#73242=CARTESIAN_POINT('Ctrl Pts',(-1.44689736863845,-4.87381170906626,
130.130081632088));
#73243=CARTESIAN_POINT('Ctrl Pts',(-1.45477966620536,-4.89101274268046,
130.2688973364));
#73244=CARTESIAN_POINT('Ctrl Pts',(-1.46266196377232,-4.90227218133672,
130.408241288838));
#73245=CARTESIAN_POINT('Ctrl Pts',(-1.47015483051776,-4.91297533898373,
130.540700848824));
#73246=CARTESIAN_POINT('Ctrl Pts',(-1.47764769726323,-4.91830982928536,
130.673637394598));
#73247=CARTESIAN_POINT('Ctrl Pts',(-1.48514056400867,-4.91824949357033,
130.806592543907));
#73248=CARTESIAN_POINT('',(-1.13985943593539,-4.91824798494418,130.799908529016));
#73249=CARTESIAN_POINT('Ctrl Pts',(-1.06997321827188,-4.76405452823403,
129.582490119308));
#73250=CARTESIAN_POINT('Ctrl Pts',(-1.0797552074402,-4.80671218538992,129.748811677139));
#73251=CARTESIAN_POINT('Ctrl Pts',(-1.08953719660859,-4.8406862486606,129.917486629869));
#73252=CARTESIAN_POINT('Ctrl Pts',(-1.09931918577689,-4.86575789899625,
130.087713472274));
#73253=CARTESIAN_POINT('Ctrl Pts',(-1.10894348654133,-4.89042538730968,
130.255196210324));
#73254=CARTESIAN_POINT('Ctrl Pts',(-1.11856778730584,-4.9064751643602,130.424181317926));
#73255=CARTESIAN_POINT('Ctrl Pts',(-1.12819208807031,-4.91374425224563,
130.593883811188));
#73256=CARTESIAN_POINT('Ctrl Pts',(-1.13208120402536,-4.9166816423341,130.662459460506));
#73257=CARTESIAN_POINT('Ctrl Pts',(-1.13597031998038,-4.9181857452644,130.731151994587));
#73258=CARTESIAN_POINT('Ctrl Pts',(-1.13985943593545,-4.91824798494418,
130.799908529016));
#73259=CARTESIAN_POINT('Ctrl Pts',(-1.13985943599124,-4.91824798494508,
130.799908530003));
#73260=CARTESIAN_POINT('Ctrl Pts',(-1.14754077984185,-4.91837091372404,
130.935708693595));
#73261=CARTESIAN_POINT('Ctrl Pts',(-1.15522212369246,-4.91286514421883,
131.0716324534));
#73262=CARTESIAN_POINT('Ctrl Pts',(-1.16290346754306,-4.90172682389837,
131.207172243981));
#73263=CARTESIAN_POINT('Ctrl Pts',(-1.17058138413356,-4.89059347327091,
131.342651559452));
#73264=CARTESIAN_POINT('Ctrl Pts',(-1.1782593007241,-4.87383260126212,131.477746849842));
#73265=CARTESIAN_POINT('Ctrl Pts',(-1.1859372173146,-4.85149242725984,131.611952278457));
#73266=CARTESIAN_POINT('Ctrl Pts',(-1.19361349098168,-4.82915703361624,
131.746128989745));
#73267=CARTESIAN_POINT('Ctrl Pts',(-1.20128976464877,-4.80124477720653,
131.879415824793));
#73268=CARTESIAN_POINT('Ctrl Pts',(-1.20896603831585,-4.76785548487302,
132.011314277764));
#73269=CARTESIAN_POINT('Ctrl Pts',(-1.21664240553569,-4.73446578561544,
132.143214338217));
#73270=CARTESIAN_POINT('Ctrl Pts',(-1.22431877275549,-4.69559901550001,
132.273725596381));
#73271=CARTESIAN_POINT('Ctrl Pts',(-1.23199513997534,-4.65140552457929,
132.402362403677));
#73272=CARTESIAN_POINT('Ctrl Pts',(-1.23967333700939,-4.60720149926447,
132.531029874105));
#73273=CARTESIAN_POINT('Ctrl Pts',(-1.24735153404347,-4.5576683573535,132.657821628027));
#73274=CARTESIAN_POINT('Ctrl Pts',(-1.25502973107751,-4.50300528134762,
132.782270246102));
#73275=CARTESIAN_POINT('Ctrl Pts',(-1.2627161116868,-4.44828394434724,132.906851503992));
#73276=CARTESIAN_POINT('Ctrl Pts',(-1.27040249229602,-4.3884219153172,133.029084273436));
#73277=CARTESIAN_POINT('Ctrl Pts',(-1.2780888729053,-4.32366539000178,133.14852372149));
#73278=CARTESIAN_POINT('Ctrl Pts',(-1.28577958631668,-4.25887236152274,
133.268030497397));
#73279=CARTESIAN_POINT('Ctrl Pts',(-1.29347029972814,-4.18917954660631,
133.384740474492));
#73280=CARTESIAN_POINT('Ctrl Pts',(-1.30116101313953,-4.11487685512454,
133.498237290627));
#73281=CARTESIAN_POINT('Ctrl Pts',(-1.30886368927773,-4.04045858752501,
133.611910648433));
#73282=CARTESIAN_POINT('Ctrl Pts',(-1.31656636541592,-3.96141635337207,
133.722360539057));
#73283=CARTESIAN_POINT('Ctrl Pts',(-1.32426904155412,-3.87808115125348,
133.829202703823));
#73284=CARTESIAN_POINT('Ctrl Pts',(-1.33009485236395,-3.81505174269055,
133.910011273114));
#73285=CARTESIAN_POINT('Ctrl Pts',(-1.33592066317378,-3.7495674144181,133.988756737511));
#73286=CARTESIAN_POINT('Ctrl Pts',(-1.34174647398362,-3.68178496192597,
134.065287258359));
#73287=CARTESIAN_POINT('Ctrl Pts',(-1.34952080810276,-3.59133172712553,
134.167414474433));
#73288=CARTESIAN_POINT('Ctrl Pts',(-1.35729514222178,-3.49648271589758,
134.265937044038));
#73289=CARTESIAN_POINT('Ctrl Pts',(-1.36506947634086,-3.39755645246117,
134.360453025651));
#73290=CARTESIAN_POINT('Ctrl Pts',(-1.37283422928794,-3.29875210680341,
134.454852524763));
#73291=CARTESIAN_POINT('Ctrl Pts',(-1.38059898223503,-3.19588078685877,
134.54525499307));
#73292=CARTESIAN_POINT('Ctrl Pts',(-1.38836373518211,-3.08930076083462,
134.63129200859));
#73293=CARTESIAN_POINT('Ctrl Pts',(-1.39612077606711,-2.98282659159468,
134.717243570934));
#73294=CARTESIAN_POINT('Ctrl Pts',(-1.4038778169521,-2.87265134892913,134.798838065001));
#73295=CARTESIAN_POINT('Ctrl Pts',(-1.4116348578371,-2.75916932483993,134.875744620502));
#73296=CARTESIAN_POINT('Ctrl Pts',(-1.41938604907723,-2.64577287842785,
134.952593180171));
#73297=CARTESIAN_POINT('Ctrl Pts',(-1.42713724031735,-2.52907493642619,
135.024760619451));
#73298=CARTESIAN_POINT('Ctrl Pts',(-1.43488843155748,-2.40950168234198,
135.091957229339));
#73299=CARTESIAN_POINT('Ctrl Pts',(-1.44263632833456,-2.28997925008049,
135.159125278876));
#73300=CARTESIAN_POINT('Ctrl Pts',(-1.45038422511167,-2.1675842764883,135.221326509952));
#73301=CARTESIAN_POINT('Ctrl Pts',(-1.45813212188875,-2.04277046414959,
135.278315455659));
#73302=CARTESIAN_POINT('Ctrl Pts',(-1.46587839797285,-1.91798276016975,
135.335292480507));
#73303=CARTESIAN_POINT('Ctrl Pts',(-1.47362467405697,-1.79077757926496,
135.387059226365));
#73304=CARTESIAN_POINT('Ctrl Pts',(-1.48137095014107,-1.66163131575496,
135.433417155674));
#73305=CARTESIAN_POINT('Ctrl Pts',(-1.48911728340643,-1.5324840989164,135.479775427187));
#73306=CARTESIAN_POINT('Ctrl Pts',(-1.49686361667177,-1.40139613885729,
135.520724670392));
#73307=CARTESIAN_POINT('Ctrl Pts',(-1.50460994993713,-1.26886143051752,
135.556115423177));
#73308=CARTESIAN_POINT('Ctrl Pts',(-1.51235801794012,-1.13629704194875,
135.591514101475));
#73309=CARTESIAN_POINT('Ctrl Pts',(-1.52010608594308,-1.00228563805597,
135.621351711527));
#73310=CARTESIAN_POINT('Ctrl Pts',(-1.52785415394607,-0.867333519892452,
135.645529446245));
#73311=CARTESIAN_POINT('Ctrl Pts',(-1.53561045668791,-0.732237973012169,
135.669732877347));
#73312=CARTESIAN_POINT('Ctrl Pts',(-1.54336675942976,-0.596200100099769,
135.688264347682));
#73313=CARTESIAN_POINT('Ctrl Pts',(-1.5511230621716,-0.45973403329057,135.701076627417));
#73314=CARTESIAN_POINT('Ctrl Pts',(-1.55888350468578,-0.323195130432044,
135.713895745452));
#73315=CARTESIAN_POINT('Ctrl Pts',(-1.56664394719994,-0.186227968542318,
135.720989570301));
#73316=CARTESIAN_POINT('Ctrl Pts',(-1.57440438971412,-0.0493478523353866,
135.722363042532));
#73317=CARTESIAN_POINT('Ctrl Pts',(-1.58217728997954,0.0877519959853531,
135.723738719582));
#73318=CARTESIAN_POINT('Ctrl Pts',(-1.58995019024499,0.224764128399301,
135.719375706269));
#73319=CARTESIAN_POINT('Ctrl Pts',(-1.59772309051041,0.361176289084986,
135.709331030392));
#73320=CARTESIAN_POINT('Ctrl Pts',(-1.60521342627248,0.492629524128983,
135.699651503785));
#73321=CARTESIAN_POINT('Ctrl Pts',(-1.61270376203451,0.623525345060253,
135.684696263298));
#73322=CARTESIAN_POINT('Ctrl Pts',(-1.62019409779657,0.753415232623536,
135.664561081513));
#73323=CARTESIAN_POINT('Ctrl Pts',(-1.62796843191566,0.888229934752388,
135.643662468191));
#73324=CARTESIAN_POINT('Ctrl Pts',(-1.63574276603476,1.02238797024958,135.6171171642));
#73325=CARTESIAN_POINT('Ctrl Pts',(-1.64351710015384,1.15537900420787,135.584975893776));
#73326=CARTESIAN_POINT('Ctrl Pts',(-1.65128185310095,1.28820613860273,135.552874234596));
#73327=CARTESIAN_POINT('Ctrl Pts',(-1.65904660604807,1.41986875672192,135.515190421982));
#73328=CARTESIAN_POINT('Ctrl Pts',(-1.66681135899518,1.54986324200278,135.472026736044));
#73329=CARTESIAN_POINT('Ctrl Pts',(-1.67456839988019,1.67972861492825,135.428905920888));
#73330=CARTESIAN_POINT('Ctrl Pts',(-1.68232544076515,1.80792878350356,135.380316186007));
#73331=CARTESIAN_POINT('Ctrl Pts',(-1.69008248165017,1.93397225272641,135.326410416958));
#73332=CARTESIAN_POINT('Ctrl Pts',(-1.69783367289029,2.0599206715883,135.272545298669));
#73333=CARTESIAN_POINT('Ctrl Pts',(-1.7055848641304,2.18371527030032,135.213372278724));
#73334=CARTESIAN_POINT('Ctrl Pts',(-1.71333605537052,2.30488194587762,135.149093322586));
#73335=CARTESIAN_POINT('Ctrl Pts',(-1.72108395214761,2.42599712238574,135.084841686718));
#73336=CARTESIAN_POINT('Ctrl Pts',(-1.72883184892476,2.54448625261087,135.015488613775));
#73337=CARTESIAN_POINT('Ctrl Pts',(-1.73657974570185,2.65989758096093,134.941283135731));
#73338=CARTESIAN_POINT('Ctrl Pts',(-1.74432602178596,2.77528476774922,134.867093179872));
#73339=CARTESIAN_POINT('Ctrl Pts',(-1.75207229787005,2.88759510458844,134.788053049148));
#73340=CARTESIAN_POINT('Ctrl Pts',(-1.75981857395416,2.99640405344108,134.704456233192));
#73341=CARTESIAN_POINT('Ctrl Pts',(-1.76756490721952,3.10521380549651,134.620858800142));
#73342=CARTESIAN_POINT('Ctrl Pts',(-1.77531124048487,3.21052180796133,134.532704852934));
#73343=CARTESIAN_POINT('Ctrl Pts',(-1.78305757375023,3.31193529779476,134.440329215577));
#73344=CARTESIAN_POINT('Ctrl Pts',(-1.79080564175319,3.41337149847581,134.347932891336));
#73345=CARTESIAN_POINT('Ctrl Pts',(-1.79855370975612,3.51091116207193,134.251313258899));
#73346=CARTESIAN_POINT('Ctrl Pts',(-1.80630177775907,3.60419749129478,134.150842876034));
#73347=CARTESIAN_POINT('Ctrl Pts',(-1.81405808050093,3.69758296633871,134.050265712051));
#73348=CARTESIAN_POINT('Ctrl Pts',(-1.82181438324286,3.78670581038964,133.94582990915));
#73349=CARTESIAN_POINT('Ctrl Pts',(-1.82957068598472,3.87124838667286,133.837942492377));
#73350=CARTESIAN_POINT('Ctrl Pts',(-1.83733112849891,3.9558360858748,133.729997492841));
#73351=CARTESIAN_POINT('Ctrl Pts',(-1.845091571013,4.03583841823812,133.618597526039));
#73352=CARTESIAN_POINT('Ctrl Pts',(-1.85285201352718,4.11098100561726,133.504178802917));
#73353=CARTESIAN_POINT('Ctrl Pts',(-1.86062491379261,4.18624421854832,133.389576404704));
#73354=CARTESIAN_POINT('Ctrl Pts',(-1.8683978140581,4.25663189615823,133.271945902051));
#73355=CARTESIAN_POINT('Ctrl Pts',(-1.87617071432354,4.32191513076584,133.151749095206));
#73356=CARTESIAN_POINT('Ctrl Pts',(-1.88366105008548,4.3848251553562,133.035921745049));
#73357=CARTESIAN_POINT('Ctrl Pts',(-1.89115138584741,4.44299527650109,132.917711710954));
#73358=CARTESIAN_POINT('Ctrl Pts',(-1.89864172160935,4.49626363477128,132.797548112292));
#73359=CARTESIAN_POINT('Ctrl Pts',(-1.90641605572843,4.5515516790364,132.672828474263));
#73360=CARTESIAN_POINT('Ctrl Pts',(-1.91419038984752,4.60173405816527,132.545609134234));
#73361=CARTESIAN_POINT('Ctrl Pts',(-1.9219647239666,4.64657759941095,132.416346869105));
#73362=CARTESIAN_POINT('Ctrl Pts',(-1.92972947691367,4.69136587499977,132.287243908166));
#73363=CARTESIAN_POINT('Ctrl Pts',(-1.93749422986068,4.73082827731791,132.156103397468));
#73364=CARTESIAN_POINT('Ctrl Pts',(-1.94525898280776,4.76477864046553,132.023404328785));
#73365=CARTESIAN_POINT('Ctrl Pts',(-1.95301602369273,4.79869528363381,131.890837058689));
#73366=CARTESIAN_POINT('Ctrl Pts',(-1.96077306457775,4.82711068612423,131.756714687477));
#73367=CARTESIAN_POINT('Ctrl Pts',(-1.96853010546272,4.84988780983042,131.621533362191));
#73368=CARTESIAN_POINT('Ctrl Pts',(-1.9762812967028,4.87264775713039,131.486453978195));
#73369=CARTESIAN_POINT('Ctrl Pts',(-1.98403248794285,4.88977782403887,131.350317613592));
#73370=CARTESIAN_POINT('Ctrl Pts',(-1.99178367918293,4.90119166557506,131.213632311918));
#73371=CARTESIAN_POINT('Ctrl Pts',(-1.99953157596002,4.91260065592421,131.077005105141));
#73372=CARTESIAN_POINT('Ctrl Pts',(-2.00727947273708,4.91829822062125,130.939829814128));
#73373=CARTESIAN_POINT('Ctrl Pts',(-2.01502736951417,4.91824969238585,130.802621121516));
#73374=CARTESIAN_POINT('Ctrl Pts',(-2.02277364559828,4.9182011743015,130.665441130004));
#73375=CARTESIAN_POINT('Ctrl Pts',(-2.03051992168244,4.91240895418478,130.528228141509));
#73376=CARTESIAN_POINT('Ctrl Pts',(-2.03826619776655,4.90089047999705,130.391497970219));
#73377=CARTESIAN_POINT('Ctrl Pts',(-2.0460125310319,4.88937192078256,130.254766789619));
#73378=CARTESIAN_POINT('Ctrl Pts',(-2.05375886429728,4.87212705597011,130.118518822921));
#73379=CARTESIAN_POINT('Ctrl Pts',(-2.06150519756264,4.84922528446493,129.983265493353));
#73380=CARTESIAN_POINT('Ctrl Pts',(-2.06925326556563,4.82631838426679,129.84798187474));
#73381=CARTESIAN_POINT('Ctrl Pts',(-2.07700133356858,4.79775212179937,129.71369372189));
#73382=CARTESIAN_POINT('Ctrl Pts',(-2.08474940157157,4.76364708281675,129.580902595045));
#73383=CARTESIAN_POINT('Ctrl Pts',(-2.09250570431343,4.72950579659288,129.447970336209));
#73384=CARTESIAN_POINT('Ctrl Pts',(-2.1002620070553,4.68981407199235,129.316538660965));
#73385=CARTESIAN_POINT('Ctrl Pts',(-2.10801830979716,4.64474266027962,129.187094813105));
#73386=CARTESIAN_POINT('Ctrl Pts',(-2.11577875231133,4.59964719259739,129.057581877166));
#73387=CARTESIAN_POINT('Ctrl Pts',(-2.12353919482551,4.5491664603238,128.930059246013));
#73388=CARTESIAN_POINT('Ctrl Pts',(-2.13129963733968,4.49351915199342,128.804993544423));
#73389=CARTESIAN_POINT('Ctrl Pts',(-2.13907253760511,4.43778251366356,128.679727076266));
#73390=CARTESIAN_POINT('Ctrl Pts',(-2.14684543787049,4.37686289937521,128.556925769641));
#73391=CARTESIAN_POINT('Ctrl Pts',(-2.15461833813592,4.31102510456372,128.437031825378));
#73392=CARTESIAN_POINT('Ctrl Pts',(-2.16210867389809,4.24758067942785,128.321496327982));
#73393=CARTESIAN_POINT('Ctrl Pts',(-2.16959900966031,4.17956960122271,128.208660746727));
#73394=CARTESIAN_POINT('Ctrl Pts',(-2.17708934542247,4.10726541125329,128.098893208037));
#73395=CARTESIAN_POINT('Ctrl Pts',(-2.18486367954157,4.03221978594608,127.984963799757));
#73396=CARTESIAN_POINT('Ctrl Pts',(-2.19263801366062,3.9523113538326,127.873978782166));
#73397=CARTESIAN_POINT('Ctrl Pts',(-2.20041234777972,3.86779837868953,127.766381229172));
#73398=CARTESIAN_POINT('Ctrl Pts',(-2.20817710072681,3.78338955823542,127.658916280546));
#73399=CARTESIAN_POINT('Ctrl Pts',(-2.21594185367394,3.69438772486799,127.554830794525));
#73400=CARTESIAN_POINT('Ctrl Pts',(-2.22370660662102,3.60109524071745,127.454540304507));
#73401=CARTESIAN_POINT('Ctrl Pts',(-2.23146364750606,3.50789541597685,127.354349424417));
#73402=CARTESIAN_POINT('Ctrl Pts',(-2.23922068839106,3.41041368566301,127.257946323774));
#73403=CARTESIAN_POINT('Ctrl Pts',(-2.2469777292761,3.30899339989057,127.165714476213));
#73404=CARTESIAN_POINT('Ctrl Pts',(-2.2547289205162,3.2076495959454,127.073552181407));
#73405=CARTESIAN_POINT('Ctrl Pts',(-2.26248011175626,3.10237343641189,126.985555140585));
#73406=CARTESIAN_POINT('Ctrl Pts',(-2.27023130299636,2.99354568113249,126.902070608165));
#73407=CARTESIAN_POINT('Ctrl Pts',(-2.27797919977346,2.88476418055157,126.818621558897));
#73408=CARTESIAN_POINT('Ctrl Pts',(-2.28572709655065,2.77243439610505,126.739681440869));
#73409=CARTESIAN_POINT('Ctrl Pts',(-2.29347499332775,2.65697060636137,126.665557619182));
#73410=CARTESIAN_POINT('Ctrl Pts',(-2.30122126941187,2.5415309691534,126.591449302601));
#73411=CARTESIAN_POINT('Ctrl Pts',(-2.30896754549594,2.42295895940206,126.522155489534));
#73412=CARTESIAN_POINT('Ctrl Pts',(-2.31671382158007,2.30169797724346,126.457940310687));
#73413=CARTESIAN_POINT('Ctrl Pts',(-2.32446015484543,2.18043609996399,126.393724657817));
#73414=CARTESIAN_POINT('Ctrl Pts',(-2.33220648811075,2.05648555617816,126.334587896943));
#73415=CARTESIAN_POINT('Ctrl Pts',(-2.3399528213761,1.93031413253364,126.280748077544));
#73416=CARTESIAN_POINT('Ctrl Pts',(-2.34770088937908,1.80411445367361,126.226896201092));
#73417=CARTESIAN_POINT('Ctrl Pts',(-2.35544895738211,1.67569326481025,126.178343779959));
#73418=CARTESIAN_POINT('Ctrl Pts',(-2.36319702538509,1.54553772232298,126.135260467497));
#73419=CARTESIAN_POINT('Ctrl Pts',(-2.37095332812695,1.41524384897629,126.092131365577));
#73420=CARTESIAN_POINT('Ctrl Pts',(-2.37870963086884,1.28321231158345,126.054483106745));
#73421=CARTESIAN_POINT('Ctrl Pts',(-2.38646593361071,1.14994533737769,126.022435400298));
#73422=CARTESIAN_POINT('Ctrl Pts',(-2.39422637612488,1.01660723457521,125.990370589025));
#73423=CARTESIAN_POINT('Ctrl Pts',(-2.40198681863897,0.882032764503286,
125.963912361724));
#73424=CARTESIAN_POINT('Ctrl Pts',(-2.40974726115314,0.746732718296827,
125.943128951627));
#73425=CARTESIAN_POINT('Ctrl Pts',(-2.41752016141858,0.611215476444824,
125.922312178155));
#73426=CARTESIAN_POINT('Ctrl Pts',(-2.42529306168403,0.474970719700355,
125.90718846917));
#73427=CARTESIAN_POINT('Ctrl Pts',(-2.43306596194947,0.338513612546228,
125.897774065122));
#73428=CARTESIAN_POINT('Ctrl Pts',(-2.44055629771141,0.207017064953346,
125.888701898375));
#73429=CARTESIAN_POINT('Ctrl Pts',(-2.44804663347336,0.0753236457449448,
125.884931156813));
#73430=CARTESIAN_POINT('Ctrl Pts',(-2.45553696923531,-0.0561090741358449,
125.886430683712));
#73431=CARTESIAN_POINT('Ctrl Pts',(-2.4633113033544,-0.192525105540563,
125.887987065629));
#73432=CARTESIAN_POINT('Ctrl Pts',(-2.4710856374735,-0.329092403527903,
125.895226179723));
#73433=CARTESIAN_POINT('Ctrl Pts',(-2.47885997159258,-0.465298599591438,
125.908170233633));
#73434=CARTESIAN_POINT('Ctrl Pts',(-2.48662472453968,-0.601336933691422,
125.921098335154));
#73435=CARTESIAN_POINT('Ctrl Pts',(-2.49438947748676,-0.737014665861168,
125.939717350605));
#73436=CARTESIAN_POINT('Ctrl Pts',(-2.50215423043386,-0.871818761966877,
125.963997500115));
#73437=CARTESIAN_POINT('Ctrl Pts',(-2.50991127131886,-1.00648896874375,
125.988253534238));
#73438=CARTESIAN_POINT('Ctrl Pts',(-2.51766831220388,-1.14028688395007,
126.018159444103));
#73439=CARTESIAN_POINT('Ctrl Pts',(-2.52542535308888,-1.27270429123198,
126.0536336364));
#73440=CARTESIAN_POINT('Ctrl Pts',(-2.53317654432907,-1.40502184151826,
126.089081077333));
#73441=CARTESIAN_POINT('Ctrl Pts',(-2.54092773556929,-1.53596057991021,
126.130088341913));
#73442=CARTESIAN_POINT('Ctrl Pts',(-2.54867892680949,-1.66502254143622,
126.176522785596));
#73443=CARTESIAN_POINT('Ctrl Pts',(-2.55642682358656,-1.79402964818452,
126.222937493402));
#73444=CARTESIAN_POINT('Ctrl Pts',(-2.56417472036356,-1.92116119748271,
126.274774660387));
#73445=CARTESIAN_POINT('Ctrl Pts',(-2.57192261714064,-2.04593466667936,
126.331851880606));
#73446=CARTESIAN_POINT('Ctrl Pts',(-2.57966889322474,-2.17068203595605,
126.388917161502));
#73447=CARTESIAN_POINT('Ctrl Pts',(-2.58741516930889,-2.29307195094467,
126.451220152881));
#73448=CARTESIAN_POINT('Ctrl Pts',(-2.59516144539299,-2.41264252239813,
126.51853057875));
#73449=CARTESIAN_POINT('Ctrl Pts',(-2.60290777865834,-2.53221397649438,
126.58584150149));
#73450=CARTESIAN_POINT('Ctrl Pts',(-2.61065411192368,-2.64896570483473,
126.65815974069));
#73451=CARTESIAN_POINT('Ctrl Pts',(-2.61840044518902,-2.76246140610562,
126.735209595267));
#73452=CARTESIAN_POINT('Ctrl Pts',(-2.626148513192,-2.87598252395188,126.812276704625));
#73453=CARTESIAN_POINT('Ctrl Pts',(-2.63389658119496,-2.9862458403693,126.894077318311));
#73454=CARTESIAN_POINT('Ctrl Pts',(-2.64164464919793,-3.09284530126687,
126.980293279648));
#73455=CARTESIAN_POINT('Ctrl Pts',(-2.6494009519398,-3.19955805734032,127.066600872335));
#73456=CARTESIAN_POINT('Ctrl Pts',(-2.65715725468168,-3.30259887476059,
127.157332940562));
#73457=CARTESIAN_POINT('Ctrl Pts',(-2.66491355742355,-3.40159557261785,
127.252131652135));
#73458=CARTESIAN_POINT('Ctrl Pts',(-2.67267399993771,-3.50064510799336,
127.346980960635));
#73459=CARTESIAN_POINT('Ctrl Pts',(-2.68043444245186,-3.59564595219568,
127.445900955519));
#73460=CARTESIAN_POINT('Ctrl Pts',(-2.68819488496604,-3.686264603589,127.548498775468));
#73461=CARTESIAN_POINT('Ctrl Pts',(-2.69596778523146,-3.77702872408616,
127.651261294547));
#73462=CARTESIAN_POINT('Ctrl Pts',(-2.70374068549691,-3.86339634776465,
127.757713132924));
#73463=CARTESIAN_POINT('Ctrl Pts',(-2.71151358576233,-3.94507535208676,
127.867429646491));
#73464=CARTESIAN_POINT('Ctrl Pts',(-2.71900392152429,-4.0237851188641,127.97315768843));
#73465=CARTESIAN_POINT('Ctrl Pts',(-2.7264942572863,-4.09814106040651,128.081916913842));
#73466=CARTESIAN_POINT('Ctrl Pts',(-2.73398459304826,-4.16792206147586,
128.193305514363));
#73467=CARTESIAN_POINT('Ctrl Pts',(-2.74197015249147,-4.24231663466434,
128.312058574176));
#73468=CARTESIAN_POINT('Ctrl Pts',(-2.74995571193477,-4.31173644726357,
128.434159702435));
#73469=CARTESIAN_POINT('Ctrl Pts',(-2.75794127137803,-4.37587548579146,
128.559166462187));
#73470=CARTESIAN_POINT('Ctrl Pts',(-2.76591645663073,-4.43993120008732,
128.684010823304));
#73471=CARTESIAN_POINT('Ctrl Pts',(-2.77389164188335,-4.49871963179323,
128.811752983107));
#73472=CARTESIAN_POINT('Ctrl Pts',(-2.78186682713604,-4.55197819272829,
128.941922002356));
#73473=CARTESIAN_POINT('Ctrl Pts',(-2.789829834859,-4.60515543170167,129.071892262948));
#73474=CARTESIAN_POINT('Ctrl Pts',(-2.79779284258203,-4.65281948972259,
129.204281665528));
#73475=CARTESIAN_POINT('Ctrl Pts',(-2.80575585030499,-4.69475414447413,
129.338595770995));
#73476=CARTESIAN_POINT('Ctrl Pts',(-2.81053681060419,-4.71993155563622,
129.419237461698));
#73477=CARTESIAN_POINT('Ctrl Pts',(-2.81531777090342,-4.74304453855751,
129.500572488431));
#73478=CARTESIAN_POINT('Ctrl Pts',(-2.82009873120262,-4.76405452823401,
129.582490119308));
#73479=CARTESIAN_POINT('Origin',(213.235140564004,0.,130.804360617566));
#73480=CARTESIAN_POINT('',(-4.91509110695617,-4.76405452823401,129.582490119308));
#73481=CARTESIAN_POINT('',(-4.56974458955163,-4.76405452823408,129.582490119308));
#73482=CARTESIAN_POINT('',(213.235140564004,-4.76405452823405,129.582490119308));
#73483=CARTESIAN_POINT('',(-3.2351405639729,-4.91824878730941,130.80781440238));
#73484=CARTESIAN_POINT('Ctrl Pts',(-3.23514056400865,-4.91824878730896,
130.80781440301));
#73485=CARTESIAN_POINT('Ctrl Pts',(-3.24719065751056,-4.91809994407063,
131.019769687541));
#73486=CARTESIAN_POINT('Ctrl Pts',(-3.25924075101248,-4.90424944354162,
131.231249688169));
#73487=CARTESIAN_POINT('Ctrl Pts',(-3.27129084451443,-4.87688073448147,
131.440927475126));
#73488=CARTESIAN_POINT('Ctrl Pts',(-3.27906517863354,-4.85922332056942,
131.576204863048));
#73489=CARTESIAN_POINT('Ctrl Pts',(-3.28683951275261,-4.83590508390784,
131.710961278448));
#73490=CARTESIAN_POINT('Ctrl Pts',(-3.29461384687173,-4.80696448749442,
131.844685316142));
#73491=CARTESIAN_POINT('Ctrl Pts',(-3.30237859981885,-4.77805955777962,
131.978244550911));
#73492=CARTESIAN_POINT('Ctrl Pts',(-3.310143352766,-4.7435461369734,132.110773561046));
#73493=CARTESIAN_POINT('Ctrl Pts',(-3.31790810571312,-4.70351439032332,
132.241766420574));
#73494=CARTESIAN_POINT('Ctrl Pts',(-3.32566514659814,-4.66352240376836,
132.372629176148));
#73495=CARTESIAN_POINT('Ctrl Pts',(-3.33342218748322,-4.61802311209007,
132.501958445902));
#73496=CARTESIAN_POINT('Ctrl Pts',(-3.34117922836825,-4.56715756229186,
132.629259207543));
#73497=CARTESIAN_POINT('Ctrl Pts',(-3.3489304196084,-4.51633037060043,132.756463970689));
#73498=CARTESIAN_POINT('Ctrl Pts',(-3.3566816108485,-4.46014512005288,132.881642908936));
#73499=CARTESIAN_POINT('Ctrl Pts',(-3.36443280208866,-4.39879234078576,
133.004317209216));
#73500=CARTESIAN_POINT('Ctrl Pts',(-3.37218069886577,-4.33746563808646,
133.126939369646));
#73501=CARTESIAN_POINT('Ctrl Pts',(-3.3799285956429,-4.27097594952999,133.247058660452));
#73502=CARTESIAN_POINT('Ctrl Pts',(-3.38767649242001,-4.19956139448581,
133.364217480057));
#73503=CARTESIAN_POINT('Ctrl Pts',(-3.39542276850415,-4.12816177782704,
133.481351792563));
#73504=CARTESIAN_POINT('Ctrl Pts',(-3.40316904458825,-4.05183954711802,
133.595526532));
#73505=CARTESIAN_POINT('Ctrl Pts',(-3.41091532067239,-3.97087791973199,
133.706310239645));
#73506=CARTESIAN_POINT('Ctrl Pts',(-3.41866165393777,-3.88991569470562,
133.81709476507));
#73507=CARTESIAN_POINT('Ctrl Pts',(-3.42640798720316,-3.80431423534883,
133.924487893098));
#73508=CARTESIAN_POINT('Ctrl Pts',(-3.43415432046854,-3.71439884402085,
134.028088938941));
#73509=CARTESIAN_POINT('Ctrl Pts',(-3.44190238847154,-3.6244633167644,134.13171318552));
#73510=CARTESIAN_POINT('Ctrl Pts',(-3.44965045647455,-3.53021219137304,
134.231543364872));
#73511=CARTESIAN_POINT('Ctrl Pts',(-3.45739852447755,-3.43200935617864,
134.327213842099));
#73512=CARTESIAN_POINT('Ctrl Pts',(-3.46515482721944,-3.33370214984237,
134.422985999047));
#73513=CARTESIAN_POINT('Ctrl Pts',(-3.47291112996132,-3.23143512438988,
134.51458934923));
#73514=CARTESIAN_POINT('Ctrl Pts',(-3.4806674327032,-3.12560756524862,134.601696579864));
#73515=CARTESIAN_POINT('Ctrl Pts',(-3.48842787521739,-3.01972352275263,
134.68885030225));
#73516=CARTESIAN_POINT('Ctrl Pts',(-3.49618831773161,-2.91027547177423,
134.771502887958));
#73517=CARTESIAN_POINT('Ctrl Pts',(-3.50394876024581,-2.79769291332397,
134.849369569996));
#73518=CARTESIAN_POINT('Ctrl Pts',(-3.51172166051126,-2.68492962735628,
134.927361250545));
#73519=CARTESIAN_POINT('Ctrl Pts',(-3.5194945607767,-2.56902210956334,135.000551465963));
#73520=CARTESIAN_POINT('Ctrl Pts',(-3.52726746104216,-2.450426534054,135.068700292557));
#73521=CARTESIAN_POINT('Ctrl Pts',(-3.53475779680389,-2.33614220644363,
135.134371737645));
#73522=CARTESIAN_POINT('Ctrl Pts',(-3.54224813256557,-2.21936213643618,
135.195361822108));
#73523=CARTESIAN_POINT('Ctrl Pts',(-3.54973846832729,-2.10051143564684,
135.251498435446));
#73524=CARTESIAN_POINT('Ctrl Pts',(-3.55751280244637,-1.97715447440831,
135.309763485543));
#73525=CARTESIAN_POINT('Ctrl Pts',(-3.56528713656548,-1.85117600913743,
135.362984326765));
#73526=CARTESIAN_POINT('Ctrl Pts',(-3.57306147068456,-1.72302708969003,
135.410916892127));
#73527=CARTESIAN_POINT('Ctrl Pts',(-3.58082622363164,-1.59503610233302,
135.458790384885));
#73528=CARTESIAN_POINT('Ctrl Pts',(-3.58859097657867,-1.46488034570736,
135.501388433669));
#73529=CARTESIAN_POINT('Ctrl Pts',(-3.59635572952575,-1.33303420618238,
135.538513431708));
#73530=CARTESIAN_POINT('Ctrl Pts',(-3.60411277041076,-1.2013190181017,135.575601556675));
#73531=CARTESIAN_POINT('Ctrl Pts',(-3.6118698112958,-1.06791716212818,135.607227343325));
#73532=CARTESIAN_POINT('Ctrl Pts',(-3.6196268521808,-0.933321353889516,
135.633241886853));
#73533=CARTESIAN_POINT('Ctrl Pts',(-3.62737804342092,-0.798827045397031,
135.659236812612));
#73534=CARTESIAN_POINT('Ctrl Pts',(-3.63512923466104,-0.663140959076525,
135.679628843866));
#73535=CARTESIAN_POINT('Ctrl Pts',(-3.64288042590115,-0.526768920116495,
135.694319468855));
#73536=CARTESIAN_POINT('Ctrl Pts',(-3.65062832267823,-0.390454842910681,
135.709003849937));
#73537=CARTESIAN_POINT('Ctrl Pts',(-3.65837621945535,-0.253455780834875,
135.717991602626));
#73538=CARTESIAN_POINT('Ctrl Pts',(-3.66612411623242,-0.116285436392451,
135.721235718663));
#73539=CARTESIAN_POINT('Ctrl Pts',(-3.67387039231652,0.0208562149709664,
135.7244791561));
#73540=CARTESIAN_POINT('Ctrl Pts',(-3.68161666840053,0.158168686827711,
135.721981337385));
#73541=CARTESIAN_POINT('Ctrl Pts',(-3.68936294448463,0.295135894826391,
135.713747327338));
#73542=CARTESIAN_POINT('Ctrl Pts',(-3.69710927774999,0.432104113886074,
135.705513256509));
#73543=CARTESIAN_POINT('Ctrl Pts',(-3.70485561101539,0.56872667374139,135.691542933315));
#73544=CARTESIAN_POINT('Ctrl Pts',(-3.71260194428075,0.704490633061288,
135.67189346393));
#73545=CARTESIAN_POINT('Ctrl Pts',(-3.72035001228372,0.84028499577837,135.652239594182));
#73546=CARTESIAN_POINT('Ctrl Pts',(-3.72809808028665,0.975219988490295,
135.626904103487));
#73547=CARTESIAN_POINT('Ctrl Pts',(-3.73584614828962,1.10879130166956,135.595995506812));
#73548=CARTESIAN_POINT('Ctrl Pts',(-3.74360245103147,1.24250457602998,135.565054060113));
#73549=CARTESIAN_POINT('Ctrl Pts',(-3.75135875377329,1.37485089414771,135.528527763557));
#73550=CARTESIAN_POINT('Ctrl Pts',(-3.75911505651513,1.50533905498266,135.48657562673));
#73551=CARTESIAN_POINT('Ctrl Pts',(-3.76687549902928,1.63589686127797,135.444601098785));
#73552=CARTESIAN_POINT('Ctrl Pts',(-3.77463594154354,1.76459416744757,135.397195095244));
#73553=CARTESIAN_POINT('Ctrl Pts',(-3.78239638405771,1.89095923516923,135.344565043958));
#73554=CARTESIAN_POINT('Ctrl Pts',(-3.79016928432313,2.01752715531576,135.291850506241));
#73555=CARTESIAN_POINT('Ctrl Pts',(-3.79794218458852,2.14175500096732,135.233895328055));
#73556=CARTESIAN_POINT('Ctrl Pts',(-3.80571508485394,2.26319434427661,135.17095361698));
#73557=CARTESIAN_POINT('Ctrl Pts',(-3.81320542061605,2.38021906157068,135.110299995643));
#73558=CARTESIAN_POINT('Ctrl Pts',(-3.82069575637814,2.49465422731484,135.045016245777));
#73559=CARTESIAN_POINT('Ctrl Pts',(-3.82818609214024,2.60612525685957,134.975366995895));
#73560=CARTESIAN_POINT('Ctrl Pts',(-3.83596042625933,2.72182274436923,134.903076973534));
#73561=CARTESIAN_POINT('Ctrl Pts',(-3.8437347603784,2.83469338305596,134.825854887478));
#73562=CARTESIAN_POINT('Ctrl Pts',(-3.85150909449749,2.94428802898831,134.743948294577));
#73563=CARTESIAN_POINT('Ctrl Pts',(-3.85927384744459,3.0537476093143,134.662142644231));
#73564=CARTESIAN_POINT('Ctrl Pts',(-3.86703860039166,3.15993891988318,134.575664205862));
#73565=CARTESIAN_POINT('Ctrl Pts',(-3.87480335333876,3.26243929110219,134.484805282871));
#73566=CARTESIAN_POINT('Ctrl Pts',(-3.88256039422377,3.36483785750751,134.394036602243));
#73567=CARTESIAN_POINT('Ctrl Pts',(-3.89031743510878,3.46355248917999,134.298896352863));
#73568=CARTESIAN_POINT('Ctrl Pts',(-3.89807447599378,3.55819158345901,134.199718583658));
#73569=CARTESIAN_POINT('Ctrl Pts',(-3.90582566723391,3.65275930966084,134.10061560518));
#73570=CARTESIAN_POINT('Ctrl Pts',(-3.91357685847406,3.74325734706025,133.997481448924));
#73571=CARTESIAN_POINT('Ctrl Pts',(-3.92132804971419,3.82932940405408,133.890688431935));
#73572=CARTESIAN_POINT('Ctrl Pts',(-3.92907594649128,3.91536487812764,133.783940804827));
#73573=CARTESIAN_POINT('Ctrl Pts',(-3.93682384326838,3.99697786845188,133.673537713754));
#73574=CARTESIAN_POINT('Ctrl Pts',(-3.94457174004546,4.07385115689435,133.559885942068));
#73575=CARTESIAN_POINT('Ctrl Pts',(-3.95231801612957,4.15070836510207,133.446257943882));
#73576=CARTESIAN_POINT('Ctrl Pts',(-3.96006429221365,4.2228276245579,133.32938294039));
#73577=CARTESIAN_POINT('Ctrl Pts',(-3.96781056829775,4.28993424023908,133.20969786563));
#73578=CARTESIAN_POINT('Ctrl Pts',(-3.9755569015631,4.35704135128605,133.090011907382));
#73579=CARTESIAN_POINT('Ctrl Pts',(-3.98330323482846,4.4191355535163,132.967516177494));
#73580=CARTESIAN_POINT('Ctrl Pts',(-3.99104956809381,4.47598763465161,132.842673095315));
#73581=CARTESIAN_POINT('Ctrl Pts',(-3.99879763609679,4.53285244741631,132.717802055393));
#73582=CARTESIAN_POINT('Ctrl Pts',(-4.00654570409979,4.58447264108795,132.590582972893));
#73583=CARTESIAN_POINT('Ctrl Pts',(-4.01429377210277,4.6306669207623,132.461498792691));
#73584=CARTESIAN_POINT('Ctrl Pts',(-4.02205007484463,4.67691029626681,132.332277420287));
#73585=CARTESIAN_POINT('Ctrl Pts',(-4.02980637758658,4.71771610617723,132.201187359119));
#73586=CARTESIAN_POINT('Ctrl Pts',(-4.03756268032845,4.75295262360015,132.068727819099));
#73587=CARTESIAN_POINT('Ctrl Pts',(-4.04532312284262,4.78820794781337,131.936197581434));
#73588=CARTESIAN_POINT('Ctrl Pts',(-4.05308356535672,4.81788797201779,131.802296789986));
#73589=CARTESIAN_POINT('Ctrl Pts',(-4.06084400787088,4.84191222505194,131.667534451387));
#73590=CARTESIAN_POINT('Ctrl Pts',(-4.06861690813632,4.86597504394984,131.532555780317));
#73591=CARTESIAN_POINT('Ctrl Pts',(-4.0763898084018,4.88436389617445,131.396713186012));
#73592=CARTESIAN_POINT('Ctrl Pts',(-4.08416270866724,4.89705018342472,131.260521294872));
#73593=CARTESIAN_POINT('Ctrl Pts',(-4.09165304442921,4.90927529217851,131.129280322022));
#73594=CARTESIAN_POINT('Ctrl Pts',(-4.09914338019111,4.91620522680309,130.997715314665));
#73595=CARTESIAN_POINT('Ctrl Pts',(-4.10663371595308,4.91786015460807,130.866284459649));
#73596=CARTESIAN_POINT('Ctrl Pts',(-4.11440805007216,4.91957782950379,130.729870363817));
#73597=CARTESIAN_POINT('Ctrl Pts',(-4.12218238419122,4.91561803869035,130.593168675059));
#73598=CARTESIAN_POINT('Ctrl Pts',(-4.1299567183103,4.90594628549177,130.456691081412));
#73599=CARTESIAN_POINT('Ctrl Pts',(-4.13772147125738,4.89628645186462,130.320381684202));
#73600=CARTESIAN_POINT('Ctrl Pts',(-4.14548622420451,4.88092868969752,130.184296218834));
#73601=CARTESIAN_POINT('Ctrl Pts',(-4.1532509771516,4.85989045888151,130.048948286337));
#73602=CARTESIAN_POINT('Ctrl Pts',(-4.1610080180366,4.83887312353292,129.913734783315));
#73603=CARTESIAN_POINT('Ctrl Pts',(-4.16876505892156,4.8121866068751,129.779257739225));
#73604=CARTESIAN_POINT('Ctrl Pts',(-4.17652209980656,4.77990028292875,129.646027182083));
#73605=CARTESIAN_POINT('Ctrl Pts',(-4.18427329104669,4.74763830635043,129.51289709514));
#73606=CARTESIAN_POINT('Ctrl Pts',(-4.19202448228685,4.70978501953334,129.381012002591));
#73607=CARTESIAN_POINT('Ctrl Pts',(-4.19977567352697,4.66646107903714,129.250872909108));
#73608=CARTESIAN_POINT('Ctrl Pts',(-4.20752357030405,4.62315555237136,129.120789128211));
#73609=CARTESIAN_POINT('Ctrl Pts',(-4.21527146708113,4.57438411985224,128.992450240581));
#73610=CARTESIAN_POINT('Ctrl Pts',(-4.22301936385821,4.52031755568503,128.866343007154));
#73611=CARTESIAN_POINT('Ctrl Pts',(-4.23076563994232,4.46626230107749,128.740262152643));
#73612=CARTESIAN_POINT('Ctrl Pts',(-4.23851191602635,4.40691427191419,128.616412382921));
#73613=CARTESIAN_POINT('Ctrl Pts',(-4.24625819211045,4.34249259380731,128.495260980212));
#73614=CARTESIAN_POINT('Ctrl Pts',(-4.25400452537579,4.27807044015423,128.374108683191));
#73615=CARTESIAN_POINT('Ctrl Pts',(-4.26175085864116,4.20857474638045,128.255655138126));
#73616=CARTESIAN_POINT('Ctrl Pts',(-4.26949719190651,4.13427066414663,128.140343136753));
#73617=CARTESIAN_POINT('Ctrl Pts',(-4.27724525990948,4.05994994202888,128.025005312057));
#73618=CARTESIAN_POINT('Ctrl Pts',(-4.28499332791247,3.98081890046283,127.912810759571));
#73619=CARTESIAN_POINT('Ctrl Pts',(-4.29274139591544,3.89718586032778,127.804173051336));
#73620=CARTESIAN_POINT('Ctrl Pts',(-4.3004976986573,3.81346393400231,127.695419881652));
#73621=CARTESIAN_POINT('Ctrl Pts',(-4.30825400139915,3.72523068987249,127.59023141798));
#73622=CARTESIAN_POINT('Ctrl Pts',(-4.316010304141,3.63283492577143,127.488988321037));
#73623=CARTESIAN_POINT('Ctrl Pts',(-4.32377074665518,3.54038984726895,127.387691187604));
#73624=CARTESIAN_POINT('Ctrl Pts',(-4.33153118916932,3.44377809721412,127.290343894173));
#73625=CARTESIAN_POINT('Ctrl Pts',(-4.33929163168349,3.34338442067241,127.197289273927));
#73626=CARTESIAN_POINT('Ctrl Pts',(-4.34706453194892,3.24282958328872,127.104085274143));
#73627=CARTESIAN_POINT('Ctrl Pts',(-4.35483743221439,3.13848098523749,127.015187971605));
#73628=CARTESIAN_POINT('Ctrl Pts',(-4.36261033247982,3.03075613820552,126.930899595014));
#73629=CARTESIAN_POINT('Ctrl Pts',(-4.37010066824191,2.9269473607048,126.849675313221));
#73630=CARTESIAN_POINT('Ctrl Pts',(-4.37759100400395,2.82000379283648,126.772730862824));
#73631=CARTESIAN_POINT('Ctrl Pts',(-4.38508133976603,2.710321821097,126.700296937677));
#73632=CARTESIAN_POINT('Ctrl Pts',(-4.39285567388512,2.5964812240627,126.625116658243));
#73633=CARTESIAN_POINT('Ctrl Pts',(-4.40063000800419,2.47932985806009,126.554557540504));
#73634=CARTESIAN_POINT('Ctrl Pts',(-4.40840434212328,2.35927957442864,126.488925187371));
#73635=CARTESIAN_POINT('Ctrl Pts',(-4.41616909507036,2.23937724204273,126.423373720248));
#73636=CARTESIAN_POINT('Ctrl Pts',(-4.42393384801746,2.11658344030295,126.36273712241));
#73637=CARTESIAN_POINT('Ctrl Pts',(-4.43169860096455,1.99133971379722,126.307278318257));
#73638=CARTESIAN_POINT('Ctrl Pts',(-4.43945564184955,1.86622038112628,126.251874596571));
#73639=CARTESIAN_POINT('Ctrl Pts',(-4.44721268273454,1.73865632123798,126.201638591722));
#73640=CARTESIAN_POINT('Ctrl Pts',(-4.45496972361954,1.60911413349843,126.156787619982));
#73641=CARTESIAN_POINT('Ctrl Pts',(-4.46272091485966,1.47966963453053,126.111970470708));
#73642=CARTESIAN_POINT('Ctrl Pts',(-4.47047210609975,1.34825034484623,126.072530398973));
#73643=CARTESIAN_POINT('Ctrl Pts',(-4.47822329733987,1.2153429916841,126.038636698258));
#73644=CARTESIAN_POINT('Ctrl Pts',(-4.48597119411694,1.08249212769231,126.00475740327));
#73645=CARTESIAN_POINT('Ctrl Pts',(-4.49371909089409,0.948154836198017,
125.976419887112));
#73646=CARTESIAN_POINT('Ctrl Pts',(-4.50146698767117,0.812832950592326,
125.953743578783));
#73647=CARTESIAN_POINT('Ctrl Pts',(-4.50921326375526,0.6775393714079,125.931072013849));
#73648=CARTESIAN_POINT('Ctrl Pts',(-4.51695953983933,0.541261993114158,
125.914059365874));
#73649=CARTESIAN_POINT('Ctrl Pts',(-4.52470581592343,0.40451239622551,125.902773855731));
#73650=CARTESIAN_POINT('Ctrl Pts',(-4.53245214918877,0.267761789882404,
125.89148826228));
#73651=CARTESIAN_POINT('Ctrl Pts',(-4.54019848245411,0.130539347629309,
125.885929923176));
#73652=CARTESIAN_POINT('Ctrl Pts',(-4.54794481571946,-0.00663907635700782,
125.886115098566));
#73653=CARTESIAN_POINT('Ctrl Pts',(-4.55569288372243,-0.143848220500248,
125.886300315424));
#73654=CARTESIAN_POINT('Ctrl Pts',(-4.5634409517254,-0.281012935871234,
125.892231605679));
#73655=CARTESIAN_POINT('Ctrl Pts',(-4.57118901972837,-0.417618617632918,
125.90387311603));
#73656=CARTESIAN_POINT('Ctrl Pts',(-4.57894532247021,-0.554369485538806,
125.915526999118));
#73657=CARTESIAN_POINT('Ctrl Pts',(-4.58670162521208,-0.690559742787245,
125.932903192314));
#73658=CARTESIAN_POINT('Ctrl Pts',(-4.59445792795393,-0.825680594987528,
125.955913998538));
#73659=CARTESIAN_POINT('Ctrl Pts',(-4.6022183704681,-0.960873565255225,
125.978937086323));
#73660=CARTESIAN_POINT('Ctrl Pts',(-4.6099788129823,-1.09499561101543,126.007600697892));
#73661=CARTESIAN_POINT('Ctrl Pts',(-4.61773925549647,-1.22755033289508,
126.041766446034));
#73662=CARTESIAN_POINT('Ctrl Pts',(-4.62551215576191,-1.36031784338194,
126.075987040069));
#73663=CARTESIAN_POINT('Ctrl Pts',(-4.63328505602736,-1.49151262781264,
126.115727307456));
#73664=CARTESIAN_POINT('Ctrl Pts',(-4.6410579562928,-1.62065473735613,126.160799345785));
#73665=CARTESIAN_POINT('Ctrl Pts',(-4.64854829205488,-1.74510220592907,
126.204232901991));
#73666=CARTESIAN_POINT('Ctrl Pts',(-4.65603862781688,-1.86764336190305,
126.252617199525));
#73667=CARTESIAN_POINT('Ctrl Pts',(-4.66352896357895,-1.98786985942046,
126.305743442866));
#73668=CARTESIAN_POINT('Ctrl Pts',(-4.67130381885714,-2.11266314619595,
126.360887680263));
#73669=CARTESIAN_POINT('Ctrl Pts',(-4.67907867413534,-2.23535778873874,
126.421315921051));
#73670=CARTESIAN_POINT('Ctrl Pts',(-4.68685352941353,-2.35547396300495,
126.486846810743));
#73671=CARTESIAN_POINT('Ctrl Pts',(-4.69461868530658,-2.47544028843246,
126.552295948517));
#73672=CARTESIAN_POINT('Ctrl Pts',(-4.70238384119963,-2.59283420623772,
126.622834883091));
#73673=CARTESIAN_POINT('Ctrl Pts',(-4.71014899709269,-2.7071957753986,126.698234207412));
#73674=CARTESIAN_POINT('Ctrl Pts',(-4.71790632321508,-2.82144203137434,
126.773557505002));
#73675=CARTESIAN_POINT('Ctrl Pts',(-4.72566364933747,-2.93266169948924,
126.853731224905));
#73676=CARTESIAN_POINT('Ctrl Pts',(-4.73342097545986,-3.04041969265861,
126.938480232066));
#73677=CARTESIAN_POINT('Ctrl Pts',(-4.7411719472867,-3.14808941750899,127.023159818368));
#73678=CARTESIAN_POINT('Ctrl Pts',(-4.74892291911353,-3.25230280751886,
127.112406988649));
#73679=CARTESIAN_POINT('Ctrl Pts',(-4.75667389094036,-3.35265438215081,
127.205903773814));
#73680=CARTESIAN_POINT('Ctrl Pts',(-4.76442139553933,-3.4529610666987,127.299358735235));
#73681=CARTESIAN_POINT('Ctrl Pts',(-4.7721689001383,-3.54940908734863,127.397059263635));
#73682=CARTESIAN_POINT('Ctrl Pts',(-4.77991640473726,-3.64162677196687,
127.498647757048));
#73683=CARTESIAN_POINT('Ctrl Pts',(-4.78766212144777,-3.73382317554775,
127.600212806925));
#73684=CARTESIAN_POINT('Ctrl Pts',(-4.79540783815827,-3.82179092344786,
127.705663746969));
#73685=CARTESIAN_POINT('Ctrl Pts',(-4.80315355486877,-3.90519617169571,
127.814607128886));
#73686=CARTESIAN_POINT('Ctrl Pts',(-4.81089916147566,-3.98860023435679,
127.923548962198));
#73687=CARTESIAN_POINT('Ctrl Pts',(-4.81864476808254,-4.0674416898175,128.035982827566));
#73688=CARTESIAN_POINT('Ctrl Pts',(-4.82639037468942,-4.1414281066588,128.151483632126));
#73689=CARTESIAN_POINT('Ctrl Pts',(-4.83414108432917,-4.21546326792204,
128.267060532005));
#73690=CARTESIAN_POINT('Ctrl Pts',(-4.84189179396892,-4.2846367881272,128.385708078921));
#73691=CARTESIAN_POINT('Ctrl Pts',(-4.84964250360866,-4.34870042526321,
128.506973476961));
#73692=CARTESIAN_POINT('Ctrl Pts',(-4.85739577780969,-4.41278525982903,
128.628278999398));
#73693=CARTESIAN_POINT('Ctrl Pts',(-4.86514905201066,-4.47175667099767,
128.752203747457));
#73694=CARTESIAN_POINT('Ctrl Pts',(-4.87290232621169,-4.52541366335418,
128.878272811149));
#73695=CARTESIAN_POINT('Ctrl Pts',(-4.88066480617851,-4.57913436475701,
129.004491561574));
#73696=CARTESIAN_POINT('Ctrl Pts',(-4.88842728614534,-4.62752789909615,
129.132859349595));
#73697=CARTESIAN_POINT('Ctrl Pts',(-4.89618976611217,-4.6704422594521,129.262883350908));
#73698=CARTESIAN_POINT('Ctrl Pts',(-4.90249021306015,-4.70527386634634,
129.368417835472));
#73699=CARTESIAN_POINT('Ctrl Pts',(-4.90879066000816,-4.73649681451379,
129.47504301176));
#73700=CARTESIAN_POINT('Ctrl Pts',(-4.91509110695614,-4.76405452823401,
129.582490119308));
#73701=CARTESIAN_POINT('Ctrl Pts',(-3.16500955108754,-4.76405452823408,
129.582490119308));
#73702=CARTESIAN_POINT('Ctrl Pts',(-3.17265462575404,-4.79768322009091,
129.713607878472));
#73703=CARTESIAN_POINT('Ctrl Pts',(-3.18029970042054,-4.82587473776987,
129.846037078759));
#73704=CARTESIAN_POINT('Ctrl Pts',(-3.18794477508703,-4.84854884266275,
129.979280510659));
#73705=CARTESIAN_POINT('Ctrl Pts',(-3.19581073990133,-4.87187807345036,
130.116373762561));
#73706=CARTESIAN_POINT('Ctrl Pts',(-3.20367670471566,-4.88936616706746,
130.254328551633));
#73707=CARTESIAN_POINT('Ctrl Pts',(-3.21154266952996,-4.90098312584827,
130.392599202848));
#73708=CARTESIAN_POINT('Ctrl Pts',(-3.21940863434426,-4.91260008462908,
130.530869854064));
#73709=CARTESIAN_POINT('Ctrl Pts',(-3.22727459915858,-4.91834594800464,
130.66945590665));
#73710=CARTESIAN_POINT('Ctrl Pts',(-3.23514056397289,-4.91824878730941,
130.80781440238));
#73711=CARTESIAN_POINT('',(-2.8898594360264,-4.91824974010731,130.805959502914));
#73712=CARTESIAN_POINT('Ctrl Pts',(-2.82009873120262,-4.76405452823401,
129.582490119308));
#73713=CARTESIAN_POINT('Ctrl Pts',(-2.82804801001931,-4.7989877331598,129.718694155128));
#73714=CARTESIAN_POINT('Ctrl Pts',(-2.83599728883601,-4.82810441912981,
129.856509573153));
#73715=CARTESIAN_POINT('Ctrl Pts',(-2.84394656765269,-4.8512666200099,129.99541362049));
#73716=CARTESIAN_POINT('Ctrl Pts',(-2.85188872461985,-4.87440806961014,
130.134193222108));
#73717=CARTESIAN_POINT('Ctrl Pts',(-2.85983088158702,-4.89160560644795,
130.274059153101));
#73718=CARTESIAN_POINT('Ctrl Pts',(-2.86777303855419,-4.90277209154466,
130.414477454464));
#73719=CARTESIAN_POINT('Ctrl Pts',(-2.87513517103323,-4.91312307591163,
130.544640852315));
#73720=CARTESIAN_POINT('Ctrl Pts',(-2.88249730351221,-4.91829222347275,
130.675278536417));
#73721=CARTESIAN_POINT('Ctrl Pts',(-2.88985943599124,-4.91824974010752,
130.80595950229));
#73722=CARTESIAN_POINT('Ctrl Pts',(-2.88985943602637,-4.91824974010731,
130.805959502914));
#73723=CARTESIAN_POINT('Ctrl Pts',(-2.89820794086171,-4.91820156483749,
130.954148995372));
#73724=CARTESIAN_POINT('Ctrl Pts',(-2.90655644569702,-4.91145165372105,
131.102143021204));
#73725=CARTESIAN_POINT('Ctrl Pts',(-2.91490495053236,-4.89807797319362,
131.249349641043));
#73726=CARTESIAN_POINT('Ctrl Pts',(-2.92328621970895,-4.88465180664131,
131.397133984442));
#73727=CARTESIAN_POINT('Ctrl Pts',(-2.93166748888556,-4.86454985974308,
131.544124447829));
#73728=CARTESIAN_POINT('Ctrl Pts',(-2.94004875806212,-4.83790179310411,
131.689735850323));
#73729=CARTESIAN_POINT('Ctrl Pts',(-2.94844645255313,-4.81120150252806,
131.835632616886));
#73730=CARTESIAN_POINT('Ctrl Pts',(-2.9568441470441,-4.77792952909772,131.980144644462));
#73731=CARTESIAN_POINT('Ctrl Pts',(-2.96524184153512,-4.73826562546462,
132.122701212799));
#73732=CARTESIAN_POINT('Ctrl Pts',(-2.97366657939604,-4.69847399086689,
132.265716860711));
#73733=CARTESIAN_POINT('Ctrl Pts',(-2.982091317257,-4.65224932172985,132.406764172971));
#73734=CARTESIAN_POINT('Ctrl Pts',(-2.99051605511792,-4.5998208444264,132.545288893424));
#73735=CARTESIAN_POINT('Ctrl Pts',(-2.99782144236563,-4.55435826317674,
132.665408562783));
#73736=CARTESIAN_POINT('Ctrl Pts',(-3.00512682961338,-4.50423170428375,
132.783631688841));
#73737=CARTESIAN_POINT('Ctrl Pts',(-3.0124322168611,-4.44961828863167,132.899612427725));
#73738=CARTESIAN_POINT('Ctrl Pts',(-3.02020655098013,-4.39149913269009,
133.023038193518));
#73739=CARTESIAN_POINT('Ctrl Pts',(-3.02798088509929,-4.32814855865314,
133.144239416373));
#73740=CARTESIAN_POINT('Ctrl Pts',(-3.03575521921837,-4.25975934281512,
133.262740857439));
#73741=CARTESIAN_POINT('Ctrl Pts',(-3.04351997216547,-4.19145441057349,
133.38109625607));
#73742=CARTESIAN_POINT('Ctrl Pts',(-3.05128472511256,-4.11812338548197,
133.496758157758));
#73743=CARTESIAN_POINT('Ctrl Pts',(-3.05904947805965,-4.04000660404017,
133.609272327729));
#73744=CARTESIAN_POINT('Ctrl Pts',(-3.06680651894463,-3.96196740928718,
133.72167474704));
#73745=CARTESIAN_POINT('Ctrl Pts',(-3.0745635598296,-3.87915213895429,133.830935337182));
#73746=CARTESIAN_POINT('Ctrl Pts',(-3.08232060071458,-3.79184625215337,
133.936625782352));
#73747=CARTESIAN_POINT('Ctrl Pts',(-3.09007179195469,-3.70460620340083,
134.042236525535));
#73748=CARTESIAN_POINT('Ctrl Pts',(-3.09782298319482,-3.61288252660651,
134.144282182351));
#73749=CARTESIAN_POINT('Ctrl Pts',(-3.10557417443493,-3.51700285169162,
134.242364981102));
#73750=CARTESIAN_POINT('Ctrl Pts',(-3.11332207121201,-3.42116392819611,
134.340406092048));
#73751=CARTESIAN_POINT('Ctrl Pts',(-3.1210699679891,-3.32117279255921,134.434487415923));
#73752=CARTESIAN_POINT('Ctrl Pts',(-3.12881786476618,-3.21739591468639,
134.524245910241));
#73753=CARTESIAN_POINT('Ctrl Pts',(-3.13656414085027,-3.11364074469925,
134.613985629017));
#73754=CARTESIAN_POINT('Ctrl Pts',(-3.14431041693429,-3.00610170311664,
134.699404061227));
#73755=CARTESIAN_POINT('Ctrl Pts',(-3.15205669301838,-2.89518022184796,
134.780176828801));
#73756=CARTESIAN_POINT('Ctrl Pts',(-3.15980302628374,-2.78425792178195,
134.860950192622));
#73757=CARTESIAN_POINT('Ctrl Pts',(-3.16754935954914,-2.6699534482558,134.93707759323));
#73758=CARTESIAN_POINT('Ctrl Pts',(-3.1752956928145,-2.55269891201957,135.008276806915));
#73759=CARTESIAN_POINT('Ctrl Pts',(-3.18304376081748,-2.43541811744293,
135.079491965171));
#73760=CARTESIAN_POINT('Ctrl Pts',(-3.19079182882045,-2.31518627966388,
135.145776537518));
#73761=CARTESIAN_POINT('Ctrl Pts',(-3.19853989682343,-2.19246155075561,
135.206893457984));
#73762=CARTESIAN_POINT('Ctrl Pts',(-3.20629619956528,-2.06960638854518,
135.268075334241));
#73763=CARTESIAN_POINT('Ctrl Pts',(-3.2140525023072,-1.94425339312259,135.324078412709));
#73764=CARTESIAN_POINT('Ctrl Pts',(-3.22180880504905,-1.81688272216531,
135.374712927443));
#73765=CARTESIAN_POINT('Ctrl Pts',(-3.22956924756322,-1.68944406964588,
135.425374467342));
#73766=CARTESIAN_POINT('Ctrl Pts',(-3.23732969007735,-1.55998596464474,
135.470661604992));
#73767=CARTESIAN_POINT('Ctrl Pts',(-3.24509013259151,-1.42900434673795,
135.510434314344));
#73768=CARTESIAN_POINT('Ctrl Pts',(-3.25286303285694,-1.29781246551009,
135.55027087038));
#73769=CARTESIAN_POINT('Ctrl Pts',(-3.26063593312233,-1.16509256287556,
135.584575210608));
#73770=CARTESIAN_POINT('Ctrl Pts',(-3.26840883338775,-1.03135228548577,
135.613258155019));
#73771=CARTESIAN_POINT('Ctrl Pts',(-3.27589916914981,-0.902473804049821,
135.640898402154));
#73772=CARTESIAN_POINT('Ctrl Pts',(-3.2833895049119,-0.772648149784768,
135.663318809151));
#73773=CARTESIAN_POINT('Ctrl Pts',(-3.29087984067397,-0.642332684473476,
135.680485286292));
#73774=CARTESIAN_POINT('Ctrl Pts',(-3.29865417479303,-0.507076268687317,
135.698302635631));
#73775=CARTESIAN_POINT('Ctrl Pts',(-3.30642850891206,-0.370863714611736,
135.71051622497));
#73776=CARTESIAN_POINT('Ctrl Pts',(-3.31420284303113,-0.234199054447876,
135.717031364257));
#73777=CARTESIAN_POINT('Ctrl Pts',(-3.32196759597819,-0.0977028212637813,
135.723538474218));
#73778=CARTESIAN_POINT('Ctrl Pts',(-3.32973234892537,0.039244022613044,
135.724361089027));
#73779=CARTESIAN_POINT('Ctrl Pts',(-3.33749710187243,0.176129408853844,
135.719455885599));
#73780=CARTESIAN_POINT('Ctrl Pts',(-3.34525414275741,0.31287883859947,135.714555554087));
#73781=CARTESIAN_POINT('Ctrl Pts',(-3.35301118364226,0.449566543996468,
135.703938739516));
#73782=CARTESIAN_POINT('Ctrl Pts',(-3.36076822452725,0.585677873207814,
135.687614091566));
#73783=CARTESIAN_POINT('Ctrl Pts',(-3.36851941576737,0.721686559807009,
135.671301754161));
#73784=CARTESIAN_POINT('Ctrl Pts',(-3.37627060700752,0.857119348751999,
135.649290197237));
#73785=CARTESIAN_POINT('Ctrl Pts',(-3.38402179824763,0.991464491473524,
135.621640059808));
#73786=CARTESIAN_POINT('Ctrl Pts',(-3.3917696950247,1.12575253392562,135.594001674425));
#73787=CARTESIAN_POINT('Ctrl Pts',(-3.39951759180175,1.25895346745419,135.560729553737));
#73788=CARTESIAN_POINT('Ctrl Pts',(-3.40726548857882,1.39056376819806,135.52193578592));
#73789=CARTESIAN_POINT('Ctrl Pts',(-3.4150117646629,1.5221465389042,135.483150132924));
#73790=CARTESIAN_POINT('Ctrl Pts',(-3.42275804074694,1.65213896386063,135.438845240648));
#73791=CARTESIAN_POINT('Ctrl Pts',(-3.43050431683102,1.78005115085772,135.389183510855));
#73792=CARTESIAN_POINT('Ctrl Pts',(-3.43825065009635,1.90796428207352,135.339521414471));
#73793=CARTESIAN_POINT('Ctrl Pts',(-3.44599698336172,2.03379678022834,135.284502543167));
#73794=CARTESIAN_POINT('Ctrl Pts',(-3.45374331662705,2.15707763610479,135.224337895145));
#73795=CARTESIAN_POINT('Ctrl Pts',(-3.46149138463001,2.28038609987415,135.164159773667));
#73796=CARTESIAN_POINT('Ctrl Pts',(-3.46923945263297,2.40114143301143,135.098833753846));
#73797=CARTESIAN_POINT('Ctrl Pts',(-3.47698752063593,2.51889654281374,135.028617152046));
#73798=CARTESIAN_POINT('Ctrl Pts',(-3.48474382337776,2.63677680414805,134.958325923207));
#73799=CARTESIAN_POINT('Ctrl Pts',(-3.49250012611962,2.75165013609627,134.883133929841));
#73800=CARTESIAN_POINT('Ctrl Pts',(-3.50025642886146,2.86309734623971,134.80334256907));
#73801=CARTESIAN_POINT('Ctrl Pts',(-3.50801687137561,2.97460403911481,134.723508621248));
#73802=CARTESIAN_POINT('Ctrl Pts',(-3.51577731388975,3.08268065856118,134.639070655166));
#73803=CARTESIAN_POINT('Ctrl Pts',(-3.5235377564039,3.18694132924324,134.550370231337));
#73804=CARTESIAN_POINT('Ctrl Pts',(-3.53131065666931,3.29136936840972,134.461527417712));
#73805=CARTESIAN_POINT('Ctrl Pts',(-3.53908355693467,3.39196893063057,134.368408738626));
#73806=CARTESIAN_POINT('Ctrl Pts',(-3.54685645720008,3.48839059082423,134.271393087611));
#73807=CARTESIAN_POINT('Ctrl Pts',(-3.55434679296228,3.58130708080083,134.177904199876));
#73808=CARTESIAN_POINT('Ctrl Pts',(-3.56183712872454,3.67034394148668,134.080796977719));
#73809=CARTESIAN_POINT('Ctrl Pts',(-3.56932746448675,3.7552252770198,133.980437786234));
#73810=CARTESIAN_POINT('Ctrl Pts',(-3.57710179860585,3.8433249141869,133.876273445502));
#73811=CARTESIAN_POINT('Ctrl Pts',(-3.58487613272495,3.92722676545942,133.768275709389));
#73812=CARTESIAN_POINT('Ctrl Pts',(-3.59265046684405,4.00657872369888,133.656817452174));
#73813=CARTESIAN_POINT('Ctrl Pts',(-3.60041521979116,4.0858328877417,133.5454965573));
#73814=CARTESIAN_POINT('Ctrl Pts',(-3.6081799727383,4.16054809110699,133.430723942408));
#73815=CARTESIAN_POINT('Ctrl Pts',(-3.61594472568541,4.23041109941507,133.312907007898));
#73816=CARTESIAN_POINT('Ctrl Pts',(-3.62370176657043,4.3002047187984,133.195207090828));
#73817=CARTESIAN_POINT('Ctrl Pts',(-3.63145880745549,4.36515553556552,133.074469205474));
#73818=CARTESIAN_POINT('Ctrl Pts',(-3.63921584834051,4.42499264505032,132.951131018366));
#73819=CARTESIAN_POINT('Ctrl Pts',(-3.64696703958066,4.48478463090539,132.827885841544));
#73820=CARTESIAN_POINT('Ctrl Pts',(-3.65471823082077,4.53947041522027,132.702044616369));
#73821=CARTESIAN_POINT('Ctrl Pts',(-3.66246942206092,4.58882440271248,132.574070668272));
#73822=CARTESIAN_POINT('Ctrl Pts',(-3.67021731883803,4.63815741344345,132.446151112517));
#73823=CARTESIAN_POINT('Ctrl Pts',(-3.67796521561518,4.68216299417844,132.316101000743));
#73824=CARTESIAN_POINT('Ctrl Pts',(-3.68571311239228,4.72066328093046,132.184404548234));
#73825=CARTESIAN_POINT('Ctrl Pts',(-3.69345938847638,4.75915551425241,132.052735643785));
#73826=CARTESIAN_POINT('Ctrl Pts',(-3.70120566456046,4.79214463453071,131.919421458609));
#73827=CARTESIAN_POINT('Ctrl Pts',(-3.70895194064457,4.8195024762636,131.784961935018));
#73828=CARTESIAN_POINT('Ctrl Pts',(-3.71669827390993,4.84686051994587,131.650501418878));
#73829=CARTESIAN_POINT('Ctrl Pts',(-3.7244446071753,4.86858712418446,131.514895930568));
#73830=CARTESIAN_POINT('Ctrl Pts',(-3.73219094044066,4.88460521575539,131.378655793164));
#73831=CARTESIAN_POINT('Ctrl Pts',(-3.73993900844365,4.90062689446686,131.242385145726));
#73832=CARTESIAN_POINT('Ctrl Pts',(-3.74768707644666,4.91093747103526,131.105479954598));
#73833=CARTESIAN_POINT('Ctrl Pts',(-3.75543514444965,4.91551176848025,130.968455457315));
#73834=CARTESIAN_POINT('Ctrl Pts',(-3.76319144719153,4.92009092754301,130.831285328765));
#73835=CARTESIAN_POINT('Ctrl Pts',(-3.77094774993344,4.91892161583052,130.693996032133));
#73836=CARTESIAN_POINT('Ctrl Pts',(-3.77870405267532,4.91203082353697,130.557103158381));
#73837=CARTESIAN_POINT('Ctrl Pts',(-3.78646449518951,4.90513635342009,130.42013722078));
#73838=CARTESIAN_POINT('Ctrl Pts',(-3.79422493770368,4.8925143538766,130.283568516771));
#73839=CARTESIAN_POINT('Ctrl Pts',(-3.80198538021787,4.87424361439373,130.147906316002));
#73840=CARTESIAN_POINT('Ctrl Pts',(-3.80975828048332,4.85594354509784,130.012026338224));
#73841=CARTESIAN_POINT('Ctrl Pts',(-3.81753118074872,4.83197668378551,129.877056156804));
#73842=CARTESIAN_POINT('Ctrl Pts',(-3.82530408101417,4.80247293152463,129.743494554166));
#73843=CARTESIAN_POINT('Ctrl Pts',(-3.83279441677603,4.77404171497462,129.614788252209));
#73844=CARTESIAN_POINT('Ctrl Pts',(-3.8402847525379,4.74046925680224,129.487390194114));
#73845=CARTESIAN_POINT('Ctrl Pts',(-3.84777508829976,4.70191466188526,129.361730528164));
#73846=CARTESIAN_POINT('Ctrl Pts',(-3.85554942241884,4.66189825778269,129.231306437783));
#73847=CARTESIAN_POINT('Ctrl Pts',(-3.86332375653792,4.61638770376544,129.102342019724));
#73848=CARTESIAN_POINT('Ctrl Pts',(-3.871098090657,4.56550638701657,128.975335059349));
#73849=CARTESIAN_POINT('Ctrl Pts',(-3.87886284360409,4.5146877769432,128.848484623702));
#73850=CARTESIAN_POINT('Ctrl Pts',(-3.88662759655121,4.45851171794416,128.72358720524));
#73851=CARTESIAN_POINT('Ctrl Pts',(-3.8943923494983,4.39715165668143,128.601126546786));
#73852=CARTESIAN_POINT('Ctrl Pts',(-3.90214939038331,4.33585253909658,128.478787517985));
#73853=CARTESIAN_POINT('Ctrl Pts',(-3.90990643126832,4.26937983964819,128.358880780116));
#73854=CARTESIAN_POINT('Ctrl Pts',(-3.91766347215332,4.19795534899483,128.241870822397));
#73855=CARTESIAN_POINT('Ctrl Pts',(-3.92541466339345,4.12658472010546,128.124949102797));
#73856=CARTESIAN_POINT('Ctrl Pts',(-3.9331658546336,4.05026993555358,128.010920147622));
#73857=CARTESIAN_POINT('Ctrl Pts',(-3.94091704587373,3.96927886438715,127.900224195283));
#73858=CARTESIAN_POINT('Ctrl Pts',(-3.94866494265082,3.88832221658647,127.789575291678));
#73859=CARTESIAN_POINT('Ctrl Pts',(-3.95641283942789,3.80269346562427,127.682256888238));
#73860=CARTESIAN_POINT('Ctrl Pts',(-3.96416073620497,3.71270385570266,127.578680357163));
#73861=CARTESIAN_POINT('Ctrl Pts',(-3.97190701228908,3.6227330696675,127.475125492066));
#73862=CARTESIAN_POINT('Ctrl Pts',(-3.97965328837316,3.52840349533988,127.375311237408));
#73863=CARTESIAN_POINT('Ctrl Pts',(-3.98739956445726,3.43006647176078,127.279615653487));
#73864=CARTESIAN_POINT('Ctrl Pts',(-3.99514589772262,3.33172872228011,127.183919363162));
#73865=CARTESIAN_POINT('Ctrl Pts',(-4.002892230988,3.22938374471073,127.092342076907));
#73866=CARTESIAN_POINT('Ctrl Pts',(-4.01063856425336,3.12341922834965,127.005224480695));
#73867=CARTESIAN_POINT('Ctrl Pts',(-4.01838663225634,3.01743098196984,126.918087375102));
#73868=CARTESIAN_POINT('Ctrl Pts',(-4.02613470025925,2.90782188580262,126.835412195125));
#73869=CARTESIAN_POINT('Ctrl Pts',(-4.03388276826223,2.79501181500518,126.757498621342));
#73870=CARTESIAN_POINT('Ctrl Pts',(-4.04163907100409,2.68208184832205,126.679502240086));
#73871=CARTESIAN_POINT('Ctrl Pts',(-4.04939537374599,2.5659444332886,126.60627779684));
#73872=CARTESIAN_POINT('Ctrl Pts',(-4.05715167648785,2.447047940042,126.538081273496));
#73873=CARTESIAN_POINT('Ctrl Pts',(-4.06491211900203,2.32808798815688,126.469848351615));
#73874=CARTESIAN_POINT('Ctrl Pts',(-4.07267256151614,2.206366370585,126.406648876912));
#73875=CARTESIAN_POINT('Ctrl Pts',(-4.08043300403031,2.0823541379467,126.348691834243));
#73876=CARTESIAN_POINT('Ctrl Pts',(-4.08820590429574,1.95814282986346,126.290641753785));
#73877=CARTESIAN_POINT('Ctrl Pts',(-4.09597880456126,1.83163391971795,126.237851073096));
#73878=CARTESIAN_POINT('Ctrl Pts',(-4.10375170482669,1.70331726199213,126.190480106814));
#73879=CARTESIAN_POINT('Ctrl Pts',(-4.11124204058866,1.57966523798585,126.144831194476));
#73880=CARTESIAN_POINT('Ctrl Pts',(-4.11873237635065,1.4543349099125,126.104214892086));
#73881=CARTESIAN_POINT('Ctrl Pts',(-4.12622271211262,1.32777417377965,126.068729845858));
#73882=CARTESIAN_POINT('Ctrl Pts',(-4.13399704623169,1.19641484886808,126.031899373317));
#73883=CARTESIAN_POINT('Ctrl Pts',(-4.14177138035076,1.06331386538916,126.000480273246));
#73884=CARTESIAN_POINT('Ctrl Pts',(-4.14954571446984,0.928956718054041,
125.97463780166));
#73885=CARTESIAN_POINT('Ctrl Pts',(-4.15731046741691,0.79476515389535,125.948827178611));
#73886=CARTESIAN_POINT('Ctrl Pts',(-4.16507522036401,0.659320886399582,
125.928579582568));
#73887=CARTESIAN_POINT('Ctrl Pts',(-4.17283997331108,0.523124654261355,
125.914010562754));
#73888=CARTESIAN_POINT('Ctrl Pts',(-4.18059701419607,0.387063694140919,
125.899456013095));
#73889=CARTESIAN_POINT('Ctrl Pts',(-4.18835405508103,0.250252641898669,
125.890568857042));
#73890=CARTESIAN_POINT('Ctrl Pts',(-4.19611109596602,0.113202168737664,
125.887413563601));
#73891=CARTESIAN_POINT('Ctrl Pts',(-4.20386228720612,-0.0237449535952466,
125.884260649592));
#73892=CARTESIAN_POINT('Ctrl Pts',(-4.21161347844621,-0.160930748194613,
125.886831003597));
#73893=CARTESIAN_POINT('Ctrl Pts',(-4.21936466968631,-0.297840040250985,
125.895137219418));
#73894=CARTESIAN_POINT('Ctrl Pts',(-4.22711256646339,-0.434691142206245,
125.903439904875));
#73895=CARTESIAN_POINT('Ctrl Pts',(-4.23486046324046,-0.571265585928096,
125.917473579735));
#73896=CARTESIAN_POINT('Ctrl Pts',(-4.24260836001753,-0.707049037241934,
125.937198742157));
#73897=CARTESIAN_POINT('Ctrl Pts',(-4.25035463610162,-0.842804085584909,
125.9569197785));
#73898=CARTESIAN_POINT('Ctrl Pts',(-4.2581009121857,-0.977768083967068,
125.982329878192));
#73899=CARTESIAN_POINT('Ctrl Pts',(-4.26584718826979,-1.11143305221947,
126.013337800574));
#73900=CARTESIAN_POINT('Ctrl Pts',(-4.27359352153513,-1.2450990071563,126.04434595185));
#73901=CARTESIAN_POINT('Ctrl Pts',(-4.28133985480043,-1.37746553197736,
126.080951919919));
#73902=CARTESIAN_POINT('Ctrl Pts',(-4.28908618806577,-1.5080364423889,126.123013679886));
#73903=CARTESIAN_POINT('Ctrl Pts',(-4.29683425606873,-1.63863659325052,
126.165084859293));
#73904=CARTESIAN_POINT('Ctrl Pts',(-4.30458232407171,-1.76743995747763,
126.212614141957));
#73905=CARTESIAN_POINT('Ctrl Pts',(-4.31233039207467,-1.89396745253293,
126.265410259692));
#73906=CARTESIAN_POINT('Ctrl Pts',(-4.32008669481651,-2.02062942251567,
126.318262489769));
#73907=CARTESIAN_POINT('Ctrl Pts',(-4.32784299755834,-2.14501033008246,
126.376392586037));
#73908=CARTESIAN_POINT('Ctrl Pts',(-4.33559930030017,-2.26665245540512,
126.439561686469));
#73909=CARTESIAN_POINT('Ctrl Pts',(-4.34335974281432,-2.38835950479265,
126.502764502152));
#73910=CARTESIAN_POINT('Ctrl Pts',(-4.35112018532849,-2.50732452027586,
126.57101148654));
#73911=CARTESIAN_POINT('Ctrl Pts',(-4.35888062784264,-2.62311706260929,
126.644019292825));
#73912=CARTESIAN_POINT('Ctrl Pts',(-4.36665352810805,-2.73909548541125,
126.717144297722));
#73913=CARTESIAN_POINT('Ctrl Pts',(-4.37442642837349,-2.85189093627025,
126.795045174349));
#73914=CARTESIAN_POINT('Ctrl Pts',(-4.3821993286389,-2.96110375962843,126.877396448234));
#73915=CARTESIAN_POINT('Ctrl Pts',(-4.3896896644011,-3.06634642176969,126.956754045885));
#73916=CARTESIAN_POINT('Ctrl Pts',(-4.39718000016326,-3.16826217097445,
127.040243896885));
#73917=CARTESIAN_POINT('Ctrl Pts',(-4.40467033592546,-3.26652591465533,
127.127542494326));
#73918=CARTESIAN_POINT('Ctrl Pts',(-4.41232756809087,-3.36697912832878,
127.216786241141));
#73919=CARTESIAN_POINT('Ctrl Pts',(-4.41998480025625,-3.46395413688269,
127.310311515935));
#73920=CARTESIAN_POINT('Ctrl Pts',(-4.42764203242166,-3.55705555686598,
127.407812542259));
#73921=CARTESIAN_POINT('Ctrl Pts',(-4.43529043724618,-3.65004964851532,
127.505201168336));
#73922=CARTESIAN_POINT('Ctrl Pts',(-4.44293884207073,-3.73917875257566,
127.606556146739));
#73923=CARTESIAN_POINT('Ctrl Pts',(-4.45058724689525,-3.82408041706777,
127.71153148774));
#73924=CARTESIAN_POINT('Ctrl Pts',(-4.4582286082714,-3.90890389525773,127.816410156505));
#73925=CARTESIAN_POINT('Ctrl Pts',(-4.46586996964758,-3.98950742243945,
127.924902247342));
#73926=CARTESIAN_POINT('Ctrl Pts',(-4.47351133102373,-4.06556571548979,
128.036625356466));
#73927=CARTESIAN_POINT('Ctrl Pts',(-4.48153076923438,-4.1453871964407,128.153876265856));
#73928=CARTESIAN_POINT('Ctrl Pts',(-4.48955020744505,-4.22020185263817,
128.274685773025));
#73929=CARTESIAN_POINT('Ctrl Pts',(-4.49756964565572,-4.28968158809207,
128.398572818261));
#73930=CARTESIAN_POINT('Ctrl Pts',(-4.50520257694934,-4.35581266025541,
128.516488971441));
#73931=CARTESIAN_POINT('Ctrl Pts',(-4.51283550824294,-4.41711080757548,
128.637192555279));
#73932=CARTESIAN_POINT('Ctrl Pts',(-4.52046843953656,-4.47333819900914,
128.760240166177));
#73933=CARTESIAN_POINT('Ctrl Pts',(-4.52809978580013,-4.5295539144429,128.883262225403));
#73934=CARTESIAN_POINT('Ctrl Pts',(-4.53573113206374,-4.58070080474959,
129.00862697483));
#73935=CARTESIAN_POINT('Ctrl Pts',(-4.54336247832731,-4.62658815136065,
129.135868741593));
#73936=CARTESIAN_POINT('Ctrl Pts',(-4.55099506589904,-4.67248296196763,
129.263131205391));
#73937=CARTESIAN_POINT('Ctrl Pts',(-4.5586276534707,-4.71311638671098,129.392270915542));
#73938=CARTESIAN_POINT('Ctrl Pts',(-4.56626024104241,-4.74834690030874,
129.522805009397));
#73939=CARTESIAN_POINT('Ctrl Pts',(-4.56742169054548,-4.7537079213421,129.54266835941));
#73940=CARTESIAN_POINT('Ctrl Pts',(-4.56858314004855,-4.7589439293273,129.562563971735));
#73941=CARTESIAN_POINT('Ctrl Pts',(-4.56974458955162,-4.76405452823407,
129.582490119308));
#73942=CARTESIAN_POINT('Origin',(213.235140564004,0.,130.804360617566));
#73943=CARTESIAN_POINT('',(-6.66542383595775,-4.76405452823408,129.582490119308));
#73944=CARTESIAN_POINT('',(-6.31979145723438,-4.76405452823404,129.582490119308));
#73945=CARTESIAN_POINT('',(213.235140564004,-4.76405452823405,129.582490119308));
#73946=CARTESIAN_POINT('',(-4.98514056403867,-4.91824846381416,130.800473370515));
#73947=CARTESIAN_POINT('Ctrl Pts',(-4.98514056403869,-4.91824846381416,
130.800473370515));
#73948=CARTESIAN_POINT('Ctrl Pts',(-4.99278994307129,-4.91835489482087,
130.935132713854));
#73949=CARTESIAN_POINT('Ctrl Pts',(-5.00043932210384,-4.9129268059493,131.069997494585));
#73950=CARTESIAN_POINT('Ctrl Pts',(-5.00808870113644,-4.9019402097927,131.20456711691));
#73951=CARTESIAN_POINT('Ctrl Pts',(-5.01573056659492,-4.89096440517935,
131.339004558724));
#73952=CARTESIAN_POINT('Ctrl Pts',(-5.02337243205339,-4.87444098482965,
131.47314701929));
#73953=CARTESIAN_POINT('Ctrl Pts',(-5.03101429751186,-4.85239799954162,
131.606493222903));
#73954=CARTESIAN_POINT('Ctrl Pts',(-5.03890637724906,-4.82963327036855,
131.744205523294));
#73955=CARTESIAN_POINT('Ctrl Pts',(-5.04679845698631,-4.80098132423921,
131.88106809453));
#73956=CARTESIAN_POINT('Ctrl Pts',(-5.05469053672351,-4.76653130125415,
132.016533219411));
#73957=CARTESIAN_POINT('Ctrl Pts',(-5.06232395247998,-4.73321038243154,
132.147558456504));
#73958=CARTESIAN_POINT('Ctrl Pts',(-5.06995736823651,-4.69446559218237,
132.277275989228));
#73959=CARTESIAN_POINT('Ctrl Pts',(-5.07759078399297,-4.65042955773849,
132.405200394374));
#73960=CARTESIAN_POINT('Ctrl Pts',(-5.08522308473622,-4.60639995563924,
132.5331061136));
#73961=CARTESIAN_POINT('Ctrl Pts',(-5.09285538547939,-4.55708077729923,
132.659218844464));
#73962=CARTESIAN_POINT('Ctrl Pts',(-5.10048768622264,-4.50265421179631,
132.783069315554));
#73963=CARTESIAN_POINT('Ctrl Pts',(-5.10812063862446,-4.44822299926237,
132.906930361204));
#73964=CARTESIAN_POINT('Ctrl Pts',(-5.11575359102633,-4.38868369523615,
133.028528393651));
#73965=CARTESIAN_POINT('Ctrl Pts',(-5.12338654342815,-4.3242659919312,133.147415609137));
#73966=CARTESIAN_POINT('Ctrl Pts',(-5.13102191450769,-4.25982787638538,
133.266340496791));
#73967=CARTESIAN_POINT('Ctrl Pts',(-5.13865728558717,-4.19050848036941,
133.382552505079));
#73968=CARTESIAN_POINT('Ctrl Pts',(-5.1462926566667,-4.11658235665875,133.495630348259));
#73969=CARTESIAN_POINT('Ctrl Pts',(-5.15393623945735,-4.04257672666535,
133.608829804728));
#73970=CARTESIAN_POINT('Ctrl Pts',(-5.16157982224803,-3.96395470252006,
133.718888031474));
#73971=CARTESIAN_POINT('Ctrl Pts',(-5.16922340503868,-3.8810330157953,133.825414372931));
#73972=CARTESIAN_POINT('Ctrl Pts',(-5.17687191233893,-3.79805790534855,
133.932009345815));
#73973=CARTESIAN_POINT('Ctrl Pts',(-5.18452041963917,-3.71077787892187,
134.035067597811));
#73974=CARTESIAN_POINT('Ctrl Pts',(-5.19216892693942,-3.61954756763109,
134.134234259036));
#73975=CARTESIAN_POINT('Ctrl Pts',(-5.19982802808361,-3.52819089447081,
134.233538274662));
#73976=CARTESIAN_POINT('Ctrl Pts',(-5.20748712922783,-3.43287330403267,
134.328939661867));
#73977=CARTESIAN_POINT('Ctrl Pts',(-5.21514623037203,-3.33398372617403,
134.420122719268));
#73978=CARTESIAN_POINT('Ctrl Pts',(-5.21690555731626,-3.31126838457515,
134.441067841512));
#73979=CARTESIAN_POINT('Ctrl Pts',(-5.21866488426048,-3.28836469566599,
134.461790565631));
#73980=CARTESIAN_POINT('Ctrl Pts',(-5.22042421120472,-3.26527758926873,
134.482287387843));
#73981=CARTESIAN_POINT('Ctrl Pts',(-5.22819854532379,-3.16325739366898,
134.572861311456));
#73982=CARTESIAN_POINT('Ctrl Pts',(-5.23597287944286,-3.05730417132377,
134.659330648952));
#73983=CARTESIAN_POINT('Ctrl Pts',(-5.24374721356193,-2.94778223953403,
134.741334446637));
#73984=CARTESIAN_POINT('Ctrl Pts',(-5.25151196650902,-2.83839528373696,
134.82323718197));
#73985=CARTESIAN_POINT('Ctrl Pts',(-5.25927671945615,-2.72544867939069,
134.900685095497));
#73986=CARTESIAN_POINT('Ctrl Pts',(-5.26704147240324,-2.60934219281335,
134.973355266556));
#73987=CARTESIAN_POINT('Ctrl Pts',(-5.27479851328823,-2.49335102483528,
135.045953260576));
#73988=CARTESIAN_POINT('Ctrl Pts',(-5.2825555541732,-2.37420654952286,135.11378274945));
#73989=CARTESIAN_POINT('Ctrl Pts',(-5.2903125950582,-2.25233980640477,135.176562403736));
#73990=CARTESIAN_POINT('Ctrl Pts',(-5.29806378629832,-2.13056496394566,
135.239294715395));
#73991=CARTESIAN_POINT('Ctrl Pts',(-5.30581497753849,-2.00607228597268,
135.296984593977));
#73992=CARTESIAN_POINT('Ctrl Pts',(-5.31356616877861,-1.87931955082755,
135.349395390632));
#73993=CARTESIAN_POINT('Ctrl Pts',(-5.32131406555568,-1.75262068897609,
135.4017839113));
#73994=CARTESIAN_POINT('Ctrl Pts',(-5.32906196233272,-1.62366404102289,
135.44889766361));
#73995=CARTESIAN_POINT('Ctrl Pts',(-5.33680985910979,-1.49292941456408,
135.490547214964));
#73996=CARTESIAN_POINT('Ctrl Pts',(-5.34455613519389,-1.36222213497082,
135.532188054129));
#73997=CARTESIAN_POINT('Ctrl Pts',(-5.35230241127793,-1.22973798891268,
135.568366847213));
#73998=CARTESIAN_POINT('Ctrl Pts',(-5.36004868736202,-1.09597369911091,
135.598943468384));
#73999=CARTESIAN_POINT('Ctrl Pts',(-5.36779502062734,-0.9622084218921,135.629520315265));
#74000=CARTESIAN_POINT('Ctrl Pts',(-5.37554135389274,-0.827163363207984,
135.654494820592));
#74001=CARTESIAN_POINT('Ctrl Pts',(-5.38328768715806,-0.691346849629597,
135.673777686991));
#74002=CARTESIAN_POINT('Ctrl Pts',(-5.39103575516105,-0.555499920883754,
135.693064871654));
#74003=CARTESIAN_POINT('Ctrl Pts',(-5.39878382316402,-0.418881580476551,
135.70665782613));
#74004=CARTESIAN_POINT('Ctrl Pts',(-5.40653189116702,-0.282006313388684,
135.714519016407));
#74005=CARTESIAN_POINT('Ctrl Pts',(-5.41428819390887,-0.144985573638679,
135.722388561651));
#74006=CARTESIAN_POINT('Ctrl Pts',(-5.42204449665068,-0.00770775267616375,
135.724514151243));
#74007=CARTESIAN_POINT('Ctrl Pts',(-5.42980079939252,0.129311059324924,
135.720910394842));
#74008=CARTESIAN_POINT('Ctrl Pts',(-5.43756124190669,0.26640300239172,135.717304715009));
#74009=CARTESIAN_POINT('Ctrl Pts',(-5.44532168442086,0.403235271173919,
135.707963622625));
#74010=CARTESIAN_POINT('Ctrl Pts',(-5.45308212693502,0.539296851950341,
135.69295366342));
#74011=CARTESIAN_POINT('Ctrl Pts',(-5.46085502720044,0.675576850855206,
135.677919608897));
#74012=CARTESIAN_POINT('Ctrl Pts',(-5.46862792746586,0.811083302785558,
135.65719856165));
#74013=CARTESIAN_POINT('Ctrl Pts',(-5.47640082773128,0.945314451684333,
135.630908415935));
#74014=CARTESIAN_POINT('Ctrl Pts',(-5.48389116349339,1.07466596021423,135.605573983237));
#74015=CARTESIAN_POINT('Ctrl Pts',(-5.49138149925551,1.2028329772479,135.575068395221));
#74016=CARTESIAN_POINT('Ctrl Pts',(-5.49887183501761,1.32938166029384,135.539540388575));
#74017=CARTESIAN_POINT('Ctrl Pts',(-5.5066461691367,1.46072847511981,135.502665326759));
#74018=CARTESIAN_POINT('Ctrl Pts',(-5.51442050325583,1.59074788242342,135.460262669096));
#74019=CARTESIAN_POINT('Ctrl Pts',(-5.52219483737491,1.71893927923828,135.412443821762));
#74020=CARTESIAN_POINT('Ctrl Pts',(-5.52995959032199,1.84697269161318,135.364683906883));
#74021=CARTESIAN_POINT('Ctrl Pts',(-5.53772434326902,1.97318221322571,135.311521218864));
#74022=CARTESIAN_POINT('Ctrl Pts',(-5.5454890962161,2.09708007831739,135.253117545925));
#74023=CARTESIAN_POINT('Ctrl Pts',(-5.55324613710109,2.22085488630264,135.194771880337));
#74024=CARTESIAN_POINT('Ctrl Pts',(-5.56100317798608,2.34232225549514,135.131195754474));
#74025=CARTESIAN_POINT('Ctrl Pts',(-5.56876021887106,2.46101250807352,135.062599748663));
#74026=CARTESIAN_POINT('Ctrl Pts',(-5.5765114101112,2.57961325540947,134.994055471633));
#74027=CARTESIAN_POINT('Ctrl Pts',(-5.58426260135137,2.69544071746994,134.920499044366));
#74028=CARTESIAN_POINT('Ctrl Pts',(-5.5920137925915,2.8080483545001,134.842187694261));
#74029=CARTESIAN_POINT('Ctrl Pts',(-5.59976168936857,2.92060813028045,134.763909628569));
#74030=CARTESIAN_POINT('Ctrl Pts',(-5.60750958614558,3.02995048258962,134.680880882344));
#74031=CARTESIAN_POINT('Ctrl Pts',(-5.61525748292266,3.13565668869202,134.593402738361));
#74032=CARTESIAN_POINT('Ctrl Pts',(-5.62300375900676,3.24134078333488,134.50594289292));
#74033=CARTESIAN_POINT('Ctrl Pts',(-5.63075003509086,3.34338994364228,134.414035750073));
#74034=CARTESIAN_POINT('Ctrl Pts',(-5.63849631117495,3.44141778702071,134.31802347528));
#74035=CARTESIAN_POINT('Ctrl Pts',(-5.64624264444027,3.53944635401828,134.222010491746));
#74036=CARTESIAN_POINT('Ctrl Pts',(-5.65398897770562,3.63345326554301,134.121892589366));
#74037=CARTESIAN_POINT('Ctrl Pts',(-5.66173531097095,3.72308863025564,134.018049170267));
#74038=CARTESIAN_POINT('Ctrl Pts',(-5.6694833789739,3.81274406818646,133.914182496155));
#74039=CARTESIAN_POINT('Ctrl Pts',(-5.67723144697684,3.89802575583708,133.806588941059));
#74040=CARTESIAN_POINT('Ctrl Pts',(-5.68497951497977,3.97862402308269,133.695681067715));
#74041=CARTESIAN_POINT('Ctrl Pts',(-5.69273581772162,4.05930795112618,133.584655320163));
#74042=CARTESIAN_POINT('Ctrl Pts',(-5.70049212046346,4.13529828527706,133.470308534572));
#74043=CARTESIAN_POINT('Ctrl Pts',(-5.7082484232053,4.20632835771104,133.3530828091));
#74044=CARTESIAN_POINT('Ctrl Pts',(-5.71600886571946,4.27739634103336,133.235794516728));
#74045=CARTESIAN_POINT('Ctrl Pts',(-5.72376930823356,4.34349859904788,133.115624565108));
#74046=CARTESIAN_POINT('Ctrl Pts',(-5.73152975074771,4.40441490316382,132.993038854148));
#74047=CARTESIAN_POINT('Ctrl Pts',(-5.73930265101313,4.46542899553902,132.870256357722));
#74048=CARTESIAN_POINT('Ctrl Pts',(-5.74707555127867,4.52124033883662,132.745050709794));
#74049=CARTESIAN_POINT('Ctrl Pts',(-5.75484845154409,4.57167690942875,132.61790777667));
#74050=CARTESIAN_POINT('Ctrl Pts',(-5.76233878730621,4.62027998363842,132.495386809418));
#74051=CARTESIAN_POINT('Ctrl Pts',(-5.7698291230683,4.66389217183814,132.371067252646));
#74052=CARTESIAN_POINT('Ctrl Pts',(-5.77731945883042,4.70240410795104,132.245394506142));
#74053=CARTESIAN_POINT('Ctrl Pts',(-5.78509379294951,4.74237623582665,132.114956839259));
#74054=CARTESIAN_POINT('Ctrl Pts',(-5.79286812706855,4.77698034457764,131.982648157344));
#74055=CARTESIAN_POINT('Ctrl Pts',(-5.80064246118764,4.80603957524248,131.84894984961));
#74056=CARTESIAN_POINT('Ctrl Pts',(-5.80840721413473,4.83506299300263,131.715416313092));
#74057=CARTESIAN_POINT('Ctrl Pts',(-5.81617196708187,4.85855504719743,131.580496936675));
#74058=CARTESIAN_POINT('Ctrl Pts',(-5.82393672002897,4.87638820553139,131.44468954199));
#74059=CARTESIAN_POINT('Ctrl Pts',(-5.831693760914,4.89420365172113,131.309017033125));
#74060=CARTESIAN_POINT('Ctrl Pts',(-5.83945080179904,4.90637133651686,131.172458646325));
#74061=CARTESIAN_POINT('Ctrl Pts',(-5.84720784268407,4.9128145547773,131.035523358656));
#74062=CARTESIAN_POINT('Ctrl Pts',(-5.85495903392422,4.91925291415673,130.898691334953));
#74063=CARTESIAN_POINT('Ctrl Pts',(-5.86271022516431,4.91997538115697,130.761483365063));
#74064=CARTESIAN_POINT('Ctrl Pts',(-5.87046141640445,4.91495700283006,130.624414173223));
#74065=CARTESIAN_POINT('Ctrl Pts',(-5.87820931318154,4.90994075744782,130.487403239446));
#74066=CARTESIAN_POINT('Ctrl Pts',(-5.88595720995869,4.89918853401159,130.350531356287));
#74067=CARTESIAN_POINT('Ctrl Pts',(-5.89370510673578,4.88272748038461,130.214313657743));
#74068=CARTESIAN_POINT('Ctrl Pts',(-5.90145138281988,4.86626987005522,130.078124453004));
#74069=CARTESIAN_POINT('Ctrl Pts',(-5.90919765890394,4.84410585166792,129.942589548589));
#74070=CARTESIAN_POINT('Ctrl Pts',(-5.91694393498804,4.81631444948453,129.808218967906));
#74071=CARTESIAN_POINT('Ctrl Pts',(-5.92469026825341,4.78852284215129,129.67384739533));
#74072=CARTESIAN_POINT('Ctrl Pts',(-5.9324366015188,4.7551038473178,129.540640546498));
#74073=CARTESIAN_POINT('Ctrl Pts',(-5.94018293478416,4.71618754192418,129.40909787102));
#74074=CARTESIAN_POINT('Ctrl Pts',(-5.94793100278713,4.6772625214939,129.277525737472));
#74075=CARTESIAN_POINT('Ctrl Pts',(-5.95567907079004,4.63283785167975,129.147618893701));
#74076=CARTESIAN_POINT('Ctrl Pts',(-5.96342713879301,4.58309324892931,129.019860874187));
#74077=CARTESIAN_POINT('Ctrl Pts',(-5.97118344153487,4.53329577702295,128.89196707193));
#74078=CARTESIAN_POINT('Ctrl Pts',(-5.97893974427676,4.47816721961135,128.766227020963));
#74079=CARTESIAN_POINT('Ctrl Pts',(-5.98669604701863,4.41793538592294,128.643104041333));
#74080=CARTESIAN_POINT('Ctrl Pts',(-5.99445648953279,4.35767140469143,128.519915347262));
#74081=CARTESIAN_POINT('Ctrl Pts',(-6.00221693204695,4.29229890609762,128.399346851316));
#74082=CARTESIAN_POINT('Ctrl Pts',(-6.00997737456112,4.22209082599729,128.281835668328));
#74083=CARTESIAN_POINT('Ctrl Pts',(-6.01775027482656,4.15177004165382,128.164135845956));
#74084=CARTESIAN_POINT('Ctrl Pts',(-6.02552317509197,4.07659837836353,128.049503471157));
#74085=CARTESIAN_POINT('Ctrl Pts',(-6.03329607535741,3.99689162623794,127.938345894888));
#74086=CARTESIAN_POINT('Ctrl Pts',(-6.04078641111939,3.92008241532195,127.831229176506));
#74087=CARTESIAN_POINT('Ctrl Pts',(-6.04827674688136,3.83906230430724,127.727339250305));
#74088=CARTESIAN_POINT('Ctrl Pts',(-6.05576708264334,3.7541469056134,127.627008878527));
#74089=CARTESIAN_POINT('Ctrl Pts',(-6.06354141676242,3.66601191376809,127.522874450208));
#74090=CARTESIAN_POINT('Ctrl Pts',(-6.07131575088151,3.57340123852914,127.422244959083));
#74091=CARTESIAN_POINT('Ctrl Pts',(-6.07909008500059,3.47662428968547,127.325529404232));
#74092=CARTESIAN_POINT('Ctrl Pts',(-6.08685483794767,3.37996660978204,127.228933042658));
#74093=CARTESIAN_POINT('Ctrl Pts',(-6.09461959089471,3.27915314640472,127.136241293592));
#74094=CARTESIAN_POINT('Ctrl Pts',(-6.10238434384181,3.17453379667028,127.047830538318));
#74095=CARTESIAN_POINT('Ctrl Pts',(-6.11014138472682,3.07001835634872,126.959507593851));
#74096=CARTESIAN_POINT('Ctrl Pts',(-6.11789842561193,2.96170484884454,126.875457432337));
#74097=CARTESIAN_POINT('Ctrl Pts',(-6.12565546649694,2.84998002997416,126.796019702518));
#74098=CARTESIAN_POINT('Ctrl Pts',(-6.13340665773708,2.73833946365863,126.716641877309));
#74099=CARTESIAN_POINT('Ctrl Pts',(-6.14115784897715,2.62329302371982,126.641869786144));
#74100=CARTESIAN_POINT('Ctrl Pts',(-6.14890904021729,2.5052602745568,126.572002643667));
#74101=CARTESIAN_POINT('Ctrl Pts',(-6.15665693699436,2.38727769246112,126.50216519659));
#74102=CARTESIAN_POINT('Ctrl Pts',(-6.16440483377139,2.26631166134219,126.437228750557));
#74103=CARTESIAN_POINT('Ctrl Pts',(-6.17215273054848,2.14281025210197,126.377448907809));
#74104=CARTESIAN_POINT('Ctrl Pts',(-6.17989900663257,2.01933467669435,126.317681569715));
#74105=CARTESIAN_POINT('Ctrl Pts',(-6.18764528271668,1.89332512973804,126.263068859642));
#74106=CARTESIAN_POINT('Ctrl Pts',(-6.19539155880076,1.76525342291417,126.213819972349));
#74107=CARTESIAN_POINT('Ctrl Pts',(-6.20313789206611,1.63718077069388,126.164570721512));
#74108=CARTESIAN_POINT('Ctrl Pts',(-6.21088422533151,1.50704629314551,126.120685512788));
#74109=CARTESIAN_POINT('Ctrl Pts',(-6.21863055859686,1.37534050113522,126.082324873479));
#74110=CARTESIAN_POINT('Ctrl Pts',(-6.22637862659983,1.243605214526,126.04395564357));
#74111=CARTESIAN_POINT('Ctrl Pts',(-6.23412669460284,1.11029828854022,126.011113554247));
#74112=CARTESIAN_POINT('Ctrl Pts',(-6.24187476260582,0.975923675562169,
125.983908767171));
#74113=CARTESIAN_POINT('Ctrl Pts',(-6.24963106534768,0.84140624764618,125.956675066524));
#74114=CARTESIAN_POINT('Ctrl Pts',(-6.25738736808949,0.705819249753642,
125.935090714277));
#74115=CARTESIAN_POINT('Ctrl Pts',(-6.26514367083135,0.569675622613875,
125.919214483877));
#74116=CARTESIAN_POINT('Ctrl Pts',(-6.27290411334552,0.433459331521099,
125.903329779855));
#74117=CARTESIAN_POINT('Ctrl Pts',(-6.28066455585962,0.296686208902539,
125.893159297259));
#74118=CARTESIAN_POINT('Ctrl Pts',(-6.28842499837378,0.159871540342711,
125.888709678668));
#74119=CARTESIAN_POINT('Ctrl Pts',(-6.29619789863921,0.0228372447312607,
125.884252917154));
#74120=CARTESIAN_POINT('Ctrl Pts',(-6.30397079890471,-0.114238338922688,
125.885535367822));
#74121=CARTESIAN_POINT('Ctrl Pts',(-6.31174369917014,-0.250841802453506,
125.89251153065));
#74122=CARTESIAN_POINT('Ctrl Pts',(-6.31923403493218,-0.382479386001982,
125.899234092386));
#74123=CARTESIAN_POINT('Ctrl Pts',(-6.32672437069419,-0.513678272261304,
125.911243563628));
#74124=CARTESIAN_POINT('Ctrl Pts',(-6.33421470645624,-0.643987902710506,
125.928454276827));
#74125=CARTESIAN_POINT('Ctrl Pts',(-6.34198904057531,-0.779238262404569,
125.946317539448));
#74126=CARTESIAN_POINT('Ctrl Pts',(-6.34976337469434,-0.913959035371852,
125.969840825432));
#74127=CARTESIAN_POINT('Ctrl Pts',(-6.35753770881342,-1.04763887555349,
125.998984893553));
#74128=CARTESIAN_POINT('Ctrl Pts',(-6.36530246176052,-1.18115396727941,
126.028093044216));
#74129=CARTESIAN_POINT('Ctrl Pts',(-6.3730672147077,-1.31363030039658,126.062808111649));
#74130=CARTESIAN_POINT('Ctrl Pts',(-6.38083196765479,-1.44456208673287,
126.103039160776));
#74131=CARTESIAN_POINT('Ctrl Pts',(-6.3885890085398,-1.5753638297735,126.143230251858));
#74132=CARTESIAN_POINT('Ctrl Pts',(-6.39634604942478,-1.70462370759048,
126.188926307981));
#74133=CARTESIAN_POINT('Ctrl Pts',(-6.4041030903098,-1.83184691311086,126.239985528967));
#74134=CARTESIAN_POINT('Ctrl Pts',(-6.41185428154995,-1.95897417862231,
126.291006245796));
#74135=CARTESIAN_POINT('Ctrl Pts',(-6.41960547279004,-2.08406746752751,
126.347381932317));
#74136=CARTESIAN_POINT('Ctrl Pts',(-6.42735666403019,-2.20664825726625,
126.40892132994));
#74137=CARTESIAN_POINT('Ctrl Pts',(-6.43510456080726,-2.32917694689906,
126.470434571678));
#74138=CARTESIAN_POINT('Ctrl Pts',(-6.44285245758438,-2.44919491262162,
126.537106984353));
#74139=CARTESIAN_POINT('Ctrl Pts',(-6.45060035436146,-2.56624491576267,
126.608699752479));
#74140=CARTESIAN_POINT('Ctrl Pts',(-6.45834663044554,-2.68327043456621,
126.680277544942));
#74141=CARTESIAN_POINT('Ctrl Pts',(-6.46609290652965,-2.79732889234739,
126.756773441787));
#74142=CARTESIAN_POINT('Ctrl Pts',(-6.47383918261374,-2.90798926189143,
126.837903569365));
#74143=CARTESIAN_POINT('Ctrl Pts',(-6.48158551587913,-3.01865044830578,
126.919034295827));
#74144=CARTESIAN_POINT('Ctrl Pts',(-6.48933184914446,-3.12591318112526,
127.004799090118));
#74145=CARTESIAN_POINT('Ctrl Pts',(-6.49707818240984,-3.22937727108092,
127.094872040481));
#74146=CARTESIAN_POINT('Ctrl Pts',(-6.50482625041282,-3.33286453110187,
127.184965162056));
#74147=CARTESIAN_POINT('Ctrl Pts',(-6.51257431841579,-3.43255116068381,
127.279368102845));
#74148=CARTESIAN_POINT('Ctrl Pts',(-6.52032238641877,-3.5280720791275,127.377716418502));
#74149=CARTESIAN_POINT('Ctrl Pts',(-6.52807868916061,-3.62369451833976,
127.476169259919));
#74150=CARTESIAN_POINT('Ctrl Pts',(-6.53583499190238,-3.71514212944284,
127.578575571652));
#74151=CARTESIAN_POINT('Ctrl Pts',(-6.54359129464422,-3.80208820767823,
127.684535570623));
#74152=CARTESIAN_POINT('Ctrl Pts',(-6.55135173715836,-3.88908069165347,
127.790552123635));
#74153=CARTESIAN_POINT('Ctrl Pts',(-6.55911217967256,-3.97156662034854,
127.900125831039));
#74154=CARTESIAN_POINT('Ctrl Pts',(-6.56687262218671,-4.04926188072924,
128.012826758955));
#74155=CARTESIAN_POINT('Ctrl Pts',(-6.57464552245213,-4.12708186443946,
128.125708604405));
#74156=CARTESIAN_POINT('Ctrl Pts',(-6.58241842271761,-4.20009560359387,
128.241727371027));
#74157=CARTESIAN_POINT('Ctrl Pts',(-6.59019132298303,-4.26806386899554,
128.360426520117));
#74158=CARTESIAN_POINT('Ctrl Pts',(-6.59768165874506,-4.33356131674822,
128.474810656152));
#74159=CARTESIAN_POINT('Ctrl Pts',(-6.60517199450702,-4.39437361120099,
128.591683407461));
#74160=CARTESIAN_POINT('Ctrl Pts',(-6.61266233026905,-4.45032928900128,
128.710619400998));
#74161=CARTESIAN_POINT('Ctrl Pts',(-6.62145591455051,-4.5160207325354,128.850249147445));
#74162=CARTESIAN_POINT('Ctrl Pts',(-6.63024949883198,-4.57520851447709,
128.993126368615));
#74163=CARTESIAN_POINT('Ctrl Pts',(-6.63904308311345,-4.62758848881774,
129.138645203499));
#74164=CARTESIAN_POINT('Ctrl Pts',(-6.64783666739492,-4.6799684631584,129.284164038383));
#74165=CARTESIAN_POINT('Ctrl Pts',(-6.65663025167633,-4.72554041934122,
129.432324193268));
#74166=CARTESIAN_POINT('Ctrl Pts',(-6.66542383595777,-4.76405452823408,
129.582490119308));
#74167=CARTESIAN_POINT('Ctrl Pts',(-4.91509110695614,-4.76405452823401,
129.582490119308));
#74168=CARTESIAN_POINT('Ctrl Pts',(-4.92286673107686,-4.79806456359889,
129.715094731021));
#74169=CARTESIAN_POINT('Ctrl Pts',(-4.93064235519757,-4.82649058400499,
129.848951090438));
#74170=CARTESIAN_POINT('Ctrl Pts',(-4.93841797931836,-4.84927328742245,
129.98354903968));
#74171=CARTESIAN_POINT('Ctrl Pts',(-4.93960418200949,-4.85274888033759,
130.004082497462));
#74172=CARTESIAN_POINT('Ctrl Pts',(-4.94079038470059,-4.856093236529,130.024633209604));
#74173=CARTESIAN_POINT('Ctrl Pts',(-4.94197658739171,-4.85930625197158,
130.045199361936));
#74174=CARTESIAN_POINT('Ctrl Pts',(-4.95490804744516,-4.89433313326069,
130.269402509782));
#74175=CARTESIAN_POINT('Ctrl Pts',(-4.96783950749871,-4.91384944124733,
130.496089496467));
#74176=CARTESIAN_POINT('Ctrl Pts',(-4.98077096755208,-4.91758650221471,
130.723576610884));
#74177=CARTESIAN_POINT('Ctrl Pts',(-4.98222749970424,-4.91800742525288,
130.749199571863));
#74178=CARTESIAN_POINT('Ctrl Pts',(-4.98368403185642,-4.91822819808973,
130.774832639892));
#74179=CARTESIAN_POINT('Ctrl Pts',(-4.98514056400859,-4.91824846381374,
130.800473369986));
#74180=CARTESIAN_POINT('',(-4.63985943596118,-4.91824845974782,130.808253006061));
#74181=CARTESIAN_POINT('Ctrl Pts',(-4.56974458955162,-4.76405452823407,
129.582490119308));
#74182=CARTESIAN_POINT('Ctrl Pts',(-4.57738283870254,-4.79766427851359,
129.713534025549));
#74183=CARTESIAN_POINT('Ctrl Pts',(-4.58502108785347,-4.82584587317406,
129.845899218852));
#74184=CARTESIAN_POINT('Ctrl Pts',(-4.59265933700439,-4.84851632270241,
129.979089431235));
#74185=CARTESIAN_POINT('Ctrl Pts',(-4.60052602016385,-4.87186476813776,
130.11626290909));
#74186=CARTESIAN_POINT('Ctrl Pts',(-4.60839270332329,-4.88936719706201,
130.254311066717));
#74187=CARTESIAN_POINT('Ctrl Pts',(-4.61625938648274,-4.90099051151931,
130.392687120122));
#74188=CARTESIAN_POINT('Ctrl Pts',(-4.6241260696422,-4.91261382597663,130.531063173527));
#74189=CARTESIAN_POINT('Ctrl Pts',(-4.6319927528017,-4.9183580602836,130.669766658435));
#74190=CARTESIAN_POINT('Ctrl Pts',(-4.63985943596117,-4.91824845974782,
130.808253006061));
#74191=CARTESIAN_POINT('Ctrl Pts',(-4.63985943599116,-4.9182484597474,130.808253006589));
#74192=CARTESIAN_POINT('Ctrl Pts',(-4.65277286871676,-4.91806854664951,
131.03558314017));
#74193=CARTESIAN_POINT('Ctrl Pts',(-4.66568630144235,-4.90212487107249,
131.262306380489));
#74194=CARTESIAN_POINT('Ctrl Pts',(-4.67859973416799,-4.87068170378865,
131.486740865579));
#74195=CARTESIAN_POINT('Ctrl Pts',(-4.68010580935812,-4.86701453215803,
131.512916338591));
#74196=CARTESIAN_POINT('Ctrl Pts',(-4.68161188454825,-4.86313657009037,
131.539060722098));
#74197=CARTESIAN_POINT('Ctrl Pts',(-4.68311795973838,-4.85904826618473,
131.565171375499));
#74198=CARTESIAN_POINT('Ctrl Pts',(-4.69089229385748,-4.83794451203547,
131.699954117383));
#74199=CARTESIAN_POINT('Ctrl Pts',(-4.69866662797662,-4.81119507309146,
131.834071600094));
#74200=CARTESIAN_POINT('Ctrl Pts',(-4.70644096209571,-4.77885145017247,
131.967013566508));
#74201=CARTESIAN_POINT('Ctrl Pts',(-4.71420571504281,-4.74654768787809,
132.099791693831));
#74202=CARTESIAN_POINT('Ctrl Pts',(-4.72197046798986,-4.70866355080931,
132.231396811139));
#74203=CARTESIAN_POINT('Ctrl Pts',(-4.72973522093696,-4.66530208537696,
132.361325458106));
#74204=CARTESIAN_POINT('Ctrl Pts',(-4.73749226182196,-4.62198368716343,
132.491125058109));
#74205=CARTESIAN_POINT('Ctrl Pts',(-4.74524930270701,-4.57319890971626,
132.619251132925));
#74206=CARTESIAN_POINT('Ctrl Pts',(-4.75300634359201,-4.51910138638564,
132.745212420787));
#74207=CARTESIAN_POINT('Ctrl Pts',(-4.76075753483213,-4.46504465841819,
132.871078720262));
#74208=CARTESIAN_POINT('Ctrl Pts',(-4.76850872607221,-4.40568331268907,
132.994783124359));
#74209=CARTESIAN_POINT('Ctrl Pts',(-4.77625991731233,-4.34122003593043,
133.115851837998));
#74210=CARTESIAN_POINT('Ctrl Pts',(-4.78400781408942,-4.27678415778394,
133.236869094205));
#74211=CARTESIAN_POINT('Ctrl Pts',(-4.79175571086649,-4.20725084486524,
133.355252543651));
#74212=CARTESIAN_POINT('Ctrl Pts',(-4.79950360764357,-4.13286981635417,
133.470550810251));
#74213=CARTESIAN_POINT('Ctrl Pts',(-4.80724988372768,-4.05850434675079,
133.585824958939));
#74214=CARTESIAN_POINT('Ctrl Pts',(-4.81499615981182,-3.97929339033991,
133.698014880101));
#74215=CARTESIAN_POINT('Ctrl Pts',(-4.82274243589592,-3.89553108248959,
133.806696482831));
#74216=CARTESIAN_POINT('Ctrl Pts',(-4.83048876916126,-3.81176815632505,
133.915378887824));
#74217=CARTESIAN_POINT('Ctrl Pts',(-4.83823510242661,-3.72345405034454,
134.020552613043));
#74218=CARTESIAN_POINT('Ctrl Pts',(-4.84598143569195,-3.63092418588913,
134.121825405446));
#74219=CARTESIAN_POINT('Ctrl Pts',(-4.85372950369494,-3.53837360001199,
134.223120877189));
#74220=CARTESIAN_POINT('Ctrl Pts',(-4.86147757169793,-3.44160564069429,
134.320513389204));
#74221=CARTESIAN_POINT('Ctrl Pts',(-4.86922563970091,-3.34099340825978,
134.413646711583));
#74222=CARTESIAN_POINT('Ctrl Pts',(-4.87698194244276,-3.24027424394748,
134.506879017166));
#74223=CARTESIAN_POINT('Ctrl Pts',(-4.88473824518457,-3.13570293218376,
134.5958428245));
#74224=CARTESIAN_POINT('Ctrl Pts',(-4.89249454792642,-3.02768698093375,
134.680221116602));
#74225=CARTESIAN_POINT('Ctrl Pts',(-4.90025499044059,-2.91961337831811,
134.764644443938));
#74226=CARTESIAN_POINT('Ctrl Pts',(-4.90801543295482,-2.80809179058428,
134.844477151874));
#74227=CARTESIAN_POINT('Ctrl Pts',(-4.915775875469,-2.69355884573146,134.91944552642));
#74228=CARTESIAN_POINT('Ctrl Pts',(-4.92354877573443,-2.5788420424278,134.994534246857));
#74229=CARTESIAN_POINT('Ctrl Pts',(-4.93132167599983,-2.46110455792531,
135.064742829358));
#74230=CARTESIAN_POINT('Ctrl Pts',(-4.93909457626526,-2.34080854029682,
135.12984306929));
#74231=CARTESIAN_POINT('Ctrl Pts',(-4.94658491202727,-2.22488558591684,
135.192576751523));
#74232=CARTESIAN_POINT('Ctrl Pts',(-4.95407524778924,-2.10658716368409,
135.250566909759));
#74233=CARTESIAN_POINT('Ctrl Pts',(-4.96156558355125,-1.98634263879519,
135.303652337804));
#74234=CARTESIAN_POINT('Ctrl Pts',(-4.96933991767032,-1.8615390061974,135.358750515989));
#74235=CARTESIAN_POINT('Ctrl Pts',(-4.97711425178939,-1.73424344444807,
135.408739230828));
#74236=CARTESIAN_POINT('Ctrl Pts',(-4.98488858590846,-1.60491308476677,
135.453386004983));
#74237=CARTESIAN_POINT('Ctrl Pts',(-4.99265333885555,-1.47574211319519,
135.497977755978));
#74238=CARTESIAN_POINT('Ctrl Pts',(-5.00041809180266,-1.34454169929636,
135.537240539066));
#74239=CARTESIAN_POINT('Ctrl Pts',(-5.00818284474974,-1.21179111760383,
135.570988917507));
#74240=CARTESIAN_POINT('Ctrl Pts',(-5.01593988563473,-1.07917238566049,
135.604703776582));
#74241=CARTESIAN_POINT('Ctrl Pts',(-5.02369692651973,-0.945006926353916,
135.632915034751));
#74242=CARTESIAN_POINT('Ctrl Pts',(-5.03145396740473,-0.809791094700726,
135.655486409116));
#74243=CARTESIAN_POINT('Ctrl Pts',(-5.03920515864486,-0.674677230358012,
135.678040762233));
#74244=CARTESIAN_POINT('Ctrl Pts',(-5.04695634988493,-0.538514954352634,
135.694963632932));
#74245=CARTESIAN_POINT('Ctrl Pts',(-5.05470754112505,-0.401812441032595,
135.70616944949));
#74246=CARTESIAN_POINT('Ctrl Pts',(-5.06245543790213,-0.265168029927377,
135.717370503277));
#74247=CARTESIAN_POINT('Ctrl Pts',(-5.07020333467922,-0.127984227037229,
135.722859303935));
#74248=CARTESIAN_POINT('Ctrl Pts',(-5.0779512314563,0.00922423283774606,
135.722601967483));
#74249=CARTESIAN_POINT('Ctrl Pts',(-5.08569750754041,0.146403991660974,
135.722344684859));
#74250=CARTESIAN_POINT('Ctrl Pts',(-5.09344378362461,0.283608006493235,
135.716343656639));
#74251=CARTESIAN_POINT('Ctrl Pts',(-5.10119005970873,0.420320490294498,
135.704617115744));
#74252=CARTESIAN_POINT('Ctrl Pts',(-5.10893639297407,0.557033983275887,
135.692890488287));
#74253=CARTESIAN_POINT('Ctrl Pts',(-5.11668272623931,0.693255548451275,
135.675438297232));
#74254=CARTESIAN_POINT('Ctrl Pts',(-5.12442905950465,0.828473868800271,
135.652330719703));
#74255=CARTESIAN_POINT('Ctrl Pts',(-5.13217712750761,0.963722470354572,
135.629217967393));
#74256=CARTESIAN_POINT('Ctrl Pts',(-5.13992519551062,1.09796699471104,135.600447374296));
#74257=CARTESIAN_POINT('Ctrl Pts',(-5.14767326351358,1.23070606572261,135.566140289316));
#74258=CARTESIAN_POINT('Ctrl Pts',(-5.15542956625543,1.36358621339864,135.531796742359));
#74259=CARTESIAN_POINT('Ctrl Pts',(-5.16318586899724,1.49495733239947,135.491905047084));
#74260=CARTESIAN_POINT('Ctrl Pts',(-5.17094217173909,1.62433243934895,135.446636696062));
#74261=CARTESIAN_POINT('Ctrl Pts',(-5.17870261425326,1.75377659768859,135.401344183958));
#74262=CARTESIAN_POINT('Ctrl Pts',(-5.18646305676743,1.8812222580913,135.350669442404));
#74263=CARTESIAN_POINT('Ctrl Pts',(-5.19422349928161,2.00620312912733,135.294831869804));
#74264=CARTESIAN_POINT('Ctrl Pts',(-5.20199639954704,2.13138463055282,135.238904661776));
#74265=CARTESIAN_POINT('Ctrl Pts',(-5.20976929981252,2.25409308569327,135.177798235347));
#74266=CARTESIAN_POINT('Ctrl Pts',(-5.21754220007796,2.3738866972044,135.111778058601));
#74267=CARTESIAN_POINT('Ctrl Pts',(-5.22503253584005,2.48932550919602,135.048157881574));
#74268=CARTESIAN_POINT('Ctrl Pts',(-5.23252287160211,2.60205745850447,134.979975165579));
#74269=CARTESIAN_POINT('Ctrl Pts',(-5.2400132073642,2.71171483541556,134.907504011829));
#74270=CARTESIAN_POINT('Ctrl Pts',(-5.24778754148327,2.82552990510076,134.832285092259));
#74271=CARTESIAN_POINT('Ctrl Pts',(-5.25556187560229,2.93639318714155,134.752207852375));
#74272=CARTESIAN_POINT('Ctrl Pts',(-5.26333620972136,3.04386200117725,134.667531229937));
#74273=CARTESIAN_POINT('Ctrl Pts',(-5.27110096266844,3.15119836950441,134.582958963869));
#74274=CARTESIAN_POINT('Ctrl Pts',(-5.27886571561556,3.25514828935673,134.493798833173));
#74275=CARTESIAN_POINT('Ctrl Pts',(-5.28663046856263,3.35529668796039,134.400353832001));
#74276=CARTESIAN_POINT('Ctrl Pts',(-5.29438750944762,3.45534561776272,134.307001641721));
#74277=CARTESIAN_POINT('Ctrl Pts',(-5.30214455033258,3.5516002561729,134.209373315182));
#74278=CARTESIAN_POINT('Ctrl Pts',(-5.30990159121757,3.64367765251988,134.107812785682));
#74279=CARTESIAN_POINT('Ctrl Pts',(-5.31765278245768,3.73568561258603,134.006328843767));
#74280=CARTESIAN_POINT('Ctrl Pts',(-5.32540397369786,3.8235223391156,133.900918889625));
#74281=CARTESIAN_POINT('Ctrl Pts',(-5.33315516493798,3.90684115754488,133.791964211119));
#74282=CARTESIAN_POINT('Ctrl Pts',(-5.34090306171504,3.99012456325373,133.683055841259));
#74283=CARTESIAN_POINT('Ctrl Pts',(-5.34865095849204,4.06889364306066,133.570606053467));
#74284=CARTESIAN_POINT('Ctrl Pts',(-5.35639885526911,4.14284166268039,133.455029593591));
#74285=CARTESIAN_POINT('Ctrl Pts',(-5.36414513135319,4.21677421396855,133.339477309818));
#74286=CARTESIAN_POINT('Ctrl Pts',(-5.37189140743731,4.28588750037997,133.220799983984));
#74287=CARTESIAN_POINT('Ctrl Pts',(-5.37963768352139,4.34991806629484,133.099441417673));
#74288=CARTESIAN_POINT('Ctrl Pts',(-5.38738401678673,4.4139491048688,132.978081955521));
#74289=CARTESIAN_POINT('Ctrl Pts',(-5.39513035005209,4.47289716563652,132.854041559185));
#74290=CARTESIAN_POINT('Ctrl Pts',(-5.40287668331743,4.52654491126077,132.727788346606));
#74291=CARTESIAN_POINT('Ctrl Pts',(-5.41062475132039,4.58020467092568,132.601506860495));
#74292=CARTESIAN_POINT('Ctrl Pts',(-5.41837281932329,4.62856160064728,132.473011931821));
#74293=CARTESIAN_POINT('Ctrl Pts',(-5.42612088732625,4.67144678864078,132.342790974585));
#74294=CARTESIAN_POINT('Ctrl Pts',(-5.43387719006808,4.71437755552243,132.212431616966));
#74295=CARTESIAN_POINT('Ctrl Pts',(-5.4416334928099,4.75182484123462,132.080342938223));
#74296=CARTESIAN_POINT('Ctrl Pts',(-5.44938979555172,4.78366970092242,131.947027347184));
#74297=CARTESIAN_POINT('Ctrl Pts',(-5.45715023806587,4.8155315571707,131.813640601601));
#74298=CARTESIAN_POINT('Ctrl Pts',(-5.46491068058014,4.84178495439893,131.679026022447));
#74299=CARTESIAN_POINT('Ctrl Pts',(-5.4726711230943,4.86236243679116,131.543694504103));
#74300=CARTESIAN_POINT('Ctrl Pts',(-5.48044402335972,4.8829729519849,131.408145739593));
#74301=CARTESIAN_POINT('Ctrl Pts',(-5.48821692362515,4.89788930213066,131.271878124907));
#74302=CARTESIAN_POINT('Ctrl Pts',(-5.49598982389057,4.90709603078913,131.135406848648));
#74303=CARTESIAN_POINT('Ctrl Pts',(-5.50348015965275,4.9159680716707,131.003896647028));
#74304=CARTESIAN_POINT('Ctrl Pts',(-5.51097049541489,4.91953839390124,130.872197641888));
#74305=CARTESIAN_POINT('Ctrl Pts',(-5.51846083117707,4.91783885051269,130.740767356225));
#74306=CARTESIAN_POINT('Ctrl Pts',(-5.52623516529617,4.91607486842003,130.604353851336));
#74307=CARTESIAN_POINT('Ctrl Pts',(-5.53400949941523,4.90862793052933,130.46779772819));
#74308=CARTESIAN_POINT('Ctrl Pts',(-5.54178383353434,4.89547660896413,130.331611388497));
#74309=CARTESIAN_POINT('Ctrl Pts',(-5.54954858648146,4.88234149522739,130.195592886297));
#74310=CARTESIAN_POINT('Ctrl Pts',(-5.55731333942858,4.86351602292483,130.059943646211));
#74311=CARTESIAN_POINT('Ctrl Pts',(-5.5650780923757,4.8390307526441,129.925176656461));
#74312=CARTESIAN_POINT('Ctrl Pts',(-5.57283513326071,4.81456980147902,129.790543519184));
#74313=CARTESIAN_POINT('Ctrl Pts',(-5.58059217414579,4.78446030859433,129.656791270617));
#74314=CARTESIAN_POINT('Ctrl Pts',(-5.5883492150308,4.74878464062306,129.524428002354));
#74315=CARTESIAN_POINT('Ctrl Pts',(-5.59610040627095,4.71313587595048,129.392164550261));
#74316=CARTESIAN_POINT('Ctrl Pts',(-5.60385159751101,4.67192939238608,129.261288369571));
#74317=CARTESIAN_POINT('Ctrl Pts',(-5.61160278875116,4.62529859213847,129.132297222816));
#74318=CARTESIAN_POINT('Ctrl Pts',(-5.61935068552825,4.57868761122494,129.00336090074));
#74319=CARTESIAN_POINT('Ctrl Pts',(-5.6270985823054,4.5266570316894,128.876308386002));
#74320=CARTESIAN_POINT('Ctrl Pts',(-5.63484647908248,4.46938999358476,128.751621923103));
#74321=CARTESIAN_POINT('Ctrl Pts',(-5.6425927551666,4.41213493450987,128.626961541925));
#74322=CARTESIAN_POINT('Ctrl Pts',(-5.65033903125069,4.34964575865998,128.504666583208));
#74323=CARTESIAN_POINT('Ctrl Pts',(-5.6580853073348,4.28215344467957,128.385198585225));
#74324=CARTESIAN_POINT('Ctrl Pts',(-5.66583164060016,4.21466063248632,128.265729705357));
#74325=CARTESIAN_POINT('Ctrl Pts',(-5.67357797386559,4.14216480077322,128.149088168262));
#74326=CARTESIAN_POINT('Ctrl Pts',(-5.68132430713095,4.06494231428161,128.03570985518));
#74327=CARTESIAN_POINT('Ctrl Pts',(-5.68907237513394,3.98770253434956,127.92230615181));
#74328=CARTESIAN_POINT('Ctrl Pts',(-5.69682044313692,3.90573421338897,127.812167449685));
#74329=CARTESIAN_POINT('Ctrl Pts',(-5.70456851113991,3.81935612565573,127.705699318244));
#74330=CARTESIAN_POINT('Ctrl Pts',(-5.71232481388179,3.73288623426282,127.599118031206));
#74331=CARTESIAN_POINT('Ctrl Pts',(-5.72008111662366,3.64199746051794,127.496215411868));
#74332=CARTESIAN_POINT('Ctrl Pts',(-5.72783741936553,3.54704820259828,127.397363096149));
#74333=CARTESIAN_POINT('Ctrl Pts',(-5.7355978618797,3.45204826740094,127.298458019972));
#74334=CARTESIAN_POINT('Ctrl Pts',(-5.74335830439388,3.35298381195137,127.203607825172));
#74335=CARTESIAN_POINT('Ctrl Pts',(-5.75111874690805,3.25024820464688,127.113145415131));
#74336=CARTESIAN_POINT('Ctrl Pts',(-5.75889164717349,3.14734767702497,127.022537786797));
#74337=CARTESIAN_POINT('Ctrl Pts',(-5.76666454743898,3.04076452509579,126.936332264708));
#74338=CARTESIAN_POINT('Ctrl Pts',(-5.77443744770443,2.93092383703761,126.854820324825));
#74339=CARTESIAN_POINT('Ctrl Pts',(-5.78192778346631,2.82507613466472,126.776271549275));
#74340=CARTESIAN_POINT('Ctrl Pts',(-5.78941811922814,2.71620387811018,126.702081206863));
#74341=CARTESIAN_POINT('Ctrl Pts',(-5.79690845499002,2.6047092117718,126.632469801088));
#74342=CARTESIAN_POINT('Ctrl Pts',(-5.8046827891091,2.48898719126885,126.560219057704));
#74343=CARTESIAN_POINT('Ctrl Pts',(-5.81245712322821,2.37007340556484,126.492672457331));
#74344=CARTESIAN_POINT('Ctrl Pts',(-5.82023145734729,2.24838737043921,126.430124993488));
#74345=CARTESIAN_POINT('Ctrl Pts',(-5.82799621029438,2.12685130247647,126.367654613805));
#74346=CARTESIAN_POINT('Ctrl Pts',(-5.83576096324147,2.00255012738952,126.310171289135));
#74347=CARTESIAN_POINT('Ctrl Pts',(-5.84352571618857,1.87593195544035,126.257926590655));
#74348=CARTESIAN_POINT('Ctrl Pts',(-5.85128275707357,1.74943954244457,126.205733782345));
#74349=CARTESIAN_POINT('Ctrl Pts',(-5.85903979795855,1.62063507129545,126.158769394023));
#74350=CARTESIAN_POINT('Ctrl Pts',(-5.86679683884356,1.4899905350182,126.117238764226));
#74351=CARTESIAN_POINT('Ctrl Pts',(-5.87454803008368,1.3594445188022,126.075739453));
#74352=CARTESIAN_POINT('Ctrl Pts',(-5.88229922132385,1.2270615704911,126.03966586216));
#74353=CARTESIAN_POINT('Ctrl Pts',(-5.89005041256397,1.0933325789532,126.009174809456));
#74354=CARTESIAN_POINT('Ctrl Pts',(-5.89779830934105,0.959660425803852,
125.978696716263));
#74355=CARTESIAN_POINT('Ctrl Pts',(-5.90554620611812,0.824643747683947,
125.953796528763));
#74356=CARTESIAN_POINT('Ctrl Pts',(-5.91329410289521,0.688787262222854,
125.934580830974));
#74357=CARTESIAN_POINT('Ctrl Pts',(-5.92104037897931,0.552959195009791,
125.915369152695));
#74358=CARTESIAN_POINT('Ctrl Pts',(-5.92878665506345,0.416292056738909,
125.901839653716));
#74359=CARTESIAN_POINT('Ctrl Pts',(-5.93653293114755,0.27929900222865,125.894047477872));
#74360=CARTESIAN_POINT('Ctrl Pts',(-5.94427926441291,0.142304936466783,
125.886255244507));
#74361=CARTESIAN_POINT('Ctrl Pts',(-5.95202559767823,0.00498533999914305,
125.884200440988));
#74362=CARTESIAN_POINT('Ctrl Pts',(-5.95977193094359,-0.132143686050491,
125.887886158288));
#74363=CARTESIAN_POINT('Ctrl Pts',(-5.96751999894657,-0.269303421194724,
125.891572700978));
#74364=CARTESIAN_POINT('Ctrl Pts',(-5.97526806694954,-0.40627211024955,
125.901002312079));
#74365=CARTESIAN_POINT('Ctrl Pts',(-5.98301613495252,-0.542536230886556,
125.916126017971));
#74366=CARTESIAN_POINT('Ctrl Pts',(-5.99077243769438,-0.678945174652538,
125.931265797518));
#74367=CARTESIAN_POINT('Ctrl Pts',(-5.9985287404362,-0.814647664945897,
125.952111717685));
#74368=CARTESIAN_POINT('Ctrl Pts',(-6.00628504317805,-0.949137310973439,
125.978563126227));
#74369=CARTESIAN_POINT('Ctrl Pts',(-6.01404548569223,-1.08369873817465,
126.005028652682));
#74370=CARTESIAN_POINT('Ctrl Pts',(-6.02180592820645,-1.21704565131129,
126.037105537568));
#74371=CARTESIAN_POINT('Ctrl Pts',(-6.02956637072063,-1.3486853441128,126.074642771322));
#74372=CARTESIAN_POINT('Ctrl Pts',(-6.03733927098606,-1.48053635663544,
126.112240263176));
#74373=CARTESIAN_POINT('Ctrl Pts',(-6.04511217125155,-1.61067430089243,
126.155315497109));
#74374=CARTESIAN_POINT('Ctrl Pts',(-6.05288507151698,-1.73862417935703,
126.203668384276));
#74375=CARTESIAN_POINT('Ctrl Pts',(-6.06037540727895,-1.8619227574521,126.2502635222));
#74376=CARTESIAN_POINT('Ctrl Pts',(-6.06786574304089,-1.98318930772456,
126.301759142789));
#74377=CARTESIAN_POINT('Ctrl Pts',(-6.07535607880286,-2.10202094546646,
126.357936098099));
#74378=CARTESIAN_POINT('Ctrl Pts',(-6.0831310787037,-2.22536868327438,126.416248013057));
#74379=CARTESIAN_POINT('Ctrl Pts',(-6.09090607860455,-2.34648353675557,
126.479788850858));
#74380=CARTESIAN_POINT('Ctrl Pts',(-6.09868107850539,-2.46489043968613,
126.548365060373));
#74381=CARTESIAN_POINT('Ctrl Pts',(-6.1064463476794,-2.58314915158864,126.616855443989));
#74382=CARTESIAN_POINT('Ctrl Pts',(-6.11421161685342,-2.69870632152533,
126.690368465248));
#74383=CARTESIAN_POINT('Ctrl Pts',(-6.12197688602743,-2.81110799311244,
126.768663042975));
#74384=CARTESIAN_POINT('Ctrl Pts',(-6.12973429422568,-2.92339587768278,
126.846878361148));
#74385=CARTESIAN_POINT('Ctrl Pts',(-6.13749170242393,-3.03253430262064,
126.929865380053));
#74386=CARTESIAN_POINT('Ctrl Pts',(-6.14524911062219,-3.13809533106104,
127.017337940624));
#74387=CARTESIAN_POINT('Ctrl Pts',(-6.15300004877302,-3.24356831658262,
127.104737544918));
#74388=CARTESIAN_POINT('Ctrl Pts',(-6.16075098692381,-3.34546954738773,
127.196614992465));
#74389=CARTESIAN_POINT('Ctrl Pts',(-6.16850192507465,-3.44340179562564,
127.292642072981));
#74390=CARTESIAN_POINT('Ctrl Pts',(-6.17624935165313,-3.54128967553431,
127.388625648307));
#74391=CARTESIAN_POINT('Ctrl Pts',(-6.18399677823165,-3.63521187206467,
127.488754842978));
#74392=CARTESIAN_POINT('Ctrl Pts',(-6.19174420481013,-3.72480597182815,
127.592662696725));
#74393=CARTESIAN_POINT('Ctrl Pts',(-6.19948979918119,-3.81437888326883,
127.696545977056));
#74394=CARTESIAN_POINT('Ctrl Pts',(-6.20723539355222,-3.89962548024037,
127.80420584196));
#74395=CARTESIAN_POINT('Ctrl Pts',(-6.21498098792327,-3.98022208394728,
127.915240470366));
#74396=CARTESIAN_POINT('Ctrl Pts',(-6.22272642785827,-4.06081708067338,
128.026272884901));
#74397=CARTESIAN_POINT('Ctrl Pts',(-6.2304718677933,-4.13676204036941,128.140679611881));
#74398=CARTESIAN_POINT('Ctrl Pts',(-6.23821730772829,-4.20777549292051,
128.25802826226));
#74399=CARTESIAN_POINT('Ctrl Pts',(-6.2459673356742,-4.2788310102863,128.375446424106));
#74400=CARTESIAN_POINT('Ctrl Pts',(-6.25371736362005,-4.34494898254698,
128.495809655774));
#74401=CARTESIAN_POINT('Ctrl Pts',(-6.26146739156596,-4.40589286324137,
128.618659096283));
#74402=CARTESIAN_POINT('Ctrl Pts',(-6.2692199660448,-4.46685676910216,128.741548903117));
#74403=CARTESIAN_POINT('Ctrl Pts',(-6.2769725405237,-4.52264303362214,128.86692619097));
#74404=CARTESIAN_POINT('Ctrl Pts',(-6.28472511500254,-4.57306289007633,
128.994311207769));
#74405=CARTESIAN_POINT('Ctrl Pts',(-6.29248568990171,-4.62353477828403,
129.121827682018));
#74406=CARTESIAN_POINT('Ctrl Pts',(-6.30024626480089,-4.66862906700021,
129.251355655095));
#74407=CARTESIAN_POINT('Ctrl Pts',(-6.30800683970006,-4.7082064619071,129.38239895333));
#74408=CARTESIAN_POINT('Ctrl Pts',(-6.31193504554483,-4.72823953368516,
129.448729741543));
#74409=CARTESIAN_POINT('Ctrl Pts',(-6.31586325138957,-4.74685991247322,
129.515448573421));
#74410=CARTESIAN_POINT('Ctrl Pts',(-6.31979145723434,-4.76405452823404,
129.582490119308));
#74411=CARTESIAN_POINT('Origin',(213.235140564004,0.,130.804360617566));
#74412=CARTESIAN_POINT('',(-8.41516596570781,-4.76405452823401,129.582490119308));
#74413=CARTESIAN_POINT('',(-8.07013341471002,-4.76405452823399,129.582490119308));
#74414=CARTESIAN_POINT('',(213.235140564004,-4.76405452823405,129.582490119308));
#74415=CARTESIAN_POINT('',(-6.73514056397329,-4.91824973727353,130.802753039002));
#74416=CARTESIAN_POINT('Ctrl Pts',(-6.73514056400862,-4.91824973727374,
130.802753039629));
#74417=CARTESIAN_POINT('Ctrl Pts',(-6.74308048856736,-4.91829580373628,
130.943689514402));
#74418=CARTESIAN_POINT('Ctrl Pts',(-6.7510204131261,-4.91227954301344,131.084575973784));
#74419=CARTESIAN_POINT('Ctrl Pts',(-6.75896033768484,-4.90024012990961,
131.224871891759));
#74420=CARTESIAN_POINT('Ctrl Pts',(-6.76690503553524,-4.88819347900021,
131.365252152266));
#74421=CARTESIAN_POINT('Ctrl Pts',(-6.77484973338559,-4.870116489556,131.505040802365));
#74422=CARTESIAN_POINT('Ctrl Pts',(-6.782794431236,-4.84610004999722,131.643704032336));
#74423=CARTESIAN_POINT('Ctrl Pts',(-6.79074523461097,-4.82206515373128,
131.782473825422));
#74424=CARTESIAN_POINT('Ctrl Pts',(-6.79869603798591,-4.79208177130108,
131.920116117517));
#74425=CARTESIAN_POINT('Ctrl Pts',(-6.80664684136087,-4.75629154989002,
132.056108896952));
#74426=CARTESIAN_POINT('Ctrl Pts',(-6.81461084874838,-4.72044189114791,
132.192327521534));
#74427=CARTESIAN_POINT('Ctrl Pts',(-6.82257485613593,-4.6787662186234,132.326890809158));
#74428=CARTESIAN_POINT('Ctrl Pts',(-6.83053886352343,-4.63145590659714,
132.459292413063));
#74429=CARTESIAN_POINT('Ctrl Pts',(-6.83851017959729,-4.58410217720377,
132.591815523861));
#74430=CARTESIAN_POINT('Ctrl Pts',(-6.84648149567114,-4.53110363311608,
132.722172659786));
#74431=CARTESIAN_POINT('Ctrl Pts',(-6.85445281174501,-4.47269898320194,
132.849879345949));
#74432=CARTESIAN_POINT('Ctrl Pts',(-6.86243872369883,-4.41418739144137,
132.977819869466));
#74433=CARTESIAN_POINT('Ctrl Pts',(-6.8704246356527,-4.35025007827006,133.103099922917));
#74434=CARTESIAN_POINT('Ctrl Pts',(-6.87841054760653,-4.28117123850171,
133.225260427373));
#74435=CARTESIAN_POINT('Ctrl Pts',(-6.88264368309837,-4.24455424471959,
133.290014705921));
#74436=CARTESIAN_POINT('Ctrl Pts',(-6.88687681859019,-4.20649331057569,
133.353892954325));
#74437=CARTESIAN_POINT('Ctrl Pts',(-6.89110995408203,-4.16703546937306,
133.41683041825));
#74438=CARTESIAN_POINT('Ctrl Pts',(-6.89888428820112,-4.09456945884271,
133.532417758676));
#74439=CARTESIAN_POINT('Ctrl Pts',(-6.90665862232015,-4.01717569231029,
133.645170747791));
#74440=CARTESIAN_POINT('Ctrl Pts',(-6.91443295643924,-3.93510240986074,
133.754640618923));
#74441=CARTESIAN_POINT('Ctrl Pts',(-6.92219770938633,-3.85313027539681,
133.863975578223));
#74442=CARTESIAN_POINT('Ctrl Pts',(-6.92996246233349,-3.76649033207073,
133.970035160362));
#74443=CARTESIAN_POINT('Ctrl Pts',(-6.93772721528057,-3.67547552617673,
134.072397141073));
#74444=CARTESIAN_POINT('Ctrl Pts',(-6.94548425616558,-3.58455111747089,
134.174657454422));
#74445=CARTESIAN_POINT('Ctrl Pts',(-6.95324129705059,-3.48926075139595,
134.273227184521));
#74446=CARTESIAN_POINT('Ctrl Pts',(-6.96099833793559,-3.38993907244603,
134.367715237528));
#74447=CARTESIAN_POINT('Ctrl Pts',(-6.96874952917572,-3.29069229274695,
134.462132036359));
#74448=CARTESIAN_POINT('Ctrl Pts',(-6.97650072041582,-3.18742053331162,
134.552473016334));
#74449=CARTESIAN_POINT('Ctrl Pts',(-6.98425191165595,-3.08049665296856,
134.638382452865));
#74450=CARTESIAN_POINT('Ctrl Pts',(-6.99199980843303,-2.97361821812679,
134.724255375594));
#74451=CARTESIAN_POINT('Ctrl Pts',(-6.99974770521013,-2.86309105382065,
134.805700256701));
#74452=CARTESIAN_POINT('Ctrl Pts',(-7.00749560198722,-2.74932242568258,
134.882400497476));
#74453=CARTESIAN_POINT('Ctrl Pts',(-7.01524187807132,-2.63557759548895,
134.959084694214));
#74454=CARTESIAN_POINT('Ctrl Pts',(-7.02298815415538,-2.51859297409999,
135.031026006298));
#74455=CARTESIAN_POINT('Ctrl Pts',(-7.03073443023948,-2.398805913088,135.097950403961));
#74456=CARTESIAN_POINT('Ctrl Pts',(-7.03848076350481,-2.27901796783529,
135.164875295645));
#74457=CARTESIAN_POINT('Ctrl Pts',(-7.04622709677017,-2.15642788298945,
135.226783008322));
#74458=CARTESIAN_POINT('Ctrl Pts',(-7.05397343003551,-2.03149842618743,
135.283445033705));
#74459=CARTESIAN_POINT('Ctrl Pts',(-7.06172149803849,-1.90654099229959,
135.340119748155));
#74460=CARTESIAN_POINT('Ctrl Pts',(-7.06946956604152,-1.7792434999694,135.391546276265));
#74461=CARTESIAN_POINT('Ctrl Pts',(-7.0772176340445,-1.65008916941539,135.437544058299));
#74462=CARTESIAN_POINT('Ctrl Pts',(-7.08497393678636,-1.52079757210191,
135.483590727323));
#74463=CARTESIAN_POINT('Ctrl Pts',(-7.09273023952818,-1.38964556323794,
135.524196993223));
#74464=CARTESIAN_POINT('Ctrl Pts',(-7.10048654227003,-1.25713255262244,
135.559231888971));
#74465=CARTESIAN_POINT('Ctrl Pts',(-7.10824698478421,-1.12454881582311,
135.594285483899));
#74466=CARTESIAN_POINT('Ctrl Pts',(-7.11600742729848,-0.990603011485884,
135.623761699524));
#74467=CARTESIAN_POINT('Ctrl Pts',(-7.12376786981267,-0.855804268115007,
135.647580839399));
#74468=CARTESIAN_POINT('Ctrl Pts',(-7.1315407700781,-0.720789133834584,
135.671438215873));
#74469=CARTESIAN_POINT('Ctrl Pts',(-7.13931367034345,-0.58491871212966,
135.6896203175));
#74470=CARTESIAN_POINT('Ctrl Pts',(-7.14708657060888,-0.448707672328128,
135.702099329185));
#74471=CARTESIAN_POINT('Ctrl Pts',(-7.15457690637087,-0.317448246918841,
135.714124697363));
#74472=CARTESIAN_POINT('Ctrl Pts',(-7.16206724213292,-0.185872845730236,
135.720854404418));
#74473=CARTESIAN_POINT('Ctrl Pts',(-7.16955757789492,-0.0544396243900029,
135.722309314919));
#74474=CARTESIAN_POINT('Ctrl Pts',(-7.177331912014,0.0819769274861851,135.723819388794));
#74475=CARTESIAN_POINT('Ctrl Pts',(-7.18510624613308,0.218672431817819,
135.719651565866));
#74476=CARTESIAN_POINT('Ctrl Pts',(-7.19288058025217,0.355135148664519,
135.709772128202));
#74477=CARTESIAN_POINT('Ctrl Pts',(-7.20064533319926,0.491429687408728,
135.699904866062));
#74478=CARTESIAN_POINT('Ctrl Pts',(-7.20841008614631,0.627491623291929,
135.684340022767));
#74479=CARTESIAN_POINT('Ctrl Pts',(-7.21617483909341,0.762807382452408,
135.6630958398));
#74480=CARTESIAN_POINT('Ctrl Pts',(-7.22393187997841,0.897988744093086,
135.641872756855));
#74481=CARTESIAN_POINT('Ctrl Pts',(-7.23168892086349,1.03242502012493,135.61498161993));
#74482=CARTESIAN_POINT('Ctrl Pts',(-7.23944596174849,1.16560628869944,135.582492579143));
#74483=CARTESIAN_POINT('Ctrl Pts',(-7.24719715298861,1.29868712424333,135.550028038594));
#74484=CARTESIAN_POINT('Ctrl Pts',(-7.25494834422869,1.4305144578134,135.51197408895));
#74485=CARTESIAN_POINT('Ctrl Pts',(-7.26269953546881,1.56058746893522,135.468452149076));
#74486=CARTESIAN_POINT('Ctrl Pts',(-7.27044743224589,1.69060519555751,135.424948707187));
#74487=CARTESIAN_POINT('Ctrl Pts',(-7.27819532902292,1.81886971275518,135.375982021204));
#74488=CARTESIAN_POINT('Ctrl Pts',(-7.2859432258,1.94489452004455,135.321723605903));
#74489=CARTESIAN_POINT('Ctrl Pts',(-7.29368950188409,2.07089296566084,135.267476540293));
#74490=CARTESIAN_POINT('Ctrl Pts',(-7.30143577796818,2.194652274369,135.207940101588));
#74491=CARTESIAN_POINT('Ctrl Pts',(-7.30918205405226,2.31570549795869,135.143334126269));
#74492=CARTESIAN_POINT('Ctrl Pts',(-7.3169283873176,2.43675961513594,135.078727674043));
#74493=CARTESIAN_POINT('Ctrl Pts',(-7.32467472058298,2.55510726241774,135.009051794613));
#74494=CARTESIAN_POINT('Ctrl Pts',(-7.33242105384832,2.67030605209712,134.934572313186));
#74495=CARTESIAN_POINT('Ctrl Pts',(-7.34016912185128,2.78553063974656,134.860076152595));
#74496=CARTESIAN_POINT('Ctrl Pts',(-7.34791718985421,2.8976046383382,134.780774461651));
#74497=CARTESIAN_POINT('Ctrl Pts',(-7.35566525785717,3.00611494552234,134.696976190264));
#74498=CARTESIAN_POINT('Ctrl Pts',(-7.36342156059901,3.1147405787524,134.613088857075));
#74499=CARTESIAN_POINT('Ctrl Pts',(-7.37117786334091,3.2197946446404,134.524695636183));
#74500=CARTESIAN_POINT('Ctrl Pts',(-7.37893416608276,3.32089701372113,134.432145904316));
#74501=CARTESIAN_POINT('Ctrl Pts',(-7.38669460859692,3.42205334418051,134.33954677587));
#74502=CARTESIAN_POINT('Ctrl Pts',(-7.39445505111111,3.51925349824792,134.242786991681));
#74503=CARTESIAN_POINT('Ctrl Pts',(-7.40221549362528,3.61215522865279,134.142251818102));
#74504=CARTESIAN_POINT('Ctrl Pts',(-7.40998839389071,3.70520609316273,134.041555256538));
#74505=CARTESIAN_POINT('Ctrl Pts',(-7.41776129415614,3.79394449195623,133.937071492759));
#74506=CARTESIAN_POINT('Ctrl Pts',(-7.42553419442157,3.87806883206359,133.82921849791));
#74507=CARTESIAN_POINT('Ctrl Pts',(-7.43302453018363,3.95913504051197,133.725286231088));
#74508=CARTESIAN_POINT('Ctrl Pts',(-7.44051486594569,4.03591665190354,133.618225690704));
#74509=CARTESIAN_POINT('Ctrl Pts',(-7.44800520170776,4.10818357588296,133.508433613871));
#74510=CARTESIAN_POINT('Ctrl Pts',(-7.45577953582679,4.1831905222498,133.394478737075));
#74511=CARTESIAN_POINT('Ctrl Pts',(-7.46355386994592,4.25357127384649,133.277220127766));
#74512=CARTESIAN_POINT('Ctrl Pts',(-7.471328204065,4.31902085488254,133.157070101882));
#74513=CARTESIAN_POINT('Ctrl Pts',(-7.47909295701211,4.38438977515945,133.037068150167));
#74514=CARTESIAN_POINT('Ctrl Pts',(-7.48685770995917,4.44483943151815,132.91418221204));
#74515=CARTESIAN_POINT('Ctrl Pts',(-7.49462246290628,4.50010757181889,132.788854231705));
#74516=CARTESIAN_POINT('Ctrl Pts',(-7.50237950379129,4.55532081902354,132.663650728887));
#74517=CARTESIAN_POINT('Ctrl Pts',(-7.51013654467625,4.60536263491645,132.536010366068));
#74518=CARTESIAN_POINT('Ctrl Pts',(-7.51789358556127,4.6500164135625,132.406400072792));
#74519=CARTESIAN_POINT('Ctrl Pts',(-7.52564477680136,4.6946365184464,132.276887519647));
#74520=CARTESIAN_POINT('Ctrl Pts',(-7.5333959680415,4.73387654672345,132.145408361069));
#74521=CARTESIAN_POINT('Ctrl Pts',(-7.54114715928159,4.76756794582284,132.012449581369));
#74522=CARTESIAN_POINT('Ctrl Pts',(-7.54889505605869,4.80124502517909,131.879547312696));
#74523=CARTESIAN_POINT('Ctrl Pts',(-7.55664295283579,4.82937807003393,131.745167051886));
#74524=CARTESIAN_POINT('Ctrl Pts',(-7.56439084961289,4.85184841523002,131.6098108135));
#74525=CARTESIAN_POINT('Ctrl Pts',(-7.572137125697,4.87431406011427,131.474482888721));
#74526=CARTESIAN_POINT('Ctrl Pts',(-7.57988340178113,4.89111929741757,131.33817977788));
#74527=CARTESIAN_POINT('Ctrl Pts',(-7.58762967786524,4.90219668488516,131.201413164719));
#74528=CARTESIAN_POINT('Ctrl Pts',(-7.5953760111306,4.91327415412351,131.064645541979));
#74529=CARTESIAN_POINT('Ctrl Pts',(-7.60312234439584,4.91862365759332,130.927414799781));
#74530=CARTESIAN_POINT('Ctrl Pts',(-7.61086867766119,4.91822972020849,130.79023681645));
#74531=CARTESIAN_POINT('Ctrl Pts',(-7.61861674566418,4.91783569460411,130.653028113061));
#74532=CARTESIAN_POINT('Ctrl Pts',(-7.62636481366724,4.91169566987101,130.515872582938));
#74533=CARTESIAN_POINT('Ctrl Pts',(-7.63411288167023,4.89984628240653,130.37928477576));
#74534=CARTESIAN_POINT('Ctrl Pts',(-7.6418691844121,4.88798430127207,130.242551801435));
#74535=CARTESIAN_POINT('Ctrl Pts',(-7.64962548715395,4.87040086980958,130.106388145501));
#74536=CARTESIAN_POINT('Ctrl Pts',(-7.65738178989582,4.84718445929574,129.971302468298));
#74537=CARTESIAN_POINT('Ctrl Pts',(-7.66514223241,4.82395565748459,129.836144691802));
#74538=CARTESIAN_POINT('Ctrl Pts',(-7.6729026749242,4.79508796818583,129.70206642249));
#74539=CARTESIAN_POINT('Ctrl Pts',(-7.68066311743837,4.76072053388455,129.569563848559));
#74540=CARTESIAN_POINT('Ctrl Pts',(-7.68843601770381,4.72629792992673,129.436848569733));
#74541=CARTESIAN_POINT('Ctrl Pts',(-7.69620891796926,4.68635805242925,129.305714415146));
#74542=CARTESIAN_POINT('Ctrl Pts',(-7.70398181823469,4.64108953398614,129.176641047117));
#74543=CARTESIAN_POINT('Ctrl Pts',(-7.71147215399671,4.59746664021308,129.052259821131));
#74544=CARTESIAN_POINT('Ctrl Pts',(-7.71896248975872,4.54889591192813,128.929792439723));
#74545=CARTESIAN_POINT('Ctrl Pts',(-7.72645282552074,4.49558676584433,128.809646930526));
#74546=CARTESIAN_POINT('Ctrl Pts',(-7.73422715963982,4.44025638728373,128.684946067829));
#74547=CARTESIAN_POINT('Ctrl Pts',(-7.74200149375893,4.37964591371896,128.562351605692));
#74548=CARTESIAN_POINT('Ctrl Pts',(-7.74977582787801,4.313937391362,128.44234299572));
#74549=CARTESIAN_POINT('Ctrl Pts',(-7.7575405808251,4.24830984888631,128.322482285635));
#74550=CARTESIAN_POINT('Ctrl Pts',(-7.76530533377214,4.17759694465666,128.205201426504));
#74551=CARTESIAN_POINT('Ctrl Pts',(-7.77307008671923,4.10202874515994,128.090959940117));
#74552=CARTESIAN_POINT('Ctrl Pts',(-7.78082712760422,4.02653560106439,127.976831919985));
#74553=CARTESIAN_POINT('Ctrl Pts',(-7.78858416848928,3.94619697269126,127.865737589123));
#74554=CARTESIAN_POINT('Ctrl Pts',(-7.79634120937428,3.86128862029136,127.758111571065));
#74555=CARTESIAN_POINT('Ctrl Pts',(-7.80409240061442,3.77644429794027,127.650566714624));
#74556=CARTESIAN_POINT('Ctrl Pts',(-7.81184359185451,3.68703735191954,127.54648527073));
#74557=CARTESIAN_POINT('Ctrl Pts',(-7.81959478309466,3.59338638914034,127.44627227435));
#74558=CARTESIAN_POINT('Ctrl Pts',(-7.82734267987174,3.49977523051866,127.346101871168));
#74559=CARTESIAN_POINT('Ctrl Pts',(-7.83509057664887,3.40192390918442,127.249796930374));
#74560=CARTESIAN_POINT('Ctrl Pts',(-7.84283847342596,3.30019064278917,127.15772863946));
#74561=CARTESIAN_POINT('Ctrl Pts',(-7.85058474951007,3.19847865679999,127.065679607247));
#74562=CARTESIAN_POINT('Ctrl Pts',(-7.85833102559416,3.09288663059767,126.977865724356));
#74563=CARTESIAN_POINT('Ctrl Pts',(-7.86607730167827,2.98380860402038,126.894620309429));
#74564=CARTESIAN_POINT('Ctrl Pts',(-7.87382363494363,2.87472977225402,126.811374280002));
#74565=CARTESIAN_POINT('Ctrl Pts',(-7.88156996820896,2.76216519956066,126.732697023022));
#74566=CARTESIAN_POINT('Ctrl Pts',(-7.88931630147431,2.64654054432316,126.658880402952));
#74567=CARTESIAN_POINT('Ctrl Pts',(-7.89706436947725,2.53088999574628,126.585047252162));
#74568=CARTESIAN_POINT('Ctrl Pts',(-7.90481243748026,2.41217833046148,126.516077114624));
#74569=CARTESIAN_POINT('Ctrl Pts',(-7.91256050548321,2.29085825655375,126.452217293768));
#74570=CARTESIAN_POINT('Ctrl Pts',(-7.92031680822508,2.16940924222726,126.388289601934));
#74571=CARTESIAN_POINT('Ctrl Pts',(-7.92807311096692,2.04534662792984,126.329483258798));
#74572=CARTESIAN_POINT('Ctrl Pts',(-7.93582941370877,1.91914618489891,126.275998774307));
#74573=CARTESIAN_POINT('Ctrl Pts',(-7.94358985622296,1.79287838489137,126.222485743536));
#74574=CARTESIAN_POINT('Ctrl Pts',(-7.95135029873719,1.66447084842675,126.174300368511));
#74575=CARTESIAN_POINT('Ctrl Pts',(-7.95911074125138,1.53441624259946,126.13159378656));
#74576=CARTESIAN_POINT('Ctrl Pts',(-7.96688364151683,1.40415286157337,126.088818648213));
#74577=CARTESIAN_POINT('Ctrl Pts',(-7.97465654178226,1.27223750403358,126.051539984623));
#74578=CARTESIAN_POINT('Ctrl Pts',(-7.9824294420477,1.13917568399913,126.019858363048));
#74579=CARTESIAN_POINT('Ctrl Pts',(-7.98991977780966,1.01095099628687,125.989328448219));
#74580=CARTESIAN_POINT('Ctrl Pts',(-7.99741011357162,0.881662054808889,
125.963995766437));
#74581=CARTESIAN_POINT('Ctrl Pts',(-8.00490044933358,0.751765339617887,
125.943904678392));
#74582=CARTESIAN_POINT('Ctrl Pts',(-8.01267478345266,0.616943550987837,
125.923051830638));
#74583=CARTESIAN_POINT('Ctrl Pts',(-8.02044911757182,0.481039916481458,
125.907779837304));
#74584=CARTESIAN_POINT('Ctrl Pts',(-8.02822345169091,0.344556212737817,
125.898194693062));
#74585=CARTESIAN_POINT('Ctrl Pts',(-8.035988204638,0.208240712961141,125.888621361654));
#74586=CARTESIAN_POINT('Ctrl Pts',(-8.043752957585,0.0713469526128881,125.884720961571));
#74587=CARTESIAN_POINT('Ctrl Pts',(-8.0515177105321,-0.0656141030554698,
125.886548314114));
#74588=CARTESIAN_POINT('Ctrl Pts',(-8.05927475141713,-0.202439127072898,
125.888373851706));
#74589=CARTESIAN_POINT('Ctrl Pts',(-8.0670317923022,-0.339330924997757,
125.895915815604));
#74590=CARTESIAN_POINT('Ctrl Pts',(-8.07478883318723,-0.475774780592142,
125.909177125535));
#74591=CARTESIAN_POINT('Ctrl Pts',(-8.08254002442735,-0.612115742813087,
125.922428435009));
#74592=CARTESIAN_POINT('Ctrl Pts',(-8.09029121566743,-0.748009047510532,
125.941390468078));
#74593=CARTESIAN_POINT('Ctrl Pts',(-8.09804240690755,-0.882941712477918,
125.966014103015));
#74594=CARTESIAN_POINT('Ctrl Pts',(-8.10579030368463,-1.01781702746325,
125.990627272251));
#74595=CARTESIAN_POINT('Ctrl Pts',(-8.11353820046181,-1.15173213098292,
126.020897187305));
#74596=CARTESIAN_POINT('Ctrl Pts',(-8.12128609723888,-1.28418110709839,
126.056723105427));
#74597=CARTESIAN_POINT('Ctrl Pts',(-8.12903237332298,-1.4166023777435,126.092541529539));
#74598=CARTESIAN_POINT('Ctrl Pts',(-8.13677864940701,-1.54755775382855,
126.133913543029));
#74599=CARTESIAN_POINT('Ctrl Pts',(-8.14452492549111,-1.67655381678383,
126.180687795888));
#74600=CARTESIAN_POINT('Ctrl Pts',(-8.15227125875646,-1.80555083195856,
126.227462394023));
#74601=CARTESIAN_POINT('Ctrl Pts',(-8.16001759202186,-1.93258813759476,
126.279639177828));
#74602=CARTESIAN_POINT('Ctrl Pts',(-8.1677639252872,-2.05719010109988,126.337017788721));
#74603=CARTESIAN_POINT('Ctrl Pts',(-8.1755119932902,-2.18181996835114,126.394409249155));
#74604=CARTESIAN_POINT('Ctrl Pts',(-8.1832600612932,-2.30401305317887,126.45700469122));
#74605=CARTESIAN_POINT('Ctrl Pts',(-8.19100812929619,-2.42331659242449,
126.524556912327));
#74606=CARTESIAN_POINT('Ctrl Pts',(-8.19876443203806,-2.54274692889118,
126.592180928738));
#74607=CARTESIAN_POINT('Ctrl Pts',(-8.20652073477992,-2.65928124427988,
126.664772054892));
#74608=CARTESIAN_POINT('Ctrl Pts',(-8.21427703752178,-2.77249367791692,
126.742038391497));
#74609=CARTESIAN_POINT('Ctrl Pts',(-8.22203748003594,-2.8857665364384,126.819345967473));
#74610=CARTESIAN_POINT('Ctrl Pts',(-8.22979792255011,-2.99571366711432,
126.901333492397));
#74611=CARTESIAN_POINT('Ctrl Pts',(-8.23755836506427,-3.10194161523259,
126.987668164906));
#74612=CARTESIAN_POINT('Ctrl Pts',(-8.2453312653297,-3.20834008988366,127.074141429496));
#74613=CARTESIAN_POINT('Ctrl Pts',(-8.25310416559509,-3.31100715830994,
127.164975527579));
#74614=CARTESIAN_POINT('Ctrl Pts',(-8.26087706586051,-3.40958496775515,
127.259799514953));
#74615=CARTESIAN_POINT('Ctrl Pts',(-8.2683674016225,-3.5045792255241,127.351176411538));
#74616=CARTESIAN_POINT('Ctrl Pts',(-8.27585773738448,-3.59577615909364,
127.446257926368));
#74617=CARTESIAN_POINT('Ctrl Pts',(-8.28334807314647,-3.68289170793955,
127.544683987885));
#74618=CARTESIAN_POINT('Ctrl Pts',(-8.29105212000108,-3.77249280078742,
127.645918300168));
#74619=CARTESIAN_POINT('Ctrl Pts',(-8.29875616685568,-3.85807248466077,
127.751025949734));
#74620=CARTESIAN_POINT('Ctrl Pts',(-8.30646021371027,-3.93927250583388,
127.859650922659));
#74621=CARTESIAN_POINT('Ctrl Pts',(-8.31415498973554,-4.02037481322738,
127.968145179402));
#74622=CARTESIAN_POINT('Ctrl Pts',(-8.32184976576084,-4.09710770232271,
128.080148026498));
#74623=CARTESIAN_POINT('Ctrl Pts',(-8.32954454178611,-4.16915061233118,
128.195267626851));
#74624=CARTESIAN_POINT('Ctrl Pts',(-8.33723045367694,-4.24111053122496,
128.310254613128));
#74625=CARTESIAN_POINT('Ctrl Pts',(-8.34491636556771,-4.3083910161016,128.428350869654));
#74626=CARTESIAN_POINT('Ctrl Pts',(-8.35260227745854,-4.37071303132848,
128.549133209903));
#74627=CARTESIAN_POINT('Ctrl Pts',(-8.3602830297844,-4.43299320968651,128.669834468773));
#74628=CARTESIAN_POINT('Ctrl Pts',(-8.36796378211028,-4.49032135574294,
128.79321787286));
#74629=CARTESIAN_POINT('Ctrl Pts',(-8.37564453443613,-4.54246292632829,
128.918833204497));
#74630=CARTESIAN_POINT('Ctrl Pts',(-8.38332211999616,-4.59458299900082,
129.044396745071));
#74631=CARTESIAN_POINT('Ctrl Pts',(-8.3909997055562,-4.64152059544803,129.172190016107));
#74632=CARTESIAN_POINT('Ctrl Pts',(-8.39867729111623,-4.68308833391675,
129.301740665871));
#74633=CARTESIAN_POINT('Ctrl Pts',(-8.40417351598012,-4.71284581899082,
129.394483299189));
#74634=CARTESIAN_POINT('Ctrl Pts',(-8.40966974084399,-4.73985231839695,
129.488126070473));
#74635=CARTESIAN_POINT('Ctrl Pts',(-8.41516596570787,-4.76405452823401,
129.582490119308));
#74636=CARTESIAN_POINT('Ctrl Pts',(-6.66542383595777,-4.76405452823408,
129.582490119308));
#74637=CARTESIAN_POINT('Ctrl Pts',(-6.67380875453969,-4.80077876456201,
129.725677359383));
#74638=CARTESIAN_POINT('Ctrl Pts',(-6.68219367312164,-4.83108614509386,
129.870687833771));
#74639=CARTESIAN_POINT('Ctrl Pts',(-6.69057859170357,-4.8548085799642,130.016949216578));
#74640=CARTESIAN_POINT('Ctrl Pts',(-6.69893588454837,-4.87845285668149,
130.162728712951));
#74641=CARTESIAN_POINT('Ctrl Pts',(-6.70729317739312,-4.89555540448016,
130.309750619291));
#74642=CARTESIAN_POINT('Ctrl Pts',(-6.7156504702379,-4.90599870086107,130.457431504274));
#74643=CARTESIAN_POINT('Ctrl Pts',(-6.72214716814968,-4.91411699263929,
130.572234002511));
#74644=CARTESIAN_POINT('Ctrl Pts',(-6.72864386606151,-4.9182120442192,130.687434348684));
#74645=CARTESIAN_POINT('Ctrl Pts',(-6.73514056397329,-4.91824973727353,
130.802753039002));
#74646=CARTESIAN_POINT('',(-6.38985943602702,-4.91824879188756,130.80091335829));
#74647=CARTESIAN_POINT('Ctrl Pts',(-6.31979145723434,-4.76405452823404,
129.582490119308));
#74648=CARTESIAN_POINT('Ctrl Pts',(-6.32756591095457,-4.79808501180636,
129.715174458272));
#74649=CARTESIAN_POINT('Ctrl Pts',(-6.33534036467476,-4.82652757312717,
129.849123030039));
#74650=CARTESIAN_POINT('Ctrl Pts',(-6.34311481839498,-4.84932004182413,
129.983825307867));
#74651=CARTESIAN_POINT('Ctrl Pts',(-6.3466777798019,-4.85976562285889,130.045558136256));
#74652=CARTESIAN_POINT('Ctrl Pts',(-6.35024074120879,-4.86902523277928,
130.107449215245));
#74653=CARTESIAN_POINT('Ctrl Pts',(-6.35380370261569,-4.87709654325472,
130.169449308584));
#74654=CARTESIAN_POINT('Ctrl Pts',(-6.36582228040754,-4.90432267953643,
130.378587960341));
#74655=CARTESIAN_POINT('Ctrl Pts',(-6.37784085819934,-4.9181006199865,130.589514655206));
#74656=CARTESIAN_POINT('Ctrl Pts',(-6.38985943599116,-4.91824879188712,
130.80091335766));
#74657=CARTESIAN_POINT('Ctrl Pts',(-6.38985943602691,-4.91824879188756,
130.80091335829));
#74658=CARTESIAN_POINT('Ctrl Pts',(-6.39751660825043,-4.91834319386872,
130.935597869267));
#74659=CARTESIAN_POINT('Ctrl Pts',(-6.40517378047407,-4.91290100334641,
131.070498104028));
#74660=CARTESIAN_POINT('Ctrl Pts',(-6.41283095269759,-4.9018955881145,131.205113291573));
#74661=CARTESIAN_POINT('Ctrl Pts',(-6.42048006870295,-4.89090175183413,
131.339586848593));
#74662=CARTESIAN_POINT('Ctrl Pts',(-6.42812918470826,-4.8743563643088,131.47377555634));
#74663=CARTESIAN_POINT('Ctrl Pts',(-6.43577830071362,-4.85228481462837,
131.607177620517));
#74664=CARTESIAN_POINT('Ctrl Pts',(-6.44342132131879,-4.83023085324548,
131.740473379734));
#74665=CARTESIAN_POINT('Ctrl Pts',(-6.45106434192404,-4.80265955527722,
131.872983346633));
#74666=CARTESIAN_POINT('Ctrl Pts',(-6.4587073625292,-4.76964817117224,132.004210352213));
#74667=CARTESIAN_POINT('Ctrl Pts',(-6.466346844853,-4.73665206944983,132.135376607196));
#74668=CARTESIAN_POINT('Ctrl Pts',(-6.47398632717679,-4.69822098652581,
132.2652606917));
#74669=CARTESIAN_POINT('Ctrl Pts',(-6.4816258095006,-4.65448328216301,132.393375544672));
#74670=CARTESIAN_POINT('Ctrl Pts',(-6.48926362075416,-4.61075514504221,
132.521462373635));
#74671=CARTESIAN_POINT('Ctrl Pts',(-6.49690143200773,-4.56172282426308,
132.647780359251));
#74672=CARTESIAN_POINT('Ctrl Pts',(-6.50453924326129,-4.50756441087217,
132.771858049417));
#74673=CARTESIAN_POINT('Ctrl Pts',(-6.51217714705102,-4.45340534132316,
132.895937242849));
#74674=CARTESIAN_POINT('Ctrl Pts',(-6.51981505084081,-4.39412021713735,
133.017775717553));
#74675=CARTESIAN_POINT('Ctrl Pts',(-6.52745295463055,-4.3299348687763,133.136922962854));
#74676=CARTESIAN_POINT('Ctrl Pts',(-6.5350927144296,-4.26573392338656,133.256099160915));
#74677=CARTESIAN_POINT('Ctrl Pts',(-6.54273247422856,-4.19663057753906,
133.372582474692));
#74678=CARTESIAN_POINT('Ctrl Pts',(-6.55037223402761,-4.12289582368305,
133.485948410191));
#74679=CARTESIAN_POINT('Ctrl Pts',(-6.55801995493309,-4.04908423361244,
133.599432480069));
#74680=CARTESIAN_POINT('Ctrl Pts',(-6.56566767583859,-3.97063182042801,
133.709792348227));
#74681=CARTESIAN_POINT('Ctrl Pts',(-6.57331539674408,-3.88785215371226,
133.816633628662));
#74682=CARTESIAN_POINT('Ctrl Pts',(-6.5809675295815,-3.80502473182085,133.923536545297));
#74683=CARTESIAN_POINT('Ctrl Pts',(-6.58861966241889,-3.71786534616613,
134.026916526027));
#74684=CARTESIAN_POINT('Ctrl Pts',(-6.59627179525631,-3.62672590476346,
134.126414541604));
#74685=CARTESIAN_POINT('Ctrl Pts',(-6.60393521482056,-3.53545203469891,
134.226059314555));
#74686=CARTESIAN_POINT('Ctrl Pts',(-6.61159863438479,-3.44018667245611,
134.321810406574));
#74687=CARTESIAN_POINT('Ctrl Pts',(-6.61926205394903,-3.34131670019117,
134.413347424348));
#74688=CARTESIAN_POINT('Ctrl Pts',(-6.62359181144222,-3.2854561278086,134.465064948788));
#74689=CARTESIAN_POINT('Ctrl Pts',(-6.62792156893545,-3.22844549308984,
134.515438032771));
#74690=CARTESIAN_POINT('Ctrl Pts',(-6.63225132642864,-3.17035867720406,
134.564414994882));
#74691=CARTESIAN_POINT('Ctrl Pts',(-6.64002566054773,-3.06606038444297,
134.652356009637));
#74692=CARTESIAN_POINT('Ctrl Pts',(-6.6477999946668,-2.9579350890547,134.736093409582));
#74693=CARTESIAN_POINT('Ctrl Pts',(-6.65557432878589,-2.84635620073457,
134.81527565544));
#74694=CARTESIAN_POINT('Ctrl Pts',(-6.66333908173298,-2.73491482342236,
134.894360316255));
#74695=CARTESIAN_POINT('Ctrl Pts',(-6.67110383468005,-2.62002863761435,
134.968900768719));
#74696=CARTESIAN_POINT('Ctrl Pts',(-6.67886858762714,-2.50210551992899,
135.038584398809));
#74697=CARTESIAN_POINT('Ctrl Pts',(-6.68662562851214,-2.38429952514637,
135.108198818134));
#74698=CARTESIAN_POINT('Ctrl Pts',(-6.6943826693972,-2.2634629355184,135.172965817181));
#74699=CARTESIAN_POINT('Ctrl Pts',(-6.70213971028221,-2.14003382933992,
135.232615157651));
#74700=CARTESIAN_POINT('Ctrl Pts',(-6.70989090152235,-2.01669780201056,
135.292219516089));
#74701=CARTESIAN_POINT('Ctrl Pts',(-6.71764209276243,-1.89077350010286,
135.346713728155));
#74702=CARTESIAN_POINT('Ctrl Pts',(-6.72539328400256,-1.76272459183064,
135.395872903933));
#74703=CARTESIAN_POINT('Ctrl Pts',(-6.73314118077964,-1.63473010776043,
135.445011185749));
#74704=CARTESIAN_POINT('Ctrl Pts',(-6.74088907755672,-1.50461317758026,
135.488818801394));
#74705=CARTESIAN_POINT('Ctrl Pts',(-6.74863697433381,-1.37285828669157,
135.527118623982));
#74706=CARTESIAN_POINT('Ctrl Pts',(-6.7563832504179,-1.24113095608592,135.565410435072));
#74707=CARTESIAN_POINT('Ctrl Pts',(-6.76412952650198,-1.10776672146095,
135.598196635653));
#74708=CARTESIAN_POINT('Ctrl Pts',(-6.77187580258607,-0.973265719594784,
135.625349821201));
#74709=CARTESIAN_POINT('Ctrl Pts',(-6.77962213585141,-0.83876372487259,
135.652503207187));
#74710=CARTESIAN_POINT('Ctrl Pts',(-6.78736846911676,-0.703125329398517,
135.674023417797));
#74711=CARTESIAN_POINT('Ctrl Pts',(-6.7951148023821,-0.566860972950257,
135.689834156523));
#74712=CARTESIAN_POINT('Ctrl Pts',(-6.80286287038507,-0.430566101044161,
135.705648435953));
#74713=CARTESIAN_POINT('Ctrl Pts',(-6.81061093838809,-0.293645377508044,
135.715750654187));
#74714=CARTESIAN_POINT('Ctrl Pts',(-6.81835900639106,-0.156614077594845,
135.720116418376));
#74715=CARTESIAN_POINT('Ctrl Pts',(-6.82611530913291,-0.019437139185406,
135.724486822551));
#74716=CARTESIAN_POINT('Ctrl Pts',(-6.83387161187477,0.117850218973723,
135.723108581255));
#74717=CARTESIAN_POINT('Ctrl Pts',(-6.84162791461662,0.254732447592913,
135.71600946929));
#74718=CARTESIAN_POINT('Ctrl Pts',(-6.84938835713079,0.391687734379148,
135.708906568316));
#74719=CARTESIAN_POINT('Ctrl Pts',(-6.85714879964494,0.528237071708814,
135.696076749069));
#74720=CARTESIAN_POINT('Ctrl Pts',(-6.86490924215911,0.663871310428023,
135.677599575968));
#74721=CARTESIAN_POINT('Ctrl Pts',(-6.87268214242455,0.799723281268265,
135.659092741669));
#74722=CARTESIAN_POINT('Ctrl Pts',(-6.88045504269001,0.934656832912526,
135.63492050647));
#74723=CARTESIAN_POINT('Ctrl Pts',(-6.88822794295544,1.06817338119907,135.605213530351));
#74724=CARTESIAN_POINT('Ctrl Pts',(-6.89571827871748,1.19683626664769,135.576586477642));
#74725=CARTESIAN_POINT('Ctrl Pts',(-6.90320861447947,1.32418308565558,135.542820180188));
#74726=CARTESIAN_POINT('Ctrl Pts',(-6.91069895024151,1.44978393256617,135.504074397295));
#74727=CARTESIAN_POINT('Ctrl Pts',(-6.91847328436059,1.58014697376257,135.463859556267));
#74728=CARTESIAN_POINT('Ctrl Pts',(-6.92624761847968,1.70904198316749,135.41815279306));
#74729=CARTESIAN_POINT('Ctrl Pts',(-6.93402195259875,1.83597136376758,135.367078252258));
#74730=CARTESIAN_POINT('Ctrl Pts',(-6.94178670554583,1.96274431524991,135.316066656262));
#74731=CARTESIAN_POINT('Ctrl Pts',(-6.9495514584929,2.08755609868336,135.259700589705));
#74732=CARTESIAN_POINT('Ctrl Pts',(-6.95731621143997,2.20992323576158,135.19815423522));
#74733=CARTESIAN_POINT('Ctrl Pts',(-6.96507325232498,2.33216883607451,135.136669009443));
#74734=CARTESIAN_POINT('Ctrl Pts',(-6.97283029320999,2.45197427496104,135.070013909326));
#74735=CARTESIAN_POINT('Ctrl Pts',(-6.98058733409499,2.56887540126814,134.998411432144));
#74736=CARTESIAN_POINT('Ctrl Pts',(-6.9883385253351,2.68568837152621,134.926862950947));
#74737=CARTESIAN_POINT('Ctrl Pts',(-6.9960897165752,2.79960105654727,134.850374722108));
#74738=CARTESIAN_POINT('Ctrl Pts',(-7.00384090781532,2.91017362607812,134.769215284332));
#74739=CARTESIAN_POINT('Ctrl Pts',(-7.01158880459239,3.02069919931746,134.688090341483));
#74740=CARTESIAN_POINT('Ctrl Pts',(-7.01933670136957,3.12788716610135,134.602298369336));
#74741=CARTESIAN_POINT('Ctrl Pts',(-7.02708459814664,3.23132662836891,134.512151237773));
#74742=CARTESIAN_POINT('Ctrl Pts',(-7.03483087423075,3.334744453331,134.422022963046));
#74743=CARTESIAN_POINT('Ctrl Pts',(-7.04257715031474,3.4344150388515,134.327541597646));
#74744=CARTESIAN_POINT('Ctrl Pts',(-7.05032342639885,3.5299608597491,134.229059055551));
#74745=CARTESIAN_POINT('Ctrl Pts',(-7.05806975966416,3.62550738594373,134.130575786481));
#74746=CARTESIAN_POINT('Ctrl Pts',(-7.06581609292956,3.71692881451989,134.028091562386));
#74747=CARTESIAN_POINT('Ctrl Pts',(-7.07356242619488,3.80388504989494,133.921994590579));
#74748=CARTESIAN_POINT('Ctrl Pts',(-7.08131049419789,3.8908607585167,133.81587385909));
#74749=CARTESIAN_POINT('Ctrl Pts',(-7.08905856220087,3.97336903637257,133.706139072298));
#74750=CARTESIAN_POINT('Ctrl Pts',(-7.09680663020387,4.05111084220871,133.593210560937));
#74751=CARTESIAN_POINT('Ctrl Pts',(-7.10456293294572,4.12893527296091,133.48016202781));
#74752=CARTESIAN_POINT('Ctrl Pts',(-7.11231923568755,4.20198289003919,133.363913312124));
#74753=CARTESIAN_POINT('Ctrl Pts',(-7.1200755384294,4.26999839418924,133.244913173059));
#74754=CARTESIAN_POINT('Ctrl Pts',(-7.12783598094358,4.33805020026185,133.125849520036));
#74755=CARTESIAN_POINT('Ctrl Pts',(-7.13559642345776,4.40106436220009,133.004031864573));
#74756=CARTESIAN_POINT('Ctrl Pts',(-7.14335686597192,4.4588326122476,132.879931574786));
#74757=CARTESIAN_POINT('Ctrl Pts',(-7.15112976623736,4.51669359701851,132.755632068197));
#74758=CARTESIAN_POINT('Ctrl Pts',(-7.15890266650275,4.56929169155139,132.629042966118));
#74759=CARTESIAN_POINT('Ctrl Pts',(-7.16667556676819,4.61646732686937,132.500654366434));
#74760=CARTESIAN_POINT('Ctrl Pts',(-7.17416590253026,4.66192800901547,132.376933015739));
#74761=CARTESIAN_POINT('Ctrl Pts',(-7.18165623829237,4.70235353294895,132.251541021696));
#74762=CARTESIAN_POINT('Ctrl Pts',(-7.18914657405443,4.73764593419014,132.124926429918));
#74763=CARTESIAN_POINT('Ctrl Pts',(-7.19692090817352,4.77427645755113,131.993511207408));
#74764=CARTESIAN_POINT('Ctrl Pts',(-7.20469524229262,4.80549296420102,131.860362563536));
#74765=CARTESIAN_POINT('Ctrl Pts',(-7.21246957641171,4.8311309371547,131.725966243941));
#74766=CARTESIAN_POINT('Ctrl Pts',(-7.22023432935881,4.85673731359805,131.591735555799));
#74767=CARTESIAN_POINT('Ctrl Pts',(-7.22799908230588,4.87677876307636,131.456260631751));
#74768=CARTESIAN_POINT('Ctrl Pts',(-7.23576383525298,4.89114049853968,131.320042385757));
#74769=CARTESIAN_POINT('Ctrl Pts',(-7.243520876138,4.90548796972489,131.183959433646));
#74770=CARTESIAN_POINT('Ctrl Pts',(-7.25127791702304,4.91416691235429,131.047135015089));
#74771=CARTESIAN_POINT('Ctrl Pts',(-7.25903495790806,4.91711363465124,130.91007989881));
#74772=CARTESIAN_POINT('Ctrl Pts',(-7.2667861491482,4.92005813480199,130.773128136861));
#74773=CARTESIAN_POINT('Ctrl Pts',(-7.27453734038829,4.91727901034634,130.635946412761));
#74774=CARTESIAN_POINT('Ctrl Pts',(-7.28228853162844,4.90876445150753,130.499049919889));
#74775=CARTESIAN_POINT('Ctrl Pts',(-7.29003642840553,4.90025351158336,130.362211611679));
#74776=CARTESIAN_POINT('Ctrl Pts',(-7.29778432518259,4.88601200991975,130.225658682972));
#74777=CARTESIAN_POINT('Ctrl Pts',(-7.30553222195968,4.86608023104083,130.089905407232));
#74778=CARTESIAN_POINT('Ctrl Pts',(-7.31327849804379,4.84615262146037,129.954180528151));
#74779=CARTESIAN_POINT('Ctrl Pts',(-7.32102477412797,4.8205371589614,129.819255355901));
#74780=CARTESIAN_POINT('Ctrl Pts',(-7.32877105021208,4.78932585715792,129.685637731209));
#74781=CARTESIAN_POINT('Ctrl Pts',(-7.33651738347744,4.7581143249597,129.552019120183));
#74782=CARTESIAN_POINT('Ctrl Pts',(-7.34426371674279,4.72130695996176,129.419708456692));
#74783=CARTESIAN_POINT('Ctrl Pts',(-7.35201005000815,4.67904654200237,129.289201708317));
#74784=CARTESIAN_POINT('Ctrl Pts',(-7.35975811801114,4.63677666011533,129.158665733861));
#74785=CARTESIAN_POINT('Ctrl Pts',(-7.36750618601411,4.58905141569424,129.029934850263));
#74786=CARTESIAN_POINT('Ctrl Pts',(-7.37525425401711,4.53606280578764,128.903487848428));
#74787=CARTESIAN_POINT('Ctrl Pts',(-7.38301055675896,4.48301787895601,128.776906457215));
#74788=CARTESIAN_POINT('Ctrl Pts',(-7.39076685950082,4.42469856343286,128.65261415779));
#74789=CARTESIAN_POINT('Ctrl Pts',(-7.39852316224267,4.36134441754186,128.531068305945));
#74790=CARTESIAN_POINT('Ctrl Pts',(-7.40628360475684,4.29795645763556,128.409457581418));
#74791=CARTESIAN_POINT('Ctrl Pts',(-7.41404404727096,4.22952850777397,128.290596563987));
#74792=CARTESIAN_POINT('Ctrl Pts',(-7.42180448978513,4.15634456949191,128.174915261192));
#74793=CARTESIAN_POINT('Ctrl Pts',(-7.42957739005055,4.08304314985527,128.059048256501));
#74794=CARTESIAN_POINT('Ctrl Pts',(-7.43735029031603,4.00497070796082,127.94637148813));
#74795=CARTESIAN_POINT('Ctrl Pts',(-7.44512319058146,3.92245332611095,127.837284115859));
#74796=CARTESIAN_POINT('Ctrl Pts',(-7.45261352634341,3.84293565894074,127.732162344345));
#74797=CARTESIAN_POINT('Ctrl Pts',(-7.46010386210534,3.75929080620236,127.630373770501));
#74798=CARTESIAN_POINT('Ctrl Pts',(-7.4675941978673,3.67184276916407,127.532242994216));
#74799=CARTESIAN_POINT('Ctrl Pts',(-7.47536853198639,3.58107911322131,127.43039155972));
#74800=CARTESIAN_POINT('Ctrl Pts',(-7.48314286610546,3.4859306725159,127.332158134229));
#74801=CARTESIAN_POINT('Ctrl Pts',(-7.49091720022454,3.38671719316323,127.237943687925));
#74802=CARTESIAN_POINT('Ctrl Pts',(-7.49868195317163,3.28762598555703,127.143845352505));
#74803=CARTESIAN_POINT('Ctrl Pts',(-7.50644670611873,3.18447998808874,127.053756407849));
#74804=CARTESIAN_POINT('Ctrl Pts',(-7.51421145906582,3.07763858865604,126.968044183783));
#74805=CARTESIAN_POINT('Ctrl Pts',(-7.52196849995084,2.97090330560716,126.882417090306));
#74806=CARTESIAN_POINT('Ctrl Pts',(-7.52972554083585,2.86048022769284,126.801158309719));
#74807=CARTESIAN_POINT('Ctrl Pts',(-7.53748258172087,2.74676465214406,126.724597510689));
#74808=CARTESIAN_POINT('Ctrl Pts',(-7.545233772961,2.63313483039553,126.648094446754));
#74809=CARTESIAN_POINT('Ctrl Pts',(-7.55298496420114,2.51621777606994,126.576282530141));
#74810=CARTESIAN_POINT('Ctrl Pts',(-7.56073615544128,2.39644055247484,126.509450171357));
#74811=CARTESIAN_POINT('Ctrl Pts',(-7.56848405221837,2.27671423739493,126.442646218108));
#74812=CARTESIAN_POINT('Ctrl Pts',(-7.57623194899544,2.15413051157663,126.380817803341));
#74813=CARTESIAN_POINT('Ctrl Pts',(-7.58397984577252,2.02914382261941,126.324209011914));
#74814=CARTESIAN_POINT('Ctrl Pts',(-7.59172612185662,1.90418327818313,126.267612061826));
#74815=CARTESIAN_POINT('Ctrl Pts',(-7.5994723979407,1.77682112631648,126.216232724562));
#74816=CARTESIAN_POINT('Ctrl Pts',(-7.60721867402481,1.64753436341259,126.170268086781));
#74817=CARTESIAN_POINT('Ctrl Pts',(-7.61496500729014,1.51824664614354,126.1243031097));
#74818=CARTESIAN_POINT('Ctrl Pts',(-7.62271134055551,1.38703465786489,126.083753042827));
#74819=CARTESIAN_POINT('Ctrl Pts',(-7.63045767382084,1.25439284613963,126.048765844033));
#74820=CARTESIAN_POINT('Ctrl Pts',(-7.63820574182383,1.12172133019977,126.013770810098));
#74821=CARTESIAN_POINT('Ctrl Pts',(-7.64595380982687,0.987619731617193,
125.984341222867));
#74822=CARTESIAN_POINT('Ctrl Pts',(-7.65370187782986,0.85259464983481,125.960574347965));
#74823=CARTESIAN_POINT('Ctrl Pts',(-7.66145818057172,0.717426061788874,
125.936782213346));
#74824=CARTESIAN_POINT('Ctrl Pts',(-7.66921448331354,0.581332415573117,
125.918664881337));
#74825=CARTESIAN_POINT('Ctrl Pts',(-7.67697078605539,0.444827984692796,
125.906268016713));
#74826=CARTESIAN_POINT('Ctrl Pts',(-7.68473122856957,0.308250697287459,
125.893864535508));
#74827=CARTESIAN_POINT('Ctrl Pts',(-7.69249167108376,0.171262578657633,
125.887187624444));
#74828=CARTESIAN_POINT('Ctrl Pts',(-7.70025211359794,0.034378916093068,
125.886230774564));
#74829=CARTESIAN_POINT('Ctrl Pts',(-7.70802501386338,-0.102724484278419,
125.885272388664));
#74830=CARTESIAN_POINT('Ctrl Pts',(-7.71579791412883,-0.239722702549963,
125.890052399568));
#74831=CARTESIAN_POINT('Ctrl Pts',(-7.72357081439426,-0.376103658845832,
125.900512220613));
#74832=CARTESIAN_POINT('Ctrl Pts',(-7.73106115015625,-0.507526823856522,
125.910591800815));
#74833=CARTESIAN_POINT('Ctrl Pts',(-7.73855148591819,-0.638376519878124,
125.925945373882));
#74834=CARTESIAN_POINT('Ctrl Pts',(-7.74604182168017,-0.768204521231687,
125.94647580254));
#74835=CARTESIAN_POINT('Ctrl Pts',(-7.75381615579923,-0.902954990717521,
125.967784648641));
#74836=CARTESIAN_POINT('Ctrl Pts',(-7.76159048991832,-1.03703161002932,
125.994738160587));
#74837=CARTESIAN_POINT('Ctrl Pts',(-7.76936482403738,-1.16992420101081,
126.027284061095));
#74838=CARTESIAN_POINT('Ctrl Pts',(-7.77712957698444,-1.3026530137507,126.059789851688));
#74839=CARTESIAN_POINT('Ctrl Pts',(-7.78489432993153,-1.43420032545401,
126.097874225473));
#74840=CARTESIAN_POINT('Ctrl Pts',(-7.7926590828786,-1.5640628331963,126.141433369976));
#74841=CARTESIAN_POINT('Ctrl Pts',(-7.80041612376361,-1.69379635966568,
126.184949250923));
#74842=CARTESIAN_POINT('Ctrl Pts',(-7.80817316464861,-1.8218480439876,126.233928957953));
#74843=CARTESIAN_POINT('Ctrl Pts',(-7.81593020553362,-1.9477268587674,126.288218110278));
#74844=CARTESIAN_POINT('Ctrl Pts',(-7.82368139677371,-2.07351074735309,
126.34246632273));
#74845=CARTESIAN_POINT('Ctrl Pts',(-7.83143258801379,-2.19712467033849,
126.402015856764));
#74846=CARTESIAN_POINT('Ctrl Pts',(-7.83918377925389,-2.31809514164815,
126.466663304847));
#74847=CARTESIAN_POINT('Ctrl Pts',(-7.84693167603096,-2.439014197281,126.531283276041));
#74848=CARTESIAN_POINT('Ctrl Pts',(-7.85467957280802,-2.5572916917749,126.600996667899));
#74849=CARTESIAN_POINT('Ctrl Pts',(-7.8624274695851,-2.67247662959794,126.675553074612));
#74850=CARTESIAN_POINT('Ctrl Pts',(-7.87017374566919,-2.78763747321492,
126.750093885732));
#74851=CARTESIAN_POINT('Ctrl Pts',(-7.87792002175328,-2.89970671887072,
126.82947548438));
#74852=CARTESIAN_POINT('Ctrl Pts',(-7.88566629783736,-3.00826072377574,
126.913403090133));
#74853=CARTESIAN_POINT('Ctrl Pts',(-7.8934126311027,-3.11681553000191,126.997331315421));
#74854=CARTESIAN_POINT('Ctrl Pts',(-7.90115896436805,-3.22185473439564,
127.085805375641));
#74855=CARTESIAN_POINT('Ctrl Pts',(-7.9089052976334,-3.32298659482447,127.178489252898));
#74856=CARTESIAN_POINT('Ctrl Pts',(-7.91665336563638,-3.42414110303239,
127.271193886068));
#74857=CARTESIAN_POINT('Ctrl Pts',(-7.92440143363943,-3.52138623790646,
127.368109948154));
#74858=CARTESIAN_POINT('Ctrl Pts',(-7.93214950164241,-3.6143663377487,127.468863797143));
#74859=CARTESIAN_POINT('Ctrl Pts',(-7.93990580438427,-3.7074452579474,127.569724728523));
#74860=CARTESIAN_POINT('Ctrl Pts',(-7.94766210712607,-3.79624982252776,
127.674431306965));
#74861=CARTESIAN_POINT('Ctrl Pts',(-7.95541840986792,-3.88046363503061,
127.782575542531));
#74862=CARTESIAN_POINT('Ctrl Pts',(-7.96317885238207,-3.96472239498071,
127.890777497931));
#74863=CARTESIAN_POINT('Ctrl Pts',(-7.97093929489626,-4.04438529359944,
128.002420448316));
#74864=CARTESIAN_POINT('Ctrl Pts',(-7.97869973741041,-4.11917928168823,
128.117067349646));
#74865=CARTESIAN_POINT('Ctrl Pts',(-7.98647263767583,-4.1940933357267,128.231898292359));
#74866=CARTESIAN_POINT('Ctrl Pts',(-7.9942455379412,-4.2641226605189,128.349742486034));
#74867=CARTESIAN_POINT('Ctrl Pts',(-8.00201843820662,-4.32903975500504,
128.470137435845));
#74868=CARTESIAN_POINT('Ctrl Pts',(-8.00950877396876,-4.39159694959138,
128.586155725975));
#74869=CARTESIAN_POINT('Ctrl Pts',(-8.01699910973094,-4.4494070106166,128.704542262371));
#74870=CARTESIAN_POINT('Ctrl Pts',(-8.02448944549309,-4.50230938549294,
128.824867435006));
#74871=CARTESIAN_POINT('Ctrl Pts',(-8.03305066556223,-4.56277514936235,
128.962395353045));
#74872=CARTESIAN_POINT('Ctrl Pts',(-8.04161188563137,-4.61699461874163,
129.102829783133));
#74873=CARTESIAN_POINT('Ctrl Pts',(-8.05017310570051,-4.66470666636355,
129.245612793419));
#74874=CARTESIAN_POINT('Ctrl Pts',(-8.05682654203701,-4.70178655319895,
129.356578013469));
#74875=CARTESIAN_POINT('Ctrl Pts',(-8.06347997837353,-4.73493695577742,
129.468961146221));
#74876=CARTESIAN_POINT('Ctrl Pts',(-8.07013341471003,-4.76405452823399,
129.582490119308));
#74877=CARTESIAN_POINT('Origin',(213.235140564004,0.,130.804360617566));
#74878=CARTESIAN_POINT('',(-10.1650489208495,-4.76405452823411,129.582490119308));
#74879=CARTESIAN_POINT('',(-9.81992175947745,-4.76405452823407,129.582490119308));
#74880=CARTESIAN_POINT('',(213.235140564004,-4.76405452823405,129.582490119308));
#74881=CARTESIAN_POINT('',(-8.48514056406485,-4.91824798673127,130.808810731474));
#74882=CARTESIAN_POINT('Ctrl Pts',(-8.48514056406486,-4.91824798673127,
130.808810731474));
#74883=CARTESIAN_POINT('Ctrl Pts',(-8.49475443834549,-4.91809419702525,
130.978778495817));
#74884=CARTESIAN_POINT('Ctrl Pts',(-8.50436831262617,-4.90912602691106,
131.148353567338));
#74885=CARTESIAN_POINT('Ctrl Pts',(-8.51398218690682,-4.89148713916088,
131.316743901762));
#74886=CARTESIAN_POINT('Ctrl Pts',(-8.52375854373859,-4.87355013939081,
131.487980174288));
#74887=CARTESIAN_POINT('Ctrl Pts',(-8.53353490057044,-4.84664689567184,
131.657991430657));
#74888=CARTESIAN_POINT('Ctrl Pts',(-8.54331125740222,-4.81097707191774,
131.825968505154));
#74889=CARTESIAN_POINT('Ctrl Pts',(-8.54947273725463,-4.78849641739771,
131.931834870098));
#74890=CARTESIAN_POINT('Ctrl Pts',(-8.55563421710703,-4.76253458499389,
132.036893713832));
#74891=CARTESIAN_POINT('Ctrl Pts',(-8.56179569695945,-4.73315119516266,
132.140946875998));
#74892=CARTESIAN_POINT('Ctrl Pts',(-8.56957003107853,-4.69607628855403,
132.27223742116));
#74893=CARTESIAN_POINT('Ctrl Pts',(-8.57734436519764,-4.65347581258836,
132.402192148277));
#74894=CARTESIAN_POINT('Ctrl Pts',(-8.58511869931672,-4.60546193514355,
132.530310624502));
#74895=CARTESIAN_POINT('Ctrl Pts',(-8.59288345226381,-4.55750723051163,
132.658271206156));
#74896=CARTESIAN_POINT('Ctrl Pts',(-8.60064820521083,-4.50415253464717,
132.784399677059));
#74897=CARTESIAN_POINT('Ctrl Pts',(-8.60841295815791,-4.44556037787898,
132.908208518231));
#74898=CARTESIAN_POINT('Ctrl Pts',(-8.61616999904292,-4.38702641566683,
133.031894390717));
#74899=CARTESIAN_POINT('Ctrl Pts',(-8.62392703992801,-4.32326551076492,
133.153264867211));
#74900=CARTESIAN_POINT('Ctrl Pts',(-8.63168408081302,-4.25448895802691,
133.271850590905));
#74901=CARTESIAN_POINT('Ctrl Pts',(-8.63943527205314,-4.18576427022242,
133.390346888181));
#74902=CARTESIAN_POINT('Ctrl Pts',(-8.64718646329319,-4.11203165845224,
133.506062275755));
#74903=CARTESIAN_POINT('Ctrl Pts',(-8.65493765453331,-4.03354902937623,
133.618550605843));
#74904=CARTESIAN_POINT('Ctrl Pts',(-8.6626855513104,-3.95509975751107,133.73099112539));
#74905=CARTESIAN_POINT('Ctrl Pts',(-8.67043344808743,-3.87190470698588,
133.840206995465));
#74906=CARTESIAN_POINT('Ctrl Pts',(-8.67818134486453,-3.78426579744953,
133.945779952318));
#74907=CARTESIAN_POINT('Ctrl Pts',(-8.68592762094864,-3.69664522008379,
134.051330825584));
#74908=CARTESIAN_POINT('Ctrl Pts',(-8.69367389703279,-3.60458288221354,
134.153240000694));
#74909=CARTESIAN_POINT('Ctrl Pts',(-8.7014201731169,-3.50842153691041,134.25112161622));
#74910=CARTESIAN_POINT('Ctrl Pts',(-8.70916650638225,-3.41225948176621,
134.349003954286));
#74911=CARTESIAN_POINT('Ctrl Pts',(-8.71691283964761,-3.31199863280413,
134.442858394548));
#74912=CARTESIAN_POINT('Ctrl Pts',(-8.72465917291296,-3.20801892418793,
134.532335623458));
#74913=CARTESIAN_POINT('Ctrl Pts',(-8.73240724091594,-3.10401593003693,
134.621832890172));
#74914=CARTESIAN_POINT('Ctrl Pts',(-8.74015530891887,-2.99629271532096,
134.706950739993));
#74915=CARTESIAN_POINT('Ctrl Pts',(-8.74790337692184,-2.88526231356341,
134.787380131004));
#74916=CARTESIAN_POINT('Ctrl Pts',(-8.75565967966369,-2.7741139073736,134.867895003329));
#74917=CARTESIAN_POINT('Ctrl Pts',(-8.76341598240553,-2.65965160984144,
134.943711233142));
#74918=CARTESIAN_POINT('Ctrl Pts',(-8.77117228514737,-2.542317924436,135.014562825726));
#74919=CARTESIAN_POINT('Ctrl Pts',(-8.77893272766154,-2.42492161450966,
135.085452233937));
#74920=CARTESIAN_POINT('Ctrl Pts',(-8.78669317017569,-2.30465120566002,
135.151371537197));
#74921=CARTESIAN_POINT('Ctrl Pts',(-8.79445361268986,-2.18197293240709,
135.212101216188));
#74922=CARTESIAN_POINT('Ctrl Pts',(-8.8022265129553,-2.05909772509906,135.272928383852));
#74923=CARTESIAN_POINT('Ctrl Pts',(-8.80999941322072,-1.93380728679309,
135.328549120838));
#74924=CARTESIAN_POINT('Ctrl Pts',(-8.81777231348616,-1.80658774502393,
135.378792143125));
#74925=CARTESIAN_POINT('Ctrl Pts',(-8.82526264924818,-1.68399295404494,
135.427208704997));
#74926=CARTESIAN_POINT('Ctrl Pts',(-8.83275298501024,-1.55960717090831,
135.470631649492));
#74927=CARTESIAN_POINT('Ctrl Pts',(-8.84024332077226,-1.43387596132223,
135.508952288481));
#74928=CARTESIAN_POINT('Ctrl Pts',(-8.84801765489135,-1.30337761470934,
135.548725866145));
#74929=CARTESIAN_POINT('Ctrl Pts',(-8.85579198901044,-1.17101642444316,
135.583128583534));
#74930=CARTESIAN_POINT('Ctrl Pts',(-8.86356632312953,-1.03727404832743,
135.611984314484));
#74931=CARTESIAN_POINT('Ctrl Pts',(-8.87133107607662,-0.903696497737537,
135.640804483324));
#74932=CARTESIAN_POINT('Ctrl Pts',(-8.87909582902364,-0.768741526647516,
135.664091185992));
#74933=CARTESIAN_POINT('Ctrl Pts',(-8.88686058197072,-0.632907150194844,
135.681717647939));
#74934=CARTESIAN_POINT('Ctrl Pts',(-8.89461762285572,-0.497207686359793,
135.699326603036));
#74935=CARTESIAN_POINT('Ctrl Pts',(-8.90237466374083,-0.36063094054836,
135.711286455124));
#74936=CARTESIAN_POINT('Ctrl Pts',(-8.91013170462583,-0.223686005967314,
135.717521273726));
#74937=CARTESIAN_POINT('Ctrl Pts',(-8.91788289586595,-0.0868443426267111,
135.723751390602));
#74938=CARTESIAN_POINT('Ctrl Pts',(-8.92563408710603,0.0503645678496878,
135.724265049593));
#74939=CARTESIAN_POINT('Ctrl Pts',(-8.93338527834615,0.187425963848421,
135.719038081101));
#74940=CARTESIAN_POINT('Ctrl Pts',(-8.94113317512323,0.324429105097622,
135.713813334209));
#74941=CARTESIAN_POINT('Ctrl Pts',(-8.94888107190029,0.461284466706592,
135.702852827518));
#74942=CARTESIAN_POINT('Ctrl Pts',(-8.95662896867736,0.597476956591937,
135.686184492804));
#74943=CARTESIAN_POINT('Ctrl Pts',(-8.96437524476146,0.733640957944369,
135.669519644746));
#74944=CARTESIAN_POINT('Ctrl Pts',(-8.97212152084555,0.869141975548753,
135.647149390972));
#74945=CARTESIAN_POINT('Ctrl Pts',(-8.97986779692965,1.00347010684969,135.619153531821));
#74946=CARTESIAN_POINT('Ctrl Pts',(-8.987614130195,1.13779922973037,135.591157466011));
#74947=CARTESIAN_POINT('Ctrl Pts',(-8.99536046346037,1.27095506629012,135.557535791728));
#74948=CARTESIAN_POINT('Ctrl Pts',(-9.00310679672572,1.40243836545145,135.518419345839));
#74949=CARTESIAN_POINT('Ctrl Pts',(-9.01085486472869,1.53395110938598,135.479294140094));
#74950=CARTESIAN_POINT('Ctrl Pts',(-9.01860293273164,1.66379019594293,135.434671825621));
#74951=CARTESIAN_POINT('Ctrl Pts',(-9.02635100073462,1.79147236469755,135.384732854516));
#74952=CARTESIAN_POINT('Ctrl Pts',(-9.03410730347647,1.91929023558056,135.334740807679));
#74953=CARTESIAN_POINT('Ctrl Pts',(-9.04186360621828,2.04494624466254,135.279420959153));
#74954=CARTESIAN_POINT('Ctrl Pts',(-9.04961990896012,2.16797741912062,135.219001822996));
#74955=CARTESIAN_POINT('Ctrl Pts',(-9.05738035147429,2.29107425902108,135.158550439328));
#74956=CARTESIAN_POINT('Ctrl Pts',(-9.0651407939885,2.4115431295362,135.092994531708));
#74957=CARTESIAN_POINT('Ctrl Pts',(-9.07290123650267,2.52894733170234,135.02260770089));
#74958=CARTESIAN_POINT('Ctrl Pts',(-9.0806741367681,2.6465400015163,134.952107878884));
#74959=CARTESIAN_POINT('Ctrl Pts',(-9.08844703703357,2.7610578450976,134.876761851681));
#74960=CARTESIAN_POINT('Ctrl Pts',(-9.096219937299,2.87209399253994,134.796886028946));
#74961=CARTESIAN_POINT('Ctrl Pts',(-9.10371027306107,2.97909369634018,134.719913893562));
#74962=CARTESIAN_POINT('Ctrl Pts',(-9.11120060882309,3.08286020342269,134.638735773584));
#74963=CARTESIAN_POINT('Ctrl Pts',(-9.11869094458515,3.1830612322387,134.553667787473));
#74964=CARTESIAN_POINT('Ctrl Pts',(-9.12646527870423,3.28706141351713,134.465374422814));
#74965=CARTESIAN_POINT('Ctrl Pts',(-9.13423961282329,3.38754985043271,134.372610713861));
#74966=CARTESIAN_POINT('Ctrl Pts',(-9.14201394694237,3.48411801524719,134.275686692473));
#74967=CARTESIAN_POINT('Ctrl Pts',(-9.14977869988946,3.58056716842908,134.178882121279));
#74968=CARTESIAN_POINT('Ctrl Pts',(-9.15754345283659,3.67310538922981,134.077927713579));
#74969=CARTESIAN_POINT('Ctrl Pts',(-9.16530820578367,3.76135682928518,133.973173938873));
#74970=CARTESIAN_POINT('Ctrl Pts',(-9.17306524666867,3.84952061676616,133.868524207092));
#74971=CARTESIAN_POINT('Ctrl Pts',(-9.18082228755367,3.93340584623148,133.760082914975));
#74972=CARTESIAN_POINT('Ctrl Pts',(-9.18857932843866,4.01267345790768,133.648237334778));
#74973=CARTESIAN_POINT('Ctrl Pts',(-9.19633051967878,4.0918812932613,133.536476098204));
#74974=CARTESIAN_POINT('Ctrl Pts',(-9.20408171091896,4.16647821674404,133.421316001093));
#74975=CARTESIAN_POINT('Ctrl Pts',(-9.21183290215907,4.23616565256411,133.303177062713));
#74976=CARTESIAN_POINT('Ctrl Pts',(-9.21958079893614,4.30582346936498,133.185088336533));
#74977=CARTESIAN_POINT('Ctrl Pts',(-9.22732869571315,4.37057575049532,133.064023623274));
#74978=CARTESIAN_POINT('Ctrl Pts',(-9.23507659249023,4.43016757589819,132.940431382302));
#74979=CARTESIAN_POINT('Ctrl Pts',(-9.24282286857433,4.48974693597583,132.816864994163));
#74980=CARTESIAN_POINT('Ctrl Pts',(-9.2505691446584,4.54416781772878,132.690772481875));
#74981=CARTESIAN_POINT('Ctrl Pts',(-9.25831542074249,4.59322174465615,132.562625974933));
#74982=CARTESIAN_POINT('Ctrl Pts',(-9.26606175400784,4.64227603368847,132.434478522043));
#74983=CARTESIAN_POINT('Ctrl Pts',(-9.27380808727318,4.68596314907174,132.304277409371));
#74984=CARTESIAN_POINT('Ctrl Pts',(-9.28155442053853,4.72412331016522,132.172513391511));
#74985=CARTESIAN_POINT('Ctrl Pts',(-9.28930248854148,4.76229201696213,132.040719866013));
#74986=CARTESIAN_POINT('Ctrl Pts',(-9.29705055654444,4.7949311978062,131.907363114325));
#74987=CARTESIAN_POINT('Ctrl Pts',(-9.3047986245474,4.82193145809311,131.772947255896));
#74988=CARTESIAN_POINT('Ctrl Pts',(-9.31255492728925,4.84896041457799,131.638388538693));
#74989=CARTESIAN_POINT('Ctrl Pts',(-9.32031123003119,4.87033840150079,131.502768850099));
#74990=CARTESIAN_POINT('Ctrl Pts',(-9.32806753277305,4.88600742609159,131.366601219691));
#74991=CARTESIAN_POINT('Ctrl Pts',(-9.33582797528721,4.9016848137126,131.230360912519));
#74992=CARTESIAN_POINT('Ctrl Pts',(-9.34358841780132,4.91164713912134,131.093572470539));
#74993=CARTESIAN_POINT('Ctrl Pts',(-9.35134886031548,4.91588854392417,130.956751188846));
#74994=CARTESIAN_POINT('Ctrl Pts',(-9.35912176058091,4.92013675740653,130.819710269486));
#74995=CARTESIAN_POINT('Ctrl Pts',(-9.36689466084635,4.91864570251984,130.682636796235));
#74996=CARTESIAN_POINT('Ctrl Pts',(-9.37466756111178,4.91146166055344,130.546044107421));
#74997=CARTESIAN_POINT('Ctrl Pts',(-9.38215789687387,4.90453877660797,130.4144169069));
#74998=CARTESIAN_POINT('Ctrl Pts',(-9.38964823263593,4.89232965690248,130.283236448937));
#74999=CARTESIAN_POINT('Ctrl Pts',(-9.39713856839802,4.87492065455812,130.152953161159));
#75000=CARTESIAN_POINT('Ctrl Pts',(-9.40491290251711,4.85685158459867,130.017730142927));
#75001=CARTESIAN_POINT('Ctrl Pts',(-9.41268723663615,4.83312330377143,129.883045324401));
#75002=CARTESIAN_POINT('Ctrl Pts',(-9.42046157075524,4.8037758314374,129.749409991329));
#75003=CARTESIAN_POINT('Ctrl Pts',(-9.42822632370233,4.77446452724018,129.615939351861));
#75004=CARTESIAN_POINT('Ctrl Pts',(-9.4359910766495,4.7395478935791,129.483516002573));
#75005=CARTESIAN_POINT('Ctrl Pts',(-9.4437558295966,4.69911763514874,129.352645592661));
#75006=CARTESIAN_POINT('Ctrl Pts',(-9.4515128704816,4.65872753262103,129.221905165086));
#75007=CARTESIAN_POINT('Ctrl Pts',(-9.45926991136655,4.61283481788281,129.092714978569));
#75008=CARTESIAN_POINT('Ctrl Pts',(-9.46702695225156,4.56158204396177,128.965569623813));
#75009=CARTESIAN_POINT('Ctrl Pts',(-9.47477814349169,4.51036792015623,128.838520150359));
#75010=CARTESIAN_POINT('Ctrl Pts',(-9.48252933473186,4.45380192822689,128.713512800508));
#75011=CARTESIAN_POINT('Ctrl Pts',(-9.490280525972,4.39207605477006,128.591025805204));
#75012=CARTESIAN_POINT('Ctrl Pts',(-9.49802842274908,4.33037641645604,128.468590870139));
#75013=CARTESIAN_POINT('Ctrl Pts',(-9.50577631952618,4.26352143407366,128.348674507458));
#75014=CARTESIAN_POINT('Ctrl Pts',(-9.51352421630327,4.19175061867122,128.231733591865));
#75015=CARTESIAN_POINT('Ctrl Pts',(-9.52127049238738,4.11999481617606,128.11481713779));
#75016=CARTESIAN_POINT('Ctrl Pts',(-9.5290167684715,4.04332543035427,128.000875225819));
#75017=CARTESIAN_POINT('Ctrl Pts',(-9.53676304455561,3.96202699047914,127.890338450661));
#75018=CARTESIAN_POINT('Ctrl Pts',(-9.54450937782097,3.88072795047751,127.779800859545));
#75019=CARTESIAN_POINT('Ctrl Pts',(-9.55225571108635,3.79480001988117,127.672668770352));
#75020=CARTESIAN_POINT('Ctrl Pts',(-9.56000204435171,3.70456971908926,127.569341875904));
#75021=CARTESIAN_POINT('Ctrl Pts',(-9.56775011235469,3.61431921184709,127.465991842114));
#75022=CARTESIAN_POINT('Ctrl Pts',(-9.5754981803576,3.51976467429511,127.366448993173));
#75023=CARTESIAN_POINT('Ctrl Pts',(-9.58324624836058,3.42127110594655,127.271077854735));
#75024=CARTESIAN_POINT('Ctrl Pts',(-9.59100255110244,3.32267285746147,127.175605354717));
#75025=CARTESIAN_POINT('Ctrl Pts',(-9.59875885384437,3.22012749661558,127.084313694483));
#75026=CARTESIAN_POINT('Ctrl Pts',(-9.60651515658623,3.11403530321438,126.99752897001));
#75027=CARTESIAN_POINT('Ctrl Pts',(-9.61427559910041,3.00788648521504,126.910697925917));
#75028=CARTESIAN_POINT('Ctrl Pts',(-9.62203604161446,2.89818737515325,126.828378845269));
#75029=CARTESIAN_POINT('Ctrl Pts',(-9.62979648412863,2.78536833878292,126.750855186485));
#75030=CARTESIAN_POINT('Ctrl Pts',(-9.63756938439406,2.67236819527996,126.673207079842));
#75031=CARTESIAN_POINT('Ctrl Pts',(-9.64534228465955,2.55623844852386,126.600369986049));
#75032=CARTESIAN_POINT('Ctrl Pts',(-9.65311518492499,2.43743600075568,126.532582439252));
#75033=CARTESIAN_POINT('Ctrl Pts',(-9.66060552068694,2.3229523212103,126.467259140528));
#75034=CARTESIAN_POINT('Ctrl Pts',(-9.66809585644888,2.20598715927923,126.406624776928));
#75035=CARTESIAN_POINT('Ctrl Pts',(-9.67558619221083,2.08696614845374,126.35085016426));
#75036=CARTESIAN_POINT('Ctrl Pts',(-9.68336052632992,1.96343241982592,126.292960840199));
#75037=CARTESIAN_POINT('Ctrl Pts',(-9.69113486044899,1.83729255214507,126.240123680606));
#75038=CARTESIAN_POINT('Ctrl Pts',(-9.69890919456807,1.70899833603373,126.192581378494));
#75039=CARTESIAN_POINT('Ctrl Pts',(-9.70667394751516,1.58086223107793,126.145097668021));
#75040=CARTESIAN_POINT('Ctrl Pts',(-9.71443870046226,1.45057742351732,126.1028959659));
#75041=CARTESIAN_POINT('Ctrl Pts',(-9.72220345340935,1.31861889897095,126.066172434117));
#75042=CARTESIAN_POINT('Ctrl Pts',(-9.72996049429436,1.18679143749127,126.029485376664));
#75043=CARTESIAN_POINT('Ctrl Pts',(-9.73771753517933,1.05329394141015,125.998265765864));
#75044=CARTESIAN_POINT('Ctrl Pts',(-9.74547457606434,0.918619577288078,
125.972661006174));
#75045=CARTESIAN_POINT('Ctrl Pts',(-9.75322576730448,0.784046772151601,
125.947075555233));
#75046=CARTESIAN_POINT('Ctrl Pts',(-9.76097695854462,0.6482992479909,125.927096600207));
#75047=CARTESIAN_POINT('Ctrl Pts',(-9.76872814978475,0.511883127487427,
125.91282111284));
#75048=CARTESIAN_POINT('Ctrl Pts',(-9.77647604656184,0.375524987474187,
125.898551692936));
#75049=CARTESIAN_POINT('Ctrl Pts',(-9.78422394333894,0.238499204341029,
125.889980959897));
#75050=CARTESIAN_POINT('Ctrl Pts',(-9.79197184011602,0.101319621288873,
125.887154358231));
#75051=CARTESIAN_POINT('Ctrl Pts',(-9.79971811620012,-0.0358312667517578,
125.88432834783));
#75052=CARTESIAN_POINT('Ctrl Pts',(-9.80746439228426,-0.173135500085666,
125.887244086905));
#75053=CARTESIAN_POINT('Ctrl Pts',(-9.81521066836837,-0.310077012167492,
125.89589493988));
#75054=CARTESIAN_POINT('Ctrl Pts',(-9.82295700163372,-0.447019535120452,
125.904545856713));
#75055=CARTESIAN_POINT('Ctrl Pts',(-9.830703334899,-0.583598941291097,125.918931947273));
#75056=CARTESIAN_POINT('Ctrl Pts',(-9.83844966816434,-0.719302465535839,
125.938994544435));
#75057=CARTESIAN_POINT('Ctrl Pts',(-9.84619773616732,-0.855036379643933,
125.959061634477));
#75058=CARTESIAN_POINT('Ctrl Pts',(-9.85394580417038,-0.989893634827646,
125.984807703521));
#75059=CARTESIAN_POINT('Ctrl Pts',(-9.86169387217336,-1.12337025417762,
126.01612270216));
#75060=CARTESIAN_POINT('Ctrl Pts',(-9.86945017491522,-1.25698873406703,
126.047470982753));
#75061=CARTESIAN_POINT('Ctrl Pts',(-9.87720647765704,-1.38922326568352,
126.084399926788));
#75062=CARTESIAN_POINT('Ctrl Pts',(-9.88496278039889,-1.51958313423272,
126.126749030372));
#75063=CARTESIAN_POINT('Ctrl Pts',(-9.89272322291307,-1.65001257976899,
126.169120736947));
#75064=CARTESIAN_POINT('Ctrl Pts',(-9.90048366542726,-1.7785650022539,126.216918231236));
#75065=CARTESIAN_POINT('Ctrl Pts',(-9.90824410794144,-1.90476929688927,
126.269932650542));
#75066=CARTESIAN_POINT('Ctrl Pts',(-9.91601700820687,-2.03117618586211,
126.3230321733));
#75067=CARTESIAN_POINT('Ctrl Pts',(-9.92378990847223,-2.15522706047216,
126.381365189872));
#75068=CARTESIAN_POINT('Ctrl Pts',(-9.93156280873765,-2.27647426836526,
126.444676228993));
#75069=CARTESIAN_POINT('Ctrl Pts',(-9.9390531444997,-2.39331383484865,126.505685752371));
#75070=CARTESIAN_POINT('Ctrl Pts',(-9.94654348026184,-2.50754976925826,
126.571317501127));
#75071=CARTESIAN_POINT('Ctrl Pts',(-9.95403381602389,-2.61880829411776,
126.641305707868));
#75072=CARTESIAN_POINT('Ctrl Pts',(-9.96180953030539,-2.73430572015671,
126.713960434702));
#75073=CARTESIAN_POINT('Ctrl Pts',(-9.96958524458686,-2.84696028917741,
126.791540348069));
#75074=CARTESIAN_POINT('Ctrl Pts',(-9.97736095886833,-2.95632337599693,
126.873796388472));
#75075=CARTESIAN_POINT('Ctrl Pts',(-9.98518129061754,-3.06631399410443,
126.956524418469));
#75076=CARTESIAN_POINT('Ctrl Pts',(-9.99300162236678,-3.17297486361209,
127.043982262013));
#75077=CARTESIAN_POINT('Ctrl Pts',(-10.000821954116,-3.27587519215888,127.135869812358));
#75078=CARTESIAN_POINT('Ctrl Pts',(-10.0085782387396,-3.37793278532302,
127.227004820013));
#75079=CARTESIAN_POINT('Ctrl Pts',(-10.0163345233631,-3.47629089186883,
127.322497000842));
#75080=CARTESIAN_POINT('Ctrl Pts',(-10.0240908079867,-3.57055927789495,
127.422010915726));
#75081=CARTESIAN_POINT('Ctrl Pts',(-10.0318417021151,-3.66476214888378,
127.521455670013));
#75082=CARTESIAN_POINT('Ctrl Pts',(-10.0395925962436,-3.75488068681802,
127.624916314611));
#75083=CARTESIAN_POINT('Ctrl Pts',(-10.0473434903721,-3.84056004153913,
127.73201922543));
#75084=CARTESIAN_POINT('Ctrl Pts',(-10.0550906764112,-3.92619840657558,
127.839070897364));
#75085=CARTESIAN_POINT('Ctrl Pts',(-10.0628378624502,-4.00740157156914,
127.94976106293));
#75086=CARTESIAN_POINT('Ctrl Pts',(-10.0705850484893,-4.08385393653115,
128.063681853541));
#75087=CARTESIAN_POINT('Ctrl Pts',(-10.0784570378526,-4.16153791117038,
128.17943785158));
#75088=CARTESIAN_POINT('Ctrl Pts',(-10.086329027216,-4.23431642523966,128.298529150419));
#75089=CARTESIAN_POINT('Ctrl Pts',(-10.0942010165793,-4.30190329678341,
128.420495879871));
#75090=CARTESIAN_POINT('Ctrl Pts',(-10.1019474751096,-4.36841239295244,
128.540517664477));
#75091=CARTESIAN_POINT('Ctrl Pts',(-10.10969393364,-4.42989403403268,128.663323485389));
#75092=CARTESIAN_POINT('Ctrl Pts',(-10.1174403921704,-4.4861215025255,128.788449675317));
#75093=CARTESIAN_POINT('Ctrl Pts',(-10.1253751469502,-4.5437157144658,128.916617357327));
#75094=CARTESIAN_POINT('Ctrl Pts',(-10.13330990173,-4.5957968533957,129.047219274615));
#75095=CARTESIAN_POINT('Ctrl Pts',(-10.1412446565099,-4.64217365544846,
129.17973548691));
#75096=CARTESIAN_POINT('Ctrl Pts',(-10.1491794112898,-4.68855045750127,
129.312251699204));
#75097=CARTESIAN_POINT('Ctrl Pts',(-10.1571141660697,-4.72922281067665,
129.446681781197));
#75098=CARTESIAN_POINT('Ctrl Pts',(-10.1650489208495,-4.76405452823411,
129.582490119308));
#75099=CARTESIAN_POINT('Ctrl Pts',(-8.41516596570787,-4.76405452823401,
129.582490119308));
#75100=CARTESIAN_POINT('Ctrl Pts',(-8.42284261422826,-4.79785806847061,
129.71428960965));
#75101=CARTESIAN_POINT('Ctrl Pts',(-8.43051926274863,-4.82618886490382,
129.847496441167));
#75102=CARTESIAN_POINT('Ctrl Pts',(-8.43819591126902,-4.84894509276012,
129.981612448381));
#75103=CARTESIAN_POINT('Ctrl Pts',(-8.44602002005897,-4.87213844359852,
130.118304681733));
#75104=CARTESIAN_POINT('Ctrl Pts',(-8.45384412884894,-4.88954077746297,
130.255940956616));
#75105=CARTESIAN_POINT('Ctrl Pts',(-8.46166823763889,-4.90109945350708,
130.393986143052));
#75106=CARTESIAN_POINT('Ctrl Pts',(-8.46949234642882,-4.91265812955118,
130.532031329489));
#75107=CARTESIAN_POINT('Ctrl Pts',(-8.47731645521872,-4.91837314617225,
130.670484989973));
#75108=CARTESIAN_POINT('Ctrl Pts',(-8.48514056400865,-4.91824798673217,
130.80881073048));
#75109=CARTESIAN_POINT('',(-8.13985943594608,-4.91824948988454,130.802120583987));
#75110=CARTESIAN_POINT('Ctrl Pts',(-8.07013341471003,-4.76405452823399,
129.582490119308));
#75111=CARTESIAN_POINT('Ctrl Pts',(-8.07865204310352,-4.80133477966088,
129.727845253815));
#75112=CARTESIAN_POINT('Ctrl Pts',(-8.087170671497,-4.83200254344879,129.875079244239));
#75113=CARTESIAN_POINT('Ctrl Pts',(-8.09568929989047,-4.8558829875021,130.023602348838));
#75114=CARTESIAN_POINT('Ctrl Pts',(-8.10417256346428,-4.87966429263794,
130.171508864407));
#75115=CARTESIAN_POINT('Ctrl Pts',(-8.11265582703813,-4.89671441550626,
130.320693571389));
#75116=CARTESIAN_POINT('Ctrl Pts',(-8.12113909061196,-4.90690919425128,
130.470556450617));
#75117=CARTESIAN_POINT('Ctrl Pts',(-8.12737920572339,-4.91440826490383,
130.580792518279));
#75118=CARTESIAN_POINT('Ctrl Pts',(-8.13361932083473,-4.91819905960549,
130.691395148153));
#75119=CARTESIAN_POINT('Ctrl Pts',(-8.13985943594614,-4.91824948988454,
130.802120583988));
#75120=CARTESIAN_POINT('Ctrl Pts',(-8.13985943599121,-4.91824948988491,
130.802120584788));
#75121=CARTESIAN_POINT('Ctrl Pts',(-8.14774011749155,-4.91831317858587,
130.941956449707));
#75122=CARTESIAN_POINT('Ctrl Pts',(-8.15562079899188,-4.91240878708701,
131.081772089033));
#75123=CARTESIAN_POINT('Ctrl Pts',(-8.16350148049222,-4.90056794172436,
131.221034244093));
#75124=CARTESIAN_POINT('Ctrl Pts',(-8.17138511948355,-4.88872265268592,
131.360348661965));
#75125=CARTESIAN_POINT('Ctrl Pts',(-8.17926875847488,-4.87093650249959,
131.499108811236));
#75126=CARTESIAN_POINT('Ctrl Pts',(-8.18715239746621,-4.84729293307246,
131.636787361181));
#75127=CARTESIAN_POINT('Ctrl Pts',(-8.19504045733832,-4.82363610512323,
131.774543116648));
#75128=CARTESIAN_POINT('Ctrl Pts',(-8.20292851721046,-4.79411537670579,
131.911215698255));
#75129=CARTESIAN_POINT('Ctrl Pts',(-8.21081657708257,-4.75886511568041,
132.046288905858));
#75130=CARTESIAN_POINT('Ctrl Pts',(-8.2187163136846,-4.72356267353772,132.181562062928));
#75131=CARTESIAN_POINT('Ctrl Pts',(-8.22661605028666,-4.68251384709882,
132.315230755384));
#75132=CARTESIAN_POINT('Ctrl Pts',(-8.23451578688869,-4.63590292928399,
132.446793901677));
#75133=CARTESIAN_POINT('Ctrl Pts',(-8.24242159928218,-4.58925616239848,
132.578458234919));
#75134=CARTESIAN_POINT('Ctrl Pts',(-8.25032741167563,-4.53703891432322,
132.708013449104));
#75135=CARTESIAN_POINT('Ctrl Pts',(-8.2582332240691,-4.47948305945182,132.834979878428));
#75136=CARTESIAN_POINT('Ctrl Pts',(-8.2661537108043,-4.42182037251302,132.962181975977));
#75137=CARTESIAN_POINT('Ctrl Pts',(-8.27407419753948,-4.35879944090511,
133.086785352617));
#75138=CARTESIAN_POINT('Ctrl Pts',(-8.28199468427468,-4.29069798952574,
133.208335206695));
#75139=CARTESIAN_POINT('Ctrl Pts',(-8.28897547928509,-4.23067613886373,
133.315464306615));
#75140=CARTESIAN_POINT('Ctrl Pts',(-8.29595627429549,-4.16670852430057,
133.420221725413));
#75141=CARTESIAN_POINT('Ctrl Pts',(-8.3029370693059,-4.09901187452849,133.522316598625));
#75142=CARTESIAN_POINT('Ctrl Pts',(-8.31071140342498,-4.0236198348989,133.636017066123));
#75143=CARTESIAN_POINT('Ctrl Pts',(-8.31848573754406,-3.94337397269968,
133.746758355859));
#75144=CARTESIAN_POINT('Ctrl Pts',(-8.32626007166314,-3.8585338990758,133.854098182043));
#75145=CARTESIAN_POINT('Ctrl Pts',(-8.33402482461024,-3.77379838326028,
133.961305721485));
#75146=CARTESIAN_POINT('Ctrl Pts',(-8.34178957755735,-3.68448016172765,
134.065119834424));
#75147=CARTESIAN_POINT('Ctrl Pts',(-8.34955433050445,-3.59088285994828,
134.165125909673));
#75148=CARTESIAN_POINT('Ctrl Pts',(-8.35731137138946,-3.49737852032841,
134.265032657478));
#75149=CARTESIAN_POINT('Ctrl Pts',(-8.36506841227445,-3.39960382366651,
134.361138610734));
#75150=CARTESIAN_POINT('Ctrl Pts',(-8.37282545315946,-3.29790328564868,
134.45306134262));
#75151=CARTESIAN_POINT('Ctrl Pts',(-8.38057664439957,-3.19627944079823,
134.544914754858));
#75152=CARTESIAN_POINT('Ctrl Pts',(-8.38832783563969,-3.09073593617419,
134.632590963668));
#75153=CARTESIAN_POINT('Ctrl Pts',(-8.39607902687979,-2.98165458677833,
134.715743875142));
#75154=CARTESIAN_POINT('Ctrl Pts',(-8.40382692365686,-2.87261959986551,
134.79886144441));
#75155=CARTESIAN_POINT('Ctrl Pts',(-8.41157482043393,-2.76005006915821,
134.877459303569));
#75156=CARTESIAN_POINT('Ctrl Pts',(-8.419322717211,-2.64436120681958,134.951231349861));
#75157=CARTESIAN_POINT('Ctrl Pts',(-8.42706899329509,-2.528696544097,135.024987964631));
#75158=CARTESIAN_POINT('Ctrl Pts',(-8.43481526937917,-2.40991417703256,
135.093920564323));
#75159=CARTESIAN_POINT('Ctrl Pts',(-8.44256154546326,-2.2884583076316,135.157766369013));
#75160=CARTESIAN_POINT('Ctrl Pts',(-8.45030787872861,-2.16700154167099,
135.221612644998));
#75161=CARTESIAN_POINT('Ctrl Pts',(-8.45805421199396,-2.04287158005791,
135.280371869137));
#75162=CARTESIAN_POINT('Ctrl Pts',(-8.4658005452593,-1.91653687094088,135.333827416741));
#75163=CARTESIAN_POINT('Ctrl Pts',(-8.47354861326226,-1.79017387004169,
135.387294935343));
#75164=CARTESIAN_POINT('Ctrl Pts',(-8.48129668126523,-1.66160549914811,
135.435456261661));
#75165=CARTESIAN_POINT('Ctrl Pts',(-8.4890447492682,-1.53131942874953,135.478143225865));
#75166=CARTESIAN_POINT('Ctrl Pts',(-8.49680105201005,-1.4008948887649,135.520875558282));
#75167=CARTESIAN_POINT('Ctrl Pts',(-8.50455735475189,-1.26874937458389,
135.558121784147));
#75168=CARTESIAN_POINT('Ctrl Pts',(-8.51231365749373,-1.13538547546737,
135.589763723324));
#75169=CARTESIAN_POINT('Ctrl Pts',(-8.5200741000079,-1.00195039602221,135.621422550756));
#75170=CARTESIAN_POINT('Ctrl Pts',(-8.52783454252209,-0.867296019547383,
135.64747105711));
#75171=CARTESIAN_POINT('Ctrl Pts',(-8.53559498503625,-0.731933342490357,
135.66784256414));
#75172=CARTESIAN_POINT('Ctrl Pts',(-8.54336788530169,-0.596353369247186,
135.688246773322));
#75173=CARTESIAN_POINT('Ctrl Pts',(-8.55114078556709,-0.46006321221134,
135.702955730082));
#75174=CARTESIAN_POINT('Ctrl Pts',(-8.55891368583252,-0.323578082909706,
135.711954762028));
#75175=CARTESIAN_POINT('Ctrl Pts',(-8.56640402159466,-0.192054531841627,
135.720626656496));
#75176=CARTESIAN_POINT('Ctrl Pts',(-8.57389435735677,-0.0603502457845487,
135.723996551126));
#75177=CARTESIAN_POINT('Ctrl Pts',(-8.58138469311891,0.0710773012681246,
135.722096995184));
#75178=CARTESIAN_POINT('Ctrl Pts',(-8.58915902723802,0.207487963711916,
135.720125417001));
#75179=CARTESIAN_POINT('Ctrl Pts',(-8.59693336135712,0.344032595755697,
135.71247067256));
#75180=CARTESIAN_POINT('Ctrl Pts',(-8.60470769547621,0.480198763673881,
135.699112113798));
#75181=CARTESIAN_POINT('Ctrl Pts',(-8.6124724484233,0.616197118959626,135.685770018266));
#75182=CARTESIAN_POINT('Ctrl Pts',(-8.62023720137033,0.751817552800991,
135.666738132711));
#75183=CARTESIAN_POINT('Ctrl Pts',(-8.62800195431743,0.886547124080211,
135.642047798367));
#75184=CARTESIAN_POINT('Ctrl Pts',(-8.63575899520243,1.02114288004988,135.617381986811));
#75185=CARTESIAN_POINT('Ctrl Pts',(-8.64351603608747,1.15484915221111,135.587068980639));
#75186=CARTESIAN_POINT('Ctrl Pts',(-8.65127307697247,1.28715797490601,135.551191919618));
#75187=CARTESIAN_POINT('Ctrl Pts',(-8.65902426821257,1.41936702248797,135.515341913767));
#75188=CARTESIAN_POINT('Ctrl Pts',(-8.66677545945276,1.55018034237151,135.473936306651));
#75189=CARTESIAN_POINT('Ctrl Pts',(-8.67452665069285,1.67910037561594,135.427109257835));
#75190=CARTESIAN_POINT('Ctrl Pts',(-8.68227454746993,1.80796561440771,135.380302111763));
#75191=CARTESIAN_POINT('Ctrl Pts',(-8.69002244424695,1.93493880033633,135.328078240179));
#75192=CARTESIAN_POINT('Ctrl Pts',(-8.69777034102404,2.05953796816633,135.270621516817));
#75193=CARTESIAN_POINT('Ctrl Pts',(-8.70551661710814,2.18411107253629,135.213176812164));
#75194=CARTESIAN_POINT('Ctrl Pts',(-8.71326289319221,2.30631079174872,135.150501596567));
#75195=CARTESIAN_POINT('Ctrl Pts',(-8.7210091692763,2.4256759395769,135.082827550786));
#75196=CARTESIAN_POINT('Ctrl Pts',(-8.72875550254166,2.5450419685318,135.015153005451));
#75197=CARTESIAN_POINT('Ctrl Pts',(-8.73650183580706,2.6615730442427,134.942479749123));
#75198=CARTESIAN_POINT('Ctrl Pts',(-8.74424816907242,2.77483370655622,134.865084809562));
#75199=CARTESIAN_POINT('Ctrl Pts',(-8.75199623707542,2.88811973280993,134.78767253794));
#75200=CARTESIAN_POINT('Ctrl Pts',(-8.75974430507841,2.99813356556575,134.705536699542));
#75201=CARTESIAN_POINT('Ctrl Pts',(-8.76749237308141,3.10447012097299,134.618996685461));
#75202=CARTESIAN_POINT('Ctrl Pts',(-8.77524867582327,3.21091969213644,134.532364695624));
#75203=CARTESIAN_POINT('Ctrl Pts',(-8.78300497856511,3.31368387507331,134.441319426857));
#75204=CARTESIAN_POINT('Ctrl Pts',(-8.79076128130697,3.41239157971579,134.346219842491));
#75205=CARTESIAN_POINT('Ctrl Pts',(-8.79852172382113,3.51115196763213,134.251069500613));
#75206=CARTESIAN_POINT('Ctrl Pts',(-8.80628216633533,3.60585129335948,134.151860814028));
#75207=CARTESIAN_POINT('Ctrl Pts',(-8.81404260884949,3.69615725254146,134.048987657302));
#75208=CARTESIAN_POINT('Ctrl Pts',(-8.82181550911492,3.78660817886623,133.945949359451));
#75209=CARTESIAN_POINT('Ctrl Pts',(-8.82958840938038,3.87265139971772,133.839235140814));
#75210=CARTESIAN_POINT('Ctrl Pts',(-8.83736130964581,3.95399608638191,133.729270532653));
#75211=CARTESIAN_POINT('Ctrl Pts',(-8.84485164540781,4.03238368879051,133.623303414984));
#75212=CARTESIAN_POINT('Ctrl Pts',(-8.85234198116975,4.10640826025097,133.514318379429));
#75213=CARTESIAN_POINT('Ctrl Pts',(-8.85983231693174,4.17584990951577,133.402717905488));
#75214=CARTESIAN_POINT('Ctrl Pts',(-8.86760665105083,4.24792446001919,133.286886065657));
#75215=CARTESIAN_POINT('Ctrl Pts',(-8.8753809851699,4.31529001563534,133.167869623226));
#75216=CARTESIAN_POINT('Ctrl Pts',(-8.88315531928899,4.37765222161807,133.046088542418));
#75217=CARTESIAN_POINT('Ctrl Pts',(-8.89092007223609,4.43993757175541,132.924457545909));
#75218=CARTESIAN_POINT('Ctrl Pts',(-8.8986848251832,4.49723166463176,132.800069034926));
#75219=CARTESIAN_POINT('Ctrl Pts',(-8.90644957813029,4.54928361131065,132.673371502061));
#75220=CARTESIAN_POINT('Ctrl Pts',(-8.91420661901531,4.60128385926237,132.546799806972));
#75221=CARTESIAN_POINT('Ctrl Pts',(-8.92196365990035,4.64805217472143,132.417924013171));
#75222=CARTESIAN_POINT('Ctrl Pts',(-8.92972070078537,4.68938393768227,132.287216425629));
#75223=CARTESIAN_POINT('Ctrl Pts',(-8.9374718920255,4.73068453203908,132.156607405696));
#75224=CARTESIAN_POINT('Ctrl Pts',(-8.94522308326565,4.7665566167952,132.024169712818));
#75225=CARTESIAN_POINT('Ctrl Pts',(-8.95297427450578,4.79684412143037,131.890394473944));
#75226=CARTESIAN_POINT('Ctrl Pts',(-8.96072217128285,4.82711875306809,131.756676093115));
#75227=CARTESIAN_POINT('Ctrl Pts',(-8.96847006805995,4.85181343933435,131.621621677496));
#75228=CARTESIAN_POINT('Ctrl Pts',(-8.97621796483702,4.87082236442745,131.485736106334));
#75229=CARTESIAN_POINT('Ctrl Pts',(-8.98396424092111,4.88982731326321,131.349878959503));
#75230=CARTESIAN_POINT('Ctrl Pts',(-8.99171051700513,4.90314881245551,131.213191389897));
#75231=CARTESIAN_POINT('Ctrl Pts',(-8.99945679308922,4.9107324991684,131.076186635657));
#75232=CARTESIAN_POINT('Ctrl Pts',(-9.00720312635456,4.91831624186233,130.93918087008));
#75233=CARTESIAN_POINT('Ctrl Pts',(-9.01494945961993,4.92016206595188,130.801858305565));
#75234=CARTESIAN_POINT('Ctrl Pts',(-9.02269579288526,4.91626766588639,130.664735047343));
#75235=CARTESIAN_POINT('Ctrl Pts',(-9.03044386088819,4.91237239369701,130.527581081319));
#75236=CARTESIAN_POINT('Ctrl Pts',(-9.03819192889114,4.90273435048658,130.390626901135));
#75237=CARTESIAN_POINT('Ctrl Pts',(-9.04593999689408,4.88740329131241,130.254385953996));
#75238=CARTESIAN_POINT('Ctrl Pts',(-9.05369629963592,4.87205593810606,130.118000208357));
#75239=CARTESIAN_POINT('Ctrl Pts',(-9.06145260237779,4.85100352598916,129.982329599147));
#75240=CARTESIAN_POINT('Ctrl Pts',(-9.06920890511964,4.82434747773057,129.847880363397));
#75241=CARTESIAN_POINT('Ctrl Pts',(-9.07696934763382,4.79767720233635,129.713359368042));
#75242=CARTESIAN_POINT('Ctrl Pts',(-9.08472979014798,4.76539742329222,129.580061424877));
#75243=CARTESIAN_POINT('Ctrl Pts',(-9.09249023266216,4.72765989980244,129.448479009792));
#75244=CARTESIAN_POINT('Ctrl Pts',(-9.10026313292758,4.68986179668988,129.316685366933));
#75245=CARTESIAN_POINT('Ctrl Pts',(-9.10803603319306,4.64658856483965,129.186613126547));
#75246=CARTESIAN_POINT('Ctrl Pts',(-9.11580893345848,4.59804101573103,129.05873698111));
#75247=CARTESIAN_POINT('Ctrl Pts',(-9.12329926922054,4.55125829231615,128.935509455659));
#75248=CARTESIAN_POINT('Ctrl Pts',(-9.13078960498258,4.49957818431132,128.814321413378));
#75249=CARTESIAN_POINT('Ctrl Pts',(-9.13827994074464,4.44322045252909,128.695575405002));
#75250=CARTESIAN_POINT('Ctrl Pts',(-9.14605427486373,4.38472590021702,128.572327105628));
#75251=CARTESIAN_POINT('Ctrl Pts',(-9.15382860898285,4.32100672478463,128.451319261524));
#75252=CARTESIAN_POINT('Ctrl Pts',(-9.16160294310194,4.25225714809689,128.333026522596));
#75253=CARTESIAN_POINT('Ctrl Pts',(-9.16936769604905,4.183592299118,128.214879568897));
#75254=CARTESIAN_POINT('Ctrl Pts',(-9.17713244899608,4.10990957864789,128.099441397363));
#75255=CARTESIAN_POINT('Ctrl Pts',(-9.18489720194319,4.03145070460736,127.987165509161));
#75256=CARTESIAN_POINT('Ctrl Pts',(-9.19265424282818,3.95306975702682,127.875001134955));
#75257=CARTESIAN_POINT('Ctrl Pts',(-9.20041128371321,3.86992231863609,127.765993112097));
#75258=CARTESIAN_POINT('Ctrl Pts',(-9.2081683245982,3.78229515087075,127.660568885565));
#75259=CARTESIAN_POINT('Ctrl Pts',(-9.21591951583831,3.69473406343451,127.555224160263));
#75260=CARTESIAN_POINT('Ctrl Pts',(-9.22367070707846,3.60270021962093,127.453458151436));
#75261=CARTESIAN_POINT('Ctrl Pts',(-9.23142189831856,3.50652245851387,127.355667631747));
#75262=CARTESIAN_POINT('Ctrl Pts',(-9.23916979509563,3.41038557552065,127.257918675637));
#75263=CARTESIAN_POINT('Ctrl Pts',(-9.2469176918727,3.31010855184853,127.164142126162));
#75264=CARTESIAN_POINT('Ctrl Pts',(-9.25466558864977,3.20605896068198,127.074699908717));
#75265=CARTESIAN_POINT('Ctrl Pts',(-9.26241186473385,3.10203113444699,126.985276400657));
#75266=CARTESIAN_POINT('Ctrl Pts',(-9.27015814081786,2.99423260665302,126.90018567595));
#75267=CARTESIAN_POINT('Ctrl Pts',(-9.27790441690195,2.88306579464535,126.819750889343));
#75268=CARTESIAN_POINT('Ctrl Pts',(-9.28565075016727,2.77189816202967,126.739315508986));
#75269=CARTESIAN_POINT('Ctrl Pts',(-9.29339708343268,2.65736251233373,126.663536364493));
#75270=CARTESIAN_POINT('Ctrl Pts',(-9.30114341669801,2.53989181329801,126.592694363072));
#75271=CARTESIAN_POINT('Ctrl Pts',(-9.308891484701,2.42239480751324,126.521836497076));
#75272=CARTESIAN_POINT('Ctrl Pts',(-9.31663955270393,2.30196177920256,126.455918176111));
#75273=CARTESIAN_POINT('Ctrl Pts',(-9.32438762070691,2.17905159986428,126.395175070594));
#75274=CARTESIAN_POINT('Ctrl Pts',(-9.33214392344877,2.05601079012475,126.334367406581));
#75275=CARTESIAN_POINT('Ctrl Pts',(-9.33990022619064,1.93048792122188,126.278746118913));
#75276=CARTESIAN_POINT('Ctrl Pts',(-9.3476565289325,1.80296372619136,126.228499511223));
#75277=CARTESIAN_POINT('Ctrl Pts',(-9.35541697144667,1.67537146765827,126.178226085407));
#75278=CARTESIAN_POINT('Ctrl Pts',(-9.36317741396091,1.54577612382916,126.133333183463));
#75279=CARTESIAN_POINT('Ctrl Pts',(-9.37093785647508,1.41467405817407,126.093959321325));
#75280=CARTESIAN_POINT('Ctrl Pts',(-9.37871075674052,1.28336153584449,126.054522252767));
#75281=CARTESIAN_POINT('Ctrl Pts',(-9.38648365700589,1.15053783734785,126.020622025165));
#75282=CARTESIAN_POINT('Ctrl Pts',(-9.39425655727132,1.01671087841746,125.992346273011));
#75283=CARTESIAN_POINT('Ctrl Pts',(-9.40174689303338,0.887748866533404,
125.965098415669));
#75284=CARTESIAN_POINT('Ctrl Pts',(-9.40923722879547,0.757855573605318,
125.943073257155));
#75285=CARTESIAN_POINT('Ctrl Pts',(-9.41672756455753,0.627488463054982,
125.926303494978));
#75286=CARTESIAN_POINT('Ctrl Pts',(-9.42450189867662,0.492178443884476,
125.908897902171));
#75287=CARTESIAN_POINT('Ctrl Pts',(-9.43227623279572,0.355929346771139,
125.897098953564));
#75288=CARTESIAN_POINT('Ctrl Pts',(-9.44005056691481,0.219245489785435,
125.890999804669));
#75289=CARTESIAN_POINT('Ctrl Pts',(-9.44781531986191,0.0827300834374924,
125.884908172431));
#75290=CARTESIAN_POINT('Ctrl Pts',(-9.45558007280897,-0.0542186298681168,
125.884502380517));
#75291=CARTESIAN_POINT('Ctrl Pts',(-9.46334482575608,-0.191088452313938,
125.889824193254));
#75292=CARTESIAN_POINT('Ctrl Pts',(-9.47110186664108,-0.327822333722208,
125.895140720291));
#75293=CARTESIAN_POINT('Ctrl Pts',(-9.47885890752611,-0.464477092059701,
125.906173516043));
#75294=CARTESIAN_POINT('Ctrl Pts',(-9.4866159484111,-0.600538104199871,
125.922912364444));
#75295=CARTESIAN_POINT('Ctrl Pts',(-9.49436713965121,-0.736496511672199,
125.93963858995));
#75296=CARTESIAN_POINT('Ctrl Pts',(-9.50211833089134,-0.871861677694062,
125.96206225574));
#75297=CARTESIAN_POINT('Ctrl Pts',(-9.50986952213145,-1.0061220406309,125.990121165497));
#75298=CARTESIAN_POINT('Ctrl Pts',(-9.51761741890853,-1.14032533933216,
126.018168149469));
#75299=CARTESIAN_POINT('Ctrl Pts',(-9.52536531568559,-1.27342438699295,
126.051845533866));
#75300=CARTESIAN_POINT('Ctrl Pts',(-9.53311321246267,-1.40491600324223,
126.091039698476));
#75301=CARTESIAN_POINT('Ctrl Pts',(-9.54085948854675,-1.53638011427986,
126.130225664511));
#75302=CARTESIAN_POINT('Ctrl Pts',(-9.54860576463082,-1.66623708826832,
126.174926003796));
#75303=CARTESIAN_POINT('Ctrl Pts',(-9.5563520407149,-1.79399752956222,126.224976824257));
#75304=CARTESIAN_POINT('Ctrl Pts',(-9.56409837398026,-1.92175891395521,
126.275028014181));
#75305=CARTESIAN_POINT('Ctrl Pts',(-9.57184470724563,-2.04742337074434,
126.330429621481));
#75306=CARTESIAN_POINT('Ctrl Pts',(-9.57959104051099,-2.17052053509985,
126.390969215344));
#75307=CARTESIAN_POINT('Ctrl Pts',(-9.58733910851394,-2.29364526621116,
126.451522366628));
#75308=CARTESIAN_POINT('Ctrl Pts',(-9.59508717651692,-2.41420121008456,
126.51721562156));
#75309=CARTESIAN_POINT('Ctrl Pts',(-9.60283524451987,-2.53174205927058,
126.587790304169));
#75310=CARTESIAN_POINT('Ctrl Pts',(-9.61059154726173,-2.64940783227035,
126.658439994391));
#75311=CARTESIAN_POINT('Ctrl Pts',(-9.6183478500036,-2.76405177357048,126.733981274381));
#75312=CARTESIAN_POINT('Ctrl Pts',(-9.62610415274546,-2.87525561004309,
126.814111472536));
#75313=CARTESIAN_POINT('Ctrl Pts',(-9.63386459525963,-2.98651879935167,
126.894284438589));
#75314=CARTESIAN_POINT('Ctrl Pts',(-9.64162503777379,-3.09433791807148,
126.979050961613));
#75315=CARTESIAN_POINT('Ctrl Pts',(-9.64938548028798,-3.19832813224702,
127.068068308207));
#75316=CARTESIAN_POINT('Ctrl Pts',(-9.65715838055341,-3.30248528074602,
127.157228553347));
#75317=CARTESIAN_POINT('Ctrl Pts',(-9.66493128081886,-3.402800955769,127.250652991577));
#75318=CARTESIAN_POINT('Ctrl Pts',(-9.6727041810843,-3.49892688707446,127.347961667588));
#75319=CARTESIAN_POINT('Ctrl Pts',(-9.68019451684633,-3.59155839865037,
127.441732928121));
#75320=CARTESIAN_POINT('Ctrl Pts',(-9.68768485260831,-3.68029928594057,
127.539110698059));
#75321=CARTESIAN_POINT('Ctrl Pts',(-9.69517518837034,-3.76487476945033,
127.639727774272));
#75322=CARTESIAN_POINT('Ctrl Pts',(-9.70290515034446,-3.85215593977986,
127.743563730066));
#75323=CARTESIAN_POINT('Ctrl Pts',(-9.71063511231849,-3.93528669078073,
127.85119007496));
#75324=CARTESIAN_POINT('Ctrl Pts',(-9.71836507429259,-4.01391671537598,
127.962238933942));
#75325=CARTESIAN_POINT('Ctrl Pts',(-9.72608557273473,-4.09245047588179,
128.073151839548));
#75326=CARTESIAN_POINT('Ctrl Pts',(-9.73380607117693,-4.16649424273253,
128.187478605739));
#75327=CARTESIAN_POINT('Ctrl Pts',(-9.74152656961905,-4.23573638300213,
128.304816587905));
#75328=CARTESIAN_POINT('Ctrl Pts',(-9.74923780683666,-4.30489546296001,
128.422013815766));
#75329=CARTESIAN_POINT('Ctrl Pts',(-9.7569490440543,-4.36926418489053,128.542214728939));
#75330=CARTESIAN_POINT('Ctrl Pts',(-9.76466028127192,-4.42857329347761,
128.664986492548));
#75331=CARTESIAN_POINT('Ctrl Pts',(-9.77236618259188,-4.48784136230359,
128.787673302531));
#75332=CARTESIAN_POINT('Ctrl Pts',(-9.78007208391177,-4.54205660962594,
128.912927070076));
#75333=CARTESIAN_POINT('Ctrl Pts',(-9.78777798523171,-4.59099495974659,
129.040289093483));
#75334=CARTESIAN_POINT('Ctrl Pts',(-9.79548001981686,-4.63990875315239,
129.167587208056));
#75335=CARTESIAN_POINT('Ctrl Pts',(-9.80318205440206,-4.6835507774132,129.296991104518));
#75336=CARTESIAN_POINT('Ctrl Pts',(-9.81088408898722,-4.72174469572343,
129.428021236851));
#75337=CARTESIAN_POINT('Ctrl Pts',(-9.8138966458173,-4.73668378074059,129.479272073982));
#75338=CARTESIAN_POINT('Ctrl Pts',(-9.81690920264739,-4.75078989188748,
129.530771503512));
#75339=CARTESIAN_POINT('Ctrl Pts',(-9.81992175947747,-4.76405452823407,
129.582490119308));
#75340=CARTESIAN_POINT('Origin',(213.235140564004,0.,130.804360617566));
#75341=CARTESIAN_POINT('',(-11.9152857535002,-4.76405452823405,129.582490119308));
#75342=CARTESIAN_POINT('',(-11.5697518023984,-4.76405452823402,129.582490119308));
#75343=CARTESIAN_POINT('',(213.235140564004,-4.76405452823405,129.582490119308));
#75344=CARTESIAN_POINT('',(-10.2351405640601,-4.91824999126511,130.804067495121));
#75345=CARTESIAN_POINT('Ctrl Pts',(-10.2351405640602,-4.91824999126511,
130.804067495121));
#75346=CARTESIAN_POINT('Ctrl Pts',(-10.2429017491463,-4.91825810842386,
130.940263875405));
#75347=CARTESIAN_POINT('Ctrl Pts',(-10.2506629342323,-4.91260460408128,
131.076679746296));
#75348=CARTESIAN_POINT('Ctrl Pts',(-10.2584241193184,-4.90126071843733,
131.212804533426));
#75349=CARTESIAN_POINT('Ctrl Pts',(-10.2661757404953,-4.88993081157252,
131.348761577475));
#75350=CARTESIAN_POINT('Ctrl Pts',(-10.2739273616722,-4.87292450676915,
131.484427864117));
#75351=CARTESIAN_POINT('Ctrl Pts',(-10.2816789828491,-4.85026501951163,
131.61929147537));
#75352=CARTESIAN_POINT('Ctrl Pts',(-10.2894229231295,-4.8276279849996,131.754021453488));
#75353=CARTESIAN_POINT('Ctrl Pts',(-10.2971668634097,-4.79934897938044,
131.887949954395));
#75354=CARTESIAN_POINT('Ctrl Pts',(-10.3049108036901,-4.76550308931971,
132.020569221459));
#75355=CARTESIAN_POINT('Ctrl Pts',(-10.3126489392927,-4.73168256935185,
132.153089080202));
#75356=CARTESIAN_POINT('Ctrl Pts',(-10.3203870748954,-4.69230356683776,
132.284301279617));
#75357=CARTESIAN_POINT('Ctrl Pts',(-10.328125210498,-4.64749234246125,132.413707686804));
#75358=CARTESIAN_POINT('Ctrl Pts',(-10.3358601234575,-4.60269978027845,
132.543060201077));
#75359=CARTESIAN_POINT('Ctrl Pts',(-10.3435950364169,-4.55247962350084,
132.670608048639));
#75360=CARTESIAN_POINT('Ctrl Pts',(-10.3513299493764,-4.49700807573169,
132.795867943514));
#75361=CARTESIAN_POINT('Ctrl Pts',(-10.3590633079488,-4.44154767537383,
132.921102666501));
#75362=CARTESIAN_POINT('Ctrl Pts',(-10.3667966665212,-4.38083814177513,
133.044049992645));
#75363=CARTESIAN_POINT('Ctrl Pts',(-10.3745300250936,-4.31510378265571,
133.164246718082));
#75364=CARTESIAN_POINT('Ctrl Pts',(-10.3822635195478,-4.24936826852709,
133.284445555479));
#75365=CARTESIAN_POINT('Ctrl Pts',(-10.3899970140019,-4.17860794137014,
133.401893351596));
#75366=CARTESIAN_POINT('Ctrl Pts',(-10.3977305084561,-4.10309281461364,
133.516151984387));
#75367=CARTESIAN_POINT('Ctrl Pts',(-10.4054658288026,-4.02755985859584,
133.630437593854));
#75368=CARTESIAN_POINT('Ctrl Pts',(-10.4132011491492,-3.94727008565719,
133.741532214494));
#75369=CARTESIAN_POINT('Ctrl Pts',(-10.4209364694957,-3.86253628486645,
133.849027514057));
#75370=CARTESIAN_POINT('Ctrl Pts',(-10.4286800326156,-3.77771219156258,
133.956637360834));
#75371=CARTESIAN_POINT('Ctrl Pts',(-10.4364235957355,-3.6884348549411,134.060639917006));
#75372=CARTESIAN_POINT('Ctrl Pts',(-10.4441671588554,-3.59505707031016,
134.160660324641));
#75373=CARTESIAN_POINT('Ctrl Pts',(-10.4519149673367,-3.50162809187508,
134.260735567858));
#75374=CARTESIAN_POINT('Ctrl Pts',(-10.4596627758181,-3.40409446597181,
134.356824037765));
#75375=CARTESIAN_POINT('Ctrl Pts',(-10.4674105842995,-3.30284439326151,
134.448589202109));
#75376=CARTESIAN_POINT('Ctrl Pts',(-10.4751706114612,-3.20143464413844,
134.540499084693));
#75377=CARTESIAN_POINT('Ctrl Pts',(-10.4829306386228,-3.0962970395167,134.628071788221));
#75378=CARTESIAN_POINT('Ctrl Pts',(-10.4906906657845,-2.98785188863263,
134.71101188868));
#75379=CARTESIAN_POINT('Ctrl Pts',(-10.4974367984062,-2.8935757534071,134.783115362765));
#75380=CARTESIAN_POINT('Ctrl Pts',(-10.5041829310279,-2.79680051840778,
134.85171829878));
#75381=CARTESIAN_POINT('Ctrl Pts',(-10.5109290636496,-2.69781790896645,
134.916654575026));
#75382=CARTESIAN_POINT('Ctrl Pts',(-10.5187033977687,-2.58374901632448,
134.991488014612));
#75383=CARTESIAN_POINT('Ctrl Pts',(-10.5264777318878,-2.46638343527605,
135.061690237066));
#75384=CARTESIAN_POINT('Ctrl Pts',(-10.5342520660069,-2.3461339454031,135.126956894426));
#75385=CARTESIAN_POINT('Ctrl Pts',(-10.542016818954,-2.22603265227925,135.192143116465));
#75386=CARTESIAN_POINT('Ctrl Pts',(-10.549781571901,-2.10305486236609,135.252405691345));
#75387=CARTESIAN_POINT('Ctrl Pts',(-10.5575463248481,-1.97764291845774,
135.307483039794));
#75388=CARTESIAN_POINT('Ctrl Pts',(-10.5653033657331,-1.85235553546042,
135.362505684645));
#75389=CARTESIAN_POINT('Ctrl Pts',(-10.5730604066181,-1.72463916532199,
135.412353195686));
#75390=CARTESIAN_POINT('Ctrl Pts',(-10.5808174475031,-1.59496106668328,
135.456809677821));
#75391=CARTESIAN_POINT('Ctrl Pts',(-10.5885686387433,-1.4653807593068,135.501232634977));
#75392=CARTESIAN_POINT('Ctrl Pts',(-10.5963198299834,-1.3338420363354,135.540272528917));
#75393=CARTESIAN_POINT('Ctrl Pts',(-10.6040710212236,-1.20083213802427,
135.573761548374));
#75394=CARTESIAN_POINT('Ctrl Pts',(-10.6118189180007,-1.06787877246845,
135.607236334103));
#75395=CARTESIAN_POINT('Ctrl Pts',(-10.6195668147777,-0.933455853563626,
135.635164842499));
#75396=CARTESIAN_POINT('Ctrl Pts',(-10.6273147115548,-0.798065575877236,
135.657429172522));
#75397=CARTESIAN_POINT('Ctrl Pts',(-10.6350609876389,-0.662703618918261,
135.679688845326));
#75398=CARTESIAN_POINT('Ctrl Pts',(-10.6428072637231,-0.526375091203496,
135.696286633038));
#75399=CARTESIAN_POINT('Ctrl Pts',(-10.6505535398072,-0.389591778518623,
135.707155872174));
#75400=CARTESIAN_POINT('Ctrl Pts',(-10.6582998730725,-0.252807456130222,
135.718025191545));
#75401=CARTESIAN_POINT('Ctrl Pts',(-10.6660462063378,-0.115568731809494,
135.723165846992));
#75402=CARTESIAN_POINT('Ctrl Pts',(-10.6737925396032,0.0216084931659148,
135.722563148524));
#75403=CARTESIAN_POINT('Ctrl Pts',(-10.6815406076061,0.158816438028989,
135.721960315087));
#75404=CARTESIAN_POINT('Ctrl Pts',(-10.6892886756092,0.29596246525475,135.715611570095));
#75405=CARTESIAN_POINT('Ctrl Pts',(-10.6970367436121,0.432532081514863,
135.70355433296));
#75406=CARTESIAN_POINT('Ctrl Pts',(-10.704793046354,0.569246845588709,135.691484281251));
#75407=CARTESIAN_POINT('Ctrl Pts',(-10.7125493490958,0.705383584858226,
135.673693652245));
#75408=CARTESIAN_POINT('Ctrl Pts',(-10.7203056518377,0.840433774209168,
135.65027169121));
#75409=CARTESIAN_POINT('Ctrl Pts',(-10.7280660943518,0.975556043912633,
135.62683722917));
#75410=CARTESIAN_POINT('Ctrl Pts',(-10.7358265368661,1.10959022625492,135.597765528998));
#75411=CARTESIAN_POINT('Ctrl Pts',(-10.7435869793802,1.24204034536529,135.563196488132));
#75412=CARTESIAN_POINT('Ctrl Pts',(-10.7513598796457,1.37470308516524,135.528571953973));
#75413=CARTESIAN_POINT('Ctrl Pts',(-10.759132779911,1.50577630620677,135.488432558865));
#75414=CARTESIAN_POINT('Ctrl Pts',(-10.7669056801764,1.63478063379225,135.442967665148));
#75415=CARTESIAN_POINT('Ctrl Pts',(-10.7743960159385,1.75909532912736,135.399155534837));
#75416=CARTESIAN_POINT('Ctrl Pts',(-10.7818863517005,1.88148865233982,135.35039848829));
#75417=CARTESIAN_POINT('Ctrl Pts',(-10.7893766874625,2.00155289496522,135.296906562924));
#75418=CARTESIAN_POINT('Ctrl Pts',(-10.7971510215816,2.12616940984285,135.24138647495));
#75419=CARTESIAN_POINT('Ctrl Pts',(-10.8049253557006,2.24867149119457,135.180589503669));
#75420=CARTESIAN_POINT('Ctrl Pts',(-10.8126996898197,2.36857996501309,135.114698424727));
#75421=CARTESIAN_POINT('Ctrl Pts',(-10.8204644427668,2.48834066235382,135.04888855065));
#75422=CARTESIAN_POINT('Ctrl Pts',(-10.8282291957139,2.60551377267246,134.977997246802));
#75423=CARTESIAN_POINT('Ctrl Pts',(-10.835993948661,2.71964012483391,134.902255278717));
#75424=CARTESIAN_POINT('Ctrl Pts',(-10.843750989546,2.83365312509364,134.826588538623));
#75425=CARTESIAN_POINT('Ctrl Pts',(-10.851508030431,2.94462506559323,134.746080936621));
#75426=CARTESIAN_POINT('Ctrl Pts',(-10.859265071316,3.05212174296428,134.661008894065));
#75427=CARTESIAN_POINT('Ctrl Pts',(-10.8670162625561,3.15953735625457,134.576001004999));
#75428=CARTESIAN_POINT('Ctrl Pts',(-10.8747674537962,3.26348261747135,134.48643576827));
#75429=CARTESIAN_POINT('Ctrl Pts',(-10.8825186450363,3.36355297698243,134.392632406817));
#75430=CARTESIAN_POINT('Ctrl Pts',(-10.8902665418134,3.46358080392139,134.298868914294));
#75431=CARTESIAN_POINT('Ctrl Pts',(-10.8980144385905,3.55973672014155,134.200871146544));
#75432=CARTESIAN_POINT('Ctrl Pts',(-10.9057623353676,3.65165008372901,134.098997885689));
#75433=CARTESIAN_POINT('Ctrl Pts',(-10.9135086114517,3.74354422102235,133.997145934523));
#75434=CARTESIAN_POINT('Ctrl Pts',(-10.9212548875358,3.83119730913693,133.891420392813));
#75435=CARTESIAN_POINT('Ctrl Pts',(-10.9290011636199,3.91427662947989,133.782215807196));
#75436=CARTESIAN_POINT('Ctrl Pts',(-10.9367474968852,3.99735656309551,133.673010415456));
#75437=CARTESIAN_POINT('Ctrl Pts',(-10.9444938301506,4.07586242485096,133.560326239718));
#75438=CARTESIAN_POINT('Ctrl Pts',(-10.952240163416,4.14950299840011,133.444589382042));
#75439=CARTESIAN_POINT('Ctrl Pts',(-10.959988231419,4.22316006324523,133.328826605899));
#75440=CARTESIAN_POINT('Ctrl Pts',(-10.9677362994219,4.29194946197168,133.210010117272));
#75441=CARTESIAN_POINT('Ctrl Pts',(-10.9754843674249,4.35562458037932,133.088593000073));
#75442=CARTESIAN_POINT('Ctrl Pts',(-10.9832406701668,4.41936737346037,132.967046839318));
#75443=CARTESIAN_POINT('Ctrl Pts',(-10.9909969729087,4.47798484632053,132.84289487544));
#75444=CARTESIAN_POINT('Ctrl Pts',(-10.9987532756505,4.53127721328623,132.716613184267));
#75445=CARTESIAN_POINT('Ctrl Pts',(-11.0065137181647,4.58459802399285,132.590264092752));
#75446=CARTESIAN_POINT('Ctrl Pts',(-11.0142741606788,4.63258792880767,132.461783375043));
#75447=CARTESIAN_POINT('Ctrl Pts',(-11.0220346031929,4.67509654033431,132.33166392767));
#75448=CARTESIAN_POINT('Ctrl Pts',(-11.0298075034584,4.71767339045786,132.201335601008));
#75449=CARTESIAN_POINT('Ctrl Pts',(-11.0375804037239,4.75475125816114,132.069363664444));
#75450=CARTESIAN_POINT('Ctrl Pts',(-11.0453533039893,4.78623034561037,131.936253784459));
#75451=CARTESIAN_POINT('Ctrl Pts',(-11.0528436397513,4.8165650889399,131.807982783894));
#75452=CARTESIAN_POINT('Ctrl Pts',(-11.0603339755134,4.84170098562771,131.678655440099));
#75453=CARTESIAN_POINT('Ctrl Pts',(-11.0678243112754,4.86159436971924,131.548728300109));
#75454=CARTESIAN_POINT('Ctrl Pts',(-11.0755986453945,4.88224201751497,131.413874933116));
#75455=CARTESIAN_POINT('Ctrl Pts',(-11.0833729795136,4.89730717096693,131.27794821461));
#75456=CARTESIAN_POINT('Ctrl Pts',(-11.0911473136327,4.9066845991462,131.141450081954));
#75457=CARTESIAN_POINT('Ctrl Pts',(-11.0989120665797,4.91605047048332,131.005120171048));
#75458=CARTESIAN_POINT('Ctrl Pts',(-11.1066768195268,4.91974253704958,130.868220633476));
#75459=CARTESIAN_POINT('Ctrl Pts',(-11.1144415724739,4.91770675521032,130.731262517326));
#75460=CARTESIAN_POINT('Ctrl Pts',(-11.1221986133589,4.91567299533828,130.594440429907));
#75461=CARTESIAN_POINT('Ctrl Pts',(-11.129955654244,4.90792271416036,130.457560268086));
#75462=CARTESIAN_POINT('Ctrl Pts',(-11.137712695129,4.89445377526414,130.321136751948));
#75463=CARTESIAN_POINT('Ctrl Pts',(-11.1454638863691,4.88099499339952,130.184816113845));
#75464=CARTESIAN_POINT('Ctrl Pts',(-11.1532150776092,4.86182617581237,130.048951823496));
#75465=CARTESIAN_POINT('Ctrl Pts',(-11.1609662688493,4.83699722484215,129.914056787759));
#75466=CARTESIAN_POINT('Ctrl Pts',(-11.1687141656264,4.81217882683846,129.779219086011));
#75467=CARTESIAN_POINT('Ctrl Pts',(-11.1764620624034,4.78170515084539,129.64535020322));
#75468=CARTESIAN_POINT('Ctrl Pts',(-11.1842099591805,4.74567770941459,129.512955901427));
#75469=CARTESIAN_POINT('Ctrl Pts',(-11.1919562352646,4.70965780414793,129.380589293668));
#75470=CARTESIAN_POINT('Ctrl Pts',(-11.1997025113488,4.6680865467765,129.249697030389));
#75471=CARTESIAN_POINT('Ctrl Pts',(-11.2074487874329,4.62111603803288,129.12077229926));
#75472=CARTESIAN_POINT('Ctrl Pts',(-11.2151951206982,4.57414518256363,128.991846616438));
#75473=CARTESIAN_POINT('Ctrl Pts',(-11.2229414539635,4.52177513002539,128.864888862092));
#75474=CARTESIAN_POINT('Ctrl Pts',(-11.2306877872288,4.46420696259896,128.740374363352));
#75475=CARTESIAN_POINT('Ctrl Pts',(-11.2384358552318,4.40662590318075,128.615831980454));
#75476=CARTESIAN_POINT('Ctrl Pts',(-11.2461839232347,4.34384457652693,128.493734296732));
#75477=CARTESIAN_POINT('Ctrl Pts',(-11.2539319912377,4.27611087396772,128.37453369862));
#75478=CARTESIAN_POINT('Ctrl Pts',(-11.2616882939795,4.20830518322311,128.255206412693));
#75479=CARTESIAN_POINT('Ctrl Pts',(-11.2694445967213,4.13553679573822,128.138782703586));
#75480=CARTESIAN_POINT('Ctrl Pts',(-11.2772008994632,4.05809825855412,128.025687987258));
#75481=CARTESIAN_POINT('Ctrl Pts',(-11.2849613419773,3.98061839009098,127.912532908875));
#75482=CARTESIAN_POINT('Ctrl Pts',(-11.2927217844916,3.89846363929077,127.802710676572));
#75483=CARTESIAN_POINT('Ctrl Pts',(-11.3004822270057,3.81196740590188,127.696614238139));
#75484=CARTESIAN_POINT('Ctrl Pts',(-11.3082551272712,3.72533232108038,127.590347484284));
#75485=CARTESIAN_POINT('Ctrl Pts',(-11.3160280275365,3.63434208638075,127.487818768779));
#75486=CARTESIAN_POINT('Ctrl Pts',(-11.323800927802,3.53936819016689,127.389385379452));
#75487=CARTESIAN_POINT('Ctrl Pts',(-11.331291263564,3.44784683430444,127.294530291765));
#75488=CARTESIAN_POINT('Ctrl Pts',(-11.3387815993262,3.35262664336714,127.203478161678));
#75489=CARTESIAN_POINT('Ctrl Pts',(-11.3462719350883,3.25406812078933,127.11651250142));
#75490=CARTESIAN_POINT('Ctrl Pts',(-11.3540462692074,3.15177272187264,127.026249511721));
#75491=CARTESIAN_POINT('Ctrl Pts',(-11.3618206033265,3.0455568073762,126.940103059907));
#75492=CARTESIAN_POINT('Ctrl Pts',(-11.3695949374456,2.93578579153237,126.858432989145));
#75493=CARTESIAN_POINT('Ctrl Pts',(-11.3773596903927,2.8261500586549,126.776863569446));
#75494=CARTESIAN_POINT('Ctrl Pts',(-11.3851244433398,2.71296825266145,126.699759785264));
#75495=CARTESIAN_POINT('Ctrl Pts',(-11.3928891962869,2.59664112087787,126.627443339014));
#75496=CARTESIAN_POINT('Ctrl Pts',(-11.4006462371719,2.4804295268415,126.555198718478));
#75497=CARTESIAN_POINT('Ctrl Pts',(-11.4084032780569,2.36107915376604,126.487732178585));
#75498=CARTESIAN_POINT('Ctrl Pts',(-11.4161603189419,2.23902189545369,126.425323735536));
#75499=CARTESIAN_POINT('Ctrl Pts',(-11.423911510182,2.11705668147029,126.36296235518));
#75500=CARTESIAN_POINT('Ctrl Pts',(-11.4316627014221,1.99238899199366,126.305651656702));
#75501=CARTESIAN_POINT('Ctrl Pts',(-11.4394138926622,1.8654773235228,126.253626894536));
#75502=CARTESIAN_POINT('Ctrl Pts',(-11.4471617894393,1.73861959589566,126.201624244281));
#75503=CARTESIAN_POINT('Ctrl Pts',(-11.4549096862163,1.60952014720512,126.154903209876));
#75504=CARTESIAN_POINT('Ctrl Pts',(-11.4626575829934,1.47865935939255,126.113651762672));
#75505=CARTESIAN_POINT('Ctrl Pts',(-11.4704038590775,1.34782594483594,126.072408944382));
#75506=CARTESIAN_POINT('Ctrl Pts',(-11.4781501351616,1.21523229663418,126.036633555044));
#75507=CARTESIAN_POINT('Ctrl Pts',(-11.4858964112457,1.08137556170259,126.006464207987));
#75508=CARTESIAN_POINT('Ctrl Pts',(-11.493642744511,0.947517838670995,125.976294638227));
#75509=CARTESIAN_POINT('Ctrl Pts',(-11.5013890777764,0.812397391702526,
125.951731279284));
#75510=CARTESIAN_POINT('Ctrl Pts',(-11.5091354110417,0.676522816804156,
125.932861880951));
#75511=CARTESIAN_POINT('Ctrl Pts',(-11.5168834790447,0.540617813736641,
125.913988256946));
#75512=CARTESIAN_POINT('Ctrl Pts',(-11.5246315470477,0.403958733858847,
125.900811184666));
#75513=CARTESIAN_POINT('Ctrl Pts',(-11.5323796150507,0.267060174009044,
125.893366632031));
#75514=CARTESIAN_POINT('Ctrl Pts',(-11.5401359177926,0.130016116740718,
125.885914167237));
#75515=CARTESIAN_POINT('Ctrl Pts',(-11.5478922205344,-0.00726753792415963,
125.884206413957));
#75516=CARTESIAN_POINT('Ctrl Pts',(-11.5556485232763,-0.144274746668937,
125.888227191796));
#75517=CARTESIAN_POINT('Ctrl Pts',(-11.5634089657904,-0.28135508028623,
125.892250115645));
#75518=CARTESIAN_POINT('Ctrl Pts',(-11.5711694083046,-0.418158284198805,
125.90200763512));
#75519=CARTESIAN_POINT('Ctrl Pts',(-11.5789298508187,-0.554173549594789,
125.917431649448));
#75520=CARTESIAN_POINT('Ctrl Pts',(-11.5867027510842,-0.690407158769655,
125.932880423773));
#75521=CARTESIAN_POINT('Ctrl Pts',(-11.5944756513496,-0.825849915303424,
125.95401381007));
#75522=CARTESIAN_POINT('Ctrl Pts',(-11.602248551615,-0.960000424292672,
125.980712387455));
#75523=CARTESIAN_POINT('Ctrl Pts',(-11.6097388873771,-1.08927422437524,
126.006440404302));
#75524=CARTESIAN_POINT('Ctrl Pts',(-11.6172292231391,-1.21734779923011,
126.037335947329));
#75525=CARTESIAN_POINT('Ctrl Pts',(-11.6247195589011,-1.34378776107863,
126.073248960072));
#75526=CARTESIAN_POINT('Ctrl Pts',(-11.6324938930202,-1.47502173251142,
126.110523625609));
#75527=CARTESIAN_POINT('Ctrl Pts',(-11.6402682271393,-1.60491147846995,
126.153321821216));
#75528=CARTESIAN_POINT('Ctrl Pts',(-11.6480425612584,-1.73295673738869,
126.201530617573));
#75529=CARTESIAN_POINT('Ctrl Pts',(-11.6558073142055,-1.8608441919692,126.249680000896));
#75530=CARTESIAN_POINT('Ctrl Pts',(-11.6635720671526,-1.98689132005251,
126.303226581038));
#75531=CARTESIAN_POINT('Ctrl Pts',(-11.6713368200997,-2.11061085056714,
126.362007085938));
#75532=CARTESIAN_POINT('Ctrl Pts',(-11.6790938609846,-2.23420750109993,
126.420729209211));
#75533=CARTESIAN_POINT('Ctrl Pts',(-11.6868509018696,-2.35548080380598,
126.484674745483));
#75534=CARTESIAN_POINT('Ctrl Pts',(-11.6946079427546,-2.47396172397353,
126.553631685863));
#75535=CARTESIAN_POINT('Ctrl Pts',(-11.7023591339947,-2.5923532967577,126.622536625278));
#75536=CARTESIAN_POINT('Ctrl Pts',(-11.7101103252348,-2.70795634185086,
126.696445250789));
#75537=CARTESIAN_POINT('Ctrl Pts',(-11.717861516475,-2.82032510447822,126.775098977073));
#75538=CARTESIAN_POINT('Ctrl Pts',(-11.725609413252,-2.93264610738423,126.853719273425));
#75539=CARTESIAN_POINT('Ctrl Pts',(-11.7333573100291,-3.04173524228455,
126.937080435574));
#75540=CARTESIAN_POINT('Ctrl Pts',(-11.7411052068062,-3.14717470538423,
127.024879907695));
#75541=CARTESIAN_POINT('Ctrl Pts',(-11.7488514828903,-3.25259211282109,
127.112661014058));
#75542=CARTESIAN_POINT('Ctrl Pts',(-11.7565977589744,-3.35436106671577,
127.204878333738));
#75543=CARTESIAN_POINT('Ctrl Pts',(-11.7643440350585,-3.4520962276984,127.301188526844));
#75544=CARTESIAN_POINT('Ctrl Pts',(-11.7720903683238,-3.54983211013938,
127.39749943089));
#75545=CARTESIAN_POINT('Ctrl Pts',(-11.7798367015891,-3.64353386177464,
127.497902994233));
#75546=CARTESIAN_POINT('Ctrl Pts',(-11.7875830348545,-3.73285274765514,
127.602018751552));
#75547=CARTESIAN_POINT('Ctrl Pts',(-11.7953311028574,-3.82219163588085,
127.706157824874));
#75548=CARTESIAN_POINT('Ctrl Pts',(-11.8030791708604,-3.90714545074154,
127.814010449726));
#75549=CARTESIAN_POINT('Ctrl Pts',(-11.8108272388633,-3.98740577924582,
127.925163122753));
#75550=CARTESIAN_POINT('Ctrl Pts',(-11.8185835416052,-4.06775140938267,
128.036433930165));
#75551=CARTESIAN_POINT('Ctrl Pts',(-11.8263398443471,-4.1433933592699,128.151011474547));
#75552=CARTESIAN_POINT('Ctrl Pts',(-11.8340961470889,-4.21406630791313,
128.268452848145));
#75553=CARTESIAN_POINT('Ctrl Pts',(-11.8418565896031,-4.28477697683697,
128.38595690374));
#75554=CARTESIAN_POINT('Ctrl Pts',(-11.8496170321173,-4.35051317267441,
128.506327491276));
#75555=CARTESIAN_POINT('Ctrl Pts',(-11.8573774746314,-4.41105608589379,
128.629098042703));
#75556=CARTESIAN_POINT('Ctrl Pts',(-11.8651503748969,-4.47169618797222,
128.752065676318));
#75557=CARTESIAN_POINT('Ctrl Pts',(-11.8729232751623,-4.52712618983217,
128.877440614833));
#75558=CARTESIAN_POINT('Ctrl Pts',(-11.8806961754277,-4.57717554745248,
129.004736470611));
#75559=CARTESIAN_POINT('Ctrl Pts',(-11.8881865111899,-4.62540548485745,
129.127404801395));
#75560=CARTESIAN_POINT('Ctrl Pts',(-11.895676846952,-4.66863908508204,129.251856522827));
#75561=CARTESIAN_POINT('Ctrl Pts',(-11.9031671827142,-4.70676833819968,
129.37764590431));
#75562=CARTESIAN_POINT('Ctrl Pts',(-11.9072067063095,-4.72733137068994,
129.445483874553));
#75563=CARTESIAN_POINT('Ctrl Pts',(-11.9112462299048,-4.74643299116131,
129.513784013706));
#75564=CARTESIAN_POINT('Ctrl Pts',(-11.9152857535001,-4.76405452823405,
129.582490119308));
#75565=CARTESIAN_POINT('Ctrl Pts',(-10.1650489208495,-4.76405452823411,
129.582490119308));
#75566=CARTESIAN_POINT('Ctrl Pts',(-10.1728097116723,-4.79812258470992,
129.715320954453));
#75567=CARTESIAN_POINT('Ctrl Pts',(-10.1805705024952,-4.82660344262438,
129.849469839351));
#75568=CARTESIAN_POINT('Ctrl Pts',(-10.188331293318,-4.84942182258588,129.984427053716));
#75569=CARTESIAN_POINT('Ctrl Pts',(-10.1961043814061,-4.87227635912964,
130.119598112869));
#75570=CARTESIAN_POINT('Ctrl Pts',(-10.2038774694941,-4.88945044079769,
130.255579672805));
#75571=CARTESIAN_POINT('Ctrl Pts',(-10.2116505575822,-4.90092071191022,
130.39185699568));
#75572=CARTESIAN_POINT('Ctrl Pts',(-10.2185941850004,-4.91116699859684,
130.513592262907));
#75573=CARTESIAN_POINT('Ctrl Pts',(-10.2255378124186,-4.91686255298458,
130.635563317364));
#75574=CARTESIAN_POINT('Ctrl Pts',(-10.2324814398368,-4.91802585029017,
130.757405336951));
#75575=CARTESIAN_POINT('Ctrl Pts',(-10.2333678145608,-4.91817434865651,
130.7729588337));
#75576=CARTESIAN_POINT('Ctrl Pts',(-10.2342541892847,-4.91824906423311,
130.788513036023));
#75577=CARTESIAN_POINT('Ctrl Pts',(-10.2351405640087,-4.91824999126505,
130.804067494219));
#75578=CARTESIAN_POINT('',(-9.88985943603245,-4.91824816614036,130.808607823354));
#75579=CARTESIAN_POINT('Ctrl Pts',(-9.81992175947747,-4.76405452823407,
129.582490119308));
#75580=CARTESIAN_POINT('Ctrl Pts',(-9.82762241378884,-4.79796140031408,
129.71469249894));
#75581=CARTESIAN_POINT('Ctrl Pts',(-9.83532306810017,-4.8263664037375,129.848327831717));
#75582=CARTESIAN_POINT('Ctrl Pts',(-9.84302372241154,-4.84916272078742,
129.982896090136));
#75583=CARTESIAN_POINT('Ctrl Pts',(-9.85082967467481,-4.87227075232277,
130.119304421026));
#75584=CARTESIAN_POINT('Ctrl Pts',(-9.85863562693807,-4.8896154804548,130.256670973928));
#75585=CARTESIAN_POINT('Ctrl Pts',(-9.86644157920134,-4.90113965557734,
130.394466559269));
#75586=CARTESIAN_POINT('Ctrl Pts',(-9.8742475314646,-4.91266383069989,130.53226214461));
#75587=CARTESIAN_POINT('Ctrl Pts',(-9.88205348372789,-4.9183674424039,130.670486339544));
#75588=CARTESIAN_POINT('Ctrl Pts',(-9.88985943599116,-4.91824816614099,
130.808607822623));
#75589=CARTESIAN_POINT('Ctrl Pts',(-9.88985943603245,-4.91824816614036,
130.808607823354));
#75590=CARTESIAN_POINT('Ctrl Pts',(-9.89918713811298,-4.91810563725986,
130.97365572547));
#75591=CARTESIAN_POINT('Ctrl Pts',(-9.90851484019353,-4.90965128715922,
131.138340451495));
#75592=CARTESIAN_POINT('Ctrl Pts',(-9.917842542274,-4.8930171587382,131.301920811707));
#75593=CARTESIAN_POINT('Ctrl Pts',(-9.92729244968566,-4.87616510106139,
131.467644292692));
#75594=CARTESIAN_POINT('Ctrl Pts',(-9.93674235709729,-4.85091759043832,
131.632234271229));
#75595=CARTESIAN_POINT('Ctrl Pts',(-9.94619226450897,-4.81746108250809,
131.794942154351));
#75596=CARTESIAN_POINT('Ctrl Pts',(-9.95533578040038,-4.78508932492308,
131.952374608467));
#75597=CARTESIAN_POINT('Ctrl Pts',(-9.96447929629182,-4.74503259162011,
132.108045180952));
#75598=CARTESIAN_POINT('Ctrl Pts',(-9.97362281218324,-4.69750201318969,
132.261295035643));
#75599=CARTESIAN_POINT('Ctrl Pts',(-9.9813971463023,-4.65708882837325,132.39159672574));
#75600=CARTESIAN_POINT('Ctrl Pts',(-9.98917148042137,-4.61118596183109,
132.520422027973));
#75601=CARTESIAN_POINT('Ctrl Pts',(-9.99694581454045,-4.55991831526217,
132.647273534835));
#75602=CARTESIAN_POINT('Ctrl Pts',(-10.0047105674876,-4.50871385148572,
132.773968708551));
#75603=CARTESIAN_POINT('Ctrl Pts',(-10.0124753204347,-4.45215790791144,
132.898694567897));
#75604=CARTESIAN_POINT('Ctrl Pts',(-10.0202400733818,-4.39042540274467,
133.020967900202));
#75605=CARTESIAN_POINT('Ctrl Pts',(-10.0279971142668,-4.32875421117238,
133.143119788909));
#75606=CARTESIAN_POINT('Ctrl Pts',(-10.0357541551517,-4.26191686475718,
133.262823651347));
#75607=CARTESIAN_POINT('Ctrl Pts',(-10.0435111960367,-4.1901365668757,133.379615675503));
#75608=CARTESIAN_POINT('Ctrl Pts',(-10.0512623872769,-4.11841039907512,
133.496319625885));
#75609=CARTESIAN_POINT('Ctrl Pts',(-10.0590135785171,-4.04174890309284,
133.610115776934));
#75610=CARTESIAN_POINT('Ctrl Pts',(-10.0667647697572,-3.96042128667038,
133.720564707576));
#75611=CARTESIAN_POINT('Ctrl Pts',(-10.0745126665343,-3.87912823665439,
133.830966694475));
#75612=CARTESIAN_POINT('Ctrl Pts',(-10.0822605633113,-3.7931732420146,133.93802397636));
#75613=CARTESIAN_POINT('Ctrl Pts',(-10.0900084600884,-3.70286879758693,
134.041326130258));
#75614=CARTESIAN_POINT('Ctrl Pts',(-10.0977547361725,-3.6125832429023,134.144606675572));
#75615=CARTESIAN_POINT('Ctrl Pts',(-10.1055010122566,-3.51795030524627,
134.244133361121));
#75616=CARTESIAN_POINT('Ctrl Pts',(-10.1132472883407,-3.41932247271796,
134.339529197714));
#75617=CARTESIAN_POINT('Ctrl Pts',(-10.1209936216061,-3.32069391214139,
134.434925738497));
#75618=CARTESIAN_POINT('Ctrl Pts',(-10.1287399548715,-3.21807067886883,
134.526191097666));
#75619=CARTESIAN_POINT('Ctrl Pts',(-10.1364862881368,-3.11184149733245,
134.612985770817));
#75620=CARTESIAN_POINT('Ctrl Pts',(-10.1442343561398,-3.0055885265074,134.699799881034));
#75621=CARTESIAN_POINT('Ctrl Pts',(-10.1519824241428,-2.89572830323321,
134.782141065681));
#75622=CARTESIAN_POINT('Ctrl Pts',(-10.1597304921458,-2.78268161284683,
134.859710923523));
#75623=CARTESIAN_POINT('Ctrl Pts',(-10.1674867948876,-2.66951477509264,
134.937363223533));
#75624=CARTESIAN_POINT('Ctrl Pts',(-10.1752430976295,-2.55315502798265,
135.010233845267));
#75625=CARTESIAN_POINT('Ctrl Pts',(-10.1829994003714,-2.434051518698,135.078068172702));
#75626=CARTESIAN_POINT('Ctrl Pts',(-10.1907598428855,-2.31488444028432,
135.14593870536));
#75627=CARTESIAN_POINT('Ctrl Pts',(-10.1985202853997,-2.19297102905751,
135.208767408594));
#75628=CARTESIAN_POINT('Ctrl Pts',(-10.2062807279139,-2.06878296953405,
135.266346732231));
#75629=CARTESIAN_POINT('Ctrl Pts',(-10.2140536281793,-1.94439555231255,
135.324018487311));
#75630=CARTESIAN_POINT('Ctrl Pts',(-10.2218265284447,-1.81772655147486,
135.376423873872));
#75631=CARTESIAN_POINT('Ctrl Pts',(-10.2295994287101,-1.68926630717658,
135.423404068968));
#75632=CARTESIAN_POINT('Ctrl Pts',(-10.2370897644721,-1.56547591633106,
135.468676415636));
#75633=CARTESIAN_POINT('Ctrl Pts',(-10.2445801002341,-1.4400225467258,135.508911067488));
#75634=CARTESIAN_POINT('Ctrl Pts',(-10.2520704359961,-1.31335439253887,
135.544010742005));
#75635=CARTESIAN_POINT('Ctrl Pts',(-10.2598447701152,-1.18188357678526,
135.580441231351));
#75636=CARTESIAN_POINT('Ctrl Pts',(-10.2676191042343,-1.0486875808879,135.611455072283));
#75637=CARTESIAN_POINT('Ctrl Pts',(-10.2753934383534,-0.914252400291646,
135.636888487228));
#75638=CARTESIAN_POINT('Ctrl Pts',(-10.2831581913005,-0.779982899040659,
135.662290557763));
#75639=CARTESIAN_POINT('Ctrl Pts',(-10.2909229442476,-0.644477632195641,
135.682125814261));
#75640=CARTESIAN_POINT('Ctrl Pts',(-10.2986876971947,-0.508237687823909,
135.696280232112));
#75641=CARTESIAN_POINT('Ctrl Pts',(-10.3064447380797,-0.372133058885759,
135.710420591595));
#75642=CARTESIAN_POINT('Ctrl Pts',(-10.3142017789646,-0.235295590896812,
135.718891300701));
#75643=CARTESIAN_POINT('Ctrl Pts',(-10.3219588198496,-0.0982361489162156,
135.72162944503));
#75644=CARTESIAN_POINT('Ctrl Pts',(-10.3297100110897,0.0387199354732024,
135.724365524503));
#75645=CARTESIAN_POINT('Ctrl Pts',(-10.3374612023299,0.175897271364438,
135.721377636034));
#75646=CARTESIAN_POINT('Ctrl Pts',(-10.34521239357,0.312780648003097,135.712654753896));
#75647=CARTESIAN_POINT('Ctrl Pts',(-10.3529602903471,0.449605845555201,
135.703935579217));
#75648=CARTESIAN_POINT('Ctrl Pts',(-10.3607081871242,0.586136942994985,
135.689486283733));
#75649=CARTESIAN_POINT('Ctrl Pts',(-10.3684560839013,0.721859728760213,
135.669347934558));
#75650=CARTESIAN_POINT('Ctrl Pts',(-10.3762023599854,0.857554124244504,
135.649213797892));
#75651=CARTESIAN_POINT('Ctrl Pts',(-10.3839486360695,0.992440157880172,
135.623393031912));
#75652=CARTESIAN_POINT('Ctrl Pts',(-10.3916949121536,1.12601012955639,135.591978422972));
#75653=CARTESIAN_POINT('Ctrl Pts',(-10.399441245419,1.25958108721579,135.560563582136));
#75654=CARTESIAN_POINT('Ctrl Pts',(-10.4071875786843,1.39183558294953,135.523554905454));
#75655=CARTESIAN_POINT('Ctrl Pts',(-10.4149339119496,1.52227786703708,135.481095927377));
#75656=CARTESIAN_POINT('Ctrl Pts',(-10.4226819799526,1.65274936276972,135.438627440906));
#75657=CARTESIAN_POINT('Ctrl Pts',(-10.4304300479556,1.78140746760162,135.390706345259));
#75658=CARTESIAN_POINT('Ctrl Pts',(-10.4381781159586,1.90777368336913,135.337525365901));
#75659=CARTESIAN_POINT('Ctrl Pts',(-10.4459344187005,2.03427420265453,135.284287865165));
#75660=CARTESIAN_POINT('Ctrl Pts',(-10.4536907214424,2.1584776060805,135.225779465453));
#75661=CARTESIAN_POINT('Ctrl Pts',(-10.4614470241842,2.27992690295286,135.162240420829));
#75662=CARTESIAN_POINT('Ctrl Pts',(-10.4692074666984,2.40144102097172,135.098667463505));
#75663=CARTESIAN_POINT('Ctrl Pts',(-10.4769679092126,2.52019776507275,135.030058706647));
#75664=CARTESIAN_POINT('Ctrl Pts',(-10.4847283517267,2.63576756041445,134.95669880586));
#75665=CARTESIAN_POINT('Ctrl Pts',(-10.4925012519922,2.75152287865143,134.883221141248));
#75666=CARTESIAN_POINT('Ctrl Pts',(-10.5002741522576,2.86408070357802,134.8049773149));
#75667=CARTESIAN_POINT('Ctrl Pts',(-10.508047052523,2.97304237211987,134.722294016193));
#75668=CARTESIAN_POINT('Ctrl Pts',(-10.5155373882851,3.07804300955293,134.642616463661));
#75669=CARTESIAN_POINT('Ctrl Pts',(-10.5230277240471,3.17970417230188,134.558816802899));
#75670=CARTESIAN_POINT('Ctrl Pts',(-10.5305180598092,3.2777017539289,134.471219528786));
#75671=CARTESIAN_POINT('Ctrl Pts',(-10.5382923939283,3.37941494364846,134.380300977401));
#75672=CARTESIAN_POINT('Ctrl Pts',(-10.5460667280474,3.47750345565743,134.285003152324));
#75673=CARTESIAN_POINT('Ctrl Pts',(-10.5538410621665,3.57156680683667,134.18564640951));
#75674=CARTESIAN_POINT('Ctrl Pts',(-10.5616058151136,3.66551423334227,134.086412115002));
#75675=CARTESIAN_POINT('Ctrl Pts',(-10.5693705680606,3.7554461030277,133.983129136937));
#75676=CARTESIAN_POINT('Ctrl Pts',(-10.5771353210077,3.84099563341799,133.87615742181));
#75677=CARTESIAN_POINT('Ctrl Pts',(-10.5848923618927,3.92646019480855,133.769291952499));
#75678=CARTESIAN_POINT('Ctrl Pts',(-10.5926494027778,4.00755083617129,133.658745340422));
#75679=CARTESIAN_POINT('Ctrl Pts',(-10.6004064436628,4.08393849079674,133.544913384051));
#75680=CARTESIAN_POINT('Ctrl Pts',(-10.6081576349029,4.16026854089763,133.431167269244));
#75681=CARTESIAN_POINT('Ctrl Pts',(-10.615908826143,4.23190244649904,133.314141064794));
#75682=CARTESIAN_POINT('Ctrl Pts',(-10.6236600173831,4.29855244734754,133.194262272426));
#75683=CARTESIAN_POINT('Ctrl Pts',(-10.6314079141602,4.36517412016782,133.074434431742));
#75684=CARTESIAN_POINT('Ctrl Pts',(-10.6391558109372,4.42681591177529,132.951756755552));
#75685=CARTESIAN_POINT('Ctrl Pts',(-10.6469037077143,4.48323442918648,132.826684062383));
#75686=CARTESIAN_POINT('Ctrl Pts',(-10.6546499837984,4.53964114506006,132.701637531726));
#75687=CARTESIAN_POINT('Ctrl Pts',(-10.6623962598826,4.59082659931321,132.574197336737));
#75688=CARTESIAN_POINT('Ctrl Pts',(-10.6701425359667,4.63659443142271,132.444840773191));
#75689=CARTESIAN_POINT('Ctrl Pts',(-10.6778888692321,4.68236260137988,132.315483254765));
#75690=CARTESIAN_POINT('Ctrl Pts',(-10.6856352024974,4.72271293898669,132.184209708128));
#75691=CARTESIAN_POINT('Ctrl Pts',(-10.6933815357627,4.7574982390087,132.051514805439));
#75692=CARTESIAN_POINT('Ctrl Pts',(-10.7011296037657,4.79229132895751,131.918790186646));
#75693=CARTESIAN_POINT('Ctrl Pts',(-10.7088776717687,4.8215168023044,131.784643956529));
#75694=CARTESIAN_POINT('Ctrl Pts',(-10.7166257397716,4.84507816449548,131.649582861966));
#75695=CARTESIAN_POINT('Ctrl Pts',(-10.7243820425135,4.86866456798266,131.514378222865));
#75696=CARTESIAN_POINT('Ctrl Pts',(-10.7321383452553,4.88657476764966,131.378257162748));
#75697=CARTESIAN_POINT('Ctrl Pts',(-10.7398946479972,4.89876388141197,131.24173402402));
#75698=CARTESIAN_POINT('Ctrl Pts',(-10.7476550905113,4.91095950087132,131.105138018783));
#75699=CARTESIAN_POINT('Ctrl Pts',(-10.7554155330256,4.91742793160717,130.968139897661));
#75700=CARTESIAN_POINT('Ctrl Pts',(-10.7631759755397,4.91817646674643,130.831254937443));
#75701=CARTESIAN_POINT('Ctrl Pts',(-10.7709488758052,4.91892620350074,130.694150237335));
#75702=CARTESIAN_POINT('Ctrl Pts',(-10.7787217760706,4.9139377101641,130.557159452068));
#75703=CARTESIAN_POINT('Ctrl Pts',(-10.7864946763361,4.90327035263295,130.420794571766));
#75704=CARTESIAN_POINT('Ctrl Pts',(-10.7939850120981,4.89299078041754,130.289386898346));
#75705=CARTESIAN_POINT('Ctrl Pts',(-10.8014753478601,4.87743809416649,130.15856071937));
#75706=CARTESIAN_POINT('Ctrl Pts',(-10.8089656836221,4.85671011316516,130.028764112172));
#75707=CARTESIAN_POINT('Ctrl Pts',(-10.8167400177412,4.83519622446397,129.894046227161));
#75708=CARTESIAN_POINT('Ctrl Pts',(-10.8245143518603,4.80803870193853,129.760010781764));
#75709=CARTESIAN_POINT('Ctrl Pts',(-10.8322886859794,4.77529059921724,129.62716787399));
#75710=CARTESIAN_POINT('Ctrl Pts',(-10.8400534389265,4.74258285560577,129.494488683227));
#75711=CARTESIAN_POINT('Ctrl Pts',(-10.8478181918735,4.70429833330681,129.362999481787));
#75712=CARTESIAN_POINT('Ctrl Pts',(-10.8555829448206,4.66054161061392,129.233203414026));
#75713=CARTESIAN_POINT('Ctrl Pts',(-10.8633399857056,4.61682834771493,129.103536261549));
#75714=CARTESIAN_POINT('Ctrl Pts',(-10.8710970265906,4.5676538245372,128.975559264285));
#75715=CARTESIAN_POINT('Ctrl Pts',(-10.8788540674756,4.51317316895114,128.84976321412));
#75716=CARTESIAN_POINT('Ctrl Pts',(-10.8866052587158,4.45873359765126,128.724062027734));
#75717=CARTESIAN_POINT('Ctrl Pts',(-10.8943564499558,4.39899601322621,128.600538872145));
#75718=CARTESIAN_POINT('Ctrl Pts',(-10.902107641196,4.33416454353856,128.479666923327));
#75719=CARTESIAN_POINT('Ctrl Pts',(-10.909855537973,4.26936062895496,128.358846348313));
#75720=CARTESIAN_POINT('Ctrl Pts',(-10.9176034347501,4.19946731961193,128.240675082697));
#75721=CARTESIAN_POINT('Ctrl Pts',(-10.9253513315272,4.12473570736615,128.125603740416));
#75722=CARTESIAN_POINT('Ctrl Pts',(-10.9330976076113,4.05001972736262,128.010556468579));
#75723=CARTESIAN_POINT('Ctrl Pts',(-10.9408438836954,3.97046767032323,127.898608157977));
#75724=CARTESIAN_POINT('Ctrl Pts',(-10.9485901597795,3.88637496104045,127.790182002305));
#75725=CARTESIAN_POINT('Ctrl Pts',(-10.9563364930448,3.8022816310044,127.681755046255));
#75726=CARTESIAN_POINT('Ctrl Pts',(-10.9640828263102,3.71364782144745,127.576850605954));
#75727=CARTESIAN_POINT('Ctrl Pts',(-10.9718291595755,3.6208101460403,127.475859911718));
#75728=CARTESIAN_POINT('Ctrl Pts',(-10.9795772275785,3.52795168027945,127.374846601316));
#75729=CARTESIAN_POINT('Ctrl Pts',(-10.9873252955815,3.43088773987947,127.277749068799));
#75730=CARTESIAN_POINT('Ctrl Pts',(-10.9950733635845,3.32999250767726,127.184922406833));
#75731=CARTESIAN_POINT('Ctrl Pts',(-11.0028296663263,3.2289900428216,127.091997087586));
#75732=CARTESIAN_POINT('Ctrl Pts',(-11.0105859690682,3.12414844019777,127.003351971428));
#75733=CARTESIAN_POINT('Ctrl Pts',(-11.01834227181,3.01587617077401,126.919302833561));
#75734=CARTESIAN_POINT('Ctrl Pts',(-11.0261027143242,2.90754611317989,126.835208836138));
#75735=CARTESIAN_POINT('Ctrl Pts',(-11.0338631568383,2.79578205870477,126.755715931333));
#75736=CARTESIAN_POINT('Ctrl Pts',(-11.0416235993525,2.68102146641663,126.681096502922));
#75737=CARTESIAN_POINT('Ctrl Pts',(-11.0493964996179,2.56607665023778,126.60635728878));
#75738=CARTESIAN_POINT('Ctrl Pts',(-11.0571693998834,2.44812602031287,126.536507383882));
#75739=CARTESIAN_POINT('Ctrl Pts',(-11.0649423001489,2.32763241715051,126.471773585188));
#75740=CARTESIAN_POINT('Ctrl Pts',(-11.0724326359109,2.211519059968,126.409393023131));
#75741=CARTESIAN_POINT('Ctrl Pts',(-11.0799229716729,2.09304468359106,126.351763193205));
#75742=CARTESIAN_POINT('Ctrl Pts',(-11.087413307435,1.9726391418837,126.299043994019));
#75743=CARTESIAN_POINT('Ctrl Pts',(-11.095187641554,1.84766838746621,126.244325930373));
#75744=CARTESIAN_POINT('Ctrl Pts',(-11.1029619756731,1.72022126688847,126.19472489098));
#75745=CARTESIAN_POINT('Ctrl Pts',(-11.1107363097922,1.59075561683369,126.150471960753));
#75746=CARTESIAN_POINT('Ctrl Pts',(-11.1185010627393,1.4614495216221,126.106273568308));
#75747=CARTESIAN_POINT('Ctrl Pts',(-11.1262658156864,1.33013021302872,126.067410296012));
#75748=CARTESIAN_POINT('Ctrl Pts',(-11.1340305686335,1.1972775277728,126.034066120998));
#75749=CARTESIAN_POINT('Ctrl Pts',(-11.1417876095185,1.06455679367658,126.000755063888));
#75750=CARTESIAN_POINT('Ctrl Pts',(-11.1495446504035,0.930306090449464,
125.9729522899));
#75751=CARTESIAN_POINT('Ctrl Pts',(-11.1573016912885,0.795022185607245,
125.950792570563));
#75752=CARTESIAN_POINT('Ctrl Pts',(-11.1650528825286,0.65984029941039,125.928649562042));
#75753=CARTESIAN_POINT('Ctrl Pts',(-11.1728040737687,0.523627146702382,
125.912141200859));
#75754=CARTESIAN_POINT('Ctrl Pts',(-11.1805552650088,0.386891159928283,
125.901351511632));
#75755=CARTESIAN_POINT('Ctrl Pts',(-11.1883031617859,0.250213289595742,
125.890566408312));
#75756=CARTESIAN_POINT('Ctrl Pts',(-11.196051058563,0.113013416110293,125.885495173385));
#75757=CARTESIAN_POINT('Ctrl Pts',(-11.2037989553401,-0.0241936249809933,
125.886170123999));
#75758=CARTESIAN_POINT('Ctrl Pts',(-11.2115452314242,-0.161371965316938,
125.886844933429));
#75759=CARTESIAN_POINT('Ctrl Pts',(-11.2192915075083,-0.298557079563732,
125.893263535678));
#75760=CARTESIAN_POINT('Ctrl Pts',(-11.2270377835924,-0.43523323856517,
125.90540612803));
#75761=CARTESIAN_POINT('Ctrl Pts',(-11.2347841168578,-0.571910406479153,
125.917548810015));
#75762=CARTESIAN_POINT('Ctrl Pts',(-11.242530450123,-0.708078222219621,
125.935415531819));
#75763=CARTESIAN_POINT('Ctrl Pts',(-11.2502767833884,-0.843225584729596,
125.95893456037));
#75764=CARTESIAN_POINT('Ctrl Pts',(-11.2580248513914,-0.978403212554175,
125.982458855843));
#75765=CARTESIAN_POINT('Ctrl Pts',(-11.2657729193944,-1.11255954731059,
126.011637909831));
#75766=CARTESIAN_POINT('Ctrl Pts',(-11.2735209873973,-1.24519358451844,
126.046348847974));
#75767=CARTESIAN_POINT('Ctrl Pts',(-11.2812772901392,-1.37796858675939,
126.081096677316));
#75768=CARTESIAN_POINT('Ctrl Pts',(-11.2890335928811,-1.50921768065986,
126.121388036311));
#75769=CARTESIAN_POINT('Ctrl Pts',(-11.296789895623,-1.63845440706377,126.167049950976));
#75770=CARTESIAN_POINT('Ctrl Pts',(-11.3045503381372,-1.76776011099997,
126.212736236779));
#75771=CARTESIAN_POINT('Ctrl Pts',(-11.3123107806512,-1.8950509446011,126.263798644362));
#75772=CARTESIAN_POINT('Ctrl Pts',(-11.3200712231654,-2.01986128637052,
126.320016357106));
#75773=CARTESIAN_POINT('Ctrl Pts',(-11.3278441234308,-2.14487198478069,
126.376324315513));
#75774=CARTESIAN_POINT('Ctrl Pts',(-11.3356170236962,-2.26739388460155,
126.437803941228));
#75775=CARTESIAN_POINT('Ctrl Pts',(-11.3433899239617,-2.38698599852874,
126.50418842272));
#75776=CARTESIAN_POINT('Ctrl Pts',(-11.3508802597237,-2.50223063788049,
126.568159661097));
#75777=CARTESIAN_POINT('Ctrl Pts',(-11.3583705954858,-2.61475454028793,
126.63668517855));
#75778=CARTESIAN_POINT('Ctrl Pts',(-11.3658609312478,-2.72419083200988,
126.709489755952));
#75779=CARTESIAN_POINT('Ctrl Pts',(-11.3736152775995,-2.83748440607882,
126.784860463902));
#75780=CARTESIAN_POINT('Ctrl Pts',(-11.3813696239513,-2.94783205967676,
126.865059207471));
#75781=CARTESIAN_POINT('Ctrl Pts',(-11.389123970303,-3.05479306362901,126.949827909065));
#75782=CARTESIAN_POINT('Ctrl Pts',(-11.3968660482348,-3.16158484087234,
127.034462495161));
#75783=CARTESIAN_POINT('Ctrl Pts',(-11.4046081261665,-3.26500033381101,
127.123652397972));
#75784=CARTESIAN_POINT('Ctrl Pts',(-11.4123502040983,-3.36462688234458,
127.217095781357));
#75785=CARTESIAN_POINT('Ctrl Pts',(-11.4200852014054,-3.46416231603767,
127.3104537048));
#75786=CARTESIAN_POINT('Ctrl Pts',(-11.4278201987125,-3.55991541288795,
127.408057104196));
#75787=CARTESIAN_POINT('Ctrl Pts',(-11.4355551960196,-3.65150556615707,
127.509563178751));
#75788=CARTESIAN_POINT('Ctrl Pts',(-11.4432848192173,-3.74303208456201,
127.610998729073));
#75789=CARTESIAN_POINT('Ctrl Pts',(-11.4510144424151,-3.8304011512328,127.716331269275));
#75790=CARTESIAN_POINT('Ctrl Pts',(-11.4587440656128,-3.91326842645912,
127.825180649021));
#75791=CARTESIAN_POINT('Ctrl Pts',(-11.4664700171059,-3.99609633829729,
127.933978323431));
#75792=CARTESIAN_POINT('Ctrl Pts',(-11.474195968599,-4.07442647678214,128.046289200421));
#75793=CARTESIAN_POINT('Ctrl Pts',(-11.4819219200921,-4.14795456296417,
128.161699836065));
#75794=CARTESIAN_POINT('Ctrl Pts',(-11.4896475068869,-4.22147917830286,
128.277105023828));
#75795=CARTESIAN_POINT('Ctrl Pts',(-11.4973730936817,-4.29020197194233,
128.395609353431));
#75796=CARTESIAN_POINT('Ctrl Pts',(-11.5050986804765,-4.35386189480628,
128.516770255754));
#75797=CARTESIAN_POINT('Ctrl Pts',(-11.5128238147382,-4.41751808873384,
128.637924060971));
#75798=CARTESIAN_POINT('Ctrl Pts',(-11.5205489489999,-4.47611182368879,
128.761733778554));
#75799=CARTESIAN_POINT('Ctrl Pts',(-11.5282740832616,-4.52942831239543,
128.887732791051));
#75800=CARTESIAN_POINT('Ctrl Pts',(-11.536003557891,-4.58277475697797,129.013802596109));
#75801=CARTESIAN_POINT('Ctrl Pts',(-11.5437330325204,-4.63083788123895,
129.142063789657));
#75802=CARTESIAN_POINT('Ctrl Pts',(-11.5514625071497,-4.67345124333323,
129.272030190182));
#75803=CARTESIAN_POINT('Ctrl Pts',(-11.5575589388993,-4.70706147767425,
129.374537970921));
#75804=CARTESIAN_POINT('Ctrl Pts',(-11.5636553706488,-4.73728242755129,
129.47810610507));
#75805=CARTESIAN_POINT('Ctrl Pts',(-11.5697518023984,-4.76405452823402,
129.582490119308));
#75806=CARTESIAN_POINT('Origin',(213.235140564004,0.,130.804360617566));
#75807=CARTESIAN_POINT('',(-13.6653609210471,-4.76405452823398,129.582490119308));
#75808=CARTESIAN_POINT('',(-13.3199629969565,-4.76405452823408,129.582490119308));
#75809=CARTESIAN_POINT('',(213.235140564004,-4.76405452823405,129.582490119308));
#75810=CARTESIAN_POINT('',(-11.9851405639703,-4.91824811303239,130.800052351862));
#75811=CARTESIAN_POINT('Ctrl Pts',(-11.9851405640086,-4.91824811303298,
130.80005235254));
#75812=CARTESIAN_POINT('Ctrl Pts',(-11.9928382668462,-4.91836740145462,
130.936230152915));
#75813=CARTESIAN_POINT('Ctrl Pts',(-12.0005359696838,-4.91282664553037,
131.072514009752));
#75814=CARTESIAN_POINT('Ctrl Pts',(-12.0082336725213,-4.90162626731536,
131.20839402963));
#75815=CARTESIAN_POINT('Ctrl Pts',(-12.015928908627,-4.89042947826595,131.344230506702));
#75816=CARTESIAN_POINT('Ctrl Pts',(-12.0236241447325,-4.87357670326283,
131.479663009321));
#75817=CARTESIAN_POINT('Ctrl Pts',(-12.0313193808382,-4.85112042706125,
131.614183848061));
#75818=CARTESIAN_POINT('Ctrl Pts',(-12.0390136106012,-4.82866708757384,
131.74868709487));
#75819=CARTESIAN_POINT('Ctrl Pts',(-12.0467078403643,-4.80061176931338,
131.882278523772));
#75820=CARTESIAN_POINT('Ctrl Pts',(-12.0544020701273,-4.76705849692604,
132.01445827866));
#75821=CARTESIAN_POINT('Ctrl Pts',(-12.0620970149627,-4.73350210622531,
132.146650317831));
#75822=CARTESIAN_POINT('Ctrl Pts',(-12.0697919597981,-4.69444684254895,
132.277430037557));
#75823=CARTESIAN_POINT('Ctrl Pts',(-12.0774869046335,-4.65004713427463,
132.40631090129));
#75824=CARTESIAN_POINT('Ctrl Pts',(-12.0851842861471,-4.60563336640595,
132.535232576387));
#75825=CARTESIAN_POINT('Ctrl Pts',(-12.0928816676608,-4.55587191651374,
132.662253824595));
#75826=CARTESIAN_POINT('Ctrl Pts',(-12.1005790491744,-4.50096588209621,
132.786906755921));
#75827=CARTESIAN_POINT('Ctrl Pts',(-12.1082850298899,-4.44599850888841,
132.911698944436));
#75828=CARTESIAN_POINT('Ctrl Pts',(-12.1159910106053,-4.38587523653585,
133.034117170521));
#75829=CARTESIAN_POINT('Ctrl Pts',(-12.1236969913208,-4.32084596472346,
133.153716531776));
#75830=CARTESIAN_POINT('Ctrl Pts',(-12.1314078195653,-4.25577578555616,
133.273391128281));
#75831=CARTESIAN_POINT('Ctrl Pts',(-12.1391186478099,-4.18579366456531,
133.390242989437));
#75832=CARTESIAN_POINT('Ctrl Pts',(-12.1468294760544,-4.11119297665866,
133.503856009518));
#75833=CARTESIAN_POINT('Ctrl Pts',(-12.1545518572617,-4.03648051619792,
133.617639253465));
#75834=CARTESIAN_POINT('Ctrl Pts',(-12.162274238469,-3.95713590338995,133.728173646549));
#75835=CARTESIAN_POINT('Ctrl Pts',(-12.1699966196763,-3.87349322778882,
133.835075595385));
#75836=CARTESIAN_POINT('Ctrl Pts',(-12.1738693486266,-3.83154691581829,
133.888686296667));
#75837=CARTESIAN_POINT('Ctrl Pts',(-12.1777420775768,-3.78852024960521,
133.941384018686));
#75838=CARTESIAN_POINT('Ctrl Pts',(-12.1816148065271,-3.74445875092837,
133.99312397114));
#75839=CARTESIAN_POINT('Ctrl Pts',(-12.1893891406461,-3.65600721793908,
134.096989664517));
#75840=CARTESIAN_POINT('Ctrl Pts',(-12.1971634747652,-3.56309069011036,
134.197336814495));
#75841=CARTESIAN_POINT('Ctrl Pts',(-12.2049378088843,-3.46601982065049,
134.293757365624));
#75842=CARTESIAN_POINT('Ctrl Pts',(-12.2127025618314,-3.36906858236177,
134.390059087041));
#75843=CARTESIAN_POINT('Ctrl Pts',(-12.2204673147785,-3.26797346414579,
134.482443565261));
#75844=CARTESIAN_POINT('Ctrl Pts',(-12.2282320677256,-3.16308550707379,
134.57053548571));
#75845=CARTESIAN_POINT('Ctrl Pts',(-12.2359891086106,-3.05830172619941,
134.658539912022));
#75846=CARTESIAN_POINT('Ctrl Pts',(-12.2437461494956,-2.94973290061633,
134.742260015163));
#75847=CARTESIAN_POINT('Ctrl Pts',(-12.2515031903806,-2.83776681812349,
134.821357325115));
#75848=CARTESIAN_POINT('Ctrl Pts',(-12.2592543816207,-2.72588517012489,
134.90039498717));
#75849=CARTESIAN_POINT('Ctrl Pts',(-12.2670055728609,-2.61061168254893,
134.974816570206));
#75850=CARTESIAN_POINT('Ctrl Pts',(-12.274756764101,-2.49236682855777,135.044324137976));
#75851=CARTESIAN_POINT('Ctrl Pts',(-12.282504660878,-2.37417223178352,135.113802163175));
#75852=CARTESIAN_POINT('Ctrl Pts',(-12.2902525576551,-2.25300911676645,
135.178370129438));
#75853=CARTESIAN_POINT('Ctrl Pts',(-12.2980004544322,-2.1293263302984,135.237773799483));
#75854=CARTESIAN_POINT('Ctrl Pts',(-12.3057467305163,-2.00566941560299,
135.297165043561));
#75855=CARTESIAN_POINT('Ctrl Pts',(-12.3134930066003,-1.87949423001065,
135.351393970956));
#75856=CARTESIAN_POINT('Ctrl Pts',(-12.3212392826844,-1.75127321973399,
135.400252823911));
#75857=CARTESIAN_POINT('Ctrl Pts',(-12.3289856159498,-1.62305126295879,
135.449112037531));
#75858=CARTESIAN_POINT('Ctrl Pts',(-12.3367319492152,-1.49278381670479,
135.492600958396));
#75859=CARTESIAN_POINT('Ctrl Pts',(-12.3444782824805,-1.360961878156,135.530560552895));
#75860=CARTESIAN_POINT('Ctrl Pts',(-12.3522263504835,-1.22911041899807,
135.568528648183));
#75861=CARTESIAN_POINT('Ctrl Pts',(-12.3599744184865,-1.09570415045801,
135.600964844957));
#75862=CARTESIAN_POINT('Ctrl Pts',(-12.3677224864895,-0.961247357880002,
135.627760515923));
#75863=CARTESIAN_POINT('Ctrl Pts',(-12.3754787892314,-0.82664766302279,
135.654584665647));
#75864=CARTESIAN_POINT('Ctrl Pts',(-12.3832350919732,-0.690995597816443,
135.675756237735));
#75865=CARTESIAN_POINT('Ctrl Pts',(-12.3909913947151,-0.554804279500532,
135.691218020228));
#75866=CARTESIAN_POINT('Ctrl Pts',(-12.3987518372292,-0.418540271777395,
135.706688055139));
#75867=CARTESIAN_POINT('Ctrl Pts',(-12.4065122797434,-0.281736827232087,
135.716442200288));
#75868=CARTESIAN_POINT('Ctrl Pts',(-12.4142727222575,-0.144909249280095,
135.72047538148));
#75869=CARTESIAN_POINT('Ctrl Pts',(-12.422045622523,-0.00786202355299234,
135.724515037092));
#75870=CARTESIAN_POINT('Ctrl Pts',(-12.4298185227884,0.129209021837687,
135.72281538144));
#75871=CARTESIAN_POINT('Ctrl Pts',(-12.4375914230538,0.265790619590803,
135.715423476972));
#75872=CARTESIAN_POINT('Ctrl Pts',(-12.4450817588159,0.397407132237124,
135.708300286851));
#75873=CARTESIAN_POINT('Ctrl Pts',(-12.4525720945779,0.528568858092386,
135.695891546957));
#75874=CARTESIAN_POINT('Ctrl Pts',(-12.4600624303399,0.658825501465144,
135.678284295787));
#75875=CARTESIAN_POINT('Ctrl Pts',(-12.467836764459,0.794020865062038,135.660009460336));
#75876=CARTESIAN_POINT('Ctrl Pts',(-12.475611098578,0.928669417221008,135.63607623962));
#75877=CARTESIAN_POINT('Ctrl Pts',(-12.4833854326971,1.0622599336885,135.606525431041));
#75878=CARTESIAN_POINT('Ctrl Pts',(-12.4911501856442,1.19568581178377,135.577011041194));
#75879=CARTESIAN_POINT('Ctrl Pts',(-12.4989149385913,1.3280558705558,135.54189292217));
#75880=CARTESIAN_POINT('Ctrl Pts',(-12.5066796915384,1.45886460095032,135.501263548072));
#75881=CARTESIAN_POINT('Ctrl Pts',(-12.5144367324234,1.58954341026992,135.46067452764));
#75882=CARTESIAN_POINT('Ctrl Pts',(-12.5221937733084,1.71866360628769,135.414585260573));
#75883=CARTESIAN_POINT('Ctrl Pts',(-12.5299508141934,1.84573081581363,135.363139052416));
#75884=CARTESIAN_POINT('Ctrl Pts',(-12.5377020054335,1.97270220296809,135.311731640245));
#75885=CARTESIAN_POINT('Ctrl Pts',(-12.5454531966737,2.09762332425186,135.254975473912));
#75886=CARTESIAN_POINT('Ctrl Pts',(-12.5532043879138,2.22001624144654,135.193063267577));
#75887=CARTESIAN_POINT('Ctrl Pts',(-12.5609522846909,2.34235713838665,135.131177375581));
#75888=CARTESIAN_POINT('Ctrl Pts',(-12.5687001814678,2.46217162030437,135.064139978325));
#75889=CARTESIAN_POINT('Ctrl Pts',(-12.5764480782449,2.5790031775185,134.992191281866));
#75890=CARTESIAN_POINT('Ctrl Pts',(-12.584194354329,2.69581029608946,134.920257635523));
#75891=CARTESIAN_POINT('Ctrl Pts',(-12.5919406304131,2.80963539836327,134.843414938289));
#75892=CARTESIAN_POINT('Ctrl Pts',(-12.5996869064972,2.92004832313543,134.761948374401));
#75893=CARTESIAN_POINT('Ctrl Pts',(-12.6074332397625,3.03046206295041,134.680481209146));
#75894=CARTESIAN_POINT('Ctrl Pts',(-12.6151795730279,3.13746326040358,134.594390341251));
#75895=CARTESIAN_POINT('Ctrl Pts',(-12.6229259062932,3.24065272004287,134.504002899001));
#75896=CARTESIAN_POINT('Ctrl Pts',(-12.6306739742962,3.34386528824633,134.413595215109));
#75897=CARTESIAN_POINT('Ctrl Pts',(-12.6384220422991,3.44326412600791,134.318889299779));
#75898=CARTESIAN_POINT('Ctrl Pts',(-12.6461701103021,3.53848526356258,134.220250706847));
#75899=CARTESIAN_POINT('Ctrl Pts',(-12.6539264130439,3.63380760327553,134.121507279645));
#75900=CARTESIAN_POINT('Ctrl Pts',(-12.6616827157857,3.72494310121309,134.018823107179));
#75901=CARTESIAN_POINT('Ctrl Pts',(-12.6694390185276,3.81156627093222,133.912598965053));
#75902=CARTESIAN_POINT('Ctrl Pts',(-12.6771994610417,3.8982356740452,133.806318127905));
#75903=CARTESIAN_POINT('Ctrl Pts',(-12.6849599035559,3.9803877159977,133.696493869246));
#75904=CARTESIAN_POINT('Ctrl Pts',(-12.6927203460701,4.05773959364234,133.583556985707));
#75905=CARTESIAN_POINT('Ctrl Pts',(-12.7004932463355,4.13521564338795,133.470438805856));
#75906=CARTESIAN_POINT('Ctrl Pts',(-12.7082661466009,4.20787592313095,133.354198347919));
#75907=CARTESIAN_POINT('Ctrl Pts',(-12.7160390468663,4.27548259432928,133.235292876615));
#75908=CARTESIAN_POINT('Ctrl Pts',(-12.7235293826285,4.34063159273945,133.120709918697));
#75909=CARTESIAN_POINT('Ctrl Pts',(-12.7310197183906,4.40108788506207,133.003652617028));
#75910=CARTESIAN_POINT('Ctrl Pts',(-12.7385100541527,4.45668130342799,132.884546864558));
#75911=CARTESIAN_POINT('Ctrl Pts',(-12.7462843882718,4.51438256314785,132.760925181284));
#75912=CARTESIAN_POINT('Ctrl Pts',(-12.7540587223909,4.56702769815066,132.634705050508));
#75913=CARTESIAN_POINT('Ctrl Pts',(-12.7618330565099,4.61437470325191,132.506338631669));
#75914=CARTESIAN_POINT('Ctrl Pts',(-12.769597809457,4.66166335740089,132.378130412968));
#75915=CARTESIAN_POINT('Ctrl Pts',(-12.7773625624042,4.70366673935454,132.247781532468));
#75916=CARTESIAN_POINT('Ctrl Pts',(-12.7851273153513,4.74018941020094,132.115767273763));
#75917=CARTESIAN_POINT('Ctrl Pts',(-12.7928843562363,4.77667580621578,131.983884133481));
#75918=CARTESIAN_POINT('Ctrl Pts',(-12.8006413971213,4.80769222040014,131.850339281055));
#75919=CARTESIAN_POINT('Ctrl Pts',(-12.8083984380063,4.83309199898311,131.715626106798));
#75920=CARTESIAN_POINT('Ctrl Pts',(-12.8161496292464,4.85847262339537,131.581014520794));
#75921=CARTESIAN_POINT('Ctrl Pts',(-12.8239008204865,4.87824497066301,131.445236749259));
#75922=CARTESIAN_POINT('Ctrl Pts',(-12.8316520117266,4.89231283938551,131.308799061862));
#75923=CARTESIAN_POINT('Ctrl Pts',(-12.8393999085037,4.90637472888857,131.172419364121));
#75924=CARTESIAN_POINT('Ctrl Pts',(-12.8471478052808,4.91473692208736,131.035380696465));
#75925=CARTESIAN_POINT('Ctrl Pts',(-12.8548957020578,4.91735475650663,130.898196970658));
#75926=CARTESIAN_POINT('Ctrl Pts',(-12.8626419781419,4.91997204333137,130.76104194073));
#75927=CARTESIAN_POINT('Ctrl Pts',(-12.870388254226,4.91684735396236,130.62374230365));
#75928=CARTESIAN_POINT('Ctrl Pts',(-12.8781345303101,4.90798810933561,130.48681411527));
#75929=CARTESIAN_POINT('Ctrl Pts',(-12.8858808635755,4.89912879931192,130.349884916117));
#75930=CARTESIAN_POINT('Ctrl Pts',(-12.8936271968408,4.88453487480433,130.213327561284));
#75931=CARTESIAN_POINT('Ctrl Pts',(-12.9013735301061,4.8642657832114,130.07765472604));
#75932=CARTESIAN_POINT('Ctrl Pts',(-12.9091215981091,4.84399215249603,129.941951507805));
#75933=CARTESIAN_POINT('Ctrl Pts',(-12.916869666112,4.8180408834798,129.807133589919));
#75934=CARTESIAN_POINT('Ctrl Pts',(-12.9246177341149,4.78652279241,129.67370478123));
#75935=CARTESIAN_POINT('Ctrl Pts',(-12.9323740368568,4.75497120353782,129.540134162816));
#75936=CARTESIAN_POINT('Ctrl Pts',(-12.9401303395986,4.71784106381872,129.407955983891));
#75937=CARTESIAN_POINT('Ctrl Pts',(-12.9478866423404,4.67529362374644,129.277660714423));
#75938=CARTESIAN_POINT('Ctrl Pts',(-12.9556470848546,4.63272347482431,129.147295902447));
#75939=CARTESIAN_POINT('Ctrl Pts',(-12.9634075273688,4.58473040098017,129.018816368474));
#75940=CARTESIAN_POINT('Ctrl Pts',(-12.971167969883,4.53152398161148,128.892692898903));
#75941=CARTESIAN_POINT('Ctrl Pts',(-12.9789408701484,4.4782321505749,128.766366964741));
#75942=CARTESIAN_POINT('Ctrl Pts',(-12.9867137704138,4.41971041723846,128.642405006701));
#75943=CARTESIAN_POINT('Ctrl Pts',(-12.9944866706793,4.35621493382028,128.521254287834));
#75944=CARTESIAN_POINT('Ctrl Pts',(-13.0019770064414,4.29502767115931,128.404507702758));
#75945=CARTESIAN_POINT('Ctrl Pts',(-13.0094673422035,4.22922215075735,128.29037178098));
#75946=CARTESIAN_POINT('Ctrl Pts',(-13.0169576779656,4.15906470852615,128.179219895092));
#75947=CARTESIAN_POINT('Ctrl Pts',(-13.0247320120847,4.08624722554948,128.063853651668));
#75948=CARTESIAN_POINT('Ctrl Pts',(-13.0325063462037,4.00851063618618,127.95133674482));
#75949=CARTESIAN_POINT('Ctrl Pts',(-13.0402806803228,3.92610454526274,127.842117183584));
#75950=CARTESIAN_POINT('Ctrl Pts',(-13.0480454332699,3.84380001248174,127.733032225697));
#75951=CARTESIAN_POINT('Ctrl Pts',(-13.0558101862169,3.75683766158096,127.627236837004));
#75952=CARTESIAN_POINT('Ctrl Pts',(-13.063574939164,3.66551172260317,127.525152348188));
#75953=CARTESIAN_POINT('Ctrl Pts',(-13.071331980049,3.57427648983543,127.423169251125));
#75954=CARTESIAN_POINT('Ctrl Pts',(-13.0790890209341,3.47868655278733,127.324890008691));
#75955=CARTESIAN_POINT('Ctrl Pts',(-13.086846061819,3.37907774475808,127.230704694372));
#75956=CARTESIAN_POINT('Ctrl Pts',(-13.0945972530592,3.27954405250567,127.136590405931));
#75957=CARTESIAN_POINT('Ctrl Pts',(-13.1023484442993,3.17599780455103,127.046564168121));
#75958=CARTESIAN_POINT('Ctrl Pts',(-13.1100996355394,3.06881294069888,126.960980569028));
#75959=CARTESIAN_POINT('Ctrl Pts',(-13.1178475323165,2.96167363327311,126.875433345248));
#75960=CARTESIAN_POINT('Ctrl Pts',(-13.1255954290936,2.85089909071917,126.794325248056));
#75961=CARTESIAN_POINT('Ctrl Pts',(-13.1333433258707,2.73689754040064,126.717971635121));
#75962=CARTESIAN_POINT('Ctrl Pts',(-13.1410896019548,2.62291983674883,126.641633993715));
#75963=CARTESIAN_POINT('Ctrl Pts',(-13.1488358780388,2.50571679261761,126.570049075806));
#75964=CARTESIAN_POINT('Ctrl Pts',(-13.1565821541229,2.38572659160582,126.503489578741));
#75965=CARTESIAN_POINT('Ctrl Pts',(-13.1643284873882,2.26573550485362,126.436929590349));
#75966=CARTESIAN_POINT('Ctrl Pts',(-13.1720748206536,2.14295756205467,126.375395286472));
#75967=CARTESIAN_POINT('Ctrl Pts',(-13.179821153919,2.01785622420303,126.319113765837));
#75968=CARTESIAN_POINT('Ctrl Pts',(-13.187569221922,1.89272687077383,126.262819641345));
#75969=CARTESIAN_POINT('Ctrl Pts',(-13.1953172899249,1.76527344341519,126.211780801218));
#75970=CARTESIAN_POINT('Ctrl Pts',(-13.2030653579279,1.63597970966912,126.166176333598));
#75971=CARTESIAN_POINT('Ctrl Pts',(-13.2108216606698,1.50654856100455,126.120523397006));
#75972=CARTESIAN_POINT('Ctrl Pts',(-13.2185779634117,1.37527356812249,126.080316500792));
#75973=CARTESIAN_POINT('Ctrl Pts',(-13.2263342661535,1.24265453712725,126.045685091345));
#75974=CARTESIAN_POINT('Ctrl Pts',(-13.2340947086677,1.10996472336154,126.011035198071));
#75975=CARTESIAN_POINT('Ctrl Pts',(-13.2418551511819,0.975929823990999,
125.981966803931));
#75976=CARTESIAN_POINT('Ctrl Pts',(-13.2496155936961,0.841059207730189,
125.95855805539));
#75977=CARTESIAN_POINT('Ctrl Pts',(-13.2573884939615,0.705972085183458,
125.935111729048));
#75978=CARTESIAN_POINT('Ctrl Pts',(-13.2651613942269,0.570046952758284,
125.917343254465));
#75979=CARTESIAN_POINT('Ctrl Pts',(-13.2729342944924,0.433798562058226,
125.905278880132));
#75980=CARTESIAN_POINT('Ctrl Pts',(-13.2804246302544,0.302503143548553,
125.893653076195));
#75981=CARTESIAN_POINT('Ctrl Pts',(-13.2879149660165,0.170907868893959,
125.887323870572));
#75982=CARTESIAN_POINT('Ctrl Pts',(-13.2954053017785,0.0394708280954393,
125.886269004325));
#75983=CARTESIAN_POINT('Ctrl Pts',(-13.3031796358976,-0.0969496880541805,
125.885174142504));
#75984=CARTESIAN_POINT('Ctrl Pts',(-13.3109539700167,-0.23363187380239,
125.88975800022));
#75985=CARTESIAN_POINT('Ctrl Pts',(-13.3187283041358,-0.370063888953388,
125.900052737692));
#75986=CARTESIAN_POINT('Ctrl Pts',(-13.3264930570828,-0.506327763838436,
125.91033478782));
#75987=CARTESIAN_POINT('Ctrl Pts',(-13.3342578100299,-0.642341695462724,
125.92631368475));
#75988=CARTESIAN_POINT('Ctrl Pts',(-13.342022562977,-0.777592167864181,
125.94796962394));
#75989=CARTESIAN_POINT('Ctrl Pts',(-13.349779603862,-0.912708307589934,
125.969604054145));
#75990=CARTESIAN_POINT('Ctrl Pts',(-13.3575366447471,-1.04706211355146,
125.996904244292));
#75991=CARTESIAN_POINT('Ctrl Pts',(-13.3652936856321,-1.180143879775,126.029798492561));
#75992=CARTESIAN_POINT('Ctrl Pts',(-13.3730448768723,-1.31312528800377,
126.062667935022));
#75993=CARTESIAN_POINT('Ctrl Pts',(-13.3807960681123,-1.44483618782624,
126.10112294546));
#75994=CARTESIAN_POINT('Ctrl Pts',(-13.3885472593525,-1.57477613064501,
126.145040581246));
#75995=CARTESIAN_POINT('Ctrl Pts',(-13.3962951561295,-1.70466084552164,
126.188939550866));
#75996=CARTESIAN_POINT('Ctrl Pts',(-13.4040430529066,-1.83277573085865,
126.238296403107));
#75997=CARTESIAN_POINT('Ctrl Pts',(-13.4117909496837,-1.95863481045777,
126.29293814325));
#75998=CARTESIAN_POINT('Ctrl Pts',(-13.4195372257678,-2.08446756305064,
126.347568453519));
#75999=CARTESIAN_POINT('Ctrl Pts',(-13.4272835018519,-2.20804509007464,
126.40748129722));
#76000=CARTESIAN_POINT('Ctrl Pts',(-13.435029777936,-2.32890111458898,126.472455417661));
#76001=CARTESIAN_POINT('Ctrl Pts',(-13.4427761112014,-2.44975803123487,
126.537430017726));
#76002=CARTESIAN_POINT('Ctrl Pts',(-13.4505224444667,-2.56789306092889,
126.60746578395));
#76003=CARTESIAN_POINT('Ctrl Pts',(-13.4582687777321,-2.68286462709367,
126.682295545883));
#76004=CARTESIAN_POINT('Ctrl Pts',(-13.4660168457351,-2.79786194034417,
126.757142065422));
#76005=CARTESIAN_POINT('Ctrl Pts',(-13.4737649137381,-2.90969405274877,
126.836784503746));
#76006=CARTESIAN_POINT('Ctrl Pts',(-13.4815129817411,-3.01794880420848,
126.920912655036));
#76007=CARTESIAN_POINT('Ctrl Pts',(-13.489269284483,-3.1263186101057,127.005130218726));
#76008=CARTESIAN_POINT('Ctrl Pts',(-13.4970255872248,-3.23110315083192,
127.093842778627));
#76009=CARTESIAN_POINT('Ctrl Pts',(-13.5047818899667,-3.33192336206522,
127.186699802644));
#76010=CARTESIAN_POINT('Ctrl Pts',(-13.5125423324809,-3.43279738408144,
127.279606387251));
#76011=CARTESIAN_POINT('Ctrl Pts',(-13.520302774995,-3.5297025844255,127.376661567089));
#76012=CARTESIAN_POINT('Ctrl Pts',(-13.5280632175092,-3.62229789003038,
127.477479035907));
#76013=CARTESIAN_POINT('Ctrl Pts',(-13.5358361177747,-3.71504183783979,
127.578458345876));
#76014=CARTESIAN_POINT('Ctrl Pts',(-13.5436090180401,-3.80346181296698,
127.683211714854));
#76015=CARTESIAN_POINT('Ctrl Pts',(-13.5513819183056,-3.88725749599962,
127.79132025569));
#76016=CARTESIAN_POINT('Ctrl Pts',(-13.5588722540675,-3.96800699488419,
127.895498778755));
#76017=CARTESIAN_POINT('Ctrl Pts',(-13.5663625898294,-4.04446239516941,
128.002792520054));
#76018=CARTESIAN_POINT('Ctrl Pts',(-13.5738529255913,-4.11639481509704,
128.112804043993));
#76019=CARTESIAN_POINT('Ctrl Pts',(-13.5817885100048,-4.19260311984398,
128.229354992098));
#76020=CARTESIAN_POINT('Ctrl Pts',(-13.5897240944183,-4.26396836570864,
128.349313981803));
#76021=CARTESIAN_POINT('Ctrl Pts',(-13.5976596788317,-4.33017842465427,
128.472250441533));
#76022=CARTESIAN_POINT('Ctrl Pts',(-13.6055853409293,-4.39630569736891,
128.595033186762));
#76023=CARTESIAN_POINT('Ctrl Pts',(-13.6135110030269,-4.45729043700007,
128.72078567151));
#76024=CARTESIAN_POINT('Ctrl Pts',(-13.6214366651244,-4.5128632937921,128.849047866612));
#76025=CARTESIAN_POINT('Ctrl Pts',(-13.6293509155556,-4.5683561346951,128.977125384982));
#76026=CARTESIAN_POINT('Ctrl Pts',(-13.6372651659867,-4.61845247250927,
129.107705077331));
#76027=CARTESIAN_POINT('Ctrl Pts',(-13.6451794164179,-4.66292880400036,
129.240302424491));
#76028=CARTESIAN_POINT('Ctrl Pts',(-13.6519065846276,-4.70073399678446,
129.353011096812));
#76029=CARTESIAN_POINT('Ctrl Pts',(-13.6586337528374,-4.73447936189535,
129.46717699462));
#76030=CARTESIAN_POINT('Ctrl Pts',(-13.6653609210472,-4.76405452823398,
129.582490119308));
#76031=CARTESIAN_POINT('Ctrl Pts',(-11.9152857535001,-4.76405452823405,
129.582490119308));
#76032=CARTESIAN_POINT('Ctrl Pts',(-11.9248052072162,-4.80558106041339,
129.744401438022));
#76033=CARTESIAN_POINT('Ctrl Pts',(-11.9343246609324,-4.83888478217968,
129.908568752554));
#76034=CARTESIAN_POINT('Ctrl Pts',(-11.9438441146484,-4.86375462011194,
130.074241409601));
#76035=CARTESIAN_POINT('Ctrl Pts',(-11.953239736843,-4.88830094474597,130.237758953781));
#76036=CARTESIAN_POINT('Ctrl Pts',(-11.9626353590377,-4.90463134586909,
130.402742953669));
#76037=CARTESIAN_POINT('Ctrl Pts',(-11.9720309812323,-4.91258887906555,
130.568450533463));
#76038=CARTESIAN_POINT('Ctrl Pts',(-11.976400842145,-4.91628989136213,130.645520370976));
#76039=CARTESIAN_POINT('Ctrl Pts',(-11.9807707030577,-4.91818039492165,
130.72274642572));
#76040=CARTESIAN_POINT('Ctrl Pts',(-11.9851405639704,-4.91824811303239,
130.800052351862));
#76041=CARTESIAN_POINT('',(-11.6398594359493,-4.91824997562219,130.804850303521));
#76042=CARTESIAN_POINT('Ctrl Pts',(-11.5697518023984,-4.76405452823402,
129.582490119308));
#76043=CARTESIAN_POINT('Ctrl Pts',(-11.5774904387069,-4.79803826805266,
129.714992205086));
#76044=CARTESIAN_POINT('Ctrl Pts',(-11.5852290750154,-4.82646319605803,
129.84880890235));
#76045=CARTESIAN_POINT('Ctrl Pts',(-11.5929677113239,-4.84925361316315,
129.983432814575));
#76046=CARTESIAN_POINT('Ctrl Pts',(-11.6007829987615,-4.87226976916243,
130.119390175544));
#76047=CARTESIAN_POINT('Ctrl Pts',(-11.6085982861991,-4.88953914801215,
130.256170419018));
#76048=CARTESIAN_POINT('Ctrl Pts',(-11.6164135736366,-4.90103760226909,
130.393248122445));
#76049=CARTESIAN_POINT('Ctrl Pts',(-11.6242288610742,-4.91253605652603,
130.530325825872));
#76050=CARTESIAN_POINT('Ctrl Pts',(-11.6320441485117,-4.9182636309454,130.667700580587));
#76051=CARTESIAN_POINT('Ctrl Pts',(-11.6398594359493,-4.91824997562219,
130.804850303521));
#76052=CARTESIAN_POINT('Ctrl Pts',(-11.6398594359912,-4.91824997562211,
130.804850304257));
#76053=CARTESIAN_POINT('Ctrl Pts',(-11.641342475681,-4.91824738436531,130.830876024256));
#76054=CARTESIAN_POINT('Ctrl Pts',(-11.6428255153709,-4.91803821598196,
130.856900563331));
#76055=CARTESIAN_POINT('Ctrl Pts',(-11.6443085550607,-4.91762251540665,
130.882921794146));
#76056=CARTESIAN_POINT('Ctrl Pts',(-11.6520828891798,-4.91544334569996,
131.019329298222));
#76057=CARTESIAN_POINT('Ctrl Pts',(-11.6598572232989,-4.9075808124374,131.155862122931));
#76058=CARTESIAN_POINT('Ctrl Pts',(-11.667631557418,-4.89401504741631,131.292007803719));
#76059=CARTESIAN_POINT('Ctrl Pts',(-11.6753963103651,-4.88046600098822,
131.427985697122));
#76060=CARTESIAN_POINT('Ctrl Pts',(-11.6831610633122,-4.86122774625856,
131.563577010627));
#76061=CARTESIAN_POINT('Ctrl Pts',(-11.6909258162592,-4.8363324050331,131.698268851406));
#76062=CARTESIAN_POINT('Ctrl Pts',(-11.6986828571442,-4.81146179021151,
131.832826914349));
#76063=CARTESIAN_POINT('Ctrl Pts',(-11.7064398980293,-4.78094534095621,
131.966486900446));
#76064=CARTESIAN_POINT('Ctrl Pts',(-11.7141969389143,-4.74486696997474,
132.098740971149));
#76065=CARTESIAN_POINT('Ctrl Pts',(-11.7219481301544,-4.70881580597349,
132.23089530803));
#76066=CARTESIAN_POINT('Ctrl Pts',(-11.7296993213945,-4.66721117120037,
132.361645464148));
#76067=CARTESIAN_POINT('Ctrl Pts',(-11.7374505126346,-4.62018798226402,
132.490494085309));
#76068=CARTESIAN_POINT('Ctrl Pts',(-11.7451984094117,-4.57318477943728,
132.619287942369));
#76069=CARTESIAN_POINT('Ctrl Pts',(-11.7529463061887,-4.52076773675328,
132.746181505422));
#76070=CARTESIAN_POINT('Ctrl Pts',(-11.7606942029658,-4.46312146120302,
132.870693089616));
#76071=CARTESIAN_POINT('Ctrl Pts',(-11.7684404790499,-4.4054872440109,132.995178628671));
#76072=CARTESIAN_POINT('Ctrl Pts',(-11.7761867551341,-4.34262613382016,
133.11728282537));
#76073=CARTESIAN_POINT('Ctrl Pts',(-11.7839330312182,-4.27477051296915,
133.236544846597));
#76074=CARTESIAN_POINT('Ctrl Pts',(-11.7916793644835,-4.20691439122345,
133.35580774819));
#76075=CARTESIAN_POINT('Ctrl Pts',(-11.7994256977489,-4.13406387859041,
133.472228092635));
#76076=CARTESIAN_POINT('Ctrl Pts',(-11.8071720310142,-4.0564966652038,133.585370841871));
#76077=CARTESIAN_POINT('Ctrl Pts',(-11.8149200990172,-3.97891208117757,
133.698538928642));
#76078=CARTESIAN_POINT('Ctrl Pts',(-11.8226681670202,-3.89660891556575,
133.808427637239));
#76079=CARTESIAN_POINT('Ctrl Pts',(-11.8304162350232,-3.80990717556159,
133.91463237034));
#76080=CARTESIAN_POINT('Ctrl Pts',(-11.838172537765,-3.72311328791638,134.020949979095));
#76081=CARTESIAN_POINT('Ctrl Pts',(-11.8459288405069,-3.63191173498627,
134.123575487633));
#76082=CARTESIAN_POINT('Ctrl Pts',(-11.8536851432488,-3.53666204442025,
134.222138352595));
#76083=CARTESIAN_POINT('Ctrl Pts',(-11.8614455857629,-3.44136151622634,
134.320753823525));
#76084=CARTESIAN_POINT('Ctrl Pts',(-11.869206028277,-3.34200882827089,134.41530206086));
#76085=CARTESIAN_POINT('Ctrl Pts',(-11.8769664707912,-3.23899836037251,
134.505451360037));
#76086=CARTESIAN_POINT('Ctrl Pts',(-11.8847393710566,-3.13582253092622,
134.595745374872));
#76087=CARTESIAN_POINT('Ctrl Pts',(-11.8925122713221,-3.02897749272747,
134.681626095212));
#76088=CARTESIAN_POINT('Ctrl Pts',(-11.9002851715875,-2.91888921913814,
134.762803340266));
#76089=CARTESIAN_POINT('Ctrl Pts',(-11.9077755073496,-2.81280293158941,
134.84102958799));
#76090=CARTESIAN_POINT('Ctrl Pts',(-11.9152658431116,-2.70370536943968,
134.91488821706));
#76091=CARTESIAN_POINT('Ctrl Pts',(-11.9227561788736,-2.59199934636086,
134.984159948989));
#76092=CARTESIAN_POINT('Ctrl Pts',(-11.9305305129927,-2.47605795546485,
135.056058139689));
#76093=CARTESIAN_POINT('Ctrl Pts',(-11.9383048471117,-2.35693913194501,
135.123242494532));
#76094=CARTESIAN_POINT('Ctrl Pts',(-11.9460791812308,-2.23506328749638,
135.185419298226));
#76095=CARTESIAN_POINT('Ctrl Pts',(-11.9538439341779,-2.11333764413367,
135.247519474566));
#76096=CARTESIAN_POINT('Ctrl Pts',(-11.961608687125,-1.98886208533451,135.304624202958));
#76097=CARTESIAN_POINT('Ctrl Pts',(-11.9693734400721,-1.86208548498143,
135.356483277284));
#76098=CARTESIAN_POINT('Ctrl Pts',(-11.9771304809571,-1.73543480093506,
135.408290844447));
#76099=CARTESIAN_POINT('Ctrl Pts',(-11.984887521842,-1.60648798295659,135.454862978729));
#76100=CARTESIAN_POINT('Ctrl Pts',(-11.992644562727,-1.47571764686486,135.495995779131));
#76101=CARTESIAN_POINT('Ctrl Pts',(-12.0003957539672,-1.34504592570083,
135.537097560968));
#76102=CARTESIAN_POINT('Ctrl Pts',(-12.0081469452074,-1.21255379497672,
135.572768056561));
#76103=CARTESIAN_POINT('Ctrl Pts',(-12.0158981364475,-1.07873261858636,
135.602851942983));
#76104=CARTESIAN_POINT('Ctrl Pts',(-12.0236460332246,-0.94496831976576,
135.63292304295));
#76105=CARTESIAN_POINT('Ctrl Pts',(-12.0313939300016,-0.809876479428558,
135.65741217079));
#76106=CARTESIAN_POINT('Ctrl Pts',(-12.0391418267787,-0.673962137271401,
135.676214279164));
#76107=CARTESIAN_POINT('Ctrl Pts',(-12.0468881028628,-0.538076225464649,
135.695012454542));
#76108=CARTESIAN_POINT('Ctrl Pts',(-12.0546343789469,-0.401368541085799,
135.708125923096));
#76109=CARTESIAN_POINT('Ctrl Pts',(-12.0623806550309,-0.264352404415259,
135.715501103113));
#76110=CARTESIAN_POINT('Ctrl Pts',(-12.0701269882963,-0.127335256322724,
135.722876337573));
#76111=CARTESIAN_POINT('Ctrl Pts',(-12.0778733215616,0.00998995820488735,
135.724513177958));
#76112=CARTESIAN_POINT('Ctrl Pts',(-12.085619654827,0.14710713102649,135.720410104146));
#76113=CARTESIAN_POINT('Ctrl Pts',(-12.09336772283,0.284255010288242,135.716306111479));
#76114=CARTESIAN_POINT('Ctrl Pts',(-12.1011157908329,0.421194364420792,
135.70645965848));
#76115=CARTESIAN_POINT('Ctrl Pts',(-12.1088638588359,0.557411822533177,
135.69092128153));
#76116=CARTESIAN_POINT('Ctrl Pts',(-12.1166201615778,0.693774054181052,
135.675366390208));
#76117=CARTESIAN_POINT('Ctrl Pts',(-12.1243764643196,0.829412468099328,
135.654107534897));
#76118=CARTESIAN_POINT('Ctrl Pts',(-12.1321327670614,0.963820982191196,
135.627246908656));
#76119=CARTESIAN_POINT('Ctrl Pts',(-12.1398932095756,1.098301234154,135.600371946091));
#76120=CARTESIAN_POINT('Ctrl Pts',(-12.1476536520898,1.23154989863293,135.567889347648));
#76121=CARTESIAN_POINT('Ctrl Pts',(-12.1554140946039,1.3630747312608,135.529951621821));
#76122=CARTESIAN_POINT('Ctrl Pts',(-12.1631869948693,1.49481069922624,135.491952994989));
#76123=CARTESIAN_POINT('Ctrl Pts',(-12.1709598951348,1.62481693449822,135.448481865441));
#76124=CARTESIAN_POINT('Ctrl Pts',(-12.1787327954002,1.75261905075177,135.399739766825));
#76125=CARTESIAN_POINT('Ctrl Pts',(-12.1862231311623,1.87577523816644,135.352769566267));
#76126=CARTESIAN_POINT('Ctrl Pts',(-12.1937134669244,1.99688449178711,135.300905090536));
#76127=CARTESIAN_POINT('Ctrl Pts',(-12.2012038026865,2.11554459578291,135.244366712804));
#76128=CARTESIAN_POINT('Ctrl Pts',(-12.2089781368055,2.2387037336868,135.185684665297));
#76129=CARTESIAN_POINT('Ctrl Pts',(-12.2167524709246,2.35961446792742,135.121781410311));
#76130=CARTESIAN_POINT('Ctrl Pts',(-12.2245268050437,2.47780244472148,135.052851891822));
#76131=CARTESIAN_POINT('Ctrl Pts',(-12.2322915579908,2.59584476539691,134.984007322805));
#76132=CARTESIAN_POINT('Ctrl Pts',(-12.240056310938,2.71117067069839,134.910149010412));
#76133=CARTESIAN_POINT('Ctrl Pts',(-12.2478210638851,2.82332702783598,134.831519362437));
#76134=CARTESIAN_POINT('Ctrl Pts',(-12.2555781047701,2.93537198969854,134.752967810536));
#76135=CARTESIAN_POINT('Ctrl Pts',(-12.263335145655,3.04425335008034,134.669654576775));
#76136=CARTESIAN_POINT('Ctrl Pts',(-12.27109218654,3.14954410090022,134.581867072754));
#76137=CARTESIAN_POINT('Ctrl Pts',(-12.2788433777801,3.25475545114572,134.494145769972));
#76138=CARTESIAN_POINT('Ctrl Pts',(-12.2865945690203,3.35638128228575,134.401957162191));
#76139=CARTESIAN_POINT('Ctrl Pts',(-12.2943457602604,3.45402532255525,134.305630691931));
#76140=CARTESIAN_POINT('Ctrl Pts',(-12.3020936570375,3.55162786150302,134.209345162992));
#76141=CARTESIAN_POINT('Ctrl Pts',(-12.3098415538146,3.64525169782699,134.108925543494));
#76142=CARTESIAN_POINT('Ctrl Pts',(-12.3175894505916,3.73453546593352,134.004739956986));
#76143=CARTESIAN_POINT('Ctrl Pts',(-12.3253357266757,3.82380055780049,133.900576163856));
#76144=CARTESIAN_POINT('Ctrl Pts',(-12.3330820027598,3.90872713296511,133.792648267293));
#76145=CARTESIAN_POINT('Ctrl Pts',(-12.3408282788439,3.98899264946551,133.681359175962));
#76146=CARTESIAN_POINT('Ctrl Pts',(-12.3485746121093,4.06925875846772,133.570069263119));
#76147=CARTESIAN_POINT('Ctrl Pts',(-12.3563209453747,4.14486351144877,133.455418423095));
#76148=CARTESIAN_POINT('Ctrl Pts',(-12.36406727864,4.21552666042864,133.337840050622));
#76149=CARTESIAN_POINT('Ctrl Pts',(-12.371815346643,4.28620563393078,133.220235347286));
#76150=CARTESIAN_POINT('Ctrl Pts',(-12.379563414646,4.35194059999564,133.099702141972));
#76151=CARTESIAN_POINT('Ctrl Pts',(-12.387311482649,4.41249658680375,132.976699664295));
#76152=CARTESIAN_POINT('Ctrl Pts',(-12.3950677853908,4.47311693323527,132.853566458122));
#76153=CARTESIAN_POINT('Ctrl Pts',(-12.4028240881327,4.52854713205572,132.727959088441));
#76154=CARTESIAN_POINT('Ctrl Pts',(-12.4105803908746,4.57859961144396,132.600358574298));
#76155=CARTESIAN_POINT('Ctrl Pts',(-12.4183408333887,4.62867880534749,132.472689955919));
#76156=CARTESIAN_POINT('Ctrl Pts',(-12.4261012759029,4.67337443325303,132.343026442804));
#76157=CARTESIAN_POINT('Ctrl Pts',(-12.433861718417,4.71254873477078,132.211864608648));
#76158=CARTESIAN_POINT('Ctrl Pts',(-12.4416346186825,4.75178592235505,132.080492221871));
#76159=CARTESIAN_POINT('Ctrl Pts',(-12.4494075189479,4.7854839756431,131.947617086806));
#76160=CARTESIAN_POINT('Ctrl Pts',(-12.4571804192134,4.81355603320446,131.813747251964));
#76161=CARTESIAN_POINT('Ctrl Pts',(-12.4646707549753,4.84060760076405,131.684743922816));
#76162=CARTESIAN_POINT('Ctrl Pts',(-12.4721610907373,4.86243505829315,131.554817261762));
#76163=CARTESIAN_POINT('Ctrl Pts',(-12.4796514264993,4.87900640450117,131.424424781453));
#76164=CARTESIAN_POINT('Ctrl Pts',(-12.4874257606184,4.89620605833752,131.28908843062));
#76165=CARTESIAN_POINT('Ctrl Pts',(-12.4952000947375,4.90779764534939,131.152821535289));
#76166=CARTESIAN_POINT('Ctrl Pts',(-12.5029744288566,4.91368877761867,131.016128554715));
#76167=CARTESIAN_POINT('Ctrl Pts',(-12.5107391818037,4.91957264959392,130.879604036023));
#76168=CARTESIAN_POINT('Ctrl Pts',(-12.5185039347507,4.91977002840923,130.742654863755));
#76169=CARTESIAN_POINT('Ctrl Pts',(-12.5262686876978,4.91423992926441,130.605793298696));
#76170=CARTESIAN_POINT('Ctrl Pts',(-12.5340257285828,4.90871532269203,130.469067666472));
#76171=CARTESIAN_POINT('Ctrl Pts',(-12.5417827694678,4.89747457443633,130.332429856415));
#76172=CARTESIAN_POINT('Ctrl Pts',(-12.5495398103528,4.88052868371991,130.196394475509));
#76173=CARTESIAN_POINT('Ctrl Pts',(-12.5572910015929,4.86359557203149,130.060461679942));
#76174=CARTESIAN_POINT('Ctrl Pts',(-12.5650421928331,4.84096592946763,129.925130795673));
#76175=CARTESIAN_POINT('Ctrl Pts',(-12.5727933840732,4.81270273078517,129.790913289091));
#76176=CARTESIAN_POINT('Ctrl Pts',(-12.5805412808503,4.7844515447161,129.65675282853));
#76177=CARTESIAN_POINT('Ctrl Pts',(-12.5882891776274,4.75057164522366,129.523705186242));
#76178=CARTESIAN_POINT('Ctrl Pts',(-12.5960370744045,4.71117741814409,129.392273369104));
#76179=CARTESIAN_POINT('Ctrl Pts',(-12.6037833504886,4.67179143148759,129.260869044669));
#76180=CARTESIAN_POINT('Ctrl Pts',(-12.6115296265727,4.62689352375542,129.131080247359));
#76181=CARTESIAN_POINT('Ctrl Pts',(-12.6192759026568,4.57664833161018,129.003396122838));
#76182=CARTESIAN_POINT('Ctrl Pts',(-12.6270222359221,4.52640276856633,128.875711055782));
#76183=CARTESIAN_POINT('Ctrl Pts',(-12.6347685691875,4.47080998550864,128.750131056326));
#76184=CARTESIAN_POINT('Ctrl Pts',(-12.6425149024528,4.41008312882091,128.627126165471));
#76185=CARTESIAN_POINT('Ctrl Pts',(-12.6502629704558,4.34934267277468,128.504093728524));
#76186=CARTESIAN_POINT('Ctrl Pts',(-12.6580110384588,4.28346602828976,128.383637898203));
#76187=CARTESIAN_POINT('Ctrl Pts',(-12.6657591064618,4.21271255024126,128.26620458778));
#76188=CARTESIAN_POINT('Ctrl Pts',(-12.6735154092036,4.14188387455432,128.148646467837));
#76189=CARTESIAN_POINT('Ctrl Pts',(-12.6812717119455,4.06616821347661,128.034117620261));
#76190=CARTESIAN_POINT('Ctrl Pts',(-12.6890280146874,3.98586887480289,127.923035857082));
#76191=CARTESIAN_POINT('Ctrl Pts',(-12.6967884572015,3.90552667795436,127.811894806221));
#76192=CARTESIAN_POINT('Ctrl Pts',(-12.7045488997157,3.82059617074404,127.704204812573));
#76193=CARTESIAN_POINT('Ctrl Pts',(-12.7123093422299,3.73142067182779,127.600350188064));
#76194=CARTESIAN_POINT('Ctrl Pts',(-12.7200822424953,3.64210202048405,127.496328846893));
#76195=CARTESIAN_POINT('Ctrl Pts',(-12.7278551427607,3.54852502705781,127.396155464125));
#76196=CARTESIAN_POINT('Ctrl Pts',(-12.7356280430262,3.45107017642426,127.300177731372));
#76197=CARTESIAN_POINT('Ctrl Pts',(-12.7431183787882,3.3571580550848,127.207689030957));
#76198=CARTESIAN_POINT('Ctrl Pts',(-12.7506087145503,3.25964534938427,127.119096438817));
#76199=CARTESIAN_POINT('Ctrl Pts',(-12.7580990503123,3.1588996801951,127.034674175305));
#76200=CARTESIAN_POINT('Ctrl Pts',(-12.7658733844314,3.05433420833807,126.947051016014));
#76201=CARTESIAN_POINT('Ctrl Pts',(-12.7736477185505,2.94595454593777,126.86364310014));
#76202=CARTESIAN_POINT('Ctrl Pts',(-12.7814220526696,2.83413517092457,126.784800828805));
#76203=CARTESIAN_POINT('Ctrl Pts',(-12.7891868056167,2.72245360329749,126.706055723522));
#76204=CARTESIAN_POINT('Ctrl Pts',(-12.7969515585638,2.60734107413781,126.631865290355));
#76205=CARTESIAN_POINT('Ctrl Pts',(-12.8047163115108,2.48920640966427,126.562540900441));
#76206=CARTESIAN_POINT('Ctrl Pts',(-12.8124733523958,2.37118907820505,126.49328536449));
#76207=CARTESIAN_POINT('Ctrl Pts',(-12.8202303932809,2.25015591981789,126.428886450452));
#76208=CARTESIAN_POINT('Ctrl Pts',(-12.8279874341659,2.1265458332809,126.369613062016));
#76209=CARTESIAN_POINT('Ctrl Pts',(-12.835738625406,2.00302896207155,126.310384372103));
#76210=CARTESIAN_POINT('Ctrl Pts',(-12.8434898166461,1.87693938180032,126.256273682709));
#76211=CARTESIAN_POINT('Ctrl Pts',(-12.8512410078862,1.74874144302091,126.207504471463));
#76212=CARTESIAN_POINT('Ctrl Pts',(-12.8589889046633,1.62059799178526,126.158755988434));
#76213=CARTESIAN_POINT('Ctrl Pts',(-12.8667368014404,1.49034832898483,126.115344606879));
#76214=CARTESIAN_POINT('Ctrl Pts',(-12.8744846982175,1.35847747689028,126.07744597826));
#76215=CARTESIAN_POINT('Ctrl Pts',(-12.8822309743016,1.22663420933517,126.039555277217));
#76216=CARTESIAN_POINT('Ctrl Pts',(-12.8899772503857,1.09317080252731,126.007175143354));
#76217=CARTESIAN_POINT('Ctrl Pts',(-12.8977235264698,0.958587778703766,
125.980431458362));
#76218=CARTESIAN_POINT('Ctrl Pts',(-12.9054698597352,0.824003761418909,
125.953687575954));
#76219=CARTESIAN_POINT('Ctrl Pts',(-12.9132161930005,0.688300494094021,
125.932580301642));
#76220=CARTESIAN_POINT('Ctrl Pts',(-12.9209625262659,0.551988646362799,
125.917184377979));
#76221=CARTESIAN_POINT('Ctrl Pts',(-12.9287105942688,0.415646272538399,
125.901785006505));
#76222=CARTESIAN_POINT('Ctrl Pts',(-12.9364586622718,0.278695435532305,
125.892099574648));
#76223=CARTESIAN_POINT('Ctrl Pts',(-12.9442067302748,0.141651482454169,
125.888150906822));
#76224=CARTESIAN_POINT('Ctrl Pts',(-12.9519630330166,0.00446187743204438,
125.884198042303));
#76225=CARTESIAN_POINT('Ctrl Pts',(-12.9597193357585,-0.132820649928944,
125.88599413271));
#76226=CARTESIAN_POINT('Ctrl Pts',(-12.9674756385003,-0.269680637264103,
125.89350983421));
#76227=CARTESIAN_POINT('Ctrl Pts',(-12.9752360810145,-0.406613670895464,
125.901029547067));
#76228=CARTESIAN_POINT('Ctrl Pts',(-12.9829965235287,-0.543123326181341,
125.914274916099));
#76229=CARTESIAN_POINT('Ctrl Pts',(-12.9907569660429,-0.678700698492902,
125.933164827581));
#76230=CARTESIAN_POINT('Ctrl Pts',(-12.9985298663083,-0.814495711638491,
125.952085062827));
#76231=CARTESIAN_POINT('Ctrl Pts',(-13.0063027665737,-0.949355066310625,
125.976667877378));
#76232=CARTESIAN_POINT('Ctrl Pts',(-13.0140756668392,-1.08278057834101,
126.006781094341));
#76233=CARTESIAN_POINT('Ctrl Pts',(-13.0215660026012,-1.21135573692979,
126.035799620017));
#76234=CARTESIAN_POINT('Ctrl Pts',(-13.0290563383631,-1.33859919308061,
126.069953360979));
#76235=CARTESIAN_POINT('Ctrl Pts',(-13.0365466741251,-1.46408152938058,
126.109081250177));
#76236=CARTESIAN_POINT('Ctrl Pts',(-13.0443210082442,-1.59432156660144,
126.149692685187));
#76237=CARTESIAN_POINT('Ctrl Pts',(-13.0520953423633,-1.72307686330869,
126.195791548754));
#76238=CARTESIAN_POINT('Ctrl Pts',(-13.0598696764824,-1.84985020264719,
126.247252182356));
#76239=CARTESIAN_POINT('Ctrl Pts',(-13.0676344294294,-1.97646730517485,
126.298649395325));
#76240=CARTESIAN_POINT('Ctrl Pts',(-13.0753991823765,-2.10110695157109,
126.355395084934));
#76241=CARTESIAN_POINT('Ctrl Pts',(-13.0831639353236,-2.22328619592103,
126.417313597813));
#76242=CARTESIAN_POINT('Ctrl Pts',(-13.0909209762086,-2.34534409012306,
126.479170612351));
#76243=CARTESIAN_POINT('Ctrl Pts',(-13.0986780170935,-2.46494609888223,
126.546190050271));
#76244=CARTESIAN_POINT('Ctrl Pts',(-13.1064350579785,-2.58162875040061,
126.618148002611));
#76245=CARTESIAN_POINT('Ctrl Pts',(-13.1141862492186,-2.69822341062366,
126.6900516909));
#76246=CARTESIAN_POINT('Ctrl Pts',(-13.1219374404587,-2.81190276415101,
126.766886276479));
#76247=CARTESIAN_POINT('Ctrl Pts',(-13.1296886316989,-2.92222780010617,
126.848381883196));
#76248=CARTESIAN_POINT('Ctrl Pts',(-13.1374365284759,-3.03250594497834,
126.929842852106));
#76249=CARTESIAN_POINT('Ctrl Pts',(-13.145184425253,-3.13943229402284,127.01596067017));
#76250=CARTESIAN_POINT('Ctrl Pts',(-13.1529323220301,-3.24259690030668,
127.10642221832));
#76251=CARTESIAN_POINT('Ctrl Pts',(-13.1606785981142,-3.34573992677886,
127.196864843863));
#76252=CARTESIAN_POINT('Ctrl Pts',(-13.1684248741983,-3.44512248185581,
127.291649134609));
#76253=CARTESIAN_POINT('Ctrl Pts',(-13.1761711502824,-3.54036811320998,
127.390422029151));
#76254=CARTESIAN_POINT('Ctrl Pts',(-13.1839174835478,-3.63561444764578,
127.489195652813));
#76255=CARTESIAN_POINT('Ctrl Pts',(-13.1916638168131,-3.7267235260394,127.59195765759));
#76256=CARTESIAN_POINT('Ctrl Pts',(-13.1994101500785,-3.81335643595306,
127.698318802832));
#76257=CARTESIAN_POINT('Ctrl Pts',(-13.2071582180815,-3.90000874670622,
127.804703766915));
#76258=CARTESIAN_POINT('Ctrl Pts',(-13.2149062860844,-3.9821826474452,127.914689172239));
#76259=CARTESIAN_POINT('Ctrl Pts',(-13.2226543540874,-4.05958037764347,
128.027853779838));
#76260=CARTESIAN_POINT('Ctrl Pts',(-13.2304106568292,-4.13706036707044,
128.141138660128));
#76261=CARTESIAN_POINT('Ctrl Pts',(-13.2381669595711,-4.20975382469447,
128.257609169177));
#76262=CARTESIAN_POINT('Ctrl Pts',(-13.2459232623129,-4.27740681831236,
128.37681577284));
#76263=CARTESIAN_POINT('Ctrl Pts',(-13.2536837048271,-4.34509592036993,
128.496086000657));
#76264=CARTESIAN_POINT('Ctrl Pts',(-13.2614441473412,-4.40773901939108,
128.618094885301));
#76265=CARTESIAN_POINT('Ctrl Pts',(-13.2692045898554,-4.46512928326653,
128.742370426945));
#76266=CARTESIAN_POINT('Ctrl Pts',(-13.2769774901208,-4.52261167508842,
128.866845466722));
#76267=CARTESIAN_POINT('Ctrl Pts',(-13.2847503903863,-4.57482423230856,
128.993594072956));
#76268=CARTESIAN_POINT('Ctrl Pts',(-13.2925232906517,-4.62160887837857,
129.122125664359));
#76269=CARTESIAN_POINT('Ctrl Pts',(-13.3000136264139,-4.66669278472115,
129.245984808664));
#76270=CARTESIAN_POINT('Ctrl Pts',(-13.307503962176,-4.70673647130985,129.37149926329));
#76271=CARTESIAN_POINT('Ctrl Pts',(-13.3149942979381,-4.74164333781551,
129.498220686529));
#76272=CARTESIAN_POINT('Ctrl Pts',(-13.3166505309442,-4.74936180415442,
129.52624081946));
#76273=CARTESIAN_POINT('Ctrl Pts',(-13.3183067639504,-4.75683259252767,
129.554331901597));
#76274=CARTESIAN_POINT('Ctrl Pts',(-13.3199629969565,-4.76405452823408,
129.582490119308));
#76275=CARTESIAN_POINT('Origin',(213.235140564004,0.,130.804360617566));
#76276=CARTESIAN_POINT('',(-15.4150128089233,-4.76405452823406,129.582490119308));
#76277=CARTESIAN_POINT('',(-15.0701040894034,-4.76405452823398,129.582490119308));
#76278=CARTESIAN_POINT('',(213.235140564004,-4.76405452823405,129.582490119308));
#76279=CARTESIAN_POINT('',(-13.7351405640513,-4.91824955803034,130.806445667775));
#76280=CARTESIAN_POINT('Ctrl Pts',(-13.7351405640514,-4.91824955803034,
130.806445667775));
#76281=CARTESIAN_POINT('Ctrl Pts',(-13.7435813121526,-4.91818605641123,
130.956234295773));
#76282=CARTESIAN_POINT('Ctrl Pts',(-13.7520220602538,-4.91127554223146,
131.10580378366));
#76283=CARTESIAN_POINT('Ctrl Pts',(-13.7604628083551,-4.89760274164466,
131.25454996388));
#76284=CARTESIAN_POINT('Ctrl Pts',(-13.7689420453452,-4.88386759458144,
131.403974410426));
#76285=CARTESIAN_POINT('Ctrl Pts',(-13.7774212823353,-4.86330843507531,
131.552567763333));
#76286=CARTESIAN_POINT('Ctrl Pts',(-13.7859005193255,-4.83606167266655,
131.699732361964));
#76287=CARTESIAN_POINT('Ctrl Pts',(-13.7943993943312,-4.80875180642613,
131.847237795586));
#76288=CARTESIAN_POINT('Ctrl Pts',(-13.8028982693369,-4.77472344426176,
131.993307603379));
#76289=CARTESIAN_POINT('Ctrl Pts',(-13.8113971443426,-4.73416301053937,
132.137358611616));
#76290=CARTESIAN_POINT('Ctrl Pts',(-13.8199248935822,-4.69346477605517,
132.281899021391));
#76291=CARTESIAN_POINT('Ctrl Pts',(-13.8284526428218,-4.64619013709462,
132.424406650554));
#76292=CARTESIAN_POINT('Ctrl Pts',(-13.8369803920614,-4.59257492080349,
132.564314781545));
#76293=CARTESIAN_POINT('Ctrl Pts',(-13.8420871111757,-4.56046822510214,
132.648096739329));
#76294=CARTESIAN_POINT('Ctrl Pts',(-13.84719383029,-4.52608867497823,132.730946953886));
#76295=CARTESIAN_POINT('Ctrl Pts',(-13.8523005494044,-4.48949472028319,
132.812748084926));
#76296=CARTESIAN_POINT('Ctrl Pts',(-13.8600748835235,-4.43378505147807,
132.937279963378));
#76297=CARTESIAN_POINT('Ctrl Pts',(-13.8678492176427,-4.37280172328451,
133.059689380234));
#76298=CARTESIAN_POINT('Ctrl Pts',(-13.8756235517618,-4.30672824035703,
133.179497440196));
#76299=CARTESIAN_POINT('Ctrl Pts',(-13.8833883047089,-4.24073618709209,
133.299157847431));
#76300=CARTESIAN_POINT('Ctrl Pts',(-13.8911530576561,-4.16966664780707,
133.416222937569));
#76301=CARTESIAN_POINT('Ctrl Pts',(-13.8989178106032,-4.09375108654948,
133.530233891193));
#76302=CARTESIAN_POINT('Ctrl Pts',(-13.9066748514882,-4.01791092569755,
133.644131607531));
#76303=CARTESIAN_POINT('Ctrl Pts',(-13.9144318923733,-3.93723453651853,
133.754980900662));
#76304=CARTESIAN_POINT('Ctrl Pts',(-13.9221889332583,-3.85199900083047,
133.862347988387));
#76305=CARTESIAN_POINT('Ctrl Pts',(-13.9299401244985,-3.7668277419229,133.969634109756));
#76306=CARTESIAN_POINT('Ctrl Pts',(-13.9376913157386,-3.67710442191587,
134.073442947563));
#76307=CARTESIAN_POINT('Ctrl Pts',(-13.9454425069788,-3.58314887903189,
134.173370438447));
#76308=CARTESIAN_POINT('Ctrl Pts',(-13.9531904037559,-3.48923326975984,
134.273255457482));
#76309=CARTESIAN_POINT('Ctrl Pts',(-13.9609383005331,-3.3910892825532,134.369262126435));
#76310=CARTESIAN_POINT('Ctrl Pts',(-13.9686861973102,-3.28907626317128,
134.461020349828));
#76311=CARTESIAN_POINT('Ctrl Pts',(-13.9764324733943,-3.18708458271387,
134.552759379378));
#76312=CARTESIAN_POINT('Ctrl Pts',(-13.9841787494784,-3.08122577035307,
134.640251469715));
#76313=CARTESIAN_POINT('Ctrl Pts',(-13.9919250255626,-2.9718948786092,134.723164503064));
#76314=CARTESIAN_POINT('Ctrl Pts',(-13.999671358828,-2.86256317980953,134.806078148459));
#76315=CARTESIAN_POINT('Ctrl Pts',(-14.0074176920934,-2.74975966200026,
134.884412433173));
#76316=CARTESIAN_POINT('Ctrl Pts',(-14.0151640253588,-2.63391086992769,
134.957876789652));
#76317=CARTESIAN_POINT('Ctrl Pts',(-14.0229120933618,-2.51803613432153,
135.031357597964));
#76318=CARTESIAN_POINT('Ctrl Pts',(-14.0306601613648,-2.39911509752582,
135.099966098564));
#76319=CARTESIAN_POINT('Ctrl Pts',(-14.0384082293678,-2.27760121823524,
135.163456367053));
#76320=CARTESIAN_POINT('Ctrl Pts',(-14.0461645321097,-2.15595819254754,
135.227014113755));
#76321=CARTESIAN_POINT('Ctrl Pts',(-14.0539208348516,-2.0317171666187,135.285442580582));
#76322=CARTESIAN_POINT('Ctrl Pts',(-14.0616771375934,-1.90535451976567,
135.338542706599));
#76323=CARTESIAN_POINT('Ctrl Pts',(-14.0694375801077,-1.77892442936332,
135.391671173752));
#76324=CARTESIAN_POINT('Ctrl Pts',(-14.0771980226219,-1.65037082796646,
135.439465497214));
#76325=CARTESIAN_POINT('Ctrl Pts',(-14.0849584651361,-1.52018684039753,
135.481776039867));
#76326=CARTESIAN_POINT('Ctrl Pts',(-14.0927313654016,-1.38979386993457,
135.52415450316));
#76327=CARTESIAN_POINT('Ctrl Pts',(-14.1005042656671,-1.25776565998818,
135.561031489105));
#76328=CARTESIAN_POINT('Ctrl Pts',(-14.1082771659326,-1.12460802832807,
135.592307969524));
#76329=CARTESIAN_POINT('Ctrl Pts',(-14.1157675016941,-0.996291011992013,
135.622447471096));
#76330=CARTESIAN_POINT('Ctrl Pts',(-14.1232578374556,-0.866925565409542,
135.647386524473));
#76331=CARTESIAN_POINT('Ctrl Pts',(-14.1307481732171,-0.736968301537565,
135.667082158538));
#76332=CARTESIAN_POINT('Ctrl Pts',(-14.1385225073362,-0.602083668497659,
135.687524558555));
#76333=CARTESIAN_POINT('Ctrl Pts',(-14.1462968414552,-0.466134180793593,
135.702382837235));
#76334=CARTESIAN_POINT('Ctrl Pts',(-14.1540711755743,-0.329621935351554,
135.711552527634));
#76335=CARTESIAN_POINT('Ctrl Pts',(-14.1618359285214,-0.193277929051758,
135.720710917209));
#76336=CARTESIAN_POINT('Ctrl Pts',(-14.1696006814684,-0.0563729313104023,
135.724194641708));
#76337=CARTESIAN_POINT('Ctrl Pts',(-14.1773654344155,0.0805819281306172,
135.721950435288));
#76338=CARTESIAN_POINT('Ctrl Pts',(-14.1851224753005,0.2174007620747,135.719708457845));
#76339=CARTESIAN_POINT('Ctrl Pts',(-14.1928795161855,0.354268970781614,
135.711749877337));
#76340=CARTESIAN_POINT('Ctrl Pts',(-14.2006365570705,0.49067183151094,135.698073340669));
#76341=CARTESIAN_POINT('Ctrl Pts',(-14.2083877483106,0.62697182978193,135.684407117584));
#76342=CARTESIAN_POINT('Ctrl Pts',(-14.2161389395507,0.762806791124726,
135.665031559873));
#76343=CARTESIAN_POINT('Ctrl Pts',(-14.2238901307908,0.897663885218503,
135.639997350373));
#76344=CARTESIAN_POINT('Ctrl Pts',(-14.2316380275678,1.03246366144986,135.61497378108));
#76345=CARTESIAN_POINT('Ctrl Pts',(-14.2393859243449,1.16628601347475,135.584296414724));
#76346=CARTESIAN_POINT('Ctrl Pts',(-14.247133821122,1.2986253343243,135.548067533423));
#76347=CARTESIAN_POINT('Ctrl Pts',(-14.254880097206,1.43093697264083,135.511846230423));
#76348=CARTESIAN_POINT('Ctrl Pts',(-14.2626263732902,1.56176581997155,135.470075825448));
#76349=CARTESIAN_POINT('Ctrl Pts',(-14.2703726493743,1.69061892068953,135.422909169601));
#76350=CARTESIAN_POINT('Ctrl Pts',(-14.2781189826396,1.81947297257183,135.375742165581));
#76351=CARTESIAN_POINT('Ctrl Pts',(-14.2858653159049,1.94635088159795,135.323178965597));
#76352=CARTESIAN_POINT('Ctrl Pts',(-14.2936116491703,2.07077762720103,135.265421374963));
#76353=CARTESIAN_POINT('Ctrl Pts',(-14.3013597171732,2.19523223731107,135.207650849916));
#76354=CARTESIAN_POINT('Ctrl Pts',(-14.3091077851762,2.31723423715463,135.144683784072));
#76355=CARTESIAN_POINT('Ctrl Pts',(-14.3168558531792,2.43633161806993,135.076768756929));
#76356=CARTESIAN_POINT('Ctrl Pts',(-14.324612155921,2.55555557709895,135.008781548886));
#76357=CARTESIAN_POINT('Ctrl Pts',(-14.3323684586629,2.67186841029072,134.9358360686));
#76358=CARTESIAN_POINT('Ctrl Pts',(-14.3401247614047,2.78484514738517,134.858225510182));
#76359=CARTESIAN_POINT('Ctrl Pts',(-14.3478852039189,2.89788218356603,134.780573528673));
#76360=CARTESIAN_POINT('Ctrl Pts',(-14.355645646433,3.00757926315111,134.698251742264));
#76361=CARTESIAN_POINT('Ctrl Pts',(-14.3634060889472,3.11354394618366,134.611594148318));
#76362=CARTESIAN_POINT('Ctrl Pts',(-14.3711789892126,3.21967873313237,134.524797443909));
#76363=CARTESIAN_POINT('Ctrl Pts',(-14.3789518894781,3.32206885826284,134.433651283324));
#76364=CARTESIAN_POINT('Ctrl Pts',(-14.3867247897435,3.42035759950287,134.338527698226));
#76365=CARTESIAN_POINT('Ctrl Pts',(-14.3942151255057,3.51507329742683,134.246862095047));
#76366=CARTESIAN_POINT('Ctrl Pts',(-14.4017054612679,3.60598041315651,134.151503448529));
#76367=CARTESIAN_POINT('Ctrl Pts',(-14.4091957970301,3.69279598341738,134.052812693149));
#76368=CARTESIAN_POINT('Ctrl Pts',(-14.4169701311492,3.78290319240956,133.950380047784));
#76369=CARTESIAN_POINT('Ctrl Pts',(-14.4247444652682,3.86888790192637,133.844033156049));
#76370=CARTESIAN_POINT('Ctrl Pts',(-14.4325187993873,3.9503908253163,133.734137979373));
#76371=CARTESIAN_POINT('Ctrl Pts',(-14.4402835523344,4.03179330363728,133.624378238681));
#76372=CARTESIAN_POINT('Ctrl Pts',(-14.4480483052815,4.10872475509251,133.511079224916));
#76373=CARTESIAN_POINT('Ctrl Pts',(-14.4558130582286,4.18086408750844,133.394642174517));
#76374=CARTESIAN_POINT('Ctrl Pts',(-14.4635700991136,4.25293177012242,133.278320771038));
#76375=CARTESIAN_POINT('Ctrl Pts',(-14.4713271399986,4.32021660094008,133.15886786358));
#76376=CARTESIAN_POINT('Ctrl Pts',(-14.4790841808836,4.38243922135144,133.036715771582));
#76377=CARTESIAN_POINT('Ctrl Pts',(-14.4868353721237,4.44461491920074,132.914655795426));
#76378=CARTESIAN_POINT('Ctrl Pts',(-14.4945865633638,4.50173582831291,132.789901033185));
#76379=CARTESIAN_POINT('Ctrl Pts',(-14.5023377546039,4.55356739228051,132.662910338843));
#76380=CARTESIAN_POINT('Ctrl Pts',(-14.510085651381,4.60537692645076,132.535973618934));
#76381=CARTESIAN_POINT('Ctrl Pts',(-14.5178335481581,4.65190143936944,132.406803218278));
#76382=CARTESIAN_POINT('Ctrl Pts',(-14.5255814449351,4.69295369096224,132.27587980432));
#76383=CARTESIAN_POINT('Ctrl Pts',(-14.5333277210192,4.73399735530899,132.144983776717));
#76384=CARTESIAN_POINT('Ctrl Pts',(-14.5410739971033,4.76957091825835,132.012335838004));
#76385=CARTESIAN_POINT('Ctrl Pts',(-14.5488202731874,4.79953652321572,131.878433345466));
#76386=CARTESIAN_POINT('Ctrl Pts',(-14.5565666064528,4.82950234937237,131.74452986449));
#76387=CARTESIAN_POINT('Ctrl Pts',(-14.5643129397182,4.85386004955198,131.609372192738));
#76388=CARTESIAN_POINT('Ctrl Pts',(-14.5720592729835,4.87252264806201,131.473469059168));
#76389=CARTESIAN_POINT('Ctrl Pts',(-14.5798073409865,4.89118942593156,131.337535491033));
#76390=CARTESIAN_POINT('Ctrl Pts',(-14.5875554089894,4.90415851109684,131.200856516144));
#76391=CARTESIAN_POINT('Ctrl Pts',(-14.5953034769923,4.9113947188073,131.063946785479));
#76392=CARTESIAN_POINT('Ctrl Pts',(-14.6030597797342,4.91863861724543,130.926891545523));
#76393=CARTESIAN_POINT('Ctrl Pts',(-14.610816082476,4.92013744619596,130.789605450921));
#76394=CARTESIAN_POINT('Ctrl Pts',(-14.6185723852178,4.91590817136375,130.652604519767));
#76395=CARTESIAN_POINT('Ctrl Pts',(-14.626332827732,4.91167663924023,130.515530467092));
#76396=CARTESIAN_POINT('Ctrl Pts',(-14.6340932702462,4.90171093987623,130.378742270879));
#76397=CARTESIAN_POINT('Ctrl Pts',(-14.6418537127604,4.88607995132916,130.242750635711));
#76398=CARTESIAN_POINT('Ctrl Pts',(-14.6496266130258,4.87042387053163,130.106540694697));
#76399=CARTESIAN_POINT('Ctrl Pts',(-14.6573995132912,4.84908438788826,129.97113025642));
#76400=CARTESIAN_POINT('Ctrl Pts',(-14.6651724135566,4.82218168718184,129.837020533465));
#76401=CARTESIAN_POINT('Ctrl Pts',(-14.6726627493187,4.79625696740963,129.70778603674));
#76402=CARTESIAN_POINT('Ctrl Pts',(-14.6801530850808,4.76516655397933,129.579759627948));
#76403=CARTESIAN_POINT('Ctrl Pts',(-14.6876434208429,4.72906116272469,129.453374466005));
#76404=CARTESIAN_POINT('Ctrl Pts',(-14.695417754962,4.691586824587,129.322197372235));
#76405=CARTESIAN_POINT('Ctrl Pts',(-14.7031920890811,4.64859100845695,129.192372908255));
#76406=CARTESIAN_POINT('Ctrl Pts',(-14.7109664232002,4.60018740483834,129.064401163192));
#76407=CARTESIAN_POINT('Ctrl Pts',(-14.7187311761473,4.55184345433523,128.936587131867));
#76408=CARTESIAN_POINT('Ctrl Pts',(-14.7264959290943,4.49810511392687,128.810621638524));
#76409=CARTESIAN_POINT('Ctrl Pts',(-14.7342606820414,4.43913639702931,128.686991705196));
#76410=CARTESIAN_POINT('Ctrl Pts',(-14.7420177229264,4.38022624869268,128.563484562861));
#76411=CARTESIAN_POINT('Ctrl Pts',(-14.7497747638115,4.31609622914609,128.442308714808));
#76412=CARTESIAN_POINT('Ctrl Pts',(-14.7575318046965,4.24695906082515,128.323932872564));
#76413=CARTESIAN_POINT('Ctrl Pts',(-14.7652829959366,4.17787402938064,128.205646298463));
#76414=CARTESIAN_POINT('Ctrl Pts',(-14.7730341871767,4.10378956129934,128.090155863583));
#76415=CARTESIAN_POINT('Ctrl Pts',(-14.7807853784168,4.02496491996688,127.977906928659));
#76416=CARTESIAN_POINT('Ctrl Pts',(-14.7885332751939,3.94617378120971,127.865705702527));
#76417=CARTESIAN_POINT('Ctrl Pts',(-14.7962811719711,3.8626467004984,127.756743555448));
#76418=CARTESIAN_POINT('Ctrl Pts',(-14.8040290687482,3.77468686913433,127.651437830296));
#76419=CARTESIAN_POINT('Ctrl Pts',(-14.8117753448323,3.68674543707079,127.546154132832));
#76420=CARTESIAN_POINT('Ctrl Pts',(-14.8195216209163,3.59437334915317,127.444525635847));
#76421=CARTESIAN_POINT('Ctrl Pts',(-14.8272678970004,3.49791453129496,127.346937155759));
#76422=CARTESIAN_POINT('Ctrl Pts',(-14.8350142302658,3.40145500139967,127.249347955295));
#76423=CARTESIAN_POINT('Ctrl Pts',(-14.8427605635311,3.30090895620719,127.155799109296));
#76424=CARTESIAN_POINT('Ctrl Pts',(-14.8505068967965,3.19665739131176,127.066638773304));
#76425=CARTESIAN_POINT('Ctrl Pts',(-14.8582549647995,3.09238248000135,126.977458470473));
#76426=CARTESIAN_POINT('Ctrl Pts',(-14.8660030328025,2.98440069479634,126.892668887323));
#76427=CARTESIAN_POINT('Ctrl Pts',(-14.8737511008054,2.87312600792428,126.812577807206));
#76428=CARTESIAN_POINT('Ctrl Pts',(-14.8815074035473,2.76173305699068,126.732401605335));
#76429=CARTESIAN_POINT('Ctrl Pts',(-14.8892637062891,2.64704053111599,126.656934110558));
#76430=CARTESIAN_POINT('Ctrl Pts',(-14.897020009031,2.52949174131606,126.586439969532));
#76431=CARTESIAN_POINT('Ctrl Pts',(-14.9047804515452,2.41188021218753,126.51590820366));
#76432=CARTESIAN_POINT('Ctrl Pts',(-14.9125408940594,2.29140972473817,126.450355267487));
#76433=CARTESIAN_POINT('Ctrl Pts',(-14.9203013365736,2.16854717946969,126.389999260256));
#76434=CARTESIAN_POINT('Ctrl Pts',(-14.928074236839,2.04548740433648,126.329546364203));
#76435=CARTESIAN_POINT('Ctrl Pts',(-14.9358471371045,1.92002825597656,126.274307225844));
#76436=CARTESIAN_POINT('Ctrl Pts',(-14.9436200373699,1.79265638100263,126.224451648804));
#76437=CARTESIAN_POINT('Ctrl Pts',(-14.9511103731319,1.66991479451543,126.176408447567));
#76438=CARTESIAN_POINT('Ctrl Pts',(-14.9586007088939,1.54539742301994,126.133364291742));
#76439=CARTESIAN_POINT('Ctrl Pts',(-14.9660910446558,1.41955016096979,126.095426512804));
#76440=CARTESIAN_POINT('Ctrl Pts',(-14.9738653787749,1.2889313617278,126.056050311446));
#76441=CARTESIAN_POINT('Ctrl Pts',(-14.9816397128939,1.15646607451228,126.022050615341));
#76442=CARTESIAN_POINT('Ctrl Pts',(-14.989414047013,1.02263649096341,125.993602083837));
#76443=CARTESIAN_POINT('Ctrl Pts',(-14.9971787999601,0.888971840415576,
125.965188612605));
#76444=CARTESIAN_POINT('Ctrl Pts',(-15.0049435529072,0.753946617715323,
125.942312774309));
#76445=CARTESIAN_POINT('Ctrl Pts',(-15.0127083058543,0.618059221551476,
125.925099827123));
#76446=CARTESIAN_POINT('Ctrl Pts',(-15.0204653467392,0.482306790665177,
125.907903976079));
#76447=CARTESIAN_POINT('Ctrl Pts',(-15.0282223876242,0.345694275792356,
125.896359872023));
#76448=CARTESIAN_POINT('Ctrl Pts',(-15.0359794285092,0.208730998887949,
125.890541895574));
#76449=CARTESIAN_POINT('Ctrl Pts',(-15.0437306197493,0.0718710070562605,
125.884728306506));
#76450=CARTESIAN_POINT('Ctrl Pts',(-15.0514818109894,-0.0653388312787332,
125.88463226662));
#76451=CARTESIAN_POINT('Ctrl Pts',(-15.0592330022295,-0.202383683323974,
125.890276378644));
#76452=CARTESIAN_POINT('Ctrl Pts',(-15.0669808990066,-0.339370287651492,
125.895918091769));
#76453=CARTESIAN_POINT('Ctrl Pts',(-15.0747287957836,-0.476191655343469,
125.907295088337));
#76454=CARTESIAN_POINT('Ctrl Pts',(-15.0824766925607,-0.612332781717113,
125.924377868935));
#76455=CARTESIAN_POINT('Ctrl Pts',(-15.0902229686448,-0.748445430301984,
125.941457076184));
#76456=CARTESIAN_POINT('Ctrl Pts',(-15.0979692447289,-0.883877732917281,
125.964239644828));
#76457=CARTESIAN_POINT('Ctrl Pts',(-15.105715520813,-1.01812003225422,125.992644222929));
#76458=CARTESIAN_POINT('Ctrl Pts',(-15.1134618540783,-1.15236332253714,
126.021049010706));
#76459=CARTESIAN_POINT('Ctrl Pts',(-15.1212081873436,-1.28541620951664,
126.055075809818));
#76460=CARTESIAN_POINT('Ctrl Pts',(-15.1289545206089,-1.41677984265017,
126.094592264456));
#76461=CARTESIAN_POINT('Ctrl Pts',(-15.1367025886119,-1.54817289375853,
126.13411756853));
#76462=CARTESIAN_POINT('Ctrl Pts',(-15.1444506566149,-1.67787556393353,
126.179134861832));
#76463=CARTESIAN_POINT('Ctrl Pts',(-15.1521987246178,-1.80540514422299,
126.229462222223));
#76464=CARTESIAN_POINT('Ctrl Pts',(-15.1599550273597,-1.93307026446818,
126.279843071132));
#76465=CARTESIAN_POINT('Ctrl Pts',(-15.1677113301015,-2.05855731693028,
126.335545117088));
#76466=CARTESIAN_POINT('Ctrl Pts',(-15.1754676328433,-2.18140402644909,
126.396338437961));
#76467=CARTESIAN_POINT('Ctrl Pts',(-15.1832280753575,-2.30431630295578,
126.45716420606));
#76468=CARTESIAN_POINT('Ctrl Pts',(-15.1909885178716,-2.42458508583469,
126.523086475831));
#76469=CARTESIAN_POINT('Ctrl Pts',(-15.1987489603858,-2.54177451089152,
126.593830318627));
#76470=CARTESIAN_POINT('Ctrl Pts',(-15.2065218606512,-2.65915205881689,
126.66468772572));
#76471=CARTESIAN_POINT('Ctrl Pts',(-15.2142947609166,-2.7734400445704,126.740381956848));
#76472=CARTESIAN_POINT('Ctrl Pts',(-15.222067661182,-2.88423256317253,126.820595365441));
#76473=CARTESIAN_POINT('Ctrl Pts',(-15.2295579969442,-2.99099749465696,
126.897892814589));
#76474=CARTESIAN_POINT('Ctrl Pts',(-15.2370483327064,-3.09451644282916,
126.979386388111));
#76475=CARTESIAN_POINT('Ctrl Pts',(-15.2445386684686,-3.19445808983532,
127.064758957658));
#76476=CARTESIAN_POINT('Ctrl Pts',(-15.2521993888874,-3.29667313602368,
127.152073519714));
#76477=CARTESIAN_POINT('Ctrl Pts',(-15.2598601093061,-3.39548998349483,
127.243739701335));
#76478=CARTESIAN_POINT('Ctrl Pts',(-15.2675208297248,-3.49050720138212,
127.3394590981));
#76479=CARTESIAN_POINT('Ctrl Pts',(-15.2751727470799,-3.58541523337387,
127.435068502083));
#76480=CARTESIAN_POINT('Ctrl Pts',(-15.2828246644349,-3.67653203411157,
127.534721579948));
#76481=CARTESIAN_POINT('Ctrl Pts',(-15.29047658179,-3.763488323915,127.63807909214));
#76482=CARTESIAN_POINT('Ctrl Pts',(-15.298121477469,-3.85036481948236,127.741341759741));
#76483=CARTESIAN_POINT('Ctrl Pts',(-15.305766373148,-3.93308813730865,127.848301796572));
#76484=CARTESIAN_POINT('Ctrl Pts',(-15.313411268827,-4.01132545497909,127.958582840448));
#76485=CARTESIAN_POINT('Ctrl Pts',(-15.3210509175266,-4.0895090754369,128.068788194298));
#76486=CARTESIAN_POINT('Ctrl Pts',(-15.3286905662262,-4.16321258705298,
128.182309694288));
#76487=CARTESIAN_POINT('Ctrl Pts',(-15.3363302149258,-4.23214348927605,
128.298738030527));
#76488=CARTESIAN_POINT('Ctrl Pts',(-15.3439670045153,-4.30104859436498,
128.415122793895));
#76489=CARTESIAN_POINT('Ctrl Pts',(-15.3516037941048,-4.36518443513168,
128.534411884905));
#76490=CARTESIAN_POINT('Ctrl Pts',(-15.3592405836943,-4.42430214705334,
128.656167522409));
#76491=CARTESIAN_POINT('Ctrl Pts',(-15.366875705914,-4.48340695157632,128.777896576535));
#76492=CARTESIAN_POINT('Ctrl Pts',(-15.3745108281337,-4.53749563414466,
128.902090741686));
#76493=CARTESIAN_POINT('Ctrl Pts',(-15.3821459503534,-4.58636587401425,
129.028288791266));
#76494=CARTESIAN_POINT('Ctrl Pts',(-15.3897827789429,-4.6352470358704,129.154515044787));
#76495=CARTESIAN_POINT('Ctrl Pts',(-15.3974196075324,-4.67890728089378,
129.282745700816));
#76496=CARTESIAN_POINT('Ctrl Pts',(-15.4050564361219,-4.71719300835156,
129.412501003791));
#76497=CARTESIAN_POINT('Ctrl Pts',(-15.4083752270557,-4.73383110932398,
129.468889688973));
#76498=CARTESIAN_POINT('Ctrl Pts',(-15.4116940179896,-4.74945482964605,
129.525566116095));
#76499=CARTESIAN_POINT('Ctrl Pts',(-15.4150128089234,-4.76405452823406,
129.582490119308));
#76500=CARTESIAN_POINT('Ctrl Pts',(-13.6653609210472,-4.76405452823398,
129.582490119308));
#76501=CARTESIAN_POINT('Ctrl Pts',(-13.6732618994108,-4.79879020631677,
129.717924000965));
#76502=CARTESIAN_POINT('Ctrl Pts',(-13.6811628777745,-4.82777218857766,
129.854940509252));
#76503=CARTESIAN_POINT('Ctrl Pts',(-13.6890638561381,-4.85086715689499,
129.993021669495));
#76504=CARTESIAN_POINT('Ctrl Pts',(-13.6969596860506,-4.87394707602353,
130.13101285302));
#76505=CARTESIAN_POINT('Ctrl Pts',(-13.7048555159631,-4.89114756217927,
130.270066943089));
#76506=CARTESIAN_POINT('Ctrl Pts',(-13.7127513458757,-4.90238621151786,
130.409655036633));
#76507=CARTESIAN_POINT('Ctrl Pts',(-13.7202144185867,-4.91300888932577,
130.541592540764));
#76508=CARTESIAN_POINT('Ctrl Pts',(-13.7276774912976,-4.91830570436068,
130.674006763662));
#76509=CARTESIAN_POINT('Ctrl Pts',(-13.7351405640086,-4.91824955803066,
130.806445667018));
#76510=CARTESIAN_POINT('',(-13.3898594359426,-4.91824795577628,130.79987642283));
#76511=CARTESIAN_POINT('Ctrl Pts',(-13.3199629969565,-4.76405452823408,
129.582490119308));
#76512=CARTESIAN_POINT('Ctrl Pts',(-13.3298371033895,-4.80711016204549,
129.750363382079));
#76513=CARTESIAN_POINT('Ctrl Pts',(-13.3397112098226,-4.84131703731055,
129.920624555717));
#76514=CARTESIAN_POINT('Ctrl Pts',(-13.3495853162557,-4.86645366289561,
130.092453454103));
#76515=CARTESIAN_POINT('Ctrl Pts',(-13.3592886505582,-4.89115555191633,
130.261310581092));
#76516=CARTESIAN_POINT('Ctrl Pts',(-13.3689919848608,-4.90709822462204,
130.431681817717));
#76517=CARTESIAN_POINT('Ctrl Pts',(-13.3786953191633,-4.91411671521435,
130.602767036937));
#76518=CARTESIAN_POINT('Ctrl Pts',(-13.3824166914231,-4.91680841019069,
130.668380749606));
#76519=CARTESIAN_POINT('Ctrl Pts',(-13.3861380636829,-4.91818798366446,
130.73409923568));
#76520=CARTESIAN_POINT('Ctrl Pts',(-13.3898594359427,-4.91824795577628,
130.79987642283));
#76521=CARTESIAN_POINT('Ctrl Pts',(-13.3898594359912,-4.91824795577706,
130.799876423688));
#76522=CARTESIAN_POINT('Ctrl Pts',(-13.3975363273454,-4.91837167339157,
130.935569464879));
#76523=CARTESIAN_POINT('Ctrl Pts',(-13.4052132186995,-4.91287556913946,
131.071391386066));
#76524=CARTESIAN_POINT('Ctrl Pts',(-13.4128901100537,-4.90175450304585,
131.206835280582));
#76525=CARTESIAN_POINT('Ctrl Pts',(-13.4205632856729,-4.89063881972146,
131.342213618143));
#76526=CARTESIAN_POINT('Ctrl Pts',(-13.4282364612921,-4.8739036210423,131.477213895897));
#76527=CARTESIAN_POINT('Ctrl Pts',(-13.4359096369112,-4.85159584056564,
131.611330791926));
#76528=CARTESIAN_POINT('Ctrl Pts',(-13.4435809797105,-4.82929338854051,
131.745415652702));
#76529=CARTESIAN_POINT('Ctrl Pts',(-13.4512523225096,-4.80142106671531,
131.878617157695));
#76530=CARTESIAN_POINT('Ctrl Pts',(-13.4589236653089,-4.76807743543659,
132.010437162475));
#76531=CARTESIAN_POINT('Ctrl Pts',(-13.4665949157291,-4.73473420568499,
132.142255579867));
#76532=CARTESIAN_POINT('Ctrl Pts',(-13.4742661661493,-4.69591989540284,
132.272692143006));
#76533=CARTESIAN_POINT('Ctrl Pts',(-13.4819374165695,-4.65178362366143,
132.401261422605));
#76534=CARTESIAN_POINT('Ctrl Pts',(-13.489610314709,-4.6076378718244,132.529858317792));
#76535=CARTESIAN_POINT('Ctrl Pts',(-13.4972832128486,-4.55816801480284,
132.65658675421));
#76536=CARTESIAN_POINT('Ctrl Pts',(-13.5049561109881,-4.50357205354791,
132.780979402512));
#76537=CARTESIAN_POINT('Ctrl Pts',(-13.5126370681599,-4.44891874882148,
132.905502703451));
#76538=CARTESIAN_POINT('Ctrl Pts',(-13.5203180253318,-4.38912874803837,
133.027684950592));
#76539=CARTESIAN_POINT('Ctrl Pts',(-13.5279989825036,-4.32444712998896,
133.147081275782));
#76540=CARTESIAN_POINT('Ctrl Pts',(-13.5356841167854,-4.25973033634509,
133.266542531887));
#76541=CARTESIAN_POINT('Ctrl Pts',(-13.5433692510673,-4.19011683222443,
133.383214506446));
#76542=CARTESIAN_POINT('Ctrl Pts',(-13.5510543853491,-4.11589548455543,
133.496680699339));
#76543=CARTESIAN_POINT('Ctrl Pts',(-13.5587516183043,-4.04155729054306,
133.610325521564));
#76544=CARTESIAN_POINT('Ctrl Pts',(-13.5664488512594,-3.96259699478743,
133.720754156435));
#76545=CARTESIAN_POINT('Ctrl Pts',(-13.5741460842146,-3.87934467018035,
133.827582076944));
#76546=CARTESIAN_POINT('Ctrl Pts',(-13.58057803006,-3.8097775352768,133.916849402422));
#76547=CARTESIAN_POINT('Ctrl Pts',(-13.5870099759055,-3.73721425178249,
134.003603028335));
#76548=CARTESIAN_POINT('Ctrl Pts',(-13.5934419217509,-3.66186656095311,
134.087638911021));
#76549=CARTESIAN_POINT('Ctrl Pts',(-13.60121625587,-3.57079332469017,134.1892136204));
#76550=CARTESIAN_POINT('Ctrl Pts',(-13.608990589989,-3.47534633594947,134.287156991757));
#76551=CARTESIAN_POINT('Ctrl Pts',(-13.6167649241081,-3.37584655978066,
134.381069029964));
#76552=CARTESIAN_POINT('Ctrl Pts',(-13.6245296770552,-3.27646940819343,
134.474865329976));
#76553=CARTESIAN_POINT('Ctrl Pts',(-13.6322944300024,-3.17304968873191,
134.564639916411));
#76554=CARTESIAN_POINT('Ctrl Pts',(-13.6400591829495,-3.06594790565478,
134.650026554996));
#76555=CARTESIAN_POINT('Ctrl Pts',(-13.6478162238345,-2.95895249757833,
134.735328386368));
#76556=CARTESIAN_POINT('Ctrl Pts',(-13.6555732647195,-2.84828260735985,
134.816250700704));
#76557=CARTESIAN_POINT('Ctrl Pts',(-13.6633303056045,-2.73433453379736,
134.892465034014));
#76558=CARTESIAN_POINT('Ctrl Pts',(-13.6710814968446,-2.62047238936337,
134.968621893503));
#76559=CARTESIAN_POINT('Ctrl Pts',(-13.6788326880847,-2.50333730581731,
135.040077622192));
#76560=CARTESIAN_POINT('Ctrl Pts',(-13.6865838793249,-2.38335722231097,
135.106545110746));
#76561=CARTESIAN_POINT('Ctrl Pts',(-13.694331776102,-2.26342813354102,135.172984348844));
#76562=CARTESIAN_POINT('Ctrl Pts',(-13.7020796728791,-2.14065679109562,
135.234439374532));
#76563=CARTESIAN_POINT('Ctrl Pts',(-13.7098275696562,-2.01549838337967,
135.290667487263));
#76564=CARTESIAN_POINT('Ctrl Pts',(-13.7175738457403,-1.89036615610433,
135.346883838286));
#76565=CARTESIAN_POINT('Ctrl Pts',(-13.7253201218245,-1.76284821314136,
135.397875290985));
#76566=CARTESIAN_POINT('Ctrl Pts',(-13.7330663979086,-1.63342214853847,
135.443446211427));
#76567=CARTESIAN_POINT('Ctrl Pts',(-13.7408127311739,-1.50399512854177,
135.489017468262));
#76568=CARTESIAN_POINT('Ctrl Pts',(-13.7485590644393,-1.37266032757259,
135.529167983153));
#76569=CARTESIAN_POINT('Ctrl Pts',(-13.7563053977047,-1.23991264123651,
135.563751303841));
#76570=CARTESIAN_POINT('Ctrl Pts',(-13.7640534657077,-1.10713522697667,
135.598342369224));
#76571=CARTESIAN_POINT('Ctrl Pts',(-13.7718015337106,-0.972944676003497,
135.627363661002));
#76572=CARTESIAN_POINT('Ctrl Pts',(-13.7795496017136,-0.83784788145648,
135.650719455915));
#76573=CARTESIAN_POINT('Ctrl Pts',(-13.7873059044555,-0.702607504428361,
135.674100073644));
#76574=CARTESIAN_POINT('Ctrl Pts',(-13.7950622071974,-0.566459345662321,
135.69180309949));
#76575=CARTESIAN_POINT('Ctrl Pts',(-13.8028185099393,-0.429917815269413,
135.703784434161));
#76576=CARTESIAN_POINT('Ctrl Pts',(-13.8105789524535,-0.293303408550549,
135.71577216363));
#76577=CARTESIAN_POINT('Ctrl Pts',(-13.8183393949676,-0.156295602219792,
135.722032099057));
#76578=CARTESIAN_POINT('Ctrl Pts',(-13.8260998374818,-0.0194096613690958,
135.722572317721));
#76579=CARTESIAN_POINT('Ctrl Pts',(-13.8338727377473,0.117696020946017,
135.723113403593));
#76580=CARTESIAN_POINT('Ctrl Pts',(-13.8416456380127,0.254679055942418,
135.717916439378));
#76581=CARTESIAN_POINT('Ctrl Pts',(-13.8494185382781,0.391027544433969,
135.707041570065));
#76582=CARTESIAN_POINT('Ctrl Pts',(-13.85690887404,0.522419421925151,135.696562029644));
#76583=CARTESIAN_POINT('Ctrl Pts',(-13.8643992098019,0.65322178086342,135.680810266229));
#76584=CARTESIAN_POINT('Ctrl Pts',(-13.8718895455638,0.782986693298438,
135.659884780889));
#76585=CARTESIAN_POINT('Ctrl Pts',(-13.8796638796829,0.917671681832088,
135.638165899413));
#76586=CARTESIAN_POINT('Ctrl Pts',(-13.887438213802,1.05166564289178,135.610804429205));
#76587=CARTESIAN_POINT('Ctrl Pts',(-13.8952125479211,1.18445855979839,135.577854200113));
#76588=CARTESIAN_POINT('Ctrl Pts',(-13.9029773008682,1.31708782130297,135.544944579235));
#76589=CARTESIAN_POINT('Ctrl Pts',(-13.9107420538153,1.44851860795529,135.506459997087));
#76590=CARTESIAN_POINT('Ctrl Pts',(-13.9185068067624,1.57824793513165,135.462505797544));
#76591=CARTESIAN_POINT('Ctrl Pts',(-13.9262638476474,1.70784841331139,135.418595253931));
#76592=CARTESIAN_POINT('Ctrl Pts',(-13.9340208885324,1.83575042712674,135.369226028493));
#76593=CARTESIAN_POINT('Ctrl Pts',(-13.9417779294174,1.96146342133941,135.31455399582));
#76594=CARTESIAN_POINT('Ctrl Pts',(-13.9495291206575,2.0870816144049,135.259923191753));
#76595=CARTESIAN_POINT('Ctrl Pts',(-13.9572803118977,2.21051371652188,135.199997695288));
#76596=CARTESIAN_POINT('Ctrl Pts',(-13.9650315031378,2.33128686291064,135.134982354144));
#76597=CARTESIAN_POINT('Ctrl Pts',(-13.9727793999148,2.45200867749061,135.069994646254));
#76598=CARTESIAN_POINT('Ctrl Pts',(-13.9805272966919,2.57007344054672,134.999921581297));
#76599=CARTESIAN_POINT('Ctrl Pts',(-13.988275193469,2.68503092078517,134.925014936594));
#76600=CARTESIAN_POINT('Ctrl Pts',(-13.9960214695531,2.7999643543968,134.850123960748));
#76601=CARTESIAN_POINT('Ctrl Pts',(-14.0037677456372,2.91179147067523,134.770401629557));
#76602=CARTESIAN_POINT('Ctrl Pts',(-14.0115140217212,3.02008952600336,134.6861440115));
#76603=CARTESIAN_POINT('Ctrl Pts',(-14.0192603549866,3.12838838076328,134.601885771473));
#76604=CARTESIAN_POINT('Ctrl Pts',(-14.0270066882519,3.23315781401694,134.513092417853));
#76605=CARTESIAN_POINT('Ctrl Pts',(-14.0347530215173,3.33400710816931,134.420101159305));
#76606=CARTESIAN_POINT('Ctrl Pts',(-14.0425010895202,3.43487898682174,134.32708907601));
#76607=CARTESIAN_POINT('Ctrl Pts',(-14.0502491575232,3.53182869210733,134.229877482093));
#76608=CARTESIAN_POINT('Ctrl Pts',(-14.0579972255262,3.62450170121326,134.128841100349));
#76609=CARTESIAN_POINT('Ctrl Pts',(-14.065753528268,3.71727320429623,134.027697335935));
#76610=CARTESIAN_POINT('Ctrl Pts',(-14.0735098310098,3.80575866673257,133.922720951939));
#76611=CARTESIAN_POINT('Ctrl Pts',(-14.0812661337517,3.88964293530966,133.814320899413));
#76612=CARTESIAN_POINT('Ctrl Pts',(-14.0890265762659,3.97357197544682,133.705862990514));
#76613=CARTESIAN_POINT('Ctrl Pts',(-14.0967870187801,4.05289470233521,133.593978090791));
#76614=CARTESIAN_POINT('Ctrl Pts',(-14.1045474612943,4.12733939825272,133.479104073326));
#76615=CARTESIAN_POINT('Ctrl Pts',(-14.1123203615597,4.2019035994049,133.36404564989));
#76616=CARTESIAN_POINT('Ctrl Pts',(-14.1200932618251,4.27157392263712,133.245988856886));
#76617=CARTESIAN_POINT('Ctrl Pts',(-14.1278661620905,4.33612427561852,133.125396879431));
#76618=CARTESIAN_POINT('Ctrl Pts',(-14.1353564978526,4.39832806067669,133.009188724109));
#76619=CARTESIAN_POINT('Ctrl Pts',(-14.1428468336146,4.45577752603527,132.890626782133));
#76620=CARTESIAN_POINT('Ctrl Pts',(-14.1503371693767,4.50831342743531,132.770141150206));
#76621=CARTESIAN_POINT('Ctrl Pts',(-14.1581115034957,4.56284124350458,132.645087268925));
#76622=CARTESIAN_POINT('Ctrl Pts',(-14.1658858376148,4.61224827263818,132.517564811591));
#76623=CARTESIAN_POINT('Ctrl Pts',(-14.1736601717339,4.65630412693997,132.388031966029));
#76624=CARTESIAN_POINT('Ctrl Pts',(-14.181424924681,4.70030568633866,132.258658758122));
#76625=CARTESIAN_POINT('Ctrl Pts',(-14.1891896776281,4.73896906799908,132.12728045831));
#76626=CARTESIAN_POINT('Ctrl Pts',(-14.1969544305751,4.77211102522948,131.994377182738));
#76627=CARTESIAN_POINT('Ctrl Pts',(-14.2047114714601,4.80522006540083,131.861605908572));
#76628=CARTESIAN_POINT('Ctrl Pts',(-14.2124685123451,4.83281850047766,131.727313049716));
#76629=CARTESIAN_POINT('Ctrl Pts',(-14.2202255532301,4.85477231508046,131.59199557821));
#76630=CARTESIAN_POINT('Ctrl Pts',(-14.2279767444702,4.87670957414084,131.456780150662));
#76631=CARTESIAN_POINT('Ctrl Pts',(-14.2357279357103,4.89301062297737,131.320542032771));
#76632=CARTESIAN_POINT('Ctrl Pts',(-14.2434791269504,4.90359221081424,131.183789784265));
#76633=CARTESIAN_POINT('Ctrl Pts',(-14.2512270237275,4.91416930119401,131.047095659112));
#76634=CARTESIAN_POINT('Ctrl Pts',(-14.2589749205045,4.91903173539689,130.909888226946));
#76635=CARTESIAN_POINT('Ctrl Pts',(-14.2667228172815,4.91814797980413,130.772682371899));
#76636=CARTESIAN_POINT('Ctrl Pts',(-14.2744690933656,4.91726440907399,130.635505217358));
#76637=CARTESIAN_POINT('Ctrl Pts',(-14.2822153694497,4.910637041867,130.49833002999));
#76638=CARTESIAN_POINT('Ctrl Pts',(-14.2899616455338,4.89828646572864,130.361672508216));
#76639=CARTESIAN_POINT('Ctrl Pts',(-14.2977079787992,4.88593579842112,130.225013977668));
#76640=CARTESIAN_POINT('Ctrl Pts',(-14.3054543120645,4.86786187307103,130.088873509717));
#76641=CARTESIAN_POINT('Ctrl Pts',(-14.3132006453299,4.84413720047614,129.953762095663));
#76642=CARTESIAN_POINT('Ctrl Pts',(-14.3209487133328,4.82040721490538,129.818620424346));
#76643=CARTESIAN_POINT('Ctrl Pts',(-14.3286967813357,4.79102403160295,129.684508650494));
#76644=CARTESIAN_POINT('Ctrl Pts',(-14.3364448493386,4.75611128722829,129.551927591013));
#76645=CARTESIAN_POINT('Ctrl Pts',(-14.3442011520805,4.72116143717333,129.419205622805));
#76646=CARTESIAN_POINT('Ctrl Pts',(-14.3519574548224,4.68067038605675,129.288017997479));
#76647=CARTESIAN_POINT('Ctrl Pts',(-14.3597137575642,4.63481184797063,129.15885091039));
#76648=CARTESIAN_POINT('Ctrl Pts',(-14.3674742000784,4.58892883380197,129.029614882938));
#76649=CARTESIAN_POINT('Ctrl Pts',(-14.3752346425925,4.53767277036861,128.902401905029));
#76650=CARTESIAN_POINT('Ctrl Pts',(-14.3829950851067,4.48126518263077,128.777677261577));
#76651=CARTESIAN_POINT('Ctrl Pts',(-14.3907679853721,4.42476704442539,128.652752399055));
#76652=CARTESIAN_POINT('Ctrl Pts',(-14.3985408856375,4.36310103242801,128.530324202637));
#76653=CARTESIAN_POINT('Ctrl Pts',(-14.4063137859029,4.2965346289699,128.410833253076));
#76654=CARTESIAN_POINT('Ctrl Pts',(-14.4138041216651,4.23238808194635,128.295686100508));
#76655=CARTESIAN_POINT('Ctrl Pts',(-14.4212944574273,4.16369140161882,128.183266612571));
#76656=CARTESIAN_POINT('Ctrl Pts',(-14.4287847931896,4.09072036511427,128.073941243745));
#76657=CARTESIAN_POINT('Ctrl Pts',(-14.4365591273086,4.01498260958352,127.960470770334));
#76658=CARTESIAN_POINT('Ctrl Pts',(-14.4443334614278,3.93440006068489,127.849974234345));
#76659=CARTESIAN_POINT('Ctrl Pts',(-14.4521077955469,3.84923367452668,127.742893129352));
#76660=CARTESIAN_POINT('Ctrl Pts',(-14.459872548494,3.76417224832787,127.635943992251));
#76661=CARTESIAN_POINT('Ctrl Pts',(-14.4676373014411,3.67453846606171,127.532402214114));
#76662=CARTESIAN_POINT('Ctrl Pts',(-14.4754020543882,3.58063721372605,127.432681480077));
#76663=CARTESIAN_POINT('Ctrl Pts',(-14.4831590952732,3.48682922543759,127.333059790078));
#76664=CARTESIAN_POINT('Ctrl Pts',(-14.4909161361583,3.38876246819827,127.237251874522));
#76665=CARTESIAN_POINT('Ctrl Pts',(-14.4986731770434,3.28678262007412,127.14563910987));
#76666=CARTESIAN_POINT('Ctrl Pts',(-14.5064243682835,3.18487967574659,127.054095431116));
#76667=CARTESIAN_POINT('Ctrl Pts',(-14.5141755595237,3.07906980377133,126.966740866538));
#76668=CARTESIAN_POINT('Ctrl Pts',(-14.5219267507639,2.96973587077239,126.883920346328));
#76669=CARTESIAN_POINT('Ctrl Pts',(-14.529674647541,2.86044840761215,126.801135027048));
#76670=CARTESIAN_POINT('Ctrl Pts',(-14.537422544318,2.74764017347205,126.722880154878));
#76671=CARTESIAN_POINT('Ctrl Pts',(-14.5451704410951,2.63172731026352,126.649460567395));
#76672=CARTESIAN_POINT('Ctrl Pts',(-14.5529167171793,2.51583869352686,126.576056337706));
#76673=CARTESIAN_POINT('Ctrl Pts',(-14.5606629932634,2.39684706953185,126.507485589972));
#76674=CARTESIAN_POINT('Ctrl Pts',(-14.5684092693475,2.27519743803797,126.444009750899));
#76675=CARTESIAN_POINT('Ctrl Pts',(-14.5761556026129,2.15354690855448,126.380533443262));
#76676=CARTESIAN_POINT('Ctrl Pts',(-14.5839019358782,2.02923867903652,126.322152300196));
#76677=CARTESIAN_POINT('Ctrl Pts',(-14.5916482691436,1.90274185479385,126.269081519592));
#76678=CARTESIAN_POINT('Ctrl Pts',(-14.5993963371466,1.77621670246445,126.215998854155));
#76679=CARTESIAN_POINT('Ctrl Pts',(-14.6071444051495,1.64750234057987,126.168229068814));
#76680=CARTESIAN_POINT('Ctrl Pts',(-14.6148924731525,1.51708694922172,126.125938848315));
#76681=CARTESIAN_POINT('Ctrl Pts',(-14.6226487758944,1.3865329508335,126.083603681267));
#76682=CARTESIAN_POINT('Ctrl Pts',(-14.6304050786364,1.25427468404155,126.046759833413));
#76683=CARTESIAN_POINT('Ctrl Pts',(-14.6381613813782,1.12081509547845,126.015523954633));
#76684=CARTESIAN_POINT('Ctrl Pts',(-14.6459218238924,0.987284275514368,
125.984271404325));
#76685=CARTESIAN_POINT('Ctrl Pts',(-14.6536822664065,0.852551240055837,
125.95863286023));
#76686=CARTESIAN_POINT('Ctrl Pts',(-14.6614427089207,0.717127186129043,
125.938673444985));
#76687=CARTESIAN_POINT('Ctrl Pts',(-14.6692156091862,0.581485737488688,
125.918681989116));
#76688=CARTESIAN_POINT('Ctrl Pts',(-14.6769885094517,0.445151442734468,
125.904387920843));
#76689=CARTESIAN_POINT('Ctrl Pts',(-14.6847614097172,0.308639555664589,
125.895804344365));
#76690=CARTESIAN_POINT('Ctrl Pts',(-14.692251745479,0.177090219546643,125.887532802513));
#76691=CARTESIAN_POINT('Ctrl Pts',(-14.6997420812408,0.0453762867405826,
125.884563786036));
#76692=CARTESIAN_POINT('Ctrl Pts',(-14.7072324170026,-0.0860448699480239,
125.886863353423));
#76693=CARTESIAN_POINT('Ctrl Pts',(-14.7150067511217,-0.222448899741297,
125.889250109607));
#76694=CARTESIAN_POINT('Ctrl Pts',(-14.7227810852407,-0.358969600910853,
125.897320413482));
#76695=CARTESIAN_POINT('Ctrl Pts',(-14.7305554193598,-0.495094479259071,
125.911093353344));
#76696=CARTESIAN_POINT('Ctrl Pts',(-14.7383201723069,-0.631051595860555,
125.924849319289));
#76697=CARTESIAN_POINT('Ctrl Pts',(-14.746084925254,-0.766613475004552,
125.944293898638));
#76698=CARTESIAN_POINT('Ctrl Pts',(-14.7538496782011,-0.901267273341114,
125.969394189089));
#76699=CARTESIAN_POINT('Ctrl Pts',(-14.7616067190861,-1.03578733162652,
125.994469549576));
#76700=CARTESIAN_POINT('Ctrl Pts',(-14.7693637599712,-1.16940072210564,
126.02518937124));
#76701=CARTESIAN_POINT('Ctrl Pts',(-14.7771208008562,-1.30159973452234,
126.061468968625));
#76702=CARTESIAN_POINT('Ctrl Pts',(-14.7848719920963,-1.43369905463559,
126.097721207284));
#76703=CARTESIAN_POINT('Ctrl Pts',(-14.7926231833364,-1.56438574417613,
126.13952477336));
#76704=CARTESIAN_POINT('Ctrl Pts',(-14.8003743745765,-1.69316265484348,
126.186743993512));
#76705=CARTESIAN_POINT('Ctrl Pts',(-14.8081222713536,-1.82188483188873,
126.233943144235));
#76706=CARTESIAN_POINT('Ctrl Pts',(-14.8158701681307,-1.94869847818551,
126.286553236623));
#76707=CARTESIAN_POINT('Ctrl Pts',(-14.8236180649078,-2.07312219037915,
126.344388930856));
#76708=CARTESIAN_POINT('Ctrl Pts',(-14.831364340992,-2.19751987581481,126.402212527108));
#76709=CARTESIAN_POINT('Ctrl Pts',(-14.8391106170761,-2.31952826721017,
126.465259386308));
#76710=CARTESIAN_POINT('Ctrl Pts',(-14.8468568931603,-2.43868688563124,
126.533296425078));
#76711=CARTESIAN_POINT('Ctrl Pts',(-14.8546032264256,-2.55784638365399,
126.601333966082));
#76712=CARTESIAN_POINT('Ctrl Pts',(-14.862349559691,-2.67415572720725,126.674361566302));
#76713=CARTESIAN_POINT('Ctrl Pts',(-14.8700958929564,-2.78718030133189,
126.752100873871));
#76714=CARTESIAN_POINT('Ctrl Pts',(-14.8778439609594,-2.90023018652624,
126.82985759062));
#76715=CARTESIAN_POINT('Ctrl Pts',(-14.8855920289624,-3.00999351646686,
126.912327892835));
#76716=CARTESIAN_POINT('Ctrl Pts',(-14.8933400969654,-3.11606618129598,
126.999191157965));
#76717=CARTESIAN_POINT('Ctrl Pts',(-14.9010963997073,-3.22225158141542,
127.086146742406));
#76718=CARTESIAN_POINT('Ctrl Pts',(-14.9088527024491,-3.32473817787577,
127.177504368281));
#76719=CARTESIAN_POINT('Ctrl Pts',(-14.916609005191,-3.42315597488899,127.272903944452));
#76720=CARTESIAN_POINT('Ctrl Pts',(-14.9243694477052,-3.52162630044404,
127.368354438249));
#76721=CARTESIAN_POINT('Ctrl Pts',(-14.9321298902195,-3.61602323041533,
127.467850897479));
#76722=CARTESIAN_POINT('Ctrl Pts',(-14.9398903327337,-3.70601566080439,
127.570998437981));
#76723=CARTESIAN_POINT('Ctrl Pts',(-14.9476632329991,-3.79615255503162,
127.674311560071));
#76724=CARTESIAN_POINT('Ctrl Pts',(-14.9554361332646,-3.88187057596333,
127.781287170382));
#76725=CARTESIAN_POINT('Ctrl Pts',(-14.96320903353,-3.96288019140338,127.89149885444));
#76726=CARTESIAN_POINT('Ctrl Pts',(-14.9706993692919,-4.04094490326898,
127.997704066172));
#76727=CARTESIAN_POINT('Ctrl Pts',(-14.9781897050536,-4.11463741889196,
128.106913902246));
#76728=CARTESIAN_POINT('Ctrl Pts',(-14.9856800408154,-4.1837390730525,128.218725215752));
#76729=CARTESIAN_POINT('Ctrl Pts',(-14.9936823409788,-4.25756382483398,
128.338178831823));
#76730=CARTESIAN_POINT('Ctrl Pts',(-15.0016846411421,-4.32637116804915,
128.460961806611));
#76731=CARTESIAN_POINT('Ctrl Pts',(-15.0096869413055,-4.38985700074989,
128.58662786192));
#76732=CARTESIAN_POINT('Ctrl Pts',(-15.0176787073992,-4.45325926195633,
128.712128492918));
#76733=CARTESIAN_POINT('Ctrl Pts',(-15.0256704734928,-4.51135379639687,
128.840504331396));
#76734=CARTESIAN_POINT('Ctrl Pts',(-15.0336622395865,-4.5638801270555,128.971280900705));
#76735=CARTESIAN_POINT('Ctrl Pts',(-15.0416415926349,-4.61632487227774,
129.101854344013));
#76736=CARTESIAN_POINT('Ctrl Pts',(-15.0496209456833,-4.66321851569826,
129.234820755411));
#76737=CARTESIAN_POINT('Ctrl Pts',(-15.0576002987317,-4.70434710270981,
129.369682465601));
#76738=CARTESIAN_POINT('Ctrl Pts',(-15.0617682289556,-4.72583018283312,
129.440126045994));
#76739=CARTESIAN_POINT('Ctrl Pts',(-15.0659361591794,-4.74574110107282,
129.511086344752));
#76740=CARTESIAN_POINT('Ctrl Pts',(-15.0701040894033,-4.76405452823398,
129.582490119308));
#76741=CARTESIAN_POINT('Origin',(213.235140564004,0.,130.804360617566));
#76742=CARTESIAN_POINT('',(-17.1650861998779,-4.76405452823408,129.582490119308));
#76743=CARTESIAN_POINT('',(-16.8197493731202,-4.76405452823399,129.582490119308));
#76744=CARTESIAN_POINT('',(213.235140564004,-4.76405452823405,129.582490119308));
#76745=CARTESIAN_POINT('',(-15.4851405639739,-4.91824870592851,130.807928408546));
#76746=CARTESIAN_POINT('Ctrl Pts',(-15.4851405640086,-4.91824870592807,
130.807928409157));
#76747=CARTESIAN_POINT('Ctrl Pts',(-15.4977558067663,-4.91808770741904,
131.029867019779));
#76748=CARTESIAN_POINT('Ctrl Pts',(-15.510371049524,-4.90290341425378,131.251269447092));
#76749=CARTESIAN_POINT('Ctrl Pts',(-15.5229862922817,-4.87291541403578,
131.470602638271));
#76750=CARTESIAN_POINT('Ctrl Pts',(-15.530760626401,-4.85443485541762,131.60577003413));
#76751=CARTESIAN_POINT('Ctrl Pts',(-15.5385349605204,-4.83029675023916,
131.740382008084));
#76752=CARTESIAN_POINT('Ctrl Pts',(-15.5463092946397,-4.80054267385402,
131.87392739856));
#76753=CARTESIAN_POINT('Ctrl Pts',(-15.5540740475871,-4.77082526670883,
132.007308206278));
#76754=CARTESIAN_POINT('Ctrl Pts',(-15.5618388005343,-4.73550574365403,
132.139624667972));
#76755=CARTESIAN_POINT('Ctrl Pts',(-15.5696035534817,-4.69467734798167,
132.270371415905));
#76756=CARTESIAN_POINT('Ctrl Pts',(-15.5773605943669,-4.65388950364741,
132.400988304325));
#76757=CARTESIAN_POINT('Ctrl Pts',(-15.5851176352523,-4.6076037909906,132.530038210809));
#76758=CARTESIAN_POINT('Ctrl Pts',(-15.5928746761375,-4.55596426774261,
132.657026980825));
#76759=CARTESIAN_POINT('Ctrl Pts',(-15.6006258673778,-4.50436368626094,
132.783919987622));
#76760=CARTESIAN_POINT('Ctrl Pts',(-15.6083770586182,-4.44741747696651,
132.908754591029));
#76761=CARTESIAN_POINT('Ctrl Pts',(-15.6161282498585,-4.38531908113688,
133.031053146659));
#76762=CARTESIAN_POINT('Ctrl Pts',(-15.6238761466358,-4.32324707878183,
133.15329972214));
#76763=CARTESIAN_POINT('Ctrl Pts',(-15.631624043413,-4.25602742190536,133.273012045811));
#76764=CARTESIAN_POINT('Ctrl Pts',(-15.6393719401903,-4.18390101101587,
133.38973397407));
#76765=CARTESIAN_POINT('Ctrl Pts',(-15.6471182162746,-4.11178968741656,
133.506431486618));
#76766=CARTESIAN_POINT('Ctrl Pts',(-15.654864492359,-4.03477385673277,133.620139515583));
#76767=CARTESIAN_POINT('Ctrl Pts',(-15.6626107684433,-3.95313935750207,
133.730428334258));
#76768=CARTESIAN_POINT('Ctrl Pts',(-15.6703571017088,-3.87150425566404,
133.840717967061));
#76769=CARTESIAN_POINT('Ctrl Pts',(-15.6781034349744,-3.78525064984824,
133.947588024965));
#76770=CARTESIAN_POINT('Ctrl Pts',(-15.6858497682399,-3.69470627546886,
134.050639810813));
#76771=CARTESIAN_POINT('Ctrl Pts',(-15.6935978362431,-3.6041416243045,134.153714674395));
#76772=CARTESIAN_POINT('Ctrl Pts',(-15.7013459042464,-3.5092845505272,134.252969270775));
#76773=CARTESIAN_POINT('Ctrl Pts',(-15.7090939722496,-3.41050116145027,
134.348040186918));
#76774=CARTESIAN_POINT('Ctrl Pts',(-15.7168502749916,-3.31161278421204,
134.443212145563));
#76775=CARTESIAN_POINT('Ctrl Pts',(-15.7246065777337,-3.20879003793378,
134.534191270137));
#76776=CARTESIAN_POINT('Ctrl Pts',(-15.7323628804758,-3.10243419309094,
134.620652684486));
#76777=CARTESIAN_POINT('Ctrl Pts',(-15.7401233229902,-2.99602158293124,
134.707160245896));
#76778=CARTESIAN_POINT('Ctrl Pts',(-15.7478837655046,-2.88607243001839,
134.789145058891));
#76779=CARTESIAN_POINT('Ctrl Pts',(-15.755644208019,-2.77301796086281,134.866324976252));
#76780=CARTESIAN_POINT('Ctrl Pts',(-15.7634171082846,-2.659782006637,134.943628789667));
#76781=CARTESIAN_POINT('Ctrl Pts',(-15.7711900085503,-2.54343110672227,
135.01611208708));
#76782=CARTESIAN_POINT('Ctrl Pts',(-15.7789629088159,-2.42442288725927,
135.083537726104));
#76783=CARTESIAN_POINT('Ctrl Pts',(-15.7864532445754,-2.30974091637957,
135.14851227329));
#76784=CARTESIAN_POINT('Ctrl Pts',(-15.7939435803349,-2.19259174611555,
135.208790354296));
#76785=CARTESIAN_POINT('Ctrl Pts',(-15.8014339160943,-2.0734015278911,135.264202449586));
#76786=CARTESIAN_POINT('Ctrl Pts',(-15.8092082502134,-1.94969217627408,
135.321715511331));
#76787=CARTESIAN_POINT('Ctrl Pts',(-15.8169825843325,-1.82339207472626,
135.374168499819));
#76788=CARTESIAN_POINT('Ctrl Pts',(-15.8247569184515,-1.69495375045156,
135.421320098256));
#76789=CARTESIAN_POINT('Ctrl Pts',(-15.8325216713986,-1.56667371493285,
135.468413586561));
#76790=CARTESIAN_POINT('Ctrl Pts',(-15.8402864243456,-1.43626106337846,
135.510218551069));
#76791=CARTESIAN_POINT('Ctrl Pts',(-15.8480511772927,-1.30419137625695,
135.546540276393));
#76792=CARTESIAN_POINT('Ctrl Pts',(-15.8558082181777,-1.17225286261054,
135.582825926469));
#76793=CARTESIAN_POINT('Ctrl Pts',(-15.8635652590626,-1.03866096312509,
135.613639072205));
#76794=CARTESIAN_POINT('Ctrl Pts',(-15.8713222999476,-0.903909290725196,
135.638833810856));
#76795=CARTESIAN_POINT('Ctrl Pts',(-15.8790734911877,-0.769259235609679,
135.664009549959));
#76796=CARTESIAN_POINT('Ctrl Pts',(-15.8868246824278,-0.633451531156165,
135.683575243676));
#76797=CARTESIAN_POINT('Ctrl Pts',(-15.8945758736679,-0.496992592850417,
135.697435461174));
#76798=CARTESIAN_POINT('Ctrl Pts',(-15.902323770445,-0.360591653233425,
135.71128978771));
#76799=CARTESIAN_POINT('Ctrl Pts',(-15.9100716672219,-0.223540418431535,
135.719443421702));
#76800=CARTESIAN_POINT('Ctrl Pts',(-15.917819563999,-0.0863528675830361,
135.721852482812));
#76801=CARTESIAN_POINT('Ctrl Pts',(-15.9255658400831,0.0508059865870601,
135.724261039999));
#76802=CARTESIAN_POINT('Ctrl Pts',(-15.9333121161673,0.188100709429822,
135.720927407573));
#76803=CARTESIAN_POINT('Ctrl Pts',(-15.9410583922514,0.325015256986704,
135.711859791812));
#76804=CARTESIAN_POINT('Ctrl Pts',(-15.9488047255167,0.461930815215674,
135.702792109116));
#76805=CARTESIAN_POINT('Ctrl Pts',(-15.956551058782,0.598465802448268,135.68799038446));
#76806=CARTESIAN_POINT('Ctrl Pts',(-15.9642973920473,0.734107634478534,
135.66751484538));
#76807=CARTESIAN_POINT('Ctrl Pts',(-15.9720454600503,0.869779842556609,
135.647034720944));
#76808=CARTESIAN_POINT('Ctrl Pts',(-15.9797935280532,1.00455811091234,135.620878312058));
#76809=CARTESIAN_POINT('Ctrl Pts',(-15.9875415960562,1.13793879992331,135.589157201553));
#76810=CARTESIAN_POINT('Ctrl Pts',(-15.995297898798,1.27146124751781,135.557402377473));
#76811=CARTESIAN_POINT('Ctrl Pts',(-16.0030542015399,1.40358276762992,135.520071128063));
#76812=CARTESIAN_POINT('Ctrl Pts',(-16.0108105042817,1.53381313625685,135.477325450041));
#76813=CARTESIAN_POINT('Ctrl Pts',(-16.0185709467958,1.66411301275285,135.434556957363));
#76814=CARTESIAN_POINT('Ctrl Pts',(-16.02633138931,1.79251936066034,135.386368415115));
#76815=CARTESIAN_POINT('Ctrl Pts',(-16.0340918318242,1.91856171306949,135.332970118908));
#76816=CARTESIAN_POINT('Ctrl Pts',(-16.0418647320896,2.04480639985224,135.279486103016));
#76817=CARTESIAN_POINT('Ctrl Pts',(-16.049637632355,2.1686791542302,135.220775788449));
#76818=CARTESIAN_POINT('Ctrl Pts',(-16.0574105326204,2.28973310348935,135.157096007787));
#76819=CARTESIAN_POINT('Ctrl Pts',(-16.0649008683828,2.40638643678201,135.09573114755));
#76820=CARTESIAN_POINT('Ctrl Pts',(-16.0723912041451,2.52042208159645,135.029752007904));
#76821=CARTESIAN_POINT('Ctrl Pts',(-16.0798815399075,2.63146707109214,134.959425492662));
#76822=CARTESIAN_POINT('Ctrl Pts',(-16.0876558740266,2.74672236511044,134.886432526224));
#76823=CARTESIAN_POINT('Ctrl Pts',(-16.0954302081456,2.85912083980922,134.8085247953));
#76824=CARTESIAN_POINT('Ctrl Pts',(-16.1032045422647,2.96821486652741,134.725952586222));
#76825=CARTESIAN_POINT('Ctrl Pts',(-16.1109692952118,3.07717444460769,134.643482140012));
#76826=CARTESIAN_POINT('Ctrl Pts',(-16.1187340481589,3.18283736889737,134.55635888724));
#76827=CARTESIAN_POINT('Ctrl Pts',(-16.126498801106,3.28478275696856,134.464877698802));
#76828=CARTESIAN_POINT('Ctrl Pts',(-16.1342558419909,3.38662689144313,134.37348737077));
#76829=CARTESIAN_POINT('Ctrl Pts',(-16.1420128828759,3.48476054845989,134.277747980137));
#76830=CARTESIAN_POINT('Ctrl Pts',(-16.1497699237609,3.57879416606433,134.177995953438));
#76831=CARTESIAN_POINT('Ctrl Pts',(-16.157521115001,3.67275687218614,134.078319150518));
#76832=CARTESIAN_POINT('Ctrl Pts',(-16.1652723062411,3.76262542598416,133.97463601786));
#76833=CARTESIAN_POINT('Ctrl Pts',(-16.1730234974812,3.84804580885601,133.867321034458));
#76834=CARTESIAN_POINT('Ctrl Pts',(-16.1807713942583,3.93342988578649,133.760051662786));
#76835=CARTESIAN_POINT('Ctrl Pts',(-16.1885192910353,4.01436930905938,133.649153815791));
#76836=CARTESIAN_POINT('Ctrl Pts',(-16.1962671878123,4.09054934262526,133.535036200283));
#76837=CARTESIAN_POINT('Ctrl Pts',(-16.2040134638964,4.16671344097048,133.420942455721));
#76838=CARTESIAN_POINT('Ctrl Pts',(-16.2117597399805,4.23811991290414,133.30363060725));
#76839=CARTESIAN_POINT('Ctrl Pts',(-16.2195060160646,4.30449672823447,133.183539252961));
#76840=CARTESIAN_POINT('Ctrl Pts',(-16.2272523493299,4.37087403354328,133.063447012185));
#76841=CARTESIAN_POINT('Ctrl Pts',(-16.2349986825953,4.43222141903552,132.940575566826));
#76842=CARTESIAN_POINT('Ctrl Pts',(-16.2427450158606,4.48831249155759,132.815388722946));
#76843=CARTESIAN_POINT('Ctrl Pts',(-16.2504930838635,4.54441612528643,132.690173844341));
#76844=CARTESIAN_POINT('Ctrl Pts',(-16.2582411518665,4.59526094389128,132.562642892145));
#76845=CARTESIAN_POINT('Ctrl Pts',(-16.2659892198695,4.64066859564943,132.433279905884));
#76846=CARTESIAN_POINT('Ctrl Pts',(-16.2737455226113,4.68612450720022,132.303779431101));
#76847=CARTESIAN_POINT('Ctrl Pts',(-16.2815018253531,4.72613157866356,132.172443402182));
#76848=CARTESIAN_POINT('Ctrl Pts',(-16.2892581280949,4.76056112441905,132.039771821647));
#76849=CARTESIAN_POINT('Ctrl Pts',(-16.297018570609,4.79500904625977,131.907029430296));
#76850=CARTESIAN_POINT('Ctrl Pts',(-16.3047790131232,4.82387342843925,131.772950448989));
#76851=CARTESIAN_POINT('Ctrl Pts',(-16.3125394556373,4.8470768997548,131.638044364777));
#76852=CARTESIAN_POINT('Ctrl Pts',(-16.3203123559028,4.87031761934244,131.502921717341));
#76853=CARTESIAN_POINT('Ctrl Pts',(-16.3280852561681,4.88787921843632,131.366969701722));
#76854=CARTESIAN_POINT('Ctrl Pts',(-16.3358581564335,4.89973623194224,131.230703108871));
#76855=CARTESIAN_POINT('Ctrl Pts',(-16.3433484921958,4.91116221314159,131.099390149901));
#76856=CARTESIAN_POINT('Ctrl Pts',(-16.350838827958,4.9172911458286,130.967785395655));
#76857=CARTESIAN_POINT('Ctrl Pts',(-16.3583291637203,4.91814598605262,130.836346901727));
#76858=CARTESIAN_POINT('Ctrl Pts',(-16.3661034978394,4.91903323780354,130.699924877357));
#76859=CARTESIAN_POINT('Ctrl Pts',(-16.3738778319585,4.9142413783758,130.563249825736));
#76860=CARTESIAN_POINT('Ctrl Pts',(-16.3816521660775,4.90373902652287,130.426833635409));
#76861=CARTESIAN_POINT('Ctrl Pts',(-16.3894169190246,4.89324961787999,130.290585565845));
#76862=CARTESIAN_POINT('Ctrl Pts',(-16.3971816719718,4.87706374940324,130.154596108883));
#76863=CARTESIAN_POINT('Ctrl Pts',(-16.4049464249188,4.8552020070954,130.019378749752));
#76864=CARTESIAN_POINT('Ctrl Pts',(-16.4127034658039,4.83336197817822,129.884295690408));
#76865=CARTESIAN_POINT('Ctrl Pts',(-16.4204605066888,4.80585735602314,129.749983586268));
#76866=CARTESIAN_POINT('Ctrl Pts',(-16.4282175475738,4.77276061805082,129.616952033597));
#76867=CARTESIAN_POINT('Ctrl Pts',(-16.435968738814,4.73968883858605,129.484020801055));
#76868=CARTESIAN_POINT('Ctrl Pts',(-16.443719930054,4.70103343111077,129.352368575731));
#76869=CARTESIAN_POINT('Ctrl Pts',(-16.4514711212942,4.65691809970679,129.222495618546));
#76870=CARTESIAN_POINT('Ctrl Pts',(-16.4592190180713,4.61282151849548,129.092677860833));
#76871=CARTESIAN_POINT('Ctrl Pts',(-16.4669669148484,4.56326975436197,128.964638236578));
#76872=CARTESIAN_POINT('Ctrl Pts',(-16.4747148116255,4.50843654139943,128.838862458148));
#76873=CARTESIAN_POINT('Ctrl Pts',(-16.4824610877096,4.45361479836297,128.7131129893));
#76874=CARTESIAN_POINT('Ctrl Pts',(-16.4902073637937,4.39351396007996,128.589626782526));
#76875=CARTESIAN_POINT('Ctrl Pts',(-16.4979536398778,4.32835599258222,128.468869777512));
#76876=CARTESIAN_POINT('Ctrl Pts',(-16.5056999731432,4.26319754410317,128.348111881097));
#76877=CARTESIAN_POINT('Ctrl Pts',(-16.5134463064085,4.1929820775735,128.230083570715));
#76878=CARTESIAN_POINT('Ctrl Pts',(-16.5211926396739,4.1179774351402,128.115226015844));
#76879=CARTESIAN_POINT('Ctrl Pts',(-16.5289407076769,4.04295599593738,128.000342739421));
#76880=CARTESIAN_POINT('Ctrl Pts',(-16.5366887756798,3.96314346040045,127.888631958751));
#76881=CARTESIAN_POINT('Ctrl Pts',(-16.5444368436828,3.87885066122662,127.780505361374));
#76882=CARTESIAN_POINT('Ctrl Pts',(-16.5521931464246,3.79446827466261,127.672263845762));
#76883=CARTESIAN_POINT('Ctrl Pts',(-16.5599494491666,3.7055963532558,127.567614431789));
#76884=CARTESIAN_POINT('Ctrl Pts',(-16.5677057519084,3.61258600556669,127.466935649888));
#76885=CARTESIAN_POINT('Ctrl Pts',(-16.5754661944226,3.51952601545441,127.366203132688));
#76886=CARTESIAN_POINT('Ctrl Pts',(-16.5832266369368,3.42232347478573,127.269445746021));
#76887=CARTESIAN_POINT('Ctrl Pts',(-16.5909870794509,3.32136520842058,127.177003974666));
#76888=CARTESIAN_POINT('Ctrl Pts',(-16.5987599797164,3.22024487488375,127.084413807572));
#76889=CARTESIAN_POINT('Ctrl Pts',(-16.6065328799819,3.1153570670575,126.99615335163));
#76890=CARTESIAN_POINT('Ctrl Pts',(-16.6143057802473,3.00712112864498,126.912522288427));
#76891=CARTESIAN_POINT('Ctrl Pts',(-16.6217961160093,2.90281983922451,126.831931425026));
#76892=CARTESIAN_POINT('Ctrl Pts',(-16.6292864517712,2.79540987006541,126.755639396084));
#76893=CARTESIAN_POINT('Ctrl Pts',(-16.6367767875332,2.68528900461896,126.683874478265));
#76894=CARTESIAN_POINT('Ctrl Pts',(-16.6445511216523,2.57099287308778,126.609388571773));
#76895=CARTESIAN_POINT('Ctrl Pts',(-16.6523254557713,2.45341416425206,126.539543894948));
#76896=CARTESIAN_POINT('Ctrl Pts',(-16.6600997898904,2.33296658211227,126.474643537981));
#76897=CARTESIAN_POINT('Ctrl Pts',(-16.6678645428375,2.2126674408526,126.409823164905));
#76898=CARTESIAN_POINT('Ctrl Pts',(-16.6756292957847,2.08950680201563,126.349935171247));
#76899=CARTESIAN_POINT('Ctrl Pts',(-16.6833940487318,1.96392780250394,126.295239788729));
#76900=CARTESIAN_POINT('Ctrl Pts',(-16.6911510896168,1.83847352982508,126.240598730436));
#76901=CARTESIAN_POINT('Ctrl Pts',(-16.6989081305018,1.71060603258315,126.191140174984));
#76902=CARTESIAN_POINT('Ctrl Pts',(-16.7066651713868,1.5807932243651,126.147078594293));
#76903=CARTESIAN_POINT('Ctrl Pts',(-16.7144163626269,1.45107830899552,126.103050240783));
#76904=CARTESIAN_POINT('Ctrl Pts',(-16.722167553867,1.31942137129501,126.064410886299));
#76905=CARTESIAN_POINT('Ctrl Pts',(-16.7299187451071,1.18631016002169,126.031326858338));
#76906=CARTESIAN_POINT('Ctrl Pts',(-16.7376666418842,1.05325552456402,125.998256891972));
#76907=CARTESIAN_POINT('Ctrl Pts',(-16.7454145386612,0.918748223524601,
125.970737650065));
#76908=CARTESIAN_POINT('Ctrl Pts',(-16.7531624354383,0.783290807994925,
125.948885504602));
#76909=CARTESIAN_POINT('Ctrl Pts',(-16.7609087115224,0.647861727236454,
125.927037930137));
#76910=CARTESIAN_POINT('Ctrl Pts',(-16.7686549876065,0.511483313029908,
125.910855156449));
#76911=CARTESIAN_POINT('Ctrl Pts',(-16.7764012636906,0.374667551691111,
125.90040228901));
#76912=CARTESIAN_POINT('Ctrl Pts',(-16.784147596956,0.237850780409443,125.889949344411));
#76913=CARTESIAN_POINT('Ctrl Pts',(-16.7918939302213,0.100597045382613,
125.885226420245));
#76914=CARTESIAN_POINT('Ctrl Pts',(-16.7996402634867,-0.0365777097900677,
125.886246636206));
#76915=CARTESIAN_POINT('Ctrl Pts',(-16.8073883314897,-0.173783184298066,
125.887267080638));
#76916=CARTESIAN_POINT('Ctrl Pts',(-16.8151363994926,-0.310909252877284,
125.894033221554));
#76917=CARTESIAN_POINT('Ctrl Pts',(-16.8228844674956,-0.447441538474306,
125.906506073774));
#76918=CARTESIAN_POINT('Ctrl Pts',(-16.8306407702374,-0.584118932209216,
125.918992182289));
#76919=CARTESIAN_POINT('Ctrl Pts',(-16.8383970729792,-0.720200892347673,
125.937197082296));
#76920=CARTESIAN_POINT('Ctrl Pts',(-16.8461533757211,-0.855179167762777,
125.961029981163));
#76921=CARTESIAN_POINT('Ctrl Pts',(-16.8539138182352,-0.990229485147588,
125.984875600365));
#76922=CARTESIAN_POINT('Ctrl Pts',(-16.8616742607495,-1.12417456239742,
126.014355119824));
#76923=CARTESIAN_POINT('Ctrl Pts',(-16.8694347032636,-1.25651885173855,
126.04932713317));
#76924=CARTESIAN_POINT('Ctrl Pts',(-16.8772076035291,-1.38907559188209,
126.084355286697));
#76925=CARTESIAN_POINT('Ctrl Pts',(-16.8849805037944,-1.52002603529006,
126.124893437679));
#76926=CARTESIAN_POINT('Ctrl Pts',(-16.8927534040598,-1.64889138583909,
126.170750765603));
#76927=CARTESIAN_POINT('Ctrl Pts',(-16.9002437398219,-1.77307215630395,
126.21494106415));
#76928=CARTESIAN_POINT('Ctrl Pts',(-16.907734075584,-1.89531651292176,126.264070408033));
#76929=CARTESIAN_POINT('Ctrl Pts',(-16.9152244113461,-2.01521738839822,
126.317927519882));
#76930=CARTESIAN_POINT('Ctrl Pts',(-16.922999300883,-2.13967323281102,126.373830634068));
#76931=CARTESIAN_POINT('Ctrl Pts',(-16.9307741904198,-2.26199828785594,
126.435004925191));
#76932=CARTESIAN_POINT('Ctrl Pts',(-16.9385490799567,-2.38171383604301,
126.501266118755));
#76933=CARTESIAN_POINT('Ctrl Pts',(-16.9463142626309,-2.50127992070713,
126.567444585959));
#76934=CARTESIAN_POINT('Ctrl Pts',(-16.9540794453051,-2.61824264233293,
126.638697130794));
#76935=CARTESIAN_POINT('Ctrl Pts',(-16.9618446279794,-2.73214346027213,
126.714791547971));
#76936=CARTESIAN_POINT('Ctrl Pts',(-16.9696019734379,-2.84592932080268,
126.790809164846));
#76937=CARTESIAN_POINT('Ctrl Pts',(-16.9773593188965,-2.9566591048909,126.871658712568));
#76938=CARTESIAN_POINT('Ctrl Pts',(-16.985116664355,-3.06389940533845,126.957062410192));
#76939=CARTESIAN_POINT('Ctrl Pts',(-16.9928676271597,-3.17105146971085,
127.042395838643));
#76940=CARTESIAN_POINT('Ctrl Pts',(-17.0006185899644,-3.27471946287186,
127.132275713058));
#76941=CARTESIAN_POINT('Ctrl Pts',(-17.0083695527691,-3.37449984907946,
127.226381602666));
#76942=CARTESIAN_POINT('Ctrl Pts',(-17.0161170377662,-3.47423546446429,
127.320445267563));
#76943=CARTESIAN_POINT('Ctrl Pts',(-17.0238645227634,-3.5700866595763,127.418730907477));
#76944=CARTESIAN_POINT('Ctrl Pts',(-17.0316120077605,-3.66168394908057,
127.520878667022));
#76945=CARTESIAN_POINT('Ctrl Pts',(-17.0393576942952,-3.75325997564768,
127.623002714498));
#76946=CARTESIAN_POINT('Ctrl Pts',(-17.0471033808298,-3.84058380117569,
127.728986806488));
#76947=CARTESIAN_POINT('Ctrl Pts',(-17.0548490673645,-3.92332398697111,
127.838435474249));
#76948=CARTESIAN_POINT('Ctrl Pts',(-17.062594633218,-4.00606288363802,127.947882436753));
#76949=CARTESIAN_POINT('Ctrl Pts',(-17.0703401990714,-4.08421804805444,
128.060793555101));
#76950=CARTESIAN_POINT('Ctrl Pts',(-17.0780857649249,-4.15749964646109,
128.176741970925));
#76951=CARTESIAN_POINT('Ctrl Pts',(-17.0858363079725,-4.23082833461591,
128.292764893608));
#76952=CARTESIAN_POINT('Ctrl Pts',(-17.0935868510201,-4.2992769905067,128.411828682534));
#76953=CARTESIAN_POINT('Ctrl Pts',(-17.1013373940677,-4.36260014823184,
128.533479068663));
#76954=CARTESIAN_POINT('Ctrl Pts',(-17.1090904973753,-4.42594422368419,
128.655169639927));
#76955=CARTESIAN_POINT('Ctrl Pts',(-17.116843600683,-4.48415925812918,128.779448158453));
#76956=CARTESIAN_POINT('Ctrl Pts',(-17.1245967039906,-4.5370471621802,128.905838531665));
#76957=CARTESIAN_POINT('Ctrl Pts',(-17.1323587136796,-4.58999582123819,
129.032374095884));
#76958=CARTESIAN_POINT('Ctrl Pts',(-17.1401207233686,-4.63760498567923,
129.161025995706));
#76959=CARTESIAN_POINT('Ctrl Pts',(-17.1478827330576,-4.67972567458143,
129.29130058136));
#76960=CARTESIAN_POINT('Ctrl Pts',(-17.1536172219977,-4.71084398470165,
129.38754603847));
#76961=CARTESIAN_POINT('Ctrl Pts',(-17.1593517109378,-4.73896766352352,
129.484676814548));
#76962=CARTESIAN_POINT('Ctrl Pts',(-17.1650861998779,-4.76405452823408,
129.582490119308));
#76963=CARTESIAN_POINT('Ctrl Pts',(-15.4150128089234,-4.76405452823406,
129.582490119308));
#76964=CARTESIAN_POINT('Ctrl Pts',(-15.4226557882312,-4.79767677092274,
129.713582733263));
#76965=CARTESIAN_POINT('Ctrl Pts',(-15.4302987675391,-4.82586457448078,
129.845988829133));
#76966=CARTESIAN_POINT('Ctrl Pts',(-15.4379417468469,-4.84853709250063,
129.979211464294));
#76967=CARTESIAN_POINT('Ctrl Pts',(-15.4458082163681,-4.87187258312357,
130.116329694869));
#76968=CARTESIAN_POINT('Ctrl Pts',(-15.4536746858893,-4.88936523239047,
130.25431249071));
#76969=CARTESIAN_POINT('Ctrl Pts',(-15.4615411554104,-4.90098435191105,
130.3926137963));
#76970=CARTESIAN_POINT('Ctrl Pts',(-15.4694076249315,-4.91260347143165,
130.530915101889));
#76971=CARTESIAN_POINT('Ctrl Pts',(-15.4772740944527,-4.91834909952949,
130.669534455329));
#76972=CARTESIAN_POINT('Ctrl Pts',(-15.4851405639739,-4.91824870592852,
130.807928408547));
#76973=CARTESIAN_POINT('',(-15.1398594360232,-4.91824978862749,130.805802548776));
#76974=CARTESIAN_POINT('Ctrl Pts',(-15.0701040894033,-4.76405452823398,
129.582490119308));
#76975=CARTESIAN_POINT('Ctrl Pts',(-15.0780695634094,-4.79905394525373,
129.718952315078));
#76976=CARTESIAN_POINT('Ctrl Pts',(-15.0860350374154,-4.82821560351136,
129.857035172868));
#76977=CARTESIAN_POINT('Ctrl Pts',(-15.0940005114215,-4.85140006569305,
129.996214303404));
#76978=CARTESIAN_POINT('Ctrl Pts',(-15.1019581955728,-4.87456185457316,
130.135257323369));
#76979=CARTESIAN_POINT('Ctrl Pts',(-15.109915879724,-4.89175803917466,130.275394125515));
#76980=CARTESIAN_POINT('Ctrl Pts',(-15.1178735638753,-4.90289998289446,
130.416089037054));
#76981=CARTESIAN_POINT('Ctrl Pts',(-15.1252021879139,-4.91316114870974,
130.545661924242));
#76982=CARTESIAN_POINT('Ctrl Pts',(-15.1325308119525,-4.91828792975117,
130.675707821371));
#76983=CARTESIAN_POINT('Ctrl Pts',(-15.1398594359911,-4.91824978862766,
130.805802548205));
#76984=CARTESIAN_POINT('Ctrl Pts',(-15.1398594360233,-4.91824978862749,
130.805802548776));
#76985=CARTESIAN_POINT('Ctrl Pts',(-15.1481808457913,-4.91820648062839,
130.953520800515));
#76986=CARTESIAN_POINT('Ctrl Pts',(-15.1565022555593,-4.91150395054456,
131.101051023692));
#76987=CARTESIAN_POINT('Ctrl Pts',(-15.1648236653272,-4.89821807427448,
131.24780481851));
#76988=CARTESIAN_POINT('Ctrl Pts',(-15.1731762609717,-4.88488240695846,
131.395108597747));
#76989=CARTESIAN_POINT('Ctrl Pts',(-15.1815288566162,-4.86491403750072,
131.541629830756));
#76990=CARTESIAN_POINT('Ctrl Pts',(-15.1898814522606,-4.83844054493169,
131.686786906647));
#76991=CARTESIAN_POINT('Ctrl Pts',(-15.1982495793767,-4.81191782547352,
131.832213898993));
#76992=CARTESIAN_POINT('Ctrl Pts',(-15.2066177064928,-4.77886588751804,
131.976271382574));
#76993=CARTESIAN_POINT('Ctrl Pts',(-15.2149858336089,-4.73946243264698,
132.118392166665));
#76994=CARTESIAN_POINT('Ctrl Pts',(-15.2233804894101,-4.69993406071453,
132.260963502891));
#76995=CARTESIAN_POINT('Ctrl Pts',(-15.2317751452115,-4.65401396770181,
132.401585572931));
#76996=CARTESIAN_POINT('Ctrl Pts',(-15.2401698010127,-4.60192935985197,
132.539707623047));
#76997=CARTESIAN_POINT('Ctrl Pts',(-15.2481557555513,-4.55238053732816,
132.671105078656));
#76998=CARTESIAN_POINT('Ctrl Pts',(-15.2561417100897,-4.49725331014482,
132.800240000642));
#76999=CARTESIAN_POINT('Ctrl Pts',(-15.2641276646283,-4.43678145503934,
132.926659697036));
#77000=CARTESIAN_POINT('Ctrl Pts',(-15.2719019987473,-4.37791204824278,
133.049729388236));
#77001=CARTESIAN_POINT('Ctrl Pts',(-15.2796763328663,-4.31382486170124,
133.170542732587));
#77002=CARTESIAN_POINT('Ctrl Pts',(-15.2874506669854,-4.24471556105109,
133.288625673527));
#77003=CARTESIAN_POINT('Ctrl Pts',(-15.2952154199324,-4.17569143143751,
133.406563087796));
#77004=CARTESIAN_POINT('Ctrl Pts',(-15.3029801728795,-4.10165769817633,
133.521776459773));
#77005=CARTESIAN_POINT('Ctrl Pts',(-15.3107449258265,-4.02285745837033,
133.633813026096));
#77006=CARTESIAN_POINT('Ctrl Pts',(-15.3185019667114,-3.94413548407349,
133.745738316121));
#77007=CARTESIAN_POINT('Ctrl Pts',(-15.3262590075964,-3.86065664789233,
133.85449276186));
#77008=CARTESIAN_POINT('Ctrl Pts',(-15.3340160484813,-3.77270901092966,
133.959649793117));
#77009=CARTESIAN_POINT('Ctrl Pts',(-15.3417672397214,-3.68482769596416,
134.064727524639));
#77010=CARTESIAN_POINT('Ctrl Pts',(-15.3495184309614,-3.59248453772077,
134.16621294273));
#77011=CARTESIAN_POINT('Ctrl Pts',(-15.3572696222014,-3.49600958139968,
134.263710277439));
#77012=CARTESIAN_POINT('Ctrl Pts',(-15.3650175189785,-3.39957562950845,
134.36116617318));
#77013=CARTESIAN_POINT('Ctrl Pts',(-15.3727654157555,-3.29901364675454,
134.454637079522));
#77014=CARTESIAN_POINT('Ctrl Pts',(-15.3805133125325,-3.19469230619625,
134.543762191512));
#77015=CARTESIAN_POINT('Ctrl Pts',(-15.3882595886166,-3.0903927874135,134.63286866045));
#77016=CARTESIAN_POINT('Ctrl Pts',(-15.3960058647007,-2.98233577203952,
134.717630889385));
#77017=CARTESIAN_POINT('Ctrl Pts',(-15.4037521407847,-2.8709246591275,134.797726949887));
#77018=CARTESIAN_POINT('Ctrl Pts',(-15.4114984740501,-2.75951272380396,
134.87782360164));
#77019=CARTESIAN_POINT('Ctrl Pts',(-15.4192448073153,-2.64474695898088,
134.95325378801));
#77020=CARTESIAN_POINT('Ctrl Pts',(-15.4269911405806,-2.52706118537816,
135.023737920896));
#77021=CARTESIAN_POINT('Ctrl Pts',(-15.4347392085835,-2.40934905686242,
135.094237838214));
#77022=CARTESIAN_POINT('Ctrl Pts',(-15.4424872765865,-2.28871595369618,
135.159789297139));
#77023=CARTESIAN_POINT('Ctrl Pts',(-15.4502353445895,-2.16562146255197,
135.220158024992));
#77024=CARTESIAN_POINT('Ctrl Pts',(-15.4579916473313,-2.04239614511773,
135.280590913448));
#77025=CARTESIAN_POINT('Ctrl Pts',(-15.465747950073,-1.91670456556245,135.335829895047));
#77026=CARTESIAN_POINT('Ctrl Pts',(-15.4735042528148,-1.78902802782657,
135.385688130215));
#77027=CARTESIAN_POINT('Ctrl Pts',(-15.481264695329,-1.66128334527823,135.435572976223));
#77028=CARTESIAN_POINT('Ctrl Pts',(-15.4890251378431,-1.53155196317589,
135.480071226578));
#77029=CARTESIAN_POINT('Ctrl Pts',(-15.4967855803573,-1.40033066428529,
135.51904587675));
#77030=CARTESIAN_POINT('Ctrl Pts',(-15.5045584806226,-1.26889871731642,
135.558083092489));
#77031=CARTESIAN_POINT('Ctrl Pts',(-15.512331380888,-1.13597245341943,135.59157889342));
#77032=CARTESIAN_POINT('Ctrl Pts',(-15.5201042811534,-1.00206005270424,
135.619447191375));
#77033=CARTESIAN_POINT('Ctrl Pts',(-15.527594616916,-0.87301570504988,135.646302406505));
#77034=CARTESIAN_POINT('Ctrl Pts',(-15.5350849526785,-0.743055976763678,
135.6679321125));
#77035=CARTESIAN_POINT('Ctrl Pts',(-15.5425752884411,-0.612638428668537,
135.684305004362));
#77036=CARTESIAN_POINT('Ctrl Pts',(-15.5503496225602,-0.477276059607541,
135.701298679393));
#77037=CARTESIAN_POINT('Ctrl Pts',(-15.5581239566793,-0.340991681649807,
135.712682877964));
#77038=CARTESIAN_POINT('Ctrl Pts',(-15.5658982907984,-0.204289894063151,
135.718365979965));
#77039=CARTESIAN_POINT('Ctrl Pts',(-15.5736630437455,-0.0677565792123065,
135.72404207805));
#77040=CARTESIAN_POINT('Ctrl Pts',(-15.5814277966925,0.0691927348470643,
135.724031043309));
#77041=CARTESIAN_POINT('Ctrl Pts',(-15.5891925496396,0.206045725553709,
135.718292670564));
#77042=CARTESIAN_POINT('Ctrl Pts',(-15.5969495905246,0.342762791940509,
135.712559997252));
#77043=CARTESIAN_POINT('Ctrl Pts',(-15.6047066314097,0.479383337267362,
135.701111322525));
#77044=CARTESIAN_POINT('Ctrl Pts',(-15.6124636722947,0.615392771885629,
135.68395842874));
#77045=CARTESIAN_POINT('Ctrl Pts',(-15.6202148635348,0.751299640731252,
135.666818470085));
#77046=CARTESIAN_POINT('Ctrl Pts',(-15.6279660547749,0.886595929825876,
135.643982903157));
#77047=CARTESIAN_POINT('Ctrl Pts',(-15.635717246015,1.02077026920864,135.615515481006));
#77048=CARTESIAN_POINT('Ctrl Pts',(-15.6434651427921,1.15488758091813,135.587060158268));
#77049=CARTESIAN_POINT('Ctrl Pts',(-15.6512130395692,1.28788350969986,135.552977822145));
#77050=CARTESIAN_POINT('Ctrl Pts',(-15.6589609363463,1.41925522333431,135.513383623832));
#77051=CARTESIAN_POINT('Ctrl Pts',(-15.6667072124304,1.55059945683831,135.473797707771));
#77052=CARTESIAN_POINT('Ctrl Pts',(-15.6744534885145,1.68031977688197,135.428702335574));
#77053=CARTESIAN_POINT('Ctrl Pts',(-15.6821997645986,1.80792728891787,135.37826288811));
#77054=CARTESIAN_POINT('Ctrl Pts',(-15.689946097864,1.93553574292325,135.327823068313));
#77055=CARTESIAN_POINT('Ctrl Pts',(-15.6976924311293,2.06103099420758,135.27203923825));
#77056=CARTESIAN_POINT('Ctrl Pts',(-15.7054387643947,2.18394332668613,135.211125259378));
#77057=CARTESIAN_POINT('Ctrl Pts',(-15.7131868323976,2.30688318452933,135.150197639243));
#77058=CARTESIAN_POINT('Ctrl Pts',(-15.7209349004006,2.42723862232567,135.084137757774));
#77059=CARTESIAN_POINT('Ctrl Pts',(-15.7286829684036,2.54456412201361,135.013205648149));
#77060=CARTESIAN_POINT('Ctrl Pts',(-15.7364392711455,2.66201431663897,134.942198151034));
#77061=CARTESIAN_POINT('Ctrl Pts',(-15.7441955738873,2.77642780524497,134.866308284224));
#77062=CARTESIAN_POINT('Ctrl Pts',(-15.7519518766292,2.88738723786942,134.785839991001));
#77063=CARTESIAN_POINT('Ctrl Pts',(-15.7597123191433,2.998405892884,134.705328749428));
#77064=CARTESIAN_POINT('Ctrl Pts',(-15.7674727616575,3.10596651205521,134.620234454727));
#77065=CARTESIAN_POINT('Ctrl Pts',(-15.7752332041716,3.20968530637265,134.530901010015));
#77066=CARTESIAN_POINT('Ctrl Pts',(-15.7830061044371,3.31357059930645,134.441424159327));
#77067=CARTESIAN_POINT('Ctrl Pts',(-15.7907790047026,3.41360145782071,134.347694827425));
#77068=CARTESIAN_POINT('Ctrl Pts',(-15.798551904968,3.50943076974038,134.250094027872));
#77069=CARTESIAN_POINT('Ctrl Pts',(-15.80604224073,3.60177644479204,134.156041263224));
#77070=CARTESIAN_POINT('Ctrl Pts',(-15.813532576492,3.69022053660507,134.058393847598));
#77071=CARTESIAN_POINT('Ctrl Pts',(-15.821022912254,3.77448938459753,133.957519818758));
#77072=CARTESIAN_POINT('Ctrl Pts',(-15.8287972463731,3.86195331157483,133.852821120454));
#77073=CARTESIAN_POINT('Ctrl Pts',(-15.8365715804922,3.94519619546707,133.744314650906));
#77074=CARTESIAN_POINT('Ctrl Pts',(-15.8443459146113,4.0238682054511,133.632375420862));
#77075=CARTESIAN_POINT('Ctrl Pts',(-15.8521106675584,4.10244325921393,133.520574145915));
#77076=CARTESIAN_POINT('Ctrl Pts',(-15.8598754205055,4.17645842479622,133.405348844843));
#77077=CARTESIAN_POINT('Ctrl Pts',(-15.8676401734526,4.24560295358366,133.287108817248));
#77078=CARTESIAN_POINT('Ctrl Pts',(-15.8753972143376,4.31467880705024,133.168986227314));
#77079=CARTESIAN_POINT('Ctrl Pts',(-15.8831542552226,4.37889345465133,133.047855204897));
#77080=CARTESIAN_POINT('Ctrl Pts',(-15.8909112961076,4.43797866094046,132.924155057491));
#77081=CARTESIAN_POINT('Ctrl Pts',(-15.8986624873477,4.49701931061592,132.800548193329));
#77082=CARTESIAN_POINT('Ctrl Pts',(-15.9064136785878,4.55093805047412,132.674376411809));
#77083=CARTESIAN_POINT('Ctrl Pts',(-15.914164869828,4.59951210980578,132.546104403044));
#77084=CARTESIAN_POINT('Ctrl Pts',(-15.9219127666051,4.64806552386653,132.417886913303));
#77085=CARTESIAN_POINT('Ctrl Pts',(-15.9296606633821,4.69127863733705,132.287571336597));
#77086=CARTESIAN_POINT('Ctrl Pts',(-15.9374085601592,4.72897653708163,132.155642961945));
#77087=CARTESIAN_POINT('Ctrl Pts',(-15.9451548362433,4.76666655123825,132.023742183866));
#77088=CARTESIAN_POINT('Ctrl Pts',(-15.9529011123275,4.79884353902041,131.890229654555));
#77089=CARTESIAN_POINT('Ctrl Pts',(-15.9606473884116,4.82538238059169,131.75560608724));
#77090=CARTESIAN_POINT('Ctrl Pts',(-15.968393721677,4.85192141806664,131.620981526165));
#77091=CARTESIAN_POINT('Ctrl Pts',(-15.9761400549423,4.87282215066489,131.485246294304));
#77092=CARTESIAN_POINT('Ctrl Pts',(-15.9838863882077,4.88801061307185,131.348911174445));
#77093=CARTESIAN_POINT('Ctrl Pts',(-15.9916344562106,4.90320247682967,131.212545523281));
#77094=CARTESIAN_POINT('Ctrl Pts',(-15.9993825242136,4.91267948161037,131.075580105283));
#77095=CARTESIAN_POINT('Ctrl Pts',(-16.0071305922166,4.91641958729721,130.938530301699));
#77096=CARTESIAN_POINT('Ctrl Pts',(-16.0148868949584,4.92016366801287,130.801334839953));
#77097=CARTESIAN_POINT('Ctrl Pts',(-16.0226431977003,4.91815865904924,130.664055204907));
#77098=CARTESIAN_POINT('Ctrl Pts',(-16.0303995004421,4.91043468864896,130.527206813672));
#77099=CARTESIAN_POINT('Ctrl Pts',(-16.0381599429563,4.90270659573309,130.390285382329));
#77100=CARTESIAN_POINT('Ctrl Pts',(-16.0459203854705,4.88925349758212,130.253796042316));
#77101=CARTESIAN_POINT('Ctrl Pts',(-16.0536808279847,4.87015728229237,130.118247574231));
#77102=CARTESIAN_POINT('Ctrl Pts',(-16.0614537282501,4.85103041206255,129.982481511711));
#77103=CARTESIAN_POINT('Ctrl Pts',(-16.0692266285156,4.82624239299752,129.847659724063));
#77104=CARTESIAN_POINT('Ctrl Pts',(-16.076999528781,4.79592615998857,129.714280193727));
#77105=CARTESIAN_POINT('Ctrl Pts',(-16.084489864543,4.76671199841156,129.585749345282));
#77106=CARTESIAN_POINT('Ctrl Pts',(-16.091980200305,4.73236465411899,129.458558012656));
#77107=CARTESIAN_POINT('Ctrl Pts',(-16.099470536067,4.69304584747548,129.333135367649));
#77108=CARTESIAN_POINT('Ctrl Pts',(-16.1072448701861,4.65223625632728,129.202957284935));
#77109=CARTESIAN_POINT('Ctrl Pts',(-16.1150192043052,4.605941502498,129.074272291947));
#77110=CARTESIAN_POINT('Ctrl Pts',(-16.1227935384242,4.5542880010454,128.947577413734));
#77111=CARTESIAN_POINT('Ctrl Pts',(-16.1305582913713,4.50269815791701,128.821038675635));
#77112=CARTESIAN_POINT('Ctrl Pts',(-16.1383230443184,4.44576285369402,128.696485530849));
#77113=CARTESIAN_POINT('Ctrl Pts',(-16.1460877972655,4.38365847650471,128.574400657417));
#77114=CARTESIAN_POINT('Ctrl Pts',(-16.1538448381505,4.32161578225834,128.452437040402));
#77115=CARTESIAN_POINT('Ctrl Pts',(-16.1616018790355,4.25441440804822,128.332937162316));
#77116=CARTESIAN_POINT('Ctrl Pts',(-16.1693589199205,4.18227896790133,128.216364153668));
#77117=CARTESIAN_POINT('Ctrl Pts',(-16.1771101111606,4.11019792565098,128.099879053632));
#77118=CARTESIAN_POINT('Ctrl Pts',(-16.1848613024007,4.03319042841998,127.986316760903));
#77119=CARTESIAN_POINT('Ctrl Pts',(-16.1926124936408,3.9515270201495,127.876115875143));
#77120=CARTESIAN_POINT('Ctrl Pts',(-16.2003603904179,3.86989832100586,127.765961827699));
#77121=CARTESIAN_POINT('Ctrl Pts',(-16.208108287195,3.78361787896377,127.659166659132));
#77122=CARTESIAN_POINT('Ctrl Pts',(-16.2158561839721,3.69299943659804,127.556139839388));
#77123=CARTESIAN_POINT('Ctrl Pts',(-16.2236024600562,3.60239994965695,127.453134570634));
#77124=CARTESIAN_POINT('Ctrl Pts',(-16.2313487361403,3.50746452533909,127.353896376196));
#77125=CARTESIAN_POINT('Ctrl Pts',(-16.2390950122244,3.4085467975363,127.258801170666));
#77126=CARTESIAN_POINT('Ctrl Pts',(-16.2468413454897,3.30962833954531,127.163705263164));
#77127=CARTESIAN_POINT('Ctrl Pts',(-16.2545876787551,3.20672780125715,127.072752676552));
#77128=CARTESIAN_POINT('Ctrl Pts',(-16.2623340120204,3.10023493863807,126.986281730515));
#77129=CARTESIAN_POINT('Ctrl Pts',(-16.2700820800234,2.99371822768091,126.899791419909));
#77130=CARTESIAN_POINT('Ctrl Pts',(-16.2778301480265,2.88360789502998,126.81778499339));
#77131=CARTESIAN_POINT('Ctrl Pts',(-16.2855782160294,2.7703256323039,126.740559570086));
#77132=CARTESIAN_POINT('Ctrl Pts',(-16.2933345187713,2.65692297184092,126.663252070683));
#77133=CARTESIAN_POINT('Ctrl Pts',(-16.3010908215131,2.54034197059532,126.590735945525));
#77134=CARTESIAN_POINT('Ctrl Pts',(-16.308847124255,2.42103254863144,126.523264442406));
#77135=CARTESIAN_POINT('Ctrl Pts',(-16.3166075667691,2.30165944763656,126.455756927715));
#77136=CARTESIAN_POINT('Ctrl Pts',(-16.3243680092832,2.17955537214382,126.393299577986));
#77137=CARTESIAN_POINT('Ctrl Pts',(-16.3321284517974,2.05519263619625,126.336098506787));
#77138=CARTESIAN_POINT('Ctrl Pts',(-16.3399013520628,1.93063026214453,126.27880561135));
#77139=CARTESIAN_POINT('Ctrl Pts',(-16.3476742523283,1.80380234405896,126.226786004393));
#77140=CARTESIAN_POINT('Ctrl Pts',(-16.3554471525937,1.67519970322636,126.180197015701));
#77141=CARTESIAN_POINT('Ctrl Pts',(-16.3629374883558,1.55127209231853,126.135301654099));
#77142=CARTESIAN_POINT('Ctrl Pts',(-16.3704278241178,1.42569684336387,126.095449025514));
#77143=CARTESIAN_POINT('Ctrl Pts',(-16.3779181598798,1.29892244455898,126.060735047865));
#77144=CARTESIAN_POINT('Ctrl Pts',(-16.3856924939989,1.16734135589116,126.024704879202));
#77145=CARTESIAN_POINT('Ctrl Pts',(-16.3934668281179,1.03405158148503,125.994096584719));
#77146=CARTESIAN_POINT('Ctrl Pts',(-16.401241162237,0.89953961301696,125.969072462025));
#77147=CARTESIAN_POINT('Ctrl Pts',(-16.4090059151841,0.765193418528343,
125.944079179327));
#77148=CARTESIAN_POINT('Ctrl Pts',(-16.4167706681312,0.629628407636705,
125.924656446124));
#77149=CARTESIAN_POINT('Ctrl Pts',(-16.4245354210783,0.493346013140051,
125.910916761362));
#77150=CARTESIAN_POINT('Ctrl Pts',(-16.4322924619633,0.357198976239042,
125.897190723049));
#77151=CARTESIAN_POINT('Ctrl Pts',(-16.4400495028484,0.220336360147173,
125.889136539361));
#77152=CARTESIAN_POINT('Ctrl Pts',(-16.4478065437334,0.083269219047094,
125.88681556951));
#77153=CARTESIAN_POINT('Ctrl Pts',(-16.4555577349735,-0.0536945586558414,
125.884496349921));
#77154=CARTESIAN_POINT('Ctrl Pts',(-16.4633089262136,-0.190862165046312,
125.887901745174));
#77155=CARTESIAN_POINT('Ctrl Pts',(-16.4710601174537,-0.327718358197829,
125.89704121282));
#77156=CARTESIAN_POINT('Ctrl Pts',(-16.4788080142308,-0.464516383816498,
125.906176795948));
#77157=CARTESIAN_POINT('Ctrl Pts',(-16.4865559110079,-0.601002870168441,
125.9210415782));
#77158=CARTESIAN_POINT('Ctrl Pts',(-16.494303807785,-0.736663733067385,
125.941592927569));
#77159=CARTESIAN_POINT('Ctrl Pts',(-16.5020500838691,-0.872296218638321,
125.962139978038));
#77160=CARTESIAN_POINT('Ctrl Pts',(-16.5097963599532,-1.00710303796139,
125.988371171106));
#77161=CARTESIAN_POINT('Ctrl Pts',(-16.5175426360373,-1.14057677568714,
126.020192175583));
#77162=CARTESIAN_POINT('Ctrl Pts',(-16.5252889693026,-1.2740514986857,126.052013414956));
#77163=CARTESIAN_POINT('Ctrl Pts',(-16.5330353025681,-1.40619274014424,
126.089424457408));
#77164=CARTESIAN_POINT('Ctrl Pts',(-16.5407816358334,-1.53650518950799,
126.132280260261));
#77165=CARTESIAN_POINT('Ctrl Pts',(-16.5485297038364,-1.66684682144125,
126.175145660374));
#77166=CARTESIAN_POINT('Ctrl Pts',(-16.5562777718393,-1.79535847500655,
126.223458125068));
#77167=CARTESIAN_POINT('Ctrl Pts',(-16.5640258398423,-1.92156224084664,
126.277023473388));
#77168=CARTESIAN_POINT('Ctrl Pts',(-16.5717821425842,-2.04790013755073,
126.330645751598));
#77169=CARTESIAN_POINT('Ctrl Pts',(-16.5795384453261,-2.17192488623211,
126.389531912739));
#77170=CARTESIAN_POINT('Ctrl Pts',(-16.5872947480679,-2.29318022956406,
126.453440312937));
#77171=CARTESIAN_POINT('Ctrl Pts',(-16.5950551905821,-2.41450029052401,
126.517382822972));
#77172=CARTESIAN_POINT('Ctrl Pts',(-16.6028156330963,-2.53304766309654,
126.586352716718));
#77173=CARTESIAN_POINT('Ctrl Pts',(-16.6105760756105,-2.64839364082366,
126.660064032409));
#77174=CARTESIAN_POINT('Ctrl Pts',(-16.6183489758759,-2.76392478215401,
126.733893676048));
#77175=CARTESIAN_POINT('Ctrl Pts',(-16.6261218761413,-2.87624393842769,
126.812479727277));
#77176=CARTESIAN_POINT('Ctrl Pts',(-16.6338947764067,-2.98495344274703,
126.895494284838));
#77177=CARTESIAN_POINT('Ctrl Pts',(-16.6413851121687,-3.08971108276091,
126.97549105413));
#77178=CARTESIAN_POINT('Ctrl Pts',(-16.6488754479307,-3.19111671727947,
127.059599748347));
#77179=CARTESIAN_POINT('Ctrl Pts',(-16.6563657836927,-3.28884722901694,
127.147494887643));
#77180=CARTESIAN_POINT('Ctrl Pts',(-16.6640225481593,-3.38874922718535,
127.237342980002));
#77181=CARTESIAN_POINT('Ctrl Pts',(-16.6716793126258,-3.48514755370028,
127.331450921984));
#77182=CARTESIAN_POINT('Ctrl Pts',(-16.6793360770924,-3.57764871411246,
127.429510585208));
#77183=CARTESIAN_POINT('Ctrl Pts',(-16.6869840046077,-3.67004311555948,
127.527457074195));
#77184=CARTESIAN_POINT('Ctrl Pts',(-16.6946319321231,-3.7585490179369,127.629345928119));
#77185=CARTESIAN_POINT('Ctrl Pts',(-16.7022798596383,-3.84280610284961,
127.734829005349));
#77186=CARTESIAN_POINT('Ctrl Pts',(-16.7099207344897,-3.92698548868614,
127.840214809599));
#77187=CARTESIAN_POINT('Ctrl Pts',(-16.7175616093411,-4.00692359733335,
127.949187933855));
#77188=CARTESIAN_POINT('Ctrl Pts',(-16.7252024841924,-4.08229750108135,
128.061364049));
#77189=CARTESIAN_POINT('Ctrl Pts',(-16.7330813916031,-4.16001949239282,
128.177034733588));
#77190=CARTESIAN_POINT('Ctrl Pts',(-16.7409602990137,-4.23288795711076,
128.296110920379));
#77191=CARTESIAN_POINT('Ctrl Pts',(-16.7488392064244,-4.30059406355323,
128.418134776823));
#77192=CARTESIAN_POINT('Ctrl Pts',(-16.7564716269968,-4.36618202553259,
128.536341190949));
#77193=CARTESIAN_POINT('Ctrl Pts',(-16.7641040475692,-4.42692558976453,
128.657313221497));
#77194=CARTESIAN_POINT('Ctrl Pts',(-16.7717364681416,-4.4825888141779,128.780606535295));
#77195=CARTESIAN_POINT('Ctrl Pts',(-16.7797386189714,-4.54094848044659,
128.909872432524));
#77196=CARTESIAN_POINT('Ctrl Pts',(-16.7877407698011,-4.59372304626322,
129.041689728486));
#77197=CARTESIAN_POINT('Ctrl Pts',(-16.7957429206309,-4.64069621712328,
129.175520022886));
#77198=CARTESIAN_POINT('Ctrl Pts',(-16.8037450714606,-4.68766938798333,
129.309350317286));
#77199=CARTESIAN_POINT('Ctrl Pts',(-16.8117472222905,-4.72884100436561,
129.445193124185));
#77200=CARTESIAN_POINT('Ctrl Pts',(-16.8197493731203,-4.76405452823399,
129.582490119308));
#77201=CARTESIAN_POINT('Origin',(213.235140564004,0.,130.804360617566));
#77202=CARTESIAN_POINT('',(-18.9154222424341,-4.76405452823411,129.582490119308));
#77203=CARTESIAN_POINT('',(-18.5697878174478,-4.76405452823411,129.582490119308));
#77204=CARTESIAN_POINT('',(213.235140564004,-4.76405452823405,129.582490119308));
#77205=CARTESIAN_POINT('',(-17.2351405640403,-4.91824853831127,130.800568797544));
#77206=CARTESIAN_POINT('Ctrl Pts',(-17.2351405640404,-4.91824853831127,
130.800568797544));
#77207=CARTESIAN_POINT('Ctrl Pts',(-17.242791346641,-4.9183523543999,130.935225327462));
#77208=CARTESIAN_POINT('Ctrl Pts',(-17.2504421292416,-4.91292188126911,
131.070090008472));
#77209=CARTESIAN_POINT('Ctrl Pts',(-17.2580929118422,-4.90193244130674,
131.204662258038));
#77210=CARTESIAN_POINT('Ctrl Pts',(-17.2657360456441,-4.89095398793478,
131.339099970249));
#77211=CARTESIAN_POINT('Ctrl Pts',(-17.2733791794459,-4.87442765347894,
131.473245433197));
#77212=CARTESIAN_POINT('Ctrl Pts',(-17.2810223132477,-4.85238079457833,
131.606597295179));
#77213=CARTESIAN_POINT('Ctrl Pts',(-17.2889847026529,-4.82941303288812,
131.745519297663));
#77214=CARTESIAN_POINT('Ctrl Pts',(-17.2969470920581,-4.80045354815532,
131.88357952074));
#77215=CARTESIAN_POINT('Ctrl Pts',(-17.3049094814632,-4.76559332951731,
132.020215576087));
#77216=CARTESIAN_POINT('Ctrl Pts',(-17.3125438327696,-4.73216929784078,
132.151222437791));
#77217=CARTESIAN_POINT('Ctrl Pts',(-17.320178184076,-4.69332116779459,132.280919711161));
#77218=CARTESIAN_POINT('Ctrl Pts',(-17.3278125353824,-4.64918135176559,
132.408821842057));
#77219=CARTESIAN_POINT('Ctrl Pts',(-17.3354456647483,-4.60504860067531,
132.53670350117));
#77220=CARTESIAN_POINT('Ctrl Pts',(-17.3430787941143,-4.55562597908057,
132.662790207729));
#77221=CARTESIAN_POINT('Ctrl Pts',(-17.3507119234802,-4.50109547417136,
132.786612517526));
#77222=CARTESIAN_POINT('Ctrl Pts',(-17.3583455971132,-4.44656108105957,
132.910443656256));
#77223=CARTESIAN_POINT('Ctrl Pts',(-17.3659792707461,-4.3869182434371,133.032009708012));
#77224=CARTESIAN_POINT('Ctrl Pts',(-17.3736129443791,-4.32239647060258,
133.150862655371));
#77225=CARTESIAN_POINT('Ctrl Pts',(-17.3812489287406,-4.25785516689618,
133.269751579759));
#77226=CARTESIAN_POINT('Ctrl Pts',(-17.3888849131021,-4.18843218417436,
133.38592541255));
#77227=CARTESIAN_POINT('Ctrl Pts',(-17.3965208974636,-4.11440191721636,
133.498962615284));
#77228=CARTESIAN_POINT('Ctrl Pts',(-17.404165046103,-4.04029249822717,133.61212067567));
#77229=CARTESIAN_POINT('Ctrl Pts',(-17.4118091947424,-3.96156618482791,
133.72213507524));
#77230=CARTESIAN_POINT('Ctrl Pts',(-17.4194533433818,-3.87853958880925,
133.828614859613));
#77231=CARTESIAN_POINT('Ctrl Pts',(-17.4271023184276,-3.79546057098146,
133.935161873804));
#77232=CARTESIAN_POINT('Ctrl Pts',(-17.4347512934735,-3.70807612667641,
134.038169524355));
#77233=CARTESIAN_POINT('Ctrl Pts',(-17.4424002685193,-3.61674080626019,
134.137282609277));
#77234=CARTESIAN_POINT('Ctrl Pts',(-17.4500599647972,-3.52527746514158,
134.236534616652));
#77235=CARTESIAN_POINT('Ctrl Pts',(-17.4577196610751,-3.42985248215683,
134.331880882519));
#77236=CARTESIAN_POINT('Ctrl Pts',(-17.4653793573529,-3.33085478546361,
134.423005316988));
#77237=CARTESIAN_POINT('Ctrl Pts',(-17.4676261245592,-3.301816456741,134.449734234641));
#77238=CARTESIAN_POINT('Ctrl Pts',(-17.4698728917655,-3.27247093466944,
134.476100191047));
#77239=CARTESIAN_POINT('Ctrl Pts',(-17.4721196589718,-3.24282850706724,
134.50209591586));
#77240=CARTESIAN_POINT('Ctrl Pts',(-17.4798939930909,-3.14025885248444,
134.592047135461));
#77241=CARTESIAN_POINT('Ctrl Pts',(-17.48766832721,-3.03378122980677,134.677869903543));
#77242=CARTESIAN_POINT('Ctrl Pts',(-17.4954426613291,-2.92376214681279,
134.759205490802));
#77243=CARTESIAN_POINT('Ctrl Pts',(-17.5032074142761,-2.81387865250606,
134.84044083922));
#77244=CARTESIAN_POINT('Ctrl Pts',(-17.5109721672232,-2.70046269336695,
134.917199779777));
#77245=CARTESIAN_POINT('Ctrl Pts',(-17.5187369201703,-2.58391599401656,
134.989161831288));
#77246=CARTESIAN_POINT('Ctrl Pts',(-17.5264939610553,-2.46748505049051,
135.061052409074));
#77247=CARTESIAN_POINT('Ctrl Pts',(-17.5342510019404,-2.34792988529786,
135.128155374986));
#77248=CARTESIAN_POINT('Ctrl Pts',(-17.5420080428254,-2.2256832425133,135.190192028655));
#77249=CARTESIAN_POINT('Ctrl Pts',(-17.5497592340655,-2.10352878687318,
135.252181900001));
#77250=CARTESIAN_POINT('Ctrl Pts',(-17.5575104253056,-1.97868724079575,
135.309112887457));
#77251=CARTESIAN_POINT('Ctrl Pts',(-17.5652616165457,-1.85161781468985,
135.360751133185));
#77252=CARTESIAN_POINT('Ctrl Pts',(-17.5730095133228,-1.72460239647992,
135.412367431281));
#77253=CARTESIAN_POINT('Ctrl Pts',(-17.5807574100999,-1.59536134301193,
135.458695314964));
#77254=CARTESIAN_POINT('Ctrl Pts',(-17.588505306877,-1.46437560612231,135.49954827587));
#77255=CARTESIAN_POINT('Ctrl Pts',(-17.5962515829611,-1.33341726862513,
135.540392691218));
#77256=CARTESIAN_POINT('Ctrl Pts',(-17.6039978590452,-1.20071534660909,
135.575764345391));
#77257=CARTESIAN_POINT('Ctrl Pts',(-17.6117441351293,-1.06676740657806,
135.60552613885));
#77258=CARTESIAN_POINT('Ctrl Pts',(-17.6194904683946,-0.932818477773584,
135.635288152003));
#77259=CARTESIAN_POINT('Ctrl Pts',(-17.62723680166,-0.797623894258367,135.659440137008));
#77260=CARTESIAN_POINT('Ctrl Pts',(-17.6349831349254,-0.66169251676377,
135.677895892473));
#77261=CARTESIAN_POINT('Ctrl Pts',(-17.6427312029284,-0.525730698379665,
135.696355780976));
#77262=CARTESIAN_POINT('Ctrl Pts',(-17.6504792709313,-0.389032145022043,
135.70911684899));
#77263=CARTESIAN_POINT('Ctrl Pts',(-17.6582273389343,-0.25211156061956,
135.716144695017));
#77264=CARTESIAN_POINT('Ctrl Pts',(-17.6659836416762,-0.115045455390599,
135.723180010323));
#77265=CARTESIAN_POINT('Ctrl Pts',(-17.673739944418,0.0222427611993643,
135.724469911472));
#77266=CARTESIAN_POINT('Ctrl Pts',(-17.6814962471599,0.1592370974715,135.720032149441));
#77267=CARTESIAN_POINT('Ctrl Pts',(-17.689256689674,0.296304551745537,135.715592018844));
#77268=CARTESIAN_POINT('Ctrl Pts',(-17.6970171321881,0.433077423462034,
135.705418162671));
#77269=CARTESIAN_POINT('Ctrl Pts',(-17.7047775747023,0.56904511345047,135.689580236105));
#77270=CARTESIAN_POINT('Ctrl Pts',(-17.7125504749677,0.705231070845705,
135.673716885094));
#77271=CARTESIAN_POINT('Ctrl Pts',(-17.7203233752332,0.840608877259587,
135.652171355525));
#77272=CARTESIAN_POINT('Ctrl Pts',(-17.7280962754986,0.974677503587224,
135.625064593802));
#77273=CARTESIAN_POINT('Ctrl Pts',(-17.7355866112607,1.10387239764918,135.598943231146));
#77274=CARTESIAN_POINT('Ctrl Pts',(-17.7430769470227,1.23185134387066,135.567658019318));
#77275=CARTESIAN_POINT('Ctrl Pts',(-17.7505672827847,1.35818141320068,135.531360333172));
#77276=CARTESIAN_POINT('Ctrl Pts',(-17.7583416169038,1.48930132550655,135.493686409222));
#77277=CARTESIAN_POINT('Ctrl Pts',(-17.7661159510229,1.61906020683902,135.450493072147));
#77278=CARTESIAN_POINT('Ctrl Pts',(-17.773890285142,1.74695814166771,135.401894773367));
#77279=CARTESIAN_POINT('Ctrl Pts',(-17.781655038089,1.87469845372195,135.353356367648));
#77280=CARTESIAN_POINT('Ctrl Pts',(-17.7894197910361,2.0005820205927,135.299426391431));
#77281=CARTESIAN_POINT('Ctrl Pts',(-17.7971845439831,2.12412207040947,135.240269599105));
#77282=CARTESIAN_POINT('Ctrl Pts',(-17.8049415848681,2.24753941850733,135.18117156214));
#77283=CARTESIAN_POINT('Ctrl Pts',(-17.8126986257531,2.36861753126765,135.116857207842));
#77284=CARTESIAN_POINT('Ctrl Pts',(-17.8204556666381,2.48688802143333,135.0475399717));
#77285=CARTESIAN_POINT('Ctrl Pts',(-17.8282068578782,2.60506932290205,134.978275008226));
#77286=CARTESIAN_POINT('Ctrl Pts',(-17.8359580491183,2.72044688009677,134.904014869152));
#77287=CARTESIAN_POINT('Ctrl Pts',(-17.8437092403584,2.83257572735218,134.825019495327));
#77288=CARTESIAN_POINT('Ctrl Pts',(-17.8514571371355,2.94465691685683,134.746057696642));
#77289=CARTESIAN_POINT('Ctrl Pts',(-17.8592050339125,3.05349182376089,134.662364890815));
#77290=CARTESIAN_POINT('Ctrl Pts',(-17.8669529306896,3.15866356708052,134.57424490392));
#77291=CARTESIAN_POINT('Ctrl Pts',(-17.8746992067737,3.26381331073868,134.486143349826));
#77292=CARTESIAN_POINT('Ctrl Pts',(-17.8824454828578,3.36530111544672,134.393616707602));
#77293=CARTESIAN_POINT('Ctrl Pts',(-17.8901917589419,3.46274268862814,134.297009488388));
#77294=CARTESIAN_POINT('Ctrl Pts',(-17.8979380922073,3.56018498110112,134.200401556041));
#77295=CARTESIAN_POINT('Ctrl Pts',(-17.9056844254726,3.65358070480708,134.099713261861));
#77296=CARTESIAN_POINT('Ctrl Pts',(-17.913430758738,3.74258228441788,133.995326130833));
#77297=CARTESIAN_POINT('Ctrl Pts',(-17.9211788267409,3.83160379531533,133.890915623032));
#77298=CARTESIAN_POINT('Ctrl Pts',(-17.9289268947439,3.91622895038564,133.782804927556));
#77299=CARTESIAN_POINT('Ctrl Pts',(-17.9366749627469,3.99615059662795,133.671408484549));
#77300=CARTESIAN_POINT('Ctrl Pts',(-17.9444312654888,4.07615718454707,133.559893648076));
#77301=CARTESIAN_POINT('Ctrl Pts',(-17.9521875682306,4.15145004943383,133.445086406333));
#77302=CARTESIAN_POINT('Ctrl Pts',(-17.9599438709725,4.22176521958163,133.32743047257));
#77303=CARTESIAN_POINT('Ctrl Pts',(-17.9677043134867,4.29211791905289,133.209711742293));
#77304=CARTESIAN_POINT('Ctrl Pts',(-17.9754647560009,4.35748744374197,133.089141633937));
#77305=CARTESIAN_POINT('Ctrl Pts',(-17.9832251985151,4.4176564052034,132.966187379373));
#77306=CARTESIAN_POINT('Ctrl Pts',(-17.9909980987805,4.47792195522324,132.843035747724));
#77307=CARTESIAN_POINT('Ctrl Pts',(-17.9987709990459,4.5329701021494,132.717492680079));
#77308=CARTESIAN_POINT('Ctrl Pts',(-18.0065438993113,4.58263178314732,132.590045080899));
#77309=CARTESIAN_POINT('Ctrl Pts',(-18.0140342350734,4.63048813695142,132.467230522968));
#77310=CARTESIAN_POINT('Ctrl Pts',(-18.0215245708356,4.67334274869021,132.342647789781));
#77311=CARTESIAN_POINT('Ctrl Pts',(-18.0290149065977,4.71108896558805,132.216742938616));
#77312=CARTESIAN_POINT('Ctrl Pts',(-18.0367892407168,4.75026634177178,132.086064366753));
#77313=CARTESIAN_POINT('Ctrl Pts',(-18.0445635748359,4.78406440888829,131.95354749118));
#77314=CARTESIAN_POINT('Ctrl Pts',(-18.0523379089549,4.81230924160563,131.819674768781));
#77315=CARTESIAN_POINT('Ctrl Pts',(-18.060102661902,4.84051926509096,131.685967032548));
#77316=CARTESIAN_POINT('Ctrl Pts',(-18.0678674148492,4.86318959149349,131.550907153072));
#77317=CARTESIAN_POINT('Ctrl Pts',(-18.0756321677963,4.88019572126216,131.414993719088));
#77318=CARTESIAN_POINT('Ctrl Pts',(-18.0833892086813,4.89718496030306,131.279215276242));
#77319=CARTESIAN_POINT('Ctrl Pts',(-18.0911462495663,4.90852114999944,131.142585351402));
#77320=CARTESIAN_POINT('Ctrl Pts',(-18.0989032904513,4.91413068491909,131.005613379129));
#77321=CARTESIAN_POINT('Ctrl Pts',(-18.1066544816915,4.9197359896448,130.868744698485));
#77322=CARTESIAN_POINT('Ctrl Pts',(-18.1144056729316,4.91962321940245,130.73153487288));
#77323=CARTESIAN_POINT('Ctrl Pts',(-18.1221568641717,4.91377055497893,130.594498768908));
#77324=CARTESIAN_POINT('Ctrl Pts',(-18.1299047609488,4.90792037809391,130.457520908936));
#77325=CARTESIAN_POINT('Ctrl Pts',(-18.1376526577259,4.89633517586987,130.320717013532));
#77326=CARTESIAN_POINT('Ctrl Pts',(-18.145400554503,4.87904523143392,130.184602041892));
#77327=CARTESIAN_POINT('Ctrl Pts',(-18.1531468305871,4.86175890368161,130.048515542569));
#77328=CARTESIAN_POINT('Ctrl Pts',(-18.1608931066712,4.83877025650969,129.913118067973));
#77329=CARTESIAN_POINT('Ctrl Pts',(-18.1686393827553,4.81016141737309,129.778919151018));
#77330=CARTESIAN_POINT('Ctrl Pts',(-18.1763857160206,4.78155236705253,129.644719243438));
#77331=CARTESIAN_POINT('Ctrl Pts',(-18.184132049286,4.7473231234982,129.511718293527));
#77332=CARTESIAN_POINT('Ctrl Pts',(-18.1918783825514,4.70760680153173,129.380414949827));
#77333=CARTESIAN_POINT('Ctrl Pts',(-18.1996264505543,4.66788158537027,129.249082201654));
#77334=CARTESIAN_POINT('Ctrl Pts',(-18.2073745185573,4.62266695881221,129.119448190329));
#77335=CARTESIAN_POINT('Ctrl Pts',(-18.2151225865603,4.572145578387,128.991995347391));
#77336=CARTESIAN_POINT('Ctrl Pts',(-18.2228788893021,4.52157050323761,128.864407046056));
#77337=CARTESIAN_POINT('Ctrl Pts',(-18.230635192044,4.46567755185105,128.739004907937));
#77338=CARTESIAN_POINT('Ctrl Pts',(-18.2383914947858,4.40469734959564,128.616250857758));
#77339=CARTESIAN_POINT('Ctrl Pts',(-18.2461519373,4.34368460036996,128.493431290046));
#77340=CARTESIAN_POINT('Ctrl Pts',(-18.2539123798142,4.27757937832064,128.373262968909));
#77341=CARTESIAN_POINT('Ctrl Pts',(-18.2616728223284,4.20665727508862,128.256181339641));
#77342=CARTESIAN_POINT('Ctrl Pts',(-18.2694457225938,4.13562132140052,128.138911760549));
#77343=CARTESIAN_POINT('Ctrl Pts',(-18.2772186228593,4.05975325106519,128.024739100873));
#77344=CARTESIAN_POINT('Ctrl Pts',(-18.2849915231247,3.97937132800418,127.91406878172));
#77345=CARTESIAN_POINT('Ctrl Pts',(-18.2924818588866,3.90191149031716,127.807421607431));
#77346=CARTESIAN_POINT('Ctrl Pts',(-18.2999721946486,3.82026047294958,127.704026798482));
#77347=CARTESIAN_POINT('Ctrl Pts',(-18.3074625304105,3.73473590809163,127.604215189728));
#77348=CARTESIAN_POINT('Ctrl Pts',(-18.3152368645296,3.64596865336136,127.50061919349));
#77349=CARTESIAN_POINT('Ctrl Pts',(-18.3230111986487,3.55274713370896,127.400555314262));
#77350=CARTESIAN_POINT('Ctrl Pts',(-18.3307855327678,3.45538324288425,127.304430660082));
#77351=CARTESIAN_POINT('Ctrl Pts',(-18.3385502857149,3.35813934435344,127.208424470947));
#77352=CARTESIAN_POINT('Ctrl Pts',(-18.3463150386619,3.25676350783038,127.11634811941));
#77353=CARTESIAN_POINT('Ctrl Pts',(-18.354079791609,3.15160791508874,127.028575849859));
#77354=CARTESIAN_POINT('Ctrl Pts',(-18.361836832494,3.04655676436411,126.940890756962));
#77355=CARTESIAN_POINT('Ctrl Pts',(-18.3695938733791,2.93773362646882,126.857501487766));
#77356=CARTESIAN_POINT('Ctrl Pts',(-18.3773509142641,2.82552731759192,126.778745330428));
#77357=CARTESIAN_POINT('Ctrl Pts',(-18.3851021055042,2.71340562436645,126.700048563721));
#77358=CARTESIAN_POINT('Ctrl Pts',(-18.3928532967442,2.59790615703109,126.625978178244));
#77359=CARTESIAN_POINT('Ctrl Pts',(-18.4006044879843,2.47945029361585,126.55683082909));
#77360=CARTESIAN_POINT('Ctrl Pts',(-18.4083523847614,2.36104477710151,126.487712869404));
#77361=CARTESIAN_POINT('Ctrl Pts',(-18.4161002815385,2.23968570062472,126.423513981058));
#77362=CARTESIAN_POINT('Ctrl Pts',(-18.4238481783156,2.11582268270914,126.364487034024));
#77363=CARTESIAN_POINT('Ctrl Pts',(-18.4315944543997,1.99198557426674,126.305472434155));
#77364=CARTESIAN_POINT('Ctrl Pts',(-18.4393407304837,1.86564591890809,126.251627791806));
#77365=CARTESIAN_POINT('Ctrl Pts',(-18.4470870065678,1.73727679300059,126.203159425812));
#77366=CARTESIAN_POINT('Ctrl Pts',(-18.4548333398332,1.60890671950155,126.154690702035));
#77367=CARTESIAN_POINT('Ctrl Pts',(-18.4625796730985,1.47850751132211,126.111598471904));
#77368=CARTESIAN_POINT('Ctrl Pts',(-18.4703260063639,1.34657064741566,126.074040273866));
#77369=CARTESIAN_POINT('Ctrl Pts',(-18.4780740743669,1.21460423716296,126.036473664931));
#77370=CARTESIAN_POINT('Ctrl Pts',(-18.4858221423698,1.08109986192609,126.004443661191));
#77371=CARTESIAN_POINT('Ctrl Pts',(-18.4935702103728,0.946562135337526,
125.978057354566));
#77372=CARTESIAN_POINT('Ctrl Pts',(-18.5013265131146,0.811881420452674,
125.95164300426));
#77373=CARTESIAN_POINT('Ctrl Pts',(-18.5090828158565,0.676165544595105,
125.930884408462));
#77374=CARTESIAN_POINT('Ctrl Pts',(-18.5168391185983,0.539927796761214,
125.915837217112));
#77375=CARTESIAN_POINT('Ctrl Pts',(-18.5245995611125,0.403617334738895,
125.900781994623));
#77376=CARTESIAN_POINT('Ctrl Pts',(-18.5323600036267,0.266784835595289,
125.891444277281));
#77377=CARTESIAN_POINT('Ctrl Pts',(-18.5401204461409,0.129945615803143,
125.887827570852));
#77378=CARTESIAN_POINT('Ctrl Pts',(-18.5478933464063,-0.00711327045281471,
125.884205058564));
#77379=CARTESIAN_POINT('Ctrl Pts',(-18.5556662466717,-0.144178507772764,
125.886321903455));
#77380=CARTESIAN_POINT('Ctrl Pts',(-18.5634391469371,-0.2807369744749,125.894129481085));
#77381=CARTESIAN_POINT('Ctrl Pts',(-18.5709294826992,-0.412331196943699,
125.901653233603));
#77382=CARTESIAN_POINT('Ctrl Pts',(-18.5784198184614,-0.543454547332617,
125.914461127196));
#77383=CARTESIAN_POINT('Ctrl Pts',(-18.5859101542235,-0.673656996951168,
125.932464753227));
#77384=CARTESIAN_POINT('Ctrl Pts',(-18.5936844883426,-0.80879611201966,
125.951150992212));
#77385=CARTESIAN_POINT('Ctrl Pts',(-18.6014588224617,-0.943371196004674,
125.975493925947));
#77386=CARTESIAN_POINT('Ctrl Pts',(-18.6092331565808,-1.07687115119386,
126.005451201227));
#77387=CARTESIAN_POINT('Ctrl Pts',(-18.6169979095279,-1.21020657962005,
126.035371556843));
#77388=CARTESIAN_POINT('Ctrl Pts',(-18.624762662475,-1.34246913778945,126.070892402127));
#77389=CARTESIAN_POINT('Ctrl Pts',(-18.6325274154221,-1.47315360044864,
126.111919724813));
#77390=CARTESIAN_POINT('Ctrl Pts',(-18.6402844563072,-1.60370826545683,
126.152906298583));
#77391=CARTESIAN_POINT('Ctrl Pts',(-18.6480414971921,-1.73268758352382,
126.199388349629));
#77392=CARTESIAN_POINT('Ctrl Pts',(-18.6557985380771,-1.8595976199223,126.251221068367));
#77393=CARTESIAN_POINT('Ctrl Pts',(-18.6635497293172,-1.9864119524746,126.303014699649));
#77394=CARTESIAN_POINT('Ctrl Pts',(-18.6713009205574,-2.11115974888513,
126.360150820014));
#77395=CARTESIAN_POINT('Ctrl Pts',(-18.6790521117975,-2.23336365970487,
126.422435261514));
#77396=CARTESIAN_POINT('Ctrl Pts',(-18.6868000085746,-2.35551563060294,
126.484693230466));
#77397=CARTESIAN_POINT('Ctrl Pts',(-18.6945479053517,-2.47512551877083,
126.552094991278));
#77398=CARTESIAN_POINT('Ctrl Pts',(-18.7022958021288,-2.59173754774647,
126.624398949548));
#77399=CARTESIAN_POINT('Ctrl Pts',(-18.7100420782129,-2.7083251839995,126.696687783389));
#77400=CARTESIAN_POINT('Ctrl Pts',(-18.7177883542969,-2.82191587630561,
126.773876569149));
#77401=CARTESIAN_POINT('Ctrl Pts',(-18.725534630381,-2.93208033345547,126.855678814652));
#77402=CARTESIAN_POINT('Ctrl Pts',(-18.7332809636464,-3.04224560381403,
126.937481664));
#77403=CARTESIAN_POINT('Ctrl Pts',(-18.7410272969117,-3.14898427465706,
127.023897807967));
#77404=CARTESIAN_POINT('Ctrl Pts',(-18.748773630177,-3.25189814804754,127.114598904769));
#77405=CARTESIAN_POINT('Ctrl Pts',(-18.75652169818,-3.35483506828656,127.205320313452));
#77406=CARTESIAN_POINT('Ctrl Pts',(-18.764269766183,-3.45394519341066,127.300328325981));
#77407=CARTESIAN_POINT('Ctrl Pts',(-18.7720178341859,-3.54886566796082,
127.399256282414));
#77408=CARTESIAN_POINT('Ctrl Pts',(-18.7797741369278,-3.64388702512104,
127.498289380657));
#77409=CARTESIAN_POINT('Ctrl Pts',(-18.7875304396697,-3.734709565626,127.601250462603));
#77410=CARTESIAN_POINT('Ctrl Pts',(-18.7952867424115,-3.82100902436337,
127.707737763837));
#77411=CARTESIAN_POINT('Ctrl Pts',(-18.8030471849257,-3.90735454372017,
127.81428190055));
#77412=CARTESIAN_POINT('Ctrl Pts',(-18.8108076274399,-3.98917193788441,
127.924355693068));
#77413=CARTESIAN_POINT('Ctrl Pts',(-18.818568069954,-4.06617971621538,128.037527485999));
#77414=CARTESIAN_POINT('Ctrl Pts',(-18.8263409702195,-4.14331111426867,
128.150880952339));
#77415=CARTESIAN_POINT('Ctrl Pts',(-18.8341138704849,-4.21561726148516,
128.267342024756));
#77416=CARTESIAN_POINT('Ctrl Pts',(-18.8418867707503,-4.28286171218099,
128.386452716749));
#77417=CARTESIAN_POINT('Ctrl Pts',(-18.8493771065123,-4.34766165771511,
128.501233435066));
#77418=CARTESIAN_POINT('Ctrl Pts',(-18.8568674422743,-4.4077613878469,128.618474202689));
#77419=CARTESIAN_POINT('Ctrl Pts',(-18.8643577780363,-4.46299203176705,
128.737748610709));
#77420=CARTESIAN_POINT('Ctrl Pts',(-18.8728685221026,-4.52574674530165,
128.87327176916));
#77421=CARTESIAN_POINT('Ctrl Pts',(-18.8813792661689,-4.58238994528214,
129.011796482427));
#77422=CARTESIAN_POINT('Ctrl Pts',(-18.8898900102352,-4.63264986635917,
129.152774023341));
#77423=CARTESIAN_POINT('Ctrl Pts',(-18.8984007543015,-4.68290978743619,
129.293751564256));
#77424=CARTESIAN_POINT('Ctrl Pts',(-18.9069114983678,-4.72678625655128,
129.437181693642));
#77425=CARTESIAN_POINT('Ctrl Pts',(-18.9154222424341,-4.76405452823411,
129.582490119308));
#77426=CARTESIAN_POINT('Ctrl Pts',(-17.1650861998779,-4.76405452823408,
129.582490119308));
#77427=CARTESIAN_POINT('Ctrl Pts',(-17.1728615289864,-4.79806952616346,
129.715114079985));
#77428=CARTESIAN_POINT('Ctrl Pts',(-17.1806368580948,-4.82649955024039,
129.848992775321));
#77429=CARTESIAN_POINT('Ctrl Pts',(-17.1884121872032,-4.8492846135786,129.983615956292));
#77430=CARTESIAN_POINT('Ctrl Pts',(-17.1901654698551,-4.85442248693634,
130.013972547563));
#77431=CARTESIAN_POINT('Ctrl Pts',(-17.1919187525071,-4.85927353984324,
130.044366983506));
#77432=CARTESIAN_POINT('Ctrl Pts',(-17.193672035159,-4.86383745032036,130.074793403828));
#77433=CARTESIAN_POINT('Ctrl Pts',(-17.2074948781088,-4.89981922296458,
130.314674651259));
#77434=CARTESIAN_POINT('Ctrl Pts',(-17.2213177210587,-4.91806097139444,
130.557281781475));
#77435=CARTESIAN_POINT('Ctrl Pts',(-17.2351405640086,-4.91824853831084,
130.800568796985));
#77436=CARTESIAN_POINT('',(-16.8898594359349,-4.91824838856106,130.808341938514));
#77437=CARTESIAN_POINT('Ctrl Pts',(-16.8197493731203,-4.76405452823399,
129.582490119308));
#77438=CARTESIAN_POINT('Ctrl Pts',(-16.8273867555103,-4.79766288588759,
129.713528595721));
#77439=CARTESIAN_POINT('Ctrl Pts',(-16.8350241379004,-4.82584429192238,
129.845891195246));
#77440=CARTESIAN_POINT('Ctrl Pts',(-16.8426615202905,-4.84851502478482,
129.97908180593));
#77441=CARTESIAN_POINT('Ctrl Pts',(-16.8505278395646,-4.87186533170469,
130.116264915853));
#77442=CARTESIAN_POINT('Ctrl Pts',(-16.8583941588386,-4.88936933475787,
130.25432599799));
#77443=CARTESIAN_POINT('Ctrl Pts',(-16.8662604781127,-4.90099312143358,
130.392718192444));
#77444=CARTESIAN_POINT('Ctrl Pts',(-16.8741267973868,-4.91261690810929,
130.531110386897));
#77445=CARTESIAN_POINT('Ctrl Pts',(-16.8819931166608,-4.91836051132978,
130.669833229029));
#77446=CARTESIAN_POINT('Ctrl Pts',(-16.8898594359349,-4.91824838856106,
130.808341938514));
#77447=CARTESIAN_POINT('Ctrl Pts',(-16.8898594359912,-4.91824838856026,
130.808341939505));
#77448=CARTESIAN_POINT('Ctrl Pts',(-16.9024630796802,-4.91806874218068,
131.030264589901));
#77449=CARTESIAN_POINT('Ctrl Pts',(-16.9150667233692,-4.90286602102809,
131.251597493366));
#77450=CARTESIAN_POINT('Ctrl Pts',(-16.9276703670583,-4.87289314661139,
131.47076548265));
#77451=CARTESIAN_POINT('Ctrl Pts',(-16.9300513805408,-4.86723083023245,
131.512169536135));
#77452=CARTESIAN_POINT('Ctrl Pts',(-16.9324323940232,-4.86104148805206,
131.553496435964));
#77453=CARTESIAN_POINT('Ctrl Pts',(-16.9348134075057,-4.85432696824674,
131.594735685399));
#77454=CARTESIAN_POINT('Ctrl Pts',(-16.9425877416248,-4.83240314429537,
131.729387465529));
#77455=CARTESIAN_POINT('Ctrl Pts',(-16.9503620757439,-4.80483778977211,
131.863339631926));
#77456=CARTESIAN_POINT('Ctrl Pts',(-16.958136409863,-4.7716855106225,131.996082250421));
#77457=CARTESIAN_POINT('Ctrl Pts',(-16.9659011628101,-4.73857408869403,
132.128661275503));
#77458=CARTESIAN_POINT('Ctrl Pts',(-16.9736659157571,-4.69988953582749,
132.260033342977));
#77459=CARTESIAN_POINT('Ctrl Pts',(-16.9814306687042,-4.65573796123039,
132.38969562912));
#77460=CARTESIAN_POINT('Ctrl Pts',(-16.9891877095892,-4.61163023859967,
132.519229132852));
#77461=CARTESIAN_POINT('Ctrl Pts',(-16.9969447504742,-4.56206642523747,
132.647055867001));
#77462=CARTESIAN_POINT('Ctrl Pts',(-17.0047017913592,-4.50720314209734,
132.772685514113));
#77463=CARTESIAN_POINT('Ctrl Pts',(-17.0124529825993,-4.45238123178581,
132.898220422931));
#77464=CARTESIAN_POINT('Ctrl Pts',(-17.0202041738394,-4.39226796206567,
133.021561185711));
#77465=CARTESIAN_POINT('Ctrl Pts',(-17.0279553650795,-4.32706890003891,
133.142235249965));
#77466=CARTESIAN_POINT('Ctrl Pts',(-17.0357032618566,-4.26189754935266,
133.262858024523));
#77467=CARTESIAN_POINT('Ctrl Pts',(-17.0434511586337,-4.19164489106718,
133.380816011586));
#77468=CARTESIAN_POINT('Ctrl Pts',(-17.0511990554108,-4.11656338738992,
133.495659363544));
#77469=CARTESIAN_POINT('Ctrl Pts',(-17.0589453314949,-4.04149758914457,
133.610478692748));
#77470=CARTESIAN_POINT('Ctrl Pts',(-17.066691607579,-3.96160516843571,133.722184355716));
#77471=CARTESIAN_POINT('Ctrl Pts',(-17.0744378836632,-3.87718283674348,
133.830354059886));
#77472=CARTESIAN_POINT('Ctrl Pts',(-17.0821842169285,-3.79275988186488,
133.938524562539));
#77473=CARTESIAN_POINT('Ctrl Pts',(-17.0899305501939,-3.7038071898228,134.043158746103));
#77474=CARTESIAN_POINT('Ctrl Pts',(-17.0976768834592,-3.61066256349931,
134.143866406608));
#77475=CARTESIAN_POINT('Ctrl Pts',(-17.1054249514622,-3.51749707808281,
134.244596619895));
#77476=CARTESIAN_POINT('Ctrl Pts',(-17.1131730194652,-3.4201380557876,134.341398273417));
#77477=CARTESIAN_POINT('Ctrl Pts',(-17.1209210874681,-3.3189607584973,134.433917415035));
#77478=CARTESIAN_POINT('Ctrl Pts',(-17.12867739021,-3.21767592877127,134.526534887099));
#77479=CARTESIAN_POINT('Ctrl Pts',(-17.1364336929518,-3.11256500652557,
134.614860490884));
#77480=CARTESIAN_POINT('Ctrl Pts',(-17.1441899956937,-3.00403742194753,
134.698579695897));
#77481=CARTESIAN_POINT('Ctrl Pts',(-17.1519504382079,-2.89545191292975,
134.782343584371));
#77482=CARTESIAN_POINT('Ctrl Pts',(-17.159710880722,-2.78344642708021,134.861495949634));
#77483=CARTESIAN_POINT('Ctrl Pts',(-17.1674713232362,-2.66845925048317,
134.935765740646));
#77484=CARTESIAN_POINT('Ctrl Pts',(-17.1752442235016,-2.55328748626217,
135.01015475612));
#77485=CARTESIAN_POINT('Ctrl Pts',(-17.183017123767,-2.43512480359333,135.079645336333));
#77486=CARTESIAN_POINT('Ctrl Pts',(-17.1907900240325,-2.31443473113332,
135.144012094105));
#77487=CARTESIAN_POINT('Ctrl Pts',(-17.1982803597945,-2.19813204680751,
135.206038958101));
#77488=CARTESIAN_POINT('Ctrl Pts',(-17.2057706955565,-2.07948281381779,
135.263307925841));
#77489=CARTESIAN_POINT('Ctrl Pts',(-17.2132610313185,-1.95891737071349,
135.315660407784));
#77490=CARTESIAN_POINT('Ctrl Pts',(-17.2210353654376,-1.83378065218863,
135.369997849991));
#77491=CARTESIAN_POINT('Ctrl Pts',(-17.2288096995567,-1.70618315343553,
135.419210754441));
#77492=CARTESIAN_POINT('Ctrl Pts',(-17.2365840336757,-1.57658341235972,
135.463069430786));
#77493=CARTESIAN_POINT('Ctrl Pts',(-17.2443487866228,-1.44714339138213,
135.506874055232));
#77494=CARTESIAN_POINT('Ctrl Pts',(-17.2521135395699,-1.31570640461834,
135.545337456714));
#77495=CARTESIAN_POINT('Ctrl Pts',(-17.259878292517,-1.18275284652813,135.578277119405));
#77496=CARTESIAN_POINT('Ctrl Pts',(-17.267635333402,-1.04993133978614,135.611184065959));
#77497=CARTESIAN_POINT('Ctrl Pts',(-17.275392374287,-0.915596636319013,
135.638578098207));
#77498=CARTESIAN_POINT('Ctrl Pts',(-17.283149415172,-0.780245911539738,
135.660325957231));
#77499=CARTESIAN_POINT('Ctrl Pts',(-17.2909006064121,-0.64499725579471,
135.682057416025));
#77500=CARTESIAN_POINT('Ctrl Pts',(-17.2986517976523,-0.508734488243535,
135.698151114762));
#77501=CARTESIAN_POINT('Ctrl Pts',(-17.3064029888924,-0.371966294718296,
135.708524576703));
#77502=CARTESIAN_POINT('Ctrl Pts',(-17.3141508856695,-0.235256231323903,
135.718893629645));
#77503=CARTESIAN_POINT('Ctrl Pts',(-17.3218987824465,-0.0980415582443893,
135.723547251862));
#77504=CARTESIAN_POINT('Ctrl Pts',(-17.3296466792236,0.039162792995575,
135.722454693338));
#77505=CARTESIAN_POINT('Ctrl Pts',(-17.3373929553077,0.176338444043044,
135.721362363354));
#77506=CARTESIAN_POINT('Ctrl Pts',(-17.3451392313919,0.313503386840421,
135.714526246537));
#77507=CARTESIAN_POINT('Ctrl Pts',(-17.352885507476,0.450141954892986,135.701967715215));
#77508=CARTESIAN_POINT('Ctrl Pts',(-17.3606318407413,0.58678153158042,135.689409091189));
#77509=CARTESIAN_POINT('Ctrl Pts',(-17.3683781740066,0.722894336445406,
135.671128004152));
#77510=CARTESIAN_POINT('Ctrl Pts',(-17.376124507272,0.857969489129146,135.647197742457));
#77511=CARTESIAN_POINT('Ctrl Pts',(-17.3838725752749,0.993074890956783,
135.623262121747));
#77512=CARTESIAN_POINT('Ctrl Pts',(-17.3916206432778,1.12714179330706,135.593674877179));
#77513=CARTESIAN_POINT('Ctrl Pts',(-17.3993687112808,1.25966956800745,135.558560407429));
#77514=CARTESIAN_POINT('Ctrl Pts',(-17.4071250140226,1.3923381948039,135.523408617603));
#77515=CARTESIAN_POINT('Ctrl Pts',(-17.4148813167645,1.52346404773039,135.482717968141));
#77516=CARTESIAN_POINT('Ctrl Pts',(-17.4226376195064,1.6525611963574,135.436662912839));
#77517=CARTESIAN_POINT('Ctrl Pts',(-17.4303980620205,1.78172724801967,135.390583276568));
#77518=CARTESIAN_POINT('Ctrl Pts',(-17.4381585045348,1.90886207561422,135.339133675991));
#77519=CARTESIAN_POINT('Ctrl Pts',(-17.4459189470489,2.03350073189098,135.282536343897));
#77520=CARTESIAN_POINT('Ctrl Pts',(-17.4536918473144,2.15833946920369,135.22584815674));
#77521=CARTESIAN_POINT('Ctrl Pts',(-17.4614647475798,2.28067367867874,135.163995901277));
#77522=CARTESIAN_POINT('Ctrl Pts',(-17.4692376478452,2.40006318713692,135.097247730017));
#77523=CARTESIAN_POINT('Ctrl Pts',(-17.4767279836073,2.51511258623958,135.032926022911));
#77524=CARTESIAN_POINT('Ctrl Pts',(-17.4842183193693,2.62742739934127,134.964058338811));
#77525=CARTESIAN_POINT('Ctrl Pts',(-17.4917086551314,2.73664159207249,134.890921012206));
#77526=CARTESIAN_POINT('Ctrl Pts',(-17.4994829892505,2.84999667411525,134.815010661634));
#77527=CARTESIAN_POINT('Ctrl Pts',(-17.5072573233696,2.96037044922866,134.734260049131));
#77528=CARTESIAN_POINT('Ctrl Pts',(-17.5150316574887,3.06732182148153,134.64893080238));
#77529=CARTESIAN_POINT('Ctrl Pts',(-17.5227964104358,3.17414138572662,134.563706716301));
#77530=CARTESIAN_POINT('Ctrl Pts',(-17.5305611633829,3.2775466366057,134.473915464869));
#77531=CARTESIAN_POINT('Ctrl Pts',(-17.53832591633,3.37712435344672,134.379862563287));
#77532=CARTESIAN_POINT('Ctrl Pts',(-17.546082957215,3.47660316829543,134.285903076374));
#77533=CARTESIAN_POINT('Ctrl Pts',(-17.5538399981,3.57226173199629,134.187690629357));
#77534=CARTESIAN_POINT('Ctrl Pts',(-17.561597038985,3.66371919459305,134.085571480292));
#77535=CARTESIAN_POINT('Ctrl Pts',(-17.5693482302251,3.75510768840584,133.983529340072));
#77536=CARTESIAN_POINT('Ctrl Pts',(-17.5770994214652,3.84230112721457,133.877586651846));
#77537=CARTESIAN_POINT('Ctrl Pts',(-17.5848506127053,3.92495516388607,133.768126806722));
#77538=CARTESIAN_POINT('Ctrl Pts',(-17.5925985094824,4.0075740703871,133.658713484952));
#77539=CARTESIAN_POINT('Ctrl Pts',(-17.6003464062594,4.08565717701009,133.545786290848));
#77540=CARTESIAN_POINT('Ctrl Pts',(-17.6080943030365,4.15890027982851,133.429761829751));
#77541=CARTESIAN_POINT('Ctrl Pts',(-17.6158405791206,4.23212806176876,133.31376163847));
#77542=CARTESIAN_POINT('Ctrl Pts',(-17.6235868552048,4.30051764510405,133.194665799261));
#77543=CARTESIAN_POINT('Ctrl Pts',(-17.6313331312889,4.36380828064201,133.072919709214));
#77544=CARTESIAN_POINT('Ctrl Pts',(-17.6390794645542,4.42709938337706,132.951172720466));
#77545=CARTESIAN_POINT('Ctrl Pts',(-17.6468257978196,4.48529128287434,132.826775788734));
#77546=CARTESIAN_POINT('Ctrl Pts',(-17.6545721310849,4.53816949539015,132.700198346279));
#77547=CARTESIAN_POINT('Ctrl Pts',(-17.6623201990879,4.59105954961502,132.573592557683));
#77548=CARTESIAN_POINT('Ctrl Pts',(-17.6700682670909,4.6386333982926,132.444805647367));
#77549=CARTESIAN_POINT('Ctrl Pts',(-17.6778163350939,4.68072509979499,132.314326048511));
#77550=CARTESIAN_POINT('Ctrl Pts',(-17.6855726378357,4.72286153685864,132.183707774385));
#77551=CARTESIAN_POINT('Ctrl Pts',(-17.6933289405775,4.7595040674805,132.051393590682));
#77552=CARTESIAN_POINT('Ctrl Pts',(-17.7010852433194,4.79053680731456,131.917886620973));
#77553=CARTESIAN_POINT('Ctrl Pts',(-17.7088456858336,4.82158611025628,131.784308394575));
#77554=CARTESIAN_POINT('Ctrl Pts',(-17.7166061283477,4.84701958391824,131.649536497636));
#77555=CARTESIAN_POINT('Ctrl Pts',(-17.7243665708619,4.86677288369339,131.514082225696));
#77556=CARTESIAN_POINT('Ctrl Pts',(-17.7321394711274,4.88655789321896,131.378410510534));
#77557=CARTESIAN_POINT('Ctrl Pts',(-17.7399123713927,4.90064446735117,131.242054620514));
#77558=CARTESIAN_POINT('Ctrl Pts',(-17.7476852716582,4.90902028603632,131.105529828781));
#77559=CARTESIAN_POINT('Ctrl Pts',(-17.7551756074202,4.91709162261487,130.973968057112));
#77560=CARTESIAN_POINT('Ctrl Pts',(-17.7626659431823,4.91986018947052,130.842249758487));
#77561=CARTESIAN_POINT('Ctrl Pts',(-17.7701562789443,4.91736062411741,130.710832253528));
#77562=CARTESIAN_POINT('Ctrl Pts',(-17.7779306130634,4.91476628698421,130.574432013925));
#77563=CARTESIAN_POINT('Ctrl Pts',(-17.7857049471825,4.9064882311872,130.437923752473));
#77564=CARTESIAN_POINT('Ctrl Pts',(-17.7934792813016,4.89250814838155,130.301819991825));
#77565=CARTESIAN_POINT('Ctrl Pts',(-17.8012440342487,4.87854529477853,130.165883966898));
#77566=CARTESIAN_POINT('Ctrl Pts',(-17.8090087871958,4.85889443584218,130.030351836073));
#77567=CARTESIAN_POINT('Ctrl Pts',(-17.8167735401429,4.83358925429883,129.895736392032));
#77568=CARTESIAN_POINT('Ctrl Pts',(-17.8245305810279,4.80830920621857,129.761254649949));
#77569=CARTESIAN_POINT('Ctrl Pts',(-17.8322876219129,4.7773860832927,129.627688164531));
#77570=CARTESIAN_POINT('Ctrl Pts',(-17.8400446627979,4.74090534352596,129.49554451657));
#77571=CARTESIAN_POINT('Ctrl Pts',(-17.847795854038,4.70445211416886,129.363500519161));
#77572=CARTESIAN_POINT('Ctrl Pts',(-17.8555470452781,4.66244971360641,129.232877598865));
#77573=CARTESIAN_POINT('Ctrl Pts',(-17.8632982365182,4.61503457159742,129.104172696935));
#77574=CARTESIAN_POINT('Ctrl Pts',(-17.8710461332953,4.56763958228862,128.975522498021));
#77575=CARTESIAN_POINT('Ctrl Pts',(-17.8787940300724,4.51483656204039,128.848789062177));
#77576=CARTESIAN_POINT('Ctrl Pts',(-17.8865419268494,4.45681158307164,128.724453510145));
#77577=CARTESIAN_POINT('Ctrl Pts',(-17.8942882029335,4.39879874167762,128.600143966431));
#77578=CARTESIAN_POINT('Ctrl Pts',(-17.9020344790176,4.33556627948259,128.478231662907));
#77579=CARTESIAN_POINT('Ctrl Pts',(-17.9097807551017,4.26734798036601,128.359176723261));
#77580=CARTESIAN_POINT('Ctrl Pts',(-17.9175270883671,4.19912917767735,128.240120904779));
#77581=CARTESIAN_POINT('Ctrl Pts',(-17.9252734216325,4.12592465900117,128.123922831486));
#77582=CARTESIAN_POINT('Ctrl Pts',(-17.9330197548979,4.04801343729121,128.011016694235));
#77583=CARTESIAN_POINT('Ctrl Pts',(-17.9407678229009,3.97008476790346,127.898085272437));
#77584=CARTESIAN_POINT('Ctrl Pts',(-17.9485158909038,3.88744752008537,127.788447575362));
#77585=CARTESIAN_POINT('Ctrl Pts',(-17.9562639589068,3.80042293100301,127.682507224467));
#77586=CARTESIAN_POINT('Ctrl Pts',(-17.9640202616486,3.71330585115176,127.576454278905));
#77587=CARTESIAN_POINT('Ctrl Pts',(-17.9717765643904,3.62179236391466,127.474106831878));
#77588=CARTESIAN_POINT('Ctrl Pts',(-17.9795328671323,3.5262431230819,127.375834330746));
#77589=CARTESIAN_POINT('Ctrl Pts',(-17.9872933096464,3.43064288474225,127.277509378621));
#77590=CARTESIAN_POINT('Ctrl Pts',(-17.9950537521606,3.33100288467038,127.183263974634));
#77591=CARTESIAN_POINT('Ctrl Pts',(-18.0028141946748,3.22771851045276,127.093428621452));
#77592=CARTESIAN_POINT('Ctrl Pts',(-18.0105870949402,3.12426833498848,127.003449056587));
#77593=CARTESIAN_POINT('Ctrl Pts',(-18.0183599952057,3.01716240031762,126.917893933583));
#77594=CARTESIAN_POINT('Ctrl Pts',(-18.0261328954711,2.90682756103946,126.837052135373));
#77595=CARTESIAN_POINT('Ctrl Pts',(-18.0336232312332,2.80050367108575,126.759149140155));
#77596=CARTESIAN_POINT('Ctrl Pts',(-18.0411135669951,2.69118181400784,126.685622908645));
#77597=CARTESIAN_POINT('Ctrl Pts',(-18.0486039027572,2.57926546902013,126.616691492286));
#77598=CARTESIAN_POINT('Ctrl Pts',(-18.0563782368763,2.46310578179614,126.545146520326));
#77599=CARTESIAN_POINT('Ctrl Pts',(-18.0641525709953,2.34378302396081,126.4783250334));
#77600=CARTESIAN_POINT('Ctrl Pts',(-18.0719269051144,2.22171849923021,126.416519465852));
#77601=CARTESIAN_POINT('Ctrl Pts',(-18.0796916580615,2.09980440811712,126.354790068142));
#77602=CARTESIAN_POINT('Ctrl Pts',(-18.0874564110086,1.97515561873021,126.298064465038));
#77603=CARTESIAN_POINT('Ctrl Pts',(-18.0952211639557,1.84822176441418,126.246591495282));
#77604=CARTESIAN_POINT('Ctrl Pts',(-18.1029782048407,1.72141398259172,126.195169649205));
#77605=CARTESIAN_POINT('Ctrl Pts',(-18.1107352457257,1.59232601232948,126.148990200399));
#77606=CARTESIAN_POINT('Ctrl Pts',(-18.1184922866107,1.46143108786168,126.108255610442));
#77607=CARTESIAN_POINT('Ctrl Pts',(-18.1262434778508,1.33063487227445,126.067551738756));
#77608=CARTESIAN_POINT('Ctrl Pts',(-18.133994669091,1.1980347865262,126.032284668857));
#77609=CARTESIAN_POINT('Ctrl Pts',(-18.1417458603311,1.06412266498436,126.00260822741));
#77610=CARTESIAN_POINT('Ctrl Pts',(-18.1494937571082,0.93026745966658,125.972944399243));
#77611=CARTESIAN_POINT('Ctrl Pts',(-18.1572416538852,0.795101708584325,
125.948866557927));
#77612=CARTESIAN_POINT('Ctrl Pts',(-18.1649895506623,0.659130768822893,
125.930478213148));
#77613=CARTESIAN_POINT('Ctrl Pts',(-18.1727358267464,0.523188271250865,
125.912093714815));
#77614=CARTESIAN_POINT('Ctrl Pts',(-18.1804821028305,0.386441307205254,
125.899396398168));
#77615=CARTESIAN_POINT('Ctrl Pts',(-18.1882283789145,0.249403357673105,
125.8924382823));
#77616=CARTESIAN_POINT('Ctrl Pts',(-18.1959747121799,0.112364396557943,
125.885480115069));
#77617=CARTESIAN_POINT('Ctrl Pts',(-18.2037210454453,-0.024965163867713,
125.884261252981));
#77618=CARTESIAN_POINT('Ctrl Pts',(-18.2114673787106,-0.162069213226618,
125.888781645296));
#77619=CARTESIAN_POINT('Ctrl Pts',(-18.2192154467136,-0.299203966086765,
125.893303049921));
#77620=CARTESIAN_POINT('Ctrl Pts',(-18.2269635147165,-0.436112716709654,
125.9035662536));
#77621=CARTESIAN_POINT('Ctrl Pts',(-18.2347115827195,-0.572282250397577,
125.919519157664));
#77622=CARTESIAN_POINT('Ctrl Pts',(-18.2424678854613,-0.708596506686528,
125.935489016663));
#77623=CARTESIAN_POINT('Ctrl Pts',(-18.2502241882032,-0.84416958769425,
125.957160610179));
#77624=CARTESIAN_POINT('Ctrl Pts',(-18.2579804909451,-0.978495724708584,
125.984430205285));
#77625=CARTESIAN_POINT('Ctrl Pts',(-18.2657409334593,-1.11289355562672,
126.011714354996));
#77626=CARTESIAN_POINT('Ctrl Pts',(-18.2735013759734,-1.24604273705096,
126.044602366081));
#77627=CARTESIAN_POINT('Ctrl Pts',(-18.2812618184876,-1.37745149107752,
126.082940232531));
#77628=CARTESIAN_POINT('Ctrl Pts',(-18.289034718753,-1.50907119410196,126.121339642327));
#77629=CARTESIAN_POINT('Ctrl Pts',(-18.2968076190184,-1.63894451602914,
126.16520626478));
#77630=CARTESIAN_POINT('Ctrl Pts',(-18.3045805192839,-1.76659768613051,
126.214337123306));
#77631=CARTESIAN_POINT('Ctrl Pts',(-18.3120708550459,-1.88961034195994,
126.261681951372));
#77632=CARTESIAN_POINT('Ctrl Pts',(-18.3195611908079,-2.01056117698658,
126.313914801778));
#77633=CARTESIAN_POINT('Ctrl Pts',(-18.32705152657,-2.12904864798273,126.370814078166));
#77634=CARTESIAN_POINT('Ctrl Pts',(-18.3348265613507,-2.25203969102043,
126.42987603039));
#77635=CARTESIAN_POINT('Ctrl Pts',(-18.3426015961315,-2.3727660408316,126.494153263206));
#77636=CARTESIAN_POINT('Ctrl Pts',(-18.3503766309122,-2.49075381185636,
126.563449334454));
#77637=CARTESIAN_POINT('Ctrl Pts',(-18.3581419274936,-2.60859380367939,
126.632658612656));
#77638=CARTESIAN_POINT('Ctrl Pts',(-18.3659072240749,-2.72370170798766,
126.706874024767));
#77639=CARTESIAN_POINT('Ctrl Pts',(-18.3736725206563,-2.83562503968742,
126.785851727841));
#77640=CARTESIAN_POINT('Ctrl Pts',(-18.3814299488222,-2.94743496177422,
126.864749404431));
#77641=CARTESIAN_POINT('Ctrl Pts',(-18.3891873769882,-3.05606641597749,
126.948399544035));
#77642=CARTESIAN_POINT('Ctrl Pts',(-18.396944805154,-3.16109321225825,127.036513385271));
#77643=CARTESIAN_POINT('Ctrl Pts',(-18.4046957368811,-3.2660320541111,127.124553435791));
#77644=CARTESIAN_POINT('Ctrl Pts',(-18.4124466686081,-3.36737195112619,
127.217049493631));
#77645=CARTESIAN_POINT('Ctrl Pts',(-18.4201976003352,-3.46471768203348,
127.313670936958));
#77646=CARTESIAN_POINT('Ctrl Pts',(-18.4279450099172,-3.56201917751277,
127.410248473984));
#77647=CARTESIAN_POINT('Ctrl Pts',(-18.4356924194992,-3.65532984134678,
127.510947391778));
#77648=CARTESIAN_POINT('Ctrl Pts',(-18.4434398290812,-3.74428950334184,
127.615398532864));
#77649=CARTESIAN_POINT('Ctrl Pts',(-18.4511853958899,-3.83322800568385,
127.719824829546));
#77650=CARTESIAN_POINT('Ctrl Pts',(-18.4589309626985,-3.91781731295466,
127.828001275673));
#77651=CARTESIAN_POINT('Ctrl Pts',(-18.4666765295072,-3.99773620201954,
127.939524091416));
#77652=CARTESIAN_POINT('Ctrl Pts',(-18.4744219313113,-4.07765338856494,
128.051044531378));
#77653=CARTESIAN_POINT('Ctrl Pts',(-18.4821673331153,-4.15290012864465,
128.16591088051));
#77654=CARTESIAN_POINT('Ctrl Pts',(-18.4899127349194,-4.22319759362039,
128.283689050753));
#77655=CARTESIAN_POINT('Ctrl Pts',(-18.4976626067608,-4.29353562876832,
128.4015351933));
#77656=CARTESIAN_POINT('Ctrl Pts',(-18.5054124786022,-4.35891848282762,
128.52229617776));
#77657=CARTESIAN_POINT('Ctrl Pts',(-18.5131623504435,-4.41911242054446,
128.645511739787));
#77658=CARTESIAN_POINT('Ctrl Pts',(-18.5209147645197,-4.47932610402394,
128.768767720921));
#77659=CARTESIAN_POINT('Ctrl Pts',(-18.5286671785959,-4.53434731955563,
128.894479527453));
#77660=CARTESIAN_POINT('Ctrl Pts',(-18.5364195926722,-4.58399023429016,
129.022166297512));
#77661=CARTESIAN_POINT('Ctrl Pts',(-18.5441797389906,-4.63368266276793,
129.149980422098));
#77662=CARTESIAN_POINT('Ctrl Pts',(-18.551939885309,-4.67798594931462,129.279773075077));
#77663=CARTESIAN_POINT('Ctrl Pts',(-18.5597000316274,-4.71676384159292,
129.411047327189));
#77664=CARTESIAN_POINT('Ctrl Pts',(-18.5630626269009,-4.73356692132093,
129.467930556134));
#77665=CARTESIAN_POINT('Ctrl Pts',(-18.5664252221743,-4.74933318412891,
129.52509182207));
#77666=CARTESIAN_POINT('Ctrl Pts',(-18.5697878174477,-4.76405452823411,
129.582490119308));
#77667=CARTESIAN_POINT('Origin',(213.235140564004,0.,130.804360617566));
#77668=CARTESIAN_POINT('',(-20.6651747065899,-4.7640545282341,129.582490119308));
#77669=CARTESIAN_POINT('',(-20.320130187517,-4.76405452823408,129.582490119308));
#77670=CARTESIAN_POINT('',(213.235140564004,-4.76405452823405,129.582490119308));
#77671=CARTESIAN_POINT('',(-18.9851405639704,-4.91824968425682,130.802598287368));
#77672=CARTESIAN_POINT('Ctrl Pts',(-18.9851405640086,-4.91824968425706,
130.802598288046));
#77673=CARTESIAN_POINT('Ctrl Pts',(-18.9930656157456,-4.91830008698088,
130.943260506847));
#77674=CARTESIAN_POINT('Ctrl Pts',(-19.0009906674826,-4.91231171566778,
131.083879878867));
#77675=CARTESIAN_POINT('Ctrl Pts',(-19.0089157192196,-4.9003219196573,131.22391770096));
#77676=CARTESIAN_POINT('Ctrl Pts',(-19.0168450820189,-4.88832560144877,
131.364031700697));
#77677=CARTESIAN_POINT('Ctrl Pts',(-19.0247744448181,-4.87032138336905,
131.503563156307));
#77678=CARTESIAN_POINT('Ctrl Pts',(-19.0327038076174,-4.8463983542322,131.641979895398));
#77679=CARTESIAN_POINT('Ctrl Pts',(-19.0406388492404,-4.82245819198274,
131.780495765312));
#77680=CARTESIAN_POINT('Ctrl Pts',(-19.0485738908634,-4.79259083272611,
131.917894968326));
#77681=CARTESIAN_POINT('Ctrl Pts',(-19.0565089324864,-4.75693616462916,
132.053656974778));
#77682=CARTESIAN_POINT('Ctrl Pts',(-19.0644567932359,-4.72122389611616,
132.189638305893));
#77683=CARTESIAN_POINT('Ctrl Pts',(-19.0724046539854,-4.67970573199247,
132.323976802585));
#77684=CARTESIAN_POINT('Ctrl Pts',(-19.0803525147348,-4.63257133438727,
132.456167475014));
#77685=CARTESIAN_POINT('Ctrl Pts',(-19.0883073765969,-4.58539541702783,
132.58847459158));
#77686=CARTESIAN_POINT('Ctrl Pts',(-19.0962622384589,-4.53259353845703,
132.718629773762));
#77687=CARTESIAN_POINT('Ctrl Pts',(-19.104217100321,-4.47440275290421,132.84614980044));
#77688=CARTESIAN_POINT('Ctrl Pts',(-19.1121865675191,-4.41610512753542,
132.973903957249));
#77689=CARTESIAN_POINT('Ctrl Pts',(-19.1201560347171,-4.35239898874052,
133.099012965156));
#77690=CARTESIAN_POINT('Ctrl Pts',(-19.1281255019152,-4.28356696116366,
133.221018878828));
#77691=CARTESIAN_POINT('Ctrl Pts',(-19.1330188018932,-4.24130368927173,
133.295931231166));
#77692=CARTESIAN_POINT('Ctrl Pts',(-19.1379121018712,-4.19710879656985,
133.369674274505));
#77693=CARTESIAN_POINT('Ctrl Pts',(-19.1428054018492,-4.15105541867314,
133.442147942883));
#77694=CARTESIAN_POINT('Ctrl Pts',(-19.1505797359683,-4.07788713782147,
133.557292020569));
#77695=CARTESIAN_POINT('Ctrl Pts',(-19.1583540700874,-3.99980844576856,
133.669571802808));
#77696=CARTESIAN_POINT('Ctrl Pts',(-19.1661284042065,-3.91707030977014,
133.778540042351));
#77697=CARTESIAN_POINT('Ctrl Pts',(-19.1738931571535,-3.83443414112981,
133.887373988278));
#77698=CARTESIAN_POINT('Ctrl Pts',(-19.1816579101006,-3.74715018826146,
133.992904203453));
#77699=CARTESIAN_POINT('Ctrl Pts',(-19.1894226630477,-3.65551396223064,
134.094710254677));
#77700=CARTESIAN_POINT('Ctrl Pts',(-19.1971797039327,-3.56396875059148,
134.196415190696));
#77701=CARTESIAN_POINT('Ctrl Pts',(-19.2049367448177,-3.46808012810207,
134.294403035021));
#77702=CARTESIAN_POINT('Ctrl Pts',(-19.2126937857027,-3.36818511375556,
134.388284738132));
#77703=CARTESIAN_POINT('Ctrl Pts',(-19.2204449769428,-3.26836543101645,
134.482095644321));
#77704=CARTESIAN_POINT('Ctrl Pts',(-19.2281961681829,-3.16454565378088,
134.571806305975));
#77705=CARTESIAN_POINT('Ctrl Pts',(-19.235947359423,-3.05710079936569,134.657063274795));
#77706=CARTESIAN_POINT('Ctrl Pts',(-19.2436952562001,-2.94970161187965,
134.742284007129));
#77707=CARTESIAN_POINT('Ctrl Pts',(-19.2514431529772,-2.83868071727795,
134.823054569031));
#77708=CARTESIAN_POINT('Ctrl Pts',(-19.2591910497543,-2.72444730087353,
134.899060846797));
#77709=CARTESIAN_POINT('Ctrl Pts',(-19.2669373258384,-2.61023777963723,
134.975051225688));
#77710=CARTESIAN_POINT('Ctrl Pts',(-19.2746836019224,-2.49281739851653,
135.046279086271));
#77711=CARTESIAN_POINT('Ctrl Pts',(-19.2824298780065,-2.37262516907755,
135.11247306614));
#77712=CARTESIAN_POINT('Ctrl Pts',(-19.2901762112718,-2.25243205240716,
135.178667534638));
#77713=CARTESIAN_POINT('Ctrl Pts',(-19.2979225445372,-2.12946738905345,
135.239827859667));
#77714=CARTESIAN_POINT('Ctrl Pts',(-19.3056688778025,-2.00419532907419,
135.295728354171));
#77715=CARTESIAN_POINT('Ctrl Pts',(-19.3134169458055,-1.87889521528567,
135.351641367203));
#77716=CARTESIAN_POINT('Ctrl Pts',(-19.3211650138084,-1.75128703361055,
135.402292046531));
#77717=CARTESIAN_POINT('Ctrl Pts',(-19.3289130818113,-1.62185509443274,
135.447502777264));
#77718=CARTESIAN_POINT('Ctrl Pts',(-19.3366693845532,-1.49228559344954,
135.4927615585));
#77719=CARTESIAN_POINT('Ctrl Pts',(-19.3444256872951,-1.36088883266296,
135.532568712557));
#77720=CARTESIAN_POINT('Ctrl Pts',(-19.3521819900369,-1.22816500985251,
135.566796314882));
#77721=CARTESIAN_POINT('Ctrl Pts',(-19.3599424325511,-1.09537034834123,
135.60104218551));
#77722=CARTESIAN_POINT('Ctrl Pts',(-19.3677028750652,-0.961247595618872,
135.62970248888));
#77723=CARTESIAN_POINT('Ctrl Pts',(-19.3754633175794,-0.826306355891596,
135.652700629231));
#77724=CARTESIAN_POINT('Ctrl Pts',(-19.3832362178448,-0.69114849650679,
135.675735688239));
#77725=CARTESIAN_POINT('Ctrl Pts',(-19.3910091181103,-0.555169912552802,
135.693090371172));
#77726=CARTESIAN_POINT('Ctrl Pts',(-19.3987820183757,-0.418885433140261,
135.70473999639));
#77727=CARTESIAN_POINT('Ctrl Pts',(-19.4062723541379,-0.287555237832218,
135.715966128388));
#77728=CARTESIAN_POINT('Ctrl Pts',(-19.4137626899,-0.155941308791479,135.721894773945));
#77729=CARTESIAN_POINT('Ctrl Pts',(-19.4212530256621,-0.0245016661486505,
135.722549586166));
#77730=CARTESIAN_POINT('Ctrl Pts',(-19.4290273597812,0.111921550492895,
135.723229225791));
#77731=CARTESIAN_POINT('Ctrl Pts',(-19.4368016939003,0.248589151452131,
135.71822937575));
#77732=CARTESIAN_POINT('Ctrl Pts',(-19.4445760280194,0.384989201019398,
135.707519433839));
#77733=CARTESIAN_POINT('Ctrl Pts',(-19.4523407809665,0.521221149716367,
135.696822690975));
#77734=CARTESIAN_POINT('Ctrl Pts',(-19.4601055339136,0.657185817068261,
135.680429888437));
#77735=CARTESIAN_POINT('Ctrl Pts',(-19.4678702868607,0.792369749769786,
135.658362393642));
#77736=CARTESIAN_POINT('Ctrl Pts',(-19.4756273277457,0.927419415883409,
135.636316816594));
#77737=CARTESIAN_POINT('Ctrl Pts',(-19.4833843686307,1.06168950713955,135.608607826131));
#77738=CARTESIAN_POINT('Ctrl Pts',(-19.4911414095157,1.19467053816105,135.575308675107));
#77739=CARTESIAN_POINT('Ctrl Pts',(-19.4988926007558,1.32755128715226,135.542034635231));
#77740=CARTESIAN_POINT('Ctrl Pts',(-19.5066437919959,1.45914453307452,135.503178920243));
#77741=CARTESIAN_POINT('Ctrl Pts',(-19.514394983236,1.58895020384354,135.458865995391));
#77742=CARTESIAN_POINT('Ctrl Pts',(-19.5221428800131,1.71870070373998,135.414571904715));
#77743=CARTESIAN_POINT('Ctrl Pts',(-19.5298907767902,1.84666477037726,135.36482534345));
#77744=CARTESIAN_POINT('Ctrl Pts',(-19.5376386735672,1.97235695634455,135.309800784659));
#77745=CARTESIAN_POINT('Ctrl Pts',(-19.5453849496513,2.09802285021613,135.254787735821));
#77746=CARTESIAN_POINT('Ctrl Pts',(-19.5531312257355,2.22141745075026,135.194499042148));
#77747=CARTESIAN_POINT('Ctrl Pts',(-19.5608775018196,2.34207515659514,135.129157378497));
#77748=CARTESIAN_POINT('Ctrl Pts',(-19.5686238350849,2.4627337531078,135.063815232509));
#77749=CARTESIAN_POINT('Ctrl Pts',(-19.5763701683503,2.58065507082735,134.993420228291));
#77750=CARTESIAN_POINT('Ctrl Pts',(-19.5841165016156,2.69539834839675,134.918240879066));
#77751=CARTESIAN_POINT('Ctrl Pts',(-19.5918645696186,2.81016732192758,134.843044693947));
#77752=CARTESIAN_POINT('Ctrl Pts',(-19.5996126376216,2.92175651214648,134.76306224604));
#77753=CARTESIAN_POINT('Ctrl Pts',(-19.6073607056246,3.02975470502338,134.678604994201));
#77754=CARTESIAN_POINT('Ctrl Pts',(-19.6151170083664,3.13786767966501,134.59405798019));
#77755=CARTESIAN_POINT('Ctrl Pts',(-19.6228733111082,3.24238172452007,134.505026903102));
#77756=CARTESIAN_POINT('Ctrl Pts',(-19.6306296138501,3.34291884392157,134.41186344715));
#77757=CARTESIAN_POINT('Ctrl Pts',(-19.6383900563643,3.44350962301081,134.318650267056));
#77758=CARTESIAN_POINT('Ctrl Pts',(-19.6461504988784,3.54011897191441,134.221300590675));
#77759=CARTESIAN_POINT('Ctrl Pts',(-19.6539109413926,3.63240699492851,134.120201760579));
#77760=CARTESIAN_POINT('Ctrl Pts',(-19.661683841658,3.7248431668701,134.018940637665));
#77761=CARTESIAN_POINT('Ctrl Pts',(-19.6694567419235,3.81294389922043,133.913918633908));
#77762=CARTESIAN_POINT('Ctrl Pts',(-19.677229642189,3.89641014890662,133.805555548589));
#77763=CARTESIAN_POINT('Ctrl Pts',(-19.684719977951,3.97684219017792,133.701131734372));
#77764=CARTESIAN_POINT('Ctrl Pts',(-19.692210313713,4.05297067108701,133.59360578611));
#77765=CARTESIAN_POINT('Ctrl Pts',(-19.699700649475,4.12456792059302,133.483375834192));
#77766=CARTESIAN_POINT('Ctrl Pts',(-19.7074749835941,4.19887980157557,133.368966480144));
#77767=CARTESIAN_POINT('Ctrl Pts',(-19.7152493177132,4.26854546274312,133.251281615754));
#77768=CARTESIAN_POINT('Ctrl Pts',(-19.7230236518323,4.33326244383982,133.130735405795));
#77769=CARTESIAN_POINT('Ctrl Pts',(-19.7307884047794,4.39789966704124,133.010337758266));
#77770=CARTESIAN_POINT('Ctrl Pts',(-19.7385531577264,4.45760016182317,132.887086122716));
#77771=CARTESIAN_POINT('Ctrl Pts',(-19.7463179106735,4.51210437114458,132.761424031561));
#77772=CARTESIAN_POINT('Ctrl Pts',(-19.7540749515585,4.56655444611685,132.635886749767));
#77773=CARTESIAN_POINT('Ctrl Pts',(-19.7618319924436,4.61581835173356,132.507944133091));
#77774=CARTESIAN_POINT('Ctrl Pts',(-19.7695890333286,4.65968232840544,132.378064420969));
#77775=CARTESIAN_POINT('Ctrl Pts',(-19.7773402245688,4.70351322691155,132.248282652148));
#77776=CARTESIAN_POINT('Ctrl Pts',(-19.7850914158088,4.74195217720557,132.116567064383));
#77777=CARTESIAN_POINT('Ctrl Pts',(-19.792842607049,4.77483359425135,131.983405658991));
#77778=CARTESIAN_POINT('Ctrl Pts',(-19.8005905038261,4.80770103581756,131.850300850749));
#77779=CARTESIAN_POINT('Ctrl Pts',(-19.8083384006033,4.83501554864285,131.715751825865));
#77780=CARTESIAN_POINT('Ctrl Pts',(-19.8160862973803,4.8566615256736,131.580261311948));
#77781=CARTESIAN_POINT('Ctrl Pts',(-19.8238325734644,4.87830297483263,131.444799139724));
#77782=CARTESIAN_POINT('Ctrl Pts',(-19.8315788495485,4.89427818505058,131.308396256015));
#77783=CARTESIAN_POINT('Ctrl Pts',(-19.8393251256326,4.90452283008644,131.171564745621));
#77784=CARTESIAN_POINT('Ctrl Pts',(-19.8470714588979,4.91476755074593,131.034732225169));
#77785=CARTESIAN_POINT('Ctrl Pts',(-19.8548177921633,4.91928159262324,130.897471461593));
#77786=CARTESIAN_POINT('Ctrl Pts',(-19.8625641254286,4.91805262121678,130.760298417862));
#77787=CARTESIAN_POINT('Ctrl Pts',(-19.8703121934316,4.91682337459069,130.623094655178));
#77788=CARTESIAN_POINT('Ctrl Pts',(-19.8780602614345,4.90984855897678,130.485979042304));
#77789=CARTESIAN_POINT('Ctrl Pts',(-19.8858083294375,4.89716794230353,130.349465896367));
#77790=CARTESIAN_POINT('Ctrl Pts',(-19.8935646321793,4.88447384851994,130.212807662634));
#77791=CARTESIAN_POINT('Ctrl Pts',(-19.9013209349212,4.86606187601619,130.076753564835));
#77792=CARTESIAN_POINT('Ctrl Pts',(-19.909077237663,4.84202359078967,129.941811715337));
#77793=CARTESIAN_POINT('Ctrl Pts',(-19.9168376801772,4.81797247560658,129.806797843312));
#77794=CARTESIAN_POINT('Ctrl Pts',(-19.9245981226914,4.78828914867807,129.672897783978));
#77795=CARTESIAN_POINT('Ctrl Pts',(-19.9323585652055,4.75311577034962,129.540606869341));
#77796=CARTESIAN_POINT('Ctrl Pts',(-19.940131465471,4.71788592859169,129.408103589582));
#77797=CARTESIAN_POINT('Ctrl Pts',(-19.9479043657364,4.67714854026842,129.277214989978));
#77798=CARTESIAN_POINT('Ctrl Pts',(-19.9556772660019,4.63109515431962,129.1484195757));
#77799=CARTESIAN_POINT('Ctrl Pts',(-19.9631676017639,4.58671592495166,129.024306199147));
#77800=CARTESIAN_POINT('Ctrl Pts',(-19.9706579375259,4.53740060285889,128.902136750585));
#77801=CARTESIAN_POINT('Ctrl Pts',(-19.9781482732879,4.48336108465437,128.782317975309));
#77802=CARTESIAN_POINT('Ctrl Pts',(-19.985922607407,4.42727264169201,128.657956234749));
#77803=CARTESIAN_POINT('Ctrl Pts',(-19.9936969415261,4.36591702381149,128.53573299716));
#77804=CARTESIAN_POINT('Ctrl Pts',(-20.0014712756452,4.29947919240989,128.416126597095));
#77805=CARTESIAN_POINT('Ctrl Pts',(-20.0092360285923,4.23312323969769,128.296667601229));
#77806=CARTESIAN_POINT('Ctrl Pts',(-20.0170007815394,4.16169772373649,128.179819364559));
#77807=CARTESIAN_POINT('Ctrl Pts',(-20.0247655344865,4.08543550399017,128.066039999881));
#77808=CARTESIAN_POINT('Ctrl Pts',(-20.0325225753715,4.00924902895561,127.952373642472));
#77809=CARTESIAN_POINT('Ctrl Pts',(-20.0402796162564,3.92823562634669,127.841770413965));
#77810=CARTESIAN_POINT('Ctrl Pts',(-20.0480366571414,3.84267369698184,127.734663251208));
#77811=CARTESIAN_POINT('Ctrl Pts',(-20.0557878483816,3.75717629053361,127.627636858796));
#77812=CARTESIAN_POINT('Ctrl Pts',(-20.0635390396218,3.66713742772582,127.524101588748));
#77813=CARTESIAN_POINT('Ctrl Pts',(-20.0712902308619,3.57287817512937,127.424460529075));
#77814=CARTESIAN_POINT('Ctrl Pts',(-20.079038127639,3.47865898522973,127.32486181951));
#77815=CARTESIAN_POINT('Ctrl Pts',(-20.0867860244161,3.38022324134464,127.229154311791));
#77816=CARTESIAN_POINT('Ctrl Pts',(-20.0945339211932,3.2779314140123,127.137707005956));
#77817=CARTESIAN_POINT('Ctrl Pts',(-20.1022801972773,3.17566098392507,127.046278828927));
#77818=CARTESIAN_POINT('Ctrl Pts',(-20.1100264733614,3.06953636606886,126.959109341658));
#77819=CARTESIAN_POINT('Ctrl Pts',(-20.1177727494455,2.9599536219864,126.876529457983));
#77820=CARTESIAN_POINT('Ctrl Pts',(-20.1255190827108,2.85037006898916,126.793948964722));
#77821=CARTESIAN_POINT('Ctrl Pts',(-20.1332654159762,2.73732865106229,126.715958377953));
#77822=CARTESIAN_POINT('Ctrl Pts',(-20.1410117492415,2.621256795364,126.642846965629));
#77823=CARTESIAN_POINT('Ctrl Pts',(-20.1487598172445,2.50515894617906,126.569719180511));
#77824=CARTESIAN_POINT('Ctrl Pts',(-20.1565078852474,2.38602963954354,126.501472952431));
#77825=CARTESIAN_POINT('Ctrl Pts',(-20.1642559532503,2.26432308056103,126.438352824474));
#77826=CARTESIAN_POINT('Ctrl Pts',(-20.1720122559922,2.14248717039847,126.375165611694));
#77827=CARTESIAN_POINT('Ctrl Pts',(-20.179768558734,2.01806888379208,126.317115562449));
#77828=CARTESIAN_POINT('Ctrl Pts',(-20.1875248614759,1.89154520372528,126.264400286818));
#77829=CARTESIAN_POINT('Ctrl Pts',(-20.19528530399,1.76495399416105,126.211656875458));
#77830=CARTESIAN_POINT('Ctrl Pts',(-20.2030457465042,1.63625551873682,126.164254046318));
#77831=CARTESIAN_POINT('Ctrl Pts',(-20.2108061890183,1.50594335543481,126.12233993492));
#77832=CARTESIAN_POINT('Ctrl Pts',(-20.2185790892837,1.37542200347953,126.08035853927));
#77833=CARTESIAN_POINT('Ctrl Pts',(-20.2263519895492,1.24328216421977,126.043883572591));
#77834=CARTESIAN_POINT('Ctrl Pts',(-20.2341248898146,1.11002995449002,126.01301252307));
#77835=CARTESIAN_POINT('Ctrl Pts',(-20.2416152255767,0.981621798226189,
125.983263713957));
#77836=CARTESIAN_POINT('Ctrl Pts',(-20.2491055613387,0.852181044947484,
125.958718520014));
#77837=CARTESIAN_POINT('Ctrl Pts',(-20.2565958971007,0.72216443628521,125.939418522385));
#77838=CARTESIAN_POINT('Ctrl Pts',(-20.2643702312198,0.587218208387621,
125.91938675948));
#77839=CARTESIAN_POINT('Ctrl Pts',(-20.2721445653389,0.451224126902702,
125.904942333098));
#77840=CARTESIAN_POINT('Ctrl Pts',(-20.279918899458,0.314684604392407,125.89618818149));
#77841=CARTESIAN_POINT('Ctrl Pts',(-20.2876836524051,0.178313354640533,
125.887444818591));
#77842=CARTESIAN_POINT('Ctrl Pts',(-20.2954484053522,0.0413983877740623,
125.884377801948));
#77843=CARTESIAN_POINT('Ctrl Pts',(-20.3032131582993,-0.0955490067097157,
125.887038841455));
#77844=CARTESIAN_POINT('Ctrl Pts',(-20.3109701991843,-0.232360383110673,
125.88969723798));
#77845=CARTESIAN_POINT('Ctrl Pts',(-20.3187272400693,-0.369203734672447,
125.898072361371));
#77846=CARTESIAN_POINT('Ctrl Pts',(-20.3264842809544,-0.50556433692043,
125.912163998078));
#77847=CARTESIAN_POINT('Ctrl Pts',(-20.3342354721944,-0.641822108576228,
125.926245008171));
#77848=CARTESIAN_POINT('Ctrl Pts',(-20.3419866634345,-0.777597468207187,
125.946033911033));
#77849=CARTESIAN_POINT('Ctrl Pts',(-20.3497378546746,-0.912377742128987,
125.971478463182));
#77850=CARTESIAN_POINT('Ctrl Pts',(-20.3574857514517,-1.04710073084009,
125.996912200717));
#77851=CARTESIAN_POINT('Ctrl Pts',(-20.3652336482288,-1.18082909165864,
126.027996734184));
#77852=CARTESIAN_POINT('Ctrl Pts',(-20.3729815450058,-1.31305753126929,
126.064628243046));
#77853=CARTESIAN_POINT('Ctrl Pts',(-20.3807278210899,-1.44525831154071,
126.101252089385));
#77854=CARTESIAN_POINT('Ctrl Pts',(-20.388474097174,-1.57595941813688,126.143420498891));
#77855=CARTESIAN_POINT('Ctrl Pts',(-20.396220373258,-1.70466836294043,126.19097912078));
#77856=CARTESIAN_POINT('Ctrl Pts',(-20.4039667065234,-1.83337825784399,
126.238538093735));
#77857=CARTESIAN_POINT('Ctrl Pts',(-20.4117130397887,-1.96009559488043,
126.291487222962));
#77858=CARTESIAN_POINT('Ctrl Pts',(-20.4194593730541,-2.08434596990911,
126.349623258279));
#77859=CARTESIAN_POINT('Ctrl Pts',(-20.427207441057,-2.20862416994745,126.407772312759));
#77860=CARTESIAN_POINT('Ctrl Pts',(-20.43495550906,-2.33043395459699,126.471110419064));
#77861=CARTESIAN_POINT('Ctrl Pts',(-20.4427035770629,-2.44932407388013,
126.53938762309));
#77862=CARTESIAN_POINT('Ctrl Pts',(-20.4504598798048,-2.56834055099749,
126.607737392941));
#77863=CARTESIAN_POINT('Ctrl Pts',(-20.4582161825467,-2.6844308244866,126.681036551603));
#77864=CARTESIAN_POINT('Ctrl Pts',(-20.4659724852885,-2.79717081843783,
126.758990612859));
#77865=CARTESIAN_POINT('Ctrl Pts',(-20.4737329278027,-2.90997098511852,
126.836986280545));
#77866=CARTESIAN_POINT('Ctrl Pts',(-20.4814933703169,-3.01941699739412,
126.919641565822));
#77867=CARTESIAN_POINT('Ctrl Pts',(-20.4892538128311,-3.12511743369867,
127.006621278421));
#77868=CARTESIAN_POINT('Ctrl Pts',(-20.4970267130965,-3.23098754972722,
127.093740618576));
#77869=CARTESIAN_POINT('Ctrl Pts',(-20.5047996133619,-3.33309978303407,
127.185197997299));
#77870=CARTESIAN_POINT('Ctrl Pts',(-20.5125725136274,-3.43109854553576,
127.28062029891));
#77871=CARTESIAN_POINT('Ctrl Pts',(-20.5200628493895,-3.52553480617799,
127.372573759504));
#77872=CARTESIAN_POINT('Ctrl Pts',(-20.5275531851516,-3.61615126191351,
127.468208654316));
#77873=CARTESIAN_POINT('Ctrl Pts',(-20.5350435209138,-3.70266604933885,
127.5671631893));
#77874=CARTESIAN_POINT('Ctrl Pts',(-20.5427532107793,-3.79171441793137,
127.669015602828));
#77875=CARTESIAN_POINT('Ctrl Pts',(-20.5504629006448,-3.87671110562716,
127.774721472327));
#77876=CARTESIAN_POINT('Ctrl Pts',(-20.5581725905103,-3.95729975157023,
127.883921996618));
#77877=CARTESIAN_POINT('Ctrl Pts',(-20.5658729677856,-4.03779105390427,
127.992990616806));
#77878=CARTESIAN_POINT('Ctrl Pts',(-20.573573345061,-4.11388466924951,128.105545180213));
#77879=CARTESIAN_POINT('Ctrl Pts',(-20.5812737223363,-4.18526216519003,
128.221191310082));
#77880=CARTESIAN_POINT('Ctrl Pts',(-20.5889651432378,-4.25655664136295,
128.336702930961));
#77881=CARTESIAN_POINT('Ctrl Pts',(-20.5966565641393,-4.32314571066714,
128.45529862336));
#77882=CARTESIAN_POINT('Ctrl Pts',(-20.6043479850409,-4.38475267177753,
128.576552935148));
#77883=CARTESIAN_POINT('Ctrl Pts',(-20.6120342090159,-4.44631800639856,
128.697725318024));
#77884=CARTESIAN_POINT('Ctrl Pts',(-20.6197204329908,-4.50290774779655,
128.821552394619));
#77885=CARTESIAN_POINT('Ctrl Pts',(-20.6274066569658,-4.55428985373553,
128.947581957989));
#77886=CARTESIAN_POINT('Ctrl Pts',(-20.6350895374991,-4.60564960889726,
129.073556699575));
#77887=CARTESIAN_POINT('Ctrl Pts',(-20.6427724180323,-4.651806083931,129.201731654703));
#77888=CARTESIAN_POINT('Ctrl Pts',(-20.6504552985656,-4.69257454021657,
129.331632792402));
#77889=CARTESIAN_POINT('Ctrl Pts',(-20.655361767907,-4.71861024127915,129.414590733344));
#77890=CARTESIAN_POINT('Ctrl Pts',(-20.6602682372484,-4.74244944925163,
129.498252244259));
#77891=CARTESIAN_POINT('Ctrl Pts',(-20.6651747065899,-4.7640545282341,129.582490119308));
#77892=CARTESIAN_POINT('Ctrl Pts',(-18.9154222424341,-4.76405452823411,
129.582490119308));
#77893=CARTESIAN_POINT('Ctrl Pts',(-18.9238373913451,-4.80090419183842,
129.72616639843));
#77894=CARTESIAN_POINT('Ctrl Pts',(-18.9322525402561,-4.83129321364356,
129.871678730157));
#77895=CARTESIAN_POINT('Ctrl Pts',(-18.9406676891671,-4.85505190900469,
130.018450938678));
#77896=CARTESIAN_POINT('Ctrl Pts',(-18.9490535319284,-4.87872786359806,
130.164712006119));
#77897=CARTESIAN_POINT('Ctrl Pts',(-18.9574393746897,-4.89581948998125,
130.31222392731));
#77898=CARTESIAN_POINT('Ctrl Pts',(-18.965825217451,-4.90620768672381,130.460399577284));
#77899=CARTESIAN_POINT('Ctrl Pts',(-18.9722636662908,-4.91418349490053,
130.57416528561));
#77900=CARTESIAN_POINT('Ctrl Pts',(-18.9787021151306,-4.91820873619813,
130.68832187259));
#77901=CARTESIAN_POINT('Ctrl Pts',(-18.9851405639703,-4.91824968425682,
130.802598287368));
#77902=CARTESIAN_POINT('',(-18.6398594360279,-4.91824887451795,130.801033335958));
#77903=CARTESIAN_POINT('Ctrl Pts',(-18.5697878174477,-4.76405452823411,
129.582490119308));
#77904=CARTESIAN_POINT('Ctrl Pts',(-18.5775620177684,-4.798089750661,129.715192934994));
#77905=CARTESIAN_POINT('Ctrl Pts',(-18.5853362180891,-4.82653616263435,
129.849162946845));
#77906=CARTESIAN_POINT('Ctrl Pts',(-18.5931104184099,-4.84933091075927,
129.983889545282));
#77907=CARTESIAN_POINT('Ctrl Pts',(-18.5972399957342,-4.86143925259346,
130.05545496461));
#77908=CARTESIAN_POINT('Ctrl Pts',(-18.6013695730585,-4.87195378562811,
130.12723379226));
#77909=CARTESIAN_POINT('Ctrl Pts',(-18.6054991503828,-4.88087106729867,
130.199149342963));
#77910=CARTESIAN_POINT('Ctrl Pts',(-18.6169525789189,-4.90560324696964,
130.398607920906));
#77911=CARTESIAN_POINT('Ctrl Pts',(-18.6284060074551,-4.9181126100524,130.599612926342));
#77912=CARTESIAN_POINT('Ctrl Pts',(-18.6398594359912,-4.91824887451751,
130.801033335313));
#77913=CARTESIAN_POINT('Ctrl Pts',(-18.6398594360279,-4.91824887451795,
130.801033335958));
#77914=CARTESIAN_POINT('Ctrl Pts',(-18.6475192066,-4.91834000481437,130.935738338606));
#77915=CARTESIAN_POINT('Ctrl Pts',(-18.6551789771722,-4.91289285644884,
131.070661083684));
#77916=CARTESIAN_POINT('Ctrl Pts',(-18.6628387477443,-4.90188026565471,
131.205300667555));
#77917=CARTESIAN_POINT('Ctrl Pts',(-18.6704903422589,-4.89087942972647,
131.33979653681));
#77918=CARTESIAN_POINT('Ctrl Pts',(-18.6781419367735,-4.87432499867613,
131.474009447759));
#77919=CARTESIAN_POINT('Ctrl Pts',(-18.685793531288,-4.85224182597472,131.607437403908));
#77920=CARTESIAN_POINT('Ctrl Pts',(-18.6934389095863,-4.83017659381875,
131.740756962122));
#77921=CARTESIAN_POINT('Ctrl Pts',(-18.7010842878844,-4.80259162042394,
131.873292438638));
#77922=CARTESIAN_POINT('Ctrl Pts',(-18.7087296661827,-4.76956362517859,
132.0045463898));
#77923=CARTESIAN_POINT('Ctrl Pts',(-18.7163713466381,-4.73655160459547,
132.135736857317));
#77924=CARTESIAN_POINT('Ctrl Pts',(-18.7240130270935,-4.69810189448041,
132.265646642174));
#77925=CARTESIAN_POINT('Ctrl Pts',(-18.7316547075489,-4.65434233516547,
132.393788341493));
#77926=CARTESIAN_POINT('Ctrl Pts',(-18.7392946056689,-4.6105929822718,132.521900153212));
#77927=CARTESIAN_POINT('Ctrl Pts',(-18.7469345037889,-4.56153637234276,
132.648244318281));
#77928=CARTESIAN_POINT('Ctrl Pts',(-18.7545744019089,-4.50735010023958,
132.772348965187));
#77929=CARTESIAN_POINT('Ctrl Pts',(-18.762214280099,-4.45316396949025,132.896453288345));
#77930=CARTESIAN_POINT('Ctrl Pts',(-18.7698541582891,-4.39384836455577,
133.018317735854));
#77931=CARTESIAN_POINT('Ctrl Pts',(-18.7774940364792,-4.32962865359607,
133.137491300674));
#77932=CARTESIAN_POINT('Ctrl Pts',(-18.7851356569152,-4.2653942975696,133.256692042583));
#77933=CARTESIAN_POINT('Ctrl Pts',(-18.7927772773512,-4.19625380309849,
133.373200327278));
#77934=CARTESIAN_POINT('Ctrl Pts',(-18.8004188977871,-4.12247774498443,
133.486591089507));
#77935=CARTESIAN_POINT('Ctrl Pts',(-18.8080684299223,-4.04862530333567,
133.600099250082));
#77936=CARTESIAN_POINT('Ctrl Pts',(-18.8157179620574,-3.97012793564836,
133.710483105901));
#77937=CARTESIAN_POINT('Ctrl Pts',(-18.8233674941926,-3.88729885673946,
133.817347617354));
#77938=CARTESIAN_POINT('Ctrl Pts',(-18.8310213335106,-3.80442313968473,
133.924272300461));
#77939=CARTESIAN_POINT('Ctrl Pts',(-18.8386751728287,-3.71721111504135,
134.02767338695));
#77940=CARTESIAN_POINT('Ctrl Pts',(-18.8463290121468,-3.62601440507188,
134.127191127344));
#77941=CARTESIAN_POINT('Ctrl Pts',(-18.8539942937547,-3.53468135840313,
134.22685764416));
#77942=CARTESIAN_POINT('Ctrl Pts',(-18.8616595753627,-3.43935201575192,
134.322628938515));
#77943=CARTESIAN_POINT('Ctrl Pts',(-18.8693248569706,-3.34041309220821,
134.414183803804));
#77944=CARTESIAN_POINT('Ctrl Pts',(-18.8741988293789,-3.27750273768657,
134.472399001901));
#77945=CARTESIAN_POINT('Ctrl Pts',(-18.8790728017874,-3.21313366910852,
134.528910295268));
#77946=CARTESIAN_POINT('Ctrl Pts',(-18.8839467741957,-3.14741141957671,
134.583644202906));
#77947=CARTESIAN_POINT('Ctrl Pts',(-18.8917211083148,-3.04257973730417,
134.670948695005));
#77948=CARTESIAN_POINT('Ctrl Pts',(-18.8994954424339,-2.93394671190642,
134.754026354128));
#77949=CARTESIAN_POINT('Ctrl Pts',(-18.9072697765529,-2.82188788607974,
134.832527920558));
#77950=CARTESIAN_POINT('Ctrl Pts',(-18.9150345295,-2.70996716274091,134.910932740824));
#77951=CARTESIAN_POINT('Ctrl Pts',(-18.9227992824472,-2.59462935661664,
134.984772467404));
#77952=CARTESIAN_POINT('Ctrl Pts',(-18.9305640353943,-2.47628423973866,
135.05373697493));
#77953=CARTESIAN_POINT('Ctrl Pts',(-18.9383210762792,-2.3580566648993,135.122632985934));
#77954=CARTESIAN_POINT('Ctrl Pts',(-18.9460781171642,-2.23682805898759,
135.186663218379));
#77955=CARTESIAN_POINT('Ctrl Pts',(-18.9538351580491,-2.11303813719905,
135.245560105682));
#77956=CARTESIAN_POINT('Ctrl Pts',(-18.9615863492893,-1.98934156635347,
135.304412578384));
#77957=CARTESIAN_POINT('Ctrl Pts',(-18.9693375405294,-1.86308787579569,
135.358139243832));
#77958=CARTESIAN_POINT('Ctrl Pts',(-18.9770887317695,-1.7347420941176,135.406518038754));
#77959=CARTESIAN_POINT('Ctrl Pts',(-18.9848366285466,-1.60645086282029,
135.454876271398));
#77960=CARTESIAN_POINT('Ctrl Pts',(-18.9925845253236,-1.47606967401502,
135.497891016704));
#77961=CARTESIAN_POINT('Ctrl Pts',(-19.0003324221007,-1.34408408234849,
135.535388100268));
#77962=CARTESIAN_POINT('Ctrl Pts',(-19.0080786981848,-1.21212609922246,
135.572877340249));
#77963=CARTESIAN_POINT('Ctrl Pts',(-19.015824974269,-1.07856475661898,135.604851107429));
#77964=CARTESIAN_POINT('Ctrl Pts',(-19.0235712503531,-0.943900957597308,
135.631185044117));
#77965=CARTESIAN_POINT('Ctrl Pts',(-19.0313175836184,-0.80923616451788,
135.657519175195));
#77966=CARTESIAN_POINT('Ctrl Pts',(-19.0390639168837,-0.673469282478845,
135.678213317675));
#77967=CARTESIAN_POINT('Ctrl Pts',(-19.0468102501491,-0.537111206239121,
135.69319428365));
#77968=CARTESIAN_POINT('Ctrl Pts',(-19.054558318152,-0.400722593554221,
135.708178604508));
#77969=CARTESIAN_POINT('Ctrl Pts',(-19.062306386155,-0.263742911772665,
135.717447160264));
#77970=CARTESIAN_POINT('Ctrl Pts',(-19.0700544541579,-0.126687575086714,
135.720978695149));
#77971=CARTESIAN_POINT('Ctrl Pts',(-19.0778107568998,0.0105134256424208,
135.724513983392));
#77972=CARTESIAN_POINT('Ctrl Pts',(-19.0855670596416,0.147789850438779,
135.722300060515));
#77973=CARTESIAN_POINT('Ctrl Pts',(-19.0933233623835,0.284626328637788,
135.714367839103));
#77974=CARTESIAN_POINT('Ctrl Pts',(-19.1010838048977,0.421535840585279,
135.706431384026));
#77975=CARTESIAN_POINT('Ctrl Pts',(-19.1088442474118,0.558004549220509,
135.692770587913));
#77976=CARTESIAN_POINT('Ctrl Pts',(-19.116604689926,0.693523799154114,135.673468113043));
#77977=CARTESIAN_POINT('Ctrl Pts',(-19.1243775901914,0.829260596618731,
135.654134652126));
#77978=CARTESIAN_POINT('Ctrl Pts',(-19.1321504904569,0.964044505000242,
135.629141485955));
#77979=CARTESIAN_POINT('Ctrl Pts',(-19.1399233907223,1.09737774473891,135.598622307112));
#77980=CARTESIAN_POINT('Ctrl Pts',(-19.1474137264845,1.22586398536982,135.569212577293));
#77981=CARTESIAN_POINT('Ctrl Pts',(-19.1549040622467,1.35300289990215,135.534671709217));
#77982=CARTESIAN_POINT('Ctrl Pts',(-19.1623943980089,1.47836556314473,135.495162076188));
#77983=CARTESIAN_POINT('Ctrl Pts',(-19.170168732128,1.60848138986436,135.454154423415));
#77984=CARTESIAN_POINT('Ctrl Pts',(-19.1779430662471,1.73709578110266,135.407663886541));
#77985=CARTESIAN_POINT('Ctrl Pts',(-19.1857174003661,1.86371190476886,135.355817636865));
#77986=CARTESIAN_POINT('Ctrl Pts',(-19.1934821533133,1.99017198537883,135.304035283058));
#77987=CARTESIAN_POINT('Ctrl Pts',(-19.2012469062603,2.11463834009371,135.246910496081));
#77988=CARTESIAN_POINT('Ctrl Pts',(-19.2090116592074,2.23662855986402,135.184620398412));
#77989=CARTESIAN_POINT('Ctrl Pts',(-19.2167687000924,2.35849761722796,135.122392168147));
#77990=CARTESIAN_POINT('Ctrl Pts',(-19.2245257409774,2.47789508788356,135.055009013283));
#77991=CARTESIAN_POINT('Ctrl Pts',(-19.2322827818624,2.59435818368148,134.982696252393));
#77992=CARTESIAN_POINT('Ctrl Pts',(-19.2400339731025,2.7107334537526,134.910438023118));
#77993=CARTESIAN_POINT('Ctrl Pts',(-19.2477851643427,2.82417842267631,134.833257792583));
#77994=CARTESIAN_POINT('Ctrl Pts',(-19.2555363555828,2.93425490301979,134.751426771889));
#77995=CARTESIAN_POINT('Ctrl Pts',(-19.2632842523598,3.04428459792318,134.669630531562));
#77996=CARTESIAN_POINT('Ctrl Pts',(-19.2710321491369,3.15094833867724,134.583187665364));
#77997=CARTESIAN_POINT('Ctrl Pts',(-19.2787800459139,3.25383713327456,134.492412538652));
#77998=CARTESIAN_POINT('Ctrl Pts',(-19.286526321998,3.35670440575394,134.401656400139));
#77999=CARTESIAN_POINT('Ctrl Pts',(-19.2942725980821,3.45579800972093,134.306570062116));
#78000=CARTESIAN_POINT('Ctrl Pts',(-19.3020188741662,3.55074256918915,134.207507730144));
#78001=CARTESIAN_POINT('Ctrl Pts',(-19.3097652074316,3.64568782951667,134.108444666916));
#78002=CARTESIAN_POINT('Ctrl Pts',(-19.317511540697,3.73648371370533,134.005405833431));
#78003=CARTESIAN_POINT('Ctrl Pts',(-19.3252578739624,3.82279249560179,133.898781500069));
#78004=CARTESIAN_POINT('Ctrl Pts',(-19.3330059419654,3.90912060575165,133.792133288927));
#78005=CARTESIAN_POINT('Ctrl Pts',(-19.3407540099683,3.99095936812634,133.68189828396));
#78006=CARTESIAN_POINT('Ctrl Pts',(-19.3485020779713,4.06801230568507,133.568498628465));
#78007=CARTESIAN_POINT('Ctrl Pts',(-19.3562583807132,4.14514713602268,133.454978450466));
#78008=CARTESIAN_POINT('Ctrl Pts',(-19.364014683455,4.21748576077008,133.338287227021));
#78009=CARTESIAN_POINT('Ctrl Pts',(-19.3717709861968,4.28477561712758,133.218875263073));
#78010=CARTESIAN_POINT('Ctrl Pts',(-19.379531428711,4.35210138810748,133.099399565365));
#78011=CARTESIAN_POINT('Ctrl Pts',(-19.3872918712252,4.41437284389436,132.977200581812));
#78012=CARTESIAN_POINT('Ctrl Pts',(-19.3950523137394,4.47138458994209,132.852750939582));
#78013=CARTESIAN_POINT('Ctrl Pts',(-19.4028252140048,4.52848785630583,132.728101519737));
#78014=CARTESIAN_POINT('Ctrl Pts',(-19.4105981142703,4.58031439252309,132.60119458353));
#78015=CARTESIAN_POINT('Ctrl Pts',(-19.4183710145357,4.62670761593839,132.472521191107));
#78016=CARTESIAN_POINT('Ctrl Pts',(-19.4258613502977,4.67141432882488,132.348525400608));
#78017=CARTESIAN_POINT('Ctrl Pts',(-19.4333516860596,4.7110758071084,132.222889648152));
#78018=CARTESIAN_POINT('Ctrl Pts',(-19.4408420218216,4.74559681550516,132.096062567385));
#78019=CARTESIAN_POINT('Ctrl Pts',(-19.4486163559407,4.78142669842783,131.964426799303));
#78020=CARTESIAN_POINT('Ctrl Pts',(-19.4563906900598,4.81183211312075,131.831090598631));
#78021=CARTESIAN_POINT('Ctrl Pts',(-19.4641650241789,4.83665150251854,131.696540703471));
#78022=CARTESIAN_POINT('Ctrl Pts',(-19.471929777126,4.86144030423708,131.562156629031));
#78023=CARTESIAN_POINT('Ctrl Pts',(-19.4796945300731,4.88065670807868,131.426562217028));
#78024=CARTESIAN_POINT('Ctrl Pts',(-19.4874592830201,4.89418897832559,131.290259070883));
#78025=CARTESIAN_POINT('Ctrl Pts',(-19.4952163239051,4.90770780813094,131.154091302945));
#78026=CARTESIAN_POINT('Ctrl Pts',(-19.5029733647901,4.9155537008885,131.017216588241));
#78027=CARTESIAN_POINT('Ctrl Pts',(-19.5107304056751,4.91766607519587,130.880146073741));
#78028=CARTESIAN_POINT('Ctrl Pts',(-19.5184815969153,4.91977685654536,130.743178925182));
#78029=CARTESIAN_POINT('Ctrl Pts',(-19.5262327881554,4.91616271948905,130.60601666006));
#78030=CARTESIAN_POINT('Ctrl Pts',(-19.5339839793956,4.9068149905973,130.469174534099));
#78031=CARTESIAN_POINT('Ctrl Pts',(-19.5417318761727,4.89747123473974,130.332390569693));
#78032=CARTESIAN_POINT('Ctrl Pts',(-19.5494797729498,4.88239876050282,130.195926863059));
#78033=CARTESIAN_POINT('Ctrl Pts',(-19.5572276697269,4.86164098219284,130.060297432908));
#78034=CARTESIAN_POINT('Ctrl Pts',(-19.564973945811,4.84088754596257,129.924696373511));
#78035=CARTESIAN_POINT('Ctrl Pts',(-19.5727202218951,4.814451230239,129.789929629702));
#78036=CARTESIAN_POINT('Ctrl Pts',(-19.5804664979792,4.78242713830198,129.656504472689));
#78037=CARTESIAN_POINT('Ctrl Pts',(-19.5882128312445,4.75040280997042,129.523078330761));
#78038=CARTESIAN_POINT('Ctrl Pts',(-19.5959591645098,4.71279071436487,129.390994175558));
#78039=CARTESIAN_POINT('Ctrl Pts',(-19.6037054977752,4.66973664777365,129.260747096331));
#78040=CARTESIAN_POINT('Ctrl Pts',(-19.6114535657782,4.62667293952267,129.130470849173));
#78041=CARTESIAN_POINT('Ctrl Pts',(-19.6192016337811,4.57816495791328,129.002032867769));
#78042=CARTESIAN_POINT('Ctrl Pts',(-19.6269497017841,4.52440761097292,128.875910765413));
#78043=CARTESIAN_POINT('Ctrl Pts',(-19.634706004526,4.47059313008457,128.749654618985));
#78044=CARTESIAN_POINT('Ctrl Pts',(-19.6424623072679,4.41151829257835,128.625719628635));
#78045=CARTESIAN_POINT('Ctrl Pts',(-19.6502186100097,4.34742543639397,128.504561683421));
#78046=CARTESIAN_POINT('Ctrl Pts',(-19.6579790525239,4.28329837192219,128.383339072563));
#78047=CARTESIAN_POINT('Ctrl Pts',(-19.6657394950381,4.21414814912197,128.264896797703));
#78048=CARTESIAN_POINT('Ctrl Pts',(-19.6734999375523,4.14026138184423,128.14966312962));
#78049=CARTESIAN_POINT('Ctrl Pts',(-19.6812728378177,4.0662560049685,128.034244478222));
#78050=CARTESIAN_POINT('Ctrl Pts',(-19.6890457380832,3.98749911410493,127.922045046604));
#78051=CARTESIAN_POINT('Ctrl Pts',(-19.6968186383486,3.90431921531321,127.813462002194));
#78052=CARTESIAN_POINT('Ctrl Pts',(-19.7043089741106,3.82416311536076,127.708826224953));
#78053=CARTESIAN_POINT('Ctrl Pts',(-19.7117993098725,3.73990019642763,127.607548706975));
#78054=CARTESIAN_POINT('Ctrl Pts',(-19.7192896456345,3.65185642971071,127.509952069848));
#78055=CARTESIAN_POINT('Ctrl Pts',(-19.7270639797536,3.56047445681761,127.408655026559));
#78056=CARTESIAN_POINT('Ctrl Pts',(-19.7348383138727,3.46472980424949,127.31100261667));
#78057=CARTESIAN_POINT('Ctrl Pts',(-19.7426126479918,3.36494465301688,127.21739385655));
#78058=CARTESIAN_POINT('Ctrl Pts',(-19.7503774009388,3.26528247806525,127.123900460861));
#78059=CARTESIAN_POINT('Ctrl Pts',(-19.7581421538859,3.16158999467696,127.034441064307));
#78060=CARTESIAN_POINT('Ctrl Pts',(-19.765906906833,3.054228820132,126.949380802214));
#78061=CARTESIAN_POINT('Ctrl Pts',(-19.773663947718,2.94697427821883,126.864405023171));
#78062=CARTESIAN_POINT('Ctrl Pts',(-19.7814209886031,2.83605860092695,126.783819924739));
#78063=CARTESIAN_POINT('Ctrl Pts',(-19.7891780294881,2.72187908495015,126.707952763188));
#78064=CARTESIAN_POINT('Ctrl Pts',(-19.7969292207283,2.60778567263452,126.632142813654));
#78065=CARTESIAN_POINT('Ctrl Pts',(-19.8046804119684,2.4904336449919,126.561043934844));
#78066=CARTESIAN_POINT('Ctrl Pts',(-19.8124316032085,2.37025181305394,126.494941932266));
#78067=CARTESIAN_POINT('Ctrl Pts',(-19.8201794999856,2.25012106160083,126.428868024802));
#78068=CARTESIAN_POINT('Ctrl Pts',(-19.8279273967627,2.1271632398655,126.367786957505));
#78069=CARTESIAN_POINT('Ctrl Pts',(-19.8356752935397,2.00183427284138,126.311940044359));
#78070=CARTESIAN_POINT('Ctrl Pts',(-19.8434215696238,1.87653152193539,126.256104813183));
#78071=CARTESIAN_POINT('Ctrl Pts',(-19.8511678457079,1.74885896918546,126.205501717427));
#78072=CARTESIAN_POINT('Ctrl Pts',(-19.858914121792,1.61929480186951,126.160324936487));
#78073=CARTESIAN_POINT('Ctrl Pts',(-19.8666604550574,1.48972967814066,126.115147822062));
#78074=CARTESIAN_POINT('Ctrl Pts',(-19.8744067883227,1.35827328114988,126.075397231103));
#78075=CARTESIAN_POINT('Ctrl Pts',(-19.882153121588,1.22542094996073,126.041218108896));
#78076=CARTESIAN_POINT('Ctrl Pts',(-19.889901189591,1.09253886741261,126.007031332512));
#78077=CARTESIAN_POINT('Ctrl Pts',(-19.897649257594,0.958260607171626,125.978418605037));
#78078=CARTESIAN_POINT('Ctrl Pts',(-19.905397325597,0.823093351378072,125.955474106477));
#78079=CARTESIAN_POINT('Ctrl Pts',(-19.9131536283389,0.68778243821655,125.932505222232));
#78080=CARTESIAN_POINT('Ctrl Pts',(-19.9209099310806,0.551581028158589,
125.915216666548));
#78081=CARTESIAN_POINT('Ctrl Pts',(-19.9286662338225,0.415003663155578,
125.903650972824));
#78082=CARTESIAN_POINT('Ctrl Pts',(-19.9364266763367,0.278353402700785,
125.892079106141));
#78083=CARTESIAN_POINT('Ctrl Pts',(-19.9441871188509,0.141327177891082,
125.886236204344));
#78084=CARTESIAN_POINT('Ctrl Pts',(-19.951947561365,0.00444022684729692,
125.886112621899));
#78085=CARTESIAN_POINT('Ctrl Pts',(-19.9597204616305,-0.132666467282743,
125.885988841068));
#78086=CARTESIAN_POINT('Ctrl Pts',(-19.9674933618959,-0.269633050011513,
125.891602710449));
#78087=CARTESIAN_POINT('Ctrl Pts',(-19.9752662621614,-0.405947807584604,
125.902892527288));
#78088=CARTESIAN_POINT('Ctrl Pts',(-19.9827565979234,-0.53730718036376,
125.913771930847));
#78089=CARTESIAN_POINT('Ctrl Pts',(-19.9902469336854,-0.66806099048736,
125.929921738687));
#78090=CARTESIAN_POINT('Ctrl Pts',(-19.9977372694475,-0.797761611883198,
125.951242086858));
#78091=CARTESIAN_POINT('Ctrl Pts',(-20.0055116035666,-0.932379871761093,
125.973370802509));
#78092=CARTESIAN_POINT('Ctrl Pts',(-20.0132859376856,-1.06628993326668,
126.001139977507));
#78093=CARTESIAN_POINT('Ctrl Pts',(-20.0210602718047,-1.19898194592276,
126.034494229935));
#78094=CARTESIAN_POINT('Ctrl Pts',(-20.0288250247518,-1.3315104275319,126.067807376228));
#78095=CARTESIAN_POINT('Ctrl Pts',(-20.0365897776989,-1.46282347157565,
126.106691810222));
#78096=CARTESIAN_POINT('Ctrl Pts',(-20.044354530646,-1.5924184163906,126.151040657619));
#78097=CARTESIAN_POINT('Ctrl Pts',(-20.052111571531,-1.72188464567939,126.195345457116));
#78098=CARTESIAN_POINT('Ctrl Pts',(-20.0598686124161,-1.84963580412119,
126.245103743613));
#78099=CARTESIAN_POINT('Ctrl Pts',(-20.067625653301,-1.97518181317857,126.30015815016));
#78100=CARTESIAN_POINT('Ctrl Pts',(-20.0753768445412,-2.10063314701426,
126.35517103975));
#78101=CARTESIAN_POINT('Ctrl Pts',(-20.0831280357812,-2.22388228480489,
126.415471943505));
#78102=CARTESIAN_POINT('Ctrl Pts',(-20.0908792270214,-2.344456987447,126.480854575416));
#78103=CARTESIAN_POINT('Ctrl Pts',(-20.0986271237984,-2.46498044262372,
126.546209417964));
#78104=CARTESIAN_POINT('Ctrl Pts',(-20.1063750205756,-2.58283138050623,
126.616641506874));
#78105=CARTESIAN_POINT('Ctrl Pts',(-20.1141229173526,-2.69756033820974,
126.69189769564));
#78106=CARTESIAN_POINT('Ctrl Pts',(-20.1218691934367,-2.81226529708873,
126.767138142433));
#78107=CARTESIAN_POINT('Ctrl Pts',(-20.1296154695208,-2.92384924803899,
126.847200467631));
#78108=CARTESIAN_POINT('Ctrl Pts',(-20.1373617456049,-3.03189035053216,
126.93178731744));
#78109=CARTESIAN_POINT('Ctrl Pts',(-20.1451080788703,-3.13993225056021,
127.016374791649));
#78110=CARTESIAN_POINT('Ctrl Pts',(-20.1528544121356,-3.24443094210425,
127.105486616101));
#78111=CARTESIAN_POINT('Ctrl Pts',(-20.160600745401,-3.34499673572624,127.19878439448));
#78112=CARTESIAN_POINT('Ctrl Pts',(-20.168348813404,-3.44558505036043,127.29210306625));
#78113=CARTESIAN_POINT('Ctrl Pts',(-20.1760968814069,-3.54223842792924,
127.389609291444));
#78114=CARTESIAN_POINT('Ctrl Pts',(-20.1838449494099,-3.63460348778926,
127.490927269957));
#78115=CARTESIAN_POINT('Ctrl Pts',(-20.1916012521518,-3.72706671433406,
127.592352930423));
#78116=CARTESIAN_POINT('Ctrl Pts',(-20.1993575548936,-3.81523225490922,
127.697598147485));
#78117=CARTESIAN_POINT('Ctrl Pts',(-20.2071138576355,-3.89878620246822,
127.806253012769));
#78118=CARTESIAN_POINT('Ctrl Pts',(-20.2148743001496,-3.98238474528457,
127.914965870425));
#78119=CARTESIAN_POINT('Ctrl Pts',(-20.2226347426638,-4.06136656560708,
128.027091683));
#78120=CARTESIAN_POINT('Ctrl Pts',(-20.230395185178,-4.13546127970726,128.142191752422));
#78121=CARTESIAN_POINT('Ctrl Pts',(-20.2381680854434,-4.20967493722053,
128.257476590694));
#78122=CARTESIAN_POINT('Ctrl Pts',(-20.2459409857088,-4.27898561347636,
128.375744889366));
#78123=CARTESIAN_POINT('Ctrl Pts',(-20.2537138859742,-4.34316862696734,
128.496532777317));
#78124=CARTESIAN_POINT('Ctrl Pts',(-20.2612042217362,-4.40501842625039,
128.612929721295));
#78125=CARTESIAN_POINT('Ctrl Pts',(-20.2686945574983,-4.4621067637387,128.73166597051));
#78126=CARTESIAN_POINT('Ctrl Pts',(-20.2761848932603,-4.51427570497735,
128.852310945567));
#78127=CARTESIAN_POINT('Ctrl Pts',(-20.2847817142089,-4.57415113128143,
128.990777802311));
#78128=CARTESIAN_POINT('Ctrl Pts',(-20.2933785351576,-4.6277091580921,129.132133849189));
#78129=CARTESIAN_POINT('Ctrl Pts',(-20.3019753561063,-4.67469033843641,
129.275814477527));
#78130=CARTESIAN_POINT('Ctrl Pts',(-20.3080269665765,-4.70776207560217,
129.376956422905));
#78131=CARTESIAN_POINT('Ctrl Pts',(-20.3140785770467,-4.73757573071408,
129.47924968965));
#78132=CARTESIAN_POINT('Ctrl Pts',(-20.320130187517,-4.76405452823408,129.582490119308));
#78133=CARTESIAN_POINT('Origin',(213.235140564004,0.,130.804360617566));
#78134=CARTESIAN_POINT('',(-22.4150500904691,-4.76405452823408,129.582490119308));
#78135=CARTESIAN_POINT('',(-22.0699306202468,-4.76405452823405,129.582490119308));
#78136=CARTESIAN_POINT('',(213.235140564004,-4.76405452823405,129.582490119308));
#78137=CARTESIAN_POINT('',(-20.7351405640401,-4.91824802158401,130.808772044207));
#78138=CARTESIAN_POINT('Ctrl Pts',(-20.7351405640403,-4.91824802158401,
130.808772044207));
#78139=CARTESIAN_POINT('Ctrl Pts',(-20.7446813187049,-4.91809669710575,
130.977481937026));
#78140=CARTESIAN_POINT('Ctrl Pts',(-20.7542220733695,-4.90926088785877,
131.145806171752));
#78141=CARTESIAN_POINT('Ctrl Pts',(-20.7637628280341,-4.89188139518882,
131.312966042139));
#78142=CARTESIAN_POINT('Ctrl Pts',(-20.7734548646572,-4.87422632644771,
131.482776465176));
#78143=CARTESIAN_POINT('Ctrl Pts',(-20.7831469012802,-4.84775452509061,
131.651385380119));
#78144=CARTESIAN_POINT('Ctrl Pts',(-20.7928389379032,-4.81266233021236,
131.817999783076));
#78145=CARTESIAN_POINT('Ctrl Pts',(-20.7997230068444,-4.78773701283744,
131.936342818823));
#78146=CARTESIAN_POINT('Ctrl Pts',(-20.8066070757855,-4.7584637302795,132.053680119585));
#78147=CARTESIAN_POINT('Ctrl Pts',(-20.8134911447266,-4.7249273209099,132.169734146905));
#78148=CARTESIAN_POINT('Ctrl Pts',(-20.8212654788457,-4.6870538984003,132.300796574077));
#78149=CARTESIAN_POINT('Ctrl Pts',(-20.8290398129648,-4.64366314041326,
132.430489572245));
#78150=CARTESIAN_POINT('Ctrl Pts',(-20.8368141470839,-4.59487025902523,
132.558313400632));
#78151=CARTESIAN_POINT('Ctrl Pts',(-20.844578900031,-4.54613751050276,132.685979697575));
#78152=CARTESIAN_POINT('Ctrl Pts',(-20.8523436529781,-4.49201602337523,
132.811781046432));
#78153=CARTESIAN_POINT('Ctrl Pts',(-20.8601084059252,-4.43267129262655,
132.935230926624));
#78154=CARTESIAN_POINT('Ctrl Pts',(-20.8678654468102,-4.37338550390114,
133.058558194655));
#78155=CARTESIAN_POINT('Ctrl Pts',(-20.8756224876953,-4.30888696380172,
133.17953829171));
#78156=CARTESIAN_POINT('Ctrl Pts',(-20.8833795285803,-4.23938982037526,
133.297703155887));
#78157=CARTESIAN_POINT('Ctrl Pts',(-20.8911307198204,-4.16994508528527,
133.41577891102));
#78158=CARTESIAN_POINT('Ctrl Pts',(-20.8988819110604,-4.09550944720151,
133.53104332332));
#78159=CARTESIAN_POINT('Ctrl Pts',(-20.9066331023006,-4.01634352383359,
133.64305182322));
#78160=CARTESIAN_POINT('Ctrl Pts',(-20.9143809990776,-3.93721124809482,
133.755012716521));
#78161=CARTESIAN_POINT('Ctrl Pts',(-20.9221288958547,-3.85335291098092,
133.863720131193));
#78162=CARTESIAN_POINT('Ctrl Pts',(-20.9298767926318,-3.76507297263704,
133.968757649106));
#78163=CARTESIAN_POINT('Ctrl Pts',(-20.9376230687159,-3.67681150055305,
134.073773195435));
#78164=CARTESIAN_POINT('Ctrl Pts',(-20.9453693448,-3.58413051831039,134.175120072823));
#78165=CARTESIAN_POINT('Ctrl Pts',(-20.9531156208841,-3.48737512147832,
134.272414513427));
#78166=CARTESIAN_POINT('Ctrl Pts',(-20.9608619541495,-3.39061901041988,
134.369709672236));
#78167=CARTESIAN_POINT('Ctrl Pts',(-20.9686082874148,-3.28978870044187,
134.462952057347));
#78168=CARTESIAN_POINT('Ctrl Pts',(-20.9763546206802,-3.1852662450395,134.551794674452));
#78169=CARTESIAN_POINT('Ctrl Pts',(-20.9841026886832,-3.08072038255823,
134.640657187245));
#78170=CARTESIAN_POINT('Ctrl Pts',(-20.9918507566862,-2.97248102719271,
134.725117718246));
#78171=CARTESIAN_POINT('Ctrl Pts',(-20.9995988246891,-2.86096308603967,
134.804869745517));
#78172=CARTESIAN_POINT('Ctrl Pts',(-21.007355127431,-2.74932662229153,134.884706534192));
#78173=CARTESIAN_POINT('Ctrl Pts',(-21.0151114301728,-2.63440493057037,
134.959824594812));
#78174=CARTESIAN_POINT('Ctrl Pts',(-21.0228677329147,-2.51664212533206,
135.029960631233));
#78175=CARTESIAN_POINT('Ctrl Pts',(-21.0306281754289,-2.39881646653865,
135.100134101369));
#78176=CARTESIAN_POINT('Ctrl Pts',(-21.0383886179431,-2.27814701651188,
135.165320063181));
#78177=CARTESIAN_POINT('Ctrl Pts',(-21.0461490604573,-2.15510133740986,
135.225301839523));
#78178=CARTESIAN_POINT('Ctrl Pts',(-21.0539219607227,-2.03185813446044,
135.285379903936));
#78179=CARTESIAN_POINT('Ctrl Pts',(-21.0616948609882,-1.906231438283,135.34023693194));
#78180=CARTESIAN_POINT('Ctrl Pts',(-21.0694677612536,-1.77870841005995,
135.38970460188));
#78181=CARTESIAN_POINT('Ctrl Pts',(-21.0769580970156,-1.65582116512497,
135.437373997415));
#78182=CARTESIAN_POINT('Ctrl Pts',(-21.0844484327775,-1.53117335878165,
135.480038965816));
#78183=CARTESIAN_POINT('Ctrl Pts',(-21.0919387685395,-1.40521121009835,
135.517593533253));
#78184=CARTESIAN_POINT('Ctrl Pts',(-21.0997131026586,-1.27447316826143,
135.556571993529));
#78185=CARTESIAN_POINT('Ctrl Pts',(-21.1074874367776,-1.14190501123633,
135.590168353381));
#78186=CARTESIAN_POINT('Ctrl Pts',(-21.1152617708967,-1.00798946003274,
135.618209421897));
#78187=CARTESIAN_POINT('Ctrl Pts',(-21.1230265238438,-0.874238947777619,
135.646215932303));
#78188=CARTESIAN_POINT('Ctrl Pts',(-21.1307912767909,-0.739144724321958,
135.668680694308));
#78189=CARTESIAN_POINT('Ctrl Pts',(-21.138556029738,-0.60320556728882,135.685479967274));
#78190=CARTESIAN_POINT('Ctrl Pts',(-21.146313070623,-0.467401426943038,
135.702262554965));
#78191=CARTESIAN_POINT('Ctrl Pts',(-21.1540701115079,-0.3307544085683,135.713390804047));
#78192=CARTESIAN_POINT('Ctrl Pts',(-21.1618271523929,-0.193774058149417,
135.718791884446));
#78193=CARTESIAN_POINT('Ctrl Pts',(-21.169578343633,-0.0568970056783372,
135.724188891848));
#78194=CARTESIAN_POINT('Ctrl Pts',(-21.1773295348731,0.0803124894226256,
135.723867311739));
#78195=CARTESIAN_POINT('Ctrl Pts',(-21.1850807261132,0.217339527950154,
135.717806108471));
#78196=CARTESIAN_POINT('Ctrl Pts',(-21.1928286228903,0.354308326331179,
135.711747481375));
#78197=CARTESIAN_POINT('Ctrl Pts',(-21.2005765196674,0.491094432612081,
135.699954100326));
#78198=CARTESIAN_POINT('Ctrl Pts',(-21.2083244164445,0.627182934281594,
135.682457032096));
#78199=CARTESIAN_POINT('Ctrl Pts',(-21.2160706925286,0.763242969170286,
135.664963623875));
#78200=CARTESIAN_POINT('Ctrl Pts',(-21.2238169686127,0.898605302170506,
135.641768951416));
#78201=CARTESIAN_POINT('Ctrl Pts',(-21.2315632446968,1.03276052594148,135.612955917501));
#78202=CARTESIAN_POINT('Ctrl Pts',(-21.2393095779621,1.16691674001583,135.584142670895));
#78203=CARTESIAN_POINT('Ctrl Pts',(-21.2470559112275,1.29986544483202,135.549711062173));
#78204=CARTESIAN_POINT('Ctrl Pts',(-21.2548022444928,1.43110819500367,135.50979496486));
#78205=CARTESIAN_POINT('Ctrl Pts',(-21.2625503124958,1.56238033607907,135.469869928614));
#78206=CARTESIAN_POINT('Ctrl Pts',(-21.2702983804987,1.69194538832479,135.424458073516));
#78207=CARTESIAN_POINT('Ctrl Pts',(-21.2780464485017,1.81932119873293,135.373742790064));
#78208=CARTESIAN_POINT('Ctrl Pts',(-21.2858027512435,1.94683238566833,135.322973605804));
#78209=CARTESIAN_POINT('Ctrl Pts',(-21.2935590539854,2.0721493190159,135.266889878434));
#78210=CARTESIAN_POINT('Ctrl Pts',(-21.3013153567272,2.19481042556054,135.205722936025));
#78211=CARTESIAN_POINT('Ctrl Pts',(-21.3090757992414,2.31753700003099,135.144523346977));
#78212=CARTESIAN_POINT('Ctrl Pts',(-21.3168362417556,2.43760458112017,135.078235325748));
#78213=CARTESIAN_POINT('Ctrl Pts',(-21.3245966842697,2.55457814344091,135.007135126334));
#78214=CARTESIAN_POINT('Ctrl Pts',(-21.3323695845352,2.67173948210831,134.935920790569));
#78215=CARTESIAN_POINT('Ctrl Pts',(-21.3401424848006,2.78579655128592,134.859879056735));
#78216=CARTESIAN_POINT('Ctrl Pts',(-21.347915385066,2.89634441468123,134.779328805369));
#78217=CARTESIAN_POINT('Ctrl Pts',(-21.3554057208282,3.00287358479019,134.701706758533));
#78218=CARTESIAN_POINT('Ctrl Pts',(-21.3628960565902,3.10614401506301,134.619898486416));
#78219=CARTESIAN_POINT('Ctrl Pts',(-21.3703863923523,3.20582535441011,134.534222124314));
#78220=CARTESIAN_POINT('Ctrl Pts',(-21.3781607264714,3.30928614203488,134.445297316904));
#78221=CARTESIAN_POINT('Ctrl Pts',(-21.3859350605905,3.40920803810672,134.35192362501));
#78222=CARTESIAN_POINT('Ctrl Pts',(-21.3937093947096,3.50518440970838,134.254413561571));
#78223=CARTESIAN_POINT('Ctrl Pts',(-21.4014741476567,3.6010424990097,134.15702367057));
#78224=CARTESIAN_POINT('Ctrl Pts',(-21.4092389006037,3.69296446715769,134.055507826906));
#78225=CARTESIAN_POINT('Ctrl Pts',(-21.4170036535508,3.78057660615906,133.95021878148));
#78226=CARTESIAN_POINT('Ctrl Pts',(-21.4247606944358,3.86810172754874,133.845034310618));
#78227=CARTESIAN_POINT('Ctrl Pts',(-21.4325177353209,3.95132528989059,133.736084394466));
#78228=CARTESIAN_POINT('Ctrl Pts',(-21.4402747762059,4.02991059712929,133.623758362058));
#78229=CARTESIAN_POINT('Ctrl Pts',(-21.4480259674461,4.10843664257649,133.511517035584));
#78230=CARTESIAN_POINT('Ctrl Pts',(-21.4557771586861,4.18233117175354,133.395904979477));
#78231=CARTESIAN_POINT('Ctrl Pts',(-21.4635283499262,4.25129817117705,133.277344022736));
#78232=CARTESIAN_POINT('Ctrl Pts',(-21.4712762467033,4.32023585778604,133.158833457565));
#78233=CARTESIAN_POINT('Ctrl Pts',(-21.4790241434803,4.38424998393468,133.03737682184));
#78234=CARTESIAN_POINT('Ctrl Pts',(-21.4867720402574,4.44308836418855,132.913424118391));
#78235=CARTESIAN_POINT('Ctrl Pts',(-21.4945183163415,4.50191443672168,132.789497343175));
#78236=CARTESIAN_POINT('Ctrl Pts',(-21.5022645924256,4.55556674927008,132.663075891736));
#78237=CARTESIAN_POINT('Ctrl Pts',(-21.5100108685097,4.6038397031817,132.534633153876));
#78238=CARTESIAN_POINT('Ctrl Pts',(-21.517757201775,4.65211301343329,132.40618946788));
#78239=CARTESIAN_POINT('Ctrl Pts',(-21.5255035350405,4.69500674826715,132.275724831662));
#78240=CARTESIAN_POINT('Ctrl Pts',(-21.5332498683058,4.73236411736538,132.143730963353));
#78241=CARTESIAN_POINT('Ctrl Pts',(-21.5409979363088,4.76972985238741,132.011707535931));
#78242=CARTESIAN_POINT('Ctrl Pts',(-21.5487460043117,4.80155664810437,131.878154571077));
#78243=CARTESIAN_POINT('Ctrl Pts',(-21.5564940723147,4.82773818065694,131.743576844815));
#78244=CARTESIAN_POINT('Ctrl Pts',(-21.5642503750566,4.85394753925388,131.608856087743));
#78245=CARTESIAN_POINT('Ctrl Pts',(-21.5720066777984,4.87449957455411,131.473108777993));
#78246=CARTESIAN_POINT('Ctrl Pts',(-21.5797629805403,4.88933941781885,131.336848288656));
#78247=CARTESIAN_POINT('Ctrl Pts',(-21.5875234230545,4.90418718155478,131.200515072993));
#78248=CARTESIAN_POINT('Ctrl Pts',(-21.5952838655686,4.91331665231312,131.063668521883));
#78249=CARTESIAN_POINT('Ctrl Pts',(-21.6030443080828,4.91672510855631,130.926823956537));
#78250=CARTESIAN_POINT('Ctrl Pts',(-21.6108172083482,4.92013903635605,130.789759716146));
#78251=CARTESIAN_POINT('Ctrl Pts',(-21.6185901086136,4.91781360395731,130.652697859023));
#78252=CARTESIAN_POINT('Ctrl Pts',(-21.626363008879,4.90979821662803,130.516151432258));
#78253=CARTESIAN_POINT('Ctrl Pts',(-21.6338533446411,4.90207420881771,130.384568812044));
#78254=CARTESIAN_POINT('Ctrl Pts',(-21.6413436804031,4.8890667826379,130.253465104929));
#78255=CARTESIAN_POINT('Ctrl Pts',(-21.6488340161652,4.87086503149063,130.123290204538));
#78256=CARTESIAN_POINT('Ctrl Pts',(-21.6566083502843,4.85197315541634,129.988179683233));
#78257=CARTESIAN_POINT('Ctrl Pts',(-21.6643826844033,4.82742544950069,129.853641800885));
#78258=CARTESIAN_POINT('Ctrl Pts',(-21.6721570185224,4.7972650447047,129.72018759016));
#78259=CARTESIAN_POINT('Ctrl Pts',(-21.6799217714695,4.76714180991215,129.586897849823));
#78260=CARTESIAN_POINT('Ctrl Pts',(-21.6876865244166,4.73141972466212,129.454689501492));
#78261=CARTESIAN_POINT('Ctrl Pts',(-21.6954512773637,4.69019356998027,129.324067626765));
#78262=CARTESIAN_POINT('Ctrl Pts',(-21.7032083182487,4.64900836169645,129.193575487525));
#78263=CARTESIAN_POINT('Ctrl Pts',(-21.7109653591336,4.60233007991013,129.064667056583));
#78264=CARTESIAN_POINT('Ctrl Pts',(-21.7187224000186,4.5503042857218,128.937836047719));
#78265=CARTESIAN_POINT('Ctrl Pts',(-21.7264735912588,4.4983177245895,128.811100683105));
#78266=CARTESIAN_POINT('Ctrl Pts',(-21.734224782499,4.44099182547712,128.686439982599));
#78267=CARTESIAN_POINT('Ctrl Pts',(-21.7419759737391,4.37852148255138,128.564330999606));
#78268=CARTESIAN_POINT('Ctrl Pts',(-21.7497238705162,4.31607769118784,128.442273916189));
#78269=CARTESIAN_POINT('Ctrl Pts',(-21.7574717672932,4.24849398253747,128.322766740533));
#78270=CARTESIAN_POINT('Ctrl Pts',(-21.7652196640703,4.17601264433699,128.206264880909));
#78271=CARTESIAN_POINT('Ctrl Pts',(-21.7729659401544,4.10354646766994,128.089787390961));
#78272=CARTESIAN_POINT('Ctrl Pts',(-21.7807122162386,4.02618490559565,127.976314298383));
#78273=CARTESIAN_POINT('Ctrl Pts',(-21.7884584923227,3.94421510326795,127.866274457895));
#78274=CARTESIAN_POINT('Ctrl Pts',(-21.796204825588,3.8622446958578,127.756233805117));
#78275=CARTESIAN_POINT('Ctrl Pts',(-21.8039511588534,3.77566621387236,127.649626768535));
#78276=CARTESIAN_POINT('Ctrl Pts',(-21.8116974921188,3.68480860470474,127.546851045946));
#78277=CARTESIAN_POINT('Ctrl Pts',(-21.8194455601218,3.59393064860564,127.444052307447));
#78278=CARTESIAN_POINT('Ctrl Pts',(-21.8271936281248,3.49877191735522,127.345086883113));
#78279=CARTESIAN_POINT('Ctrl Pts',(-21.8349416961277,3.39969962267526,127.250317069988));
#78280=CARTESIAN_POINT('Ctrl Pts',(-21.8426979988696,3.3005220327814,127.155446534378));
#78281=CARTESIAN_POINT('Ctrl Pts',(-21.8504543016114,3.19742285361602,127.064780788284));
#78282=CARTESIAN_POINT('Ctrl Pts',(-21.8582106043532,3.09080434260711,126.978643485025));
#78283=CARTESIAN_POINT('Ctrl Pts',(-21.8659710468674,2.98412892608866,126.892460207693));
#78284=CARTESIAN_POINT('Ctrl Pts',(-21.8737314893816,2.87393074888859,126.810810421846));
#78285=CARTESIAN_POINT('Ctrl Pts',(-21.8814919318958,2.76064189427898,126.733974960893));
#78286=CARTESIAN_POINT('Ctrl Pts',(-21.8892648321612,2.64717117834265,126.657016156836));
#78287=CARTESIAN_POINT('Ctrl Pts',(-21.8970377324267,2.53060020313822,126.584887327276));
#78288=CARTESIAN_POINT('Ctrl Pts',(-21.9048106326921,2.41138731446645,126.517824220645));
#78289=CARTESIAN_POINT('Ctrl Pts',(-21.9123009684541,2.29650811457737,126.453199026862));
#78290=CARTESIAN_POINT('Ctrl Pts',(-21.9197913042162,2.17917602115765,126.393277786815));
#78291=CARTESIAN_POINT('Ctrl Pts',(-21.9272816399782,2.05981769961689,126.338228722196));
#78292=CARTESIAN_POINT('Ctrl Pts',(-21.9350559740973,1.93593387103638,126.281092455559));
#78293=CARTESIAN_POINT('Ctrl Pts',(-21.9428303082163,1.80947470564764,126.229024124094));
#78294=CARTESIAN_POINT('Ctrl Pts',(-21.9506046423354,1.68089346304385,126.182263666138));
#78295=CARTESIAN_POINT('Ctrl Pts',(-21.9583693952825,1.55247068532992,126.135560836268));
#78296=CARTESIAN_POINT('Ctrl Pts',(-21.9661341482296,1.42193139790572,126.09415299665));
#78297=CARTESIAN_POINT('Ctrl Pts',(-21.9738989011767,1.28975177168359,126.058233414262));
#78298=CARTESIAN_POINT('Ctrl Pts',(-21.9816559420617,1.15770342812981,126.022349507711));
#78299=CARTESIAN_POINT('Ctrl Pts',(-21.9894129829468,1.02401836281609,125.991943112488));
#78300=CARTESIAN_POINT('Ctrl Pts',(-21.9971700238318,0.889190630458458,
125.967158628275));
#78301=CARTESIAN_POINT('Ctrl Pts',(-22.0049212150719,0.754464572742602,
125.942392834234));
#78302=CARTESIAN_POINT('Ctrl Pts',(-22.012672406312,0.618597946099293,125.923240583081));
#78303=CARTESIAN_POINT('Ctrl Pts',(-22.0204235975521,0.482097454127241,
125.909795763851));
#78304=CARTESIAN_POINT('Ctrl Pts',(-22.0281714943292,0.345654978505546,
125.896356659028));
#78305=CARTESIAN_POINT('Ctrl Pts',(-22.0359193911062,0.208579561658239,
125.888620199619));
#78306=CARTESIAN_POINT('Ctrl Pts',(-22.0436672878833,0.0713853138995451,
125.886628701382));
#78307=CARTESIAN_POINT('Ctrl Pts',(-22.0514135639674,-0.0657802357800839,
125.884637619723));
#78308=CARTESIAN_POINT('Ctrl Pts',(-22.0591598400515,-0.203064176253083,
125.888389114617));
#78309=CARTESIAN_POINT('Ctrl Pts',(-22.0669061161356,-0.339950490928263,
125.897873409163));
#78310=CARTESIAN_POINT('Ctrl Pts',(-22.074652449401,-0.476837816067122,
125.907357773721));
#78311=CARTESIAN_POINT('Ctrl Pts',(-22.0823987826663,-0.613327119521069,
125.922574995352));
#78312=CARTESIAN_POINT('Ctrl Pts',(-22.0901451159317,-0.748906002770302,
125.94346328667));
#78313=CARTESIAN_POINT('Ctrl Pts',(-22.0978931839347,-0.884515247970401,
125.964356255776));
#78314=CARTESIAN_POINT('Ctrl Pts',(-22.1056412519377,-1.0192132809315,125.990922762194));
#78315=CARTESIAN_POINT('Ctrl Pts',(-22.1133893199406,-1.15249680398375,
126.023049690706));
#78316=CARTESIAN_POINT('Ctrl Pts',(-22.1211456226825,-1.2859219823504,126.0552107641));
#78317=CARTESIAN_POINT('Ctrl Pts',(-22.1289019254244,-1.41792926700313,
126.092943973055));
#78318=CARTESIAN_POINT('Ctrl Pts',(-22.1366582281662,-1.54802892927213,
126.136085829527));
#78319=CARTESIAN_POINT('Ctrl Pts',(-22.1444186706804,-1.67819802964829,
126.179250712108));
#78320=CARTESIAN_POINT('Ctrl Pts',(-22.1521791131944,-1.80645711344013,
126.227829855904));
#78321=CARTESIAN_POINT('Ctrl Pts',(-22.1599395557086,-1.9323363559845,126.281611534338));
#78322=CARTESIAN_POINT('Ctrl Pts',(-22.167712455974,-2.05841767106386,126.335479547897));
#78323=CARTESIAN_POINT('Ctrl Pts',(-22.1754853562395,-2.18211115766965,
126.394566616576));
#78324=CARTESIAN_POINT('Ctrl Pts',(-22.1832582565049,-2.30297072686775,
126.458614548858));
#78325=CARTESIAN_POINT('Ctrl Pts',(-22.1907485922669,-2.4194367462991,126.520334177475));
#78326=CARTESIAN_POINT('Ctrl Pts',(-22.198238928029,-2.53327104509812,126.586660096784));
#78327=CARTESIAN_POINT('Ctrl Pts',(-22.2057292637911,-2.64410147051529,
126.657324269025));
#78328=CARTESIAN_POINT('Ctrl Pts',(-22.2135050158773,-2.75915504608735,
126.730681072002));
#78329=CARTESIAN_POINT('Ctrl Pts',(-22.2212807679636,-2.87133580835104,
126.808945712742));
#78330=CARTESIAN_POINT('Ctrl Pts',(-22.2290565200499,-2.98019665006642,
126.891866401668));
#78331=CARTESIAN_POINT('Ctrl Pts',(-22.2368199666371,-3.0888852143012,126.974655864645));
#78332=CARTESIAN_POINT('Ctrl Pts',(-22.2445834132244,-3.19426401401315,
127.062086465408));
#78333=CARTESIAN_POINT('Ctrl Pts',(-22.2523468598116,-3.29591328084603,
127.153862198495));
#78334=CARTESIAN_POINT('Ctrl Pts',(-22.2601032064868,-3.39746958628009,
127.245553999835));
#78335=CARTESIAN_POINT('Ctrl Pts',(-22.267859553162,-3.49530285553143,127.341582768679));
#78336=CARTESIAN_POINT('Ctrl Pts',(-22.2756158998372,-3.58902465571209,
127.441610986209));
#78337=CARTESIAN_POINT('Ctrl Pts',(-22.2833668330945,-3.68268104426293,
127.541569390647));
#78338=CARTESIAN_POINT('Ctrl Pts',(-22.2911177663518,-3.77223140701409,
127.645521405863));
#78339=CARTESIAN_POINT('Ctrl Pts',(-22.298868699609,-3.85732289862148,127.75309151795));
#78340=CARTESIAN_POINT('Ctrl Pts',(-22.3066159019005,-3.94237343084635,
127.860609850415));
#78341=CARTESIAN_POINT('Ctrl Pts',(-22.3143631041919,-4.02296912173825,
127.971742507572));
#78342=CARTESIAN_POINT('Ctrl Pts',(-22.3221103064834,-4.09879655867963,
128.08607994165));
#78343=CARTESIAN_POINT('Ctrl Pts',(-22.3298572073455,-4.17462104531473,
128.200412927069));
#78344=CARTESIAN_POINT('Ctrl Pts',(-22.3376041082076,-4.24567742114018,
128.317950122415));
#78345=CARTESIAN_POINT('Ctrl Pts',(-22.3453510090697,-4.31169491968724,
128.438252001707));
#78346=CARTESIAN_POINT('Ctrl Pts',(-22.3530973593788,-4.37770772653487,
128.558545331443));
#78347=CARTESIAN_POINT('Ctrl Pts',(-22.3608437096879,-4.43868218493249,
128.681602608968));
#78348=CARTESIAN_POINT('Ctrl Pts',(-22.368590059997,-4.49439330747625,128.806959340854));
#78349=CARTESIAN_POINT('Ctrl Pts',(-22.3763411935889,-4.55013883100134,
128.932393479088));
#78350=CARTESIAN_POINT('Ctrl Pts',(-22.3840923271808,-4.60061436663891,
129.060129550598));
#78351=CARTESIAN_POINT('Ctrl Pts',(-22.3918434607727,-4.64564283081932,
129.189682398552));
#78352=CARTESIAN_POINT('Ctrl Pts',(-22.3995790040048,-4.69058072631766,
129.318974668427));
#78353=CARTESIAN_POINT('Ctrl Pts',(-22.407314547237,-4.73009335830748,129.450076033197));
#78354=CARTESIAN_POINT('Ctrl Pts',(-22.4150500904691,-4.76405452823408,
129.582490119308));
#78355=CARTESIAN_POINT('Ctrl Pts',(-20.6651747065899,-4.7640545282341,129.582490119308));
#78356=CARTESIAN_POINT('Ctrl Pts',(-20.6728565465615,-4.79788063571959,
129.714377599012));
#78357=CARTESIAN_POINT('Ctrl Pts',(-20.6805383865331,-4.82622772596712,
129.847678318042));
#78358=CARTESIAN_POINT('Ctrl Pts',(-20.6882202265047,-4.8489928090036,129.981893718091));
#78359=CARTESIAN_POINT('Ctrl Pts',(-20.6960402827554,-4.87216749508839,
130.118524002238));
#78360=CARTESIAN_POINT('Ctrl Pts',(-20.703860339006,-4.88955727877376,130.256101781898));
#78361=CARTESIAN_POINT('Ctrl Pts',(-20.7116803952567,-4.90110841950362,
130.394093237958));
#78362=CARTESIAN_POINT('Ctrl Pts',(-20.7195004515073,-4.91265956023348,
130.532084694017));
#78363=CARTESIAN_POINT('Ctrl Pts',(-20.727320507758,-4.91837205430769,130.670489392195));
#78364=CARTESIAN_POINT('Ctrl Pts',(-20.7351405640086,-4.91824802158451,
130.808772043649));
#78365=CARTESIAN_POINT('',(-20.3898594359439,-4.91824942229388,130.80197679587));
#78366=CARTESIAN_POINT('Ctrl Pts',(-20.320130187517,-4.76405452823408,129.582490119308));
#78367=CARTESIAN_POINT('Ctrl Pts',(-20.3286835810525,-4.80147986759645,
129.728410949473));
#78368=CARTESIAN_POINT('Ctrl Pts',(-20.3372369745881,-4.83224103412311,
129.87622469168));
#78369=CARTESIAN_POINT('Ctrl Pts',(-20.3457903681237,-4.85616156344646,
130.025336913045));
#78370=CARTESIAN_POINT('Ctrl Pts',(-20.3543062507495,-4.87997718928168,
130.173795202721));
#78371=CARTESIAN_POINT('Ctrl Pts',(-20.3628221333753,-4.89701194625247,
130.323540373495));
#78372=CARTESIAN_POINT('Ctrl Pts',(-20.3713380160011,-4.90714008083112,
130.473967988107));
#78373=CARTESIAN_POINT('Ctrl Pts',(-20.3775118226487,-4.9144827307169,130.583024329991));
#78374=CARTESIAN_POINT('Ctrl Pts',(-20.3836856292964,-4.91819633051015,
130.692438974677));
#78375=CARTESIAN_POINT('Ctrl Pts',(-20.389859435944,-4.91824942229388,130.80197679587));
#78376=CARTESIAN_POINT('Ctrl Pts',(-20.3898594359911,-4.91824942229429,
130.801976796707));
#78377=CARTESIAN_POINT('Ctrl Pts',(-20.3977271603077,-4.91831708093587,
130.941568693342));
#78378=CARTESIAN_POINT('Ctrl Pts',(-20.4055948846243,-4.91243745220422,
131.081147358311));
#78379=CARTESIAN_POINT('Ctrl Pts',(-20.413462608941,-4.90064040371127,131.220181126936));
#78380=CARTESIAN_POINT('Ctrl Pts',(-20.4213329011031,-4.88883950493117,
131.359260273007));
#78381=CARTESIAN_POINT('Ctrl Pts',(-20.4292031932653,-4.87111737031541,
131.497793796023));
#78382=CARTESIAN_POINT('Ctrl Pts',(-20.4370734854275,-4.84755570480307,
131.63525576819));
#78383=CARTESIAN_POINT('Ctrl Pts',(-20.4449478339736,-4.82398189550227,
131.772788588877));
#78384=CARTESIAN_POINT('Ctrl Pts',(-20.4528221825198,-4.79456262260292,
131.909248390416));
#78385=CARTESIAN_POINT('Ctrl Pts',(-20.4606965310659,-4.7594305555103,132.044120211106));
#78386=CARTESIAN_POINT('Ctrl Pts',(-20.4685822234648,-4.72424787686653,
132.179186329275));
#78387=CARTESIAN_POINT('Ctrl Pts',(-20.4764679158635,-4.68333605498181,
132.312659533615));
#78388=CARTESIAN_POINT('Ctrl Pts',(-20.4843536082624,-4.63687773177912,
132.444039843217));
#78389=CARTESIAN_POINT('Ctrl Pts',(-20.4922451030626,-4.59038522390083,
132.575516824265));
#78390=CARTESIAN_POINT('Ctrl Pts',(-20.5001365978628,-4.53833821785165,
132.704897494192));
#78391=CARTESIAN_POINT('Ctrl Pts',(-20.508028092663,-4.48096699767772,132.831703170817));
#78392=CARTESIAN_POINT('Ctrl Pts',(-20.5159342962008,-4.4234888448823,132.958745197016));
#78393=CARTESIAN_POINT('Ctrl Pts',(-20.5238404997386,-4.36066681064876,
133.083202302654));
#78394=CARTESIAN_POINT('Ctrl Pts',(-20.5317467032764,-4.29277712002305,
133.204620532722));
#78395=CARTESIAN_POINT('Ctrl Pts',(-20.5393753078754,-4.22727114061728,
133.321775582408));
#78396=CARTESIAN_POINT('Ctrl Pts',(-20.5470039124743,-4.15704756176367,
133.436101329416));
#78397=CARTESIAN_POINT('Ctrl Pts',(-20.5546325170732,-4.08239095982688,
133.547218089916));
#78398=CARTESIAN_POINT('Ctrl Pts',(-20.5624068511923,-4.00630819001947,
133.660457518064));
#78399=CARTESIAN_POINT('Ctrl Pts',(-20.5701811853113,-3.92538970092749,
133.77070827668));
#78400=CARTESIAN_POINT('Ctrl Pts',(-20.5779555194304,-3.83989779120505,
133.877529668497));
#78401=CARTESIAN_POINT('Ctrl Pts',(-20.5857202723775,-3.75451124262072,
133.984219412495));
#78402=CARTESIAN_POINT('Ctrl Pts',(-20.5934850253246,-3.66456272997648,
134.087487896633));
#78403=CARTESIAN_POINT('Ctrl Pts',(-20.6012497782717,-3.57035839697324,
134.186922365659));
#78404=CARTESIAN_POINT('Ctrl Pts',(-20.6090068191567,-3.47624762904158,
134.286258074969));
#78405=CARTESIAN_POINT('Ctrl Pts',(-20.6167638600417,-3.37788971970297,
134.381767065273));
#78406=CARTESIAN_POINT('Ctrl Pts',(-20.6245209009267,-3.275631506201,134.473069014002));
#78407=CARTESIAN_POINT('Ctrl Pts',(-20.6322720921668,-3.17345040641329,
134.564302111222));
#78408=CARTESIAN_POINT('Ctrl Pts',(-20.640023283407,-3.06737514729707,134.651334222326));
#78409=CARTESIAN_POINT('Ctrl Pts',(-20.6477744746471,-2.95778964355184,
134.733821584034));
#78410=CARTESIAN_POINT('Ctrl Pts',(-20.6555223714242,-2.848250716569,134.816273886414));
#78411=CARTESIAN_POINT('Ctrl Pts',(-20.6632702682012,-2.73520482403686,
134.894185046652));
#78412=CARTESIAN_POINT('Ctrl Pts',(-20.6710181649782,-2.61906903376005,
134.967251495177));
#78413=CARTESIAN_POINT('Ctrl Pts',(-20.6787644410624,-2.50295753658696,
135.040302659777));
#78414=CARTESIAN_POINT('Ctrl Pts',(-20.6865107171464,-2.38375775798487,
135.108510920324));
#78415=CARTESIAN_POINT('Ctrl Pts',(-20.6942569932305,-2.26191549134503,
135.171616205749));
#78416=CARTESIAN_POINT('Ctrl Pts',(-20.7020033264959,-2.1400723252936,135.234721957002));
#78417=CARTESIAN_POINT('Ctrl Pts',(-20.7097496597612,-2.01558697944628,
135.29272447816));
#78418=CARTESIAN_POINT('Ctrl Pts',(-20.7174959930266,-1.88892921192834,
135.345410000123));
#78419=CARTESIAN_POINT('Ctrl Pts',(-20.7252440610295,-1.76224308028137,
135.398107320644));
#78420=CARTESIAN_POINT('Ctrl Pts',(-20.7329921290325,-1.63338391979895,
135.445485122478));
#78421=CARTESIAN_POINT('Ctrl Pts',(-20.7407401970354,-1.50284041563251,
135.487378207501));
#78422=CARTESIAN_POINT('Ctrl Pts',(-20.7484964997773,-1.37215816827617,
135.529315816994));
#78423=CARTESIAN_POINT('Ctrl Pts',(-20.7562528025191,-1.23978837409685,
135.56575694552));
#78424=CARTESIAN_POINT('Ctrl Pts',(-20.764009105261,-1.10623433243964,135.596586474538));
#78425=CARTESIAN_POINT('Ctrl Pts',(-20.7717695477751,-0.972609008969159,
135.627432458204));
#78426=CARTESIAN_POINT('Ctrl Pts',(-20.7795299902893,-0.837798562676585,
135.652660802529));
#78427=CARTESIAN_POINT('Ctrl Pts',(-20.7872904328035,-0.702314386431186,
135.672207941087));
#78428=CARTESIAN_POINT('Ctrl Pts',(-20.7950633330689,-0.566612718958359,
135.691786458447));
#78429=CARTESIAN_POINT('Ctrl Pts',(-20.8028362333343,-0.430235549468906,
135.705665505815));
#78430=CARTESIAN_POINT('Ctrl Pts',(-20.8106091335997,-0.293698169259079,
135.713833547308));
#78431=CARTESIAN_POINT('Ctrl Pts',(-20.8180994693619,-0.162124266735123,
135.72170465992));
#78432=CARTESIAN_POINT('Ctrl Pts',(-20.825589805124,-0.0304019073486875,
135.724272770742));
#78433=CARTESIAN_POINT('Ctrl Pts',(-20.8330801408861,0.10101164151941,135.721573213212));
#78434=CARTESIAN_POINT('Ctrl Pts',(-20.8408544750052,0.237407775033773,
135.718771301138));
#78435=CARTESIAN_POINT('Ctrl Pts',(-20.8486288091243,0.373903280619894,
135.71028551259));
#78436=CARTESIAN_POINT('Ctrl Pts',(-20.8564031432434,0.509985608355766,
135.696098319219));
#78437=CARTESIAN_POINT('Ctrl Pts',(-20.8641678961905,0.645900226784547,
135.681928610295));
#78438=CARTESIAN_POINT('Ctrl Pts',(-20.8719326491376,0.781402295404141,
135.662071517282));
#78439=CARTESIAN_POINT('Ctrl Pts',(-20.8796974020847,0.915979073383363,
135.636561503252));
#78440=CARTESIAN_POINT('Ctrl Pts',(-20.8874544429697,1.0504221878095,135.611076826127));
#78441=CARTESIAN_POINT('Ctrl Pts',(-20.8952114838547,1.18394145883076,135.579950473556));
#78442=CARTESIAN_POINT('Ctrl Pts',(-20.9029685247397,1.31602943629607,135.543268675896));
#78443=CARTESIAN_POINT('Ctrl Pts',(-20.9107197159798,1.44801780519044,135.506614540265));
#78444=CARTESIAN_POINT('Ctrl Pts',(-20.9184709072199,1.57857665372421,135.464413402491));
#78445=CARTESIAN_POINT('Ctrl Pts',(-20.9262220984601,1.70720924884263,135.416802448437));
#78446=CARTESIAN_POINT('Ctrl Pts',(-20.9339699952372,1.83578717167639,135.369211730308));
#78447=CARTESIAN_POINT('Ctrl Pts',(-20.9417178920143,1.96244010355671,135.316215904489));
#78448=CARTESIAN_POINT('Ctrl Pts',(-20.9494657887914,2.08668720746943,135.258001775168));
#78449=CARTESIAN_POINT('Ctrl Pts',(-20.9572120648755,2.21090832156646,135.199799822987));
#78450=CARTESIAN_POINT('Ctrl Pts',(-20.9649583409596,2.33272425487457,135.136381904241));
#78451=CARTESIAN_POINT('Ctrl Pts',(-20.9727046170437,2.45167524001829,135.067982502769));
#78452=CARTESIAN_POINT('Ctrl Pts',(-20.9804509503091,2.57062710323117,134.999582596388));
#78453=CARTESIAN_POINT('Ctrl Pts',(-20.9881972835744,2.68671363715254,134.926201328794));
#78454=CARTESIAN_POINT('Ctrl Pts',(-20.9959436168398,2.79950107604371,134.848118373383));
#78455=CARTESIAN_POINT('Ctrl Pts',(-21.0036916848427,2.91231377289981,134.770017931836));
#78456=CARTESIAN_POINT('Ctrl Pts',(-21.0114397528457,3.02182558319254,134.687213929799));
#78457=CARTESIAN_POINT('Ctrl Pts',(-21.0191878208487,3.12763337480069,134.600028218309));
#78458=CARTESIAN_POINT('Ctrl Pts',(-21.0269441235906,3.23355362018904,134.512749844808));
#78459=CARTESIAN_POINT('Ctrl Pts',(-21.0347004263324,3.33576168075101,134.42108070815));
#78460=CARTESIAN_POINT('Ctrl Pts',(-21.0424567290743,3.43388865840592,134.325382023944));
#78461=CARTESIAN_POINT('Ctrl Pts',(-21.0502171715884,3.53206800938322,134.229632262468));
#78462=CARTESIAN_POINT('Ctrl Pts',(-21.0579776141026,3.62616166911746,134.129848952317));
#78463=CARTESIAN_POINT('Ctrl Pts',(-21.0657380566168,3.71583973703538,134.026427983586));
#78464=CARTESIAN_POINT('Ctrl Pts',(-21.0735109568822,3.80566176414928,133.922840994334));
#78465=CARTESIAN_POINT('Ctrl Pts',(-21.0812838571477,3.89105379108128,133.815604983357));
#78466=CARTESIAN_POINT('Ctrl Pts',(-21.0890567574131,3.97172758483533,133.70514724439));
#78467=CARTESIAN_POINT('Ctrl Pts',(-21.096547093175,4.04946868298019,133.598704922461));
#78468=CARTESIAN_POINT('Ctrl Pts',(-21.104037428937,4.12282846009108,133.48927129757));
#78469=CARTESIAN_POINT('Ctrl Pts',(-21.1115277646989,4.19158947900152,133.3772501803));
#78470=CARTESIAN_POINT('Ctrl Pts',(-21.119302098818,4.26295759284442,133.260981748318));
#78471=CARTESIAN_POINT('Ctrl Pts',(-21.1270764329371,4.3295974134669,133.141557437729));
#78472=CARTESIAN_POINT('Ctrl Pts',(-21.1348507670562,4.39121714801795,133.019398996794));
#78473=CARTESIAN_POINT('Ctrl Pts',(-21.1426155200032,4.45276094175319,132.89739110522));
#78474=CARTESIAN_POINT('Ctrl Pts',(-21.1503802729504,4.50929678493063,132.772656133463));
#78475=CARTESIAN_POINT('Ctrl Pts',(-21.1581450258975,4.56057652336387,132.645644093037));
#78476=CARTESIAN_POINT('Ctrl Pts',(-21.1659020667825,4.61180533003799,132.51875820276));
#78477=CARTESIAN_POINT('Ctrl Pts',(-21.1736591076675,4.65778827545224,132.389600104719));
#78478=CARTESIAN_POINT('Ctrl Pts',(-21.1814161485524,4.69832361844659,132.258643340714));
#78479=CARTESIAN_POINT('Ctrl Pts',(-21.1891673397926,4.73882839342353,132.127785332223));
#78480=CARTESIAN_POINT('Ctrl Pts',(-21.1969185310327,4.77389362772621,131.995131729547));
#78481=CARTESIAN_POINT('Ctrl Pts',(-21.2046697222728,4.80336624335519,131.861174600581));
#78482=CARTESIAN_POINT('Ctrl Pts',(-21.2124176190499,4.83282633233631,131.727274406968));
#78483=CARTESIAN_POINT('Ctrl Pts',(-21.220165515827,4.85669844650645,131.59207217003));
#78484=CARTESIAN_POINT('Ctrl Pts',(-21.2279134126041,4.87487984536769,131.45607340379));
#78485=CARTESIAN_POINT('Ctrl Pts',(-21.2356596886882,4.89305744107224,131.32010308556));
#78486=CARTESIAN_POINT('Ctrl Pts',(-21.2434059647723,4.90554663741534,131.183336956711));
#78487=CARTESIAN_POINT('Ctrl Pts',(-21.2511522408564,4.9122961967945,131.046288576798));
#78488=CARTESIAN_POINT('Ctrl Pts',(-21.2588985741217,4.91904580599737,130.909239185226));
#78489=CARTESIAN_POINT('Ctrl Pts',(-21.2666449073871,4.92005567446114,130.771907928925));
#78490=CARTESIAN_POINT('Ctrl Pts',(-21.2743912406524,4.91532663835688,130.634810917598));
#78491=CARTESIAN_POINT('Ctrl Pts',(-21.2821393086554,4.91059654321776,130.497683204345));
#78492=CARTESIAN_POINT('Ctrl Pts',(-21.2898873766584,4.90012499961088,130.360790231109));
#78493=CARTESIAN_POINT('Ctrl Pts',(-21.2976354446614,4.88396488717058,130.224645132707));
#78494=CARTESIAN_POINT('Ctrl Pts',(-21.3053917474032,4.86778759957049,130.088355337675));
#78495=CARTESIAN_POINT('Ctrl Pts',(-21.3131480501451,4.8459097119998,129.952815394135));
#78496=CARTESIAN_POINT('Ctrl Pts',(-21.320904352887,4.81843572695672,129.81853091235));
#78497=CARTESIAN_POINT('Ctrl Pts',(-21.3286647954012,4.7909470782206,129.684174758893));
#78498=CARTESIAN_POINT('Ctrl Pts',(-21.3364252379153,4.75785647483153,129.551075781608));
#78499=CARTESIAN_POINT('Ctrl Pts',(-21.3441856804295,4.71931867102253,129.419725523457));
#78500=CARTESIAN_POINT('Ctrl Pts',(-21.3519585806949,4.68071900290958,129.288164410211));
#78501=CARTESIAN_POINT('Ctrl Pts',(-21.3597314809604,4.63665478616584,129.158357996207));
#78502=CARTESIAN_POINT('Ctrl Pts',(-21.3675043812258,4.58732971813785,129.030779742728));
#78503=CARTESIAN_POINT('Ctrl Pts',(-21.3749947169879,4.53979774057481,128.907839280114));
#78504=CARTESIAN_POINT('Ctrl Pts',(-21.3824850527499,4.48738088407196,128.786968074653));
#78505=CARTESIAN_POINT('Ctrl Pts',(-21.389975388512,4.43030135581073,128.668567331875));
#78506=CARTESIAN_POINT('Ctrl Pts',(-21.3977497226311,4.37105763988686,128.545677388949));
#78507=CARTESIAN_POINT('Ctrl Pts',(-21.4055240567502,4.30660303593,128.425059663547));
#78508=CARTESIAN_POINT('Ctrl Pts',(-21.4132983908692,4.23713465153532,128.307187614497));
#78509=CARTESIAN_POINT('Ctrl Pts',(-21.4210631438163,4.16775188071584,128.189460832212));
#78510=CARTESIAN_POINT('Ctrl Pts',(-21.4288278967634,4.09336782050057,128.074473327113));
#78511=CARTESIAN_POINT('Ctrl Pts',(-21.4365926497105,4.01422694492218,127.962677120559));
#78512=CARTESIAN_POINT('Ctrl Pts',(-21.4443496905955,3.93516467317721,127.850991951574));
#78513=CARTESIAN_POINT('Ctrl Pts',(-21.4521067314806,3.85135521254061,127.74249209044));
#78514=CARTESIAN_POINT('Ctrl Pts',(-21.4598637723656,3.76308792111388,127.637603228616));
#78515=CARTESIAN_POINT('Ctrl Pts',(-21.4676149636057,3.67488719273787,127.532793464299));
#78516=CARTESIAN_POINT('Ctrl Pts',(-21.4753661548458,3.58223557551724,127.43158957709));
#78517=CARTESIAN_POINT('Ctrl Pts',(-21.4831173460859,3.48546431771102,127.334386330563));
#78518=CARTESIAN_POINT('Ctrl Pts',(-21.490865242863,3.38873419027122,127.237224398008));
#78519=CARTESIAN_POINT('Ctrl Pts',(-21.4986131396401,3.28788818002643,127.144060000701));
#78520=CARTESIAN_POINT('Ctrl Pts',(-21.5063610364172,3.18329605649346,127.055252819808));
#78521=CARTESIAN_POINT('Ctrl Pts',(-21.5141073125013,3.07872581137784,126.966464215462));
#78522=CARTESIAN_POINT('Ctrl Pts',(-21.5218535885854,2.97041130944767,126.882031267525));
#78523=CARTESIAN_POINT('Ctrl Pts',(-21.5295998646695,2.858756927727,126.802274675126));
#78524=CARTESIAN_POINT('Ctrl Pts',(-21.5373461979348,2.7471017217992,126.722517493983));
#78525=CARTESIAN_POINT('Ctrl Pts',(-21.5450925312002,2.632106905022,126.64743696451));
#78526=CARTESIAN_POINT('Ctrl Pts',(-21.5528388644655,2.51420714707588,126.577311353115));
#78527=CARTESIAN_POINT('Ctrl Pts',(-21.5605869324685,2.39628098629643,126.507170037576));
#78528=CARTESIAN_POINT('Ctrl Pts',(-21.5683350004714,2.27544892580137,126.441986047951));
#78529=CARTESIAN_POINT('Ctrl Pts',(-21.5760830684744,2.15217126317994,126.38199225701));
#78530=CARTESIAN_POINT('Ctrl Pts',(-21.5838393712163,2.02876257959166,126.321934703955));
#78531=CARTESIAN_POINT('Ctrl Pts',(-21.5915956739581,1.90290345377174,126.267078540152));
#78532=CARTESIAN_POINT('Ctrl Pts',(-21.5993519767,1.77507575610665,126.217609139386));
#78533=CARTESIAN_POINT('Ctrl Pts',(-21.6071124192141,1.64717983295033,126.168113335313));
#78534=CARTESIAN_POINT('Ctrl Pts',(-21.6148728617283,1.51731361438653,126.124010148772));
#78535=CARTESIAN_POINT('Ctrl Pts',(-21.6226333042425,1.38597429787458,126.085435071625));
#78536=CARTESIAN_POINT('Ctrl Pts',(-21.6304062045079,1.25442414383201,126.04679807034));
#78537=CARTESIAN_POINT('Ctrl Pts',(-21.6381791047734,1.12139654594342,126.013707006383));
#78538=CARTESIAN_POINT('Ctrl Pts',(-21.6459520050388,0.987399943987629,
125.986246420796));
#78539=CARTESIAN_POINT('Ctrl Pts',(-21.6534423408008,0.858274456030554,
125.959784096665));
#78540=CARTESIAN_POINT('Ctrl Pts',(-21.6609326765628,0.728249496334088,
125.938550043569));
#78541=CARTESIAN_POINT('Ctrl Pts',(-21.6684230123248,0.597782718883282,
125.922574173701));
#78542=CARTESIAN_POINT('Ctrl Pts',(-21.6761973464439,0.462369253910339,
125.905992573872));
#78543=CARTESIAN_POINT('Ctrl Pts',(-21.683971680563,0.326050857628112,125.895023230798));
#78544=CARTESIAN_POINT('Ctrl Pts',(-21.6917460146821,0.189332405827244,
125.88975622834));
#78545=CARTESIAN_POINT('Ctrl Pts',(-21.6995107676292,0.052782447299527,
125.884495716991));
#78546=CARTESIAN_POINT('Ctrl Pts',(-21.7072755205762,-0.0841661988337974,
125.884923578284));
#78547=CARTESIAN_POINT('Ctrl Pts',(-21.7150402735233,-0.221001090013797,
125.891078457878));
#78548=CARTESIAN_POINT('Ctrl Pts',(-21.7227973144083,-0.357700074850843,
125.897227224358));
#78549=CARTESIAN_POINT('Ctrl Pts',(-21.7305543552934,-0.494285141532955,
125.909091671999));
#78550=CARTESIAN_POINT('Ctrl Pts',(-21.7383113961784,-0.630241738656434,
125.926658452268));
#78551=CARTESIAN_POINT('Ctrl Pts',(-21.7460625874186,-0.766095809853174,
125.944211985291));
#78552=CARTESIAN_POINT('Ctrl Pts',(-21.7538137786586,-0.901321968654677,
125.96745924181));
#78553=CARTESIAN_POINT('Ctrl Pts',(-21.7615649698988,-1.03540904151109,
125.996334912637));
#78554=CARTESIAN_POINT('Ctrl Pts',(-21.7693128666759,-1.16943912378393,
126.025198310534));
#78555=CARTESIAN_POINT('Ctrl Pts',(-21.777060763453,-1.30233070163004,126.059685282648));
#78556=CARTESIAN_POINT('Ctrl Pts',(-21.7848086602301,-1.43358129563961,
126.099679147871));
#78557=CARTESIAN_POINT('Ctrl Pts',(-21.7925549363142,-1.5648044348547,126.139664647239));
#78558=CARTESIAN_POINT('Ctrl Pts',(-21.8003012123983,-1.69438689924198,
126.18515463459));
#78559=CARTESIAN_POINT('Ctrl Pts',(-21.8080474884824,-1.82184029988104,
126.235982241793));
#78560=CARTESIAN_POINT('Ctrl Pts',(-21.8157938217477,-1.94929464135147,
126.286810224194));
#78561=CARTESIAN_POINT('Ctrl Pts',(-21.8235401550131,-2.07461952456006,
126.342975760247));
#78562=CARTESIAN_POINT('Ctrl Pts',(-21.8312864882784,-2.19734588651852,
126.40426355983));
#78563=CARTESIAN_POINT('Ctrl Pts',(-21.8390345562814,-2.32009973219481,
126.46556508439));
#78564=CARTESIAN_POINT('Ctrl Pts',(-21.8467826242843,-2.44025354895704,
126.531990980426));
#78565=CARTESIAN_POINT('Ctrl Pts',(-21.8545306922873,-2.55736261225882,
126.603279859961));
#78566=CARTESIAN_POINT('Ctrl Pts',(-21.8622869950291,-2.67459614046701,
126.674644506165));
#78567=CARTESIAN_POINT('Ctrl Pts',(-21.870043297771,-2.78877811646778,126.750882256761));
#78568=CARTESIAN_POINT('Ctrl Pts',(-21.8777996005128,-2.89949211733087,
126.831687899604));
#78569=CARTESIAN_POINT('Ctrl Pts',(-21.885560043027,-3.01026520958991,126.912536670852));
#78570=CARTESIAN_POINT('Ctrl Pts',(-21.8933204855411,-3.11756633278576,
126.997957948927));
#78571=CARTESIAN_POINT('Ctrl Pts',(-21.9010809280553,-3.22101274640848,
127.087606664185));
#78572=CARTESIAN_POINT('Ctrl Pts',(-21.9088538283207,-3.32462522139788,
127.177399291519));
#78573=CARTESIAN_POINT('Ctrl Pts',(-21.9166267285861,-3.42437033673121,
127.271432648797));
#78574=CARTESIAN_POINT('Ctrl Pts',(-21.9243996288516,-3.51990214151541,
127.369324667732));
#78575=CARTESIAN_POINT('Ctrl Pts',(-21.9318899646136,-3.61196112456562,
127.463658065203));
#78576=CARTESIAN_POINT('Ctrl Pts',(-21.9393803003756,-3.70010760156797,
127.561574221925));
#78577=CARTESIAN_POINT('Ctrl Pts',(-21.9468706361377,-3.78406903338846,
127.66270426891));
#78578=CARTESIAN_POINT('Ctrl Pts',(-21.9546076688493,-3.87079576569405,
127.767165071004));
#78579=CARTESIAN_POINT('Ctrl Pts',(-21.962344701561,-3.95334046479952,127.875396627304));
#78580=CARTESIAN_POINT('Ctrl Pts',(-21.9700817342727,-4.03135472329717,
127.987028163373));
#78581=CARTESIAN_POINT('Ctrl Pts',(-21.9778092501755,-4.10927302164879,
128.098522388921));
#78582=CARTESIAN_POINT('Ctrl Pts',(-21.9855367660781,-4.18267173935463,
128.213407955476));
#78583=CARTESIAN_POINT('Ctrl Pts',(-21.9932642819809,-4.25124137468817,
128.331279576306));
#78584=CARTESIAN_POINT('Ctrl Pts',(-22.0009824375401,-4.31972795159038,
128.449008419187));
#78585=CARTESIAN_POINT('Ctrl Pts',(-22.0087005930991,-4.38339689614496,
128.569715775096));
#78586=CARTESIAN_POINT('Ctrl Pts',(-22.0164187486583,-4.44198128320627,
128.692966447321));
#78587=CARTESIAN_POINT('Ctrl Pts',(-22.0241315180154,-4.50052478649122,
128.816131107672));
#78588=CARTESIAN_POINT('Ctrl Pts',(-22.0318442873726,-4.55399062093118,
128.941835199043));
#78589=CARTESIAN_POINT('Ctrl Pts',(-22.0395570567297,-4.60215720039006,
129.069617937686));
#78590=CARTESIAN_POINT('Ctrl Pts',(-22.0472658083821,-4.65029868910855,
129.197334112259));
#78591=CARTESIAN_POINT('Ctrl Pts',(-22.0549745600344,-4.69314627838737,
129.327126410124));
#78592=CARTESIAN_POINT('Ctrl Pts',(-22.0626833116868,-4.73052625149337,
129.458513506475));
#78593=CARTESIAN_POINT('Ctrl Pts',(-22.0650990812068,-4.74224039196137,
129.499687610532));
#78594=CARTESIAN_POINT('Ctrl Pts',(-22.0675148507268,-4.75341793402174,
129.541018199907));
#78595=CARTESIAN_POINT('Ctrl Pts',(-22.0699306202468,-4.76405452823405,
129.582490119308));
#78596=CARTESIAN_POINT('Origin',(213.235140564004,0.,130.804360617566));
#78597=CARTESIAN_POINT('',(-24.1652761364937,-4.76405452823408,129.582490119308));
#78598=CARTESIAN_POINT('',(-23.8197459990105,-4.76405452823405,129.582490119308));
#78599=CARTESIAN_POINT('',(213.235140564004,-4.76405452823405,129.582490119308));
#78600=CARTESIAN_POINT('',(-22.4851405640465,-4.91824999885107,130.804254309485));
#78601=CARTESIAN_POINT('Ctrl Pts',(-22.4851405640464,-4.91824999885107,
130.804254309485));
#78602=CARTESIAN_POINT('Ctrl Pts',(-22.4929100480016,-4.91825294584514,
130.940594401862));
#78603=CARTESIAN_POINT('Ctrl Pts',(-22.5006795319569,-4.91258231712604,
131.077151886514));
#78604=CARTESIAN_POINT('Ctrl Pts',(-22.5084490159121,-4.90120978706623,
131.213415241872));
#78605=CARTESIAN_POINT('Ctrl Pts',(-22.516208922518,-4.88985127578729,131.349510627033));
#78606=CARTESIAN_POINT('Ctrl Pts',(-22.523968829124,-4.87280488002072,131.485312217893));
#78607=CARTESIAN_POINT('Ctrl Pts',(-22.5317287357299,-4.85009425012328,
131.620307201247));
#78608=CARTESIAN_POINT('Ctrl Pts',(-22.5394809393304,-4.82740616432516,
131.755168179498));
#78609=CARTESIAN_POINT('Ctrl Pts',(-22.547233142931,-4.79906509809244,131.889223760036));
#78610=CARTESIAN_POINT('Ctrl Pts',(-22.5549853465315,-4.76514656917072,
132.021965330443));
#78611=CARTESIAN_POINT('Ctrl Pts',(-22.5627317147411,-4.73125357206994,
132.15460698101));
#78612=CARTESIAN_POINT('Ctrl Pts',(-22.5704780829507,-4.69179156525008,
132.285936212367));
#78613=CARTESIAN_POINT('Ctrl Pts',(-22.5782244511603,-4.64688723496165,
132.41545406242));
#78614=CARTESIAN_POINT('Ctrl Pts',(-22.5859675484736,-4.60200186548225,
132.544917223689));
#78615=CARTESIAN_POINT('Ctrl Pts',(-22.5937106457868,-4.55167887093173,
132.672570155688));
#78616=CARTESIAN_POINT('Ctrl Pts',(-22.6014537431001,-4.49609487543769,
132.797928758755));
#78617=CARTESIAN_POINT('Ctrl Pts',(-22.6091952422889,-4.44052235211583,
132.923261488628));
#78618=CARTESIAN_POINT('Ctrl Pts',(-22.6169367414778,-4.37969114618855,
133.046300473741));
#78619=CARTESIAN_POINT('Ctrl Pts',(-22.6246782406666,-4.31382598535281,
133.166581697523));
#78620=CARTESIAN_POINT('Ctrl Pts',(-22.6324198242689,-4.2479601063212,133.286864232856));
#78621=CARTESIAN_POINT('Ctrl Pts',(-22.6401614078713,-4.17706035102051,
133.404388603519));
#78622=CARTESIAN_POINT('Ctrl Pts',(-22.6479029914736,-4.10139715885603,
133.518715864734));
#78623=CARTESIAN_POINT('Ctrl Pts',(-22.6556463417301,-4.02571670010955,
133.633069215795));
#78624=CARTESIAN_POINT('Ctrl Pts',(-22.6633896919866,-3.94527085754286,
133.744223679236));
#78625=CARTESIAN_POINT('Ctrl Pts',(-22.671133042243,-3.86037286112385,133.851770080634));
#78626=CARTESIAN_POINT('Ctrl Pts',(-22.6788846293804,-3.77538455564472,
133.959430883018));
#78627=CARTESIAN_POINT('Ctrl Pts',(-22.6866362165177,-3.68593487914394,
134.063475649012));
#78628=CARTESIAN_POINT('Ctrl Pts',(-22.694387803655,-3.59237710244734,134.16352864199));
#78629=CARTESIAN_POINT('Ctrl Pts',(-22.7021435681625,-3.49876890698442,
134.26363555404));
#78630=CARTESIAN_POINT('Ctrl Pts',(-22.7098993326699,-3.40104847917913,
134.359746132506));
#78631=CARTESIAN_POINT('Ctrl Pts',(-22.7176550971774,-3.29960453595577,
134.451522934875));
#78632=CARTESIAN_POINT('Ctrl Pts',(-22.7254232328219,-3.19799878058225,
134.543446129442));
#78633=CARTESIAN_POINT('Ctrl Pts',(-22.7331913684666,-3.09265794297792,
134.631021484481));
#78634=CARTESIAN_POINT('Ctrl Pts',(-22.7409595041112,-2.98400294132002,
134.713952605062));
#78635=CARTESIAN_POINT('Ctrl Pts',(-22.7481811732131,-2.88299151410723,
134.791049754042));
#78636=CARTESIAN_POINT('Ctrl Pts',(-22.7554028423149,-2.77911632718114,
134.864133413423));
#78637=CARTESIAN_POINT('Ctrl Pts',(-22.7626245114168,-2.67273522412218,
134.933000767087));
#78638=CARTESIAN_POINT('Ctrl Pts',(-22.7703988455359,-2.55821291252541,
135.007138450457));
#78639=CARTESIAN_POINT('Ctrl Pts',(-22.778173179655,-2.44042216513535,135.076624934622));
#78640=CARTESIAN_POINT('Ctrl Pts',(-22.7859475137741,-2.31977760653852,
135.141158389967));
#78641=CARTESIAN_POINT('Ctrl Pts',(-22.7937122667212,-2.19928173157784,
135.205612313595));
#78642=CARTESIAN_POINT('Ctrl Pts',(-22.8014770196682,-2.07593938476042,
135.265125171237));
#78643=CARTESIAN_POINT('Ctrl Pts',(-22.8092417726153,-1.95019449299208,
135.319438081132));
#78644=CARTESIAN_POINT('Ctrl Pts',(-22.8169988135003,-1.8245744928231,135.37369704668));
#78645=CARTESIAN_POINT('Ctrl Pts',(-22.8247558543854,-1.69655705302487,
135.422766188367));
#78646=CARTESIAN_POINT('Ctrl Pts',(-22.8325128952704,-1.56661073779577,
135.466432459432));
#78647=CARTESIAN_POINT('Ctrl Pts',(-22.8402640865106,-1.43676241609329,
135.510065801424));
#78648=CARTESIAN_POINT('Ctrl Pts',(-22.8480152777506,-1.30498848331449,
135.548304258503));
#78649=CARTESIAN_POINT('Ctrl Pts',(-22.8557664689908,-1.17177719220194,
135.580982988482));
#78650=CARTESIAN_POINT('Ctrl Pts',(-22.8635143657679,-1.03862251944218,
135.613647829129));
#78651=CARTESIAN_POINT('Ctrl Pts',(-22.871262262545,-0.904032082325198,
135.640757549613));
#78652=CARTESIAN_POINT('Ctrl Pts',(-22.8790101593221,-0.768508783811016,
135.66219730808));
#78653=CARTESIAN_POINT('Ctrl Pts',(-22.8867564354062,-0.63301383384934,
135.683632581812));
#78654=CARTESIAN_POINT('Ctrl Pts',(-22.8945027114902,-0.496586796541796,
135.699400191562));
#78655=CARTESIAN_POINT('Ctrl Pts',(-22.9022489875743,-0.359739853991382,
135.709436590469));
#78656=CARTESIAN_POINT('Ctrl Pts',(-22.9099953208397,-0.22289190126774,
135.719473063462));
#78657=CARTESIAN_POINT('Ctrl Pts',(-22.9177416541051,-0.0856244270340815,
135.723778212596));
#78658=CARTESIAN_POINT('Ctrl Pts',(-22.9254879873704,0.0515465875682617,
135.722340488591));
#78659=CARTESIAN_POINT('Ctrl Pts',(-22.9332360553734,0.188748320668248,
135.720902442618));
#78660=CARTESIAN_POINT('Ctrl Pts',(-22.9409841233763,0.325853160283593,
135.713718968459));
#78661=CARTESIAN_POINT('Ctrl Pts',(-22.9487321913793,0.462346850400912,
135.700830616701));
#78662=CARTESIAN_POINT('Ctrl Pts',(-22.9564884941211,0.598985607636197,
135.687928567048));
#78663=CARTESIAN_POINT('Ctrl Pts',(-22.9642447968631,0.735011527998921,
135.669309564689));
#78664=CARTESIAN_POINT('Ctrl Pts',(-22.9720010996049,0.869916639057891,
135.645065948774));
#78665=CARTESIAN_POINT('Ctrl Pts',(-22.9797615421191,1.00489375303692,135.620809393312));
#78666=CARTESIAN_POINT('Ctrl Pts',(-22.9875219846333,1.13874848434594,135.59092232766));
#78667=CARTESIAN_POINT('Ctrl Pts',(-22.9952824271475,1.27098571789894,135.55554766581));
#78668=CARTESIAN_POINT('Ctrl Pts',(-23.0030553274129,1.40343523039835,135.520116217411));
#78669=CARTESIAN_POINT('Ctrl Pts',(-23.0108282276783,1.53426168306555,135.479179686094));
#78670=CARTESIAN_POINT('Ctrl Pts',(-23.0186011279437,1.66298686278692,135.432930348779));
#78671=CARTESIAN_POINT('Ctrl Pts',(-23.0260914637057,1.78703255798572,135.38836229137));
#78672=CARTESIAN_POINT('Ctrl Pts',(-23.0335817994677,1.9091268155518,135.33886110528));
#78673=CARTESIAN_POINT('Ctrl Pts',(-23.0410721352297,2.02886321313201,135.284639305873));
#78674=CARTESIAN_POINT('Ctrl Pts',(-23.0488464693488,2.15313945262027,135.228361670461));
#78675=CARTESIAN_POINT('Ctrl Pts',(-23.0566208034678,2.27526917587172,135.166820120668));
#78676=CARTESIAN_POINT('Ctrl Pts',(-23.0643951375869,2.39477433036429,135.10020034562));
#78677=CARTESIAN_POINT('Ctrl Pts',(-23.072159890534,2.51413220543427,135.033662673491));
#78678=CARTESIAN_POINT('Ctrl Pts',(-23.0799246434811,2.63087160931883,134.962059417115));
#78679=CARTESIAN_POINT('Ctrl Pts',(-23.0876893964281,2.74453478412558,134.885624132854));
#78680=CARTESIAN_POINT('Ctrl Pts',(-23.0954464373132,2.85808506706504,134.809264765196));
#78681=CARTESIAN_POINT('Ctrl Pts',(-23.1032034781982,2.9685648788877,134.728083137114));
#78682=CARTESIAN_POINT('Ctrl Pts',(-23.1109605190832,3.07554170692518,134.642358307959));
#78683=CARTESIAN_POINT('Ctrl Pts',(-23.1187117103234,3.18243786290462,134.556698124565));
#78684=CARTESIAN_POINT('Ctrl Pts',(-23.1264629015635,3.28583598923935,134.466501802965));
#78685=CARTESIAN_POINT('Ctrl Pts',(-23.1342140928037,3.38533348699316,134.372091022788));
#78686=CARTESIAN_POINT('Ctrl Pts',(-23.1419619895808,3.48478869565584,134.277720369711));
#78687=CARTESIAN_POINT('Ctrl Pts',(-23.1497098863579,3.58034629010211,134.179139089279));
#78688=CARTESIAN_POINT('Ctrl Pts',(-23.157457783135,3.67163781929383,134.076708213166));
#78689=CARTESIAN_POINT('Ctrl Pts',(-23.1652040592191,3.76291025226577,133.974298763385));
#78690=CARTESIAN_POINT('Ctrl Pts',(-23.1729503353032,3.84991813499068,133.868041611299));
#78691=CARTESIAN_POINT('Ctrl Pts',(-23.1806966113873,3.93233115675755,133.758333321586));
#78692=CARTESIAN_POINT('Ctrl Pts',(-23.1884429446526,4.0147447868785,133.648624222031));
#78693=CARTESIAN_POINT('Ctrl Pts',(-23.196189277918,4.09256325354067,133.535464246608));
#78694=CARTESIAN_POINT('Ctrl Pts',(-23.2039356111833,4.16549793959766,133.419281262195));
#78695=CARTESIAN_POINT('Ctrl Pts',(-23.2116836791863,4.2384489588721,133.303072259408));
#78696=CARTESIAN_POINT('Ctrl Pts',(-23.2194317471893,4.3065138133998,133.18383923158));
#78697=CARTESIAN_POINT('Ctrl Pts',(-23.2271798151923,4.36944865160021,133.062036755441));
#78698=CARTESIAN_POINT('Ctrl Pts',(-23.2349361179341,4.43245037769543,132.940104826181));
#78699=CARTESIAN_POINT('Ctrl Pts',(-23.242692420676,4.49031101626684,132.815598341356));
#78700=CARTESIAN_POINT('Ctrl Pts',(-23.2504487234178,4.54283368335113,132.688994584126));
#78701=CARTESIAN_POINT('Ctrl Pts',(-23.258209165932,4.59538438336426,132.562323254658));
#78702=CARTESIAN_POINT('Ctrl Pts',(-23.2659696084462,4.64259130044129,132.433552789228));
#78703=CARTESIAN_POINT('Ctrl Pts',(-23.2737300509604,4.68430705037323,132.303176990683));
#78704=CARTESIAN_POINT('Ctrl Pts',(-23.2815029512258,4.72608976613036,132.172591901332));
#78705=CARTESIAN_POINT('Ctrl Pts',(-23.2892758514912,4.76236359623064,132.040396706397));
#78706=CARTESIAN_POINT('Ctrl Pts',(-23.2970487517566,4.79303182282468,131.907097670489));
#78707=CARTESIAN_POINT('Ctrl Pts',(-23.3045390875186,4.82258518213326,131.778644390297));
#78708=CARTESIAN_POINT('Ctrl Pts',(-23.3120294232806,4.84693336086172,131.649166433302));
#78709=CARTESIAN_POINT('Ctrl Pts',(-23.3195197590426,4.86603547299593,131.519120603887));
#78710=CARTESIAN_POINT('Ctrl Pts',(-23.3272940931617,4.88586184751777,131.384144047322));
#78711=CARTESIAN_POINT('Ctrl Pts',(-23.3350684272807,4.9000992973312,131.248128141357));
#78712=CARTESIAN_POINT('Ctrl Pts',(-23.3428427613998,4.9086456488922,131.111575454629));
#78713=CARTESIAN_POINT('Ctrl Pts',(-23.3506075143469,4.91718146783871,130.975191056883));
#78714=CARTESIAN_POINT('Ctrl Pts',(-23.3583722672941,4.9200401196576,130.838271581084));
#78715=CARTESIAN_POINT('Ctrl Pts',(-23.3661370202412,4.91717067261028,130.701328394833));
#78716=CARTESIAN_POINT('Ctrl Pts',(-23.3738940611262,4.91430407553822,130.564521222484));
#78717=CARTESIAN_POINT('Ctrl Pts',(-23.3816511020111,4.90572070955883,130.427690774897));
#78718=CARTESIAN_POINT('Ctrl Pts',(-23.3894081428961,4.89142157154652,130.291351775625));
#78719=CARTESIAN_POINT('Ctrl Pts',(-23.3971593341362,4.87713321662544,130.155115590653));
#78720=CARTESIAN_POINT('Ctrl Pts',(-23.4049105253764,4.85713770969391,130.019370503589));
#78721=CARTESIAN_POINT('Ctrl Pts',(-23.4126617166165,4.83148807437643,129.884629108016));
#78722=CARTESIAN_POINT('Ctrl Pts',(-23.4204096133935,4.80584934083815,129.749944981131));
#78723=CARTESIAN_POINT('Ctrl Pts',(-23.4281575101706,4.77456133156568,129.616264080537));
#78724=CARTESIAN_POINT('Ctrl Pts',(-23.4359054069477,4.73772863594695,129.484091540965));
#78725=CARTESIAN_POINT('Ctrl Pts',(-23.4436516830318,4.70090364493413,129.35194664904));
#78726=CARTESIAN_POINT('Ctrl Pts',(-23.4513979591159,4.65853637942354,129.221309866934));
#78727=CARTESIAN_POINT('Ctrl Pts',(-23.4591442352,4.61078193950301,129.0926734473));
#78728=CARTESIAN_POINT('Ctrl Pts',(-23.4668905684654,4.56302714706993,128.964036078101));
#78729=CARTESIAN_POINT('Ctrl Pts',(-23.4746369017308,4.50988523694162,128.837399467362));
#78730=CARTESIAN_POINT('Ctrl Pts',(-23.4823832349961,4.45156018102447,128.713237709362));
#78731=CARTESIAN_POINT('Ctrl Pts',(-23.4901313029991,4.39322206361529,128.589048146196));
#78732=CARTESIAN_POINT('Ctrl Pts',(-23.4978793710021,4.32969865689708,128.467334892415));
#78733=CARTESIAN_POINT('Ctrl Pts',(-23.5056274390051,4.26124060141183,128.348548817085));
#78734=CARTESIAN_POINT('Ctrl Pts',(-23.513383741747,4.19270978789084,128.229636494502));
#78735=CARTESIAN_POINT('Ctrl Pts',(-23.5211400444888,4.11923404447307,128.113657904285));
#78736=CARTESIAN_POINT('Ctrl Pts',(-23.5288963472307,4.04110850240705,128.001036673696));
#78737=CARTESIAN_POINT('Ctrl Pts',(-23.5366567897449,3.96294126238692,127.888355333766));
#78738=CARTESIAN_POINT('Ctrl Pts',(-23.5444172322591,3.88011951462452,127.779035235501));
#78739=CARTESIAN_POINT('Ctrl Pts',(-23.5521776747732,3.79297904467585,127.673467289912));
#78740=CARTESIAN_POINT('Ctrl Pts',(-23.5599505750387,3.70569868910885,127.567729877285));
#78741=CARTESIAN_POINT('Ctrl Pts',(-23.5677234753041,3.61408601885497,127.465756944784));
#78742=CARTESIAN_POINT('Ctrl Pts',(-23.5754963755695,3.51851469030773,127.367903512263));
#78743=CARTESIAN_POINT('Ctrl Pts',(-23.5829867113315,3.42641762028361,127.273607298493));
#78744=CARTESIAN_POINT('Ctrl Pts',(-23.5904770470935,3.33064493339792,127.183136487722));
#78745=CARTESIAN_POINT('Ctrl Pts',(-23.5979673828554,3.23155885222512,127.096772392438));
#78746=CARTESIAN_POINT('Ctrl Pts',(-23.6057417169745,3.12871589216721,127.007133776232));
#78747=CARTESIAN_POINT('Ctrl Pts',(-23.6135160510936,3.02197754770216,126.921635486931));
#78748=CARTESIAN_POINT('Ctrl Pts',(-23.6212903852127,2.91171141675949,126.840635136656));
#78749=CARTESIAN_POINT('Ctrl Pts',(-23.6290551381598,2.8015811789686,126.759734612074));
#78750=CARTESIAN_POINT('Ctrl Pts',(-23.6368198911069,2.68793211735317,126.683321226224));
#78751=CARTESIAN_POINT('Ctrl Pts',(-23.644584644054,2.57116693010801,126.6117142361));
#78752=CARTESIAN_POINT('Ctrl Pts',(-23.652341684939,2.45451771569293,126.540178367048));
#78753=CARTESIAN_POINT('Ctrl Pts',(-23.660098725824,2.3347588659261,126.47343959675));
#78754=CARTESIAN_POINT('Ctrl Pts',(-23.667855766709,2.21232397114588,126.41177530716));
#78755=CARTESIAN_POINT('Ctrl Pts',(-23.6756069579492,2.08998140547188,126.350157519091));
#78756=CARTESIAN_POINT('Ctrl Pts',(-23.6833581491893,1.96496715930937,126.293606770058));
#78757=CARTESIAN_POINT('Ctrl Pts',(-23.6911093404294,1.83774115272297,126.242355519137));
#78758=CARTESIAN_POINT('Ctrl Pts',(-23.6988572372065,1.71056922058358,126.191126051366));
#78759=CARTESIAN_POINT('Ctrl Pts',(-23.7066051339836,1.58118775960948,126.14519174758));
#78760=CARTESIAN_POINT('Ctrl Pts',(-23.7143530307606,1.45007828707664,126.104737651428));
#78761=CARTESIAN_POINT('Ctrl Pts',(-23.7220993068447,1.31899623981923,126.064292017401));
#78762=CARTESIAN_POINT('Ctrl Pts',(-23.7298455829289,1.18618727332162,126.02932442607));
#78763=CARTESIAN_POINT('Ctrl Pts',(-23.737591859013,1.05214936906679,125.99997046192));
#78764=CARTESIAN_POINT('Ctrl Pts',(-23.7453381922783,0.918110475374609,
125.970616281085));
#78765=CARTESIAN_POINT('Ctrl Pts',(-23.7530845255436,0.782843007737389,
125.946875893757));
#78766=CARTESIAN_POINT('Ctrl Pts',(-23.7608308588089,0.646856086896882,
125.928833952133));
#78767=CARTESIAN_POINT('Ctrl Pts',(-23.7685789268119,0.510838712728319,
125.910787970142));
#78768=CARTESIAN_POINT('Ctrl Pts',(-23.7763269948149,0.374101952248003,
125.89844302461));
#78769=CARTESIAN_POINT('Ctrl Pts',(-23.7840750628178,0.237160611706851,
125.891831950295));
#78770=CARTESIAN_POINT('Ctrl Pts',(-23.7918313655597,0.100073728279162,
125.885213849653));
#78771=CARTESIAN_POINT('Ctrl Pts',(-23.7995876683015,-0.0372177784163698,
125.884341812584));
#78772=CARTESIAN_POINT('Ctrl Pts',(-23.8073439710434,-0.17419797311882,
125.889196517695));
#78773=CARTESIAN_POINT('Ctrl Pts',(-23.8151044135576,-0.311251278275576,
125.894053813908));
#78774=CARTESIAN_POINT('Ctrl Pts',(-23.8228648560717,-0.447992550750946,
125.90464391253));
#78775=CARTESIAN_POINT('Ctrl Pts',(-23.8306252985859,-0.583911405745882,
125.920895604613));
#78776=CARTESIAN_POINT('Ctrl Pts',(-23.8383981988513,-0.720048449753165,
125.937173385354));
#78777=CARTESIAN_POINT('Ctrl Pts',(-23.8461710991167,-0.855360051925455,
125.9591308586));
#78778=CARTESIAN_POINT('Ctrl Pts',(-23.8539439993822,-0.989345553597839,
125.986645553547));
#78779=CARTESIAN_POINT('Ctrl Pts',(-23.8614343351442,-1.11846034479641,
126.013160020027));
#78780=CARTESIAN_POINT('Ctrl Pts',(-23.8689246709063,-1.24634347680606,
126.044834610834));
#78781=CARTESIAN_POINT('Ctrl Pts',(-23.8764150066684,-1.37256248331411,
126.081516634128));
#78782=CARTESIAN_POINT('Ctrl Pts',(-23.8841893407875,-1.50356712181625,
126.119589467484));
#78783=CARTESIAN_POINT('Ctrl Pts',(-23.8919636749066,-1.63319393645424,
126.163177545891));
#78784=CARTESIAN_POINT('Ctrl Pts',(-23.8997380090257,-1.76094336236402,
126.212164896884));
#78785=CARTESIAN_POINT('Ctrl Pts',(-23.9075027619728,-1.88853534852383,
126.261091875346));
#78786=CARTESIAN_POINT('Ctrl Pts',(-23.9152675149198,-2.01425418801448,
126.31540474804));
#78787=CARTESIAN_POINT('Ctrl Pts',(-23.9230322678669,-2.13761361267586,
126.374937279771));
#78788=CARTESIAN_POINT('Ctrl Pts',(-23.9307893087519,-2.26085051501727,
126.434410682952));
#78789=CARTESIAN_POINT('Ctrl Pts',(-23.9385463496369,-2.38173231618071,
126.499093259477));
#78790=CARTESIAN_POINT('Ctrl Pts',(-23.9463033905219,-2.49979128070281,
126.568770149234));
#78791=CARTESIAN_POINT('Ctrl Pts',(-23.9540545817621,-2.61776121604219,
126.638394495108));
#78792=CARTESIAN_POINT('Ctrl Pts',(-23.9618057730022,-2.73291221649801,
126.713005459811));
#78793=CARTESIAN_POINT('Ctrl Pts',(-23.9695569642424,-2.84480010963653,
126.792341749376));
#78794=CARTESIAN_POINT('Ctrl Pts',(-23.9773048610195,-2.9566404474353,126.871644318901));
#78795=CARTESIAN_POINT('Ctrl Pts',(-23.9850527577966,-3.0652201181117,126.955667993089));
#78796=CARTESIAN_POINT('Ctrl Pts',(-23.9928006545737,-3.17012316735488,
127.044107678427));
#78797=CARTESIAN_POINT('Ctrl Pts',(-24.0005469306578,-3.2750042731416,127.132528864091));
#78798=CARTESIAN_POINT('Ctrl Pts',(-24.0082932067419,-3.37620998849391,
127.225363971705));
#78799=CARTESIAN_POINT('Ctrl Pts',(-24.016039482826,-3.47335707118877,127.322267322072));
#78800=CARTESIAN_POINT('Ctrl Pts',(-24.0237858160913,-3.5705048710016,127.419171387758));
#78801=CARTESIAN_POINT('Ctrl Pts',(-24.0315321493568,-3.66359370157296,
127.520143480014));
#78802=CARTESIAN_POINT('Ctrl Pts',(-24.0392784826221,-3.75227715041547,
127.62480101772));
#78803=CARTESIAN_POINT('Ctrl Pts',(-24.0470265506251,-3.84098045930134,
127.729481992757));
#78804=CARTESIAN_POINT('Ctrl Pts',(-24.0547746186282,-3.92527617062519,
127.837849757334));
#78805=CARTESIAN_POINT('Ctrl Pts',(-24.0625226866312,-4.0048583942221,127.949488938361));
#78806=CARTESIAN_POINT('Ctrl Pts',(-24.070278989373,-4.08452519875317,128.061246770837));
#78807=CARTESIAN_POINT('Ctrl Pts',(-24.0780352921148,-4.15946828113642,
128.176282646382));
#78808=CARTESIAN_POINT('Ctrl Pts',(-24.0857915948567,-4.22942502139845,
128.294152050361));
#78809=CARTESIAN_POINT('Ctrl Pts',(-24.0935520373709,-4.29941909967912,
128.41208436479));
#78810=CARTESIAN_POINT('Ctrl Pts',(-24.1013124798851,-4.36442134764529,
128.532852877021));
#78811=CARTESIAN_POINT('Ctrl Pts',(-24.1090729223993,-4.42421579995151,
128.655989695691));
#78812=CARTESIAN_POINT('Ctrl Pts',(-24.1168458226647,-4.48410623962088,
128.779324184513));
#78813=CARTESIAN_POINT('Ctrl Pts',(-24.12461872293,-4.53877202165465,128.905034218276));
#78814=CARTESIAN_POINT('Ctrl Pts',(-24.1323916231955,-4.58804556597105,
129.032632380202));
#78815=CARTESIAN_POINT('Ctrl Pts',(-24.1398819589574,-4.63552789283838,
129.15559202754));
#78816=CARTESIAN_POINT('Ctrl Pts',(-24.1473722947194,-4.67800311909113,
129.280304618362));
#78817=CARTESIAN_POINT('Ctrl Pts',(-24.1548626304813,-4.71536595009257,
129.406323772841));
#78818=CARTESIAN_POINT('Ctrl Pts',(-24.1583337991521,-4.73268061962758,
129.464723523514));
#78819=CARTESIAN_POINT('Ctrl Pts',(-24.1618049678229,-4.74891401369239,
129.5234574829));
#78820=CARTESIAN_POINT('Ctrl Pts',(-24.1652761364937,-4.76405452823407,
129.582490119308));
#78821=CARTESIAN_POINT('Ctrl Pts',(-22.4150500904691,-4.76405452823408,
129.582490119308));
#78822=CARTESIAN_POINT('Ctrl Pts',(-22.4228105212612,-4.79812496141817,
129.715330221202));
#78823=CARTESIAN_POINT('Ctrl Pts',(-22.4305709520533,-4.8266080734547,129.849491122361));
#78824=CARTESIAN_POINT('Ctrl Pts',(-22.4383313828454,-4.84942792020898,
129.984463118364));
#78825=CARTESIAN_POINT('Ctrl Pts',(-22.4461042768808,-4.87228441561213,
130.119651879245));
#78826=CARTESIAN_POINT('Ctrl Pts',(-22.4538771709163,-4.88945942155506,
130.255653949909));
#78827=CARTESIAN_POINT('Ctrl Pts',(-22.4616500649517,-4.90092891478267,
130.391954464912));
#78828=CARTESIAN_POINT('Ctrl Pts',(-22.4691590058357,-4.9120089251653,130.523626465707));
#78829=CARTESIAN_POINT('Ctrl Pts',(-22.4766679467197,-4.91776464845334,
130.655576656357));
#78830=CARTESIAN_POINT('Ctrl Pts',(-22.4841768876037,-4.91822056078252,
130.787343626173));
#78831=CARTESIAN_POINT('Ctrl Pts',(-22.484498113072,-4.91824006428557,130.792980493906));
#78832=CARTESIAN_POINT('Ctrl Pts',(-22.4848193385403,-4.91824987700829,
130.798617395189));
#78833=CARTESIAN_POINT('Ctrl Pts',(-22.4851405640086,-4.91824999885106,
130.80425430882));
#78834=CARTESIAN_POINT('',(-22.139859436035,-4.91824822085812,130.808543980559));
#78835=CARTESIAN_POINT('Ctrl Pts',(-22.0699306202468,-4.76405452823405,
129.582490119308));
#78836=CARTESIAN_POINT('Ctrl Pts',(-22.0776378832166,-4.79798948271468,
129.714801991793));
#78837=CARTESIAN_POINT('Ctrl Pts',(-22.0853451461864,-4.82641450282772,
129.848553263949));
#78838=CARTESIAN_POINT('Ctrl Pts',(-22.0930524091562,-4.84922153977913,
129.983243378286));
#78839=CARTESIAN_POINT('Ctrl Pts',(-22.1008535802954,-4.87230646618314,
130.11957460726));
#78840=CARTESIAN_POINT('Ctrl Pts',(-22.1086547514346,-4.88963550117929,
130.256867306196));
#78841=CARTESIAN_POINT('Ctrl Pts',(-22.1164559225737,-4.90115030148244,
130.394593873212));
#78842=CARTESIAN_POINT('Ctrl Pts',(-22.1242570937129,-4.91266510178558,
130.532320440228));
#78843=CARTESIAN_POINT('Ctrl Pts',(-22.132058264852,-4.91836565489243,130.670480456408));
#78844=CARTESIAN_POINT('Ctrl Pts',(-22.1398594359911,-4.91824822085878,
130.808543979782));
#78845=CARTESIAN_POINT('Ctrl Pts',(-22.139859436035,-4.91824822085812,130.808543980559));
#78846=CARTESIAN_POINT('Ctrl Pts',(-22.1491261022749,-4.91810872613641,
130.972543535006));
#78847=CARTESIAN_POINT('Ctrl Pts',(-22.1583927685146,-4.90976258893785,
131.136186978294));
#78848=CARTESIAN_POINT('Ctrl Pts',(-22.1676594347545,-4.89333921015692,
131.298743502424));
#78849=CARTESIAN_POINT('Ctrl Pts',(-22.1772692389539,-4.87630768551886,
131.467319377263));
#78850=CARTESIAN_POINT('Ctrl Pts',(-22.1868790431532,-4.85058951655298,
131.634726219696));
#78851=CARTESIAN_POINT('Ctrl Pts',(-22.1964888473526,-4.81638261423217,
131.800172635882));
#78852=CARTESIAN_POINT('Ctrl Pts',(-22.2060986515519,-4.78217571191136,
131.965619052067));
#78853=CARTESIAN_POINT('Ctrl Pts',(-22.2157084557512,-4.73948020609989,
132.129105063668));
#78854=CARTESIAN_POINT('Ctrl Pts',(-22.2253182599506,-4.68854620602673,
132.289863070089));
#78855=CARTESIAN_POINT('Ctrl Pts',(-22.2330925940696,-4.64734058660124,
132.41991633947));
#78856=CARTESIAN_POINT('Ctrl Pts',(-22.2408669281887,-4.60065437435307,
132.548459831092));
#78857=CARTESIAN_POINT('Ctrl Pts',(-22.2486412623078,-4.54861549652774,
132.674996906973));
#78858=CARTESIAN_POINT('Ctrl Pts',(-22.256406015255,-4.49664075196847,132.801378037217));
#78859=CARTESIAN_POINT('Ctrl Pts',(-22.264170768202,-4.43932661453742,132.925757313601));
#78860=CARTESIAN_POINT('Ctrl Pts',(-22.2719355211491,-4.37685094065176,
133.047652597183));
#78861=CARTESIAN_POINT('Ctrl Pts',(-22.2796925620342,-4.31443731848607,
133.169426812652));
#78862=CARTESIAN_POINT('Ctrl Pts',(-22.2874496029192,-4.24687253902505,
133.288721599357));
#78863=CARTESIAN_POINT('Ctrl Pts',(-22.2952066438042,-4.17438262486525,
133.405074512581));
#78864=CARTESIAN_POINT('Ctrl Pts',(-22.3029578350444,-4.1019473759137,133.521339683168));
#78865=CARTESIAN_POINT('Ctrl Pts',(-22.3107090262846,-4.02459459082052,
133.634667065552));
#78866=CARTESIAN_POINT('Ctrl Pts',(-22.3184602175247,-3.94259614722024,
133.744618885546));
#78867=CARTESIAN_POINT('Ctrl Pts',(-22.3262081143018,-3.86063255514586,
133.854523973083));
#78868=CARTESIAN_POINT('Ctrl Pts',(-22.3339560110789,-3.77402746499148,
133.961056038995));
#78869=CARTESIAN_POINT('Ctrl Pts',(-22.341703907856,-3.68309586416433,134.063806570159));
#78870=CARTESIAN_POINT('Ctrl Pts',(-22.3494501839402,-3.59218328426782,
134.166535608127));
#78871=CARTESIAN_POINT('Ctrl Pts',(-22.3571964600242,-3.49694625275671,
134.265484392125));
#78872=CARTESIAN_POINT('Ctrl Pts',(-22.3649427361083,-3.39773954603953,
134.360278085644));
#78873=CARTESIAN_POINT('Ctrl Pts',(-22.3726890693737,-3.29853210700111,
134.455072478907));
#78874=CARTESIAN_POINT('Ctrl Pts',(-22.3804354026391,-3.19535521695379,
134.545711450391));
#78875=CARTESIAN_POINT('Ctrl Pts',(-22.3881817359045,-3.08859965978725,
134.631857868259));
#78876=CARTESIAN_POINT('Ctrl Pts',(-22.3959298039074,-2.98182019545387,
134.718023578019));
#78877=CARTESIAN_POINT('Ctrl Pts',(-22.4036778719104,-2.8714607734729,134.799694486714));
#78878=CARTESIAN_POINT('Ctrl Pts',(-22.4114259399134,-2.75794398783813,
134.876574760075));
#78879=CARTESIAN_POINT('Ctrl Pts',(-22.4191822426552,-2.64430655521256,
134.953536742705));
#78880=CARTESIAN_POINT('Ctrl Pts',(-22.4269385453972,-2.52750537982127,
135.025697699508));
#78881=CARTESIAN_POINT('Ctrl Pts',(-22.4346948481391,-2.40799115044376,
135.092805753263));
#78882=CARTESIAN_POINT('Ctrl Pts',(-22.4424552906532,-2.28841313272353,
135.159949624607));
#78883=CARTESIAN_POINT('Ctrl Pts',(-22.4502157331673,-2.16611952412009,
135.222035042234));
#78884=CARTESIAN_POINT('Ctrl Pts',(-22.4579761756815,-2.04158326382754,
135.278857331092));
#78885=CARTESIAN_POINT('Ctrl Pts',(-22.4657490759469,-1.91684708687399,
135.335770836134));
#78886=CARTESIAN_POINT('Ctrl Pts',(-22.4735219762125,-1.78986142645664,
135.387404181583));
#78887=CARTESIAN_POINT('Ctrl Pts',(-22.481294876478,-1.66111758044659,135.433601532277));
#78888=CARTESIAN_POINT('Ctrl Pts',(-22.4887852122399,-1.53705389752832,
135.478119492907));
#78889=CARTESIAN_POINT('Ctrl Pts',(-22.4962755480017,-1.41135793253972,
135.517589729034));
#78890=CARTESIAN_POINT('Ctrl Pts',(-22.5037658837635,-1.28447846354116,
135.551917688229));
#78891=CARTESIAN_POINT('Ctrl Pts',(-22.5115402178826,-1.15278832090854,
135.58754720243));
#78892=CARTESIAN_POINT('Ctrl Pts',(-22.5193145520017,-1.0194060027721,135.617749666915));
#78893=CARTESIAN_POINT('Ctrl Pts',(-22.5270888861207,-0.884818492532877,
135.642364265536));
#78894=CARTESIAN_POINT('Ctrl Pts',(-22.5348536390678,-0.750396849371779,
135.666948528865));
#78895=CARTESIAN_POINT('Ctrl Pts',(-22.5426183920149,-0.614773350289618,
135.685958558841));
#78896=CARTESIAN_POINT('Ctrl Pts',(-22.550383144962,-0.478449768169881,
135.699283383232));
#78897=CARTESIAN_POINT('Ctrl Pts',(-22.5581401858469,-0.342261584553731,
135.71259497322));
#78898=CARTESIAN_POINT('Ctrl Pts',(-22.5658972267319,-0.205375088235683,
135.720232556877));
#78899=CARTESIAN_POINT('Ctrl Pts',(-22.5736542676169,-0.0683015177875444,
135.722136330749));
#78900=CARTESIAN_POINT('Ctrl Pts',(-22.581405458857,0.0686686844150285,
135.72403866897));
#78901=CARTESIAN_POINT('Ctrl Pts',(-22.5891566500972,0.205825290602621,
135.72021579848));
#78902=CARTESIAN_POINT('Ctrl Pts',(-22.5969078413373,0.34265303244978,135.710659829992));
#78903=CARTESIAN_POINT('Ctrl Pts',(-22.6046557381143,0.479422618856468,
135.701107923046));
#78904=CARTESIAN_POINT('Ctrl Pts',(-22.6124036348914,0.61586322972809,135.685827791731));
#78905=CARTESIAN_POINT('Ctrl Pts',(-22.6201515316685,0.751460913016745,
135.664863632554));
#78906=CARTESIAN_POINT('Ctrl Pts',(-22.6278978077526,0.887030232193389,
135.643903858627));
#78907=CARTESIAN_POINT('Ctrl Pts',(-22.6356440838367,1.02175658837179,135.617262481474));
#78908=CARTESIAN_POINT('Ctrl Pts',(-22.6433903599207,1.1551328556645,135.585035376244));
#78909=CARTESIAN_POINT('Ctrl Pts',(-22.6511366931861,1.28851010751034,135.552808033122));
#78910=CARTESIAN_POINT('Ctrl Pts',(-22.6588830264514,1.42053687055499,135.514994971471));
#78911=CARTESIAN_POINT('Ctrl Pts',(-22.6666293597168,1.55071827799797,135.471742740853));
#78912=CARTESIAN_POINT('Ctrl Pts',(-22.6743774277197,1.68092883866453,135.428480824199));
#78913=CARTESIAN_POINT('Ctrl Pts',(-22.6821254957227,1.8092928504486,135.379777438017));
#78914=CARTESIAN_POINT('Ctrl Pts',(-22.6898735637256,1.93533299722661,135.325828216957));
#78915=CARTESIAN_POINT('Ctrl Pts',(-22.6976298664675,2.0615071009725,135.271821658023));
#78916=CARTESIAN_POINT('Ctrl Pts',(-22.7053861692093,2.18535204596109,135.212558280967));
#78917=CARTESIAN_POINT('Ctrl Pts',(-22.7131424719511,2.30641231245985,135.148281117234));
#78918=CARTESIAN_POINT('Ctrl Pts',(-22.7209029144653,2.42753719246822,135.083969646842));
#78919=CARTESIAN_POINT('Ctrl Pts',(-22.7286633569794,2.54587409530542,135.014639255138));
#78920=CARTESIAN_POINT('Ctrl Pts',(-22.7364237994936,2.66099518686844,134.940577207393));
#78921=CARTESIAN_POINT('Ctrl Pts',(-22.744196699759,2.77630108102745,134.866396268675));
#78922=CARTESIAN_POINT('Ctrl Pts',(-22.7519696000244,2.88838052813893,134.787468720576));
#78923=CARTESIAN_POINT('Ctrl Pts',(-22.7597425002898,2.99683686116581,134.704123673196));
#78924=CARTESIAN_POINT('Ctrl Pts',(-22.767232836052,3.10135053330376,134.623808428221));
#78925=CARTESIAN_POINT('Ctrl Pts',(-22.7747231718141,3.20249970018748,134.539391479719));
#78926=CARTESIAN_POINT('Ctrl Pts',(-22.7822135075762,3.29996223667653,134.451199289486));
#78927=CARTESIAN_POINT('Ctrl Pts',(-22.7899878416953,3.40112009485836,134.359663265555));
#78928=CARTESIAN_POINT('Ctrl Pts',(-22.7977621758145,3.49862668460454,134.263770113513));
#78929=CARTESIAN_POINT('Ctrl Pts',(-22.8055365099335,3.59208348031357,134.163842621232));
#78930=CARTESIAN_POINT('Ctrl Pts',(-22.8133012628806,3.68542509887436,134.064038280655));
#78931=CARTESIAN_POINT('Ctrl Pts',(-22.8210660158277,3.77472658952797,133.960209775368));
#78932=CARTESIAN_POINT('Ctrl Pts',(-22.8288307687748,3.85962336769156,133.852719277906));
#78933=CARTESIAN_POINT('Ctrl Pts',(-22.8365878096598,3.94443582517813,133.745335541522));
#78934=CARTESIAN_POINT('Ctrl Pts',(-22.8443448505448,4.02485203551462,133.634297355867));
#78935=CARTESIAN_POINT('Ctrl Pts',(-22.8521018914298,4.10054534742606,133.520002515203));
#78936=CARTESIAN_POINT('Ctrl Pts',(-22.8598530826699,4.17618157842229,133.405793865168));
#78937=CARTESIAN_POINT('Ctrl Pts',(-22.8676042739101,4.24710178509104,133.288333773027));
#78938=CARTESIAN_POINT('Ctrl Pts',(-22.8753554651503,4.31302081483474,133.168051484262));
#78939=CARTESIAN_POINT('Ctrl Pts',(-22.8831033619274,4.37891182723236,133.047820318679));
#78940=CARTESIAN_POINT('Ctrl Pts',(-22.8908512587045,4.43980570292522,132.92476968434));
#78941=CARTESIAN_POINT('Ctrl Pts',(-22.8985991554815,4.49546182204881,132.799355872949));
#78942=CARTESIAN_POINT('Ctrl Pts',(-22.9063454315657,4.55110629911209,132.673968295424));
#78943=CARTESIAN_POINT('Ctrl Pts',(-22.9140917076498,4.60151504037863,132.546218881219));
#78944=CARTESIAN_POINT('Ctrl Pts',(-22.9218379837339,4.64649459439816,132.416586112566));
#78945=CARTESIAN_POINT('Ctrl Pts',(-22.9295843169993,4.69147448044653,132.286952386993));
#78946=CARTESIAN_POINT('Ctrl Pts',(-22.9373306502646,4.73102497111685,132.155435648594));
#78947=CARTESIAN_POINT('Ctrl Pts',(-22.94507698353,4.76500187511187,132.022531456439));
#78948=CARTESIAN_POINT('Ctrl Pts',(-22.9528250515329,4.79898638799897,131.889597501312));
#78949=CARTESIAN_POINT('Ctrl Pts',(-22.960573119536,4.82739473368754,131.755275852862));
#78950=CARTESIAN_POINT('Ctrl Pts',(-22.968321187539,4.85013350412361,131.620073835969));
#78951=CARTESIAN_POINT('Ctrl Pts',(-22.9760774902808,4.87289644159549,131.484728124763));
#78952=CARTESIAN_POINT('Ctrl Pts',(-22.9838337930227,4.88997770189924,131.348500562186));
#78953=CARTESIAN_POINT('Ctrl Pts',(-22.9915900957646,4.90133553473013,131.21190575432));
#78954=CARTESIAN_POINT('Ctrl Pts',(-22.9993505382788,4.91269942957839,131.075238041692));
#78955=CARTESIAN_POINT('Ctrl Pts',(-23.0071109807929,4.91833379402113,130.938203083654));
#78956=CARTESIAN_POINT('Ctrl Pts',(-23.0148714233071,4.91824905768622,130.801316103051));
#78957=CARTESIAN_POINT('Ctrl Pts',(-23.0226443235725,4.91816418532502,130.664209379315));
#78958=CARTESIAN_POINT('Ctrl Pts',(-23.030417223838,4.91234188262093,130.527251498545));
#78959=CARTESIAN_POINT('Ctrl Pts',(-23.0381901241034,4.9008446309997,130.390954080001));
#78960=CARTESIAN_POINT('Ctrl Pts',(-23.0456804598654,4.88976533343487,130.259611415936));
#78961=CARTESIAN_POINT('Ctrl Pts',(-23.0531707956273,4.87341655925481,130.128882334483));
#78962=CARTESIAN_POINT('Ctrl Pts',(-23.0606611313893,4.85189885350642,129.99921430922));
#78963=CARTESIAN_POINT('Ctrl Pts',(-23.0684354655083,4.82956529740414,129.864629881366));
#78964=CARTESIAN_POINT('Ctrl Pts',(-23.0762097996274,4.80159236624469,129.730762234883));
#78965=CARTESIAN_POINT('Ctrl Pts',(-23.0839841337465,4.76803621778487,129.598121135377));
#78966=CARTESIAN_POINT('Ctrl Pts',(-23.0917488866936,4.73452142427907,129.465643504171));
#78967=CARTESIAN_POINT('Ctrl Pts',(-23.0995136396408,4.69543719921333,129.334389787675));
#78968=CARTESIAN_POINT('Ctrl Pts',(-23.1072783925879,4.65089118172614,129.204862484325));
#78969=CARTESIAN_POINT('Ctrl Pts',(-23.1150354334729,4.60638940797152,129.075463829319));
#78970=CARTESIAN_POINT('Ctrl Pts',(-23.1227924743578,4.55643676357715,128.947788542452));
#78971=CARTESIAN_POINT('Ctrl Pts',(-23.1305495152428,4.5011913611288,128.82232646221));
#78972=CARTESIAN_POINT('Ctrl Pts',(-23.138300706483,4.44598761966818,128.696958993898));
#78973=CARTESIAN_POINT('Ctrl Pts',(-23.1460518977231,4.38549922153395,128.573801766538));
#78974=CARTESIAN_POINT('Ctrl Pts',(-23.1538030889632,4.31993317116313,128.453326704756));
#78975=CARTESIAN_POINT('Ctrl Pts',(-23.1615509857403,4.25439498811275,128.332902848088));
#78976=CARTESIAN_POINT('Ctrl Pts',(-23.1692988825174,4.18378363169591,128.215159232324));
#78977=CARTESIAN_POINT('Ctrl Pts',(-23.1770467792945,4.10835293213205,128.100544934584));
#78978=CARTESIAN_POINT('Ctrl Pts',(-23.1847930553786,4.03293801104444,127.985954611683));
#78979=CARTESIAN_POINT('Ctrl Pts',(-23.1925393314627,3.9527059667789,127.874492631175));
#78980=CARTESIAN_POINT('Ctrl Pts',(-23.2002856075468,3.8679547947545,127.766580380578));
#78981=CARTESIAN_POINT('Ctrl Pts',(-23.2080319408121,3.7832029971162,127.658667333397));
#78982=CARTESIAN_POINT('Ctrl Pts',(-23.2157782740776,3.69393224663472,127.554304375888));
#78983=CARTESIAN_POINT('Ctrl Pts',(-23.2235246073429,3.60048153227411,127.453880682056));
#78984=CARTESIAN_POINT('Ctrl Pts',(-23.2312726753459,3.50700989027408,127.353434499035));
#78985=CARTESIAN_POINT('Ctrl Pts',(-23.2390207433488,3.40935668800406,127.256929621265));
#78986=CARTESIAN_POINT('Ctrl Pts',(-23.2467688113518,3.30789826291805,127.164718857079));
#78987=CARTESIAN_POINT('Ctrl Pts',(-23.2545251140936,3.20633200661035,127.072410090194));
#78988=CARTESIAN_POINT('Ctrl Pts',(-23.2622814168355,3.10095273847587,126.984404817018));
#78989=CARTESIAN_POINT('Ctrl Pts',(-23.2700377195774,2.99217084412811,126.901016320422));
#78990=CARTESIAN_POINT('Ctrl Pts',(-23.2777981620916,2.88333088960783,126.817583316874));
#78991=CARTESIAN_POINT('Ctrl Pts',(-23.2855586046057,2.77108500998726,126.73877222441));
#78992=CARTESIAN_POINT('Ctrl Pts',(-23.2933190471199,2.65587231430665,126.664852758822));
#78993=CARTESIAN_POINT('Ctrl Pts',(-23.3010919473853,2.54047466897883,126.590814631146));
#78994=CARTESIAN_POINT('Ctrl Pts',(-23.3088648476508,2.42210102820884,126.521684019369));
#78995=CARTESIAN_POINT('Ctrl Pts',(-23.3166377479162,2.30121560450737,126.457684898804));
#78996=CARTESIAN_POINT('Ctrl Pts',(-23.3241280836782,2.18472467045093,126.396012307477));
#78997=CARTESIAN_POINT('Ctrl Pts',(-23.3316184194401,2.06590167999925,126.339104732456));
#78998=CARTESIAN_POINT('Ctrl Pts',(-23.3391087552021,1.94517745240033,126.287119452743));
#78999=CARTESIAN_POINT('Ctrl Pts',(-23.3468830893211,1.81987592901743,126.233163135348));
#79000=CARTESIAN_POINT('Ctrl Pts',(-23.3546574234402,1.6921292341346,126.184338821745));
#79001=CARTESIAN_POINT('Ctrl Pts',(-23.3624317575593,1.5623966026319,126.140874805581));
#79002=CARTESIAN_POINT('Ctrl Pts',(-23.3701965105064,1.43282385500317,126.097464354933));
#79003=CARTESIAN_POINT('Ctrl Pts',(-23.3779612634534,1.30127040768345,126.059401180587));
#79004=CARTESIAN_POINT('Ctrl Pts',(-23.3857260164005,1.16821720842277,126.026866335367));
#79005=CARTESIAN_POINT('Ctrl Pts',(-23.3934830572855,1.03529615947513,125.994363804214));
#79006=CARTESIAN_POINT('Ctrl Pts',(-23.4012400981705,0.900878700226168,
125.967378767481));
#79007=CARTESIAN_POINT('Ctrl Pts',(-23.4089971390555,0.765462409380287,
125.946042970239));
#79008=CARTESIAN_POINT('Ctrl Pts',(-23.4167483302956,0.630148237012718,
125.924723262488));
#79009=CARTESIAN_POINT('Ctrl Pts',(-23.4244995215357,0.493837116938609,
125.909044375288));
#79010=CARTESIAN_POINT('Ctrl Pts',(-23.4322507127758,0.357037983664662,
125.899087236732));
#79011=CARTESIAN_POINT('Ctrl Pts',(-23.4399986095529,0.220296993671779,
125.889134330225));
#79012=CARTESIAN_POINT('Ctrl Pts',(-23.4477465063301,0.0830687921361914,
125.884898363828));
#79013=CARTESIAN_POINT('Ctrl Pts',(-23.4554944031071,-0.0541315982100819,
125.88640852014));
#79014=CARTESIAN_POINT('Ctrl Pts',(-23.4632406791912,-0.19130328919258,
125.887918360561));
#79015=CARTESIAN_POINT('Ctrl Pts',(-23.4709869552753,-0.328446789863249,
125.895171928616));
#79016=CARTESIAN_POINT('Ctrl Pts',(-23.4787332313594,-0.465046501165917,
125.908146282567));
#79017=CARTESIAN_POINT('Ctrl Pts',(-23.4864795646247,-0.601647220816437,
125.921120732291));
#79018=CARTESIAN_POINT('Ctrl Pts',(-23.49422589789,-0.737703753875519,125.93981601521));
#79019=CARTESIAN_POINT('Ctrl Pts',(-23.5019722311554,-0.872705445415273,
125.964157288361));
#79020=CARTESIAN_POINT('Ctrl Pts',(-23.5097202991583,-1.00773736964763,
125.988504012573));
#79021=CARTESIAN_POINT('Ctrl Pts',(-23.5174683671613,-1.14171359761394,
126.018499173628));
#79022=CARTESIAN_POINT('Ctrl Pts',(-23.5252164351643,-1.27413388208736,
126.054016849688));
#79023=CARTESIAN_POINT('Ctrl Pts',(-23.5329727379061,-1.40669490441529,
126.089572274357));
#79024=CARTESIAN_POINT('Ctrl Pts',(-23.540729040648,-1.53769630163585,126.130661837334));
#79025=CARTESIAN_POINT('Ctrl Pts',(-23.5484853433898,-1.66665267654765,
126.177109606625));
#79026=CARTESIAN_POINT('Ctrl Pts',(-23.556245785904,-1.79567787935972,126.223582166488));
#79027=CARTESIAN_POINT('Ctrl Pts',(-23.5640062284182,-1.9226555231884,126.275418483437));
#79028=CARTESIAN_POINT('Ctrl Pts',(-23.5717666709324,-2.04712133933738,
126.332394910572));
#79029=CARTESIAN_POINT('Ctrl Pts',(-23.5795395711978,-2.17178695906383,
126.389462801326));
#79030=CARTESIAN_POINT('Ctrl Pts',(-23.5873124714632,-2.29393234490585,
126.451687113547));
#79031=CARTESIAN_POINT('Ctrl Pts',(-23.5950853717286,-2.4131181418871,126.518798356229));
#79032=CARTESIAN_POINT('Ctrl Pts',(-23.6025757074908,-2.52797123493895,
126.583469936198));
#79033=CARTESIAN_POINT('Ctrl Pts',(-23.6100660432529,-2.64007591826598,
126.652679148965));
#79034=CARTESIAN_POINT('Ctrl Pts',(-23.617556379015,-2.74906700026126,126.726148547237));
#79035=CARTESIAN_POINT('Ctrl Pts',(-23.6253031721824,-2.86178976678577,
126.802133423033));
#79036=CARTESIAN_POINT('Ctrl Pts',(-23.6330499653498,-2.97154496364008,
126.882920231638));
#79037=CARTESIAN_POINT('Ctrl Pts',(-23.6407967585171,-3.07789393071905,
126.968249042841));
#79038=CARTESIAN_POINT('Ctrl Pts',(-23.6485312997414,-3.18407470155647,
127.053442902235));
#79039=CARTESIAN_POINT('Ctrl Pts',(-23.6562658409657,-3.28685966616888,
127.143164214412));
#79040=CARTESIAN_POINT('Ctrl Pts',(-23.6640003821899,-3.38583845623077,
127.237109433418));
#79041=CARTESIAN_POINT('Ctrl Pts',(-23.6717278517343,-3.48472675012762,
127.330968758445));
#79042=CARTESIAN_POINT('Ctrl Pts',(-23.6794553212787,-3.57981550709763,
127.429044039738));
#79043=CARTESIAN_POINT('Ctrl Pts',(-23.6871827908231,-3.67072663227632,
127.530990938841));
#79044=CARTESIAN_POINT('Ctrl Pts',(-23.6949049018569,-3.76157471634971,
127.632867144228));
#79045=CARTESIAN_POINT('Ctrl Pts',(-23.7026270128907,-3.84825067058314,
127.738609333425));
#79046=CARTESIAN_POINT('Ctrl Pts',(-23.7103491239246,-3.930412875896,127.847836021441));
#79047=CARTESIAN_POINT('Ctrl Pts',(-23.7180675854749,-4.01253625120348,
127.957011088729));
#79048=CARTESIAN_POINT('Ctrl Pts',(-23.7257860470253,-4.09014988648217,
128.069667063224));
#79049=CARTESIAN_POINT('Ctrl Pts',(-23.7335045085756,-4.16295241656001,
128.18538939971));
#79050=CARTESIAN_POINT('Ctrl Pts',(-23.7412225938894,-4.23575139787648,
128.301106095307));
#79051=CARTESIAN_POINT('Ctrl Pts',(-23.748940679203,-4.30373952188243,128.419888527669));
#79052=CARTESIAN_POINT('Ctrl Pts',(-23.7566587645167,-4.3666588322444,128.541293295262));
#79053=CARTESIAN_POINT('Ctrl Pts',(-23.7643764315985,-4.42957473309934,
128.662691484104));
#79054=CARTESIAN_POINT('Ctrl Pts',(-23.7720940986803,-4.48742219024157,
128.786711372921));
#79055=CARTESIAN_POINT('Ctrl Pts',(-23.779811765762,-4.53998965728447,128.91288580297));
#79056=CARTESIAN_POINT('Ctrl Pts',(-23.7875336500506,-4.59258584905459,
129.0391291792));
#79057=CARTESIAN_POINT('Ctrl Pts',(-23.7952555343392,-4.63989613882725,
129.167529082938));
#79058=CARTESIAN_POINT('Ctrl Pts',(-23.8029774186278,-4.6817574591316,129.29759913798));
#79059=CARTESIAN_POINT('Ctrl Pts',(-23.8085669454221,-4.71205899729742,
129.391751035445));
#79060=CARTESIAN_POINT('Ctrl Pts',(-23.8141564722163,-4.73950647488403,
129.486777631865));
#79061=CARTESIAN_POINT('Ctrl Pts',(-23.8197459990105,-4.76405452823405,
129.582490119308));
#79062=CARTESIAN_POINT('Origin',(213.235140564004,0.,130.804360617566));
#79063=CARTESIAN_POINT('',(-25.9153671414536,-4.76405452823411,129.582490119308));
#79064=CARTESIAN_POINT('',(-25.5699526237868,-4.76405452823406,129.582490119308));
#79065=CARTESIAN_POINT('',(213.235140564004,-4.76405452823405,129.582490119308));
#79066=CARTESIAN_POINT('',(-24.2351405639732,-4.91824806745606,130.800000633076));
#79067=CARTESIAN_POINT('Ctrl Pts',(-24.2351405640086,-4.91824806745661,
130.800000633701));
#79068=CARTESIAN_POINT('Ctrl Pts',(-24.2428327878828,-4.91836867782199,
130.936054278564));
#79069=CARTESIAN_POINT('Ctrl Pts',(-24.250525011757,-4.9128395587903,131.072219580756));
#79070=CARTESIAN_POINT('Ctrl Pts',(-24.2582172356313,-4.90165976709171,
131.207987413226));
#79071=CARTESIAN_POINT('Ctrl Pts',(-24.2659066851318,-4.8904840076367,131.34370627797));
#79072=CARTESIAN_POINT('Ctrl Pts',(-24.2735961346324,-4.87366165881892,
131.479027562654));
#79073=CARTESIAN_POINT('Ctrl Pts',(-24.2812855841329,-4.85124384364944,
131.613444192948));
#79074=CARTESIAN_POINT('Ctrl Pts',(-24.288973822721,-4.82882955877303,131.747839655698));
#79075=CARTESIAN_POINT('Ctrl Pts',(-24.2966620613091,-4.80082162501622,
131.88133035557));
#79076=CARTESIAN_POINT('Ctrl Pts',(-24.3043502998972,-4.76732272740965,
132.013416892197));
#79077=CARTESIAN_POINT('Ctrl Pts',(-24.3120390541298,-4.73382158305711,
132.145512287768));
#79078=CARTESIAN_POINT('Ctrl Pts',(-24.3197278083623,-4.69482883996834,
132.276202947606));
#79079=CARTESIAN_POINT('Ctrl Pts',(-24.3274165625948,-4.65049762531464,
132.40500264483));
#79080=CARTESIAN_POINT('Ctrl Pts',(-24.3351075590924,-4.60615348238504,
132.533839903803));
#79081=CARTESIAN_POINT('Ctrl Pts',(-24.3427985555901,-4.5564679003707,132.66078472772));
#79082=CARTESIAN_POINT('Ctrl Pts',(-24.3504895520877,-4.5016427275876,132.785369404941));
#79083=CARTESIAN_POINT('Ctrl Pts',(-24.358189014574,-4.44675720510963,132.910091220759));
#79084=CARTESIAN_POINT('Ctrl Pts',(-24.3658884770604,-4.38672095606205,
133.032447338702));
#79085=CARTESIAN_POINT('Ctrl Pts',(-24.3735879395467,-4.32178269779036,
133.151992908957));
#79086=CARTESIAN_POINT('Ctrl Pts',(-24.3812920853721,-4.25680493963322,
133.271611194995));
#79087=CARTESIAN_POINT('Ctrl Pts',(-24.3889962311975,-4.1869194381364,133.388415188816));
#79088=CARTESIAN_POINT('Ctrl Pts',(-24.396700377023,-4.11241846104265,133.501988735705));
#79089=CARTESIAN_POINT('Ctrl Pts',(-24.4044162002136,-4.03780456096723,
133.615734428841));
#79090=CARTESIAN_POINT('Ctrl Pts',(-24.4121320234043,-3.9585614471088,133.726239575841));
#79091=CARTESIAN_POINT('Ctrl Pts',(-24.4198478465949,-3.87502221888228,
133.83312040759));
#79092=CARTESIAN_POINT('Ctrl Pts',(-24.4243353158279,-3.8264363833653,133.895281557765));
#79093=CARTESIAN_POINT('Ctrl Pts',(-24.4288227850611,-3.7763981025758,133.956217445617));
#79094=CARTESIAN_POINT('Ctrl Pts',(-24.4333102542941,-3.72497846716922,
134.01585847396));
#79095=CARTESIAN_POINT('Ctrl Pts',(-24.4410845884132,-3.63589631302594,
134.11918381336));
#79096=CARTESIAN_POINT('Ctrl Pts',(-24.4488589225323,-3.5423706651416,134.21896349486));
#79097=CARTESIAN_POINT('Ctrl Pts',(-24.4566332566513,-3.44471465491814,
134.314791361605));
#79098=CARTESIAN_POINT('Ctrl Pts',(-24.4643980095984,-3.34717899699938,
134.410501129069));
#79099=CARTESIAN_POINT('Ctrl Pts',(-24.4721627625455,-3.24552338130106,
134.502268500939));
#79100=CARTESIAN_POINT('Ctrl Pts',(-24.4799275154926,-3.14010112703675,
134.589720306484));
#79101=CARTESIAN_POINT('Ctrl Pts',(-24.4876845563776,-3.034783579642,134.677085253661));
#79102=CARTESIAN_POINT('Ctrl Pts',(-24.4954415972625,-2.92570713755785,
134.760142916406));
#79103=CARTESIAN_POINT('Ctrl Pts',(-24.5031986381475,-2.81326164176152,
134.838557191544));
#79104=CARTESIAN_POINT('Ctrl Pts',(-24.5109498293877,-2.70090094198781,
134.916912333867));
#79105=CARTESIAN_POINT('Ctrl Pts',(-24.5187010206279,-2.58517656486285,
134.990630835607));
#79106=CARTESIAN_POINT('Ctrl Pts',(-24.526452211868,-2.46651078938088,135.059417325574));
#79107=CARTESIAN_POINT('Ctrl Pts',(-24.5342001086451,-2.34789545001916,
135.128174579449));
#79108=CARTESIAN_POINT('Ctrl Pts',(-24.5419480054221,-2.22634153633676,
135.192003795146));
#79109=CARTESIAN_POINT('Ctrl Pts',(-24.5496959021992,-2.10229943442395,
135.250653472352));
#79110=CARTESIAN_POINT('Ctrl Pts',(-24.5574421782833,-1.97828327944482,
135.30929088131));
#79111=CARTESIAN_POINT('Ctrl Pts',(-24.5651884543674,-1.85178032471338,
135.362750739801));
#79112=CARTESIAN_POINT('Ctrl Pts',(-24.5729347304515,-1.72326427236933,
135.410828169832));
#79113=CARTESIAN_POINT('Ctrl Pts',(-24.5806810637168,-1.59474727134916,
135.458905954758));
#79114=CARTESIAN_POINT('Ctrl Pts',(-24.5884273969821,-1.46421750924465,
135.501601094955));
#79115=CARTESIAN_POINT('Ctrl Pts',(-24.5961737302475,-1.33216694222551,
135.538757548595));
#79116=CARTESIAN_POINT('Ctrl Pts',(-24.6039217982504,-1.20008680339781,
135.575922323166));
#79117=CARTESIAN_POINT('Ctrl Pts',(-24.6116698662534,-1.06648555823141,
135.607545837151));
#79118=CARTESIAN_POINT('Ctrl Pts',(-24.6194179342563,-0.931868143972421,
135.633522534995));
#79119=CARTESIAN_POINT('Ctrl Pts',(-24.6271742369982,-0.79710765672322,
135.659526841184));
#79120=CARTESIAN_POINT('Ctrl Pts',(-24.63493053974,-0.661329227467334,135.679872268388));
#79121=CARTESIAN_POINT('Ctrl Pts',(-24.6426868424819,-0.525046312202897,
135.694504729199));
#79122=CARTESIAN_POINT('Ctrl Pts',(-24.650447284996,-0.388690658642998,
135.709144999796));
#79123=CARTESIAN_POINT('Ctrl Pts',(-24.6582077275102,-0.251830372498786,
135.718066202827));
#79124=CARTESIAN_POINT('Ctrl Pts',(-24.6659681700243,-0.114980778526438,
135.72126640099));
#79125=CARTESIAN_POINT('Ctrl Pts',(-24.6737410702898,0.0220884985630899,
135.724471736395));
#79126=CARTESIAN_POINT('Ctrl Pts',(-24.6815139705552,0.159146658058194,
135.721937721875));
#79127=CARTESIAN_POINT('Ctrl Pts',(-24.6892868708206,0.29568072864988,135.713714543411));
#79128=CARTESIAN_POINT('Ctrl Pts',(-24.6967772065827,0.427251441869022,
135.705790298196));
#79129=CARTESIAN_POINT('Ctrl Pts',(-24.7042675423449,0.558335202081555,
135.692583369554));
#79130=CARTESIAN_POINT('Ctrl Pts',(-24.711757878107,0.688482251766975,135.674183535445));
#79131=CARTESIAN_POINT('Ctrl Pts',(-24.719532212226,0.82356386639702,135.655086066034));
#79132=CARTESIAN_POINT('Ctrl Pts',(-24.7273065463451,0.958064235523123,
135.63033364479));
#79133=CARTESIAN_POINT('Ctrl Pts',(-24.7350808804642,1.09147239270891,135.599970180328));
#79134=CARTESIAN_POINT('Ctrl Pts',(-24.7428456334113,1.2247161362638,135.569644136123));
#79135=CARTESIAN_POINT('Ctrl Pts',(-24.7506103863585,1.35686996856732,135.533720893638));
#79136=CARTESIAN_POINT('Ctrl Pts',(-24.7583751393056,1.48742895284718,135.492296002438));
#79137=CARTESIAN_POINT('Ctrl Pts',(-24.7661321801906,1.61785826410365,135.450912255023));
#79138=CARTESIAN_POINT('Ctrl Pts',(-24.7738892210757,1.74669550937336,135.404037850602));
#79139=CARTESIAN_POINT('Ctrl Pts',(-24.7816462619608,1.8734471969674,135.351819101453));
#79140=CARTESIAN_POINT('Ctrl Pts',(-24.7893974532009,2.00010330012767,135.299639730869));
#79141=CARTESIAN_POINT('Ctrl Pts',(-24.797148644441,2.12467661601915,135.242124185774));
#79142=CARTESIAN_POINT('Ctrl Pts',(-24.8048998356812,2.24669038838435,135.179468086102));
#79143=CARTESIAN_POINT('Ctrl Pts',(-24.8126477324583,2.36865230164146,135.116838616944));
#79144=CARTESIAN_POINT('Ctrl Pts',(-24.8203956292353,2.48805648801008,135.049073116977));
#79145=CARTESIAN_POINT('Ctrl Pts',(-24.8281435260124,2.60444790846954,134.97641456671));
#79146=CARTESIAN_POINT('Ctrl Pts',(-24.8358898020966,2.72081498235294,134.903771215046));
#79147=CARTESIAN_POINT('Ctrl Pts',(-24.8436360781807,2.8341702124029,134.826237055824));
#79148=CARTESIAN_POINT('Ctrl Pts',(-24.8513823542648,2.94408518138219,134.744099886511));
#79149=CARTESIAN_POINT('Ctrl Pts',(-24.8591286875302,3.05400096172865,134.66196211088));
#79150=CARTESIAN_POINT('Ctrl Pts',(-24.8668750207955,3.16047611714944,134.575221491389));
#79151=CARTESIAN_POINT('Ctrl Pts',(-24.8746213540609,3.26311345091137,134.484207580278));
#79152=CARTESIAN_POINT('Ctrl Pts',(-24.8823694220639,3.36577376959242,134.393173287233));
#79153=CARTESIAN_POINT('Ctrl Pts',(-24.8901174900669,3.4645942639364,134.297864057646));
#79154=CARTESIAN_POINT('Ctrl Pts',(-24.8978655580699,3.55921319615178,134.198647654167));
#79155=CARTESIAN_POINT('Ctrl Pts',(-24.9056218608118,3.65393269049443,134.099325802314));
#79156=CARTESIAN_POINT('Ctrl Pts',(-24.9133781635536,3.74444143219922,133.996088764704));
#79157=CARTESIAN_POINT('Ctrl Pts',(-24.9211344662955,3.83041638048846,133.889339290845));
#79158=CARTESIAN_POINT('Ctrl Pts',(-24.9288949088097,3.91643721619638,133.782532841577));
#79159=CARTESIAN_POINT('Ctrl Pts',(-24.9366553513239,3.99791920462755,133.67221053491));
#79160=CARTESIAN_POINT('Ctrl Pts',(-24.9444157938381,4.07458217025562,133.558804880995));
#79161=CARTESIAN_POINT('Ctrl Pts',(-24.9521886941035,4.15136820208194,133.445217178256));
#79162=CARTESIAN_POINT('Ctrl Pts',(-24.9599615943689,4.22331954693774,133.328536570238));
#79163=CARTESIAN_POINT('Ctrl Pts',(-24.9677344946344,4.29020115418773,133.209221760981));
#79164=CARTESIAN_POINT('Ctrl Pts',(-24.9752248303963,4.35465144654804,133.094244345578));
#79165=CARTESIAN_POINT('Ctrl Pts',(-24.9827151661581,4.41439405773337,132.976821198102));
#79166=CARTESIAN_POINT('Ctrl Pts',(-24.99020550192,4.46926141555867,132.857379239473));
#79167=CARTESIAN_POINT('Ctrl Pts',(-24.997979836039,4.52620908593361,132.733408602677));
#79168=CARTESIAN_POINT('Ctrl Pts',(-25.0057541701581,4.57808490778234,132.606870344589));
#79169=CARTESIAN_POINT('Ctrl Pts',(-25.0135285042772,4.62464963282695,132.478218089424));
#79170=CARTESIAN_POINT('Ctrl Pts',(-25.0212932572243,4.67115697100956,132.349724386665));
#79171=CARTESIAN_POINT('Ctrl Pts',(-25.0290580101713,4.71236610410475,132.21912223472));
#79172=CARTESIAN_POINT('Ctrl Pts',(-25.0368227631184,4.74808449000776,132.08688809807));
#79173=CARTESIAN_POINT('Ctrl Pts',(-25.0445798040034,4.7837673999064,131.954785298229));
#79174=CARTESIAN_POINT('Ctrl Pts',(-25.0523368448885,4.81397031400719,131.821054114362));
#79175=CARTESIAN_POINT('Ctrl Pts',(-25.0600938857735,4.83854958466325,131.686188820367));
#79176=CARTESIAN_POINT('Ctrl Pts',(-25.0678450770137,4.86311031990014,131.551425229339));
#79177=CARTESIAN_POINT('Ctrl Pts',(-25.0755962682538,4.8820557829984,131.41552961356));
#79178=CARTESIAN_POINT('Ctrl Pts',(-25.0833474594939,4.89529285614709,131.279008818927));
#79179=CARTESIAN_POINT('Ctrl Pts',(-25.091095356271,4.90852430318652,131.142546049274));
#79180=CARTESIAN_POINT('Ctrl Pts',(-25.098843253048,4.91605214818696,131.005459017584));
#79181=CARTESIAN_POINT('Ctrl Pts',(-25.1065911498251,4.91783485782742,130.868261897973));
#79182=CARTESIAN_POINT('Ctrl Pts',(-25.1143374259092,4.91961719456345,130.731093477041));
#79183=CARTESIAN_POINT('Ctrl Pts',(-25.1220837019932,4.9156567812265,130.593815404678));
#79184=CARTESIAN_POINT('Ctrl Pts',(-25.1298299780773,4.90596417999352,130.456943681996));
#79185=CARTESIAN_POINT('Ctrl Pts',(-25.1375763113426,4.89627150721195,130.320070948959));
#79186=CARTESIAN_POINT('Ctrl Pts',(-25.145322644608,4.88084658971753,130.183604961579));
#79187=CARTESIAN_POINT('Ctrl Pts',(-25.1530689778733,4.85975199460728,130.048058023752));
#79188=CARTESIAN_POINT('Ctrl Pts',(-25.1608170458763,4.83865267550872,129.912480731127));
#79189=CARTESIAN_POINT('Ctrl Pts',(-25.1685651138793,4.81188121237726,129.777823283845));
#79190=CARTESIAN_POINT('Ctrl Pts',(-25.1763131818822,4.77955148623449,129.644588806849));
#79191=CARTESIAN_POINT('Ctrl Pts',(-25.1840694846241,4.74718739967403,129.511212726666));
#79192=CARTESIAN_POINT('Ctrl Pts',(-25.1918257873658,4.70925334179871,129.379263018396));
#79193=CARTESIAN_POINT('Ctrl Pts',(-25.1995820901077,4.66591354574455,129.249229161342));
#79194=CARTESIAN_POINT('Ctrl Pts',(-25.2073425326218,4.62255061793624,129.119125901303));
#79195=CARTESIAN_POINT('Ctrl Pts',(-25.2151029751361,4.57377634190246,128.99094089522));
#79196=CARTESIAN_POINT('Ctrl Pts',(-25.2228634176502,4.5198031589681,128.865143645002));
#79197=CARTESIAN_POINT('Ctrl Pts',(-25.2306363179157,4.46574333348898,128.739144453869));
#79198=CARTESIAN_POINT('Ctrl Pts',(-25.2384092181811,4.40646809280162,128.615541030958));
#79199=CARTESIAN_POINT('Ctrl Pts',(-25.2461821184465,4.34223630699538,128.494779071764));
#79200=CARTESIAN_POINT('Ctrl Pts',(-25.2536724542086,4.2803395083926,128.378407113965));
#79201=CARTESIAN_POINT('Ctrl Pts',(-25.2611627899707,4.21384042946294,128.264673883742));
#79202=CARTESIAN_POINT('Ctrl Pts',(-25.2686531257328,4.1430076740085,128.153951125505));
#79203=CARTESIAN_POINT('Ctrl Pts',(-25.2764274598519,4.06948927310268,128.039030280237));
#79204=CARTESIAN_POINT('Ctrl Pts',(-25.2842017939709,3.99106920167037,127.926988662751));
#79205=CARTESIAN_POINT('Ctrl Pts',(-25.29197612809,3.90799978707162,127.818272754366));
#79206=CARTESIAN_POINT('Ctrl Pts',(-25.2997408810371,3.82503274810234,127.709690828623));
#79207=CARTESIAN_POINT('Ctrl Pts',(-25.3075056339842,3.73742800185325,127.604426764586));
#79208=CARTESIAN_POINT('Ctrl Pts',(-25.3152703869312,3.64548233767515,127.502900094071));
#79209=CARTESIAN_POINT('Ctrl Pts',(-25.3230274278162,3.55362799522716,127.401474261276));
#79210=CARTESIAN_POINT('Ctrl Pts',(-25.3307844687012,3.45744157559582,127.303778722807));
#79211=CARTESIAN_POINT('Ctrl Pts',(-25.3385415095861,3.35726128034615,127.210201500611));
#79212=CARTESIAN_POINT('Ctrl Pts',(-25.3462927008263,3.25715653183559,127.116694845726));
#79213=CARTESIAN_POINT('Ctrl Pts',(-25.3540438920664,3.15306418709066,127.027300591294));
#79214=CARTESIAN_POINT('Ctrl Pts',(-25.3617950833066,3.04536033746614,126.942371042556));
#79215=CARTESIAN_POINT('Ctrl Pts',(-25.3695429800837,2.93770226485124,126.857477591141));
#79216=CARTESIAN_POINT('Ctrl Pts',(-25.3772908768608,2.82643604668417,126.777045312777));
#79217=CARTESIAN_POINT('Ctrl Pts',(-25.3850387736379,2.71197182243664,126.701387074292));
#79218=CARTESIAN_POINT('Ctrl Pts',(-25.392785049722,2.59753154163711,126.625744661879));
#79219=CARTESIAN_POINT('Ctrl Pts',(-25.4005313258061,2.47989491129314,126.554874518468));
#79220=CARTESIAN_POINT('Ctrl Pts',(-25.4082776018902,2.35950176687121,126.489046669007));
#79221=CARTESIAN_POINT('Ctrl Pts',(-25.4160239351555,2.23910773373444,126.423218333619));
#79222=CARTESIAN_POINT('Ctrl Pts',(-25.4237702684209,2.11595748895299,126.362432554017));
#79223=CARTESIAN_POINT('Ctrl Pts',(-25.4315166016863,1.99051586734849,126.3069136035));
#79224=CARTESIAN_POINT('Ctrl Pts',(-25.4392646696893,1.86504615396242,126.251382219898));
#79225=CARTESIAN_POINT('Ctrl Pts',(-25.4470127376922,1.73728440011416,126.20112017059));
#79226=CARTESIAN_POINT('Ctrl Pts',(-25.4547608056952,1.607715454543,126.15630359557));
#79227=CARTESIAN_POINT('Ctrl Pts',(-25.4625171084371,1.47800880155494,126.111439388961));
#79228=CARTESIAN_POINT('Ctrl Pts',(-25.4702734111789,1.34649149010508,126.072032345829));
#79229=CARTESIAN_POINT('Ctrl Pts',(-25.4780297139208,1.21366410501443,126.038208867705));
#79230=CARTESIAN_POINT('Ctrl Pts',(-25.485790156435,1.08076582594882,126.004367336973));
#79231=CARTESIAN_POINT('Ctrl Pts',(-25.4935505989491,0.946556462369149,
125.976115389879));
#79232=CARTESIAN_POINT('Ctrl Pts',(-25.5013110414633,0.811545849252267,
125.953528070769));
#79233=CARTESIAN_POINT('Ctrl Pts',(-25.5090839417287,0.676318505113714,
125.93090449249));
#79234=CARTESIAN_POINT('Ctrl Pts',(-25.5168568419941,0.540287729318321,
125.913963761978));
#79235=CARTESIAN_POINT('Ctrl Pts',(-25.5246297422595,0.403968423714513,
125.902728993796));
#79236=CARTESIAN_POINT('Ctrl Pts',(-25.5321200780216,0.272604668236464,
125.891902637736));
#79237=CARTESIAN_POINT('Ctrl Pts',(-25.5396104137837,0.14097330406644,125.886374607167));
#79238=CARTESIAN_POINT('Ctrl Pts',(-25.5471007495457,0.00953227722159142,
125.886119855038));
#79239=CARTESIAN_POINT('Ctrl Pts',(-25.5548750836648,-0.126892376106331,
125.885855443904));
#79240=CARTESIAN_POINT('Ctrl Pts',(-25.5626494177839,-0.263544126207083,
125.891271239952));
#79241=CARTESIAN_POINT('Ctrl Pts',(-25.570423751903,-0.399910946599676,
125.902396287087));
#79242=CARTESIAN_POINT('Ctrl Pts',(-25.5781885048501,-0.536109707073772,
125.913507623595));
#79243=CARTESIAN_POINT('Ctrl Pts',(-25.5859532577971,-0.672023850594534,
125.93031417988));
#79244=CARTESIAN_POINT('Ctrl Pts',(-25.5937180107443,-0.807139991270013,
125.95279302585));
#79245=CARTESIAN_POINT('Ctrl Pts',(-25.6014750516293,-0.94212193268977,
125.975249545513));
#79246=CARTESIAN_POINT('Ctrl Pts',(-25.6092320925143,-1.07630706538066,
126.003367079601));
#79247=CARTESIAN_POINT('Ctrl Pts',(-25.6169891333993,-1.20918612928194,
126.037070824901));
#79248=CARTESIAN_POINT('Ctrl Pts',(-25.6247403246395,-1.34196498804748,
126.070749153944));
#79249=CARTESIAN_POINT('Ctrl Pts',(-25.6324915158796,-1.47343936100866,
126.11000521353));
#79250=CARTESIAN_POINT('Ctrl Pts',(-25.6402427071197,-1.60310955722688,
126.154713016938));
#79251=CARTESIAN_POINT('Ctrl Pts',(-25.6479906038968,-1.73272464015265,
126.199401818337));
#79252=CARTESIAN_POINT('Ctrl Pts',(-25.655738500674,-1.86053670264897,126.24953762778));
#79253=CARTESIAN_POINT('Ctrl Pts',(-25.6634863974511,-1.98606083058957,
126.304944495479));
#79254=CARTESIAN_POINT('Ctrl Pts',(-25.6712326735352,-2.11155870158841,
126.360339773255));
#79255=CARTESIAN_POINT('Ctrl Pts',(-25.6789789496193,-2.23476923252213,
126.421003758393));
#79256=CARTESIAN_POINT('Ctrl Pts',(-25.6867252257034,-2.35522750194124,
126.486712359938));
#79257=CARTESIAN_POINT('Ctrl Pts',(-25.6944715589688,-2.47568666055592,
126.552421446529));
#79258=CARTESIAN_POINT('Ctrl Pts',(-25.7022178922341,-2.59339317389404,
126.62317503661));
#79259=CARTESIAN_POINT('Ctrl Pts',(-25.7099642254995,-2.70790709990199,
126.698703276676));
#79260=CARTESIAN_POINT('Ctrl Pts',(-25.7177122935025,-2.82244667050953,
126.774248430769));
#79261=CARTESIAN_POINT('Ctrl Pts',(-25.7254603615054,-2.93379190479616,
126.854570147313));
#79262=CARTESIAN_POINT('Ctrl Pts',(-25.7332084295084,-3.04153253861013,
126.939355717301));
#79263=CARTESIAN_POINT('Ctrl Pts',(-25.7409647322503,-3.14938768045215,
127.024231398402));
#79264=CARTESIAN_POINT('Ctrl Pts',(-25.7487210349921,-3.25363026123202,
127.113580167905));
#79265=CARTESIAN_POINT('Ctrl Pts',(-25.756477337734,-3.35388335743939,127.207049192739));
#79266=CARTESIAN_POINT('Ctrl Pts',(-25.7642377802481,-3.45418996174249,
127.300568104805));
#79267=CARTESIAN_POINT('Ctrl Pts',(-25.7719982227624,-3.55050256422987,
127.398211375895));
#79268=CARTESIAN_POINT('Ctrl Pts',(-25.7797586652765,-3.6424824497096,127.499590630705));
#79269=CARTESIAN_POINT('Ctrl Pts',(-25.787531565542,-3.73460998946734,127.601132628495));
#79270=CARTESIAN_POINT('Ctrl Pts',(-25.7953044658074,-3.82239066288767,
127.706422294122));
#79271=CARTESIAN_POINT('Ctrl Pts',(-25.8030773660728,-3.90552670600746,
127.815038920063));
#79272=CARTESIAN_POINT('Ctrl Pts',(-25.8105677018348,-3.98564054455155,
127.919707058061));
#79273=CARTESIAN_POINT('Ctrl Pts',(-25.8180580375966,-4.0614414008384,128.027464217177));
#79274=CARTESIAN_POINT('Ctrl Pts',(-25.8255483733586,-4.13270281665368,
128.137911575915));
#79275=CARTESIAN_POINT('Ctrl Pts',(-25.833499057336,-4.20834388468305,128.255146914006));
#79276=CARTESIAN_POINT('Ctrl Pts',(-25.8414497413134,-4.27910134301528,
128.375771468827));
#79277=CARTESIAN_POINT('Ctrl Pts',(-25.8494004252908,-4.34466498045625,
128.499351014528));
#79278=CARTESIAN_POINT('Ctrl Pts',(-25.8573410544048,-4.41014570258818,
128.622774274877));
#79279=CARTESIAN_POINT('Ctrl Pts',(-25.8652816835188,-4.4704455054632,128.749144767636));
#79280=CARTESIAN_POINT('Ctrl Pts',(-25.8732223126328,-4.52529716041595,
128.877999106211));
#79281=CARTESIAN_POINT('Ctrl Pts',(-25.8811512875611,-4.58006831149897,
129.006664329746));
#79282=CARTESIAN_POINT('Ctrl Pts',(-25.8890802624895,-4.62940710430368,
129.137805799789));
#79283=CARTESIAN_POINT('Ctrl Pts',(-25.8970092374178,-4.67309232257847,
129.270935951285));
#79284=CARTESIAN_POINT('Ctrl Pts',(-25.9031285387631,-4.70680702307544,
129.373681075656));
#79285=CARTESIAN_POINT('Ctrl Pts',(-25.9092478401083,-4.7371552205288,129.477610126819));
#79286=CARTESIAN_POINT('Ctrl Pts',(-25.9153671414536,-4.76405452823411,
129.582490119308));
#79287=CARTESIAN_POINT('Ctrl Pts',(-24.1652761364937,-4.76405452823407,
129.582490119308));
#79288=CARTESIAN_POINT('Ctrl Pts',(-24.1748731237573,-4.80591458719474,
129.745701853881));
#79289=CARTESIAN_POINT('Ctrl Pts',(-24.1844701110211,-4.8394173052575,129.911198225682));
#79290=CARTESIAN_POINT('Ctrl Pts',(-24.1940670982847,-4.86434929394215,
130.078213931955));
#79291=CARTESIAN_POINT('Ctrl Pts',(-24.2035307701994,-4.8889349430225,130.24290956042));
#79292=CARTESIAN_POINT('Ctrl Pts',(-24.212994442114,-4.90518630260743,130.409082652632));
#79293=CARTESIAN_POINT('Ctrl Pts',(-24.2224581140287,-4.9129445827565,130.575978067305));
#79294=CARTESIAN_POINT('Ctrl Pts',(-24.2266855973436,-4.91641025656448,
130.650531326042));
#79295=CARTESIAN_POINT('Ctrl Pts',(-24.2309130806584,-4.91818178254436,
130.725228431567));
#79296=CARTESIAN_POINT('Ctrl Pts',(-24.2351405639733,-4.91824806745606,
130.800000633076));
#79297=CARTESIAN_POINT('',(-23.8898594359345,-4.91824995370166,130.805035460958));
#79298=CARTESIAN_POINT('Ctrl Pts',(-23.8197459990105,-4.76405452823405,
129.582490119308));
#79299=CARTESIAN_POINT('Ctrl Pts',(-23.8274769694886,-4.79800736229832,
129.714871704019));
#79300=CARTESIAN_POINT('Ctrl Pts',(-23.8352079399666,-4.82641147466578,
129.848565479955));
#79301=CARTESIAN_POINT('Ctrl Pts',(-23.8429389104446,-4.84919130876466,
129.983064864806));
#79302=CARTESIAN_POINT('Ctrl Pts',(-23.8507589980263,-4.87223373251392,
130.119114662461));
#79303=CARTESIAN_POINT('Ctrl Pts',(-23.8585790856079,-4.88952135646728,
130.255988344086));
#79304=CARTESIAN_POINT('Ctrl Pts',(-23.8663991731895,-4.90103010817356,
130.393158792088));
#79305=CARTESIAN_POINT('Ctrl Pts',(-23.8742192607711,-4.91253885987984,
130.53032924009));
#79306=CARTESIAN_POINT('Ctrl Pts',(-23.8820393483529,-4.91826878461024,
130.667796041645));
#79307=CARTESIAN_POINT('Ctrl Pts',(-23.8898594359345,-4.91824995370166,
130.805035460958));
#79308=CARTESIAN_POINT('Ctrl Pts',(-23.8898594359911,-4.91824995370153,
130.805035461952));
#79309=CARTESIAN_POINT('Ctrl Pts',(-23.8919076249367,-4.91824502161922,
130.840980361367));
#79310=CARTESIAN_POINT('Ctrl Pts',(-23.8939558138823,-4.91784604244065,
130.876922193558));
#79311=CARTESIAN_POINT('Ctrl Pts',(-23.896004002828,-4.91705317907111,130.912855302628));
#79312=CARTESIAN_POINT('Ctrl Pts',(-23.903778336947,-4.91404369854502,131.049247014164));
#79313=CARTESIAN_POINT('Ctrl Pts',(-23.911552671066,-4.90535019690039,131.185729447764));
#79314=CARTESIAN_POINT('Ctrl Pts',(-23.9193270051851,-4.89095592581988,
131.321790027425));
#79315=CARTESIAN_POINT('Ctrl Pts',(-23.9270917581322,-4.87657939439202,
131.457682924582));
#79316=CARTESIAN_POINT('Ctrl Pts',(-23.9348565110792,-4.85651611329203,
131.593154617177));
#79317=CARTESIAN_POINT('Ctrl Pts',(-23.9426212640263,-4.83080132585475,
131.727692417419));
#79318=CARTESIAN_POINT('Ctrl Pts',(-23.9503783049113,-4.8051120787068,131.862096592822));
#79319=CARTESIAN_POINT('Ctrl Pts',(-23.9581353457964,-4.77378256857804,
131.99556834022));
#79320=CARTESIAN_POINT('Ctrl Pts',(-23.9658923866814,-4.73689979797866,
132.127600341278));
#79321=CARTESIAN_POINT('Ctrl Pts',(-23.9736435779215,-4.70004484096355,
132.259532775977));
#79322=CARTESIAN_POINT('Ctrl Pts',(-23.9813947691616,-4.65764506371638,
132.390027250377));
#79323=CARTESIAN_POINT('Ctrl Pts',(-23.9891459604017,-4.60983840788225,
132.518587240774));
#79324=CARTESIAN_POINT('Ctrl Pts',(-23.9968938571788,-4.56205207115219,
132.647092589744));
#79325=CARTESIAN_POINT('Ctrl Pts',(-24.0046417539559,-4.50886356249979,
132.773664724337));
#79326=CARTESIAN_POINT('Ctrl Pts',(-24.012389650733,-4.45046041764813,132.897823092378));
#79327=CARTESIAN_POINT('Ctrl Pts',(-24.020135926817,-4.39206948947535,133.021955489166));
#79328=CARTESIAN_POINT('Ctrl Pts',(-24.0278822029011,-4.32846626105303,
133.143674770136));
#79329=CARTESIAN_POINT('Ctrl Pts',(-24.0356284789852,-4.25988591563597,
133.262521525291));
#79330=CARTESIAN_POINT('Ctrl Pts',(-24.0433748122505,-4.19130506397438,
133.381369157745));
#79331=CARTESIAN_POINT('Ctrl Pts',(-24.0511211455159,-4.11774721741212,
133.497343883443));
#79332=CARTESIAN_POINT('Ctrl Pts',(-24.0588674787812,-4.03949270913817,
133.610012362762));
#79333=CARTESIAN_POINT('Ctrl Pts',(-24.0666155467842,-3.96122067630978,
133.722706073405));
#79334=CARTESIAN_POINT('Ctrl Pts',(-24.0743636147871,-3.87825011182596,
133.832091743289));
#79335=CARTESIAN_POINT('Ctrl Pts',(-24.0821116827901,-3.79090347984968,
133.937766730562));
#79336=CARTESIAN_POINT('Ctrl Pts',(-24.0898679855319,-3.70346401483337,
134.04355403047));
#79337=CARTESIAN_POINT('Ctrl Pts',(-24.0976242882737,-3.61163944105797,
134.145622467855));
#79338=CARTESIAN_POINT('Ctrl Pts',(-24.1053805910155,-3.51579153511385,
134.243603694774));
#79339=CARTESIAN_POINT('Ctrl Pts',(-24.1131410335297,-3.41989247225626,
134.341637217224));
#79340=CARTESIAN_POINT('Ctrl Pts',(-24.1209014760439,-3.31996608311959,
134.435578914787));
#79341=CARTESIAN_POINT('Ctrl Pts',(-24.128661918558,-3.21640875939532,134.525099489751));
#79342=CARTESIAN_POINT('Ctrl Pts',(-24.1364348188235,-3.11268519626163,
134.614763771088));
#79343=CARTESIAN_POINT('Ctrl Pts',(-24.1442077190889,-3.00531935733366,
134.699992504184));
#79344=CARTESIAN_POINT('Ctrl Pts',(-24.1519806193543,-2.89473897449381,
134.780498106643));
#79345=CARTESIAN_POINT('Ctrl Pts',(-24.1594709551165,-2.78817846710343,
134.858077127674));
#79346=CARTESIAN_POINT('Ctrl Pts',(-24.1669612908786,-2.67863332783829,
134.931270280489));
#79347=CARTESIAN_POINT('Ctrl Pts',(-24.1744516266408,-2.56650769771754,
134.999860742707));
#79348=CARTESIAN_POINT('Ctrl Pts',(-24.1822259607599,-2.45013079025304,
135.071051833145));
#79349=CARTESIAN_POINT('Ctrl Pts',(-24.1900002948789,-2.33060520349197,
135.137509833129));
#79350=CARTESIAN_POINT('Ctrl Pts',(-24.197774628998,-2.20835312926849,135.198943591973));
#79351=CARTESIAN_POINT('Ctrl Pts',(-24.2055393819451,-2.0862517198005,135.2603016392));
#79352=CARTESIAN_POINT('Ctrl Pts',(-24.2133041348922,-1.96143085455517,
135.316647591517));
#79353=CARTESIAN_POINT('Ctrl Pts',(-24.2210688878393,-1.83434092217407,
135.367733979865));
#79354=CARTESIAN_POINT('Ctrl Pts',(-24.2288259287243,-1.70737721730547,
135.418769628492));
#79355=CARTESIAN_POINT('Ctrl Pts',(-24.2365829696093,-1.57814929061276,
135.46455596402));
#79356=CARTESIAN_POINT('Ctrl Pts',(-24.2443400104943,-1.44713099036155,
135.504891966173));
#79357=CARTESIAN_POINT('Ctrl Pts',(-24.2520912017344,-1.31621149202973,
135.545197550633));
#79358=CARTESIAN_POINT('Ctrl Pts',(-24.2598423929745,-1.18350467964676,
135.580060868129));
#79359=CARTESIAN_POINT('Ctrl Pts',(-24.2675935842147,-1.04950285349737,
135.609329589682));
#79360=CARTESIAN_POINT('Ctrl Pts',(-24.2753414809917,-0.915557981698705,
135.638585871248));
#79361=CARTESIAN_POINT('Ctrl Pts',(-24.2830893777689,-0.780319572028402,
135.662252202986));
#79362=CARTESIAN_POINT('Ctrl Pts',(-24.2908372745459,-0.644293294278856,
135.680226613822));
#79363=CARTESIAN_POINT('Ctrl Pts',(-24.29858355063,-0.508295470294227,135.698197264799));
#79364=CARTESIAN_POINT('Ctrl Pts',(-24.306329826714,-0.371510493386991,
135.710478311914));
#79365=CARTESIAN_POINT('Ctrl Pts',(-24.3140761027981,-0.234452000494012,
135.717019299173));
#79366=CARTESIAN_POINT('Ctrl Pts',(-24.3218224360635,-0.0973924958663737,
135.723560334716));
#79367=CARTESIAN_POINT('Ctrl Pts',(-24.3295687693289,0.0399401382551061,
135.724361207216));
#79368=CARTESIAN_POINT('Ctrl Pts',(-24.3373151025942,0.177029794038206,
135.719423538274));
#79369=CARTESIAN_POINT('Ctrl Pts',(-24.3450631705972,0.314150150099393,
135.714484763576));
#79370=CARTESIAN_POINT('Ctrl Pts',(-24.3528112386002,0.451027028908924,
135.703804904293));
#79371=CARTESIAN_POINT('Ctrl Pts',(-24.3605593066032,0.587147376716695,
135.687437620903));
#79372=CARTESIAN_POINT('Ctrl Pts',(-24.368315609345,0.723412394849784,135.671052942168));
#79373=CARTESIAN_POINT('Ctrl Pts',(-24.3760719120869,0.858918887016169,
135.648968811211));
#79374=CARTESIAN_POINT('Ctrl Pts',(-24.3838282148287,0.993161402573715,
135.62129049986));
#79375=CARTESIAN_POINT('Ctrl Pts',(-24.3915886573429,1.12747556740396,135.593597415761));
#79376=CARTESIAN_POINT('Ctrl Pts',(-24.3993490998571,1.26052403229758,135.560304296705));
#79377=CARTESIAN_POINT('Ctrl Pts',(-24.4071095423712,1.39181549037001,135.521566644789));
#79378=CARTESIAN_POINT('Ctrl Pts',(-24.4148824426367,1.52331770914627,135.482766807755));
#79379=CARTESIAN_POINT('Ctrl Pts',(-24.422655342902,1.6530569145997,135.438505098772));
#79380=CARTESIAN_POINT('Ctrl Pts',(-24.4304282431675,1.78055995598714,135.388985935478));
#79381=CARTESIAN_POINT('Ctrl Pts',(-24.4379185789295,1.90342794066004,135.3412669185));
#79382=CARTESIAN_POINT('Ctrl Pts',(-24.4454089146916,2.02421923662176,135.288666177296));
#79383=CARTESIAN_POINT('Ctrl Pts',(-24.4528992504537,2.1425329769676,135.231406529357));
#79384=CARTESIAN_POINT('Ctrl Pts',(-24.4606735845728,2.26533261873883,135.171975864463));
#79385=CARTESIAN_POINT('Ctrl Pts',(-24.4684479186918,2.3858521155326,135.107337775498));
#79386=CARTESIAN_POINT('Ctrl Pts',(-24.4762222528109,2.50361830903366,135.037690090354));
#79387=CARTESIAN_POINT('Ctrl Pts',(-24.483987005758,2.62123936622628,134.968128239756));
#79388=CARTESIAN_POINT('Ctrl Pts',(-24.4917517587051,2.73611353829486,134.893569274268));
#79389=CARTESIAN_POINT('Ctrl Pts',(-24.4995165116522,2.84778917644996,134.814258355538));
#79390=CARTESIAN_POINT('Ctrl Pts',(-24.5072735525372,2.95935389678676,134.735026209531));
#79391=CARTESIAN_POINT('Ctrl Pts',(-24.5150305934222,3.06772608854799,134.651051727626));
#79392=CARTESIAN_POINT('Ctrl Pts',(-24.5227876343072,3.17248050111997,134.562624915419));
#79393=CARTESIAN_POINT('Ctrl Pts',(-24.5305388255473,3.2771559175747,134.474264786558));
#79394=CARTESIAN_POINT('Ctrl Pts',(-24.5382900167875,3.37821868760179,134.381459261539));
#79395=CARTESIAN_POINT('Ctrl Pts',(-24.5460412080277,3.47527455218835,134.284540188998));
#79396=CARTESIAN_POINT('Ctrl Pts',(-24.5537891048047,3.57228916544327,134.187662309649));
#79397=CARTESIAN_POINT('Ctrl Pts',(-24.5615370015818,3.66529998440791,134.086674635829));
#79398=CARTESIAN_POINT('Ctrl Pts',(-24.5692848983589,3.75394789105644,133.981947484));
#79399=CARTESIAN_POINT('Ctrl Pts',(-24.577031174443,3.84257725447391,133.877242238834));
#79400=CARTESIAN_POINT('Ctrl Pts',(-24.5847774505271,3.92684526840573,133.768799369756));
#79401=CARTESIAN_POINT('Ctrl Pts',(-24.5925237266112,4.00643184948538,133.657023741373));
#79402=CARTESIAN_POINT('Ctrl Pts',(-24.6002700598766,4.0860190180551,133.545247287888));
#79403=CARTESIAN_POINT('Ctrl Pts',(-24.6080163931418,4.16092445805009,133.430138344488));
#79404=CARTESIAN_POINT('Ctrl Pts',(-24.6157627264072,4.23087056487944,133.312132003824));
#79405=CARTESIAN_POINT('Ctrl Pts',(-24.6235107944102,4.30083233565444,133.194099236459));
#79406=CARTESIAN_POINT('Ctrl Pts',(-24.6312588624131,4.36583236397042,133.07316811695));
#79407=CARTESIAN_POINT('Ctrl Pts',(-24.6390069304161,4.42563847782243,132.949799296745));
#79408=CARTESIAN_POINT('Ctrl Pts',(-24.646763233158,4.48550815432402,132.82629935869));
#79409=CARTESIAN_POINT('Ctrl Pts',(-24.6545195358999,4.54017271844043,132.700356896869));
#79410=CARTESIAN_POINT('Ctrl Pts',(-24.6622758386418,4.58944752992524,132.57245406322));
#79411=CARTESIAN_POINT('Ctrl Pts',(-24.6700362811559,4.63874864086059,132.444482963976));
#79412=CARTESIAN_POINT('Ctrl Pts',(-24.6777967236701,4.68265414205246,132.314549778253));
#79413=CARTESIAN_POINT('Ctrl Pts',(-24.6855571661843,4.72102929844848,132.183151909129));
#79414=CARTESIAN_POINT('Ctrl Pts',(-24.6933300664497,4.75946605805232,132.051543108481));
#79415=CARTESIAN_POINT('Ctrl Pts',(-24.7011029667151,4.79235463833192,131.91846530567));
#79416=CARTESIAN_POINT('Ctrl Pts',(-24.7088758669805,4.8196112721016,131.784427068543));
#79417=CARTESIAN_POINT('Ctrl Pts',(-24.7163662027426,4.84587705857844,131.655261458958));
#79418=CARTESIAN_POINT('Ctrl Pts',(-24.7238565385046,4.86691321123197,131.525204335214));
#79419=CARTESIAN_POINT('Ctrl Pts',(-24.7313468742666,4.88269051437392,131.394713396286));
#79420=CARTESIAN_POINT('Ctrl Pts',(-24.7391212083857,4.89906601875989,131.259274853748));
#79421=CARTESIAN_POINT('Ctrl Pts',(-24.7468955425048,4.90982789573741,131.122939921847));
#79422=CARTESIAN_POINT('Ctrl Pts',(-24.7546698766239,4.91488682988674,130.986213612883));
#79423=CARTESIAN_POINT('Ctrl Pts',(-24.762434629571,4.91993952935187,130.849655806875));
#79424=CARTESIAN_POINT('Ctrl Pts',(-24.770199382518,4.91930325602775,130.712707970458));
#79425=CARTESIAN_POINT('Ctrl Pts',(-24.7779641354651,4.91294014415034,130.575882604409));
#79426=CARTESIAN_POINT('Ctrl Pts',(-24.7857211763501,4.90658335220537,130.439193135243));
#79427=CARTESIAN_POINT('Ctrl Pts',(-24.7934782172352,4.89451105908241,130.302626282394));
#79428=CARTESIAN_POINT('Ctrl Pts',(-24.8012352581202,4.87673739635905,130.166696576355));
#79429=CARTESIAN_POINT('Ctrl Pts',(-24.8089864493603,4.858977136893,130.030869375965));
#79430=CARTESIAN_POINT('Ctrl Pts',(-24.8167376406004,4.83552411609995,129.895678752121));
#79431=CARTESIAN_POINT('Ctrl Pts',(-24.8244888318405,4.80644442101107,129.761635778391));
#79432=CARTESIAN_POINT('Ctrl Pts',(-24.8322367286176,4.77737708556832,129.627649776501));
#79433=CARTESIAN_POINT('Ctrl Pts',(-24.8399846253946,4.74268791502992,129.494810835842));
#79434=CARTESIAN_POINT('Ctrl Pts',(-24.8477325221717,4.70249435505845,129.363621257674));
#79435=CARTESIAN_POINT('Ctrl Pts',(-24.8554787982558,4.66230920271324,129.232459121536));
#79436=CARTESIAN_POINT('Ctrl Pts',(-24.8632250743399,4.61662206558767,129.102946035221));
#79437=CARTESIAN_POINT('Ctrl Pts',(-24.870971350424,4.56560055486246,128.975570133137));
#79438=CARTESIAN_POINT('Ctrl Pts',(-24.8787176836893,4.51457866750805,128.848193290793));
#79439=CARTESIAN_POINT('Ctrl Pts',(-24.8864640169547,4.45822247335537,128.722954027093));
#79440=CARTESIAN_POINT('Ctrl Pts',(-24.8942103502201,4.39674797611212,128.600321076847));
#79441=CARTESIAN_POINT('Ctrl Pts',(-24.901958418223,4.33525971208145,128.477660663802));
#79442=CARTESIAN_POINT('Ctrl Pts',(-24.909706486226,4.26865103930964,128.357608075082));
#79443=CARTESIAN_POINT('Ctrl Pts',(-24.917454554229,4.19718402226721,128.240607636929));
#79444=CARTESIAN_POINT('Ctrl Pts',(-24.9252108569708,4.12564104922859,128.123482849318));
#79445=CARTESIAN_POINT('Ctrl Pts',(-24.9329671597127,4.04922962138445,128.009417026417));
#79446=CARTESIAN_POINT('Ctrl Pts',(-24.9407234624545,3.96825558425035,127.898826126192));
#79447=CARTESIAN_POINT('Ctrl Pts',(-24.9484839049687,3.88723832883445,127.788176200273));
#79448=CARTESIAN_POINT('Ctrl Pts',(-24.9562443474829,3.80165385563229,127.681005197974));
#79449=CARTESIAN_POINT('Ctrl Pts',(-24.964004789997,3.71184781635464,127.577695334224));
#79450=CARTESIAN_POINT('Ctrl Pts',(-24.9717776902625,3.62189761245014,127.47421962831));
#79451=CARTESIAN_POINT('Ctrl Pts',(-24.9795505905278,3.52771256897532,127.374617731242));
#79452=CARTESIAN_POINT('Ctrl Pts',(-24.9873234907933,3.42967528025342,127.279235012071));
#79453=CARTESIAN_POINT('Ctrl Pts',(-24.9948138265553,3.33520189391731,127.187319694996));
#79454=CARTESIAN_POINT('Ctrl Pts',(-25.0023041623174,3.23715170664756,127.099322331787));
#79455=CARTESIAN_POINT('Ctrl Pts',(-25.0097944980795,3.13589400176253,127.015514899909));
#79456=CARTESIAN_POINT('Ctrl Pts',(-25.0175688321986,3.03079708022061,126.928529883778));
#79457=CARTESIAN_POINT('Ctrl Pts',(-25.0253431663177,2.92191169818666,126.845783251027));
#79458=CARTESIAN_POINT('Ctrl Pts',(-25.0331175004367,2.80961445964391,126.767623116729));
#79459=CARTESIAN_POINT('Ctrl Pts',(-25.0408822533838,2.69745561741137,126.689559307812));
#79460=CARTESIAN_POINT('Ctrl Pts',(-25.0486470063309,2.58189360279594,126.61607097186));
#79461=CARTESIAN_POINT('Ctrl Pts',(-25.056411759278,2.46333912984626,126.547466985601));
#79462=CARTESIAN_POINT('Ctrl Pts',(-25.064168800163,2.3449024068706,126.478931137787));
#79463=CARTESIAN_POINT('Ctrl Pts',(-25.071925841048,2.22347947647936,126.415270180101));
#79464=CARTESIAN_POINT('Ctrl Pts',(-25.0796828819329,2.09951086621194,126.356750339545));
#79465=CARTESIAN_POINT('Ctrl Pts',(-25.0874340731731,1.97563574163769,126.298274629256));
#79466=CARTESIAN_POINT('Ctrl Pts',(-25.0951852644132,1.84921911038972,126.244932485471));
#79467=CARTESIAN_POINT('Ctrl Pts',(-25.1029364556533,1.72072667479015,126.196944555046));
#79468=CARTESIAN_POINT('Ctrl Pts',(-25.1106843524304,1.59228885190337,126.148977020772));
#79469=CARTESIAN_POINT('Ctrl Pts',(-25.1184322492075,1.46177734492655,126.106359310197));
#79470=CARTESIAN_POINT('Ctrl Pts',(-25.1261801459845,1.32967823638432,126.069264119058));
#79471=CARTESIAN_POINT('Ctrl Pts',(-25.1339264220686,1.19760676012787,126.032176687433));
#79472=CARTESIAN_POINT('Ctrl Pts',(-25.1416726981526,1.0639487190226,126.000609583137));
#79473=CARTESIAN_POINT('Ctrl Pts',(-25.1494189742367,0.929205392309645,
125.974685638708));
#79474=CARTESIAN_POINT('Ctrl Pts',(-25.1571653075021,0.794461070952247,
125.948761502915));
#79475=CARTESIAN_POINT('Ctrl Pts',(-25.1649116407674,0.658631831925272,
125.928480683977));
#79476=CARTESIAN_POINT('Ctrl Pts',(-25.1726579740328,0.522228790380028,
125.913914814472));
#79477=CARTESIAN_POINT('Ctrl Pts',(-25.1804060420357,0.385795202319383,
125.899345683041));
#79478=CARTESIAN_POINT('Ctrl Pts',(-25.1881541100387,0.248787944722713,
125.890494089249));
#79479=CARTESIAN_POINT('Ctrl Pts',(-25.1959021780417,0.111722494090165,
125.887379720022));
#79480=CARTESIAN_POINT('Ctrl Pts',(-25.2036584807836,-0.0254886313346032,
125.884262040806));
#79481=CARTESIAN_POINT('Ctrl Pts',(-25.2114147835254,-0.162757681856225,
125.886893775644));
#79482=CARTESIAN_POINT('Ctrl Pts',(-25.2191710862672,-0.299569383284561,
125.895242443484));
#79483=CARTESIAN_POINT('Ctrl Pts',(-25.2269315287814,-0.436454105237271,
125.90359556726));
#79484=CARTESIAN_POINT('Ctrl Pts',(-25.2346919712955,-0.572880602994445,
125.917671663903));
#79485=CARTESIAN_POINT('Ctrl Pts',(-25.2424524138096,-0.708340475118342,
125.937386523346));
#79486=CARTESIAN_POINT('Ctrl Pts',(-25.2502253140751,-0.844017799454534,
125.957133030831));
#79487=CARTESIAN_POINT('Ctrl Pts',(-25.2579982143405,-0.9787250129254,125.982536317089));
#79488=CARTESIAN_POINT('Ctrl Pts',(-25.265771114606,-1.11196474519111,126.013461175086));
#79489=CARTESIAN_POINT('Ctrl Pts',(-25.2732614503681,-1.24036087757994,
126.043261836601));
#79490=CARTESIAN_POINT('Ctrl Pts',(-25.2807517861302,-1.36739407269115,
126.078189511808));
#79491=CARTESIAN_POINT('Ctrl Pts',(-25.2882421218923,-1.49263590152876,
126.118080522654));
#79492=CARTESIAN_POINT('Ctrl Pts',(-25.2960164560114,-1.62262631237189,
126.159484013301));
#79493=CARTESIAN_POINT('Ctrl Pts',(-25.3037907901305,-1.75109860667504,
126.2063657928));
#79494=CARTESIAN_POINT('Ctrl Pts',(-25.3115651242496,-1.87755634171447,
126.258597178254));
#79495=CARTESIAN_POINT('Ctrl Pts',(-25.3193298771967,-2.00385822889731,
126.310764193193));
#79496=CARTESIAN_POINT('Ctrl Pts',(-25.3270946301438,-2.12815013889102,
126.368267548341));
#79497=CARTESIAN_POINT('Ctrl Pts',(-25.3348593830909,-2.24995020398048,
126.430928653752));
#79498=CARTESIAN_POINT('Ctrl Pts',(-25.3426164239759,-2.37162929552822,
126.49352752327));
#79499=CARTESIAN_POINT('Ctrl Pts',(-25.3503734648609,-2.49082112199857,
126.56127377085));
#79500=CARTESIAN_POINT('Ctrl Pts',(-25.3581305057459,-2.60706358317803,
126.633940670394));
#79501=CARTESIAN_POINT('Ctrl Pts',(-25.365881696986,-2.72321838501295,126.706552771265));
#79502=CARTESIAN_POINT('Ctrl Pts',(-25.3736328882262,-2.83642791839467,
126.784077931768));
#79503=CARTESIAN_POINT('Ctrl Pts',(-25.3813840794663,-2.94625482339331,
126.866243608368));
#79504=CARTESIAN_POINT('Ctrl Pts',(-25.3891319762434,-3.05603504902789,
126.948374362364));
#79505=CARTESIAN_POINT('Ctrl Pts',(-25.3968798730204,-3.16243519337324,
127.0351414759));
#79506=CARTESIAN_POINT('Ctrl Pts',(-25.4046277697975,-3.26504722313634,
127.126229340247));
#79507=CARTESIAN_POINT('Ctrl Pts',(-25.4123740458817,-3.36763778867489,
127.217298150977));
#79508=CARTESIAN_POINT('Ctrl Pts',(-25.4201203219658,-3.46644152354261,
127.31268565541));
#79509=CARTESIAN_POINT('Ctrl Pts',(-25.4278665980499,-3.56108413157174,
127.412036507112));
#79510=CARTESIAN_POINT('Ctrl Pts',(-25.4356129313153,-3.65572743823111,
127.511388092199));
#79511=CARTESIAN_POINT('Ctrl Pts',(-25.4433592645806,-3.74620928709418,
127.614702799855));
#79512=CARTESIAN_POINT('Ctrl Pts',(-25.451105597846,-3.83219314142072,127.721589333583));
#79513=CARTESIAN_POINT('Ctrl Pts',(-25.458853665849,-3.91819625123514,127.82849980381));
#79514=CARTESIAN_POINT('Ctrl Pts',(-25.4666017338519,-3.99969911710219,
127.938983387217));
#79515=CARTESIAN_POINT('Ctrl Pts',(-25.4743498018549,-4.07640654821327,
128.052617040089));
#79516=CARTESIAN_POINT('Ctrl Pts',(-25.4821061045968,-4.15319550489508,
128.166371464161));
#79517=CARTESIAN_POINT('Ctrl Pts',(-25.4898624073387,-4.22517862663083,
128.28328232099));
#79518=CARTESIAN_POINT('Ctrl Pts',(-25.4976187100806,-4.29210472236403,
128.402898539006));
#79519=CARTESIAN_POINT('Ctrl Pts',(-25.5053791525948,-4.35906653856971,
128.522578599799));
#79520=CARTESIAN_POINT('Ctrl Pts',(-25.5131395951089,-4.42096577424825,
128.644966550226));
#79521=CARTESIAN_POINT('Ctrl Pts',(-25.5209000376231,-4.47759847431941,
128.769589140158));
#79522=CARTESIAN_POINT('Ctrl Pts',(-25.5286729378886,-4.53432208622826,
128.894411785335));
#79523=CARTESIAN_POINT('Ctrl Pts',(-25.536445838154,-4.58576212132881,129.021475875867));
#79524=CARTESIAN_POINT('Ctrl Pts',(-25.5442187384194,-4.63176349230904,
129.150289877297));
#79525=CARTESIAN_POINT('Ctrl Pts',(-25.5517090741814,-4.67609259758325,
129.274421165311));
#79526=CARTESIAN_POINT('Ctrl Pts',(-25.5591994099434,-4.71537150014363,
129.400177051728));
#79527=CARTESIAN_POINT('Ctrl Pts',(-25.5666897457053,-4.74950633063405,
129.527108615114));
#79528=CARTESIAN_POINT('Ctrl Pts',(-25.5677773717325,-4.75446284143058,
129.545539574205));
#79529=CARTESIAN_POINT('Ctrl Pts',(-25.5688649977596,-4.7593123489355,129.564000434196));
#79530=CARTESIAN_POINT('Ctrl Pts',(-25.5699526237868,-4.76405452823406,
129.582490119308));
#79531=CARTESIAN_POINT('Origin',(213.235140564004,0.,130.804360617566));
#79532=CARTESIAN_POINT('',(-27.6650164504902,-4.76405452823402,129.582490119308));
#79533=CARTESIAN_POINT('',(-27.320109157184,-4.76405452823409,129.582490119308));
#79534=CARTESIAN_POINT('',(213.235140564004,-4.76405452823405,129.582490119308));
#79535=CARTESIAN_POINT('',(-25.9851405640488,-4.91824961917714,130.806296066854));
#79536=CARTESIAN_POINT('Ctrl Pts',(-25.9851405640487,-4.91824961917714,
130.806296066854));
#79537=CARTESIAN_POINT('Ctrl Pts',(-25.9935514421844,-4.91819087722613,
130.955567649422));
#79538=CARTESIAN_POINT('Ctrl Pts',(-26.0019623203201,-4.91133226515802,
131.104627492812));
#79539=CARTESIAN_POINT('Ctrl Pts',(-26.0103731984557,-4.89775637761353,
131.252875420049));
#79540=CARTESIAN_POINT('Ctrl Pts',(-26.0188206508137,-4.88412145609892,
131.401767994913));
#79541=CARTESIAN_POINT('Ctrl Pts',(-26.0272681031716,-4.86371079700626,
131.549841309758));
#79542=CARTESIAN_POINT('Ctrl Pts',(-26.0357155555295,-4.83665867837743,
131.696501801111));
#79543=CARTESIAN_POINT('Ctrl Pts',(-26.0441815759815,-4.80954709729033,
131.843484662532));
#79544=CARTESIAN_POINT('Ctrl Pts',(-26.0526475964335,-4.77576494785516,
131.989048229664));
#79545=CARTESIAN_POINT('Ctrl Pts',(-26.0611136168855,-4.73549654337785,
132.13261343618));
#79546=CARTESIAN_POINT('Ctrl Pts',(-26.0696079068611,-4.69509367565232,
132.27665803204));
#79547=CARTESIAN_POINT('Ctrl Pts',(-26.0781021968367,-4.64816129120635,
132.41869065189));
#79548=CARTESIAN_POINT('Ctrl Pts',(-26.0865964868123,-4.59493312340749,
132.558148704512));
#79549=CARTESIAN_POINT('Ctrl Pts',(-26.0923963235987,-4.5585893340428,132.653369605386));
#79550=CARTESIAN_POINT('Ctrl Pts',(-26.0981961603851,-4.51931140517969,
132.747390694804));
#79551=CARTESIAN_POINT('Ctrl Pts',(-26.1039959971716,-4.47718591578177,
132.840039702792));
#79552=CARTESIAN_POINT('Ctrl Pts',(-26.1117703312906,-4.42071921825757,
132.964230153389));
#79553=CARTESIAN_POINT('Ctrl Pts',(-26.1195446654097,-4.35899187907983,
133.086266079454));
#79554=CARTESIAN_POINT('Ctrl Pts',(-26.1273189995288,-4.29219031467474,
133.205669711605));
#79555=CARTESIAN_POINT('Ctrl Pts',(-26.1350837524759,-4.22547107722756,
133.32492618945));
#79556=CARTESIAN_POINT('Ctrl Pts',(-26.142848505423,-4.1536902462662,133.441556490185));
#79557=CARTESIAN_POINT('Ctrl Pts',(-26.1506132583701,-4.07708207451369,
133.555103211881));
#79558=CARTESIAN_POINT('Ctrl Pts',(-26.1583702992551,-4.00054999107736,
133.668537157372));
#79559=CARTESIAN_POINT('Ctrl Pts',(-26.16612734014,-3.91920032553539,133.778893296642));
#79560=CARTESIAN_POINT('Ctrl Pts',(-26.1738843810251,-3.8333127951275,133.885739542205));
#79561=CARTESIAN_POINT('Ctrl Pts',(-26.1816355722652,-3.7474900331744,133.992505214183));
#79562=CARTESIAN_POINT('Ctrl Pts',(-26.1893867635054,-3.65713646167303,
134.095765957337));
#79563=CARTESIAN_POINT('Ctrl Pts',(-26.1971379547455,-3.5625743725684,134.195119662738));
#79564=CARTESIAN_POINT('Ctrl Pts',(-26.2048858515226,-3.46805247487416,
134.294431140165));
#79565=CARTESIAN_POINT('Ctrl Pts',(-26.2126337482997,-3.36932588620517,
134.38983860003));
#79566=CARTESIAN_POINT('Ctrl Pts',(-26.2203816450768,-3.26675619853912,
134.480974141151));
#79567=CARTESIAN_POINT('Ctrl Pts',(-26.2281279211609,-3.16420796624058,
134.572090618681));
#79568=CARTESIAN_POINT('Ctrl Pts',(-26.235874197245,-3.05781852601209,134.658936695355));
#79569=CARTESIAN_POINT('Ctrl Pts',(-26.2436204733291,-2.94798494474973,
134.741182664348));
#79570=CARTESIAN_POINT('Ctrl Pts',(-26.2513668065944,-2.83815055272083,
134.823429240462));
#79571=CARTESIAN_POINT('Ctrl Pts',(-26.2591131398598,-2.72487228187536,
134.901075406792));
#79572=CARTESIAN_POINT('Ctrl Pts',(-26.2668594731251,-2.60857843782391,
134.973833197668));
#79573=CARTESIAN_POINT('Ctrl Pts',(-26.2746075411281,-2.49225855057241,
135.046607282146));
#79574=CARTESIAN_POINT('Ctrl Pts',(-26.2823556091311,-2.37292207769225,
135.114490605484));
#79575=CARTESIAN_POINT('Ctrl Pts',(-26.2901036771341,-2.25102396648818,
135.177240008173));
#79576=CARTESIAN_POINT('Ctrl Pts',(-26.297859979876,-2.12899630052091,135.240056101674));
#79577=CARTESIAN_POINT('Ctrl Pts',(-26.3056162826178,-2.0044019058299,135.297727195568));
#79578=CARTESIAN_POINT('Ctrl Pts',(-26.3133725853597,-1.87771836464632,
135.350057132466));
#79579=CARTESIAN_POINT('Ctrl Pts',(-26.3211330278739,-1.75096720864244,
135.402414999426));
#79580=CARTESIAN_POINT('Ctrl Pts',(-26.328893470388,-1.62212505143446,135.44942589511));
#79581=CARTESIAN_POINT('Ctrl Pts',(-26.3366539129022,-1.49168591959197,
135.490943186965));
#79582=CARTESIAN_POINT('Ctrl Pts',(-26.3444268131676,-1.3610373952752,135.532527126062));
#79583=CARTESIAN_POINT('Ctrl Pts',(-26.3521997134331,-1.22878715082634,
135.568599735574));
#79584=CARTESIAN_POINT('Ctrl Pts',(-26.3599726136985,-1.09544159745608,
135.599065068214));
#79585=CARTESIAN_POINT('Ctrl Pts',(-26.3674629494605,-0.9669434908291,135.628422909274));
#79586=CARTESIAN_POINT('Ctrl Pts',(-26.3749532852224,-0.837428629984786,
135.652574016398));
#79587=CARTESIAN_POINT('Ctrl Pts',(-26.3824436209844,-0.707353880997542,
135.671478198798));
#79588=CARTESIAN_POINT('Ctrl Pts',(-26.3902179551035,-0.572347308366123,
135.691099139019));
#79589=CARTESIAN_POINT('Ctrl Pts',(-26.3979922892225,-0.43630989293138,
135.705129579291));
#79590=CARTESIAN_POINT('Ctrl Pts',(-26.4057666233416,-0.299744358236747,
135.713468111012));
#79591=CARTESIAN_POINT('Ctrl Pts',(-26.4135313762887,-0.163347128358413,
135.721796366237));
#79592=CARTESIAN_POINT('Ctrl Pts',(-26.4212961292358,-0.0264234607293649,
135.724446646612));
#79593=CARTESIAN_POINT('Ctrl Pts',(-26.4290608821829,0.11051520013423,135.72136879867));
#79594=CARTESIAN_POINT('Ctrl Pts',(-26.4368179230678,0.247317851589359,
135.718294007689));
#79595=CARTESIAN_POINT('Ctrl Pts',(-26.4445749639529,0.384135078307084,
135.709502419001));
#79596=CARTESIAN_POINT('Ctrl Pts',(-26.4523320048379,0.52045215884695,135.694995812799));
#79597=CARTESIAN_POINT('Ctrl Pts',(-26.460083196078,0.656666441615988,135.680500146142));
#79598=CARTESIAN_POINT('Ctrl Pts',(-26.467834387318,0.792380941732509,135.66029808145));
#79599=CARTESIAN_POINT('Ctrl Pts',(-26.4755855785582,0.927083146898066,
135.634443422367));
#79600=CARTESIAN_POINT('Ctrl Pts',(-26.4833334753352,1.06172810003313,135.608599752205));
#79601=CARTESIAN_POINT('Ctrl Pts',(-26.4910813721124,1.19536123080366,135.577108339589));
#79602=CARTESIAN_POINT('Ctrl Pts',(-26.4988292688894,1.3274775642288,135.540074542516));
#79603=CARTESIAN_POINT('Ctrl Pts',(-26.5065755449735,1.45956626176509,135.503048492116));
#79604=CARTESIAN_POINT('Ctrl Pts',(-26.5143218210576,1.59013841682948,135.460482468722));
#79605=CARTESIAN_POINT('Ctrl Pts',(-26.5220680971417,1.71870201337645,135.412532321367));
#79606=CARTESIAN_POINT('Ctrl Pts',(-26.5298144304071,1.84726655895069,135.364581820056));
#79607=CARTESIAN_POINT('Ctrl Pts',(-26.5375607636724,1.97382215010562,135.311247252101));
#79608=CARTESIAN_POINT('Ctrl Pts',(-26.5453070969378,2.09789500352166,135.252733310664));
#79609=CARTESIAN_POINT('Ctrl Pts',(-26.5530551649407,2.22199564219279,135.194206265435));
#79610=CARTESIAN_POINT('Ctrl Pts',(-26.5608032329437,2.34361208321983,135.130497705424));
#79611=CARTESIAN_POINT('Ctrl Pts',(-26.5685513009467,2.46229383948965,135.061858957027));
#79612=CARTESIAN_POINT('Ctrl Pts',(-26.5763076036885,2.58110173214252,134.993147258551));
#79613=CARTESIAN_POINT('Ctrl Pts',(-26.5840639064303,2.69696837048407,134.919495100546));
#79614=CARTESIAN_POINT('Ctrl Pts',(-26.5918202091721,2.80947057688375,134.841198258607));
#79615=CARTESIAN_POINT('Ctrl Pts',(-26.5995806516863,2.92203282909851,134.762859627286));
#79616=CARTESIAN_POINT('Ctrl Pts',(-26.6073410942005,3.03122676017127,134.67987160885));
#79617=CARTESIAN_POINT('Ctrl Pts',(-26.6151015367147,3.13666197055301,134.592570583366));
#79618=CARTESIAN_POINT('Ctrl Pts',(-26.6228744369801,3.24226643489442,134.505129414526));
#79619=CARTESIAN_POINT('Ctrl Pts',(-26.6306473372456,3.34409983042321,134.413361664914));
#79620=CARTESIAN_POINT('Ctrl Pts',(-26.638420237511,3.44180770633878,134.31764153077));
#79621=CARTESIAN_POINT('Ctrl Pts',(-26.6459105732731,3.53596365485444,134.225401064607));
#79622=CARTESIAN_POINT('Ctrl Pts',(-26.6534009090351,3.62628861113713,134.129490807449));
#79623=CARTESIAN_POINT('Ctrl Pts',(-26.6608912447972,3.71250181426558,134.030273409564));
#79624=CARTESIAN_POINT('Ctrl Pts',(-26.6686655789163,3.80198381719383,133.927294153882));
#79625=CARTESIAN_POINT('Ctrl Pts',(-26.6764399130354,3.8873195698984,133.820425819176));
#79626=CARTESIAN_POINT('Ctrl Pts',(-26.6842142471545,3.96815202009563,133.710036547175));
#79627=CARTESIAN_POINT('Ctrl Pts',(-26.6919790001016,4.0488848515222,133.599783320087));
#79628=CARTESIAN_POINT('Ctrl Pts',(-26.6997437530487,4.12512519436103,133.486018101909));
#79629=CARTESIAN_POINT('Ctrl Pts',(-26.7075085059958,4.19655440482771,133.369144076227));
#79630=CARTESIAN_POINT('Ctrl Pts',(-26.7152655468808,4.26791267079559,133.252386131475));
#79631=CARTESIAN_POINT('Ctrl Pts',(-26.7230225877658,4.33446911122874,133.132525855339));
#79632=CARTESIAN_POINT('Ctrl Pts',(-26.7307796286508,4.39594700434421,133.009997259785));
#79633=CARTESIAN_POINT('Ctrl Pts',(-26.7385308198909,4.45737853650225,132.887561063997));
#79634=CARTESIAN_POINT('Ctrl Pts',(-26.7462820111311,4.5137389696489,132.762460901986));
#79635=CARTESIAN_POINT('Ctrl Pts',(-26.7540332023712,4.56479654489694,132.635157047046));
#79636=CARTESIAN_POINT('Ctrl Pts',(-26.7617810991483,4.6158324193135,132.50790729964));
#79637=CARTESIAN_POINT('Ctrl Pts',(-26.7695289959254,4.66156977334897,132.378456084297));
#79638=CARTESIAN_POINT('Ctrl Pts',(-26.7772768927025,4.70182429635734,132.247285199339));
#79639=CARTESIAN_POINT('Ctrl Pts',(-26.7850231687866,4.74207039898729,132.116141752502));
#79640=CARTESIAN_POINT('Ctrl Pts',(-26.7927694448707,4.77683583718795,131.983279725073));
#79641=CARTESIAN_POINT('Ctrl Pts',(-26.8005157209548,4.80598578447387,131.849197304295));
#79642=CARTESIAN_POINT('Ctrl Pts',(-26.8082620542201,4.83513594693807,131.715113893751));
#79643=CARTESIAN_POINT('Ctrl Pts',(-26.8160083874854,4.85867045271556,131.579810453923));
#79644=CARTESIAN_POINT('Ctrl Pts',(-26.8237547207508,4.87650542450284,131.443796233789));
#79645=CARTESIAN_POINT('Ctrl Pts',(-26.8315027887538,4.89434439030839,131.307751554213));
#79646=CARTESIAN_POINT('Ctrl Pts',(-26.8392508567568,4.9064812314722,131.170996165166));
#79647=CARTESIAN_POINT('Ctrl Pts',(-26.8469989247598,4.9128838967222,131.034044922271));
#79648=CARTESIAN_POINT('Ctrl Pts',(-26.8547552275016,4.91929336680103,130.896948125965));
#79649=CARTESIAN_POINT('Ctrl Pts',(-26.8625115302436,4.91995646855731,130.759655451158));
#79650=CARTESIAN_POINT('Ctrl Pts',(-26.8702678329854,4.9148933085302,130.622682803111));
#79651=CARTESIAN_POINT('Ctrl Pts',(-26.8780282754996,4.90982744614213,130.485637048638));
#79652=CARTESIAN_POINT('Ctrl Pts',(-26.8857887180137,4.89902926284382,130.348912050833));
#79653=CARTESIAN_POINT('Ctrl Pts',(-26.8935491605279,4.88257074422027,130.213018085539));
#79654=CARTESIAN_POINT('Ctrl Pts',(-26.9013220607934,4.86608580492153,130.076905971187));
#79655=CARTESIAN_POINT('Ctrl Pts',(-26.9090949610588,4.84392243587731,129.94162794124));
#79656=CARTESIAN_POINT('Ctrl Pts',(-26.9168678613242,4.81620386966694,129.807684467402));
#79657=CARTESIAN_POINT('Ctrl Pts',(-26.9243581970861,4.78949294315743,129.678610176223));
#79658=CARTESIAN_POINT('Ctrl Pts',(-26.9318485328481,4.75762377267252,129.550775395638));
#79659=CARTESIAN_POINT('Ctrl Pts',(-26.9393388686101,4.72074970801481,129.424612359086));
#79660=CARTESIAN_POINT('Ctrl Pts',(-26.9471132027291,4.6824775519876,129.293665812656));
#79661=CARTESIAN_POINT('Ctrl Pts',(-26.9548875368482,4.63869225410969,129.164105481759));
#79662=CARTESIAN_POINT('Ctrl Pts',(-26.9626618709673,4.5895105469629,129.03643075419));
#79663=CARTESIAN_POINT('Ctrl Pts',(-26.9704266239144,4.54038945187474,128.908913374312));
#79664=CARTESIAN_POINT('Ctrl Pts',(-26.9781913768615,4.48588531940227,128.783277335349));
#79665=CARTESIAN_POINT('Ctrl Pts',(-26.9859561298086,4.4261651245641,128.660008651915));
#79666=CARTESIAN_POINT('Ctrl Pts',(-26.9937131706936,4.36650424466528,128.536862400675));
#79667=CARTESIAN_POINT('Ctrl Pts',(-27.0014702115786,4.30163778151859,128.416079175361));
#79668=CARTESIAN_POINT('Ctrl Pts',(-27.0092272524636,4.23178130679853,128.298126383914));
#79669=CARTESIAN_POINT('Ctrl Pts',(-27.0169784437037,4.16197751138945,128.180262541584));
#79670=CARTESIAN_POINT('Ctrl Pts',(-27.0247296349438,4.08719139286464,128.065225219659));
#79671=CARTESIAN_POINT('Ctrl Pts',(-27.0324808261839,4.00768492084337,127.953458192413));
#79672=CARTESIAN_POINT('Ctrl Pts',(-27.040228722961,3.92821224119373,127.841738669135));
#79673=CARTESIAN_POINT('Ctrl Pts',(-27.0479766197382,3.84402342452957,127.73328699392));
#79674=CARTESIAN_POINT('Ctrl Pts',(-27.0557245165153,3.75542419701934,127.628518656299));
#79675=CARTESIAN_POINT('Ctrl Pts',(-27.0634707925994,3.6668435025574,127.523772233956));
#79676=CARTESIAN_POINT('Ctrl Pts',(-27.0712170686834,3.57385448457397,127.422707915029));
#79677=CARTESIAN_POINT('Ctrl Pts',(-27.0789633447675,3.47680340509713,127.325708415232));
#79678=CARTESIAN_POINT('Ctrl Pts',(-27.0867096780328,3.3797516092114,127.228708199407));
#79679=CARTESIAN_POINT('Ctrl Pts',(-27.0944560112982,3.27863796852657,127.135773138967));
#79680=CARTESIAN_POINT('Ctrl Pts',(-27.1022023445635,3.17384559089952,127.047249063775));
#79681=CARTESIAN_POINT('Ctrl Pts',(-27.1099504125665,3.06902974574608,126.958705164231));
#79682=CARTESIAN_POINT('Ctrl Pts',(-27.1176984805694,2.96053382293475,126.87457446781));
#79683=CARTESIAN_POINT('Ctrl Pts',(-27.1254465485724,2.84877366058778,126.795162232198));
#79684=CARTESIAN_POINT('Ctrl Pts',(-27.1332028513143,2.73689471821015,126.715665596316));
#79685=CARTESIAN_POINT('Ctrl Pts',(-27.1409591540561,2.62174492526147,126.640897665735));
#79686=CARTESIAN_POINT('Ctrl Pts',(-27.148715456798,2.5037691955234,126.57112038365));
#79687=CARTESIAN_POINT('Ctrl Pts',(-27.1564758993121,2.38573049858618,126.501305859328));
#79688=CARTESIAN_POINT('Ctrl Pts',(-27.1642363418263,2.26486320384756,126.43648747575));
#79689=CARTESIAN_POINT('Ctrl Pts',(-27.1719967843405,2.14163553079064,126.376880485961));
#79690=CARTESIAN_POINT('Ctrl Pts',(-27.1797696846059,2.01821004173328,126.317177809741));
#79691=CARTESIAN_POINT('Ctrl Pts',(-27.1875425848713,1.89241696152696,126.262703400281));
#79692=CARTESIAN_POINT('Ctrl Pts',(-27.1953154851368,1.7647439614108,126.213624095703));
#79693=CARTESIAN_POINT('Ctrl Pts',(-27.2028058208989,1.64171219643653,126.16632894747));
#79694=CARTESIAN_POINT('Ctrl Pts',(-27.2102961566609,1.5169351099634,126.124043561736));
#79695=CARTESIAN_POINT('Ctrl Pts',(-27.217786492423,1.39085924154083,126.0868725537));
#79696=CARTESIAN_POINT('Ctrl Pts',(-27.2255608265422,1.2600031682482,126.048292195597));
#79697=CARTESIAN_POINT('Ctrl Pts',(-27.2333351606612,1.12733336950668,126.015099483229));
#79698=CARTESIAN_POINT('Ctrl Pts',(-27.2411094947803,0.993333091223592,
125.98746613747));
#79699=CARTESIAN_POINT('Ctrl Pts',(-27.2488742477274,0.859497956307722,
125.95986684734));
#79700=CARTESIAN_POINT('Ctrl Pts',(-27.2566390006746,0.724335983591141,
125.937813369736));
#79701=CARTESIAN_POINT('Ctrl Pts',(-27.2644037536217,0.588346325010557,
125.921427926616));
#79702=CARTESIAN_POINT('Ctrl Pts',(-27.2721607945067,0.452491733275992,
125.905058757749));
#79703=CARTESIAN_POINT('Ctrl Pts',(-27.2799178353917,0.315811477278347,
125.894346466732));
#79704=CARTESIAN_POINT('Ctrl Pts',(-27.2876748762767,0.178815322311946,
125.889362332418));
#79705=CARTESIAN_POINT('Ctrl Pts',(-27.2954260675168,0.0419224772116804,
125.884381956679));
#79706=CARTESIAN_POINT('Ctrl Pts',(-27.3031772587569,-0.0952854035653323,
125.885121153803));
#79707=CARTESIAN_POINT('Ctrl Pts',(-27.3109284499971,-0.232293359175477,
125.891599392167));
#79708=CARTESIAN_POINT('Ctrl Pts',(-27.3186763467742,-0.369243082749681,
125.898074877107));
#79709=CARTESIAN_POINT('Ctrl Pts',(-27.3264242435513,-0.505992660451609,
125.910284533385));
#79710=CARTESIAN_POINT('Ctrl Pts',(-27.3341721403284,-0.642027276711597,
125.928195727157));
#79711=CARTESIAN_POINT('Ctrl Pts',(-27.3419184164125,-0.77803343746243,
125.946103174293));
#79712=CARTESIAN_POINT('Ctrl Pts',(-27.3496646924965,-0.913324546869294,
125.969709735695));
#79713=CARTESIAN_POINT('Ctrl Pts',(-27.3574109685806,-1.04739145227851,
125.998930958504));
#79714=CARTESIAN_POINT('Ctrl Pts',(-27.365157301846,-1.18145934733917,126.028152397017));
#79715=CARTESIAN_POINT('Ctrl Pts',(-27.3729036351113,-1.3143026383731,126.06298849638));
#79716=CARTESIAN_POINT('Ctrl Pts',(-27.3806499683767,-1.44542328976766,
126.10330386659));
#79717=CARTESIAN_POINT('Ctrl Pts',(-27.3883980363797,-1.5765733047228,126.143628265148));
#79718=CARTESIAN_POINT('Ctrl Pts',(-27.3961461043827,-1.70599953876617,
126.189434261352));
#79719=CARTESIAN_POINT('Ctrl Pts',(-27.4038941723857,-1.83322039930074,
126.240536998046));
#79720=CARTESIAN_POINT('Ctrl Pts',(-27.4116504751275,-1.96057647168002,
126.291694047337));
#79721=CARTESIAN_POINT('Ctrl Pts',(-27.4194067778694,-2.08572212499398,
126.34815893657));
#79722=CARTESIAN_POINT('Ctrl Pts',(-27.4271630806113,-2.20819649224858,
126.409698933873));
#79723=CARTESIAN_POINT('Ctrl Pts',(-27.4349235231255,-2.33073622776078,
126.471271776925));
#79724=CARTESIAN_POINT('Ctrl Pts',(-27.4426839656396,-2.45060149477074,
126.537924935528));
#79725=CARTESIAN_POINT('Ctrl Pts',(-27.4504444081538,-2.56735811072846,
126.609380832898));
#79726=CARTESIAN_POINT('Ctrl Pts',(-27.4582173084192,-2.68430215477111,
126.680951437617));
#79727=CARTESIAN_POINT('Ctrl Pts',(-27.4659902086847,-2.79812725076357,
126.757339969715));
#79728=CARTESIAN_POINT('Ctrl Pts',(-27.4737631089501,-2.90842943485161,
126.838226317648));
#79729=CARTESIAN_POINT('Ctrl Pts',(-27.4812534447121,-3.01472185671256,
126.916172243092));
#79730=CARTESIAN_POINT('Ctrl Pts',(-27.488743780474,-3.11774281240201,126.998294455943));
#79731=CARTESIAN_POINT('Ctrl Pts',(-27.4962341162359,-3.21716292065497,
127.084273816904));
#79732=CARTESIAN_POINT('Ctrl Pts',(-27.5038934172043,-3.31882572398132,
127.172192679768));
#79733=CARTESIAN_POINT('Ctrl Pts',(-27.5115527181727,-3.41706547671011,
127.264441057515));
#79734=CARTESIAN_POINT('Ctrl Pts',(-27.519212019141,-3.51148264535747,127.360718258979));
#79735=CARTESIAN_POINT('Ctrl Pts',(-27.5268625104388,-3.6057912160842,127.456884723127));
#79736=CARTESIAN_POINT('Ctrl Pts',(-27.5345130017364,-3.69628566326201,
127.557070515036));
#79737=CARTESIAN_POINT('Ctrl Pts',(-27.5421634930342,-3.78259884884492,
127.660934300437));
#79738=CARTESIAN_POINT('Ctrl Pts',(-27.5498069570394,-3.86883275219898,
127.764702682658));
#79739=CARTESIAN_POINT('Ctrl Pts',(-27.5574504210446,-3.95089277429838,
127.872142033216));
#79740=CARTESIAN_POINT('Ctrl Pts',(-27.5650938850498,-4.02844845775133,
127.98287411472));
#79741=CARTESIAN_POINT('Ctrl Pts',(-27.5727320974051,-4.10595085446164,
128.093530114735));
#79742=CARTESIAN_POINT('Ctrl Pts',(-27.5803703097604,-4.1789548374162,128.207474016999));
#79743=CARTESIAN_POINT('Ctrl Pts',(-27.5880085221157,-4.2471704704547,128.324294881059));
#79744=CARTESIAN_POINT('Ctrl Pts',(-27.5956438189238,-4.31536006521479,
128.441071153959));
#79745=CARTESIAN_POINT('Ctrl Pts',(-27.6032791157318,-4.37876474033592,
128.560721857964));
#79746=CARTESIAN_POINT('Ctrl Pts',(-27.6109144125398,-4.43713837373944,
128.682807857254));
#79747=CARTESIAN_POINT('Ctrl Pts',(-27.6185480443435,-4.49549927779408,
128.804867233646));
#79748=CARTESIAN_POINT('Ctrl Pts',(-27.6261816761471,-4.54883115212521,
128.929360483547));
#79749=CARTESIAN_POINT('Ctrl Pts',(-27.6338153079508,-4.59693455979449,
129.055825311812));
#79750=CARTESIAN_POINT('Ctrl Pts',(-27.6414504912618,-4.64504774430282,
129.182315843585));
#79751=CARTESIAN_POINT('Ctrl Pts',(-27.6490856745728,-4.68793019774338,
129.310778376485));
#79752=CARTESIAN_POINT('Ctrl Pts',(-27.6567208578838,-4.72543132371363,
129.440732417738));
#79753=CARTESIAN_POINT('Ctrl Pts',(-27.6594860554192,-4.73901292573772,
129.487797246435));
#79754=CARTESIAN_POINT('Ctrl Pts',(-27.6622512529547,-4.75188916809314,
129.535057564754));
#79755=CARTESIAN_POINT('Ctrl Pts',(-27.6650164504902,-4.76405452823402,
129.582490119308));
#79756=CARTESIAN_POINT('Ctrl Pts',(-25.9153671414536,-4.76405452823411,
129.582490119308));
#79757=CARTESIAN_POINT('Ctrl Pts',(-25.923282705383,-4.79884987132734,129.718156633936));
#79758=CARTESIAN_POINT('Ctrl Pts',(-25.9311982693124,-4.82787263050501,
129.855414641848));
#79759=CARTESIAN_POINT('Ctrl Pts',(-25.9391138332419,-4.85098804002467,
129.993744741804));
#79760=CARTESIAN_POINT('Ctrl Pts',(-25.9470236550876,-4.87408668123604,
130.13197449477));
#79761=CARTESIAN_POINT('Ctrl Pts',(-25.9549334769334,-4.89128645037956,
130.271274429011));
#79762=CARTESIAN_POINT('Ctrl Pts',(-25.9628432987791,-4.90250346835763,
130.411114123314));
#79763=CARTESIAN_POINT('Ctrl Pts',(-25.9702757205222,-4.9130434792377,130.542513743276));
#79764=CARTESIAN_POINT('Ctrl Pts',(-25.9777081422654,-4.91830152752587,
130.67438958289));
#79765=CARTESIAN_POINT('Ctrl Pts',(-25.9851405640086,-4.91824961917742,
130.806296066141));
#79766=CARTESIAN_POINT('',(-25.6398594359502,-4.91824793218808,130.799850625585));
#79767=CARTESIAN_POINT('Ctrl Pts',(-25.5699526237868,-4.76405452823406,
129.582490119308));
#79768=CARTESIAN_POINT('Ctrl Pts',(-25.5799243591641,-4.80753248471586,
129.752010011761));
#79769=CARTESIAN_POINT('Ctrl Pts',(-25.5898960945415,-4.84198469666304,
129.923954638454));
#79770=CARTESIAN_POINT('Ctrl Pts',(-25.5998678299188,-4.86718685273507,
130.097483539806));
#79771=CARTESIAN_POINT('Ctrl Pts',(-25.6096542149229,-4.891920561856,130.267786959792));
#79772=CARTESIAN_POINT('Ctrl Pts',(-25.6194405999269,-4.9077449112389,130.439616485704));
#79773=CARTESIAN_POINT('Ctrl Pts',(-25.6292269849311,-4.91449288853822,
130.612155750283));
#79774=CARTESIAN_POINT('Ctrl Pts',(-25.6327711352708,-4.9169366761092,130.674641039071));
#79775=CARTESIAN_POINT('Ctrl Pts',(-25.6363152856105,-4.91819049968701,
130.737219188364));
#79776=CARTESIAN_POINT('Ctrl Pts',(-25.6398594359502,-4.91824793218808,
130.799850625585));
#79777=CARTESIAN_POINT('Ctrl Pts',(-25.6398594359912,-4.91824793218874,
130.799850626309));
#79778=CARTESIAN_POINT('Ctrl Pts',(-25.6475321901618,-4.91837226816469,
130.935441832968));
#79779=CARTESIAN_POINT('Ctrl Pts',(-25.6552049443324,-4.91288521422851,
131.071167098629));
#79780=CARTESIAN_POINT('Ctrl Pts',(-25.6628776985029,-4.90178036831504,
131.206520142259));
#79781=CARTESIAN_POINT('Ctrl Pts',(-25.6705464539726,-4.89068130975733,
131.341802645854));
#79782=CARTESIAN_POINT('Ctrl Pts',(-25.6782152094422,-4.87397031425118,
131.476712915772));
#79783=CARTESIAN_POINT('Ctrl Pts',(-25.6858839649119,-4.85169305430979,
131.61074611425));
#79784=CARTESIAN_POINT('Ctrl Pts',(-25.6935507019143,-4.82942165789072,
131.744744034302));
#79785=CARTESIAN_POINT('Ctrl Pts',(-25.7012174389168,-4.80158697541088,
131.877864947818));
#79786=CARTESIAN_POINT('Ctrl Pts',(-25.7088841759192,-4.7682863246519,132.009611043261));
#79787=CARTESIAN_POINT('Ctrl Pts',(-25.7165506385416,-4.73498686566862,
132.141352423727));
#79788=CARTESIAN_POINT('Ctrl Pts',(-25.7242171011641,-4.69622192537889,
132.271718696317));
#79789=CARTESIAN_POINT('Ctrl Pts',(-25.7318835637865,-4.65213941487484,
132.400224624011));
#79790=CARTESIAN_POINT('Ctrl Pts',(-25.7395514956454,-4.60804845619458,
132.528755179176));
#79791=CARTESIAN_POINT('Ctrl Pts',(-25.7472194275042,-4.55863803045239,
132.655424302297));
#79792=CARTESIAN_POINT('Ctrl Pts',(-25.754887359363,-4.5041049791734,132.77976472789));
#79793=CARTESIAN_POINT('Ctrl Pts',(-25.7625632282976,-4.44951548073676,
132.904233858249));
#79794=CARTESIAN_POINT('Ctrl Pts',(-25.7702390972321,-4.3897929272935,133.026369110101));
#79795=CARTESIAN_POINT('Ctrl Pts',(-25.7779149661667,-4.32518130200142,
133.145725554375));
#79796=CARTESIAN_POINT('Ctrl Pts',(-25.7855948590658,-4.26053580498894,
133.265144569557));
#79797=CARTESIAN_POINT('Ctrl Pts',(-25.7932747519649,-4.19099633650859,
133.381781532978));
#79798=CARTESIAN_POINT('Ctrl Pts',(-25.8009546448639,-4.11685074135035,
133.495219780722));
#79799=CARTESIAN_POINT('Ctrl Pts',(-25.8086467760269,-4.04258699176298,
133.608838797552));
#79800=CARTESIAN_POINT('Ctrl Pts',(-25.8163389071898,-3.96370268422352,
133.71924859037));
#79801=CARTESIAN_POINT('Ctrl Pts',(-25.8240310383528,-3.88052698662211,
133.826064337092));
#79802=CARTESIAN_POINT('Ctrl Pts',(-25.8310664820746,-3.80445210865978,
133.923761081822));
#79803=CARTESIAN_POINT('Ctrl Pts',(-25.8381019257964,-3.72478791801777,
134.018451483989));
#79804=CARTESIAN_POINT('Ctrl Pts',(-25.8451373695182,-3.64181246816916,
134.109868900597));
#79805=CARTESIAN_POINT('Ctrl Pts',(-25.8529117036373,-3.55012260519602,
134.210887339394));
#79806=CARTESIAN_POINT('Ctrl Pts',(-25.8606860377563,-3.45408117576585,
134.308247883175));
#79807=CARTESIAN_POINT('Ctrl Pts',(-25.8684603718754,-3.35401157386546,
134.40155249803));
#79808=CARTESIAN_POINT('Ctrl Pts',(-25.8762251248225,-3.2540652988062,134.494742123286));
#79809=CARTESIAN_POINT('Ctrl Pts',(-25.8839898777696,-3.15010101208414,
134.583885501219));
#79810=CARTESIAN_POINT('Ctrl Pts',(-25.8917546307167,-3.0424814406506,134.668618598834));
#79811=CARTESIAN_POINT('Ctrl Pts',(-25.8995116716017,-2.93496875849244,
134.753267538343));
#79812=CARTESIAN_POINT('Ctrl Pts',(-25.9072687124867,-2.82380832163516,
134.833514674342));
#79813=CARTESIAN_POINT('Ctrl Pts',(-25.9150257533717,-2.70939842098782,
134.909033961311));
#79814=CARTESIAN_POINT('Ctrl Pts',(-25.9227769446118,-2.59507479773668,
134.984496298598));
#79815=CARTESIAN_POINT('Ctrl Pts',(-25.9305281358518,-2.477506913131,135.055237668877));
#79816=CARTESIAN_POINT('Ctrl Pts',(-25.9382793270919,-2.35712444610986,
135.120973573119));
#79817=CARTESIAN_POINT('Ctrl Pts',(-25.946027223869,-2.23679314484834,135.186681537849));
#79818=CARTESIAN_POINT('Ctrl Pts',(-25.9537751206461,-2.11364998288739,
135.247388080909));
#79819=CARTESIAN_POINT('Ctrl Pts',(-25.9615230174232,-1.98815161758541,
135.302853277112));
#79820=CARTESIAN_POINT('Ctrl Pts',(-25.9692692935073,-1.86267950383601,
135.358306871192));
#79821=CARTESIAN_POINT('Ctrl Pts',(-25.9770155695914,-1.73485352403987,
135.408521141224));
#79822=CARTESIAN_POINT('Ctrl Pts',(-25.9847618456755,-1.60515245427527,
135.453303364152));
#79823=CARTESIAN_POINT('Ctrl Pts',(-25.9925081789408,-1.47545042708684,
135.498085917652));
#79824=CARTESIAN_POINT('Ctrl Pts',(-26.0002545122062,-1.34387365186748,
135.537436216435));
#79825=CARTESIAN_POINT('Ctrl Pts',(-26.0080008454715,-1.21091790655001,
135.57121082353));
#79826=CARTESIAN_POINT('Ctrl Pts',(-26.0157489134745,-1.07793238671522,
135.604992994213));
#79827=CARTESIAN_POINT('Ctrl Pts',(-26.0234969814775,-0.943567661142076,
135.633196892322));
#79828=CARTESIAN_POINT('Ctrl Pts',(-26.0312450494805,-0.808331196273148,
135.655729881973));
#79829=CARTESIAN_POINT('Ctrl Pts',(-26.0390013522223,-0.672951000480024,
135.678286819953));
#79830=CARTESIAN_POINT('Ctrl Pts',(-26.046757654964,-0.536697600881362,
135.695160745317));
#79831=CARTESIAN_POINT('Ctrl Pts',(-26.0545139577059,-0.400085666502281,
135.706310690951));
#79832=CARTESIAN_POINT('Ctrl Pts',(-26.0622744002201,-0.263400818220329,
135.717466587647));
#79833=CARTESIAN_POINT('Ctrl Pts',(-26.0700348427343,-0.126357444323342,
135.722892401686));
#79834=CARTESIAN_POINT('Ctrl Pts',(-26.0777952852485,0.0105292488120982,
135.722599346768));
#79835=CARTESIAN_POINT('Ctrl Pts',(-26.0855681855139,0.147635684619589,
135.722305821411));
#79836=CARTESIAN_POINT('Ctrl Pts',(-26.0933410857793,0.284584546241221,
135.716275098869));
#79837=CARTESIAN_POINT('Ctrl Pts',(-26.1011139860448,0.42086431009477,135.704570439093));
#79838=CARTESIAN_POINT('Ctrl Pts',(-26.1086043218068,0.552189961265159,
135.693291273182));
#79839=CARTESIAN_POINT('Ctrl Pts',(-26.116094657569,0.682894011287214,135.676743570525));
#79840=CARTESIAN_POINT('Ctrl Pts',(-26.123584993331,0.812529140113618,135.655028557032));
#79841=CARTESIAN_POINT('Ctrl Pts',(-26.1313593274501,0.947079424250089,
135.632490212203));
#79842=CARTESIAN_POINT('Ctrl Pts',(-26.1391336615691,1.08090434567657,135.604313589666));
#79843=CARTESIAN_POINT('Ctrl Pts',(-26.1469079956882,1.21349422484095,135.57055562289));
#79844=CARTESIAN_POINT('Ctrl Pts',(-26.1546727486353,1.34592069882933,135.536839259791));
#79845=CARTESIAN_POINT('Ctrl Pts',(-26.1624375015824,1.47711478379883,135.497555334171));
#79846=CARTESIAN_POINT('Ctrl Pts',(-26.1702022545295,1.60657414570291,135.452812249761));
#79847=CARTESIAN_POINT('Ctrl Pts',(-26.1779592954145,1.73590492674369,135.408113604814));
#79848=CARTESIAN_POINT('Ctrl Pts',(-26.1857163362995,1.86350404634305,135.357966718211));
#79849=CARTESIAN_POINT('Ctrl Pts',(-26.1934733771845,1.98888190720445,135.302530447807));
#79850=CARTESIAN_POINT('Ctrl Pts',(-26.2012245684247,2.11416521964568,135.247135982326));
#79851=CARTESIAN_POINT('Ctrl Pts',(-26.2089757596649,2.23723025134615,135.186460229902));
#79852=CARTESIAN_POINT('Ctrl Pts',(-26.216726950905,2.35760539325344,135.12071091292));
#79853=CARTESIAN_POINT('Ctrl Pts',(-26.2244748476821,2.47792937251415,135.054989541152));
#79854=CARTESIAN_POINT('Ctrl Pts',(-26.2322227444591,2.59556539346812,134.984199080762));
#79855=CARTESIAN_POINT('Ctrl Pts',(-26.2399706412362,2.71006476580336,134.908594045096));
#79856=CARTESIAN_POINT('Ctrl Pts',(-26.2477169173203,2.82454018733822,134.833004824373));
#79857=CARTESIAN_POINT('Ctrl Pts',(-26.2554631934044,2.93587993926146,134.752603246854));
#79858=CARTESIAN_POINT('Ctrl Pts',(-26.2632094694885,3.0436630880413,134.667687948895));
#79859=CARTESIAN_POINT('Ctrl Pts',(-26.2709558027539,3.15144703245185,134.58277202411));
#79860=CARTESIAN_POINT('Ctrl Pts',(-26.2787021360192,3.25567401422449,134.493342554348));
#79861=CARTESIAN_POINT('Ctrl Pts',(-26.2864484692846,3.35595537568815,134.399739120435));
#79862=CARTESIAN_POINT('Ctrl Pts',(-26.2941965372875,3.45625919446753,134.306114724682));
#79863=CARTESIAN_POINT('Ctrl Pts',(-26.3019446052905,3.55261534893573,134.208314771496));
#79864=CARTESIAN_POINT('Ctrl Pts',(-26.3096926732935,3.64467160389241,134.106716134811));
#79865=CARTESIAN_POINT('Ctrl Pts',(-26.3174489760354,3.73682569733222,134.005009517886));
#79866=CARTESIAN_POINT('Ctrl Pts',(-26.3252052787772,3.82467049929258,133.899496442735));
#79867=CARTESIAN_POINT('Ctrl Pts',(-26.332961581519,3.90789335180106,133.790587771258));
#79868=CARTESIAN_POINT('Ctrl Pts',(-26.3407220240332,3.99116062285183,133.681620971944));
#79869=CARTESIAN_POINT('Ctrl Pts',(-26.3484824665474,4.0698008049323,133.569255285236));
#79870=CARTESIAN_POINT('Ctrl Pts',(-26.3562429090615,4.14354485081241,133.453930230127));
#79871=CARTESIAN_POINT('Ctrl Pts',(-26.364015809327,4.21740727718156,133.338420045001));
#79872=CARTESIAN_POINT('Ctrl Pts',(-26.3717887095925,4.28635766437638,133.219941336283));
#79873=CARTESIAN_POINT('Ctrl Pts',(-26.3795616098579,4.35017274379426,133.098958656798));
#79874=CARTESIAN_POINT('Ctrl Pts',(-26.3870519456199,4.4116679843349,132.98237400245));
#79875=CARTESIAN_POINT('Ctrl Pts',(-26.3945422813819,4.46839466509504,132.86346454595));
#79876=CARTESIAN_POINT('Ctrl Pts',(-26.4020326171439,4.52019616288691,132.7426613454));
#79877=CARTESIAN_POINT('Ctrl Pts',(-26.409806951263,4.5739617302122,132.617277854784));
#79878=CARTESIAN_POINT('Ctrl Pts',(-26.4175812853821,4.62259157855505,132.489457005536));
#79879=CARTESIAN_POINT('Ctrl Pts',(-26.4253556195011,4.66585811340718,132.359658379428));
#79880=CARTESIAN_POINT('Ctrl Pts',(-26.4331203724482,4.70907132612194,132.230019718526));
#79881=CARTESIAN_POINT('Ctrl Pts',(-26.4408851253953,4.74693425443892,132.098408497871));
#79882=CARTESIAN_POINT('Ctrl Pts',(-26.4486498783424,4.77926657766478,131.965305940187));
#79883=CARTESIAN_POINT('Ctrl Pts',(-26.4564069192274,4.81156678797144,131.83233558184));
#79884=CARTESIAN_POINT('Ctrl Pts',(-26.4641639601125,4.83834723296443,131.697877211612));
#79885=CARTESIAN_POINT('Ctrl Pts',(-26.4719210009975,4.8594769249571,131.562428608125));
#79886=CARTESIAN_POINT('Ctrl Pts',(-26.4796721922376,4.88059068288468,131.427082147482));
#79887=CARTESIAN_POINT('Ctrl Pts',(-26.4874233834778,4.89606210960789,131.290747324657));
#79888=CARTESIAN_POINT('Ctrl Pts',(-26.4951745747179,4.90581105164078,131.153933196724));
#79889=CARTESIAN_POINT('Ctrl Pts',(-26.502922471495,4.91555585011323,131.017177218445));
#79890=CARTESIAN_POINT('Ctrl Pts',(-26.510670368272,4.91958297364262,130.879942729398));
#79891=CARTESIAN_POINT('Ctrl Pts',(-26.5184182650491,4.91786402344031,130.742744796128));
#79892=CARTESIAN_POINT('Ctrl Pts',(-26.5261645411332,4.91614543280533,130.605575561708));
#79893=CARTESIAN_POINT('Ctrl Pts',(-26.5339108172173,4.90868316408747,130.468443258544));
#79894=CARTESIAN_POINT('Ctrl Pts',(-26.5416570933014,4.89550094365343,130.331863450179));
#79895=CARTESIAN_POINT('Ctrl Pts',(-26.5494034265667,4.88231862591124,130.195282633614));
#79896=CARTESIAN_POINT('Ctrl Pts',(-26.557149759832,4.86341630975927,130.059254709144));
#79897=CARTESIAN_POINT('Ctrl Pts',(-26.5648960930973,4.83886961520092,129.924290217209));
#79898=CARTESIAN_POINT('Ctrl Pts',(-26.5726441611003,4.81431742358058,129.789295500911));
#79899=CARTESIAN_POINT('Ctrl Pts',(-26.5803922291033,4.78411840824743,129.655365075616));
#79900=CARTESIAN_POINT('Ctrl Pts',(-26.5881402971062,4.74839925218484,129.52299899634));
#79901=CARTESIAN_POINT('Ctrl Pts',(-26.5958965998481,4.71264213337798,129.39049223682));
#79902=CARTESIAN_POINT('Ctrl Pts',(-26.6036529025899,4.67135325615571,129.259553522617));
#79903=CARTESIAN_POINT('Ctrl Pts',(-26.6114092053318,4.62470929100075,129.130667982632));
#79904=CARTESIAN_POINT('Ctrl Pts',(-26.6191696478459,4.5780404305571,129.001713652554));
#79905=CARTESIAN_POINT('Ctrl Pts',(-26.6269300903601,4.52601093527567,128.874815041814));
#79906=CARTESIAN_POINT('Ctrl Pts',(-26.6346905328743,4.46884515833365,128.750436078218));
#79907=CARTESIAN_POINT('Ctrl Pts',(-26.6424634331397,4.41158761381155,128.625857450467));
#79908=CARTESIAN_POINT('Ctrl Pts',(-26.6502363334052,4.34917748916139,128.503806900878));
#79909=CARTESIAN_POINT('Ctrl Pts',(-26.6580092336706,4.28188494369869,128.384723373799));
#79910=CARTESIAN_POINT('Ctrl Pts',(-26.6654995694327,4.2170386517627,128.269968832881));
#79911=CARTESIAN_POINT('Ctrl Pts',(-26.6729899051948,4.14765891489515,128.15796960401));
#79912=CARTESIAN_POINT('Ctrl Pts',(-26.6804802409569,4.0740237358259,128.049090456143));
#79913=CARTESIAN_POINT('Ctrl Pts',(-26.688254575076,3.99759665656185,127.936083122292));
#79914=CARTESIAN_POINT('Ctrl Pts',(-26.696028909195,3.91634297689393,127.826079162396));
#79915=CARTESIAN_POINT('Ctrl Pts',(-26.7038032433141,3.83052633559218,127.719518473333));
#79916=CARTESIAN_POINT('Ctrl Pts',(-26.7115679962612,3.74481545563165,127.613089110797));
#79917=CARTESIAN_POINT('Ctrl Pts',(-26.7193327492083,3.6545530458801,127.510094877324));
#79918=CARTESIAN_POINT('Ctrl Pts',(-26.7270975021554,3.56004650490541,127.410947594456));
#79919=CARTESIAN_POINT('Ctrl Pts',(-26.7348545430404,3.46563382915901,127.311898786068));
#79920=CARTESIAN_POINT('Ctrl Pts',(-26.7426115839254,3.36698567889441,127.216689605797));
#79921=CARTESIAN_POINT('Ctrl Pts',(-26.7503686248104,3.26445004731979,127.125699318798));
#79922=CARTESIAN_POINT('Ctrl Pts',(-26.7581198160506,3.16199173866268,127.034777648283));
#79923=CARTESIAN_POINT('Ctrl Pts',(-26.7658710072906,3.05565207507122,126.948068796906));
#79924=CARTESIAN_POINT('Ctrl Pts',(-26.7736221985307,2.94581601576378,126.865915357851));
#79925=CARTESIAN_POINT('Ctrl Pts',(-26.7813700953078,2.83602663971152,126.783796836199));
#79926=CARTESIAN_POINT('Ctrl Pts',(-26.789117992085,2.72274413602858,126.706230109651));
#79927=CARTESIAN_POINT('Ctrl Pts',(-26.7968658888621,2.6063864945491,126.633517476961));
#79928=CARTESIAN_POINT('Ctrl Pts',(-26.8046121649462,2.49005319257984,126.560820054186));
#79929=CARTESIAN_POINT('Ctrl Pts',(-26.8123584410303,2.37064636362032,126.492974912698));
#79930=CARTESIAN_POINT('Ctrl Pts',(-26.8201047171144,2.24861259056381,126.430240765521));
#79931=CARTESIAN_POINT('Ctrl Pts',(-26.8278510503798,2.12657791668171,126.367506155254));
#79932=CARTESIAN_POINT('Ctrl Pts',(-26.8355973836451,2.00191660771909,126.309882793331));
#79933=CARTESIAN_POINT('Ctrl Pts',(-26.8433437169105,1.87509907026491,126.25758301808));
#79934=CARTESIAN_POINT('Ctrl Pts',(-26.8510917849134,1.74825313290234,126.205271530656));
#79935=CARTESIAN_POINT('Ctrl Pts',(-26.8588398529165,1.61925036755467,126.158286151231));
#79936=CARTESIAN_POINT('Ctrl Pts',(-26.8665879209194,1.48857995991605,126.116790589776));
#79937=CARTESIAN_POINT('Ctrl Pts',(-26.8743442236613,1.35777067421338,126.075250926344));
#79938=CARTESIAN_POINT('Ctrl Pts',(-26.8821005264031,1.22529057890167,126.03921285473));
#79939=CARTESIAN_POINT('Ctrl Pts',(-26.889856829145,1.09164332137603,126.008789961075));
#79940=CARTESIAN_POINT('Ctrl Pts',(-26.8976172716592,0.957924732285,125.978350829806));
#79941=CARTESIAN_POINT('Ctrl Pts',(-26.9053777141734,0.823038124023069,
125.953532918962));
#79942=CARTESIAN_POINT('Ctrl Pts',(-26.9131381566875,0.687495080565086,
125.934398238173));
#79943=CARTESIAN_POINT('Ctrl Pts',(-26.920911056953,0.551734451380798,125.915232840697));
#79944=CARTESIAN_POINT('Ctrl Pts',(-26.9286839572184,0.41531567053489,125.901768942808));
#79945=CARTESIAN_POINT('Ctrl Pts',(-26.9364568574838,0.278754062048078,
125.894016511967));
#79946=CARTESIAN_POINT('Ctrl Pts',(-26.9439471932458,0.147156812008808,
125.886545901514));
#79947=CARTESIAN_POINT('Ctrl Pts',(-26.9514375290078,0.0154272463080015,
125.884378720139));
#79948=CARTESIAN_POINT('Ctrl Pts',(-26.9589278647697,-0.115977477334406,
125.887478242803));
#79949=CARTESIAN_POINT('Ctrl Pts',(-26.9667021988888,-0.25236445101447,
125.890695284812));
#79950=CARTESIAN_POINT('Ctrl Pts',(-26.9744765330078,-0.388833496541188,
125.89959647942));
#79951=CARTESIAN_POINT('Ctrl Pts',(-26.9822508671269,-0.524872013016396,
125.914197794873));
#79952=CARTESIAN_POINT('Ctrl Pts',(-26.990015620074,-0.660742874177605,
125.928781115509));
#79953=CARTESIAN_POINT('Ctrl Pts',(-26.9977803730211,-0.796183876999741,
125.949050538231));
#79954=CARTESIAN_POINT('Ctrl Pts',(-27.0055451259682,-0.930682387920349,
125.97497003952));
#79955=CARTESIAN_POINT('Ctrl Pts',(-27.0133021668531,-1.06504731302363,
126.000863797196));
#79956=CARTESIAN_POINT('Ctrl Pts',(-27.0210592077381,-1.19847122768184,
126.032396392324));
#79957=CARTESIAN_POINT('Ctrl Pts',(-27.028816248623,-1.33044694654991,126.069480050443));
#79958=CARTESIAN_POINT('Ctrl Pts',(-27.0365674398632,-1.46232314150229,
126.106535743488));
#79959=CARTESIAN_POINT('Ctrl Pts',(-27.0443186311033,-1.59275293954911,
126.149134062013));
#79960=CARTESIAN_POINT('Ctrl Pts',(-27.0520698223434,-1.721240027483,126.197136308908));
#79961=CARTESIAN_POINT('Ctrl Pts',(-27.0598177191205,-1.84967250497719,
126.245118153568));
#79962=CARTESIAN_POINT('Ctrl Pts',(-27.0675656158976,-1.97616354914584,
126.298499221871));
#79963=CARTESIAN_POINT('Ctrl Pts',(-27.0753135126747,-2.10023289376968,
126.357091246994));
#79964=CARTESIAN_POINT('Ctrl Pts',(-27.0830597887588,-2.22427628576092,
126.415671015928));
#79965=CARTESIAN_POINT('Ctrl Pts',(-27.0908060648428,-2.34589863249586,
126.479459406724));
#79966=CARTESIAN_POINT('Ctrl Pts',(-27.0985523409269,-2.46464088241683,
126.548220537256));
#79967=CARTESIAN_POINT('Ctrl Pts',(-27.1062986741922,-2.58338400886595,
126.616982175367));
#79968=CARTESIAN_POINT('Ctrl Pts',(-27.1140450074575,-2.69924665774559,
126.690716430541));
#79969=CARTESIAN_POINT('Ctrl Pts',(-27.1217913407229,-2.81179591655585,
126.769142310443));
#79970=CARTESIAN_POINT('Ctrl Pts',(-27.1295394087258,-2.92437037999225,
126.847585753277));
#79971=CARTESIAN_POINT('Ctrl Pts',(-27.1372874767288,-3.03362965613461,
126.930722688052));
#79972=CARTESIAN_POINT('Ctrl Pts',(-27.1450355447318,-3.13917159433288,
127.018230038223));
#79973=CARTESIAN_POINT('Ctrl Pts',(-27.1527918474736,-3.24482570375917,
127.105830392248));
#79974=CARTESIAN_POINT('Ctrl Pts',(-27.1605481502154,-3.34675428158102,
127.197810190479));
#79975=CARTESIAN_POINT('Ctrl Pts',(-27.1683044529572,-3.44458953084251,
127.293807096181));
#79976=CARTESIAN_POINT('Ctrl Pts',(-27.1760648954714,-3.54247699772243,
127.389855238322));
#79977=CARTESIAN_POINT('Ctrl Pts',(-27.1838253379856,-3.63626651554925,
127.489924475017));
#79978=CARTESIAN_POINT('Ctrl Pts',(-27.1915857804997,-3.72562939023108,
127.5936179139));
#79979=CARTESIAN_POINT('Ctrl Pts',(-27.1993586807651,-3.81513571813261,
127.697477810696));
#79980=CARTESIAN_POINT('Ctrl Pts',(-27.2071315810306,-3.90020096000481,
127.804973228919));
#79981=CARTESIAN_POINT('Ctrl Pts',(-27.214904481296,-3.98053818472183,127.915675999531));
#79982=CARTESIAN_POINT('Ctrl Pts',(-27.2223948170582,-4.05795494896487,
128.02235444559));
#79983=CARTESIAN_POINT('Ctrl Pts',(-27.2298851528203,-4.13098130797035,
128.132010845523));
#79984=CARTESIAN_POINT('Ctrl Pts',(-27.2373754885825,-4.19940105463946,
128.244240728812));
#79985=CARTESIAN_POINT('Ctrl Pts',(-27.2453950705407,-4.27265514943476,
128.36440046207));
#79986=CARTESIAN_POINT('Ctrl Pts',(-27.2534146524989,-4.34084847910697,
128.487870880693));
#79987=CARTESIAN_POINT('Ctrl Pts',(-27.2614342344571,-4.40367885088525,
128.614201801232));
#79988=CARTESIAN_POINT('Ctrl Pts',(-27.2694431127645,-4.46642536363424,
128.740364109234));
#79989=CARTESIAN_POINT('Ctrl Pts',(-27.2774519910719,-4.52382301045794,
128.869379001647));
#79990=CARTESIAN_POINT('Ctrl Pts',(-27.2854608693793,-4.57561342169677,
129.000768402655));
#79991=CARTESIAN_POINT('Ctrl Pts',(-27.2934571006645,-4.62732204938768,
129.131950323337));
#79992=CARTESIAN_POINT('Ctrl Pts',(-27.3014533319497,-4.67344095730387,
129.265498949696));
#79993=CARTESIAN_POINT('Ctrl Pts',(-27.3094495632349,-4.71375845183941,
129.400913318872));
#79994=CARTESIAN_POINT('Ctrl Pts',(-27.3130027612179,-4.73167389664767,
129.461085923473));
#79995=CARTESIAN_POINT('Ctrl Pts',(-27.3165559592009,-4.74844444045746,
129.521626623983));
#79996=CARTESIAN_POINT('Ctrl Pts',(-27.3201091571839,-4.76405452823409,
129.582490119308));
#79997=CARTESIAN_POINT('Origin',(213.235140564004,0.,130.804360617566));
#79998=CARTESIAN_POINT('',(-29.4150816029337,-4.76405452823407,129.582490119308));
#79999=CARTESIAN_POINT('',(-29.0697544875928,-4.76405452823408,129.582490119308));
#80000=CARTESIAN_POINT('',(213.235140564004,-4.76405452823405,129.582490119308));
#80001=CARTESIAN_POINT('',(-27.7351405639751,-4.9182486262395,130.808036619917));
#80002=CARTESIAN_POINT('Ctrl Pts',(-27.7351405640086,-4.91824862623906,
130.808036620505));
#80003=CARTESIAN_POINT('Ctrl Pts',(-27.748320956022,-4.91807527927719,131.039963382041));
#80004=CARTESIAN_POINT('Ctrl Pts',(-27.7615013480354,-4.90149533204166,
131.271289001323));
#80005=CARTESIAN_POINT('Ctrl Pts',(-27.7746817400487,-4.86876952591759,
131.500253113571));
#80006=CARTESIAN_POINT('Ctrl Pts',(-27.7824560741679,-4.84946650739838,
131.635305508681));
#80007=CARTESIAN_POINT('Ctrl Pts',(-27.7902304082869,-4.82450942815123,
131.769768053086));
#80008=CARTESIAN_POINT('Ctrl Pts',(-27.798004742406,-4.79394297434503,131.903129847763));
#80009=CARTESIAN_POINT('Ctrl Pts',(-27.8057694953531,-4.76341419096134,
132.036327285947));
#80010=CARTESIAN_POINT('Ctrl Pts',(-27.8135342483003,-4.72728987443892,
132.168426296159));
#80011=CARTESIAN_POINT('Ctrl Pts',(-27.8212990012474,-4.68566634265908,
132.298922087621));
#80012=CARTESIAN_POINT('Ctrl Pts',(-27.8290560421324,-4.64408415195784,
132.429288268823));
#80013=CARTESIAN_POINT('Ctrl Pts',(-27.8368130830173,-4.59701373346094,
132.558054030036));
#80014=CARTESIAN_POINT('Ctrl Pts',(-27.8445701239023,-4.54460215028954,
132.684726102807));
#80015=CARTESIAN_POINT('Ctrl Pts',(-27.8523213151424,-4.49223009110064,
132.811302651181));
#80016=CARTESIAN_POINT('Ctrl Pts',(-27.8600725063826,-4.434525033227,132.93578829395));
#80017=CARTESIAN_POINT('Ctrl Pts',(-27.8678236976228,-4.37168332191907,
133.057706573107));
#80018=CARTESIAN_POINT('Ctrl Pts',(-27.8755715943998,-4.30886832001488,
133.179573033744));
#80019=CARTESIAN_POINT('Ctrl Pts',(-27.8833194911769,-4.24092118567372,
133.298873954289));
#80020=CARTESIAN_POINT('Ctrl Pts',(-27.8910673879539,-4.16808559161616,
133.415154666024));
#80021=CARTESIAN_POINT('Ctrl Pts',(-27.898813664038,-4.09526523319463,133.531411054341));
#80022=CARTESIAN_POINT('Ctrl Pts',(-27.9065599401222,-4.01755865639306,
133.644648159335));
#80023=CARTESIAN_POINT('Ctrl Pts',(-27.9143062162063,-3.93525431032151,
133.754438002245));
#80024=CARTESIAN_POINT('Ctrl Pts',(-27.9220525494716,-3.85294935669797,
133.864228655599));
#80025=CARTESIAN_POINT('Ctrl Pts',(-27.929798882737,-3.76604680059003,133.970571683266));
#80026=CARTESIAN_POINT('Ctrl Pts',(-27.9375452160024,-3.6748767983224,134.073070390497));
#80027=CARTESIAN_POINT('Ctrl Pts',(-27.9452932840054,-3.5836863791649,134.175592051602));
#80028=CARTESIAN_POINT('Ctrl Pts',(-27.9530413520084,-3.48822687197404,
134.27426738709));
#80029=CARTESIAN_POINT('Ctrl Pts',(-27.9607894200113,-3.38886658947828,
134.368735219262));
#80030=CARTESIAN_POINT('Ctrl Pts',(-27.9685457227532,-3.28940070569189,
134.463303452971));
#80031=CARTESIAN_POINT('Ctrl Pts',(-27.976302025495,-3.18602604873139,134.553654980671));
#80032=CARTESIAN_POINT('Ctrl Pts',(-27.9840583282369,-3.07914585925095,
134.639467374875));
#80033=CARTESIAN_POINT('Ctrl Pts',(-27.9918187707511,-2.97220862459528,
134.725325569738));
#80034=CARTESIAN_POINT('Ctrl Pts',(-27.9995792132653,-2.86176244396381,
134.806639572044));
#80035=CARTESIAN_POINT('Ctrl Pts',(-28.0073396557794,-2.74824025338752,
134.883129864797));
#80036=CARTESIAN_POINT('Ctrl Pts',(-28.0151125560449,-2.6345358269129,134.959742946559));
#80037=CARTESIAN_POINT('Ctrl Pts',(-28.0228854563103,-2.51774585631129,
135.031516640074));
#80038=CARTESIAN_POINT('Ctrl Pts',(-28.0306583565757,-2.39832940279758,
135.098216593047));
#80039=CARTESIAN_POINT('Ctrl Pts',(-28.0381486923377,-2.28325403816147,
135.162491834723));
#80040=CARTESIAN_POINT('Ctrl Pts',(-28.0456390280997,-2.16574010857344,
135.222055678687));
#80041=CARTESIAN_POINT('Ctrl Pts',(-28.0531293638617,-2.04621478947577,
135.276741202649));
#80042=CARTESIAN_POINT('Ctrl Pts',(-28.0609036979808,-1.92215763157506,
135.333500144874));
#80043=CARTESIAN_POINT('Ctrl Pts',(-28.0686780320999,-1.79554057384626,
135.385183336964));
#80044=CARTESIAN_POINT('Ctrl Pts',(-28.0764523662189,-1.66681760407285,
135.431552221255));
#80045=CARTESIAN_POINT('Ctrl Pts',(-28.084217119166,-1.53825327385538,135.477863960041));
#80046=CARTESIAN_POINT('Ctrl Pts',(-28.0919818721132,-1.40758855986009,
135.518874291174));
#80047=CARTESIAN_POINT('Ctrl Pts',(-28.0997466250603,-1.27530021903194,
135.55439139787));
#80048=CARTESIAN_POINT('Ctrl Pts',(-28.1075036659453,-1.14314326884901,
135.589873228475));
#80049=CARTESIAN_POINT('Ctrl Pts',(-28.1152607068303,-1.00936627614765,
135.619872591505));
#80050=CARTESIAN_POINT('Ctrl Pts',(-28.1230177477153,-0.874463732858376,
135.644246591679));
#80051=CARTESIAN_POINT('Ctrl Pts',(-28.1307689389554,-0.739662920626569,
135.66860221123));
#80052=CARTESIAN_POINT('Ctrl Pts',(-28.1385201301955,-0.60373863044392,
135.687340842396));
#80053=CARTESIAN_POINT('Ctrl Pts',(-28.1462713214356,-0.467197849328054,
135.700370138807));
#80054=CARTESIAN_POINT('Ctrl Pts',(-28.1540192182127,-0.330715101686322,
135.713393897419));
#80055=CARTESIAN_POINT('Ctrl Pts',(-28.1617671149898,-0.19361677264173,
135.720713110577));
#80056=CARTESIAN_POINT('Ctrl Pts',(-28.1695150117668,-0.0564170989217934,
135.722287027492));
#80057=CARTESIAN_POINT('Ctrl Pts',(-28.1772612878509,0.0807538755842706,
135.723860615178));
#80058=CARTESIAN_POINT('Ctrl Pts',(-28.1850075639351,0.218025761907662,
135.71969129257));
#80059=CARTESIAN_POINT('Ctrl Pts',(-28.1927538400192,0.354882575604865,
135.709790407098));
#80060=CARTESIAN_POINT('Ctrl Pts',(-28.2005001732845,0.491740399547791,
135.699889448541));
#80061=CARTESIAN_POINT('Ctrl Pts',(-28.2082465065499,0.628182754804501,
135.684256870906));
#80062=CARTESIAN_POINT('Ctrl Pts',(-28.2159928398152,0.763697433288137,
135.662956020858));
#80063=CARTESIAN_POINT('Ctrl Pts',(-28.2237409078182,0.899242459344428,
135.641650400632));
#80064=CARTESIAN_POINT('Ctrl Pts',(-28.2314889758212,1.03385900908642,135.614674042789));
#80065=CARTESIAN_POINT('Ctrl Pts',(-28.2392370438242,1.16704413145933,135.58214159389));
#80066=CARTESIAN_POINT('Ctrl Pts',(-28.246993346566,1.30037080456523,135.549574569117));
#80067=CARTESIAN_POINT('Ctrl Pts',(-28.2547496493079,1.43226263086088,135.511439750175));
#80068=CARTESIAN_POINT('Ctrl Pts',(-28.2625059520497,1.56223038154622,135.467902114913));
#80069=CARTESIAN_POINT('Ctrl Pts',(-28.2702663945639,1.69226749993354,135.424341242303));
#80070=CARTESIAN_POINT('Ctrl Pts',(-28.278026837078,1.82037813143489,135.375371946991));
#80071=CARTESIAN_POINT('Ctrl Pts',(-28.2857872795922,1.94609309798619,135.321207384556));
#80072=CARTESIAN_POINT('Ctrl Pts',(-28.2935601798576,2.07200987336224,135.266955872357));
#80073=CARTESIAN_POINT('Ctrl Pts',(-28.3013330801231,2.19552294631646,135.207492596941));
#80074=CARTESIAN_POINT('Ctrl Pts',(-28.3091059803886,2.31618701582715,135.143077106369));
#80075=CARTESIAN_POINT('Ctrl Pts',(-28.3165963161506,2.43246464247684,135.081003281133));
#80076=CARTESIAN_POINT('Ctrl Pts',(-28.3240866519126,2.54609654071978,135.014331196593));
#80077=CARTESIAN_POINT('Ctrl Pts',(-28.3315769876746,2.65671137534498,134.943330021972));
#80078=CARTESIAN_POINT('Ctrl Pts',(-28.3393513217937,2.77152020504548,134.869636816236));
#80079=CARTESIAN_POINT('Ctrl Pts',(-28.3471256559128,2.88344235079026,134.791046327344));
#80080=CARTESIAN_POINT('Ctrl Pts',(-28.3548999900319,2.99203171577573,134.707811561832));
#80081=CARTESIAN_POINT('Ctrl Pts',(-28.362664742979,3.10048725407376,134.62467937573));
#80082=CARTESIAN_POINT('Ctrl Pts',(-28.3704294959261,3.20561787670635,134.536914536939));
#80083=CARTESIAN_POINT('Ctrl Pts',(-28.3781942488732,3.30700450400641,134.444814472923));
#80084=CARTESIAN_POINT('Ctrl Pts',(-28.3859512897582,3.4082904326788,134.352805883988));
#80085=CARTESIAN_POINT('Ctrl Pts',(-28.3937083306432,3.50583947866144,134.25647089976));
#80086=CARTESIAN_POINT('Ctrl Pts',(-28.4014653715282,3.59926413514131,134.156148311914));
#80087=CARTESIAN_POINT('Ctrl Pts',(-28.4092165627683,3.69261833936099,134.055901378113));
#80088=CARTESIAN_POINT('Ctrl Pts',(-28.4169677540084,3.78185407944575,133.951673111068));
#80089=CARTESIAN_POINT('Ctrl Pts',(-28.4247189452485,3.8666196229123,133.843840137847));
#80090=CARTESIAN_POINT('Ctrl Pts',(-28.4324668420256,3.95134913876168,133.736052996517));
#80091=CARTESIAN_POINT('Ctrl Pts',(-28.4402147388027,4.0316119957434,133.624664502959));
#80092=CARTESIAN_POINT('Ctrl Pts',(-28.4479626355798,4.10709595155373,133.510085272299));
#80093=CARTESIAN_POINT('Ctrl Pts',(-28.4557089116639,4.18256411774785,133.395530009145));
#80094=CARTESIAN_POINT('Ctrl Pts',(-28.463455187748,4.25325515616629,133.277785662728));
#80095=CARTESIAN_POINT('Ctrl Pts',(-28.4712014638321,4.31889971152841,133.157292478938));
#80096=CARTESIAN_POINT('Ctrl Pts',(-28.4789477970974,4.38454475146363,133.036798405695));
#80097=CARTESIAN_POINT('Ctrl Pts',(-28.4866941303628,4.44514304696789,132.913555797911));
#80098=CARTESIAN_POINT('Ctrl Pts',(-28.4944404636281,4.50047103240126,132.788029831174));
#80099=CARTESIAN_POINT('Ctrl Pts',(-28.5021885316311,4.55581140815335,132.662475753768));
#80100=CARTESIAN_POINT('Ctrl Pts',(-28.5099365996341,4.60587896761775,132.534637657583));
#80101=CARTESIAN_POINT('Ctrl Pts',(-28.517684667637,4.65049830886217,132.405000658853));
#80102=CARTESIAN_POINT('Ctrl Pts',(-28.5254409703789,4.69516507207344,132.275225880378));
#80103=CARTESIAN_POINT('Ctrl Pts',(-28.5331972731208,4.73437192261259,132.143648750411));
#80104=CARTESIAN_POINT('Ctrl Pts',(-28.5409535758627,4.76799322090075,132.010770045557));
#80105=CARTESIAN_POINT('Ctrl Pts',(-28.5487140183768,4.80163246388817,131.877820419336));
#80106=CARTESIAN_POINT('Ctrl Pts',(-28.5564744608909,4.82968013446193,131.743568216514));
#80107=CARTESIAN_POINT('Ctrl Pts',(-28.5642349034051,4.85206196424514,131.608523385683));
#80108=CARTESIAN_POINT('Ctrl Pts',(-28.5720078036705,4.87447972332848,131.4732617689));
#80109=CARTESIAN_POINT('Ctrl Pts',(-28.579780703936,4.89121341853944,131.337205369718));
#80110=CARTESIAN_POINT('Ctrl Pts',(-28.5875536042014,4.90224071893429,131.200869124565));
#80111=CARTESIAN_POINT('Ctrl Pts',(-28.5950439399634,4.91286714918369,131.069489045334));
#80112=CARTESIAN_POINT('Ctrl Pts',(-28.6025342757255,4.91819485282245,130.937849420869));
#80113=CARTESIAN_POINT('Ctrl Pts',(-28.6100246114875,4.91824957378903,130.806408158542));
#80114=CARTESIAN_POINT('Ctrl Pts',(-28.6177989456066,4.91830636951769,130.669983260803));
#80115=CARTESIAN_POINT('Ctrl Pts',(-28.6255732797256,4.9126826190398,130.533339910863));
#80116=CARTESIAN_POINT('Ctrl Pts',(-28.6333476138447,4.90135005770111,130.396990178809));
#80117=CARTESIAN_POINT('Ctrl Pts',(-28.6411123667918,4.89003146273146,130.260808485614));
#80118=CARTESIAN_POINT('Ctrl Pts',(-28.6488771197389,4.87301808771849,130.124920076197));
#80119=CARTESIAN_POINT('Ctrl Pts',(-28.656641872686,4.85033364401388,129.989838300961));
#80120=CARTESIAN_POINT('Ctrl Pts',(-28.664398913571,4.82767173081856,129.854890690849));
#80121=CARTESIAN_POINT('Ctrl Pts',(-28.672155954456,4.7993500223603,129.720748503643));
#80122=CARTESIAN_POINT('Ctrl Pts',(-28.679912995341,4.76544409677402,129.587920884977));
#80123=CARTESIAN_POINT('Ctrl Pts',(-28.6876641865811,4.73156373990992,129.455193432651));
#80124=CARTESIAN_POINT('Ctrl Pts',(-28.6954153778213,4.69210764416697,129.323778952975));
#80125=CARTESIAN_POINT('Ctrl Pts',(-28.7031665690614,4.64720255656525,129.194176944579));
#80126=CARTESIAN_POINT('Ctrl Pts',(-28.7109144658385,4.60231655482371,129.064630020494));
#80127=CARTESIAN_POINT('Ctrl Pts',(-28.7186623626156,4.55198629523495,128.93689440417));
#80128=CARTESIAN_POINT('Ctrl Pts',(-28.7264102593927,4.49638846534228,128.811454741405));
#80129=CARTESIAN_POINT('Ctrl Pts',(-28.7341565354767,4.44080226531707,128.686041317914));
#80130=CARTESIAN_POINT('Ctrl Pts',(-28.7419028115608,4.37995084497337,128.562923249914));
#80131=CARTESIAN_POINT('Ctrl Pts',(-28.7496490876449,4.31405900253759,128.44256511729));
#80132=CARTESIAN_POINT('Ctrl Pts',(-28.7573954209103,4.2481666737032,128.322206096209));
#80133=CARTESIAN_POINT('Ctrl Pts',(-28.7651417541756,4.17723403627797,128.204607394093));
#80134=CARTESIAN_POINT('Ctrl Pts',(-28.772888087441,4.10153161297023,128.090208541815));
#80135=CARTESIAN_POINT('Ctrl Pts',(-28.7806361554439,4.02581223662968,127.975784070706));
#80136=CARTESIAN_POINT('Ctrl Pts',(-28.7883842234469,3.94532116460504,127.864561201335));
#80137=CARTESIAN_POINT('Ctrl Pts',(-28.7961322914499,3.86037172989342,127.756949721487));
#80138=CARTESIAN_POINT('Ctrl Pts',(-28.8038885941917,3.77533200991168,127.649223870878));
#80139=CARTESIAN_POINT('Ctrl Pts',(-28.8116448969336,3.68582470441006,127.545117384427));
#80140=CARTESIAN_POINT('Ctrl Pts',(-28.8194011996754,3.59220321966602,127.445006648256));
#80141=CARTESIAN_POINT('Ctrl Pts',(-28.8271616421896,3.49853176631657,127.34484247997));
#80142=CARTESIAN_POINT('Ctrl Pts',(-28.8349220847038,3.40074203691041,127.248678585448));
#80143=CARTESIAN_POINT('Ctrl Pts',(-28.842682527218,3.29922292176801,127.156853088447));
#80144=CARTESIAN_POINT('Ctrl Pts',(-28.8504554274834,3.19754083912955,127.064880185006));
#80145=CARTESIAN_POINT('Ctrl Pts',(-28.8582283277487,3.09211770818492,126.977259846182));
#80146=CARTESIAN_POINT('Ctrl Pts',(-28.8660012280141,2.98337468911472,126.894289195348));
#80147=CARTESIAN_POINT('Ctrl Pts',(-28.8734915637762,2.87858475269455,126.814334736661));
#80148=CARTESIAN_POINT('Ctrl Pts',(-28.8809818995384,2.77071236235782,126.738697956201));
#80149=CARTESIAN_POINT('Ctrl Pts',(-28.8884722353004,2.66015668377066,126.667604704983));
#80150=CARTESIAN_POINT('Ctrl Pts',(-28.8962465694195,2.54540925302752,126.593815931537));
#80151=CARTESIAN_POINT('Ctrl Pts',(-28.9040209035385,2.4274075582807,126.524688283744));
#80152=CARTESIAN_POINT('Ctrl Pts',(-28.9117952376576,2.30656714086174,126.460522327851));
#80153=CARTESIAN_POINT('Ctrl Pts',(-28.9195599906047,2.18587564845742,126.396435450763));
#80154=CARTESIAN_POINT('Ctrl Pts',(-28.9273247435519,2.06235273628625,126.337298280457));
#80155=CARTESIAN_POINT('Ctrl Pts',(-28.935089496499,1.93644311714481,126.283368346331));
#80156=CARTESIAN_POINT('Ctrl Pts',(-28.942846537384,1.81065855321212,126.229491976177));
#80157=CARTESIAN_POINT('Ctrl Pts',(-28.950603578269,1.68249235679357,126.180812702825));
#80158=CARTESIAN_POINT('Ctrl Pts',(-28.958360619154,1.55241373835822,126.137542145903));
#80159=CARTESIAN_POINT('Ctrl Pts',(-28.9661118103941,1.4224332132209,126.094304219644));
#80160=CARTESIAN_POINT('Ctrl Pts',(-28.9738630016343,1.29054350610047,126.056467014205));
#80161=CARTESIAN_POINT('Ctrl Pts',(-28.9816141928744,1.15723336920089,126.02419388494));
#80162=CARTESIAN_POINT('Ctrl Pts',(-28.9893620896515,1.02397989266566,125.991934472615));
#80163=CARTESIAN_POINT('Ctrl Pts',(-28.9971099864285,0.88930756629846,125.965234524695));
#80164=CARTESIAN_POINT('Ctrl Pts',(-29.0048578832056,0.753719640269004,
125.944207351837));
#80165=CARTESIAN_POINT('Ctrl Pts',(-29.0126041592897,0.618160076310736,
125.923184577411));
#80166=CARTESIAN_POINT('Ctrl Pts',(-29.0203504353738,0.481685679743536,
125.907832277669));
#80167=CARTESIAN_POINT('Ctrl Pts',(-29.0280967114579,0.344808823712795,
125.89821244027));
#80168=CARTESIAN_POINT('Ctrl Pts',(-29.0358430447232,0.207930957288196,
125.888592531859));
#80169=CARTESIAN_POINT('Ctrl Pts',(-29.0435893779887,0.0706510154751086,
125.88470519764));
#80170=CARTESIAN_POINT('Ctrl Pts',(-29.051335711254,-0.0665149878230809,
125.886560416369));
#80171=CARTESIAN_POINT('Ctrl Pts',(-29.059083779257,-0.203711708496667,
125.888416050561));
#80172=CARTESIAN_POINT('Ctrl Pts',(-29.0668318472599,-0.340794049027356,
125.896016791416));
#80173=CARTESIAN_POINT('Ctrl Pts',(-29.0745799152629,-0.477247879205806,
125.909320523318));
#80174=CARTESIAN_POINT('Ctrl Pts',(-29.0823362180048,-0.613846734138791,
125.922638394585));
#80175=CARTESIAN_POINT('Ctrl Pts',(-29.0900925207466,-0.749815354600336,
125.941671326813));
#80176=CARTESIAN_POINT('Ctrl Pts',(-29.0978488234885,-0.884646051560765,
125.966325435185));
#80177=CARTESIAN_POINT('Ctrl Pts',(-29.1056092660027,-1.01954871172402,
125.990992702197));
#80178=CARTESIAN_POINT('Ctrl Pts',(-29.1133697085168,-1.15331185707987,
126.021287037173));
#80179=CARTESIAN_POINT('Ctrl Pts',(-29.121130151031,-1.28544080981666,126.057064019821));
#80180=CARTESIAN_POINT('Ctrl Pts',(-29.1289030512965,-1.41778186767807,
126.092898434859));
#80181=CARTESIAN_POINT('Ctrl Pts',(-29.1366759515619,-1.54848311764643,
126.134232967281));
#80182=CARTESIAN_POINT('Ctrl Pts',(-29.1444488518273,-1.67706693404797,
126.18087388554));
#80183=CARTESIAN_POINT('Ctrl Pts',(-29.1519391875893,-1.80097640483918,
126.225819288938));
#80184=CARTESIAN_POINT('Ctrl Pts',(-29.1594295233512,-1.92291943228982,
126.275691858664));
#80185=CARTESIAN_POINT('Ctrl Pts',(-29.1669198591132,-2.04249024275295,
126.330277843325));
#80186=CARTESIAN_POINT('Ctrl Pts',(-29.1746947830569,-2.16660403241195,
126.386937770546));
#80187=CARTESIAN_POINT('Ctrl Pts',(-29.1824697070006,-2.28855496587655,
126.448855852897));
#80188=CARTESIAN_POINT('Ctrl Pts',(-29.1902446309443,-2.40786544995348,
126.51584490261));
#80189=CARTESIAN_POINT('Ctrl Pts',(-29.1980098405491,-2.52702686215729,
126.582750253199));
#80190=CARTESIAN_POINT('Ctrl Pts',(-29.2057750501539,-2.64355405184961,
126.654713774174));
#80191=CARTESIAN_POINT('Ctrl Pts',(-29.2135402597586,-2.75698989575442,
126.731500470543));
#80192=CARTESIAN_POINT('Ctrl Pts',(-29.221297624704,-2.870311143195,126.808209594571));
#80193=CARTESIAN_POINT('Ctrl Pts',(-29.2290549896493,-2.98054693844968,
126.889731978877));
#80194=CARTESIAN_POINT('Ctrl Pts',(-29.2368123545947,-3.08726557027292,
126.975787206868));
#80195=CARTESIAN_POINT('Ctrl Pts',(-29.2445633089976,-3.19389601179866,
127.061771320414));
#80196=CARTESIAN_POINT('Ctrl Pts',(-29.2523142634005,-3.29701477442576,
127.152280574189));
#80197=CARTESIAN_POINT('Ctrl Pts',(-29.2600652178033,-3.39622028205886,
127.246992087566));
#80198=CARTESIAN_POINT('Ctrl Pts',(-29.2678126838207,-3.49538114137613,
127.341660975189));
#80199=CARTESIAN_POINT('Ctrl Pts',(-29.2755601498379,-3.59063196760138,
127.440528090245));
#80200=CARTESIAN_POINT('Ctrl Pts',(-29.2833076158553,-3.68160547577825,
127.543231337206));
#80201=CARTESIAN_POINT('Ctrl Pts',(-29.2910532728381,-3.77255774162731,
127.645910602944));
#80202=CARTESIAN_POINT('Ctrl Pts',(-29.298798929821,-3.85923441827731,127.752423925421));
#80203=CARTESIAN_POINT('Ctrl Pts',(-29.3065445868038,-3.94130648447086,
127.862373830042));
#80204=CARTESIAN_POINT('Ctrl Pts',(-29.31429011253,-4.02337715988486,127.972321871469));
#80205=CARTESIAN_POINT('Ctrl Pts',(-29.3220356382563,-4.10084314747055,
128.085706065174));
#80206=CARTESIAN_POINT('Ctrl Pts',(-29.3297811639825,-4.17341722173141,
128.202097803042));
#80207=CARTESIAN_POINT('Ctrl Pts',(-29.3375315429424,-4.24603676985053,
128.318562470278));
#80208=CARTESIAN_POINT('Ctrl Pts',(-29.3452819219022,-4.3137580736368,128.438038114628));
#80209=CARTESIAN_POINT('Ctrl Pts',(-29.353032300862,-4.37633845182278,128.560069010489));
#80210=CARTESIAN_POINT('Ctrl Pts',(-29.3607852357813,-4.43893946808426,
128.682140150319));
#80211=CARTESIAN_POINT('Ctrl Pts',(-29.3685381707006,-4.49639601355354,
128.806767867301));
#80212=CARTESIAN_POINT('Ctrl Pts',(-29.3762911056198,-4.5485129116741,128.93347490357));
#80213=CARTESIAN_POINT('Ctrl Pts',(-29.384052654986,-4.60068771796163,129.060322726656));
#80214=CARTESIAN_POINT('Ctrl Pts',(-29.3918142043521,-4.64751088883166,
129.18925411777));
#80215=CARTESIAN_POINT('Ctrl Pts',(-29.3995757537182,-4.6888364732971,129.319774618313));
#80216=CARTESIAN_POINT('Ctrl Pts',(-29.4047443701234,-4.71635624850492,
129.406691594356));
#80217=CARTESIAN_POINT('Ctrl Pts',(-29.4099129865286,-4.7414391129661,129.494312958415));
#80218=CARTESIAN_POINT('Ctrl Pts',(-29.4150816029337,-4.76405452823407,
129.582490119308));
#80219=CARTESIAN_POINT('Ctrl Pts',(-27.6650164504902,-4.76405452823402,
129.582490119308));
#80220=CARTESIAN_POINT('Ctrl Pts',(-27.6726576270515,-4.79767153518427,
129.713562319198));
#80221=CARTESIAN_POINT('Ctrl Pts',(-27.6802988036129,-4.82585647153979,
129.845950237151));
#80222=CARTESIAN_POINT('Ctrl Pts',(-27.6879399801743,-4.84852785224846,
129.979157170851));
#80223=CARTESIAN_POINT('Ctrl Pts',(-27.6958067441411,-4.87186855107991,
130.11629671968));
#80224=CARTESIAN_POINT('Ctrl Pts',(-27.7036735081079,-4.88936504333653,
130.254303931843));
#80225=CARTESIAN_POINT('Ctrl Pts',(-27.7115402720748,-4.90098591852434,
130.392632443978));
#80226=CARTESIAN_POINT('Ctrl Pts',(-27.7194070360416,-4.91260679371213,
130.530960956112));
#80227=CARTESIAN_POINT('Ctrl Pts',(-27.7272738000084,-4.91835208897519,
130.669610305378));
#80228=CARTESIAN_POINT('Ctrl Pts',(-27.7351405639752,-4.9182486262395,130.808036619917));
#80229=CARTESIAN_POINT('',(-27.38985943602,-4.9182498326282,130.80564372033));
#80230=CARTESIAN_POINT('Ctrl Pts',(-27.3201091571839,-4.76405452823409,
129.582490119308));
#80231=CARTESIAN_POINT('Ctrl Pts',(-27.3280913567537,-4.79912232815121,
129.719218938957));
#80232=CARTESIAN_POINT('Ctrl Pts',(-27.3360735563233,-4.82833034249597,
129.857577834223));
#80233=CARTESIAN_POINT('Ctrl Pts',(-27.344055755893,-4.85153765587541,129.99704070816));
#80234=CARTESIAN_POINT('Ctrl Pts',(-27.3520294712711,-4.87472030245806,
130.13635534855));
#80235=CARTESIAN_POINT('Ctrl Pts',(-27.3600031866493,-4.89191490313895,
130.276771277517));
#80236=CARTESIAN_POINT('Ctrl Pts',(-27.3679769020273,-4.90303131735161,
130.417751042453));
#80237=CARTESIAN_POINT('Ctrl Pts',(-27.3752710800153,-4.91320036653513,
130.546716204787));
#80238=CARTESIAN_POINT('Ctrl Pts',(-27.3825652580032,-4.91828361497706,
130.676152846472));
#80239=CARTESIAN_POINT('Ctrl Pts',(-27.3898594359911,-4.91824983262833,
130.805643719816));
#80240=CARTESIAN_POINT('Ctrl Pts',(-27.3898594360201,-4.9182498326282,130.80564372033));
#80241=CARTESIAN_POINT('Ctrl Pts',(-27.3981545579858,-4.91821141447941,
130.95290398593));
#80242=CARTESIAN_POINT('Ctrl Pts',(-27.4064496799514,-4.91155496272104,
131.09998366834));
#80243=CARTESIAN_POINT('Ctrl Pts',(-27.4147448019172,-4.89835427534359,
131.246297780207));
#80244=CARTESIAN_POINT('Ctrl Pts',(-27.423167994457,-4.88494977907478,131.394870874207));
#80245=CARTESIAN_POINT('Ctrl Pts',(-27.4315911869969,-4.86479739107107,
131.542654243628));
#80246=CARTESIAN_POINT('Ctrl Pts',(-27.4400143795368,-4.83802743156649,
131.689049056459));
#80247=CARTESIAN_POINT('Ctrl Pts',(-27.448354056866,-4.81152289384773,131.83399237764));
#80248=CARTESIAN_POINT('Ctrl Pts',(-27.4566937341952,-4.77853157841535,
131.977574290635));
#80249=CARTESIAN_POINT('Ctrl Pts',(-27.4650334115245,-4.73922973640288,
132.119231169406));
#80250=CARTESIAN_POINT('Ctrl Pts',(-27.4734983616696,-4.69933752953261,
132.263015919004));
#80251=CARTESIAN_POINT('Ctrl Pts',(-27.4819633118148,-4.65294382769438,
132.404817037884));
#80252=CARTESIAN_POINT('Ctrl Pts',(-27.49042826196,-4.60028281832949,132.544067792318));
#80253=CARTESIAN_POINT('Ctrl Pts',(-27.4988932121051,-4.54762180896466,
132.683318546751));
#80254=CARTESIAN_POINT('Ctrl Pts',(-27.5073581622503,-4.48869367965767,
132.820018676014));
#80255=CARTESIAN_POINT('Ctrl Pts',(-27.5158231123954,-4.42378021487808,
132.953628323775));
#80256=CARTESIAN_POINT('Ctrl Pts',(-27.5235974465145,-4.36416273865318,
133.076337379991));
#80257=CARTESIAN_POINT('Ctrl Pts',(-27.5313717806336,-4.2993413143803,133.196758369057));
#80258=CARTESIAN_POINT('Ctrl Pts',(-27.5391461147527,-4.22951448978743,
133.314418434266));
#80259=CARTESIAN_POINT('Ctrl Pts',(-27.5469108676998,-4.15977372051527,
133.431933493961));
#80260=CARTESIAN_POINT('Ctrl Pts',(-27.5546756206469,-4.08504002243042,
133.546694066953));
#80261=CARTESIAN_POINT('Ctrl Pts',(-27.562440373594,-4.00555924423072,133.658248878073));
#80262=CARTESIAN_POINT('Ctrl Pts',(-27.570197414479,-3.92615740746052,133.769692891381));
#80263=CARTESIAN_POINT('Ctrl Pts',(-27.577954455364,-3.84201809876874,133.877937162782));
#80264=CARTESIAN_POINT('Ctrl Pts',(-27.585711496249,-3.75343197057496,133.982556883495));
#80265=CARTESIAN_POINT('Ctrl Pts',(-27.5934626874891,-3.66491264586956,
134.087097709663));
#80266=CARTESIAN_POINT('Ctrl Pts',(-27.6012138787292,-3.57195342798532,
134.18801912845));
#80267=CARTESIAN_POINT('Ctrl Pts',(-27.6089650699693,-3.47488676517149,
134.284927386317));
#80268=CARTESIAN_POINT('Ctrl Pts',(-27.6167129667464,-3.37786135827857,
134.38179445559));
#80269=CARTESIAN_POINT('Ctrl Pts',(-27.6244608635235,-3.27673225476734,
134.474651480802));
#80270=CARTESIAN_POINT('Ctrl Pts',(-27.6322087603006,-3.17187031718759,
134.5631399079));
#80271=CARTESIAN_POINT('Ctrl Pts',(-27.6399550363847,-3.06703031446462,
134.651609825127));
#80272=CARTESIAN_POINT('Ctrl Pts',(-27.6477013124688,-2.95845932939005,
134.735712709892));
#80273=CARTESIAN_POINT('Ctrl Pts',(-27.6554475885529,-2.84656271321275,
134.815129095333));
#80274=CARTESIAN_POINT('Ctrl Pts',(-27.6631939218182,-2.7346652710402,134.894546067007));
#80275=CARTESIAN_POINT('Ctrl Pts',(-27.6709402550836,-2.61944246760607,
134.969276244046));
#80276=CARTESIAN_POINT('Ctrl Pts',(-27.6786865883489,-2.50132981752473,
135.039042684317));
#80277=CARTESIAN_POINT('Ctrl Pts',(-27.6864346563519,-2.38319071693433,
135.108824748298));
#80278=CARTESIAN_POINT('Ctrl Pts',(-27.6941827243548,-2.26216081848309,
135.173640664767));
#80279=CARTESIAN_POINT('Ctrl Pts',(-27.7019307923578,-2.13870112641277,
135.233258963022));
#80280=CARTESIAN_POINT('Ctrl Pts',(-27.7096870950996,-2.01511021991237,
135.292940624313));
#80281=CARTESIAN_POINT('Ctrl Pts',(-27.7174433978415,-1.88908471377028,
135.347413462141));
#80282=CARTESIAN_POINT('Ctrl Pts',(-27.7251997005833,-1.76110704035503,
135.396493570227));
#80283=CARTESIAN_POINT('Ctrl Pts',(-27.7329601430975,-1.63306106140197,
135.445599873844));
#80284=CARTESIAN_POINT('Ctrl Pts',(-27.7407205856117,-1.50306120944049,
135.489307588004));
#80285=CARTESIAN_POINT('Ctrl Pts',(-27.7484810281259,-1.37160509201754,
135.527482734773));
#80286=CARTESIAN_POINT('Ctrl Pts',(-27.7562539283913,-1.23993794956496,
135.565719163677));
#80287=CARTESIAN_POINT('Ctrl Pts',(-27.7640268286567,-1.10681025003527,
135.59840518411));
#80288=CARTESIAN_POINT('Ctrl Pts',(-27.7717997289222,-0.97273068816611,
135.625457802938));
#80289=CARTESIAN_POINT('Ctrl Pts',(-27.7792900646843,-0.843525256095834,
135.65152699093));
#80290=CARTESIAN_POINT('Ctrl Pts',(-27.7867804004464,-0.713436269511016,
135.672365194421));
#80291=CARTESIAN_POINT('Ctrl Pts',(-27.7942707362085,-0.582921471319326,
135.687943894298));
#80292=CARTESIAN_POINT('Ctrl Pts',(-27.8020450703275,-0.447458164886229,
135.704113265315));
#80293=CARTESIAN_POINT('Ctrl Pts',(-27.8098194044467,-0.311107013114465,
135.714667651273));
#80294=CARTESIAN_POINT('Ctrl Pts',(-27.8175937385658,-0.174373163640406,
135.719518505396));
#80295=CARTESIAN_POINT('Ctrl Pts',(-27.8253584915129,-0.0378078264155682,
135.724363381276));
#80296=CARTESIAN_POINT('Ctrl Pts',(-27.8331232444599,0.0991388831185796,
135.723518697394));
#80297=CARTESIAN_POINT('Ctrl Pts',(-27.840887997407,0.235954407152601,135.71694736797));
#80298=CARTESIAN_POINT('Ctrl Pts',(-27.848645038292,0.372634044079205,135.710382565283));
#80299=CARTESIAN_POINT('Ctrl Pts',(-27.8564020791771,0.509182366811173,
135.698102454637));
#80300=CARTESIAN_POINT('Ctrl Pts',(-27.8641591200621,0.645084866956548,
135.680121950622));
#80301=CARTESIAN_POINT('Ctrl Pts',(-27.8719103113022,0.780884881969396,
135.662155005845));
#80302=CARTESIAN_POINT('Ctrl Pts',(-27.8796615025422,0.916039657759709,
135.638496275094));
#80303=CARTESIAN_POINT('Ctrl Pts',(-27.8874126937823,1.05003822192403,135.609212623091));
#80304=CARTESIAN_POINT('Ctrl Pts',(-27.8951605905594,1.18397983312424,135.579941417421));
#80305=CARTESIAN_POINT('Ctrl Pts',(-27.9029084873365,1.3167658289457,135.545050128798));
#80306=CARTESIAN_POINT('Ctrl Pts',(-27.9106563841136,1.4478940874432,135.504656967164));
#80307=CARTESIAN_POINT('Ctrl Pts',(-27.9184026601977,1.57899491673583,135.464272254909));
#80308=CARTESIAN_POINT('Ctrl Pts',(-27.9261489362819,1.70843832503221,135.418388073818));
#80309=CARTESIAN_POINT('Ctrl Pts',(-27.933895212366,1.83573643356326,135.367172777735));
#80310=CARTESIAN_POINT('Ctrl Pts',(-27.9416415456313,1.96303548177987,135.315957103593));
#80311=CARTESIAN_POINT('Ctrl Pts',(-27.9493878788966,2.08818883592086,135.25941038186));
#80312=CARTESIAN_POINT('Ctrl Pts',(-27.9571342121619,2.21072809043967,135.197749329328));
#80313=CARTESIAN_POINT('Ctrl Pts',(-27.9648822801649,2.3332947867749,135.136074468232));
#80314=CARTESIAN_POINT('Ctrl Pts',(-27.9726303481679,2.45324586941514,135.069283172988));
#80315=CARTESIAN_POINT('Ctrl Pts',(-27.9803784161709,2.57013741144903,134.997638183954));
#80316=CARTESIAN_POINT('Ctrl Pts',(-27.9881347189127,2.68715318720497,134.925917049772));
#80317=CARTESIAN_POINT('Ctrl Pts',(-27.9958910216545,2.80110259283458,134.849332121646));
#80318=CARTESIAN_POINT('Ctrl Pts',(-28.0036473243964,2.9115701362972,134.768189877754));
#80319=CARTESIAN_POINT('Ctrl Pts',(-28.0114077669105,3.02209663961389,134.687004325803));
#80320=CARTESIAN_POINT('Ctrl Pts',(-28.0191682094248,3.12913727281141,134.601256855685));
#80321=CARTESIAN_POINT('Ctrl Pts',(-28.026928651939,3.23231034742593,134.511293700375));
#80322=CARTESIAN_POINT('Ctrl Pts',(-28.0347015522044,3.3356490446191,134.421186128222));
#80323=CARTESIAN_POINT('Ctrl Pts',(-28.0424744524698,3.43510749274633,134.326849616679));
#80324=CARTESIAN_POINT('Ctrl Pts',(-28.0502473527352,3.53034090540144,134.228667285221));
#80325=CARTESIAN_POINT('Ctrl Pts',(-28.0577376884972,3.62211234362779,134.134054128819));
#80326=CARTESIAN_POINT('Ctrl Pts',(-28.0652280242593,3.70996038924204,134.035870138083));
#80327=CARTESIAN_POINT('Ctrl Pts',(-28.0727183600213,3.79361362708284,133.934485009808));
#80328=CARTESIAN_POINT('Ctrl Pts',(-28.0804926941403,3.88043860286236,133.82925583358));
#80329=CARTESIAN_POINT('Ctrl Pts',(-28.0882670282594,3.96301943477866,133.720244651344));
#80330=CARTESIAN_POINT('Ctrl Pts',(-28.0960413623785,4.04100858128699,133.607828596421));
#80331=CARTESIAN_POINT('Ctrl Pts',(-28.1038061153256,4.11890161314245,133.495551084238));
#80332=CARTESIAN_POINT('Ctrl Pts',(-28.1115708682726,4.19221399828266,133.379877366704));
#80333=CARTESIAN_POINT('Ctrl Pts',(-28.1193356212197,4.2606374853736,133.26121862745));
#80334=CARTESIAN_POINT('Ctrl Pts',(-28.1270926621047,4.32899301329248,133.142677741728));
#80335=CARTESIAN_POINT('Ctrl Pts',(-28.1348497029898,4.39246911223033,133.021158070802));
#80336=CARTESIAN_POINT('Ctrl Pts',(-28.1426067438748,4.45080022589988,132.897100546852));
#80337=CARTESIAN_POINT('Ctrl Pts',(-28.1503579351149,4.50908735162287,132.773136575647));
#80338=CARTESIAN_POINT('Ctrl Pts',(-28.1581091263551,4.56223704904577,132.646638913125));
#80339=CARTESIAN_POINT('Ctrl Pts',(-28.1658603175952,4.61002938028732,132.518073596856));
#80340=CARTESIAN_POINT('Ctrl Pts',(-28.1736082143723,4.65780139851319,132.389562924277));
#80341=CARTESIAN_POINT('Ctrl Pts',(-28.1813561111493,4.70022044344138,132.258986711529));
#80342=CARTESIAN_POINT('Ctrl Pts',(-28.1891040079264,4.73711455926891,132.12683130339));
#80343=CARTESIAN_POINT('Ctrl Pts',(-28.1968502840105,4.77400095764276,131.994703539312));
#80344=CARTESIAN_POINT('Ctrl Pts',(-28.2045965600946,4.80536462059856,131.860997613222));
#80345=CARTESIAN_POINT('Ctrl Pts',(-28.2123428361787,4.83108347860162,131.726214990709));
#80346=CARTESIAN_POINT('Ctrl Pts',(-28.220089169444,4.85680252645544,131.591431373261));
#80347=CARTESIAN_POINT('Ctrl Pts',(-28.2278355027094,4.87687661292898,131.455571427568));
#80348=CARTESIAN_POINT('Ctrl Pts',(-28.2355818359747,4.89123488335785,131.319146377201));
#80349=CARTESIAN_POINT('Ctrl Pts',(-28.2433299039777,4.90559636922183,131.18269077539));
#80350=CARTESIAN_POINT('Ctrl Pts',(-28.2510779719806,4.91423945104085,131.045670205827));
#80351=CARTESIAN_POINT('Ctrl Pts',(-28.2588260399836,4.91714522637847,130.908600174374));
#80352=CARTESIAN_POINT('Ctrl Pts',(-28.2665823427254,4.92005409000869,130.77138446326));
#80353=CARTESIAN_POINT('Ctrl Pts',(-28.2743386454673,4.91721345809016,130.634119576746));
#80354=CARTESIAN_POINT('Ctrl Pts',(-28.2820949482092,4.90865659579756,130.497320738995));
#80355=CARTESIAN_POINT('Ctrl Pts',(-28.2898553907234,4.90009516644991,130.360448887584));
#80356=CARTESIAN_POINT('Ctrl Pts',(-28.2976158332376,4.88581146820079,130.22404396923));
#80357=CARTESIAN_POINT('Ctrl Pts',(-28.3053762757518,4.86589048472126,130.088614256626));
#80358=CARTESIAN_POINT('Ctrl Pts',(-28.3131491760172,4.84593752231055,129.952967140225));
#80359=CARTESIAN_POINT('Ctrl Pts',(-28.3209220762826,4.82032926402175,129.818298742219));
#80360=CARTESIAN_POINT('Ctrl Pts',(-28.328694976548,4.78920167364366,129.685106226612));
#80361=CARTESIAN_POINT('Ctrl Pts',(-28.3361853123101,4.75920564958139,129.556755594439));
#80362=CARTESIAN_POINT('Ctrl Pts',(-28.3436756480721,4.72408469192248,129.429775700407));
#80363=CARTESIAN_POINT('Ctrl Pts',(-28.3511659838342,4.6840031305258,129.304594723926));
#80364=CARTESIAN_POINT('Ctrl Pts',(-28.3589403179533,4.64240186454643,129.174667472675));
#80365=CARTESIAN_POINT('Ctrl Pts',(-28.3667146520724,4.59532462637429,129.046266673229));
#80366=CARTESIAN_POINT('Ctrl Pts',(-28.3744889861914,4.54290085425753,128.919888571903));
#80367=CARTESIAN_POINT('Ctrl Pts',(-28.3822537391385,4.49054168975466,128.793666220292));
#80368=CARTESIAN_POINT('Ctrl Pts',(-28.3900184920856,4.43284925006628,128.669461964544));
#80369=CARTESIAN_POINT('Ctrl Pts',(-28.3977832450327,4.37000285825083,128.547757400033));
#80370=CARTESIAN_POINT('Ctrl Pts',(-28.4055402859177,4.30721888635772,128.426173714211));
#80371=CARTESIAN_POINT('Ctrl Pts',(-28.4132973268027,4.23929132755739,128.30708512402));
#80372=CARTESIAN_POINT('Ctrl Pts',(-28.4210543676877,4.16644761092212,128.190953384098));
#80373=CARTESIAN_POINT('Ctrl Pts',(-28.4288055589278,4.0936588263002,128.074909220025));
#80374=CARTESIAN_POINT('Ctrl Pts',(-28.4365567501679,4.0159614699311,127.961817797835));
#80375=CARTESIAN_POINT('Ctrl Pts',(-28.444307941408,3.93362875062406,127.852116062187));
#80376=CARTESIAN_POINT('Ctrl Pts',(-28.4520558381851,3.85133102491902,127.742460952703));
#80377=CARTESIAN_POINT('Ctrl Pts',(-28.4598037349622,3.76440208895066,127.636192976344));
#80378=CARTESIAN_POINT('Ctrl Pts',(-28.4675516317393,3.67315817204063,127.533719685628));
#80379=CARTESIAN_POINT('Ctrl Pts',(-28.4752979078234,3.58193334139091,127.431267830115));
#80380=CARTESIAN_POINT('Ctrl Pts',(-28.4830441839076,3.48639558494988,127.332609373204));
#80381=CARTESIAN_POINT('Ctrl Pts',(-28.4907904599917,3.38690081835619,127.238118069853));
#80382=CARTESIAN_POINT('Ctrl Pts',(-28.498536793257,3.28740531731487,127.143626068989));
#80383=CARTESIAN_POINT('Ctrl Pts',(-28.5062831265224,3.18395303132537,127.0533015523));
#80384=CARTESIAN_POINT('Ctrl Pts',(-28.5140294597877,3.07693576858063,126.967480460651));
#80385=CARTESIAN_POINT('Ctrl Pts',(-28.5217775277907,2.9698945400619,126.881640149963));
#80386=CARTESIAN_POINT('Ctrl Pts',(-28.5295255957936,2.859287051106,126.800305515681));
#80387=CARTESIAN_POINT('Ctrl Pts',(-28.5372736637966,2.74553679416704,126.723771104472));
#80388=CARTESIAN_POINT('Ctrl Pts',(-28.5450299665384,2.63166564210137,126.647155351579));
#80389=CARTESIAN_POINT('Ctrl Pts',(-28.5527862692802,2.51464537459536,126.575350231621));
#80390=CARTESIAN_POINT('Ctrl Pts',(-28.5605425720221,2.39492744496857,126.508606248909));
#80391=CARTESIAN_POINT('Ctrl Pts',(-28.5683030145362,2.2751456182781,126.441826642923));
#80392=CARTESIAN_POINT('Ctrl Pts',(-28.5760634570504,2.15266360947595,126.38011373255));
#80393=CARTESIAN_POINT('Ctrl Pts',(-28.5838238995646,2.02795497852603,126.323670752426));
#80394=CARTESIAN_POINT('Ctrl Pts',(-28.59159679983,1.90304615421043,126.267137165019));
#80395=CARTESIAN_POINT('Ctrl Pts',(-28.5993697000955,1.77590392783999,126.215890559401));
#80396=CARTESIAN_POINT('Ctrl Pts',(-28.607142600361,1.64702006931879,126.170085274671));
#80397=CARTESIAN_POINT('Ctrl Pts',(-28.614632936123,1.52282146369298,126.125945127418));
#80398=CARTESIAN_POINT('Ctrl Pts',(-28.622123271885,1.39700594709441,126.086857649393));
#80399=CARTESIAN_POINT('Ctrl Pts',(-28.6296136076471,1.27002258328984,126.052916026662));
#80400=CARTESIAN_POINT('Ctrl Pts',(-28.6373879417662,1.13822460665161,126.017687496988));
#80401=CARTESIAN_POINT('Ctrl Pts',(-28.6451622758853,1.0047509804201,125.987891142294));
#80402=CARTESIAN_POINT('Ctrl Pts',(-28.6529366100044,0.870089175209734,
125.963686295771));
#80403=CARTESIAN_POINT('Ctrl Pts',(-28.6607013629515,0.735593328639214,
125.939511279558));
#80404=CARTESIAN_POINT('Ctrl Pts',(-28.6684661158986,0.599912597763412,
125.920914128914));
#80405=CARTESIAN_POINT('Ctrl Pts',(-28.6762308688457,0.463549090902945,
125.908004288333));
#80406=CARTESIAN_POINT('Ctrl Pts',(-28.6839879097307,0.327321022200065,
125.895107269988));
#80407=CARTESIAN_POINT('Ctrl Pts',(-28.6917449506157,0.190411913753323,
125.887886357116));
#80408=CARTESIAN_POINT('Ctrl Pts',(-28.6995019915007,0.0533331837876476,
125.886399796859));
#80409=CARTESIAN_POINT('Ctrl Pts',(-28.7072531827408,-0.0836421740414438,
125.884914357629));
#80410=CARTESIAN_POINT('Ctrl Pts',(-28.7150043739809,-0.220786509426215,
125.889154667941));
#80411=CARTESIAN_POINT('Ctrl Pts',(-28.722755565221,-0.357584532415619,
125.899127048746));
#80412=CARTESIAN_POINT('Ctrl Pts',(-28.7305034619981,-0.494324412596046,
125.909095191023));
#80413=CARTESIAN_POINT('Ctrl Pts',(-28.7382513587751,-0.630717884020645,
125.924790529847));
#80414=CARTESIAN_POINT('Ctrl Pts',(-28.7459992555522,-0.766251131541064,
125.946167304624));
#80415=CARTESIAN_POINT('Ctrl Pts',(-28.7537455316363,-0.901756028427861,
125.967539607841));
#80416=CARTESIAN_POINT('Ctrl Pts',(-28.7614918077204,-1.03640067337513,
125.994590922277));
#80417=CARTESIAN_POINT('Ctrl Pts',(-28.7692380838045,-1.16967823465537,
126.027223829711));
#80418=CARTESIAN_POINT('Ctrl Pts',(-28.7769844170699,-1.30295677976047,
126.059856978034));
#80419=CARTESIAN_POINT('Ctrl Pts',(-28.7847307503352,-1.43486784131396,
126.098071708589));
#80420=CARTESIAN_POINT('Ctrl Pts',(-28.7924770836006,-1.56491700085398,
126.141719966289));
#80421=CARTESIAN_POINT('Ctrl Pts',(-28.8002251516036,-1.69499528400158,
126.185377998714));
#80422=CARTESIAN_POINT('Ctrl Pts',(-28.8079732196066,-1.82321046485832,
126.234471855202));
#80423=CARTESIAN_POINT('Ctrl Pts',(-28.8157212876095,-1.94908582495608,
126.288804449224));
#80424=CARTESIAN_POINT('Ctrl Pts',(-28.8234775903514,-2.07509496688448,
126.343194788573));
#80425=CARTESIAN_POINT('Ctrl Pts',(-28.8312338930932,-2.19875896089797,
126.402834832537));
#80426=CARTESIAN_POINT('Ctrl Pts',(-28.8389901958351,-2.31962302907808,
126.467480164352));
#80427=CARTESIAN_POINT('Ctrl Pts',(-28.8467506383492,-2.44055160605051,
126.532159999327));
#80428=CARTESIAN_POINT('Ctrl Pts',(-28.8545110808634,-2.55867694289546,
126.601850246724));
#80429=CARTESIAN_POINT('Ctrl Pts',(-28.8622715233776,-2.67357208182827,
126.676262340421));
#80430=CARTESIAN_POINT('Ctrl Pts',(-28.870044423643,-2.78865166063801,126.750793887016));
#80431=CARTESIAN_POINT('Ctrl Pts',(-28.8778173239085,-2.9004903602987,126.830062200812));
#80432=CARTESIAN_POINT('Ctrl Pts',(-28.8855902241739,-3.00869251730853,
126.913736965914));
#80433=CARTESIAN_POINT('Ctrl Pts',(-28.8930805599359,-3.11296125336598,
126.994369942541));
#80434=CARTESIAN_POINT('Ctrl Pts',(-28.9005708956979,-3.21385301557886,
127.079094363298));
#80435=CARTESIAN_POINT('Ctrl Pts',(-28.9080612314599,-3.31104667393621,
127.167582787465));
#80436=CARTESIAN_POINT('Ctrl Pts',(-28.9157178265862,-3.41039769297248,
127.258035346433));
#80437=CARTESIAN_POINT('Ctrl Pts',(-28.9233744217124,-3.50621937401956,
127.352726200813));
#80438=CARTESIAN_POINT('Ctrl Pts',(-28.9310310168386,-3.59812010972619,
127.45134484986));
#80439=CARTESIAN_POINT('Ctrl Pts',(-28.9386787643668,-3.68991464930377,
127.549849539876));
#80440=CARTESIAN_POINT('Ctrl Pts',(-28.9463265118951,-3.77779697796692,
127.652272710351));
#80441=CARTESIAN_POINT('Ctrl Pts',(-28.9539742594233,-3.86140890898757,
127.758264049811));
#80442=CARTESIAN_POINT('Ctrl Pts',(-28.9616149438516,-3.94494361996105,
127.864157500654));
#80443=CARTESIAN_POINT('Ctrl Pts',(-28.9692556282801,-4.02421552685795,
127.973612253527));
#80444=CARTESIAN_POINT('Ctrl Pts',(-28.9768963127084,-4.09890405487364,
128.08624203821));
#80445=CARTESIAN_POINT('Ctrl Pts',(-28.9846344939487,-4.17454562491685,
128.200309003692));
#80446=CARTESIAN_POINT('Ctrl Pts',(-28.992372675189,-4.24548573850194,128.317632293919));
#80447=CARTESIAN_POINT('Ctrl Pts',(-29.0001108564294,-4.31143403894221,
128.437776667999));
#80448=CARTESIAN_POINT('Ctrl Pts',(-29.0077430609832,-4.3764791578535,128.556275629251));
#80449=CARTESIAN_POINT('Ctrl Pts',(-29.0153752655371,-4.43666813624174,
128.677518522198));
#80450=CARTESIAN_POINT('Ctrl Pts',(-29.0230074700909,-4.49176690799423,
128.801060064292));
#80451=CARTESIAN_POINT('Ctrl Pts',(-29.0307986396745,-4.54801328760144,
128.927174753474));
#80452=CARTESIAN_POINT('Ctrl Pts',(-29.0385898092582,-4.5989548535771,129.055684531569));
#80453=CARTESIAN_POINT('Ctrl Pts',(-29.0463809788419,-4.64439333110353,
129.186091898069));
#80454=CARTESIAN_POINT('Ctrl Pts',(-29.0541721484255,-4.68983180862997,
129.31649926457));
#80455=CARTESIAN_POINT('Ctrl Pts',(-29.0619633180091,-4.72976705823019,
129.448803794148));
#80456=CARTESIAN_POINT('Ctrl Pts',(-29.0697544875927,-4.76405452823408,
129.582490119308));
#80457=CARTESIAN_POINT('Origin',(213.235140564004,0.,130.804360617566));
#80458=CARTESIAN_POINT('',(-31.1654202583464,-4.76405452823401,129.582490119308));
#80459=CARTESIAN_POINT('',(-30.8197844671783,-4.7640545282341,129.582490119308));
#80460=CARTESIAN_POINT('',(213.235140564004,-4.76405452823405,129.582490119308));
#80461=CARTESIAN_POINT('',(-29.4851405640419,-4.91824861549777,130.800670271478));
#80462=CARTESIAN_POINT('Ctrl Pts',(-29.4851405640418,-4.91824861549777,
130.800670271479));
#80463=CARTESIAN_POINT('Ctrl Pts',(-29.4927930356503,-4.91834965534574,
130.935329482471));
#80464=CARTESIAN_POINT('Ctrl Pts',(-29.5004455072588,-4.9129161848214,131.070199397566));
#80465=CARTESIAN_POINT('Ctrl Pts',(-29.5080979788673,-4.90192287276748,
131.204779413252));
#80466=CARTESIAN_POINT('Ctrl Pts',(-29.5157426700542,-4.89094073783477,
131.339222598733));
#80467=CARTESIAN_POINT('Ctrl Pts',(-29.523387361241,-4.87441003651631,131.473376071944));
#80468=CARTESIAN_POINT('Ctrl Pts',(-29.5310320524279,-4.85235746788152,
131.60673837548));
#80469=CARTESIAN_POINT('Ctrl Pts',(-29.5390646796908,-4.82918582370335,
131.746868257648));
#80470=CARTESIAN_POINT('Ctrl Pts',(-29.5470973069538,-4.79991719261537,
131.886124119136));
#80471=CARTESIAN_POINT('Ctrl Pts',(-29.5551299342168,-4.76464445377761,
132.023928693397));
#80472=CARTESIAN_POINT('Ctrl Pts',(-29.5627655150732,-4.7311152184967,132.154921696647));
#80473=CARTESIAN_POINT('Ctrl Pts',(-29.5704010959297,-4.69216129203358,
132.284602997777));
#80474=CARTESIAN_POINT('Ctrl Pts',(-29.5780366767862,-4.64791490469885,
132.41248688785));
#80475=CARTESIAN_POINT('Ctrl Pts',(-29.5856709314088,-4.60367620257575,
132.540348565607));
#80476=CARTESIAN_POINT('Ctrl Pts',(-29.5933051860314,-4.55414699898319,
132.666413071893));
#80477=CARTESIAN_POINT('Ctrl Pts',(-29.600939440654,-4.49950911101767,132.790210768602));
#80478=CARTESIAN_POINT('Ctrl Pts',(-29.6085741346125,-4.44486807875266,
132.914015589617));
#80479=CARTESIAN_POINT('Ctrl Pts',(-29.616208828571,-4.38511794075102,133.035552972723));
#80480=CARTESIAN_POINT('Ctrl Pts',(-29.6238435225295,-4.3204880540809,133.154374667959));
#80481=CARTESIAN_POINT('Ctrl Pts',(-29.6314804215562,-4.25583950087188,
133.273230681525));
#80482=CARTESIAN_POINT('Ctrl Pts',(-29.639117320583,-4.18630858960663,133.38936909364));
#80483=CARTESIAN_POINT('Ctrl Pts',(-29.6467542196097,-4.11216958661395,
133.502368095952));
#80484=CARTESIAN_POINT('Ctrl Pts',(-29.6543992370009,-4.03795177055231,
133.615487221247));
#80485=CARTESIAN_POINT('Ctrl Pts',(-29.6620442543922,-3.95911630688897,
133.725459938272));
#80486=CARTESIAN_POINT('Ctrl Pts',(-29.6696892717835,-3.8759797160554,133.831894977937));
#80487=CARTESIAN_POINT('Ctrl Pts',(-29.6773390192001,-3.79279168803573,
133.9383958697));
#80488=CARTESIAN_POINT('Ctrl Pts',(-29.6849887666167,-3.70529749652613,
134.041354421144));
#80489=CARTESIAN_POINT('Ctrl Pts',(-29.6926385140333,-3.61385163861373,
134.140415083037));
#80490=CARTESIAN_POINT('Ctrl Pts',(-29.7002991120519,-3.52227607150229,
134.239616255167));
#80491=CARTESIAN_POINT('Ctrl Pts',(-29.7079597100705,-3.42673793667808,
134.334908220911));
#80492=CARTESIAN_POINT('Ctrl Pts',(-29.7156203080891,-3.32762618744494,
134.42597448698));
#80493=CARTESIAN_POINT('Ctrl Pts',(-29.7183519076392,-3.29228513326763,
134.458446700091));
#80494=CARTESIAN_POINT('Ctrl Pts',(-29.7210835071891,-3.25648998315958,
134.490382017532));
#80495=CARTESIAN_POINT('Ctrl Pts',(-29.7238151067391,-3.22025926066219,
134.521767422937));
#80496=CARTESIAN_POINT('Ctrl Pts',(-29.7315894408582,-3.11714394785248,
134.61109260535));
#80497=CARTESIAN_POINT('Ctrl Pts',(-29.7393637749773,-3.01014587040966,
134.696265623824));
#80498=CARTESIAN_POINT('Ctrl Pts',(-29.7471381090964,-2.89963371300888,
134.776929986738));
#80499=CARTESIAN_POINT('Ctrl Pts',(-29.7549028620435,-2.78925775196533,
134.857494938034));
#80500=CARTESIAN_POINT('Ctrl Pts',(-29.7626676149905,-2.67537664070298,
134.933562061292));
#80501=CARTESIAN_POINT('Ctrl Pts',(-29.7704323679376,-2.55839404725985,
135.004813326673));
#80502=CARTESIAN_POINT('Ctrl Pts',(-29.7781894088226,-2.44152764257769,
135.075993824293));
#80503=CARTESIAN_POINT('Ctrl Pts',(-29.7859464497077,-2.32156621766588,
135.142367780719));
#80504=CARTESIAN_POINT('Ctrl Pts',(-29.7937034905927,-2.19894420510965,
135.203659134979));
#80505=CARTESIAN_POINT('Ctrl Pts',(-29.8014546818328,-2.07641466276745,
135.264904268953));
#80506=CARTESIAN_POINT('Ctrl Pts',(-29.809205873073,-1.95122887463564,135.321074255684));
#80507=CARTESIAN_POINT('Ctrl Pts',(-29.8169570643131,-1.82384746617401,
135.371938037012));
#80508=CARTESIAN_POINT('Ctrl Pts',(-29.8247049610902,-1.69652019820863,
135.422780199876));
#80509=CARTESIAN_POINT('Ctrl Pts',(-29.8324528578671,-1.56699952830063,
135.468320498235));
#80510=CARTESIAN_POINT('Ctrl Pts',(-29.8402007546442,-1.43576753470486,
135.508375354872));
#80511=CARTESIAN_POINT('Ctrl Pts',(-29.8479470307283,-1.30456299201311,
135.548421832896));
#80512=CARTESIAN_POINT('Ctrl Pts',(-29.8556933068124,-1.17164821135772,
135.58298503745));
#80513=CARTESIAN_POINT('Ctrl Pts',(-29.8634395828965,-1.0375215845876,135.611930900361));
#80514=CARTESIAN_POINT('Ctrl Pts',(-29.8711859161619,-0.903393967725188,
135.640876976944));
#80515=CARTESIAN_POINT('Ctrl Pts',(-29.8789322494272,-0.768054869064787,
135.664205546666));
#80516=CARTESIAN_POINT('Ctrl Pts',(-29.8866785826926,-0.632013664642088,
135.681833507312));
#80517=CARTESIAN_POINT('Ctrl Pts',(-29.8944266506956,-0.495941994734903,
135.699465415617));
#80518=CARTESIAN_POINT('Ctrl Pts',(-29.9021747186985,-0.359168293842022,
135.711394124304));
#80519=CARTESIAN_POINT('Ctrl Pts',(-29.9099227867015,-0.222207465767521,
135.717588365662));
#80520=CARTESIAN_POINT('Ctrl Pts',(-29.9176790894434,-0.0851010740949017,
135.723789190333));
#80521=CARTESIAN_POINT('Ctrl Pts',(-29.9254353921852,0.052192450856806,
135.724243355241));
#80522=CARTESIAN_POINT('Ctrl Pts',(-29.9331916949271,0.189157235024127,
135.718971752024));
#80523=CARTESIAN_POINT('Ctrl Pts',(-29.9409521374413,0.326195121420689,
135.713697335193));
#80524=CARTESIAN_POINT('Ctrl Pts',(-29.9487125799554,0.462903527902638,
135.702691092227));
#80525=CARTESIAN_POINT('Ctrl Pts',(-29.9564730224696,0.598772288770548,
135.68602578518));
#80526=CARTESIAN_POINT('Ctrl Pts',(-29.964245922735,0.734859158235081,135.669333725503));
#80527=CARTESIAN_POINT('Ctrl Pts',(-29.9720188230004,0.870103302657755,
135.646964511991));
#80528=CARTESIAN_POINT('Ctrl Pts',(-29.9797917232658,1.00400443845168,135.619042138712));
#80529=CARTESIAN_POINT('Ctrl Pts',(-29.9872820590279,1.13303793068343,135.592134814035));
#80530=CARTESIAN_POINT('Ctrl Pts',(-29.9947723947899,1.26082406378781,135.560071137679));
#80531=CARTESIAN_POINT('Ctrl Pts',(-30.002262730552,1.3869308381967,135.523005117055));
#80532=CARTESIAN_POINT('Ctrl Pts',(-30.0100370646711,1.51781898928626,135.484533726994));
#80533=CARTESIAN_POINT('Ctrl Pts',(-30.0178113987902,1.64731253638487,135.44055131105));
#80534=CARTESIAN_POINT('Ctrl Pts',(-30.0255857329093,1.77491226992272,135.391175361653));
#80535=CARTESIAN_POINT('Ctrl Pts',(-30.0333504858564,1.9023547481929,135.341860263702));
#80536=CARTESIAN_POINT('Ctrl Pts',(-30.0411152388034,2.02790769566083,135.28716499768));
#80537=CARTESIAN_POINT('Ctrl Pts',(-30.0488799917505,2.15108535238151,135.227257278044));
#80538=CARTESIAN_POINT('Ctrl Pts',(-30.0566370326355,2.27414066731688,135.167409059601));
#80539=CARTESIAN_POINT('Ctrl Pts',(-30.0643940735206,2.39482503705114,135.10235886006));
#80540=CARTESIAN_POINT('Ctrl Pts',(-30.0721511144056,2.51267138224773,135.032322962163));
#80541=CARTESIAN_POINT('Ctrl Pts',(-30.0799023056457,2.63042885859885,134.962339878882));
#80542=CARTESIAN_POINT('Ctrl Pts',(-30.0876534968858,2.74535223557114,134.887378779737));
#80543=CARTESIAN_POINT('Ctrl Pts',(-30.0954046881259,2.85699813807721,134.807702309393));
#80544=CARTESIAN_POINT('Ctrl Pts',(-30.103152584903,2.96859658809631,134.728059703675));
#80545=CARTESIAN_POINT('Ctrl Pts',(-30.11090048168,3.07692001667762,134.643705939512));
#80546=CARTESIAN_POINT('Ctrl Pts',(-30.1186483784571,3.18155340003668,134.554947375023));
#80547=CARTESIAN_POINT('Ctrl Pts',(-30.1263946545412,3.28616489634743,134.466207376913));
#80548=CARTESIAN_POINT('Ctrl Pts',(-30.1341409306253,3.38708758478787,134.37306466392));
#80549=CARTESIAN_POINT('Ctrl Pts',(-30.1418872067094,3.48393927703865,134.275866080101));
#80550=CARTESIAN_POINT('Ctrl Pts',(-30.1496335399748,3.58079168422675,134.178666778783));
#80551=CARTESIAN_POINT('Ctrl Pts',(-30.1573798732401,3.67357275930074,134.077411823844));
#80552=CARTESIAN_POINT('Ctrl Pts',(-30.1651262065054,3.76193725582314,133.972484848992));
#80553=CARTESIAN_POINT('Ctrl Pts',(-30.1728742745084,3.85032154096186,133.867534376471));
#80554=CARTESIAN_POINT('Ctrl Pts',(-30.1806223425114,3.93428702763511,133.758910546698));
#80555=CARTESIAN_POINT('Ctrl Pts',(-30.1883704105143,4.01352909134764,133.647029661863));
#80556=CARTESIAN_POINT('Ctrl Pts',(-30.1961267132562,4.09285537446848,133.535029868693));
#80557=CARTESIAN_POINT('Ctrl Pts',(-30.2038830159981,4.16744798008595,133.419766425023));
#80558=CARTESIAN_POINT('Ctrl Pts',(-30.2116393187399,4.23704564239276,133.301684642754));
#80559=CARTESIAN_POINT('Ctrl Pts',(-30.2193997612541,4.30668045106768,133.183539836682));
#80560=CARTESIAN_POINT('Ctrl Pts',(-30.2271602037682,4.3713148201394,133.06257403936));
#80561=CARTESIAN_POINT('Ctrl Pts',(-30.2349206462824,4.43073420936317,132.939255797306));
#80562=CARTESIAN_POINT('Ctrl Pts',(-30.2426935465478,4.49024898386537,132.815739593864));
#80563=CARTESIAN_POINT('Ctrl Pts',(-30.2504664468134,4.54453189459061,132.689863758546));
#80564=CARTESIAN_POINT('Ctrl Pts',(-30.2582393470788,4.59341684576232,132.562116215926));
#80565=CARTESIAN_POINT('Ctrl Pts',(-30.2657296828408,4.6405247058253,132.439012618257));
#80566=CARTESIAN_POINT('Ctrl Pts',(-30.2732200186028,4.68262015310914,132.314171325116));
#80567=CARTESIAN_POINT('Ctrl Pts',(-30.2807103543649,4.71959925209145,132.188039034742));
#80568=CARTESIAN_POINT('Ctrl Pts',(-30.2884846884839,4.75798042485118,132.057124400241));
#80569=CARTESIAN_POINT('Ctrl Pts',(-30.296259022603,4.79097119793339,131.924404241471));
#80570=CARTESIAN_POINT('Ctrl Pts',(-30.3040333567221,4.81840058608051,131.79036206511));
#80571=CARTESIAN_POINT('Ctrl Pts',(-30.3117981096692,4.84579616995811,131.656485083752));
#80572=CARTESIAN_POINT('Ctrl Pts',(-30.3195628626163,4.86764392851099,131.521289705912));
#80573=CARTESIAN_POINT('Ctrl Pts',(-30.3273276155633,4.88382239954593,131.385275268951));
#80574=CARTESIAN_POINT('Ctrl Pts',(-30.3350846564484,4.89998480189542,131.249395923445));
#80575=CARTESIAN_POINT('Ctrl Pts',(-30.3428416973333,4.91048907642576,131.112699523437));
#80576=CARTESIAN_POINT('Ctrl Pts',(-30.3505987382184,4.91526472014121,130.975695942106));
#80577=CARTESIAN_POINT('Ctrl Pts',(-30.3583499294585,4.92003676250659,130.838795676241));
#80578=CARTESIAN_POINT('Ctrl Pts',(-30.3661011206987,4.91908875920035,130.70158907928));
#80579=CARTESIAN_POINT('Ctrl Pts',(-30.3738523119389,4.91240202555274,130.564591141099));
#80580=CARTESIAN_POINT('Ctrl Pts',(-30.381600208716,4.90571813394531,130.427651430696));
#80581=CARTESIAN_POINT('Ctrl Pts',(-30.389348105493,4.89330038222731,130.290920592366));
#80582=CARTESIAN_POINT('Ctrl Pts',(-30.3970960022701,4.87518218766754,130.15491339142));
#80583=CARTESIAN_POINT('Ctrl Pts',(-30.4048422783542,4.85706778304351,130.018934640248));
#80584=CARTESIAN_POINT('Ctrl Pts',(-30.4125885544383,4.83325535893973,129.883679612674));
#80585=CARTESIAN_POINT('Ctrl Pts',(-30.4203348305223,4.80383014296098,129.749657332239));
#80586=CARTESIAN_POINT('Ctrl Pts',(-30.4280811637876,4.77440470977205,129.615634062482));
#80587=CARTESIAN_POINT('Ctrl Pts',(-30.435827497053,4.73936648587419,129.482843939892));
#80588=CARTESIAN_POINT('Ctrl Pts',(-30.4435738303184,4.69885161903793,129.351784793464));
#80589=CARTESIAN_POINT('Ctrl Pts',(-30.4513218983214,4.65832767917798,129.220696297249));
#80590=CARTESIAN_POINT('Ctrl Pts',(-30.4590699663244,4.61232477132086,129.091339922007));
#80591=CARTESIAN_POINT('Ctrl Pts',(-30.4668180343274,4.56102848530953,128.964196978458));
#80592=CARTESIAN_POINT('Ctrl Pts',(-30.4745743370693,4.50967768099499,128.836918905875));
#80593=CARTESIAN_POINT('Ctrl Pts',(-30.482330639811,4.45302240676723,128.711859327427));
#80594=CARTESIAN_POINT('Ctrl Pts',(-30.4900869425529,4.39129609558846,128.589478755396));
#80595=CARTESIAN_POINT('Ctrl Pts',(-30.4978473850671,4.32953683921888,128.467032865169));
#80596=CARTESIAN_POINT('Ctrl Pts',(-30.5056078275813,4.26270134326782,128.347269171722));
#80597=CARTESIAN_POINT('Ctrl Pts',(-30.5133682700954,4.19106784494925,128.230621434678));
#80598=CARTESIAN_POINT('Ctrl Pts',(-30.5211411703609,4.11931935417987,128.113786444332));
#80599=CARTESIAN_POINT('Ctrl Pts',(-30.5289140706263,4.04275768811868,128.000077730489));
#80600=CARTESIAN_POINT('Ctrl Pts',(-30.5366869708918,3.96170357270389,127.889898769381));
#80601=CARTESIAN_POINT('Ctrl Pts',(-30.5441773066538,3.88359597854754,127.783725091034));
#80602=CARTESIAN_POINT('Ctrl Pts',(-30.5516676424158,3.80131708043434,127.680829230668));
#80603=CARTESIAN_POINT('Ctrl Pts',(-30.5591579781778,3.7151865185552,127.581540083493));
#80604=CARTESIAN_POINT('Ctrl Pts',(-30.5669323122969,3.62579029024359,127.478486358123));
#80605=CARTESIAN_POINT('Ctrl Pts',(-30.574706646416,3.53196138053587,127.378991798697));
#80606=CARTESIAN_POINT('Ctrl Pts',(-30.5824809805351,3.43401415558535,127.283461607123));
#80607=CARTESIAN_POINT('Ctrl Pts',(-30.5902457334821,3.33618764183565,127.188049147972));
#80608=CARTESIAN_POINT('Ctrl Pts',(-30.5980104864293,3.23425318868581,127.096591605888));
#80609=CARTESIAN_POINT('Ctrl Pts',(-30.6057752393764,3.12856524951621,127.009461074492));
#80610=CARTESIAN_POINT('Ctrl Pts',(-30.6135322802613,3.02298228109817,126.92241708237));
#80611=CARTESIAN_POINT('Ctrl Pts',(-30.6212893211463,2.91365354529384,126.839691795512));
#80612=CARTESIAN_POINT('Ctrl Pts',(-30.6290463620313,2.80096990425718,126.761620128993));
#80613=CARTESIAN_POINT('Ctrl Pts',(-30.6367975532714,2.68837123882986,126.683607336925));
#80614=CARTESIAN_POINT('Ctrl Pts',(-30.6445487445116,2.57242302397057,126.61024140184));
#80615=CARTESIAN_POINT('Ctrl Pts',(-30.6522999357518,2.45354843572592,126.541816408288));
#80616=CARTESIAN_POINT('Ctrl Pts',(-30.6600478325288,2.334724372353,126.473420497184));
#80617=CARTESIAN_POINT('Ctrl Pts',(-30.6677957293059,2.21297674752372,126.40996154544));
#80618=CARTESIAN_POINT('Ctrl Pts',(-30.675543626083,2.08875671072263,126.351689681385));
#80619=CARTESIAN_POINT('Ctrl Pts',(-30.6832899021671,1.96456265807554,126.293430006548));
#80620=CARTESIAN_POINT('Ctrl Pts',(-30.6910361782511,1.83789757587744,126.240355427158));
#80621=CARTESIAN_POINT('Ctrl Pts',(-30.6987824543352,1.70923578765204,126.192669378475));
#80622=CARTESIAN_POINT('Ctrl Pts',(-30.7065287876006,1.58057304967456,126.144982977784));
#80623=CARTESIAN_POINT('Ctrl Pts',(-30.7142751208659,1.44991394285471,126.102685323045));
#80624=CARTESIAN_POINT('Ctrl Pts',(-30.7220214541313,1.31775089602114,126.065930958013));
#80625=CARTESIAN_POINT('Ctrl Pts',(-30.7297695221342,1.18555825218942,126.029168362095));
#80626=CARTESIAN_POINT('Ctrl Pts',(-30.7375175901372,1.05186137475576,125.997951630822));
#80627=CARTESIAN_POINT('Ctrl Pts',(-30.7452656581402,0.917165519902225,
125.972384782403));
#80628=CARTESIAN_POINT('Ctrl Pts',(-30.753021960882,0.782326508691256,125.946790761232));
#80629=CARTESIAN_POINT('Ctrl Pts',(-30.7607782636239,0.646486783869696,
125.9268586911));
#80630=CARTESIAN_POINT('Ctrl Pts',(-30.7685345663657,0.510159963680854,
125.91264109638));
#80631=CARTESIAN_POINT('Ctrl Pts',(-30.7762950088799,0.373760381763356,
125.898415913301));
#80632=CARTESIAN_POINT('Ctrl Pts',(-30.7840554513941,0.236873576473364,
125.889911307225));
#80633=CARTESIAN_POINT('Ctrl Pts',(-30.7918158939082,0.100014876076593,
125.887127646975));
#80634=CARTESIAN_POINT('Ctrl Pts',(-30.7995887941737,-0.0370635220559864,
125.884339518147));
#80635=CARTESIAN_POINT('Ctrl Pts',(-30.8073616944391,-0.17411333403871,
125.887290678821));
#80636=CARTESIAN_POINT('Ctrl Pts',(-30.8151345947045,-0.310621743687501,
125.895929381942));
#80637=CARTESIAN_POINT('Ctrl Pts',(-30.8226249304666,-0.44216772880218,
125.904254046445));
#80638=CARTESIAN_POINT('Ctrl Pts',(-30.8301152662286,-0.573210684494612,
125.917859887788));
#80639=CARTESIAN_POINT('Ctrl Pts',(-30.8376056019907,-0.703301128580765,
125.936655759521));
#80640=CARTESIAN_POINT('Ctrl Pts',(-30.8453799361097,-0.838323991393825,
125.956164282443));
#80641=CARTESIAN_POINT('Ctrl Pts',(-30.8531542702288,-0.972748399667074,
125.981325961893));
#80642=CARTESIAN_POINT('Ctrl Pts',(-30.8609286043479,-1.10606352297363,
126.012095334253));
#80643=CARTESIAN_POINT('Ctrl Pts',(-30.868693357295,-1.23921434730562,126.042826786112));
#80644=CARTESIAN_POINT('Ctrl Pts',(-30.876458110242,-1.3712582294884,126.079152093009));
#80645=CARTESIAN_POINT('Ctrl Pts',(-30.8842228631891,-1.50169052590856,
126.12097416897));
#80646=CARTESIAN_POINT('Ctrl Pts',(-30.8919799040741,-1.63199327513315,
126.162754706655));
#80647=CARTESIAN_POINT('Ctrl Pts',(-30.8997369449592,-1.76068725407411,
126.210021030214));
#80648=CARTESIAN_POINT('Ctrl Pts',(-30.9074939858442,-1.88727941865261,
126.262625326025));
#80649=CARTESIAN_POINT('Ctrl Pts',(-30.9152451770844,-2.01377611909574,
126.315189952528));
#80650=CARTESIAN_POINT('Ctrl Pts',(-30.9229963683245,-2.13817380043774,
126.373084389537));
#80651=CARTESIAN_POINT('Ctrl Pts',(-30.9307475595647,-2.25999630402923,
126.436111566942));
#80652=CARTESIAN_POINT('Ctrl Pts',(-30.9384954563418,-2.38176702980647,
126.499111956116));
#80653=CARTESIAN_POINT('Ctrl Pts',(-30.9462433531189,-2.50096440823137,
126.567240567468));
#80654=CARTESIAN_POINT('Ctrl Pts',(-30.9539912498959,-2.61713414194007,
126.640253036632));
#80655=CARTESIAN_POINT('Ctrl Pts',(-30.96173752598,-2.73327957544448,126.713250233161));
#80656=CARTESIAN_POINT('Ctrl Pts',(-30.9694838020642,-2.8463982931303,126.791129047577));
#80657=CARTESIAN_POINT('Ctrl Pts',(-30.9772300781483,-2.95606275570117,
126.873600379793));
#80658=CARTESIAN_POINT('Ctrl Pts',(-30.9849764114136,-3.06572802779019,
126.956072320793));
#80659=CARTESIAN_POINT('Ctrl Pts',(-30.992722744679,-3.17193868141687,127.043136612255));
#80660=CARTESIAN_POINT('Ctrl Pts',(-31.0004690779443,-3.27429852473151,
127.134462494533));
#80661=CARTESIAN_POINT('Ctrl Pts',(-31.0082171459473,-3.37668129082363,
127.22580882861));
#80662=CARTESIAN_POINT('Ctrl Pts',(-31.0159652139503,-3.47521123892816,
127.321418392323));
#80663=CARTESIAN_POINT('Ctrl Pts',(-31.0237132819533,-3.5695277522721,127.420922323721));
#80664=CARTESIAN_POINT('Ctrl Pts',(-31.0314695846951,-3.66394450632867,
127.52053200908));
#80665=CARTESIAN_POINT('Ctrl Pts',(-31.039225887437,-3.75413861077265,127.624044045979));
#80666=CARTESIAN_POINT('Ctrl Pts',(-31.0469821901788,-3.83978825215359,
127.73105470355));
#80667=CARTESIAN_POINT('Ctrl Pts',(-31.054742632693,-3.92548360732699,127.838122475931));
#80668=CARTESIAN_POINT('Ctrl Pts',(-31.0625030752072,-4.00662943518677,
127.948692274737));
#80669=CARTESIAN_POINT('Ctrl Pts',(-31.0702635177213,-4.08294687791647,
128.062330739061));
#80670=CARTESIAN_POINT('Ctrl Pts',(-31.0780364179868,-4.15938683218039,
128.176151625937));
#80671=CARTESIAN_POINT('Ctrl Pts',(-31.0858093182522,-4.230982708128,128.293050688641));
#80672=CARTESIAN_POINT('Ctrl Pts',(-31.0935822185176,-4.29750085235006,
128.412568509846));
#80673=CARTESIAN_POINT('Ctrl Pts',(-31.1010725542795,-4.36160089447973,
128.527741557202));
#80674=CARTESIAN_POINT('Ctrl Pts',(-31.1085628900415,-4.42098583327287,
128.645345996741));
#80675=CARTESIAN_POINT('Ctrl Pts',(-31.1160532258035,-4.47548939672102,
128.764954399487));
#80676=CARTESIAN_POINT('Ctrl Pts',(-31.1245404803809,-4.53724705793451,
128.900481964068));
#80677=CARTESIAN_POINT('Ctrl Pts',(-31.1330277349583,-4.59290752930504,
129.038954402169));
#80678=CARTESIAN_POINT('Ctrl Pts',(-31.1415149895357,-4.64220592367311,
129.179827692472));
#80679=CARTESIAN_POINT('Ctrl Pts',(-31.1494834124726,-4.68849067368878,
129.312089302797));
#80680=CARTESIAN_POINT('Ctrl Pts',(-31.1574518354095,-4.72916767521412,
129.446466808865));
#80681=CARTESIAN_POINT('Ctrl Pts',(-31.1654202583464,-4.76405452823401,
129.582490119308));
#80682=CARTESIAN_POINT('Ctrl Pts',(-29.4150816029337,-4.76405452823407,
129.582490119308));
#80683=CARTESIAN_POINT('Ctrl Pts',(-29.4228566469627,-4.7980744352381,129.715133220393));
#80684=CARTESIAN_POINT('Ctrl Pts',(-29.4306316909917,-4.82650842637683,
129.849034037413));
#80685=CARTESIAN_POINT('Ctrl Pts',(-29.4384067350207,-4.84929583035118,
129.983682232181));
#80686=CARTESIAN_POINT('Ctrl Pts',(-29.4407269843226,-4.85609610800431,
130.0238643043));
#80687=CARTESIAN_POINT('Ctrl Pts',(-29.4430472336244,-4.86239387499183,
130.064112915958));
#80688=CARTESIAN_POINT('Ctrl Pts',(-29.4453674829263,-4.86818841738373,
130.104414480102));
#80689=CARTESIAN_POINT('Ctrl Pts',(-29.4586251766203,-4.90129790612179,
130.33469395584));
#80690=CARTESIAN_POINT('Ctrl Pts',(-29.4718828703144,-4.91807356675018,
130.567376942442));
#80691=CARTESIAN_POINT('Ctrl Pts',(-29.4851405640086,-4.91824861549733,
130.800670270894));
#80692=CARTESIAN_POINT('',(-29.1398594359388,-4.9182483209296,130.808424627057));
#80693=CARTESIAN_POINT('Ctrl Pts',(-29.0697544875927,-4.76405452823408,
129.582490119308));
#80694=CARTESIAN_POINT('Ctrl Pts',(-29.0773912973827,-4.79766268985716,
129.713527831402));
#80695=CARTESIAN_POINT('Ctrl Pts',(-29.0850281071728,-4.82584473991743,
129.845892683461));
#80696=CARTESIAN_POINT('Ctrl Pts',(-29.0926649169627,-4.84851619709028,
129.979088693257));
#80697=CARTESIAN_POINT('Ctrl Pts',(-29.1005306701254,-4.87186732025087,
130.116277776672));
#80698=CARTESIAN_POINT('Ctrl Pts',(-29.108396423288,-4.88937218816657,130.254348176387));
#80699=CARTESIAN_POINT('Ctrl Pts',(-29.1162621764507,-4.9009960473005,130.392753029146));
#80700=CARTESIAN_POINT('Ctrl Pts',(-29.1241279296134,-4.91261990643446,
130.531157881905));
#80701=CARTESIAN_POINT('Ctrl Pts',(-29.1319936827761,-4.91836278825225,
130.669896722895));
#80702=CARTESIAN_POINT('Ctrl Pts',(-29.1398594359388,-4.9182483209296,130.808424627058));
#80703=CARTESIAN_POINT('Ctrl Pts',(-29.1398594359911,-4.91824832092884,
130.80842462798));
#80704=CARTESIAN_POINT('Ctrl Pts',(-29.1521788354858,-4.91806904133954,
131.025388033418));
#80705=CARTESIAN_POINT('Ctrl Pts',(-29.1644982349803,-4.90353032655609,
131.241777625956));
#80706=CARTESIAN_POINT('Ctrl Pts',(-29.1768176344749,-4.87487472503856,
131.456111703242));
#80707=CARTESIAN_POINT('Ctrl Pts',(-29.1800480414075,-4.86736062065044,
131.512314628512));
#80708=CARTESIAN_POINT('Ctrl Pts',(-29.1832784483402,-4.85887604229768,
131.568376420214));
#80709=CARTESIAN_POINT('Ctrl Pts',(-29.1865088552728,-4.84942579143849,
131.624270707656));
#80710=CARTESIAN_POINT('Ctrl Pts',(-29.1942831893919,-4.82668271008041,
131.758786536462));
#80711=CARTESIAN_POINT('Ctrl Pts',(-29.202057523511,-4.79830246142229,131.892568422899));
#80712=CARTESIAN_POINT('Ctrl Pts',(-29.2098318576301,-4.76434275451195,
132.025106774648));
#80713=CARTESIAN_POINT('Ctrl Pts',(-29.2175966105772,-4.73042489990527,
132.157481784724));
#80714=CARTESIAN_POINT('Ctrl Pts',(-29.2253613635244,-4.6909413647112,132.288615934325));
#80715=CARTESIAN_POINT('Ctrl Pts',(-29.2331261164715,-4.64600131700206,
132.41800705496));
#80716=CARTESIAN_POINT('Ctrl Pts',(-29.2408831573565,-4.60110590438204,
132.547269662509));
#80717=CARTESIAN_POINT('Ctrl Pts',(-29.2486401982414,-4.55076489171014,
132.674792319326));
#80718=CARTESIAN_POINT('Ctrl Pts',(-29.2563972391264,-4.49513788173963,
132.800085670435));
#80719=CARTESIAN_POINT('Ctrl Pts',(-29.2641484303666,-4.43955282052989,
132.925284536854));
#80720=CARTESIAN_POINT('Ctrl Pts',(-29.2718996216067,-4.37868985433787,
133.048257087881));
#80721=CARTESIAN_POINT('Ctrl Pts',(-29.2796508128469,-4.31275742301797,
133.168532031128));
#80722=CARTESIAN_POINT('Ctrl Pts',(-29.287398709624,-4.24685301474019,133.288755854316));
#80723=CARTESIAN_POINT('Ctrl Pts',(-29.295146606401,-4.17588361432586,133.406284008019));
#80724=CARTESIAN_POINT('Ctrl Pts',(-29.3028945031781,-4.100104417655,133.520668189772));
#80725=CARTESIAN_POINT('Ctrl Pts',(-29.3106407792622,-4.02434107235847,
133.635028444821));
#80726=CARTESIAN_POINT('Ctrl Pts',(-29.3183870553464,-3.94377014779473,
133.7462457103));
#80727=CARTESIAN_POINT('Ctrl Pts',(-29.3261333314306,-3.8586909205612,133.853899507641));
#80728=CARTESIAN_POINT('Ctrl Pts',(-29.3338796646959,-3.77361106529214,
133.961554099657));
#80729=CARTESIAN_POINT('Ctrl Pts',(-29.3416259979612,-3.68402308336316,
134.065644864308));
#80730=CARTESIAN_POINT('Ctrl Pts',(-29.3493723312266,-3.59026714667992,
134.165783661155));
#80731=CARTESIAN_POINT('Ctrl Pts',(-29.3571203992296,-3.49649021400472,
134.265944883392));
#80732=CARTESIAN_POINT('Ctrl Pts',(-29.3648684672326,-3.39854373640565,
134.362152091401));
#80733=CARTESIAN_POINT('Ctrl Pts',(-29.3726165352356,-3.29680512342074,
134.454053623928));
#80734=CARTESIAN_POINT('Ctrl Pts',(-29.3803728379774,-3.19495838142724,
134.546052830497));
#80735=CARTESIAN_POINT('Ctrl Pts',(-29.3881291407194,-3.08931174362308,
134.633736957796));
#80736=CARTESIAN_POINT('Ctrl Pts',(-29.3958854434613,-2.98027654724618,
134.716793973476));
#80737=CARTESIAN_POINT('Ctrl Pts',(-29.4036458859754,-2.87118315550183,
134.799895319185));
#80738=CARTESIAN_POINT('Ctrl Pts',(-29.4114063284895,-2.75869792194067,
134.878364408755));
#80739=CARTESIAN_POINT('Ctrl Pts',(-29.4191667710037,-2.64326077449113,
134.951932864138));
#80740=CARTESIAN_POINT('Ctrl Pts',(-29.4269396712691,-2.52763831708462,
135.025619418138));
#80741=CARTESIAN_POINT('Ctrl Pts',(-29.4347125715347,-2.40905481481085,
135.094389421063));
#80742=CARTESIAN_POINT('Ctrl Pts',(-29.4424854718001,-2.28797515973411,
135.158020311541));
#80743=CARTESIAN_POINT('Ctrl Pts',(-29.4499758075619,-2.1712970551036,135.219338058871));
#80744=CARTESIAN_POINT('Ctrl Pts',(-29.4574661433238,-2.05230140795038,
135.275883713991));
#80745=CARTESIAN_POINT('Ctrl Pts',(-29.4649564790856,-1.93141951423011,
135.327501309889));
#80746=CARTESIAN_POINT('Ctrl Pts',(-29.4727308132047,-1.80595434676516,
135.381076002626));
#80747=CARTESIAN_POINT('Ctrl Pts',(-29.4805051473238,-1.67805963918038,
135.429511273083));
#80748=CARTESIAN_POINT('Ctrl Pts',(-29.4882794814429,-1.54819531907598,
135.47258022642));
#80749=CARTESIAN_POINT('Ctrl Pts',(-29.49604423439,-1.41849104513997,135.515596101121));
#80750=CARTESIAN_POINT('Ctrl Pts',(-29.5038089873371,-1.28682235595714,
135.55325869572));
#80751=CARTESIAN_POINT('Ctrl Pts',(-29.5115737402841,-1.15367074811228,
135.585388422071));
#80752=CARTESIAN_POINT('Ctrl Pts',(-29.5193307811692,-1.02065138832126,
135.617486236725));
#80753=CARTESIAN_POINT('Ctrl Pts',(-29.5270878220542,-0.886152418515271,
135.644062027956));
#80754=CARTESIAN_POINT('Ctrl Pts',(-29.5348448629392,-0.750671816080639,
135.664985565764));
#80755=CARTESIAN_POINT('Ctrl Pts',(-29.5425960541793,-0.615293380622188,
135.685893324969));
#80756=CARTESIAN_POINT('Ctrl Pts',(-29.5503472454194,-0.478935170792394,
135.701157255385));
#80757=CARTESIAN_POINT('Ctrl Pts',(-29.5580984366596,-0.342106365057883,
135.710697978316));
#80758=CARTESIAN_POINT('Ctrl Pts',(-29.5658463334367,-0.205335715215836,
135.720234646185));
#80759=CARTESIAN_POINT('Ctrl Pts',(-29.5735942302137,-0.0680952564869745,
135.72405291752));
#80760=CARTESIAN_POINT('Ctrl Pts',(-29.5813421269908,0.0690999019604429,
135.722125177409));
#80761=CARTESIAN_POINT('Ctrl Pts',(-29.5890884030749,0.206266362138298,
135.72019784054));
#80762=CARTESIAN_POINT('Ctrl Pts',(-29.5968346791591,0.343387150203734,
135.712526888442));
#80763=CARTESIAN_POINT('Ctrl Pts',(-29.6045809552432,0.479946739315554,
135.699136832054));
#80764=CARTESIAN_POINT('Ctrl Pts',(-29.6123272885085,0.616507336479052,
135.685746676824));
#80765=CARTESIAN_POINT('Ctrl Pts',(-29.6200736217739,0.752506337323381,
135.666637371216));
#80766=CARTESIAN_POINT('Ctrl Pts',(-29.6278199550392,0.887433317082195,
135.641885312101));
#80767=CARTESIAN_POINT('Ctrl Pts',(-29.6355680230422,1.02239051280261,135.617127709933));
#80768=CARTESIAN_POINT('Ctrl Pts',(-29.6433160910451,1.15627482524811,135.586724910262));
#80769=CARTESIAN_POINT('Ctrl Pts',(-29.6510641590481,1.2885863927717,135.550804356921));
#80770=CARTESIAN_POINT('Ctrl Pts',(-29.6588204617899,1.42103858260379,135.514845626789));
#80771=CARTESIAN_POINT('Ctrl Pts',(-29.6665767645318,1.55191431053923,135.473357530945));
#80772=CARTESIAN_POINT('Ctrl Pts',(-29.6743330672737,1.68072871710143,135.426517477952));
#80773=CARTESIAN_POINT('Ctrl Pts',(-29.6820935097878,1.80961187579113,135.379652425011));
#80774=CARTESIAN_POINT('Ctrl Pts',(-29.6898539523019,1.93643115955007,135.327429871896));
#80775=CARTESIAN_POINT('Ctrl Pts',(-29.6976143948161,2.06072298253663,135.270074877541));
#80776=CARTESIAN_POINT('Ctrl Pts',(-29.7053872950815,2.18521432979157,135.212627811858));
#80777=CARTESIAN_POINT('Ctrl Pts',(-29.713160195347,2.30716976046241,135.150032019318));
#80778=CARTESIAN_POINT('Ctrl Pts',(-29.7209330956125,2.42615074184579,135.082558326922));
#80779=CARTESIAN_POINT('Ctrl Pts',(-29.7284234313746,2.54080646486216,135.0175374732));
#80780=CARTESIAN_POINT('Ctrl Pts',(-29.7359137671366,2.65269997989081,134.947987372913));
#80781=CARTESIAN_POINT('Ctrl Pts',(-29.7434041028988,2.7614669414705,134.874186583583));
#80782=CARTESIAN_POINT('Ctrl Pts',(-29.7511784370179,2.87435783545621,134.797587614895));
#80783=CARTESIAN_POINT('Ctrl Pts',(-29.7589527711369,2.98423801370107,134.716166622017));
#80784=CARTESIAN_POINT('Ctrl Pts',(-29.766727105256,3.09066798104836,134.630187912861));
#80785=CARTESIAN_POINT('Ctrl Pts',(-29.7744918582031,3.19696678297281,134.544315164779));
#80786=CARTESIAN_POINT('Ctrl Pts',(-29.7822566111502,3.29982353315876,134.453896119859));
#80787=CARTESIAN_POINT('Ctrl Pts',(-29.7900213640973,3.39882687834791,134.359238803034));
#80788=CARTESIAN_POINT('Ctrl Pts',(-29.7977784049823,3.49773189201893,134.264675501191));
#80789=CARTESIAN_POINT('Ctrl Pts',(-29.8055354458673,3.5927908363472,134.165882572995));
#80790=CARTESIAN_POINT('Ctrl Pts',(-29.8132924867523,3.68362497620382,134.063208588427));
#80791=CARTESIAN_POINT('Ctrl Pts',(-29.8210436779925,3.77439061732898,133.96061203111));
#80792=CARTESIAN_POINT('Ctrl Pts',(-29.8287948692326,3.86093753743193,133.854140534547));
#80793=CARTESIAN_POINT('Ctrl Pts',(-29.8365460604727,3.94292372956989,133.744179578879));
#80794=CARTESIAN_POINT('Ctrl Pts',(-29.8442939572498,4.02487507538914,133.63426535955));
#80795=CARTESIAN_POINT('Ctrl Pts',(-29.8520418540269,4.10226931542995,133.520864943693));
#80796=CARTESIAN_POINT('Ctrl Pts',(-29.859789750804,4.17480478739694,133.404396780704));
#80797=CARTESIAN_POINT('Ctrl Pts',(-29.8675360268881,4.24732508650688,133.287952980345));
#80798=CARTESIAN_POINT('Ctrl Pts',(-29.8752823029722,4.31498843256487,133.168443040901));
#80799=CARTESIAN_POINT('Ctrl Pts',(-29.8830285790563,4.37753679246813,133.046313938464));
#80800=CARTESIAN_POINT('Ctrl Pts',(-29.8907749123216,4.44008561408918,132.924183934499));
#80801=CARTESIAN_POINT('Ctrl Pts',(-29.898521245587,4.49751919599378,132.799435076945));
#80802=CARTESIAN_POINT('Ctrl Pts',(-29.9062675788523,4.54962591597954,132.672538094988));
#80803=CARTESIAN_POINT('Ctrl Pts',(-29.9140156468553,4.60174430490396,132.545612695332));
#80804=CARTESIAN_POINT('Ctrl Pts',(-29.9217637148583,4.64853330967106,132.416538575619));
#80805=CARTESIAN_POINT('Ctrl Pts',(-29.9295117828613,4.68982996495887,132.285805170114));
#80806=CARTESIAN_POINT('Ctrl Pts',(-29.9372680856031,4.73117051082336,132.15493281959));
#80807=CARTESIAN_POINT('Ctrl Pts',(-29.9450243883451,4.76700692855247,132.022398033878));
#80808=CARTESIAN_POINT('Ctrl Pts',(-29.9527806910869,4.79722639860321,131.888704632648));
#80809=CARTESIAN_POINT('Ctrl Pts',(-29.9605411336011,4.82746199769505,131.754939875225));
#80810=CARTESIAN_POINT('Ctrl Pts',(-29.9683015761152,4.85207460534403,131.620015654524));
#80811=CARTESIAN_POINT('Ctrl Pts',(-29.9760620186294,4.87100299053636,131.484443648295));
#80812=CARTESIAN_POINT('Ctrl Pts',(-29.9838349188948,4.88996176125298,131.348654009847));
#80813=CARTESIAN_POINT('Ctrl Pts',(-29.9916078191603,4.90321803738849,131.212214897211));
#80814=CARTESIAN_POINT('Ctrl Pts',(-29.9993807194257,4.91076263573133,131.07564164898));
#80815=CARTESIAN_POINT('Ctrl Pts',(-30.0068710551877,4.91803296892063,130.944033182331));
#80816=CARTESIAN_POINT('Ctrl Pts',(-30.0143613909496,4.91999967781119,130.81230047109));
#80817=CARTESIAN_POINT('Ctrl Pts',(-30.0218517267116,4.91670018311583,130.680900616559));
#80818=CARTESIAN_POINT('Ctrl Pts',(-30.0296260608306,4.91327558707621,130.544518696603));
#80819=CARTESIAN_POINT('Ctrl Pts',(-30.0374003949497,4.90416672011928,130.408063355208));
#80820=CARTESIAN_POINT('Ctrl Pts',(-30.0451747290688,4.8893583941103,130.27204721698));
#80821=CARTESIAN_POINT('Ctrl Pts',(-30.0529394820159,4.87456831803966,130.136198706486));
#80822=CARTESIAN_POINT('Ctrl Pts',(-30.060704234963,4.85409280063932,130.000788707113));
#80823=CARTESIAN_POINT('Ctrl Pts',(-30.0684689879101,4.82796864552613,129.866329797008));
#80824=CARTESIAN_POINT('Ctrl Pts',(-30.076226028795,4.80187043729209,129.732004433388));
#80825=CARTESIAN_POINT('Ctrl Pts',(-30.08398306968,4.77013483019267,129.598628660474));
#80826=CARTESIAN_POINT('Ctrl Pts',(-30.091740110565,4.73285037043758,129.466709529446));
#80827=CARTESIAN_POINT('Ctrl Pts',(-30.0994913018051,4.69559402718363,129.334889879661));
#80828=CARTESIAN_POINT('Ctrl Pts',(-30.1072424930453,4.65279726603736,129.204525060039));
#80829=CARTESIAN_POINT('Ctrl Pts',(-30.1149936842854,4.60459953925229,129.076111172139));
#80830=CARTESIAN_POINT('Ctrl Pts',(-30.1227415810625,4.55642229778682,128.947751863568));
#80831=CARTESIAN_POINT('Ctrl Pts',(-30.1304894778395,4.50284879346106,128.821342202773));
#80832=CARTESIAN_POINT('Ctrl Pts',(-30.1382373746166,4.44406802376494,128.697362168907));
#80833=CARTESIAN_POINT('Ctrl Pts',(-30.1459836507007,4.38529954973868,128.573408068992));
#80834=CARTESIAN_POINT('Ctrl Pts',(-30.1537299267847,4.32132614430036,128.451882938166));
#80835=CARTESIAN_POINT('Ctrl Pts',(-30.1614762028688,4.25238438790143,128.333245468482));
#80836=CARTESIAN_POINT('Ctrl Pts',(-30.1692225361342,4.18344212259021,128.214607123043));
#80837=CARTESIAN_POINT('Ctrl Pts',(-30.1769688693995,4.10953162957136,128.098856819315));
#80838=CARTESIAN_POINT('Ctrl Pts',(-30.1847152026649,4.03093455967212,127.986427041674));
#80839=CARTESIAN_POINT('Ctrl Pts',(-30.1924632706678,3.95231988850402,127.873972086163));
#80840=CARTESIAN_POINT('Ctrl Pts',(-30.2002113386707,3.86901677598191,127.764839456803));
#80841=CARTESIAN_POINT('Ctrl Pts',(-30.2079594066737,3.78134891027844,127.659430812112));
#80842=CARTESIAN_POINT('Ctrl Pts',(-30.2157157094155,3.69358787012391,127.553910137857));
#80843=CARTESIAN_POINT('Ctrl Pts',(-30.2234720121574,3.60145306046009,127.452121655662));
#80844=CARTESIAN_POINT('Ctrl Pts',(-30.2312283148993,3.50530737732605,127.354432610641));
#80845=CARTESIAN_POINT('Ctrl Pts',(-30.2389887574134,3.40911037834604,127.256691426036));
#80846=CARTESIAN_POINT('Ctrl Pts',(-30.2467491999277,3.30889852584867,127.163054305159));
#80847=CARTESIAN_POINT('Ctrl Pts',(-30.2545096424419,3.20506921195834,127.07384933772));
#80848=CARTESIAN_POINT('Ctrl Pts',(-30.2622825427073,3.10107322203582,126.984501170548));
#80849=CARTESIAN_POINT('Ctrl Pts',(-30.2700554429727,2.99344847347289,126.899599616908));
#80850=CARTESIAN_POINT('Ctrl Pts',(-30.2778283432381,2.88262357147262,126.819430955992));
#80851=CARTESIAN_POINT('Ctrl Pts',(-30.2853186790002,2.77582743380993,126.742176627832));
#80852=CARTESIAN_POINT('Ctrl Pts',(-30.2928090147623,2.66606002717133,126.669317231765));
#80853=CARTESIAN_POINT('Ctrl Pts',(-30.3002993505244,2.55372615063673,126.601068359103));
#80854=CARTESIAN_POINT('Ctrl Pts',(-30.3080736846435,2.43713310103148,126.530231809691));
#80855=CARTESIAN_POINT('Ctrl Pts',(-30.3158480187625,2.31740579261338,126.464137912308));
#80856=CARTESIAN_POINT('Ctrl Pts',(-30.3236223528816,2.19496730142352,126.403076531281));
#80857=CARTESIAN_POINT('Ctrl Pts',(-30.3313871058287,2.07267970473141,126.34209040295));
#80858=CARTESIAN_POINT('Ctrl Pts',(-30.3391518587758,1.94768791995112,126.286124623402));
#80859=CARTESIAN_POINT('Ctrl Pts',(-30.3469166117229,1.82044308684874,126.235425289719));
#80860=CARTESIAN_POINT('Ctrl Pts',(-30.3546736526079,1.69332463510843,126.18477631133));
#80861=CARTESIAN_POINT('Ctrl Pts',(-30.3624306934929,1.56395794913512,126.139383513238));
#80862=CARTESIAN_POINT('Ctrl Pts',(-30.3701877343779,1.43281748683617,126.099446472556));
#80863=CARTESIAN_POINT('Ctrl Pts',(-30.377938925618,1.30177591857979,126.059539548707));
#80864=CARTESIAN_POINT('Ctrl Pts',(-30.3856901168582,1.16896360893954,126.025080306583));
#80865=CARTESIAN_POINT('Ctrl Pts',(-30.3934413080983,1.03487331955688,125.996219576065));
#80866=CARTESIAN_POINT('Ctrl Pts',(-30.4011892048754,0.900840022124366,
125.967371112127));
#80867=CARTESIAN_POINT('Ctrl Pts',(-30.4089371016525,0.765530206696216,
125.944116509209));
#80868=CARTESIAN_POINT('Ctrl Pts',(-30.4166849984296,0.629449851087463,
125.926556198827));
#80869=CARTESIAN_POINT('Ctrl Pts',(-30.4244312745137,0.493397960555551,
125.908999561684));
#80870=CARTESIAN_POINT('Ctrl Pts',(-30.4321775505977,0.356576237944092,
125.897134897872));
#80871=CARTESIAN_POINT('Ctrl Pts',(-30.4399238266818,0.219498471381506,
125.891011099817));
#80872=CARTESIAN_POINT('Ctrl Pts',(-30.4476701599472,0.0824196929418009,
125.884887256558));
#80873=CARTESIAN_POINT('Ctrl Pts',(-30.4554164932126,-0.0549147426448532,
125.884504381065));
#80874=CARTESIAN_POINT('Ctrl Pts',(-30.4631628264779,-0.191988734872408,
125.889859280891));
#80875=CARTESIAN_POINT('Ctrl Pts',(-30.4709108944809,-0.329093423869931,
125.895215379909));
#80876=CARTESIAN_POINT('Ctrl Pts',(-30.4786589624839,-0.465937162856939,
125.906311795859));
#80877=CARTESIAN_POINT('Ctrl Pts',(-30.4864070304868,-0.602007063783788,
125.923093306953));
#80878=CARTESIAN_POINT('Ctrl Pts',(-30.4941633332287,-0.738221581420594,
125.939892653637));
#80879=CARTESIAN_POINT('Ctrl Pts',(-30.5019196359706,-0.873660229432092,
125.962389117453));
#80880=CARTESIAN_POINT('Ctrl Pts',(-30.5096759387124,-1.0078178799286,125.990475888639));
#80881=CARTESIAN_POINT('Ctrl Pts',(-30.5174363812266,-1.14204713440277,
126.018577650581));
#80882=CARTESIAN_POINT('Ctrl Pts',(-30.5251968237407,-1.27499365022287,
126.052275569187));
#80883=CARTESIAN_POINT('Ctrl Pts',(-30.5329572662549,-1.40616659607493,
126.091412647709));
#80884=CARTESIAN_POINT('Ctrl Pts',(-30.5407301665203,-1.53755011238465,
126.130612552543));
#80885=CARTESIAN_POINT('Ctrl Pts',(-30.5485030667857,-1.66715399947828,
126.175268938022));
#80886=CARTESIAN_POINT('Ctrl Pts',(-30.5562759670512,-1.79450573098123,
126.225175947346));
#80887=CARTESIAN_POINT('Ctrl Pts',(-30.5637663028132,-1.91722790626457,
126.273268711173));
#80888=CARTESIAN_POINT('Ctrl Pts',(-30.5712566385752,-2.0378585441665,126.326236855888));
#80889=CARTESIAN_POINT('Ctrl Pts',(-30.5787469743373,-2.15599745781895,
126.383856344932));
#80890=CARTESIAN_POINT('Ctrl Pts',(-30.5865220441461,-2.27862724772009,
126.443666153717));
#80891=CARTESIAN_POINT('Ctrl Pts',(-30.594297113955,-2.39896061875612,126.508677407539));
#80892=CARTESIAN_POINT('Ctrl Pts',(-30.6020721837638,-2.51652488359778,
126.5786907804));
#80893=CARTESIAN_POINT('Ctrl Pts',(-30.609837507902,-2.63394178736863,126.648616394914));
#80894=CARTESIAN_POINT('Ctrl Pts',(-30.6176028320401,-2.74859615878053,
126.723531454025));
#80895=CARTESIAN_POINT('Ctrl Pts',(-30.6253681561782,-2.86003700080638,
126.803189361981));
#80896=CARTESIAN_POINT('Ctrl Pts',(-30.6334688358033,-2.97629055858908,
126.886287398905));
#80897=CARTESIAN_POINT('Ctrl Pts',(-30.6415695154282,-3.08904642401237,
126.974546941627));
#80898=CARTESIAN_POINT('Ctrl Pts',(-30.6496701950532,-3.197822017491,127.067635124979));
#80899=CARTESIAN_POINT('Ctrl Pts',(-30.6574209290212,-3.30189855505178,
127.15670194136));
#80900=CARTESIAN_POINT('Ctrl Pts',(-30.6651716629892,-3.40233117176396,
127.250188660896));
#80901=CARTESIAN_POINT('Ctrl Pts',(-30.6729223969572,-3.49872814195416,
127.347760488653));
#80902=CARTESIAN_POINT('Ctrl Pts',(-30.6806696726043,-3.59508210052151,
127.445288780575));
#80903=CARTESIAN_POINT('Ctrl Pts',(-30.6884169482515,-3.6874037212943,127.546898276432));
#80904=CARTESIAN_POINT('Ctrl Pts',(-30.6961642238987,-3.77533674529737,
127.652216026639));
#80905=CARTESIAN_POINT('Ctrl Pts',(-30.7039097205091,-3.86324957690148,
127.757509592326));
#80906=CARTESIAN_POINT('Ctrl Pts',(-30.7116552171195,-3.94677556751609,
127.866509417449));
#80907=CARTESIAN_POINT('Ctrl Pts',(-30.7194007137299,-4.02559777753427,
127.978808353669));
#80908=CARTESIAN_POINT('Ctrl Pts',(-30.727146109024,-4.10441895650438,128.091105820943));
#80909=CARTESIAN_POINT('Ctrl Pts',(-30.7348915043181,-4.17853625430074,
128.20670199259));
#80910=CARTESIAN_POINT('Ctrl Pts',(-30.7426368996122,-4.24767545038139,
128.325159873228));
#80911=CARTESIAN_POINT('Ctrl Pts',(-30.7503866983179,-4.31685395347359,
128.443685099533));
#80912=CARTESIAN_POINT('Ctrl Pts',(-30.7581364970237,-4.38104850528407,
128.565074946332));
#80913=CARTESIAN_POINT('Ctrl Pts',(-30.7658862957294,-4.44003026842972,
128.688866756093));
#80914=CARTESIAN_POINT('Ctrl Pts',(-30.7736386990034,-4.49903185428767,
128.812700170062));
#80915=CARTESIAN_POINT('Ctrl Pts',(-30.7813911022774,-4.55281700442514,
128.938936797377));
#80916=CARTESIAN_POINT('Ctrl Pts',(-30.7891435055514,-4.60120499790612,
129.067093905244));
#80917=CARTESIAN_POINT('Ctrl Pts',(-30.7969033255299,-4.64963928405729,
129.195373620689));
#80918=CARTESIAN_POINT('Ctrl Pts',(-30.8046631455085,-4.69266597925393,
129.325577115149));
#80919=CARTESIAN_POINT('Ctrl Pts',(-30.812422965487,-4.73015412448565,129.457206201357));
#80920=CARTESIAN_POINT('Ctrl Pts',(-30.8148767993841,-4.74200873989752,
129.498830351722));
#80921=CARTESIAN_POINT('Ctrl Pts',(-30.8173306332813,-4.75330989944343,
129.540596974726));
#80922=CARTESIAN_POINT('Ctrl Pts',(-30.8197844671784,-4.7640545282341,129.582490119308));
#80923=CARTESIAN_POINT('Origin',(213.235140564004,0.,130.804360617566));
#80924=CARTESIAN_POINT('',(-32.9151834992122,-4.76405452823401,129.582490119308));
#80925=CARTESIAN_POINT('',(-32.5701265742934,-4.76405452823409,129.582490119308));
#80926=CARTESIAN_POINT('',(213.235140564004,-4.76405452823405,129.582490119308));
#80927=CARTESIAN_POINT('',(-31.2351405639676,-4.91824962726525,130.802445831626));
#80928=CARTESIAN_POINT('Ctrl Pts',(-31.2351405640085,-4.91824962726554,
130.802445832352));
#80929=CARTESIAN_POINT('Ctrl Pts',(-31.243051214989,-4.91830428636559,130.942841264952));
#80930=CARTESIAN_POINT('Ctrl Pts',(-31.2509618659695,-4.91234303963147,
131.083200981546));
#80931=CARTESIAN_POINT('Ctrl Pts',(-31.25887251695,-4.90040142640427,131.222988044516));
#80932=CARTESIAN_POINT('Ctrl Pts',(-31.2667870358457,-4.8884539743217,131.362843456413));
#80933=CARTESIAN_POINT('Ctrl Pts',(-31.2747015547414,-4.87052035993673,
131.502125290756));
#80934=CARTESIAN_POINT('Ctrl Pts',(-31.2826160736371,-4.8466878869723,131.640302953362));
#80935=CARTESIAN_POINT('Ctrl Pts',(-31.2905358609123,-4.82283954968131,
131.778572595325));
#80936=CARTESIAN_POINT('Ctrl Pts',(-31.2984556481875,-4.79308459129735,
131.915736239297));
#80937=CARTESIAN_POINT('Ctrl Pts',(-31.3063754354627,-4.75756115508497,
132.051274775849));
#80938=CARTESIAN_POINT('Ctrl Pts',(-31.3143076703234,-4.72198188643707,
132.187026339276));
#80939=CARTESIAN_POINT('Ctrl Pts',(-31.3222399051842,-4.68061611918711,
132.321147336433));
#80940=CARTESIAN_POINT('Ctrl Pts',(-31.3301721400449,-4.6336518177189,132.453134069151));
#80941=CARTESIAN_POINT('Ctrl Pts',(-31.3381110771738,-4.58664783420092,
132.585232322831));
#80942=CARTESIAN_POINT('Ctrl Pts',(-31.3460500143026,-4.53403602217863,
132.715192376689));
#80943=CARTESIAN_POINT('Ctrl Pts',(-31.3539889514314,-4.47605179660929,
132.842532194389));
#80944=CARTESIAN_POINT('Ctrl Pts',(-31.3619425090092,-4.41796078654283,
132.970106522739));
#80945=CARTESIAN_POINT('Ctrl Pts',(-31.369896066587,-4.35447775671424,133.095050644233));
#80946=CARTESIAN_POINT('Ctrl Pts',(-31.3778496241648,-4.28588377862541,
133.216907673815));
#80947=CARTESIAN_POINT('Ctrl Pts',(-31.3834000326486,-4.23801531294763,
133.301945882717));
#80948=CARTESIAN_POINT('Ctrl Pts',(-31.3889504411325,-4.18765875834085,
133.385481264039));
#80949=CARTESIAN_POINT('Ctrl Pts',(-31.3945008496164,-4.13492154908751,
133.467367723338));
#80950=CARTESIAN_POINT('Ctrl Pts',(-31.4022751837355,-4.06105370919175,
133.582064271578));
#80951=CARTESIAN_POINT('Ctrl Pts',(-31.4100495178546,-3.98229298485263,
133.693866686373));
#80952=CARTESIAN_POINT('Ctrl Pts',(-31.4178238519737,-3.898893061197,133.80232925647));
#80953=CARTESIAN_POINT('Ctrl Pts',(-31.4255886049208,-3.81559592049373,
133.910658156142));
#80954=CARTESIAN_POINT('Ctrl Pts',(-31.4333533578679,-3.72767119242189,
134.015655093891));
#80955=CARTESIAN_POINT('Ctrl Pts',(-31.441118110815,-3.63541694186813,134.116901443168));
#80956=CARTESIAN_POINT('Ctrl Pts',(-31.4488751517,-3.54325431953646,134.218047233143));
#80957=CARTESIAN_POINT('Ctrl Pts',(-31.456632192585,-3.44677099382002,134.315449560719));
#80958=CARTESIAN_POINT('Ctrl Pts',(-31.4643892334701,-3.34630634572266,
134.408721435114));
#80959=CARTESIAN_POINT('Ctrl Pts',(-31.4721404247102,-3.24591745879792,
134.501922972463));
#80960=CARTESIAN_POINT('Ctrl Pts',(-31.4798916159503,-3.14155351084147,
134.590999991535));
#80961=CARTESIAN_POINT('Ctrl Pts',(-31.4876428071904,-3.03359166376204,
134.675601333416));
#80962=CARTESIAN_POINT('Ctrl Pts',(-31.4953907039675,-2.92567570334774,
134.760166717469));
#80963=CARTESIAN_POINT('Ctrl Pts',(-31.5031386007447,-2.81416519237015,
134.840259967183));
#80964=CARTESIAN_POINT('Ctrl Pts',(-31.5108864975218,-2.69947122066022,
134.9155694655));
#80965=CARTESIAN_POINT('Ctrl Pts',(-31.5186327736059,-2.58480124045666,
134.990863210693));
#80966=CARTESIAN_POINT('Ctrl Pts',(-31.5263790496899,-2.46694945065919,
135.061374980401));
#80967=CARTESIAN_POINT('Ctrl Pts',(-31.534125325774,-2.34635650656006,135.126836089633));
#80968=CARTESIAN_POINT('Ctrl Pts',(-31.5418716590394,-2.22576267227138,
135.192297682085));
#80969=CARTESIAN_POINT('Ctrl Pts',(-31.5496179923047,-2.10242798690988,
135.252708353148));
#80970=CARTESIAN_POINT('Ctrl Pts',(-31.5573643255701,-1.97681796575485,
135.307845245359));
#80971=CARTESIAN_POINT('Ctrl Pts',(-31.565112393573,-1.85117981510634,135.362994485095));
#80972=CARTESIAN_POINT('Ctrl Pts',(-31.572860461576,-1.72326567265324,135.412867438762));
#80973=CARTESIAN_POINT('Ctrl Pts',(-31.580608529579,-1.5935609209986,135.457289442894));
#80974=CARTESIAN_POINT('Ctrl Pts',(-31.5883648323209,-1.46371831759039,
135.50175865926));
#80975=CARTESIAN_POINT('Ctrl Pts',(-31.5961211350627,-1.33208167383569,
135.540765226405));
#80976=CARTESIAN_POINT('Ctrl Pts',(-31.6038774378046,-1.19915195695956,
135.574184266992));
#80977=CARTESIAN_POINT('Ctrl Pts',(-31.6116378803188,-1.06615129149093,
135.607621144326));
#80978=CARTESIAN_POINT('Ctrl Pts',(-31.619398322833,-0.93185656035094,135.635464473422));
#80979=CARTESIAN_POINT('Ctrl Pts',(-31.6271587653472,-0.796777824564119,
135.657640762044));
#80980=CARTESIAN_POINT('Ctrl Pts',(-31.6349316656126,-0.661482248398888,
135.679852650013));
#80981=CARTESIAN_POINT('Ctrl Pts',(-31.642704565878,-0.525400540932047,
135.696379271167));
#80982=CARTESIAN_POINT('Ctrl Pts',(-31.6504774661435,-0.389047671979803,
135.707199078236));
#80983=CARTESIAN_POINT('Ctrl Pts',(-31.6579678019054,-0.257651573267969,
135.717625558064));
#80984=CARTESIAN_POINT('Ctrl Pts',(-31.6654581376674,-0.126003993383963,
135.722752922434));
#80985=CARTESIAN_POINT('Ctrl Pts',(-31.6729484734293,0.0054372000108684,
135.722607612112));
#80986=CARTESIAN_POINT('Ctrl Pts',(-31.6807228075484,0.141862026205495,
135.722456792304));
#80987=CARTESIAN_POINT('Ctrl Pts',(-31.6884971416674,0.278496659524296,
135.71662510042));
#80988=CARTESIAN_POINT('Ctrl Pts',(-31.6962714757865,0.414828987458322,
135.705085051123));
#80989=CARTESIAN_POINT('Ctrl Pts',(-31.7040362287336,0.550993297982538,
135.693559223905));
#80990=CARTESIAN_POINT('Ctrl Pts',(-31.7118009816807,0.686855658581828,
135.676339069567));
#80991=CARTESIAN_POINT('Ctrl Pts',(-31.7195657346278,0.821902755533517,
135.653449080664));
#80992=CARTESIAN_POINT('Ctrl Pts',(-31.7273227755128,0.956815721804867,
135.63058182642));
#80993=CARTESIAN_POINT('Ctrl Pts',(-31.7350798163978,1.09091465285752,135.602056009184));
#80994=CARTESIAN_POINT('Ctrl Pts',(-31.7428368572828,1.22369051866483,135.567947981836));
#80995=CARTESIAN_POINT('Ctrl Pts',(-31.750588048523,1.35636625715889,135.533865675616));
#80996=CARTESIAN_POINT('Ctrl Pts',(-31.7583392397631,1.48772053919776,135.494209635095));
#80997=CARTESIAN_POINT('Ctrl Pts',(-31.7660904310032,1.61725405961764,135.449107367298));
#80998=CARTESIAN_POINT('Ctrl Pts',(-31.7738383277803,1.74673252483575,135.404024269169));
#80999=CARTESIAN_POINT('Ctrl Pts',(-31.7815862245574,1.8743913991571,135.353499675998));
#81000=CARTESIAN_POINT('Ctrl Pts',(-31.7893341213344,1.99974630623212,135.297711012673));
#81001=CARTESIAN_POINT('Ctrl Pts',(-31.7970803974185,2.12507499176275,135.241934019135));
#81002=CARTESIAN_POINT('Ctrl Pts',(-31.8048266735026,2.24810031169022,135.180895304515));
#81003=CARTESIAN_POINT('Ctrl Pts',(-31.8125729495867,2.36835802877431,135.114820373792));
#81004=CARTESIAN_POINT('Ctrl Pts',(-31.820319282852,2.48861663357372,135.048744955318));
#81005=CARTESIAN_POINT('Ctrl Pts',(-31.8280656161174,2.60610725211323,134.977633434826));
#81006=CARTESIAN_POINT('Ctrl Pts',(-31.8358119493828,2.72039076571828,134.901757003601));
#81007=CARTESIAN_POINT('Ctrl Pts',(-31.8435600173857,2.83469987232367,134.825863580376));
#81008=CARTESIAN_POINT('Ctrl Pts',(-31.8513080853887,2.94580011919107,134.745203339285));
#81009=CARTESIAN_POINT('Ctrl Pts',(-31.8590561533917,3.0532821958477,134.66009023659));
#81010=CARTESIAN_POINT('Ctrl Pts',(-31.8668124561335,3.1608785057346,134.574886674676));
#81011=CARTESIAN_POINT('Ctrl Pts',(-31.8745687588753,3.2648486567501,134.485221040473));
#81012=CARTESIAN_POINT('Ctrl Pts',(-31.8823250616172,3.36481680103221,134.391447312642));
#81013=CARTESIAN_POINT('Ctrl Pts',(-31.8900855041314,3.46483830132291,134.29762353495));
#81014=CARTESIAN_POINT('Ctrl Pts',(-31.8978459466455,3.56085326516767,134.199687573705));
#81015=CARTESIAN_POINT('Ctrl Pts',(-31.9056063891596,3.65252416102431,134.098028833345));
#81016=CARTESIAN_POINT('Ctrl Pts',(-31.913379289425,3.74434221514114,133.99620690135));
#81017=CARTESIAN_POINT('Ctrl Pts',(-31.9211521896905,3.83180201644321,133.890650549244));
#81018=CARTESIAN_POINT('Ctrl Pts',(-31.9289250899559,3.91460708283561,133.78178138889));
#81019=CARTESIAN_POINT('Ctrl Pts',(-31.936415425718,3.99440197649193,133.676869896739));
#81020=CARTESIAN_POINT('Ctrl Pts',(-31.9439057614801,4.06987450595057,133.568882525012));
#81021=CARTESIAN_POINT('Ctrl Pts',(-31.9513960972422,4.14079942792155,133.45821878262));
#81022=CARTESIAN_POINT('Ctrl Pts',(-31.9591704313612,4.21441348986561,133.343359190801));
#81023=CARTESIAN_POINT('Ctrl Pts',(-31.9669447654803,4.28336147911722,133.225252432186));
#81024=CARTESIAN_POINT('Ctrl Pts',(-31.9747190995994,4.34734346216295,133.104314505036));
#81025=CARTESIAN_POINT('Ctrl Pts',(-31.9824838525465,4.4112465931329,132.983525623073));
#81026=CARTESIAN_POINT('Ctrl Pts',(-31.9902486054936,4.47019571411436,132.859912857233));
#81027=CARTESIAN_POINT('Ctrl Pts',(-31.9980133584407,4.523933972783,132.733921311714));
#81028=CARTESIAN_POINT('Ctrl Pts',(-32.0057703993257,4.57761885785548,132.608054902774));
#81029=CARTESIAN_POINT('Ctrl Pts',(-32.0135274402108,4.62610302770397,132.479814773202));
#81030=CARTESIAN_POINT('Ctrl Pts',(-32.0212844810958,4.66917557700601,132.349670454974));
#81031=CARTESIAN_POINT('Ctrl Pts',(-32.0290356723359,4.71221564496364,132.219624279589));
#81032=CARTESIAN_POINT('Ctrl Pts',(-32.0367868635759,4.74985209290475,132.087677143409));
#81033=CARTESIAN_POINT('Ctrl Pts',(-32.0445380548161,4.78192230946361,131.954318046671));
#81034=CARTESIAN_POINT('Ctrl Pts',(-32.0522859515932,4.81397889532488,131.821015631107));
#81035=CARTESIAN_POINT('Ctrl Pts',(-32.0600338483702,4.84047386397152,131.686302827913));
#81036=CARTESIAN_POINT('Ctrl Pts',(-32.0677817451473,4.86129467073749,131.550683059115));
#81037=CARTESIAN_POINT('Ctrl Pts',(-32.0755280212314,4.88211112223951,131.415091659049));
#81038=CARTESIAN_POINT('Ctrl Pts',(-32.0832742973155,4.89725571340494,131.27859405693));
#81039=CARTESIAN_POINT('Ctrl Pts',(-32.0910205733996,4.90666723639013,131.141702719646));
#81040=CARTESIAN_POINT('Ctrl Pts',(-32.0987669066649,4.91607882884905,131.004810371861));
#81041=CARTESIAN_POINT('Ctrl Pts',(-32.1065132399303,4.91975724186456,130.867524673155));
#81042=CARTESIAN_POINT('Ctrl Pts',(-32.1142595731956,4.91769328197664,130.73036165202));
#81043=CARTESIAN_POINT('Ctrl Pts',(-32.1220076411986,4.91562885987921,130.593167914178));
#81044=CARTESIAN_POINT('Ctrl Pts',(-32.1297557092016,4.90781951183897,130.456097299421));
#81045=CARTESIAN_POINT('Ctrl Pts',(-32.1375037772045,4.89430813584194,130.31966387327));
#81046=CARTESIAN_POINT('Ctrl Pts',(-32.1452600799464,4.88078239979366,130.183085444049));
#81047=CARTESIAN_POINT('Ctrl Pts',(-32.1530163826882,4.86154256851119,130.04714594592));
#81048=CARTESIAN_POINT('Ctrl Pts',(-32.16077268543,4.83668329931962,129.912352924447));
#81049=CARTESIAN_POINT('Ctrl Pts',(-32.1685331279442,4.81181076198754,129.777487959881));
#81050=CARTESIAN_POINT('Ctrl Pts',(-32.1762935704584,4.78131289735586,129.643771072241));
#81051=CARTESIAN_POINT('Ctrl Pts',(-32.1840540129726,4.74533487836266,129.511696718985));
#81052=CARTESIAN_POINT('Ctrl Pts',(-32.191826913238,4.70929910425938,129.379410348252));
#81053=CARTESIAN_POINT('Ctrl Pts',(-32.1995998135034,4.66776571464926,129.248772153755));
#81054=CARTESIAN_POINT('Ctrl Pts',(-32.2073727137688,4.62092916771991,129.120259465789));
#81055=CARTESIAN_POINT('Ctrl Pts',(-32.2148630495309,4.5757952472452,128.996418537734));
#81056=CARTESIAN_POINT('Ctrl Pts',(-32.222353385293,4.52573715874137,128.874551549051));
#81057=CARTESIAN_POINT('Ctrl Pts',(-32.2298437210551,4.47096927086958,128.755063947623));
#81058=CARTESIAN_POINT('Ctrl Pts',(-32.2376180551742,4.41412484188327,128.631045937471));
#81059=CARTESIAN_POINT('Ctrl Pts',(-32.2453923892933,4.35202635324192,128.509198453455));
#81060=CARTESIAN_POINT('Ctrl Pts',(-32.2531667234124,4.28486167467389,128.389998695357));
#81061=CARTESIAN_POINT('Ctrl Pts',(-32.2609314763595,4.21777977056952,128.270945840308));
#81062=CARTESIAN_POINT('Ctrl Pts',(-32.2686962293065,4.14564428957568,128.154534555954));
#81063=CARTESIAN_POINT('Ctrl Pts',(-32.2764609822536,4.06869087550451,128.041221529122));
#81064=CARTESIAN_POINT('Ctrl Pts',(-32.2842180231386,3.99181389264904,127.928021046385));
#81065=CARTESIAN_POINT('Ctrl Pts',(-32.2919750640237,3.91012871778607,127.817913018676));
#81066=CARTESIAN_POINT('Ctrl Pts',(-32.2997321049087,3.82391638198536,127.711328680116));
#81067=CARTESIAN_POINT('Ctrl Pts',(-32.3074832961488,3.73776905957771,127.604824717635));
#81068=CARTESIAN_POINT('Ctrl Pts',(-32.315234487389,3.6471016164059,127.50183945797));
#81069=CARTESIAN_POINT('Ctrl Pts',(-32.3229856786291,3.55223756680335,127.402774027239));
#81070=CARTESIAN_POINT('Ctrl Pts',(-32.3307335754062,3.45741383695245,127.30375070196));
#81071=CARTESIAN_POINT('Ctrl Pts',(-32.3384814721833,3.35839731808918,127.208644173791));
#81072=CARTESIAN_POINT('Ctrl Pts',(-32.3462293689604,3.255550720281,127.11782124165));
#81073=CARTESIAN_POINT('Ctrl Pts',(-32.3539756450445,3.15272563576397,127.027017307709));
#81074=CARTESIAN_POINT('Ctrl Pts',(-32.3617219211285,3.04607235874047,126.94049544616));
#81075=CARTESIAN_POINT('Ctrl Pts',(-32.3694681972126,2.93598895778154,126.858584153765));
#81076=CARTESIAN_POINT('Ctrl Pts',(-32.377214530478,2.82590474421194,126.77667225672));
#81077=CARTESIAN_POINT('Ctrl Pts',(-32.3849608637434,2.71239066984251,126.699371230132));
#81078=CARTESIAN_POINT('Ctrl Pts',(-32.3927071970087,2.59587591476838,126.626967734723));
#81079=CARTESIAN_POINT('Ctrl Pts',(-32.4004552650117,2.47933506702335,126.554548025054));
#81080=CARTESIAN_POINT('Ctrl Pts',(-32.4082033330147,2.35979253341687,126.487028235321));
#81081=CARTESIAN_POINT('Ctrl Pts',(-32.4159514010176,2.2377039992403,126.424650139203));
#81082=CARTESIAN_POINT('Ctrl Pts',(-32.4237077037595,2.11548570791608,126.362205746902));
#81083=CARTESIAN_POINT('Ctrl Pts',(-32.4314640065013,1.99071635936602,126.304914142614));
#81084=CARTESIAN_POINT('Ctrl Pts',(-32.4392203092432,1.8638741306448,126.252970029228));
#81085=CARTESIAN_POINT('Ctrl Pts',(-32.4469807517573,1.73696420240696,126.200998191704));
#81086=CARTESIAN_POINT('Ctrl Pts',(-32.4547411942715,1.60797955699168,126.154379664978));
#81087=CARTESIAN_POINT('Ctrl Pts',(-32.4625016367857,1.47741466497931,126.113259577277));
#81088=CARTESIAN_POINT('Ctrl Pts',(-32.4702745370511,1.34664017861128,126.07207347996));
#81089=CARTESIAN_POINT('Ctrl Pts',(-32.4780474373166,1.21428075412166,126.036403561786));
#81090=CARTESIAN_POINT('Ctrl Pts',(-32.485820337582,1.08084309240601,126.006344228255));
#81091=CARTESIAN_POINT('Ctrl Pts',(-32.493310673344,0.952256225803273,125.977377627213));
#81092=CARTESIAN_POINT('Ctrl Pts',(-32.500801009106,0.8226684571998,125.95362083064));
#81093=CARTESIAN_POINT('Ctrl Pts',(-32.508291344868,0.69253677288075,125.935112638596));
#81094=CARTESIAN_POINT('Ctrl Pts',(-32.5160656789871,0.557471106197878,
125.915902702824));
#81095=CARTESIAN_POINT('Ctrl Pts',(-32.5238400131062,0.421391617045269,
125.902286378638));
#81096=CARTESIAN_POINT('Ctrl Pts',(-32.5316143472252,0.284801335290685,
125.894363544052));
#81097=CARTESIAN_POINT('Ctrl Pts',(-32.5393791001723,0.148379388850939,
125.886450473651));
#81098=CARTESIAN_POINT('Ctrl Pts',(-32.5471438531194,0.0114482889012248,
125.884216954098));
#81099=CARTESIAN_POINT('Ctrl Pts',(-32.5549086060664,-0.125480369761398,
125.887711581962));
#81100=CARTESIAN_POINT('Ctrl Pts',(-32.5626656469514,-0.262273028949322,
125.891202738913));
#81101=CARTESIAN_POINT('Ctrl Pts',(-32.5704226878364,-0.399062863366618,
125.900410711454));
#81102=CARTESIAN_POINT('Ctrl Pts',(-32.5781797287214,-0.535335159375257,
125.915332152765));
#81103=CARTESIAN_POINT('Ctrl Pts',(-32.5859309199615,-0.671504691386174,
125.9302423417));
#81104=CARTESIAN_POINT('Ctrl Pts',(-32.5936821112017,-0.807157074746824,
125.950857381072));
#81105=CARTESIAN_POINT('Ctrl Pts',(-32.6014333024418,-0.941779963292485,
125.977121907574));
#81106=CARTESIAN_POINT('Ctrl Pts',(-32.6091811992189,-1.07634563351915,
126.003375270953));
#81107=CARTESIAN_POINT('Ctrl Pts',(-32.616929095996,-1.2098822962827,126.035273270984));
#81108=CARTESIAN_POINT('Ctrl Pts',(-32.6246769927731,-1.34188529961477,
126.072709013192));
#81109=CARTESIAN_POINT('Ctrl Pts',(-32.6324232688572,-1.47386069076437,
126.110136924649));
#81110=CARTESIAN_POINT('Ctrl Pts',(-32.6401695449412,-1.60430268469447,
126.153100167605));
#81111=CARTESIAN_POINT('Ctrl Pts',(-32.6479158210253,-1.73271974198939,
126.201441396222));
#81112=CARTESIAN_POINT('Ctrl Pts',(-32.6556621542907,-1.8611377472302,126.249782981683));
#81113=CARTESIAN_POINT('Ctrl Pts',(-32.6634084875561,-1.9875304201102,126.303502494282));
#81114=CARTESIAN_POINT('Ctrl Pts',(-32.6711548208215,-2.11142460251992,
126.362393799773));
#81115=CARTESIAN_POINT('Ctrl Pts',(-32.6789028888245,-2.2353465301726,126.421298293564));
#81116=CARTESIAN_POINT('Ctrl Pts',(-32.6866509568275,-2.35676850093917,
126.485376717094));
#81117=CARTESIAN_POINT('Ctrl Pts',(-32.6943990248305,-2.47524079474421,
126.554376374003));
#81118=CARTESIAN_POINT('Ctrl Pts',(-32.7021553275723,-2.59383900231279,
126.623449364568));
#81119=CARTESIAN_POINT('Ctrl Pts',(-32.7099116303142,-2.70948093213436,
126.697453839612));
#81120=CARTESIAN_POINT('Ctrl Pts',(-32.717667933056,-2.82174430877767,126.776092736903));
#81121=CARTESIAN_POINT('Ctrl Pts',(-32.7254283755702,-2.93406760376544,
126.854773606141));
#81122=CARTESIAN_POINT('Ctrl Pts',(-32.7331888180844,-3.04300844207798,
126.938093588948));
#81123=CARTESIAN_POINT('Ctrl Pts',(-32.7409492605986,-3.14817744979978,
127.025715118571));
#81124=CARTESIAN_POINT('Ctrl Pts',(-32.748722160864,-3.25351528414911,127.113477306053));
#81125=CARTESIAN_POINT('Ctrl Pts',(-32.7564950611295,-3.35506889852955,
127.20555457643));
#81126=CARTESIAN_POINT('Ctrl Pts',(-32.7642679613949,-3.45248498270692,
127.301571656369));
#81127=CARTESIAN_POINT('Ctrl Pts',(-32.7717582971569,-3.54635974684788,
127.3940982736));
#81128=CARTESIAN_POINT('Ctrl Pts',(-32.7792486329189,-3.63639236691941,
127.490283004602));
#81129=CARTESIAN_POINT('Ctrl Pts',(-32.7867389686809,-3.72230318708338,
127.589762346253));
#81130=CARTESIAN_POINT('Ctrl Pts',(-32.7944546360175,-3.81079846020092,
127.692234322334));
#81131=CARTESIAN_POINT('Ctrl Pts',(-32.8021703033541,-3.89521147350888,
127.798539935146));
#81132=CARTESIAN_POINT('Ctrl Pts',(-32.8098859706907,-3.97518776059449,
127.90831757049));
#81133=CARTESIAN_POINT('Ctrl Pts',(-32.817592281136,-4.05506705938423,128.01796207705));
#81134=CARTESIAN_POINT('Ctrl Pts',(-32.8252985915813,-4.13052010076039,
128.131069914492));
#81135=CARTESIAN_POINT('Ctrl Pts',(-32.8330049020266,-4.20123058136087,
128.247244142953));
#81136=CARTESIAN_POINT('Ctrl Pts',(-32.8407021623806,-4.27185802140532,
128.36328193941));
#81137=CARTESIAN_POINT('Ctrl Pts',(-32.8483994227347,-4.33775378375465,
128.482378620389));
#81138=CARTESIAN_POINT('Ctrl Pts',(-32.8560966830887,-4.39864350046135,
128.60410644626));
#81139=CARTESIAN_POINT('Ctrl Pts',(-32.8637887063279,-4.45949178860543,
128.725751450119));
#81140=CARTESIAN_POINT('Ctrl Pts',(-32.8714807295672,-4.51534062785411,
128.850023684835));
#81141=CARTESIAN_POINT('Ctrl Pts',(-32.8791727528065,-4.56596047428187,
128.976468933194));
#81142=CARTESIAN_POINT('Ctrl Pts',(-32.8868612619777,-4.61655719524825,
129.102856415579));
#81143=CARTESIAN_POINT('Ctrl Pts',(-32.8945497711488,-4.66192952821856,
129.231414568632));
#81144=CARTESIAN_POINT('Ctrl Pts',(-32.90223828032,-4.70189537228377,129.361667659728));
#81145=CARTESIAN_POINT('Ctrl Pts',(-32.906553353284,-4.72432566785483,129.434770465402));
#81146=CARTESIAN_POINT('Ctrl Pts',(-32.9108684262481,-4.74505385564512,
129.508406785259));
#81147=CARTESIAN_POINT('Ctrl Pts',(-32.9151834992122,-4.76405452823401,
129.582490119308));
#81148=CARTESIAN_POINT('Ctrl Pts',(-31.1654202583464,-4.76405452823401,
129.582490119308));
#81149=CARTESIAN_POINT('Ctrl Pts',(-31.1738666463901,-4.80103397831636,
129.726672433938));
#81150=CARTESIAN_POINT('Ctrl Pts',(-31.1823130344338,-4.83150726471108,
129.872703889186));
#81151=CARTESIAN_POINT('Ctrl Pts',(-31.1907594224775,-4.8553031000455,130.020004276871));
#81152=CARTESIAN_POINT('Ctrl Pts',(-31.1991747260673,-4.87901136178704,
130.16676256868));
#81153=CARTESIAN_POINT('Ctrl Pts',(-31.207590029657,-4.89609112909457,130.314780213512));
#81154=CARTESIAN_POINT('Ctrl Pts',(-31.2160053332468,-4.90642171873993,
130.463466234542));
#81155=CARTESIAN_POINT('Ctrl Pts',(-31.222383743487,-4.91425182707523,130.576163349865));
#81156=CARTESIAN_POINT('Ctrl Pts',(-31.2287621537274,-4.91820555525443,
130.689244065148));
#81157=CARTESIAN_POINT('Ctrl Pts',(-31.2351405639676,-4.91824962726525,
130.802445831626));
#81158=CARTESIAN_POINT('',(-30.8898594360284,-4.91824895780906,130.801158819624));
#81159=CARTESIAN_POINT('Ctrl Pts',(-30.8197844671784,-4.7640545282341,129.582490119308));
#81160=CARTESIAN_POINT('Ctrl Pts',(-30.8275584240133,-4.79809443636444,
129.715211204481));
#81161=CARTESIAN_POINT('Ctrl Pts',(-30.8353323808482,-4.82654466266992,
129.849202443635));
#81162=CARTESIAN_POINT('Ctrl Pts',(-30.8431063376831,-4.84934167116051,
129.983953146338));
#81163=CARTESIAN_POINT('Ctrl Pts',(-30.8478024245054,-4.86311287332117,
130.06535326377));
#81164=CARTESIAN_POINT('Ctrl Pts',(-30.8524985113278,-4.8748221571778,130.147030419108));
#81165=CARTESIAN_POINT('Ctrl Pts',(-30.8571945981501,-4.88446472887062,
130.22887180367));
#81166=CARTESIAN_POINT('Ctrl Pts',(-30.8680828774305,-4.90682185673984,
130.41862805936));
#81167=CARTESIAN_POINT('Ctrl Pts',(-30.8789711567108,-4.91812432521411,
130.609712008915));
#81168=CARTESIAN_POINT('Ctrl Pts',(-30.8898594359911,-4.91824895780864,
130.801158818967));
#81169=CARTESIAN_POINT('Ctrl Pts',(-30.8898594360285,-4.91824895780906,
130.801158819624));
#81170=CARTESIAN_POINT('Ctrl Pts',(-30.8975220895259,-4.91833666828801,
130.935889986125));
#81171=CARTESIAN_POINT('Ctrl Pts',(-30.9051847430233,-4.91288394704376,
131.070840739474));
#81172=CARTESIAN_POINT('Ctrl Pts',(-30.9128473965207,-4.90186313858186,
131.205510007585));
#81173=CARTESIAN_POINT('Ctrl Pts',(-30.9205017579385,-4.89085425620024,
131.340033544417));
#81174=CARTESIAN_POINT('Ctrl Pts',(-30.9281561193564,-4.87428930275188,
131.474275803935));
#81175=CARTESIAN_POINT('Ctrl Pts',(-30.9358104807742,-4.85219263597003,
131.607734556612));
#81176=CARTESIAN_POINT('Ctrl Pts',(-30.9434585087382,-4.8301142526492,131.741082881417));
#81177=CARTESIAN_POINT('Ctrl Pts',(-30.9511065367022,-4.80251332647413,
131.873648593866));
#81178=CARTESIAN_POINT('Ctrl Pts',(-30.9587545646662,-4.76946608516426,
132.00493394934));
#81179=CARTESIAN_POINT('Ctrl Pts',(-30.966398738977,-4.73643549554682,132.136153153352));
#81180=CARTESIAN_POINT('Ctrl Pts',(-30.9740429132878,-4.69796414544094,
132.266092893788));
#81181=CARTESIAN_POINT('Ctrl Pts',(-30.9816870875985,-4.65417939426002,
132.394265403566));
#81182=CARTESIAN_POINT('Ctrl Pts',(-30.989329371168,-4.61040547297844,132.522406210631));
#81183=CARTESIAN_POINT('Ctrl Pts',(-30.9969716547374,-4.56132089337728,
132.648780275366));
#81184=CARTESIAN_POINT('Ctrl Pts',(-31.0046139383068,-4.50710279138551,
132.772915287974));
#81185=CARTESIAN_POINT('Ctrl Pts',(-31.0122560921489,-4.4528856097433,132.897048193396));
#81186=CARTESIAN_POINT('Ctrl Pts',(-31.0198982459908,-4.3935352402735,133.018941753405));
#81187=CARTESIAN_POINT('Ctrl Pts',(-31.0275403998329,-4.32927662460057,
133.138144448641));
#81188=CARTESIAN_POINT('Ctrl Pts',(-31.0351841846384,-4.26500429506366,
133.257372583727));
#81189=CARTESIAN_POINT('Ctrl Pts',(-31.0428279694441,-4.1958218277138,133.373908358008));
#81190=CARTESIAN_POINT('Ctrl Pts',(-31.0504717542497,-4.12199941387091,
133.48732612136));
#81191=CARTESIAN_POINT('Ctrl Pts',(-31.0581234028725,-4.04810105257745,
133.600860567295));
#81192=CARTESIAN_POINT('Ctrl Pts',(-31.0657750514952,-3.96955343324428,
133.711270259487));
#81193=CARTESIAN_POINT('Ctrl Pts',(-31.073426700118,-3.88666944840212,133.818159492965));
#81194=CARTESIAN_POINT('Ctrl Pts',(-31.0810825530534,-3.8037399217166,133.925107458329));
#81195=CARTESIAN_POINT('Ctrl Pts',(-31.0887384059889,-3.71646954504271,
134.02853080672));
#81196=CARTESIAN_POINT('Ctrl Pts',(-31.0963942589243,-3.62520968580912,
134.12806905791));
#81197=CARTESIAN_POINT('Ctrl Pts',(-31.1040617118269,-3.53381155179644,
134.227758127103));
#81198=CARTESIAN_POINT('Ctrl Pts',(-31.1117291647294,-3.43841214779178,
134.323550059335));
#81199=CARTESIAN_POINT('Ctrl Pts',(-31.119396617632,-3.33939805141746,134.415122824731));
#81200=CARTESIAN_POINT('Ctrl Pts',(-31.1248118190757,-3.26946853447863,
134.479796840687));
#81201=CARTESIAN_POINT('Ctrl Pts',(-31.1302270205194,-3.19773671950685,
134.542367169959));
#81202=CARTESIAN_POINT('Ctrl Pts',(-31.1356422219631,-3.1243475334576,134.602733368189));
#81203=CARTESIAN_POINT('Ctrl Pts',(-31.1434165560821,-3.01898634624972,
134.689398102534));
#81204=CARTESIAN_POINT('Ctrl Pts',(-31.1511908902012,-2.90984961627873,
134.771812942361));
#81205=CARTESIAN_POINT('Ctrl Pts',(-31.1589652243203,-2.79731500532604,
134.84963092046));
#81206=CARTESIAN_POINT('Ctrl Pts',(-31.1667299772674,-2.68491908322369,
134.927352994856));
#81207=CARTESIAN_POINT('Ctrl Pts',(-31.1744947302146,-2.5691339306675,135.000489259395));
#81208=CARTESIAN_POINT('Ctrl Pts',(-31.1822594831617,-2.45037119991824,
135.068732088851));
#81209=CARTESIAN_POINT('Ctrl Pts',(-31.1900165240467,-2.33172642598775,
135.136907138567));
#81210=CARTESIAN_POINT('Ctrl Pts',(-31.1977735649317,-2.21011029596223,
135.200198231747));
#81211=CARTESIAN_POINT('Ctrl Pts',(-31.2055306058166,-2.08596414564402,
135.258340483437));
#81212=CARTESIAN_POINT('Ctrl Pts',(-31.2132817970567,-1.96191161490399,
135.316438889603));
#81213=CARTESIAN_POINT('Ctrl Pts',(-31.2210329882969,-1.83533321407292,
135.36939601757));
#81214=CARTESIAN_POINT('Ctrl Pts',(-31.228784179537,-1.70669531488896,135.416992638943));
#81215=CARTESIAN_POINT('Ctrl Pts',(-31.2365320763141,-1.57811209024298,
135.464569030483));
#81216=CARTESIAN_POINT('Ctrl Pts',(-31.2442799730911,-1.44747147413522,
135.506789311523));
#81217=CARTESIAN_POINT('Ctrl Pts',(-31.2520278698682,-1.3152600724652,135.543482266593));
#81218=CARTESIAN_POINT('Ctrl Pts',(-31.2597741459523,-1.18307632657025,
135.580167546289));
#81219=CARTESIAN_POINT('Ctrl Pts',(-31.2675204220364,-1.04932282515283,
135.611327695267));
#81220=CARTESIAN_POINT('Ctrl Pts',(-31.2752666981205,-0.914501218992165,
135.636841407281));
#81221=CARTESIAN_POINT('Ctrl Pts',(-31.2830130313859,-0.77967861760885,
135.662355307631));
#81222=CARTESIAN_POINT('Ctrl Pts',(-31.2907593646513,-0.643788279896508,
135.682222615149));
#81223=CARTESIAN_POINT('Ctrl Pts',(-31.2985056979167,-0.507341536663927,
135.696373253248));
#81224=CARTESIAN_POINT('Ctrl Pts',(-31.3062537659197,-0.37086423712907,
135.710527060285));
#81225=CARTESIAN_POINT('Ctrl Pts',(-31.3140018339226,-0.23383067293322,
135.718961610113));
#81226=CARTESIAN_POINT('Ctrl Pts',(-31.3217499019256,-0.0967563781090899,
135.721658784832));
#81227=CARTESIAN_POINT('Ctrl Pts',(-31.3295062046675,0.0404636009064103,
135.724358826139));
#81228=CARTESIAN_POINT('Ctrl Pts',(-31.3372625074094,0.177724005511788,
135.72130930372));
#81229=CARTESIAN_POINT('Ctrl Pts',(-31.3450188101512,0.314509662764759,
135.712544266792));
#81230=CARTESIAN_POINT('Ctrl Pts',(-31.3527792526654,0.451368326641543,
135.7037745517));
#81231=CARTESIAN_POINT('Ctrl Pts',(-31.3605396951796,0.587751349684457,
135.689283284926));
#81232=CARTESIAN_POINT('Ctrl Pts',(-31.3683001376938,0.723150589117112,
135.669156223546));
#81233=CARTESIAN_POINT('Ctrl Pts',(-31.3760730379592,0.858767183429083,
135.64899685242));
#81234=CARTESIAN_POINT('Ctrl Pts',(-31.3838459382246,0.993396454080462,
135.623183681408));
#81235=CARTESIAN_POINT('Ctrl Pts',(-31.39161883849,1.12654144455891,135.59185343074));
#81236=CARTESIAN_POINT('Ctrl Pts',(-31.399109174252,1.25484627926058,135.5616621136));
#81237=CARTESIAN_POINT('Ctrl Pts',(-31.406599510014,1.38177257813163,135.526347954828));
#81238=CARTESIAN_POINT('Ctrl Pts',(-31.414089845776,1.50689241234026,135.486075935709));
#81239=CARTESIAN_POINT('Ctrl Pts',(-31.421864179895,1.63675620309353,135.444276990744));
#81240=CARTESIAN_POINT('Ctrl Pts',(-31.4296385140142,1.76508521031181,135.397004402927));
#81241=CARTESIAN_POINT('Ctrl Pts',(-31.4374128481333,1.89138338523731,135.344388365559));
#81242=CARTESIAN_POINT('Ctrl Pts',(-31.4451776010804,2.01752590894998,135.291837172755));
#81243=CARTESIAN_POINT('Ctrl Pts',(-31.4529423540275,2.14164222279959,135.233955782139));
#81244=CARTESIAN_POINT('Ctrl Pts',(-31.4607071069747,2.2632510048694,135.170924249469));
#81245=CARTESIAN_POINT('Ctrl Pts',(-31.4684641478597,2.38473900338198,135.107955320606));
#81246=CARTESIAN_POINT('Ctrl Pts',(-31.4762211887447,2.50372408148981,135.039846607903));
#81247=CARTESIAN_POINT('Ctrl Pts',(-31.4839782296297,2.61974483119606,134.96682624288));
#81248=CARTESIAN_POINT('Ctrl Pts',(-31.4917294208699,2.73567808875276,134.893860943083));
#81249=CARTESIAN_POINT('Ctrl Pts',(-31.4994806121099,2.84865113783499,134.815991570792));
#81250=CARTESIAN_POINT('Ctrl Pts',(-31.50723180335,2.95822745006749,134.733491999458));
#81251=CARTESIAN_POINT('Ctrl Pts',(-31.5149797001271,3.0677571894441,134.651027492642));
#81252=CARTESIAN_POINT('Ctrl Pts',(-31.5227275969042,3.17389275170417,134.563936935566));
#81253=CARTESIAN_POINT('Ctrl Pts',(-31.5304754936813,3.2762270660491,134.47253717741));
#81254=CARTESIAN_POINT('Ctrl Pts',(-31.5382217697654,3.37853997426153,134.381156538113));
#81255=CARTESIAN_POINT('Ctrl Pts',(-31.5459680458496,3.47705292472543,134.285468750926));
#81256=CARTESIAN_POINT('Ctrl Pts',(-31.5537143219337,3.57139270455902,134.185830299867));
#81257=CARTESIAN_POINT('Ctrl Pts',(-31.5614606551991,3.66573318078744,134.0861911133));
#81258=CARTESIAN_POINT('Ctrl Pts',(-31.5692069884645,3.75590015611331,133.982601488568));
#81259=CARTESIAN_POINT('Ctrl Pts',(-31.5769533217299,3.84155828632714,133.875453744655));
#81260=CARTESIAN_POINT('Ctrl Pts',(-31.5847013897329,3.92723559908567,133.768282005747));
#81261=CARTESIAN_POINT('Ctrl Pts',(-31.5924494577359,4.00840181341415,133.657550867404));
#81262=CARTESIAN_POINT('Ctrl Pts',(-31.6001975257389,4.08476302747088,133.54368426984));
#81263=CARTESIAN_POINT('Ctrl Pts',(-31.6079538284808,4.16120539913441,133.429696653501));
#81264=CARTESIAN_POINT('Ctrl Pts',(-31.6157101312226,4.23283235101661,133.312567246333));
#81265=CARTESIAN_POINT('Ctrl Pts',(-31.6234664339645,4.2993940661312,133.192747882357));
#81266=CARTESIAN_POINT('Ctrl Pts',(-31.6312268764787,4.36599130723727,133.072864567179));
#81267=CARTESIAN_POINT('Ctrl Pts',(-31.6389873189928,4.42751774938116,132.950288783664));
#81268=CARTESIAN_POINT('Ctrl Pts',(-31.646747761507,4.48377087883792,132.825494400517));
#81269=CARTESIAN_POINT('Ctrl Pts',(-31.6545206617725,4.540114310812,132.700499686347));
#81270=CARTESIAN_POINT('Ctrl Pts',(-31.6622935620379,4.5911673682623,132.573279618595));
#81271=CARTESIAN_POINT('Ctrl Pts',(-31.6700664623034,4.63677646065695,132.444326201472));
#81272=CARTESIAN_POINT('Ctrl Pts',(-31.6775567980652,4.68072754765951,132.32006056588));
#81273=CARTESIAN_POINT('Ctrl Pts',(-31.6850471338271,4.7196235106219,132.19418571049));
#81274=CARTESIAN_POINT('Ctrl Pts',(-31.6925374695889,4.75337184698519,132.067150840362));
#81275=CARTESIAN_POINT('Ctrl Pts',(-31.700311803708,4.78839976178011,131.935299404518));
#81276=CARTESIAN_POINT('Ctrl Pts',(-31.7080861378271,4.8179929578323,131.801780587867));
#81277=CARTESIAN_POINT('Ctrl Pts',(-31.7158604719462,4.84199284398262,131.667082102937));
#81278=CARTESIAN_POINT('Ctrl Pts',(-31.7236252248933,4.86596315241815,131.532549621852));
#81279=CARTESIAN_POINT('Ctrl Pts',(-31.7313899778404,4.88435379855211,131.396840746395));
#81280=CARTESIAN_POINT('Ctrl Pts',(-31.7391547307874,4.89705610213931,131.260457750861));
#81281=CARTESIAN_POINT('Ctrl Pts',(-31.7469117716724,4.90974578961949,131.124210212842));
#81282=CARTESIAN_POINT('Ctrl Pts',(-31.7546688125574,4.91675834177269,130.987290273934));
#81283=CARTESIAN_POINT('Ctrl Pts',(-31.7624258534424,4.91803628981564,130.850209440412));
#81284=CARTESIAN_POINT('Ctrl Pts',(-31.7701770446825,4.91931327414804,130.713231980613));
#81285=CARTESIAN_POINT('Ctrl Pts',(-31.7779282359226,4.91486425841429,130.576094257069));
#81286=CARTESIAN_POINT('Ctrl Pts',(-31.7856794271627,4.90468370585328,130.439311568756));
#81287=CARTESIAN_POINT('Ctrl Pts',(-31.7934273239398,4.89450748029868,130.302587016733));
#81288=CARTESIAN_POINT('Ctrl Pts',(-31.801175220717,4.87860459200456,130.166217588884));
#81289=CARTESIAN_POINT('Ctrl Pts',(-31.808923117494,4.85702158345065,130.030717030121));
#81290=CARTESIAN_POINT('Ctrl Pts',(-31.8166693935781,4.83544308959683,129.895244815154));
#81291=CARTESIAN_POINT('Ctrl Pts',(-31.8244156696621,4.80818690025611,129.760641493618));
#81292=CARTESIAN_POINT('Ctrl Pts',(-31.8321619457462,4.77535120485009,129.627413748401));
#81293=CARTESIAN_POINT('Ctrl Pts',(-31.8399082790116,4.74251526705855,129.494185019728));
#81294=CARTESIAN_POINT('Ctrl Pts',(-31.8476546122769,4.70409983457553,129.36233226724));
#81295=CARTESIAN_POINT('Ctrl Pts',(-31.8554009455423,4.66025371473688,129.232349683513));
#81296=CARTESIAN_POINT('Ctrl Pts',(-31.8631490135452,4.61639777586364,129.102337991088));
#81297=CARTESIAN_POINT('Ctrl Pts',(-31.8708970815482,4.5671088545472,128.974197671195));
#81298=CARTESIAN_POINT('Ctrl Pts',(-31.8786451495512,4.51258476257148,128.848405141818));
#81299=CARTESIAN_POINT('Ctrl Pts',(-31.886401452293,4.45800272174188,128.722478918644));
#81300=CARTESIAN_POINT('Ctrl Pts',(-31.8941577550348,4.39817455129249,128.598905829826));
#81301=CARTESIAN_POINT('Ctrl Pts',(-31.9019140577767,4.33334535979917,128.478140280795));
#81302=CARTESIAN_POINT('Ctrl Pts',(-31.9096745002908,4.26848156701429,128.357310275554));
#81303=CARTESIAN_POINT('Ctrl Pts',(-31.9174349428051,4.19861163366287,128.23929113219));
#81304=CARTESIAN_POINT('Ctrl Pts',(-31.9251953853192,4.12402477529131,128.124509368843));
#81305=CARTESIAN_POINT('Ctrl Pts',(-31.9329682855847,4.04931818347317,128.00954334762));
#81306=CARTESIAN_POINT('Ctrl Pts',(-31.9407411858501,3.96987976200627,127.897825410346));
#81307=CARTESIAN_POINT('Ctrl Pts',(-31.9485140861155,3.88604042853469,127.789750717381));
#81308=CARTESIAN_POINT('Ctrl Pts',(-31.9560044218776,3.80524886601265,127.685604811728));
#81309=CARTESIAN_POINT('Ctrl Pts',(-31.9634947576397,3.72037100327695,127.584842102491));
#81310=CARTESIAN_POINT('Ctrl Pts',(-31.9709850934018,3.63173476937418,127.487783220999));
#81311=CARTESIAN_POINT('Ctrl Pts',(-31.9787594275209,3.53973786572348,127.387044322516));
#81312=CARTESIAN_POINT('Ctrl Pts',(-31.98653376164,3.44340054914609,127.289976546777));
#81313=CARTESIAN_POINT('Ctrl Pts',(-31.994308095759,3.34304742360918,127.196976941548));
#81314=CARTESIAN_POINT('Ctrl Pts',(-32.0020728487061,3.24281797433095,127.104091950022));
#81315=CARTESIAN_POINT('Ctrl Pts',(-32.0098376016531,3.13858284738608,127.015265416521));
#81316=CARTESIAN_POINT('Ctrl Pts',(-32.0176023546002,3.03070587603699,126.93086026834));
#81317=CARTESIAN_POINT('Ctrl Pts',(-32.0253593954852,2.92293604961649,126.846538952542));
#81318=CARTESIAN_POINT('Ctrl Pts',(-32.0331164363702,2.81153188296877,126.766630522374));
#81319=CARTESIAN_POINT('Ctrl Pts',(-32.0408734772552,2.69689265752841,126.691459809588));
#81320=CARTESIAN_POINT('Ctrl Pts',(-32.0486246684953,2.58233988241957,126.616345783621));
#81321=CARTESIAN_POINT('Ctrl Pts',(-32.0563758597354,2.464557229983,126.54596257721));
#81322=CARTESIAN_POINT('Ctrl Pts',(-32.0641270509756,2.34397524308472,126.480593380271));
#81323=CARTESIAN_POINT('Ctrl Pts',(-32.0718749477526,2.22344450674766,126.415251966985));
#81324=CARTESIAN_POINT('Ctrl Pts',(-32.0796228445297,2.10011714534268,126.354920510539));
#81325=CARTESIAN_POINT('Ctrl Pts',(-32.0873707413067,1.97445054436269,126.299837545101));
#81326=CARTESIAN_POINT('Ctrl Pts',(-32.0951170173908,1.84881023012673,126.244766101833));
#81327=CARTESIAN_POINT('Ctrl Pts',(-32.102863293475,1.72083200744713,126.194941122702));
#81328=CARTESIAN_POINT('Ctrl Pts',(-32.110609569559,1.59099523676721,126.150553872644));
#81329=CARTESIAN_POINT('Ctrl Pts',(-32.1183559028244,1.46115750766157,126.106166294929));
#81330=CARTESIAN_POINT('Ctrl Pts',(-32.1261022360897,1.32946157312347,126.067216652856));
#81331=CARTESIAN_POINT('Ctrl Pts',(-32.1338485693551,1.19640364536209,126.033846873758));
#81332=CARTESIAN_POINT('Ctrl Pts',(-32.141596637358,1.06331592020052,126.000469621728));
#81333=CARTESIAN_POINT('Ctrl Pts',(-32.1493447053609,0.928865974031862,
125.972674814263));
#81334=CARTESIAN_POINT('Ctrl Pts',(-32.1570927733639,0.793561552899899,
125.950553542263));
#81335=CARTESIAN_POINT('Ctrl Pts',(-32.1648490761057,0.658113328618644,
125.928408759512));
#81336=CARTESIAN_POINT('Ctrl Pts',(-32.1726053788476,0.521809201712001,
125.911949620786));
#81337=CARTESIAN_POINT('Ctrl Pts',(-32.1803616815894,0.38516396351098,125.901215526534));
#81338=CARTESIAN_POINT('Ctrl Pts',(-32.1881221241036,0.248445793631837,
125.890475703172));
#81339=CARTESIAN_POINT('Ctrl Pts',(-32.1958825666177,0.111386540198871,
125.885467027153));
#81340=CARTESIAN_POINT('Ctrl Pts',(-32.2036430091319,-0.0254986269283883,
125.886176716722));
#81341=CARTESIAN_POINT('Ctrl Pts',(-32.2114159093973,-0.162603534277642,
125.886887545546));
#81342=CARTESIAN_POINT('Ctrl Pts',(-32.2191888096628,-0.299533406116201,
125.893335065381));
#81343=CARTESIAN_POINT('Ctrl Pts',(-32.2269617099282,-0.435776913772694,
125.905454459665));
#81344=CARTESIAN_POINT('Ctrl Pts',(-32.2344520456904,-0.56706762675232,
125.91713328344));
#81345=CARTESIAN_POINT('Ctrl Pts',(-32.2419423814526,-0.697720705849254,
125.934078727617));
#81346=CARTESIAN_POINT('Ctrl Pts',(-32.2494327172147,-0.827289141184968,
125.956188205267));
#81347=CARTESIAN_POINT('Ctrl Pts',(-32.2572070513338,-0.961770203125248,
125.979135970482));
#81348=CARTESIAN_POINT('Ctrl Pts',(-32.2649813854529,-1.0955087447375,126.007719779533));
#81349=CARTESIAN_POINT('Ctrl Pts',(-32.272755719572,-1.22799526211631,126.041881147928));
#81350=CARTESIAN_POINT('Ctrl Pts',(-32.2805204725191,-1.36031850170311,
126.07600041549));
#81351=CARTESIAN_POINT('Ctrl Pts',(-32.2882852254662,-1.49139241223421,
126.115683468815));
#81352=CARTESIAN_POINT('Ctrl Pts',(-32.2960499784134,-1.62071499193351,
126.160820375744));
#81353=CARTESIAN_POINT('Ctrl Pts',(-32.3038070192984,-1.74990912662388,
126.20591245206));
#81354=CARTESIAN_POINT('Ctrl Pts',(-32.3115640601834,-1.87735502532025,
126.256447474214));
#81355=CARTESIAN_POINT('Ctrl Pts',(-32.3193211010685,-2.00256357650255,
126.312265094921));
#81356=CARTESIAN_POINT('Ctrl Pts',(-32.3270722923086,-2.12767770694225,
126.368040623127));
#81357=CARTESIAN_POINT('Ctrl Pts',(-32.3348234835488,-2.25055749249534,
126.429090662129));
#81358=CARTESIAN_POINT('Ctrl Pts',(-32.3425746747889,-2.37073195852932,
126.49520605509));
#81359=CARTESIAN_POINT('Ctrl Pts',(-32.350322571566,-2.49085534720916,126.561293347245));
#81360=CARTESIAN_POINT('Ctrl Pts',(-32.3580704683431,-2.60827536147061,
126.632441523321));
#81361=CARTESIAN_POINT('Ctrl Pts',(-32.3658183651202,-2.72254408773107,
126.708394705493));
#81362=CARTESIAN_POINT('Ctrl Pts',(-32.3735646412043,-2.83678891143734,
126.784331999898));
#81363=CARTESIAN_POINT('Ctrl Pts',(-32.3813109172884,-2.94788343289747,
126.865072084907));
#81364=CARTESIAN_POINT('Ctrl Pts',(-32.3890571933725,-3.05540762947576,
126.950315044374));
#81365=CARTESIAN_POINT('Ctrl Pts',(-32.3968035266379,-3.16293261977325,
127.035558633085));
#81366=CARTESIAN_POINT('Ctrl Pts',(-32.4045498599032,-3.26688692623008,
127.125304919697));
#81367=CARTESIAN_POINT('Ctrl Pts',(-32.4122961931685,-3.36688292654267,
127.219213142014));
#81368=CARTESIAN_POINT('Ctrl Pts',(-32.4200442611715,-3.46690132026594,
127.313142394427));
#81369=CARTESIAN_POINT('Ctrl Pts',(-32.4277923291744,-3.56295935900285,
127.411235169598));
#81370=CARTESIAN_POINT('Ctrl Pts',(-32.4355403971774,-3.65470595625923,
127.513113523259));
#81371=CARTESIAN_POINT('Ctrl Pts',(-32.4432966999192,-3.74655006289123,
127.615100154447));
#81372=CARTESIAN_POINT('Ctrl Pts',(-32.4510530026612,-3.83407331245463,
127.720880110229));
#81373=CARTESIAN_POINT('Ctrl Pts',(-32.458809305403,-3.91696429894751,127.830041578984));
#81374=CARTESIAN_POINT('Ctrl Pts',(-32.4665697479172,-3.9998995268559,127.939261310502));
#81375=CARTESIAN_POINT('Ctrl Pts',(-32.4743301904314,-4.07819734218227,
128.051865830404));
#81376=CARTESIAN_POINT('Ctrl Pts',(-32.4820906329456,-4.15159003668739,
128.167414802844));
#81377=CARTESIAN_POINT('Ctrl Pts',(-32.4898635332111,-4.22510054766113,
128.283149264754));
#81378=CARTESIAN_POINT('Ctrl Pts',(-32.4976364334765,-4.29369000704804,
128.401837285947));
#81379=CARTESIAN_POINT('Ctrl Pts',(-32.505409333742,-4.3571365612187,128.523013636199));
#81380=CARTESIAN_POINT('Ctrl Pts',(-32.5128996695039,-4.41827667333174,
128.639784920892));
#81381=CARTESIAN_POINT('Ctrl Pts',(-32.5203900052657,-4.47464117185407,
128.758866483112));
#81382=CARTESIAN_POINT('Ctrl Pts',(-32.5278803410276,-4.52607474631596,
128.879826790048));
#81383=CARTESIAN_POINT('Ctrl Pts',(-32.5365140061901,-4.5853591728265,129.01925055171));
#81384=CARTESIAN_POINT('Ctrl Pts',(-32.5451476713527,-4.63825300021984,
129.161546301435));
#81385=CARTESIAN_POINT('Ctrl Pts',(-32.5537813365152,-4.6844984378688,129.306142526598));
#81386=CARTESIAN_POINT('Ctrl Pts',(-32.5592297491079,-4.71368236150979,
129.39739228892));
#81387=CARTESIAN_POINT('Ctrl Pts',(-32.5646781617006,-4.74021949285508,
129.489557678113));
#81388=CARTESIAN_POINT('Ctrl Pts',(-32.5701265742934,-4.76405452823409,
129.582490119308));
#81389=CARTESIAN_POINT('Origin',(213.235140564004,0.,130.804360617566));
#81390=CARTESIAN_POINT('',(-34.6650476268334,-4.76405452823403,129.582490119308));
#81391=CARTESIAN_POINT('',(-34.31993947219,-4.764054528234,129.582490119308));
#81392=CARTESIAN_POINT('',(213.235140564004,-4.76405452823405,129.582490119308));
#81393=CARTESIAN_POINT('',(-32.9851405640433,-4.91824806159545,130.808727208065));
#81394=CARTESIAN_POINT('Ctrl Pts',(-32.9851405640433,-4.91824806159545,
130.808727208065));
#81395=CARTESIAN_POINT('Ctrl Pts',(-32.9946113937143,-4.91809934263803,
130.976234723177));
#81396=CARTESIAN_POINT('Ctrl Pts',(-33.0040822233852,-4.90938940149991,
131.143363614817));
#81397=CARTESIAN_POINT('Ctrl Pts',(-33.0135530530561,-4.89225623805502,
131.309347710185));
#81398=CARTESIAN_POINT('Ctrl Pts',(-33.0231650569598,-4.87486768397501,
131.477806000332));
#81399=CARTESIAN_POINT('Ctrl Pts',(-33.0327770608635,-4.84880296886926,
131.645085156236));
#81400=CARTESIAN_POINT('Ctrl Pts',(-33.0423890647672,-4.81425522540968,
131.810407180661));
#81401=CARTESIAN_POINT('Ctrl Pts',(-33.0499882406761,-4.7869420467601,131.941109493914));
#81402=CARTESIAN_POINT('Ctrl Pts',(-33.057587416585,-4.75432763833278,132.070588999782));
#81403=CARTESIAN_POINT('Ctrl Pts',(-33.0651865924938,-4.71652836273839,
132.198470823391));
#81404=CARTESIAN_POINT('Ctrl Pts',(-33.0729609266129,-4.67785782774121,
132.329300276008));
#81405=CARTESIAN_POINT('Ctrl Pts',(-33.0807352607321,-4.633678395593,132.458726739406));
#81406=CARTESIAN_POINT('Ctrl Pts',(-33.0885095948512,-4.58410831829956,
132.586251183397));
#81407=CARTESIAN_POINT('Ctrl Pts',(-33.0962743477984,-4.53459933169618,
132.713618464907));
#81408=CARTESIAN_POINT('Ctrl Pts',(-33.1040391007455,-4.47971305879685,
132.839088030104));
#81409=CARTESIAN_POINT('Ctrl Pts',(-33.1118038536927,-4.4196179531081,132.962174374836));
#81410=CARTESIAN_POINT('Ctrl Pts',(-33.1195608945777,-4.3595825347256,133.085138468476));
#81411=CARTESIAN_POINT('Ctrl Pts',(-33.1273179354628,-4.29434874944517,
133.20572370313));
#81412=CARTESIAN_POINT('Ctrl Pts',(-33.1350749763478,-4.22413359057179,
133.323463329149));
#81413=CARTESIAN_POINT('Ctrl Pts',(-33.142826167588,-4.15397138149572,133.4411141668));
#81414=CARTESIAN_POINT('Ctrl Pts',(-33.1505773588282,-4.07883547533745,
133.555923332661));
#81415=CARTESIAN_POINT('Ctrl Pts',(-33.1583285500684,-3.9989891911991,133.667447851859));
#81416=CARTESIAN_POINT('Ctrl Pts',(-33.1660764468455,-3.91917684386148,
133.778924970162));
#81417=CARTESIAN_POINT('Ctrl Pts',(-33.1738243436226,-3.83465832755951,
133.887119901237));
#81418=CARTESIAN_POINT('Ctrl Pts',(-33.1815722403998,-3.74574063165275,
133.991618088008));
#81419=CARTESIAN_POINT('Ctrl Pts',(-33.189318516484,-3.65684153541113,134.09609441601));
#81420=CARTESIAN_POINT('Ctrl Pts',(-33.1970647925681,-3.56354534312323,
134.196875240231));
#81421=CARTESIAN_POINT('Ctrl Pts',(-33.2048110686523,-3.46619948006827,
134.293578900631));
#81422=CARTESIAN_POINT('Ctrl Pts',(-33.2125574019177,-3.36885289842826,
134.390283274876));
#81423=CARTESIAN_POINT('Ctrl Pts',(-33.2203037351831,-3.26745686373794,
134.482910149706));
#81424=CARTESIAN_POINT('Ctrl Pts',(-33.2280500684485,-3.16239553466678,
134.57111486291));
#81425=CARTESIAN_POINT('Ctrl Pts',(-33.2357981364515,-3.05731067783942,
134.659339328948));
#81426=CARTESIAN_POINT('Ctrl Pts',(-33.2435462044546,-2.94855919267224,
134.743139411413));
#81427=CARTESIAN_POINT('Ctrl Pts',(-33.2512942724577,-2.83655784446072,
134.822211119704));
#81428=CARTESIAN_POINT('Ctrl Pts',(-33.2590505751996,-2.72443745988365,
134.901366866347));
#81429=CARTESIAN_POINT('Ctrl Pts',(-33.2668068779414,-2.6090606324382,134.975783974247));
#81430=CARTESIAN_POINT('Ctrl Pts',(-33.2745631806833,-2.4908730711102,135.045201855589));
#81431=CARTESIAN_POINT('Ctrl Pts',(-33.2823236231975,-2.372622429522,135.114656787345));
#81432=CARTESIAN_POINT('Ctrl Pts',(-33.2900840657117,-2.25155840976807,
135.179106992219));
#81433=CARTESIAN_POINT('Ctrl Pts',(-33.2978445082259,-2.12814988431899,
135.238338643264));
#81434=CARTESIAN_POINT('Ctrl Pts',(-33.3056174084914,-2.00454325254916,
135.297665378213));
#81435=CARTESIAN_POINT('Ctrl Pts',(-33.313390308757,-1.87858495364245,135.351756664486));
#81436=CARTESIAN_POINT('Ctrl Pts',(-33.3211632090225,-1.75076316437698,
135.400447149036));
#81437=CARTESIAN_POINT('Ctrl Pts',(-33.3286535447839,-1.62758801912603,
135.447367611824));
#81438=CARTESIAN_POINT('Ctrl Pts',(-33.3361438805453,-1.50268280845453,
135.489273023162));
#81439=CARTESIAN_POINT('Ctrl Pts',(-33.3436342163067,-1.37649438825613,
135.526060127446));
#81440=CARTESIAN_POINT('Ctrl Pts',(-33.3514085504258,-1.24552149574123,
135.564242025973));
#81441=CARTESIAN_POINT('Ctrl Pts',(-33.3591828845448,-1.11275128431885,
135.597030783363));
#81442=CARTESIAN_POINT('Ctrl Pts',(-33.3669572186639,-0.978667520317207,
135.624256150373));
#81443=CARTESIAN_POINT('Ctrl Pts',(-33.374721971611,-0.844749002571108,
135.651447964552));
#81444=CARTESIAN_POINT('Ctrl Pts',(-33.3824867245581,-0.709520532715764,
135.673089953455));
#81445=CARTESIAN_POINT('Ctrl Pts',(-33.3902514775052,-0.573481632377448,
135.689061414936));
#81446=CARTESIAN_POINT('Ctrl Pts',(-33.3980085183901,-0.437577847792946,
135.705017013336));
#81447=CARTESIAN_POINT('Ctrl Pts',(-33.4057655592752,-0.300865620360074,
135.715313247052));
#81448=CARTESIAN_POINT('Ctrl Pts',(-33.4135226001601,-0.163854929960267,
135.719880389109));
#81449=CARTESIAN_POINT('Ctrl Pts',(-33.4212737914003,-0.0269475603878786,
135.724444087048));
#81450=CARTESIAN_POINT('Ctrl Pts',(-33.4290249826404,0.110257434989688,
135.723287279756));
#81451=CARTESIAN_POINT('Ctrl Pts',(-33.4367761738805,0.247245038459042,
135.716392066311));
#81452=CARTESIAN_POINT('Ctrl Pts',(-33.4445240706576,0.384174418542658,
135.709499783515));
#81453=CARTESIAN_POINT('Ctrl Pts',(-33.4522719674346,0.52088620083598,135.696873965117));
#81454=CARTESIAN_POINT('Ctrl Pts',(-33.4600198642117,0.656865671480133,
135.67854881173));
#81455=CARTESIAN_POINT('Ctrl Pts',(-33.4677661402958,0.792816698150591,
135.660227491571));
#81456=CARTESIAN_POINT('Ctrl Pts',(-33.47551241638,0.92803533064574,135.636209259914));
#81457=CARTESIAN_POINT('Ctrl Pts',(-33.4832586924641,1.06201267571571,135.606580118913));
#81458=CARTESIAN_POINT('Ctrl Pts',(-33.4910050257294,1.19599100977583,135.576950759197));
#81459=CARTESIAN_POINT('Ctrl Pts',(-33.4987513589948,1.32872765638524,135.541710491911));
#81460=CARTESIAN_POINT('Ctrl Pts',(-33.5064976922601,1.45972499431876,135.500996222279));
#81461=CARTESIAN_POINT('Ctrl Pts',(-33.5142457602631,1.59075166819785,135.46027283497));
#81462=CARTESIAN_POINT('Ctrl Pts',(-33.5219938282661,1.72003788505195,135.414073122));
#81463=CARTESIAN_POINT('Ctrl Pts',(-33.5297418962691,1.84710261715635,135.362583405473));
#81464=CARTESIAN_POINT('Ctrl Pts',(-33.5374981990109,1.97430239517012,135.311038965062));
#81465=CARTESIAN_POINT('Ctrl Pts',(-33.5452545017528,2.09927560911814,135.254193437051));
#81466=CARTESIAN_POINT('Ctrl Pts',(-33.5530108044946,2.22156210249681,135.192280954953));
#81467=CARTESIAN_POINT('Ctrl Pts',(-33.5607712470088,2.34391386385896,135.130335428298));
#81468=CARTESIAN_POINT('Ctrl Pts',(-33.5685316895229,2.46357570637388,135.063317749788));
#81469=CARTESIAN_POINT('Ctrl Pts',(-33.5762921320371,2.58011429435089,134.991506816421));
#81470=CARTESIAN_POINT('Ctrl Pts',(-33.5840650323025,2.69683996041528,134.919580605769));
#81471=CARTESIAN_POINT('Ctrl Pts',(-33.5918379325679,2.81043202876259,134.842845983059));
#81472=CARTESIAN_POINT('Ctrl Pts',(-33.5996108328333,2.92048751171914,134.761624287881));
#81473=CARTESIAN_POINT('Ctrl Pts',(-33.6071011685954,3.02654220065749,134.683355205907));
#81474=CARTESIAN_POINT('Ctrl Pts',(-33.6145915043575,3.12931272739518,134.600919813088));
#81475=CARTESIAN_POINT('Ctrl Pts',(-33.6220818401195,3.22847068354311,134.514638249766));
#81476=CARTESIAN_POINT('Ctrl Pts',(-33.6298561742386,3.3313882437361,134.425085294747));
#81477=CARTESIAN_POINT('Ctrl Pts',(-33.6376305083577,3.43073989632107,134.331105079909));
#81478=CARTESIAN_POINT('Ctrl Pts',(-33.6454048424768,3.5261209182697,134.233012587691));
#81479=CARTESIAN_POINT('Ctrl Pts',(-33.6531695954238,3.62138439163323,134.135040985702));
#81480=CARTESIAN_POINT('Ctrl Pts',(-33.6609343483709,3.71268670092573,134.032967467781));
#81481=CARTESIAN_POINT('Ctrl Pts',(-33.6686991013179,3.79965629237272,133.92714705316));
#81482=CARTESIAN_POINT('Ctrl Pts',(-33.6764561422029,3.88653950439544,133.821431740867));
#81483=CARTESIAN_POINT('Ctrl Pts',(-33.6842131830879,3.96909831573404,133.71197723786));
#81484=CARTESIAN_POINT('Ctrl Pts',(-33.6919702239729,4.04699840652773,133.599174915522));
#81485=CARTESIAN_POINT('Ctrl Pts',(-33.699721415213,4.12483975225699,133.486457658294));
#81486=CARTESIAN_POINT('Ctrl Pts',(-33.7074726064531,4.19802914893938,133.370397927238));
#81487=CARTESIAN_POINT('Ctrl Pts',(-33.7152237976932,4.26627315636882,133.251419345457));
#81488=CARTESIAN_POINT('Ctrl Pts',(-33.7229716944703,4.33448815827464,133.132491332747));
#81489=CARTESIAN_POINT('Ctrl Pts',(-33.7307195912473,4.39776175737465,133.010647275178));
#81490=CARTESIAN_POINT('Ctrl Pts',(-33.7384674880243,4.45584451220179,132.886338702364));
#81491=CARTESIAN_POINT('Ctrl Pts',(-33.7462137641084,4.51391511736875,132.762056132225));
#81492=CARTESIAN_POINT('Ctrl Pts',(-33.7539600401925,4.56679687260656,132.635310426228));
#81493=CARTESIAN_POINT('Ctrl Pts',(-33.7617063162766,4.61428706473051,132.506576216943));
#81494=CARTESIAN_POINT('Ctrl Pts',(-33.7694526495419,4.66177760741627,132.37784105737));
#81495=CARTESIAN_POINT('Ctrl Pts',(-33.7771989828073,4.70387637225777,132.247117732022));
#81496=CARTESIAN_POINT('Ctrl Pts',(-33.7849453160726,4.74042956506992,132.114898904344));
#81497=CARTESIAN_POINT('Ctrl Pts',(-33.7926933840755,4.77699094371617,131.982650467177));
#81498=CARTESIAN_POINT('Ctrl Pts',(-33.8004414520785,4.8080041749526,131.848906238011));
#81499=CARTESIAN_POINT('Ctrl Pts',(-33.8081895200814,4.83336600960478,131.714171630742));
#81500=CARTESIAN_POINT('Ctrl Pts',(-33.8159458228232,4.85875479911663,131.57929382593));
#81501=CARTESIAN_POINT('Ctrl Pts',(-33.8237021255651,4.87848012123137,131.443423925191));
#81502=CARTESIAN_POINT('Ctrl Pts',(-33.8314584283069,4.89249023327454,131.307075626108));
#81503=CARTESIAN_POINT('Ctrl Pts',(-33.8392188708211,4.90650782293634,131.170654553832));
#81504=CARTESIAN_POINT('Ctrl Pts',(-33.8469793133352,4.91480410074876,131.033754964492));
#81505=CARTESIAN_POINT('Ctrl Pts',(-33.8547397558494,4.91737948213112,130.896892186319));
#81506=CARTESIAN_POINT('Ctrl Pts',(-33.8625126561148,4.9199589977443,130.759809703864));
#81507=CARTESIAN_POINT('Ctrl Pts',(-33.8702855563802,4.91679927400373,130.622764541747));
#81508=CARTESIAN_POINT('Ctrl Pts',(-33.8780584566456,4.90795283832523,130.486269436809));
#81509=CARTESIAN_POINT('Ctrl Pts',(-33.8855487924079,4.89942799286611,130.35473627274));
#81510=CARTESIAN_POINT('Ctrl Pts',(-33.8930391281702,4.88562274220658,130.223714174563));
#81511=CARTESIAN_POINT('Ctrl Pts',(-33.9005294639325,4.86662891672818,130.093652485232));
#81512=CARTESIAN_POINT('Ctrl Pts',(-33.9083037980516,4.84691493458444,129.958659467424));
#81513=CARTESIAN_POINT('Ctrl Pts',(-33.9160781321707,4.82154871320462,129.824273506605));
#81514=CARTESIAN_POINT('Ctrl Pts',(-33.9238524662898,4.7905764935515,129.691005363421));
#81515=CARTESIAN_POINT('Ctrl Pts',(-33.9316172192369,4.75964244439104,129.557901461314));
#81516=CARTESIAN_POINT('Ctrl Pts',(-33.939381972184,4.72311623124687,129.425913012969));
#81517=CARTESIAN_POINT('Ctrl Pts',(-33.9471467251311,4.68109570796365,129.295544513667));
#81518=CARTESIAN_POINT('Ctrl Pts',(-33.9549037660161,4.6391169200566,129.165305498197));
#81519=CARTESIAN_POINT('Ctrl Pts',(-33.9626608069012,4.59165480090288,129.03668359958));
#81520=CARTESIAN_POINT('Ctrl Pts',(-33.9704178477862,4.538857914282,128.910171636377));
#81521=CARTESIAN_POINT('Ctrl Pts',(-33.9781690390263,4.48610084220394,128.783755076828));
#81522=CARTESIAN_POINT('Ctrl Pts',(-33.9859202302664,4.42801716014065,128.659445645015));
#81523=CARTESIAN_POINT('Ctrl Pts',(-33.9936714215066,4.36480466260737,128.537719199128));
#81524=CARTESIAN_POINT('Ctrl Pts',(-34.0014193182837,4.3016190320718,128.416044490227));
#81525=CARTESIAN_POINT('Ctrl Pts',(-34.0091672150607,4.23330910149245,128.296950929979));
#81526=CARTESIAN_POINT('Ctrl Pts',(-34.0169151118378,4.1601199263164,128.180892443342));
#81527=CARTESIAN_POINT('Ctrl Pts',(-34.0246613879219,4.08694606073803,128.064858233639));
#81528=CARTESIAN_POINT('Ctrl Pts',(-34.0324076640061,4.00889518907209,127.95185816524));
#81529=CARTESIAN_POINT('Ctrl Pts',(-34.0401539400902,3.92625706171269,127.842319336987));
#81530=CARTESIAN_POINT('Ctrl Pts',(-34.0479002733555,3.84361832433741,127.732779700144));
#81531=CARTESIAN_POINT('Ctrl Pts',(-34.0556466066209,3.75639249916016,127.626701666538));
#81532=CARTESIAN_POINT('Ctrl Pts',(-34.0633929398863,3.66491094837876,127.5244809242));
#81533=CARTESIAN_POINT('Ctrl Pts',(-34.0711410078892,3.57340891093847,127.422237290236));
#81534=CARTESIAN_POINT('Ctrl Pts',(-34.0788890758922,3.47764951213106,127.323852957708));
#81535=CARTESIAN_POINT('Ctrl Pts',(-34.0866371438952,3.37800216227966,127.229687981627));
#81536=CARTESIAN_POINT('Ctrl Pts',(-34.094393446637,3.27824890603889,127.135422925888));
#81537=CARTESIAN_POINT('Ctrl Pts',(-34.1021497493789,3.17459972893179,127.045386453586));
#81538=CARTESIAN_POINT('Ctrl Pts',(-34.1099060521208,3.06745885110309,126.95989976339));
#81539=CARTESIAN_POINT('Ctrl Pts',(-34.117666494635,2.96026078896195,126.874367446374));
#81540=CARTESIAN_POINT('Ctrl Pts',(-34.1254269371491,2.8495676280572,126.793389980891));
#81541=CARTESIAN_POINT('Ctrl Pts',(-34.1331873796633,2.73581315316811,126.717245564934));
#81542=CARTESIAN_POINT('Ctrl Pts',(-34.1409602799287,2.62187606949727,126.6409789152));
#81543=CARTESIAN_POINT('Ctrl Pts',(-34.1487331801942,2.50486818542463,126.569561022633));
#81544=CARTESIAN_POINT('Ctrl Pts',(-34.1565060804596,2.38524927332648,126.503224841216));
#81545=CARTESIAN_POINT('Ctrl Pts',(-34.1639964162215,2.26997880998739,126.439300147086));
#81546=CARTESIAN_POINT('Ctrl Pts',(-34.1714867519834,2.15228413286571,126.380094250997));
#81547=CARTESIAN_POINT('Ctrl Pts',(-34.1789770877453,2.03259292347908,126.325772774292));
#81548=CARTESIAN_POINT('Ctrl Pts',(-34.1867514218644,1.90836358550693,126.269391682285));
#81549=CARTESIAN_POINT('Ctrl Pts',(-34.1945257559835,1.78158980840141,126.218094108359));
#81550=CARTESIAN_POINT('Ctrl Pts',(-34.2023000901025,1.65272630393062,126.172117227286));
#81551=CARTESIAN_POINT('Ctrl Pts',(-34.2100648430496,1.52402161221223,126.12619700861));
#81552=CARTESIAN_POINT('Ctrl Pts',(-34.2178295959967,1.39323268210615,126.085584565877));
#81553=CARTESIAN_POINT('Ctrl Pts',(-34.2255943489438,1.26083685217334,126.050470263898));
#81554=CARTESIAN_POINT('Ctrl Pts',(-34.2333513898288,1.12857251964528,126.015390837938));
#81555=CARTESIAN_POINT('Ctrl Pts',(-34.2411084307137,0.994704838848106,
125.985798785012));
#81556=CARTESIAN_POINT('Ctrl Pts',(-34.2488654715987,0.859728734345996,
125.961835494674));
#81557=CARTESIAN_POINT('Ctrl Pts',(-34.2566166628389,0.724854416374068,
125.937890275239));
#81558=CARTESIAN_POINT('Ctrl Pts',(-34.2643678540791,0.58887372183565,125.919565437653));
#81559=CARTESIAN_POINT('Ctrl Pts',(-34.2721190453193,0.452293916470628,
125.906951784762));
#81560=CARTESIAN_POINT('Ctrl Pts',(-34.2798669420963,0.315772161166458,
125.894343493011));
#81561=CARTESIAN_POINT('Ctrl Pts',(-34.2876148388734,0.178652189984851,
125.887441593909));
#81562=CARTESIAN_POINT('Ctrl Pts',(-34.2953627356504,0.0414483613027857,
125.886285272897));
#81563=CARTESIAN_POINT('Ctrl Pts',(-34.3031090117345,-0.0957267672960914,
125.885129193761));
#81564=CARTESIAN_POINT('Ctrl Pts',(-34.3108552878186,-0.232985327801419,
125.88971630546));
#81565=CARTESIAN_POINT('Ctrl Pts',(-34.3186015639027,-0.36981137269736,
125.900033690135));
#81566=CARTESIAN_POINT('Ctrl Pts',(-34.3263478971681,-0.506638427612083,
125.910351150971));
#81567=CARTESIAN_POINT('Ctrl Pts',(-34.3340942304334,-0.643032570688132,
125.926398939792));
#81568=CARTESIAN_POINT('Ctrl Pts',(-34.3418405636988,-0.778481789016616,
125.948112151242));
#81569=CARTESIAN_POINT('Ctrl Pts',(-34.3495886317017,-0.913961340258221,
125.969830225216));
#81570=CARTESIAN_POINT('Ctrl Pts',(-34.3573366997047,-1.04849515971152,
125.997216184577));
#81571=CARTESIAN_POINT('Ctrl Pts',(-34.3650847677077,-1.18158064759604,
126.030153852487));
#81572=CARTESIAN_POINT('Ctrl Pts',(-34.3728410704495,-1.31480758032101,
126.063126526942));
#81573=CARTESIAN_POINT('Ctrl Pts',(-34.3805973731914,-1.44658272643163,
126.101662602597));
#81574=CARTESIAN_POINT('Ctrl Pts',(-34.3883536759332,-1.57641736152975,
126.145595613322));
#81575=CARTESIAN_POINT('Ctrl Pts',(-34.3961141184474,-1.70632129328187,
126.189552072418));
#81576=CARTESIAN_POINT('Ctrl Pts',(-34.4038745609615,-1.83428228569309,
126.238911065602));
#81577=CARTESIAN_POINT('Ctrl Pts',(-34.4116350034757,-1.95983181164479,
126.293458010264));
#81578=CARTESIAN_POINT('Ctrl Pts',(-34.4194079037411,-2.08558288084148,
126.348092518524));
#81579=CARTESIAN_POINT('Ctrl Pts',(-34.4271808040066,-2.20891439593567,
126.407931449818));
#81580=CARTESIAN_POINT('Ctrl Pts',(-34.4349537042721,-2.32938184794327,
126.472713901942));
#81581=CARTESIAN_POINT('Ctrl Pts',(-34.4424440400341,-2.44547000463184,
126.535141348755));
#81582=CARTESIAN_POINT('Ctrl Pts',(-34.4499343757961,-2.5588984496489,126.602158980885));
#81583=CARTESIAN_POINT('Ctrl Pts',(-34.4574247115582,-2.66929666876196,
126.67349650014));
#81584=CARTESIAN_POINT('Ctrl Pts',(-34.4651967991377,-2.78384755871116,
126.747517407208));
#81585=CARTESIAN_POINT('Ctrl Pts',(-34.4729688867172,-2.89549949137508,
126.82642457917));
#81586=CARTESIAN_POINT('Ctrl Pts',(-34.4807409742967,-3.00380714388975,
126.909963911423));
#81587=CARTESIAN_POINT('Ctrl Pts',(-34.4885007573929,-3.1119433277124,126.993370987278));
#81588=CARTESIAN_POINT('Ctrl Pts',(-34.4962605404892,-3.21674546924396,
127.081395380739));
#81589=CARTESIAN_POINT('Ctrl Pts',(-34.5040203235855,-3.31779583247672,
127.173738924729));
#81590=CARTESIAN_POINT('Ctrl Pts',(-34.5117730050702,-3.41875371626542,
127.265997957597));
#81591=CARTESIAN_POINT('Ctrl Pts',(-34.5195256865548,-3.51596636494148,
127.362568015953));
#81592=CARTESIAN_POINT('Ctrl Pts',(-34.5272783680395,-3.60904761639883,
127.463109599599));
#81593=CARTESIAN_POINT('Ctrl Pts',(-34.5350256379881,-3.70206389516783,
127.563581003086));
#81594=CARTESIAN_POINT('Ctrl Pts',(-34.5427729079366,-3.79095424973157,
127.668018130206));
#81595=CARTESIAN_POINT('Ctrl Pts',(-34.5505201778852,-3.87536832769674,
127.776043694392));
#81596=CARTESIAN_POINT('Ctrl Pts',(-34.5582637223173,-3.95974181251877,
127.884017311114));
#81597=CARTESIAN_POINT('Ctrl Pts',(-34.5660072667493,-4.03964306452908,
127.995575622787));
#81598=CARTESIAN_POINT('Ctrl Pts',(-34.5737508111814,-4.11476136648118,
128.110307544701));
#81599=CARTESIAN_POINT('Ctrl Pts',(-34.581494001961,-4.18987623773411,128.225034226737));
#81600=CARTESIAN_POINT('Ctrl Pts',(-34.5892371927407,-4.26020836969045,
128.342933909747));
#81601=CARTESIAN_POINT('Ctrl Pts',(-34.5969803835203,-4.32548987863497,
128.4635658012));
#81602=CARTESIAN_POINT('Ctrl Pts',(-34.6047230389637,-4.39076687425237,
128.584189352601));
#81603=CARTESIAN_POINT('Ctrl Pts',(-34.6124656944072,-4.45099375982855,
128.707544389925));
#81604=CARTESIAN_POINT('Ctrl Pts',(-34.6202083498507,-4.50594858202552,
128.833165437316));
#81605=CARTESIAN_POINT('Ctrl Pts',(-34.6279556026154,-4.560936034497,128.958861074143));
#81606=CARTESIAN_POINT('Ctrl Pts',(-34.6357028553801,-4.61064501347426,
129.086825049675));
#81607=CARTESIAN_POINT('Ctrl Pts',(-34.6434501081448,-4.65490160907204,
129.216571565973));
#81608=CARTESIAN_POINT('Ctrl Pts',(-34.650649281041,-4.69602726911979,129.337139157076));
#81609=CARTESIAN_POINT('Ctrl Pts',(-34.6578484539372,-4.73244513292729,
129.459245566747));
#81610=CARTESIAN_POINT('Ctrl Pts',(-34.6650476268334,-4.76405452823403,
129.582490119308));
#81611=CARTESIAN_POINT('Ctrl Pts',(-32.9151834992122,-4.76405452823401,
129.582490119308));
#81612=CARTESIAN_POINT('Ctrl Pts',(-32.9228708627559,-4.79790449531073,
129.714470627195));
#81613=CARTESIAN_POINT('Ctrl Pts',(-32.9305582262996,-4.82626875440093,
129.847870405711));
#81614=CARTESIAN_POINT('Ctrl Pts',(-32.9382455898434,-4.84904313388873,
129.982190472045));
#81615=CARTESIAN_POINT('Ctrl Pts',(-32.9460614188709,-4.8721981018139,130.118755195107));
#81616=CARTESIAN_POINT('Ctrl Pts',(-32.9538772478985,-4.88957459330449,
130.256270826341));
#81617=CARTESIAN_POINT('Ctrl Pts',(-32.961693076926,-4.90111776738139,130.394204924251));
#81618=CARTESIAN_POINT('Ctrl Pts',(-32.9695089059535,-4.91266094145829,
130.532139022162));
#81619=CARTESIAN_POINT('Ctrl Pts',(-32.977324734981,-4.91837079231979,130.670491155864));
#81620=CARTESIAN_POINT('Ctrl Pts',(-32.9851405640085,-4.918248061596,130.808727207449));
#81621=CARTESIAN_POINT('',(-32.6398594359421,-4.91824935210416,130.801836132062));
#81622=CARTESIAN_POINT('Ctrl Pts',(-32.5701265742934,-4.76405452823409,
129.582490119308));
#81623=CARTESIAN_POINT('Ctrl Pts',(-32.5787159453649,-4.80163023673377,
129.728997236458));
#81624=CARTESIAN_POINT('Ctrl Pts',(-32.5873053164363,-4.83248793567468,
129.877411663971));
#81625=CARTESIAN_POINT('Ctrl Pts',(-32.5958946875078,-4.8564495174955,130.02713404409));
#81626=CARTESIAN_POINT('Ctrl Pts',(-32.6044442660324,-4.8803000909132,130.176162795446));
#81627=CARTESIAN_POINT('Ctrl Pts',(-32.6129938445571,-4.89731819714702,
130.326487182374));
#81628=CARTESIAN_POINT('Ctrl Pts',(-32.6215434230817,-4.90737648749908,
130.477498150401));
#81629=CARTESIAN_POINT('Ctrl Pts',(-32.6276487607019,-4.91455921098699,
130.585336559217));
#81630=CARTESIAN_POINT('Ctrl Pts',(-32.633754098322,-4.91819375699317,130.693524708538));
#81631=CARTESIAN_POINT('Ctrl Pts',(-32.6398594359422,-4.91824935210415,
130.801836132062));
#81632=CARTESIAN_POINT('Ctrl Pts',(-32.6398594359911,-4.9182493521046,130.801836132932));
#81633=CARTESIAN_POINT('Ctrl Pts',(-32.6477146369204,-4.91832088141948,
130.941190915199));
#81634=CARTESIAN_POINT('Ctrl Pts',(-32.6555698378496,-4.91246529782376,
131.080539411816));
#81635=CARTESIAN_POINT('Ctrl Pts',(-32.6634250387788,-4.9007107268889,131.21935150163));
#81636=CARTESIAN_POINT('Ctrl Pts',(-32.6712824326159,-4.88895287447336,
131.358202343108));
#81637=CARTESIAN_POINT('Ctrl Pts',(-32.679139826453,-4.87129278575712,131.496516105238));
#81638=CARTESIAN_POINT('Ctrl Pts',(-32.68699722029,-4.84781044438552,131.633768212061));
#81639=CARTESIAN_POINT('Ctrl Pts',(-32.6948583187497,-4.82431703150399,
131.771085030833));
#81640=CARTESIAN_POINT('Ctrl Pts',(-32.7027194172094,-4.79499596115353,
131.907338827296));
#81641=CARTESIAN_POINT('Ctrl Pts',(-32.7105805156691,-4.75997821932935,
132.042015825615));
#81642=CARTESIAN_POINT('Ctrl Pts',(-32.7185594697667,-4.72443548238876,
132.178711936609));
#81643=CARTESIAN_POINT('Ctrl Pts',(-32.7265384238643,-4.68302399350987,
132.313783201881));
#81644=CARTESIAN_POINT('Ctrl Pts',(-32.7345173779619,-4.63593256907531,
132.446710238532));
#81645=CARTESIAN_POINT('Ctrl Pts',(-32.7423951192043,-4.58943849831233,
132.57795109868));
#81646=CARTESIAN_POINT('Ctrl Pts',(-32.7502728604466,-4.53740795696268,
132.707101490471));
#81647=CARTESIAN_POINT('Ctrl Pts',(-32.758150601689,-4.48007028516977,132.833683978304));
#81648=CARTESIAN_POINT('Ctrl Pts',(-32.7661801622142,-4.42162760574246,
132.962705955065));
#81649=CARTESIAN_POINT('Ctrl Pts',(-32.7742097227395,-4.35767134368835,
133.089059673188));
#81650=CARTESIAN_POINT('Ctrl Pts',(-32.7822392832647,-4.2884918207682,133.212268623638));
#81651=CARTESIAN_POINT('Ctrl Pts',(-32.79026884379,-4.21931229784813,133.335477574087));
#81652=CARTESIAN_POINT('Ctrl Pts',(-32.7982984043152,-4.14490978357858,
133.455541446482));
#81653=CARTESIAN_POINT('Ctrl Pts',(-32.8063279648404,-4.0656187706269,133.572017943614));
#81654=CARTESIAN_POINT('Ctrl Pts',(-32.8141022989595,-3.98884808991657,
133.684792136283));
#81655=CARTESIAN_POINT('Ctrl Pts',(-32.8218766330786,-3.90725997239606,
133.794548278398));
#81656=CARTESIAN_POINT('Ctrl Pts',(-32.8296509671977,-3.82111939450904,
133.900847277542));
#81657=CARTESIAN_POINT('Ctrl Pts',(-32.8374157201448,-3.73508497718567,
134.007015272669));
#81658=CARTESIAN_POINT('Ctrl Pts',(-32.8451804730919,-3.64450950650486,
134.109734301355));
#81659=CARTESIAN_POINT('Ctrl Pts',(-32.852945226039,-3.54970163305374,134.208593479577));
#81660=CARTESIAN_POINT('Ctrl Pts',(-32.860702266924,-3.45498792411934,134.30735446947));
#81661=CARTESIAN_POINT('Ctrl Pts',(-32.868459307809,-3.35605044679242,134.402262957702));
#81662=CARTESIAN_POINT('Ctrl Pts',(-32.876216348694,-3.25323834702194,134.492940740048));
#81663=CARTESIAN_POINT('Ctrl Pts',(-32.8839675399341,-3.15050377865551,
134.583550141572));
#81664=CARTESIAN_POINT('Ctrl Pts',(-32.8917187311742,-3.04390069570522,
134.669934929962));
#81665=CARTESIAN_POINT('Ctrl Pts',(-32.8994699224144,-2.93381509834212,
134.751753685306));
#81666=CARTESIAN_POINT('Ctrl Pts',(-32.9072178191914,-2.82377629029454,
134.833537665496));
#81667=CARTESIAN_POINT('Ctrl Pts',(-32.9149657159685,-2.71025822489476,
134.910759239786));
#81668=CARTESIAN_POINT('Ctrl Pts',(-32.9227136127456,-2.59367981013424,
134.983117383041));
#81669=CARTESIAN_POINT('Ctrl Pts',(-32.9304598888296,-2.47712578106495,
135.055460390532));
#81670=CARTESIAN_POINT('Ctrl Pts',(-32.9382061649138,-2.3575130079169,135.122941784453));
#81671=CARTESIAN_POINT('Ctrl Pts',(-32.9459524409979,-2.23528885894826,
135.185304212222));
#81672=CARTESIAN_POINT('Ctrl Pts',(-32.9536987742632,-2.11306380774889,
135.247667100337));
#81673=CARTESIAN_POINT('Ctrl Pts',(-32.9614451075285,-1.98822769051716,
135.304910769209));
#81674=CARTESIAN_POINT('Ctrl Pts',(-32.9691914407938,-1.86125155794798,
135.356824313252));
#81675=CARTESIAN_POINT('Ctrl Pts',(-32.9769395087968,-1.73424698995447,
135.408749482972));
#81676=CARTESIAN_POINT('Ctrl Pts',(-32.9846875767997,-1.60510181480681,
135.45534200472));
#81677=CARTESIAN_POINT('Ctrl Pts',(-32.9924356448027,-1.4743057142101,135.496439658199));
#81678=CARTESIAN_POINT('Ctrl Pts',(-33.0001919475445,-1.34337060196082,
135.537580990753));
#81679=CARTESIAN_POINT('Ctrl Pts',(-33.0079482502864,-1.21078143279462,
135.573215671602));
#81680=CARTESIAN_POINT('Ctrl Pts',(-33.0157045530282,-1.07704219749085,
135.603231648061));
#81681=CARTESIAN_POINT('Ctrl Pts',(-33.0234649955424,-0.943231581530391,
135.633263644951));
#81682=CARTESIAN_POINT('Ctrl Pts',(-33.0312254380566,-0.808270060870548,
135.657670892403));
#81683=CARTESIAN_POINT('Ctrl Pts',(-33.0389858805707,-0.672669405852567,
135.676392938162));
#81684=CARTESIAN_POINT('Ctrl Pts',(-33.0467587808362,-0.536851072624907,
135.69514503821));
#81685=CARTESIAN_POINT('Ctrl Pts',(-33.0545316811016,-0.400391944187662,
135.708193661892));
#81686=CARTESIAN_POINT('Ctrl Pts',(-33.062304581367,-0.263807372512092,
135.715530410264));
#81687=CARTESIAN_POINT('Ctrl Pts',(-33.0697949171291,-0.132187994051589,
135.722600449352));
#81688=CARTESIAN_POINT('Ctrl Pts',(-33.0772852528912,-0.000452442356223659,
135.724366681204));
#81689=CARTESIAN_POINT('Ctrl Pts',(-33.0847755886533,0.130942238749945,
135.720867222119));
#81690=CARTESIAN_POINT('Ctrl Pts',(-33.0925499227724,0.267318789125649,
135.717235079979));
#81691=CARTESIAN_POINT('Ctrl Pts',(-33.1003242568915,0.403760110362607,
135.707918561769));
#81692=CARTESIAN_POINT('Ctrl Pts',(-33.1080985910106,0.539753555335134,
135.6929032595));
#81693=CARTESIAN_POINT('Ctrl Pts',(-33.1158633439577,0.675579400540446,
135.677906462248));
#81694=CARTESIAN_POINT('Ctrl Pts',(-33.1236280969047,0.810958082858944,
135.65722489759));
#81695=CARTESIAN_POINT('Ctrl Pts',(-33.1313928498518,0.945377080745844,
135.630896149156));
#81696=CARTESIAN_POINT('Ctrl Pts',(-33.1391498907368,1.07966257178925,135.604593550806));
#81697=CARTESIAN_POINT('Ctrl Pts',(-33.1469069316218,1.21298989406473,135.572655005234));
#81698=CARTESIAN_POINT('Ctrl Pts',(-33.1546639725068,1.34485213173174,135.535169830193));
#81699=CARTESIAN_POINT('Ctrl Pts',(-33.1624151637469,1.47661493105923,135.497712923014));
#81700=CARTESIAN_POINT('Ctrl Pts',(-33.170166354987,1.60691447033537,135.454717818362));
#81701=CARTESIAN_POINT('Ctrl Pts',(-33.1779175462271,1.73525486079802,135.406324723312));
#81702=CARTESIAN_POINT('Ctrl Pts',(-33.1856654430042,1.86354070317147,135.357952196618));
#81703=CARTESIAN_POINT('Ctrl Pts',(-33.1934133397814,1.98986868783246,135.304186380345));
#81704=CARTESIAN_POINT('Ctrl Pts',(-33.2011612365584,2.11375912380571,135.245217002209));
#81705=CARTESIAN_POINT('Ctrl Pts',(-33.2089075126425,2.23762364457053,135.186259959197));
#81706=CARTESIAN_POINT('Ctrl Pts',(-33.2166537887266,2.35905127803991,135.122101687277));
#81707=CARTESIAN_POINT('Ctrl Pts',(-33.2244000648107,2.4775836927265,135.052979464678));
#81708=CARTESIAN_POINT('Ctrl Pts',(-33.232146398076,2.59611698239213,134.983856731835));
#81709=CARTESIAN_POINT('Ctrl Pts',(-33.2398927313413,2.71175467289462,134.909770172145));
#81710=CARTESIAN_POINT('Ctrl Pts',(-33.2476390646066,2.82406470898329,134.831002094278));
#81711=CARTESIAN_POINT('Ctrl Pts',(-33.2553871326096,2.93639989612568,134.752216376845));
#81712=CARTESIAN_POINT('Ctrl Pts',(-33.2631352006125,3.04540562595478,134.668747279503));
#81713=CARTESIAN_POINT('Ctrl Pts',(-33.2708832686155,3.15068073301714,134.580919101304));
#81714=CARTESIAN_POINT('Ctrl Pts',(-33.2786395713573,3.2560677277165,134.492997578272));
#81715=CARTESIAN_POINT('Ctrl Pts',(-33.2863958740992,3.35771587854612,134.400707970556));
#81716=CARTESIAN_POINT('Ctrl Pts',(-33.2941521768411,3.45525849308206,134.304413732661));
#81717=CARTESIAN_POINT('Ctrl Pts',(-33.3019126193552,3.55285316904847,134.208068099631));
#81718=CARTESIAN_POINT('Ctrl Pts',(-33.3096730618694,3.64633767611456,134.107713863419));
#81719=CARTESIAN_POINT('Ctrl Pts',(-33.3174335043836,3.73538452971476,134.003748914986));
#81720=CARTESIAN_POINT('Ctrl Pts',(-33.325206404649,3.82457432922944,133.899617072788));
#81721=CARTESIAN_POINT('Ctrl Pts',(-33.3329793049144,3.90931199800893,133.791863243141));
#81722=CARTESIAN_POINT('Ctrl Pts',(-33.3407522051798,3.98931190945571,133.68091646642));
#81723=CARTESIAN_POINT('Ctrl Pts',(-33.348242540942,4.06640362261519,133.574002884488));
#81724=CARTESIAN_POINT('Ctrl Pts',(-33.3557328767041,4.13909588700599,133.46412472536));
#81725=CARTESIAN_POINT('Ctrl Pts',(-33.3632232124663,4.20717372759986,133.351687115739));
#81726=CARTESIAN_POINT('Ctrl Pts',(-33.3709975465854,4.27783276021036,133.234986399977));
#81727=CARTESIAN_POINT('Ctrl Pts',(-33.3787718807045,4.34374437647595,133.11515864654));
#81728=CARTESIAN_POINT('Ctrl Pts',(-33.3865462148236,4.40461935625323,132.992627372105));
#81729=CARTESIAN_POINT('Ctrl Pts',(-33.3943109677707,4.46541931305849,132.870247106514));
#81730=CARTESIAN_POINT('Ctrl Pts',(-33.4020757207177,4.52119481158055,132.745170296083));
#81731=CARTESIAN_POINT('Ctrl Pts',(-33.4098404736648,4.57170044157857,132.617848454572));
#81732=CARTESIAN_POINT('Ctrl Pts',(-33.4175975145498,4.62215590867286,132.49065307091));
#81733=CARTESIAN_POINT('Ctrl Pts',(-33.4253545554347,4.66735178012736,132.36121745463));
#81734=CARTESIAN_POINT('Ctrl Pts',(-33.4331115963197,4.70708920110316,132.230016366812));
#81735=CARTESIAN_POINT('Ctrl Pts',(-33.4408627875599,4.74679665578085,132.098914218754));
#81736=CARTESIAN_POINT('Ctrl Pts',(-33.4486139788001,4.78105374027489,131.966049621808));
#81737=CARTESIAN_POINT('Ctrl Pts',(-33.4563651700402,4.80971037477895,131.83191556658));
#81738=CARTESIAN_POINT('Ctrl Pts',(-33.4641130668173,4.83835482944879,131.697838521905));
#81739=CARTESIAN_POINT('Ctrl Pts',(-33.4718609635944,4.86140348693259,131.562493473616));
#81740=CARTESIAN_POINT('Ctrl Pts',(-33.4796088603714,4.87875668584335,131.426386551783));
#81741=CARTESIAN_POINT('Ctrl Pts',(-33.4873551364555,4.89610625483896,131.290308100584));
#81742=CARTESIAN_POINT('Ctrl Pts',(-33.4951014125396,4.9077626855409,131.153468480412));
#81743=CARTESIAN_POINT('Ctrl Pts',(-33.5028476886236,4.91367786747877,131.016381553205));
#81744=CARTESIAN_POINT('Ctrl Pts',(-33.510594021889,4.91959309308118,130.879293614054));
#81745=CARTESIAN_POINT('Ctrl Pts',(-33.5183403551543,4.91976696849799,130.741958754827));
#81746=CARTESIAN_POINT('Ctrl Pts',(-33.5260866884197,4.91420347159105,130.604893070575));
#81747=CARTESIAN_POINT('Ctrl Pts',(-33.5338347564226,4.90863872877755,130.467796691414));
#81748=CARTESIAN_POINT('Ctrl Pts',(-33.5415828244256,4.89733407280118,130.330969997746));
#81749=CARTESIAN_POINT('Ctrl Pts',(-33.5493308924285,4.88034550591383,130.194925792989));
#81750=CARTESIAN_POINT('Ctrl Pts',(-33.5570871951704,4.8633388833754,130.058736998833));
#81751=CARTESIAN_POINT('Ctrl Pts',(-33.5648434979122,4.84063633104417,129.923332743445));
#81752=CARTESIAN_POINT('Ctrl Pts',(-33.572599800654,4.81234542727534,129.789217991586));
#81753=CARTESIAN_POINT('Ctrl Pts',(-33.5803602431682,4.78403942379938,129.655031658645));
#81754=CARTESIAN_POINT('Ctrl Pts',(-33.5881206856823,4.75013922224993,129.522136579271));
#81755=CARTESIAN_POINT('Ctrl Pts',(-33.5958811281965,4.71080256615432,129.391023345287));
#81756=CARTESIAN_POINT('Ctrl Pts',(-33.6036540284619,4.67140276336609,129.259699636699));
#81757=CARTESIAN_POINT('Ctrl Pts',(-33.6114269287274,4.62654919454484,129.130163859102));
#81758=CARTESIAN_POINT('Ctrl Pts',(-33.6191998289928,4.57644843535629,129.002888225042));
#81759=CARTESIAN_POINT('Ctrl Pts',(-33.6266901647549,4.52816896496011,128.880239380868));
#81760=CARTESIAN_POINT('Ctrl Pts',(-33.6341805005169,4.4750173022852,128.759689491154));
#81761=CARTESIAN_POINT('Ctrl Pts',(-33.641670836279,4.41721809264798,128.641638401357));
#81762=CARTESIAN_POINT('Ctrl Pts',(-33.6494451703981,4.35722740841002,128.519111368611));
#81763=CARTESIAN_POINT('Ctrl Pts',(-33.6572195045172,4.29203976431774,128.398888231444));
#81764=CARTESIAN_POINT('Ctrl Pts',(-33.6649938386363,4.22185514639264,128.281441240063));
#81765=CARTESIAN_POINT('Ctrl Pts',(-33.6727585915834,4.15175702473647,128.164138991603));
#81766=CARTESIAN_POINT('Ctrl Pts',(-33.6805233445305,4.07667438110451,128.049606413842));
#81767=CARTESIAN_POINT('Ctrl Pts',(-33.6882880974777,3.99685443658223,127.938294031586));
#81768=CARTESIAN_POINT('Ctrl Pts',(-33.6960451383627,3.91711377035411,127.827092206356));
#81769=CARTESIAN_POINT('Ctrl Pts',(-33.7038021792477,3.83264539306175,127.719104527448));
#81770=CARTESIAN_POINT('Ctrl Pts',(-33.7115592201327,3.74374124875022,127.614754917028));
#81771=CARTESIAN_POINT('Ctrl Pts',(-33.7193104113729,3.65490414774548,127.510483997461));
#81772=CARTESIAN_POINT('Ctrl Pts',(-33.727061602613,3.56163819035822,127.409845982017));
#81773=CARTESIAN_POINT('Ctrl Pts',(-33.7348127938532,3.46427702174812,127.313233610554));
#81774=CARTESIAN_POINT('Ctrl Pts',(-33.7425606906303,3.36695723423201,127.216662301926));
#81775=CARTESIAN_POINT('Ctrl Pts',(-33.7503085874073,3.26554597430036,127.124113509026));
#81776=CARTESIAN_POINT('Ctrl Pts',(-33.7580564841844,3.16041519410034,127.035944655467));
#81777=CARTESIAN_POINT('Ctrl Pts',(-33.7658027602685,3.05530640499318,126.947794244932));
#81778=CARTESIAN_POINT('Ctrl Pts',(-33.7735490363527,2.94647994256069,126.864022202458));
#81779=CARTESIAN_POINT('Ctrl Pts',(-33.7812953124368,2.83434212852143,126.784946759677));
#81780=CARTESIAN_POINT('Ctrl Pts',(-33.7890416457021,2.7222034867063,126.705870733179));
#81781=CARTESIAN_POINT('Ctrl Pts',(-33.7967879789676,2.60675376402312,126.631491600864));
#81782=CARTESIAN_POINT('Ctrl Pts',(-33.8045343122329,2.48842931598555,126.562084978025));
#81783=CARTESIAN_POINT('Ctrl Pts',(-33.8122823802359,2.37007837000825,126.492662812054));
#81784=CARTESIAN_POINT('Ctrl Pts',(-33.8200304482388,2.24885175480483,126.428215569186));
#81785=CARTESIAN_POINT('Ctrl Pts',(-33.8277785162418,2.12521117699891,126.368973315914));
#81786=CARTESIAN_POINT('Ctrl Pts',(-33.8355348189837,2.00143919251555,126.30966809927));
#81787=CARTESIAN_POINT('Ctrl Pts',(-33.8432911217256,1.87524847353427,126.255579092046));
#81788=CARTESIAN_POINT('Ctrl Pts',(-33.8510474244675,1.74712200993646,126.206888731312));
#81789=CARTESIAN_POINT('Ctrl Pts',(-33.8588078669816,1.61892716138704,126.158172383066));
#81790=CARTESIAN_POINT('Ctrl Pts',(-33.8665683094958,1.48879488032868,126.114860546189));
#81791=CARTESIAN_POINT('Ctrl Pts',(-33.87432875201,1.35722317978619,126.077085683447));
#81792=CARTESIAN_POINT('Ctrl Pts',(-33.8821016522755,1.22544026866979,126.039250181142));
#81793=CARTESIAN_POINT('Ctrl Pts',(-33.8898745525409,1.09221370077561,126.006969507032));
#81794=CARTESIAN_POINT('Ctrl Pts',(-33.8976474528064,0.958052421087607,
125.980325105575));
#81795=CARTESIAN_POINT('Ctrl Pts',(-33.9051377885683,0.828768241850493,
125.954649295225));
#81796=CARTESIAN_POINT('Ctrl Pts',(-33.9126281243302,0.69861643350888,125.934207134382));
#81797=CARTESIAN_POINT('Ctrl Pts',(-33.9201184600921,0.568054823652561,
125.919025748816));
#81798=CARTESIAN_POINT('Ctrl Pts',(-33.9278927942112,0.432542930672723,
125.903268756401));
#81799=CARTESIAN_POINT('Ctrl Pts',(-33.9356671283302,0.29616028654971,125.893129425334));
#81800=CARTESIAN_POINT('Ctrl Pts',(-33.9434414624493,0.159412306085997,
125.888694764483));
#81801=CARTESIAN_POINT('Ctrl Pts',(-33.9512062153964,0.0228328552870593,
125.884265568954));
#81802=CARTESIAN_POINT('Ctrl Pts',(-33.9589709683435,-0.114110648991904,
125.8855270676));
#81803=CARTESIAN_POINT('Ctrl Pts',(-33.9667357212906,-0.250905538439235,
125.892514785979));
#81804=CARTESIAN_POINT('Ctrl Pts',(-33.9744927621756,-0.387564561274083,
125.899495564057));
#81805=CARTESIAN_POINT('Ctrl Pts',(-33.9822498030606,-0.524074875091091,
125.912191223946));
#81806=CARTESIAN_POINT('Ctrl Pts',(-33.9900068439456,-0.659922019276341,
125.930585285139));
#81807=CARTESIAN_POINT('Ctrl Pts',(-33.9977580351857,-0.795666720072131,
125.948965475227));
#81808=CARTESIAN_POINT('Ctrl Pts',(-34.0055092264257,-0.930748860795491,
125.973035461038));
#81809=CARTESIAN_POINT('Ctrl Pts',(-34.0132604176658,-1.06465767492297,
126.002726822937));
#81810=CARTESIAN_POINT('Ctrl Pts',(-34.0210083144429,-1.19850957423359,
126.032405565215));
#81811=CARTESIAN_POINT('Ctrl Pts',(-34.02875621122,-1.33118875791891,126.067700847119));
#81812=CARTESIAN_POINT('Ctrl Pts',(-34.0365041079971,-1.46219346614992,
126.108492930967));
#81813=CARTESIAN_POINT('Ctrl Pts',(-34.0442503840812,-1.59317077102029,
126.14927648199));
#81814=CARTESIAN_POINT('Ctrl Pts',(-34.0519966601652,-1.72247392408005,
126.195554431757));
#81815=CARTESIAN_POINT('Ctrl Pts',(-34.0597429362493,-1.84961556123117,
126.247156942268));
#81816=CARTESIAN_POINT('Ctrl Pts',(-34.0674892695146,-1.9767581369121,126.298759833696));
#81817=CARTESIAN_POINT('Ctrl Pts',(-34.07523560278,-2.1017388025811,126.355687217268));
#81818=CARTESIAN_POINT('Ctrl Pts',(-34.0829819360453,-2.22408981447257,
126.417720951528));
#81819=CARTESIAN_POINT('Ctrl Pts',(-34.0907300040483,-2.34646822602566,
126.479768577813));
#81820=CARTESIAN_POINT('Ctrl Pts',(-34.0984780720513,-2.46621546333353,
126.546924653518));
#81821=CARTESIAN_POINT('Ctrl Pts',(-34.1062261400543,-2.58288840123231,
126.618925088343));
#81822=CARTESIAN_POINT('Ctrl Pts',(-34.1139824427961,-2.6996853405176,126.691002046087));
#81823=CARTESIAN_POINT('Ctrl Pts',(-34.121738745538,-2.8134011201641,126.767933442271));
#81824=CARTESIAN_POINT('Ctrl Pts',(-34.1294950482799,-2.92362118286983,
126.84941153552));
#81825=CARTESIAN_POINT('Ctrl Pts',(-34.1372554907941,-3.03390007334213,
126.930933116082));
#81826=CARTESIAN_POINT('Ctrl Pts',(-34.1450159333082,-3.14067922493189,
127.017005983891));
#81827=CARTESIAN_POINT('Ctrl Pts',(-34.1527763758224,-3.24357800475732,
127.107282745847));
#81828=CARTESIAN_POINT('Ctrl Pts',(-34.1605492760878,-3.34664196683876,
127.197704428075));
#81829=CARTESIAN_POINT('Ctrl Pts',(-34.1683221763533,-3.44581282639051,
127.292343219961));
#81830=CARTESIAN_POINT('Ctrl Pts',(-34.1760950766187,-3.5407469646873,127.390814954394));
#81831=CARTESIAN_POINT('Ctrl Pts',(-34.1835854123808,-3.6322300079326,127.485706993246));
#81832=CARTESIAN_POINT('Ctrl Pts',(-34.1910757481428,-3.71977880834725,
127.584157908433));
#81833=CARTESIAN_POINT('Ctrl Pts',(-34.1985660839049,-3.80312307725695,
127.68579717878));
#81834=CARTESIAN_POINT('Ctrl Pts',(-34.206310538568,-3.88929490352841,127.79088468703));
#81835=CARTESIAN_POINT('Ctrl Pts',(-34.2140549932311,-3.97125274011145,
127.899723368308));
#81836=CARTESIAN_POINT('Ctrl Pts',(-34.2217994478943,-4.04865008092329,
128.011939520249));
#81837=CARTESIAN_POINT('Ctrl Pts',(-34.2295343293618,-4.12595174813202,
128.124016957818));
#81838=CARTESIAN_POINT('Ctrl Pts',(-34.2372692108293,-4.19870391135565,
128.239463240276));
#81839=CARTESIAN_POINT('Ctrl Pts',(-34.2450040922969,-4.26659920068892,
128.357870412562));
#81840=CARTESIAN_POINT('Ctrl Pts',(-34.252729512362,-4.33441143966738,128.476132747735));
#81841=CARTESIAN_POINT('Ctrl Pts',(-34.2604549324272,-4.39737844007198,
128.597348421123));
#81842=CARTESIAN_POINT('Ctrl Pts',(-34.2681803524924,-4.45523560581082,
128.721079849351));
#81843=CARTESIAN_POINT('Ctrl Pts',(-34.2759003324996,-4.51305202990301,
128.844724148836));
#81844=CARTESIAN_POINT('Ctrl Pts',(-34.2836203125069,-4.56576561011797,
128.970880324095));
#81845=CARTESIAN_POINT('Ctrl Pts',(-34.2913402925141,-4.61315724699001,
129.099085485207));
#81846=CARTESIAN_POINT('Ctrl Pts',(-34.299056110084,-4.66052333137096,129.227221521015));
#81847=CARTESIAN_POINT('Ctrl Pts',(-34.3067719276538,-4.70257304827278,
129.357403974628));
#81848=CARTESIAN_POINT('Ctrl Pts',(-34.3144877452236,-4.73913529537912,
129.489149716383));
#81849=CARTESIAN_POINT('Ctrl Pts',(-34.3163049875457,-4.74774649726812,
129.520178694907));
#81850=CARTESIAN_POINT('Ctrl Pts',(-34.3181222298679,-4.7560535205127,129.551294311635));
#81851=CARTESIAN_POINT('Ctrl Pts',(-34.31993947219,-4.764054528234,129.582490119308));
#81852=CARTESIAN_POINT('Origin',(213.235140564004,0.,130.804360617566));
#81853=CARTESIAN_POINT('',(-36.4152663115527,-4.76405452823401,129.582490119308));
#81854=CARTESIAN_POINT('',(-36.0696835869212,-4.76181538791775,129.583090555045));
#81855=CARTESIAN_POINT('',(213.235140564004,-4.76405452823405,129.582490119308));
#81856=CARTESIAN_POINT('',(-34.7351405639796,-4.91824999933744,130.804441346932));
#81857=CARTESIAN_POINT('Ctrl Pts',(-34.7351405640085,-4.91824999933744,
130.804441347438));
#81858=CARTESIAN_POINT('Ctrl Pts',(-34.7353844877961,-4.91824992907732,
130.808721755457));
#81859=CARTESIAN_POINT('Ctrl Pts',(-34.7356284115836,-4.91824427088825,
130.813002158059));
#81860=CARTESIAN_POINT('Ctrl Pts',(-34.7358723353711,-4.91823302480335,
130.817282545971));
#81861=CARTESIAN_POINT('Ctrl Pts',(-34.7436466694902,-4.91787458980837,
130.953706984666));
#81862=CARTESIAN_POINT('Ctrl Pts',(-34.7514210036093,-4.91183497002536,
131.090332584922));
#81863=CARTESIAN_POINT('Ctrl Pts',(-34.7591953377284,-4.90008745949622,
131.226647192995));
#81864=CARTESIAN_POINT('Ctrl Pts',(-34.7669600906755,-4.8883544267239,131.362793805497));
#81865=CARTESIAN_POINT('Ctrl Pts',(-34.7747248436226,-4.87092753294101,
131.498629802626));
#81866=CARTESIAN_POINT('Ctrl Pts',(-34.7824895965697,-4.84783205185145,
131.633641908529));
#81867=CARTESIAN_POINT('Ctrl Pts',(-34.7902466374547,-4.82475950951933,
131.768519918505));
#81868=CARTESIAN_POINT('Ctrl Pts',(-34.7980036783397,-4.79602964957033,
131.902575282835));
#81869=CARTESIAN_POINT('Ctrl Pts',(-34.8057607192247,-4.76171959945346,
132.035299088279));
#81870=CARTESIAN_POINT('Ctrl Pts',(-34.8135119104649,-4.72743542281228,
132.167922805668));
#81871=CARTESIAN_POINT('Ctrl Pts',(-34.8212631017049,-4.6875795293558,132.299216585858));
#81872=CARTESIAN_POINT('Ctrl Pts',(-34.8290142929451,-4.64228018581905,
132.428681318306));
#81873=CARTESIAN_POINT('Ctrl Pts',(-34.8367621897222,-4.59700009571163,
132.558091024789));
#81874=CARTESIAN_POINT('Ctrl Pts',(-34.8445100864992,-4.54628128597217,
132.685672861454));
#81875=CARTESIAN_POINT('Ctrl Pts',(-34.8522579832763,-4.49030191842068,
132.810942722522));
#81876=CARTESIAN_POINT('Ctrl Pts',(-34.8600042593604,-4.43433426054609,
132.936186379835));
#81877=CARTESIAN_POINT('Ctrl Pts',(-34.8677505354446,-4.3731083930137,133.059118666768));
#81878=CARTESIAN_POINT('Ctrl Pts',(-34.8754968115287,-4.30685052703,133.179275689799));
#81879=CARTESIAN_POINT('Ctrl Pts',(-34.883243144794,-4.24059217194589,133.299433599802));
#81880=CARTESIAN_POINT('Ctrl Pts',(-34.8909894780594,-4.16930193307872,
133.416815862661));
#81881=CARTESIAN_POINT('Ctrl Pts',(-34.8987358113247,-4.09325166966457,
133.530983772916));
#81882=CARTESIAN_POINT('Ctrl Pts',(-34.9064838793277,-4.01718437532132,
133.645177250282));
#81883=CARTESIAN_POINT('Ctrl Pts',(-34.9142319473306,-3.93635515197055,
133.756154617341));
#81884=CARTESIAN_POINT('Ctrl Pts',(-34.9219800153336,-3.85107857841109,
133.863507041882));
#81885=CARTESIAN_POINT('Ctrl Pts',(-34.9297363180754,-3.76571137189434,
133.970973561857));
#81886=CARTESIAN_POINT('Ctrl Pts',(-34.9374926208173,-3.67588761665074,
134.074807136645));
#81887=CARTESIAN_POINT('Ctrl Pts',(-34.9452489235591,-3.5819618629107,134.174632457515));
#81888=CARTESIAN_POINT('Ctrl Pts',(-34.9530093660733,-3.48798597816771,
134.274511058165));
#81889=CARTESIAN_POINT('Ctrl Pts',(-34.9607698085874,-3.38990401190089,
134.370376868964));
#81890=CARTESIAN_POINT('Ctrl Pts',(-34.9685302511016,-3.2881058817618,134.46189295137));
#81891=CARTESIAN_POINT('Ctrl Pts',(-34.976303151367,-3.186144336227,134.553555943516));
#81892=CARTESIAN_POINT('Ctrl Pts',(-34.9840760516325,-3.08045500742379,
134.640855004742));
#81893=CARTESIAN_POINT('Ctrl Pts',(-34.9918489518979,-2.9714599579233,134.723494294918));
#81894=CARTESIAN_POINT('Ctrl Pts',(-34.99933928766,-2.86642715301413,134.803129438741));
#81895=CARTESIAN_POINT('Ctrl Pts',(-35.006829623422,-2.75832504999342,134.878437542406));
#81896=CARTESIAN_POINT('Ctrl Pts',(-35.014319959184,-2.6475535000912,134.949193970869));
#81897=CARTESIAN_POINT('Ctrl Pts',(-35.0220942933031,-2.53258201320617,
135.022633150823));
#81898=CARTESIAN_POINT('Ctrl Pts',(-35.0298686274221,-2.4143704642541,135.091401321853));
#81899=CARTESIAN_POINT('Ctrl Pts',(-35.0376429615412,-2.29333530746205,
135.155199183871));
#81900=CARTESIAN_POINT('Ctrl Pts',(-35.0454077144883,-2.17244931568352,
135.218918420726));
#81901=CARTESIAN_POINT('Ctrl Pts',(-35.0531724674355,-2.04874698245789,
135.277679355858));
#81902=CARTESIAN_POINT('Ctrl Pts',(-35.0609372203826,-1.92267380235278,
135.331225814614));
#81903=CARTESIAN_POINT('Ctrl Pts',(-35.0686942612676,-1.79672583990764,
135.384719090272));
#81904=CARTESIAN_POINT('Ctrl Pts',(-35.0764513021525,-1.66841207418315,
135.43300804433));
#81905=CARTESIAN_POINT('Ctrl Pts',(-35.0842083430375,-1.53820235757236,
135.475882486257));
#81906=CARTESIAN_POINT('Ctrl Pts',(-35.0919595342776,-1.40809083312157,
135.518724596234));
#81907=CARTESIAN_POINT('Ctrl Pts',(-35.0997107255179,-1.27608657346729,
135.556160199513));
#81908=CARTESIAN_POINT('Ctrl Pts',(-35.107461916758,-1.1426788257471,135.588027429091));
#81909=CARTESIAN_POINT('Ctrl Pts',(-35.1152098135351,-1.00932777987864,
135.619881114247));
#81910=CARTESIAN_POINT('Ctrl Pts',(-35.122957710312,-0.874574811847501,
135.646171042259));
#81911=CARTESIAN_POINT('Ctrl Pts',(-35.1307056070891,-0.738923514371043,
135.666785434713));
#81912=CARTESIAN_POINT('Ctrl Pts',(-35.1384518831732,-0.603300592221713,
135.687395515081));
#81913=CARTESIAN_POINT('Ctrl Pts',(-35.1461981592574,-0.466780100675269,
135.702332362595));
#81914=CARTESIAN_POINT('Ctrl Pts',(-35.1539444353415,-0.329874599172941,
135.711535549369));
#81915=CARTESIAN_POINT('Ctrl Pts',(-35.1616907686068,-0.192968087065114,
135.72073880408));
#81916=CARTESIAN_POINT('Ctrl Pts',(-35.1694371018721,-0.0556769494151028,
135.724208287373));
#81917=CARTESIAN_POINT('Ctrl Pts',(-35.1771834351375,0.0814827718919483,
135.721935591106));
#81918=CARTESIAN_POINT('Ctrl Pts',(-35.1849315031405,0.218673209167401,
135.719662385884));
#81919=CARTESIAN_POINT('Ctrl Pts',(-35.1926795711435,0.355731780701311,
135.711644448745));
#81920=CARTESIAN_POINT('Ctrl Pts',(-35.2004276391465,0.492144486851199,
135.697925459944));
#81921=CARTESIAN_POINT('Ctrl Pts',(-35.2081839418883,0.628702174048701,
135.684191890439));
#81922=CARTESIAN_POINT('Ctrl Pts',(-35.2159402446302,0.764612235014296,
135.664745204661));
#81923=CARTESIAN_POINT('Ctrl Pts',(-35.223696547372,0.899367268822977,135.639680832223));
#81924=CARTESIAN_POINT('Ctrl Pts',(-35.2314569898862,1.0341942254506,135.614603082175));
#81925=CARTESIAN_POINT('Ctrl Pts',(-35.2392174324004,1.16786454568972,135.583901758519));
#81926=CARTESIAN_POINT('Ctrl Pts',(-35.2469778749146,1.29988399358569,135.547722786505));
#81927=CARTESIAN_POINT('Ctrl Pts',(-35.25475077518,1.43211537081956,135.511485736793));
#81928=CARTESIAN_POINT('Ctrl Pts',(-35.2625236754455,1.5626902072905,135.469753586184));
#81929=CARTESIAN_POINT('Ctrl Pts',(-35.2702965757109,1.69113146918927,135.422721519057));
#81930=CARTESIAN_POINT('Ctrl Pts',(-35.2777869114729,1.81490356769382,135.377399186036));
#81931=CARTESIAN_POINT('Ctrl Pts',(-35.2852772472349,1.93669423536678,135.327155694687));
#81932=CARTESIAN_POINT('Ctrl Pts',(-35.2927675829969,2.05609835102641,135.272206030448));
#81933=CARTESIAN_POINT('Ctrl Pts',(-35.300541917116,2.18002971002338,135.215172932986));
#81934=CARTESIAN_POINT('Ctrl Pts',(-35.308316251235,2.30178254961261,135.152889085126));
#81935=CARTESIAN_POINT('Ctrl Pts',(-35.3160905853541,2.42087995647165,135.085543082593));
#81936=CARTESIAN_POINT('Ctrl Pts',(-35.3238553383012,2.53983058642062,135.018280077989));
#81937=CARTESIAN_POINT('Ctrl Pts',(-35.3316200912483,2.65613195804929,134.94596752237));
#81938=CARTESIAN_POINT('Ctrl Pts',(-35.3393848441954,2.76932774367032,134.868841754272));
#81939=CARTESIAN_POINT('Ctrl Pts',(-35.3471418850803,2.8824111016413,134.791792588574));
#81940=CARTESIAN_POINT('Ctrl Pts',(-35.3548989259652,2.99239469091629,134.709939942627));
#81941=CARTESIAN_POINT('Ctrl Pts',(-35.3626559668502,3.09884770555388,134.62356550344));
#81942=CARTESIAN_POINT('Ctrl Pts',(-35.3704071580904,3.20522044314504,134.537256199889));
#81943=CARTESIAN_POINT('Ctrl Pts',(-35.3781583493305,3.30806760314114,134.446432135675));
#81944=CARTESIAN_POINT('Ctrl Pts',(-35.3859095405706,3.40698855222042,134.351417435202));
#81945=CARTESIAN_POINT('Ctrl Pts',(-35.3936574373477,3.50586745725754,134.256443118512));
#81946=CARTESIAN_POINT('Ctrl Pts',(-35.4014053341248,3.60082318900819,134.157281978362));
#81947=CARTESIAN_POINT('Ctrl Pts',(-35.4091532309019,3.69148950096306,134.054297282607));
#81948=CARTESIAN_POINT('Ctrl Pts',(-35.4168995069859,3.78213684748001,133.95133412903));
#81949=CARTESIAN_POINT('Ctrl Pts',(-35.4246457830701,3.86849630070615,133.844549303965));
#81950=CARTESIAN_POINT('Ctrl Pts',(-35.4323920591542,3.95023997005212,133.734341375438));
#81951=CARTESIAN_POINT('Ctrl Pts',(-35.4401383924195,4.03198424281128,133.624132633381));
#81952=CARTESIAN_POINT('Ctrl Pts',(-35.4478847256848,4.10911243078851,133.510501051456));
#81953=CARTESIAN_POINT('Ctrl Pts',(-35.4556310589501,4.18133852673198,133.39387624551));
#81954=CARTESIAN_POINT('Ctrl Pts',(-35.4633791269531,4.25358079720886,133.277225322247));
#81955=CARTESIAN_POINT('Ctrl Pts',(-35.471127194956,4.3209185853696,133.157580173443));
#81956=CARTESIAN_POINT('Ctrl Pts',(-35.478875262959,4.38311081128926,133.035396851799));
#81957=CARTESIAN_POINT('Ctrl Pts',(-35.4866315657008,4.44536913584672,132.913083672267));
#81958=CARTESIAN_POINT('Ctrl Pts',(-35.4943878684427,4.50247079608237,132.788227280129));
#81959=CARTESIAN_POINT('Ctrl Pts',(-35.5021441711845,4.55422181703875,132.661306148191));
#81960=CARTESIAN_POINT('Ctrl Pts',(-35.5099046136987,4.60600045907328,132.534317274624));
#81961=CARTESIAN_POINT('Ctrl Pts',(-35.5176650562128,4.65242263914321,132.405261833109));
#81962=CARTESIAN_POINT('Ctrl Pts',(-35.525425498727,4.69334398168834,132.274634514515));
#81963=CARTESIAN_POINT('Ctrl Pts',(-35.5331983989924,4.73433101480536,132.143797501353));
#81964=CARTESIAN_POINT('Ctrl Pts',(-35.5409712992579,4.76979946316274,132.01138394659));
#81965=CARTESIAN_POINT('Ctrl Pts',(-35.5487441995233,4.79965569247943,131.877900694205));
#81966=CARTESIAN_POINT('Ctrl Pts',(-35.5562345352855,4.82842657265772,131.749269894265));
#81967=CARTESIAN_POINT('Ctrl Pts',(-35.5637248710476,4.85198613119707,131.619646121919));
#81968=CARTESIAN_POINT('Ctrl Pts',(-35.5712152068098,4.87029626353875,131.48948642197));
#81969=CARTESIAN_POINT('Ctrl Pts',(-35.5789895409288,4.88930063011309,131.354391677439));
#81970=CARTESIAN_POINT('Ctrl Pts',(-35.586763875048,4.90270984871404,131.218291624136));
#81971=CARTESIAN_POINT('Ctrl Pts',(-35.5945382091671,4.91042480696855,131.081689443345));
#81972=CARTESIAN_POINT('Ctrl Pts',(-35.6023029621142,4.91813025722651,130.945255612533));
#81973=CARTESIAN_POINT('Ctrl Pts',(-35.6100677150612,4.92015538836963,130.80832127211));
#81974=CARTESIAN_POINT('Ctrl Pts',(-35.6178324680083,4.91645238244269,130.671398090237));
#81975=CARTESIAN_POINT('Ctrl Pts',(-35.6255895088933,4.91275305439344,130.534610902399));
#81976=CARTESIAN_POINT('Ctrl Pts',(-35.6333465497784,4.90333692167235,130.397835239348));
#81977=CARTESIAN_POINT('Ctrl Pts',(-35.6411035906634,4.88820811440373,130.261585809034));
#81978=CARTESIAN_POINT('Ctrl Pts',(-35.6488547819035,4.87309071588636,130.125439125474));
#81979=CARTESIAN_POINT('Ctrl Pts',(-35.6566059731437,4.85226926055118,129.989818271777));
#81980=CARTESIAN_POINT('Ctrl Pts',(-35.6643571643838,4.82579989134293,129.855235509261));
#81981=CARTESIAN_POINT('Ctrl Pts',(-35.6721050611609,4.79934177232264,129.720709948009));
#81982=CARTESIAN_POINT('Ctrl Pts',(-35.6798529579379,4.76724058915932,129.587221983205));
#81983=CARTESIAN_POINT('Ctrl Pts',(-35.687600854715,4.72960400420158,129.455276103556));
#81984=CARTESIAN_POINT('Ctrl Pts',(-35.6953471307991,4.69197529200606,129.323357824142));
#81985=CARTESIAN_POINT('Ctrl Pts',(-35.7030934068832,4.6488135882908,129.192981364004));
#81986=CARTESIAN_POINT('Ctrl Pts',(-35.7108396829673,4.60027698675157,129.064638022534));
#81987=CARTESIAN_POINT('Ctrl Pts',(-35.7185860162327,4.55174002692618,128.936293733664));
#81988=CARTESIAN_POINT('Ctrl Pts',(-35.7263323494981,4.49782822840101,128.809982959098));
#81989=CARTESIAN_POINT('Ctrl Pts',(-35.7340786827635,4.43874844524977,128.686178542698));
#81990=CARTESIAN_POINT('Ctrl Pts',(-35.7418267507664,4.37965543159079,128.562346401157));
#81991=CARTESIAN_POINT('Ctrl Pts',(-35.7495748187694,4.31539229869233,128.441022087448));
#81992=CARTESIAN_POINT('Ctrl Pts',(-35.7573228867724,4.24621242702055,128.322654936564));
#81993=CARTESIAN_POINT('Ctrl Pts',(-35.7650791895143,4.17695903015782,128.204161983664));
#81994=CARTESIAN_POINT('Ctrl Pts',(-35.7728354922561,4.10277865347802,128.088632809967));
#81995=CARTESIAN_POINT('Ctrl Pts',(-35.780591794998,4.02396900150094,127.976489238338));
#81996=CARTESIAN_POINT('Ctrl Pts',(-35.7883522375122,3.94511728643959,127.864285812307));
#81997=CARTESIAN_POINT('Ctrl Pts',(-35.7961126800264,3.86163161070525,127.755471898977));
#81998=CARTESIAN_POINT('Ctrl Pts',(-35.8038731225406,3.77385013321886,127.650436358091));
#81999=CARTESIAN_POINT('Ctrl Pts',(-35.811646022806,3.68592774111206,127.545232204831));
#82000=CARTESIAN_POINT('Ctrl Pts',(-35.8194189230713,3.59369603004515,127.443818833979));
#82001=CARTESIAN_POINT('Ctrl Pts',(-35.8271918233368,3.49753081059526,127.346548984258));
#82002=CARTESIAN_POINT('Ctrl Pts',(-35.8346821590988,3.40486143909886,127.252815138584));
#82003=CARTESIAN_POINT('Ctrl Pts',(-35.8421724948608,3.30853980515541,127.162928999557));
#82004=CARTESIAN_POINT('Ctrl Pts',(-35.8496628306227,3.20892983705715,127.0771696695));
#82005=CARTESIAN_POINT('Ctrl Pts',(-35.8574371647418,3.10554312674165,126.988158748378));
#82006=CARTESIAN_POINT('Ctrl Pts',(-35.8652114988609,2.99828630753648,126.903311789761));
#82007=CARTESIAN_POINT('Ctrl Pts',(-35.87298583298,2.88752914744693,126.822984161471));
#82008=CARTESIAN_POINT('Ctrl Pts',(-35.8807505859271,2.77690848565869,126.742755529804));
#82009=CARTESIAN_POINT('Ctrl Pts',(-35.8885153388742,2.66279637972862,126.667035373814));
#82010=CARTESIAN_POINT('Ctrl Pts',(-35.8962800918213,2.54559746379843,126.596140493238));
#82011=CARTESIAN_POINT('Ctrl Pts',(-35.9040371327063,2.42851495148375,126.525316026456));
#82012=CARTESIAN_POINT('Ctrl Pts',(-35.9117941735913,2.30835206273338,126.459307498783));
#82013=CARTESIAN_POINT('Ctrl Pts',(-35.9195512144763,2.1855440683549,126.398389647646));
#82014=CARTESIAN_POINT('Ctrl Pts',(-35.9273024057165,2.06282868444028,126.337517735134));
#82015=CARTESIAN_POINT('Ctrl Pts',(-35.9350535969566,1.93747251404203,126.281729031055));
#82016=CARTESIAN_POINT('Ctrl Pts',(-35.9428047881967,1.80993688374789,126.231253190515));
#82017=CARTESIAN_POINT('Ctrl Pts',(-35.9505526849738,1.68245545949875,126.180798803553));
#82018=CARTESIAN_POINT('Ctrl Pts',(-35.958300581751,1.55279678051847,126.1356529325));
#82019=CARTESIAN_POINT('Ctrl Pts',(-35.9660484785281,1.42144348157484,126.095997686441));
#82020=CARTESIAN_POINT('Ctrl Pts',(-35.9737947546122,1.29011765890953,126.056350735405));
#82021=CARTESIAN_POINT('Ctrl Pts',(-35.9815410306963,1.15709829540054,126.022192237817));
#82022=CARTESIAN_POINT('Ctrl Pts',(-35.9892873067804,1.02288418864571,125.993654744296));
#82023=CARTESIAN_POINT('Ctrl Pts',(-35.9970336400458,0.888669091153008,
125.965117040117));
#82024=CARTESIAN_POINT('Ctrl Pts',(-36.0047799733111,0.753259615232364,
125.942200504113));
#82025=CARTESIAN_POINT('Ctrl Pts',(-36.0125263065764,0.617165387494643,
125.924986687749));
#82026=CARTESIAN_POINT('Ctrl Pts',(-36.0202743745794,0.48104068239823,125.90776901647));
#82027=CARTESIAN_POINT('Ctrl Pts',(-36.0280224425825,0.344231308145707,
125.896256655134));
#82028=CARTESIAN_POINT('Ctrl Pts',(-36.0357705105855,0.207252261324314,
125.890479304116));
#82029=CARTESIAN_POINT('Ctrl Pts',(-36.0435268133273,0.0701276315418873,
125.88469581286));
#82030=CARTESIAN_POINT('Ctrl Pts',(-36.0512831160691,-0.0671666397972779,
125.884659524318));
#82031=CARTESIAN_POINT('Ctrl Pts',(-36.059039418811,-0.204114744606161,
125.890347976808));
#82032=CARTESIAN_POINT('Ctrl Pts',(-36.0667998613252,-0.341135942742196,
125.896039465395));
#82033=CARTESIAN_POINT('Ctrl Pts',(-36.0745603038393,-0.477810216782652,
125.907461750745));
#82034=CARTESIAN_POINT('Ctrl Pts',(-36.0823207463535,-0.61362762485381,
125.92454051837));
#82035=CARTESIAN_POINT('Ctrl Pts',(-36.0900936466189,-0.749663059085706,
125.94164670235));
#82036=CARTESIAN_POINT('Ctrl Pts',(-36.0978665468844,-0.884838492875758,
125.964427448903));
#82037=CARTESIAN_POINT('Ctrl Pts',(-36.1056394471499,-1.01865402234965,
125.992757241845));
#82038=CARTESIAN_POINT('Ctrl Pts',(-36.1131297829118,-1.1476050202642,126.020057175454));
#82039=CARTESIAN_POINT('Ctrl Pts',(-36.1206201186737,-1.27529297066829,
126.052509640326));
#82040=CARTESIAN_POINT('Ctrl Pts',(-36.1281104544356,-1.40128634474042,
126.089959314904));
#82041=CARTESIAN_POINT('Ctrl Pts',(-36.1358847885547,-1.53205679588701,
126.128828905276));
#82042=CARTESIAN_POINT('Ctrl Pts',(-36.1436591226738,-1.66141587583529,
126.17320525131));
#82043=CARTESIAN_POINT('Ctrl Pts',(-36.1514334567928,-1.78886473493432,
126.222969341697));
#82044=CARTESIAN_POINT('Ctrl Pts',(-36.1591982097399,-1.91615652470476,
126.27267210229));
#82045=CARTESIAN_POINT('Ctrl Pts',(-36.166962962687,-2.04154241704425,126.327749254951));
#82046=CARTESIAN_POINT('Ctrl Pts',(-36.1747277156341,-2.1645371647229,126.388031607513));
#82047=CARTESIAN_POINT('Ctrl Pts',(-36.1824847565191,-2.28740975228439,
126.448254086793));
#82048=CARTESIAN_POINT('Ctrl Pts',(-36.1902417974041,-2.40789557258581,
126.513671306734));
#82049=CARTESIAN_POINT('Ctrl Pts',(-36.1979988382891,-2.52552820674429,
126.584065563966));
#82050=CARTESIAN_POINT('Ctrl Pts',(-36.2057500295292,-2.64307213321831,
126.654406736342));
#82051=CARTESIAN_POINT('Ctrl Pts',(-36.2135012207693,-2.75776682207294,
126.7297172755));
#82052=CARTESIAN_POINT('Ctrl Pts',(-36.2212524120094,-2.86916969967449,
126.80973318851));
#82053=CARTESIAN_POINT('Ctrl Pts',(-36.2290003087865,-2.98052522808114,
126.889715092622));
#82054=CARTESIAN_POINT('Ctrl Pts',(-36.2367482055636,-3.08859141107396,
126.974398165319));
#82055=CARTESIAN_POINT('Ctrl Pts',(-36.2444961023407,-3.19295415923958,
127.063474786711));
#82056=CARTESIAN_POINT('Ctrl Pts',(-36.2522423784248,-3.29729507696807,
127.152532775193));
#82057=CARTESIAN_POINT('Ctrl Pts',(-36.2599886545088,-3.39793380356293,
127.245982230703));
#82058=CARTESIAN_POINT('Ctrl Pts',(-36.2677349305929,-3.49448920814908,
127.343475147541));
#82059=CARTESIAN_POINT('Ctrl Pts',(-36.2754812638583,-3.59104532548529,
127.44096878405));
#82060=CARTESIAN_POINT('Ctrl Pts',(-36.2832275971236,-3.68351778555101,
127.542505663659));
#82061=CARTESIAN_POINT('Ctrl Pts',(-36.290973930389,-3.77156251115694,127.647701103628));
#82062=CARTESIAN_POINT('Ctrl Pts',(-36.298721998392,-3.8596269537687,127.752920101386));
#82063=CARTESIAN_POINT('Ctrl Pts',(-36.3064700663949,-3.9432614379467,127.86179899008));
#82064=CARTESIAN_POINT('Ctrl Pts',(-36.3142181343979,-4.02216260768733,
127.973920542274));
#82065=CARTESIAN_POINT('Ctrl Pts',(-36.3219744371397,-4.1011476345301,128.086161258587));
#82066=CARTESIAN_POINT('Ctrl Pts',(-36.3297307398815,-4.17538907236613,
128.201651202597));
#82067=CARTESIAN_POINT('Ctrl Pts',(-36.3374870426233,-4.24462701197451,
128.319944269263));
#82068=CARTESIAN_POINT('Ctrl Pts',(-36.3452474851375,-4.31390190595607,
128.4383004725));
#82069=CARTESIAN_POINT('Ctrl Pts',(-36.3530079276517,-4.37816779736918,
128.559462434303));
#82070=CARTESIAN_POINT('Ctrl Pts',(-36.3607683701658,-4.43721157305724,
128.682960957335));
#82071=CARTESIAN_POINT('Ctrl Pts',(-36.3685412704313,-4.49635013105569,
128.806657731161));
#82072=CARTESIAN_POINT('Ctrl Pts',(-36.3763141706967,-4.55024966760307,
128.932698201938));
#82073=CARTESIAN_POINT('Ctrl Pts',(-36.3840870709621,-4.59874557276672,
129.060593941815));
#82074=CARTESIAN_POINT('Ctrl Pts',(-36.3915774067242,-4.64547852962464,
129.1838403494));
#82075=CARTESIAN_POINT('Ctrl Pts',(-36.3990677424864,-4.68719380797315,
129.308809188348));
#82076=CARTESIAN_POINT('Ctrl Pts',(-36.4065580782486,-4.72378883236707,
129.435053446145));
#82077=CARTESIAN_POINT('Ctrl Pts',(-36.4094608226833,-4.73797057358291,
129.483977129726));
#82078=CARTESIAN_POINT('Ctrl Pts',(-36.412363567118,-4.75139468639191,129.533129588106));
#82079=CARTESIAN_POINT('Ctrl Pts',(-36.4152663115528,-4.76405452823402,
129.582490119308));
#82080=CARTESIAN_POINT('Ctrl Pts',(-34.6650476268334,-4.76405452823403,
129.582490119308));
#82081=CARTESIAN_POINT('Ctrl Pts',(-34.6728041571113,-4.79811111157992,
129.715276220893));
#82082=CARTESIAN_POINT('Ctrl Pts',(-34.6805606873892,-4.82658522312024,
129.84938326537));
#82083=CARTESIAN_POINT('Ctrl Pts',(-34.688317217667,-4.84940066901136,129.984301952657));
#82084=CARTESIAN_POINT('Ctrl Pts',(-34.6961211087191,-4.87235542425136,
130.120044443019));
#82085=CARTESIAN_POINT('Ctrl Pts',(-34.7039249997712,-4.88958214057927,
130.256608121163));
#82086=CARTESIAN_POINT('Ctrl Pts',(-34.7117288908233,-4.90105633548391,
130.393471509761));
#82087=CARTESIAN_POINT('Ctrl Pts',(-34.7195327818754,-4.91253053038855,
130.530334898358));
#82088=CARTESIAN_POINT('Ctrl Pts',(-34.7273366729275,-4.91825224716583,
130.667497598343));
#82089=CARTESIAN_POINT('Ctrl Pts',(-34.7351405639796,-4.91824999933744,
130.804441346932));
#82090=CARTESIAN_POINT('',(-34.3898612108785,-4.91451134145429,130.808502671262));
#82091=CARTESIAN_POINT('Ctrl Pts',(-34.31993947219,-4.764054528234,129.582490119308));
#82092=CARTESIAN_POINT('Ctrl Pts',(-34.3276536921924,-4.79801892200384,
129.714916775135));
#82093=CARTESIAN_POINT('Ctrl Pts',(-34.3353679121948,-4.82646487016461,
129.848789404461));
#82094=CARTESIAN_POINT('Ctrl Pts',(-34.3430821321972,-4.84928307828942,
129.983606885247));
#82095=CARTESIAN_POINT('Ctrl Pts',(-34.3508783494962,-4.87234382958494,
130.119857390881));
#82096=CARTESIAN_POINT('Ctrl Pts',(-34.3586745667951,-4.88965640799597,
130.25707255254));
#82097=CARTESIAN_POINT('Ctrl Pts',(-34.3664707840941,-4.90116138148723,
130.394726420851));
#82098=CARTESIAN_POINT('Ctrl Pts',(-34.3742670013931,-4.91266635497847,
130.532380289162));
#82099=CARTESIAN_POINT('Ctrl Pts',(-34.3820632186921,-4.91836370896115,
130.670472449304));
#82100=CARTESIAN_POINT('Ctrl Pts',(-34.3898594359911,-4.9182482795467,130.808474403648));
#82101=CARTESIAN_POINT('Ctrl Pts',(-34.3898612383632,-4.91445347382228,
130.808503108995));
#82102=CARTESIAN_POINT('Ctrl Pts',(-34.4189120614814,-4.91848817089666,
131.322342766133));
#82103=CARTESIAN_POINT('Ctrl Pts',(-34.5407787592039,-4.6074576551442,133.47310541816));
#82104=CARTESIAN_POINT('Ctrl Pts',(-34.7554613315307,-1.48508419419027,
136.428967694209));
#82105=CARTESIAN_POINT('Ctrl Pts',(-35.0339089553435,3.92941694857211,135.094041523499));
#82106=CARTESIAN_POINT('Ctrl Pts',(-35.3123565791566,5.73297587828731,129.817108162799));
#82107=CARTESIAN_POINT('Ctrl Pts',(-35.5908042029694,2.26821004729653,125.447411578065));
#82108=CARTESIAN_POINT('Ctrl Pts',(-35.8432465388909,-2.7626746087458,125.948835401795));
#82109=CARTESIAN_POINT('Ctrl Pts',(-36.0028730002082,-4.45755648309024,
128.442094762146));
#82110=CARTESIAN_POINT('Ctrl Pts',(-36.0696835869212,-4.76181538791761,
129.583090555045));
#82111=CARTESIAN_POINT('Origin',(213.235140564004,0.,130.804360617566));
#82112=CARTESIAN_POINT('',(-38.1653731028237,-4.76405452823409,129.582490119308));
#82113=CARTESIAN_POINT('',(-37.8199424078995,-4.77192532739619,129.580475997939));
#82114=CARTESIAN_POINT('',(213.235140564004,-4.76405452823405,129.582490119308));
#82115=CARTESIAN_POINT('',(-36.4851405639765,-4.91824802675748,130.799954962542));
#82116=CARTESIAN_POINT('Ctrl Pts',(-36.4851405640085,-4.91824802675798,
130.799954963109));
#82117=CARTESIAN_POINT('Ctrl Pts',(-36.4928276338665,-4.91836979410064,
130.935889816499));
#82118=CARTESIAN_POINT('Ctrl Pts',(-36.5005147037245,-4.91285169280305,
131.071941831601));
#82119=CARTESIAN_POINT('Ctrl Pts',(-36.5082017735825,-4.90169143817275,
131.207602613697));
#82120=CARTESIAN_POINT('Ctrl Pts',(-36.5158857677113,-4.89053564895279,
131.343209115575));
#82121=CARTESIAN_POINT('Ctrl Pts',(-36.5235697618401,-4.87374222681335,
131.478424299786));
#82122=CARTESIAN_POINT('Ctrl Pts',(-36.5312537559689,-4.85136095628237,
131.612741675211));
#82123=CARTESIAN_POINT('Ctrl Pts',(-36.538936339408,-4.82898379468568,131.747034391568));
#82124=CARTESIAN_POINT('Ctrl Pts',(-36.5466189228472,-4.80102088990743,
131.880429234494));
#82125=CARTESIAN_POINT('Ctrl Pts',(-36.5543015062863,-4.76757360973981,
132.012427229228));
#82126=CARTESIAN_POINT('Ctrl Pts',(-36.5619844103365,-4.7341249337437,132.144430732529));
#82127=CARTESIAN_POINT('Ctrl Pts',(-36.5696673143867,-4.69519152486053,
132.275036885866));
#82128=CARTESIAN_POINT('Ctrl Pts',(-36.5773502184369,-4.65092523053898,
132.403759742999));
#82129=CARTESIAN_POINT('Ctrl Pts',(-36.5850351743359,-4.60664711415884,
132.532516977737));
#82130=CARTESIAN_POINT('Ctrl Pts',(-36.592720130235,-4.55703340891382,132.659389539654));
#82131=CARTESIAN_POINT('Ctrl Pts',(-36.600405086134,-4.50228473464615,132.783909866934));
#82132=CARTESIAN_POINT('Ctrl Pts',(-36.6080983775956,-4.44747667669282,
132.908565256406));
#82133=CARTESIAN_POINT('Ctrl Pts',(-36.6157916690573,-4.38752268863135,
133.030862952023));
#82134=CARTESIAN_POINT('Ctrl Pts',(-36.623484960519,-4.32267032552709,133.150358128074));
#82135=CARTESIAN_POINT('Ctrl Pts',(-36.6311827738555,-4.25777984424232,
133.269923539632));
#82136=CARTESIAN_POINT('Ctrl Pts',(-36.638880587192,-4.18798545839921,133.386682810443));
#82137=CARTESIAN_POINT('Ctrl Pts',(-36.6465784005286,-4.11357834835301,
133.500219707812));
#82138=CARTESIAN_POINT('Ctrl Pts',(-36.6542880192234,-4.03905712764318,
133.613930725244));
#82139=CARTESIAN_POINT('Ctrl Pts',(-36.6619976379181,-3.95990928697845,
133.724409177488));
#82140=CARTESIAN_POINT('Ctrl Pts',(-36.6697072566129,-3.87646695557892,
133.831271089451));
#82141=CARTESIAN_POINT('Ctrl Pts',(-36.6748067384291,-3.82127451759782,
133.901954270872));
#82142=CARTESIAN_POINT('Ctrl Pts',(-36.6799062202452,-3.7642040135486,133.971055898711));
#82143=CARTESIAN_POINT('Ctrl Pts',(-36.6850057020614,-3.70536015296158,
134.038473973549));
#82144=CARTESIAN_POINT('Ctrl Pts',(-36.6927800361805,-3.61565067863599,
134.141255130212));
#82145=CARTESIAN_POINT('Ctrl Pts',(-36.7005543702996,-3.521519376323,134.240463645861));
#82146=CARTESIAN_POINT('Ctrl Pts',(-36.7083287044187,-3.423281844015,134.335695277286));
#82147=CARTESIAN_POINT('Ctrl Pts',(-36.7160934573658,-3.32516538068582,
134.430809544235));
#82148=CARTESIAN_POINT('Ctrl Pts',(-36.7238582103129,-3.22295303439132,
134.521956409283));
#82149=CARTESIAN_POINT('Ctrl Pts',(-36.73162296326,-3.11700038939506,134.608764859364));
#82150=CARTESIAN_POINT('Ctrl Pts',(-36.739380004145,-3.01115297805947,134.695487090068));
#82151=CARTESIAN_POINT('Ctrl Pts',(-36.74713704503,-2.90157296134098,134.777879234684));
#82152=CARTESIAN_POINT('Ctrl Pts',(-36.754894085915,-2.78865221894935,134.855607569339));
#82153=CARTESIAN_POINT('Ctrl Pts',(-36.7626452771551,-2.67581663096857,
134.933277288451));
#82154=CARTESIAN_POINT('Ctrl Pts',(-36.7703964683952,-2.55964565250498,
135.006289977227));
#82155=CARTESIAN_POINT('Ctrl Pts',(-36.7781476596353,-2.44056335273725,
135.074352840483));
#82156=CARTESIAN_POINT('Ctrl Pts',(-36.7858955564124,-2.32153166612289,
135.142386775207));
#82157=CARTESIAN_POINT('Ctrl Pts',(-36.7936434531895,-2.19959145799996,
135.205474875124));
#82158=CARTESIAN_POINT('Ctrl Pts',(-36.8013913499666,-2.0751946370679,135.263368386205));
#82159=CARTESIAN_POINT('Ctrl Pts',(-36.8091376260507,-1.95082383726926,
135.321249787212));
#82160=CARTESIAN_POINT('Ctrl Pts',(-36.8168839021347,-1.82399780101219,
135.373938595825));
#82161=CARTESIAN_POINT('Ctrl Pts',(-36.8246301782188,-1.69519146881032,
135.421232821404));
#82162=CARTESIAN_POINT('Ctrl Pts',(-36.8323765114841,-1.56638418578972,
135.468527396098));
#82163=CARTESIAN_POINT('Ctrl Pts',(-36.8401228447495,-1.43559694466283,
135.510427173542));
#82164=CARTESIAN_POINT('Ctrl Pts',(-36.8478691780148,-1.30332264235544,
135.546779109477));
#82165=CARTESIAN_POINT('Ctrl Pts',(-36.8556172460178,-1.17101871813535,
135.583139186177));
#82166=CARTESIAN_POINT('Ctrl Pts',(-36.8633653140207,-1.03722744698512,
135.613948845551));
#82167=CARTESIAN_POINT('Ctrl Pts',(-36.8711133820236,-0.902454399342149,
135.639105607698));
#82168=CARTESIAN_POINT('Ctrl Pts',(-36.8788696847655,-0.767538113299777,
135.664289106751));
#82169=CARTESIAN_POINT('Ctrl Pts',(-36.8866259875073,-0.631638351313373,
135.683807635165));
#82170=CARTESIAN_POINT('Ctrl Pts',(-36.8943822902492,-0.495268889113341,
135.697610232084));
#82171=CARTESIAN_POINT('Ctrl Pts',(-36.9021427327633,-0.358826642425143,
135.711420195864));
#82172=CARTESIAN_POINT('Ctrl Pts',(-36.9099031752775,-0.221914586089837,
135.719508126199));
#82173=CARTESIAN_POINT('Ctrl Pts',(-36.9176636177917,-0.0850480471087371,
135.721875222748));
#82174=CARTESIAN_POINT('Ctrl Pts',(-36.9254365180571,0.0520382021909894,
135.724246119172));
#82175=CARTESIAN_POINT('Ctrl Pts',(-36.9332094183226,0.189078397050262,
135.720877839682));
#82176=CARTESIAN_POINT('Ctrl Pts',(-36.940982318588,0.325559881160564,135.711823691933));
#82177=CARTESIAN_POINT('Ctrl Pts',(-36.9484726543501,0.457079919549005,
135.703098685261));
#82178=CARTESIAN_POINT('Ctrl Pts',(-36.9559629901122,0.588080856759524,
135.689094057259));
#82179=CARTESIAN_POINT('Ctrl Pts',(-36.9634533258743,0.718113490108519,
135.669902322024));
#82180=CARTESIAN_POINT('Ctrl Pts',(-36.9712276599934,0.853076350271984,
135.649982926316));
#82181=CARTESIAN_POINT('Ctrl Pts',(-36.9790019941125,0.987423552403778,
135.624412221754));
#82182=CARTESIAN_POINT('Ctrl Pts',(-36.9867763282316,1.12064440681875,135.593237226539));
#82183=CARTESIAN_POINT('Ctrl Pts',(-36.9945410811787,1.25370107843695,135.562100651719));
#82184=CARTESIAN_POINT('Ctrl Pts',(-37.0023058341258,1.38563378726269,135.525373616921));
#82185=CARTESIAN_POINT('Ctrl Pts',(-37.0100705870729,1.51593818751635,135.483154743634));
#82186=CARTESIAN_POINT('Ctrl Pts',(-37.0178276279579,1.64611316760271,135.440977802727));
#82187=CARTESIAN_POINT('Ctrl Pts',(-37.0255846688429,1.77466268801198,135.393319997899));
#82188=CARTESIAN_POINT('Ctrl Pts',(-37.0333417097279,1.90109415684289,135.340330642745));
#82189=CARTESIAN_POINT('Ctrl Pts',(-37.041092900968,2.02743028271915,135.287381247275));
#82190=CARTESIAN_POINT('Ctrl Pts',(-37.0488440922081,2.15165117710705,135.229108454678));
#82191=CARTESIAN_POINT('Ctrl Pts',(-37.0565952834482,2.27328128337633,135.165710783415));
#82192=CARTESIAN_POINT('Ctrl Pts',(-37.0643431802253,2.39485969360619,135.102340057853));
#82193=CARTESIAN_POINT('Ctrl Pts',(-37.0720910770023,2.51384915985902,135.033848966251));
#82194=CARTESIAN_POINT('Ctrl Pts',(-37.0798389737794,2.6297961306363,134.960483254567));
#82195=CARTESIAN_POINT('Ctrl Pts',(-37.0875852498635,2.74571884780682,134.887132889408));
#82196=CARTESIAN_POINT('Ctrl Pts',(-37.0953315259476,2.85860000521263,134.808910141256));
#82197=CARTESIAN_POINT('Ctrl Pts',(-37.1030778020317,2.96801294545895,134.726105410141));
#82198=CARTESIAN_POINT('Ctrl Pts',(-37.110824135297,3.07742669336659,134.64330006778));
#82199=CARTESIAN_POINT('Ctrl Pts',(-37.1185704685623,3.18337186127836,134.5559129109));
#82200=CARTESIAN_POINT('Ctrl Pts',(-37.1263168018276,3.28545326589827,134.464275903484));
#82201=CARTESIAN_POINT('Ctrl Pts',(-37.1340648698306,3.38755753094068,134.372618374597));
#82202=CARTESIAN_POINT('Ctrl Pts',(-37.1418129378335,3.48579602003702,134.276709362472));
#82203=CARTESIAN_POINT('Ctrl Pts',(-37.1495610058365,3.57980924077354,134.176918824947));
#82204=CARTESIAN_POINT('Ctrl Pts',(-37.1573173085783,3.67392237988009,134.077022228851));
#82205=CARTESIAN_POINT('Ctrl Pts',(-37.1650736113202,3.76380101151736,133.973236151585));
#82206=CARTESIAN_POINT('Ctrl Pts',(-37.172829914062,3.8491245525434,133.865965301634));
#82207=CARTESIAN_POINT('Ctrl Pts',(-37.1805903565762,3.93449363331256,133.758637198001));
#82208=CARTESIAN_POINT('Ctrl Pts',(-37.1883507990903,4.0153025488774,133.647820931359));
#82209=CARTESIAN_POINT('Ctrl Pts',(-37.1961112416045,4.09127376171465,133.533950709357));
#82210=CARTESIAN_POINT('Ctrl Pts',(-37.2038841418699,4.16736693028706,133.419897692766));
#82211=CARTESIAN_POINT('Ctrl Pts',(-37.2116570421354,4.23860667407224,133.302781258312));
#82212=CARTESIAN_POINT('Ctrl Pts',(-37.2194299424008,4.3047607390515,133.183061532356));
#82213=CARTESIAN_POINT('Ctrl Pts',(-37.2269202781629,4.36850993713755,133.067693919992));
#82214=CARTESIAN_POINT('Ctrl Pts',(-37.234410613925,4.42753665340542,132.94990927786));
#82215=CARTESIAN_POINT('Ctrl Pts',(-37.2419009496871,4.48167591756359,132.83013553903));
#82216=CARTESIAN_POINT('Ctrl Pts',(-37.2496752838062,4.53786788837688,132.705820542489));
#82217=CARTESIAN_POINT('Ctrl Pts',(-37.2574496179253,4.58897247479398,132.57896884601));
#82218=CARTESIAN_POINT('Ctrl Pts',(-37.2652239520444,4.63475319430905,132.450035521775));
#82219=CARTESIAN_POINT('Ctrl Pts',(-37.2729887049914,4.68047749317892,132.321261096338));
#82220=CARTESIAN_POINT('Ctrl Pts',(-37.2807534579385,4.72089085039618,132.190410512459));
#82221=CARTESIAN_POINT('Ctrl Pts',(-37.2885182108856,4.75580362779796,132.057961397848));
#82222=CARTESIAN_POINT('Ctrl Pts',(-37.2962752517706,4.79068172933704,131.925643833565));
#82223=CARTESIAN_POINT('Ctrl Pts',(-37.3040322926557,4.82007002417415,131.791731273717));
#82224=CARTESIAN_POINT('Ctrl Pts',(-37.3117893335407,4.84382787610935,131.656718857466));
#82225=CARTESIAN_POINT('Ctrl Pts',(-37.3195405247808,4.86756781206351,131.521808255129));
#82226=CARTESIAN_POINT('Ctrl Pts',(-37.3272917160209,4.88568568896112,131.385799830772));
#82227=CARTESIAN_POINT('Ctrl Pts',(-37.335042907261,4.89809147603133,131.249200987732));
#82228=CARTESIAN_POINT('Ctrl Pts',(-37.3427908040381,4.91049199031114,131.112660202844));
#82229=CARTESIAN_POINT('Ctrl Pts',(-37.3505387008151,4.91718520816626,130.975529886929));
#82230=CARTESIAN_POINT('Ctrl Pts',(-37.3582865975922,4.918132726969,130.838324457403));
#82231=CARTESIAN_POINT('Ctrl Pts',(-37.3660328736763,4.91908004757123,130.701147728295));
#82232=CARTESIAN_POINT('Ctrl Pts',(-37.3737791497605,4.91428405702093,130.563896307536));
#82233=CARTESIAN_POINT('Ctrl Pts',(-37.3815254258446,4.90375845834459,130.427086122385));
#82234=CARTESIAN_POINT('Ctrl Pts',(-37.3892717591099,4.89323278197069,130.290274927333));
#82235=CARTESIAN_POINT('Ctrl Pts',(-37.3970180923752,4.87697744306541,130.153905364202));
#82236=CARTESIAN_POINT('Ctrl Pts',(-37.4047644256406,4.85505812610579,130.018489346534));
#82237=CARTESIAN_POINT('Ctrl Pts',(-37.4125124936435,4.83313390046718,129.883043003387));
#82238=CARTESIAN_POINT('Ctrl Pts',(-37.4202605616464,4.80554323524706,129.74855101649));
#82239=CARTESIAN_POINT('Ctrl Pts',(-37.4280086296494,4.77240307202143,129.61551580824));
#82240=CARTESIAN_POINT('Ctrl Pts',(-37.4357649323912,4.7392276870358,129.482339208588));
#82241=CARTESIAN_POINT('Ctrl Pts',(-37.4435212351331,4.70049111666466,129.350622860418));
#82242=CARTESIAN_POINT('Ctrl Pts',(-37.4512775378749,4.65636057060059,129.220855234229));
#82243=CARTESIAN_POINT('Ctrl Pts',(-37.4590379803891,4.61220647073529,129.091018347152));
#82244=CARTESIAN_POINT('Ctrl Pts',(-37.4667984229033,4.56265279986055,128.963132618902));
#82245=CARTESIAN_POINT('Ctrl Pts',(-37.4745588654175,4.50791485335659,128.837666249499));
#82246=CARTESIAN_POINT('Ctrl Pts',(-37.4823317656829,4.45308903664149,128.711998470341));
#82247=CARTESIAN_POINT('Ctrl Pts',(-37.4901046659483,4.39306248506888,128.58875816273));
#82248=CARTESIAN_POINT('Ctrl Pts',(-37.4978775662137,4.32809677700681,128.468389438086));
#82249=CARTESIAN_POINT('Ctrl Pts',(-37.5053679019758,4.26549273607101,128.352396419772));
#82250=CARTESIAN_POINT('Ctrl Pts',(-37.512858237738,4.19830256276164,128.23907009553));
#82251=CARTESIAN_POINT('Ctrl Pts',(-37.5203485735001,4.12679711881795,128.128780567817));
#82252=CARTESIAN_POINT('Ctrl Pts',(-37.5281229076191,4.05258052423415,128.014309379139));
#82253=CARTESIAN_POINT('Ctrl Pts',(-37.5358972417382,3.97347987661718,127.902747202758));
#82254=CARTESIAN_POINT('Ctrl Pts',(-37.5436715758573,3.88975021651057,127.794538975731));
#82255=CARTESIAN_POINT('Ctrl Pts',(-37.5514363288044,3.80612374572714,127.686464105674));
#82256=CARTESIAN_POINT('Ctrl Pts',(-37.5592010817515,3.7178798503558,127.581735266892));
#82257=CARTESIAN_POINT('Ctrl Pts',(-37.5669658346985,3.62531786805777,127.480770176786));
#82258=CARTESIAN_POINT('Ctrl Pts',(-37.5747228755835,3.53284781962546,127.379905366632));
#82259=CARTESIAN_POINT('Ctrl Pts',(-37.5824799164686,3.43606848163346,127.282797152272));
#82260=CARTESIAN_POINT('Ctrl Pts',(-37.5902369573535,3.33532041138046,127.189831489736));
#82261=CARTESIAN_POINT('Ctrl Pts',(-37.5979881485937,3.23464831603053,127.09693593333));
#82262=CARTESIAN_POINT('Ctrl Pts',(-37.6057393398338,3.13001373167596,127.008176974815));
#82263=CARTESIAN_POINT('Ctrl Pts',(-37.6134905310739,3.02179488728543,126.923904623527));
#82264=CARTESIAN_POINT('Ctrl Pts',(-37.621238427851,2.91362203879075,126.839668090236));
#82265=CARTESIAN_POINT('Ctrl Pts',(-37.628986324628,2.80186826802107,126.759914611147));
#82266=CARTESIAN_POINT('Ctrl Pts',(-37.6367342214051,2.68694561135834,126.684954550655));
#82267=CARTESIAN_POINT('Ctrl Pts',(-37.6444804974892,2.57204699403793,126.610010170192));
#82268=CARTESIAN_POINT('Ctrl Pts',(-37.6522267735734,2.45398113654999,126.539857427399));
#82269=CARTESIAN_POINT('Ctrl Pts',(-37.6599730496575,2.33318950993037,126.474763664817));
#82270=CARTESIAN_POINT('Ctrl Pts',(-37.6677193829229,2.21239699165456,126.409669421728));
#82271=CARTESIAN_POINT('Ctrl Pts',(-37.6754657161882,2.08887900826863,126.34963441884));
#82272=CARTESIAN_POINT('Ctrl Pts',(-37.6832120494535,1.96310175119711,126.294880095716));
#82273=CARTESIAN_POINT('Ctrl Pts',(-37.6909601174565,1.83729632718076,126.24011351074));
#82274=CARTESIAN_POINT('Ctrl Pts',(-37.6987081854595,1.70923098110191,126.190630114731));
#82275=CARTESIAN_POINT('Ctrl Pts',(-37.7064562534625,1.57939162493083,126.146603093006));
#82276=CARTESIAN_POINT('Ctrl Pts',(-37.7142125562043,1.4494142739469,126.102529278838));
#82277=CARTESIAN_POINT('Ctrl Pts',(-37.7219688589462,1.31765951735152,126.063923549032));
#82278=CARTESIAN_POINT('Ctrl Pts',(-37.7297251616881,1.18462870013296,126.030909255572));
#82279=CARTESIAN_POINT('Ctrl Pts',(-37.7374856042022,1.05152688036194,125.99787734139));
#82280=CARTESIAN_POINT('Ctrl Pts',(-37.7452460467163,0.91714802575034,125.970442888229));
#82281=CARTESIAN_POINT('Ctrl Pts',(-37.7530064892305,0.782002418645201,
125.948677835533));
#82282=CARTESIAN_POINT('Ctrl Pts',(-37.7607793894959,0.646639863813688,
125.926877843642));
#82283=CARTESIAN_POINT('Ctrl Pts',(-37.7685522897614,0.510508485318408,
125.910765484945));
#82284=CARTESIAN_POINT('Ctrl Pts',(-37.7763251900268,0.374123316172745,
125.900360739222));
#82285=CARTESIAN_POINT('Ctrl Pts',(-37.7838155257889,0.242696091459036,
125.890334232215));
#82286=CARTESIAN_POINT('Ctrl Pts',(-37.7913058615508,0.111033515422634,
125.885607581543));
#82287=CARTESIAN_POINT('Ctrl Pts',(-37.7987961973129,-0.0204066268725122,
125.886152952971));
#82288=CARTESIAN_POINT('Ctrl Pts',(-37.806570531432,-0.156830362113137,
125.886719002323));
#82289=CARTESIAN_POINT('Ctrl Pts',(-37.8143448655511,-0.293446612885683,
125.892966536018));
#82290=CARTESIAN_POINT('Ctrl Pts',(-37.8221191996702,-0.429743185397317,
125.904921480572));
#82291=CARTESIAN_POINT('Ctrl Pts',(-37.8298839526173,-0.565871784564505,
125.916861691726));
#82292=CARTESIAN_POINT('Ctrl Pts',(-37.8376487055644,-0.701681103632381,
125.934495284593));
#82293=CARTESIAN_POINT('Ctrl Pts',(-37.8454134585115,-0.836657905802827,
125.95779620438));
#82294=CARTESIAN_POINT('Ctrl Pts',(-37.8531704993965,-0.971500647110885,
125.981073981366));
#82295=CARTESIAN_POINT('Ctrl Pts',(-37.8609275402815,-1.1055121342515,126.01000781749));
#82296=CARTESIAN_POINT('Ctrl Pts',(-37.8686845811665,-1.23818357194774,
126.044519810915));
#82297=CARTESIAN_POINT('Ctrl Pts',(-37.8764357724066,-1.37075496107898,
126.079005778577));
#82298=CARTESIAN_POINT('Ctrl Pts',(-37.8841869636466,-1.50198793534603,
126.119061432664));
#82299=CARTESIAN_POINT('Ctrl Pts',(-37.8919381548866,-1.63138357998536,
126.164557747028));
#82300=CARTESIAN_POINT('Ctrl Pts',(-37.8996860516637,-1.76072422802539,
126.210034724245));
#82301=CARTESIAN_POINT('Ctrl Pts',(-37.9074339484408,-1.88822873155778,
126.26094763309));
#82302=CARTESIAN_POINT('Ctrl Pts',(-37.9151818452179,-2.01341325649687,
126.317117575222));
#82303=CARTESIAN_POINT('Ctrl Pts',(-37.922928121302,-2.13857159553202,126.373275767813));
#82304=CARTESIAN_POINT('Ctrl Pts',(-37.9306743973861,-2.26141056476401,
126.434688646461));
#82305=CARTESIAN_POINT('Ctrl Pts',(-37.9384206734702,-2.38146661546252,
126.501129294254));
#82306=CARTESIAN_POINT('Ctrl Pts',(-37.9461670067355,-2.50152355238737,
126.567570432496));
#82307=CARTESIAN_POINT('Ctrl Pts',(-37.9539133400008,-2.61879718771126,
126.639039224632));
#82308=CARTESIAN_POINT('Ctrl Pts',(-37.9616596732662,-2.73284923020659,
126.715263144106));
#82309=CARTESIAN_POINT('Ctrl Pts',(-37.9694077412691,-2.84692681386574,
126.791504133397));
#82310=CARTESIAN_POINT('Ctrl Pts',(-37.9771558092721,-2.95778104409628,
126.87250215181));
#82311=CARTESIAN_POINT('Ctrl Pts',(-37.9849038772751,-3.06500356789617,
126.957941998736));
#82312=CARTESIAN_POINT('Ctrl Pts',(-37.9926601800169,-3.17234004907076,
127.043472652148));
#82313=CARTESIAN_POINT('Ctrl Pts',(-38.0004164827588,-3.2760368071569,127.133454320402));
#82314=CARTESIAN_POINT('Ctrl Pts',(-38.0081727855006,-3.37571907342281,
127.227531882523));
#82315=CARTESIAN_POINT('Ctrl Pts',(-38.0159332280148,-3.47545454311545,
127.321659656671));
#82316=CARTESIAN_POINT('Ctrl Pts',(-38.0236936705289,-3.57117097884798,
127.419887400805));
#82317=CARTESIAN_POINT('Ctrl Pts',(-38.0314541130431,-3.66253203585477,
127.521824684962));
#82318=CARTESIAN_POINT('Ctrl Pts',(-38.0392270133085,-3.75403975374105,
127.623925607897));
#82319=CARTESIAN_POINT('Ctrl Pts',(-38.0469999135739,-3.84117787270947,
127.729747668624));
#82320=CARTESIAN_POINT('Ctrl Pts',(-38.0547728138393,-3.92365119527987,
127.838868354842));
#82321=CARTESIAN_POINT('Ctrl Pts',(-38.0622631496015,-4.00312640483864,
127.944022229259));
#82322=CARTESIAN_POINT('Ctrl Pts',(-38.0697534853637,-4.07826990830115,
128.052238813215));
#82323=CARTESIAN_POINT('Ctrl Pts',(-38.0772438211259,-4.14885767938843,
128.163117914087));
#82324=CARTESIAN_POINT('Ctrl Pts',(-38.0852101053287,-4.22393071530854,
128.28104245816));
#82325=CARTESIAN_POINT('Ctrl Pts',(-38.0931763895316,-4.29407895943621,
128.402337430133));
#82326=CARTESIAN_POINT('Ctrl Pts',(-38.1011426737345,-4.35899411609593,
128.52656489399));
#82327=CARTESIAN_POINT('Ctrl Pts',(-38.109098762519,-4.42382619297043,128.650633368922));
#82328=CARTESIAN_POINT('Ctrl Pts',(-38.1170548513034,-4.48343834476155,
128.777626545651));
#82329=CARTESIAN_POINT('Ctrl Pts',(-38.1250109400879,-4.53756546112957,
128.907077626427));
#82330=CARTESIAN_POINT('Ctrl Pts',(-38.1329551346756,-4.59161165851954,
129.036335180376));
#82331=CARTESIAN_POINT('Ctrl Pts',(-38.1408993292633,-4.64018902028521,
129.168042981875));
#82332=CARTESIAN_POINT('Ctrl Pts',(-38.148843523851,-4.68307861145244,129.301710365027));
#82333=CARTESIAN_POINT('Ctrl Pts',(-38.1543533835086,-4.71282557012691,
129.39441812965));
#82334=CARTESIAN_POINT('Ctrl Pts',(-38.1598632431662,-4.73983742116825,
129.488067986405));
#82335=CARTESIAN_POINT('Ctrl Pts',(-38.1653731028237,-4.76405452823409,
129.582490119308));
#82336=CARTESIAN_POINT('Ctrl Pts',(-36.4152663115528,-4.76405452823402,
129.582490119308));
#82337=CARTESIAN_POINT('Ctrl Pts',(-36.4249449713455,-4.806266409085,129.747073602091));
#82338=CARTESIAN_POINT('Ctrl Pts',(-36.4346236311382,-4.83997782400976,
129.913971994365));
#82339=CARTESIAN_POINT('Ctrl Pts',(-36.444302290931,-4.86497297357822,130.08240422771));
#82340=CARTESIAN_POINT('Ctrl Pts',(-36.4538371830679,-4.88959684301709,
130.248334553985));
#82341=CARTESIAN_POINT('Ctrl Pts',(-36.4633720752047,-4.90576145259318,
130.415753566812));
#82342=CARTESIAN_POINT('Ctrl Pts',(-36.4729069673416,-4.91330612857632,
130.583893047628));
#82343=CARTESIAN_POINT('Ctrl Pts',(-36.4769848328865,-4.91653282205094,
130.655802638813));
#82344=CARTESIAN_POINT('Ctrl Pts',(-36.4810626984315,-4.91818343115418,
130.727843733526));
#82345=CARTESIAN_POINT('Ctrl Pts',(-36.4851405639764,-4.91824802675748,
130.799954962542));
#82346=CARTESIAN_POINT('',(-36.1398594359911,-4.92619932659902,130.805220646693));
#82347=CARTESIAN_POINT('Ctrl Pts',(-36.0696835869212,-4.76181538791761,
129.583090555045));
#82348=CARTESIAN_POINT('Ctrl Pts',(-36.0930755366112,-4.86834354976456,
129.982579879972));
#82349=CARTESIAN_POINT('Ctrl Pts',(-36.1164674863011,-4.92520919812032,
130.394016325281));
#82350=CARTESIAN_POINT('Ctrl Pts',(-36.1398594359911,-4.92619932659902,
130.805220646693));
#82351=CARTESIAN_POINT('Ctrl Pts',(-36.1398594359911,-4.92619932659902,
130.805220646693));
#82352=CARTESIAN_POINT('Ctrl Pts',(-36.1424727741925,-4.92630994331169,
130.851160210344));
#82353=CARTESIAN_POINT('Ctrl Pts',(-36.2379019869981,-4.90488295595626,
132.528593278985));
#82354=CARTESIAN_POINT('Ctrl Pts',(-36.426147074408,-3.00542925083882,135.785231510157));
#82355=CARTESIAN_POINT('Ctrl Pts',(-36.7045946982209,2.56603982576222,136.025195746457));
#82356=CARTESIAN_POINT('Ctrl Pts',(-36.9830423220338,5.77944366050238,131.467467551281));
#82357=CARTESIAN_POINT('Ctrl Pts',(-37.2614899458467,3.68182111275986,126.300376478595));
#82358=CARTESIAN_POINT('Ctrl Pts',(-37.5399375696596,-1.79921517064808,
125.272226797766));
#82359=CARTESIAN_POINT('Ctrl Pts',(-37.7260883903438,-4.35811414719312,
127.983527806903));
#82360=CARTESIAN_POINT('Ctrl Pts',(-37.8194233364238,-4.76966346126612,
129.571636985164));
#82361=CARTESIAN_POINT('Ctrl Pts',(-37.8199424078995,-4.77192532739619,
129.580475997939));
#82362=CARTESIAN_POINT('Origin',(213.235140564004,0.,130.804360617566));
#82363=CARTESIAN_POINT('',(-39.9150204635389,-4.76405452823403,129.582490119308));
#82364=CARTESIAN_POINT('',(-39.5701139254339,-4.76405452823409,129.582490119308));
#82365=CARTESIAN_POINT('',(213.235140564004,-4.76405452823405,129.582490119308));
#82366=CARTESIAN_POINT('',(-38.235140564046,-4.91824967668966,130.806143940884));
#82367=CARTESIAN_POINT('Ctrl Pts',(-38.2351405640459,-4.91824967668966,
130.806143940884));
#82368=CARTESIAN_POINT('Ctrl Pts',(-38.2435224758346,-4.91819573390039,
130.954913433905));
#82369=CARTESIAN_POINT('Ctrl Pts',(-38.2519043876232,-4.91138754394824,
131.103478602525));
#82370=CARTESIAN_POINT('Ctrl Pts',(-38.2602862994119,-4.89790558294522,
131.25124311113));
#82371=CARTESIAN_POINT('Ctrl Pts',(-38.2687029849859,-4.88436768973608,
131.399620645908));
#82372=CARTESIAN_POINT('Ctrl Pts',(-38.2771196705599,-4.86410061939569,
131.547190589583));
#82373=CARTESIAN_POINT('Ctrl Pts',(-38.2855363561339,-4.8372365346784,131.693363300392));
#82374=CARTESIAN_POINT('Ctrl Pts',(-38.2939705996134,-4.81031640924787,
131.839840939624));
#82375=CARTESIAN_POINT('Ctrl Pts',(-38.3024048430931,-4.7767718368876,131.984915250611));
#82376=CARTESIAN_POINT('Ctrl Pts',(-38.3108390865726,-4.73678503963418,
132.128011081547));
#82377=CARTESIAN_POINT('Ctrl Pts',(-38.3193010235034,-4.69666694756791,
132.271576761075));
#82378=CARTESIAN_POINT('Ctrl Pts',(-38.3277629604342,-4.65006438485824,
132.41315069266));
#82379=CARTESIAN_POINT('Ctrl Pts',(-38.3362248973649,-4.5972090155243,132.552174203187));
#82380=CARTESIAN_POINT('Ctrl Pts',(-38.3427137465562,-4.5566780444993,132.658781307593));
#82381=CARTESIAN_POINT('Ctrl Pts',(-38.3492025957475,-4.51247125317275,
132.763889122567));
#82382=CARTESIAN_POINT('Ctrl Pts',(-38.3556914449387,-4.46471120750986,
132.86725588782));
#82383=CARTESIAN_POINT('Ctrl Pts',(-38.3634657790578,-4.40748957366053,
132.991100308641));
#82384=CARTESIAN_POINT('Ctrl Pts',(-38.3712401131769,-4.34502051082752,
133.112758221829));
#82385=CARTESIAN_POINT('Ctrl Pts',(-38.379014447296,-4.277493340301,133.231753001624));
#82386=CARTESIAN_POINT('Ctrl Pts',(-38.3867792002431,-4.21004939097709,
133.350601130987));
#82387=CARTESIAN_POINT('Ctrl Pts',(-38.3945439531902,-4.13755992820406,
133.466792320541));
#82388=CARTESIAN_POINT('Ctrl Pts',(-38.4023087061373,-4.06026198470017,
133.579870602794));
#82389=CARTESIAN_POINT('Ctrl Pts',(-38.4100657470223,-3.98304081460369,
133.692836574102));
#82390=CARTESIAN_POINT('Ctrl Pts',(-38.4178227879073,-3.90102088714029,
133.802695470224));
#82391=CARTESIAN_POINT('Ctrl Pts',(-38.4255798287923,-3.81448454460635,
133.909016914398));
#82392=CARTESIAN_POINT('Ctrl Pts',(-38.4333310200324,-3.72801345980123,
134.015258180744));
#82393=CARTESIAN_POINT('Ctrl Pts',(-38.4410822112725,-3.63703298488982,
134.11796700288));
#82394=CARTESIAN_POINT('Ctrl Pts',(-38.4488334025126,-3.54186785359698,
134.216743241211));
#82395=CARTESIAN_POINT('Ctrl Pts',(-38.4565812992897,-3.44674317002368,
134.315477497006));
#82396=CARTESIAN_POINT('Ctrl Pts',(-38.4643291960668,-3.3474376382418,134.410282212424));
#82397=CARTESIAN_POINT('Ctrl Pts',(-38.4720770928439,-3.24431508304851,
134.500791694213));
#82398=CARTESIAN_POINT('Ctrl Pts',(-38.479823368928,-3.14121409887057,134.59128224337));
#82399=CARTESIAN_POINT('Ctrl Pts',(-38.4875696450121,-3.03429797307346,
134.677479088268));
#82400=CARTESIAN_POINT('Ctrl Pts',(-38.4953159210962,-2.92396577221555,
134.759054945249));
#82401=CARTESIAN_POINT('Ctrl Pts',(-38.5030622543616,-2.81363275691055,
134.840631404406));
#82402=CARTESIAN_POINT('Ctrl Pts',(-38.5108085876269,-2.6998839305962,134.917586575146));
#82403=CARTESIAN_POINT('Ctrl Pts',(-38.5185549208923,-2.58314934387634,
134.989635104351));
#82404=CARTESIAN_POINT('Ctrl Pts',(-38.5263029888952,-2.46638861525516,
135.061699768325));
#82405=CARTESIAN_POINT('Ctrl Pts',(-38.5340510568982,-2.3466411283469,135.12885539896));
#82406=CARTESIAN_POINT('Ctrl Pts',(-38.5417991249012,-2.22436330220813,
135.190861610646));
#82407=CARTESIAN_POINT('Ctrl Pts',(-38.549555427643,-2.10195551774045,135.252933723271));
#82408=CARTESIAN_POINT('Ctrl Pts',(-38.5573117303849,-1.97701237117749,
135.30984530721));
#82409=CARTESIAN_POINT('Ctrl Pts',(-38.5650680331267,-1.85001262996764,
135.361403115882));
#82410=CARTESIAN_POINT('Ctrl Pts',(-38.5728284756409,-1.72294510517185,
135.41298844251));
#82411=CARTESIAN_POINT('Ctrl Pts',(-38.5805889181551,-1.59381916644517,
135.459214168411));
#82412=CARTESIAN_POINT('Ctrl Pts',(-38.5883493606693,-1.463129723798,135.499936671027));
#82413=CARTESIAN_POINT('Ctrl Pts',(-38.5961222609347,-1.3322304868556,135.54072454502));
#82414=CARTESIAN_POINT('Ctrl Pts',(-38.6038951612002,-1.19976310848476,
135.575991441416));
#82415=CARTESIAN_POINT('Ctrl Pts',(-38.6116680614656,-1.06623457457192,
135.605644497372));
#82416=CARTESIAN_POINT('Ctrl Pts',(-38.6191583972276,-0.937560139205245,
135.634219590053));
#82417=CARTESIAN_POINT('Ctrl Pts',(-38.6266487329896,-0.807900663326651,
135.657581855994));
#82418=CARTESIAN_POINT('Ctrl Pts',(-38.6341390687516,-0.677713249198604,
135.675693886227));
#82419=CARTESIAN_POINT('Ctrl Pts',(-38.6419134028707,-0.542589739693904,
135.69449263959));
#82420=CARTESIAN_POINT('Ctrl Pts',(-38.6496877369898,-0.406469437444971,
135.707694721551));
#82421=CARTESIAN_POINT('Ctrl Pts',(-38.6574620711089,-0.269855673983883,
135.715201785606));
#82422=CARTESIAN_POINT('Ctrl Pts',(-38.6652268240559,-0.133410274776922,
135.722699597876));
#82423=CARTESIAN_POINT('Ctrl Pts',(-38.672991577003,0.00352698898255541,
135.724516335918));
#82424=CARTESIAN_POINT('Ctrl Pts',(-38.68075632995,0.140444376955893,135.720604960505));
#82425=CARTESIAN_POINT('Ctrl Pts',(-38.688513370835,0.277225776649299,135.716697469925));
#82426=CARTESIAN_POINT('Ctrl Pts',(-38.69627041172,0.413986951564987,135.707073198832));
#82427=CARTESIAN_POINT('Ctrl Pts',(-38.704027452605,0.550213200635643,135.691737060643));
#82428=CARTESIAN_POINT('Ctrl Pts',(-38.7117786438452,0.686336720432375,
135.676412487556));
#82429=CARTESIAN_POINT('Ctrl Pts',(-38.7195298350853,0.821925730371897,
135.655384664479));
#82430=CARTESIAN_POINT('Ctrl Pts',(-38.7272810263255,0.956468055169481,
135.628710513867));
#82431=CARTESIAN_POINT('Ctrl Pts',(-38.7350289231026,1.09095319588981,135.602047700481));
#82432=CARTESIAN_POINT('Ctrl Pts',(-38.7427768198796,1.224392153581,135.569743408532));
#82433=CARTESIAN_POINT('Ctrl Pts',(-38.7505247166567,1.35628060396224,135.531906067989));
#82434=CARTESIAN_POINT('Ctrl Pts',(-38.7582709927408,1.48814146612284,135.494076642202));
#82435=CARTESIAN_POINT('Ctrl Pts',(-38.7660172688249,1.61845209052152,135.450716577689));
#82436=CARTESIAN_POINT('Ctrl Pts',(-38.773763544909,1.74672141892598,135.401984715637));
#82437=CARTESIAN_POINT('Ctrl Pts',(-38.7815098781744,1.87499169418549,135.353252493857));
#82438=CARTESIAN_POINT('Ctrl Pts',(-38.7892562114397,2.00122027790512,135.299148534265));
#82439=CARTESIAN_POINT('Ctrl Pts',(-38.797002544705,2.12493464156878,135.23988041028));
#82440=CARTESIAN_POINT('Ctrl Pts',(-38.804750612708,2.2486767102064,135.180599013611));
#82441=CARTESIAN_POINT('Ctrl Pts',(-38.8124986807109,2.36990308587518,135.116151320176));
#82442=CARTESIAN_POINT('Ctrl Pts',(-38.8202467487139,2.48816481970358,135.046791393959));
#82443=CARTESIAN_POINT('Ctrl Pts',(-38.8280030514558,2.60655224351019,134.977357751188));
#82444=CARTESIAN_POINT('Ctrl Pts',(-38.8357593541977,2.72196839352068,134.903001644672));
#82445=CARTESIAN_POINT('Ctrl Pts',(-38.8435156569396,2.83399190041499,134.82402142053));
#82446=CARTESIAN_POINT('Ctrl Pts',(-38.8512760994538,2.94607519762788,134.744999042264));
#82447=CARTESIAN_POINT('Ctrl Pts',(-38.8590365419678,3.05476193396696,134.661347866952));
#82448=CARTESIAN_POINT('Ctrl Pts',(-38.866796984482,3.15966376475733,134.573406644902));
#82449=CARTESIAN_POINT('Ctrl Pts',(-38.8745698847474,3.26473399327922,134.485324251796));
#82450=CARTESIAN_POINT('Ctrl Pts',(-38.8823427850129,3.36600688573248,134.392938313645));
#82451=CARTESIAN_POINT('Ctrl Pts',(-38.8901156852783,3.46313027572235,134.2966251774));
#82452=CARTESIAN_POINT('Ctrl Pts',(-38.8976060210403,3.55672298584717,134.203813266256));
#82453=CARTESIAN_POINT('Ctrl Pts',(-38.9050963568024,3.64646243565909,134.107354952448));
#82454=CARTESIAN_POINT('Ctrl Pts',(-38.9125866925644,3.7320700769938,134.007614588594));
#82455=CARTESIAN_POINT('Ctrl Pts',(-38.9203610266835,3.82092355806935,133.904092538529));
#82456=CARTESIAN_POINT('Ctrl Pts',(-38.9281353608026,3.90560719181378,133.796706720899));
#82457=CARTESIAN_POINT('Ctrl Pts',(-38.9359096949217,3.98576617354197,133.685827444088));
#82458=CARTESIAN_POINT('Ctrl Pts',(-38.9436744478688,4.06582636648919,133.575084816077));
#82459=CARTESIAN_POINT('Ctrl Pts',(-38.9514392008159,4.14137277559752,133.4608576091));
#82460=CARTESIAN_POINT('Ctrl Pts',(-38.959203953763,4.21208921727919,133.343550938944));
#82461=CARTESIAN_POINT('Ctrl Pts',(-38.966960994648,4.28273542239405,133.226360779427));
#82462=CARTESIAN_POINT('Ctrl Pts',(-38.974718035533,4.34856100616923,133.106097576081));
#82463=CARTESIAN_POINT('Ctrl Pts',(-38.982475076418,4.40929189390279,132.983197017313));
#82464=CARTESIAN_POINT('Ctrl Pts',(-38.9902262676581,4.4699769840015,132.860389138812));
#82465=CARTESIAN_POINT('Ctrl Pts',(-38.9979774588982,4.52557485272603,132.734948212664));
#82466=CARTESIAN_POINT('Ctrl Pts',(-39.0057286501384,4.57585654729728,132.607335914417));
#82467=CARTESIAN_POINT('Ctrl Pts',(-39.0134765469154,4.62611687080704,132.479777854802));
#82468=CARTESIAN_POINT('Ctrl Pts',(-39.0212244436925,4.67106537114485,132.350050621634));
#82469=CARTESIAN_POINT('Ctrl Pts',(-39.0289723404696,4.71052067392268,132.218637126261));
#82470=CARTESIAN_POINT('Ctrl Pts',(-39.0367186165536,4.74996772350172,132.087251119759));
#82471=CARTESIAN_POINT('Ctrl Pts',(-39.0444648926377,4.78392374870767,131.954179926866));
#82472=CARTESIAN_POINT('Ctrl Pts',(-39.0522111687218,4.8122569581602,131.819922546322));
#82473=CARTESIAN_POINT('Ctrl Pts',(-39.0599575019871,4.84059037676205,131.685664174721));
#82474=CARTESIAN_POINT('Ctrl Pts',(-39.0677038352525,4.86330081605778,131.550219980535));
#82475=CARTESIAN_POINT('Ctrl Pts',(-39.0754501685179,4.88030750024101,131.414099713894));
#82476=CARTESIAN_POINT('Ctrl Pts',(-39.0831982365209,4.89731799295323,131.277948964064));
#82477=CARTESIAN_POINT('Ctrl Pts',(-39.0909463045238,4.90862214038062,131.14112222838));
#82478=CARTESIAN_POINT('Ctrl Pts',(-39.0986943725268,4.91419102591724,131.004134548033));
#82479=CARTESIAN_POINT('Ctrl Pts',(-39.1064506752687,4.91976583013169,130.86700127555));
#82480=CARTESIAN_POINT('Ctrl Pts',(-39.1142069780105,4.91959318012247,130.729707107971));
#82481=CARTESIAN_POINT('Ctrl Pts',(-39.1219632807524,4.91369632251795,130.592767818602));
#82482=CARTESIAN_POINT('Ctrl Pts',(-39.1297237232665,4.90779631758299,130.455755440611));
#82483=CARTESIAN_POINT('Ctrl Pts',(-39.1374841657807,4.89616605048132,130.319098707611));
#82484=CARTESIAN_POINT('Ctrl Pts',(-39.1452446082948,4.87888061165811,130.183307447792));
#82485=CARTESIAN_POINT('Ctrl Pts',(-39.1530175085603,4.86156742471398,130.047298203787));
#82486=CARTESIAN_POINT('Ctrl Pts',(-39.1607904088257,4.83858099054103,129.912157594946));
#82487=CARTESIAN_POINT('Ctrl Pts',(-39.1685633090911,4.8100475859487,129.778385333551));
#82488=CARTESIAN_POINT('Ctrl Pts',(-39.1760536448532,4.78255144248439,129.649476030809));
#82489=CARTESIAN_POINT('Ctrl Pts',(-39.1835439806153,4.74990469586761,129.52183761539));
#82490=CARTESIAN_POINT('Ctrl Pts',(-39.1910343163774,4.71226332418739,129.395901379243));
#82491=CARTESIAN_POINT('Ctrl Pts',(-39.1988086504965,4.67319476845935,129.265190232426));
#82492=CARTESIAN_POINT('Ctrl Pts',(-39.2065829846156,4.62862161131375,129.135898835517));
#82493=CARTESIAN_POINT('Ctrl Pts',(-39.2143573187347,4.5786636230849,129.008525856476));
#82494=CARTESIAN_POINT('Ctrl Pts',(-39.2221220716818,4.52876720361166,128.881309853248));
#82495=CARTESIAN_POINT('Ctrl Pts',(-39.2298868246288,4.47349929874544,128.756007924153));
#82496=CARTESIAN_POINT('Ctrl Pts',(-39.2376515775759,4.41302983892011,128.633105058379));
#82497=CARTESIAN_POINT('Ctrl Pts',(-39.2454086184609,4.35262043821475,128.510324261463));
#82498=CARTESIAN_POINT('Ctrl Pts',(-39.2531656593459,4.28701993511846,128.389938134555));
#82499=CARTESIAN_POINT('Ctrl Pts',(-39.2609227002309,4.21644674255645,128.27241276469));
#82500=CARTESIAN_POINT('Ctrl Pts',(-39.2686738914711,4.14592676978804,128.15497602162));
#82501=CARTESIAN_POINT('Ctrl Pts',(-39.2764250827112,4.07044177204677,128.0403960754));
#82502=CARTESIAN_POINT('Ctrl Pts',(-39.2841762739513,3.9902564154782,127.9291150974));
#82503=CARTESIAN_POINT('Ctrl Pts',(-39.2919241707284,3.91010513982509,127.817881416784));
#82504=CARTESIAN_POINT('Ctrl Pts',(-39.2996720675055,3.82525770685523,127.70994423215));
#82505=CARTESIAN_POINT('Ctrl Pts',(-39.3074199642826,3.73602236627537,127.605717164289));
#82506=CARTESIAN_POINT('Ctrl Pts',(-39.3151662403667,3.64680569180507,127.501511898484));
#82507=CARTESIAN_POINT('Ctrl Pts',(-39.3229125164508,3.55320318949789,127.40101550259));
#82508=CARTESIAN_POINT('Ctrl Pts',(-39.3306587925349,3.45556344466568,127.304608577437));
#82509=CARTESIAN_POINT('Ctrl Pts',(-39.3384051258003,3.35792297907919,127.208200940629));
#82510=CARTESIAN_POINT('Ctrl Pts',(-39.3461514590656,3.25624548970483,127.115883109491));
#82511=CARTESIAN_POINT('Ctrl Pts',(-39.3538977923309,3.15091618246592,127.027998575392));
#82512=CARTESIAN_POINT('Ctrl Pts',(-39.3616458603339,3.04556328745881,126.94009436016));
#82513=CARTESIAN_POINT('Ctrl Pts',(-39.3693939283369,2.93655724739715,126.856625667964));
#82514=CARTESIAN_POINT('Ctrl Pts',(-39.3771419963399,2.82431575088884,126.777895219505));
#82515=CARTESIAN_POINT('Ctrl Pts',(-39.3848982990817,2.71195496278234,126.699081095389));
#82516=CARTESIAN_POINT('Ctrl Pts',(-39.3926546018236,2.59635216967742,126.625015499558));
#82517=CARTESIAN_POINT('Ctrl Pts',(-39.4004109045655,2.47795387163507,126.555957662037));
#82518=CARTESIAN_POINT('Ctrl Pts',(-39.4081713470797,2.35949238085615,126.486862966268));
#82519=CARTESIAN_POINT('Ctrl Pts',(-39.4159317895937,2.23823275760998,126.422781537154));
#82520=CARTESIAN_POINT('Ctrl Pts',(-39.4236922321079,2.11464452301101,126.363925773567));
#82521=CARTESIAN_POINT('Ctrl Pts',(-39.4314651323733,1.99085789360621,126.304975529483));
#82522=CARTESIAN_POINT('Ctrl Pts',(-39.4392380326388,1.86473554286216,126.251267867491));
#82523=CARTESIAN_POINT('Ctrl Pts',(-39.4470109329042,1.73676614857357,126.20296665403));
#82524=CARTESIAN_POINT('Ctrl Pts',(-39.4545012686662,1.61344876410352,126.156421311341));
#82525=CARTESIAN_POINT('Ctrl Pts',(-39.4619916044282,1.48841658631768,126.114896262598));
#82526=CARTESIAN_POINT('Ctrl Pts',(-39.4694819401902,1.36211678331456,126.078493402852));
#82527=CARTESIAN_POINT('Ctrl Pts',(-39.4772562743093,1.23102828489201,126.040710317613));
#82528=CARTESIAN_POINT('Ctrl Pts',(-39.4850306084284,1.0981588907535,126.00832581895));
#82529=CARTESIAN_POINT('Ctrl Pts',(-39.4928049425475,0.96399288316662,125.981508682901));
#82530=CARTESIAN_POINT('Ctrl Pts',(-39.5005696954946,0.829992223193326,
125.954724596575));
#82531=CARTESIAN_POINT('Ctrl Pts',(-39.5083344484416,0.694698508937481,
125.933494296862));
#82532=CARTESIAN_POINT('Ctrl Pts',(-39.5160992013887,0.55861162708742,125.917936964977));
#82533=CARTESIAN_POINT('Ctrl Pts',(-39.5238562422737,0.422659908646901,
125.902395084853));
#82534=CARTESIAN_POINT('Ctrl Pts',(-39.5316132831587,0.285916976262028,
125.892515003822));
#82535=CARTESIAN_POINT('Ctrl Pts',(-39.5393703240437,0.14889301967697,125.888364896332));
#82536=CARTESIAN_POINT('Ctrl Pts',(-39.5471215152838,0.0119723939232769,
125.88421791847));
#82537=CARTESIAN_POINT('Ctrl Pts',(-39.554872706524,-0.125228445006856,
125.885792325214));
#82538=CARTESIAN_POINT('Ctrl Pts',(-39.5626238977641,-0.262194427301316,
125.893104449864));
#82539=CARTESIAN_POINT('Ctrl Pts',(-39.5703717945412,-0.399102195399427,
125.900413466666));
#82540=CARTESIAN_POINT('Ctrl Pts',(-39.5781196913183,-0.535774915805013,
125.913455330221));
#82541=CARTESIAN_POINT('Ctrl Pts',(-39.5858675880954,-0.671697981138233,
125.93219427346));
#82542=CARTESIAN_POINT('Ctrl Pts',(-39.5936138641795,-0.807592614296347,
125.950929296917));
#82543=CARTESIAN_POINT('Ctrl Pts',(-39.6013601402636,-0.942737517232608,
125.975358976327));
#82544=CARTESIAN_POINT('Ctrl Pts',(-39.6091064163477,-1.07662406081528,
126.00539576104));
#82545=CARTESIAN_POINT('Ctrl Pts',(-39.616852749613,-1.210511592718,126.035432767477));
#82546=CARTESIAN_POINT('Ctrl Pts',(-39.6245990828783,-1.34314036524885,
126.071076876226));
#82547=CARTESIAN_POINT('Ctrl Pts',(-39.6323454161437,-1.47401317618001,
126.112189668107));
#82548=CARTESIAN_POINT('Ctrl Pts',(-39.6400934841467,-1.60491529516978,
126.153311666913));
#82549=CARTESIAN_POINT('Ctrl Pts',(-39.6478415521496,-1.7340602971447,126.19990466866));
#82550=CARTESIAN_POINT('Ctrl Pts',(-39.6555896201526,-1.86096772370854,
126.251780888026));
#82551=CARTESIAN_POINT('Ctrl Pts',(-39.6633459228944,-1.98801002899555,
126.303712242056));
#82552=CARTESIAN_POINT('Ctrl Pts',(-39.6711022256363,-2.11280964584294,
126.360937882237));
#82553=CARTESIAN_POINT('Ctrl Pts',(-39.6788585283782,-2.2349071325004,126.423222275582));
#82554=CARTESIAN_POINT('Ctrl Pts',(-39.6866189708923,-2.35706978626293,
126.485539911984));
#82555=CARTESIAN_POINT('Ctrl Pts',(-39.6943794134065,-2.47652709575224,
126.55292148956));
#82556=CARTESIAN_POINT('Ctrl Pts',(-39.7021398559207,-2.59284657615135,
126.625086793677));
#82557=CARTESIAN_POINT('Ctrl Pts',(-39.7099127561861,-2.70935278290675,
126.697367943948));
#82558=CARTESIAN_POINT('Ctrl Pts',(-39.7176856564515,-2.82271077130739,
126.77444794641));
#82559=CARTESIAN_POINT('Ctrl Pts',(-39.7254585567169,-2.93251853359339,
126.856004236408));
#82560=CARTESIAN_POINT('Ctrl Pts',(-39.732948892479,-3.03833450713154,126.934595749837));
#82561=CARTESIAN_POINT('Ctrl Pts',(-39.7404392282411,-3.14085365286397,
127.017343558953));
#82562=CARTESIAN_POINT('Ctrl Pts',(-39.7479295640031,-3.23974853831984,
127.103926525334));
#82563=CARTESIAN_POINT('Ctrl Pts',(-39.7555877436823,-3.34085946661956,
127.192449648298));
#82564=CARTESIAN_POINT('Ctrl Pts',(-39.7632459233616,-3.438522303563,127.285280320083));
#82565=CARTESIAN_POINT('Ctrl Pts',(-39.7709041030409,-3.53233941002593,
127.382115542345));
#82566=CARTESIAN_POINT('Ctrl Pts',(-39.77855346555,-3.62604850108378,127.478839274323));
#82567=CARTESIAN_POINT('Ctrl Pts',(-39.7862028280591,-3.71592038553408,
127.579558105399));
#82568=CARTESIAN_POINT('Ctrl Pts',(-39.7938521905683,-3.80159006410806,
127.683928588668));
#82569=CARTESIAN_POINT('Ctrl Pts',(-39.8014945190874,-3.88718096491826,
127.788203097801));
#82570=CARTESIAN_POINT('Ctrl Pts',(-39.8091368476064,-3.96857708869918,
127.896122273078));
#82571=CARTESIAN_POINT('Ctrl Pts',(-39.8167791761255,-4.0454503397911,128.007305986211));
#82572=CARTESIAN_POINT('Ctrl Pts',(-39.824416247059,-4.12227070547103,128.118413209845));
#82573=CARTESIAN_POINT('Ctrl Pts',(-39.8320533179927,-4.1945741585436,128.232780173941));
#82574=CARTESIAN_POINT('Ctrl Pts',(-39.8396903889262,-4.2620733229811,128.349994293638));
#82575=CARTESIAN_POINT('Ctrl Pts',(-39.8473244869759,-4.32954621200796,
128.467162785375));
#82576=CARTESIAN_POINT('Ctrl Pts',(-39.8549585850255,-4.39221832954647,
128.587175880213));
#82577=CARTESIAN_POINT('Ctrl Pts',(-39.8625926830752,-4.44984629012379,
128.709593075147));
#82578=CARTESIAN_POINT('Ctrl Pts',(-39.8702251171496,-4.50746168975395,
128.831983587272));
#82579=CARTESIAN_POINT('Ctrl Pts',(-39.8778575512241,-4.56003495129283,
128.956776790592));
#82580=CARTESIAN_POINT('Ctrl Pts',(-39.8854899852985,-4.60736951399532,
129.083509309635));
#82581=CARTESIAN_POINT('Ctrl Pts',(-39.893123820201,-4.65471276430396,129.210265088685));
#82582=CARTESIAN_POINT('Ctrl Pts',(-39.9007576551033,-4.69681525624594,
129.338960515656));
#82583=CARTESIAN_POINT('Ctrl Pts',(-39.9083914900058,-4.73352938745337,
129.469114347916));
#82584=CARTESIAN_POINT('Ctrl Pts',(-39.9106011478501,-4.74415650594061,
129.506788130503));
#82585=CARTESIAN_POINT('Ctrl Pts',(-39.9128108056945,-4.75433248306291,
129.544584012739));
#82586=CARTESIAN_POINT('Ctrl Pts',(-39.9150204635388,-4.76405452823403,
129.582490119308));
#82587=CARTESIAN_POINT('Ctrl Pts',(-38.1653731028237,-4.76405452823409,
129.582490119308));
#82588=CARTESIAN_POINT('Ctrl Pts',(-38.1733037435307,-4.79891152769259,
129.718397031168));
#82589=CARTESIAN_POINT('Ctrl Pts',(-38.1812343842377,-4.82797634339808,
129.855904430386));
#82590=CARTESIAN_POINT('Ctrl Pts',(-38.1891650249446,-4.85111275434098,
129.994491426171));
#82591=CARTESIAN_POINT('Ctrl Pts',(-38.1970893081135,-4.87423061815535,
130.132967324742));
#82592=CARTESIAN_POINT('Ctrl Pts',(-38.2050135912824,-4.89142948732574,
130.272520736319));
#82593=CARTESIAN_POINT('Ctrl Pts',(-38.2129378744513,-4.90262400013599,
130.412619662609));
#82594=CARTESIAN_POINT('Ctrl Pts',(-38.2203387709704,-4.91307913268544,
130.543465271456));
#82595=CARTESIAN_POINT('Ctrl Pts',(-38.2277396674894,-4.91829730602107,
130.674786363234));
#82596=CARTESIAN_POINT('Ctrl Pts',(-38.2351405640085,-4.9182496766899,130.806143940219));
#82597=CARTESIAN_POINT('',(-37.8898589934247,-4.91743469503477,130.799824135819));
#82598=CARTESIAN_POINT('Ctrl Pts',(-37.8199424078995,-4.77192532739619,
129.580475997939));
#82599=CARTESIAN_POINT('Ctrl Pts',(-37.8432478679745,-4.87347941629538,
129.977333211189));
#82600=CARTESIAN_POINT('Ctrl Pts',(-37.8665533280494,-4.9207712278546,130.388155924214));
#82601=CARTESIAN_POINT('Ctrl Pts',(-37.8898587881243,-4.91705745387562,
130.799820856863));
#82602=CARTESIAN_POINT('Ctrl Pts',(-37.8898594359911,-4.91824791434055,
130.799831204269));
#82603=CARTESIAN_POINT('Ctrl Pts',(-37.8975283655907,-4.91837269683403,
130.935325847404));
#82604=CARTESIAN_POINT('Ctrl Pts',(-37.9051972951903,-4.9128940792562,131.070959621141));
#82605=CARTESIAN_POINT('Ctrl Pts',(-37.9128662247899,-4.90180442327651,
131.206226837155));
#82606=CARTESIAN_POINT('Ctrl Pts',(-37.9205314994772,-4.89072005248292,
131.34142958657));
#82607=CARTESIAN_POINT('Ctrl Pts',(-37.9281967741646,-4.87402998909565,
131.476265727456));
#82608=CARTESIAN_POINT('Ctrl Pts',(-37.935862048852,-4.85177868278434,131.610230753369));
#82609=CARTESIAN_POINT('Ctrl Pts',(-37.9435245019742,-4.82953556711341,
131.74414646715));
#82610=CARTESIAN_POINT('Ctrl Pts',(-37.9511869550964,-4.80173534968034,
131.877191309779));
#82611=CARTESIAN_POINT('Ctrl Pts',(-37.9588494082187,-4.7684741342957,132.008867775308));
#82612=CARTESIAN_POINT('Ctrl Pts',(-37.9665114089083,-4.73521488283284,
132.140536465949));
#82613=CARTESIAN_POINT('Ctrl Pts',(-37.974173409598,-4.69649537264059,132.270836552027));
#82614=CARTESIAN_POINT('Ctrl Pts',(-37.9818354102876,-4.65246233438006,
132.399282963536));
#82615=CARTESIAN_POINT('Ctrl Pts',(-37.9894987053801,-4.60842185726729,
132.527751074522));
#82616=CARTESIAN_POINT('Ctrl Pts',(-37.9971620004726,-4.55906619690956,
132.654364509553));
#82617=CARTESIAN_POINT('Ctrl Pts',(-38.0048252955652,-4.50459106188987,
132.778656043191));
#82618=CARTESIAN_POINT('Ctrl Pts',(-38.0124964083817,-4.45006035396499,
132.903074373056));
#82619=CARTESIAN_POINT('Ctrl Pts',(-38.0201675211983,-4.39039990053984,
133.025165702982));
#82620=CARTESIAN_POINT('Ctrl Pts',(-38.0278386340148,-4.32585261457259,
133.144485020134));
#82621=CARTESIAN_POINT('Ctrl Pts',(-38.0355136202747,-4.26127273616834,
133.263864586254));
#82622=CARTESIAN_POINT('Ctrl Pts',(-38.0431886065347,-4.19180131578868,
133.380469008353));
#82623=CARTESIAN_POINT('Ctrl Pts',(-38.0508635927947,-4.11772520068029,
133.493881436259));
#82624=CARTESIAN_POINT('Ctrl Pts',(-38.0585509603689,-4.04352958572797,
133.607476821484));
#82625=CARTESIAN_POINT('Ctrl Pts',(-38.0662383279431,-3.96471466712519,
133.717869598399));
#82626=CARTESIAN_POINT('Ctrl Pts',(-38.0739256955174,-3.88160873183472,
133.824674626977));
#82627=CARTESIAN_POINT('Ctrl Pts',(-38.0815614027734,-3.79906128148991,
133.930761908978));
#82628=CARTESIAN_POINT('Ctrl Pts',(-38.0891971100294,-3.71228063013956,
134.033309287622));
#82629=CARTESIAN_POINT('Ctrl Pts',(-38.0968328172854,-3.62162342668443,
134.131976403349));
#82630=CARTESIAN_POINT('Ctrl Pts',(-38.1046071514045,-3.52932033460267,
134.232434828287));
#82631=CARTESIAN_POINT('Ctrl Pts',(-38.1123814855235,-3.43268802333354,
134.329208936762));
#82632=CARTESIAN_POINT('Ctrl Pts',(-38.1201558196426,-3.33205230381746,
134.421902670829));
#82633=CARTESIAN_POINT('Ctrl Pts',(-38.1279205725897,-3.23154060883189,
134.514482168152));
#82634=CARTESIAN_POINT('Ctrl Pts',(-38.1356853255368,-3.12703560728388,
134.602991034343));
#82635=CARTESIAN_POINT('Ctrl Pts',(-38.1434500784839,-3.01890223537644,
134.687067451173));
#82636=CARTESIAN_POINT('Ctrl Pts',(-38.1512071193689,-2.91087626305824,
134.77106036212));
#82637=CARTESIAN_POINT('Ctrl Pts',(-38.1589641602539,-2.79922939865271,
134.850629346196));
#82638=CARTESIAN_POINT('Ctrl Pts',(-38.1667212011389,-2.68436191042112,
134.925450788429));
#82639=CARTESIAN_POINT('Ctrl Pts',(-38.174472392379,-2.56958104465596,135.00021580723));
#82640=CARTESIAN_POINT('Ctrl Pts',(-38.1822235836191,-2.45158471551103,
135.070240197752));
#82641=CARTESIAN_POINT('Ctrl Pts',(-38.1899747748592,-2.33080432579081,
135.135242081815));
#82642=CARTESIAN_POINT('Ctrl Pts',(-38.1977226716363,-2.21007527095797,
135.200216338343));
#82643=CARTESIAN_POINT('Ctrl Pts',(-38.2054705684135,-2.08656485259624,
135.260172149273));
#82644=CARTESIAN_POINT('Ctrl Pts',(-38.2132184651906,-1.96073118009593,
135.314872373664));
#82645=CARTESIAN_POINT('Ctrl Pts',(-38.2209647412747,-1.83492382928724,
135.369561155948));
#82646=CARTESIAN_POINT('Ctrl Pts',(-38.2287110173588,-1.70679454929606,
135.418996382606));
#82647=CARTESIAN_POINT('Ctrl Pts',(-38.2364572934429,-1.57682328049001,
135.462988248597));
#82648=CARTESIAN_POINT('Ctrl Pts',(-38.2442036267083,-1.44685105226558,
135.506980439326));
#82649=CARTESIAN_POINT('Ctrl Pts',(-38.2519499599735,-1.3150371784213,135.545529063864));
#82650=CARTESIAN_POINT('Ctrl Pts',(-38.2596962932389,-1.18187830084589,
135.578493705833));
#82651=CARTESIAN_POINT('Ctrl Pts',(-38.2674443612419,-1.04868960326346,
135.611465730006));
#82652=CARTESIAN_POINT('Ctrl Pts',(-38.2751924292448,-0.914155682024639,
135.63885118934));
#82653=CARTESIAN_POINT('Ctrl Pts',(-38.2829404972478,-0.778784558070727,
135.660560538761));
#82654=CARTESIAN_POINT('Ctrl Pts',(-38.2906967999897,-0.643269560075155,
135.682292961136));
#82655=CARTESIAN_POINT('Ctrl Pts',(-38.2984531027315,-0.506915968563318,
135.698337160748));
#82656=CARTESIAN_POINT('Ctrl Pts',(-38.3062094054733,-0.370238692403159,
135.70865530418));
#82657=CARTESIAN_POINT('Ctrl Pts',(-38.3139698479875,-0.233488467465254,
135.718978954715));
#82658=CARTESIAN_POINT('Ctrl Pts',(-38.3217302905017,-0.0964146041944834,
135.723570446313));
#82659=CARTESIAN_POINT('Ctrl Pts',(-38.3294907330158,0.0404677688391133,
135.722444128669));
#82660=CARTESIAN_POINT('Ctrl Pts',(-38.3372636332813,0.17756987760975,135.721316002961));
#82661=CARTESIAN_POINT('Ctrl Pts',(-38.3450365335467,0.314479491166332,
135.714451745563));
#82662=CARTESIAN_POINT('Ctrl Pts',(-38.3528094338121,0.45068548048526,135.701917729043));
#82663=CARTESIAN_POINT('Ctrl Pts',(-38.3602997695741,0.581940039010632,
135.689839355595));
#82664=CARTESIAN_POINT('Ctrl Pts',(-38.3677901053363,0.712540936825952,
135.672496326879));
#82665=CARTESIAN_POINT('Ctrl Pts',(-38.3752804410983,0.842041478362543,
135.649992589891));
#82666=CARTESIAN_POINT('Ctrl Pts',(-38.3830547752174,0.976452072291771,
135.626635616876));
#82667=CARTESIAN_POINT('Ctrl Pts',(-38.3908291093365,1.11010299515356,135.597644886106));
#82668=CARTESIAN_POINT('Ctrl Pts',(-38.3986034434556,1.24248492340916,135.563080432558));
#82669=CARTESIAN_POINT('Ctrl Pts',(-38.4063681964026,1.3747037027695,135.528558576611));
#82670=CARTESIAN_POINT('Ctrl Pts',(-38.4141329493498,1.50565622461094,135.488476763199));
#82671=CARTESIAN_POINT('Ctrl Pts',(-38.4218977022969,1.63484082407832,135.442946451894));
#82672=CARTESIAN_POINT('Ctrl Pts',(-38.4296547431819,1.76389711558032,135.397461361936));
#82673=CARTESIAN_POINT('Ctrl Pts',(-38.4374117840668,1.89118861273123,135.346538672381));
#82674=CARTESIAN_POINT('Ctrl Pts',(-38.4451688249518,2.01622669431847,135.290340218458));
#82675=CARTESIAN_POINT('Ctrl Pts',(-38.4529200161919,2.14117048371573,135.234184144226));
#82676=CARTESIAN_POINT('Ctrl Pts',(-38.4606712074321,2.26386388477921,135.172760384204));
#82677=CARTESIAN_POINT('Ctrl Pts',(-38.4684223986722,2.38383656165944,135.10627952775));
#82678=CARTESIAN_POINT('Ctrl Pts',(-38.4761702954493,2.50375824695161,135.039826927432));
#82679=CARTESIAN_POINT('Ctrl Pts',(-38.4839181922263,2.62096116675749,134.968321694778));
#82680=CARTESIAN_POINT('Ctrl Pts',(-38.4916660890034,2.7349981883732,134.892021069719));
#82681=CARTESIAN_POINT('Ctrl Pts',(-38.4994123650875,2.84901135590235,134.815736405106));
#82682=CARTESIAN_POINT('Ctrl Pts',(-38.5071586411715,2.95985961773483,134.734658560571));
#82683=CARTESIAN_POINT('Ctrl Pts',(-38.5149049172556,3.06712386602207,134.649088729277));
#82684=CARTESIAN_POINT('Ctrl Pts',(-38.522651250521,3.17438890610948,134.563518266325));
#82685=CARTESIAN_POINT('Ctrl Pts',(-38.5303975837863,3.27806957423187,134.473455994262));
#82686=CARTESIAN_POINT('Ctrl Pts',(-38.5381439170516,3.37777928704401,134.379243853494));
#82687=CARTESIAN_POINT('Ctrl Pts',(-38.5458919850545,3.47751132915458,134.28501061457));
#82688=CARTESIAN_POINT('Ctrl Pts',(-38.5536400530575,3.57327036229184,134.186625926131));
#82689=CARTESIAN_POINT('Ctrl Pts',(-38.5613881210605,3.66470645192017,134.084468799281));
#82690=CARTESIAN_POINT('Ctrl Pts',(-38.5691444238023,3.75623972091328,133.982203098621));
#82691=CARTESIAN_POINT('Ctrl Pts',(-38.5769007265442,3.8434406072765,133.876157242139));
#82692=CARTESIAN_POINT('Ctrl Pts',(-38.584657029286,3.92599895986322,133.766743987364));
#82693=CARTESIAN_POINT('Ctrl Pts',(-38.5924174718002,4.00860137632839,133.657272335439));
#82694=CARTESIAN_POINT('Ctrl Pts',(-38.6001779143143,4.08655609956023,133.544430025498));
#82695=CARTESIAN_POINT('Ctrl Pts',(-38.6079383568285,4.15959676279037,133.428658206157));
#82696=CARTESIAN_POINT('Ctrl Pts',(-38.6157112570939,4.23275467737736,133.312700539613));
#82697=CARTESIAN_POINT('Ctrl Pts',(-38.6234841573593,4.30098257355306,133.193804305454));
#82698=CARTESIAN_POINT('Ctrl Pts',(-38.6312570576248,4.36406001471642,133.072435406997));
#82699=CARTESIAN_POINT('Ctrl Pts',(-38.6387473933869,4.42484443201185,132.955478573707));
#82700=CARTESIAN_POINT('Ctrl Pts',(-38.646237729149,4.48084622614649,132.836226008916));
#82701=CARTESIAN_POINT('Ctrl Pts',(-38.6537280649111,4.53191140080741,132.715109716148));
#82702=CARTESIAN_POINT('Ctrl Pts',(-38.6615023990302,4.58491272708586,132.589401262329));
#82703=CARTESIAN_POINT('Ctrl Pts',(-38.6692767331493,4.63276359264101,132.461286757615));
#82704=CARTESIAN_POINT('Ctrl Pts',(-38.6770510672684,4.67523920478611,132.331227160696));
#82705=CARTESIAN_POINT('Ctrl Pts',(-38.6848158202155,4.71766246953545,132.201327850607));
#82706=CARTESIAN_POINT('Ctrl Pts',(-38.6925805731626,4.75472354148426,132.069488586011));
#82707=CARTESIAN_POINT('Ctrl Pts',(-38.7003453261097,4.78624503261944,131.936191678381));
#82708=CARTESIAN_POINT('Ctrl Pts',(-38.7081023669947,4.81773521616519,131.803027163119));
#82709=CARTESIAN_POINT('Ctrl Pts',(-38.7158594078797,4.84369667871507,131.668408263923));
#82710=CARTESIAN_POINT('Ctrl Pts',(-38.7236164487647,4.86400146512909,131.532833547552));
#82711=CARTESIAN_POINT('Ctrl Pts',(-38.7313676400049,4.88429093954567,131.397361069129));
#82712=CARTESIAN_POINT('Ctrl Pts',(-38.7391188312449,4.89893217085611,131.260934593307));
#82713=CARTESIAN_POINT('Ctrl Pts',(-38.746870022485,4.90784810583442,131.124063655646));
#82714=CARTESIAN_POINT('Ctrl Pts',(-38.7546179192621,4.91676025130254,130.987250891784));
#82715=CARTESIAN_POINT('Ctrl Pts',(-38.7623658160393,4.91995191493199,130.84999443113));
#82716=CARTESIAN_POINT('Ctrl Pts',(-38.7701137128164,4.91739783381656,130.712809503558));
#82717=CARTESIAN_POINT('Ctrl Pts',(-38.7778599889005,4.91484428695985,130.575653272115));
#82718=CARTESIAN_POINT('Ctrl Pts',(-38.7856062649846,4.90654739324831,130.438568934642));
#82719=CARTESIAN_POINT('Ctrl Pts',(-38.7933525410687,4.89253401699069,130.302071900702));
#82720=CARTESIAN_POINT('Ctrl Pts',(-38.801098874334,4.87852053728949,130.165573859172));
#82721=CARTESIAN_POINT('Ctrl Pts',(-38.8088452075994,4.85879053076791,130.029663518748));
#82722=CARTESIAN_POINT('Ctrl Pts',(-38.8165915408647,4.83342272383283,129.894850950088));
#82723=CARTESIAN_POINT('Ctrl Pts',(-38.8243396088677,4.80804923595334,129.760008191088));
#82724=CARTESIAN_POINT('Ctrl Pts',(-38.8320876768707,4.77703550762498,129.626264077191));
#82725=CARTESIAN_POINT('Ctrl Pts',(-38.8398357448737,4.7405112634608,129.494117882993));
#82726=CARTESIAN_POINT('Ctrl Pts',(-38.8475920476156,4.70394820089523,129.361831242247));
#82727=CARTESIAN_POINT('Ctrl Pts',(-38.8553483503574,4.66186302754181,129.23114629115));
#82728=CARTESIAN_POINT('Ctrl Pts',(-38.8631046530992,4.61443536372731,129.102547074171));
#82729=CARTESIAN_POINT('Ctrl Pts',(-38.8708650956134,4.56698238634054,128.973879219918));
#82730=CARTESIAN_POINT('Ctrl Pts',(-38.8786255381276,4.51418138718322,128.84729967862));
#82731=CARTESIAN_POINT('Ctrl Pts',(-38.8863859806418,4.45625953933603,128.723271003788));
#82732=CARTESIAN_POINT('Ctrl Pts',(-38.8941588809072,4.3982447101967,128.599043227115));
#82733=CARTESIAN_POINT('Ctrl Pts',(-38.9019317811727,4.335092785524,128.477374846983));
#82734=CARTESIAN_POINT('Ctrl Pts',(-38.9097046814381,4.26707659160689,128.35870315507));
#82735=CARTESIAN_POINT('Ctrl Pts',(-38.9171950172001,4.20153295766167,128.244345478075));
#82736=CARTESIAN_POINT('Ctrl Pts',(-38.924685352962,4.13147273514576,128.132770658444));
#82737=CARTESIAN_POINT('Ctrl Pts',(-38.932175688724,4.05717614209043,128.024341766092));
#82738=CARTESIAN_POINT('Ctrl Pts',(-38.9399500228431,3.98006257112689,127.911801759329));
#82739=CARTESIAN_POINT('Ctrl Pts',(-38.9477243569622,3.89814077157495,127.802294451762));
#82740=CARTESIAN_POINT('Ctrl Pts',(-38.9554986910813,3.8116770550972,127.696258127276));
#82741=CARTESIAN_POINT('Ctrl Pts',(-38.9632634440284,3.7253198974223,127.590352483083));
#82742=CARTESIAN_POINT('Ctrl Pts',(-38.9710281969755,3.63443220489126,127.487909610761));
#82743=CARTESIAN_POINT('Ctrl Pts',(-38.9787929499226,3.53932387725116,127.389339453002));
#82744=CARTESIAN_POINT('Ctrl Pts',(-38.9865499908076,3.44431001254313,127.290867196513));
#82745=CARTESIAN_POINT('Ctrl Pts',(-38.9943070316927,3.34508412469663,127.196260279539));
#82746=CARTESIAN_POINT('Ctrl Pts',(-39.0020640725777,3.24199650916696,127.105895841872));
#82747=CARTESIAN_POINT('Ctrl Pts',(-39.0098152638178,3.13898663280965,127.01559954873));
#82748=CARTESIAN_POINT('Ctrl Pts',(-39.0175664550579,3.03212111805632,126.929539623583));
#82749=CARTESIAN_POINT('Ctrl Pts',(-39.025317646298,2.92178700245488,126.848056309909));
#82750=CARTESIAN_POINT('Ctrl Pts',(-39.0330655430751,2.81149978179627,126.766607628817));
#82751=CARTESIAN_POINT('Ctrl Pts',(-39.0408134398523,2.69774720629531,126.689731922154));
#82752=CARTESIAN_POINT('Ctrl Pts',(-39.0485613366293,2.58094909822007,126.617728938651));
#82753=CARTESIAN_POINT('Ctrl Pts',(-39.0563076127135,2.46417542179101,126.545741016619));
#82754=CARTESIAN_POINT('Ctrl Pts',(-39.0640538887975,2.34435781253047,126.478623995404));
#82755=CARTESIAN_POINT('Ctrl Pts',(-39.0718001648816,2.22194441991716,126.416633864759));
#82756=CARTESIAN_POINT('Ctrl Pts',(-39.079546498147,2.09953012367601,126.354643276517));
#82757=CARTESIAN_POINT('Ctrl Pts',(-39.0872928314123,1.97452035463921,126.297779830993));
#82758=CARTESIAN_POINT('Ctrl Pts',(-39.0950391646777,1.84738680324385,126.24625299908));
#82759=CARTESIAN_POINT('Ctrl Pts',(-39.1027872326807,1.72022478117166,126.194714628091));
#82760=CARTESIAN_POINT('Ctrl Pts',(-39.1105353006836,1.59093839260654,126.148515395645));
#82761=CARTESIAN_POINT('Ctrl Pts',(-39.1182833686866,1.46001781072822,126.107816030867));
#82762=CARTESIAN_POINT('Ctrl Pts',(-39.1260396714284,1.32895808489714,126.067073410319));
#82763=CARTESIAN_POINT('Ctrl Pts',(-39.1337959741703,1.1962610701642,126.031842450349));
#82764=CARTESIAN_POINT('Ctrl Pts',(-39.1415522769121,1.06243109602415,126.00223366915));
#82765=CARTESIAN_POINT('Ctrl Pts',(-39.1493127194263,0.928529692797354,
125.972609084853));
#82766=CARTESIAN_POINT('Ctrl Pts',(-39.1570731619404,0.793494510004567,
125.948612726898));
#82767=CARTESIAN_POINT('Ctrl Pts',(-39.1648336044546,0.657837499612393,
125.930303489607));
#82768=CARTESIAN_POINT('Ctrl Pts',(-39.17260650472,0.521962720544074,125.911964860704));
#82769=CARTESIAN_POINT('Ctrl Pts',(-39.1803794049855,0.385464508654437,
125.89933163211));
#82770=CARTESIAN_POINT('Ctrl Pts',(-39.188152305251,0.24885823909118,125.892410634175));
#82771=CARTESIAN_POINT('Ctrl Pts',(-39.195642641013,0.117217951516797,125.885741231948));
#82772=CARTESIAN_POINT('Ctrl Pts',(-39.203132976775,-0.0145223657895349,
125.884375965981));
#82773=CARTESIAN_POINT('Ctrl Pts',(-39.210623312537,-0.145905787133676,
125.888275329069));
#82774=CARTESIAN_POINT('Ctrl Pts',(-39.2183976466561,-0.282270650831207,
125.892322537692));
#82775=CARTESIAN_POINT('Ctrl Pts',(-39.2261719807751,-0.41868298380456,
125.902054293197));
#82776=CARTESIAN_POINT('Ctrl Pts',(-39.2339463148942,-0.554630097449639,
125.917483443183));
#82777=CARTESIAN_POINT('Ctrl Pts',(-39.2417110678413,-0.690409668426355,
125.932893578121));
#82778=CARTESIAN_POINT('Ctrl Pts',(-39.2494758207884,-0.825724776110992,
125.953987093124));
#82779=CARTESIAN_POINT('Ctrl Pts',(-39.2572405737355,-0.960063015724354,
125.980724844797));
#82780=CARTESIAN_POINT('Ctrl Pts',(-39.2649976146204,-1.09426782870466,
126.007436040157));
#82781=CARTESIAN_POINT('Ctrl Pts',(-39.2727546555054,-1.22749732347055,
126.039780240298));
#82782=CARTESIAN_POINT('Ctrl Pts',(-39.2805116963904,-1.35924485838201,
126.077666585003));
#82783=CARTESIAN_POINT('Ctrl Pts',(-39.2882628876306,-1.4908930414529,126.115524359321));
#82784=CARTESIAN_POINT('Ctrl Pts',(-39.2960140788707,-1.62106111488213,
126.158915851799));
#82785=CARTESIAN_POINT('Ctrl Pts',(-39.3037652701108,-1.74925361894652,
126.207699346697));
#82786=CARTESIAN_POINT('Ctrl Pts',(-39.3115131668879,-1.87739163777705,
126.256462107309));
#82787=CARTESIAN_POINT('Ctrl Pts',(-39.319261063665,-2.0035553926455,126.310612173473));
#82788=CARTESIAN_POINT('Ctrl Pts',(-39.327008960442,-2.12726577226441,126.369958358337));
#82789=CARTESIAN_POINT('Ctrl Pts',(-39.3347552365261,-2.25095027433863,
126.429292129259));
#82790=CARTESIAN_POINT('Ctrl Pts',(-39.3425015126102,-2.37218206965326,
126.493819687949));
#82791=CARTESIAN_POINT('Ctrl Pts',(-39.3502477886943,-2.49050355103721,
126.563302362275));
#82792=CARTESIAN_POINT('Ctrl Pts',(-39.3579941219597,-2.60882590584362,
126.632785549507));
#82793=CARTESIAN_POINT('Ctrl Pts',(-39.3657404552251,-2.72423756671765,
126.707223727385));
#82794=CARTESIAN_POINT('Ctrl Pts',(-39.3734867884904,-2.83630733966034,
126.786333273522));
#82795=CARTESIAN_POINT('Ctrl Pts',(-39.3812348564934,-2.94840220985179,
126.865460535693));
#82796=CARTESIAN_POINT('Ctrl Pts',(-39.3889829244964,-3.05715338355428,
126.949261022358));
#82797=CARTESIAN_POINT('Ctrl Pts',(-39.3967309924994,-3.16216068422731,
127.037409214956));
#82798=CARTESIAN_POINT('Ctrl Pts',(-39.4044872952412,-3.2672795879088,127.125651092502));
#82799=CARTESIAN_POINT('Ctrl Pts',(-39.4122435979831,-3.3686463700914,127.218249654744));
#82800=CARTESIAN_POINT('Ctrl Pts',(-39.4199999007249,-3.46589544628015,
127.314840332777));
#82801=CARTESIAN_POINT('Ctrl Pts',(-39.4277603432391,-3.56319642722884,
127.411482564163));
#82802=CARTESIAN_POINT('Ctrl Pts',(-39.4355207857532,-3.65637505750607,
127.512120870223));
#82803=CARTESIAN_POINT('Ctrl Pts',(-39.4432812282674,-3.74510506510637,
127.616356365089));
#82804=CARTESIAN_POINT('Ctrl Pts',(-39.4510541285328,-3.83397750999219,
127.720759188024));
#82805=CARTESIAN_POINT('Ctrl Pts',(-39.4588270287982,-3.91838682068088,
127.828770430879));
#82806=CARTESIAN_POINT('Ctrl Pts',(-39.4665999290637,-3.99804867774925,
127.939960185914));
#82807=CARTESIAN_POINT('Ctrl Pts',(-39.4740902648257,-4.0748146256575,128.047107913285));
#82808=CARTESIAN_POINT('Ctrl Pts',(-39.4815806005878,-4.1471721220219,128.157206813712));
#82809=CARTESIAN_POINT('Ctrl Pts',(-39.4890709363498,-4.21490742587628,
128.269851108057));
#82810=CARTESIAN_POINT('Ctrl Pts',(-39.4971083552182,-4.28759001668972,
128.390722775968));
#82811=CARTESIAN_POINT('Ctrl Pts',(-39.5051457740864,-4.35516775034002,
128.514886492627));
#82812=CARTESIAN_POINT('Ctrl Pts',(-39.5131831929548,-4.41734034050855,
128.641888102454));
#82813=CARTESIAN_POINT('Ctrl Pts',(-39.5212097282743,-4.47942874215494,
128.768717738139));
#82814=CARTESIAN_POINT('Ctrl Pts',(-39.5292362635939,-4.53612641755964,
128.898377300592));
#82815=CARTESIAN_POINT('Ctrl Pts',(-39.5372627989135,-4.58717710024377,
129.030385050232));
#82816=CARTESIAN_POINT('Ctrl Pts',(-39.545276454415,-4.63814586420752,129.16218097301));
#82817=CARTESIAN_POINT('Ctrl Pts',(-39.5532901099165,-4.68348556729917,
129.296317244772));
#82818=CARTESIAN_POINT('Ctrl Pts',(-39.5613037654181,-4.72298676985517,
129.432289542777));
#82819=CARTESIAN_POINT('Ctrl Pts',(-39.5642404854233,-4.73746255706055,
129.482118558715));
#82820=CARTESIAN_POINT('Ctrl Pts',(-39.5671772054286,-4.75115471100942,
129.532193927731));
#82821=CARTESIAN_POINT('Ctrl Pts',(-39.5701139254339,-4.76405452823409,
129.582490119308));
#82822=CARTESIAN_POINT('Origin',(213.235140564004,0.,130.804360617566));
#82823=CARTESIAN_POINT('',(-41.6650773111923,-4.76405452823405,129.582490119308));
#82824=CARTESIAN_POINT('',(-41.3197599198393,-4.76405452823404,129.582490119308));
#82825=CARTESIAN_POINT('',(213.235140564004,-4.76405452823405,129.582490119308));
#82826=CARTESIAN_POINT('',(-39.9851405639765,-4.91824854872011,130.808138912485));
#82827=CARTESIAN_POINT('Ctrl Pts',(-39.9851405640085,-4.91824854871968,
130.808138913047));
#82828=CARTESIAN_POINT('Ctrl Pts',(-39.9988861052777,-4.91806270117596,
131.050058693222));
#82829=CARTESIAN_POINT('Ctrl Pts',(-40.012631646547,-4.90002514730396,131.291308336928));
#82830=CARTESIAN_POINT('Ctrl Pts',(-40.0263771878162,-4.86444322375335,
131.529877802325));
#82831=CARTESIAN_POINT('Ctrl Pts',(-40.0341515219352,-4.84431846061283,
131.664810192274));
#82832=CARTESIAN_POINT('Ctrl Pts',(-40.0419258560543,-4.81854333208972,
131.799118324574));
#82833=CARTESIAN_POINT('Ctrl Pts',(-40.0497001901734,-4.78716563351233,
131.932291581685));
#82834=CARTESIAN_POINT('Ctrl Pts',(-40.0574649431205,-4.75582660514417,
132.065300714659));
#82835=CARTESIAN_POINT('Ctrl Pts',(-40.0652296960675,-4.71889883375243,
132.197177378413));
#82836=CARTESIAN_POINT('Ctrl Pts',(-40.0729944490145,-4.67648170823861,
132.327417377838));
#82837=CARTESIAN_POINT('Ctrl Pts',(-40.0807514898996,-4.63410671201165,
132.457528021059));
#82838=CARTESIAN_POINT('Ctrl Pts',(-40.0885085307846,-4.58625333188387,
132.586004865544));
#82839=CARTESIAN_POINT('Ctrl Pts',(-40.0962655716696,-4.5330716309168,132.712355547192));
#82840=CARTESIAN_POINT('Ctrl Pts',(-40.1040167629097,-4.4799300346842,132.838610946807));
#82841=CARTESIAN_POINT('Ctrl Pts',(-40.1117679541499,-4.42146826651086,
132.962743016079));
#82842=CARTESIAN_POINT('Ctrl Pts',(-40.11951914539,-4.35788556834454,133.084276501039));
#82843=CARTESIAN_POINT('Ctrl Pts',(-40.1272670421671,-4.29432989452124,
133.205758331027));
#82844=CARTESIAN_POINT('Ctrl Pts',(-40.1350149389442,-4.22565780051822,
133.324643427709));
#82845=CARTESIAN_POINT('Ctrl Pts',(-40.1427628357212,-4.15211572223893,
133.440478614097));
#82846=CARTESIAN_POINT('Ctrl Pts',(-40.1505091118053,-4.07858902737693,
133.556289570262));
#82847=CARTESIAN_POINT('Ctrl Pts',(-40.1582553878894,-4.00019458389978,
133.669051555246));
#82848=CARTESIAN_POINT('Ctrl Pts',(-40.1660016639735,-3.91722344080143,
133.778338354089));
#82849=CARTESIAN_POINT('Ctrl Pts',(-40.1737479972388,-3.83425168522907,
133.887625959662));
#82850=CARTESIAN_POINT('Ctrl Pts',(-40.1814943305042,-3.74670339903135,
133.993438016515));
#82851=CARTESIAN_POINT('Ctrl Pts',(-40.1892406637695,-3.65491114720952,
134.095379847));
#82852=CARTESIAN_POINT('Ctrl Pts',(-40.1969887317725,-3.56309833914934,
134.197344506651));
#82853=CARTESIAN_POINT('Ctrl Pts',(-40.2047367997754,-3.46703993582788,
134.2954369248));
#82854=CARTESIAN_POINT('Ctrl Pts',(-40.2124848677783,-3.36710644174079,
134.38929817246));
#82855=CARTESIAN_POINT('Ctrl Pts',(-40.2202411705202,-3.26706673714696,
134.483259176971));
#82856=CARTESIAN_POINT('Ctrl Pts',(-40.227997473262,-3.16314400008589,134.572979759788));
#82857=CARTESIAN_POINT('Ctrl Pts',(-40.2357537760038,-3.05574342644822,
134.658139954038));
#82858=CARTESIAN_POINT('Ctrl Pts',(-40.243514218518,-2.9482855298905,134.743345600848));
#82859=CARTESIAN_POINT('Ctrl Pts',(-40.2512746610322,-2.8373464141595,134.823985779344));
#82860=CARTESIAN_POINT('Ctrl Pts',(-40.2590351035464,-2.72336070876421,
134.899783613113));
#82861=CARTESIAN_POINT('Ctrl Pts',(-40.2668080038118,-2.60919202339545,
134.975703124295));
#82862=CARTESIAN_POINT('Ctrl Pts',(-40.2745809040772,-2.49196730979754,
135.04676455431));
#82863=CARTESIAN_POINT('Ctrl Pts',(-40.2823538043426,-2.37214704724894,
135.11273634964));
#82864=CARTESIAN_POINT('Ctrl Pts',(-40.2898441401047,-2.25668255305155,
135.176309904039));
#82865=CARTESIAN_POINT('Ctrl Pts',(-40.2973344758668,-2.13880821869824,
135.23515730378));
#82866=CARTESIAN_POINT('Ctrl Pts',(-40.3048248116289,-2.01895222782011,
135.289114230005));
#82867=CARTESIAN_POINT('Ctrl Pts',(-40.312599145748,-1.89455186061979,135.345116949486));
#82868=CARTESIAN_POINT('Ctrl Pts',(-40.3203734798671,-1.76762253855215,
135.396028430037));
#82869=CARTESIAN_POINT('Ctrl Pts',(-40.3281478139862,-1.63861969315752,
135.441612881967));
#82870=CARTESIAN_POINT('Ctrl Pts',(-40.3359125669333,-1.50977583224052,
135.487141155135));
#82871=CARTESIAN_POINT('Ctrl Pts',(-40.3436773198804,-1.37886389763405,
135.52735533324));
#82872=CARTESIAN_POINT('Ctrl Pts',(-40.3514420728275,-1.24636180509307,
135.562066505208));
#82873=CARTESIAN_POINT('Ctrl Pts',(-40.3591991137125,-1.11399131549854,
135.596743201551));
#82874=CARTESIAN_POINT('Ctrl Pts',(-40.3669561545976,-0.980034186737435,
135.625927670236));
#82875=CARTESIAN_POINT('Ctrl Pts',(-40.3747131954826,-0.844985771422639,
135.649480028746));
#82876=CARTESIAN_POINT('Ctrl Pts',(-40.3824643867227,-0.710039197168354,
135.673014626239));
#82877=CARTESIAN_POINT('Ctrl Pts',(-40.3902155779628,-0.574003357981259,
135.690925500487));
#82878=CARTESIAN_POINT('Ctrl Pts',(-40.3979667692029,-0.437385793624253,
135.703123393006));
#82879=CARTESIAN_POINT('Ctrl Pts',(-40.40571466598,-0.300826295376491,135.715316101095));
#82880=CARTESIAN_POINT('Ctrl Pts',(-40.413462562757,-0.163685952318491,
135.721800622202));
#82881=CARTESIAN_POINT('Ctrl Pts',(-40.4212104595341,-0.0264792397117674,
135.722539336601));
#82882=CARTESIAN_POINT('Ctrl Pts',(-40.4289567356182,0.110698772208513,
135.723277896476));
#82883=CARTESIAN_POINT('Ctrl Pts',(-40.4367030117023,0.247942735351468,
135.718273038181));
#82884=CARTESIAN_POINT('Ctrl Pts',(-40.4444492877864,0.384736743908612,
135.707539249881));
#82885=CARTESIAN_POINT('Ctrl Pts',(-40.4521956210518,0.521531762248052,
135.696805382346));
#82886=CARTESIAN_POINT('Ctrl Pts',(-40.4599419543171,0.6578764296068,135.680342531003));
#82887=CARTESIAN_POINT('Ctrl Pts',(-40.4676882875824,0.793258932997148,
135.658217159299));
#82888=CARTESIAN_POINT('Ctrl Pts',(-40.4754363555854,0.92867175436027,135.636086832771));
#82889=CARTESIAN_POINT('Ctrl Pts',(-40.4831844235883,1.0631215972222,135.60829152559));
#82890=CARTESIAN_POINT('Ctrl Pts',(-40.4909324915913,1.19610621773281,135.5749489438));
#82891=CARTESIAN_POINT('Ctrl Pts',(-40.4986887943332,1.32923217588082,135.541570925117));
#82892=CARTESIAN_POINT('Ctrl Pts',(-40.506445097075,1.46088942105955,135.502633949742));
#82893=CARTESIAN_POINT('Ctrl Pts',(-40.5142013998169,1.59058973780019,135.458305970544));
#82894=CARTESIAN_POINT('Ctrl Pts',(-40.5219618423311,1.72035927950526,135.413954332168));
#82895=CARTESIAN_POINT('Ctrl Pts',(-40.5297222848452,1.84816944741361,135.364206098367));
#82896=CARTESIAN_POINT('Ctrl Pts',(-40.5374827273594,1.97355236969247,135.309277276793));
#82897=CARTESIAN_POINT('Ctrl Pts',(-40.5452556276249,2.09913656776914,135.254260278598));
#82898=CARTESIAN_POINT('Ctrl Pts',(-40.5530285278902,2.22228538247704,135.194046245766));
#82899=CARTESIAN_POINT('Ctrl Pts',(-40.5608014281557,2.34255510098758,135.128897432225));
#82900=CARTESIAN_POINT('Ctrl Pts',(-40.5682917639177,2.45845271228946,135.066116942155));
#82901=CARTESIAN_POINT('Ctrl Pts',(-40.5757820996798,2.57167665329429,134.998754383277));
#82902=CARTESIAN_POINT('Ctrl Pts',(-40.5832724354419,2.68185723418049,134.92708118025));
#82903=CARTESIAN_POINT('Ctrl Pts',(-40.5910467695609,2.79621534527919,134.852690465945));
#82904=CARTESIAN_POINT('Ctrl Pts',(-40.59882110368,2.90765701475315,134.773420131284));
#82905=CARTESIAN_POINT('Ctrl Pts',(-40.6065954377991,3.01573769418655,134.689525893634));
#82906=CARTESIAN_POINT('Ctrl Pts',(-40.6143601907462,3.12368517384198,134.605735048134));
#82907=CARTESIAN_POINT('Ctrl Pts',(-40.6221249436933,3.22827959916315,134.517331875483));
#82908=CARTESIAN_POINT('Ctrl Pts',(-40.6298896966404,3.32910370877294,134.42461634869));
#82909=CARTESIAN_POINT('Ctrl Pts',(-40.6376467375254,3.4298276784557,134.331992908265));
#82910=CARTESIAN_POINT('Ctrl Pts',(-40.6454037784103,3.52678849868834,134.23506590017));
#82911=CARTESIAN_POINT('Ctrl Pts',(-40.6531608192953,3.61960073215858,134.134176468669));
#82912=CARTESIAN_POINT('Ctrl Pts',(-40.6609120105354,3.71234297520158,134.033363118673));
#82913=CARTESIAN_POINT('Ctrl Pts',(-40.6686632017757,3.80094259490978,133.928593579458));
#82914=CARTESIAN_POINT('Ctrl Pts',(-40.6764143930158,3.88505015795253,133.820246612211));
#82915=CARTESIAN_POINT('Ctrl Pts',(-40.6841622897929,3.96912197303734,133.711945695314));
#82916=CARTESIAN_POINT('Ctrl Pts',(-40.6919101865699,4.04870528955814,133.600070682735));
#82917=CARTESIAN_POINT('Ctrl Pts',(-40.6996580833469,4.12349037052715,133.485034082699));
#82918=CARTESIAN_POINT('Ctrl Pts',(-40.707404359431,4.1982598080694,133.37002154584));
#82919=CARTESIAN_POINT('Ctrl Pts',(-40.7151506355151,4.2682327934901,133.251849064539));
#82920=CARTESIAN_POINT('Ctrl Pts',(-40.7228969115992,4.33314265640084,133.130958516168));
#82921=CARTESIAN_POINT('Ctrl Pts',(-40.7306432448646,4.39805299846145,133.010067075411));
#82922=CARTESIAN_POINT('Ctrl Pts',(-40.7383895781299,4.45789995848569,132.886457872002));
#82923=CARTESIAN_POINT('Ctrl Pts',(-40.7461359113953,4.51246280663164,132.76059743382));
#82924=CARTESIAN_POINT('Ctrl Pts',(-40.7538839793982,4.56703787374912,132.634708810065));
#82925=CARTESIAN_POINT('Ctrl Pts',(-40.7616320474012,4.61632631880141,132.506568306978));
#82926=CARTESIAN_POINT('Ctrl Pts',(-40.7693801154042,4.66015569614619,132.376662099527));
#82927=CARTESIAN_POINT('Ctrl Pts',(-40.777136418146,4.70403165587479,132.246617826212));
#82928=CARTESIAN_POINT('Ctrl Pts',(-40.7848927208879,4.74243683266572,132.114804470838));
#82929=CARTESIAN_POINT('Ctrl Pts',(-40.7926490236297,4.77524863763722,131.981723565532));
#82930=CARTESIAN_POINT('Ctrl Pts',(-40.8004094661439,4.80807795525697,131.848571630941));
#82931=CARTESIAN_POINT('Ctrl Pts',(-40.808169908658,4.83530787490849,131.71415118137));
#82932=CARTESIAN_POINT('Ctrl Pts',(-40.8159303511722,4.8568672337927,131.578972608056));
#82933=CARTESIAN_POINT('Ctrl Pts',(-40.8237032514376,4.87846120167374,131.443577034096));
#82934=CARTESIAN_POINT('Ctrl Pts',(-40.8314761517031,4.89436637292891,131.307421292971));
#82935=CARTESIAN_POINT('Ctrl Pts',(-40.8392490519686,4.9045635515924,131.171020447506));
#82936=CARTESIAN_POINT('Ctrl Pts',(-40.8467393877306,4.91439003712641,131.039578116345));
#82937=CARTESIAN_POINT('Ctrl Pts',(-40.8542297234927,4.91891631429733,130.907908499613));
#82938=CARTESIAN_POINT('Ctrl Pts',(-40.8617200592547,4.91817091397879,130.776469339485));
#82939=CARTESIAN_POINT('Ctrl Pts',(-40.8694943933738,4.91739725158062,130.640046623651));
#82940=CARTESIAN_POINT('Ctrl Pts',(-40.877268727493,4.91094181844268,130.503440038761));
#82941=CARTESIAN_POINT('Ctrl Pts',(-40.8850430616121,4.8987794675504,130.367161817469));
#82942=CARTESIAN_POINT('Ctrl Pts',(-40.8928078145592,4.88663210566861,130.231051546905));
#82943=CARTESIAN_POINT('Ctrl Pts',(-40.9005725675062,4.86879185455618,130.095269220428));
#82944=CARTESIAN_POINT('Ctrl Pts',(-40.9083373204533,4.84528555003507,129.960328034592));
#82945=CARTESIAN_POINT('Ctrl Pts',(-40.9160943613383,4.82180259230702,129.825520874244));
#82946=CARTESIAN_POINT('Ctrl Pts',(-40.9238514022233,4.79266484701677,129.691553574661));
#82947=CARTESIAN_POINT('Ctrl Pts',(-40.9316084431083,4.75795099021294,129.558934811975));
#82948=CARTESIAN_POINT('Ctrl Pts',(-40.9393596343484,4.72326331139855,129.42641605813));
#82949=CARTESIAN_POINT('Ctrl Pts',(-40.9471108255886,4.68300798944803,129.295244193714));
#82950=CARTESIAN_POINT('Ctrl Pts',(-40.9548620168287,4.63731480962308,129.165917936557));
#82951=CARTESIAN_POINT('Ctrl Pts',(-40.9626099136058,4.5916410506184,129.03664664651));
#82952=CARTESIAN_POINT('Ctrl Pts',(-40.9703578103828,4.54053416058043,128.909219771406));
#82953=CARTESIAN_POINT('Ctrl Pts',(-40.9781057071599,4.4841737739554,128.784120872518));
#82954=CARTESIAN_POINT('Ctrl Pts',(-40.985851983244,4.42782517670834,128.659048141624));
#82955=CARTESIAN_POINT('Ctrl Pts',(-40.9935982593281,4.3662254291755,128.536302774585));
#82956=CARTESIAN_POINT('Ctrl Pts',(-41.0013445354122,4.29960215344792,128.416347974265));
#82957=CARTESIAN_POINT('Ctrl Pts',(-41.0090908686776,4.23297838592236,128.296392288466));
#82958=CARTESIAN_POINT('Ctrl Pts',(-41.0168372019429,4.16133120603621,128.179227552278));
#82959=CARTESIAN_POINT('Ctrl Pts',(-41.0245835352083,4.08493380703481,128.065291641683));
#82960=CARTESIAN_POINT('Ctrl Pts',(-41.0323316032113,4.00851929936571,127.951330215931));
#82961=CARTESIAN_POINT('Ctrl Pts',(-41.0400796712143,3.92735267347948,127.840599379263));
#82962=CARTESIAN_POINT('Ctrl Pts',(-41.0478277392172,3.84174975106248,127.733507004528));
#82963=CARTESIAN_POINT('Ctrl Pts',(-41.0555840419591,3.75605584884073,127.626300810741));
#82964=CARTESIAN_POINT('Ctrl Pts',(-41.0633403447009,3.66591647597003,127.522741109516));
#82965=CARTESIAN_POINT('Ctrl Pts',(-41.0710966474428,3.57168732334919,127.423202128715));
#82966=CARTESIAN_POINT('Ctrl Pts',(-41.0788570899569,3.47740787779242,127.323610020964));
#82967=CARTESIAN_POINT('Ctrl Pts',(-41.0866175324712,3.37903458328288,127.228043181974));
#82968=CARTESIAN_POINT('Ctrl Pts',(-41.0943779749853,3.27695838119108,127.136837361956));
#82969=CARTESIAN_POINT('Ctrl Pts',(-41.1021508752508,3.17471831731777,127.045485130258));
#82970=CARTESIAN_POINT('Ctrl Pts',(-41.1099237755162,3.06876376974749,126.958508155357));
#82971=CARTESIAN_POINT('Ctrl Pts',(-41.1176966757817,2.959517699532,126.876200991398));
#82972=CARTESIAN_POINT('Ctrl Pts',(-41.1251870115437,2.85424299914339,126.796885900169));
#82973=CARTESIAN_POINT('Ctrl Pts',(-41.1326773473057,2.74591218488185,126.721907170942));
#82974=CARTESIAN_POINT('Ctrl Pts',(-41.1401676830677,2.63492578983711,126.651488220712));
#82975=CARTESIAN_POINT('Ctrl Pts',(-41.1479420171867,2.51973131189035,126.578399314581));
#82976=CARTESIAN_POINT('Ctrl Pts',(-41.1557163513058,2.40131100382872,126.509991257373));
#82977=CARTESIAN_POINT('Ctrl Pts',(-41.1634906854249,2.28008222891679,126.446562080245));
#82978=CARTESIAN_POINT('Ctrl Pts',(-41.171255438372,2.15900285763557,126.383211073909));
#82979=CARTESIAN_POINT('Ctrl Pts',(-41.1790201913191,2.03512224931721,126.324826918304));
#82980=CARTESIAN_POINT('Ctrl Pts',(-41.1867849442662,1.90888667617337,126.271664430965));
#82981=CARTESIAN_POINT('Ctrl Pts',(-41.1945419851512,1.78277648198039,126.218554745357));
#82982=CARTESIAN_POINT('Ctrl Pts',(-41.2022990260361,1.65431633563104,126.170656557936));
#82983=CARTESIAN_POINT('Ctrl Pts',(-41.2100560669211,1.52397672708972,126.128178628187));
#82984=CARTESIAN_POINT('Ctrl Pts',(-41.2178072581612,1.39373540866109,126.085732731376));
#82985=CARTESIAN_POINT('Ctrl Pts',(-41.2255584494014,1.26161781934262,126.048699077056));
#82986=CARTESIAN_POINT('Ctrl Pts',(-41.2333096406415,1.12811369667322,126.017238042378));
#82987=CARTESIAN_POINT('Ctrl Pts',(-41.2410575374186,0.99466631681729,125.985790379479));
#82988=CARTESIAN_POINT('Ctrl Pts',(-41.2488054341957,0.859833955455193,
125.959910714922));
#82989=CARTESIAN_POINT('Ctrl Pts',(-41.2565533309727,0.72412054318671,125.939709293839));
#82990=CARTESIAN_POINT('Ctrl Pts',(-41.2642996070568,0.588435519238431,
125.919512098459));
#82991=CARTESIAN_POINT('Ctrl Pts',(-41.2720458831409,0.451870197419816,
125.904990841547));
#82992=CARTESIAN_POINT('Ctrl Pts',(-41.279792159225,0.314937318719655,125.896204390654));
#82993=CARTESIAN_POINT('Ctrl Pts',(-41.2875384924904,0.17800342921209,125.887417874901));
#82994=CARTESIAN_POINT('Ctrl Pts',(-41.2952848257557,0.0407023675717651,
125.884366274676));
#82995=CARTESIAN_POINT('Ctrl Pts',(-41.3030311590211,-0.0964498011149574,
125.887056427426));
#82996=CARTESIAN_POINT('Ctrl Pts',(-41.310779227024,-0.233632684078911,
125.889747182618));
#82997=CARTESIAN_POINT('Ctrl Pts',(-41.3185272950269,-0.370666216924256,
125.898182241764));
#82998=CARTESIAN_POINT('Ctrl Pts',(-41.3262753630299,-0.507036535337007,
125.912316360373));
#82999=CARTESIAN_POINT('Ctrl Pts',(-41.3340316657718,-0.643551789746993,
125.926465500891));
#83000=CARTESIAN_POINT('Ctrl Pts',(-41.3417879685136,-0.779402032164128,
125.946325760069));
#83001=CARTESIAN_POINT('Ctrl Pts',(-41.3495442712555,-0.914080154468566,
125.971800164379));
#83002=CARTESIAN_POINT('Ctrl Pts',(-41.3573047137696,-1.04883015854214,
125.997288165146));
#83003=CARTESIAN_POINT('Ctrl Pts',(-41.3650651562838,-1.18240641536105,
126.02839619307));
#83004=CARTESIAN_POINT('Ctrl Pts',(-41.372825598798,-1.31431513540615,126.064976819292));
#83005=CARTESIAN_POINT('Ctrl Pts',(-41.3805984990634,-1.44643560703898,
126.101616167983));
#83006=CARTESIAN_POINT('Ctrl Pts',(-41.3883713993288,-1.57688282038497,
126.143745550177));
#83007=CARTESIAN_POINT('Ctrl Pts',(-41.3961442995943,-1.70518033791856,
126.191168330475));
#83008=CARTESIAN_POINT('Ctrl Pts',(-41.4036346353563,-1.82881391752839,
126.236867173258));
#83009=CARTESIAN_POINT('Ctrl Pts',(-41.4111249711184,-1.9504510971713,126.287481120781));
#83010=CARTESIAN_POINT('Ctrl Pts',(-41.4186153068805,-2.06968741188378,
126.342793955553));
#83011=CARTESIAN_POINT('Ctrl Pts',(-41.4263902653792,-2.19345454701301,
126.400208604035));
#83012=CARTESIAN_POINT('Ctrl Pts',(-41.4341652238779,-2.31502683861591,
126.462868190964));
#83013=CARTESIAN_POINT('Ctrl Pts',(-41.4419401823766,-2.43392783549776,
126.530582622151));
#83014=CARTESIAN_POINT('Ctrl Pts',(-41.4497054190613,-2.55268015848356,
126.598212383163));
#83015=CARTESIAN_POINT('Ctrl Pts',(-41.457470655746,-2.66876749656911,126.670884219826));
#83016=CARTESIAN_POINT('Ctrl Pts',(-41.4652358924307,-2.78173416079713,
126.748360356083));
#83017=CARTESIAN_POINT('Ctrl Pts',(-41.4729932770136,-2.89458659466821,
126.825758149522));
#83018=CARTESIAN_POINT('Ctrl Pts',(-41.4807506615965,-3.00432431453443,
126.907950354258));
#83019=CARTESIAN_POINT('Ctrl Pts',(-41.4885080461793,-3.11051732110719,
126.994653928385));
#83020=CARTESIAN_POINT('Ctrl Pts',(-41.4962589928004,-3.21662219662083,
127.081285546004));
#83021=CARTESIAN_POINT('Ctrl Pts',(-41.5040099394213,-3.3191879152424,127.172420831183));
#83022=CARTESIAN_POINT('Ctrl Pts',(-41.5117608860424,-3.41781487530316,
127.267734465333));
#83023=CARTESIAN_POINT('Ctrl Pts',(-41.5195083337016,-3.51639731280616,
127.36300507264));
#83024=CARTESIAN_POINT('Ctrl Pts',(-41.5272557813608,-3.61104424889036,
127.462450005041));
#83025=CARTESIAN_POINT('Ctrl Pts',(-41.53500322902,-3.70139061247776,127.565704940227));
#83026=CARTESIAN_POINT('Ctrl Pts',(-41.5427488570747,-3.7917157568632,127.668935624439));
#83027=CARTESIAN_POINT('Ctrl Pts',(-41.5504944851293,-3.87774208194308,
127.77597423644));
#83028=CARTESIAN_POINT('Ctrl Pts',(-41.5582401131839,-3.95914299596626,
127.886421310454));
#83029=CARTESIAN_POINT('Ctrl Pts',(-41.5659855994087,-4.04054241946133,
127.996866362076));
#83030=CARTESIAN_POINT('Ctrl Pts',(-41.5737310856335,-4.11731636978816,
128.110719436078));
#83031=CARTESIAN_POINT('Ctrl Pts',(-41.5814765718583,-4.18918024022112,
128.227550190421));
#83032=CARTESIAN_POINT('Ctrl Pts',(-41.5892267892329,-4.26108800702499,
128.344452308109));
#83033=CARTESIAN_POINT('Ctrl Pts',(-41.5969770066076,-4.3280794971936,128.464335406502));
#83034=CARTESIAN_POINT('Ctrl Pts',(-41.6047272239822,-4.38991482252266,
128.586742320046));
#83035=CARTESIAN_POINT('Ctrl Pts',(-41.6124799930164,-4.45177050633902,
128.709189534495));
#83036=CARTESIAN_POINT('Ctrl Pts',(-41.6202327620507,-4.50846647793683,
128.834161865338));
#83037=CARTESIAN_POINT('Ctrl Pts',(-41.6279855310849,-4.55981048029157,
128.961180906761));
#83038=CARTESIAN_POINT('Ctrl Pts',(-41.6357466300772,-4.61120964917867,
129.088336423717));
#83039=CARTESIAN_POINT('Ctrl Pts',(-41.6435077290694,-4.65724522892415,
129.217542676514));
#83040=CARTESIAN_POINT('Ctrl Pts',(-41.6512688280616,-4.69777430233468,
129.348304414384));
#83041=CARTESIAN_POINT('Ctrl Pts',(-41.6558716557719,-4.72181063305927,
129.425854481857));
#83042=CARTESIAN_POINT('Ctrl Pts',(-41.6604744834821,-4.74391114867854,
129.50395138814));
#83043=CARTESIAN_POINT('Ctrl Pts',(-41.6650773111923,-4.76405452823405,
129.582490119308));
#83044=CARTESIAN_POINT('Ctrl Pts',(-39.9150204635388,-4.76405452823403,
129.582490119308));
#83045=CARTESIAN_POINT('Ctrl Pts',(-39.9226601301531,-4.79766750777594,
129.713546616394));
#83046=CARTESIAN_POINT('Ctrl Pts',(-39.9302997967672,-4.82585041976442,
129.845921259423));
#83047=CARTESIAN_POINT('Ctrl Pts',(-39.9379394633814,-4.84852111043041,
129.979117559909));
#83048=CARTESIAN_POINT('Ctrl Pts',(-39.9458063134806,-4.87186596749284,
130.116274766186));
#83049=CARTESIAN_POINT('Ctrl Pts',(-39.9536731635798,-4.88936559114322,
130.254302799531));
#83050=CARTESIAN_POINT('Ctrl Pts',(-39.961540013679,-4.90098781854546,130.392655061411));
#83051=CARTESIAN_POINT('Ctrl Pts',(-39.9694068637782,-4.91261004594769,
130.531007323291));
#83052=CARTESIAN_POINT('Ctrl Pts',(-39.9772737138774,-4.91835491299647,
130.669683350103));
#83053=CARTESIAN_POINT('Ctrl Pts',(-39.9851405639765,-4.91824854872011,
130.808138912485));
#83054=CARTESIAN_POINT('',(-39.6398594360423,-4.91824987188027,130.80548322601));
#83055=CARTESIAN_POINT('Ctrl Pts',(-39.5701139254339,-4.76405452823409,
129.582490119308));
#83056=CARTESIAN_POINT('Ctrl Pts',(-39.5781133945864,-4.79919294448669,
129.719494270977));
#83057=CARTESIAN_POINT('Ctrl Pts',(-39.5861128637389,-4.82844873500477,
129.858138048181));
#83058=CARTESIAN_POINT('Ctrl Pts',(-39.5941123328914,-4.85167949962034,
129.997893572075));
#83059=CARTESIAN_POINT('Ctrl Pts',(-39.6021025955522,-4.87488352823167,
130.137488253037));
#83060=CARTESIAN_POINT('Ctrl Pts',(-39.6100928582131,-4.89207629594091,
130.278191781637));
#83061=CARTESIAN_POINT('Ctrl Pts',(-39.6180831208739,-4.90316615218488,
130.419464856913));
#83062=CARTESIAN_POINT('Ctrl Pts',(-39.6253418925796,-4.91324075650532,
130.547804693176));
#83063=CARTESIAN_POINT('Ctrl Pts',(-39.6326006642854,-4.91827928667657,
130.67661421901));
#83064=CARTESIAN_POINT('Ctrl Pts',(-39.6398594359911,-4.91824987188048,
130.8054832251));
#83065=CARTESIAN_POINT('Ctrl Pts',(-39.6398594360424,-4.91824987188027,
130.80548322601));
#83066=CARTESIAN_POINT('Ctrl Pts',(-39.6481290507699,-4.91821636080731,
130.952298289754));
#83067=CARTESIAN_POINT('Ctrl Pts',(-39.6563986654975,-4.9116047325426,131.098940220869));
#83068=CARTESIAN_POINT('Ctrl Pts',(-39.6646682802251,-4.89848671975691,
131.244827323306));
#83069=CARTESIAN_POINT('Ctrl Pts',(-39.6732391368865,-4.88489084969848,
131.396028737753));
#83070=CARTESIAN_POINT('Ctrl Pts',(-39.681809993548,-4.86430572391944,131.546418918438));
#83071=CARTESIAN_POINT('Ctrl Pts',(-39.6903808502094,-4.83686829731992,
131.695364622541));
#83072=CARTESIAN_POINT('Ctrl Pts',(-39.6986930973762,-4.81025874351182,
131.839816169898));
#83073=CARTESIAN_POINT('Ctrl Pts',(-39.707005344543,-4.77720456139641,131.982908891268));
#83074=CARTESIAN_POINT('Ctrl Pts',(-39.7153175917098,-4.73788102594566,
132.124082727135));
#83075=CARTESIAN_POINT('Ctrl Pts',(-39.7240177531187,-4.69672234782602,
132.271844834553));
#83076=CARTESIAN_POINT('Ctrl Pts',(-39.7327179145274,-4.64869527844162,
132.417504279031));
#83077=CARTESIAN_POINT('Ctrl Pts',(-39.7414180759363,-4.59405636483465,
132.560444094859));
#83078=CARTESIAN_POINT('Ctrl Pts',(-39.7501182373451,-4.53941745122775,
132.703383910688));
#83079=CARTESIAN_POINT('Ctrl Pts',(-39.7588183987539,-4.47816691515689,
132.84360378822));
#83080=CARTESIAN_POINT('Ctrl Pts',(-39.7675185601628,-4.41061504991322,
132.980517308611));
#83081=CARTESIAN_POINT('Ctrl Pts',(-39.7752928942818,-4.35025171340783,
133.102861182813));
#83082=CARTESIAN_POINT('Ctrl Pts',(-39.783067228401,-4.28469845338574,133.222885354349));
#83083=CARTESIAN_POINT('Ctrl Pts',(-39.7908415625201,-4.2141566923093,133.340118183889));
#83084=CARTESIAN_POINT('Ctrl Pts',(-39.7986063154672,-4.14370186764889,
133.457206534444));
#83085=CARTESIAN_POINT('Ctrl Pts',(-39.8063710684142,-4.06827097402557,
133.571510055957));
#83086=CARTESIAN_POINT('Ctrl Pts',(-39.8141358213613,-3.98811260262222,
133.682578978168));
#83087=CARTESIAN_POINT('Ctrl Pts',(-39.8218928622463,-3.90803384564349,
133.793537585159));
#83088=CARTESIAN_POINT('Ctrl Pts',(-39.8296499031313,-3.82323718225476,
133.901267671191));
#83089=CARTESIAN_POINT('Ctrl Pts',(-39.8374069440163,-3.7340158454221,134.005346204637));
#83090=CARTESIAN_POINT('Ctrl Pts',(-39.8451581352565,-3.64486179109347,
134.109346251651));
#83091=CARTESIAN_POINT('Ctrl Pts',(-39.8529093264966,-3.55128995820697,
134.209699931454));
#83092=CARTESIAN_POINT('Ctrl Pts',(-39.8606605177367,-3.45363518574191,
134.306015521509));
#83093=CARTESIAN_POINT('Ctrl Pts',(-39.8684084145138,-3.35602191916003,
134.402290174868));
#83094=CARTESIAN_POINT('Ctrl Pts',(-39.8761563112909,-3.25432944226823,
134.494529878097));
#83095=CARTESIAN_POINT('Ctrl Pts',(-39.883904208068,-3.14893079336533,134.582378341333));
#83096=CARTESIAN_POINT('Ctrl Pts',(-39.8916504841521,-3.04355419158781,
134.670208428563));
#83097=CARTESIAN_POINT('Ctrl Pts',(-39.8993967602362,-2.93447325995125,
134.753648852694));
#83098=CARTESIAN_POINT('Ctrl Pts',(-39.9071430363203,-2.82209528687978,
134.83238262027));
#83099=CARTESIAN_POINT('Ctrl Pts',(-39.9148893695857,-2.70971648425965,
134.911116969042));
#83100=CARTESIAN_POINT('Ctrl Pts',(-39.922635702851,-2.59404091183839,134.985144367595));
#83101=CARTESIAN_POINT('Ctrl Pts',(-39.9303820361164,-2.47550576198666,
135.05419053003));
#83102=CARTESIAN_POINT('Ctrl Pts',(-39.9381301041194,-2.35694406700999,
135.123252154874));
#83103=CARTESIAN_POINT('Ctrl Pts',(-39.9458781721224,-2.23552185808173,
135.18733012711));
#83104=CARTESIAN_POINT('Ctrl Pts',(-39.9536262401253,-2.11170153993017,
135.246195786588));
#83105=CARTESIAN_POINT('Ctrl Pts',(-39.9613825428672,-1.98774962407101,
135.305124009189));
#83106=CARTESIAN_POINT('Ctrl Pts',(-39.9691388456091,-1.86139486126452,
135.358828684735));
#83107=CARTESIAN_POINT('Ctrl Pts',(-39.976895148351,-1.73312079443059,135.407128847057));
#83108=CARTESIAN_POINT('Ctrl Pts',(-39.9846555908651,-1.60477826386476,
135.45545478863));
#83109=CARTESIAN_POINT('Ctrl Pts',(-39.9924160333793,-1.47451475923758,
135.49837034699));
#83110=CARTESIAN_POINT('Ctrl Pts',(-40.0001764758935,-1.34282869443821,
135.535744575764));
#83111=CARTESIAN_POINT('Ctrl Pts',(-40.0079493761589,-1.21093123547708,
135.573178800968));
#83112=CARTESIAN_POINT('Ctrl Pts',(-40.0157222764243,-1.07760703341135,
135.605053829711));
#83113=CARTESIAN_POINT('Ctrl Pts',(-40.0234951766897,-0.94336527875647,
135.631289766967));
#83114=CARTESIAN_POINT('Ctrl Pts',(-40.0309855124517,-0.814003550019504,
135.656571961819));
#83115=CARTESIAN_POINT('Ctrl Pts',(-40.0384758482137,-0.683790125625639,
135.676617890641));
#83116=CARTESIAN_POINT('Ctrl Pts',(-40.0459661839756,-0.553182913605547,
135.691401821259));
#83117=CARTESIAN_POINT('Ctrl Pts',(-40.0537405180947,-0.417623689442982,
135.7067462891));
#83118=CARTESIAN_POINT('Ctrl Pts',(-40.0615148522138,-0.281210816399245,
135.716470471348));
#83119=CARTESIAN_POINT('Ctrl Pts',(-40.0692891863329,-0.144449971760837,
135.720488897845));
#83120=CARTESIAN_POINT('Ctrl Pts',(-40.0770539392799,-0.00785767264096399,
135.724502371991));
#83121=CARTESIAN_POINT('Ctrl Pts',(-40.0848186922271,0.12908135775712,135.722824070268));
#83122=CARTESIAN_POINT('Ctrl Pts',(-40.0925834451741,0.265854345368811,
135.715420027668));
#83123=CARTESIAN_POINT('Ctrl Pts',(-40.1003404860591,0.402491488121046,
135.708023338867));
#83124=CARTESIAN_POINT('Ctrl Pts',(-40.1080975269441,0.538962528409856,
135.694912247346));
#83125=CARTESIAN_POINT('Ctrl Pts',(-40.1158545678291,0.674753058165272,
135.676104799376));
#83126=CARTESIAN_POINT('Ctrl Pts',(-40.1236057590692,0.810441187225903,
135.657311534249));
#83127=CARTESIAN_POINT('Ctrl Pts',(-40.1313569503093,0.945449441502048,
135.632830516358));
#83128=CARTESIAN_POINT('Ctrl Pts',(-40.1391081415495,1.07926726508193,135.60273171962));
#83129=CARTESIAN_POINT('Ctrl Pts',(-40.1468560383265,1.21302821251708,135.572645715673));
#83130=CARTESIAN_POINT('Ctrl Pts',(-40.1546039351036,1.34559935494425,135.536946767459));
#83131=CARTESIAN_POINT('Ctrl Pts',(-40.1623518318806,1.47647929929888,135.495756139289));
#83132=CARTESIAN_POINT('Ctrl Pts',(-40.1700981079647,1.60733186639079,135.45457412731));
#83133=CARTESIAN_POINT('Ctrl Pts',(-40.1778443840488,1.73649356636687,135.40790283758));
#83134=CARTESIAN_POINT('Ctrl Pts',(-40.1855906601329,1.86347755431497,135.35591359068));
#83135=CARTESIAN_POINT('Ctrl Pts',(-40.1933369933983,1.99046247962985,135.303923960007));
#83136=CARTESIAN_POINT('Ctrl Pts',(-40.2010833266636,2.11526929902405,135.246616441965));
#83137=CARTESIAN_POINT('Ctrl Pts',(-40.2088296599289,2.23743093484609,135.184210600647));
#83138=CARTESIAN_POINT('Ctrl Pts',(-40.2165777279319,2.35961992791946,135.121790783974));
#83139=CARTESIAN_POINT('Ctrl Pts',(-40.2243257959349,2.47916221057224,135.054270549932));
#83140=CARTESIAN_POINT('Ctrl Pts',(-40.2320738639379,2.59561546349312,134.981915336319));
#83141=CARTESIAN_POINT('Ctrl Pts',(-40.2398301666797,2.71219248431702,134.909483222724));
#83142=CARTESIAN_POINT('Ctrl Pts',(-40.2475864694216,2.82567358453307,134.832206071165));
#83143=CARTESIAN_POINT('Ctrl Pts',(-40.2553427721634,2.93564514541842,134.750392883359));
#83144=CARTESIAN_POINT('Ctrl Pts',(-40.2631032146776,3.04567540143714,134.668536029392));
#83145=CARTESIAN_POINT('Ctrl Pts',(-40.2708636571918,3.15219208223108,134.58213856126));
#83146=CARTESIAN_POINT('Ctrl Pts',(-40.278624099706,3.25481561402661,134.49154902897));
#83147=CARTESIAN_POINT('Ctrl Pts',(-40.2863969999714,3.35760388622587,134.40081407432));
#83148=CARTESIAN_POINT('Ctrl Pts',(-40.2941699002368,3.45648623849685,134.305873878812));
#83149=CARTESIAN_POINT('Ctrl Pts',(-40.3019428005022,3.55112022297843,134.207113653632));
#83150=CARTESIAN_POINT('Ctrl Pts',(-40.3094331362643,3.64231402375677,134.111943611398));
#83151=CARTESIAN_POINT('Ctrl Pts',(-40.3169234720264,3.72956276793215,134.013226683794));
#83152=CARTESIAN_POINT('Ctrl Pts',(-40.3244138077886,3.81259729582122,133.911334212947));
#83153=CARTESIAN_POINT('Ctrl Pts',(-40.3321881419077,3.89878010307179,133.8055784581));
#83154=CARTESIAN_POINT('Ctrl Pts',(-40.3399624760268,3.98069582294925,133.696066602626));
#83155=CARTESIAN_POINT('Ctrl Pts',(-40.3477368101459,4.05799921606556,133.583177888441));
#83156=CARTESIAN_POINT('Ctrl Pts',(-40.355501563093,4.13520733965865,133.470428299506));
#83157=CARTESIAN_POINT('Ctrl Pts',(-40.36326631604,4.20781422773934,133.354310451841));
#83158=CARTESIAN_POINT('Ctrl Pts',(-40.3710310689871,4.27551413767626,133.235237397872));
#83159=CARTESIAN_POINT('Ctrl Pts',(-40.3787881098721,4.34314680710823,133.116282608938));
#83160=CARTESIAN_POINT('Ctrl Pts',(-40.3865451507571,4.40588200525265,132.994378792459));
#83161=CARTESIAN_POINT('Ctrl Pts',(-40.3943021916421,4.46345686482174,132.869968488963));
#83162=CARTESIAN_POINT('Ctrl Pts',(-40.4020533828823,4.52098830674137,132.745652004244));
#83163=CARTESIAN_POINT('Ctrl Pts',(-40.4098045741223,4.57336699224735,132.618833148137));
#83164=CARTESIAN_POINT('Ctrl Pts',(-40.4175557653624,4.62037582443633,132.4899792884));
#83165=CARTESIAN_POINT('Ctrl Pts',(-40.4253036621395,4.66736467661769,132.361180194991));
#83166=CARTESIAN_POINT('Ctrl Pts',(-40.4330515589168,4.70898808115027,132.230348184752));
#83167=CARTESIAN_POINT('Ctrl Pts',(-40.4407994556938,4.74507704593572,132.09797064019));
#83168=CARTESIAN_POINT('Ctrl Pts',(-40.448545731778,4.78115846168768,131.965620786158));
#83169=CARTESIAN_POINT('Ctrl Pts',(-40.456292007862,4.81170763762495,131.83172641781));
#83170=CARTESIAN_POINT('Ctrl Pts',(-40.4640382839461,4.83660555903792,131.696789734518));
#83171=CARTESIAN_POINT('Ctrl Pts',(-40.4717846172115,4.86150366424168,131.561852055154));
#83172=CARTESIAN_POINT('Ctrl Pts',(-40.4795309504768,4.88075036073767,131.425872429969));
#83173=CARTESIAN_POINT('Ctrl Pts',(-40.4872772837422,4.89427790713727,131.289362504375));
#83174=CARTESIAN_POINT('Ctrl Pts',(-40.4950253517452,4.90780848293709,131.152822008329));
#83175=CARTESIAN_POINT('Ctrl Pts',(-40.5027734197482,4.91561732152165,131.015751364547));
#83176=CARTESIAN_POINT('Ctrl Pts',(-40.5105214877512,4.91768865883524,130.878666184405));
#83177=CARTESIAN_POINT('Ctrl Pts',(-40.5182777904931,4.91976219759078,130.741435308502));
#83178=CARTESIAN_POINT('Ctrl Pts',(-40.5260340932349,4.91608604797777,130.604190256921));
#83179=CARTESIAN_POINT('Ctrl Pts',(-40.5337903959767,4.90669661087029,130.467446041784));
#83180=CARTESIAN_POINT('Ctrl Pts',(-40.5415508384909,4.89730216233751,130.330628842143));
#83181=CARTESIAN_POINT('Ctrl Pts',(-40.5493112810051,4.88218839327771,130.194313399981));
#83182=CARTESIAN_POINT('Ctrl Pts',(-40.5570717235192,4.86144337978754,130.059007461257));
#83183=CARTESIAN_POINT('Ctrl Pts',(-40.5648446237847,4.84066506456003,129.923484317428));
#83184=CARTESIAN_POINT('Ctrl Pts',(-40.5726175240501,4.81423751597063,129.788974299253));
#83185=CARTESIAN_POINT('Ctrl Pts',(-40.5803904243155,4.78229972166743,129.655973733872));
#83186=CARTESIAN_POINT('Ctrl Pts',(-40.5878807600775,4.75152294663399,129.527808074053));
#83187=CARTESIAN_POINT('Ctrl Pts',(-40.5953710958395,4.71562967702933,129.401044323904));
#83188=CARTESIAN_POINT('Ctrl Pts',(-40.6028614316014,4.67478684611728,129.27610965458));
#83189=CARTESIAN_POINT('Ctrl Pts',(-40.6106357657205,4.63239544685687,129.146438049293));
#83190=CARTESIAN_POINT('Ctrl Pts',(-40.6184100998396,4.58453746880618,129.018326201327));
#83191=CARTESIAN_POINT('Ctrl Pts',(-40.6261844339586,4.53134536860734,128.892269559875));
#83192=CARTESIAN_POINT('Ctrl Pts',(-40.6339491869057,4.47821882291807,128.766368271968));
#83193=CARTESIAN_POINT('Ctrl Pts',(-40.6417139398528,4.41977138557886,128.642517507693));
#83194=CARTESIAN_POINT('Ctrl Pts',(-40.6494786927999,4.35618530793343,128.521197761911));
#83195=CARTESIAN_POINT('Ctrl Pts',(-40.6572357336849,4.29266238487672,128.39999851261));
#83196=CARTESIAN_POINT('Ctrl Pts',(-40.6649927745699,4.22401115856685,128.281325623185));
#83197=CARTESIAN_POINT('Ctrl Pts',(-40.6727498154549,4.1504618646939,128.165639455294));
#83198=CARTESIAN_POINT('Ctrl Pts',(-40.680501006695,4.0769680349156,128.050040527243));
#83199=CARTESIAN_POINT('Ctrl Pts',(-40.6882521979351,3.9985836985125,127.937424166236));
#83200=CARTESIAN_POINT('Ctrl Pts',(-40.6960033891752,3.91558471903809,127.828225645738));
#83201=CARTESIAN_POINT('Ctrl Pts',(-40.7037512859523,3.83262101634403,127.719073537525));
#83202=CARTESIAN_POINT('Ctrl Pts',(-40.7114991827294,3.74504680763295,127.613336691172));
#83203=CARTESIAN_POINT('Ctrl Pts',(-40.7192470795065,3.65318079725539,127.511420726668));
#83204=CARTESIAN_POINT('Ctrl Pts',(-40.7269933555906,3.5613340032668,127.409526080788));
#83205=CARTESIAN_POINT('Ctrl Pts',(-40.7347396316747,3.46519745488942,127.31145101723));
#83206=CARTESIAN_POINT('Ctrl Pts',(-40.7424859077588,3.36512933632013,127.217567117469));
#83207=CARTESIAN_POINT('Ctrl Pts',(-40.7502322410242,3.26506047907071,127.123682524678));
#83208=CARTESIAN_POINT('Ctrl Pts',(-40.7579785742895,3.16106027884223,127.033989424922));
#83209=CARTESIAN_POINT('Ctrl Pts',(-40.7657249075548,3.0535225815357,126.948821367792));
#83210=CARTESIAN_POINT('Ctrl Pts',(-40.7734729755578,2.94596080190748,126.863634237866));
#83211=CARTESIAN_POINT('Ctrl Pts',(-40.7812210435608,2.83486025524777,126.782974409706));
#83212=CARTESIAN_POINT('Ctrl Pts',(-40.7889691115638,2.72064621915353,126.707133846602));
#83213=CARTESIAN_POINT('Ctrl Pts',(-40.7967254143056,2.60631079502256,126.631212679245));
#83214=CARTESIAN_POINT('Ctrl Pts',(-40.8044817170475,2.48885559748517,126.560121225252));
#83215=CARTESIAN_POINT('Ctrl Pts',(-40.8122380197893,2.36873359638736,126.494107236169));
#83216=CARTESIAN_POINT('Ctrl Pts',(-40.8199984623035,2.24854748256076,126.428058013432));
#83217=CARTESIAN_POINT('Ctrl Pts',(-40.8277589048176,2.12569207906489,126.367091829208));
#83218=CARTESIAN_POINT('Ctrl Pts',(-40.8355193473317,2.00064217423662,126.311409031674));
#83219=CARTESIAN_POINT('Ctrl Pts',(-40.8432922475972,1.87539152819971,126.255636847171));
#83220=CARTESIAN_POINT('Ctrl Pts',(-40.8510651478626,1.7479397048465,126.205165141853));
#83221=CARTESIAN_POINT('Ctrl Pts',(-40.858838048128,1.61877940447563,126.160145258418));
#83222=CARTESIAN_POINT('Ctrl Pts',(-40.8663283838901,1.49431440635718,126.116761961144));
#83223=CARTESIAN_POINT('Ctrl Pts',(-40.8738187196522,1.36826328425528,126.078441082079));
#83224=CARTESIAN_POINT('Ctrl Pts',(-40.8813090554143,1.24107566086662,126.045273071985));
#83225=CARTESIAN_POINT('Ctrl Pts',(-40.8890833895334,1.10906568008046,126.010847486707));
#83226=CARTESIAN_POINT('Ctrl Pts',(-40.8968577236525,0.975413147937866,
125.981864175918));
#83227=CARTESIAN_POINT('Ctrl Pts',(-40.9046320577716,0.84060649592791,125.958479502484));
#83228=CARTESIAN_POINT('Ctrl Pts',(-40.9123968107187,0.705965981068539,
125.935123648571));
#83229=CARTESIAN_POINT('Ctrl Pts',(-40.9201615636658,0.570174557907952,
125.917352769608));
#83230=CARTESIAN_POINT('Ctrl Pts',(-40.9279263166129,0.433734991683567,
125.905273251588));
#83231=CARTESIAN_POINT('Ctrl Pts',(-40.9356833574979,0.297430939159817,
125.893205731115));
#83232=CARTESIAN_POINT('Ctrl Pts',(-40.9434403983829,0.160480411575381,
125.886818356632));
#83233=CARTESIAN_POINT('Ctrl Pts',(-40.9511974392679,0.0233951722466785,
125.886166261055));
#83234=CARTESIAN_POINT('Ctrl Pts',(-40.958948630508,-0.113586690036492,
125.885514657228));
#83235=CARTESIAN_POINT('Ctrl Pts',(-40.9666998217481,-0.250702672481956,
125.890589725473));
#83236=CARTESIAN_POINT('Ctrl Pts',(-40.9744510129883,-0.387437456208372,
125.901394649907));
#83237=CARTESIAN_POINT('Ctrl Pts',(-40.9821989097653,-0.52411412400437,
125.912194981959));
#83238=CARTESIAN_POINT('Ctrl Pts',(-40.9899468065424,-0.66040952639174,
125.928720295759));
#83239=CARTESIAN_POINT('Ctrl Pts',(-40.9976947033195,-0.795810136299649,
125.95092170382));
#83240=CARTESIAN_POINT('Ctrl Pts',(-41.0054409794036,-0.931182423318865,
125.973118467826));
#83241=CARTESIAN_POINT('Ctrl Pts',(-41.0131872554878,-1.06565990458383,
126.000988901235));
#83242=CARTESIAN_POINT('Ctrl Pts',(-41.0209335315719,-1.19873635076984,
126.034432502401));
#83243=CARTESIAN_POINT('Ctrl Pts',(-41.0286798648372,-1.33181377929576,
126.06787635044));
#83244=CARTESIAN_POINT('Ctrl Pts',(-41.0364261981025,-1.46348977293108,
126.106893353037));
#83245=CARTESIAN_POINT('Ctrl Pts',(-41.0441725313679,-1.59327082362771,
126.151332448182));
#83246=CARTESIAN_POINT('Ctrl Pts',(-41.0519205993709,-1.72308093789099,
126.195781495155));
#83247=CARTESIAN_POINT('Ctrl Pts',(-41.0596686673738,-1.85099489497844,
126.245654924245));
#83248=CARTESIAN_POINT('Ctrl Pts',(-41.0674167353768,-1.97653718497606,
126.300752750655));
#83249=CARTESIAN_POINT('Ctrl Pts',(-41.0751730381187,-2.10221290281345,
126.35590913569));
#83250=CARTESIAN_POINT('Ctrl Pts',(-41.0829293408606,-2.22551155974407,
126.416300852494));
#83251=CARTESIAN_POINT('Ctrl Pts',(-41.0906856436024,-2.34597987410962,
126.481680720468));
#83252=CARTESIAN_POINT('Ctrl Pts',(-41.0984460861166,-2.46651248604193,
126.547095483647));
#83253=CARTESIAN_POINT('Ctrl Pts',(-41.1062065286308,-2.58421140998175,
126.617503502299));
#83254=CARTESIAN_POINT('Ctrl Pts',(-41.113966971145,-2.69865145263887,126.692613616634));
#83255=CARTESIAN_POINT('Ctrl Pts',(-41.1217398714104,-2.81327520461181,
126.767844304393));
#83256=CARTESIAN_POINT('Ctrl Pts',(-41.1295127716758,-2.92462930343529,
126.847791943439));
#83257=CARTESIAN_POINT('Ctrl Pts',(-41.1372856719413,-3.03232010366483,
126.932123815482));
#83258=CARTESIAN_POINT('Ctrl Pts',(-41.1447760077032,-3.13609607204853,
127.013390011558));
#83259=CARTESIAN_POINT('Ctrl Pts',(-41.1522663434652,-3.23647022337348,
127.09872701936));
#83260=CARTESIAN_POINT('Ctrl Pts',(-41.1597566792272,-3.33312342680312,
127.187805449427));
#83261=CARTESIAN_POINT('Ctrl Pts',(-41.1674134037402,-3.43192366426608,
127.278862649096));
#83262=CARTESIAN_POINT('Ctrl Pts',(-41.1750701282532,-3.52716869389441,
127.37413670988));
#83263=CARTESIAN_POINT('Ctrl Pts',(-41.1827268527662,-3.61846879384522,
127.473314738196));
#83264=CARTESIAN_POINT('Ctrl Pts',(-41.1903747179501,-3.70966325363188,
127.572378011072));
#83265=CARTESIAN_POINT('Ctrl Pts',(-41.198022583134,-3.79692158697122,127.67533597854));
#83266=CARTESIAN_POINT('Ctrl Pts',(-41.2056704483179,-3.87988773714554,
127.781836141297));
#83267=CARTESIAN_POINT('Ctrl Pts',(-41.2133112386969,-3.96277713788632,
127.888237784029));
#83268=CARTESIAN_POINT('Ctrl Pts',(-41.220952029076,-4.04138200396901,127.998174790541));
#83269=CARTESIAN_POINT('Ctrl Pts',(-41.2285928194551,-4.11538411119943,
128.111258933673));
#83270=CARTESIAN_POINT('Ctrl Pts',(-41.2362283501721,-4.18933527787853,
128.2242652335));
#83271=CARTESIAN_POINT('Ctrl Pts',(-41.243863880889,-4.2586897672421,128.340414024735));
#83272=CARTESIAN_POINT('Ctrl Pts',(-41.251499411606,-4.32317089112018,128.45928567022));
#83273=CARTESIAN_POINT('Ctrl Pts',(-41.2591316827896,-4.38762448863661,
128.578106570561));
#83274=CARTESIAN_POINT('Ctrl Pts',(-41.2667639539732,-4.44720866698158,
128.699647658746));
#83275=CARTESIAN_POINT('Ctrl Pts',(-41.2743962251567,-4.50169145460962,
128.823462561129));
#83276=CARTESIAN_POINT('Ctrl Pts',(-41.2820290199258,-4.55617797984057,
128.947285957405));
#83277=CARTESIAN_POINT('Ctrl Pts',(-41.2896618146949,-4.60556224143734,
129.073383114953));
#83278=CARTESIAN_POINT('Ctrl Pts',(-41.2972946094639,-4.64965950561795,
129.201285589903));
#83279=CARTESIAN_POINT('Ctrl Pts',(-41.3047830462557,-4.69292276442373,
129.326769063277));
#83280=CARTESIAN_POINT('Ctrl Pts',(-41.3122714830475,-4.73109715056116,
129.45398980396));
#83281=CARTESIAN_POINT('Ctrl Pts',(-41.3197599198393,-4.76405452823403,
129.582490119308));
#83282=CARTESIAN_POINT('Origin',(213.235140564004,0.,130.804360617566));
#83283=CARTESIAN_POINT('',(-43.4154178838317,-4.76405452823406,129.582490119308));
#83284=CARTESIAN_POINT('',(-43.0697814015304,-4.7640545282341,129.582490119308));
#83285=CARTESIAN_POINT('',(213.235140564004,-4.76405452823405,129.582490119308));
#83286=CARTESIAN_POINT('',(-41.7351405640431,-4.91824869491783,130.800777680352));
#83287=CARTESIAN_POINT('Ctrl Pts',(-41.7351405640431,-4.91824869491783,
130.800777680352));
#83288=CARTESIAN_POINT('Ctrl Pts',(-41.7427950097377,-4.91834679994633,
130.935445105295));
#83289=CARTESIAN_POINT('Ctrl Pts',(-41.7504494554324,-4.91290971845572,
131.070325623503));
#83290=CARTESIAN_POINT('Ctrl Pts',(-41.758103901127,-4.90191150312827,131.204918575918));
#83291=CARTESIAN_POINT('Ctrl Pts',(-41.7657504384142,-4.89092465091859,
131.339372469809));
#83292=CARTESIAN_POINT('Ctrl Pts',(-41.7733969757012,-4.87438812458713,
131.473538989973));
#83293=CARTESIAN_POINT('Ctrl Pts',(-41.7810435129884,-4.85232800297637,
131.606916543363));
#83294=CARTESIAN_POINT('Ctrl Pts',(-41.7886841035495,-4.83028503756258,
131.740190368785));
#83295=CARTESIAN_POINT('Ctrl Pts',(-41.7963246941106,-4.8027270877807,131.872676051988));
#83296=CARTESIAN_POINT('Ctrl Pts',(-41.8039652846717,-4.7697320877363,132.003876717382));
#83297=CARTESIAN_POINT('Ctrl Pts',(-41.8116025319927,-4.73675152508488,
132.135019974213));
#83298=CARTESIAN_POINT('Ctrl Pts',(-41.8192397793138,-4.6983387395161,132.264878940731));
#83299=CARTESIAN_POINT('Ctrl Pts',(-41.8268770266347,-4.65462275942882,
132.392966934407));
#83300=CARTESIAN_POINT('Ctrl Pts',(-41.8345127392591,-4.61091556402089,
132.521029188938));
#83301=CARTESIAN_POINT('Ctrl Pts',(-41.8421484518834,-4.56190742286855,
132.647320796677));
#83302=CARTESIAN_POINT('Ctrl Pts',(-41.8497841645077,-4.50777706630277,
132.77137078099));
#83303=CARTESIAN_POINT('Ctrl Pts',(-41.8574201072333,-4.45364507852555,
132.895424503535));
#83304=CARTESIAN_POINT('Ctrl Pts',(-41.8650560499588,-4.39439072996786,
133.017236098825));
#83305=CARTESIAN_POINT('Ctrl Pts',(-41.8726919926844,-4.33024044805813,
133.136355627102));
#83306=CARTESIAN_POINT('Ctrl Pts',(-41.8803299302943,-4.26607340693537,
133.255506275266));
#83307=CARTESIAN_POINT('Ctrl Pts',(-41.887967867904,-4.197008080667,133.371963103274));
#83308=CARTESIAN_POINT('Ctrl Pts',(-41.8956058055139,-4.12331600337679,
133.485302280265));
#83309=CARTESIAN_POINT('Ctrl Pts',(-41.9032517650887,-4.04954652885077,
133.598760495006));
#83310=CARTESIAN_POINT('Ctrl Pts',(-41.9108977246635,-3.97114082297043,
133.709094184074));
#83311=CARTESIAN_POINT('Ctrl Pts',(-41.9185436842382,-3.88841291985857,
133.815909725115));
#83312=CARTESIAN_POINT('Ctrl Pts',(-41.926194183097,-3.80563590251286,133.922788680835));
#83313=CARTESIAN_POINT('Ctrl Pts',(-41.9338446819558,-3.71853183935376,
134.026145023419));
#83314=CARTESIAN_POINT('Ctrl Pts',(-41.9414951808145,-3.62745301867817,
134.125620568215));
#83315=CARTESIAN_POINT('Ctrl Pts',(-41.9491567837371,-3.53624200465687,
134.225240493503));
#83316=CARTESIAN_POINT('Ctrl Pts',(-41.9568183866597,-3.44104500103126,
134.320968093023));
#83317=CARTESIAN_POINT('Ctrl Pts',(-41.9644799895823,-3.3422491270763,134.41248392963));
#83318=CARTESIAN_POINT('Ctrl Pts',(-41.9681568445569,-3.29483632008411,
134.456402997543));
#83319=CARTESIAN_POINT('Ctrl Pts',(-41.9718336995316,-3.2465951175301,134.499352671356));
#83320=CARTESIAN_POINT('Ctrl Pts',(-41.9755105545062,-3.19757068636793,
134.541301180136));
#83321=CARTESIAN_POINT('Ctrl Pts',(-41.9832848886253,-3.09391353630704,
134.629997015383));
#83322=CARTESIAN_POINT('Ctrl Pts',(-41.9910592227443,-2.98639896895209,
134.714517128132));
#83323=CARTESIAN_POINT('Ctrl Pts',(-41.9988335568634,-2.87539783221303,
134.794507277653));
#83324=CARTESIAN_POINT('Ctrl Pts',(-42.0065983098106,-2.76453349445439,
134.874398846464));
#83325=CARTESIAN_POINT('Ctrl Pts',(-42.0143630627577,-2.65019145097514,
134.949771333727));
#83326=CARTESIAN_POINT('Ctrl Pts',(-42.0221278157049,-2.53277729827217,
135.020309172738));
#83327=CARTESIAN_POINT('Ctrl Pts',(-42.0298848565899,-2.41547976296108,
135.090776952572));
#83328=CARTESIAN_POINT('Ctrl Pts',(-42.0376418974749,-2.2951165235444,135.15641944));
#83329=CARTESIAN_POINT('Ctrl Pts',(-42.04539893836,-2.17212368501981,135.216963223679));
#83330=CARTESIAN_POINT('Ctrl Pts',(-42.0531501296002,-2.04922359635099,
135.27746135082));
#83331=CARTESIAN_POINT('Ctrl Pts',(-42.0609013208404,-1.92369820496837,
135.332868255428));
#83332=CARTESIAN_POINT('Ctrl Pts',(-42.0686525120805,-1.79600953431401,
135.38295568758));
#83333=CARTESIAN_POINT('Ctrl Pts',(-42.0764004088577,-1.66837513475141,
135.433021831236));
#83334=CARTESIAN_POINT('Ctrl Pts',(-42.0841483056347,-1.53857964783893,
135.477772856759));
#83335=CARTESIAN_POINT('Ctrl Pts',(-42.0918962024118,-1.40710626038626,
135.517028124879));
#83336=CARTESIAN_POINT('Ctrl Pts',(-42.099642478496,-1.275660374332,135.556275181643));
#83337=CARTESIAN_POINT('Ctrl Pts',(-42.1073887545801,-1.14253766024279,
135.590028655825));
#83338=CARTESIAN_POINT('Ctrl Pts',(-42.1151350306642,-1.00823731684453,
135.61815751559));
#83339=CARTESIAN_POINT('Ctrl Pts',(-42.1228813639296,-0.873935982071649,
135.646286582995));
#83340=CARTESIAN_POINT('Ctrl Pts',(-42.130627697195,-0.738457383305424,
135.668790872985));
#83341=CARTESIAN_POINT('Ctrl Pts',(-42.1383740304604,-0.602311393010782,
135.685590385601));
#83342=CARTESIAN_POINT('Ctrl Pts',(-42.1461220984634,-0.466134913765027,
135.702393660351));
#83343=CARTESIAN_POINT('Ctrl Pts',(-42.1538701664664,-0.329291133535421,
135.713489567688));
#83344=CARTESIAN_POINT('Ctrl Pts',(-42.1616182344695,-0.192295136921508,
135.718849974846));
#83345=CARTESIAN_POINT('Ctrl Pts',(-42.1693745372114,-0.0551535393326823,
135.724216079108));
#83346=CARTESIAN_POINT('Ctrl Pts',(-42.1771308399532,0.0821402065189988,
135.723834490947));
#83347=CARTESIAN_POINT('Ctrl Pts',(-42.184887142695,0.219070363301342,135.717729241883));
#83348=CARTESIAN_POINT('Ctrl Pts',(-42.1926475852092,0.356073603831433,
135.711620734264));
#83349=CARTESIAN_POINT('Ctrl Pts',(-42.2004080277235,0.49271247929883,135.699782512345));
#83350=CARTESIAN_POINT('Ctrl Pts',(-42.2081684702377,0.628477276379563,
135.682290442356));
#83351=CARTESIAN_POINT('Ctrl Pts',(-42.2159413705032,0.764460015165017,
135.664770292543));
#83352=CARTESIAN_POINT('Ctrl Pts',(-42.2237142707686,0.899565486075578,
135.641578223986));
#83353=CARTESIAN_POINT('Ctrl Pts',(-42.231487171034,1.03329416958053,135.612841273824));
#83354=CARTESIAN_POINT('Ctrl Pts',(-42.2389775067958,1.16216147859261,135.585148984186));
#83355=CARTESIAN_POINT('Ctrl Pts',(-42.2464678425575,1.28975006341186,135.552308031435));
#83356=CARTESIAN_POINT('Ctrl Pts',(-42.2539581783193,1.41562886996102,135.514475049831));
#83357=CARTESIAN_POINT('Ctrl Pts',(-42.2617325124384,1.5462804097255,135.475207619229));
#83358=CARTESIAN_POINT('Ctrl Pts',(-42.2695068465575,1.67550382415904,135.430437754202));
#83359=CARTESIAN_POINT('Ctrl Pts',(-42.2772811806765,1.80280062815081,135.380285983832));
#83360=CARTESIAN_POINT('Ctrl Pts',(-42.2850459336236,1.92994055020849,135.330196021037));
#83361=CARTESIAN_POINT('Ctrl Pts',(-42.2928106865707,2.05515822586244,135.274737491965));
#83362=CARTESIAN_POINT('Ctrl Pts',(-42.3005754395178,2.17796892509315,135.214081064922));
#83363=CARTESIAN_POINT('Ctrl Pts',(-42.3083324804028,2.30065764700606,135.153484882698));
#83364=CARTESIAN_POINT('Ctrl Pts',(-42.3160895212879,2.42094380171056,135.087701248374));
#83365=CARTESIAN_POINT('Ctrl Pts',(-42.3238465621729,2.53836163509838,135.016949283928));
#83366=CARTESIAN_POINT('Ctrl Pts',(-42.331597753413,2.65569092278451,134.946250674089));
#83367=CARTESIAN_POINT('Ctrl Pts',(-42.3393489446531,2.77015586100561,134.870591392585));
#83368=CARTESIAN_POINT('Ctrl Pts',(-42.3471001358932,2.88131468168165,134.790236778164));
#83369=CARTESIAN_POINT('Ctrl Pts',(-42.3548480326703,2.99242625689379,134.709916316598));
#83370=CARTESIAN_POINT('Ctrl Pts',(-42.3625959294474,3.10023419318805,134.62490471986));
#83371=CARTESIAN_POINT('Ctrl Pts',(-42.3703438262245,3.20432533935822,134.535510866758));
#83372=CARTESIAN_POINT('Ctrl Pts',(-42.3780901023086,3.30839471190456,134.446135712924));
#83373=CARTESIAN_POINT('Ctrl Pts',(-42.3858363783927,3.40874854435049,134.3523803806));
#83374=CARTESIAN_POINT('Ctrl Pts',(-42.3935826544768,3.50500676679596,134.254594033904));
#83375=CARTESIAN_POINT('Ctrl Pts',(-42.4013289877421,3.60126569979764,134.156806965372));
#83376=CARTESIAN_POINT('Ctrl Pts',(-42.4090753210075,3.69342868820284,134.054989101715));
#83377=CARTESIAN_POINT('Ctrl Pts',(-42.4168216542728,3.78115282725794,133.949526171145));
#83378=CARTESIAN_POINT('Ctrl Pts',(-42.4245697222758,3.86889661152588,133.844039622883));
#83379=CARTESIAN_POINT('Ctrl Pts',(-42.4323177902788,3.95219931843022,133.734906683908));
#83380=CARTESIAN_POINT('Ctrl Pts',(-42.4400658582817,4.03075886326929,133.622545503033));
#83381=CARTESIAN_POINT('Ctrl Pts',(-42.4478221610236,4.10940190212737,133.510064903359));
#83382=CARTESIAN_POINT('Ctrl Pts',(-42.4555784637654,4.18329148441925,133.394349528891));
#83383=CARTESIAN_POINT('Ctrl Pts',(-42.4633347665072,4.25216905991821,133.275846273679));
#83384=CARTESIAN_POINT('Ctrl Pts',(-42.4710952090214,4.32108339745308,133.157279769712));
#83385=CARTESIAN_POINT('Ctrl Pts',(-42.4788556515356,4.38498021585691,133.035922765856));
#83386=CARTESIAN_POINT('Ctrl Pts',(-42.4866160940498,4.44364783103554,132.912245105918));
#83387=CARTESIAN_POINT('Ctrl Pts',(-42.4943889943152,4.5024096246784,132.788368907619));
#83388=CARTESIAN_POINT('Ctrl Pts',(-42.5021618945807,4.55592528772964,132.662164969004));
#83389=CARTESIAN_POINT('Ctrl Pts',(-42.5099347948461,4.60403169762542,132.534122216677));
#83390=CARTESIAN_POINT('Ctrl Pts',(-42.5174251306081,4.65038931834863,132.410734140918));
#83391=CARTESIAN_POINT('Ctrl Pts',(-42.5249154663701,4.69172404131558,132.285638913862));
#83392=CARTESIAN_POINT('Ctrl Pts',(-42.5324058021321,4.72793465210855,132.159283858156));
#83393=CARTESIAN_POINT('Ctrl Pts',(-42.5401801362512,4.76551819921577,132.028138012108));
#83394=CARTESIAN_POINT('Ctrl Pts',(-42.5479544703703,4.79770045577841,131.895219488136));
#83395=CARTESIAN_POINT('Ctrl Pts',(-42.5557288044893,4.82431338294927,131.761012824795));
#83396=CARTESIAN_POINT('Ctrl Pts',(-42.5634935574364,4.85089351206586,131.626971559173));
#83397=CARTESIAN_POINT('Ctrl Pts',(-42.5712583103834,4.87191789319248,131.491645692683));
#83398=CARTESIAN_POINT('Ctrl Pts',(-42.5790230633305,4.88726810599457,131.355535292808));
#83399=CARTESIAN_POINT('Ctrl Pts',(-42.5867801042155,4.90260307274888,131.219560079702));
#83400=CARTESIAN_POINT('Ctrl Pts',(-42.5945371451005,4.91227504287343,131.082802269862));
#83401=CARTESIAN_POINT('Ctrl Pts',(-42.6022941859855,4.91621661842149,130.945772156191));
#83402=CARTESIAN_POINT('Ctrl Pts',(-42.6100453772256,4.92015522159677,130.808845377995));
#83403=CARTESIAN_POINT('Ctrl Pts',(-42.6177965684657,4.91837202035535,130.671647093921));
#83404=CARTESIAN_POINT('Ctrl Pts',(-42.6255477597058,4.91085146526319,130.53469239804));
#83405=CARTESIAN_POINT('Ctrl Pts',(-42.6332956564829,4.90333410660755,130.397795911558));
#83406=CARTESIAN_POINT('Ctrl Pts',(-42.64104355326,4.8900842655401,130.261143196913));
#83407=CARTESIAN_POINT('Ctrl Pts',(-42.6487914500371,4.87113849223304,130.125248806459));
#83408=CARTESIAN_POINT('Ctrl Pts',(-42.6565377261212,4.85219668197333,129.989382842181));
#83409=CARTESIAN_POINT('Ctrl Pts',(-42.6642840022053,4.82756136331593,129.854275273553));
#83410=CARTESIAN_POINT('Ctrl Pts',(-42.6720302782894,4.79732086085732,129.720434595882));
#83411=CARTESIAN_POINT('Ctrl Pts',(-42.6797766115547,4.76708013517024,129.58659293023));
#83412=CARTESIAN_POINT('Ctrl Pts',(-42.68752294482,4.73123422928303,129.454018555547));
#83413=CARTESIAN_POINT('Ctrl Pts',(-42.6952692780854,4.68992231887011,129.323208462835));
#83414=CARTESIAN_POINT('Ctrl Pts',(-42.7030173460883,4.64860115694135,129.19236907611));
#83415=CARTESIAN_POINT('Ctrl Pts',(-42.7107654140913,4.60181167244005,129.0632951303));
#83416=CARTESIAN_POINT('Ctrl Pts',(-42.7185134820942,4.54974238164558,128.936466797469));
#83417=CARTESIAN_POINT('Ctrl Pts',(-42.726269784836,4.49761775098907,128.809503669975));
#83418=CARTESIAN_POINT('Ctrl Pts',(-42.734026087578,4.44020225330236,128.684791285326));
#83419=CARTESIAN_POINT('Ctrl Pts',(-42.7417823903198,4.37773212049169,128.5627887263));
#83420=CARTESIAN_POINT('Ctrl Pts',(-42.749542832834,4.3152286454901,128.440721050834));
#83421=CARTESIAN_POINT('Ctrl Pts',(-42.7573032753481,4.24766535225111,128.321366422965));
#83422=CARTESIAN_POINT('Ctrl Pts',(-42.7650637178623,4.17532311325151,128.20515690057));
#83423=CARTESIAN_POINT('Ctrl Pts',(-42.7728366181277,4.10286474406773,128.088760828333));
#83424=CARTESIAN_POINT('Ctrl Pts',(-42.7806095183931,4.02561231930156,127.975520273841));
#83425=CARTESIAN_POINT('Ctrl Pts',(-42.7883824186585,3.94388901502325,127.865836753501));
#83426=CARTESIAN_POINT('Ctrl Pts',(-42.7958727544207,3.86513655870292,127.7601405054));
#83427=CARTESIAN_POINT('Ctrl Pts',(-42.8033630901828,3.78223282871864,127.657747406461));
#83428=CARTESIAN_POINT('Ctrl Pts',(-42.8108534259449,3.6954994614176,127.558984400059));
#83429=CARTESIAN_POINT('Ctrl Pts',(-42.818627760064,3.60547757213457,127.456476764252));
#83430=CARTESIAN_POINT('Ctrl Pts',(-42.8264020941831,3.51104474923607,127.357555211434));
#83431=CARTESIAN_POINT('Ctrl Pts',(-42.8341764283022,3.41251781962994,127.262623022372));
#83432=CARTESIAN_POINT('Ctrl Pts',(-42.8419411812493,3.31411231565869,127.167807828749));
#83433=CARTESIAN_POINT('Ctrl Pts',(-42.8497059341964,3.2116230231006,127.07697248511));
#83434=CARTESIAN_POINT('Ctrl Pts',(-42.8574706871435,3.10540665380837,126.990486920525));
#83435=CARTESIAN_POINT('Ctrl Pts',(-42.8652277280285,2.9992957801115,126.904087254622));
#83436=CARTESIAN_POINT('Ctrl Pts',(-42.8729847689135,2.88946549761346,126.822029015518));
#83437=CARTESIAN_POINT('Ctrl Pts',(-42.8807418097985,2.77630869994954,126.744644732792));
#83438=CARTESIAN_POINT('Ctrl Pts',(-42.8884930010386,2.66323723470773,126.667318806157));
#83439=CARTESIAN_POINT('Ctrl Pts',(-42.8962441922787,2.54684456883082,126.594660040068));
#83440=CARTESIAN_POINT('Ctrl Pts',(-42.9039953835188,2.42755566070103,126.526959937632));
#83441=CARTESIAN_POINT('Ctrl Pts',(-42.9117432802959,2.30831745353868,126.459288609546));
#83442=CARTESIAN_POINT('Ctrl Pts',(-42.919491177073,2.18618579175968,126.396571945897));
#83443=CARTESIAN_POINT('Ctrl Pts',(-42.9272390738501,2.06161333909198,126.339057324107));
#83444=CARTESIAN_POINT('Ctrl Pts',(-42.9349853499342,1.93706694429607,126.281554733135));
#83445=CARTESIAN_POINT('Ctrl Pts',(-42.9427316260183,1.8100811288793,126.229252183401));
#83446=CARTESIAN_POINT('Ctrl Pts',(-42.9504779021024,1.68113144594543,126.182350219054));
#83447=CARTESIAN_POINT('Ctrl Pts',(-42.9582242353677,1.55218081113428,126.135447908487));
#83448=CARTESIAN_POINT('Ctrl Pts',(-42.9659705686331,1.42126664729498,126.093946396493));
#83449=CARTESIAN_POINT('Ctrl Pts',(-42.9737169018984,1.28888231488431,126.057997226413));
#83450=CARTESIAN_POINT('Ctrl Pts',(-42.9814649699014,1.1564683359201,126.022040005765));
#83451=CARTESIAN_POINT('Ctrl Pts',(-42.9892130379044,1.02258391047611,125.991637703707));
#83452=CARTESIAN_POINT('Ctrl Pts',(-42.9969611059074,0.887734918561544,
125.966891260881));
#83453=CARTESIAN_POINT('Ctrl Pts',(-43.0047174086493,0.752742607533467,
125.942118517242));
#83454=CARTESIAN_POINT('Ctrl Pts',(-43.0124737113911,0.616784067338725,
125.923013711365));
#83455=CARTESIAN_POINT('Ctrl Pts',(-43.0202300141329,0.480373226435244,
125.909626240113));
#83456=CARTESIAN_POINT('Ctrl Pts',(-43.0279904566471,0.343889578958907,
125.896231623564));
#83457=CARTESIAN_POINT('Ctrl Pts',(-43.0357508991613,0.2069535399131,125.888560443896));
#83458=CARTESIAN_POINT('Ctrl Pts',(-43.0435113416754,0.0700804302608409,
125.886609932975));
#83459=CARTESIAN_POINT('Ctrl Pts',(-43.0512842419409,-0.0670124002582414,
125.884656290921));
#83460=CARTESIAN_POINT('Ctrl Pts',(-43.0590571422064,-0.204041708472887,
125.888441658022));
#83461=CARTESIAN_POINT('Ctrl Pts',(-43.0668300424718,-0.340495002699345,
125.897911166523));
#83462=CARTESIAN_POINT('Ctrl Pts',(-43.0743203782338,-0.47198787597483,
125.907036434538));
#83463=CARTESIAN_POINT('Ctrl Pts',(-43.0818107139958,-0.602945581125637,
125.921439719462));
#83464=CARTESIAN_POINT('Ctrl Pts',(-43.0893010497578,-0.732919199129937,
125.941027140408));
#83465=CARTESIAN_POINT('Ctrl Pts',(-43.0970753838769,-0.867820806365882,
125.961357224372));
#83466=CARTESIAN_POINT('Ctrl Pts',(-43.1048497179959,-1.00208955778166,
125.987336717162));
#83467=CARTESIAN_POINT('Ctrl Pts',(-43.112624052115,-1.13521490916483,126.018917046432));
#83468=CARTESIAN_POINT('Ctrl Pts',(-43.1203888050621,-1.26817619545018,
126.050458455768));
#83469=CARTESIAN_POINT('Ctrl Pts',(-43.1281535580092,-1.39999650871206,
126.087586878231));
#83470=CARTESIAN_POINT('Ctrl Pts',(-43.1359183109563,-1.53017180567683,
126.130202157735));
#83471=CARTESIAN_POINT('Ctrl Pts',(-43.1436753518413,-1.66021781070133,
126.172775111142));
#83472=CARTESIAN_POINT('Ctrl Pts',(-43.1514323927263,-1.78862168171332,
126.220823955743));
#83473=CARTESIAN_POINT('Ctrl Pts',(-43.1591894336113,-1.91489128355243,
126.274197879355));
#83474=CARTESIAN_POINT('Ctrl Pts',(-43.1669406248513,-2.04106566450204,
126.327531553276));
#83475=CARTESIAN_POINT('Ctrl Pts',(-43.1746918160914,-2.16510862117123,
126.386182161629));
#83476=CARTESIAN_POINT('Ctrl Pts',(-43.1824430073315,-2.28654520335439,
126.449949739443));
#83477=CARTESIAN_POINT('Ctrl Pts',(-43.1901909041086,-2.40793017175136,
126.513690214335));
#83478=CARTESIAN_POINT('Ctrl Pts',(-43.1979388008856,-2.52671062353022,
126.582543151696));
#83479=CARTESIAN_POINT('Ctrl Pts',(-43.2056866976626,-2.64243375725943,
126.65626142625));
#83480=CARTESIAN_POINT('Ctrl Pts',(-43.2134329737467,-2.75813268420361,
126.72996428053));
#83481=CARTESIAN_POINT('Ctrl Pts',(-43.2211792498309,-2.8707752356136,126.808530237773));
#83482=CARTESIAN_POINT('Ctrl Pts',(-43.228925525915,-2.97993563994864,126.891667600696));
#83483=CARTESIAN_POINT('Ctrl Pts',(-43.2366718591804,-3.08909685008129,
126.97480557732));
#83484=CARTESIAN_POINT('Ctrl Pts',(-43.2444181924457,-3.19477555081695,
127.062514790077));
#83485=CARTESIAN_POINT('Ctrl Pts',(-43.2521645257111,-3.29657757107428,
127.154462073717));
#83486=CARTESIAN_POINT('Ctrl Pts',(-43.2599125937141,-3.39840238918834,
127.246429948314));
#83487=CARTESIAN_POINT('Ctrl Pts',(-43.2676606617171,-3.49634850920976,
127.342637520364));
#83488=CARTESIAN_POINT('Ctrl Pts',(-43.2754087297201,-3.59005756641433,
127.442713739571));
#83489=CARTESIAN_POINT('Ctrl Pts',(-43.2831650324619,-3.68386621871967,
127.542896320975));
#83490=CARTESIAN_POINT('Ctrl Pts',(-43.2909213352037,-3.77342854492692,
127.646955477149));
#83491=CARTESIAN_POINT('Ctrl Pts',(-43.2986776379456,-3.85842519517247,
127.754485525737));
#83492=CARTESIAN_POINT('Ctrl Pts',(-43.3064380804597,-3.94346721068957,
127.86207296635));
#83493=CARTESIAN_POINT('Ctrl Pts',(-43.3141985229738,-4.02393846535643,
127.97313467424));
#83494=CARTESIAN_POINT('Ctrl Pts',(-43.321958965488,-4.09956274451401,128.087235599041));
#83495=CARTESIAN_POINT('Ctrl Pts',(-43.3297318657534,-4.17530842247811,
128.201519688777));
#83496=CARTESIAN_POINT('Ctrl Pts',(-43.3375047660189,-4.24619137414552,
128.31885241003));
#83497=CARTESIAN_POINT('Ctrl Pts',(-43.3452776662843,-4.3119807470397,128.438772931671));
#83498=CARTESIAN_POINT('Ctrl Pts',(-43.3527680020464,-4.37537851051663,
128.55433404029));
#83499=CARTESIAN_POINT('Ctrl Pts',(-43.3602583378085,-4.43404645744239,
128.672297793872));
#83500=CARTESIAN_POINT('Ctrl Pts',(-43.3677486735707,-4.48782092077067,
128.792235759215));
#83501=CARTESIAN_POINT('Ctrl Pts',(-43.376268988075,-4.54898978614722,128.928666116704));
#83502=CARTESIAN_POINT('Ctrl Pts',(-43.3847893025794,-4.60399456945207,
129.068023789314));
#83503=CARTESIAN_POINT('Ctrl Pts',(-43.3933096170837,-4.6525721106131,129.209758529882));
#83504=CARTESIAN_POINT('Ctrl Pts',(-43.4006790393331,-4.69458797897907,
129.332348271155));
#83505=CARTESIAN_POINT('Ctrl Pts',(-43.4080484615824,-4.73179629584008,
129.456715760791));
#83506=CARTESIAN_POINT('Ctrl Pts',(-43.4154178838317,-4.76405452823406,
129.582490119308));
#83507=CARTESIAN_POINT('Ctrl Pts',(-41.6650773111923,-4.76405452823405,
129.582490119308));
#83508=CARTESIAN_POINT('Ctrl Pts',(-41.67285208007,-4.79807929090603,129.715152152568));
#83509=CARTESIAN_POINT('Ctrl Pts',(-41.6806268489478,-4.82651721256817,
129.849074877393));
#83510=CARTESIAN_POINT('Ctrl Pts',(-41.6884016178255,-4.84930693794822,
129.983747868416));
#83511=CARTESIAN_POINT('Ctrl Pts',(-41.6912887221148,-4.85776973792735,
130.0337577113));
#83512=CARTESIAN_POINT('Ctrl Pts',(-41.6941758264041,-4.86545419363686,
130.083870981395));
#83513=CARTESIAN_POINT('Ctrl Pts',(-41.6970629306933,-4.87235899193441,
130.134061493133));
#83514=CARTESIAN_POINT('Ctrl Pts',(-41.7097554751317,-4.90271447980346,
130.354713481002));
#83515=CARTESIAN_POINT('Ctrl Pts',(-41.7224480195701,-4.91808601786737,
130.577473165781));
#83516=CARTESIAN_POINT('Ctrl Pts',(-41.7351405640085,-4.91824869491739,
130.800777679744));
#83517=CARTESIAN_POINT('',(-41.3898594359429,-4.91824825723657,130.808500990674));
#83518=CARTESIAN_POINT('Ctrl Pts',(-41.3197599198393,-4.76405452823403,
129.582490119308));
#83519=CARTESIAN_POINT('Ctrl Pts',(-41.3273964518608,-4.79766368818847,
129.71353172388));
#83520=CARTESIAN_POINT('Ctrl Pts',(-41.3350329838823,-4.82584721264061,
129.845903662855));
#83521=CARTESIAN_POINT('Ctrl Pts',(-41.3426695159038,-4.84851983346089,
129.979110057411));
#83522=CARTESIAN_POINT('Ctrl Pts',(-41.350534502577,-4.87187072887995,130.116301457253));
#83523=CARTESIAN_POINT('Ctrl Pts',(-41.3583994892502,-4.88937575275814,
130.254377564647));
#83524=CARTESIAN_POINT('Ctrl Pts',(-41.3662644759234,-4.9009992852771,130.39279158543));
#83525=CARTESIAN_POINT('Ctrl Pts',(-41.3741294625966,-4.91262281779606,
130.531205606213));
#83526=CARTESIAN_POINT('Ctrl Pts',(-41.3819944492698,-4.91836488890507,
130.669957075579));
#83527=CARTESIAN_POINT('Ctrl Pts',(-41.389859435943,-4.91824825723657,130.808500990674));
#83528=CARTESIAN_POINT('Ctrl Pts',(-41.3898594359911,-4.91824825723585,
130.808500991522));
#83529=CARTESIAN_POINT('Ctrl Pts',(-41.4019188502082,-4.91806942541481,
131.020930907655));
#83530=CARTESIAN_POINT('Ctrl Pts',(-41.4139782644253,-4.90412471843964,
131.232801737864));
#83531=CARTESIAN_POINT('Ctrl Pts',(-41.4260376786424,-4.87664726816819,
131.442713564115));
#83532=CARTESIAN_POINT('Ctrl Pts',(-41.4300932201083,-4.86740669172328,
131.513306223113));
#83533=CARTESIAN_POINT('Ctrl Pts',(-41.4341487615742,-4.85663595382896,
131.583677646618));
#83534=CARTESIAN_POINT('Ctrl Pts',(-41.4382043030401,-4.84434491737359,
131.653775347846));
#83535=CARTESIAN_POINT('Ctrl Pts',(-41.4459786371593,-4.82078342136201,
131.788150240794));
#83536=CARTESIAN_POINT('Ctrl Pts',(-41.4537529712782,-4.79158933020956,
131.921756889933));
#83537=CARTESIAN_POINT('Ctrl Pts',(-41.4615273053973,-4.75682345392793,
132.054086063679));
#83538=CARTESIAN_POINT('Ctrl Pts',(-41.4692920583445,-4.72210042348165,
132.186252153544));
#83539=CARTESIAN_POINT('Ctrl Pts',(-41.4770568112917,-4.68181936903707,
132.317143526048));
#83540=CARTESIAN_POINT('Ctrl Pts',(-41.4848215642388,-4.63609251348601,
132.44625868654));
#83541=CARTESIAN_POINT('Ctrl Pts',(-41.4925786051239,-4.59041107449259,
132.575245608033));
#83542=CARTESIAN_POINT('Ctrl Pts',(-41.5003356460088,-4.53929472791557,
132.702459462118));
#83543=CARTESIAN_POINT('Ctrl Pts',(-41.5080926868939,-4.4829060523938,132.827411874433));
#83544=CARTESIAN_POINT('Ctrl Pts',(-41.515843878134,-4.42655990001088,132.952270059162));
#83545=CARTESIAN_POINT('Ctrl Pts',(-41.5235950693742,-4.36494949264671,
133.074869841642));
#83546=CARTESIAN_POINT('Ctrl Pts',(-41.5313462606143,-4.29828613518435,
133.19474120705));
#83547=CARTESIAN_POINT('Ctrl Pts',(-41.5390941573914,-4.23165111142721,
133.31456162393));
#83548=CARTESIAN_POINT('Ctrl Pts',(-41.5468420541685,-4.15996759868137,
133.431655589225));
#83549=CARTESIAN_POINT('Ctrl Pts',(-41.5545899509456,-4.08349351704301,
133.545576362225));
#83550=CARTESIAN_POINT('Ctrl Pts',(-41.5623362270297,-4.00703543213384,
133.659473305456));
#83551=CARTESIAN_POINT('Ctrl Pts',(-41.5700825031138,-3.92578898930033,
133.770198052251));
#83552=CARTESIAN_POINT('Ctrl Pts',(-41.5778287791979,-3.84005601916743,
133.877331953611));
#83553=CARTESIAN_POINT('Ctrl Pts',(-41.5855751124633,-3.75432241617333,
133.98446664581));
#83554=CARTESIAN_POINT('Ctrl Pts',(-41.5933214457287,-3.66410246407318,
134.088010134425));
#83555=CARTESIAN_POINT('Ctrl Pts',(-41.6010677789941,-3.56973869119103,
134.187576356935));
#83556=CARTESIAN_POINT('Ctrl Pts',(-41.6088158469971,-3.47535378619622,
134.28716487661));
#83557=CARTESIAN_POINT('Ctrl Pts',(-41.6165639150001,-3.37682348273643,
134.382774074112));
#83558=CARTESIAN_POINT('Ctrl Pts',(-41.6243119830031,-3.27452732401904,
134.474054592103));
#83559=CARTESIAN_POINT('Ctrl Pts',(-41.6320682857449,-3.17212244372682,
134.565432124114));
#83560=CARTESIAN_POINT('Ctrl Pts',(-41.6398245884867,-3.0659440051395,134.652471525759));
#83561=CARTESIAN_POINT('Ctrl Pts',(-41.6475808912286,-2.95640523730333,
134.734863274396));
#83562=CARTESIAN_POINT('Ctrl Pts',(-41.6553413337428,-2.84680800532847,
134.81729899799));
#83563=CARTESIAN_POINT('Ctrl Pts',(-41.663101776257,-2.73384719223768,134.895081904165));
#83564=CARTESIAN_POINT('Ctrl Pts',(-41.6708622187712,-2.61796435150189,
134.967946297814));
#83565=CARTESIAN_POINT('Ctrl Pts',(-41.6786351190367,-2.50189548534255,
135.040927659856));
#83566=CARTESIAN_POINT('Ctrl Pts',(-41.6864080193021,-2.3828955576191,135.108974537196));
#83567=CARTESIAN_POINT('Ctrl Pts',(-41.6941809195676,-2.26143080657674,
135.171867202514));
#83568=CARTESIAN_POINT('Ctrl Pts',(-41.7016712553294,-2.14438160518978,
135.232473561029));
#83569=CARTESIAN_POINT('Ctrl Pts',(-41.7091615910912,-2.0250439532986,135.288293808208));
#83570=CARTESIAN_POINT('Ctrl Pts',(-41.716651926853,-1.90385008828339,135.339174605355));
#83571=CARTESIAN_POINT('Ctrl Pts',(-41.7244262609721,-1.7780611210365,135.391984563391));
#83572=CARTESIAN_POINT('Ctrl Pts',(-41.7322005950912,-1.64987394380568,
135.439640405068));
#83573=CARTESIAN_POINT('Ctrl Pts',(-41.7399749292103,-1.51974985684307,
135.481918039461));
#83574=CARTESIAN_POINT('Ctrl Pts',(-41.7477396821574,-1.38978613618811,
135.524143570448));
#83575=CARTESIAN_POINT('Ctrl Pts',(-41.7555044351044,-1.25789062361781,
135.561003962563));
#83576=CARTESIAN_POINT('Ctrl Pts',(-41.7632691880515,-1.12454589999998,
135.592322561994));
#83577=CARTESIAN_POINT('Ctrl Pts',(-41.7710262289364,-0.991333616241483,
135.623610055351));
#83578=CARTESIAN_POINT('Ctrl Pts',(-41.7787832698215,-0.856675364005673,
135.64936662079));
#83579=CARTESIAN_POINT('Ctrl Pts',(-41.7865403107065,-0.721069904199495,
135.669465062052));
#83580=CARTESIAN_POINT('Ctrl Pts',(-41.7942915019466,-0.585566705525228,
135.689548346923));
#83581=CARTESIAN_POINT('Ctrl Pts',(-41.8020426931867,-0.449118106220323,
135.703981943407));
#83582=CARTESIAN_POINT('Ctrl Pts',(-41.8097938844269,-0.312233758518155,
135.712689573794));
#83583=CARTESIAN_POINT('Ctrl Pts',(-41.8175417812039,-0.175407590315456,
135.721393503205));
#83584=CARTESIAN_POINT('Ctrl Pts',(-41.825289677981,-0.038146431433194,
135.72437628217));
#83585=CARTESIAN_POINT('Ctrl Pts',(-41.8330375747581,0.0990344504043435,
135.721613431906));
#83586=CARTESIAN_POINT('Ctrl Pts',(-41.8407838508422,0.236186636958678,
135.71885115957));
#83587=CARTESIAN_POINT('Ctrl Pts',(-41.8485301269263,0.373258189230657,
135.710345656441));
#83588=CARTESIAN_POINT('Ctrl Pts',(-41.8562764030104,0.50973373913565,135.696124571161));
#83589=CARTESIAN_POINT('Ctrl Pts',(-41.8640227362758,0.646210296471964,
135.681903380904));
#83590=CARTESIAN_POINT('Ctrl Pts',(-41.8717690695411,0.782090453802543,
135.661966564827));
#83591=CARTESIAN_POINT('Ctrl Pts',(-41.8795154028064,0.916864260867472,
135.636393625488));
#83592=CARTESIAN_POINT('Ctrl Pts',(-41.8872634708094,1.05166824959204,135.610814959265));
#83593=CARTESIAN_POINT('Ctrl Pts',(-41.8950115388123,1.18536501100023,135.579597731077));
#83594=CARTESIAN_POINT('Ctrl Pts',(-41.9027596068153,1.31745546849312,135.542872425195));
#83595=CARTESIAN_POINT('Ctrl Pts',(-41.9105159095571,1.44968631329632,135.506108087221));
#83596=CARTESIAN_POINT('Ctrl Pts',(-41.918272212299,1.58030706659254,135.463824082352));
#83597=CARTESIAN_POINT('Ctrl Pts',(-41.9260285150408,1.7088339578248,135.416200767342));
#83598=CARTESIAN_POINT('Ctrl Pts',(-41.933788957555,1.83742944772879,135.368552034334));
#83599=CARTESIAN_POINT('Ctrl Pts',(-41.9415494000692,1.96392848831663,135.315558463806));
#83600=CARTESIAN_POINT('Ctrl Pts',(-41.9493098425833,2.08786887233352,135.257447932502));
#83601=CARTESIAN_POINT('Ctrl Pts',(-41.9570827428487,2.21200821645775,135.199244117014));
#83602=CARTESIAN_POINT('Ctrl Pts',(-41.9648556431142,2.33358034922079,135.135907106908));
#83603=CARTESIAN_POINT('Ctrl Pts',(-41.9726285433796,2.45214839464508,135.067710393639));
#83604=CARTESIAN_POINT('Ctrl Pts',(-41.9801188791417,2.5664061929646,135.001992802674));
#83605=CARTESIAN_POINT('Ctrl Pts',(-41.9876092149038,2.67787426366432,134.931762863403));
#83606=CARTESIAN_POINT('Ctrl Pts',(-41.9950995506659,2.78618996369219,134.857301346064));
#83607=CARTESIAN_POINT('Ctrl Pts',(-42.002873884785,2.89861248640719,134.780016597665));
#83608=CARTESIAN_POINT('Ctrl Pts',(-42.0106482189041,3.00799499613306,134.697928241496));
#83609=CARTESIAN_POINT('Ctrl Pts',(-42.0184225530231,3.11389961477315,134.611303255907));
#83610=CARTESIAN_POINT('Ctrl Pts',(-42.0261873059702,3.21967371543574,134.52478502787));
#83611=CARTESIAN_POINT('Ctrl Pts',(-42.0339520589173,3.32197815353384,134.433741539973));
#83612=CARTESIAN_POINT('Ctrl Pts',(-42.0417168118644,3.42040345846579,134.338483315466));
#83613=CARTESIAN_POINT('Ctrl Pts',(-42.0494738527494,3.51873100599732,134.243319702772));
#83614=CARTESIAN_POINT('Ctrl Pts',(-42.0572308936343,3.61318680850876,134.143949954204));
#83615=CARTESIAN_POINT('Ctrl Pts',(-42.0649879345193,3.70339425973269,134.040724938757));
#83616=CARTESIAN_POINT('Ctrl Pts',(-42.0727391257594,3.79353368481595,133.937577766097));
#83617=CARTESIAN_POINT('Ctrl Pts',(-42.0804903169997,3.87943087918509,133.830581406537));
#83618=CARTESIAN_POINT('Ctrl Pts',(-42.0882415082398,3.960746188761,133.720123414968));
#83619=CARTESIAN_POINT('Ctrl Pts',(-42.0959894050168,4.04202693716118,133.609712370993));
#83620=CARTESIAN_POINT('Ctrl Pts',(-42.1037373017938,4.11872944274777,133.495842935477));
#83621=CARTESIAN_POINT('Ctrl Pts',(-42.1114851985709,4.19055459603477,133.378935386368));
#83622=CARTESIAN_POINT('Ctrl Pts',(-42.119231474655,4.26236472504806,133.262052291798));
#83623=CARTESIAN_POINT('Ctrl Pts',(-42.1269777507391,4.32929932653864,133.142132680604));
#83624=CARTESIAN_POINT('Ctrl Pts',(-42.1347240268231,4.3911030930548,133.019625091317));
#83625=CARTESIAN_POINT('Ctrl Pts',(-42.1424703600885,4.45290731579233,132.897116597707));
#83626=CARTESIAN_POINT('Ctrl Pts',(-42.1502166933538,4.50958045188186,132.772020436946));
#83627=CARTESIAN_POINT('Ctrl Pts',(-42.1579630266192,4.56091374850402,132.644808617703));
#83628=CARTESIAN_POINT('Ctrl Pts',(-42.1657110946221,4.61225854086198,132.517568310255));
#83629=CARTESIAN_POINT('Ctrl Pts',(-42.1734591626251,4.65826096793492,132.388211764034));
#83630=CARTESIAN_POINT('Ctrl Pts',(-42.1812072306281,4.69876104674554,132.257229396254));
#83631=CARTESIAN_POINT('Ctrl Pts',(-42.1889635333699,4.73930416952194,132.126107818855));
#83632=CARTESIAN_POINT('Ctrl Pts',(-42.1967198361118,4.77433314642686,131.99335734226));
#83633=CARTESIAN_POINT('Ctrl Pts',(-42.2044761388536,4.80373822690096,131.859482463568));
#83634=CARTESIAN_POINT('Ctrl Pts',(-42.2122365813678,4.83315900175188,131.725536131822));
#83635=CARTESIAN_POINT('Ctrl Pts',(-42.2199970238819,4.85694983135891,131.590464587026));
#83636=CARTESIAN_POINT('Ctrl Pts',(-42.2277574663961,4.87505260057043,131.45477987018));
#83637=CARTESIAN_POINT('Ctrl Pts',(-42.2355303666615,4.89318442995417,131.318877340182));
#83638=CARTESIAN_POINT('Ctrl Pts',(-42.2433032669269,4.90560991687712,131.182360060731));
#83639=CARTESIAN_POINT('Ctrl Pts',(-42.2510761671923,4.91232301531016,131.045743416775));
#83640=CARTESIAN_POINT('Ctrl Pts',(-42.2585665029544,4.91879207570596,130.914093131942));
#83641=CARTESIAN_POINT('Ctrl Pts',(-42.2660568387165,4.91995685375458,130.782350889485));
#83642=CARTESIAN_POINT('Ctrl Pts',(-42.2735471744786,4.91585755198091,130.650973554447));
#83643=CARTESIAN_POINT('Ctrl Pts',(-42.2813215085977,4.91160282393456,130.51461500782));
#83644=CARTESIAN_POINT('Ctrl Pts',(-42.2890958427168,4.9016634833501,130.378217642885));
#83645=CARTESIAN_POINT('Ctrl Pts',(-42.2968701768359,4.88602746286568,130.242294167204));
#83646=CARTESIAN_POINT('Ctrl Pts',(-42.304634929783,4.87041071237908,130.106538205059));
#83647=CARTESIAN_POINT('Ctrl Pts',(-42.3123996827301,4.84911129524245,129.971255354806));
#83648=CARTESIAN_POINT('Ctrl Pts',(-42.3201644356772,4.82216913459946,129.836957961059));
#83649=CARTESIAN_POINT('Ctrl Pts',(-42.3279214765622,4.79525373329024,129.702793953378));
#83650=CARTESIAN_POINT('Ctrl Pts',(-42.3356785174472,4.76270681799171,129.569613835256));
#83651=CARTESIAN_POINT('Ctrl Pts',(-42.3434355583323,4.72462001983748,129.437924109472));
#83652=CARTESIAN_POINT('Ctrl Pts',(-42.3511867495724,4.68656194323402,129.306333691936));
#83653=CARTESIAN_POINT('Ctrl Pts',(-42.3589379408125,4.64297240735345,129.176231803704));
#83654=CARTESIAN_POINT('Ctrl Pts',(-42.3666891320527,4.59399388177659,129.048113688259));
#83655=CARTESIAN_POINT('Ctrl Pts',(-42.3744370288298,4.54503617337964,128.920050026431));
#83656=CARTESIAN_POINT('Ctrl Pts',(-42.3821849256069,4.49069417016202,128.793968824841));
#83657=CARTESIAN_POINT('Ctrl Pts',(-42.389932822384,4.43115978788133,128.670348903267));
#83658=CARTESIAN_POINT('Ctrl Pts',(-42.3976790984681,4.37163785891,128.546754840317));
#83659=CARTESIAN_POINT('Ctrl Pts',(-42.4054253745522,4.30692588078618,128.425621385346));
#83660=CARTESIAN_POINT('Ctrl Pts',(-42.4131716506363,4.23726322176676,128.307405781778));
#83661=CARTESIAN_POINT('Ctrl Pts',(-42.4209179839017,4.16760004851341,128.18918930557));
#83662=CARTESIAN_POINT('Ctrl Pts',(-42.428664317167,4.09298631993178,128.073891060576));
#83663=CARTESIAN_POINT('Ctrl Pts',(-42.4364106504324,4.0137063142859,127.961941808671));
#83664=CARTESIAN_POINT('Ctrl Pts',(-42.4441587184353,3.93440855443244,127.849967486507));
#83665=CARTESIAN_POINT('Ctrl Pts',(-42.4519067864384,3.85044266403317,127.741343968812));
#83666=CARTESIAN_POINT('Ctrl Pts',(-42.4596548544414,3.76213477027295,127.636470936279));
#83667=CARTESIAN_POINT('Ctrl Pts',(-42.4674111571833,3.67373302183235,127.53148644344));
#83668=CARTESIAN_POINT('Ctrl Pts',(-42.4751674599251,3.58098030383065,127.430260697887));
#83669=CARTESIAN_POINT('Ctrl Pts',(-42.482923762667,3.48424174110856,127.33315872888));
#83670=CARTESIAN_POINT('Ctrl Pts',(-42.4906842051811,3.38745154610281,127.236004933629));
#83671=CARTESIAN_POINT('Ctrl Pts',(-42.4984446476954,3.28667155456641,127.142979565621));
#83672=CARTESIAN_POINT('Ctrl Pts',(-42.5062050902095,3.1823011484362,127.054408289447));
#83673=CARTESIAN_POINT('Ctrl Pts',(-42.513977990475,3.07776319766451,126.965694830799));
#83674=CARTESIAN_POINT('Ctrl Pts',(-42.5217508907404,2.96962362328354,126.881449992579));
#83675=CARTESIAN_POINT('Ctrl Pts',(-42.5295237910058,2.85831276521803,126.801957439638));
#83676=CARTESIAN_POINT('Ctrl Pts',(-42.5370141267678,2.75104833721968,126.725354641226));
#83677=CARTESIAN_POINT('Ctrl Pts',(-42.5445044625297,2.64083944849535,126.653164780436));
#83678=CARTESIAN_POINT('Ctrl Pts',(-42.5519947982916,2.52809220299046,126.58560098046));
#83679=CARTESIAN_POINT('Ctrl Pts',(-42.5597691324108,2.41107011140215,126.515475478471));
#83680=CARTESIAN_POINT('Ctrl Pts',(-42.5675434665299,2.29094268894056,126.450111619763));
#83681=CARTESIAN_POINT('Ctrl Pts',(-42.5753178006489,2.16813476829461,126.389796687911));
#83682=CARTESIAN_POINT('Ctrl Pts',(-42.583082553596,2.0454781974352,126.329556088822));
#83683=CARTESIAN_POINT('Ctrl Pts',(-42.5908473065431,1.92014804887794,126.27435220666));
#83684=CARTESIAN_POINT('Ctrl Pts',(-42.5986120594902,1.79259695209313,126.224428387735));
#83685=CARTESIAN_POINT('Ctrl Pts',(-42.6063691003752,1.6651725408558,126.17455415385));
#83686=CARTESIAN_POINT('Ctrl Pts',(-42.6141261412602,1.53553193290139,126.129949688517));
#83687=CARTESIAN_POINT('Ctrl Pts',(-42.6218831821452,1.40415079222919,126.090811676992));
#83688=CARTESIAN_POINT('Ctrl Pts',(-42.6296343733854,1.27286872709735,126.051703179747));
#83689=CARTESIAN_POINT('Ctrl Pts',(-42.6373855646255,1.13984911497429,126.018053042298));
#83690=CARTESIAN_POINT('Ctrl Pts',(-42.6451367558656,1.00558562651601,125.990009092153));
#83691=CARTESIAN_POINT('Ctrl Pts',(-42.6528846526427,0.871379203621746,
125.961977061435));
#83692=CARTESIAN_POINT('Ctrl Pts',(-42.6606325494197,0.735930337802519,
125.939546558623));
#83693=CARTESIAN_POINT('Ctrl Pts',(-42.6683804461968,0.599745608853917,
125.922814933343));
#83694=CARTESIAN_POINT('Ctrl Pts',(-42.6761267222809,0.463589366814808,
125.906086807957));
#83695=CARTESIAN_POINT('Ctrl Pts',(-42.683872998365,0.326697955616605,125.89505523663));
#83696=CARTESIAN_POINT('Ctrl Pts',(-42.6916192744492,0.189585451490489,
125.889765983307));
#83697=CARTESIAN_POINT('Ctrl Pts',(-42.6993656077145,0.0524719352312011,
125.884476690941));
#83698=CARTESIAN_POINT('Ctrl Pts',(-42.7071119409799,-0.0848622865380212,
125.884929816231));
#83699=CARTESIAN_POINT('Ctrl Pts',(-42.7148582742452,-0.221901142306615,
125.89111902514));
#83700=CARTESIAN_POINT('Ctrl Pts',(-42.7226063422482,-0.358970686976984,
125.89730962008));
#83701=CARTESIAN_POINT('Ctrl Pts',(-42.7303544102512,-0.495744343533176,
125.909238837119));
#83702=CARTESIAN_POINT('Ctrl Pts',(-42.7381024782542,-0.63170956957887,
125.926848333399));
#83703=CARTESIAN_POINT('Ctrl Pts',(-42.745858780996,-0.767819301084812,
125.944476545261));
#83704=CARTESIAN_POINT('Ctrl Pts',(-42.7536150837379,-0.903118497371499,
125.967797045761));
#83705=CARTESIAN_POINT('Ctrl Pts',(-42.7613713864798,-1.03710269008942,
125.996699952262));
#83706=CARTESIAN_POINT('Ctrl Pts',(-42.7691318289939,-1.17115839420536,
126.025618285115));
#83707=CARTESIAN_POINT('Ctrl Pts',(-42.7768922715081,-1.30389731803941,
126.060124862553));
#83708=CARTESIAN_POINT('Ctrl Pts',(-42.7846527140223,-1.43482959505532,
126.100059702908));
#83709=CARTESIAN_POINT('Ctrl Pts',(-42.7924256142878,-1.56597205618575,
126.140058650214));
#83710=CARTESIAN_POINT('Ctrl Pts',(-42.8001985145531,-1.69530170592608,
126.185503143961));
#83711=CARTESIAN_POINT('Ctrl Pts',(-42.8079714148186,-1.8223472797653,126.23618445476));
#83712=CARTESIAN_POINT('Ctrl Pts',(-42.8154617505806,-1.94477442698611,
126.285023372252));
#83713=CARTESIAN_POINT('Ctrl Pts',(-42.8229520863426,-2.06508039774963,
126.338724848522));
#83714=CARTESIAN_POINT('Ctrl Pts',(-42.8304424221045,-2.18286637637645,
126.397062415109));
#83715=CARTESIAN_POINT('Ctrl Pts',(-42.8382175270897,-2.30513036809968,
126.457617872061));
#83716=CARTESIAN_POINT('Ctrl Pts',(-42.845992632075,-2.42506629975389,126.523360745701));
#83717=CARTESIAN_POINT('Ctrl Pts',(-42.8537677370602,-2.54220269976336,
126.594088833487));
#83718=CARTESIAN_POINT('Ctrl Pts',(-42.8615330889043,-2.65919216312966,
126.66472819951));
#83719=CARTESIAN_POINT('Ctrl Pts',(-42.8692984407485,-2.77338875112387,
126.740340135858));
#83720=CARTESIAN_POINT('Ctrl Pts',(-42.8770637925927,-2.88434297150766,
126.820675303034));
#83721=CARTESIAN_POINT('Ctrl Pts',(-42.8850936929651,-2.99907715914755,
126.903747313392));
#83722=CARTESIAN_POINT('Ctrl Pts',(-42.8931235933375,-3.11034374475109,
126.991869935696));
#83723=CARTESIAN_POINT('Ctrl Pts',(-42.9011534937099,-3.21767452558208,
127.084716318722));
#83724=CARTESIAN_POINT('Ctrl Pts',(-42.9089042614454,-3.3212743106991,127.174335207693));
#83725=CARTESIAN_POINT('Ctrl Pts',(-42.9166550291809,-3.42120701176852,
127.268354664679));
#83726=CARTESIAN_POINT('Ctrl Pts',(-42.9244057969164,-3.51708264249682,
127.366437880164));
#83727=CARTESIAN_POINT('Ctrl Pts',(-42.9321530804166,-3.6129151738474,127.464477003886));
#83728=CARTESIAN_POINT('Ctrl Pts',(-42.9399003639166,-3.70469399111762,
127.566575972256));
#83729=CARTESIAN_POINT('Ctrl Pts',(-42.9476476474167,-3.79206477075871,
127.672360005039));
#83730=CARTESIAN_POINT('Ctrl Pts',(-42.9553931259917,-3.8794151951721,127.778119392762));
#83731=CARTESIAN_POINT('Ctrl Pts',(-42.9631386045667,-3.96235937759712,
127.887561834711));
#83732=CARTESIAN_POINT('Ctrl Pts',(-42.9708840831417,-4.04058248929738,
128.000278555699));
#83733=CARTESIAN_POINT('Ctrl Pts',(-42.9786294345188,-4.11880431640182,
128.11299342563));
#83734=CARTESIAN_POINT('Ctrl Pts',(-42.9863747858959,-4.19230500583251,
128.228982145526));
#83735=CARTESIAN_POINT('Ctrl Pts',(-42.994120137273,-4.26081260070424,128.347806314445));
#83736=CARTESIAN_POINT('Ctrl Pts',(-43.0018697678768,-4.32935804531452,
128.466696132491));
#83737=CARTESIAN_POINT('Ctrl Pts',(-43.0096193984806,-4.39290469076406,
128.588424189267));
#83738=CARTESIAN_POINT('Ctrl Pts',(-43.0173690290843,-4.45122610263049,
128.712526674405));
#83739=CARTESIAN_POINT('Ctrl Pts',(-43.0251212462136,-4.50956697991787,
128.83667058013));
#83740=CARTESIAN_POINT('Ctrl Pts',(-43.0328734633429,-4.56267899430795,
128.963190134387));
#83741=CARTESIAN_POINT('Ctrl Pts',(-43.0406256804722,-4.61038392677963,
129.091601699857));
#83742=CARTESIAN_POINT('Ctrl Pts',(-43.0483850744578,-4.65813302357772,
129.220132146331));
#83743=CARTESIAN_POINT('Ctrl Pts',(-43.0561444684436,-4.70046492196504,
129.350557730384));
#83744=CARTESIAN_POINT('Ctrl Pts',(-43.0639038624292,-4.73725125030763,
129.482379659322));
#83745=CARTESIAN_POINT('Ctrl Pts',(-43.0658630421296,-4.74653947924328,
129.515663553363));
#83746=CARTESIAN_POINT('Ctrl Pts',(-43.06782222183,-4.75547442177194,129.549036414434));
#83747=CARTESIAN_POINT('Ctrl Pts',(-43.0697814015304,-4.7640545282341,129.582490119308));
#83748=CARTESIAN_POINT('Origin',(213.235140564004,0.,130.804360617566));
#83749=CARTESIAN_POINT('',(-45.1651923290374,-4.76405452823407,129.582490119308));
#83750=CARTESIAN_POINT('',(-44.8201225776941,-4.76405452823406,129.582490119308));
#83751=CARTESIAN_POINT('',(213.235140564004,-4.76405452823405,129.582490119308));
#83752=CARTESIAN_POINT('',(-43.4851405639651,-4.91824956659705,130.802295873524));
#83753=CARTESIAN_POINT('Ctrl Pts',(-43.4851405640086,-4.91824956659737,
130.802295874294));
#83754=CARTESIAN_POINT('Ctrl Pts',(-43.4930372764877,-4.91830839744131,
130.942431830506));
#83755=CARTESIAN_POINT('Ctrl Pts',(-43.500933988967,-4.91237352301066,131.082539161257));
#83756=CARTESIAN_POINT('Ctrl Pts',(-43.5088307014462,-4.90047868839197,
131.22208263891));
#83757=CARTESIAN_POINT('Ctrl Pts',(-43.5167308566085,-4.88857866805239,
131.361686952511));
#83758=CARTESIAN_POINT('Ctrl Pts',(-43.5246310117707,-4.87071354147857,
131.500726555114));
#83759=CARTESIAN_POINT('Ctrl Pts',(-43.5325311669331,-4.84696884207495,
131.638672373719));
#83760=CARTESIAN_POINT('Ctrl Pts',(-43.5404361953534,-4.82320949561139,
131.776703285027));
#83761=CARTESIAN_POINT('Ctrl Pts',(-43.5483412237738,-4.79356341218359,
131.913638704233));
#83762=CARTESIAN_POINT('Ctrl Pts',(-43.5562462521941,-4.75816700446225,
132.04896088277));
#83763=CARTESIAN_POINT('Ctrl Pts',(-43.564163369394,-4.72271646671761,132.184490003005));
#83764=CARTESIAN_POINT('Ctrl Pts',(-43.572080486594,-4.68149812895479,132.31840059567));
#83765=CARTESIAN_POINT('Ctrl Pts',(-43.5799976037939,-4.63469827231357,
132.450190191706));
#83766=CARTESIAN_POINT('Ctrl Pts',(-43.5879211327744,-4.5878605141987,132.582086519263));
#83767=CARTESIAN_POINT('Ctrl Pts',(-43.5958446617549,-4.5354323630066,132.711858083544));
#83768=CARTESIAN_POINT('Ctrl Pts',(-43.6037681907354,-4.47764760974547,
132.839023966978));
#83769=CARTESIAN_POINT('Ctrl Pts',(-43.6117063611401,-4.41975607943011,
132.966424832785));
#83770=CARTESIAN_POINT('Ctrl Pts',(-43.6196445315447,-4.35648833193795,
133.091210065452));
#83771=CARTESIAN_POINT('Ctrl Pts',(-43.6275827019493,-4.28812390246818,
133.212923770066));
#83772=CARTESIAN_POINT('Ctrl Pts',(-43.6337872337607,-4.234689766415,133.308056088178));
#83773=CARTESIAN_POINT('Ctrl Pts',(-43.6399917655722,-4.17814293966459,
133.401312488867));
#83774=CARTESIAN_POINT('Ctrl Pts',(-43.6461962973837,-4.11863445846413,
133.492488825084));
#83775=CARTESIAN_POINT('Ctrl Pts',(-43.6539706315028,-4.04406979672443,
133.606733593754));
#83776=CARTESIAN_POINT('Ctrl Pts',(-43.6617449656219,-3.96462995860692,
133.718054498226));
#83777=CARTESIAN_POINT('Ctrl Pts',(-43.669519299741,-3.88057133770916,133.826007379755));
#83778=CARTESIAN_POINT('Ctrl Pts',(-43.6772840526881,-3.79661631154923,
133.933827219007));
#83779=CARTESIAN_POINT('Ctrl Pts',(-43.6850488056352,-3.70805406635717,
134.038286988629));
#83780=CARTESIAN_POINT('Ctrl Pts',(-43.6928135585823,-3.61518520979579,
134.138969884238));
#83781=CARTESIAN_POINT('Ctrl Pts',(-43.7005705994673,-3.52240859189197,
134.239552780175));
#83782=CARTESIAN_POINT('Ctrl Pts',(-43.7083276403523,-3.42533413817417,
134.336365981722));
#83783=CARTESIAN_POINT('Ctrl Pts',(-43.7160846812373,-3.32430357908102,
134.429024571177));
#83784=CARTESIAN_POINT('Ctrl Pts',(-43.7238358724774,-3.22334920791825,
134.521613286069));
#83785=CARTESIAN_POINT('Ctrl Pts',(-43.7315870637176,-3.11844495648586,
134.610053361777));
#83786=CARTESIAN_POINT('Ctrl Pts',(-43.7393382549577,-3.00997011730864,
134.693995941785));
#83787=CARTESIAN_POINT('Ctrl Pts',(-43.7470861517348,-2.90154138283189,
134.777902843956));
#83788=CARTESIAN_POINT('Ctrl Pts',(-43.754834048512,-2.78954538754161,134.857315813596));
#83789=CARTESIAN_POINT('Ctrl Pts',(-43.762581945289,-2.6743951105537,134.931925741843));
#83790=CARTESIAN_POINT('Ctrl Pts',(-43.7703282213731,-2.55926892052122,
135.006520063301));
#83791=CARTESIAN_POINT('Ctrl Pts',(-43.7780744974572,-2.44099008908846,
135.076313129294));
#83792=CARTESIAN_POINT('Ctrl Pts',(-43.7858207735414,-2.32000089894515,
135.141038942205));
#83793=CARTESIAN_POINT('Ctrl Pts',(-43.7935671068067,-2.19901081568729,
135.205765232907));
#83794=CARTESIAN_POINT('Ctrl Pts',(-43.8013134400721,-2.07531067853034,
135.265424011464));
#83795=CARTESIAN_POINT('Ctrl Pts',(-43.8090597733374,-1.94936735072531,
135.319795258265));
#83796=CARTESIAN_POINT('Ctrl Pts',(-43.8168078413404,-1.82339581878525,
135.37417868113));
#83797=CARTESIAN_POINT('Ctrl Pts',(-43.8245559093433,-1.69518045546037,
135.423272061075));
#83798=CARTESIAN_POINT('Ctrl Pts',(-43.8323039773463,-1.56520769758678,
135.466903692532));
#83799=CARTESIAN_POINT('Ctrl Pts',(-43.8400602800882,-1.43509680311924,
135.510581696207));
#83800=CARTESIAN_POINT('Ctrl Pts',(-43.84781658283,-1.30322515424092,135.548786231037));
#83801=CARTESIAN_POINT('Ctrl Pts',(-43.8555728855719,-1.17009446905893,
135.581395471529));
#83802=CARTESIAN_POINT('Ctrl Pts',(-43.8633333280861,-1.03689272802176,
135.614022116555));
#83803=CARTESIAN_POINT('Ctrl Pts',(-43.8710937706003,-0.902430994805061,
135.641047439633));
#83804=CARTESIAN_POINT('Ctrl Pts',(-43.8788542131145,-0.767219768351191,
135.662401054774));
#83805=CARTESIAN_POINT('Ctrl Pts',(-43.8866271133799,-0.631791488833129,
135.683788948635));
#83806=CARTESIAN_POINT('Ctrl Pts',(-43.8944000136453,-0.495611700411419,
135.699486895612));
#83807=CARTESIAN_POINT('Ctrl Pts',(-43.9021729139107,-0.359195494525443,
135.709476483599));
#83808=CARTESIAN_POINT('Ctrl Pts',(-43.9096632496726,-0.227738361337324,
135.719102924902));
#83809=CARTESIAN_POINT('Ctrl Pts',(-43.9171535854345,-0.0960620088562741,
135.723428818088));
#83810=CARTESIAN_POINT('Ctrl Pts',(-43.9246439211965,0.0353758646920503,
135.722483390606));
#83811=CARTESIAN_POINT('Ctrl Pts',(-43.9324182553156,0.171797245167937,
135.721502116954));
#83812=CARTESIAN_POINT('Ctrl Pts',(-43.9401925894346,0.308393847800017,
135.714838799324));
#83813=CARTESIAN_POINT('Ctrl Pts',(-43.9479669235537,0.444653402256518,
135.702469070261));
#83814=CARTESIAN_POINT('Ctrl Pts',(-43.9557316765008,0.580745028990202,
135.690114585784));
#83815=CARTESIAN_POINT('Ctrl Pts',(-43.963496429448,0.716500048407952,135.672067717744));
#83816=CARTESIAN_POINT('Ctrl Pts',(-43.9712611823951,0.851405305390756,
135.648356082929));
#83817=CARTESIAN_POINT('Ctrl Pts',(-43.9790182232801,0.986176572570312,
135.624667998844));
#83818=CARTESIAN_POINT('Ctrl Pts',(-43.986775264165,1.12009937433432,135.59532641187));
#83819=CARTESIAN_POINT('Ctrl Pts',(-43.9945323050501,1.25266515486895,135.560410772083));
#83820=CARTESIAN_POINT('Ctrl Pts',(-44.0022834962902,1.38513096651745,135.525521462451));
#83821=CARTESIAN_POINT('Ctrl Pts',(-44.0100346875303,1.51624141729157,135.485066565867));
#83822=CARTESIAN_POINT('Ctrl Pts',(-44.0177858787705,1.64549798744993,135.439176626406));
#83823=CARTESIAN_POINT('Ctrl Pts',(-44.0255337755476,1.77469962011776,135.393306191393));
#83824=CARTESIAN_POINT('Ctrl Pts',(-44.0332816723247,1.90204857167684,135.342005438524));
#83825=CARTESIAN_POINT('Ctrl Pts',(-44.0410295691018,2.02706155478761,135.285454737935));
#83826=CARTESIAN_POINT('Ctrl Pts',(-44.0487758451859,2.15204838787728,135.228915866533));
#83827=CARTESIAN_POINT('Ctrl Pts',(-44.05652212127,2.27469986845013,135.167129392778));
#83828=CARTESIAN_POINT('Ctrl Pts',(-44.0642683973541,2.39455314057997,135.100323643412));
#83829=CARTESIAN_POINT('Ctrl Pts',(-44.0720147306195,2.51440729743944,135.033517400902));
#83830=CARTESIAN_POINT('Ctrl Pts',(-44.0797610638849,2.63146286314099,134.961691999199));
#83831=CARTESIAN_POINT('Ctrl Pts',(-44.0875073971502,2.74528237796421,134.885121297603));
#83832=CARTESIAN_POINT('Ctrl Pts',(-44.0952554651532,2.85912738187861,134.80853344853));
#83833=CARTESIAN_POINT('Ctrl Pts',(-44.1030035331562,2.96973456853441,134.72719840315));
#83834=CARTESIAN_POINT('Ctrl Pts',(-44.1107516011591,3.07669654618326,134.641432603495));
#83835=CARTESIAN_POINT('Ctrl Pts',(-44.118507903901,3.18377220429482,134.555575650928));
#83836=CARTESIAN_POINT('Ctrl Pts',(-44.126264206643,3.28719460881878,134.465278782201));
#83837=CARTESIAN_POINT('Ctrl Pts',(-44.1340205093848,3.38659007362532,134.370898257312));
#83838=CARTESIAN_POINT('Ctrl Pts',(-44.141780951899,3.4860385887843,134.276467358694));
#83839=CARTESIAN_POINT('Ctrl Pts',(-44.1495413944132,3.5814556097007,134.177948741638));
#83840=CARTESIAN_POINT('Ctrl Pts',(-44.1573018369274,3.67250598150133,134.075733858017));
#83841=CARTESIAN_POINT('Ctrl Pts',(-44.1650747371929,3.76370251544173,133.97335488999));
#83842=CARTESIAN_POINT('Ctrl Pts',(-44.1728476374583,3.85051814484051,133.867268100963));
#83843=CARTESIAN_POINT('Ctrl Pts',(-44.1806205377237,3.93265895956695,133.75789689976));
#83844=CARTESIAN_POINT('Ctrl Pts',(-44.1881108734857,4.01181374877653,133.652501617212));
#83845=CARTESIAN_POINT('Ctrl Pts',(-44.1956012092476,4.08662753011999,133.544056823535));
#83846=CARTESIAN_POINT('Ctrl Pts',(-44.2030915450095,4.15687749640477,133.432963391357));
#83847=CARTESIAN_POINT('Ctrl Pts',(-44.2108658791286,4.22979101151448,133.317657817931));
#83848=CARTESIAN_POINT('Ctrl Pts',(-44.2186402132476,4.29801877395729,133.19913354158));
#83849=CARTESIAN_POINT('Ctrl Pts',(-44.2264145473667,4.36126338807634,133.077808378638));
#83850=CARTESIAN_POINT('Ctrl Pts',(-44.2341793003138,4.42443005886066,132.956632738118));
#83851=CARTESIAN_POINT('Ctrl Pts',(-44.2419440532609,4.48262562166015,132.832663422505));
#83852=CARTESIAN_POINT('Ctrl Pts',(-44.249708806208,4.53559593838496,132.706347091284));
#83853=CARTESIAN_POINT('Ctrl Pts',(-44.257465847093,4.58851364424459,132.580156219223));
#83854=CARTESIAN_POINT('Ctrl Pts',(-44.265222887978,4.63621628172619,132.451623328741));
#83855=CARTESIAN_POINT('Ctrl Pts',(-44.272979928863,4.67849580758928,132.321219226952));
#83856=CARTESIAN_POINT('Ctrl Pts',(-44.2807311201031,4.72074345013275,132.190913463912));
#83857=CARTESIAN_POINT('Ctrl Pts',(-44.2884823113432,4.75757600108842,132.058739668667));
#83858=CARTESIAN_POINT('Ctrl Pts',(-44.2962335025833,4.78883382878659,131.925187822254));
#83859=CARTESIAN_POINT('Ctrl Pts',(-44.3039813993604,4.82007837107434,131.791692738938));
#83860=CARTESIAN_POINT('Ctrl Pts',(-44.3117292961374,4.8457528137615,131.656821149266));
#83861=CARTESIAN_POINT('Ctrl Pts',(-44.3194771929145,4.86574767873999,131.521077151027));
#83862=CARTESIAN_POINT('Ctrl Pts',(-44.3272234689986,4.88573836122371,131.385361547507));
#83863=CARTESIAN_POINT('Ctrl Pts',(-44.3349697450827,4.9000517721482,131.248774284948));
#83864=CARTESIAN_POINT('Ctrl Pts',(-44.3427160211668,4.9086298243352,131.111828193331));
#83865=CARTESIAN_POINT('Ctrl Pts',(-44.3504623544322,4.91720793984345,130.97488109081));
#83866=CARTESIAN_POINT('Ctrl Pts',(-44.3582086876976,4.92005058769212,130.837575544146));
#83867=CARTESIAN_POINT('Ctrl Pts',(-44.3659550209629,4.91715171580341,130.700427628233));
#83868=CARTESIAN_POINT('Ctrl Pts',(-44.3737030889658,4.91425219473244,130.563248998997));
#83869=CARTESIAN_POINT('Ctrl Pts',(-44.3814511569688,4.905608603644,130.426228461559));
#83870=CARTESIAN_POINT('Ctrl Pts',(-44.3891992249717,4.89126696899205,130.289879810784));
#83871=CARTESIAN_POINT('Ctrl Pts',(-44.3969555277135,4.87691009188006,130.153386247039));
#83872=CARTESIAN_POINT('Ctrl Pts',(-44.4047118304553,4.85684311475774,130.017566385868));
#83873=CARTESIAN_POINT('Ctrl Pts',(-44.4124681331972,4.8311637827703,129.882927187226));
#83874=CARTESIAN_POINT('Ctrl Pts',(-44.4202285757113,4.80547074495019,129.748216127589));
#83875=CARTESIAN_POINT('Ctrl Pts',(-44.4279890182255,4.7741594727249,129.614687366572));
#83876=CARTESIAN_POINT('Ctrl Pts',(-44.4357494607397,4.73737814624568,129.482834468762));
#83877=CARTESIAN_POINT('Ctrl Pts',(-44.4435223610051,4.70053777511584,129.350769908974));
#83878=CARTESIAN_POINT('Ctrl Pts',(-44.4512952612706,4.65820992325379,129.220386960431));
#83879=CARTESIAN_POINT('Ctrl Pts',(-44.459068161536,4.61059195088929,129.092161760863));
#83880=CARTESIAN_POINT('Ctrl Pts',(-44.4665584972981,4.56470501176229,128.968597870278));
#83881=CARTESIAN_POINT('Ctrl Pts',(-44.4740488330602,4.51390601176882,128.8470378573));
#83882=CARTESIAN_POINT('Ctrl Pts',(-44.4815391688223,4.45841178367465,128.72788585738));
#83883=CARTESIAN_POINT('Ctrl Pts',(-44.4893135029414,4.40081347505575,128.604216173168));
#83884=CARTESIAN_POINT('Ctrl Pts',(-44.4970878370605,4.33797441673603,128.48274895783));
#83885=CARTESIAN_POINT('Ctrl Pts',(-44.5048621711796,4.27008537981359,128.36396025869));
#83886=CARTESIAN_POINT('Ctrl Pts',(-44.5126269241266,4.20228001006175,128.245317956005));
#83887=CARTESIAN_POINT('Ctrl Pts',(-44.5203916770737,4.12943723704211,128.12934793763));
#83888=CARTESIAN_POINT('Ctrl Pts',(-44.5281564300208,4.05179548018321,128.016505447499));
#83889=CARTESIAN_POINT('Ctrl Pts',(-44.5359134709058,3.97423083821178,127.903775034121));
#83890=CARTESIAN_POINT('Ctrl Pts',(-44.5436705117908,3.89187691796901,127.794166287303));
#83891=CARTESIAN_POINT('Ctrl Pts',(-44.5514275526758,3.80501737036232,127.688108722462));
#83892=CARTESIAN_POINT('Ctrl Pts',(-44.5591787439159,3.71822332421578,127.582131136455));
#83893=CARTESIAN_POINT('Ctrl Pts',(-44.5669299351561,3.62693066039519,127.479699703329));
#83894=CARTESIAN_POINT('Ctrl Pts',(-44.5746811263963,3.53146532900853,127.381213572446));
#83895=CARTESIAN_POINT('Ctrl Pts',(-44.5824290231733,3.43604057293472,127.282769300798));
#83896=CARTESIAN_POINT('Ctrl Pts',(-44.5901769199504,3.33644694818695,127.188267276387));
#83897=CARTESIAN_POINT('Ctrl Pts',(-44.5979248167275,3.23304939092162,127.098072083417));
#83898=CARTESIAN_POINT('Ctrl Pts',(-44.6056710928116,3.12967346219642,127.007895757338));
#83899=CARTESIAN_POINT('Ctrl Pts',(-44.6134173688957,3.02249547808234,126.922024727607));
#83900=CARTESIAN_POINT('Ctrl Pts',(-44.6211636449798,2.91191549942818,126.840785061747));
#83901=CARTESIAN_POINT('Ctrl Pts',(-44.6289099782451,2.80133470449758,126.759544796193));
#83902=CARTESIAN_POINT('Ctrl Pts',(-44.6366563115104,2.68735217999173,126.682936194203));
#83903=CARTESIAN_POINT('Ctrl Pts',(-44.6444026447758,2.57039884303922,126.611243298649));
#83904=CARTESIAN_POINT('Ctrl Pts',(-44.6521507127788,2.45341931519795,126.539534347968));
#83905=CARTESIAN_POINT('Ctrl Pts',(-44.6598987807817,2.33346798431292,126.472743498552));
#83906=CARTESIAN_POINT('Ctrl Pts',(-44.6676468487847,2.2110019989777,126.411109745715));
#83907=CARTESIAN_POINT('Ctrl Pts',(-44.6754031515265,2.0884058553359,126.349410487793));
#83908=CARTESIAN_POINT('Ctrl Pts',(-44.6831594542683,1.96329006821664,126.292879451425));
#83909=CARTESIAN_POINT('Ctrl Pts',(-44.6909157570102,1.8361339910268,126.241708425091));
#83910=CARTESIAN_POINT('Ctrl Pts',(-44.6986761995243,1.7089100468098,126.19051008724));
#83911=CARTESIAN_POINT('Ctrl Pts',(-44.7064366420385,1.57964401097734,126.144677590393));
#83912=CARTESIAN_POINT('Ctrl Pts',(-44.7141970845527,1.44883122838508,126.104353050109));
#83913=CARTESIAN_POINT('Ctrl Pts',(-44.7219699848181,1.3178084535012,126.063963777292));
#83914=CARTESIAN_POINT('Ctrl Pts',(-44.7297428850836,1.18523434840905,126.029100229383));
#83915=CARTESIAN_POINT('Ctrl Pts',(-44.737515785349,1.05161617928934,125.999853725703));
#83916=CARTESIAN_POINT('Ctrl Pts',(-44.7450061211111,0.9228553671799,125.971670406099));
#83917=CARTESIAN_POINT('Ctrl Pts',(-44.7524964568731,0.793125385172624,
125.948702887214));
#83918=CARTESIAN_POINT('Ctrl Pts',(-44.7599867926352,0.662883447272754,
125.930987186581));
#83919=CARTESIAN_POINT('Ctrl Pts',(-44.7677611267543,0.527703346711997,
125.912599789774));
#83920=CARTESIAN_POINT('Ctrl Pts',(-44.7755354608734,0.391543492366668,
125.899812072342));
#83921=CARTESIAN_POINT('Ctrl Pts',(-44.7833097949925,0.254907512770367,
125.892720848361));
#83922=CARTESIAN_POINT('Ctrl Pts',(-44.7910745479396,0.118439924807596,
125.885638363681));
#83923=CARTESIAN_POINT('Ctrl Pts',(-44.7988393008868,-0.0185022341936729,
125.88423842398));
#83924=CARTESIAN_POINT('Ctrl Pts',(-44.8066040538339,-0.155407083093876,
125.888566510708));
#83925=CARTESIAN_POINT('Ctrl Pts',(-44.8143610947189,-0.292175956168876,
125.892890298718));
#83926=CARTESIAN_POINT('Ctrl Pts',(-44.8221181356039,-0.428907204646427,
125.902930779205));
#83927=CARTESIAN_POINT('Ctrl Pts',(-44.829875176489,-0.565086144798041,
125.918681472201));
#83928=CARTESIAN_POINT('Ctrl Pts',(-44.8376263677291,-0.701162391350457,
125.934420287476));
#83929=CARTESIAN_POINT('Ctrl Pts',(-44.8453775589691,-0.836686771790337,
125.955860699459));
#83930=CARTESIAN_POINT('Ctrl Pts',(-44.8531287502092,-0.971147286457694,
125.982944227074));
#83931=CARTESIAN_POINT('Ctrl Pts',(-44.8608766469863,-1.10555065181983,
126.010016243467));
#83932=CARTESIAN_POINT('Ctrl Pts',(-44.8686245437635,-1.23889066827852,
126.042726528072));
#83933=CARTESIAN_POINT('Ctrl Pts',(-44.8763724405406,-1.37066334391245,
126.08096511643));
#83934=CARTESIAN_POINT('Ctrl Pts',(-44.8841187166247,-1.50240845554332,
126.119195706099));
#83935=CARTESIAN_POINT('Ctrl Pts',(-44.8918649927088,-1.63258650323105,
126.162952190487));
#83936=CARTESIAN_POINT('Ctrl Pts',(-44.8996112687929,-1.76070691447579,
126.21207423453));
#83937=CARTESIAN_POINT('Ctrl Pts',(-44.9073576020582,-1.88882827147647,
126.261196641181));
#83938=CARTESIAN_POINT('Ctrl Pts',(-44.9151039353236,-2.01489159667214,
126.315684546556));
#83939=CARTESIAN_POINT('Ctrl Pts',(-44.9228502685889,-2.1384249955175,126.375328939982));
#83940=CARTESIAN_POINT('Ctrl Pts',(-44.9305983365919,-2.26198605881085,
126.434986690355));
#83941=CARTESIAN_POINT('Ctrl Pts',(-44.938346404595,-2.38301571635764,126.499803056661));
#83942=CARTESIAN_POINT('Ctrl Pts',(-44.9460944725979,-2.50106579464921,
126.569522609645));
#83943=CARTESIAN_POINT('Ctrl Pts',(-44.9538507753398,-2.61924133796896,
126.639316261399));
#83944=CARTESIAN_POINT('Ctrl Pts',(-44.9616070780816,-2.73443063896892,
126.714023310562));
#83945=CARTESIAN_POINT('Ctrl Pts',(-44.9693633808235,-2.84621323834376,
126.793344129894));
#83946=CARTESIAN_POINT('Ctrl Pts',(-44.9771238233376,-2.95805549945745,
126.872707285136));
#83947=CARTESIAN_POINT('Ctrl Pts',(-44.9848842658519,-3.06648712696398,
126.95668887802));
#83948=CARTESIAN_POINT('Ctrl Pts',(-44.9926447083661,-3.17112080902666,
127.04494897782));
#83949=CARTESIAN_POINT('Ctrl Pts',(-45.0004176086316,-3.27592245836488,
127.133350760568));
#83950=CARTESIAN_POINT('Ctrl Pts',(-45.0081905088969,-3.37691369071269,
127.226044510642));
#83951=CARTESIAN_POINT('Ctrl Pts',(-45.0159634091624,-3.47374348677721,
127.322652810961));
#83952=CARTESIAN_POINT('Ctrl Pts',(-45.0234537449243,-3.56705327585367,
127.415749156221));
#83953=CARTESIAN_POINT('Ctrl Pts',(-45.0309440806862,-3.65649872407,127.512480159255));
#83954=CARTESIAN_POINT('Ctrl Pts',(-45.0384344164481,-3.74180239351616,
127.612480621329));
#83955=CARTESIAN_POINT('Ctrl Pts',(-45.04615639937,-3.82974417604411,127.715573711527));
#83956=CARTESIAN_POINT('Ctrl Pts',(-45.0538783822918,-3.91357280490112,
127.822480679164));
#83957=CARTESIAN_POINT('Ctrl Pts',(-45.0616003652137,-3.99293570973049,
127.932837070656));
#83958=CARTESIAN_POINT('Ctrl Pts',(-45.0693129442786,-4.07220196614547,
128.04305906976));
#83959=CARTESIAN_POINT('Ctrl Pts',(-45.0770255233434,-4.14701308527094,
128.156721819437));
#83960=CARTESIAN_POINT('Ctrl Pts',(-45.0847381024084,-4.21705489348378,
128.273425792675));
#83961=CARTESIAN_POINT('Ctrl Pts',(-45.0924415360908,-4.28701364788033,
128.389991381275));
#83962=CARTESIAN_POINT('Ctrl Pts',(-45.1001449697733,-4.35221414822146,
128.509590675735));
#83963=CARTESIAN_POINT('Ctrl Pts',(-45.1078484034558,-4.4123843589793,128.631793626393));
#83964=CARTESIAN_POINT('Ctrl Pts',(-45.1155465568533,-4.47251332632922,
128.753912813573));
#83965=CARTESIAN_POINT('Ctrl Pts',(-45.1232447102508,-4.52761868702478,
128.878631753324));
#83966=CARTESIAN_POINT('Ctrl Pts',(-45.1309428636483,-4.57747339277889,
129.005494196483));
#83967=CARTESIAN_POINT('Ctrl Pts',(-45.1386373384577,-4.62730427529659,
129.132296018002));
#83968=CARTESIAN_POINT('Ctrl Pts',(-45.146331813267,-4.67188935044903,129.261238936517));
#83969=CARTESIAN_POINT('Ctrl Pts',(-45.1540262880764,-4.71104914957288,
129.391845494529));
#83970=CARTESIAN_POINT('Ctrl Pts',(-45.1577483017301,-4.72999174287846,
129.455023216755));
#83971=CARTESIAN_POINT('Ctrl Pts',(-45.1614703153837,-4.74766559605856,
129.518589921493));
#83972=CARTESIAN_POINT('Ctrl Pts',(-45.1651923290374,-4.76405452823407,
129.582490119308));
#83973=CARTESIAN_POINT('Ctrl Pts',(-43.4154178838317,-4.76405452823406,
129.582490119308));
#83974=CARTESIAN_POINT('Ctrl Pts',(-43.423896563135,-4.80116832061884,129.727196232536));
#83975=CARTESIAN_POINT('Ctrl Pts',(-43.4323752424382,-4.83172860360835,
129.873764859095));
#83976=CARTESIAN_POINT('Ctrl Pts',(-43.4408539217414,-4.85556247859763,
130.021611565229));
#83977=CARTESIAN_POINT('Ctrl Pts',(-43.4492996326952,-4.87930367836105,
130.168883386797));
#83978=CARTESIAN_POINT('Ctrl Pts',(-43.4577453436491,-4.89637057697915,
130.317423117939));
#83979=CARTESIAN_POINT('Ctrl Pts',(-43.4661910546028,-4.90664090648471,
130.46663576312));
#83980=CARTESIAN_POINT('Ctrl Pts',(-43.4725075577236,-4.91432203229262,
130.578231121296));
#83981=CARTESIAN_POINT('Ctrl Pts',(-43.4788240608444,-4.91820250836251,
130.690202491997));
#83982=CARTESIAN_POINT('Ctrl Pts',(-43.4851405639651,-4.91824956659705,
130.802295873524));
#83983=CARTESIAN_POINT('',(-43.1398594360288,-4.91824904124129,130.801289652058));
#83984=CARTESIAN_POINT('Ctrl Pts',(-43.0697814015304,-4.7640545282341,129.582490119308));
#83985=CARTESIAN_POINT('Ctrl Pts',(-43.0775551247889,-4.79809906899389,
129.715229267033));
#83986=CARTESIAN_POINT('Ctrl Pts',(-43.0853288480475,-4.82655307337718,
129.849241521043));
#83987=CARTESIAN_POINT('Ctrl Pts',(-43.0931025713061,-4.84935232322232,
129.984016112033));
#83988=CARTESIAN_POINT('Ctrl Pts',(-43.0983650628433,-4.86478647946545,
130.075252977679));
#83989=CARTESIAN_POINT('Ctrl Pts',(-43.1036275543804,-4.87763029253095,
130.166839069195));
#83990=CARTESIAN_POINT('Ctrl Pts',(-43.1088900459175,-4.88787739480595,
130.258615589329));
#83991=CARTESIAN_POINT('Ctrl Pts',(-43.119213175942,-4.90797855191232,130.438648363512));
#83992=CARTESIAN_POINT('Ctrl Pts',(-43.1295363059665,-4.91813572606594,
130.619811829999));
#83993=CARTESIAN_POINT('Ctrl Pts',(-43.1398594359911,-4.91824904124087,
130.801289651394));
#83994=CARTESIAN_POINT('Ctrl Pts',(-43.1398594360288,-4.91824904124129,
130.801289652058));
#83995=CARTESIAN_POINT('Ctrl Pts',(-43.1475252570698,-4.91833318758668,
130.936052703421));
#83996=CARTESIAN_POINT('Ctrl Pts',(-43.1551910781108,-4.91287427796632,
131.071037008464));
#83997=CARTESIAN_POINT('Ctrl Pts',(-43.1628568991518,-4.90184420580349,
131.205741290408));
#83998=CARTESIAN_POINT('Ctrl Pts',(-43.1705143159875,-4.89082622614698,
131.340297893137));
#83999=CARTESIAN_POINT('Ctrl Pts',(-43.1781717328232,-4.87424926385755,
131.474574685797));
#84000=CARTESIAN_POINT('Ctrl Pts',(-43.185829149659,-4.85213722165147,131.608069174671));
#84001=CARTESIAN_POINT('Ctrl Pts',(-43.1934801194527,-4.83004379633255,
131.741451269954));
#84002=CARTESIAN_POINT('Ctrl Pts',(-43.2011310892465,-4.80242462678519,
131.874051976868));
#84003=CARTESIAN_POINT('Ctrl Pts',(-43.2087820590402,-4.76935548930471,
132.005373223303));
#84004=CARTESIAN_POINT('Ctrl Pts',(-43.2164290232409,-4.7363036648593,132.136625717737));
#84005=CARTESIAN_POINT('Ctrl Pts',(-43.2240759874416,-4.69780764424593,
132.266599694645));
#84006=CARTESIAN_POINT('Ctrl Pts',(-43.2317229516423,-4.65399434532609,
132.394807000244));
#84007=CARTESIAN_POINT('Ctrl Pts',(-43.2393679196004,-4.61019248388249,
132.522980837283));
#84008=CARTESIAN_POINT('Ctrl Pts',(-43.2470128875585,-4.56107623362987,
132.649388539521));
#84009=CARTESIAN_POINT('Ctrl Pts',(-43.2546578555166,-4.50682230966105,
132.773557339999));
#84010=CARTESIAN_POINT('Ctrl Pts',(-43.2623025866572,-4.45257006631166,
132.89772229411));
#84011=CARTESIAN_POINT('Ctrl Pts',(-43.2699473177977,-4.39318062689535,
133.019648115778));
#84012=CARTESIAN_POINT('Ctrl Pts',(-43.2775920489383,-4.32887854308547,
133.138882757473));
#84013=CARTESIAN_POINT('Ctrl Pts',(-43.285238302273,-4.26456365565251,133.258141140784));
#84014=CARTESIAN_POINT('Ctrl Pts',(-43.2928845556078,-4.19533436993311,
133.374706924719));
#84015=CARTESIAN_POINT('Ctrl Pts',(-43.3005308089425,-4.12146052871224,
133.488153860863));
#84016=CARTESIAN_POINT('Ctrl Pts',(-43.3081848797822,-4.04751115911255,
133.601716784792));
#84017=CARTESIAN_POINT('Ctrl Pts',(-43.3158389506219,-3.96890797140104,
133.712154155884));
#84018=CARTESIAN_POINT('Ctrl Pts',(-43.3234930214615,-3.88596356903981,
133.819069592342));
#84019=CARTESIAN_POINT('Ctrl Pts',(-43.3311511956406,-3.80297470027136,
133.926042346053));
#84020=CARTESIAN_POINT('Ctrl Pts',(-43.3388093698195,-3.71564024226348,
134.029489098929));
#84021=CARTESIAN_POINT('Ctrl Pts',(-43.3464675439986,-3.62431133920984,
134.129048629842));
#84022=CARTESIAN_POINT('Ctrl Pts',(-43.354137477867,-3.53284219391221,134.228761041734));
#84023=CARTESIAN_POINT('Ctrl Pts',(-43.3618074117354,-3.43736663688643,
134.324574025734));
#84024=CARTESIAN_POINT('Ctrl Pts',(-43.3694773456038,-3.33827113849234,
134.416164719176));
#84025=CARTESIAN_POINT('Ctrl Pts',(-43.3754307869793,-3.26135271254595,
134.487257877645));
#84026=CARTESIAN_POINT('Ctrl Pts',(-43.3813842283549,-3.18225401859903,
134.555807905523));
#84027=CARTESIAN_POINT('Ctrl Pts',(-43.3873376697304,-3.10116787349353,
134.621681783372));
#84028=CARTESIAN_POINT('Ctrl Pts',(-43.3951120038495,-2.9952810855481,134.707703548568));
#84029=CARTESIAN_POINT('Ctrl Pts',(-43.4028863379686,-2.88564469510584,
134.789452515187));
#84030=CARTESIAN_POINT('Ctrl Pts',(-43.4106606720877,-2.77263846903882,
134.866584021381));
#84031=CARTESIAN_POINT('Ctrl Pts',(-43.4184254250348,-2.65977151304591,
134.943620469888));
#84032=CARTESIAN_POINT('Ctrl Pts',(-43.4261901779818,-2.54354330452,135.016050562293));
#84033=CARTESIAN_POINT('Ctrl Pts',(-43.4339549309289,-2.42436736069691,
135.083569184917));
#84034=CARTESIAN_POINT('Ctrl Pts',(-43.4417119718139,-2.30530978410148,
135.151020747092));
#84035=CARTESIAN_POINT('Ctrl Pts',(-43.4494690126989,-2.18331063649303,
135.213570355733));
#84036=CARTESIAN_POINT('Ctrl Pts',(-43.4572260535839,-2.05881285792689,
135.270955817328));
#84037=CARTESIAN_POINT('Ctrl Pts',(-43.464977244824,-1.93440896410333,135.3282980041));
#84038=CARTESIAN_POINT('Ctrl Pts',(-43.4727284360641,-1.80751054340688,
135.380483632242));
#84039=CARTESIAN_POINT('Ctrl Pts',(-43.4804796273042,-1.67858529344036,
135.427296316356));
#84040=CARTESIAN_POINT('Ctrl Pts',(-43.4882275240813,-1.5497148401448,135.47408910383));
#84041=CARTESIAN_POINT('Ctrl Pts',(-43.4959754208584,-1.41881963767101,
135.515513356115));
#84042=CARTESIAN_POINT('Ctrl Pts',(-43.5037233176355,-1.28638732514,135.551400823022));
#84043=CARTESIAN_POINT('Ctrl Pts',(-43.5114695937196,-1.15398271459386,
135.587280783045));
#84044=CARTESIAN_POINT('Ctrl Pts',(-43.5192158698037,-1.02004201064806,
135.617626159171));
#84045=CARTESIAN_POINT('Ctrl Pts',(-43.5269621458878,-0.885067593212989,
135.642318701091));
#84046=CARTESIAN_POINT('Ctrl Pts',(-43.5347084791532,-0.750092179427247,
135.667011425286));
#84047=CARTESIAN_POINT('Ctrl Pts',(-43.5424548124186,-0.614083421508419,
135.686051161653));
#84048=CARTESIAN_POINT('Ctrl Pts',(-43.5502011456839,-0.477553067367593,
135.699370947519));
#84049=CARTESIAN_POINT('Ctrl Pts',(-43.5579492136869,-0.340992138200592,
135.712693716259));
#84050=CARTESIAN_POINT('Ctrl Pts',(-43.5656972816898,-0.203909769420831,
135.720293947615));
#84051=CARTESIAN_POINT('Ctrl Pts',(-43.5734453496928,-0.0668215957981928,
135.722156662222));
#84052=CARTESIAN_POINT('Ctrl Pts',(-43.5812016524346,0.0704122767665552,
135.724021356544));
#84053=CARTESIAN_POINT('Ctrl Pts',(-43.5889579551765,0.207651574945859,
135.720136347583));
#84054=CARTESIAN_POINT('Ctrl Pts',(-43.5967142579183,0.344381342609671,
135.710538819931));
#84055=CARTESIAN_POINT('Ctrl Pts',(-43.6044747004325,0.481184087067524,
135.70093616979));
#84056=CARTESIAN_POINT('Ctrl Pts',(-43.6122351429467,0.617476370794974,
135.685614969333));
#84057=CARTESIAN_POINT('Ctrl Pts',(-43.6199955854609,0.752750582458009,
135.66466406726));
#84058=CARTESIAN_POINT('Ctrl Pts',(-43.6277684857263,0.888241948294685,
135.643679532939));
#84059=CARTESIAN_POINT('Ctrl Pts',(-43.6355413859918,1.02271159247896,135.617047313602));
#84060=CARTESIAN_POINT('Ctrl Pts',(-43.6433142862572,1.15566339996077,135.584907152063));
#84061=CARTESIAN_POINT('Ctrl Pts',(-43.6508046220192,1.28378207435486,135.553935366352));
#84062=CARTESIAN_POINT('Ctrl Pts',(-43.6582949577812,1.41049105426834,135.517849225462));
#84063=CARTESIAN_POINT('Ctrl Pts',(-43.6657852935432,1.53536342308586,135.476816312546));
#84064=CARTESIAN_POINT('Ctrl Pts',(-43.6735596276623,1.66497036572161,135.434227624265));
#84065=CARTESIAN_POINT('Ctrl Pts',(-43.6813339617814,1.79300923364071,135.386174737209));
#84066=CARTESIAN_POINT('Ctrl Pts',(-43.6891082959005,1.9189847797996,135.332790861856));
#84067=CARTESIAN_POINT('Ctrl Pts',(-43.6968730488476,2.04480507235661,135.279472777358));
#84068=CARTESIAN_POINT('Ctrl Pts',(-43.7046378017946,2.16856674616459,135.22083692792));
#84069=CARTESIAN_POINT('Ctrl Pts',(-43.7124025547417,2.28978958427508,135.157066295905));
#84070=CARTESIAN_POINT('Ctrl Pts',(-43.7201595956267,2.41089202215381,135.093359001781));
#84071=CARTESIAN_POINT('Ctrl Pts',(-43.7279166365118,2.52946029867803,135.024527255032));
#84072=CARTESIAN_POINT('Ctrl Pts',(-43.7356736773968,2.64503440310105,134.950801991674));
#84073=CARTESIAN_POINT('Ctrl Pts',(-43.7434248686368,2.7605213521921,134.87713232511));
#84074=CARTESIAN_POINT('Ctrl Pts',(-43.7511760598769,2.87301829517336,134.798576696545));
#84075=CARTESIAN_POINT('Ctrl Pts',(-43.758927251117,2.98209037890282,134.715411631623));
#84076=CARTESIAN_POINT('Ctrl Pts',(-43.7666751478941,3.09111610408784,134.632281914072));
#84077=CARTESIAN_POINT('Ctrl Pts',(-43.7744230446712,3.19671955496161,134.544546893289));
#84078=CARTESIAN_POINT('Ctrl Pts',(-43.7821709414483,3.29849559701849,134.452525890542));
#84079=CARTESIAN_POINT('Ctrl Pts',(-43.7899172175324,3.40025034972128,134.360524136605));
#84080=CARTESIAN_POINT('Ctrl Pts',(-43.7976634936165,3.49817899624824,134.264238446001));
#84081=CARTESIAN_POINT('Ctrl Pts',(-43.8054097697006,3.59191050065179,134.164027567995));
#84082=CARTESIAN_POINT('Ctrl Pts',(-43.8131561029659,3.68564269695988,134.063815950256));
#84083=CARTESIAN_POINT('Ctrl Pts',(-43.8209024362313,3.77517742225239,133.959679372829));
#84084=CARTESIAN_POINT('Ctrl Pts',(-43.8286487694966,3.86018172668997,133.852012188765));
#84085=CARTESIAN_POINT('Ctrl Pts',(-43.8363968374996,3.94520506725216,133.744320893381));
#84086=CARTESIAN_POINT('Ctrl Pts',(-43.8441449055025,4.02569572588994,133.633097724846));
#84087=CARTESIAN_POINT('Ctrl Pts',(-43.8518929735054,4.10136238685134,133.518768404583));
#84088=CARTESIAN_POINT('Ctrl Pts',(-43.8596492762473,4.17710946724056,133.404317573758));
#84089=CARTESIAN_POINT('Ctrl Pts',(-43.8674055789892,4.24802209209454,133.286754323141));
#84090=CARTESIAN_POINT('Ctrl Pts',(-43.875161881731,4.31385319949746,133.166531999089));
#84091=CARTESIAN_POINT('Ctrl Pts',(-43.8829223242452,4.37971944294453,133.046245508762));
#84092=CARTESIAN_POINT('Ctrl Pts',(-43.8906827667594,4.44049859156064,132.923297467377));
#84093=CARTESIAN_POINT('Ctrl Pts',(-43.8984432092736,4.49599101994625,132.798162967615));
#84094=CARTESIAN_POINT('Ctrl Pts',(-43.906216109539,4.55157252970437,132.672827590846));
#84095=CARTESIAN_POINT('Ctrl Pts',(-43.9139890098044,4.60185021659823,132.545299105736));
#84096=CARTESIAN_POINT('Ctrl Pts',(-43.9217619100698,4.64667348791094,132.416070442331));
#84097=CARTESIAN_POINT('Ctrl Pts',(-43.9292522458319,4.68986732040879,132.291539566348));
#84098=CARTESIAN_POINT('Ctrl Pts',(-43.936742581594,4.72799632674821,132.165430272357));
#84099=CARTESIAN_POINT('Ctrl Pts',(-43.9442329173561,4.76097074052283,132.038192320184));
#84100=CARTESIAN_POINT('Ctrl Pts',(-43.9520072514752,4.79519538921773,131.906130102383));
#84101=CARTESIAN_POINT('Ctrl Pts',(-43.9597815855943,4.82397527004242,131.772433617343));
#84102=CARTESIAN_POINT('Ctrl Pts',(-43.9675559197134,4.84715476362069,131.637591533945));
#84103=CARTESIAN_POINT('Ctrl Pts',(-43.9753206726604,4.8703056905447,131.502915631363));
#84104=CARTESIAN_POINT('Ctrl Pts',(-43.9830854256075,4.88786989749892,131.367097321195));
#84105=CARTESIAN_POINT('Ctrl Pts',(-43.9908501785546,4.89974176373797,131.230639529995));
#84106=CARTESIAN_POINT('Ctrl Pts',(-43.9986072194395,4.91160183867211,131.094317270598));
#84107=CARTESIAN_POINT('Ctrl Pts',(-44.0063642603246,4.91778079036836,130.957357181104));
#84108=CARTESIAN_POINT('Ctrl Pts',(-44.0141213012096,4.91822426479209,130.820271108139));
#84109=CARTESIAN_POINT('Ctrl Pts',(-44.0218724924497,4.91866740478831,130.683288412848));
#84110=CARTESIAN_POINT('Ctrl Pts',(-44.0296236836898,4.91338367523699,130.546180312571));
#84111=CARTESIAN_POINT('Ctrl Pts',(-44.03737487493,4.9023706762507,130.409462130436));
#84112=CARTESIAN_POINT('Ctrl Pts',(-44.045122771707,4.89136235808281,130.272802057177));
#84113=CARTESIAN_POINT('Ctrl Pts',(-44.0528706684841,4.87462964501886,130.136531961333));
#84114=CARTESIAN_POINT('Ctrl Pts',(-44.0606185652611,4.85222220598737,130.001165294981));
#84115=CARTESIAN_POINT('Ctrl Pts',(-44.0683648413452,4.82981945410904,129.865826944417));
#84116=CARTESIAN_POINT('Ctrl Pts',(-44.0761111174292,4.80174440113933,129.73139203293));
#84117=CARTESIAN_POINT('Ctrl Pts',(-44.0838573935133,4.76809831900315,129.598366636313));
#84118=CARTESIAN_POINT('Ctrl Pts',(-44.0916037267786,4.73445198849929,129.465340257732));
#84119=CARTESIAN_POINT('Ctrl Pts',(-44.099350060044,4.69523464263664,129.333723793812));
#84120=CARTESIAN_POINT('Ctrl Pts',(-44.1070963933093,4.65059809428449,129.204010522138));
#84121=CARTESIAN_POINT('Ctrl Pts',(-44.1148444613123,4.60595154988658,129.074268202075));
#84122=CARTESIAN_POINT('Ctrl Pts',(-44.1225925293153,4.55588351528176,128.946430291979));
#84123=CARTESIAN_POINT('Ctrl Pts',(-44.1303405973183,4.50059469868046,128.820971996869));
#84124=CARTESIAN_POINT('Ctrl Pts',(-44.1380969000601,4.44524712046716,128.695380363191));
#84125=CARTESIAN_POINT('Ctrl Pts',(-44.145853202802,4.38466783402944,128.572173754951));
#84126=CARTESIAN_POINT('Ctrl Pts',(-44.1536095055439,4.3191047094967,128.451805077116));
#84127=CARTESIAN_POINT('Ctrl Pts',(-44.161369948058,4.25350659195023,128.331372154892));
#84128=CARTESIAN_POINT('Ctrl Pts',(-44.1691303905721,4.1829195371035,128.213780516265));
#84129=CARTESIAN_POINT('Ctrl Pts',(-44.1768908330862,4.10763535148138,128.099454910936));
#84130=CARTESIAN_POINT('Ctrl Pts',(-44.1846637333516,4.03223031300107,127.984945779996));
#84131=CARTESIAN_POINT('Ctrl Pts',(-44.1924366336171,3.95211330455078,127.873713476816));
#84132=CARTESIAN_POINT('Ctrl Pts',(-44.2002095338825,3.86761764309672,127.766151140044));
#84133=CARTESIAN_POINT('Ctrl Pts',(-44.2076998696447,3.78619361176687,127.662498965145));
#84134=CARTESIAN_POINT('Ctrl Pts',(-44.2151902054068,3.70070395040982,127.562254798448));
#84135=CARTESIAN_POINT('Ctrl Pts',(-44.222680541169,3.61147853377034,127.465737269146));
#84136=CARTESIAN_POINT('Ctrl Pts',(-44.2304548752881,3.5188701083408,127.365560248386));
#84137=CARTESIAN_POINT('Ctrl Pts',(-44.2382292094072,3.42194369756848,127.269080703677));
#84138=CARTESIAN_POINT('Ctrl Pts',(-44.2460035435263,3.32102631634885,127.176693699474));
#84139=CARTESIAN_POINT('Ctrl Pts',(-44.2537682964734,3.22023330678206,127.084420553997));
#84140=CARTESIAN_POINT('Ctrl Pts',(-44.2615330494204,3.11545939875045,126.996230175049));
#84141=CARTESIAN_POINT('Ctrl Pts',(-44.2692978023676,3.00707062801688,126.912483268443));
#84142=CARTESIAN_POINT('Ctrl Pts',(-44.2770548432526,2.89878951053901,126.828819540445));
#84143=CARTESIAN_POINT('Ctrl Pts',(-44.2848118841376,2.78690098265716,126.749590739578));
#84144=CARTESIAN_POINT('Ctrl Pts',(-44.2925689250226,2.67180629575129,126.675119261035));
#84145=CARTESIAN_POINT('Ctrl Pts',(-44.3003201162627,2.55679840264411,126.600703942013));
#84146=CARTESIAN_POINT('Ctrl Pts',(-44.3080713075028,2.43858948989276,126.531039016076));
#84147=CARTESIAN_POINT('Ctrl Pts',(-44.315822498743,2.3176118162437,126.466405047057));
#84148=CARTESIAN_POINT('Ctrl Pts',(-44.3235703955201,2.19668556133264,126.401798549199));
#84149=CARTESIAN_POINT('Ctrl Pts',(-44.3313182922971,2.0729932301979,126.342218939208));
#84150=CARTESIAN_POINT('Ctrl Pts',(-44.3390661890742,1.9469936518833,126.287901962599));
#84151=CARTESIAN_POINT('Ctrl Pts',(-44.3468124651583,1.82102042996425,126.23359634793));
#84152=CARTESIAN_POINT('Ctrl Pts',(-44.3545587412426,1.69274127963389,126.184551331707));
#84153=CARTESIAN_POINT('Ctrl Pts',(-44.3623050173267,1.56263671673807,126.140955257317));
#84154=CARTESIAN_POINT('Ctrl Pts',(-44.3700513505921,1.43253119343992,126.09735886111));
#84155=CARTESIAN_POINT('Ctrl Pts',(-44.3777976838574,1.30060060139527,126.059211611218));
#84156=CARTESIAN_POINT('Ctrl Pts',(-44.3855440171227,1.16734200757159,126.026652411757));
#84157=CARTESIAN_POINT('Ctrl Pts',(-44.3932920851257,1.03405357140977,125.994085920888));
#84158=CARTESIAN_POINT('Ctrl Pts',(-44.4010401531287,0.899436921404208,
125.967110063381));
#84159=CARTESIAN_POINT('Ctrl Pts',(-44.4087882211317,0.764000348687499,
125.945812837652));
#84160=CARTESIAN_POINT('Ctrl Pts',(-44.4165445238736,0.628419832369775,
125.924492976979));
#84161=CARTESIAN_POINT('Ctrl Pts',(-44.4243008266155,0.492018039413514,
125.908863865111));
#84162=CARTESIAN_POINT('Ctrl Pts',(-44.4320571293573,0.355309991453566,
125.898961768087));
#84163=CARTESIAN_POINT('Ctrl Pts',(-44.4398175718715,0.218528978291663,
125.889054386015));
#84164=CARTESIAN_POINT('Ctrl Pts',(-44.4475780143858,0.0814417750159961,
125.884880121373));
#84165=CARTESIAN_POINT('Ctrl Pts',(-44.4553384569,-0.0554365358649684,125.886423056658));
#84166=CARTESIAN_POINT('Ctrl Pts',(-44.4631113571654,-0.192534575961671,
125.887968468799));
#84167=CARTESIAN_POINT('Ctrl Pts',(-44.4708842574308,-0.329422662924207,
125.895249400172));
#84168=CARTESIAN_POINT('Ctrl Pts',(-44.4786571576963,-0.465589872111775,
125.908197922813));
#84169=CARTESIAN_POINT('Ctrl Pts',(-44.4861474934582,-0.596807060257929,
125.920675734042));
#84170=CARTESIAN_POINT('Ctrl Pts',(-44.49363782922,-0.727354566922098,125.938416186634));
#84171=CARTESIAN_POINT('Ctrl Pts',(-44.5011281649819,-0.856786014983597,
125.961313974488));
#84172=CARTESIAN_POINT('Ctrl Pts',(-44.5089024991011,-0.991124895741017,
125.985079938928));
#84173=CARTESIAN_POINT('Ctrl Pts',(-44.5166768332201,-1.12468696172905,
126.014477322851));
#84174=CARTESIAN_POINT('Ctrl Pts',(-44.5244511673392,-1.25696307449394,
126.04944454135));
#84175=CARTESIAN_POINT('Ctrl Pts',(-44.5322159202863,-1.38907616877134,
126.084368665877));
#84176=CARTESIAN_POINT('Ctrl Pts',(-44.5399806732334,-1.51990608879708,
126.124848868064));
#84177=CARTESIAN_POINT('Ctrl Pts',(-44.5477454261805,-1.64895151128427,
126.170772161959));
#84178=CARTESIAN_POINT('Ctrl Pts',(-44.5555024670654,-1.77786876403828,
126.216649844191));
#84179=CARTESIAN_POINT('Ctrl Pts',(-44.5632595079504,-1.90500468043288,
126.267959729406));
#84180=CARTESIAN_POINT('Ctrl Pts',(-44.5710165488354,-2.02987113408955,
126.324538495931));
#84181=CARTESIAN_POINT('Ctrl Pts',(-44.5787677400755,-2.1546434249827,126.381074595968));
#84182=CARTESIAN_POINT('Ctrl Pts',(-44.5865189313157,-2.27714930494219,
126.442871507987));
#84183=CARTESIAN_POINT('Ctrl Pts',(-44.5942701225558,-2.39691908125864,
126.509717212067));
#84184=CARTESIAN_POINT('Ctrl Pts',(-44.6020180193329,-2.51663795222535,
126.576534504939));
#84185=CARTESIAN_POINT('Ctrl Pts',(-44.6097659161099,-2.63362269182408,
126.648396131759));
#84186=CARTESIAN_POINT('Ctrl Pts',(-44.617513812887,-2.74742695237193,126.725043492865));
#84187=CARTESIAN_POINT('Ctrl Pts',(-44.6252600889711,-2.86120740752135,
126.801674820995));
#84188=CARTESIAN_POINT('Ctrl Pts',(-44.6330063650553,-2.97180838284285,
126.883089673962));
#84189=CARTESIAN_POINT('Ctrl Pts',(-44.6407526411394,-3.07881168915751,
126.968985584377));
#84190=CARTESIAN_POINT('Ctrl Pts',(-44.6484989744048,-3.1858157853464,127.054882128857));
#84191=CARTESIAN_POINT('Ctrl Pts',(-44.65624530767,-3.28922185465103,127.145259552047));
#84192=CARTESIAN_POINT('Ctrl Pts',(-44.6639916409354,-3.38864435626574,
127.239774738498));
#84193=CARTESIAN_POINT('Ctrl Pts',(-44.6717397089384,-3.4880891228606,127.334311090971));
#84194=CARTESIAN_POINT('Ctrl Pts',(-44.6794877769414,-3.58354826330052,
127.432986781257));
#84195=CARTESIAN_POINT('Ctrl Pts',(-44.6872358449444,-3.67467299825015,
127.535421734927));
#84196=CARTESIAN_POINT('Ctrl Pts',(-44.6949921476863,-3.76589458165249,
127.637965557684));
#84197=CARTESIAN_POINT('Ctrl Pts',(-44.7027484504281,-3.85277229699821,
127.744276332471));
#84198=CARTESIAN_POINT('Ctrl Pts',(-44.7105047531699,-3.93499725086926,
127.853940359679));
#84199=CARTESIAN_POINT('Ctrl Pts',(-44.7182651956841,-4.01726609067383,
127.96366291788));
#84200=CARTESIAN_POINT('Ctrl Pts',(-44.7260256381983,-4.09487699964931,
128.076741972505));
#84201=CARTESIAN_POINT('Ctrl Pts',(-44.7337860807125,-4.16756495496575,
128.192735566254));
#84202=CARTESIAN_POINT('Ctrl Pts',(-44.7415589809779,-4.2403695954411,128.308915363216));
#84203=CARTESIAN_POINT('Ctrl Pts',(-44.7493318812434,-4.30823529635164,
128.428018708903));
#84204=CARTESIAN_POINT('Ctrl Pts',(-44.7571047815088,-4.37094304016679,
128.549579031222));
#84205=CARTESIAN_POINT('Ctrl Pts',(-44.7645951172708,-4.43137119954257,
128.666720329631));
#84206=CARTESIAN_POINT('Ctrl Pts',(-44.7720854530329,-4.48700977049351,
128.786142792248));
#84207=CARTESIAN_POINT('Ctrl Pts',(-44.7795757887949,-4.53770607229015,
128.907413948837));
#84208=CARTESIAN_POINT('Ctrl Pts',(-44.788247599836,-4.5963988683989,129.047813603552));
#84209=CARTESIAN_POINT('Ctrl Pts',(-44.7969194108771,-4.64862565067612,
129.191068172679));
#84210=CARTESIAN_POINT('Ctrl Pts',(-44.8055912219183,-4.69413025906848,
129.33659899748));
#84211=CARTESIAN_POINT('Ctrl Pts',(-44.8104350071769,-4.71954762001937,
129.417887676454));
#84212=CARTESIAN_POINT('Ctrl Pts',(-44.8152787924355,-4.74286849138426,
129.499886083174));
#84213=CARTESIAN_POINT('Ctrl Pts',(-44.8201225776941,-4.76405452823406,
129.582490119308));
#84214=CARTESIAN_POINT('Origin',(213.235140564004,0.,130.804360617566));
#84215=CARTESIAN_POINT('',(-46.915040585789,-4.76405452823398,129.582490119308));
#84216=CARTESIAN_POINT('',(-46.5699483010518,-4.76405452823402,129.582490119308));
#84217=CARTESIAN_POINT('',(213.235140564004,-4.76405452823405,129.582490119308));
#84218=CARTESIAN_POINT('',(-45.2351405640464,-4.91824810652024,130.808676311034));
#84219=CARTESIAN_POINT('Ctrl Pts',(-45.2351405640464,-4.91824810652024,
130.808676311034));
#84220=CARTESIAN_POINT('Ctrl Pts',(-45.2445444544636,-4.91810213064542,
130.9750332535));
#84221=CARTESIAN_POINT('Ctrl Pts',(-45.2539483448808,-4.90951205841258,
131.141018612161));
#84222=CARTESIAN_POINT('Ctrl Pts',(-45.263352235298,-4.8926131430149,131.305878010383));
#84223=CARTESIAN_POINT('Ctrl Pts',(-45.272888149729,-4.87547697871907,131.473051918717));
#84224=CARTESIAN_POINT('Ctrl Pts',(-45.28242406416,-4.84979708838166,131.639068048438));
#84225=CARTESIAN_POINT('Ctrl Pts',(-45.291959978591,-4.8157635036038,131.803162369596));
#84226=CARTESIAN_POINT('Ctrl Pts',(-45.300267332481,-4.78611463930858,131.946115581588));
#84227=CARTESIAN_POINT('Ctrl Pts',(-45.3085746863711,-4.75012670806714,
132.087610656431));
#84228=CARTESIAN_POINT('Ctrl Pts',(-45.3168820402611,-4.70795463187301,
132.227155840613));
#84229=CARTESIAN_POINT('Ctrl Pts',(-45.3246563743801,-4.66848841733956,
132.35774747074));
#84230=CARTESIAN_POINT('Ctrl Pts',(-45.3324307084993,-4.62352194811584,
132.486902603422));
#84231=CARTESIAN_POINT('Ctrl Pts',(-45.3402050426184,-4.57317651175509,
132.614122937549));
#84232=CARTESIAN_POINT('Ctrl Pts',(-45.3479697955655,-4.52289312164516,
132.741186483985));
#84233=CARTESIAN_POINT('Ctrl Pts',(-45.3557345485126,-4.46724409680583,
132.866319616198));
#84234=CARTESIAN_POINT('Ctrl Pts',(-45.3634993014597,-4.40640084302413,
132.98903786446));
#84235=CARTESIAN_POINT('Ctrl Pts',(-45.3712563423447,-4.34561801962,133.111634227227));
#84236=CARTESIAN_POINT('Ctrl Pts',(-45.3790133832296,-4.27965140642154,
133.231820131149));
#84237=CARTESIAN_POINT('Ctrl Pts',(-45.3867704241146,-4.20872083395094,
133.349130156123));
#84238=CARTESIAN_POINT('Ctrl Pts',(-45.3945216153548,-4.1378437507766,133.466351716695));
#84239=CARTESIAN_POINT('Ctrl Pts',(-45.402272806595,-4.06201036073395,133.580701381821));
#84240=CARTESIAN_POINT('Ctrl Pts',(-45.4100239978351,-3.98148667456019,
133.691737787733));
#84241=CARTESIAN_POINT('Ctrl Pts',(-45.4177718946122,-3.90099721310121,
133.80272700021));
#84242=CARTESIAN_POINT('Ctrl Pts',(-45.4255197913893,-3.81582164947759,
133.910405438486));
#84243=CARTESIAN_POINT('Ctrl Pts',(-45.4332676881664,-3.72626949088769,
134.014360421893));
#84244=CARTESIAN_POINT('Ctrl Pts',(-45.4410139642505,-3.63673606467872,
134.118293660159));
#84245=CARTESIAN_POINT('Ctrl Pts',(-45.4487602403346,-3.54282811947194,
134.218504696741));
#84246=CARTESIAN_POINT('Ctrl Pts',(-45.4565065164187,-3.44489539738257,
134.314613993548));
#84247=CARTESIAN_POINT('Ctrl Pts',(-45.4642528496841,-3.34696195237609,
134.410723999812));
#84248=CARTESIAN_POINT('Ctrl Pts',(-45.4719991829495,-3.24500395024257,
134.502731932038));
#84249=CARTESIAN_POINT('Ctrl Pts',(-45.4797455162149,-3.13940764059065,
134.590295472883));
#84250=CARTESIAN_POINT('Ctrl Pts',(-45.4874935842179,-3.03378768337762,
134.677878622975));
#84251=CARTESIAN_POINT('Ctrl Pts',(-45.4952416522208,-2.92452809823754,
134.761015151661));
#84252=CARTESIAN_POINT('Ctrl Pts',(-45.5029897202237,-2.81204749322128,
134.839403610939));
#84253=CARTESIAN_POINT('Ctrl Pts',(-45.5107460229656,-2.69944734247932,
134.917875382405));
#84254=CARTESIAN_POINT('Ctrl Pts',(-45.5185023257074,-2.58361965464235,
134.991588780032));
#84255=CARTESIAN_POINT('Ctrl Pts',(-45.5262586284493,-2.46501171671025,
135.06028593399));
#84256=CARTESIAN_POINT('Ctrl Pts',(-45.5340190709635,-2.3463404741503,135.129019753688));
#84257=CARTESIAN_POINT('Ctrl Pts',(-45.5417795134777,-2.22488637074305,
135.192731813399));
#84258=CARTESIAN_POINT('Ctrl Pts',(-45.5495399559919,-2.10111957189729,
135.251211144297));
#84259=CARTESIAN_POINT('Ctrl Pts',(-45.5573128562573,-1.97715409159852,
135.309784351409));
#84260=CARTESIAN_POINT('Ctrl Pts',(-45.5650857565228,-1.8508688573959,135.363107891579));
#84261=CARTESIAN_POINT('Ctrl Pts',(-45.5728586567882,-1.72275304357371,
135.411019386496));
#84262=CARTESIAN_POINT('Ctrl Pts',(-45.5803489925501,-1.5992945622903,135.45718917789));
#84263=CARTESIAN_POINT('Ctrl Pts',(-45.587839328312,-1.47413657568182,135.498333479351));
#84264=CARTESIAN_POINT('Ctrl Pts',(-45.5953296640739,-1.34772655990897,
135.534351757327));
#84265=CARTESIAN_POINT('Ctrl Pts',(-45.603103998193,-1.21652366996474,135.57173567926));
#84266=CARTESIAN_POINT('Ctrl Pts',(-45.6108783323121,-1.08355632399403,
135.60371561919));
#84267=CARTESIAN_POINT('Ctrl Pts',(-45.6186526664312,-0.949309315717473,
135.630124275848));
#84268=CARTESIAN_POINT('Ctrl Pts',(-45.6264174193783,-0.815227754880802,
135.656500386196));
#84269=CARTESIAN_POINT('Ctrl Pts',(-45.6341821723253,-0.679870049566951,
135.677318800045));
#84270=CARTESIAN_POINT('Ctrl Pts',(-45.6419469252724,-0.54373644689543,
135.692461858213));
#84271=CARTESIAN_POINT('Ctrl Pts',(-45.6497039661574,-0.407738054037044,
135.707589876083));
#84272=CARTESIAN_POINT('Ctrl Pts',(-45.6574610070424,-0.270965683468014,
135.717053712901));
#84273=CARTESIAN_POINT('Ctrl Pts',(-45.6652180479274,-0.133929730068915,
135.720786747379));
#84274=CARTESIAN_POINT('Ctrl Pts',(-45.6729692391675,0.00300288345174166,
135.724516966746));
#84275=CARTESIAN_POINT('Ctrl Pts',(-45.6807204304076,0.140198294924244,
135.722524975136));
#84276=CARTESIAN_POINT('Ctrl Pts',(-45.6884716216477,0.277141387209298,
135.714796007019));
#84277=CARTESIAN_POINT('Ctrl Pts',(-45.6962195184248,0.414026275027054,
135.70707032392));
#84278=CARTESIAN_POINT('Ctrl Pts',(-45.703967415202,0.550658667427509,135.693612536027));
#84279=CARTESIAN_POINT('Ctrl Pts',(-45.711715311979,0.686524068277104,135.674459976529));
#84280=CARTESIAN_POINT('Ctrl Pts',(-45.7194615880631,0.822361049013761,
135.655311423335));
#84281=CARTESIAN_POINT('Ctrl Pts',(-45.7272078641471,0.957430970427422,
135.630470522485));
#84282=CARTESIAN_POINT('Ctrl Pts',(-45.7349541402312,1.09122547221634,135.600026372316));
#84283=CARTESIAN_POINT('Ctrl Pts',(-45.7427004734966,1.22502096164588,135.569581997416));
#84284=CARTESIAN_POINT('Ctrl Pts',(-45.7504468067619,1.35754063144337,135.533534377408));
#84285=CARTESIAN_POINT('Ctrl Pts',(-45.7581931400272,1.48828770298435,135.49202344414));
#84286=CARTESIAN_POINT('Ctrl Pts',(-45.7659412080302,1.61906405442546,135.450503214787));
#84287=CARTESIAN_POINT('Ctrl Pts',(-45.7736892760332,1.74806664513958,135.403517355894));
#84288=CARTESIAN_POINT('Ctrl Pts',(-45.7814373440362,1.87481559050982,135.351255114262));
#84289=CARTESIAN_POINT('Ctrl Pts',(-45.789193646778,2.00169924616753,135.298937327698));
#84290=CARTESIAN_POINT('Ctrl Pts',(-45.7969499495199,2.12632410978771,135.241332105477));
#84291=CARTESIAN_POINT('Ctrl Pts',(-45.8047062522618,2.24823145862955,135.17867637788));
#84292=CARTESIAN_POINT('Ctrl Pts',(-45.8124666947759,2.37020387309402,135.115987209034));
#84293=CARTESIAN_POINT('Ctrl Pts',(-45.8202271372901,2.48945554292122,135.048242356606));
#84294=CARTESIAN_POINT('Ctrl Pts',(-45.8279875798042,2.60555483817438,134.975723350267));
#84295=CARTESIAN_POINT('Ctrl Pts',(-45.8357604800696,2.72184050632309,134.903087929981));
#84296=CARTESIAN_POINT('Ctrl Pts',(-45.843533380335,2.83496336464404,134.825663261825));
#84297=CARTESIAN_POINT('Ctrl Pts',(-45.8513062806004,2.94452238901528,134.743773132534));
#84298=CARTESIAN_POINT('Ctrl Pts',(-45.8587966163625,3.05009866688914,134.664859915711));
#84299=CARTESIAN_POINT('Ctrl Pts',(-45.8662869521247,3.15236548189355,134.581800456862));
#84300=CARTESIAN_POINT('Ctrl Pts',(-45.8737772878868,3.25099638050922,134.494916889514));
#84301=CARTESIAN_POINT('Ctrl Pts',(-45.8815516220059,3.35336689962325,134.404739105303));
#84302=CARTESIAN_POINT('Ctrl Pts',(-45.8893259561249,3.45214462721011,134.310155849992));
#84303=CARTESIAN_POINT('Ctrl Pts',(-45.897100290244,3.54692676512755,134.211484563847));
#84304=CARTESIAN_POINT('Ctrl Pts',(-45.9048650431911,3.64159209253094,134.112934881244));
#84305=CARTESIAN_POINT('Ctrl Pts',(-45.9126297961382,3.7322713597279,134.010307471436));
#84306=CARTESIAN_POINT('Ctrl Pts',(-45.9203945490853,3.81859518093083,133.903959608834));
#84307=CARTESIAN_POINT('Ctrl Pts',(-45.9281515899703,3.90483326409748,133.797717372429));
#84308=CARTESIAN_POINT('Ctrl Pts',(-45.9359086308553,3.98672426518592,133.687762338442));
#84309=CARTESIAN_POINT('Ctrl Pts',(-45.9436656717403,4.06393625291824,133.574487906107));
#84310=CARTESIAN_POINT('Ctrl Pts',(-45.9514168629804,4.1410900144901,133.461298894902));
#84311=CARTESIAN_POINT('Ctrl Pts',(-45.9591680542206,4.21357156661799,133.344795789532));
#84312=CARTESIAN_POINT('Ctrl Pts',(-45.9669192454607,4.28109005324667,133.225403991505));
#84313=CARTESIAN_POINT('Ctrl Pts',(-45.9746671422378,4.34857984271733,133.106062938177));
#84314=CARTESIAN_POINT('Ctrl Pts',(-45.9824150390148,4.41111057014216,132.983835973739));
#84315=CARTESIAN_POINT('Ctrl Pts',(-45.9901629357919,4.46843554726462,132.85917613786));
#84316=CARTESIAN_POINT('Ctrl Pts',(-45.997909211876,4.52574853323773,132.734542378132));
#84317=CARTESIAN_POINT('Ctrl Pts',(-46.0056554879601,4.57785777161193,132.607477114185));
#84318=CARTESIAN_POINT('Ctrl Pts',(-46.0134017640442,4.62456344218149,132.478456203767));
#84319=CARTESIAN_POINT('Ctrl Pts',(-46.0211480973096,4.67126945752163,132.349434340946));
#84320=CARTESIAN_POINT('Ctrl Pts',(-46.0288944305749,4.71257169238525,132.218457170467));
#84321=CARTESIAN_POINT('Ctrl Pts',(-46.0366407638403,4.74831935441895,132.086018282838));
#84322=CARTESIAN_POINT('Ctrl Pts',(-46.0443888318432,4.78407502189371,131.953549736438));
#84323=CARTESIAN_POINT('Ctrl Pts',(-46.0521368998463,4.8142735394425,131.819619198902));
#84324=CARTESIAN_POINT('Ctrl Pts',(-46.0598849678492,4.83881473640168,131.684732703267));
#84325=CARTESIAN_POINT('Ctrl Pts',(-46.0676412705911,4.86338201603706,131.549702848659));
#84326=CARTESIAN_POINT('Ctrl Pts',(-46.075397573333,4.88227989403673,131.41371539164));
#84327=CARTESIAN_POINT('Ctrl Pts',(-46.0831538760748,4.89545975570788,131.277284335246));
#84328=CARTESIAN_POINT('Ctrl Pts',(-46.090914318589,4.90864665186805,131.14078046149));
#84329=CARTESIAN_POINT('Ctrl Pts',(-46.0986747611032,4.91610942931226,131.003832906784));
#84330=CARTESIAN_POINT('Ctrl Pts',(-46.1064352036173,4.91785164040135,130.866956987283));
#84331=CARTESIAN_POINT('Ctrl Pts',(-46.1142081038828,4.91959664824235,130.729861342404));
#84332=CARTESIAN_POINT('Ctrl Pts',(-46.1219810041482,4.91560275024385,130.592837953552));
#84333=CARTESIAN_POINT('Ctrl Pts',(-46.1297539044137,4.90592559402316,130.456399228316));
#84334=CARTESIAN_POINT('Ctrl Pts',(-46.1372442401757,4.89660022680639,130.324920394412));
#84335=CARTESIAN_POINT('Ctrl Pts',(-46.1447345759377,4.88199766322645,130.193984760255));
#84336=CARTESIAN_POINT('Ctrl Pts',(-46.1522249116997,4.86221246724157,130.064041101478));
#84337=CARTESIAN_POINT('Ctrl Pts',(-46.1599992458188,4.84167710953731,129.929170589383));
#84338=CARTESIAN_POINT('Ctrl Pts',(-46.1677735799379,4.81549331264808,129.794941529813));
#84339=CARTESIAN_POINT('Ctrl Pts',(-46.175547914057,4.78371042582497,129.661864392472));
#84340=CARTESIAN_POINT('Ctrl Pts',(-46.1833126670041,4.75196670856935,129.528951260809));
#84341=CARTESIAN_POINT('Ctrl Pts',(-46.1910774199511,4.71463772102353,129.397187603332));
#84342=CARTESIAN_POINT('Ctrl Pts',(-46.1988421728982,4.67182438622515,129.267077310309));
#84343=CARTESIAN_POINT('Ctrl Pts',(-46.2065992137832,4.62905357423451,129.137096244663));
#84344=CARTESIAN_POINT('Ctrl Pts',(-46.2143562546683,4.58080937643992,129.008765644503));
#84345=CARTESIAN_POINT('Ctrl Pts',(-46.2221132955533,4.5272433537948,128.882577414907));
#84346=CARTESIAN_POINT('Ctrl Pts',(-46.2298644867934,4.47371772570404,128.756484344838));
#84347=CARTESIAN_POINT('Ctrl Pts',(-46.2376156780334,4.41487841300241,128.632530788049));
#84348=CARTESIAN_POINT('Ctrl Pts',(-46.2453668692735,4.35092610322437,128.511191389885));
#84349=CARTESIAN_POINT('Ctrl Pts',(-46.2531147660506,4.28700097488397,128.389903564203));
#84350=CARTESIAN_POINT('Ctrl Pts',(-46.2608626628277,4.2179673536257,128.271228032419));
#84351=CARTESIAN_POINT('Ctrl Pts',(-46.2686105596048,4.14407305352638,128.155617219361));
#84352=CARTESIAN_POINT('Ctrl Pts',(-46.2763568356888,4.07019421052167,128.040030589592));
#84353=CARTESIAN_POINT('Ctrl Pts',(-46.2841031117729,3.99145692146836,127.927507732632));
#84354=CARTESIAN_POINT('Ctrl Pts',(-46.291849387857,3.90815353126402,127.818473975617));
#84355=CARTESIAN_POINT('Ctrl Pts',(-46.2995957211224,3.82484952613298,127.709439413739));
#84356=CARTESIAN_POINT('Ctrl Pts',(-46.3073420543878,3.73697958994952,127.603894313869));
#84357=CARTESIAN_POINT('Ctrl Pts',(-46.3150883876531,3.64487748743746,127.502232339611));
#84358=CARTESIAN_POINT('Ctrl Pts',(-46.3228364556561,3.55275475929814,127.400547598858));
#84359=CARTESIAN_POINT('Ctrl Pts',(-46.3305845236591,3.45639824133398,127.302748003804));
#84360=CARTESIAN_POINT('Ctrl Pts',(-46.3383325916621,3.35617952878086,127.209191354083));
#84361=CARTESIAN_POINT('Ctrl Pts',(-46.3460888944039,3.25585430258727,127.115535271241));
#84362=CARTESIAN_POINT('Ctrl Pts',(-46.3538451971457,3.15165896829736,127.026131409067));
#84363=CARTESIAN_POINT('Ctrl Pts',(-46.3616014998876,3.04399969379405,126.941298499675));
#84364=CARTESIAN_POINT('Ctrl Pts',(-46.3693619424018,2.93628295829437,126.856420312405));
#84365=CARTESIAN_POINT('Ctrl Pts',(-46.3771223849159,2.82509891546129,126.776118167936));
#84366=CARTESIAN_POINT('Ctrl Pts',(-46.3848828274301,2.71088303550717,126.700667618535));
#84367=CARTESIAN_POINT('Ctrl Pts',(-46.3926557276955,2.59648380608293,126.625095949213));
#84368=CARTESIAN_POINT('Ctrl Pts',(-46.4004286279609,2.47904334891283,126.554391640055));
#84369=CARTESIAN_POINT('Ctrl Pts',(-46.4082015282264,2.35902284591166,126.488784841964));
#84370=CARTESIAN_POINT('Ctrl Pts',(-46.4156918639884,2.24336539050798,126.425563016236));
#84371=CARTESIAN_POINT('Ctrl Pts',(-46.4231821997504,2.12531249089972,126.367074658));
#84372=CARTESIAN_POINT('Ctrl Pts',(-46.4306725355125,2.00529282886471,126.313482782108));
#84373=CARTESIAN_POINT('Ctrl Pts',(-46.4384468696315,1.88072258486446,126.257858953954));
#84374=CARTESIAN_POINT('Ctrl Pts',(-46.4462212037507,1.75363889369082,126.207334038416));
#84375=CARTESIAN_POINT('Ctrl Pts',(-46.4539955378698,1.62449790243732,126.162142437916));
#84376=CARTESIAN_POINT('Ctrl Pts',(-46.4617602908169,1.49551606591388,126.117006532024));
#84377=CARTESIAN_POINT('Ctrl Pts',(-46.469525043764,1.36448233955753,126.077190991085));
#84378=CARTESIAN_POINT('Ctrl Pts',(-46.4772897967111,1.23187521188992,126.042883270688));
#84379=CARTESIAN_POINT('Ctrl Pts',(-46.4850468375961,1.09939979149095,126.008609625203));
#84380=CARTESIAN_POINT('Ctrl Pts',(-46.492803878481,0.965354455726345,125.979833011118));
#84381=CARTESIAN_POINT('Ctrl Pts',(-46.5005609193661,0.830234980668827,
125.956691802623));
#84382=CARTESIAN_POINT('Ctrl Pts',(-46.5083121106062,0.695217400258342,
125.933568045093));
#84383=CARTESIAN_POINT('Ctrl Pts',(-46.5160633018463,0.559127676639525,
125.916071300107));
#84384=CARTESIAN_POINT('Ctrl Pts',(-46.5238144930865,0.422473618896509,
125.904289280959));
#84385=CARTESIAN_POINT('Ctrl Pts',(-46.5315623898636,0.285877642773586,
125.892512269484));
#84386=CARTESIAN_POINT('Ctrl Pts',(-46.5393102866406,0.148718198288503,
125.886445186443));
#84387=CARTESIAN_POINT('Ctrl Pts',(-46.5470581834177,0.0115098728212643,
125.886124085502));
#84388=CARTESIAN_POINT('Ctrl Pts',(-46.5548044595018,-0.125669751622156,
125.885803051729));
#84389=CARTESIAN_POINT('Ctrl Pts',(-46.5625507355859,-0.262897845993511,
125.891225610255));
#84390=CARTESIAN_POINT('Ctrl Pts',(-46.57029701167,-0.399658550970937,125.902375702745));
#84391=CARTESIAN_POINT('Ctrl Pts',(-46.5780433449354,-0.536420265484821,
125.913525877541));
#84392=CARTESIAN_POINT('Ctrl Pts',(-46.5857896782008,-0.672714194047978,
125.930403638896));
#84393=CARTESIAN_POINT('Ctrl Pts',(-46.5935360114661,-0.808028728335253,
125.952940965888));
#84394=CARTESIAN_POINT('Ctrl Pts',(-46.6012840794691,-0.943373565374276,
125.975483339958));
#84395=CARTESIAN_POINT('Ctrl Pts',(-46.6090321474721,-1.07773818612011,
126.003687737466));
#84396=CARTESIAN_POINT('Ctrl Pts',(-46.6167802154751,-1.2106207073057,126.037434924256));
#84397=CARTESIAN_POINT('Ctrl Pts',(-46.6245365182169,-1.34364445761613,
126.071217977957));
#84398=CARTESIAN_POINT('Ctrl Pts',(-46.6322928209588,-1.47518258220828,
126.110555492345));
#84399=CARTESIAN_POINT('Ctrl Pts',(-46.6400491237006,-1.60474737906548,
126.155278029368));
#84400=CARTESIAN_POINT('Ctrl Pts',(-46.6478095662148,-1.73438132855607,
126.200024436156));
#84401=CARTESIAN_POINT('Ctrl Pts',(-46.655570008729,-1.86203948794549,126.250161449713));
#84402=CARTESIAN_POINT('Ctrl Pts',(-46.6633304512431,-1.98725464502111,
126.305471639347));
#84403=CARTESIAN_POINT('Ctrl Pts',(-46.6711033515086,-2.11267080858278,
126.360870617807));
#84404=CARTESIAN_POINT('Ctrl Pts',(-46.6788762517741,-2.23563578207047,
126.421459194362));
#84405=CARTESIAN_POINT('Ctrl Pts',(-46.6866491520395,-2.35570665292161,
126.486973765791));
#84406=CARTESIAN_POINT('Ctrl Pts',(-46.6941394878016,-2.47141264517719,
126.550106717527));
#84407=CARTESIAN_POINT('Ctrl Pts',(-46.7016298235635,-2.5844310332787,126.617813579115));
#84408=CARTESIAN_POINT('Ctrl Pts',(-46.7091201593256,-2.69439295524025,
126.689821801945));
#84409=CARTESIAN_POINT('Ctrl Pts',(-46.7168839525298,-2.80836937092695,
126.764458903514));
#84410=CARTESIAN_POINT('Ctrl Pts',(-46.724647745734,-2.91942549512991,126.843955537909));
#84411=CARTESIAN_POINT('Ctrl Pts',(-46.7324115389382,-3.02711811027867,
126.928055803839));
#84412=CARTESIAN_POINT('Ctrl Pts',(-46.7401630440496,-3.13464027564649,
127.012022960624));
#84413=CARTESIAN_POINT('Ctrl Pts',(-46.7479145491609,-3.23880922797593,
127.100578998185));
#84414=CARTESIAN_POINT('Ctrl Pts',(-46.7556660542723,-3.33920955541522,
127.193424089804));
#84415=CARTESIAN_POINT('Ctrl Pts',(-46.7634104675609,-3.43951802697391,
127.2861842378));
#84416=CARTESIAN_POINT('Ctrl Pts',(-46.7711548808495,-3.53606444594628,
127.383225370047));
#84417=CARTESIAN_POINT('Ctrl Pts',(-46.7788992941381,-3.6284651924949,127.484206493229));
#84418=CARTESIAN_POINT('Ctrl Pts',(-46.7866383135098,-3.72080158272198,
127.585117283931));
#84419=CARTESIAN_POINT('Ctrl Pts',(-46.7943773328816,-3.80899778156704,
127.689962317673));
#84420=CARTESIAN_POINT('Ctrl Pts',(-46.8021163522533,-3.89270618738852,
127.798363012582));
#84421=CARTESIAN_POINT('Ctrl Pts',(-46.8098516715358,-3.97637457152954,
127.906711880224));
#84422=CARTESIAN_POINT('Ctrl Pts',(-46.8175869908184,-4.05555919375947,
128.018612715882));
#84423=CARTESIAN_POINT('Ctrl Pts',(-46.825322310101,-4.12995228204412,128.133653368439));
#84424=CARTESIAN_POINT('Ctrl Pts',(-46.8330572732535,-4.20434194530896,
128.248688724584));
#84425=CARTESIAN_POINT('Ctrl Pts',(-46.8407922364058,-4.27394029121761,
128.366863286923));
#84426=CARTESIAN_POINT('Ctrl Pts',(-46.8485271995583,-4.33848256268185,
128.487735461049));
#84427=CARTESIAN_POINT('Ctrl Pts',(-46.8562616664843,-4.40302069352118,
128.60859988078));
#84428=CARTESIAN_POINT('Ctrl Pts',(-46.8639961334103,-4.46250321509175,
128.732161219404));
#84429=CARTESIAN_POINT('Ctrl Pts',(-46.8717306003363,-4.51671145296347,
128.85795348822));
#84430=CARTESIAN_POINT('Ctrl Pts',(-46.8794695499381,-4.57095110837883,
128.983818662636));
#84431=CARTESIAN_POINT('Ctrl Pts',(-46.8872084995397,-4.61991021949255,
129.111916988931));
#84432=CARTESIAN_POINT('Ctrl Pts',(-46.8949474491414,-4.66341829462873,
129.241762501664));
#84433=CARTESIAN_POINT('Ctrl Pts',(-46.9016451613573,-4.70107257348113,
129.354137942978));
#84434=CARTESIAN_POINT('Ctrl Pts',(-46.9083428735732,-4.73464468864475,
129.467821601106));
#84435=CARTESIAN_POINT('Ctrl Pts',(-46.9150405857891,-4.76405452823398,
129.582490119308));
#84436=CARTESIAN_POINT('Ctrl Pts',(-45.1651923290374,-4.76405452823407,
129.582490119308));
#84437=CARTESIAN_POINT('Ctrl Pts',(-45.1728855518329,-4.79792966098168,
129.714568747764));
#84438=CARTESIAN_POINT('Ctrl Pts',(-45.1805787746285,-4.82631197159566,
129.84807280976));
#84439=CARTESIAN_POINT('Ctrl Pts',(-45.188271997424,-4.84909609083771,129.982502865688));
#84440=CARTESIAN_POINT('Ctrl Pts',(-45.1960834251881,-4.87223028392675,
130.118998414968));
#84441=CARTESIAN_POINT('Ctrl Pts',(-45.2038948529522,-4.88959273668898,
130.256448238861));
#84442=CARTESIAN_POINT('Ctrl Pts',(-45.2117062807163,-4.90112750835848,
130.394321339799));
#84443=CARTESIAN_POINT('Ctrl Pts',(-45.2195177084804,-4.91266228002797,
130.532194440737));
#84444=CARTESIAN_POINT('Ctrl Pts',(-45.2273291362445,-4.91836936270034,
130.6704903914));
#84445=CARTESIAN_POINT('Ctrl Pts',(-45.2351405640086,-4.91824810652082,
130.808676310364));
#84446=CARTESIAN_POINT('',(-44.8898594359405,-4.91824927968631,130.801698782662));
#84447=CARTESIAN_POINT('Ctrl Pts',(-44.8201225776941,-4.76405452823406,
129.582490119308));
#84448=CARTESIAN_POINT('Ctrl Pts',(-44.8287491969274,-4.80178614993221,
129.729605139652));
#84449=CARTESIAN_POINT('Ctrl Pts',(-44.8373758161607,-4.83274365385713,
129.878642232481));
#84450=CARTESIAN_POINT('Ctrl Pts',(-44.846002435394,-4.85674727733277,130.028996866401));
#84451=CARTESIAN_POINT('Ctrl Pts',(-44.8545868334649,-4.88063342015264,
130.178615621382));
#84452=CARTESIAN_POINT('Ctrl Pts',(-44.8631712315358,-4.89763348754675,
130.329538834179));
#84453=CARTESIAN_POINT('Ctrl Pts',(-44.8717556296067,-4.90761853185545,
130.481152622168));
#84454=CARTESIAN_POINT('Ctrl Pts',(-44.8777902317179,-4.91463775078828,
130.587733057691));
#84455=CARTESIAN_POINT('Ctrl Pts',(-44.8838248338292,-4.91819134554488,
130.694654371707));
#84456=CARTESIAN_POINT('Ctrl Pts',(-44.8898594359405,-4.91824927968631,
130.801698782662));
#84457=CARTESIAN_POINT('Ctrl Pts',(-44.8898594359911,-4.9182492796868,130.80169878356));
#84458=CARTESIAN_POINT('Ctrl Pts',(-44.8977025392354,-4.91832457600144,
130.940823178404));
#84459=CARTESIAN_POINT('Ctrl Pts',(-44.9055456424797,-4.91249232923136,
131.079948183281));
#84460=CARTESIAN_POINT('Ctrl Pts',(-44.913388745724,-4.90077893990125,131.218545171503));
#84461=CARTESIAN_POINT('Ctrl Pts',(-44.9212336807835,-4.88906281482177,
131.357174530085));
#84462=CARTESIAN_POINT('Ctrl Pts',(-44.929078615843,-4.87146284270923,131.495275250381));
#84463=CARTESIAN_POINT('Ctrl Pts',(-44.9369235509025,-4.84805730189472,
131.632324058815));
#84464=CARTESIAN_POINT('Ctrl Pts',(-44.944771850857,-4.82464172184031,131.769431651017));
#84465=CARTESIAN_POINT('Ctrl Pts',(-44.9526201508114,-4.79541567671351,
131.905486060992));
#84466=CARTESIAN_POINT('Ctrl Pts',(-44.9604684507658,-4.76050848440808,
132.03997464807));
#84467=CARTESIAN_POINT('Ctrl Pts',(-44.9685980309193,-4.72435023110115,
132.179283256907));
#84468=CARTESIAN_POINT('Ctrl Pts',(-44.9767276110727,-4.68209613988705,
132.316911285416));
#84469=CARTESIAN_POINT('Ctrl Pts',(-44.9848571912262,-4.63394568844649,
132.452307952595));
#84470=CARTESIAN_POINT('Ctrl Pts',(-44.992721685211,-4.58736530808628,132.583289658228));
#84471=CARTESIAN_POINT('Ctrl Pts',(-45.0005861791959,-4.53526728341086,
132.71218292079));
#84472=CARTESIAN_POINT('Ctrl Pts',(-45.0084506731807,-4.47788036622893,
132.838511666097));
#84473=CARTESIAN_POINT('Ctrl Pts',(-45.0167127964186,-4.41759196332404,
132.971227599791));
#84474=CARTESIAN_POINT('Ctrl Pts',(-45.0249749196563,-4.35146616301392,
133.101112505185));
#84475=CARTESIAN_POINT('Ctrl Pts',(-45.0332370428942,-4.27982097372728,
133.227646711973));
#84476=CARTESIAN_POINT('Ctrl Pts',(-45.041499166132,-4.20817578444064,133.35418091876));
#84477=CARTESIAN_POINT('Ctrl Pts',(-45.0497612893698,-4.1310115217808,133.477364064907));
#84478=CARTESIAN_POINT('Ctrl Pts',(-45.0580234126077,-4.04869592842835,
133.596715240752));
#84479=CARTESIAN_POINT('Ctrl Pts',(-45.0657977467268,-3.971240181581,133.709020019053));
#84480=CARTESIAN_POINT('Ctrl Pts',(-45.0735720808459,-3.88898545890976,
133.818277477611));
#84481=CARTESIAN_POINT('Ctrl Pts',(-45.0813464149649,-3.80219940482909,
133.924050145134));
#84482=CARTESIAN_POINT('Ctrl Pts',(-45.089111167912,-3.71552030680378,134.029692457297));
#84483=CARTESIAN_POINT('Ctrl Pts',(-45.0968759208591,-3.62432123439391,
134.131858224238));
#84484=CARTESIAN_POINT('Ctrl Pts',(-45.1046406738062,-3.52891333363567,
134.230138448393));
#84485=CARTESIAN_POINT('Ctrl Pts',(-45.1123977146912,-3.43360019334961,
134.328321059244));
#84486=CARTESIAN_POINT('Ctrl Pts',(-45.1201547555763,-3.33408681419874,
134.422625528536));
#84487=CARTESIAN_POINT('Ctrl Pts',(-45.1279117964613,-3.23072463789963,
134.5126757844));
#84488=CARTESIAN_POINT('Ctrl Pts',(-45.1356629877014,-3.12744040782129,
134.602658132665));
#84489=CARTESIAN_POINT('Ctrl Pts',(-45.1434141789415,-3.02031345125291,
134.688392397322));
#84490=CARTESIAN_POINT('Ctrl Pts',(-45.1511653701816,-2.90973183953378,
134.769539514476));
#84491=CARTESIAN_POINT('Ctrl Pts',(-45.1589132669587,-2.79919722794979,
134.850652141941));
#84492=CARTESIAN_POINT('Ctrl Pts',(-45.1666611637359,-2.68521119613585,
134.927181268811));
#84493=CARTESIAN_POINT('Ctrl Pts',(-45.174409060513,-2.56819447674748,134.998828425537));
#84494=CARTESIAN_POINT('Ctrl Pts',(-45.1821553365971,-2.45120223473422,
135.070460595222));
#84495=CARTESIAN_POINT('Ctrl Pts',(-45.1899016126811,-2.33118089933533,
135.137212621969));
#84496=CARTESIAN_POINT('Ctrl Pts',(-45.1976478887652,-2.20857939709849,
135.198829881221));
#84497=CARTESIAN_POINT('Ctrl Pts',(-45.2053942220306,-2.08597698984522,
135.260447595318));
#84498=CARTESIAN_POINT('Ctrl Pts',(-45.213140555296,-1.96079472707713,135.316930290719));
#84499=CARTESIAN_POINT('Ctrl Pts',(-45.2208868885614,-1.83350493460382,
135.368069933165));
#84500=CARTESIAN_POINT('Ctrl Pts',(-45.2286349565643,-1.7061866364644,135.419221027978));
#84501=CARTESIAN_POINT('Ctrl Pts',(-45.2363830245672,-1.5767602321731,135.465026543138));
#84502=CARTESIAN_POINT('Ctrl Pts',(-45.2441310925702,-1.44571638184337,
135.505327242184));
#84503=CARTESIAN_POINT('Ctrl Pts',(-45.2518873953121,-1.31453325654971,
135.545670773292));
#84504=CARTESIAN_POINT('Ctrl Pts',(-45.2596436980539,-1.18172962553687,
135.580497686006));
#84505=CARTESIAN_POINT('Ctrl Pts',(-45.2674000007957,-1.04781015234293,
135.609698997654));
#84506=CARTESIAN_POINT('Ctrl Pts',(-45.2751604433099,-0.913819202293729,
135.638915894921));
#84507=CARTESIAN_POINT('Ctrl Pts',(-45.2829208858241,-0.778711608315073,
135.662501141081));
#84508=CARTESIAN_POINT('Ctrl Pts',(-45.2906813283383,-0.642999499256316,
135.680397400288));
#84509=CARTESIAN_POINT('Ctrl Pts',(-45.2984542286037,-0.507069533072328,
135.698322388159));
#84510=CARTESIAN_POINT('Ctrl Pts',(-45.3062271288692,-0.370533502230687,
135.710540104633));
#84511=CARTESIAN_POINT('Ctrl Pts',(-45.3140000291346,-0.233906800281148,
135.717045288017));
#84512=CARTESIAN_POINT('Ctrl Pts',(-45.3214903648966,-0.102246823090481,
135.723313991599));
#84513=CARTESIAN_POINT('Ctrl Pts',(-45.3289807006585,0.0294970394025631,
135.724278279032));
#84514=CARTESIAN_POINT('Ctrl Pts',(-45.3364710364205,0.16086798386666,135.719979048066));
#84515=CARTESIAN_POINT('Ctrl Pts',(-45.3442453705396,0.297219897620416,
135.71551681045));
#84516=CARTESIAN_POINT('Ctrl Pts',(-45.3520197046586,0.433601978624816,
135.705369907805));
#84517=CARTESIAN_POINT('Ctrl Pts',(-45.3597940387777,0.56950150154682,135.689527053035));
#84518=CARTESIAN_POINT('Ctrl Pts',(-45.3675587917248,0.705233540452327,
135.673703723168));
#84519=CARTESIAN_POINT('Ctrl Pts',(-45.3753235446718,0.840483819963181,
135.652198453227));
#84520=CARTESIAN_POINT('Ctrl Pts',(-45.3830882976189,0.974740056812664,
135.625051946011));
#84521=CARTESIAN_POINT('Ctrl Pts',(-45.3908453385039,1.10886294847503,135.597932401089));
#84522=CARTESIAN_POINT('Ctrl Pts',(-45.3986023793889,1.24199338151171,135.565182846011));
#84523=CARTESIAN_POINT('Ctrl Pts',(-45.4063594202739,1.37362499317664,135.526895682615));
#84524=CARTESIAN_POINT('Ctrl Pts',(-45.414110611514,1.50515734041982,135.488637391868));
#84525=CARTESIAN_POINT('Ctrl Pts',(-45.4218618027542,1.63519274214251,135.444849913537));
#84526=CARTESIAN_POINT('Ctrl Pts',(-45.4296129939943,1.76323617225048,135.395676470714));
#84527=CARTESIAN_POINT('Ctrl Pts',(-45.4373608907714,1.89122518048464,135.346523927916));
#84528=CARTESIAN_POINT('Ctrl Pts',(-45.4451087875485,2.01722353679644,135.2919901135));
#84529=CARTESIAN_POINT('Ctrl Pts',(-45.4528566843256,2.14075271402463,135.232267671683));
#84530=CARTESIAN_POINT('Ctrl Pts',(-45.4606029604097,2.2642560516121,135.172557722513));
#84531=CARTESIAN_POINT('Ctrl Pts',(-45.4683492364939,2.38529088569735,135.107661474826));
#84532=CARTESIAN_POINT('Ctrl Pts',(-45.476095512578,2.50340033766479,135.037818992451));
#84533=CARTESIAN_POINT('Ctrl Pts',(-45.4838418458434,2.62151066148953,134.967975994513));
#84534=CARTESIAN_POINT('Ctrl Pts',(-45.4915881791086,2.73669522357693,134.893186888031));
#84535=CARTESIAN_POINT('Ctrl Pts',(-45.499334512374,2.84852369517427,134.813736606486));
#84536=CARTESIAN_POINT('Ctrl Pts',(-45.5070825803769,2.96037720998231,134.734268532602));
#84537=CARTESIAN_POINT('Ctrl Pts',(-45.51483064838,3.06887282010134,134.650137432931));
#84538=CARTESIAN_POINT('Ctrl Pts',(-45.522578716383,3.17361134161095,134.561670042527));
#84539=CARTESIAN_POINT('Ctrl Pts',(-45.5303350191248,3.27846118046748,134.473108627928));
#84540=CARTESIAN_POINT('Ctrl Pts',(-45.5380913218667,3.37954565495509,134.380201968979));
#84541=CARTESIAN_POINT('Ctrl Pts',(-45.5458476246086,3.47650029189455,134.283315745612));
#84542=CARTESIAN_POINT('Ctrl Pts',(-45.5536080671227,3.573506676443,134.18637781115));
#84543=CARTESIAN_POINT('Ctrl Pts',(-45.5613685096368,3.6663785667377,134.085456367541));
#84544=CARTESIAN_POINT('Ctrl Pts',(-45.569128952151,3.75479090635583,133.980951291866));
#84545=CARTESIAN_POINT('Ctrl Pts',(-45.5769018524164,3.84334517331038,133.876278455365));
#84546=CARTESIAN_POINT('Ctrl Pts',(-45.5846747526819,3.92742534395177,133.768010799906));
#84547=CARTESIAN_POINT('Ctrl Pts',(-45.5924476529473,4.006748408665,133.656579096603));
#84548=CARTESIAN_POINT('Ctrl Pts',(-45.5999379887094,4.08318788017349,133.549198216395));
#84549=CARTESIAN_POINT('Ctrl Pts',(-45.6074283244714,4.15520993820216,133.43887959461));
#84550=CARTESIAN_POINT('Ctrl Pts',(-45.6149186602334,4.22260207782701,133.32602965906));
#84551=CARTESIAN_POINT('Ctrl Pts',(-45.6226929943525,4.29254941090894,133.208900983905));
#84552=CARTESIAN_POINT('Ctrl Pts',(-45.6304673284716,4.35773038043868,133.088674227883));
#84553=CARTESIAN_POINT('Ctrl Pts',(-45.6382416625907,4.41785834969763,132.965774660388));
#84554=CARTESIAN_POINT('Ctrl Pts',(-45.6460064155378,4.47791221660827,132.843026555626));
#84555=CARTESIAN_POINT('Ctrl Pts',(-45.6537711684849,4.53292530369345,132.717612541287));
#84556=CARTESIAN_POINT('Ctrl Pts',(-45.661535921432,4.58265495375163,132.589985616651));
#84557=CARTESIAN_POINT('Ctrl Pts',(-45.669292962317,4.63233521162038,132.462485452874));
#84558=CARTESIAN_POINT('Ctrl Pts',(-45.6770500032021,4.67674233436563,132.332777114638));
#84559=CARTESIAN_POINT('Ctrl Pts',(-45.6848070440871,4.71568036083824,132.201336564712));
#84560=CARTESIAN_POINT('Ctrl Pts',(-45.6925582353273,4.75458902384208,132.069995135127));
#84561=CARTESIAN_POINT('Ctrl Pts',(-45.7003094265673,4.78803668911843,131.936924467258));
#84562=CARTESIAN_POINT('Ctrl Pts',(-45.7080606178074,4.81587628061533,131.802618456156));
#84563=CARTESIAN_POINT('Ctrl Pts',(-45.7158085145845,4.8437040395432,131.668369528692));
#84564=CARTESIAN_POINT('Ctrl Pts',(-45.7235564113615,4.8659283862643,131.532886684314));
#84565=CARTESIAN_POINT('Ctrl Pts',(-45.7313043081386,4.8824527421955,131.396676650379));
#84566=CARTESIAN_POINT('Ctrl Pts',(-45.7390505842227,4.89897364158768,131.260495108648));
#84567=CARTESIAN_POINT('Ctrl Pts',(-45.7467968603069,4.90979687471523,131.123587067794));
#84568=CARTESIAN_POINT('Ctrl Pts',(-45.754543136391,4.91487746002262,130.986466673098));
#84569=CARTESIAN_POINT('Ctrl Pts',(-45.7622894696563,4.91995808283373,130.849345266212));
#84570=CARTESIAN_POINT('Ctrl Pts',(-45.7700358029217,4.91929595876057,130.712011893053));
#84571=CARTESIAN_POINT('Ctrl Pts',(-45.7777821361871,4.91289820720832,130.574982614895));
#84572=CARTESIAN_POINT('Ctrl Pts',(-45.7855302041901,4.90649902292397,130.437922649981));
#84573=CARTESIAN_POINT('Ctrl Pts',(-45.793278272193,4.89436167347615,130.301167306044));
#84574=CARTESIAN_POINT('Ctrl Pts',(-45.801026340196,4.87654528165912,130.165229036099));
#84575=CARTESIAN_POINT('Ctrl Pts',(-45.8087826429378,4.85870995436887,130.029146289344));
#84576=CARTESIAN_POINT('Ctrl Pts',(-45.8165389456797,4.83518357852838,129.893882739564));
#84577=CARTESIAN_POINT('Ctrl Pts',(-45.8242952484215,4.80607680436346,129.759942687301));
#84578=CARTESIAN_POINT('Ctrl Pts',(-45.8320556909357,4.77695449503674,129.625931147199));
#84579=CARTESIAN_POINT('Ctrl Pts',(-45.8398161334499,4.742245951511,129.493244890212));
#84580=CARTESIAN_POINT('Ctrl Pts',(-45.847576575964,4.70211190076259,129.362373538842));
#84581=CARTESIAN_POINT('Ctrl Pts',(-45.8553494762295,4.661913423273,129.231292101161));
#84582=CARTESIAN_POINT('Ctrl Pts',(-45.863122376495,4.61627216443944,129.102031759966));
#84583=CARTESIAN_POINT('Ctrl Pts',(-45.8708952767604,4.5653975705921,128.975063461571));
#84584=CARTESIAN_POINT('Ctrl Pts',(-45.8783856125224,4.51637239637668,128.852710780637));
#84585=CARTESIAN_POINT('Ctrl Pts',(-45.8858759482844,4.46248789708463,128.732486673691));
#84586=CARTESIAN_POINT('Ctrl Pts',(-45.8933662840464,4.40397114784299,128.614789611303));
#84587=CARTESIAN_POINT('Ctrl Pts',(-45.9011406181655,4.34323571826789,128.492630029022));
#84588=CARTESIAN_POINT('Ctrl Pts',(-45.9089149522845,4.27731744959246,128.372805935004));
#84589=CARTESIAN_POINT('Ctrl Pts',(-45.9166892864036,4.20641919885393,128.255788353334));
#84590=CARTESIAN_POINT('Ctrl Pts',(-45.9244540393507,4.13560832387318,128.138914985375));
#84591=CARTESIAN_POINT('Ctrl Pts',(-45.9322187922978,4.05982987904001,128.024841579002));
#84592=CARTESIAN_POINT('Ctrl Pts',(-45.9399835452449,3.97933382333182,127.914017145764));
#84593=CARTESIAN_POINT('Ctrl Pts',(-45.9477405861299,3.89891771744073,127.803302784916));
#84594=CARTESIAN_POINT('Ctrl Pts',(-45.9554976270149,3.81379355349988,127.695831289756));
#84595=CARTESIAN_POINT('Ctrl Pts',(-45.9632546678999,3.72425585067987,127.592024797454));
#84596=CARTESIAN_POINT('Ctrl Pts',(-45.97100585914,3.63478566893794,127.488296586434));
#84597=CARTESIAN_POINT('Ctrl Pts',(-45.9787570503801,3.54090882738847,127.388228171935));
#84598=CARTESIAN_POINT('Ctrl Pts',(-45.9865082416203,3.44296135572847,127.292210255543));
#84599=CARTESIAN_POINT('Ctrl Pts',(-45.9942561383973,3.34505551435703,127.196233149327));
#84600=CARTESIAN_POINT('Ctrl Pts',(-46.0020040351744,3.24308276257053,127.104303390265));
#84601=CARTESIAN_POINT('Ctrl Pts',(-46.0097519319515,3.13741722136372,127.01677613117));
#84602=CARTESIAN_POINT('Ctrl Pts',(-46.0174982080355,3.03177378311039,126.92926718089));
#84603=CARTESIAN_POINT('Ctrl Pts',(-46.0252444841197,2.92243939278076,126.846159148084));
#84604=CARTESIAN_POINT('Ctrl Pts',(-46.0329907602038,2.80982230173143,126.76776778509));
#84605=CARTESIAN_POINT('Ctrl Pts',(-46.0407370934691,2.69720437936831,126.68937584343));
#84606=CARTESIAN_POINT('Ctrl Pts',(-46.0484834267344,2.58130402881186,126.615700864419));
#84607=CARTESIAN_POINT('Ctrl Pts',(-46.0562297599997,2.46255927523958,126.547015802023));
#84608=CARTESIAN_POINT('Ctrl Pts',(-46.0639778280026,2.34378792960338,126.478315358084));
#84609=CARTESIAN_POINT('Ctrl Pts',(-46.0717258960056,2.22217125178955,126.414607250089));
#84610=CARTESIAN_POINT('Ctrl Pts',(-46.0794739640085,2.09817234034742,126.35611872973));
#84611=CARTESIAN_POINT('Ctrl Pts',(-46.0872302667504,1.97404164138593,126.297568047074));
#84612=CARTESIAN_POINT('Ctrl Pts',(-46.0949865694922,1.84752400528735,126.244248200718));
#84613=CARTESIAN_POINT('Ctrl Pts',(-46.1027428722341,1.71910352353059,126.196338684254));
#84614=CARTESIAN_POINT('Ctrl Pts',(-46.1105033147482,1.59061449989605,126.148403597038));
#84615=CARTESIAN_POINT('Ctrl Pts',(-46.1182637572625,1.4602209784434,126.10588471476));
#84616=CARTESIAN_POINT('Ctrl Pts',(-46.1260241997767,1.32842176930888,126.068911466184));
#84617=CARTESIAN_POINT('Ctrl Pts',(-46.1337971000421,1.19641098438327,126.031878864867));
#84618=CARTESIAN_POINT('Ctrl Pts',(-46.1415700003075,1.06299038324338,126.000409776776));
#84619=CARTESIAN_POINT('Ctrl Pts',(-46.149342900573,0.928669397219115,125.974582546767));
#84620=CARTESIAN_POINT('Ctrl Pts',(-46.1568332363351,0.799231317370065,
125.949694201624));
#84621=CARTESIAN_POINT('Ctrl Pts',(-46.1643235720971,0.668957483201672,
125.930044690525));
#84622=CARTESIAN_POINT('Ctrl Pts',(-46.1718139078592,0.538305878943531,
125.915658351811));
#84623=CARTESIAN_POINT('Ctrl Pts',(-46.1795882419783,0.402700579400201,
125.900726550693));
#84624=CARTESIAN_POINT('Ctrl Pts',(-46.1873625760974,0.266258741145796,
125.891417607349));
#84625=CARTESIAN_POINT('Ctrl Pts',(-46.1951369102165,0.129486299266316,
125.887815452432));
#84626=CARTESIAN_POINT('Ctrl Pts',(-46.2029016631636,-0.00711758280243635,
125.884217736849));
#84627=CARTESIAN_POINT('Ctrl Pts',(-46.2106664161107,-0.144050870735498,
125.886312826102));
#84628=CARTESIAN_POINT('Ctrl Pts',(-46.2184311690578,-0.280800689465603,
125.894133124334));
#84629=CARTESIAN_POINT('Ctrl Pts',(-46.2261882099428,-0.41741468634754,
125.901945655335));
#84630=CARTESIAN_POINT('Ctrl Pts',(-46.2339452508278,-0.553845188859211,
125.915472057029));
#84631=CARTESIAN_POINT('Ctrl Pts',(-46.2417022917128,-0.689577846239994,
125.934692717547));
#84632=CARTESIAN_POINT('Ctrl Pts',(-46.2494534829529,-0.825208146567447,
125.953898883615));
#84633=CARTESIAN_POINT('Ctrl Pts',(-46.257204674193,-0.960141263696641,
125.978790706797));
#84634=CARTESIAN_POINT('Ctrl Pts',(-46.2649558654331,-1.09386685705719,
126.009296659543));
#84635=CARTESIAN_POINT('Ctrl Pts',(-46.2727037622101,-1.22753561347404,
126.039789646445));
#84636=CARTESIAN_POINT('Ctrl Pts',(-46.2804516589872,-1.35999748652241,
126.07589193026));
#84637=CARTESIAN_POINT('Ctrl Pts',(-46.2881995557643,-1.49075145454704,
126.117480721167));
#84638=CARTESIAN_POINT('Ctrl Pts',(-46.2959458318484,-1.62147807165992,
126.159060812596));
#84639=CARTESIAN_POINT('Ctrl Pts',(-46.3036921079325,-1.75049712201573,
126.206125009933));
#84640=CARTESIAN_POINT('Ctrl Pts',(-46.3114383840166,-1.87732228439825,
126.258500511601));
#84641=CARTESIAN_POINT('Ctrl Pts',(-46.3191847172819,-2.00414838297548,
126.310876399894));
#84642=CARTESIAN_POINT('Ctrl Pts',(-46.3269310505472,-2.12878019990099,
126.368563521518));
#84643=CARTESIAN_POINT('Ctrl Pts',(-46.3346773838125,-2.25075132796435,
126.431340891774));
#84644=CARTESIAN_POINT('Ctrl Pts',(-46.3424254518155,-2.37274977061549,
126.494132320586));
#84645=CARTESIAN_POINT('Ctrl Pts',(-46.3501735198185,-2.49208599118945,
126.562016087466));
#84646=CARTESIAN_POINT('Ctrl Pts',(-46.3579215878214,-2.60831848032506,
126.634725409578));
#84647=CARTESIAN_POINT('Ctrl Pts',(-46.3656778905632,-2.72467450273394,
126.707512008023));
#84648=CARTESIAN_POINT('Ctrl Pts',(-46.3734341933051,-2.83791987224614,
126.785134199073));
#84649=CARTESIAN_POINT('Ctrl Pts',(-46.381190496047,-2.94764191254957,126.867281723528));
#84650=CARTESIAN_POINT('Ctrl Pts',(-46.3889509385611,-3.05742251480973,
126.94947309259));
#84651=CARTESIAN_POINT('Ctrl Pts',(-46.3967113810753,-3.16367573805213,
127.036194360671));
#84652=CARTESIAN_POINT('Ctrl Pts',(-46.4044718235894,-3.26602307112765,
127.127095824087));
#84653=CARTESIAN_POINT('Ctrl Pts',(-46.4122447238549,-3.36853470122818,
127.218143210601));
#84654=CARTESIAN_POINT('Ctrl Pts',(-46.4200176241203,-3.46712763018577,
127.313383930219));
#84655=CARTESIAN_POINT('Ctrl Pts',(-46.4277905243858,-3.56146058417582,
127.412431731245));
#84656=CARTESIAN_POINT('Ctrl Pts',(-46.4352808601479,-3.65236429767885,
127.507878895217));
#84657=CARTESIAN_POINT('Ctrl Pts',(-46.44277119591,-3.7393121773532,127.606860920735));
#84658=CARTESIAN_POINT('Ctrl Pts',(-46.4502615316721,-3.82203619499996,
127.709005648163));
#84659=CARTESIAN_POINT('Ctrl Pts',(-46.4580137640801,-3.90765262541002,
127.814721825838));
#84660=CARTESIAN_POINT('Ctrl Pts',(-46.4657659964882,-3.98902275759095,
127.924169647303));
#84661=CARTESIAN_POINT('Ctrl Pts',(-46.4735182288962,-4.06580198842802,
128.036972452997));
#84662=CARTESIAN_POINT('Ctrl Pts',(-46.4815540682425,-4.14539010339482,
128.153902025881));
#84663=CARTESIAN_POINT('Ctrl Pts',(-46.4895899075888,-4.22004469059768,
128.27443647339));
#84664=CARTESIAN_POINT('Ctrl Pts',(-46.4976257469351,-4.28942536002038,
128.398116003377));
#84665=CARTESIAN_POINT('Ctrl Pts',(-46.5053585457352,-4.35618960631028,
128.517131439085));
#84666=CARTESIAN_POINT('Ctrl Pts',(-46.5130913445354,-4.41807022567004,
128.639058690767));
#84667=CARTESIAN_POINT('Ctrl Pts',(-46.5208241433355,-4.47480662911583,
128.763456726022));
#84668=CARTESIAN_POINT('Ctrl Pts',(-46.5285515023032,-4.53150311990737,
128.88776725034));
#84669=CARTESIAN_POINT('Ctrl Pts',(-46.536278861271,-4.58306243067394,129.014544744627));
#84670=CARTESIAN_POINT('Ctrl Pts',(-46.5440062202387,-4.6292697277998,129.143323336294));
#84671=CARTESIAN_POINT('Ctrl Pts',(-46.5517293393805,-4.67545167203406,
129.27203127008));
#84672=CARTESIAN_POINT('Ctrl Pts',(-46.5594524585223,-4.7162873165601,129.402737746014));
#84673=CARTESIAN_POINT('Ctrl Pts',(-46.5671755776641,-4.75161003122865,
129.534957145999));
#84674=CARTESIAN_POINT('Ctrl Pts',(-46.5680998187933,-4.75583717120834,
129.550780106295));
#84675=CARTESIAN_POINT('Ctrl Pts',(-46.5690240599226,-4.75998541624853,
129.566624713434));
#84676=CARTESIAN_POINT('Ctrl Pts',(-46.5699483010518,-4.76405452823401,
129.582490119308));
#84677=CARTESIAN_POINT('Origin',(213.235140564004,0.,130.804360617566));
#84678=CARTESIAN_POINT('',(-48.6652562953714,-4.76405452823406,129.582490119308));
#84679=CARTESIAN_POINT('',(-48.3197360547346,-4.76405452823404,129.582490119308));
#84680=CARTESIAN_POINT('',(213.235140564004,-4.76405452823405,129.582490119308));
#84681=CARTESIAN_POINT('',(-46.9851405639615,-4.91824999272014,130.804628214911));
#84682=CARTESIAN_POINT('Ctrl Pts',(-46.9851405640085,-4.91824999272009,
130.804628215736));
#84683=CARTESIAN_POINT('Ctrl Pts',(-46.9859496370517,-4.9182492202234,130.818826114959));
#84684=CARTESIAN_POINT('Ctrl Pts',(-46.986758710095,-4.91818696861465,130.833023819215));
#84685=CARTESIAN_POINT('Ctrl Pts',(-46.9875677831383,-4.91806324189077,
130.84722098694));
#84686=CARTESIAN_POINT('Ctrl Pts',(-46.9953421172574,-4.91687435925656,
130.983640716111));
#84687=CARTESIAN_POINT('Ctrl Pts',(-47.0031164513764,-4.91000317256601,
131.120227020131));
#84688=CARTESIAN_POINT('Ctrl Pts',(-47.0108907854955,-4.897426093981,131.256467592179));
#84689=CARTESIAN_POINT('Ctrl Pts',(-47.0186555384426,-4.8848645155213,131.392540259899));
#84690=CARTESIAN_POINT('Ctrl Pts',(-47.0264202913897,-4.86661107234901,
131.528267657853));
#84691=CARTESIAN_POINT('Ctrl Pts',(-47.0341850443368,-4.84269416215559,
131.663136673546));
#84692=CARTESIAN_POINT('Ctrl Pts',(-47.0419420852218,-4.81880100657457,
131.797871735431));
#84693=CARTESIAN_POINT('Ctrl Pts',(-47.0496991261068,-4.78925564587121,
131.931749729213));
#84694=CARTESIAN_POINT('Ctrl Pts',(-47.0574561669918,-4.75413830396486,
132.064262220579));
#84695=CARTESIAN_POINT('Ctrl Pts',(-47.065207358232,-4.71904744431921,132.196674783244));
#84696=CARTESIAN_POINT('Ctrl Pts',(-47.0729585494721,-4.67839306679449,
132.327723516728));
#84697=CARTESIAN_POINT('Ctrl Pts',(-47.0807097407122,-4.63230647397676,
132.456910100533));
#84698=CARTESIAN_POINT('Ctrl Pts',(-47.0884576374893,-4.58623946919031,
132.586041776593));
#84699=CARTESIAN_POINT('Ctrl Pts',(-47.0962055342664,-4.53474497230109,
132.713312509672));
#84700=CARTESIAN_POINT('Ctrl Pts',(-47.1039534310435,-4.47800408871746,
132.83823928748));
#84701=CARTESIAN_POINT('Ctrl Pts',(-47.1116997071276,-4.42127507410349,
132.963139933299));
#84702=CARTESIAN_POINT('Ctrl Pts',(-47.1194459832117,-4.35930201722169,
133.085697243348));
#84703=CARTESIAN_POINT('Ctrl Pts',(-47.1271922592958,-4.29231394893896,
133.205448709712));
#84704=CARTESIAN_POINT('Ctrl Pts',(-47.1349385925612,-4.22532538616561,
133.325201060053));
#84705=CARTESIAN_POINT('Ctrl Pts',(-47.1426849258266,-4.15332192899037,
133.442147184172));
#84706=CARTESIAN_POINT('Ctrl Pts',(-47.1504312590919,-4.076578102137,133.55585003962));
#84707=CARTESIAN_POINT('Ctrl Pts',(-47.1581793270949,-3.99981708903582,
133.669578358035));
#84708=CARTESIAN_POINT('Ctrl Pts',(-47.1659273950978,-3.91831381253091,
133.780061638516));
#84709=CARTESIAN_POINT('Ctrl Pts',(-47.1736754631008,-3.83238533427041,
133.886892971357));
#84710=CARTESIAN_POINT('Ctrl Pts',(-47.1814317658427,-3.74636553020042,
133.993837845811));
#84711=CARTESIAN_POINT('Ctrl Pts',(-47.1891880685845,-3.6559113747416,134.09712271411));
#84712=CARTESIAN_POINT('Ctrl Pts',(-47.1969443713264,-3.56137969616614,
134.196374432726));
#84713=CARTESIAN_POINT('Ctrl Pts',(-47.2047048138406,-3.46679756318753,
134.295679124972));
#84714=CARTESIAN_POINT('Ctrl Pts',(-47.2124652563547,-3.36813385175206,
134.390946106833));
#84715=CARTESIAN_POINT('Ctrl Pts',(-47.2202256988689,-3.26578052332756,
134.481840819546));
#84716=CARTESIAN_POINT('Ctrl Pts',(-47.2279985991343,-3.16326288825377,
134.572881444521));
#84717=CARTESIAN_POINT('Ctrl Pts',(-47.2357714993997,-3.0570441034649,134.659535527355));
#84718=CARTESIAN_POINT('Ctrl Pts',(-47.2435443996651,-2.94754802457509,
134.741509802614));
#84719=CARTESIAN_POINT('Ctrl Pts',(-47.2510347354271,-2.84203240395706,
134.820504106486));
#84720=CARTESIAN_POINT('Ctrl Pts',(-47.2585250711892,-2.73347388201609,
134.895152766682));
#84721=CARTESIAN_POINT('Ctrl Pts',(-47.2660154069513,-2.62227366999117,
134.965233586328));
#84722=CARTESIAN_POINT('Ctrl Pts',(-47.2737897410703,-2.50685726812874,
135.03797154155));
#84723=CARTESIAN_POINT('Ctrl Pts',(-47.2815640751894,-2.38822929798725,
135.106018851214));
#84724=CARTESIAN_POINT('Ctrl Pts',(-47.2893384093084,-2.2668080280024,135.169078755852));
#84725=CARTESIAN_POINT('Ctrl Pts',(-47.2971031622555,-2.14553639888107,
135.232060944793));
#84726=CARTESIAN_POINT('Ctrl Pts',(-47.3048679152026,-2.02147866308284,
135.290067780008));
#84727=CARTESIAN_POINT('Ctrl Pts',(-47.3126326681497,-1.8950818663292,135.342845803441));
#84728=CARTESIAN_POINT('Ctrl Pts',(-47.3203897090347,-1.7688106086558,135.395571406997));
#84729=CARTESIAN_POINT('Ctrl Pts',(-47.3281467499197,-1.64020527171864,
135.443078384061));
#84730=CARTESIAN_POINT('Ctrl Pts',(-47.3359037908047,-1.50973697869491,
135.485159408121));
#84731=CARTESIAN_POINT('Ctrl Pts',(-47.3436549820449,-1.37936707282603,
135.527208698553));
#84732=CARTESIAN_POINT('Ctrl Pts',(-47.351406173285,-1.24713737776247,135.563840060841));
#84733=CARTESIAN_POINT('Ctrl Pts',(-47.3591573645251,-1.1135381169076,135.594894609168));
#84734=CARTESIAN_POINT('Ctrl Pts',(-47.3669052613022,-0.979995639302471,
135.625935958483));
#84735=CARTESIAN_POINT('Ctrl Pts',(-47.3746531580793,-0.845085133677955,
135.651405119839));
#84736=CARTESIAN_POINT('Ctrl Pts',(-47.3824010548563,-0.709310863847926,
135.671193382407));
#84737=CARTESIAN_POINT('Ctrl Pts',(-47.3901473309404,-0.573564995068006,
135.690977505696));
#84738=CARTESIAN_POINT('Ctrl Pts',(-47.3978936070245,-0.436956108099488,
135.705083037484));
#84739=CARTESIAN_POINT('Ctrl Pts',(-47.4056398831086,-0.299997120728754,
135.713452671098));
#84740=CARTESIAN_POINT('Ctrl Pts',(-47.413386216374,-0.163037122358075,
135.721822366496));
#84741=CARTESIAN_POINT('Ctrl Pts',(-47.4211325496393,-0.025727408665489,
135.724456055384));
#84742=CARTESIAN_POINT('Ctrl Pts',(-47.4288788829047,0.111415936842174,
135.721348471071));
#84743=CARTESIAN_POINT('Ctrl Pts',(-47.4366269509077,0.248589994651179,
135.718240190836));
#84744=CARTESIAN_POINT('Ctrl Pts',(-47.4443750189106,0.385597219348077,
135.709388087824));
#84745=CARTESIAN_POINT('Ctrl Pts',(-47.4521230869136,0.521923886707727,
135.694838970343));
#84746=CARTESIAN_POINT('Ctrl Pts',(-47.4598793896554,0.658395443671755,
135.680274389888));
#84747=CARTESIAN_POINT('Ctrl Pts',(-47.4676356923973,0.794184609042562,
135.660000741295));
#84748=CARTESIAN_POINT('Ctrl Pts',(-47.4753919951391,0.928784572203252,
135.634116541103));
#84749=CARTESIAN_POINT('Ctrl Pts',(-47.4831524376533,1.06345637541719,135.608218525734));
#84750=CARTESIAN_POINT('Ctrl Pts',(-47.4909128801675,1.19693733138371,135.576704081723));
#84751=CARTESIAN_POINT('Ctrl Pts',(-47.4986733226816,1.32873410159363,135.53972214017));
#84752=CARTESIAN_POINT('Ctrl Pts',(-47.5064462229471,1.46074244367946,135.502680831922));
#84753=CARTESIAN_POINT('Ctrl Pts',(-47.5142191232125,1.59106082545536,135.460154608423));
#84754=CARTESIAN_POINT('Ctrl Pts',(-47.521992023478,1.71921341009314,135.412341554273));
#84755=CARTESIAN_POINT('Ctrl Pts',(-47.52948235924,1.8427073254828,135.366266625075));
#84756=CARTESIAN_POINT('Ctrl Pts',(-47.536972695002,1.96418989026465,135.31528269026));
#84757=CARTESIAN_POINT('Ctrl Pts',(-47.5444630307641,2.08325729944026,135.259607197367));
#84758=CARTESIAN_POINT('Ctrl Pts',(-47.5522373648832,2.20683918562417,135.201820751239));
#84759=CARTESIAN_POINT('Ctrl Pts',(-47.5600116990023,2.32821062995524,135.138796913261));
#84760=CARTESIAN_POINT('Ctrl Pts',(-47.5677860331213,2.44689587598283,135.070727178775));
#84761=CARTESIAN_POINT('Ctrl Pts',(-47.5755507860684,2.56543485305188,135.002741334152));
#84762=CARTESIAN_POINT('Ctrl Pts',(-47.5833155390155,2.68129388283498,134.929722158857));
#84763=CARTESIAN_POINT('Ctrl Pts',(-47.5910802919626,2.79401808475923,134.851908764845));
#84764=CARTESIAN_POINT('Ctrl Pts',(-47.5988373328476,2.90663032741685,134.774172656193));
#84765=CARTESIAN_POINT('Ctrl Pts',(-47.6065943737326,3.01611361866234,134.69165202546));
#84766=CARTESIAN_POINT('Ctrl Pts',(-47.6143514146176,3.12203887524488,134.604631176876));
#84767=CARTESIAN_POINT('Ctrl Pts',(-47.6221026058578,3.22788425276761,134.517675951391));
#84768=CARTESIAN_POINT('Ctrl Pts',(-47.6298537970979,3.33017663538644,134.426227510081));
#84769=CARTESIAN_POINT('Ctrl Pts',(-47.637604988338,3.42851737023967,134.330612410116));
#84770=CARTESIAN_POINT('Ctrl Pts',(-47.6453528851151,3.52681630765726,134.23503794912));
#84771=CARTESIAN_POINT('Ctrl Pts',(-47.6531007818922,3.62116665809292,134.135300623705));
#84772=CARTESIAN_POINT('Ctrl Pts',(-47.6608486786693,3.71120439313757,134.031765924443));
#84773=CARTESIAN_POINT('Ctrl Pts',(-47.6685949547534,3.80122329422903,133.928252882407));
#84774=CARTESIAN_POINT('Ctrl Pts',(-47.6763412308376,3.88693111787532,133.820944341314));
#84775=CARTESIAN_POINT('Ctrl Pts',(-47.6840875069217,3.96800240575882,133.710240857767));
#84776=CARTESIAN_POINT('Ctrl Pts',(-47.691833840187,4.04907429209216,133.599536557033));
#84777=CARTESIAN_POINT('Ctrl Pts',(-47.6995801734523,4.1255093433711,133.485437579265));
#84778=CARTESIAN_POINT('Ctrl Pts',(-47.7073265067177,4.19702417283647,133.36837527336));
#84779=CARTESIAN_POINT('Ctrl Pts',(-47.7150745747207,4.26855501755195,133.251286752163));
#84780=CARTESIAN_POINT('Ctrl Pts',(-47.7228226427236,4.33516324411925,133.131233915876));
#84781=CARTESIAN_POINT('Ctrl Pts',(-47.7305707107266,4.39661055320231,133.008674276275));
#84782=CARTESIAN_POINT('Ctrl Pts',(-47.7383270134684,4.45812316921677,132.885984378829));
#84783=CARTESIAN_POINT('Ctrl Pts',(-47.7460833162103,4.51446373519345,132.760782705978));
#84784=CARTESIAN_POINT('Ctrl Pts',(-47.7538396189522,4.56544119236859,132.633548902441));
#84785=CARTESIAN_POINT('Ctrl Pts',(-47.7616000614664,4.61644585774753,132.506247190392));
#84786=CARTESIAN_POINT('Ctrl Pts',(-47.7693605039805,4.66208158061902,132.37691155499));
#84787=CARTESIAN_POINT('Ctrl Pts',(-47.7771209464946,4.70220699942155,132.24603755679));
#84788=CARTESIAN_POINT('Ctrl Pts',(-47.7848938467601,4.7423968311085,132.114953468031));
#84789=CARTESIAN_POINT('Ctrl Pts',(-47.7926667470255,4.7770585834262,131.982326460072));
#84790=CARTESIAN_POINT('Ctrl Pts',(-47.800439647291,4.80610170913157,131.84866393748));
#84791=CARTESIAN_POINT('Ctrl Pts',(-47.807929983053,4.83408904406217,131.71986038426));
#84792=CARTESIAN_POINT('Ctrl Pts',(-47.815420318815,4.85685910940292,131.590095599825));
#84793=CARTESIAN_POINT('Ctrl Pts',(-47.822910654577,4.87437658346252,131.459826852465));
#84794=CARTESIAN_POINT('Ctrl Pts',(-47.8306849886961,4.8925582378755,131.324618925953));
#84795=CARTESIAN_POINT('Ctrl Pts',(-47.8384593228152,4.90513872838041,131.18843976855));
#84796=CARTESIAN_POINT('Ctrl Pts',(-47.8462336569342,4.91202200744782,131.05179315554));
#84797=CARTESIAN_POINT('Ctrl Pts',(-47.8539984098813,4.91889680348895,130.915314947269));
#84798=CARTESIAN_POINT('Ctrl Pts',(-47.8617631628284,4.92008833891436,130.778370816374));
#84799=CARTESIAN_POINT('Ctrl Pts',(-47.8695279157755,4.9155519113241,130.641472712619));
#84800=CARTESIAN_POINT('Ctrl Pts',(-47.8772849566605,4.91101998937768,130.504710577991));
#84801=CARTESIAN_POINT('Ctrl Pts',(-47.8850419975454,4.90077143883322,130.367994767749));
#84802=CARTESIAN_POINT('Ctrl Pts',(-47.8927990384304,4.88481352291191,130.231839955164));
#84803=CARTESIAN_POINT('Ctrl Pts',(-47.9005502296705,4.86886764097912,130.095787817983));
#84804=CARTESIAN_POINT('Ctrl Pts',(-47.9083014209108,4.84722100878712,129.960296223135));
#84805=CARTESIAN_POINT('Ctrl Pts',(-47.9160526121509,4.81993288652047,129.825877080689));
#84806=CARTESIAN_POINT('Ctrl Pts',(-47.923800508928,4.79265636243372,129.691515069965));
#84807=CARTESIAN_POINT('Ctrl Pts',(-47.931548405705,4.75974319490094,129.558224987397));
#84808=CARTESIAN_POINT('Ctrl Pts',(-47.9392963024821,4.72130411524199,129.426510656976));
#84809=CARTESIAN_POINT('Ctrl Pts',(-47.9470425785662,4.68287307620985,129.294823878353));
#84810=CARTESIAN_POINT('Ctrl Pts',(-47.9547888546502,4.63891853366306,129.16471257133));
#84811=CARTESIAN_POINT('Ctrl Pts',(-47.9625351307343,4.58960156904713,129.036667063836));
#84812=CARTESIAN_POINT('Ctrl Pts',(-47.9702814639997,4.54028424038465,128.908620611139));
#84813=CARTESIAN_POINT('Ctrl Pts',(-47.978027797265,4.48560455118449,128.782640353239));
#84814=CARTESIAN_POINT('Ctrl Pts',(-47.9857741305303,4.42577223002262,128.659197866057));
#84815=CARTESIAN_POINT('Ctrl Pts',(-47.9935221985333,4.36592650982727,128.535727734786));
#84816=CARTESIAN_POINT('Ctrl Pts',(-48.0012702665362,4.3009260320426,128.414796856866));
#84817=CARTESIAN_POINT('Ctrl Pts',(-48.0090183345392,4.23102690766987,128.296853016566));
#84818=CARTESIAN_POINT('Ctrl Pts',(-48.0167746372811,4.16105349367586,128.178783824149));
#84819=CARTESIAN_POINT('Ctrl Pts',(-48.0245309400229,4.08617123251555,128.063708347948));
#84820=CARTESIAN_POINT('Ctrl Pts',(-48.0322872427647,4.00668039094847,127.952046590799));
#84821=CARTESIAN_POINT('Ctrl Pts',(-48.0400476852789,3.92714712272583,127.84032523641));
#84822=CARTESIAN_POINT('Ctrl Pts',(-48.0478081277931,3.84300061261264,127.732021540153));
#84823=CARTESIAN_POINT('Ctrl Pts',(-48.0555685703073,3.7545813803642,127.627522296102));
#84824=CARTESIAN_POINT('Ctrl Pts',(-48.0633414705727,3.66602020971466,127.522855300587));
#84825=CARTESIAN_POINT('Ctrl Pts',(-48.071114370838,3.57317287551519,127.422005249294));
#84826=CARTESIAN_POINT('Ctrl Pts',(-48.0788872711035,3.47641732860077,127.325322586744));
#84827=CARTESIAN_POINT('Ctrl Pts',(-48.0863776068656,3.38317908952815,127.232154582506));
#84828=CARTESIAN_POINT('Ctrl Pts',(-48.0938679426277,3.28631207775877,127.142856445984));
#84829=CARTESIAN_POINT('Ctrl Pts',(-48.1013582783898,3.18618191381722,127.057705058996));
#84830=CARTESIAN_POINT('Ctrl Pts',(-48.1091326125089,3.08225528427696,126.96932513129));
#84831=CARTESIAN_POINT('Ctrl Pts',(-48.116906946628,2.97448396477283,126.885132647393));
#84832=CARTESIAN_POINT('Ctrl Pts',(-48.1246812807471,2.86323987968398,126.805480717658));
#84833=CARTESIAN_POINT('Ctrl Pts',(-48.1324460336942,2.75213289298782,126.725926951808));
#84834=CARTESIAN_POINT('Ctrl Pts',(-48.1402107866413,2.63756197120931,126.650902831514));
#84835=CARTESIAN_POINT('Ctrl Pts',(-48.1479755395884,2.51993366944313,126.580722687522));
#84836=CARTESIAN_POINT('Ctrl Pts',(-48.1557325804734,2.4024221977647,126.510612247439));
#84837=CARTESIAN_POINT('Ctrl Pts',(-48.1634896213584,2.28185972271108,126.445336408361));
#84838=CARTESIAN_POINT('Ctrl Pts',(-48.1712466622434,2.15868317943003,126.385167253009));
#84839=CARTESIAN_POINT('Ctrl Pts',(-48.1789978534836,2.03559952453826,126.325043471685));
#84840=CARTESIAN_POINT('Ctrl Pts',(-48.1867490447236,1.90990607502303,126.270018879831));
#84841=CARTESIAN_POINT('Ctrl Pts',(-48.1945002359638,1.78206554690058,126.220320320072));
#84842=CARTESIAN_POINT('Ctrl Pts',(-48.2022481327408,1.65427935441301,126.170642883526));
#84843=CARTESIAN_POINT('Ctrl Pts',(-48.2099960295179,1.52434826197686,126.126287118102));
#84844=CARTESIAN_POINT('Ctrl Pts',(-48.217743926295,1.39275600396752,126.087432191576));
#84845=CARTESIAN_POINT('Ctrl Pts',(-48.2254902023791,1.26119127222158,126.048585392663));
#84846=CARTESIAN_POINT('Ctrl Pts',(-48.2332364784633,1.1279664407833,126.015237254574));
#84847=CARTESIAN_POINT('Ctrl Pts',(-48.2409827545474,0.993581104882178,
125.987517289148));
#84848=CARTESIAN_POINT('Ctrl Pts',(-48.2487290878127,0.859194776979217,
125.9597971191));
#84849=CARTESIAN_POINT('Ctrl Pts',(-48.2564754210781,0.723648310423534,
125.9377052836));
#84850=CARTESIAN_POINT('Ctrl Pts',(-48.2642217543434,0.587451818810714,
125.921320230361));
#84851=CARTESIAN_POINT('Ctrl Pts',(-48.2719698223464,0.451224826937732,
125.904931507803));
#84852=CARTESIAN_POINT('Ctrl Pts',(-48.2797178903493,0.314347908434946,
125.894252157255));
#84853=CARTESIAN_POINT('Ctrl Pts',(-48.2874659583523,0.177336231142527,
125.889308743616));
#84854=CARTESIAN_POINT('Ctrl Pts',(-48.2952222610942,0.0401789362092088,
125.884360076057));
#84855=CARTESIAN_POINT('Ctrl Pts',(-48.302978563836,-0.0971130122836188,
125.885159537386));
#84856=CARTESIAN_POINT('Ctrl Pts',(-48.3107348665779,-0.234023952536301,
125.891681526465));
#84857=CARTESIAN_POINT('Ctrl Pts',(-48.318495309092,-0.371007966280291,
125.898206996527));
#84858=CARTESIAN_POINT('Ctrl Pts',(-48.3262557516063,-0.507610177369921,
125.910461045347));
#84859=CARTESIAN_POINT('Ctrl Pts',(-48.3340161941204,-0.643321105752883,
125.928366255654));
#84860=CARTESIAN_POINT('Ctrl Pts',(-48.3417890943859,-0.779249889365936,
125.946300208996));
#84861=CARTESIAN_POINT('Ctrl Pts',(-48.3495619946513,-0.914284145797944,
125.969903384707));
#84862=CARTESIAN_POINT('Ctrl Pts',(-48.3573348949168,-1.04792474448931,
125.999047225873));
#84863=CARTESIAN_POINT('Ctrl Pts',(-48.3648252306788,-1.17670717079752,
126.027131615003));
#84864=CARTESIAN_POINT('Ctrl Pts',(-48.3723155664407,-1.30419520807634,
126.060360751402));
#84865=CARTESIAN_POINT('Ctrl Pts',(-48.3798059022027,-1.42995828098586,
126.098576689554));
#84866=CARTESIAN_POINT('Ctrl Pts',(-48.3875802363218,-1.56048969902998,
126.138241596616));
#84867=CARTESIAN_POINT('Ctrl Pts',(-48.3953545704409,-1.6895762508405,126.183404565895));
#84868=CARTESIAN_POINT('Ctrl Pts',(-48.40312890456,-1.81671982046462,126.233943551648));
#84869=CARTESIAN_POINT('Ctrl Pts',(-48.4108936575071,-1.94370669700215,
126.284420252618));
#84870=CARTESIAN_POINT('Ctrl Pts',(-48.4186584104542,-2.06875499597062,
126.340259644343));
#84871=CARTESIAN_POINT('Ctrl Pts',(-48.4264231634013,-2.1913805090514,126.401289583952));
#84872=CARTESIAN_POINT('Ctrl Pts',(-48.4341802042863,-2.31388422874404,
126.462258907765));
#84873=CARTESIAN_POINT('Ctrl Pts',(-48.4419372451712,-2.43396960353701,
126.528408347062));
#84874=CARTESIAN_POINT('Ctrl Pts',(-48.4496942860562,-2.55117154841131,
126.599517363285));
#84875=CARTESIAN_POINT('Ctrl Pts',(-48.4574454772963,-2.66828511038713,
126.670572755645));
#84876=CARTESIAN_POINT('Ctrl Pts',(-48.4651966685365,-2.78251923758726,
126.746580078598));
#84877=CARTESIAN_POINT('Ctrl Pts',(-48.4729478597766,-2.89343297157776,
126.827272650034));
#84878=CARTESIAN_POINT('Ctrl Pts',(-48.4806957565537,-3.00429956427274,
126.907930924975));
#84879=CARTESIAN_POINT('Ctrl Pts',(-48.4884436533308,-3.11184825515029,
126.99327025822));
#84880=CARTESIAN_POINT('Ctrl Pts',(-48.4961915501079,-3.21566683503874,
127.082980514898));
#84881=CARTESIAN_POINT('Ctrl Pts',(-48.503937826192,-3.3194636983182,127.172672006125));
#84882=CARTESIAN_POINT('Ctrl Pts',(-48.5116841022761,-3.4195317069508,127.266732346726));
#84883=CARTESIAN_POINT('Ctrl Pts',(-48.5194303783602,-3.51549185553239,
127.3648112174));
#84884=CARTESIAN_POINT('Ctrl Pts',(-48.5271767116256,-3.61145271247001,
127.462890812069));
#84885=CARTESIAN_POINT('Ctrl Pts',(-48.5349230448908,-3.70330537542946,
127.564988716547));
#84886=CARTESIAN_POINT('Ctrl Pts',(-48.5426693781561,-3.79070811526944,
127.670718160723));
#84887=CARTESIAN_POINT('Ctrl Pts',(-48.5504174461591,-3.878130428347,127.776471282275));
#84888=CARTESIAN_POINT('Ctrl Pts',(-48.5581655141622,-3.96110058627273,
127.885857260538));
#84889=CARTESIAN_POINT('Ctrl Pts',(-48.5659135821652,-4.03931777844532,
127.998457029195));
#84890=CARTESIAN_POINT('Ctrl Pts',(-48.573669884907,-4.11761810078055,128.111176470225));
#84891=CARTESIAN_POINT('Ctrl Pts',(-48.5814261876489,-4.19115514302552,
128.227116203178));
#84892=CARTESIAN_POINT('Ctrl Pts',(-48.5891824903907,-4.25967171634283,
128.345828549138));
#84893=CARTESIAN_POINT('Ctrl Pts',(-48.5969429329049,-4.32822485901841,
128.464604255451));
#84894=CARTESIAN_POINT('Ctrl Pts',(-48.604703375419,-4.39175201248198,128.586155177126));
#84895=CARTESIAN_POINT('Ctrl Pts',(-48.6124638179332,-4.4500429236628,128.710010828238));
#84896=CARTESIAN_POINT('Ctrl Pts',(-48.6202367181986,-4.50842740858908,
128.834065303437));
#84897=CARTESIAN_POINT('Ctrl Pts',(-48.6280096184641,-4.56155870238263,
128.960431540754));
#84898=CARTESIAN_POINT('Ctrl Pts',(-48.6357825187295,-4.60927517135961,
129.088620119359));
#84899=CARTESIAN_POINT('Ctrl Pts',(-48.6432728544915,-4.65525702649881,
129.212148720244));
#84900=CARTESIAN_POINT('Ctrl Pts',(-48.6507631902536,-4.69621081116611,
129.337369176547));
#84901=CARTESIAN_POINT('Ctrl Pts',(-48.6582535260156,-4.73203667290888,
129.463833859629));
#84902=CARTESIAN_POINT('Ctrl Pts',(-48.6605877824675,-4.74320129243672,
129.503244776816));
#84903=CARTESIAN_POINT('Ctrl Pts',(-48.6629220389195,-4.75387503723625,
129.542800438403));
#84904=CARTESIAN_POINT('Ctrl Pts',(-48.6652562953714,-4.76405452823406,
129.582490119308));
#84905=CARTESIAN_POINT('Ctrl Pts',(-46.9150405857891,-4.76405452823398,
129.582490119308));
#84906=CARTESIAN_POINT('Ctrl Pts',(-46.922788768966,-4.7980770148678,129.71514327833));
#84907=CARTESIAN_POINT('Ctrl Pts',(-46.9305369521428,-4.82652808527651,
129.849114315221));
#84908=CARTESIAN_POINT('Ctrl Pts',(-46.9382851353198,-4.84933180294816,
129.983894818513));
#84909=CARTESIAN_POINT('Ctrl Pts',(-46.9460943734267,-4.87231521169769,
130.119737379066));
#84910=CARTESIAN_POINT('Ctrl Pts',(-46.9539036115337,-4.88956184041191,
130.256401813749));
#84911=CARTESIAN_POINT('Ctrl Pts',(-46.9617128496407,-4.90104738870751,
130.393364807194));
#84912=CARTESIAN_POINT('Ctrl Pts',(-46.9695220877476,-4.91253293700309,
130.530327800639));
#84913=CARTESIAN_POINT('Ctrl Pts',(-46.9773313258545,-4.91825744889735,
130.667588949323));
#84914=CARTESIAN_POINT('Ctrl Pts',(-46.9851405639614,-4.91824999272014,
130.80462821491));
#84915=CARTESIAN_POINT('',(-46.6398594360395,-4.91824834186539,130.808399211173));
#84916=CARTESIAN_POINT('Ctrl Pts',(-46.5699483010518,-4.76405452823401,
129.582490119308));
#84917=CARTESIAN_POINT('Ctrl Pts',(-46.5776698308829,-4.7980497363981,129.715036919991));
#84918=CARTESIAN_POINT('Ctrl Pts',(-46.5853913607139,-4.82651753434675,
129.849036394156));
#84919=CARTESIAN_POINT('Ctrl Pts',(-46.593112890545,-4.84934736789346,129.983986819834));
#84920=CARTESIAN_POINT('Ctrl Pts',(-46.6009039814527,-4.87238286894861,
130.1201529757));
#84921=CARTESIAN_POINT('Ctrl Pts',(-46.6086950723604,-4.88967822118436,
130.257286906837));
#84922=CARTESIAN_POINT('Ctrl Pts',(-46.6164861632681,-4.90117291008143,
130.394864380729));
#84923=CARTESIAN_POINT('Ctrl Pts',(-46.6242772541758,-4.9126675989785,130.53244185462));
#84924=CARTESIAN_POINT('Ctrl Pts',(-46.6320683450834,-4.91836160787432,
130.670462460698));
#84925=CARTESIAN_POINT('Ctrl Pts',(-46.6398594359911,-4.91824834186609,
130.808399210317));
#84926=CARTESIAN_POINT('Ctrl Pts',(-46.6398594360394,-4.91824834186539,
130.808399211173));
#84927=CARTESIAN_POINT('Ctrl Pts',(-46.6490111898273,-4.91811529466422,
130.970425708587));
#84928=CARTESIAN_POINT('Ctrl Pts',(-46.6581629436152,-4.90997173897153,
131.132110276553));
#84929=CARTESIAN_POINT('Ctrl Pts',(-46.6673146974032,-4.89394191360149,
131.292741215865));
#84930=CARTESIAN_POINT('Ctrl Pts',(-46.6765304058137,-4.87780006801593,
131.454494682217));
#84931=CARTESIAN_POINT('Ctrl Pts',(-46.6857461142242,-4.85366144978944,
131.615179685457));
#84932=CARTESIAN_POINT('Ctrl Pts',(-46.6949618226347,-4.82170173736842,
131.774090176958));
#84933=CARTESIAN_POINT('Ctrl Pts',(-46.7042476070203,-4.78949900423655,
131.934209019151));
#84934=CARTESIAN_POINT('Ctrl Pts',(-46.7135333914058,-4.7493558473027,132.092526207359));
#84935=CARTESIAN_POINT('Ctrl Pts',(-46.7228191757913,-4.70150009146582,
132.248341210388));
#84936=CARTESIAN_POINT('Ctrl Pts',(-46.7247825023559,-4.69138177805227,
132.281285733102));
#84937=CARTESIAN_POINT('Ctrl Pts',(-46.7267458289205,-4.68091884761776,
132.3141184762));
#84938=CARTESIAN_POINT('Ctrl Pts',(-46.7287091554851,-4.67011372258824,
132.346832944901));
#84939=CARTESIAN_POINT('Ctrl Pts',(-46.7364834896042,-4.62732784392044,
132.47637492472));
#84940=CARTESIAN_POINT('Ctrl Pts',(-46.7442578237232,-4.57908015914792,
132.604340516058));
#84941=CARTESIAN_POINT('Ctrl Pts',(-46.7520321578423,-4.52550463227619,
132.730234675169));
#84942=CARTESIAN_POINT('Ctrl Pts',(-46.7597969107894,-4.47199513245315,
132.85597368098));
#84943=CARTESIAN_POINT('Ctrl Pts',(-46.7675616637365,-4.41317100671473,
132.979645977692));
#84944=CARTESIAN_POINT('Ctrl Pts',(-46.7753264166836,-4.34921596802157,
133.100771627382));
#84945=CARTESIAN_POINT('Ctrl Pts',(-46.7830834575686,-4.28532445037463,
133.221776973369));
#84946=CARTESIAN_POINT('Ctrl Pts',(-46.7908404984536,-4.21631234259891,
133.340240362392));
#84947=CARTESIAN_POINT('Ctrl Pts',(-46.7985975393385,-4.14241128050061,
133.455702135681));
#84948=CARTESIAN_POINT('Ctrl Pts',(-46.8063487305787,-4.06856594776781,
133.571076838349));
#84949=CARTESIAN_POINT('Ctrl Pts',(-46.8140999218189,-3.98983920897081,
133.683454102768));
#84950=CARTESIAN_POINT('Ctrl Pts',(-46.821851113059,-3.906508251208,133.792399497123));
#84951=CARTESIAN_POINT('Ctrl Pts',(-46.8295990098361,-3.8232127113254,133.901298586779));
#84952=CARTESIAN_POINT('Ctrl Pts',(-46.8373469066131,-3.73531708166364,
134.006768397599));
#84953=CARTESIAN_POINT('Ctrl Pts',(-46.8450948033902,-3.64314129966474,
134.108404281499));
#84954=CARTESIAN_POINT('Ctrl Pts',(-46.8528410794743,-3.55098479885237,
134.210018905364));
#84955=CARTESIAN_POINT('Ctrl Pts',(-46.8605873555584,-3.45455018901577,
134.30780090806));
#84956=CARTESIAN_POINT('Ctrl Pts',(-46.8683336316425,-3.35419678365892,
134.401379800027));
#84957=CARTESIAN_POINT('Ctrl Pts',(-46.8760799649079,-3.25384263751602,
134.494959382772));
#84958=CARTESIAN_POINT('Ctrl Pts',(-46.8838262981731,-3.14956992406675,
134.584335526241));
#84959=CARTESIAN_POINT('Ctrl Pts',(-46.8915726314385,-3.0417735025981,134.669175881119));
#84960=CARTESIAN_POINT('Ctrl Pts',(-46.8993206994415,-2.93395294086827,
134.754035235406));
#84961=CARTESIAN_POINT('Ctrl Pts',(-46.9070687674445,-2.82260740804753,
134.834356538108));
#84962=CARTESIAN_POINT('Ctrl Pts',(-46.9148168354475,-2.70816306839881,
134.909849121686));
#84963=CARTESIAN_POINT('Ctrl Pts',(-46.9225731381893,-2.593597095944,134.98542193968));
#84964=CARTESIAN_POINT('Ctrl Pts',(-46.9303294409311,-2.47592606451947,
135.056155571163));
#84965=CARTESIAN_POINT('Ctrl Pts',(-46.938085743673,-2.35560369594359,135.121803644423));
#84966=CARTESIAN_POINT('Ctrl Pts',(-46.9458461861872,-2.2352171076966,135.187486756036));
#84967=CARTESIAN_POINT('Ctrl Pts',(-46.9536066287013,-2.11217671316505,
135.248078728282));
#84968=CARTESIAN_POINT('Ctrl Pts',(-46.9613670712155,-1.98695790827754,
135.303380659001));
#84969=CARTESIAN_POINT('Ctrl Pts',(-46.9691399714809,-1.86153809104803,
135.358771365289));
#84970=CARTESIAN_POINT('Ctrl Pts',(-46.9769128717463,-1.73393323953328,
135.408854917317));
#84971=CARTESIAN_POINT('Ctrl Pts',(-46.9846857720118,-1.60463651238487,
135.453481472698));
#84972=CARTESIAN_POINT('Ctrl Pts',(-46.9921761077738,-1.48004004694693,
135.496485740383));
#84973=CARTESIAN_POINT('Ctrl Pts',(-46.9996664435359,-1.35387287313202,
135.534422785692));
#84974=CARTESIAN_POINT('Ctrl Pts',(-47.0071567792979,-1.2265848868552,135.567203526779));
#84975=CARTESIAN_POINT('Ctrl Pts',(-47.014931113417,-1.09447073789053,135.601227159628));
#84976=CARTESIAN_POINT('Ctrl Pts',(-47.0227054475361,-0.960730609589093,
135.629803543835));
#84977=CARTESIAN_POINT('Ctrl Pts',(-47.0304797816552,-0.825853407092362,
135.652777803875));
#84978=CARTESIAN_POINT('Ctrl Pts',(-47.0382445346023,-0.691142428693386,
135.675723750193));
#84979=CARTESIAN_POINT('Ctrl Pts',(-47.0460092875494,-0.55529754606672,
135.69308124446));
#84980=CARTESIAN_POINT('Ctrl Pts',(-47.0537740404964,-0.418821845923377,
135.704745431423));
#84981=CARTESIAN_POINT('Ctrl Pts',(-47.0615310813814,-0.282481695369571,
135.71639803335));
#84982=CARTESIAN_POINT('Ctrl Pts',(-47.0692881222665,-0.145512361160019,
135.72236854795));
#84983=CARTESIAN_POINT('Ctrl Pts',(-47.0770451631515,-0.00842577204631309,
135.722603400193));
#84984=CARTESIAN_POINT('Ctrl Pts',(-47.0847963543916,0.128557439004164,
135.722838075333));
#84985=CARTESIAN_POINT('Ctrl Pts',(-47.0925475456317,0.265657339575808,
135.717345696711));
#84986=CARTESIAN_POINT('Ctrl Pts',(-47.1002987368718,0.402358603482833,
135.706124648678));
#84987=CARTESIAN_POINT('Ctrl Pts',(-47.1080466336489,0.539001765706071,
135.69490836989));
#84988=CARTESIAN_POINT('Ctrl Pts',(-47.115794530426,0.675246239411549,135.677968296313));
#84989=CARTESIAN_POINT('Ctrl Pts',(-47.123542427203,0.810578648703746,135.655354878206));
#84990=CARTESIAN_POINT('Ctrl Pts',(-47.1312887032871,0.945882749373532,
135.632746190339));
#84991=CARTESIAN_POINT('Ctrl Pts',(-47.1390349793713,1.08027477973574,135.604466582829));
#84992=CARTESIAN_POINT('Ctrl Pts',(-47.1467812554554,1.21324881870292,135.570618097646));
#84993=CARTESIAN_POINT('Ctrl Pts',(-47.1545275887208,1.34622383925407,135.5367693626));
#84994=CARTESIAN_POINT('Ctrl Pts',(-47.1622739219861,1.47778046864058,135.497351764298));
#84995=CARTESIAN_POINT('Ctrl Pts',(-47.1700202552514,1.60742566088105,135.452517866115));
#84996=CARTESIAN_POINT('Ctrl Pts',(-47.1777683232544,1.73709988626343,135.407673927692));
#84997=CARTESIAN_POINT('Ctrl Pts',(-47.1855163912574,1.8648614532996,135.357411403528));
#84998=CARTESIAN_POINT('Ctrl Pts',(-47.1932644592604,1.99023546296301,135.301931724782));
#84999=CARTESIAN_POINT('Ctrl Pts',(-47.2010207620023,2.11574272161586,135.246393081573));
#85000=CARTESIAN_POINT('Ctrl Pts',(-47.2087770647441,2.23885699582329,135.185626365801));
#85001=CARTESIAN_POINT('Ctrl Pts',(-47.2165333674859,2.3591257583593,135.119880136552));
#85002=CARTESIAN_POINT('Ctrl Pts',(-47.2242938100001,2.47945871195526,135.05409881656));
#85003=CARTESIAN_POINT('Ctrl Pts',(-47.2320542525142,2.59694279293212,134.983332888996));
#85004=CARTESIAN_POINT('Ctrl Pts',(-47.2398146950284,2.7111536961594,134.907874806441));
#85005=CARTESIAN_POINT('Ctrl Pts',(-47.2475875952938,2.82554794086771,134.832295591874));
#85006=CARTESIAN_POINT('Ctrl Pts',(-47.2553604955592,2.9366581907942,134.752009399567));
#85007=CARTESIAN_POINT('Ctrl Pts',(-47.2631333958247,3.04409181499776,134.667350144392));
#85008=CARTESIAN_POINT('Ctrl Pts',(-47.2706237315867,3.14761995635256,134.585768466385));
#85009=CARTESIAN_POINT('Ctrl Pts',(-47.2781140673488,3.24773390625493,134.500126349468));
#85010=CARTESIAN_POINT('Ctrl Pts',(-47.2856044031108,3.34411553789474,134.410754152902));
#85011=CARTESIAN_POINT('Ctrl Pts',(-47.2933787372299,3.4441515083926,134.317993382339));
#85012=CARTESIAN_POINT('Ctrl Pts',(-47.3011530713489,3.5404834358823,134.220920258363));
#85013=CARTESIAN_POINT('Ctrl Pts',(-47.308927405468,3.63271675402707,134.119862396711));
#85014=CARTESIAN_POINT('Ctrl Pts',(-47.3166921584151,3.72483640285035,134.018929079841));
#85015=CARTESIAN_POINT('Ctrl Pts',(-47.3244569113623,3.81286723162271,133.914021082392));
#85016=CARTESIAN_POINT('Ctrl Pts',(-47.3322216643093,3.89644909199301,133.805504988636));
#85017=CARTESIAN_POINT('Ctrl Pts',(-47.3399787051943,3.9799479376813,133.697096674594));
#85018=CARTESIAN_POINT('Ctrl Pts',(-47.3477357460793,4.05900637151,133.58508770353));
#85019=CARTESIAN_POINT('Ctrl Pts',(-47.3554927869643,4.13330260929571,133.469879816988));
#85020=CARTESIAN_POINT('Ctrl Pts',(-47.3632439782044,4.20754281971057,133.354758809611));
#85021=CARTESIAN_POINT('Ctrl Pts',(-47.3709951694446,4.27702777113424,133.236444015585));
#85022=CARTESIAN_POINT('Ctrl Pts',(-47.3787463606847,4.34147755788319,133.115368120128));
#85023=CARTESIAN_POINT('Ctrl Pts',(-47.3864942574618,4.40589995175351,132.994343685156));
#85024=CARTESIAN_POINT('Ctrl Pts',(-47.3942421542388,4.46529125407996,132.870560827231));
#85025=CARTESIAN_POINT('Ctrl Pts',(-47.4019900510159,4.5194164178817,132.74447873363));
#85026=CARTESIAN_POINT('Ctrl Pts',(-47.4097363271,4.57353025986597,132.618423013686));
#85027=CARTESIAN_POINT('Ctrl Pts',(-47.417482603184,4.62238000026643,132.490069373735));
#85028=CARTESIAN_POINT('Ctrl Pts',(-47.4252288792681,4.66577802717588,132.359898615695));
#85029=CARTESIAN_POINT('Ctrl Pts',(-47.4329752125335,4.7091763744397,132.229726896764));
#85030=CARTESIAN_POINT('Ctrl Pts',(-47.4407215457988,4.74712280425592,132.097738403872));
#85031=CARTESIAN_POINT('Ctrl Pts',(-47.4484678790641,4.77947916911898,131.964430414801));
#85032=CARTESIAN_POINT('Ctrl Pts',(-47.4562159470671,4.81184277996561,131.831092572331));
#85033=CARTESIAN_POINT('Ctrl Pts',(-47.4639640150702,4.83861374261053,131.696435025546));
#85034=CARTESIAN_POINT('Ctrl Pts',(-47.4717120830731,4.85970483226885,131.560966198911));
#85035=CARTESIAN_POINT('Ctrl Pts',(-47.479468385815,4.88081833778825,131.425353394395));
#85036=CARTESIAN_POINT('Ctrl Pts',(-47.4872246885568,4.89623985124863,131.288927974543));
#85037=CARTESIAN_POINT('Ctrl Pts',(-47.4949809912987,4.90593389042989,131.152205015582));
#85038=CARTESIAN_POINT('Ctrl Pts',(-47.5027414338128,4.91563310361174,131.015409083463));
#85039=CARTESIAN_POINT('Ctrl Pts',(-47.510501876327,4.91959874003263,130.878315686412));
#85040=CARTESIAN_POINT('Ctrl Pts',(-47.5182623188411,4.91784750104666,130.74143988212));
#85041=CARTESIAN_POINT('Ctrl Pts',(-47.5260352191065,4.91609345081641,130.604344352635));
#85042=CARTESIAN_POINT('Ctrl Pts',(-47.533808119372,4.90860420750972,130.467467504525));
#85043=CARTESIAN_POINT('Ctrl Pts',(-47.5415810196374,4.89544847654975,130.331320158465));
#85044=CARTESIAN_POINT('Ctrl Pts',(-47.5490713553995,4.88277098954736,130.200122111367));
#85045=CARTESIAN_POINT('Ctrl Pts',(-47.5565616911615,4.86483188641534,130.06960175382));
#85046=CARTESIAN_POINT('Ctrl Pts',(-47.5640520269236,4.84173715244562,129.94020530217));
#85047=CARTESIAN_POINT('Ctrl Pts',(-47.5718263610427,4.81776677461811,129.805902744727));
#85048=CARTESIAN_POINT('Ctrl Pts',(-47.5796006951618,4.78816616600944,129.672385571216));
#85049=CARTESIAN_POINT('Ctrl Pts',(-47.5873750292809,4.7529976862754,129.540162825778));
#85050=CARTESIAN_POINT('Ctrl Pts',(-47.595139782228,4.71787254854954,129.408103033058));
#85051=CARTESIAN_POINT('Ctrl Pts',(-47.6029045351751,4.67719329237095,129.277334868508));
#85052=CARTESIAN_POINT('Ctrl Pts',(-47.6106692881222,4.63107366648888,129.148359482888));
#85053=CARTESIAN_POINT('Ctrl Pts',(-47.6184263290072,4.58499984726946,129.019512197441));
#85054=CARTESIAN_POINT('Ctrl Pts',(-47.6261833698922,4.5334965422479,128.892454513178));
#85055=CARTESIAN_POINT('Ctrl Pts',(-47.6339404107772,4.47672781575351,128.767674307365));
#85056=CARTESIAN_POINT('Ctrl Pts',(-47.6416916020174,4.42000189899729,128.642988199277));
#85057=CARTESIAN_POINT('Ctrl Pts',(-47.6494427932575,4.3580186254431,128.520576505557));
#85058=CARTESIAN_POINT('Ctrl Pts',(-47.6571939844976,4.29099072955867,128.400908595715));
#85059=CARTESIAN_POINT('Ctrl Pts',(-47.6649418812747,4.22399132231802,128.281291547926));
#85060=CARTESIAN_POINT('Ctrl Pts',(-47.6726897780518,4.15195174785371,128.164416304957));
#85061=CARTESIAN_POINT('Ctrl Pts',(-47.6804376748289,4.07513128479229,128.050728820428));
#85062=CARTESIAN_POINT('Ctrl Pts',(-47.688183950913,3.99832689091568,127.937065116871));
#85063=CARTESIAN_POINT('Ctrl Pts',(-47.695930226997,3.91674381636887,127.82658816917));
#85064=CARTESIAN_POINT('Ctrl Pts',(-47.7036765030811,3.83068516460228,127.719715705717));
#85065=CARTESIAN_POINT('Ctrl Pts',(-47.7114228363465,3.74462587757039,127.612842453356));
#85066=CARTESIAN_POINT('Ctrl Pts',(-47.7191691696119,3.6540911926013,127.509574042847));
#85067=CARTESIAN_POINT('Ctrl Pts',(-47.7269155028772,3.55942481147405,127.410295492386));
#85068=CARTESIAN_POINT('Ctrl Pts',(-47.7346635708802,3.46473723046698,127.310994709182));
#85069=CARTESIAN_POINT('Ctrl Pts',(-47.7424116388831,3.36591638188401,127.215685846886));
#85070=CARTESIAN_POINT('Ctrl Pts',(-47.7501597068861,3.26334287049806,127.124717106019));
#85071=CARTESIAN_POINT('Ctrl Pts',(-47.7579160096279,3.16066034276356,127.033651682492));
#85072=CARTESIAN_POINT('Ctrl Pts',(-47.7656723123699,3.05421747798942,126.946935854651));
#85073=CARTESIAN_POINT('Ctrl Pts',(-47.7734286151118,2.94442844538828,126.864877885977));
#85074=CARTESIAN_POINT('Ctrl Pts',(-47.781189057626,2.83458081507476,126.782776120494));
#85075=CARTESIAN_POINT('Ctrl Pts',(-47.7889495001401,2.72138378080093,126.705337388462));
#85076=CARTESIAN_POINT('Ctrl Pts',(-47.7967099426542,2.60527970267697,126.632826039821));
#85077=CARTESIAN_POINT('Ctrl Pts',(-47.8044828429197,2.48898924397957,126.560198289526));
#85078=CARTESIAN_POINT('Ctrl Pts',(-47.8122557431851,2.36978275616859,126.49251392222));
#85079=CARTESIAN_POINT('Ctrl Pts',(-47.8200286434506,2.24812714410402,126.429991245137));
#85080=CARTESIAN_POINT('Ctrl Pts',(-47.8275189792126,2.13089401997065,126.369741424851));
#85081=CARTESIAN_POINT('Ctrl Pts',(-47.8350093149745,2.01138702320944,126.314284658988));
#85082=CARTESIAN_POINT('Ctrl Pts',(-47.8424996507365,1.89003885590877,126.263772969953));
#85083=CARTESIAN_POINT('Ctrl Pts',(-47.8502739848556,1.76408973596122,126.211346114876));
#85084=CARTESIAN_POINT('Ctrl Pts',(-47.8580483189747,1.63575810449533,126.16408065161));
#85085=CARTESIAN_POINT('Ctrl Pts',(-47.8658226530938,1.50550594168224,126.122199266004));
#85086=CARTESIAN_POINT('Ctrl Pts',(-47.8735874060409,1.37541430301884,126.080369495463));
#85087=CARTESIAN_POINT('Ctrl Pts',(-47.881352158988,1.24340721102521,126.043910718653));
#85088=CARTESIAN_POINT('Ctrl Pts',(-47.8891169119351,1.10996778200734,126.012998119757));
#85089=CARTESIAN_POINT('Ctrl Pts',(-47.8968739528201,0.976660886911533,
125.982116223691));
#85090=CARTESIAN_POINT('Ctrl Pts',(-47.9046309937051,0.841924864278071,
125.956769630954));
#85091=CARTESIAN_POINT('Ctrl Pts',(-47.9123880345901,0.706258859845322,
125.93708401916));
#85092=CARTESIAN_POINT('Ctrl Pts',(-47.9201392258302,0.570695162202028,
125.917413252439));
#85093=CARTESIAN_POINT('Ctrl Pts',(-47.9278904170704,0.434203264015171,
125.903395025411));
#85094=CARTESIAN_POINT('Ctrl Pts',(-47.9356416083105,0.297293047320565,
125.895104064226));
#85095=CARTESIAN_POINT('Ctrl Pts',(-47.9433895050876,0.160441021120067,
125.88681662692));
#85096=CARTESIAN_POINT('Ctrl Pts',(-47.9511374018646,0.0231714194688175,
125.884251637523));
#85097=CARTESIAN_POINT('Ctrl Pts',(-47.9588852986417,-0.114000417790578,
125.887432006406));
#85098=CARTESIAN_POINT('Ctrl Pts',(-47.9666315747258,-0.251143561658701,
125.890611710025));
#85099=CARTESIAN_POINT('Ctrl Pts',(-47.9743778508099,-0.388188591199009,
125.899534372412));
#85100=CARTESIAN_POINT('Ctrl Pts',(-47.982124126894,-0.524620224866981,
125.914170776449));
#85101=CARTESIAN_POINT('Ctrl Pts',(-47.9898704601594,-0.661052865642094,
125.928807288529));
#85102=CARTESIAN_POINT('Ctrl Pts',(-47.9976167934247,-0.796871712775053,
125.949157584718));
#85103=CARTESIAN_POINT('Ctrl Pts',(-48.0053631266901,-0.931567060346423,
125.975140610714));
#85104=CARTESIAN_POINT('Ctrl Pts',(-48.0131111946931,-1.06629257200715,
126.001129455429));
#85105=CARTESIAN_POINT('Ctrl Pts',(-48.0208592626961,-1.19989369963706,
126.032753465974));
#85106=CARTESIAN_POINT('Ctrl Pts',(-48.0286073306991,-1.33187176609815,
126.069880639662));
#85107=CARTESIAN_POINT('Ctrl Pts',(-48.0363636334409,-1.46399010041865,
126.107047272553));
#85108=CARTESIAN_POINT('Ctrl Pts',(-48.0441199361827,-1.59448155072266,
126.149728646206));
#85109=CARTESIAN_POINT('Ctrl Pts',(-48.0518762389246,-1.72286289763792,
126.197742932274));
#85110=CARTESIAN_POINT('Ctrl Pts',(-48.0596366814387,-1.85131276554368,
126.245782845013));
#85111=CARTESIAN_POINT('Ctrl Pts',(-48.067397123953,-1.97764992599705,126.299161189645));
#85112=CARTESIAN_POINT('Ctrl Pts',(-48.0751575664671,-2.10141286746253,
126.35764868368));
#85113=CARTESIAN_POINT('Ctrl Pts',(-48.0829304667326,-2.2253744841888,126.416230067033));
#85114=CARTESIAN_POINT('Ctrl Pts',(-48.090703366998,-2.34675327776635,126.47993680752));
#85115=CARTESIAN_POINT('Ctrl Pts',(-48.0984762672634,-2.46511320665511,
126.548494085252));
#85116=CARTESIAN_POINT('Ctrl Pts',(-48.1059666030254,-2.57917045399778,
126.614559133252));
#85117=CARTESIAN_POINT('Ctrl Pts',(-48.1134569387875,-2.69042425260649,
126.685128017685));
#85118=CARTESIAN_POINT('Ctrl Pts',(-48.1209472745495,-2.79851281567694,
126.759918865854));
#85119=CARTESIAN_POINT('Ctrl Pts',(-48.1286799548003,-2.91009850736653,
126.837129518747));
#85120=CARTESIAN_POINT('Ctrl Pts',(-48.136412635051,-3.01867289244847,126.919090705006));
#85121=CARTESIAN_POINT('Ctrl Pts',(-48.1441453153018,-3.12380140471801,
127.005538715136));
#85122=CARTESIAN_POINT('Ctrl Pts',(-48.1518657761139,-3.22876378941267,
127.091850117243));
#85123=CARTESIAN_POINT('Ctrl Pts',(-48.1595862369259,-3.33029084180872,
127.182633975219));
#85124=CARTESIAN_POINT('Ctrl Pts',(-48.1673066977379,-3.42797673765221,
127.277583257338));
#85125=CARTESIAN_POINT('Ctrl Pts',(-48.175020103386,-3.52557336550705,127.37244577226));
#85126=CARTESIAN_POINT('Ctrl Pts',(-48.1827335090342,-3.61933553607707,
127.471465867113));
#85127=CARTESIAN_POINT('Ctrl Pts',(-48.1904469146823,-3.7088901410447,127.574296069579));
#85128=CARTESIAN_POINT('Ctrl Pts',(-48.1981549902434,-3.79838286234331,
127.677055214726));
#85129=CARTESIAN_POINT('Ctrl Pts',(-48.2058630658044,-3.88367354310419,
127.783618932773));
#85130=CARTESIAN_POINT('Ctrl Pts',(-48.2135711413654,-3.96442596832126,
127.893603017868));
#85131=CARTESIAN_POINT('Ctrl Pts',(-48.2212756076997,-4.04514058204955,
128.003535604051));
#85132=CARTESIAN_POINT('Ctrl Pts',(-48.228980074034,-4.12132093532961,128.116885051816));
#85133=CARTESIAN_POINT('Ctrl Pts',(-48.2366845403683,-4.19267145129361,
128.233234567757));
#85134=CARTESIAN_POINT('Ctrl Pts',(-48.244388596637,-4.264018169669,128.349577891064));
#85135=CARTESIAN_POINT('Ctrl Pts',(-48.2520926529056,-4.330535347054,128.468920632802));
#85136=CARTESIAN_POINT('Ctrl Pts',(-48.2597967091743,-4.39197116966303,
128.590817686573));
#85137=CARTESIAN_POINT('Ctrl Pts',(-48.2675004098361,-4.45340415649271,
128.712709113771));
#85138=CARTESIAN_POINT('Ctrl Pts',(-48.2752041104979,-4.50975608213834,
128.837154262443));
#85139=CARTESIAN_POINT('Ctrl Pts',(-48.2829078111596,-4.56082183334964,
128.963684853902));
#85140=CARTESIAN_POINT('Ctrl Pts',(-48.2906154750572,-4.61191385578068,
129.090280540124));
#85141=CARTESIAN_POINT('Ctrl Pts',(-48.2983231389547,-4.65771412821306,
129.218963443053));
#85142=CARTESIAN_POINT('Ctrl Pts',(-48.3060308028522,-4.69806627517386,
129.349246760655));
#85143=CARTESIAN_POINT('Ctrl Pts',(-48.3105992201464,-4.72198343716756,
129.426467118105));
#85144=CARTESIAN_POINT('Ctrl Pts',(-48.3151676374405,-4.74398758183023,
129.504249399838));
#85145=CARTESIAN_POINT('Ctrl Pts',(-48.3197360547346,-4.76405452823404,
129.582490119308));
#85146=CARTESIAN_POINT('Origin',(213.235140564004,0.,130.804360617566));
#85147=CARTESIAN_POINT('',(-50.4153787949643,-4.76405452823401,129.582490119308));
#85148=CARTESIAN_POINT('',(-50.0699315015413,-4.76405452823402,129.582490119308));
#85149=CARTESIAN_POINT('',(213.235140564004,-4.76405452823405,129.582490119308));
#85150=CARTESIAN_POINT('',(-48.7351405639799,-4.91824799118596,130.799915429687));
#85151=CARTESIAN_POINT('Ctrl Pts',(-48.7351405640085,-4.91824799118642,
130.799915430193));
#85152=CARTESIAN_POINT('Ctrl Pts',(-48.7428228016083,-4.91837074863296,
130.93573682854));
#85153=CARTESIAN_POINT('Ctrl Pts',(-48.7505050392081,-4.91286304742632,
131.071680793918));
#85154=CARTESIAN_POINT('Ctrl Pts',(-48.7581872768079,-4.90172128579977,
131.207239630221));
#85155=CARTESIAN_POINT('Ctrl Pts',(-48.7658661433431,-4.89058441332145,
131.342738981563));
#85156=CARTESIAN_POINT('Ctrl Pts',(-48.7735450098783,-4.87381842854621,
131.477853143451));
#85157=CARTESIAN_POINT('Ctrl Pts',(-48.7812238764135,-4.85147180124849,
131.612076176529));
#85158=CARTESIAN_POINT('Ctrl Pts',(-48.7889011370898,-4.82912984723533,
131.746271139938));
#85159=CARTESIAN_POINT('Ctrl Pts',(-48.7965783977663,-4.80120963665041,
131.879574952118));
#85160=CARTESIAN_POINT('Ctrl Pts',(-48.8042556584427,-4.76781124290074,
132.011489034334));
#85161=CARTESIAN_POINT('Ctrl Pts',(-48.8119330489346,-4.73441228441417,
132.143405347099));
#85162=CARTESIAN_POINT('Ctrl Pts',(-48.8196104394266,-4.69553505633905,
132.273931496716));
#85163=CARTESIAN_POINT('Ctrl Pts',(-48.8272878299186,-4.65133014834854,
132.402581789233));
#85164=CARTESIAN_POINT('Ctrl Pts',(-48.8349670857104,-4.60711450032767,
132.531263338642));
#85165=CARTESIAN_POINT('Ctrl Pts',(-48.8426463415022,-4.55756872745563,
132.65806774763));
#85166=CARTESIAN_POINT('Ctrl Pts',(-48.850325597294,-4.50289224223815,132.782527576468));
#85167=CARTESIAN_POINT('Ctrl Pts',(-48.8580130609432,-4.4481573168793,132.907120432328));
#85168=CARTESIAN_POINT('Ctrl Pts',(-48.8657005245923,-4.38828088881619,
133.029363338446));
#85169=CARTESIAN_POINT('Ctrl Pts',(-48.8733879882415,-4.32350937127147,
133.148811465638));
#85170=CARTESIAN_POINT('Ctrl Pts',(-48.8810798149675,-4.25870109217349,
133.268327386498));
#85171=CARTESIAN_POINT('Ctrl Pts',(-48.8887716416935,-4.18899239512965,
133.38504502804));
#85172=CARTESIAN_POINT('Ctrl Pts',(-48.8964634684195,-4.11467339318653,
133.498548051636));
#85173=CARTESIAN_POINT('Ctrl Pts',(-48.9041672321142,-4.04023905536352,
133.612227220913));
#85174=CARTESIAN_POINT('Ctrl Pts',(-48.911870995809,-3.96118035448186,133.722681484809));
#85175=CARTESIAN_POINT('Ctrl Pts',(-48.9195747595037,-3.87782846972253,
133.829526633161));
#85176=CARTESIAN_POINT('Ctrl Pts',(-48.9252835562787,-3.81606139199834,
133.908703158104));
#85177=CARTESIAN_POINT('Ctrl Pts',(-48.9309923530537,-3.75193760199575,
133.985898461072));
#85178=CARTESIAN_POINT('Ctrl Pts',(-48.9367011498286,-3.68560453527068,
134.060969631877));
#85179=CARTESIAN_POINT('Ctrl Pts',(-48.9444754839477,-3.59527106498049,
134.163202797211));
#85180=CARTESIAN_POINT('Ctrl Pts',(-48.9522498180668,-3.50053759630902,
134.261836470801));
#85181=CARTESIAN_POINT('Ctrl Pts',(-48.9600241521859,-3.40172218214453,
134.356468338062));
#85182=CARTESIAN_POINT('Ctrl Pts',(-48.967788905133,-3.30302854914647,134.450983580004));
#85183=CARTESIAN_POINT('Ctrl Pts',(-48.9755536580801,-3.20026325977176,
134.541506560748));
#85184=CARTESIAN_POINT('Ctrl Pts',(-48.9833184110272,-3.09378415015764,
134.627668438646));
#85185=CARTESIAN_POINT('Ctrl Pts',(-48.9910754519122,-2.98741079709658,
134.713744739352));
#85186=CARTESIAN_POINT('Ctrl Pts',(-48.9988324927972,-2.8773312662722,134.795468312768));
#85187=CARTESIAN_POINT('Ctrl Pts',(-49.0065895336822,-2.76393946160558,
134.872507826687));
#85188=CARTESIAN_POINT('Ctrl Pts',(-49.0143407249223,-2.65063316658077,
134.949489244509));
#85189=CARTESIAN_POINT('Ctrl Pts',(-49.0220919161624,-2.53401989153566,
135.021793414811));
#85190=CARTESIAN_POINT('Ctrl Pts',(-49.0298431074025,-2.41452548011929,
135.089130129261));
#85191=CARTESIAN_POINT('Ctrl Pts',(-49.0375910041796,-2.29508185701555,
135.156438223812));
#85192=CARTESIAN_POINT('Ctrl Pts',(-49.0453389009567,-2.17275987299166,
135.218782870194));
#85193=CARTESIAN_POINT('Ctrl Pts',(-49.0530867977338,-2.04801294261065,
135.275918069886));
#85194=CARTESIAN_POINT('Ctrl Pts',(-49.0608330738179,-1.92329210659824,
135.333041318126));
#85195=CARTESIAN_POINT('Ctrl Pts',(-49.068579349902,-1.79614768840098,135.384957124457));
#85196=CARTESIAN_POINT('Ctrl Pts',(-49.0763256259861,-1.66705584930732,
135.431466393079));
#85197=CARTESIAN_POINT('Ctrl Pts',(-49.0840719592515,-1.53796305728667,
135.477976005023));
#85198=CARTESIAN_POINT('Ctrl Pts',(-49.0918182925168,-1.40692318350586,
135.519078867102));
#85199=CARTESIAN_POINT('Ctrl Pts',(-49.0995646257822,-1.27443004738224,
135.554624938299));
#85200=CARTESIAN_POINT('Ctrl Pts',(-49.1073126937851,-1.14190724033979,
135.590178969792));
#85201=CARTESIAN_POINT('Ctrl Pts',(-49.115060761788,-1.00793090088994,135.620173632892));
#85202=CARTESIAN_POINT('Ctrl Pts',(-49.122808829791,-0.873007213927309,
135.644509527148));
#85203=CARTESIAN_POINT('Ctrl Pts',(-49.1305651325329,-0.737940128464558,
135.668871285883));
#85204=CARTESIAN_POINT('Ctrl Pts',(-49.1383214352748,-0.601924069563516,
135.687562192238));
#85205=CARTESIAN_POINT('Ctrl Pts',(-49.1460777380166,-0.465473113648684,
135.700534413804));
#85206=CARTESIAN_POINT('Ctrl Pts',(-49.1538381805308,-0.328949329750221,
135.713513559035));
#85207=CARTESIAN_POINT('Ctrl Pts',(-49.161598623045,-0.19199057655083,135.720767916972));
#85208=CARTESIAN_POINT('Ctrl Pts',(-49.1693590655591,-0.0551121642013376,
135.722301824195));
#85209=CARTESIAN_POINT('Ctrl Pts',(-49.1771319658246,0.0819859775273392,
135.723838193781));
#85210=CARTESIAN_POINT('Ctrl Pts',(-49.18490486609,0.219003129676087,135.719635774135));
#85211=CARTESIAN_POINT('Ctrl Pts',(-49.1926777663554,0.355426969933536,
135.709750992607));
#85212=CARTESIAN_POINT('Ctrl Pts',(-49.2001681021175,0.48689145996634,135.700225547785));
#85213=CARTESIAN_POINT('Ctrl Pts',(-49.2076584378794,0.617804719885413,
135.685423739369));
#85214=CARTESIAN_POINT('Ctrl Pts',(-49.2151487736414,0.747718118489417,
135.665440814167));
#85215=CARTESIAN_POINT('Ctrl Pts',(-49.2229231077605,0.882557223088012,
135.644700230282));
#85216=CARTESIAN_POINT('Ctrl Pts',(-49.2306974418796,1.01674627994064,135.618312189934));
#85217=CARTESIAN_POINT('Ctrl Pts',(-49.2384717759986,1.14977489503716,135.586326819166));
#85218=CARTESIAN_POINT('Ctrl Pts',(-49.2462365289457,1.28263956425468,135.554380867508));
#85219=CARTESIAN_POINT('Ctrl Pts',(-49.2540012818929,1.41434626078754,135.516851401332));
#85220=CARTESIAN_POINT('Ctrl Pts',(-49.26176603484,1.54439124853745,135.473840110394));
#85221=CARTESIAN_POINT('Ctrl Pts',(-49.2695230757249,1.67430707377222,135.430871538876));
#85222=CARTESIAN_POINT('Ctrl Pts',(-49.2772801166099,1.80256410587156,135.38243209962));
#85223=CARTESIAN_POINT('Ctrl Pts',(-49.2850371574949,1.92867067097503,135.328674101999));
#85224=CARTESIAN_POINT('Ctrl Pts',(-49.2927883487351,2.05468213813697,135.274956643702));
#85225=CARTESIAN_POINT('Ctrl Pts',(-49.3005395399752,2.1785460079716,135.215928762922));
#85226=CARTESIAN_POINT('Ctrl Pts',(-49.3082907312154,2.29978794109783,135.151791869292));
#85227=CARTESIAN_POINT('Ctrl Pts',(-49.3160386279924,2.42097834316809,135.087682235552));
#85228=CARTESIAN_POINT('Ctrl Pts',(-49.3237865247695,2.53954868010703,135.018468090276));
#85229=CARTESIAN_POINT('Ctrl Pts',(-49.3315344215465,2.65504690474479,134.944397935768));
#85230=CARTESIAN_POINT('Ctrl Pts',(-49.3392806976306,2.77052096964366,134.87034327514));
#85231=CARTESIAN_POINT('Ctrl Pts',(-49.3470269737147,2.88292387155265,134.791434836629));
#85232=CARTESIAN_POINT('Ctrl Pts',(-49.3547732497987,2.99183072872938,134.707965612072));
#85233=CARTESIAN_POINT('Ctrl Pts',(-49.3625195830641,3.10073838983164,134.624495771363));
#85234=CARTESIAN_POINT('Ctrl Pts',(-49.3702659163295,3.20614964439734,134.536465315257));
#85235=CARTESIAN_POINT('Ctrl Pts',(-49.3780122495948,3.30767133721131,134.444208607179));
#85236=CARTESIAN_POINT('Ctrl Pts',(-49.3857603175978,3.40921576510476,134.351931238851));
#85237=CARTESIAN_POINT('Ctrl Pts',(-49.3935083856007,3.5068686086908,134.255425998131));
#85238=CARTESIAN_POINT('Ctrl Pts',(-49.4012564536037,3.60027263425461,134.155065024334));
#85239=CARTESIAN_POINT('Ctrl Pts',(-49.4090127563455,3.69377593072818,134.054597385701));
#85240=CARTESIAN_POINT('Ctrl Pts',(-49.4167690590874,3.78302112181224,133.950266114609));
#85241=CARTESIAN_POINT('Ctrl Pts',(-49.4245253618292,3.86769009387992,133.842477863527));
#85242=CARTESIAN_POINT('Ctrl Pts',(-49.4322858043434,3.95240425632756,133.734632082609));
#85243=CARTESIAN_POINT('Ctrl Pts',(-49.4400462468576,4.03253710462189,133.623325962331));
#85244=CARTESIAN_POINT('Ctrl Pts',(-49.4478066893718,4.10781374952696,133.508995391745));
#85245=CARTESIAN_POINT('Ctrl Pts',(-49.4555795896372,4.18321123518507,133.394481287577));
#85246=CARTESIAN_POINT('Ctrl Pts',(-49.4633524899026,4.25373673808465,133.276933366479));
#85247=CARTESIAN_POINT('Ctrl Pts',(-49.4711253901681,4.31916080942989,133.156813160081));
#85248=CARTESIAN_POINT('Ctrl Pts',(-49.4786157259302,4.38220655098914,133.041059625749));
#85249=CARTESIAN_POINT('Ctrl Pts',(-49.4861060616922,4.44051518508065,132.922917853518));
#85250=CARTESIAN_POINT('Ctrl Pts',(-49.4935963974544,4.49392434941947,132.802816772751));
#85251=CARTESIAN_POINT('Ctrl Pts',(-49.5013707315734,4.54935853845701,132.678162023003));
#85252=CARTESIAN_POINT('Ctrl Pts',(-49.5091450656925,4.59968999574327,132.551001588669));
#85253=CARTESIAN_POINT('Ctrl Pts',(-49.5169193998116,4.64468501330742,132.421791973036));
#85254=CARTESIAN_POINT('Ctrl Pts',(-49.5246841527587,4.68962457853374,132.292741596706));
#85255=CARTESIAN_POINT('Ctrl Pts',(-49.5324489057057,4.72924066234118,132.161647429609));
#85256=CARTESIAN_POINT('Ctrl Pts',(-49.5402136586528,4.76334653753586,132.028988244988));
#85257=CARTESIAN_POINT('Ctrl Pts',(-49.5479706995379,4.79741853829448,131.896460819339));
#85258=CARTESIAN_POINT('Ctrl Pts',(-49.5557277404229,4.82599112487382,131.762371845689));
#85259=CARTESIAN_POINT('Ctrl Pts',(-49.5634847813079,4.84892667773223,131.627217310117));
#85260=CARTESIAN_POINT('Ctrl Pts',(-49.571235972548,4.87184493471168,131.492164695633));
#85261=CARTESIAN_POINT('Ctrl Pts',(-49.5789871637882,4.88913455404411,131.356048502538));
#85262=CARTESIAN_POINT('Ctrl Pts',(-49.5867383550283,4.90070859533483,131.219376672811));
#85263=CARTESIAN_POINT('Ctrl Pts',(-49.5944862518054,4.91227771734933,131.082762932257));
#85264=CARTESIAN_POINT('Ctrl Pts',(-49.6022341485824,4.91813606003942,130.945594413533));
#85265=CARTESIAN_POINT('Ctrl Pts',(-49.6099820453595,4.91824835289376,130.80838575829));
#85266=CARTESIAN_POINT('Ctrl Pts',(-49.6177283214436,4.91836062225885,130.671205804139));
#85267=CARTESIAN_POINT('Ctrl Pts',(-49.6254745975277,4.91272923221237,130.533986120887));
#85268=CARTESIAN_POINT('Ctrl Pts',(-49.6332208736118,4.90137102612259,130.397242542819));
#85269=CARTESIAN_POINT('Ctrl Pts',(-49.6409672068772,4.89001273618913,130.260497955341));
#85270=CARTESIAN_POINT('Ctrl Pts',(-49.6487135401425,4.87292757822051,130.124229869683));
#85271=CARTESIAN_POINT('Ctrl Pts',(-49.6564598734078,4.8501843516398,129.988949790063));
#85272=CARTESIAN_POINT('Ctrl Pts',(-49.6642079414108,4.82743603187119,129.853639415408));
#85273=CARTESIAN_POINT('Ctrl Pts',(-49.6719560094138,4.79902718694441,129.719317872546));
#85274=CARTESIAN_POINT('Ctrl Pts',(-49.6797040774168,4.76507781465651,129.586486862709));
#85275=CARTESIAN_POINT('Ctrl Pts',(-49.6874603801587,4.73109236057169,129.453514678495));
#85276=CARTESIAN_POINT('Ctrl Pts',(-49.6952166829005,4.69155471310247,129.322036571222));
#85277=CARTESIAN_POINT('Ctrl Pts',(-49.7029729856423,4.646635052302,129.192539984487));
#85278=CARTESIAN_POINT('Ctrl Pts',(-49.7107334281565,4.601691416526,129.062974281525));
#85279=CARTESIAN_POINT('Ctrl Pts',(-49.7184938706707,4.55136018703969,128.935392569961));
#85280=CARTESIAN_POINT('Ctrl Pts',(-49.7262543131849,4.49585950530076,128.810261730575));
#85281=CARTESIAN_POINT('Ctrl Pts',(-49.7340272134503,4.44026972894046,128.684930020058));
#85282=CARTESIAN_POINT('Ctrl Pts',(-49.7418001137157,4.3794940907885,128.562057394461));
#85283=CARTESIAN_POINT('Ctrl Pts',(-49.7495730139812,4.3137968677988,128.442086364676));
#85284=CARTESIAN_POINT('Ctrl Pts',(-49.7570633497432,4.25048790434618,128.326476584011));
#85285=CARTESIAN_POINT('Ctrl Pts',(-49.7645536855052,4.18260912641421,128.213561365101));
#85286=CARTESIAN_POINT('Ctrl Pts',(-49.7720440212672,4.11043364364238,128.103709154731));
#85287=CARTESIAN_POINT('Ctrl Pts',(-49.7798183553863,4.03552160550398,127.989691864416));
#85288=CARTESIAN_POINT('Ctrl Pts',(-49.7875926895054,3.95574331280614,127.878613263117));
#85289=CARTESIAN_POINT('Ctrl Pts',(-49.7953670236245,3.87135650982524,127.770916727145));
#85290=CARTESIAN_POINT('Ctrl Pts',(-49.8031317765716,3.78707370603716,127.663352917528));
#85291=CARTESIAN_POINT('Ctrl Pts',(-49.8108965295187,3.69819393145342,127.559163184767));
#85292=CARTESIAN_POINT('Ctrl Pts',(-49.8186612824657,3.6050190609536,127.458763416368));
#85293=CARTESIAN_POINT('Ctrl Pts',(-49.8264183233507,3.51193673304882,127.358463366436));
#85294=CARTESIAN_POINT('Ctrl Pts',(-49.8341753642357,3.41456806289036,127.261946074566));
#85295=CARTESIAN_POINT('Ctrl Pts',(-49.8419324051207,3.31325595089106,127.169595416568));
#85296=CARTESIAN_POINT('Ctrl Pts',(-49.8496835963609,3.21202023914311,127.07731440092));
#85297=CARTESIAN_POINT('Ctrl Pts',(-49.857434787601,3.10684729245172,126.989194027316));
#85298=CARTESIAN_POINT('Ctrl Pts',(-49.8651859788411,2.99811746338405,126.905581996222));
#85299=CARTESIAN_POINT('Ctrl Pts',(-49.8729338756182,2.88943384739435,126.822005502471));
#85300=CARTESIAN_POINT('Ctrl Pts',(-49.8806817723953,2.77719666509922,126.742933777951));
#85301=CARTESIAN_POINT('Ctrl Pts',(-49.8884296691724,2.66181983452268,126.668674673126));
#85302=CARTESIAN_POINT('Ctrl Pts',(-49.8961759452565,2.54646713829201,126.594431101704));
#85303=CARTESIAN_POINT('Ctrl Pts',(-49.9039222213406,2.42797642863396,126.524998359065));
#85304=CARTESIAN_POINT('Ctrl Pts',(-49.9116684974247,2.30679079579489,126.460641095436));
#85305=CARTESIAN_POINT('Ctrl Pts',(-49.9194148306901,2.18560426839068,126.396283356736));
#85306=CARTESIAN_POINT('Ctrl Pts',(-49.9271611639554,2.06172312340398,126.337001355181));
#85307=CARTESIAN_POINT('Ctrl Pts',(-49.9349074972207,1.93561489158732,126.28301368839));
#85308=CARTESIAN_POINT('Ctrl Pts',(-49.9426555652237,1.80947841870703,126.229013931437));
#85309=CARTESIAN_POINT('Ctrl Pts',(-49.9504036332267,1.68111422590616,126.180311022351));
#85310=CARTESIAN_POINT('Ctrl Pts',(-49.9581517012296,1.55100927038034,126.137075185359));
#85311=CARTESIAN_POINT('Ctrl Pts',(-49.9659080039715,1.42076603775934,126.093793396804));
#85312=CARTESIAN_POINT('Ctrl Pts',(-49.9736643067134,1.28877871823962,126.055990410872));
#85313=CARTESIAN_POINT('Ctrl Pts',(-49.9814206094553,1.15554939839926,126.023786525434));
#85314=CARTESIAN_POINT('Ctrl Pts',(-49.9891810519695,1.02224897005926,125.991565451813));
#85315=CARTESIAN_POINT('Ctrl Pts',(-49.9969414944835,0.887705603873172,
125.964949509178));
#85316=CARTESIAN_POINT('Ctrl Pts',(-50.0047019369977,0.752430010649473,
125.944007529407));
#85317=CARTESIAN_POINT('Ctrl Pts',(-50.0124748372631,0.616937261034513,
125.923031931712));
#85318=CARTESIAN_POINT('Ctrl Pts',(-50.0202477375286,0.48071032423789,125.907748541879));
#85319=CARTESIAN_POINT('Ctrl Pts',(-50.028020637794,0.344264345353241,125.898174204167));
#85320=CARTESIAN_POINT('Ctrl Pts',(-50.0355109735561,0.212778521487179,
125.888947917748));
#85321=CARTESIAN_POINT('Ctrl Pts',(-50.0430013093181,0.0810896123887326,
125.88502282212));
#85322=CARTESIAN_POINT('Ctrl Pts',(-50.0504916450801,-0.0503447747947326,
125.886368296898));
#85323=CARTESIAN_POINT('Ctrl Pts',(-50.0582659791992,-0.186762536716492,
125.88776478576));
#85324=CARTESIAN_POINT('Ctrl Pts',(-50.0660403133184,-0.323338225795499,
125.894843825598));
#85325=CARTESIAN_POINT('Ctrl Pts',(-50.0738146474374,-0.459559499906637,
125.907628224577));
#85326=CARTESIAN_POINT('Ctrl Pts',(-50.0815794003846,-0.595612893472248,
125.920396867927));
#85327=CARTESIAN_POINT('Ctrl Pts',(-50.0893441533316,-0.731312355623601,
125.938856843957));
#85328=CARTESIAN_POINT('Ctrl Pts',(-50.0971089062787,-0.866144817674582,
125.962978974139));
#85329=CARTESIAN_POINT('Ctrl Pts',(-50.1048659471638,-1.00084336222308,
125.98707714588));
#85330=CARTESIAN_POINT('Ctrl Pts',(-50.1126229880488,-1.134676237968,126.016826211887));
#85331=CARTESIAN_POINT('Ctrl Pts',(-50.1203800289338,-1.2671351332698,126.052145174582));
#85332=CARTESIAN_POINT('Ctrl Pts',(-50.1281312201739,-1.39949414028773,
126.087437502973));
#85333=CARTESIAN_POINT('Ctrl Pts',(-50.135882411414,-1.53048085297704,126.128291267284));
#85334=CARTESIAN_POINT('Ctrl Pts',(-50.1436336026541,-1.65959715123671,
126.174574406724));
#85335=CARTESIAN_POINT('Ctrl Pts',(-50.1513814994312,-1.78865857162569,
126.220837874594));
#85336=CARTESIAN_POINT('Ctrl Pts',(-50.1591293962082,-1.91585079146782,
126.272525996244));
#85337=CARTESIAN_POINT('Ctrl Pts',(-50.1668772929853,-2.04069107464674,
126.329456931412));
#85338=CARTESIAN_POINT('Ctrl Pts',(-50.1746235690694,-2.16550524392966,
126.386375957855));
#85339=CARTESIAN_POINT('Ctrl Pts',(-50.1823698451535,-2.28796809961651,
126.448535454336));
#85340=CARTESIAN_POINT('Ctrl Pts',(-50.1901161212376,-2.40761748287308,
126.515705686394));
#85341=CARTESIAN_POINT('Ctrl Pts',(-50.197862454503,-2.5272677493547,126.582876414288));
#85342=CARTESIAN_POINT('Ctrl Pts',(-50.2056087877684,-2.64410416104717,
126.655057760178));
#85343=CARTESIAN_POINT('Ctrl Pts',(-50.2133551210337,-2.75769009378995,
126.731974534554));
#85344=CARTESIAN_POINT('Ctrl Pts',(-50.2211031890367,-2.87130146331436,
126.808908533908));
#85345=CARTESIAN_POINT('Ctrl Pts',(-50.2288512570397,-2.98166058174492,
126.890579852778));
#85346=CARTESIAN_POINT('Ctrl Pts',(-50.2365993250426,-3.08836102236103,
126.976670810638));
#85347=CARTESIAN_POINT('Ctrl Pts',(-50.2443556277845,-3.19517486547518,
127.062853266992));
#85348=CARTESIAN_POINT('Ctrl Pts',(-50.2521119305263,-3.29832195834583,
127.153464499694));
#85349=CARTESIAN_POINT('Ctrl Pts',(-50.2598682332681,-3.39742970090696,
127.248147113023));
#85350=CARTESIAN_POINT('Ctrl Pts',(-50.2676286757823,-3.4965903402545,127.342880261314));
#85351=CARTESIAN_POINT('Ctrl Pts',(-50.2753891182965,-3.59170706242428,
127.441688838627));
#85352=CARTESIAN_POINT('Ctrl Pts',(-50.2831495608107,-3.68244590554037,
127.544180374808));
#85353=CARTESIAN_POINT('Ctrl Pts',(-50.2909224610761,-3.77333041070297,
127.646836439502));
#85354=CARTESIAN_POINT('Ctrl Pts',(-50.2986953613416,-3.85982274628432,
127.753186974054));
#85355=CARTESIAN_POINT('Ctrl Pts',(-50.306468261607,-3.94163029222587,127.862807677042));
#85356=CARTESIAN_POINT('Ctrl Pts',(-50.313958597369,-4.02046392781113,127.968443391357));
#85357=CARTESIAN_POINT('Ctrl Pts',(-50.321448933131,-4.09494729397454,128.077115390142));
#85358=CARTESIAN_POINT('Ctrl Pts',(-50.328939268893,-4.16485880467396,128.188422124476));
#85359=CARTESIAN_POINT('Ctrl Pts',(-50.336921665962,-4.23936299992356,128.30704091249));
#85360=CARTESIAN_POINT('Ctrl Pts',(-50.344904063031,-4.30890056710795,128.429011375594));
#85361=CARTESIAN_POINT('Ctrl Pts',(-50.3528864600999,-4.37316512444513,
128.553891809331));
#85362=CARTESIAN_POINT('Ctrl Pts',(-50.3608585126971,-4.43734640067066,
128.678610409209));
#85363=CARTESIAN_POINT('Ctrl Pts',(-50.3688305652943,-4.49626810400048,
128.806231154193));
#85364=CARTESIAN_POINT('Ctrl Pts',(-50.3768026178915,-4.54966723934897,
128.936283779292));
#85365=CARTESIAN_POINT('Ctrl Pts',(-50.3847625385116,-4.60298511117318,
129.066138488553));
#85366=CARTESIAN_POINT('Ctrl Pts',(-50.3927224591317,-4.65079702562367,
129.198417369794));
#85367=CARTESIAN_POINT('Ctrl Pts',(-50.4006823797517,-4.69288632300249,
129.33262659884));
#85368=CARTESIAN_POINT('Ctrl Pts',(-50.4055811848226,-4.71878950385977,
129.415223509437));
#85369=CARTESIAN_POINT('Ctrl Pts',(-50.4104799898935,-4.74252609117121,
129.49855106994));
#85370=CARTESIAN_POINT('Ctrl Pts',(-50.4153787949644,-4.76405452823401,
129.582490119308));
#85371=CARTESIAN_POINT('Ctrl Pts',(-48.6652562953714,-4.76405452823406,
129.582490119308));
#85372=CARTESIAN_POINT('Ctrl Pts',(-48.6750211380865,-4.80663816484833,
129.74852307217));
#85373=CARTESIAN_POINT('Ctrl Pts',(-48.6847859808016,-4.8405687531086,129.916903017672));
#85374=CARTESIAN_POINT('Ctrl Pts',(-48.6945508235167,-4.86562797313288,
130.086831879767));
#85375=CARTESIAN_POINT('Ctrl Pts',(-48.7041603425565,-4.8902885907148,130.254057782258));
#85376=CARTESIAN_POINT('Ctrl Pts',(-48.7137698615963,-4.90635781315228,
130.422783822178));
#85377=CARTESIAN_POINT('Ctrl Pts',(-48.723379380636,-4.91367303920693,130.592227814184));
#85378=CARTESIAN_POINT('Ctrl Pts',(-48.727299775084,-4.91665743119279,130.661355861357));
#85379=CARTESIAN_POINT('Ctrl Pts',(-48.731220169532,-4.91818534567931,130.73060314286));
#85380=CARTESIAN_POINT('Ctrl Pts',(-48.7351405639799,-4.91824799118596,
130.799915429687));
#85381=CARTESIAN_POINT('',(-48.3898594359496,-4.91824988988752,130.805401348769));
#85382=CARTESIAN_POINT('Ctrl Pts',(-48.3197360547346,-4.76405452823404,
129.582490119308));
#85383=CARTESIAN_POINT('Ctrl Pts',(-48.327452615951,-4.79794981633546,129.714647333183));
#85384=CARTESIAN_POINT('Ctrl Pts',(-48.3351691771674,-4.82631527570629,
129.848112744647));
#85385=CARTESIAN_POINT('Ctrl Pts',(-48.3428857383838,-4.84907548571991,
129.982381301348));
#85386=CARTESIAN_POINT('Ctrl Pts',(-48.3507146879782,-4.87216718835205,
130.118605421527));
#85387=CARTESIAN_POINT('Ctrl Pts',(-48.3585436375725,-4.88948903909917,
130.255655842828));
#85388=CARTESIAN_POINT('Ctrl Pts',(-48.3663725871668,-4.9010169722093,130.393002257232));
#85389=CARTESIAN_POINT('Ctrl Pts',(-48.374201536761,-4.91254490531941,130.530348671637));
#85390=CARTESIAN_POINT('Ctrl Pts',(-48.3820304863554,-4.91827896681453,
130.667990658427));
#85391=CARTESIAN_POINT('Ctrl Pts',(-48.3898594359497,-4.91824988988752,
130.805401348769));
#85392=CARTESIAN_POINT('Ctrl Pts',(-48.3898594359911,-4.91824988988736,
130.805401349497));
#85393=CARTESIAN_POINT('Ctrl Pts',(-48.3930379234482,-4.91823808489216,
130.861188929996));
#85394=CARTESIAN_POINT('Ctrl Pts',(-48.3962164109053,-4.91727711705718,
130.916965370821));
#85395=CARTESIAN_POINT('Ctrl Pts',(-48.3993948983624,-4.91536792460722,
130.972709149613));
#85396=CARTESIAN_POINT('Ctrl Pts',(-48.4071692324815,-4.91069818775784,
131.109054114708));
#85397=CARTESIAN_POINT('Ctrl Pts',(-48.4149435666005,-4.90034374655151,
131.245420595926));
#85398=CARTESIAN_POINT('Ctrl Pts',(-48.4227179007196,-4.88429409418772,
131.381295851351));
#85399=CARTESIAN_POINT('Ctrl Pts',(-48.4304826536667,-4.86826422158607,
131.517003652667));
#85400=CARTESIAN_POINT('Ctrl Pts',(-48.4382474066139,-4.84655314864596,
131.652221048201));
#85401=CARTESIAN_POINT('Ctrl Pts',(-48.446012159561,-4.81920235772692,131.786435817222));
#85402=CARTESIAN_POINT('Ctrl Pts',(-48.453769200446,-4.791878731999,131.920517282242));
#85403=CARTESIAN_POINT('Ctrl Pts',(-48.461526241331,-4.75892661298791,132.053597721868));
#85404=CARTESIAN_POINT('Ctrl Pts',(-48.469283282216,-4.72043917302311,132.185170914562));
#85405=CARTESIAN_POINT('Ctrl Pts',(-48.4770344734562,-4.68198075673611,
132.316644886887));
#85406=CARTESIAN_POINT('Ctrl Pts',(-48.4847856646964,-4.63799543736451,
132.446613500943));
#85407=CARTESIAN_POINT('Ctrl Pts',(-48.4925368559365,-4.58862719118,132.574581949169));
#85408=CARTESIAN_POINT('Ctrl Pts',(-48.5002847527136,-4.53927992781713,
132.702496007392));
#85409=CARTESIAN_POINT('Ctrl Pts',(-48.5080326494907,-4.48455442850029,
132.828411226618));
#85410=CARTESIAN_POINT('Ctrl Pts',(-48.5157805462678,-4.42464406546086,
132.951849373411));
#85411=CARTESIAN_POINT('Ctrl Pts',(-48.5235268223519,-4.36474623437785,
133.075261699606));
#85412=CARTESIAN_POINT('Ctrl Pts',(-48.5312730984361,-4.29966586742658,
133.196197632493));
#85413=CARTESIAN_POINT('Ctrl Pts',(-48.5390193745202,-4.22964372344691,
133.314200659323));
#85414=CARTESIAN_POINT('Ctrl Pts',(-48.5467657077855,-4.15962106257968,
133.432204557224));
#85415=CARTESIAN_POINT('Ctrl Pts',(-48.5545120410509,-4.08465675140677,
133.547275169641));
#85416=CARTESIAN_POINT('Ctrl Pts',(-48.5622583743163,-4.00503637796646,
133.658982601939));
#85417=CARTESIAN_POINT('Ctrl Pts',(-48.5700064423192,-3.92539817409556,
133.770715050342));
#85418=CARTESIAN_POINT('Ctrl Pts',(-48.5777545103223,-3.8411020599975,133.879082501613));
#85419=CARTESIAN_POINT('Ctrl Pts',(-48.5855025783253,-3.75247537783706,
133.983686269528));
#85420=CARTESIAN_POINT('Ctrl Pts',(-48.5932588810671,-3.66375450218415,
134.088401211574));
#85421=CARTESIAN_POINT('Ctrl Pts',(-48.601015183809,-3.57069411745731,134.189344180888));
#85422=CARTESIAN_POINT('Ctrl Pts',(-48.6087714865509,-3.47366045782954,
134.286151261216));
#85423=CARTESIAN_POINT('Ctrl Pts',(-48.616531929065,-3.376575008416,134.383010010399));
#85424=CARTESIAN_POINT('Ctrl Pts',(-48.6242923715792,-3.2755123464647,134.475728207892));
#85425=CARTESIAN_POINT('Ctrl Pts',(-48.6320528140934,-3.17087284327355,
134.563981406195));
#85426=CARTESIAN_POINT('Ctrl Pts',(-48.6398257143588,-3.06606536346241,
134.652376276366));
#85427=CARTESIAN_POINT('Ctrl Pts',(-48.6475986146243,-2.95766987766794,
134.736291584703));
#85428=CARTESIAN_POINT('Ctrl Pts',(-48.6553715148898,-2.84611758719976,
134.815444977478));
#85429=CARTESIAN_POINT('Ctrl Pts',(-48.6628618506516,-2.73862050347623,
134.891720945048));
#85430=CARTESIAN_POINT('Ctrl Pts',(-48.6703521864134,-2.62819240412949,
134.963575033512));
#85431=CARTESIAN_POINT('Ctrl Pts',(-48.6778425221753,-2.51524003989757,
135.030795356704));
#85432=CARTESIAN_POINT('Ctrl Pts',(-48.6856168562944,-2.39800505244169,
135.100564358884));
#85433=CARTESIAN_POINT('Ctrl Pts',(-48.6933911904134,-2.27767924130043,
135.165562288279));
#85434=CARTESIAN_POINT('Ctrl Pts',(-48.7011655245325,-2.15468831158728,
135.22550315569));
#85435=CARTESIAN_POINT('Ctrl Pts',(-48.7089302774796,-2.03184895720299,
135.285370151339));
#85436=CARTESIAN_POINT('Ctrl Pts',(-48.7166950304267,-1.90635136753844,
135.34019231594));
#85437=CARTESIAN_POINT('Ctrl Pts',(-48.7244597833738,-1.77864891062985,
135.389727681958));
#85438=CARTESIAN_POINT('Ctrl Pts',(-48.7322168242588,-1.65107328960193,
135.439213848753));
#85439=CARTESIAN_POINT('Ctrl Pts',(-48.7399738651438,-1.52129752148494,
135.483423526065));
#85440=CARTESIAN_POINT('Ctrl Pts',(-48.7477309060287,-1.38979786671721,
135.522161477307));
#85441=CARTESIAN_POINT('Ctrl Pts',(-48.7554820972689,-1.25839737686206,
135.560870215957));
#85442=CARTESIAN_POINT('Ctrl Pts',(-48.763233288509,-1.12527596143351,135.594115331598));
#85443=CARTESIAN_POINT('Ctrl Pts',(-48.7709844797491,-0.990927738736999,
135.621750499971));
#85444=CARTESIAN_POINT('Ctrl Pts',(-48.7787323765262,-0.85663661761881,
135.649373922661));
#85445=CARTESIAN_POINT('Ctrl Pts',(-48.7864802733034,-0.721120108454675,
135.671392061821));
#85446=CARTESIAN_POINT('Ctrl Pts',(-48.7942281700805,-0.584885084992501,
135.687709110133));
#85447=CARTESIAN_POINT('Ctrl Pts',(-48.8019744461645,-0.448678558960533,
135.70402274527));
#85448=CARTESIAN_POINT('Ctrl Pts',(-48.8097207222486,-0.311754205525746,
135.714637615132));
#85449=CARTESIAN_POINT('Ctrl Pts',(-48.8174669983327,-0.174626237827864,
135.719509520658));
#85450=CARTESIAN_POINT('Ctrl Pts',(-48.825213331598,-0.0374972578822876,
135.724381462146));
#85451=CARTESIAN_POINT('Ctrl Pts',(-48.8329596648634,0.0998349486068893,
135.723510340824));
#85452=CARTESIAN_POINT('Ctrl Pts',(-48.8407059981288,0.23685433179815,135.716904061446));
#85453=CARTESIAN_POINT('Ctrl Pts',(-48.8484540661317,0.373904399530065,
135.710296302637));
#85454=CARTESIAN_POINT('Ctrl Pts',(-48.8562021341346,0.51064111412667,135.697950848891));
#85455=CARTESIAN_POINT('Ctrl Pts',(-48.8639502021375,0.646552113141298,
135.679927602799));
#85456=CARTESIAN_POINT('Ctrl Pts',(-48.8717065048794,0.782607559983041,
135.661885201387));
#85457=CARTESIAN_POINT('Ctrl Pts',(-48.8794628076213,0.917835149991321,
135.638153004693));
#85458=CARTESIAN_POINT('Ctrl Pts',(-48.8872191103631,1.05173075159825,135.608842430274));
#85459=CARTESIAN_POINT('Ctrl Pts',(-48.8949795528773,1.18569781731946,135.579516211919));
#85460=CARTESIAN_POINT('Ctrl Pts',(-48.9027399953915,1.31833110016377,135.54460578269));
#85461=CARTESIAN_POINT('Ctrl Pts',(-48.9105004379057,1.44914122279315,135.504272614498));
#85462=CARTESIAN_POINT('Ctrl Pts',(-48.9182733381712,1.58016133344414,135.463874699923));
#85463=CARTESIAN_POINT('Ctrl Pts',(-48.9260462384365,1.70935206673169,135.418036781706));
#85464=CARTESIAN_POINT('Ctrl Pts',(-48.933819138702,1.83624279562809,135.366969022635));
#85465=CARTESIAN_POINT('Ctrl Pts',(-48.9413094744641,1.95852072691203,135.317757705237));
#85466=CARTESIAN_POINT('Ctrl Pts',(-48.9487998102262,2.07866269160748,135.263690307716));
#85467=CARTESIAN_POINT('Ctrl Pts',(-48.9562901459883,2.19627056517438,135.204994511342));
#85468=CARTESIAN_POINT('Ctrl Pts',(-48.9640644801074,2.31833757701233,135.144073246008));
#85469=CARTESIAN_POINT('Ctrl Pts',(-48.9718388142264,2.43806121589239,135.077972701792));
#85470=CARTESIAN_POINT('Ctrl Pts',(-48.9796131483455,2.55497076698948,135.006896452313));
#85471=CARTESIAN_POINT('Ctrl Pts',(-48.9873779012926,2.67173623751335,134.935907797959));
#85472=CARTESIAN_POINT('Ctrl Pts',(-48.9951426542397,2.78569418989876,134.85995584057));
#85473=CARTESIAN_POINT('Ctrl Pts',(-49.0029074071868,2.89639599350979,134.779291222153));
#85474=CARTESIAN_POINT('Ctrl Pts',(-49.0106644480718,3.00698784652871,134.698706720972));
#85475=CARTESIAN_POINT('Ctrl Pts',(-49.0184214889568,3.11432967275093,134.613419102283));
#85476=CARTESIAN_POINT('Ctrl Pts',(-49.0261785298418,3.21799978370546,134.523723527336));
#85477=CARTESIAN_POINT('Ctrl Pts',(-49.0339297210819,3.32159171622301,134.43409559252));
#85478=CARTESIAN_POINT('Ctrl Pts',(-49.041680912322,3.42151715027272,134.340066572586));
#85479=CARTESIAN_POINT('Ctrl Pts',(-49.0494321035622,3.51738589609908,134.241973091424));
#85480=CARTESIAN_POINT('Ctrl Pts',(-49.0571800003393,3.61321389515108,134.143921302608));
#85481=CARTESIAN_POINT('Ctrl Pts',(-49.0649278971164,3.70498836259032,134.04180876746));
#85482=CARTESIAN_POINT('Ctrl Pts',(-49.0726757938935,3.79235471536453,133.936010147024));
#85483=CARTESIAN_POINT('Ctrl Pts',(-49.0804220699776,3.87970279298113,133.830233657378));
#85484=CARTESIAN_POINT('Ctrl Pts',(-49.0881683460616,3.96264434121974,133.720772917377));
#85485=CARTESIAN_POINT('Ctrl Pts',(-49.0959146221457,4.04086422939547,133.608036658426));
#85486=CARTESIAN_POINT('Ctrl Pts',(-49.1036609554111,4.11908469497254,133.495299567282));
#85487=CARTESIAN_POINT('Ctrl Pts',(-49.1114072886765,4.19258320806575,133.37928723016));
#85488=CARTESIAN_POINT('Ctrl Pts',(-49.1191536219418,4.26108748162426,133.260438087119));
#85489=CARTESIAN_POINT('Ctrl Pts',(-49.1269016899448,4.32960709623995,133.141562328636));
#85490=CARTESIAN_POINT('Ctrl Pts',(-49.1346497579477,4.39313005058105,133.019848838757));
#85491=CARTESIAN_POINT('Ctrl Pts',(-49.1423978259507,4.4514297979772,132.895761061331));
#85492=CARTESIAN_POINT('Ctrl Pts',(-49.1501541286925,4.50979150703867,132.771541401939));
#85493=CARTESIAN_POINT('Ctrl Pts',(-49.1579104314345,4.56291875334618,132.644942768616));
#85494=CARTESIAN_POINT('Ctrl Pts',(-49.1656667341763,4.61063278021964,132.51644952544));
#85495=CARTESIAN_POINT('Ctrl Pts',(-49.1734271766905,4.65837227350588,132.387887701551));
#85496=CARTESIAN_POINT('Ctrl Pts',(-49.1811876192046,4.70069266980552,132.257429624591));
#85497=CARTESIAN_POINT('Ctrl Pts',(-49.1889480617188,4.73746529960663,132.125574301087));
#85498=CARTESIAN_POINT('Ctrl Pts',(-49.1967209619842,4.77429696009762,131.993507311713));
#85499=CARTESIAN_POINT('Ctrl Pts',(-49.2044938622497,4.80556296830533,131.860038974476));
#85500=CARTESIAN_POINT('Ctrl Pts',(-49.2122667625151,4.83118575473103,131.725678839346));
#85501=CARTESIAN_POINT('Ctrl Pts',(-49.2197570982771,4.85587708833012,131.596203033561));
#85502=CARTESIAN_POINT('Ctrl Pts',(-49.2272474340391,4.87532832207602,131.465899447038));
#85503=CARTESIAN_POINT('Ctrl Pts',(-49.2347377698011,4.88951581462955,131.335226100516));
#85504=CARTESIAN_POINT('Ctrl Pts',(-49.2425121039201,4.90424123027552,131.199598234342));
#85505=CARTESIAN_POINT('Ctrl Pts',(-49.2502864380392,4.91334252158849,131.063142387458));
#85506=CARTESIAN_POINT('Ctrl Pts',(-49.2580607721582,4.91673652796036,130.926364622092));
#85507=CARTESIAN_POINT('Ctrl Pts',(-49.2658255251053,4.92012635152271,130.789755423098));
#85508=CARTESIAN_POINT('Ctrl Pts',(-49.2735902780525,4.91782287554224,130.6528254821));
#85509=CARTESIAN_POINT('Ctrl Pts',(-49.2813550309996,4.90979447642093,130.516087722887));
#85510=CARTESIAN_POINT('Ctrl Pts',(-49.2891120718846,4.90177405121882,130.379485773544));
#85511=CARTESIAN_POINT('Ctrl Pts',(-49.2968691127695,4.88804004118779,130.243076013898));
#85512=CARTESIAN_POINT('Ctrl Pts',(-49.3046261536545,4.86861284092837,130.107372764266));
#85513=CARTESIAN_POINT('Ctrl Pts',(-49.3123773448947,4.84920029087179,129.971771849511));
#85514=CARTESIAN_POINT('Ctrl Pts',(-49.3201285361348,4.82410315127968,129.836876769749));
#85515=CARTESIAN_POINT('Ctrl Pts',(-49.3278797273749,4.79339372626994,129.703197756107));
#85516=CARTESIAN_POINT('Ctrl Pts',(-49.335627624152,4.76269735358503,129.569575559612));
#85517=CARTESIAN_POINT('Ctrl Pts',(-49.3433755209291,4.72639352715479,129.437168781483));
#85518=CARTESIAN_POINT('Ctrl Pts',(-49.3511234177061,4.68460579912524,129.306478255929));
#85519=CARTESIAN_POINT('Ctrl Pts',(-49.3588696937902,4.64282681218755,129.175815068017));
#85520=CARTESIAN_POINT('Ctrl Pts',(-49.3666159698744,4.59556632431853,129.046867790759));
#85521=CARTESIAN_POINT('Ctrl Pts',(-49.3743622459585,4.54299787699253,128.920122481835));
#85522=CARTESIAN_POINT('Ctrl Pts',(-49.3821085792239,4.4904290416182,128.793376237307));
#85523=CARTESIAN_POINT('Ctrl Pts',(-49.3898549124891,4.43255231838501,128.668832354682));
#85524=CARTESIAN_POINT('Ctrl Pts',(-49.3976012457545,4.36958940153057,128.54695690433));
#85525=CARTESIAN_POINT('Ctrl Pts',(-49.4053493137575,4.30661238456745,128.425054160816));
#85526=CARTESIAN_POINT('Ctrl Pts',(-49.4130973817605,4.2385470868824,128.305821385968));
#85527=CARTESIAN_POINT('Ctrl Pts',(-49.4208454497634,4.16566096290401,128.189699682638));
#85528=CARTESIAN_POINT('Ctrl Pts',(-49.4286017525053,4.09269737468571,128.07345456378));
#85529=CARTESIAN_POINT('Ctrl Pts',(-49.4363580552471,4.01490293334614,127.960327453165));
#85530=CARTESIAN_POINT('Ctrl Pts',(-49.444114357989,3.93258852574926,127.850730554466));
#85531=CARTESIAN_POINT('Ctrl Pts',(-49.4518748005031,3.8502301844746,127.741075160603));
#85532=CARTESIAN_POINT('Ctrl Pts',(-49.4596352430173,3.76334731749674,127.634954035408));
#85533=CARTESIAN_POINT('Ctrl Pts',(-49.4673956855314,3.67229020412545,127.532745157402));
#85534=CARTESIAN_POINT('Ctrl Pts',(-49.4751685857969,3.58108691779199,127.430372204632));
#85535=CARTESIAN_POINT('Ctrl Pts',(-49.4829414860623,3.48569626680652,127.331924330005));
#85536=CARTESIAN_POINT('Ctrl Pts',(-49.4907143863278,3.38650502177914,127.237742219144));
#85537=CARTESIAN_POINT('Ctrl Pts',(-49.4982047220898,3.29091962835577,127.146983865242));
#85538=CARTESIAN_POINT('Ctrl Pts',(-49.5056950578519,3.19180539758634,127.060186720045));
#85539=CARTESIAN_POINT('Ctrl Pts',(-49.513185393614,3.08953489656831,126.977618245079));
#85540=CARTESIAN_POINT('Ctrl Pts',(-49.520959727733,2.98338677842018,126.891919161289));
#85541=CARTESIAN_POINT('Ctrl Pts',(-49.5287340618521,2.87350208007221,126.810504268785));
#85542=CARTESIAN_POINT('Ctrl Pts',(-49.5365083959712,2.76026161566952,126.733717071938));
#85543=CARTESIAN_POINT('Ctrl Pts',(-49.5442731489183,2.64716071001861,126.657024508449));
#85544=CARTESIAN_POINT('Ctrl Pts',(-49.5520379018654,2.53071258756723,126.58494851022));
#85545=CARTESIAN_POINT('Ctrl Pts',(-49.5598026548125,2.41133169229693,126.517792930917));
#85546=CARTESIAN_POINT('Ctrl Pts',(-49.5675596956975,2.29206936781495,126.450704051482));
#85547=CARTESIAN_POINT('Ctrl Pts',(-49.5753167365826,2.16988040580546,126.388526056006));
#85548=CARTESIAN_POINT('Ctrl Pts',(-49.5830737774675,2.04520854229898,126.331519788629));
#85549=CARTESIAN_POINT('Ctrl Pts',(-49.5908249687077,1.9206306948144,126.274556510122));
#85550=CARTESIAN_POINT('Ctrl Pts',(-49.5985761599478,1.79357402680211,126.222757358842));
#85551=CARTESIAN_POINT('Ctrl Pts',(-49.6063273511879,1.66450689230132,126.176337295673));
#85552=CARTESIAN_POINT('Ctrl Pts',(-49.614075247965,1.53549461477584,126.12993696227));
#85553=CARTESIAN_POINT('Ctrl Pts',(-49.621823144742,1.40447393742505,126.08891130183));
#85554=CARTESIAN_POINT('Ctrl Pts',(-49.6295710415191,1.27193300920695,126.053427079556));
#85555=CARTESIAN_POINT('Ctrl Pts',(-49.6373173176032,1.13941980569379,126.017950279816));
#85556=CARTESIAN_POINT('Ctrl Pts',(-49.6450635936874,1.00538736126562,125.988012713677));
#85557=CARTESIAN_POINT('Ctrl Pts',(-49.6528098697715,0.870338413419094,
125.963731101829));
#85558=CARTESIAN_POINT('Ctrl Pts',(-49.6605562030368,0.735288468671917,
125.939449310739));
#85559=CARTESIAN_POINT('Ctrl Pts',(-49.6683025363021,0.599222390328442,
125.920823626437));
#85560=CARTESIAN_POINT('Ctrl Pts',(-49.6760488695675,0.462652127740718,
125.9079194537));
#85561=CARTESIAN_POINT('Ctrl Pts',(-49.6837969375705,0.3260512811896,125.895012391164));
#85562=CARTESIAN_POINT('Ctrl Pts',(-49.6915450055734,0.188946414876321,
125.887829426588));
#85563=CARTESIAN_POINT('Ctrl Pts',(-49.6992930735764,0.0518532067744206,
125.886383969853));
#85564=CARTESIAN_POINT('Ctrl Pts',(-49.7070493763183,-0.0853857056206671,
125.88493697687));
#85565=CARTESIAN_POINT('Ctrl Pts',(-49.7148056790601,-0.222612543486195,
125.889239677051));
#85566=CARTESIAN_POINT('Ctrl Pts',(-49.722561981802,-0.359312466254466,
125.899253318628));
#85567=CARTESIAN_POINT('Ctrl Pts',(-49.7303224243162,-0.496085349887473,
125.909272304787));
#85568=CARTESIAN_POINT('Ctrl Pts',(-49.7380828668303,-0.63233036985443,
125.925008261105));
#85569=CARTESIAN_POINT('Ctrl Pts',(-49.7458433093445,-0.767540187597426,
125.946370794303));
#85570=CARTESIAN_POINT('Ctrl Pts',(-49.7536162096099,-0.902967056143042,
125.967767620536));
#85571=CARTESIAN_POINT('Ctrl Pts',(-49.7613891098753,-1.03735501815833,
125.994808995856));
#85572=CARTESIAN_POINT('Ctrl Pts',(-49.7691620101407,-1.17020838622026,
126.027353668092));
#85573=CARTESIAN_POINT('Ctrl Pts',(-49.7766523459027,-1.29823219971588,
126.058715259518));
#85574=CARTESIAN_POINT('Ctrl Pts',(-49.7841426816648,-1.42483075892259,
126.095186891809));
#85575=CARTESIAN_POINT('Ctrl Pts',(-49.7916330174268,-1.54957765926795,
126.1365996832));
#85576=CARTESIAN_POINT('Ctrl Pts',(-49.7994073543303,-1.67905442262962,
126.179582668558));
#85577=CARTESIAN_POINT('Ctrl Pts',(-49.8071816912339,-1.80694648626056,
126.228025058616));
#85578=CARTESIAN_POINT('Ctrl Pts',(-49.8149560281375,-1.93275901032833,
126.281792135996));
#85579=CARTESIAN_POINT('Ctrl Pts',(-49.8227207832134,-2.05841647114915,
126.335492945747));
#85580=CARTESIAN_POINT('Ctrl Pts',(-49.8304855382893,-2.18199913599579,
126.394505232937));
#85581=CARTESIAN_POINT('Ctrl Pts',(-49.8382502933652,-2.30302734669305,
126.458644554259));
#85582=CARTESIAN_POINT('Ctrl Pts',(-49.8460073357261,-2.42393534032146,
126.522720166127));
#85583=CARTESIAN_POINT('Ctrl Pts',(-49.853764378087,-2.54229358599368,126.591912495585));
#85584=CARTESIAN_POINT('Ctrl Pts',(-49.8615214204479,-2.6576427777372,126.665989207405));
#85585=CARTESIAN_POINT('Ctrl Pts',(-49.8692726125132,-2.77290497409687,
126.740010051196));
#85586=CARTESIAN_POINT('Ctrl Pts',(-49.8770238045784,-2.88516230599961,
126.818907734636));
#85587=CARTESIAN_POINT('Ctrl Pts',(-49.8847749966436,-2.99398076385158,
126.902404409689));
#85588=CARTESIAN_POINT('Ctrl Pts',(-49.8925228908177,-3.10275292283416,
126.985865559504));
#85589=CARTESIAN_POINT('Ctrl Pts',(-49.9002707849918,-3.20808880831806,
127.073921571624));
#85590=CARTESIAN_POINT('Ctrl Pts',(-49.9080186791658,-3.30958426000976,
127.166251893463));
#85591=CARTESIAN_POINT('Ctrl Pts',(-49.91576495172,-3.41105846889104,127.258562890736));
#85592=CARTESIAN_POINT('Ctrl Pts',(-49.9235112242741,-3.50869355375994,
127.355146155383));
#85593=CARTESIAN_POINT('Ctrl Pts',(-49.9312574968283,-3.60211957281576,
127.455641810972));
#85594=CARTESIAN_POINT('Ctrl Pts',(-49.9390038256361,-3.69554627033357,
127.556138196362));
#85595=CARTESIAN_POINT('Ctrl Pts',(-49.9467501544438,-3.78476357485034,
127.660546743044));
#85596=CARTESIAN_POINT('Ctrl Pts',(-49.9544964832516,-3.86943973891063,
127.768472087096));
#85597=CARTESIAN_POINT('Ctrl Pts',(-49.9622445458679,-3.95413485546566,
127.87642158735));
#85598=CARTESIAN_POINT('Ctrl Pts',(-49.9699926084842,-4.03428656774275,
127.987889143755));
#85599=CARTESIAN_POINT('Ctrl Pts',(-49.9777406711005,-4.10960485765943,
128.102448151108));
#85600=CARTESIAN_POINT('Ctrl Pts',(-49.9854969553295,-4.18500306920807,
128.217128719145));
#85601=CARTESIAN_POINT('Ctrl Pts',(-49.9932532395585,-4.25555739792462,
128.334906963841));
#85602=CARTESIAN_POINT('Ctrl Pts',(-50.0010095237875,-4.32102216451849,
128.455328792273));
#85603=CARTESIAN_POINT('Ctrl Pts',(-50.0087699474057,-4.38652186847922,
128.575814887666));
#85604=CARTESIAN_POINT('Ctrl Pts',(-50.0165303710239,-4.44692642594108,
128.69894702717));
#85605=CARTESIAN_POINT('Ctrl Pts',(-50.0242907946421,-4.50203765966367,
128.824249516271));
#85606=CARTESIAN_POINT('Ctrl Pts',(-50.0320636447594,-4.5572371411067,128.949752647933));
#85607=CARTESIAN_POINT('Ctrl Pts',(-50.0398364948765,-4.60712621879869,
129.077432709554));
#85608=CARTESIAN_POINT('Ctrl Pts',(-50.0476093449938,-4.65155580344958,
129.206796324683));
#85609=CARTESIAN_POINT('Ctrl Pts',(-50.055050063843,-4.69408692690964,129.330632276099));
#85610=CARTESIAN_POINT('Ctrl Pts',(-50.0624907826922,-4.73161543421519,
129.456010584061));
#85611=CARTESIAN_POINT('Ctrl Pts',(-50.0699315015413,-4.76405452823403,
129.582490119308));
#85612=CARTESIAN_POINT('Origin',(213.235140564004,0.,130.804360617566));
#85613=CARTESIAN_POINT('',(-52.1650248355919,-4.76405452823407,129.582490119308));
#85614=CARTESIAN_POINT('',(-51.8201183854057,-4.76405452823404,129.582490119308));
#85615=CARTESIAN_POINT('',(213.235140564004,-4.76405452823405,129.582490119308));
#85616=CARTESIAN_POINT('',(-50.4851405640431,-4.9182497302669,130.805989491289));
#85617=CARTESIAN_POINT('Ctrl Pts',(-50.4851405640431,-4.9182497302669,130.805989491289));
#85618=CARTESIAN_POINT('Ctrl Pts',(-50.4934943809599,-4.91820062086283,
130.954271282496));
#85619=CARTESIAN_POINT('Ctrl Pts',(-50.5018481978766,-4.91144143289579,
131.10235617592));
#85620=CARTESIAN_POINT('Ctrl Pts',(-50.5102020147934,-4.89805053678207,
131.249651535539));
#85621=CARTESIAN_POINT('Ctrl Pts',(-50.5185889108578,-4.88460661587328,
131.397530150094));
#85622=CARTESIAN_POINT('Ctrl Pts',(-50.5269758069222,-4.8644784451024,131.544612685482));
#85623=CARTESIAN_POINT('Ctrl Pts',(-50.5353627029866,-4.83779608759408,
131.690313255893));
#85624=CARTESIAN_POINT('Ctrl Pts',(-50.5437662021802,-4.81106090832361,
131.83630226262));
#85625=CARTESIAN_POINT('Ctrl Pts',(-50.5521697013737,-4.77774568641162,
131.980903561024));
#85626=CARTESIAN_POINT('Ctrl Pts',(-50.5605732005673,-4.73803057145959,
132.123545732102));
#85627=CARTESIAN_POINT('Ctrl Pts',(-50.569003845401,-4.69818716563829,132.266648677074));
#85628=CARTESIAN_POINT('Ctrl Pts',(-50.5774344902347,-4.65190258321221,
132.407779556749));
#85629=CARTESIAN_POINT('Ctrl Pts',(-50.5858651350684,-4.59940644198817,
132.546383419913));
#85630=CARTESIAN_POINT('Ctrl Pts',(-50.5930390542809,-4.55473570996948,
132.664326108343));
#85631=CARTESIAN_POINT('Ctrl Pts',(-50.6002129734934,-4.505568117783,132.78043930485));
#85632=CARTESIAN_POINT('Ctrl Pts',(-50.6073868927059,-4.45207105772289,
132.894395631504));
#85633=CARTESIAN_POINT('Ctrl Pts',(-50.615161226825,-4.39409660791693,133.017889433448));
#85634=CARTESIAN_POINT('Ctrl Pts',(-50.6229355609442,-4.33088813624253,
133.139164825681));
#85635=CARTESIAN_POINT('Ctrl Pts',(-50.6307098950633,-4.26263786183846,
133.257746343725));
#85636=CARTESIAN_POINT('Ctrl Pts',(-50.6384746480104,-4.19447169979789,
133.376181720646));
#85637=CARTESIAN_POINT('Ctrl Pts',(-50.6462394009575,-4.12127629133662,
133.491929493512));
#85638=CARTESIAN_POINT('Ctrl Pts',(-50.6540041539047,-4.04329144038476,
133.604535146164));
#85639=CARTESIAN_POINT('Ctrl Pts',(-50.6617611947897,-3.96538404508604,
133.717028957295));
#85640=CARTESIAN_POINT('Ctrl Pts',(-50.6695182356748,-3.88269689497874,
133.826386539409));
#85641=CARTESIAN_POINT('Ctrl Pts',(-50.6772752765598,-3.79551494695359,
133.932179242415));
#85642=CARTESIAN_POINT('Ctrl Pts',(-50.6850264678,-3.70839874351374,134.03789216632));
#85643=CARTESIAN_POINT('Ctrl Pts',(-50.6927776590402,-3.61679473650666,
134.140045261526));
#85644=CARTESIAN_POINT('Ctrl Pts',(-50.7005288502804,-3.52103008940392,
134.238240372597));
#85645=CARTESIAN_POINT('Ctrl Pts',(-50.7082767470575,-3.42530614483094,
134.336393748126));
#85646=CARTESIAN_POINT('Ctrl Pts',(-50.7160246438346,-3.3254253497384,134.430592206075));
#85647=CARTESIAN_POINT('Ctrl Pts',(-50.7237725406117,-3.22175374826125,
134.52047227467));
#85648=CARTESIAN_POINT('Ctrl Pts',(-50.7315188166958,-3.11810383264824,
134.610333542292));
#85649=CARTESIAN_POINT('Ctrl Pts',(-50.73926509278,-3.0106649830983,134.695877961358));
#85650=CARTESIAN_POINT('Ctrl Pts',(-50.7470113688641,-2.89983825104456,
134.776780683506));
#85651=CARTESIAN_POINT('Ctrl Pts',(-50.7547577021295,-2.78901070089305,
134.857684002858));
#85652=CARTESIAN_POINT('Ctrl Pts',(-50.7625040353948,-2.67479553411351,
134.933945326406));
#85653=CARTESIAN_POINT('Ctrl Pts',(-50.7702503686602,-2.55762453036736,
135.005281924156));
#85654=CARTESIAN_POINT('Ctrl Pts',(-50.7779984366632,-2.44042728698732,
135.076634497243));
#85655=CARTESIAN_POINT('Ctrl Pts',(-50.7857465046662,-2.32027322333718,
135.143059946699));
#85656=CARTESIAN_POINT('Ctrl Pts',(-50.7934945726692,-2.19762021331256,
135.204320669719));
#85657=CARTESIAN_POINT('Ctrl Pts',(-50.8012508754111,-2.07483684620931,
135.265646501364));
#85658=CARTESIAN_POINT('Ctrl Pts',(-50.809007178153,-1.949549577588,135.321796466466));
#85659=CARTESIAN_POINT('Ctrl Pts',(-50.8167634808949,-1.82223834237338,
135.37258023642));
#85660=CARTESIAN_POINT('Ctrl Pts',(-50.8245239234091,-1.69485915731925,
135.423391111201));
#85661=CARTESIAN_POINT('Ctrl Pts',(-50.8322843659232,-1.56545422188273,
135.468829954407));
#85662=CARTESIAN_POINT('Ctrl Pts',(-50.8400448084374,-1.43451931117596,
135.508756158798));
#85663=CARTESIAN_POINT('Ctrl Pts',(-50.8478177087029,-1.3033742121265,135.548746456277));
#85664=CARTESIAN_POINT('Ctrl Pts',(-50.8555906089684,-1.17069460846028,
135.583206332728));
#85665=CARTESIAN_POINT('Ctrl Pts',(-50.8633635092338,-1.03698804195296,
135.612046013195));
#85666=CARTESIAN_POINT('Ctrl Pts',(-50.8708538449955,-0.90814204593158,
135.639837298634));
#85667=CARTESIAN_POINT('Ctrl Pts',(-50.8783441807572,-0.778342759604827,
135.662409857694));
#85668=CARTESIAN_POINT('Ctrl Pts',(-50.8858345165188,-0.64804750448508,
135.67972906461));
#85669=CARTESIAN_POINT('Ctrl Pts',(-50.8936088506379,-0.51281206515897,
135.697704934521));
#85670=CARTESIAN_POINT('Ctrl Pts',(-50.901383184757,-0.376613920084245,
135.710078168962));
#85671=CARTESIAN_POINT('Ctrl Pts',(-50.909157518876,-0.239956990130485,
135.716753487175));
#85672=CARTESIAN_POINT('Ctrl Pts',(-50.9169222718231,-0.103468477629513,
135.723420578655));
#85673=CARTESIAN_POINT('Ctrl Pts',(-50.9246870247701,0.0334773079995623,
135.724403707046));
#85674=CARTESIAN_POINT('Ctrl Pts',(-50.9324517777172,0.170368349558318,
135.719658949099));
#85675=CARTESIAN_POINT('Ctrl Pts',(-50.9402088186022,0.307123429004959,
135.714918903712));
#85676=CARTESIAN_POINT('Ctrl Pts',(-50.9479658594872,0.443823484383001,
135.704462306846));
#85677=CARTESIAN_POINT('Ctrl Pts',(-50.9557229003722,0.57995385407072,135.688297204956));
#85678=CARTESIAN_POINT('Ctrl Pts',(-50.9634740916123,0.715981566787347,
135.672144293296));
#85679=CARTESIAN_POINT('Ctrl Pts',(-50.9712252828524,0.851440062248544,
135.650291491028));
#85680=CARTESIAN_POINT('Ctrl Pts',(-50.9789764740925,0.98581752116214,135.622798837308));
#85681=CARTESIAN_POINT('Ctrl Pts',(-50.9867243708696,1.12013786607125,135.595317868699));
#85682=CARTESIAN_POINT('Ctrl Pts',(-50.9944722676467,1.25337770605331,135.562201894464));
#85683=CARTESIAN_POINT('Ctrl Pts',(-51.0022201644237,1.38503338621548,135.523562412528));
#85684=CARTESIAN_POINT('Ctrl Pts',(-51.0099664405078,1.51666152684771,135.484931013138));
#85685=CARTESIAN_POINT('Ctrl Pts',(-51.0177127165919,1.64670579187263,135.440778514229));
#85686=CARTESIAN_POINT('Ctrl Pts',(-51.0254589926761,1.7746760990675,135.391266743257));
#85687=CARTESIAN_POINT('Ctrl Pts',(-51.0332053259414,1.90264735090993,135.341754606799));
#85688=CARTESIAN_POINT('Ctrl Pts',(-51.0409516592067,2.02854424974756,135.28688326041));
#85689=CARTESIAN_POINT('Ctrl Pts',(-51.048697992472,2.15189553937748,135.226863150082));
#85690=CARTESIAN_POINT('Ctrl Pts',(-51.056446060475,2.27527445267345,135.166829598665));
#85691=CARTESIAN_POINT('Ctrl Pts',(-51.064194128478,2.39610627089577,135.10164515994));
#85692=CARTESIAN_POINT('Ctrl Pts',(-51.0719421964809,2.51394360005048,135.031566626062));
#85693=CARTESIAN_POINT('Ctrl Pts',(-51.0796984992228,2.63190616812089,134.961413611884));
#85694=CARTESIAN_POINT('Ctrl Pts',(-51.0874548019646,2.74686755301205,134.886356312151));
#85695=CARTESIAN_POINT('Ctrl Pts',(-51.0952111047065,2.85840820932839,134.806695632447));
#85696=CARTESIAN_POINT('Ctrl Pts',(-51.1029715472206,2.97000839825158,134.72699243544));
#85697=CARTESIAN_POINT('Ctrl Pts',(-51.1107319897348,3.07818391242994,134.642681202978));
#85698=CARTESIAN_POINT('Ctrl Pts',(-51.1184924322489,3.18254847645298,134.554103043057));
#85699=CARTESIAN_POINT('Ctrl Pts',(-51.1262653325144,3.28708057573924,134.46538268961));
#85700=CARTESIAN_POINT('Ctrl Pts',(-51.1340382327799,3.38778921241254,134.372381986316));
#85701=CARTESIAN_POINT('Ctrl Pts',(-51.1418111330453,3.48432451753367,134.275479416889));
#85702=CARTESIAN_POINT('Ctrl Pts',(-51.1493014688075,3.57735052115772,134.182099499942));
#85703=CARTESIAN_POINT('Ctrl Pts',(-51.1567918045696,3.66650113917274,134.085096703779));
#85704=CARTESIAN_POINT('Ctrl Pts',(-51.1642821403318,3.75150004649306,133.98483706987));
#85705=CARTESIAN_POINT('Ctrl Pts',(-51.1720564744509,3.83972171321756,133.880776061471));
#85706=CARTESIAN_POINT('Ctrl Pts',(-51.1798308085699,3.92375009001871,133.772876740136));
#85707=CARTESIAN_POINT('Ctrl Pts',(-51.187605142689,4.00323263295736,133.661511567188));
#85708=CARTESIAN_POINT('Ctrl Pts',(-51.1953698956361,4.0826172207654,133.550283641863));
#85709=CARTESIAN_POINT('Ctrl Pts',(-51.2031346485832,4.15746689674329,133.435598678816));
#85710=CARTESIAN_POINT('Ctrl Pts',(-51.2108994015303,4.22746794921622,133.317863711029));
#85711=CARTESIAN_POINT('Ctrl Pts',(-51.2186564424153,4.297399475657,133.200245679272));
#85712=CARTESIAN_POINT('Ctrl Pts',(-51.2264134833002,4.36249176358301,133.079584005113));
#85713=CARTESIAN_POINT('Ctrl Pts',(-51.2341705241852,4.42247339552931,132.956316037257));
#85714=CARTESIAN_POINT('Ctrl Pts',(-51.2419217154253,4.48240979486037,132.833141026734));
#85715=CARTESIAN_POINT('Ctrl Pts',(-51.2496729066655,4.5372430389633,132.707363984707));
#85716=CARTESIAN_POINT('Ctrl Pts',(-51.2574240979056,4.58674698965109,132.579447971875));
#85717=CARTESIAN_POINT('Ctrl Pts',(-51.2651719946827,4.63622989983927,132.45158632676));
#85718=CARTESIAN_POINT('Ctrl Pts',(-51.2729198914598,4.68038788089619,132.321587882857));
#85719=CARTESIAN_POINT('Ctrl Pts',(-51.2806677882369,4.71904250141271,132.189936646646));
#85720=CARTESIAN_POINT('Ctrl Pts',(-51.2884140643209,4.75768903621591,132.058312949035));
#85721=CARTESIAN_POINT('Ctrl Pts',(-51.296160340405,4.7908343901741,131.92503752168));
#85722=CARTESIAN_POINT('Ctrl Pts',(-51.3039066164891,4.81834981189573,131.790610156326));
#85723=CARTESIAN_POINT('Ctrl Pts',(-51.3116529497545,4.84586543672995,131.65618179866));
#85724=CARTESIAN_POINT('Ctrl Pts',(-51.3193992830199,4.86775096800018,131.520601869052));
#85725=CARTESIAN_POINT('Ctrl Pts',(-51.3271456162852,4.88392873439036,131.384380599891));
#85726=CARTESIAN_POINT('Ctrl Pts',(-51.3348936842882,4.90011012367915,131.248128824921));
#85727=CARTESIAN_POINT('Ctrl Pts',(-51.3426417522911,4.9105811584907,131.111235812766));
#85728=CARTESIAN_POINT('Ctrl Pts',(-51.3503898202941,4.91531605795677,130.974216771097));
#85729=CARTESIAN_POINT('Ctrl Pts',(-51.3581461230359,4.92005598973034,130.83705210396));
#85730=CARTESIAN_POINT('Ctrl Pts',(-51.3659024257777,4.91904759435314,130.699761531093));
#85731=CARTESIAN_POINT('Ctrl Pts',(-51.3736587285196,4.91231725768135,130.562860674738));
#85732=CARTESIAN_POINT('Ctrl Pts',(-51.3814191710338,4.90558332882623,130.425886750274));
#85733=CARTESIAN_POINT('Ctrl Pts',(-51.3891796135479,4.89312140888488,130.289303345944));
#85734=CARTESIAN_POINT('Ctrl Pts',(-51.3969400560621,4.87500969038011,130.153619823394));
#85735=CARTESIAN_POINT('Ctrl Pts',(-51.4047129563275,4.85686889733693,130.017718489608));
#85736=CARTESIAN_POINT('Ctrl Pts',(-51.4124858565929,4.83306024980587,129.882720309559));
#85737=CARTESIAN_POINT('Ctrl Pts',(-51.4202587568583,4.80371306414723,129.749124217587));
#85738=CARTESIAN_POINT('Ctrl Pts',(-51.4277490926204,4.77543272260815,129.620384680065));
#85739=CARTESIAN_POINT('Ctrl Pts',(-51.4352394283825,4.74200960959721,129.492947359503));
#85740=CARTESIAN_POINT('Ctrl Pts',(-51.4427297641446,4.70360232571002,129.367242590376));
#85741=CARTESIAN_POINT('Ctrl Pts',(-51.4505040982636,4.6637388179809,129.236771686721));
#85742=CARTESIAN_POINT('Ctrl Pts',(-51.4582784323828,4.61837945324241,129.107754014742));
#85743=CARTESIAN_POINT('Ctrl Pts',(-51.4660527665019,4.56764703514317,128.980687504081));
#85744=CARTESIAN_POINT('Ctrl Pts',(-51.473817519449,4.51697714021509,128.853777591538));
#85745=CARTESIAN_POINT('Ctrl Pts',(-51.481582272396,4.46094751092773,128.728814415422));
#85746=CARTESIAN_POINT('Ctrl Pts',(-51.4893470253431,4.39973102683338,128.606281921518));
#85747=CARTESIAN_POINT('Ctrl Pts',(-51.4971040662281,4.33857534381411,128.483871128615));
#85748=CARTESIAN_POINT('Ctrl Pts',(-51.5048611071132,4.27224323161904,128.363886561065));
#85749=CARTESIAN_POINT('Ctrl Pts',(-51.5126181479982,4.20095593633078,128.246792967726));
#85750=CARTESIAN_POINT('Ctrl Pts',(-51.5203693392383,4.12972239934643,128.129787675577));
#85751=CARTESIAN_POINT('Ctrl Pts',(-51.5281205304784,4.05354131951291,128.015669350865));
#85752=CARTESIAN_POINT('Ctrl Pts',(-51.5358717217185,3.97268004969477,127.904878545668));
#85753=CARTESIAN_POINT('Ctrl Pts',(-51.5436196184956,3.89185314807334,127.794134829519));
#85754=CARTESIAN_POINT('Ctrl Pts',(-51.5513675152727,3.80635024285079,127.686716135119));
#85755=CARTESIAN_POINT('Ctrl Pts',(-51.5591154120498,3.71648209584986,127.58303419919));
#85756=CARTESIAN_POINT('Ctrl Pts',(-51.5668616881339,3.62663274732795,127.479373951287));
#85757=CARTESIAN_POINT('Ctrl Pts',(-51.574607964218,3.53242022917225,127.379449202358));
#85758=CARTESIAN_POINT('Ctrl Pts',(-51.5823542403021,3.4341954370614,127.283638424242));
#85759=CARTESIAN_POINT('Ctrl Pts',(-51.5901005735675,3.33596991987745,127.187826938872));
#85760=CARTESIAN_POINT('Ctrl Pts',(-51.5978469068328,3.23373234951027,127.096129757907));
#85761=CARTESIAN_POINT('Ctrl Pts',(-51.6055932400982,3.12787001567564,127.008888021494));
#85762=CARTESIAN_POINT('Ctrl Pts',(-51.6133413081011,3.02198397470535,126.921626747898));
#85763=CARTESIAN_POINT('Ctrl Pts',(-51.6210893761042,2.9124718566525,126.838823152889));
#85764=CARTESIAN_POINT('Ctrl Pts',(-51.6288374441072,2.79975318513301,126.76077740897));
#85765=CARTESIAN_POINT('Ctrl Pts',(-51.6365937468491,2.68691471486791,126.682648717106));
#85766=CARTESIAN_POINT('Ctrl Pts',(-51.6443500495908,2.57086320531068,126.609288200553));
#85767=CARTESIAN_POINT('Ctrl Pts',(-51.6521063523327,2.45204672625646,126.540952366559));
#85768=CARTESIAN_POINT('Ctrl Pts',(-51.6598667948469,2.33316683126987,126.472580059673));
#85769=CARTESIAN_POINT('Ctrl Pts',(-51.667627237361,2.21151937283599,126.409237959584));
#85770=CARTESIAN_POINT('Ctrl Pts',(-51.6753876798752,2.08757515630237,126.35113560312));
#85771=CARTESIAN_POINT('Ctrl Pts',(-51.6831605801407,1.96343197350912,126.292939975595));
#85772=CARTESIAN_POINT('Ctrl Pts',(-51.6909334804062,1.83698502573734,126.240001051229));
#85773=CARTESIAN_POINT('Ctrl Pts',(-51.6987063806716,1.70872397922919,126.192479718702));
#85774=CARTESIAN_POINT('Ctrl Pts',(-51.7061967164335,1.58512554483359,126.146685906312));
#85775=CARTESIAN_POINT('Ctrl Pts',(-51.7136870521954,1.45984290884758,126.105922733287));
#85776=CARTESIAN_POINT('Ctrl Pts',(-51.7211773879573,1.33332385134872,126.070289370751));
#85777=CARTESIAN_POINT('Ctrl Pts',(-51.7289517220764,1.20200778532849,126.033304958442));
#85778=CARTESIAN_POINT('Ctrl Pts',(-51.7367260561955,1.06894371931695,126.001729873504));
#85779=CARTESIAN_POINT('Ctrl Pts',(-51.7445003903146,0.934616953996705,
125.975729940883));
#85780=CARTESIAN_POINT('Ctrl Pts',(-51.7522651432617,0.800455734409594,
125.949762050856));
#85781=CARTESIAN_POINT('Ctrl Pts',(-51.7600298962088,0.665035291972695,
125.929355715731));
#85782=CARTESIAN_POINT('Ctrl Pts',(-51.7677946491559,0.528856229602482,
125.914627071563));
#85783=CARTESIAN_POINT('Ctrl Pts',(-51.7755516900409,0.392812422196804,
125.899913056092));
#85784=CARTESIAN_POINT('Ctrl Pts',(-51.7833087309258,0.25601188048422,125.890865551157));
#85785=CARTESIAN_POINT('Ctrl Pts',(-51.7910657718108,0.118965199753478,
125.887549624275));
#85786=CARTESIAN_POINT('Ctrl Pts',(-51.798816963051,-0.0179781330094434,
125.884236197959));
#85787=CARTESIAN_POINT('Ctrl Pts',(-51.8065681542912,-0.155166846065093,
125.886645755981));
#85788=CARTESIAN_POINT('Ctrl Pts',(-51.8143193455313,-0.292085779718963,
125.894791495964));
#85789=CARTESIAN_POINT('Ctrl Pts',(-51.8220672423084,-0.428946519173413,
125.902933773791));
#85790=CARTESIAN_POINT('Ctrl Pts',(-51.8298151390855,-0.565537317824866,
125.916807361352));
#85791=CARTESIAN_POINT('Ctrl Pts',(-51.8375630358625,-0.701343795552268,
125.93637335968));
#85792=CARTESIAN_POINT('Ctrl Pts',(-51.8453093119466,-0.837121865492178,
125.955935265223));
#85793=CARTESIAN_POINT('Ctrl Pts',(-51.8530555880307,-0.972115554113877,
125.981187157391));
#85794=CARTESIAN_POINT('Ctrl Pts',(-51.8608018641148,-1.105816774655,126.012038390984));
#85795=CARTESIAN_POINT('Ctrl Pts',(-51.8685481973802,-1.23951898214817,
126.042889852314));
#85796=CARTESIAN_POINT('Ctrl Pts',(-51.8762945306455,-1.37192832156811,
126.079340649642));
#85797=CARTESIAN_POINT('Ctrl Pts',(-51.8840408639108,-1.50254844249584,
126.121249339745));
#85798=CARTESIAN_POINT('Ctrl Pts',(-51.8917889319138,-1.633197814894,126.163167415008));
#85799=CARTESIAN_POINT('Ctrl Pts',(-51.8995369999168,-1.76205679928488,
126.210545695777));
#85800=CARTESIAN_POINT('Ctrl Pts',(-51.9072850679198,-1.88864608927655,
126.263193475524));
#85801=CARTESIAN_POINT('Ctrl Pts',(-51.9150413706616,-2.01536991987205,
126.315897209958));
#85802=CARTESIAN_POINT('Ctrl Pts',(-51.9227976734035,-2.13981887575725,
126.37388148057));
#85803=CARTESIAN_POINT('Ctrl Pts',(-51.9305539761453,-2.26153495745039,
126.436907961986));
#85804=CARTESIAN_POINT('Ctrl Pts',(-51.9383144186595,-2.38331600268113,
126.499968082533));
#85805=CARTESIAN_POINT('Ctrl Pts',(-51.9460748611737,-2.50236092811516,
126.568075582234));
#85806=CARTESIAN_POINT('Ctrl Pts',(-51.9538353036879,-2.61823896269446,
126.640947618988));
#85807=CARTESIAN_POINT('Ctrl Pts',(-51.9616082039533,-2.7343030149822,126.713936636405));
#85808=CARTESIAN_POINT('Ctrl Pts',(-51.9693811042187,-2.847189695269,126.791705253004));
#85809=CARTESIAN_POINT('Ctrl Pts',(-51.9771540044841,-2.95649896678588,
126.873928462968));
#85810=CARTESIAN_POINT('Ctrl Pts',(-51.9846443402462,-3.06183457095012,
126.953162652144));
#85811=CARTESIAN_POINT('Ctrl Pts',(-51.9921346760082,-3.16384810783968,
127.036532991273));
#85812=CARTESIAN_POINT('Ctrl Pts',(-51.9996250117703,-3.26221410591101,
127.12371635471));
#85813=CARTESIAN_POINT('Ctrl Pts',(-52.0072823682229,-3.36277348455108,
127.212843746561));
#85814=CARTESIAN_POINT('Ctrl Pts',(-52.0149397246753,-3.45985953892064,
127.306256855097));
#85815=CARTESIAN_POINT('Ctrl Pts',(-52.0225970811278,-3.55307652160224,
127.40365035438));
#85816=CARTESIAN_POINT('Ctrl Pts',(-52.0302456119749,-3.64618606559832,
127.500931601269));
#85817=CARTESIAN_POINT('Ctrl Pts',(-52.037894142822,-3.73543512631841,127.602183831351));
#85818=CARTESIAN_POINT('Ctrl Pts',(-52.045542673669,-3.82046084072659,127.707061467181));
#85819=CARTESIAN_POINT('Ctrl Pts',(-52.0531841627059,-3.90540827409576,
127.811842544807));
#85820=CARTESIAN_POINT('Ctrl Pts',(-52.0608256517427,-3.98613983993017,
127.920242080387));
#85821=CARTESIAN_POINT('Ctrl Pts',(-52.0684671407796,-4.0623298012738,128.031878039049));
#85822=CARTESIAN_POINT('Ctrl Pts',(-52.0761033649914,-4.13846726933831,
128.143437082885));
#85823=CARTESIAN_POINT('Ctrl Pts',(-52.0837395892031,-4.21006912986374,
128.258227782799));
#85824=CARTESIAN_POINT('Ctrl Pts',(-52.0913758134149,-4.27685056291799,
128.375835895648));
#85825=CARTESIAN_POINT('Ctrl Pts',(-52.099009006558,-4.34360548822308,128.493397325965));
#85826=CARTESIAN_POINT('Ctrl Pts',(-52.1066421997011,-4.40554359168371,
128.613773595245));
#85827=CARTESIAN_POINT('Ctrl Pts',(-52.1142753928442,-4.46242421877927,
128.736522820699));
#85828=CARTESIAN_POINT('Ctrl Pts',(-52.1219069216737,-4.51929244383109,
128.859245282361));
#85829=CARTESIAN_POINT('Ctrl Pts',(-52.1295384505033,-4.57110522009044,
128.984339303371));
#85830=CARTESIAN_POINT('Ctrl Pts',(-52.1371699793328,-4.61766885556299,
129.111340416014));
#85831=CARTESIAN_POINT('Ctrl Pts',(-52.1448027627309,-4.66424014576289,
129.238362406727));
#85832=CARTESIAN_POINT('Ctrl Pts',(-52.152435546129,-4.70556043530697,129.367291735476));
#85833=CARTESIAN_POINT('Ctrl Pts',(-52.1600683295271,-4.74148510574168,
129.497646396885));
#85834=CARTESIAN_POINT('Ctrl Pts',(-52.1617204982154,-4.74926124879883,
129.525862563742));
#85835=CARTESIAN_POINT('Ctrl Pts',(-52.1633726669036,-4.75678477467003,
129.554145460496));
#85836=CARTESIAN_POINT('Ctrl Pts',(-52.1650248355919,-4.76405452823407,
129.582490119308));
#85837=CARTESIAN_POINT('Ctrl Pts',(-50.4153787949644,-4.76405452823401,
129.582490119308));
#85838=CARTESIAN_POINT('Ctrl Pts',(-50.4233250152514,-4.79897522845777,
129.718645399485));
#85839=CARTESIAN_POINT('Ctrl Pts',(-50.4312712355385,-4.82808341113277,
129.856410290236));
#85840=CARTESIAN_POINT('Ctrl Pts',(-50.4392174558255,-4.85124139258481,
129.995262345802));
#85841=CARTESIAN_POINT('Ctrl Pts',(-50.4471566799911,-4.87437898496585,
130.133992151316));
#85842=CARTESIAN_POINT('Ctrl Pts',(-50.4550959041567,-4.89157675695739,
130.273806857429));
#85843=CARTESIAN_POINT('Ctrl Pts',(-50.4630351283223,-4.90274785718882,
130.414172827738));
#85844=CARTESIAN_POINT('Ctrl Pts',(-50.4704036068844,-4.91311587437202,
130.544447980763));
#85845=CARTESIAN_POINT('Ctrl Pts',(-50.4777720854464,-4.9182930471674,130.675197637016));
#85846=CARTESIAN_POINT('Ctrl Pts',(-50.4851405640085,-4.9182497302671,130.805989490675));
#85847=CARTESIAN_POINT('',(-50.139859435941,-4.91824790236153,130.799818215517));
#85848=CARTESIAN_POINT('Ctrl Pts',(-50.0699315015413,-4.76405452823403,
129.582490119308));
#85849=CARTESIAN_POINT('Ctrl Pts',(-50.0699812147741,-4.76427126162551,
129.583335159512));
#85850=CARTESIAN_POINT('Ctrl Pts',(-50.0700309280068,-4.76448776799205,
129.584180248854));
#85851=CARTESIAN_POINT('Ctrl Pts',(-50.0700806412396,-4.76470404731428,
129.585025387202));
#85852=CARTESIAN_POINT('Ctrl Pts',(-50.0802659710137,-4.80901571441495,
129.758178736929));
#85853=CARTESIAN_POINT('Ctrl Pts',(-50.0904513007877,-4.84390632131328,
129.933834040213));
#85854=CARTESIAN_POINT('Ctrl Pts',(-50.1006366305617,-4.8691456428026,130.111104696801));
#85855=CARTESIAN_POINT('Ctrl Pts',(-50.1106019485555,-4.89383977349548,
130.284546156533));
#85856=CARTESIAN_POINT('Ctrl Pts',(-50.1205672665494,-4.90929511545234,
130.459534200369));
#85857=CARTESIAN_POINT('Ctrl Pts',(-50.1305325845432,-4.91534060276653,
130.635216237539));
#85858=CARTESIAN_POINT('Ctrl Pts',(-50.1336415350092,-4.91722665603788,
130.690025000456));
#85859=CARTESIAN_POINT('Ctrl Pts',(-50.1367504854751,-4.918197181964,130.744901128459));
#85860=CARTESIAN_POINT('Ctrl Pts',(-50.139859435941,-4.91824790236153,130.799818215517));
#85861=CARTESIAN_POINT('Ctrl Pts',(-50.139859435991,-4.91824790236235,130.7998182164));
#85862=CARTESIAN_POINT('Ctrl Pts',(-50.1475248510763,-4.91837295833512,
130.935221553372));
#85863=CARTESIAN_POINT('Ctrl Pts',(-50.1551902661616,-4.9129021639932,131.070768982495));
#85864=CARTESIAN_POINT('Ctrl Pts',(-50.1628556812468,-4.90182667104543,
131.20595537541));
#85865=CARTESIAN_POINT('Ctrl Pts',(-50.1705920389054,-4.89064867562888,
131.342392903519));
#85866=CARTESIAN_POINT('Ctrl Pts',(-50.178328396564,-4.87376167017608,131.478462266883));
#85867=CARTESIAN_POINT('Ctrl Pts',(-50.1860647542226,-4.85121043588478,
131.613644479547));
#85868=CARTESIAN_POINT('Ctrl Pts',(-50.1937232281112,-4.82888623028358,
131.747465780419));
#85869=CARTESIAN_POINT('Ctrl Pts',(-50.2013817019996,-4.80101139998182,
131.880417309493));
#85870=CARTESIAN_POINT('Ctrl Pts',(-50.2090401758882,-4.76768135676842,
132.012001931377));
#85871=CARTESIAN_POINT('Ctrl Pts',(-50.2166980399471,-4.73435396756279,
132.143576075428));
#85872=CARTESIAN_POINT('Ctrl Pts',(-50.224355904006,-4.69557232760295,132.273783140227));
#85873=CARTESIAN_POINT('Ctrl Pts',(-50.2320137680649,-4.65148249520225,
132.402138342823));
#85874=CARTESIAN_POINT('Ctrl Pts',(-50.2396727720677,-4.60738609962224,
132.530512652278));
#85875=CARTESIAN_POINT('Ctrl Pts',(-50.2473317760705,-4.55798007063612,
132.657034172352));
#85876=CARTESIAN_POINT('Ctrl Pts',(-50.2549907800733,-4.50345947224149,
132.781235890409));
#85877=CARTESIAN_POINT('Ctrl Pts',(-50.2627855704882,-4.44797227865465,
132.907639579594));
#85878=CARTESIAN_POINT('Ctrl Pts',(-50.2705803609032,-4.38718761060133,
133.031640032764));
#85879=CARTESIAN_POINT('Ctrl Pts',(-50.2783751513181,-4.32136051551518,
133.152769942502));
#85880=CARTESIAN_POINT('Ctrl Pts',(-50.2860456817218,-4.25658279765894,
133.271968869732));
#85881=CARTESIAN_POINT('Ctrl Pts',(-50.2937162121256,-4.18692249311526,
133.38838778584));
#85882=CARTESIAN_POINT('Ctrl Pts',(-50.3013867425293,-4.11266659077473,
133.501610434625));
#85883=CARTESIAN_POINT('Ctrl Pts',(-50.3092436629499,-4.03660630749094,
133.617584336622));
#85884=CARTESIAN_POINT('Ctrl Pts',(-50.3171005833704,-3.95572449336865,
133.73020428153));
#85885=CARTESIAN_POINT('Ctrl Pts',(-50.324957503791,-3.87037285449671,133.8390594543));
#85886=CARTESIAN_POINT('Ctrl Pts',(-50.3328144242115,-3.78502121562477,
133.94791462707));
#85887=CARTESIAN_POINT('Ctrl Pts',(-50.3406713446321,-3.69520009384722,
134.053004736021));
#85888=CARTESIAN_POINT('Ctrl Pts',(-50.3485282650526,-3.60130018461268,
134.153960600073));
#85889=CARTESIAN_POINT('Ctrl Pts',(-50.3563025991717,-3.50838728374742,
134.253855288628));
#85890=CARTESIAN_POINT('Ctrl Pts',(-50.3640769332908,-3.41116767138523,
134.350039375797));
#85891=CARTESIAN_POINT('Ctrl Pts',(-50.3718512674099,-3.30996956334717,
134.442118794275));
#85892=CARTESIAN_POINT('Ctrl Pts',(-50.379616020357,-3.20889617293307,134.534084733099));
#85893=CARTESIAN_POINT('Ctrl Pts',(-50.387380773304,-3.10385432903034,134.621955807819));
#85894=CARTESIAN_POINT('Ctrl Pts',(-50.3951455262511,-2.99521116357081,
134.705372428381));
#85895=CARTESIAN_POINT('Ctrl Pts',(-50.402902567136,-2.88667590403512,134.788706198379));
#85896=CARTESIAN_POINT('Ctrl Pts',(-50.410659608021,-2.77454674919739,134.867594082073));
#85897=CARTESIAN_POINT('Ctrl Pts',(-50.418416648906,-2.65922592983904,134.941714907033));
#85898=CARTESIAN_POINT('Ctrl Pts',(-50.4261678401461,-2.54399207480686,
135.015779836903));
#85899=CARTESIAN_POINT('Ctrl Pts',(-50.4339190313863,-2.42557167351986,
135.085084652889));
#85900=CARTESIAN_POINT('Ctrl Pts',(-50.4416702226264,-2.30439783666213,
135.149350108104));
#85901=CARTESIAN_POINT('Ctrl Pts',(-50.4494181194035,-2.18327550191782,
135.213588248786));
#85902=CARTESIAN_POINT('Ctrl Pts',(-50.4571660161806,-2.05940240387961,
135.272791105901));
#85903=CARTESIAN_POINT('Ctrl Pts',(-50.4649139129577,-1.9332380869943,135.326724331543));
#85904=CARTESIAN_POINT('Ctrl Pts',(-50.4726601890417,-1.80710016096448,
135.380646275517));
#85905=CARTESIAN_POINT('Ctrl Pts',(-50.4804064651258,-1.67867232865637,
135.42930062696));
#85906=CARTESIAN_POINT('Ctrl Pts',(-50.4881527412099,-1.54843567694259,
135.47250050588));
#85907=CARTESIAN_POINT('Ctrl Pts',(-50.4958990744753,-1.41819806385125,
135.515700703693));
#85908=CARTESIAN_POINT('Ctrl Pts',(-50.5036454077406,-1.28615197579398,
135.55344622555));
#85909=CARTESIAN_POINT('Ctrl Pts',(-50.511391741006,-1.15279490021219,135.585599680878));
#85910=CARTESIAN_POINT('Ctrl Pts',(-50.5191398090089,-1.01940796023851,
135.61776033675));
#85911=CARTESIAN_POINT('Ctrl Pts',(-50.5268878770118,-0.884709828538143,
135.644326342531));
#85912=CARTESIAN_POINT('Ctrl Pts',(-50.5346359450147,-0.749209061726243,
135.665211247273));
#85913=CARTESIAN_POINT('Ctrl Pts',(-50.5423922477565,-0.613564283086526,
135.686118348741));
#85914=CARTESIAN_POINT('Ctrl Pts',(-50.5501485504984,-0.477115552294207,
135.701332228078));
#85915=CARTESIAN_POINT('Ctrl Pts',(-50.5579048532402,-0.340377998979923,
135.710818186965));
#85916=CARTESIAN_POINT('Ctrl Pts',(-50.5656652957544,-0.203567464716348,
135.720309208793));
#85917=CARTESIAN_POINT('Ctrl Pts',(-50.5734257382685,-0.0664681913946131,
135.724066207809));
#85918=CARTESIAN_POINT('Ctrl Pts',(-50.5811861807827,0.0704047893100568,
135.722106669178));
#85919=CARTESIAN_POINT('Ctrl Pts',(-50.5889590810481,0.207497490674553,
135.720143984921));
#85920=CARTESIAN_POINT('Ctrl Pts',(-50.5967319813135,0.344362782929777,
135.712446447024));
#85921=CARTESIAN_POINT('Ctrl Pts',(-50.6045048815789,0.480489950550833,
135.699083538214));
#85922=CARTESIAN_POINT('Ctrl Pts',(-50.6119952173411,0.611668552747988,
135.686206404798));
#85923=CARTESIAN_POINT('Ctrl Pts',(-50.6194855531033,0.742161458894984,
135.668068692674));
#85924=CARTESIAN_POINT('Ctrl Pts',(-50.6269758888655,0.87152261445422,135.644777066075));
#85925=CARTESIAN_POINT('Ctrl Pts',(-50.6347502229845,1.00578853754267,135.620602330375));
#85926=CARTESIAN_POINT('Ctrl Pts',(-50.6425245571037,1.1392605093561,135.590798565633));
#85927=CARTESIAN_POINT('Ctrl Pts',(-50.6502988912228,1.27142958124231,135.555428906114));
#85928=CARTESIAN_POINT('Ctrl Pts',(-50.6580636441699,1.40343576655988,135.520102836538));
#85929=CARTESIAN_POINT('Ctrl Pts',(-50.665828397117,1.53414187278016,135.479224620579));
#85930=CARTESIAN_POINT('Ctrl Pts',(-50.6735931500641,1.66304692282871,135.432908769521));
#85931=CARTESIAN_POINT('Ctrl Pts',(-50.6813501909492,1.79182394256414,135.38663892002));
#85932=CARTESIAN_POINT('Ctrl Pts',(-50.6891072318342,1.91880310043388,135.334942314472));
#85933=CARTESIAN_POINT('Ctrl Pts',(-50.6968642727192,2.04349676941535,135.277983759482));
#85934=CARTESIAN_POINT('Ctrl Pts',(-50.7046154639594,2.1680964059314,135.221068157382));
#85935=CARTESIAN_POINT('Ctrl Pts',(-50.7123666551995,2.29041362990957,135.158898665844));
#85936=CARTESIAN_POINT('Ctrl Pts',(-50.7201178464397,2.4099793961318,135.091688733388));
#85937=CARTESIAN_POINT('Ctrl Pts',(-50.7278657432168,2.5294943437137,135.024507366947));
#85938=CARTESIAN_POINT('Ctrl Pts',(-50.735613639994,2.64625981937454,134.952290011679));
#85939=CARTESIAN_POINT('Ctrl Pts',(-50.7433615367711,2.7598302645873,134.875296624576));
#85940=CARTESIAN_POINT('Ctrl Pts',(-50.7511078128552,2.87337695331105,134.798319342829));
#85941=CARTESIAN_POINT('Ctrl Pts',(-50.7588540889393,2.98372961752984,134.716568235646));
#85942=CARTESIAN_POINT('Ctrl Pts',(-50.7666003650234,3.09047099060843,134.630347041837));
#85943=CARTESIAN_POINT('Ctrl Pts',(-50.7743466982888,3.1972131516276,134.544125211563));
#85944=CARTESIAN_POINT('Ctrl Pts',(-50.7820930315542,3.30034366417484,134.45343347449));
#85945=CARTESIAN_POINT('Ctrl Pts',(-50.7898393648196,3.39947803355569,134.358616117931));
#85946=CARTESIAN_POINT('Ctrl Pts',(-50.7975874328226,3.49863460339162,134.263777527681));
#85947=CARTESIAN_POINT('Ctrl Pts',(-50.8053355008256,3.59379296681325,134.164811749667));
#85948=CARTESIAN_POINT('Ctrl Pts',(-50.8130835688286,3.68460550291662,134.06209991812));
#85949=CARTESIAN_POINT('Ctrl Pts',(-50.8208398715705,3.77551455566367,133.959278923218));
#85950=CARTESIAN_POINT('Ctrl Pts',(-50.8285961743123,3.86206829516841,133.852704214974));
#85951=CARTESIAN_POINT('Ctrl Pts',(-50.8363524770542,3.94395908860282,133.742790431247));
#85952=CARTESIAN_POINT('Ctrl Pts',(-50.8441129195684,4.02589358961959,133.632817983223));
#85953=CARTESIAN_POINT('Ctrl Pts',(-50.8518733620827,4.10315996536191,133.519503231461));
#85954=CARTESIAN_POINT('Ctrl Pts',(-50.8596338045969,4.1754945393934,133.403288937854));
#85955=CARTESIAN_POINT('Ctrl Pts',(-50.8674067048623,4.24794523130448,133.286888086746));
#85956=CARTESIAN_POINT('Ctrl Pts',(-50.8751796051278,4.31544810825091,133.167578732889));
#85957=CARTESIAN_POINT('Ctrl Pts',(-50.8829525053933,4.37778557380154,133.045828112828));
#85958=CARTESIAN_POINT('Ctrl Pts',(-50.890442841155,4.43785691545828,132.928503434482));
#85959=CARTESIAN_POINT('Ctrl Pts',(-50.8979331769167,4.4931317477964,132.808912180355));
#85960=CARTESIAN_POINT('Ctrl Pts',(-50.9054235126785,4.54345870708427,132.687487283385));
#85961=CARTESIAN_POINT('Ctrl Pts',(-50.9131978467976,4.59569382833208,132.561458524536));
#85962=CARTESIAN_POINT('Ctrl Pts',(-50.9209721809166,4.64276393796802,132.433055111687));
#85963=CARTESIAN_POINT('Ctrl Pts',(-50.9287465150357,4.68444705345657,132.302739363365));
#85964=CARTESIAN_POINT('Ctrl Pts',(-50.9365112679828,4.72607879823062,132.172584217556));
#85965=CARTESIAN_POINT('Ctrl Pts',(-50.9442760209298,4.76233664049947,132.040521794372));
#85966=CARTESIAN_POINT('Ctrl Pts',(-50.9520407738769,4.79304613150344,131.907035476162));
#85967=CARTESIAN_POINT('Ctrl Pts',(-50.9597978147619,4.82372512140802,131.773681738445));
#85968=CARTESIAN_POINT('Ctrl Pts',(-50.9675548556469,4.84886663950332,131.638907298634));
#85969=CARTESIAN_POINT('Ctrl Pts',(-50.9753118965319,4.86834576793745,131.503211493151));
#85970=CARTESIAN_POINT('Ctrl Pts',(-50.9830630877721,4.88781020700935,131.367618016929));
#85971=CARTESIAN_POINT('Ctrl Pts',(-50.9908142790122,4.90162070037098,131.231104943442));
#85972=CARTESIAN_POINT('Ctrl Pts',(-50.9985654702523,4.90970329791155,131.094182267855));
#85973=CARTESIAN_POINT('Ctrl Pts',(-51.0063133670294,4.91778246013251,130.957317788059));
#85974=CARTESIAN_POINT('Ctrl Pts',(-51.0140612638065,4.92013854559381,130.820044441887));
#85975=CARTESIAN_POINT('Ctrl Pts',(-51.0218091605836,4.91674942820777,130.68287760345));
#85976=CARTESIAN_POINT('Ctrl Pts',(-51.0295554366676,4.91336101975203,130.54573945736));
#85977=CARTESIAN_POINT('Ctrl Pts',(-51.0373017127517,4.9042298084914,130.408708165289));
#85978=CARTESIAN_POINT('Ctrl Pts',(-51.0450479888358,4.88938579568122,130.272298963722));
#85979=CARTESIAN_POINT('Ctrl Pts',(-51.0527943221011,4.87454167329593,130.135888755214));
#85980=CARTESIAN_POINT('Ctrl Pts',(-51.0605406553664,4.85398470750775,130.000101035044));
#85981=CARTESIAN_POINT('Ctrl Pts',(-51.0682869886317,4.82779672820983,129.865445385191));
#85982=CARTESIAN_POINT('Ctrl Pts',(-51.0760350566347,4.80160288429546,129.730759580138));
#85983=CARTESIAN_POINT('Ctrl Pts',(-51.0837831246377,4.76977559219737,129.597206733576));
#85984=CARTESIAN_POINT('Ctrl Pts',(-51.0915311926407,4.73244761335131,129.465285321182));
#85985=CARTESIAN_POINT('Ctrl Pts',(-51.0992874953825,4.69507996188511,129.333223701141));
#85986=CARTESIAN_POINT('Ctrl Pts',(-51.1070437981243,4.65220005188253,129.202797355729));
#85987=CARTESIAN_POINT('Ctrl Pts',(-51.1148001008662,4.60399044685841,129.074489227047));
#85988=CARTESIAN_POINT('Ctrl Pts',(-51.1225605433803,4.55575511091647,128.946112616453));
#85989=CARTESIAN_POINT('Ctrl Pts',(-51.1303209858946,4.50218456444414,128.81985683505));
#85990=CARTESIAN_POINT('Ctrl Pts',(-51.1380814284088,4.44350879200761,128.69618304491));
#85991=CARTESIAN_POINT('Ctrl Pts',(-51.1458543286742,4.38473882801225,128.572310722622));
#85992=CARTESIAN_POINT('Ctrl Pts',(-51.1536272289396,4.32084744343521,128.451029020414));
#85993=CARTESIAN_POINT('Ctrl Pts',(-51.161400129205,4.25211012142916,128.33277356109));
#85994=CARTESIAN_POINT('Ctrl Pts',(-51.1688904649671,4.18587157421624,128.218816985579));
#85995=CARTESIAN_POINT('Ctrl Pts',(-51.1763808007292,4.11513346215704,128.107670709628));
#85996=CARTESIAN_POINT('Ctrl Pts',(-51.1838711364913,4.04017820820069,127.999696090661));
#85997=CARTESIAN_POINT('Ctrl Pts',(-51.1916454706104,3.96238100300919,127.887627581198));
#85998=CARTESIAN_POINT('Ctrl Pts',(-51.1994198047294,3.8797941192154,127.778620983794));
#85999=CARTESIAN_POINT('Ctrl Pts',(-51.2071941388485,3.7926865315062,127.673112953099));
#86000=CARTESIAN_POINT('Ctrl Pts',(-51.2149588917955,3.70568629611372,127.567734951622));
#86001=CARTESIAN_POINT('Ctrl Pts',(-51.2227236447427,3.61417668868066,127.465847236511));
#86002=CARTESIAN_POINT('Ctrl Pts',(-51.2304883976898,3.5184700986499,127.367857856414));
#86003=CARTESIAN_POINT('Ctrl Pts',(-51.2382454385747,3.42285856575384,127.269965800751));
#86004=CARTESIAN_POINT('Ctrl Pts',(-51.2460024794598,3.32305861717709,127.175964652766));
#86005=CARTESIAN_POINT('Ctrl Pts',(-51.2537595203447,3.21942283764176,127.086229412919));
#86006=CARTESIAN_POINT('Ctrl Pts',(-51.2615107115849,3.11586521065353,126.996561843114));
#86007=CARTESIAN_POINT('Ctrl Pts',(-51.269261902825,3.00847780467973,126.911154033178));
#86008=CARTESIAN_POINT('Ctrl Pts',(-51.2770130940651,2.89764972125601,126.830343864279));
#86009=CARTESIAN_POINT('Ctrl Pts',(-51.2847609908422,2.78686874272463,126.749568041858));
#86010=CARTESIAN_POINT('Ctrl Pts',(-51.2925088876193,2.67265031054922,126.673386203738));
#86011=CARTESIAN_POINT('Ctrl Pts',(-51.3002567843964,2.55541606387512,126.602095537518));
#86012=CARTESIAN_POINT('Ctrl Pts',(-51.3080030604805,2.43820634007814,126.530819783769));
#86013=CARTESIAN_POINT('Ctrl Pts',(-51.3157493365645,2.31798239040251,126.464433369873));
#86014=CARTESIAN_POINT('Ctrl Pts',(-51.3234956126486,2.19519391430608,126.403189552827));
#86015=CARTESIAN_POINT('Ctrl Pts',(-51.3312419459139,2.07240453181317,126.341945283694));
#86016=CARTESIAN_POINT('Ctrl Pts',(-51.3389882791793,1.94705093498571,126.285843861664));
#86017=CARTESIAN_POINT('Ctrl Pts',(-51.3467346124446,1.81960608063025,126.235091882436));
#86018=CARTESIAN_POINT('Ctrl Pts',(-51.3544826804476,1.69213268588278,126.184328537655));
#86019=CARTESIAN_POINT('Ctrl Pts',(-51.3622307484505,1.56256746485369,126.138917164117));
#86020=CARTESIAN_POINT('Ctrl Pts',(-51.3699788164535,1.43140156004473,126.099015504144));
#86021=CARTESIAN_POINT('Ctrl Pts',(-51.3777351191953,1.30009625055143,126.059071436213));
#86022=CARTESIAN_POINT('Ctrl Pts',(-51.3854914219372,1.16718723353377,126.024648893384));
#86023=CARTESIAN_POINT('Ctrl Pts',(-51.3932477246791,1.03317950189805,125.995855321805));
#86024=CARTESIAN_POINT('Ctrl Pts',(-51.4010081671932,0.899100246300877,
125.96704638223));
#86025=CARTESIAN_POINT('Ctrl Pts',(-51.4087686097074,0.76392149275524,125.943872466357));
#86026=CARTESIAN_POINT('Ctrl Pts',(-51.4165290522215,0.628155542248925,
125.926389351021));
#86027=CARTESIAN_POINT('Ctrl Pts',(-51.424301952487,0.492171648186308,125.908878170236));
#86028=CARTESIAN_POINT('Ctrl Pts',(-51.4320748527524,0.355599063244194,
125.897076079064));
#86029=CARTESIAN_POINT('Ctrl Pts',(-51.4398477530179,0.218953194599875,
125.890986770496));
#86030=CARTESIAN_POINT('Ctrl Pts',(-51.4473380887799,0.0872747474698428,
125.885118823631));
#86031=CARTESIAN_POINT('Ctrl Pts',(-51.454828424542,-0.044471439755898,
125.884555523664));
#86032=CARTESIAN_POINT('Ctrl Pts',(-51.4623187603041,-0.175828690340573,
125.889254582682));
#86033=CARTESIAN_POINT('Ctrl Pts',(-51.4700930944232,-0.312166391005563,
125.894131807951));
#86034=CARTESIAN_POINT('Ctrl Pts',(-51.4778674285423,-0.448516956616542,
125.904693763738));
#86035=CARTESIAN_POINT('Ctrl Pts',(-51.4856417626614,-0.584367629861358,
125.920950176525));
#86036=CARTESIAN_POINT('Ctrl Pts',(-51.4934065156085,-0.720050879292724,
125.937186554736));
#86037=CARTESIAN_POINT('Ctrl Pts',(-51.5011712685556,-0.855235077689818,
125.959103380393));
#86038=CARTESIAN_POINT('Ctrl Pts',(-51.5089360215027,-0.989408068044108,
125.986658391671));
#86039=CARTESIAN_POINT('Ctrl Pts',(-51.5166930623877,-1.12344779589251,
126.014186034924));
#86040=CARTESIAN_POINT('Ctrl Pts',(-51.5244501032727,-1.25647793389795,
126.047340641552));
#86041=CARTESIAN_POINT('Ctrl Pts',(-51.5322071441577,-1.38799240289921,
126.08602826895));
#86042=CARTESIAN_POINT('Ctrl Pts',(-51.5399583353979,-1.51940769581708,
126.124686721708));
#86043=CARTESIAN_POINT('Ctrl Pts',(-51.5477095266381,-1.64930922120316,
126.168869780251));
#86044=CARTESIAN_POINT('Ctrl Pts',(-51.5554607178782,-1.77720239117796,
126.218432715463));
#86045=CARTESIAN_POINT('Ctrl Pts',(-51.5632086146553,-1.90504120314334,
126.267974585104));
#86046=CARTESIAN_POINT('Ctrl Pts',(-51.5709565114324,-2.03087299366717,
126.322891642578));
#86047=CARTESIAN_POINT('Ctrl Pts',(-51.5787044082095,-2.15421982414746,
126.382989788089));
#86048=CARTESIAN_POINT('Ctrl Pts',(-51.5864506842936,-2.27754085313004,
126.443075362363));
#86049=CARTESIAN_POINT('Ctrl Pts',(-51.5941969603778,-2.39837760473566,
126.508339697855));
#86050=CARTESIAN_POINT('Ctrl Pts',(-51.6019432364619,-2.51627393313666,
126.57854134127));
#86051=CARTESIAN_POINT('Ctrl Pts',(-51.6096895697273,-2.63417113182158,
126.648743502897));
#86052=CARTESIAN_POINT('Ctrl Pts',(-51.6174359029926,-2.74912752806806,
126.723882845146));
#86053=CARTESIAN_POINT('Ctrl Pts',(-51.625182236258,-2.86071366235615,126.803673126083));
#86054=CARTESIAN_POINT('Ctrl Pts',(-51.632930304261,-2.97232478558532,126.8834812755));
#86055=CARTESIAN_POINT('Ctrl Pts',(-51.6406783722639,-3.08056382703257,
126.967942208798));
#86056=CARTESIAN_POINT('Ctrl Pts',(-51.6484264402669,-3.18503259909559,
127.056727977459));
#86057=CARTESIAN_POINT('Ctrl Pts',(-51.6561827430087,-3.28961240181262,
127.14560810869));
#86058=CARTESIAN_POINT('Ctrl Pts',(-51.6639390457507,-3.39041363217254,
127.23882200367));
#86059=CARTESIAN_POINT('Ctrl Pts',(-51.6716953484925,-3.48707293168823,
127.336002874831));
#86060=CARTESIAN_POINT('Ctrl Pts',(-51.6794557910067,-3.5837838211823,127.433235614349));
#86061=CARTESIAN_POINT('Ctrl Pts',(-51.6872162335209,-3.67634811114175,
127.534439260585));
#86062=CARTESIAN_POINT('Ctrl Pts',(-51.6949766760351,-3.76444196373765,
127.639212948949));
#86063=CARTESIAN_POINT('Ctrl Pts',(-51.7027495763005,-3.85267723240659,
127.74415482934));
#86064=CARTESIAN_POINT('Ctrl Pts',(-51.7105224765659,-3.93642748409369,
127.852677894429));
#86065=CARTESIAN_POINT('Ctrl Pts',(-51.7182953768314,-4.01541102161395,
127.964350513711));
#86066=CARTESIAN_POINT('Ctrl Pts',(-51.7257857125933,-4.09152330859643,
128.071963551993));
#86067=CARTESIAN_POINT('Ctrl Pts',(-51.7332760483551,-4.1632092610856,128.182500873158));
#86068=CARTESIAN_POINT('Ctrl Pts',(-51.7407663841171,-4.23025761216825,
128.295555404483));
#86069=CARTESIAN_POINT('Ctrl Pts',(-51.7488222097794,-4.30236784119367,
128.417145093335));
#86070=CARTESIAN_POINT('Ctrl Pts',(-51.7568780354418,-4.369328357198,128.542008231541));
#86071=CARTESIAN_POINT('Ctrl Pts',(-51.7649338611041,-4.43084077719799,
128.669686621467));
#86072=CARTESIAN_POINT('Ctrl Pts',(-51.7729786123424,-4.4922686354595,128.797189490635));
#86073=CARTESIAN_POINT('Ctrl Pts',(-51.7810233635806,-4.54826315846495,
128.927499591582));
#86074=CARTESIAN_POINT('Ctrl Pts',(-51.7890681148189,-4.59857017835228,
129.060131453359));
#86075=CARTESIAN_POINT('Ctrl Pts',(-51.7970997542386,-4.64879520483839,
129.192547143766));
#86076=CARTESIAN_POINT('Ctrl Pts',(-51.8051313936585,-4.693351078895,129.327276726197));
#86077=CARTESIAN_POINT('Ctrl Pts',(-51.8131630330782,-4.73203060737242,
129.463812448573));
#86078=CARTESIAN_POINT('Ctrl Pts',(-51.8154814838541,-4.74319602181914,
129.50322549178));
#86079=CARTESIAN_POINT('Ctrl Pts',(-51.8177999346299,-4.75387207661904,
129.542788895002));
#86080=CARTESIAN_POINT('Ctrl Pts',(-51.8201183854058,-4.76405452823404,
129.582490119308));
#86081=CARTESIAN_POINT('Origin',(213.235140564004,0.,130.804360617566));
#86082=CARTESIAN_POINT('',(-53.9150733197311,-4.76405452823399,129.582490119308));
#86083=CARTESIAN_POINT('',(-53.5697656565505,-4.76405452823409,129.582490119308));
#86084=CARTESIAN_POINT('',(213.235140564004,-4.76405452823405,129.582490119308));
#86085=CARTESIAN_POINT('',(-52.2351405639781,-4.91824847382902,130.808235172839));
#86086=CARTESIAN_POINT('Ctrl Pts',(-52.2351405640084,-4.9182484738286,130.808235173372));
#86087=CARTESIAN_POINT('Ctrl Pts',(-52.2481165697295,-4.91806852435966,
131.036657796555));
#86088=CARTESIAN_POINT('Ctrl Pts',(-52.2610925754504,-4.90197300803857,
131.264470097888));
#86089=CARTESIAN_POINT('Ctrl Pts',(-52.2740685811715,-4.87022848596664,
131.489968054062));
#86090=CARTESIAN_POINT('Ctrl Pts',(-52.2754032659754,-4.86696331083278,
131.513162302115));
#86091=CARTESIAN_POINT('Ctrl Pts',(-52.2767379507793,-4.86353260158788,
131.536332098239));
#86092=CARTESIAN_POINT('Ctrl Pts',(-52.2780726355832,-4.85993666785756,
131.559475606765));
#86093=CARTESIAN_POINT('Ctrl Pts',(-52.2858469697023,-4.83899090582646,
131.694282991584));
#86094=CARTESIAN_POINT('Ctrl Pts',(-52.2936213038213,-4.81239868313447,
131.828431734942));
#86095=CARTESIAN_POINT('Ctrl Pts',(-52.3013956379403,-4.78021090249829,
131.961411519703));
#86096=CARTESIAN_POINT('Ctrl Pts',(-52.3091603908874,-4.74806279042503,
132.094227418765));
#86097=CARTESIAN_POINT('Ctrl Pts',(-52.3169251438343,-4.71033293253625,
132.225876849324));
#86098=CARTESIAN_POINT('Ctrl Pts',(-52.3246898967814,-4.66712378507074,
132.35585623062));
#86099=CARTESIAN_POINT('Ctrl Pts',(-52.3324469376664,-4.62395755353964,
132.485706514563));
#86100=CARTESIAN_POINT('Ctrl Pts',(-52.3402039785514,-4.57532298500618,
132.613889681561));
#86101=CARTESIAN_POINT('Ctrl Pts',(-52.3479610194363,-4.52137313691162,
132.739914290114));
#86102=CARTESIAN_POINT('Ctrl Pts',(-52.3557122106764,-4.46746397281724,
132.865843862529));
#86103=CARTESIAN_POINT('Ctrl Pts',(-52.3634634019165,-4.40824766066713,
132.989617758544));
#86104=CARTESIAN_POINT('Ctrl Pts',(-52.3712145931566,-4.34392633172333,
133.110761945839));
#86105=CARTESIAN_POINT('Ctrl Pts',(-52.3789624899336,-4.27963234106016,
133.231854643623));
#86106=CARTESIAN_POINT('Ctrl Pts',(-52.3867103867107,-4.21023783206539,
133.350319511113));
#86107=CARTESIAN_POINT('Ctrl Pts',(-52.3944582834877,-4.13599199469353,
133.465704879839));
#86108=CARTESIAN_POINT('Ctrl Pts',(-52.4022045595718,-4.06176168795028,
133.581066112433));
#86109=CARTESIAN_POINT('Ctrl Pts',(-52.4099508356558,-3.98268228273301,
133.69334879897));
#86110=CARTESIAN_POINT('Ctrl Pts',(-52.4176971117398,-3.89904741713465,
133.802128504083));
#86111=CARTESIAN_POINT('Ctrl Pts',(-52.4254434450052,-3.8154119341627,133.910909012184));
#86112=CARTESIAN_POINT('Ctrl Pts',(-52.4331897782705,-3.72722116200948,
134.016186177316));
#86113=CARTESIAN_POINT('Ctrl Pts',(-52.4409361115358,-3.63481006202942,
134.117567353565));
#86114=CARTESIAN_POINT('Ctrl Pts',(-52.4486841795387,-3.54237826722425,
134.218971233425));
#86115=CARTESIAN_POINT('Ctrl Pts',(-52.4564322475416,-3.44572452725197,
134.316477099382));
#86116=CARTESIAN_POINT('Ctrl Pts',(-52.4641803155446,-3.34522152464625,
134.409728284468));
#86117=CARTESIAN_POINT('Ctrl Pts',(-52.4719366182864,-3.24461170625323,
134.503078578023));
#86118=CARTESIAN_POINT('Ctrl Pts',(-52.4796929210283,-3.14014473998698,
134.592164891329));
#86119=CARTESIAN_POINT('Ctrl Pts',(-52.4874492237701,-3.03222776196002,
134.676669729982));
#86120=CARTESIAN_POINT('Ctrl Pts',(-52.4952096662842,-2.92425318539241,
134.761219671412));
#86121=CARTESIAN_POINT('Ctrl Pts',(-52.5029701087983,-2.81282524545193,
134.841183037947));
#86122=CARTESIAN_POINT('Ctrl Pts',(-52.5107305513125,-2.69838024902019,
134.916285604017));
#86123=CARTESIAN_POINT('Ctrl Pts',(-52.5185034515779,-2.58375153532038,
134.991508731393));
#86124=CARTESIAN_POINT('Ctrl Pts',(-52.5262763518433,-2.46609642253151,
135.0618552647));
#86125=CARTESIAN_POINT('Ctrl Pts',(-52.5340492521087,-2.34587679093241,
135.127096457779));
#86126=CARTESIAN_POINT('Ctrl Pts',(-52.5415395878712,-2.23002744574942,
135.189965969162));
#86127=CARTESIAN_POINT('Ctrl Pts',(-52.5490299236337,-2.11179707450387,
135.24809474407));
#86128=CARTESIAN_POINT('Ctrl Pts',(-52.5565202593961,-1.99161485314921,
135.301321073164));
#86129=CARTESIAN_POINT('Ctrl Pts',(-52.5642945935152,-1.86687588635034,
135.356565494701));
#86130=CARTESIAN_POINT('Ctrl Pts',(-52.5720689276343,-1.73963900335625,
135.40670337717));
#86131=CARTESIAN_POINT('Ctrl Pts',(-52.5798432617534,-1.61036106258794,
135.451501707591));
#86132=CARTESIAN_POINT('Ctrl Pts',(-52.5876080147005,-1.48124244532791,
135.496244828074));
#86133=CARTESIAN_POINT('Ctrl Pts',(-52.5953727676477,-1.35008814109999,
135.535661363));
#86134=CARTESIAN_POINT('Ctrl Pts',(-52.6031375205948,-1.2173772067598,135.569565314005));
#86135=CARTESIAN_POINT('Ctrl Pts',(-52.6108945614798,-1.0847980827905,135.603435591127));
#86136=CARTESIAN_POINT('Ctrl Pts',(-52.6186516023648,-0.950665781799995,
135.631804084028));
#86137=CARTESIAN_POINT('Ctrl Pts',(-52.6264086432498,-0.815476498728038,
135.654533928132));
#86138=CARTESIAN_POINT('Ctrl Pts',(-52.63415983449,-0.680389162945881,135.677246631483));
#86139=CARTESIAN_POINT('Ctrl Pts',(-52.64191102573,-0.544246815612059,135.69432908512));
#86140=CARTESIAN_POINT('Ctrl Pts',(-52.6496622169702,-0.407557530427672,
135.705695121749));
#86141=CARTESIAN_POINT('Ctrl Pts',(-52.6574101137473,-0.27092634183598,
135.717056327509));
#86142=CARTESIAN_POINT('Ctrl Pts',(-52.6651580105245,-0.133749066550099,
135.72270591628));
#86143=CARTESIAN_POINT('Ctrl Pts',(-52.6729059073016,0.00345960069853902,
135.722609400788));
#86144=CARTESIAN_POINT('Ctrl Pts',(-52.6806521833857,0.140639566851865,
135.722512905485));
#86145=CARTESIAN_POINT('Ctrl Pts',(-52.6883984594698,0.277850521189361,
135.71667269696));
#86146=CARTESIAN_POINT('Ctrl Pts',(-52.6961447355539,0.414576655654646,
135.705106403575));
#86147=CARTESIAN_POINT('Ctrl Pts',(-52.7038910688192,0.551303799401197,
135.69354002481));
#86148=CARTESIAN_POINT('Ctrl Pts',(-52.7116374020846,0.687545726560492,
135.676247509796));
#86149=CARTESIAN_POINT('Ctrl Pts',(-52.71938373535,0.822791038209392,135.653298436299));
#86150=CARTESIAN_POINT('Ctrl Pts',(-52.7271318033529,0.95806663710811,135.630344223516));
#86151=CARTESIAN_POINT('Ctrl Pts',(-52.7348798713559,1.09234479100224,135.601730996964));
#86152=CARTESIAN_POINT('Ctrl Pts',(-52.7426279393589,1.22512398185717,135.567579517803));
#86153=CARTESIAN_POINT('Ctrl Pts',(-52.7503842421007,1.35804429201622,135.533391742045));
#86154=CARTESIAN_POINT('Ctrl Pts',(-52.7581405448427,1.48946207747062,135.493654053061));
#86155=CARTESIAN_POINT('Ctrl Pts',(-52.7658968475845,1.61889015417386,135.448537372516));
#86156=CARTESIAN_POINT('Ctrl Pts',(-52.7736572900987,1.74838731053865,135.40339661184));
#86157=CARTESIAN_POINT('Ctrl Pts',(-52.7814177326129,1.87589227880128,135.35287128299));
#86158=CARTESIAN_POINT('Ctrl Pts',(-52.7891781751271,2.00093851069744,135.297180237683));
#86159=CARTESIAN_POINT('Ctrl Pts',(-52.7969510753925,2.12618547790612,135.241399792166));
#86160=CARTESIAN_POINT('Ctrl Pts',(-52.8047239756579,2.24896547104311,135.180437233172));
#86161=CARTESIAN_POINT('Ctrl Pts',(-52.8124968759234,2.36883638191488,135.114557510774));
#86162=CARTESIAN_POINT('Ctrl Pts',(-52.8199872116853,2.48434968323808,135.051072682227));
#86163=CARTESIAN_POINT('Ctrl Pts',(-52.8274775474471,2.59716147144785,134.983022145156));
#86164=CARTESIAN_POINT('Ctrl Pts',(-52.834967883209,2.70690371581109,134.910679569599));
#86165=CARTESIAN_POINT('Ctrl Pts',(-52.8427422173282,2.8208068707264,134.835594103301));
#86166=CARTESIAN_POINT('Ctrl Pts',(-52.8505165514472,2.93176393441776,134.755646860263));
#86167=CARTESIAN_POINT('Ctrl Pts',(-52.8582908855663,3.03933192332999,134.671096259206));
#86168=CARTESIAN_POINT('Ctrl Pts',(-52.8660556385134,3.14676734430951,134.586649859208));
#86169=CARTESIAN_POINT('Ctrl Pts',(-52.8738203914605,3.25082169653457,134.497611628508));
#86170=CARTESIAN_POINT('Ctrl Pts',(-52.8815851444076,3.35107955237981,134.404284074547));
#86171=CARTESIAN_POINT('Ctrl Pts',(-52.8893421852926,3.45123783070923,134.311049214828));
#86172=CARTESIAN_POINT('Ctrl Pts',(-52.8970992261777,3.54760683227307,134.213533774532));
#86173=CARTESIAN_POINT('Ctrl Pts',(-52.9048562670627,3.63980320354225,134.11208123787));
#86174=CARTESIAN_POINT('Ctrl Pts',(-52.9126074583028,3.73193004881067,134.010705207355));
#86175=CARTESIAN_POINT('Ctrl Pts',(-52.9203586495429,3.81989026505082,133.905398278244));
#86176=CARTESIAN_POINT('Ctrl Pts',(-52.928109840783,3.90333673103308,133.796541331806));
#86177=CARTESIAN_POINT('Ctrl Pts',(-52.9358577375601,3.98674773004128,133.687730652474));
#86178=CARTESIAN_POINT('Ctrl Pts',(-52.9436056343373,4.06564855711208,133.575373266443));
#86179=CARTESIAN_POINT('Ctrl Pts',(-52.9513535311144,4.13973199205104,133.459883559754));
#86180=CARTESIAN_POINT('Ctrl Pts',(-52.9590998071985,4.21379993033247,133.344418011023));
#86181=CARTESIAN_POINT('Ctrl Pts',(-52.9668460832825,4.28305226988077,133.22582177376));
#86182=CARTESIAN_POINT('Ctrl Pts',(-52.9745923593666,4.34722503508131,133.104538340452));
#86183=CARTESIAN_POINT('Ctrl Pts',(-52.982338692632,4.41139827399062,132.983254011858));
#86184=CARTESIAN_POINT('Ctrl Pts',(-52.9900850258973,4.47049168088363,132.859282793209));
#86185=CARTESIAN_POINT('Ctrl Pts',(-52.9978313591627,4.52428736989566,132.733092547385));
#86186=CARTESIAN_POINT('Ctrl Pts',(-53.0055794271657,4.57809510607925,132.60687404213));
#86187=CARTESIAN_POINT('Ctrl Pts',(-53.0133274951687,4.62660261031784,132.478435880436));
#86188=CARTESIAN_POINT('Ctrl Pts',(-53.0210755631716,4.66964039964916,132.348265277985));
#86189=CARTESIAN_POINT('Ctrl Pts',(-53.0288318659135,4.71272393005514,132.217956328669));
#86190=CARTESIAN_POINT('Ctrl Pts',(-53.0365881686554,4.75032600997975,132.085911632279));
#86191=CARTESIAN_POINT('Ctrl Pts',(-53.0443444713972,4.78232710578093,131.952633457884));
#86192=CARTESIAN_POINT('Ctrl Pts',(-53.0521049139114,4.81434528153053,131.819284148915));
#86193=CARTESIAN_POINT('Ctrl Pts',(-53.0598653564256,4.840756441245,131.684700433594));
#86194=CARTESIAN_POINT('Ctrl Pts',(-53.0676257989398,4.8614925303401,131.549393126889));
#86195=CARTESIAN_POINT('Ctrl Pts',(-53.0753986992053,4.88226190684624,131.413868612883));
#86196=CARTESIAN_POINT('Ctrl Pts',(-53.0831715994707,4.89733796477343,131.277618575117));
#86197=CARTESIAN_POINT('Ctrl Pts',(-53.0909444997361,4.90670464384513,131.141158183722));
#86198=CARTESIAN_POINT('Ctrl Pts',(-53.0984348354981,4.91573082053923,131.009658471279));
#86199=CARTESIAN_POINT('Ctrl Pts',(-53.10592517126,4.91945550351924,130.877963741348));
#86200=CARTESIAN_POINT('Ctrl Pts',(-53.113415507022,4.91791000953669,130.746531553949));
#86201=CARTESIAN_POINT('Ctrl Pts',(-53.121189841141,4.91630591768004,130.610116075215));
#86202=CARTESIAN_POINT('Ctrl Pts',(-53.1289641752601,4.90901904109058,130.473551317383));
#86203=CARTESIAN_POINT('Ctrl Pts',(-53.1367385093792,4.89602735132519,130.337349656693));
#86204=CARTESIAN_POINT('Ctrl Pts',(-53.1445032623262,4.88305167265633,130.201315852377));
#86205=CARTESIAN_POINT('Ctrl Pts',(-53.1522680152733,4.86438520652166,130.065644640305));
#86206=CARTESIAN_POINT('Ctrl Pts',(-53.1600327682204,4.840057912219,129.930849044165));
#86207=CARTESIAN_POINT('Ctrl Pts',(-53.1677898091054,4.81575478012801,129.79618732891));
#86208=CARTESIAN_POINT('Ctrl Pts',(-53.1755468499903,4.78580207771579,129.662399881156));
#86209=CARTESIAN_POINT('Ctrl Pts',(-53.1833038908753,4.75028157602928,129.529994888689));
#86210=CARTESIAN_POINT('Ctrl Pts',(-53.1910550821154,4.71478786062946,129.397689743856));
#86211=CARTESIAN_POINT('Ctrl Pts',(-53.1988062733556,4.67373480414731,129.266765355322));
#86212=CARTESIAN_POINT('Ctrl Pts',(-53.2065574645957,4.62725522527689,129.137719641636));
#86213=CARTESIAN_POINT('Ctrl Pts',(-53.2143053613728,4.58079540146732,129.008728775821));
#86214=CARTESIAN_POINT('Ctrl Pts',(-53.2220532581497,4.52891377476509,128.881615363788));
#86215=CARTESIAN_POINT('Ctrl Pts',(-53.2298011549268,4.47179291986293,128.756861864364));
#86216=CARTESIAN_POINT('Ctrl Pts',(-53.2375474310109,4.41468401341223,128.632134460683));
#86217=CARTESIAN_POINT('Ctrl Pts',(-53.245293707095,4.35233822129179,128.509766342978));
#86218=CARTESIAN_POINT('Ctrl Pts',(-53.2530399831791,4.28498598102263,128.390219319933));
#86219=CARTESIAN_POINT('Ctrl Pts',(-53.2607863164444,4.21763324357454,128.270671414418));
#86220=CARTESIAN_POINT('Ctrl Pts',(-53.2685326497097,4.14527417614053,128.153944985742));
#86221=CARTESIAN_POINT('Ctrl Pts',(-53.2762789829751,4.06818463237967,128.040476238767));
#86222=CARTESIAN_POINT('Ctrl Pts',(-53.284027050978,3.99107782494998,127.926982081253));
#86223=CARTESIAN_POINT('Ctrl Pts',(-53.291775118981,3.90923865286163,127.816747380461));
#86224=CARTESIAN_POINT('Ctrl Pts',(-53.299523186984,3.82298541478731,127.710178079185));
#86225=CARTESIAN_POINT('Ctrl Pts',(-53.3072794897258,3.73664050574514,127.603495514787));
#86226=CARTESIAN_POINT('Ctrl Pts',(-53.3150357924677,3.64587240565352,127.50048643623));
#86227=CARTESIAN_POINT('Ctrl Pts',(-53.3227920952095,3.55103907685237,127.401522899254));
#86228=CARTESIAN_POINT('Ctrl Pts',(-53.3305525377237,3.45615513264814,127.302506542458));
#86229=CARTESIAN_POINT('Ctrl Pts',(-53.3383129802378,3.35720191829415,127.207540300266));
#86230=CARTESIAN_POINT('Ctrl Pts',(-53.346073422752,3.25457241172448,127.116957536895));
#86231=CARTESIAN_POINT('Ctrl Pts',(-53.3538463230174,3.15177815515998,127.026229362031));
#86232=CARTESIAN_POINT('Ctrl Pts',(-53.3616192232828,3.04529611714926,126.939898974016));
#86233=CARTESIAN_POINT('Ctrl Pts',(-53.3693921235482,2.9355510439423,126.858258346855));
#86234=CARTESIAN_POINT('Ctrl Pts',(-53.3768824593104,2.82979548057489,126.77958556213));
#86235=CARTESIAN_POINT('Ctrl Pts',(-53.3843727950726,2.72101025662343,126.705267662498));
#86236=CARTESIAN_POINT('Ctrl Pts',(-53.3918631308348,2.60959725775939,126.635525622655));
#86237=CARTESIAN_POINT('Ctrl Pts',(-53.3996374649539,2.49396000118262,126.563139292175));
#86238=CARTESIAN_POINT('Ctrl Pts',(-53.407411799073,2.37512546791411,126.495453360436));
#86239=CARTESIAN_POINT('Ctrl Pts',(-53.4151861331921,2.25351282768591,126.432763312466));
#86240=CARTESIAN_POINT('Ctrl Pts',(-53.4229508861392,2.13205006416796,126.370150524377));
#86241=CARTESIAN_POINT('Ctrl Pts',(-53.4307156390863,2.00781635014345,126.31252154692));
#86242=CARTESIAN_POINT('Ctrl Pts',(-53.4384803920334,1.88125950070231,126.260128476322));
#86243=CARTESIAN_POINT('Ctrl Pts',(-53.4462374329184,1.75482834930836,126.20778744326));
#86244=CARTESIAN_POINT('Ctrl Pts',(-53.4539944738035,1.62607901316586,126.160672116653));
#86245=CARTESIAN_POINT('Ctrl Pts',(-53.4617515146885,1.49548324430038,126.118988388114));
#86246=CARTESIAN_POINT('Ctrl Pts',(-53.4695027059286,1.36498595871992,126.0773360936));
#86247=CARTESIAN_POINT('Ctrl Pts',(-53.4772538971687,1.23264538286877,126.041107362692));
#86248=CARTESIAN_POINT('Ctrl Pts',(-53.4850050884088,1.09895222147341,126.010459588402));
#86249=CARTESIAN_POINT('Ctrl Pts',(-53.4927529851859,0.965315883238017,
125.979824840234));
#86250=CARTESIAN_POINT('Ctrl Pts',(-53.5005008819631,0.830328483143253,
125.954766418021));
#86251=CARTESIAN_POINT('Ctrl Pts',(-53.5082487787402,0.694494613545642,
125.935391497284));
#86252=CARTESIAN_POINT('Ctrl Pts',(-53.5159950548243,0.558689157465312,
125.916020629364));
#86253=CARTESIAN_POINT('Ctrl Pts',(-53.5237413309084,0.42203797087301,125.902330953373));
#86254=CARTESIAN_POINT('Ctrl Pts',(-53.5314876069926,0.285054143601113,
125.894378214571));
#86255=CARTESIAN_POINT('Ctrl Pts',(-53.5392339402579,0.148069305145721,
125.886425417065));
#86256=CARTESIAN_POINT('Ctrl Pts',(-53.5469802735232,0.0107522114190008,
125.884209663912));
#86257=CARTESIAN_POINT('Ctrl Pts',(-53.5547266067886,-0.126381040432686,
125.887734650999));
#86258=CARTESIAN_POINT('Ctrl Pts',(-53.5624746747916,-0.263545002325309,
125.891260427483));
#86259=CARTESIAN_POINT('Ctrl Pts',(-53.5702227427946,-0.400524649657835,
125.900529492357));
#86260=CARTESIAN_POINT('Ctrl Pts',(-53.5779708107976,-0.536806403053045,
125.915493473928));
#86261=CARTESIAN_POINT('Ctrl Pts',(-53.5857271135395,-0.673232998317537,
125.930473359397));
#86262=CARTESIAN_POINT('Ctrl Pts',(-53.5934834162814,-0.808959828710015,
125.951160209594));
#86263=CARTESIAN_POINT('Ctrl Pts',(-53.6012397190233,-0.943480385811545,
125.97745396588));
#86264=CARTESIAN_POINT('Ctrl Pts',(-53.6090001615375,-1.07807274058492,
126.003761755935));
#86265=CARTESIAN_POINT('Ctrl Pts',(-53.6167606040516,-1.21145715914997,
126.035682324089));
#86266=CARTESIAN_POINT('Ctrl Pts',(-53.6245210465658,-1.34314075857766,
126.073065238376));
#86267=CARTESIAN_POINT('Ctrl Pts',(-53.6322939468312,-1.47503574820929,
126.110508163036));
#86268=CARTESIAN_POINT('Ctrl Pts',(-53.6400668470967,-1.60522409116347,
126.153430833884));
#86269=CARTESIAN_POINT('Ctrl Pts',(-53.6478397473621,-1.73323055571743,
126.201633718952));
#86270=CARTESIAN_POINT('Ctrl Pts',(-53.655330083124,-1.85658366285307,126.248084307731));
#86271=CARTESIAN_POINT('Ctrl Pts',(-53.6628204188859,-1.97791048737297,
126.29943775753));
#86272=CARTESIAN_POINT('Ctrl Pts',(-53.6703107546477,-2.09680788798463,
126.355475392773));
#86273=CARTESIAN_POINT('Ctrl Pts',(-53.6780857478496,-2.22022378159239,
126.413642642801));
#86274=CARTESIAN_POINT('Ctrl Pts',(-53.6858607410514,-2.34141292501956,
126.477041420202));
#86275=CARTESIAN_POINT('Ctrl Pts',(-53.6936357342533,-2.45990002673024,
126.54547873132));
#86276=CARTESIAN_POINT('Ctrl Pts',(-53.7014009981672,-2.57823885884242,
126.613830402968));
#86277=CARTESIAN_POINT('Ctrl Pts',(-53.7091662620812,-2.69388204188799,
126.687207868635));
#86278=CARTESIAN_POINT('Ctrl Pts',(-53.7169315259951,-2.80637533812242,
126.765370579936));
#86279=CARTESIAN_POINT('Ctrl Pts',(-53.724688930366,-2.91875477526293,126.84345417954));
#86280=CARTESIAN_POINT('Ctrl Pts',(-53.7324463347369,-3.02799035158682,
126.926313163742));
#86281=CARTESIAN_POINT('Ctrl Pts',(-53.7402037391077,-3.13365379570381,
127.013661875755));
#86282=CARTESIAN_POINT('Ctrl Pts',(-53.7479546785665,-3.2392291813876,127.100937792575));
#86283=CARTESIAN_POINT('Ctrl Pts',(-53.7557056180253,-3.34123806288523,
127.192695738132));
#86284=CARTESIAN_POINT('Ctrl Pts',(-53.7634565574841,-3.43928282766282,
127.28860796787));
#86285=CARTESIAN_POINT('Ctrl Pts',(-53.7712039874065,-3.53728319889611,
127.384476769652));
#86286=CARTESIAN_POINT('Ctrl Pts',(-53.7789514173288,-3.63132274580799,
127.484495840307));
#86287=CARTESIAN_POINT('Ctrl Pts',(-53.7866988472512,-3.72103862461811,
127.588298644189));
#86288=CARTESIAN_POINT('Ctrl Pts',(-53.7944444470007,-3.81073330987601,
127.692076926769));
#86289=CARTESIAN_POINT('Ctrl Pts',(-53.8021900467503,-3.89610610462482,
127.799636867971));
#86290=CARTESIAN_POINT('Ctrl Pts',(-53.8099356464998,-3.97683285860141,
127.91057702558));
#86291=CARTESIAN_POINT('Ctrl Pts',(-53.8176810938486,-4.05755802421499,
128.021515000354));
#86292=CARTESIAN_POINT('Ctrl Pts',(-53.8254265411972,-4.13363710231795,
128.135832742306));
#86293=CARTESIAN_POINT('Ctrl Pts',(-53.833171988546,-4.20478811536839,128.253098191363));
#86294=CARTESIAN_POINT('Ctrl Pts',(-53.840922046836,-4.27598148532006,128.3704334497));
#86295=CARTESIAN_POINT('Ctrl Pts',(-53.8486721051261,-4.34224072672372,
128.490719586115));
#86296=CARTESIAN_POINT('Ctrl Pts',(-53.8564221634162,-4.40332875277113,
128.61349801176));
#86297=CARTESIAN_POINT('Ctrl Pts',(-53.8641747690669,-4.46443685779391,
128.736316793349));
#86298=CARTESIAN_POINT('Ctrl Pts',(-53.8719273747176,-4.5203701980571,128.861629141036));
#86299=CARTESIAN_POINT('Ctrl Pts',(-53.8796799803683,-4.57093944266997,
128.988955518437));
#86300=CARTESIAN_POINT('Ctrl Pts',(-53.8874406389297,-4.62156121537877,
129.116414154332));
#86301=CARTESIAN_POINT('Ctrl Pts',(-53.895201297491,-4.66680763261751,129.245890630247));
#86302=CARTESIAN_POINT('Ctrl Pts',(-53.9029619560525,-4.70653881476726,
129.376888919917));
#86303=CARTESIAN_POINT('Ctrl Pts',(-53.9069990772786,-4.72720711211976,
129.445034679924));
#86304=CARTESIAN_POINT('Ctrl Pts',(-53.9110361985049,-4.74638375651336,
129.513592048561));
#86305=CARTESIAN_POINT('Ctrl Pts',(-53.9150733197311,-4.76405452823399,
129.582490119308));
#86306=CARTESIAN_POINT('Ctrl Pts',(-52.1650248355919,-4.76405452823407,
129.582490119308));
#86307=CARTESIAN_POINT('Ctrl Pts',(-52.1726632853586,-4.79766468427344,
129.713535607601));
#86308=CARTESIAN_POINT('Ctrl Pts',(-52.1803017351253,-4.82584641107061,
129.845901857919));
#86309=CARTESIAN_POINT('Ctrl Pts',(-52.187940184892,-4.8485168568208,129.979092569218));
#86310=CARTESIAN_POINT('Ctrl Pts',(-52.1958069147397,-4.87186482371074,
130.116263772277));
#86311=CARTESIAN_POINT('Ctrl Pts',(-52.2036736445873,-4.88936686806602,
130.254309027462));
#86312=CARTESIAN_POINT('Ctrl Pts',(-52.211540374435,-4.90099004563023,130.39268157373));
#86313=CARTESIAN_POINT('Ctrl Pts',(-52.2194071042827,-4.91261322319444,
130.531054119999));
#86314=CARTESIAN_POINT('Ctrl Pts',(-52.2272738341305,-4.91835756854535,
130.669753493166));
#86315=CARTESIAN_POINT('Ctrl Pts',(-52.2351405639781,-4.91824847382902,
130.808235172838));
#86316=CARTESIAN_POINT('',(-51.8898594360354,-4.91824990617988,130.805321274443));
#86317=CARTESIAN_POINT('Ctrl Pts',(-51.8201183854058,-4.76405452823404,
129.582490119308));
#86318=CARTESIAN_POINT('Ctrl Pts',(-51.828135682534,-4.79926586027597,129.719778568533));
#86319=CARTESIAN_POINT('Ctrl Pts',(-51.8361529796623,-4.82857088525035,
129.858716332355));
#86320=CARTESIAN_POINT('Ctrl Pts',(-51.8441702767905,-4.85182571170561,
129.998773672704));
#86321=CARTESIAN_POINT('Ctrl Pts',(-51.8521776154136,-4.8750516527016,130.138657043979));
#86322=CARTESIAN_POINT('Ctrl Pts',(-51.8601849540367,-4.89224231988163,
130.279656873771));
#86323=CARTESIAN_POINT('Ctrl Pts',(-51.8681922926598,-4.90330454694982,
130.421231941582));
#86324=CARTESIAN_POINT('Ctrl Pts',(-51.8754146737702,-4.91328234651313,
130.548928438958));
#86325=CARTESIAN_POINT('Ctrl Pts',(-51.8826370548806,-4.91827495242315,
130.677092572184));
#86326=CARTESIAN_POINT('Ctrl Pts',(-51.889859435991,-4.91824990618003,130.805321273655));
#86327=CARTESIAN_POINT('Ctrl Pts',(-51.8898594360354,-4.91824990617988,
130.805321274443));
#86328=CARTESIAN_POINT('Ctrl Pts',(-51.8981042988535,-4.91822131408472,
130.951703476768));
#86329=CARTESIAN_POINT('Ctrl Pts',(-51.9063491616717,-4.91165329920825,
131.097920000058));
#86330=CARTESIAN_POINT('Ctrl Pts',(-51.9145940244898,-4.89861554147768,
131.243392324044));
#86331=CARTESIAN_POINT('Ctrl Pts',(-51.9228547446132,-4.8855527082899,131.389144434257));
#86332=CARTESIAN_POINT('Ctrl Pts',(-51.9311154647366,-4.86599530976217,
131.534149180284));
#86333=CARTESIAN_POINT('Ctrl Pts',(-51.93937618486,-4.84006424513526,131.677837100056));
#86334=CARTESIAN_POINT('Ctrl Pts',(-51.9476611144281,-4.81405718511522,
131.821946121704));
#86335=CARTESIAN_POINT('Ctrl Pts',(-51.9559460439962,-4.7816391523339,131.9647302936));
#86336=CARTESIAN_POINT('Ctrl Pts',(-51.9642309735642,-4.74298172897772,
132.105632065452));
#86337=CARTESIAN_POINT('Ctrl Pts',(-51.9725292725657,-4.70426192393872,
132.246761211218));
#86338=CARTESIAN_POINT('Ctrl Pts',(-51.9808275715673,-4.65928271751152,
132.386001598625));
#86339=CARTESIAN_POINT('Ctrl Pts',(-51.9891258705688,-4.60826434017012,
132.522814234518));
#86340=CARTESIAN_POINT('Ctrl Pts',(-51.9974438725248,-4.55712482803094,
132.659951709653));
#86341=CARTESIAN_POINT('Ctrl Pts',(-52.0057618744809,-4.49991759387119,
132.794649623649));
#86342=CARTESIAN_POINT('Ctrl Pts',(-52.014079876437,-4.43691017137636,132.92639058758));
#86343=CARTESIAN_POINT('Ctrl Pts',(-52.0157912536013,-4.42394678610545,
132.953495471477));
#86344=CARTESIAN_POINT('Ctrl Pts',(-52.0175026307656,-4.41073802523113,
132.980475279727));
#86345=CARTESIAN_POINT('Ctrl Pts',(-52.0192140079299,-4.39728644798685,
133.007325655158));
#86346=CARTESIAN_POINT('Ctrl Pts',(-52.026988342049,-4.33617948798705,133.129299813848));
#86347=CARTESIAN_POINT('Ctrl Pts',(-52.0347626761681,-4.2698968213164,133.248922720314));
#86348=CARTESIAN_POINT('Ctrl Pts',(-52.0425370102871,-4.19864273770781,
133.365723970078));
#86349=CARTESIAN_POINT('Ctrl Pts',(-52.0503017632342,-4.12747646838921,
133.482381272742));
#86350=CARTESIAN_POINT('Ctrl Pts',(-52.0580665161812,-4.0513511743476,133.596223507215));
#86351=CARTESIAN_POINT('Ctrl Pts',(-52.0658312691282,-3.97051818003925,
133.706802424817));
#86352=CARTESIAN_POINT('Ctrl Pts',(-52.0735883100132,-3.88976547020052,
133.817271513879));
#86353=CARTESIAN_POINT('Ctrl Pts',(-52.0813453508981,-3.80431459428713,
133.924483422563));
#86354=CARTESIAN_POINT('Ctrl Pts',(-52.089102391783,-3.71446135494585,134.028016912073));
#86355=CARTESIAN_POINT('Ctrl Pts',(-52.0968535830231,-3.62467587463107,
134.131472326173));
#86356=CARTESIAN_POINT('Ctrl Pts',(-52.1046047742632,-3.53049489408182,
134.231254548349));
#86357=CARTESIAN_POINT('Ctrl Pts',(-52.1123559655033,-3.4322556305999,134.32697390158));
#86358=CARTESIAN_POINT('Ctrl Pts',(-52.1201038622804,-3.3340581214257,134.422652571534));
#86359=CARTESIAN_POINT('Ctrl Pts',(-52.1278517590574,-3.23180603940663,
134.514271534803));
#86360=CARTESIAN_POINT('Ctrl Pts',(-52.1355996558344,-3.12587458476752,
134.601476778919));
#86361=CARTESIAN_POINT('Ctrl Pts',(-52.1433459319185,-3.01996528870496,
134.688663781577));
#86362=CARTESIAN_POINT('Ctrl Pts',(-52.1510922080025,-2.91037845254127,
134.771438653157));
#86363=CARTESIAN_POINT('Ctrl Pts',(-52.1588384840866,-2.79752328678356,
134.849486885361));
#86364=CARTESIAN_POINT('Ctrl Pts',(-52.1665848173519,-2.68466728795466,
134.927535693699));
#86365=CARTESIAN_POINT('Ctrl Pts',(-52.1743311506172,-2.56854323294814,
135.000857570654));
#86366=CARTESIAN_POINT('Ctrl Pts',(-52.1820774838825,-2.44958997569059,
135.069180896722));
#86367=CARTESIAN_POINT('Ctrl Pts',(-52.1898255518854,-2.33061007967616,
135.137519523324));
#86368=CARTESIAN_POINT('Ctrl Pts',(-52.1975736198884,-2.20880005961682,
135.200857176895));
#86369=CARTESIAN_POINT('Ctrl Pts',(-52.2053216878913,-2.0846237035928,135.258968016307));
#86370=CARTESIAN_POINT('Ctrl Pts',(-52.2130779906331,-1.96031537145971,
135.317140616611));
#86371=CARTESIAN_POINT('Ctrl Pts',(-52.220834293375,-1.83363603411204,135.37007513983));
#86372=CARTESIAN_POINT('Ctrl Pts',(-52.2285905961168,-1.70507032710317,
135.417593566609));
#86373=CARTESIAN_POINT('Ctrl Pts',(-52.2363510386309,-1.57643600070525,
135.465137355403));
#86374=CARTESIAN_POINT('Ctrl Pts',(-52.244111481145,-1.44591367037546,135.507259167711));
#86375=CARTESIAN_POINT('Ctrl Pts',(-52.2518719236591,-1.31400253787622,
135.543831093574));
#86376=CARTESIAN_POINT('Ctrl Pts',(-52.2596448239245,-1.18187964991658,
135.580461727939));
#86377=CARTESIAN_POINT('Ctrl Pts',(-52.26741772419,-1.04836388569331,135.611524583853));
#86378=CARTESIAN_POINT('Ctrl Pts',(-52.2751906244553,-0.913964912631464,
135.636942867355));
#86379=CARTESIAN_POINT('Ctrl Pts',(-52.2826809602179,-0.784451680762086,
135.661437132229));
#86380=CARTESIAN_POINT('Ctrl Pts',(-52.2901712959803,-0.654118643653161,
135.680690043575));
#86381=CARTESIAN_POINT('Ctrl Pts',(-52.2976616317428,-0.523423857490555,
135.694678657112));
#86382=CARTESIAN_POINT('Ctrl Pts',(-52.3054359658619,-0.387773738795743,
135.709197653182));
#86383=CARTESIAN_POINT('Ctrl Pts',(-52.313210299981,-0.251304199309538,
135.718091271386));
#86384=CARTESIAN_POINT('Ctrl Pts',(-52.3209846341001,-0.114521427230507,
135.721277121352));
#86385=CARTESIAN_POINT('Ctrl Pts',(-52.3287493870472,0.0220927723065638,
135.724459045043));
#86386=CARTESIAN_POINT('Ctrl Pts',(-52.3365141399942,0.159019049242489,
135.72194718767));
#86387=CARTESIAN_POINT('Ctrl Pts',(-52.3442788929413,0.295744432258527,
135.713710706253));
#86388=CARTESIAN_POINT('Ctrl Pts',(-52.3520359338263,0.432334017696848,
135.705482405425));
#86389=CARTESIAN_POINT('Ctrl Pts',(-52.3597929747113,0.568722718557942,
135.691540818865));
#86390=CARTESIAN_POINT('Ctrl Pts',(-52.3675500155963,0.7043962461554,135.671907123857));
#86391=CARTESIAN_POINT('Ctrl Pts',(-52.3753012068364,0.839967461290311,
135.652288234771));
#86392=CARTESIAN_POINT('Ctrl Pts',(-52.3830523980765,0.974824191271789,
135.626985836893));
#86393=CARTESIAN_POINT('Ctrl Pts',(-52.3908035893166,1.10845631559856,135.596073010741));
#86394=CARTESIAN_POINT('Ctrl Pts',(-52.3985514860937,1.24203164270757,135.565173323366));
#86395=CARTESIAN_POINT('Ctrl Pts',(-52.4062993828708,1.37438301926801,135.528668038398));
#86396=CARTESIAN_POINT('Ctrl Pts',(-52.4140472796479,1.5050097996753,135.486681470026));
#86397=CARTESIAN_POINT('Ctrl Pts',(-52.421793555732,1.63560925577612,135.444703684339));
#86398=CARTESIAN_POINT('Ctrl Pts',(-52.4295398318161,1.76448446129726,135.397247015391));
#86399=CARTESIAN_POINT('Ctrl Pts',(-52.4372861079002,1.89114962322367,135.344485744155));
#86400=CARTESIAN_POINT('Ctrl Pts',(-52.4450324411655,2.01781572016353,135.291724083446));
#86401=CARTESIAN_POINT('Ctrl Pts',(-52.4527787744308,2.14227138004817,135.233657892645));
#86402=CARTESIAN_POINT('Ctrl Pts',(-52.4605251076962,2.26405087042892,135.170509575012));
#86403=CARTESIAN_POINT('Ctrl Pts',(-52.4682731756991,2.38585763248201,135.107347115752));
#86404=CARTESIAN_POINT('Ctrl Pts',(-52.476021243702,2.50498668546375,135.039100444899));
#86405=CARTESIAN_POINT('Ctrl Pts',(-52.4837693117049,2.62099733405319,134.966037687857));
#86406=CARTESIAN_POINT('Ctrl Pts',(-52.4915256144468,2.73713128014065,134.892897278847));
#86407=CARTESIAN_POINT('Ctrl Pts',(-52.4992819171886,2.85013986985923,134.814930767388));
#86408=CARTESIAN_POINT('Ctrl Pts',(-52.5070382199305,2.95961137313065,134.732449667287));
#86409=CARTESIAN_POINT('Ctrl Pts',(-52.5147986624446,3.06914130463963,134.649924544539));
#86410=CARTESIAN_POINT('Ctrl Pts',(-52.5225591049588,3.17513008601504,134.562880279883));
#86411=CARTESIAN_POINT('Ctrl Pts',(-52.5303195474729,3.27720027223872,134.471667727441));
#86412=CARTESIAN_POINT('Ctrl Pts',(-52.5380924477384,3.37943431058668,134.380308752512));
#86413=CARTESIAN_POINT('Ctrl Pts',(-52.5458653480038,3.47773690287933,134.284768391082));
#86414=CARTESIAN_POINT('Ctrl Pts',(-52.5536382482693,3.57176795249014,134.185433931776));
#86415=CARTESIAN_POINT('Ctrl Pts',(-52.5611285840314,3.66238073659946,134.089710530273));
#86416=CARTESIAN_POINT('Ctrl Pts',(-52.5686189197935,3.74902694630057,133.990464323796));
#86417=CARTESIAN_POINT('Ctrl Pts',(-52.5761092555557,3.83143968736196,133.88806828604));
#86418=CARTESIAN_POINT('Ctrl Pts',(-52.5838835896748,3.91697713254828,133.781789871393));
#86419=CARTESIAN_POINT('Ctrl Pts',(-52.5916579237939,3.99822470497009,133.671781400682));
#86420=CARTESIAN_POINT('Ctrl Pts',(-52.599432257913,4.07483948018898,133.558424210367));
#86421=CARTESIAN_POINT('Ctrl Pts',(-52.6071970108602,4.15135983454468,133.445206722659));
#86422=CARTESIAN_POINT('Ctrl Pts',(-52.6149617638072,4.22325853509124,133.328649047652));
#86423=CARTESIAN_POINT('Ctrl Pts',(-52.6227265167543,4.29023235922937,133.209166091263));
#86424=CARTESIAN_POINT('Ctrl Pts',(-52.6304835576394,4.35713966402121,133.08980180703));
#86425=CARTESIAN_POINT('Ctrl Pts',(-52.6382405985244,4.41913163669655,132.967518362188));
#86426=CARTESIAN_POINT('Ctrl Pts',(-52.6459976394094,4.47594810870774,132.842759889214));
#86427=CARTESIAN_POINT('Ctrl Pts',(-52.6537488306496,4.53272173497543,132.718095497575));
#86428=CARTESIAN_POINT('Ctrl Pts',(-52.6615000218899,4.58432746765317,132.590960147201));
#86429=CARTESIAN_POINT('Ctrl Pts',(-52.66925121313,4.63055105886011,132.461822518724));
#86430=CARTESIAN_POINT('Ctrl Pts',(-52.6769991099071,4.67675500380774,132.332739777183));
#86431=CARTESIAN_POINT('Ctrl Pts',(-52.6847470066842,4.71758122557412,132.20165681748));
#86432=CARTESIAN_POINT('Ctrl Pts',(-52.6924949034613,4.75286370202761,132.069062041796));
#86433=CARTESIAN_POINT('Ctrl Pts',(-52.7002411795455,4.78813879814762,131.93649500208));
#86434=CARTESIAN_POINT('Ctrl Pts',(-52.7079874556296,4.81787235505548,131.802417152979));
#86435=CARTESIAN_POINT('Ctrl Pts',(-52.7157337317137,4.84194841727673,131.667331409037));
#86436=CARTESIAN_POINT('Ctrl Pts',(-52.7234800649791,4.86602465722201,131.532244667922));
#86437=CARTESIAN_POINT('Ctrl Pts',(-52.7312263982445,4.88444325054703,131.396150402019));
#86438=CARTESIAN_POINT('Ctrl Pts',(-52.7389727315098,4.89713957164911,131.259560659623));
#86439=CARTESIAN_POINT('Ctrl Pts',(-52.7467207995128,4.90983873600426,131.122940328901));
#86440=CARTESIAN_POINT('Ctrl Pts',(-52.7544688675158,4.91681304199492,130.985824690103));
#86441=CARTESIAN_POINT('Ctrl Pts',(-52.7622169355188,4.91804986453024,130.848729441013));
#86442=CARTESIAN_POINT('Ctrl Pts',(-52.7699732382607,4.91928800157527,130.711488485461));
#86443=CARTESIAN_POINT('Ctrl Pts',(-52.7777295410026,4.91477647048875,130.574268354479));
#86444=CARTESIAN_POINT('Ctrl Pts',(-52.7854858437445,4.90455480649529,130.437583829064));
#86445=CARTESIAN_POINT('Ctrl Pts',(-52.7932462862587,4.894327686892,130.300826351003));
#86446=CARTESIAN_POINT('Ctrl Pts',(-52.8010067287729,4.87838440706759,130.164605436252));
#86447=CARTESIAN_POINT('Ctrl Pts',(-52.8087671712871,4.85681613228064,130.029428285218));
#86448=CARTESIAN_POINT('Ctrl Pts',(-52.8165400715525,4.83521323418427,129.894034135821));
#86449=CARTESIAN_POINT('Ctrl Pts',(-52.8243129718181,4.80796737457661,129.759687481794));
#86450=CARTESIAN_POINT('Ctrl Pts',(-52.8320858720835,4.77522055981481,129.626883795025));
#86451=CARTESIAN_POINT('Ctrl Pts',(-52.8395762078452,4.74366417425527,129.498907856787));
#86452=CARTESIAN_POINT('Ctrl Pts',(-52.8470665436069,4.70699992274369,129.372364947801));
#86453=CARTESIAN_POINT('Ctrl Pts',(-52.8545568793686,4.66539733576304,129.247681215134));
#86454=CARTESIAN_POINT('Ctrl Pts',(-52.8623312134877,4.62221737405043,129.118270060842));
#86455=CARTESIAN_POINT('Ctrl Pts',(-52.8701055476068,4.57358042951609,128.990451911587));
#86456=CARTESIAN_POINT('Ctrl Pts',(-52.8778798817259,4.5196219722879,128.864721401085));
#86457=CARTESIAN_POINT('Ctrl Pts',(-52.885644634673,4.46573001403592,128.739145842199));
#86458=CARTESIAN_POINT('Ctrl Pts',(-52.89340938762,4.40652974483713,128.615653158733));
#86459=CARTESIAN_POINT('Ctrl Pts',(-52.9011741405671,4.3422063375672,128.494722727227));
#86460=CARTESIAN_POINT('Ctrl Pts',(-52.9089311814521,4.27794681721208,128.37391240553));
#86461=CARTESIAN_POINT('Ctrl Pts',(-52.9166882223371,4.20857446728899,128.255659614338));
#86462=CARTESIAN_POINT('Ctrl Pts',(-52.9244452632221,4.13432232157438,128.140423305272));
#86463=CARTESIAN_POINT('Ctrl Pts',(-52.9321964544622,4.06012616998055,128.025273896803));
#86464=CARTESIAN_POINT('Ctrl Pts',(-52.9399476457024,3.98105775810385,127.913136770021));
#86465=CARTESIAN_POINT('Ctrl Pts',(-52.9476988369425,3.89739559401976,127.804445511065));
#86466=CARTESIAN_POINT('Ctrl Pts',(-52.9554467337196,3.81376898858717,127.695800448793));
#86467=CARTESIAN_POINT('Ctrl Pts',(-52.9631946304966,3.72555275222789,127.590598650564));
#86468=CARTESIAN_POINT('Ctrl Pts',(-52.9709425272737,3.63306805251157,127.489243788807));
#86469=CARTESIAN_POINT('Ctrl Pts',(-52.9786888033578,3.5406026986007,127.387910128303));
#86470=CARTESIAN_POINT('Ctrl Pts',(-52.986435079442,3.44387092066199,127.290422092306));
#86471=CARTESIAN_POINT('Ctrl Pts',(-52.9941813555261,3.34323315817787,127.197149075036));
#86472=CARTESIAN_POINT('Ctrl Pts',(-53.0019276887914,3.24259465280851,127.103875369246));
#86473=CARTESIAN_POINT('Ctrl Pts',(-53.0096740220567,3.13805039210655,127.014817010033));
#86474=CARTESIAN_POINT('Ctrl Pts',(-53.0174203553221,3.02999624508699,126.930305143356));
#86475=CARTESIAN_POINT('Ctrl Pts',(-53.025168423325,2.92191790009055,126.845774350832));
#86476=CARTESIAN_POINT('Ctrl Pts',(-53.032916491328,2.81032841259863,126.765792317674));
#86477=CARTESIAN_POINT('Ctrl Pts',(-53.040664559331,2.6956548295922,126.690648412976));
#86478=CARTESIAN_POINT('Ctrl Pts',(-53.0484208620729,2.58085937013712,126.615424644441));
#86479=CARTESIAN_POINT('Ctrl Pts',(-53.0561771648148,2.46297359491387,126.545049490733));
#86480=CARTESIAN_POINT('Ctrl Pts',(-53.0639334675567,2.34245197350996,126.479767941452));
#86481=CARTESIAN_POINT('Ctrl Pts',(-53.0716939100708,2.2218660260877,126.414451549442));
#86482=CARTESIAN_POINT('Ctrl Pts',(-53.0794543525849,2.0986417803501,126.354234350491));
#86483=CARTESIAN_POINT('Ctrl Pts',(-53.0872147950991,1.9732552354135,126.299313798895));
#86484=CARTESIAN_POINT('Ctrl Pts',(-53.0949876953645,1.84766740886368,126.244305083955));
#86485=CARTESIAN_POINT('Ctrl Pts',(-53.10276059563,1.71991071130153,126.194610149184));
#86486=CARTESIAN_POINT('Ctrl Pts',(-53.1105334958954,1.59047875516304,126.150377335272));
#86487=CARTESIAN_POINT('Ctrl Pts',(-53.1180238316574,1.46575197664943,126.107752495561));
#86488=CARTESIAN_POINT('Ctrl Pts',(-53.1255141674195,1.33946991991614,126.070199635451));
#86489=CARTESIAN_POINT('Ctrl Pts',(-53.1330045031815,1.21208274992882,126.037806467048));
#86490=CARTESIAN_POINT('Ctrl Pts',(-53.1407788373006,1.07986565667348,126.004185101818));
#86491=CARTESIAN_POINT('Ctrl Pts',(-53.1485531714196,0.946039171163907,
125.976015908921));
#86492=CARTESIAN_POINT('Ctrl Pts',(-53.1563275055387,0.811092667664798,
125.953452275105));
#86493=CARTESIAN_POINT('Ctrl Pts',(-53.1640922584857,0.676312473670737,
125.930916448951));
#86494=CARTESIAN_POINT('Ctrl Pts',(-53.1718570114329,0.54041539002685,125.913972500176));
#86495=CARTESIAN_POINT('Ctrl Pts',(-53.17962176438,0.40390482025721,125.902723752327));
#86496=CARTESIAN_POINT('Ctrl Pts',(-53.1873788052649,0.267529834709927,
125.891486176892));
#86497=CARTESIAN_POINT('Ctrl Pts',(-53.1951358461499,0.130542962740503,
125.885932577486));
#86498=CARTESIAN_POINT('Ctrl Pts',(-53.2028928870349,-0.00654370620673618,
125.886114970752));
#86499=CARTESIAN_POINT('Ctrl Pts',(-53.210644078275,-0.143526997030357,
125.886297226473));
#86500=CARTESIAN_POINT('Ctrl Pts',(-53.2183952695151,-0.280609545653028,
125.892206864592));
#86501=CARTESIAN_POINT('Ctrl Pts',(-53.2261464607552,-0.417276023358432,
125.903843932274));
#86502=CARTESIAN_POINT('Ctrl Pts',(-53.2338943575323,-0.553884414165485,
125.915476053891));
#86503=CARTESIAN_POINT('Ctrl Pts',(-53.2416422543094,-0.690076697039048,
125.932830730314));
#86504=CARTESIAN_POINT('Ctrl Pts',(-53.2493901510864,-0.825339652014751,
125.955855948979));
#86505=CARTESIAN_POINT('Ctrl Pts',(-53.2571364271705,-0.960574312896021,
125.978876351264));
#86506=CARTESIAN_POINT('Ctrl Pts',(-53.2648827032546,-1.09487964736569,
126.007564870896));
#86507=CARTESIAN_POINT('Ctrl Pts',(-53.2726289793387,-1.22775004726036,
126.041817926529));
#86508=CARTESIAN_POINT('Ctrl Pts',(-53.280375312604,-1.36062142797415,126.07607123501));
#86509=CARTESIAN_POINT('Ctrl Pts',(-53.2881216458693,-1.49205747438903,
126.115889063859));
#86510=CARTESIAN_POINT('Ctrl Pts',(-53.2958679791347,-1.62156560715783,
126.161117349743));
#86511=CARTESIAN_POINT('Ctrl Pts',(-53.3036160471376,-1.75110274237485,
126.206355764188));
#86512=CARTESIAN_POINT('Ctrl Pts',(-53.3113641151406,-1.87871073579389,
126.257006917801));
#86513=CARTESIAN_POINT('Ctrl Pts',(-53.3191121831436,-2.00391530367527,
126.312867934927));
#86514=CARTESIAN_POINT('Ctrl Pts',(-53.3268684858854,-2.12925294046152,
126.368788321808));
#86515=CARTESIAN_POINT('Ctrl Pts',(-53.3346247886273,-2.252181691432,126.429929473614));
#86516=CARTESIAN_POINT('Ctrl Pts',(-53.3423810913692,-2.37224978798514,
126.496041455073));
#86517=CARTESIAN_POINT('Ctrl Pts',(-53.3501415338833,-2.49238196849675,
126.562188722488));
#86518=CARTESIAN_POINT('Ctrl Pts',(-53.3579019763974,-2.60965011815424,
126.633311903399));
#86519=CARTESIAN_POINT('Ctrl Pts',(-53.3656624189116,-2.72363082391754,
126.709117255139));
#86520=CARTESIAN_POINT('Ctrl Pts',(-53.373435319177,-2.83779450162847,126.785044296359));
#86521=CARTESIAN_POINT('Ctrl Pts',(-53.3812082194424,-2.94865987334772,
126.865668298165));
#86522=CARTESIAN_POINT('Ctrl Pts',(-53.3889811197078,-3.05583532627483,
126.950654152202));
#86523=CARTESIAN_POINT('Ctrl Pts',(-53.39647145547,-3.15911468153169,127.032550556379));
#86524=CARTESIAN_POINT('Ctrl Pts',(-53.4039617912322,-3.25896750257098,
127.118496989036));
#86525=CARTESIAN_POINT('Ctrl Pts',(-53.4114521269944,-3.35507666955602,
127.20816212417));
#86526=CARTESIAN_POINT('Ctrl Pts',(-53.4191092801371,-3.45332628524492,
127.299824192879));
#86527=CARTESIAN_POINT('Ctrl Pts',(-53.4267664332797,-3.54799461589064,
127.395681804218));
#86528=CARTESIAN_POINT('Ctrl Pts',(-53.4344235864223,-3.63869382386666,
127.495419651236));
#86529=CARTESIAN_POINT('Ctrl Pts',(-53.4420718673701,-3.72928794042992,
127.595041933946));
#86530=CARTESIAN_POINT('Ctrl Pts',(-53.449720148318,-3.81592180784249,127.69853521981));
#86531=CARTESIAN_POINT('Ctrl Pts',(-53.4573684292659,-3.89824149798524,
127.805544803634));
#86532=CARTESIAN_POINT('Ctrl Pts',(-53.465009622384,-3.98048490066586,127.912455219331));
#86533=CARTESIAN_POINT('Ctrl Pts',(-53.4726508155022,-4.05842183125482,
128.022875136013));
#86534=CARTESIAN_POINT('Ctrl Pts',(-53.4802920086204,-4.1317364140721,128.136414353652));
#86535=CARTESIAN_POINT('Ctrl Pts',(-53.4879278738848,-4.20499987799149,
128.2498744056));
#86536=CARTESIAN_POINT('Ctrl Pts',(-53.4955637391492,-4.27364718674857,
128.366449094643));
#86537=CARTESIAN_POINT('Ctrl Pts',(-53.5031996044137,-4.33740419922716,
128.48571707553));
#86538=CARTESIAN_POINT('Ctrl Pts',(-53.5108322038416,-4.4011339430232,128.60493404586));
#86539=CARTESIAN_POINT('Ctrl Pts',(-53.5184648032694,-4.45997736130885,
128.726841661266));
#86540=CARTESIAN_POINT('Ctrl Pts',(-53.5260974026973,-4.5137051911607,128.850992114239));
#86541=CARTESIAN_POINT('Ctrl Pts',(-53.5337303321047,-4.56743534382382,
128.9751479346));
#86542=CARTESIAN_POINT('Ctrl Pts',(-53.5413632615123,-4.61604929520416,
129.101546420496));
#86543=CARTESIAN_POINT('Ctrl Pts',(-53.5489961909197,-4.6593651655302,129.229718017881));
#86544=CARTESIAN_POINT('Ctrl Pts',(-53.55591934613,-4.6986531606534,129.34597113839));
#86545=CARTESIAN_POINT('Ctrl Pts',(-53.5628425013403,-4.73358309749759,
129.463682473335));
#86546=CARTESIAN_POINT('Ctrl Pts',(-53.5697656565506,-4.76405452823409,
129.582490119308));
#86547=CARTESIAN_POINT('Origin',(213.235140564004,0.,130.804360617566));
#86548=CARTESIAN_POINT('',(-55.665415119611,-4.764054528234,129.582490119308));
#86549=CARTESIAN_POINT('',(-55.3197786156161,-4.76405452823412,129.582490119309));
#86550=CARTESIAN_POINT('',(213.235140564004,-4.76405452823405,129.582490119308));
#86551=CARTESIAN_POINT('',(-53.9851405640441,-4.91824877609614,130.800890901613));
#86552=CARTESIAN_POINT('Ctrl Pts',(-53.9851405640439,-4.91824877609614,
130.800890901613));
#86553=CARTESIAN_POINT('Ctrl Pts',(-53.9927972686402,-4.91834379071892,
130.935572114287));
#86554=CARTESIAN_POINT('Ctrl Pts',(-54.0004539732365,-4.91290248423804,
131.070468642337));
#86555=CARTESIAN_POINT('Ctrl Pts',(-54.0081106778327,-4.90189833130391,
131.205079736226));
#86556=CARTESIAN_POINT('Ctrl Pts',(-54.0157593497178,-4.89090572291623,
131.339549608521));
#86557=CARTESIAN_POINT('Ctrl Pts',(-54.0234080216029,-4.87436190749982,
131.473734243646));
#86558=CARTESIAN_POINT('Ctrl Pts',(-54.031056693488,-4.85229238178572,131.607131882725));
#86559=CARTESIAN_POINT('Ctrl Pts',(-54.0386992936412,-4.8302403754848,131.740423626987));
#86560=CARTESIAN_POINT('Ctrl Pts',(-54.0463418937945,-4.80267145024832,
131.872929222193));
#86561=CARTESIAN_POINT('Ctrl Pts',(-54.0539844939477,-4.76966296323101,
132.004151549221));
#86562=CARTESIAN_POINT('Ctrl Pts',(-54.061623586964,-4.73666962358229,132.135313659222));
#86563=CARTESIAN_POINT('Ctrl Pts',(-54.0692626799804,-4.6982417827371,132.265193281768));
#86564=CARTESIAN_POINT('Ctrl Pts',(-54.0769017729967,-4.65450790482404,
132.393303419063));
#86565=CARTESIAN_POINT('Ctrl Pts',(-54.0845392166914,-4.61078346929268,
132.521385896685));
#86566=CARTESIAN_POINT('Ctrl Pts',(-54.0921766603861,-4.56175540431634,
132.647699267331));
#86567=CARTESIAN_POINT('Ctrl Pts',(-54.0998141040808,-4.50760190068792,
132.771772157487));
#86568=CARTESIAN_POINT('Ctrl Pts',(-54.1074516622702,-4.45344758523193,
132.895846907648));
#86569=CARTESIAN_POINT('Ctrl Pts',(-54.1150892204595,-4.39416783982267,
133.01768074119));
#86570=CARTESIAN_POINT('Ctrl Pts',(-54.1227267786489,-4.32998858797518,
133.136823241169));
#86571=CARTESIAN_POINT('Ctrl Pts',(-54.1303662150348,-4.26579355343277,
133.255995040177));
#86572=CARTESIAN_POINT('Ctrl Pts',(-54.1380056514206,-4.19669680812159,
133.372473835057));
#86573=CARTESIAN_POINT('Ctrl Pts',(-54.1456450878066,-4.12296942876577,
133.485835240225));
#86574=CARTESIAN_POINT('Ctrl Pts',(-54.1532924949838,-4.04916512416028,
133.599314923765));
#86575=CARTESIAN_POINT('Ctrl Pts',(-54.160939902161,-3.97072076004615,133.709670386039));
#86576=CARTESIAN_POINT('Ctrl Pts',(-54.1685873093382,-3.88794997798313,
133.816507365519));
#86577=CARTESIAN_POINT('Ctrl Pts',(-54.1762391488307,-3.80513122329416,
133.923406266008));
#86578=CARTESIAN_POINT('Ctrl Pts',(-54.1838909883232,-3.7179813182745,134.026782316829));
#86579=CARTESIAN_POINT('Ctrl Pts',(-54.1915428278157,-3.62685222945442,
134.126276626167));
#86580=CARTESIAN_POINT('Ctrl Pts',(-54.1992059243301,-3.53558907585785,
134.225917306796));
#86581=CARTESIAN_POINT('Ctrl Pts',(-54.2068690208445,-3.44033533527844,
134.321664560761));
#86582=CARTESIAN_POINT('Ctrl Pts',(-54.2145321173589,-3.34147792538912,
134.413198150157));
#86583=CARTESIAN_POINT('Ctrl Pts',(-54.2187567456638,-3.2869783100992,134.463660178383));
#86584=CARTESIAN_POINT('Ctrl Pts',(-54.2229813739687,-3.23138400646271,
134.51284229533));
#86585=CARTESIAN_POINT('Ctrl Pts',(-54.2272060022736,-3.17476362491381,
134.56069646363));
#86586=CARTESIAN_POINT('Ctrl Pts',(-54.2349803363927,-3.07056847865618,
134.648759665055));
#86587=CARTESIAN_POINT('Ctrl Pts',(-54.2427546705117,-2.96254140538158,
134.732623740153));
#86588=CARTESIAN_POINT('Ctrl Pts',(-54.2505290046308,-2.85105540249286,
134.811936712217));
#86589=CARTESIAN_POINT('Ctrl Pts',(-54.2582937575779,-2.73970679613877,
134.891151938131));
#86590=CARTESIAN_POINT('Ctrl Pts',(-54.266058510525,-2.62490805742996,134.965826996443));
#86591=CARTESIAN_POINT('Ctrl Pts',(-54.2738232634721,-2.50706669629267,
135.035648795277));
#86592=CARTESIAN_POINT('Ctrl Pts',(-54.281580304357,-2.38934237685669,135.105401246116));
#86593=CARTESIAN_POINT('Ctrl Pts',(-54.2893373452421,-2.26858178304,135.170309832139));
#86594=CARTESIAN_POINT('Ctrl Pts',(-54.2970943861271,-2.14522267609269,
135.230103801764));
#86595=CARTESIAN_POINT('Ctrl Pts',(-54.3048455773673,-2.02195659520702,
135.289852680292));
#86596=CARTESIAN_POINT('Ctrl Pts',(-54.3125967686073,-1.89609625196496,
135.344494449653));
#86597=CARTESIAN_POINT('Ctrl Pts',(-54.3203479598475,-1.7681050506704,135.393803676619));
#86598=CARTESIAN_POINT('Ctrl Pts',(-54.3280958566245,-1.6401682490512,135.443091945849));
#86599=CARTESIAN_POINT('Ctrl Pts',(-54.3358437534017,-1.51010275475476,
135.48705204027));
#86600=CARTESIAN_POINT('Ctrl Pts',(-54.3435916501788,-1.37839284524093,
135.525506265255));
#86601=CARTESIAN_POINT('Ctrl Pts',(-54.3513379262628,-1.24671048660084,
135.563952446444));
#86602=CARTESIAN_POINT('Ctrl Pts',(-54.3590842023469,-1.11338477198998,
135.596894939508));
#86603=CARTESIAN_POINT('Ctrl Pts',(-54.366830478431,-0.978915688513234,
135.6242057538));
#86604=CARTESIAN_POINT('Ctrl Pts',(-54.3745768116964,-0.844445612415897,
135.651516769695));
#86605=CARTESIAN_POINT('Ctrl Pts',(-54.3823231449617,-0.708832533753829,
135.67319594605));
#86606=CARTESIAN_POINT('Ctrl Pts',(-54.3900694782271,-0.572586802527636,
135.689166388123));
#86607=CARTESIAN_POINT('Ctrl Pts',(-54.3978175462301,-0.436310560014969,
135.705140406667));
#86608=CARTESIAN_POINT('Ctrl Pts',(-54.4055656142329,-0.299401771247377,
135.715403101492));
#86609=CARTESIAN_POINT('Ctrl Pts',(-54.4133136822359,-0.16237568253322,
135.719929475819));
#86610=CARTESIAN_POINT('Ctrl Pts',(-54.4210699849777,-0.0252039608615334,
135.724460660829));
#86611=CARTESIAN_POINT('Ctrl Pts',(-54.4288262877196,0.112084918418896,
135.723243333739));
#86612=CARTESIAN_POINT('Ctrl Pts',(-54.4365825904614,0.24897537381797,135.716304665062));
#86613=CARTESIAN_POINT('Ctrl Pts',(-54.4443430329756,0.385938891775156,
135.709362293009));
#86614=CARTESIAN_POINT('Ctrl Pts',(-54.4521034754898,0.522503173023274,
135.696692530807));
#86615=CARTESIAN_POINT('Ctrl Pts',(-54.4598639180039,0.658158975501423,
135.678374346052));
#86616=CARTESIAN_POINT('Ctrl Pts',(-54.4676368182694,0.794032544716666,
135.66002675532));
#86617=CARTESIAN_POINT('Ctrl Pts',(-54.4754097185348,0.92899433573148,135.636012691109));
#86618=CARTESIAN_POINT('Ctrl Pts',(-54.4831826188003,1.06254561158124,135.606462228924));
#86619=CARTESIAN_POINT('Ctrl Pts',(-54.4906729545623,1.19124196215814,135.577986000473));
#86620=CARTESIAN_POINT('Ctrl Pts',(-54.4981632903242,1.31862827086018,135.544368988257));
#86621=CARTESIAN_POINT('Ctrl Pts',(-54.5056536260862,1.4442744450737,135.505770447586));
#86622=CARTESIAN_POINT('Ctrl Pts',(-54.5134279602053,1.57468453217258,135.465708431513));
#86623=CARTESIAN_POINT('Ctrl Pts',(-54.5212022943244,1.70363302552022,135.420152776365));
#86624=CARTESIAN_POINT('Ctrl Pts',(-54.5289766284435,1.83062218293633,135.369227043415));
#86625=CARTESIAN_POINT('Ctrl Pts',(-54.5367413813906,1.95745483756511,135.318364071879));
#86626=CARTESIAN_POINT('Ctrl Pts',(-54.5445061343378,2.0823326014182,135.262144334791));
#86627=CARTESIAN_POINT('Ctrl Pts',(-54.5522708872849,2.20477179236346,135.200741447988));
#86628=CARTESIAN_POINT('Ctrl Pts',(-54.5600279281699,2.32708937497868,135.139399547397));
#86629=CARTESIAN_POINT('Ctrl Pts',(-54.5677849690549,2.44697285740616,135.072884915926));
#86630=CARTESIAN_POINT('Ctrl Pts',(-54.57554200994,2.56395782802465,135.001419506671));
#86631=CARTESIAN_POINT('Ctrl Pts',(-54.5832932011801,2.68085457936631,134.930007990037));
#86632=CARTESIAN_POINT('Ctrl Pts',(-54.5910443924203,2.79485683729627,134.853653329756));
#86633=CARTESIAN_POINT('Ctrl Pts',(-54.5987955836605,2.90552445711169,134.772623548828));
#86634=CARTESIAN_POINT('Ctrl Pts',(-54.6065434804376,3.01614504023667,134.691628207718));
#86635=CARTESIAN_POINT('Ctrl Pts',(-54.6142913772147,3.12343348938125,134.605961928539));
#86636=CARTESIAN_POINT('Ctrl Pts',(-54.6220392739918,3.22697854122691,134.515936099347));
#86637=CARTESIAN_POINT('Ctrl Pts',(-54.6297855500759,3.3305019336799,134.425929101618));
#86638=CARTESIAN_POINT('Ctrl Pts',(-54.63753182616,3.43028319148311,134.331564624101));
#86639=CARTESIAN_POINT('Ctrl Pts',(-54.6452781022441,3.52594437723939,134.233194138038));
#86640=CARTESIAN_POINT('Ctrl Pts',(-54.6530244355095,3.62160626914468,134.134822925827));
#86641=CARTESIAN_POINT('Ctrl Pts',(-54.6607707687749,3.71314775574784,134.032445926349));
#86642=CARTESIAN_POINT('Ctrl Pts',(-54.6685171020402,3.8002282866856,133.92645094803));
#86643=CARTESIAN_POINT('Ctrl Pts',(-54.6762651700432,3.88732831870449,133.82043223287));
#86644=CARTESIAN_POINT('Ctrl Pts',(-54.6840132380463,3.96996515902742,133.710794228654));
#86645=CARTESIAN_POINT('Ctrl Pts',(-54.6917613060492,4.04783927394014,133.597956915324));
#86646=CARTESIAN_POINT('Ctrl Pts',(-54.6995176087911,4.12579615438902,133.484999677155));
#86647=CARTESIAN_POINT('Ctrl Pts',(-54.707273911533,4.19897997534989,133.368836659765));
#86648=CARTESIAN_POINT('Ctrl Pts',(-54.7150302142748,4.26713491175729,133.249916322792));
#86649=CARTESIAN_POINT('Ctrl Pts',(-54.722790656789,4.33532622450636,133.130932514454));
#86650=CARTESIAN_POINT('Ctrl Pts',(-54.7305510993032,4.3984831245225,133.009188800992));
#86651=CARTESIAN_POINT('Ctrl Pts',(-54.7383115418174,4.45639679170617,132.885156306088));
#86652=CARTESIAN_POINT('Ctrl Pts',(-54.7460844420828,4.51440342704965,132.760924703212));
#86653=CARTESIAN_POINT('Ctrl Pts',(-54.7538573423483,4.56714985938415,132.634397337832));
#86654=CARTESIAN_POINT('Ctrl Pts',(-54.7616302426137,4.61447594540314,132.50606412047));
#86655=CARTESIAN_POINT('Ctrl Pts',(-54.7691205783756,4.66008160898704,132.382396138813));
#86656=CARTESIAN_POINT('Ctrl Pts',(-54.7766109141375,4.70065407596304,132.257051613294));
#86657=CARTESIAN_POINT('Ctrl Pts',(-54.7841012498994,4.73609485676863,132.130478474391));
#86658=CARTESIAN_POINT('Ctrl Pts',(-54.7918755840184,4.77287938555128,131.999106276453));
#86659=CARTESIAN_POINT('Ctrl Pts',(-54.7996499181375,4.80425193306907,131.865994312623));
#86660=CARTESIAN_POINT('Ctrl Pts',(-54.8074242522565,4.83004741311189,131.731628135379));
#86661=CARTESIAN_POINT('Ctrl Pts',(-54.8151890052036,4.85581110253089,131.597427552441));
#86662=CARTESIAN_POINT('Ctrl Pts',(-54.8229537581507,4.87601132716498,131.46197621185));
#86663=CARTESIAN_POINT('Ctrl Pts',(-54.8307185110978,4.89053271292637,131.325774892684));
#86664=CARTESIAN_POINT('Ctrl Pts',(-54.8384755519828,4.90503967584271,131.189708850588));
#86665=CARTESIAN_POINT('Ctrl Pts',(-54.8462325928678,4.91387898316304,131.052894698526));
#86666=CARTESIAN_POINT('Ctrl Pts',(-54.8539896337528,4.91698634448713,130.915843130218));
#86667=CARTESIAN_POINT('Ctrl Pts',(-54.8617408249929,4.92009136252587,130.778894913562));
#86668=CARTESIAN_POINT('Ctrl Pts',(-54.8694920162329,4.91747302942635,130.641710026306));
#86669=CARTESIAN_POINT('Ctrl Pts',(-54.877243207473,4.90911893156643,130.504803647632));
#86670=CARTESIAN_POINT('Ctrl Pts',(-54.8849911042501,4.90076838442096,130.367955457821));
#86671=CARTESIAN_POINT('Ctrl Pts',(-54.8927390010272,4.88668694498166,130.231385930578));
#86672=CARTESIAN_POINT('Ctrl Pts',(-54.9004868978043,4.86691429496976,130.095609386231));
#86673=CARTESIAN_POINT('Ctrl Pts',(-54.9082331738884,4.84714578097,129.95986124341));
#86674=CARTESIAN_POINT('Ctrl Pts',(-54.9159794499725,4.82168848062965,129.82490614019));
#86675=CARTESIAN_POINT('Ctrl Pts',(-54.9237257260566,4.79063381226401,129.691252024799));
#86676=CARTESIAN_POINT('Ctrl Pts',(-54.931472059322,4.75957891465986,129.557596922803));
#86677=CARTESIAN_POINT('Ctrl Pts',(-54.9392183925873,4.72292665506641,129.425243208619));
#86678=CARTESIAN_POINT('Ctrl Pts',(-54.9469647258526,4.68081923190478,129.29468701684));
#86679=CARTESIAN_POINT('Ctrl Pts',(-54.9547127938556,4.63870237907779,129.164101587906));
#86680=CARTESIAN_POINT('Ctrl Pts',(-54.9624608618585,4.59112805173356,129.035314854411));
#86681=CARTESIAN_POINT('Ctrl Pts',(-54.9702089298615,4.53828768560231,128.908805831966));
#86682=CARTESIAN_POINT('Ctrl Pts',(-54.9779652326033,4.48539116010098,128.782162354227));
#86683=CARTESIAN_POINT('Ctrl Pts',(-54.9857215353451,4.42721756650751,128.657801784641));
#86684=CARTESIAN_POINT('Ctrl Pts',(-54.993477838087,4.36400592691846,128.536181759468));
#86685=CARTESIAN_POINT('Ctrl Pts',(-55.0012382806012,4.30076054937409,128.414496822027));
#86686=CARTESIAN_POINT('Ctrl Pts',(-55.0089987231153,4.23247196242981,128.295555682466));
#86687=CARTESIAN_POINT('Ctrl Pts',(-55.0167591656295,4.15942366341745,128.179788680906));
#86688=CARTESIAN_POINT('Ctrl Pts',(-55.0245320658949,4.08625810079059,128.063835839878));
#86689=CARTESIAN_POINT('Ctrl Pts',(-55.0323049661603,4.00831777993626,127.951067640908));
#86690=CARTESIAN_POINT('Ctrl Pts',(-55.0400778664257,3.9259283150813,127.841883625699));
#86691=CARTESIAN_POINT('Ctrl Pts',(-55.0475682021878,3.84653391479925,127.736668724458));
#86692=CARTESIAN_POINT('Ctrl Pts',(-55.05505853795,3.76300842497322,127.634782181162));
#86693=CARTESIAN_POINT('Ctrl Pts',(-55.0625488737121,3.67567546618837,127.536548975234));
#86694=CARTESIAN_POINT('Ctrl Pts',(-55.0703232078312,3.58503125172818,127.434591227447));
#86695=CARTESIAN_POINT('Ctrl Pts',(-55.0780975419503,3.48999801488191,127.336246346813));
#86696=CARTESIAN_POINT('Ctrl Pts',(-55.0858718760694,3.39089503157182,127.241915678011));
#86697=CARTESIAN_POINT('Ctrl Pts',(-55.0936366290165,3.29191418383131,127.147701263327));
#86698=CARTESIAN_POINT('Ctrl Pts',(-55.1014013819636,3.18887384964357,127.05749148407));
#86699=CARTESIAN_POINT('Ctrl Pts',(-55.1091661349107,3.0821329861155,126.97165409105));
#86700=CARTESIAN_POINT('Ctrl Pts',(-55.1169231757957,2.97549813911787,126.885901952939));
#86701=CARTESIAN_POINT('Ctrl Pts',(-55.1246802166807,2.86517037972825,126.804513802287));
#86702=CARTESIAN_POINT('Ctrl Pts',(-55.1324372575657,2.75154461850447,126.727819770858));
#86703=CARTESIAN_POINT('Ctrl Pts',(-55.1401884488058,2.63800454335172,126.651183574995));
#86704=CARTESIAN_POINT('Ctrl Pts',(-55.1479396400459,2.52117173942896,126.579234670298));
#86705=CARTESIAN_POINT('Ctrl Pts',(-55.155690831286,2.40147293170706,126.51226196763));
#86706=CARTESIAN_POINT('Ctrl Pts',(-55.1634387280631,2.28182499917135,126.445317730148));
#86707=CARTESIAN_POINT('Ctrl Pts',(-55.1711866248403,2.15931382607675,126.383345678585));
#86708=CARTESIAN_POINT('Ctrl Pts',(-55.1789345216173,2.03439357362095,126.326590430284));
#86709=CARTESIAN_POINT('Ctrl Pts',(-55.1866807977014,1.90949945178884,126.269847053958));
#86710=CARTESIAN_POINT('Ctrl Pts',(-55.1944270737855,1.78219760865962,126.218318471971));
#86711=CARTESIAN_POINT('Ctrl Pts',(-55.2021733498696,1.65296480929534,126.172202329928));
#86712=CARTESIAN_POINT('Ctrl Pts',(-55.2099196831349,1.52373105596406,126.126085847467));
#86713=CARTESIAN_POINT('Ctrl Pts',(-55.2176660164002,1.39256668617812,126.085382016074));
#86714=CARTESIAN_POINT('Ctrl Pts',(-55.2254123496656,1.25996597374079,126.050239373055));
#86715=CARTESIAN_POINT('Ctrl Pts',(-55.2331604176685,1.12733556629384,126.015088860084));
#86716=CARTESIAN_POINT('Ctrl Pts',(-55.2409084856714,0.993268553977209,
125.985502113809));
#86717=CARTESIAN_POINT('Ctrl Pts',(-55.2486565536744,0.858271421881679,
125.961576993566));
#86718=CARTESIAN_POINT('Ctrl Pts',(-55.2564128564162,0.723130813226935,
125.937626445421));
#86719=CARTESIAN_POINT('Ctrl Pts',(-55.2641691591581,0.587058495653427,
125.919349611736));
#86720=CARTESIAN_POINT('Ctrl Pts',(-55.2719254618999,0.450568688789894,
125.906792760029));
#86721=CARTESIAN_POINT('Ctrl Pts',(-55.2796859044141,0.314006033206624,
125.894229206352));
#86722=CARTESIAN_POINT('Ctrl Pts',(-55.2874463469283,0.177025834620456,
125.88739173735));
#86723=CARTESIAN_POINT('Ctrl Pts',(-55.2952067894425,0.0401433875962681,
125.886274448035));
#86724=CARTESIAN_POINT('Ctrl Pts',(-55.3029796897079,-0.0969587952835497,
125.885155365148));
#86725=CARTESIAN_POINT('Ctrl Pts',(-55.3107525899733,-0.233962522058218,
125.889774798408));
#86726=CARTESIAN_POINT('Ctrl Pts',(-55.3185254902387,-0.370355644534846,
125.900074761393));
#86727=CARTESIAN_POINT('Ctrl Pts',(-55.3260158260008,-0.501790533457566,
125.910000294779));
#86728=CARTESIAN_POINT('Ctrl Pts',(-55.333506161763,-0.632658135384008,
125.925200489566));
#86729=CARTESIAN_POINT('Ctrl Pts',(-55.3409964975251,-0.762510111089371,
125.945578733906));
#86730=CARTESIAN_POINT('Ctrl Pts',(-55.3487708316442,-0.897285463919555,
125.966729625573));
#86731=CARTESIAN_POINT('Ctrl Pts',(-55.3565451657633,-1.03139358309989,
125.993525969023));
#86732=CARTESIAN_POINT('Ctrl Pts',(-55.3643194998823,-1.16432422955083,
126.025916084982));
#86733=CARTESIAN_POINT('Ctrl Pts',(-55.3720842528294,-1.29709105086072,
126.058266283018));
#86734=CARTESIAN_POINT('Ctrl Pts',(-55.3798490057765,-1.42868291055205,
126.096196445239));
#86735=CARTESIAN_POINT('Ctrl Pts',(-55.3876137587236,-1.55859638436842,
126.139603349161));
#86736=CARTESIAN_POINT('Ctrl Pts',(-55.3953707996087,-1.68838082629131,
126.182967140735));
#86737=CARTESIAN_POINT('Ctrl Pts',(-55.4031278404937,-1.81648983132267,
126.23179672591));
#86738=CARTESIAN_POINT('Ctrl Pts',(-55.4108848813787,-1.94243219145681,
126.285938299534));
#86739=CARTESIAN_POINT('Ctrl Pts',(-55.4186360726188,-2.06827957747696,
126.340039044575));
#86740=CARTESIAN_POINT('Ctrl Pts',(-55.4263872638589,-2.191963213018,126.399443650954));
#86741=CARTESIAN_POINT('Ctrl Pts',(-55.434138455099,-2.31300937391758,126.463949266246));
#86742=CARTESIAN_POINT('Ctrl Pts',(-55.4418863518761,-2.43400408696978,
126.528427464931));
#86743=CARTESIAN_POINT('Ctrl Pts',(-55.4496342486532,-2.5523632106494,126.59800217693));
#86744=CARTESIAN_POINT('Ctrl Pts',(-55.4573821454303,-2.66763545623592,
126.672423525217));
#86745=CARTESIAN_POINT('Ctrl Pts',(-55.4651284215144,-2.7828835893538,126.746829306161));
#86746=CARTESIAN_POINT('Ctrl Pts',(-55.4728746975985,-2.89504580047696,
126.826079494942));
#86747=CARTESIAN_POINT('Ctrl Pts',(-55.4806209736826,-3.00369810159739,
126.909879807887));
#86748=CARTESIAN_POINT('Ctrl Pts',(-55.4883673069479,-3.11235120476458,
126.993680739427));
#86749=CARTESIAN_POINT('Ctrl Pts',(-55.4961136402133,-3.21749403664578,
127.082031623382));
#86750=CARTESIAN_POINT('Ctrl Pts',(-55.5038599734786,-3.31873446153417,
127.174596901244));
#86751=CARTESIAN_POINT('Ctrl Pts',(-55.5116080414816,-3.41999755851294,
127.267182908458));
#86752=CARTESIAN_POINT('Ctrl Pts',(-55.5193561094845,-3.51735622102066,
127.363984923837));
#86753=CARTESIAN_POINT('Ctrl Pts',(-55.5271041774875,-3.61045434966125,
127.464629722492));
#86754=CARTESIAN_POINT('Ctrl Pts',(-55.5348604802293,-3.70365142410148,
127.565381487637));
#86755=CARTESIAN_POINT('Ctrl Pts',(-55.5426167829712,-3.79257865330724,
127.669983907137));
#86756=CARTESIAN_POINT('Ctrl Pts',(-55.5503730857131,-3.8769191628354,127.778029362178));
#86757=CARTESIAN_POINT('Ctrl Pts',(-55.5581335282272,-3.96130468743271,
127.886132484331));
#86758=CARTESIAN_POINT('Ctrl Pts',(-55.5658939707413,-4.04109838701436,
127.997681985872));
#86759=CARTESIAN_POINT('Ctrl Pts',(-55.5736544132554,-4.11602670031402,
128.112241143099));
#86760=CARTESIAN_POINT('Ctrl Pts',(-55.5814273135208,-4.19107529519421,
128.226984200857));
#86761=CARTESIAN_POINT('Ctrl Pts',(-55.5892002137863,-4.2612426959874,128.344746232852));
#86762=CARTESIAN_POINT('Ctrl Pts',(-55.5969731140517,-4.32630085970409,
128.46506501123));
#86763=CARTESIAN_POINT('Ctrl Pts',(-55.6044634498137,-4.38899399529805,
128.581009898949));
#86764=CARTESIAN_POINT('Ctrl Pts',(-55.6119537855758,-4.44694277639168,
128.699328595379));
#86765=CARTESIAN_POINT('Ctrl Pts',(-55.6194441213379,-4.49998614696551,
128.819591678969));
#86766=CARTESIAN_POINT('Ctrl Pts',(-55.6279986247142,-4.56056549975874,
128.956940789518));
#86767=CARTESIAN_POINT('Ctrl Pts',(-55.6365531280906,-4.61491201809283,
129.09719976048));
#86768=CARTESIAN_POINT('Ctrl Pts',(-55.645107631467,-4.66276424856004,129.239811920705));
#86769=CARTESIAN_POINT('Ctrl Pts',(-55.6518767941817,-4.70062963010714,
129.352660659571));
#86770=CARTESIAN_POINT('Ctrl Pts',(-55.6586459568963,-4.73442942243786,
129.466982281433));
#86771=CARTESIAN_POINT('Ctrl Pts',(-55.665415119611,-4.764054528234,129.582490119308));
#86772=CARTESIAN_POINT('Ctrl Pts',(-53.9150733197311,-4.76405452823399,
129.582490119308));
#86773=CARTESIAN_POINT('Ctrl Pts',(-53.922847823381,-4.79808409324873,129.71517087683));
#86774=CARTESIAN_POINT('Ctrl Pts',(-53.930622327031,-4.82652590896521,129.849115295931));
#86775=CARTESIAN_POINT('Ctrl Pts',(-53.9383968306809,-4.84931793657393,
129.983812866047));
#86776=CARTESIAN_POINT('Ctrl Pts',(-53.9418506799408,-4.85944337110096,
130.043652712268));
#86777=CARTESIAN_POINT('Ctrl Pts',(-53.9453045292007,-4.86845444587565,
130.103641154042));
#86778=CARTESIAN_POINT('Ctrl Pts',(-53.9487583784606,-4.87634901943149,
130.163733344349));
#86779=CARTESIAN_POINT('Ctrl Pts',(-53.9608857736432,-4.90406899390232,
130.374733212729));
#86780=CARTESIAN_POINT('Ctrl Pts',(-53.9730131688258,-4.91809828314246,
130.587570370039));
#86781=CARTESIAN_POINT('Ctrl Pts',(-53.9851405640084,-4.9182487760957,130.800890900986));
#86782=CARTESIAN_POINT('',(-53.6398594359473,-4.9182481978369,130.808570958887));
#86783=CARTESIAN_POINT('Ctrl Pts',(-53.5697656565506,-4.76405452823409,
129.582490119308));
#86784=CARTESIAN_POINT('Ctrl Pts',(-53.5774022064258,-4.7976658793482,129.713540267179));
#86785=CARTESIAN_POINT('Ctrl Pts',(-53.5850387563011,-4.82585170671341,
129.845924118334));
#86786=CARTESIAN_POINT('Ctrl Pts',(-53.5926753061764,-4.84852592904176,
129.979145871024));
#86787=CARTESIAN_POINT('Ctrl Pts',(-53.6005393278049,-4.87187555390005,
130.116335932197));
#86788=CARTESIAN_POINT('Ctrl Pts',(-53.6084033494333,-4.889380025036,130.254414134824));
#86789=CARTESIAN_POINT('Ctrl Pts',(-53.6162673710618,-4.90100283232545,
130.392833826168));
#86790=CARTESIAN_POINT('Ctrl Pts',(-53.6241313926903,-4.9126256396149,130.531253517513));
#86791=CARTESIAN_POINT('Ctrl Pts',(-53.6319954143188,-4.91836681143365,
130.670014232959));
#86792=CARTESIAN_POINT('Ctrl Pts',(-53.6398594359473,-4.9182481978369,130.808570958887));
#86793=CARTESIAN_POINT('Ctrl Pts',(-53.639859435991,-4.91824819783625,130.808570959657));
#86794=CARTESIAN_POINT('Ctrl Pts',(-53.6516810374523,-4.91806989174917,
131.016856550807));
#86795=CARTESIAN_POINT('Ctrl Pts',(-53.6635026389136,-4.90465736337878,
131.224596674198));
#86796=CARTESIAN_POINT('Ctrl Pts',(-53.6753242403749,-4.87823520261405,
131.4304631415));
#86797=CARTESIAN_POINT('Ctrl Pts',(-53.6801827438523,-4.86737608505906,
131.515071216857));
#86798=CARTESIAN_POINT('Ctrl Pts',(-53.6850412473298,-4.85432000492346,
131.599363263414));
#86799=CARTESIAN_POINT('Ctrl Pts',(-53.6898997508072,-4.83908453432629,
131.683248512661));
#86800=CARTESIAN_POINT('Ctrl Pts',(-53.6976740849262,-4.81470549674104,
131.817477490439));
#86801=CARTESIAN_POINT('Ctrl Pts',(-53.7054484190455,-4.78469864489195,
131.950903951438));
#86802=CARTESIAN_POINT('Ctrl Pts',(-53.7132227531646,-4.74912788750124,
132.083019043674));
#86803=CARTESIAN_POINT('Ctrl Pts',(-53.7209875061117,-4.71360096789001,
132.214971315867));
#86804=CARTESIAN_POINT('Ctrl Pts',(-53.7287522590588,-4.67252388682418,
132.345615061045));
#86805=CARTESIAN_POINT('Ctrl Pts',(-53.7365170120059,-4.62601191785663,
132.474449476983));
#86806=CARTESIAN_POINT('Ctrl Pts',(-53.744274052891,-4.57954614523229,132.603155932763));
#86807=CARTESIAN_POINT('Ctrl Pts',(-53.7520310937759,-4.52765635888517,
132.730056270159));
#86808=CARTESIAN_POINT('Ctrl Pts',(-53.759788134661,-4.47050810731524,132.854663113523));
#86809=CARTESIAN_POINT('Ctrl Pts',(-53.7675393259011,-4.41340295168643,
132.979175989897));
#86810=CARTESIAN_POINT('Ctrl Pts',(-53.7752905171413,-4.35104738614633,
133.101398460851));
#86811=CARTESIAN_POINT('Ctrl Pts',(-53.7830417083814,-4.28365557277662,
133.220861806541));
#86812=CARTESIAN_POINT('Ctrl Pts',(-53.7907896051585,-4.21629240272533,
133.340274377123));
#86813=CARTESIAN_POINT('Ctrl Pts',(-53.7985375019356,-4.1438974339068,133.456929815051));
#86814=CARTESIAN_POINT('Ctrl Pts',(-53.8062853987127,-4.06673130107604,
133.570382957922));
#86815=CARTESIAN_POINT('Ctrl Pts',(-53.8140316747969,-3.98958130973666,
133.683812368842));
#86816=CARTESIAN_POINT('Ctrl Pts',(-53.821777950881,-3.9076623592502,133.794040494006));
#86817=CARTESIAN_POINT('Ctrl Pts',(-53.8295242269652,-3.82127882308466,
133.9006505295));
#86818=CARTESIAN_POINT('Ctrl Pts',(-53.8372705602306,-3.73489464925548,
134.007261351966));
#86819=CARTESIAN_POINT('Ctrl Pts',(-53.8450168934961,-3.6440460701174,134.110253727704));
#86820=CARTESIAN_POINT('Ctrl Pts',(-53.8527632267615,-3.54907795772038,
134.209243686413));
#86821=CARTESIAN_POINT('Ctrl Pts',(-53.8605112947645,-3.45408857787319,
134.308255813237));
#86822=CARTESIAN_POINT('Ctrl Pts',(-53.8682593627674,-3.35497809962917,
134.4032634574));
#86823=CARTESIAN_POINT('Ctrl Pts',(-53.8760074307704,-3.25212818580093,
134.49391957842));
#86824=CARTESIAN_POINT('Ctrl Pts',(-53.8837637335123,-3.14916896186021,
134.584672049845));
#86825=CARTESIAN_POINT('Ctrl Pts',(-53.8915200362542,-3.04246265697053,
134.671063500558));
#86826=CARTESIAN_POINT('Ctrl Pts',(-53.8992763389961,-2.93242437667412,
134.752786929097));
#86827=CARTESIAN_POINT('Ctrl Pts',(-53.9070367815104,-2.82232736563432,
134.834553975889));
#86828=CARTESIAN_POINT('Ctrl Pts',(-53.9147972240246,-2.70889515881823,
134.911647816396));
#86829=CARTESIAN_POINT('Ctrl Pts',(-53.9225576665388,-2.59257091887731,
134.983805448293));
#86830=CARTESIAN_POINT('Ctrl Pts',(-53.9303305668043,-2.47605994493967,
135.056078914027));
#86831=CARTESIAN_POINT('Ctrl Pts',(-53.9381034670698,-2.35664800135264,
135.12340014428));
#86832=CARTESIAN_POINT('Ctrl Pts',(-53.9458763673353,-2.23480265526569,
135.185552253927));
#86833=CARTESIAN_POINT('Ctrl Pts',(-53.9533667030969,-2.11738669442517,
135.245444977833));
#86834=CARTESIAN_POINT('Ctrl Pts',(-53.9608570388586,-1.99771145989837,
135.300537748633));
#86835=CARTESIAN_POINT('Ctrl Pts',(-53.9683473746203,-1.87621011447327,
135.350679861619));
#86836=CARTESIAN_POINT('Ctrl Pts',(-53.9761217087393,-1.75010200860079,
135.402723128063));
#86837=CARTESIAN_POINT('Ctrl Pts',(-53.9838960428584,-1.62162711174686,
135.449597775056));
#86838=CARTESIAN_POINT('Ctrl Pts',(-53.9916703769775,-1.49124807972184,
135.491082523891));
#86839=CARTESIAN_POINT('Ctrl Pts',(-53.9994351299246,-1.36102972820148,
135.532516146481));
#86840=CARTESIAN_POINT('Ctrl Pts',(-54.0071998828717,-1.22891227968052,
135.568572970236));
#86841=CARTESIAN_POINT('Ctrl Pts',(-54.0149646358188,-1.09537938142757,
135.599079282226));
#86842=CARTESIAN_POINT('Ctrl Pts',(-54.0227216767038,-0.961979109931653,
135.629555294917));
#86843=CARTESIAN_POINT('Ctrl Pts',(-54.0304787175888,-0.827166565076972,
135.654491680145));
#86844=CARTESIAN_POINT('Ctrl Pts',(-54.0382357584738,-0.691441272809314,
135.673764280106));
#86845=CARTESIAN_POINT('Ctrl Pts',(-54.0459869497139,-0.55581833204016,
135.69302234645));
#86846=CARTESIAN_POINT('Ctrl Pts',(-54.0537381409541,-0.419284399413234,
135.70662507416));
#86847=CARTESIAN_POINT('Ctrl Pts',(-54.0614893321942,-0.282349582043312,
135.714499289337));
#86848=CARTESIAN_POINT('Ctrl Pts',(-54.0692372289713,-0.145472965623814,
135.722370157763));
#86849=CARTESIAN_POINT('Ctrl Pts',(-54.0769851257483,-0.00819619285073767,
135.724517333831));
#86850=CARTESIAN_POINT('Ctrl Pts',(-54.0847330225254,0.128965329089036,
135.720919475791));
#86851=CARTESIAN_POINT('Ctrl Pts',(-54.0924792986095,0.26609815979528,135.717322370346));
#86852=CARTESIAN_POINT('Ctrl Pts',(-54.1002255746936,0.403115397037173,
135.707982631359));
#86853=CARTESIAN_POINT('Ctrl Pts',(-54.1079718507777,0.5395018505838,135.692931044155));
#86854=CARTESIAN_POINT('Ctrl Pts',(-54.1157181840431,0.675889310904245,
135.677879345842));
#86855=CARTESIAN_POINT('Ctrl Pts',(-54.1234645173084,0.811645589632215,
135.657115758064));
#86856=CARTESIAN_POINT('Ctrl Pts',(-54.1312108505737,0.946261229910615,
135.630722886114));
#86857=CARTESIAN_POINT('Ctrl Pts',(-54.1389589185766,1.08090701642811,135.604324103664));
#86858=CARTESIAN_POINT('Ctrl Pts',(-54.1467069865796,1.21441127261649,135.572293603724));
#86859=CARTESIAN_POINT('Ctrl Pts',(-54.1544550545826,1.34627572541837,135.534764906171));
#86860=CARTESIAN_POINT('Ctrl Pts',(-54.1622113573245,1.47828032533025,135.497196322671));
#86861=CARTESIAN_POINT('Ctrl Pts',(-54.1699676600663,1.60864126378737,135.454117975627));
#86862=CARTESIAN_POINT('Ctrl Pts',(-54.1777239628081,1.73687587707863,135.405713163299));
#86863=CARTESIAN_POINT('Ctrl Pts',(-54.1854844053223,1.86517893304407,135.357282515865));
#86864=CARTESIAN_POINT('Ctrl Pts',(-54.1932448478364,1.99135304299268,135.30351989162));
#86865=CARTESIAN_POINT('Ctrl Pts',(-54.2010052903506,2.11493739538371,135.244655976673));
#86866=CARTESIAN_POINT('Ctrl Pts',(-54.208778190616,2.23872013634849,135.185697568145));
#86867=CARTESIAN_POINT('Ctrl Pts',(-54.2165510908815,2.35990446630394,135.121621687448));
#86868=CARTESIAN_POINT('Ctrl Pts',(-54.2243239911469,2.47805518218693,135.05270448036));
#86869=CARTESIAN_POINT('Ctrl Pts',(-54.231814326909,2.59191082194435,134.986292587341));
#86870=CARTESIAN_POINT('Ctrl Pts',(-54.239304662671,2.70294931782431,134.915385411484));
#86871=CARTESIAN_POINT('Ctrl Pts',(-54.246794998433,2.81080974262181,134.840265925336));
#86872=CARTESIAN_POINT('Ctrl Pts',(-54.2545693325521,2.92275972820834,134.762298261038));
#86873=CARTESIAN_POINT('Ctrl Pts',(-54.2623436666712,3.03164051620622,134.679545583393));
#86874=CARTESIAN_POINT('Ctrl Pts',(-54.2701180007903,3.13701586180466,134.592277531291));
#86875=CARTESIAN_POINT('Ctrl Pts',(-54.2778827537374,3.24226134170732,134.505117029264));
#86876=CARTESIAN_POINT('Ctrl Pts',(-54.2856475066844,3.3440096767891,134.41345247204));
#86877=CARTESIAN_POINT('Ctrl Pts',(-54.2934122596315,3.44185329427804,134.31759686968));
#86878=CARTESIAN_POINT('Ctrl Pts',(-54.3011693005165,3.53959973210662,134.221836472456));
#86879=CARTESIAN_POINT('Ctrl Pts',(-54.3089263414015,3.63344889270668,134.1218935857));
#86880=CARTESIAN_POINT('Ctrl Pts',(-54.3166833822865,3.72302631262759,134.018121364414));
#86881=CARTESIAN_POINT('Ctrl Pts',(-54.3244345735266,3.81253618151946,133.914427398567));
#86882=CARTESIAN_POINT('Ctrl Pts',(-54.3321857647668,3.89778046720273,133.806910140799));
#86883=CARTESIAN_POINT('Ctrl Pts',(-54.3399369560069,3.97842188104792,133.695959206392));
#86884=CARTESIAN_POINT('Ctrl Pts',(-54.347684852784,4.05902902014103,133.585055429092));
#86885=CARTESIAN_POINT('Ctrl Pts',(-54.355432749561,4.13503694903388,133.47072119339));
#86886=CARTESIAN_POINT('Ctrl Pts',(-54.3631806463381,4.20614912213341,133.353378590213));
#86887=CARTESIAN_POINT('Ctrl Pts',(-54.3709269224222,4.27724642009922,133.236060532579));
#86888=CARTESIAN_POINT('Ctrl Pts',(-54.3786731985063,4.343449796736,133.1157356933));
#86889=CARTESIAN_POINT('Ctrl Pts',(-54.3864194745904,4.40450667970366,132.992854156726));
#86890=CARTESIAN_POINT('Ctrl Pts',(-54.3941658078557,4.46556401337945,132.869971713069));
#86891=CARTESIAN_POINT('Ctrl Pts',(-54.4019121411211,4.52147460360996,132.744532884584));
#86892=CARTESIAN_POINT('Ctrl Pts',(-54.4096584743865,4.57203257469429,132.617010941935));
#86893=CARTESIAN_POINT('Ctrl Pts',(-54.4174065423894,4.62260186788564,132.48946044163));
#86894=CARTESIAN_POINT('Ctrl Pts',(-54.4251546103924,4.66781601262755,132.359826262256));
#86895=CARTESIAN_POINT('Ctrl Pts',(-54.4329026783953,4.70751801421561,132.228599785801));
#86896=CARTESIAN_POINT('Ctrl Pts',(-54.4406589811372,4.74726221156342,132.097233840286));
#86897=CARTESIAN_POINT('Ctrl Pts',(-54.448415283879,4.78148244963238,131.964272591924));
#86898=CARTESIAN_POINT('Ctrl Pts',(-54.4561715866209,4.8100720509136,131.830221196553));
#86899=CARTESIAN_POINT('Ctrl Pts',(-54.463932029135,4.83867691132587,131.696098253916));
#86900=CARTESIAN_POINT('Ctrl Pts',(-54.4716924716492,4.86164508131289,131.56088439015));
#86901=CARTESIAN_POINT('Ctrl Pts',(-54.4794529141634,4.87892156373866,131.425091990533));
#86902=CARTESIAN_POINT('Ctrl Pts',(-54.4872258144288,4.89622577990776,131.289081604902));
#86903=CARTESIAN_POINT('Ctrl Pts',(-54.4949987146943,4.90782001718698,131.152491217335));
#86904=CARTESIAN_POINT('Ctrl Pts',(-54.5027716149597,4.91370136695366,131.015836240033));
#86905=CARTESIAN_POINT('Ctrl Pts',(-54.5102619507218,4.91936891484217,130.884149015367));
#86906=CARTESIAN_POINT('Ctrl Pts',(-54.5177522864839,4.91973171888739,130.752402123454));
#86907=CARTESIAN_POINT('Ctrl Pts',(-54.5252426222461,4.91483276193648,130.621052176146));
#86908=CARTESIAN_POINT('Ctrl Pts',(-54.5330169563651,4.90974805954385,130.484722055665));
#86909=CARTESIAN_POINT('Ctrl Pts',(-54.5407912904842,4.89897861363779,130.348387721445));
#86910=CARTESIAN_POINT('Ctrl Pts',(-54.5485656246032,4.88251547807646,130.212561945006));
#86911=CARTESIAN_POINT('Ctrl Pts',(-54.5563303775503,4.86607263185836,130.076903561698));
#86912=CARTESIAN_POINT('Ctrl Pts',(-54.5640951304975,4.84395010424328,129.94175287352));
#86913=CARTESIAN_POINT('Ctrl Pts',(-54.5718598834446,4.81619093642229,129.807621972572));
#86914=CARTESIAN_POINT('Ctrl Pts',(-54.5796169243296,4.78845933939812,129.673624292327));
#86915=CARTESIAN_POINT('Ctrl Pts',(-54.5873739652145,4.75510232193858,129.540644764035));
#86916=CARTESIAN_POINT('Ctrl Pts',(-54.5951310060995,4.71621459670577,129.409189323309));
#86917=CARTESIAN_POINT('Ctrl Pts',(-54.6028821973396,4.67735619700906,129.277833014153));
#86918=CARTESIAN_POINT('Ctrl Pts',(-54.6106333885798,4.63297550162076,129.147998878285));
#86919=CARTESIAN_POINT('Ctrl Pts',(-54.6183845798199,4.58321799216971,129.020181282759));
#86920=CARTESIAN_POINT('Ctrl Pts',(-54.626132476597,4.5334816309875,128.892418013121));
#86921=CARTESIAN_POINT('Ctrl Pts',(-54.6338803733741,4.47837314254132,128.766669942722));
#86922=CARTESIAN_POINT('Ctrl Pts',(-54.6416282701511,4.41808735374489,128.643414714222));
#86923=CARTESIAN_POINT('Ctrl Pts',(-54.6493745462352,4.35781417543587,128.520185268059));
#86924=CARTESIAN_POINT('Ctrl Pts',(-54.6571208223193,4.29236602255315,128.399447977589));
#86925=CARTESIAN_POINT('Ctrl Pts',(-54.6648670984034,4.22198504228919,128.281658620661));
#86926=CARTESIAN_POINT('Ctrl Pts',(-54.6726134316687,4.15160354248891,128.163868394239));
#86927=CARTESIAN_POINT('Ctrl Pts',(-54.680359764934,4.07628934318438,128.049026480399));
#86928=CARTESIAN_POINT('Ctrl Pts',(-54.6881060981993,3.99632933954245,127.937561902551));
#86929=CARTESIAN_POINT('Ctrl Pts',(-54.6958541662023,3.9163514294121,127.826072362984));
#86930=CARTESIAN_POINT('Ctrl Pts',(-54.7036022342053,3.8317258725235,127.717961982038));
#86931=CARTESIAN_POINT('Ctrl Pts',(-54.7113503022083,3.74278122298893,127.613628447775));
#86932=CARTESIAN_POINT('Ctrl Pts',(-54.7191066049501,3.65374204202226,127.509184026589));
#86933=CARTESIAN_POINT('Ctrl Pts',(-54.7268629076919,3.56037485266949,127.408524768636));
#86934=CARTESIAN_POINT('Ctrl Pts',(-54.7346192104337,3.46304699504312,127.312013473793));
#86935=CARTESIAN_POINT('Ctrl Pts',(-54.7423796529479,3.36566719060865,127.215450667966));
#86936=CARTESIAN_POINT('Ctrl Pts',(-54.7501400954621,3.26432279447367,127.123040499916));
#86937=CARTESIAN_POINT('Ctrl Pts',(-54.7579005379763,3.15941516358818,127.035106197049));
#86938=CARTESIAN_POINT('Ctrl Pts',(-54.7656734382417,3.05433912566033,126.947030734233));
#86939=CARTESIAN_POINT('Ctrl Pts',(-54.7734463385071,2.94568873261387,126.863445733158));
#86940=CARTESIAN_POINT('Ctrl Pts',(-54.7812192387725,2.83389604314877,126.784632233816));
#86941=CARTESIAN_POINT('Ctrl Pts',(-54.7887095745346,2.7261672995333,126.708683803693));
#86942=CARTESIAN_POINT('Ctrl Pts',(-54.7961999102967,2.61552101254961,126.637166153199));
#86943=CARTESIAN_POINT('Ctrl Pts',(-54.8036902460588,2.50236457596035,126.570289929507));
#86944=CARTESIAN_POINT('Ctrl Pts',(-54.8114645801779,2.38491777868549,126.500878073468));
#86945=CARTESIAN_POINT('Ctrl Pts',(-54.819238914297,2.2643946935461,126.436246675518));
#86946=CARTESIAN_POINT('Ctrl Pts',(-54.8270132484161,2.14122189413659,126.376680427831));
#86947=CARTESIAN_POINT('Ctrl Pts',(-54.8347780013632,2.01820089419409,126.317187590222));
#86948=CARTESIAN_POINT('Ctrl Pts',(-54.8425427543104,1.89253702601445,126.262747651047));
#86949=CARTESIAN_POINT('Ctrl Pts',(-54.8503075072575,1.76468439199987,126.213601196824));
#86950=CARTESIAN_POINT('Ctrl Pts',(-54.8580645481425,1.6369587430238,126.164503555552));
#86951=CARTESIAN_POINT('Ctrl Pts',(-54.8658215890276,1.50704901696855,126.120689075813));
#86952=CARTESIAN_POINT('Ctrl Pts',(-54.8735786299126,1.37543206629944,126.082351543719));
#86953=CARTESIAN_POINT('Ctrl Pts',(-54.8813298211528,1.24391436899649,126.044042922255));
#86954=CARTESIAN_POINT('Ctrl Pts',(-54.8890810123929,1.11069238348038,126.011203136401));
#86955=CARTESIAN_POINT('Ctrl Pts',(-54.8968322036331,0.97626067112854,125.983977005808));
#86956=CARTESIAN_POINT('Ctrl Pts',(-54.9045801004102,0.841886095840717,
125.956762447047));
#86957=CARTESIAN_POINT('Ctrl Pts',(-54.9123279971873,0.706303198737797,
125.935156875512));
#86958=CARTESIAN_POINT('Ctrl Pts',(-54.9200758939644,0.570019142824407,
125.919254555328));
#86959=CARTESIAN_POINT('Ctrl Pts',(-54.9278221700485,0.43376359459757,125.903355561567));
#86960=CARTESIAN_POINT('Ctrl Pts',(-54.9355684461327,0.296807567374053,
125.893157491504));
#86961=CARTESIAN_POINT('Ctrl Pts',(-54.9433147222168,0.159665406438524,
125.888702978909));
#86962=CARTESIAN_POINT('Ctrl Pts',(-54.9510610554822,0.0225222331507177,
125.884248433431));
#86963=CARTESIAN_POINT('Ctrl Pts',(-54.9588073887475,-0.114806685831678,
125.885537542715));
#86964=CARTESIAN_POINT('Ctrl Pts',(-54.9665537220128,-0.251805327116809,
125.892560831364));
#86965=CARTESIAN_POINT('Ctrl Pts',(-54.9743017900158,-0.388834648297774,
125.899585692829));
#86966=CARTESIAN_POINT('Ctrl Pts',(-54.9820498580189,-0.525533154225138,
125.912347268917));
#86967=CARTESIAN_POINT('Ctrl Pts',(-54.9897979260219,-0.661388667148345,
125.930784097856));
#86968=CARTESIAN_POINT('Ctrl Pts',(-54.9975542287637,-0.797388568927388,
125.949240521677));
#86969=CARTESIAN_POINT('Ctrl Pts',(-55.0053105315057,-0.932543299927897,
125.973384194713));
#86970=CARTESIAN_POINT('Ctrl Pts',(-55.0130668342476,-1.0663490700338,126.003102165521));
#86971=CARTESIAN_POINT('Ctrl Pts',(-55.0208272767618,-1.2002262563082,126.032835997704));
#86972=CARTESIAN_POINT('Ctrl Pts',(-55.0285877192759,-1.33275266946667,
126.06814995532));
#86973=CARTESIAN_POINT('Ctrl Pts',(-55.0363481617901,-1.46343942590286,
126.108881077709));
#86974=CARTESIAN_POINT('Ctrl Pts',(-55.0441210620555,-1.59433597232213,
126.149677585312));
#86975=CARTESIAN_POINT('Ctrl Pts',(-55.051893962321,-1.72338659235167,126.195908503363));
#86976=CARTESIAN_POINT('Ctrl Pts',(-55.0596668625865,-1.85012130080695,
126.247362237623));
#86977=CARTESIAN_POINT('Ctrl Pts',(-55.0671571983483,-1.97224888338046,
126.296945499037));
#86978=CARTESIAN_POINT('Ctrl Pts',(-55.0746475341101,-2.09222572902183,
126.351378316933));
#86979=CARTESIAN_POINT('Ctrl Pts',(-55.0821378698719,-2.20965440801859,
126.410431799341));
#86980=CARTESIAN_POINT('Ctrl Pts',(-55.0899130101817,-2.33154807001562,
126.471730668459));
#86981=CARTESIAN_POINT('Ctrl Pts',(-55.0976881504915,-2.45108211634481,
126.538202733636));
#86982=CARTESIAN_POINT('Ctrl Pts',(-55.1054632908013,-2.56778630866249,
126.609642923186));
#86983=CARTESIAN_POINT('Ctrl Pts',(-55.1132286705009,-2.68434399505456,
126.680993429488));
#86984=CARTESIAN_POINT('Ctrl Pts',(-55.1209940502005,-2.79807856601499,
126.757299447498));
#86985=CARTESIAN_POINT('Ctrl Pts',(-55.1287594299001,-2.90854205076117,
126.838308903146));
#86986=CARTESIAN_POINT('Ctrl Pts',(-55.1367185626383,-3.02176169639659,
126.921339615808));
#86987=CARTESIAN_POINT('Ctrl Pts',(-55.1446776953764,-3.1315444928007,127.009311406704));
#86988=CARTESIAN_POINT('Ctrl Pts',(-55.1526368281145,-3.23743631109765,
127.101903434277));
#86989=CARTESIAN_POINT('Ctrl Pts',(-55.1603876305625,-3.34055641117398,
127.192071865636));
#86990=CARTESIAN_POINT('Ctrl Pts',(-55.1681384330106,-3.4399863653504,127.286621408679));
#86991=CARTESIAN_POINT('Ctrl Pts',(-55.1758892354586,-3.53533793702208,
127.385213248184));
#86992=CARTESIAN_POINT('Ctrl Pts',(-55.1836365277603,-3.63064632633007,
127.483760437888));
#86993=CARTESIAN_POINT('Ctrl Pts',(-55.191383820062,-3.7218797371152,127.586346001037));
#86994=CARTESIAN_POINT('Ctrl Pts',(-55.1991311123636,-3.8086857906305,127.692593336623));
#86995=CARTESIAN_POINT('Ctrl Pts',(-55.2068765738559,-3.89547133048362,
127.79881556426));
#86996=CARTESIAN_POINT('Ctrl Pts',(-55.2146220353483,-3.97783134877193,
127.908697539246));
#86997=CARTESIAN_POINT('Ctrl Pts',(-55.2223674968406,-4.05545313597058,
128.021828870317));
#86998=CARTESIAN_POINT('Ctrl Pts',(-55.2304850900719,-4.13680427237365,
128.140395611404));
#86999=CARTESIAN_POINT('Ctrl Pts',(-55.2386026833031,-4.21295029522901,
128.262531324154));
#87000=CARTESIAN_POINT('Ctrl Pts',(-55.2467202765344,-4.28358197502536,
128.387728968816));
#87001=CARTESIAN_POINT('Ctrl Pts',(-55.2544698307117,-4.3510113242947,128.507250346958));
#87002=CARTESIAN_POINT('Ctrl Pts',(-55.2622193848892,-4.41341520153701,
128.629561734039));
#87003=CARTESIAN_POINT('Ctrl Pts',(-55.2699689390666,-4.47057185358703,
128.75419712057));
#87004=CARTESIAN_POINT('Ctrl Pts',(-55.2777211340661,-4.52774798295818,
128.878874979208));
#87005=CARTESIAN_POINT('Ctrl Pts',(-55.2854733290657,-4.57967317347573,
129.005878054953));
#87006=CARTESIAN_POINT('Ctrl Pts',(-55.2932255240652,-4.6261740823844,129.134721009155));
#87007=CARTESIAN_POINT('Ctrl Pts',(-55.3009846094251,-4.67271632255723,
129.263678482456));
#87008=CARTESIAN_POINT('Ctrl Pts',(-55.308743694785,-4.71382453847262,129.394478726866));
#87009=CARTESIAN_POINT('Ctrl Pts',(-55.3165027801449,-4.74937539568687,
129.526621828398));
#87010=CARTESIAN_POINT('Ctrl Pts',(-55.317594725302,-4.75437850940002,129.545218481621));
#87011=CARTESIAN_POINT('Ctrl Pts',(-55.318686670459,-4.75927164097778,129.563841714487));
#87012=CARTESIAN_POINT('Ctrl Pts',(-55.3197786156161,-4.76405452823412,
129.582490119309));
#87013=CARTESIAN_POINT('Origin',(213.235140564004,0.,130.804360617566));
#87014=CARTESIAN_POINT('',(-57.4152011815765,-4.76405452823411,129.582490119308));
#87015=CARTESIAN_POINT('',(-57.0701182010014,-4.76405452823404,129.582490119308));
#87016=CARTESIAN_POINT('',(213.235140564004,-4.76405452823405,129.582490119308));
#87017=CARTESIAN_POINT('',(-55.7351405639628,-4.9182495025703,130.802148612358));
#87018=CARTESIAN_POINT('Ctrl Pts',(-55.7351405640085,-4.91824950257066,
130.802148613168));
#87019=CARTESIAN_POINT('Ctrl Pts',(-55.7430237908748,-4.91831241585365,
130.942032251313));
#87020=CARTESIAN_POINT('Ctrl Pts',(-55.7509070177411,-4.91240317315693,
131.08189431191));
#87021=CARTESIAN_POINT('Ctrl Pts',(-55.7587902446074,-4.90055374134223,
131.221201223454));
#87022=CARTESIAN_POINT('Ctrl Pts',(-55.7666765057547,-4.88869974864066,
131.360561754705));
#87023=CARTESIAN_POINT('Ctrl Pts',(-55.7745627669019,-4.87090104280418,
131.499366341054));
#87024=CARTESIAN_POINT('Ctrl Pts',(-55.7824490280492,-4.84724140196124,
131.63708737564));
#87025=CARTESIAN_POINT('Ctrl Pts',(-55.7903397817841,-4.82356828286713,
131.774886866138));
#87026=CARTESIAN_POINT('Ctrl Pts',(-55.798230535519,-4.79402763944753,131.911601209291));
#87027=CARTESIAN_POINT('Ctrl Pts',(-55.8061212892539,-4.7587541683001,132.046713960294));
#87028=CARTESIAN_POINT('Ctrl Pts',(-55.8140237851165,-4.72342820715993,
132.18202777082));
#87029=CARTESIAN_POINT('Ctrl Pts',(-55.8219262809793,-4.68235246769653,
132.315734867519));
#87030=CARTESIAN_POINT('Ctrl Pts',(-55.8298287768419,-4.63571156242695,
132.447333950424));
#87031=CARTESIAN_POINT('Ctrl Pts',(-55.8377374019982,-4.5890344817761,132.579035103538));
#87032=CARTESIAN_POINT('Ctrl Pts',(-55.8456460271544,-4.53678376848017,
132.708624639214));
#87033=CARTESIAN_POINT('Ctrl Pts',(-55.8535546523107,-4.47919160491059,
132.835622695437));
#87034=CARTESIAN_POINT('Ctrl Pts',(-55.8614779459022,-4.42149262291089,
132.962856299905));
#87035=CARTESIAN_POINT('Ctrl Pts',(-55.8694012394938,-4.35843255734479,
133.08748848667));
#87036=CARTESIAN_POINT('Ctrl Pts',(-55.8773245330854,-4.29028942379935,
133.209064283828));
#87037=CARTESIAN_POINT('Ctrl Pts',(-55.8841802704406,-4.23132765231517,
133.314259392962));
#87038=CARTESIAN_POINT('Ctrl Pts',(-55.8910360077956,-4.1685610800927,133.417166569318));
#87039=CARTESIAN_POINT('Ctrl Pts',(-55.8978917451508,-4.10219475032617,
133.51751031725));
#87040=CARTESIAN_POINT('Ctrl Pts',(-55.9056660792698,-4.02693602976367,
133.63129907297));
#87041=CARTESIAN_POINT('Ctrl Pts',(-55.913440413389,-3.94682002154035,133.74213434208));
#87042=CARTESIAN_POINT('Ctrl Pts',(-55.9212147475081,-3.86210581822375,
133.849573534809));
#87043=CARTESIAN_POINT('Ctrl Pts',(-55.9289795004551,-3.77749601759184,
133.956880318334));
#87044=CARTESIAN_POINT('Ctrl Pts',(-55.9367442534022,-3.68829953698645,
134.060799049036));
#87045=CARTESIAN_POINT('Ctrl Pts',(-55.9445090063493,-3.59481951570741,
134.160914760134));
#87046=CARTESIAN_POINT('Ctrl Pts',(-55.9522660472343,-3.50143234010321,
134.260931034896));
#87047=CARTESIAN_POINT('Ctrl Pts',(-55.9600230881193,-3.40377035551371,
134.357151522967));
#87048=CARTESIAN_POINT('Ctrl Pts',(-55.9677801290043,-3.30217762914935,
134.449193393983));
#87049=CARTESIAN_POINT('Ctrl Pts',(-55.9755313202444,-3.20066151465049,
134.541165855509));
#87050=CARTESIAN_POINT('Ctrl Pts',(-55.9832825114845,-3.09522084700842,
134.628965710673));
#87051=CARTESIAN_POINT('Ctrl Pts',(-55.9910337027246,-2.98623703530915,
134.712246418283));
#87052=CARTESIAN_POINT('Ctrl Pts',(-55.9987815995017,-2.87729954463678,
134.795491729372));
#87053=CARTESIAN_POINT('Ctrl Pts',(-56.0065294962788,-2.76482221508682,
134.874221476262));
#87054=CARTESIAN_POINT('Ctrl Pts',(-56.0142773930559,-2.64921989975699,
134.94812906974));
#87055=CARTESIAN_POINT('Ctrl Pts',(-56.02202366914,-2.53364176593942,135.022021203342));
#87056=CARTESIAN_POINT('Ctrl Pts',(-56.029769945224,-2.4149402757375,135.091092979413));
#87057=CARTESIAN_POINT('Ctrl Pts',(-56.0375162213081,-2.29355932284947,
135.155081097564));
#87058=CARTESIAN_POINT('Ctrl Pts',(-56.0452625545734,-2.17217747395497,
135.219069688059));
#87059=CARTESIAN_POINT('Ctrl Pts',(-56.0530088878387,-2.04811646875717,
135.277974363432));
#87060=CARTESIAN_POINT('Ctrl Pts',(-56.0607552211041,-1.92184450117899,
135.331577950077));
#87061=CARTESIAN_POINT('Ctrl Pts',(-56.068503289107,-1.79554425586936,135.385193540873));
#87062=CARTESIAN_POINT('Ctrl Pts',(-56.0762513571101,-1.66703242274066,
135.433505527923));
#87063=CARTESIAN_POINT('Ctrl Pts',(-56.083999425113,-1.53679647483696,135.476345169919));
#87064=CARTESIAN_POINT('Ctrl Pts',(-56.0917557278549,-1.40642211061765,
135.519230342397));
#87065=CARTESIAN_POINT('Ctrl Pts',(-56.0995120305967,-1.27432034316865,
135.556631429229));
#87066=CARTESIAN_POINT('Ctrl Pts',(-56.1072683333386,-1.14099362288777,
135.588429661281));
#87067=CARTESIAN_POINT('Ctrl Pts',(-56.1150287758527,-1.0075957421217,135.620244865006));
#87068=CARTESIAN_POINT('Ctrl Pts',(-56.1227892183669,-0.872971989357373,
135.646451180632));
#87069=CARTESIAN_POINT('Ctrl Pts',(-56.130549660881,-0.737633282538259,
135.666981331028));
#87070=CARTESIAN_POINT('Ctrl Pts',(-56.1383225611465,-0.602077318012338,
135.687544438244));
#87071=CARTESIAN_POINT('Ctrl Pts',(-56.1460954614119,-0.465804494828162,
135.70241312935));
#87072=CARTESIAN_POINT('Ctrl Pts',(-56.1538683616773,-0.329330006961362,
135.71157212809));
#87073=CARTESIAN_POINT('Ctrl Pts',(-56.1613586974394,-0.197816710484977,
135.720398174155));
#87074=CARTESIAN_POINT('Ctrl Pts',(-56.1688490332016,-0.0661164647181106,
135.723922435861));
#87075=CARTESIAN_POINT('Ctrl Pts',(-56.1763393689637,0.0653132185093781,
135.722176926253));
#87076=CARTESIAN_POINT('Ctrl Pts',(-56.1841137030828,0.201726098121702,
135.720365235117));
#87077=CARTESIAN_POINT('Ctrl Pts',(-56.1918880372019,0.338279608429306,
135.712870538652));
#87078=CARTESIAN_POINT('Ctrl Pts',(-56.199662371321,0.474461340259999,135.699671588189));
#87079=CARTESIAN_POINT('Ctrl Pts',(-56.2074271242681,0.610475240277306,
135.686488904252));
#87080=CARTESIAN_POINT('Ctrl Pts',(-56.2151918772151,0.746117888060793,
135.667615991243));
#87081=CARTESIAN_POINT('Ctrl Pts',(-56.2229566301623,0.880876306110258,
135.64308358916));
#87082=CARTESIAN_POINT('Ctrl Pts',(-56.2307136710473,1.01550088019879,135.618575553005));
#87083=CARTESIAN_POINT('Ctrl Pts',(-56.2384707119323,1.14924259011514,135.588419283556));
#87084=CARTESIAN_POINT('Ctrl Pts',(-56.2462277528172,1.281593373103,135.552697325143));
#87085=CARTESIAN_POINT('Ctrl Pts',(-56.2539789440574,1.41384434933568,135.517002304936));
#87086=CARTESIAN_POINT('Ctrl Pts',(-56.2617301352975,1.54470611049822,135.47575005136));
#87087=CARTESIAN_POINT('Ctrl Pts',(-56.2694813265376,1.67368094074449,135.429074140703));
#87088=CARTESIAN_POINT('Ctrl Pts',(-56.2772292233147,1.80260095324756,135.382418068554));
#87089=CARTESIAN_POINT('Ctrl Pts',(-56.2849771200917,1.92963526308168,135.330343056955));
#87090=CARTESIAN_POINT('Ctrl Pts',(-56.2927250168688,2.0543016898257,135.273032414608));
#87091=CARTESIAN_POINT('Ctrl Pts',(-56.3004712929529,2.17894203904075,135.215733760412));
#87092=CARTESIAN_POINT('Ctrl Pts',(-56.308217569037,2.30121513536269,135.153201817043));
#87093=CARTESIAN_POINT('Ctrl Pts',(-56.3159638451211,2.42065952133068,135.085667724548));
#87094=CARTESIAN_POINT('Ctrl Pts',(-56.3237101783865,2.54010478901016,135.018133133531));
#87095=CARTESIAN_POINT('Ctrl Pts',(-56.3314565116518,2.6567209643365,134.945596512133));
#87096=CARTESIAN_POINT('Ctrl Pts',(-56.3392028449172,2.77007226275375,134.868334377523));
#87097=CARTESIAN_POINT('Ctrl Pts',(-56.3469509129202,2.88344894540867,134.791054940594));
#87098=CARTESIAN_POINT('Ctrl Pts',(-56.3546989809232,2.99355897326287,134.709048104824));
#87099=CARTESIAN_POINT('Ctrl Pts',(-56.3624470489262,3.09999688838854,134.622632786294));
#87100=CARTESIAN_POINT('Ctrl Pts',(-56.370203351668,3.20654792699661,134.536125624535));
#87101=CARTESIAN_POINT('Ctrl Pts',(-56.3779596544098,3.30941875267354,134.445200867269));
#87102=CARTESIAN_POINT('Ctrl Pts',(-56.3857159571517,3.4082378548688,134.350217042626));
#87103=CARTESIAN_POINT('Ctrl Pts',(-56.3934763996659,3.50710969979443,134.255182522256));
#87104=CARTESIAN_POINT('Ctrl Pts',(-56.4012368421801,3.60192524206938,134.156084900034));
#87105=CARTESIAN_POINT('Ctrl Pts',(-56.4089972846943,3.69235171590876,134.053317660761));
#87106=CARTESIAN_POINT('Ctrl Pts',(-56.4167701849597,3.78292335035164,133.950385450393));
#87107=CARTESIAN_POINT('Ctrl Pts',(-56.4245430852252,3.8690915908621,133.843772155531));
#87108=CARTESIAN_POINT('Ctrl Pts',(-56.4323159854906,3.95056511016457,133.73390296627));
#87109=CARTESIAN_POINT('Ctrl Pts',(-56.4398063212526,4.02907686182065,133.628027798783));
#87110=CARTESIAN_POINT('Ctrl Pts',(-56.4472966570145,4.10322912279955,133.519129601613));
#87111=CARTESIAN_POINT('Ctrl Pts',(-56.4547869927765,4.17280153026225,133.407610596254));
#87112=CARTESIAN_POINT('Ctrl Pts',(-56.4625613268956,4.24501179670018,133.291863313911));
#87113=CARTESIAN_POINT('Ctrl Pts',(-56.4703356610147,4.31251680412911,133.172925911786));
#87114=CARTESIAN_POINT('Ctrl Pts',(-56.4781099951338,4.37502170576884,133.051218008802));
#87115=CARTESIAN_POINT('Ctrl Pts',(-56.4858747480809,4.43744957570352,132.929660099931));
#87116=CARTESIAN_POINT('Ctrl Pts',(-56.493639501028,4.49488942386328,132.805338828274));
#87117=CARTESIAN_POINT('Ctrl Pts',(-56.5014042539751,4.54708983580989,132.67870239205));
#87118=CARTESIAN_POINT('Ctrl Pts',(-56.5091612948601,4.59923840157152,132.552191732919));
#87119=CARTESIAN_POINT('Ctrl Pts',(-56.5169183357451,4.6461577390474,132.423370844359));
#87120=CARTESIAN_POINT('Ctrl Pts',(-56.5246753766301,4.68764267478816,132.292711791182));
#87121=CARTESIAN_POINT('Ctrl Pts',(-56.5324265678702,4.72909632641622,132.162151269014));
#87122=CARTESIAN_POINT('Ctrl Pts',(-56.5401777591103,4.76512361554327,132.02975571245));
#87123=CARTESIAN_POINT('Ctrl Pts',(-56.5479289503505,4.79556789611087,131.896016065173));
#87124=CARTESIAN_POINT('Ctrl Pts',(-56.5556768471276,4.82599923704705,131.762333260815));
#87125=CARTESIAN_POINT('Ctrl Pts',(-56.5634247439046,4.85085220239881,131.627307882381));
#87126=CARTESIAN_POINT('Ctrl Pts',(-56.5711726406817,4.87002038467275,131.491444684745));
#87127=CARTESIAN_POINT('Ctrl Pts',(-56.5789189167658,4.88918455737618,131.355609906762));
#87128=CARTESIAN_POINT('Ctrl Pts',(-56.5866651928499,4.90266625767106,131.218938045054));
#87129=CARTESIAN_POINT('Ctrl Pts',(-56.5944114689341,4.91041052119701,131.081942273692));
#87130=CARTESIAN_POINT('Ctrl Pts',(-56.6021578021994,4.91815484188936,130.944945491059));
#87131=CARTESIAN_POINT('Ctrl Pts',(-56.6099041354648,4.92016161923581,130.807625184344));
#87132=CARTESIAN_POINT('Ctrl Pts',(-56.6176504687301,4.91642794276504,130.670497455721));
#87133=CARTESIAN_POINT('Ctrl Pts',(-56.6253985367331,4.91269343016331,130.533339018294));
#87134=CARTESIAN_POINT('Ctrl Pts',(-56.6331466047362,4.90321591631798,130.39637363552));
#87135=CARTESIAN_POINT('Ctrl Pts',(-56.6408946727392,4.88804455444544,130.260114812569));
#87136=CARTESIAN_POINT('Ctrl Pts',(-56.648650975481,4.87285706826897,130.123711172121));
#87137=CARTESIAN_POINT('Ctrl Pts',(-56.6564072782229,4.85196368889586,129.988015980762));
#87138=CARTESIAN_POINT('Ctrl Pts',(-56.6641635809648,4.82546524566948,129.853535594054));
#87139=CARTESIAN_POINT('Ctrl Pts',(-56.6719240234789,4.79895265942614,129.718983431115));
#87140=CARTESIAN_POINT('Ctrl Pts',(-56.6796844659931,4.76682913985776,129.585647744679));
#87141=CARTESIAN_POINT('Ctrl Pts',(-56.6874449085073,4.72924586883788,129.454021188171));
#87142=CARTESIAN_POINT('Ctrl Pts',(-56.6952178087727,4.69160226581481,129.322183333029));
#87143=CARTESIAN_POINT('Ctrl Pts',(-56.702990709038,4.6484815201748,129.192060461829));
#87144=CARTESIAN_POINT('Ctrl Pts',(-56.7107636093035,4.60008388687645,129.06412750209));
#87145=CARTESIAN_POINT('Ctrl Pts',(-56.7182539450655,4.55344562945511,128.940845227682));
#87146=CARTESIAN_POINT('Ctrl Pts',(-56.7257442808275,4.50190760034834,128.819596694863));
#87147=CARTESIAN_POINT('Ctrl Pts',(-56.7332346165894,4.44568908839166,128.700784711673));
#87148=CARTESIAN_POINT('Ctrl Pts',(-56.7410089507085,4.38733903446656,128.577467936026));
#87149=CARTESIAN_POINT('Ctrl Pts',(-56.7487832848276,4.32376173499277,128.456385490379));
#87150=CARTESIAN_POINT('Ctrl Pts',(-56.7565576189467,4.25515085536902,128.338012251955));
#87151=CARTESIAN_POINT('Ctrl Pts',(-56.7643223718938,4.18662453252238,128.219784897968));
#87152=CARTESIAN_POINT('Ctrl Pts',(-56.7720871248408,4.11307716669244,128.104260442884));
#87153=CARTESIAN_POINT('Ctrl Pts',(-56.7798518777879,4.0347499440894,127.991892670874));
#87154=CARTESIAN_POINT('Ctrl Pts',(-56.7876089186729,3.95650051718817,127.87963650412));
#87155=CARTESIAN_POINT('Ctrl Pts',(-56.795365959558,3.87348090322022,127.770531099785));
#87156=CARTESIAN_POINT('Ctrl Pts',(-56.803123000443,3.78597736241983,127.665004238665));
#87157=CARTESIAN_POINT('Ctrl Pts',(-56.8108741916832,3.69853980872012,127.559556956172));
#87158=CARTESIAN_POINT('Ctrl Pts',(-56.8186253829233,3.60662530713444,127.45768314522));
#87159=CARTESIAN_POINT('Ctrl Pts',(-56.8263765741634,3.51056223146715,127.359779963626));
#87160=CARTESIAN_POINT('Ctrl Pts',(-56.8341244709405,3.41453998516973,127.261918393497));
#87161=CARTESIAN_POINT('Ctrl Pts',(-56.8418723677175,3.3143729450157,127.168024374652));
#87162=CARTESIAN_POINT('Ctrl Pts',(-56.8496202644946,3.21042825972758,127.078460263069));
#87163=CARTESIAN_POINT('Ctrl Pts',(-56.8573665405787,3.10650531742684,126.988914886367));
#87164=CARTESIAN_POINT('Ctrl Pts',(-56.8651128166628,2.99880659774137,126.903697870438));
#87165=CARTESIAN_POINT('Ctrl Pts',(-56.8728590927469,2.88773413897328,126.823132841476));
#87166=CARTESIAN_POINT('Ctrl Pts',(-56.8806054260123,2.77666086029354,126.742567217802));
#87167=CARTESIAN_POINT('Ctrl Pts',(-56.8883517592776,2.66221410931545,126.666653879171));
#87168=CARTESIAN_POINT('Ctrl Pts',(-56.896098092543,2.5448265242333,126.595674240077));
#87169=CARTESIAN_POINT('Ctrl Pts',(-56.9038461605459,2.4274126510157,126.524678705586));
#87170=CARTESIAN_POINT('Ctrl Pts',(-56.9115942285489,2.30705696769329,126.458619271447));
#87171=CARTESIAN_POINT('Ctrl Pts',(-56.9193422965518,2.18421806922206,126.397732145754));
#87172=CARTESIAN_POINT('Ctrl Pts',(-56.9270985992937,2.0612486161074,126.336780308499));
#87173=CARTESIAN_POINT('Ctrl Pts',(-56.9348549020356,1.93579102662994,126.281011934829));
#87174=CARTESIAN_POINT('Ctrl Pts',(-56.9426112047774,1.80832581278619,126.230615891708));
#87175=CARTESIAN_POINT('Ctrl Pts',(-56.9503716472916,1.6807925669199,126.180192950702));
#87176=CARTESIAN_POINT('Ctrl Pts',(-56.9581320898057,1.55124993067059,126.135148182076));
#87177=CARTESIAN_POINT('Ctrl Pts',(-56.9658925323198,1.42019410481406,126.095620683449));
#87178=CARTESIAN_POINT('Ctrl Pts',(-56.9736654325852,1.28892789651127,126.056029731771));
#87179=CARTESIAN_POINT('Ctrl Pts',(-56.9814383328508,1.15614402339869,126.02197384601));
#87180=CARTESIAN_POINT('Ctrl Pts',(-56.9892112331162,1.02235029814514,125.993541255921));
#87181=CARTESIAN_POINT('Ctrl Pts',(-56.9967015688783,0.893420311809538,
125.966142262098));
#87182=CARTESIAN_POINT('Ctrl Pts',(-57.0041919046403,0.763552923591962,
125.94396487197));
#87183=CARTESIAN_POINT('Ctrl Pts',(-57.0116822404024,0.633205558275497,
125.927042319211));
#87184=CARTESIAN_POINT('Ctrl Pts',(-57.0194565745215,0.497916032985787,
125.909478142721));
#87185=CARTESIAN_POINT('Ctrl Pts',(-57.0272309086405,0.361680858901798,
125.897519505895));
#87186=CARTESIAN_POINT('Ctrl Pts',(-57.0350052427596,0.225004244560835,
125.891260155289));
#87187=CARTESIAN_POINT('Ctrl Pts',(-57.0427699957067,0.0884960719324635,
125.885008518772));
#87188=CARTESIAN_POINT('Ctrl Pts',(-57.0505347486538,-0.0484520716775091,
125.8844422108));
#87189=CARTESIAN_POINT('Ctrl Pts',(-57.0582995016008,-0.18532803775502,
125.889603596011));
#87190=CARTESIAN_POINT('Ctrl Pts',(-57.0660565424858,-0.322068056693224,
125.894759854862));
#87191=CARTESIAN_POINT('Ctrl Pts',(-57.0738135833707,-0.458735652601401,
125.90563247124));
#87192=CARTESIAN_POINT('Ctrl Pts',(-57.0815706242557,-0.594816190732355,
125.922211832273));
#87193=CARTESIAN_POINT('Ctrl Pts',(-57.0893218154959,-0.730794109472061,
125.93877869068));
#87194=CARTESIAN_POINT('Ctrl Pts',(-57.097073006736,-0.866185465086569,
125.961043680792));
#87195=CARTESIAN_POINT('Ctrl Pts',(-57.1048241979762,-1.00047862339296,
125.988945205929));
#87196=CARTESIAN_POINT('Ctrl Pts',(-57.1125720947532,-1.13471470352413,
126.016834872173));
#87197=CARTESIAN_POINT('Ctrl Pts',(-57.1203199915304,-1.26785313271433,
126.050356229258));
#87198=CARTESIAN_POINT('Ctrl Pts',(-57.1280678883075,-1.3993905977649,126.089396246822));
#87199=CARTESIAN_POINT('Ctrl Pts',(-57.1358141643916,-1.53090054801376,
126.128428098055));
#87200=CARTESIAN_POINT('Ctrl Pts',(-57.1435604404757,-1.66080982566395,
126.172976202462));
#87201=CARTESIAN_POINT('Ctrl Pts',(-57.1513067165598,-1.78862884330984,
126.222877241695));
#87202=CARTESIAN_POINT('Ctrl Pts',(-57.1590530498252,-1.91644880448669,
126.272778649286));
#87203=CARTESIAN_POINT('Ctrl Pts',(-57.1667993830905,-2.04217811067544,
126.328032928369));
#87204=CARTESIAN_POINT('Ctrl Pts',(-57.1745457163558,-2.16534614838121,
126.388428199583));
#87205=CARTESIAN_POINT('Ctrl Pts',(-57.1822937843588,-2.28854176871487,
126.4488369959));
#87206=CARTESIAN_POINT('Ctrl Pts',(-57.1900418523619,-2.4091746282437,126.514388903186));
#87207=CARTESIAN_POINT('Ctrl Pts',(-57.1977899203649,-2.52679811663301,
126.584825768761));
#87208=CARTESIAN_POINT('Ctrl Pts',(-57.2055462231068,-2.64454661666551,
126.655337495475));
#87209=CARTESIAN_POINT('Ctrl Pts',(-57.2133025258485,-2.75927902046179,
126.730744350459));
#87210=CARTESIAN_POINT('Ctrl Pts',(-57.2210588285904,-2.87057670042268,
126.81074415257));
#87211=CARTESIAN_POINT('Ctrl Pts',(-57.2288192711045,-2.98193378330632,
126.890786652984));
#87212=CARTESIAN_POINT('Ctrl Pts',(-57.2365797136187,-3.08985218203316,
126.975426743976));
#87213=CARTESIAN_POINT('Ctrl Pts',(-57.2443401561329,-3.19394666119732,
127.064322143442));
#87214=CARTESIAN_POINT('Ctrl Pts',(-57.2521130563983,-3.29820824206064,
127.153360245695));
#87215=CARTESIAN_POINT('Ctrl Pts',(-57.2598859566637,-3.39863335010845,
127.246667040664));
#87216=CARTESIAN_POINT('Ctrl Pts',(-57.2676588569292,-3.49487326999634,
127.343862981508));
#87217=CARTESIAN_POINT('Ctrl Pts',(-57.2751491926912,-3.58761462638258,
127.43752560508));
#87218=CARTESIAN_POINT('Ctrl Pts',(-57.2826395284532,-3.67646958831234,
127.534799295745));
#87219=CARTESIAN_POINT('Ctrl Pts',(-57.2901298642152,-3.76116294608421,
127.635317172691));
#87220=CARTESIAN_POINT('Ctrl Pts',(-57.2978585046994,-3.84855081952744,
127.739033021732));
#87221=CARTESIAN_POINT('Ctrl Pts',(-57.3055871451837,-3.93179432220579,
127.84654304682));
#87222=CARTESIAN_POINT('Ctrl Pts',(-57.3133157856679,-4.01054278145833,
127.957479928005));
#87223=CARTESIAN_POINT('Ctrl Pts',(-57.3210349725339,-4.0891949161544,128.068281111985));
#87224=CARTESIAN_POINT('Ctrl Pts',(-57.3287541594,-4.16336271619009,128.182500495525));
#87225=CARTESIAN_POINT('Ctrl Pts',(-57.336473346266,-4.23273413835902,128.299735939801));
#87226=CARTESIAN_POINT('Ctrl Pts',(-57.3441832907805,-4.302022500605,128.416831015511));
#87227=CARTESIAN_POINT('Ctrl Pts',(-57.351893235295,-4.36652571901792,128.536934623359));
#87228=CARTESIAN_POINT('Ctrl Pts',(-57.3596031798095,-4.42597408949314,
128.659614380447));
#87229=CARTESIAN_POINT('Ctrl Pts',(-57.3673077977208,-4.48538138861153,
128.782209381233));
#87230=CARTESIAN_POINT('Ctrl Pts',(-57.3750124156322,-4.53974061357756,
128.907376636773));
#87231=CARTESIAN_POINT('Ctrl Pts',(-57.3827170335435,-4.58882720901201,
129.034657843558));
#87232=CARTESIAN_POINT('Ctrl Pts',(-57.3904178145022,-4.63788935898501,
129.161875663429));
#87233=CARTESIAN_POINT('Ctrl Pts',(-57.3981185954609,-4.68168396286949,
129.291204970892));
#87234=CARTESIAN_POINT('Ctrl Pts',(-57.4058193764196,-4.7200341787311,129.422166559515));
#87235=CARTESIAN_POINT('Ctrl Pts',(-57.4089466448052,-4.73560810795835,
129.475349741589));
#87236=CARTESIAN_POINT('Ctrl Pts',(-57.4120739131909,-4.75028473236229,
129.52880189419));
#87237=CARTESIAN_POINT('Ctrl Pts',(-57.4152011815765,-4.76405452823411,
129.582490119308));
#87238=CARTESIAN_POINT('Ctrl Pts',(-55.665415119611,-4.764054528234,129.582490119308));
#87239=CARTESIAN_POINT('Ctrl Pts',(-55.6739271886917,-4.8013074290267,129.727738614107));
#87240=CARTESIAN_POINT('Ctrl Pts',(-55.6824392577724,-4.83195755642185,
129.87486329597));
#87241=CARTESIAN_POINT('Ctrl Pts',(-55.6909513268531,-4.8558303914332,130.023275300758));
#87242=CARTESIAN_POINT('Ctrl Pts',(-55.699428429661,-4.87960516050402,130.171077651818));
#87243=CARTESIAN_POINT('Ctrl Pts',(-55.7079055324689,-4.89665810257531,
130.320156528335));
#87244=CARTESIAN_POINT('Ctrl Pts',(-55.7163826352768,-4.90686536188065,
130.469912739899));
#87245=CARTESIAN_POINT('Ctrl Pts',(-55.7226352781722,-4.91439415430214,
130.580371717865));
#87246=CARTESIAN_POINT('Ctrl Pts',(-55.7288879210675,-4.91819960239075,
130.691198813367));
#87247=CARTESIAN_POINT('Ctrl Pts',(-55.7351405639629,-4.9182495025703,130.802148612358));
#87248=CARTESIAN_POINT('',(-55.3898594360289,-4.9182491242873,130.801425664894));
#87249=CARTESIAN_POINT('Ctrl Pts',(-55.3197786156161,-4.76405452823412,
129.582490119309));
#87250=CARTESIAN_POINT('Ctrl Pts',(-55.3275521152037,-4.79810364862538,
129.715247122947));
#87251=CARTESIAN_POINT('Ctrl Pts',(-55.3353256147913,-4.82656139489736,
129.849280179693));
#87252=CARTESIAN_POINT('Ctrl Pts',(-55.3430991143789,-4.84936286713653,
129.98407844335));
#87253=CARTESIAN_POINT('Ctrl Pts',(-55.3489279074809,-4.86646006545832,
130.085154050354));
#87254=CARTESIAN_POINT('Ctrl Pts',(-55.3547567005828,-4.88037813522813,
130.186659715631));
#87255=CARTESIAN_POINT('Ctrl Pts',(-55.3605854936848,-4.89110893864667,
130.288379597769));
#87256=CARTESIAN_POINT('Ctrl Pts',(-55.3703434744535,-4.90907337340337,
130.458668821684));
#87257=CARTESIAN_POINT('Ctrl Pts',(-55.3801014552224,-4.91814677411089,
130.629912319547));
#87258=CARTESIAN_POINT('Ctrl Pts',(-55.389859435991,-4.9182491242869,130.801425664228));
#87259=CARTESIAN_POINT('Ctrl Pts',(-55.389859436029,-4.9182491242873,130.801425664894));
#87260=CARTESIAN_POINT('Ctrl Pts',(-55.3975287093647,-4.91832956626769,
130.936226373385));
#87261=CARTESIAN_POINT('Ctrl Pts',(-55.4051979827003,-4.91286385231857,
131.071249821404));
#87262=CARTESIAN_POINT('Ctrl Pts',(-55.412867256036,-4.90182346626275,131.205994490759));
#87263=CARTESIAN_POINT('Ctrl Pts',(-55.4205280170279,-4.89079533424426,
131.340589603187));
#87264=CARTESIAN_POINT('Ctrl Pts',(-55.4281887780199,-4.87420486859583,
131.474906155198));
#87265=CARTESIAN_POINT('Ctrl Pts',(-55.4358495390118,-4.8520755586004,131.608441357376));
#87266=CARTESIAN_POINT('Ctrl Pts',(-55.4435037431039,-4.82996518923872,
131.741862265824));
#87267=CARTESIAN_POINT('Ctrl Pts',(-55.4511579471961,-4.80232547147055,
131.874502760349));
#87268=CARTESIAN_POINT('Ctrl Pts',(-55.4588121512882,-4.76923177128743,
132.005864414581));
#87269=CARTESIAN_POINT('Ctrl Pts',(-55.4664622018516,-4.73615602929184,
132.137154785845));
#87270=CARTESIAN_POINT('Ctrl Pts',(-55.4741122524151,-4.69763228838224,
132.267167308161));
#87271=CARTESIAN_POINT('Ctrl Pts',(-55.4817623029785,-4.65378706511144,
132.395413418419));
#87272=CARTESIAN_POINT('Ctrl Pts',(-55.489410254756,-4.60995387074702,132.523624344446));
#87273=CARTESIAN_POINT('Ctrl Pts',(-55.4970582065333,-4.56080222634519,
132.650069441839));
#87274=CARTESIAN_POINT('Ctrl Pts',(-55.5047061583108,-4.50650846512339,
132.774275467571));
#87275=CARTESIAN_POINT('Ctrl Pts',(-55.5123537689327,-4.452217125807,132.898475952791));
#87276=CARTESIAN_POINT('Ctrl Pts',(-55.5200013795547,-4.3927842868615,133.020437196672));
#87277=CARTESIAN_POINT('Ctrl Pts',(-55.5276489901766,-4.32843414743316,
133.139706607743));
#87278=CARTESIAN_POINT('Ctrl Pts',(-55.5352980167735,-4.26407209340924,
133.258998101855));
#87279=CARTESIAN_POINT('Ctrl Pts',(-55.5429470433704,-4.19479111958725,
133.375596418511));
#87280=CARTESIAN_POINT('Ctrl Pts',(-55.5505960699673,-4.12086075596664,
133.489074697768));
#87281=CARTESIAN_POINT('Ctrl Pts',(-55.5582528693755,-4.04685526556292,
133.60266829173));
#87282=CARTESIAN_POINT('Ctrl Pts',(-55.5659096687836,-3.9681911697162,133.713135179273));
#87283=CARTESIAN_POINT('Ctrl Pts',(-55.5735664681918,-3.88518081679781,
133.820078290573));
#87284=CARTESIAN_POINT('Ctrl Pts',(-55.5812272718838,-3.80212705187374,
133.927077330017));
#87285=CARTESIAN_POINT('Ctrl Pts',(-55.5888880755759,-3.71472276315588,
134.030548617135));
#87286=CARTESIAN_POINT('Ctrl Pts',(-55.5965488792679,-3.62331890390447,
134.130130180105));
#87287=CARTESIAN_POINT('Ctrl Pts',(-55.6042216043421,-3.53177280626968,
134.229866707216));
#87288=CARTESIAN_POINT('Ctrl Pts',(-55.6118943294162,-3.43621498977593,
134.32570113535));
#87289=CARTESIAN_POINT('Ctrl Pts',(-55.6195670544903,-3.33703184835501,
134.417309759965));
#87290=CARTESIAN_POINT('Ctrl Pts',(-55.6260557421594,-3.25315442273412,
134.49478155091));
#87291=CARTESIAN_POINT('Ctrl Pts',(-55.6325444298286,-3.16668492983673,
134.569231755106));
#87292=CARTESIAN_POINT('Ctrl Pts',(-55.6390331174976,-3.07787329861358,
134.640488746315));
#87293=CARTESIAN_POINT('Ctrl Pts',(-55.6468074516167,-2.97146483360443,
134.725864354795));
#87294=CARTESIAN_POINT('Ctrl Pts',(-55.6545817857358,-2.86133284530761,
134.806944418968));
#87295=CARTESIAN_POINT('Ctrl Pts',(-55.6623561198549,-2.74785919161345,
134.883386595121));
#87296=CARTESIAN_POINT('Ctrl Pts',(-55.670120872802,-2.63452538405605,134.959734563124));
#87297=CARTESIAN_POINT('Ctrl Pts',(-55.677885625749,-2.51785842643888,135.031455799473));
#87298=CARTESIAN_POINT('Ctrl Pts',(-55.6856503786961,-2.39827368564984,
135.098247713336));
#87299=CARTESIAN_POINT('Ctrl Pts',(-55.6934074195811,-2.27880771811121,
135.164973288529));
#87300=CARTESIAN_POINT('Ctrl Pts',(-55.7011644604662,-2.15643007364254,
135.226779094832));
#87301=CARTESIAN_POINT('Ctrl Pts',(-55.7089215013512,-2.03158528013885,
135.283405639892));
#87302=CARTESIAN_POINT('Ctrl Pts',(-55.7166726925913,-1.90683463306543,
135.339989482434));
#87303=CARTESIAN_POINT('Ctrl Pts',(-55.7244238838314,-1.77962089477293,
135.391401676992));
#87304=CARTESIAN_POINT('Ctrl Pts',(-55.7321750750715,-1.65041307139816,
135.437428689185));
#87305=CARTESIAN_POINT('Ctrl Pts',(-55.7399229718486,-1.52126016479489,
135.483436138671));
#87306=CARTESIAN_POINT('Ctrl Pts',(-55.7476708686257,-1.39011522632476,
135.524062827211));
#87307=CARTESIAN_POINT('Ctrl Pts',(-55.7554187654028,-1.25746691026064,
135.559143476131));
#87308=CARTESIAN_POINT('Ctrl Pts',(-55.7631650414869,-1.12484634136466,
135.594216786935));
#87309=CARTESIAN_POINT('Ctrl Pts',(-55.770911317571,-0.990723398112361,
135.62374626575));
#87310=CARTESIAN_POINT('Ctrl Pts',(-55.7786575936551,-0.855601170929385,
135.647616722585));
#87311=CARTESIAN_POINT('Ctrl Pts',(-55.7864039269204,-0.720477946304455,
135.671487355627));
#87312=CARTESIAN_POINT('Ctrl Pts',(-55.7941502601859,-0.584355808033334,
135.689698815318));
#87313=CARTESIAN_POINT('Ctrl Pts',(-55.8018965934512,-0.447746902166392,
135.702187255382));
#87314=CARTESIAN_POINT('Ctrl Pts',(-55.8096446614542,-0.311107403682347,
135.714678492146));
#87315=CARTESIAN_POINT('Ctrl Pts',(-55.8173927294571,-0.173981309955912,
135.721444123399));
#87316=CARTESIAN_POINT('Ctrl Pts',(-55.8251407974601,-0.0368843373871096,
135.722472308871));
#87317=CARTESIAN_POINT('Ctrl Pts',(-55.832897100202,0.100358343475614,135.723501587111));
#87318=CARTESIAN_POINT('Ctrl Pts',(-55.8406534029438,0.237571449776515,
135.718781235569));
#87319=CARTESIAN_POINT('Ctrl Pts',(-55.8484097056857,0.37424026127967,135.708351572833));
#87320=CARTESIAN_POINT('Ctrl Pts',(-55.8561701481998,0.510982017042356,
135.697916343471));
#87321=CARTESIAN_POINT('Ctrl Pts',(-55.8639305907141,0.647178511093406,
135.681765777066));
#87322=CARTESIAN_POINT('Ctrl Pts',(-55.8716910332282,0.78232268235092,135.659991810643));
#87323=CARTESIAN_POINT('Ctrl Pts',(-55.8794639334937,0.917683799029857,
135.638182890715));
#87324=CARTESIAN_POINT('Ctrl Pts',(-55.8872368337591,1.05198883392483,135.610732609921));
#87325=CARTESIAN_POINT('Ctrl Pts',(-55.8950097340245,1.18474253183181,135.577783728476));
#87326=CARTESIAN_POINT('Ctrl Pts',(-55.9025000697865,1.31267029843313,135.546032621865));
#87327=CARTESIAN_POINT('Ctrl Pts',(-55.9099904055485,1.43915726414061,135.509175836042));
#87328=CARTESIAN_POINT('Ctrl Pts',(-55.9174807413105,1.5637775403749,135.467383549819));
#87329=CARTESIAN_POINT('Ctrl Pts',(-55.9252550754296,1.69312283226049,135.424006696361));
#87330=CARTESIAN_POINT('Ctrl Pts',(-55.9330294095487,1.82086681635337,135.375175290683));
#87331=CARTESIAN_POINT('Ctrl Pts',(-55.9408037436678,1.94651506567573,135.321025555504));
#87332=CARTESIAN_POINT('Ctrl Pts',(-55.9485684966149,2.07200846476013,135.266942555034));
#87333=CARTESIAN_POINT('Ctrl Pts',(-55.9563332495619,2.1954109124924,135.207554419546));
#87334=CARTESIAN_POINT('Ctrl Pts',(-55.964098002509,2.31624331468696,135.143047051231));
#87335=CARTESIAN_POINT('Ctrl Pts',(-55.971855043394,2.43695570443622,135.078603752543));
#87336=CARTESIAN_POINT('Ctrl Pts',(-55.9796120842791,2.55510278578551,135.009051522334));
#87337=CARTESIAN_POINT('Ctrl Pts',(-55.9873691251641,2.67022596228412,134.934624092557));
#87338=CARTESIAN_POINT('Ctrl Pts',(-55.9951203164042,2.78526232349981,134.860252789083));
#87339=CARTESIAN_POINT('Ctrl Pts',(-56.0028715076443,2.89727899176605,134.781013815149));
#87340=CARTESIAN_POINT('Ctrl Pts',(-56.0106226988844,3.00584280528774,134.69718633835));
#87341=CARTESIAN_POINT('Ctrl Pts',(-56.0183705956615,3.11436047629266,134.613394490466));
#87342=CARTESIAN_POINT('Ctrl Pts',(-56.0261184924385,3.21942790260524,134.525018257031));
#87343=CARTESIAN_POINT('Ctrl Pts',(-56.0338663892156,3.32064190102524,134.432379419565));
#87344=CARTESIAN_POINT('Ctrl Pts',(-56.0416126652997,3.42183472765869,134.339759960146));
#87345=CARTESIAN_POINT('Ctrl Pts',(-56.0493589413838,3.51917544146678,134.242879934026));
#87346=CARTESIAN_POINT('Ctrl Pts',(-56.0571052174679,3.61229519718496,134.142100342424));
#87347=CARTESIAN_POINT('Ctrl Pts',(-56.0648515507332,3.70541564029203,134.04132000689));
#87348=CARTESIAN_POINT('Ctrl Pts',(-56.0725978839986,3.79431479780925,133.936640335587));
#87349=CARTESIAN_POINT('Ctrl Pts',(-56.0803442172639,3.87866212660504,133.828457701017));
#87350=CARTESIAN_POINT('Ctrl Pts',(-56.0880922852668,3.96302834440007,133.720250839698));
#87351=CARTESIAN_POINT('Ctrl Pts',(-56.0958403532697,4.04284046473646,133.608539762386));
#87352=CARTESIAN_POINT('Ctrl Pts',(-56.1035884212727,4.11780976874678,133.493751955939));
#87353=CARTESIAN_POINT('Ctrl Pts',(-56.1113447240145,4.19285875102576,133.378842151644));
#87354=CARTESIAN_POINT('Ctrl Pts',(-56.1191010267564,4.26305442115808,133.260849413927));
#87355=CARTESIAN_POINT('Ctrl Pts',(-56.1268573294983,4.32815248145335,133.14022858468));
#87356=CARTESIAN_POINT('Ctrl Pts',(-56.1346177720125,4.39328528654363,133.019543376464));
#87357=CARTESIAN_POINT('Ctrl Pts',(-56.1423782145267,4.45331488943827,132.896227633092));
#87358=CARTESIAN_POINT('Ctrl Pts',(-56.1501386570409,4.50804456046034,132.770757653621));
#87359=CARTESIAN_POINT('Ctrl Pts',(-56.1579115573063,4.56286208840893,132.645086258599));
#87360=CARTESIAN_POINT('Ctrl Pts',(-56.1656844575717,4.61236254168788,132.517254081746));
#87361=CARTESIAN_POINT('Ctrl Pts',(-56.1734573578372,4.6563983309755,132.387754960675));
#87362=CARTESIAN_POINT('Ctrl Pts',(-56.1809476935992,4.69883330840324,132.262963458842));
#87363=CARTESIAN_POINT('Ctrl Pts',(-56.1884380293612,4.73619394523367,132.136624399281));
#87364=CARTESIAN_POINT('Ctrl Pts',(-56.1959283651233,4.7683932145393,132.009188079917));
#87365=CARTESIAN_POINT('Ctrl Pts',(-56.2037026992424,4.80181332892722,131.876919973772));
#87366=CARTESIAN_POINT('Ctrl Pts',(-56.2114770333615,4.82977882807532,131.743050774515));
#87367=CARTESIAN_POINT('Ctrl Pts',(-56.2192513674806,4.85213707015684,131.608070089272));
#87368=CARTESIAN_POINT('Ctrl Pts',(-56.2270161204276,4.87446775770323,131.47325575566));
#87369=CARTESIAN_POINT('Ctrl Pts',(-56.2347808733747,4.89120487462955,131.337333043576));
#87370=CARTESIAN_POINT('Ctrl Pts',(-56.2425456263218,4.90224586360402,131.200805513204));
#87371=CARTESIAN_POINT('Ctrl Pts',(-56.2503026672068,4.91327588651257,131.0644135839));
#87372=CARTESIAN_POINT('Ctrl Pts',(-56.2580597080919,4.91862100878843,130.927418418926));
#87373=CARTESIAN_POINT('Ctrl Pts',(-56.2658167489769,4.91822999315974,130.790332186294));
#87374=CARTESIAN_POINT('Ctrl Pts',(-56.273567940217,4.91783927239897,130.653349331456));
#87375=CARTESIAN_POINT('Ctrl Pts',(-56.2813191314571,4.91172102482053,130.516275935035));
#87376=CARTESIAN_POINT('Ctrl Pts',(-56.2890703226972,4.89987598749963,130.379627325223));
#87377=CARTESIAN_POINT('Ctrl Pts',(-56.2968182194743,4.88803598463561,130.243036794715));
#87378=CARTESIAN_POINT('Ctrl Pts',(-56.3045661162514,4.8704740668385,130.106871080414));
#87379=CARTESIAN_POINT('Ctrl Pts',(-56.3123140130284,4.84724302764511,129.971643322534));
#87380=CARTESIAN_POINT('Ctrl Pts',(-56.3200602891125,4.82401684788429,129.836443851385));
#87381=CARTESIAN_POINT('Ctrl Pts',(-56.3278065651966,4.79512397161675,129.702182331482));
#87382=CARTESIAN_POINT('Ctrl Pts',(-56.3355528412807,4.76066874951808,129.569364212769));
#87383=CARTESIAN_POINT('Ctrl Pts',(-56.343299174546,4.72621327307883,129.436545113623));
#87384=CARTESIAN_POINT('Ctrl Pts',(-56.3510455078113,4.68619546704952,129.305169815366));
#87385=CARTESIAN_POINT('Ctrl Pts',(-56.3587918410767,4.64077014420735,129.175730662317));
#87386=CARTESIAN_POINT('Ctrl Pts',(-56.3665399090796,4.59533464867928,129.046262522268));
#87387=CARTESIAN_POINT('Ctrl Pts',(-56.3742879770826,4.54448935607604,128.918731759051));
#87388=CARTESIAN_POINT('Ctrl Pts',(-56.3820360450855,4.48843786359724,128.793612347114));
#87389=CARTESIAN_POINT('Ctrl Pts',(-56.3897923478274,4.43232679892491,128.668359956776));
#87390=CARTESIAN_POINT('Ctrl Pts',(-56.3975486505692,4.37099864128637,128.54552439458));
#87391=CARTESIAN_POINT('Ctrl Pts',(-56.4053049533111,4.30470401317964,128.425557048245));
#87392=CARTESIAN_POINT('Ctrl Pts',(-56.4130653958252,4.2383740016338,128.305525671725));
#87393=CARTESIAN_POINT('Ctrl Pts',(-56.4208258383394,4.16707244092084,128.188365895236));
#87394=CARTESIAN_POINT('Ctrl Pts',(-56.4285862808536,4.09109371773113,128.074500684302));
#87395=CARTESIAN_POINT('Ctrl Pts',(-56.436359181119,4.01499302674978,127.960452686822));
#87396=CARTESIAN_POINT('Ctrl Pts',(-56.4441320813844,3.93420040008097,127.849710139489));
#87397=CARTESIAN_POINT('Ctrl Pts',(-56.4519049816498,3.84905154166185,127.742664144672));
#87398=CARTESIAN_POINT('Ctrl Pts',(-56.459395317412,3.76699805872237,127.639509541398));
#87399=CARTESIAN_POINT('Ctrl Pts',(-56.4668856531741,3.68089976659567,127.539787631828));
#87400=CARTESIAN_POINT('Ctrl Pts',(-56.4743759889362,3.59108847350101,127.443815031208));
#87401=CARTESIAN_POINT('Ctrl Pts',(-56.4821503230553,3.49787195793229,127.344203600268));
#87402=CARTESIAN_POINT('Ctrl Pts',(-56.4899246571744,3.40036004460926,127.248315861675));
#87403=CARTESIAN_POINT('Ctrl Pts',(-56.4976989912935,3.29888214723805,127.156544881933));
#87404=CARTESIAN_POINT('Ctrl Pts',(-56.5054637442406,3.19752931230587,127.064887001721));
#87405=CARTESIAN_POINT('Ctrl Pts',(-56.5132284971876,3.09222050562441,126.977336045254));
#87406=CARTESIAN_POINT('Ctrl Pts',(-56.5209932501348,2.9833239518934,126.894250483496));
#87407=CARTESIAN_POINT('Ctrl Pts',(-56.5287502910198,2.87453555575457,126.811247443489));
#87408=CARTESIAN_POINT('Ctrl Pts',(-56.5365073319048,2.76216681270894,126.732701207775));
#87409=CARTESIAN_POINT('Ctrl Pts',(-56.5442643727898,2.64662092921322,126.658931723042));
#87410=CARTESIAN_POINT('Ctrl Pts',(-56.55201556403,2.53116217976675,126.585217868452));
#87411=CARTESIAN_POINT('Ctrl Pts',(-56.5597667552701,2.41253138697458,126.516273804448));
#87412=CARTESIAN_POINT('Ctrl Pts',(-56.5675179465103,2.29116250944611,126.452377458383));
#87413=CARTESIAN_POINT('Ctrl Pts',(-56.5752658432873,2.16984521692886,126.388508269971));
#87414=CARTESIAN_POINT('Ctrl Pts',(-56.5830137400645,2.04579249953019,126.32968271418));
#87415=CARTESIAN_POINT('Ctrl Pts',(-56.5907616368416,1.91946461284274,126.276133739135));
#87416=CARTESIAN_POINT('Ctrl Pts',(-56.5985079129257,1.79316315122587,126.222595965381));
#87417=CARTESIAN_POINT('Ctrl Pts',(-56.6062541890097,1.6645878266771,126.174332729446));
#87418=CARTESIAN_POINT('Ctrl Pts',(-56.6140004650938,1.53422029263908,126.131529446193));
#87419=CARTESIAN_POINT('Ctrl Pts',(-56.6217467983592,1.40385179625754,126.088725846976));
#87420=CARTESIAN_POINT('Ctrl Pts',(-56.6294931316245,1.27169143544405,126.051382402824));
#87421=CARTESIAN_POINT('Ctrl Pts',(-56.6372394648899,1.13823711350541,126.019634989493));
#87422=CARTESIAN_POINT('Ctrl Pts',(-56.6449875328929,1.00475290539631,125.987880466549));
#87423=CARTESIAN_POINT('Ctrl Pts',(-56.6527356008959,0.869974539824291,
125.961724558599));
#87424=CARTESIAN_POINT('Ctrl Pts',(-56.6604836688989,0.73441083417581,125.941252168318));
#87425=CARTESIAN_POINT('Ctrl Pts',(-56.6682399716407,0.598703049808107,
125.920758019738));
#87426=CARTESIAN_POINT('Ctrl Pts',(-56.6759962743826,0.462208645221434,
125.905959513871));
#87427=CARTESIAN_POINT('Ctrl Pts',(-56.6837525771244,0.325442853270143,
125.896889780999));
#87428=CARTESIAN_POINT('Ctrl Pts',(-56.6915130196386,0.188604065297934,
125.887815207338));
#87429=CARTESIAN_POINT('Ctrl Pts',(-56.6992734621528,0.0514939919980021,
125.884475508752));
#87430=CARTESIAN_POINT('Ctrl Pts',(-56.7070339046669,-0.0853723905588257,
125.886851632579));
#87431=CARTESIAN_POINT('Ctrl Pts',(-56.7148068049324,-0.222458483183733,
125.88923157077));
#87432=CARTESIAN_POINT('Ctrl Pts',(-56.7225797051977,-0.359299712830921,
125.897345643882));
#87433=CARTESIAN_POINT('Ctrl Pts',(-56.7303526054631,-0.495385577822631,
125.911122815069));
#87434=CARTESIAN_POINT('Ctrl Pts',(-56.7378429412251,-0.626524378841732,
125.92439915138));
#87435=CARTESIAN_POINT('Ctrl Pts',(-56.7453332769872,-0.756961475594774,
125.942933955011));
#87436=CARTESIAN_POINT('Ctrl Pts',(-56.7528236127492,-0.886251140259517,
125.966619204583));
#87437=CARTESIAN_POINT('Ctrl Pts',(-56.7605979468683,-1.02044286185734,
125.991202487592));
#87438=CARTESIAN_POINT('Ctrl Pts',(-56.7683722809874,-1.15382350302958,
126.021412357054));
#87439=CARTESIAN_POINT('Ctrl Pts',(-56.7761466151065,-1.28588430964043,
126.057184129935));
#87440=CARTESIAN_POINT('Ctrl Pts',(-56.7839113680536,-1.4177823631101,126.092911817302));
#87441=CARTESIAN_POINT('Ctrl Pts',(-56.7916761210007,-1.54836344468064,
126.134187668342));
#87442=CARTESIAN_POINT('Ctrl Pts',(-56.7994408739478,-1.67712692813105,
126.180895647499));
#87443=CARTESIAN_POINT('Ctrl Pts',(-56.8071979148328,-1.8057625218741,126.227557235632));
#87444=CARTESIAN_POINT('Ctrl Pts',(-56.8149549557177,-1.93258374490037,
126.279640082603));
#87445=CARTESIAN_POINT('Ctrl Pts',(-56.8227119966027,-2.05710347406054,
126.336977898399));
#87446=CARTESIAN_POINT('Ctrl Pts',(-56.8304631878428,-2.18152930192365,
126.394272475303));
#87447=CARTESIAN_POINT('Ctrl Pts',(-56.838214379083,-2.30365673678873,126.45681397043));
#87448=CARTESIAN_POINT('Ctrl Pts',(-56.845965570323,-2.42301738527417,126.524387508637));
#87449=CARTESIAN_POINT('Ctrl Pts',(-56.8537134671001,-2.54232730230045,
126.591932326287));
#87450=CARTESIAN_POINT('Ctrl Pts',(-56.8614613638772,-2.65887243232339,
126.664504740991));
#87451=CARTESIAN_POINT('Ctrl Pts',(-56.8692092606543,-2.77220801009941,
126.741843440834));
#87452=CARTESIAN_POINT('Ctrl Pts',(-56.8769555367384,-2.8855198805158,126.819165963089));
#87453=CARTESIAN_POINT('Ctrl Pts',(-56.8847018128225,-2.99562321133926,
126.901252567156));
#87454=CARTESIAN_POINT('Ctrl Pts',(-56.8924480889065,-3.10210166234376,
126.987798245616));
#87455=CARTESIAN_POINT('Ctrl Pts',(-56.9001944221719,-3.20858089934814,
127.074344562937));
#87456=CARTESIAN_POINT('Ctrl Pts',(-56.9079407554373,-3.3114348997508,127.165349773736));
#87457=CARTESIAN_POINT('Ctrl Pts',(-56.9156870887026,-3.4102802185304,127.260468422027));
#87458=CARTESIAN_POINT('Ctrl Pts',(-56.9234351567056,-3.50914767303394,
127.35560837148));
#87459=CARTESIAN_POINT('Ctrl Pts',(-56.9311832247086,-3.60400437790277,
127.454863320417));
#87460=CARTESIAN_POINT('Ctrl Pts',(-56.9389312927115,-3.69450387388461,
127.55785107833));
#87461=CARTESIAN_POINT('Ctrl Pts',(-56.9466875954534,-3.7850995538076,127.660948292857));
#87462=CARTESIAN_POINT('Ctrl Pts',(-56.9544438981952,-3.87132851564963,
127.767785947264));
#87463=CARTESIAN_POINT('Ctrl Pts',(-56.9622002009371,-3.95288439002263,
127.877948469283));
#87464=CARTESIAN_POINT('Ctrl Pts',(-56.9699606434512,-4.03448379322138,
127.988169788358));
#87465=CARTESIAN_POINT('Ctrl Pts',(-56.9777210859654,-4.11140491994529,
128.101719187522));
#87466=CARTESIAN_POINT('Ctrl Pts',(-56.9854815284796,-4.18338544259421,
128.218153104393));
#87467=CARTESIAN_POINT('Ctrl Pts',(-56.993254428745,-4.25548151476821,128.334773931324));
#87468=CARTESIAN_POINT('Ctrl Pts',(-57.0010273290105,-4.32262094241365,
128.454288188086));
#87469=CARTESIAN_POINT('Ctrl Pts',(-57.0088002292759,-4.38458755221458,
128.576227978008));
#87470=CARTESIAN_POINT('Ctrl Pts',(-57.0162905650379,-4.44430151966453,
128.693734949418));
#87471=CARTESIAN_POINT('Ctrl Pts',(-57.0237809007999,-4.49921210133561,
128.813493887187));
#87472=CARTESIAN_POINT('Ctrl Pts',(-57.0312712365619,-4.54916925189624,
128.935071399681));
#87473=CARTESIAN_POINT('Ctrl Pts',(-57.0399825578534,-4.60726982350856,
129.076467033576));
#87474=CARTESIAN_POINT('Ctrl Pts',(-57.0486938791448,-4.65882662131957,
129.220700646112));
#87475=CARTESIAN_POINT('Ctrl Pts',(-57.0574052004363,-4.70358508809922,
129.367186173906));
#87476=CARTESIAN_POINT('Ctrl Pts',(-57.0616428672913,-4.72535807348324,
129.438444809089));
#87477=CARTESIAN_POINT('Ctrl Pts',(-57.0658805341464,-4.74552299645481,
129.510235958156));
#87478=CARTESIAN_POINT('Ctrl Pts',(-57.0701182010015,-4.76405452823404,
129.582490119308));
#87479=CARTESIAN_POINT('Origin',(213.235140564004,0.,130.804360617566));
#87480=CARTESIAN_POINT('',(-59.165034112149,-4.76405452823398,129.582490119308));
#87481=CARTESIAN_POINT('',(-58.8199570926743,-4.76405452823407,129.582490119308));
#87482=CARTESIAN_POINT('',(213.235140564004,-4.76405452823405,129.582490119308));
#87483=CARTESIAN_POINT('',(-57.4851405640492,-4.91824815608763,130.808619448461));
#87484=CARTESIAN_POINT('Ctrl Pts',(-57.4851405640492,-4.91824815608763,
130.808619448461));
#87485=CARTESIAN_POINT('Ctrl Pts',(-57.494480310666,-4.91810505791892,130.973874261755));
#87486=CARTESIAN_POINT('Ctrl Pts',(-57.5038200572828,-4.90962930027124,
131.138764540297));
#87487=CARTESIAN_POINT('Ctrl Pts',(-57.5131598038996,-4.89295343983749,
131.302547026536));
#87488=CARTESIAN_POINT('Ctrl Pts',(-57.5226232671053,-4.87605668684078,
131.46849901601));
#87489=CARTESIAN_POINT('Ctrl Pts',(-57.5320867303109,-4.8507412115729,131.633313665362));
#87490=CARTESIAN_POINT('Ctrl Pts',(-57.5415501935165,-4.81719403868288,
131.796239973223));
#87491=CARTESIAN_POINT('Ctrl Pts',(-57.5505592916871,-4.78525755123167,
131.951343772983));
#87492=CARTESIAN_POINT('Ctrl Pts',(-57.5595683898577,-4.74586126885286,
132.104736401066));
#87493=CARTESIAN_POINT('Ctrl Pts',(-57.5685774880283,-4.69920644601773,
132.255788135634));
#87494=CARTESIAN_POINT('Ctrl Pts',(-57.5763518221473,-4.65894601438298,
132.386137104151));
#87495=CARTESIAN_POINT('Ctrl Pts',(-57.5841261562665,-4.61319417433263,
132.515016120226));
#87496=CARTESIAN_POINT('Ctrl Pts',(-57.5919004903855,-4.56207524447303,
132.641927630294));
#87497=CARTESIAN_POINT('Ctrl Pts',(-57.5996652433326,-4.51101931412586,
132.768682733268));
#87498=CARTESIAN_POINT('Ctrl Pts',(-57.6074299962796,-4.45460959944137,
132.893474795645));
#87499=CARTESIAN_POINT('Ctrl Pts',(-57.6151947492267,-4.3930204521356,133.015820400067));
#87500=CARTESIAN_POINT('Ctrl Pts',(-57.6229517901117,-4.33149247603928,
133.138044489109));
#87501=CARTESIAN_POINT('Ctrl Pts',(-57.6307088309968,-4.26479547933942,
133.257826608766));
#87502=CARTESIAN_POINT('Ctrl Pts',(-57.6384658718818,-4.19315212162949,
133.37470268573));
#87503=CARTESIAN_POINT('Ctrl Pts',(-57.6462170631219,-4.12156279073292,
133.491490625535));
#87504=CARTESIAN_POINT('Ctrl Pts',(-57.653968254362,-4.04503472683967,133.605376552657));
#87505=CARTESIAN_POINT('Ctrl Pts',(-57.6617194456021,-3.96383662246492,
133.715920730788));
#87506=CARTESIAN_POINT('Ctrl Pts',(-57.6694673423792,-3.88267302945044,
133.826417924695));
#87507=CARTESIAN_POINT('Ctrl Pts',(-57.6772152391563,-3.79684357471622,
133.933575880107));
#87508=CARTESIAN_POINT('Ctrl Pts',(-57.6849631359334,-3.7066602718305,134.036983808062));
#87509=CARTESIAN_POINT('Ctrl Pts',(-57.6927094120175,-3.61649583334775,
134.140370105308));
#87510=CARTESIAN_POINT('Ctrl Pts',(-57.7004556881016,-3.52197961501504,
134.240007640895));
#87511=CARTESIAN_POINT('Ctrl Pts',(-57.7082019641857,-3.42346366282378,
134.335519012742));
#87512=CARTESIAN_POINT('Ctrl Pts',(-57.715948297451,-3.32494698341013,134.431031089634));
#87513=CARTESIAN_POINT('Ctrl Pts',(-57.7236946307164,-3.22243079192417,
134.522416669868));
#87514=CARTESIAN_POINT('Ctrl Pts',(-57.7314409639817,-3.11630341460103,
134.609335793654));
#87515=CARTESIAN_POINT('Ctrl Pts',(-57.7391890319847,-3.01015227078757,
134.696274382376));
#87516=CARTESIAN_POINT('Ctrl Pts',(-57.7469370999877,-2.90038863432754,
134.778744276628));
#87517=CARTESIAN_POINT('Ctrl Pts',(-57.7546851679907,-2.78743294051551,
134.856446582181));
#87518=CARTESIAN_POINT('Ctrl Pts',(-57.7624414707325,-2.6743571960479,134.934231470669));
#87519=CARTESIAN_POINT('Ctrl Pts',(-57.7701977734744,-2.55808293985622,
135.007238426546));
#87520=CARTESIAN_POINT('Ctrl Pts',(-57.7779540762162,-2.43905902038,135.075212307522));
#87521=CARTESIAN_POINT('Ctrl Pts',(-57.7857145187304,-2.31997157425404,
135.143222468205));
#87522=CARTESIAN_POINT('Ctrl Pts',(-57.7934749612445,-2.19813188771915,
135.20619402188));
#87523=CARTESIAN_POINT('Ctrl Pts',(-57.8012354037586,-2.07401140170014,
135.263918865657));
#87524=CARTESIAN_POINT('Ctrl Pts',(-57.8090083040241,-1.94969166645807,
135.321736374479));
#87525=CARTESIAN_POINT('Ctrl Pts',(-57.8167812042895,-1.82308417650453,
135.374290192622));
#87526=CARTESIAN_POINT('Ctrl Pts',(-57.8245541045549,-1.6946790855034,135.421420922528));
#87527=CARTESIAN_POINT('Ctrl Pts',(-57.8320444403169,-1.57094184299306,
135.466838331687));
#87528=CARTESIAN_POINT('Ctrl Pts',(-57.839534776079,-1.44553571822913,135.507219998651));
#87529=CARTESIAN_POINT('Ctrl Pts',(-57.847025111841,-1.31890879105788,135.542468115647));
#87530=CARTESIAN_POINT('Ctrl Pts',(-57.8547994459601,-1.18748076545568,
135.579052675712));
#87531=CARTESIAN_POINT('Ctrl Pts',(-57.8625737800792,-1.05432121209059,
135.610222613152));
#87532=CARTESIAN_POINT('Ctrl Pts',(-57.8703481141983,-0.919915934111412,
135.635813580875));
#87533=CARTESIAN_POINT('Ctrl Pts',(-57.8781128671453,-0.785676298625387,
135.661373010018));
#87534=CARTESIAN_POINT('Ctrl Pts',(-57.8858776200924,-0.650194373582241,
135.681367077378));
#87535=CARTESIAN_POINT('Ctrl Pts',(-57.8936423730395,-0.513971113057892,
135.695681171102));
#87536=CARTESIAN_POINT('Ctrl Pts',(-57.9013994139245,-0.377883151396122,
135.709981047866));
#87537=CARTESIAN_POINT('Ctrl Pts',(-57.9091564548095,-0.241055705841468,
135.718612137101));
#87538=CARTESIAN_POINT('Ctrl Pts',(-57.9169134956945,-0.103999567360767,
135.72151092567));
#87539=CARTESIAN_POINT('Ctrl Pts',(-57.9246646869346,0.0329532160197648,
135.72440752824));
#87540=CARTESIAN_POINT('Ctrl Pts',(-57.9324158781747,0.170133959760733,
135.721580426127));
#87541=CARTESIAN_POINT('Ctrl Pts',(-57.9401670694149,0.307027466384795,
135.713017989739));
#87542=CARTESIAN_POINT('Ctrl Pts',(-57.9479149661919,0.443862789616787,
135.704459192614));
#87543=CARTESIAN_POINT('Ctrl Pts',(-57.9556628629691,0.580410729160785,
135.690169933908));
#87544=CARTESIAN_POINT('Ctrl Pts',(-57.9634107597462,0.71615702567338,135.670190678006));
#87545=CARTESIAN_POINT('Ctrl Pts',(-57.9711570358303,0.851874926987096,
135.650215601333));
#87546=CARTESIAN_POINT('Ctrl Pts',(-57.9789033119143,0.986791132253789,
135.624552951778));
#87547=CARTESIAN_POINT('Ctrl Pts',(-57.9866495879984,1.12039783295732,135.593294920561));
#87548=CARTESIAN_POINT('Ctrl Pts',(-57.9943959212637,1.25400551991517,135.562036658605));
#87549=CARTESIAN_POINT('Ctrl Pts',(-58.0021422545291,1.38630330233558,135.525183021632));
#87550=CARTESIAN_POINT('Ctrl Pts',(-58.0098885877944,1.51679526260314,135.482876962931));
#87551=CARTESIAN_POINT('Ctrl Pts',(-58.0176366557974,1.64731644564044,135.440561430081));
#87552=CARTESIAN_POINT('Ctrl Pts',(-58.0253847238003,1.77603062997607,135.392791166342));
#87553=CARTESIAN_POINT('Ctrl Pts',(-58.0331327918033,1.90245909188332,135.339758336202));
#87554=CARTESIAN_POINT('Ctrl Pts',(-58.0408890945451,2.02902192346439,135.28666914214));
#87555=CARTESIAN_POINT('Ctrl Pts',(-58.0486453972871,2.15329381873653,135.228306360293));
#87556=CARTESIAN_POINT('Ctrl Pts',(-58.0564017000289,2.27481750571984,135.164909708927));
#87557=CARTESIAN_POINT('Ctrl Pts',(-58.0641621425431,2.3964060535539,135.10147922086));
#87558=CARTESIAN_POINT('Ctrl Pts',(-58.0719225850572,2.51524313177885,135.033009704825));
#87559=CARTESIAN_POINT('Ctrl Pts',(-58.0796830275714,2.63089883220604,134.959785312732));
#87560=CARTESIAN_POINT('Ctrl Pts',(-58.0874559278368,2.74674019343098,134.886443374344));
#87561=CARTESIAN_POINT('Ctrl Pts',(-58.0952288281023,2.85938964991657,134.808331529741));
#87562=CARTESIAN_POINT('Ctrl Pts',(-58.1030017283677,2.96844815595266,134.725776000807));
#87563=CARTESIAN_POINT('Ctrl Pts',(-58.1104920641298,3.07354211059357,134.646221573294));
#87564=CARTESIAN_POINT('Ctrl Pts',(-58.1179823998919,3.17530142432966,134.562541126215));
#87565=CARTESIAN_POINT('Ctrl Pts',(-58.125472735654,3.27340161060828,134.475058774343));
#87566=CARTESIAN_POINT('Ctrl Pts',(-58.1332470697731,3.37522129526569,134.384259502511));
#87567=CARTESIAN_POINT('Ctrl Pts',(-58.1410214038922,3.47342143760903,134.289076711545));
#87568=CARTESIAN_POINT('Ctrl Pts',(-58.1487957380113,3.56760117930796,134.189830287774));
#87569=CARTESIAN_POINT('Ctrl Pts',(-58.1565604909584,3.66166485289234,134.090706176351));
#87570=CARTESIAN_POINT('Ctrl Pts',(-58.1643252439054,3.75171771783988,133.987528677555));
#87571=CARTESIAN_POINT('Ctrl Pts',(-58.1720899968525,3.83739257003756,133.880657307731));
#87572=CARTESIAN_POINT('Ctrl Pts',(-58.1798470377375,3.92298232876423,133.773892084058));
#87573=CARTESIAN_POINT('Ctrl Pts',(-58.1876040786226,4.00420248510135,133.663440593516));
#87574=CARTESIAN_POINT('Ctrl Pts',(-58.1953611195076,4.08072350865371,133.549698248609));
#87575=CARTESIAN_POINT('Ctrl Pts',(-58.2031123107477,4.15718682710698,133.436041677689));
#87576=CARTESIAN_POINT('Ctrl Pts',(-58.2108635019878,4.22895784884965,133.319099515071));
#87577=CARTESIAN_POINT('Ctrl Pts',(-58.2186146932279,4.29574831275511,133.199298924905));
#87578=CARTESIAN_POINT('Ctrl Pts',(-58.226362590005,4.36251038893172,133.079549253186));
#87579=CARTESIAN_POINT('Ctrl Pts',(-58.2341104867821,4.42429592758238,132.956943911044));
#87580=CARTESIAN_POINT('Ctrl Pts',(-58.2418583835592,4.48086100280215,132.831937431417));
#87581=CARTESIAN_POINT('Ctrl Pts',(-58.2496046596433,4.5374142458276,132.706957100451));
#87582=CARTESIAN_POINT('Ctrl Pts',(-58.2573509357274,4.5887490364112,132.579576987005));
#87583=CARTESIAN_POINT('Ctrl Pts',(-58.2650972118115,4.63466845473061,132.450274156372));
#87584=CARTESIAN_POINT('Ctrl Pts',(-58.2728435450768,4.68058821201673,132.320970371255));
#87585=CARTESIAN_POINT('Ctrl Pts',(-58.2805898783422,4.72109238643315,132.189744209053));
#87586=CARTESIAN_POINT('Ctrl Pts',(-58.2883362116076,4.75603319304583,132.057090169044));
#87587=CARTESIAN_POINT('Ctrl Pts',(-58.2960842796105,4.79098182440989,131.924406422083));
#87588=CARTESIAN_POINT('Ctrl Pts',(-58.3038323476136,4.82036450925408,131.790294539021));
#87589=CARTESIAN_POINT('Ctrl Pts',(-58.3115804156165,4.8440841591374,131.655261153289));
#87590=CARTESIAN_POINT('Ctrl Pts',(-58.3193367183584,4.86782901854688,131.520084252468));
#87591=CARTESIAN_POINT('Ctrl Pts',(-58.3270930211003,4.88589875216386,131.383984278234));
#87592=CARTESIAN_POINT('Ctrl Pts',(-58.3348493238422,4.89824787507861,131.247475520032));
#87593=CARTESIAN_POINT('Ctrl Pts',(-58.3426097663563,4.91060358909209,131.110893902997));
#87594=CARTESIAN_POINT('Ctrl Pts',(-58.3503702088704,4.91723258963241,130.973903457567));
#87595=CARTESIAN_POINT('Ctrl Pts',(-58.3581306513846,4.91814156587027,130.837019468727));
#87596=CARTESIAN_POINT('Ctrl Pts',(-58.36590355165,4.91905200127748,130.699915741555));
#87597=CARTESIAN_POINT('Ctrl Pts',(-58.3736764519155,4.91422407701677,130.562919203419));
#87598=CARTESIAN_POINT('Ctrl Pts',(-58.3814493521809,4.90371655884486,130.426541913674));
#87599=CARTESIAN_POINT('Ctrl Pts',(-58.3889396879429,4.89359101542543,130.295122281925));
#87600=CARTESIAN_POINT('Ctrl Pts',(-58.3964300237048,4.87819168002817,130.164277963653));
#87601=CARTESIAN_POINT('Ctrl Pts',(-58.4039203594668,4.85761584668391,130.034457150536));
#87602=CARTESIAN_POINT('Ctrl Pts',(-58.4116946935859,4.83625987436435,129.89971414183));
#87603=CARTESIAN_POINT('Ctrl Pts',(-58.419469027705,4.80925947221593,129.765646957418));
#87604=CARTESIAN_POINT('Ctrl Pts',(-58.4272433618241,4.77666709594936,129.632765757141));
#87605=CARTESIAN_POINT('Ctrl Pts',(-58.4350081147711,4.74411488687367,129.500048321068));
#87606=CARTESIAN_POINT('Ctrl Pts',(-58.4427728677182,4.70598450816555,129.368514337008));
#87607=CARTESIAN_POINT('Ctrl Pts',(-58.4505376206653,4.66237994831585,129.238667071548));
#87608=CARTESIAN_POINT('Ctrl Pts',(-58.4582946615503,4.61881869712969,129.108948772223));
#87609=CARTESIAN_POINT('Ctrl Pts',(-58.4660517024353,4.56979420840062,128.980914225856));
#87610=CARTESIAN_POINT('Ctrl Pts',(-58.4738087433203,4.51546103463981,128.855054405821));
#87611=CARTESIAN_POINT('Ctrl Pts',(-58.4815599345604,4.46116883394798,128.729289497654));
#87612=CARTESIAN_POINT('Ctrl Pts',(-58.4893111258005,4.40157607092016,128.605696409035));
#87613=CARTESIAN_POINT('Ctrl Pts',(-58.4970623170406,4.33688631867345,128.48474855487));
#87614=CARTESIAN_POINT('Ctrl Pts',(-58.5048102138177,4.2722240612971,128.36385210677));
#87615=CARTESIAN_POINT('Ctrl Pts',(-58.5125581105949,4.20246930742585,128.245599001017));
#87616=CARTESIAN_POINT('Ctrl Pts',(-58.5203060073719,4.12787262058341,128.130440145537));
#87617=CARTESIAN_POINT('Ctrl Pts',(-58.528052283456,4.05329153775974,128.015305378807));
#87618=CARTESIAN_POINT('Ctrl Pts',(-58.5357985595401,3.97387074895792,127.903263902862));
#87619=CARTESIAN_POINT('Ctrl Pts',(-58.5435448356242,3.88990518274603,127.79473925737));
#87620=CARTESIAN_POINT('Ctrl Pts',(-58.5512911688896,3.8059389967194,127.686213810774));
#87621=CARTESIAN_POINT('Ctrl Pts',(-58.5590375021549,3.71742820558215,127.581205555652));
#87622=CARTESIAN_POINT('Ctrl Pts',(-58.5667838354203,3.6247089642163,127.480106116594));
#87623=CARTESIAN_POINT('Ctrl Pts',(-58.5745319034233,3.53196895901921,127.378984037018));
#87624=CARTESIAN_POINT('Ctrl Pts',(-58.5822799714262,3.43501889242421,127.281772803438));
#87625=CARTESIAN_POINT('Ctrl Pts',(-58.5900280394292,3.33423253081029,127.188827946854));
#87626=CARTESIAN_POINT('Ctrl Pts',(-58.5977843421711,3.23333905225187,127.09578430737));
#87627=CARTESIAN_POINT('Ctrl Pts',(-58.6055406449129,3.12860142177541,127.007016368217));
#87628=CARTESIAN_POINT('Ctrl Pts',(-58.6132969476547,3.02042773995131,126.922840383143));
#87629=CARTESIAN_POINT('Ctrl Pts',(-58.6210573901689,2.91219632257618,126.838619470812));
#87630=CARTESIAN_POINT('Ctrl Pts',(-58.628817832683,2.80052551778018,126.758995622983));
#87631=CARTESIAN_POINT('Ctrl Pts',(-58.6365782751972,2.6858524650723,126.684241735984));
#87632=CARTESIAN_POINT('Ctrl Pts',(-58.6443511754626,2.570995329,126.60936784741));
#87633=CARTESIAN_POINT('Ctrl Pts',(-58.652124075728,2.4531266505316,126.539379741636));
#87634=CARTESIAN_POINT('Ctrl Pts',(-58.6598969759935,2.33270900403111,126.474504757954));
#87635=CARTESIAN_POINT('Ctrl Pts',(-58.6673873117556,2.21666884229353,126.411988143339));
#87636=CARTESIAN_POINT('Ctrl Pts',(-58.6748776475177,2.09826209469348,126.354219490263));
#87637=CARTESIAN_POINT('Ctrl Pts',(-58.6823679832798,1.97791842738403,126.301359201053));
#87638=CARTESIAN_POINT('Ctrl Pts',(-58.6901423173988,1.85301189335193,126.246494697912));
#87639=CARTESIAN_POINT('Ctrl Pts',(-58.6979166515179,1.72562299724315,126.196744312983));
#87640=CARTESIAN_POINT('Ctrl Pts',(-58.705690985637,1.59620930457392,126.152339667646));
#87641=CARTESIAN_POINT('Ctrl Pts',(-58.7134557385841,1.46695510271487,126.107989747067));
#87642=CARTESIAN_POINT('Ctrl Pts',(-58.7212204915311,1.33568143561125,126.068972583302));
#87643=CARTESIAN_POINT('Ctrl Pts',(-58.7289852444783,1.2028679240148,126.035472715772));
#87644=CARTESIAN_POINT('Ctrl Pts',(-58.7367422853633,1.07018632467041,126.002006120783));
#87645=CARTESIAN_POINT('Ctrl Pts',(-58.7444993262484,0.935968301037668,
125.974046011868));
#87646=CARTESIAN_POINT('Ctrl Pts',(-58.7522563671334,0.800710462326672,
125.951727742722));
#87647=CARTESIAN_POINT('Ctrl Pts',(-58.7600075583735,0.665554622603999,
125.929426303956));
#87648=CARTESIAN_POINT('Ctrl Pts',(-58.7677587496135,0.529360912759822,
125.912758299918));
#87649=CARTESIAN_POINT('Ctrl Pts',(-58.7755099408537,0.392637666405466,
125.901808351101));
#87650=CARTESIAN_POINT('Ctrl Pts',(-58.7832578376307,0.255972531078022,
125.890863056304));
#87651=CARTESIAN_POINT('Ctrl Pts',(-58.791005734408,0.118778695783228,125.885631014141));
#87652=CARTESIAN_POINT('Ctrl Pts',(-58.7987536311851,-0.0184290421641127,
125.886145145171));
#87653=CARTESIAN_POINT('Ctrl Pts',(-58.8064999072692,-0.155608079210532,
125.886659168656));
#87654=CARTESIAN_POINT('Ctrl Pts',(-58.8142461833532,-0.292800622410291,
125.892916973076));
#87655=CARTESIAN_POINT('Ctrl Pts',(-58.8219924594373,-0.429490919750866,
125.904899360208));
#87656=CARTESIAN_POINT('Ctrl Pts',(-58.8297387927026,-0.566182226108165,
125.916881835792));
#87657=CARTESIAN_POINT('Ctrl Pts',(-58.837485125968,-0.702370889736662,
125.934588944269));
#87658=CARTESIAN_POINT('Ctrl Pts',(-58.8452314592334,-0.837545725852771,
125.957949551673));
#87659=CARTESIAN_POINT('Ctrl Pts',(-58.8529795272363,-0.972750833436009,
125.981315390524));
#87660=CARTESIAN_POINT('Ctrl Pts',(-58.8607275952393,-1.10694127654346,
126.010337181053));
#87661=CARTESIAN_POINT('Ctrl Pts',(-58.8684756632423,-1.23961590701895,
126.044892636209));
#87662=CARTESIAN_POINT('Ctrl Pts',(-58.8762319659841,-1.37243154567073,
126.079484817313));
#87663=CARTESIAN_POINT('Ctrl Pts',(-58.883988268726,-1.5037277745507,126.119622312767));
#87664=CARTESIAN_POINT('Ctrl Pts',(-58.8917445714679,-1.63301793209567,
126.165132718879));
#87665=CARTESIAN_POINT('Ctrl Pts',(-58.8995050139821,-1.76237709569076,
126.210667415265));
#87666=CARTESIAN_POINT('Ctrl Pts',(-58.9072654564963,-1.88972769163806,
126.261580591349));
#87667=CARTESIAN_POINT('Ctrl Pts',(-58.9150258990104,-2.01460383994363,
126.317651976414));
#87668=CARTESIAN_POINT('Ctrl Pts',(-58.9227987992759,-2.13968045052828,
126.373813372245));
#87669=CARTESIAN_POINT('Ctrl Pts',(-58.9305716995413,-2.26227432589723,
126.435149348929));
#87670=CARTESIAN_POINT('Ctrl Pts',(-58.9383445998068,-2.38194416632168,
126.501393611996));
#87671=CARTESIAN_POINT('Ctrl Pts',(-58.9458349355687,-2.49726370661558,
126.56522972924));
#87672=CARTESIAN_POINT('Ctrl Pts',(-58.9533252713306,-2.60986784986305,
126.633623311383));
#87673=CARTESIAN_POINT('Ctrl Pts',(-58.9608156070926,-2.7193893999931,126.706299569496));
#87674=CARTESIAN_POINT('Ctrl Pts',(-58.968571446223,-2.83279306454415,126.78155191925));
#87675=CARTESIAN_POINT('Ctrl Pts',(-58.9763272853535,-2.94325496047855,
126.861637362605));
#87676=CARTESIAN_POINT('Ctrl Pts',(-58.9840831244839,-3.05033395842733,
126.9462981758));
#87677=CARTESIAN_POINT('Ctrl Pts',(-58.9918266920159,-3.15724353170873,
127.030825035275));
#87678=CARTESIAN_POINT('Ctrl Pts',(-58.9995702595479,-3.26078056114886,
127.11991260563));
#87679=CARTESIAN_POINT('Ctrl Pts',(-59.0073138270799,-3.36053194376454,
127.213259377356));
#87680=CARTESIAN_POINT('Ctrl Pts',(-59.0150503122169,-3.4601920921144,127.306520772579));
#87681=CARTESIAN_POINT('Ctrl Pts',(-59.0227867973538,-3.55607319546732,
127.404033354081));
#87682=CARTESIAN_POINT('Ctrl Pts',(-59.0305232824907,-3.6477941619193,127.505454614848));
#87683=CARTESIAN_POINT('Ctrl Pts',(-59.0382543904089,-3.73945137801255,
127.606805383099));
#87684=CARTESIAN_POINT('Ctrl Pts',(-59.0459854983271,-3.82695394721599,
127.712059135335));
#87685=CARTESIAN_POINT('Ctrl Pts',(-59.0537166062452,-3.90995700446654,
127.820835976186));
#87686=CARTESIAN_POINT('Ctrl Pts',(-59.061444038016,-3.99292059370397,127.929561093571));
#87687=CARTESIAN_POINT('Ctrl Pts',(-59.0691714697868,-4.07138869102997,
128.04180565369));
#87688=CARTESIAN_POINT('Ctrl Pts',(-59.0768989015577,-4.14505645487896,
128.157156422879));
#87689=CARTESIAN_POINT('Ctrl Pts',(-59.0846259704071,-4.21872075889714,
128.272501774582));
#87690=CARTESIAN_POINT('Ctrl Pts',(-59.0923530392565,-4.28758495728074,
128.390952719827));
#87691=CARTESIAN_POINT('Ctrl Pts',(-59.100080108106,-4.351387403744,128.512066848208));
#87692=CARTESIAN_POINT('Ctrl Pts',(-59.1078067175771,-4.41518605711833,
128.63317377629));
#87693=CARTESIAN_POINT('Ctrl Pts',(-59.1155333270482,-4.47392337873462,
128.756943222097));
#87694=CARTESIAN_POINT('Ctrl Pts',(-59.1232599365194,-4.52738395536537,
128.882908670938));
#87695=CARTESIAN_POINT('Ctrl Pts',(-59.1309909096984,-4.58087472458491,
129.008945260482));
#87696=CARTESIAN_POINT('Ctrl Pts',(-59.1387218828775,-4.62908264408669,
129.137179967326));
#87697=CARTESIAN_POINT('Ctrl Pts',(-59.1464528560566,-4.67184062006425,
129.267126646039));
#87698=CARTESIAN_POINT('Ctrl Pts',(-59.1526466080874,-4.70609663084208,
129.37123482059));
#87699=CARTESIAN_POINT('Ctrl Pts',(-59.1588403601182,-4.7368554690376,129.476441400305));
#87700=CARTESIAN_POINT('Ctrl Pts',(-59.165034112149,-4.76405452823398,129.582490119308));
#87701=CARTESIAN_POINT('Ctrl Pts',(-57.4152011815765,-4.76405452823411,
129.582490119308));
#87702=CARTESIAN_POINT('Ctrl Pts',(-57.4229006030558,-4.79795614748395,
129.714672018235));
#87703=CARTESIAN_POINT('Ctrl Pts',(-57.4306000245351,-4.82635740057608,
129.848285643771));
#87704=CARTESIAN_POINT('Ctrl Pts',(-57.4382994460144,-4.84915170512526,
129.982831066557));
#87705=CARTESIAN_POINT('Ctrl Pts',(-57.4461062990135,-4.87226406302232,
130.119253827696));
#87706=CARTESIAN_POINT('Ctrl Pts',(-57.4539131520124,-4.88961172564464,
130.256634178774));
#87707=CARTESIAN_POINT('Ctrl Pts',(-57.4617200050115,-4.90113765442327,
130.394442631995));
#87708=CARTESIAN_POINT('Ctrl Pts',(-57.4695268580105,-4.91266358320189,
130.532251085217));
#87709=CARTESIAN_POINT('Ctrl Pts',(-57.4773337110095,-4.91836776813177,
130.670487216997));
#87710=CARTESIAN_POINT('Ctrl Pts',(-57.4851405640085,-4.91824815608826,
130.808619447741));
#87711=CARTESIAN_POINT('',(-57.139859435939,-4.91824920542422,130.801564934464));
#87712=CARTESIAN_POINT('Ctrl Pts',(-57.0701182010015,-4.76405452823404,
129.582490119308));
#87713=CARTESIAN_POINT('Ctrl Pts',(-57.0787834017356,-4.80194788990491,
129.730235761351));
#87714=CARTESIAN_POINT('Ctrl Pts',(-57.0874486024699,-4.83300862439036,
129.87991862542));
#87715=CARTESIAN_POINT('Ctrl Pts',(-57.0961138032041,-4.85705530084033,
130.030928741394));
#87716=CARTESIAN_POINT('Ctrl Pts',(-57.1047341945617,-4.88097762742078,
130.181157955764));
#87717=CARTESIAN_POINT('Ctrl Pts',(-57.1133545859192,-4.89795815486478,
130.332700521287));
#87718=CARTESIAN_POINT('Ctrl Pts',(-57.1219749772768,-4.90786633239802,
130.484937503478));
#87719=CARTESIAN_POINT('Ctrl Pts',(-57.1279364634976,-4.91471839530177,
130.590217952354));
#87720=CARTESIAN_POINT('Ctrl Pts',(-57.1338979497183,-4.91818910252655,
130.695830121914));
#87721=CARTESIAN_POINT('Ctrl Pts',(-57.139859435939,-4.91824920542422,130.801564934464));
#87722=CARTESIAN_POINT('Ctrl Pts',(-57.139859435991,-4.91824920542475,130.801564935387));
#87723=CARTESIAN_POINT('Ctrl Pts',(-57.1476908595179,-4.91832816075135,
130.940465549757));
#87724=CARTESIAN_POINT('Ctrl Pts',(-57.1555222830448,-4.91251855116177,
131.079373617091));
#87725=CARTESIAN_POINT('Ctrl Pts',(-57.1633537065717,-4.90084506944486,
131.217761957426));
#87726=CARTESIAN_POINT('Ctrl Pts',(-57.1711866138629,-4.8891693760361,131.356176517219));
#87727=CARTESIAN_POINT('Ctrl Pts',(-57.179019521154,-4.87162762925993,131.494070776241));
#87728=CARTESIAN_POINT('Ctrl Pts',(-57.1868524284452,-4.84829641842778,
131.630922715391));
#87729=CARTESIAN_POINT('Ctrl Pts',(-57.194688372281,-4.8249561629001,131.767827707257));
#87730=CARTESIAN_POINT('Ctrl Pts',(-57.2025243161168,-4.79582203705538,
131.903689201124));
#87731=CARTESIAN_POINT('Ctrl Pts',(-57.2103602599526,-4.76102170627262,
132.037995642564));
#87732=CARTESIAN_POINT('Ctrl Pts',(-57.2182007948159,-4.72620098620692,
132.172380773256));
#87733=CARTESIAN_POINT('Ctrl Pts',(-57.2260413296791,-4.68570754438162,
132.305208670745));
#87734=CARTESIAN_POINT('Ctrl Pts',(-57.2338818645424,-4.63971874720671,
132.435983432226));
#87735=CARTESIAN_POINT('Ctrl Pts',(-57.2417332379249,-4.5936663765037,132.566938972798));
#87736=CARTESIAN_POINT('Ctrl Pts',(-57.2495846113074,-4.54210360681127,
132.695835352532));
#87737=CARTESIAN_POINT('Ctrl Pts',(-57.25743598469,-4.48525600926085,132.822196486483));
#87738=CARTESIAN_POINT('Ctrl Pts',(-57.2652937880904,-4.42836185538808,
132.948661106069));
#87739=CARTESIAN_POINT('Ctrl Pts',(-57.2731515914908,-4.3661744177312,133.072586004796));
#87740=CARTESIAN_POINT('Ctrl Pts',(-57.2810093948912,-4.29896459324919,
133.193520823264));
#87741=CARTESIAN_POINT('Ctrl Pts',(-57.2888794534532,-4.23164994720188,
133.314644253695));
#87742=CARTESIAN_POINT('Ctrl Pts',(-57.2967495120151,-4.15929747147366,
133.432767971077));
#87743=CARTESIAN_POINT('Ctrl Pts',(-57.304619570577,-4.08222093126828,133.547471138638));
#87744=CARTESIAN_POINT('Ctrl Pts',(-57.306319333843,-4.06557405746394,133.572244554132));
#87745=CARTESIAN_POINT('Ctrl Pts',(-57.308019097109,-4.04870696780659,133.596858538697));
#87746=CARTESIAN_POINT('Ctrl Pts',(-57.3097188603751,-4.03162306031359,
133.621309066162));
#87747=CARTESIAN_POINT('Ctrl Pts',(-57.3174931944941,-3.95348511748049,
133.7331402686));
#87748=CARTESIAN_POINT('Ctrl Pts',(-57.3252675286132,-3.87056683763764,
133.841894995027));
#87749=CARTESIAN_POINT('Ctrl Pts',(-57.3330418627323,-3.78313852325258,
133.947137411483));
#87750=CARTESIAN_POINT('Ctrl Pts',(-57.3408066156794,-3.69581795645107,
134.052250126066));
#87751=CARTESIAN_POINT('Ctrl Pts',(-57.3485713686265,-3.60399866172716,
134.153858845474));
#87752=CARTESIAN_POINT('Ctrl Pts',(-57.3563361215736,-3.5079942690365,134.251556473752));
#87753=CARTESIAN_POINT('Ctrl Pts',(-57.3640931624586,-3.41208522926223,
134.349157067369));
#87754=CARTESIAN_POINT('Ctrl Pts',(-57.3718502033437,-3.31199963579226,
134.442854023233));
#87755=CARTESIAN_POINT('Ctrl Pts',(-57.3796072442287,-3.20809121308795,
134.532273415769));
#87756=CARTESIAN_POINT('Ctrl Pts',(-57.3873584354688,-3.10426114853378,
134.621625376446));
#87757=CARTESIAN_POINT('Ctrl Pts',(-57.3951096267088,-2.9966142879771,134.706705940454));
#87758=CARTESIAN_POINT('Ctrl Pts',(-57.4028608179489,-2.88554075954532,
134.787178412482));
#87759=CARTESIAN_POINT('Ctrl Pts',(-57.410608714726,-2.77451444032595,134.867616681564));
#87760=CARTESIAN_POINT('Ctrl Pts',(-57.4183566115031,-2.66006466589254,
134.943450525197));
#87761=CARTESIAN_POINT('Ctrl Pts',(-57.4261045082801,-2.54261397797426,
135.014384040483));
#87762=CARTESIAN_POINT('Ctrl Pts',(-57.4338507843642,-2.42518785820794,
135.085302718007));
#87763=CARTESIAN_POINT('Ctrl Pts',(-57.4415970604484,-2.3047624079933,135.151322904059));
#87764=CARTESIAN_POINT('Ctrl Pts',(-57.4493433365325,-2.18178809553241,
135.212192711543));
#87765=CARTESIAN_POINT('Ctrl Pts',(-57.4570896697978,-2.05881287530308,
135.273062968354));
#87766=CARTESIAN_POINT('Ctrl Pts',(-57.4648360030631,-1.93328910567397,
135.328782597298));
#87767=CARTESIAN_POINT('Ctrl Pts',(-57.4725823363285,-1.80569037006717,
135.379146443148));
#87768=CARTESIAN_POINT('Ctrl Pts',(-57.4803304043315,-1.67806305960806,
135.429521567633));
#87769=CARTESIAN_POINT('Ctrl Pts',(-57.4880784723345,-1.548360222116,135.474538378864));
#87770=CARTESIAN_POINT('Ctrl Pts',(-57.4958265403374,-1.41707347793118,
135.514040630119));
#87771=CARTESIAN_POINT('Ctrl Pts',(-57.5035828430793,-1.2856472006323,135.553584864837));
#87772=CARTESIAN_POINT('Ctrl Pts',(-57.5113391458211,-1.15263402886043,
135.587602718894));
#87773=CARTESIAN_POINT('Ctrl Pts',(-57.519095448563,-1.01853928021185,135.615988283665));
#87774=CARTESIAN_POINT('Ctrl Pts',(-57.5268558910771,-0.884372961158409,
135.644388998666));
#87775=CARTESIAN_POINT('Ctrl Pts',(-57.5346163335913,-0.749124300323084,
135.667151369573));
#87776=CARTESIAN_POINT('Ctrl Pts',(-57.5423767761054,-0.613305766086227,
135.684221179076));
#87777=CARTESIAN_POINT('Ctrl Pts',(-57.5501496763709,-0.477269203880809,
135.701318390554));
#87778=CARTESIAN_POINT('Ctrl Pts',(-57.5579225766363,-0.340661330027623,
135.712704747089));
#87779=CARTESIAN_POINT('Ctrl Pts',(-57.5656954769018,-0.203997560556797,
135.718378124432));
#87780=CARTESIAN_POINT('Ctrl Pts',(-57.5731858126638,-0.0723018633416816,
135.723845260219));
#87781=CARTESIAN_POINT('Ctrl Pts',(-57.5806761484258,0.0594454281349506,
135.724007567502));
#87782=CARTESIAN_POINT('Ctrl Pts',(-57.5881664841878,0.190787767961467,
135.718908723964));
#87783=CARTESIAN_POINT('Ctrl Pts',(-57.5959408183069,0.327109992523338,
135.713616556223));
#87784=CARTESIAN_POINT('Ctrl Pts',(-57.6037151524259,0.463427779607381,
135.702639645139));
#87785=CARTESIAN_POINT('Ctrl Pts',(-57.611489486545,0.599228344672425,135.685969824932));
#87786=CARTESIAN_POINT('Ctrl Pts',(-57.6192542394921,0.734861547677503,
135.669320548788));
#87787=CARTESIAN_POINT('Ctrl Pts',(-57.6270189924393,0.869978412631856,
135.64699237045));
#87788=CARTESIAN_POINT('Ctrl Pts',(-57.6347837453863,1.00406691352968,135.619029110376));
#87789=CARTESIAN_POINT('Ctrl Pts',(-57.6425407862713,1.13802223583827,135.591093623805));
#87790=CARTESIAN_POINT('Ctrl Pts',(-57.6502978271563,1.27095084643934,135.557534272768));
#87791=CARTESIAN_POINT('Ctrl Pts',(-57.6580548680413,1.40234695444476,135.518446539763));
#87792=CARTESIAN_POINT('Ctrl Pts',(-57.6658060592814,1.53364397562319,135.479388283122));
#87793=CARTESIAN_POINT('Ctrl Pts',(-57.6735572505215,1.66341042128189,135.434810053673));
#87794=CARTESIAN_POINT('Ctrl Pts',(-57.6813084417617,1.79115214633792,135.384858085218));
#87795=CARTESIAN_POINT('Ctrl Pts',(-57.6890563385388,1.91883957775318,135.334927347683));
#87796=CARTESIAN_POINT('Ctrl Pts',(-57.6968042353158,2.04450363680051,135.279627555894));
#87797=CARTESIAN_POINT('Ctrl Pts',(-57.7045521320929,2.1676669778647,135.219154263432));
#87798=CARTESIAN_POINT('Ctrl Pts',(-57.712298408177,2.29080455581303,135.158693620678));
#87799=CARTESIAN_POINT('Ctrl Pts',(-57.7200446842612,2.41144210552369,135.09306180198));
#87800=CARTESIAN_POINT('Ctrl Pts',(-57.7277909603453,2.52912421818262,135.022501647866));
#87801=CARTESIAN_POINT('Ctrl Pts',(-57.7355372936106,2.64680719954401,134.951940972893));
#87802=CARTESIAN_POINT('Ctrl Pts',(-57.7432836268759,2.76153436500908,134.876452090958));
#87803=CARTESIAN_POINT('Ctrl Pts',(-57.7510299601413,2.87287712826909,134.796322549795));
#87804=CARTESIAN_POINT('Ctrl Pts',(-57.7587780281442,2.98424482596878,134.716175064178));
#87805=CARTESIAN_POINT('Ctrl Pts',(-57.7665260961472,3.0922262960322,134.631385079688));
#87806=CARTESIAN_POINT('Ctrl Pts',(-57.7742741641501,3.19642435086389,134.542281755271));
#87807=CARTESIAN_POINT('Ctrl Pts',(-57.782030466892,3.30073314862851,134.453083730781));
#87808=CARTESIAN_POINT('Ctrl Pts',(-57.789786769634,3.40125020105201,134.35956346329));
#87809=CARTESIAN_POINT('Ctrl Pts',(-57.7975430723758,3.49761326770551,134.262088844606));
#87810=CARTESIAN_POINT('Ctrl Pts',(-57.80530351489,3.59402776622913,134.164562200783));
#87811=CARTESIAN_POINT('Ctrl Pts',(-57.8130639574041,3.68628359835076,134.063077289458));
#87812=CARTESIAN_POINT('Ctrl Pts',(-57.8208243999183,3.7740581478354,133.958035959014));
#87813=CARTESIAN_POINT('Ctrl Pts',(-57.8285973001837,3.86197360081913,133.852826006901));
#87814=CARTESIAN_POINT('Ctrl Pts',(-57.8363702004491,3.94539315770099,133.744048537527));
#87815=CARTESIAN_POINT('Ctrl Pts',(-57.8441431007145,4.02403643633555,133.632136036786));
#87816=CARTESIAN_POINT('Ctrl Pts',(-57.8516334364766,4.09982083370139,133.524291837337));
#87817=CARTESIAN_POINT('Ctrl Pts',(-57.8591237722386,4.17117001656507,133.413536840791));
#87818=CARTESIAN_POINT('Ctrl Pts',(-57.8666141080007,4.23787395798125,133.300278761008));
#87819=CARTESIAN_POINT('Ctrl Pts',(-57.8743884421198,4.30710699961025,133.182726466706));
#87820=CARTESIAN_POINT('Ctrl Pts',(-57.8821627762388,4.37155490709918,133.062105163146));
#87821=CARTESIAN_POINT('Ctrl Pts',(-57.8899371103579,4.43093363777566,132.93884185668));
#87822=CARTESIAN_POINT('Ctrl Pts',(-57.897701863305,4.49023918947333,132.815730461223));
#87823=CARTESIAN_POINT('Ctrl Pts',(-57.9054666162521,4.54448782659129,132.68998389024));
#87824=CARTESIAN_POINT('Ctrl Pts',(-57.9132313691992,4.59343965395904,132.56205661174));
#87825=CARTESIAN_POINT('Ctrl Pts',(-57.9209884100842,4.64234286168181,132.434256392417));
#87826=CARTESIAN_POINT('Ctrl Pts',(-57.9287454509691,4.68595959019541,132.304280138616));
#87827=CARTESIAN_POINT('Ctrl Pts',(-57.9365024918541,4.72409677930186,132.17260499716));
#87828=CARTESIAN_POINT('Ctrl Pts',(-57.9442536830942,4.7622052088574,132.041029152952));
#87829=CARTESIAN_POINT('Ctrl Pts',(-57.9520048743344,4.79484221550081,131.907757345141));
#87830=CARTESIAN_POINT('Ctrl Pts',(-57.9597560655746,4.82186373238449,131.773284354924));
#87831=CARTESIAN_POINT('Ctrl Pts',(-57.9675039623516,4.84887376440267,131.638868519314));
#87832=CARTESIAN_POINT('Ctrl Pts',(-57.9752518591287,4.87027297682982,131.503252899212));
#87833=CARTESIAN_POINT('Ctrl Pts',(-57.9829997559058,4.88596787746547,131.366944800489));
#87834=CARTESIAN_POINT('Ctrl Pts',(-57.9907460319899,4.90165949506622,131.230665214483));
#87835=CARTESIAN_POINT('Ctrl Pts',(-57.998492308074,4.91164912956055,131.093693826126));
#87836=CARTESIAN_POINT('Ctrl Pts',(-58.0062385841581,4.91589492997459,130.956545044989));
#87837=CARTESIAN_POINT('Ctrl Pts',(-58.0139849174234,4.92014076173016,130.819395251451));
#87838=CARTESIAN_POINT('Ctrl Pts',(-58.0217312506888,4.9186426627024,130.682068453299));
#87839=CARTESIAN_POINT('Ctrl Pts',(-58.0294775839542,4.91141089357604,130.545080658906));
#87840=CARTESIAN_POINT('Ctrl Pts',(-58.0372256519571,4.90417750494514,130.408062187047));
#87841=CARTESIAN_POINT('Ctrl Pts',(-58.0449737199599,4.89120791178008,130.271383260361));
#87842=CARTESIAN_POINT('Ctrl Pts',(-58.0527217879629,4.87256435522666,130.135555962473));
#87843=CARTESIAN_POINT('Ctrl Pts',(-58.0604780907047,4.85390098407946,129.999584305715));
#87844=CARTESIAN_POINT('Ctrl Pts',(-58.0682343934466,4.82955165650847,129.864466473782));
#87845=CARTESIAN_POINT('Ctrl Pts',(-58.0759906961885,4.79963009050997,129.730706084315));
#87846=CARTESIAN_POINT('Ctrl Pts',(-58.0837511387027,4.76969255447069,129.596874302899));
#87847=CARTESIAN_POINT('Ctrl Pts',(-58.0915115812168,4.73417695510684,129.464401785036));
#87848=CARTESIAN_POINT('Ctrl Pts',(-58.0992720237309,4.69324699688804,129.333777165768));
#87849=CARTESIAN_POINT('Ctrl Pts',(-58.1070449239964,4.65225133426672,129.202942856265));
#87850=CARTESIAN_POINT('Ctrl Pts',(-58.1148178242619,4.60582407667476,129.073962741261));
#87851=CARTESIAN_POINT('Ctrl Pts',(-58.1225907245274,4.55417753334568,128.947306483388));
#87852=CARTESIAN_POINT('Ctrl Pts',(-58.1300810602895,4.50440847195605,128.825254499514));
#87853=CARTESIAN_POINT('Ctrl Pts',(-58.1375713960515,4.44979313275573,128.705360630282));
#87854=CARTESIAN_POINT('Ctrl Pts',(-58.1450617318136,4.39056101226808,128.588021956609));
#87855=CARTESIAN_POINT('Ctrl Pts',(-58.1528360659327,4.32908308792936,128.46623435146));
#87856=CARTESIAN_POINT('Ctrl Pts',(-58.1606104000518,4.26243663729623,128.346813740717));
#87857=CARTESIAN_POINT('Ctrl Pts',(-58.1683847341709,4.19082738090478,128.230229904887));
#87858=CARTESIAN_POINT('Ctrl Pts',(-58.176149487118,4.11930637652203,128.113789748215));
#87859=CARTESIAN_POINT('Ctrl Pts',(-58.183914240065,4.04283493848531,128.00017974026));
#87860=CARTESIAN_POINT('Ctrl Pts',(-58.1916789930121,3.9616657544016,127.889847362681));
#87861=CARTESIAN_POINT('Ctrl Pts',(-58.1994360338971,3.88057718869581,127.779624568775));
#87862=CARTESIAN_POINT('Ctrl Pts',(-58.2071930747821,3.79480039241356,127.67267323976));
#87863=CARTESIAN_POINT('Ctrl Pts',(-58.2149501156671,3.70463244893746,127.569413712163));
#87864=CARTESIAN_POINT('Ctrl Pts',(-58.2227013069072,3.61453250180882,127.466232053378));
#87865=CARTESIAN_POINT('Ctrl Pts',(-58.2304524981473,3.52004825473804,127.366736947894));
#87866=CARTESIAN_POINT('Ctrl Pts',(-58.2382036893875,3.42151810950774,127.271317044553));
#87867=CARTESIAN_POINT('Ctrl Pts',(-58.2459515861645,3.32302984221768,127.175937697216));
#87868=CARTESIAN_POINT('Ctrl Pts',(-58.2536994829416,3.22049937721389,127.084630378483));
#87869=CARTESIAN_POINT('Ctrl Pts',(-58.2614473797186,3.1143029904755,126.997747957206));
#87870=CARTESIAN_POINT('Ctrl Pts',(-58.2691936558027,3.00812881773203,126.910883709858));
#87871=CARTESIAN_POINT('Ctrl Pts',(-58.2769399318869,2.89829055093085,126.828442766318));
#87872=CARTESIAN_POINT('Ctrl Pts',(-58.284686207971,2.78519835593871,126.750738387933));
#87873=CARTESIAN_POINT('Ctrl Pts',(-58.2924325412363,2.67210532612552,126.673033435952));
#87874=CARTESIAN_POINT('Ctrl Pts',(-58.3001788745017,2.55575864242525,126.600065340297));
#87875=CARTESIAN_POINT('Ctrl Pts',(-58.307925207767,2.4365979834481,126.532104383495));
#87876=CARTESIAN_POINT('Ctrl Pts',(-58.31567327577,2.31741063926789,126.464128207309));
#87877=CARTESIAN_POINT('Ctrl Pts',(-58.3234213437728,2.19540840539337,126.401161594914));
#87878=CARTESIAN_POINT('Ctrl Pts',(-58.3311694117758,2.07105575513923,126.343428974781));
#87879=CARTESIAN_POINT('Ctrl Pts',(-58.3389257145176,1.94657094140841,126.285634995731));
#87880=CARTESIAN_POINT('Ctrl Pts',(-58.3466820172595,1.81973107635018,126.233086286029));
#87881=CARTESIAN_POINT('Ctrl Pts',(-58.3544383200013,1.69102133510279,126.18595938914));
#87882=CARTESIAN_POINT('Ctrl Pts',(-58.3621987625155,1.56224289759094,126.138807339207));
#87883=CARTESIAN_POINT('Ctrl Pts',(-58.3699592050297,1.43159296752367,126.09708298708));
#87884=CARTESIAN_POINT('Ctrl Pts',(-58.3777196475439,1.29957113366506,126.060912722728));
#87885=CARTESIAN_POINT('Ctrl Pts',(-58.3854925478093,1.16733736663822,126.024684394656));
#87886=CARTESIAN_POINT('Ctrl Pts',(-58.3932654480747,1.03372767620185,125.994028058683));
#87887=CARTESIAN_POINT('Ctrl Pts',(-58.4010383483401,0.899251961154634,
125.96901895716));
#87888=CARTESIAN_POINT('Ctrl Pts',(-58.4085286841022,0.769664777072177,
125.944918999471));
#87889=CARTESIAN_POINT('Ctrl Pts',(-58.4160190198644,0.639273744424748,
125.926062866237));
#87890=CARTESIAN_POINT('Ctrl Pts',(-58.4235093556265,0.508536987110952,
125.912472107467));
#87891=CARTESIAN_POINT('Ctrl Pts',(-58.4312836897455,0.372843305908174,
125.898366050948));
#87892=CARTESIAN_POINT('Ctrl Pts',(-58.4390580238647,0.236347329424679,
125.889887840273));
#87893=CARTESIAN_POINT('Ctrl Pts',(-58.4468323579838,0.0995554942823636,
125.88711832477));
#87894=CARTESIAN_POINT('Ctrl Pts',(-58.4545971109309,-0.0370677571485767,
125.884352222448));
#87895=CARTESIAN_POINT('Ctrl Pts',(-58.4623618638779,-0.173985754621854,
125.887280824673));
#87896=CARTESIAN_POINT('Ctrl Pts',(-58.470126616825,-0.310685435319369,
125.895933412974));
#87897=CARTESIAN_POINT('Ctrl Pts',(-58.47788365771,-0.447249343966886,125.904577407402));
#87898=CARTESIAN_POINT('Ctrl Pts',(-58.4856406985951,-0.58359497969117,
125.918934049676));
#87899=CARTESIAN_POINT('Ctrl Pts',(-58.4933977394801,-0.71920812064433,
125.93898059729));
#87900=CARTESIAN_POINT('Ctrl Pts',(-58.5011489307201,-0.854718994672243,
125.959012027647));
#87901=CARTESIAN_POINT('Ctrl Pts',(-58.5089001219603,-0.989498088210454,
125.984724765824));
#87902=CARTESIAN_POINT('Ctrl Pts',(-58.5166513132004,-1.1230355055525,126.016044179008));
#87903=CARTESIAN_POINT('Ctrl Pts',(-58.5243992099774,-1.25651616593068,
126.047350280606));
#87904=CARTESIAN_POINT('Ctrl Pts',(-58.5321471067545,-1.38875581991871,
126.084258228547));
#87905=CARTESIAN_POINT('Ctrl Pts',(-58.5398950035315,-1.51925420260059,
126.126642185426));
#87906=CARTESIAN_POINT('Ctrl Pts',(-58.5476412796156,-1.64972528783386,
126.169017276496));
#87907=CARTESIAN_POINT('Ctrl Pts',(-58.5553875556997,-1.77845545463806,
126.216865977421));
#87908=CARTESIAN_POINT('Ctrl Pts',(-58.5631338317838,-1.90495944269964,
126.270012529454));
#87909=CARTESIAN_POINT('Ctrl Pts',(-58.5708801650492,-2.0314643645851,126.323159473802));
#87910=CARTESIAN_POINT('Ctrl Pts',(-58.5786264983145,-2.15574271448898,
126.381604195862));
#87911=CARTESIAN_POINT('Ctrl Pts',(-58.5863728315799,-2.27732943903889,
126.445122875875));
#87912=CARTESIAN_POINT('Ctrl Pts',(-58.5941208995829,-2.39894339209292,
126.508655780455));
#87913=CARTESIAN_POINT('Ctrl Pts',(-58.6018689675858,-2.51786417388733,
126.577264723053));
#87914=CARTESIAN_POINT('Ctrl Pts',(-58.6096170355888,-2.63365190722394,
126.650680238182));
#87915=CARTESIAN_POINT('Ctrl Pts',(-58.6173733383307,-2.74956270114128,
126.724173780195));
#87916=CARTESIAN_POINT('Ctrl Pts',(-58.6251296410725,-2.8623334641704,126.802483889793));
#87917=CARTESIAN_POINT('Ctrl Pts',(-58.6328859438143,-2.97155341628101,
126.885297801447));
#87918=CARTESIAN_POINT('Ctrl Pts',(-58.6406463863285,-3.08083166236861,
126.968155913379));
#87919=CARTESIAN_POINT('Ctrl Pts',(-58.6484068288427,-3.18655502001154,
127.055522368244));
#87920=CARTESIAN_POINT('Ctrl Pts',(-58.6561672713569,-3.2883471138192,127.147045164732));
#87921=CARTESIAN_POINT('Ctrl Pts',(-58.6639401716223,-3.39030261333251,
127.238714881738));
#87922=CARTESIAN_POINT('Ctrl Pts',(-58.6717130718878,-3.48831395829851,
127.334553999909));
#87923=CARTESIAN_POINT('Ctrl Pts',(-58.6794859721532,-3.58204223243934,
127.434174197274));
#87924=CARTESIAN_POINT('Ctrl Pts',(-58.6869763079152,-3.67236324772761,
127.530172949536));
#87925=CARTESIAN_POINT('Ctrl Pts',(-58.6944666436772,-3.7587069847742,127.629682417567));
#87926=CARTESIAN_POINT('Ctrl Pts',(-58.7019569794392,-3.84080768578747,
127.732328817064));
#87927=CARTESIAN_POINT('Ctrl Pts',(-58.7097173502063,-3.92586820915285,
127.838675734386));
#87928=CARTESIAN_POINT('Ctrl Pts',(-58.7174777209734,-4.00664976386243,
127.948734816506));
#87929=CARTESIAN_POINT('Ctrl Pts',(-58.7252380917405,-4.0828096513879,128.062126416584));
#87930=CARTESIAN_POINT('Ctrl Pts',(-58.7331313418183,-4.16027360977096,
128.177459598851));
#87931=CARTESIAN_POINT('Ctrl Pts',(-58.741024591896,-4.23295586205342,128.29624021107));
#87932=CARTESIAN_POINT('Ctrl Pts',(-58.7489178419738,-4.30053666294926,
128.418031329071));
#87933=CARTESIAN_POINT('Ctrl Pts',(-58.7566587308323,-4.36681297036912,
128.537471546864));
#87934=CARTESIAN_POINT('Ctrl Pts',(-58.7643996196907,-4.42818275921784,
128.659806752579));
#87935=CARTESIAN_POINT('Ctrl Pts',(-58.7721405085491,-4.48438690609844,
128.784594012507));
#87936=CARTESIAN_POINT('Ctrl Pts',(-58.7801099392367,-4.54225042295116,
128.913065488699));
#87937=CARTESIAN_POINT('Ctrl Pts',(-58.7880793699241,-4.59463830909258,
129.044135708188));
#87938=CARTESIAN_POINT('Ctrl Pts',(-58.7960488006117,-4.6413181232458,129.177292966443));
#87939=CARTESIAN_POINT('Ctrl Pts',(-58.8040182312992,-4.68799793739903,
129.310450224698));
#87940=CARTESIAN_POINT('Ctrl Pts',(-58.8119876619867,-4.72896949444375,
129.44569410505));
#87941=CARTESIAN_POINT('Ctrl Pts',(-58.8199570926742,-4.76405452823407,
129.582490119308));
#87942=CARTESIAN_POINT('Origin',(213.235140564004,0.,130.804360617566));
#87943=CARTESIAN_POINT('',(-60.9152461054369,-4.76405452823402,129.582490119308));
#87944=CARTESIAN_POINT('',(-60.5697319016605,-4.76405452823403,129.582490119308));
#87945=CARTESIAN_POINT('',(213.235140564004,-4.76405452823405,129.582490119308));
#87946=CARTESIAN_POINT('',(-59.2351405639695,-4.91824997905427,130.804814525752));
#87947=CARTESIAN_POINT('Ctrl Pts',(-59.2351405640084,-4.91824997905421,
130.804814526437));
#87948=CARTESIAN_POINT('Ctrl Pts',(-59.2365147863075,-4.91824775337627,
130.828930469497));
#87949=CARTESIAN_POINT('Ctrl Pts',(-59.2378890086065,-4.91806815542009,
130.853045470433));
#87950=CARTESIAN_POINT('Ctrl Pts',(-59.2392632309054,-4.91771121833615,
130.877157839702));
#87951=CARTESIAN_POINT('Ctrl Pts',(-59.2470375650245,-4.9156919321172,131.013567804266));
#87952=CARTESIAN_POINT('Ctrl Pts',(-59.2548118991436,-4.90798943313343,
131.150109750795));
#87953=CARTESIAN_POINT('Ctrl Pts',(-59.2625862332627,-4.89458325254077,
131.286271238374));
#87954=CARTESIAN_POINT('Ctrl Pts',(-59.2703509862099,-4.88119359386754,
131.422264919089));
#87955=CARTESIAN_POINT('Ctrl Pts',(-59.278115739157,-4.86211427769381,131.55787868844));
#87956=CARTESIAN_POINT('Ctrl Pts',(-59.2858804921042,-4.8373768246463,131.692599616302));
#87957=CARTESIAN_POINT('Ctrl Pts',(-59.2936375329892,-4.8126639411859,131.827186737439));
#87958=CARTESIAN_POINT('Ctrl Pts',(-59.3013945738742,-4.78230417454216,
131.960882399776));
#87959=CARTESIAN_POINT('Ctrl Pts',(-59.3091516147592,-4.74638084213209,
132.093178666765));
#87960=CARTESIAN_POINT('Ctrl Pts',(-59.3169028059993,-4.71048459978648,
132.22537516811));
#87961=CARTESIAN_POINT('Ctrl Pts',(-59.3246539972396,-4.66903324465619,
132.356173998829));
#87962=CARTESIAN_POINT('Ctrl Pts',(-59.3324051884797,-4.62216111031285,
132.485077646935));
#87963=CARTESIAN_POINT('Ctrl Pts',(-59.3401530852568,-4.57530889787697,
132.613926507552));
#87964=CARTESIAN_POINT('Ctrl Pts',(-59.3479009820339,-4.52304062198529,
132.74088142098));
#87965=CARTESIAN_POINT('Ctrl Pts',(-59.355648878811,-4.46554032492361,132.865460486321));
#87966=CARTESIAN_POINT('Ctrl Pts',(-59.3633951548951,-4.4080520556845,132.990013492407));
#87967=CARTESIAN_POINT('Ctrl Pts',(-59.3711414309793,-4.34533410588747,
133.112191284166));
#87968=CARTESIAN_POINT('Ctrl Pts',(-59.3788877070634,-4.27761831757293,
133.231532756427));
#87969=CARTESIAN_POINT('Ctrl Pts',(-59.3866340403288,-4.20990202939593,
133.35087510964));
#87970=CARTESIAN_POINT('Ctrl Pts',(-59.3943803735941,-4.1371880220269,133.467380761537));
#87971=CARTESIAN_POINT('Ctrl Pts',(-59.4021267068594,-4.05975347550475,
133.580614348879));
#87972=CARTESIAN_POINT('Ctrl Pts',(-59.4098747748624,-3.98230158805259,
133.693873294097));
#87973=CARTESIAN_POINT('Ctrl Pts',(-59.4176228428654,-3.90012727852677,
133.803858394002));
#87974=CARTESIAN_POINT('Ctrl Pts',(-59.4253709108685,-3.81355007967587,
133.91016467647));
#87975=CARTESIAN_POINT('Ctrl Pts',(-59.4331272136103,-3.72688086554775,
134.01658394252));
#87976=CARTESIAN_POINT('Ctrl Pts',(-59.4408835163522,-3.63579966168534,
134.119316277072));
#87977=CARTESIAN_POINT('Ctrl Pts',(-59.4486398190941,-3.54066556118018,
134.217990715625));
#87978=CARTESIAN_POINT('Ctrl Pts',(-59.4564002616083,-3.44548068474116,
134.316717819696));
#87979=CARTESIAN_POINT('Ctrl Pts',(-59.4641607041225,-3.34623888415661,
134.411382442465));
#87980=CARTESIAN_POINT('Ctrl Pts',(-59.4719211466367,-3.24333415018636,
134.501652417348));
#87981=CARTESIAN_POINT('Ctrl Pts',(-59.4796940469022,-3.1402642244017,134.592067301608));
#87982=CARTESIAN_POINT('Ctrl Pts',(-59.4874669471676,-3.03351991960272,
134.678073195052));
#87983=CARTESIAN_POINT('Ctrl Pts',(-59.4952398474331,-2.92352686874046,
134.759379417806));
#87984=CARTESIAN_POINT('Ctrl Pts',(-59.5027301831948,-2.81753234233684,
134.837729954562));
#87985=CARTESIAN_POINT('Ctrl Pts',(-59.5102205189566,-2.7085214241549,134.911716405154));
#87986=CARTESIAN_POINT('Ctrl Pts',(-59.5177108547184,-2.59689667057551,
134.981119019108));
#87987=CARTESIAN_POINT('Ctrl Pts',(-59.5254851888375,-2.48103963053278,
135.053153054268));
#87988=CARTESIAN_POINT('Ctrl Pts',(-59.5332595229566,-2.36199963500479,
135.120476981048));
#87989=CARTESIAN_POINT('Ctrl Pts',(-59.5410338570756,-2.2401967511368,135.182796591598));
#87990=CARTESIAN_POINT('Ctrl Pts',(-59.5487986100227,-2.11854397843751,
135.245039398798));
#87991=CARTESIAN_POINT('Ctrl Pts',(-59.5565633629697,-1.99413543707173,
135.302289984631));
#87992=CARTESIAN_POINT('Ctrl Pts',(-59.5643281159168,-1.86741970734935,
135.354297617031));
#87993=CARTESIAN_POINT('Ctrl Pts',(-59.5720851568018,-1.74082983347594,
135.406253594718));
#87994=CARTESIAN_POINT('Ctrl Pts',(-59.5798421976869,-1.61193769084453,
135.452976834399));
#87995=CARTESIAN_POINT('Ctrl Pts',(-59.5875992385719,-1.48121565595883,
135.494262881264));
#87996=CARTESIAN_POINT('Ctrl Pts',(-59.595350429812,-1.35059219957668,135.535517794));
#87997=CARTESIAN_POINT('Ctrl Pts',(-59.6031016210521,-1.21814196892384,
135.571343557909));
#87998=CARTESIAN_POINT('Ctrl Pts',(-59.6108528122922,-1.08435614550405,
135.601584274246));
#87999=CARTESIAN_POINT('Ctrl Pts',(-59.6186007090693,-0.950627184627884,
135.631812137472));
#88000=CARTESIAN_POINT('Ctrl Pts',(-59.6263486058464,-0.815564140568402,
135.656459588403));
#88001=CARTESIAN_POINT('Ctrl Pts',(-59.6340965026235,-0.679671929550312,
135.675420987822));
#88002=CARTESIAN_POINT('Ctrl Pts',(-59.6418427787076,-0.543808144253269,
135.694378420925));
#88003=CARTESIAN_POINT('Ctrl Pts',(-59.6495890547916,-0.407115923955601,
135.707652114301));
#88004=CARTESIAN_POINT('Ctrl Pts',(-59.6573353308757,-0.270108525782485,
135.715187884616));
#88005=CARTESIAN_POINT('Ctrl Pts',(-59.665081664141,-0.13310011625188,135.722723710558));
#88006=CARTESIAN_POINT('Ctrl Pts',(-59.6728279974064,0.00422308542152605,
135.72452150745));
#88007=CARTESIAN_POINT('Ctrl Pts',(-59.6805743306718,0.141344973232886,
135.720579150244));
#88008=CARTESIAN_POINT('Ctrl Pts',(-59.6883223986747,0.278497568540284,
135.716635910173));
#88009=CARTESIAN_POINT('Ctrl Pts',(-59.6960704666777,0.415448369547073,
135.706949969306));
#88010=CARTESIAN_POINT('Ctrl Pts',(-59.7038185346807,0.551683946481696,
135.691571262269));
#88011=CARTESIAN_POINT('Ctrl Pts',(-59.7115748374226,0.688064316208524,
135.676176210558));
#88012=CARTESIAN_POINT('Ctrl Pts',(-59.7193311401644,0.823727554267093,
135.655076350398));
#88013=CARTESIAN_POINT('Ctrl Pts',(-59.7270874429062,0.958167459128667,
135.628373281601));
#88014=CARTESIAN_POINT('Ctrl Pts',(-59.7348478854204,1.09267911861574,135.601655960571));
#88015=CARTESIAN_POINT('Ctrl Pts',(-59.7426083279345,1.22596576412376,135.569329563985));
#88016=CARTESIAN_POINT('Ctrl Pts',(-59.7503687704487,1.35753497286985,135.531546023274));
#88017=CARTESIAN_POINT('Ctrl Pts',(-59.7581416707141,1.4893153881898,135.493701829069));
#88018=CARTESIAN_POINT('Ctrl Pts',(-59.7659145709796,1.61937248627495,135.450383108503));
#88019=CARTESIAN_POINT('Ctrl Pts',(-59.773687471245,1.74723164491043,135.401790839062));
#88020=CARTESIAN_POINT('Ctrl Pts',(-59.7811778070071,1.87044280107329,135.354965021011));
#88021=CARTESIAN_POINT('Ctrl Pts',(-59.7886681427692,1.99161276138343,135.303242531957));
#88022=CARTESIAN_POINT('Ctrl Pts',(-59.7961584785313,2.11033905198889,135.246843273486));
#88023=CARTESIAN_POINT('Ctrl Pts',(-59.8039328126504,2.23356688598718,135.188305619989));
#88024=CARTESIAN_POINT('Ctrl Pts',(-59.8117071467694,2.35455243759627,135.124544127266));
#88025=CARTESIAN_POINT('Ctrl Pts',(-59.8194814808885,2.47282112486666,135.055753183175));
#88026=CARTESIAN_POINT('Ctrl Pts',(-59.8272462338356,2.59094405654997,134.987047017774));
#88027=CARTESIAN_POINT('Ctrl Pts',(-59.8350109867828,2.70635645128811,134.913323928556));
#88028=CARTESIAN_POINT('Ctrl Pts',(-59.8427757397299,2.81860489247843,134.834825792034));
#88029=CARTESIAN_POINT('Ctrl Pts',(-59.8505327806149,2.93074184693438,134.756405620968));
#88030=CARTESIAN_POINT('Ctrl Pts',(-59.8582898214998,3.03972078320653,134.673220063283));
#88031=CARTESIAN_POINT('Ctrl Pts',(-59.8660468623848,3.14511435663451,134.585556029892));
#88032=CARTESIAN_POINT('Ctrl Pts',(-59.8737980536249,3.25042845194907,134.49795810463));
#88033=CARTESIAN_POINT('Ctrl Pts',(-59.881549244865,3.35216226670846,134.405888674881));
#88034=CARTESIAN_POINT('Ctrl Pts',(-59.8893004361052,3.44991914328328,134.309676718477));
#88035=CARTESIAN_POINT('Ctrl Pts',(-59.8970483328823,3.54763447057779,134.213505654721));
#88036=CARTESIAN_POINT('Ctrl Pts',(-59.9047962296594,3.6413759435113,134.113195839846));
#88037=CARTESIAN_POINT('Ctrl Pts',(-59.9125441264365,3.73078176526413,134.009114973593));
#88038=CARTESIAN_POINT('Ctrl Pts',(-59.9202904025206,3.8201688852463,133.905055878813));
#88039=CARTESIAN_POINT('Ctrl Pts',(-59.9280366786046,3.90522190337754,133.79722759805));
#88040=CARTESIAN_POINT('Ctrl Pts',(-59.9357829546887,3.98561780567198,133.686032661642));
#88041=CARTESIAN_POINT('Ctrl Pts',(-59.9435292879541,4.06601430143071,133.574836904419));
#88042=CARTESIAN_POINT('Ctrl Pts',(-59.9512756212194,4.14175338368226,133.46027475879));
#88043=CARTESIAN_POINT('Ctrl Pts',(-59.9590219544847,4.21255429666111,133.342779290713));
#88044=CARTESIAN_POINT('Ctrl Pts',(-59.9667700224877,4.28337106501353,133.225257510341));
#88045=CARTESIAN_POINT('Ctrl Pts',(-59.9745180904906,4.34924726179517,133.104801435175));
#88046=CARTESIAN_POINT('Ctrl Pts',(-59.9822661584936,4.40994737708912,132.981870019108));
#88047=CARTESIAN_POINT('Ctrl Pts',(-59.9900224612354,4.47071200518795,132.85880795007));
#88048=CARTESIAN_POINT('Ctrl Pts',(-59.9977787639773,4.52628938918531,132.733265635899));
#88049=CARTESIAN_POINT('Ctrl Pts',(-60.0055350667191,4.57649139359088,132.605723875459));
#88050=CARTESIAN_POINT('Ctrl Pts',(-60.0132955092333,4.62672019231781,132.478114042142));
#88051=CARTESIAN_POINT('Ctrl Pts',(-60.0210559517474,4.67156776694264,132.348503005431));
#88052=CARTESIAN_POINT('Ctrl Pts',(-60.0288163942616,4.7108957751407,132.217387177211));
#88053=CARTESIAN_POINT('Ctrl Pts',(-60.036589294527,4.75028691614889,132.086060870223));
#88054=CARTESIAN_POINT('Ctrl Pts',(-60.0443621947924,4.78414068802326,131.953225323611));
#88055=CARTESIAN_POINT('Ctrl Pts',(-60.0521350950579,4.81236963391396,131.819388483727));
#88056=CARTESIAN_POINT('Ctrl Pts',(-60.05962543082,4.83957238651753,131.690416950085));
#88057=CARTESIAN_POINT('Ctrl Pts',(-60.0671157665822,4.86155211490772,131.560515962038));
#88058=CARTESIAN_POINT('Ctrl Pts',(-60.0746061023443,4.87827628156955,131.430142994416));
#88059=CARTESIAN_POINT('Ctrl Pts',(-60.0823804364634,4.89563455009333,131.294826896102));
#88060=CARTESIAN_POINT('Ctrl Pts',(-60.0901547705824,4.90738584632752,131.158573680767));
#88061=CARTESIAN_POINT('Ctrl Pts',(-60.0979291047015,4.91343719114534,131.021887699029));
#88062=CARTESIAN_POINT('Ctrl Pts',(-60.1056938576486,4.9194810782215,130.885370170548));
#88063=CARTESIAN_POINT('Ctrl Pts',(-60.1134586105958,4.91983897377632,130.748421323696));
#88064=CARTESIAN_POINT('Ctrl Pts',(-60.1212233635429,4.91446929262161,130.611553370868));
#88065=CARTESIAN_POINT('Ctrl Pts',(-60.1289804044279,4.90910494470992,130.47482135722));
#88066=CARTESIAN_POINT('Ctrl Pts',(-60.1367374453128,4.89802435610577,130.338170465841));
#88067=CARTESIAN_POINT('Ctrl Pts',(-60.1444944861978,4.88123792285803,130.202115316254));
#88068=CARTESIAN_POINT('Ctrl Pts',(-60.152245677438,4.86446414839018,130.066162766913));
#88069=CARTESIAN_POINT('Ctrl Pts',(-60.1599968686781,4.84199314146508,129.930805451605));
#88070=CARTESIAN_POINT('Ctrl Pts',(-60.1677480599182,4.81388727731124,129.796554910179));
#88071=CARTESIAN_POINT('Ctrl Pts',(-60.1754959566953,4.78579335889941,129.662361428816));
#88072=CARTESIAN_POINT('Ctrl Pts',(-60.1832438534725,4.75206942660643,129.529274167597));
#88073=CARTESIAN_POINT('Ctrl Pts',(-60.1909917502496,4.71282927662019,129.397796267125));
#88074=CARTESIAN_POINT('Ctrl Pts',(-60.1987380263337,4.67359733482741,129.266345868996));
#88075=CARTESIAN_POINT('Ctrl Pts',(-60.2064843024177,4.62885158220049,129.13650453641));
#88076=CARTESIAN_POINT('Ctrl Pts',(-60.2142305785018,4.57875608196576,129.008761607664));
#88077=CARTESIAN_POINT('Ctrl Pts',(-60.2219769117672,4.52866021193743,128.881017735948));
#88078=CARTESIAN_POINT('Ctrl Pts',(-60.2297232450325,4.47321465823772,128.755372662959));
#88079=CARTESIAN_POINT('Ctrl Pts',(-60.2374695782978,4.41263201617326,128.632296679202));
#88080=CARTESIAN_POINT('Ctrl Pts',(-60.2452176463008,4.35203580704625,128.509193133431));
#88081=CARTESIAN_POINT('Ctrl Pts',(-60.2529657143038,4.2863003929915,128.388660172438));
#88082=CARTESIAN_POINT('Ctrl Pts',(-60.2607137823068,4.21568460605508,128.271144013173));
#88083=CARTESIAN_POINT('Ctrl Pts',(-60.2684700850486,4.14499376781987,128.153502956337));
#88084=CARTESIAN_POINT('Ctrl Pts',(-60.2762263877906,4.06941239696825,128.038885441795));
#88085=CARTESIAN_POINT('Ctrl Pts',(-60.2839826905324,3.98924331137297,127.927709636796));
#88086=CARTESIAN_POINT('Ctrl Pts',(-60.2917431330466,3.90903143712277,127.816474493922));
#88087=CARTESIAN_POINT('Ctrl Pts',(-60.2995035755607,3.82422721070979,127.708685027972));
#88088=CARTESIAN_POINT('Ctrl Pts',(-60.3072640180749,3.73517350010559,127.604725953013));
#88089=CARTESIAN_POINT('Ctrl Pts',(-60.3150369183403,3.64597683257943,127.500599993718));
#88090=CARTESIAN_POINT('Ctrl Pts',(-60.3228098186058,3.55251731573888,127.400316999019));
#88091=CARTESIAN_POINT('Ctrl Pts',(-60.3305827188712,3.45517502667162,127.304225106252));
#88092=CARTESIAN_POINT('Ctrl Pts',(-60.3380730546332,3.36137137500331,127.211626395828));
#88093=CARTESIAN_POINT('Ctrl Pts',(-60.3455633903951,3.26396257485432,127.12291957079));
#88094=CARTESIAN_POINT('Ctrl Pts',(-60.3530537261571,3.16331592543335,127.03837928219));
#88095=CARTESIAN_POINT('Ctrl Pts',(-60.3608280602762,3.05885322770767,126.950633622851));
#88096=CARTESIAN_POINT('Ctrl Pts',(-60.3686023943952,2.95057140141032,126.867098733457));
#88097=CARTESIAN_POINT('Ctrl Pts',(-60.3763767285143,2.8388445135125,126.788125453809));
#88098=CARTESIAN_POINT('Ctrl Pts',(-60.3841414814614,2.7272553190187,126.70924950167));
#88099=CARTESIAN_POINT('Ctrl Pts',(-60.3919062344085,2.6122298268594,126.634924197119));
#88100=CARTESIAN_POINT('Ctrl Pts',(-60.3996709873556,2.49417649801723,126.565461390262));
#88101=CARTESIAN_POINT('Ctrl Pts',(-60.4074280282406,2.37624042140569,126.496067574845));
#88102=CARTESIAN_POINT('Ctrl Pts',(-60.4151850691257,2.25528282753555,126.431526843182));
#88103=CARTESIAN_POINT('Ctrl Pts',(-60.4229421100107,2.13174229970388,126.372108613206));
#88104=CARTESIAN_POINT('Ctrl Pts',(-60.4306933012508,2.00829493474525,126.312735190979));
#88105=CARTESIAN_POINT('Ctrl Pts',(-60.4384444924909,1.88226886373024,126.258476750307));
#88106=CARTESIAN_POINT('Ctrl Pts',(-60.446195683731,1.75412817495747,126.209557312927));
#88107=CARTESIAN_POINT('Ctrl Pts',(-60.4539435805081,1.6260419493957,126.160658667613));
#88108=CARTESIAN_POINT('Ctrl Pts',(-60.4616914772852,1.49584325814796,126.117094651436));
#88109=CARTESIAN_POINT('Ctrl Pts',(-60.4694393740623,1.36401691727227,126.079041484227));
#88110=CARTESIAN_POINT('Ctrl Pts',(-60.4771856501464,1.23221815162525,126.040996276921));
#88111=CARTESIAN_POINT('Ctrl Pts',(-60.4849319262304,1.09879278895285,126.008459734058));
#88112=CARTESIAN_POINT('Ctrl Pts',(-60.4926782023145,0.964241203603525,
125.981558323902));
#88113=CARTESIAN_POINT('Ctrl Pts',(-60.5004245355799,0.829688625024966,
125.954656715165));
#88114=CARTESIAN_POINT('Ctrl Pts',(-60.5081708688453,0.694010190558273,
125.93339039879));
#88115=CARTESIAN_POINT('Ctrl Pts',(-60.5159172021106,0.557716481881299,
125.91783471583));
#88116=CARTESIAN_POINT('Ctrl Pts',(-60.5236652701136,0.421392251173261,
125.902275549282));
#88117=CARTESIAN_POINT('Ctrl Pts',(-60.5314133381165,0.284452860444995,
125.892429605251));
#88118=CARTESIAN_POINT('Ctrl Pts',(-60.5391614061195,0.147413629699876,
125.88832031217));
#88119=CARTESIAN_POINT('Ctrl Pts',(-60.5469177088614,0.0102287520295327,
125.884206651683));
#88120=CARTESIAN_POINT('Ctrl Pts',(-60.5546740116033,-0.127055786213454,
125.885841833258));
#88121=CARTESIAN_POINT('Ctrl Pts',(-60.5624303143452,-0.26392448862483,
125.893197117253));
#88122=CARTESIAN_POINT('Ctrl Pts',(-60.5701907568593,-0.400866241983907,
125.900556326985));
#88123=CARTESIAN_POINT('Ctrl Pts',(-60.5779511993734,-0.537391328277675,
125.913641685197));
#88124=CARTESIAN_POINT('Ctrl Pts',(-60.5857116418876,-0.672990748154215,
125.932372674703));
#88125=CARTESIAN_POINT('Ctrl Pts',(-60.593484542153,-0.808807844257492,
125.951133732857));
#88126=CARTESIAN_POINT('Ctrl Pts',(-60.6012574424185,-0.943695919587552,
125.975558463103));
#88127=CARTESIAN_POINT('Ctrl Pts',(-60.609030342684,-1.07715663539498,126.005515272556));
#88128=CARTESIAN_POINT('Ctrl Pts',(-60.616520678446,-1.20576571801572,126.034383076529));
#88129=CARTESIAN_POINT('Ctrl Pts',(-60.624011014208,-1.33304911805222,126.068387653138));
#88130=CARTESIAN_POINT('Ctrl Pts',(-60.63150134997,-1.45857722960131,126.107368438757));
#88131=CARTESIAN_POINT('Ctrl Pts',(-60.6392756840891,-1.58886477765286,
126.147827192712));
#88132=CARTESIAN_POINT('Ctrl Pts',(-60.6470500182082,-1.71767401797561,
126.193775111706));
#88133=CARTESIAN_POINT('Ctrl Pts',(-60.6548243523273,-1.84450758677274,
126.245087120084));
#88134=CARTESIAN_POINT('Ctrl Pts',(-60.6625891052744,-1.97118484453177,
126.296335890999));
#88135=CARTESIAN_POINT('Ctrl Pts',(-60.6703538582214,-2.09589091641836,
126.352935452637));
#88136=CARTESIAN_POINT('Ctrl Pts',(-60.6781186111685,-2.21814265096764,
126.414710717807));
#88137=CARTESIAN_POINT('Ctrl Pts',(-60.6858756520535,-2.34027296337055,
126.476424626912));
#88138=CARTESIAN_POINT('Ctrl Pts',(-60.6936326929386,-2.45995344284691,
126.543303834373));
#88139=CARTESIAN_POINT('Ctrl Pts',(-60.7013897338236,-2.57672035547545,
126.615124974614));
#88140=CARTESIAN_POINT('Ctrl Pts',(-60.7091409250637,-2.69339921326718,
126.686891953975));
#88141=CARTESIAN_POINT('Ctrl Pts',(-60.7168921163037,-2.80716854582542,
126.763593244244));
#88142=CARTESIAN_POINT('Ctrl Pts',(-60.7246433075438,-2.91758902625588,
126.844959484014));
#88143=CARTESIAN_POINT('Ctrl Pts',(-60.7323912043209,-3.02796257503643,
126.926291140962));
#88144=CARTESIAN_POINT('Ctrl Pts',(-60.740139101098,-3.13498978854208,127.012283572473));
#88145=CARTESIAN_POINT('Ctrl Pts',(-60.7478869978751,-3.23826035311738,
127.102624140191));
#88146=CARTESIAN_POINT('Ctrl Pts',(-60.7556332739592,-3.34150931571683,
127.19294581061));
#88147=CARTESIAN_POINT('Ctrl Pts',(-60.7633795500433,-3.44100289833029,
127.287613550862));
#88148=CARTESIAN_POINT('Ctrl Pts',(-60.7711258261274,-3.53636423506873,
127.386274741022));
#88149=CARTESIAN_POINT('Ctrl Pts',(-60.7788721593927,-3.6317262757429,127.484936659477));
#88150=CARTESIAN_POINT('Ctrl Pts',(-60.7866184926581,-3.72295573796189,
127.587591805548));
#88151=CARTESIAN_POINT('Ctrl Pts',(-60.7943648259235,-3.80971325329529,
127.693851336087));
#88152=CARTESIAN_POINT('Ctrl Pts',(-60.8021128939264,-3.8964901973727,127.800134662712));
#88153=CARTESIAN_POINT('Ctrl Pts',(-60.8098609619293,-3.97879295455648,
127.910023677207));
#88154=CARTESIAN_POINT('Ctrl Pts',(-60.8176090299323,-4.05632327079427,
128.0230974899));
#88155=CARTESIAN_POINT('Ctrl Pts',(-60.8253653326742,-4.13393598717477,
128.136291478787));
#88156=CARTESIAN_POINT('Ctrl Pts',(-60.833121635416,-4.2067659088866,128.252676704494));
#88157=CARTESIAN_POINT('Ctrl Pts',(-60.8408779381578,-4.27455857700611,
128.371803930818));
#88158=CARTESIAN_POINT('Ctrl Pts',(-60.848638380672,-4.34238742811379,128.490994738929));
#88159=CARTESIAN_POINT('Ctrl Pts',(-60.8563988231862,-4.40517348960581,
128.612930116361));
#88160=CARTESIAN_POINT('Ctrl Pts',(-60.8641592657004,-4.46270937628829,
128.737138306036));
#88161=CARTESIAN_POINT('Ctrl Pts',(-60.8719321659658,-4.52033762468387,
128.861545885723));
#88162=CARTESIAN_POINT('Ctrl Pts',(-60.8797050662311,-4.57269870692403,
128.988233207032));
#88163=CARTESIAN_POINT('Ctrl Pts',(-60.8874779664966,-4.61963397156314,
129.11670987429));
#88164=CARTESIAN_POINT('Ctrl Pts',(-60.8949683022587,-4.66486302111027,
129.240516091081));
#88165=CARTESIAN_POINT('Ctrl Pts',(-60.9024586380208,-4.7050537945398,129.365983524651));
#88166=CARTESIAN_POINT('Ctrl Pts',(-60.9099489737829,-4.7401091660917,129.492663946825));
#88167=CARTESIAN_POINT('Ctrl Pts',(-60.9117146843342,-4.74837283295475,
129.522526554482));
#88168=CARTESIAN_POINT('Ctrl Pts',(-60.9134803948856,-4.75635509691311,
129.552470153443));
#88169=CARTESIAN_POINT('Ctrl Pts',(-60.9152461054369,-4.76405452823402,
129.582490119308));
#88170=CARTESIAN_POINT('Ctrl Pts',(-59.165034112149,-4.76405452823398,129.582490119308));
#88171=CARTESIAN_POINT('Ctrl Pts',(-59.1727742599865,-4.79804438416839,
129.715016051728));
#88172=CARTESIAN_POINT('Ctrl Pts',(-59.1805144078242,-4.82647343551534,
129.848857094792));
#88173=CARTESIAN_POINT('Ctrl Pts',(-59.1882545556616,-4.84926594987579,
129.983505691361));
#88174=CARTESIAN_POINT('Ctrl Pts',(-59.1960688903796,-4.87227692331144,
130.119444852341));
#88175=CARTESIAN_POINT('Ctrl Pts',(-59.2038832250975,-4.88954270213659,
130.256206719216));
#88176=CARTESIAN_POINT('Ctrl Pts',(-59.2116975598155,-4.90103911891263,
130.393266203364));
#88177=CARTESIAN_POINT('Ctrl Pts',(-59.2195118945334,-4.91253553568865,
130.530325687512));
#88178=CARTESIAN_POINT('Ctrl Pts',(-59.2273262292515,-4.91826263506064,
130.667682381086));
#88179=CARTESIAN_POINT('Ctrl Pts',(-59.2351405639694,-4.91824997905427,
130.804814525752));
#88180=CARTESIAN_POINT('',(-58.8898594360411,-4.91824840746026,130.808318522891));
#88181=CARTESIAN_POINT('Ctrl Pts',(-58.8199570926742,-4.76405452823407,
129.582490119308));
#88182=CARTESIAN_POINT('Ctrl Pts',(-58.8276862897791,-4.79808194527658,
129.715162501919));
#88183=CARTESIAN_POINT('Ctrl Pts',(-58.8354154868839,-4.82657252583923,
129.849294383098));
#88184=CARTESIAN_POINT('Ctrl Pts',(-58.8431446839888,-4.84941444227015,
129.984383404711));
#88185=CARTESIAN_POINT('Ctrl Pts',(-58.8509304759891,-4.87242361227952,
130.120461578102));
#88186=CARTESIAN_POINT('Ctrl Pts',(-58.8587162679895,-4.8897009621754,130.257510574267));
#88187=CARTESIAN_POINT('Ctrl Pts',(-58.8665020599899,-4.90118490255336,
130.395007941402));
#88188=CARTESIAN_POINT('Ctrl Pts',(-58.8742878519903,-4.91266884293131,
130.532505308536));
#88189=CARTESIAN_POINT('Ctrl Pts',(-58.8820736439906,-4.91835935506972,
130.670450640487));
#88190=CARTESIAN_POINT('Ctrl Pts',(-58.889859435991,-4.91824840746098,130.808318522003));
#88191=CARTESIAN_POINT('Ctrl Pts',(-58.8898594360411,-4.91824840746026,
130.808318522891));
#88192=CARTESIAN_POINT('Ctrl Pts',(-58.8989570390533,-4.91811876650329,
130.969415461274));
#88193=CARTESIAN_POINT('Ctrl Pts',(-58.9080546420654,-4.91007019755224,
131.130177591142));
#88194=CARTESIAN_POINT('Ctrl Pts',(-58.9171522450775,-4.89422441324256,
131.289902021898));
#88195=CARTESIAN_POINT('Ctrl Pts',(-58.9263092006774,-4.8782752513397,131.450668491779));
#88196=CARTESIAN_POINT('Ctrl Pts',(-58.9354661562772,-4.85442691080236,
131.610383603236));
#88197=CARTESIAN_POINT('Ctrl Pts',(-58.9446231118771,-4.82285244834712,
131.768350930781));
#88198=CARTESIAN_POINT('Ctrl Pts',(-58.9538470483144,-4.79104702660448,
131.927473749775));
#88199=CARTESIAN_POINT('Ctrl Pts',(-58.9630709847519,-4.75140211119584,
132.084823050191));
#88200=CARTESIAN_POINT('Ctrl Pts',(-58.9722949211893,-4.70414275297314,
132.239708666699));
#88201=CARTESIAN_POINT('Ctrl Pts',(-58.9749981485436,-4.69029261526219,
132.285100462076));
#88202=CARTESIAN_POINT('Ctrl Pts',(-58.9777013758979,-4.67578879778627,
132.33028080118));
#88203=CARTESIAN_POINT('Ctrl Pts',(-58.9804046032522,-4.66063772933524,
132.375232674227));
#88204=CARTESIAN_POINT('Ctrl Pts',(-58.9881789373714,-4.61706408459059,
132.504511804147));
#88205=CARTESIAN_POINT('Ctrl Pts',(-58.9959532714905,-4.56803833085984,
132.632181327229));
#88206=CARTESIAN_POINT('Ctrl Pts',(-59.0037276056097,-4.51369744313826,
132.757747024375));
#88207=CARTESIAN_POINT('Ctrl Pts',(-59.0114923585569,-4.45942352570428,
132.883157973022));
#88208=CARTESIAN_POINT('Ctrl Pts',(-59.0192571115041,-4.39984766146744,
133.006469899225));
#88209=CARTESIAN_POINT('Ctrl Pts',(-59.0270218644513,-4.33515648150296,
133.127203992265));
#88210=CARTESIAN_POINT('Ctrl Pts',(-59.0347789053364,-4.27052955373041,
133.247818170502));
#88211=CARTESIAN_POINT('Ctrl Pts',(-59.0425359462215,-4.20079760431519,
133.365859268386));
#88212=CARTESIAN_POINT('Ctrl Pts',(-59.0502929871065,-4.12619506284523,
133.480869045696));
#88213=CARTESIAN_POINT('Ctrl Pts',(-59.0580441783467,-4.05164877973211,
133.595792093239));
#88214=CARTESIAN_POINT('Ctrl Pts',(-59.0657953695868,-3.97223942725329,
133.707688043563));
#88215=CARTESIAN_POINT('Ctrl Pts',(-59.0735465608271,-3.8882468318813,133.816124160221));
#88216=CARTESIAN_POINT('Ctrl Pts',(-59.0812944576042,-3.8042899356028,133.924514188636));
#88217=CARTESIAN_POINT('Ctrl Pts',(-59.0890423543815,-3.71575390976769,
134.029446999701));
#88218=CARTESIAN_POINT('Ctrl Pts',(-59.0967902511586,-3.62296114909805,
134.130519900376));
#88219=CARTESIAN_POINT('Ctrl Pts',(-59.1045365272428,-3.53018779867356,
134.23157165878));
#88220=CARTESIAN_POINT('Ctrl Pts',(-59.112282803327,-3.43315974874112,134.328764824962));
#88221=CARTESIAN_POINT('Ctrl Pts',(-59.1200290794112,-3.33223856142256,
134.421731103467));
#88222=CARTESIAN_POINT('Ctrl Pts',(-59.1277754126766,-3.23131662912672,
134.514698068228));
#88223=CARTESIAN_POINT('Ctrl Pts',(-59.135521745942,-3.12650178965439,134.603437818162));
#88224=CARTESIAN_POINT('Ctrl Pts',(-59.1432680792074,-3.01819091808133,
134.687620413731));
#88225=CARTESIAN_POINT('Ctrl Pts',(-59.1510161472105,-2.90985579103955,
134.771821861409));
#88226=CARTESIAN_POINT('Ctrl Pts',(-59.1587642152136,-2.79802338262443,
134.851463884081));
#88227=CARTESIAN_POINT('Ctrl Pts',(-59.1665122832166,-2.68312161857887,
134.926258413778));
#88228=CARTESIAN_POINT('Ctrl Pts',(-59.1742685859586,-2.56809773557113,
135.00113243599));
#88229=CARTESIAN_POINT('Ctrl Pts',(-59.1820248887005,-2.44999830862501,
135.071148459976));
#88230=CARTESIAN_POINT('Ctrl Pts',(-59.1897811914424,-2.32927855088701,
135.13606288052));
#88231=CARTESIAN_POINT('Ctrl Pts',(-59.1975416339566,-2.2084943613795,135.201011947844));
#88232=CARTESIAN_POINT('Ctrl Pts',(-59.205302076471,-2.08508740596666,135.260853815656));
#88233=CARTESIAN_POINT('Ctrl Pts',(-59.2130625189852,-1.95953428254303,
135.315392479351));
#88234=CARTESIAN_POINT('Ctrl Pts',(-59.2208354192507,-1.8337796100996,135.370018693351));
#88235=CARTESIAN_POINT('Ctrl Pts',(-59.2286083195162,-1.70587225000887,
135.419324550496));
#88236=CARTESIAN_POINT('Ctrl Pts',(-59.2363812197817,-1.5763062639185,135.463163213173));
#88237=CARTESIAN_POINT('Ctrl Pts',(-59.2438715555428,-1.45145032779531,
135.505408230033));
#88238=CARTESIAN_POINT('Ctrl Pts',(-59.2513618913041,-1.325054558018,135.542576557053));
#88239=CARTESIAN_POINT('Ctrl Pts',(-59.2588522270652,-1.19756938443239,
135.574581852684));
#88240=CARTESIAN_POINT('Ctrl Pts',(-59.2666265611843,-1.06525057172689,
135.60780063883));
#88241=CARTESIAN_POINT('Ctrl Pts',(-59.2744008953034,-0.931338968758862,
135.635562379462));
#88242=CARTESIAN_POINT('Ctrl Pts',(-59.2821752294224,-0.796324414382764,
135.657715178028));
#88243=CARTESIAN_POINT('Ctrl Pts',(-59.2899399823695,-0.661476253378521,
135.67984067525));
#88244=CARTESIAN_POINT('Ctrl Pts',(-59.2977047353166,-0.525528227649034,
135.696370921565));
#88245=CARTESIAN_POINT('Ctrl Pts',(-59.3054694882636,-0.388984052867978,
135.707204126094));
#88246=CARTESIAN_POINT('Ctrl Pts',(-59.3132265291486,-0.252575495686064,
135.718026570932));
#88247=CARTESIAN_POINT('Ctrl Pts',(-59.3209835700337,-0.115572354984052,
135.723163203698));
#88248=CARTESIAN_POINT('Ctrl Pts',(-59.3287406109187,0.0215131238449157,
135.722563566612));
#88249=CARTESIAN_POINT('Ctrl Pts',(-59.3364918021588,0.158495225447929,
135.721964381717));
#88250=CARTESIAN_POINT('Ctrl Pts',(-59.3442429933989,0.295559152208349,
135.715637538848));
#88251=CARTESIAN_POINT('Ctrl Pts',(-59.351994184639,0.432189577653266,135.703584559321));
#88252=CARTESIAN_POINT('Ctrl Pts',(-59.3597420814161,0.568761931522634,
135.691536702632));
#88253=CARTESIAN_POINT('Ctrl Pts',(-59.3674899781933,0.704900761897533,
135.673767584134));
#88254=CARTESIAN_POINT('Ctrl Pts',(-59.3752378749703,0.840093009499151,
135.650330778214));
#88255=CARTESIAN_POINT('Ctrl Pts',(-59.3829841510544,0.975256977796978,
135.626898874769));
#88256=CARTESIAN_POINT('Ctrl Pts',(-59.3907304271384,1.10947437218832,135.597801708781));
#88257=CARTESIAN_POINT('Ctrl Pts',(-59.3984767032225,1.2422399021177,135.563144400014));
#88258=CARTESIAN_POINT('Ctrl Pts',(-59.4062230364878,1.37500641209207,135.528486835414));
#88259=CARTESIAN_POINT('Ctrl Pts',(-59.4139693697532,1.50632065793001,135.488269144885));
#88260=CARTESIAN_POINT('Ctrl Pts',(-59.4217157030186,1.63569053148172,135.442646890288));
#88261=CARTESIAN_POINT('Ctrl Pts',(-59.4294637710216,1.76508937651963,135.397014418903));
#88262=CARTESIAN_POINT('Ctrl Pts',(-59.4372118390245,1.89254261417908,135.345975105066));
#88263=CARTESIAN_POINT('Ctrl Pts',(-59.4449599070274,2.01757658040093,135.289733267048));
#88264=CARTESIAN_POINT('Ctrl Pts',(-59.4527162097693,2.14274343421001,135.233431654535));
#88265=CARTESIAN_POINT('Ctrl Pts',(-59.4604725125112,2.26548552314852,135.171916633098));
#88266=CARTESIAN_POINT('Ctrl Pts',(-59.468228815253,2.38535184142447,135.10543951188));
#88267=CARTESIAN_POINT('Ctrl Pts',(-59.4759892577672,2.50528213596359,135.038926909821));
#88268=CARTESIAN_POINT('Ctrl Pts',(-59.4837497002814,2.62233326794553,134.967447134438));
#88269=CARTESIAN_POINT('Ctrl Pts',(-59.4915101427955,2.73608272034308,134.891295215763));
#88270=CARTESIAN_POINT('Ctrl Pts',(-59.499283043061,2.85001477345983,134.815021051267));
#88271=CARTESIAN_POINT('Ctrl Pts',(-59.5070559433264,2.96063423993009,134.73405998685));
#88272=CARTESIAN_POINT('Ctrl Pts',(-59.5148288435918,3.06755052872188,134.64874832125));
#88273=CARTESIAN_POINT('Ctrl Pts',(-59.5223191793539,3.17058014111122,134.566537949581));
#88274=CARTESIAN_POINT('Ctrl Pts',(-59.529809515116,3.270170908261,134.480287997385));
#88275=CARTESIAN_POINT('Ctrl Pts',(-59.5372998508781,3.36600672024583,134.39033075433));
#88276=CARTESIAN_POINT('Ctrl Pts',(-59.5450741849972,3.46547617616961,134.296962755063));
#88277=CARTESIAN_POINT('Ctrl Pts',(-59.5528485191162,3.56121540719336,134.199305029842));
#88278=CARTESIAN_POINT('Ctrl Pts',(-59.5606228532352,3.65283184858071,134.097687590172));
#88279=CARTESIAN_POINT('Ctrl Pts',(-59.5683876061823,3.74433538089192,133.996195384914));
#88280=CARTESIAN_POINT('Ctrl Pts',(-59.5761523591294,3.83172597389976,133.890753462527));
#88281=CARTESIAN_POINT('Ctrl Pts',(-59.5839171120765,3.91464571742834,133.781730592816));
#88282=CARTESIAN_POINT('Ctrl Pts',(-59.5916741529615,3.9974831038988,133.672816006156));
#88283=CARTESIAN_POINT('Ctrl Pts',(-59.5994311938464,4.07585824255894,133.560327859232));
#88284=CARTESIAN_POINT('Ctrl Pts',(-59.6071882347314,4.14945180070211,133.444669844939));
#88285=CARTESIAN_POINT('Ctrl Pts',(-59.6149394259715,4.22298986137051,133.329099049254));
#88286=CARTESIAN_POINT('Ctrl Pts',(-59.6226906172117,4.29175330966586,133.210363472707));
#88287=CARTESIAN_POINT('Ctrl Pts',(-59.6304418084518,4.35546487896835,133.088897496361));
#88288=CARTESIAN_POINT('Ctrl Pts',(-59.6381897052288,4.41914936915441,132.967483146295));
#88289=CARTESIAN_POINT('Ctrl Pts',(-59.6459376020059,4.47778606970764,132.843341050065));
#88290=CARTESIAN_POINT('Ctrl Pts',(-59.6536854987829,4.53114273320537,132.716931817239));
#88291=CARTESIAN_POINT('Ctrl Pts',(-59.661431774867,4.58448823563932,132.5905490265));
#88292=CARTESIAN_POINT('Ctrl Pts',(-59.6691780509511,4.63255574592978,132.46190040241));
#88293=CARTESIAN_POINT('Ctrl Pts',(-59.6769243270352,4.6751605824233,132.331467880025));
#88294=CARTESIAN_POINT('Ctrl Pts',(-59.6846706603005,4.71776573341598,132.201034394817));
#88295=CARTESIAN_POINT('Ctrl Pts',(-59.6924169935658,4.75490800875374,132.068817356678));
#88296=CARTESIAN_POINT('Ctrl Pts',(-59.7001633268311,4.78645229056156,131.935314875119));
#88297=CARTESIAN_POINT('Ctrl Pts',(-59.7079113948341,4.81800363649258,131.801782496605));
#88298=CARTESIAN_POINT('Ctrl Pts',(-59.7156594628371,4.843954404426,131.666964482266));
#88299=CARTESIAN_POINT('Ctrl Pts',(-59.72340753084,4.86422046611703,131.531369778105));
#88300=CARTESIAN_POINT('Ctrl Pts',(-59.7311638335819,4.88450806681962,131.39563096228));
#88301=CARTESIAN_POINT('Ctrl Pts',(-59.7389201363237,4.89909883430244,131.259114194945));
#88302=CARTESIAN_POINT('Ctrl Pts',(-59.7466764390656,4.90796042241798,131.122334758777));
#88303=CARTESIAN_POINT('Ctrl Pts',(-59.7544368815797,4.91682674022992,130.985482319305));
#88304=CARTESIAN_POINT('Ctrl Pts',(-59.7621973240938,4.91995777675734,130.848367322324));
#88305=CARTESIAN_POINT('Ctrl Pts',(-59.769957766608,4.91737336834726,130.711504714312));
#88306=CARTESIAN_POINT('Ctrl Pts',(-59.7777306668734,4.91478481121536,130.574422402291));
#88307=CARTESIAN_POINT('Ctrl Pts',(-59.7855035671388,4.90646249844249,130.437593679342));
#88308=CARTESIAN_POINT('Ctrl Pts',(-59.7932764674042,4.89247824368927,130.301528938446));
#88309=CARTESIAN_POINT('Ctrl Pts',(-59.8007668031665,4.87900235182013,130.170410493602));
#88310=CARTESIAN_POINT('Ctrl Pts',(-59.8082571389287,4.86026906659534,130.040001754705));
#88311=CARTESIAN_POINT('Ctrl Pts',(-59.8157474746909,4.83638708758873,129.910748284669));
#88312=CARTESIAN_POINT('Ctrl Pts',(-59.82352180881,4.81159961608998,129.776594130035));
#88313=CARTESIAN_POINT('Ctrl Pts',(-59.8312961429291,4.7811867989801,129.643259617594));
#88314=CARTESIAN_POINT('Ctrl Pts',(-59.8390704770482,4.74521409345568,129.511253402456));
#88315=CARTESIAN_POINT('Ctrl Pts',(-59.8468352299953,4.7092857210759,129.379409873181));
#88316=CARTESIAN_POINT('Ctrl Pts',(-59.8545999829424,4.66781119565562,129.24889175764));
#88317=CARTESIAN_POINT('Ctrl Pts',(-59.8623647358895,4.62090731448351,129.120199504889));
#88318=CARTESIAN_POINT('Ctrl Pts',(-59.8701217767746,4.57405001890742,128.991635071098));
#88319=CARTESIAN_POINT('Ctrl Pts',(-59.8778788176595,4.52177423193532,128.864893256156));
#88320=CARTESIAN_POINT('Ctrl Pts',(-59.8856358585445,4.46424698470419,128.740460929582));
#88321=CARTESIAN_POINT('Ctrl Pts',(-59.8933870497847,4.40676311921778,128.616122438394));
#88322=CARTESIAN_POINT('Ctrl Pts',(-59.9011382410247,4.34403583934589,128.49409032246));
#88323=CARTESIAN_POINT('Ctrl Pts',(-59.9088894322648,4.27628073280018,128.374832647613));
#88324=CARTESIAN_POINT('Ctrl Pts',(-59.9166373290419,4.20855442398208,128.25562566046));
#88325=CARTESIAN_POINT('Ctrl Pts',(-59.9243852258191,4.13580473146711,128.139191108256));
#88326=CARTESIAN_POINT('Ctrl Pts',(-59.9321331225962,4.05829364372423,128.025973358056));
#88327=CARTESIAN_POINT('Ctrl Pts',(-59.9398793986803,3.98079876962997,127.912779290569));
#88328=CARTESIAN_POINT('Ctrl Pts',(-59.9476256747643,3.89854470209081,127.802801009081));
#88329=CARTESIAN_POINT('Ctrl Pts',(-59.9553719508484,3.81183708177263,127.696454389167));
#88330=CARTESIAN_POINT('Ctrl Pts',(-59.9631182841138,3.7251288213985,127.590106984226));
#88331=CARTESIAN_POINT('Ctrl Pts',(-59.9708646173791,3.63396718970146,127.487391597365));
#88332=CARTESIAN_POINT('Ctrl Pts',(-59.9786109506444,3.53869822580756,127.388691147438));
#88333=CARTESIAN_POINT('Ctrl Pts',(-59.9863590186474,3.44340792708988,127.289968594229));
#88334=CARTESIAN_POINT('Ctrl Pts',(-59.9941070866505,3.34400873733179,127.195263048339));
#88335=CARTESIAN_POINT('Ctrl Pts',(-60.0018551546534,3.2408833738499,127.10492038699));
#88336=CARTESIAN_POINT('Ctrl Pts',(-60.0096114573953,3.13764840750435,127.014481708386));
#88337=CARTESIAN_POINT('Ctrl Pts',(-60.0173677601372,3.030679651013,126.928415435118));
#88338=CARTESIAN_POINT('Ctrl Pts',(-60.025124062879,2.92039314240219,126.847027303791));
#88339=CARTESIAN_POINT('Ctrl Pts',(-60.0328845053932,2.81004777056107,126.765595733168));
#88340=CARTESIAN_POINT('Ctrl Pts',(-60.0406449479074,2.69638144202449,126.688847498374));
#88341=CARTESIAN_POINT('Ctrl Pts',(-60.0484053904216,2.57983811787982,126.617044251678));
#88342=CARTESIAN_POINT('Ctrl Pts',(-60.0561782906871,2.46310770804485,126.545125740036));
#88343=CARTESIAN_POINT('Ctrl Pts',(-60.0639511909524,2.34349141489891,126.478168270491));
#88344=CARTESIAN_POINT('Ctrl Pts',(-60.0717240912179,2.22145746354942,126.416387304049));
#88345=CARTESIAN_POINT('Ctrl Pts',(-60.0792144269798,2.10385975371761,126.356852231354));
#88346=CARTESIAN_POINT('Ctrl Pts',(-60.0867047627418,1.98401739007027,126.302123965985));
#88347=CARTESIAN_POINT('Ctrl Pts',(-60.0941950985038,1.86236399208234,126.252351893552));
#88348=CARTESIAN_POINT('Ctrl Pts',(-60.1019694326229,1.73609806853288,126.200692697865));
#88349=CARTESIAN_POINT('Ctrl Pts',(-60.1097437667419,1.60748109646445,126.154209301384));
#88350=CARTESIAN_POINT('Ctrl Pts',(-60.117518100861,1.47697640304071,126.113121573629));
#88351=CARTESIAN_POINT('Ctrl Pts',(-60.1252828538081,1.34663254498807,126.072084482826));
#88352=CARTESIAN_POINT('Ctrl Pts',(-60.1330476067553,1.21440596385744,126.036429946149));
#88353=CARTESIAN_POINT('Ctrl Pts',(-60.1408123597024,1.08078083339959,126.006330203672));
#88354=CARTESIAN_POINT('Ctrl Pts',(-60.1485694005874,0.947288421305109,
125.976260356682));
#88355=CARTESIAN_POINT('Ctrl Pts',(-60.1563264414724,0.812400603113867,
125.951734409972));
#88356=CARTESIAN_POINT('Ctrl Pts',(-60.1640834823574,0.676617280351525,
125.932875000382));
#88357=CARTESIAN_POINT('Ctrl Pts',(-60.1718346735975,0.540936352849304,
125.91402981282));
#88358=CARTESIAN_POINT('Ctrl Pts',(-60.1795858648377,0.404361650614417,
125.900842710442));
#88359=CARTESIAN_POINT('Ctrl Pts',(-60.1873370560778,0.267403501115037,
125.893385314218));
#88360=CARTESIAN_POINT('Ctrl Pts',(-60.1950849528549,0.130503562482486,
125.885931087587));
#88361=CARTESIAN_POINT('Ctrl Pts',(-60.2028328496319,-0.00677910969947318,
125.884201744739));
#88362=CARTESIAN_POINT('Ctrl Pts',(-60.210580746409,-0.143929045674341,
125.888217058605));
#88363=CARTESIAN_POINT('Ctrl Pts',(-60.2183270224931,-0.281050292839214,
125.892231532554));
#88364=CARTESIAN_POINT('Ctrl Pts',(-60.2260732985772,-0.418038468474032,
125.901988261618));
#88365=CARTESIAN_POINT('Ctrl Pts',(-60.2338195746613,-0.554378478434141,
125.917454892555));
#88366=CARTESIAN_POINT('Ctrl Pts',(-60.2415659079266,-0.690719494825046,
125.932921637662));
#88367=CARTESIAN_POINT('Ctrl Pts',(-60.249312241192,-0.826411947520334,
125.95409832468));
#88368=CARTESIAN_POINT('Ctrl Pts',(-60.2570585744574,-0.960946633444781,
125.980900798083));
#88369=CARTESIAN_POINT('Ctrl Pts',(-60.2648066424604,-1.09551144747953,
126.007709273713));
#88370=CARTESIAN_POINT('Ctrl Pts',(-60.2725547104634,-1.22891759546181,
126.040145966323));
#88371=CARTESIAN_POINT('Ctrl Pts',(-60.2803027784663,-1.36066721303082,
126.078075840081));
#88372=CARTESIAN_POINT('Ctrl Pts',(-60.2880590812082,-1.49255685566103,
126.116046026161));
#88373=CARTESIAN_POINT('Ctrl Pts',(-60.29581538395,-1.62278607462486,126.159520947523));
#88374=CARTESIAN_POINT('Ctrl Pts',(-60.3035716866918,-1.75087276634372,
126.208315837695));
#88375=CARTESIAN_POINT('Ctrl Pts',(-60.311332129206,-1.87902782178674,126.25713677117));
#88376=CARTESIAN_POINT('Ctrl Pts',(-60.3190925717202,-2.00503771237078,
126.311283176979));
#88377=CARTESIAN_POINT('Ctrl Pts',(-60.3268530142343,-2.12844233081867,
126.37052296753));
#88378=CARTESIAN_POINT('Ctrl Pts',(-60.3346259144998,-2.25204504931544,
126.429857855051));
#88379=CARTESIAN_POINT('Ctrl Pts',(-60.3423988147652,-2.3730337930136,126.494302282368));
#88380=CARTESIAN_POINT('Ctrl Pts',(-60.3501717150307,-2.49097420135859,
126.563578780373));
#88381=CARTESIAN_POINT('Ctrl Pts',(-60.3576620507927,-2.60462717878596,
126.630336903179));
#88382=CARTESIAN_POINT('Ctrl Pts',(-60.3651523865547,-2.71544934329007,
126.701581713584));
#88383=CARTESIAN_POINT('Ctrl Pts',(-60.3726427223167,-2.82308063060881,
126.777029141814));
#88384=CARTESIAN_POINT('Ctrl Pts',(-60.3803688363466,-2.93409989936158,
126.854851478795));
#88385=CARTESIAN_POINT('Ctrl Pts',(-60.3880949503766,-3.04208577092471,
126.937399034632));
#88386=CARTESIAN_POINT('Ctrl Pts',(-60.3958210644065,-3.14660570564304,
127.024406173963));
#88387=CARTESIAN_POINT('Ctrl Pts',(-60.4035349748601,-3.250960548701,127.1112758835));
#88388=CARTESIAN_POINT('Ctrl Pts',(-60.4112488853137,-3.35186005432657,
127.202590898686));
#88389=CARTESIAN_POINT('Ctrl Pts',(-60.4189627957674,-3.44890065211306,
127.298042412617));
#88390=CARTESIAN_POINT('Ctrl Pts',(-60.4266696585593,-3.54585259067578,
127.39340671916));
#88391=CARTESIAN_POINT('Ctrl Pts',(-60.4343765213512,-3.63895235232623,
127.492899732487));
#88392=CARTESIAN_POINT('Ctrl Pts',(-60.442083384143,-3.72782930482369,127.596172384841));
#88393=CARTESIAN_POINT('Ctrl Pts',(-60.4497849296654,-3.81664493759624,
127.699373785307));
#88394=CARTESIAN_POINT('Ctrl Pts',(-60.4574864751878,-3.90124329931633,
127.806349338136));
#88395=CARTESIAN_POINT('Ctrl Pts',(-60.4651880207102,-3.9812908597072,127.916713451981));
#88396=CARTESIAN_POINT('Ctrl Pts',(-60.4728859750974,-4.06130109491251,
128.027026104407));
#88397=CARTESIAN_POINT('Ctrl Pts',(-60.4805839294846,-4.13676451924996,
128.140723853293));
#88398=CARTESIAN_POINT('Ctrl Pts',(-60.4882818838717,-4.20738843157316,
128.257388758993));
#88399=CARTESIAN_POINT('Ctrl Pts',(-60.4959794064094,-4.27800838194788,
128.374047119879));
#88400=CARTESIAN_POINT('Ctrl Pts',(-60.503676928947,-4.34378914721932,128.493671972289));
#88401=CARTESIAN_POINT('Ctrl Pts',(-60.5113744514847,-4.40448196449461,
128.615817337907));
#88402=CARTESIAN_POINT('Ctrl Pts',(-60.5190716469134,-4.46517220260643,
128.737957512912));
#88403=CARTESIAN_POINT('Ctrl Pts',(-60.526768842342,-4.52077475164605,128.862617630379));
#88404=CARTESIAN_POINT('Ctrl Pts',(-60.5344660377707,-4.57108769168258,
128.989328833423));
#88405=CARTESIAN_POINT('Ctrl Pts',(-60.5421670668684,-4.62142569060738,
129.116103146314));
#88406=CARTESIAN_POINT('Ctrl Pts',(-60.5498680959661,-4.66646867744965,
129.244930214439));
#88407=CARTESIAN_POINT('Ctrl Pts',(-60.5575691250638,-4.70606359539469,
129.375323004835));
#88408=CARTESIAN_POINT('Ctrl Pts',(-60.5616233839294,-4.72690860780455,
129.443969171439));
#88409=CARTESIAN_POINT('Ctrl Pts',(-60.5656776427949,-4.74624448496707,
129.513049030915));
#88410=CARTESIAN_POINT('Ctrl Pts',(-60.5697319016604,-4.76405452823403,
129.582490119308));
#88411=CARTESIAN_POINT('Origin',(213.235140564004,0.,130.804360617566));
#88412=CARTESIAN_POINT('',(-62.6653842080088,-4.76405452823406,129.582490119308));
#88413=CARTESIAN_POINT('',(-62.3199210724795,-4.76405452823405,129.582490119308));
#88414=CARTESIAN_POINT('',(213.235140564004,-4.76405452823405,129.582490119308));
#88415=CARTESIAN_POINT('',(-60.9851405639584,-4.91824796096415,130.799882116478));
#88416=CARTESIAN_POINT('Ctrl Pts',(-60.9851405640084,-4.91824796096495,
130.799882117362));
#88417=CARTESIAN_POINT('Ctrl Pts',(-60.9928182880772,-4.91837153989948,
130.93559537294));
#88418=CARTESIAN_POINT('Ctrl Pts',(-61.0004960121458,-4.91287362247503,
131.071436499204));
#88419=CARTESIAN_POINT('Ctrl Pts',(-61.0081737362145,-4.9017493146528,131.206898465229));
#88420=CARTESIAN_POINT('Ctrl Pts',(-61.0158477996582,-4.89063031073562,
131.342295844996));
#88421=CARTESIAN_POINT('Ctrl Pts',(-61.0235218631019,-4.8738902832785,131.477314027108));
#88422=CARTESIAN_POINT('Ctrl Pts',(-61.0311959265456,-4.85157641150895,
131.611447592922));
#88423=CARTESIAN_POINT('Ctrl Pts',(-61.0388681933982,-4.82926776368656,
131.745549756447));
#88424=CARTESIAN_POINT('Ctrl Pts',(-61.0465404602509,-4.80138793153318,
131.878767321949));
#88425=CARTESIAN_POINT('Ctrl Pts',(-61.0542127271036,-4.76803571740963,
132.010602077642));
#88426=CARTESIAN_POINT('Ctrl Pts',(-61.0618849370681,-4.73468375058525,
132.14243585581));
#88427=CARTESIAN_POINT('Ctrl Pts',(-61.0695571470326,-4.69585958036707,
132.27288645754));
#88428=CARTESIAN_POINT('Ctrl Pts',(-61.0772293569972,-4.65171256107439,
132.40146841344));
#88429=CARTESIAN_POINT('Ctrl Pts',(-61.0849032494586,-4.60755586044814,
132.53007856705));
#88430=CARTESIAN_POINT('Ctrl Pts',(-61.0925771419201,-4.55807411889652,
132.656818882375));
#88431=CARTESIAN_POINT('Ctrl Pts',(-61.1002510343815,-4.50346556316825,
132.781222014796));
#88432=CARTESIAN_POINT('Ctrl Pts',(-61.1079330096527,-4.44879948896839,
132.905756179395));
#88433=CARTESIAN_POINT('Ctrl Pts',(-61.1156149849239,-4.38899597707964,
133.027947878844));
#88434=CARTESIAN_POINT('Ctrl Pts',(-61.1232969601951,-4.32430031971325,
133.147352253793));
#88435=CARTESIAN_POINT('Ctrl Pts',(-61.1309831423546,-4.25956923299425,
133.266822018288));
#88436=CARTESIAN_POINT('Ctrl Pts',(-61.1386693245141,-4.18994086992982,
133.383501076189));
#88437=CARTESIAN_POINT('Ctrl Pts',(-61.1463555066737,-4.11570429665684,
133.49697295598));
#88438=CARTESIAN_POINT('Ctrl Pts',(-61.1540537610474,-4.04135112455874,
133.610623059082));
#88439=CARTESIAN_POINT('Ctrl Pts',(-61.1617520154212,-3.96237551682344,
133.721055597784));
#88440=CARTESIAN_POINT('Ctrl Pts',(-61.1694502697949,-3.87910772298163,
133.827886098855));
#88441=CARTESIAN_POINT('Ctrl Pts',(-61.1757657123952,-3.81079704540008,
133.915526993105));
#88442=CARTESIAN_POINT('Ctrl Pts',(-61.1820811549954,-3.73959848333886,
134.000744235032));
#88443=CARTESIAN_POINT('Ctrl Pts',(-61.1883965975958,-3.6657123461508,134.083344615358));
#88444=CARTESIAN_POINT('Ctrl Pts',(-61.1961709317149,-3.57475822723578,
134.185026001075));
#88445=CARTESIAN_POINT('Ctrl Pts',(-61.2039452658339,-3.47942610258915,
134.2830811777));
#88446=CARTESIAN_POINT('Ctrl Pts',(-61.211719599953,-3.38003646820944,134.377109774178));
#88447=CARTESIAN_POINT('Ctrl Pts',(-61.2194843529001,-3.28076932267154,
134.471022488815));
#88448=CARTESIAN_POINT('Ctrl Pts',(-61.2272491058473,-3.17745489822238,
134.560918230894));
#88449=CARTESIAN_POINT('Ctrl Pts',(-61.2350138587944,-3.07045326961318,
134.646430343849));
#88450=CARTESIAN_POINT('Ctrl Pts',(-61.2427708996794,-2.96355791652997,
134.731857524969));
#88451=CARTESIAN_POINT('Ctrl Pts',(-61.2505279405644,-2.85298295063678,
134.812909498888));
#88452=CARTESIAN_POINT('Ctrl Pts',(-61.2582849814494,-2.73912428546976,
134.889257337344));
#88453=CARTESIAN_POINT('Ctrl Pts',(-61.2660361726895,-2.62535148200784,
134.9655476013));
#88454=CARTESIAN_POINT('Ctrl Pts',(-61.2737873639297,-2.50830023152952,
135.037140573869));
#88455=CARTESIAN_POINT('Ctrl Pts',(-61.2815385551698,-2.3883981363744,135.103748644328));
#88456=CARTESIAN_POINT('Ctrl Pts',(-61.2892864519469,-2.26854700280806,
135.17032840458));
#88457=CARTESIAN_POINT('Ctrl Pts',(-61.2970343487241,-2.14584777556872,
135.231927287224));
#88458=CARTESIAN_POINT('Ctrl Pts',(-61.3047822455012,-2.0207553582815,135.288302058361));
#88459=CARTESIAN_POINT('Ctrl Pts',(-61.3125285215853,-1.89568910763129,
135.34466503711));
#88460=CARTESIAN_POINT('Ctrl Pts',(-61.3202747976694,-1.76823101887653,
135.3958059174));
#88461=CARTESIAN_POINT('Ctrl Pts',(-61.3280210737535,-1.63885845643614,
135.441528505649));
#88462=CARTESIAN_POINT('Ctrl Pts',(-61.3357674070189,-1.50948493899706,
135.487251431411));
#88463=CARTESIAN_POINT('Ctrl Pts',(-61.3435137402843,-1.37819728829377,
135.527555855044));
#88464=CARTESIAN_POINT('Ctrl Pts',(-61.3512600735496,-1.24549022793658,
135.562294744329));
#88465=CARTESIAN_POINT('Ctrl Pts',(-61.3590081415526,-1.11275344875334,
135.597041413147));
#88466=CARTESIAN_POINT('Ctrl Pts',(-61.3667562095556,-0.978597005546652,
135.62621996851));
#88467=CARTESIAN_POINT('Ctrl Pts',(-61.3745042775585,-0.84352767891142,
135.6497340931));
#88468=CARTESIAN_POINT('Ctrl Pts',(-61.3822605803004,-0.708314798988495,
135.673273208782));
#88469=CARTESIAN_POINT('Ctrl Pts',(-61.3900168830423,-0.57218748329756,
135.691135800482));
#88470=CARTESIAN_POINT('Ctrl Pts',(-61.3977731857842,-0.435660089907948,
135.703277166004));
#88471=CARTESIAN_POINT('Ctrl Pts',(-61.4055336282984,-0.299059827737351,
135.715425011739));
#88472=CARTESIAN_POINT('Ctrl Pts',(-61.4132940708126,-0.162059452729946,
135.721845528465));
#88473=CARTESIAN_POINT('Ctrl Pts',(-61.4210545133268,-0.0251742390910713,
135.722546189521));
#88474=CARTESIAN_POINT('Ctrl Pts',(-61.4288274135922,0.111930714844648,
135.72324797534));
#88475=CARTESIAN_POINT('Ctrl Pts',(-61.4366003138577,0.248919747062051,
135.71821157126));
#88476=CARTESIAN_POINT('Ctrl Pts',(-61.4443732141231,0.385280888231227,
135.707496522236));
#88477=CARTESIAN_POINT('Ctrl Pts',(-61.451863549885,0.516684958442969,135.697170992234));
#88478=CARTESIAN_POINT('Ctrl Pts',(-61.4593538856468,0.647505690031206,
135.68157255189));
#88479=CARTESIAN_POINT('Ctrl Pts',(-61.4668442214087,0.777295039901073,
135.660799177194));
#88480=CARTESIAN_POINT('Ctrl Pts',(-61.4746185555278,0.912005392422351,
135.639238173683));
#88481=CARTESIAN_POINT('Ctrl Pts',(-61.4823928896469,1.0460313315711,135.612033775368));
#88482=CARTESIAN_POINT('Ctrl Pts',(-61.490167223766,1.17886277792507,135.579239214276));
#88483=CARTESIAN_POINT('Ctrl Pts',(-61.497931976713,1.31153052139307,135.54648506955));
#88484=CARTESIAN_POINT('Ctrl Pts',(-61.5056967296601,1.4430063251933,135.508154562664));
#88485=CARTESIAN_POINT('Ctrl Pts',(-61.5134614826072,1.57278708157492,135.464352447873));
#88486=CARTESIAN_POINT('Ctrl Pts',(-61.5212185234922,1.70243893787972,135.420593837961));
#88487=CARTESIAN_POINT('Ctrl Pts',(-61.5289755643773,1.83039872905795,135.371374559217));
#88488=CARTESIAN_POINT('Ctrl Pts',(-61.5367326052623,1.95617571750912,135.316849911152));
#88489=CARTESIAN_POINT('Ctrl Pts',(-61.5444837965024,2.08185785655506,135.262366380548));
#88490=CARTESIAN_POINT('Ctrl Pts',(-61.5522349877425,2.20536011201475,135.202585598886));
#88491=CARTESIAN_POINT('Ctrl Pts',(-61.5599861789826,2.32620937933313,135.137711859504));
#88492=CARTESIAN_POINT('Ctrl Pts',(-61.5677340757597,2.44700728248898,135.072865693191));
#88493=CARTESIAN_POINT('Ctrl Pts',(-61.5754819725368,2.56515409644669,135.002931058998));
#88494=CARTESIAN_POINT('Ctrl Pts',(-61.5832298693139,2.68019929511584,134.928159206363));
#88495=CARTESIAN_POINT('Ctrl Pts',(-61.590976145398,2.79522042880952,134.853402994387));
#88496=CARTESIAN_POINT('Ctrl Pts',(-61.5987224214821,2.90714091009121,134.773811789499));
#88497=CARTESIAN_POINT('Ctrl Pts',(-61.6064686975662,3.01553764861504,134.689681164482));
#88498=CARTESIAN_POINT('Ctrl Pts',(-61.6142150308315,3.12393518729883,134.605549918431));
#88499=CARTESIAN_POINT('Ctrl Pts',(-61.6219613640969,3.22880862246597,134.516879425099));
#88500=CARTESIAN_POINT('Ctrl Pts',(-61.6297076973622,3.32976684155063,134.424006434964));
#88501=CARTESIAN_POINT('Ctrl Pts',(-61.6374557653652,3.43074766952845,134.331112646568));
#88502=CARTESIAN_POINT('Ctrl Pts',(-61.6452038333682,3.52781124904164,134.23401475329));
#88503=CARTESIAN_POINT('Ctrl Pts',(-61.6529519013712,3.62060261831174,134.133087062135));
#88504=CARTESIAN_POINT('Ctrl Pts',(-61.660708204113,3.71349260735333,134.032052103829));
#88505=CARTESIAN_POINT('Ctrl Pts',(-61.6684645068548,3.8021010508708,133.927179504945));
#88506=CARTESIAN_POINT('Ctrl Pts',(-61.6762208095966,3.88611231654023,133.818877846864));
#88507=CARTESIAN_POINT('Ctrl Pts',(-61.6839812521108,3.97016842155167,133.710518384927));
#88508=CARTESIAN_POINT('Ctrl Pts',(-61.691741694625,4.04962223322311,133.598726535502));
#88509=CARTESIAN_POINT('Ctrl Pts',(-61.6995021371392,4.12420152079204,133.483939852893));
#88510=CARTESIAN_POINT('Ctrl Pts',(-61.7072750374046,4.19890052965431,133.368968904511));
#88511=CARTESIAN_POINT('Ctrl Pts',(-61.7150479376701,4.26870917831983,133.250993852549));
#88512=CARTESIAN_POINT('Ctrl Pts',(-61.7228208379355,4.33340083171799,133.130477616809));
#88513=CARTESIAN_POINT('Ctrl Pts',(-61.7303111736975,4.3957407805665,133.0143424498));
#88514=CARTESIAN_POINT('Ctrl Pts',(-61.7378015094595,4.45332917183307,132.895847925258));
#88515=CARTESIAN_POINT('Ctrl Pts',(-61.7452918452215,4.50600625725573,132.775423952944));
#88516=CARTESIAN_POINT('Ctrl Pts',(-61.7530661793406,4.56068061038311,132.650434069118));
#88517=CARTESIAN_POINT('Ctrl Pts',(-61.7608405134597,4.61023707348776,132.522969608907));
#88518=CARTESIAN_POINT('Ctrl Pts',(-61.7686148475788,4.65444472179399,132.393488489785));
#88519=CARTESIAN_POINT('Ctrl Pts',(-61.7763796005259,4.69859788812463,132.264166944571));
#88520=CARTESIAN_POINT('Ctrl Pts',(-61.7841443534729,4.73741523053368,132.132834051999));
#88521=CARTESIAN_POINT('Ctrl Pts',(-61.79190910642,4.77071293971553,131.999969713103));
#88522=CARTESIAN_POINT('Ctrl Pts',(-61.799666147305,4.80397757714325,131.867237336941));
#88523=CARTESIAN_POINT('Ctrl Pts',(-61.8074231881901,4.83173339669718,131.732976918205));
#88524=CARTESIAN_POINT('Ctrl Pts',(-61.8151802290751,4.8538458005935,131.597685271513));
#88525=CARTESIAN_POINT('Ctrl Pts',(-61.8229314203152,4.87594152935406,131.462495649305));
#88526=CARTESIAN_POINT('Ctrl Pts',(-61.8306826115553,4.89240225044825,131.326276731306));
#88527=CARTESIAN_POINT('Ctrl Pts',(-61.8384338027955,4.9031441170792,131.189536979317));
#88528=CARTESIAN_POINT('Ctrl Pts',(-61.8461816995726,4.91388141813024,131.05285534537));
#88529=CARTESIAN_POINT('Ctrl Pts',(-61.8539295963496,4.91890466857223,130.915653706666));
#88530=CARTESIAN_POINT('Ctrl Pts',(-61.8616774931267,4.91818173131711,130.778446910024));
#88531=CARTESIAN_POINT('Ctrl Pts',(-61.8694237692108,4.91745894528488,130.641268814085));
#88532=CARTESIAN_POINT('Ctrl Pts',(-61.8771700452949,4.91099236441548,130.504085953065));
#88533=CARTESIAN_POINT('Ctrl Pts',(-61.8849163213791,4.89880197179482,130.367414049163));
#88534=CARTESIAN_POINT('Ctrl Pts',(-61.8926626546444,4.88661148918747,130.23074113638));
#88535=CARTESIAN_POINT('Ctrl Pts',(-61.9004089879097,4.8686971452524,130.094579577661));
#88536=CARTESIAN_POINT('Ctrl Pts',(-61.9081553211751,4.84513085180934,129.959440448943));
#88537=CARTESIAN_POINT('Ctrl Pts',(-61.915903389178,4.8215592808583,129.824271056755));
#88538=CARTESIAN_POINT('Ctrl Pts',(-61.9236514571809,4.79233330892533,129.690124935263));
#88539=CARTESIAN_POINT('Ctrl Pts',(-61.9313995251839,4.757575985582,129.557503045943));
#88540=CARTESIAN_POINT('Ctrl Pts',(-61.9391558279257,4.7227817217417,129.424740204501));
#88541=CARTESIAN_POINT('Ctrl Pts',(-61.9469121306677,4.68244446225671,129.293505210095));
#88542=CARTESIAN_POINT('Ctrl Pts',(-61.9546684334095,4.63673735123466,129.164284461357));
#88543=CARTESIAN_POINT('Ctrl Pts',(-61.9624288759237,4.59100584495119,129.034994743614));
#88544=CARTESIAN_POINT('Ctrl Pts',(-61.9701893184378,4.53989892189582,128.907721776324));
#88545=CARTESIAN_POINT('Ctrl Pts',(-61.977949760952,4.48363756152041,128.782931103726));
#88546=CARTESIAN_POINT('Ctrl Pts',(-61.9857226612174,4.42728588541475,128.657940106062));
#88547=CARTESIAN_POINT('Ctrl Pts',(-61.9934955614829,4.36576341274733,128.53543971557));
#88548=CARTESIAN_POINT('Ctrl Pts',(-62.0012684617483,4.29933710926502,128.415870826213));
#88549=CARTESIAN_POINT('Ctrl Pts',(-62.0087587975104,4.23532556923152,128.300648567159));
#88550=CARTESIAN_POINT('Ctrl Pts',(-62.0162491332724,4.16676070194888,128.188148637693));
#88551=CARTESIAN_POINT('Ctrl Pts',(-62.0237394690345,4.09391785483666,128.078737815278));
#88552=CARTESIAN_POINT('Ctrl Pts',(-62.0315138031536,4.0183131490365,127.965178648278));
#88553=CARTESIAN_POINT('Ctrl Pts',(-62.0392881372726,3.93786016747144,127.854587738119));
#88554=CARTESIAN_POINT('Ctrl Pts',(-62.0470624713917,3.85281934859991,127.747406883936));
#88555=CARTESIAN_POINT('Ctrl Pts',(-62.0548272243388,3.76788333493756,127.640358120577));
#88556=CARTESIAN_POINT('Ctrl Pts',(-62.062591977286,3.67837097461425,127.536711354624));
#88557=CARTESIAN_POINT('Ctrl Pts',(-62.070356730233,3.58458666854186,127.436880628284));
#88558=CARTESIAN_POINT('Ctrl Pts',(-62.0781137711181,3.490895510364,127.337149055229));
#88559=CARTESIAN_POINT('Ctrl Pts',(-62.0858708120032,3.39294111607042,127.241226262332));
#88560=CARTESIAN_POINT('Ctrl Pts',(-62.0936278528882,3.29106871648181,127.149494030959));
#88561=CARTESIAN_POINT('Ctrl Pts',(-62.1013790441283,3.18927313966261,127.057830975576));
#88562=CARTESIAN_POINT('Ctrl Pts',(-62.1091302353684,3.0835657278569,126.970352452217));
#88563=CARTESIAN_POINT('Ctrl Pts',(-62.1168814266085,2.9743289431362,126.887403839591));
#88564=CARTESIAN_POINT('Ctrl Pts',(-62.1246293233856,2.86513858696298,126.804490482338));
#88565=CARTESIAN_POINT('Ctrl Pts',(-62.1323772201626,2.75242215213261,126.72610344242));
#88566=CARTESIAN_POINT('Ctrl Pts',(-62.1401251169397,2.63659542297332,126.652548044959));
#88567=CARTESIAN_POINT('Ctrl Pts',(-62.1478713930238,2.52079292226884,126.579008033702));
#88568=CARTESIAN_POINT('Ctrl Pts',(-62.1556176691079,2.40188175115738,126.510297864072));
#88569=CARTESIAN_POINT('Ctrl Pts',(-62.1633639451919,2.28030660267691,126.446679484178));
#88570=CARTESIAN_POINT('Ctrl Pts',(-62.1711102784573,2.15873055675664,126.383060634667));
#88571=CARTESIAN_POINT('Ctrl Pts',(-62.1788566117226,2.03449084063159,126.324533831162));
#88572=CARTESIAN_POINT('Ctrl Pts',(-62.1866029449879,1.90805630705779,126.271314821239));
#88573=CARTESIAN_POINT('Ctrl Pts',(-62.1943510129909,1.7815934593465,126.218083893288));
#88574=CARTESIAN_POINT('Ctrl Pts',(-62.2020990809939,1.6529351764055,126.17016327583));
#88575=CARTESIAN_POINT('Ctrl Pts',(-62.2098471489968,1.52256944261142,126.12772022569));
#88576=CARTESIAN_POINT('Ctrl Pts',(-62.2176034517387,1.39206515456409,126.085232066571));
#88577=CARTESIAN_POINT('Ctrl Pts',(-62.2253597544806,1.25985016295856,126.048233225318));
#88578=CARTESIAN_POINT('Ctrl Pts',(-62.2331160572224,1.1264272773577,126.016840941228));
#88579=CARTESIAN_POINT('Ctrl Pts',(-62.2408764997366,0.992933179945151,
125.985431902131));
#88580=CARTESIAN_POINT('Ctrl Pts',(-62.2486369422508,0.858230287738499,
125.959635456285));
#88581=CARTESIAN_POINT('Ctrl Pts',(-62.256397384765,0.722829721083129,125.939517325453));
#88582=CARTESIAN_POINT('Ctrl Pts',(-62.2641702850304,0.58721179741805,125.919366899211));
#88583=CARTESIAN_POINT('Ctrl Pts',(-62.2719431852958,0.450894350258999,
125.904913044574));
#88584=CARTESIAN_POINT('Ctrl Pts',(-62.2797160855613,0.314392617690945,
125.896169469654));
#88585=CARTESIAN_POINT('Ctrl Pts',(-62.2872064213233,0.182853066928855,
125.887743745707));
#88586=CARTESIAN_POINT('Ctrl Pts',(-62.2946967570852,0.0511427045500864,
125.884620350569));
#88587=CARTESIAN_POINT('Ctrl Pts',(-62.3021870928473,-0.0802810571713846,
125.886765878839));
#88588=CARTESIAN_POINT('Ctrl Pts',(-62.3099614269664,-0.216687790763728,
125.888992755464));
#88589=CARTESIAN_POINT('Ctrl Pts',(-62.3177357610855,-0.353217857286612,
125.896903039128));
#88590=CARTESIAN_POINT('Ctrl Pts',(-62.3255100952046,-0.489358785267645,
125.910516418801));
#88591=CARTESIAN_POINT('Ctrl Pts',(-62.3332748481517,-0.625331931722389,
125.924113021201));
#88592=CARTESIAN_POINT('Ctrl Pts',(-62.3410396010986,-0.760916508562987,
125.943398696353));
#88593=CARTESIAN_POINT('Ctrl Pts',(-62.3488043540457,-0.895599634227301,
125.968341143073));
#88594=CARTESIAN_POINT('Ctrl Pts',(-62.3565613949307,-1.03014899071269,
125.993258816604));
#88595=CARTESIAN_POINT('Ctrl Pts',(-62.3643184358159,-1.16379829583602,
126.023822010131));
#88596=CARTESIAN_POINT('Ctrl Pts',(-62.3720754767009,-1.29603974043084,
126.05994663334));
#88597=CARTESIAN_POINT('Ctrl Pts',(-62.379826667941,-1.42818146072253,126.096044014689));
#88598=CARTESIAN_POINT('Ctrl Pts',(-62.3875778591811,-1.55891705807206,
126.137694375373));
#88599=CARTESIAN_POINT('Ctrl Pts',(-62.3953290504212,-1.68774922549897,
126.184762624848));
#88600=CARTESIAN_POINT('Ctrl Pts',(-62.4030769471982,-1.81652663581871,
126.231810869061));
#88601=CARTESIAN_POINT('Ctrl Pts',(-62.4108248439753,-1.94340185881632,
126.284272288193));
#88602=CARTESIAN_POINT('Ctrl Pts',(-62.4185727407524,-2.06789327423267,
126.3419621068));
#88603=CARTESIAN_POINT('Ctrl Pts',(-62.4263190168365,-2.19235864872882,
126.399639857941));
#88604=CARTESIAN_POINT('Ctrl Pts',(-62.4340652929205,-2.31444085296472,
126.462543668912));
#88605=CARTESIAN_POINT('Ctrl Pts',(-62.4418115690046,-2.43367913512781,
126.530440996218));
#88606=CARTESIAN_POINT('Ctrl Pts',(-62.44955790227,-2.55291829748064,126.598338824726));
#88607=CARTESIAN_POINT('Ctrl Pts',(-62.4573042355354,-2.66931315612464,
126.671230049663));
#88608=CARTESIAN_POINT('Ctrl Pts',(-62.4650505688007,-2.78242877014554,
126.748836828761));
#88609=CARTESIAN_POINT('Ctrl Pts',(-62.4727986368036,-2.89556971562268,
126.826460987358));
#88610=CARTESIAN_POINT('Ctrl Pts',(-62.4805467048065,-3.00542963285425,
126.908802580325));
#88611=CARTESIAN_POINT('Ctrl Pts',(-62.4882947728094,-3.11160403646128,
126.995541458984));
#88612=CARTESIAN_POINT('Ctrl Pts',(-62.4960510755512,-3.21789128348912,
127.082372524757));
#88613=CARTESIAN_POINT('Ctrl Pts',(-62.5038073782931,-3.32048488899119,
127.173609964274));
#88614=CARTESIAN_POINT('Ctrl Pts',(-62.511563681035,-3.41901443537407,127.268894120312));
#88615=CARTESIAN_POINT('Ctrl Pts',(-62.5193241235491,-3.51759656994239,
127.364229132374));
#88616=CARTESIAN_POINT('Ctrl Pts',(-62.5270845660633,-3.6121100539642,127.463614881478));
#88617=CARTESIAN_POINT('Ctrl Pts',(-62.5348450085774,-3.70222332082832,
127.56665687182));
#88618=CARTESIAN_POINT('Ctrl Pts',(-62.5426179088429,-3.79248124550855,
127.669864274314));
#88619=CARTESIAN_POINT('Ctrl Pts',(-62.5503908091083,-3.8783245926976,127.776739341833));
#88620=CARTESIAN_POINT('Ctrl Pts',(-62.5581637093737,-3.95946333060175,
127.886855999554));
#88621=CARTESIAN_POINT('Ctrl Pts',(-62.5656540451359,-4.03765247100836,
127.992969639402));
#88622=CARTESIAN_POINT('Ctrl Pts',(-62.5731443808981,-4.11147293986799,
128.10209302614));
#88623=CARTESIAN_POINT('Ctrl Pts',(-62.5806347166602,-4.18070559958617,
128.21382326943));
#88624=CARTESIAN_POINT('Ctrl Pts',(-62.588633751821,-4.25464013295595,128.333141571435));
#88625=CARTESIAN_POINT('Ctrl Pts',(-62.5966327869818,-4.32356552374327,
128.455792831829));
#88626=CARTESIAN_POINT('Ctrl Pts',(-62.6046318221426,-4.3871773021134,128.58133151692));
#88627=CARTESIAN_POINT('Ctrl Pts',(-62.6126203547539,-4.45070555967966,
128.7067053726));
#88628=CARTESIAN_POINT('Ctrl Pts',(-62.6206088873652,-4.50893393109456,
128.834958788006));
#88629=CARTESIAN_POINT('Ctrl Pts',(-62.6285974199765,-4.56160153313018,
128.965617972321));
#88630=CARTESIAN_POINT('Ctrl Pts',(-62.63657358476,-4.61418759530553,129.096074870387));
#88631=CARTESIAN_POINT('Ctrl Pts',(-62.6445497495436,-4.6612299106076,129.228929782936));
#88632=CARTESIAN_POINT('Ctrl Pts',(-62.6525259143271,-4.702514088301,129.363685667471));
#88633=CARTESIAN_POINT('Ctrl Pts',(-62.656812012221,-4.72469868852751,129.436098528611));
#88634=CARTESIAN_POINT('Ctrl Pts',(-62.6610981101149,-4.74522136577641,
129.509059904719));
#88635=CARTESIAN_POINT('Ctrl Pts',(-62.6653842080088,-4.76405452823406,
129.582490119308));
#88636=CARTESIAN_POINT('Ctrl Pts',(-60.9152461054369,-4.76405452823402,
129.582490119308));
#88637=CARTESIAN_POINT('Ctrl Pts',(-60.9251020627235,-4.80703171165325,
129.75005750519));
#88638=CARTESIAN_POINT('Ctrl Pts',(-60.9349580200101,-4.84119281879953,
129.920005984769));
#88639=CARTESIAN_POINT('Ctrl Pts',(-60.9448139772968,-4.86631688391131,
130.091519086888));
#88640=CARTESIAN_POINT('Ctrl Pts',(-60.9545017912762,-4.89101233074943,
130.260106163723));
#88641=CARTESIAN_POINT('Ctrl Pts',(-60.9641896052557,-4.90697645570549,
130.430205070139));
#88642=CARTESIAN_POINT('Ctrl Pts',(-60.9738774192352,-4.91404468006025,
130.601018676807));
#88643=CARTESIAN_POINT('Ctrl Pts',(-60.9776318008096,-4.91678387502598,
130.667215185008));
#88644=CARTESIAN_POINT('Ctrl Pts',(-60.981386182384,-4.9181875312636,130.73351878516));
#88645=CARTESIAN_POINT('Ctrl Pts',(-60.9851405639584,-4.91824796096415,
130.799882116478));
#88646=CARTESIAN_POINT('',(-60.6398594359436,-4.91824984849176,130.805581400405));
#88647=CARTESIAN_POINT('Ctrl Pts',(-60.5697319016604,-4.76405452823403,
129.582490119308));
#88648=CARTESIAN_POINT('Ctrl Pts',(-60.5774417162904,-4.79792314311371,
129.714543334696));
#88649=CARTESIAN_POINT('Ctrl Pts',(-60.5851515309204,-4.82627074302898,
129.847903162596));
#88650=CARTESIAN_POINT('Ctrl Pts',(-60.5928613455504,-4.84902190340704,
129.982065267477));
#88651=CARTESIAN_POINT('Ctrl Pts',(-60.6006943606159,-4.87213662023907,
130.11837124099));
#88652=CARTESIAN_POINT('Ctrl Pts',(-60.6085273756815,-4.88947445874853,
130.255504925166));
#88653=CARTESIAN_POINT('Ctrl Pts',(-60.616360390747,-4.90101128615102,130.392934517859));
#88654=CARTESIAN_POINT('Ctrl Pts',(-60.6241934058126,-4.91254811355353,
130.530364110552));
#88655=CARTESIAN_POINT('Ctrl Pts',(-60.6320264208781,-4.91828397610615,
130.668089187314));
#88656=CARTESIAN_POINT('Ctrl Pts',(-60.6398594359436,-4.91824984849176,
130.805581400405));
#88657=CARTESIAN_POINT('Ctrl Pts',(-60.639859435991,-4.91824984849156,130.805581401237));
#88658=CARTESIAN_POINT('Ctrl Pts',(-60.643603072704,-4.91823353785304,130.871293121737));
#88659=CARTESIAN_POINT('Ctrl Pts',(-60.6473467094168,-4.91690034492517,
130.936986903404));
#88660=CARTESIAN_POINT('Ctrl Pts',(-60.6510903461297,-4.91425206892654,
131.002627270211));
#88661=CARTESIAN_POINT('Ctrl Pts',(-60.6588646802487,-4.9087524480947,131.138941283136));
#88662=CARTESIAN_POINT('Ctrl Pts',(-60.6666390143678,-4.89756809725561,
131.275242207376));
#88663=CARTESIAN_POINT('Ctrl Pts',(-60.6744133484869,-4.88069163100898,
131.411017246557));
#88664=CARTESIAN_POINT('Ctrl Pts',(-60.682178101434,-4.86383596349872,131.546624955137));
#88665=CARTESIAN_POINT('Ctrl Pts',(-60.6899428543811,-4.84130218614871,
131.681707683942));
#88666=CARTESIAN_POINT('Ctrl Pts',(-60.6977076073282,-4.81313489858287,
131.815753474246));
#88667=CARTESIAN_POINT('Ctrl Pts',(-60.7054646482132,-4.78499558716413,
131.949666128382));
#88668=CARTESIAN_POINT('Ctrl Pts',(-60.7132216890982,-4.7512339802709,132.082543513434));
#88669=CARTESIAN_POINT('Ctrl Pts',(-60.7209787299832,-4.71194633002055,
132.213879984409));
#88670=CARTESIAN_POINT('Ctrl Pts',(-60.7287299212233,-4.67268830689292,
132.34511741353));
#88671=CARTESIAN_POINT('Ctrl Pts',(-60.7364811124633,-4.62791264662451,
132.474815868444));
#88672=CARTESIAN_POINT('Ctrl Pts',(-60.7442323037035,-4.57776633485353,
132.602481427184));
#88673=CARTESIAN_POINT('Ctrl Pts',(-60.7519802004805,-4.52764133660268,
132.730092724656));
#88674=CARTESIAN_POINT('Ctrl Pts',(-60.7597280972577,-4.47215036954447,
132.855672481317));
#88675=CARTESIAN_POINT('Ctrl Pts',(-60.7674759940348,-4.41148971347016,
132.978743649703));
#88676=CARTESIAN_POINT('Ctrl Pts',(-60.7752222701188,-4.35084174629741,
133.101789074254));
#88677=CARTESIAN_POINT('Ctrl Pts',(-60.7829685462029,-4.28502641378575,
133.222326603813));
#88678=CARTESIAN_POINT('Ctrl Pts',(-60.790714822287,-4.21428724923702,133.339901199655));
#88679=CARTESIAN_POINT('Ctrl Pts',(-60.7984611555523,-4.14354756250775,
133.457476663405));
#88680=CARTESIAN_POINT('Ctrl Pts',(-60.8062074888176,-4.06788417277146,
133.572088814791));
#88681=CARTESIAN_POINT('Ctrl Pts',(-60.813953822083,-3.98758527966579,133.683309505597));
#88682=CARTESIAN_POINT('Ctrl Pts',(-60.821701890086,-3.90726840417987,133.794555103505));
#88683=CARTESIAN_POINT('Ctrl Pts',(-60.829449958089,-3.82231418845972,133.902407412605));
#88684=CARTESIAN_POINT('Ctrl Pts',(-60.837198026092,-3.73305239552146,134.006469746686));
#88685=CARTESIAN_POINT('Ctrl Pts',(-60.8449543288338,-3.64369573408743,
134.110642679453));
#88686=CARTESIAN_POINT('Ctrl Pts',(-60.8527106315756,-3.55002260504918,
134.211017293552));
#88687=CARTESIAN_POINT('Ctrl Pts',(-60.8604669343175,-3.45240145105574,
134.307231908842));
#88688=CARTESIAN_POINT('Ctrl Pts',(-60.8682273768316,-3.3547281937131,134.40349787677));
#88689=CARTESIAN_POINT('Ctrl Pts',(-60.8759878193458,-3.2531030022346,134.495599159301));
#88690=CARTESIAN_POINT('Ctrl Pts',(-60.8837482618599,-3.14792821550424,
134.58321375212));
#88691=CARTESIAN_POINT('Ctrl Pts',(-60.8915211621254,-3.0425845928691,134.670968991662));
#88692=CARTESIAN_POINT('Ctrl Pts',(-60.8992940623908,-2.9336802990924,134.754222911155));
#88693=CARTESIAN_POINT('Ctrl Pts',(-60.9070669626563,-2.82164824626189,
134.832695786946));
#88694=CARTESIAN_POINT('Ctrl Pts',(-60.9145572984184,-2.71368884074286,
134.908315976042));
#88695=CARTESIAN_POINT('Ctrl Pts',(-60.9220476341804,-2.60282539113857,
134.979496526034));
#88696=CARTESIAN_POINT('Ctrl Pts',(-60.9295379699425,-2.48946593046216,
135.046028030691));
#88697=CARTESIAN_POINT('Ctrl Pts',(-60.9373123040616,-2.37180841137968,
135.115082097569));
#88698=CARTESIAN_POINT('Ctrl Pts',(-60.9450866381807,-2.25108916875184,
135.179346365338));
#88699=CARTESIAN_POINT('Ctrl Pts',(-60.9528609722998,-2.12773564070224,
135.238537441486));
#88700=CARTESIAN_POINT('Ctrl Pts',(-60.9606257252469,-2.0045341348517,135.297655569922));
#88701=CARTESIAN_POINT('Ctrl Pts',(-60.9683904781941,-1.87870515229034,
135.351712779346));
#88702=CARTESIAN_POINT('Ctrl Pts',(-60.9761552311412,-1.75070352557956,
135.400469866488));
#88703=CARTESIAN_POINT('Ctrl Pts',(-60.9839122720262,-1.62282903188912,
135.449178527403));
#88704=CARTESIAN_POINT('Ctrl Pts',(-60.9916693129111,-1.49278655136236,
135.492597403677));
#88705=CARTESIAN_POINT('Ctrl Pts',(-60.9994263537961,-1.36105352407415,
135.530534161471));
#88706=CARTESIAN_POINT('Ctrl Pts',(-61.0071775450362,-1.22941983768637,
135.568442310861));
#88707=CARTESIAN_POINT('Ctrl Pts',(-61.0149287362764,-1.09609851623398,
135.600876462706));
#88708=CARTESIAN_POINT('Ctrl Pts',(-61.0226799275165,-0.96158455958484,
135.6276933033));
#88709=CARTESIAN_POINT('Ctrl Pts',(-61.0304278242936,-0.827127774955552,
135.654498746021));
#88710=CARTESIAN_POINT('Ctrl Pts',(-61.0381757210708,-0.691479745935739,
135.67569154978));
#88711=CARTESIAN_POINT('Ctrl Pts',(-61.0459236178479,-0.555147920088452,
135.691178994519));
#88712=CARTESIAN_POINT('Ctrl Pts',(-61.053669893932,-0.418844611920158,
135.706663199618));
#88713=CARTESIAN_POINT('Ctrl Pts',(-61.061416170016,-0.281858179650459,
135.716444375408));
#88714=CARTESIAN_POINT('Ctrl Pts',(-61.0691624461001,-0.144703095944134,
135.720481453807));
#88715=CARTESIAN_POINT('Ctrl Pts',(-61.0769087793655,-0.00754699979032486,
135.724518562007));
#88716=CARTESIAN_POINT('Ctrl Pts',(-61.0846551126309,0.129777359488358,
135.722811476705));
#88717=CARTESIAN_POINT('Ctrl Pts',(-61.0924014458962,0.266753989730087,
135.715371243849));
#88718=CARTESIAN_POINT('Ctrl Pts',(-61.1001495138992,0.403761294938243,
135.707929344805));
#88719=CARTESIAN_POINT('Ctrl Pts',(-61.1078975819022,0.540420325839154,
135.694751764598));
#88720=CARTESIAN_POINT('Ctrl Pts',(-61.1156456499051,0.676219094123127,
135.675901523608));
#88721=CARTESIAN_POINT('Ctrl Pts',(-61.123401952647,0.812162190954428,135.657031248358));
#88722=CARTESIAN_POINT('Ctrl Pts',(-61.1311582553888,0.947242810891693,
135.632476322644));
#88723=CARTESIAN_POINT('Ctrl Pts',(-61.1389145581307,1.08095750993771,135.602351230751));
#88724=CARTESIAN_POINT('Ctrl Pts',(-61.1466750006449,1.21474357654487,135.572210060189));
#88725=CARTESIAN_POINT('Ctrl Pts',(-61.1544354431591,1.34716189231044,135.53649290133));
#88726=CARTESIAN_POINT('Ctrl Pts',(-61.1621958856732,1.47772407188877,135.495364202073));
#88727=CARTESIAN_POINT('Ctrl Pts',(-61.1699687859387,1.60849584146835,135.454169479377));
#88728=CARTESIAN_POINT('Ctrl Pts',(-61.1777416862041,1.73740515273237,135.407545989768));
#88729=CARTESIAN_POINT('Ctrl Pts',(-61.1855145864695,1.8639826666933,135.355706756981));
#88730=CARTESIAN_POINT('Ctrl Pts',(-61.1930049222315,1.98595876919103,135.305752010881));
#88731=CARTESIAN_POINT('Ctrl Pts',(-61.2004952579934,2.10576938433685,135.250954276866));
#88732=CARTESIAN_POINT('Ctrl Pts',(-61.2079855937554,2.22301778092754,135.191543655482));
#88733=CARTESIAN_POINT('Ctrl Pts',(-61.2157599278745,2.34471168611271,135.129880462331));
#88734=CARTESIAN_POINT('Ctrl Pts',(-61.2235342619936,2.46403073401666,135.063052351033));
#88735=CARTESIAN_POINT('Ctrl Pts',(-61.2313085961127,2.58050545774597,134.991265756812));
#88736=CARTESIAN_POINT('Ctrl Pts',(-61.2390733490598,2.69683663678778,134.919567633153));
#88737=CARTESIAN_POINT('Ctrl Pts',(-61.2468381020068,2.81033013667362,134.842923388576));
#88738=CARTESIAN_POINT('Ctrl Pts',(-61.2546028549539,2.92053886080871,134.761586391389));
#88739=CARTESIAN_POINT('Ctrl Pts',(-61.2623598958389,3.03063812408547,134.680330179253));
#88740=CARTESIAN_POINT('Ctrl Pts',(-61.2701169367239,3.13745879156984,134.594390720583));
#88741=CARTESIAN_POINT('Ctrl Pts',(-61.2778739776089,3.24058097933402,134.504065738096));
#88742=CARTESIAN_POINT('Ctrl Pts',(-61.285625168849,3.34362540185424,134.413808870382));
#88743=CARTESIAN_POINT('Ctrl Pts',(-61.2933763600892,3.44297660318405,134.319173318109));
#88744=CARTESIAN_POINT('Ctrl Pts',(-61.3011275513293,3.53824644992244,134.220498074126));
#88745=CARTESIAN_POINT('Ctrl Pts',(-61.3088754481064,3.63347580443455,134.121864769753));
#88746=CARTESIAN_POINT('Ctrl Pts',(-61.3166233448835,3.72462698352099,134.019195469282));
#88747=CARTESIAN_POINT('Ctrl Pts',(-61.3243712416605,3.81134769136716,133.912866985263));
#88748=CARTESIAN_POINT('Ctrl Pts',(-61.3321175177446,3.89805025911073,133.806560742869));
#88749=CARTESIAN_POINT('Ctrl Pts',(-61.3398637938287,3.98032395204148,133.696597142177));
#88750=CARTESIAN_POINT('Ctrl Pts',(-61.3476100699127,4.05785613337724,133.583386825307));
#88751=CARTESIAN_POINT('Ctrl Pts',(-61.3553564031781,4.13538888703794,133.470175672745));
#88752=CARTESIAN_POINT('Ctrl Pts',(-61.3631027364434,4.20817983834974,133.353718078752));
#88753=CARTESIAN_POINT('Ctrl Pts',(-61.3708490697087,4.27595937421572,133.234454132754));
#88754=CARTESIAN_POINT('Ctrl Pts',(-61.3785971377117,4.34375408883881,133.115163478421));
#88755=CARTESIAN_POINT('Ctrl Pts',(-61.3863452057147,4.4065349616874,132.993065561358));
#88756=CARTESIAN_POINT('Ctrl Pts',(-61.3940932737177,4.4640782714028,132.868625195882));
#88757=CARTESIAN_POINT('Ctrl Pts',(-61.4018495764595,4.52168273883254,132.744052573704));
#88758=CARTESIAN_POINT('Ctrl Pts',(-61.4096058792014,4.57403835900126,132.617132885334));
#88759=CARTESIAN_POINT('Ctrl Pts',(-61.4173621819433,4.62096932700243,132.488351574015));
#88760=CARTESIAN_POINT('Ctrl Pts',(-61.4251226244574,4.66792534347429,132.359501528233));
#88761=CARTESIAN_POINT('Ctrl Pts',(-61.4328830669716,4.70945082033221,132.228788252095));
#88762=CARTESIAN_POINT('Ctrl Pts',(-61.4406435094857,4.74542012804259,132.096711526131));
#88763=CARTESIAN_POINT('Ctrl Pts',(-61.4484164097512,4.7814471768789,131.964422778881));
#88764=CARTESIAN_POINT('Ctrl Pts',(-61.4561893100165,4.81190014614841,131.830766589437));
#88765=CARTESIAN_POINT('Ctrl Pts',(-61.4639622102819,4.83670456956486,131.696252970516));
#88766=CARTESIAN_POINT('Ctrl Pts',(-61.471452546044,4.86060728971179,131.56662926046));
#88767=CARTESIAN_POINT('Ctrl Pts',(-61.4789428818062,4.87926496815599,131.436209682978));
#88768=CARTESIAN_POINT('Ctrl Pts',(-61.4864332175682,4.89265675209853,131.305452394234));
#88769=CARTESIAN_POINT('Ctrl Pts',(-61.4942075516873,4.90655628959947,131.169737403146));
#88770=CARTESIAN_POINT('Ctrl Pts',(-61.5019818858064,4.91482676681583,131.033228682329));
#88771=CARTESIAN_POINT('Ctrl Pts',(-61.5097562199255,4.91738810522468,130.896432790858));
#88772=CARTESIAN_POINT('Ctrl Pts',(-61.5175209728726,4.91994628701287,130.759805488098));
#88773=CARTESIAN_POINT('Ctrl Pts',(-61.5252857258198,4.91680932229427,130.622892106008));
#88774=CARTESIAN_POINT('Ctrl Pts',(-61.5330504787669,4.90794871036947,130.486205751372));
#88775=CARTESIAN_POINT('Ctrl Pts',(-61.5408075196518,4.89909689892936,130.349655155552));
#88776=CARTESIAN_POINT('Ctrl Pts',(-61.5485645605368,4.88453277843306,130.213331526079));
#88777=CARTESIAN_POINT('Ctrl Pts',(-61.5563216014218,4.86427987391699,130.077749049597));
#88778=CARTESIAN_POINT('Ctrl Pts',(-61.5640727926619,4.84404224227374,129.942268816915));
#88779=CARTESIAN_POINT('Ctrl Pts',(-61.5718239839022,4.81812442303516,129.807529009858));
#88780=CARTESIAN_POINT('Ctrl Pts',(-61.5795751751423,4.78660182490122,129.674039409965));
#88781=CARTESIAN_POINT('Ctrl Pts',(-61.5873230719194,4.75509262471238,129.540606546713));
#88782=CARTESIAN_POINT('Ctrl Pts',(-61.5950709686964,4.71798347326789,129.40842321347));
#88783=CARTESIAN_POINT('Ctrl Pts',(-61.6028188654734,4.67540096914463,129.27798948307));
#88784=CARTESIAN_POINT('Ctrl Pts',(-61.6105651415575,4.63282737236327,129.147583036595));
#88785=CARTESIAN_POINT('Ctrl Pts',(-61.6183114176416,4.58478282144526,129.018925836436));
#88786=CARTESIAN_POINT('Ctrl Pts',(-61.6260576937257,4.53144381342069,128.892502874869));
#88787=CARTESIAN_POINT('Ctrl Pts',(-61.633804026991,4.47810441165976,128.766078980076));
#88788=CARTESIAN_POINT('Ctrl Pts',(-61.6415503602565,4.41947062678487,128.641889717003));
#88789=CARTESIAN_POINT('Ctrl Pts',(-61.6492966935218,4.35576698602873,128.520399797867));
#88790=CARTESIAN_POINT('Ctrl Pts',(-61.6570447615248,4.29204907928385,128.398882671905));
#88791=CARTESIAN_POINT('Ctrl Pts',(-61.6647928295278,4.22325923894819,128.280066438951));
#88792=CARTESIAN_POINT('Ctrl Pts',(-61.6725408975308,4.14966759961328,128.164390565611));
#88793=CARTESIAN_POINT('Ctrl Pts',(-61.6802972002726,4.07599774620843,128.048591750577));
#88794=CARTESIAN_POINT('Ctrl Pts',(-61.6880535030144,3.99751610938801,127.93594029279));
#88795=CARTESIAN_POINT('Ctrl Pts',(-61.6958098057562,3.91453607945671,127.826846495831));
#88796=CARTESIAN_POINT('Ctrl Pts',(-61.7035702482704,3.83151176058484,127.717694472227));
#88797=CARTESIAN_POINT('Ctrl Pts',(-61.7113306907846,3.74398451393526,127.612104193882));
#88798=CARTESIAN_POINT('Ctrl Pts',(-61.7190911332987,3.65230691319044,127.510451500064));
#88799=CARTESIAN_POINT('Ctrl Pts',(-61.7268640335642,3.56048214342215,127.408635624318));
#88800=CARTESIAN_POINT('Ctrl Pts',(-61.7346369338296,3.46449397964875,127.310770243671));
#88801=CARTESIAN_POINT('Ctrl Pts',(-61.7424098340951,3.36473125916445,127.217193683048));
#88802=CARTESIAN_POINT('Ctrl Pts',(-61.7499001698571,3.26859516485716,127.127018866109));
#88803=CARTESIAN_POINT('Ctrl Pts',(-61.7573905056191,3.16895441158675,127.040826665518));
#88804=CARTESIAN_POINT('Ctrl Pts',(-61.7648808413811,3.06618318766209,126.958882269922));
#88805=CARTESIAN_POINT('Ctrl Pts',(-61.7726551755002,2.95951536154539,126.873830927661));
#88806=CARTESIAN_POINT('Ctrl Pts',(-61.7804295096194,2.84913710354739,126.793086442934));
#88807=CARTESIAN_POINT('Ctrl Pts',(-61.7882038437384,2.73543131176619,126.716989995625));
#88808=CARTESIAN_POINT('Ctrl Pts',(-61.7959685966855,2.62186565221118,126.640987330385));
#88809=CARTESIAN_POINT('Ctrl Pts',(-61.8037333496326,2.50498094021496,126.569621520331));
#88810=CARTESIAN_POINT('Ctrl Pts',(-61.8114981025797,2.38519346172388,126.503193890659));
#88811=CARTESIAN_POINT('Ctrl Pts',(-61.8192551434647,2.26552495784531,126.436832237845));
#88812=CARTESIAN_POINT('Ctrl Pts',(-61.8270121843497,2.14295976460758,126.375399193277));
#88813=CARTESIAN_POINT('Ctrl Pts',(-61.8347692252347,2.01794319765212,126.319152895113));
#88814=CARTESIAN_POINT('Ctrl Pts',(-61.8425204164749,1.8930209066623,126.262949012721));
#88815=CARTESIAN_POINT('Ctrl Pts',(-61.850271607715,1.76565127657975,126.21192425116));
#88816=CARTESIAN_POINT('Ctrl Pts',(-61.8580227989551,1.6363039612941,126.16629071633));
#88817=CARTESIAN_POINT('Ctrl Pts',(-61.8657706957322,1.5070116220679,126.120676576969));
#88818=CARTESIAN_POINT('Ctrl Pts',(-61.8735185925092,1.37574363738721,126.08044923669));
#88819=CARTESIAN_POINT('Ctrl Pts',(-61.8812664892863,1.24298916231292,126.045772486106));
#88820=CARTESIAN_POINT('Ctrl Pts',(-61.8890127653704,1.11026245661296,126.011102989151));
#88821=CARTESIAN_POINT('Ctrl Pts',(-61.8967590414545,0.976050257033153,
125.981981871217));
#88822=CARTESIAN_POINT('Ctrl Pts',(-61.9045053175386,0.840856002267571,
125.958522790528));
#88823=CARTESIAN_POINT('Ctrl Pts',(-61.912251650804,0.705660749528713,125.935063536669));
#88824=CARTESIAN_POINT('Ctrl Pts',(-61.9199979840693,0.56948381234757,125.917266470297));
#88825=CARTESIAN_POINT('Ctrl Pts',(-61.9277443173346,0.432837528728403,
125.905193878597));
#88826=CARTESIAN_POINT('Ctrl Pts',(-61.9354923853376,0.296160644121458,
125.893118583323));
#88827=CARTESIAN_POINT('Ctrl Pts',(-61.9432404533407,0.15901459329965,125.886770348067));
#88828=CARTESIAN_POINT('Ctrl Pts',(-61.9509885213436,0.0219151263119513,
125.886159443383));
#88829=CARTESIAN_POINT('Ctrl Pts',(-61.9587448240855,-0.115330051620767,
125.885547889421));
#88830=CARTESIAN_POINT('Ctrl Pts',(-61.9665011268274,-0.252528155233385,
125.890685848596));
#88831=CARTESIAN_POINT('Ctrl Pts',(-61.9742574295692,-0.389164589390033,
125.901531435873));
#88832=CARTESIAN_POINT('Ctrl Pts',(-61.9820178720834,-0.525873950525634,
125.912382811766));
#88833=CARTESIAN_POINT('Ctrl Pts',(-61.9897783145975,-0.662020656955246,
125.928947838641));
#88834=CARTESIAN_POINT('Ctrl Pts',(-61.9975387571116,-0.797097929770319,
125.951133036579));
#88835=CARTESIAN_POINT('Ctrl Pts',(-62.0053116573771,-0.932392040615496,
125.973353848165));
#88836=CARTESIAN_POINT('Ctrl Pts',(-62.0130845576424,-1.06661290420646,
126.001212780139));
#88837=CARTESIAN_POINT('Ctrl Pts',(-62.0208574579079,-1.19926570214619,
126.034565565558));
#88838=CARTESIAN_POINT('Ctrl Pts',(-62.0283477936699,-1.32709623674894,
126.066705893217));
#88839=CARTESIAN_POINT('Ctrl Pts',(-62.035838129432,-1.45347043720029,126.103947491135));
#88840=CARTESIAN_POINT('Ctrl Pts',(-62.0433284651941,-1.57796293485931,
126.146118885033));
#88841=CARTESIAN_POINT('Ctrl Pts',(-62.0511028340312,-1.70717618043334,
126.189889415614));
#88842=CARTESIAN_POINT('Ctrl Pts',(-62.0588772028683,-1.8347715093924,126.239109648032));
#88843=CARTESIAN_POINT('Ctrl Pts',(-62.0666515717054,-1.96025490507105,
126.293641853373));
#88844=CARTESIAN_POINT('Ctrl Pts',(-62.0744163512153,-2.08558352273938,
126.348106795741));
#88845=CARTESIAN_POINT('Ctrl Pts',(-62.0821811307252,-2.2088050351323,126.407870519972));
#88846=CARTESIAN_POINT('Ctrl Pts',(-62.0899459102351,-2.32944091129757,
126.47274566431));
#88847=CARTESIAN_POINT('Ctrl Pts',(-62.097702969562,-2.44995684445031,126.537556306109));
#88848=CARTESIAN_POINT('Ctrl Pts',(-62.1054600288888,-2.56789191527144,
126.607468070453));
#88849=CARTESIAN_POINT('Ctrl Pts',(-62.1132170882156,-2.68278823776849,
126.682245828554));
#88850=CARTESIAN_POINT('Ctrl Pts',(-62.1209682898026,-2.79759779635957,
126.756967118265));
#88851=CARTESIAN_POINT('Ctrl Pts',(-62.1287194913898,-2.9093728477812,126.836546875309));
#88852=CARTESIAN_POINT('Ctrl Pts',(-62.1364706929768,-3.01768108050096,
126.920704613375));
#88853=CARTESIAN_POINT('Ctrl Pts',(-62.144218557716,-3.12594268714839,127.004826122019));
#88854=CARTESIAN_POINT('Ctrl Pts',(-62.1519664224551,-3.23074013560302,
127.093521452251));
#88855=CARTESIAN_POINT('Ctrl Pts',(-62.1597142871944,-3.33167122921823,
127.186467600505));
#88856=CARTESIAN_POINT('Ctrl Pts',(-62.167460519711,-3.43258105994205,127.279394168035));
#88857=CARTESIAN_POINT('Ctrl Pts',(-62.1752067522277,-3.52962586860398,
127.376569507626));
#88858=CARTESIAN_POINT('Ctrl Pts',(-62.1829529847444,-3.62243791678548,
127.477631503025));
#88859=CARTESIAN_POINT('Ctrl Pts',(-62.1906992629046,-3.71525051184835,
127.578694093917));
#88860=CARTESIAN_POINT('Ctrl Pts',(-62.1984455410648,-3.80383003225941,
127.683643098332));
#88861=CARTESIAN_POINT('Ctrl Pts',(-62.206191819225,-3.88784714979851,127.792081148077));
#88862=CARTESIAN_POINT('Ctrl Pts',(-62.213939820567,-3.97188295718589,127.900543320177));
#88863=CARTESIAN_POINT('Ctrl Pts',(-62.221687821909,-4.05135410281197,128.012495773005));
#88864=CARTESIAN_POINT('Ctrl Pts',(-62.229435823251,-4.12597317726844,128.127510154249));
#88865=CARTESIAN_POINT('Ctrl Pts',(-62.2371918970811,-4.20066999585148,
128.242644366684));
#88866=CARTESIAN_POINT('Ctrl Pts',(-62.2449479709113,-4.27050443231383,
128.360846551381));
#88867=CARTESIAN_POINT('Ctrl Pts',(-62.2527040447415,-4.33523359464394,
128.481661165986));
#88868=CARTESIAN_POINT('Ctrl Pts',(-62.2604642535788,-4.39999726612839,
128.602540190666));
#88869=CARTESIAN_POINT('Ctrl Pts',(-62.2682244624161,-4.45965007018302,
128.72603406863));
#88870=CARTESIAN_POINT('Ctrl Pts',(-62.2759846712534,-4.51399674250588,
128.85166594836));
#88871=CARTESIAN_POINT('Ctrl Pts',(-62.283756953163,-4.56842796555643,128.977493281949));
#88872=CARTESIAN_POINT('Ctrl Pts',(-62.2915292350726,-4.61753642212146,
129.105464898438));
#88873=CARTESIAN_POINT('Ctrl Pts',(-62.2993015169822,-4.66117605574161,
129.235086632603));
#88874=CARTESIAN_POINT('Ctrl Pts',(-62.306174702148,-4.69976746119073,129.349713738361));
#88875=CARTESIAN_POINT('Ctrl Pts',(-62.3130478873137,-4.73408281986375,
129.465630883257));
#88876=CARTESIAN_POINT('Ctrl Pts',(-62.3199210724795,-4.76405452823405,
129.582490119308));
#88877=CARTESIAN_POINT('Origin',(213.235140564004,0.,130.804360617566));
#88878=CARTESIAN_POINT('',(-64.4150295539547,-4.76405452823403,129.582490119308));
#88879=CARTESIAN_POINT('',(-64.0701225287273,-4.76405452823399,129.582490119308));
#88880=CARTESIAN_POINT('',(213.235140564004,-4.76405452823405,129.582490119308));
#88881=CARTESIAN_POINT('',(-62.7351405640401,-4.91824977962896,130.805832921769));
#88882=CARTESIAN_POINT('Ctrl Pts',(-62.7351405640401,-4.91824977962896,
130.805832921769));
#88883=CARTESIAN_POINT('Ctrl Pts',(-62.7434671272577,-4.9182055325362,130.953640863794));
#88884=CARTESIAN_POINT('Ctrl Pts',(-62.7517936904754,-4.91149398221606,
131.101259344452));
#88885=CARTESIAN_POINT('Ctrl Pts',(-62.760120253693,-4.89819140610862,131.24809929249));
#88886=CARTESIAN_POINT('Ctrl Pts',(-62.7684782995291,-4.8848385331479,131.395494440308));
#88887=CARTESIAN_POINT('Ctrl Pts',(-62.7768363453653,-4.8648447801471,131.542104870886));
#88888=CARTESIAN_POINT('Ctrl Pts',(-62.7851943912014,-4.83833812578196,
131.687348297607));
#88889=CARTESIAN_POINT('Ctrl Pts',(-62.7935681368434,-4.81178168115064,
131.832864550494));
#88890=CARTESIAN_POINT('Ctrl Pts',(-62.8019418824853,-4.77868796388197,
131.977008386601));
#88891=CARTESIAN_POINT('Ctrl Pts',(-62.8103156281273,-4.73923506913203,
132.119211948329));
#88892=CARTESIAN_POINT('Ctrl Pts',(-62.8187159994217,-4.69965672764547,
132.261867668837));
#88893=CARTESIAN_POINT('Ctrl Pts',(-62.8271163707161,-4.6536788351441,132.402570489922));
#88894=CARTESIAN_POINT('Ctrl Pts',(-62.8355167420105,-4.6015289851969,132.540768997209));
#88895=CARTESIAN_POINT('Ctrl Pts',(-62.843371941498,-4.55276358421359,132.669998623563));
#88896=CARTESIAN_POINT('Ctrl Pts',(-62.8512271409856,-4.49860188638689,
132.797038484982));
#88897=CARTESIAN_POINT('Ctrl Pts',(-62.8590823404731,-4.43926593480472,
132.921457928174));
#88898=CARTESIAN_POINT('Ctrl Pts',(-62.8668566745922,-4.3805408173069,133.044596535133));
#88899=CARTESIAN_POINT('Ctrl Pts',(-62.8746310087113,-4.31659527900452,
133.165484912506));
#88900=CARTESIAN_POINT('Ctrl Pts',(-62.8824053428304,-4.24762442976221,
133.283648774717));
#88901=CARTESIAN_POINT('Ctrl Pts',(-62.8901700957775,-4.17873858092748,
133.401667010528));
#88902=CARTESIAN_POINT('Ctrl Pts',(-62.8979348487247,-4.10483993906106,
133.516967077629));
#88903=CARTESIAN_POINT('Ctrl Pts',(-62.9056996016718,-4.02617107041891,
133.629095928037));
#88904=CARTESIAN_POINT('Ctrl Pts',(-62.9134566425568,-3.94758033680614,
133.74111341049));
#88905=CARTESIAN_POINT('Ctrl Pts',(-62.9212136834419,-3.86422902805879,
133.849965626309));
#88906=CARTESIAN_POINT('Ctrl Pts',(-62.9289707243269,-3.77640470510279,
133.955225667957));
#88907=CARTESIAN_POINT('Ctrl Pts',(-62.936721915567,-3.68864661115214,134.06040633219));
#88908=CARTESIAN_POINT('Ctrl Pts',(-62.9444731068072,-3.59642246647058,
134.161999915144));
#88909=CARTESIAN_POINT('Ctrl Pts',(-62.9522242980474,-3.50006185215328,
134.259610260298));
#88910=CARTESIAN_POINT('Ctrl Pts',(-62.9599721948245,-3.40374219366731,
134.357179118452));
#88911=CARTESIAN_POINT('Ctrl Pts',(-62.9677200916015,-3.30328983638444,
134.450767828373));
#88912=CARTESIAN_POINT('Ctrl Pts',(-62.9754679883787,-3.19907303021354,
134.540015153234));
#88913=CARTESIAN_POINT('Ctrl Pts',(-62.9832142644628,-3.09487802395183,
134.62924380948));
#88914=CARTESIAN_POINT('Ctrl Pts',(-62.9909605405468,-2.98692043183581,
134.714132632834));
#88915=CARTESIAN_POINT('Ctrl Pts',(-62.998706816631,-2.87560327531221,134.794359222267));
#88916=CARTESIAN_POINT('Ctrl Pts',(-63.0064531498964,-2.76428529707065,
134.874586403914));
#88917=CARTESIAN_POINT('Ctrl Pts',(-63.0141994831618,-2.64960802211177,
134.950151054378));
#88918=CARTESIAN_POINT('Ctrl Pts',(-63.0219458164272,-2.53200494315482,
135.020773077269));
#88919=CARTESIAN_POINT('Ctrl Pts',(-63.0296938844302,-2.41437552780391,
135.091410915473));
#88920=CARTESIAN_POINT('Ctrl Pts',(-63.0374419524331,-2.29381933976595,
135.15710372233));
#88921=CARTESIAN_POINT('Ctrl Pts',(-63.0451900204361,-2.17079569080896,
135.217616686645));
#88922=CARTESIAN_POINT('Ctrl Pts',(-63.052946323178,-2.04764129085369,135.278193964859));
#88923=CARTESIAN_POINT('Ctrl Pts',(-63.0607026259199,-1.92201454274061,
135.333580230468));
#88924=CARTESIAN_POINT('Ctrl Pts',(-63.0684589286618,-1.7943965310866,135.383588079892));
#88925=CARTESIAN_POINT('Ctrl Pts',(-63.076219371176,-1.66671040585743,135.433622620012));
#88926=CARTESIAN_POINT('Ctrl Pts',(-63.0839798136902,-1.53703126885931,
135.478272896769));
#88927=CARTESIAN_POINT('Ctrl Pts',(-63.0917402562044,-1.40585574193498,
135.517401323455));
#88928=CARTESIAN_POINT('Ctrl Pts',(-63.0995131564698,-1.27446964040944,
135.556592562565));
#88929=CARTESIAN_POINT('Ctrl Pts',(-63.1072860567353,-1.14158272794049,
135.590244142148));
#88930=CARTESIAN_POINT('Ctrl Pts',(-63.1150589570007,-1.00770308338584,
135.618269378462));
#88931=CARTESIAN_POINT('Ctrl Pts',(-63.1225492927625,-0.87869030113794,
135.645275826844));
#88932=CARTESIAN_POINT('Ctrl Pts',(-63.1300396285242,-0.748756014115618,
135.667057842591));
#88933=CARTESIAN_POINT('Ctrl Pts',(-63.137529964286,-0.618357746135029,
135.683583584422));
#88934=CARTESIAN_POINT('Ctrl Pts',(-63.1453042984051,-0.483015388185867,
135.700735904778));
#88935=CARTESIAN_POINT('Ctrl Pts',(-63.1530786325242,-0.346744447157127,
135.712279833206));
#88936=CARTESIAN_POINT('Ctrl Pts',(-63.1608529666433,-0.210049414582917,
135.71812315822));
#88937=CARTESIAN_POINT('Ctrl Pts',(-63.1686177195904,-0.0735228464197539,
135.723959281858));
#88938=CARTESIAN_POINT('Ctrl Pts',(-63.1763824725374,0.063426386502673,
135.724108764167));
#88939=CARTESIAN_POINT('Ctrl Pts',(-63.1841472254845,0.200286009099147,
135.718530799505));
#88940=CARTESIAN_POINT('Ctrl Pts',(-63.1919042663694,0.337009700789261,
135.712958374956));
#88941=CARTESIAN_POINT('Ctrl Pts',(-63.1996613072545,0.473643571158825,
135.701669839789));
#88942=CARTESIAN_POINT('Ctrl Pts',(-63.2074183481395,0.609673017102681,
135.684676373203));
#88943=CARTESIAN_POINT('Ctrl Pts',(-63.2151695393796,0.745599882183011,
135.667695721522));
#88944=CARTESIAN_POINT('Ctrl Pts',(-63.2229207306197,0.880922843702231,
135.645018749826));
#88945=CARTESIAN_POINT('Ctrl Pts',(-63.2306719218598,1.01513045732638,135.616708611748));
#88946=CARTESIAN_POINT('Ctrl Pts',(-63.2384198186369,1.14928102913481,135.588410506234));
#88947=CARTESIAN_POINT('Ctrl Pts',(-63.246167715414,1.28231681415679,135.554484076837));
#88948=CARTESIAN_POINT('Ctrl Pts',(-63.2539156121911,1.41373484555055,135.515043885307));
#88949=CARTESIAN_POINT('Ctrl Pts',(-63.2616618882752,1.54512538712519,135.475611943815));
#88950=CARTESIAN_POINT('Ctrl Pts',(-63.2694081643592,1.67489847393822,135.430668646598));
#88951=CARTESIAN_POINT('Ctrl Pts',(-63.2771544404433,1.80256501793662,135.380378801382));
#88952=CARTESIAN_POINT('Ctrl Pts',(-63.2849007737086,1.93023250434044,135.330088584937));
#88953=CARTESIAN_POINT('Ctrl Pts',(-63.292647106974,2.05579305314045,135.27445188503));
#88954=CARTESIAN_POINT('Ctrl Pts',(-63.3003934402393,2.17877669790947,135.213682012423));
#88955=CARTESIAN_POINT('Ctrl Pts',(-63.3081415082423,2.30178788401303,135.152898530825));
#88956=CARTESIAN_POINT('Ctrl Pts',(-63.3158895762454,2.42222066732166,135.086979762243));
#88957=CARTESIAN_POINT('Ctrl Pts',(-63.3236376442484,2.5396292252973,135.016185217489));
#88958=CARTESIAN_POINT('Ctrl Pts',(-63.3313939469902,2.65716256648553,134.94531543145));
#88959=CARTESIAN_POINT('Ctrl Pts',(-63.3391502497319,2.7716649263213,134.869559719775));
#88960=CARTESIAN_POINT('Ctrl Pts',(-63.3469065524738,2.88271859887994,134.789221536365));
#88961=CARTESIAN_POINT('Ctrl Pts',(-63.3546669949879,2.99383154412738,134.708840474047));
#88962=CARTESIAN_POINT('Ctrl Pts',(-63.3624274375021,3.10149182766155,134.623872308619));
#88963=CARTESIAN_POINT('Ctrl Pts',(-63.3701878800163,3.20531525764995,134.534660493122));
#88964=CARTESIAN_POINT('Ctrl Pts',(-63.3779607802817,3.30930535422517,134.4453054669));
#88965=CARTESIAN_POINT('Ctrl Pts',(-63.3857336805471,3.40944600332291,134.351693444638));
#88966=CARTESIAN_POINT('Ctrl Pts',(-63.3935065808125,3.50538964642401,134.254205032789));
#88967=CARTESIAN_POINT('Ctrl Pts',(-63.4009969165746,3.5978454964321,134.160260570268));
#88968=CARTESIAN_POINT('Ctrl Pts',(-63.4084872523367,3.68640397913906,134.062716886227));
#88969=CARTESIAN_POINT('Ctrl Pts',(-63.4159775880989,3.77079100277721,133.961941697424));
#88970=CARTESIAN_POINT('Ctrl Pts',(-63.423751922218,3.85837758606461,133.857345586707));
#88971=CARTESIAN_POINT('Ctrl Pts',(-63.4315262563371,3.94174759222032,133.748936759917));
#88972=CARTESIAN_POINT('Ctrl Pts',(-63.4393005904562,4.02055075111479,133.637089817509));
#88973=CARTESIAN_POINT('Ctrl Pts',(-63.4470653434033,4.09925679215876,133.525380716462));
#88974=CARTESIAN_POINT('Ctrl Pts',(-63.4548300963504,4.17340696142413,133.410242247039));
#88975=CARTESIAN_POINT('Ctrl Pts',(-63.4625948492975,4.24269003077375,133.292083344333));
#88976=CARTESIAN_POINT('Ctrl Pts',(-63.4703518901825,4.31190428720207,133.174041798715));
#88977=CARTESIAN_POINT('Ctrl Pts',(-63.4781089310675,4.37626086726032,133.052986124905));
#88978=CARTESIAN_POINT('Ctrl Pts',(-63.4858659719525,4.43549102077797,132.9293553157));
#88979=CARTESIAN_POINT('Ctrl Pts',(-63.4936171631926,4.49467650837611,132.80581773745));
#88980=CARTESIAN_POINT('Ctrl Pts',(-63.5013683544327,4.54874309599145,132.679709240261));
#88981=CARTESIAN_POINT('Ctrl Pts',(-63.5091195456729,4.5974674684087,132.551494252817));
#88982=CARTESIAN_POINT('Ctrl Pts',(-63.5168674424499,4.64617113166797,132.423333760162));
#88983=CARTESIAN_POINT('Ctrl Pts',(-63.524615339227,4.68953695715384,132.293068922665));
#88984=CARTESIAN_POINT('Ctrl Pts',(-63.5323632360041,4.72738946304791,132.161184823999));
#88985=CARTESIAN_POINT('Ctrl Pts',(-63.5401095120882,4.76523405101375,132.029328312644));
#88986=CARTESIAN_POINT('Ctrl Pts',(-63.5478557881724,4.79756750551092,131.895853589396));
#88987=CARTESIAN_POINT('Ctrl Pts',(-63.5556020642565,4.82426411990756,131.761261220488));
#88988=CARTESIAN_POINT('Ctrl Pts',(-63.5633483975218,4.85096093137253,131.62666785805));
#88989=CARTESIAN_POINT('Ctrl Pts',(-63.5710947307872,4.87202074364083,131.490957216983));
#88990=CARTESIAN_POINT('Ctrl Pts',(-63.5788410640526,4.88736899276481,131.35463999303));
#88991=CARTESIAN_POINT('Ctrl Pts',(-63.5865891320555,4.90272067902274,131.21829224178));
#88992=CARTESIAN_POINT('Ctrl Pts',(-63.5943372000585,4.91235821321032,131.081338025775));
#88993=CARTESIAN_POINT('Ctrl Pts',(-63.6020852680615,4.91625895115228,130.944292700074));
#88994=CARTESIAN_POINT('Ctrl Pts',(-63.6098415708034,4.92016383484496,130.80710172097));
#88995=CARTESIAN_POINT('Ctrl Pts',(-63.6175978735453,4.91831973146611,130.669819830168));
#88996=CARTESIAN_POINT('Ctrl Pts',(-63.6253541762871,4.910756165122,130.532962479738));
#88997=CARTESIAN_POINT('Ctrl Pts',(-63.6331146188013,4.90318856187479,130.39603208442));
#88998=CARTESIAN_POINT('Ctrl Pts',(-63.6408750613154,4.88989545087465,130.259527069908));
#88999=CARTESIAN_POINT('Ctrl Pts',(-63.6486355038296,4.87095812382458,130.12395631243));
#89000=CARTESIAN_POINT('Ctrl Pts',(-63.656408404095,4.85199039689594,129.988167924738));
#89001=CARTESIAN_POINT('Ctrl Pts',(-63.6641813043605,4.82736041824475,129.853317175887));
#89002=CARTESIAN_POINT('Ctrl Pts',(-63.6719542046259,4.79720053899032,129.719902203789));
#89003=CARTESIAN_POINT('Ctrl Pts',(-63.6794445403879,4.76813704731518,129.59133720198));
#89004=CARTESIAN_POINT('Ctrl Pts',(-63.6869348761499,4.73393880641623,129.464105698514));
#89005=CARTESIAN_POINT('Ctrl Pts',(-63.6944252119119,4.69476703351866,129.338637054446));
#89006=CARTESIAN_POINT('Ctrl Pts',(-63.7021995460309,4.65411005094539,129.208411228601));
#89007=CARTESIAN_POINT('Ctrl Pts',(-63.7099738801501,4.60796615942195,129.079672062348));
#89008=CARTESIAN_POINT('Ctrl Pts',(-63.7177482142692,4.55646119136074,128.952916728564));
#89009=CARTESIAN_POINT('Ctrl Pts',(-63.7255129672163,4.50501969856954,128.8263176094));
#89010=CARTESIAN_POINT('Ctrl Pts',(-63.7332777201633,4.44823042105971,128.701697816819));
#89011=CARTESIAN_POINT('Ctrl Pts',(-63.7410424731104,4.38626918109586,128.579540235272));
#89012=CARTESIAN_POINT('Ctrl Pts',(-63.7487995139954,4.32436948190903,128.457503982358));
#89013=CARTESIAN_POINT('Ctrl Pts',(-63.7565565548804,4.25730821857601,128.337925420239));
#89014=CARTESIAN_POINT('Ctrl Pts',(-63.7643135957654,4.18530946213846,128.221267942373));
#89015=CARTESIAN_POINT('Ctrl Pts',(-63.7720647870055,4.1133650005232,128.10469843682));
#89016=CARTESIAN_POINT('Ctrl Pts',(-63.7798159782456,4.03649066151548,127.991045962311));
#89017=CARTESIAN_POINT('Ctrl Pts',(-63.7875671694858,3.95495647479197,127.880749435312));
#89018=CARTESIAN_POINT('Ctrl Pts',(-63.7953150662628,3.87345694227282,127.770499787279));
#89019=CARTESIAN_POINT('Ctrl Pts',(-63.80306296304,3.7873017331392,127.663603563551));
#89020=CARTESIAN_POINT('Ctrl Pts',(-63.8108108598171,3.69680410981446,127.560470601527));
#89021=CARTESIAN_POINT('Ctrl Pts',(-63.8185571359012,3.6063254166416,127.457359212695));
#89022=CARTESIAN_POINT('Ctrl Pts',(-63.8263034119853,3.51150637371691,127.358009813479));
#89023=CARTESIAN_POINT('Ctrl Pts',(-63.8340496880694,3.41270017408323,127.262798732703));
#89024=CARTESIAN_POINT('Ctrl Pts',(-63.8417960213347,3.31389324508463,127.167586949101));
#89025=CARTESIAN_POINT('Ctrl Pts',(-63.8495423546001,3.21109938217554,127.076513816182));
#89026=CARTESIAN_POINT('Ctrl Pts',(-63.8572886878655,3.10470794451307,126.989918110229));
#89027=CARTESIAN_POINT('Ctrl Pts',(-63.8650367558684,2.99829268122594,126.903303011769));
#89028=CARTESIAN_POINT('Ctrl Pts',(-63.8727848238713,2.88827854319387,126.821167582264));
#89029=CARTESIAN_POINT('Ctrl Pts',(-63.8805328918743,2.77508687349521,126.743809434899));
#89030=CARTESIAN_POINT('Ctrl Pts',(-63.8882891946162,2.66177490234284,126.666369070375));
#89031=CARTESIAN_POINT('Ctrl Pts',(-63.896045497358,2.54527897666502,126.593716351501));
#89032=CARTESIAN_POINT('Ctrl Pts',(-63.9038018000999,2.4260487193876,126.526105053243));
#89033=CARTESIAN_POINT('Ctrl Pts',(-63.9115622426141,2.30675482533191,126.4584576688));
#89034=CARTESIAN_POINT('Ctrl Pts',(-63.9193226851284,2.18472403940201,126.395857244901));
#89035=CARTESIAN_POINT('Ctrl Pts',(-63.9270831276425,2.06042843373263,126.338510448565));
#89036=CARTESIAN_POINT('Ctrl Pts',(-63.934856027908,1.9359332977226,126.28107159406));
#89037=CARTESIAN_POINT('Ctrl Pts',(-63.9426289281733,1.80916643846161,126.228903368991));
#89038=CARTESIAN_POINT('Ctrl Pts',(-63.9504018284387,1.68061849249453,126.182163678319));
#89039=CARTESIAN_POINT('Ctrl Pts',(-63.9578921642007,1.55674358815696,126.137123093134));
#89040=CARTESIAN_POINT('Ctrl Pts',(-63.9653824999627,1.43121513636299,126.09712330632));
#89041=CARTESIAN_POINT('Ctrl Pts',(-63.9728728357247,1.30448151257663,126.0622607614));
#89042=CARTESIAN_POINT('Ctrl Pts',(-63.9806471698438,1.17294274492381,126.026076392493));
#89043=CARTESIAN_POINT('Ctrl Pts',(-63.9884215039629,1.03968893777712,125.995311891306));
#89044=CARTESIAN_POINT('Ctrl Pts',(-63.9961958380819,0.905206392251208,
125.970130125551));
#89045=CARTESIAN_POINT('Ctrl Pts',(-64.003960591029,0.770889584443603,125.944979394072));
#89046=CARTESIAN_POINT('Ctrl Pts',(-64.0117253439761,0.635347431879937,
125.925397779699));
#89047=CARTESIAN_POINT('Ctrl Pts',(-64.0194900969232,0.499081235154803,
125.911498369023));
#89048=CARTESIAN_POINT('Ctrl Pts',(-64.0272471378082,0.362950379937272,
125.897612763438));
#89049=CARTESIAN_POINT('Ctrl Pts',(-64.0350041786931,0.226097298091355,
125.889398169859));
#89050=CARTESIAN_POINT('Ctrl Pts',(-64.0427612195781,0.0890329715300792,
125.886916546457));
#89051=CARTESIAN_POINT('Ctrl Pts',(-64.0505124108182,-0.0479279937563315,
125.884436794467));
#89052=CARTESIAN_POINT('Ctrl Pts',(-64.0582636020584,-0.185099497359099,
125.887681414481));
#89053=CARTESIAN_POINT('Ctrl Pts',(-64.0660147932985,-0.321966308790757,
125.896660467954));
#89054=CARTESIAN_POINT('Ctrl Pts',(-64.0737626900756,-0.458774948176515,
125.90563570509));
#89055=CARTESIAN_POINT('Ctrl Pts',(-64.0815105868526,-0.595278763651564,
125.920340502566));
#89056=CARTESIAN_POINT('Ctrl Pts',(-64.0892584836297,-0.730963621414174,
125.940732830958));
#89057=CARTESIAN_POINT('Ctrl Pts',(-64.0970047597138,-0.866620096829568,
125.961120893714));
#89058=CARTESIAN_POINT('Ctrl Pts',(-64.1047510357979,-1.00145756889593,
125.987194062921));
#89059=CARTESIAN_POINT('Ctrl Pts',(-64.112497311882,-1.13496851204762,126.018858602191));
#89060=CARTESIAN_POINT('Ctrl Pts',(-64.1202436451473,-1.26848044074658,
126.050523375201));
#89061=CARTESIAN_POINT('Ctrl Pts',(-64.1279899784126,-1.40066544057867,
126.087779510412));
#89062=CARTESIAN_POINT('Ctrl Pts',(-64.135736311678,-1.53102803132618,126.130482545794));
#89063=CARTESIAN_POINT('Ctrl Pts',(-64.1434843796809,-1.66141981587202,
126.173195144225));
#89064=CARTESIAN_POINT('Ctrl Pts',(-64.1512324476839,-1.78998800776162,
126.221356948396));
#89065=CARTESIAN_POINT('Ctrl Pts',(-64.1589805156869,-1.91625447036826,
126.27477433764));
#89066=CARTESIAN_POINT('Ctrl Pts',(-64.1667368184287,-2.04265513047413,
126.328248499521));
#89067=CARTESIAN_POINT('Ctrl Pts',(-64.1744931211706,-2.16674881389534,
126.386989251936));
#89068=CARTESIAN_POINT('Ctrl Pts',(-64.1822494239125,-2.28807898039,126.450755485954));
#89069=CARTESIAN_POINT('Ctrl Pts',(-64.1900098664266,-2.4094739044477,126.514555753931));
#89070=CARTESIAN_POINT('Ctrl Pts',(-64.1977703089408,-2.52810203457313,
126.583386652007));
#89071=CARTESIAN_POINT('Ctrl Pts',(-64.2055307514549,-2.64353432942961,
126.656962721098));
#89072=CARTESIAN_POINT('Ctrl Pts',(-64.2133036517203,-2.75915192645339,
126.730656901027));
#89073=CARTESIAN_POINT('Ctrl Pts',(-64.2210765519858,-2.87156311556875,
126.809111250017));
#89074=CARTESIAN_POINT('Ctrl Pts',(-64.2288494522512,-2.98036984582112,
126.891998333137));
#89075=CARTESIAN_POINT('Ctrl Pts',(-64.2363397880134,-3.08522117736238,
126.971872262007));
#89076=CARTESIAN_POINT('Ctrl Pts',(-64.2438301237754,-3.18672532526037,
127.055862041832));
#89077=CARTESIAN_POINT('Ctrl Pts',(-64.2513204595375,-3.28455879095931,
127.143642571713));
#89078=CARTESIAN_POINT('Ctrl Pts',(-64.2589772908735,-3.38456690403458,
127.23337429179));
#89079=CARTESIAN_POINT('Ctrl Pts',(-64.2666341222094,-3.48107626436257,
127.327370025791));
#89080=CARTESIAN_POINT('Ctrl Pts',(-64.2742909535454,-3.57369301393172,
127.425322099781));
#89081=CARTESIAN_POINT('Ctrl Pts',(-64.2819389498596,-3.66620289540336,
127.523161149379));
#89082=CARTESIAN_POINT('Ctrl Pts',(-64.2895869461738,-3.75482882032915,
127.624947174461));
#89083=CARTESIAN_POINT('Ctrl Pts',(-64.297234942488,-3.83921005965763,127.730332449132));
#89084=CARTESIAN_POINT('Ctrl Pts',(-64.3048758880061,-3.92351350672683,
127.835620567626));
#89085=CARTESIAN_POINT('Ctrl Pts',(-64.3125168335242,-4.00357979839632,
127.944501025308));
#89086=CARTESIAN_POINT('Ctrl Pts',(-64.3201577790423,-4.07908555363194,
128.056589865001));
#89087=CARTESIAN_POINT('Ctrl Pts',(-64.328063760285,-4.15721032015385,128.172566645889));
#89088=CARTESIAN_POINT('Ctrl Pts',(-64.3359697415278,-4.23045213663244,
128.291978101722));
#89089=CARTESIAN_POINT('Ctrl Pts',(-64.3438757227705,-4.29849852397049,
128.414361976997));
#89090=CARTESIAN_POINT('Ctrl Pts',(-64.3515082187794,-4.36419103750313,
128.532512325563));
#89091=CARTESIAN_POINT('Ctrl Pts',(-64.3591407147881,-4.42504138323864,
128.653432480606));
#89092=CARTESIAN_POINT('Ctrl Pts',(-64.3667732107969,-4.48081325641169,
128.776678289472));
#89093=CARTESIAN_POINT('Ctrl Pts',(-64.3744040968274,-4.53657336521397,
128.899898101194));
#89094=CARTESIAN_POINT('Ctrl Pts',(-64.3820349828578,-4.58725696986167,
129.025442221674));
#89095=CARTESIAN_POINT('Ctrl Pts',(-64.3896658688882,-4.63267495053891,
129.152844385387));
#89096=CARTESIAN_POINT('Ctrl Pts',(-64.3972978797951,-4.67809962632558,
129.28026532958));
#89097=CARTESIAN_POINT('Ctrl Pts',(-64.404929890702,-4.71825699590313,129.409544482713));
#89098=CARTESIAN_POINT('Ctrl Pts',(-64.4125619016089,-4.75300719352354,
129.54019857067));
#89099=CARTESIAN_POINT('Ctrl Pts',(-64.4133844523908,-4.75675244527613,
129.554279999997));
#89100=CARTESIAN_POINT('Ctrl Pts',(-64.4142070031727,-4.760434936853,129.568377387448));
#89101=CARTESIAN_POINT('Ctrl Pts',(-64.4150295539547,-4.76405452823403,
129.582490119308));
#89102=CARTESIAN_POINT('Ctrl Pts',(-62.6653842080088,-4.76405452823406,
129.582490119308));
#89103=CARTESIAN_POINT('Ctrl Pts',(-62.6733465228717,-4.799041029491,129.718901956715));
#89104=CARTESIAN_POINT('Ctrl Pts',(-62.6813088377347,-4.82819392202019,
129.856932659022));
#89105=CARTESIAN_POINT('Ctrl Pts',(-62.6892711525976,-4.85137405232088,
129.996058157488));
#89106=CARTESIAN_POINT('Ctrl Pts',(-62.6972258082262,-4.87453188482843,
130.135049826182));
#89107=CARTESIAN_POINT('Ctrl Pts',(-62.7051804638548,-4.89172834729019,
130.27513383785));
#89108=CARTESIAN_POINT('Ctrl Pts',(-62.7131351194834,-4.90287509196743,
130.415774854747));
#89109=CARTESIAN_POINT('Ctrl Pts',(-62.7204702676585,-4.91315372974815,
130.54546276917));
#89110=CARTESIAN_POINT('Ctrl Pts',(-62.7278054158335,-4.91828875835897,
130.675623958895));
#89111=CARTESIAN_POINT('Ctrl Pts',(-62.7351405640086,-4.91824977962913,
130.805832921208));
#89112=CARTESIAN_POINT('',(-62.3898594359577,-4.91824789635182,130.799811713202));
#89113=CARTESIAN_POINT('Ctrl Pts',(-62.3199210724795,-4.76405452823405,
129.582490119308));
#89114=CARTESIAN_POINT('Ctrl Pts',(-62.320539411322,-4.76675090131487,129.593003237027));
#89115=CARTESIAN_POINT('Ctrl Pts',(-62.3211577501644,-4.76941214013832,
129.603523977018));
#89116=CARTESIAN_POINT('Ctrl Pts',(-62.3217760890069,-4.77203820801996,
129.614052084581));
#89117=CARTESIAN_POINT('Ctrl Pts',(-62.3320725719393,-4.81576708491634,
129.789364506159));
#89118=CARTESIAN_POINT('Ctrl Pts',(-62.3423690548716,-4.84985192258178,
129.967171340743));
#89119=CARTESIAN_POINT('Ctrl Pts',(-62.352665537804,-4.87406213141582,130.14656019069));
#89120=CARTESIAN_POINT('Ctrl Pts',(-62.3627208266703,-4.89770521856867,
130.32174687506));
#89121=CARTESIAN_POINT('Ctrl Pts',(-62.3727761155366,-4.91193093972787,
130.498442635262));
#89122=CARTESIAN_POINT('Ctrl Pts',(-62.3828314044028,-4.9165688058078,130.67577508083));
#89123=CARTESIAN_POINT('Ctrl Pts',(-62.3851740815878,-4.91764933399519,
130.717089923189));
#89124=CARTESIAN_POINT('Ctrl Pts',(-62.3875167587727,-4.91820963078576,
130.758439214522));
#89125=CARTESIAN_POINT('Ctrl Pts',(-62.3898594359577,-4.91824789635182,
130.799811713202));
#89126=CARTESIAN_POINT('Ctrl Pts',(-62.389859435991,-4.91824789635236,130.799811713791));
#89127=CARTESIAN_POINT('Ctrl Pts',(-62.3975216442029,-4.91837305175083,
130.935128991462));
#89128=CARTESIAN_POINT('Ctrl Pts',(-62.4051838524148,-4.91290946822373,
131.070595210122));
#89129=CARTESIAN_POINT('Ctrl Pts',(-62.4128460606267,-4.90184711431266,
131.205705768782));
#89130=CARTESIAN_POINT('Ctrl Pts',(-62.4206534628014,-4.89057513584456,
131.343376586429));
#89131=CARTESIAN_POINT('Ctrl Pts',(-62.4284608649761,-4.87349000832848,
131.480677707847));
#89132=CARTESIAN_POINT('Ctrl Pts',(-62.4362682671508,-4.850636834558,131.617075427157));
#89133=CARTESIAN_POINT('Ctrl Pts',(-62.4439230751124,-4.82823032178836,
131.750807278591));
#89134=CARTESIAN_POINT('Ctrl Pts',(-62.4515778830739,-4.80027924671348,
131.88367030643));
#89135=CARTESIAN_POINT('Ctrl Pts',(-62.4592326910355,-4.76687835307637,
132.01516771594));
#89136=CARTESIAN_POINT('Ctrl Pts',(-62.4668867353449,-4.73348079154956,
132.146652007122));
#89137=CARTESIAN_POINT('Ctrl Pts',(-62.4745407796543,-4.69463459126161,
132.276770562044));
#89138=CARTESIAN_POINT('Ctrl Pts',(-62.4821948239637,-4.65048516148636,
132.405038856718));
#89139=CARTESIAN_POINT('Ctrl Pts',(-62.4898498570664,-4.60633002823537,
132.533323721824));
#89140=CARTESIAN_POINT('Ctrl Pts',(-62.497504890169,-4.55687043391876,132.659757472053));
#89141=CARTESIAN_POINT('Ctrl Pts',(-62.5051599232716,-4.50230082056917,
132.783873280724));
#89142=CARTESIAN_POINT('Ctrl Pts',(-62.5130819057339,-4.44582823395357,
132.912317305251));
#89143=CARTESIAN_POINT('Ctrl Pts',(-62.5210038881964,-4.38388293208794,
133.038278356155));
#89144=CARTESIAN_POINT('Ctrl Pts',(-62.5289258706588,-4.31673285920018,
133.161265470292));
#89145=CARTESIAN_POINT('Ctrl Pts',(-62.5365922686147,-4.25174922865379,
133.280284688639));
#89146=CARTESIAN_POINT('Ctrl Pts',(-62.5442586665705,-4.181891737911,133.396518584788));
#89147=CARTESIAN_POINT('Ctrl Pts',(-62.5519250645265,-4.10744755791259,
133.509551483567));
#89148=CARTESIAN_POINT('Ctrl Pts',(-62.559974839242,-4.02928061676058,133.628236865653));
#89149=CARTESIAN_POINT('Ctrl Pts',(-62.5680246139576,-3.94605672524618,
133.743392429204));
#89150=CARTESIAN_POINT('Ctrl Pts',(-62.5760743886732,-3.85815549910716,
133.854576873376));
#89151=CARTESIAN_POINT('Ctrl Pts',(-62.5841241633887,-3.77025427296802,
133.965761317548));
#89152=CARTESIAN_POINT('Ctrl Pts',(-62.5921739381043,-3.67767610052967,
134.072974313002));
#89153=CARTESIAN_POINT('Ctrl Pts',(-62.6002237128198,-3.58084349503747,
134.175820676138));
#89154=CARTESIAN_POINT('Ctrl Pts',(-62.6079980469389,-3.48732422831018,
134.275147926678));
#89155=CARTESIAN_POINT('Ctrl Pts',(-62.615772381058,-3.38952091736318,134.370738428404));
#89156=CARTESIAN_POINT('Ctrl Pts',(-62.6235467151771,-3.28776417073599,
134.462200119256));
#89157=CARTESIAN_POINT('Ctrl Pts',(-62.6313114681242,-3.18613283020502,
134.553549091749));
#89158=CARTESIAN_POINT('Ctrl Pts',(-62.6390762210712,-3.08055803631173,
134.640779118903));
#89159=CARTESIAN_POINT('Ctrl Pts',(-62.6468409740183,-2.97140910311259,
134.723532852163));
#89160=CARTESIAN_POINT('Ctrl Pts',(-62.6545980149033,-2.86236857817234,
134.806204393249));
#89161=CARTESIAN_POINT('Ctrl Pts',(-62.6623550557884,-2.7497612878884,134.884408253342));
#89162=CARTESIAN_POINT('Ctrl Pts',(-62.6701120966734,-2.63399141065753,
134.957825714456));
#89163=CARTESIAN_POINT('Ctrl Pts',(-62.6778632879135,-2.5183088363918,135.031187810891));
#89164=CARTESIAN_POINT('Ctrl Pts',(-62.6856144791536,-2.3994687510749,135.099770484225));
#89165=CARTESIAN_POINT('Ctrl Pts',(-62.6933656703938,-2.27790595722141,
135.163297129211));
#89166=CARTESIAN_POINT('Ctrl Pts',(-62.7011135671709,-2.15639483079794,
135.22679677368));
#89167=CARTESIAN_POINT('Ctrl Pts',(-62.7088614639479,-2.03216364324611,
135.285244483195));
#89168=CARTESIAN_POINT('Ctrl Pts',(-62.716609360725,-1.90567335704063,135.338408711573));
#89169=CARTESIAN_POINT('Ctrl Pts',(-62.7243556368091,-1.77920952987621,
135.39156181914));
#89170=CARTESIAN_POINT('Ctrl Pts',(-62.7321019128933,-1.65048790419101,
135.439433492463));
#89171=CARTESIAN_POINT('Ctrl Pts',(-62.7398481889774,-1.51999069553578,
135.481839783525));
#89172=CARTESIAN_POINT('Ctrl Pts',(-62.7475945222427,-1.38949252357979,
135.524246387621));
#89173=CARTESIAN_POINT('Ctrl Pts',(-62.7553408555081,-1.25721911432547,
135.561187408124));
#89174=CARTESIAN_POINT('Ctrl Pts',(-62.7630871887734,-1.12366878233238,
135.592528485353));
#89175=CARTESIAN_POINT('Ctrl Pts',(-62.7708352567764,-0.990088542668778,
135.623876581199));
#89176=CARTESIAN_POINT('Ctrl Pts',(-62.7785833247793,-0.855231191794881,
135.649622149014));
#89177=CARTESIAN_POINT('Ctrl Pts',(-62.7863313927823,-0.719605803154936,
135.66968183518));
#89178=CARTESIAN_POINT('Ctrl Pts',(-62.7940876955241,-0.583836270237611,
135.689762841019));
#89179=CARTESIAN_POINT('Ctrl Pts',(-62.8018439982661,-0.44729745632209,
135.704145836325));
#89180=CARTESIAN_POINT('Ctrl Pts',(-62.8096003010079,-0.310504692713374,
135.712799259161));
#89181=CARTESIAN_POINT('Ctrl Pts',(-62.8173607435221,-0.173638918687783,
135.721457300589));
#89182=CARTESIAN_POINT('Ctrl Pts',(-62.8251211860363,-0.036519315578075,
135.724379667806));
#89183=CARTESIAN_POINT('Ctrl Pts',(-62.8328816285504,0.100339200920041,
135.721586980797));
#89184=CARTESIAN_POINT('Ctrl Pts',(-62.8406545288159,0.237417414858382,
135.718789810719));
#89185=CARTESIAN_POINT('Ctrl Pts',(-62.8484274290813,0.37423331421897,135.710259277559));
#89186=CARTESIAN_POINT('Ctrl Pts',(-62.8562003293468,0.510276615900347,
135.696067971626));
#89187=CARTESIAN_POINT('Ctrl Pts',(-62.8636906651088,0.641374400893024,
135.682392555409));
#89188=CARTESIAN_POINT('Ctrl Pts',(-62.8711810008708,0.771754479904198,
135.663460831977));
#89189=CARTESIAN_POINT('Ctrl Pts',(-62.8786713366328,0.900971455956128,
135.639382178847));
#89190=CARTESIAN_POINT('Ctrl Pts',(-62.8864456707519,1.03508773293009,135.614390576265));
#89191=CARTESIAN_POINT('Ctrl Pts',(-62.894220004871,1.16837580784162,135.583774881943));
#89192=CARTESIAN_POINT('Ctrl Pts',(-62.9019943389901,1.30032712578436,135.547601327086));
#89193=CARTESIAN_POINT('Ctrl Pts',(-62.9097590919372,1.43211582552037,135.511472352903));
#89194=CARTESIAN_POINT('Ctrl Pts',(-62.9175238448843,1.56257067275564,135.469799249156));
#89195=CARTESIAN_POINT('Ctrl Pts',(-62.9252885978314,1.69119139676037,135.422699574596));
#89196=CARTESIAN_POINT('Ctrl Pts',(-62.9330456387164,1.8196843728486,135.375646680098));
#89197=CARTESIAN_POINT('Ctrl Pts',(-62.9408026796013,1.94634648617702,135.323178074193));
#89198=CARTESIAN_POINT('Ctrl Pts',(-62.9485597204863,2.07069112198224,135.265461528759));
#89199=CARTESIAN_POINT('Ctrl Pts',(-62.9563109117264,2.19494198853017,135.20778850782));
#89200=CARTESIAN_POINT('Ctrl Pts',(-62.9640621029666,2.31687850291183,135.144875588479));
#89201=CARTESIAN_POINT('Ctrl Pts',(-62.9718132942067,2.43603292792123,135.076939070513));
#89202=CARTESIAN_POINT('Ctrl Pts',(-62.9795611909838,2.55513670912177,135.009031427379));
#89203=CARTESIAN_POINT('Ctrl Pts',(-62.9873090877608,2.67146041384924,134.936104625539));
#89204=CARTESIAN_POINT('Ctrl Pts',(-62.9950569845379,2.78456007426379,134.85842132941));
#89205=CARTESIAN_POINT('Ctrl Pts',(-63.002803260622,2.89763607666753,134.780754282952));
#89206=CARTESIAN_POINT('Ctrl Pts',(-63.0105495367062,3.00748905411379,134.698332942439));
#89207=CARTESIAN_POINT('Ctrl Pts',(-63.0182958127903,3.11370359664268,134.611463581074));
#89208=CARTESIAN_POINT('Ctrl Pts',(-63.0260421460557,3.21991892322334,134.52459357846));
#89209=CARTESIAN_POINT('Ctrl Pts',(-63.033788479321,3.32249545865616,134.433275736993));
#89210=CARTESIAN_POINT('Ctrl Pts',(-63.0415348125864,3.42105081114509,134.337856678136));
#89211=CARTESIAN_POINT('Ctrl Pts',(-63.0492828805894,3.51962823442173,134.242416250842));
#89212=CARTESIAN_POINT('Ctrl Pts',(-63.0570309485923,3.61418240199828,134.142873050468));
#89213=CARTESIAN_POINT('Ctrl Pts',(-63.0647790165953,3.70436801948363,134.039610320252));
#89214=CARTESIAN_POINT('Ctrl Pts',(-63.0725353193371,3.79464948731646,133.936237841177));
#89215=CARTESIAN_POINT('Ctrl Pts',(-63.080291622079,3.88055287268232,133.829138230337));
#89216=CARTESIAN_POINT('Ctrl Pts',(-63.0880479248209,3.96177307247127,133.718727990555));
#89217=CARTESIAN_POINT('Ctrl Pts',(-63.095808367335,4.04303662192633,133.608258821503));
#89218=CARTESIAN_POINT('Ctrl Pts',(-63.1035688098493,4.11961178704503,133.494475826842));
#89219=CARTESIAN_POINT('Ctrl Pts',(-63.1113292523634,4.1912375914936,133.377823365334));
#89220=CARTESIAN_POINT('Ctrl Pts',(-63.1191021526289,4.26297837604221,133.260983642939));
#89221=CARTESIAN_POINT('Ctrl Pts',(-63.1268750528943,4.32975373241596,133.141265590436));
#89222=CARTESIAN_POINT('Ctrl Pts',(-63.1346479531597,4.39134891241674,133.019137760286));
#89223=CARTESIAN_POINT('Ctrl Pts',(-63.1421382889217,4.45070495247501,132.901449584385));
#89224=CARTESIAN_POINT('Ctrl Pts',(-63.1496286246837,4.50525077479246,132.781524072409));
#89225=CARTESIAN_POINT('Ctrl Pts',(-63.1571189604456,4.55483765382755,132.659795070673));
#89226=CARTESIAN_POINT('Ctrl Pts',(-63.1648932945647,4.60630463445315,132.533450676835));
#89227=CARTESIAN_POINT('Ctrl Pts',(-63.1726676286837,4.65259224396969,132.404763113887));
#89228=CARTESIAN_POINT('Ctrl Pts',(-63.1804419628028,4.69348131821857,132.274196043059));
#89229=CARTESIAN_POINT('Ctrl Pts',(-63.1882067157499,4.7343200003378,132.143789884476));
#89230=CARTESIAN_POINT('Ctrl Pts',(-63.1959714686969,4.76977326937909,132.011509196327));
#89231=CARTESIAN_POINT('Ctrl Pts',(-63.203736221644,4.79966962230043,131.877838413921));
#89232=CARTESIAN_POINT('Ctrl Pts',(-63.211493262529,4.82953628174255,131.74430039522));
#89233=CARTESIAN_POINT('Ctrl Pts',(-63.219250303414,4.85385692375506,131.609375408912));
#89234=CARTESIAN_POINT('Ctrl Pts',(-63.2270073442989,4.87250967240302,131.473563542574));
#89235=CARTESIAN_POINT('Ctrl Pts',(-63.234758535539,4.89114835486813,131.337854093021));
#89236=CARTESIAN_POINT('Ctrl Pts',(-63.2425097267792,4.90412759852797,131.201259480413));
#89237=CARTESIAN_POINT('Ctrl Pts',(-63.2502609180193,4.91137655912721,131.064290140621));
#89238=CARTESIAN_POINT('Ctrl Pts',(-63.2580088147964,4.91862243872484,130.927379016453));
#89239=CARTESIAN_POINT('Ctrl Pts',(-63.2657567115734,4.92014285871247,130.790093871477));
#89240=CARTESIAN_POINT('Ctrl Pts',(-63.2735046083505,4.91591883064088,130.652950204944));
#89241=CARTESIAN_POINT('Ctrl Pts',(-63.2812508844346,4.91169568614492,130.51583522591));
#89242=CARTESIAN_POINT('Ctrl Pts',(-63.2889971605186,4.90173049569564,130.378862056986));
#89243=CARTESIAN_POINT('Ctrl Pts',(-63.2967434366027,4.88605639638326,130.242545742485));
#89244=CARTESIAN_POINT('Ctrl Pts',(-63.304489769868,4.87038218136826,130.106228421728));
#89245=CARTESIAN_POINT('Ctrl Pts',(-63.3122361031334,4.84899901805933,129.970568353476));
#89246=CARTESIAN_POINT('Ctrl Pts',(-63.3199824363988,4.82199183680364,129.836074612142));
#89247=CARTESIAN_POINT('Ctrl Pts',(-63.3277305044017,4.79497860747696,129.701550751868));
#89248=CARTESIAN_POINT('Ctrl Pts',(-63.3354785724047,4.76233893098125,129.568194121493));
#89249=CARTESIAN_POINT('Ctrl Pts',(-63.3432266404076,4.72420860065541,129.4365023793));
#89250=CARTESIAN_POINT('Ctrl Pts',(-63.3509829431495,4.68603774496064,129.304670673555));
#89251=CARTESIAN_POINT('Ctrl Pts',(-63.3587392458913,4.64236468723968,129.174507766824));
#89252=CARTESIAN_POINT('Ctrl Pts',(-63.3664955486331,4.59337492743055,129.046495480944));
#89253=CARTESIAN_POINT('Ctrl Pts',(-63.3742559911473,4.54435902031156,128.918414871052));
#89254=CARTESIAN_POINT('Ctrl Pts',(-63.3820164336614,4.49002091160054,128.792487527998));
#89255=CARTESIAN_POINT('Ctrl Pts',(-63.3897768761755,4.43059338882702,128.669173205327));
#89256=CARTESIAN_POINT('Ctrl Pts',(-63.397549776441,4.37107046771821,128.545660927559));
#89257=CARTESIAN_POINT('Ctrl Pts',(-63.4053226767064,4.30644199075551,128.424770397412));
#89258=CARTESIAN_POINT('Ctrl Pts',(-63.4130955769718,4.23698608774719,128.306935552677));
#89259=CARTESIAN_POINT('Ctrl Pts',(-63.420585912734,4.17005508176039,128.193384301353));
#89260=CARTESIAN_POINT('Ctrl Pts',(-63.4280762484963,4.09864170138477,128.08267068765));
#89261=CARTESIAN_POINT('Ctrl Pts',(-63.4355665842585,4.02303056402202,127.975154343106));
#89262=CARTESIAN_POINT('Ctrl Pts',(-63.4433409183776,3.94455260740644,127.863561483682));
#89263=CARTESIAN_POINT('Ctrl Pts',(-63.4511152524967,3.86130369965797,127.75505963572));
#89264=CARTESIAN_POINT('Ctrl Pts',(-63.4588895866158,3.77355546852083,127.650083808455));
#89265=CARTESIAN_POINT('Ctrl Pts',(-63.4666543395629,3.68591537923628,127.545237354515));
#89266=CARTESIAN_POINT('Ctrl Pts',(-63.47441909251,3.59378724782314,127.443908572101));
#89267=CARTESIAN_POINT('Ctrl Pts',(-63.4821838454571,3.49748594184438,127.346503600698));
#89268=CARTESIAN_POINT('Ctrl Pts',(-63.4899408863421,3.40128028368033,127.249195373287));
#89269=CARTESIAN_POINT('Ctrl Pts',(-63.497697927227,3.30090997249661,127.155803477539));
#89270=CARTESIAN_POINT('Ctrl Pts',(-63.505454968112,3.196729869217,127.066700760683));
#89271=CARTESIAN_POINT('Ctrl Pts',(-63.5132061593522,3.09262832896409,126.977665236879));
#89272=CARTESIAN_POINT('Ctrl Pts',(-63.5209573505924,2.98472301105,126.892912706973));
#89273=CARTESIAN_POINT('Ctrl Pts',(-63.5287085418325,2.87340506657975,126.8127786773));
#89274=CARTESIAN_POINT('Ctrl Pts',(-63.5364564386095,2.7621344352051,126.732678706728));
#89275=CARTESIAN_POINT('Ctrl Pts',(-63.5442043353866,2.64745437876083,126.657193560096));
#89276=CARTESIAN_POINT('Ctrl Pts',(-63.5519522321636,2.52978833764556,126.586617852862));
#89277=CARTESIAN_POINT('Ctrl Pts',(-63.5596985082478,2.41214690972935,126.516056908544));
#89278=CARTESIAN_POINT('Ctrl Pts',(-63.5674447843318,2.29152107458051,126.450403561939));
#89279=CARTESIAN_POINT('Ctrl Pts',(-63.575191060416,2.16836206497228,126.389908327905));
#89280=CARTESIAN_POINT('Ctrl Pts',(-63.5829373936813,2.04520214623256,126.32941264731));
#89281=CARTESIAN_POINT('Ctrl Pts',(-63.5906837269467,1.91950936663725,126.274075327632));
#89282=CARTESIAN_POINT('Ctrl Pts',(-63.598430060212,1.79175793183678,126.224100081723));
#89283=CARTESIAN_POINT('Ctrl Pts',(-63.6061781282149,1.66397788798843,126.174113644204));
#89284=CARTESIAN_POINT('Ctrl Pts',(-63.6139261962179,1.53413863558321,126.129491812309));
#89285=CARTESIAN_POINT('Ctrl Pts',(-63.6216742642209,1.4027322682454,126.090389335714));
#89286=CARTESIAN_POINT('Ctrl Pts',(-63.6294305669628,1.2711862406561,126.051245300542));
#89287=CARTESIAN_POINT('Ctrl Pts',(-63.6371868697047,1.13807014634592,126.017632450394));
#89288=CARTESIAN_POINT('Ctrl Pts',(-63.6449431724465,1.00388962291999,125.989655155391));
#89289=CARTESIAN_POINT('Ctrl Pts',(-63.6527036149607,0.869637483308436,
125.961662928064));
#89290=CARTESIAN_POINT('Ctrl Pts',(-63.6604640574749,0.734320168108235,
125.939312312991));
#89291=CARTESIAN_POINT('Ctrl Pts',(-63.6682244999891,0.598450308344868,
125.922655967452));
#89292=CARTESIAN_POINT('Ctrl Pts',(-63.6759974002545,0.462362338220836,
125.905972883669));
#89293=CARTESIAN_POINT('Ctrl Pts',(-63.6837703005199,0.325720440973305,
125.895002367252));
#89294=CARTESIAN_POINT('Ctrl Pts',(-63.6915432007854,0.189040036710512,
125.889744973691));
#89295=CARTESIAN_POINT('Ctrl Pts',(-63.6990335365474,0.0573283094200115,
125.884678699629));
#89296=CARTESIAN_POINT('Ctrl Pts',(-63.7065238723094,-0.0744188658198374,
125.884917386534));
#89297=CARTESIAN_POINT('Ctrl Pts',(-63.7140142080714,-0.205745078151946,
125.890415967357));
#89298=CARTESIAN_POINT('Ctrl Pts',(-63.7217885421905,-0.342050563740365,
125.896123028543));
#89299=CARTESIAN_POINT('Ctrl Pts',(-63.7295628763096,-0.478334309468239,
125.907514793235));
#89300=CARTESIAN_POINT('Ctrl Pts',(-63.7373372104286,-0.614083508315742,
125.924597866436));
#89301=CARTESIAN_POINT('Ctrl Pts',(-63.7451019633757,-0.74966540840792,
125.941659886276));
#89302=CARTESIAN_POINT('Ctrl Pts',(-63.7528667163229,-0.884713688216192,
125.96439921045));
#89303=CARTESIAN_POINT('Ctrl Pts',(-63.76063146927,-1.01871645748081,125.992770460273));
#89304=CARTESIAN_POINT('Ctrl Pts',(-63.768388510155,-1.15258613330643,126.021113531371));
#89305=CARTESIAN_POINT('Ctrl Pts',(-63.7761455510401,-1.28541198507125,
126.055077315929));
#89306=CARTESIAN_POINT('Ctrl Pts',(-63.7839025919251,-1.41668851484582,
126.094564792437));
#89307=CARTESIAN_POINT('Ctrl Pts',(-63.7916537831653,-1.54786604796828,
126.134022491131));
#89308=CARTESIAN_POINT('Ctrl Pts',(-63.7994049744055,-1.67749621176206,
126.178995478521));
#89309=CARTESIAN_POINT('Ctrl Pts',(-63.8071561656456,-1.80508530851847,
126.229336017471));
#89310=CARTESIAN_POINT('Ctrl Pts',(-63.8149040624227,-1.93262017650468,
126.27965516035));
#89311=CARTESIAN_POINT('Ctrl Pts',(-63.8226519591998,-2.05811533994081,
126.335337174163));
#89312=CARTESIAN_POINT('Ctrl Pts',(-63.8303998559769,-2.18109405062049,
126.396185053362));
#89313=CARTESIAN_POINT('Ctrl Pts',(-63.8381461320611,-2.30404703680535,
126.457020204496));
#89314=CARTESIAN_POINT('Ctrl Pts',(-63.8458924081452,-2.42448426705172,
126.523018898396));
#89315=CARTESIAN_POINT('Ctrl Pts',(-63.8536386842294,-2.54195107377796,
126.59393690955));
#89316=CARTESIAN_POINT('Ctrl Pts',(-63.8613850174948,-2.65941874761765,
126.664855444206));
#89317=CARTESIAN_POINT('Ctrl Pts',(-63.8691313507602,-2.77391561948534,
126.74069316651));
#89318=CARTESIAN_POINT('Ctrl Pts',(-63.8768776840256,-2.88501398025388,
126.82116122559));
#89319=CARTESIAN_POINT('Ctrl Pts',(-63.8846257520287,-2.99613722073015,
126.901647304934));
#89320=CARTESIAN_POINT('Ctrl Pts',(-63.8923738200316,-3.10386011908522,
126.986765555134));
#89321=CARTESIAN_POINT('Ctrl Pts',(-63.9001218880346,-3.20778649141001,
127.076185609868));
#89322=CARTESIAN_POINT('Ctrl Pts',(-63.9078781907765,-3.31182331791933,
127.165700701299));
#89323=CARTESIAN_POINT('Ctrl Pts',(-63.9156344935184,-3.41205526122974,
127.259526474941));
#89324=CARTESIAN_POINT('Ctrl Pts',(-63.9233907962602,-3.50812120232632,
127.357293938157));
#89325=CARTESIAN_POINT('Ctrl Pts',(-63.9311512387744,-3.60423841670828,
127.455113582813));
#89326=CARTESIAN_POINT('Ctrl Pts',(-63.9389116812886,-3.69618493634622,
127.556878819085));
#89327=CARTESIAN_POINT('Ctrl Pts',(-63.9466721238028,-3.7836393695877,127.662186818521));
#89328=CARTESIAN_POINT('Ctrl Pts',(-63.9544450240683,-3.87123419244937,
127.767663867706));
#89329=CARTESIAN_POINT('Ctrl Pts',(-63.9622179243337,-3.95432228173845,
127.876694733667));
#89330=CARTESIAN_POINT('Ctrl Pts',(-63.9699908245991,-4.03262457294653,
127.988846079126));
#89331=CARTESIAN_POINT('Ctrl Pts',(-63.9774811603609,-4.10808037863444,
128.09692044068));
#89332=CARTESIAN_POINT('Ctrl Pts',(-63.9849714961226,-4.17909213089906,
128.207892086581));
#89333=CARTESIAN_POINT('Ctrl Pts',(-63.9924618318844,-4.24545104470866,
128.321352665609));
#89334=CARTESIAN_POINT('Ctrl Pts',(-64.0005366497677,-4.31698804398247,
128.443666743606));
#89335=CARTESIAN_POINT('Ctrl Pts',(-64.008611467651,-4.38332968069564,128.569235709413));
#89336=CARTESIAN_POINT('Ctrl Pts',(-64.0166862855343,-4.44417947166694,
128.697597250191));
#89337=CARTESIAN_POINT('Ctrl Pts',(-64.0247498264294,-4.50494428209864,
128.825779526047));
#89338=CARTESIAN_POINT('Ctrl Pts',(-64.0328133673244,-4.56023237056421,
128.95674629851));
#89339=CARTESIAN_POINT('Ctrl Pts',(-64.0408769082194,-4.60979166284431,
129.09000829448));
#89340=CARTESIAN_POINT('Ctrl Pts',(-64.0489271056746,-4.65926894506919,
129.223049770277));
#89341=CARTESIAN_POINT('Ctrl Pts',(-64.0569773031299,-4.70303620408986,
129.35837857463));
#89342=CARTESIAN_POINT('Ctrl Pts',(-64.0650275005851,-4.74088848545256,
129.495483453351));
#89343=CARTESIAN_POINT('Ctrl Pts',(-64.0667258432992,-4.74887414625427,
129.524408342851));
#89344=CARTESIAN_POINT('Ctrl Pts',(-64.0684241860133,-4.75659671139267,
129.553412204632));
#89345=CARTESIAN_POINT('Ctrl Pts',(-64.0701225287274,-4.764054528234,129.582490119308));
#89346=CARTESIAN_POINT('Origin',(213.235140564004,0.,130.804360617566));
#89347=CARTESIAN_POINT('',(-66.1650696236363,-4.76405452823402,129.582490119308));
#89348=CARTESIAN_POINT('',(-65.8197716842485,-4.76405452823398,129.582490119308));
#89349=CARTESIAN_POINT('',(213.235140564004,-4.76405452823405,129.582490119308));
#89350=CARTESIAN_POINT('',(-64.48514056398,-4.91824840200337,130.808325298039));
#89351=CARTESIAN_POINT('Ctrl Pts',(-64.4851405640085,-4.91824840200297,
130.808325298541));
#89352=CARTESIAN_POINT('Ctrl Pts',(-64.4978018550894,-4.91806869548702,
131.031254026103));
#89353=CARTESIAN_POINT('Ctrl Pts',(-64.5104631461705,-4.90272945504267,
131.253589797038));
#89354=CARTESIAN_POINT('Ctrl Pts',(-64.5231244372515,-4.87248571274956,
131.473737971195));
#89355=CARTESIAN_POINT('Ctrl Pts',(-64.5253389859512,-4.86719586989387,
131.512243432423));
#89356=CARTESIAN_POINT('Ctrl Pts',(-64.5275535346509,-4.86145014892634,
131.550682063995));
#89357=CARTESIAN_POINT('Ctrl Pts',(-64.5297680833505,-4.85525002522065,
131.589045430147));
#89358=CARTESIAN_POINT('Ctrl Pts',(-64.5375424174696,-4.83348404045158,
131.723722814499));
#89359=CARTESIAN_POINT('Ctrl Pts',(-64.5453167515887,-4.80607570897494,
131.857707197984));
#89360=CARTESIAN_POINT('Ctrl Pts',(-64.5530910857078,-4.77307903900955,
131.990488582782));
#89361=CARTESIAN_POINT('Ctrl Pts',(-64.5608558386549,-4.74012303449089,
132.12310632639));
#89362=CARTESIAN_POINT('Ctrl Pts',(-64.568620591602,-4.70159248819834,132.254523645437));
#89363=CARTESIAN_POINT('Ctrl Pts',(-64.576385344549,-4.65759291991145,132.384237592172));
#89364=CARTESIAN_POINT('Ctrl Pts',(-64.584142385434,-4.61363705261601,132.513822705187));
#89365=CARTESIAN_POINT('Ctrl Pts',(-64.591899426319,-4.5642230978478,132.641707444826));
#89366=CARTESIAN_POINT('Ctrl Pts',(-64.599656467204,-4.50950710175618,132.767401310397));
#89367=CARTESIAN_POINT('Ctrl Pts',(-64.6074076584441,-4.45483236742284,
132.893000389246));
#89368=CARTESIAN_POINT('Ctrl Pts',(-64.6151588496842,-4.39486370557697,
133.016411525519));
#89369=CARTESIAN_POINT('Ctrl Pts',(-64.6229100409244,-4.32980612930487,
133.137161926108));
#89370=CARTESIAN_POINT('Ctrl Pts',(-64.6306579377015,-4.26477620423823,
133.257861004555));
#89371=CARTESIAN_POINT('Ctrl Pts',(-64.6384058344785,-4.19466185168961,
133.375901253092));
#89372=CARTESIAN_POINT('Ctrl Pts',(-64.6461537312556,-4.11971500643078,
133.49083252851));
#89373=CARTESIAN_POINT('Ctrl Pts',(-64.6539000073397,-4.04478383843631,
133.605739762782));
#89374=CARTESIAN_POINT('Ctrl Pts',(-64.6616462834238,-3.96502240179397,
133.717538990196));
#89375=CARTESIAN_POINT('Ctrl Pts',(-64.6693925595079,-3.88072691281483,
133.825807570709));
#89376=CARTESIAN_POINT('Ctrl Pts',(-64.6771388927733,-3.79643080158565,
133.934076950435));
#89377=CARTESIAN_POINT('Ctrl Pts',(-64.6848852260386,-3.70760081141714,
134.038815322764));
#89378=CARTESIAN_POINT('Ctrl Pts',(-64.6926315593039,-3.61457428760482,
134.139632088059));
#89379=CARTESIAN_POINT('Ctrl Pts',(-64.7003796273069,-3.52152693114749,
134.24047143057));
#89380=CARTESIAN_POINT('Ctrl Pts',(-64.7081276953098,-3.42428143606292,
134.337387131221));
#89381=CARTESIAN_POINT('Ctrl Pts',(-64.7158757633128,-3.32321264911289,
134.430024798275));
#89382=CARTESIAN_POINT('Ctrl Pts',(-64.7236320660546,-3.22203644505322,
134.522760921744));
#89383=CARTESIAN_POINT('Ctrl Pts',(-64.7313883687965,-3.11702912064238,
134.611209664412));
#89384=CARTESIAN_POINT('Ctrl Pts',(-64.7391446715383,-3.00859973712811,
134.69505601611));
#89385=CARTESIAN_POINT('Ctrl Pts',(-64.7469051140525,-2.90011248158711,
134.778947119131));
#89386=CARTESIAN_POINT('Ctrl Pts',(-64.7546655565666,-2.78819984643927,
134.858230710632));
#89387=CARTESIAN_POINT('Ctrl Pts',(-64.7624259990808,-2.67329979977132,
134.932635226049));
#89388=CARTESIAN_POINT('Ctrl Pts',(-64.7701988993462,-2.55821530534812,
135.007159182199));
#89389=CARTESIAN_POINT('Ctrl Pts',(-64.7779717996116,-2.44013415312025,
135.076788212081));
#89390=CARTESIAN_POINT('Ctrl Pts',(-64.785744699877,-2.31951960725176,135.141296385372));
#89391=CARTESIAN_POINT('Ctrl Pts',(-64.7932350356391,-2.20328970393415,
135.203459524078));
#89392=CARTESIAN_POINT('Ctrl Pts',(-64.8007253714012,-2.08470767687764,
135.260867520164));
#89393=CARTESIAN_POINT('Ctrl Pts',(-64.8082157071633,-1.9642036784546,135.313361279802));
#89394=CARTESIAN_POINT('Ctrl Pts',(-64.8159900412824,-1.83913073430618,
135.367845356291));
#89395=CARTESIAN_POINT('Ctrl Pts',(-64.8237643754015,-1.71159100519587,
135.4172077828));
#89396=CARTESIAN_POINT('Ctrl Pts',(-64.8315387095206,-1.5820427594963,135.461218331693));
#89397=CARTESIAN_POINT('Ctrl Pts',(-64.8393034624677,-1.45265417043149,
135.505174641518));
#89398=CARTESIAN_POINT('Ctrl Pts',(-64.8470682154147,-1.3212623565535,135.543792072671));
#89399=CARTESIAN_POINT('Ctrl Pts',(-64.8548329683618,-1.18834749806699,
135.576887546389));
#89400=CARTESIAN_POINT('Ctrl Pts',(-64.8625900092468,-1.0555646524917,135.609950149215));
#89401=CARTESIAN_POINT('Ctrl Pts',(-64.8703470501318,-0.921262149594142,
135.637501615126));
#89402=CARTESIAN_POINT('Ctrl Pts',(-64.8781040910168,-0.785937008254221,
135.659408102561));
#89403=CARTESIAN_POINT('Ctrl Pts',(-64.8858552822569,-0.65071391665606,
135.681298070143));
#89404=CARTESIAN_POINT('Ctrl Pts',(-64.8936064734971,-0.514470105981229,
135.697551470172));
#89405=CARTESIAN_POINT('Ctrl Pts',(-64.9013576647372,-0.377714165042159,
135.708085229739));
#89406=CARTESIAN_POINT('Ctrl Pts',(-64.9091055615143,-0.241016349026072,
135.718614512176));
#89407=CARTESIAN_POINT('Ctrl Pts',(-64.9168534582913,-0.103807224667278,
135.723428959263));
#89408=CARTESIAN_POINT('Ctrl Pts',(-64.9246013550684,0.0333983129050693,
135.722497217458));
#89409=CARTESIAN_POINT('Ctrl Pts',(-64.9323476311525,0.170575150036766,
135.721565670552));
#89410=CARTESIAN_POINT('Ctrl Pts',(-64.9400939072366,0.307748011165861,
135.714890328209));
#89411=CARTESIAN_POINT('Ctrl Pts',(-64.9478401833207,0.444401205101536,
135.702491958333));
#89412=CARTESIAN_POINT('Ctrl Pts',(-64.955586516586,0.581055407780045,135.690093496935));
#89413=CARTESIAN_POINT('Ctrl Pts',(-64.9633328498514,0.717189546244628,
135.671971959031));
#89414=CARTESIAN_POINT('Ctrl Pts',(-64.9710791831168,0.85229265458679,135.648200034128));
#89415=CARTESIAN_POINT('Ctrl Pts',(-64.9788272511197,0.987426018333327,
135.624422785667));
#89416=CARTESIAN_POINT('Ctrl Pts',(-64.9865753191227,1.12152750753259,135.594992700016));
#89417=CARTESIAN_POINT('Ctrl Pts',(-64.9943233871257,1.25409634854941,135.560033588982));
#89418=CARTESIAN_POINT('Ctrl Pts',(-65.0020796898676,1.38680608530805,135.525037322988));
#89419=CARTESIAN_POINT('Ctrl Pts',(-65.0098359926094,1.5179795413033,135.484500392892));
#89420=CARTESIAN_POINT('Ctrl Pts',(-65.0175922953512,1.64713058196371,135.438596682816));
#89421=CARTESIAN_POINT('Ctrl Pts',(-65.0253527378654,1.77635055442337,135.392668472547));
#89422=CARTESIAN_POINT('Ctrl Pts',(-65.0331131803797,1.90354559829671,135.341367920882));
#89423=CARTESIAN_POINT('Ctrl Pts',(-65.0408736228938,2.028250506176,135.284916715496));
#89424=CARTESIAN_POINT('Ctrl Pts',(-65.0486465231592,2.15315560144404,135.228374889623));
#89425=CARTESIAN_POINT('Ctrl Pts',(-65.0564194234247,2.27556222335211,135.166666063457));
#89426=CARTESIAN_POINT('Ctrl Pts',(-65.0641923236901,2.39502988472424,135.1000578734));
#89427=CARTESIAN_POINT('Ctrl Pts',(-65.0716826594522,2.51015459568542,135.035871058827));
#89428=CARTESIAN_POINT('Ctrl Pts',(-65.0791729952142,2.62255005082217,134.967135065199));
#89429=CARTESIAN_POINT('Ctrl Pts',(-65.0866633309762,2.7318498921273,134.894125797791));
#89430=CARTESIAN_POINT('Ctrl Pts',(-65.0944376650953,2.84529387013583,134.818348361819));
#89431=CARTESIAN_POINT('Ctrl Pts',(-65.1022119992144,2.95576221648972,134.737727172878));
#89432=CARTESIAN_POINT('Ctrl Pts',(-65.1099863333335,3.06281352890933,134.652523341468));
#89433=CARTESIAN_POINT('Ctrl Pts',(-65.1177510862806,3.16973291015384,134.567424516165));
#89434=CARTESIAN_POINT('Ctrl Pts',(-65.1255158392277,3.27324333351046,134.477754526762));
#89435=CARTESIAN_POINT('Ctrl Pts',(-65.1332805921748,3.37293122049939,134.383818403919));
#89436=CARTESIAN_POINT('Ctrl Pts',(-65.1410376330598,3.47252009607348,134.289975579757));
#89437=CARTESIAN_POINT('Ctrl Pts',(-65.1487946739449,3.56829370797957,134.191875320732));
#89438=CARTESIAN_POINT('Ctrl Pts',(-65.1565517148299,3.65987080067712,134.08986343827));
#89439=CARTESIAN_POINT('Ctrl Pts',(-65.16430290607,3.7513788343767,133.987928483762));
#89440=CARTESIAN_POINT('Ctrl Pts',(-65.1720540973101,3.83869638775054,133.882088066942));
#89441=CARTESIAN_POINT('Ctrl Pts',(-65.1798052885502,3.92147866453274,133.772725175048));
#89442=CARTESIAN_POINT('Ctrl Pts',(-65.1875531853272,4.00422575663903,133.6634087653));
#89443=CARTESIAN_POINT('Ctrl Pts',(-65.1953010821043,4.0824411705606,133.550573169262));
#89444=CARTESIAN_POINT('Ctrl Pts',(-65.2030489788814,4.15582021428058,133.434634635435));
#89445=CARTESIAN_POINT('Ctrl Pts',(-65.2107952549654,4.22918390868647,133.31872035345));
#89446=CARTESIAN_POINT('Ctrl Pts',(-65.2185415310496,4.29771303619146,133.199704754854));
#89447=CARTESIAN_POINT('Ctrl Pts',(-65.2262878071337,4.36114632573639,133.078032930811));
#89448=CARTESIAN_POINT('Ctrl Pts',(-65.234034140399,4.42458008353146,132.956360208614));
#89449=CARTESIAN_POINT('Ctrl Pts',(-65.2417804736644,4.48291774756538,132.832031568524));
#89450=CARTESIAN_POINT('Ctrl Pts',(-65.2495268069298,4.53594428402451,132.705516191086));
#89451=CARTESIAN_POINT('Ctrl Pts',(-65.2572748749327,4.58898269540883,132.578972481406));
#89452=CARTESIAN_POINT('Ctrl Pts',(-65.2650229429357,4.63670746137042,132.450241420426));
#89453=CARTESIAN_POINT('Ctrl Pts',(-65.2727710109387,4.6789520679073,132.319811246497));
#89454=CARTESIAN_POINT('Ctrl Pts',(-65.2805273136805,4.72124157251472,132.189242449826));
#89455=CARTESIAN_POINT('Ctrl Pts',(-65.2882836164224,4.75803916221425,132.056971305385));
#89456=CARTESIAN_POINT('Ctrl Pts',(-65.2960399191643,4.78922836303293,131.923500800573));
#89457=CARTESIAN_POINT('Ctrl Pts',(-65.3038003616784,4.82043421046721,131.789959058534));
#89458=CARTESIAN_POINT('Ctrl Pts',(-65.3115608041926,4.84602563156959,131.655217064512));
#89459=CARTESIAN_POINT('Ctrl Pts',(-65.3193212467067,4.86593768249237,131.519786038278));
#89460=CARTESIAN_POINT('Ctrl Pts',(-65.3270941469722,4.885881698007,131.384137606138));
#89461=CARTESIAN_POINT('Ctrl Pts',(-65.3348670472376,4.90012808395764,131.247798320526));
#89462=CARTESIAN_POINT('Ctrl Pts',(-65.342639947503,4.90866391635209,131.111283439792));
#89463=CARTESIAN_POINT('Ctrl Pts',(-65.3501302832651,4.91688944973854,130.979731218833));
#89464=CARTESIAN_POINT('Ctrl Pts',(-65.3576206190271,4.91981240050838,130.848016255696));
#89465=CARTESIAN_POINT('Ctrl Pts',(-65.3651109547891,4.91746687013063,130.71659591129));
#89466=CARTESIAN_POINT('Ctrl Pts',(-65.3728852889082,4.91503240825569,130.580192724581));
#89467=CARTESIAN_POINT('Ctrl Pts',(-65.3806596230273,4.9069143582325,130.443674854263));
#89468=CARTESIAN_POINT('Ctrl Pts',(-65.3884339571464,4.8930938110057,130.307554801177));
#89469=CARTESIAN_POINT('Ctrl Pts',(-65.3961987100935,4.87929029636818,130.171602503891));
#89470=CARTESIAN_POINT('Ctrl Pts',(-65.4039634630406,4.85979830690382,130.03604743357));
#89471=CARTESIAN_POINT('Ctrl Pts',(-65.4117282159877,4.83465092427619,129.901402422025));
#89472=CARTESIAN_POINT('Ctrl Pts',(-65.4194852568727,4.80952851838354,129.766891141803));
#89473=CARTESIAN_POINT('Ctrl Pts',(-65.4272422977577,4.77876196875752,129.633288503421));
#89474=CARTESIAN_POINT('Ctrl Pts',(-65.4349993386427,4.74243613841335,129.501102187487));
#89475=CARTESIAN_POINT('Ctrl Pts',(-65.4427505298828,4.70613770166041,129.369015554282));
#89476=CARTESIAN_POINT('Ctrl Pts',(-65.4505017211229,4.66428843188234,129.238343493081));
#89477=CARTESIAN_POINT('Ctrl Pts',(-65.458252912363,4.61702417628389,129.109583104702));
#89478=CARTESIAN_POINT('Ctrl Pts',(-65.4660008091401,4.5697800092549,128.980877442923));
#89479=CARTESIAN_POINT('Ctrl Pts',(-65.4737487059172,4.51712556838073,128.854082204194));
#89480=CARTESIAN_POINT('Ctrl Pts',(-65.4814966026942,4.45924636183527,128.72967872702));
#89481=CARTESIAN_POINT('Ctrl Pts',(-65.4892428787783,4.40137926237209,128.605301272372));
#89482=CARTESIAN_POINT('Ctrl Pts',(-65.4969891548625,4.3382897359099,128.483314938397));
#89483=CARTESIAN_POINT('Ctrl Pts',(-65.5047354309466,4.27021102686079,128.364180122484));
#89484=CARTESIAN_POINT('Ctrl Pts',(-65.5124817642119,4.20213181527012,128.245044427145));
#89485=CARTESIAN_POINT('Ctrl Pts',(-65.5202280974773,4.12906354157955,128.128760631321));
#89486=CARTESIAN_POINT('Ctrl Pts',(-65.5279744307426,4.05128470964006,128.015763252593));
#89487=CARTESIAN_POINT('Ctrl Pts',(-65.5357224987456,3.97348845967044,127.902740568885));
#89488=CARTESIAN_POINT('Ctrl Pts',(-65.5434705667486,3.89097977396011,127.793006088756));
#89489=CARTESIAN_POINT('Ctrl Pts',(-65.5512186347516,3.80407941637344,127.686963809904));
#89490=CARTESIAN_POINT('Ctrl Pts',(-65.5589749374934,3.71708670005261,127.580808828056));
#89491=CARTESIAN_POINT('Ctrl Pts',(-65.5667312402352,3.62569323618477,127.478354189207));
#89492=CARTESIAN_POINT('Ctrl Pts',(-65.5744875429771,3.53025924528654,127.379969763185));
#89493=CARTESIAN_POINT('Ctrl Pts',(-65.5822479854913,3.43477431839377,127.281532826432));
#89494=CARTESIAN_POINT('Ctrl Pts',(-65.5900084280054,3.33524485094255,127.187170700047));
#89495=CARTESIAN_POINT('Ctrl Pts',(-65.5977688705196,3.23206584286858,127.097214349901));
#89496=CARTESIAN_POINT('Ctrl Pts',(-65.605541770785,3.12872120269104,127.007113593836));
#89497=CARTESIAN_POINT('Ctrl Pts',(-65.6133146710505,3.02171561997012,126.921432991711));
#89498=CARTESIAN_POINT('Ctrl Pts',(-65.6210875713159,2.91147561041485,126.840461926573));
#89499=CARTESIAN_POINT('Ctrl Pts',(-65.628577907078,2.80524310288459,126.762434363605));
#89500=CARTESIAN_POINT('Ctrl Pts',(-65.63606824284,2.69600750032462,126.688780047448));
#89501=CARTESIAN_POINT('Ctrl Pts',(-65.643558578602,2.58417202609608,126.619717502312));
#89502=CARTESIAN_POINT('Ctrl Pts',(-65.6513329127211,2.46809627587051,126.548036429786));
#89503=CARTESIAN_POINT('Ctrl Pts',(-65.6591072468402,2.34885192085261,126.481075131644));
#89504=CARTESIAN_POINT('Ctrl Pts',(-65.6668815809593,2.22685992170939,126.419126535834));
#89505=CARTESIAN_POINT('Ctrl Pts',(-65.6746463339064,2.10501826680254,126.357254286132));
#89506=CARTESIAN_POINT('Ctrl Pts',(-65.6824110868535,1.98043605059833,126.300382622285));
#89507=CARTESIAN_POINT('Ctrl Pts',(-65.6901758398006,1.85356261447099,126.248760909873));
#89508=CARTESIAN_POINT('Ctrl Pts',(-65.6979328806856,1.72681519082901,126.197190468873));
#89509=CARTESIAN_POINT('Ctrl Pts',(-65.7056899215706,1.59778143574751,126.150859748956));
#89510=CARTESIAN_POINT('Ctrl Pts',(-65.7134469624556,1.46693434583226,126.109971766233));
#89511=CARTESIAN_POINT('Ctrl Pts',(-65.7211981536957,1.33618592872536,126.069114617456));
#89512=CARTESIAN_POINT('Ctrl Pts',(-65.7289493449359,1.20362727027075,126.033692152431));
#89513=CARTESIAN_POINT('Ctrl Pts',(-65.736700536176,1.06975002419918,126.003858774193));
#89514=CARTESIAN_POINT('Ctrl Pts',(-65.7444484329531,0.935929679528493,
125.974038075937));
#89515=CARTESIAN_POINT('Ctrl Pts',(-65.7521963297302,0.800792242709317,
125.949801824617));
#89516=CARTESIAN_POINT('Ctrl Pts',(-65.7599442265073,0.664842949157073,
125.931254122171));
#89517=CARTESIAN_POINT('Ctrl Pts',(-65.7676905025914,0.528922093266312,
125.912710299506));
#89518=CARTESIAN_POINT('Ctrl Pts',(-65.7754367786755,0.392190105560796,
125.899852711712));
#89519=CARTESIAN_POINT('Ctrl Pts',(-65.7831830547596,0.255160405703753,
125.892733979693));
#89520=CARTESIAN_POINT('Ctrl Pts',(-65.790929388025,0.118129694324595,125.885615195126));
#89521=CARTESIAN_POINT('Ctrl Pts',(-65.7986757212904,-0.01919834315263,
125.88423537115));
#89522=CARTESIAN_POINT('Ctrl Pts',(-65.8064220545557,-0.156307596645724,
125.888595061955));
#89523=CARTESIAN_POINT('Ctrl Pts',(-65.8141701225587,-0.293447554805489,
125.892955729082));
#89524=CARTESIAN_POINT('Ctrl Pts',(-65.8219181905617,-0.430368240793513,
125.903058456214));
#89525=CARTESIAN_POINT('Ctrl Pts',(-65.8296662585647,-0.566556379200238,
125.918851746252));
#89526=CARTESIAN_POINT('Ctrl Pts',(-65.8374225613066,-0.702889259981121,
125.934661821586));
#89527=CARTESIAN_POINT('Ctrl Pts',(-65.8451788640484,-0.838487648940886,
125.956174496244));
#89528=CARTESIAN_POINT('Ctrl Pts',(-65.8529351667903,-0.972845656130369,
125.98328663018));
#89529=CARTESIAN_POINT('Ctrl Pts',(-65.8606956093045,-1.10727537423391,
126.010413234678));
#89530=CARTESIAN_POINT('Ctrl Pts',(-65.8684560518186,-1.24046301193602,
126.043145160232));
#89531=CARTESIAN_POINT('Ctrl Pts',(-65.8762164943327,-1.37191661116169,
126.081328977346));
#89532=CARTESIAN_POINT('Ctrl Pts',(-65.8839893945982,-1.50358123137457,
126.119574090513));
#89533=CARTESIAN_POINT('Ctrl Pts',(-65.8917622948637,-1.63350587975983,
126.163288459499));
#89534=CARTESIAN_POINT('Ctrl Pts',(-65.8995351951291,-1.76121654800737,
126.212269663161));
#89535=CARTESIAN_POINT('Ctrl Pts',(-65.9070255308911,-1.88428461177913,
126.259470276694));
#89536=CARTESIAN_POINT('Ctrl Pts',(-65.914515866653,-2.00529658537079,126.311561325851));
#89537=CARTESIAN_POINT('Ctrl Pts',(-65.922006202415,-2.12385066609942,126.368321685071));
#89538=CARTESIAN_POINT('Ctrl Pts',(-65.9297812304682,-2.24691074414967,
126.427239389067));
#89539=CARTESIAN_POINT('Ctrl Pts',(-65.9375562585214,-2.36771224722287,
126.491375015461));
#89540=CARTESIAN_POINT('Ctrl Pts',(-65.9453312865747,-2.48578106105976,
126.560532678196));
#89541=CARTESIAN_POINT('Ctrl Pts',(-65.9530965778673,-2.60370201590915,
126.629603733963));
#89542=CARTESIAN_POINT('Ctrl Pts',(-65.9608618691598,-2.71889675688229,
126.703684115817));
#89543=CARTESIAN_POINT('Ctrl Pts',(-65.9686271604524,-2.8309125142882,126.782530511887));
#89544=CARTESIAN_POINT('Ctrl Pts',(-65.9763845847619,-2.94281478901344,
126.861297029013));
#89545=CARTESIAN_POINT('Ctrl Pts',(-65.9841420090715,-3.05154417219573,
126.944819727021));
#89546=CARTESIAN_POINT('Ctrl Pts',(-65.991899433381,-3.1566741362209,127.032810344772));
#89547=CARTESIAN_POINT('Ctrl Pts',(-65.9996503662968,-3.26171612774944,
127.120727332189));
#89548=CARTESIAN_POINT('Ctrl Pts',(-66.0074012992125,-3.36316439949768,
127.213104544159));
#89549=CARTESIAN_POINT('Ctrl Pts',(-66.0151522321284,-3.46062334270266,
127.309611822239));
#89550=CARTESIAN_POINT('Ctrl Pts',(-66.0228996449348,-3.55803802463637,
127.406075271249));
#89551=CARTESIAN_POINT('Ctrl Pts',(-66.0306470577412,-3.65146670569653,
127.506664779914));
#89552=CARTESIAN_POINT('Ctrl Pts',(-66.0383944705476,-3.74054878273879,
127.611011612767));
#89553=CARTESIAN_POINT('Ctrl Pts',(-66.0461400426149,-3.82960969441067,
127.715333653434));
#89554=CARTESIAN_POINT('Ctrl Pts',(-66.0538856146823,-3.91432580411637,
127.823410944299));
#89555=CARTESIAN_POINT('Ctrl Pts',(-66.0616311867496,-3.99437541497384,
127.934840081526));
#89556=CARTESIAN_POINT('Ctrl Pts',(-66.0693765958471,-4.0744233415569,128.046266874242));
#89557=CARTESIAN_POINT('Ctrl Pts',(-66.0771220049447,-4.14980473803786,
128.161045054669));
#89558=CARTESIAN_POINT('Ctrl Pts',(-66.0848674140422,-4.22024026637581,
128.278740860643));
#89559=CARTESIAN_POINT('Ctrl Pts',(-66.0926173157467,-4.29071664977332,
128.396504934284));
#89560=CARTESIAN_POINT('Ctrl Pts',(-66.1003672174513,-4.35624123371674,
128.517189678217));
#89561=CARTESIAN_POINT('Ctrl Pts',(-66.1081171191558,-4.41657974103042,
128.64033509701));
#89562=CARTESIAN_POINT('Ctrl Pts',(-66.1158695639228,-4.47693804789723,
128.763520924893));
#89563=CARTESIAN_POINT('Ctrl Pts',(-66.1236220086897,-4.53210672686887,
128.889168680153));
#89564=CARTESIAN_POINT('Ctrl Pts',(-66.1313744534567,-4.58189937968992,
129.016797713247));
#89565=CARTESIAN_POINT('Ctrl Pts',(-66.1391346815246,-4.63174202334797,
129.144554883362));
#89566=CARTESIAN_POINT('Ctrl Pts',(-66.1468949095925,-4.67619773291773,
129.274296935016));
#89567=CARTESIAN_POINT('Ctrl Pts',(-66.1546551376604,-4.71512967005692,
129.405527083135));
#89568=CARTESIAN_POINT('Ctrl Pts',(-66.1581266329857,-4.73254565791201,
129.464232167798));
#89569=CARTESIAN_POINT('Ctrl Pts',(-66.1615981283111,-4.74885692234884,
129.523234884618));
#89570=CARTESIAN_POINT('Ctrl Pts',(-66.1650696236364,-4.76405452823402,
129.582490119308));
#89571=CARTESIAN_POINT('Ctrl Pts',(-64.4150295539547,-4.76405452823403,
129.582490119308));
#89572=CARTESIAN_POINT('Ctrl Pts',(-64.4226670803882,-4.79766306093323,
129.713529278222));
#89573=CARTESIAN_POINT('Ctrl Pts',(-64.4303046068217,-4.82584443848221,
129.845892000019));
#89574=CARTESIAN_POINT('Ctrl Pts',(-64.4379421332552,-4.8485150824566,129.979082144752));
#89575=CARTESIAN_POINT('Ctrl Pts',(-64.445808538376,-4.87186511226066,130.116263684571));
#89576=CARTESIAN_POINT('Ctrl Pts',(-64.4536749434968,-4.88936886737709,
130.254322558506));
#89577=CARTESIAN_POINT('Ctrl Pts',(-64.4615413486176,-4.90099259422966,
130.392711915629));
#89578=CARTESIAN_POINT('Ctrl Pts',(-64.4694077537384,-4.91261632108222,
130.531101272753));
#89579=CARTESIAN_POINT('Ctrl Pts',(-64.4772741588592,-4.91836005286657,
130.669820648485));
#89580=CARTESIAN_POINT('Ctrl Pts',(-64.48514056398,-4.91824840200337,130.808325298039));
#89581=CARTESIAN_POINT('',(-64.1398594360283,-4.91824993534877,130.805158077164));
#89582=CARTESIAN_POINT('Ctrl Pts',(-64.0701225287274,-4.764054528234,129.582490119308));
#89583=CARTESIAN_POINT('Ctrl Pts',(-64.0781582273743,-4.79934114512443,
129.720072103015));
#89584=CARTESIAN_POINT('Ctrl Pts',(-64.0861939260212,-4.82869690305613,
129.859313232665));
#89585=CARTESIAN_POINT('Ctrl Pts',(-64.0942296246681,-4.85197641295532,
129.999681830331));
#89586=CARTESIAN_POINT('Ctrl Pts',(-64.1022545812035,-4.87522480283589,
130.139862783439));
#89587=CARTESIAN_POINT('Ctrl Pts',(-64.1102795377389,-4.89241308219218,
130.281167856988));
#89588=CARTESIAN_POINT('Ctrl Pts',(-64.1183044942743,-4.90344656354808,
130.42305383697));
#89589=CARTESIAN_POINT('Ctrl Pts',(-64.1254894748465,-4.91332516523728,
130.550088544902));
#89590=CARTESIAN_POINT('Ctrl Pts',(-64.1326744554187,-4.91827061982955,
130.677588566443));
#89591=CARTESIAN_POINT('Ctrl Pts',(-64.139859435991,-4.91824993534888,130.805158076502));
#89592=CARTESIAN_POINT('Ctrl Pts',(-64.1398594360282,-4.91824993534877,
130.805158077163));
#89593=CARTESIAN_POINT('Ctrl Pts',(-64.1480802783964,-4.91822626875783,
130.951119339359));
#89594=CARTESIAN_POINT('Ctrl Pts',(-64.1563011207648,-4.91170069888442,
131.09692237697));
#89595=CARTESIAN_POINT('Ctrl Pts',(-64.164521963133,-4.89874086550328,131.24199173523));
#89596=CARTESIAN_POINT('Ctrl Pts',(-64.172757650151,-4.88575763011782,131.38732305008));
#89597=CARTESIAN_POINT('Ctrl Pts',(-64.180993337169,-4.86631695936606,131.531917728935));
#89598=CARTESIAN_POINT('Ctrl Pts',(-64.189229024187,-4.84053774569423,131.675209281232));
#89599=CARTESIAN_POINT('Ctrl Pts',(-64.1974879554785,-4.81468577317552,
131.818905257351));
#89600=CARTESIAN_POINT('Ctrl Pts',(-64.2057468867699,-4.78245953336674,
131.961290441817));
#89601=CARTESIAN_POINT('Ctrl Pts',(-64.2140058180614,-4.74402862355473,
132.101810224061));
#89602=CARTESIAN_POINT('Ctrl Pts',(-64.2222775043416,-4.70553836153289,
132.242547023275));
#89603=CARTESIAN_POINT('Ctrl Pts',(-64.2305491906217,-4.66082439267892,
132.381412370845));
#89604=CARTESIAN_POINT('Ctrl Pts',(-64.2388208769019,-4.61010499468608,
132.51787017414));
#89605=CARTESIAN_POINT('Ctrl Pts',(-64.2471120720283,-4.5592659745388,132.654649814386));
#89606=CARTESIAN_POINT('Ctrl Pts',(-64.2554032671548,-4.50239332614663,
132.789010268259));
#89607=CARTESIAN_POINT('Ctrl Pts',(-64.2636944622812,-4.43975267442496,
132.920436999088));
#89608=CARTESIAN_POINT('Ctrl Pts',(-64.2660994600866,-4.42158272092387,
132.958559488595));
#89609=CARTESIAN_POINT('Ctrl Pts',(-64.2685044578918,-4.40292774055166,
132.996435315707));
#89610=CARTESIAN_POINT('Ctrl Pts',(-64.2709094556971,-4.38379490299275,
133.034052370027));
#89611=CARTESIAN_POINT('Ctrl Pts',(-64.2786837898162,-4.32194658383872,
133.15565229341));
#89612=CARTESIAN_POINT('Ctrl Pts',(-64.2864581239353,-4.25493696664731,
133.274869502135));
#89613=CARTESIAN_POINT('Ctrl Pts',(-64.2942324580544,-4.18297320085201,
133.391234844013));
#89614=CARTESIAN_POINT('Ctrl Pts',(-64.3019972110015,-4.11109812396646,
133.507456776006));
#89615=CARTESIAN_POINT('Ctrl Pts',(-64.3097619639486,-4.03428125035618,
133.620833504975));
#89616=CARTESIAN_POINT('Ctrl Pts',(-64.3175267168957,-3.95277662843796,
133.730918320427));
#89617=CARTESIAN_POINT('Ctrl Pts',(-64.3252837577807,-3.87135295805923,
133.840893798088));
#89618=CARTESIAN_POINT('Ctrl Pts',(-64.3330407986656,-3.78525103603341,
133.947583556649));
#89619=CARTESIAN_POINT('Ctrl Pts',(-64.3407978395506,-3.69476922372682,
134.050568165752));
#89620=CARTESIAN_POINT('Ctrl Pts',(-64.3485490307907,-3.60435564445885,
134.15347511336));
#89621=CARTESIAN_POINT('Ctrl Pts',(-64.3563002220309,-3.50956900615667,
134.252682180442));
#89622=CARTESIAN_POINT('Ctrl Pts',(-64.364051413271,-3.41074889194883,134.347801749936));
#89623=CARTESIAN_POINT('Ctrl Pts',(-64.371799310048,-3.31197077892551,134.442880891075));
#89624=CARTESIAN_POINT('Ctrl Pts',(-64.3795472068252,-3.209162880766,134.533875719412));
#89625=CARTESIAN_POINT('Ctrl Pts',(-64.3872951036023,-3.10270254571794,
134.620434512985));
#89626=CARTESIAN_POINT('Ctrl Pts',(-64.3950413796864,-2.99626447987694,
134.706975200324));
#89627=CARTESIAN_POINT('Ctrl Pts',(-64.4027876557703,-2.88617579996529,
134.789081452102));
#89628=CARTESIAN_POINT('Ctrl Pts',(-64.4105339318544,-2.77284762340966,
134.866441256826));
#89629=CARTESIAN_POINT('Ctrl Pts',(-64.4182802651198,-2.65951861029118,
134.943801632603));
#89630=CARTESIAN_POINT('Ctrl Pts',(-64.4260265983852,-2.54295037571757,
135.016415270991));
#89631=CARTESIAN_POINT('Ctrl Pts',(-64.4337729316505,-2.42358341890949,
135.084013228945));
#89632=CARTESIAN_POINT('Ctrl Pts',(-64.4415209996535,-2.30418973069908,
135.151626324994));
#89633=CARTESIAN_POINT('Ctrl Pts',(-64.4492690676565,-2.18199641322166,
135.214221312899));
#89634=CARTESIAN_POINT('Ctrl Pts',(-64.4570171356595,-2.05746862072361,
135.271575178927));
#89635=CARTESIAN_POINT('Ctrl Pts',(-64.4647734384013,-1.93280847860578,
135.328990001327));
#89636=CARTESIAN_POINT('Ctrl Pts',(-64.4725297411432,-1.80580926086457,
135.381152410709));
#89637=CARTESIAN_POINT('Ctrl Pts',(-64.4802860438851,-1.67695667772851,
135.427887341131));
#89638=CARTESIAN_POINT('Ctrl Pts',(-64.4880464863992,-1.54803532208916,
135.474647215393));
#89639=CARTESIAN_POINT('Ctrl Pts',(-64.4958069289134,-1.41725900260808,
135.51597372081));
#89640=CARTESIAN_POINT('Ctrl Pts',(-64.5035673714276,-1.28512769042289,
135.551741988576));
#89641=CARTESIAN_POINT('Ctrl Pts',(-64.511340271693,-1.15278426932531,135.587567674739));
#89642=CARTESIAN_POINT('Ctrl Pts',(-64.5191131719584,-1.01908189041864,
135.617817206777));
#89643=CARTESIAN_POINT('Ctrl Pts',(-64.5268860722238,-0.884530679151612,
135.64241689464));
#89644=CARTESIAN_POINT('Ctrl Pts',(-64.5343764079859,-0.754870743326913,
135.666122321888));
#89645=CARTESIAN_POINT('Ctrl Pts',(-64.541866743748,-0.624422923058458,
135.684581502331));
#89646=CARTESIAN_POINT('Ctrl Pts',(-64.5493570795101,-0.493645405713664,
135.697774280431));
#89647=CARTESIAN_POINT('Ctrl Pts',(-64.5571314136292,-0.357909419051108,
135.711467266723));
#89648=CARTESIAN_POINT('Ctrl Pts',(-64.5649057477483,-0.221388270050871,
135.719529991327));
#89649=CARTESIAN_POINT('Ctrl Pts',(-64.5726800818674,-0.084588639066603,
135.72188314671));
#89650=CARTESIAN_POINT('Ctrl Pts',(-64.5804448348145,0.0520423985984248,
135.724233402039));
#89651=CARTESIAN_POINT('Ctrl Pts',(-64.5882095877615,0.188950848218802,
135.720888082093));
#89652=CARTESIAN_POINT('Ctrl Pts',(-64.5959743407086,0.325623560229994,
135.711819467065));
#89653=CARTESIAN_POINT('Ctrl Pts',(-64.6037313815936,0.462160526977055,
135.702759859113));
#89654=CARTESIAN_POINT('Ctrl Pts',(-64.6114884224786,0.598461834476933,
135.687988294124));
#89655=CARTESIAN_POINT('Ctrl Pts',(-64.6192454633636,0.734013332483941,
135.667529079612));
#89656=CARTESIAN_POINT('Ctrl Pts',(-64.6269966546037,0.869462610051866,
135.647085293552));
#89657=CARTESIAN_POINT('Ctrl Pts',(-64.6347478458438,1.00416281857292,135.620962453276));
#89658=CARTESIAN_POINT('Ctrl Pts',(-64.6424990370839,1.13760429185905,135.589236743198));
#89659=CARTESIAN_POINT('Ctrl Pts',(-64.650246933861,1.27098904895936,135.557524517393));
#89660=CARTESIAN_POINT('Ctrl Pts',(-64.6579948306382,1.40311575532449,135.520214248389));
#89661=CARTESIAN_POINT('Ctrl Pts',(-64.6657427274153,1.53348453136136,135.477433295641));
#89662=CARTESIAN_POINT('Ctrl Pts',(-64.6734890034994,1.66382603706071,135.434661291747));
#89663=CARTESIAN_POINT('Ctrl Pts',(-64.6812352795833,1.79240997260925,135.386421002107));
#89664=CARTESIAN_POINT('Ctrl Pts',(-64.6889815556674,1.91875161489029,135.332889661622));
#89665=CARTESIAN_POINT('Ctrl Pts',(-64.6967278889328,2.04509418979662,135.27935792598));
#89666=CARTESIAN_POINT('Ctrl Pts',(-64.7044742221981,2.16919407842172,135.220535214085));
#89667=CARTESIAN_POINT('Ctrl Pts',(-64.7122205554635,2.29058691077764,135.156646760121));
#89668=CARTESIAN_POINT('Ctrl Pts',(-64.7199686234664,2.41200692821669,135.09274399878));
#89669=CARTESIAN_POINT('Ctrl Pts',(-64.7277166914694,2.53071833715708,135.023773420022));
#89670=CARTESIAN_POINT('Ctrl Pts',(-64.7354647594724,2.64628208259835,134.950005826917));
#89671=CARTESIAN_POINT('Ctrl Pts',(-64.7432210622142,2.76196865056351,134.876159832737));
#89672=CARTESIAN_POINT('Ctrl Pts',(-64.7509773649561,2.87450054220997,134.797506850455));
#89673=CARTESIAN_POINT('Ctrl Pts',(-64.758733667698,2.98346793136081,134.714360894426));
#89674=CARTESIAN_POINT('Ctrl Pts',(-64.7664941102121,3.09249347968819,134.631170560896));
#89675=CARTESIAN_POINT('Ctrl Pts',(-64.7742545527263,3.19795043419182,134.543482725172));
#89676=CARTESIAN_POINT('Ctrl Pts',(-64.7820149952404,3.29946349259535,134.451650532493));
#89677=CARTESIAN_POINT('Ctrl Pts',(-64.7897878955058,3.40113950877214,134.359670922626));
#89678=CARTESIAN_POINT('Ctrl Pts',(-64.7975607957713,3.49885869844773,134.263533935556));
#89679=CARTESIAN_POINT('Ctrl Pts',(-64.8053336960367,3.59228332883262,134.163628923));
#89680=CARTESIAN_POINT('Ctrl Pts',(-64.8128240317988,3.68231173858146,134.067355709294));
#89681=CARTESIAN_POINT('Ctrl Pts',(-64.8203143675609,3.76835220309984,133.967583901549));
#89682=CARTESIAN_POINT('Ctrl Pts',(-64.827804703323,3.85014010349792,133.864688091209));
#89683=CARTESIAN_POINT('Ctrl Pts',(-64.835579037442,3.93502901699755,133.757890954948));
#89684=CARTESIAN_POINT('Ctrl Pts',(-64.8433533715611,4.01560543130416,133.647389945406));
#89685=CARTESIAN_POINT('Ctrl Pts',(-64.8511277056802,4.09152874963622,133.533568479456));
#89686=CARTESIAN_POINT('Ctrl Pts',(-64.8588924586272,4.16735849926379,133.41988728829));
#89687=CARTESIAN_POINT('Ctrl Pts',(-64.8666572115743,4.23854634804271,133.30289410503));
#89688=CARTESIAN_POINT('Ctrl Pts',(-64.8744219645214,4.30479160464176,133.183005673707));
#89689=CARTESIAN_POINT('Ctrl Pts',(-64.8821790054063,4.37097106551806,133.063236317265));
#89690=CARTESIAN_POINT('Ctrl Pts',(-64.8899360462913,4.43221751558849,132.94057777532));
#89691=CARTESIAN_POINT('Ctrl Pts',(-64.8976930871763,4.48827349468616,132.815475755841));
#89692=CARTESIAN_POINT('Ctrl Pts',(-64.9054442784164,4.54428720153394,132.690468076768));
#89693=CARTESIAN_POINT('Ctrl Pts',(-64.9131954696565,4.5951180691138,132.563020943177));
#89694=CARTESIAN_POINT('Ctrl Pts',(-64.9209466608966,4.64055470650643,132.433604331202));
#89695=CARTESIAN_POINT('Ctrl Pts',(-64.9286945576737,4.68597203211618,132.304242724739));
#89696=CARTESIAN_POINT('Ctrl Pts',(-64.9364424544508,4.72599955828581,132.172913672901));
#89697=CARTESIAN_POINT('Ctrl Pts',(-64.9441903512278,4.7604742390024,132.040106579443));
#89698=CARTESIAN_POINT('Ctrl Pts',(-64.9519366273119,4.79494170835893,131.907327266366));
#89699=CARTESIAN_POINT('Ctrl Pts',(-64.9596829033959,4.82385854444972,131.773070904818));
#89700=CARTESIAN_POINT('Ctrl Pts',(-64.96742917948,4.8471118553323,131.637841105878));
#89701=CARTESIAN_POINT('Ctrl Pts',(-64.9751755127453,4.87036533786557,131.502610308703));
#89702=CARTESIAN_POINT('Ctrl Pts',(-64.9829218460106,4.88795514551239,131.366406445107));
#89703=CARTESIAN_POINT('Ctrl Pts',(-64.990668179276,4.89981977085075,131.229741947293));
#89704=CARTESIAN_POINT('Ctrl Pts',(-64.9984162472789,4.91168705318969,131.093046844412));
#89705=CARTESIAN_POINT('Ctrl Pts',(-65.0061643152819,4.91782656815173,130.95589129147));
#89706=CARTESIAN_POINT('Ctrl Pts',(-65.0139123832849,4.91822883007871,130.818791053548));
#89707=CARTESIAN_POINT('Ctrl Pts',(-65.0216686860267,4.91863151953444,130.681545103863));
#89708=CARTESIAN_POINT('Ctrl Pts',(-65.0294249887685,4.91328477415181,130.544354978223));
#89709=CARTESIAN_POINT('Ctrl Pts',(-65.0371812915103,4.90223126204096,130.407735207427));
#89710=CARTESIAN_POINT('Ctrl Pts',(-65.0449417340245,4.89117185033789,130.271042518545));
#89711=CARTESIAN_POINT('Ctrl Pts',(-65.0527021765387,4.87439965053415,130.134921178923));
#89712=CARTESIAN_POINT('Ctrl Pts',(-65.0604626190529,4.8520089136721,129.99987782462));
#89713=CARTESIAN_POINT('Ctrl Pts',(-65.0682355193183,4.82958223321147,129.864617686736));
#89714=CARTESIAN_POINT('Ctrl Pts',(-65.0760084195836,4.80151907219228,129.730439375123));
#89715=CARTESIAN_POINT('Ctrl Pts',(-65.083781319849,4.76796445041862,129.597837488055));
#89716=CARTESIAN_POINT('Ctrl Pts',(-65.0912716556113,4.73562962366439,129.470056013582));
#89717=CARTESIAN_POINT('Ctrl Pts',(-65.0987619913735,4.69819574885011,129.343738634839));
#89718=CARTESIAN_POINT('Ctrl Pts',(-65.1062523271358,4.65583494739597,129.21931045902));
#89719=CARTESIAN_POINT('Ctrl Pts',(-65.1140266612549,4.61186802328036,129.090164551098));
#89720=CARTESIAN_POINT('Ctrl Pts',(-65.121800995374,4.56245391452202,128.962644836904));
#89721=CARTESIAN_POINT('Ctrl Pts',(-65.1295753294932,4.5077310997147,128.83724511634));
#89722=CARTESIAN_POINT('Ctrl Pts',(-65.1373400824403,4.45307572588598,128.711999939724));
#89723=CARTESIAN_POINT('Ctrl Pts',(-65.1451048353875,4.39312481851497,128.588869913132));
#89724=CARTESIAN_POINT('Ctrl Pts',(-65.1528695883346,4.32806646514757,128.468333277023));
#89725=CARTESIAN_POINT('Ctrl Pts',(-65.1606266292196,4.26307272865399,128.347916359601));
#89726=CARTESIAN_POINT('Ctrl Pts',(-65.1683836701047,4.19298182573539,128.230088048543));
#89727=CARTESIAN_POINT('Ctrl Pts',(-65.1761407109897,4.11802957961944,128.115305868425));
#89728=CARTESIAN_POINT('Ctrl Pts',(-65.1838919022299,4.04313385557522,128.000610246441));
#89729=CARTESIAN_POINT('Ctrl Pts',(-65.1916430934701,3.9633842981334,127.888956509165));
#89730=CARTESIAN_POINT('Ctrl Pts',(-65.1993942847103,3.87906204957123,127.780776539344));
#89731=CARTESIAN_POINT('Ctrl Pts',(-65.2071421814874,3.79477564021407,127.672642548897));
#89732=CARTESIAN_POINT('Ctrl Pts',(-65.2148900782645,3.70592064509094,127.567979697082));
#89733=CARTESIAN_POINT('Ctrl Pts',(-65.2226379750416,3.61282068308968,127.467189693813));
#89734=CARTESIAN_POINT('Ctrl Pts',(-65.2303842511257,3.51974019559346,127.366420773641));
#89735=CARTESIAN_POINT('Ctrl Pts',(-65.2381305272098,3.42241677252422,127.269523377659));
#89736=CARTESIAN_POINT('Ctrl Pts',(-65.2458768032939,3.32121309529373,127.176864699147));
#89737=CARTESIAN_POINT('Ctrl Pts',(-65.2536231365593,3.22000867100068,127.084205336649));
#89738=CARTESIAN_POINT('Ctrl Pts',(-65.2613694698248,3.11492422375067,126.995785018068));
#89739=CARTESIAN_POINT('Ctrl Pts',(-65.2691158030902,3.00635763100361,126.911932473463));
#89740=CARTESIAN_POINT('Ctrl Pts',(-65.2768638710932,2.89776672552087,126.828061150661));
#89741=CARTESIAN_POINT('Ctrl Pts',(-65.2846119390962,2.78569243218529,126.748759876268));
#89742=CARTESIAN_POINT('Ctrl Pts',(-65.2923600070992,2.67056355153748,126.67431541446));
#89743=CARTESIAN_POINT('Ctrl Pts',(-65.3001163098411,2.55531231054527,126.599791832192));
#89744=CARTESIAN_POINT('Ctrl Pts',(-65.307872612583,2.4370003259359,126.530135586547));
#89745=CARTESIAN_POINT('Ctrl Pts',(-65.3156289153249,2.31608355019785,126.465588896099));
#89746=CARTESIAN_POINT('Ctrl Pts',(-65.3233893578391,2.19510223753569,126.401007755139));
#89747=CARTESIAN_POINT('Ctrl Pts',(-65.3311498003534,2.07151371567519,126.341541772832));
#89748=CARTESIAN_POINT('Ctrl Pts',(-65.3389102428676,1.94579517687389,126.287385502275));
#89749=CARTESIAN_POINT('Ctrl Pts',(-65.346683143133,1.81987482351351,126.233142295265));
#89750=CARTESIAN_POINT('Ctrl Pts',(-65.3544560433985,1.69181798581307,126.184225972507));
#89751=CARTESIAN_POINT('Ctrl Pts',(-65.362228943664,1.56211917005494,126.140781867181));
#89752=CARTESIAN_POINT('Ctrl Pts',(-65.3697192794256,1.43713523294842,126.098917064514));
#89753=CARTESIAN_POINT('Ctrl Pts',(-65.3772096151873,1.31062692101751,126.062133614897));
#89754=CARTESIAN_POINT('Ctrl Pts',(-65.3846999509489,1.18304492481576,126.030516488526));
#89755=CARTESIAN_POINT('Ctrl Pts',(-65.3924742850679,1.05062561844378,125.997700589197));
#89756=CARTESIAN_POINT('Ctrl Pts',(-65.400248619187,0.916630138556373,125.970346558012));
#89757=CARTESIAN_POINT('Ctrl Pts',(-65.4080229533061,0.781548784059955,
125.948604799917));
#89758=CARTESIAN_POINT('Ctrl Pts',(-65.4157877062532,0.646633905260386,
125.926889836595));
#89759=CARTESIAN_POINT('Ctrl Pts',(-65.4235524592003,0.510636196849151,
125.910773445873));
#89760=CARTESIAN_POINT('Ctrl Pts',(-65.4313172121473,0.374059681983171,
125.900355885022));
#89761=CARTESIAN_POINT('Ctrl Pts',(-65.4390742530323,0.237618816837148,
125.889948671039));
#89762=CARTESIAN_POINT('Ctrl Pts',(-65.4468312939173,0.100600676581215,
125.885229052499));
#89763=CARTESIAN_POINT('Ctrl Pts',(-65.4545883348023,-0.0364823421880473,
125.886245927849));
#89764=CARTESIAN_POINT('Ctrl Pts',(-65.4623395260424,-0.173461985586505,
125.887262036366));
#89765=CARTESIAN_POINT('Ctrl Pts',(-65.4700907172825,-0.310506020742713,
125.894006025375));
#89766=CARTESIAN_POINT('Ctrl Pts',(-65.4778419085227,-0.44709912820108,
125.906474805089));
#89767=CARTESIAN_POINT('Ctrl Pts',(-65.4855898052997,-0.583634179945036,
125.91893828524));
#89768=CARTESIAN_POINT('Ctrl Pts',(-65.4933377020768,-0.719718296649652,
125.937121681203));
#89769=CARTESIAN_POINT('Ctrl Pts',(-65.5010855988538,-0.854838584474578,
125.960969857262));
#89770=CARTESIAN_POINT('Ctrl Pts',(-65.5088318749379,-0.989930608048148,
125.984813044798));
#89771=CARTESIAN_POINT('Ctrl Pts',(-65.516578151022,-1.12405881898928,126.01431858759));
#89772=CARTESIAN_POINT('Ctrl Pts',(-65.5243244271061,-1.25671824903137,
126.04937982843));
#89773=CARTESIAN_POINT('Ctrl Pts',(-65.5320707603714,-1.38937865833506,
126.084441328085));
#89774=CARTESIAN_POINT('Ctrl Pts',(-65.5398170936368,-1.52056988711839,
126.125058507722));
#89775=CARTESIAN_POINT('Ctrl Pts',(-65.5475634269021,-1.64980030298776,
126.171074308394));
#89776=CARTESIAN_POINT('Ctrl Pts',(-65.555311494905,-1.77905965911274,126.217100413985));
#89777=CARTESIAN_POINT('Ctrl Pts',(-65.563059562908,-1.90635696030263,126.268527415225));
#89778=CARTESIAN_POINT('Ctrl Pts',(-65.5708076309109,-2.03121916656682,
126.325149553118));
#89779=CARTESIAN_POINT('Ctrl Pts',(-65.5785639336528,-2.15621407786988,
126.381831869693));
#89780=CARTESIAN_POINT('Ctrl Pts',(-65.5863202363946,-2.27876836771029,
126.443720190894));
#89781=CARTESIAN_POINT('Ctrl Pts',(-65.5940765391365,-2.39843179728367,
126.510561836035));
#89782=CARTESIAN_POINT('Ctrl Pts',(-65.6018369816506,-2.51815909483241,
126.577439156574));
#89783=CARTESIAN_POINT('Ctrl Pts',(-65.6095974241648,-2.6349921247931,126.649274864249));
#89784=CARTESIAN_POINT('Ctrl Pts',(-65.617357866679,-2.74850927006552,126.725772644399));
#89785=CARTESIAN_POINT('Ctrl Pts',(-65.6251307669444,-2.86220864313711,
126.802393225576));
#89786=CARTESIAN_POINT('Ctrl Pts',(-65.6329036672098,-2.97258117959476,
126.883690602592));
#89787=CARTESIAN_POINT('Ctrl Pts',(-65.6406765674752,-3.07923731379335,
126.969327289439));
#89788=CARTESIAN_POINT('Ctrl Pts',(-65.6481669032373,-3.18201622886439,
127.051850867015));
#89789=CARTESIAN_POINT('Ctrl Pts',(-65.6556572389994,-3.2813440195308,127.138403539745));
#89790=CARTESIAN_POINT('Ctrl Pts',(-65.6631475747615,-3.37690558870681,
127.22865205737));
#89791=CARTESIAN_POINT('Ctrl Pts',(-65.6708054564397,-3.47460470567242,
127.320919278968));
#89792=CARTESIAN_POINT('Ctrl Pts',(-65.6784633381179,-3.56869624901928,
127.417360836562));
#89793=CARTESIAN_POINT('Ctrl Pts',(-65.6861212197961,-3.65879426432663,
127.517658989211));
#89794=CARTESIAN_POINT('Ctrl Pts',(-65.6937702152272,-3.74878772941223,
127.617840755345));
#89795=CARTESIAN_POINT('Ctrl Pts',(-65.7014192106583,-3.83479661182774,
127.721869923546));
#89796=CARTESIAN_POINT('Ctrl Pts',(-65.7090682060894,-3.91646911087059,
127.829389564581));
#89797=CARTESIAN_POINT('Ctrl Pts',(-65.7167100992922,-3.99806577554587,
127.936809371719));
#89798=CARTESIAN_POINT('Ctrl Pts',(-65.7243519924951,-4.07533382051231,
128.047712888317));
#89799=CARTESIAN_POINT('Ctrl Pts',(-65.7319938856979,-4.14795971669204,
128.16170792544));
#89800=CARTESIAN_POINT('Ctrl Pts',(-65.7396303820591,-4.2205343231654,128.27562245723));
#89801=CARTESIAN_POINT('Ctrl Pts',(-65.7472668784203,-4.28847308626001,
128.392623827514));
#89802=CARTESIAN_POINT('Ctrl Pts',(-65.7549033747815,-4.3515044086014,128.512288968506));
#89803=CARTESIAN_POINT('Ctrl Pts',(-65.7625365975673,-4.41450871098772,
128.631902812039));
#89804=CARTESIAN_POINT('Ctrl Pts',(-65.7701698203531,-4.47260956978139,
128.754177798339));
#89805=CARTESIAN_POINT('Ctrl Pts',(-65.7778030431388,-4.52558042577481,
128.87866467263));
#89806=CARTESIAN_POINT('Ctrl Pts',(-65.7854364070183,-4.57855226088996,
129.003153847956));
#89807=CARTESIAN_POINT('Ctrl Pts',(-65.7930697708978,-4.62639373549626,
129.129854626074));
#89808=CARTESIAN_POINT('Ctrl Pts',(-65.8007031347773,-4.66892581622505,
129.258296328771));
#89809=CARTESIAN_POINT('Ctrl Pts',(-65.8070593179343,-4.70434161710013,
129.36524773319));
#89810=CARTESIAN_POINT('Ctrl Pts',(-65.8134155010914,-4.73607689232854,
129.473405741533));
#89811=CARTESIAN_POINT('Ctrl Pts',(-65.8197716842484,-4.76405452823398,
129.582490119308));
#89812=CARTESIAN_POINT('Origin',(213.235140564004,0.,130.804360617566));
#89813=CARTESIAN_POINT('',(-67.9154119669996,-4.76405452823407,129.582490119308));
#89814=CARTESIAN_POINT('',(-67.5697761045558,-4.76405452823408,129.582490119308));
#89815=CARTESIAN_POINT('',(213.235140564004,-4.76405452823405,129.582490119308));
#89816=CARTESIAN_POINT('',(-66.235140564045,-4.91824885854051,130.801009801995));
#89817=CARTESIAN_POINT('Ctrl Pts',(-66.235140564045,-4.91824885854051,130.801009801996));
#89818=CARTESIAN_POINT('Ctrl Pts',(-66.2427998121925,-4.91834063041699,
130.935710419581));
#89819=CARTESIAN_POINT('Ctrl Pts',(-66.25045906034,-4.91289448446255,131.070628404356));
#89820=CARTESIAN_POINT('Ctrl Pts',(-66.2581183084876,-4.9018833561888,131.205262880991));
#89821=CARTESIAN_POINT('Ctrl Pts',(-66.2657694033577,-4.89088394927227,
131.339754039089));
#89822=CARTESIAN_POINT('Ctrl Pts',(-66.2734204982278,-4.87433137425639,
131.473961890991));
#89823=CARTESIAN_POINT('Ctrl Pts',(-66.2810715930979,-4.85225058466901,
131.60738448152));
#89824=CARTESIAN_POINT('Ctrl Pts',(-66.2887164947383,-4.83018766852416,
131.740699072242));
#89825=CARTESIAN_POINT('Ctrl Pts',(-66.2963613963786,-4.80260550492369,
131.873229270524));
#89826=CARTESIAN_POINT('Ctrl Pts',(-66.3040062980189,-4.76958091247342,
132.004477687634));
#89827=CARTESIAN_POINT('Ctrl Pts',(-66.3116475322512,-4.73657216256244,
132.135663142326));
#89828=CARTESIAN_POINT('Ctrl Pts',(-66.3192887664834,-4.69812627272704,
132.265567648643));
#89829=CARTESIAN_POINT('Ctrl Pts',(-66.3269300007157,-4.65437118034599,
132.393703871261));
#89830=CARTESIAN_POINT('Ctrl Pts',(-66.3345694738153,-4.61062617252976,
132.521810561361));
#89831=CARTESIAN_POINT('Ctrl Pts',(-66.3422089469151,-4.56157452489964,
132.648149396986));
#89832=CARTESIAN_POINT('Ctrl Pts',(-66.3498484200148,-4.50739392498528,
132.772248588845));
#89833=CARTESIAN_POINT('Ctrl Pts',(-66.357487894633,-4.45321331430047,132.896347805374));
#89834=CARTESIAN_POINT('Ctrl Pts',(-66.3651273692513,-4.39390391070185,
133.018207008109));
#89835=CARTESIAN_POINT('Ctrl Pts',(-66.3727668438696,-4.32969116860841,
133.137375286824));
#89836=CARTESIAN_POINT('Ctrl Pts',(-66.3804080824465,-4.26546359976,133.256571081557));
#89837=CARTESIAN_POINT('Ctrl Pts',(-66.3880493210234,-4.19633063253334,
133.373074362418));
#89838=CARTESIAN_POINT('Ctrl Pts',(-66.3956905596002,-4.12256291951449,
133.486460175216));
#89839=CARTESIAN_POINT('Ctrl Pts',(-66.4033397192723,-4.04871873707678,
133.599963526525));
#89840=CARTESIAN_POINT('Ctrl Pts',(-66.4109888789443,-3.97023043644532,
133.710342619686));
#89841=CARTESIAN_POINT('Ctrl Pts',(-66.4186380386163,-3.88741129824348,
133.817202541861));
#89842=CARTESIAN_POINT('Ctrl Pts',(-66.4262915254948,-3.80454530842361,
133.924122915767));
#89843=CARTESIAN_POINT('Ctrl Pts',(-66.4339450123733,-3.71734386289516,
134.027519848115));
#89844=CARTESIAN_POINT('Ctrl Pts',(-66.4415984992518,-3.62615863655848,
134.127033728935));
#89845=CARTESIAN_POINT('Ctrl Pts',(-66.4492633983006,-3.53483744326241,
134.226695995631));
#89846=CARTESIAN_POINT('Ctrl Pts',(-66.4569282973494,-3.43952089224874,
134.322463365574));
#89847=CARTESIAN_POINT('Ctrl Pts',(-66.4645931963983,-3.34059572849287,
134.414014789544));
#89848=CARTESIAN_POINT('Ctrl Pts',(-66.4693626142791,-3.2790403913808,134.470981880136));
#89849=CARTESIAN_POINT('Ctrl Pts',(-66.4741320321599,-3.21608850216308,
134.52631743402));
#89850=CARTESIAN_POINT('Ctrl Pts',(-66.4789014500408,-3.1518389214251,134.579952554718));
#89851=CARTESIAN_POINT('Ctrl Pts',(-66.4866757841598,-3.04710963995969,
134.667379859107));
#89852=CARTESIAN_POINT('Ctrl Pts',(-66.4944501182789,-2.93857406374783,
134.750584788941));
#89853=CARTESIAN_POINT('Ctrl Pts',(-66.502224452398,-2.82660732586373,134.829217644576));
#89854=CARTESIAN_POINT('Ctrl Pts',(-66.5099892053451,-2.71477857697762,
134.907753592244));
#89855=CARTESIAN_POINT('Ctrl Pts',(-66.5177539582921,-2.59952739694863,
134.981728454494));
#89856=CARTESIAN_POINT('Ctrl Pts',(-66.5255187112392,-2.48126319403188,
135.050831625879));
#89857=CARTESIAN_POINT('Ctrl Pts',(-66.5332757521242,-2.36311645278838,
135.11986616302));
#89858=CARTESIAN_POINT('Ctrl Pts',(-66.5410327930092,-2.24196297939929,
135.184038442426));
#89859=CARTESIAN_POINT('Ctrl Pts',(-66.5487898338942,-2.11824217514571,
135.243080382311));
#89860=CARTESIAN_POINT('Ctrl Pts',(-66.5565410251343,-1.99461466971319,
135.302077798209));
#89861=CARTESIAN_POINT('Ctrl Pts',(-66.5642922163745,-1.86842403841305,
135.35595240755));
#89862=CARTESIAN_POINT('Ctrl Pts',(-66.5720434076146,-1.7401350492394,135.404481602161));
#89863=CARTESIAN_POINT('Ctrl Pts',(-66.5797913043917,-1.6119005863082,135.452990170569));
#89864=CARTESIAN_POINT('Ctrl Pts',(-66.5875392011687,-1.48156990425189,
135.49615770493));
#89865=CARTESIAN_POINT('Ctrl Pts',(-66.5952870979458,-1.3496283532354,135.533809461844));
#89866=CARTESIAN_POINT('Ctrl Pts',(-66.6030333740299,-1.21771440154723,
135.571453342822));
#89867=CARTESIAN_POINT('Ctrl Pts',(-66.6107796501141,-1.08419062684762,
135.60358363407));
#89868=CARTESIAN_POINT('Ctrl Pts',(-66.6185259261982,-0.949557786093246,
135.630075390879));
#89869=CARTESIAN_POINT('Ctrl Pts',(-66.6262722594635,-0.814923951509823,
135.656567343244));
#89870=CARTESIAN_POINT('Ctrl Pts',(-66.6340185927289,-0.679181418144645,
135.677420602631));
#89871=CARTESIAN_POINT('Ctrl Pts',(-66.6417649259942,-0.542840994622834,
135.692561382373));
#89872=CARTESIAN_POINT('Ctrl Pts',(-66.6495129939972,-0.406470038608121,
135.707705552787));
#89873=CARTESIAN_POINT('Ctrl Pts',(-66.6572610620002,-0.269501314506633,
135.717134654811));
#89874=CARTESIAN_POINT('Ctrl Pts',(-66.6650091300032,-0.13245021124291,
135.72082682858));
#89875=CARTESIAN_POINT('Ctrl Pts',(-66.6727654327451,0.00474655156410364,
135.724522926435));
#89876=CARTESIAN_POINT('Ctrl Pts',(-66.6805217354869,0.142025476984417,
135.722469905523));
#89877=CARTESIAN_POINT('Ctrl Pts',(-66.6882780382287,0.278871158475106,
135.714698074347));
#89878=CARTESIAN_POINT('Ctrl Pts',(-66.6960384807429,0.41578987862635,135.706922095111));
#89879=CARTESIAN_POINT('Ctrl Pts',(-66.7037989232571,0.552274505215999,
135.69342126211));
#89880=CARTESIAN_POINT('Ctrl Pts',(-66.7115593657713,0.687816286316394,
135.674277641374));
#89881=CARTESIAN_POINT('Ctrl Pts',(-66.7193322660367,0.823575651116645,
135.655103289599));
#89882=CARTESIAN_POINT('Ctrl Pts',(-66.7271051663021,0.958388761177205,
135.630268119585));
#89883=CARTESIAN_POINT('Ctrl Pts',(-66.7348780665676,1.09175768058041,135.599905240379));
#89884=CARTESIAN_POINT('Ctrl Pts',(-66.7423684023296,1.22027830382709,135.570646128312));
#89885=CARTESIAN_POINT('Ctrl Pts',(-66.7498587380916,1.34745761606107,135.536254302324));
#89886=CARTESIAN_POINT('Ctrl Pts',(-66.7573490738536,1.47286650206953,135.496891632869));
#89887=CARTESIAN_POINT('Ctrl Pts',(-66.7651234079727,1.60303030410823,135.456036515837));
#89888=CARTESIAN_POINT('Ctrl Pts',(-66.7728977420918,1.73169909813534,135.409696758652));
#89889=CARTESIAN_POINT('Ctrl Pts',(-66.7806720762109,1.85837590334509,135.357998950193));
#89890=CARTESIAN_POINT('Ctrl Pts',(-66.788436829158,1.98489659071403,135.306364854661));
#89891=CARTESIAN_POINT('Ctrl Pts',(-66.796201582105,2.10942981537455,135.249385992802));
#89892=CARTESIAN_POINT('Ctrl Pts',(-66.8039663350521,2.23149296100489,135.187238921545));
#89893=CARTESIAN_POINT('Ctrl Pts',(-66.8117233759371,2.35343487179804,135.125153575634));
#89894=CARTESIAN_POINT('Ctrl Pts',(-66.8194804168222,2.47291123962067,135.057910411741));
#89895=CARTESIAN_POINT('Ctrl Pts',(-66.8272374577072,2.58945901254748,134.985734205854));
#89896=CARTESIAN_POINT('Ctrl Pts',(-66.8349886489473,2.70591889589228,134.913612428606));
#89897=CARTESIAN_POINT('Ctrl Pts',(-66.8427398401874,2.81945424913524,134.836565218898));
#89898=CARTESIAN_POINT('Ctrl Pts',(-66.8504910314275,2.92962656726045,134.754863274052));
#89899=CARTESIAN_POINT('Ctrl Pts',(-66.8582389282046,3.03975205921122,134.673196054712));
#89900=CARTESIAN_POINT('Ctrl Pts',(-66.8659868249817,3.14651704559254,134.586878267489));
#89901=CARTESIAN_POINT('Ctrl Pts',(-66.8737347217587,3.24951216621316,134.496223798147));
#89902=CARTESIAN_POINT('Ctrl Pts',(-66.8814809978428,3.35248574247486,134.405588291767));
#89903=CARTESIAN_POINT('Ctrl Pts',(-66.8892272739268,3.45169072820364,134.310618165768));
#89904=CARTESIAN_POINT('Ctrl Pts',(-66.8969735500109,3.54675133250987,134.211667185493));
#89905=CARTESIAN_POINT('Ctrl Pts',(-66.9047198832763,3.64181263853189,134.112715474785));
#89906=CARTESIAN_POINT('Ctrl Pts',(-66.9124662165416,3.73272923122931,134.009783133105));
#89907=CARTESIAN_POINT('Ctrl Pts',(-66.9202125498069,3.81916292724842,133.903260034719));
#89908=CARTESIAN_POINT('Ctrl Pts',(-66.9279606178099,3.90561597949447,133.796713081224));
#89909=CARTESIAN_POINT('Ctrl Pts',(-66.9357086858128,3.98758389109744,133.686574074445));
#89910=CARTESIAN_POINT('Ctrl Pts',(-66.9434567538158,4.06476969042986,133.573264809889));
#89911=CARTESIAN_POINT('Ctrl Pts',(-66.9512130565576,4.14203752374834,133.459835118898));
#89912=CARTESIAN_POINT('Ctrl Pts',(-66.9589693592995,4.21451287152458,133.343228763051));
#89913=CARTESIAN_POINT('Ctrl Pts',(-66.9667256620413,4.28194264333406,133.223895750954));
#89914=CARTESIAN_POINT('Ctrl Pts',(-66.9744861045555,4.34940840444312,133.104499047235));
#89915=CARTESIAN_POINT('Ctrl Pts',(-66.9822465470696,4.41182304576945,132.982373135426));
#89916=CARTESIAN_POINT('Ctrl Pts',(-66.9900069895838,4.46898061894604,132.857990401628));
#89917=CARTESIAN_POINT('Ctrl Pts',(-66.9977798898492,4.5262299465333,132.733407997622));
#89918=CARTESIAN_POINT('Ctrl Pts',(-67.0055527901146,4.578205193613,132.606561893998));
#89919=CARTESIAN_POINT('Ctrl Pts',(-67.0133256903801,4.6247492020701,132.477942967034));
#89920=CARTESIAN_POINT('Ctrl Pts',(-67.0208160261422,4.66960121858307,132.353999662036));
#89921=CARTESIAN_POINT('Ctrl Pts',(-67.0283063619043,4.70940992614292,132.228410482733));
#89922=CARTESIAN_POINT('Ctrl Pts',(-67.0357966976664,4.74407956369188,132.101623950842));
#89923=CARTESIAN_POINT('Ctrl Pts',(-67.0435710317855,4.78006371108571,131.970030269058));
#89924=CARTESIAN_POINT('Ctrl Pts',(-67.0513453659046,4.81062538703736,131.836729797883));
#89925=CARTESIAN_POINT('Ctrl Pts',(-67.0591197000237,4.83560246409114,131.702209085725));
#89926=CARTESIAN_POINT('Ctrl Pts',(-67.0668844529708,4.86054875912971,131.567854158322));
#89927=CARTESIAN_POINT('Ctrl Pts',(-67.0746492059179,4.87992407874462,131.43228236283));
#89928=CARTESIAN_POINT('Ctrl Pts',(-67.082413958865,4.89361609937007,131.295995171362));
#89929=CARTESIAN_POINT('Ctrl Pts',(-67.09017099975,4.90729452088759,131.159843342254));
#89930=CARTESIAN_POINT('Ctrl Pts',(-67.097928040635,4.91530083785992,131.022977917668));
#89931=CARTESIAN_POINT('Ctrl Pts',(-67.10568508152,4.91757386981557,130.885909973217));
#89932=CARTESIAN_POINT('Ctrl Pts',(-67.1134362727602,4.91984518766016,130.748945392768));
#89933=CARTESIAN_POINT('Ctrl Pts',(-67.1211874640003,4.91639181972575,130.611778985766));
#89934=CARTESIAN_POINT('Ctrl Pts',(-67.1289386552404,4.90720448866213,130.474925997415));
#89935=CARTESIAN_POINT('Ctrl Pts',(-67.1366865520175,4.89802106245932,130.338131175234));
#89936=CARTESIAN_POINT('Ctrl Pts',(-67.1444344487947,4.88310854644099,130.201649896027));
#89937=CARTESIAN_POINT('Ctrl Pts',(-67.1521823455718,4.86250975240698,130.065996229038));
#89938=CARTESIAN_POINT('Ctrl Pts',(-67.1599286216559,4.84191526719659,129.930370937871));
#89939=CARTESIAN_POINT('Ctrl Pts',(-67.1676748977398,4.81563692850278,129.795573300869));
#89940=CARTESIAN_POINT('Ctrl Pts',(-67.1754211738239,4.78376924497211,129.662110700359));
#89941=CARTESIAN_POINT('Ctrl Pts',(-67.1831675070893,4.75190132620147,129.528647114659));
#89942=CARTESIAN_POINT('Ctrl Pts',(-67.1909138403547,4.71444407106468,129.39651896539));
#89943=CARTESIAN_POINT('Ctrl Pts',(-67.19866017362,4.67154269546031,129.266221512351));
#89944=CARTESIAN_POINT('Ctrl Pts',(-67.206408241623,4.62863171239034,129.135894880101));
#89945=CARTESIAN_POINT('Ctrl Pts',(-67.214156309626,4.58027430508712,129.007400131158));
#89946=CARTESIAN_POINT('Ctrl Pts',(-67.221904377629,4.52666482163802,128.881215106939));
#89947=CARTESIAN_POINT('Ctrl Pts',(-67.2296606803708,4.47299836139194,128.754895971775));
#89948=CARTESIAN_POINT('Ctrl Pts',(-67.2374169831126,4.41406882753546,128.630891825478));
#89949=CARTESIAN_POINT('Ctrl Pts',(-67.2451732858545,4.35011802349843,128.509658840835));
#89950=CARTESIAN_POINT('Ctrl Pts',(-67.2529337283686,4.28613308699168,128.388361150497));
#89951=CARTESIAN_POINT('Ctrl Pts',(-67.2606941708829,4.21712173680047,128.269837906651));
#89952=CARTESIAN_POINT('Ctrl Pts',(-67.2684546133971,4.14337008460657,128.154517715716));
#89953=CARTESIAN_POINT('Ctrl Pts',(-67.2762275136625,4.0695000397132,128.039012402572));
#89954=CARTESIAN_POINT('Ctrl Pts',(-67.2840004139279,3.99087471087767,127.926720737791));
#89955=CARTESIAN_POINT('Ctrl Pts',(-67.2917733141934,3.9078221384177,127.818040273565));
#89956=CARTESIAN_POINT('Ctrl Pts',(-67.2992636499554,3.8277887361638,127.713310617965));
#89957=CARTESIAN_POINT('Ctrl Pts',(-67.3067539857174,3.7436445815651,127.611934405756));
#89958=CARTESIAN_POINT('Ctrl Pts',(-67.3142443214794,3.65571526745278,127.514234640371));
#89959=CARTESIAN_POINT('Ctrl Pts',(-67.3220186555985,3.56445208666996,127.412830558687));
#89960=CARTESIAN_POINT('Ctrl Pts',(-67.3297929897175,3.46882195736728,127.315065994442));
#89961=CARTESIAN_POINT('Ctrl Pts',(-67.3375673238366,3.36914659265055,127.221340341356));
#89962=CARTESIAN_POINT('Ctrl Pts',(-67.3453320767837,3.26959406891244,127.127730196761));
#89963=CARTESIAN_POINT('Ctrl Pts',(-67.3530968297308,3.1660065112925,127.038149324643));
#89964=CARTESIAN_POINT('Ctrl Pts',(-67.3608615826779,3.05874510885052,126.952963283924));
#89965=CARTESIAN_POINT('Ctrl Pts',(-67.3686186235629,2.95159023994586,126.867861851182));
#89966=CARTESIAN_POINT('Ctrl Pts',(-67.3763756644479,2.84076909190066,126.78714680485));
#89967=CARTESIAN_POINT('Ctrl Pts',(-67.3841327053329,2.72667857756171,126.711145866644));
#89968=CARTESIAN_POINT('Ctrl Pts',(-67.391883896573,2.6126740997679,126.635202241337));
#89969=CARTESIAN_POINT('Ctrl Pts',(-67.399635087813,2.49540548708247,126.563965864125));
#89970=CARTESIAN_POINT('Ctrl Pts',(-67.4073862790531,2.37530121525251,126.497723042924));
#89971=CARTESIAN_POINT('Ctrl Pts',(-67.4151341758302,2.25524799094115,126.431508376688));
#89972=CARTESIAN_POINT('Ctrl Pts',(-67.4228820726073,2.13236184622706,126.370283233607));
#89973=CARTESIAN_POINT('Ctrl Pts',(-67.4306299693844,2.00709842294861,126.314289461883));
#89974=CARTESIAN_POINT('Ctrl Pts',(-67.4383762454685,1.88186120207777,126.258307402849));
#89975=CARTESIAN_POINT('Ctrl Pts',(-67.4461225215526,1.75424804845261,126.207554698018));
#89976=CARTESIAN_POINT('Ctrl Pts',(-67.4538687976367,1.62473692142669,126.162226087131));
#89977=CARTESIAN_POINT('Ctrl Pts',(-67.461615130902,1.49522483837958,126.116897141639));
#89978=CARTESIAN_POINT('Ctrl Pts',(-67.4693614641674,1.36381512299099,126.076992499141));
#89979=CARTESIAN_POINT('Ctrl Pts',(-67.4771077974327,1.23100294409522,126.042657685407));
#89980=CARTESIAN_POINT('Ctrl Pts',(-67.4848558654357,1.09816102283176,126.00831518263));
#89981=CARTESIAN_POINT('Ctrl Pts',(-67.4926039334387,0.963916391542621,
125.979545088484));
#89982=CARTESIAN_POINT('Ctrl Pts',(-67.5003520014418,0.828776121632136,
125.956442177378));
#89983=CARTESIAN_POINT('Ctrl Pts',(-67.5081083041836,0.693492223035338,
125.933314712224));
#89984=CARTESIAN_POINT('Ctrl Pts',(-67.5158646069254,0.557311170292499,
125.915866527985));
#89985=CARTESIAN_POINT('Ctrl Pts',(-67.5236209096673,0.420747455148574,
125.904140761122));
#89986=CARTESIAN_POINT('Ctrl Pts',(-67.5313813521815,0.28411085183821,125.892408735865));
#89987=CARTESIAN_POINT('Ctrl Pts',(-67.5391417946956,0.147091569563719,
125.886405230893));
#89988=CARTESIAN_POINT('Ctrl Pts',(-67.5469022372098,0.0102048573974459,
125.886121204586));
#89989=CARTESIAN_POINT('Ctrl Pts',(-67.5546751374752,-0.126901597471801,
125.885836722335));
#89990=CARTESIAN_POINT('Ctrl Pts',(-67.5624480377406,-0.263874666083487,
125.891290050579));
#89991=CARTESIAN_POINT('Ctrl Pts',(-67.570220938006,-0.400202562713456,
125.902420086379));
#89992=CARTESIAN_POINT('Ctrl Pts',(-67.5777112737681,-0.531574596912417,
125.913145517342));
#89993=CARTESIAN_POINT('Ctrl Pts',(-67.5852016095302,-0.662347246264545,
125.929142058742));
#89994=CARTESIAN_POINT('Ctrl Pts',(-67.5926919452923,-0.792072767955476,
125.950310371353));
#89995=CARTESIAN_POINT('Ctrl Pts',(-67.6004662794114,-0.926716872229778,
125.97228128697));
#89996=CARTESIAN_POINT('Ctrl Pts',(-67.6082406135304,-1.06065938974916,
125.999893488132));
#89997=CARTESIAN_POINT('Ctrl Pts',(-67.6160149476495,-1.19339040547402,
126.033092190552));
#89998=CARTESIAN_POINT('Ctrl Pts',(-67.6237797005965,-1.32595784208378,
126.066249978538));
#89999=CARTESIAN_POINT('Ctrl Pts',(-67.6315444535437,-1.45731637201854,
126.104980475001));
#90000=CARTESIAN_POINT('Ctrl Pts',(-67.6393092064907,-1.58696320869375,
126.149177394883));
#90001=CARTESIAN_POINT('Ctrl Pts',(-67.6470662473757,-1.71648127830342,
126.19333041776));
#90002=CARTESIAN_POINT('Ctrl Pts',(-67.6548232882607,-1.84429067022652,
126.242938934112));
#90003=CARTESIAN_POINT('Ctrl Pts',(-67.6625803291456,-1.96990112181394,
126.29784615151));
#90004=CARTESIAN_POINT('Ctrl Pts',(-67.6703315203858,-2.0954168495827,126.352711962947));
#90005=CARTESIAN_POINT('Ctrl Pts',(-67.6780827116259,-2.21873658085227,
126.412868366091));
#90006=CARTESIAN_POINT('Ctrl Pts',(-67.6858339028661,-2.3393878350576,126.478109628582));
#90007=CARTESIAN_POINT('Ctrl Pts',(-67.6935817996431,-2.45998780926175,
126.543323161796));
#90008=CARTESIAN_POINT('Ctrl Pts',(-67.7013296964201,-2.57792121900156,
126.613617070318));
#90009=CARTESIAN_POINT('Ctrl Pts',(-67.7090775931972,-2.69273830499027,
126.688738734626));
#90010=CARTESIAN_POINT('Ctrl Pts',(-67.7168238692813,-2.80753137371962,
126.763844685101));
#90011=CARTESIAN_POINT('Ctrl Pts',(-67.7245701453654,-2.91920908834374,
126.843776168773));
#90012=CARTESIAN_POINT('Ctrl Pts',(-67.7323164214496,-3.02734926009838,
126.928236326488));
#90013=CARTESIAN_POINT('Ctrl Pts',(-67.7400627547149,-3.13549023011905,
127.012697107669));
#90014=CARTESIAN_POINT('Ctrl Pts',(-67.7478090879802,-3.2400932970392,127.101686388947));
#90015=CARTESIAN_POINT('Ctrl Pts',(-67.7555554212455,-3.34076837505722,
127.194866230991));
#90016=CARTESIAN_POINT('Ctrl Pts',(-67.7633034892485,-3.44146599856053,
127.288066940014));
#90017=CARTESIAN_POINT('Ctrl Pts',(-67.7710515572514,-3.53823359589458,
127.385459811688));
#90018=CARTESIAN_POINT('Ctrl Pts',(-67.7787996252544,-3.63071734618682,
127.486669460361));
#90019=CARTESIAN_POINT('Ctrl Pts',(-67.7865559279962,-3.72329938930995,
127.587986675853));
#90020=CARTESIAN_POINT('Ctrl Pts',(-67.7943122307381,-3.81158822628296,
127.693128482597));
#90021=CARTESIAN_POINT('Ctrl Pts',(-67.8020685334799,-3.8952694698251,127.801685340426));
#90022=CARTESIAN_POINT('Ctrl Pts',(-67.8098289759941,-3.97899537656674,
127.910300138319));
#90023=CARTESIAN_POINT('Ctrl Pts',(-67.8175894185082,-4.05810856427903,
128.022333300004));
#90024=CARTESIAN_POINT('Ctrl Pts',(-67.8253498610224,-4.13233813522523,
128.137346444626));
#90025=CARTESIAN_POINT('Ctrl Pts',(-67.8331227612879,-4.20668686606839,
128.252544218558));
#90026=CARTESIAN_POINT('Ctrl Pts',(-67.8408956615533,-4.2761361159087,128.370731197581));
#90027=CARTESIAN_POINT('Ctrl Pts',(-67.8486685618188,-4.34046065969393,
128.491443774238));
#90028=CARTESIAN_POINT('Ctrl Pts',(-67.8561588975809,-4.40244684428977,
128.607768144679));
#90029=CARTESIAN_POINT('Ctrl Pts',(-67.863649233343,-4.45967431223964,128.726437399618));
#90030=CARTESIAN_POINT('Ctrl Pts',(-67.8711395691052,-4.51198462451892,
128.847021145066));
#90031=CARTESIAN_POINT('Ctrl Pts',(-67.8797294403174,-4.57197377050905,
128.985305846391));
#90032=CARTESIAN_POINT('Ctrl Pts',(-67.8883193115296,-4.62565936726916,
129.126483064055));
#90033=CARTESIAN_POINT('Ctrl Pts',(-67.8969091827418,-4.67278164609967,
129.269989492194));
#90034=CARTESIAN_POINT('Ctrl Pts',(-67.9030767774944,-4.70661581106723,
129.373028230644));
#90035=CARTESIAN_POINT('Ctrl Pts',(-67.9092443722471,-4.73706726407475,
129.47726718594));
#90036=CARTESIAN_POINT('Ctrl Pts',(-67.9154119669996,-4.76405452823407,
129.582490119308));
#90037=CARTESIAN_POINT('Ctrl Pts',(-66.1650696236364,-4.76405452823402,
129.582490119308));
#90038=CARTESIAN_POINT('Ctrl Pts',(-66.1728438719774,-4.79808884234628,
129.715189393489));
#90039=CARTESIAN_POINT('Ctrl Pts',(-66.1806181203184,-4.82653451571629,
129.849155293682));
#90040=CARTESIAN_POINT('Ctrl Pts',(-66.1883923686595,-4.84932882642928,
129.983877226106));
#90041=CARTESIAN_POINT('Ctrl Pts',(-66.1924128545156,-4.861117001929,130.053549250984));
#90042=CARTESIAN_POINT('Ctrl Pts',(-66.1964333403718,-4.87139458023908,
130.12342340788));
#90043=CARTESIAN_POINT('Ctrl Pts',(-66.200453826228,-4.88015835202264,130.193428934246));
#90044=CARTESIAN_POINT('Ctrl Pts',(-66.2120160721548,-4.905361496178,130.394753137599));
#90045=CARTESIAN_POINT('Ctrl Pts',(-66.2235783180815,-4.91811032154685,
130.597668476328));
#90046=CARTESIAN_POINT('Ctrl Pts',(-66.2351405640084,-4.91824885854007,
130.801009801352));
#90047=CARTESIAN_POINT('',(-65.889859435952,-4.91824814305622,130.808634471095));
#90048=CARTESIAN_POINT('Ctrl Pts',(-65.8197716842484,-4.76405452823398,
129.582490119308));
#90049=CARTESIAN_POINT('Ctrl Pts',(-65.8274085485116,-4.79766926250685,
129.713553458063));
#90050=CARTESIAN_POINT('Ctrl Pts',(-65.8350454127747,-4.82585821990346,
129.845954040388));
#90051=CARTESIAN_POINT('Ctrl Pts',(-65.8426822770379,-4.84853448028878,
129.979196115209));
#90052=CARTESIAN_POINT('Ctrl Pts',(-65.8505451368569,-4.87188179280929,
130.116381184918));
#90053=CARTESIAN_POINT('Ctrl Pts',(-65.858407996676,-4.88938500251125,130.254457868088));
#90054=CARTESIAN_POINT('Ctrl Pts',(-65.866270856495,-4.90100668618583,130.392879725589));
#90055=CARTESIAN_POINT('Ctrl Pts',(-65.874133716314,-4.91262836986042,130.531301583091));
#90056=CARTESIAN_POINT('Ctrl Pts',(-65.8819965761329,-4.91836855425554,
130.670068150686));
#90057=CARTESIAN_POINT('Ctrl Pts',(-65.8898594359519,-4.91824814305622,
130.808634471095));
#90058=CARTESIAN_POINT('Ctrl Pts',(-65.8898594359911,-4.91824814305563,
130.808634471784));
#90059=CARTESIAN_POINT('Ctrl Pts',(-65.9014631194068,-4.91807044515766,
131.013124918148));
#90060=CARTESIAN_POINT('Ctrl Pts',(-65.9130668028225,-4.90513620346425,
131.217082535833));
#90061=CARTESIAN_POINT('Ctrl Pts',(-65.9246704862381,-4.87966224002228,
131.419242301958));
#90062=CARTESIAN_POINT('Ctrl Pts',(-65.9303120570168,-4.86727710655853,
131.517529939458));
#90063=CARTESIAN_POINT('Ctrl Pts',(-65.9359536277956,-4.85192848519588,
131.615393185222));
#90064=CARTESIAN_POINT('Ctrl Pts',(-65.9415951985743,-4.83364483722309,
131.712689109956));
#90065=CARTESIAN_POINT('Ctrl Pts',(-65.9493695326934,-4.80844916143868,
131.84676719866));
#90066=CARTESIAN_POINT('Ctrl Pts',(-65.9571438668125,-4.77763066080824,
131.980008527351));
#90067=CARTESIAN_POINT('Ctrl Pts',(-65.9649182009316,-4.74125634039637,
132.111904642504));
#90068=CARTESIAN_POINT('Ctrl Pts',(-65.9726829538787,-4.70492684808359,
132.243638207482));
#90069=CARTESIAN_POINT('Ctrl Pts',(-65.9804477068258,-4.66305526252321,
132.374029484283));
#90070=CARTESIAN_POINT('Ctrl Pts',(-65.9882124597729,-4.61575990365766,
132.502578381661));
#90071=CARTESIAN_POINT('Ctrl Pts',(-65.9959695006579,-4.56851151920922,
132.630999602461));
#90072=CARTESIAN_POINT('Ctrl Pts',(-66.003726541543,-4.51585021588766,132.757581720831));
#90073=CARTESIAN_POINT('Ctrl Pts',(-66.011483582428,-4.45794450591964,132.88183837789));
#90074=CARTESIAN_POINT('Ctrl Pts',(-66.0192347736681,-4.40008246309811,
133.006001332037));
#90075=CARTESIAN_POINT('Ctrl Pts',(-66.0269859649082,-4.33698404999113,
133.127841962465));
#90076=CARTESIAN_POINT('Ctrl Pts',(-66.0347371561483,-4.26886627794321,
133.246892861681));
#90077=CARTESIAN_POINT('Ctrl Pts',(-66.0424850529254,-4.20077745776532,
133.365893161088));
#90078=CARTESIAN_POINT('Ctrl Pts',(-66.0502329497024,-4.12767371549681,
133.482105748937));
#90079=CARTESIAN_POINT('Ctrl Pts',(-66.0579808464795,-4.04981839089362,
133.595087057631));
#90080=CARTESIAN_POINT('Ctrl Pts',(-66.0657271225636,-3.97197935194598,
133.708044733072));
#90081=CARTESIAN_POINT('Ctrl Pts',(-66.0734733986479,-3.88939092934408,
133.817772152061));
#90082=CARTESIAN_POINT('Ctrl Pts',(-66.081219674732,-3.8023600281203,133.923854371215));
#90083=CARTESIAN_POINT('Ctrl Pts',(-66.0889660079974,-3.71532848445418,
134.029937373444));
#90084=CARTESIAN_POINT('Ctrl Pts',(-66.0967123412627,-3.62385464470653,
134.132374819885));
#90085=CARTESIAN_POINT('Ctrl Pts',(-66.104458674528,-3.52828571187385,134.230784846684));
#90086=CARTESIAN_POINT('Ctrl Pts',(-66.112206742531,-3.43269537704155,134.329216911726));
#90087=CARTESIAN_POINT('Ctrl Pts',(-66.119954810534,-3.33300839658943,134.423619482005));
#90088=CARTESIAN_POINT('Ctrl Pts',(-66.127702878537,-3.22960853879268,134.513647846759));
#90089=CARTESIAN_POINT('Ctrl Pts',(-66.1354591812789,-3.12609878639644,
134.603771894732));
#90090=CARTESIAN_POINT('Ctrl Pts',(-66.1432154840207,-3.01886856924686,
134.689512193247));
#90091=CARTESIAN_POINT('Ctrl Pts',(-66.1509717867625,-2.90833485400029,
134.770564273394));
#90092=CARTESIAN_POINT('Ctrl Pts',(-66.1587322292767,-2.79774214358164,
134.851659613478));
#90093=CARTESIAN_POINT('Ctrl Pts',(-66.1664926717908,-2.68384274631323,
134.928061531575));
#90094=CARTESIAN_POINT('Ctrl Pts',(-66.174253114305,-2.56708141760555,134.999509727894));
#90095=CARTESIAN_POINT('Ctrl Pts',(-66.1820260145704,-2.45013265324744,
135.0710726192));
#90096=CARTESIAN_POINT('Ctrl Pts',(-66.1897989148359,-2.3303131186512,135.137665707753));
#90097=CARTESIAN_POINT('Ctrl Pts',(-66.1975718151014,-2.20809169254464,
135.19907495866));
#90098=CARTESIAN_POINT('Ctrl Pts',(-66.2050621508634,-2.09031332313426,
135.258251828616));
#90099=CARTESIAN_POINT('Ctrl Pts',(-66.2125524866254,-1.97030494057341,
135.312615081556));
#90100=CARTESIAN_POINT('Ctrl Pts',(-66.2200428223875,-1.84850061700697,
135.362016652352));
#90101=CARTESIAN_POINT('Ctrl Pts',(-66.2278171565065,-1.72207804549089,
135.41329129872));
#90102=CARTESIAN_POINT('Ctrl Pts',(-66.2355914906256,-1.59332018969813,
135.459383014073));
#90103=CARTESIAN_POINT('Ctrl Pts',(-66.2433658247447,-1.46269104385342,
135.500073340117));
#90104=CARTESIAN_POINT('Ctrl Pts',(-66.2511305776918,-1.3322228867563,135.540713518972));
#90105=CARTESIAN_POINT('Ctrl Pts',(-66.2588953306389,-1.19988839794507,
135.57596543827));
#90106=CARTESIAN_POINT('Ctrl Pts',(-66.266660083586,-1.0661722731674,135.605658332396));
#90107=CARTESIAN_POINT('Ctrl Pts',(-66.274417124471,-0.932588957130112,
135.635321735121));
#90108=CARTESIAN_POINT('Ctrl Pts',(-66.282174165356,-0.797627115184929,
135.659437016109));
#90109=CARTESIAN_POINT('Ctrl Pts',(-66.289931206241,-0.661787019806354,
135.677883060616));
#90110=CARTESIAN_POINT('Ctrl Pts',(-66.2976823974811,-0.526049362500386,
135.696315194818));
#90111=CARTESIAN_POINT('Ctrl Pts',(-66.3054335887212,-0.389435155866664,
135.7090865497));
#90112=CARTESIAN_POINT('Ctrl Pts',(-66.3131847799613,-0.252454942999151,
135.716127057886));
#90113=CARTESIAN_POINT('Ctrl Pts',(-66.3209326767384,-0.115532950375987,
135.723164573669));
#90114=CARTESIAN_POINT('Ctrl Pts',(-66.3286805735155,0.0217543494468244,
135.724476067275));
#90115=CARTESIAN_POINT('Ctrl Pts',(-66.3364284702926,0.158891428918405,
135.72004333478));
#90116=CARTESIAN_POINT('Ctrl Pts',(-66.3441747463767,0.295999822269294,
135.715611529517));
#90117=CARTESIAN_POINT('Ctrl Pts',(-66.3519210224609,0.432957667257184,
135.705437900761));
#90118=CARTESIAN_POINT('Ctrl Pts',(-66.359667298545,0.569249970595441,135.689556369373));
#90119=CARTESIAN_POINT('Ctrl Pts',(-66.3674136318104,0.705543280012333,
135.673674720752));
#90120=CARTESIAN_POINT('Ctrl Pts',(-66.3751599650757,0.841170649638669,
135.652085130674));
#90121=CARTESIAN_POINT('Ctrl Pts',(-66.3829062983411,0.975623134898289,
135.624873304112));
#90122=CARTESIAN_POINT('Ctrl Pts',(-66.390654366344,1.11010572985975,135.597655383651));
#90123=CARTESIAN_POINT('Ctrl Pts',(-66.398402434347,1.24341253377916,135.564812798861));
#90124=CARTESIAN_POINT('Ctrl Pts',(-66.40615050235,1.37504609560438,135.526482100275));
#90125=CARTESIAN_POINT('Ctrl Pts',(-66.4139068050918,1.50681955914575,135.488110663367));
#90126=CARTESIAN_POINT('Ctrl Pts',(-66.4216631078336,1.63691585219103,135.444239570432));
#90127=CARTESIAN_POINT('Ctrl Pts',(-66.4294194105755,1.76485343576031,135.395055054444));
#90128=CARTESIAN_POINT('Ctrl Pts',(-66.4371798530897,1.89285930347006,135.345844287199));
#90129=CARTESIAN_POINT('Ctrl Pts',(-66.4449402956039,2.01870380735118,135.291314601431));
#90130=CARTESIAN_POINT('Ctrl Pts',(-66.4527007381181,2.1419275486525,135.231699484066));
#90131=CARTESIAN_POINT('Ctrl Pts',(-66.4604736383835,2.26534909964264,135.171988667222));
#90132=CARTESIAN_POINT('Ctrl Pts',(-66.468246538649,2.38614113626038,135.10717629029));
#90133=CARTESIAN_POINT('Ctrl Pts',(-66.4760194389144,2.50387014448361,135.037541143136));
#90134=CARTESIAN_POINT('Ctrl Pts',(-66.4835097746765,2.61731940671614,134.970437408981));
#90135=CARTESIAN_POINT('Ctrl Pts',(-66.4910001104383,2.72792421320384,134.898855624029));
#90136=CARTESIAN_POINT('Ctrl Pts',(-66.4984904462003,2.83532536596307,134.823080952651));
#90137=CARTESIAN_POINT('Ctrl Pts',(-66.5062647803194,2.94679866607336,134.744433261576));
#90138=CARTESIAN_POINT('Ctrl Pts',(-66.5140391144386,3.05517369772571,134.661019328886));
#90139=CARTESIAN_POINT('Ctrl Pts',(-66.5218134485577,3.16001586556039,134.573111444021));
#90140=CARTESIAN_POINT('Ctrl Pts',(-66.5295782015048,3.26472882479324,134.485311897768));
#90141=CARTESIAN_POINT('Ctrl Pts',(-66.5373429544518,3.3659172865368,134.39302966788));
#90142=CARTESIAN_POINT('Ctrl Pts',(-66.5451077073989,3.46317559095159,134.296580239631));
#90143=CARTESIAN_POINT('Ctrl Pts',(-66.5528647482839,3.5603372970472,134.200226606315));
#90144=CARTESIAN_POINT('Ctrl Pts',(-66.5606217891689,3.6535763381209,134.099714284791));
#90145=CARTESIAN_POINT('Ctrl Pts',(-66.5683788300539,3.74252040741471,133.995398702983));
#90146=CARTESIAN_POINT('Ctrl Pts',(-66.5761300212941,3.83139740329399,133.891161786367));
#90147=CARTESIAN_POINT('Ctrl Pts',(-66.5838812125341,3.91598562153294,133.783127614483));
#90148=CARTESIAN_POINT('Ctrl Pts',(-66.5916324037742,3.99595015145007,133.671687848565));
#90149=CARTESIAN_POINT('Ctrl Pts',(-66.5993803005513,4.07588069430896,133.56029544752));
#90150=CARTESIAN_POINT('Ctrl Pts',(-66.6071281973284,4.15119123000632,133.44550064833));
#90151=CARTESIAN_POINT('Ctrl Pts',(-66.6148760941055,4.22158778783065,133.327727339257));
#90152=CARTESIAN_POINT('Ctrl Pts',(-66.6226223701896,4.29196962021257,133.209978665823));
#90153=CARTESIAN_POINT('Ctrl Pts',(-66.6303686462738,4.35743931880516,133.089253057139));
#90154=CARTESIAN_POINT('Ctrl Pts',(-66.6381149223579,4.41774705573912,132.966002126699));
#90155=CARTESIAN_POINT('Ctrl Pts',(-66.6458612556232,4.47805523785109,132.842750286449));
#90156=CARTESIAN_POINT('Ctrl Pts',(-66.6536075888885,4.533201210435,132.716973438423));
#90157=CARTESIAN_POINT('Ctrl Pts',(-66.6613539221539,4.58298198253718,132.58914609774));
#90158=CARTESIAN_POINT('Ctrl Pts',(-66.6691019901569,4.63277390269812,132.46129013101));
#90159=CARTESIAN_POINT('Ctrl Pts',(-66.6768500581599,4.67719808968219,132.331383122124));
#90160=CARTESIAN_POINT('Ctrl Pts',(-66.6845981261629,4.71610054287537,132.199917399639));
#90161=CARTESIAN_POINT('Ctrl Pts',(-66.6923544289047,4.75504434205875,132.06831195382));
#90162=CARTESIAN_POINT('Ctrl Pts',(-66.7001107316464,4.78845457324821,131.935144860621));
#90163=CARTESIAN_POINT('Ctrl Pts',(-66.7078670343883,4.8162276359383,131.800921915893));
#90164=CARTESIAN_POINT('Ctrl Pts',(-66.7156274769024,4.84401552194822,131.666627332339));
#90165=CARTESIAN_POINT('Ctrl Pts',(-66.7233879194166,4.86616018122114,131.531276160003));
#90166=CARTESIAN_POINT('Ctrl Pts',(-66.7311483619308,4.88260973667466,131.395381109453));
#90167=CARTESIAN_POINT('Ctrl Pts',(-66.7389212621962,4.89908569841491,131.259267908103));
#90168=CARTESIAN_POINT('Ctrl Pts',(-66.7466941624616,4.90984825642155,131.122609473826));
#90169=CARTESIAN_POINT('Ctrl Pts',(-66.7544670627271,4.91489763958616,130.985921226979));
#90170=CARTESIAN_POINT('Ctrl Pts',(-66.7619573984891,4.91976346495411,130.854201942202));
#90171=CARTESIAN_POINT('Ctrl Pts',(-66.7694477342512,4.91932428155204,130.722455282764));
#90172=CARTESIAN_POINT('Ctrl Pts',(-66.7769380700132,4.91362585095671,130.591137590409));
#90173=CARTESIAN_POINT('Ctrl Pts',(-66.7847124041323,4.90771136263336,130.454840947836));
#90174=CARTESIAN_POINT('Ctrl Pts',(-66.7924867382513,4.89611221047146,130.318574696249));
#90175=CARTESIAN_POINT('Ctrl Pts',(-66.8002610723704,4.87882256988073,130.182851652126));
#90176=CARTESIAN_POINT('Ctrl Pts',(-66.8080258253175,4.86155423722683,130.047295874525));
#90177=CARTESIAN_POINT('Ctrl Pts',(-66.8157905782647,4.83860941889166,129.912282356481));
#90178=CARTESIAN_POINT('Ctrl Pts',(-66.8235553312117,4.81003427251879,129.778322918602));
#90179=CARTESIAN_POINT('Ctrl Pts',(-66.8313123720967,4.78148750738413,129.644496531126));
#90180=CARTESIAN_POINT('Ctrl Pts',(-66.8390694129817,4.74732162382006,129.51172252027));
#90181=CARTESIAN_POINT('Ctrl Pts',(-66.8468264538667,4.7076344125075,129.380506235729));
#90182=CARTESIAN_POINT('Ctrl Pts',(-66.8545776451068,4.66797712962972,129.24938890241));
#90183=CARTESIAN_POINT('Ctrl Pts',(-66.8623288363469,4.62280691927656,129.119827329957));
#90184=CARTESIAN_POINT('Ctrl Pts',(-66.8700800275871,4.57227226973397,128.992314990679));
#90185=CARTESIAN_POINT('Ctrl Pts',(-66.8778279243642,4.5217590987655,128.864856847546));
#90186=CARTESIAN_POINT('Ctrl Pts',(-66.8855758211412,4.46588616715587,128.739446567977));
#90187=CARTESIAN_POINT('Ctrl Pts',(-66.8933237179183,4.40485120575558,128.616560599819));
#90188=CARTESIAN_POINT('Ctrl Pts',(-66.9010699940024,4.34382901155337,128.493700336756));
#90189=CARTESIAN_POINT('Ctrl Pts',(-66.9088162700866,4.2776471091168,128.373363684752));
#90190=CARTESIAN_POINT('Ctrl Pts',(-66.9165625461707,4.20655041560103,128.256004939191));
#90191=CARTESIAN_POINT('Ctrl Pts',(-66.924308879436,4.13545319726571,128.138645327315));
#90192=CARTESIAN_POINT('Ctrl Pts',(-66.9320552127014,4.05944131803315,128.024264000137));
#90193=CARTESIAN_POINT('Ctrl Pts',(-66.9398015459667,3.97880427934194,127.913288226706));
#90194=CARTESIAN_POINT('Ctrl Pts',(-66.9475496139697,3.89814918254502,127.802287601021));
#90195=CARTESIAN_POINT('Ctrl Pts',(-66.9552976819727,3.81286709499761,127.694694362895));
#90196=CARTESIAN_POINT('Ctrl Pts',(-66.9630457499757,3.72328898556474,127.590904193017));
#90197=CARTESIAN_POINT('Ctrl Pts',(-66.9708020527175,3.63361567145118,127.487003713712));
#90198=CARTESIAN_POINT('Ctrl Pts',(-66.9785583554593,3.53963747050244,127.386914673324));
#90199=CARTESIAN_POINT('Ctrl Pts',(-66.9863146582012,3.44172392449089,127.290997628906));
#90200=CARTESIAN_POINT('Ctrl Pts',(-66.9940751007153,3.34375811907158,127.195029390673));
#90201=CARTESIAN_POINT('Ctrl Pts',(-67.0018355432295,3.24185307369125,127.103237846874));
#90202=CARTESIAN_POINT('Ctrl Pts',(-67.0095959857437,3.13641210544066,127.015943775751));
#90203=CARTESIAN_POINT('Ctrl Pts',(-67.0173688860091,3.03080187398722,126.928509572436));
#90204=CARTESIAN_POINT('Ctrl Pts',(-67.0251417862746,2.92164468835486,126.845587505779));
#90205=CARTESIAN_POINT('Ctrl Pts',(-67.03291468654,2.80937431000866,126.7674559805));
#90206=CARTESIAN_POINT('Ctrl Pts',(-67.0404050223021,2.70118524270706,126.692164732966));
#90207=CARTESIAN_POINT('Ctrl Pts',(-67.0478953580641,2.59010565750581,126.621321942883));
#90208=CARTESIAN_POINT('Ctrl Pts',(-67.0553856938261,2.4765442228886,126.5551357736));
#90209=CARTESIAN_POINT('Ctrl Pts',(-67.0631600279452,2.35867707196212,126.486440135592));
#90210=CARTESIAN_POINT('Ctrl Pts',(-67.0709343620643,2.23776279017286,126.42254359334));
#90211=CARTESIAN_POINT('Ctrl Pts',(-67.0787086961834,2.11422967621388,126.363728237069));
#90212=CARTESIAN_POINT('Ctrl Pts',(-67.0864734491305,1.99084880577738,126.304985365468));
#90213=CARTESIAN_POINT('Ctrl Pts',(-67.0942382020775,1.86485587449695,126.251311386574));
#90214=CARTESIAN_POINT('Ctrl Pts',(-67.1020029550246,1.73670644087972,126.202944118192));
#90215=CARTESIAN_POINT('Ctrl Pts',(-67.1097599959096,1.60868428708672,126.154624888864));
#90216=CARTESIAN_POINT('Ctrl Pts',(-67.1175170367946,1.47851025678424,126.111602018282));
#90217=CARTESIAN_POINT('Ctrl Pts',(-67.1252740776796,1.34666237323368,126.074066386229));
#90218=CARTESIAN_POINT('Ctrl Pts',(-67.1330252689197,1.21491391719774,126.036559060089));
#90219=CARTESIAN_POINT('Ctrl Pts',(-67.1407764601597,1.08149449487975,126.004530842718));
#90220=CARTESIAN_POINT('Ctrl Pts',(-67.1485276513999,0.946899540052417,
125.978123540552));
#90221=CARTESIAN_POINT('Ctrl Pts',(-67.1562755481769,0.812361791671318,
125.951727462193));
#90222=CARTESIAN_POINT('Ctrl Pts',(-67.164023444954,0.676649887359797,125.930947622537));
#90223=CARTESIAN_POINT('Ctrl Pts',(-67.1717713417311,0.540271554538408,
125.915875196717));
#90224=CARTESIAN_POINT('Ctrl Pts',(-67.1795176178152,0.403921749124083,
125.900805923723));
#90225=CARTESIAN_POINT('Ctrl Pts',(-67.1872638938993,0.266906180831998,
125.891441732817));
#90226=CARTESIAN_POINT('Ctrl Pts',(-67.1950101699834,0.129739444941043,
125.887822126013));
#90227=CARTESIAN_POINT('Ctrl Pts',(-67.2027565032487,-0.00742830348359602,
125.884202492489));
#90228=CARTESIAN_POINT('Ctrl Pts',(-67.2105028365141,-0.144746830904619,
125.886327537996));
#90229=CARTESIAN_POINT('Ctrl Pts',(-67.2182491697795,-0.281700181170313,
125.894184646134));
#90230=CARTESIAN_POINT('Ctrl Pts',(-67.2259972377824,-0.41868420118923,
125.902043513816));
#90231=CARTESIAN_POINT('Ctrl Pts',(-67.2337453057854,-0.555302491073616,
125.915636976066));
#90232=CARTESIAN_POINT('Ctrl Pts',(-67.2414933737884,-0.691043256697624,
125.934900454481));
#90233=CARTESIAN_POINT('Ctrl Pts',(-67.2492496765302,-0.826928289222488,
125.95418440635));
#90234=CARTESIAN_POINT('Ctrl Pts',(-67.2570059792721,-0.961933546727675,
125.979150357268));
#90235=CARTESIAN_POINT('Ctrl Pts',(-67.2647622820139,-1.09555593599869,
126.009682291171));
#90236=CARTESIAN_POINT('Ctrl Pts',(-67.272522724528,-1.22924964356233,126.040230520887));
#90237=CARTESIAN_POINT('Ctrl Pts',(-67.2802831670421,-1.36155863522941,
126.076350550109));
#90238=CARTESIAN_POINT('Ctrl Pts',(-67.2880436095563,-1.49199502843927,
126.117876445224));
#90239=CARTESIAN_POINT('Ctrl Pts',(-67.2958165098217,-1.62264080972711,
126.159469001392));
#90240=CARTESIAN_POINT('Ctrl Pts',(-67.3035894100872,-1.75140761802711,
126.206484630644));
#90241=CARTESIAN_POINT('Ctrl Pts',(-67.3113623103526,-1.87782676489667,
126.258708881727));
#90242=CARTESIAN_POINT('Ctrl Pts',(-67.3188526461147,-1.99965025734861,
126.309034649738));
#90243=CARTESIAN_POINT('Ctrl Pts',(-67.3263429818768,-2.11929353208964,
126.364196792235));
#90244=CARTESIAN_POINT('Ctrl Pts',(-67.333833317639,-2.23636056010105,126.423964002221));
#90245=CARTESIAN_POINT('Ctrl Pts',(-67.3416084934216,-2.35787937448386,
126.486004019978));
#90246=CARTESIAN_POINT('Ctrl Pts',(-67.3493836692043,-2.47700710437234,
126.553202821404));
#90247=CARTESIAN_POINT('Ctrl Pts',(-67.357158844987,-2.59327476208843,126.625352473184));
#90248=CARTESIAN_POINT('Ctrl Pts',(-67.3649242526913,-2.7093963508775,126.697411482196));
#90249=CARTESIAN_POINT('Ctrl Pts',(-67.3726896603956,-2.8226646882478,126.774408760587));
#90250=CARTESIAN_POINT('Ctrl Pts',(-67.3804550681,-2.9326333414837,126.856089508977));
#90251=CARTESIAN_POINT('Ctrl Pts',(-67.388343444619,-3.04434339909278,126.939063709713));
#90252=CARTESIAN_POINT('Ctrl Pts',(-67.396231821138,-3.15264800295381,127.026870814925));
#90253=CARTESIAN_POINT('Ctrl Pts',(-67.404120197657,-3.25710679850231,127.11919598547));
#90254=CARTESIAN_POINT('Ctrl Pts',(-67.411871035762,-3.35974429444228,127.209911413187));
#90255=CARTESIAN_POINT('Ctrl Pts',(-67.4196218738671,-3.4586686846207,127.304988375594));
#90256=CARTESIAN_POINT('Ctrl Pts',(-67.4273727119721,-3.55349349238493,
127.404086060699));
#90257=CARTESIAN_POINT('Ctrl Pts',(-67.4351200140234,-3.64827503958724,
127.503138535888));
#90258=CARTESIAN_POINT('Ctrl Pts',(-67.4428673160746,-3.7389604562633,127.60620780199));
#90259=CARTESIAN_POINT('Ctrl Pts',(-67.450614618126,-3.8251993177929,127.712915447155));
#90260=CARTESIAN_POINT('Ctrl Pts',(-67.4583600634878,-3.91141751163871,
127.819597519164));
#90261=CARTESIAN_POINT('Ctrl Pts',(-67.4661055088497,-3.99319102630841,
127.929915930614));
#90262=CARTESIAN_POINT('Ctrl Pts',(-67.4738509542115,-4.07020927977448,
128.043458684984));
#90263=CARTESIAN_POINT('Ctrl Pts',(-67.4818447167402,-4.14969672043453,
128.160641593504));
#90264=CARTESIAN_POINT('Ctrl Pts',(-67.489838479269,-4.22411861333894,128.281258709124));
#90265=CARTESIAN_POINT('Ctrl Pts',(-67.4978322417977,-4.29318177250914,
128.404824551845));
#90266=CARTESIAN_POINT('Ctrl Pts',(-67.5055816027224,-4.36013339198612,
128.524612487724));
#90267=CARTESIAN_POINT('Ctrl Pts',(-67.513330963647,-4.42204900608833,128.647171103629));
#90268=CARTESIAN_POINT('Ctrl Pts',(-67.5210803245717,-4.47870852322668,
128.772033619645));
#90269=CARTESIAN_POINT('Ctrl Pts',(-67.5291962879024,-4.53804845691893,
128.902803061309));
#90270=CARTESIAN_POINT('Ctrl Pts',(-67.5373122512332,-4.5916226393496,129.036099274335));
#90271=CARTESIAN_POINT('Ctrl Pts',(-67.5454282145639,-4.63923546684187,
129.171364185942));
#90272=CARTESIAN_POINT('Ctrl Pts',(-67.5535441778946,-4.68684829433408,
129.306629097549));
#90273=CARTESIAN_POINT('Ctrl Pts',(-67.5616601412252,-4.72849966024031,
129.443862228621));
#90274=CARTESIAN_POINT('Ctrl Pts',(-67.5697761045559,-4.76405452823408,
129.582490119308));
#90275=CARTESIAN_POINT('Origin',(213.235140564004,0.,130.804360617566));
#90276=CARTESIAN_POINT('',(-69.6652100424012,-4.76405452823405,129.582490119308));
#90277=CARTESIAN_POINT('',(-69.3201134481353,-4.76405452823409,129.582490119308));
#90278=CARTESIAN_POINT('',(213.235140564004,-4.76405452823405,129.582490119308));
#90279=CARTESIAN_POINT('',(-67.9851405639607,-4.91824943552146,130.802004244757));
#90280=CARTESIAN_POINT('Ctrl Pts',(-67.9851405640084,-4.91824943552187,
130.802004245604));
#90281=CARTESIAN_POINT('Ctrl Pts',(-67.9930107492047,-4.91831633734571,
130.941642580585));
#90282=CARTESIAN_POINT('Ctrl Pts',(-68.0008809344009,-4.91243199672117,
131.081266340895));
#90283=CARTESIAN_POINT('Ctrl Pts',(-68.0087511195972,-4.9006266186085,131.220343558906));
#90284=CARTESIAN_POINT('Ctrl Pts',(-68.0166239464927,-4.88881727791327,
131.359467459451));
#90285=CARTESIAN_POINT('Ctrl Pts',(-68.0244967733882,-4.87108297174089,
131.498044080167));
#90286=CARTESIAN_POINT('Ctrl Pts',(-68.0323696002838,-4.84750573826796,
131.635547227154));
#90287=CARTESIAN_POINT('Ctrl Pts',(-68.0402465527333,-4.82391614974754,
131.773122429157));
#90288=CARTESIAN_POINT('Ctrl Pts',(-68.0481235051828,-4.79447759725055,
131.909622669071));
#90289=CARTESIAN_POINT('Ctrl Pts',(-68.0560004576324,-4.75932307605186,
132.044532750885));
#90290=CARTESIAN_POINT('Ctrl Pts',(-68.0638888171598,-4.72411764552476,
132.179638203917));
#90291=CARTESIAN_POINT('Ctrl Pts',(-68.0717771766871,-4.68317980188223,
132.313148535996));
#90292=CARTESIAN_POINT('Ctrl Pts',(-68.0796655362145,-4.63669250378297,
132.444563558626));
#90293=CARTESIAN_POINT('Ctrl Pts',(-68.0875597502083,-4.59017070442584,
132.576076112922));
#90294=CARTESIAN_POINT('Ctrl Pts',(-68.0954539642021,-4.53809137900341,
132.70548991166));
#90295=CARTESIAN_POINT('Ctrl Pts',(-68.1033481781959,-4.48068511658272,
132.832326087818));
#90296=CARTESIAN_POINT('Ctrl Pts',(-68.1112570938165,-4.42317194479173,
132.959398474716));
#90297=CARTESIAN_POINT('Ctrl Pts',(-68.1191660094372,-4.36031217509731,
133.083883310427));
#90298=CARTESIAN_POINT('Ctrl Pts',(-68.1270749250578,-4.29238232005271,
133.205326481755));
#90299=CARTESIAN_POINT('Ctrl Pts',(-68.1345790143446,-4.2279295275402,133.320553454027));
#90300=CARTESIAN_POINT('Ctrl Pts',(-68.1420831036313,-4.15891291511128,
133.433042176827));
#90301=CARTESIAN_POINT('Ctrl Pts',(-68.1495871929181,-4.08560303385224,
133.542431272658));
#90302=CARTESIAN_POINT('Ctrl Pts',(-68.1573615270372,-4.00965304320633,
133.655759798943));
#90303=CARTESIAN_POINT('Ctrl Pts',(-68.1651358611562,-3.92886383360519,
133.766105325651));
#90304=CARTESIAN_POINT('Ctrl Pts',(-68.1729101952753,-3.84349718698554,
133.873026848379));
#90305=CARTESIAN_POINT('Ctrl Pts',(-68.1806749482224,-3.7582357471284,133.979816599887));
#90306=CARTESIAN_POINT('Ctrl Pts',(-68.1884397011695,-3.6684083363175,134.083190440921));
#90307=CARTESIAN_POINT('Ctrl Pts',(-68.1962044541166,-3.57432061425678,
134.182735257685));
#90308=CARTESIAN_POINT('Ctrl Pts',(-68.2039614950016,-3.48032634144814,
134.282181205133));
#90309=CARTESIAN_POINT('Ctrl Pts',(-68.2117185358867,-3.38208044488746,
134.377805414241));
#90310=CARTESIAN_POINT('Ctrl Pts',(-68.2194755767717,-3.27992931580752,
134.469227156174));
#90311=CARTESIAN_POINT('Ctrl Pts',(-68.2272267680118,-3.17785521968835,
134.56057995626));
#90312=CARTESIAN_POINT('Ctrl Pts',(-68.2349779592519,-3.07188204297807,
134.647736337425));
#90313=CARTESIAN_POINT('Ctrl Pts',(-68.242729150492,-2.96239329719065,134.730352086642));
#90314=CARTESIAN_POINT('Ctrl Pts',(-68.2504770472691,-2.85295108704103,
134.812932721962));
#90315=CARTESIAN_POINT('Ctrl Pts',(-68.2582249440463,-2.73999659111978,
134.890976328743));
#90316=CARTESIAN_POINT('Ctrl Pts',(-68.2659728408234,-2.62394652113391,
134.964178848779));
#90317=CARTESIAN_POINT('Ctrl Pts',(-68.2737191169075,-2.50792072632093,
135.037366056426));
#90318=CARTESIAN_POINT('Ctrl Pts',(-68.2814653929915,-2.38880097587663,
135.105713983094));
#90319=CARTESIAN_POINT('Ctrl Pts',(-68.2892116690756,-2.26703275805912,
135.16896203538));
#90320=CARTESIAN_POINT('Ctrl Pts',(-68.2969580023409,-2.14526364137646,
135.232210554549));
#90321=CARTESIAN_POINT('Ctrl Pts',(-68.3047043356064,-2.02084636526339,
135.290358944003));
#90322=CARTESIAN_POINT('Ctrl Pts',(-68.3124506688717,-1.89425043696567,
135.343192884191));
#90323=CARTESIAN_POINT('Ctrl Pts',(-68.3201987368747,-1.76762615838722,
135.396038656173));
#90324=CARTESIAN_POINT('Ctrl Pts',(-68.3279468048776,-1.63882261750664,
135.443567460109));
#90325=CARTESIAN_POINT('Ctrl Pts',(-68.3356948728806,-1.50832830551248,
135.485613525206));
#90326=CARTESIAN_POINT('Ctrl Pts',(-68.3434511756225,-1.37769530261081,
135.527704277361));
#90327=CARTESIAN_POINT('Ctrl Pts',(-68.3512074783644,-1.24536831167013,
135.564300530284));
#90328=CARTESIAN_POINT('Ctrl Pts',(-68.3589637811063,-1.11185049676045,
135.595286575599));
#90329=CARTESIAN_POINT('Ctrl Pts',(-68.3667242236205,-0.978261419372801,
135.626289159099));
#90330=CARTESIAN_POINT('Ctrl Pts',(-68.3744846661345,-0.843480635593314,
135.651675496189));
#90331=CARTESIAN_POINT('Ctrl Pts',(-68.3822451086487,-0.708019463434344,
135.671381421086));
#90332=CARTESIAN_POINT('Ctrl Pts',(-68.3900180089141,-0.572340836976147,
135.691118979684));
#90333=CARTESIAN_POINT('Ctrl Pts',(-68.3977909091796,-0.43598002866856,
135.705157863953));
#90334=CARTESIAN_POINT('Ctrl Pts',(-68.405563809445,-0.299452315932775,
135.713485934054));
#90335=CARTESIAN_POINT('Ctrl Pts',(-68.413054145207,-0.167887729448603,
135.721511257829));
#90336=CARTESIAN_POINT('Ctrl Pts',(-68.4205444809689,-0.0361684706039233,
135.724233757462));
#90337=CARTESIAN_POINT('Ctrl Pts',(-68.4280348167309,0.0952481521205627,
135.721688230408));
#90338=CARTESIAN_POINT('Ctrl Pts',(-68.43580915085,0.231647476039649,135.719046188922));
#90339=CARTESIAN_POINT('Ctrl Pts',(-68.443583484969,0.368152833981991,135.71072039134));
#90340=CARTESIAN_POINT('Ctrl Pts',(-68.4513578190881,0.504251696922477,
135.696692708568));
#90341=CARTESIAN_POINT('Ctrl Pts',(-68.4591225720352,0.640182830177709,
135.682682313662));
#90342=CARTESIAN_POINT('Ctrl Pts',(-68.4668873249823,0.775708080038133,
135.662984055028));
#90343=CARTESIAN_POINT('Ctrl Pts',(-68.4746520779293,0.91031466563093,135.637631794733));
#90344=CARTESIAN_POINT('Ctrl Pts',(-68.4824091188143,1.04478755806548,135.612304714662));
#90345=CARTESIAN_POINT('Ctrl Pts',(-68.4901661596993,1.17834322028607,135.58133488019));
#90346=CARTESIAN_POINT('Ctrl Pts',(-68.4979232005843,1.31047410142037,135.54480792684));
#90347=CARTESIAN_POINT('Ctrl Pts',(-68.5056743918244,1.44250534162884,135.50830851875));
#90348=CARTESIAN_POINT('Ctrl Pts',(-68.5134255830644,1.57311356404928,135.4662604368));
#90349=CARTESIAN_POINT('Ctrl Pts',(-68.5211767743045,1.70180187517385,135.418800284541));
#90350=CARTESIAN_POINT('Ctrl Pts',(-68.5289246710816,1.83043549033384,135.371360304113));
#90351=CARTESIAN_POINT('Ctrl Pts',(-68.5366725678587,1.9571504511401,135.318512963443));
#90352=CARTESIAN_POINT('Ctrl Pts',(-68.5444204646357,2.08146570195725,135.260444503006));
#90353=CARTESIAN_POINT('Ctrl Pts',(-68.5521667407198,2.20575494870385,135.202388189239));
#90354=CARTESIAN_POINT('Ctrl Pts',(-68.5599130168039,2.32764512990048,135.139113093399));
#90355=CARTESIAN_POINT('Ctrl Pts',(-68.567659292888,2.44667620365112,135.070853160275));
#90356=CARTESIAN_POINT('Ctrl Pts',(-68.5754056261533,2.56570815606228,135.002592723271));
#90357=CARTESIAN_POINT('Ctrl Pts',(-68.5831519594186,2.68188061975816,134.92934757005));
#90358=CARTESIAN_POINT('Ctrl Pts',(-68.590898292684,2.79475950149538,134.851396865402));
#90359=CARTESIAN_POINT('Ctrl Pts',(-68.5986463606869,2.90766366167506,134.773428704235));
#90360=CARTESIAN_POINT('Ctrl Pts',(-68.6063944286899,3.01727245055912,134.69075311687));
#90361=CARTESIAN_POINT('Ctrl Pts',(-68.6141424966928,3.1231823590646,134.603691481617));
#90362=CARTESIAN_POINT('Ctrl Pts',(-68.6218987994347,3.22920482988147,134.516537316221));
#90363=CARTESIAN_POINT('Ctrl Pts',(-68.6296551021765,3.33152026479532,134.424988039666));
#90364=CARTESIAN_POINT('Ctrl Pts',(-68.6374114049183,3.42975934260136,134.32940443493));
#90365=CARTESIAN_POINT('Ctrl Pts',(-68.6451718474325,3.52805085356128,134.233769814347));
#90366=CARTESIAN_POINT('Ctrl Pts',(-68.6529322899467,3.62226140377021,134.134096859057));
#90367=CARTESIAN_POINT('Ctrl Pts',(-68.6606927324609,3.71206062886231,134.030781072211));
#90368=CARTESIAN_POINT('Ctrl Pts',(-68.6684656327263,3.80200400764254,133.927299433692));
#90369=CARTESIAN_POINT('Ctrl Pts',(-68.6762385329917,3.88752166626892,133.820163583591));
#90370=CARTESIAN_POINT('Ctrl Pts',(-68.6840114332571,3.9683248711163,133.709800477515));
#90371=CARTESIAN_POINT('Ctrl Pts',(-68.6915017690193,4.04619067593868,133.603449348329));
#90372=CARTESIAN_POINT('Ctrl Pts',(-68.6989921047816,4.11967866881516,133.494101782929));
#90373=CARTESIAN_POINT('Ctrl Pts',(-68.7064824405438,4.1885709394259,133.382161336764));
#90374=CARTESIAN_POINT('Ctrl Pts',(-68.7142567746629,4.26007528141438,133.265976634562));
#90375=CARTESIAN_POINT('Ctrl Pts',(-68.722031108782,4.3268550324068,133.14663051393));
#90376=CARTESIAN_POINT('Ctrl Pts',(-68.7298054429011,4.38861790542529,133.024544380834));
#90377=CARTESIAN_POINT('Ctrl Pts',(-68.7375701958482,4.45030466122261,132.902608707987));
#90378=CARTESIAN_POINT('Ctrl Pts',(-68.7453349487953,4.50698666628786,132.777940087056));
#90379=CARTESIAN_POINT('Ctrl Pts',(-68.7530997017424,4.55841523915072,132.650988238387));
#90380=CARTESIAN_POINT('Ctrl Pts',(-68.7608567426274,4.60979273243,132.524162480084));
#90381=CARTESIAN_POINT('Ctrl Pts',(-68.7686137835124,4.65592703128676,132.395058366953));
#90382=CARTESIAN_POINT('Ctrl Pts',(-68.7763708243974,4.69661583966551,132.264149204007));
#90383=CARTESIAN_POINT('Ctrl Pts',(-68.7841220156376,4.73727396429746,132.133338760679));
#90384=CARTESIAN_POINT('Ctrl Pts',(-68.7918732068777,4.7724946565911,132.000726348763));
#90385=CARTESIAN_POINT('Ctrl Pts',(-68.7996243981179,4.80212426190384,131.866803856396));
#90386=CARTESIAN_POINT('Ctrl Pts',(-68.8073722948949,4.83174127384384,131.73293828466));
#90387=CARTESIAN_POINT('Ctrl Pts',(-68.8151201916721,4.85577184092432,131.597764120879));
#90388=CARTESIAN_POINT('Ctrl Pts',(-68.8228680884492,4.87411263020959,131.461786758308));
#90389=CARTESIAN_POINT('Ctrl Pts',(-68.8306143645333,4.89244958299714,131.32583783927));
#90390=CARTESIAN_POINT('Ctrl Pts',(-68.8383606406174,4.90509907309294,131.189086442838));
#90391=CARTESIAN_POINT('Ctrl Pts',(-68.8461069167015,4.91200926099124,131.052046068161));
#90392=CARTESIAN_POINT('Ctrl Pts',(-68.8538532499669,4.91891949989897,130.915004681882));
#90393=CARTESIAN_POINT('Ctrl Pts',(-68.8615995832321,4.92009033238127,130.777674703572));
#90394=CARTESIAN_POINT('Ctrl Pts',(-68.8693459164975,4.91552198968117,130.640572243556));
#90395=CARTESIAN_POINT('Ctrl Pts',(-68.8770939845005,4.91095262393239,130.503439080395));
#90396=CARTESIAN_POINT('Ctrl Pts',(-68.8848420525035,4.90064153852303,130.36653392759));
#90397=CARTESIAN_POINT('Ctrl Pts',(-68.8925901205065,4.88464101161046,130.230369981586));
#90398=CARTESIAN_POINT('Ctrl Pts',(-68.9003464232484,4.86862347914747,130.094061318919));
#90399=CARTESIAN_POINT('Ctrl Pts',(-68.9081027259903,4.84690447173551,129.958495825609));
#90400=CARTESIAN_POINT('Ctrl Pts',(-68.9158590287322,4.81958789917982,129.824179234056));
#90401=CARTESIAN_POINT('Ctrl Pts',(-68.9236194712464,4.79225674694683,129.689790953694));
#90402=CARTESIAN_POINT('Ctrl Pts',(-68.9313799137605,4.75932217038413,129.55665328264));
#90403=CARTESIAN_POINT('Ctrl Pts',(-68.9391403562747,4.72093834748541,129.425257944905));
#90404=CARTESIAN_POINT('Ctrl Pts',(-68.9469132565401,4.68249290746666,129.293651679709));
#90405=CARTESIAN_POINT('Ctrl Pts',(-68.9546861568056,4.63858086590374,129.163793707602));
#90406=CARTESIAN_POINT('Ctrl Pts',(-68.962459057071,4.58940536506362,129.036157728295));
#90407=CARTESIAN_POINT('Ctrl Pts',(-68.9699493928329,4.54201751754565,128.913161638334));
#90408=CARTESIAN_POINT('Ctrl Pts',(-68.9774397285948,4.4897423690861,128.792229078583));
#90409=CARTESIAN_POINT('Ctrl Pts',(-68.9849300643567,4.43280165646442,128.673761514744));
#90410=CARTESIAN_POINT('Ctrl Pts',(-68.9927043984758,4.37370201941584,128.550802217212));
#90411=CARTESIAN_POINT('Ctrl Pts',(-69.0004787325948,4.30938883466821,128.430109028009));
#90412=CARTESIAN_POINT('Ctrl Pts',(-69.0082530667139,4.24005865474453,128.312155636665));
#90413=CARTESIAN_POINT('Ctrl Pts',(-69.016017819661,4.1708139180712,128.194347612335));
#90414=CARTESIAN_POINT('Ctrl Pts',(-69.0237825726081,4.09656468475564,128.079273001342));
#90415=CARTESIAN_POINT('Ctrl Pts',(-69.0315473255552,4.0175548988525,127.967384111282));
#90416=CARTESIAN_POINT('Ctrl Pts',(-69.0393043664402,3.93862358658277,127.855606350846));
#90417=CARTESIAN_POINT('Ctrl Pts',(-69.0470614073253,3.85494135521198,127.747008331936));
#90418=CARTESIAN_POINT('Ctrl Pts',(-69.0548184482103,3.76679706369379,127.642016084874));
#90419=CARTESIAN_POINT('Ctrl Pts',(-69.0625696394504,3.67871924247137,127.537103013282));
#90420=CARTESIAN_POINT('Ctrl Pts',(-69.0703208306905,3.586186309046,127.435790599475));
#90421=CARTESIAN_POINT('Ctrl Pts',(-69.0780720219306,3.4895290487504,127.338473995008));
#90422=CARTESIAN_POINT('Ctrl Pts',(-69.0858199187077,3.39291287036898,127.241198752694));
#90423=CARTESIAN_POINT('Ctrl Pts',(-69.0935678154847,3.29217612653519,127.147916218692));
#90424=CARTESIAN_POINT('Ctrl Pts',(-69.1013157122618,3.18768816493279,127.058986507327));
#90425=CARTESIAN_POINT('Ctrl Pts',(-69.1090619883459,3.0832220599596,126.970075398141));
#90426=CARTESIAN_POINT('Ctrl Pts',(-69.1168082644301,2.97500659551866,126.885515553761));
#90427=CARTESIAN_POINT('Ctrl Pts',(-69.1245545405142,2.86344577246775,126.805628147065));
#90428=CARTESIAN_POINT('Ctrl Pts',(-69.1323008737796,2.75188412590004,126.725740150659));
#90429=CARTESIAN_POINT('Ctrl Pts',(-69.1400472070448,2.63697738931614,126.650524888384));
#90430=CARTESIAN_POINT('Ctrl Pts',(-69.1477935403101,2.51915990594445,126.580261135927));
#90431=CARTESIAN_POINT('Ctrl Pts',(-69.1555416083131,2.4013160381641,126.50998164839));
#90432=CARTESIAN_POINT('Ctrl Pts',(-69.1632896763162,2.28056046222771,126.444656077385));
#90433=CARTESIAN_POINT('Ctrl Pts',(-69.1710377443192,2.1573532024603,126.38451783503));
#90434=CARTESIAN_POINT('Ctrl Pts',(-69.1787940470611,2.03401499655103,126.324315677036));
#90435=CARTESIAN_POINT('Ctrl Pts',(-69.1865503498029,1.90822025359245,126.26931203258));
#90436=CARTESIAN_POINT('Ctrl Pts',(-69.1943066525447,1.78045062636509,126.219692840117));
#90437=CARTESIAN_POINT('Ctrl Pts',(-69.2020670950589,1.65261280464061,126.170047164397));
#90438=CARTESIAN_POINT('Ctrl Pts',(-69.209827537573,1.52279836822426,126.125791793142));
#90439=CARTESIAN_POINT('Ctrl Pts',(-69.2175879800872,1.39150435542503,126.087062800878));
#90440=CARTESIAN_POINT('Ctrl Pts',(-69.2253608803526,1.25999957782091,126.048271637397));
#90441=CARTESIAN_POINT('Ctrl Pts',(-69.2331337806181,1.12701085704306,126.015024675736));
#90442=CARTESIAN_POINT('Ctrl Pts',(-69.2409066808835,0.993046533431332,
125.987407052818));
#90443=CARTESIAN_POINT('Ctrl Pts',(-69.2483970166455,0.863952150418478,
125.960793400057));
#90444=CARTESIAN_POINT('Ctrl Pts',(-69.2558873524076,0.733952168275309,
125.939406960477));
#90445=CARTESIAN_POINT('Ctrl Pts',(-69.2633776881696,0.603504205612691,
125.923278182664));
#90446=CARTESIAN_POINT('Ctrl Pts',(-69.2711520222887,0.468110268797287,
125.906537877338));
#90447=CARTESIAN_POINT('Ctrl Pts',(-69.2789263564076,0.331804823219269,
125.895408764251));
#90448=CARTESIAN_POINT('Ctrl Pts',(-69.2867006905267,0.195092638736001,
125.88998151896));
#90449=CARTESIAN_POINT('Ctrl Pts',(-69.2944654434738,0.0585489398019751,
125.884560962265));
#90450=CARTESIAN_POINT('Ctrl Pts',(-69.302230196421,-0.0784001137534861,
125.884828307005));
#90451=CARTESIAN_POINT('Ctrl Pts',(-69.3099949493681,-0.215242125019637,
125.890822799444));
#90452=CARTESIAN_POINT('Ctrl Pts',(-69.3177519902531,-0.351948222871249,
125.896811338068));
#90453=CARTESIAN_POINT('Ctrl Pts',(-69.325509031138,-0.488547101943895,
125.908515687449));
#90454=CARTESIAN_POINT('Ctrl Pts',(-69.333266072023,-0.624524195541667,
125.925923102164));
#90455=CARTESIAN_POINT('Ctrl Pts',(-69.3410172632631,-0.760398747754854,
125.943317389812));
#90456=CARTESIAN_POINT('Ctrl Pts',(-69.3487684545031,-0.895652061565506,
125.966406133015));
#90457=CARTESIAN_POINT('Ctrl Pts',(-69.3565196457432,-1.02977288722657,
125.995124621773));
#90458=CARTESIAN_POINT('Ctrl Pts',(-69.3642675425203,-1.1638367079593,126.023830904407));
#90459=CARTESIAN_POINT('Ctrl Pts',(-69.3720154392973,-1.29676861638737,
126.058162091826));
#90460=CARTESIAN_POINT('Ctrl Pts',(-69.3797633360744,-1.42806599668528,
126.098002091953));
#90461=CARTESIAN_POINT('Ctrl Pts',(-69.3875096121585,-1.55933591240186,
126.137833758411));
#90462=CARTESIAN_POINT('Ctrl Pts',(-69.3952558882426,-1.68897160617778,
126.18317183209));
#90463=CARTESIAN_POINT('Ctrl Pts',(-69.4030021643267,-1.81648449384346,
126.233850017411));
#90464=CARTESIAN_POINT('Ctrl Pts',(-69.4107484975921,-1.94399832278066,
126.284528576828));
#90465=CARTESIAN_POINT('Ctrl Pts',(-69.4184948308574,-2.06938895101667,
126.340547182149));
#90466=CARTESIAN_POINT('Ctrl Pts',(-69.4262411641227,-2.19218706354579,
126.401691093184));
#90467=CARTESIAN_POINT('Ctrl Pts',(-69.4339892321257,-2.31501267586012,
126.462848696973));
#90468=CARTESIAN_POINT('Ctrl Pts',(-69.4417373001286,-2.4352442672754,126.529133716189));
#90469=CARTESIAN_POINT('Ctrl Pts',(-69.4494853681315,-2.55243680718027,
126.600285284291));
#90470=CARTESIAN_POINT('Ctrl Pts',(-69.4572416708734,-2.66975390071147,
126.671512473126));
#90471=CARTESIAN_POINT('Ctrl Pts',(-69.4649979736152,-2.78402515585255,
126.747616339702));
#90472=CARTESIAN_POINT('Ctrl Pts',(-69.472754276357,-2.89483379222295,126.828292160169));
#90473=CARTESIAN_POINT('Ctrl Pts',(-69.4805147188711,-3.00570157049881,
126.909011039751));
#90474=CARTESIAN_POINT('Ctrl Pts',(-69.4882751613853,-3.11310274148995,
126.994306492482));
#90475=CARTESIAN_POINT('Ctrl Pts',(-69.4960356038994,-3.21665416049633,
127.083833897562));
#90476=CARTESIAN_POINT('Ctrl Pts',(-69.5038085041648,-3.32037180943349,
127.173505019981));
#90477=CARTESIAN_POINT('Ctrl Pts',(-69.5115814044303,-3.42022707189196,
127.267421402327));
#90478=CARTESIAN_POINT('Ctrl Pts',(-69.5193543046957,-3.51587354939758,
127.365201382063));
#90479=CARTESIAN_POINT('Ctrl Pts',(-69.5268446404579,-3.60804303653003,
127.459426813245));
#90480=CARTESIAN_POINT('Ctrl Pts',(-69.5343349762202,-3.69630421962132,
127.55723958703));
#90481=CARTESIAN_POINT('Ctrl Pts',(-69.5418253119825,-3.78038412737664,
127.658271154124));
#90482=CARTESIAN_POINT('Ctrl Pts',(-69.5495609560854,-3.86721765036528,
127.762611502943));
#90483=CARTESIAN_POINT('Ctrl Pts',(-69.5572966001884,-3.94987525363598,
127.870726382361));
#90484=CARTESIAN_POINT('Ctrl Pts',(-69.5650322442914,-4.02800816387792,
127.98224557841));
#90485=CARTESIAN_POINT('Ctrl Pts',(-69.5727583820808,-4.10604505678381,
128.093627728799));
#90486=CARTESIAN_POINT('Ctrl Pts',(-69.5804845198703,-4.17956809177795,
128.208405554353));
#90487=CARTESIAN_POINT('Ctrl Pts',(-69.5882106576597,-4.24826735672974,
128.326174279083));
#90488=CARTESIAN_POINT('Ctrl Pts',(-69.5959274543373,-4.31688356239112,
128.443800618203));
#90489=CARTESIAN_POINT('Ctrl Pts',(-69.6036442510148,-4.38068741280281,
128.564410317273));
#90490=CARTESIAN_POINT('Ctrl Pts',(-69.6113610476923,-4.43941153423827,
128.687568636248));
#90491=CARTESIAN_POINT('Ctrl Pts',(-69.6190724681238,-4.49809474292947,
128.810641151558));
#90492=CARTESIAN_POINT('Ctrl Pts',(-69.6267838885552,-4.55170509224803,
128.936258400123));
#90493=CARTESIAN_POINT('Ctrl Pts',(-69.6344953089866,-4.60002051692417,
129.063960000933));
#90494=CARTESIAN_POINT('Ctrl Pts',(-69.642202740298,-4.648310948017,129.191595541667));
#90495=CARTESIAN_POINT('Ctrl Pts',(-69.6499101716094,-4.69131176676075,
129.321312919831));
#90496=CARTESIAN_POINT('Ctrl Pts',(-69.6576176029209,-4.72884875237447,
129.452631155112));
#90497=CARTESIAN_POINT('Ctrl Pts',(-69.660148416081,-4.74117440191244,129.495750828137));
#90498=CARTESIAN_POINT('Ctrl Pts',(-69.6626792292411,-4.75291133001434,
129.539042958571));
#90499=CARTESIAN_POINT('Ctrl Pts',(-69.6652100424012,-4.76405452823405,
129.582490119308));
#90500=CARTESIAN_POINT('Ctrl Pts',(-67.9154119669996,-4.76405452823407,
129.582490119308));
#90501=CARTESIAN_POINT('Ctrl Pts',(-67.9239585741172,-4.80145152871823,
129.728300456617));
#90502=CARTESIAN_POINT('Ctrl Pts',(-67.9325051812348,-4.83219447185872,
129.876000973547));
#90503=CARTESIAN_POINT('Ctrl Pts',(-67.9410517883524,-4.85610720839616,
130.024998158204));
#90504=CARTESIAN_POINT('Ctrl Pts',(-67.9495613079844,-4.87991617705707,
130.173348778573));
#90505=CARTESIAN_POINT('Ctrl Pts',(-67.9580708276163,-4.89695398951606,
130.322984601923));
#90506=CARTESIAN_POINT('Ctrl Pts',(-67.9665803472483,-4.90709519897987,
130.473302056812));
#90507=CARTESIAN_POINT('Ctrl Pts',(-67.9727670861524,-4.9144682373931,130.582588466192));
#90508=CARTESIAN_POINT('Ctrl Pts',(-67.9789538250566,-4.91819684409512,
130.692234792326));
#90509=CARTESIAN_POINT('Ctrl Pts',(-67.9851405639607,-4.91824943552146,
130.802004244757));
#90510=CARTESIAN_POINT('',(-67.6398594360288,-4.91824920641527,130.801566678494));
#90511=CARTESIAN_POINT('Ctrl Pts',(-67.5697761045559,-4.76405452823408,
129.582490119308));
#90512=CARTESIAN_POINT('Ctrl Pts',(-67.5775493903736,-4.79810817533265,
129.715264772509));
#90513=CARTESIAN_POINT('Ctrl Pts',(-67.5853226761914,-4.82656962736789,
129.849318420193));
#90514=CARTESIAN_POINT('Ctrl Pts',(-67.5930959620091,-4.84937330309023,
129.984140141245));
#90515=CARTESIAN_POINT('Ctrl Pts',(-67.5994909551566,-4.86813362573884,
130.095056425874));
#90516=CARTESIAN_POINT('Ctrl Pts',(-67.6058859483039,-4.88306562724851,
130.206492331211));
#90517=CARTESIAN_POINT('Ctrl Pts',(-67.6122809414514,-4.89415924064579,
130.318162726064));
#90518=CARTESIAN_POINT('Ctrl Pts',(-67.6214737729647,-4.91010635997548,
130.478689422689));
#90519=CARTESIAN_POINT('Ctrl Pts',(-67.630666604478,-4.91815743186786,130.64001341048));
#90520=CARTESIAN_POINT('Ctrl Pts',(-67.639859435991,-4.9182492064149,130.80156667783));
#90521=CARTESIAN_POINT('Ctrl Pts',(-67.6398594360288,-4.91824920641527,
130.801566678494));
#90522=CARTESIAN_POINT('Ctrl Pts',(-67.6475324466333,-4.91832580815699,
130.93641087006));
#90523=CARTESIAN_POINT('Ctrl Pts',(-67.6552054572378,-4.91285267348217,
131.071479102557));
#90524=CARTESIAN_POINT('Ctrl Pts',(-67.6628784678423,-4.90180091895616,
131.206269579174));
#90525=CARTESIAN_POINT('Ctrl Pts',(-67.6705428620542,-4.89076157497681,
131.340908693082));
#90526=CARTESIAN_POINT('Ctrl Pts',(-67.678207256266,-4.87415610287449,131.475270274707));
#90527=CARTESIAN_POINT('Ctrl Pts',(-67.6858716504779,-4.85200762096918,
131.608851207043));
#90528=CARTESIAN_POINT('Ctrl Pts',(-67.6935293817549,-4.82987839353959,
131.742316012647));
#90529=CARTESIAN_POINT('Ctrl Pts',(-67.701187113032,-4.80221580742792,131.875001124938));
#90530=CARTESIAN_POINT('Ctrl Pts',(-67.708844844309,-4.76909486034099,132.006407736264));
#90531=CARTESIAN_POINT('Ctrl Pts',(-67.7164982782742,-4.73599249983397,
132.137740605752));
#90532=CARTESIAN_POINT('Ctrl Pts',(-67.7241517122395,-4.69743796800965,
132.267796012838));
#90533=CARTESIAN_POINT('Ctrl Pts',(-67.7318051462048,-4.6535574212547,132.396084962289));
#90534=CARTESIAN_POINT('Ctrl Pts',(-67.7394563818591,-4.60968947839604,
132.524337063052));
#90535=CARTESIAN_POINT('Ctrl Pts',(-67.7471076175133,-4.56049869176321,
132.650823335254));
#90536=CARTESIAN_POINT('Ctrl Pts',(-67.7547588531676,-4.50616105254587,
132.77507004085));
#90537=CARTESIAN_POINT('Ctrl Pts',(-67.7624096461324,-4.45182655722647,
132.899309557708));
#90538=CARTESIAN_POINT('Ctrl Pts',(-67.7700604390972,-4.39234596244396,
133.021309397682));
#90539=CARTESIAN_POINT('Ctrl Pts',(-67.7777112320619,-4.32794315310324,
133.140616409642));
#90540=CARTESIAN_POINT('Ctrl Pts',(-67.7853633373754,-4.26352929667955,
133.259943886461));
#90541=CARTESIAN_POINT('Ctrl Pts',(-67.793015442689,-4.19419173776662,133.376577263501));
#90542=CARTESIAN_POINT('Ctrl Pts',(-67.8006675480025,-4.12019973015244,
133.490089056212));
#90543=CARTESIAN_POINT('Ctrl Pts',(-67.8083273831058,-4.04613297935969,
133.603715513094));
#90544=CARTESIAN_POINT('Ctrl Pts',(-67.8159872182092,-3.96740260915268,
133.714213750862));
#90545=CARTESIAN_POINT('Ctrl Pts',(-67.8236470533126,-3.88432074757255,
133.821186000726));
#90546=CARTESIAN_POINT('Ctrl Pts',(-67.8313107955854,-3.80119650715437,
133.928212815564));
#90547=CARTESIAN_POINT('Ctrl Pts',(-67.8389745378581,-3.71371661445925,
134.031709754582));
#90548=CARTESIAN_POINT('Ctrl Pts',(-67.846638280131,-3.62223186484096,134.131314085806));
#90549=CARTESIAN_POINT('Ctrl Pts',(-67.8543141073698,-3.53060285279229,
134.231075483239));
#90550=CARTESIAN_POINT('Ctrl Pts',(-67.8619899346086,-3.43495665154634,
134.326931726454));
#90551=CARTESIAN_POINT('Ctrl Pts',(-67.8696657618474,-3.3356796100937,134.418558260378));
#90552=CARTESIAN_POINT('Ctrl Pts',(-67.8766866963198,-3.24487277182504,
134.502367323635));
#90553=CARTESIAN_POINT('Ctrl Pts',(-67.8837076307923,-3.15102880541874,
134.582637975888));
#90554=CARTESIAN_POINT('Ctrl Pts',(-67.8907285652647,-3.05446467201014,
134.659153560117));
#90555=CARTESIAN_POINT('Ctrl Pts',(-67.8985028993838,-2.94753847294181,
134.743879848256));
#90556=CARTESIAN_POINT('Ctrl Pts',(-67.9062772335028,-2.8369149677715,134.824288005531));
#90557=CARTESIAN_POINT('Ctrl Pts',(-67.914051567622,-2.72297809125792,134.90003801905));
#90558=CARTESIAN_POINT('Ctrl Pts',(-67.9218163205691,-2.60918163176197,
134.975694677448));
#90559=CARTESIAN_POINT('Ctrl Pts',(-67.9295810735162,-2.4920802481906,135.046704400084));
#90560=CARTESIAN_POINT('Ctrl Pts',(-67.9373458264633,-2.37209114169222,
135.112767130188));
#90561=CARTESIAN_POINT('Ctrl Pts',(-67.9451028673483,-2.25222121006596,
135.178764245858));
#90562=CARTESIAN_POINT('Ctrl Pts',(-67.9528599082333,-2.12946960348594,
135.239823959586));
#90563=CARTESIAN_POINT('Ctrl Pts',(-67.9606169491183,-2.00428242121468,
135.295689489794));
#90564=CARTESIAN_POINT('Ctrl Pts',(-67.9683681403585,-1.87918964357122,
135.351512891372));
#90565=CARTESIAN_POINT('Ctrl Pts',(-67.9761193315986,-1.7516653016332,135.402149747249));
#90566=CARTESIAN_POINT('Ctrl Pts',(-67.9838705228388,-1.62217969269224,
135.447389381974));
#90567=CARTESIAN_POINT('Ctrl Pts',(-67.9916184196159,-1.49274911858922,
135.492609788647));
#90568=CARTESIAN_POINT('Ctrl Pts',(-67.999366316393,-1.3613593037462,135.532437408005));
#90569=CARTESIAN_POINT('Ctrl Pts',(-68.0071142131701,-1.2284998994806,135.566709939012));
#90570=CARTESIAN_POINT('Ctrl Pts',(-68.0148604892543,-1.09566828653826,
135.600975300944));
#90571=CARTESIAN_POINT('Ctrl Pts',(-68.0226067653384,-0.961368073953953,
135.629687788222));
#90572=CARTESIAN_POINT('Ctrl Pts',(-68.0303530414225,-0.826103044026408,
135.652735275444));
#90573=CARTESIAN_POINT('Ctrl Pts',(-68.0380993746879,-0.690837015602955,
135.675782932797));
#90574=CARTESIAN_POINT('Ctrl Pts',(-68.0458457079532,-0.554606541035317,
135.69316544098));
#90575=CARTESIAN_POINT('Ctrl Pts',(-68.0535920412186,-0.417924145535406,
135.704822072478));
#90576=CARTESIAN_POINT('Ctrl Pts',(-68.0613401092216,-0.281211140961272,
135.716481314398));
#90577=CARTESIAN_POINT('Ctrl Pts',(-68.0690881772245,-0.144046403546104,
135.722412094846));
#90578=CARTESIAN_POINT('Ctrl Pts',(-68.0768362452275,-0.00694571220998101,
135.722605713084));
#90579=CARTESIAN_POINT('Ctrl Pts',(-68.0845925479694,0.130300691372787,
135.722799537101));
#90580=CARTESIAN_POINT('Ctrl Pts',(-68.0923488507113,0.267482521313254,
135.717244017892));
#90581=CARTESIAN_POINT('Ctrl Pts',(-68.1001051534531,0.404085312342746,
135.705982606546));
#90582=CARTESIAN_POINT('Ctrl Pts',(-68.1078655959673,0.540761012394842,
135.694715184645));
#90583=CARTESIAN_POINT('Ctrl Pts',(-68.1156260384815,0.676856669958941,
135.677735850756));
#90584=CARTESIAN_POINT('Ctrl Pts',(-68.1233864809957,0.811865792994566,
135.655139626825));
#90585=CARTESIAN_POINT('Ctrl Pts',(-68.1311593812611,0.947091644660035,
135.632507129429));
#90586=CARTESIAN_POINT('Ctrl Pts',(-68.1389322815266,1.08122709354346,135.604239804356));
#90587=CARTESIAN_POINT('Ctrl Pts',(-68.146705181792,1.21377776263872,135.570483423938));
#90588=CARTESIAN_POINT('Ctrl Pts',(-68.1541955175539,1.34150988103487,135.537954172977));
#90589=CARTESIAN_POINT('Ctrl Pts',(-68.1616858533158,1.46777014551341,135.500328107964));
#90590=CARTESIAN_POINT('Ctrl Pts',(-68.1691761890777,1.59213371131244,135.457777997063));
#90591=CARTESIAN_POINT('Ctrl Pts',(-68.1769505231968,1.72121255951112,135.413614585773));
#90592=CARTESIAN_POINT('Ctrl Pts',(-68.1847248573159,1.84865692617802,135.364006470938));
#90593=CARTESIAN_POINT('Ctrl Pts',(-68.192499191435,1.97397322272228,135.309092882471));
#90594=CARTESIAN_POINT('Ctrl Pts',(-68.2002639443821,2.09913507813072,135.254246970094));
#90595=CARTESIAN_POINT('Ctrl Pts',(-68.2080286973293,2.22217372706486,135.194108749205));
#90596=CARTESIAN_POINT('Ctrl Pts',(-68.2157934502764,2.34261121585499,135.128867034933));
#90597=CARTESIAN_POINT('Ctrl Pts',(-68.2235504911614,2.46292908443322,135.063690119652));
#90598=CARTESIAN_POINT('Ctrl Pts',(-68.2313075320465,2.58065059262441,134.993419983266));
#90599=CARTESIAN_POINT('Ctrl Pts',(-68.2390645729315,2.69531857526733,134.918293145005));
#90600=CARTESIAN_POINT('Ctrl Pts',(-68.2468157641717,2.80990008589334,134.843222960476));
#90601=CARTESIAN_POINT('Ctrl Pts',(-68.2545669554119,2.92143232862603,134.763303577402));
#90602=CARTESIAN_POINT('Ctrl Pts',(-68.2623181466521,3.02948384906819,134.678816794984));
#90603=CARTESIAN_POINT('Ctrl Pts',(-68.2700660434292,3.13748944473136,134.594365921704));
#90604=CARTESIAN_POINT('Ctrl Pts',(-68.2778139402063,3.24201695317114,134.50535175043));
#90605=CARTESIAN_POINT('Ctrl Pts',(-68.2855618369834,3.34266515743276,134.412098511009));
#90606=CARTESIAN_POINT('Ctrl Pts',(-68.2933081130676,3.44329230825992,134.318864778156));
#90607=CARTESIAN_POINT('Ctrl Pts',(-68.3010543891517,3.54004148235356,134.221394006444));
#90608=CARTESIAN_POINT('Ctrl Pts',(-68.3088006652359,3.6325460387999,134.12004943567));
#90609=CARTESIAN_POINT('Ctrl Pts',(-68.3165469985013,3.72505127809398,134.018704116793));
#90610=CARTESIAN_POINT('Ctrl Pts',(-68.3242933317666,3.81331157364519,133.913485230556));
#90611=CARTESIAN_POINT('Ctrl Pts',(-68.3320396650321,3.89699880127807,133.804791154229));
#90612=CARTESIAN_POINT('Ctrl Pts',(-68.3397877330351,3.980704770085,133.696072736617));
#90613=CARTESIAN_POINT('Ctrl Pts',(-68.3475358010381,4.05983539465274,133.583877890021));
#90614=CARTESIAN_POINT('Ctrl Pts',(-68.3552838690411,4.13410456369698,133.468635850893));
#90615=CARTESIAN_POINT('Ctrl Pts',(-68.363040171783,4.2084526668979,133.353271331154));
#90616=CARTESIAN_POINT('Ctrl Pts',(-68.3707964745248,4.27792878118196,133.2348534786));
#90617=CARTESIAN_POINT('Ctrl Pts',(-68.3785527772667,4.34229138213674,133.113838613807));
#90618=CARTESIAN_POINT('Ctrl Pts',(-68.3863132197809,4.40668833534957,132.992759159737));
#90619=CARTESIAN_POINT('Ctrl Pts',(-68.3940736622951,4.46596616810311,132.869080283888));
#90620=CARTESIAN_POINT('Ctrl Pts',(-68.4018341048093,4.51993105373295,132.743279474043));
#90621=CARTESIAN_POINT('Ctrl Pts',(-68.4096070050748,4.57398256858806,132.617276717569));
#90622=CARTESIAN_POINT('Ctrl Pts',(-68.4173799053403,4.62270395399424,132.48914558584));
#90623=CARTESIAN_POINT('Ctrl Pts',(-68.4251528056057,4.66595062949402,132.359380805739));
#90624=CARTESIAN_POINT('Ctrl Pts',(-68.4326431413674,4.70762517940513,132.234333302259));
#90625=CARTESIAN_POINT('Ctrl Pts',(-68.4401334771289,4.74421606231217,132.107769158674));
#90626=CARTESIAN_POINT('Ctrl Pts',(-68.4476238128906,4.77563899399134,131.980139194327));
#90627=CARTESIAN_POINT('Ctrl Pts',(-68.4553981470096,4.80825333567764,131.847670101082));
#90628=CARTESIAN_POINT('Ctrl Pts',(-68.4631724811287,4.83540341687729,131.71363314818));
#90629=CARTESIAN_POINT('Ctrl Pts',(-68.4709468152477,4.8569395789692,131.578518862851));
#90630=CARTESIAN_POINT('Ctrl Pts',(-68.4787115681948,4.87844919966604,131.443571093803));
#90631=CARTESIAN_POINT('Ctrl Pts',(-68.4864763211419,4.89435860636441,131.307549016472));
#90632=CARTESIAN_POINT('Ctrl Pts',(-68.494241074089,4.90456830894643,131.170956806005));
#90633=CARTESIAN_POINT('Ctrl Pts',(-68.501998114974,4.91476787110791,131.034500260848));
#90634=CARTESIAN_POINT('Ctrl Pts',(-68.5097551558589,4.91927896589805,130.897475096801));
#90635=CARTESIAN_POINT('Ctrl Pts',(-68.5175121967439,4.91805347470634,130.760393784284));
#90636=CARTESIAN_POINT('Ctrl Pts',(-68.525263387984,4.91682890766706,130.623415845849));
#90637=CARTESIAN_POINT('Ctrl Pts',(-68.5330145792241,4.90987636877563,130.486382232591));
#90638=CARTESIAN_POINT('Ctrl Pts',(-68.5407657704642,4.89719973204254,130.349808258665));
#90639=CARTESIAN_POINT('Ctrl Pts',(-68.5485136672413,4.88452848321827,130.213292332322));
#90640=CARTESIAN_POINT('Ctrl Pts',(-68.5562615640183,4.86613801145158,130.077236045234));
#90641=CARTESIAN_POINT('Ctrl Pts',(-68.5640094607954,4.84208423293126,129.94215220674));
#90642=CARTESIAN_POINT('Ctrl Pts',(-68.5717557368795,4.81803548594288,129.807096624874));
#90643=CARTESIAN_POINT('Ctrl Pts',(-68.5795020129636,4.78832585701402,129.673013471665));
#90644=CARTESIAN_POINT('Ctrl Pts',(-68.5872482890477,4.75306277170416,129.54040755248));
#90645=CARTESIAN_POINT('Ctrl Pts',(-68.594994622313,4.71779942609027,129.407800654429));
#90646=CARTESIAN_POINT('Ctrl Pts',(-68.6027409555783,4.67698264276923,129.276671389996));
#90647=CARTESIAN_POINT('Ctrl Pts',(-68.6104872888436,4.63077022868955,129.147511151989));
#90648=CARTESIAN_POINT('Ctrl Pts',(-68.6182353568466,4.58454746566014,129.018321989442));
#90649=CARTESIAN_POINT('Ctrl Pts',(-68.6259834248494,4.53292679914924,128.891103098802));
#90650=CARTESIAN_POINT('Ctrl Pts',(-68.6337314928524,4.47611470780124,128.766327206381));
#90651=CARTESIAN_POINT('Ctrl Pts',(-68.6414877955942,4.4192422358864,128.641418700657));
#90652=CARTESIAN_POINT('Ctrl Pts',(-68.6492440983361,4.35716747958491,128.518958736222));
#90653=CARTESIAN_POINT('Ctrl Pts',(-68.6570004010779,4.29014380447648,128.399397166823));
#90654=CARTESIAN_POINT('Ctrl Pts',(-68.6647608435921,4.22308435681443,128.279771783813));
#90655=CARTESIAN_POINT('Ctrl Pts',(-68.6725212861063,4.15107093234099,128.163048210861));
#90656=CARTESIAN_POINT('Ctrl Pts',(-68.6802817286204,4.07440048700341,128.049647613639));
#90657=CARTESIAN_POINT('Ctrl Pts',(-68.6880546288858,3.99760696346071,127.936064975711));
#90658=CARTESIAN_POINT('Ctrl Pts',(-68.6958275291512,3.91614171237452,127.825816287831));
#90659=CARTESIAN_POINT('Ctrl Pts',(-68.7036004294166,3.83034281221331,127.719290601598));
#90660=CARTESIAN_POINT('Ctrl Pts',(-68.7110907651789,3.7476629181841,127.616637392377));
#90661=CARTESIAN_POINT('Ctrl Pts',(-68.7185811009413,3.6609591856893,127.517441435162));
#90662=CARTESIAN_POINT('Ctrl Pts',(-68.7260714367036,3.57056534412745,127.422017319523));
#90663=CARTESIAN_POINT('Ctrl Pts',(-68.7338457708226,3.4767441925916,127.32297516954));
#90664=CARTESIAN_POINT('Ctrl Pts',(-68.7416201049417,3.37865039005745,127.227682790218));
#90665=CARTESIAN_POINT('Ctrl Pts',(-68.7493944390608,3.2766157368352,127.136531235544));
#90666=CARTESIAN_POINT('Ctrl Pts',(-68.7571591920079,3.17470683220396,127.045492017015));
#90667=CARTESIAN_POINT('Ctrl Pts',(-68.764923944955,3.06886702912894,126.95858372726));
#90668=CARTESIAN_POINT('Ctrl Pts',(-68.7726886979021,2.95946672760206,126.876162589116));
#90669=CARTESIAN_POINT('Ctrl Pts',(-68.7804457387871,2.85017508399679,126.793823312809));
#90670=CARTESIAN_POINT('Ctrl Pts',(-68.7882027796721,2.73733028965298,126.715962552808));
#90671=CARTESIAN_POINT('Ctrl Pts',(-68.7959598205571,2.62133749116316,126.642897795442));
#90672=CARTESIAN_POINT('Ctrl Pts',(-68.8037110117972,2.50543216374482,126.569888136777));
#90673=CARTESIAN_POINT('Ctrl Pts',(-68.8114622030374,2.38638388682055,126.501667489455));
#90674=CARTESIAN_POINT('Ctrl Pts',(-68.8192133942775,2.26462830278217,126.438511134048));
#90675=CARTESIAN_POINT('Ctrl Pts',(-68.8269612910546,2.14292446811527,126.375381621776));
#90676=CARTESIAN_POINT('Ctrl Pts',(-68.8347091878316,2.01851596127136,126.317312299988));
#90677=CARTESIAN_POINT('Ctrl Pts',(-68.8424570846087,1.89186444733695,126.264533310784));
#90678=CARTESIAN_POINT('Ctrl Pts',(-68.8502033606928,1.76523942616896,126.211765361807));
#90679=CARTESIAN_POINT('Ctrl Pts',(-68.8579496367769,1.63637269180727,126.164285694572));
#90680=CARTESIAN_POINT('Ctrl Pts',(-68.865695912861,1.50574701744352,126.122276788547));
#90681=CARTESIAN_POINT('Ctrl Pts',(-68.8734422461264,1.37512037883055,126.080267572422));
#90682=CARTESIAN_POINT('Ctrl Pts',(-68.8811885793917,1.24273514649838,126.043729317785));
#90683=CARTESIAN_POINT('Ctrl Pts',(-68.8889349126571,1.10909004164311,126.012794866997));
#90684=CARTESIAN_POINT('Ctrl Pts',(-68.8966829806601,0.975415007893047,
125.981853488653));
#90685=CARTESIAN_POINT('Ctrl Pts',(-68.904431048663,0.840479921016337,125.956518499477));
#90686=CARTESIAN_POINT('Ctrl Pts',(-68.912179116666,0.704794105798939,125.936871703256));
#90687=CARTESIAN_POINT('Ctrl Pts',(-68.9199354194078,0.568964082082815,
125.917204026187));
#90688=CARTESIAN_POINT('Ctrl Pts',(-68.9276917221497,0.432382123715796,
125.903236674684));
#90689=CARTESIAN_POINT('Ctrl Pts',(-68.9354480248915,0.295563655679571,
125.894999642048));
#90690=CARTESIAN_POINT('Ctrl Pts',(-68.9432084674057,0.15867216350743,125.886758213059));
#90691=CARTESIAN_POINT('Ctrl Pts',(-68.9509689099199,0.0215443008461921,
125.884253204283));
#90692=CARTESIAN_POINT('Ctrl Pts',(-68.9587293524341,-0.115305081753601,
125.887462428604));
#90693=CARTESIAN_POINT('Ctrl Pts',(-68.9665022526995,-0.252374147131448,
125.890676804656));
#90694=CARTESIAN_POINT('Ctrl Pts',(-68.9742751529649,-0.389163448761537,
125.899623718838));
#90695=CARTESIAN_POINT('Ctrl Pts',(-68.9820480532303,-0.525162926845925,
125.914229028052));
#90696=CARTESIAN_POINT('Ctrl Pts',(-68.9895383889923,-0.656218481339564,
125.928303397487));
#90697=CARTESIAN_POINT('Ctrl Pts',(-68.9970287247543,-0.786540334784979,
125.947631865341));
#90698=CARTESIAN_POINT('Ctrl Pts',(-69.0045190605163,-0.915683425175047,
125.972103698966));
#90699=CARTESIAN_POINT('Ctrl Pts',(-69.0122933946355,-1.04972301509146,
125.997503389601));
#90700=CARTESIAN_POINT('Ctrl Pts',(-69.0200677287547,-1.18291728898096,
126.028524625166));
#90701=CARTESIAN_POINT('Ctrl Pts',(-69.0278420628739,-1.31475789587773,
126.065099626892));
#90702=CARTESIAN_POINT('Ctrl Pts',(-69.0356068158211,-1.44643602100944,
126.101629553197));
#90703=CARTESIAN_POINT('Ctrl Pts',(-69.0433715687683,-1.5767634253954,126.143699523598));
#90704=CARTESIAN_POINT('Ctrl Pts',(-69.0511363217155,-1.70524019843139,
126.191190457237));
#90705=CARTESIAN_POINT('Ctrl Pts',(-69.0588933626006,-1.8335893665252,126.23863422221));
#90706=CARTESIAN_POINT('Ctrl Pts',(-69.0666504034856,-1.96009119677698,
126.291488100988));
#90707=CARTESIAN_POINT('Ctrl Pts',(-69.0744074443707,-2.08425958731718,
126.349582841383));
#90708=CARTESIAN_POINT('Ctrl Pts',(-69.082158635611,-2.20833434150801,126.407633772082));
#90709=CARTESIAN_POINT('Ctrl Pts',(-69.0899098268512,-2.33007880580415,
126.470917532822));
#90710=CARTESIAN_POINT('Ctrl Pts',(-69.0976610180914,-2.44902590350822,
126.539216401195));
#90711=CARTESIAN_POINT('Ctrl Pts',(-69.1054089148686,-2.5679224455229,126.607486240726));
#90712=CARTESIAN_POINT('Ctrl Pts',(-69.1131568116458,-2.68402364734899,
126.680766754119));
#90713=CARTESIAN_POINT('Ctrl Pts',(-69.120904708423,-2.79688634266317,126.758793926888));
#90714=CARTESIAN_POINT('Ctrl Pts',(-69.1286509845072,-2.90972542953453,
126.836804778054));
#90715=CARTESIAN_POINT('Ctrl Pts',(-69.1363972605914,-3.01932703594144,
126.919560091474));
#90716=CARTESIAN_POINT('Ctrl Pts',(-69.1441435366756,-3.12527668603847,
127.006752330999));
#90717=CARTESIAN_POINT('Ctrl Pts',(-69.1518898699411,-3.23122711823145,
127.093945214156));
#90718=CARTESIAN_POINT('Ctrl Pts',(-69.1596362032066,-3.3335252384397,127.185574840336));
#90719=CARTESIAN_POINT('Ctrl Pts',(-69.167382536472,-3.43178971163483,127.281293425811));
#90720=CARTESIAN_POINT('Ctrl Pts',(-69.1751306044752,-3.53007619047781,
127.377033446801));
#90721=CARTESIAN_POINT('Ctrl Pts',(-69.1828786724782,-3.62432694482605,
127.476863976462));
#90722=CARTESIAN_POINT('Ctrl Pts',(-69.1906267404813,-3.71419784834841,
127.580400722371));
#90723=CARTESIAN_POINT('Ctrl Pts',(-69.1983830432233,-3.80416426773626,
127.684047508366));
#90724=CARTESIAN_POINT('Ctrl Pts',(-69.2061393459651,-3.88974128082898,
127.791408083486));
#90725=CARTESIAN_POINT('Ctrl Pts',(-69.2138956487071,-3.97062505362117,
127.902065018207));
#90726=CARTESIAN_POINT('Ctrl Pts',(-69.2216560912214,-4.05155199651826,
128.012781013867));
#90727=CARTESIAN_POINT('Ctrl Pts',(-69.2294165337357,-4.12778049064987,
128.126796549957));
#90728=CARTESIAN_POINT('Ctrl Pts',(-69.23717697625,-4.19905091336629,128.243666475452));
#90729=CARTESIAN_POINT('Ctrl Pts',(-69.2449498765156,-4.27043574569225,
128.360724010926));
#90730=CARTESIAN_POINT('Ctrl Pts',(-69.2527227767811,-4.336846412196,128.48064475012));
#90731=CARTESIAN_POINT('Ctrl Pts',(-69.2604956770466,-4.39806959178665,
128.602959489125));
#90732=CARTESIAN_POINT('Ctrl Pts',(-69.2679860128077,-4.45706715457859,
128.720827779257));
#90733=CARTESIAN_POINT('Ctrl Pts',(-69.2754763485687,-4.51124771223012,
128.840918754452));
#90734=CARTESIAN_POINT('Ctrl Pts',(-69.2829666843298,-4.56046386036755,
128.962798117736));
#90735=CARTESIAN_POINT('Ctrl Pts',(-69.2917189477579,-4.61797165536622,
129.105210998539));
#90736=CARTESIAN_POINT('Ctrl Pts',(-69.300471211186,-4.66885543046119,129.250445070519));
#90737=CARTESIAN_POINT('Ctrl Pts',(-69.3092234746142,-4.7128622013437,129.397906589293));
#90738=CARTESIAN_POINT('Ctrl Pts',(-69.312853465788,-4.73111395886884,129.45906608432));
#90739=CARTESIAN_POINT('Ctrl Pts',(-69.3164834569616,-4.74818330114657,
129.520608445774));
#90740=CARTESIAN_POINT('Ctrl Pts',(-69.3201134481353,-4.76405452823409,
129.582490119308));
#90741=CARTESIAN_POINT('Origin',(213.235140564004,0.,130.804360617566));
#90742=CARTESIAN_POINT('',(-71.4150282010452,-4.76405452823412,129.582490119309));
#90743=CARTESIAN_POINT('',(-71.0699658330087,-4.76405452823398,129.582490119308));
#90744=CARTESIAN_POINT('',(213.235140564004,-4.76405452823405,129.582490119308));
#90745=CARTESIAN_POINT('',(-69.7351405640517,-4.91824821000367,130.808556722393));
#90746=CARTESIAN_POINT('Ctrl Pts',(-69.7351405640517,-4.91824821000367,
130.808556722393));
#90747=CARTESIAN_POINT('Ctrl Pts',(-69.7444187886688,-4.91810812104566,
130.972754781138));
#90748=CARTESIAN_POINT('Ctrl Pts',(-69.7536970132858,-4.90974152552505,
131.136595367194));
#90749=CARTESIAN_POINT('Ctrl Pts',(-69.7629752379029,-4.89327832969581,
131.299345718988));
#90750=CARTESIAN_POINT('Ctrl Pts',(-69.7725248542183,-4.87633357895065,
131.466856582214));
#90751=CARTESIAN_POINT('Ctrl Pts',(-69.7820744705337,-4.85081157199009,
131.633212407593));
#90752=CARTESIAN_POINT('Ctrl Pts',(-69.7916240868491,-4.81690610697297,
131.797637325793));
#90753=CARTESIAN_POINT('Ctrl Pts',(-69.8011737031644,-4.78300064195585,
131.962062243994));
#90754=CARTESIAN_POINT('Ctrl Pts',(-69.8107233194799,-4.74071184323133,
132.124556280918));
#90755=CARTESIAN_POINT('Ctrl Pts',(-69.8202729357953,-4.69028412933995,
132.284366647473));
#90756=CARTESIAN_POINT('Ctrl Pts',(-69.8280472699145,-4.64923097246828,
132.414468124253));
#90757=CARTESIAN_POINT('Ctrl Pts',(-69.8358216040337,-4.60269545694166,
132.543066248064));
#90758=CARTESIAN_POINT('Ctrl Pts',(-69.8435959381529,-4.55080492781291,
132.669664231323));
#90759=CARTESIAN_POINT('Ctrl Pts',(-69.8513606911001,-4.49897834912372,
132.796106193881));
#90760=CARTESIAN_POINT('Ctrl Pts',(-69.8591254440473,-4.44181003487559,
132.920552562208));
#90761=CARTESIAN_POINT('Ctrl Pts',(-69.8668901969945,-4.37947727625291,
133.042520989229));
#90762=CARTESIAN_POINT('Ctrl Pts',(-69.8746472378797,-4.31720642740474,
133.16436827549));
#90763=CARTESIAN_POINT('Ctrl Pts',(-69.8824042787648,-4.24978151868362,
133.283742172314));
#90764=CARTESIAN_POINT('Ctrl Pts',(-69.8901613196499,-4.17742803050364,
133.400179970384));
#90765=CARTESIAN_POINT('Ctrl Pts',(-69.8979125108902,-4.10512910465191,
133.516529961804));
#90766=CARTESIAN_POINT('Ctrl Pts',(-69.9056637021304,-4.02790920268156,
133.629947930839));
#90767=CARTESIAN_POINT('Ctrl Pts',(-69.9134148933707,-3.94603968892922,
133.739995784935));
#90768=CARTESIAN_POINT('Ctrl Pts',(-69.9211627901479,-3.86420497190416,
133.849996865758));
#90769=CARTESIAN_POINT('Ctrl Pts',(-69.9289106869252,-3.77772480649938,
133.956630367531));
#90770=CARTESIAN_POINT('Ctrl Pts',(-69.9366585837024,-3.68691370109126,
134.059487408216));
#90771=CARTESIAN_POINT('Ctrl Pts',(-69.9444048597866,-3.59612159140873,
134.162322933425));
#90772=CARTESIAN_POINT('Ctrl Pts',(-69.9521511358708,-3.50100060228079,
134.261383275912));
#90773=CARTESIAN_POINT('Ctrl Pts',(-69.959897411955,-3.40190507052986,134.356293183593));
#90774=CARTESIAN_POINT('Ctrl Pts',(-69.9676437452204,-3.30280880727835,
134.451203791877));
#90775=CARTESIAN_POINT('Ctrl Pts',(-69.975390078486,-3.19973822521254,134.541963633793));
#90776=CARTESIAN_POINT('Ctrl Pts',(-69.9831364117515,-3.09308371280454,
134.628235119702));
#90777=CARTESIAN_POINT('Ctrl Pts',(-69.9908844797546,-2.98640531585798,
134.714525925511));
#90778=CARTESIAN_POINT('Ctrl Pts',(-69.9986325477576,-2.87614169540752,
134.796326129377));
#90779=CARTESIAN_POINT('Ctrl Pts',(-70.0063806157607,-2.76271509841206,
134.873339401918));
#90780=CARTESIAN_POINT('Ctrl Pts',(-70.0141369185026,-2.64916795027937,
134.950434525081));
#90781=CARTESIAN_POINT('Ctrl Pts',(-70.0218932212446,-2.53245143431552,
135.022732333908));
#90782=CARTESIAN_POINT('Ctrl Pts',(-70.0296495239866,-2.41301594376746,
135.089980423105));
#90783=CARTESIAN_POINT('Ctrl Pts',(-70.0374099665009,-2.29351670690197,
135.157264404631));
#90784=CARTESIAN_POINT('Ctrl Pts',(-70.0451704090152,-2.17129595205114,
135.219493118833));
#90785=CARTESIAN_POINT('Ctrl Pts',(-70.0529308515295,-2.04682637818646,
135.276461336474));
#90786=CARTESIAN_POINT('Ctrl Pts',(-70.060703751795,-1.92215699471192,135.333521004556));
#90787=CARTESIAN_POINT('Ctrl Pts',(-70.0684766520606,-1.79523194049187,
135.385303153271));
#90788=CARTESIAN_POINT('Ctrl Pts',(-70.0762495523261,-1.66654233040697,
135.431651371718));
#90789=CARTESIAN_POINT('Ctrl Pts',(-70.0837398880869,-1.54253091182139,
135.476314715672));
#90790=CARTESIAN_POINT('Ctrl Pts',(-70.0912302238476,-1.41688129589539,
135.515932251774));
#90791=CARTESIAN_POINT('Ctrl Pts',(-70.0987205596083,-1.29004214955684,
135.550408901651));
#90792=CARTESIAN_POINT('Ctrl Pts',(-70.1064948937274,-1.15839385841048,
135.586192744193));
#90793=CARTESIAN_POINT('Ctrl Pts',(-70.1142692278464,-1.02504703192719,
135.61655152413));
#90794=CARTESIAN_POINT('Ctrl Pts',(-70.1220435619655,-0.890488464682378,
135.641323854636));
#90795=CARTESIAN_POINT('Ctrl Pts',(-70.1298083149126,-0.756095728846037,
135.666065655459));
#90796=CARTESIAN_POINT('Ctrl Pts',(-70.1375730678597,-0.620494604406137,
135.685234635443));
#90797=CARTESIAN_POINT('Ctrl Pts',(-70.1453378208068,-0.484186733831959,
135.698719234308));
#90798=CARTESIAN_POINT('Ctrl Pts',(-70.1530948616917,-0.348014246156439,
135.71219044008));
#90799=CARTESIAN_POINT('Ctrl Pts',(-70.1608519025767,-0.211136795807643,
135.719988461904));
#90800=CARTESIAN_POINT('Ctrl Pts',(-70.1686089434617,-0.0740655509111302,
135.722052897149));
#90801=CARTESIAN_POINT('Ctrl Pts',(-70.1763601347018,0.0629023274937205,
135.724115775587));
#90802=CARTESIAN_POINT('Ctrl Pts',(-70.184111325942,0.200063320220439,135.72045366773));
#90803=CARTESIAN_POINT('Ctrl Pts',(-70.1918625171822,0.336902168544469,
135.711058080354));
#90804=CARTESIAN_POINT('Ctrl Pts',(-70.1996104139592,0.47368285670748,135.701666486353));
#90805=CARTESIAN_POINT('Ctrl Pts',(-70.2073583107363,0.610141283560909,
135.686546286329));
#90806=CARTESIAN_POINT('Ctrl Pts',(-70.2151062075134,0.745763445607566,
135.66574107436));
#90807=CARTESIAN_POINT('Ctrl Pts',(-70.2228524835975,0.881357238421598,
135.644940214392));
#90808=CARTESIAN_POINT('Ctrl Pts',(-70.2305987596815,1.01611472817172,135.618456767071));
#90809=CARTESIAN_POINT('Ctrl Pts',(-70.2383450357656,1.14952867694443,135.586386013084));
#90810=CARTESIAN_POINT('Ctrl Pts',(-70.2460913690309,1.2829436105486,135.554315022358));
#90811=CARTESIAN_POINT('Ctrl Pts',(-70.2538377022963,1.41501460324895,135.516656734046));
#90812=CARTESIAN_POINT('Ctrl Pts',(-70.2615840355616,1.54524661681551,135.473557117578));
#90813=CARTESIAN_POINT('Ctrl Pts',(-70.2693321035646,1.67550779493854,135.430447849249));
#90814=CARTESIAN_POINT('Ctrl Pts',(-70.2770801715676,1.80392880334425,135.381894950809));
#90815=CARTESIAN_POINT('Ctrl Pts',(-70.2848282395705,1.93003209693533,135.328093497312));
#90816=CARTESIAN_POINT('Ctrl Pts',(-70.2925845423124,2.05626941460749,135.274234862991));
#90817=CARTESIAN_POINT('Ctrl Pts',(-70.3003408450543,2.18018373659078,135.215116684173));
#90818=CARTESIAN_POINT('Ctrl Pts',(-70.3080971477962,2.30131925861064,135.150981458225));
#90819=CARTESIAN_POINT('Ctrl Pts',(-70.3158575903103,2.42251943430592,135.086812001375));
#90820=CARTESIAN_POINT('Ctrl Pts',(-70.3236180328245,2.54093751737697,135.017620358898));
#90821=CARTESIAN_POINT('Ctrl Pts',(-70.3313784753387,2.65614533731364,134.943693294407));
#90822=CARTESIAN_POINT('Ctrl Pts',(-70.3391513756041,2.77153809907055,134.86964755563));
#90823=CARTESIAN_POINT('Ctrl Pts',(-70.3469242758695,2.88370997945372,134.790851429044));
#90824=CARTESIAN_POINT('Ctrl Pts',(-70.3546971761349,2.99226392595159,134.707633559592));
#90825=CARTESIAN_POINT('Ctrl Pts',(-70.362187511897,3.0968716630644,134.627440869306));
#90826=CARTESIAN_POINT('Ctrl Pts',(-70.3696778476591,3.19811970480336,134.543142534807));
#90827=CARTESIAN_POINT('Ctrl Pts',(-70.3771681834212,3.29568554360642,134.455064640102));
#90828=CARTESIAN_POINT('Ctrl Pts',(-70.3849425175403,3.39695062084092,134.363647245251));
#90829=CARTESIAN_POINT('Ctrl Pts',(-70.3927168516593,3.49456953909797,134.267868445663));
#90830=CARTESIAN_POINT('Ctrl Pts',(-70.4004911857783,3.58814339471309,134.16805056188));
#90831=CARTESIAN_POINT('Ctrl Pts',(-70.4082559387254,3.68160192891411,134.068355694718));
#90832=CARTESIAN_POINT('Ctrl Pts',(-70.4160206916725,3.77102505466988,133.964631930213));
#90833=CARTESIAN_POINT('Ctrl Pts',(-70.4237854446195,3.8560477631489,133.857241013326));
#90834=CARTESIAN_POINT('Ctrl Pts',(-70.4315424855045,3.94098602587525,133.749956758611));
#90835=CARTESIAN_POINT('Ctrl Pts',(-70.4392995263896,4.02153232781797,133.639012904335));
#90836=CARTESIAN_POINT('Ctrl Pts',(-70.4470565672745,4.09735955167546,133.524806861621));
#90837=CARTESIAN_POINT('Ctrl Pts',(-70.4548077585146,4.17312959363359,133.410686942572));
#90838=CARTESIAN_POINT('Ctrl Pts',(-70.4625589497547,4.24418742548935,133.293310056042));
#90839=CARTESIAN_POINT('Ctrl Pts',(-70.4703101409948,4.31024739172633,133.173105112993));
#90840=CARTESIAN_POINT('Ctrl Pts',(-70.4780580377718,4.37627928071545,133.052951260251));
#90841=CARTESIAN_POINT('Ctrl Pts',(-70.4858059345489,4.43731734110599,132.929972083592));
#90842=CARTESIAN_POINT('Ctrl Pts',(-70.493553831326,4.49312041838339,132.804623592379));
#90843=CARTESIAN_POINT('Ctrl Pts',(-70.50130010741,4.54891182286,132.679301321367));
#90844=CARTESIAN_POINT('Ctrl Pts',(-70.5090463834941,4.59947026342356,132.551611078539));
#90845=CARTESIAN_POINT('Ctrl Pts',(-70.5167926595782,4.64460172793202,132.422031119056));
#90846=CARTESIAN_POINT('Ctrl Pts',(-70.5245389928435,4.6897335255907,132.292450203043));
#90847=CARTESIAN_POINT('Ctrl Pts',(-70.5322853261088,4.72943813866297,132.160979911752));
#90848=CARTESIAN_POINT('Ctrl Pts',(-70.5400316593741,4.76357079511038,132.028115634909));
#90849=CARTESIAN_POINT('Ctrl Pts',(-70.547779727377,4.79771109532954,131.895221604032));
#90850=CARTESIAN_POINT('Ctrl Pts',(-70.55552779538,4.82627685868318,131.760933345011));
#90851=CARTESIAN_POINT('Ctrl Pts',(-70.5632758633829,4.8491740825506,131.625758072894));
#90852=CARTESIAN_POINT('Ctrl Pts',(-70.5710321661248,4.87209564186003,131.490439134889));
#90853=CARTESIAN_POINT('Ctrl Pts',(-70.5787884688667,4.88933656151407,131.354231686676));
#90854=CARTESIAN_POINT('Ctrl Pts',(-70.5865447716085,4.90085448807156,131.21765028505));
#90855=CARTESIAN_POINT('Ctrl Pts',(-70.5943052141227,4.91237856209326,131.080995985817));
#90856=CARTESIAN_POINT('Ctrl Pts',(-70.6020656566367,4.9181735400901,130.943967725896));
#90857=CARTESIAN_POINT('Ctrl Pts',(-70.6098260991509,4.91824924779478,130.807080740003));
#90858=CARTESIAN_POINT('Ctrl Pts',(-70.6175989994163,4.91832507703219,130.669974010967));
#90859=CARTESIAN_POINT('Ctrl Pts',(-70.6253718996817,4.91266330541031,130.533009400006));
#90860=CARTESIAN_POINT('Ctrl Pts',(-70.6331447999471,4.90132581464771,130.396698599262));
#90861=CARTESIAN_POINT('Ctrl Pts',(-70.6406351357094,4.8904004702313,130.265343039465));
#90862=CARTESIAN_POINT('Ctrl Pts',(-70.6481254714717,4.87420493364416,130.134594885555));
#90863=CARTESIAN_POINT('Ctrl Pts',(-70.6556158072341,4.85283922538445,130.004901728648));
#90864=CARTESIAN_POINT('Ctrl Pts',(-70.6633901413531,4.83066342980289,129.870291216283));
#90865=CARTESIAN_POINT('Ctrl Pts',(-70.6711644754722,4.80284742290493,129.736390874936));
#90866=CARTESIAN_POINT('Ctrl Pts',(-70.6789388095913,4.76944676491718,129.603710535685));
#90867=CARTESIAN_POINT('Ctrl Pts',(-70.6867035625384,4.7360872702553,129.471193713094));
#90868=CARTESIAN_POINT('Ctrl Pts',(-70.6944683154855,4.69715691331984,129.339894276492));
#90869=CARTESIAN_POINT('Ctrl Pts',(-70.7022330684326,4.65276274420152,129.210314850133));
#90870=CARTESIAN_POINT('Ctrl Pts',(-70.7099901093176,4.60841266799781,129.080864123887));
#90871=CARTESIAN_POINT('Ctrl Pts',(-70.7177471502026,4.55860970495447,128.953130375682));
#90872=CARTESIAN_POINT('Ctrl Pts',(-70.7255041910877,4.50351139341343,128.827603628987));
#90873=CARTESIAN_POINT('Ctrl Pts',(-70.7332553823278,4.44845463193781,128.702171542988));
#90874=CARTESIAN_POINT('Ctrl Pts',(-70.741006573568,4.38811062681534,128.578943502326));
#90875=CARTESIAN_POINT('Ctrl Pts',(-70.7487577648081,4.32268582920232,128.458391673928));
#90876=CARTESIAN_POINT('Ctrl Pts',(-70.7565056615852,4.25728883887346,128.337891083273));
#90877=CARTESIAN_POINT('Ctrl Pts',(-70.7642535583623,4.18681553717697,128.220064785461));
#90878=CARTESIAN_POINT('Ctrl Pts',(-70.7720014551394,4.11151922779875,128.105362154813));
#90879=CARTESIAN_POINT('Ctrl Pts',(-70.7797477312235,4.03623866878526,127.990683517484));
#90880=CARTESIAN_POINT('Ctrl Pts',(-70.7874940073077,3.95613732320112,127.879127574292));
#90881=CARTESIAN_POINT('Ctrl Pts',(-70.7952402833918,3.87151269235626,127.771116061744));
#90882=CARTESIAN_POINT('Ctrl Pts',(-70.8029866166572,3.7868874368316,127.66310375188));
#90883=CARTESIAN_POINT('Ctrl Pts',(-70.8107329499225,3.6977390705401,127.558636232625));
#90884=CARTESIAN_POINT('Ctrl Pts',(-70.8184792831879,3.60440612606566,127.458103075045));
#90885=CARTESIAN_POINT('Ctrl Pts',(-70.8262273511909,3.51105228032543,127.357547403761));
#90886=CARTESIAN_POINT('Ctrl Pts',(-70.8339754191939,3.41351225761958,127.260928133853));
#90887=CARTESIAN_POINT('Ctrl Pts',(-70.8417234871969,3.31216198162016,127.168598514511));
#90888=CARTESIAN_POINT('Ctrl Pts',(-70.8494797899388,3.21070398934133,127.076170766151));
#90889=CARTESIAN_POINT('Ctrl Pts',(-70.8572360926807,3.10542794376917,126.988042039347));
#90890=CARTESIAN_POINT('Ctrl Pts',(-70.8649923954226,2.99674386303928,126.904526097764));
#90891=CARTESIAN_POINT('Ctrl Pts',(-70.8727528379368,2.88800177434309,126.820965581209));
#90892=CARTESIAN_POINT('Ctrl Pts',(-70.8805132804509,2.77584834558633,126.74202298051));
#90893=CARTESIAN_POINT('Ctrl Pts',(-70.8882737229651,2.66072236937621,126.667968525948));
#90894=CARTESIAN_POINT('Ctrl Pts',(-70.8960466232305,2.54541158272867,126.593795192601));
#90895=CARTESIAN_POINT('Ctrl Pts',(-70.9038195234959,2.42711905062857,126.524525883645));
#90896=CARTESIAN_POINT('Ctrl Pts',(-70.9115924237614,2.30630872274831,126.46038511834));
#90897=CARTESIAN_POINT('Ctrl Pts',(-70.9190827595232,2.18989015459214,126.398576031416));
#90898=CARTESIAN_POINT('Ctrl Pts',(-70.9265730952851,2.07113394661053,126.341529224142));
#90899=CARTESIAN_POINT('Ctrl Pts',(-70.934063431047,1.95047073341027,126.289402480372));
#90900=CARTESIAN_POINT('Ctrl Pts',(-70.9418377651661,1.82523253780426,126.235299335269));
#90901=CARTESIAN_POINT('Ctrl Pts',(-70.9496120992851,1.6975431572031,126.186325324467));
#90902=CARTESIAN_POINT('Ctrl Pts',(-70.9573864334042,1.5678615585905,126.142709279725));
#90903=CARTESIAN_POINT('Ctrl Pts',(-70.9651511863513,1.43833978095839,126.099146987861));
#90904=CARTESIAN_POINT('Ctrl Pts',(-70.9729159392983,1.30683103750208,126.060929647065));
#90905=CARTESIAN_POINT('Ctrl Pts',(-70.9806806922454,1.17381606343087,126.028238873752));
#90906=CARTESIAN_POINT('Ctrl Pts',(-70.9884377331304,1.0409332017071,125.995580569376));
#90907=CARTESIAN_POINT('Ctrl Pts',(-70.9961947740153,0.906547463705026,
125.968438001702));
#90908=CARTESIAN_POINT('Ctrl Pts',(-71.0039518149003,0.771156273370085,
125.946943498917));
#90909=CARTESIAN_POINT('Ctrl Pts',(-71.0117030061404,0.635867182584781,
125.925465205304));
#90910=CARTESIAN_POINT('Ctrl Pts',(-71.0194541973806,0.499574533223449,
125.909626559854));
#90911=CARTESIAN_POINT('Ctrl Pts',(-71.0272053886207,0.362787164588129,
125.899509087121));
#90912=CARTESIAN_POINT('Ctrl Pts',(-71.0349532853977,0.226057934233588,
125.889395914584));
#90913=CARTESIAN_POINT('Ctrl Pts',(-71.0427011821748,0.08883479189768,125.884999107173));
#90914=CARTESIAN_POINT('Ctrl Pts',(-71.0504490789519,-0.0483672742460088,
125.886348451123));
#90915=CARTESIAN_POINT('Ctrl Pts',(-71.0581953550359,-0.185540640675194,
125.887697512819));
#90916=CARTESIAN_POINT('Ctrl Pts',(-71.0659416311199,-0.32269254898266,
125.894790331246));
#90917=CARTESIAN_POINT('Ctrl Pts',(-71.0736879072039,-0.459307373576597,
125.907604569009));
#90918=CARTESIAN_POINT('Ctrl Pts',(-71.0814342404693,-0.59592320663032,
125.920418901364));
#90919=CARTESIAN_POINT('Ctrl Pts',(-71.0891805737347,-0.732001558802787,
125.93895470082));
#90920=CARTESIAN_POINT('Ctrl Pts',(-71.096926907,-0.867031687794124,125.963137723001));
#90921=CARTESIAN_POINT('Ctrl Pts',(-71.1046749750029,-1.00209205584643,
125.987326160802));
#90922=CARTESIAN_POINT('Ctrl Pts',(-71.1124230430058,-1.13610334883913,
126.017164268939));
#90923=CARTESIAN_POINT('Ctrl Pts',(-71.1201711110088,-1.26856517229714,
126.052526711995));
#90924=CARTESIAN_POINT('Ctrl Pts',(-71.1279274137506,-1.40116777775763,
126.087926738676));
#90925=CARTESIAN_POINT('Ctrl Pts',(-71.1356837164925,-1.53221724569505,
126.128862727887));
#90926=CARTESIAN_POINT('Ctrl Pts',(-71.1434400192343,-1.66122797303317,
126.175159316681));
#90927=CARTESIAN_POINT('Ctrl Pts',(-71.1512004617484,-1.79030755728091,
126.22148061536));
#90928=CARTESIAN_POINT('Ctrl Pts',(-71.1589609042626,-1.91734587076247,
126.273168067364));
#90929=CARTESIAN_POINT('Ctrl Pts',(-71.1667213467767,-2.04187838296597,
126.329998570114));
#90930=CARTESIAN_POINT('Ctrl Pts',(-71.1744942470421,-2.16661080581352,
126.386920302233));
#90931=CARTESIAN_POINT('Ctrl Pts',(-71.1822671473075,-2.28882904030236,
126.449001406219));
#90932=CARTESIAN_POINT('Ctrl Pts',(-71.1900400475729,-2.40809341588997,
126.515972906217));
#90933=CARTESIAN_POINT('Ctrl Pts',(-71.1975303833351,-2.52302223102001,
126.580509823502));
#90934=CARTESIAN_POINT('Ctrl Pts',(-71.2050207190974,-2.63520795683101,
126.649587591853));
#90935=CARTESIAN_POINT('Ctrl Pts',(-71.2125110548596,-2.74428507677346,
126.722929192208));
#90936=CARTESIAN_POINT('Ctrl Pts',(-71.220259276429,-2.85711762798235,126.798795880678));
#90937=CARTESIAN_POINT('Ctrl Pts',(-71.2280074979985,-2.96698678927996,
126.879469506545));
#90938=CARTESIAN_POINT('Ctrl Pts',(-71.2357557195679,-3.07345350336626,
126.964690498253));
#90939=CARTESIAN_POINT('Ctrl Pts',(-71.2434916860282,-3.17975182252658,
127.049776698701));
#90940=CARTESIAN_POINT('Ctrl Pts',(-71.2512276524884,-3.28265810680815,
127.139395697583));
#90941=CARTESIAN_POINT('Ctrl Pts',(-71.2589636189487,-3.3817615476813,127.233244279903));
#90942=CARTESIAN_POINT('Ctrl Pts',(-71.2666925120404,-3.48077437348095,
127.32700705192));
#90943=CARTESIAN_POINT('Ctrl Pts',(-71.2744214051321,-3.57599098767044,
127.424991446448));
#90944=CARTESIAN_POINT('Ctrl Pts',(-71.2821502982237,-3.6670328127386,127.526853422639));
#90945=CARTESIAN_POINT('Ctrl Pts',(-71.2898738298731,-3.75801148316269,
127.628644738375));
#90946=CARTESIAN_POINT('Ctrl Pts',(-71.2975973615224,-3.84482086439671,
127.734307991986));
#90947=CARTESIAN_POINT('Ctrl Pts',(-71.3053208931718,-3.92711881451436,
127.843461956823));
#90948=CARTESIAN_POINT('Ctrl Pts',(-71.3130407711693,-4.00937783321157,
127.952564285881));
#90949=CARTESIAN_POINT('Ctrl Pts',(-71.3207606491669,-4.08712943133494,
128.065153725941));
#90950=CARTESIAN_POINT('Ctrl Pts',(-71.3284805271644,-4.16007168372777,
128.180815945039));
#90951=CARTESIAN_POINT('Ctrl Pts',(-71.3362000314408,-4.23301040496854,
128.296472564901));
#90952=CARTESIAN_POINT('Ctrl Pts',(-71.343919535717,-4.30114002466459,128.41520134041));
#90953=CARTESIAN_POINT('Ctrl Pts',(-71.3516390399934,-4.36420199213107,
128.536559031364));
#90954=CARTESIAN_POINT('Ctrl Pts',(-71.3593581195935,-4.42726049034381,
128.657910046019));
#90955=CARTESIAN_POINT('Ctrl Pts',(-71.3670771991937,-4.48525171412237,
128.781889336178));
#90956=CARTESIAN_POINT('Ctrl Pts',(-71.3747962787938,-4.53796349435114,
128.908029848308));
#90957=CARTESIAN_POINT('Ctrl Pts',(-71.3825195995503,-4.59070423643966,
129.034239666838));
#90958=CARTESIAN_POINT('Ctrl Pts',(-71.3902429203067,-4.63815959149372,
129.16261271424));
#90959=CARTESIAN_POINT('Ctrl Pts',(-71.3979662410631,-4.68016584382023,
129.292662652747));
#90960=CARTESIAN_POINT('Ctrl Pts',(-71.4036535610572,-4.71109852242625,
129.388429181008));
#90961=CARTESIAN_POINT('Ctrl Pts',(-71.4093408810511,-4.73907738275365,
129.485104608161));
#90962=CARTESIAN_POINT('Ctrl Pts',(-71.4150282010451,-4.76405452823412,
129.582490119309));
#90963=CARTESIAN_POINT('Ctrl Pts',(-69.6652100424012,-4.76405452823405,
129.582490119308));
#90964=CARTESIAN_POINT('Ctrl Pts',(-69.6729160059501,-4.79798397061735,
129.71478050021));
#90965=CARTESIAN_POINT('Ctrl Pts',(-69.6806219694989,-4.826405066055,129.848509029593));
#90966=CARTESIAN_POINT('Ctrl Pts',(-69.6883279330478,-4.84921000393715,
129.983175254681));
#90967=CARTESIAN_POINT('Ctrl Pts',(-69.6961300382079,-4.87229946217271,
130.11952161072));
#90968=CARTESIAN_POINT('Ctrl Pts',(-69.703932143368,-4.88963157798843,130.256828815998));
#90969=CARTESIAN_POINT('Ctrl Pts',(-69.7117342485281,-4.90114821834125,
130.394568957877));
#90970=CARTESIAN_POINT('Ctrl Pts',(-69.7195363536882,-4.91266485869405,
130.532309099757));
#90971=CARTESIAN_POINT('Ctrl Pts',(-69.7273384588484,-4.91836601148334,
130.670481758551));
#90972=CARTESIAN_POINT('Ctrl Pts',(-69.7351405640084,-4.91824821000432,
130.808556721627));
#90973=CARTESIAN_POINT('',(-69.3898594359379,-4.91824912971278,130.801434770766));
#90974=CARTESIAN_POINT('Ctrl Pts',(-69.3201134481353,-4.76405452823409,
129.582490119308));
#90975=CARTESIAN_POINT('Ctrl Pts',(-69.3288186313557,-4.80211576120071,
129.730890288985));
#90976=CARTESIAN_POINT('Ctrl Pts',(-69.3375238145761,-4.8332833158892,129.88124324352));
#90977=CARTESIAN_POINT('Ctrl Pts',(-69.3462289977965,-4.85737407892202,
130.032933291166));
#90978=CARTESIAN_POINT('Ctrl Pts',(-69.3548866098648,-4.88133319333549,
130.183794399301));
#90979=CARTESIAN_POINT('Ctrl Pts',(-69.3635442219332,-4.89829255583419,
130.335977826698));
#90980=CARTESIAN_POINT('Ctrl Pts',(-69.3722018340016,-4.90812000793932,
130.488859349477));
#90981=CARTESIAN_POINT('Ctrl Pts',(-69.3780877013137,-4.91480118961508,
130.592795671693));
#90982=CARTESIAN_POINT('Ctrl Pts',(-69.3839735686258,-4.91818703416645,
130.697054265705));
#90983=CARTESIAN_POINT('Ctrl Pts',(-69.389859435938,-4.91824912971278,130.801434770766));
#90984=CARTESIAN_POINT('Ctrl Pts',(-69.389859435991,-4.91824912971334,130.801434771708));
#90985=CARTESIAN_POINT('Ctrl Pts',(-69.3976795903753,-4.91833163184545,
130.940118099247));
#90986=CARTESIAN_POINT('Ctrl Pts',(-69.4054997447596,-4.91254396783923,
131.078815667496));
#90987=CARTESIAN_POINT('Ctrl Pts',(-69.4133198991439,-4.9009091403827,131.21700169673));
#90988=CARTESIAN_POINT('Ctrl Pts',(-69.4211412015346,-4.88927260492193,
131.35520801181));
#90989=CARTESIAN_POINT('Ctrl Pts',(-69.4289625039254,-4.87178722802085,
131.492902259086));
#90990=CARTESIAN_POINT('Ctrl Pts',(-69.4367838063161,-4.84852792659058,
131.62956362748));
#90991=CARTESIAN_POINT('Ctrl Pts',(-69.4446078276649,-4.82526053941436,
131.766272504141));
#90992=CARTESIAN_POINT('Ctrl Pts',(-69.4524318490137,-4.79621529426033,
131.901947411878));
#90993=CARTESIAN_POINT('Ctrl Pts',(-69.4602558703624,-4.76151821987119,
132.036077835248));
#90994=CARTESIAN_POINT('Ctrl Pts',(-69.4680841830829,-4.72680211459782,
132.170281827373));
#90995=CARTESIAN_POINT('Ctrl Pts',(-69.4759124958035,-4.68642810193007,
132.302939280281));
#90996=CARTESIAN_POINT('Ctrl Pts',(-69.483740808524,-4.64057196066345,132.433555185567));
#90997=CARTESIAN_POINT('Ctrl Pts',(-69.4915797216638,-4.59465372500422,
132.564347959536));
#90998=CARTESIAN_POINT('Ctrl Pts',(-69.4994186348035,-4.54323866303483,
132.693093306502));
#90999=CARTESIAN_POINT('Ctrl Pts',(-69.5072575479433,-4.48655081755768,
132.819315908378));
#91000=CARTESIAN_POINT('Ctrl Pts',(-69.5151026597042,-4.42981814616346,
132.945638320784));
#91001=CARTESIAN_POINT('Ctrl Pts',(-69.5229477714649,-4.36780455241388,
133.069433673841));
#91002=CARTESIAN_POINT('Ctrl Pts',(-69.5307928832258,-4.30077947142102,
133.190252274935));
#91003=CARTESIAN_POINT('Ctrl Pts',(-69.5386503213002,-4.2336490799887,133.311260707354));
#91004=CARTESIAN_POINT('Ctrl Pts',(-69.5465077593746,-4.16149167580229,
133.429282725199));
#91005=CARTESIAN_POINT('Ctrl Pts',(-69.554365197449,-4.08461966215346,133.543898038017));
#91006=CARTESIAN_POINT('Ctrl Pts',(-69.5567149010135,-4.06163170567629,
133.578172824088));
#91007=CARTESIAN_POINT('Ctrl Pts',(-69.5590646045779,-4.03822240922261,
133.612143192054));
#91008=CARTESIAN_POINT('Ctrl Pts',(-69.5614143081424,-4.01440079892208,
133.645798508514));
#91009=CARTESIAN_POINT('Ctrl Pts',(-69.5691886422613,-3.9355835555347,133.75715199114));
#91010=CARTESIAN_POINT('Ctrl Pts',(-69.5769629763802,-3.85200479108893,
133.865399955488));
#91011=CARTESIAN_POINT('Ctrl Pts',(-69.5847373104992,-3.76393745608926,
133.970108221079));
#91012=CARTESIAN_POINT('Ctrl Pts',(-69.5925020634461,-3.67597865620906,
134.074687443091));
#91013=CARTESIAN_POINT('Ctrl Pts',(-69.6002668163931,-3.58354254157078,
134.175735349814));
#91014=CARTESIAN_POINT('Ctrl Pts',(-69.6080315693401,-3.48694521442781,
134.272846761993));
#91015=CARTESIAN_POINT('Ctrl Pts',(-69.6157886102249,-3.39044382911221,
134.369861721747));
#91016=CARTESIAN_POINT('Ctrl Pts',(-69.6235456511098,-3.28978973003388,
134.462947692207));
#91017=CARTESIAN_POINT('Ctrl Pts',(-69.6313026919946,-3.18533891129155,
134.551732907947));
#91018=CARTESIAN_POINT('Ctrl Pts',(-69.6390538832347,-3.08096685972415,
134.640451170064));
#91019=CARTESIAN_POINT('Ctrl Pts',(-69.6468050744747,-2.97280408407458,
134.724874880731));
#91020=CARTESIAN_POINT('Ctrl Pts',(-69.6545562657147,-2.86124275480197,
134.804669725697));
#91021=CARTESIAN_POINT('Ctrl Pts',(-69.6623041624916,-2.74972884207,134.884430655725));
#91022=CARTESIAN_POINT('Ctrl Pts',(-69.6700520592686,-2.63481956599732,
134.95956640607));
#91023=CARTESIAN_POINT('Ctrl Pts',(-69.6777999560456,-2.51693926172928,
135.029783651449));
#91024=CARTESIAN_POINT('Ctrl Pts',(-69.6855462321295,-2.39908361548001,
135.099986208893));
#91025=CARTESIAN_POINT('Ctrl Pts',(-69.6932925082135,-2.27825851286104,
135.165272107847));
#91026=CARTESIAN_POINT('Ctrl Pts',(-69.7010387842975,-2.15491594703655,
135.22539220801));
#91027=CARTESIAN_POINT('Ctrl Pts',(-69.7087851175627,-2.03157247072508,
135.285512751967));
#91028=CARTESIAN_POINT('Ctrl Pts',(-69.716531450828,-1.90571184556632,135.340467249741));
#91029=CARTESIAN_POINT('Ctrl Pts',(-69.7242777840933,-1.77780889504602,
135.390053432746));
#91030=CARTESIAN_POINT('Ctrl Pts',(-69.7320258520962,-1.64987730154659,
135.439650720233));
#91031=CARTESIAN_POINT('Ctrl Pts',(-69.739773920099,-1.51990283704257,135.483877159422));
#91032=CARTESIAN_POINT('Ctrl Pts',(-69.7475219881019,-1.38837806388366,
135.522579499117));
#91033=CARTESIAN_POINT('Ctrl Pts',(-69.7552782908436,-1.25671350463086,
135.56132297212));
#91034=CARTESIAN_POINT('Ctrl Pts',(-69.7630345935854,-1.12349572095419,
135.594530506975));
#91035=CARTESIAN_POINT('Ctrl Pts',(-69.7707908963272,-0.989230665783423,
135.622099273032));
#91036=CARTESIAN_POINT('Ctrl Pts',(-69.7785513388412,-0.85489394931007,
135.64968275337));
#91037=CARTESIAN_POINT('Ctrl Pts',(-69.7863117813552,-0.71950923330896,
135.671621405558));
#91038=CARTESIAN_POINT('Ctrl Pts',(-69.7940722238693,-0.583589306701709,
135.687864132831));
#91039=CARTESIAN_POINT('Ctrl Pts',(-69.8018451241346,-0.447451189362046,
135.704132934372));
#91040=CARTESIAN_POINT('Ctrl Pts',(-69.8096180244,-0.310776534554623,135.714687509043));
#91041=CARTESIAN_POINT('Ctrl Pts',(-69.8173909246653,-0.174080761691003,
135.719528870119));
#91042=CARTESIAN_POINT('Ctrl Pts',(-69.8248812604285,-0.0423542244631702,
135.724194235527));
#91043=CARTESIAN_POINT('Ctrl Pts',(-69.8323715961918,0.0893916140735198,
135.723554556645));
#91044=CARTESIAN_POINT('Ctrl Pts',(-69.839861931955,0.220700482344392,135.717656289474));
#91045=CARTESIAN_POINT('Ctrl Pts',(-69.8476362660741,0.356987966243205,
135.711534387712));
#91046=CARTESIAN_POINT('Ctrl Pts',(-69.8554106001932,0.493236408100186,
135.699727874943));
#91047=CARTESIAN_POINT('Ctrl Pts',(-69.8631849343122,0.628932983167448,
135.682231707005));
#91048=CARTESIAN_POINT('Ctrl Pts',(-69.8709496872593,0.764462324333305,
135.66475710153));
#91049=CARTESIAN_POINT('Ctrl Pts',(-69.8787144402063,0.899440767925499,
135.641606842174));
#91050=CARTESIAN_POINT('Ctrl Pts',(-69.8864791931533,1.03335656417244,135.61282786543));
#91051=CARTESIAN_POINT('Ctrl Pts',(-69.8942362340383,1.16713935336285,135.584077472372));
#91052=CARTESIAN_POINT('Ctrl Pts',(-69.9019932749233,1.2998612158091,135.549709568929));
#91053=CARTESIAN_POINT('Ctrl Pts',(-69.9097503158083,1.43101695122329,135.509822714726));
#91054=CARTESIAN_POINT('Ctrl Pts',(-69.9175015070484,1.5620737810768,135.46996593951));
#91055=CARTESIAN_POINT('Ctrl Pts',(-69.9252526982883,1.6915664621274,135.424598610806));
#91056=CARTESIAN_POINT('Ctrl Pts',(-69.9330038895284,1.8190017486142,135.373869967708));
#91057=CARTESIAN_POINT('Ctrl Pts',(-69.9407517863054,1.94638287170496,135.323162885637));
#91058=CARTESIAN_POINT('Ctrl Pts',(-69.9484996830824,2.07170797695909,135.267099165631));
#91059=CARTESIAN_POINT('Ctrl Pts',(-69.9562475798595,2.19450091799564,135.205877263384));
#91060=CARTESIAN_POINT('Ctrl Pts',(-69.9639938559435,2.31726817339603,135.14466816744));
#91061=CARTESIAN_POINT('Ctrl Pts',(-69.9717401320276,2.4375039684628,135.078303209742));
#91062=CARTESIAN_POINT('Ctrl Pts',(-69.9794864081117,2.5547543810588,135.007027998523));
#91063=CARTESIAN_POINT('Ctrl Pts',(-69.987232741377,2.67200565917056,134.935752261167));
#91064=CARTESIAN_POINT('Ctrl Pts',(-69.9949790746423,2.7862711767559,134.859566401047));
#91065=CARTESIAN_POINT('Ctrl Pts',(-70.0027254079076,2.89712410583148,134.778760569497));
#91066=CARTESIAN_POINT('Ctrl Pts',(-70.0104734759105,3.00800185965223,134.697936642041));
#91067=CARTESIAN_POINT('Ctrl Pts',(-70.0182215439134,3.11546518836735,134.612490914657));
#91068=CARTESIAN_POINT('Ctrl Pts',(-70.0259696119163,3.2191189154243,134.522754957985));
#91069=CARTESIAN_POINT('Ctrl Pts',(-70.0337259146581,3.32288280689571,134.43292362887));
#91070=CARTESIAN_POINT('Ctrl Pts',(-70.0414822174,3.42282871255838,134.338793218266));
#91071=CARTESIAN_POINT('Ctrl Pts',(-70.0492385201418,3.51859663815677,134.240733816224));
#91072=CARTESIAN_POINT('Ctrl Pts',(-70.0569989626559,3.61441567798057,134.142622076926));
#91073=CARTESIAN_POINT('Ctrl Pts',(-70.0647594051701,3.70605203335514,134.040577458447));
#91074=CARTESIAN_POINT('Ctrl Pts',(-70.0725198476842,3.79318554018795,133.93500376558));
#91075=CARTESIAN_POINT('Ctrl Pts',(-70.0802927479495,3.88045892146129,133.829260596449));
#91076=CARTESIAN_POINT('Ctrl Pts',(-70.0880656482149,3.9632147734412,133.719977343951));
#91077=CARTESIAN_POINT('Ctrl Pts',(-70.0958385484803,4.04117535184151,133.607588192732));
#91078=CARTESIAN_POINT('Ctrl Pts',(-70.1033288842428,4.11630186685181,133.499284670242));
#91079=CARTESIAN_POINT('Ctrl Pts',(-70.1108192200053,4.18697553068549,133.388097402995));
#91080=CARTESIAN_POINT('Ctrl Pts',(-70.1183095557679,4.25298880215847,133.27443537579));
#91081=CARTESIAN_POINT('Ctrl Pts',(-70.126083889887,4.32150498687929,133.156463818284));
#91082=CARTESIAN_POINT('Ctrl Pts',(-70.1338582240061,4.38521744418695,133.03545243685));
#91083=CARTESIAN_POINT('Ctrl Pts',(-70.1416325581253,4.44384473598061,132.911829958979));
#91084=CARTESIAN_POINT('Ctrl Pts',(-70.1493973110724,4.50239977487689,132.788359834764));
#91085=CARTESIAN_POINT('Ctrl Pts',(-70.1571620640195,4.55588195182488,132.662285366721));
#91086=CARTESIAN_POINT('Ctrl Pts',(-70.1649268169667,4.60405414257455,132.534062474749));
#91087=CARTESIAN_POINT('Ctrl Pts',(-70.1726838578518,4.65217848802519,132.405966935561));
#91088=CARTESIAN_POINT('Ctrl Pts',(-70.1804408987369,4.69500320607329,132.275727582511));
#91089=CARTESIAN_POINT('Ctrl Pts',(-70.1881979396219,4.73233814462599,132.143822728795));
#91090=CARTESIAN_POINT('Ctrl Pts',(-70.1959491308621,4.7696449286113,132.012017345554));
#91091=CARTESIAN_POINT('Ctrl Pts',(-70.2037003221023,4.80147006724533,131.878549336237));
#91092=CARTESIAN_POINT('Ctrl Pts',(-70.2114515133426,4.82767250822328,131.743914349848));
#91093=CARTESIAN_POINT('Ctrl Pts',(-70.2191994101197,4.85386381246473,131.60933658692));
#91094=CARTESIAN_POINT('Ctrl Pts',(-70.2269473068968,4.87443709764183,131.473593216381));
#91095=CARTESIAN_POINT('Ctrl Pts',(-70.2346952036739,4.88930196140111,131.337192103816));
#91096=CARTESIAN_POINT('Ctrl Pts',(-70.2424414797581,4.90416371575131,131.200819523423));
#91097=CARTESIAN_POINT('Ctrl Pts',(-70.2501877558423,4.9133193814423,131.063789863088));
#91098=CARTESIAN_POINT('Ctrl Pts',(-70.2579340319265,4.91673023963269,130.926617777608));
#91099=CARTESIAN_POINT('Ctrl Pts',(-70.2656803651919,4.92014112300127,130.789444679554));
#91100=CARTESIAN_POINT('Ctrl Pts',(-70.2734266984572,4.91780710453085,130.652129545102));
#91101=CARTESIAN_POINT('Ctrl Pts',(-70.2811730317226,4.90974158580548,130.515188310607));
#91102=CARTESIAN_POINT('Ctrl Pts',(-70.2889210997256,4.90167426086311,130.378216409071));
#91103=CARTESIAN_POINT('Ctrl Pts',(-70.2966691677287,4.8878729045729,130.241618964322));
#91104=CARTESIAN_POINT('Ctrl Pts',(-70.3044172357317,4.86840287412582,130.105907671618));
#91105=CARTESIAN_POINT('Ctrl Pts',(-70.3121735384736,4.8489121506987,129.970052143337));
#91106=CARTESIAN_POINT('Ctrl Pts',(-70.3199298412155,4.82374077366935,129.835085036092));
#91107=CARTESIAN_POINT('Ctrl Pts',(-70.3276861439574,4.79300552459065,129.701509265958));
#91108=CARTESIAN_POINT('Ctrl Pts',(-70.3354465864716,4.76225387118414,129.567862202414));
#91109=CARTESIAN_POINT('Ctrl Pts',(-70.3432070289859,4.72593253202465,129.435608332494));
#91110=CARTESIAN_POINT('Ctrl Pts',(-70.3509674715001,4.68420818300894,129.30523528567));
#91111=CARTESIAN_POINT('Ctrl Pts',(-70.3587403717655,4.64241685436408,129.174652952458));
#91112=CARTESIAN_POINT('Ctrl Pts',(-70.366513272031,4.59520531839163,129.045957843051));
#91113=CARTESIAN_POINT('Ctrl Pts',(-70.3742861722965,4.54278873936122,128.919618318992));
#91114=CARTESIAN_POINT('Ctrl Pts',(-70.3817765080579,4.49227763501229,128.797871554874));
#91115=CARTESIAN_POINT('Ctrl Pts',(-70.3892668438194,4.43693347970021,128.678312366079));
#91116=CARTESIAN_POINT('Ctrl Pts',(-70.3967571795808,4.37698818284047,128.56133642916));
#91117=CARTESIAN_POINT('Ctrl Pts',(-70.4045315136999,4.31477004182549,128.439925314029));
#91118=CARTESIAN_POINT('Ctrl Pts',(-70.412305847819,4.24739787884373,128.320912611734));
#91119=CARTESIAN_POINT('Ctrl Pts',(-70.4200801819381,4.17508027030704,128.204766841802));
#91120=CARTESIAN_POINT('Ctrl Pts',(-70.4278449348851,4.10285178675966,128.088764211151));
#91121=CARTESIAN_POINT('Ctrl Pts',(-70.4356096878322,4.02569018919691,127.975621811474));
#91122=CARTESIAN_POINT('Ctrl Pts',(-70.4433744407793,3.94385088449194,127.865785577961));
#91123=CARTESIAN_POINT('Ctrl Pts',(-70.4511314816642,3.86209286373847,127.756058435343));
#91124=CARTESIAN_POINT('Ctrl Pts',(-70.4588885225492,3.77566661360599,127.649631235595));
#91125=CARTESIAN_POINT('Ctrl Pts',(-70.4666455634342,3.68487177068056,127.546922499022));
#91126=CARTESIAN_POINT('Ctrl Pts',(-70.4743967546743,3.59414539685198,127.444291215906));
#91127=CARTESIAN_POINT('Ctrl Pts',(-70.4821479459145,3.49905724540849,127.345373106266));
#91128=CARTESIAN_POINT('Ctrl Pts',(-70.4898991371546,3.39994807767874,127.250554751795));
#91129=CARTESIAN_POINT('Ctrl Pts',(-70.4976470339317,3.30088103398923,127.155776697654));
#91130=CARTESIAN_POINT('Ctrl Pts',(-70.5053949307087,3.19779665507245,127.065095202676));
#91131=CARTESIAN_POINT('Ctrl Pts',(-70.5131428274857,3.09107335794886,126.978860838677));
#91132=CARTESIAN_POINT('Ctrl Pts',(-70.5208891035698,2.98437238503833,126.892644513048));
#91133=CARTESIAN_POINT('Ctrl Pts',(-70.5286353796538,2.87403431186303,126.810873713653));
#91134=CARTESIAN_POINT('Ctrl Pts',(-70.5363816557379,2.760471203601,126.733859199241));
#91135=CARTESIAN_POINT('Ctrl Pts',(-70.5441279890032,2.64690725704221,126.656844116324));
#91136=CARTESIAN_POINT('Ctrl Pts',(-70.5518743222686,2.53011855146796,126.584585607887));
#91137=CARTESIAN_POINT('Ctrl Pts',(-70.559620655534,2.41054640262869,126.517351274997));
#91138=CARTESIAN_POINT('Ctrl Pts',(-70.567368723537,2.29094747643493,126.450101885444));
#91139=CARTESIAN_POINT('Ctrl Pts',(-70.5751167915398,2.1685642073369,126.387879101901));
#91140=CARTESIAN_POINT('Ctrl Pts',(-70.5828648595428,2.04386242620345,126.330904521296));
#91141=CARTESIAN_POINT('Ctrl Pts',(-70.5906211622846,1.91902811053372,126.273869387429));
#91142=CARTESIAN_POINT('Ctrl Pts',(-70.5983774650265,1.79187071661352,126.222093761593));
#91143=CARTESIAN_POINT('Ctrl Pts',(-70.6061337677683,1.66287648526213,126.175751230584));
#91144=CARTESIAN_POINT('Ctrl Pts',(-70.6138942102825,1.53381340580536,126.129383965169));
#91145=CARTESIAN_POINT('Ctrl Pts',(-70.6216546527966,1.40291190840469,126.088455689305));
#91146=CARTESIAN_POINT('Ctrl Pts',(-70.6294150953108,1.27067234193961,126.053089749479));
#91147=CARTESIAN_POINT('Ctrl Pts',(-70.6371879955762,1.13822049278277,126.017667037107));
#91148=CARTESIAN_POINT('Ctrl Pts',(-70.6449608958416,1.00442666400649,125.987824589233));
#91149=CARTESIAN_POINT('Ctrl Pts',(-70.652733796107,0.869801202983778,125.963634542917));
#91150=CARTESIAN_POINT('Ctrl Pts',(-70.6602241318692,0.740069716566674,
125.940323865715));
#91151=CARTESIAN_POINT('Ctrl Pts',(-70.6677144676315,0.609566317125854,
125.922261809065));
#91152=CARTESIAN_POINT('Ctrl Pts',(-70.6752048033937,0.478749251252998,
125.90946713385));
#91153=CARTESIAN_POINT('Ctrl Pts',(-70.6829791375128,0.342972216569107,
125.896187344635));
#91154=CARTESIAN_POINT('Ctrl Pts',(-70.6907534716319,0.206427159764203,
125.888540180794));
#91155=CARTESIAN_POINT('Ctrl Pts',(-70.6985278057511,0.069621000229875,
125.88660340733));
#91156=CARTESIAN_POINT('Ctrl Pts',(-70.7062925586982,-0.0670165579389881,
125.884669020767));
#91157=CARTESIAN_POINT('Ctrl Pts',(-70.7140573116453,-0.203914191406301,
125.888431027445));
#91158=CARTESIAN_POINT('Ctrl Pts',(-70.7218220645924,-0.340558668614846,
125.89791558519));
#91159=CARTESIAN_POINT('Ctrl Pts',(-70.7295791054775,-0.477067428602092,
125.907390722738));
#91160=CARTESIAN_POINT('Ctrl Pts',(-70.7373361463625,-0.613323145201315,
125.922577073601));
#91161=CARTESIAN_POINT('Ctrl Pts',(-70.7450931872475,-0.74881174453205,
125.94344876548));
#91162=CARTESIAN_POINT('Ctrl Pts',(-70.7528443784877,-0.884198170856636,
125.964304717854));
#91163=CARTESIAN_POINT('Ctrl Pts',(-70.7605955697279,-1.01881824651647,
125.990837418231));
#91164=CARTESIAN_POINT('Ctrl Pts',(-70.7683467609681,-1.15216253956335,
126.022969131301));
#91165=CARTESIAN_POINT('Ctrl Pts',(-70.7760946577453,-1.28545015772879,
126.055087187536));
#91166=CARTESIAN_POINT('Ctrl Pts',(-70.7838425545224,-1.41746269246836,
126.092799431967));
#91167=CARTESIAN_POINT('Ctrl Pts',(-70.7915904512995,-1.5477006541428,126.135976984266));
#91168=CARTESIAN_POINT('Ctrl Pts',(-70.7993367273837,-1.6779113728429,126.179145504751));
#91169=CARTESIAN_POINT('Ctrl Pts',(-70.8070830034678,-1.80634788595232,
126.227776936215));
#91170=CARTESIAN_POINT('Ctrl Pts',(-70.814829279552,-1.93252601204163,126.281692569247));
#91171=CARTESIAN_POINT('Ctrl Pts',(-70.8225756128174,-2.05870506954937,
126.335608600272));
#91172=CARTESIAN_POINT('Ctrl Pts',(-70.8303219460828,-2.18262534725211,
126.394808757078));
#91173=CARTESIAN_POINT('Ctrl Pts',(-70.8380682793482,-2.30382316284822,
126.459066393141));
#91174=CARTESIAN_POINT('Ctrl Pts',(-70.8458163473512,-2.42504811985448,
126.523338419255));
#91175=CARTESIAN_POINT('Ctrl Pts',(-70.8535644153542,-2.54354905621517,
126.592669995241));
#91176=CARTESIAN_POINT('Ctrl Pts',(-70.8613124833572,-2.65888774319492,
126.666788982949));
#91177=CARTESIAN_POINT('Ctrl Pts',(-70.8690687860991,-2.7743490135039,126.740986745199));
#91178=CARTESIAN_POINT('Ctrl Pts',(-70.876825088841,-2.88664099128814,126.819981871536));
#91179=CARTESIAN_POINT('Ctrl Pts',(-70.8845813915829,-2.99535480802067,
126.90345910169));
#91180=CARTESIAN_POINT('Ctrl Pts',(-70.8923418340972,-3.10412664859066,
126.986980886155));
#91181=CARTESIAN_POINT('Ctrl Pts',(-70.9001022766114,-3.20931622301673,
127.074989290409));
#91182=CARTESIAN_POINT('Ctrl Pts',(-70.9078627191256,-3.3105493056135,127.16713002856));
#91183=CARTESIAN_POINT('Ctrl Pts',(-70.9156356193911,-3.41194489654151,
127.259418679203));
#91184=CARTESIAN_POINT('Ctrl Pts',(-70.9234085196567,-3.50937102566989,
127.355852644575));
#91185=CARTESIAN_POINT('Ctrl Pts',(-70.9311814199222,-3.60249114682615,
127.456041546817));
#91186=CARTESIAN_POINT('Ctrl Pts',(-70.9386717556838,-3.69222611701703,
127.552588330097));
#91187=CARTESIAN_POINT('Ctrl Pts',(-70.9461620914453,-3.77796251193308,
127.652621553277));
#91188=CARTESIAN_POINT('Ctrl Pts',(-70.9536524272069,-3.85943685403772,
127.755765821238));
#91189=CARTESIAN_POINT('Ctrl Pts',(-70.9614213020186,-3.94394093827576,
127.862745659103));
#91190=CARTESIAN_POINT('Ctrl Pts',(-70.9691901768302,-4.02413301129352,
127.973418231407));
#91191=CARTESIAN_POINT('Ctrl Pts',(-70.9769590516418,-4.09967228073009,
128.087400873088));
#91192=CARTESIAN_POINT('Ctrl Pts',(-70.984715528078,-4.17509099677335,128.201201609459));
#91193=CARTESIAN_POINT('Ctrl Pts',(-70.9924720045142,-4.24587148194348,
128.318301572758));
#91194=CARTESIAN_POINT('Ctrl Pts',(-71.0002284809504,-4.31171306470087,
128.438285067169));
#91195=CARTESIAN_POINT('Ctrl Pts',(-71.0079778176759,-4.37749404134967,
128.558158118719));
#91196=CARTESIAN_POINT('Ctrl Pts',(-71.0157271544014,-4.4383449695204,128.680909082619));
#91197=CARTESIAN_POINT('Ctrl Pts',(-71.023476491127,-4.49400821765804,128.806093067381));
#91198=CARTESIAN_POINT('Ctrl Pts',(-71.0312247147739,-4.54966347058655,
128.9312590713));
#91199=CARTESIAN_POINT('Ctrl Pts',(-71.0389729384209,-4.60013233288696,
129.058857060701));
#91200=CARTESIAN_POINT('Ctrl Pts',(-71.0467211620678,-4.64520277425386,
129.188416853518));
#91201=CARTESIAN_POINT('Ctrl Pts',(-71.0544693857148,-4.6902732156207,129.317976646336));
#91202=CARTESIAN_POINT('Ctrl Pts',(-71.0622176093617,-4.72994507621285,
129.449497883561));
#91203=CARTESIAN_POINT('Ctrl Pts',(-71.0699658330086,-4.76405452823398,
129.582490119308));
#91204=CARTESIAN_POINT('Origin',(213.235140564004,0.,130.804360617566));
#91205=CARTESIAN_POINT('',(-73.1652357600351,-4.76405452823407,129.582490119308));
#91206=CARTESIAN_POINT('',(-72.8197282857816,-4.76405452823409,129.582490119308));
#91207=CARTESIAN_POINT('',(213.235140564004,-4.76405452823405,129.582490119308));
#91208=CARTESIAN_POINT('',(-71.4851405639545,-4.91824995845192,130.804999904443));
#91209=CARTESIAN_POINT('Ctrl Pts',(-71.4851405640084,-4.91824995845179,
130.804999905388));
#91210=CARTESIAN_POINT('Ctrl Pts',(-71.4870799355632,-4.91824553450007,
130.839034810544));
#91211=CARTESIAN_POINT('Ctrl Pts',(-71.489019307118,-4.91788782706535,130.873067104726));
#91212=CARTESIAN_POINT('Ctrl Pts',(-71.4909586786726,-4.9171769671839,130.907091994935));
#91213=CARTESIAN_POINT('Ctrl Pts',(-71.4987330127917,-4.91432735220566,
131.043487140169));
#91214=CARTESIAN_POINT('Ctrl Pts',(-71.5065073469109,-4.90579382634764,
131.179979669595));
#91215=CARTESIAN_POINT('Ctrl Pts',(-71.51428168103,-4.89155904051835,131.316057027191));
#91216=CARTESIAN_POINT('Ctrl Pts',(-71.5220464339771,-4.87734179779038,
131.451966681605));
#91217=CARTESIAN_POINT('Ctrl Pts',(-71.5298111869242,-4.8574373156064,131.587461797135));
#91218=CARTESIAN_POINT('Ctrl Pts',(-71.5375759398713,-4.83188023636037,
131.722029645032));
#91219=CARTESIAN_POINT('Ctrl Pts',(-71.5453329807564,-4.80634854076567,
131.856463838246));
#91220=CARTESIAN_POINT('Ctrl Pts',(-71.5530900216415,-4.775175493174,131.989972214996));
#91221=CARTESIAN_POINT('Ctrl Pts',(-71.5608470625266,-4.73844750141264,
132.122047355321));
#91222=CARTESIAN_POINT('Ctrl Pts',(-71.5685982537667,-4.70174720651567,
132.254022896755));
#91223=CARTESIAN_POINT('Ctrl Pts',(-71.5763494450069,-4.65950040977517,
132.384566977912));
#91224=CARTESIAN_POINT('Ctrl Pts',(-71.584100636247,-4.61184447077059,132.513182913746));
#91225=CARTESIAN_POINT('Ctrl Pts',(-71.5918485330241,-4.56420878681129,
132.641744184377));
#91226=CARTESIAN_POINT('Ctrl Pts',(-71.5995964298013,-4.51116866873738,
132.768378573794));
#91227=CARTESIAN_POINT('Ctrl Pts',(-71.6073443265784,-4.45291108889233,
132.892605310345));
#91228=CARTESIAN_POINT('Ctrl Pts',(-71.6150906026625,-4.39466569527709,
133.016806061341));
#91229=CARTESIAN_POINT('Ctrl Pts',(-71.6228368787467,-4.33120517660153,
133.138599807467));
#91230=CARTESIAN_POINT('Ctrl Pts',(-71.6305831548308,-4.26276417748866,
133.257526863384));
#91231=CARTESIAN_POINT('Ctrl Pts',(-71.6383294880962,-4.19432267315998,
133.376454797193));
#91232=CARTESIAN_POINT('Ctrl Pts',(-71.6460758213616,-4.12090081004148,
133.492515659709));
#91233=CARTESIAN_POINT('Ctrl Pts',(-71.653822154627,-4.04277841321618,133.605275783031));
#91234=CARTESIAN_POINT('Ctrl Pts',(-71.66157022263,-3.96463852142177,133.718061158202));
#91235=CARTESIAN_POINT('Ctrl Pts',(-71.6693182906329,-3.8817962238749,133.827544001991));
#91236=CARTESIAN_POINT('Ctrl Pts',(-71.6770663586359,-3.79457351258423,
133.933321294867));
#91237=CARTESIAN_POINT('Ctrl Pts',(-71.6848226613778,-3.70725809995791,
134.039211009108));
#91238=CARTESIAN_POINT('Ctrl Pts',(-71.6925789641197,-3.61555322273975,
134.141387003128));
#91239=CARTESIAN_POINT('Ctrl Pts',(-71.7003352668616,-3.51982022553436,
134.2394805052));
#91240=CARTESIAN_POINT('Ctrl Pts',(-71.7080957093758,-3.4240361327459,134.337626362727));
#91241=CARTESIAN_POINT('Ctrl Pts',(-71.71585615189,-3.32421992045408,134.431685118572));
#91242=CARTESIAN_POINT('Ctrl Pts',(-71.7236165944042,-3.22076759411128,
134.521327010637));
#91243=CARTESIAN_POINT('Ctrl Pts',(-71.7313894946697,-3.11714919691017,
134.611112803827));
#91244=CARTESIAN_POINT('Ctrl Pts',(-71.7391623949351,-3.00988332755102,
134.696467320899));
#91245=CARTESIAN_POINT('Ctrl Pts',(-71.7469352952005,-2.89939738054973,
134.777102478317));
#91246=CARTESIAN_POINT('Ctrl Pts',(-71.7544256309622,-2.79292787602493,
134.854806344651));
#91247=CARTESIAN_POINT('Ctrl Pts',(-71.7619159667239,-2.68346860103983,
134.928127844043));
#91248=CARTESIAN_POINT('Ctrl Pts',(-71.7694063024856,-2.57142344220033,
134.996849680569));
#91249=CARTESIAN_POINT('Ctrl Pts',(-71.7771806366047,-2.45513005710246,
135.068177126418));
#91250=CARTESIAN_POINT('Ctrl Pts',(-71.7849549707237,-2.33568244725872,
135.134775175601));
#91251=CARTESIAN_POINT('Ctrl Pts',(-71.7927293048428,-2.21350246295819,
135.196352182788));
#91252=CARTESIAN_POINT('Ctrl Pts',(-71.8004940577899,-2.09147305456877,
135.257853301816));
#91253=CARTESIAN_POINT('Ctrl Pts',(-71.808258810737,-1.96671831763929,135.314345516826));
#91254=CARTESIAN_POINT('Ctrl Pts',(-71.8160235636841,-1.83968835044573,
135.365580831032));
#91255=CARTESIAN_POINT('Ctrl Pts',(-71.8237806045691,-1.71278455120639,
135.416765257603));
#91256=CARTESIAN_POINT('Ctrl Pts',(-71.8315376454541,-1.58361037902625,
135.462703028554));
#91257=CARTESIAN_POINT('Ctrl Pts',(-71.8392946863391,-1.4526394462314,135.503192568355));
#91258=CARTESIAN_POINT('Ctrl Pts',(-71.8470458775792,-1.32176727963596,
135.543651574678));
#91259=CARTESIAN_POINT('Ctrl Pts',(-71.8547970688194,-1.18910142138563,
135.578670412671));
#91260=CARTESIAN_POINT('Ctrl Pts',(-71.8625482600595,-1.05513399288357,
135.608096176437));
#91261=CARTESIAN_POINT('Ctrl Pts',(-71.8702961568366,-0.921223504111953,
135.637509433469));
#91262=CARTESIAN_POINT('Ctrl Pts',(-71.8780440536136,-0.786012926428039,
135.661334260656));
#91263=CARTESIAN_POINT('Ctrl Pts',(-71.8857919503907,-0.650007809757516,
135.679468094305));
#91264=CARTESIAN_POINT('Ctrl Pts',(-71.8935382264748,-0.514031142425655,
135.697598134746));
#91265=CARTESIAN_POINT('Ctrl Pts',(-71.9012845025588,-0.377260653979112,
135.710039497848));
#91266=CARTESIAN_POINT('Ctrl Pts',(-71.9090307786429,-0.240209921862925,
135.716741125623));
#91267=CARTESIAN_POINT('Ctrl Pts',(-71.9167771119083,-0.103158178069368,
135.723442802868));
#91268=CARTESIAN_POINT('Ctrl Pts',(-71.9245234451736,0.0341734230231403,
135.724404641145));
#91269=CARTESIAN_POINT('Ctrl Pts',(-71.932269778439,0.171268772036229,135.71962765713));
#91270=CARTESIAN_POINT('Ctrl Pts',(-71.940017846442,0.308394822602178,135.714849603343));
#91271=CARTESIAN_POINT('Ctrl Pts',(-71.9477659144449,0.445284125156572,
135.704330183536));
#91272=CARTESIAN_POINT('Ctrl Pts',(-71.9555139824479,0.581423563406765,
135.688122456806));
#91273=CARTESIAN_POINT('Ctrl Pts',(-71.9632702851898,0.717707692272011,
135.67189750431));
#91274=CARTESIAN_POINT('Ctrl Pts',(-71.9710265879316,0.853239975967523,
135.649972214446));
#91275=CARTESIAN_POINT('Ctrl Pts',(-71.9787828906735,0.987514840810215,
135.622451266535));
#91276=CARTESIAN_POINT('Ctrl Pts',(-71.9865433331877,1.12186137219139,135.594915629865));
#91277=CARTESIAN_POINT('Ctrl Pts',(-71.9943037757019,1.25494876825523,135.561778478569));
#91278=CARTESIAN_POINT('Ctrl Pts',(-72.0020642182161,1.38628554019205,135.523194738782));
#91279=CARTESIAN_POINT('Ctrl Pts',(-72.0098371184815,1.51783314557453,135.484549060951));
#91280=CARTESIAN_POINT('Ctrl Pts',(-72.0176100187469,1.64762414065546,135.44043944851));
#91281=CARTESIAN_POINT('Ctrl Pts',(-72.0253829190123,1.77518513542065,135.391069764382));
#91282=CARTESIAN_POINT('Ctrl Pts',(-72.0328732547744,1.89810896672022,135.343494792626));
#91283=CARTESIAN_POINT('Ctrl Pts',(-72.0403635905365,2.01896183255949,135.291035665929));
#91284=CARTESIAN_POINT('Ctrl Pts',(-72.0478539262985,2.13734260514679,135.233914731777));
#91285=CARTESIAN_POINT('Ctrl Pts',(-72.0556282604176,2.26021182070693,135.174628040045));
#91286=CARTESIAN_POINT('Ctrl Pts',(-72.0634025945367,2.38080699643011,135.110131255283));
#91287=CARTESIAN_POINT('Ctrl Pts',(-72.0711769286558,2.49865474245378,135.04062165066));
#91288=CARTESIAN_POINT('Ctrl Pts',(-72.0789416816028,2.61635725166268,134.971197710413));
#91289=CARTESIAN_POINT('Ctrl Pts',(-72.0867064345499,2.73131873470714,134.896773439108));
#91290=CARTESIAN_POINT('Ctrl Pts',(-72.094471187497,2.84308725575626,134.817593468854));
#91291=CARTESIAN_POINT('Ctrl Pts',(-72.102228228382,2.95474476673477,134.738492141262));
#91292=CARTESIAN_POINT('Ctrl Pts',(-72.109985269267,3.06321530977931,134.654644739096));
#91293=CARTESIAN_POINT('Ctrl Pts',(-72.117742310152,3.16807329465536,134.56634076932));
#91294=CARTESIAN_POINT('Ctrl Pts',(-72.1254935013921,3.27285220530935,134.478103390255));
#91295=CARTESIAN_POINT('Ctrl Pts',(-72.1332446926322,3.37402368242551,134.385416383734));
#91296=CARTESIAN_POINT('Ctrl Pts',(-72.1409958838723,3.471193078305,134.28861113606));
#91297=CARTESIAN_POINT('Ctrl Pts',(-72.1487437806494,3.56832117459916,134.191847033199));
#91298=CARTESIAN_POINT('Ctrl Pts',(-72.1564916774265,3.66145029640585,134.09096844588));
#91299=CARTESIAN_POINT('Ctrl Pts',(-72.1642395742036,3.75022089190135,133.986345269391));
#91300=CARTESIAN_POINT('Ctrl Pts',(-72.1719858502877,3.83897291850182,133.881743977815));
#91301=CARTESIAN_POINT('Ctrl Pts',(-72.1797321263717,3.92336797944733,133.773399952997));
#91302=CARTESIAN_POINT('Ctrl Pts',(-72.1874784024558,4.00308551705314,133.661717684098));
#91303=CARTESIAN_POINT('Ctrl Pts',(-72.1952247357211,4.0828036431157,133.550034590786));
#91304=CARTESIAN_POINT('Ctrl Pts',(-72.2029710689865,4.15784394980044,133.435013522437));
#91305=CARTESIAN_POINT('Ctrl Pts',(-72.2107174022518,4.22792832273901,133.317089246026));
#91306=CARTESIAN_POINT('Ctrl Pts',(-72.2184654702547,4.29802839058697,133.199138561291));
#91307=CARTESIAN_POINT('Ctrl Pts',(-72.2262135382578,4.36317011651623,133.078283710789));
#91308=CARTESIAN_POINT('Ctrl Pts',(-72.2339616062607,4.42312078875598,132.954985073526));
#91309=CARTESIAN_POINT('Ctrl Pts',(-72.2417179090026,4.4831351772836,132.831555393005));
#91310=CARTESIAN_POINT('Ctrl Pts',(-72.2494742117444,4.53794731986127,132.705677089531));
#91311=CARTESIAN_POINT('Ctrl Pts',(-72.2572305144863,4.58737201124352,132.577832098295));
#91312=CARTESIAN_POINT('Ctrl Pts',(-72.2649909570004,4.63682308207178,132.449918872338));
#91313=CARTESIAN_POINT('Ctrl Pts',(-72.2727513995146,4.68088084660649,132.320037237103));
#91314=CARTESIAN_POINT('Ctrl Pts',(-72.2805118420287,4.71940998688618,132.188684437407));
#91315=CARTESIAN_POINT('Ctrl Pts',(-72.2882847422942,4.75800097756231,132.057120778536));
#91316=CARTESIAN_POINT('Ctrl Pts',(-72.2960576425596,4.79104551452926,131.924081615541));
#91317=CARTESIAN_POINT('Ctrl Pts',(-72.303830542825,4.81845923457119,131.790075417737));
#91318=CARTESIAN_POINT('Ctrl Pts',(-72.3113208785872,4.84487639683905,131.660940682762));
#91319=CARTESIAN_POINT('Ctrl Pts',(-72.3188112143493,4.86606497381129,131.530908304634));
#91320=CARTESIAN_POINT('Ctrl Pts',(-72.3263015501114,4.88199521335488,131.400435947772));
#91321=CARTESIAN_POINT('Ctrl Pts',(-72.3340758842305,4.89852945277239,131.265016691845));
#91322=CARTESIAN_POINT('Ctrl Pts',(-72.3418502183495,4.90945111928723,131.128694467491));
#91323=CARTESIAN_POINT('Ctrl Pts',(-72.3496245524686,4.91467030562071,130.991974181974));
#91324=CARTESIAN_POINT('Ctrl Pts',(-72.3573893054157,4.91988305977349,130.855422391991));
#91325=CARTESIAN_POINT('Ctrl Pts',(-72.3651540583628,4.91940730219587,130.718473903873));
#91326=CARTESIAN_POINT('Ctrl Pts',(-72.3729188113099,4.91320456645233,130.581641173664));
#91327=CARTESIAN_POINT('Ctrl Pts',(-72.3806758521949,4.90700799135338,130.444944347652));
#91328=CARTESIAN_POINT('Ctrl Pts',(-72.3884328930799,4.89509577528495,130.308363438786));
#91329=CARTESIAN_POINT('Ctrl Pts',(-72.3961899339649,4.87748144673841,130.172412993769));
#91330=CARTESIAN_POINT('Ctrl Pts',(-72.403941125205,4.85988040129402,130.03656507004));
#91331=CARTESIAN_POINT('Ctrl Pts',(-72.4116923164452,4.83658585230741,129.901347049987));
#91332=CARTESIAN_POINT('Ctrl Pts',(-72.4194435076854,4.80766328773967,129.767270084285));
#91333=CARTESIAN_POINT('Ctrl Pts',(-72.4271914044625,4.77875301603337,129.633250104871));
#91334=CARTESIAN_POINT('Ctrl Pts',(-72.4349393012395,4.74421956863301,129.500370596598));
#91335=CARTESIAN_POINT('Ctrl Pts',(-72.4426871980166,4.70417980237779,129.369133998038));
#91336=CARTESIAN_POINT('Ctrl Pts',(-72.4504334741007,4.66414841157861,129.237924851346));
#91337=CARTESIAN_POINT('Ctrl Pts',(-72.4581797501848,4.61861310694212,129.108358304516));
#91338=CARTESIAN_POINT('Ctrl Pts',(-72.4659260262689,4.56774092739604,128.980922688079));
#91339=CARTESIAN_POINT('Ctrl Pts',(-72.4736723595343,4.51686837232302,128.853486130941));
#91340=CARTESIAN_POINT('Ctrl Pts',(-72.4814186927997,4.46065900867942,128.728180898687));
#91341=CARTESIAN_POINT('Ctrl Pts',(-72.4891650260651,4.39932829062478,128.60547597898));
#91342=CARTESIAN_POINT('Ctrl Pts',(-72.4969130940681,4.33798383798115,128.482743580358));
#91343=CARTESIAN_POINT('Ctrl Pts',(-72.5046611620709,4.2715159235065,128.362613002684));
#91344=CARTESIAN_POINT('Ctrl Pts',(-72.5124092300739,4.20018609070058,128.24552887906));
#91345=CARTESIAN_POINT('Ctrl Pts',(-72.5201655328157,4.12878044769942,128.128320317036));
#91346=CARTESIAN_POINT('Ctrl Pts',(-72.5279218355576,4.05250276785224,128.014165011349));
#91347=CARTESIAN_POINT('Ctrl Pts',(-72.5356781382995,3.97165840892398,127.903479278158));
#91348=CARTESIAN_POINT('Ctrl Pts',(-72.5434385808136,3.89077090092719,127.792734468659));
#91349=CARTESIAN_POINT('Ctrl Pts',(-72.5511990233279,3.80531210066674,127.685463227196));
#91350=CARTESIAN_POINT('Ctrl Pts',(-72.558959465842,3.71562721162532,127.58204817357));
#91351=CARTESIAN_POINT('Ctrl Pts',(-72.5667323661075,3.62579835243816,127.47846710892));
#91352=CARTESIAN_POINT('Ctrl Pts',(-72.5745052663729,3.53173011613359,127.378754886839));
#91353=CARTESIAN_POINT('Ctrl Pts',(-72.5822781666383,3.43380469196813,127.283257324574));
#91354=CARTESIAN_POINT('Ctrl Pts',(-72.5897685024003,3.3394391036306,127.191231339242));
#91355=CARTESIAN_POINT('Ctrl Pts',(-72.5972588381623,3.24149212461839,127.10311911275));
#91356=CARTESIAN_POINT('Ctrl Pts',(-72.6047491739243,3.1403327192139,127.019193055207));
#91357=CARTESIAN_POINT('Ctrl Pts',(-72.6125235080434,3.03533782420661,126.932084915684));
#91358=CARTESIAN_POINT('Ctrl Pts',(-72.6202978421625,2.92654950353909,126.849210716208));
#91359=CARTESIAN_POINT('Ctrl Pts',(-72.6280721762816,2.81434395291338,126.77091901303));
#91360=CARTESIAN_POINT('Ctrl Pts',(-72.6358369292286,2.70227668560072,126.69272379738));
#91361=CARTESIAN_POINT('Ctrl Pts',(-72.6436016821758,2.58680088537269,126.619100062723));
#91362=CARTESIAN_POINT('Ctrl Pts',(-72.6513664351229,2.46832690396422,126.550357166972));
#91363=CARTESIAN_POINT('Ctrl Pts',(-72.6591234760079,2.34997059258428,126.481682547634));
#91364=CARTESIAN_POINT('Ctrl Pts',(-72.6668805168929,2.22862236202573,126.417879314967));
#91365=CARTESIAN_POINT('Ctrl Pts',(-72.6746375577779,2.10472242748314,126.359214212131));
#91366=CARTESIAN_POINT('Ctrl Pts',(-72.682388749018,1.98091592684482,126.300593349106));
#91367=CARTESIAN_POINT('Ctrl Pts',(-72.6901399402581,1.85456190427208,126.247103070181));
#91368=CARTESIAN_POINT('Ctrl Pts',(-72.6978911314983,1.72612580314898,126.198964567908));
#91369=CARTESIAN_POINT('Ctrl Pts',(-72.7056390282753,1.59774429079517,126.150846525783));
#91370=CARTESIAN_POINT('Ctrl Pts',(-72.7133869250524,1.4672828252962,126.108075873135));
#91371=CARTESIAN_POINT('Ctrl Pts',(-72.7211348218295,1.3352272864277,126.070825875317));
#91372=CARTESIAN_POINT('Ctrl Pts',(-72.7288810979135,1.20319937073114,126.033583669395));
#91373=CARTESIAN_POINT('Ctrl Pts',(-72.7366273739976,1.06957842095028,126.001859927412));
#91374=CARTESIAN_POINT('Ctrl Pts',(-72.7443736500817,0.934865572011036,
125.975778069367));
#91375=CARTESIAN_POINT('Ctrl Pts',(-72.752119983347,0.800151728652323,125.949696018792));
#91376=CARTESIAN_POINT('Ctrl Pts',(-72.7598663166124,0.664346353889069,
125.929256009573));
#91377=CARTESIAN_POINT('Ctrl Pts',(-72.7676126498777,0.527960478561605,
125.914530273313));
#91378=CARTESIAN_POINT('Ctrl Pts',(-72.7753607178807,0.391544060562809,
125.899801239326));
#91379=CARTESIAN_POINT('Ctrl Pts',(-72.7831087858837,0.254547271948345,
125.890789066658));
#91380=CARTESIAN_POINT('Ctrl Pts',(-72.7908568538867,0.117485565789411,
125.887514046406));
#91381=CARTESIAN_POINT('Ctrl Pts',(-72.7986131566285,-0.0197218111816969,
125.884235545423));
#91382=CARTESIAN_POINT('Ctrl Pts',(-72.8063694593703,-0.156993852045623,
125.886706386652));
#91383=CARTESIAN_POINT('Ctrl Pts',(-72.8141257621122,-0.293815244895422,
125.894894693011));
#91384=CARTESIAN_POINT('Ctrl Pts',(-72.8218862046264,-0.430709663442571,
125.903087369715));
#91385=CARTESIAN_POINT('Ctrl Pts',(-72.8296466471405,-0.567152565953215,
125.917003552436));
#91386=CARTESIAN_POINT('Ctrl Pts',(-72.8374070896547,-0.702635452636977,
125.936559627057));
#91387=CARTESIAN_POINT('Ctrl Pts',(-72.8451799899201,-0.83833582847805,
125.956147094825));
#91388=CARTESIAN_POINT('Ctrl Pts',(-72.8529528901856,-0.973072724378941,
125.981392474538));
#91389=CARTESIAN_POINT('Ctrl Pts',(-72.860725790451,-1.10634861186653,126.012161142218));
#91390=CARTESIAN_POINT('Ctrl Pts',(-72.8682161262131,-1.23477958514297,
126.041811291328));
#91391=CARTESIAN_POINT('Ctrl Pts',(-72.8757064619751,-1.36185363140396,
126.076590048094));
#91392=CARTESIAN_POINT('Ctrl Pts',(-72.8831967977372,-1.48714213010228,
126.116334236734));
#91393=CARTESIAN_POINT('Ctrl Pts',(-72.8909711318562,-1.61718098030739,
126.157585338366));
#91394=CARTESIAN_POINT('Ctrl Pts',(-72.8987454659753,-1.74570813606772,
126.204316504457));
#91395=CARTESIAN_POINT('Ctrl Pts',(-72.9065198000943,-1.8722270041725,126.256399634076));
#91396=CARTESIAN_POINT('Ctrl Pts',(-72.9142845530413,-1.99858994907999,
126.308418575892));
#91397=CARTESIAN_POINT('Ctrl Pts',(-72.9220493059884,-2.1229491728547,126.365776210127));
#91398=CARTESIAN_POINT('Ctrl Pts',(-72.9298140589354,-2.24482259878887,
126.428294511751));
#91399=CARTESIAN_POINT('Ctrl Pts',(-72.9375710998203,-2.36657497831796,
126.490750719316));
#91400=CARTESIAN_POINT('Ctrl Pts',(-72.9453281407052,-2.48584612767307,
126.558357216707));
#91401=CARTESIAN_POINT('Ctrl Pts',(-72.9530851815901,-2.60217368121453,
126.630887819608));
#91402=CARTESIAN_POINT('Ctrl Pts',(-72.9608363728302,-2.71841351124344,
126.703363726617));
#91403=CARTESIAN_POINT('Ctrl Pts',(-72.9685875640703,-2.83171383339463,
126.780756142008));
#91404=CARTESIAN_POINT('Ctrl Pts',(-72.9763387553104,-2.94163696859287,
126.862793035054));
#91405=CARTESIAN_POINT('Ctrl Pts',(-72.9840866520875,-3.0515133835262,126.944795060233));
#91406=CARTESIAN_POINT('Ctrl Pts',(-72.9918345488645,-3.15801515372683,
127.03143740353));
#91407=CARTESIAN_POINT('Ctrl Pts',(-72.9995824456416,-3.26073387625993,
127.122404934683));
#91408=CARTESIAN_POINT('Ctrl Pts',(-73.0073287217256,-3.36343111225064,
127.213353437391));
#91409=CARTESIAN_POINT('Ctrl Pts',(-73.0150749978097,-3.46234658207325,
127.308625069345));
#91410=CARTESIAN_POINT('Ctrl Pts',(-73.0228212738938,-3.55710557331878,
127.407864923065));
#91411=CARTESIAN_POINT('Ctrl Pts',(-73.030567607159,-3.65186526405352,127.50710550935));
#91412=CARTESIAN_POINT('Ctrl Pts',(-73.0383139404243,-3.74246814499035,
127.610314093088));
#91413=CARTESIAN_POINT('Ctrl Pts',(-73.0460602736896,-3.82857722098516,
127.717099772504));
#91414=CARTESIAN_POINT('Ctrl Pts',(-73.0538083416925,-3.91470558051061,
127.823909365832));
#91415=CARTESIAN_POINT('Ctrl Pts',(-73.0615564096954,-3.99633788719332,
127.934297344581));
#91416=CARTESIAN_POINT('Ctrl Pts',(-73.0693044776983,-4.07317845458179,
128.047841011318));
#91417=CARTESIAN_POINT('Ctrl Pts',(-73.0770607804401,-4.15010068903981,
128.161505353615));
#91418=CARTESIAN_POINT('Ctrl Pts',(-73.0848170831818,-4.22222079147901,
128.278331759377));
#91419=CARTESIAN_POINT('Ctrl Pts',(-73.0925733859236,-4.28928704231855,
128.397869451761));
#91420=CARTESIAN_POINT('Ctrl Pts',(-73.1003338284377,-4.3563890884355,128.517470945011));
#91421=CARTESIAN_POINT('Ctrl Pts',(-73.1080942709519,-4.41843173139561,
128.639786259838));
#91422=CARTESIAN_POINT('Ctrl Pts',(-73.115854713466,-4.4752104615666,128.764342385494));
#91423=CARTESIAN_POINT('Ctrl Pts',(-73.1236276137314,-4.53208033799584,
128.889098459701));
#91424=CARTESIAN_POINT('Ctrl Pts',(-73.1314005139968,-4.58366926842381,
129.016102170556));
#91425=CARTESIAN_POINT('Ctrl Pts',(-73.1391734142622,-4.62982158952197,
129.144862165715));
#91426=CARTESIAN_POINT('Ctrl Pts',(-73.1466637500247,-4.67429615750091,
129.268941410732));
#91427=CARTESIAN_POINT('Ctrl Pts',(-73.1541540857872,-4.7137224304112,129.394651172334));
#91428=CARTESIAN_POINT('Ctrl Pts',(-73.1616444215497,-4.74800601278444,
129.521542639417));
#91429=CARTESIAN_POINT('Ctrl Pts',(-73.1628415343781,-4.75348524863795,
129.541822558486));
#91430=CARTESIAN_POINT('Ctrl Pts',(-73.1640386472066,-4.75883489886877,
129.562138863632));
#91431=CARTESIAN_POINT('Ctrl Pts',(-73.1652357600351,-4.76405452823407,
129.582490119308));
#91432=CARTESIAN_POINT('Ctrl Pts',(-71.4150282010451,-4.76405452823412,
129.582490119309));
#91433=CARTESIAN_POINT('Ctrl Pts',(-71.4227606235564,-4.79801320159563,
129.71489447135));
#91434=CARTESIAN_POINT('Ctrl Pts',(-71.4304930460676,-4.826421244122,129.848611458346));
#91435=CARTESIAN_POINT('Ctrl Pts',(-71.4382254685788,-4.84920307574022,
129.983134343795));
#91436=CARTESIAN_POINT('Ctrl Pts',(-71.4460446511415,-4.8722405261997,130.119166615525));
#91437=CARTESIAN_POINT('Ctrl Pts',(-71.4538638337041,-4.88952469595008,
130.256022567493));
#91438=CARTESIAN_POINT('Ctrl Pts',(-71.4616830162667,-4.90103150184777,
130.393175403343));
#91439=CARTESIAN_POINT('Ctrl Pts',(-71.4695021988293,-4.91253830774546,
130.530328239193));
#91440=CARTESIAN_POINT('Ctrl Pts',(-71.4773213813919,-4.9182677949696,130.667777546891));
#91441=CARTESIAN_POINT('Ctrl Pts',(-71.4851405639546,-4.91824995845192,
130.804999904443));
#91442=CARTESIAN_POINT('',(-71.1398594360428,-4.9182484759593,130.808232467773));
#91443=CARTESIAN_POINT('Ctrl Pts',(-71.0699658330086,-4.76405452823398,
129.582490119308));
#91444=CARTESIAN_POINT('Ctrl Pts',(-71.0777030597182,-4.79811556922247,
129.715293601174));
#91445=CARTESIAN_POINT('Ctrl Pts',(-71.0854402864279,-4.82662987703852,
129.849563530845));
#91446=CARTESIAN_POINT('Ctrl Pts',(-71.0931775131375,-4.84948433727197,
129.984796876876));
#91447=CARTESIAN_POINT('Ctrl Pts',(-71.1009578336131,-4.8724660892081,130.120783427432));
#91448=CARTESIAN_POINT('Ctrl Pts',(-71.1087381540886,-4.88972465357151,
130.257743771572));
#91449=CARTESIAN_POINT('Ctrl Pts',(-71.1165184745642,-4.9011973749989,130.395157301592));
#91450=CARTESIAN_POINT('Ctrl Pts',(-71.1242987950398,-4.9126700964263,130.532570831613));
#91451=CARTESIAN_POINT('Ctrl Pts',(-71.1320791155154,-4.91835695415469,
130.670437145927));
#91452=CARTESIAN_POINT('Ctrl Pts',(-71.139859435991,-4.91824847596002,130.808232466857));
#91453=CARTESIAN_POINT('Ctrl Pts',(-71.1398594360427,-4.9182484759593,130.808232467773));
#91454=CARTESIAN_POINT('Ctrl Pts',(-71.1489049275806,-4.91812235791222,
130.96843491873));
#91455=CARTESIAN_POINT('Ctrl Pts',(-71.1579504191185,-4.91016493917958,
131.12830970416));
#91456=CARTESIAN_POINT('Ctrl Pts',(-71.1669959106564,-4.89449543925293,
131.287162292824));
#91457=CARTESIAN_POINT('Ctrl Pts',(-71.176096553043,-4.8787304015419,131.446983414271));
#91458=CARTESIAN_POINT('Ctrl Pts',(-71.1851971954297,-4.85515906191396,
131.605769743764));
#91459=CARTESIAN_POINT('Ctrl Pts',(-71.1942978378163,-4.82395190626533,
131.762833918466));
#91460=CARTESIAN_POINT('Ctrl Pts',(-71.2034625668571,-4.79252499006506,
131.921004137887));
#91461=CARTESIAN_POINT('Ctrl Pts',(-71.2126272958978,-4.75335441236356,
132.077427772717));
#91462=CARTESIAN_POINT('Ctrl Pts',(-71.2217920249387,-4.70666251969357,
132.231424382158));
#91463=CARTESIAN_POINT('Ctrl Pts',(-71.2252280336323,-4.68915695587144,
132.289160261361));
#91464=CARTESIAN_POINT('Ctrl Pts',(-71.228664042326,-4.67059465505894,132.346555214575));
#91465=CARTESIAN_POINT('Ctrl Pts',(-71.2321000510196,-4.65098903443619,
132.403574194314));
#91466=CARTESIAN_POINT('Ctrl Pts',(-71.2398743851383,-4.60662923825511,
132.532585683841));
#91467=CARTESIAN_POINT('Ctrl Pts',(-71.2476487192571,-4.5568272322371,132.659954407817));
#91468=CARTESIAN_POINT('Ctrl Pts',(-71.2554230533758,-4.50172299729148,
132.785186990108));
#91469=CARTESIAN_POINT('Ctrl Pts',(-71.2631878063226,-4.44668667339078,
132.910265234433));
#91470=CARTESIAN_POINT('Ctrl Pts',(-71.2709525592692,-4.38636127826588,
133.03321222075));
#91471=CARTESIAN_POINT('Ctrl Pts',(-71.278717312216,-4.32093635419087,133.153550283287));
#91472=CARTESIAN_POINT('Ctrl Pts',(-71.2864743531007,-4.25557641107269,
133.273768824365));
#91473=CARTESIAN_POINT('Ctrl Pts',(-71.2942313939854,-4.18512720396693,
133.391383257047));
#91474=CARTESIAN_POINT('Ctrl Pts',(-71.3019884348701,-4.1098259475563,133.505936776643));
#91475=CARTESIAN_POINT('Ctrl Pts',(-71.3097396261099,-4.03458147640898,
133.620403910539));
#91476=CARTESIAN_POINT('Ctrl Pts',(-71.3174908173498,-3.95449245279771,
133.731814400418));
#91477=CARTESIAN_POINT('Ctrl Pts',(-71.3252420085896,-3.86984133219999,
133.839737221234));
#91478=CARTESIAN_POINT('Ctrl Pts',(-71.3329899053664,-3.78522619058667,
133.947614171972));
#91479=CARTESIAN_POINT('Ctrl Pts',(-71.3407378021431,-3.69605304932102,
134.052006094952));
#91480=CARTESIAN_POINT('Ctrl Pts',(-71.3484856989199,-3.60264674845865,
134.152512267106));
#91481=CARTESIAN_POINT('Ctrl Pts',(-71.3562319750037,-3.50925998618094,
134.252997415536));
#91482=CARTESIAN_POINT('Ctrl Pts',(-71.3639782510876,-3.41164209157134,
134.349598143671));
#91483=CARTESIAN_POINT('Ctrl Pts',(-71.3717245271714,-3.31015686197168,
134.441948363812));
#91484=CARTESIAN_POINT('Ctrl Pts',(-71.3794708604364,-3.20867088323112,
134.534299265662));
#91485=CARTESIAN_POINT('Ctrl Pts',(-71.3872171937014,-3.1033178016973,134.622399333774));
#91486=CARTESIAN_POINT('Ctrl Pts',(-71.3949635269665,-2.99449649352841,
134.705921050617));
#91487=CARTESIAN_POINT('Ctrl Pts',(-71.4027115949692,-2.88565081558206,
134.789461471568));
#91488=CARTESIAN_POINT('Ctrl Pts',(-71.4104596629718,-2.77333567557318,
134.868421263047));
#91489=CARTESIAN_POINT('Ctrl Pts',(-71.4182077309745,-2.65798074486767,
134.942514967323));
#91490=CARTESIAN_POINT('Ctrl Pts',(-71.4259640337161,-2.54250321356905,
135.01668741927));
#91491=CARTESIAN_POINT('Ctrl Pts',(-71.4337203364577,-2.42397976732895,
135.08598324129));
#91492=CARTESIAN_POINT('Ctrl Pts',(-71.4414766391992,-2.30286709375386,
135.150161603691));
#91493=CARTESIAN_POINT('Ctrl Pts',(-71.4492370817131,-2.18168977869824,
135.214374220017));
#91494=CARTESIAN_POINT('Ctrl Pts',(-71.456997524227,-2.05792083530419,135.273463765935));
#91495=CARTESIAN_POINT('Ctrl Pts',(-71.4647579667409,-1.93203804577157,
135.327237141659));
#91496=CARTESIAN_POINT('Ctrl Pts',(-71.472530867006,-1.80595317800983,135.38109683918));
#91497=CARTESIAN_POINT('Ctrl Pts',(-71.4803037672712,-1.67774804900742,
135.4296231744));
#91498=CARTESIAN_POINT('Ctrl Pts',(-71.4880766675364,-1.54791760510034,
135.472672319918));
#91499=CARTESIAN_POINT('Ctrl Pts',(-71.4955670033018,-1.42280682479164,
135.514156520584));
#91500=CARTESIAN_POINT('Ctrl Pts',(-71.5030573390671,-1.29618714260848,
135.550554752058));
#91501=CARTESIAN_POINT('Ctrl Pts',(-71.5105476748325,-1.16850950563759,
135.581783416287));
#91502=CARTESIAN_POINT('Ctrl Pts',(-71.5183220089516,-1.03599093231318,
135.614196124796));
#91503=CARTESIAN_POINT('Ctrl Pts',(-71.5260963430708,-0.901912816821885,
135.641142193132));
#91504=CARTESIAN_POINT('Ctrl Pts',(-71.5338706771899,-0.766765913580014,
135.662472709343));
#91505=CARTESIAN_POINT('Ctrl Pts',(-71.541635430137,-0.631785566817964,
135.6837769376));
#91506=CARTESIAN_POINT('Ctrl Pts',(-71.549400183084,-0.495739435588995,
135.699479323429));
#91507=CARTESIAN_POINT('Ctrl Pts',(-71.5571649360311,-0.359131845864075,
135.709481144096));
#91508=CARTESIAN_POINT('Ctrl Pts',(-71.5649219769161,-0.222659936723285,
135.719473030814));
#91509=CARTESIAN_POINT('Ctrl Pts',(-71.5726790178012,-0.0856280662305558,
135.723775591406));
#91510=CARTESIAN_POINT('Ctrl Pts',(-71.5804360586862,0.051451222560865,
135.722341487211));
#91511=CARTESIAN_POINT('Ctrl Pts',(-71.5881872499263,0.188427138794287,
135.720908464485));
#91512=CARTESIAN_POINT('Ctrl Pts',(-71.5959384411664,0.3254500127893,135.713747391813));
#91513=CARTESIAN_POINT('Ctrl Pts',(-71.6036896324065,0.462004536881481,
135.70086292742));
#91514=CARTESIAN_POINT('Ctrl Pts',(-71.6114375291836,0.598501021658397,
135.687983939267));
#91515=CARTESIAN_POINT('Ctrl Pts',(-71.6191854259607,0.734529164028518,
135.669386434288));
#91516=CARTESIAN_POINT('Ctrl Pts',(-71.6269333227378,0.869576240341327,
135.645127109015));
#91517=CARTESIAN_POINT('Ctrl Pts',(-71.6346795988218,1.00459506771705,135.620872858269));
#91518=CARTESIAN_POINT('Ctrl Pts',(-71.642425874906,1.13863285266302,135.590959212009));
#91519=CARTESIAN_POINT('Ctrl Pts',(-71.6501721509901,1.27118495387946,135.555494363898));
#91520=CARTESIAN_POINT('Ctrl Pts',(-71.6579184842554,1.40373803356522,135.520029253993));
#91521=CARTESIAN_POINT('Ctrl Pts',(-71.6656648175208,1.53480502995698,135.479012961518));
#91522=CARTESIAN_POINT('Ctrl Pts',(-71.6734111507861,1.66389479097174,135.432604041056));
#91523=CARTESIAN_POINT('Ctrl Pts',(-71.6811592187891,1.79301346074362,135.386184727638));
#91524=CARTESIAN_POINT('Ctrl Pts',(-71.688907286792,1.92015364619997,135.334370515407));
#91525=CARTESIAN_POINT('Ctrl Pts',(-71.696655354795,2.04484293580088,135.277368602178));
#91526=CARTESIAN_POINT('Ctrl Pts',(-71.7044116575368,2.16966474666243,135.220306106638));
#91527=CARTESIAN_POINT('Ctrl Pts',(-71.7121679602786,2.29203010207884,135.158045058998));
#91528=CARTESIAN_POINT('Ctrl Pts',(-71.7199242630204,2.41148953440427,135.090839509146));
#91529=CARTESIAN_POINT('Ctrl Pts',(-71.7276847055346,2.53101272582576,135.023598089668));
#91530=CARTESIAN_POINT('Ctrl Pts',(-71.7354451480488,2.6476265714404,134.951407115176));
#91531=CARTESIAN_POINT('Ctrl Pts',(-71.743205590563,2.76091035798079,134.874564182217));
#91532=CARTESIAN_POINT('Ctrl Pts',(-71.7509784908284,2.87437599771219,134.797597894159));
#91533=CARTESIAN_POINT('Ctrl Pts',(-71.7587513910938,2.98450058168153,134.715964957672));
#91534=CARTESIAN_POINT('Ctrl Pts',(-71.7665242913592,3.09089557323945,134.630004042904));
#91535=CARTESIAN_POINT('Ctrl Pts',(-71.7740146271212,3.19342283886114,134.547168023909));
#91536=CARTESIAN_POINT('Ctrl Pts',(-71.7815049628832,3.29248673288394,134.460313432458));
#91537=CARTESIAN_POINT('Ctrl Pts',(-71.7889952986452,3.38777317398078,134.369774476315));
#91538=CARTESIAN_POINT('Ctrl Pts',(-71.7967696327644,3.48667242945431,134.275802708129));
#91539=CARTESIAN_POINT('Ctrl Pts',(-71.8045439668835,3.58181541636068,134.177564000405));
#91540=CARTESIAN_POINT('Ctrl Pts',(-71.8123183010026,3.67281158611053,134.075390748187));
#91541=CARTESIAN_POINT('Ctrl Pts',(-71.8200830539498,3.76369561121373,133.973343415371));
#91542=CARTESIAN_POINT('Ctrl Pts',(-71.8278478068969,3.85044273016745,133.867371475233));
#91543=CARTESIAN_POINT('Ctrl Pts',(-71.8356125598441,3.93269728423352,133.757845869448));
#91544=CARTESIAN_POINT('Ctrl Pts',(-71.8433696007291,4.0148701419168,133.648429046038));
#91545=CARTESIAN_POINT('Ctrl Pts',(-71.8511266416141,4.09255908118916,133.535465891543));
#91546=CARTESIAN_POINT('Ctrl Pts',(-71.8588836824992,4.1654472326537,133.419362035248));
#91547=CARTESIAN_POINT('Ctrl Pts',(-71.8666348737393,4.23828041859632,133.303345733773));
#91548=CARTESIAN_POINT('Ctrl Pts',(-71.8743860649795,4.3063198157089,133.184193774492));
#91549=CARTESIAN_POINT('Ctrl Pts',(-71.8821372562197,4.36929080670958,133.062342218222));
#91550=CARTESIAN_POINT('Ctrl Pts',(-71.8898851529968,4.43223503335927,132.940542452115));
#91551=CARTESIAN_POINT('Ctrl Pts',(-71.8976330497739,4.49011495933476,132.81604571771));
#91552=CARTESIAN_POINT('Ctrl Pts',(-71.905380946551,4.54270114537755,132.689314029798));
#91553=CARTESIAN_POINT('Ctrl Pts',(-71.9131272226352,4.59527633152385,132.562608851423));
#91554=CARTESIAN_POINT('Ctrl Pts',(-71.9208734987194,4.64255983054481,132.433670010315));
#91555=CARTESIAN_POINT('Ctrl Pts',(-71.9286197748035,4.68436989788417,132.302980556809));
#91556=CARTESIAN_POINT('Ctrl Pts',(-71.9363661080689,4.72618027385595,132.172290138583));
#91557=CARTESIAN_POINT('Ctrl Pts',(-71.9441124413343,4.7625170183942,132.039849454546));
#91558=CARTESIAN_POINT('Ctrl Pts',(-71.9518587745997,4.79324804826132,131.906157427481));
#91559=CARTESIAN_POINT('Ctrl Pts',(-71.9596068426028,4.82398596012951,131.772435461013));
#91560=CARTESIAN_POINT('Ctrl Pts',(-71.9673549106058,4.84911557173555,131.637461974848));
#91561=CARTESIAN_POINT('Ctrl Pts',(-71.9751029786089,4.86855585449216,131.501746417672));
#91562=CARTESIAN_POINT('Ctrl Pts',(-71.9828592813508,4.88801679861261,131.365886620388));
#91563=CARTESIAN_POINT('Ctrl Pts',(-71.9906155840927,4.90177627945069,131.229283564248));
#91564=CARTESIAN_POINT('Ctrl Pts',(-71.9983718868346,4.90980508813009,131.092452719283));
#91565=CARTESIAN_POINT('Ctrl Pts',(-72.0061323293488,4.91783818202642,130.955548843576));
#91566=CARTESIAN_POINT('Ctrl Pts',(-72.0138927718629,4.92013450263755,130.818417327509));
#91567=CARTESIAN_POINT('Ctrl Pts',(-72.0216532143772,4.91671702056835,130.681572987271));
#91568=CARTESIAN_POINT('Ctrl Pts',(-72.0294261146426,4.91329405245355,130.544508972349));
#91569=CARTESIAN_POINT('Ctrl Pts',(-72.0371990149082,4.90413897859954,130.407733444799));
#91570=CARTESIAN_POINT('Ctrl Pts',(-72.0449719151737,4.88932671824339,130.271756350993));
#91571=CARTESIAN_POINT('Ctrl Pts',(-72.0524622509352,4.87505292086205,130.140722367063));
#91572=CARTESIAN_POINT('Ctrl Pts',(-72.0599525866967,4.85552614771494,130.010430079174));
#91573=CARTESIAN_POINT('Ctrl Pts',(-72.0674429224582,4.83085780862984,129.881324380303));
#91574=CARTESIAN_POINT('Ctrl Pts',(-72.0752172565773,4.80525416196891,129.74732359961));
#91575=CARTESIAN_POINT('Ctrl Pts',(-72.0829915906964,4.77403026331621,129.614176688999));
#91576=CARTESIAN_POINT('Ctrl Pts',(-72.0907659248155,4.73725466498359,129.4823918957));
#91577=CARTESIAN_POINT('Ctrl Pts',(-72.0985306777626,4.70052438928919,129.350769515381));
#91578=CARTESIAN_POINT('Ctrl Pts',(-72.1062954307096,4.65825613148131,129.220506285248));
#91579=CARTESIAN_POINT('Ctrl Pts',(-72.1140601836566,4.61056973306006,129.092101934104));
#91580=CARTESIAN_POINT('Ctrl Pts',(-72.1218172245416,4.56293069744198,128.963825115972));
#91581=CARTESIAN_POINT('Ctrl Pts',(-72.1295742654266,4.5098843656183,128.837403866816));
#91582=CARTESIAN_POINT('Ctrl Pts',(-72.1373313063116,4.45160072934423,128.713324030368));
#91583=CARTESIAN_POINT('Ctrl Pts',(-72.1450824975517,4.39336104521358,128.589337763489));
#91584=CARTESIAN_POINT('Ctrl Pts',(-72.1528336887919,4.32989208340656,128.467689747284));
#91585=CARTESIAN_POINT('Ctrl Pts',(-72.160584880032,4.26141227689011,128.348846726571));
#91586=CARTESIAN_POINT('Ctrl Pts',(-72.168332776809,4.19296157611827,128.230054217312));
#91587=CARTESIAN_POINT('Ctrl Pts',(-72.176080673586,4.11950446131969,128.114064670398));
#91588=CARTESIAN_POINT('Ctrl Pts',(-72.1838285703631,4.04130562109771,128.001320849852));
#91589=CARTESIAN_POINT('Ctrl Pts',(-72.1915748464472,3.96312313838734,127.888600612884));
#91590=CARTESIAN_POINT('Ctrl Pts',(-72.1993211225312,3.88020112581105,127.779125072895));
#91591=CARTESIAN_POINT('Ctrl Pts',(-72.2070673986153,3.79284774992457,127.673308237232));
#91592=CARTESIAN_POINT('Ctrl Pts',(-72.2148137318806,3.70549372921544,127.567490620455));
#91593=CARTESIAN_POINT('Ctrl Pts',(-72.2225600651459,3.61370852881903,127.4653320634));
#91594=CARTESIAN_POINT('Ctrl Pts',(-72.2303063984112,3.51784051238584,127.367213371387));
#91595=CARTESIAN_POINT('Ctrl Pts',(-72.2380544664141,3.42195102697495,127.269072706373));
#91596=CARTESIAN_POINT('Ctrl Pts',(-72.2458025344171,3.3219771793156,127.174973986238));
#91597=CARTESIAN_POINT('Ctrl Pts',(-72.25355060242,3.21830378508636,127.085260752088));
#91598=CARTESIAN_POINT('Ctrl Pts',(-72.2613069051618,3.11452020554015,126.995452169645));
#91599=CARTESIAN_POINT('Ctrl Pts',(-72.2690632079037,3.00702952109897,126.910038640168));
#91600=CARTESIAN_POINT('Ctrl Pts',(-72.2768195106455,2.89624962318642,126.829323362056));
#91601=CARTESIAN_POINT('Ctrl Pts',(-72.2845799531597,2.78541059870654,126.748565003769));
#91602=CARTESIAN_POINT('Ctrl Pts',(-72.2923403956737,2.67127918785532,126.672510110146));
#91603=CARTESIAN_POINT('Ctrl Pts',(-72.3001008381879,2.5543009362462,126.601417626091));
#91604=CARTESIAN_POINT('Ctrl Pts',(-72.3078737384533,2.43713490076275,126.530211018069));
#91605=CARTESIAN_POINT('Ctrl Pts',(-72.3156466387187,2.31711323470843,126.463982927418));
#91606=CARTESIAN_POINT('Ctrl Pts',(-72.3234195389842,2.19470546608784,126.402945960933));
#91607=CARTESIAN_POINT('Ctrl Pts',(-72.3309098747465,2.07674752817853,126.34412784192));
#91608=CARTESIAN_POINT('Ctrl Pts',(-72.3384002105088,1.95657423844223,126.29013010502));
#91609=CARTESIAN_POINT('Ctrl Pts',(-72.3458905462711,1.83462011767261,126.241099493509));
#91610=CARTESIAN_POINT('Ctrl Pts',(-72.3536648803902,1.70804206935098,126.190209871462));
#91611=CARTESIAN_POINT('Ctrl Pts',(-72.3614392145093,1.57914452262869,126.144510264225));
#91612=CARTESIAN_POINT('Ctrl Pts',(-72.3692135486284,1.44839213449318,126.104217716841));
#91613=CARTESIAN_POINT('Ctrl Pts',(-72.3769783015756,1.31780088699037,126.06397482642));
#91614=CARTESIAN_POINT('Ctrl Pts',(-72.3847430545227,1.18535971642677,126.029125851069));
#91615=CARTESIAN_POINT('Ctrl Pts',(-72.3925078074698,1.05155383605675,125.999840080366));
#91616=CARTESIAN_POINT('Ctrl Pts',(-72.4002648483548,0.917880853573456,
125.970583396704));
#91617=CARTESIAN_POINT('Ctrl Pts',(-72.4080218892398,0.782846238141581,
125.946879004837));
#91618=CARTESIAN_POINT('Ctrl Pts',(-72.4157789301248,0.646950628550035,
125.928846496294));
#91619=CARTESIAN_POINT('Ctrl Pts',(-72.423530121365,0.51115749889498,125.910827586207));
#91620=CARTESIAN_POINT('Ctrl Pts',(-72.4312813126053,0.374505053437303,
125.898472097132));
#91621=CARTESIAN_POINT('Ctrl Pts',(-72.4390325038454,0.237504046167165,
125.891848542206));
#91622=CARTESIAN_POINT('Ctrl Pts',(-72.4467804006225,0.100561267979552,
125.885227802468));
#91623=CARTESIAN_POINT('Ctrl Pts',(-72.4545282973996,-0.0367293876737959,
125.884334170252));
#91624=CARTESIAN_POINT('Ctrl Pts',(-72.4622761941767,-0.173852340223402,
125.889184280312));
#91625=CARTESIAN_POINT('Ctrl Pts',(-72.4700224702608,-0.31094660960699,
125.894033375834));
#91626=CARTESIAN_POINT('Ctrl Pts',(-72.4777687463449,-0.447872855189297,
125.904623810035));
#91627=CARTESIAN_POINT('Ctrl Pts',(-72.485515022429,-0.584116189312538,
125.92092009475));
#91628=CARTESIAN_POINT('Ctrl Pts',(-72.4932613556944,-0.720360529153307,
125.93721649976));
#91629=CARTESIAN_POINT('Ctrl Pts',(-72.5010076889599,-0.85592155927776,
125.959218792897));
#91630=CARTESIAN_POINT('Ctrl Pts',(-72.5087540222252,-0.990290598323581,
125.986839720531));
#91631=CARTESIAN_POINT('Ctrl Pts',(-72.5165020902283,-1.12468972838423,
126.01446683368));
#91632=CARTESIAN_POINT('Ctrl Pts',(-72.5242501582312,-1.25789595330558,
126.047715006402));
#91633=CARTESIAN_POINT('Ctrl Pts',(-72.5319982262342,-1.3894122399525,126.086446174725));
#91634=CARTESIAN_POINT('Ctrl Pts',(-72.5397545289761,-1.52106830367375,
126.125218506995));
#91635=CARTESIAN_POINT('Ctrl Pts',(-72.547510831718,-1.65103046560631,126.169485365087));
#91636=CARTESIAN_POINT('Ctrl Pts',(-72.5552671344599,-1.7788177558298,126.219059051252));
#91637=CARTESIAN_POINT('Ctrl Pts',(-72.5630275769741,-1.90667324997769,
126.268659196385));
#91638=CARTESIAN_POINT('Ctrl Pts',(-72.5707880194884,-2.03235120134987,
126.323571656958));
#91639=CARTESIAN_POINT('Ctrl Pts',(-72.5785484620026,-2.15539292397695,
126.383561548872));
#91640=CARTESIAN_POINT('Ctrl Pts',(-72.5863213622681,-2.27863216410032,
126.443647741886));
#91641=CARTESIAN_POINT('Ctrl Pts',(-72.5940942625335,-2.39922637463695,
126.508827468021));
#91642=CARTESIAN_POINT('Ctrl Pts',(-72.601867162799,-2.5167428921132,126.578820619235));
#91643=CARTESIAN_POINT('Ctrl Pts',(-72.6093574985607,-2.62998738816753,
126.646269343097));
#91644=CARTESIAN_POINT('Ctrl Pts',(-72.6168478343224,-2.74037381200635,
126.718187439468));
#91645=CARTESIAN_POINT('Ctrl Pts',(-72.6243381700841,-2.8475438352521,126.794288652025));
#91646=CARTESIAN_POINT('Ctrl Pts',(-72.6320580407129,-2.95799799125557,
126.872721920482));
#91647=CARTESIAN_POINT('Ctrl Pts',(-72.6397779113418,-3.06539650939066,
126.955855338688));
#91648=CARTESIAN_POINT('Ctrl Pts',(-72.6474977819705,-3.16930886403994,
127.043421321749));
#91649=CARTESIAN_POINT('Ctrl Pts',(-72.6552054645287,-3.27305716268682,
127.130849056331));
#91650=CARTESIAN_POINT('Ctrl Pts',(-72.6629131470869,-3.37332995652509,
127.222695167493));
#91651=CARTESIAN_POINT('Ctrl Pts',(-72.6706208296451,-3.46972591784802,
127.318649052116));
#91652=CARTESIAN_POINT('Ctrl Pts',(-72.6783214714962,-3.56603382472385,
127.414515286113));
#91653=CARTESIAN_POINT('Ctrl Pts',(-72.6860221133473,-3.65847166227832,
127.514481553219));
#91654=CARTESIAN_POINT('Ctrl Pts',(-72.6937227551985,-3.74667126376606,
127.6181971717));
#91655=CARTESIAN_POINT('Ctrl Pts',(-72.7014180916617,-3.83481009978596,
127.721841334892));
#91656=CARTESIAN_POINT('Ctrl Pts',(-72.7091134281248,-3.9187162518825,127.829229409806));
#91657=CARTESIAN_POINT('Ctrl Pts',(-72.716808764588,-3.99805886377508,127.939974403333));
#91658=CARTESIAN_POINT('Ctrl Pts',(-72.7245005266803,-4.07736462218924,
128.050667957435));
#91659=CARTESIAN_POINT('Ctrl Pts',(-72.7321922887727,-4.15211082771811,
128.164715005133));
#91660=CARTESIAN_POINT('Ctrl Pts',(-72.7398840508651,-4.22200764339674,
128.281696446179));
#91661=CARTESIAN_POINT('Ctrl Pts',(-72.7475753563879,-4.29190031012319,
128.398670943412));
#91662=CARTESIAN_POINT('Ctrl Pts',(-72.7552666619107,-4.35694394839456,
128.518579151306));
#91663=CARTESIAN_POINT('Ctrl Pts',(-72.7629579674336,-4.41689283330309,
128.640974206955));
#91664=CARTESIAN_POINT('Ctrl Pts',(-72.7706489725695,-4.47683937688444,
128.763364482417));
#91665=CARTESIAN_POINT('Ctrl Pts',(-72.7783399777055,-4.53169139357884,
128.888241053135));
#91666=CARTESIAN_POINT('Ctrl Pts',(-72.7860309828414,-4.58125014194578,
129.015134472155));
#91667=CARTESIAN_POINT('Ctrl Pts',(-72.7937256911257,-4.63083275239513,
129.142088989191));
#91668=CARTESIAN_POINT('Ctrl Pts',(-72.80142039941,-4.67511686576179,129.271061921659));
#91669=CARTESIAN_POINT('Ctrl Pts',(-72.8091151076943,-4.71395272631355,
129.401565993759));
#91670=CARTESIAN_POINT('Ctrl Pts',(-72.8126528337234,-4.73180793662982,
129.461566663794));
#91671=CARTESIAN_POINT('Ctrl Pts',(-72.8161905597525,-4.74851219113345,
129.521890782841));
#91672=CARTESIAN_POINT('Ctrl Pts',(-72.8197282857817,-4.76405452823409,
129.582490119308));
#91673=CARTESIAN_POINT('Origin',(213.235140564004,0.,130.804360617566));
#91674=CARTESIAN_POINT('',(-74.915389332428,-4.7640545282341,129.582490119308));
#91675=CARTESIAN_POINT('',(-74.5699110322191,-4.76405452823404,129.582490119308));
#91676=CARTESIAN_POINT('',(213.235140564004,-4.76405452823405,129.582490119308));
#91677=CARTESIAN_POINT('',(-73.235140563966,-4.9182479362882,130.799855099079));
#91678=CARTESIAN_POINT('Ctrl Pts',(-73.2351405640085,-4.91824793628889,
130.79985509983));
#91679=CARTESIAN_POINT('Ctrl Pts',(-73.2428140903957,-4.91837216652081,
130.935465504126));
#91680=CARTESIAN_POINT('Ctrl Pts',(-73.2504876167828,-4.91288341773544,
131.071208978493));
#91681=CARTESIAN_POINT('Ctrl Pts',(-73.25816114317,-4.90177552888557,131.206579124001));
#91682=CARTESIAN_POINT('Ctrl Pts',(-73.2658307249217,-4.89067335013165,
131.341879681441));
#91683=CARTESIAN_POINT('Ctrl Pts',(-73.2735003066735,-4.87395780832335,
131.476806894329));
#91684=CARTESIAN_POINT('Ctrl Pts',(-73.2811698884252,-4.85167481683329,
131.610855834046));
#91685=CARTESIAN_POINT('Ctrl Pts',(-73.2888374871321,-4.82939758682722,
131.744870114107));
#91686=CARTESIAN_POINT('Ctrl Pts',(-73.296505085839,-4.80155583470916,131.878006178507));
#91687=CARTESIAN_POINT('Ctrl Pts',(-73.3041726845459,-4.76824711562812,
132.009766153809));
#91688=CARTESIAN_POINT('Ctrl Pts',(-73.3118400436167,-4.73493943754669,
132.141522011207));
#91689=CARTESIAN_POINT('Ctrl Pts',(-73.3195074026876,-4.69616523023003,
132.271901477481));
#91690=CARTESIAN_POINT('Ctrl Pts',(-73.3271747617585,-4.65207263555085,
132.400419280667));
#91691=CARTESIAN_POINT('Ctrl Pts',(-73.3348436241561,-4.60797139570735,
132.528962282132));
#91692=CARTESIAN_POINT('Ctrl Pts',(-73.3425124865538,-4.55854982451355,
132.655642516577));
#91693=CARTESIAN_POINT('Ctrl Pts',(-73.3501813489515,-4.50400498499601,
132.779992708222));
#91694=CARTESIAN_POINT('Ctrl Pts',(-73.3578581717088,-4.44940352736258,
132.904471976671));
#91695=CARTESIAN_POINT('Ctrl Pts',(-73.365534994466,-4.38966834096258,133.026616005201));
#91696=CARTESIAN_POINT('Ctrl Pts',(-73.3732118172233,-4.32504361823655,
133.14597987843));
#91697=CARTESIAN_POINT('Ctrl Pts',(-73.3808926932371,-4.26038477454887,
133.265406774138));
#91698=CARTESIAN_POINT('Ctrl Pts',(-73.3885735692509,-4.19083145789736,
133.382050248324));
#91699=CARTESIAN_POINT('Ctrl Pts',(-73.3962544452647,-4.11667170824701,
133.495493670579));
#91700=CARTESIAN_POINT('Ctrl Pts',(-73.4039475323815,-4.04239405897969,
133.60911744587));
#91701=CARTESIAN_POINT('Ctrl Pts',(-73.4116406194982,-3.9634955791439,133.719530680906));
#91702=CARTESIAN_POINT('Ctrl Pts',(-73.4193337066149,-3.880305609263,133.82634861245));
#91703=CARTESIAN_POINT('Ctrl Pts',(-73.4262531528642,-3.80548148257161,
133.922424599185));
#91704=CARTESIAN_POINT('Ctrl Pts',(-73.4331725991135,-3.72718626888421,
134.015592341138));
#91705=CARTESIAN_POINT('Ctrl Pts',(-73.4400920453628,-3.64568432271109,
134.105598094882));
#91706=CARTESIAN_POINT('Ctrl Pts',(-73.447866379482,-3.55411292550965,134.206723933142));
#91707=CARTESIAN_POINT('Ctrl Pts',(-73.4556407136011,-3.4581856774549,134.30419697933));
#91708=CARTESIAN_POINT('Ctrl Pts',(-73.4634150477202,-3.35822550577957,
134.397618820761));
#91709=CARTESIAN_POINT('Ctrl Pts',(-73.4711798006673,-3.25838852608214,
134.490925528123));
#91710=CARTESIAN_POINT('Ctrl Pts',(-73.4789445536145,-3.15452879491227,
134.580190700416));
#91711=CARTESIAN_POINT('Ctrl Pts',(-73.4867093065616,-3.0470086122924,134.665049879747));
#91712=CARTESIAN_POINT('Ctrl Pts',(-73.4944663474467,-2.93959522023339,
134.749824775744));
#91713=CARTESIAN_POINT('Ctrl Pts',(-73.5022233883317,-2.82852891666714,
134.830202146756));
#91714=CARTESIAN_POINT('Ctrl Pts',(-73.5099804292167,-2.71420761007415,
134.905855480651));
#91715=CARTESIAN_POINT('Ctrl Pts',(-73.5177316204569,-2.59997251406759,
134.98145176378));
#91716=CARTESIAN_POINT('Ctrl Pts',(-73.5254828116971,-2.48248762553258,
135.052330885712));
#91717=CARTESIAN_POINT('Ctrl Pts',(-73.5332340029373,-2.36218228965434,
135.118207843992));
#91718=CARTESIAN_POINT('Ctrl Pts',(-73.5409818997144,-2.24192808675326,
135.184056802808));
#91719=CARTESIAN_POINT('Ctrl Pts',(-73.5487297964914,-2.1188561629635,135.244907639145));
#91720=CARTESIAN_POINT('Ctrl Pts',(-73.5564776932685,-1.99342289411566,
135.300519892738));
#91721=CARTESIAN_POINT('Ctrl Pts',(-73.5642239693527,-1.86801586320364,
135.356120513446));
#91722=CARTESIAN_POINT('Ctrl Pts',(-73.5719702454369,-1.74024882689782,
135.406484572651));
#91723=CARTESIAN_POINT('Ctrl Pts',(-73.579716521521,-1.6106003350587,135.451418786258));
#91724=CARTESIAN_POINT('Ctrl Pts',(-73.5874628547864,-1.48095088618404,
135.496353331559));
#91725=CARTESIAN_POINT('Ctrl Pts',(-73.5952091880518,-1.34942032347004,
135.535857823251));
#91726=CARTESIAN_POINT('Ctrl Pts',(-73.6029555213172,-1.2165042563878,135.569788243361));
#91727=CARTESIAN_POINT('Ctrl Pts',(-73.6107035893202,-1.08355842367373,
135.603726261954));
#91728=CARTESIAN_POINT('Ctrl Pts',(-73.6184516573232,-0.949226847926304,
135.632087628358));
#91729=CARTESIAN_POINT('Ctrl Pts',(-73.6261997253262,-0.814016886661847,
135.654779111957));
#91730=CARTESIAN_POINT('Ctrl Pts',(-73.6339560280681,-0.678663222641723,
135.677494712335));
#91731=CARTESIAN_POINT('Ctrl Pts',(-73.64171233081,-0.542429694408645,135.694528327474));
#91732=CARTESIAN_POINT('Ctrl Pts',(-73.6494686335518,-0.405830922617038,
135.70583838705));
#91733=CARTESIAN_POINT('Ctrl Pts',(-73.657229076066,-0.269159243947644,
135.717154483146));
#91734=CARTESIAN_POINT('Ctrl Pts',(-73.6649895185803,-0.132122323731912,
135.722740920746));
#91735=CARTESIAN_POINT('Ctrl Pts',(-73.6727499610945,0.00476461886399771,
135.722608309672));
#91736=CARTESIAN_POINT('Ctrl Pts',(-73.68052286136,0.141871304532413,135.722475485719));
#91737=CARTESIAN_POINT('Ctrl Pts',(-73.6882957616255,0.27882714063965,135.71660528383));
#91738=CARTESIAN_POINT('Ctrl Pts',(-73.696068661891,0.415120529808438,135.70506036436));
#91739=CARTESIAN_POINT('Ctrl Pts',(-73.7035589976526,0.546459310971236,
135.693935131794));
#91740=CARTESIAN_POINT('Ctrl Pts',(-73.7110493334143,0.677182666616575,
135.677540637529));
#91741=CARTESIAN_POINT('Ctrl Pts',(-73.7185396691759,0.806843158358512,
135.655977583105));
#91742=CARTESIAN_POINT('Ctrl Pts',(-73.726314003295,0.941419767061309,135.633596958918));
#91743=CARTESIAN_POINT('Ctrl Pts',(-73.734088337414,1.0752776221262,135.605577210705));
#91744=CARTESIAN_POINT('Ctrl Pts',(-73.7418626715331,1.20790697761996,135.571974674504));
#91745=CARTESIAN_POINT('Ctrl Pts',(-73.7496274244803,1.3403728792865,135.538413550427));
#91746=CARTESIAN_POINT('Ctrl Pts',(-73.7573921774274,1.47161291846988,135.499283423181));
#91747=CARTESIAN_POINT('Ctrl Pts',(-73.7651569303745,1.60112463440961,135.454692107641));
#91748=CARTESIAN_POINT('Ctrl Pts',(-73.7729139712595,1.73050771748727,135.410145080825));
#91749=CARTESIAN_POINT('Ctrl Pts',(-73.7806710121444,1.85816552614729,135.360147786432));
#91750=CARTESIAN_POINT('Ctrl Pts',(-73.7884280530294,1.9836082772336,135.304858508354));
#91751=CARTESIAN_POINT('Ctrl Pts',(-73.7961792442696,2.10895643096535,135.249610924351));
#91752=CARTESIAN_POINT('Ctrl Pts',(-73.8039304355098,2.2320924956283,135.189079457005));
#91753=CARTESIAN_POINT('Ctrl Pts',(-73.81168162675,2.35254461902446,135.123471275792));
#91754=CARTESIAN_POINT('Ctrl Pts',(-73.8194295235271,2.47294554705551,135.057890979805));
#91755=CARTESIAN_POINT('Ctrl Pts',(-73.8271774203041,2.59066446005866,134.987238448148));
#91756=CARTESIAN_POINT('Ctrl Pts',(-73.8349253170813,2.70525236971734,134.911767668083));
#91757=CARTESIAN_POINT('Ctrl Pts',(-73.8426715931654,2.81981631005555,134.836312674879));
#91758=CARTESIAN_POINT('Ctrl Pts',(-73.8504178692497,2.93125022345547,134.756041652895));
#91759=CARTESIAN_POINT('Ctrl Pts',(-73.8581641453338,3.03913282664551,134.671252744909));
#91760=CARTESIAN_POINT('Ctrl Pts',(-73.8659104785992,3.14701622620056,134.58646321103));
#91761=CARTESIAN_POINT('Ctrl Pts',(-73.8736568118645,3.25134795584579,134.497155966189));
#91762=CARTESIAN_POINT('Ctrl Pts',(-73.8814031451299,3.35173896015751,134.403670135441));
#91763=CARTESIAN_POINT('Ctrl Pts',(-73.8891512131329,3.45215244633845,134.310163369188));
#91764=CARTESIAN_POINT('Ctrl Pts',(-73.8968992811359,3.54862316505258,134.21247642135));
#91765=CARTESIAN_POINT('Ctrl Pts',(-73.9046473491389,3.64079843961101,134.110985752749));
#91766=CARTESIAN_POINT('Ctrl Pts',(-73.9124036518808,3.73307167914802,134.009387218658));
#91767=CARTESIAN_POINT('Ctrl Pts',(-73.9201599546227,3.82104009168055,133.903977178074));
#91768=CARTESIAN_POINT('Ctrl Pts',(-73.9279162573646,3.90439053788344,133.795166126152));
#91769=CARTESIAN_POINT('Ctrl Pts',(-73.9356766998788,3.98778547072932,133.686296998495));
#91770=CARTESIAN_POINT('Ctrl Pts',(-73.943437142393,4.06655730158809,133.57402356241));
#91771=CARTESIAN_POINT('Ctrl Pts',(-73.9511975849072,4.14043646825831,133.458785021239));
#91772=CARTESIAN_POINT('Ctrl Pts',(-73.9589704851727,4.21443423232534,133.343361488933));
#91773=CARTESIAN_POINT('Ctrl Pts',(-73.9667433854382,4.28352343997149,133.224963677717));
#91774=CARTESIAN_POINT('Ctrl Pts',(-73.9745162857036,4.34748027824938,133.104055878407));
#91775=CARTESIAN_POINT('Ctrl Pts',(-73.9820066214654,4.40911212435572,132.987543382155));
#91776=CARTESIAN_POINT('Ctrl Pts',(-73.9894969572271,4.46597813883685,132.868700496163));
#91777=CARTESIAN_POINT('Ctrl Pts',(-73.9969872929888,4.51792119337332,132.747958094661));
#91778=CARTESIAN_POINT('Ctrl Pts',(-74.0047616271079,4.57183368461235,132.622637708301));
#91779=CARTESIAN_POINT('Ctrl Pts',(-74.012535961227,4.62061331720246,132.494873945455));
#91780=CARTESIAN_POINT('Ctrl Pts',(-74.0203102953461,4.66403195812012,132.365126120816));
#91781=CARTESIAN_POINT('Ctrl Pts',(-74.0280750482931,4.70739708944318,132.235538198775));
#91782=CARTESIAN_POINT('Ctrl Pts',(-74.0358398012402,4.74541425206288,132.103971447317));
#91783=CARTESIAN_POINT('Ctrl Pts',(-74.0436045541872,4.77790256137297,131.970906877483));
#91784=CARTESIAN_POINT('Ctrl Pts',(-74.0513615950722,4.81035860283625,131.837974469255));
#91785=CARTESIAN_POINT('Ctrl Pts',(-74.0591186359572,4.83729662686257,131.703547580502));
#91786=CARTESIAN_POINT('Ctrl Pts',(-74.0668756768422,4.85858506241349,131.568123835974));
#91787=CARTESIAN_POINT('Ctrl Pts',(-74.0746268680823,4.87985744418964,131.432802215544));
#91788=CARTESIAN_POINT('Ctrl Pts',(-74.0823780593223,4.89548865708745,131.296485620285));
#91789=CARTESIAN_POINT('Ctrl Pts',(-74.0901292505625,4.90539795101484,131.159683012975));
#91790=CARTESIAN_POINT('Ctrl Pts',(-74.0978771473395,4.91530303322795,131.022938550424));
#91791=CARTESIAN_POINT('Ctrl Pts',(-74.1056250441167,4.91949100528358,130.885708875797));
#91792=CARTESIAN_POINT('Ctrl Pts',(-74.1133729408938,4.91793286470779,130.748509022002));
#91793=CARTESIAN_POINT('Ctrl Pts',(-74.1211192169778,4.91637505006142,130.61133786746));
#91794=CARTESIAN_POINT('Ctrl Pts',(-74.1288654930619,4.90907351799069,130.474196912034));
#91795=CARTESIAN_POINT('Ctrl Pts',(-74.136611769146,4.89605139055868,130.337601746725));
#91796=CARTESIAN_POINT('Ctrl Pts',(-74.1443581024113,4.88302916700034,130.201005573103));
#91797=CARTESIAN_POINT('Ctrl Pts',(-74.1521044356767,4.86428630092153,130.064955586839));
#91798=CARTESIAN_POINT('Ctrl Pts',(-74.159850768942,4.83989781387392,129.929962416654));
#91799=CARTESIAN_POINT('Ctrl Pts',(-74.167598836945,4.81550386519363,129.794939015683));
#91800=CARTESIAN_POINT('Ctrl Pts',(-74.1753469049479,4.7854618492335,129.660973286394));
#91801=CARTESIAN_POINT('Ctrl Pts',(-74.1830949729508,4.74989786277997,129.528565431943));
#91802=CARTESIAN_POINT('Ctrl Pts',(-74.1908512756927,4.71429607849847,129.396016852849));
#91803=CARTESIAN_POINT('Ctrl Pts',(-74.1986075784345,4.67316070170972,129.265029834271));
#91804=CARTESIAN_POINT('Ctrl Pts',(-74.2063638811764,4.62666783415993,129.136089711853));
#91805=CARTESIAN_POINT('Ctrl Pts',(-74.2141243236905,4.58015015196686,129.007080770208));
#91806=CARTESIAN_POINT('Ctrl Pts',(-74.2218847662046,4.52826942912837,128.880121263338));
#91807=CARTESIAN_POINT('Ctrl Pts',(-74.2296452087188,4.471249474902,128.755675381692));
#91808=CARTESIAN_POINT('Ctrl Pts',(-74.2374181089842,4.41413798718311,128.631029728469));
#91809=CARTESIAN_POINT('Ctrl Pts',(-74.2451910092496,4.35187095973814,128.508906112379));
#91810=CARTESIAN_POINT('Ctrl Pts',(-74.252963909515,4.28471803721438,128.38974379412));
#91811=CARTESIAN_POINT('Ctrl Pts',(-74.2604542452772,4.2200062925709,128.274913326279));
#91812=CARTESIAN_POINT('Ctrl Pts',(-74.2679445810394,4.15075787663367,128.162832854982));
#91813=CARTESIAN_POINT('Ctrl Pts',(-74.2754349168016,4.07725036439922,128.053867474781));
#91814=CARTESIAN_POINT('Ctrl Pts',(-74.2832092509206,4.00095579249872,127.940770639074));
#91815=CARTESIAN_POINT('Ctrl Pts',(-74.2909835850395,3.91983110328264,127.830671518044));
#91816=CARTESIAN_POINT('Ctrl Pts',(-74.2987579191585,3.83413941974083,127.724010317277));
#91817=CARTESIAN_POINT('Ctrl Pts',(-74.3065226721056,3.74855334354026,127.617480566907));
#91818=CARTESIAN_POINT('Ctrl Pts',(-74.3142874250526,3.65841171439173,127.514380608434));
#91819=CARTESIAN_POINT('Ctrl Pts',(-74.3220521779996,3.56402144795968,127.415122623417));
#91820=CARTESIAN_POINT('Ctrl Pts',(-74.3298092188845,3.46972493127143,127.31596322283));
#91821=CARTESIAN_POINT('Ctrl Pts',(-74.3375662597694,3.37118844258138,127.220638483363));
#91822=CARTESIAN_POINT('Ctrl Pts',(-74.3453233006543,3.26875953032542,127.129528077789));
#91823=CARTESIAN_POINT('Ctrl Pts',(-74.3530744918943,3.16640786050911,127.03848637928));
#91824=CARTESIAN_POINT('Ctrl Pts',(-74.3608256831343,3.06016990061778,126.951652947715));
#91825=CARTESIAN_POINT('Ctrl Pts',(-74.3685768743743,2.95043020805505,126.869370827249));
#91826=CARTESIAN_POINT('Ctrl Pts',(-74.3763247711513,2.84073715778861,126.787123678879));
#91827=CARTESIAN_POINT('Ctrl Pts',(-74.3840726679282,2.7275456471735,126.709424228223));
#91828=CARTESIAN_POINT('Ctrl Pts',(-74.3918205647052,2.6112733114351,126.63657526375));
#91829=CARTESIAN_POINT('Ctrl Pts',(-74.3995668407892,2.49502529736279,126.563741537709));
#91830=CARTESIAN_POINT('Ctrl Pts',(-74.4073131168733,2.37569807109688,126.495756487169));
#91831=CARTESIAN_POINT('Ctrl Pts',(-74.4150593929573,2.25373791198869,126.432879348412));
#91832=CARTESIAN_POINT('Ctrl Pts',(-74.4228057262226,2.13177685259849,126.37000174551));
#91833=CARTESIAN_POINT('Ctrl Pts',(-74.4305520594878,2.00718316908452,126.312232308786));
#91834=CARTESIAN_POINT('Ctrl Pts',(-74.438298392753,1.8804270188328,126.25978392778));
#91835=CARTESIAN_POINT('Ctrl Pts',(-74.4460464607559,1.75364248242062,126.207323801323));
#91836=CARTESIAN_POINT('Ctrl Pts',(-74.4537945287587,1.62469487682233,126.160187251209));
#91837=CARTESIAN_POINT('Ctrl Pts',(-74.4615425967615,1.49407319551313,126.118538560664));
#91838=CARTESIAN_POINT('Ctrl Pts',(-74.4692988995033,1.36331268792573,126.076845605395));
#91839=CARTESIAN_POINT('Ctrl Pts',(-74.4770552022451,1.23087492351143,126.040652279824));
#91840=CARTESIAN_POINT('Ctrl Pts',(-74.4848115049868,1.0972634161861,126.010072760334));
#91841=CARTESIAN_POINT('Ctrl Pts',(-74.4925719475009,0.96358059637597,125.979476919634));
#91842=CARTESIAN_POINT('Ctrl Pts',(-74.500332390015,0.828723169616098,125.954500926474));
#91843=CARTESIAN_POINT('Ctrl Pts',(-74.5080928325291,0.693202646848998,
125.935207390063));
#91844=CARTESIAN_POINT('Ctrl Pts',(-74.5158657327944,0.557464574508172,
125.915882881955));
#91845=CARTESIAN_POINT('Ctrl Pts',(-74.5236386330597,0.421061668282188,
125.902259098105));
#91846=CARTESIAN_POINT('Ctrl Pts',(-74.531411533325,0.284509240154991,125.894346609972));
#91847=CARTESIAN_POINT('Ctrl Pts',(-74.5389018690881,0.152920836725796,
125.886721760712));
#91848=CARTESIAN_POINT('Ctrl Pts',(-74.5463922048511,0.0211939016250774,
125.884400181803));
#91849=CARTESIAN_POINT('Ctrl Pts',(-74.5538825406141,-0.110214364695965,
125.887345684061));
#91850=CARTESIAN_POINT('Ctrl Pts',(-74.5616568747333,-0.246605015360688,
125.890402865932));
#91851=CARTESIAN_POINT('Ctrl Pts',(-74.5694312088526,-0.38308440015906,
125.899144100303));
#91852=CARTESIAN_POINT('Ctrl Pts',(-74.5772055429719,-0.51913993726121,
125.913585956222));
#91853=CARTESIAN_POINT('Ctrl Pts',(-74.5849702959192,-0.655027798073519,
125.928010013845));
#91854=CARTESIAN_POINT('Ctrl Pts',(-74.5927350488664,-0.790492465470328,
125.948120673481));
#91855=CARTESIAN_POINT('Ctrl Pts',(-74.6004998018137,-0.925021264018458,
125.973882512491));
#91856=CARTESIAN_POINT('Ctrl Pts',(-74.6082568426989,-1.05941644666771,
125.999618764478));
#91857=CARTESIAN_POINT('Ctrl Pts',(-74.6160138835841,-1.19287722874811,
126.030994952995));
#91858=CARTESIAN_POINT('Ctrl Pts',(-74.6237709244693,-1.32489632238328,
126.067923898107));
#91859=CARTESIAN_POINT('Ctrl Pts',(-74.6315221157096,-1.45681585939281,
126.104824994815));
#91860=CARTESIAN_POINT('Ctrl Pts',(-74.63927330695,-1.58729549695094,126.147270408505));
#91861=CARTESIAN_POINT('Ctrl Pts',(-74.6470244981903,-1.7158387596256,126.195122023886));
#91862=CARTESIAN_POINT('Ctrl Pts',(-74.6547723949676,-1.84432738798479,
126.242953301055));
#91863=CARTESIAN_POINT('Ctrl Pts',(-74.6625202917448,-1.97088091273265,
126.296186073695));
#91864=CARTESIAN_POINT('Ctrl Pts',(-74.6702681885221,-2.09501884731395,
126.354632638026));
#91865=CARTESIAN_POINT('Ctrl Pts',(-74.6780144646064,-2.2191308149151,126.413066976596));
#91866=CARTESIAN_POINT('Ctrl Pts',(-74.6857607406907,-2.34082784390101,
126.476712771136));
#91867=CARTESIAN_POINT('Ctrl Pts',(-74.693507016775,-2.45965060655395,126.545334677732));
#91868=CARTESIAN_POINT('Ctrl Pts',(-74.7012533500405,-2.57847424632969,
126.613957090879));
#91869=CARTESIAN_POINT('Ctrl Pts',(-74.7089996833061,-2.69442323887346,
126.687555493855));
#91870=CARTESIAN_POINT('Ctrl Pts',(-74.7167460165716,-2.80706434263411,
126.765849401931));
#91871=CARTESIAN_POINT('Ctrl Pts',(-74.7244940845748,-2.9197306715888,126.844160843385));
#91872=CARTESIAN_POINT('Ctrl Pts',(-74.732242152578,-3.02908731672551,126.927169659255));
#91873=CARTESIAN_POINT('Ctrl Pts',(-74.7399902205811,-3.13473174899534,
127.01455324458));
#91874=CARTESIAN_POINT('Ctrl Pts',(-74.7477465233232,-3.24048846142483,
127.102029702219));
#91875=CARTESIAN_POINT('Ctrl Pts',(-74.7555028260651,-3.34252477791533,
127.193889967716));
#91876=CARTESIAN_POINT('Ctrl Pts',(-74.7632591288072,-3.44047247707194,
127.289772135679));
#91877=CARTESIAN_POINT('Ctrl Pts',(-74.7710195713215,-3.53847245386502,
127.385705478843));
#91878=CARTESIAN_POINT('Ctrl Pts',(-74.7787800138359,-3.63237919750787,
127.485664716967));
#91879=CARTESIAN_POINT('Ctrl Pts',(-74.7865404563503,-3.72186354894042,
127.589253343218));
#91880=CARTESIAN_POINT('Ctrl Pts',(-74.7943133566159,-3.81149154859769,
127.693008259127));
#91881=CARTESIAN_POINT('Ctrl Pts',(-74.8020862568816,-3.89668272643745,
127.800403899322));
#91882=CARTESIAN_POINT('Ctrl Pts',(-74.8098591571472,-3.97714964967791,
127.911012431369));
#91883=CARTESIAN_POINT('Ctrl Pts',(-74.8173494929076,-4.0546913975557,128.017600064645));
#91884=CARTESIAN_POINT('Ctrl Pts',(-74.8248398286679,-4.12784623364636,
128.1271707957));
#91885=CARTESIAN_POINT('Ctrl Pts',(-74.8323301644283,-4.19639747692351,
128.239320407712));
#91886=CARTESIAN_POINT('Ctrl Pts',(-74.8403463761326,-4.26976151510246,
128.359343736597));
#91887=CARTESIAN_POINT('Ctrl Pts',(-74.8483625878368,-4.33807319262493,
128.48268134349));
#91888=CARTESIAN_POINT('Ctrl Pts',(-74.8563787995411,-4.40102994931516,
128.60888380199));
#91889=CARTESIAN_POINT('Ctrl Pts',(-74.8643843410293,-4.4639029055492,128.734918274969));
#91890=CARTESIAN_POINT('Ctrl Pts',(-74.8723898825175,-4.52143497228248,
128.86380969095));
#91891=CARTESIAN_POINT('Ctrl Pts',(-74.8803954240057,-4.57336737440473,
128.995080672054));
#91892=CARTESIAN_POINT('Ctrl Pts',(-74.8883883634197,-4.62521802615655,
129.126145010468));
#91893=CARTESIAN_POINT('Ctrl Pts',(-74.8963813028338,-4.67148644927185,
129.259581118436));
#91894=CARTESIAN_POINT('Ctrl Pts',(-74.9043742422479,-4.71196051533489,
129.394888672324));
#91895=CARTESIAN_POINT('Ctrl Pts',(-74.9080459389746,-4.73055298653757,
129.457044567292));
#91896=CARTESIAN_POINT('Ctrl Pts',(-74.9117176357013,-4.74792338859597,
129.519595050684));
#91897=CARTESIAN_POINT('Ctrl Pts',(-74.915389332428,-4.7640545282341,129.582490119308));
#91898=CARTESIAN_POINT('Ctrl Pts',(-73.1652357600351,-4.76405452823407,
129.582490119308));
#91899=CARTESIAN_POINT('Ctrl Pts',(-73.1751882435279,-4.80744916394512,
129.75168514534));
#91900=CARTESIAN_POINT('Ctrl Pts',(-73.1851407270206,-4.84185311265486,
129.923297623253));
#91901=CARTESIAN_POINT('Ctrl Pts',(-73.1950932105134,-4.8670426185736,130.096491129957));
#91902=CARTESIAN_POINT('Ctrl Pts',(-73.2048632772353,-4.89177043185747,
130.266510212886));
#91903=CARTESIAN_POINT('Ctrl Pts',(-73.2146333439573,-4.90761850293709,
130.438053071438));
#91904=CARTESIAN_POINT('Ctrl Pts',(-73.2244034106792,-4.91442021846172,
130.610306555834));
#91905=CARTESIAN_POINT('Ctrl Pts',(-73.2279824617749,-4.9169118787639,130.673407867176));
#91906=CARTESIAN_POINT('Ctrl Pts',(-73.2315615128704,-4.91818999338173,
130.736604314292));
#91907=CARTESIAN_POINT('Ctrl Pts',(-73.235140563966,-4.9182479362882,130.799855099079));
#91908=CARTESIAN_POINT('',(-72.8898594359386,-4.91824980117577,130.805759093339));
#91909=CARTESIAN_POINT('Ctrl Pts',(-72.8197282857817,-4.76405452823409,
129.582490119308));
#91910=CARTESIAN_POINT('Ctrl Pts',(-72.827431657208,-4.79789784864164,129.714444711933));
#91911=CARTESIAN_POINT('Ctrl Pts',(-72.8351350286343,-4.82622855293165,
129.847704598932));
#91912=CARTESIAN_POINT('Ctrl Pts',(-72.8428384000606,-4.84897116631987,
129.981766130167));
#91913=CARTESIAN_POINT('Ctrl Pts',(-72.8506752393736,-4.87210781608252,
130.118150398848));
#91914=CARTESIAN_POINT('Ctrl Pts',(-72.8585120786865,-4.88946089590854,
130.255363917468));
#91915=CARTESIAN_POINT('Ctrl Pts',(-72.8663489179995,-4.90100615995804,
130.39287345792));
#91916=CARTESIAN_POINT('Ctrl Pts',(-72.8741857573126,-4.91255142400755,
130.530382998373));
#91917=CARTESIAN_POINT('Ctrl Pts',(-72.8820225966256,-4.91828891867964,
130.66818813263));
#91918=CARTESIAN_POINT('Ctrl Pts',(-72.8898594359387,-4.91824980117577,
130.805759093339));
#91919=CARTESIAN_POINT('Ctrl Pts',(-72.889859435991,-4.91824980117551,130.80575909426));
#91920=CARTESIAN_POINT('Ctrl Pts',(-72.8941682219596,-4.91822829389993,
130.881397218446));
#91921=CARTESIAN_POINT('Ctrl Pts',(-72.8984770079282,-4.91646201598752,
130.957008388749));
#91922=CARTESIAN_POINT('Ctrl Pts',(-72.9027857938971,-4.91295411382803,
131.03253804397));
#91923=CARTESIAN_POINT('Ctrl Pts',(-72.9105601280161,-4.90662481280411,
131.168816053557));
#91924=CARTESIAN_POINT('Ctrl Pts',(-72.9183344621351,-4.89461096677241,
131.305046370138));
#91925=CARTESIAN_POINT('Ctrl Pts',(-72.9261087962542,-4.87690831200657,
131.440716161882));
#91926=CARTESIAN_POINT('Ctrl Pts',(-72.9338735492012,-4.85922747418064,
131.576218752732));
#91927=CARTESIAN_POINT('Ctrl Pts',(-72.9416383021482,-4.83587182741818,
131.711161809267));
#91928=CARTESIAN_POINT('Ctrl Pts',(-72.9494030550952,-4.80688908695483,
131.845033653738));
#91929=CARTESIAN_POINT('Ctrl Pts',(-72.9571600959802,-4.77793513255782,
131.978772534806));
#91930=CARTESIAN_POINT('Ctrl Pts',(-72.9649171368652,-4.74336528883123,
132.111441941463));
#91931=CARTESIAN_POINT('Ctrl Pts',(-72.9726741777502,-4.70327888411369,
132.242536823999));
#91932=CARTESIAN_POINT('Ctrl Pts',(-72.9804253689903,-4.66322270886582,
132.373532846864));
#91933=CARTESIAN_POINT('Ctrl Pts',(-72.9881765602303,-4.61765836687906,
132.502956336613));
#91934=CARTESIAN_POINT('Ctrl Pts',(-72.9959277514704,-4.56673584771151,
132.630314275173));
#91935=CARTESIAN_POINT('Ctrl Pts',(-73.0036756482475,-4.51583497197294,
132.757618083211));
#91936=CARTESIAN_POINT('Ctrl Pts',(-73.0114235450245,-4.45958059341154,
132.882857723903));
#91937=CARTESIAN_POINT('Ctrl Pts',(-73.0191714418016,-4.39817189210529,
133.005557353434));
#91938=CARTESIAN_POINT('Ctrl Pts',(-73.0269177178857,-4.3367760361757,133.128231316847));
#91939=CARTESIAN_POINT('Ctrl Pts',(-73.0346639939697,-4.27022817691521,
133.248365976514));
#91940=CARTESIAN_POINT('Ctrl Pts',(-73.0424102700538,-4.1987746130634,133.365507784598));
#91941=CARTESIAN_POINT('Ctrl Pts',(-73.0501566033191,-4.12732052175752,
133.482650457395));
#91942=CARTESIAN_POINT('Ctrl Pts',(-73.0579029365845,-4.05096085719293,
133.596799900753));
#91943=CARTESIAN_POINT('Ctrl Pts',(-73.0656492698498,-3.9699864199273,133.707529728743));
#91944=CARTESIAN_POINT('Ctrl Pts',(-73.0733973378527,-3.88899384899776,
133.81828435391));
#91945=CARTESIAN_POINT('Ctrl Pts',(-73.0811454058556,-3.8033846796653,133.925617524333));
#91946=CARTESIAN_POINT('Ctrl Pts',(-73.0888934738586,-3.71349108357781,
134.02913456851));
#91947=CARTESIAN_POINT('Ctrl Pts',(-73.0966497766004,-3.62350194750678,
134.132761631834));
#91948=CARTESIAN_POINT('Ctrl Pts',(-73.1044060793422,-3.5292195452495,134.2325641713));
#91949=CARTESIAN_POINT('Ctrl Pts',(-73.112162382084,-3.43101451427831,134.328182756283));
#91950=CARTESIAN_POINT('Ctrl Pts',(-73.1199228245981,-3.3327570683252,134.423852375784));
#91951=CARTESIAN_POINT('Ctrl Pts',(-73.1276832671123,-3.23057311307851,
134.515333330507));
#91952=CARTESIAN_POINT('Ctrl Pts',(-73.1354437096265,-3.12486694009949,
134.602306071252));
#91953=CARTESIAN_POINT('Ctrl Pts',(-73.1432166098919,-3.01899107818746,
134.689418428361));
#91954=CARTESIAN_POINT('Ctrl Pts',(-73.1509895101572,-2.90958201191764,
134.772007874004));
#91955=CARTESIAN_POINT('Ctrl Pts',(-73.1587624104226,-2.79707434811417,
134.849797324971));
#91956=CARTESIAN_POINT('Ctrl Pts',(-73.166252746185,-2.68865662127357,134.92475893346));
#91957=CARTESIAN_POINT('Ctrl Pts',(-73.1737430819474,-2.57736192949597,
134.99526330736));
#91958=CARTESIAN_POINT('Ctrl Pts',(-73.1812334177098,-2.46359957294985,
135.061103528133));
#91959=CARTESIAN_POINT('Ctrl Pts',(-73.1890077518289,-2.34552388208411,
135.129440100884));
#91960=CARTESIAN_POINT('Ctrl Pts',(-73.196782085948,-2.22441568126635,135.192968325691));
#91961=CARTESIAN_POINT('Ctrl Pts',(-73.2045564200671,-2.1007041257914,135.251407417228));
#91962=CARTESIAN_POINT('Ctrl Pts',(-73.2123211730141,-1.97714503375216,
135.309774487807));
#91963=CARTESIAN_POINT('Ctrl Pts',(-73.2200859259612,-1.85098932093365,
135.363064738945));
#91964=CARTESIAN_POINT('Ctrl Pts',(-73.2278506789083,-1.72269326756848,
135.411041740498));
#91965=CARTESIAN_POINT('Ctrl Pts',(-73.2356077197933,-1.59452463965217,
135.458971090616));
#91966=CARTESIAN_POINT('Ctrl Pts',(-73.2433647606783,-1.46422026548786,
135.501597556949));
#91967=CARTESIAN_POINT('Ctrl Pts',(-73.2511218015633,-1.33225874709521,
135.538731715535));
#91968=CARTESIAN_POINT('Ctrl Pts',(-73.2588729928034,-1.20039674190991,
135.575837870964));
#91969=CARTESIAN_POINT('Ctrl Pts',(-73.2666241840436,-1.06688045470472,
135.607459857155));
#91970=CARTESIAN_POINT('Ctrl Pts',(-73.2743753752838,-0.932205748567533,
135.633457376261));
#91971=CARTESIAN_POINT('Ctrl Pts',(-73.2821232720609,-0.797588282772833,
135.659443845728));
#91972=CARTESIAN_POINT('Ctrl Pts',(-73.2898711688378,-0.661813760385015,
135.679810528779));
#91973=CARTESIAN_POINT('Ctrl Pts',(-73.2976190656149,-0.52539018397863,
135.694467796052));
#91974=CARTESIAN_POINT('Ctrl Pts',(-73.305365341699,-0.388995144443849,
135.70912199734));
#91975=CARTESIAN_POINT('Ctrl Pts',(-73.3131116177832,-0.251951709422492,
135.718069116613));
#91976=CARTESIAN_POINT('Ctrl Pts',(-73.3208578938673,-0.114774592040411,
135.721271218291));
#91977=CARTESIAN_POINT('Ctrl Pts',(-73.3286042271327,0.0224035379521743,
135.724473343606));
#91978=CARTESIAN_POINT('Ctrl Pts',(-73.336350560398,0.159714961415861,135.72193035758));
#91979=CARTESIAN_POINT('Ctrl Pts',(-73.3440968936634,0.296643762988791,
135.713656446947));
#91980=CARTESIAN_POINT('Ctrl Pts',(-73.3518449616663,0.433603228817248,
135.70538068343));
#91981=CARTESIAN_POINT('Ctrl Pts',(-73.3595930296693,0.570179512071966,
135.691371465064));
#91982=CARTESIAN_POINT('Ctrl Pts',(-73.3673410976723,0.705861017552133,
135.671694927679));
#91983=CARTESIAN_POINT('Ctrl Pts',(-73.3750974004141,0.841686726951139,
135.651997477835));
#91984=CARTESIAN_POINT('Ctrl Pts',(-73.3828537031559,0.976615371354942,
135.626620732993));
#91985=CARTESIAN_POINT('Ctrl Pts',(-73.3906100058978,1.11014421299232,135.595682239922));
#91986=CARTESIAN_POINT('Ctrl Pts',(-73.398370448412,1.24374432299296,135.564727234047));
#91987=CARTESIAN_POINT('Ctrl Pts',(-73.4061308909262,1.37594276486986,135.528204669071));
#91988=CARTESIAN_POINT('Ctrl Pts',(-73.4138913334404,1.50625216336704,135.486281962789));
#91989=CARTESIAN_POINT('Ctrl Pts',(-73.4216642337058,1.63677074607902,135.444291958456));
#91990=CARTESIAN_POINT('Ctrl Pts',(-73.4294371339712,1.76539385853742,135.396884625106));
#91991=CARTESIAN_POINT('Ctrl Pts',(-73.4372100342366,1.8916534671864,135.344275839526));
#91992=CARTESIAN_POINT('Ctrl Pts',(-73.4447003699987,2.01332322103189,135.293579515815));
#91993=CARTESIAN_POINT('Ctrl Pts',(-73.4521907057606,2.13279804700486,135.238053475853));
#91994=CARTESIAN_POINT('Ctrl Pts',(-73.4596810415227,2.24968262193993,135.177930230942));
#91995=CARTESIAN_POINT('Ctrl Pts',(-73.4674553756417,2.37099891105981,135.115527394925));
#91996=CARTESIAN_POINT('Ctrl Pts',(-73.4752297097608,2.48990894657635,135.047974192886));
#91997=CARTESIAN_POINT('Ctrl Pts',(-73.4830040438799,2.60594452692407,134.975479914001));
#91998=CARTESIAN_POINT('Ctrl Pts',(-73.490768796827,2.72183710378941,134.903074977837));
#91999=CARTESIAN_POINT('Ctrl Pts',(-73.498533549774,2.83486194563252,134.825741286154));
#92000=CARTESIAN_POINT('Ctrl Pts',(-73.506298302721,2.94457350646707,134.743734924168));
#92001=CARTESIAN_POINT('Ctrl Pts',(-73.514055343606,3.05417610023273,134.661810012056));
#92002=CARTESIAN_POINT('Ctrl Pts',(-73.521812384491,3.16047165069988,134.575221897923));
#92003=CARTESIAN_POINT('Ctrl Pts',(-73.529569425376,3.2630420940429,134.484270854923));
#92004=CARTESIAN_POINT('Ctrl Pts',(-73.5373206166161,3.36553518821685,134.393388398812));
#92005=CARTESIAN_POINT('Ctrl Pts',(-73.5450718078563,3.46430847533151,134.298149820955));
#92006=CARTESIAN_POINT('Ctrl Pts',(-73.5528229990964,3.55897589272276,134.198896470598));
#92007=CARTESIAN_POINT('Ctrl Pts',(-73.5605708958735,3.65360307393616,134.099685305562));
#92008=CARTESIAN_POINT('Ctrl Pts',(-73.5683187926505,3.74412758702922,133.996463044217));
#92009=CARTESIAN_POINT('Ctrl Pts',(-73.5760666894276,3.83019943647956,133.889608636655));
#92010=CARTESIAN_POINT('Ctrl Pts',(-73.5838129655116,3.91625328155449,133.782776580731));
#92011=CARTESIAN_POINT('Ctrl Pts',(-73.5915592415957,3.99785607049535,133.672314194089));
#92012=CARTESIAN_POINT('Ctrl Pts',(-73.5993055176798,4.07469767200758,133.558634014351));
#92013=CARTESIAN_POINT('Ctrl Pts',(-73.6070518509452,4.15153984074716,133.444952995451));
#92014=CARTESIAN_POINT('Ctrl Pts',(-73.6147981842105,4.22362053298201,133.328054459966));
#92015=CARTESIAN_POINT('Ctrl Pts',(-73.6225445174758,4.29067281955979,133.20838013038));
#92016=CARTESIAN_POINT('Ctrl Pts',(-73.6302925854788,4.35774012203214,133.088679000558));
#92017=CARTESIAN_POINT('Ctrl Pts',(-73.6380406534817,4.41977658701986,132.966201180694));
#92018=CARTESIAN_POINT('Ctrl Pts',(-73.6457887214846,4.47656132676596,132.841412838351));
#92019=CARTESIAN_POINT('Ctrl Pts',(-73.6535450242265,4.5334064180093,132.716491869472));
#92020=CARTESIAN_POINT('Ctrl Pts',(-73.6613013269683,4.58498847198252,132.589255829109));
#92021=CARTESIAN_POINT('Ctrl Pts',(-73.6690576297102,4.63113464206716,132.460191221688));
#92022=CARTESIAN_POINT('Ctrl Pts',(-73.6768180722243,4.67730544175221,132.331057728599));
#92023=CARTESIAN_POINT('Ctrl Pts',(-73.6845785147384,4.71803446042663,132.200094096911));
#92024=CARTESIAN_POINT('Ctrl Pts',(-73.6923389572526,4.75319911319038,132.067800862637));
#92025=CARTESIAN_POINT('Ctrl Pts',(-73.700111857518,4.78842021537651,131.935295259519));
#92026=CARTESIAN_POINT('Ctrl Pts',(-73.7078847577834,4.81805901726189,131.801456170549));
#92027=CARTESIAN_POINT('Ctrl Pts',(-73.7156576580489,4.84204415853208,131.666794052287));
#92028=CARTESIAN_POINT('Ctrl Pts',(-73.7231479938111,4.86515737950295,131.537027241214));
#92029=CARTESIAN_POINT('Ctrl Pts',(-73.7306383295734,4.88302081127843,131.406496505518));
#92030=CARTESIAN_POINT('Ctrl Pts',(-73.7381286653356,4.89561639037252,131.275660119811));
#92031=CARTESIAN_POINT('Ctrl Pts',(-73.7459029994547,4.90868953467592,131.139863032776));
#92032=CARTESIAN_POINT('Ctrl Pts',(-73.7536773335738,4.91612889133002,131.003306496408));
#92033=CARTESIAN_POINT('Ctrl Pts',(-73.7614516676929,4.91785746686445,130.866497547854));
#92034=CARTESIAN_POINT('Ctrl Pts',(-73.76921642064,4.91958391208402,130.729857204102));
#92035=CARTESIAN_POINT('Ctrl Pts',(-73.7769811735872,4.91561357486859,130.592965454294));
#92036=CARTESIAN_POINT('Ctrl Pts',(-73.7847459265343,4.90592107847343,130.4563355692));
#92037=CARTESIAN_POINT('Ctrl Pts',(-73.7925029674193,4.89623820880233,130.319841386834));
#92038=CARTESIAN_POINT('Ctrl Pts',(-73.8002600083042,4.88084451751945,130.183608939058));
#92039=CARTESIAN_POINT('Ctrl Pts',(-73.8080170491892,4.85976665922539,130.048152259783));
#92040=CARTESIAN_POINT('Ctrl Pts',(-73.8157682404293,4.8387046959082,129.912797729443));
#92041=CARTESIAN_POINT('Ctrl Pts',(-73.8235194316695,4.81196715741731,129.778218187925));
#92042=CARTESIAN_POINT('Ctrl Pts',(-73.8312706229097,4.77963255424048,129.644922948286));
#92043=CARTESIAN_POINT('Ctrl Pts',(-73.8390185196868,4.74731169413259,129.511684362681));
#92044=CARTESIAN_POINT('Ctrl Pts',(-73.8467664164639,4.70939859276699,129.379729372427));
#92045=CARTESIAN_POINT('Ctrl Pts',(-73.854514313241,4.66602289046028,129.249557270451));
#92046=CARTESIAN_POINT('Ctrl Pts',(-73.8622605893251,4.62265626141541,129.119412397673));
#92047=CARTESIAN_POINT('Ctrl Pts',(-73.8700068654092,4.57382942775682,128.991050042051));
#92048=CARTESIAN_POINT('Ctrl Pts',(-73.8777531414933,4.51972183553017,128.86495411249));
#92049=CARTESIAN_POINT('Ctrl Pts',(-73.8854994747586,4.46561384389348,128.738857252117));
#92050=CARTESIAN_POINT('Ctrl Pts',(-73.8932458080241,4.40622517007299,128.615027210473));
#92051=CARTESIAN_POINT('Ctrl Pts',(-73.9009921412894,4.34178316597662,128.493927324406));
#92052=CARTESIAN_POINT('Ctrl Pts',(-73.9087402092924,4.27732673054034,128.372800318859));
#92053=CARTESIAN_POINT('Ctrl Pts',(-73.9164882772954,4.20781489658678,128.254405030577));
#92054=CARTESIAN_POINT('Ctrl Pts',(-73.9242363452983,4.1335204688605,128.13917927364));
#92055=CARTESIAN_POINT('Ctrl Pts',(-73.9319926480402,4.05914708013222,128.023831053397));
#92056=CARTESIAN_POINT('Ctrl Pts',(-73.9397489507821,3.97998115599643,127.91165942278));
#92057=CARTESIAN_POINT('Ctrl Pts',(-73.947505253524,3.89633857858578,127.803072770071));
#92058=CARTESIAN_POINT('Ctrl Pts',(-73.9552656960382,3.81265135861313,127.694428161395));
#92059=CARTESIAN_POINT('Ctrl Pts',(-73.9630261385524,3.72448297564591,127.589372642587));
#92060=CARTESIAN_POINT('Ctrl Pts',(-73.9707865810666,3.63218828467451,127.488279899735));
#92061=CARTESIAN_POINT('Ctrl Pts',(-73.9785594813321,3.53974543407164,127.387024873837));
#92062=CARTESIAN_POINT('Ctrl Pts',(-73.9863323815975,3.44316331438664,127.289745613606));
#92063=CARTESIAN_POINT('Ctrl Pts',(-73.9941052818629,3.34283281518932,127.196778070736));
#92064=CARTESIAN_POINT('Ctrl Pts',(-74.0015956176248,3.24614958235809,127.107190132223));
#92065=CARTESIAN_POINT('Ctrl Pts',(-74.0090859533866,3.14598599881325,127.021606070122));
#92066=CARTESIAN_POINT('Ctrl Pts',(-74.0165762891484,3.04271786020936,126.940288790379));
#92067=CARTESIAN_POINT('Ctrl Pts',(-74.0243506232675,2.93553427873976,126.855888341255));
#92068=CARTESIAN_POINT('Ctrl Pts',(-74.0321249573865,2.82466655119882,126.775817256323));
#92069=CARTESIAN_POINT('Ctrl Pts',(-74.0398992915056,2.71049964544922,126.700414378332));
#92070=CARTESIAN_POINT('Ctrl Pts',(-74.0476640444527,2.59647344020756,126.62510442765));
#92071=CARTESIAN_POINT('Ctrl Pts',(-74.0554287973997,2.47915646987265,126.554451450257));
#92072=CARTESIAN_POINT('Ctrl Pts',(-74.0631935503468,2.35896684693005,126.488754231717));
#92073=CARTESIAN_POINT('Ctrl Pts',(-74.0709505912318,2.23889659801533,126.423122264579));
#92074=CARTESIAN_POINT('Ctrl Pts',(-74.0787076321169,2.11595971524768,126.362436447342));
#92075=CARTESIAN_POINT('Ctrl Pts',(-74.0864646730019,1.99060307737814,126.306952202619));
#92076=CARTESIAN_POINT('Ctrl Pts',(-74.094215864242,1.86534097192417,126.251509798997));
#92077=CARTESIAN_POINT('Ctrl Pts',(-74.1019670554821,1.7376630994995,126.201261317897));
#92078=CARTESIAN_POINT('Ctrl Pts',(-74.1097182467223,1.60804039644098,126.156416002372));
#92079=CARTESIAN_POINT('Ctrl Pts',(-74.1174661434994,1.47847278648923,126.111589747302));
#92080=CARTESIAN_POINT('Ctrl Pts',(-74.1252140402764,1.3469623586621,126.072162217823));
#92081=CARTESIAN_POINT('Ctrl Pts',(-74.1329619370535,1.2139992559975,126.038294223889));
#92082=CARTESIAN_POINT('Ctrl Pts',(-74.1407082131376,1.08106396634763,126.004433314409));
#92083=CARTESIAN_POINT('Ctrl Pts',(-74.1484544892217,0.94667698489861,125.976129723776));
#92084=CARTESIAN_POINT('Ctrl Pts',(-74.1562007653058,0.811342432886796,
125.95349404353));
#92085=CARTESIAN_POINT('Ctrl Pts',(-74.1639470985711,0.676006881866248,
125.930858196193));
#92086=CARTESIAN_POINT('Ctrl Pts',(-74.1716934318364,0.53972413193411,125.913890407228));
#92087=CARTESIAN_POINT('Ctrl Pts',(-74.1794397651018,0.403006890761979,
125.902649843918));
#92088=CARTESIAN_POINT('Ctrl Pts',(-74.1871878331047,0.266259032711431,
125.891406763362));
#92089=CARTESIAN_POINT('Ctrl Pts',(-74.1949359011077,0.129076879378445,
125.885893492662));
#92090=CARTESIAN_POINT('Ctrl Pts',(-74.2026839691107,-0.00802376622388518,
125.886117162665));
#92091=CARTESIAN_POINT('Ctrl Pts',(-74.2104402718526,-0.145270124023693,
125.886341070387));
#92092=CARTESIAN_POINT('Ctrl Pts',(-74.2181965745945,-0.282434409457219,
125.892314098165));
#92093=CARTESIAN_POINT('Ctrl Pts',(-74.2259528773363,-0.419002291888928,
125.903991229255));
#92094=CARTESIAN_POINT('Ctrl Pts',(-74.2337133198505,-0.555643064711471,
125.915674592782));
#92095=CARTESIAN_POINT('Ctrl Pts',(-74.2414737623646,-0.69168641263746,
125.933068076391));
#92096=CARTESIAN_POINT('Ctrl Pts',(-74.2492342048788,-0.826626135186591,
125.956075116987));
#92097=CARTESIAN_POINT('Ctrl Pts',(-74.2570071051442,-0.961782474958112,
125.979119090527));
#92098=CARTESIAN_POINT('Ctrl Pts',(-74.2647800054095,-1.09583126652113,
126.007794546833));
#92099=CARTESIAN_POINT('Ctrl Pts',(-74.272552905675,-1.22827857884026,126.041954209534));
#92100=CARTESIAN_POINT('Ctrl Pts',(-74.2800432414371,-1.35591109774303,
126.074872082454));
#92101=CARTESIAN_POINT('Ctrl Pts',(-74.2875335771992,-1.48205625659689,
126.112882265999));
#92102=CARTESIAN_POINT('Ctrl Pts',(-74.2950239129613,-1.60628973845464,
126.155810699728));
#92103=CARTESIAN_POINT('Ctrl Pts',(-74.3027983138802,-1.73523467846636,
126.20036716091));
#92104=CARTESIAN_POINT('Ctrl Pts',(-74.3105727147991,-1.86252854432281,
126.25036341917));
#92105=CARTESIAN_POINT('Ctrl Pts',(-74.318347115718,-1.98767816082537,126.305658739082));
#92106=CARTESIAN_POINT('Ctrl Pts',(-74.3261119198117,-2.11267329095542,
126.360885801706));
#92107=CARTESIAN_POINT('Ctrl Pts',(-74.3338767239053,-2.23552908409832,
126.421398754283));
#92108=CARTESIAN_POINT('Ctrl Pts',(-74.341641527999,-2.35576815425472,126.487007323486));
#92109=CARTESIAN_POINT('Ctrl Pts',(-74.3493986044432,-2.4758875606859,126.552550598059));
#92110=CARTESIAN_POINT('Ctrl Pts',(-74.3571556808874,-2.59339508567163,
126.623179211116));
#92111=CARTESIAN_POINT('Ctrl Pts',(-74.3649127573317,-2.70783428016457,
126.698655248976));
#92112=CARTESIAN_POINT('Ctrl Pts',(-74.3726639685936,-2.82218694634474,
126.774074218852));
#92113=CARTESIAN_POINT('Ctrl Pts',(-74.3804151798554,-2.93347557482508,
126.854333103745));
#92114=CARTESIAN_POINT('Ctrl Pts',(-74.3881663911174,-3.04126956814847,
126.939148789431));
#92115=CARTESIAN_POINT('Ctrl Pts',(-74.3959142270513,-3.14901662170038,
127.023927541436));
#92116=CARTESIAN_POINT('Ctrl Pts',(-74.4036620629853,-3.25327176059354,
127.113258905812));
#92117=CARTESIAN_POINT('Ctrl Pts',(-74.4114098989192,-3.35363476659757,
127.206817439956));
#92118=CARTESIAN_POINT('Ctrl Pts',(-74.4191560920303,-3.45397649199642,
127.30035613629));
#92119=CARTESIAN_POINT('Ctrl Pts',(-74.4269022851414,-3.5504274403712,127.39811995302));
#92120=CARTESIAN_POINT('Ctrl Pts',(-74.4346484782525,-3.64262209016361,
127.499744547468));
#92121=CARTESIAN_POINT('Ctrl Pts',(-74.4423947063997,-3.73481715695257,
127.601369601563));
#92122=CARTESIAN_POINT('Ctrl Pts',(-74.4501409345468,-3.82275562414257,
127.70685517861));
#92123=CARTESIAN_POINT('Ctrl Pts',(-74.4578871626939,-3.90611059478766,
127.815801920838));
#92124=CARTESIAN_POINT('Ctrl Pts',(-74.4656351033989,-3.9894839937832,127.924772749317));
#92125=CARTESIAN_POINT('Ctrl Pts',(-74.4733830441038,-4.06827164247307,
128.037205955102));
#92126=CARTESIAN_POINT('Ctrl Pts',(-74.4811309848088,-4.14218875059206,
128.152671454604));
#92127=CARTESIAN_POINT('Ctrl Pts',(-74.4888868507763,-4.21618146750984,
128.268255062187));
#92128=CARTESIAN_POINT('Ctrl Pts',(-74.4966427167438,-4.28529348184605,
128.386876829015));
#92129=CARTESIAN_POINT('Ctrl Pts',(-74.5043985827114,-4.34928469720025,
128.508079779951));
#92130=CARTESIAN_POINT('Ctrl Pts',(-74.5121585793053,-4.41330999305588,
128.629347281267));
#92131=CARTESIAN_POINT('Ctrl Pts',(-74.5199185758991,-4.47220888794963,
128.753198353049));
#92132=CARTESIAN_POINT('Ctrl Pts',(-74.527678572493,-4.52578903711485,128.879155004123));
#92133=CARTESIAN_POINT('Ctrl Pts',(-74.5354502962407,-4.5794501583059,129.005302004896));
#92134=CARTESIAN_POINT('Ctrl Pts',(-74.5432220199882,-4.62777633689152,
129.13356057663));
#92135=CARTESIAN_POINT('Ctrl Pts',(-74.5509937437359,-4.67062455285026,
129.263435782017));
#92136=CARTESIAN_POINT('Ctrl Pts',(-74.5572995065636,-4.70539041640939,
129.368812950451));
#92137=CARTESIAN_POINT('Ctrl Pts',(-74.5636052693913,-4.73655093449785,
129.475254024756));
#92138=CARTESIAN_POINT('Ctrl Pts',(-74.5699110322191,-4.76405452823404,
129.582490119308));
#92139=CARTESIAN_POINT('Origin',(213.235140564004,0.,130.804360617566));
#92140=CARTESIAN_POINT('',(-76.6650346057277,-4.76405452823402,129.582490119308));
#92141=CARTESIAN_POINT('',(-76.3201263474126,-4.76405452823413,129.582490119309));
#92142=CARTESIAN_POINT('',(213.235140564004,-4.76405452823405,129.582490119308));
#92143=CARTESIAN_POINT('',(-74.9851405640369,-4.91824982451843,130.8056744381));
#92144=CARTESIAN_POINT('Ctrl Pts',(-74.9851405640368,-4.91824982451843,
130.8056744381));
#92145=CARTESIAN_POINT('Ctrl Pts',(-74.9934406861383,-4.91821046334308,
130.95302187926));
#92146=CARTESIAN_POINT('Ctrl Pts',(-75.0017408082398,-4.91154523835553,
131.100187303183));
#92147=CARTESIAN_POINT('Ctrl Pts',(-75.0100409303413,-4.8983283466603,131.246585075058));
#92148=CARTESIAN_POINT('Ctrl Pts',(-75.0184356684995,-4.8849607908953,131.394651687431));
#92149=CARTESIAN_POINT('Ctrl Pts',(-75.0268304066577,-4.86489136275868,
131.541932729236));
#92150=CARTESIAN_POINT('Ctrl Pts',(-75.0352251448159,-4.83824912343897,
131.687835847576));
#92151=CARTESIAN_POINT('Ctrl Pts',(-75.0435702033672,-4.81176455145261,
131.832875519143));
#92152=CARTESIAN_POINT('Ctrl Pts',(-75.0519152619184,-4.7787849177952,131.976553268964));
#92153=CARTESIAN_POINT('Ctrl Pts',(-75.0602603204696,-4.73948666356753,
132.118304767203));
#92154=CARTESIAN_POINT('Ctrl Pts',(-75.0686798984314,-4.6998374851705,132.261322072989));
#92155=CARTESIAN_POINT('Ctrl Pts',(-75.0770994763931,-4.65375642235025,
132.402378272524));
#92156=CARTESIAN_POINT('Ctrl Pts',(-75.0855190543548,-4.60147351414362,
132.540915989886));
#92157=CARTESIAN_POINT('Ctrl Pts',(-75.0939386323165,-4.54919060593713,
132.679453707249));
#92158=CARTESIAN_POINT('Ctrl Pts',(-75.1023582102783,-4.49070603386983,
132.815472690386));
#92159=CARTESIAN_POINT('Ctrl Pts',(-75.11077778824,-4.42629631325821,132.948441775017));
#92160=CARTESIAN_POINT('Ctrl Pts',(-75.1185521223595,-4.36682270414599,
133.071220624052));
#92161=CARTESIAN_POINT('Ctrl Pts',(-75.1263264564791,-4.30214246873719,
133.191717507008));
#92162=CARTESIAN_POINT('Ctrl Pts',(-75.1341007905987,-4.23245360039246,
133.309459334788));
#92163=CARTESIAN_POINT('Ctrl Pts',(-75.1418655435463,-4.1628506173495,133.427056056287));
#92164=CARTESIAN_POINT('Ctrl Pts',(-75.1496302964939,-4.08825148041425,
133.541904145143));
#92165=CARTESIAN_POINT('Ctrl Pts',(-75.1573950494414,-4.00890150918022,
133.653552038337));
#92166=CARTESIAN_POINT('Ctrl Pts',(-75.1651520903268,-3.92963034945668,
133.765089041268));
#92167=CARTESIAN_POINT('Ctrl Pts',(-75.1729091312123,-3.84561797067704,
133.873431857237));
#92168=CARTESIAN_POINT('Ctrl Pts',(-75.1806661720977,-3.75715452714677,
133.978155337084));
#92169=CARTESIAN_POINT('Ctrl Pts',(-75.1884173633383,-3.66875779458705,
134.08279984414));
#92170=CARTESIAN_POINT('Ctrl Pts',(-75.1961685545787,-3.5759169296235,134.18383015026));
#92171=CARTESIAN_POINT('Ctrl Pts',(-75.2039197458193,-3.47896391876216,
134.280852112515));
#92172=CARTESIAN_POINT('Ctrl Pts',(-75.2116676425968,-3.38205211551686,
134.377832837847));
#92173=CARTESIAN_POINT('Ctrl Pts',(-75.2194155393744,-3.28103191833573,
134.470808331778));
#92174=CARTESIAN_POINT('Ctrl Pts',(-75.2271634361519,-3.17627376925593,
134.559419605816));
#92175=CARTESIAN_POINT('Ctrl Pts',(-75.2349097122365,-3.07153753332231,
134.648012344286));
#92176=CARTESIAN_POINT('Ctrl Pts',(-75.2426559883209,-2.96306519904072,
134.732242426343));
#92177=CARTESIAN_POINT('Ctrl Pts',(-75.2504022644054,-2.85126174293748,
134.811789910237));
#92178=CARTESIAN_POINT('Ctrl Pts',(-75.2581485976711,-2.73945746152668,
134.891337981333));
#92179=CARTESIAN_POINT('Ctrl Pts',(-75.2658949309369,-2.62432232778905,
134.966203158637));
#92180=CARTESIAN_POINT('Ctrl Pts',(-75.2736412642027,-2.5062915314385,135.036107989744));
#92181=CARTESIAN_POINT('Ctrl Pts',(-75.281389332206,-2.38823430290965,135.106028475554));
#92182=CARTESIAN_POINT('Ctrl Pts',(-75.2891374002094,-2.2672804577293,135.17098620554));
#92183=CARTESIAN_POINT('Ctrl Pts',(-75.2968854682128,-2.14389072851793,
135.23074916882));
#92184=CARTESIAN_POINT('Ctrl Pts',(-75.3046417709551,-2.02036985923383,
135.290575648889));
#92185=CARTESIAN_POINT('Ctrl Pts',(-75.3123980736973,-1.89440828676583,
135.345196162643));
#92186=CARTESIAN_POINT('Ctrl Pts',(-75.3201543764395,-1.76648822759623,
135.394426238476));
#92187=CARTESIAN_POINT('Ctrl Pts',(-75.3279148189541,-1.63849989363911,
135.443682589883));
#92188=CARTESIAN_POINT('Ctrl Pts',(-75.3356752614688,-1.50855136037819,
135.487542645658));
#92189=CARTESIAN_POINT('Ctrl Pts',(-75.3434357039834,-1.37714007798435,
135.525871844717));
#92190=CARTESIAN_POINT('Ctrl Pts',(-75.3512086042492,-1.24551784253424,
135.564262573208));
#92191=CARTESIAN_POINT('Ctrl Pts',(-75.358981504515,-1.11242854542716,135.597104608947));
#92192=CARTESIAN_POINT('Ctrl Pts',(-75.3667544047809,-0.978380783775875,
135.624314362618));
#92193=CARTESIAN_POINT('Ctrl Pts',(-75.3742447405384,-0.849205995991428,
135.650534973188));
#92194=CARTESIAN_POINT('Ctrl Pts',(-75.381735076296,-0.719141523111381,
135.671525638464));
#92195=CARTESIAN_POINT('Ctrl Pts',(-75.3892254120535,-0.588645074301121,
135.687257302834));
#92196=CARTESIAN_POINT('Ctrl Pts',(-75.3969997461725,-0.453200812889957,
135.70358543805));
#92197=CARTESIAN_POINT('Ctrl Pts',(-75.4047740802916,-0.316862125477234,
135.714299632698));
#92198=CARTESIAN_POINT('Ctrl Pts',(-75.4125484144106,-0.180134055567478,
135.719310747987));
#92199=CARTESIAN_POINT('Ctrl Pts',(-75.4203131673577,-0.0435744907845177,
135.724315687524));
#92200=CARTESIAN_POINT('Ctrl Pts',(-75.4280779203047,0.0933731147268622,
135.723631518211));
#92201=CARTESIAN_POINT('Ctrl Pts',(-75.4358426732518,0.230196246977213,
135.717220553528));
#92202=CARTESIAN_POINT('Ctrl Pts',(-75.4435997141367,0.366883484563744,
135.710815956305));
#92203=CARTESIAN_POINT('Ctrl Pts',(-75.4513567550218,0.503446106906145,
135.698695901137));
#92204=CARTESIAN_POINT('Ctrl Pts',(-75.4591137959067,0.639369588484622,
135.680874699553));
#92205=CARTESIAN_POINT('Ctrl Pts',(-75.4668649871469,0.775190569108495,
135.663066937076));
#92206=CARTESIAN_POINT('Ctrl Pts',(-75.474616178387,0.910372982243449,135.639566636256));
#92207=CARTESIAN_POINT('Ctrl Pts',(-75.4823673696271,1.04440577746549,135.610440062862));
#92208=CARTESIAN_POINT('Ctrl Pts',(-75.4901152664042,1.1783816051743,135.581325869039));
#92209=CARTESIAN_POINT('Ctrl Pts',(-75.4978631631813,1.31120840554609,135.546590241636));
#92210=CARTESIAN_POINT('Ctrl Pts',(-75.5056110599584,1.44238391842779,135.506350801984));
#92211=CARTESIAN_POINT('Ctrl Pts',(-75.5133573360425,1.57353199221965,135.466119779555));
#92212=CARTESIAN_POINT('Ctrl Pts',(-75.5211036121266,1.70302909203099,135.420387349419));
#92213=CARTESIAN_POINT('Ctrl Pts',(-75.5288498882107,1.83038714210187,135.369321293468));
#92214=CARTESIAN_POINT('Ctrl Pts',(-75.536596221476,1.95774613230111,135.318254860558));
#92215=CARTESIAN_POINT('Ctrl Pts',(-75.5443425547414,2.08296567837085,135.261854868771));
#92216=CARTESIAN_POINT('Ctrl Pts',(-75.5520888880068,2.2055771210745,135.200337485737));
#92217=CARTESIAN_POINT('Ctrl Pts',(-75.5598369560098,2.32821602176044,135.138806326311));
#92218=CARTESIAN_POINT('Ctrl Pts',(-75.5675850240127,2.44824530747384,135.072155670516));
#92219=CARTESIAN_POINT('Ctrl Pts',(-75.5753330920157,2.5652207436527,135.000647738204));
#92220=CARTESIAN_POINT('Ctrl Pts',(-75.5830893947575,2.68232050271731,134.929063806411));
#92221=CARTESIAN_POINT('Ctrl Pts',(-75.5908456974994,2.79635959457038,134.85261248995));
#92222=CARTESIAN_POINT('Ctrl Pts',(-75.5986020002413,2.9069221682364,134.771599779794));
#92223=CARTESIAN_POINT('Ctrl Pts',(-75.6063624427555,3.01754375247696,134.690543830716));
#92224=CARTESIAN_POINT('Ctrl Pts',(-75.6141228852696,3.12468481597546,134.604921880847));
#92225=CARTESIAN_POINT('Ctrl Pts',(-75.6218833277838,3.22796326471374,134.515079715552));
#92226=CARTESIAN_POINT('Ctrl Pts',(-75.6296562280493,3.33140750518657,134.425093327638));
#92227=CARTESIAN_POINT('Ctrl Pts',(-75.6374291283147,3.43097645596009,134.330873455235));
#92228=CARTESIAN_POINT('Ctrl Pts',(-75.6452020285801,3.52632488181411,134.232802813433));
#92229=CARTESIAN_POINT('Ctrl Pts',(-75.6526923643421,3.61820715221963,134.138297286485));
#92230=CARTESIAN_POINT('Ctrl Pts',(-75.6601827001042,3.70617021805039,134.040216329085));
#92231=CARTESIAN_POINT('Ctrl Pts',(-75.6676730358662,3.78994223101326,133.93892931965));
#92232=CARTESIAN_POINT('Ctrl Pts',(-75.6754473699852,3.87689048530829,133.833801982467));
#92233=CARTESIAN_POINT('Ctrl Pts',(-75.6832217041041,3.95959903151038,133.724887667353));
#92234=CARTESIAN_POINT('Ctrl Pts',(-75.690996038223,4.03771988627897,133.612563100018));
#92235=CARTESIAN_POINT('Ctrl Pts',(-75.6987607911699,4.11574446407592,133.500376962672));
#92236=CARTESIAN_POINT('Ctrl Pts',(-75.7065255441169,4.18919237896562,133.384789253375));
#92237=CARTESIAN_POINT('Ctrl Pts',(-75.7142902970638,4.25775489788121,133.266210794175));
#92238=CARTESIAN_POINT('Ctrl Pts',(-75.7220473379487,4.32624931953645,133.147750108772));
#92239=CARTESIAN_POINT('Ctrl Pts',(-75.7298043788335,4.38986780696952,133.026304921076));
#92240=CARTESIAN_POINT('Ctrl Pts',(-75.7375614197184,4.44834428726299,132.902315851711));
#92241=CARTESIAN_POINT('Ctrl Pts',(-75.7453126109584,4.5067766699877,132.778420283467));
#92242=CARTESIAN_POINT('Ctrl Pts',(-75.7530638021983,4.56007459765794,132.651985004114));
#92243=CARTESIAN_POINT('Ctrl Pts',(-75.7608149934383,4.60801758630512,132.523475793115));
#92244=CARTESIAN_POINT('Ctrl Pts',(-75.7685628902152,4.65594019790314,132.395021201959));
#92245=CARTESIAN_POINT('Ctrl Pts',(-75.7763107869921,4.69851226088147,132.264494797883));
#92246=CARTESIAN_POINT('Ctrl Pts',(-75.784058683769,4.73556124951496,132.13238272378));
#92247=CARTESIAN_POINT('Ctrl Pts',(-75.7918049598529,4.77260248829882,132.000298284674));
#92248=CARTESIAN_POINT('Ctrl Pts',(-75.7995512359368,4.80412284520769,131.866629211492));
#92249=CARTESIAN_POINT('Ctrl Pts',(-75.8072975120208,4.82999966302748,131.731876826402));
#92250=CARTESIAN_POINT('Ctrl Pts',(-75.8150438452859,4.85587667186404,131.597123446602));
#92251=CARTESIAN_POINT('Ctrl Pts',(-75.8227901785511,4.87610998475256,131.461287122887));
#92252=CARTESIAN_POINT('Ctrl Pts',(-75.8305365118163,4.89062814787684,131.324878995431));
#92253=CARTESIAN_POINT('Ctrl Pts',(-75.8382845798191,4.90514956224307,131.18844032032));
#92254=CARTESIAN_POINT('Ctrl Pts',(-75.8460326478219,4.91395323868608,131.051429975356));
#92255=CARTESIAN_POINT('Ctrl Pts',(-75.8537807158247,4.91701967056269,130.914363443891));
#92256=CARTESIAN_POINT('Ctrl Pts',(-75.8615370185664,4.92008936147959,130.777151236486));
#92257=CARTESIAN_POINT('Ctrl Pts',(-75.869293321308,4.9174096184353,130.639883114783));
#92258=CARTESIAN_POINT('Ctrl Pts',(-75.8770496240497,4.90901310269211,130.503074341581));
#92259=CARTESIAN_POINT('Ctrl Pts',(-75.8848100665637,4.90061210547565,130.366192549417));
#92260=CARTESIAN_POINT('Ctrl Pts',(-75.8925705090777,4.8864882960006,130.229770982968));
#92261=CARTESIAN_POINT('Ctrl Pts',(-75.9003309515917,4.86672606213781,130.09431801419));
#92262=CARTESIAN_POINT('Ctrl Pts',(-75.908103851857,4.84693210418281,129.958647604282));
#92263=CARTESIAN_POINT('Ctrl Pts',(-75.9158767521223,4.82148170708765,129.823949283577));
#92264=CARTESIAN_POINT('Ctrl Pts',(-75.9236496523875,4.79051025182633,129.690720375097));
#92265=CARTESIAN_POINT('Ctrl Pts',(-75.9311399881513,4.76066468696842,129.56233467299));
#92266=CARTESIAN_POINT('Ctrl Pts',(-75.9386303239151,4.72569258540207,129.435313701197));
#92267=CARTESIAN_POINT('Ctrl Pts',(-75.9461206596789,4.68575777500824,129.310085831441));
#92268=CARTESIAN_POINT('Ctrl Pts',(-75.953894993798,4.64430882414992,129.180109908971));
#92269=CARTESIAN_POINT('Ctrl Pts',(-75.9616693279171,4.59738211571997,129.05165401892));
#92270=CARTESIAN_POINT('Ctrl Pts',(-75.9694436620362,4.54510650623184,128.925214558977));
#92271=CARTESIAN_POINT('Ctrl Pts',(-75.9772084149834,4.49289532176025,128.798930924368));
#92272=CARTESIAN_POINT('Ctrl Pts',(-75.9849731679306,4.43534850037472,128.674659133153));
#92273=CARTESIAN_POINT('Ctrl Pts',(-75.9927379208778,4.37264480053699,128.552880990557));
#92274=CARTESIAN_POINT('Ctrl Pts',(-76.0004949617629,4.31000337889791,128.431223799729));
#92275=CARTESIAN_POINT('Ctrl Pts',(-76.008252002648,4.24221544940581,128.312055674066));
#92276=CARTESIAN_POINT('Ctrl Pts',(-76.016009043533,4.16950789975838,128.195838634459));
#92277=CARTESIAN_POINT('Ctrl Pts',(-76.0237602347732,4.09685517943981,128.079709235026));
#92278=CARTESIAN_POINT('Ctrl Pts',(-76.0315114260135,4.01929042986386,127.966526822155));
#92279=CARTESIAN_POINT('Ctrl Pts',(-76.0392626172537,3.93708634751327,127.856728660431));
#92280=CARTESIAN_POINT('Ctrl Pts',(-76.0470105140308,3.85491720409044,127.746977165854));
#92281=CARTESIAN_POINT('Ctrl Pts',(-76.054758410808,3.76811288355754,127.640607373877));
#92282=CARTESIAN_POINT('Ctrl Pts',(-76.0625063075852,3.67698913733047,127.538027207387));
#92283=CARTESIAN_POINT('Ctrl Pts',(-76.0702525836694,3.5858844522267,127.435468498456));
#92284=CARTESIAN_POINT('Ctrl Pts',(-76.0779988597536,3.49046239808624,127.33669813038));
#92285=CARTESIAN_POINT('Ctrl Pts',(-76.0857451358378,3.39107845222846,127.242090275027));
#92286=CARTESIAN_POINT('Ctrl Pts',(-76.0934914691032,3.29169377274112,127.1474817213));
#92287=CARTESIAN_POINT('Ctrl Pts',(-76.1012378023685,3.18834742635329,127.057036011175));
#92288=CARTESIAN_POINT('Ctrl Pts',(-76.108984135634,3.08143082723557,126.971089544519));
#92289=CARTESIAN_POINT('Ctrl Pts',(-76.116732203637,2.97449028488692,126.885123830747));
#92290=CARTESIAN_POINT('Ctrl Pts',(-76.1244802716402,2.86397820348854,126.803659610305));
#92291=CARTESIAN_POINT('Ctrl Pts',(-76.1322283396432,2.75031772996819,126.726991926029));
#92292=CARTESIAN_POINT('Ctrl Pts',(-76.1399846423851,2.63653645674385,126.650242758426));
#92293=CARTESIAN_POINT('Ctrl Pts',(-76.147740945127,2.5196004317433,126.578300529403));
#92294=CARTESIAN_POINT('Ctrl Pts',(-76.1554972478689,2.39996081436219,126.511416272245));
#92295=CARTESIAN_POINT('Ctrl Pts',(-76.1632576903832,2.28025734171468,126.444496316944));
#92296=CARTESIAN_POINT('Ctrl Pts',(-76.1710181328975,2.15784775018252,126.382639888916));
#92297=CARTESIAN_POINT('Ctrl Pts',(-76.1787785754117,2.03320536119487,126.326050777715));
#92298=CARTESIAN_POINT('Ctrl Pts',(-76.1865514756772,1.90836288517918,126.269370824648));
#92299=CARTESIAN_POINT('Ctrl Pts',(-76.1943243759428,1.78128081181966,126.217975231988));
#92300=CARTESIAN_POINT('Ctrl Pts',(-76.2020972762083,1.65245072978312,126.172018915129));
#92301=CARTESIAN_POINT('Ctrl Pts',(-76.2095876119696,1.52830394574665,126.127733226149));
#92302=CARTESIAN_POINT('Ctrl Pts',(-76.2170779477308,1.40253432966097,126.088498307759));
#92303=CARTESIAN_POINT('Ctrl Pts',(-76.224568283492,1.27559083576169,126.054407872304));
#92304=CARTESIAN_POINT('Ctrl Pts',(-76.2323426176111,1.14383424069293,126.019024887623));
#92305=CARTESIAN_POINT('Ctrl Pts',(-76.2401169517302,1.01039563017916,125.989072110177));
#92306=CARTESIAN_POINT('Ctrl Pts',(-76.2478912858494,0.875762287746976,
125.964709444407));
#92307=CARTESIAN_POINT('Ctrl Pts',(-76.2556560387965,0.741294868876446,
125.940376803445));
#92308=CARTESIAN_POINT('Ctrl Pts',(-76.2634207917437,0.605636028749181,
125.921620635428));
#92309=CARTESIAN_POINT('Ctrl Pts',(-76.2711855446908,0.469287747062014,
125.908550973293));
#92310=CARTESIAN_POINT('Ctrl Pts',(-76.2789425855759,0.333074888410762,
125.89549429213));
#92311=CARTESIAN_POINT('Ctrl Pts',(-76.2866996264608,0.196174337572018,
125.888112914302));
#92312=CARTESIAN_POINT('Ctrl Pts',(-76.2944566673459,0.0590974441484794,
125.886465686338));
#92313=CARTESIAN_POINT('Ctrl Pts',(-76.3022078585861,-0.077876078523613,
125.884819700562));
#92314=CARTESIAN_POINT('Ctrl Pts',(-76.3099590498262,-0.215025289734102,
125.888899262337));
#92315=CARTESIAN_POINT('Ctrl Pts',(-76.3177102410664,-0.35183490729462,
125.898711296578));
#92316=CARTESIAN_POINT('Ctrl Pts',(-76.3254581378435,-0.488586377117973,
125.908519160443));
#92317=CARTESIAN_POINT('Ctrl Pts',(-76.3332060346206,-0.624998151218251,
125.924054622943));
#92318=CARTESIAN_POINT('Ctrl Pts',(-76.3409539313978,-0.760556361164459,
125.945272525754));
#92319=CARTESIAN_POINT('Ctrl Pts',(-76.3487002074819,-0.896086215255443,
125.966485990237));
#92320=CARTESIAN_POINT('Ctrl Pts',(-76.3564464835661,-1.03076247431502,
125.993379470333));
#92321=CARTESIAN_POINT('Ctrl Pts',(-76.3641927596503,-1.16407819278082,
126.025856141938));
#92322=CARTESIAN_POINT('Ctrl Pts',(-76.3719390929156,-1.29739489535279,
126.058333053279));
#92323=CARTESIAN_POINT('Ctrl Pts',(-76.379685426181,-1.42935065743405,126.096393145834));
#92324=CARTESIAN_POINT('Ctrl Pts',(-76.3874317594463,-1.55945088736836,
126.139888944119));
#92325=CARTESIAN_POINT('Ctrl Pts',(-76.3951798274494,-1.68958025234729,
126.183394482988));
#92326=CARTESIAN_POINT('Ctrl Pts',(-76.4029278954524,-1.81785288759488,
126.23233802591));
#92327=CARTESIAN_POINT('Ctrl Pts',(-76.4106759634554,-1.94379184396714,
126.28652304525));
#92328=CARTESIAN_POINT('Ctrl Pts',(-76.4184322661973,-2.06986464976076,
126.340765653074));
#92329=CARTESIAN_POINT('Ctrl Pts',(-76.4261885689392,-2.1935984623812,126.400260710634));
#92330=CARTESIAN_POINT('Ctrl Pts',(-76.4339448716811,-2.31453821774371,
126.464764334373));
#92331=CARTESIAN_POINT('Ctrl Pts',(-76.4417053141953,-2.43554252229542,
126.529302385638));
#92332=CARTESIAN_POINT('Ctrl Pts',(-76.4494657567095,-2.55374946130381,
126.598854131537));
#92333=CARTESIAN_POINT('Ctrl Pts',(-76.4572261992238,-2.66873173905181,
126.673131506578));
#92334=CARTESIAN_POINT('Ctrl Pts',(-76.4649990994892,-2.78389859655938,
126.747528118254));
#92335=CARTESIAN_POINT('Ctrl Pts',(-76.4727719997547,-2.89583012906565,
126.826665292482));
#92336=CARTESIAN_POINT('Ctrl Pts',(-76.4805449000202,-3.00413028618033,
126.910213177348));
#92337=CARTESIAN_POINT('Ctrl Pts',(-76.4880352357818,-3.10849345978609,
126.99072388615));
#92338=CARTESIAN_POINT('Ctrl Pts',(-76.4955255715434,-3.2094844574116,127.075329994392));
#92339=CARTESIAN_POINT('Ctrl Pts',(-76.5030159073051,-3.30678176547625,
127.163704437972));
#92340=CARTESIAN_POINT('Ctrl Pts',(-76.5106725118287,-3.40623885695652,
127.254040597261));
#92341=CARTESIAN_POINT('Ctrl Pts',(-76.5183291163523,-3.50217156810879,
127.348619192693));
#92342=CARTESIAN_POINT('Ctrl Pts',(-76.5259857208759,-3.59418792836113,
127.447130181906));
#92343=CARTESIAN_POINT('Ctrl Pts',(-76.5336334799343,-3.68609798463603,
127.545527364074));
#92344=CARTESIAN_POINT('Ctrl Pts',(-76.5412812389926,-3.77410041135327,
127.647847617771));
#92345=CARTESIAN_POINT('Ctrl Pts',(-76.548928998051,-3.85783661147684,127.753741050716));
#92346=CARTESIAN_POINT('Ctrl Pts',(-76.5565696961159,-3.94149549996518,
127.859536714781));
#92347=CARTESIAN_POINT('Ctrl Pts',(-76.5642103941809,-4.02089574503894,
127.968898684209));
#92348=CARTESIAN_POINT('Ctrl Pts',(-76.5718510922459,-4.09571631903511,
128.081441063762));
#92349=CARTESIAN_POINT('Ctrl Pts',(-76.5796163850361,-4.17175697119375,
128.195818640404));
#92350=CARTESIAN_POINT('Ctrl Pts',(-76.5873816778263,-4.24306698472555,
128.313480961797));
#92351=CARTESIAN_POINT('Ctrl Pts',(-76.5951469706164,-4.30935250625322,
128.433988486581));
#92352=CARTESIAN_POINT('Ctrl Pts',(-76.602779193841,-4.37450212913653,128.552430939977));
#92353=CARTESIAN_POINT('Ctrl Pts',(-76.6104114170654,-4.4347978936474,128.673621490505));
#92354=CARTESIAN_POINT('Ctrl Pts',(-76.61804364029,-4.4900053734628,128.797115039971));
#92355=CARTESIAN_POINT('Ctrl Pts',(-76.625875467863,-4.54665668592162,128.923838297052));
#92356=CARTESIAN_POINT('Ctrl Pts',(-76.633707295436,-4.59794967749869,129.052986292388));
#92357=CARTESIAN_POINT('Ctrl Pts',(-76.6415391230089,-4.64368268703469,
129.184053805683));
#92358=CARTESIAN_POINT('Ctrl Pts',(-76.6493709505819,-4.68941569657056,
129.315121318978));
#92359=CARTESIAN_POINT('Ctrl Pts',(-76.6572027781548,-4.72958858089092,
129.448107913711));
#92360=CARTESIAN_POINT('Ctrl Pts',(-76.6650346057277,-4.76405452823403,
129.582490119308));
#92361=CARTESIAN_POINT('Ctrl Pts',(-74.915389332428,-4.7640545282341,129.582490119308));
#92362=CARTESIAN_POINT('Ctrl Pts',(-74.9233682696944,-4.79910898964202,
129.719166932312));
#92363=CARTESIAN_POINT('Ctrl Pts',(-74.9313472069608,-4.82830796905041,
129.857471997866));
#92364=CARTESIAN_POINT('Ctrl Pts',(-74.9393261442272,-4.85151083619154,
129.996879553506));
#92365=CARTESIAN_POINT('Ctrl Pts',(-74.9472967331157,-4.87468942612653,
130.136141246742));
#92366=CARTESIAN_POINT('Ctrl Pts',(-74.9552673220041,-4.89188435059366,
130.276502779105));
#92367=CARTESIAN_POINT('Ctrl Pts',(-74.9632379108926,-4.9030057590873,130.417427045933));
#92368=CARTESIAN_POINT('Ctrl Pts',(-74.9705387952646,-4.91319272501936,
130.546510579372));
#92369=CARTESIAN_POINT('Ctrl Pts',(-74.9778396796365,-4.918284447055,130.67606590687));
#92370=CARTESIAN_POINT('Ctrl Pts',(-74.9851405640085,-4.91824982451857,
130.805674437596));
#92371=CARTESIAN_POINT('',(-74.6398594359583,-4.91824789637572,130.799811739049));
#92372=CARTESIAN_POINT('Ctrl Pts',(-74.5699110322191,-4.76405452823404,
129.582490119308));
#92373=CARTESIAN_POINT('Ctrl Pts',(-74.5710978670709,-4.76923109837905,
129.602673487738));
#92374=CARTESIAN_POINT('Ctrl Pts',(-74.5722847019227,-4.77427818705792,
129.622885011757));
#92375=CARTESIAN_POINT('Ctrl Pts',(-74.5734715367745,-4.77919553909627,
129.643122889285));
#92376=CARTESIAN_POINT('Ctrl Pts',(-74.5838863897011,-4.82234686566057,
129.820716694929));
#92377=CARTESIAN_POINT('Ctrl Pts',(-74.5943012426276,-4.85561496466627,
130.000798665939));
#92378=CARTESIAN_POINT('Ctrl Pts',(-74.6047160955543,-4.87876862660314,
130.182428345873));
#92379=CARTESIAN_POINT('Ctrl Pts',(-74.6148654039255,-4.90133194617918,
130.3594270653));
#92380=CARTESIAN_POINT('Ctrl Pts',(-74.6250147122967,-4.91429008969093,
130.537895936914));
#92381=CARTESIAN_POINT('Ctrl Pts',(-74.6351640206679,-4.91747302611252,
130.716941512356));
#92382=CARTESIAN_POINT('Ctrl Pts',(-74.6367291590981,-4.91796387099888,
130.744552370221));
#92383=CARTESIAN_POINT('Ctrl Pts',(-74.6382942975283,-4.91822233695506,
130.77217689094));
#92384=CARTESIAN_POINT('Ctrl Pts',(-74.6398594359584,-4.91824789637572,
130.799811739049));
#92385=CARTESIAN_POINT('Ctrl Pts',(-74.639859435991,-4.91824789637626,130.799811739625));
#92386=CARTESIAN_POINT('Ctrl Pts',(-74.647518742692,-4.91837297631381,130.935048197454));
#92387=CARTESIAN_POINT('Ctrl Pts',(-74.6551780493929,-4.91291599175694,
131.070438329716));
#92388=CARTESIAN_POINT('Ctrl Pts',(-74.6628373560939,-4.90186575537136,
131.205478030324));
#92389=CARTESIAN_POINT('Ctrl Pts',(-74.6707157646144,-4.89049941636793,
131.344380671179));
#92390=CARTESIAN_POINT('Ctrl Pts',(-74.678594173135,-4.87321496953365,131.482912101015));
#92391=CARTESIAN_POINT('Ctrl Pts',(-74.6864725816555,-4.85005783070138,
131.620523653578));
#92392=CARTESIAN_POINT('Ctrl Pts',(-74.6941240345815,-4.82756778627012,
131.754170990316));
#92393=CARTESIAN_POINT('Ctrl Pts',(-74.7017754875075,-4.79953883076809,
131.886950297796));
#92394=CARTESIAN_POINT('Ctrl Pts',(-74.7094269404335,-4.76606506433638,
132.018365092439));
#92395=CARTESIAN_POINT('Ctrl Pts',(-74.7170774793527,-4.73259529652388,
132.149764188888));
#92396=CARTESIAN_POINT('Ctrl Pts',(-74.724728018272,-4.69368211011505,132.279798707484));
#92397=CARTESIAN_POINT('Ctrl Pts',(-74.7323785571913,-4.64947028911381,
132.407984355588));
#92398=CARTESIAN_POINT('Ctrl Pts',(-74.7400299369695,-4.60525360885936,
132.536184092379));
#92399=CARTESIAN_POINT('Ctrl Pts',(-74.7476813167477,-4.55573726714946,
132.662534175001));
#92400=CARTESIAN_POINT('Ctrl Pts',(-74.7553326965259,-4.5011151071118,132.786567936448));
#92401=CARTESIAN_POINT('Ctrl Pts',(-74.763381568531,-4.44365530410517,132.917045301203));
#92402=CARTESIAN_POINT('Ctrl Pts',(-74.7714304405361,-4.38054516848821,
133.044958770821));
#92403=CARTESIAN_POINT('Ctrl Pts',(-74.7794793125412,-4.31206593385308,
133.169793018757));
#92404=CARTESIAN_POINT('Ctrl Pts',(-74.7871418965388,-4.24687321030787,
133.288636119998));
#92405=CARTESIAN_POINT('Ctrl Pts',(-74.7948044805363,-4.17681500123564,
133.404688359622));
#92406=CARTESIAN_POINT('Ctrl Pts',(-74.8024670645338,-4.10217867923782,
133.517534616061));
#92407=CARTESIAN_POINT('Ctrl Pts',(-74.810134790174,-4.02749227579267,133.630456593056));
#92408=CARTESIAN_POINT('Ctrl Pts',(-74.8178025158143,-3.94822187912135,
133.74016798076));
#92409=CARTESIAN_POINT('Ctrl Pts',(-74.8254702414545,-3.86469534440186,
133.846286480808));
#92410=CARTESIAN_POINT('Ctrl Pts',(-74.8331485005768,-3.78105406571581,
133.952550760369));
#92411=CARTESIAN_POINT('Ctrl Pts',(-74.840826759699,-3.69314524463562,134.055212002915));
#92412=CARTESIAN_POINT('Ctrl Pts',(-74.8485050188213,-3.60133386345812,
134.153924390121));
#92413=CARTESIAN_POINT('Ctrl Pts',(-74.8496430660766,-3.58772587124415,
134.168555227597));
#92414=CARTESIAN_POINT('Ctrl Pts',(-74.8507811133319,-3.57403220584152,
134.183099387927));
#92415=CARTESIAN_POINT('Ctrl Pts',(-74.8519191605872,-3.56025411598836,
134.197555821513));
#92416=CARTESIAN_POINT('Ctrl Pts',(-74.8596934947062,-3.46613194879049,
134.296311953427));
#92417=CARTESIAN_POINT('Ctrl Pts',(-74.8674678288253,-3.367748563397,134.391305327569));
#92418=CARTESIAN_POINT('Ctrl Pts',(-74.8752421629444,-3.26543694881502,
134.482145901648));
#92419=CARTESIAN_POINT('Ctrl Pts',(-74.8830069158914,-3.16325142415417,
134.57287452284));
#92420=CARTESIAN_POINT('Ctrl Pts',(-74.8907716688385,-3.05714759238342,
134.659460270087));
#92421=CARTESIAN_POINT('Ctrl Pts',(-74.8985364217855,-2.9474969359988,134.741548049576));
#92422=CARTESIAN_POINT('Ctrl Pts',(-74.9062934626705,-2.8379551861919,134.823554298325));
#92423=CARTESIAN_POINT('Ctrl Pts',(-74.9140505035554,-2.72487393316754,
134.901071236943));
#92424=CARTESIAN_POINT('Ctrl Pts',(-74.9218075444404,-2.60865928796078,
134.973782613699));
#92425=CARTESIAN_POINT('Ctrl Pts',(-74.9295587356805,-2.49253228112216,
135.04643915824));
#92426=CARTESIAN_POINT('Ctrl Pts',(-74.9373099269205,-2.37327691543874,
135.114297147565));
#92427=CARTESIAN_POINT('Ctrl Pts',(-74.9450611181606,-2.25132966914383,
135.17708262832));
#92428=CARTESIAN_POINT('Ctrl Pts',(-74.9528090149377,-2.12943425368182,
135.239841423571));
#92429=CARTESIAN_POINT('Ctrl Pts',(-74.9605569117147,-2.00484958004986,
135.297531819686));
#92430=CARTESIAN_POINT('Ctrl Pts',(-74.9683048084917,-1.87803801166946,
135.349925080779));
#92431=CARTESIAN_POINT('Ctrl Pts',(-74.9760510845758,-1.75125296953507,
135.402307382332));
#92432=CARTESIAN_POINT('Ctrl Pts',(-74.9837973606599,-1.62224232030099,
135.449394603632));
#92433=CARTESIAN_POINT('Ctrl Pts',(-74.991543636744,-1.49148939032738,135.491005735456));
#92434=CARTESIAN_POINT('Ctrl Pts',(-74.9992899700093,-1.36073549516517,
135.532617174443));
#92435=CARTESIAN_POINT('Ctrl Pts',(-75.0070363032746,-1.22823966615429,
135.568752324729));
#92436=CARTESIAN_POINT('Ctrl Pts',(-75.01478263654,-1.09450102650723,135.599279862504));
#92437=CARTESIAN_POINT('Ctrl Pts',(-75.0225307045429,-0.960732437019272,
135.629814236709));
#92438=CARTESIAN_POINT('Ctrl Pts',(-75.0302787725459,-0.825720864161248,
135.654738412547));
#92439=CARTESIAN_POINT('Ctrl Pts',(-75.0380268405489,-0.68997587934256,
135.673972136817));
#92440=CARTESIAN_POINT('Ctrl Pts',(-75.0457831432907,-0.554086623138806,
135.693226302919));
#92441=CARTESIAN_POINT('Ctrl Pts',(-75.0535394460325,-0.417462785597245,
135.706777881227));
#92442=CARTESIAN_POINT('Ctrl Pts',(-75.0612957487743,-0.280619880601453,
135.714598447357));
#92443=CARTESIAN_POINT('Ctrl Pts',(-75.0690561912885,-0.14370393842663,
135.722423187559));
#92444=CARTESIAN_POINT('Ctrl Pts',(-75.0768166338027,-0.00656908654743849,
135.724510814688));
#92445=CARTESIAN_POINT('Ctrl Pts',(-75.0845770763168,0.130269894400301,
135.720885082787));
#92446=CARTESIAN_POINT('Ctrl Pts',(-75.0923499765822,0.26732854142788,135.717253530538));
#92447=CARTESIAN_POINT('Ctrl Pts',(-75.1001228768476,0.404089978129397,
135.707890318218));
#92448=CARTESIAN_POINT('Ctrl Pts',(-75.107895777113,0.540044372735581,135.692871141026));
#92449=CARTESIAN_POINT('Ctrl Pts',(-75.1153861128753,0.671056482655628,
135.678397948755));
#92450=CARTESIAN_POINT('Ctrl Pts',(-75.1228764486377,0.801318903257601,
135.658672915536));
#92451=CARTESIAN_POINT('Ctrl Pts',(-75.1303667844,0.930386911627887,135.633808128117));
#92452=CARTESIAN_POINT('Ctrl Pts',(-75.1381411185191,1.06434857275906,135.608000584728));
#92453=CARTESIAN_POINT('Ctrl Pts',(-75.1459154526382,1.19744781172977,135.576574095299));
#92454=CARTESIAN_POINT('Ctrl Pts',(-75.1536897867573,1.32917648622411,135.539597985531));
#92455=CARTESIAN_POINT('Ctrl Pts',(-75.1614545397044,1.46074281690008,135.502667445512));
#92456=CARTESIAN_POINT('Ctrl Pts',(-75.1692192926515,1.59094157109824,135.460200998189));
#92457=CARTESIAN_POINT('Ctrl Pts',(-75.1769840455986,1.71927320297116,135.412319245423));
#92458=CARTESIAN_POINT('Ctrl Pts',(-75.1847410864836,1.84747737405814,135.36448504949));
#92459=CARTESIAN_POINT('Ctrl Pts',(-75.1924981273685,1.97381774933448,135.311246387472));
#92460=CARTESIAN_POINT('Ctrl Pts',(-75.2002551682535,2.09780874432766,135.2527739903));
#92461=CARTESIAN_POINT('Ctrl Pts',(-75.2080063594936,2.22170623674717,135.194345687618));
#92462=CARTESIAN_POINT('Ctrl Pts',(-75.2157575507338,2.34325752313116,135.130691671734));
#92463=CARTESIAN_POINT('Ctrl Pts',(-75.223508741974,2.46199619161785,135.062031085669));
#92464=CARTESIAN_POINT('Ctrl Pts',(-75.231256638751,2.58068439300282,134.993399682185));
#92465=CARTESIAN_POINT('Ctrl Pts',(-75.2390045355282,2.69656201637946,134.919766136103));
#92466=CARTESIAN_POINT('Ctrl Pts',(-75.2467524323052,2.80918670104647,134.841395809531));
#92467=CARTESIAN_POINT('Ctrl Pts',(-75.2544987083893,2.92178782705705,134.763041876342));
#92468=CARTESIAN_POINT('Ctrl Pts',(-75.2622449844732,3.03113704708802,134.679953356652));
#92469=CARTESIAN_POINT('Ctrl Pts',(-75.2699912605573,3.13682082324802,134.592439046709));
#92470=CARTESIAN_POINT('Ctrl Pts',(-75.2777375938226,3.2425053795415,134.504924090755));
#92471=CARTESIAN_POINT('Ctrl Pts',(-75.285483927088,3.34452413684802,134.412983528711));
#92472=CARTESIAN_POINT('Ctrl Pts',(-75.2932302603533,3.44249682043959,134.316966303344));
#92473=CARTESIAN_POINT('Ctrl Pts',(-75.3009783283563,3.54049144433476,134.220927575586));
#92474=CARTESIAN_POINT('Ctrl Pts',(-75.3087263963593,3.6344379123272,134.120810641461));
#92475=CARTESIAN_POINT('Ctrl Pts',(-75.3164744643623,3.72399326933371,134.017000839013));
#92476=CARTESIAN_POINT('Ctrl Pts',(-75.3242307671041,3.81364380683923,133.913080706271));
#92477=CARTESIAN_POINT('Ctrl Pts',(-75.3319870698459,3.8988936548846,133.80546016145));
#92478=CARTESIAN_POINT('Ctrl Pts',(-75.3397433725878,3.97944025138362,133.694557556906));
#92479=CARTESIAN_POINT('Ctrl Pts',(-75.3475038151019,4.06002983802662,133.583595760301));
#92480=CARTESIAN_POINT('Ctrl Pts',(-75.3552642576161,4.13591095500109,133.469348739011));
#92481=CARTESIAN_POINT('Ctrl Pts',(-75.3630247001303,4.20682533574648,133.352262432201));
#92482=CARTESIAN_POINT('Ctrl Pts',(-75.3707976003957,4.27785355455113,133.234988168058));
#92483=CARTESIAN_POINT('Ctrl Pts',(-75.3785705006611,4.34389891596651,133.114865853107));
#92484=CARTESIAN_POINT('Ctrl Pts',(-75.3863434009265,4.40474952798511,132.99236533836));
#92485=CARTESIAN_POINT('Ctrl Pts',(-75.3938337366886,4.46338806698439,132.874318025882));
#92486=CARTESIAN_POINT('Ctrl Pts',(-75.4013240724508,4.5172028580651,132.754062699943));
#92487=CARTESIAN_POINT('Ctrl Pts',(-75.4088144082129,4.56604781938688,132.632034104153));
#92488=CARTESIAN_POINT('Ctrl Pts',(-75.416588742332,4.61674475226264,132.505378757065));
#92489=CARTESIAN_POINT('Ctrl Pts',(-75.424363076451,4.66224814645558,132.376411812581));
#92490=CARTESIAN_POINT('Ctrl Pts',(-75.4321374105701,4.70234166430523,132.245598257457));
#92491=CARTESIAN_POINT('Ctrl Pts',(-75.4399021635172,4.74238577047718,132.114945918349));
#92492=CARTESIAN_POINT('Ctrl Pts',(-75.4476669164643,4.77703315255691,131.982451866943));
#92493=CARTESIAN_POINT('Ctrl Pts',(-75.4554316694114,4.80611525957518,131.848601573562));
#92494=CARTESIAN_POINT('Ctrl Pts',(-75.4631887102964,4.83516848183493,131.714884222178));
#92495=CARTESIAN_POINT('Ctrl Pts',(-75.4709457511815,4.85866734655437,131.579813689065));
#92496=CARTESIAN_POINT('Ctrl Pts',(-75.4787027920665,4.87649302423167,131.44389079443));
#92497=CARTESIAN_POINT('Ctrl Pts',(-75.4864539833067,4.8943052594268,131.308070400307));
#92498=CARTESIAN_POINT('Ctrl Pts',(-75.4942051745467,4.90645277243412,131.17139931014));
#92499=CARTESIAN_POINT('Ctrl Pts',(-75.5019563657869,4.91286782747891,131.034388381592));
#92500=CARTESIAN_POINT('Ctrl Pts',(-75.509704262564,4.91928015595417,130.897435686343));
#92501=CARTESIAN_POINT('Ctrl Pts',(-75.5174521593412,4.91996485412807,130.760143829714));
#92502=CARTESIAN_POINT('Ctrl Pts',(-75.5252000561183,4.91490607189348,130.623028416993));
#92503=CARTESIAN_POINT('Ctrl Pts',(-75.5329463322024,4.90984834784707,130.48594168586));
#92504=CARTESIAN_POINT('Ctrl Pts',(-75.5406926082865,4.89904954747252,130.349031715674));
#92505=CARTESIAN_POINT('Ctrl Pts',(-75.5484388843706,4.88254594246699,130.21281333949));
#92506=CARTESIAN_POINT('Ctrl Pts',(-75.556185217636,4.86604221563561,130.076593957773));
#92507=CARTESIAN_POINT('Ctrl Pts',(-75.5639315509014,4.84383364716639,129.941066568371));
#92508=CARTESIAN_POINT('Ctrl Pts',(-75.5716778841667,4.8160082647134,129.806739719272));
#92509=CARTESIAN_POINT('Ctrl Pts',(-75.5794259521697,4.78817665095897,129.672382788608));
#92510=CARTESIAN_POINT('Ctrl Pts',(-75.5871740201726,4.75472579954021,129.539227315997));
#92511=CARTESIAN_POINT('Ctrl Pts',(-75.5949220881756,4.71579453066731,129.407770123889));
#92512=CARTESIAN_POINT('Ctrl Pts',(-75.6026783909175,4.6768218851784,129.276173217513));
#92513=CARTESIAN_POINT('Ctrl Pts',(-75.6104346936593,4.63235729805957,129.146278572697));
#92514=CARTESIAN_POINT('Ctrl Pts',(-75.6181909964012,4.58258919879826,129.018566873161));
#92515=CARTESIAN_POINT('Ctrl Pts',(-75.6259514389154,4.53279453680388,128.890787010045));
#92516=CARTESIAN_POINT('Ctrl Pts',(-75.6337118814296,4.4776908793719,128.765192771623));
#92517=CARTESIAN_POINT('Ctrl Pts',(-75.6414723239438,4.41751380836918,128.642242485879));
#92518=CARTESIAN_POINT('Ctrl Pts',(-75.6492452242093,4.35724013578982,128.519094829422));
#92519=CARTESIAN_POINT('Ctrl Pts',(-75.6570181244747,4.29187696127257,128.39859995098));
#92520=CARTESIAN_POINT('Ctrl Pts',(-75.6647910247401,4.2217050509751,128.281190087247));
#92521=CARTESIAN_POINT('Ctrl Pts',(-75.672281360502,4.15408406637082,128.168048367801));
#92522=CARTESIAN_POINT('Ctrl Pts',(-75.6797716962639,4.08199806393175,128.057771518885));
#92523=CARTESIAN_POINT('Ctrl Pts',(-75.6872620320258,4.00573384496549,127.950717432829));
#92524=CARTESIAN_POINT('Ctrl Pts',(-75.6950363661449,3.92657804495567,127.839604358559));
#92525=CARTESIAN_POINT('Ctrl Pts',(-75.702810700264,3.84267019807177,127.731611280616));
#92526=CARTESIAN_POINT('Ctrl Pts',(-75.7105850343831,3.75428457505002,127.627171546698));
#92527=CARTESIAN_POINT('Ctrl Pts',(-75.7183497873301,3.6660078794094,127.522860525419));
#92528=CARTESIAN_POINT('Ctrl Pts',(-75.7261145402773,3.57326463785824,127.422094430478));
#92529=CARTESIAN_POINT('Ctrl Pts',(-75.7338792932244,3.47637218441209,127.325277477147));
#92530=CARTESIAN_POINT('Ctrl Pts',(-75.7416363341094,3.37957596591663,127.228556683779));
#92531=CARTESIAN_POINT('Ctrl Pts',(-75.7493933749943,3.27863901138534,127.13577750094));
#92532=CARTESIAN_POINT('Ctrl Pts',(-75.7571504158793,3.17391844479411,127.04731060881));
#92533=CARTESIAN_POINT('Ctrl Pts',(-75.7649016071194,3.06927684879631,126.95891043025));
#92534=CARTESIAN_POINT('Ctrl Pts',(-75.7726527983595,2.96085761741198,126.874816320909));
#92535=CARTESIAN_POINT('Ctrl Pts',(-75.7804039895996,2.84905393682134,126.795361399858));
#92536=CARTESIAN_POINT('Ctrl Pts',(-75.7881518863767,2.73729777577787,126.715940249268));
#92537=CARTESIAN_POINT('Ctrl Pts',(-75.7958997831539,2.62216034457671,126.641154591255));
#92538=CARTESIAN_POINT('Ctrl Pts',(-75.8036476799309,2.504066869179,126.571296458215));
#92539=CARTESIAN_POINT('Ctrl Pts',(-75.811393956015,2.38599809639087,126.501452937991));
#92540=CARTESIAN_POINT('Ctrl Pts',(-75.819140232099,2.26497484560452,126.436535091487));
#92541=CARTESIAN_POINT('Ctrl Pts',(-75.8268865081831,2.14144986618793,126.376790682138));
#92542=CARTESIAN_POINT('Ctrl Pts',(-75.8346328414484,2.01792397493783,126.31704583177));
#92543=CARTESIAN_POINT('Ctrl Pts',(-75.8423791747138,1.89189667016723,126.26247466499));
#92544=CARTESIAN_POINT('Ctrl Pts',(-75.8501255079791,1.76384338879855,126.21327800425));
#92545=CARTESIAN_POINT('Ctrl Pts',(-75.8578735759821,1.63576143078589,126.164070326259));
#92546=CARTESIAN_POINT('Ctrl Pts',(-75.8656216439849,1.50565295824583,126.120239689486));
#92547=CARTESIAN_POINT('Ctrl Pts',(-75.8733697119879,1.37401099769051,126.081937845225));
#92548=CARTESIAN_POINT('Ctrl Pts',(-75.8811260147297,1.24222912649241,126.043595293308));
#92549=CARTESIAN_POINT('Ctrl Pts',(-75.8888823174716,1.10891088755632,126.010793381377));
#92550=CARTESIAN_POINT('Ctrl Pts',(-75.8966386202135,0.974562544449634,
125.98363339966));
#92551=CARTESIAN_POINT('Ctrl Pts',(-75.9043990627276,0.840142495586718,
125.956458921843));
#92552=CARTESIAN_POINT('Ctrl Pts',(-75.9121595052417,0.704691632965476,
125.93493243578));
#92553=CARTESIAN_POINT('Ctrl Pts',(-75.9199199477559,0.568722898653324,
125.919103477246));
#92554=CARTESIAN_POINT('Ctrl Pts',(-75.9276928480213,0.432535895258117,
125.903249108662));
#92555=CARTESIAN_POINT('Ctrl Pts',(-75.9354657482868,0.295829749021376,
125.893110573515));
#92556=CARTESIAN_POINT('Ctrl Pts',(-75.9432386485522,0.15911987388323,125.888685289777));
#92557=CARTESIAN_POINT('Ctrl Pts',(-75.9507289843144,0.0273797470562648,
125.884420876249));
#92558=CARTESIAN_POINT('Ctrl Pts',(-75.9582193200764,-0.104363534260139,
125.885461541182));
#92559=CARTESIAN_POINT('Ctrl Pts',(-75.9657096558385,-0.23565384200104,
125.891759440058));
#92560=CARTESIAN_POINT('Ctrl Pts',(-75.9734839899576,-0.37192206166341,
125.898296125685));
#92561=CARTESIAN_POINT('Ctrl Pts',(-75.9812583240767,-0.508133937464272,
125.910517277156));
#92562=CARTESIAN_POINT('Ctrl Pts',(-75.9890326581958,-0.643776631678409,
125.928426377751));
#92563=CARTESIAN_POINT('Ctrl Pts',(-75.9967974111429,-0.779252158393926,
125.946313406979));
#92564=CARTESIAN_POINT('Ctrl Pts',(-76.0045621640899,-0.914159515349397,
125.969874387057));
#92565=CARTESIAN_POINT('Ctrl Pts',(-76.012326917037,-1.04798709800216,125.999060824117));
#92566=CARTESIAN_POINT('Ctrl Pts',(-76.020083957922,-1.18168176121428,126.028218272797));
#92567=CARTESIAN_POINT('Ctrl Pts',(-76.0278409988071,-1.31429840482707,
126.062989976745));
#92568=CARTESIAN_POINT('Ctrl Pts',(-76.0355980396921,-1.44533213087425,
126.103275839139));
#92569=CARTESIAN_POINT('Ctrl Pts',(-76.0433492309323,-1.57626704336844,
126.14353132165));
#92570=CARTESIAN_POINT('Ctrl Pts',(-76.0511004221724,-1.70562104207544,
126.189292571394));
#92571=CARTESIAN_POINT('Ctrl Pts',(-76.0588516134125,-1.8329013377515,126.240408848696));
#92572=CARTESIAN_POINT('Ctrl Pts',(-76.0665995101897,-1.96012753590745,
126.291503400218));
#92573=CARTESIAN_POINT('Ctrl Pts',(-76.0743474069668,-2.08528142198677,
126.347948307052));
#92574=CARTESIAN_POINT('Ctrl Pts',(-76.0820953037439,-2.20788745584483,
126.409543665198));
#92575=CARTESIAN_POINT('Ctrl Pts',(-76.089841579828,-2.33046784316369,126.471126138922));
#92576=CARTESIAN_POINT('Ctrl Pts',(-76.0975878559121,-2.45050108920477,
126.537856745624));
#92577=CARTESIAN_POINT('Ctrl Pts',(-76.1053341319962,-2.56753402148043,
126.609488496626));
#92578=CARTESIAN_POINT('Ctrl Pts',(-76.1130804652616,-2.68456781766612,
126.681120776397));
#92579=CARTESIAN_POINT('Ctrl Pts',(-76.1208267985271,-2.79860092243051,
126.75765406856));
#92580=CARTESIAN_POINT('Ctrl Pts',(-76.1285731317924,-2.9092073928881,126.838796924008));
#92581=CARTESIAN_POINT('Ctrl Pts',(-76.1363211997954,-3.01983863289801,
126.919957950836));
#92582=CARTESIAN_POINT('Ctrl Pts',(-76.1440692677984,-3.12704139644846,
127.005730363849));
#92583=CARTESIAN_POINT('Ctrl Pts',(-76.1518173358014,-3.23042151800431,
127.095781391162));
#92584=CARTESIAN_POINT('Ctrl Pts',(-76.1595736385433,-3.33391151318373,
127.185928125778));
#92585=CARTESIAN_POINT('Ctrl Pts',(-76.1673299412852,-3.43357045531373,
127.280362301335));
#92586=CARTESIAN_POINT('Ctrl Pts',(-76.1750862440271,-3.52903947823306,
127.378712733797));
#92587=CARTESIAN_POINT('Ctrl Pts',(-76.1828466865413,-3.62455945584444,
127.477115658846));
#92588=CARTESIAN_POINT('Ctrl Pts',(-76.1906071290555,-3.71588479804903,
127.579438714207));
#92589=CARTESIAN_POINT('Ctrl Pts',(-76.1983675715697,-3.80269657128017,
127.685277122487));
#92590=CARTESIAN_POINT('Ctrl Pts',(-76.2061404718352,-3.8896477024765,127.791285431976));
#92591=CARTESIAN_POINT('Ctrl Pts',(-76.2139133721006,-3.97207055050816,
127.900820058631));
#92592=CARTESIAN_POINT('Ctrl Pts',(-76.221686272366,-4.04968869388416,128.013445974456));
#92593=CARTESIAN_POINT('Ctrl Pts',(-76.2291766081279,-4.12448522223826,
128.12197765455));
#92594=CARTESIAN_POINT('Ctrl Pts',(-76.2366669438898,-4.19482014291475,
128.233379513098));
#92595=CARTESIAN_POINT('Ctrl Pts',(-76.2441572796517,-4.26048716050001,
128.347241935509));
#92596=CARTESIAN_POINT('Ctrl Pts',(-76.2522516915477,-4.33145005258056,
128.470287066698));
#92597=CARTESIAN_POINT('Ctrl Pts',(-76.2603461034436,-4.39717110738405,
128.596568562782));
#92598=CARTESIAN_POINT('Ctrl Pts',(-76.2684405153396,-4.4573557375553,128.725619919118));
#92599=CARTESIAN_POINT('Ctrl Pts',(-76.2765234352285,-4.51745492085225,
128.854488055337));
#92600=CARTESIAN_POINT('Ctrl Pts',(-76.2846063551175,-4.57203318722553,
128.986117909908));
#92601=CARTESIAN_POINT('Ctrl Pts',(-76.2926892750064,-4.62084055069108,
129.120016333404));
#92602=CARTESIAN_POINT('Ctrl Pts',(-76.3007586197631,-4.66956594298494,
129.25368987668));
#92603=CARTESIAN_POINT('Ctrl Pts',(-76.3088279645198,-4.71253963181309,
129.389624072026));
#92604=CARTESIAN_POINT('Ctrl Pts',(-76.3168973092765,-4.7495588931892,129.527304086857));
#92605=CARTESIAN_POINT('Ctrl Pts',(-76.3179736553219,-4.75449678304108,
129.545668817075));
#92606=CARTESIAN_POINT('Ctrl Pts',(-76.3190500013673,-4.75932880030024,
129.564064577817));
#92607=CARTESIAN_POINT('Ctrl Pts',(-76.3201263474126,-4.76405452823413,
129.582490119309));
#92608=CARTESIAN_POINT('Origin',(213.235140564004,0.,130.804360617566));
#92609=CARTESIAN_POINT('',(-78.4150662180022,-4.76405452823401,129.582490119308));
#92610=CARTESIAN_POINT('',(-78.0697779892986,-4.76405452823406,129.582490119308));
#92611=CARTESIAN_POINT('',(213.235140564004,-4.76405452823405,129.582490119308));
#92612=CARTESIAN_POINT('',(-76.7351405639554,-4.9182483336571,130.808409194994));
#92613=CARTESIAN_POINT('Ctrl Pts',(-76.7351405640085,-4.91824833365633,
130.808409195929));
#92614=CARTESIAN_POINT('Ctrl Pts',(-76.74751275176,-4.91806897685328,131.026293405774));
#92615=CARTESIAN_POINT('Ctrl Pts',(-76.7598849395115,-4.90340809633497,
131.243600830494));
#92616=CARTESIAN_POINT('Ctrl Pts',(-76.7722571272631,-4.8745101616524,131.458832730377));
#92617=CARTESIAN_POINT('Ctrl Pts',(-76.7753259285481,-4.86734230897611,
131.512218917541));
#92618=CARTESIAN_POINT('Ctrl Pts',(-76.778394729833,-4.85929871632235,131.565477593643));
#92619=CARTESIAN_POINT('Ctrl Pts',(-76.781463531118,-4.85038346950786,131.618586176748));
#92620=CARTESIAN_POINT('Ctrl Pts',(-76.7892378652371,-4.82779806854749,
131.753128570112));
#92621=CARTESIAN_POINT('Ctrl Pts',(-76.7970121993562,-4.79957464391219,
131.886943628883));
#92622=CARTESIAN_POINT('Ctrl Pts',(-76.8047865334752,-4.76577030732162,
132.019521693453));
#92623=CARTESIAN_POINT('Ctrl Pts',(-76.8125512864222,-4.73200763155472,
132.151936367408));
#92624=CARTESIAN_POINT('Ctrl Pts',(-76.8203160393692,-4.69267782462236,
132.283116705224));
#92625=CARTESIAN_POINT('Ctrl Pts',(-76.8280807923163,-4.64788946593474,
132.412560410798));
#92626=CARTESIAN_POINT('Ctrl Pts',(-76.8358378332013,-4.60314559167637,
132.54187555106));
#92627=CARTESIAN_POINT('Ctrl Pts',(-76.8435948740863,-4.55295408172638,
132.669457124522));
#92628=CARTESIAN_POINT('Ctrl Pts',(-76.8513519149712,-4.49747396515987,
132.794815589478));
#92629=CARTESIAN_POINT('Ctrl Pts',(-76.8591031062113,-4.44203568658076,
132.92007952064));
#92630=CARTESIAN_POINT('Ctrl Pts',(-76.8668542974514,-4.38131689720084,
133.043123324124));
#92631=CARTESIAN_POINT('Ctrl Pts',(-76.8746054886915,-4.31552548433383,
133.163475463555));
#92632=CARTESIAN_POINT('Ctrl Pts',(-76.8823533854685,-4.24976203457241,
133.283776450116));
#92633=CARTESIAN_POINT('Ctrl Pts',(-76.8901012822456,-4.17893043658405,
133.401387705676));
#92634=CARTESIAN_POINT('Ctrl Pts',(-76.8978491790226,-4.1032853606222,133.515860628963));
#92635=CARTESIAN_POINT('Ctrl Pts',(-76.9055954551067,-4.02765610797952,
133.630309606982));
#92636=CARTESIAN_POINT('Ctrl Pts',(-76.9133417311908,-3.94721559550259,
133.741621232511));
#92637=CARTESIAN_POINT('Ctrl Pts',(-76.9210880072748,-3.86226260674418,
133.84937467649));
#92638=CARTESIAN_POINT('Ctrl Pts',(-76.9288343405402,-3.77730899088221,
133.95712891588));
#92639=CARTESIAN_POINT('Ctrl Pts',(-76.9365806738055,-3.68784307432745,
134.061324614286));
#92640=CARTESIAN_POINT('Ctrl Pts',(-76.9443270070708,-3.59420457381605,
134.161573232826));
#92641=CARTESIAN_POINT('Ctrl Pts',(-76.9520750750737,-3.50054510361182,
134.261844301348));
#92642=CARTESIAN_POINT('Ctrl Pts',(-76.9598231430766,-3.40271145688383,
134.358166245445));
#92643=CARTESIAN_POINT('Ctrl Pts',(-76.9675712110796,-3.30108063073189,
134.450186961745));
#92644=CARTESIAN_POINT('Ctrl Pts',(-76.9753275138214,-3.19934179012809,
134.542305478757));
#92645=CARTESIAN_POINT('Ctrl Pts',(-76.9830838165633,-3.09379799865874,
134.630113373286));
#92646=CARTESIAN_POINT('Ctrl Pts',(-76.9908401193051,-2.98486022754893,
134.713298131072));
#92647=CARTESIAN_POINT('Ctrl Pts',(-76.9986005618192,-2.87586431307063,
134.796527287069));
#92648=CARTESIAN_POINT('Ctrl Pts',(-77.0063610043333,-2.76347112968022,
134.875128165654));
#92649=CARTESIAN_POINT('Ctrl Pts',(-77.0141214468475,-2.64812029044048,
134.94883187333));
#92650=CARTESIAN_POINT('Ctrl Pts',(-77.0218943471129,-2.53258427979354,
135.022653896742));
#92651=CARTESIAN_POINT('Ctrl Pts',(-77.0296672473782,-2.41408146366862,
135.09156284307));
#92652=CARTESIAN_POINT('Ctrl Pts',(-77.0374401476436,-2.29307647294854,
135.155335606199));
#92653=CARTESIAN_POINT('Ctrl Pts',(-77.0449304834059,-2.17647031842908,
135.216790068757));
#92654=CARTESIAN_POINT('Ctrl Pts',(-77.0524208191683,-2.05754102965276,
135.273475158751));
#92655=CARTESIAN_POINT('Ctrl Pts',(-77.0599111549306,-1.93671971947156,
135.325234403762));
#92656=CARTESIAN_POINT('Ctrl Pts',(-77.0676854890497,-1.81131743259711,
135.378956116276));
#92657=CARTESIAN_POINT('Ctrl Pts',(-77.0754598231688,-1.68347958340171,
135.427541257682));
#92658=CARTESIAN_POINT('Ctrl Pts',(-77.0832341572879,-1.55366583322831,
135.47076239422));
#92659=CARTESIAN_POINT('Ctrl Pts',(-77.090998910235,-1.4240120669002,135.513930264569));
#92660=CARTESIAN_POINT('Ctrl Pts',(-77.0987636631821,-1.29238761214385,
135.551747160967));
#92661=CARTESIAN_POINT('Ctrl Pts',(-77.1065284161292,-1.15927375471972,
135.584032931032));
#92662=CARTESIAN_POINT('Ctrl Pts',(-77.1142854570142,-1.02629210785535,
135.616286634416));
#92663=CARTESIAN_POINT('Ctrl Pts',(-77.1220424978991,-0.891824379679084,
135.643020052407));
#92664=CARTESIAN_POINT('Ctrl Pts',(-77.1297995387841,-0.756368394593804,
135.664102371421));
#92665=CARTESIAN_POINT('Ctrl Pts',(-77.1375507300242,-0.621014557920387,
135.685168792093));
#92666=CARTESIAN_POINT('Ctrl Pts',(-77.1453019212643,-0.484674332468407,
135.700592536238));
#92667=CARTESIAN_POINT('Ctrl Pts',(-77.1530531125045,-0.347856803315691,
135.71029362841));
#92668=CARTESIAN_POINT('Ctrl Pts',(-77.1608010092816,-0.211097425262406,
135.719990597359));
#92669=CARTESIAN_POINT('Ctrl Pts',(-77.1685489060586,-0.0738615361646152,
135.723969724361));
#92670=CARTESIAN_POINT('Ctrl Pts',(-77.1762968028357,0.0633357875304305,
135.722202790767));
#92671=CARTESIAN_POINT('Ctrl Pts',(-77.1840430789198,0.200504412502617,
135.720436226778));
#92672=CARTESIAN_POINT('Ctrl Pts',(-77.191789355004,0.337634097432755,135.712925997974));
#92673=CARTESIAN_POINT('Ctrl Pts',(-77.1995356310881,0.474209287104718,
135.699696011032));
#92674=CARTESIAN_POINT('Ctrl Pts',(-77.2072819643534,0.610785484943892,
135.68646592643));
#92675=CARTESIAN_POINT('Ctrl Pts',(-77.2150282976188,0.746806790213627,
135.667516037135));
#92676=CARTESIAN_POINT('Ctrl Pts',(-77.2227746308841,0.881762688954109,
135.642922141704));
#92677=CARTESIAN_POINT('Ctrl Pts',(-77.2305226988871,1.01674881013221,135.61832273864));
#92678=CARTESIAN_POINT('Ctrl Pts',(-77.2382707668901,1.15066866545685,135.588076884433));
#92679=CARTESIAN_POINT('Ctrl Pts',(-77.246018834893,1.28302224424862,135.552311436947));
#92680=CARTESIAN_POINT('Ctrl Pts',(-77.2537751376349,1.41551648999914,135.516507977518));
#92681=CARTESIAN_POINT('Ctrl Pts',(-77.2615314403767,1.54644075585497,135.475173308419));
#92682=CARTESIAN_POINT('Ctrl Pts',(-77.2692877431186,1.67530997473362,135.42848426979));
#92683=CARTESIAN_POINT('Ctrl Pts',(-77.2770481856327,1.80424797499456,135.381770311815));
#92684=CARTESIAN_POINT('Ctrl Pts',(-77.284808628147,1.9311283812195,135.329696438297));
#92685=CARTESIAN_POINT('Ctrl Pts',(-77.2925690706611,2.05548734409571,135.272487164651));
#92686=CARTESIAN_POINT('Ctrl Pts',(-77.3003419709266,2.1800459390192,135.2151860536));
#92687=CARTESIAN_POINT('Ctrl Pts',(-77.308114871192,2.30207465387628,135.152733246904));
#92688=CARTESIAN_POINT('Ctrl Pts',(-77.3158877714574,2.42113463883094,135.085399057379));
#92689=CARTESIAN_POINT('Ctrl Pts',(-77.3233781072194,2.53586649343817,135.020512635247));
#92690=CARTESIAN_POINT('Ctrl Pts',(-77.3308684429814,2.6478414506437,134.951093732102));
#92691=CARTESIAN_POINT('Ctrl Pts',(-77.3383587787434,2.7566948387418,134.87742047823));
#92692=CARTESIAN_POINT('Ctrl Pts',(-77.3461331128625,2.86967543613508,134.800953880545));
#92693=CARTESIAN_POINT('Ctrl Pts',(-77.3539074469815,2.97965097170614,134.719661733149));
#92694=CARTESIAN_POINT('Ctrl Pts',(-77.3616817811006,3.08618164080724,134.633807828645));
#92695=CARTESIAN_POINT('Ctrl Pts',(-77.3694465340477,3.19258102037958,134.548059731406));
#92696=CARTESIAN_POINT('Ctrl Pts',(-77.3772112869949,3.29554367925083,134.457761306053));
#92697=CARTESIAN_POINT('Ctrl Pts',(-77.384976039942,3.39465790341201,134.363220095166));
#92698=CARTESIAN_POINT('Ctrl Pts',(-77.392733080827,3.4936736859285,134.268772783942));
#92699=CARTESIAN_POINT('Ctrl Pts',(-77.400490121712,3.58884835925057,134.170091341328));
#92700=CARTESIAN_POINT('Ctrl Pts',(-77.408247162597,3.67980277995377,134.067523893154));
#92701=CARTESIAN_POINT('Ctrl Pts',(-77.4159983538371,3.77068861122066,133.96503379189));
#92702=CARTESIAN_POINT('Ctrl Pts',(-77.4237495450771,3.85736026614413,133.858663809318));
#92703=CARTESIAN_POINT('Ctrl Pts',(-77.4315007363172,3.93947528619857,133.74879902445));
#92704=CARTESIAN_POINT('Ctrl Pts',(-77.4392486330943,4.02155540517911,133.638980935045));
#92705=CARTESIAN_POINT('Ctrl Pts',(-77.4469965298715,4.09908250765063,133.525671310165));
#92706=CARTESIAN_POINT('Ctrl Pts',(-77.4547444266485,4.17175444106424,133.409288245344));
#92707=CARTESIAN_POINT('Ctrl Pts',(-77.4624907027327,4.24441117307601,133.292929525351));
#92708=CARTESIAN_POINT('Ctrl Pts',(-77.4702369788167,4.31221454916572,133.173498975588));
#92709=CARTESIAN_POINT('Ctrl Pts',(-77.4779832549008,4.37490601251123,133.051443269404));
#92710=CARTESIAN_POINT('Ctrl Pts',(-77.4857295881662,4.43759793863097,132.929386662233));
#92711=CARTESIAN_POINT('Ctrl Pts',(-77.4934759214315,4.49517769808231,132.804705207746));
#92712=CARTESIAN_POINT('Ctrl Pts',(-77.5012222546968,4.54743311707082,132.677869386766));
#92713=CARTESIAN_POINT('Ctrl Pts',(-77.5089703226998,4.59970023829804,132.551005161783));
#92714=CARTESIAN_POINT('Ctrl Pts',(-77.5167183907029,4.64664049752387,132.421985971696));
#92715=CARTESIAN_POINT('Ctrl Pts',(-77.5244664587059,4.68809035587684,132.291301059425));
#92716=CARTESIAN_POINT('Ctrl Pts',(-77.5322227614477,4.72958426763247,132.160477253673));
#92717=CARTESIAN_POINT('Ctrl Pts',(-77.5399790641896,4.76557600355863,132.027984562538));
#92718=CARTESIAN_POINT('Ctrl Pts',(-77.5477353669314,4.79595215366741,131.894326673108));
#92719=CARTESIAN_POINT('Ctrl Pts',(-77.5554958094456,4.8263445164422,131.760597446437));
#92720=CARTESIAN_POINT('Ctrl Pts',(-77.5632562519597,4.85111525063289,131.625702166628));
#92721=CARTESIAN_POINT('Ctrl Pts',(-77.5710166944739,4.87020252553492,131.490152439312));
#92722=CARTESIAN_POINT('Ctrl Pts',(-77.5787895947393,4.88932044102506,131.35438511554));
#92723=CARTESIAN_POINT('Ctrl Pts',(-77.5865624950047,4.90273662709394,131.217961634185));
#92724=CARTESIAN_POINT('Ctrl Pts',(-77.5943353952701,4.91044129651265,131.081397322721));
#92725=CARTESIAN_POINT('Ctrl Pts',(-77.6018257310322,4.91786588179118,130.949797467962));
#92726=CARTESIAN_POINT('Ctrl Pts',(-77.6093160667943,4.91998699203978,130.818067152367));
#92727=CARTESIAN_POINT('Ctrl Pts',(-77.6168064025564,4.91684151218128,130.686663520784));
#92728=CARTESIAN_POINT('Ctrl Pts',(-77.6245807366755,4.91357677049793,130.550277680571));
#92729=CARTESIAN_POINT('Ctrl Pts',(-77.6323550707945,4.90462784785839,130.413811756488));
#92730=CARTESIAN_POINT('Ctrl Pts',(-77.6401294049136,4.88997895529572,130.277778354985));
#92731=CARTESIAN_POINT('Ctrl Pts',(-77.6478941578607,4.87534811618393,130.141912602492));
#92732=CARTESIAN_POINT('Ctrl Pts',(-77.6556589108078,4.85503132567286,130.006478696965));
#92733=CARTESIAN_POINT('Ctrl Pts',(-77.6634236637549,4.82906478656594,129.871989259335));
#92734=CARTESIAN_POINT('Ctrl Pts',(-77.6711807046399,4.80312403779173,129.737633398511));
#92735=CARTESIAN_POINT('Ctrl Pts',(-77.6789377455248,4.77154478101786,129.604220520198));
#92736=CARTESIAN_POINT('Ctrl Pts',(-77.6866947864098,4.73441496808316,129.47225777901));
#92737=CARTESIAN_POINT('Ctrl Pts',(-77.69444597765,4.69731315502918,129.340394551951));
#92738=CARTESIAN_POINT('Ctrl Pts',(-77.7021971688902,4.6546692226954,129.209979660183));
#92739=CARTESIAN_POINT('Ctrl Pts',(-77.7099483601303,4.60662204176346,129.081509368375));
#92740=CARTESIAN_POINT('Ctrl Pts',(-77.7176962569074,4.55859528216505,128.953093679868));
#92741=CARTESIAN_POINT('Ctrl Pts',(-77.7254441536844,4.50516997824864,128.826621312887));
#92742=CARTESIAN_POINT('Ctrl Pts',(-77.7331920504615,4.44653456479516,128.70257246778));
#92743=CARTESIAN_POINT('Ctrl Pts',(-77.7409383265456,4.3879114166063,128.578549571017));
#92744=CARTESIAN_POINT('Ctrl Pts',(-77.7486846026298,4.32408049360813,128.456949541021));
#92745=CARTESIAN_POINT('Ctrl Pts',(-77.7564308787139,4.25527783846084,128.338231346825));
#92746=CARTESIAN_POINT('Ctrl Pts',(-77.7641772119792,4.18647467542789,128.219512276279));
#92747=CARTESIAN_POINT('Ctrl Pts',(-77.7719235452446,4.11269990305261,128.103675422245));
#92748=CARTESIAN_POINT('Ctrl Pts',(-77.77966987851,4.03423466505778,127.991153598922));
#92749=CARTESIAN_POINT('Ctrl Pts',(-77.7874179465129,3.95575185531706,127.878606577118));
#92750=CARTESIAN_POINT('Ctrl Pts',(-77.7951660145158,3.87257671337463,127.769376383903));
#92751=CARTESIAN_POINT('Ctrl Pts',(-77.8029140825188,3.78503245640052,127.663865056911));
#92752=CARTESIAN_POINT('Ctrl Pts',(-77.8106703852607,3.69739515634819,127.558241591224));
#92753=CARTESIAN_POINT('Ctrl Pts',(-77.8184266880025,3.60537971532263,127.456345188578));
#92754=CARTESIAN_POINT('Ctrl Pts',(-77.8261829907443,3.50934859866901,127.358543519181));
#92755=CARTESIAN_POINT('Ctrl Pts',(-77.8339434332585,3.413266227317,127.260689650089));
#92756=CARTESIAN_POINT('Ctrl Pts',(-77.8417038757728,3.31316419486976,127.166935136134));
#92757=CARTESIAN_POINT('Ctrl Pts',(-77.8494643182869,3.20943950862779,127.077608532578));
#92758=CARTESIAN_POINT('Ctrl Pts',(-77.8572372185524,3.10554831431123,126.988138534029));
#92759=CARTESIAN_POINT('Ctrl Pts',(-77.8650101188178,2.99802315201168,126.903110892722));
#92760=CARTESIAN_POINT('Ctrl Pts',(-77.8727830190832,2.88729229109259,126.822812390017));
#92761=CARTESIAN_POINT('Ctrl Pts',(-77.8802733548452,2.78058677588241,126.745432940146));
#92762=CARTESIAN_POINT('Ctrl Pts',(-77.8877636906072,2.67090484247756,126.672444936751));
#92763=CARTESIAN_POINT('Ctrl Pts',(-77.8952540263692,2.55865103698725,126.604064445458));
#92764=CARTESIAN_POINT('Ctrl Pts',(-77.9030283604883,2.4421410943428,126.533091287054));
#92765=CARTESIAN_POINT('Ctrl Pts',(-77.9108026946074,2.32249133621925,126.466857103785));
#92766=CARTESIAN_POINT('Ctrl Pts',(-77.9185770287264,2.20012449861976,126.405652255663));
#92767=CARTESIAN_POINT('Ctrl Pts',(-77.9263417816735,2.07790846721136,126.344522837047));
#92768=CARTESIAN_POINT('Ctrl Pts',(-77.9341065346207,1.95298236526729,126.288410594211));
#92769=CARTESIAN_POINT('Ctrl Pts',(-77.9418712875677,1.8257970437956,126.237562152846));
#92770=CARTESIAN_POINT('Ctrl Pts',(-77.9496283284527,1.6987380445782,126.18676421487));
#92771=CARTESIAN_POINT('Ctrl Pts',(-77.9573853693377,1.56942465195114,126.141219818446));
#92772=CARTESIAN_POINT('Ctrl Pts',(-77.9651424102227,1.43833108957336,126.101129096658));
#92773=CARTESIAN_POINT('Ctrl Pts',(-77.9728936014628,1.30733638587056,126.061068607594));
#92774=CARTESIAN_POINT('Ctrl Pts',(-77.980644792703,1.17456455682217,126.026453721044));
#92775=CARTESIAN_POINT('Ctrl Pts',(-77.9883959839431,1.04050818694485,125.997435844346));
#92776=CARTESIAN_POINT('Ctrl Pts',(-77.9961438807202,0.906508794600613,
125.968430301018));
#92777=CARTESIAN_POINT('Ctrl Pts',(-78.0038917774972,0.771226328624115,
125.945017118674));
#92778=CARTESIAN_POINT('Ctrl Pts',(-78.0116396742743,0.635166648767972,
125.927297321812));
#92779=CARTESIAN_POINT('Ctrl Pts',(-78.0193859503584,0.499135429664119,
125.909581231549));
#92780=CARTESIAN_POINT('Ctrl Pts',(-78.0271322264427,0.362327707499512,
125.897556208394));
#92781=CARTESIAN_POINT('Ctrl Pts',(-78.0348785025268,0.22525721274329,125.891271746946));
#92782=CARTESIAN_POINT('Ctrl Pts',(-78.0426248357921,0.0881857061636275,
125.884987239108));
#92783=CARTESIAN_POINT('Ctrl Pts',(-78.0503711690574,-0.0491481863233042,
125.884443395439));
#92784=CARTESIAN_POINT('Ctrl Pts',(-78.0581175023228,-0.186228360824128,
125.889637628411));
#92785=CARTESIAN_POINT('Ctrl Pts',(-78.0658655703258,-0.323339233479397,
125.894833024596));
#92786=CARTESIAN_POINT('Ctrl Pts',(-78.0736136383287,-0.460195884476491,
125.905769039626));
#92787=CARTESIAN_POINT('Ctrl Pts',(-78.0813617063316,-0.596285361393116,
125.922391052904));
#92788=CARTESIAN_POINT('Ctrl Pts',(-78.0891180090735,-0.732519475825479,
125.939030732255));
#92789=CARTESIAN_POINT('Ctrl Pts',(-78.0968743118153,-0.867984398704479,
125.961368434214));
#92790=CARTESIAN_POINT('Ctrl Pts',(-78.1046306145572,-1.00217487729666,
125.98929794115));
#92791=CARTESIAN_POINT('Ctrl Pts',(-78.1123910570713,-1.13643697738766,
126.017242354905));
#92792=CARTESIAN_POINT('Ctrl Pts',(-78.1201514995856,-1.26942289890986,
126.050784424965));
#92793=CARTESIAN_POINT('Ctrl Pts',(-78.1279119420998,-1.40064162687198,
126.089767729991));
#92794=CARTESIAN_POINT('Ctrl Pts',(-78.1356848423652,-1.53207099878528,
126.128813614479));
#92795=CARTESIAN_POINT('Ctrl Pts',(-78.1434577426306,-1.66172713819609,
126.17331806175));
#92796=CARTESIAN_POINT('Ctrl Pts',(-78.151230642896,-1.78913727777151,126.22307576899));
#92797=CARTESIAN_POINT('Ctrl Pts',(-78.158720978658,-1.91191573784624,126.27102465824));
#92798=CARTESIAN_POINT('Ctrl Pts',(-78.1662113144201,-2.03260837636572,
126.323851376502));
#92799=CARTESIAN_POINT('Ctrl Pts',(-78.1737016501821,-2.15081474414552,
126.381332356423));
#92800=CARTESIAN_POINT('Ctrl Pts',(-78.1814767132349,-2.27351444572606,
126.440998339022));
#92801=CARTESIAN_POINT('Ctrl Pts',(-78.1892517762878,-2.39392383056797,
126.505868445645));
#92802=CARTESIAN_POINT('Ctrl Pts',(-78.1970268393407,-2.51156997926362,
126.575743905004));
#92803=CARTESIAN_POINT('Ctrl Pts',(-78.2047921581613,-2.62906868588906,
126.645531791734));
#92804=CARTESIAN_POINT('Ctrl Pts',(-78.2125574769819,-2.74381071431604,
126.720312350925));
#92805=CARTESIAN_POINT('Ctrl Pts',(-78.2203227958026,-2.85534477969413,
126.799839516164));
#92806=CARTESIAN_POINT('Ctrl Pts',(-78.2284371050609,-2.97189143028495,
126.882940806413));
#92807=CARTESIAN_POINT('Ctrl Pts',(-78.2365514143192,-3.08493467246098,
126.971225110819));
#92808=CARTESIAN_POINT('Ctrl Pts',(-78.2446657235775,-3.19398912335395,
127.064358406016));
#92809=CARTESIAN_POINT('Ctrl Pts',(-78.2524164511523,-3.29815712000958,
127.153318633711));
#92810=CARTESIAN_POINT('Ctrl Pts',(-78.260167178727,-3.39868566738597,127.246702473511));
#92811=CARTESIAN_POINT('Ctrl Pts',(-78.2679179063017,-3.49518270608593,
127.344175519399));
#92812=CARTESIAN_POINT('Ctrl Pts',(-78.2756651805459,-3.59163675060628,
127.441605136247));
#92813=CARTESIAN_POINT('Ctrl Pts',(-78.28341245479,-3.684062586047,127.543120056786));
#92814=CARTESIAN_POINT('Ctrl Pts',(-78.2911597290342,-3.77210358185438,
127.648347685042));
#92815=CARTESIAN_POINT('Ctrl Pts',(-78.2989052292268,-3.86012441711724,
127.753551217179));
#92816=CARTESIAN_POINT('Ctrl Pts',(-78.3066507294194,-3.94376216087564,
127.862465465105));
#92817=CARTESIAN_POINT('Ctrl Pts',(-78.314396229612,-4.02269946804459,127.974683594955));
#92818=CARTESIAN_POINT('Ctrl Pts',(-78.3221416334722,-4.10163579345397,
128.086900329125));
#92819=CARTESIAN_POINT('Ctrl Pts',(-78.3298870373324,-4.17587157524765,
128.202420542839));
#92820=CARTESIAN_POINT('Ctrl Pts',(-78.3376324411926,-4.24513215785856,
128.320807512675));
#92821=CARTESIAN_POINT('Ctrl Pts',(-78.3453822725759,-4.31443233205588,
128.439262156327));
#92822=CARTESIAN_POINT('Ctrl Pts',(-78.3531321039591,-4.37875142946373,
128.560586491384));
#92823=CARTESIAN_POINT('Ctrl Pts',(-78.3608819353423,-4.43786015067658,
128.684318083668));
#92824=CARTESIAN_POINT('Ctrl Pts',(-78.3686343747685,-4.49698876368704,
128.808091315218));
#92825=CARTESIAN_POINT('Ctrl Pts',(-78.3763868141946,-4.55090335005497,
128.934273060221));
#92826=CARTESIAN_POINT('Ctrl Pts',(-78.3841392536207,-4.59942270762946,
129.062380761471));
#92827=CARTESIAN_POINT('Ctrl Pts',(-78.3918991566564,-4.64798877689356,
129.19061179756));
#92828=CARTESIAN_POINT('Ctrl Pts',(-78.3996590596922,-4.69114912104015,
129.320772122251));
#92829=CARTESIAN_POINT('Ctrl Pts',(-78.407418962728,-4.72877228316011,129.452363666195));
#92830=CARTESIAN_POINT('Ctrl Pts',(-78.4099680478194,-4.74113128316439,
129.495590758245));
#92831=CARTESIAN_POINT('Ctrl Pts',(-78.4125171329109,-4.75289318270538,
129.538972202489));
#92832=CARTESIAN_POINT('Ctrl Pts',(-78.4150662180023,-4.76405452823401,
129.582490119308));
#92833=CARTESIAN_POINT('Ctrl Pts',(-76.6650346057277,-4.76405452823403,
129.582490119308));
#92834=CARTESIAN_POINT('Ctrl Pts',(-76.672671502873,-4.79766263469746,129.713527616335));
#92835=CARTESIAN_POINT('Ctrl Pts',(-76.6803084000183,-4.8258444961389,129.845891658541));
#92836=CARTESIAN_POINT('Ctrl Pts',(-76.6879452971636,-4.84851577964765,
129.979086240763));
#92837=CARTESIAN_POINT('Ctrl Pts',(-76.6958111749622,-4.87186682683677,
130.116274458343));
#92838=CARTESIAN_POINT('Ctrl Pts',(-76.7036770527608,-4.88937158334248,
130.254343344525));
#92839=CARTESIAN_POINT('Ctrl Pts',(-76.7115429305594,-4.9009954595654,130.392746031066));
#92840=CARTESIAN_POINT('Ctrl Pts',(-76.719408808358,-4.91261933578832,130.531148717607));
#92841=CARTESIAN_POINT('Ctrl Pts',(-76.7272746861567,-4.91836236347926,
130.669884739713));
#92842=CARTESIAN_POINT('Ctrl Pts',(-76.7351405639554,-4.9182483336571,130.808409194994));
#92843=CARTESIAN_POINT('',(-76.3898594360211,-4.91824995923563,130.804993846394));
#92844=CARTESIAN_POINT('Ctrl Pts',(-76.3201263474126,-4.76405452823413,
129.582490119309));
#92845=CARTESIAN_POINT('Ctrl Pts',(-76.3281810370973,-4.79941887244748,
129.720375160668));
#92846=CARTESIAN_POINT('Ctrl Pts',(-76.336235726782,-4.82882690419295,129.859929325067));
#92847=CARTESIAN_POINT('Ctrl Pts',(-76.3442904164667,-4.85213173058735,
130.000618910593));
#92848=CARTESIAN_POINT('Ctrl Pts',(-76.3523335468215,-4.87540311209611,
130.141106591715));
#92849=CARTESIAN_POINT('Ctrl Pts',(-76.3603766771764,-4.89258869526852,
130.282726105568));
#92850=CARTESIAN_POINT('Ctrl Pts',(-76.3684198075313,-4.90359226627961,
130.42493216768));
#92851=CARTESIAN_POINT('Ctrl Pts',(-76.3755663503513,-4.91336924215022,
130.551286170078));
#92852=CARTESIAN_POINT('Ctrl Pts',(-76.3827128931711,-4.91826629653936,
130.678102890917));
#92853=CARTESIAN_POINT('Ctrl Pts',(-76.3898594359911,-4.9182499592357,130.804993845861));
#92854=CARTESIAN_POINT('Ctrl Pts',(-76.3898594360212,-4.91824995923563,
130.804993846394));
#92855=CARTESIAN_POINT('Ctrl Pts',(-76.3980569668082,-4.91823121931258,
130.950545693764));
#92856=CARTESIAN_POINT('Ctrl Pts',(-76.4062544975953,-4.91174696503634,
131.09594676965));
#92857=CARTESIAN_POINT('Ctrl Pts',(-76.4144520283824,-4.89886280865999,
131.240624579438));
#92858=CARTESIAN_POINT('Ctrl Pts',(-76.4226634473724,-4.88595682403033,
131.385547501423));
#92859=CARTESIAN_POINT('Ctrl Pts',(-76.4308748663625,-4.86662931813862,
131.529744395062));
#92860=CARTESIAN_POINT('Ctrl Pts',(-76.4390862853525,-4.84099718955688,
131.672651624776));
#92861=CARTESIAN_POINT('Ctrl Pts',(-76.4473200301227,-4.81529537055134,
131.815947400662));
#92862=CARTESIAN_POINT('Ctrl Pts',(-76.455553774893,-4.78325470441282,131.957946186527));
#92863=CARTESIAN_POINT('Ctrl Pts',(-76.4637875196632,-4.74504281851426,
132.098096182883));
#92864=CARTESIAN_POINT('Ctrl Pts',(-76.4720334309119,-4.70677446935404,
132.238453269932));
#92865=CARTESIAN_POINT('Ctrl Pts',(-76.4802793421606,-4.66231679228311,
132.376955811759));
#92866=CARTESIAN_POINT('Ctrl Pts',(-76.4885252534092,-4.61188613012242,
132.513070477456));
#92867=CARTESIAN_POINT('Ctrl Pts',(-76.4967904872647,-4.5613372940174,132.649504100038));
#92868=CARTESIAN_POINT('Ctrl Pts',(-76.5050557211203,-4.50478760996428,
132.783538365348));
#92869=CARTESIAN_POINT('Ctrl Pts',(-76.5133209549758,-4.44250081567044,
132.914661440972));
#92870=CARTESIAN_POINT('Ctrl Pts',(-76.516415604472,-4.41917954007774,132.963756235749));
#92871=CARTESIAN_POINT('Ctrl Pts',(-76.5195102539682,-4.39505443429168,
133.012443189383));
#92872=CARTESIAN_POINT('Ctrl Pts',(-76.5226049034644,-4.37014091486708,
133.060696462848));
#92873=CARTESIAN_POINT('Ctrl Pts',(-76.5303792375834,-4.30755352837156,
133.181917644992));
#92874=CARTESIAN_POINT('Ctrl Pts',(-76.5381535717026,-4.23981944372601,
133.300724738339));
#92875=CARTESIAN_POINT('Ctrl Pts',(-76.5459279058216,-4.16714866238844,
133.416649860367));
#92876=CARTESIAN_POINT('Ctrl Pts',(-76.5536926587687,-4.09456744129409,
133.532432115043));
#92877=CARTESIAN_POINT('Ctrl Pts',(-76.5614574117157,-4.01706183459346,
133.645339137291));
#92878=CARTESIAN_POINT('Ctrl Pts',(-76.5692221646627,-3.93488860524996,
133.754925771358));
#92879=CARTESIAN_POINT('Ctrl Pts',(-76.5769792055477,-3.85279699151607,
133.864403562436));
#92880=CARTESIAN_POINT('Ctrl Pts',(-76.5847362464327,-3.76604721391699,
133.970567217445));
#92881=CARTESIAN_POINT('Ctrl Pts',(-76.5924932873177,-3.67494018148277,
134.072999130009));
#92882=CARTESIAN_POINT('Ctrl Pts',(-76.6002444785578,-3.58390185357053,
134.17535379787));
#92883=CARTESIAN_POINT('Ctrl Pts',(-76.6079956697979,-3.48851306986965,
134.273982033704));
#92884=CARTESIAN_POINT('Ctrl Pts',(-76.615746861038,-3.38911576675206,134.368498294768));
#92885=CARTESIAN_POINT('Ctrl Pts',(-76.6234947578151,-3.28976071013994,
134.4629743839));
#92886=CARTESIAN_POINT('Ctrl Pts',(-76.6312426545922,-3.18640080542552,
134.553341705457));
#92887=CARTESIAN_POINT('Ctrl Pts',(-76.6389905513692,-3.07941553489647,
134.639250841019));
#92888=CARTESIAN_POINT('Ctrl Pts',(-76.6467368274533,-2.97245264337967,
134.725142006242));
#92889=CARTESIAN_POINT('Ctrl Pts',(-76.6544831035374,-2.86186619909756,
134.80657659574));
#92890=CARTESIAN_POINT('Ctrl Pts',(-76.6622293796214,-2.74806921116227,
134.883245106389));
#92891=CARTESIAN_POINT('Ctrl Pts',(-76.6699757128868,-2.63427138320362,
134.959914182988));
#92892=CARTESIAN_POINT('Ctrl Pts',(-76.6777220461521,-2.51726328854291,
135.031816892083));
#92893=CARTESIAN_POINT('Ctrl Pts',(-76.6854683794175,-2.397487055372,135.098686977058));
#92894=CARTESIAN_POINT('Ctrl Pts',(-76.6932164474204,-2.2776839991443,135.165572037124));
#92895=CARTESIAN_POINT('Ctrl Pts',(-76.7009645154233,-2.15511191216886,
135.227422039882));
#92896=CARTESIAN_POINT('Ctrl Pts',(-76.7087125834262,-2.03023729762168,
135.284016807258));
#92897=CARTESIAN_POINT('Ctrl Pts',(-76.7164688861681,-1.90522996484762,
135.340671724226));
#92898=CARTESIAN_POINT('Ctrl Pts',(-76.7242251889098,-1.77791557271667,
135.392060086875));
#92899=CARTESIAN_POINT('Ctrl Pts',(-76.7319814916517,-1.64878088813436,
135.438009789161));
#92900=CARTESIAN_POINT('Ctrl Pts',(-76.7397419341658,-1.51957728048273,
135.483984016187));
#92901=CARTESIAN_POINT('Ctrl Pts',(-76.74750237668,-1.38855181781587,135.524513683345));
#92902=CARTESIAN_POINT('Ctrl Pts',(-76.7552628191941,-1.25620522211999,
135.559476967606));
#92903=CARTESIAN_POINT('Ctrl Pts',(-76.7630357194596,-1.12364617191951,
135.594496378035));
#92904=CARTESIAN_POINT('Ctrl Pts',(-76.770808619725,-0.989762132721141,
135.62393146529));
#92905=CARTESIAN_POINT('Ctrl Pts',(-76.7785815199905,-0.855063669094408,
135.647711645965));
#92906=CARTESIAN_POINT('Ctrl Pts',(-76.7860718557528,-0.725261833900718,
135.670627357175));
#92907=CARTESIAN_POINT('Ctrl Pts',(-76.7935621915151,-0.594704064254259,
135.688292122706));
#92908=CARTESIAN_POINT('Ctrl Pts',(-76.8010525272773,-0.463848661725816,
135.700688576508));
#92909=CARTESIAN_POINT('Ctrl Pts',(-76.8088268613964,-0.328031836842645,
135.713555045623));
#92910=CARTESIAN_POINT('Ctrl Pts',(-76.8166011955156,-0.191464137169983,
135.72078657786));
#92911=CARTESIAN_POINT('Ctrl Pts',(-76.8243755296346,-0.0546527164413332,
135.722306951462));
#92912=CARTESIAN_POINT('Ctrl Pts',(-76.8321402825817,0.0819900964384566,
135.72382545134));
#92913=CARTESIAN_POINT('Ctrl Pts',(-76.8399050355288,0.218875645550496,
135.719646792782));
#92914=CARTESIAN_POINT('Ctrl Pts',(-76.8476697884759,0.355490622099401,
135.709746380184));
#92915=CARTESIAN_POINT('Ctrl Pts',(-76.8554268293609,0.491969910727664,
135.699855800816));
#92916=CARTESIAN_POINT('Ctrl Pts',(-76.8631838702459,0.628178774171234,
135.684254804764));
#92917=CARTESIAN_POINT('Ctrl Pts',(-76.8709409111309,0.763603219677173,
135.662970828871));
#92918=CARTESIAN_POINT('Ctrl Pts',(-76.878692102371,0.898925540555123,135.64170290339));
#92919=CARTESIAN_POINT('Ctrl Pts',(-76.8864432936111,1.0334642362498,135.614760588708));
#92920=CARTESIAN_POINT('Ctrl Pts',(-76.8941944848512,1.16671011377224,135.582223170311));
#92921=CARTESIAN_POINT('Ctrl Pts',(-76.9019423816283,1.29989935824246,135.549699581184));
#92922=CARTESIAN_POINT('Ctrl Pts',(-76.9096902784053,1.43179649840839,135.511585710689));
#92923=CARTESIAN_POINT('Ctrl Pts',(-76.9174381751824,1.56190243921174,135.468011958831));
#92924=CARTESIAN_POINT('Ctrl Pts',(-76.9251844512665,1.69198116465704,135.424447321663));
#92925=CARTESIAN_POINT('Ctrl Pts',(-76.9329307273506,1.82026906550781,135.375425198891));
#92926=CARTESIAN_POINT('Ctrl Pts',(-76.9406770034347,1.94628250650731,135.321125772781));
#92927=CARTESIAN_POINT('Ctrl Pts',(-76.9484233367,2.07229687770957,135.266825945845));
#92928=CARTESIAN_POINT('Ctrl Pts',(-76.9561696699653,2.19603639650815,135.207248892552));
#92929=CARTESIAN_POINT('Ctrl Pts',(-76.9639160032307,2.31703807258324,135.142622669667));
#92930=CARTESIAN_POINT('Ctrl Pts',(-76.9716640712337,2.43806684614456,135.077981974188));
#92931=CARTESIAN_POINT('Ctrl Pts',(-76.9794121392367,2.55635621214841,135.008290043254));
#92932=CARTESIAN_POINT('Ctrl Pts',(-76.9871602072397,2.67146877218419,134.933820347572));
#92933=CARTESIAN_POINT('Ctrl Pts',(-76.9949165099815,2.78670367521847,134.859271504612));
#92934=CARTESIAN_POINT('Ctrl Pts',(-77.0026728127233,2.89875469888196,134.779934966023));
#92935=CARTESIAN_POINT('Ctrl Pts',(-77.0104291154651,3.00721393608535,134.696127235069));
#92936=CARTESIAN_POINT('Ctrl Pts',(-77.0181895579793,3.11573106124958,134.612274773406));
#92937=CARTESIAN_POINT('Ctrl Pts',(-77.0259500004935,3.22065228113544,134.523946615921));
#92938=CARTESIAN_POINT('Ctrl Pts',(-77.0337104430077,3.32160445011535,134.43149818588));
#92939=CARTESIAN_POINT('Ctrl Pts',(-77.0414833432731,3.42271867647901,134.338901349412));
#92940=CARTESIAN_POINT('Ctrl Pts',(-77.0492562435386,3.51985084251727,134.242171299094));
#92941=CARTESIAN_POINT('Ctrl Pts',(-77.057029143804,3.61266559179242,134.141699435304));
#92942=CARTESIAN_POINT('Ctrl Pts',(-77.0645194795661,3.70210629114568,134.044879976835));
#92943=CARTESIAN_POINT('Ctrl Pts',(-77.0720098153281,3.78753782222094,133.944586264901));
#92944=CARTESIAN_POINT('Ctrl Pts',(-77.0795001510902,3.86869785127562,133.84119449482));
#92945=CARTESIAN_POINT('Ctrl Pts',(-77.0872744852092,3.95293508749937,133.733882594351));
#92946=CARTESIAN_POINT('Ctrl Pts',(-77.0950488193283,4.03283735790277,133.622893140632));
#92947=CARTESIAN_POINT('Ctrl Pts',(-77.1028231534474,4.10806640598207,133.508611616741));
#92948=CARTESIAN_POINT('Ctrl Pts',(-77.1105879063945,4.18320274098303,133.394470934615));
#92949=CARTESIAN_POINT('Ctrl Pts',(-77.1183526593416,4.25367710010306,133.277046578327));
#92950=CARTESIAN_POINT('Ctrl Pts',(-77.1261174122887,4.31919133442124,133.156757114579));
#92951=CARTESIAN_POINT('Ctrl Pts',(-77.1338744531737,4.3846404990783,133.036587124023));
#92952=CARTESIAN_POINT('Ctrl Pts',(-77.1416314940587,4.44513915703453,132.913558030131));
#92953=CARTESIAN_POINT('Ctrl Pts',(-77.1493885349437,4.50043256604408,132.788117099847));
#92954=CARTESIAN_POINT('Ctrl Pts',(-77.1571397261838,4.55568427786385,132.662770765544));
#92955=CARTESIAN_POINT('Ctrl Pts',(-77.164890917424,4.60573839678961,132.535016571333));
#92956=CARTESIAN_POINT('Ctrl Pts',(-77.1726421086641,4.65038639669676,132.40532577144));
#92957=CARTESIAN_POINT('Ctrl Pts',(-77.1803900054412,4.69501542001298,132.275690093595));
#92958=CARTESIAN_POINT('Ctrl Pts',(-77.1881379022182,4.73424276735112,132.144119816067));
#92959=CARTESIAN_POINT('Ctrl Pts',(-77.1958857989953,4.76790837485868,132.011105326049));
#92960=CARTESIAN_POINT('Ctrl Pts',(-77.2036320750794,4.8015669402468,131.878118659796));
#92961=CARTESIAN_POINT('Ctrl Pts',(-77.2113783511636,4.82966598399625,131.743688760718));
#92962=CARTESIAN_POINT('Ctrl Pts',(-77.2191246272477,4.85209568187975,131.60831991777));
#92963=CARTESIAN_POINT('Ctrl Pts',(-77.2268709605131,4.87452554533422,131.472950075559));
#92964=CARTESIAN_POINT('Ctrl Pts',(-77.2346172937784,4.89128591550549,131.336641661353));
#92965=CARTESIAN_POINT('Ctrl Pts',(-77.2423636270438,4.9023184054314,131.199907472273));
#92966=CARTESIAN_POINT('Ctrl Pts',(-77.2501116950468,4.91335336600692,131.063142662519));
#92967=CARTESIAN_POINT('Ctrl Pts',(-77.2578597630497,4.91865786243756,130.925952277782));
#92968=CARTESIAN_POINT('Ctrl Pts',(-77.2656078310526,4.91822554884936,130.788852131327));
#92969=CARTESIAN_POINT('Ctrl Pts',(-77.2733641337945,4.91779277579313,130.651606273205));
#92970=CARTESIAN_POINT('Ctrl Pts',(-77.2811204365364,4.911611014239,130.514451236537));
#92971=CARTESIAN_POINT('Ctrl Pts',(-77.2888767392783,4.89972606360162,130.377901282854));
#92972=CARTESIAN_POINT('Ctrl Pts',(-77.2966371817924,4.88783476960823,130.241278448349));
#92973=CARTESIAN_POINT('Ctrl Pts',(-77.3043976243067,4.87023427132397,130.10526172788));
#92974=CARTESIAN_POINT('Ctrl Pts',(-77.3121580668208,4.84702190208244,129.970357174388));
#92975=CARTESIAN_POINT('Ctrl Pts',(-77.3199309670863,4.8237722702851,129.83523606013));
#92976=CARTESIAN_POINT('Ctrl Pts',(-77.3277038673517,4.79489284774365,129.701231062956));
#92977=CARTESIAN_POINT('Ctrl Pts',(-77.3354767676172,4.76053166233539,129.568835889201));
#92978=CARTESIAN_POINT('Ctrl Pts',(-77.3429671033792,4.72741959256741,129.441253613495));
#92979=CARTESIAN_POINT('Ctrl Pts',(-77.3504574391411,4.68921748157953,129.315166445745));
#92980=CARTESIAN_POINT('Ctrl Pts',(-77.3579477749031,4.64610003535104,129.190998437517));
#92981=CARTESIAN_POINT('Ctrl Pts',(-77.3657221090222,4.60134777804347,129.062122561518));
#92982=CARTESIAN_POINT('Ctrl Pts',(-77.3734964431412,4.55115833611975,128.934906007674));
#92983=CARTESIAN_POINT('Ctrl Pts',(-77.3812707772603,4.49567319150811,128.809841723784));
#92984=CARTESIAN_POINT('Ctrl Pts',(-77.3890355302074,4.44025642737835,128.684931570445));
#92985=CARTESIAN_POINT('Ctrl Pts',(-77.3968002831545,4.37955710333887,128.562168763357));
#92986=CARTESIAN_POINT('Ctrl Pts',(-77.4045650361016,4.31376621463617,128.442030389176));
#92987=CARTESIAN_POINT('Ctrl Pts',(-77.4123220769866,4.24804067037162,128.322011338123));
#92988=CARTESIAN_POINT('Ctrl Pts',(-77.4200791178717,4.17723381170246,128.204611873372));
#92989=CARTESIAN_POINT('Ctrl Pts',(-77.4278361587567,4.10158424256904,128.090288075498));
#92990=CARTESIAN_POINT('Ctrl Pts',(-77.4355873499968,4.02599172136406,127.976050490089));
#92991=CARTESIAN_POINT('Ctrl Pts',(-77.4433385412369,3.94556397350741,127.86488427969));
#92992=CARTESIAN_POINT('Ctrl Pts',(-77.451089732477,3.8605847650603,127.757219607655));
#92993=CARTESIAN_POINT('Ctrl Pts',(-77.4588376292541,3.77564167504356,127.649600695977));
#92994=CARTESIAN_POINT('Ctrl Pts',(-77.4665855260312,3.68615121371228,127.545480668898));
#92995=CARTESIAN_POINT('Ctrl Pts',(-77.4743334228083,3.59243943928063,127.445259258928));
#92996=CARTESIAN_POINT('Ctrl Pts',(-77.4820796988924,3.49874726733225,127.345058813118));
#92997=CARTESIAN_POINT('Ctrl Pts',(-77.4898259749765,3.40083580548928,127.24875564772));
#92998=CARTESIAN_POINT('Ctrl Pts',(-77.4975722510606,3.29906996365355,127.156714741467));
#92999=CARTESIAN_POINT('Ctrl Pts',(-77.505318584326,3.19730337060536,127.064673155789));
#93000=CARTESIAN_POINT('Ctrl Pts',(-77.5130649175913,3.09168263075157,126.976894154289));
#93001=CARTESIAN_POINT('Ctrl Pts',(-77.5208112508567,2.98260761525354,126.893704038942));
#93002=CARTESIAN_POINT('Ctrl Pts',(-77.5285593188596,2.87350817316222,126.810495293746));
#93003=CARTESIAN_POINT('Ctrl Pts',(-77.5363073868626,2.760953226939,126.731877716656));
#93004=CARTESIAN_POINT('Ctrl Pts',(-77.5440554548656,2.64537331479475,126.658135456305));
#93005=CARTESIAN_POINT('Ctrl Pts',(-77.5518117576074,2.52967056294429,126.584314821803));
#93006=CARTESIAN_POINT('Ctrl Pts',(-77.5595680603493,2.41093675304473,126.515380065358));
#93007=CARTESIAN_POINT('Ctrl Pts',(-77.5673243630912,2.28962930359001,126.451570625545));
#93008=CARTESIAN_POINT('Ctrl Pts',(-77.5750848056053,2.16825710869702,126.387727128712));
#93009=CARTESIAN_POINT('Ctrl Pts',(-77.5828452481195,2.04430889033384,126.329014566584));
#93010=CARTESIAN_POINT('Ctrl Pts',(-77.5906056906337,1.91826301621665,126.275624583846));
#93011=CARTESIAN_POINT('Ctrl Pts',(-77.5983785908991,1.79201480207251,126.222148894768));
#93012=CARTESIAN_POINT('Ctrl Pts',(-77.6061514911646,1.66366256942882,126.174012996633));
#93013=CARTESIAN_POINT('Ctrl Pts',(-77.61392439143,1.53370170009022,126.13135920973));
#93014=CARTESIAN_POINT('Ctrl Pts',(-77.621414727192,1.40846523570411,126.090255995419));
#93015=CARTESIAN_POINT('Ctrl Pts',(-77.628905062954,1.28173535637487,126.054243319314));
#93016=CARTESIAN_POINT('Ctrl Pts',(-77.636395398716,1.15396326154357,126.023403406556));
#93017=CARTESIAN_POINT('Ctrl Pts',(-77.6441697328351,1.02134664890106,125.991394189133));
#93018=CARTESIAN_POINT('Ctrl Pts',(-77.6519440669542,0.887187139887614,
125.964856333272));
#93019=CARTESIAN_POINT('Ctrl Pts',(-77.6597184010733,0.751975939883148,
125.943937256547));
#93020=CARTESIAN_POINT('Ctrl Pts',(-77.6674831540203,0.616931375598516,
125.923043960715));
#93021=CARTESIAN_POINT('Ctrl Pts',(-77.6752479069674,0.480838081865013,
125.907755725244));
#93022=CARTESIAN_POINT('Ctrl Pts',(-77.6830126599145,0.344200682795646,
125.898169737416));
#93023=CARTESIAN_POINT('Ctrl Pts',(-77.6907697007995,0.207698993917285,
125.888593270527));
#93024=CARTESIAN_POINT('Ctrl Pts',(-77.6985267416845,0.0706546626323717,
125.884707807741));
#93025=CARTESIAN_POINT('Ctrl Pts',(-77.7062837825695,-0.0664196262973008,
125.886559127495));
#93026=CARTESIAN_POINT('Ctrl Pts',(-77.7140349738096,-0.203390546439595,
125.888409051155));
#93027=CARTESIAN_POINT('Ctrl Pts',(-77.7217861650498,-0.340390989912295,
125.895987141153));
#93028=CARTESIAN_POINT('Ctrl Pts',(-77.72953735629,-0.476905665615885,125.909287170864));
#93029=CARTESIAN_POINT('Ctrl Pts',(-77.7372852530671,-0.613362318940467,
125.922581547709));
#93030=CARTESIAN_POINT('Ctrl Pts',(-77.7450331498441,-0.749333226829437,
125.941592989419));
#93031=CARTESIAN_POINT('Ctrl Pts',(-77.7527810466212,-0.884305840571931,
125.966263239171));
#93032=CARTESIAN_POINT('Ctrl Pts',(-77.7605273227053,-1.0192502209533,125.990928328439));
#93033=CARTESIAN_POINT('Ctrl Pts',(-77.7682735987894,-1.15319633819584,
126.021249801051));
#93034=CARTESIAN_POINT('Ctrl Pts',(-77.7760198748735,-1.28563988264154,
126.057117927892));
#93035=CARTESIAN_POINT('Ctrl Pts',(-77.7837662081388,-1.41808440475557,
126.092986319504));
#93036=CARTESIAN_POINT('Ctrl Pts',(-77.7915125414042,-1.5490259545688,126.134401344845));
#93037=CARTESIAN_POINT('Ctrl Pts',(-77.7992588746696,-1.67797386485884,
126.181202955172));
#93038=CARTESIAN_POINT('Ctrl Pts',(-77.8070069426725,-1.80695065213915,
126.228015046395));
#93039=CARTESIAN_POINT('Ctrl Pts',(-77.8147550106755,-1.93393254405191,
126.280215989616));
#93040=CARTESIAN_POINT('Ctrl Pts',(-77.8225030786785,-2.05844776188428,
126.337597150122));
#93041=CARTESIAN_POINT('Ctrl Pts',(-77.8302593814203,-2.18309531597174,
126.395039296008));
#93042=CARTESIAN_POINT('Ctrl Pts',(-77.8380156841621,-2.30527060338783,
126.457672493309));
#93043=CARTESIAN_POINT('Ctrl Pts',(-77.8457719869039,-2.42452493180908,
126.525241325289));
#93044=CARTESIAN_POINT('Ctrl Pts',(-77.8535324294181,-2.54384290985642,
126.59284622079));
#93045=CARTESIAN_POINT('Ctrl Pts',(-77.8612928719323,-2.66023649082991,
126.66539179333));
#93046=CARTESIAN_POINT('Ctrl Pts',(-77.8690533144465,-2.77328586919239,
126.742579167237));
#93047=CARTESIAN_POINT('Ctrl Pts',(-77.876826214712,-2.88651672445306,126.819890449168));
#93048=CARTESIAN_POINT('Ctrl Pts',(-77.8845991149773,-2.99639233575464,
126.901858188889));
#93049=CARTESIAN_POINT('Ctrl Pts',(-77.8923720152428,-3.10252519904289,
126.988142535249));
#93050=CARTESIAN_POINT('Ctrl Pts',(-77.8998623510048,-3.20479986541835,
127.071290228281));
#93051=CARTESIAN_POINT('Ctrl Pts',(-77.9073526867669,-3.30359894508477,
127.158445933845));
#93052=CARTESIAN_POINT('Ctrl Pts',(-77.914843022529,-3.39860937538332,127.249274489769));
#93053=CARTESIAN_POINT('Ctrl Pts',(-77.9225019334602,-3.49575808090294,
127.342147204948));
#93054=CARTESIAN_POINT('Ctrl Pts',(-77.9301608443915,-3.5892727087008,127.439173157499));
#93055=CARTESIAN_POINT('Ctrl Pts',(-77.9378197553226,-3.67876918681696,
127.540032151767));
#93056=CARTESIAN_POINT('Ctrl Pts',(-77.9454697647136,-3.76816164798992,
127.640773923051));
#93057=CARTESIAN_POINT('Ctrl Pts',(-77.9531197741044,-3.85354497834343,
127.745339581697));
#93058=CARTESIAN_POINT('Ctrl Pts',(-77.9607697834954,-3.93456950362442,
127.85336995617));
#93059=CARTESIAN_POINT('Ctrl Pts',(-77.9684126748289,-4.01551863851188,
127.961299812282));
#93060=CARTESIAN_POINT('Ctrl Pts',(-77.9760555661625,-4.09211679237984,
128.072687653498));
#93061=CARTESIAN_POINT('Ctrl Pts',(-77.983698457496,-4.16405278101098,128.187139285799));
#93062=CARTESIAN_POINT('Ctrl Pts',(-77.9913358822161,-4.23593731709264,
128.30150905604));
#93063=CARTESIAN_POINT('Ctrl Pts',(-77.9989733069363,-4.30316610786869,
128.418937917682));
#93064=CARTESIAN_POINT('Ctrl Pts',(-78.0066107316564,-4.365470096523,128.539001065781));
#93065=CARTESIAN_POINT('Ctrl Pts',(-78.0142448735701,-4.42774730495529,
128.659012606948));
#93066=CARTESIAN_POINT('Ctrl Pts',(-78.0218790154838,-4.48510373684876,
128.781655824646));
#93067=CARTESIAN_POINT('Ctrl Pts',(-78.0295131573976,-4.53731553191086,
128.906480003202));
#93068=CARTESIAN_POINT('Ctrl Pts',(-78.0371472564263,-4.5895270336716,129.031303480553));
#93069=CARTESIAN_POINT('Ctrl Pts',(-78.044781355455,-4.63659379080224,129.158307526332));
#93070=CARTESIAN_POINT('Ctrl Pts',(-78.0524154544837,-4.6783396088294,129.287020323842));
#93071=CARTESIAN_POINT('Ctrl Pts',(-78.0582029660887,-4.70998766649555,
129.384599200733));
#93072=CARTESIAN_POINT('Ctrl Pts',(-78.0639904776936,-4.73857855460141,
129.483159684766));
#93073=CARTESIAN_POINT('Ctrl Pts',(-78.0697779892986,-4.76405452823406,
129.582490119308));
#93074=CARTESIAN_POINT('Origin',(213.235140564004,0.,130.804360617566));
#93075=CARTESIAN_POINT('',(-80.1654084279177,-4.76405452823404,129.582490119308));
#93076=CARTESIAN_POINT('',(-79.8197738634776,-4.76405452823417,129.582490119309));
#93077=CARTESIAN_POINT('',(213.235140564004,-4.76405452823405,129.582490119308));
#93078=CARTESIAN_POINT('',(-78.4851405640458,-4.9182489417445,130.801134237387));
#93079=CARTESIAN_POINT('Ctrl Pts',(-78.485140564046,-4.9182489417445,130.801134237387));
#93080=CARTESIAN_POINT('Ctrl Pts',(-78.4928026403242,-4.91833732203731,
130.935859922949));
#93081=CARTESIAN_POINT('Ctrl Pts',(-78.5004647166025,-4.91288572166285,
131.070804853923));
#93082=CARTESIAN_POINT('Ctrl Pts',(-78.5081267928807,-4.90186657667286,
131.205467993461));
#93083=CARTESIAN_POINT('Ctrl Pts',(-78.5157805991188,-4.89085932516567,
131.339985784723));
#93084=CARTESIAN_POINT('Ctrl Pts',(-78.5234344053569,-4.87429651307583,
131.4742219915));
#93085=CARTESIAN_POINT('Ctrl Pts',(-78.5310882115949,-4.85220259044985,
131.607674431546));
#93086=CARTESIAN_POINT('Ctrl Pts',(-78.5387357066714,-4.83012688599015,
131.741016829624));
#93087=CARTESIAN_POINT('Ctrl Pts',(-78.5463832017478,-4.80252920910269,
131.873576351376));
#93088=CARTESIAN_POINT('Ctrl Pts',(-78.5540306968244,-4.76948587907409,
132.004855312187));
#93089=CARTESIAN_POINT('Ctrl Pts',(-78.5616743679513,-4.73645907158338,
132.13606863005));
#93090=CARTESIAN_POINT('Ctrl Pts',(-78.5693180390784,-4.69799212318942,
132.266002270696));
#93091=CARTESIAN_POINT('Ctrl Pts',(-78.5769617102053,-4.65421248287121,
132.394168538916));
#93092=CARTESIAN_POINT('Ctrl Pts',(-78.5846035112398,-4.6104435536333,132.522303450112));
#93093=CARTESIAN_POINT('Ctrl Pts',(-78.5922453122742,-4.56136464652823,
132.648671467787));
#93094=CARTESIAN_POINT('Ctrl Pts',(-78.5998871133087,-4.50715298291554,
132.772800368002));
#93095=CARTESIAN_POINT('Ctrl Pts',(-78.6075288055478,-4.45294209110812,
132.896927501008));
#93096=CARTESIAN_POINT('Ctrl Pts',(-78.6151704977868,-4.39359874940335,
133.018815211029));
#93097=CARTESIAN_POINT('Ctrl Pts',(-78.6228121900258,-4.32934797873513,
133.138012078586));
#93098=CARTESIAN_POINT('Ctrl Pts',(-78.6304555344611,-4.26508331652608,
133.257234717479));
#93099=CARTESIAN_POINT('Ctrl Pts',(-78.6380988788963,-4.19590930687053,
133.373765002907));
#93100=CARTESIAN_POINT('Ctrl Pts',(-78.6457422233316,-4.12209621223419,
133.487177398411));
#93101=CARTESIAN_POINT('Ctrl Pts',(-78.653393440683,-4.0482070874896,133.600706612709));
#93102=CARTESIAN_POINT('Ctrl Pts',(-78.6610446580344,-3.96966955657373,
133.711111186798));
#93103=CARTESIAN_POINT('Ctrl Pts',(-78.6686958753859,-3.88679657151321,
133.817995544722));
#93104=CARTESIAN_POINT('Ctrl Pts',(-78.6763513167103,-3.80387783513793,
133.92493890981));
#93105=CARTESIAN_POINT('Ctrl Pts',(-78.6840067580348,-3.71661913874972,
134.028357882526));
#93106=CARTESIAN_POINT('Ctrl Pts',(-78.6916621993592,-3.62537189640952,
134.127892124145));
#93107=CARTESIAN_POINT('Ctrl Pts',(-78.6993292101295,-3.5339867547656,134.227576788969));
#93108=CARTESIAN_POINT('Ctrl Pts',(-78.7069962208997,-3.43860131396968,
134.323364714613));
#93109=CARTESIAN_POINT('Ctrl Pts',(-78.71466323167,-3.33960217578401,134.414934030474));
#93110=CARTESIAN_POINT('Ctrl Pts',(-78.7199744537161,-3.27102180971564,
134.478367483709));
#93111=CARTESIAN_POINT('Ctrl Pts',(-78.7252856757622,-3.20070799148809,
134.539777330131));
#93112=CARTESIAN_POINT('Ctrl Pts',(-78.7305968978083,-3.12879742538389,
134.599068739861));
#93113=CARTESIAN_POINT('Ctrl Pts',(-78.7383712319274,-3.02353788949273,
134.685856907562));
#93114=CARTESIAN_POINT('Ctrl Pts',(-78.7461455660464,-2.9144978321693,134.768399608943));
#93115=CARTESIAN_POINT('Ctrl Pts',(-78.7539199001655,-2.80205450825847,
134.84634943438));
#93116=CARTESIAN_POINT('Ctrl Pts',(-78.7616846531126,-2.68974976069563,
134.924203193623));
#93117=CARTESIAN_POINT('Ctrl Pts',(-78.7694494060597,-2.57405041002116,
134.997475118645));
#93118=CARTESIAN_POINT('Ctrl Pts',(-78.7772141590067,-2.45536774764835,
135.065857101937));
#93119=CARTESIAN_POINT('Ctrl Pts',(-78.7849711998917,-2.33680296256829,
135.13417116728));
#93120=CARTESIAN_POINT('Ctrl Pts',(-78.7927282407768,-2.21526109899332,
135.197604762143));
#93121=CARTESIAN_POINT('Ctrl Pts',(-78.8004852816618,-2.0911831819534,135.255892484465));
#93122=CARTESIAN_POINT('Ctrl Pts',(-78.8082364729019,-1.96719883303608,
135.314136251562));
#93123=CARTESIAN_POINT('Ctrl Pts',(-78.815987664142,-1.84068258971744,135.367241704542));
#93124=CARTESIAN_POINT('Ctrl Pts',(-78.8237388553821,-1.71210056645969,
135.414989068529));
#93125=CARTESIAN_POINT('Ctrl Pts',(-78.8314867521592,-1.5835731939917,135.462716138612));
#93126=CARTESIAN_POINT('Ctrl Pts',(-78.8392346489363,-1.45298215362688,
135.505089513325));
#93127=CARTESIAN_POINT('Ctrl Pts',(-78.8469825457134,-1.32081385025044,
135.541937406969));
#93128=CARTESIAN_POINT('Ctrl Pts',(-78.8547288217975,-1.18867319363385,
135.578777592827));
#93129=CARTESIAN_POINT('Ctrl Pts',(-78.8624750978815,-1.05495630661775,
135.61009449166));
#93130=CARTESIAN_POINT('Ctrl Pts',(-78.8702213739656,-0.920164697454836,
135.635766209323));
#93131=CARTESIAN_POINT('Ctrl Pts',(-78.877967707231,-0.78537209329107,135.661438116488));
#93132=CARTESIAN_POINT('Ctrl Pts',(-78.8857140404963,-0.649505135211773,
135.681464686184));
#93133=CARTESIAN_POINT('Ctrl Pts',(-78.8934603737617,-0.51307507153837,
135.695775242546));
#93134=CARTESIAN_POINT('Ctrl Pts',(-78.9012084417646,-0.376614455298332,
135.710089003657));
#93135=CARTESIAN_POINT('Ctrl Pts',(-78.9089565097676,-0.239590871290205,
135.718684163482));
#93136=CARTESIAN_POINT('Ctrl Pts',(-78.9167045777706,-0.102519831956767,
135.721541999878));
#93137=CARTESIAN_POINT('Ctrl Pts',(-78.9244608805124,0.0346968881086265,
135.724402873616));
#93138=CARTESIAN_POINT('Ctrl Pts',(-78.9322171832543,0.171960772747315,
135.721514234959));
#93139=CARTESIAN_POINT('Ctrl Pts',(-78.9399734859961,0.308756609462109,
135.712909529272));
#93140=CARTESIAN_POINT('Ctrl Pts',(-78.9477339285103,0.445625458234173,
135.704300230995));
#93141=CARTESIAN_POINT('Ctrl Pts',(-78.9554943710244,0.582025372677596,
135.689968827472));
#93142=CARTESIAN_POINT('Ctrl Pts',(-78.9632548135386,0.717448109849961,
135.67000048013));
#93143=CARTESIAN_POINT('Ctrl Pts',(-78.971027713804,0.853088239621932,135.650000077825));
#93144=CARTESIAN_POINT('Ctrl Pts',(-78.9788006140696,0.987747673178774,
135.624344722283));
#93145=CARTESIAN_POINT('Ctrl Pts',(-78.986573514335,1.12092929410096,135.593170551164));
#93146=CARTESIAN_POINT('Ctrl Pts',(-78.9940638500969,1.24926942763691,135.563129639688));
#93147=CARTESIAN_POINT('Ctrl Pts',(-79.0015541858588,1.3762370307251,135.52796427433));
#93148=CARTESIAN_POINT('Ctrl Pts',(-79.0090445216208,1.50140398145464,135.48783893469));
#93149=CARTESIAN_POINT('Ctrl Pts',(-79.0168188557399,1.63131667516605,135.446192230601));
#93150=CARTESIAN_POINT('Ctrl Pts',(-79.0245931898589,1.75970100200358,135.399070088515));
#93151=CARTESIAN_POINT('Ctrl Pts',(-79.032367523978,1.8860607609518,135.346602120227));
#93152=CARTESIAN_POINT('Ctrl Pts',(-79.0401322769251,2.01226479278987,135.294198814022));
#93153=CARTESIAN_POINT('Ctrl Pts',(-79.0478970298721,2.13644886363297,135.236462938764));
#93154=CARTESIAN_POINT('Ctrl Pts',(-79.0556617828192,2.25813144085323,135.173573985935));
#93155=CARTESIAN_POINT('Ctrl Pts',(-79.0634188237041,2.37969316122237,135.1107474953));
#93156=CARTESIAN_POINT('Ctrl Pts',(-79.0711758645891,2.49875798719979,135.042778290705));
#93157=CARTESIAN_POINT('Ctrl Pts',(-79.0789329054741,2.61486424371473,134.969893962702));
#93158=CARTESIAN_POINT('Ctrl Pts',(-79.0866840967142,2.73088294359829,134.897064597339));
#93159=CARTESIAN_POINT('Ctrl Pts',(-79.0944352879544,2.84394718505944,134.819327693217));
#93160=CARTESIAN_POINT('Ctrl Pts',(-79.1021864791944,2.95362011901819,134.736956611948));
#93161=CARTESIAN_POINT('Ctrl Pts',(-79.1099343759715,3.06324643905482,134.654620540586));
#93162=CARTESIAN_POINT('Ctrl Pts',(-79.1176822727486,3.1694840064577,134.567654443856));
#93163=CARTESIAN_POINT('Ctrl Pts',(-79.1254301695256,3.2719253793318,134.476374693599));
#93164=CARTESIAN_POINT('Ctrl Pts',(-79.1331764456097,3.3743453236788,134.385114037098));
#93165=CARTESIAN_POINT('Ctrl Pts',(-79.1409227216938,3.47297036125623,134.28954178177));
#93166=CARTESIAN_POINT('Ctrl Pts',(-79.1486689977778,3.56742686160703,134.190013973949));
#93167=CARTESIAN_POINT('Ctrl Pts',(-79.1564153310432,3.66188405921439,134.090485431435));
#93168=CARTESIAN_POINT('Ctrl Pts',(-79.1641616643085,3.75217238905854,133.987001561748));
#93169=CARTESIAN_POINT('Ctrl Pts',(-79.1719079975739,3.83795604732683,133.879954290548));
#93170=CARTESIAN_POINT('Ctrl Pts',(-79.1796560655769,3.92375891625072,133.772883046854));
#93171=CARTESIAN_POINT('Ctrl Pts',(-79.1874041335798,4.00505486178291,133.662247118752));
#93172=CARTESIAN_POINT('Ctrl Pts',(-79.1951522015828,4.08154948538709,133.548470101686));
#93173=CARTESIAN_POINT('Ctrl Pts',(-79.2029085043246,4.15812540838744,133.434572161052));
#93174=CARTESIAN_POINT('Ctrl Pts',(-79.2106648070665,4.22988959737858,133.317526787637));
#93175=CARTESIAN_POINT('Ctrl Pts',(-79.2184211098083,4.29659170595529,133.197785522345));
#93176=CARTESIAN_POINT('Ctrl Pts',(-79.2261815523225,4.3633294154557,133.077980347534));
#93177=CARTESIAN_POINT('Ctrl Pts',(-79.2339419948366,4.42499948529468,132.955476762799));
#93178=CARTESIAN_POINT('Ctrl Pts',(-79.2417024373508,4.4813988464692,132.830748399153));
#93179=CARTESIAN_POINT('Ctrl Pts',(-79.2494753376162,4.53788874490518,132.705819810465));
#93180=CARTESIAN_POINT('Ctrl Pts',(-79.2572482378816,4.58909088076802,132.578659668924));
#93181=CARTESIAN_POINT('Ctrl Pts',(-79.265021138147,4.63485108695769,132.449759798381));
#93182=CARTESIAN_POINT('Ctrl Pts',(-79.2725114739093,4.6789477943906,132.325545762809));
#93183=CARTESIAN_POINT('Ctrl Pts',(-79.2800018096714,4.71799126740704,132.199716583479));
#93184=CARTESIAN_POINT('Ctrl Pts',(-79.2874921454337,4.75188847700245,132.072721356722));
#93185=CARTESIAN_POINT('Ctrl Pts',(-79.2952664795528,4.78707090960166,131.940911067346));
#93186=CARTESIAN_POINT('Ctrl Pts',(-79.3030408136719,4.81682058151303,131.807427028324));
#93187=CARTESIAN_POINT('Ctrl Pts',(-79.310815147791,4.84097833004299,131.672756765965));
#93188=CARTESIAN_POINT('Ctrl Pts',(-79.318579900738,4.86510630630679,131.53825247267));
#93189=CARTESIAN_POINT('Ctrl Pts',(-79.3263446536852,4.88365600294281,131.40256524594));
#93190=CARTESIAN_POINT('Ctrl Pts',(-79.3341094066322,4.8965181510694,131.266197232342));
#93191=CARTESIAN_POINT('Ctrl Pts',(-79.3418664475172,4.90936752432922,131.129964661377));
#93192=CARTESIAN_POINT('Ctrl Pts',(-79.3496234884022,4.91654055427657,130.993053035867));
#93193=CARTESIAN_POINT('Ctrl Pts',(-79.3573805292873,4.9179791726358,130.855973794376));
#93194=CARTESIAN_POINT('Ctrl Pts',(-79.3651317205274,4.91941670612174,130.718997925408));
#93195=CARTESIAN_POINT('Ctrl Pts',(-79.3728829117675,4.91512843131837,130.581855081413));
#93196=CARTESIAN_POINT('Ctrl Pts',(-79.3806341030077,4.90510820749114,130.445060554523));
#93197=CARTESIAN_POINT('Ctrl Pts',(-79.3883819997848,4.89509224252636,130.308324168955));
#93198=CARTESIAN_POINT('Ctrl Pts',(-79.3961298965618,4.87934920251789,130.171936195148));
#93199=CARTESIAN_POINT('Ctrl Pts',(-79.4038777933389,4.85792502775777,130.036410432212));
#93200=CARTESIAN_POINT('Ctrl Pts',(-79.411624069423,4.83650533447316,129.900913018345));
#93201=CARTESIAN_POINT('Ctrl Pts',(-79.4193703455071,4.8094069311796,129.766277842538));
#93202=CARTESIAN_POINT('Ctrl Pts',(-79.4271166215912,4.77672741335286,129.633011702416));
#93203=CARTESIAN_POINT('Ctrl Pts',(-79.4348629548566,4.7440476542932,129.499744578553));
#93204=CARTESIAN_POINT('Ctrl Pts',(-79.442609288122,4.70578679160541,129.367846890256));
#93205=CARTESIAN_POINT('Ctrl Pts',(-79.4503556213873,4.6620930532845,129.237813004176));
#93206=CARTESIAN_POINT('Ctrl Pts',(-79.4581036893903,4.61838953005391,129.10774999791));
#93207=CARTESIAN_POINT('Ctrl Pts',(-79.4658517573933,4.56925083469331,128.979551994941));
#93208=CARTESIAN_POINT('Ctrl Pts',(-79.4735998253963,4.51487422044557,128.85369564478));
#93209=CARTESIAN_POINT('Ctrl Pts',(-79.4813561281381,4.4604398140852,128.727705532992));
#93210=CARTESIAN_POINT('Ctrl Pts',(-79.4891124308801,4.40075652362129,128.604062405003));
#93211=CARTESIAN_POINT('Ctrl Pts',(-79.4968687336219,4.33606892485685,128.483220953222));
#93212=CARTESIAN_POINT('Ctrl Pts',(-79.5046291761361,4.27134680037325,128.36231500472));
#93213=CARTESIAN_POINT('Ctrl Pts',(-79.5123896186502,4.20161524417627,128.244214048511));
#93214=CARTESIAN_POINT('Ctrl Pts',(-79.5201500611643,4.12716297169562,128.129344941432));
#93215=CARTESIAN_POINT('Ctrl Pts',(-79.5279229614298,4.05259118181761,128.014291436264));
#93216=CARTESIAN_POINT('Ctrl Pts',(-79.5356958616953,3.97328375849158,127.90248046668));
#93217=CARTESIAN_POINT('Ctrl Pts',(-79.5434687619607,3.88957115597044,127.794307580634));
#93218=CARTESIAN_POINT('Ctrl Pts',(-79.5509590977227,3.80890171741095,127.690067051468));
#93219=CARTESIAN_POINT('Ctrl Pts',(-79.5584494334847,3.72414201603116,127.589204926877));
#93220=CARTESIAN_POINT('Ctrl Pts',(-79.5659397692466,3.63561960484334,127.492042222336));
#93221=CARTESIAN_POINT('Ctrl Pts',(-79.5737141033657,3.54374083952863,127.391195564319));
#93222=CARTESIAN_POINT('Ctrl Pts',(-79.5814884374847,3.44751736137916,127.294014939165));
#93223=CARTESIAN_POINT('Ctrl Pts',(-79.5892627716038,3.34727330876307,127.200897774835));
#93224=CARTESIAN_POINT('Ctrl Pts',(-79.5970275245509,3.24715279798331,127.107895369088));
#93225=CARTESIAN_POINT('Ctrl Pts',(-79.604792277498,3.14302185540678,127.018946723562));
#93226=CARTESIAN_POINT('Ctrl Pts',(-79.6125570304451,3.03524388866223,126.934415191744));
#93227=CARTESIAN_POINT('Ctrl Pts',(-79.6203140713301,2.92757296851336,126.849967617836));
#93228=CARTESIAN_POINT('Ctrl Pts',(-79.6280711122151,2.81626253833069,126.76992866675));
#93229=CARTESIAN_POINT('Ctrl Pts',(-79.6358281531001,2.70171149854224,126.694623638008));
#93230=CARTESIAN_POINT('Ctrl Pts',(-79.6435793443402,2.5872468425835,126.619375397374));
#93231=CARTESIAN_POINT('Ctrl Pts',(-79.6513305355804,2.46954676656517,126.548854187337));
#93232=CARTESIAN_POINT('Ctrl Pts',(-79.6590817268206,2.34904148113322,126.483343702254));
#93233=CARTESIAN_POINT('Ctrl Pts',(-79.6668296235977,2.22858741366232,126.417861060874));
#93234=CARTESIAN_POINT('Ctrl Pts',(-79.6745775203748,2.10533085091978,126.357385094995));
#93235=CARTESIAN_POINT('Ctrl Pts',(-79.6823254171519,1.97972889850062,126.302154874717));
#93236=CARTESIAN_POINT('Ctrl Pts',(-79.690071693236,1.85415321930225,126.246936207411));
#93237=CARTESIAN_POINT('Ctrl Pts',(-79.69781796932,1.72623348393338,126.196961260398));
#93238=CARTESIAN_POINT('Ctrl Pts',(-79.7055642454041,1.59644882832818,126.152421860335));
#93239=CARTESIAN_POINT('Ctrl Pts',(-79.7133105786695,1.46666321468231,126.107882131492));
#93240=CARTESIAN_POINT('Ctrl Pts',(-79.7210569119348,1.33501302312562,126.068778156571));
#93241=CARTESIAN_POINT('Ctrl Pts',(-79.7288032452002,1.20199429917472,126.035252444411));
#93242=CARTESIAN_POINT('Ctrl Pts',(-79.7365513132031,1.06894578660307,126.001719224401));
#93243=CARTESIAN_POINT('Ctrl Pts',(-79.7442993812062,0.934528510827687,
125.973766848473));
#93244=CARTESIAN_POINT('Ctrl Pts',(-79.7520474492092,0.799250110776796,
125.951487002591));
#93245=CARTESIAN_POINT('Ctrl Pts',(-79.7598037519511,0.663827935232313,
125.929183477423));
#93246=CARTESIAN_POINT('Ctrl Pts',(-79.767560054693,0.52754319355888,125.91256458918));
#93247=CARTESIAN_POINT('Ctrl Pts',(-79.7753163574348,0.390910630552998,
125.901670341664));
#93248=CARTESIAN_POINT('Ctrl Pts',(-79.783076799949,0.254205142633941,125.890770279561));
#93249=CARTESIAN_POINT('Ctrl Pts',(-79.7908372424631,0.117151853969851,
125.885600961082));
#93250=CARTESIAN_POINT('Ctrl Pts',(-79.7985976849773,-0.0197340509522312,
125.886150208308));
#93251=CARTESIAN_POINT('Ctrl Pts',(-79.8063705852427,-0.156839697280681,
125.886700337234));
#93252=CARTESIAN_POINT('Ctrl Pts',(-79.8141434855082,-0.293777032141836,
125.892987358387));
#93253=CARTESIAN_POINT('Ctrl Pts',(-79.8219163857736,-0.430034651244678,
125.904947054574));
#93254=CARTESIAN_POINT('Ctrl Pts',(-79.8294067215356,-0.561338962679421,
125.91647198568));
#93255=CARTESIAN_POINT('Ctrl Pts',(-79.8368970572976,-0.692011813627218,
125.933264280935));
#93256=CARTESIAN_POINT('Ctrl Pts',(-79.8443873930595,-0.821606074275422,
125.955221877417));
#93257=CARTESIAN_POINT('Ctrl Pts',(-79.8521617271786,-0.95611394070676,
125.978012002843));
#93258=CARTESIAN_POINT('Ctrl Pts',(-79.8599360612977,-1.08988589327567,
126.006439038537));
#93259=CARTESIAN_POINT('Ctrl Pts',(-79.8677103954168,-1.22241235987757,
126.040445097228));
#93260=CARTESIAN_POINT('Ctrl Pts',(-79.8754751483639,-1.35477549945361,
126.074409246491));
#93261=CARTESIAN_POINT('Ctrl Pts',(-79.8832399013109,-1.48589583209466,
126.113938642024));
#93262=CARTESIAN_POINT('Ctrl Pts',(-79.891004654258,-1.61527122751894,126.158923940132));
#93263=CARTESIAN_POINT('Ctrl Pts',(-79.898761695143,-1.74451812547697,126.203864558208));
#93264=CARTESIAN_POINT('Ctrl Pts',(-79.9065187360281,-1.87202316826902,
126.254250167474));
#93265=CARTESIAN_POINT('Ctrl Pts',(-79.9142757769132,-1.99729705676941,
126.30992099404));
#93266=CARTESIAN_POINT('Ctrl Pts',(-79.9220269681533,-2.12247647525617,
126.365549838803));
#93267=CARTESIAN_POINT('Ctrl Pts',(-79.9297781593934,-2.24542773259705,
126.426455809595));
#93268=CARTESIAN_POINT('Ctrl Pts',(-79.9375293506336,-2.36567960933227,
126.492430301746));
#93269=CARTESIAN_POINT('Ctrl Pts',(-79.9452772474107,-2.48588037581157,
126.558376752977));
#93270=CARTESIAN_POINT('Ctrl Pts',(-79.9530251441878,-2.60338370154532,
126.629387253254));
#93271=CARTESIAN_POINT('Ctrl Pts',(-79.9607730409649,-2.71774137334648,
126.705206449924));
#93272=CARTESIAN_POINT('Ctrl Pts',(-79.968519317049,-2.83207512398796,126.781009786851));
#93273=CARTESIAN_POINT('Ctrl Pts',(-79.9762655931331,-2.94326420385429,
126.861619603525));
#93274=CARTESIAN_POINT('Ctrl Pts',(-79.9840118692172,-3.05088823906931,
126.946736476309));
#93275=CARTESIAN_POINT('Ctrl Pts',(-79.9917582024826,-3.15851306874066,
127.031853977406));
#93276=CARTESIAN_POINT('Ctrl Pts',(-79.9995045357479,-3.26257249459517,
127.121478358478));
#93277=CARTESIAN_POINT('Ctrl Pts',(-80.0072508690133,-3.36267849519126,
127.21526931189));
#93278=CARTESIAN_POINT('Ctrl Pts',(-80.0149989370163,-3.46280691383196,
127.309081269136));
#93279=CARTESIAN_POINT('Ctrl Pts',(-80.0227470050192,-3.55897986023369,
127.407061388177));
#93280=CARTESIAN_POINT('Ctrl Pts',(-80.0304950730222,-3.6508458051584,127.508832136509));
#93281=CARTESIAN_POINT('Ctrl Pts',(-80.038251375764,-3.74280938630247,127.610711048003));
#93282=CARTESIAN_POINT('Ctrl Pts',(-80.046007678506,-3.83045655946711,127.716388345923));
#93283=CARTESIAN_POINT('Ctrl Pts',(-80.0537639812478,-3.91347543618363,
127.825452583926));
#93284=CARTESIAN_POINT('Ctrl Pts',(-80.061524423762,-3.99653862257453,127.934575032796));
#93285=CARTESIAN_POINT('Ctrl Pts',(-80.0692848662762,-4.07496836684843,
128.047087703195));
#93286=CARTESIAN_POINT('Ctrl Pts',(-80.0770453087904,-4.14849644483638,
128.162550573358));
#93287=CARTESIAN_POINT('Ctrl Pts',(-80.0848182090559,-4.22214255662263,
128.27819879477));
#93288=CARTESIAN_POINT('Ctrl Pts',(-80.0925911093213,-4.29087108204223,
128.396806341357));
#93289=CARTESIAN_POINT('Ctrl Pts',(-80.1003640095867,-4.354459622326,128.517908243246));
#93290=CARTESIAN_POINT('Ctrl Pts',(-80.1078543453488,-4.41573655900041,
128.634607785964));
#93291=CARTESIAN_POINT('Ctrl Pts',(-80.1153446811107,-4.47224059321952,
128.753623202075));
#93292=CARTESIAN_POINT('Ctrl Pts',(-80.1228350168728,-4.52381590882459,
128.874523141102));
#93293=CARTESIAN_POINT('Ctrl Pts',(-80.131461488494,-4.58321418021869,129.013761210818));
#93294=CARTESIAN_POINT('Ctrl Pts',(-80.1400879601153,-4.63623611515082,
129.155874571086));
#93295=CARTESIAN_POINT('Ctrl Pts',(-80.1487144317366,-4.68262360601552,
129.300293056954));
#93296=CARTESIAN_POINT('Ctrl Pts',(-80.1542790971303,-4.71254671669702,
129.39345287777));
#93297=CARTESIAN_POINT('Ctrl Pts',(-80.159843762524,-4.73971004719732,129.487571357225));
#93298=CARTESIAN_POINT('Ctrl Pts',(-80.1654084279176,-4.76405452823404,
129.582490119308));
#93299=CARTESIAN_POINT('Ctrl Pts',(-78.4150662180023,-4.76405452823401,
129.582490119308));
#93300=CARTESIAN_POINT('Ctrl Pts',(-78.4228402209491,-4.79809353827815,
129.715207702856));
#93301=CARTESIAN_POINT('Ctrl Pts',(-78.430614223896,-4.82654303296878,129.849194871298));
#93302=CARTESIAN_POINT('Ctrl Pts',(-78.4383882268428,-4.84933960771396,
129.983940949618));
#93303=CARTESIAN_POINT('Ctrl Pts',(-78.4429752425603,-4.86279062482549,
130.06344727131));
#93304=CARTESIAN_POINT('Ctrl Pts',(-78.4475622582779,-4.87427454369444,
130.143217716642));
#93305=CARTESIAN_POINT('Ctrl Pts',(-78.4521492739955,-4.88378684855164,
130.223147162445));
#93306=CARTESIAN_POINT('Ctrl Pts',(-78.4631463706665,-4.90659203225248,
130.41477324277));
#93307=CARTESIAN_POINT('Ctrl Pts',(-78.4741434673374,-4.91812209273009,
130.607767408421));
#93308=CARTESIAN_POINT('Ctrl Pts',(-78.4851405640086,-4.91824894174407,
130.801134236732));
#93309=CARTESIAN_POINT('',(-78.1398594359569,-4.91824809318944,130.80869147642));
#93310=CARTESIAN_POINT('Ctrl Pts',(-78.0697779892986,-4.76405452823406,
129.582490119308));
#93311=CARTESIAN_POINT('Ctrl Pts',(-78.0774154655189,-4.797673837549,129.713571296083));
#93312=CARTESIAN_POINT('Ctrl Pts',(-78.0850529417394,-4.82586675114046,
129.845993425159));
#93313=CARTESIAN_POINT('Ctrl Pts',(-78.0926904179597,-4.84854548498732,
129.979260779662));
#93314=CARTESIAN_POINT('Ctrl Pts',(-78.1005519209593,-4.87188944430299,
130.116437207704));
#93315=CARTESIAN_POINT('Ctrl Pts',(-78.1084134239588,-4.88939068370309,
130.254508754735));
#93316=CARTESIAN_POINT('Ctrl Pts',(-78.1162749269583,-4.90101084537413,
130.392929267247));
#93317=CARTESIAN_POINT('Ctrl Pts',(-78.1241364299578,-4.91263100704514,
130.531349779759));
#93318=CARTESIAN_POINT('Ctrl Pts',(-78.1319979329574,-4.91837011605548,
130.670118794076));
#93319=CARTESIAN_POINT('Ctrl Pts',(-78.1398594359569,-4.91824809318944,
130.80869147642));
#93320=CARTESIAN_POINT('Ctrl Pts',(-78.1398594359912,-4.91824809318891,
130.808691477025));
#93321=CARTESIAN_POINT('Ctrl Pts',(-78.1512629029101,-4.91807109345862,
131.009697442304));
#93322=CARTESIAN_POINT('Ctrl Pts',(-78.1626663698291,-4.90556839729258,
131.210182371441));
#93323=CARTESIAN_POINT('Ctrl Pts',(-78.174069836748,-4.8809497333259,131.408937133191));
#93324=CARTESIAN_POINT('Ctrl Pts',(-78.1804767732793,-4.86711795579357,
131.520605729495));
#93325=CARTESIAN_POINT('Ctrl Pts',(-78.1868837098105,-4.84946236679947,
131.631728881281));
#93326=CARTESIAN_POINT('Ctrl Pts',(-78.1932906463418,-4.82802602763092,
131.742096048814));
#93327=CARTESIAN_POINT('Ctrl Pts',(-78.2010649804609,-4.80201464728211,
131.876018280132));
#93328=CARTESIAN_POINT('Ctrl Pts',(-78.20883931458,-4.77038563986094,132.009069539209));
#93329=CARTESIAN_POINT('Ctrl Pts',(-78.2166136486991,-4.73320910429146,
132.140741789819));
#93330=CARTESIAN_POINT('Ctrl Pts',(-78.2243784016461,-4.6960783854796,132.272251766148));
#93331=CARTESIAN_POINT('Ctrl Pts',(-78.2321431545932,-4.65341384699147,
132.402385742874));
#93332=CARTESIAN_POINT('Ctrl Pts',(-78.2399079075403,-4.60533685077465,
132.530644358264));
#93333=CARTESIAN_POINT('Ctrl Pts',(-78.2476649484253,-4.55730760530798,
132.658775585389));
#93334=CARTESIAN_POINT('Ctrl Pts',(-78.2554219893103,-4.50387673639554,
132.785034794185));
#93335=CARTESIAN_POINT('Ctrl Pts',(-78.2631790301953,-4.44521571374638,
132.908936660564));
#93336=CARTESIAN_POINT('Ctrl Pts',(-78.2709302214354,-4.3865989278308,133.032745091582));
#93337=CARTESIAN_POINT('Ctrl Pts',(-78.2786814126755,-4.32276000529121,
133.154199366635));
#93338=CARTESIAN_POINT('Ctrl Pts',(-78.2864326039156,-4.25391879869345,
133.272833407901));
#93339=CARTESIAN_POINT('Ctrl Pts',(-78.2941805006927,-4.18510685144499,
133.391417026534));
#93340=CARTESIAN_POINT('Ctrl Pts',(-78.3019283974698,-4.11129704461234,
133.507182458003));
#93341=CARTESIAN_POINT('Ctrl Pts',(-78.3096762942469,-4.0327554131942,133.619687745957));
#93342=CARTESIAN_POINT('Ctrl Pts',(-78.317422570331,-3.95423021099219,133.732169500229));
#93343=CARTESIAN_POINT('Ctrl Pts',(-78.3251688464151,-3.8709753766189,133.841392147053));
#93344=CARTESIAN_POINT('Ctrl Pts',(-78.3329151224992,-3.78330033529861,
133.946942618951));
#93345=CARTESIAN_POINT('Ctrl Pts',(-78.3406614557645,-3.69562464678121,
134.052493869999));
#93346=CARTESIAN_POINT('Ctrl Pts',(-78.3484077890298,-3.60352893602056,
134.154372591285));
#93347=CARTESIAN_POINT('Ctrl Pts',(-78.3561541222952,-3.50736272409399,
134.252199039554));
#93348=CARTESIAN_POINT('Ctrl Pts',(-78.3639021902981,-3.41117497641089,
134.350047395378));
#93349=CARTESIAN_POINT('Ctrl Pts',(-78.3716502583012,-3.31091518768766,
134.443841393651));
#93350=CARTESIAN_POINT('Ctrl Pts',(-78.3793983263041,-3.20696921744136,
134.533238666106));
#93351=CARTESIAN_POINT('Ctrl Pts',(-78.387154629046,-3.10291277218105,134.622730951046));
#93352=CARTESIAN_POINT('Ctrl Pts',(-78.3949109317877,-2.99516261622621,
134.707816920224));
#93353=CARTESIAN_POINT('Ctrl Pts',(-78.4026672345296,-2.88413756189644,
134.788194648567));
#93354=CARTESIAN_POINT('Ctrl Pts',(-78.4104276770437,-2.77305325015197,
134.868615276923));
#93355=CARTESIAN_POINT('Ctrl Pts',(-78.418188119558,-2.65869088301477,134.94432244151));
#93356=CARTESIAN_POINT('Ctrl Pts',(-78.4259485620721,-2.54149679217376,
135.01505855471));
#93357=CARTESIAN_POINT('Ctrl Pts',(-78.4337214623376,-2.42411457097413,
135.085908219799));
#93358=CARTESIAN_POINT('Ctrl Pts',(-78.441494362603,-2.30389188532504,135.15177069902));
#93359=CARTESIAN_POINT('Ctrl Pts',(-78.4492672628685,-2.18129890815822,
135.212434815645));
#93360=CARTESIAN_POINT('Ctrl Pts',(-78.4567575986306,-2.0631624945035,135.270893638827));
#93361=CARTESIAN_POINT('Ctrl Pts',(-78.4642479343927,-1.94282541086829,
135.324525359456));
#93362=CARTESIAN_POINT('Ctrl Pts',(-78.4717382701548,-1.8207226226696,135.373184557466));
#93363=CARTESIAN_POINT('Ctrl Pts',(-78.4795126042738,-1.69399027014527,
135.423688683757));
#93364=CARTESIAN_POINT('Ctrl Pts',(-78.4872869383929,-1.56495422658384,
135.468995759522));
#93365=CARTESIAN_POINT('Ctrl Pts',(-78.495061272512,-1.43407980743096,135.508890154982));
#93366=CARTESIAN_POINT('Ctrl Pts',(-78.5028260254591,-1.3033666793031,135.548735384164));
#93367=CARTESIAN_POINT('Ctrl Pts',(-78.5105907784062,-1.17082005390523,
135.583181092731));
#93368=CARTESIAN_POINT('Ctrl Pts',(-78.5183555313533,-1.03692565750349,
135.612059468712));
#93369=CARTESIAN_POINT('Ctrl Pts',(-78.5261125722382,-0.903164246903833,
135.640909162282));
#93370=CARTESIAN_POINT('Ctrl Pts',(-78.5338696131232,-0.768058108928924,
135.664202445432));
#93371=CARTESIAN_POINT('Ctrl Pts',(-78.5416266540082,-0.63210824404421,
135.68182125096));
#93372=CARTESIAN_POINT('Ctrl Pts',(-78.5493778452483,-0.496260900009957,
135.69942677001));
#93373=CARTESIAN_POINT('Ctrl Pts',(-78.5571290364885,-0.35957148165881,
135.711366278817));
#93374=CARTESIAN_POINT('Ctrl Pts',(-78.5648802277286,-0.222550949145562,
135.717572819124));
#93375=CARTESIAN_POINT('Ctrl Pts',(-78.5726281245057,-0.0855886540139603,
135.723776721485));
#93376=CARTESIAN_POINT('Ctrl Pts',(-78.5803760212827,0.0517040856267704,
135.724252484031));
#93377=CARTESIAN_POINT('Ctrl Pts',(-78.5881239180598,0.188811640964827,
135.718985041338));
#93378=CARTESIAN_POINT('Ctrl Pts',(-78.5958701941439,0.325890516358004,
135.71371870048));
#93379=CARTESIAN_POINT('Ctrl Pts',(-78.603616470228,0.462783894068173,135.702711558942));
#93380=CARTESIAN_POINT('Ctrl Pts',(-78.6113627463122,0.598976996836243,
135.686000671868));
#93381=CARTESIAN_POINT('Ctrl Pts',(-78.6191090795775,0.735171104951045,
135.669289661437));
#93382=CARTESIAN_POINT('Ctrl Pts',(-78.6268554128428,0.870664539753861,
135.646874869069));
#93383=CARTESIAN_POINT('Ctrl Pts',(-78.6346017461082,1.00494888780859,135.61884509624));
#93384=CARTESIAN_POINT('Ctrl Pts',(-78.6423498141112,1.13926330791182,135.590809046337));
#93385=CARTESIAN_POINT('Ctrl Pts',(-78.6500978821142,1.27236771982945,135.557155593692));
#93386=CARTESIAN_POINT('Ctrl Pts',(-78.6578459501171,1.4037655129478,135.518024314433));
#93387=CARTESIAN_POINT('Ctrl Pts',(-78.665602252859,1.53530295720451,135.478851445984));
#93388=CARTESIAN_POINT('Ctrl Pts',(-78.6733585556009,1.665129784072,135.434189232817));
#93389=CARTESIAN_POINT('Ctrl Pts',(-78.6811148583427,1.79276559714513,135.384226835721));
#93390=CARTESIAN_POINT('Ctrl Pts',(-78.6888753008569,1.92046953329473,135.334237772188));
#93391=CARTESIAN_POINT('Ctrl Pts',(-78.696635743371,2.04597976789403,135.278943045515));
#93392=CARTESIAN_POINT('Ctrl Pts',(-78.7043961858852,2.16883833200463,135.218578934791));
#93393=CARTESIAN_POINT('Ctrl Pts',(-78.7121690861506,2.29189411958921,135.158117922239));
#93394=CARTESIAN_POINT('Ctrl Pts',(-78.7199419864161,2.41228938687595,135.092571450718));
#93395=CARTESIAN_POINT('Ctrl Pts',(-78.7277148866815,2.5295923249478,135.022220943853));
#93396=CARTESIAN_POINT('Ctrl Pts',(-78.7352052224436,2.64263100575247,134.954427855115));
#93397=CARTESIAN_POINT('Ctrl Pts',(-78.7426955582056,2.75279802434725,134.882174113557));
#93398=CARTESIAN_POINT('Ctrl Pts',(-78.7501858939676,2.85973592528007,134.805747064807));
#93399=CARTESIAN_POINT('Ctrl Pts',(-78.7579602280867,2.97072840922998,134.726422261274));
#93400=CARTESIAN_POINT('Ctrl Pts',(-78.7657345622058,3.07859366866015,134.642350164472));
#93401=CARTESIAN_POINT('Ctrl Pts',(-78.7735088963248,3.18289877376601,134.553805704303));
#93402=CARTESIAN_POINT('Ctrl Pts',(-78.7812736492719,3.28707533215155,134.465370367268));
#93403=CARTESIAN_POINT('Ctrl Pts',(-78.789038402219,3.38770017098097,134.372473884269));
#93404=CARTESIAN_POINT('Ctrl Pts',(-78.7968031551661,3.48436955837914,134.275434204101));
#93405=CARTESIAN_POINT('Ctrl Pts',(-78.8045601960511,3.58094293237893,134.178490905111));
#93406=CARTESIAN_POINT('Ctrl Pts',(-78.8123172369362,3.67356839891922,134.077412873341));
#93407=CARTESIAN_POINT('Ctrl Pts',(-78.8200742778212,3.76187582173067,133.972557796464));
#93408=CARTESIAN_POINT('Ctrl Pts',(-78.8278254690613,3.85011665122776,133.867781791616));
#93409=CARTESIAN_POINT('Ctrl Pts',(-78.8355766603014,3.93404566757502,133.759234708861));
#93410=CARTESIAN_POINT('Ctrl Pts',(-78.8433278515415,4.01333035044917,133.647310240873));
#93411=CARTESIAN_POINT('Ctrl Pts',(-78.8510757483186,4.09258133521822,133.53543334377));
#93412=CARTESIAN_POINT('Ctrl Pts',(-78.8588236450958,4.16719168706052,133.420182234855));
#93413=CARTESIAN_POINT('Ctrl Pts',(-78.8665715418728,4.23687002103937,133.301982584021));
#93414=CARTESIAN_POINT('Ctrl Pts',(-78.8743178179569,4.30653377981264,133.183807658006));
#93415=CARTESIAN_POINT('Ctrl Pts',(-78.882064094041,4.37126737435724,133.062685753451));
#93416=CARTESIAN_POINT('Ctrl Pts',(-78.8898103701251,4.4308237305321,132.939069996253));
#93417=CARTESIAN_POINT('Ctrl Pts',(-78.8975567033905,4.49038052633853,132.815453326551));
#93418=CARTESIAN_POINT('Ctrl Pts',(-78.9053030366558,4.54475983782165,132.689343119692));
#93419=CARTESIAN_POINT('Ctrl Pts',(-78.9130493699211,4.59376156629696,132.561215117664));
#93420=CARTESIAN_POINT('Ctrl Pts',(-78.9207974379241,4.64277426836968,132.433058422257));
#93421=CARTESIAN_POINT('Ctrl Pts',(-78.9285455059271,4.6864068514414,132.302883397612));
#93422=CARTESIAN_POINT('Ctrl Pts',(-78.9362935739301,4.72450831469506,132.171183300608));
#93423=CARTESIAN_POINT('Ctrl Pts',(-78.944049876672,4.76265027263722,132.039343231173));
#93424=CARTESIAN_POINT('Ctrl Pts',(-78.9518061794138,4.79524925891879,131.905975227691));
#93425=CARTESIAN_POINT('Ctrl Pts',(-78.9595624821557,4.82220475387671,131.771585707289));
#93426=CARTESIAN_POINT('Ctrl Pts',(-78.9673229246699,4.84917463579392,131.637124459152));
#93427=CARTESIAN_POINT('Ctrl Pts',(-78.975083367184,4.87049496377423,131.501640993734));
#93428=CARTESIAN_POINT('Ctrl Pts',(-78.9828438096982,4.88611698271115,131.365648327891));
#93429=CARTESIAN_POINT('Ctrl Pts',(-78.9906167099636,4.90176407949974,131.229437354548));
#93430=CARTESIAN_POINT('Ctrl Pts',(-78.9983896102291,4.91169455942326,131.09271593749));
#93431=CARTESIAN_POINT('Ctrl Pts',(-79.0061625104945,4.91591178887908,130.955999486131));
#93432=CARTESIAN_POINT('Ctrl Pts',(-79.0136528462565,4.91997571142159,130.824253022148));
#93433=CARTESIAN_POINT('Ctrl Pts',(-79.0211431820185,4.91873455684636,130.692511477106));
#93434=CARTESIAN_POINT('Ctrl Pts',(-79.0286335177804,4.91223686376402,130.561230905729));
#93435=CARTESIAN_POINT('Ctrl Pts',(-79.0364078518995,4.90549280867349,130.424972791586));
#93436=CARTESIAN_POINT('Ctrl Pts',(-79.0441821860186,4.89306438006664,130.288779672029));
#93437=CARTESIAN_POINT('Ctrl Pts',(-79.0519565201377,4.87494887512056,130.15316438949));
#93438=CARTESIAN_POINT('Ctrl Pts',(-79.0597212730848,4.8568556959153,130.017716240666));
#93439=CARTESIAN_POINT('Ctrl Pts',(-79.0674860260318,4.83308943708872,129.882844895731));
#93440=CARTESIAN_POINT('Ctrl Pts',(-79.0752507789789,4.80369937102654,129.749061884837));
#93441=CARTESIAN_POINT('Ctrl Pts',(-79.0830078198639,4.7743384955923,129.615411749115));
#93442=CARTESIAN_POINT('Ctrl Pts',(-79.0907648607489,4.73936501195307,129.482848175685));
#93443=CARTESIAN_POINT('Ctrl Pts',(-79.0985219016339,4.698879785185,129.351875909598));
#93444=CARTESIAN_POINT('Ctrl Pts',(-79.106273092874,4.65842508864131,129.221002410716));
#93445=CARTESIAN_POINT('Ctrl Pts',(-79.1140242841143,4.61246703712198,129.091718202631));
#93446=CARTESIAN_POINT('Ctrl Pts',(-79.1217754753544,4.56115712006781,128.964515844615));
#93447=CARTESIAN_POINT('Ctrl Pts',(-79.1295233721315,4.50986901109719,128.837367550995));
#93448=CARTESIAN_POINT('Ctrl Pts',(-79.1372712689084,4.45323370671615,128.712299709382));
#93449=CARTESIAN_POINT('Ctrl Pts',(-79.1450191656855,4.39145183438493,128.58978755515));
#93450=CARTESIAN_POINT('Ctrl Pts',(-79.1527654417696,4.32968288548955,128.46730102782));
#93451=CARTESIAN_POINT('Ctrl Pts',(-79.1605117178537,4.26276968589406,128.3473694734));
#93452=CARTESIAN_POINT('Ctrl Pts',(-79.1682579939378,4.19095991364083,128.230445687978));
#93453=CARTESIAN_POINT('Ctrl Pts',(-79.1760043272032,4.11914961130408,128.113521039451));
#93454=CARTESIAN_POINT('Ctrl Pts',(-79.1837506604685,4.04244286879164,127.999604537378));
#93455=CARTESIAN_POINT('Ctrl Pts',(-79.1914969937339,3.96113178308632,127.889121680614));
#93456=CARTESIAN_POINT('Ctrl Pts',(-79.1992450617368,3.87980248832723,127.77861408198));
#93457=CARTESIAN_POINT('Ctrl Pts',(-79.2069931297399,3.79386703028029,127.67154197358));
#93458=CARTESIAN_POINT('Ctrl Pts',(-79.2147411977429,3.70365878029909,127.568299014071));
#93459=CARTESIAN_POINT('Ctrl Pts',(-79.2224975004847,3.6133546559162,127.464946326716));
#93460=CARTESIAN_POINT('Ctrl Pts',(-79.2302538032266,3.5187689257682,127.365431212729));
#93461=CARTESIAN_POINT('Ctrl Pts',(-79.2380101059685,3.42027331959384,127.270111972978));
#93462=CARTESIAN_POINT('Ctrl Pts',(-79.2457705484826,3.32172514334882,127.174741858478));
#93463=CARTESIAN_POINT('Ctrl Pts',(-79.2535309909968,3.21926322485227,127.083572340298));
#93464=CARTESIAN_POINT('Ctrl Pts',(-79.2612914335109,3.11329282639065,126.996921735634));
#93465=CARTESIAN_POINT('Ctrl Pts',(-79.2690643337764,3.00715231483781,126.910132031727));
#93466=CARTESIAN_POINT('Ctrl Pts',(-79.2768372340418,2.89749238147942,126.827875972196));
#93467=CARTESIAN_POINT('Ctrl Pts',(-79.2846101343073,2.78474847447253,126.750429316172));
#93468=CARTESIAN_POINT('Ctrl Pts',(-79.2921004700693,2.67610309247011,126.675798041171));
#93469=CARTESIAN_POINT('Ctrl Pts',(-79.2995908058313,2.56459432514578,126.605632736604));
#93470=CARTESIAN_POINT('Ctrl Pts',(-79.3070811415933,2.45063210056094,126.540139074283));
#93471=CARTESIAN_POINT('Ctrl Pts',(-79.3148554757124,2.33234896359275,126.472162199848));
#93472=CARTESIAN_POINT('Ctrl Pts',(-79.3226298098315,2.21104796567604,126.409002881004));
#93473=CARTESIAN_POINT('Ctrl Pts',(-79.3304041439506,2.08715911473177,126.350940595573));
#93474=CARTESIAN_POINT('Ctrl Pts',(-79.3381688968977,1.96342294572437,126.292949866719));
#93475=CARTESIAN_POINT('Ctrl Pts',(-79.3459336498449,1.8371056200571,126.240043837013));
#93476=CARTESIAN_POINT('Ctrl Pts',(-79.3536984027919,1.70866413546114,126.192457546741));
#93477=CARTESIAN_POINT('Ctrl Pts',(-79.3614554436769,1.58035022075839,126.144918519843));
#93478=CARTESIAN_POINT('Ctrl Pts',(-79.369212484562,1.44991670985441,126.102688852645));
#93479=CARTESIAN_POINT('Ctrl Pts',(-79.376969525447,1.31784277909337,126.065956511531));
#93480=CARTESIAN_POINT('Ctrl Pts',(-79.3847207166871,1.18586844631073,126.029251870561));
#93481=CARTESIAN_POINT('Ctrl Pts',(-79.3924719079271,1.05225653109541,125.998036408491));
#93482=CARTESIAN_POINT('Ctrl Pts',(-79.4002230991673,0.917503321256874,
125.972448913283));
#93483=CARTESIAN_POINT('Ctrl Pts',(-79.4079709959444,0.782807385127366,
125.946872293444));
#93484=CARTESIAN_POINT('Ctrl Pts',(-79.4157188927214,0.646971502460888,
125.926918955671));
#93485=CARTESIAN_POINT('Ctrl Pts',(-79.4234667894985,0.510503946279892,
125.912676982729));
#93486=CARTESIAN_POINT('Ctrl Pts',(-79.4312130655826,0.374064936169748,
125.8984379889));
#93487=CARTESIAN_POINT('Ctrl Pts',(-79.4389593416668,0.23699490397085,125.889908024145));
#93488=CARTESIAN_POINT('Ctrl Pts',(-79.4467056177509,0.099808675887804,
125.887123457258));
#93489=CARTESIAN_POINT('Ctrl Pts',(-79.4544519510163,-0.0373785648730006,
125.884338869815));
#93490=CARTESIAN_POINT('Ctrl Pts',(-79.4621982842816,-0.174681612344805,
125.887299772803));
#93491=CARTESIAN_POINT('Ctrl Pts',(-79.469944617547,-0.311584596734984,
125.895990409281));
#93492=CARTESIAN_POINT('Ctrl Pts',(-79.47769268555,-0.448518239599112,125.904682991968));
#93493=CARTESIAN_POINT('Ctrl Pts',(-79.4854407535529,-0.585051251000035,
125.91910783667));
#93494=CARTESIAN_POINT('Ctrl Pts',(-79.4931888215558,-0.720672239401334,
125.939197250745));
#93495=CARTESIAN_POINT('Ctrl Pts',(-79.5009451242977,-0.856437367403201,
125.959308016089));
#93496=CARTESIAN_POINT('Ctrl Pts',(-79.5087014270396,-0.991288148744622,
125.985095319768));
#93497=CARTESIAN_POINT('Ctrl Pts',(-79.5164577297814,-1.12472220575496,
126.016440085395));
#93498=CARTESIAN_POINT('Ctrl Pts',(-79.5242181722956,-1.25822748053915,
126.047801580668));
#93499=CARTESIAN_POINT('Ctrl Pts',(-79.5319786148098,-1.39031414795729,
126.084726343056));
#93500=CARTESIAN_POINT('Ctrl Pts',(-79.539739057324,-1.52049534457306,126.12704547214));
#93501=CARTESIAN_POINT('Ctrl Pts',(-79.5475119575894,-1.65088551960258,
126.169432535647));
#93502=CARTESIAN_POINT('Ctrl Pts',(-79.5552848578548,-1.77936374467216,
126.217231133919));
#93503=CARTESIAN_POINT('Ctrl Pts',(-79.5630577581203,-1.90546264544854,
126.270223966637));
#93504=CARTESIAN_POINT('Ctrl Pts',(-79.5705480938823,-2.0269775335574,126.321290376404));
#93505=CARTESIAN_POINT('Ctrl Pts',(-79.5780384296443,-2.14628280396557,
126.377179799445));
#93506=CARTESIAN_POINT('Ctrl Pts',(-79.5855287654063,-2.26298384302322,
126.43765852231));
#93507=CARTESIAN_POINT('Ctrl Pts',(-79.5933039768102,-2.38412330573238,
126.500437397736));
#93508=CARTESIAN_POINT('Ctrl Pts',(-79.601079188214,-2.50284030305716,126.568360453214));
#93509=CARTESIAN_POINT('Ctrl Pts',(-79.6088543996178,-2.61866711537292,
126.641216901411));
#93510=CARTESIAN_POINT('Ctrl Pts',(-79.6166198354763,-2.73434830203286,
126.71398174933));
#93511=CARTESIAN_POINT('Ctrl Pts',(-79.6243852713348,-2.84714620647429,
126.791667441216));
#93512=CARTESIAN_POINT('Ctrl Pts',(-79.6321507071932,-2.95661595060341,
126.874016461752));
#93513=CARTESIAN_POINT('Ctrl Pts',(-79.6399683387051,-3.06682149951219,
126.95691899416));
#93514=CARTESIAN_POINT('Ctrl Pts',(-79.6477859702169,-3.1736536130799,127.044547616851));
#93515=CARTESIAN_POINT('Ctrl Pts',(-79.6556036017287,-3.27668541495413,
127.136593482929));
#93516=CARTESIAN_POINT('Ctrl Pts',(-79.6633544764349,-3.3788374012524,127.227853345217));
#93517=CARTESIAN_POINT('Ctrl Pts',(-79.6711053511411,-3.47725342455917,
127.323455045077));
#93518=CARTESIAN_POINT('Ctrl Pts',(-79.6788562258473,-3.57154877839179,
127.423055782733));
#93519=CARTESIAN_POINT('Ctrl Pts',(-79.6866035385961,-3.66580079827105,
127.522610748317));
#93520=CARTESIAN_POINT('Ctrl Pts',(-79.6943508513448,-3.75593564865222,
127.626160811545));
#93521=CARTESIAN_POINT('Ctrl Pts',(-79.7020981640935,-3.84160486831608,
127.7333257597));
#93522=CARTESIAN_POINT('Ctrl Pts',(-79.7098435942767,-3.92725327070679,
127.840464667207));
#93523=CARTESIAN_POINT('Ctrl Pts',(-79.7175890244597,-4.00843795881415,
127.951216405861));
#93524=CARTESIAN_POINT('Ctrl Pts',(-79.7253344546428,-4.08485048633842,
128.06516738474));
#93525=CARTESIAN_POINT('Ctrl Pts',(-79.733204405379,-4.16249147115516,128.180950313373));
#93526=CARTESIAN_POINT('Ctrl Pts',(-79.7410743561153,-4.2352052709196,128.300035912439));
#93527=CARTESIAN_POINT('Ctrl Pts',(-79.7489443068515,-4.30271412888976,
128.421959688345));
#93528=CARTESIAN_POINT('Ctrl Pts',(-79.7566934781813,-4.36918693465726,
128.542012311333));
#93529=CARTESIAN_POINT('Ctrl Pts',(-79.7644426495111,-4.43061327347606,
128.664816244655));
#93530=CARTESIAN_POINT('Ctrl Pts',(-79.7721918208409,-4.4867747180714,128.789903943479));
#93531=CARTESIAN_POINT('Ctrl Pts',(-79.7801221612803,-4.54424917001703,
128.917916087518));
#93532=CARTESIAN_POINT('Ctrl Pts',(-79.7880525017197,-4.59620932889364,
129.048319707534));
#93533=CARTESIAN_POINT('Ctrl Pts',(-79.7959828421592,-4.64247390309608,
129.18059366336));
#93534=CARTESIAN_POINT('Ctrl Pts',(-79.8039131825986,-4.68873847729852,
129.312867619186));
#93535=CARTESIAN_POINT('Ctrl Pts',(-79.8118435230381,-4.72930737185479,
129.447011483947));
#93536=CARTESIAN_POINT('Ctrl Pts',(-79.8197738634775,-4.76405452823417,
129.582490119309));
#93537=CARTESIAN_POINT('Origin',(213.235140564004,0.,130.804360617566));
#93538=CARTESIAN_POINT('',(-81.9152188971548,-4.76405452823409,129.582490119308));
#93539=CARTESIAN_POINT('',(-81.5701083236629,-4.76405452823402,129.582490119308));
#93540=CARTESIAN_POINT('',(213.235140564004,-4.76405452823405,129.582490119308));
#93541=CARTESIAN_POINT('',(-80.2351405639591,-4.91824936580377,130.801862964505));
#93542=CARTESIAN_POINT('Ctrl Pts',(-80.2351405640087,-4.91824936580422,
130.801862965385));
#93543=CARTESIAN_POINT('Ctrl Pts',(-80.2429981429322,-4.91832015776003,
130.941262876391));
#93544=CARTESIAN_POINT('Ctrl Pts',(-80.2508557218557,-4.91245999970312,
131.080655168156));
#93545=CARTESIAN_POINT('Ctrl Pts',(-80.2587133007792,-4.90069735131702,
131.219509426181));
#93546=CARTESIAN_POINT('Ctrl Pts',(-80.2665731437013,-4.88893131376744,
131.358403692184));
#93547=CARTESIAN_POINT('Ctrl Pts',(-80.2744329866233,-4.87125942953433,
131.496759241733));
#93548=CARTESIAN_POINT('Ctrl Pts',(-80.2822928295454,-4.84776201245914,
131.634051242473));
#93549=CARTESIAN_POINT('Ctrl Pts',(-80.290156443864,-4.82425332059426,131.771409120173));
#93550=CARTESIAN_POINT('Ctrl Pts',(-80.2980200581826,-4.79491359097808,
131.907702062928));
#93551=CARTESIAN_POINT('Ctrl Pts',(-80.3058836725012,-4.75987413255851,
132.042416070565));
#93552=CARTESIAN_POINT('Ctrl Pts',(-80.3138335865165,-4.72445013154641,
132.178608504984));
#93553=CARTESIAN_POINT('Ctrl Pts',(-80.3217835005318,-4.68320065663003,
132.313186761867));
#93554=CARTESIAN_POINT('Ctrl Pts',(-80.3297334145472,-4.63631250990897,
132.445637368441));
#93555=CARTESIAN_POINT('Ctrl Pts',(-80.3376137588887,-4.58983468121998,
132.576928900152));
#93556=CARTESIAN_POINT('Ctrl Pts',(-80.3454941032303,-4.53781668310194,
132.706129550449));
#93557=CARTESIAN_POINT('Ctrl Pts',(-80.3533744475718,-4.48048797077733,
132.832761614958));
#93558=CARTESIAN_POINT('Ctrl Pts',(-80.361359146424,-4.42240008988507,132.961070589327));
#93559=CARTESIAN_POINT('Ctrl Pts',(-80.3693438452763,-4.35886003026248,
133.086742111878));
#93560=CARTESIAN_POINT('Ctrl Pts',(-80.3773285441286,-4.29015297255464,
133.209307713571));
#93561=CARTESIAN_POINT('Ctrl Pts',(-80.3853132429809,-4.22144591484662,
133.331873315263));
#93562=CARTESIAN_POINT('Ctrl Pts',(-80.3932979418332,-4.14757212034963,
133.451332694959));
#93563=CARTESIAN_POINT('Ctrl Pts',(-80.4012826406855,-4.06885992385342,
133.567250767854));
#93564=CARTESIAN_POINT('Ctrl Pts',(-80.4090569748045,-3.99222147747906,
133.680114865273));
#93565=CARTESIAN_POINT('Ctrl Pts',(-80.4168313089237,-3.91076206017412,
133.789966560684));
#93566=CARTESIAN_POINT('Ctrl Pts',(-80.4246056430427,-3.82474613354405,
133.896366451396));
#93567=CARTESIAN_POINT('Ctrl Pts',(-80.4323703959898,-3.73883621385586,
134.002635213753));
#93568=CARTESIAN_POINT('Ctrl Pts',(-80.4401351489369,-3.64838120142737,
134.105460334563));
#93569=CARTESIAN_POINT('Ctrl Pts',(-80.447899901884,-3.55368926504029,134.204430568323));
#93570=CARTESIAN_POINT('Ctrl Pts',(-80.455656942769,-3.45909137801935,134.303302503451));
#93571=CARTESIAN_POINT('Ctrl Pts',(-80.463413983654,-3.36026521002513,134.398326890205));
#93572=CARTESIAN_POINT('Ctrl Pts',(-80.471171024539,-3.25755946347702,134.489125115388));
#93573=CARTESIAN_POINT('Ctrl Pts',(-80.4789222157791,-3.15493116813146,
134.579854868924));
#93574=CARTESIAN_POINT('Ctrl Pts',(-80.4866734070194,-3.0484294092288,134.666364546477));
#93575=CARTESIAN_POINT('Ctrl Pts',(-80.4944245982595,-2.93843978649981,
134.748312275943));
#93576=CARTESIAN_POINT('Ctrl Pts',(-80.5021724950366,-2.8284969122944,134.830225175438));
#93577=CARTESIAN_POINT('Ctrl Pts',(-80.5099203918136,-2.71506943557235,
134.907579750174));
#93578=CARTESIAN_POINT('Ctrl Pts',(-80.5176682885907,-2.59857591120857,
134.980074484222));
#93579=CARTESIAN_POINT('Ctrl Pts',(-80.5254145646748,-2.48210675477877,
135.052554053935));
#93580=CARTESIAN_POINT('Ctrl Pts',(-80.5331608407589,-2.36257315811835,
135.120175598543));
#93581=CARTESIAN_POINT('Ctrl Pts',(-80.540907116843,-2.24042218753757,135.182681241286));
#93582=CARTESIAN_POINT('Ctrl Pts',(-80.5486534501083,-2.11827031526657,
135.24518734543));
#93583=CARTESIAN_POINT('Ctrl Pts',(-80.5563997833736,-1.99350137856661,
135.302577294256));
#93584=CARTESIAN_POINT('Ctrl Pts',(-80.5641461166389,-1.86658618060849,
135.354639630205));
#93585=CARTESIAN_POINT('Ctrl Pts',(-80.5718941846418,-1.73964256087193,
135.406713625153));
#93586=CARTESIAN_POINT('Ctrl Pts',(-80.5796422526449,-1.61055208510356,
135.453457484778));
#93587=CARTESIAN_POINT('Ctrl Pts',(-80.5873903206479,-1.47980424453522,
135.494708414943));
#93588=CARTESIAN_POINT('Ctrl Pts',(-80.5951466233897,-1.34891744360548,
135.536003187087));
#93589=CARTESIAN_POINT('Ctrl Pts',(-80.6029029261314,-1.21637013259876,
135.571793250013));
#93590=CARTESIAN_POINT('Ctrl Pts',(-80.6106592288733,-1.08266617061231,
135.601965960392));
#93591=CARTESIAN_POINT('Ctrl Pts',(-80.6184196713874,-0.948890846795597,
135.632154774854));
#93592=CARTESIAN_POINT('Ctrl Pts',(-80.6261801139018,-0.813958026352576,
135.656720192708));
#93593=CARTESIAN_POINT('Ctrl Pts',(-80.6339405564159,-0.678379408417407,
135.675601161897));
#93594=CARTESIAN_POINT('Ctrl Pts',(-80.6417134566814,-0.542583147648625,
135.694512440494));
#93595=CARTESIAN_POINT('Ctrl Pts',(-80.6494863569467,-0.406139407117813,
135.707720997712));
#93596=CARTESIAN_POINT('Ctrl Pts',(-80.6572592572121,-0.269563528597922,
135.715217830574));
#93597=CARTESIAN_POINT('Ctrl Pts',(-80.6647495929741,-0.137952527276476,
135.722442134678));
#93598=CARTESIAN_POINT('Ctrl Pts',(-80.6722399287361,-0.00621913625590731,
135.724362771354));
#93599=CARTESIAN_POINT('Ctrl Pts',(-80.6797302644981,0.125179556277915,
135.72101732118));
#93600=CARTESIAN_POINT('Ctrl Pts',(-80.6875045986172,0.261560270176754,
135.717545027245));
#93601=CARTESIAN_POINT('Ctrl Pts',(-80.6952789327363,0.398012417497684,
135.708388437062));
#93602=CARTESIAN_POINT('Ctrl Pts',(-80.7030532668554,0.534023368354635,
135.693532541783));
#93603=CARTESIAN_POINT('Ctrl Pts',(-80.7108180198025,0.669866697870671,
135.678694955067));
#93604=CARTESIAN_POINT('Ctrl Pts',(-80.7185827727496,0.805269527871059,
135.658172080733));
#93605=CARTESIAN_POINT('Ctrl Pts',(-80.7263475256966,0.939719293111635,
135.632000901665));
#93606=CARTESIAN_POINT('Ctrl Pts',(-80.7341045665816,1.07403552094997,135.605855716181));
#93607=CARTESIAN_POINT('Ctrl Pts',(-80.7418616074666,1.20740018652085,135.574073464285));
#93608=CARTESIAN_POINT('Ctrl Pts',(-80.7496186483516,1.33930626964343,135.536742869518));
#93609=CARTESIAN_POINT('Ctrl Pts',(-80.7573698395917,1.47111288136246,135.499440426043));
#93610=CARTESIAN_POINT('Ctrl Pts',(-80.7651210308318,1.60146272530599,135.456598073826));
#93611=CARTESIAN_POINT('Ctrl Pts',(-80.7728722220719,1.72985974871705,135.408355438617));
#93612=CARTESIAN_POINT('Ctrl Pts',(-80.780620118849,1.85820219996823,135.360133307816));
#93613=CARTESIAN_POINT('Ctrl Pts',(-80.7883680156261,1.98459311627731,135.306515596352));
#93614=CARTESIAN_POINT('Ctrl Pts',(-80.7961159124032,2.10855258462038,135.247691469572));
#93615=CARTESIAN_POINT('Ctrl Pts',(-80.8038621884873,2.23248612331493,135.188879647532));
#93616=CARTESIAN_POINT('Ctrl Pts',(-80.8116084645714,2.3539888727009,135.124863743903));
#93617=CARTESIAN_POINT('Ctrl Pts',(-80.8193547406555,2.47260222349409,135.055880499546));
#93618=CARTESIAN_POINT('Ctrl Pts',(-80.8271010739208,2.59121644986393,134.986896745971));
#93619=CARTESIAN_POINT('Ctrl Pts',(-80.8348474071862,2.70694089711576,134.912945775053));
#93620=CARTESIAN_POINT('Ctrl Pts',(-80.8425937404515,2.81934317940427,134.834309388859));
#93621=CARTESIAN_POINT('Ctrl Pts',(-80.8503418084545,2.9317706334047,134.755655392592));
#93622=CARTESIAN_POINT('Ctrl Pts',(-80.8580898764575,3.04087412172568,134.672314117205));
#93623=CARTESIAN_POINT('Ctrl Pts',(-80.8658379444604,3.14625209908134,134.584609391328));
#93624=CARTESIAN_POINT('Ctrl Pts',(-80.8735942472023,3.2517420734052,134.496811451824));
#93625=CARTESIAN_POINT('Ctrl Pts',(-80.8813505499442,3.35349832621974,134.404641048372));
#93626=CARTESIAN_POINT('Ctrl Pts',(-80.889106852686,3.4511537393512,134.308461205429));
#93627=CARTESIAN_POINT('Ctrl Pts',(-80.8968672952002,3.54886127411726,134.212230028408));
#93628=CARTESIAN_POINT('Ctrl Pts',(-80.9046277377143,3.64246334125349,134.111985433467));
#93629=CARTESIAN_POINT('Ctrl Pts',(-80.9123881802285,3.73163199005489,134.008124927452));
#93630=CARTESIAN_POINT('Ctrl Pts',(-80.9201610804939,3.82094378028736,133.904097695332));
#93631=CARTESIAN_POINT('Ctrl Pts',(-80.9279339807593,3.90580768814124,133.79644325995));
#93632=CARTESIAN_POINT('Ctrl Pts',(-80.9357068810247,3.98593758434089,133.685590326603));
#93633=CARTESIAN_POINT('Ctrl Pts',(-80.9431972167869,4.06315455697952,133.578767176604));
#93634=CARTESIAN_POINT('Ctrl Pts',(-80.950687552549,4.13597555862536,133.468974294892));
#93635=CARTESIAN_POINT('Ctrl Pts',(-80.9581778883111,4.20418513955255,133.35661655592));
#93636=CARTESIAN_POINT('Ctrl Pts',(-80.9659522224301,4.27498090747135,133.239998739128));
#93637=CARTESIAN_POINT('Ctrl Pts',(-80.9737265565493,4.34103292747858,133.120248322405));
#93638=CARTESIAN_POINT('Ctrl Pts',(-80.9815008906683,4.40205148322949,132.997788483145));
#93639=CARTESIAN_POINT('Ctrl Pts',(-80.9892656436154,4.46299483906398,132.875479564691));
#93640=CARTESIAN_POINT('Ctrl Pts',(-80.9970303965624,4.51891690066217,132.750468214128));
#93641=CARTESIAN_POINT('Ctrl Pts',(-81.0047951495095,4.56957172873663,132.623205657263));
#93642=CARTESIAN_POINT('Ctrl Pts',(-81.0125521903944,4.62017624572146,132.496069499364));
#93643=CARTESIAN_POINT('Ctrl Pts',(-81.0203092312795,4.66552379643557,132.366686945663));
#93644=CARTESIAN_POINT('Ctrl Pts',(-81.0280662721644,4.70541496971352,132.235532523836));
#93645=CARTESIAN_POINT('Ctrl Pts',(-81.0358174634046,4.74527606074778,132.104477006578));
#93646=CARTESIAN_POINT('Ctrl Pts',(-81.0435686546447,4.7796888510925,131.971652653312));
#93647=CARTESIAN_POINT('Ctrl Pts',(-81.0513198458848,4.80850268321464,131.8375522784));
#93648=CARTESIAN_POINT('Ctrl Pts',(-81.0590677426619,4.83730426868938,131.703508899726));
#93649=CARTESIAN_POINT('Ctrl Pts',(-81.066815639439,4.8605115470373,131.568190959527));
#93650=CARTESIAN_POINT('Ctrl Pts',(-81.0745635362161,4.8780242637094,131.432104470712));
#93651=CARTESIAN_POINT('Ctrl Pts',(-81.0823098123002,4.89553331709871,131.296046448256));
#93652=CARTESIAN_POINT('Ctrl Pts',(-81.0900560883843,4.90735012826414,131.159220584475));
#93653=CARTESIAN_POINT('Ctrl Pts',(-81.0978023644684,4.91342598447547,131.022140684563));
#93654=CARTESIAN_POINT('Ctrl Pts',(-81.1055486977337,4.91950188553737,130.885059772759));
#93655=CARTESIAN_POINT('Ctrl Pts',(-81.1132950309991,4.91983672977018,130.747725211666));
#93656=CARTESIAN_POINT('Ctrl Pts',(-81.1210413642644,4.91443389012269,130.61065310064));
#93657=CARTESIAN_POINT('Ctrl Pts',(-81.1287894322674,4.90902984054669,130.473550293265));
#93658=CARTESIAN_POINT('Ctrl Pts',(-81.1365375002703,4.89788556565461,130.336710443499));
#93659=CARTESIAN_POINT('Ctrl Pts',(-81.1442855682733,4.88105646660766,130.200646420046));
#93660=CARTESIAN_POINT('Ctrl Pts',(-81.1520418710152,4.86420948139404,130.06443778613));
#93661=CARTESIAN_POINT('Ctrl Pts',(-81.159798173757,4.84166565074942,129.929007014297));
#93662=CARTESIAN_POINT('Ctrl Pts',(-81.1675544764989,4.81353196109052,129.794859195051));
#93663=CARTESIAN_POINT('Ctrl Pts',(-81.175314919013,4.78538325563429,129.660639777074));
#93664=CARTESIAN_POINT('Ctrl Pts',(-81.1830753615273,4.75163884248064,129.527705054868));
#93665=CARTESIAN_POINT('Ctrl Pts',(-81.1908358040414,4.71245589003037,129.396545804809));
#93666=CARTESIAN_POINT('Ctrl Pts',(-81.1986087043069,4.67321003762633,129.265176006278));
#93667=CARTESIAN_POINT('Ctrl Pts',(-81.2063816045722,4.62850832731785,129.1355877452));
#93668=CARTESIAN_POINT('Ctrl Pts',(-81.2141545048376,4.57855678115273,129.008253475923));
#93669=CARTESIAN_POINT('Ctrl Pts',(-81.2216448405997,4.53042109951067,128.88554812807));
#93670=CARTESIAN_POINT('Ctrl Pts',(-81.2291351763618,4.47741076877118,128.764936022581));
#93671=CARTESIAN_POINT('Ctrl Pts',(-81.2366255121239,4.41974996544118,128.646817267948));
#93672=CARTESIAN_POINT('Ctrl Pts',(-81.244399846243,4.35990293522789,128.524220004832));
#93673=CARTESIAN_POINT('Ctrl Pts',(-81.2521741803621,4.2948562483551,128.403920544404));
#93674=CARTESIAN_POINT('Ctrl Pts',(-81.2599485144812,4.22480933718678,128.286391370947));
#93675=CARTESIAN_POINT('Ctrl Pts',(-81.2677132674283,4.15484875257602,128.169007041692));
#93676=CARTESIAN_POINT('Ctrl Pts',(-81.2754780203754,4.07990040310759,128.054386538923));
#93677=CARTESIAN_POINT('Ctrl Pts',(-81.2832427733225,4.00021098164112,127.942980676898));
#93678=CARTESIAN_POINT('Ctrl Pts',(-81.2909998142075,3.92060070883148,127.831685464746));
#93679=CARTESIAN_POINT('Ctrl Pts',(-81.2987568550926,3.83625896093346,127.723598855399));
#93680=CARTESIAN_POINT('Ctrl Pts',(-81.3065138959776,3.74747718491634,127.619145112921));
#93681=CARTESIAN_POINT('Ctrl Pts',(-81.3142650872177,3.65876235992774,127.514770139823));
#93682=CARTESIAN_POINT('Ctrl Pts',(-81.3220162784578,3.56561442350507,127.41402287733));
#93683=CARTESIAN_POINT('Ctrl Pts',(-81.3297674696979,3.46836656025204,127.317296456094));
#93684=CARTESIAN_POINT('Ctrl Pts',(-81.337515366475,3.37116002993441,127.220611146165));
#93685=CARTESIAN_POINT('Ctrl Pts',(-81.345263263252,3.26985731525767,127.127943553625));
#93686=CARTESIAN_POINT('Ctrl Pts',(-81.3530111600291,3.16482994918056,127.0396515378));
#93687=CARTESIAN_POINT('Ctrl Pts',(-81.3607574361132,3.05982455256459,126.951377990763));
#93688=CARTESIAN_POINT('Ctrl Pts',(-81.3685037121973,2.95109635333172,126.867478451328));
#93689=CARTESIAN_POINT('Ctrl Pts',(-81.3762499882814,2.839051299925,126.788271627156));
#93690=CARTESIAN_POINT('Ctrl Pts',(-81.3839963215468,2.727005419427,126.709064218296));
#93691=CARTESIAN_POINT('Ctrl Pts',(-81.3917426548122,2.6116429551485,126.634549819506));
#93692=CARTESIAN_POINT('Ctrl Pts',(-81.3994889880775,2.49339993925729,126.565004557336));
#93693=CARTESIAN_POINT('Ctrl Pts',(-81.4072370560806,2.37513044366202,126.495443720986));
#93694=CARTESIAN_POINT('Ctrl Pts',(-81.4149851240835,2.25397944975393,126.430854433777));
#93695=CARTESIAN_POINT('Ctrl Pts',(-81.4227331920866,2.13040839418066,126.371467303205));
#93696=CARTESIAN_POINT('Ctrl Pts',(-81.4304894948284,2.00670600581951,126.312017055284));
#93697=CARTESIAN_POINT('Ctrl Pts',(-81.4382457975703,1.8805787707504,126.257780178224));
#93698=CARTESIAN_POINT('Ctrl Pts',(-81.4460021003122,1.75250946469014,126.208939675076));
#93699=CARTESIAN_POINT('Ctrl Pts',(-81.4537625428264,1.62437180418514,126.160073104282));
#93700=CARTESIAN_POINT('Ctrl Pts',(-81.4615229853405,1.49429037792357,126.116608770296));
#93701=CARTESIAN_POINT('Ctrl Pts',(-81.4692834278547,1.36276304332975,126.078679719512));
#93702=CARTESIAN_POINT('Ctrl Pts',(-81.4770563281201,1.231024569382,126.040689781648));
#93703=CARTESIAN_POINT('Ctrl Pts',(-81.4848292283855,1.09783592888468,126.008252976067));
#93704=CARTESIAN_POINT('Ctrl Pts',(-81.492602128651,0.963705971011835,125.981451343701));
#93705=CARTESIAN_POINT('Ctrl Pts',(-81.500092464413,0.834451974961738,125.95562401818));
#93706=CARTESIAN_POINT('Ctrl Pts',(-81.5075828001749,0.704324216090279,
125.935029321632));
#93707=CARTESIAN_POINT('Ctrl Pts',(-81.5150731359369,0.573780489878895,
125.919694916422));
#93708=CARTESIAN_POINT('Ctrl Pts',(-81.522847470056,0.438287158609339,125.903779102578));
#93709=CARTESIAN_POINT('Ctrl Pts',(-81.5306218041751,0.301916492385118,
125.893479925623));
#93710=CARTESIAN_POINT('Ctrl Pts',(-81.5383961382941,0.165173803679244,
125.888884986757));
#93711=CARTESIAN_POINT('Ctrl Pts',(-81.5461608912412,0.0285996381161548,
125.884295710743));
#93712=CARTESIAN_POINT('Ctrl Pts',(-81.5539256441882,-0.108345250687616,
125.88539669829));
#93713=CARTESIAN_POINT('Ctrl Pts',(-81.5616903971353,-0.245148236411733,
125.892224075827));
#93714=CARTESIAN_POINT('Ctrl Pts',(-81.5694474380203,-0.381815347482217,
125.899044672317));
#93715=CARTESIAN_POINT('Ctrl Pts',(-81.5772044789055,-0.518340447997844,
125.911580320992));
#93716=CARTESIAN_POINT('Ctrl Pts',(-81.5849615197905,-0.654209058381405,
125.929815144352));
#93717=CARTESIAN_POINT('Ctrl Pts',(-81.5927127110307,-0.789975209189526,
125.94803621669));
#93718=CARTESIAN_POINT('Ctrl Pts',(-81.6004639022708,-0.92508546933795,
125.971947857423));
#93719=CARTESIAN_POINT('Ctrl Pts',(-81.608215093511,-1.05902899246004,126.001482245628));
#93720=CARTESIAN_POINT('Ctrl Pts',(-81.6159629902881,-1.19291558601083,
126.03100408093));
#93721=CARTESIAN_POINT('Ctrl Pts',(-81.6237108870652,-1.32563604783668,
126.06614382653));
#93722=CARTESIAN_POINT('Ctrl Pts',(-81.6314587838422,-1.45668847810984,
126.106782332934));
#93723=CARTESIAN_POINT('Ctrl Pts',(-81.6392050599264,-1.58771349504011,
126.14741233864));
#93724=CARTESIAN_POINT('Ctrl Pts',(-81.6469513360104,-1.71707080124438,
126.193538701573));
#93725=CARTESIAN_POINT('Ctrl Pts',(-81.6546976120946,-1.8442728338938,126.244992155086));
#93726=CARTESIAN_POINT('Ctrl Pts',(-81.6624439453599,-1.97147580551956,
126.296445988416));
#93727=CARTESIAN_POINT('Ctrl Pts',(-81.6701902786253,-2.096523109407,126.353226844186));
#93728=CARTESIAN_POINT('Ctrl Pts',(-81.6779366118907,-2.21894674643024,
126.415117129332));
#93729=CARTESIAN_POINT('Ctrl Pts',(-81.6856846798936,-2.34139779937766,
126.477021274377));
#93730=CARTESIAN_POINT('Ctrl Pts',(-81.6934327478966,-2.46122366745418,
126.544036949308));
#93731=CARTESIAN_POINT('Ctrl Pts',(-81.7011808158995,-2.5779809162625,126.61590058339));
#93732=CARTESIAN_POINT('Ctrl Pts',(-81.7089371186414,-2.69486225606475,
126.687840594998));
#93733=CARTESIAN_POINT('Ctrl Pts',(-81.7166934213832,-2.80866812818763,
126.76463865311));
#93734=CARTESIAN_POINT('Ctrl Pts',(-81.7244497241251,-2.91898361491308,
126.845987502463));
#93735=CARTESIAN_POINT('Ctrl Pts',(-81.7322101666393,-3.02935798033532,
126.927379770146));
#93736=CARTESIAN_POINT('Ctrl Pts',(-81.7399706091535,-3.13623794380125,
127.013327423963));
#93737=CARTESIAN_POINT('Ctrl Pts',(-81.7477310516677,-3.23924246551425,
127.103483517187));
#93738=CARTESIAN_POINT('Ctrl Pts',(-81.7555039519331,-3.34241233922981,
127.193784336976));
#93739=CARTESIAN_POINT('Ctrl Pts',(-81.7632768521986,-3.44169405592559,
127.288306826595));
#93740=CARTESIAN_POINT('Ctrl Pts',(-81.771049752464,-3.53674354683358,127.386667221951));
#93741=CARTESIAN_POINT('Ctrl Pts',(-81.778540088226,-3.62833774933107,127.48145196918));
#93742=CARTESIAN_POINT('Ctrl Pts',(-81.7860304239879,-3.71600188302689,
127.57980020159));
#93743=CARTESIAN_POINT('Ctrl Pts',(-81.7935207597499,-3.79946522514793,
127.681341715063));
#93744=CARTESIAN_POINT('Ctrl Pts',(-81.8012637578307,-3.88574393392626,
127.786308403997));
#93745=CARTESIAN_POINT('Ctrl Pts',(-81.8090067559115,-3.96781483318949,
127.89503003215));
#93746=CARTESIAN_POINT('Ctrl Pts',(-81.8167497539922,-4.0453310506335,128.007133463172));
#93747=CARTESIAN_POINT('Ctrl Pts',(-81.8244831899834,-4.12275154068426,
128.119098453883));
#93748=CARTESIAN_POINT('Ctrl Pts',(-81.8322166259745,-4.19562831494933,
128.234436619325));
#93749=CARTESIAN_POINT('Ctrl Pts',(-81.8399500619657,-4.26365359300274,
128.352740520289));
#93750=CARTESIAN_POINT('Ctrl Pts',(-81.84767405617,-4.33159581868827,128.470899983487));
#93751=CARTESIAN_POINT('Ctrl Pts',(-81.8553980503743,-4.39469814749423,
128.592017632574));
#93752=CARTESIAN_POINT('Ctrl Pts',(-81.8631220445786,-4.45269553496809,
128.715656345685));
#93753=CARTESIAN_POINT('Ctrl Pts',(-81.8708406093801,-4.51065215452198,
128.839208149826));
#93754=CARTESIAN_POINT('Ctrl Pts',(-81.8785591741816,-4.56351080343583,
128.965277137834));
#93755=CARTESIAN_POINT('Ctrl Pts',(-81.8862777389832,-4.6110519036736,129.093400827235));
#93756=CARTESIAN_POINT('Ctrl Pts',(-81.8939921687289,-4.65856753478472,
129.221455877113));
#93757=CARTESIAN_POINT('Ctrl Pts',(-81.9017065984746,-4.70077115122349,
129.351563068366));
#93758=CARTESIAN_POINT('Ctrl Pts',(-81.9094210282204,-4.73749114772036,
129.483239620923));
#93759=CARTESIAN_POINT('Ctrl Pts',(-81.9113536511985,-4.74669026046447,
129.516227299798));
#93760=CARTESIAN_POINT('Ctrl Pts',(-81.9132862741767,-4.75554545824106,
129.549313384549));
#93761=CARTESIAN_POINT('Ctrl Pts',(-81.9152188971548,-4.76405452823409,
129.582490119308));
#93762=CARTESIAN_POINT('Ctrl Pts',(-80.1654084279176,-4.76405452823404,
129.582490119308));
#93763=CARTESIAN_POINT('Ctrl Pts',(-80.1739907747347,-4.80160086113247,
129.728882701434));
#93764=CARTESIAN_POINT('Ctrl Pts',(-80.1825731215518,-4.83243972327195,
129.877179793995));
#93765=CARTESIAN_POINT('Ctrl Pts',(-80.1911554683689,-4.85639332437589,
130.026783006355));
#93766=CARTESIAN_POINT('Ctrl Pts',(-80.1996984730164,-4.88023712024129,
130.175700425528));
#93767=CARTESIAN_POINT('Ctrl Pts',(-80.2082414776637,-4.89725853709734,
130.32591178946));
#93768=CARTESIAN_POINT('Ctrl Pts',(-80.2167844823112,-4.90733053367499,
130.476808948724));
#93769=CARTESIAN_POINT('Ctrl Pts',(-80.2229031761938,-4.9145443262912,130.584884920049));
#93770=CARTESIAN_POINT('Ctrl Pts',(-80.2290218700766,-4.91819424011381,
130.693312303923));
#93771=CARTESIAN_POINT('Ctrl Pts',(-80.2351405639592,-4.91824936580377,
130.801862964505));
#93772=CARTESIAN_POINT('',(-79.8898594360288,-4.91824928709222,130.801712501838));
#93773=CARTESIAN_POINT('Ctrl Pts',(-79.8197738634775,-4.76405452823417,
129.582490119309));
#93774=CARTESIAN_POINT('Ctrl Pts',(-79.827546945423,-4.79811264918998,129.715282216011));
#93775=CARTESIAN_POINT('Ctrl Pts',(-79.8353200273684,-4.82657777092677,
129.849356243151));
#93776=CARTESIAN_POINT('Ctrl Pts',(-79.8430931093139,-4.84938363127091,
129.984201206682));
#93777=CARTESIAN_POINT('Ctrl Pts',(-79.8500542026156,-4.86980715475825,
130.104960048412));
#93778=CARTESIAN_POINT('Ctrl Pts',(-79.8570152959173,-4.88569270901646,
130.226336888437));
#93779=CARTESIAN_POINT('Ctrl Pts',(-79.863976389219,-4.89702818777626,130.347963870618));
#93780=CARTESIAN_POINT('Ctrl Pts',(-79.8726040714764,-4.91107754823396,
130.498710155822));
#93781=CARTESIAN_POINT('Ctrl Pts',(-79.8812317537339,-4.91816766298115,
130.650115038787));
#93782=CARTESIAN_POINT('Ctrl Pts',(-79.8898594359913,-4.91824928709186,
130.80171250118));
#93783=CARTESIAN_POINT('Ctrl Pts',(-79.8898594360288,-4.91824928709222,
130.801712501838));
#93784=CARTESIAN_POINT('Ctrl Pts',(-79.8975364691867,-4.91832191735719,
130.936606058499));
#93785=CARTESIAN_POINT('Ctrl Pts',(-79.9052135023444,-4.91284074513111,
131.071724769537));
#93786=CARTESIAN_POINT('Ctrl Pts',(-79.9128905355022,-4.90177656295177,
131.206566521795));
#93787=CARTESIAN_POINT('Ctrl Pts',(-79.9205588524238,-4.89072494265981,
131.341255179421));
#93788=CARTESIAN_POINT('Ctrl Pts',(-79.9282271693454,-4.87410295193499,
131.475667107368));
#93789=CARTESIAN_POINT('Ctrl Pts',(-79.935895486267,-4.85193338151652,131.609298828751));
#93790=CARTESIAN_POINT('Ctrl Pts',(-79.9435570381454,-4.82978336924923,
131.742812659288));
#93791=CARTESIAN_POINT('Ctrl Pts',(-79.9512185900237,-4.80209557838459,
131.875547258887));
#93792=CARTESIAN_POINT('Ctrl Pts',(-79.9588801419021,-4.76894468128677,
132.007003411303));
#93793=CARTESIAN_POINT('Ctrl Pts',(-79.9665372570022,-4.73581298175884,
132.138383437915));
#93794=CARTESIAN_POINT('Ctrl Pts',(-79.9741943721024,-4.6972245660148,132.268486101928));
#93795=CARTESIAN_POINT('Ctrl Pts',(-79.9818514872026,-4.6533052723407,132.396821953017));
#93796=CARTESIAN_POINT('Ctrl Pts',(-79.9895063075543,-4.60939914076901,
132.525119343341));
#93797=CARTESIAN_POINT('Ctrl Pts',(-79.997161127906,-4.56016543717282,132.651650594194));
#93798=CARTESIAN_POINT('Ctrl Pts',(-80.0048159482576,-4.50577985147171,
132.775941453487));
#93799=CARTESIAN_POINT('Ctrl Pts',(-80.0124702272485,-4.45139811200396,
132.900223522737));
#93800=CARTESIAN_POINT('Ctrl Pts',(-80.0201245062393,-4.39186537579566,
133.022265147927));
#93801=CARTESIAN_POINT('Ctrl Pts',(-80.0277787852301,-4.32740525268059,
133.141612602606));
#93802=CARTESIAN_POINT('Ctrl Pts',(-80.035434275585,-4.26293492812495,133.260978945178));
#93803=CARTESIAN_POINT('Ctrl Pts',(-80.0430897659398,-4.19353585685992,
133.377649916452));
#93804=CARTESIAN_POINT('Ctrl Pts',(-80.0507452562946,-4.11947705388346,
133.49119739434));
#93805=CARTESIAN_POINT('Ctrl Pts',(-80.0584084351493,-4.04534387277225,
133.604858909308));
#93806=CARTESIAN_POINT('Ctrl Pts',(-80.066071614004,-3.96654183206233,133.715390328504));
#93807=CARTESIAN_POINT('Ctrl Pts',(-80.0737347928587,-3.88338287503102,
133.822393173457));
#93808=CARTESIAN_POINT('Ctrl Pts',(-80.0814017837352,-3.80018255086408,
133.929449246605));
#93809=CARTESIAN_POINT('Ctrl Pts',(-80.0890687746115,-3.71262125321013,
134.032972943804));
#93810=CARTESIAN_POINT('Ctrl Pts',(-80.096735765488,-3.62104965329249,134.132600763783));
#93811=CARTESIAN_POINT('Ctrl Pts',(-80.1044150067211,-3.52933173981188,
134.232387769594));
#93812=CARTESIAN_POINT('Ctrl Pts',(-80.1120942479542,-3.433591005632,134.328266177521));
#93813=CARTESIAN_POINT('Ctrl Pts',(-80.1197734891873,-3.33421378696513,
134.419910573702));
#93814=CARTESIAN_POINT('Ctrl Pts',(-80.1273236638021,-3.23650682205786,
134.510014683292));
#93815=CARTESIAN_POINT('Ctrl Pts',(-80.134873838417,-3.13528498592989,134.596025828627));
#93816=CARTESIAN_POINT('Ctrl Pts',(-80.1424240130319,-3.030942861091,134.677675533152));
#93817=CARTESIAN_POINT('Ctrl Pts',(-80.150198347151,-2.92350289015378,134.761749361386));
#93818=CARTESIAN_POINT('Ctrl Pts',(-80.15797268127,-2.81239196730528,134.841482632209));
#93819=CARTESIAN_POINT('Ctrl Pts',(-80.1657470153891,-2.69799608994582,
134.916537676149));
#93820=CARTESIAN_POINT('Ctrl Pts',(-80.1735117683362,-2.58374119528136,
134.991500221455));
#93821=CARTESIAN_POINT('Ctrl Pts',(-80.1812765212833,-2.46620972499101,
135.061795799086));
#93822=CARTESIAN_POINT('Ctrl Pts',(-80.1890412742304,-2.34582069902412,
135.127126897453));
#93823=CARTESIAN_POINT('Ctrl Pts',(-80.1967983151154,-2.22555124513501,
135.192393108052));
#93824=CARTESIAN_POINT('Ctrl Pts',(-80.2045553560003,-2.10243022504993,
135.252704466614));
#93825=CARTESIAN_POINT('Ctrl Pts',(-80.2123123968853,-1.97690529286855,
135.307806911853));
#93826=CARTESIAN_POINT('Ctrl Pts',(-80.2200635881254,-1.85147502001514,
135.362867803909));
#93827=CARTESIAN_POINT('Ctrl Pts',(-80.2278147793656,-1.72364479989424,
135.412727444737));
#93828=CARTESIAN_POINT('Ctrl Pts',(-80.2355659706057,-1.5938862035252,135.457178025622));
#93829=CARTESIAN_POINT('Ctrl Pts',(-80.2433138673828,-1.46418275802087,
135.501609713825));
#93830=CARTESIAN_POINT('Ctrl Pts',(-80.25106176416,-1.33255293550377,135.540636788173));
#93831=CARTESIAN_POINT('Ctrl Pts',(-80.258809660937,-1.1994873661917,135.574099931286));
#93832=CARTESIAN_POINT('Ctrl Pts',(-80.2665559370211,-1.06644963132817,
135.607556074631));
#93833=CARTESIAN_POINT('Ctrl Pts',(-80.2743022131051,-0.931977125956554,
135.635450506419));
#93834=CARTESIAN_POINT('Ctrl Pts',(-80.2820484891892,-0.796574305580768,
135.657674169995));
#93835=CARTESIAN_POINT('Ctrl Pts',(-80.2897948224546,-0.661170485692306,
135.67989799762));
#93836=CARTESIAN_POINT('Ctrl Pts',(-80.2975411557199,-0.524836722899564,
135.696450910181));
#93837=CARTESIAN_POINT('Ctrl Pts',(-80.3052874889853,-0.388085902584176,
135.707275301172));
#93838=CARTESIAN_POINT('Ctrl Pts',(-80.3130355569882,-0.251304457870929,
135.71810211621));
#93839=CARTESIAN_POINT('Ctrl Pts',(-80.3207836249912,-0.114106159457105,
135.723197826087));
#93840=CARTESIAN_POINT('Ctrl Pts',(-80.3285316929941,0.0229931703295307,
135.722556869915));
#93841=CARTESIAN_POINT('Ctrl Pts',(-80.336287995736,0.160238210915554,135.721915232527));
#93842=CARTESIAN_POINT('Ctrl Pts',(-80.3440442984779,0.297383681171619,
135.715524751514));
#93843=CARTESIAN_POINT('Ctrl Pts',(-80.3518006012197,0.433915389860011,
135.703432008855));
#93844=CARTESIAN_POINT('Ctrl Pts',(-80.3595610437339,0.570519969632221,
135.691332811935));
#93845=CARTESIAN_POINT('Ctrl Pts',(-80.367321486248,0.706509747633785,135.673525339737));
#93846=CARTESIAN_POINT('Ctrl Pts',(-80.3750819287622,0.841378819633916,
135.65010769561));
#93847=CARTESIAN_POINT('Ctrl Pts',(-80.3828548290276,0.976464395441904,
135.626652459401));
#93848=CARTESIAN_POINT('Ctrl Pts',(-80.3906277292929,1.11042528787508,135.597569137508));
#93849=CARTESIAN_POINT('Ctrl Pts',(-80.3984006295584,1.24276801644454,135.563006508973));
#93850=CARTESIAN_POINT('Ctrl Pts',(-80.4058909653205,1.37029975348108,135.529700319042));
#93851=CARTESIAN_POINT('Ctrl Pts',(-80.4133813010827,1.4963286381162,135.491306369086));
#93852=CARTESIAN_POINT('Ctrl Pts',(-80.4208716368449,1.62043088514817,135.448000010215));
#93853=CARTESIAN_POINT('Ctrl Pts',(-80.4286459709639,1.74923850659444,135.403051677585));
#93854=CARTESIAN_POINT('Ctrl Pts',(-80.436420305083,1.87637853333625,135.352668691841));
#93855=CARTESIAN_POINT('Ctrl Pts',(-80.4441946392021,2.0013582334598,135.29699328493));
#93856=CARTESIAN_POINT('Ctrl Pts',(-80.4519593921492,2.12618390727271,135.241386492982));
#93857=CARTESIAN_POINT('Ctrl Pts',(-80.4597241450963,2.24885419816539,135.180500415137));
#93858=CARTESIAN_POINT('Ctrl Pts',(-80.4674888980434,2.36889231069481,135.114526772464));
#93859=CARTESIAN_POINT('Ctrl Pts',(-80.4752459389284,2.48881119967895,135.048618655744));
#93860=CARTESIAN_POINT('Ctrl Pts',(-80.4830029798134,2.60610277249812,134.977633217067));
#93861=CARTESIAN_POINT('Ctrl Pts',(-80.4907600206984,2.72031131222097,134.901809754176));
#93862=CARTESIAN_POINT('Ctrl Pts',(-80.4985112119386,2.83443372639576,134.826043470347));
#93863=CARTESIAN_POINT('Ctrl Pts',(-80.5062624031788,2.94547741072523,134.745446639576));
#93864=CARTESIAN_POINT('Ctrl Pts',(-80.5140135944189,3.05301263419777,134.66030368223));
#93865=CARTESIAN_POINT('Ctrl Pts',(-80.521761491196,3.16050215233159,134.575196912912));
#93866=CARTESIAN_POINT('Ctrl Pts',(-80.5295093879731,3.26448586959285,134.485548102252));
#93867=CARTESIAN_POINT('Ctrl Pts',(-80.5372572847502,3.3645645501395,134.391683916412));
#93868=CARTESIAN_POINT('Ctrl Pts',(-80.5450035608343,3.46462229638362,134.297839364936));
#93869=CARTESIAN_POINT('Ctrl Pts',(-80.5527498369184,3.56077634568605,134.199781459449));
#93870=CARTESIAN_POINT('Ctrl Pts',(-80.5604961130025,3.65266227506975,134.097875664865));
#93871=CARTESIAN_POINT('Ctrl Pts',(-80.5682424462679,3.74454888273413,133.995969118036));
#93872=CARTESIAN_POINT('Ctrl Pts',(-80.5759887795332,3.83216704580072,133.890214915791));
#93873=CARTESIAN_POINT('Ctrl Pts',(-80.5837351127986,3.91519107120897,133.781013425407));
#93874=CARTESIAN_POINT('Ctrl Pts',(-80.5914831808015,3.99823368927219,133.671787480105));
#93875=CARTESIAN_POINT('Ctrl Pts',(-80.5992312488045,4.07667988585684,133.559113021649));
#93876=CARTESIAN_POINT('Ctrl Pts',(-80.6069793168075,4.1502461678637,133.443421020178));
#93877=CARTESIAN_POINT('Ctrl Pts',(-80.6147356195494,4.22389063699063,133.32760605987));
#93878=CARTESIAN_POINT('Ctrl Pts',(-80.6224919222911,4.29264462096392,133.208767480497));
#93879=CARTESIAN_POINT('Ctrl Pts',(-80.630248225033,4.35626937759889,133.08736306441));
#93880=CARTESIAN_POINT('Ctrl Pts',(-80.6380086675472,4.41992809268218,132.96589385113));
#93881=CARTESIAN_POINT('Ctrl Pts',(-80.6457691100614,4.4784519587335,132.841856425771));
#93882=CARTESIAN_POINT('Ctrl Pts',(-80.6535295525756,4.53165005928323,132.715729447148));
#93883=CARTESIAN_POINT('Ctrl Pts',(-80.661302452841,4.58493355814667,132.589399998302));
#93884=CARTESIAN_POINT('Ctrl Pts',(-80.6690753531064,4.63287407029189,132.460974659645));
#93885=CARTESIAN_POINT('Ctrl Pts',(-80.6768482533718,4.67533002948314,132.330949028996));
#93886=CARTESIAN_POINT('Ctrl Pts',(-80.6843385891338,4.71624260761744,132.205650157537));
#93887=CARTESIAN_POINT('Ctrl Pts',(-80.6918289248958,4.75206238071695,132.078865619797));
#93888=CARTESIAN_POINT('Ctrl Pts',(-80.6993192606578,4.78270781038475,131.951046739826));
#93889=CARTESIAN_POINT('Ctrl Pts',(-80.7070935947769,4.81451517083294,131.818381568172));
#93890=CARTESIAN_POINT('Ctrl Pts',(-80.7148679288959,4.84084882802785,131.684181828415));
#93891=CARTESIAN_POINT('Ctrl Pts',(-80.722642263015,4.86156211209968,131.548938949709));
#93892=CARTESIAN_POINT('Ctrl Pts',(-80.7304070159621,4.88224986890008,131.413862745765));
#93893=CARTESIAN_POINT('Ctrl Pts',(-80.7381717689091,4.89733097584156,131.277746343533));
#93894=CARTESIAN_POINT('Ctrl Pts',(-80.7459365218562,4.9067090137068,131.141094514447));
#93895=CARTESIAN_POINT('Ctrl Pts',(-80.7536935627412,4.91607773717265,131.004578409883));
#93896=CARTESIAN_POINT('Ctrl Pts',(-80.7614506036261,4.91975463731667,130.86752832428));
#93897=CARTESIAN_POINT('Ctrl Pts',(-80.7692076445111,4.91769471597277,130.730457011474));
#93898=CARTESIAN_POINT('Ctrl Pts',(-80.7769588357512,4.91563634803158,130.593489065211));
#93899=CARTESIAN_POINT('Ctrl Pts',(-80.7847100269913,4.90784977545585,130.456500312946));
#93900=CARTESIAN_POINT('Ctrl Pts',(-80.7924612182315,4.89434200904784,130.320006035705));
#93901=CARTESIAN_POINT('Ctrl Pts',(-80.8002091150085,4.88083998380091,130.183569772174));
#93902=CARTESIAN_POINT('Ctrl Pts',(-80.8079570117856,4.86162163953014,130.047627953916));
#93903=CARTESIAN_POINT('Ctrl Pts',(-80.8157049085627,4.83674601300432,129.91269304039));
#93904=CARTESIAN_POINT('Ctrl Pts',(-80.8234511846467,4.81187558992331,129.77778635234));
#93905=CARTESIAN_POINT('Ctrl Pts',(-80.8311974607308,4.78135030923411,129.643886534325));
#93906=CARTESIAN_POINT('Ctrl Pts',(-80.8389437368149,4.74528066739942,129.51149772843));
#93907=CARTESIAN_POINT('Ctrl Pts',(-80.8466900700802,4.70921075930687,129.379107945271));
#93908=CARTESIAN_POINT('Ctrl Pts',(-80.8544364033455,4.66759651117477,129.248229573706));
#93909=CARTESIAN_POINT('Ctrl Pts',(-80.8621827366108,4.62059871827531,129.11935303682));
#93910=CARTESIAN_POINT('Ctrl Pts',(-80.8699308046138,4.57359040054592,128.990447638927));
#93911=CARTESIAN_POINT('Ctrl Pts',(-80.8776788726167,4.52119627295,128.863545335007));
#93912=CARTESIAN_POINT('Ctrl Pts',(-80.8854269406196,4.46362568792565,128.73911758572));
#93913=CARTESIAN_POINT('Ctrl Pts',(-80.8931832433614,4.40599391619835,128.61455759314));
#93914=CARTESIAN_POINT('Ctrl Pts',(-80.9009395461033,4.3431748614365,128.492477764265));
#93915=CARTESIAN_POINT('Ctrl Pts',(-80.9086958488452,4.27542462291296,128.373326402198));
#93916=CARTESIAN_POINT('Ctrl Pts',(-80.9164562913593,4.20763822404721,128.254111445462));
#93917=CARTESIAN_POINT('Ctrl Pts',(-80.9242167338734,4.13491560429727,128.137828401283));
#93918=CARTESIAN_POINT('Ctrl Pts',(-80.9319771763876,4.05755627786348,128.024896619873));
#93919=CARTESIAN_POINT('Ctrl Pts',(-80.939750076653,3.98007276737126,127.911783550343));
#93920=CARTESIAN_POINT('Ctrl Pts',(-80.9475229769183,3.8979379105921,127.802032807222));
#93921=CARTESIAN_POINT('Ctrl Pts',(-80.9552958771837,3.81149214799814,127.696031376921));
#93922=CARTESIAN_POINT('Ctrl Pts',(-80.962786212946,3.7281889066154,127.59388336561));
#93923=CARTESIAN_POINT('Ctrl Pts',(-80.9702765487083,3.64088294659379,127.495217036496));
#93924=CARTESIAN_POINT('Ctrl Pts',(-80.9777668844705,3.5499099061446,127.400344941815));
#93925=CARTESIAN_POINT('Ctrl Pts',(-80.9855412185896,3.45548759521866,127.301875742832));
#93926=CARTESIAN_POINT('Ctrl Pts',(-80.9933155527087,3.35681553837506,127.207182253876));
#93927=CARTESIAN_POINT('Ctrl Pts',(-81.0010898868278,3.25422791023313,127.116653501924));
#93928=CARTESIAN_POINT('Ctrl Pts',(-81.008854639775,3.15176671217408,127.026236318567));
#93929=CARTESIAN_POINT('Ctrl Pts',(-81.0166193927221,3.04539983463761,126.939973915944));
#93930=CARTESIAN_POINT('Ctrl Pts',(-81.0243841456692,2.93549983918251,126.858220255559));
#93931=CARTESIAN_POINT('Ctrl Pts',(-81.0321411865543,2.82570899795221,126.776547794063));
#93932=CARTESIAN_POINT('Ctrl Pts',(-81.0398982274394,2.7123923338149,126.699375394933));
#93933=CARTESIAN_POINT('Ctrl Pts',(-81.0476552683244,2.59595691848611,126.627018072375));
#93934=CARTESIAN_POINT('Ctrl Pts',(-81.0554064595647,2.47960930800865,126.554715315036));
#93935=CARTESIAN_POINT('Ctrl Pts',(-81.0631576508049,2.36014795832808,126.487220612334));
#93936=CARTESIAN_POINT('Ctrl Pts',(-81.0709088420451,2.23801017947578,126.424806587866));
#93937=CARTESIAN_POINT('Ctrl Pts',(-81.0786567388222,2.11592431243879,126.362419091023));
#93938=CARTESIAN_POINT('Ctrl Pts',(-81.0864046355994,1.9911646261518,126.305108155018));
#93939=CARTESIAN_POINT('Ctrl Pts',(-81.0941525323765,1.86419417808803,126.253101107399));
#93940=CARTESIAN_POINT('Ctrl Pts',(-81.1018988084606,1.73725028950484,126.201104938534));
#93941=CARTESIAN_POINT('Ctrl Pts',(-81.1096450845448,1.60809692053365,126.154410599377));
#93942=CARTESIAN_POINT('Ctrl Pts',(-81.1173913606289,1.47721794622575,126.113197627235));
#93943=CARTESIAN_POINT('Ctrl Pts',(-81.1251376938944,1.34633800579881,126.071984350869));
#93944=CARTESIAN_POINT('Ctrl Pts',(-81.1328840271597,1.21373280753077,126.036252639686));
#93945=CARTESIAN_POINT('Ctrl Pts',(-81.1406303604251,1.07990187202671,126.006132297728));
#93946=CARTESIAN_POINT('Ctrl Pts',(-81.1483784284282,0.946040966012017,
125.976005210528));
#93947=CARTESIAN_POINT('Ctrl Pts',(-81.1561264964312,0.810954157898682,
125.951492078924));
#93948=CARTESIAN_POINT('Ctrl Pts',(-81.1638745644343,0.675151260998935,
125.932671604783));
#93949=CARTESIAN_POINT('Ctrl Pts',(-81.1716308671762,0.539204031165215,
125.913831128018));
#93950=CARTESIAN_POINT('Ctrl Pts',(-81.179387169918,0.402539580111882,125.900695448445));
#93951=CARTESIAN_POINT('Ctrl Pts',(-81.1871434726599,0.265673505848731,
125.893291421272));
#93952=CARTESIAN_POINT('Ctrl Pts',(-81.1949039151741,0.128734382040788,
125.885883442346));
#93953=CARTESIAN_POINT('Ctrl Pts',(-81.2026643576884,-0.00840618865881398,
125.884213216204));
#93954=CARTESIAN_POINT('Ctrl Pts',(-81.2104248002026,-0.145233500297805,
125.8882554221));
#93955=CARTESIAN_POINT('Ctrl Pts',(-81.218197700468,-0.282280459284768,
125.892304116903));
#93956=CARTESIAN_POINT('Ctrl Pts',(-81.2259706007335,-0.419012764120642,
125.902083540625));
#93957=CARTESIAN_POINT('Ctrl Pts',(-81.2337435009989,-0.554920815787799,
125.917516446661));
#93958=CARTESIAN_POINT('Ctrl Pts',(-81.2412338367602,-0.685888267431147,
125.932388327688));
#93959=CARTESIAN_POINT('Ctrl Pts',(-81.2487241725215,-0.816090048431828,
125.95250974354));
#93960=CARTESIAN_POINT('Ctrl Pts',(-81.2562145082828,-0.945081779089869,
125.977767254403));
#93961=CARTESIAN_POINT('Ctrl Pts',(-81.2639888424019,-1.07896427043575,
126.003982411469));
#93962=CARTESIAN_POINT('Ctrl Pts',(-81.271763176521,-1.21196724147693,126.035813863631));
#93963=CARTESIAN_POINT('Ctrl Pts',(-81.2795375106402,-1.34358276325477,
126.073190738901));
#93964=CARTESIAN_POINT('Ctrl Pts',(-81.2873022635873,-1.47503608066449,
126.110521550513));
#93965=CARTESIAN_POINT('Ctrl Pts',(-81.2950670165344,-1.60510497853336,
126.153384081356));
#93966=CARTESIAN_POINT('Ctrl Pts',(-81.3028317694815,-1.73329028039838,
126.20165620968));
#93967=CARTESIAN_POINT('Ctrl Pts',(-81.3105888103664,-1.86134826681414,
126.249880393445));
#93968=CARTESIAN_POINT('Ctrl Pts',(-81.3183458512514,-1.98752601671655,
126.303503345507));
#93969=CARTESIAN_POINT('Ctrl Pts',(-81.3261028921363,-2.11133846752849,
126.362352857776));
#93970=CARTESIAN_POINT('Ctrl Pts',(-81.3338540833765,-2.23505755040899,
126.42115799117));
#93971=CARTESIAN_POINT('Ctrl Pts',(-81.3416052746167,-2.35641453284803,
126.485181672517));
#93972=CARTESIAN_POINT('Ctrl Pts',(-81.3493564658569,-2.47494367214014,
126.554203340213));
#93973=CARTESIAN_POINT('Ctrl Pts',(-81.357104362634,-2.59342243338602,126.62319567186));
#93974=CARTESIAN_POINT('Ctrl Pts',(-81.364852259411,-2.70907540484057,126.697181568502));
#93975=CARTESIAN_POINT('Ctrl Pts',(-81.3726001561881,-2.82146103552243,
126.775894322867));
#93976=CARTESIAN_POINT('Ctrl Pts',(-81.3803464322722,-2.93382315755311,
126.85459061222));
#93977=CARTESIAN_POINT('Ctrl Pts',(-81.3880927083564,-3.04291897821407,
126.938011568461));
#93978=CARTESIAN_POINT('Ctrl Pts',(-81.3958389844405,-3.14833590139897,
127.025847138106));
#93979=CARTESIAN_POINT('Ctrl Pts',(-81.4035853177059,-3.25375360274751,
127.113683356132));
#93980=CARTESIAN_POINT('Ctrl Pts',(-81.4113316509712,-3.35549205206618,
127.205934002319));
#93981=CARTESIAN_POINT('Ctrl Pts',(-81.4190779842366,-3.45317203845016,
127.302248978088));
#93982=CARTESIAN_POINT('Ctrl Pts',(-81.4268260522395,-3.55087389958968,
127.398585522928));
#93983=CARTESIAN_POINT('Ctrl Pts',(-81.4345741202425,-3.64451521091992,
127.498987934051));
#93984=CARTESIAN_POINT('Ctrl Pts',(-81.4423221882455,-3.73375419178265,
127.60306983136));
#93985=CARTESIAN_POINT('Ctrl Pts',(-81.4500784909873,-3.82308801689633,
127.707262348149));
#93986=CARTESIAN_POINT('Ctrl Pts',(-81.4578347937292,-3.90800991015203,
127.815141865692));
#93987=CARTESIAN_POINT('Ctrl Pts',(-81.4655910964711,-3.98821858418567,
127.926289112677));
#93988=CARTESIAN_POINT('Ctrl Pts',(-81.4733515389853,-4.06847006800367,
128.037495682294));
#93989=CARTESIAN_POINT('Ctrl Pts',(-81.4811119814996,-4.14400310486857,
128.151973130418));
#93990=CARTESIAN_POINT('Ctrl Pts',(-81.4888724240137,-4.21456078670153,
128.269274733873));
#93991=CARTESIAN_POINT('Ctrl Pts',(-81.4966453242792,-4.28523173398918,
128.386764640276));
#93992=CARTESIAN_POINT('Ctrl Pts',(-81.5044182245446,-4.3509111784808,128.507087418191));
#93993=CARTESIAN_POINT('Ctrl Pts',(-81.51219112481,-4.41138865921522,128.629772573856));
#93994=CARTESIAN_POINT('Ctrl Pts',(-81.5196814605727,-4.46966763119614,
128.747997815097));
#93995=CARTESIAN_POINT('Ctrl Pts',(-81.5271717963353,-4.52311615716766,
128.868416377742));
#93996=CARTESIAN_POINT('Ctrl Pts',(-81.534662132098,-4.57158947917601,128.990593075573));
#93997=CARTESIAN_POINT('Ctrl Pts',(-81.5434568423525,-4.62850399351063,
129.134045744628));
#93998=CARTESIAN_POINT('Ctrl Pts',(-81.552251552607,-4.67871160297205,129.280302977208));
#93999=CARTESIAN_POINT('Ctrl Pts',(-81.5610462628615,-4.72196086392718,
129.428763052128));
#94000=CARTESIAN_POINT('Ctrl Pts',(-81.5640669497953,-4.73681552925252,
129.47975409055));
#94001=CARTESIAN_POINT('Ctrl Pts',(-81.567087636729,-4.75084972363613,129.531004786592));
#94002=CARTESIAN_POINT('Ctrl Pts',(-81.5701083236628,-4.76405452823403,
129.582490119308));
#94003=CARTESIAN_POINT('Origin',(213.235140564004,0.,130.804360617566));
#94004=CARTESIAN_POINT('',(-83.6650228471445,-4.76405452823415,129.582490119309));
#94005=CARTESIAN_POINT('',(-83.3199745081269,-4.76405452823405,129.582490119308));
#94006=CARTESIAN_POINT('',(213.235140564004,-4.76405452823405,129.582490119308));
#94007=CARTESIAN_POINT('',(-81.9851405640544,-4.91824826795288,130.808488241399));
#94008=CARTESIAN_POINT('Ctrl Pts',(-81.9851405640544,-4.91824826795288,
130.8084882414));
#94009=CARTESIAN_POINT('Ctrl Pts',(-81.9943597297253,-4.91811131641968,
130.971672113781));
#94010=CARTESIAN_POINT('Ctrl Pts',(-82.0035788953962,-4.90984909429807,
131.134505591539));
#94011=CARTESIAN_POINT('Ctrl Pts',(-82.0127980610671,-4.89358889978316,
131.296265834472));
#94012=CARTESIAN_POINT('Ctrl Pts',(-82.0220872629018,-4.87720517981175,
131.459254937725));
#94013=CARTESIAN_POINT('Ctrl Pts',(-82.0313764647366,-4.85270160936032,
131.62115440444));
#94014=CARTESIAN_POINT('Ctrl Pts',(-82.0406656665714,-4.82025706733785,
131.781245906267));
#94015=CARTESIAN_POINT('Ctrl Pts',(-82.0500289215405,-4.78755387876324,
131.942613650949));
#94016=CARTESIAN_POINT('Ctrl Pts',(-82.0593921765095,-4.74678266151788,
132.102144461393));
#94017=CARTESIAN_POINT('Ctrl Pts',(-82.0687554314786,-4.69817465004165,
132.259124522881));
#94018=CARTESIAN_POINT('Ctrl Pts',(-82.0698264155067,-4.69261478820944,
132.277080152535));
#94019=CARTESIAN_POINT('Ctrl Pts',(-82.0708973995348,-4.68695244725871,
132.295002433936));
#94020=CARTESIAN_POINT('Ctrl Pts',(-82.0719683835628,-4.68118801245724,
132.31289031715));
#94021=CARTESIAN_POINT('Ctrl Pts',(-82.0797427176819,-4.6393436515898,132.44273948123));
#94022=CARTESIAN_POINT('Ctrl Pts',(-82.087517051801,-4.59202618497923,132.571051947522));
#94023=CARTESIAN_POINT('Ctrl Pts',(-82.09529138592,-4.53936597940594,132.697331712832));
#94024=CARTESIAN_POINT('Ctrl Pts',(-82.1030561388671,-4.48677067282964,
132.823455849617));
#94025=CARTESIAN_POINT('Ctrl Pts',(-82.1108208918142,-4.42884587741305,
132.947551912483));
#94026=CARTESIAN_POINT('Ctrl Pts',(-82.1185856447613,-4.3657718172393,133.069138642517));
#94027=CARTESIAN_POINT('Ctrl Pts',(-82.1263426856463,-4.30276040311129,
133.190604610896));
#94028=CARTESIAN_POINT('Ctrl Pts',(-82.1340997265313,-4.23461008082681,
133.309565861439));
#94029=CARTESIAN_POINT('Ctrl Pts',(-82.1418567674163,-4.16154914326525,
133.425561065965));
#94030=CARTESIAN_POINT('Ctrl Pts',(-82.1496079586564,-4.08854330152494,
133.541468797605));
#94031=CARTESIAN_POINT('Ctrl Pts',(-82.1573591498966,-4.01063442289286,
133.654414605805));
#94032=CARTESIAN_POINT('Ctrl Pts',(-82.1651103411367,-3.92809653347163,
133.763962058002));
#94033=CARTESIAN_POINT('Ctrl Pts',(-82.1728582379138,-3.84559372485506,
133.873462949608));
#94034=CARTESIAN_POINT('Ctrl Pts',(-82.1806061346908,-3.75846605333776,
133.979568046395));
#94035=CARTESIAN_POINT('Ctrl Pts',(-82.1883540314679,-3.66703051045002,
134.081870388403));
#94036=CARTESIAN_POINT('Ctrl Pts',(-82.196100307552,-3.57561409390672,134.184151330965));
#94037=CARTESIAN_POINT('Ctrl Pts',(-82.2038465836361,-3.47989185873097,
134.282630809634));
#94038=CARTESIAN_POINT('Ctrl Pts',(-82.2115928597202,-3.38022041944603,
134.376935736225));
#94039=CARTESIAN_POINT('Ctrl Pts',(-82.2193391929856,-3.28054824440958,
134.471241358953));
#94040=CARTESIAN_POINT('Ctrl Pts',(-82.2270855262509,-3.17692709108684,
134.561372099411));
#94041=CARTESIAN_POINT('Ctrl Pts',(-82.2348318595163,-3.06974939572087,
134.646992750619));
#94042=CARTESIAN_POINT('Ctrl Pts',(-82.2425799275192,-2.96254769865299,
134.732632575978));
#94043=CARTESIAN_POINT('Ctrl Pts',(-82.2503279955222,-2.85178818007577,
134.813760058322));
#94044=CARTESIAN_POINT('Ctrl Pts',(-82.2580760635252,-2.73789488296588,
134.890081444095));
#94045=CARTESIAN_POINT('Ctrl Pts',(-82.265832366267,-2.62388053870433,134.966483945144));
#94046=CARTESIAN_POINT('Ctrl Pts',(-82.2735886690088,-2.50672608794671,
135.0380699279));
#94047=CARTESIAN_POINT('Ctrl Pts',(-82.2813449717507,-2.38688345205788,
135.104589733415));
#94048=CARTESIAN_POINT('Ctrl Pts',(-82.2891054142648,-2.26697685254588,
135.171145042552));
#94049=CARTESIAN_POINT('Ctrl Pts',(-82.2968658567791,-2.14437955831906,
135.232628611376));
#94050=CARTESIAN_POINT('Ctrl Pts',(-82.3046262992932,-2.01956550887947,
135.288838091904));
#94051=CARTESIAN_POINT('Ctrl Pts',(-82.3123991995587,-1.89455109684725,
135.34513780488));
#94052=CARTESIAN_POINT('Ctrl Pts',(-82.3201720998241,-1.7673131816202,135.396146365363));
#94053=CARTESIAN_POINT('Ctrl Pts',(-82.3279450000896,-1.63834382109731,
135.441710354902));
#94054=CARTESIAN_POINT('Ctrl Pts',(-82.3354353358516,-1.51406282168399,
135.485617978653));
#94055=CARTESIAN_POINT('Ctrl Pts',(-82.3429256716135,-1.38817437054623,
135.524469915866));
#94056=CARTESIAN_POINT('Ctrl Pts',(-82.3504160073755,-1.2611277050684,135.558173821091));
#94057=CARTESIAN_POINT('Ctrl Pts',(-82.3581903414946,-1.12926402665379,
135.593155620127));
#94058=CARTESIAN_POINT('Ctrl Pts',(-82.3659646756136,-0.99573486826807,
135.622702117604));
#94059=CARTESIAN_POINT('Ctrl Pts',(-82.3737390097327,-0.861027997874883,
135.646654892946));
#94060=CARTESIAN_POINT('Ctrl Pts',(-82.3815037626798,-0.726487141660357,
135.670578148632));
#94061=CARTESIAN_POINT('Ctrl Pts',(-82.3892685156269,-0.590771842573108,
135.688921330927));
#94062=CARTESIAN_POINT('Ctrl Pts',(-82.397033268574,-0.454384412887237,
135.701575935257));
#94063=CARTESIAN_POINT('Ctrl Pts',(-82.404790309459,-0.318132445119255,
135.714217970855));
#94064=CARTESIAN_POINT('Ctrl Pts',(-82.412547350344,-0.181210062020253,
135.721182636309));
#94065=CARTESIAN_POINT('Ctrl Pts',(-82.420304391229,-0.0441287899329816,
135.722412641732));
#94066=CARTESIAN_POINT('Ctrl Pts',(-82.4280555824691,0.0928491081004854,
135.723641719598));
#94067=CARTESIAN_POINT('Ctrl Pts',(-82.4358067737092,0.229985267261336,
135.719144741698));
#94068=CARTESIAN_POINT('Ctrl Pts',(-82.4435579649493,0.366764386670902,
135.70891635149));
#94069=CARTESIAN_POINT('Ctrl Pts',(-82.4513058617264,0.503485371306202,
135.698692308622));
#94070=CARTESIAN_POINT('Ctrl Pts',(-82.4590537585035,0.639849228951849,
135.682741727565));
#94071=CARTESIAN_POINT('Ctrl Pts',(-82.4668016552806,0.775342231003463,
135.661111330473));
#94072=CARTESIAN_POINT('Ctrl Pts',(-82.4745479313647,0.910806890839939,
135.639485457994));
#94073=CARTESIAN_POINT('Ctrl Pts',(-82.4822942074486,1.04540067158514,135.612182194261));
#94074=CARTESIAN_POINT('Ctrl Pts',(-82.4900404835327,1.17861692472409,135.579299905898));
#94075=CARTESIAN_POINT('Ctrl Pts',(-82.4977868167981,1.31183416123534,135.546417374804));
#94076=CARTESIAN_POINT('Ctrl Pts',(-82.5055331500635,1.4436734702766,135.507955830594));
#94077=CARTESIAN_POINT('Ctrl Pts',(-82.5132794833288,1.57364071134718,135.464064253431));
#94078=CARTESIAN_POINT('Ctrl Pts',(-82.5210275513318,1.70363705768009,135.420162847053));
#94079=CARTESIAN_POINT('Ctrl Pts',(-82.5287756193348,1.83176013146819,135.370829113058));
#94080=CARTESIAN_POINT('Ctrl Pts',(-82.5365236873378,1.9575335839392,135.316261029837));
#94081=CARTESIAN_POINT('Ctrl Pts',(-82.5442799900796,2.08344070993205,135.261634951008));
#94082=CARTESIAN_POINT('Ctrl Pts',(-82.5520362928215,2.20699286693559,135.201763565864));
#94083=CARTESIAN_POINT('Ctrl Pts',(-82.5597925955633,2.32773573527054,135.136892141888));
#94084=CARTESIAN_POINT('Ctrl Pts',(-82.5675530380775,2.44854304771014,135.07198609408));
#94085=CARTESIAN_POINT('Ctrl Pts',(-82.5753134805917,2.56653774760186,135.00207488908));
#94086=CARTESIAN_POINT('Ctrl Pts',(-82.5830739231058,2.68129341798007,134.927447891587));
#94087=CARTESIAN_POINT('Ctrl Pts',(-82.5908468233713,2.7962333043479,134.852701096213));
#94088=CARTESIAN_POINT('Ctrl Pts',(-82.5986197236367,2.90792345205854,134.773223607462));
#94089=CARTESIAN_POINT('Ctrl Pts',(-82.6063926239022,3.01596881651194,134.68934648116));
#94090=CARTESIAN_POINT('Ctrl Pts',(-82.6138829596642,3.1200864598182,134.608518499673));
#94091=CARTESIAN_POINT('Ctrl Pts',(-82.6213732954263,3.22081947777635,134.523605401459));
#94092=CARTESIAN_POINT('Ctrl Pts',(-82.6288636311884,3.31784735376558,134.434935227681));
#94093=CARTESIAN_POINT('Ctrl Pts',(-82.6366379653074,3.41855407116322,134.342903097314));
#94094=CARTESIAN_POINT('Ctrl Pts',(-82.6444122994266,3.5155881480297,134.246531838222));
#94095=CARTESIAN_POINT('Ctrl Pts',(-82.6521866335457,3.60855265014795,134.146146193214));
#94096=CARTESIAN_POINT('Ctrl Pts',(-82.6599513864927,3.70140258182582,134.045884264542));
#94097=CARTESIAN_POINT('Ctrl Pts',(-82.6677161394397,3.79019265478353,133.941618077851));
#94098=CARTESIAN_POINT('Ctrl Pts',(-82.6754808923868,3.87456006899657,133.833711593309));
#94099=CARTESIAN_POINT('Ctrl Pts',(-82.6832379332718,3.95884368830444,133.72591228301));
#94100=CARTESIAN_POINT('Ctrl Pts',(-82.6909949741569,4.03871315118027,133.614480176064));
#94101=CARTESIAN_POINT('Ctrl Pts',(-82.6987520150419,4.11384376553748,133.499814667489));
#94102=CARTESIAN_POINT('Ctrl Pts',(-82.706503206282,4.18891772331408,133.385235629066));
#94103=CARTESIAN_POINT('Ctrl Pts',(-82.7142543975221,4.2592597322091,133.267428368066));
#94104=CARTESIAN_POINT('Ctrl Pts',(-82.7220055887622,4.32458675290145,133.146823526371));
#94105=CARTESIAN_POINT('Ctrl Pts',(-82.7297534855393,4.38988600786726,133.026269944952));
#94106=CARTESIAN_POINT('Ctrl Pts',(-82.7375013823165,4.45017432820992,132.902921490813));
#94107=CARTESIAN_POINT('Ctrl Pts',(-82.7452492790935,4.50521333974134,132.777235632846));
#94108=CARTESIAN_POINT('Ctrl Pts',(-82.7529955551776,4.56024083829805,132.651576065651));
#94109=CARTESIAN_POINT('Ctrl Pts',(-82.7607418312618,4.61002105537983,132.523580425049));
#94110=CARTESIAN_POINT('Ctrl Pts',(-82.7684881073459,4.65436289371413,132.393728138348));
#94111=CARTESIAN_POINT('Ctrl Pts',(-82.7762344406112,4.69870505936975,132.263874893107));
#94112=CARTESIAN_POINT('Ctrl Pts',(-82.7839807738764,4.73760863982853,132.132165344406));
#94113=CARTESIAN_POINT('Ctrl Pts',(-82.7917271071418,4.77093188131216,131.999095754062));
#94114=CARTESIAN_POINT('Ctrl Pts',(-82.7994751751448,4.80426258530472,131.865996363706));
#94115=CARTESIAN_POINT('Ctrl Pts',(-82.8072232431478,4.83201036865254,131.731536704826));
#94116=CARTESIAN_POINT('Ctrl Pts',(-82.8149713111508,4.85408431803855,131.596224555293));
#94117=CARTESIAN_POINT('Ctrl Pts',(-82.8227276138926,4.87618172788062,131.460768594397));
#94118=CARTESIAN_POINT('Ctrl Pts',(-82.8304839166344,4.89259319470256,131.32445871942));
#94119=CARTESIAN_POINT('Ctrl Pts',(-82.8382402193763,4.90327949810117,131.187809735443));
#94120=CARTESIAN_POINT('Ctrl Pts',(-82.8460006618904,4.9139715051017,131.051087817788));
#94121=CARTESIAN_POINT('Ctrl Pts',(-82.8537611044047,4.91893224581936,130.914026821007));
#94122=CARTESIAN_POINT('Ctrl Pts',(-82.8615215469189,4.91817468218478,130.777141910458));
#94123=CARTESIAN_POINT('Ctrl Pts',(-82.8692944471843,4.9174159024418,130.640037260098));
#94124=CARTESIAN_POINT('Ctrl Pts',(-82.8770673474496,4.91092049325699,130.503109651584));
#94125=CARTESIAN_POINT('Ctrl Pts',(-82.8848402477151,4.89875345001772,130.366870390887));
#94126=CARTESIAN_POINT('Ctrl Pts',(-82.8923305834772,4.88702870944704,130.235583770481));
#94127=CARTESIAN_POINT('Ctrl Pts',(-82.8998209192393,4.8700375718024,130.104936625863));
#94128=CARTESIAN_POINT('Ctrl Pts',(-82.9073112550014,4.847882780343,129.975375931004));
#94129=CARTESIAN_POINT('Ctrl Pts',(-82.9150855891205,4.82488798323177,129.840902903022));
#94130=CARTESIAN_POINT('Ctrl Pts',(-82.9228599232395,4.79625740231677,129.707174366468));
#94131=CARTESIAN_POINT('Ctrl Pts',(-82.9306342573586,4.76204970028167,129.574699804761));
#94132=CARTESIAN_POINT('Ctrl Pts',(-82.9383990103057,4.72788415618218,129.442388506113));
#94133=CARTESIAN_POINT('Ctrl Pts',(-82.9461637632528,4.68815526359836,129.311328482318));
#94134=CARTESIAN_POINT('Ctrl Pts',(-82.9539285161999,4.64297313025405,129.182021696675));
#94135=CARTESIAN_POINT('Ctrl Pts',(-82.9616855570848,4.59783587244154,129.052843340353));
#94136=CARTESIAN_POINT('Ctrl Pts',(-82.96944259797,4.54725628055144,128.925415123531));
#94137=CARTESIAN_POINT('Ctrl Pts',(-82.977199638855,4.49139487291884,128.800226101617));
#94138=CARTESIAN_POINT('Ctrl Pts',(-82.9849508300951,4.43557559080819,128.675131485718));
#94139=CARTESIAN_POINT('Ctrl Pts',(-82.9927020213352,4.37448257966063,128.552273059273));
#94140=CARTESIAN_POINT('Ctrl Pts',(-83.0004532125753,4.30832516102148,128.432121723734));
#94141=CARTESIAN_POINT('Ctrl Pts',(-83.0082011093524,4.24219586104996,128.312021455718));
#94142=CARTESIAN_POINT('Ctrl Pts',(-83.0159490061295,4.1710066229427,128.194626331944));
#94143=CARTESIAN_POINT('Ctrl Pts',(-83.0236969029066,4.0950134811615,128.080384176477));
#94144=CARTESIAN_POINT('Ctrl Pts',(-83.0314431789907,4.01903623550754,127.966165918007));
#94145=CARTESIAN_POINT('Ctrl Pts',(-83.0391894550748,3.93825730132652,127.855099641315));
#94146=CARTESIAN_POINT('Ctrl Pts',(-83.0469357311589,3.85297674164616,127.747605264118));
#94147=CARTESIAN_POINT('Ctrl Pts',(-83.0546820644242,3.76769555244396,127.640110093421));
#94148=CARTESIAN_POINT('Ctrl Pts',(-83.0624283976896,3.67791291442427,127.536187181117));
#94149=CARTESIAN_POINT('Ctrl Pts',(-83.070174730955,3.5839697253284,127.436224030307));
#94150=CARTESIAN_POINT('Ctrl Pts',(-83.077922798958,3.49000549830656,127.336238493443));
#94151=CARTESIAN_POINT('Ctrl Pts',(-83.0856708669609,3.39187913387172,127.24021476747));
#94152=CARTESIAN_POINT('Ctrl Pts',(-83.0934189349639,3.28996869905902,127.148503806679));
#94153=CARTESIAN_POINT('Ctrl Pts',(-83.1011752377057,3.18794995262359,127.056695374387));
#94154=CARTESIAN_POINT('Ctrl Pts',(-83.1089315404476,3.08213939299894,126.969209125574));
#94155=CARTESIAN_POINT('Ctrl Pts',(-83.1166878431895,2.97294894069247,126.886356322196));
#94156=CARTESIAN_POINT('Ctrl Pts',(-83.1244482857036,2.86370021015395,126.803459297783));
#94157=CARTESIAN_POINT('Ctrl Pts',(-83.1322087282178,2.75106831332362,126.72520086946));
#94158=CARTESIAN_POINT('Ctrl Pts',(-83.139969170732,2.63549367964732,126.65184859145));
#94159=CARTESIAN_POINT('Ctrl Pts',(-83.1477420709974,2.5197335153088,126.578378561851));
#94160=CARTESIAN_POINT('Ctrl Pts',(-83.1555149712629,2.40102151295096,126.509830616513));
#94161=CARTESIAN_POINT('Ctrl Pts',(-83.1632878715283,2.27982298036273,126.446426446343));
#94162=CARTESIAN_POINT('Ctrl Pts',(-83.1707782072903,2.16303031971576,126.385327177465));
#94163=CARTESIAN_POINT('Ctrl Pts',(-83.1782685430522,2.04392905190227,126.329004329881));
#94164=CARTESIAN_POINT('Ctrl Pts',(-83.1857588788141,1.9229507640255,126.277613063125));
#94165=CARTESIAN_POINT('Ctrl Pts',(-83.1935332129332,1.79738554759209,126.224273280871));
#94166=CARTESIAN_POINT('Ctrl Pts',(-83.2013075470523,1.66940041407463,126.176077458946));
#94167=CARTESIAN_POINT('Ctrl Pts',(-83.2090818811714,1.53945571491708,126.133251631007));
#94168=CARTESIAN_POINT('Ctrl Pts',(-83.2168466341185,1.40967116098809,126.090478582074));
#94169=CARTESIAN_POINT('Ctrl Pts',(-83.2246113870656,1.27793221428302,126.053062480406));
#94170=CARTESIAN_POINT('Ctrl Pts',(-83.2323761400127,1.1447207066549,126.021182012678));
#94171=CARTESIAN_POINT('Ctrl Pts',(-83.2401331808977,1.01164150657411,125.989333209081));
#94172=CARTESIAN_POINT('Ctrl Pts',(-83.2478902217827,0.87709303391469,125.963009188427));
#94173=CARTESIAN_POINT('Ctrl Pts',(-83.2556472626677,0.741573508925192,
125.942339248489));
#94174=CARTESIAN_POINT('Ctrl Pts',(-83.2633984539079,0.606156180263492,
125.921684895914));
#94175=CARTESIAN_POINT('Ctrl Pts',(-83.271149645148,0.469769641758475,125.906676195959));
#94176=CARTESIAN_POINT('Ctrl Pts',(-83.2789008363881,0.332923219547658,
125.897391574217));
#94177=CARTESIAN_POINT('Ctrl Pts',(-83.2866487331652,0.196134960716965,
125.888110898687));
#94178=CARTESIAN_POINT('Ctrl Pts',(-83.2943966299423,0.0588875961929768,
125.884549488956));
#94179=CARTESIAN_POINT('Ctrl Pts',(-83.3021445267193,-0.0783037140750059,
125.886733995824));
#94180=CARTESIAN_POINT('Ctrl Pts',(-83.3098908028034,-0.215466326878383,
125.888918045741));
#94181=CARTESIAN_POINT('Ctrl Pts',(-83.3176370788876,-0.352572518080116,
125.896845615349));
#94182=CARTESIAN_POINT('Ctrl Pts',(-83.3253833549717,-0.489106807615796,
125.910491228908));
#94183=CARTESIAN_POINT('Ctrl Pts',(-83.3331296882371,-0.62564210501677,
125.924136943196));
#94184=CARTESIAN_POINT('Ctrl Pts',(-83.3408760215024,-0.761605103300574,
125.943500746779));
#94185=CARTESIAN_POINT('Ctrl Pts',(-83.3486223547678,-0.896485521576785,
125.968505287627));
#94186=CARTESIAN_POINT('Ctrl Pts',(-83.3563704227708,-1.03139614538729,
125.993515428067));
#94187=CARTESIAN_POINT('Ctrl Pts',(-83.3641184907737,-1.16522332242821,
126.024168748151));
#94188=CARTESIAN_POINT('Ctrl Pts',(-83.3718665587766,-1.29746743044787,
126.06033686874));
#94189=CARTESIAN_POINT('Ctrl Pts',(-83.3796228615185,-1.42985208907943,
126.096543429238));
#94190=CARTESIAN_POINT('Ctrl Pts',(-83.3873791642604,-1.56064993998876,
126.138276395307));
#94191=CARTESIAN_POINT('Ctrl Pts',(-83.3951354670022,-1.68937645658072,
126.185357451249));
#94192=CARTESIAN_POINT('Ctrl Pts',(-83.4028959095164,-1.81817167839047,
126.232463635767));
#94193=CARTESIAN_POINT('Ctrl Pts',(-83.4106563520306,-1.94489300195566,
126.284923448395));
#94194=CARTESIAN_POINT('Ctrl Pts',(-83.4184167945448,-2.06907726345978,
126.342510962957));
#94195=CARTESIAN_POINT('Ctrl Pts',(-83.4261896948102,-2.19346087656504,
126.40019092211));
#94196=CARTESIAN_POINT('Ctrl Pts',(-83.4339625950757,-2.31529894133267,
126.46301485296));
#94197=CARTESIAN_POINT('Ctrl Pts',(-83.4417354953411,-2.43415343269864,
126.530711108238));
#94198=CARTESIAN_POINT('Ctrl Pts',(-83.4492258311031,-2.54868726392673,
126.595946434119));
#94199=CARTESIAN_POINT('Ctrl Pts',(-83.4567161668651,-2.66045041520976,
126.665705828973));
#94200=CARTESIAN_POINT('Ctrl Pts',(-83.4642065026271,-2.76907906306409,
126.739710053864));
#94201=CARTESIAN_POINT('Ctrl Pts',(-83.4719474395665,-2.88134205628105,
126.816190208604));
#94202=CARTESIAN_POINT('Ctrl Pts',(-83.4796883765059,-2.99061989283231,
126.897451418079));
#94203=CARTESIAN_POINT('Ctrl Pts',(-83.4874293134452,-3.09647557227514,
126.983232238042));
#94204=CARTESIAN_POINT('Ctrl Pts',(-83.4951580116616,-3.20216388976515,
127.068877435188));
#94205=CARTESIAN_POINT('Ctrl Pts',(-83.502886709878,-3.3044405208091,127.159027766624));
#94206=CARTESIAN_POINT('Ctrl Pts',(-83.5106154080944,-3.40289693775067,
127.253378289597));
#94207=CARTESIAN_POINT('Ctrl Pts',(-83.5183370415297,-3.50126335595945,
127.347642567024));
#94208=CARTESIAN_POINT('Ctrl Pts',(-83.526058674965,-3.59581622232154,127.44609912865));
#94209=CARTESIAN_POINT('Ctrl Pts',(-83.5337803084002,-3.68617946093688,
127.548402380078));
#94210=CARTESIAN_POINT('Ctrl Pts',(-83.5414965952463,-3.77648013052249,
127.65063479501));
#94211=CARTESIAN_POINT('Ctrl Pts',(-83.5492128820924,-3.86259668317436,
127.756708306345));
#94212=CARTESIAN_POINT('Ctrl Pts',(-83.5569291689385,-3.94418968735834,
127.866240338776));
#94213=CARTESIAN_POINT('Ctrl Pts',(-83.5646418232168,-4.02574428030597,
127.975720807218));
#94214=CARTESIAN_POINT('Ctrl Pts',(-83.5723544774951,-4.10277932737506,
128.088656240637));
#94215=CARTESIAN_POINT('Ctrl Pts',(-83.5800671317734,-4.17499580640857,
128.204631193381));
#94216=CARTESIAN_POINT('Ctrl Pts',(-83.5877793978067,-4.24720865015867,
128.320600308098));
#94217=CARTESIAN_POINT('Ctrl Pts',(-83.5954916638401,-4.31460319117812,
128.439608308166));
#94218=CARTESIAN_POINT('Ctrl Pts',(-83.6032039298734,-4.37692395977381,
128.561211110097));
#94219=CARTESIAN_POINT('Ctrl Pts',(-83.6109158038908,-4.4392415605924,128.682807730933));
#94220=CARTESIAN_POINT('Ctrl Pts',(-83.6186276779081,-4.49648572694092,
128.806998537271));
#94221=CARTESIAN_POINT('Ctrl Pts',(-83.6263395519254,-4.5484475173092,128.933315924144));
#94222=CARTESIAN_POINT('Ctrl Pts',(-83.6340555416557,-4.60043703891545,
129.059700724735));
#94223=CARTESIAN_POINT('Ctrl Pts',(-83.6417715313859,-4.64713840675758,
129.188214005921));
#94224=CARTESIAN_POINT('Ctrl Pts',(-83.6494875211162,-4.68839126405798,
129.318369225396));
#94225=CARTESIAN_POINT('Ctrl Pts',(-83.6546659631256,-4.71607734668912,
129.405720463517));
#94226=CARTESIAN_POINT('Ctrl Pts',(-83.6598444051351,-4.74131034347372,
129.493810888119));
#94227=CARTESIAN_POINT('Ctrl Pts',(-83.6650228471445,-4.76405452823415,
129.582490119309));
#94228=CARTESIAN_POINT('Ctrl Pts',(-81.9152188971548,-4.76405452823409,
129.582490119308));
#94229=CARTESIAN_POINT('Ctrl Pts',(-81.9229317503212,-4.79801314726194,
129.714894259504));
#94230=CARTESIAN_POINT('Ctrl Pts',(-81.9306446034876,-4.82645499448301,
129.848743097592));
#94231=CARTESIAN_POINT('Ctrl Pts',(-81.9383574566541,-4.84927101642369,
129.983535622958));
#94232=CARTESIAN_POINT('Ctrl Pts',(-81.9461546412132,-4.87233650595616,
130.119801953302));
#94233=CARTESIAN_POINT('Ctrl Pts',(-81.9539518257724,-4.88965231265043,
130.257032331246));
#94234=CARTESIAN_POINT('Ctrl Pts',(-81.9617490103315,-4.90115921366017,
130.394700484219));
#94235=CARTESIAN_POINT('Ctrl Pts',(-81.9695461948906,-4.91266611466992,
130.532368637192));
#94236=CARTESIAN_POINT('Ctrl Pts',(-81.9773433794496,-4.91836409580708,
130.670474149571));
#94237=CARTESIAN_POINT('Ctrl Pts',(-81.9851405640087,-4.91824826795356,
130.808488240592));
#94238=CARTESIAN_POINT('',(-81.6398594359374,-4.91824905295598,130.801308471165));
#94239=CARTESIAN_POINT('Ctrl Pts',(-81.5701083236628,-4.76405452823403,
129.582490119308));
#94240=CARTESIAN_POINT('Ctrl Pts',(-81.5788549634402,-4.80229009242161,
129.73157000377));
#94241=CARTESIAN_POINT('Ctrl Pts',(-81.5876016032175,-4.83356823313081,
129.882618677574));
#94242=CARTESIAN_POINT('Ctrl Pts',(-81.5963482429949,-4.85770413863388,
130.035014425011));
#94243=CARTESIAN_POINT('Ctrl Pts',(-81.6050443608007,-4.88170063133802,
130.186529910561));
#94244=CARTESIAN_POINT('Ctrl Pts',(-81.6137404786066,-4.89863706784531,
130.33937676233));
#94245=CARTESIAN_POINT('Ctrl Pts',(-81.6224365964124,-4.90837967686126,
130.492925214512));
#94246=CARTESIAN_POINT('Ctrl Pts',(-81.6282442095874,-4.91488617846839,
130.595470975022));
#94247=CARTESIAN_POINT('Ctrl Pts',(-81.6340518227623,-4.9181851465564,130.698329272967));
#94248=CARTESIAN_POINT('Ctrl Pts',(-81.6398594359373,-4.91824905295597,
130.801308471165));
#94249=CARTESIAN_POINT('Ctrl Pts',(-81.6398594359913,-4.91824905295657,
130.801308472121));
#94250=CARTESIAN_POINT('Ctrl Pts',(-81.6476687247406,-4.91833498556877,
130.939780899548));
#94251=CARTESIAN_POINT('Ctrl Pts',(-81.6554780134899,-4.9125685830178,131.078274297816));
#94252=CARTESIAN_POINT('Ctrl Pts',(-81.6632873022392,-4.90097117585682,
131.21626424212));
#94253=CARTESIAN_POINT('Ctrl Pts',(-81.6710974148324,-4.88937254522282,
131.354268743727));
#94254=CARTESIAN_POINT('Ctrl Pts',(-81.6789075274256,-4.87194171643958,
131.49176930486));
#94255=CARTESIAN_POINT('Ctrl Pts',(-81.6867176400188,-4.84875195097137,
131.628246277383));
#94256=CARTESIAN_POINT('Ctrl Pts',(-81.6945301641732,-4.82555502510229,
131.764765390471));
#94257=CARTESIAN_POINT('Ctrl Pts',(-81.7023426883276,-4.79659568558305,
131.900259909069));
#94258=CARTESIAN_POINT('Ctrl Pts',(-81.710155212482,-4.7619983407032,132.034220311043));
#94259=CARTESIAN_POINT('Ctrl Pts',(-81.7179717371523,-4.7273832797523,132.16824930938));
#94260=CARTESIAN_POINT('Ctrl Pts',(-81.7257882618226,-4.6871245600809,132.300742257428));
#94261=CARTESIAN_POINT('Ctrl Pts',(-81.733604786493,-4.64139638868414,132.431204994146));
#94262=CARTESIAN_POINT('Ctrl Pts',(-81.7414316799484,-4.59560755790249,
132.561840792438));
#94263=CARTESIAN_POINT('Ctrl Pts',(-81.7492585734038,-4.54433491332346,
132.690440640849));
#94264=CARTESIAN_POINT('Ctrl Pts',(-81.7570854668591,-4.48780098528893,
132.816529939204));
#94265=CARTESIAN_POINT('Ctrl Pts',(-81.7649183325838,-4.43122391934212,
132.942715449325));
#94266=CARTESIAN_POINT('Ctrl Pts',(-81.7727511983086,-4.36937774052998,
133.066386251551));
#94267=CARTESIAN_POINT('Ctrl Pts',(-81.7805840640333,-4.30253043869562,
133.187093268662));
#94268=CARTESIAN_POINT('Ctrl Pts',(-81.7884293310176,-4.23557730193732,
133.307991393232));
#94269=CARTESIAN_POINT('Ctrl Pts',(-81.796274598002,-4.1636074284083,133.425916037209));
#94270=CARTESIAN_POINT('Ctrl Pts',(-81.8041198649863,-4.08693187737184,
133.540447402049));
#94271=CARTESIAN_POINT('Ctrl Pts',(-81.8071164952938,-4.05764437440562,
133.584194563199));
#94272=CARTESIAN_POINT('Ctrl Pts',(-81.8101131256012,-4.02767073475177,
133.627446999452));
#94273=CARTESIAN_POINT('Ctrl Pts',(-81.8131097559086,-3.99702978244563,
133.670182660321));
#94274=CARTESIAN_POINT('Ctrl Pts',(-81.8208840900277,-3.91753615910348,
133.781054296896));
#94275=CARTESIAN_POINT('Ctrl Pts',(-81.8286584241468,-3.83330000709396,
133.888791488001));
#94276=CARTESIAN_POINT('Ctrl Pts',(-81.8364327582659,-3.74459691484425,
133.992961722728));
#94277=CARTESIAN_POINT('Ctrl Pts',(-81.844197511213,-3.65600314122812,134.09700357695));
#94278=CARTESIAN_POINT('Ctrl Pts',(-81.85196226416,-3.56295363192653,134.197486926625));
#94279=CARTESIAN_POINT('Ctrl Pts',(-81.8597270171071,-3.46576694977739,
134.294008524208));
#94280=CARTESIAN_POINT('Ctrl Pts',(-81.8674840579921,-3.36867679481105,
134.390434255179));
#94281=CARTESIAN_POINT('Ctrl Pts',(-81.8752410988771,-3.26745791989503,
134.482905790904));
#94282=CARTESIAN_POINT('Ctrl Pts',(-81.8829981397621,-3.16246857557404,
134.57105353988));
#94283=CARTESIAN_POINT('Ctrl Pts',(-81.8907493310022,-3.05755840453444,
134.659134815952));
#94284=CARTESIAN_POINT('Ctrl Pts',(-81.8985005222424,-2.94888372179954,
134.742898544929));
#94285=CARTESIAN_POINT('Ctrl Pts',(-81.9062517134825,-2.83683872562821,
134.822012806006));
#94286=CARTESIAN_POINT('Ctrl Pts',(-81.9139996102596,-2.72484135156899,
134.901093441411));
#94287=CARTESIAN_POINT('Ctrl Pts',(-81.9217475070366,-2.60947683185872,
134.975528314288));
#94288=CARTESIAN_POINT('Ctrl Pts',(-81.9294954038137,-2.49117127933511,
135.045026687833));
#94289=CARTESIAN_POINT('Ctrl Pts',(-81.9372416798978,-2.37289047378271,
135.114510523817));
#94290=CARTESIAN_POINT('Ctrl Pts',(-81.944987955982,-2.25167019597342,135.179059716482));
#94291=CARTESIAN_POINT('Ctrl Pts',(-81.9527342320661,-2.1279639472848,135.238427881552));
#94292=CARTESIAN_POINT('Ctrl Pts',(-81.9604805653315,-2.00425678542459,
135.297796484866));
#94293=CARTESIAN_POINT('Ctrl Pts',(-81.9682268985968,-1.87806396854338,
135.351983815112));
#94294=CARTESIAN_POINT('Ctrl Pts',(-81.9759732318621,-1.74986154259587,
135.400790497837));
#94295=CARTESIAN_POINT('Ctrl Pts',(-81.9837212998651,-1.62163040660414,
135.449608110479));
#94296=CARTESIAN_POINT('Ctrl Pts',(-81.9914693678681,-1.49138913133547,
135.493042538798));
#94297=CARTESIAN_POINT('Ctrl Pts',(-81.9992174358711,-1.3596312028971,135.530943532803));
#94298=CARTESIAN_POINT('Ctrl Pts',(-82.0069737386129,-1.22773324056462,
135.568884808435));
#94299=CARTESIAN_POINT('Ctrl Pts',(-82.0147300413549,-1.0943157814127,135.60128079357));
#94300=CARTESIAN_POINT('Ctrl Pts',(-82.0224863440967,-0.959885394956362,
135.628031739341));
#94301=CARTESIAN_POINT('Ctrl Pts',(-82.0302467866109,-0.82538325895515,
135.654796962898));
#94302=CARTESIAN_POINT('Ctrl Pts',(-82.0380072291249,-0.689867504514324,
135.675911083419));
#94303=CARTESIAN_POINT('Ctrl Pts',(-82.0457676716391,-0.553851222095246,
135.691326126579));
#94304=CARTESIAN_POINT('Ctrl Pts',(-82.0535405719045,-0.417616594264671,
135.706765915335));
#94305=CARTESIAN_POINT('Ctrl Pts',(-82.06131347217,-0.280880223027997,135.716488317037));
#94306=CARTESIAN_POINT('Ctrl Pts',(-82.0690863724354,-0.144157512079178,
135.720497482444));
#94307=CARTESIAN_POINT('Ctrl Pts',(-82.076576708198,-0.0124050160477781,
135.72436090459));
#94308=CARTESIAN_POINT('Ctrl Pts',(-82.0840670439605,0.119334487624514,
135.722919263247));
#94309=CARTESIAN_POINT('Ctrl Pts',(-82.0915573797231,0.25060501860766,135.716221791006));
#94310=CARTESIAN_POINT('Ctrl Pts',(-82.0993317138421,0.386852711662048,
135.70927038207));
#94311=CARTESIAN_POINT('Ctrl Pts',(-82.1071060479612,0.523026759557225,
135.696634705111));
#94312=CARTESIAN_POINT('Ctrl Pts',(-82.1148803820803,0.658614316341515,
135.678312837768));
#94313=CARTESIAN_POINT('Ctrl Pts',(-82.1226451350273,0.794034773579877,
135.660013550489));
#94314=CARTESIAN_POINT('Ctrl Pts',(-82.1304098879745,0.928869794135261,
135.636042067955));
#94315=CARTESIAN_POINT('Ctrl Pts',(-82.1381746409216,1.06260792343337,135.606448440957));
#94316=CARTESIAN_POINT('Ctrl Pts',(-82.1459316818066,1.19621322213645,135.576884206766));
#94317=CARTESIAN_POINT('Ctrl Pts',(-82.1536887226916,1.32872341837167,135.541709024433));
#94318=CARTESIAN_POINT('Ctrl Pts',(-82.1614457635766,1.45963392117172,135.501024527052));
#94319=CARTESIAN_POINT('Ctrl Pts',(-82.1691969548168,1.59044570334346,135.460370710167));
#94320=CARTESIAN_POINT('Ctrl Pts',(-82.1769481460569,1.7196598213891,135.414215963309));
#94321=CARTESIAN_POINT('Ctrl Pts',(-82.184699337297,1.84678394714717,135.362712525335));
#94322=CARTESIAN_POINT('Ctrl Pts',(-82.1924472340741,1.97385404176047,135.311230977696));
#94323=CARTESIAN_POINT('Ctrl Pts',(-82.2001951308512,2.09883554925481,135.254405406932));
#94324=CARTESIAN_POINT('Ctrl Pts',(-82.2079430276283,2.22125354012725,135.1924371635));
#94325=CARTESIAN_POINT('Ctrl Pts',(-82.2156893037124,2.34364592379502,135.130481882487));
#94326=CARTESIAN_POINT('Ctrl Pts',(-82.2234355797966,2.4634755088373,135.063386244966));
#94327=CARTESIAN_POINT('Ctrl Pts',(-82.2311818558807,2.58028987661407,134.991398617769));
#94328=CARTESIAN_POINT('Ctrl Pts',(-82.2389281891461,2.6971051066878,134.919410459176));
#94329=CARTESIAN_POINT('Ctrl Pts',(-82.2466745224114,2.81090474224335,134.842530443964));
#94330=CARTESIAN_POINT('Ctrl Pts',(-82.2544208556768,2.92126372943901,134.761051316315));
#94331=CARTESIAN_POINT('Ctrl Pts',(-82.2621689236798,3.03164743076482,134.679553941979));
#94332=CARTESIAN_POINT('Ctrl Pts',(-82.2699169916828,3.13858863603834,134.593455637922));
#94333=CARTESIAN_POINT('Ctrl Pts',(-82.2776650596858,3.2416941943933,134.50309037419));
#94334=CARTESIAN_POINT('Ctrl Pts',(-82.2854213624277,3.34490933456251,134.412629069181));
#94335=CARTESIAN_POINT('Ctrl Pts',(-82.2931776651695,3.4442803899321,134.317892003498));
#94336=CARTESIAN_POINT('Ctrl Pts',(-82.3009339679114,3.53944962575954,134.219251451723));
#94337=CARTESIAN_POINT('Ctrl Pts',(-82.3086944104256,3.6346696562739,134.120558252515));
#94338=CARTESIAN_POINT('Ctrl Pts',(-82.3164548529398,3.72568313928251,134.01795770818));
#94339=CARTESIAN_POINT('Ctrl Pts',(-82.324215295454,3.81217237469915,133.91185556496));
#94340=CARTESIAN_POINT('Ctrl Pts',(-82.3319881957195,3.8988004503144,133.805583097161));
#94341=CARTESIAN_POINT('Ctrl Pts',(-82.3397610959849,3.98088953084325,133.695798111066));
#94342=CARTESIAN_POINT('Ctrl Pts',(-82.3475339962503,4.05816452015065,133.582936473988));
#94343=CARTESIAN_POINT('Ctrl Pts',(-82.355024332012,4.13263036894901,133.474177641704));
#94344=CARTESIAN_POINT('Ctrl Pts',(-82.3625146677737,4.20262589489997,133.362562223861));
#94345=CARTESIAN_POINT('Ctrl Pts',(-82.3700050035353,4.26794605027134,133.248500461043));
#94346=CARTESIAN_POINT('Ctrl Pts',(-82.3777793376544,4.33574283919023,133.130114011815));
#94347=CARTESIAN_POINT('Ctrl Pts',(-82.3855536717735,4.398717485427,133.008717036632));
#94348=CARTESIAN_POINT('Ctrl Pts',(-82.3933280058925,4.4565911658811,132.884739968235));
#94349=CARTESIAN_POINT('Ctrl Pts',(-82.4010927588396,4.51439352219653,132.760915690495));
#94350=CARTESIAN_POINT('Ctrl Pts',(-82.4088575117866,4.56710725717209,132.63451799713));
#94351=CARTESIAN_POINT('Ctrl Pts',(-82.4166222647337,4.61449802626495,132.506004243034));
#94352=CARTESIAN_POINT('Ctrl Pts',(-82.4243793056187,4.66184172617772,132.377618130611));
#94353=CARTESIAN_POINT('Ctrl Pts',(-82.4321363465037,4.70387284687444,132.247120504383));
#94354=CARTESIAN_POINT('Ctrl Pts',(-82.4398933873887,4.7404041514135,132.114990826191));
#94355=CARTESIAN_POINT('Ctrl Pts',(-82.4476445786287,4.77690790741148,131.982960788019));
#94356=CARTESIAN_POINT('Ctrl Pts',(-82.4553957698688,4.80791999874377,131.849301522906));
#94357=CARTESIAN_POINT('Ctrl Pts',(-82.4631469611089,4.8333023928751,131.714509529298));
#94358=CARTESIAN_POINT('Ctrl Pts',(-82.4708948578859,4.85867399881194,131.579774825884));
#94359=CARTESIAN_POINT('Ctrl Pts',(-82.4786427546629,4.87842059438907,131.44390873493));
#94360=CARTESIAN_POINT('Ctrl Pts',(-82.48639065144,4.89245487044994,131.307419662918));
#94361=CARTESIAN_POINT('Ctrl Pts',(-82.494136927524,4.9064862108428,131.170959141478));
#94362=CARTESIAN_POINT('Ctrl Pts',(-82.5018832036081,4.91480756846505,131.03387628685));
#94363=CARTESIAN_POINT('Ctrl Pts',(-82.5096294796922,4.91738335804249,130.89668597999));
#94364=CARTESIAN_POINT('Ctrl Pts',(-82.5173758129575,4.91995916663382,130.759494660423));
#94365=CARTESIAN_POINT('Ctrl Pts',(-82.5251221462228,4.91678931521013,130.622196277936));
#94366=CARTESIAN_POINT('Ctrl Pts',(-82.5328684794881,4.90789034575819,130.485306677748));
#94367=CARTESIAN_POINT('Ctrl Pts',(-82.540616547491,4.89898938344374,130.348386422082));
#94368=CARTESIAN_POINT('Ctrl Pts',(-82.548364615494,4.88435677544462,130.211875520943));
#94369=CARTESIAN_POINT('Ctrl Pts',(-82.5561126834969,4.86406099257518,130.076285262257));
#94370=CARTESIAN_POINT('Ctrl Pts',(-82.5638689862388,4.84374363910614,129.94055089663));
#94371=CARTESIAN_POINT('Ctrl Pts',(-82.5716252889806,4.81775114535535,129.805739515331));
#94372=CARTESIAN_POINT('Ctrl Pts',(-82.5793815917225,4.78620335210486,129.672353314233));
#94373=CARTESIAN_POINT('Ctrl Pts',(-82.5871420342366,4.75463872084722,129.538895920903));
#94374=CARTESIAN_POINT('Ctrl Pts',(-82.5949024767508,4.71751298779507,129.406865599642));
#94375=CARTESIAN_POINT('Ctrl Pts',(-82.6026629192649,4.67499579409606,129.276748956284));
#94376=CARTESIAN_POINT('Ctrl Pts',(-82.6104358195303,4.63241034802323,129.14642343814));
#94377=CARTESIAN_POINT('Ctrl Pts',(-82.6182087197958,4.58441628311373,129.018018103176));
#94378=CARTESIAN_POINT('Ctrl Pts',(-82.6259816200612,4.53123161070032,128.89199999449));
#94379=CARTESIAN_POINT('Ctrl Pts',(-82.6334719558235,4.47998033509123,128.770562961471));
#94380=CARTESIAN_POINT('Ctrl Pts',(-82.6409622915858,4.42390941445499,128.6513428834));
#94381=CARTESIAN_POINT('Ctrl Pts',(-82.6484526273481,4.3632531625059,128.534734017796));
#94382=CARTESIAN_POINT('Ctrl Pts',(-82.6562269614672,4.30029711033031,128.413703891615));
#94383=CARTESIAN_POINT('Ctrl Pts',(-82.6640012955862,4.23220173149967,128.295103507828));
#94384=CARTESIAN_POINT('Ctrl Pts',(-82.6717756297053,4.15917845057275,128.179400107617));
#94385=CARTESIAN_POINT('Ctrl Pts',(-82.6795403826524,4.08624516431329,128.063839301506));
#94386=CARTESIAN_POINT('Ctrl Pts',(-82.6873051355995,4.00839626647538,127.951168702641));
#94387=CARTESIAN_POINT('Ctrl Pts',(-82.6950698885466,3.92588987373413,127.841832683215));
#94388=CARTESIAN_POINT('Ctrl Pts',(-82.7028269294317,3.84346542750507,127.732605257864));
#94389=CARTESIAN_POINT('Ctrl Pts',(-82.7105839703167,3.75639292607726,127.62670613108));
#94390=CARTESIAN_POINT('Ctrl Pts',(-82.7183410112018,3.66497454813711,127.524551991441));
#94391=CARTESIAN_POINT('Ctrl Pts',(-82.7260922024419,3.57362510950677,127.422474887033));
#94392=CARTESIAN_POINT('Ctrl Pts',(-82.7338433936822,3.47793657721598,127.324137438683));
#94393=CARTESIAN_POINT('Ctrl Pts',(-82.7415945849224,3.37825205951236,127.22992414661));
#94394=CARTESIAN_POINT('Ctrl Pts',(-82.7493424816995,3.27860991038807,127.1357508977));
#94395=CARTESIAN_POINT('Ctrl Pts',(-82.7570903784765,3.17497543738677,127.045698586713));
#94396=CARTESIAN_POINT('Ctrl Pts',(-82.7648382752536,3.06772918454784,126.960115475438));
#94397=CARTESIAN_POINT('Ctrl Pts',(-82.7725845513377,2.96050536531304,126.874550266305));
#94398=CARTESIAN_POINT('Ctrl Pts',(-82.7803308274219,2.84967157438043,126.793452641103));
#94399=CARTESIAN_POINT('Ctrl Pts',(-82.7880771035061,2.73564176097019,126.717130844463));
#94400=CARTESIAN_POINT('Ctrl Pts',(-82.7958234367714,2.62161110581824,126.640808484434));
#94401=CARTESIAN_POINT('Ctrl Pts',(-82.8035697700368,2.50438470601706,126.569262240779));
#94402=CARTESIAN_POINT('Ctrl Pts',(-82.8113161033021,2.38440549810417,126.502757023194));
#94403=CARTESIAN_POINT('Ctrl Pts',(-82.8190641713051,2.26439942168004,126.436236912228));
#94404=CARTESIAN_POINT('Ctrl Pts',(-82.826812239308,2.14163965231658,126.374760263225));
#94405=CARTESIAN_POINT('Ctrl Pts',(-82.834560307311,2.01659336117531,126.318545833364));
#94406=CARTESIAN_POINT('Ctrl Pts',(-82.8423166100528,1.8914141693469,126.262271658138));
#94407=CARTESIAN_POINT('Ctrl Pts',(-82.8500729127948,1.76394395842746,126.211271034733));
#94408=CARTESIAN_POINT('Ctrl Pts',(-82.8578292155367,1.63467001689946,126.165714586842));
#94409=CARTESIAN_POINT('Ctrl Pts',(-82.8655896580509,1.50532707797614,126.120133824103));
#94410=CARTESIAN_POINT('Ctrl Pts',(-82.8733501005651,1.3741788638437,126.080003141114));
#94411=CARTESIAN_POINT('Ctrl Pts',(-82.8811105430793,1.24172646495639,126.045442836313));
#94412=CARTESIAN_POINT('Ctrl Pts',(-82.8888834433448,1.10906144172018,126.010827052242));
#94413=CARTESIAN_POINT('Ctrl Pts',(-82.8966563436102,0.975088432382155,
125.981799598291));
#94414=CARTESIAN_POINT('Ctrl Pts',(-82.9044292438757,0.840318213978551,
125.958429503553));
#94415=CARTESIAN_POINT('Ctrl Pts',(-82.9119195796375,0.710447232484356,
125.935908970626));
#94416=CARTESIAN_POINT('Ctrl Pts',(-82.9194099153993,0.579836302111344,
125.91864165986));
#94417=CARTESIAN_POINT('Ctrl Pts',(-82.9269002511611,0.448943775163659,
125.906643542311));
#94418=CARTESIAN_POINT('Ctrl Pts',(-82.9346745852802,0.31308841826842,125.894190512489));
#94419=CARTESIAN_POINT('Ctrl Pts',(-82.9424489193992,0.176499340871205,
125.887374678848));
#94420=CARTESIAN_POINT('Ctrl Pts',(-82.9502232535183,0.0396839263492316,
125.886270719192));
#94421=CARTESIAN_POINT('Ctrl Pts',(-82.9579880064654,-0.0969628754018883,
125.885168120067));
#94422=CARTESIAN_POINT('Ctrl Pts',(-82.9657527594125,-0.233835072070384,
125.889763391795));
#94423=CARTESIAN_POINT('Ctrl Pts',(-82.9735175123596,-0.37041928237792,
125.90007956753));
#94424=CARTESIAN_POINT('Ctrl Pts',(-82.9812745532446,-0.506867835322649,
125.910385497094));
#94425=CARTESIAN_POINT('Ctrl Pts',(-82.9890315941297,-0.64302858379119,
125.92640099381));
#94426=CARTESIAN_POINT('Ctrl Pts',(-82.9967886350147,-0.778387620919688,
125.948097056545));
#94427=CARTESIAN_POINT('Ctrl Pts',(-83.0045398262549,-0.913644582744795,
125.969776758111));
#94428=CARTESIAN_POINT('Ctrl Pts',(-83.012291017495,-1.04810065212751,125.997128437508));
#94429=CARTESIAN_POINT('Ctrl Pts',(-83.0200422087351,-1.18124687975515,
126.030071259811));
#94430=CARTESIAN_POINT('Ctrl Pts',(-83.0277901055122,-1.31433651668442,
126.063000080536));
#94431=CARTESIAN_POINT('Ctrl Pts',(-83.0355380022893,-1.44611704040084,
126.101515224015));
#94432=CARTESIAN_POINT('Ctrl Pts',(-83.0432858990664,-1.57608975505062,
126.145484771772));
#94433=CARTESIAN_POINT('Ctrl Pts',(-83.0510321751505,-1.70603528221039,
126.189445122047));
#94434=CARTESIAN_POINT('Ctrl Pts',(-83.0587784512346,-1.83417338236171,
126.238857481993));
#94435=CARTESIAN_POINT('Ctrl Pts',(-83.0665247273187,-1.96002097090085,
126.29354019816));
#94436=CARTESIAN_POINT('Ctrl Pts',(-83.074271060584,-2.08586948841779,126.348223317982));
#94437=CARTESIAN_POINT('Ctrl Pts',(-83.0820173938494,-2.20942710200628,
126.408176715849));
#94438=CARTESIAN_POINT('Ctrl Pts',(-83.0897637271148,-2.3302315176174,126.473170926869));
#94439=CARTESIAN_POINT('Ctrl Pts',(-83.0975117951177,-2.45106298653962,
126.538179692891));
#94440=CARTESIAN_POINT('Ctrl Pts',(-83.1052598631206,-2.56913968636999,
126.608231333157));
#94441=CARTESIAN_POINT('Ctrl Pts',(-83.1130079311236,-2.68402505307463,
126.683051046936));
#94442=CARTESIAN_POINT('Ctrl Pts',(-83.1207642338654,-2.79903252131463,
126.757950279997));
#94443=CARTESIAN_POINT('Ctrl Pts',(-83.1285205366073,-2.91084155283274,
126.837627495877));
#94444=CARTESIAN_POINT('Ctrl Pts',(-83.1362768393492,-3.01904520575611,
126.921764951249));
#94445=CARTESIAN_POINT('Ctrl Pts',(-83.1440372818633,-3.12730661022699,
127.005947313315));
#94446=CARTESIAN_POINT('Ctrl Pts',(-83.1517977243776,-3.23195850359698,
127.094594405772));
#94447=CARTESIAN_POINT('Ctrl Pts',(-83.1595581668917,-3.33262882375305,
127.187349671275));
#94448=CARTESIAN_POINT('Ctrl Pts',(-83.1673310671572,-3.43346074884413,
127.280253835764));
#94449=CARTESIAN_POINT('Ctrl Pts',(-83.1751039674226,-3.53029805197323,
127.377279074937));
#94450=CARTESIAN_POINT('Ctrl Pts',(-83.182876867688,-3.62280656954413,127.478032969518));
#94451=CARTESIAN_POINT('Ctrl Pts',(-83.1903672034502,-3.71195216948843,
127.57512420625));
#94452=CARTESIAN_POINT('Ctrl Pts',(-83.1978575392124,-3.79707804529234,
127.675677477826));
#94453=CARTESIAN_POINT('Ctrl Pts',(-83.2053478749746,-3.8779230094375,127.779315792216));
#94454=CARTESIAN_POINT('Ctrl Pts',(-83.2131256248477,-3.96187010200848,
127.886930846092));
#94455=CARTESIAN_POINT('Ctrl Pts',(-83.2209033747207,-4.04147175796609,
127.998219251153));
#94456=CARTESIAN_POINT('Ctrl Pts',(-83.2286811245938,-4.116389092648,128.112795292253));
#94457=CARTESIAN_POINT('Ctrl Pts',(-83.2364463580136,-4.1911858655564,128.227186950248));
#94458=CARTESIAN_POINT('Ctrl Pts',(-83.2442115914335,-4.26131311791541,
128.3448553847));
#94459=CARTESIAN_POINT('Ctrl Pts',(-83.2519768248532,-4.32647231475834,
128.465382128539));
#94460=CARTESIAN_POINT('Ctrl Pts',(-83.2597348559254,-4.39157107566005,
128.58579708237));
#94461=CARTESIAN_POINT('Ctrl Pts',(-83.2674928869975,-4.4517107608616,128.709064732525));
#94462=CARTESIAN_POINT('Ctrl Pts',(-83.2752509180696,-4.50663606226283,
128.834737693042));
#94463=CARTESIAN_POINT('Ctrl Pts',(-83.2830025719219,-4.56151621422867,
128.960307348468));
#94464=CARTESIAN_POINT('Ctrl Pts',(-83.2907542257741,-4.61119035866945,
129.088278022726));
#94465=CARTESIAN_POINT('Ctrl Pts',(-83.2985058796263,-4.65544934868352,
129.218178274851));
#94466=CARTESIAN_POINT('Ctrl Pts',(-83.3056620891265,-4.6963085783192,129.338100221321));
#94467=CARTESIAN_POINT('Ctrl Pts',(-83.3128182986267,-4.73255301784986,
129.459666208422));
#94468=CARTESIAN_POINT('Ctrl Pts',(-83.3199745081269,-4.76405452823405,
129.582490119308));
#94469=CARTESIAN_POINT('Origin',(213.235140564004,0.,130.804360617566));
#94470=CARTESIAN_POINT('',(-85.4152252782566,-4.76405452823408,129.582490119308));
#94471=CARTESIAN_POINT('',(-85.069725199937,-4.76405452823396,129.582490119308));
#94472=CARTESIAN_POINT('',(213.235140564004,-4.76405452823405,129.582490119308));
#94473=CARTESIAN_POINT('',(-83.7351405639751,-4.91824993107876,130.80518399099));
#94474=CARTESIAN_POINT('Ctrl Pts',(-83.7351405640088,-4.91824993107866,
130.805183991582));
#94475=CARTESIAN_POINT('Ctrl Pts',(-83.7376450848192,-4.91824257246219,
130.849139125296));
#94476=CARTESIAN_POINT('Ctrl Pts',(-83.7401496056296,-4.91764597711713,
130.893088715047));
#94477=CARTESIAN_POINT('Ctrl Pts',(-83.74265412644,-4.91646050823067,130.937022343426));
#94478=CARTESIAN_POINT('Ctrl Pts',(-83.7504284605591,-4.91278067008646,
131.073397615159));
#94479=CARTESIAN_POINT('Ctrl Pts',(-83.7582027946782,-4.903416433567,131.2098356697));
#94480=CARTESIAN_POINT('Ctrl Pts',(-83.7659771287973,-4.88835356997622,
131.345823854915));
#94481=CARTESIAN_POINT('Ctrl Pts',(-83.7737418817444,-4.87330927001864,
131.481644446846));
#94482=CARTESIAN_POINT('Ctrl Pts',(-83.7815066346914,-4.85258035939235,
131.617015887731));
#94483=CARTESIAN_POINT('Ctrl Pts',(-83.7892713876385,-4.82620460097485,
131.751425669201));
#94484=CARTESIAN_POINT('Ctrl Pts',(-83.7970284285235,-4.79985503933245,
131.885701952982));
#94485=CARTESIAN_POINT('Ctrl Pts',(-83.8047854694086,-4.76786986592196,
132.019018096942));
#94486=CARTESIAN_POINT('Ctrl Pts',(-83.8125425102936,-4.73033857577903,
132.150867216509));
#94487=CARTESIAN_POINT('Ctrl Pts',(-83.8202937015337,-4.692835588274,132.282616907629));
#94488=CARTESIAN_POINT('Ctrl Pts',(-83.8280448927738,-4.64979491539434,
132.412901401863));
#94489=CARTESIAN_POINT('Ctrl Pts',(-83.8357960840139,-4.60135693763739,
132.541224859514));
#94490=CARTESIAN_POINT('Ctrl Pts',(-83.8435439807909,-4.55293954731305,
132.669493776272));
#94491=CARTESIAN_POINT('Ctrl Pts',(-83.8512918775679,-4.49912955247868,
132.795802949193));
#94492=CARTESIAN_POINT('Ctrl Pts',(-83.859039774345,-4.44011684860706,132.919672753686));
#94493=CARTESIAN_POINT('Ctrl Pts',(-83.8667860504291,-4.38111648892092,
133.043516647286));
#94494=CARTESIAN_POINT('Ctrl Pts',(-83.8745323265132,-4.31691575292055,
133.164921834666));
#94495=CARTESIAN_POINT('Ctrl Pts',(-83.8822786025973,-4.24775207911664,
133.283430067352));
#94496=CARTESIAN_POINT('Ctrl Pts',(-83.8900249358627,-4.17858789476211,
133.401939174839));
#94497=CARTESIAN_POINT('Ctrl Pts',(-83.8977712691281,-4.10446089656903,
133.517550947295));
#94498=CARTESIAN_POINT('Ctrl Pts',(-83.9055176023934,-4.02565354429549,
133.62983342823));
#94499=CARTESIAN_POINT('Ctrl Pts',(-83.9132656703964,-3.94682854366193,
133.742141054048));
#94500=CARTESIAN_POINT('Ctrl Pts',(-83.9210137383994,-3.86332132784651,
133.851117584795));
#94501=CARTESIAN_POINT('Ctrl Pts',(-83.9287618064024,-3.7754563361864,133.956361968462));
#94502=CARTESIAN_POINT('Ctrl Pts',(-83.9365181091442,-3.68749796056742,
134.061718207112));
#94503=CARTESIAN_POINT('Ctrl Pts',(-83.944274411886,-3.59517280815231,134.163334074431));
#94504=CARTESIAN_POINT('Ctrl Pts',(-83.9520307146279,-3.49884446166895,
134.260843005131));
#94505=CARTESIAN_POINT('Ctrl Pts',(-83.959791157142,-3.40246470184669,134.358403979284));
#94506=CARTESIAN_POINT('Ctrl Pts',(-83.9675515996562,-3.30207777657493,
134.451853382821));
#94507=CARTESIAN_POINT('Ctrl Pts',(-83.9753120421704,-3.19808169132444,
134.540863870357));
#94508=CARTESIAN_POINT('Ctrl Pts',(-83.9830849424358,-3.09391866232556,
134.630017245429));
#94509=CARTESIAN_POINT('Ctrl Pts',(-83.9908578427013,-2.98613520318335,
134.714717223287));
#94510=CARTESIAN_POINT('Ctrl Pts',(-83.9986307429667,-2.87516045414131,
134.794678327403));
#94511=CARTESIAN_POINT('Ctrl Pts',(-84.0061210787287,-2.76821991675548,
134.871732643975));
#94512=CARTESIAN_POINT('Ctrl Pts',(-84.0136114144907,-2.65831634101399,
134.944386475219));
#94513=CARTESIAN_POINT('Ctrl Pts',(-84.0211017502528,-2.54585492878171,
135.012424987808));
#94514=CARTESIAN_POINT('Ctrl Pts',(-84.0288760843718,-2.42912950792289,
135.083043201281));
#94515=CARTESIAN_POINT('Ctrl Pts',(-84.0366504184909,-2.30927870993854,
135.148912905052));
#94516=CARTESIAN_POINT('Ctrl Pts',(-84.04442475261,-2.18672615262975,135.209745027116));
#94517=CARTESIAN_POINT('Ctrl Pts',(-84.0521895055571,-2.064324630395,135.270502179026));
#94518=CARTESIAN_POINT('Ctrl Pts',(-84.0599542585042,-1.93922832073468,
135.326233929872));
#94519=CARTESIAN_POINT('Ctrl Pts',(-84.0677190114513,-1.8118888232123,135.376695027342));
#94520=CARTESIAN_POINT('Ctrl Pts',(-84.0754760523363,-1.68467580107403,
135.427106006138));
#94521=CARTESIAN_POINT('Ctrl Pts',(-84.0832330932213,-1.55522438594163,
135.472256606118));
#94522=CARTESIAN_POINT('Ctrl Pts',(-84.0909901341063,-1.42400940841375,
135.5119481385));
#94523=CARTESIAN_POINT('Ctrl Pts',(-84.0987413253464,-1.29289338112131,
135.551609739187));
#94524=CARTESIAN_POINT('Ctrl Pts',(-84.1064925165865,-1.16001681125566,
135.585820353627));
#94525=CARTESIAN_POINT('Ctrl Pts',(-84.1142437078267,-1.02587274188369,
135.614430074441));
#94526=CARTESIAN_POINT('Ctrl Pts',(-84.1219916046037,-0.891785687319422,
135.64302763536));
#94527=CARTESIAN_POINT('Ctrl Pts',(-84.1297395013808,-0.75643258628915,
135.666028955964));
#94528=CARTESIAN_POINT('Ctrl Pts',(-84.1374873981579,-0.6203196036862,135.683334551887));
#94529=CARTESIAN_POINT('Ctrl Pts',(-84.145233674242,-0.484235092984954,
135.700636527852));
#94530=CARTESIAN_POINT('Ctrl Pts',(-84.1529799503261,-0.347391404470298,
135.712245099661));
#94531=CARTESIAN_POINT('Ctrl Pts',(-84.1607262264102,-0.210302416876331,
135.718112336564));
#94532=CARTESIAN_POINT('Ctrl Pts',(-84.1684725596755,-0.0732124173227867,
135.723979616778));
#94533=CARTESIAN_POINT('Ctrl Pts',(-84.1762188929409,0.0641224943156463,
135.724105460799));
#94534=CARTESIAN_POINT('Ctrl Pts',(-84.1839652262063,0.201186224411701,
135.718494026989));
#94535=CARTESIAN_POINT('Ctrl Pts',(-84.1917132942092,0.338280648979591,
135.712881336537));
#94536=CARTESIAN_POINT('Ctrl Pts',(-84.1994613622121,0.475103380597773,
135.701528827593));
#94537=CARTESIAN_POINT('Ctrl Pts',(-84.2072094302151,0.611141635466226,
135.684492681752));
#94538=CARTESIAN_POINT('Ctrl Pts',(-84.214965732957,0.747324473411385,135.667438429693));
#94539=CARTESIAN_POINT('Ctrl Pts',(-84.2227220356988,0.882720780545246,
135.644688522574));
#94540=CARTESIAN_POINT('Ctrl Pts',(-84.2304783384407,1.01682562976458,135.616350715348));
#94541=CARTESIAN_POINT('Ctrl Pts',(-84.2382387809549,1.15100205477976,135.587997783382));
#94542=CARTESIAN_POINT('Ctrl Pts',(-84.245999223469,1.28388526979703,135.554051105286));
#94543=CARTESIAN_POINT('Ctrl Pts',(-84.2537596659832,1.41498473819222,135.514668596158));
#94544=CARTESIAN_POINT('Ctrl Pts',(-84.2615325662486,1.54629465909254,135.475222866729));
#94545=CARTESIAN_POINT('Ctrl Pts',(-84.269305466514,1.67581474171641,135.430323996911));
#94546=CARTESIAN_POINT('Ctrl Pts',(-84.2770783667795,1.80307284579192,135.380178727507));
#94547=CARTESIAN_POINT('Ctrl Pts',(-84.2845687025416,1.9257047972415,135.331856364954));
#94548=CARTESIAN_POINT('Ctrl Pts',(-84.2920590383037,2.04623609036355,135.278662544507));
#94549=CARTESIAN_POINT('Ctrl Pts',(-84.2995493740658,2.16426695829061,135.22082205131));
#94550=CARTESIAN_POINT('Ctrl Pts',(-84.3073237081849,2.28677300244897,135.160788518234));
#94551=CARTESIAN_POINT('Ctrl Pts',(-84.315098042304,2.40697333358794,135.095558831384));
#94552=CARTESIAN_POINT('Ctrl Pts',(-84.3228723764231,2.52439577147361,135.025333141934));
#94553=CARTESIAN_POINT('Ctrl Pts',(-84.3306371293702,2.6416734966986,134.955193999369));
#94554=CARTESIAN_POINT('Ctrl Pts',(-84.3384018823172,2.7561798081096,134.880071303797));
#94555=CARTESIAN_POINT('Ctrl Pts',(-84.3461666352643,2.8674642673941,134.800212433852));
#94556=CARTESIAN_POINT('Ctrl Pts',(-84.3539236761493,2.9786381973848,134.720432880863));
#94557=CARTESIAN_POINT('Ctrl Pts',(-84.3616807170344,3.08659632778562,134.635926741212));
#94558=CARTESIAN_POINT('Ctrl Pts',(-84.3694377579194,3.19091483855833,134.546986107188));
#94559=CARTESIAN_POINT('Ctrl Pts',(-84.3771889491595,3.29515468193073,134.458112543988));
#94560=CARTESIAN_POINT('Ctrl Pts',(-84.3849401403995,3.39576007245741,134.364811395245));
#94561=CARTESIAN_POINT('Ctrl Pts',(-84.3926913316397,3.49233838699389,134.267416443456));
#94562=CARTESIAN_POINT('Ctrl Pts',(-84.4004392284168,3.58887565317052,134.170062887119));
#94563=CARTESIAN_POINT('Ctrl Pts',(-84.4081871251939,3.68138897291665,134.068619265448));
#94564=CARTESIAN_POINT('Ctrl Pts',(-84.415935021971,3.76952105272785,133.963457655573));
#94565=CARTESIAN_POINT('Ctrl Pts',(-84.4236812980551,3.85763469720762,133.858318043239));
#94566=CARTESIAN_POINT('Ctrl Pts',(-84.4314275741392,3.94136867367733,133.749462289095));
#94567=CARTESIAN_POINT('Ctrl Pts',(-84.4391738502233,4.02040489263177,133.637296826132));
#94568=CARTESIAN_POINT('Ctrl Pts',(-84.4469201834886,4.09944169501374,133.525130535188));
#94569=CARTESIAN_POINT('Ctrl Pts',(-84.454666516754,4.17378044548553,133.409654806267));
#94570=CARTESIAN_POINT('Ctrl Pts',(-84.4624128500193,4.2431456813816,133.291306091249));
#94571=CARTESIAN_POINT('Ctrl Pts',(-84.4701609180223,4.31252645114139,133.172930872857));
#94572=CARTESIAN_POINT('Ctrl Pts',(-84.4779089860252,4.37693129236773,133.05168172534));
#94573=CARTESIAN_POINT('Ctrl Pts',(-84.4856570540282,4.43613030005905,132.928020435757));
#94574=CARTESIAN_POINT('Ctrl Pts',(-84.4934133567701,4.49539222516014,132.804227717484));
#94575=CARTESIAN_POINT('Ctrl Pts',(-84.501169659512,4.54943709523391,132.678018089174));
#94576=CARTESIAN_POINT('Ctrl Pts',(-84.5089259622539,4.59808264214261,132.549874604484));
#94577=CARTESIAN_POINT('Ctrl Pts',(-84.516686404768,4.64675415264437,132.421662725758));
#94578=CARTESIAN_POINT('Ctrl Pts',(-84.5244468472822,4.69002047451208,132.291515304811));
#94579=CARTESIAN_POINT('Ctrl Pts',(-84.5322072897963,4.72774931916171,132.159930400966));
#94580=CARTESIAN_POINT('Ctrl Pts',(-84.5399801900618,4.76553872950219,132.02813426535));
#94581=CARTESIAN_POINT('Ctrl Pts',(-84.5477530903272,4.79777280708402,131.894896415787));
#94582=CARTESIAN_POINT('Ctrl Pts',(-84.5555259905927,4.82437028545145,131.760725825712));
#94583=CARTESIAN_POINT('Ctrl Pts',(-84.5630163263546,4.85000087848501,131.631432674544));
#94584=CARTESIAN_POINT('Ctrl Pts',(-84.5705066621165,4.87039751888811,131.501273724736));
#94585=CARTESIAN_POINT('Ctrl Pts',(-84.5779969978785,4.88553324101221,131.370706813337));
#94586=CARTESIAN_POINT('Ctrl Pts',(-84.5857713319976,4.90124283864115,131.235189417808));
#94587=CARTESIAN_POINT('Ctrl Pts',(-84.5935456661167,4.91133447073031,131.098803235904));
#94588=CARTESIAN_POINT('Ctrl Pts',(-84.6013200002357,4.91572130518057,130.96205371283));
#94589=CARTESIAN_POINT('Ctrl Pts',(-84.6090847531828,4.92010273324944,130.82547272132));
#94590=CARTESIAN_POINT('Ctrl Pts',(-84.61684950613,4.91879334016872,130.688529666612));
#94591=CARTESIAN_POINT('Ctrl Pts',(-84.624614259077,4.91175777968097,130.55173722941));
#94592=CARTESIAN_POINT('Ctrl Pts',(-84.632371299962,4.90472920701109,130.415080656385));
#94593=CARTESIAN_POINT('Ctrl Pts',(-84.640128340847,4.89198580488988,130.278574791087));
#94594=CARTESIAN_POINT('Ctrl Pts',(-84.647885381732,4.87354423374991,130.142734088334));
#94595=CARTESIAN_POINT('Ctrl Pts',(-84.6556365729722,4.85511656954221,130.006995824113));
#94596=CARTESIAN_POINT('Ctrl Pts',(-84.6633877642123,4.8309993416822,129.871922109868));
#94597=CARTESIAN_POINT('Ctrl Pts',(-84.6711389554524,4.80126114843691,129.738023688162));
#94598=CARTESIAN_POINT('Ctrl Pts',(-84.6788868522295,4.771535594717,129.604182176858));
#94599=CARTESIAN_POINT('Ctrl Pts',(-84.6866347490066,4.73619391185903,129.471515345431));
#94600=CARTESIAN_POINT('Ctrl Pts',(-84.6943826457837,4.69535601302328,129.340524911803));
#94601=CARTESIAN_POINT('Ctrl Pts',(-84.7021289218678,4.65452665659561,129.20956187855));
#94602=CARTESIAN_POINT('Ctrl Pts',(-84.7098751979518,4.60820348727698,129.080274918612));
#94603=CARTESIAN_POINT('Ctrl Pts',(-84.7176214740359,4.55655651350683,128.953151336658));
#94604=CARTESIAN_POINT('Ctrl Pts',(-84.7253678073012,4.50490915849052,128.826026816307));
#94605=CARTESIAN_POINT('Ctrl Pts',(-84.7331141405666,4.44793806776186,128.701066068019));
#94606=CARTESIAN_POINT('Ctrl Pts',(-84.740860473832,4.38586154634956,128.578736759239));
#94607=CARTESIAN_POINT('Ctrl Pts',(-84.7486085418349,4.32377112333078,128.456380055659));
#94608=CARTESIAN_POINT('Ctrl Pts',(-84.7563566098379,4.25657317142948,128.336656312788));
#94609=CARTESIAN_POINT('Ctrl Pts',(-84.7641046778409,4.18453193590752,128.2200085634));
#94610=CARTESIAN_POINT('Ctrl Pts',(-84.7718609805827,4.11241413410304,128.103236839396));
#94611=CARTESIAN_POINT('Ctrl Pts',(-84.7796172833246,4.03544297175806,127.98954797263));
#94612=CARTESIAN_POINT('Ctrl Pts',(-84.7873735860664,3.95392633521457,127.879356412749));
#94613=CARTESIAN_POINT('Ctrl Pts',(-84.7951340285806,3.87236619078753,127.769106040314));
#94614=CARTESIAN_POINT('Ctrl Pts',(-84.8028944710948,3.78625598338683,127.662356998312));
#94615=CARTESIAN_POINT('Ctrl Pts',(-84.8106549136089,3.69594323921468,127.559489798103));
#94616=CARTESIAN_POINT('Ctrl Pts',(-84.8184278138744,3.605485517008,127.456457466332));
#94617=CARTESIAN_POINT('Ctrl Pts',(-84.8262007141398,3.51081204697257,127.357319711741));
#94618=CARTESIAN_POINT('Ctrl Pts',(-84.8339736144053,3.41230711637157,127.262420018677));
#94619=CARTESIAN_POINT('Ctrl Pts',(-84.8414639501674,3.31738308811578,127.170970168492));
#94620=CARTESIAN_POINT('Ctrl Pts',(-84.8489542859295,3.21890155970101,127.083455805576));
#94621=CARTESIAN_POINT('Ctrl Pts',(-84.8564446216916,3.11723314681125,127.000147089));
#94622=CARTESIAN_POINT('Ctrl Pts',(-84.8642189558106,3.01170994514667,126.913679697116));
#94623=CARTESIAN_POINT('Ctrl Pts',(-84.8719932899298,2.90241916130007,126.831469258493));
#94624=CARTESIAN_POINT('Ctrl Pts',(-84.8797676240489,2.78973910576426,126.753862032914));
#94625=CARTESIAN_POINT('Ctrl Pts',(-84.8875323769959,2.67719791832639,126.676350451304));
#94626=CARTESIAN_POINT('Ctrl Pts',(-84.895297129943,2.56127608902775,126.603431014697));
#94627=CARTESIAN_POINT('Ctrl Pts',(-84.9030618828901,2.44238584514977,126.535410577344));
#94628=CARTESIAN_POINT('Ctrl Pts',(-84.9108189237751,2.32361368473807,126.467457698848));
#94629=CARTESIAN_POINT('Ctrl Pts',(-84.9185759646601,2.20187931409443,126.40439432943));
#94630=CARTESIAN_POINT('Ctrl Pts',(-84.926333005545,2.07762456399858,126.346484527591));
#94631=CARTESIAN_POINT('Ctrl Pts',(-84.9340841967852,1.95346351537617,126.288618395984));
#94632=CARTESIAN_POINT('Ctrl Pts',(-84.9418353880253,1.82678622334068,126.23589826091));
#94633=CARTESIAN_POINT('Ctrl Pts',(-84.9495865792654,1.69805946911441,126.188542477534));
#94634=CARTESIAN_POINT('Ctrl Pts',(-84.9573344760425,1.56938742719277,126.141206821629));
#94635=CARTESIAN_POINT('Ctrl Pts',(-84.9650823728196,1.4386680217402,126.099231117392));
#94636=CARTESIAN_POINT('Ctrl Pts',(-84.9728302695966,1.30638817824548,126.062785669277));
#94637=CARTESIAN_POINT('Ctrl Pts',(-84.9805765456808,1.17413600484203,126.026347844764));
#94638=CARTESIAN_POINT('Ctrl Pts',(-84.9883228217649,1.04032441932584,125.995438079196));
#94639=CARTESIAN_POINT('Ctrl Pts',(-84.996069097849,0.905455298630496,125.970176739735));
#94640=CARTESIAN_POINT('Ctrl Pts',(-85.0038154311144,0.770585182362128,
125.9449152138));
#94641=CARTESIAN_POINT('Ctrl Pts',(-85.0115617643797,0.634657899619902,
125.92530226915));
#94642=CARTESIAN_POINT('Ctrl Pts',(-85.0193080976451,0.498184911470203,
125.911407025258));
#94643=CARTESIAN_POINT('Ctrl Pts',(-85.0270561656481,0.361681361141231,
125.897508669622));
#94644=CARTESIAN_POINT('Ctrl Pts',(-85.034804233651,0.224632251107003,125.889330602264));
#94645=CARTESIAN_POINT('Ctrl Pts',(-85.042552301654,0.0875531484062345,
125.886889976199));
#94646=CARTESIAN_POINT('Ctrl Pts',(-85.0503086043958,-0.0496716435959595,
125.884446756208));
#94647=CARTESIAN_POINT('Ctrl Pts',(-85.0580649071377,-0.186926100415,125.887753165533));
#94648=CARTESIAN_POINT('Ctrl Pts',(-85.0658212098795,-0.323695113736321,
125.896774190834));
#94649=CARTESIAN_POINT('Ctrl Pts',(-85.0735816523937,-0.460537124798459,
125.905800030928));
#94650=CARTESIAN_POINT('Ctrl Pts',(-85.0813420949078,-0.596892787583985,
125.920546522489));
#94651=CARTESIAN_POINT('Ctrl Pts',(-85.089102537422,-0.732254120706716,
125.940926957567));
#94652=CARTESIAN_POINT('Ctrl Pts',(-85.0968754376874,-0.867832747858191,
125.961340109129));
#94653=CARTESIAN_POINT('Ctrl Pts',(-85.1046483379529,-1.00241347160462,
125.987405202831));
#94654=CARTESIAN_POINT('Ctrl Pts',(-85.1124212382183,-1.1354995921853,126.018984588595));
#94655=CARTESIAN_POINT('Ctrl Pts',(-85.1199115739803,-1.26374769705952,
126.049415984143));
#94656=CARTESIAN_POINT('Ctrl Pts',(-85.1274019097423,-1.39060768076853,
126.084967632327));
#94657=CARTESIAN_POINT('Ctrl Pts',(-85.1348922455044,-1.51565192400376,
126.125473751252));
#94658=CARTESIAN_POINT('Ctrl Pts',(-85.1426665796235,-1.6454372577271,126.167515671988));
#94659=CARTESIAN_POINT('Ctrl Pts',(-85.1504409137426,-1.77367756630603,
126.215028353537));
#94660=CARTESIAN_POINT('Ctrl Pts',(-85.1582152478616,-1.89987704551724,
126.267880674436));
#94661=CARTESIAN_POINT('Ctrl Pts',(-85.1659800008087,-2.02592099514908,
126.320667859574));
#94662=CARTESIAN_POINT('Ctrl Pts',(-85.1737447537559,-2.14992876263638,
126.378781440998));
#94663=CARTESIAN_POINT('Ctrl Pts',(-85.181509506703,-2.27141936389203,126.442040462438));
#94664=CARTESIAN_POINT('Ctrl Pts',(-85.189266547588,-2.39278929897012,126.505236654127));
#94665=CARTESIAN_POINT('Ctrl Pts',(-85.1970235884729,-2.51164669856962,
126.573567936267));
#94666=CARTESIAN_POINT('Ctrl Pts',(-85.2047806293579,-2.62753058246556,
126.646805314181));
#94667=CARTESIAN_POINT('Ctrl Pts',(-85.2125318205981,-2.74332707742305,
126.719987463218));
#94668=CARTESIAN_POINT('Ctrl Pts',(-85.2202830118382,-2.85615419078308,
126.798068135926));
#94669=CARTESIAN_POINT('Ctrl Pts',(-85.2280342030784,-2.9655759075078,126.880772642344));
#94670=CARTESIAN_POINT('Ctrl Pts',(-85.2357820998554,-3.07495111708415,
126.96344199714));
#94671=CARTESIAN_POINT('Ctrl Pts',(-85.2435299966326,-3.18092349751863,
127.05073104166));
#94672=CARTESIAN_POINT('Ctrl Pts',(-85.2512778934097,-3.28308657173051,
127.142322165416));
#94673=CARTESIAN_POINT('Ctrl Pts',(-85.2590241694938,-3.38522827562965,
127.233894130284));
#94674=CARTESIAN_POINT('Ctrl Pts',(-85.2667704455778,-3.48356196731321,
127.329766123617));
#94675=CARTESIAN_POINT('Ctrl Pts',(-85.2745167216619,-3.57771510173734,
127.429580963529));
#94676=CARTESIAN_POINT('Ctrl Pts',(-85.2822630549272,-3.67186893117813,
127.529396540251));
#94677=CARTESIAN_POINT('Ctrl Pts',(-85.2900093881926,-3.76184187351027,
127.633154737226));
#94678=CARTESIAN_POINT('Ctrl Pts',(-85.2977557214579,-3.84729931936343,
127.740462608538));
#94679=CARTESIAN_POINT('Ctrl Pts',(-85.3055037894609,-3.93277590281919,
127.847794510704));
#94680=CARTESIAN_POINT('Ctrl Pts',(-85.3132518574639,-4.01373473408586,
127.958677363241));
#94681=CARTESIAN_POINT('Ctrl Pts',(-85.3209999254669,-4.0898827052696,128.072686676621));
#94682=CARTESIAN_POINT('Ctrl Pts',(-85.3287562282087,-4.1661116074234,128.186817160457));
#94683=CARTESIAN_POINT('Ctrl Pts',(-85.3365125309506,-4.23751921815287,
128.304080417231));
#94684=CARTESIAN_POINT('Ctrl Pts',(-85.3442688336925,-4.30385656654757,
128.424024146164));
#94685=CARTESIAN_POINT('Ctrl Pts',(-85.3520292762067,-4.37022932118248,
128.544031892677));
#94686=CARTESIAN_POINT('Ctrl Pts',(-85.3597897187208,-4.43152624659729,
128.666722612464));
#94687=CARTESIAN_POINT('Ctrl Pts',(-85.367550161235,-4.48754571629947,128.791622058631));
#94688=CARTESIAN_POINT('Ctrl Pts',(-85.3753230615004,-4.5436551134276,128.916722004478));
#94689=CARTESIAN_POINT('Ctrl Pts',(-85.3830959617658,-4.59446998039584,
129.044037398712));
#94690=CARTESIAN_POINT('Ctrl Pts',(-85.3908688620313,-4.6398376477609,129.173075950526));
#94691=CARTESIAN_POINT('Ctrl Pts',(-85.3983591977933,-4.68355608614274,
129.297423625952));
#94692=CARTESIAN_POINT('Ctrl Pts',(-85.4058495335553,-4.72221639757264,
129.423371057348));
#94693=CARTESIAN_POINT('Ctrl Pts',(-85.4133398693172,-4.75572692037172,
129.550468867313));
#94694=CARTESIAN_POINT('Ctrl Pts',(-85.4139683389637,-4.75853858957919,
129.561132890694));
#94695=CARTESIAN_POINT('Ctrl Pts',(-85.4145968086102,-4.76131447935733,
129.571806710324));
#94696=CARTESIAN_POINT('Ctrl Pts',(-85.4152252782566,-4.76405452823408,
129.582490119308));
#94697=CARTESIAN_POINT('Ctrl Pts',(-83.6650228471445,-4.76405452823415,
129.582490119309));
#94698=CARTESIAN_POINT('Ctrl Pts',(-83.6727478526518,-4.7979834497542,129.714778469372));
#94699=CARTESIAN_POINT('Ctrl Pts',(-83.6804728581592,-4.82637148214606,
129.848377264129));
#94700=CARTESIAN_POINT('Ctrl Pts',(-83.6881978636665,-4.84914314726169,
129.982780554599));
#94701=CARTESIAN_POINT('Ctrl Pts',(-83.6960216470513,-4.87220598844752,
130.118902429184));
#94702=CARTESIAN_POINT('Ctrl Pts',(-83.7038454304361,-4.88950779304398,
130.255849098009));
#94703=CARTESIAN_POINT('Ctrl Pts',(-83.7116692138208,-4.9010245141228,130.393092123189));
#94704=CARTESIAN_POINT('Ctrl Pts',(-83.7194929972056,-4.91254123520162,
130.530335148369));
#94705=CARTESIAN_POINT('Ctrl Pts',(-83.7273167805903,-4.91827291838221,
130.667874113824));
#94706=CARTESIAN_POINT('Ctrl Pts',(-83.7351405639751,-4.91824993107876,
130.805183990989));
#94707=CARTESIAN_POINT('',(-83.3898594360444,-4.91824854697785,130.808141179725));
#94708=CARTESIAN_POINT('Ctrl Pts',(-83.3199745081269,-4.76405452823405,
129.582490119308));
#94709=CARTESIAN_POINT('Ctrl Pts',(-83.3277201319047,-4.79815063006876,
129.715430302881));
#94710=CARTESIAN_POINT('Ctrl Pts',(-83.3354657556824,-4.82668962234322,
129.849844006803));
#94711=CARTESIAN_POINT('Ctrl Pts',(-83.3432113794602,-4.8495570910012,129.985227488203));
#94712=CARTESIAN_POINT('Ctrl Pts',(-83.3509860555487,-4.87251033103457,
130.121118766403));
#94713=CARTESIAN_POINT('Ctrl Pts',(-83.3587607316373,-4.88974931916973,
130.257986727359));
#94714=CARTESIAN_POINT('Ctrl Pts',(-83.3665354077258,-4.90121034433255,
130.395312670367));
#94715=CARTESIAN_POINT('Ctrl Pts',(-83.3743100838143,-4.91267136949533,
130.532638613375));
#94716=CARTESIAN_POINT('Ctrl Pts',(-83.3820847599029,-4.91835440890207,
130.670422141569));
#94717=CARTESIAN_POINT('Ctrl Pts',(-83.3898594359914,-4.91824854697857,
130.808141178786));
#94718=CARTESIAN_POINT('Ctrl Pts',(-83.3898594360443,-4.91824854697785,
130.808141179725));
#94719=CARTESIAN_POINT('Ctrl Pts',(-83.3988547443525,-4.91812606459202,
130.967482248801));
#94720=CARTESIAN_POINT('Ctrl Pts',(-83.4078500526607,-4.91025620410759,
131.126502818401));
#94721=CARTESIAN_POINT('Ctrl Pts',(-83.4168453609689,-4.89475572259842,
131.284516299184));
#94722=CARTESIAN_POINT('Ctrl Pts',(-83.4258919752923,-4.87916683189729,
131.443431032237));
#94723=CARTESIAN_POINT('Ctrl Pts',(-83.4349385896156,-4.85586013639439,
131.601327047096));
#94724=CARTESIAN_POINT('Ctrl Pts',(-83.443985203939,-4.82500359745644,131.757525528288));
#94725=CARTESIAN_POINT('Ctrl Pts',(-83.4530931965809,-4.79393770699704,
131.914783765073));
#94726=CARTESIAN_POINT('Ctrl Pts',(-83.4622011892227,-4.75521925941508,
132.070321249573));
#94727=CARTESIAN_POINT('Ctrl Pts',(-83.4713091818646,-4.70906796023881,
132.223466677151));
#94728=CARTESIAN_POINT('Ctrl Pts',(-83.4754712875057,-4.68797806807494,
132.293449984462));
#94729=CARTESIAN_POINT('Ctrl Pts',(-83.4796333931467,-4.66533667133282,
132.362934075846));
#94730=CARTESIAN_POINT('Ctrl Pts',(-83.4837954987878,-4.64116799542365,
132.431856454966));
#94731=CARTESIAN_POINT('Ctrl Pts',(-83.4915698329069,-4.59602369156994,
132.560595523544));
#94732=CARTESIAN_POINT('Ctrl Pts',(-83.499344167026,-4.54544727869063,132.687658728732));
#94733=CARTESIAN_POINT('Ctrl Pts',(-83.507118501145,-4.48958173842214,132.812553555639));
#94734=CARTESIAN_POINT('Ctrl Pts',(-83.5148832540921,-4.43378504743918,
132.937294460834));
#94735=CARTESIAN_POINT('Ctrl Pts',(-83.5226480070392,-4.37271235679831,
133.05987195143));
#94736=CARTESIAN_POINT('Ctrl Pts',(-83.5304127599863,-4.306556112949,133.179809524304));
#94737=CARTESIAN_POINT('Ctrl Pts',(-83.5381698008712,-4.24046557641391,
133.299627973489));
#94738=CARTESIAN_POINT('Ctrl Pts',(-83.5459268417562,-4.16930172213016,
133.416811382731));
#94739=CARTESIAN_POINT('Ctrl Pts',(-83.5536838826411,-4.09330454108528,
133.530904399798));
#94740=CARTESIAN_POINT('Ctrl Pts',(-83.5614350738812,-4.01736467010568,
133.644911378434));
#94741=CARTESIAN_POINT('Ctrl Pts',(-83.5691862651213,-3.93659894307991,
133.75583227952));
#94742=CARTESIAN_POINT('Ctrl Pts',(-83.5769374563614,-3.85129243402407,
133.86323780538));
#94743=CARTESIAN_POINT('Ctrl Pts',(-83.5846853531385,-3.76602218251008,
133.970597681027));
#94744=CARTESIAN_POINT('Ctrl Pts',(-83.5924332499156,-3.67621523014584,
134.074444847647));
#94745=CARTESIAN_POINT('Ctrl Pts',(-83.6001811466927,-3.58219885028352,
134.174380566992));
#94746=CARTESIAN_POINT('Ctrl Pts',(-83.6079274227768,-3.4882021366211,134.274295381938));
#94747=CARTESIAN_POINT('Ctrl Pts',(-83.6156736988608,-3.38999801458852,
134.370300092455));
#94748=CARTESIAN_POINT('Ctrl Pts',(-83.6234199749449,-3.2879525032671,134.462030832164));
#94749=CARTESIAN_POINT('Ctrl Pts',(-83.6311663082103,-3.18590623866902,
134.553762249009));
#94750=CARTESIAN_POINT('Ctrl Pts',(-83.6389126414756,-3.0800188189575,134.641219370721));
#94751=CARTESIAN_POINT('Ctrl Pts',(-83.646658974741,-2.97069110659266,134.72407711391));
#94752=CARTESIAN_POINT('Ctrl Pts',(-83.654407042744,-2.86133891104451,134.806953412516));
#94753=CARTESIAN_POINT('Ctrl Pts',(-83.6621551107469,-2.74854520130655,
134.885228046916));
#94754=CARTESIAN_POINT('Ctrl Pts',(-83.6699031787499,-2.6327413784461,134.958618180202));
#94755=CARTESIAN_POINT('Ctrl Pts',(-83.6776594814917,-2.51681447790479,
135.032086313395));
#94756=CARTESIAN_POINT('Ctrl Pts',(-83.6854157842335,-2.39787140428618,
135.100659365664));
#94757=CARTESIAN_POINT('Ctrl Pts',(-83.6931720869753,-2.27637030273414,
135.164099291768));
#94758=CARTESIAN_POINT('Ctrl Pts',(-83.7009325294894,-2.15480435238587,
135.22757307767));
#94759=CARTESIAN_POINT('Ctrl Pts',(-83.7086929720037,-2.03067800729966,
135.285908112105));
#94760=CARTESIAN_POINT('Ctrl Pts',(-83.7164534145178,-1.90447021627643,
135.338914207261));
#94761=CARTESIAN_POINT('Ctrl Pts',(-83.7242263147832,-1.77805982530285,
135.392005392507));
#94762=CARTESIAN_POINT('Ctrl Pts',(-83.7319992150486,-1.64956167806223,
135.439750407634));
#94763=CARTESIAN_POINT('Ctrl Pts',(-83.739772115314,-1.51947158723861,135.482008440786));
#94764=CARTESIAN_POINT('Ctrl Pts',(-83.7472624510759,-1.39411059889536,
135.522730287991));
#94765=CARTESIAN_POINT('Ctrl Pts',(-83.7547527868379,-1.26727169637365,
135.558357075127));
#94766=CARTESIAN_POINT('Ctrl Pts',(-83.7622431225998,-1.13940632728965,
135.588807950731));
#94767=CARTESIAN_POINT('Ctrl Pts',(-83.7700174567189,-1.00669290387129,
135.620413380539));
#94768=CARTESIAN_POINT('Ctrl Pts',(-83.7777917908379,-0.872453244171115,
135.646542778081));
#94769=CARTESIAN_POINT('Ctrl Pts',(-83.785566124957,-0.737178999982175,
135.667050221529));
#94770=CARTESIAN_POINT('Ctrl Pts',(-83.7933308779041,-0.602071469209758,
135.687532391384));
#94771=CARTESIAN_POINT('Ctrl Pts',(-83.8010956308511,-0.465932273721789,
135.702406334869));
#94772=CARTESIAN_POINT('Ctrl Pts',(-83.8088603837982,-0.329266331098542,
135.711576401053));
#94773=CARTESIAN_POINT('Ctrl Pts',(-83.8166174246832,-0.192736127016161,
135.720737359398));
#94774=CARTESIAN_POINT('Ctrl Pts',(-83.8243744655681,-0.0556806044995665,
135.724205688384));
#94775=CARTESIAN_POINT('Ctrl Pts',(-83.8321315064531,0.081387414730357,
135.721937170221));
#94776=CARTESIAN_POINT('Ctrl Pts',(-83.8398826976932,0.218352069900932,
135.719670362765));
#94777=CARTESIAN_POINT('Ctrl Pts',(-83.8476338889332,0.355328813697248,
135.711675325645));
#94778=CARTESIAN_POINT('Ctrl Pts',(-83.8553850801734,0.491802376358289,
135.697959853824));
#94779=CARTESIAN_POINT('Ctrl Pts',(-83.8631329769504,0.628217934114462,
135.684250211445));
#94780=CARTESIAN_POINT('Ctrl Pts',(-83.8708808737275,0.764130347906118,
135.664825009123));
#94781=CARTESIAN_POINT('Ctrl Pts',(-83.8786287705045,0.899027248710216,
135.639744063434));
#94782=CARTESIAN_POINT('Ctrl Pts',(-83.8863750465886,1.03389593199071,135.614668364139));
#94783=CARTESIAN_POINT('Ctrl Pts',(-83.8941213226727,1.16774914067108,135.583939346068));
#94784=CARTESIAN_POINT('Ctrl Pts',(-83.9018675987568,1.30008290140695,135.547668272776));
#94785=CARTESIAN_POINT('Ctrl Pts',(-83.9096139320221,1.43241763900075,135.511396931738));
#94786=CARTESIAN_POINT('Ctrl Pts',(-83.9173602652875,1.56323252921032,135.469583557192));
#94787=CARTESIAN_POINT('Ctrl Pts',(-83.9251065985528,1.69203739421934,135.422389690565));
#94788=CARTESIAN_POINT('Ctrl Pts',(-83.9328546665557,1.82087110418464,135.375185255198));
#94789=CARTESIAN_POINT('Ctrl Pts',(-83.9406027345587,1.94769352621084,135.32259806457));
#94790=CARTESIAN_POINT('Ctrl Pts',(-83.9483508025616,2.07203351878264,135.264838188358));
#94791=CARTESIAN_POINT('Ctrl Pts',(-83.9561071053035,2.19650566137838,135.207016924263));
#94792=CARTESIAN_POINT('Ctrl Pts',(-83.9638634080453,2.31848974897926,135.144012157526));
#94793=CARTESIAN_POINT('Ctrl Pts',(-83.9716197107872,2.43753786874083,135.076080669366));
#94794=CARTESIAN_POINT('Ctrl Pts',(-83.9793801533013,2.55664952806839,135.008112924126));
#94795=CARTESIAN_POINT('Ctrl Pts',(-83.9871405958155,2.67282176614634,134.935213425589));
#94796=CARTESIAN_POINT('Ctrl Pts',(-83.9949010383297,2.78563568905678,134.857682325789));
#94797=CARTESIAN_POINT('Ctrl Pts',(-84.0026739385951,2.89863071089142,134.780026766185));
#94798=CARTESIAN_POINT('Ctrl Pts',(-84.0104468388605,3.0082563316525,134.697724982568));
#94799=CARTESIAN_POINT('Ctrl Pts',(-84.0182197391259,3.11412608347067,134.611118003945));
#94800=CARTESIAN_POINT('Ctrl Pts',(-84.0257100748881,3.2161472031436,134.527659407141));
#94801=CARTESIAN_POINT('Ctrl Pts',(-84.0332004106503,3.31468055319453,134.440203394861));
#94802=CARTESIAN_POINT('Ctrl Pts',(-84.0406907464125,3.40941409253309,134.34908608058));
#94803=CARTESIAN_POINT('Ctrl Pts',(-84.0484650805316,3.5077394828064,134.254514025635));
#94804=CARTESIAN_POINT('Ctrl Pts',(-84.0562394146507,3.60228270003551,134.155697975682));
#94805=CARTESIAN_POINT('Ctrl Pts',(-84.0640137487698,3.69265522625002,134.052972696985));
#94806=CARTESIAN_POINT('Ctrl Pts',(-84.0717785017169,3.7829163764028,133.950374018014));
#94807=CARTESIAN_POINT('Ctrl Pts',(-84.0795432546639,3.86901680685477,133.843875986957));
#94808=CARTESIAN_POINT('Ctrl Pts',(-84.087308007611,3.95060312348455,133.73385170361));
#94809=CARTESIAN_POINT('Ctrl Pts',(-84.095065048496,4.03210840743449,133.623936697934));
#94810=CARTESIAN_POINT('Ctrl Pts',(-84.102822089381,4.10910826852633,133.510502721761));
#94811=CARTESIAN_POINT('Ctrl Pts',(-84.110579130266,4.18128831241459,133.393957325736));
#94812=CARTESIAN_POINT('Ctrl Pts',(-84.1183303215061,4.25341392477017,133.277499817501));
#94813=CARTESIAN_POINT('Ctrl Pts',(-84.1260815127463,4.32072674947453,133.157935890709));
#94814=CARTESIAN_POINT('Ctrl Pts',(-84.1338327039864,4.38295482875981,133.035703269771));
#94815=CARTESIAN_POINT('Ctrl Pts',(-84.1415806007634,4.44515645945148,132.913522600959));
#94816=CARTESIAN_POINT('Ctrl Pts',(-84.1493284975406,4.50227746608728,132.788675841654));
#94817=CARTESIAN_POINT('Ctrl Pts',(-84.1570763943177,4.55409122607484,132.661626394747));
#94818=CARTESIAN_POINT('Ctrl Pts',(-84.1648226704018,4.6058941477408,132.534603523846));
#94819=CARTESIAN_POINT('Ctrl Pts',(-84.1725689464858,4.65239188338515,132.405379243598));
#94820=CARTESIAN_POINT('Ctrl Pts',(-84.1803152225699,4.69340563228344,132.274437701718));
#94821=CARTESIAN_POINT('Ctrl Pts',(-84.1880615558352,4.73441968393585,132.143495193259));
#94822=CARTESIAN_POINT('Ctrl Pts',(-84.1958078891006,4.76994955120377,132.010835770965));
#94823=CARTESIAN_POINT('Ctrl Pts',(-84.2035542223659,4.79986619038137,131.876959152403));
#94824=CARTESIAN_POINT('Ctrl Pts',(-84.2113022903689,4.82978952918292,131.7430525531));
#94825=CARTESIAN_POINT('Ctrl Pts',(-84.2190503583718,4.85409705327559,131.607928596603));
#94826=CARTESIAN_POINT('Ctrl Pts',(-84.2267984263748,4.87271083673212,131.472097215405));
#94827=CARTESIAN_POINT('Ctrl Pts',(-84.2345547291166,4.89134440313919,131.336121470998));
#94828=CARTESIAN_POINT('Ctrl Pts',(-84.2423110318584,4.90427208747126,131.199437187933));
#94829=CARTESIAN_POINT('Ctrl Pts',(-84.2500673346003,4.91146781920559,131.06256000449));
#94830=CARTESIAN_POINT('Ctrl Pts',(-84.2578277771145,4.91866739151862,130.925609765573));
#94831=CARTESIAN_POINT('Ctrl Pts',(-84.2655882196287,4.92012891112413,130.78846681188));
#94832=CARTESIAN_POINT('Ctrl Pts',(-84.2733486621429,4.91587848203368,130.651645810235));
#94833=CARTESIAN_POINT('Ctrl Pts',(-84.2811215624083,4.91162122977712,130.514605171371));
#94834=CARTESIAN_POINT('Ctrl Pts',(-84.2888944626737,4.90163373408856,130.377887907488));
#94835=CARTESIAN_POINT('Ctrl Pts',(-84.2966673629391,4.88599401700529,130.242003499456));
#94836=CARTESIAN_POINT('Ctrl Pts',(-84.3041576987012,4.87092284303194,130.111058831928));
#94837=CARTESIAN_POINT('Ctrl Pts',(-84.3116480344633,4.8506033055318,129.980887823054));
#94838=CARTESIAN_POINT('Ctrl Pts',(-84.3191383702254,4.82514952045834,129.851934679385));
#94839=CARTESIAN_POINT('Ctrl Pts',(-84.3269127043446,4.79873064738741,129.718092238079));
#94840=CARTESIAN_POINT('Ctrl Pts',(-84.3346870384637,4.76669682420443,129.585137863104));
#94841=CARTESIAN_POINT('Ctrl Pts',(-84.3424613725828,4.72911969579625,129.453579374976));
#94842=CARTESIAN_POINT('Ctrl Pts',(-84.3502261255299,4.69158887784058,129.322183020928));
#94843=CARTESIAN_POINT('Ctrl Pts',(-84.357990878477,4.64852845391031,129.192179503152));
#94844=CARTESIAN_POINT('Ctrl Pts',(-84.3657556314241,4.60006130527624,129.064067811685));
#94845=CARTESIAN_POINT('Ctrl Pts',(-84.3735126723091,4.55164229489746,128.936083362557));
#94846=CARTESIAN_POINT('Ctrl Pts',(-84.3812697131942,4.49782738387271,128.80998736377));
#94847=CARTESIAN_POINT('Ctrl Pts',(-84.3890267540792,4.43878951827638,128.686264615271));
#94848=CARTESIAN_POINT('Ctrl Pts',(-84.3967779453193,4.37979617359383,128.562635167058));
#94849=CARTESIAN_POINT('Ctrl Pts',(-84.4045291365595,4.31558788171681,128.441375758293));
#94850=CARTESIAN_POINT('Ctrl Pts',(-84.4122803277997,4.2463859127734,128.322951795485));
#94851=CARTESIAN_POINT('Ctrl Pts',(-84.4200282245768,4.17721335651271,128.20457816602));
#94852=CARTESIAN_POINT('Ctrl Pts',(-84.4277761213537,4.10305154140986,128.089037922431));
#94853=CARTESIAN_POINT('Ctrl Pts',(-84.4355240181308,4.02416784639441,127.976772209303));
#94854=CARTESIAN_POINT('Ctrl Pts',(-84.443270294215,3.94530065214742,127.864529979742));
#94855=CARTESIAN_POINT('Ctrl Pts',(-84.4510165702991,3.86171376723845,127.755561237907));
#94856=CARTESIAN_POINT('Ctrl Pts',(-84.4587628463832,3.77371787269385,127.650278107578));
#94857=CARTESIAN_POINT('Ctrl Pts',(-84.4665091796486,3.68572132858368,127.544994200073));
#94858=CARTESIAN_POINT('Ctrl Pts',(-84.4742555129139,3.59331596062078,127.443396258346));
#94859=CARTESIAN_POINT('Ctrl Pts',(-84.4820018461793,3.49685244407135,127.345862960072));
#94860=CARTESIAN_POINT('Ctrl Pts',(-84.4897499141823,3.4003673251861,127.248307819891));
#94861=CARTESIAN_POINT('Ctrl Pts',(-84.4974979821853,3.29982252419184,127.154819412375));
#94862=CARTESIAN_POINT('Ctrl Pts',(-84.5052460501883,3.19560494086963,127.065738929779));
#94863=CARTESIAN_POINT('Ctrl Pts',(-84.5130023529302,3.0912765938598,126.976563771387));
#94864=CARTESIAN_POINT('Ctrl Pts',(-84.520758655672,2.9832679645739,126.891806150731));
#94865=CARTESIAN_POINT('Ctrl Pts',(-84.5285149584139,2.8719987823477,126.811766716768));
#94866=CARTESIAN_POINT('Ctrl Pts',(-84.5362754009281,2.7606702124084,126.731684563348));
#94867=CARTESIAN_POINT('Ctrl Pts',(-84.5440358434422,2.64607794842242,126.656325829138));
#94868=CARTESIAN_POINT('Ctrl Pts',(-84.5517962859564,2.52866910401943,126.585946742082));
#94869=CARTESIAN_POINT('Ctrl Pts',(-84.5595691862219,2.41107178451633,126.515454676267));
#94870=CARTESIAN_POINT('Ctrl Pts',(-84.5673420864874,2.29064919299887,126.449958418617));
#94871=CARTESIAN_POINT('Ctrl Pts',(-84.5751149867528,2.16787214297028,126.389667713837));
#94872=CARTESIAN_POINT('Ctrl Pts',(-84.5826053225147,2.04955834797027,126.331568728041));
#94873=CARTESIAN_POINT('Ctrl Pts',(-84.5900956582766,1.92905858522301,126.278303520521));
#94874=CARTESIAN_POINT('Ctrl Pts',(-84.5975859940384,1.80680826073937,126.230016186784));
#94875=CARTESIAN_POINT('Ctrl Pts',(-84.6053603281575,1.6799227780427,126.179898024111));
#94876=CARTESIAN_POINT('Ctrl Pts',(-84.6131346622766,1.55074943301358,126.134983899535));
#94877=CARTESIAN_POINT('Ctrl Pts',(-84.6209089963956,1.41975419524518,126.095488025577));
#94878=CARTESIAN_POINT('Ctrl Pts',(-84.6286737493427,1.28892039739995,126.056040826754));
#94879=CARTESIAN_POINT('Ctrl Pts',(-84.6364385022899,1.15626954506074,126.021998704071));
#94880=CARTESIAN_POINT('Ctrl Pts',(-84.644203255237,1.02228787300575,125.993527990338));
#94881=CARTESIAN_POINT('Ctrl Pts',(-84.651960296122,0.88843927343626,125.965085554119));
#94882=CARTESIAN_POINT('Ctrl Pts',(-84.6597173370069,0.753262864522192,
125.942203595472));
#94883=CARTESIAN_POINT('Ctrl Pts',(-84.6674743778919,0.617260003764343,
125.924998656177));
#94884=CARTESIAN_POINT('Ctrl Pts',(-84.675225569132,0.481359703821925,125.90780669126));
#94885=CARTESIAN_POINT('Ctrl Pts',(-84.6829767603722,0.344634578849199,
125.896283273327));
#94886=CARTESIAN_POINT('Ctrl Pts',(-84.6907279516123,0.207595790432129,
125.890493805137));
#94887=CARTESIAN_POINT('Ctrl Pts',(-84.6984758483894,0.0706152471555784,
125.884706797625));
#94888=CARTESIAN_POINT('Ctrl Pts',(-84.7062237451666,-0.0666783046123071,
125.884648909155));
#94889=CARTESIAN_POINT('Ctrl Pts',(-84.7139716419437,-0.203769192594108,
125.890333635686));
#94890=CARTESIAN_POINT('Ctrl Pts',(-84.7217179180278,-0.340831404117481,
125.896017173094));
#94891=CARTESIAN_POINT('Ctrl Pts',(-84.7294641941118,-0.477690645794539,
125.90744092));
#94892=CARTESIAN_POINT('Ctrl Pts',(-84.7372104701959,-0.613832255533716,
125.924566254628));
#94893=CARTESIAN_POINT('Ctrl Pts',(-84.7449568034612,-0.749974870239143,
125.94169171567));
#94894=CARTESIAN_POINT('Ctrl Pts',(-84.7527031367266,-0.885399454527858,
125.964518799622));
#94895=CARTESIAN_POINT('Ctrl Pts',(-84.760449469992,-1.01959786759984,125.992957157983));
#94896=CARTESIAN_POINT('Ctrl Pts',(-84.768197537995,-1.15382633347579,126.021401884917));
#94897=CARTESIAN_POINT('Ctrl Pts',(-84.7759456059979,-1.28682769932916,
126.055460305726));
#94898=CARTESIAN_POINT('Ctrl Pts',(-84.7836936740009,-1.41810578166829,
126.094991333416));
#94899=CARTESIAN_POINT('Ctrl Pts',(-84.7914499767427,-1.54952338791573,
126.134564375152));
#94900=CARTESIAN_POINT('Ctrl Pts',(-84.7992062794846,-1.67921367702035,
126.179621529649));
#94901=CARTESIAN_POINT('Ctrl Pts',(-84.8069625822265,-1.80669683054255,
126.229972174833));
#94902=CARTESIAN_POINT('Ctrl Pts',(-84.8147230247407,-1.93424802566257,
126.280349693673));
#94903=CARTESIAN_POINT('Ctrl Pts',(-84.8224834672548,-2.05958938077981,
126.336026174206));
#94904=CARTESIAN_POINT('Ctrl Pts',(-84.830243909769,-2.18226364822946,126.396763944535));
#94905=CARTESIAN_POINT('Ctrl Pts',(-84.8380168100344,-2.3051348433034,126.457599216524));
#94906=CARTESIAN_POINT('Ctrl Pts',(-84.8457897102998,-2.42533005201508,
126.523511826218));
#94907=CARTESIAN_POINT('Ctrl Pts',(-84.8535626105653,-2.54241832400425,
126.594219037017));
#94908=CARTESIAN_POINT('Ctrl Pts',(-84.8610529463274,-2.65525014238096,
126.662355862604));
#94909=CARTESIAN_POINT('Ctrl Pts',(-84.8685432820896,-2.76519673515625,
126.734944579998));
#94910=CARTESIAN_POINT('Ctrl Pts',(-84.8760336178517,-2.87190152311498,
126.81169675693));
#94911=CARTESIAN_POINT('Ctrl Pts',(-84.8841041004386,-2.98687088637196,
126.89439359818));
#94912=CARTESIAN_POINT('Ctrl Pts',(-84.8921745830254,-3.09847089327534,
126.982208319673));
#94913=CARTESIAN_POINT('Ctrl Pts',(-84.9002450656123,-3.20621148892957,
127.074831029165));
#94914=CARTESIAN_POINT('Ctrl Pts',(-84.9079464759637,-3.30902498610363,
127.163217998096));
#94915=CARTESIAN_POINT('Ctrl Pts',(-84.9156478863152,-3.4083238454004,127.255982692074));
#94916=CARTESIAN_POINT('Ctrl Pts',(-84.9233492966666,-3.50371041895164,
127.352810768204));
#94917=CARTESIAN_POINT('Ctrl Pts',(-84.9310437533059,-3.59901086661893,
127.449551416897));
#94918=CARTESIAN_POINT('Ctrl Pts',(-84.9387382099451,-3.69040577616813,
127.550347870198));
#94919=CARTESIAN_POINT('Ctrl Pts',(-84.9464326665844,-3.77753108436507,
127.654846056692));
#94920=CARTESIAN_POINT('Ctrl Pts',(-84.9541219091619,-3.86459735307908,
127.759273431169));
#94921=CARTESIAN_POINT('Ctrl Pts',(-84.9618111517394,-3.94739952192053,
127.867397244793));
#94922=CARTESIAN_POINT('Ctrl Pts',(-84.9695003943169,-4.0256112273304,127.97882751585));
#94923=CARTESIAN_POINT('Ctrl Pts',(-84.9771861581981,-4.10378754892108,
128.090207374651));
#94924=CARTESIAN_POINT('Ctrl Pts',(-84.9848719220792,-4.1773773117728,128.204890389145));
#94925=CARTESIAN_POINT('Ctrl Pts',(-84.9925576859603,-4.2460955201551,128.322454919072));
#94926=CARTESIAN_POINT('Ctrl Pts',(-85.0002430415961,-4.31481007842572,
128.440013204312));
#94927=CARTESIAN_POINT('Ctrl Pts',(-85.0079283972319,-4.37865338911832,
128.560452361462));
#94928=CARTESIAN_POINT('Ctrl Pts',(-85.0156137528677,-4.43738487790799,
128.683323487336));
#94929=CARTESIAN_POINT('Ctrl Pts',(-85.0232989048597,-4.49611481045222,
128.806191357416));
#94930=CARTESIAN_POINT('Ctrl Pts',(-85.0309840568516,-4.54973302457026,
128.931490706482));
#94931=CARTESIAN_POINT('Ctrl Pts',(-85.0386692088436,-4.59804617841052,
129.05875057987));
#94932=CARTESIAN_POINT('Ctrl Pts',(-85.0463579175028,-4.64638169144558,
129.186069348778));
#94933=CARTESIAN_POINT('Ctrl Pts',(-85.054046626162,-4.68940710720134,129.315350079358));
#94934=CARTESIAN_POINT('Ctrl Pts',(-85.0617353348212,-4.72697827914892,
129.446104599374));
#94935=CARTESIAN_POINT('Ctrl Pts',(-85.0643986231931,-4.73999254068507,
129.491396599392));
#94936=CARTESIAN_POINT('Ctrl Pts',(-85.0670619115651,-4.75235281418266,
129.53686531382));
#94937=CARTESIAN_POINT('Ctrl Pts',(-85.069725199937,-4.76405452823396,129.582490119308));
#94938=CARTESIAN_POINT('Origin',(213.235140564004,0.,130.804360617566));
#94939=CARTESIAN_POINT('',(-87.1653941590426,-4.76405452823403,129.582490119308));
#94940=CARTESIAN_POINT('',(-86.8199013756722,-4.76405452823401,129.582490119308));
#94941=CARTESIAN_POINT('',(213.235140564004,-4.76405452823405,129.582490119308));
#94942=CARTESIAN_POINT('',(-85.4851405639742,-4.91824791732384,130.799834444828));
#94943=CARTESIAN_POINT('Ctrl Pts',(-85.4851405640089,-4.91824791732441,
130.79983444544));
#94944=CARTESIAN_POINT('Ctrl Pts',(-85.4928102058359,-4.91837262725987,
130.93534727246));
#94945=CARTESIAN_POINT('Ctrl Pts',(-85.5004798476629,-4.91289243297851,
131.070998262037));
#94946=CARTESIAN_POINT('Ctrl Pts',(-85.5081494894899,-4.90179993215824,
131.206281614272));
#94947=CARTESIAN_POINT('Ctrl Pts',(-85.5158149080154,-4.89071353944266,
131.341490472497));
#94948=CARTESIAN_POINT('Ctrl Pts',(-85.5234803265409,-4.87402101912933,
131.476331698243));
#94949=CARTESIAN_POINT('Ctrl Pts',(-85.5311457450664,-4.85176704392226,
131.61030082255));
#94950=CARTESIAN_POINT('Ctrl Pts',(-85.5388089982247,-4.82951935513341,
131.744232102565));
#94951=CARTESIAN_POINT('Ctrl Pts',(-85.5464722513831,-4.80171340041526,
131.8772913765));
#94952=CARTESIAN_POINT('Ctrl Pts',(-85.5541355045414,-4.76844551204447,
132.008981081099));
#94953=CARTESIAN_POINT('Ctrl Pts',(-85.5617983391458,-4.73517944070992,
132.140663593028));
#94954=CARTESIAN_POINT('Ctrl Pts',(-85.5694611737501,-4.69645212696236,
132.270976296331));
#94955=CARTESIAN_POINT('Ctrl Pts',(-85.5771240083544,-4.65241052363223,
132.399434089885));
#94956=CARTESIAN_POINT('Ctrl Pts',(-85.5847881706427,-4.60836128953188,
132.527914140392));
#94957=CARTESIAN_POINT('Ctrl Pts',(-85.592452332931,-4.55899606467394,132.654538263487));
#94958=CARTESIAN_POINT('Ctrl Pts',(-85.6001164952193,-4.50451077086627,
132.77883922663));
#94959=CARTESIAN_POINT('Ctrl Pts',(-85.607788497958,-4.44996973851463,132.903267349859));
#94960=CARTESIAN_POINT('Ctrl Pts',(-85.6154605006967,-4.39029833615977,
133.025367198979));
#94961=CARTESIAN_POINT('Ctrl Pts',(-85.6231325034355,-4.32573967813694,
133.144693777501));
#94962=CARTESIAN_POINT('Ctrl Pts',(-85.6308084083052,-4.26114818431489,
133.26408104786));
#94963=CARTESIAN_POINT('Ctrl Pts',(-85.6384843131749,-4.19166468913342,
133.380691894912));
#94964=CARTESIAN_POINT('Ctrl Pts',(-85.6461602180447,-4.1175762274804,133.494109504245));
#94965=CARTESIAN_POINT('Ctrl Pts',(-85.6538484765497,-4.04336852752947,
133.60770964838));
#94966=CARTESIAN_POINT('Ctrl Pts',(-85.6615367350547,-3.96454128652445,
133.718105961257));
#94967=CARTESIAN_POINT('Ctrl Pts',(-85.6692249935597,-3.88142295689908,
133.824913363697));
#94968=CARTESIAN_POINT('Ctrl Pts',(-85.6767458267499,-3.80011467469848,
133.929394847598));
#94969=CARTESIAN_POINT('Ctrl Pts',(-85.68426665994,-3.71470056573458,134.030441917186));
#94970=CARTESIAN_POINT('Ctrl Pts',(-85.6917874931301,-3.62552120709613,
134.12772924584));
#94971=CARTESIAN_POINT('Ctrl Pts',(-85.6995618272492,-3.53333592482057,
134.228295789385));
#94972=CARTESIAN_POINT('Ctrl Pts',(-85.7073361613683,-3.43681710797767,
134.325183093237));
#94973=CARTESIAN_POINT('Ctrl Pts',(-85.7151104954874,-3.33629010306817,
134.417994717841));
#94974=CARTESIAN_POINT('Ctrl Pts',(-85.7228752484345,-3.23588698870785,
134.510691960412));
#94975=CARTESIAN_POINT('Ctrl Pts',(-85.7306400013816,-3.13148579937848,
134.599323255166));
#94976=CARTESIAN_POINT('Ctrl Pts',(-85.7384047543287,-3.02345104694852,
134.683526356382));
#94977=CARTESIAN_POINT('Ctrl Pts',(-85.7461617952137,-2.91552359615741,
134.767645825892));
#94978=CARTESIAN_POINT('Ctrl Pts',(-85.7539188360988,-2.80397007052181,
134.847345615583));
#94979=CARTESIAN_POINT('Ctrl Pts',(-85.7616758769838,-2.68919035872191,
134.922301641556));
#94980=CARTESIAN_POINT('Ctrl Pts',(-85.7694270682239,-2.574497203196,134.997201142606));
#94981=CARTESIAN_POINT('Ctrl Pts',(-85.777178259464,-2.45658303005188,135.067363787449));
#94982=CARTESIAN_POINT('Ctrl Pts',(-85.7849294507041,-2.33587891141086,
135.132507192455));
#94983=CARTESIAN_POINT('Ctrl Pts',(-85.7926773474812,-2.21522609523998,
135.197622909777));
#94984=CARTESIAN_POINT('Ctrl Pts',(-85.8004252442582,-2.09178603537643,
135.257723444957));
#94985=CARTESIAN_POINT('Ctrl Pts',(-85.8081731410353,-1.96601656294511,
135.312571120274));
#94986=CARTESIAN_POINT('Ctrl Pts',(-85.8159194171194,-1.84027339877615,
135.367407322639));
#94987=CARTESIAN_POINT('Ctrl Pts',(-85.8236656932035,-1.71220214937502,
135.4169926945));
#94988=CARTESIAN_POINT('Ctrl Pts',(-85.8314119692876,-1.58228253231092,
135.461136868412));
#94989=CARTESIAN_POINT('Ctrl Pts',(-85.8391583025529,-1.4523619562099,135.505281368186));
#94990=CARTESIAN_POINT('Ctrl Pts',(-85.8469046358182,-1.32059335539978,
135.543984464083));
#94991=CARTESIAN_POINT('Ctrl Pts',(-85.8546509690836,-1.18747320684742,
135.577105157715));
#94992=CARTESIAN_POINT('Ctrl Pts',(-85.8623990370865,-1.05432324696095,
135.610233268496));
#94993=CARTESIAN_POINT('Ctrl Pts',(-85.8701471050894,-0.919821516380451,
135.637776395001));
#94994=CARTESIAN_POINT('Ctrl Pts',(-85.8778951730924,-0.784475930743299,
135.659644396768));
#94995=CARTESIAN_POINT('Ctrl Pts',(-85.8856514758342,-0.648986498206545,
135.681535640108));
#94996=CARTESIAN_POINT('Ctrl Pts',(-85.8934077785761,-0.51265180561555,
135.6977396475));
#94997=CARTESIAN_POINT('Ctrl Pts',(-85.901164081318,-0.375986717140373,
135.708217982033));
#94998=CARTESIAN_POINT('Ctrl Pts',(-85.9089245238322,-0.23924868639257,
135.718701909168));
#94999=CARTESIAN_POINT('Ctrl Pts',(-85.9166849663464,-0.10218029892303,
135.723454060636));
#95000=CARTESIAN_POINT('Ctrl Pts',(-85.9244454088605,0.0347033002329159,
135.722488182346));
#95001=CARTESIAN_POINT('Ctrl Pts',(-85.9322183091259,0.17180663709381,135.721520753544));
#95002=CARTESIAN_POINT('Ctrl Pts',(-85.9399912093913,0.308724202140494,
135.714816971369));
#95003=CARTESIAN_POINT('Ctrl Pts',(-85.9477641096567,0.444944788905772,
135.702442609257));
#95004=CARTESIAN_POINT('Ctrl Pts',(-85.9552544454188,0.576213414224647,
135.690518086376));
#95005=CARTESIAN_POINT('Ctrl Pts',(-85.962744781181,0.706834549936867,135.673328145693));
#95006=CARTESIAN_POINT('Ctrl Pts',(-85.9702351169431,0.836361378945249,
135.650976210566));
#95007=CARTESIAN_POINT('Ctrl Pts',(-85.9780094510622,0.970799257042992,
135.627776795025));
#95008=CARTESIAN_POINT('Ctrl Pts',(-85.9857837851813,1.10448406787116,135.598942735196));
#95009=CARTESIAN_POINT('Ctrl Pts',(-85.9935581193003,1.23690641787442,135.564533469041));
#95010=CARTESIAN_POINT('Ctrl Pts',(-86.0013228722474,1.36916556916623,135.530166609232));
#95011=CARTESIAN_POINT('Ctrl Pts',(-86.0090876251945,1.50016498058434,135.490238311607));
#95012=CARTESIAN_POINT('Ctrl Pts',(-86.0168523781416,1.62940285697743,135.444859447668));
#95013=CARTESIAN_POINT('Ctrl Pts',(-86.0246094190266,1.75851237248976,135.399525654655));
#95014=CARTESIAN_POINT('Ctrl Pts',(-86.0323664599116,1.88586346822408,135.348752197281));
#95015=CARTESIAN_POINT('Ctrl Pts',(-86.0401235007966,2.01096733361788,135.292700337955));
#95016=CARTESIAN_POINT('Ctrl Pts',(-86.0478746920367,2.13597685721379,135.236690747772));
#95017=CARTESIAN_POINT('Ctrl Pts',(-86.0556258832769,2.25874216822816,135.175410837758));
#95018=CARTESIAN_POINT('Ctrl Pts',(-86.063377074517,2.3787926843047,135.109070645849));
#95019=CARTESIAN_POINT('Ctrl Pts',(-86.0711249712941,2.49879217570929,135.042758650291));
#95020=CARTESIAN_POINT('Ctrl Pts',(-86.0788728680711,2.61607882563935,134.971390839226));
#95021=CARTESIAN_POINT('Ctrl Pts',(-86.0866207648482,2.73020520018958,134.89522392833));
#95022=CARTESIAN_POINT('Ctrl Pts',(-86.0943670409323,2.84430770196254,134.819072949911));
#95023=CARTESIAN_POINT('Ctrl Pts',(-86.1021133170164,2.95525091825526,134.738125085304));
#95024=CARTESIAN_POINT('Ctrl Pts',(-86.1098595931005,3.06261538848128,134.652681036234));
#95025=CARTESIAN_POINT('Ctrl Pts',(-86.1176059263659,3.16998065124757,134.567236356435));
#95026=CARTESIAN_POINT('Ctrl Pts',(-86.1253522596313,3.2737668093194,134.477295669401));
#95027=CARTESIAN_POINT('Ctrl Pts',(-86.1330985928966,3.37358687883183,134.383200462191));
#95028=CARTESIAN_POINT('Ctrl Pts',(-86.1408466608996,3.47342930235659,134.289084183012));
#95029=CARTESIAN_POINT('Ctrl Pts',(-86.1485947289026,3.56930358551315,134.190811800441));
#95030=CARTESIAN_POINT('Ctrl Pts',(-86.1563427969056,3.66085934977078,134.088761915169));
#95031=CARTESIAN_POINT('Ctrl Pts',(-86.1640990996475,3.75251242058432,133.986603570064));
#95032=CARTESIAN_POINT('Ctrl Pts',(-86.1718554023893,3.83983754243001,133.880659993789));
#95033=CARTESIAN_POINT('Ctrl Pts',(-86.1796117051311,3.92252408058497,133.77134358006));
#95034=CARTESIAN_POINT('Ctrl Pts',(-86.1873721476453,4.00525475103477,133.661968820871));
#95035=CARTESIAN_POINT('Ctrl Pts',(-86.1951325901594,4.08334168216125,133.549217958461));
#95036=CARTESIAN_POINT('Ctrl Pts',(-86.2028930326735,4.15651799031273,133.433531828938));
#95037=CARTESIAN_POINT('Ctrl Pts',(-86.210665932939,4.22981176757055,133.31765998977));
#95038=CARTESIAN_POINT('Ctrl Pts',(-86.2184388332043,4.29817897407176,133.198843806574));
#95039=CARTESIAN_POINT('Ctrl Pts',(-86.2262117334697,4.36139862728571,133.077548923978));
#95040=CARTESIAN_POINT('Ctrl Pts',(-86.2337020692318,4.42232008686481,132.960663415888));
#95041=CARTESIAN_POINT('Ctrl Pts',(-86.2411924049939,4.47846161737434,132.841476572204));
#95042=CARTESIAN_POINT('Ctrl Pts',(-86.248682740756,4.52966871625975,132.720420215657));
#95043=CARTESIAN_POINT('Ctrl Pts',(-86.2564570748751,4.58281734786325,132.594773970558));
#95044=CARTESIAN_POINT('Ctrl Pts',(-86.2642314089941,4.63081834239162,132.466715639409));
#95045=CARTESIAN_POINT('Ctrl Pts',(-86.2720057431132,4.67344636702702,132.336705917106));
#95046=CARTESIAN_POINT('Ctrl Pts',(-86.2797704960603,4.71602185643184,132.206856420166));
#95047=CARTESIAN_POINT('Ctrl Pts',(-86.2875352490074,4.75323743052242,132.075060685075));
#95048=CARTESIAN_POINT('Ctrl Pts',(-86.2953000019545,4.78491513609461,131.941800815059));
#95049=CARTESIAN_POINT('Ctrl Pts',(-86.3030570428395,4.81656137892306,131.808673300624));
#95050=CARTESIAN_POINT('Ctrl Pts',(-86.3108140837245,4.84268060922345,131.674084923091));
#95051=CARTESIAN_POINT('Ctrl Pts',(-86.3185711246095,4.86314428757814,131.538534098901));
#95052=CARTESIAN_POINT('Ctrl Pts',(-86.3263223158496,4.88359253411395,131.403085494641));
#95053=CARTESIAN_POINT('Ctrl Pts',(-86.3340735070898,4.89839365959494,131.266676273383));
#95054=CARTESIAN_POINT('Ctrl Pts',(-86.34182469833,4.90747001362606,131.129815880023));
#95055=CARTESIAN_POINT('Ctrl Pts',(-86.3495725951071,4.91654250996454,130.993013655983));
#95056=CARTESIAN_POINT('Ctrl Pts',(-86.3573204918842,4.91989504844671,130.85576103053));
#95057=CARTESIAN_POINT('Ctrl Pts',(-86.3650683886613,4.9175017622875,130.718573203574));
#95058=CARTESIAN_POINT('Ctrl Pts',(-86.3728146647454,4.91510897675215,130.581414073355));
#95059=CARTESIAN_POINT('Ctrl Pts',(-86.3805609408294,4.90697276404083,130.444320105332));
#95060=CARTESIAN_POINT('Ctrl Pts',(-86.3883072169135,4.89311938433697,130.307806740201));
#95061=CARTESIAN_POINT('Ctrl Pts',(-86.3960535501788,4.87926590237063,130.171292367361));
#95062=CARTESIAN_POINT('Ctrl Pts',(-86.4037998834442,4.85969520867153,130.035358994933));
#95063=CARTESIAN_POINT('Ctrl Pts',(-86.4115462167096,4.8344854317433,129.900516785501));
#95064=CARTESIAN_POINT('Ctrl Pts',(-86.4192942847126,4.80927000926015,129.76564437909));
#95065=CARTESIAN_POINT('Ctrl Pts',(-86.4270423527155,4.77841306249044,129.631864006154));
#95066=CARTESIAN_POINT('Ctrl Pts',(-86.4347904207185,4.74204373076291,129.499675092992));
#95067=CARTESIAN_POINT('Ctrl Pts',(-86.4425467234604,4.70563574527696,129.367345687882));
#95068=CARTESIAN_POINT('Ctrl Pts',(-86.4503030262024,4.66370377547049,129.236611498904));
#95069=CARTESIAN_POINT('Ctrl Pts',(-86.4580593289442,4.61642687420275,129.107956780728));
#95070=CARTESIAN_POINT('Ctrl Pts',(-86.4658197714584,4.56912473982932,128.979233395655));
#95071=CARTESIAN_POINT('Ctrl Pts',(-86.4735802139725,4.51647213966634,128.852592053736));
#95072=CARTESIAN_POINT('Ctrl Pts',(-86.4813406564867,4.45869570448371,128.728495574429));
#95073=CARTESIAN_POINT('Ctrl Pts',(-86.4891135567521,4.40082652143816,128.604199884437));
#95074=CARTESIAN_POINT('Ctrl Pts',(-86.4968864570175,4.3378172465426,128.482457568084));
#95075=CARTESIAN_POINT('Ctrl Pts',(-86.504659357283,4.26994019335295,128.363706236526));
#95076=CARTESIAN_POINT('Ctrl Pts',(-86.5121496930449,4.20453064201928,128.249271814988));
#95077=CARTESIAN_POINT('Ctrl Pts',(-86.5196400288069,4.13460124345565,128.137614955049));
#95078=CARTESIAN_POINT('Ctrl Pts',(-86.5271303645689,4.06043178994989,128.029099054818));
#95079=CARTESIAN_POINT('Ctrl Pts',(-86.5349046986879,3.9834501790708,127.916468741247));
#95080=CARTESIAN_POINT('Ctrl Pts',(-86.5426790328071,3.90165678830704,127.806865489107));
#95081=CARTESIAN_POINT('Ctrl Pts',(-86.5504533669261,3.81531741542974,127.700727894124));
#95082=CARTESIAN_POINT('Ctrl Pts',(-86.5582181198732,3.72908444811291,127.594721104241));
#95083=CARTESIAN_POINT('Ctrl Pts',(-86.5659828728202,3.63831689036867,127.492171773653));
#95084=CARTESIAN_POINT('Ctrl Pts',(-86.5737476257673,3.54332416124115,127.393490207998));
#95085=CARTESIAN_POINT('Ctrl Pts',(-86.5815046666522,3.44842578023163,127.294906654267));
#95086=CARTESIAN_POINT('Ctrl Pts',(-86.5892617075373,3.34931084844771,127.20018350052));
#95087=CARTESIAN_POINT('Ctrl Pts',(-86.5970187484222,3.24632921906197,127.109698296871));
#95088=CARTESIAN_POINT('Ctrl Pts',(-86.6047699396623,3.14342524892417,127.019281328818));
#95089=CARTESIAN_POINT('Ctrl Pts',(-86.6125211309025,3.03666067763057,126.933096206691));
#95090=CARTESIAN_POINT('Ctrl Pts',(-86.6202723221426,2.92642214366695,126.851483627378));
#95091=CARTESIAN_POINT('Ctrl Pts',(-86.6280202189197,2.81623046402053,126.769905735588));
#95092=CARTESIAN_POINT('Ctrl Pts',(-86.6357681156966,2.70256807197049,126.692896753375));
#95093=CARTESIAN_POINT('Ctrl Pts',(-86.6435160124737,2.58585443816379,126.620756921334));
#95094=CARTESIAN_POINT('Ctrl Pts',(-86.6512622885578,2.46916521833323,126.54863217939));
#95095=CARTESIAN_POINT('Ctrl Pts',(-86.6590085646419,2.34942635862366,126.48137476715));
#95096=CARTESIAN_POINT('Ctrl Pts',(-86.666754840726,2.22708570816272,126.419241199466));
#95097=CARTESIAN_POINT('Ctrl Pts',(-86.6745011739913,2.10474415461105,126.357107173126));
#95098=CARTESIAN_POINT('Ctrl Pts',(-86.6822475072567,1.97980112056938,126.300097243851));
#95099=CARTESIAN_POINT('Ctrl Pts',(-86.6899938405221,1.85272805063187,126.248421435257));
#95100=CARTESIAN_POINT('Ctrl Pts',(-86.697741908525,1.72562652356157,126.196734054223));
#95101=CARTESIAN_POINT('Ctrl Pts',(-86.705489976528,1.596394373502,126.150383318115));
#95102=CARTESIAN_POINT('Ctrl Pts',(-86.7132380445309,1.46552158490703,126.109530530473));
#95103=CARTESIAN_POINT('Ctrl Pts',(-86.7209943472728,1.33450970315441,126.068634324002));
#95104=CARTESIAN_POINT('Ctrl Pts',(-86.7287506500146,1.2018540734575,126.033247855273));
#95105=CARTESIAN_POINT('Ctrl Pts',(-86.7365069527565,1.06805889542725,126.00348223352));
#95106=CARTESIAN_POINT('Ctrl Pts',(-86.7442673952706,0.934192306881998,
125.973700724959));
#95107=CARTESIAN_POINT('Ctrl Pts',(-86.7520278377849,0.799185342756793,
125.949546109981));
#95108=CARTESIAN_POINT('Ctrl Pts',(-86.759788280299,0.663549885637091,125.931077882923));
#95109=CARTESIAN_POINT('Ctrl Pts',(-86.7675611805645,0.527696694440839,
125.912580009028));
#95110=CARTESIAN_POINT('Ctrl Pts',(-86.7753340808298,0.391213383603855,
125.899786800802));
#95111=CARTESIAN_POINT('Ctrl Pts',(-86.7831069810952,0.254615319914042,
125.892705692659));
#95112=CARTESIAN_POINT('Ctrl Pts',(-86.7905973168574,0.122982939906159,
125.885882000633));
#95113=CARTESIAN_POINT('Ctrl Pts',(-86.7980876526196,-0.0087556866946793,
125.88436232398));
#95114=CARTESIAN_POINT('Ctrl Pts',(-86.8055779883818,-0.140143588202138,
125.88810769108));
#95115=CARTESIAN_POINT('Ctrl Pts',(-86.8133523225008,-0.276513101926866,
125.891995064911));
#95116=CARTESIAN_POINT('Ctrl Pts',(-86.8211266566199,-0.41293674770034,
125.90156692608));
#95117=CARTESIAN_POINT('Ctrl Pts',(-86.828900990739,-0.54890185232917,125.916836723097));
#95118=CARTESIAN_POINT('Ctrl Pts',(-86.8366657436861,-0.684699392118095,
125.932087701453));
#95119=CARTESIAN_POINT('Ctrl Pts',(-86.8444304966332,-0.820039130371874,
125.953022600364));
#95120=CARTESIAN_POINT('Ctrl Pts',(-86.8521952495803,-0.954408616783686,
125.979602877046));
#95121=CARTESIAN_POINT('Ctrl Pts',(-86.8599522904653,-1.08864464552732,
126.006156753822));
#95122=CARTESIAN_POINT('Ctrl Pts',(-86.8677093313503,-1.22191195911997,
126.038344774671));
#95123=CARTESIAN_POINT('Ctrl Pts',(-86.8754663722353,-1.35370380977322,
126.076076673268));
#95124=CARTESIAN_POINT('Ctrl Pts',(-86.8832175634754,-1.48539627516723,
126.113780117947));
#95125=CARTESIAN_POINT('Ctrl Pts',(-86.8909687547155,-1.61561511795681,
126.157019011809));
#95126=CARTESIAN_POINT('Ctrl Pts',(-86.8987199459557,-1.74386471265541,
126.205652219934));
#95127=CARTESIAN_POINT('Ctrl Pts',(-86.9064678427328,-1.87205979785491,
126.254264757647));
#95128=CARTESIAN_POINT('Ctrl Pts',(-86.9142157395099,-1.99828693486013,
126.30826691123));
#95129=CARTESIAN_POINT('Ctrl Pts',(-86.921963636287,-2.12206678862434,126.367468055522));
#95130=CARTESIAN_POINT('Ctrl Pts',(-86.9297099123711,-2.24582075031153,
126.426656816211));
#95131=CARTESIAN_POINT('Ctrl Pts',(-86.9374561884552,-2.36712809451514,
126.491042235897));
#95132=CARTESIAN_POINT('Ctrl Pts',(-86.9452024645393,-2.48553093463297,
126.560386178967));
#95133=CARTESIAN_POINT('Ctrl Pts',(-86.9529487978047,-2.60393464877382,
126.629730633918));
#95134=CARTESIAN_POINT('Ctrl Pts',(-86.96069513107,-2.71943347868095,126.704033487711));
#95135=CARTESIAN_POINT('Ctrl Pts',(-86.9684414643354,-2.83159589822037,
126.783011623549));
#95136=CARTESIAN_POINT('Ctrl Pts',(-86.9761895323384,-2.94378343575612,
126.862007445993));
#95137=CARTESIAN_POINT('Ctrl Pts',(-86.9839376003414,-3.05263275654347,
126.945680408838));
#95138=CARTESIAN_POINT('Ctrl Pts',(-86.9916856683444,-3.15774330277944,
127.033705462788));
#95139=CARTESIAN_POINT('Ctrl Pts',(-86.9994419710863,-3.26296556175435,
127.121824070813));
#95140=CARTESIAN_POINT('Ctrl Pts',(-87.0071982738281,-3.36444080823806,
127.214303758369));
#95141=CARTESIAN_POINT('Ctrl Pts',(-87.0149545765699,-3.46180303067885,
127.3107803853));
#95142=CARTESIAN_POINT('Ctrl Pts',(-87.0227150190841,-3.55921721826955,
127.407308504711));
#95143=CARTESIAN_POINT('Ctrl Pts',(-87.0304754615983,-3.65251374178303,
127.507837527821));
#95144=CARTESIAN_POINT('Ctrl Pts',(-87.0382359041124,-3.74136586190748,
127.611968951455));
#95145=CARTESIAN_POINT('Ctrl Pts',(-87.0460088043779,-3.83036061534283,
127.716267536095));
#95146=CARTESIAN_POINT('Ctrl Pts',(-87.0537817046434,-3.91489646704285,
127.824179769374));
#95147=CARTESIAN_POINT('Ctrl Pts',(-87.0615546049088,-3.99468859388868,
127.935276077097));
#95148=CARTESIAN_POINT('Ctrl Pts',(-87.0690449406707,-4.07158007593813,
128.042333754199));
#95149=CARTESIAN_POINT('Ctrl Pts',(-87.0765352764325,-4.14406656851509,
128.152347769435));
#95150=CARTESIAN_POINT('Ctrl Pts',(-87.0840256121944,-4.21193385519023,
128.264912594471));
#95151=CARTESIAN_POINT('Ctrl Pts',(-87.092059552798,-4.28472655332906,128.385646717364));
#95152=CARTESIAN_POINT('Ctrl Pts',(-87.1000934934016,-4.35242294254361,
128.50967647454));
#95153=CARTESIAN_POINT('Ctrl Pts',(-87.1081274340052,-4.41472236966481,
128.636548480576));
#95154=CARTESIAN_POINT('Ctrl Pts',(-87.1161505265311,-4.47693767505077,
128.763249173748));
#95155=CARTESIAN_POINT('Ctrl Pts',(-87.124173619057,-4.53377037157371,128.892784159149));
#95156=CARTESIAN_POINT('Ctrl Pts',(-87.1321967115828,-4.58496378813763,
129.024672407804));
#95157=CARTESIAN_POINT('Ctrl Pts',(-87.1402069690404,-4.63607530722921,
129.156349666161));
#95158=CARTESIAN_POINT('Ctrl Pts',(-87.148217226498,-4.68156539790506,129.290372355991));
#95159=CARTESIAN_POINT('Ctrl Pts',(-87.1562274839556,-4.72122418707915,
129.426236806786));
#95160=CARTESIAN_POINT('Ctrl Pts',(-87.159283042318,-4.73635225824825,129.478063075913));
#95161=CARTESIAN_POINT('Ctrl Pts',(-87.1623386006803,-4.7506323121341,129.530157102445));
#95162=CARTESIAN_POINT('Ctrl Pts',(-87.1653941590427,-4.76405452823403,
129.582490119308));
#95163=CARTESIAN_POINT('Ctrl Pts',(-85.4152252782566,-4.76405452823408,
129.582490119308));
#95164=CARTESIAN_POINT('Ctrl Pts',(-85.4252802492457,-4.80789294130721,
129.75341542654));
#95165=CARTESIAN_POINT('Ctrl Pts',(-85.4353352202348,-4.84255315743214,
129.926797078868));
#95166=CARTESIAN_POINT('Ctrl Pts',(-85.4453901912239,-4.86780846451807,
130.101776946203));
#95167=CARTESIAN_POINT('Ctrl Pts',(-85.4552467903679,-4.89256551637552,
130.273304682329));
#95168=CARTESIAN_POINT('Ctrl Pts',(-85.4651033895119,-4.90828512320806,
130.446368405372));
#95169=CARTESIAN_POINT('Ctrl Pts',(-85.4749599886558,-4.91479857163483,
130.620137755911));
#95170=CARTESIAN_POINT('Ctrl Pts',(-85.4783535137619,-4.91704108453822,
130.679964745436));
#95171=CARTESIAN_POINT('Ctrl Pts',(-85.481747038868,-4.9181927379082,130.739875167581));
#95172=CARTESIAN_POINT('Ctrl Pts',(-85.4851405639742,-4.91824791732385,
130.799834444828));
#95173=CARTESIAN_POINT('',(-85.1398594359628,-4.91824974829331,130.805934120905));
#95174=CARTESIAN_POINT('Ctrl Pts',(-85.069725199937,-4.76405452823396,129.582490119308));
#95175=CARTESIAN_POINT('Ctrl Pts',(-85.0774224301562,-4.79787391781389,
129.714351405999));
#95176=CARTESIAN_POINT('Ctrl Pts',(-85.0851196603755,-4.82618868007886,
129.847516930377));
#95177=CARTESIAN_POINT('Ctrl Pts',(-85.0928168905947,-4.84892324497919,
129.981483696757));
#95178=CARTESIAN_POINT('Ctrl Pts',(-85.1006573148227,-4.87208074818226,
130.117942689271));
#95179=CARTESIAN_POINT('Ctrl Pts',(-85.1084977390507,-4.88944832579167,
130.255232597457));
#95180=CARTESIAN_POINT('Ctrl Pts',(-85.1163381632788,-4.90100157360506,
130.392818835944));
#95181=CARTESIAN_POINT('Ctrl Pts',(-85.1241785875068,-4.91255482141848,
130.530405074431));
#95182=CARTESIAN_POINT('Ctrl Pts',(-85.1320190117348,-4.91829378588438,
130.668287211764));
#95183=CARTESIAN_POINT('Ctrl Pts',(-85.1398594359628,-4.91824974829331,
130.805934120905));
#95184=CARTESIAN_POINT('Ctrl Pts',(-85.1398594359914,-4.91824974829315,
130.805934121408));
#95185=CARTESIAN_POINT('Ctrl Pts',(-85.1447333712156,-4.91822237267818,
130.891501190161));
#95186=CARTESIAN_POINT('Ctrl Pts',(-85.1496073064404,-4.91596211462244,
130.977029819251));
#95187=CARTESIAN_POINT('Ctrl Pts',(-85.1544812416651,-4.91147410740755,
131.062440362539));
#95188=CARTESIAN_POINT('Ctrl Pts',(-85.1622555757842,-4.90431536072584,
131.198677318959));
#95189=CARTESIAN_POINT('Ctrl Pts',(-85.1700299099032,-4.89147246467867,
131.334831979816));
#95190=CARTESIAN_POINT('Ctrl Pts',(-85.1778042440223,-4.87294427737159,
131.470391496829));
#95191=CARTESIAN_POINT('Ctrl Pts',(-85.1855689969693,-4.85443892439945,
131.605783948852));
#95192=CARTESIAN_POINT('Ctrl Pts',(-85.1933337499163,-4.830262273676,131.740582332754));
#95193=CARTESIAN_POINT('Ctrl Pts',(-85.2010985028634,-4.80046515428053,
131.874275270722));
#95194=CARTESIAN_POINT('Ctrl Pts',(-85.2088555437484,-4.77069762980412,
132.00783542298));
#95195=CARTESIAN_POINT('Ctrl Pts',(-85.2166125846333,-4.73532083024184,
132.14029193513));
#95196=CARTESIAN_POINT('Ctrl Pts',(-85.2243696255183,-4.69443715647294,
132.271140371458));
#95197=CARTESIAN_POINT('Ctrl Pts',(-85.2321208167584,-4.65358431340052,
132.401890133961));
#95198=CARTESIAN_POINT('Ctrl Pts',(-85.2398720079985,-4.60723297809819,
132.53103386271));
#95199=CARTESIAN_POINT('Ctrl Pts',(-85.2476231992386,-4.55553613848605,
132.658079461794));
#95200=CARTESIAN_POINT('Ctrl Pts',(-85.2553710960156,-4.50386127140973,
132.78507106311));
#95201=CARTESIAN_POINT('Ctrl Pts',(-85.2631189927927,-4.44684556587112,
132.909965947032));
#95202=CARTESIAN_POINT('Ctrl Pts',(-85.2708668895697,-4.3846910948542,133.032289491028));
#95203=CARTESIAN_POINT('Ctrl Pts',(-85.2786131656538,-4.32254962521273,
133.154587447576));
#95204=CARTESIAN_POINT('Ctrl Pts',(-85.2863594417378,-4.25527170515766,
133.274314785718));
#95205=CARTESIAN_POINT('Ctrl Pts',(-85.2941057178219,-4.18310638973966,
133.391019465311));
#95206=CARTESIAN_POINT('Ctrl Pts',(-85.3018520510872,-4.1109405416136,133.507725006392));
#95207=CARTESIAN_POINT('Ctrl Pts',(-85.3095983843526,-4.03388743175491,
133.621407511873));
#95208=CARTESIAN_POINT('Ctrl Pts',(-85.3173447176179,-3.95224045086554,
133.731642373913));
#95209=CARTESIAN_POINT('Ctrl Pts',(-85.3250927856209,-3.8705751857008,133.841901922286));
#95210=CARTESIAN_POINT('Ctrl Pts',(-85.3328408536239,-3.78431423503414,
133.948711976761));
#95211=CARTESIAN_POINT('Ctrl Pts',(-85.3405889216268,-3.69379216683655,
134.051679895173));
#95212=CARTESIAN_POINT('Ctrl Pts',(-85.3483452243687,-3.60317389070803,
134.154757249113));
#95213=CARTESIAN_POINT('Ctrl Pts',(-85.3561015271104,-3.5082857088998,134.253984015726));
#95214=CARTESIAN_POINT('Ctrl Pts',(-85.3638578298523,-3.40950043997338,
134.349003027221));
#95215=CARTESIAN_POINT('Ctrl Pts',(-85.3716182723664,-3.31066244637429,
134.444072753223));
#95216=CARTESIAN_POINT('Ctrl Pts',(-85.3793787148806,-3.20792351382213,
134.534929990277));
#95217=CARTESIAN_POINT('Ctrl Pts',(-85.3871391573947,-3.10168987157424,
134.62125765614));
#95218=CARTESIAN_POINT('Ctrl Pts',(-85.3949120576601,-2.99528569365313,
134.707723902836));
#95219=CARTESIAN_POINT('Ctrl Pts',(-85.4026849579255,-2.88537590908218,
134.789645814247));
#95220=CARTESIAN_POINT('Ctrl Pts',(-85.4104578581909,-2.77239680331742,
134.866748957872));
#95221=CARTESIAN_POINT('Ctrl Pts',(-85.417948193953,-2.6635247726235,134.941049208016));
#95222=CARTESIAN_POINT('Ctrl Pts',(-85.4254385297151,-2.55180296274842,
135.010874793252));
#95223=CARTESIAN_POINT('Ctrl Pts',(-85.4329288654771,-2.43764192584907,
135.076021290401));
#95224=CARTESIAN_POINT('Ctrl Pts',(-85.4407031995962,-2.31915243853834,
135.143637836789));
#95225=CARTESIAN_POINT('Ctrl Pts',(-85.4484775337152,-2.1976597672397,135.206427664572));
#95226=CARTESIAN_POINT('Ctrl Pts',(-85.4562518678343,-2.07359476851667,
135.264112606016));
#95227=CARTESIAN_POINT('Ctrl Pts',(-85.4640166207813,-1.94968266881657,
135.321726455925));
#95228=CARTESIAN_POINT('Ctrl Pts',(-85.4717813737284,-1.82320490048748,
135.374247774086));
#95229=CARTESIAN_POINT('Ctrl Pts',(-85.4795461266754,-1.69461917452559,
135.421442912244));
#95230=CARTESIAN_POINT('Ctrl Pts',(-85.4873031675604,-1.56616116171946,
135.468591175526));
#95231=CARTESIAN_POINT('Ctrl Pts',(-85.4950602084454,-1.43559972239451,
135.510423652379));
#95232=CARTESIAN_POINT('Ctrl Pts',(-85.5028172493303,-1.3034146027804,135.546753835737));
#95233=CARTESIAN_POINT('Ctrl Pts',(-85.5105684405704,-1.17132916499342,
135.583056622222));
#95234=CARTESIAN_POINT('Ctrl Pts',(-85.5183196318105,-1.03762285953132,
135.613865270995));
#95235=CARTESIAN_POINT('Ctrl Pts',(-85.5260708230506,-0.90279239432758,
135.639042505265));
#95236=CARTESIAN_POINT('Ctrl Pts',(-85.5338187198277,-0.768019235668091,
135.664209038539));
#95237=CARTESIAN_POINT('Ctrl Pts',(-85.5415666166046,-0.632123251088051,
135.683748846188));
#95238=CARTESIAN_POINT('Ctrl Pts',(-85.5493145133817,-0.495612979349267,
135.697575392865));
#95239=CARTESIAN_POINT('Ctrl Pts',(-85.5570607894658,-0.359131262616511,
135.711399047325));
#95240=CARTESIAN_POINT('Ctrl Pts',(-85.5648070655498,-0.222035903038514,
135.719511778543));
#95241=CARTESIAN_POINT('Ctrl Pts',(-85.5725533416339,-0.0848418351293324,
135.721878784844));
#95242=CARTESIAN_POINT('Ctrl Pts',(-85.5802996748992,0.0523532455151055,
135.724245808619));
#95243=CARTESIAN_POINT('Ctrl Pts',(-85.5880460081645,0.18964664503765,135.7208670161));
#95244=CARTESIAN_POINT('Ctrl Pts',(-85.5957923414298,0.326522543993857,
135.711759734284));
#95245=CARTESIAN_POINT('Ctrl Pts',(-85.6035404094328,0.46342909535879,135.702650412955));
#95246=CARTESIAN_POINT('Ctrl Pts',(-85.6112884774358,0.599917570082481,
135.687810075547));
#95247=CARTESIAN_POINT('Ctrl Pts',(-85.6190365454387,0.735476785030354,
135.667307970888));
#95248=CARTESIAN_POINT('Ctrl Pts',(-85.6267928481806,0.871180073925235,
135.646784076348));
#95249=CARTESIAN_POINT('Ctrl Pts',(-85.6345491509224,1.00595174296484,135.620586452722));
#95250=CARTESIAN_POINT('Ctrl Pts',(-85.6423054536642,1.13928977923307,135.588835704912));
#95251=CARTESIAN_POINT('Ctrl Pts',(-85.6500658961784,1.272698982026,135.557068010772));
#95252=CARTESIAN_POINT('Ctrl Pts',(-85.6578263386926,1.40467265135236,135.519741393037));
#95253=CARTESIAN_POINT('Ctrl Pts',(-85.6655867812067,1.53472444010577,135.477026233191));
#95254=CARTESIAN_POINT('Ctrl Pts',(-85.6733596814721,1.66498499953558,135.434242503178));
#95255=CARTESIAN_POINT('Ctrl Pts',(-85.6811325817374,1.79331714701117,135.386053082784));
#95256=CARTESIAN_POINT('Ctrl Pts',(-85.6889054820028,1.91925417175156,135.332676693848));
#95257=CARTESIAN_POINT('Ctrl Pts',(-85.6963958177651,2.04061306843187,135.281240671095));
#95258=CARTESIAN_POINT('Ctrl Pts',(-85.7038861535275,2.15974767805275,135.224988382724));
#95259=CARTESIAN_POINT('Ctrl Pts',(-85.7113764892898,2.27626410013549,135.16415474217));
#95260=CARTESIAN_POINT('Ctrl Pts',(-85.7191508234089,2.39719827777097,135.101014575648));
#95261=CARTESIAN_POINT('Ctrl Pts',(-85.726925157528,2.51569489464556,135.032738786076));
#95262=CARTESIAN_POINT('Ctrl Pts',(-85.7346994916471,2.63128703187111,134.95953950883));
#95263=CARTESIAN_POINT('Ctrl Pts',(-85.7424642445942,2.74673671211829,134.886430443151));
#95264=CARTESIAN_POINT('Ctrl Pts',(-85.7502289975413,2.85928870774192,134.80841016999));
#95265=CARTESIAN_POINT('Ctrl Pts',(-85.7579937504884,2.96849903987399,134.725737481981));
#95266=CARTESIAN_POINT('Ctrl Pts',(-85.7657507913734,3.0776009027646,134.643146905651));
#95267=CARTESIAN_POINT('Ctrl Pts',(-85.7735078322584,3.18336739739423,134.555913344608));
#95268=CARTESIAN_POINT('Ctrl Pts',(-85.7812648731434,3.28538229553097,134.464339611319));
#95269=CARTESIAN_POINT('Ctrl Pts',(-85.7890160643835,3.38732026343959,134.372834934494));
#95270=CARTESIAN_POINT('Ctrl Pts',(-85.7967672556236,3.48551197625884,134.276996860153));
#95271=CARTESIAN_POINT('Ctrl Pts',(-85.8045184468638,3.57957345636716,134.177169081291));
#95272=CARTESIAN_POINT('Ctrl Pts',(-85.8122663436409,3.67359495783713,134.077383731897));
#95273=CARTESIAN_POINT('Ctrl Pts',(-85.8200142404179,3.76348945051798,133.973612334616));
#95274=CARTESIAN_POINT('Ctrl Pts',(-85.827762137195,3.84890925214866,133.86623596304));
#95275=CARTESIAN_POINT('Ctrl Pts',(-85.8355084132791,3.93431118579828,133.758882052287));
#95276=CARTESIAN_POINT('Ctrl Pts',(-85.8432546893632,4.01524004692808,133.647924972919));
#95277=CARTESIAN_POINT('Ctrl Pts',(-85.8510009654473,4.09138822122309,133.533779142772));
#95278=CARTESIAN_POINT('Ctrl Pts',(-85.8587472987127,4.16753695762672,133.419632470026));
#95279=CARTESIAN_POINT('Ctrl Pts',(-85.866493631978,4.23890471980806,133.302297324768));
#95280=CARTESIAN_POINT('Ctrl Pts',(-85.8742399652434,4.30522727245043,133.182217046169));
#95281=CARTESIAN_POINT('Ctrl Pts',(-85.8819880332464,4.37156467756852,133.062109876425));
#95282=CARTESIAN_POINT('Ctrl Pts',(-85.8897361012494,4.43285443591132,132.93925669222));
#95283=CARTESIAN_POINT('Ctrl Pts',(-85.8974841692524,4.48887850150865,132.814124997088));
#95284=CARTESIAN_POINT('Ctrl Pts',(-85.9052404719942,4.54496211014951,132.6888603105));
#95285=CARTESIAN_POINT('Ctrl Pts',(-85.912996774736,4.59576868653493,132.561312632923));
#95286=CARTESIAN_POINT('Ctrl Pts',(-85.9207530774779,4.64112834873941,132.431969511934));
#95287=CARTESIAN_POINT('Ctrl Pts',(-85.9285135199921,4.68651222076149,132.302557356627));
#95288=CARTESIAN_POINT('Ctrl Pts',(-85.9362739625062,4.7264432720234,132.171348222295));
#95289=CARTESIAN_POINT('Ctrl Pts',(-85.9440344050204,4.76080196680109,132.038843381886));
#95290=CARTESIAN_POINT('Ctrl Pts',(-85.9518073052858,4.79521581720586,131.906125832943));
#95291=CARTESIAN_POINT('Ctrl Pts',(-85.9595802055512,4.82403935343005,131.772108803901));
#95292=CARTESIAN_POINT('Ctrl Pts',(-85.9673531058166,4.84720432377537,131.637303176254));
#95293=CARTESIAN_POINT('Ctrl Pts',(-85.9748434415787,4.86952718909967,131.507398072726));
#95294=CARTESIAN_POINT('Ctrl Pts',(-85.9823337773408,4.88659571226928,131.376761015686));
#95295=CARTESIAN_POINT('Ctrl Pts',(-85.9898241131028,4.89839461978055,131.245850381213));
#95296=CARTESIAN_POINT('Ctrl Pts',(-85.9975984472219,4.91064088645626,131.109976230245));
#95297=CARTESIAN_POINT('Ctrl Pts',(-86.005372781341,4.91724884688008,130.973376938477));
#95298=CARTESIAN_POINT('Ctrl Pts',(-86.01314711546,4.91814459548718,130.836560002346));
#95299=CARTESIAN_POINT('Ctrl Pts',(-86.0209118684071,4.91903924016418,130.699911680862));
#95300=CARTESIAN_POINT('Ctrl Pts',(-86.0286766213543,4.91423567757437,130.563046635911));
#95301=CARTESIAN_POINT('Ctrl Pts',(-86.0364413743013,4.90371165586805,130.426478283229));
#95302=CARTESIAN_POINT('Ctrl Pts',(-86.0441984151863,4.89319808676846,130.290045572161));
#95303=CARTESIAN_POINT('Ctrl Pts',(-86.0519554560713,4.87697539511814,130.153909354224));
#95304=CARTESIAN_POINT('Ctrl Pts',(-86.0597124969563,4.85507336409417,130.018583491554));
#95305=CARTESIAN_POINT('Ctrl Pts',(-86.0674636881964,4.83318784956213,129.88335967917));
#95306=CARTESIAN_POINT('Ctrl Pts',(-86.0752148794366,4.80563158258861,129.748945390085));
#95307=CARTESIAN_POINT('Ctrl Pts',(-86.0829660706767,4.77248617253988,129.615849450006));
#95308=CARTESIAN_POINT('Ctrl Pts',(-86.0907139674538,4.73935485017465,129.482810079252));
#95309=CARTESIAN_POINT('Ctrl Pts',(-86.0984618642309,4.70063920377225,129.351088321627));
#95310=CARTESIAN_POINT('Ctrl Pts',(-86.1062097610079,4.65647191058508,129.221182671651));
#95311=CARTESIAN_POINT('Ctrl Pts',(-86.113956037092,4.61231385624351,129.091304195136));
#95312=CARTESIAN_POINT('Ctrl Pts',(-86.121702313176,4.56270654914106,128.963241440567));
#95313=CARTESIAN_POINT('Ctrl Pts',(-86.1294485892601,4.5078323776895,128.837477215543));
#95314=CARTESIAN_POINT('Ctrl Pts',(-86.1371949225255,4.4529578011692,128.711712062156));
#95315=CARTESIAN_POINT('Ctrl Pts',(-86.1449412557909,4.39281643907293,128.58824583051));
#95316=CARTESIAN_POINT('Ctrl Pts',(-86.1526875890563,4.32763845955921,128.467540464913));
#95317=CARTESIAN_POINT('Ctrl Pts',(-86.1604356570593,4.26244588388899,128.346808068187));
#95318=CARTESIAN_POINT('Ctrl Pts',(-86.1681837250622,4.19221463210468,128.228838111759));
#95319=CARTESIAN_POINT('Ctrl Pts',(-86.1759317930652,4.11722016899497,128.114066740957));
#95320=CARTESIAN_POINT('Ctrl Pts',(-86.183688095807,4.04214600087753,127.999173389776));
#95321=CARTESIAN_POINT('Ctrl Pts',(-86.1914443985488,3.96229872294989,127.887485742891));
#95322=CARTESIAN_POINT('Ctrl Pts',(-86.1992007012906,3.8779966974675,127.77941025815));
#95323=CARTESIAN_POINT('Ctrl Pts',(-86.2069611438048,3.79364967745559,127.671277090269));
#95324=CARTESIAN_POINT('Ctrl Pts',(-86.214721586319,3.70484342528343,127.566760223868));
#95325=CARTESIAN_POINT('Ctrl Pts',(-86.2224820288331,3.61193506410006,127.466231178011));
#95326=CARTESIAN_POINT('Ctrl Pts',(-86.2302549290986,3.5188775581673,127.365540754005));
#95327=CARTESIAN_POINT('Ctrl Pts',(-86.238027829364,3.42170506145758,127.268851218909));
#95328=CARTESIAN_POINT('Ctrl Pts',(-86.2458007296295,3.32081050133173,127.176496138738));
#95329=CARTESIAN_POINT('Ctrl Pts',(-86.2532910653915,3.22358371260424,127.087498398359));
#95330=CARTESIAN_POINT('Ctrl Pts',(-86.2607814011535,3.12290101037792,127.002525646093));
#95331=CARTESIAN_POINT('Ctrl Pts',(-86.2682717369156,3.01913978372785,126.921838495438));
#95332=CARTESIAN_POINT('Ctrl Pts',(-86.2760460710347,2.91144441863196,126.838092066942));
#95333=CARTESIAN_POINT('Ctrl Pts',(-86.2838204051537,2.80009132979206,126.758697348867));
#95334=CARTESIAN_POINT('Ctrl Pts',(-86.2915947392728,2.68546754057026,126.683990834277));
#95335=CARTESIAN_POINT('Ctrl Pts',(-86.2993594922199,2.57098501492446,126.609376388789));
#95336=CARTESIAN_POINT('Ctrl Pts',(-86.3071242451671,2.45324013347387,126.539438862129));
#95337=CARTESIAN_POINT('Ctrl Pts',(-86.3148889981142,2.33265281974991,126.474474489154));
#95338=CARTESIAN_POINT('Ctrl Pts',(-86.3226460389993,2.21218527504593,126.409574639711));
#95339=CARTESIAN_POINT('Ctrl Pts',(-86.3304030798843,2.08888125821942,126.34963829854));
#95340=CARTESIAN_POINT('Ctrl Pts',(-86.3381601207693,1.96318919457174,126.294918163247));
#95341=CARTESIAN_POINT('Ctrl Pts',(-86.3459113120094,1.83759191628716,126.240239292833));
#95342=CARTESIAN_POINT('Ctrl Pts',(-86.3536625032496,1.70961053267106,126.19076895417));
#95343=CARTESIAN_POINT('Ctrl Pts',(-86.3614136944897,1.57971724505676,126.14671351971));
#95344=CARTESIAN_POINT('Ctrl Pts',(-86.3691615912668,1.44987916555454,126.102676809984));
#95345=CARTESIAN_POINT('Ctrl Pts',(-86.3769094880439,1.31813116774786,126.064050552307));
#95346=CARTESIAN_POINT('Ctrl Pts',(-86.384657384821,1.18496436448925,126.030992570014));
#95347=CARTESIAN_POINT('Ctrl Pts',(-86.3924036609051,1.05182541685513,125.997941502738));
#95348=CARTESIAN_POINT('Ctrl Pts',(-86.4001499369893,0.917268633295511,
125.970456488204));
#95349=CARTESIAN_POINT('Ctrl Pts',(-86.4078962130734,0.781798798908662,
125.948645047176));
#95350=CARTESIAN_POINT('Ctrl Pts',(-86.4156425463388,0.646327964514085,
125.926833445141));
#95351=CARTESIAN_POINT('Ctrl Pts',(-86.4233888796041,0.5099444518374,125.91069556233));
#95352=CARTESIAN_POINT('Ctrl Pts',(-86.4311352128695,0.373161319218978,
125.900287443934));
#95353=CARTESIAN_POINT('Ctrl Pts',(-86.4388832808725,0.23634755496658,125.889876994712));
#95354=CARTESIAN_POINT('Ctrl Pts',(-86.4466313488755,0.0991343824571351,
125.885198892865));
#95355=CARTESIAN_POINT('Ctrl Pts',(-86.4543794168785,-0.0379623614454079,
125.886257129268));
#95356=CARTESIAN_POINT('Ctrl Pts',(-86.4621357196204,-0.175204813399029,
125.887316490377));
#95357=CARTESIAN_POINT('Ctrl Pts',(-86.4698920223623,-0.312330197981408,
125.894124365426));
#95358=CARTESIAN_POINT('Ctrl Pts',(-86.4776483251042,-0.448824468116052,
125.906632607629));
#95359=CARTESIAN_POINT('Ctrl Pts',(-86.4854087676184,-0.585391589352429,
125.919147525858));
#95360=CARTESIAN_POINT('Ctrl Pts',(-86.4931692101326,-0.721326537639481,
125.937368821679));
#95361=CARTESIAN_POINT('Ctrl Pts',(-86.5009296526468,-0.856123709682584,
125.9611968524));
#95362=CARTESIAN_POINT('Ctrl Pts',(-86.5087025529123,-0.991137270112981,
125.985063133991));
#95363=CARTESIAN_POINT('Ctrl Pts',(-86.5164754531777,-1.12500902242117,
126.014554052049));
#95364=CARTESIAN_POINT('Ctrl Pts',(-86.5242483534431,-1.25724594123624,
126.049519326235));
#95365=CARTESIAN_POINT('Ctrl Pts',(-86.531738689205,-1.38467571496373,126.083213524631));
#95366=CARTESIAN_POINT('Ctrl Pts',(-86.5392290249669,-1.51058715785964,
126.121990885321));
#95367=CARTESIAN_POINT('Ctrl Pts',(-86.5467193607287,-1.63455702039369,
126.165674768149));
#95368=CARTESIAN_POINT('Ctrl Pts',(-86.5544937938774,-1.7632288769528,126.211015516217));
#95369=CARTESIAN_POINT('Ctrl Pts',(-86.562268227026,-1.89021656238627,126.261785955074));
#95370=CARTESIAN_POINT('Ctrl Pts',(-86.5700426601747,-2.01502776123146,
126.317842347909));
#95371=CARTESIAN_POINT('Ctrl Pts',(-86.5778074890018,-2.13968477174234,
126.373829490213));
#95372=CARTESIAN_POINT('Ctrl Pts',(-86.5855723178289,-2.26217029233569,
126.4350894347));
#95373=CARTESIAN_POINT('Ctrl Pts',(-86.593337146656,-2.38200809965312,126.501429003458));
#95374=CARTESIAN_POINT('Ctrl Pts',(-86.6010942403688,-2.50172652776018,
126.567702486517));
#95375=CARTESIAN_POINT('Ctrl Pts',(-86.6088513340816,-2.61880215171673,
126.639045335571));
#95376=CARTESIAN_POINT('Ctrl Pts',(-86.6166084277944,-2.73277997633288,
126.715216860805));
#95377=CARTESIAN_POINT('Ctrl Pts',(-86.6243596488841,-2.8466715123427,126.791330719255));
#95378=CARTESIAN_POINT('Ctrl Pts',(-86.6321108699738,-2.95746959339661,
126.872265761093));
#95379=CARTESIAN_POINT('Ctrl Pts',(-86.6398620910635,-3.06474535206361,
126.957736254634));
#95380=CARTESIAN_POINT('Ctrl Pts',(-86.6476098988209,-3.17197387071528,
127.043169110338));
#95381=CARTESIAN_POINT('Ctrl Pts',(-86.6553577065785,-3.27568284748481,
127.133133201471));
#95382=CARTESIAN_POINT('Ctrl Pts',(-86.663105514336,-3.3754740572554,127.227300658424));
#95383=CARTESIAN_POINT('Ctrl Pts',(-86.6708516686727,-3.47524397108448,
127.321448019573));
#95384=CARTESIAN_POINT('Ctrl Pts',(-86.6785978230093,-3.57109749695532,
127.419796693971));
#95385=CARTESIAN_POINT('Ctrl Pts',(-86.686343977346,-3.66267134356729,127.521980125985));
#95386=CARTESIAN_POINT('Ctrl Pts',(-86.6940901561138,-3.75424547899967,
127.624163880282));
#95387=CARTESIAN_POINT('Ctrl Pts',(-86.7018363348816,-3.8415396474482,127.730182125101));
#95388=CARTESIAN_POINT('Ctrl Pts',(-86.7095825136493,-3.92422939519156,
127.839633527864));
#95389=CARTESIAN_POINT('Ctrl Pts',(-86.7173303943538,-4.00693731095241,
127.949108978529));
#95390=CARTESIAN_POINT('Ctrl Pts',(-86.7250782750582,-4.08503855757133,
128.062018776099));
#95391=CARTESIAN_POINT('Ctrl Pts',(-86.7328261557626,-4.15825097429988,
128.177931121609));
#95392=CARTESIAN_POINT('Ctrl Pts',(-86.7405818164013,-4.23153690633054,
128.293959859002));
#95393=CARTESIAN_POINT('Ctrl Pts',(-86.74833747704,-4.2999239947759,128.412996835063));
#95394=CARTESIAN_POINT('Ctrl Pts',(-86.7560931376787,-4.36317494708238,
128.534583658556));
#95395=CARTESIAN_POINT('Ctrl Pts',(-86.7638529245643,-4.42645955081553,
128.65623516993));
#95396=CARTESIAN_POINT('Ctrl Pts',(-86.7716127114498,-4.48460240798662,
128.780438878062));
#95397=CARTESIAN_POINT('Ctrl Pts',(-86.7793724983354,-4.53741409986099,
128.90671566951));
#95398=CARTESIAN_POINT('Ctrl Pts',(-86.787143673959,-4.59030330140581,129.033177792504));
#95399=CARTESIAN_POINT('Ctrl Pts',(-86.7949148495828,-4.63784557115586,
129.161718710619));
#95400=CARTESIAN_POINT('Ctrl Pts',(-86.8026860252064,-4.67990092905662,
129.291842731154));
#95401=CARTESIAN_POINT('Ctrl Pts',(-86.8084244753616,-4.71095576384141,
129.387929892481));
#95402=CARTESIAN_POINT('Ctrl Pts',(-86.8141629255169,-4.7390197636557,129.484879952173));
#95403=CARTESIAN_POINT('Ctrl Pts',(-86.8199013756722,-4.76405452823401,
129.582490119308));
#95404=CARTESIAN_POINT('Origin',(213.235140564004,0.,130.804360617566));
#95405=CARTESIAN_POINT('',(-88.9150399778173,-4.76405452823403,129.582490119308));
#95406=CARTESIAN_POINT('',(-88.5701298338732,-4.76405452823396,129.582490119308));
#95407=CARTESIAN_POINT('',(213.235140564004,-4.76405452823405,129.582490119308));
#95408=CARTESIAN_POINT('',(-87.2351405640591,-4.91824986470146,130.805514248378));
#95409=CARTESIAN_POINT('Ctrl Pts',(-87.235140564059,-4.91824986470146,130.805514248378));
#95410=CARTESIAN_POINT('Ctrl Pts',(-87.2434150306343,-4.9182154076984,130.95241406143));
#95411=CARTESIAN_POINT('Ctrl Pts',(-87.2516894972096,-4.91159524424352,
131.099139306973));
#95412=CARTESIAN_POINT('Ctrl Pts',(-87.2599639637848,-4.89846150369965,
131.245107664377));
#95413=CARTESIAN_POINT('Ctrl Pts',(-87.2685064031367,-4.88490242033887,
131.395803280715));
#95414=CARTESIAN_POINT('Ctrl Pts',(-87.2770488424886,-4.86440086237666,
131.545691795828));
#95415=CARTESIAN_POINT('Ctrl Pts',(-87.2855912818405,-4.83709249482959,
131.694146692397));
#95416=CARTESIAN_POINT('Ctrl Pts',(-87.2939087439399,-4.81050333186161,
131.838691818775));
#95417=CARTESIAN_POINT('Ctrl Pts',(-87.3022262060394,-4.77746153715247,
131.98187763293));
#95418=CARTESIAN_POINT('Ctrl Pts',(-87.3105436681389,-4.73814257228153,
132.123143399996));
#95419=CARTESIAN_POINT('Ctrl Pts',(-87.319198596117,-4.69722831201058,132.270140768316));
#95420=CARTESIAN_POINT('Ctrl Pts',(-87.327853524095,-4.64951700377619,132.415058660253));
#95421=CARTESIAN_POINT('Ctrl Pts',(-87.336508452073,-4.59526078202615,132.557289996541));
#95422=CARTESIAN_POINT('Ctrl Pts',(-87.3451633800511,-4.54100456027611,
132.699521332828));
#95423=CARTESIAN_POINT('Ctrl Pts',(-87.3538183080292,-4.48020363982355,
132.839065813765));
#95424=CARTESIAN_POINT('Ctrl Pts',(-87.3624732360073,-4.41316267366985,
132.975346172153));
#95425=CARTESIAN_POINT('Ctrl Pts',(-87.3702475701264,-4.35294277676666,
133.097760713634));
#95426=CARTESIAN_POINT('Ctrl Pts',(-87.3780219042455,-4.2875302410094,133.217861637103));
#95427=CARTESIAN_POINT('Ctrl Pts',(-87.3857962383646,-4.2171259359179,133.335177067471));
#95428=CARTESIAN_POINT('Ctrl Pts',(-87.3935609913117,-4.14680839784021,
133.452347917055));
#95429=CARTESIAN_POINT('Ctrl Pts',(-87.4013257442588,-4.07151153014495,
133.566739771915));
#95430=CARTESIAN_POINT('Ctrl Pts',(-87.4090904972059,-3.99148339667264,
133.677902570729));
#95431=CARTESIAN_POINT('Ctrl Pts',(-87.4168475380909,-3.91153474827069,
133.788954961083));
#95432=CARTESIAN_POINT('Ctrl Pts',(-87.4246045789759,-3.82686441257948,
133.896784362512));
#95433=CARTESIAN_POINT('Ctrl Pts',(-87.4323616198609,-3.73776512653218,
134.000967399981));
#95434=CARTESIAN_POINT('Ctrl Pts',(-87.440112811101,-3.6487330309497,134.105071872211));
#95435=CARTESIAN_POINT('Ctrl Pts',(-87.4478640023411,-3.55527888597019,
134.205535157772));
#95436=CARTESIAN_POINT('Ctrl Pts',(-87.4556151935812,-3.45773707120855,
134.301965141936));
#95437=CARTESIAN_POINT('Ctrl Pts',(-87.4633630903583,-3.36023671432006,
134.398354140783));
#95438=CARTESIAN_POINT('Ctrl Pts',(-87.4711109871354,-3.25865242059542,
134.490712973477));
#95439=CARTESIAN_POINT('Ctrl Pts',(-87.4788588839125,-3.15335681047315,
134.578684913164));
#95440=CARTESIAN_POINT('Ctrl Pts',(-87.4866051599966,-3.0480832259226,134.666638451018));
#95441=CARTESIAN_POINT('Ctrl Pts',(-87.4943514360806,-2.93910016897346,
134.750206670598));
#95442=CARTESIAN_POINT('Ctrl Pts',(-87.5020977121647,-2.82681455622494,
134.829072101289));
#95443=CARTESIAN_POINT('Ctrl Pts',(-87.5098440454301,-2.71452811460937,
134.907938114147));
#95444=CARTESIAN_POINT('Ctrl Pts',(-87.5175903786955,-2.59893938848384,
134.982101044134));
#95445=CARTESIAN_POINT('Ctrl Pts',(-87.5253367119608,-2.48048524843065,
135.051286093109));
#95446=CARTESIAN_POINT('Ctrl Pts',(-87.5330847799638,-2.36200458139394,
135.120486635596));
#95447=CARTESIAN_POINT('Ctrl Pts',(-87.5408328479669,-2.24065756107677,
135.184706881681));
#95448=CARTESIAN_POINT('Ctrl Pts',(-87.5485809159699,-2.11690632387932,
135.243717629389));
#95449=CARTESIAN_POINT('Ctrl Pts',(-87.5563372187118,-1.99302356239449,
135.302791094422));
#95450=CARTESIAN_POINT('Ctrl Pts',(-87.5640935214537,-1.866731833141,135.356643832343));
#95451=CARTESIAN_POINT('Ctrl Pts',(-87.5718498241955,-1.7385144665978,135.405094310351));
#95452=CARTESIAN_POINT('Ctrl Pts',(-87.5796102667097,-1.61022866658553,
135.453570647839));
#95453=CARTESIAN_POINT('Ctrl Pts',(-87.5873707092238,-1.48001555237063,
135.496638857385));
#95454=CARTESIAN_POINT('Ctrl Pts',(-87.595131151738,-1.34837338401885,135.534167408522));
#95455=CARTESIAN_POINT('Ctrl Pts',(-87.6029040520034,-1.21651989197179,
135.57175620382));
#95456=CARTESIAN_POINT('Ctrl Pts',(-87.6106769522689,-1.0832331419167,135.603787478749));
#95457=CARTESIAN_POINT('Ctrl Pts',(-87.6184498525343,-0.949022230375064,
135.630180741519));
#95458=CARTESIAN_POINT('Ctrl Pts',(-87.6259401882964,-0.819690223524848,
135.655614542707));
#95459=CARTESIAN_POINT('Ctrl Pts',(-87.6334305240584,-0.689500384223107,
135.675813079727));
#95460=CARTESIAN_POINT('Ctrl Pts',(-87.6409208598204,-0.558910590025547,
135.690750083711));
#95461=CARTESIAN_POINT('Ctrl Pts',(-87.6486951939395,-0.423369444088893,
135.706253428742));
#95462=CARTESIAN_POINT('Ctrl Pts',(-87.6564695280586,-0.28696806237198,
135.716137492594));
#95463=CARTESIAN_POINT('Ctrl Pts',(-87.6642438621777,-0.150212021635176,
135.720316212469));
#95464=CARTESIAN_POINT('Ctrl Pts',(-87.6720086151248,-0.0136245204967136,
135.724489782445));
#95465=CARTESIAN_POINT('Ctrl Pts',(-87.6797733680718,0.123316382960341,
135.722971986863));
#95466=CARTESIAN_POINT('Ctrl Pts',(-87.6875381210189,0.260097954833687,
135.715728259719));
#95467=CARTESIAN_POINT('Ctrl Pts',(-87.6952951619039,0.396743673321566,
135.708491727147));
#95468=CARTESIAN_POINT('Ctrl Pts',(-87.703052202789,0.533229987259395,135.695540601093));
#95469=CARTESIAN_POINT('Ctrl Pts',(-87.710809243674,0.669042467778677,135.676892324883));
#95470=CARTESIAN_POINT('Ctrl Pts',(-87.7185604349141,0.804752531050118,
135.658258111483));
#95471=CARTESIAN_POINT('Ctrl Pts',(-87.7263116261543,0.939789386567182,
135.63393535235));
#95472=CARTESIAN_POINT('Ctrl Pts',(-87.7340628173944,1.073642396753,135.603993422937));
#95473=CARTESIAN_POINT('Ctrl Pts',(-87.7418107141715,1.20743851583903,135.574064219642));
#95474=CARTESIAN_POINT('Ctrl Pts',(-87.7495586109486,1.34005140961509,135.538520681376));
#95475=CARTESIAN_POINT('Ctrl Pts',(-87.7573065077257,1.47097954322825,135.497483484688));
#95476=CARTESIAN_POINT('Ctrl Pts',(-87.7650527838098,1.60188028949799,135.456454872097));
#95477=CARTESIAN_POINT('Ctrl Pts',(-87.7727990598939,1.73109660374572,135.409935003676));
#95478=CARTESIAN_POINT('Ctrl Pts',(-87.780545335978,1.8581414405904,135.35809462926));
#95479=CARTESIAN_POINT('Ctrl Pts',(-87.7882916692433,1.98518721525138,135.306253872171));
#95480=CARTESIAN_POINT('Ctrl Pts',(-87.7960380025087,2.11006111853508,135.249092678427));
#95481=CARTESIAN_POINT('Ctrl Pts',(-87.8037843357741,2.23229581576175,135.186830064514));
#95482=CARTESIAN_POINT('Ctrl Pts',(-87.811532403777,2.35455788660119,135.124553507321));
#95483=CARTESIAN_POINT('Ctrl Pts',(-87.8192804717799,2.47417922699072,135.057173434077));
#95484=CARTESIAN_POINT('Ctrl Pts',(-87.8270285397829,2.59071720680562,134.98495476396));
#95485=CARTESIAN_POINT('Ctrl Pts',(-87.8347848425248,2.70737904457244,134.91265933898));
#95486=CARTESIAN_POINT('Ctrl Pts',(-87.8425411452667,2.82095064268278,134.835515250664));
#95487=CARTESIAN_POINT('Ctrl Pts',(-87.8502974480085,2.93101802051978,134.753831015719));
#95488=CARTESIAN_POINT('Ctrl Pts',(-87.8580578905227,3.04114414463041,134.672103183438));
#95489=CARTESIAN_POINT('Ctrl Pts',(-87.8658183330368,3.14776201794214,134.585830621882));
#95490=CARTESIAN_POINT('Ctrl Pts',(-87.873578775551,3.25049165840981,134.495361435922));
#95491=CARTESIAN_POINT('Ctrl Pts',(-87.8813516758164,3.35338620961626,134.404747020794));
#95492=CARTESIAN_POINT('Ctrl Pts',(-87.8891245760819,3.45237977250185,134.309922789603));
#95493=CARTESIAN_POINT('Ctrl Pts',(-87.8968974763473,3.54712944793814,134.211273551891));
#95494=CARTESIAN_POINT('Ctrl Pts',(-87.9043878121093,3.63843473401178,134.116210462453));
#95495=CARTESIAN_POINT('Ctrl Pts',(-87.9118781478713,3.72579912346444,134.017595866117));
#95496=CARTESIAN_POINT('Ctrl Pts',(-87.9193684836333,3.80895302155096,133.915800789274));
#95497=CARTESIAN_POINT('Ctrl Pts',(-87.9271428177524,3.89525972495811,133.810146121152));
#95498=CARTESIAN_POINT('Ctrl Pts',(-87.9349171518714,3.97730374641448,133.700730353569));
#95499=CARTESIAN_POINT('Ctrl Pts',(-87.9426914859905,4.05473940226316,133.587932323528));
#95500=CARTESIAN_POINT('Ctrl Pts',(-87.9504562389376,4.13207962558642,133.475273306979));
#95501=CARTESIAN_POINT('Ctrl Pts',(-87.9582209918847,4.20482256446318,133.359240640946));
#95502=CARTESIAN_POINT('Ctrl Pts',(-87.9659857448318,4.27266199233714,133.240247019215));
#95503=CARTESIAN_POINT('Ctrl Pts',(-87.9737427857168,4.34043404113496,133.121371583626));
#95504=CARTESIAN_POINT('Ctrl Pts',(-87.9814998266019,4.40331207853759,132.999541382236));
#95505=CARTESIAN_POINT('Ctrl Pts',(-87.9892568674869,4.46103271874009,132.875198647164));
#95506=CARTESIAN_POINT('Ctrl Pts',(-87.997008058727,4.5187098313589,132.750949679917));
#95507=CARTESIAN_POINT('Ctrl Pts',(-88.0047592499672,4.57123712411015,132.6241923035));
#95508=CARTESIAN_POINT('Ctrl Pts',(-88.0125104412073,4.61839695244212,132.495393630896));
#95509=CARTESIAN_POINT('Ctrl Pts',(-88.0202583379844,4.66553673658896,132.366649701165));
#95510=CARTESIAN_POINT('Ctrl Pts',(-88.0280062347614,4.70731345953583,132.235866567206));
#95511=CARTESIAN_POINT('Ctrl Pts',(-88.0357541315385,4.74355755804388,132.103531413122));
#95512=CARTESIAN_POINT('Ctrl Pts',(-88.0435004076226,4.77979407506785,131.971223940698));
#95513=CARTESIAN_POINT('Ctrl Pts',(-88.0512466837067,4.81050016638838,131.837365470733));
#95514=CARTESIAN_POINT('Ctrl Pts',(-88.0589929597908,4.83555622875427,131.702458062755));
#95515=CARTESIAN_POINT('Ctrl Pts',(-88.0667392930562,4.86061247607836,131.567549658922));
#95516=CARTESIAN_POINT('Ctrl Pts',(-88.0744856263215,4.88001853983181,131.431592686018));
#95517=CARTESIAN_POINT('Ctrl Pts',(-88.0822319595869,4.89370607897761,131.295098709706));
#95518=CARTESIAN_POINT('Ctrl Pts',(-88.0899800275899,4.90739668335288,131.158574166515));
#95519=CARTESIAN_POINT('Ctrl Pts',(-88.0977280955928,4.91536617582449,131.021512769555));
#95520=CARTESIAN_POINT('Ctrl Pts',(-88.1054761635958,4.91759818800414,130.884430111372));
#95521=CARTESIAN_POINT('Ctrl Pts',(-88.1132324663377,4.91983257239291,130.747201760109));
#95522=CARTESIAN_POINT('Ctrl Pts',(-88.1209887690795,4.91631728897776,130.60995249402));
#95523=CARTESIAN_POINT('Ctrl Pts',(-88.1287450718213,4.90708813496676,130.473197367539));
#95524=CARTESIAN_POINT('Ctrl Pts',(-88.1365055143355,4.89785405507839,130.33636925073));
#95525=CARTESIAN_POINT('Ctrl Pts',(-88.1442659568497,4.88290007048621,130.200036187492));
#95526=CARTESIAN_POINT('Ctrl Pts',(-88.1520263993639,4.86231366210198,130.064706026668));
#95527=CARTESIAN_POINT('Ctrl Pts',(-88.1597992996293,4.84169420658744,129.929158621856));
#95528=CARTESIAN_POINT('Ctrl Pts',(-88.1675721998948,4.81542433411614,129.794617720587));
#95529=CARTESIAN_POINT('Ctrl Pts',(-88.1753451001602,4.78364245050019,129.661579812568));
#95530=CARTESIAN_POINT('Ctrl Pts',(-88.1828354359222,4.7530159184075,129.533378167607));
#95531=CARTESIAN_POINT('Ctrl Pts',(-88.1903257716842,4.71727125209247,129.406572434357));
#95532=CARTESIAN_POINT('Ctrl Pts',(-88.1978161074462,4.67657488402088,129.281589979339));
#95533=CARTESIAN_POINT('Ctrl Pts',(-88.2055904415653,4.63433550078439,129.151868776552));
#95534=CARTESIAN_POINT('Ctrl Pts',(-88.2133647756844,4.58662771433529,129.023700922686));
#95535=CARTESIAN_POINT('Ctrl Pts',(-88.2211391098034,4.53358340051323,128.897582021847));
#95536=CARTESIAN_POINT('Ctrl Pts',(-88.2289038627505,4.48060445906725,128.771618551282));
#95537=CARTESIAN_POINT('Ctrl Pts',(-88.2366686156977,4.4223022262262,128.647699366372));
#95538=CARTESIAN_POINT('Ctrl Pts',(-88.2444333686447,4.35885839002497,128.526305175262));
#95539=CARTESIAN_POINT('Ctrl Pts',(-88.2521904095297,4.29547756713627,128.405031554575));
#95540=CARTESIAN_POINT('Ctrl Pts',(-88.2599474504147,4.22696548339365,128.28627828119));
#95541=CARTESIAN_POINT('Ctrl Pts',(-88.2677044912997,4.15355183474339,128.170505986308));
#95542=CARTESIAN_POINT('Ctrl Pts',(-88.2754556825398,4.08019354789676,128.054820996214));
#95543=CARTESIAN_POINT('Ctrl Pts',(-88.28320687378,4.00194126194501,127.942112838998));
#95544=CARTESIAN_POINT('Ctrl Pts',(-88.2909580650201,3.91907033007207,127.832817111163));
#95545=CARTESIAN_POINT('Ctrl Pts',(-88.2987059617972,3.83623462055573,127.723567836926));
#95546=CARTESIAN_POINT('Ctrl Pts',(-88.3064538585743,3.74878440519206,127.617728418273));
#95547=CARTESIAN_POINT('Ctrl Pts',(-88.3142017553514,3.65703791268919,127.515704848463));
#95548=CARTESIAN_POINT('Ctrl Pts',(-88.3219480314355,3.56531061157473,127.413702619785));
#95549=CARTESIAN_POINT('Ctrl Pts',(-88.3296943075194,3.46928908212053,127.315514942824));
#95550=CARTESIAN_POINT('Ctrl Pts',(-88.3374405836035,3.36933107275015,127.221513818622));
#95551=CARTESIAN_POINT('Ctrl Pts',(-88.3451869168689,3.2693723255126,127.127512000526));
#95552=CARTESIAN_POINT('Ctrl Pts',(-88.3529332501342,3.16547732518568,127.037697064694));
#95553=CARTESIAN_POINT('Ctrl Pts',(-88.3606795833996,3.05803952644947,126.952403022112));
#95554=CARTESIAN_POINT('Ctrl Pts',(-88.3684276514025,2.95057766776329,126.867089878521));
#95555=CARTESIAN_POINT('Ctrl Pts',(-88.3761757194055,2.83957173806734,126.78629988583));
#95556=CARTESIAN_POINT('Ctrl Pts',(-88.3839237874084,2.72544667245893,126.710325505591));
#95557=CARTESIAN_POINT('Ctrl Pts',(-88.3916800901502,2.61120031337254,126.634270378877));
#95558=CARTESIAN_POINT('Ctrl Pts',(-88.3994363928921,2.49382852215972,126.563041305552));
#95559=CARTESIAN_POINT('Ctrl Pts',(-88.4071926956339,2.37378397796804,126.496886567912));
#95560=CARTESIAN_POINT('Ctrl Pts',(-88.4149531381481,2.25367536238832,126.430696521497));
#95561=CARTESIAN_POINT('Ctrl Pts',(-88.4227135806623,2.13089150118981,126.369586381453));
#95562=CARTESIAN_POINT('Ctrl Pts',(-88.4304740231765,2.00590694755695,126.313757052315));
#95563=CARTESIAN_POINT('Ctrl Pts',(-88.4382469234419,1.880721757623,126.257838100983));
#95564=CARTESIAN_POINT('Ctrl Pts',(-88.4460198237073,1.75332917924145,126.207217045214));
#95565=CARTESIAN_POINT('Ctrl Pts',(-88.4537927239727,1.6242217349851,126.162045805093));
#95566=CARTESIAN_POINT('Ctrl Pts',(-88.4612830597348,1.49980767152809,126.11851665333));
#95567=CARTESIAN_POINT('Ctrl Pts',(-88.468773395497,1.37380155156294,126.080048057218));
#95568=CARTESIAN_POINT('Ctrl Pts',(-88.4762637312591,1.246652891461,126.046730994454));
#95569=CARTESIAN_POINT('Ctrl Pts',(-88.4840380653782,1.1146833512666,126.012150705129));
#95570=CARTESIAN_POINT('Ctrl Pts',(-88.4918123994972,0.981064882003765,
125.983010761335));
#95571=CARTESIAN_POINT('Ctrl Pts',(-88.4995867336163,0.846285731554575,
125.959468098318));
#95572=CARTESIAN_POINT('Ctrl Pts',(-88.5073514865634,0.71167268436312,125.935954449529));
#95573=CARTESIAN_POINT('Ctrl Pts',(-88.5151162395104,0.575902183562834,
125.918024422884));
#95574=CARTESIAN_POINT('Ctrl Pts',(-88.5228809924575,0.439476869351736,
125.905784993591));
#95575=CARTESIAN_POINT('Ctrl Pts',(-88.5306380333425,0.303187054685602,
125.893557720671));
#95576=CARTESIAN_POINT('Ctrl Pts',(-88.5383950742276,0.166244107755559,
125.887009832112));
#95577=CARTESIAN_POINT('Ctrl Pts',(-88.5461521151126,0.0291597269057145,
125.886197060625));
#95578=CARTESIAN_POINT('Ctrl Pts',(-88.5539033063528,-0.107821277545984,
125.885384902055));
#95579=CARTESIAN_POINT('Ctrl Pts',(-88.5616544975928,-0.244943114247928,
125.890299254421));
#95580=CARTESIAN_POINT('Ctrl Pts',(-88.569405688833,-0.381690468404819,
125.900943905841));
#95581=CARTESIAN_POINT('Ctrl Pts',(-88.5771535856101,-0.518379701288525,
125.911584032999));
#95582=CARTESIAN_POINT('Ctrl Pts',(-88.5849014823872,-0.654694379224354,
125.92794958485));
#95583=CARTESIAN_POINT('Ctrl Pts',(-88.5926493791643,-0.790120918193643,
125.949992275842));
#95584=CARTESIAN_POINT('Ctrl Pts',(-88.6003956552484,-0.925519128850438,
125.972030355978));
#95585=CARTESIAN_POINT('Ctrl Pts',(-88.6081419313325,-1.06002918442376,
125.999743150414));
#95586=CARTESIAN_POINT('Ctrl Pts',(-88.6158882074166,-1.19314473813956,
126.03303075092));
#95587=CARTESIAN_POINT('Ctrl Pts',(-88.623634540682,-1.32626127448395,126.066318597147));
#95588=CARTESIAN_POINT('Ctrl Pts',(-88.6313808739474,-1.45798290914398,
126.105181236712));
#95589=CARTESIAN_POINT('Ctrl Pts',(-88.6391272072127,-1.58781595735216,
126.149468186147));
#95590=CARTESIAN_POINT('Ctrl Pts',(-88.6468752752157,-1.71767808077147,
126.193765053338));
#95591=CARTESIAN_POINT('Ctrl Pts',(-88.6546233432187,-1.84565040618618,
126.243488521388));
#95592=CARTESIAN_POINT('Ctrl Pts',(-88.6623714112216,-1.97125718960859,
126.298439162978));
#95593=CARTESIAN_POINT('Ctrl Pts',(-88.6701277139635,-2.09699746941498,
126.353448206764));
#95594=CARTESIAN_POINT('Ctrl Pts',(-88.6778840167053,-2.22036682623198,
126.413695364854));
#95595=CARTESIAN_POINT('Ctrl Pts',(-88.6856403194471,-2.34091168899455,
126.478933988108));
#95596=CARTESIAN_POINT('Ctrl Pts',(-88.6934007619613,-2.46152089017991,
126.544207431178));
#95597=CARTESIAN_POINT('Ctrl Pts',(-88.7011612044755,-2.57930225786841,
126.614477447632));
#95598=CARTESIAN_POINT('Ctrl Pts',(-88.7089216469896,-2.69383025779619,
126.689453376244));
#95599=CARTESIAN_POINT('Ctrl Pts',(-88.7166945472551,-2.80854210823678,
126.764549662873));
#95600=CARTESIAN_POINT('Ctrl Pts',(-88.7244674475205,-2.91998983646938,
126.84436672988));
#95601=CARTESIAN_POINT('Ctrl Pts',(-88.7322403477859,-3.02777940734386,
126.928572320592));
#95602=CARTESIAN_POINT('Ctrl Pts',(-88.7397306835478,-3.13165055581004,
127.009716825979));
#95603=CARTESIAN_POINT('Ctrl Pts',(-88.7472210193098,-3.2321246609155,127.094936127536));
#95604=CARTESIAN_POINT('Ctrl Pts',(-88.7547113550717,-3.32888220596853,
127.183901210076));
#95605=CARTESIAN_POINT('Ctrl Pts',(-88.7623680314278,-3.42778848080405,
127.274841972366));
#95606=CARTESIAN_POINT('Ctrl Pts',(-88.7700247077838,-3.52314454494613,
127.370003713737));
#95607=CARTESIAN_POINT('Ctrl Pts',(-88.7776813841399,-3.61456031361364,
127.469074002933));
#95608=CARTESIAN_POINT('Ctrl Pts',(-88.7853292035122,-3.70587033561802,
127.568029690976));
#95609=CARTESIAN_POINT('Ctrl Pts',(-88.7929770228845,-3.79324885201695,
127.670884646024));
#95610=CARTESIAN_POINT('Ctrl Pts',(-88.8006248422568,-3.87633939608425,
127.777286791432));
#95611=CARTESIAN_POINT('Ctrl Pts',(-88.8082655891791,-3.95935310076816,
127.88359053966));
#95612=CARTESIAN_POINT('Ctrl Pts',(-88.8159063361015,-4.03808647091666,
127.993434639985));
#95613=CARTESIAN_POINT('Ctrl Pts',(-88.8235470830237,-4.11222082990317,
128.106431243285));
#95614=CARTESIAN_POINT('Ctrl Pts',(-88.8311825833212,-4.18630428350404,
128.2193502559));
#95615=CARTESIAN_POINT('Ctrl Pts',(-88.8388180836185,-4.25579478629175,
128.335417129918));
#95616=CARTESIAN_POINT('Ctrl Pts',(-88.8464535839159,-4.32041515927868,
128.454212555427));
#95617=CARTESIAN_POINT('Ctrl Pts',(-88.8540858257332,-4.38500795526401,
128.572957284515));
#95618=CARTESIAN_POINT('Ctrl Pts',(-88.8617180675505,-4.44473456326938,
128.694427894813));
#95619=CARTESIAN_POINT('Ctrl Pts',(-88.8693503093677,-4.49936248964123,
128.818178287237));
#95620=CARTESIAN_POINT('Ctrl Pts',(-88.8769831125742,-4.55399443416758,
128.941937782116));
#95621=CARTESIAN_POINT('Ctrl Pts',(-88.8846159157806,-4.6035267735283,129.06797702981));
#95622=CARTESIAN_POINT('Ctrl Pts',(-88.8922487189871,-4.64777422352981,
129.195827798631));
#95623=CARTESIAN_POINT('Ctrl Pts',(-88.8998458052638,-4.69181462206964,
129.323080302725));
#95624=CARTESIAN_POINT('Ctrl Pts',(-88.9074428915406,-4.73061939022566,
129.452127023663));
#95625=CARTESIAN_POINT('Ctrl Pts',(-88.9150399778173,-4.76405452823403,
129.582490119308));
#95626=CARTESIAN_POINT('Ctrl Pts',(-87.1653941590427,-4.76405452823403,
129.582490119308));
#95627=CARTESIAN_POINT('Ctrl Pts',(-87.1733902600484,-4.79917917091089,
129.719440568014));
#95628=CARTESIAN_POINT('Ctrl Pts',(-87.181386361054,-4.82842565015031,129.858028792729));
#95629=CARTESIAN_POINT('Ctrl Pts',(-87.1893824620597,-4.85165185218374,
129.997727263618));
#95630=CARTESIAN_POINT('Ctrl Pts',(-87.197369497904,-4.87485172272489,130.137267358669));
#95631=CARTESIAN_POINT('Ctrl Pts',(-87.2053565337483,-4.89204486357648,
130.277914841835));
#95632=CARTESIAN_POINT('Ctrl Pts',(-87.2133435695926,-4.90313991537456,
130.419130773498));
#95633=CARTESIAN_POINT('Ctrl Pts',(-87.2206092343981,-4.91323288715235,
130.547592401148));
#95634=CARTESIAN_POINT('Ctrl Pts',(-87.2278748992035,-4.91828012077182,
130.676524083358));
#95635=CARTESIAN_POINT('Ctrl Pts',(-87.2351405640089,-4.91824986470167,
130.805514247488));
#95636=CARTESIAN_POINT('',(-86.8898594360246,-4.9182479024669,130.799818329603));
#95637=CARTESIAN_POINT('Ctrl Pts',(-86.8199013756722,-4.76405452823401,
129.582490119308));
#95638=CARTESIAN_POINT('Ctrl Pts',(-86.8216565786288,-4.77171183841665,
129.612345855494));
#95639=CARTESIAN_POINT('Ctrl Pts',(-86.8234117815855,-4.77908585800606,
129.642263334497));
#95640=CARTESIAN_POINT('Ctrl Pts',(-86.8251669845421,-4.78617577532478,
129.672236724083));
#95641=CARTESIAN_POINT('Ctrl Pts',(-86.8359490597836,-4.82972858595405,
129.85636092496));
#95642=CARTESIAN_POINT('Ctrl Pts',(-86.846731135025,-4.86267186386441,130.043083385357));
#95643=CARTESIAN_POINT('Ctrl Pts',(-86.8575132102665,-4.88475779004073,
130.231364635786));
#95644=CARTESIAN_POINT('Ctrl Pts',(-86.8682952855081,-4.90684371621709,
130.419645886214));
#95645=CARTESIAN_POINT('Ctrl Pts',(-86.8790773607497,-4.91807212000454,
130.609486579959));
#95646=CARTESIAN_POINT('Ctrl Pts',(-86.8898594359914,-4.91824790246636,
130.799818329018));
#95647=CARTESIAN_POINT('Ctrl Pts',(-86.8898594360245,-4.9182479024669,130.799818329603));
#95648=CARTESIAN_POINT('Ctrl Pts',(-86.8975161444314,-4.91837273139357,
130.934979202668));
#95649=CARTESIAN_POINT('Ctrl Pts',(-86.9051728528383,-4.91292173440832,
131.070298365521));
#95650=CARTESIAN_POINT('Ctrl Pts',(-86.9128295612452,-4.90188259609975,
131.205272174589));
#95651=CARTESIAN_POINT('Ctrl Pts',(-86.920778938208,-4.89042149988227,131.345405196689));
#95652=CARTESIAN_POINT('Ctrl Pts',(-86.9287283151711,-4.87293651889991,
131.485165501218));
#95653=CARTESIAN_POINT('Ctrl Pts',(-86.9366776921339,-4.84947337498785,
131.623989221132));
#95654=CARTESIAN_POINT('Ctrl Pts',(-86.9443260986553,-4.82689856645291,
131.757556952248));
#95655=CARTESIAN_POINT('Ctrl Pts',(-86.9519745051767,-4.7987900901287,131.890257291798));
#95656=CARTESIAN_POINT('Ctrl Pts',(-86.9596229116981,-4.76524142747747,
132.021594038218));
#95657=CARTESIAN_POINT('Ctrl Pts',(-86.9672702572283,-4.7316974187152,132.152912565532));
#95658=CARTESIAN_POINT('Ctrl Pts',(-86.9749176027584,-4.69271482354635,
132.282867486452));
#95659=CARTESIAN_POINT('Ctrl Pts',(-86.9825649482887,-4.64843782494699,
132.410974712519));
#95660=CARTESIAN_POINT('Ctrl Pts',(-86.9902129898755,-4.60415679628284,
132.539093598826));
#95661=CARTESIAN_POINT('Ctrl Pts',(-86.9978610314625,-4.5545805375101,132.665364076015));
#95662=CARTESIAN_POINT('Ctrl Pts',(-87.0055090730494,-4.49990231636308,
132.789319611019));
#95663=CARTESIAN_POINT('Ctrl Pts',(-87.0131595680623,-4.44520655491211,
132.913314909894));
#95664=CARTESIAN_POINT('Ctrl Pts',(-87.0208100630751,-4.38540573883924,
133.034993422437));
#95665=CARTESIAN_POINT('Ctrl Pts',(-87.0284605580881,-4.32074000539837,
133.153911397662));
#95666=CARTESIAN_POINT('Ctrl Pts',(-87.0361193562716,-4.25600408949026,
133.272958435938));
#95667=CARTESIAN_POINT('Ctrl Pts',(-87.0437781544552,-4.18639291050616,
133.389238604206));
#95668=CARTESIAN_POINT('Ctrl Pts',(-87.0514369526387,-4.11219115716434,
133.502335218899));
#95669=CARTESIAN_POINT('Ctrl Pts',(-87.0591006870272,-4.03794157973197,
133.615504725977));
#95670=CARTESIAN_POINT('Ctrl Pts',(-87.0667644214155,-3.95909577203372,
133.725486269763));
#95671=CARTESIAN_POINT('Ctrl Pts',(-87.0744281558039,-3.87597913792231,
133.831895718088));
#95672=CARTESIAN_POINT('Ctrl Pts',(-87.0821026387063,-3.79274593135937,
133.93845440742));
#95673=CARTESIAN_POINT('Ctrl Pts',(-87.0897771216088,-3.70523020533087,
134.041430700128));
#95674=CARTESIAN_POINT('Ctrl Pts',(-87.0974516045112,-3.61379480714271,
134.140476645879));
#95675=CARTESIAN_POINT('Ctrl Pts',(-87.0995059391258,-3.58931903387138,
134.166989639312));
#95676=CARTESIAN_POINT('Ctrl Pts',(-87.1015602737403,-3.56456258369106,
134.193221227023));
#95677=CARTESIAN_POINT('Ctrl Pts',(-87.1036146083549,-3.53953281040988,
134.219165230795));
#95678=CARTESIAN_POINT('Ctrl Pts',(-87.111388942474,-3.44481123047191,134.317346584641));
#95679=CARTESIAN_POINT('Ctrl Pts',(-87.1191632765931,-3.34585141626337,
134.411739311184));
#95680=CARTESIAN_POINT('Ctrl Pts',(-87.1269376107121,-3.24298872491999,
134.501955402361));
#95681=CARTESIAN_POINT('Ctrl Pts',(-87.1347023636592,-3.14025280265087,
134.592060310268));
#95682=CARTESIAN_POINT('Ctrl Pts',(-87.1424671166063,-3.0336238647186,134.677998569143));
#95683=CARTESIAN_POINT('Ctrl Pts',(-87.1502318695533,-2.92347554829333,
134.759417353067));
#95684=CARTESIAN_POINT('Ctrl Pts',(-87.1579889104383,-2.81343663272846,
134.840755270707));
#95685=CARTESIAN_POINT('Ctrl Pts',(-87.1657459513234,-2.69988560722988,
134.917582415432));
#95686=CARTESIAN_POINT('Ctrl Pts',(-87.1735029922084,-2.58323050042245,
134.989585013484));
#95687=CARTESIAN_POINT('Ctrl Pts',(-87.1812541834485,-2.46666336413866,
135.061533313816));
#95688=CARTESIAN_POINT('Ctrl Pts',(-87.1890053746886,-2.34699713713889,
135.12866410463));
#95689=CARTESIAN_POINT('Ctrl Pts',(-87.1967565659287,-2.22466995720138,
135.190706094615));
#95690=CARTESIAN_POINT('Ctrl Pts',(-87.2045044627058,-2.10239476957835,
135.252721715099));
#95691=CARTESIAN_POINT('Ctrl Pts',(-87.2122523594829,-1.97746122639522,
135.309652660074));
#95692=CARTESIAN_POINT('Ctrl Pts',(-87.22000025626,-1.85033307488721,135.361273012431));
#95693=CARTESIAN_POINT('Ctrl Pts',(-87.2277465323441,-1.72323151584793,
135.412882566924));
#95694=CARTESIAN_POINT('Ctrl Pts',(-87.2354928084281,-1.59393662360072,
135.459183591368));
#95695=CARTESIAN_POINT('Ctrl Pts',(-87.2432390845122,-1.46293281740536,
135.499998022036));
#95696=CARTESIAN_POINT('Ctrl Pts',(-87.2509854177776,-1.33192804416949,
135.540812753987));
#95697=CARTESIAN_POINT('Ctrl Pts',(-87.258731751043,-1.19921470508263,135.576140695054));
#95698=CARTESIAN_POINT('Ctrl Pts',(-87.2664780843084,-1.06529271351499,
135.605853562165));
#95699=CARTESIAN_POINT('Ctrl Pts',(-87.2742261523114,-0.931340731045698,
135.635573083266));
#95700=CARTESIAN_POINT('Ctrl Pts',(-87.2819742203143,-0.796179939105779,
135.659674943551));
#95701=CARTESIAN_POINT('Ctrl Pts',(-87.2897222883173,-0.660320388187454,
135.678081993214));
#95702=CARTESIAN_POINT('Ctrl Pts',(-87.2974785910592,-0.524316444122219,
135.696508606107));
#95703=CARTESIAN_POINT('Ctrl Pts',(-87.305234893801,-0.38761264559977,135.709228265258));
#95704=CARTESIAN_POINT('Ctrl Pts',(-87.3129911965429,-0.250724669979703,
135.716215684887));
#95705=CARTESIAN_POINT('Ctrl Pts',(-87.320751639057,-0.11376363312543,135.723206833912));
#95706=CARTESIAN_POINT('Ctrl Pts',(-87.3285120815712,0.023381385941645,
135.724459643595));
#95707=CARTESIAN_POINT('Ctrl Pts',(-87.3362725240853,0.160195760720989,
135.720001001153));
#95708=CARTESIAN_POINT('Ctrl Pts',(-87.3440454243508,0.297229762080538,
135.715535201302));
#95709=CARTESIAN_POINT('Ctrl Pts',(-87.3518183246162,0.433931668378921,
135.705339656776));
#95710=CARTESIAN_POINT('Ctrl Pts',(-87.3595912248817,0.569792118071048,
135.689493164865));
#95711=CARTESIAN_POINT('Ctrl Pts',(-87.3670815606435,0.700713698202832,
135.674222732851));
#95712=CARTESIAN_POINT('Ctrl Pts',(-87.3745718964054,0.830853633460133,
135.653705120765));
#95713=CARTESIAN_POINT('Ctrl Pts',(-87.3820622321673,0.959767891472947,
135.628055120434));
#95714=CARTESIAN_POINT('Ctrl Pts',(-87.3898365662864,1.09356997276304,135.601432592544));
#95715=CARTESIAN_POINT('Ctrl Pts',(-87.3976109004055,1.22647544375197,135.56919647253));
#95716=CARTESIAN_POINT('Ctrl Pts',(-87.4053852345246,1.35797659354375,135.531419178012));
#95717=CARTESIAN_POINT('Ctrl Pts',(-87.4131499874716,1.48931567992064,135.493688440634));
#95718=CARTESIAN_POINT('Ctrl Pts',(-87.4209147404187,1.61925351651872,135.450430223343));
#95719=CARTESIAN_POINT('Ctrl Pts',(-87.4286794933657,1.74729130088375,135.401768166648));
#95720=CARTESIAN_POINT('Ctrl Pts',(-87.4364365342506,1.87520191631599,135.353154441793));
#95721=CARTESIAN_POINT('Ctrl Pts',(-87.4441935751356,2.00121587195041,135.299147696441));
#95722=CARTESIAN_POINT('Ctrl Pts',(-87.4519506160206,2.12484863159888,135.239921614249));
#95723=CARTESIAN_POINT('Ctrl Pts',(-87.4597018072607,2.24838815882208,135.180740194905));
#95724=CARTESIAN_POINT('Ctrl Pts',(-87.4674529985008,2.36954971308005,135.116347441203));
#95725=CARTESIAN_POINT('Ctrl Pts',(-87.4752041897409,2.48786822513832,135.046965331282));
#95726=CARTESIAN_POINT('Ctrl Pts',(-87.482952086518,2.60613644867287,134.977612710609));
#95727=CARTESIAN_POINT('Ctrl Pts',(-87.490699983295,2.72156369681083,134.903275148803));
#95728=CARTESIAN_POINT('Ctrl Pts',(-87.4984478800721,2.8337092323813,134.82422069583));
#95729=CARTESIAN_POINT('Ctrl Pts',(-87.5061941561562,2.945831309523,134.745182779344));
#95730=CARTESIAN_POINT('Ctrl Pts',(-87.5139404322402,3.05467272016352,134.661430159353));
#95731=CARTESIAN_POINT('Ctrl Pts',(-87.5216867083243,3.15982181380379,134.573274143705));
#95732=CARTESIAN_POINT('Ctrl Pts',(-87.5294330415897,3.26497168363092,134.485117477309));
#95733=CARTESIAN_POINT('Ctrl Pts',(-87.537179374855,3.36642888246945,134.392557601578));
#95734=CARTESIAN_POINT('Ctrl Pts',(-87.5449257081203,3.46381526675065,134.295945767655));
#95735=CARTESIAN_POINT('Ctrl Pts',(-87.5526737761233,3.56122346003751,134.199312298182));
#95736=CARTESIAN_POINT('Ctrl Pts',(-87.5604218441263,3.65455874722492,134.098625340176));
#95737=CARTESIAN_POINT('Ctrl Pts',(-87.5681699121293,3.74348052524587,133.994272312207));
#95738=CARTESIAN_POINT('Ctrl Pts',(-87.5759262148711,3.83249681039056,133.889808376597));
#95739=CARTESIAN_POINT('Ctrl Pts',(-87.583682517613,3.91708996215104,133.781670885714));
#95740=CARTESIAN_POINT('Ctrl Pts',(-87.5914388203548,3.99695997067645,133.670280025943));
#95741=CARTESIAN_POINT('Ctrl Pts',(-87.599199262869,4.07687260823024,133.558829713516));
#95742=CARTESIAN_POINT('Ctrl Pts',(-87.606959705383,4.15205686525745,133.444122899062));
#95743=CARTESIAN_POINT('Ctrl Pts',(-87.6147201478972,4.22225719454089,133.326607085627));
#95744=CARTESIAN_POINT('Ctrl Pts',(-87.6224930481626,4.29257021562499,133.208902625377));
#95745=CARTESIAN_POINT('Ctrl Pts',(-87.630265948428,4.357883134747,133.088380499153));
#95746=CARTESIAN_POINT('Ctrl Pts',(-87.6380388486934,4.41798692394173,132.96551183911));
#95747=CARTESIAN_POINT('Ctrl Pts',(-87.6455291844556,4.47590578900855,132.847109764343));
#95748=CARTESIAN_POINT('Ctrl Pts',(-87.6530195202179,4.52898755472494,132.726529080548));
#95749=CARTESIAN_POINT('Ctrl Pts',(-87.6605098559801,4.57708878836483,132.604205412521));
#95750=CARTESIAN_POINT('Ctrl Pts',(-87.6682841900992,4.62701379489702,132.477243805443));
#95751=CARTESIAN_POINT('Ctrl Pts',(-87.6760585242182,4.67173128762119,132.348002258342));
#95752=CARTESIAN_POINT('Ctrl Pts',(-87.6838328583374,4.71102776339145,132.216947066267));
#95753=CARTESIAN_POINT('Ctrl Pts',(-87.6915976112844,4.75027580976704,132.086053388005));
#95754=CARTESIAN_POINT('Ctrl Pts',(-87.6993623642315,4.78411602101374,131.953350882958));
#95755=CARTESIAN_POINT('Ctrl Pts',(-87.7071271171785,4.81238280448082,131.819326038473));
#95756=CARTESIAN_POINT('Ctrl Pts',(-87.7148841580635,4.84062151298023,131.685434309352));
#95757=CARTESIAN_POINT('Ctrl Pts',(-87.7226411989485,4.86329772964747,131.550223234525));
#95758=CARTESIAN_POINT('Ctrl Pts',(-87.7303982398335,4.8802956758171,131.414194348267));
#95759=CARTESIAN_POINT('Ctrl Pts',(-87.7381494310736,4.89728080370324,131.278268042452));
#95760=CARTESIAN_POINT('Ctrl Pts',(-87.7459006223137,4.90859613592757,131.141525539124));
#95761=CARTESIAN_POINT('Ctrl Pts',(-87.7536518135538,4.91417704770595,131.004478098812));
#95762=CARTESIAN_POINT('Ctrl Pts',(-87.7613997103309,4.91975558744796,130.867488907316));
#95763=CARTESIAN_POINT('Ctrl Pts',(-87.7691476071078,4.9196045384368,130.730195426436));
#95764=CARTESIAN_POINT('Ctrl Pts',(-87.7768955038849,4.91371118949469,130.593113348389));
#95765=CARTESIAN_POINT('Ctrl Pts',(-87.784641779969,4.90781907331414,130.456059944958));
#95766=CARTESIAN_POINT('Ctrl Pts',(-87.7923880560532,4.89618706316837,130.31921824676));
#95767=CARTESIAN_POINT('Ctrl Pts',(-87.8001343321373,4.87885456401745,130.183102856515));
#95768=CARTESIAN_POINT('Ctrl Pts',(-87.8078806654027,4.86152193692189,130.046986461496));
#95769=CARTESIAN_POINT('Ctrl Pts',(-87.8156269986681,4.83848878623959,129.911596772963));
#95770=CARTESIAN_POINT('Ctrl Pts',(-87.8233733319334,4.80984623366961,129.77744179363));
#95771=CARTESIAN_POINT('Ctrl Pts',(-87.8311213999364,4.78119726679885,129.643256771221));
#95772=CARTESIAN_POINT('Ctrl Pts',(-87.8388694679392,4.74693647999147,129.5103073905));
#95773=CARTESIAN_POINT('Ctrl Pts',(-87.8466175359422,4.70720571518489,129.379089619674));
#95774=CARTESIAN_POINT('Ctrl Pts',(-87.854373838684,4.66743272404841,129.247732389039));
#95775=CARTESIAN_POINT('Ctrl Pts',(-87.8621301414259,4.62217825518426,129.118110819433));
#95776=CARTESIAN_POINT('Ctrl Pts',(-87.8698864441678,4.57163366064695,128.990704438645));
#95777=CARTESIAN_POINT('Ctrl Pts',(-87.877646886682,4.52106208893767,128.863230057235));
#95778=CARTESIAN_POINT('Ctrl Pts',(-87.8854073291962,4.46519492467207,128.737973577387));
#95779=CARTESIAN_POINT('Ctrl Pts',(-87.8931677717103,4.40427053532475,128.615391884539));
#95780=CARTESIAN_POINT('Ctrl Pts',(-87.9009406719758,4.34324834473903,128.492613412676));
#95781=CARTESIAN_POINT('Ctrl Pts',(-87.9087135722412,4.27715289472485,128.372518650919));
#95782=CARTESIAN_POINT('Ctrl Pts',(-87.9164864725066,4.20626757738537,128.255538118855));
#95783=CARTESIAN_POINT('Ctrl Pts',(-87.9239768082687,4.13795911987975,128.142810123786));
#95784=CARTESIAN_POINT('Ctrl Pts',(-87.9314671440308,4.06520316654555,128.032974125998));
#95785=CARTESIAN_POINT('Ctrl Pts',(-87.9389574797929,3.98828869196884,127.92638626535));
#95786=CARTESIAN_POINT('Ctrl Pts',(-87.946731813912,3.90845798171169,127.81575709357));
#95787=CARTESIAN_POINT('Ctrl Pts',(-87.9545061480312,3.82389430492806,127.708276787368));
#95788=CARTESIAN_POINT('Ctrl Pts',(-87.9622804821502,3.73487456518304,127.60437701685));
#95789=CARTESIAN_POINT('Ctrl Pts',(-87.9700452350973,3.64596453431157,127.500605293515));
#95790=CARTESIAN_POINT('Ctrl Pts',(-87.9778099880444,3.55260961925711,127.400405619971));
#95791=CARTESIAN_POINT('Ctrl Pts',(-87.9855747409915,3.45512960872882,127.3041802723));
#95792=CARTESIAN_POINT('Ctrl Pts',(-87.9933317818765,3.35774641672068,127.208050497));
#95793=CARTESIAN_POINT('Ctrl Pts',(-88.0010888227616,3.25624655909695,127.115887465035));
#95794=CARTESIAN_POINT('Ctrl Pts',(-88.0088458636466,3.15098940965234,127.028059675803));
#95795=CARTESIAN_POINT('Ctrl Pts',(-88.0165970548867,3.04581163544361,126.940298118191));
#95796=CARTESIAN_POINT('Ctrl Pts',(-88.0243482461268,2.93688250810477,126.856865545554));
#95797=CARTESIAN_POINT('Ctrl Pts',(-88.032099437367,2.82459723432153,126.778092677356));
#95798=CARTESIAN_POINT('Ctrl Pts',(-88.0398473341441,2.71235968477449,126.699353289728));
#95799=CARTESIAN_POINT('Ctrl Pts',(-88.0475952309212,2.59676914527587,126.625269891544));
#95800=CARTESIAN_POINT('Ctrl Pts',(-88.0553431276983,2.47825261159246,126.556131921317));
#95801=CARTESIAN_POINT('Ctrl Pts',(-88.0630894037824,2.35976086901298,126.487008413263));
#95802=CARTESIAN_POINT('Ctrl Pts',(-88.0708356798666,2.23834468714888,126.422828472414));
#95803=CARTESIAN_POINT('Ctrl Pts',(-88.0785819559507,2.11445831518612,126.363837101601));
#95804=CARTESIAN_POINT('Ctrl Pts',(-88.086328289216,1.99057102872246,126.304845295327));
#95805=CARTESIAN_POINT('Ctrl Pts',(-88.0940746224814,1.86421386876416,126.251042303599));
#95806=CARTESIAN_POINT('Ctrl Pts',(-88.1018209557468,1.73586348588816,126.202626051029));
#95807=CARTESIAN_POINT('Ctrl Pts',(-88.1095690237498,1.60748435983365,126.154198955975));
#95808=CARTESIAN_POINT('Ctrl Pts',(-88.1173170917527,1.47711148837441,126.111161138483));
#95809=CARTESIAN_POINT('Ctrl Pts',(-88.1250651597557,1.34523881264115,126.073661345845));
#95810=CARTESIAN_POINT('Ctrl Pts',(-88.1328214624976,1.21322598105863,126.036121697981));
#95811=CARTESIAN_POINT('Ctrl Pts',(-88.1405777652395,1.07971053765166,126.004131939754));
#95812=CARTESIAN_POINT('Ctrl Pts',(-88.1483340679814,0.945199353190114,
125.977790277746));
#95813=CARTESIAN_POINT('Ctrl Pts',(-88.1560945104956,0.810616376059364,
125.9514345564));
#95814=CARTESIAN_POINT('Ctrl Pts',(-88.1638549530098,0.67503698519777,125.930732997019));
#95815=CARTESIAN_POINT('Ctrl Pts',(-88.171615395524,0.53897441470745,125.915732012038));
#95816=CARTESIAN_POINT('Ctrl Pts',(-88.1793882957895,0.402693424499912,
125.900706946143));
#95817=CARTESIAN_POINT('Ctrl Pts',(-88.1871611960548,0.265928094969845,
125.891400767954));
#95818=CARTESIAN_POINT('Ctrl Pts',(-88.1949340963203,0.12919381479039,125.887807758019));
#95819=CARTESIAN_POINT('Ctrl Pts',(-88.2024244320822,-0.00256982988834706,
125.884345363046));
#95820=CARTESIAN_POINT('Ctrl Pts',(-88.2099147678441,-0.134304335479741,
125.886187967444));
#95821=CARTESIAN_POINT('Ctrl Pts',(-88.217405103606,-0.265553873613018,
125.893284951003));
#95822=CARTESIAN_POINT('Ctrl Pts',(-88.2251794377251,-0.401779777880308,
125.90065101885));
#95823=CARTESIAN_POINT('Ctrl Pts',(-88.2329537718442,-0.537914736372974,
125.913701104242));
#95824=CARTESIAN_POINT('Ctrl Pts',(-88.2407281059633,-0.67344589966379,
125.932435568602));
#95825=CARTESIAN_POINT('Ctrl Pts',(-88.2484928589103,-0.808810032907883,
125.951146944409));
#95826=CARTESIAN_POINT('Ctrl Pts',(-88.2562576118575,-0.943571467969517,
125.975528707329));
#95827=CARTESIAN_POINT('Ctrl Pts',(-88.2640223648046,-1.07721890498082,
126.005529250113));
#95828=CARTESIAN_POINT('Ctrl Pts',(-88.2717794056896,-1.21073360147394,
126.035499995935));
#95829=CARTESIAN_POINT('Ctrl Pts',(-88.2795364465746,-1.3431361227756,126.071078330794));
#95830=CARTESIAN_POINT('Ctrl Pts',(-88.2872934874596,-1.47392218959192,
126.112161086266));
#95831=CARTESIAN_POINT('Ctrl Pts',(-88.2950446786997,-1.60460962961841,
126.153212860913));
#95832=CARTESIAN_POINT('Ctrl Pts',(-88.3027958699398,-1.7336826699805,126.199760677313));
#95833=CARTESIAN_POINT('Ctrl Pts',(-88.31054706118,-1.86064944815984,126.251650798836));
#95834=CARTESIAN_POINT('Ctrl Pts',(-88.3182949579571,-1.98756226207099,
126.303518865673));
#95835=CARTESIAN_POINT('Ctrl Pts',(-88.3260428547341,-2.11237023316926,
126.360724573941));
#95836=CARTESIAN_POINT('Ctrl Pts',(-88.3337907515112,-2.23459904699309,
126.423065128595));
#95837=CARTESIAN_POINT('Ctrl Pts',(-88.3415370275953,-2.35680229318368,
126.485392642949));
#95838=CARTESIAN_POINT('Ctrl Pts',(-88.3492833036794,-2.47642710714252,
126.552852689725));
#95839=CARTESIAN_POINT('Ctrl Pts',(-88.3570295797635,-2.59302182826836,
126.625195526232));
#95840=CARTESIAN_POINT('Ctrl Pts',(-88.3647759130289,-2.70961741007011,
126.697538896758));
#95841=CARTESIAN_POINT('Ctrl Pts',(-88.3725222462942,-2.8231825221929,126.774764922812));
#95842=CARTESIAN_POINT('Ctrl Pts',(-88.3802685795596,-2.93329300377644,
126.85657956785));
#95843=CARTESIAN_POINT('Ctrl Pts',(-88.3880166475625,-3.04342814383873,
126.938412534711));
#95844=CARTESIAN_POINT('Ctrl Pts',(-88.3957647155655,-3.15010680014675,
127.024835932209));
#95845=CARTESIAN_POINT('Ctrl Pts',(-88.4035127835685,-3.25293684014523,
127.115514595227));
#95846=CARTESIAN_POINT('Ctrl Pts',(-88.4112690863104,-3.35587616913378,
127.206289632607));
#95847=CARTESIAN_POINT('Ctrl Pts',(-88.4190253890522,-3.45495841718359,
127.301328710784));
#95848=CARTESIAN_POINT('Ctrl Pts',(-88.426781691794,-3.54982698428493,127.400258468079));
#95849=CARTESIAN_POINT('Ctrl Pts',(-88.4345421343082,-3.64474618559723,
127.499241027165));
#95850=CARTESIAN_POINT('Ctrl Pts',(-88.4423025768223,-3.73544696627377,
127.602118109995));
#95851=CARTESIAN_POINT('Ctrl Pts',(-88.4500630193365,-3.82161286265189,
127.708483005238));
#95852=CARTESIAN_POINT('Ctrl Pts',(-88.457835919602,-3.90791708017656,127.815018646854));
#95853=CARTESIAN_POINT('Ctrl Pts',(-88.4656088198673,-3.9896716327417,127.925052975355));
#95854=CARTESIAN_POINT('Ctrl Pts',(-88.4733817201328,-4.06660275211667,
128.038149288152));
#95855=CARTESIAN_POINT('Ctrl Pts',(-88.4808720558949,-4.1407372315256,128.147134265108));
#95856=CARTESIAN_POINT('Ctrl Pts',(-88.4883623916571,-4.21039271432896,
128.258962208267));
#95857=CARTESIAN_POINT('Ctrl Pts',(-88.4958527274192,-4.27536540237552,
128.37322225485));
#95858=CARTESIAN_POINT('Ctrl Pts',(-88.5039673523599,-4.3457533010789,128.497005413998));
#95859=CARTESIAN_POINT('Ctrl Pts',(-88.5120819773005,-4.41085202937009,
128.624006454679));
#95860=CARTESIAN_POINT('Ctrl Pts',(-88.5201966022411,-4.47036889127372,
128.753754600206));
#95861=CARTESIAN_POINT('Ctrl Pts',(-88.5285188075131,-4.53140825483455,
128.886821834817));
#95862=CARTESIAN_POINT('Ctrl Pts',(-88.5368410127851,-4.58657609156948,
129.022778347369));
#95863=CARTESIAN_POINT('Ctrl Pts',(-88.5451632180572,-4.63560448481789,
129.161085192436));
#95864=CARTESIAN_POINT('Ctrl Pts',(-88.5534854233292,-4.68463287806617,
129.299392037503));
#95865=CARTESIAN_POINT('Ctrl Pts',(-88.5618076286012,-4.72752162291951,
129.440048875951));
#95866=CARTESIAN_POINT('Ctrl Pts',(-88.5701298338733,-4.76405452823397,
129.582490119308));
#95867=CARTESIAN_POINT('Origin',(213.235140564004,0.,130.804360617566));
#95868=CARTESIAN_POINT('',(-90.6650630979317,-4.76405452823406,129.582490119308));
#95869=CARTESIAN_POINT('',(-90.3197845579208,-4.76405452823393,129.582490119308));
#95870=CARTESIAN_POINT('',(213.235140564004,-4.76405452823405,129.582490119308));
#95871=CARTESIAN_POINT('',(-88.98514056396,-4.91824826917725,130.808486782246));
#95872=CARTESIAN_POINT('Ctrl Pts',(-88.985140564009,-4.91824826917653,130.808486783108));
#95873=CARTESIAN_POINT('Ctrl Pts',(-88.9972482442412,-4.9180693451276,131.021758132721));
#95874=CARTESIAN_POINT('Ctrl Pts',(-89.0093559244733,-4.90401532505547,
131.234467650703));
#95875=CARTESIAN_POINT('Ctrl Pts',(-89.0214636047054,-4.87632108299787,
131.445200502413));
#95876=CARTESIAN_POINT('Ctrl Pts',(-89.0253620627651,-4.86740402877369,
131.513052739048));
#95877=CARTESIAN_POINT('Ctrl Pts',(-89.0292605208248,-4.85707316178395,
131.580700345055));
#95878=CARTESIAN_POINT('Ctrl Pts',(-89.0331589788845,-4.84533718105517,
131.648096751902));
#95879=CARTESIAN_POINT('Ctrl Pts',(-89.0409333130037,-4.82193320081409,
131.782499168762));
#95880=CARTESIAN_POINT('Ctrl Pts',(-89.0487076471227,-4.79289572884961,
131.916139944255));
#95881=CARTESIAN_POINT('Ctrl Pts',(-89.0564819812418,-4.75828497826597,
132.04850977587));
#95882=CARTESIAN_POINT('Ctrl Pts',(-89.0642467341889,-4.72371688233916,
132.180716473498));
#95883=CARTESIAN_POINT('Ctrl Pts',(-89.072011487136,-4.68358927214729,132.311654969149));
#95884=CARTESIAN_POINT('Ctrl Pts',(-89.0797762400831,-4.63801378270779,
132.440823636981));
#95885=CARTESIAN_POINT('Ctrl Pts',(-89.0875332809681,-4.5924835594869,132.569864012671));
#95886=CARTESIAN_POINT('Ctrl Pts',(-89.0952903218531,-4.54151635421954,
132.697137692376));
#95887=CARTESIAN_POINT('Ctrl Pts',(-89.1030473627381,-4.48527417301372,
132.822156111514));
#95888=CARTESIAN_POINT('Ctrl Pts',(-89.1107985539783,-4.42907440447432,
132.947080253289));
#95889=CARTESIAN_POINT('Ctrl Pts',(-89.1185497452184,-4.36760773751705,
133.069752164552));
#95890=CARTESIAN_POINT('Ctrl Pts',(-89.1263009364585,-4.30108492597971,
133.189701583133));
#95891=CARTESIAN_POINT('Ctrl Pts',(-89.1340488332356,-4.23459038841173,
133.309600020011));
#95892=CARTESIAN_POINT('Ctrl Pts',(-89.1417967300127,-4.16304416967384,
133.426777924466));
#95893=CARTESIAN_POINT('Ctrl Pts',(-89.1495446267898,-4.08670366606434,
133.540788253787));
#95894=CARTESIAN_POINT('Ctrl Pts',(-89.1572909028739,-4.01037913124248,
133.654774734606));
#95895=CARTESIAN_POINT('Ctrl Pts',(-89.165037178958,-3.92926252368292,133.765594633558));
#95896=CARTESIAN_POINT('Ctrl Pts',(-89.1727834550421,-3.84365518310861,
133.872828948161));
#95897=CARTESIAN_POINT('Ctrl Pts',(-89.1805297883074,-3.75804721060048,
133.980064054342));
#95898=CARTESIAN_POINT('Ctrl Pts',(-89.1882761215728,-3.66794868285102,
134.083713217816));
#95899=CARTESIAN_POINT('Ctrl Pts',(-89.1960224548381,-3.57370167544866,
134.183389974851));
#95900=CARTESIAN_POINT('Ctrl Pts',(-89.2037705228411,-3.47943356208258,
134.283089053805));
#95901=CARTESIAN_POINT('Ctrl Pts',(-89.2115185908439,-3.38101538897182,
134.378813672103));
#95902=CARTESIAN_POINT('Ctrl Pts',(-89.2192666588469,-3.27882628958447,
134.470214027787));
#95903=CARTESIAN_POINT('Ctrl Pts',(-89.2270229615887,-3.17652858240609,
134.561711524857));
#95904=CARTESIAN_POINT('Ctrl Pts',(-89.2347792643307,-3.07045223484165,
134.648875317493));
#95905=CARTESIAN_POINT('Ctrl Pts',(-89.2425355670725,-2.9610101128649,134.731395398926));
#95906=CARTESIAN_POINT('Ctrl Pts',(-89.2502960095867,-2.85150957833211,
134.813959523811));
#95907=CARTESIAN_POINT('Ctrl Pts',(-89.2580564521008,-2.73864001146899,
134.891874776896));
#95908=CARTESIAN_POINT('Ctrl Pts',(-89.265816894615,-2.62284265402436,134.964874945715));
#95909=CARTESIAN_POINT('Ctrl Pts',(-89.2735897948804,-2.50685940838154,
135.037992300885));
#95910=CARTESIAN_POINT('Ctrl Pts',(-89.281362695146,-2.38793931952346,135.106178610214));
#95911=CARTESIAN_POINT('Ctrl Pts',(-89.2891355954114,-2.26654836783466,
135.169213600058));
#95912=CARTESIAN_POINT('Ctrl Pts',(-89.2966259311736,-2.14957028300346,
135.229957109246));
#95913=CARTESIAN_POINT('Ctrl Pts',(-89.3041162669356,-2.03029813948232,
135.285917192658));
#95914=CARTESIAN_POINT('Ctrl Pts',(-89.3116066026978,-1.90916399462772,
135.33694000508));
#95915=CARTESIAN_POINT('Ctrl Pts',(-89.3193809368168,-1.78343701185497,
135.389897362942));
#95916=CARTESIAN_POINT('Ctrl Pts',(-89.3271552709359,-1.65530577965287,
135.437703418906));
#95917=CARTESIAN_POINT('Ctrl Pts',(-89.334929605055,-1.52523133530176,135.480133541513));
#95918=CARTESIAN_POINT('Ctrl Pts',(-89.3426943580021,-1.39531719607823,
135.522511372786));
#95919=CARTESIAN_POINT('Ctrl Pts',(-89.3504591109492,-1.26346497783599,
135.559526333108));
#95920=CARTESIAN_POINT('Ctrl Pts',(-89.3582238638963,-1.13015705405705,
135.591001203161));
#95921=CARTESIAN_POINT('Ctrl Pts',(-89.3659809047813,-0.996981533586957,
135.622444811929));
#95922=CARTESIAN_POINT('Ctrl Pts',(-89.3737379456663,-0.862353562882643,
135.648359191384));
#95923=CARTESIAN_POINT('Ctrl Pts',(-89.3814949865514,-0.726771753422879,
135.668616560763));
#95924=CARTESIAN_POINT('Ctrl Pts',(-89.3892461777915,-0.591292187260485,
135.688858653902));
#95925=CARTESIAN_POINT('Ctrl Pts',(-89.3969973690316,-0.454860599168647,
135.703452170629));
#95926=CARTESIAN_POINT('Ctrl Pts',(-89.4047485602717,-0.317986551626253,
135.712320235929));
#95927=CARTESIAN_POINT('Ctrl Pts',(-89.4124964570488,-0.181170679205113,
135.721184532065));
#95928=CARTESIAN_POINT('Ctrl Pts',(-89.420244353826,-0.0439131106949756,
135.724328191534));
#95929=CARTESIAN_POINT('Ctrl Pts',(-89.4279922506031,0.0932709152251658,
135.721726131627));
#95930=CARTESIAN_POINT('Ctrl Pts',(-89.4357385266872,0.23042624520443,135.719124616015));
#95931=CARTESIAN_POINT('Ctrl Pts',(-89.4434848027712,0.36750767254513,135.710779779043));
#95932=CARTESIAN_POINT('Ctrl Pts',(-89.4512310788553,0.503999797109908,
135.696718665278));
#95933=CARTESIAN_POINT('Ctrl Pts',(-89.4589774121207,0.640492929228357,
135.682657447717));
#95934=CARTESIAN_POINT('Ctrl Pts',(-89.4667237453861,0.776396360983598,
135.662879909228));
#95935=CARTESIAN_POINT('Ctrl Pts',(-89.4744700786514,0.911200049281774,
135.637464954603));
#95936=CARTESIAN_POINT('Ctrl Pts',(-89.4822181466544,1.04603392593147,135.612044308476));
#95937=CARTESIAN_POINT('Ctrl Pts',(-89.4899662146574,1.17976718493234,135.580983806484));
#95938=CARTESIAN_POINT('Ctrl Pts',(-89.4977142826604,1.31190059708888,135.544413347848));
#95939=CARTESIAN_POINT('Ctrl Pts',(-89.5054705854023,1.44417444220809,135.507804021694));
#95940=CARTESIAN_POINT('Ctrl Pts',(-89.5132268881441,1.57484466647749,135.465673145264));
#95941=CARTESIAN_POINT('Ctrl Pts',(-89.520983190886,1.70342728827788,135.418200508162));
#95942=CARTESIAN_POINT('Ctrl Pts',(-89.5287436334001,1.83207853849507,135.370702533484));
#95943=CARTESIAN_POINT('Ctrl Pts',(-89.5365040759143,1.95863960547145,135.317857267727));
#95944=CARTESIAN_POINT('Ctrl Pts',(-89.5442645184285,2.08264801517743,135.259892045732));
#95945=CARTESIAN_POINT('Ctrl Pts',(-89.5520374186939,2.20685549419162,135.201833772817));
#95946=CARTESIAN_POINT('Ctrl Pts',(-89.5598103189593,2.32850178017859,135.138639299804));
#95947=CARTESIAN_POINT('Ctrl Pts',(-89.5675832192248,2.44714967690405,135.070581605903));
#95948=CARTESIAN_POINT('Ctrl Pts',(-89.5750735549867,2.56148442372623,135.004997980603));
#95949=CARTESIAN_POINT('Ctrl Pts',(-89.5825638907487,2.67303473372726,134.934898740284));
#95950=CARTESIAN_POINT('Ctrl Pts',(-89.5900542265106,2.78143763501597,134.860564229938));
#95951=CARTESIAN_POINT('Ctrl Pts',(-89.5978285606297,2.89395066525651,134.783411304038));
#95952=CARTESIAN_POINT('Ctrl Pts',(-89.6056028947488,3.00342931486091,134.701451210497));
#95953=CARTESIAN_POINT('Ctrl Pts',(-89.6133772288678,3.10943539311046,134.614950414247));
#95954=CARTESIAN_POINT('Ctrl Pts',(-89.6211419818149,3.21531082834259,134.528556222498));
#95955=CARTESIAN_POINT('Ctrl Pts',(-89.6289067347621,3.31772190740933,134.437632707237));
#95956=CARTESIAN_POINT('Ctrl Pts',(-89.6366714877092,3.41625879602881,134.342489911565));
#95957=CARTESIAN_POINT('Ctrl Pts',(-89.6444285285941,3.51469781642138,134.247441613059));
#95958=CARTESIAN_POINT('Ctrl Pts',(-89.6521855694791,3.60927002442683,134.148182643533));
#95959=CARTESIAN_POINT('Ctrl Pts',(-89.6599426103641,3.69959840278609,134.045063430322));
#95960=CARTESIAN_POINT('Ctrl Pts',(-89.6676938016043,3.7898586638127,133.942021980111));
#95961=CARTESIAN_POINT('Ctrl Pts',(-89.6754449928444,3.87588120863602,133.835126373364));
#95962=CARTESIAN_POINT('Ctrl Pts',(-89.6831961840846,3.95732592916066,133.724763766601));
#95963=CARTESIAN_POINT('Ctrl Pts',(-89.6909440808617,4.03873603350658,133.61444806689));
#95964=CARTESIAN_POINT('Ctrl Pts',(-89.6986919776387,4.11557195173285,133.500668611897));
#95965=CARTESIAN_POINT('Ctrl Pts',(-89.7064398744158,4.18753408195496,133.383845328698));
#95966=CARTESIAN_POINT('Ctrl Pts',(-89.7141861504999,4.25948115925054,133.267046482412));
#95967=CARTESIAN_POINT('Ctrl Pts',(-89.7219324265841,4.32655627144583,133.147205407026));
#95968=CARTESIAN_POINT('Ctrl Pts',(-89.7296787026682,4.38850358553658,133.024770341521));
#95969=CARTESIAN_POINT('Ctrl Pts',(-89.7374250359335,4.45045135690841,132.902334372227));
#95970=CARTESIAN_POINT('Ctrl Pts',(-89.7451713691989,4.50727107813781,132.777304723459));
#95971=CARTESIAN_POINT('Ctrl Pts',(-89.7529177024643,4.55875344331177,132.650153158886));
#95972=CARTESIAN_POINT('Ctrl Pts',(-89.7606657704672,4.61024733760439,132.522973119602));
#95973=CARTESIAN_POINT('Ctrl Pts',(-89.7684138384702,4.65640135070579,132.39367058126));
#95974=CARTESIAN_POINT('Ctrl Pts',(-89.7761619064732,4.69705492493503,132.262735773225));
#95975=CARTESIAN_POINT('Ctrl Pts',(-89.783918209215,4.7377517062668,132.131661806117));
#95976=CARTESIAN_POINT('Ctrl Pts',(-89.7916745119568,4.77293625473262,131.998952477852));
#95977=CARTESIAN_POINT('Ctrl Pts',(-89.7994308146987,4.80249822853209,131.865112156545));
#95978=CARTESIAN_POINT('Ctrl Pts',(-89.8071912572129,4.83207598044706,131.731200400629));
#95979=CARTESIAN_POINT('Ctrl Pts',(-89.8149516997271,4.85602510983729,131.596156833627));
#95980=CARTESIAN_POINT('Ctrl Pts',(-89.8227121422413,4.87428690143246,131.460493428073));
#95981=CARTESIAN_POINT('Ctrl Pts',(-89.8304850425067,4.89257800847671,131.324612243577));
#95982=CARTESIAN_POINT('Ctrl Pts',(-89.8382579427722,4.90516349752205,131.1881096217));
#95983=CARTESIAN_POINT('Ctrl Pts',(-89.8460308430376,4.91203671846552,131.051500939947));
#95984=CARTESIAN_POINT('Ctrl Pts',(-89.8535211787996,4.91866008051508,130.919858327872));
#95985=CARTESIAN_POINT('Ctrl Pts',(-89.8610115145615,4.91997927164379,130.788117541136));
#95986=CARTESIAN_POINT('Ctrl Pts',(-89.8685018503236,4.91603395886155,130.656735491588));
#95987=CARTESIAN_POINT('Ctrl Pts',(-89.8762761844426,4.91193905834601,130.520372051698));
#95988=CARTESIAN_POINT('Ctrl Pts',(-89.8840505185617,4.90215959469573,130.383963130644));
#95989=CARTESIAN_POINT('Ctrl Pts',(-89.8918248526808,4.88668289961727,130.248021421492));
#95990=CARTESIAN_POINT('Ctrl Pts',(-89.8995896056279,4.87122527818231,130.112247248347));
#95991=CARTESIAN_POINT('Ctrl Pts',(-89.907354358575,4.85008443947064,129.976939526167));
#95992=CARTESIAN_POINT('Ctrl Pts',(-89.9151191115221,4.82329970608404,129.842610646009));
#95993=CARTESIAN_POINT('Ctrl Pts',(-89.9228761524071,4.79654157567223,129.708415183189));
#95994=CARTESIAN_POINT('Ctrl Pts',(-89.9306331932921,4.76415078193144,129.575197008606));
#95995=CARTESIAN_POINT('Ctrl Pts',(-89.9383902341771,4.72621836226506,129.443462732092));
#95996=CARTESIAN_POINT('Ctrl Pts',(-89.9461414254172,4.68831454773138,129.31182779742));
#95997=CARTESIAN_POINT('Ctrl Pts',(-89.9538926166574,4.64487753302853,129.181674907658));
#95998=CARTESIAN_POINT('Ctrl Pts',(-89.9616438078975,4.59604920716909,129.053499472935));
#95999=CARTESIAN_POINT('Ctrl Pts',(-89.9693917046746,4.54724163465076,128.92537851619));
#96000=CARTESIAN_POINT('Ctrl Pts',(-89.9771396014517,4.49304744738668,128.799233707439));
#96001=CARTESIAN_POINT('Ctrl Pts',(-89.9848874982287,4.43365799978234,128.675544091074));
#96002=CARTESIAN_POINT('Ctrl Pts',(-89.9926337743128,4.37428097517015,128.55188034791));
#96003=CARTESIAN_POINT('Ctrl Pts',(-90.0003800503969,4.30971102091436,128.430671127827));
#96004=CARTESIAN_POINT('Ctrl Pts',(-90.0081263264809,4.24018696917661,128.312373954495));
#96005=CARTESIAN_POINT('Ctrl Pts',(-90.0158726597463,4.17066240422801,128.19407590792));
#96006=CARTESIAN_POINT('Ctrl Pts',(-90.0236189930117,4.09618386691946,128.078690288053));
#96007=CARTESIAN_POINT('Ctrl Pts',(-90.0313653262771,4.0170351304277,127.966648189675));
#96008=CARTESIAN_POINT('Ctrl Pts',(-90.0391133942801,3.93786866912529,127.854581000245));
#96009=CARTESIAN_POINT('Ctrl Pts',(-90.046861462283,3.85403015303628,127.745859141509));
#96010=CARTESIAN_POINT('Ctrl Pts',(-90.054609530286,3.7658452406594,127.640882676138));
#96011=CARTESIAN_POINT('Ctrl Pts',(-90.0623658330278,3.67756660430836,127.53579464053));
#96012=CARTESIAN_POINT('Ctrl Pts',(-90.0701221357696,3.58493259579151,127.434460249894));
#96013=CARTESIAN_POINT('Ctrl Pts',(-90.0778784385115,3.48830791185131,127.3372449612));
#96014=CARTESIAN_POINT('Ctrl Pts',(-90.0856388810256,3.39163165640772,127.23997778578));
#96015=CARTESIAN_POINT('Ctrl Pts',(-90.0933993235398,3.29096076828217,127.146834358362));
#96016=CARTESIAN_POINT('Ctrl Pts',(-90.101159766054,3.18669424742868,127.058140811427));
#96017=CARTESIAN_POINT('Ctrl Pts',(-90.1089326663194,3.08226034869956,126.969304885737));
#96018=CARTESIAN_POINT('Ctrl Pts',(-90.1167055665849,2.9742195912059,126.884933355977));
#96019=CARTESIAN_POINT('Ctrl Pts',(-90.1244784668503,2.86300198209583,126.805310391198));
#96020=CARTESIAN_POINT('Ctrl Pts',(-90.1319688026124,2.75582741321686,126.728581921746));
#96021=CARTESIAN_POINT('Ctrl Pts',(-90.1394591383744,2.64570321327045,126.656262935709));
#96022=CARTESIAN_POINT('Ctrl Pts',(-90.1469494741364,2.53303523612335,126.588567032124));
#96023=CARTESIAN_POINT('Ctrl Pts',(-90.1547238082555,2.41609541837882,126.518304417778));
#96024=CARTESIAN_POINT('Ctrl Pts',(-90.1624981423746,2.29604469081544,126.452799803714));
#96025=CARTESIAN_POINT('Ctrl Pts',(-90.1702724764937,2.17330754910786,126.392340971249));
#96026=CARTESIAN_POINT('Ctrl Pts',(-90.1780372294408,2.0507216699581,126.331956648891));
#96027=CARTESIAN_POINT('Ctrl Pts',(-90.1858019823878,1.92545631145703,126.276605906326));
#96028=CARTESIAN_POINT('Ctrl Pts',(-90.1935667353348,1.79796381754005,126.226532620217));
#96029=CARTESIAN_POINT('Ctrl Pts',(-90.2013237762198,1.67059795096502,126.176509067601));
#96030=CARTESIAN_POINT('Ctrl Pts',(-90.2090808171048,1.54100971254757,126.131752682333));
#96031=CARTESIAN_POINT('Ctrl Pts',(-90.2168378579898,1.40967453542727,126.092460707056));
#96032=CARTESIAN_POINT('Ctrl Pts',(-90.2245890492299,1.27843839918586,126.053198362163));
#96033=CARTESIAN_POINT('Ctrl Pts',(-90.2323402404701,1.14545831945303,126.019392336755));
#96034=CARTESIAN_POINT('Ctrl Pts',(-90.2400914317102,1.01122779327843,125.991191036863));
#96035=CARTESIAN_POINT('Ctrl Pts',(-90.2478393284873,0.877054318657992,
125.963001723277));
#96036=CARTESIAN_POINT('Ctrl Pts',(-90.2555872252643,0.741631836466278,
125.940412477493));
#96037=CARTESIAN_POINT('Ctrl Pts',(-90.2633351220414,0.605466812048298,
125.923521242826));
#96038=CARTESIAN_POINT('Ctrl Pts',(-90.2710813981255,0.469330270418419,
125.906633541442));
#96039=CARTESIAN_POINT('Ctrl Pts',(-90.2788276742095,0.332451883255404,
125.895441528519));
#96040=CARTESIAN_POINT('Ctrl Pts',(-90.2865739502936,0.195345672797809,
125.889991570514));
#96041=CARTESIAN_POINT('Ctrl Pts',(-90.2943202835589,0.0582384502531272,
125.884541572279));
#96042=CARTESIAN_POINT('Ctrl Pts',(-90.3020666168243,-0.0790962082852262,
125.88483372907));
#96043=CARTESIAN_POINT('Ctrl Pts',(-90.3098129500896,-0.216142224237108,
125.890862311735));
#96044=CARTESIAN_POINT('Ctrl Pts',(-90.3175610180925,-0.353218930693866,
125.896892244459));
#96045=CARTESIAN_POINT('Ctrl Pts',(-90.3253090860955,-0.490006475426297,
125.90866114215));
#96046=CARTESIAN_POINT('Ctrl Pts',(-90.3330571540984,-0.625992248007013,
125.926111262732));
#96047=CARTESIAN_POINT('Ctrl Pts',(-90.3408134568403,-0.762122547885265,
125.943579929511));
#96048=CARTESIAN_POINT('Ctrl Pts',(-90.3485697595821,-0.897448984980592,
125.966741831039));
#96049=CARTESIAN_POINT('Ctrl Pts',(-90.356326062324,-1.03146696249758,125.995487676036));
#96050=CARTESIAN_POINT('Ctrl Pts',(-90.3640865048381,-1.16555646944436,
126.024248863557));
#96051=CARTESIAN_POINT('Ctrl Pts',(-90.3718469473523,-1.29833574694426,
126.05859983521));
#96052=CARTESIAN_POINT('Ctrl Pts',(-90.3796073898664,-1.42931474128445,
126.098381183607));
#96053=CARTESIAN_POINT('Ctrl Pts',(-90.3873802901318,-1.56050399473413,
126.138226392555));
#96054=CARTESIAN_POINT('Ctrl Pts',(-90.3951531903973,-1.68988682071423,
126.183519268983));
#96055=CARTESIAN_POINT('Ctrl Pts',(-90.4029260906627,-1.81699171038766,
126.234051636011));
#96056=CARTESIAN_POINT('Ctrl Pts',(-90.4104164264249,-1.939476017167,126.282747024215));
#96057=CARTESIAN_POINT('Ctrl Pts',(-90.4179067621871,-2.05984484830673,
126.336307454068));
#96058=CARTESIAN_POINT('Ctrl Pts',(-90.4253970979493,-2.17769912295971,
126.394506924714));
#96059=CARTESIAN_POINT('Ctrl Pts',(-90.4331721961499,-2.30003390044828,
126.454918982846));
#96060=CARTESIAN_POINT('Ctrl Pts',(-90.4409472943505,-2.4200467036457,126.520521173735));
#96061=CARTESIAN_POINT('Ctrl Pts',(-90.448722392551,-2.53726582552732,126.591111848135));
#96062=CARTESIAN_POINT('Ctrl Pts',(-90.4564877390489,-2.65433792855479,
126.661613986126));
#96063=CARTESIAN_POINT('Ctrl Pts',(-90.4642530855467,-2.76862299067614,
126.73709195787));
#96064=CARTESIAN_POINT('Ctrl Pts',(-90.4720184320446,-2.87967122861419,
126.817296951459));
#96065=CARTESIAN_POINT('Ctrl Pts',(-90.4800619597899,-2.99469759391117,
126.900375161996));
#96066=CARTESIAN_POINT('Ctrl Pts',(-90.4881054875353,-3.10625051128023,
126.988525230945));
#96067=CARTESIAN_POINT('Ctrl Pts',(-90.4961490152806,-3.21385903343552,
127.081419149358));
#96068=CARTESIAN_POINT('Ctrl Pts',(-90.5038997764408,-3.31755084385011,
127.170931934998));
#96069=CARTESIAN_POINT('Ctrl Pts',(-90.511650537601,-3.41758002234671,127.264849021001));
#96070=CARTESIAN_POINT('Ctrl Pts',(-90.5194012987613,-3.51355624691792,
127.362833985061));
#96071=CARTESIAN_POINT('Ctrl Pts',(-90.5271485806756,-3.60948938863803,
127.460774964565));
#96072=CARTESIAN_POINT('Ctrl Pts',(-90.5348958625898,-3.70137292352647,
127.562779910086));
#96073=CARTESIAN_POINT('Ctrl Pts',(-90.5426431445041,-3.78885215464494,
127.668474393108));
#96074=CARTESIAN_POINT('Ctrl Pts',(-90.5503886264776,-3.87631106154699,
127.77414431993));
#96075=CARTESIAN_POINT('Ctrl Pts',(-90.5581341084511,-3.95936745262888,
127.883501776978));
#96076=CARTESIAN_POINT('Ctrl Pts',(-90.5658795904246,-4.03770609206386,
127.996138301472));
#96077=CARTESIAN_POINT('Ctrl Pts',(-90.5736249501833,-4.11604349540499,
128.10877304869));
#96078=CARTESIAN_POINT('Ctrl Pts',(-90.581370309942,-4.1896630736576,128.224686438558));
#96079=CARTESIAN_POINT('Ctrl Pts',(-90.5891156697007,-4.25829243351487,
128.343440339871));
#96080=CARTESIAN_POINT('Ctrl Pts',(-90.596865332462,-4.32695992101522,128.462260215956));
#96081=CARTESIAN_POINT('Ctrl Pts',(-90.6046149952232,-4.39063145769388,
128.583923416421));
#96082=CARTESIAN_POINT('Ctrl Pts',(-90.6123646579845,-4.44908014600279,
128.707966351941));
#96083=CARTESIAN_POINT('Ctrl Pts',(-90.6201169107451,-4.50754836833084,
128.832050743602));
#96084=CARTESIAN_POINT('Ctrl Pts',(-90.6278691635057,-4.5607901095426,128.958516096289));
#96085=CARTESIAN_POINT('Ctrl Pts',(-90.6356214162662,-4.6086266685323,129.086878945875));
#96086=CARTESIAN_POINT('Ctrl Pts',(-90.6433808915753,-4.65650779545359,
129.215361387398));
#96087=CARTESIAN_POINT('Ctrl Pts',(-90.6511403668844,-4.69897356303453,
129.345744484816));
#96088=CARTESIAN_POINT('Ctrl Pts',(-90.6588998421936,-4.73589510125555,
129.4775295611));
#96089=CARTESIAN_POINT('Ctrl Pts',(-90.6609542607729,-4.74567054238756,
129.512421315814));
#96090=CARTESIAN_POINT('Ctrl Pts',(-90.6630086793523,-4.75505761478963,
129.547411290336));
#96091=CARTESIAN_POINT('Ctrl Pts',(-90.6650630979317,-4.76405452823406,
129.582490119308));
#96092=CARTESIAN_POINT('Ctrl Pts',(-88.9150399778173,-4.76405452823403,
129.582490119308));
#96093=CARTESIAN_POINT('Ctrl Pts',(-88.9226765403677,-4.7976634032,129.713530612715));
#96094=CARTESIAN_POINT('Ctrl Pts',(-88.9303131029181,-4.82584657930655,
129.84590081179));
#96095=CARTESIAN_POINT('Ctrl Pts',(-88.9379496654685,-4.84851894198989,
129.979104819849));
#96096=CARTESIAN_POINT('Ctrl Pts',(-88.9458148152171,-4.87186996235847,
130.116296057869));
#96097=CARTESIAN_POINT('Ctrl Pts',(-88.9536799649657,-4.889375011302,130.254371347012));
#96098=CARTESIAN_POINT('Ctrl Pts',(-88.9615451147143,-4.9009986377072,130.392783874185));
#96099=CARTESIAN_POINT('Ctrl Pts',(-88.9694102644628,-4.91262226411238,
130.531196401358));
#96100=CARTESIAN_POINT('Ctrl Pts',(-88.9772754142115,-4.91836449822501,
130.669945701738));
#96101=CARTESIAN_POINT('Ctrl Pts',(-88.9851405639601,-4.91824826917725,
130.808486782245));
#96102=CARTESIAN_POINT('',(-88.6398594360367,-4.91824997771658,130.804828795773));
#96103=CARTESIAN_POINT('Ctrl Pts',(-88.5701298338733,-4.76405452823397,
129.582490119308));
#96104=CARTESIAN_POINT('Ctrl Pts',(-88.5782041209728,-4.79949911971491,
129.720688043545));
#96105=CARTESIAN_POINT('Ctrl Pts',(-88.5862784080723,-4.8289610107534,129.860565217491));
#96106=CARTESIAN_POINT('Ctrl Pts',(-88.5943526951718,-4.85229179860094,
130.001585827397));
#96107=CARTESIAN_POINT('Ctrl Pts',(-88.6024145699402,-4.87558672080988,
130.142389651045));
#96108=CARTESIAN_POINT('Ctrl Pts',(-88.6104764447087,-4.89276927693621,
130.28433306948));
#96109=CARTESIAN_POINT('Ctrl Pts',(-88.6185383194771,-4.90374172190632,
130.426868647671));
#96110=CARTESIAN_POINT('Ctrl Pts',(-88.6256453583152,-4.91341460753055,
130.552522533289));
#96111=CARTESIAN_POINT('Ctrl Pts',(-88.6327523971533,-4.91826199021932,
130.678636265036));
#96112=CARTESIAN_POINT('Ctrl Pts',(-88.6398594359915,-4.91824997771666,
130.804828794969));
#96113=CARTESIAN_POINT('Ctrl Pts',(-88.6398594360368,-4.91824997771658,
130.804828795773));
#96114=CARTESIAN_POINT('Ctrl Pts',(-88.6480343427133,-4.91823616025208,
130.949982379278));
#96115=CARTESIAN_POINT('Ctrl Pts',(-88.6562092493898,-4.91179212857453,
131.094992640823));
#96116=CARTESIAN_POINT('Ctrl Pts',(-88.6643841560662,-4.89898148010898,
131.239289945215));
#96117=CARTESIAN_POINT('Ctrl Pts',(-88.6725720466721,-4.88615048492125,
131.383816432164));
#96118=CARTESIAN_POINT('Ctrl Pts',(-88.6807599372779,-4.86693271592382,
131.527627381295));
#96119=CARTESIAN_POINT('Ctrl Pts',(-88.6889478278838,-4.84144309063563,
131.670161901139));
#96120=CARTESIAN_POINT('Ctrl Pts',(-88.6971571696266,-4.81588668606677,
131.813069841643));
#96121=CARTESIAN_POINT('Ctrl Pts',(-88.7053665113696,-4.78402562367715,
131.95469434762));
#96122=CARTESIAN_POINT('Ctrl Pts',(-88.7135758531125,-4.74602557556677,
132.094486308561));
#96123=CARTESIAN_POINT('Ctrl Pts',(-88.7217967973305,-4.70797182100498,
132.234475841098));
#96124=CARTESIAN_POINT('Ctrl Pts',(-88.7300177415486,-4.66376185868199,
132.372627352328));
#96125=CARTESIAN_POINT('Ctrl Pts',(-88.7382386857666,-4.61361011382306,
132.508410141532));
#96126=CARTESIAN_POINT('Ctrl Pts',(-88.7464787748588,-4.56334157595128,
132.644509140693));
#96127=CARTESIAN_POINT('Ctrl Pts',(-88.754718863951,-4.50710371254321,132.778228090842));
#96128=CARTESIAN_POINT('Ctrl Pts',(-88.7629589530432,-4.44515839478008,
132.909057723521));
#96129=CARTESIAN_POINT('Ctrl Pts',(-88.7667394191062,-4.41673853560815,
132.969080980654));
#96130=CARTESIAN_POINT('Ctrl Pts',(-88.7705198851692,-4.38711794729714,
133.028496445633));
#96131=CARTESIAN_POINT('Ctrl Pts',(-88.7743003512322,-4.35632498955899,
133.087256946321));
#96132=CARTESIAN_POINT('Ctrl Pts',(-88.7820746853513,-4.29300085491992,
133.208094895332));
#96133=CARTESIAN_POINT('Ctrl Pts',(-88.7898490194703,-4.22454481273088,
133.32648747086));
#96134=CARTESIAN_POINT('Ctrl Pts',(-88.7976233535894,-4.15116970869277,
133.441968077392));
#96135=CARTESIAN_POINT('Ctrl Pts',(-88.8053881065365,-4.07788503291266,
133.557306364398));
#96136=CARTESIAN_POINT('Ctrl Pts',(-88.8131528594836,-3.99969356511958,
133.669739496114));
#96137=CARTESIAN_POINT('Ctrl Pts',(-88.8209176124307,-3.91685477330913,
133.778823888024));
#96138=CARTESIAN_POINT('Ctrl Pts',(-88.8286746533157,-3.83409825815476,
133.887799935779));
#96139=CARTESIAN_POINT('Ctrl Pts',(-88.8364316942006,-3.74670383952713,
133.993433553302));
#96140=CARTESIAN_POINT('Ctrl Pts',(-88.8441887350856,-3.65497496296968,
134.095308973673));
#96141=CARTESIAN_POINT('Ctrl Pts',(-88.8519399263257,-3.56331525987146,
134.197107568998));
#96142=CARTESIAN_POINT('Ctrl Pts',(-88.8596911175658,-3.46732786543789,
134.295153318878));
#96143=CARTESIAN_POINT('Ctrl Pts',(-88.8674423088059,-3.36735705661374,
134.389062769178));
#96144=CARTESIAN_POINT('Ctrl Pts',(-88.875190205583,-3.26742873805002,134.482932305458));
#96145=CARTESIAN_POINT('Ctrl Pts',(-88.8829381023602,-3.16352065681897,
134.57266877164));
#96146=CARTESIAN_POINT('Ctrl Pts',(-88.8906859991373,-3.05601441518644,
134.657925065797));
#96147=CARTESIAN_POINT('Ctrl Pts',(-88.8984322752214,-2.94853066154209,
134.743163526176));
#96148=CARTESIAN_POINT('Ctrl Pts',(-88.9061785513054,-2.83745055070981,
134.823923435804));
#96149=CARTESIAN_POINT('Ctrl Pts',(-88.9139248273895,-2.723188968183,134.899897811399));
#96150=CARTESIAN_POINT('Ctrl Pts',(-88.9216711606549,-2.60892654220331,
134.975872747818));
#96151=CARTESIAN_POINT('Ctrl Pts',(-88.9294174939203,-2.49148292323219,
135.04706186324));
#96152=CARTESIAN_POINT('Ctrl Pts',(-88.9371638271856,-2.37130185204952,
135.113201597338));
#96153=CARTESIAN_POINT('Ctrl Pts',(-88.9449118951886,-2.25109386714939,
135.179356142972));
#96154=CARTESIAN_POINT('Ctrl Pts',(-88.9526599631916,-2.1281475526282,135.240458868709));
#96155=CARTESIAN_POINT('Ctrl Pts',(-88.9604080311945,-2.00293074330515,
135.296292440293));
#96156=CARTESIAN_POINT('Ctrl Pts',(-88.9681643339364,-1.87758085206688,
135.35218535246));
#96157=CARTESIAN_POINT('Ctrl Pts',(-88.9759206366782,-1.74995600322717,
135.40279776416));
#96158=CARTESIAN_POINT('Ctrl Pts',(-88.9836769394201,-1.62054400233121,
135.447960535626));
#96159=CARTESIAN_POINT('Ctrl Pts',(-88.9914373819342,-1.49106293035351,
135.493147411824));
#96160=CARTESIAN_POINT('Ctrl Pts',(-88.9991978244484,-1.35979317969662,
135.532878738879));
#96161=CARTESIAN_POINT('Ctrl Pts',(-89.0069582669626,-1.22723620464085,
135.567035744059));
#96162=CARTESIAN_POINT('Ctrl Pts',(-89.014731167228,-1.09446643736122,135.601247581096));
#96163=CARTESIAN_POINT('Ctrl Pts',(-89.0225040674935,-0.960405698992884,
135.629867132839));
#96164=CARTESIAN_POINT('Ctrl Pts',(-89.0302769677589,-0.825564974306989,
135.652826925142));
#96165=CARTESIAN_POINT('Ctrl Pts',(-89.0377673035208,-0.695626049608546,
135.674952071162));
#96166=CARTESIAN_POINT('Ctrl Pts',(-89.0452576392827,-0.564963168459875,
135.691821767204));
#96167=CARTESIAN_POINT('Ctrl Pts',(-89.0527479750446,-0.434034729652507,
135.703421437351));
#96168=CARTESIAN_POINT('Ctrl Pts',(-89.0605223091637,-0.298142099291189,
135.715460912518));
#96169=CARTESIAN_POINT('Ctrl Pts',(-89.0682966432828,-0.161532909512511,
135.721860984421));
#96170=CARTESIAN_POINT('Ctrl Pts',(-89.0760709774019,-0.0247147686370575,
135.722548519905));
#96171=CARTESIAN_POINT('Ctrl Pts',(-89.083835730349,0.111934756107555,135.723235208062));
#96172=CARTESIAN_POINT('Ctrl Pts',(-89.091600483296,0.248792332366639,135.718223365735));
#96173=CARTESIAN_POINT('Ctrl Pts',(-89.0993652362431,0.385344511134806,
135.707491522431));
#96174=CARTESIAN_POINT('Ctrl Pts',(-89.1071222771281,0.521761064353973,
135.696770338144));
#96175=CARTESIAN_POINT('Ctrl Pts',(-89.1148793180131,0.657872436471643,
135.68034048913));
#96176=CARTESIAN_POINT('Ctrl Pts',(-89.1226363588981,0.793164811273817,
135.658232540542));
#96177=CARTESIAN_POINT('Ctrl Pts',(-89.1303875501382,0.928355161043546,
135.63614126373));
#96178=CARTESIAN_POINT('Ctrl Pts',(-89.1381387413784,1.06272735853112,135.608380473));
#96179=CARTESIAN_POINT('Ctrl Pts',(-89.1458899326185,1.19577270281499,135.575032551969));
#96180=CARTESIAN_POINT('Ctrl Pts',(-89.1536378293955,1.32876149927861,135.541698804695));
#96181=CARTESIAN_POINT('Ctrl Pts',(-89.1613857261727,1.46042418574826,135.502782745032));
#96182=CARTESIAN_POINT('Ctrl Pts',(-89.1691336229498,1.59026247019454,135.458417808705));
#96183=CARTESIAN_POINT('Ctrl Pts',(-89.1768798990338,1.72007359527036,135.414062152566));
#96184=CARTESIAN_POINT('Ctrl Pts',(-89.1846261751177,1.84806070766761,135.364260013196));
#96185=CARTESIAN_POINT('Ctrl Pts',(-89.1923724512018,1.97374127791077,135.309194513546));
#96186=CARTESIAN_POINT('Ctrl Pts',(-89.2001187844671,2.09942277589953,135.254128607415));
#96187=CARTESIAN_POINT('Ctrl Pts',(-89.2078651177326,2.22279733965769,135.193799420375));
#96188=CARTESIAN_POINT('Ctrl Pts',(-89.2156114509979,2.34340337568982,135.128437823318));
#96189=CARTESIAN_POINT('Ctrl Pts',(-89.2233595190009,2.46403642060733,135.063061588985));
#96190=CARTESIAN_POINT('Ctrl Pts',(-89.2311075870038,2.58189936041836,134.992650888336));
#96191=CARTESIAN_POINT('Ctrl Pts',(-89.2388556550067,2.69655646951008,134.91748184958));
#96192=CARTESIAN_POINT('Ctrl Pts',(-89.2466119577486,2.81133543754193,134.842232920275));
#96193=CARTESIAN_POINT('Ctrl Pts',(-89.2543682604904,2.92290144113071,134.762215765223));
#96194=CARTESIAN_POINT('Ctrl Pts',(-89.2621245632322,3.03084850738987,134.677749364871));
#96195=CARTESIAN_POINT('Ctrl Pts',(-89.2698850057464,3.13885318824882,134.593237882258));
#96196=CARTESIAN_POINT('Ctrl Pts',(-89.2776454482605,3.24323478562238,134.504272676044));
#96197=CARTESIAN_POINT('Ctrl Pts',(-89.2854058907747,3.34362232435879,134.411211434352));
#96198=CARTESIAN_POINT('Ctrl Pts',(-89.2931787910401,3.4441710140841,134.318000802494));
#96199=CARTESIAN_POINT('Ctrl Pts',(-89.3009516913055,3.54071255721653,134.220681273296));
#96200=CARTESIAN_POINT('Ctrl Pts',(-89.3087245915709,3.63291398609695,134.119646281294));
#96201=CARTESIAN_POINT('Ctrl Pts',(-89.3162149273331,3.72176366079819,134.022284165741));
#96202=CARTESIAN_POINT('Ctrl Pts',(-89.3237052630953,3.80658309273496,133.921472266038));
#96203=CARTESIAN_POINT('Ctrl Pts',(-89.3311955988575,3.88711224303279,133.817588367432));
#96204=CARTESIAN_POINT('Ctrl Pts',(-89.3389699329766,3.9706946805387,133.709765679238));
#96205=CARTESIAN_POINT('Ctrl Pts',(-89.3467442670956,4.04991984623069,133.598291894098));
#96206=CARTESIAN_POINT('Ctrl Pts',(-89.3545186012147,4.12445183641704,133.483554547011));
#96207=CARTESIAN_POINT('Ctrl Pts',(-89.3622833541618,4.1988919725866,133.36895860345));
#96208=CARTESIAN_POINT('Ctrl Pts',(-89.3700481071089,4.2686502305942,133.251107425337));
#96209=CARTESIAN_POINT('Ctrl Pts',(-89.377812860056,4.33343101497726,133.130421386534));
#96210=CARTESIAN_POINT('Ctrl Pts',(-89.385569900941,4.39814745817201,133.009855214807));
#96211=CARTESIAN_POINT('Ctrl Pts',(-89.393326941826,4.45789608221385,132.886460127857));
#96212=CARTESIAN_POINT('Ctrl Pts',(-89.401083982711,4.51242487221753,132.760684935028));
#96213=CARTESIAN_POINT('Ctrl Pts',(-89.4088351739511,4.56691254163658,132.63500459025));
#96214=CARTESIAN_POINT('Ctrl Pts',(-89.4165863651913,4.61618805713429,132.5069480694));
#96215=CARTESIAN_POINT('Ctrl Pts',(-89.4243375564314,4.66004576510778,132.376987887329));
#96216=CARTESIAN_POINT('Ctrl Pts',(-89.4320854532085,4.70388483238538,132.247082941801));
#96217=CARTESIAN_POINT('Ctrl Pts',(-89.4398333499855,4.74231054730809,132.115276313968));
#96218=CARTESIAN_POINT('Ctrl Pts',(-89.4475812467626,4.77516583411507,131.982059356293));
#96219=CARTESIAN_POINT('Ctrl Pts',(-89.4553275228466,4.80801424830433,131.848870264734));
#96220=CARTESIAN_POINT('Ctrl Pts',(-89.4630737989308,4.83529445849214,131.714271809476));
#96221=CARTESIAN_POINT('Ctrl Pts',(-89.4708200750149,4.85689971223601,131.578768938661));
#96222=CARTESIAN_POINT('Ctrl Pts',(-89.4785664082802,4.87850512546497,131.443265067595));
#96223=CARTESIAN_POINT('Ctrl Pts',(-89.4863127415455,4.8944354370992,131.306857153738));
#96224=CARTESIAN_POINT('Ctrl Pts',(-89.4940590748109,4.90463538279991,131.170058340128));
#96225=CARTESIAN_POINT('Ctrl Pts',(-89.5018071428139,4.91483761270772,131.033228891373));
#96226=CARTESIAN_POINT('Ctrl Pts',(-89.5095552108169,4.91930689404716,130.89600875848));
#96227=CARTESIAN_POINT('Ctrl Pts',(-89.5173032788199,4.9180400209636,130.758913783789));
#96228=CARTESIAN_POINT('Ctrl Pts',(-89.5250595815617,4.91677180143226,130.621673102928));
#96229=CARTESIAN_POINT('Ctrl Pts',(-89.5328158843034,4.90975525277446,130.484558237562));
#96230=CARTESIAN_POINT('Ctrl Pts',(-89.5405721870453,4.89703930401219,130.348083160902));
#96231=CARTESIAN_POINT('Ctrl Pts',(-89.5483326295595,4.88431656836516,130.211535243384));
#96232=CARTESIAN_POINT('Ctrl Pts',(-89.5560930720736,4.86588842379378,130.075628182218));
#96233=CARTESIAN_POINT('Ctrl Pts',(-89.5638535145878,4.84185528231614,129.940867428475));
#96234=CARTESIAN_POINT('Ctrl Pts',(-89.5716264148532,4.81778356070624,129.805890344806));
#96235=CARTESIAN_POINT('Ctrl Pts',(-89.5793993151186,4.7880889467807,129.672063627676));
#96236=CARTESIAN_POINT('Ctrl Pts',(-89.5871722153841,4.75292247100479,129.539880073185));
#96237=CARTESIAN_POINT('Ctrl Pts',(-89.5946625511461,4.71903438520224,129.41250172385));
#96238=CARTESIAN_POINT('Ctrl Pts',(-89.6021528869083,4.68006545363289,129.286649439295));
#96239=CARTESIAN_POINT('Ctrl Pts',(-89.6096432226703,4.6361929603614,129.162746199746));
#96240=CARTESIAN_POINT('Ctrl Pts',(-89.6174175567894,4.59065702817282,129.034145131209));
#96241=CARTESIAN_POINT('Ctrl Pts',(-89.6251918909085,4.53969411287146,128.907236451772));
#96242=CARTESIAN_POINT('Ctrl Pts',(-89.6329662250276,4.48344869447733,128.782512238857));
#96243=CARTESIAN_POINT('Ctrl Pts',(-89.6407309779746,4.42727259353472,128.657941737387));
#96244=CARTESIAN_POINT('Ctrl Pts',(-89.6484957309217,4.36582710206212,128.535550698823));
#96245=CARTESIAN_POINT('Ctrl Pts',(-89.6562604838688,4.2993061159292,128.415815038341));
#96246=CARTESIAN_POINT('Ctrl Pts',(-89.6640175247538,4.2328511993775,128.296198301006));
#96247=CARTESIAN_POINT('Ctrl Pts',(-89.6717745656389,4.16133100873153,128.179232032841));
#96248=CARTESIAN_POINT('Ctrl Pts',(-89.6795316065239,4.08498691980275,128.065370853522));
#96249=CARTESIAN_POINT('Ctrl Pts',(-89.687282797764,4.00870040254521,127.951595537803));
#96250=CARTESIAN_POINT('Ctrl Pts',(-89.6950339890041,3.92759744455299,127.840920973586));
#96251=CARTESIAN_POINT('Ctrl Pts',(-89.7027851802443,3.84196442515621,127.733775588889));
#96252=CARTESIAN_POINT('Ctrl Pts',(-89.7105330770214,3.75636780207689,127.626675743839));
#96253=CARTESIAN_POINT('Ctrl Pts',(-89.7182809737985,3.66624519063893,127.523102399702));
#96254=CARTESIAN_POINT('Ctrl Pts',(-89.7260288705756,3.57192507630068,127.423453296773));
#96255=CARTESIAN_POINT('Ctrl Pts',(-89.7337751466597,3.47762469169703,127.323825038287));
#96256=CARTESIAN_POINT('Ctrl Pts',(-89.7415214227438,3.37912881922449,127.228119672023));
#96257=CARTESIAN_POINT('Ctrl Pts',(-89.7492676988279,3.27680458375309,127.136699948639));
#96258=CARTESIAN_POINT('Ctrl Pts',(-89.7570140320933,3.17447959294757,127.045279550415));
#96259=CARTESIAN_POINT('Ctrl Pts',(-89.7647603653587,3.06832647430463,126.958145118679));
#96260=CARTESIAN_POINT('Ctrl Pts',(-89.772506698624,2.95874707786966,126.875620515231));
#96261=CARTESIAN_POINT('Ctrl Pts',(-89.780254766627,2.84914314188848,126.79307743097));
#96262=CARTESIAN_POINT('Ctrl Pts',(-89.7880028346301,2.73611171354127,126.715146464385));
#96263=CARTESIAN_POINT('Ctrl Pts',(-89.7957509026331,2.62008505275539,126.642109138039));
#96264=CARTESIAN_POINT('Ctrl Pts',(-89.803507205375,2.50393507745386,126.568994186753));
#96265=CARTESIAN_POINT('Ctrl Pts',(-89.8112635081168,2.38478384198821,126.50078347391));
#96266=CARTESIAN_POINT('Ctrl Pts',(-89.8190198108586,2.26309021390805,126.437713649214));
#96267=CARTESIAN_POINT('Ctrl Pts',(-89.8267802533728,2.14133163427447,126.374610162254));
#96268=CARTESIAN_POINT('Ctrl Pts',(-89.834540695887,2.01702831235432,126.31665319592));
#96269=CARTESIAN_POINT('Ctrl Pts',(-89.8423011384012,1.89065977359634,126.264031479386));
#96270=CARTESIAN_POINT('Ctrl Pts',(-89.8500740386666,1.76408837684147,126.211325289802));
#96271=CARTESIAN_POINT('Ctrl Pts',(-89.8578469389321,1.63544550539274,126.163971599985));
#96272=CARTESIAN_POINT('Ctrl Pts',(-89.8656198391975,1.50522739822047,126.122109712056));
#96273=CARTESIAN_POINT('Ctrl Pts',(-89.8731101749595,1.37974304724494,126.081769609198));
#96274=CARTESIAN_POINT('Ctrl Pts',(-89.8806005107214,1.25279629654676,126.046529041071));
#96275=CARTESIAN_POINT('Ctrl Pts',(-89.8880908464834,1.12483883773506,126.016467484713));
#96276=CARTESIAN_POINT('Ctrl Pts',(-89.8958651806025,0.992029832979374,
125.985266135308));
#96277=CARTESIAN_POINT('Ctrl Pts',(-89.9036395147215,0.85771126616984,125.959545438143));
#96278=CARTESIAN_POINT('Ctrl Pts',(-89.9114138488406,0.722375230958079,
125.939449817952));
#96279=CARTESIAN_POINT('Ctrl Pts',(-89.9191786017877,0.587205985314387,
125.919378963817));
#96280=CARTESIAN_POINT('Ctrl Pts',(-89.9269433547348,0.451022149245679,
125.904919450109));
#96281=CARTESIAN_POINT('Ctrl Pts',(-89.9347081076819,0.314328929122017,
125.896165390518));
#96282=CARTESIAN_POINT('Ctrl Pts',(-89.9424651485669,0.177771474631618,
125.887420025583));
#96283=CARTESIAN_POINT('Ctrl Pts',(-89.9502221894519,0.0407060305458466,
125.884368862527));
#96284=CARTESIAN_POINT('Ctrl Pts',(-89.9579792303369,-0.0963544492060208,
125.887054558084));
#96285=CARTESIAN_POINT('Ctrl Pts',(-89.965730421577,-0.233311570584119,
125.889738228337));
#96286=CARTESIAN_POINT('Ctrl Pts',(-89.9734816128173,-0.370263345771275,
125.898150138515));
#96287=CARTESIAN_POINT('Ctrl Pts',(-89.9812328040574,-0.506694531118351,
125.912280925387));
#96288=CARTESIAN_POINT('Ctrl Pts',(-89.9889807008345,-0.643067729572047,
125.926405706297));
#96289=CARTESIAN_POINT('Ctrl Pts',(-89.9967285976115,-0.778920390193332,
125.946244489279));
#96290=CARTESIAN_POINT('Ctrl Pts',(-90.0044764943886,-0.913740328393507,
125.971735898558));
#96291=CARTESIAN_POINT('Ctrl Pts',(-90.0122227704727,-1.04853206516899,
125.997221975584));
#96292=CARTESIAN_POINT('Ctrl Pts',(-90.0199690465567,-1.18229112529025,
126.028358254444));
#96293=CARTESIAN_POINT('Ctrl Pts',(-90.0277153226408,-1.31451387639524,
126.065031938179));
#96294=CARTESIAN_POINT('Ctrl Pts',(-90.0354616559061,-1.44673760353836,
126.10170589263));
#96295=CARTESIAN_POINT('Ctrl Pts',(-90.0432079891715,-1.57742462229343,
126.143917229027));
#96296=CARTESIAN_POINT('Ctrl Pts',(-90.0509543224368,-1.70608524879114,
126.191502914758));
#96297=CARTESIAN_POINT('Ctrl Pts',(-90.0587023904398,-1.83477468794392,
126.239099256973));
#96298=CARTESIAN_POINT('Ctrl Pts',(-90.0664504584427,-1.9614364652183,126.292072207849));
#96299=CARTESIAN_POINT('Ctrl Pts',(-90.0741985264457,-2.08560008066112,
126.350210264688));
#96300=CARTESIAN_POINT('Ctrl Pts',(-90.0819548291875,-2.2098956586725,126.408410111345));
#96301=CARTESIAN_POINT('Ctrl Pts',(-90.0897111319294,-2.33168741641451,
126.47178586385));
#96302=CARTESIAN_POINT('Ctrl Pts',(-90.0974674346713,-2.45052822467107,
126.540079378882));
#96303=CARTESIAN_POINT('Ctrl Pts',(-90.1052278771855,-2.56943246184523,
126.60840934422));
#96304=CARTESIAN_POINT('Ctrl Pts',(-90.1129883196996,-2.68538228082437,
126.681662093423));
#96305=CARTESIAN_POINT('Ctrl Pts',(-90.1207487622138,-2.7979597031904,126.75953620088));
#96306=CARTESIAN_POINT('Ctrl Pts',(-90.1285216624792,-2.91071784482865,
126.837535318767));
#96307=CARTESIAN_POINT('Ctrl Pts',(-90.1362945627447,-3.0200924594925,126.920170383848));
#96308=CARTESIAN_POINT('Ctrl Pts',(-90.1440674630101,-3.12569811907768,
127.007099192421));
#96309=CARTESIAN_POINT('Ctrl Pts',(-90.1515577987722,-3.22746474693347,
127.090867919843));
#96310=CARTESIAN_POINT('Ctrl Pts',(-90.1590481345343,-3.32573145456485,
127.178623428655));
#96311=CARTESIAN_POINT('Ctrl Pts',(-90.1665384702964,-3.42018722534059,
127.270028657193));
#96312=CARTESIAN_POINT('Ctrl Pts',(-90.1741987121588,-3.51678557185298,
127.363507264871));
#96313=CARTESIAN_POINT('Ctrl Pts',(-90.1818589540213,-3.60972311669065,
127.46111811559));
#96314=CARTESIAN_POINT('Ctrl Pts',(-90.1895191958837,-3.69861766985977,
127.562538538133));
#96315=CARTESIAN_POINT('Ctrl Pts',(-90.1971705196152,-3.7874087310932,127.663840885997));
#96316=CARTESIAN_POINT('Ctrl Pts',(-90.2048218433467,-3.87216589474051,
127.768943689028));
#96317=CARTESIAN_POINT('Ctrl Pts',(-90.2124731670783,-3.9525416122317,127.87748551499));
#96318=CARTESIAN_POINT('Ctrl Pts',(-90.2201173554329,-4.03284237392931,
127.985926118358));
#96319=CARTESIAN_POINT('Ctrl Pts',(-90.2277615437875,-4.10876957591086,
128.097799045613));
#96320=CARTESIAN_POINT('Ctrl Pts',(-90.2354057321421,-4.18001437723478,
128.212708081324));
#96321=CARTESIAN_POINT('Ctrl Pts',(-90.2430443833342,-4.25120757150529,
128.327533881253));
#96322=CARTESIAN_POINT('Ctrl Pts',(-90.2506830345264,-4.31772490130267,
128.445391072843));
#96323=CARTESIAN_POINT('Ctrl Pts',(-90.2583216857185,-4.37929984730207,
128.565853099169));
#96324=CARTESIAN_POINT('Ctrl Pts',(-90.2659570433207,-4.44084824376795,
128.686263185367));
#96325=CARTESIAN_POINT('Ctrl Pts',(-90.273592400923,-4.49745831256911,128.809275513571));
#96326=CARTESIAN_POINT('Ctrl Pts',(-90.2812277585251,-4.5489088876211,128.934437893328));
#96327=CARTESIAN_POINT('Ctrl Pts',(-90.2888628943485,-4.60035796822437,
129.059596637581));
#96328=CARTESIAN_POINT('Ctrl Pts',(-90.2964980301717,-4.64664769166659,
129.186904939655));
#96329=CARTESIAN_POINT('Ctrl Pts',(-90.304133165995,-4.68760469495257,129.315889829691));
#96330=CARTESIAN_POINT('Ctrl Pts',(-90.3093502966369,-4.71559084238847,
129.404025920222));
#96331=CARTESIAN_POINT('Ctrl Pts',(-90.3145674272788,-4.74108810602048,
129.492944387662));
#96332=CARTESIAN_POINT('Ctrl Pts',(-90.3197845579208,-4.76405452823393,
129.582490119308));
#96333=CARTESIAN_POINT('Origin',(213.235140564004,0.,130.804360617566));
#96334=CARTESIAN_POINT('',(-92.4154045049002,-4.764054528234,129.582490119308));
#96335=CARTESIAN_POINT('',(-92.069771887517,-4.76405452823417,129.582490119309));
#96336=CARTESIAN_POINT('',(213.235140564004,-4.76405452823405,129.582490119308));
#96337=CARTESIAN_POINT('',(-90.7351405640466,-4.91824902519036,130.801264052685));
#96338=CARTESIAN_POINT('Ctrl Pts',(-90.7351405640468,-4.91824902519036,
130.801264052685));
#96339=CARTESIAN_POINT('Ctrl Pts',(-90.7428057530588,-4.91833386882775,
130.93602051764));
#96340=CARTESIAN_POINT('Ctrl Pts',(-90.7504709420708,-4.9128761986244,131.070997929296));
#96341=CARTESIAN_POINT('Ctrl Pts',(-90.7581361310829,-4.90184799165934,
131.205695053125));
#96342=CARTESIAN_POINT('Ctrl Pts',(-90.7657929371722,-4.89083184553285,
131.340244867398));
#96343=CARTESIAN_POINT('Ctrl Pts',(-90.7734497432615,-4.87425731142311,
131.474514605884));
#96344=CARTESIAN_POINT('Ctrl Pts',(-90.7811065493508,-4.85214837645269,
131.608001828174));
#96345=CARTESIAN_POINT('Ctrl Pts',(-90.7887569299817,-4.8300579949156,131.741377030311));
#96346=CARTESIAN_POINT('Ctrl Pts',(-90.7964073106126,-4.80244251677769,
131.873970627672));
#96347=CARTESIAN_POINT('Ctrl Pts',(-90.8040576912435,-4.76937780208517,
132.005284613278));
#96348=CARTESIAN_POINT('Ctrl Pts',(-90.8117040952299,-4.73633027433065,
132.136530342274));
#96349=CARTESIAN_POINT('Ctrl Pts',(-90.8193504992163,-4.69783924039402,
132.266497393015));
#96350=CARTESIAN_POINT('Ctrl Pts',(-90.8269969032026,-4.65403170005497,
132.394697687933));
#96351=CARTESIAN_POINT('Ctrl Pts',(-90.8346413310321,-4.61023548145241,
132.522864850428));
#96352=CARTESIAN_POINT('Ctrl Pts',(-90.8422857588617,-4.56112561799244,
132.649265784427));
#96353=CARTESIAN_POINT('Ctrl Pts',(-90.8499301866912,-4.50687890279669,
132.773427812465));
#96354=CARTESIAN_POINT('Ctrl Pts',(-90.8575743981105,-4.45263372330044,
132.897586325533));
#96355=CARTESIAN_POINT('Ctrl Pts',(-90.8652186095297,-4.39325214244064,
133.019505690027));
#96356=CARTESIAN_POINT('Ctrl Pts',(-90.872862820949,-4.32895878409133,133.138733961343));
#96357=CARTESIAN_POINT('Ctrl Pts',(-90.8805085753086,-4.26465244849602,
133.257986298203));
#96358=CARTESIAN_POINT('Ctrl Pts',(-90.8881543296682,-4.19543255524392,
133.374546107872));
#96359=CARTESIAN_POINT('Ctrl Pts',(-90.8958000840277,-4.12156901147522,
133.487987258168));
#96360=CARTESIAN_POINT('Ctrl Pts',(-90.9034536646853,-4.0476298599804,133.601544528365));
#96361=CARTESIAN_POINT('Ctrl Pts',(-90.9111072453428,-3.96903778608739,
133.711976427007));
#96362=CARTESIAN_POINT('Ctrl Pts',(-90.9187608260003,-3.88610544629988,
133.818886703494));
#96363=CARTESIAN_POINT('Ctrl Pts',(-90.9264185292908,-3.80312843466327,
133.925854567645));
#96364=CARTESIAN_POINT('Ctrl Pts',(-90.9340762325813,-3.71580676153998,
134.029296725865));
#96365=CARTESIAN_POINT('Ctrl Pts',(-90.9417339358718,-3.62449161161779,
134.128852100457));
#96366=CARTESIAN_POINT('Ctrl Pts',(-90.9494033679423,-3.53303660053156,
134.228559957201));
#96367=CARTESIAN_POINT('Ctrl Pts',(-90.9570728000127,-3.43757618066661,
134.324368856597));
#96368=CARTESIAN_POINT('Ctrl Pts',(-90.9647422320831,-3.33849684065856,
134.415956097048));
#96369=CARTESIAN_POINT('Ctrl Pts',(-90.9705922699137,-3.26292176782947,
134.485816396549));
#96370=CARTESIAN_POINT('Ctrl Pts',(-90.9764423077442,-3.18524185082494,
134.553221231407));
#96371=CARTESIAN_POINT('Ctrl Pts',(-90.9822923455748,-3.10563999061448,
134.618044310689));
#96372=CARTESIAN_POINT('Ctrl Pts',(-90.990066679694,-2.99985410072831,134.704190125736));
#96373=CARTESIAN_POINT('Ctrl Pts',(-90.9978410138131,-2.89031360281266,
134.786067540014));
#96374=CARTESIAN_POINT('Ctrl Pts',(-91.0056153479322,-2.77739785950375,
134.863331446794));
#96375=CARTESIAN_POINT('Ctrl Pts',(-91.0133801008793,-2.66462127475689,
134.940500132714));
#96376=CARTESIAN_POINT('Ctrl Pts',(-91.0211448538265,-2.5484780407179,135.01306640539));
#96377=CARTESIAN_POINT('Ctrl Pts',(-91.0289096067736,-2.4293813167176,135.080724666672));
#96378=CARTESIAN_POINT('Ctrl Pts',(-91.0366666476586,-2.31040288126287,
135.148315728814));
#96379=CARTESIAN_POINT('Ctrl Pts',(-91.0444236885437,-2.18847713128068,
135.211008288578));
#96380=CARTESIAN_POINT('Ctrl Pts',(-91.0521807294287,-2.06404669920747,
135.268539633465));
#96381=CARTESIAN_POINT('Ctrl Pts',(-91.0599319206688,-1.93971010109084,
135.326027593517));
#96382=CARTESIAN_POINT('Ctrl Pts',(-91.0676831119089,-1.8128729338595,135.378361922294));
#96383=CARTESIAN_POINT('Ctrl Pts',(-91.0754343031491,-1.68400264117168,
135.425325686361));
#96384=CARTESIAN_POINT('Ctrl Pts',(-91.0831821999262,-1.55518712179581,
135.472269489576));
#96385=CARTESIAN_POINT('Ctrl Pts',(-91.0909300967033,-1.42434056222138,
135.51384713448));
#96386=CARTESIAN_POINT('Ctrl Pts',(-91.0986779934804,-1.29195040402995,
135.549889799441));
#96387=CARTESIAN_POINT('Ctrl Pts',(-91.1064242695645,-1.15958793900563,
135.585924925053));
#96388=CARTESIAN_POINT('Ctrl Pts',(-91.1141705456486,-1.0256828946015,135.616427271012));
#96389=CARTESIAN_POINT('Ctrl Pts',(-91.1219168217328,-0.890737511782772,
135.641277998254));
#96390=CARTESIAN_POINT('Ctrl Pts',(-91.1296631549981,-0.755791132827696,
135.666128908938));
#96391=CARTESIAN_POINT('Ctrl Pts',(-91.1374094882635,-0.61980478463389,
135.685328046851));
#96392=CARTESIAN_POINT('Ctrl Pts',(-91.1451558215289,-0.483290136274591,
135.69880784955));
#96393=CARTESIAN_POINT('Ctrl Pts',(-91.1529038895319,-0.346744916406505,
135.712290670958));
#96394=CARTESIAN_POINT('Ctrl Pts',(-91.1606519575349,-0.209671549949994,
135.720051570087));
#96395=CARTESIAN_POINT('Ctrl Pts',(-91.1684000255379,-0.0725856537635758,
135.722074963212));
#96396=CARTESIAN_POINT('Ctrl Pts',(-91.1761563282797,0.0646459389448387,
135.724100506823));
#96397=CARTESIAN_POINT('Ctrl Pts',(-91.1839126310217,0.201889696438832,
135.720376357459));
#96398=CARTESIAN_POINT('Ctrl Pts',(-91.1916689337636,0.338630619358337,
135.710939096112));
#96399=CARTESIAN_POINT('Ctrl Pts',(-91.1994293762778,0.475444525025594,
135.701496797815));
#96400=CARTESIAN_POINT('Ctrl Pts',(-91.2071898187919,0.611754672973703,
135.686335354825));
#96401=CARTESIAN_POINT('Ctrl Pts',(-91.2149502613061,0.747053348078596,
135.665543020812));
#96402=CARTESIAN_POINT('Ctrl Pts',(-91.2227231615715,0.882569216628018,
135.644717309098));
#96403=CARTESIAN_POINT('Ctrl Pts',(-91.230496061837,1.0170699838269,135.618242718698));
#96404=CARTESIAN_POINT('Ctrl Pts',(-91.2382689621025,1.15005937117471,135.586258410835));
#96405=CARTESIAN_POINT('Ctrl Pts',(-91.2457592978643,1.27821425930877,135.555436813128));
#96406=CARTESIAN_POINT('Ctrl Pts',(-91.2532496336261,1.40496544841964,135.519499211466));
#96407=CARTESIAN_POINT('Ctrl Pts',(-91.260739969388,1.52988582576255,135.4786126885));
#96408=CARTESIAN_POINT('Ctrl Pts',(-91.2685143035071,1.65954259718496,135.436175940588));
#96409=CARTESIAN_POINT('Ctrl Pts',(-91.2762886376263,1.78763769950532,135.388273159727));
#96410=CARTESIAN_POINT('Ctrl Pts',(-91.2840629717454,1.91367572988546,135.335036975832));
#96411=CARTESIAN_POINT('Ctrl Pts',(-91.2918277246925,2.03955842965785,135.281866400775));
#96412=CARTESIAN_POINT('Ctrl Pts',(-91.2995924776396,2.16338874499898,135.223375651541));
#96413=CARTESIAN_POINT('Ctrl Pts',(-91.3073572305868,2.28468624481829,135.159747147512));
#96414=CARTESIAN_POINT('Ctrl Pts',(-91.3151142714718,2.40586327025045,135.096181840211));
#96415=CARTESIAN_POINT('Ctrl Pts',(-91.3228713123569,2.52451214239294,135.027489113537));
#96416=CARTESIAN_POINT('Ctrl Pts',(-91.3306283532419,2.64017258013704,134.953899364173));
#96417=CARTESIAN_POINT('Ctrl Pts',(-91.3383795444821,2.75574579744518,134.880365109412));
#96418=CARTESIAN_POINT('Ctrl Pts',(-91.3461307357222,2.86833473748875,134.801941391445));
#96419=CARTESIAN_POINT('Ctrl Pts',(-91.3538819269624,2.97750422331127,134.718904226042));
#96420=CARTESIAN_POINT('Ctrl Pts',(-91.3616298237395,3.08662730919027,134.63590235365));
#96421=CARTESIAN_POINT('Ctrl Pts',(-91.3693777205167,3.19233352094263,134.548291169973));
#96422=CARTESIAN_POINT('Ctrl Pts',(-91.3771256172938,3.29421735006745,134.456389521205));
#96423=CARTESIAN_POINT('Ctrl Pts',(-91.3848718933779,3.39607986729158,134.36450709628));
#96424=CARTESIAN_POINT('Ctrl Pts',(-91.392618169462,3.49412130213105,134.268336253087));
#96425=CARTESIAN_POINT('Ctrl Pts',(-91.4003644455462,3.58797019840641,134.168235305756));
#96426=CARTESIAN_POINT('Ctrl Pts',(-91.4081107788116,3.68181978745312,134.068133619503));
#96427=CARTESIAN_POINT('Ctrl Pts',(-91.4158571120769,3.77147650877684,133.964102056441));
#96428=CARTESIAN_POINT('Ctrl Pts',(-91.4236034453423,3.85660695054932,133.856534579101));
#96429=CARTESIAN_POINT('Ctrl Pts',(-91.4313515133453,3.94175645669388,133.748943012772));
#96430=CARTESIAN_POINT('Ctrl Pts',(-91.4390995813483,4.02237742370374,133.637814263001));
#96431=CARTESIAN_POINT('Ctrl Pts',(-91.4468476493513,4.09817803704285,133.523573709473));
#96432=CARTESIAN_POINT('Ctrl Pts',(-91.4546039520932,4.17405921217595,133.409211739725));
#96433=CARTESIAN_POINT('Ctrl Pts',(-91.4623602548352,4.24510958313337,133.291731685901));
#96434=CARTESIAN_POINT('Ctrl Pts',(-91.4701165575771,4.31108155680585,133.171586604469));
#96435=CARTESIAN_POINT('Ctrl Pts',(-91.4778770000913,4.37708874170706,133.051377397989));
#96436=CARTESIAN_POINT('Ctrl Pts',(-91.4856374426056,4.43801195485126,132.928500679741));
#96437=CARTESIAN_POINT('Ctrl Pts',(-91.4933978851198,4.49365101412424,132.803431308102));
#96438=CARTESIAN_POINT('Ctrl Pts',(-91.5011707853853,4.54937939015457,132.678161164005));
#96439=CARTESIAN_POINT('Ctrl Pts',(-91.5089436856507,4.59980651748605,132.550691696511));
#96440=CARTESIAN_POINT('Ctrl Pts',(-91.5167165859162,4.64478122574641,132.42151565882));
#96441=CARTESIAN_POINT('Ctrl Pts',(-91.5242069216778,4.68812099007425,132.297035495482));
#96442=CARTESIAN_POINT('Ctrl Pts',(-91.5316972574393,4.72639778177273,132.170970978784));
#96443=CARTESIAN_POINT('Ctrl Pts',(-91.5391875932009,4.75952130733774,132.043771763029));
#96444=CARTESIAN_POINT('Ctrl Pts',(-91.54696192732,4.79390072144421,131.91174975034));
#96445=CARTESIAN_POINT('Ctrl Pts',(-91.5547362614391,4.8228372869302,131.778087089771));
#96446=CARTESIAN_POINT('Ctrl Pts',(-91.5625105955582,4.84617481176206,131.643272267469));
#96447=CARTESIAN_POINT('Ctrl Pts',(-91.5702753485052,4.86948357518022,131.508623592387));
#96448=CARTESIAN_POINT('Ctrl Pts',(-91.5780401014523,4.88720696147164,131.372825962359));
#96449=CARTESIAN_POINT('Ctrl Pts',(-91.5858048543994,4.89923876048785,131.236382179798));
#96450=CARTESIAN_POINT('Ctrl Pts',(-91.5935618952843,4.91125860935166,131.100073915126));
#96451=CARTESIAN_POINT('Ctrl Pts',(-91.6013189361692,4.91759808647479,130.963121162003));
#96452=CARTESIAN_POINT('Ctrl Pts',(-91.6090759770542,4.91820223792918,130.826035702995));
#96453=CARTESIAN_POINT('Ctrl Pts',(-91.6168271682943,4.91880593378827,130.689053621199));
#96454=CARTESIAN_POINT('Ctrl Pts',(-91.6245783595346,4.91368291101969,130.55193942209));
#96455=CARTESIAN_POINT('Ctrl Pts',(-91.6323295507746,4.90283016573214,130.415208425632));
#96456=CARTESIAN_POINT('Ctrl Pts',(-91.6400774475517,4.89198203315083,130.278535543495));
#96457=CARTESIAN_POINT('Ctrl Pts',(-91.6478253443288,4.87540905251657,130.142245928994));
#96458=CARTESIAN_POINT('Ctrl Pts',(-91.6555732411058,4.85316029091126,130.00685309207));
#96459=CARTESIAN_POINT('Ctrl Pts',(-91.6633195171899,4.83091618326719,129.871488576409));
#96460=CARTESIAN_POINT('Ctrl Pts',(-91.6710657932739,4.80299871951531,129.737020850752));
#96461=CARTESIAN_POINT('Ctrl Pts',(-91.678812069358,4.76950857834417,129.603956109243));
#96462=CARTESIAN_POINT('Ctrl Pts',(-91.6865584026234,4.73601818995646,129.470890385481));
#96463=CARTESIAN_POINT('Ctrl Pts',(-91.6943047358886,4.69695513748856,129.339228045675));
#96464=CARTESIAN_POINT('Ctrl Pts',(-91.702051069154,4.65247065553931,129.209462545009));
#96465=CARTESIAN_POINT('Ctrl Pts',(-91.7097991371569,4.60797621159882,129.07966798426));
#96466=CARTESIAN_POINT('Ctrl Pts',(-91.71754720516,4.55805804903395,128.951771477689));
#96467=CARTESIAN_POINT('Ctrl Pts',(-91.7252952731629,4.50291631893379,128.82624846524));
#96468=CARTESIAN_POINT('Ctrl Pts',(-91.7330515759048,4.4477159835466,128.700592045439));
#96469=CARTESIAN_POINT('Ctrl Pts',(-91.7408078786465,4.38728114806209,128.577314517401));
#96470=CARTESIAN_POINT('Ctrl Pts',(-91.7485641813884,4.32185915159361,128.456869076306));
#96471=CARTESIAN_POINT('Ctrl Pts',(-91.7563246239026,4.25640223743562,128.336359349853));
#96472=CARTESIAN_POINT('Ctrl Pts',(-91.7640850664167,4.18595305916165,128.218685057556));
#96473=CARTESIAN_POINT('Ctrl Pts',(-91.7718455089309,4.11080292525089,128.104271290849));
#96474=CARTESIAN_POINT('Ctrl Pts',(-91.7796184091963,4.03553215367387,127.989673857008));
#96475=CARTESIAN_POINT('Ctrl Pts',(-91.7873913094617,3.95554557462359,127.878347725819));
#96476=CARTESIAN_POINT('Ctrl Pts',(-91.7951642097271,3.8711760440431,127.770686426337));
#96477=CARTESIAN_POINT('Ctrl Pts',(-91.8026545454893,3.78987355841094,127.666938886272));
#96478=CARTESIAN_POINT('Ctrl Pts',(-91.8101448812516,3.70450145104887,127.56659458678));
#96479=CARTESIAN_POINT('Ctrl Pts',(-91.8176352170138,3.61538922301267,127.469972543477));
#96480=CARTESIAN_POINT('Ctrl Pts',(-91.8254095511329,3.52289827776763,127.369687046038));
#96481=CARTESIAN_POINT('Ctrl Pts',(-91.833183885252,3.42608501636788,127.273093961039));
#96482=CARTESIAN_POINT('Ctrl Pts',(-91.8409582193711,3.32527599043282,127.180588735955));
#96483=CARTESIAN_POINT('Ctrl Pts',(-91.8487229723181,3.2245912026132,127.088197515295));
#96484=CARTESIAN_POINT('Ctrl Pts',(-91.8564877252652,3.1199207336899,126.999884392384));
#96485=CARTESIAN_POINT('Ctrl Pts',(-91.8642524782123,3.01163019639435,126.916010501814));
#96486=CARTESIAN_POINT('Ctrl Pts',(-91.8720095190973,2.90344721478708,126.832219915976));
#96487=CARTESIAN_POINT('Ctrl Pts',(-91.8797665599822,2.79165162711616,126.752860026009));
#96488=CARTESIAN_POINT('Ctrl Pts',(-91.8875236008672,2.67664430660942,126.678253697188));
#96489=CARTESIAN_POINT('Ctrl Pts',(-91.8952747921073,2.56172371401755,126.603703629579));
#96490=CARTESIAN_POINT('Ctrl Pts',(-91.9030259833474,2.44359653608789,126.533900199907));
#96491=CARTESIAN_POINT('Ctrl Pts',(-91.9107771745875,2.32269470242368,126.469124478457));
#96492=CARTESIAN_POINT('Ctrl Pts',(-91.9185250713646,2.20184425526378,126.404376288417));
#96493=CARTESIAN_POINT('Ctrl Pts',(-91.9262729681418,2.07822184181082,126.344651740699));
#96494=CARTESIAN_POINT('Ctrl Pts',(-91.9340208649188,1.9522860144783,126.290187118444));
#96495=CARTESIAN_POINT('Ctrl Pts',(-91.941767141003,1.82637653020564,126.235733889014));
#96496=CARTESIAN_POINT('Ctrl Pts',(-91.949513417087,1.69815495320619,126.186538551658));
#96497=CARTESIAN_POINT('Ctrl Pts',(-91.9572596931712,1.56810157824014,126.142790012843));
#96498=CARTESIAN_POINT('Ctrl Pts',(-91.9650060264365,1.4380472432505,126.099041151086));
#96499=CARTESIAN_POINT('Ctrl Pts',(-91.9727523597018,1.30616145387334,126.060739292754));
#96500=CARTESIAN_POINT('Ctrl Pts',(-91.9804986929671,1.17294111392645,126.028023924476));
#96501=CARTESIAN_POINT('Ctrl Pts',(-91.9882467609701,1.03969094020721,125.995301229817));
#96502=CARTESIAN_POINT('Ctrl Pts',(-91.995994828973,0.905106000826217,125.968167607892));
#96503=CARTESIAN_POINT('Ctrl Pts',(-92.003742896976,0.769694483424782,125.946711652821));
#96504=CARTESIAN_POINT('Ctrl Pts',(-92.0114991997179,0.634139049051788,
125.925232894106));
#96505=CARTESIAN_POINT('Ctrl Pts',(-92.0192555024598,0.497755668529646,
125.909443917677));
#96506=CARTESIAN_POINT('Ctrl Pts',(-92.0270118052017,0.361059320632334,
125.899381593199));
#96507=CARTESIAN_POINT('Ctrl Pts',(-92.0347722477158,0.224290013777929,
125.889313898154));
#96508=CARTESIAN_POINT('Ctrl Pts',(-92.04253269023,0.0872077972854539,125.88497895772));
#96509=CARTESIAN_POINT('Ctrl Pts',(-92.0502931327442,-0.0496722280336851,
125.886361458125));
#96510=CARTESIAN_POINT('Ctrl Pts',(-92.0580660330096,-0.186771985321104,
125.887746177843));
#96511=CARTESIAN_POINT('Ctrl Pts',(-92.065838933275,-0.323668512168345,
125.894866658936));
#96512=CARTESIAN_POINT('Ctrl Pts',(-92.0736118335404,-0.459850804667805,
125.90765557234));
#96513=CARTESIAN_POINT('Ctrl Pts',(-92.0811021693025,-0.591082527813524,
125.919979576528));
#96514=CARTESIAN_POINT('Ctrl Pts',(-92.0885925050647,-0.721650738231154,
125.937567003394));
#96515=CARTESIAN_POINT('Ctrl Pts',(-92.0960828408268,-0.851108935678263,
125.9603130701));
#96516=CARTESIAN_POINT('Ctrl Pts',(-92.1038571749458,-0.985475580027133,
125.983921560839));
#96517=CARTESIAN_POINT('Ctrl Pts',(-92.1116315090648,-1.11907201067563,
126.013162377689));
#96518=CARTESIAN_POINT('Ctrl Pts',(-92.1194058431838,-1.25138901733661,
126.047974532544));
#96519=CARTESIAN_POINT('Ctrl Pts',(-92.1271705961309,-1.38354295511239,
126.08274378453));
#96520=CARTESIAN_POINT('Ctrl Pts',(-92.1349353490778,-1.51442023174586,
126.123070614355));
#96521=CARTESIAN_POINT('Ctrl Pts',(-92.1427001020249,-1.64351939186472,
126.168842623742));
#96522=CARTESIAN_POINT('Ctrl Pts',(-92.1504571429097,-1.77249032887706,
126.214569171724));
#96523=CARTESIAN_POINT('Ctrl Pts',(-92.1582141837946,-1.89968629778918,
126.265730006846));
#96524=CARTESIAN_POINT('Ctrl Pts',(-92.1659712246795,-2.02461898113001,
126.322162379676));
#96525=CARTESIAN_POINT('Ctrl Pts',(-92.1737224159196,-2.14945745176335,
126.378552196414));
#96526=CARTESIAN_POINT('Ctrl Pts',(-92.1814736071597,-2.27203567916957,
126.44020547796));
#96527=CARTESIAN_POINT('Ctrl Pts',(-92.1892247983997,-2.39188372245534,
126.50691075506));
#96528=CARTESIAN_POINT('Ctrl Pts',(-92.1969726951767,-2.51168082712517,
126.573587680638));
#96529=CARTESIAN_POINT('Ctrl Pts',(-92.2047205919537,-2.62874971472295,
126.645312141349));
#96530=CARTESIAN_POINT('Ctrl Pts',(-92.2124684887307,-2.7426437347701,126.721826060869));
#96531=CARTESIAN_POINT('Ctrl Pts',(-92.2202147648147,-2.85651393064383,
126.798323975327));
#96532=CARTESIAN_POINT('Ctrl Pts',(-92.2279610408988,-2.96721025559948,
126.879609137975));
#96533=CARTESIAN_POINT('Ctrl Pts',(-92.2357073169828,-3.07431416622612,
126.965379571788));
#96534=CARTESIAN_POINT('Ctrl Pts',(-92.2434536502481,-3.18141886746964,
127.05115063874));
#96535=CARTESIAN_POINT('Ctrl Pts',(-92.2511999835133,-3.28493079629746,
127.141406798538));
#96536=CARTESIAN_POINT('Ctrl Pts',(-92.2589463167786,-3.3844640100063,127.235805387859));
#96537=CARTESIAN_POINT('Ctrl Pts',(-92.2666943847815,-3.4840195134881,127.330225117089));
#96538=CARTESIAN_POINT('Ctrl Pts',(-92.2744424527843,-3.57959424523284,
127.428788852805));
#96539=CARTESIAN_POINT('Ctrl Pts',(-92.2821905207872,-3.67083898066302,
127.53111692964));
#96540=CARTESIAN_POINT('Ctrl Pts',(-92.289946823529,-3.76218069208396,127.633553761973));
#96541=CARTESIAN_POINT('Ctrl Pts',(-92.2977031262709,-3.84918295364231,
127.739762635156));
#96542=CARTESIAN_POINT('Ctrl Pts',(-92.3054594290127,-3.93153638723861,
127.849330211916));
#96543=CARTESIAN_POINT('Ctrl Pts',(-92.3132198715268,-4.01393377534204,
127.95895626819));
#96544=CARTESIAN_POINT('Ctrl Pts',(-92.3209803140407,-4.09167716993482,
128.071944278102));
#96545=CARTESIAN_POINT('Ctrl Pts',(-92.3287407565548,-4.16450103035498,
128.187852595283));
#96546=CARTESIAN_POINT('Ctrl Pts',(-92.3365136568202,-4.23744179410088,
128.303946978785));
#96547=CARTESIAN_POINT('Ctrl Pts',(-92.3442865570856,-4.30544704833943,
128.422970697889));
#96548=CARTESIAN_POINT('Ctrl Pts',(-92.3520594573509,-4.36829722882561,
128.544457437531));
#96549=CARTESIAN_POINT('Ctrl Pts',(-92.3595497931137,-4.42886264694771,
128.661527828193));
#96550=CARTESIAN_POINT('Ctrl Pts',(-92.3670401288763,-4.48464115366571,
128.780884995329));
#96551=CARTESIAN_POINT('Ctrl Pts',(-92.3745304646391,-4.53547956146055,
128.902096647957));
#96552=CARTESIAN_POINT('Ctrl Pts',(-92.3831948267737,-4.59428632118831,
129.042306871712));
#96553=CARTESIAN_POINT('Ctrl Pts',(-92.3918591889083,-4.6466417660541,129.185375286934));
#96554=CARTESIAN_POINT('Ctrl Pts',(-92.4005235510429,-4.69228942413747,
129.330724630415));
#96555=CARTESIAN_POINT('Ctrl Pts',(-92.4054838689954,-4.71842255365836,
129.413936636866));
#96556=CARTESIAN_POINT('Ctrl Pts',(-92.4104441869478,-4.74235801714723,
129.497895751871));
#96557=CARTESIAN_POINT('Ctrl Pts',(-92.4154045049002,-4.764054528234,129.582490119308));
#96558=CARTESIAN_POINT('Ctrl Pts',(-90.6650630979317,-4.76405452823406,
129.582490119308));
#96559=CARTESIAN_POINT('Ctrl Pts',(-90.6728368653943,-4.7980981811203,129.715225805227));
#96560=CARTESIAN_POINT('Ctrl Pts',(-90.680610632857,-4.82655146086384,129.849234029403));
#96561=CARTESIAN_POINT('Ctrl Pts',(-90.6883844003196,-4.84935028061991,
129.984004037565));
#96562=CARTESIAN_POINT('Ctrl Pts',(-90.6935378408002,-4.86446423420885,
130.073346717156));
#96563=CARTESIAN_POINT('Ctrl Pts',(-90.6986912812809,-4.87709428164181,
130.163024053761));
#96564=CARTESIAN_POINT('Ctrl Pts',(-90.7038447217616,-4.88723437455985,
130.252886927694));
#96565=CARTESIAN_POINT('Ctrl Pts',(-90.7142766691775,-4.90776064560362,
130.434793515931));
#96566=CARTESIAN_POINT('Ctrl Pts',(-90.7247086165934,-4.91813355712363,
130.617867092848));
#96567=CARTESIAN_POINT('Ctrl Pts',(-90.735140564009,-4.91824902518994,130.801264052022));
#96568=CARTESIAN_POINT('',(-90.3898594359623,-4.9182480484996,130.808741933566));
#96569=CARTESIAN_POINT('Ctrl Pts',(-90.3197845579208,-4.76405452823393,
129.582490119308));
#96570=CARTESIAN_POINT('Ctrl Pts',(-90.3274229448282,-4.79767960507908,
129.713593783595));
#96571=CARTESIAN_POINT('Ctrl Pts',(-90.3350613317357,-4.82587730052624,
129.846042274493));
#96572=CARTESIAN_POINT('Ctrl Pts',(-90.3426997186431,-4.84855894226438,
129.979339862743));
#96573=CARTESIAN_POINT('Ctrl Pts',(-90.3505596715296,-4.87189850827637,
130.116504001748));
#96574=CARTESIAN_POINT('Ctrl Pts',(-90.3584196244162,-4.88939706813633,
130.254566794181));
#96575=CARTESIAN_POINT('Ctrl Pts',(-90.3662795773027,-4.90101530917749,
130.392982443974));
#96576=CARTESIAN_POINT('Ctrl Pts',(-90.3741395301893,-4.91263355021866,
130.531398093767));
#96577=CARTESIAN_POINT('Ctrl Pts',(-90.3819994830757,-4.91837149578089,
130.670166137992));
#96578=CARTESIAN_POINT('Ctrl Pts',(-90.3898594359622,-4.9182480484996,130.808741933566));
#96579=CARTESIAN_POINT('Ctrl Pts',(-90.3898594359916,-4.91824804849914,
130.808741934084));
#96580=CARTESIAN_POINT('Ctrl Pts',(-90.4010783904105,-4.91807184520559,
131.006538989173));
#96581=CARTESIAN_POINT('Ctrl Pts',(-90.4122973448293,-4.90596017356694,
131.203826077175));
#96582=CARTESIAN_POINT('Ctrl Pts',(-90.4235162992482,-4.8821162522506,131.399443773109));
#96583=CARTESIAN_POINT('Ctrl Pts',(-90.4306728975352,-4.86690615689988,
131.524228776714));
#96584=CARTESIAN_POINT('Ctrl Pts',(-90.4378294958223,-4.84692287525181,
131.648335290403));
#96585=CARTESIAN_POINT('Ctrl Pts',(-90.4449860941093,-4.82222831375912,
131.77146823954));
#96586=CARTESIAN_POINT('Ctrl Pts',(-90.4527604282283,-4.79540219270726,
131.905229650933));
#96587=CARTESIAN_POINT('Ctrl Pts',(-90.4605347623474,-4.76296385051995,
132.038085910132));
#96588=CARTESIAN_POINT('Ctrl Pts',(-90.4683090964665,-4.72498647738317,
132.169529417036));
#96589=CARTESIAN_POINT('Ctrl Pts',(-90.4760738494135,-4.68705590796465,
132.300810931565));
#96590=CARTESIAN_POINT('Ctrl Pts',(-90.4838386023605,-4.64359999749885,
132.430682786054));
#96591=CARTESIAN_POINT('Ctrl Pts',(-90.4916033553075,-4.59474314544142,
132.558646366787));
#96592=CARTESIAN_POINT('Ctrl Pts',(-90.4993603961925,-4.54593481869822,
132.686482852287));
#96593=CARTESIAN_POINT('Ctrl Pts',(-90.5071174370776,-4.49173636409581,
132.812414472927));
#96594=CARTESIAN_POINT('Ctrl Pts',(-90.5148744779625,-4.43232220247175,
132.935956957396));
#96595=CARTESIAN_POINT('Ctrl Pts',(-90.5226256692026,-4.37295284552907,
133.059406277516));
#96596=CARTESIAN_POINT('Ctrl Pts',(-90.5303768604427,-4.30837577913205,
133.180469696662));
#96597=CARTESIAN_POINT('Ctrl Pts',(-90.5381280516828,-4.23881368892118,
133.298682483949));
#96598=CARTESIAN_POINT('Ctrl Pts',(-90.5458759484599,-4.16928116445436,
133.416845027647));
#96599=CARTESIAN_POINT('Ctrl Pts',(-90.5536238452369,-4.0947680281073,133.532159013008));
#96600=CARTESIAN_POINT('Ctrl Pts',(-90.561371742014,-4.01554300026345,133.644184111295));
#96601=CARTESIAN_POINT('Ctrl Pts',(-90.569118018098,-3.93633454458753,133.756185776347));
#96602=CARTESIAN_POINT('Ctrl Pts',(-90.5768642941821,-3.85241638348156,
133.86489960372));
#96603=CARTESIAN_POINT('Ctrl Pts',(-90.5846105702662,-3.76410045089587,
133.969914417151));
#96604=CARTESIAN_POINT('Ctrl Pts',(-90.5923569035315,-3.67578386638214,
134.074930005776));
#96605=CARTESIAN_POINT('Ctrl Pts',(-90.6001032367967,-3.58306969724902,
134.176246226755));
#96606=CARTESIAN_POINT('Ctrl Pts',(-90.607849570062,-3.48630976970296,134.273485471499));
#96607=CARTESIAN_POINT('Ctrl Pts',(-90.615597638065,-3.38952817344214,134.370746492297));
#96608=CARTESIAN_POINT('Ctrl Pts',(-90.6233457060679,-3.28869929161189,
134.463928442994));
#96609=CARTESIAN_POINT('Ctrl Pts',(-90.6310937740708,-3.184211060673,134.5526913105));
#96610=CARTESIAN_POINT('Ctrl Pts',(-90.6388500768127,-3.07961177839841,
134.641548516238));
#96611=CARTESIAN_POINT('Ctrl Pts',(-90.6466063795545,-2.97134567635988,
134.725977003188));
#96612=CARTESIAN_POINT('Ctrl Pts',(-90.6543626822963,-2.85983339702102,
134.805677401299));
#96613=CARTESIAN_POINT('Ctrl Pts',(-90.6621231248104,-2.7482616002211,134.885420337912));
#96614=CARTESIAN_POINT('Ctrl Pts',(-90.6698835673247,-2.63344050095503,
134.960429943632));
#96615=CARTESIAN_POINT('Ctrl Pts',(-90.6776440098388,-2.51581799065118,
135.030451352562));
#96616=CARTESIAN_POINT('Ctrl Pts',(-90.6854169101042,-2.39800666225207,
135.100585166073));
#96617=CARTESIAN_POINT('Ctrl Pts',(-90.6931898103695,-2.27738528044665,
135.165714595404));
#96618=CARTESIAN_POINT('Ctrl Pts',(-90.7009627106349,-2.15442529494813,
135.225631329815));
#96619=CARTESIAN_POINT('Ctrl Pts',(-90.7084530463972,-2.03593521463467,
135.283369940011));
#96620=CARTESIAN_POINT('Ctrl Pts',(-90.7159433821596,-1.91527388905724,
135.336268140986));
#96621=CARTESIAN_POINT('Ctrl Pts',(-90.7234337179219,-1.79287716078718,
135.384183163127));
#96622=CARTESIAN_POINT('Ctrl Pts',(-90.731208052041,-1.66583972336827,135.433914897893));
#96623=CARTESIAN_POINT('Ctrl Pts',(-90.7389823861601,-1.53653027351599,
135.478435655201));
#96624=CARTESIAN_POINT('Ctrl Pts',(-90.7467567202791,-1.40541543065441,
135.517532641774));
#96625=CARTESIAN_POINT('Ctrl Pts',(-90.7545214732262,-1.27446217511859,
135.556581444805));
#96626=CARTESIAN_POINT('Ctrl Pts',(-90.7622862261733,-1.14170832469778,
135.590219666243));
#96627=CARTESIAN_POINT('Ctrl Pts',(-90.7700509791204,-1.00764061817782,
135.618282453979));
#96628=CARTESIAN_POINT('Ctrl Pts',(-90.7778080200054,-0.873706069594,135.64631736936));
#96629=CARTESIAN_POINT('Ctrl Pts',(-90.7855650608904,-0.73846064199694,
135.668787791529));
#96630=CARTESIAN_POINT('Ctrl Pts',(-90.7933221017754,-0.602406045278277,
135.685578705207));
#96631=CARTESIAN_POINT('Ctrl Pts',(-90.8010732930155,-0.466454048389164,
135.702356956726));
#96632=CARTESIAN_POINT('Ctrl Pts',(-90.8088244842557,-0.329694483397402,
135.713464177035));
#96633=CARTESIAN_POINT('Ctrl Pts',(-90.8165756754958,-0.192638708584791,
135.718836519476));
#96634=CARTESIAN_POINT('Ctrl Pts',(-90.8243235722729,-0.0556411861327437,
135.724206578528));
#96635=CARTESIAN_POINT('Ctrl Pts',(-90.8320714690499,0.0816519058931658,
135.723846592386));
#96636=CARTESIAN_POINT('Ctrl Pts',(-90.839819365827,0.218724856527024,135.717744634681));
#96637=CARTESIAN_POINT('Ctrl Pts',(-90.8475656419111,0.355769134454561,
135.711643953374));
#96638=CARTESIAN_POINT('Ctrl Pts',(-90.8553119179952,0.492592972252758,
135.699803706927));
#96639=CARTESIAN_POINT('Ctrl Pts',(-90.8630581940793,0.628681827765329,
135.682264083394));
#96640=CARTESIAN_POINT('Ctrl Pts',(-90.8708045273446,0.764771687855103,
135.664724330387));
#96641=CARTESIAN_POINT('Ctrl Pts',(-90.87855086061,0.900126167075165,135.641485166318));
#96642=CARTESIAN_POINT('Ctrl Pts',(-90.8862971938754,1.03423740196892,135.612638485875));
#96643=CARTESIAN_POINT('Ctrl Pts',(-90.8940452618784,1.16837867014369,135.583785345417));
#96644=CARTESIAN_POINT('Ctrl Pts',(-90.9017933298814,1.3012757578266,135.549322271957));
#96645=CARTESIAN_POINT('Ctrl Pts',(-90.9095413978843,1.43243291324453,135.509391862048));
#96646=CARTESIAN_POINT('Ctrl Pts',(-90.9172977006262,1.56372946404785,135.469419013624));
#96647=CARTESIAN_POINT('Ctrl Pts',(-90.925054003368,1.69328201395639,135.423967335201));
#96648=CARTESIAN_POINT('Ctrl Pts',(-90.9328103061098,1.82061132694102,135.37322890837));
#96649=CARTESIAN_POINT('Ctrl Pts',(-90.940570748624,1.94800859941416,135.322463400913));
#96650=CARTESIAN_POINT('Ctrl Pts',(-90.9483311911382,2.07317991390372,135.266405682301));
#96651=CARTESIAN_POINT('Ctrl Pts',(-90.9560916336523,2.19566874825433,135.205294815034));
#96652=CARTESIAN_POINT('Ctrl Pts',(-90.9638645339178,2.3183542125559,135.144085847177));
#96653=CARTESIAN_POINT('Ctrl Pts',(-90.9716374341832,2.43834824922074,135.077807709916));
#96654=CARTESIAN_POINT('Ctrl Pts',(-90.9794103344487,2.55522077043769,135.006744450205));
#96655=CARTESIAN_POINT('Ctrl Pts',(-90.9869006702107,2.66784468112461,134.938264518981));
#96656=CARTESIAN_POINT('Ctrl Pts',(-90.9943910059728,2.77756982954708,134.865341498206));
#96657=CARTESIAN_POINT('Ctrl Pts',(-91.0018813417348,2.88404051603024,134.788264904117));
#96658=CARTESIAN_POINT('Ctrl Pts',(-91.0096556758539,2.99454807095201,134.708265927535));
#96659=CARTESIAN_POINT('Ctrl Pts',(-91.017430009973,3.10189956117272,134.623538781946));
#96660=CARTESIAN_POINT('Ctrl Pts',(-91.025204344092,3.20566373848533,134.53436102752));
#96661=CARTESIAN_POINT('Ctrl Pts',(-91.0329690970391,3.30930003572306,134.445293176708));
#96662=CARTESIAN_POINT('Ctrl Pts',(-91.0407338499863,3.40935752294812,134.35178588291));
#96663=CARTESIAN_POINT('Ctrl Pts',(-91.0484986029334,3.50543441121012,134.254159546664));
#96664=CARTESIAN_POINT('Ctrl Pts',(-91.0562556438184,3.60141587455225,134.156630174271));
#96665=CARTESIAN_POINT('Ctrl Pts',(-91.0640126847033,3.69342433428844,134.054990177737));
#96666=CARTESIAN_POINT('Ctrl Pts',(-91.0717697255883,3.78109183835352,133.949599491235));
#96667=CARTESIAN_POINT('Ctrl Pts',(-91.0795209168284,3.86869323167196,133.844288280669));
#96668=CARTESIAN_POINT('Ctrl Pts',(-91.0872721080687,3.95195993610689,133.735232309295));
#96669=CARTESIAN_POINT('Ctrl Pts',(-91.0950232993088,4.03056183401493,133.62282728664));
#96670=CARTESIAN_POINT('Ctrl Pts',(-91.1027711960859,4.10913032401948,133.510470039119));
#96671=CARTESIAN_POINT('Ctrl Pts',(-91.1105190928628,4.18303772729247,133.394766891152));
#96672=CARTESIAN_POINT('Ctrl Pts',(-91.1182669896399,4.25199525546935,133.276145278487));
#96673=CARTESIAN_POINT('Ctrl Pts',(-91.126013265724,4.32093835921788,133.157548478907));
#96674=CARTESIAN_POINT('Ctrl Pts',(-91.1337595418081,4.38493345098744,133.036034766697));
#96675=CARTESIAN_POINT('Ctrl Pts',(-91.1415058178922,4.44373621952061,132.912058763369));
#96676=CARTESIAN_POINT('Ctrl Pts',(-91.1492521511576,4.50253942212255,132.788081844878));
#96677=CARTESIAN_POINT('Ctrl Pts',(-91.156998484423,4.55615005745953,132.661642952245));
#96678=CARTESIAN_POINT('Ctrl Pts',(-91.1647448176884,4.60437092653096,132.533219036702));
#96679=CARTESIAN_POINT('Ctrl Pts',(-91.1724928856914,4.65260259433161,132.404766361514));
#96680=CARTESIAN_POINT('Ctrl Pts',(-91.1802409536943,4.69544195666949,132.274328144793));
#96681=CARTESIAN_POINT('Ctrl Pts',(-91.1879890216973,4.73274101811986,132.142398553465));
#96682=CARTESIAN_POINT('Ctrl Pts',(-91.1957453244391,4.77007972145655,132.010328745799));
#96683=CARTESIAN_POINT('Ctrl Pts',(-91.2035016271809,4.80186625486287,131.876764774035));
#96684=CARTESIAN_POINT('Ctrl Pts',(-91.2112579299227,4.82800318324298,131.74221365781));
#96685=CARTESIAN_POINT('Ctrl Pts',(-91.2190183724369,4.8541540616888,131.607590727604));
#96686=CARTESIAN_POINT('Ctrl Pts',(-91.2267788149511,4.87464926834414,131.471979989492));
#96687=CARTESIAN_POINT('Ctrl Pts',(-91.2345392574652,4.88944317188505,131.335894747615));
#96688=CARTESIAN_POINT('Ctrl Pts',(-91.2423121577307,4.90426082391327,131.199591049626));
#96689=CARTESIAN_POINT('Ctrl Pts',(-91.2500850579961,4.91335885777632,131.06281171605));
#96690=CARTESIAN_POINT('Ctrl Pts',(-91.2578579582616,4.91674377725259,130.926072126257));
#96691=CARTESIAN_POINT('Ctrl Pts',(-91.2653482940236,4.92000564637981,130.79430336498));
#96692=CARTESIAN_POINT('Ctrl Pts',(-91.2728386297856,4.91796256662295,130.662571816062));
#96693=CARTESIAN_POINT('Ctrl Pts',(-91.2803289655477,4.9106658518279,130.531333230311));
#96694=CARTESIAN_POINT('Ctrl Pts',(-91.2881032996668,4.90309247987363,130.395118693693));
#96695=CARTESIAN_POINT('Ctrl Pts',(-91.2958776337859,4.88983523536181,130.259003752851));
#96696=CARTESIAN_POINT('Ctrl Pts',(-91.3036519679049,4.87089453733705,130.123501257169));
#96697=CARTESIAN_POINT('Ctrl Pts',(-91.311416720852,4.85197718202983,129.988165756203));
#96698=CARTESIAN_POINT('Ctrl Pts',(-91.3191814737991,4.82739036337932,129.853441582085));
#96699=CARTESIAN_POINT('Ctrl Pts',(-91.3269462267462,4.79718646668753,129.719839955554));
#96700=CARTESIAN_POINT('Ctrl Pts',(-91.3347032676312,4.76701256893165,129.586371024042));
#96701=CARTESIAN_POINT('Ctrl Pts',(-91.3424603085162,4.73123278117247,129.454022800229));
#96702=CARTESIAN_POINT('Ctrl Pts',(-91.3502173494012,4.68995103914371,129.323299405821));
#96703=CARTESIAN_POINT('Ctrl Pts',(-91.3579685406414,4.64870042799779,129.192674590942));
#96704=CARTESIAN_POINT('Ctrl Pts',(-91.3657197318814,4.60195623830484,129.063672537898));
#96705=CARTESIAN_POINT('Ctrl Pts',(-91.3734709231216,4.54987295504699,128.936784874676));
#96706=CARTESIAN_POINT('Ctrl Pts',(-91.3812188198986,4.49781180857398,128.809951142096));
#96707=CARTESIAN_POINT('Ctrl Pts',(-91.3889667166757,4.44041623006354,128.685230372873));
#96708=CARTESIAN_POINT('Ctrl Pts',(-91.3967146134528,4.37788973615141,128.5630965723));
#96709=CARTESIAN_POINT('Ctrl Pts',(-91.4044608895368,4.31537632143389,128.440988319486));
#96710=CARTESIAN_POINT('Ctrl Pts',(-91.412207165621,4.24773430417261,128.321466306758));
#96711=CARTESIAN_POINT('Ctrl Pts',(-91.4199534417051,4.17521411411934,128.204981814129));
#96712=CARTESIAN_POINT('Ctrl Pts',(-91.4276997749704,4.1026933887384,128.088496461638));
#96713=CARTESIAN_POINT('Ctrl Pts',(-91.4354461082358,4.02529462534275,127.975049005887));
#96714=CARTESIAN_POINT('Ctrl Pts',(-91.4431924415012,3.94331250563561,127.865063159771));
#96715=CARTESIAN_POINT('Ctrl Pts',(-91.4509405095041,3.8613120266013,127.755052683089));
#96716=CARTESIAN_POINT('Ctrl Pts',(-91.458688577507,3.77472638242484,127.648505672012));
#96717=CARTESIAN_POINT('Ctrl Pts',(-91.46643664551,3.6838913345952,127.545813748578));
#96718=CARTESIAN_POINT('Ctrl Pts',(-91.4741929482519,3.59295974619566,127.443012682945));
#96719=CARTESIAN_POINT('Ctrl Pts',(-91.4819492509938,3.49776999175757,127.344075182929));
#96720=CARTESIAN_POINT('Ctrl Pts',(-91.4897055537357,3.39869597521147,127.249357279933));
#96721=CARTESIAN_POINT('Ctrl Pts',(-91.4974659962499,3.29956907987941,127.15458882314));
#96722=CARTESIAN_POINT('Ctrl Pts',(-91.505226438764,3.19655408503046,127.064044708901));
#96723=CARTESIAN_POINT('Ctrl Pts',(-91.5129868812782,3.09005818312961,126.978040781565));
#96724=CARTESIAN_POINT('Ctrl Pts',(-91.5207597815437,2.98339132455306,126.89189879309));
#96725=CARTESIAN_POINT('Ctrl Pts',(-91.5285326818091,2.87323270695781,126.810311788713));
#96726=CARTESIAN_POINT('Ctrl Pts',(-91.5363055820745,2.76001944905717,126.733552871759));
#96727=CARTESIAN_POINT('Ctrl Pts',(-91.5437959178365,2.65092177824852,126.65958433478));
#96728=CARTESIAN_POINT('Ctrl Pts',(-91.5512862535985,2.5389879607995,126.590099115731));
#96729=CARTESIAN_POINT('Ctrl Pts',(-91.5587765893605,2.42462916915919,126.525300387263));
#96730=CARTESIAN_POINT('Ctrl Pts',(-91.5665509234796,2.30593442917507,126.45804479531));
#96731=CARTESIAN_POINT('Ctrl Pts',(-91.5743252575987,2.18425120998468,126.395625040265));
#96732=CARTESIAN_POINT('Ctrl Pts',(-91.5820995917178,2.06001121280276,126.338317977193));
#96733=CARTESIAN_POINT('Ctrl Pts',(-91.5898643446648,1.93592433031373,126.281081539955));
#96734=CARTESIAN_POINT('Ctrl Pts',(-91.597629097612,1.80928729099459,126.228945419889));
#96735=CARTESIAN_POINT('Ctrl Pts',(-91.6053938505591,1.68055851486637,126.182141871054));
#96736=CARTESIAN_POINT('Ctrl Pts',(-91.6131508914441,1.55195759397336,126.135384808163));
#96737=CARTESIAN_POINT('Ctrl Pts',(-91.6209079323291,1.42126943572979,126.093949909185));
#96738=CARTESIAN_POINT('Ctrl Pts',(-91.6286649732141,1.28897435180654,126.05802222014));
#96739=CARTESIAN_POINT('Ctrl Pts',(-91.6364161644542,1.156779032635,126.022121624444));
#96740=CARTESIAN_POINT('Ctrl Pts',(-91.6441673556943,1.02297957556137,125.991720074376));
#96741=CARTESIAN_POINT('Ctrl Pts',(-91.6519185469345,0.888073104041771,
125.966953334281));
#96742=CARTESIAN_POINT('Ctrl Pts',(-91.6596664437115,0.753223971371501,
125.942197120712));
#96743=CARTESIAN_POINT('Ctrl Pts',(-91.6674143404886,0.617269143798842,
125.923071024201));
#96744=CARTESIAN_POINT('Ctrl Pts',(-91.6751622372657,0.480717421113914,
125.909660031878));
#96745=CARTESIAN_POINT('Ctrl Pts',(-91.6829085133498,0.344194262105658,
125.896251844845));
#96746=CARTESIAN_POINT('Ctrl Pts',(-91.6906547894339,0.207074845180411,
125.888556422322));
#96747=CARTESIAN_POINT('Ctrl Pts',(-91.698401065518,0.0698742083914101,
125.886606998534));
#96748=CARTESIAN_POINT('Ctrl Pts',(-91.7061473987833,-0.0673274411813373,
125.884657560356));
#96749=CARTESIAN_POINT('Ctrl Pts',(-91.7138937320486,-0.204609920888443,
125.888454211106));
#96750=CARTESIAN_POINT('Ctrl Pts',(-91.7216400653139,-0.341457466412116,
125.897978053891));
#96751=CARTESIAN_POINT('Ctrl Pts',(-91.7293881333169,-0.478335657994589,
125.907504029475));
#96752=CARTESIAN_POINT('Ctrl Pts',(-91.7371362013198,-0.61477833163074,
125.922759722111));
#96753=CARTESIAN_POINT('Ctrl Pts',(-91.7448842693228,-0.750274517323372,
125.943674327426));
#96754=CARTESIAN_POINT('Ctrl Pts',(-91.7526405720646,-0.885914709974768,
125.964611161033));
#96755=CARTESIAN_POINT('Ctrl Pts',(-91.7603968748065,-1.02060601820641,
125.991218861914));
#96756=CARTESIAN_POINT('Ctrl Pts',(-91.7681531775484,-1.15384679850733,
126.023375297773));
#96757=CARTESIAN_POINT('Ctrl Pts',(-91.7759136200625,-1.2871586934245,126.055548896491));
#96758=CARTESIAN_POINT('Ctrl Pts',(-91.7836740625767,-1.41901814207316,
126.093277023784));
#96759=CARTESIAN_POINT('Ctrl Pts',(-91.7914345050908,-1.54893931818225,
126.136387818685));
#96760=CARTESIAN_POINT('Ctrl Pts',(-91.7992074053563,-1.67906905529709,
126.179567818862));
#96761=CARTESIAN_POINT('Ctrl Pts',(-91.8069803056217,-1.80725393632791,
126.22814761496));
#96762=CARTESIAN_POINT('Ctrl Pts',(-91.8147532058871,-1.93302791836956,
126.281907065643));
#96763=CARTESIAN_POINT('Ctrl Pts',(-91.8222435416493,-2.05422969936048,
126.333712224882));
#96764=CARTESIAN_POINT('Ctrl Pts',(-91.8297338774114,-2.17319254453902,
126.390326857467));
#96765=CARTESIAN_POINT('Ctrl Pts',(-91.8372242131735,-2.28952327024669,
126.45151485215));
#96766=CARTESIAN_POINT('Ctrl Pts',(-91.8449994603469,-2.41027889121765,
126.515030266921));
#96767=CARTESIAN_POINT('Ctrl Pts',(-91.8527747075203,-2.52858075501139,
126.583675067432));
#96768=CARTESIAN_POINT('Ctrl Pts',(-91.8605499546937,-2.64396242739829,
126.657235620052));
#96769=CARTESIAN_POINT('Ctrl Pts',(-91.8683154188557,-2.75919892366504,
126.730703616936));
#96770=CARTESIAN_POINT('Ctrl Pts',(-91.8760808830178,-2.87152221321195,
126.809074849936));
#96771=CARTESIAN_POINT('Ctrl Pts',(-91.8838463471797,-2.98048898906497,
126.892089097264));
#96772=CARTESIAN_POINT('Ctrl Pts',(-91.8916025221625,-3.08932541702299,
126.975004041551));
#96773=CARTESIAN_POINT('Ctrl Pts',(-91.8993586971453,-3.19481301885132,
127.062550703165));
#96774=CARTESIAN_POINT('Ctrl Pts',(-91.9071148721281,-3.29653663340567,
127.154425099353));
#96775=CARTESIAN_POINT('Ctrl Pts',(-91.9148657790816,-3.39819115681903,
127.246237094034));
#96776=CARTESIAN_POINT('Ctrl Pts',(-91.9226166860351,-3.49608648998639,
127.342370714792));
#96777=CARTESIAN_POINT('Ctrl Pts',(-91.9303675929886,-3.58983974795637,
127.44248113631));
#96778=CARTESIAN_POINT('Ctrl Pts',(-91.9381149140952,-3.68354963231496,
127.542545243165));
#96779=CARTESIAN_POINT('Ctrl Pts',(-91.9458622352018,-3.77312098801117,
127.646582205093));
#96780=CARTESIAN_POINT('Ctrl Pts',(-91.9536095563085,-3.85820737238423,
127.754209976339));
#96781=CARTESIAN_POINT('Ctrl Pts',(-91.9613549709857,-3.94327281904472,
127.861811262978));
#96782=CARTESIAN_POINT('Ctrl Pts',(-91.969100385663,-4.02385524938429,127.973001293432));
#96783=CARTESIAN_POINT('Ctrl Pts',(-91.9768458003403,-4.09964841115681,
128.087364856178));
#96784=CARTESIAN_POINT('Ctrl Pts',(-91.984593776484,-4.17546663829348,128.201766239807));
#96785=CARTESIAN_POINT('Ctrl Pts',(-91.9923417526278,-4.24649221036113,
128.319342930459));
#96786=CARTESIAN_POINT('Ctrl Pts',(-92.0000897287715,-4.31246207454953,
128.439650504662));
#96787=CARTESIAN_POINT('Ctrl Pts',(-92.0078387166846,-4.3784405534115,128.559973789227));
#96788=CARTESIAN_POINT('Ctrl Pts',(-92.0155877045976,-4.43936182826284,
128.683028320924));
#96789=CARTESIAN_POINT('Ctrl Pts',(-92.0233366925106,-4.49500920693038,
128.808345764888));
#96790=CARTESIAN_POINT('Ctrl Pts',(-92.0310930625346,-4.55070959834326,
128.933782593123));
#96791=CARTESIAN_POINT('Ctrl Pts',(-92.0388494325587,-4.60112590169011,
129.061486280616));
#96792=CARTESIAN_POINT('Ctrl Pts',(-92.0466058025827,-4.64608972588001,
129.190968748995));
#96793=CARTESIAN_POINT('Ctrl Pts',(-92.0543278308942,-4.69085447051105,
129.319877927331));
#96794=CARTESIAN_POINT('Ctrl Pts',(-92.0620498592056,-4.7302148646397,129.450549784542));
#96795=CARTESIAN_POINT('Ctrl Pts',(-92.0697718875171,-4.76405452823417,
129.582490119309));
#96796=CARTESIAN_POINT('Origin',(213.235140564004,0.,130.804360617566));
#96797=CARTESIAN_POINT('',(-94.1652277315646,-4.76405452823406,129.582490119308));
#96798=CARTESIAN_POINT('',(-93.8201028328085,-4.76405452823393,129.582490119308));
#96799=CARTESIAN_POINT('',(213.235140564004,-4.76405452823405,129.582490119308));
#96800=CARTESIAN_POINT('',(-92.4851405639578,-4.91824929378548,130.801724962307));
#96801=CARTESIAN_POINT('Ctrl Pts',(-92.485140564009,-4.91824929378596,130.801724963215));
#96802=CARTESIAN_POINT('Ctrl Pts',(-92.4929859638921,-4.91832387304165,
130.940893201087));
#96803=CARTESIAN_POINT('Ctrl Pts',(-92.5008313637752,-4.91248718749969,
131.08006072528));
#96804=CARTESIAN_POINT('Ctrl Pts',(-92.5086767636583,-4.90076596850035,
131.218698625102));
#96805=CARTESIAN_POINT('Ctrl Pts',(-92.5165240638458,-4.88904191039983,
131.357370105649));
#96806=CARTESIAN_POINT('Ctrl Pts',(-92.5243713640332,-4.87143051122289,
131.495511330634));
#96807=CARTESIAN_POINT('Ctrl Pts',(-92.5322186642207,-4.84801037639572,
131.632598779485));
#96808=CARTESIAN_POINT('Ctrl Pts',(-92.5400693938123,-4.82458000656991,
131.769746137891));
#96809=CARTESIAN_POINT('Ctrl Pts',(-92.547920123404,-4.7953359082831,131.905838431539));
#96810=CARTESIAN_POINT('Ctrl Pts',(-92.5557708529956,-4.76040771941291,
132.040362805045));
#96811=CARTESIAN_POINT('Ctrl Pts',(-92.5638714559503,-4.72436783462716,
132.179168826166));
#96812=CARTESIAN_POINT('Ctrl Pts',(-92.5719720589049,-4.68227613829448,
132.316305040936));
#96813=CARTESIAN_POINT('Ctrl Pts',(-92.5800726618596,-4.63433002919282,
132.451226806126));
#96814=CARTESIAN_POINT('Ctrl Pts',(-92.5879396713312,-4.58776652070624,
132.582257892405));
#96815=CARTESIAN_POINT('Ctrl Pts',(-92.5958066808029,-4.53568179255408,
132.711200161232));
#96816=CARTESIAN_POINT('Ctrl Pts',(-92.6036736902745,-4.47830470860807,
132.837577280728));
#96817=CARTESIAN_POINT('Ctrl Pts',(-92.6118910899708,-4.41837209585412,
132.969583134682));
#96818=CARTESIAN_POINT('Ctrl Pts',(-92.6201084896671,-4.35266507332881,
133.098789662325));
#96819=CARTESIAN_POINT('Ctrl Pts',(-92.6283258893634,-4.28149618872812,
133.224685688379));
#96820=CARTESIAN_POINT('Ctrl Pts',(-92.6365432890597,-4.21032730412744,
133.350581714433));
#96821=CARTESIAN_POINT('Ctrl Pts',(-92.6447606887559,-4.13369686372427,
133.473166887299));
#96822=CARTESIAN_POINT('Ctrl Pts',(-92.6529780884522,-4.05196604076127,
133.591967883129));
#96823=CARTESIAN_POINT('Ctrl Pts',(-92.6607524225715,-3.97464197852288,
133.704363369464));
#96824=CARTESIAN_POINT('Ctrl Pts',(-92.6685267566907,-3.89251537202124,
133.813717162985));
#96825=CARTESIAN_POINT('Ctrl Pts',(-92.6763010908099,-3.80585335273085,
133.919591478996));
#96826=CARTESIAN_POINT('Ctrl Pts',(-92.6840658437571,-3.71929813663427,
134.025335314375));
#96827=CARTESIAN_POINT('Ctrl Pts',(-92.6918305967042,-3.62821887443087,
134.12760790474));
#96828=CARTESIAN_POINT('Ctrl Pts',(-92.6995953496514,-3.53292623256085,
134.225999888118));
#96829=CARTESIAN_POINT('Ctrl Pts',(-92.7073523905365,-3.43772823668586,
134.324294147191));
#96830=CARTESIAN_POINT('Ctrl Pts',(-92.7151094314216,-3.33832545929679,
134.41871519043));
#96831=CARTESIAN_POINT('Ctrl Pts',(-92.7228664723067,-3.23506890107839,
134.508886534303));
#96832=CARTESIAN_POINT('Ctrl Pts',(-92.730617663547,-3.1318902094339,134.598989879264));
#96833=CARTESIAN_POINT('Ctrl Pts',(-92.7383688547872,-3.02486381479887,
134.684849647559));
#96834=CARTESIAN_POINT('Ctrl Pts',(-92.7461200460275,-2.91437739083234,
134.766126320672));
#96835=CARTESIAN_POINT('Ctrl Pts',(-92.7538679428047,-2.80393792654287,
134.847368449031));
#96836=CARTESIAN_POINT('Ctrl Pts',(-92.7616158395819,-2.69004167211494,
134.924031125321));
#96837=CARTESIAN_POINT('Ctrl Pts',(-92.7693637363591,-2.57310901008165,
134.995815387063));
#96838=CARTESIAN_POINT('Ctrl Pts',(-92.7771100124433,-2.4562008078408,135.067584633084));
#96839=CARTESIAN_POINT('Ctrl Pts',(-92.7848562885275,-2.33625779432396,
135.134477289891));
#96840=CARTESIAN_POINT('Ctrl Pts',(-92.7926025646117,-2.21372859732735,
135.196238206921));
#96841=CARTESIAN_POINT('Ctrl Pts',(-92.8003488978771,-2.09119849584788,
135.257999579855));
#96842=CARTESIAN_POINT('Ctrl Pts',(-92.8080952311427,-1.9660825219171,135.314628961446));
#96843=CARTESIAN_POINT('Ctrl Pts',(-92.8158415644081,-1.83885275718515,
135.365917763968));
#96844=CARTESIAN_POINT('Ctrl Pts',(-92.8235896324112,-1.71159450022936,
135.417218052262));
#96845=CARTESIAN_POINT('Ctrl Pts',(-92.8313377004143,-1.5822218730646,135.463175235465));
#96846=CARTESIAN_POINT('Ctrl Pts',(-92.8390857684174,-1.45122534882768,
135.503629502129));
#96847=CARTESIAN_POINT('Ctrl Pts',(-92.8468420711594,-1.32008959992611,
135.544126764069));
#96848=CARTESIAN_POINT('Ctrl Pts',(-92.8545983739013,-1.1873268804404,135.579109310784));
#96849=CARTESIAN_POINT('Ctrl Pts',(-92.8623546766433,-1.05344172582442,
135.608467568165));
#96850=CARTESIAN_POINT('Ctrl Pts',(-92.8701151191575,-0.919485112670212,
135.637841494932));
#96851=CARTESIAN_POINT('Ctrl Pts',(-92.8778755616718,-0.784405255546721,
135.661585083268));
#96852=CARTESIAN_POINT('Ctrl Pts',(-92.8856360041861,-0.64871421574871,
135.679640397105));
#96853=CARTESIAN_POINT('Ctrl Pts',(-92.8934089044516,-0.512805352647534,
135.697724694936));
#96854=CARTESIAN_POINT('Ctrl Pts',(-92.9011818047172,-0.376283735864319,
135.710102435652));
#96855=CARTESIAN_POINT('Ctrl Pts',(-92.9089547049827,-0.239664752427623,
135.716767753476));
#96856=CARTESIAN_POINT('Ctrl Pts',(-92.9164450407436,-0.108012213183497,
135.723190770208));
#96857=CARTESIAN_POINT('Ctrl Pts',(-92.9239353765044,0.0237304285630812,
135.724309472757));
#96858=CARTESIAN_POINT('Ctrl Pts',(-92.9314257122653,0.155106321858892,
135.720164223429));
#96859=CARTESIAN_POINT('Ctrl Pts',(-92.9392000463844,0.291463372101913,
135.715861805713));
#96860=CARTESIAN_POINT('Ctrl Pts',(-92.9469743805035,0.427857252518841,
135.70587476223));
#96861=CARTESIAN_POINT('Ctrl Pts',(-92.9547487146226,0.56377525135831,135.690191204934));
#96862=CARTESIAN_POINT('Ctrl Pts',(-92.9625134675698,0.699525743411182,
135.674526976219));
#96863=CARTESIAN_POINT('Ctrl Pts',(-92.9702782205169,0.8348011361504,135.653180246668));
#96864=CARTESIAN_POINT('Ctrl Pts',(-92.9780429734641,0.969089098953742,
135.626191118609));
#96865=CARTESIAN_POINT('Ctrl Pts',(-92.9858000143491,1.1032436850593,135.599228796532));
#96866=CARTESIAN_POINT('Ctrl Pts',(-92.9935570552341,1.23641241210438,135.566635304915));
#96867=CARTESIAN_POINT('Ctrl Pts',(-93.0013140961192,1.36808880938738,135.52850245203));
#96868=CARTESIAN_POINT('Ctrl Pts',(-93.0090652873593,1.49966590847509,135.490398355425));
#96869=CARTESIAN_POINT('Ctrl Pts',(-93.0168164785995,1.62975254378082,135.446763320479));
#96870=CARTESIAN_POINT('Ctrl Pts',(-93.0245676698397,1.75785352167992,135.397739989969));
#96871=CARTESIAN_POINT('Ctrl Pts',(-93.0323155666168,1.88590005324603,135.348737495682));
#96872=CARTESIAN_POINT('Ctrl Pts',(-93.040063463394,2.01196224159648,135.294351400248));
#96873=CARTESIAN_POINT('Ctrl Pts',(-93.0478113601711,2.13556133410218,135.234773786875));
#96874=CARTESIAN_POINT('Ctrl Pts',(-93.0555576362552,2.25913457234221,135.175208635854));
#96875=CARTESIAN_POINT('Ctrl Pts',(-93.0633039123394,2.38024538758876,135.110454296569));
#96876=CARTESIAN_POINT('Ctrl Pts',(-93.0710501884235,2.49843662016344,135.040750297178));
#96877=CARTESIAN_POINT('Ctrl Pts',(-93.0787965216889,2.61662872519879,134.971045783249));
#96878=CARTESIAN_POINT('Ctrl Pts',(-93.0865428549543,2.73190086779516,134.896391734913));
#96879=CARTESIAN_POINT('Ctrl Pts',(-93.0942891882197,2.84382238552751,134.817072581073));
#96880=CARTESIAN_POINT('Ctrl Pts',(-93.1020372562227,2.95576896730729,134.737735664259));
#96881=CARTESIAN_POINT('Ctrl Pts',(-93.1097853242257,3.06436311219457,134.653731789092));
#96882=CARTESIAN_POINT('Ctrl Pts',(-93.1175333922287,3.16920525357997,134.565387222521));
#96883=CARTESIAN_POINT('Ctrl Pts',(-93.1252896949706,3.27415882244158,134.476948762293));
#96884=CARTESIAN_POINT('Ctrl Pts',(-93.1330459977124,3.3753521225419,134.384160647352));
#96885=CARTESIAN_POINT('Ctrl Pts',(-93.1408023004543,3.47242025234193,134.28738813018));
#96886=CARTESIAN_POINT('Ctrl Pts',(-93.1485627429686,3.56954019032549,134.190563962602));
#96887=CARTESIAN_POINT('Ctrl Pts',(-93.1563231854829,3.66253030592995,134.08975144261));
#96888=CARTESIAN_POINT('Ctrl Pts',(-93.1640836279971,3.75106507426348,133.985350066015));
#96889=CARTESIAN_POINT('Ctrl Pts',(-93.1718565282626,3.83974196646688,133.880781095061));
#96890=CARTESIAN_POINT('Ctrl Pts',(-93.179629428528,3.92394897888479,133.77261206357));
#96891=CARTESIAN_POINT('Ctrl Pts',(-93.1874023287935,4.00340259719374,133.661273410649));
#96892=CARTESIAN_POINT('Ctrl Pts',(-93.1948926645551,4.07996787634084,133.553982198214));
#96893=CARTESIAN_POINT('Ctrl Pts',(-93.2023830003167,4.15211918834305,133.44374806861));
#96894=CARTESIAN_POINT('Ctrl Pts',(-93.2098733360783,4.21964355205206,133.330977200296));
#96895=CARTESIAN_POINT('Ctrl Pts',(-93.2176476701974,4.28972812253835,133.213930590228));
#96896=CARTESIAN_POINT('Ctrl Pts',(-93.2254220043165,4.35504996397883,133.093780314809));
#96897=CARTESIAN_POINT('Ctrl Pts',(-93.2331963384355,4.41532194139743,132.970951307178));
#96898=CARTESIAN_POINT('Ctrl Pts',(-93.2409610913826,4.47551963899051,132.848273675322));
#96899=CARTESIAN_POINT('Ctrl Pts',(-93.2487258443297,4.53067968490899,132.722924227468));
#96900=CARTESIAN_POINT('Ctrl Pts',(-93.2564905972767,4.58055889116168,132.595355678168));
#96901=CARTESIAN_POINT('Ctrl Pts',(-93.2642476381617,4.63038855668341,132.467913831749));
#96902=CARTESIAN_POINT('Ctrl Pts',(-93.2720046790466,4.67494767888497,132.338257631794));
#96903=CARTESIAN_POINT('Ctrl Pts',(-93.2797617199315,4.71403973888023,132.206862811061));
#96904=CARTESIAN_POINT('Ctrl Pts',(-93.2875129111716,4.753102319249,132.075567076184));
#96905=CARTESIAN_POINT('Ctrl Pts',(-93.2952641024116,4.78670593246589,131.942535703424));
#96906=CARTESIAN_POINT('Ctrl Pts',(-93.3030152936517,4.8147029236901,131.808262415109));
#96907=CARTESIAN_POINT('Ctrl Pts',(-93.3107631904288,4.84268801544614,131.674046196523));
#96908=CARTESIAN_POINT('Ctrl Pts',(-93.3185110872058,4.86507114510722,131.538589494163));
#96909=CARTESIAN_POINT('Ctrl Pts',(-93.3262589839829,4.88175514022601,131.402398921838));
#96910=CARTESIAN_POINT('Ctrl Pts',(-93.3340052600669,4.89843564541268,131.266236837646));
#96911=CARTESIAN_POINT('Ctrl Pts',(-93.341751536151,4.90941933977151,131.129341576648));
#96912=CARTESIAN_POINT('Ctrl Pts',(-93.349497812235,4.91466063915287,130.992227231049));
#96913=CARTESIAN_POINT('Ctrl Pts',(-93.3572441455003,4.9199019772243,130.855111873303));
#96914=CARTESIAN_POINT('Ctrl Pts',(-93.3649904787656,4.91940082079996,130.71777781841));
#96915=CARTESIAN_POINT('Ctrl Pts',(-93.3727368120309,4.91316368440942,130.580741135632));
#96916=CARTESIAN_POINT('Ctrl Pts',(-93.3804848800338,4.9069251512554,130.443673764439));
#96917=CARTESIAN_POINT('Ctrl Pts',(-93.3882329480367,4.89494809983603,130.306904288363));
#96918=CARTESIAN_POINT('Ctrl Pts',(-93.3959810160396,4.87729105226344,130.170945229364));
#96919=CARTESIAN_POINT('Ctrl Pts',(-93.4037373187814,4.85961523857064,130.03484167146));
#96920=CARTESIAN_POINT('Ctrl Pts',(-93.4114936215232,4.83624742006354,129.899550639542));
#96921=CARTESIAN_POINT('Ctrl Pts',(-93.419249924265,4.80729765580588,129.765576563499));
#96922=CARTESIAN_POINT('Ctrl Pts',(-93.4270103667791,4.7783324401873,129.631530981458));
#96923=CARTESIAN_POINT('Ctrl Pts',(-93.4347708092933,4.74377944085467,129.498804134045));
#96924=CARTESIAN_POINT('Ctrl Pts',(-93.4425312518074,4.70379881079189,129.367885831817));
#96925=CARTESIAN_POINT('Ctrl Pts',(-93.4503041520727,4.66375400027242,129.236757367908));
#96926=CARTESIAN_POINT('Ctrl Pts',(-93.4580770523382,4.61826427765711,129.107443619798));
#96927=CARTESIAN_POINT('Ctrl Pts',(-93.4658499526036,4.56753853714037,128.980415778971));
#96928=CARTESIAN_POINT('Ctrl Pts',(-93.4733402883661,4.51865680505869,128.858005720113));
#96929=CARTESIAN_POINT('Ctrl Pts',(-93.4808306241285,4.46491325635545,128.737718538211));
#96930=CARTESIAN_POINT('Ctrl Pts',(-93.488320959891,4.40653449895807,128.619952969714));
#96931=CARTESIAN_POINT('Ctrl Pts',(-93.4960952940101,4.34594229323363,128.497722283901));
#96932=CARTESIAN_POINT('Ctrl Pts',(-93.5038696281292,4.28016451456443,128.377821009989));
#96933=CARTESIAN_POINT('Ctrl Pts',(-93.5116439622483,4.20940346776533,128.260720409505));
#96934=CARTESIAN_POINT('Ctrl Pts',(-93.5194087151954,4.13872962763252,128.143764125046));
#96935=CARTESIAN_POINT('Ctrl Pts',(-93.5271734681424,4.06308493925008,128.029601977805));
#96936=CARTESIAN_POINT('Ctrl Pts',(-93.5349382210895,3.98271883514135,127.918683272));
#96937=CARTESIAN_POINT('Ctrl Pts',(-93.5426952619745,3.90243255177997,127.807874732217));
#96938=CARTESIAN_POINT('Ctrl Pts',(-93.5504523028595,3.81743441266948,127.700303537624));
#96939=CARTESIAN_POINT('Ctrl Pts',(-93.5582093437446,3.72801844199509,127.596392170302));
#96940=CARTESIAN_POINT('Ctrl Pts',(-93.5659605349847,3.63866990059985,127.492559163349));
#96941=CARTESIAN_POINT('Ctrl Pts',(-93.573711726225,3.5449104128099,127.392380785397));
#96942=CARTESIAN_POINT('Ctrl Pts',(-93.5814629174651,3.44707555015369,127.296248131623));
#96943=CARTESIAN_POINT('Ctrl Pts',(-93.5892108142422,3.34928226992381,127.20015633679));
#96944=CARTESIAN_POINT('Ctrl Pts',(-93.5969587110193,3.24741733821374,127.108107119542));
#96945=CARTESIAN_POINT('Ctrl Pts',(-93.6047066077964,3.14185445948987,127.020456070952));
#96946=CARTESIAN_POINT('Ctrl Pts',(-93.6124528838805,3.03631366224456,126.932823357072));
#96947=CARTESIAN_POINT('Ctrl Pts',(-93.6201991599646,2.92707675718301,126.849587231511));
#96948=CARTESIAN_POINT('Ctrl Pts',(-93.6279454360487,2.81455162529098,126.7710639249));
#96949=CARTESIAN_POINT('Ctrl Pts',(-93.6356917693141,2.70202566276414,126.692540038647));
#96950=CARTESIAN_POINT('Ctrl Pts',(-93.6434381025795,2.58621174558976,126.6187292645));
#96951=CARTESIAN_POINT('Ctrl Pts',(-93.6511844358448,2.46754757871762,126.549905069642));
#96952=CARTESIAN_POINT('Ctrl Pts',(-93.6589325038479,2.34885683782791,126.481065462082));
#96953=CARTESIAN_POINT('Ctrl Pts',(-93.6666805718508,2.2273149152436,126.41721485205));
#96954=CARTESIAN_POINT('Ctrl Pts',(-93.6744286398538,2.10338464283626,126.358581033873));
#96955=CARTESIAN_POINT('Ctrl Pts',(-93.6821849425957,1.97932265586078,126.299884898977));
#96956=CARTESIAN_POINT('Ctrl Pts',(-93.6899412453376,1.85286760237231,126.246416799079));
#96957=CARTESIAN_POINT('Ctrl Pts',(-93.6976975480794,1.72450336313443,126.198356795049));
#96958=CARTESIAN_POINT('Ctrl Pts',(-93.7054579905936,1.59607061203674,126.150271139948));
#96959=CARTESIAN_POINT('Ctrl Pts',(-93.7132184331078,1.46572701614474,126.107599453819));
#96960=CARTESIAN_POINT('Ctrl Pts',(-93.720978875622,1.33397123354978,126.07047174999));
#96961=CARTESIAN_POINT('Ctrl Pts',(-93.7287517758875,1.20200394487588,126.033284445474));
#96962=CARTESIAN_POINT('Ctrl Pts',(-93.736524676153,1.06862032001299,126.00165899793));
#96963=CARTESIAN_POINT('Ctrl Pts',(-93.7442975764185,0.934329698113822,
125.97567434926));
#96964=CARTESIAN_POINT('Ctrl Pts',(-93.7517879121804,0.804920878580893,
125.950634308022));
#96965=CARTESIAN_POINT('Ctrl Pts',(-93.7592782479422,0.674670164913171,
125.930832117648));
#96966=CARTESIAN_POINT('Ctrl Pts',(-93.7667685837041,0.544035512498864,
125.916292653264));
#96967=CARTESIAN_POINT('Ctrl Pts',(-93.7745429178232,0.408447807531721,
125.901201920668));
#96968=CARTESIAN_POINT('Ctrl Pts',(-93.7823172519422,0.272016973927845,
125.891733061484));
#96969=CARTESIAN_POINT('Ctrl Pts',(-93.7900915860612,0.135248848051348,
125.887970599311));
#96970=CARTESIAN_POINT('Ctrl Pts',(-93.7978563390082,-0.00135072333332237,
125.884212774035));
#96971=CARTESIAN_POINT('Ctrl Pts',(-93.8056210919553,-0.138286372840629,
125.886147363591));
#96972=CARTESIAN_POINT('Ctrl Pts',(-93.8133858449023,-0.275045263736215,
125.893807373236));
#96973=CARTESIAN_POINT('Ctrl Pts',(-93.8211428857872,-0.411668323773028,
125.901459774852));
#96974=CARTESIAN_POINT('Ctrl Pts',(-93.8288999266721,-0.548114586741336,
125.914826258307));
#96975=CARTESIAN_POINT('Ctrl Pts',(-93.836656967557,-0.683869679246917,
125.933887814613));
#96976=CARTESIAN_POINT('Ctrl Pts',(-93.8444081587971,-0.819522397781403,
125.95293499645));
#96977=CARTESIAN_POINT('Ctrl Pts',(-93.8521593500371,-0.954484597703345,
125.977668648658));
#96978=CARTESIAN_POINT('Ctrl Pts',(-93.8599105412771,-1.08824585495615,
126.008017841901));
#96979=CARTESIAN_POINT('Ctrl Pts',(-93.8676584380541,-1.2219502601066,126.038354135928));
#96980=CARTESIAN_POINT('Ctrl Pts',(-93.8754063348312,-1.35445435732335,
126.07430113759));
#96981=CARTESIAN_POINT('Ctrl Pts',(-93.8831542316082,-1.48525698137443,
126.115736644397));
#96982=CARTESIAN_POINT('Ctrl Pts',(-93.8909005076922,-1.61603224433669,
126.157163483789));
#96983=CARTESIAN_POINT('Ctrl Pts',(-93.8986467837762,-1.7451063695853,126.204076426745));
#96984=CARTESIAN_POINT('Ctrl Pts',(-93.9063930598602,-1.87199283369897,
126.25630324182));
#96985=CARTESIAN_POINT('Ctrl Pts',(-93.9141393931255,-1.99888023445917,
126.308530442421));
#96986=CARTESIAN_POINT('Ctrl Pts',(-93.9218857263907,-2.12357958032309,
126.366071444604));
#96987=CARTESIAN_POINT('Ctrl Pts',(-93.929632059656,-2.2456242053865,126.428705810491));
#96988=CARTESIAN_POINT('Ctrl Pts',(-93.9373801276589,-2.36769616149799,
126.491354202909));
#96989=CARTESIAN_POINT('Ctrl Pts',(-93.9451281956619,-2.48711186604396,
126.559098050264));
#96990=CARTESIAN_POINT('Ctrl Pts',(-93.9528762636648,-2.6034294972728,126.631671087391));
#96991=CARTESIAN_POINT('Ctrl Pts',(-93.9606325664066,-2.71987075226446,
126.704321256006));
#96992=CARTESIAN_POINT('Ctrl Pts',(-93.9683888691484,-2.83320702425014,
126.781810659872));
#96993=CARTESIAN_POINT('Ctrl Pts',(-93.9761451718902,-2.94302527354926,
126.863829523697));
#96994=CARTESIAN_POINT('Ctrl Pts',(-93.9839056144043,-3.05290213615429,
126.945892163458));
#96995=CARTESIAN_POINT('Ctrl Pts',(-93.9916660569184,-3.15925693161789,
127.032488833536));
#96996=CARTESIAN_POINT('Ctrl Pts',(-93.9994264994325,-3.26171073916644,
127.123270274134));
#96997=CARTESIAN_POINT('Ctrl Pts',(-94.0071993996978,-3.36432901466257,
127.214197445161));
#96998=CARTESIAN_POINT('Ctrl Pts',(-94.0149722999632,-3.46303350667502,
127.309322539484));
#96999=CARTESIAN_POINT('Ctrl Pts',(-94.0227452002286,-3.55748248889155,
127.408259705677));
#97000=CARTESIAN_POINT('Ctrl Pts',(-94.0302355359913,-3.64849801271059,
127.503600256681));
#97001=CARTESIAN_POINT('Ctrl Pts',(-94.0377258717539,-3.73556184859653,
127.602480303399));
#97002=CARTESIAN_POINT('Ctrl Pts',(-94.0452162075166,-3.81840553232964,
127.704528000605));
#97003=CARTESIAN_POINT('Ctrl Pts',(-94.0529669144684,-3.90412894123516,
127.810122972741));
#97004=CARTESIAN_POINT('Ctrl Pts',(-94.0607176214202,-3.98561230062312,
127.919453344993));
#97005=CARTESIAN_POINT('Ctrl Pts',(-94.068468328372,-4.06251064084263,128.032143029508));
#97006=CARTESIAN_POINT('Ctrl Pts',(-94.0765316119714,-4.14251019822082,
128.149377352856));
#97007=CARTESIAN_POINT('Ctrl Pts',(-94.0845948955708,-4.21754685391524,
128.270247352509));
#97008=CARTESIAN_POINT('Ctrl Pts',(-94.0926581791702,-4.28727613769913,
128.394288755232));
#97009=CARTESIAN_POINT('Ctrl Pts',(-94.1003894614796,-4.35413435637868,
128.513222821072));
#97010=CARTESIAN_POINT('Ctrl Pts',(-94.1081207437889,-4.41611330721045,
128.635071952975));
#97011=CARTESIAN_POINT('Ctrl Pts',(-94.1158520260983,-4.47295211812505,
128.759395480587));
#97012=CARTESIAN_POINT('Ctrl Pts',(-94.1235778857442,-4.52975106272427,
128.883631808609));
#97013=CARTESIAN_POINT('Ctrl Pts',(-94.1313037453902,-4.58141687585617,
129.010338723938));
#97014=CARTESIAN_POINT('Ctrl Pts',(-94.1390296050361,-4.62773442138493,
129.139050680158));
#97015=CARTESIAN_POINT('Ctrl Pts',(-94.1467512564063,-4.67402673774634,
129.267692526976));
#97016=CARTESIAN_POINT('Ctrl Pts',(-94.1544729077765,-4.7149764535067,129.398336871008));
#97017=CARTESIAN_POINT('Ctrl Pts',(-94.1621945591467,-4.75041662047909,
129.530498382324));
#97018=CARTESIAN_POINT('Ctrl Pts',(-94.1632056166193,-4.75505708453684,
129.547803344334));
#97019=CARTESIAN_POINT('Ctrl Pts',(-94.164216674092,-4.75960315778423,129.565134293483));
#97020=CARTESIAN_POINT('Ctrl Pts',(-94.1652277315646,-4.76405452823406,
129.582490119308));
#97021=CARTESIAN_POINT('Ctrl Pts',(-92.4154045049002,-4.764054528234,129.582490119308));
#97022=CARTESIAN_POINT('Ctrl Pts',(-92.424023850493,-4.80175568549997,129.729486359293));
#97023=CARTESIAN_POINT('Ctrl Pts',(-92.4326431960858,-4.83269371092977,
129.878401800015));
#97024=CARTESIAN_POINT('Ctrl Pts',(-92.4412625416786,-4.85668916151153,
130.028632926326));
#97025=CARTESIAN_POINT('Ctrl Pts',(-92.4498401457289,-4.88056840754981,
130.17813651725));
#97026=CARTESIAN_POINT('Ctrl Pts',(-92.4584177497793,-4.89757206130976,
130.32894286188));
#97027=CARTESIAN_POINT('Ctrl Pts',(-92.4669953538296,-4.90757148331663,
130.480439024218));
#97028=CARTESIAN_POINT('Ctrl Pts',(-92.4730437572057,-4.91462246602353,
130.587264880759));
#97029=CARTESIAN_POINT('Ctrl Pts',(-92.4790921605817,-4.91819179696133,
130.694433345267));
#97030=CARTESIAN_POINT('Ctrl Pts',(-92.4851405639579,-4.91824929378548,
130.801724962307));
#97031=CARTESIAN_POINT('',(-92.1398594360289,-4.91824936578745,130.801862932376));
#97032=CARTESIAN_POINT('Ctrl Pts',(-92.0697718875171,-4.76405452823417,
129.582490119309));
#97033=CARTESIAN_POINT('Ctrl Pts',(-92.0775447754838,-4.79811707026865,
129.71529945373));
#97034=CARTESIAN_POINT('Ctrl Pts',(-92.0853176634505,-4.82658582570716,
129.849393649157));
#97035=CARTESIAN_POINT('Ctrl Pts',(-92.0930905514173,-4.84939385186018,
129.984261640588));
#97036=CARTESIAN_POINT('Ctrl Pts',(-92.1006176466071,-4.87148064697149,
130.114864862183));
#97037=CARTESIAN_POINT('Ctrl Pts',(-92.1081447417968,-4.88825931939402,
130.246193359425));
#97038=CARTESIAN_POINT('Ctrl Pts',(-92.1156718369866,-4.89971567372624,
130.377781927121));
#97039=CARTESIAN_POINT('Ctrl Pts',(-92.1237343699882,-4.91198697262083,
130.51873101079));
#97040=CARTESIAN_POINT('Ctrl Pts',(-92.1317969029898,-4.91817743232996,
130.660217143608));
#97041=CARTESIAN_POINT('Ctrl Pts',(-92.1398594359916,-4.91824936578712,
130.80186293172));
#97042=CARTESIAN_POINT('Ctrl Pts',(-92.1398594360288,-4.91824936578745,
130.801862932376));
#97043=CARTESIAN_POINT('Ctrl Pts',(-92.1475407774203,-4.91831789825695,
130.93681179459));
#97044=CARTESIAN_POINT('Ctrl Pts',(-92.1552221188117,-4.91282807124698,
131.0719867331));
#97045=CARTESIAN_POINT('Ctrl Pts',(-92.1629034602031,-4.90175039741188,
131.20688528013));
#97046=CARTESIAN_POINT('Ctrl Pts',(-92.1705759898489,-4.89068543146713,
131.341629076626));
#97047=CARTESIAN_POINT('Ctrl Pts',(-92.1782485194948,-4.8740454003861,131.47609671642));
#97048=CARTESIAN_POINT('Ctrl Pts',(-92.1859210491406,-4.85185281164743,
131.609784330036));
#97049=CARTESIAN_POINT('Ctrl Pts',(-92.193586715678,-4.82968007426798,131.743352359547));
#97050=CARTESIAN_POINT('Ctrl Pts',(-92.2012523822153,-4.80196472494574,
131.876141357745));
#97051=CARTESIAN_POINT('Ctrl Pts',(-92.2089180487527,-4.76878115459254,
132.007651672175));
#97052=CARTESIAN_POINT('Ctrl Pts',(-92.2166347742547,-4.7353765573092,132.140037941808));
#97053=CARTESIAN_POINT('Ctrl Pts',(-92.2243514997566,-4.69643065403239,
132.271128020614));
#97054=CARTESIAN_POINT('Ctrl Pts',(-92.2320682252585,-4.65207195115217,
132.4004212755));
#97055=CARTESIAN_POINT('Ctrl Pts',(-92.23972692109,-4.60804682511228,132.528742246872));
#97056=CARTESIAN_POINT('Ctrl Pts',(-92.2473856169216,-4.55869017428788,
132.65529294547));
#97057=CARTESIAN_POINT('Ctrl Pts',(-92.255044312753,-4.50417778488755,132.779598715777));
#97058=CARTESIAN_POINT('Ctrl Pts',(-92.2627023841936,-4.4496698397213,132.903894351802));
#97059=CARTESIAN_POINT('Ctrl Pts',(-92.2703604556343,-4.39000715277736,
133.025945056422));
#97060=CARTESIAN_POINT('Ctrl Pts',(-92.278018527075,-4.32541343863651,133.145296679778));
#97061=CARTESIAN_POINT('Ctrl Pts',(-92.2856777243033,-4.26081022878763,
133.26466584862));
#97062=CARTESIAN_POINT('Ctrl Pts',(-92.2933369215316,-4.19127474119288,
133.381334794752));
#97063=CARTESIAN_POINT('Ctrl Pts',(-92.3009961187599,-4.11707610984384,
133.494874949112));
#97064=CARTESIAN_POINT('Ctrl Pts',(-92.3087563972632,-4.04189825155601,
133.609913535124));
#97065=CARTESIAN_POINT('Ctrl Pts',(-92.3165166757665,-3.96193351289705,
133.72173979682));
#97066=CARTESIAN_POINT('Ctrl Pts',(-92.3242769542698,-3.87750578463183,
133.829940223633));
#97067=CARTESIAN_POINT('Ctrl Pts',(-92.3319475927844,-3.79405329206241,
133.936890813209));
#97068=CARTESIAN_POINT('Ctrl Pts',(-92.3396182312991,-3.70624068100972,
134.040298626305));
#97069=CARTESIAN_POINT('Ctrl Pts',(-92.3472888698137,-3.61441924797575,
134.139800103205));
#97070=CARTESIAN_POINT('Ctrl Pts',(-92.3550939683113,-3.52098826075632,
134.241045759143));
#97071=CARTESIAN_POINT('Ctrl Pts',(-92.362899066809,-3.42340690801974,134.33824654365));
#97072=CARTESIAN_POINT('Ctrl Pts',(-92.3707041653066,-3.322081168469,134.431061566446));
#97073=CARTESIAN_POINT('Ctrl Pts',(-92.3785092638042,-3.22075542891826,
134.523876589241));
#97074=CARTESIAN_POINT('Ctrl Pts',(-92.3863143623019,-3.11568567483839,
134.612305625749));
#97075=CARTESIAN_POINT('Ctrl Pts',(-92.3941194607995,-3.00730873746807,
134.696053979079));
#97076=CARTESIAN_POINT('Ctrl Pts',(-92.4018937949185,-2.89935897588927,
134.779472232022));
#97077=CARTESIAN_POINT('Ctrl Pts',(-92.4096681290376,-2.78776475261839,
134.858527661847));
#97078=CARTESIAN_POINT('Ctrl Pts',(-92.4174424631567,-2.67291411339402,
134.932884955016));
#97079=CARTESIAN_POINT('Ctrl Pts',(-92.4252072161037,-2.55820501731832,
135.007150609467));
#97080=CARTESIAN_POINT('Ctrl Pts',(-92.4329719690508,-2.44024781548098,
135.076729437264));
#97081=CARTESIAN_POINT('Ctrl Pts',(-92.4407367219978,-2.31946333110538,
135.141326483025));
#97082=CARTESIAN_POINT('Ctrl Pts',(-92.4484937628828,-2.19879881158243,
135.20585937009));
#97083=CARTESIAN_POINT('Ctrl Pts',(-92.4562508037678,-2.07531294028713,
135.265420138627));
#97084=CARTESIAN_POINT('Ctrl Pts',(-92.4640078446527,-1.94945490956833,
135.319757457054));
#97085=CARTESIAN_POINT('Ctrl Pts',(-92.4717590358928,-1.82369178936936,
135.374053799287));
#97086=CARTESIAN_POINT('Ctrl Pts',(-92.4795102271329,-1.69556042786087,
135.423134377499));
#97087=CARTESIAN_POINT('Ctrl Pts',(-92.487261418373,-1.56553365231574,135.466794257412));
#97088=CARTESIAN_POINT('Ctrl Pts',(-92.4950093151501,-1.43556214161862,
135.510435580711));
#97089=CARTESIAN_POINT('Ctrl Pts',(-92.5027572119271,-1.30369718901858,
135.548660663888));
#97090=CARTESIAN_POINT('Ctrl Pts',(-92.5105051087042,-1.17043038545329,
135.581313179117));
#97091=CARTESIAN_POINT('Ctrl Pts',(-92.5182513847883,-1.03719145843076,
135.613958864144));
#97092=CARTESIAN_POINT('Ctrl Pts',(-92.5259976608723,-0.902551643199964,
135.641034206805));
#97093=CARTESIAN_POINT('Ctrl Pts',(-92.5337439369564,-0.767016049777256,
135.662433223228));
#97094=CARTESIAN_POINT('Ctrl Pts',(-92.5414902702217,-0.631479455861401,
135.683832397613));
#97095=CARTESIAN_POINT('Ctrl Pts',(-92.5492366034871,-0.495047456740555,
135.699555101177));
#97096=CARTESIAN_POINT('Ctrl Pts',(-92.5569829367524,-0.358233278960902,
135.709546850559));
#97097=CARTESIAN_POINT('Ctrl Pts',(-92.5647310047553,-0.221388462595671,
135.719540837524));
#97098=CARTESIAN_POINT('Ctrl Pts',(-92.5724790727582,-0.0841616871169833,
135.723801288006));
#97099=CARTESIAN_POINT('Ctrl Pts',(-92.5802271407611,0.0529312008536751,
135.722325781175));
#97100=CARTESIAN_POINT('Ctrl Pts',(-92.5879834435029,0.19016979277803,135.720848706159));
#97101=CARTESIAN_POINT('Ctrl Pts',(-92.5957397462448,0.327273821374372,
135.713623500143));
#97102=CARTESIAN_POINT('Ctrl Pts',(-92.6034960489866,0.463729388489498,
135.700699874271));
#97103=CARTESIAN_POINT('Ctrl Pts',(-92.6112564915008,0.600257786049763,
135.687769350671));
#97104=CARTESIAN_POINT('Ctrl Pts',(-92.619016934015,0.736136645338421,135.669134400028));
#97105=CARTESIAN_POINT('Ctrl Pts',(-92.6267773765292,0.870860668680839,
135.644896203454));
#97106=CARTESIAN_POINT('Ctrl Pts',(-92.6345502767946,1.0058009629854,135.620619097575));
#97107=CARTESIAN_POINT('Ctrl Pts',(-92.6423231770599,1.13958233499793,135.590720856553));
#97108=CARTESIAN_POINT('Ctrl Pts',(-92.6500960773253,1.27171221903285,135.555353260632));
#97109=CARTESIAN_POINT('Ctrl Pts',(-92.6575864130876,1.39903884897194,135.521271365906));
#97110=CARTESIAN_POINT('Ctrl Pts',(-92.6650767488499,1.52483168371457,135.482110953708));
#97111=CARTESIAN_POINT('Ctrl Pts',(-92.6725670846121,1.64866801332278,135.438049951601));
#97112=CARTESIAN_POINT('Ctrl Pts',(-92.6803414187312,1.77719963500352,135.392318363208));
#97113=CARTESIAN_POINT('Ctrl Pts',(-92.6881157528502,1.90403061060044,135.341162373514));
#97114=CARTESIAN_POINT('Ctrl Pts',(-92.6958900869693,2.02866908313515,135.284727211231));
#97115=CARTESIAN_POINT('Ctrl Pts',(-92.7036548399164,2.15315394989138,135.228361600242));
#97116=CARTESIAN_POINT('Ctrl Pts',(-92.7114195928634,2.27545133714997,135.166729921597));
#97117=CARTESIAN_POINT('Ctrl Pts',(-92.7191843458105,2.39508562536236,135.100026795202));
#97118=CARTESIAN_POINT('Ctrl Pts',(-92.7269413866955,2.51460109111315,135.033389919292));
#97119=CARTESIAN_POINT('Ctrl Pts',(-92.7346984275805,2.63145838227722,134.961691808717));
#97120=CARTESIAN_POINT('Ctrl Pts',(-92.7424554684655,2.74520324703989,134.885174530861));
#97121=CARTESIAN_POINT('Ctrl Pts',(-92.7502066597056,2.85886233591539,134.80871495528));
#97122=CARTESIAN_POINT('Ctrl Pts',(-92.7579578509456,2.96941334707704,134.727443663357));
#97123=CARTESIAN_POINT('Ctrl Pts',(-92.7657090421858,3.07642828882265,134.641647686086));
#97124=CARTESIAN_POINT('Ctrl Pts',(-92.7734569389628,3.18339774636316,134.555888174394));
#97125=CARTESIAN_POINT('Ctrl Pts',(-92.7812048357399,3.28683381929068,134.465608046319));
#97126=CARTESIAN_POINT('Ctrl Pts',(-92.788952732517,3.38633926766975,134.371136392231));
#97127=CARTESIAN_POINT('Ctrl Pts',(-92.7966990086011,3.4858239016541,134.276684499577));
#97128=CARTESIAN_POINT('Ctrl Pts',(-92.8044452846851,3.58137926314151,134.178043093886));
#97129=CARTESIAN_POINT('Ctrl Pts',(-92.8121915607692,3.67264316059553,134.075579851648));
#97130=CARTESIAN_POINT('Ctrl Pts',(-92.8199378940345,3.76390773173878,133.973115853051));
#97131=CARTESIAN_POINT('Ctrl Pts',(-92.8276842273,3.85088051559807,133.86683025356));
#97132=CARTESIAN_POINT('Ctrl Pts',(-92.8354305605653,3.93323826229641,133.757125395619));
#97133=CARTESIAN_POINT('Ctrl Pts',(-92.8431786285683,4.01561445244121,133.647395970035));
#97134=CARTESIAN_POINT('Ctrl Pts',(-92.8509266965711,4.09337331419015,133.534246074912));
#97135=CARTESIAN_POINT('Ctrl Pts',(-92.8586747645741,4.16623398313402,133.418108398106));
#97136=CARTESIAN_POINT('Ctrl Pts',(-92.8664310673159,4.239172089264,133.301847288796));
#97137=CARTESIAN_POINT('Ctrl Pts',(-92.8741873700578,4.30720139522228,133.182592386212));
#97138=CARTESIAN_POINT('Ctrl Pts',(-92.8819436727996,4.37008594989862,133.060802917515));
#97139=CARTESIAN_POINT('Ctrl Pts',(-92.8897041153138,4.43300406795539,132.938948446111));
#97140=CARTESIAN_POINT('Ctrl Pts',(-92.897464557828,4.49077179868117,132.814557067495));
#97141=CARTESIAN_POINT('Ctrl Pts',(-92.9052250003422,4.54320114287566,132.688108593775));
#97142=CARTESIAN_POINT('Ctrl Pts',(-92.9129979006076,4.59571465130776,132.56145713374));
#97143=CARTESIAN_POINT('Ctrl Pts',(-92.920770800873,4.64287251373869,132.432742347004));
#97144=CARTESIAN_POINT('Ctrl Pts',(-92.9285437011385,4.68453618340016,132.302460683955));
#97145=CARTESIAN_POINT('Ctrl Pts',(-92.9360340369007,4.72468527372622,132.176915087514));
#97146=CARTESIAN_POINT('Ctrl Pts',(-92.9435243726629,4.75973260970269,132.049914853668));
#97147=CARTESIAN_POINT('Ctrl Pts',(-92.9510147084252,4.78959940178096,131.921911794452));
#97148=CARTESIAN_POINT('Ctrl Pts',(-92.9587890425443,4.82059860235787,131.789055460344));
#97149=CARTESIAN_POINT('Ctrl Pts',(-92.9665633766633,4.84611485974488,131.654697906551));
#97150=CARTESIAN_POINT('Ctrl Pts',(-92.9743377107824,4.86600449825838,131.519331445942));
#97151=CARTESIAN_POINT('Ctrl Pts',(-92.9821024637295,4.88586962456994,131.384131812399));
#97152=CARTESIAN_POINT('Ctrl Pts',(-92.9898672166766,4.90012187291857,131.247926129111));
#97153=CARTESIAN_POINT('Ctrl Pts',(-92.9976319696237,4.90866789856035,131.111219745087));
#97154=CARTESIAN_POINT('Ctrl Pts',(-93.0053890105087,4.91720543616898,130.974649139772));
#97155=CARTESIAN_POINT('Ctrl Pts',(-93.0131460513937,4.92004800541794,130.837579211055));
#97156=CARTESIAN_POINT('Ctrl Pts',(-93.0209030922787,4.91715373025298,130.700522977188));
#97157=CARTESIAN_POINT('Ctrl Pts',(-93.0286542835189,4.91426163768341,130.563570098493));
#97158=CARTESIAN_POINT('Ctrl Pts',(-93.036405474759,4.90564131995753,130.426631283388));
#97159=CARTESIAN_POINT('Ctrl Pts',(-93.0441566659992,4.89130292440958,130.290221760678));
#97160=CARTESIAN_POINT('Ctrl Pts',(-93.0519045627763,4.87697062306229,130.153870215654));
#97161=CARTESIAN_POINT('Ctrl Pts',(-93.0596524595533,4.85692511842995,130.018047903598));
#97162=CARTESIAN_POINT('Ctrl Pts',(-93.0674003563304,4.83122856567375,129.883266915102));
#97163=CARTESIAN_POINT('Ctrl Pts',(-93.0751466324145,4.80553738808243,129.748514119884));
#97164=CARTESIAN_POINT('Ctrl Pts',(-93.0828929084987,4.77419758675797,129.61480259877));
#97165=CARTESIAN_POINT('Ctrl Pts',(-93.0906391845828,4.73732272497176,129.48263581188));
#97166=CARTESIAN_POINT('Ctrl Pts',(-93.0983855178482,4.70044759098376,129.350468049365));
#97167=CARTESIAN_POINT('Ctrl Pts',(-93.1061318511135,4.65803742007127,129.219845420412));
#97168=CARTESIAN_POINT('Ctrl Pts',(-93.1138781843789,4.61025598987186,129.091257360214));
#97169=CARTESIAN_POINT('Ctrl Pts',(-93.1216262523819,4.56246385935238,128.962640503611));
#97170=CARTESIAN_POINT('Ctrl Pts',(-93.1293743203848,4.50929821215446,128.836059488822));
#97171=CARTESIAN_POINT('Ctrl Pts',(-93.1371223883878,4.45097126675221,128.711984493384));
#97172=CARTESIAN_POINT('Ctrl Pts',(-93.1448786911296,4.39258233077837,128.587777629564));
#97173=CARTESIAN_POINT('Ctrl Pts',(-93.1526349938715,4.3290213053387,128.466082459962));
#97174=CARTESIAN_POINT('Ctrl Pts',(-93.1603912966134,4.26054701390939,128.347345720426));
#97175=CARTESIAN_POINT('Ctrl Pts',(-93.1681517391275,4.19203617568902,128.228545607517));
#97176=CARTESIAN_POINT('Ctrl Pts',(-93.1759121816417,4.11860705542509,128.11270740102));
#97177=CARTESIAN_POINT('Ctrl Pts',(-93.1836726241559,4.04056171447239,128.000248620152));
#97178=CARTESIAN_POINT('Ctrl Pts',(-93.1914455244213,3.96239108820964,127.887609310465));
#97179=CARTESIAN_POINT('Ctrl Pts',(-93.1992184246868,3.87958966927376,127.778360578957));
#97180=CARTESIAN_POINT('Ctrl Pts',(-93.2069913249523,3.79250024752544,127.67288733251));
#97181=CARTESIAN_POINT('Ctrl Pts',(-93.2144816607142,3.70857674562457,127.571248304245));
#97182=CARTESIAN_POINT('Ctrl Pts',(-93.221971996476,3.62067179323408,127.473115259353));
#97183=CARTESIAN_POINT('Ctrl Pts',(-93.2294623322379,3.52912292494078,127.378798701156));
#97184=CARTESIAN_POINT('Ctrl Pts',(-93.237236666357,3.43410295347847,127.280906101986));
#97185=CARTESIAN_POINT('Ctrl Pts',(-93.245011000476,3.33485629865505,127.186815012297));
#97186=CARTESIAN_POINT('Ctrl Pts',(-93.2527853345951,3.23171949701599,127.096912417644));
#97187=CARTESIAN_POINT('Ctrl Pts',(-93.2605500875422,3.12870980226791,127.007120619904));
#97188=CARTESIAN_POINT('Ctrl Pts',(-93.2683148404893,3.02181979173525,126.921507300897));
#97189=CARTESIAN_POINT('Ctrl Pts',(-93.2760795934364,2.91142417473824,126.840424147685));
#97190=CARTESIAN_POINT('Ctrl Pts',(-93.2838366343214,2.80113820422434,126.759421527404));
#97191=CARTESIAN_POINT('Ctrl Pts',(-93.2915936752062,2.68735386928573,126.682940348799));
#97192=CARTESIAN_POINT('Ctrl Pts',(-93.2993507160912,2.57048015167668,126.611293142276));
#97193=CARTESIAN_POINT('Ctrl Pts',(-93.3071019073313,2.45369456944706,126.539699965469));
#97194=CARTESIAN_POINT('Ctrl Pts',(-93.3148530985715,2.33382457369807,126.472933708431));
#97195=CARTESIAN_POINT('Ctrl Pts',(-93.3226042898116,2.21130912589593,126.411264327678));
#97196=CARTESIAN_POINT('Ctrl Pts',(-93.3303521865887,2.08884575042714,126.349621158056));
#97197=CARTESIAN_POINT('Ctrl Pts',(-93.3381000833658,1.96373950771476,126.293070731511));
#97198=CARTESIAN_POINT('Ctrl Pts',(-93.3458479801428,1.83645483045995,126.241837552618));
#97199=CARTESIAN_POINT('Ctrl Pts',(-93.353594256227,1.70919677841534,126.190615090602));
#97200=CARTESIAN_POINT('Ctrl Pts',(-93.361340532311,1.57976156066156,126.144707809798));
#97201=CARTESIAN_POINT('Ctrl Pts',(-93.3690868083952,1.44863413617935,126.104292298701));
#97202=CARTESIAN_POINT('Ctrl Pts',(-93.3768331416605,1.31750574374517,126.063876489267));
#97203=CARTESIAN_POINT('Ctrl Pts',(-93.3845794749259,1.18468549327806,126.02895264559));
#97204=CARTESIAN_POINT('Ctrl Pts',(-93.3923258081912,1.0506736862822,125.999647528582));
#97205=CARTESIAN_POINT('Ctrl Pts',(-93.4000738761942,0.916631868270413,
125.970335848896));
#97206=CARTESIAN_POINT('Ctrl Pts',(-93.4078219441971,0.781398344614256,
125.946645483206));
#97207=CARTESIAN_POINT('Ctrl Pts',(-93.4155700122001,0.645483398260895,
125.928652028543));
#97208=CARTESIAN_POINT('Ctrl Pts',(-93.4233263149419,0.509423999885697,
125.910639450223));
#97209=CARTESIAN_POINT('Ctrl Pts',(-93.4310826176839,0.372682120299041,
125.898335929327));
#97210=CARTESIAN_POINT('Ctrl Pts',(-93.4388389204257,0.235773511433159,
125.891765181973));
#97211=CARTESIAN_POINT('Ctrl Pts',(-93.4465993629399,0.0987918303201126,
125.885190927614));
#97212=CARTESIAN_POINT('Ctrl Pts',(-93.4543598054541,-0.0383563666225004,
125.884355545996));
#97213=CARTESIAN_POINT('Ctrl Pts',(-93.4621202479683,-0.175156537113291,
125.88923058368));
#97214=CARTESIAN_POINT('Ctrl Pts',(-93.4698931482337,-0.312176311382302,
125.894113447208));
#97215=CARTESIAN_POINT('Ctrl Pts',(-93.477666048499,-0.44884655275655,125.904725018088));
#97216=CARTESIAN_POINT('Ctrl Pts',(-93.4854389487645,-0.584658141882119,
125.920984949073));
#97217=CARTESIAN_POINT('Ctrl Pts',(-93.4929292845266,-0.715532637655331,
125.936653790611));
#97218=CARTESIAN_POINT('Ctrl Pts',(-93.5004196202887,-0.845609521563356,
125.957567408858));
#97219=CARTESIAN_POINT('Ctrl Pts',(-93.5079099560508,-0.97444511267973,
125.983609661037));
#97220=CARTESIAN_POINT('Ctrl Pts',(-93.5156842901699,-1.1081655443907,126.010639313123));
#97221=CARTESIAN_POINT('Ctrl Pts',(-93.5234586242889,-1.24097228411011,
126.043279802357));
#97222=CARTESIAN_POINT('Ctrl Pts',(-93.531232958408,-1.37235784370795,126.081457166159));
#97223=CARTESIAN_POINT('Ctrl Pts',(-93.5389977113552,-1.50358148234658,
126.119587479772));
#97224=CARTESIAN_POINT('Ctrl Pts',(-93.5467624643023,-1.63338705394936,
126.163240982771));
#97225=CARTESIAN_POINT('Ctrl Pts',(-93.5545272172494,-1.76127613469166,
126.21229251704));
#97226=CARTESIAN_POINT('Ctrl Pts',(-93.5622842581345,-1.8890381941957,126.261295332634));
#97227=CARTESIAN_POINT('Ctrl Pts',(-93.5700412990195,-2.01488718818781,
126.315685370965));
#97228=CARTESIAN_POINT('Ctrl Pts',(-93.5777983399045,-2.13833911135747,
126.37528747442));
#97229=CARTESIAN_POINT('Ctrl Pts',(-93.5855495311446,-2.26169793847139,
126.434844631465));
#97230=CARTESIAN_POINT('Ctrl Pts',(-93.5933007223848,-2.38266294212549,
126.499605860998));
#97231=CARTESIAN_POINT('Ctrl Pts',(-93.6010519136249,-2.50076973086457,
126.569347770396));
#97232=CARTESIAN_POINT('Ctrl Pts',(-93.608799810402,-2.61882632106767,126.639060037623));
#97233=CARTESIAN_POINT('Ctrl Pts',(-93.6165477071791,-2.73402677658734,
126.713748575941));
#97234=CARTESIAN_POINT('Ctrl Pts',(-93.6242956039561,-2.84593117814597,
126.793143995174));
#97235=CARTESIAN_POINT('Ctrl Pts',(-93.6320418800403,-2.95781217171647,
126.872522806596));
#97236=CARTESIAN_POINT('Ctrl Pts',(-93.6397881561243,-3.06639816404589,
126.956606314466));
#97237=CARTESIAN_POINT('Ctrl Pts',(-93.6475344322085,-3.17127845405589,
127.045081959453));
#97238=CARTESIAN_POINT('Ctrl Pts',(-93.6552807654738,-3.27615951826795,
127.133558257548));
#97239=CARTESIAN_POINT('Ctrl Pts',(-93.6630270987391,-3.37733452674099,
127.226426505361));
#97240=CARTESIAN_POINT('Ctrl Pts',(-93.6707734320044,-3.47442640674552,
127.323334302439));
#97241=CARTESIAN_POINT('Ctrl Pts',(-93.6785215000074,-3.57154002980351,
127.420263801346));
#97242=CARTESIAN_POINT('Ctrl Pts',(-93.6862695680104,-3.66456842820272,
127.521234373485));
#97243=CARTESIAN_POINT('Ctrl Pts',(-93.6940176360134,-3.75317217962262,
127.625857565403));
#97244=CARTESIAN_POINT('Ctrl Pts',(-93.7017739387553,-3.84187010016406,
127.730591952095));
#97245=CARTESIAN_POINT('Ctrl Pts',(-93.7095302414971,-3.9261337267703,127.838986414549));
#97246=CARTESIAN_POINT('Ctrl Pts',(-93.717286544239,-4.00566432988292,127.950619855197));
#97247=CARTESIAN_POINT('Ctrl Pts',(-93.7250469867532,-4.08523738087325,
128.062312877975));
#97248=CARTESIAN_POINT('Ctrl Pts',(-93.7328074292674,-4.1600721615665,128.177247996132));
#97249=CARTESIAN_POINT('Ctrl Pts',(-93.7405678717816,-4.22991448797448,
128.294976930896));
#97250=CARTESIAN_POINT('Ctrl Pts',(-93.748340772047,-4.29986893148494,128.412894854598));
#97251=CARTESIAN_POINT('Ctrl Pts',(-93.7561136723125,-4.3648147201874,128.533615212631));
#97252=CARTESIAN_POINT('Ctrl Pts',(-93.7638865725779,-4.42454426104911,
128.656666238815));
#97253=CARTESIAN_POINT('Ctrl Pts',(-93.7713769083399,-4.48210248265039,
128.77524405025));
#97254=CARTESIAN_POINT('Ctrl Pts',(-93.7788672441018,-4.53481699637019,
128.895985738155));
#97255=CARTESIAN_POINT('Ctrl Pts',(-93.7863575798638,-4.58254569603886,
129.018455243193));
#97256=CARTESIAN_POINT('Ctrl Pts',(-93.7951963202617,-4.63886648048808,
129.162971616836));
#97257=CARTESIAN_POINT('Ctrl Pts',(-93.8040350606597,-4.68839467034822,
129.310276098878));
#97258=CARTESIAN_POINT('Ctrl Pts',(-93.8128738010576,-4.73088032785859,
129.459758674246));
#97259=CARTESIAN_POINT('Ctrl Pts',(-93.8152834783079,-4.74246305545977,
129.50051162602));
#97260=CARTESIAN_POINT('Ctrl Pts',(-93.8176931555582,-4.75352260960667,
129.541426328424));
#97261=CARTESIAN_POINT('Ctrl Pts',(-93.8201028328085,-4.76405452823393,
129.582490119308));
#97262=CARTESIAN_POINT('Origin',(213.235140564004,0.,130.804360617566));
#97263=CARTESIAN_POINT('',(-95.9150180446607,-4.76405452823415,129.582490119309));
#97264=CARTESIAN_POINT('',(-95.5699831042333,-4.76405452823397,129.582490119308));
#97265=CARTESIAN_POINT('',(213.235140564004,-4.76405452823405,129.582490119308));
#97266=CARTESIAN_POINT('',(-94.2351405640567,-4.91824832960019,130.808414120368));
#97267=CARTESIAN_POINT('Ctrl Pts',(-94.2351405640567,-4.91824832960019,
130.808414120368));
#97268=CARTESIAN_POINT('Ctrl Pts',(-94.2443029884524,-4.9181146402537,130.970623803505));
#97269=CARTESIAN_POINT('Ctrl Pts',(-94.2534654128481,-4.90995233268537,
131.132490188506));
#97270=CARTESIAN_POINT('Ctrl Pts',(-94.2626278372439,-4.89388613611978,
131.293299825643));
#97271=CARTESIAN_POINT('Ctrl Pts',(-94.2718551523956,-4.87770615442514,
131.455248359919));
#97272=CARTESIAN_POINT('Ctrl Pts',(-94.2810824675474,-4.85351003632696,
131.616125071655));
#97273=CARTESIAN_POINT('Ctrl Pts',(-94.2903097826992,-4.82147397135044,
131.775221990827));
#97274=CARTESIAN_POINT('Ctrl Pts',(-94.2996077942268,-4.78919245754591,
131.935537853473));
#97275=CARTESIAN_POINT('Ctrl Pts',(-94.3089058057544,-4.74895046713222,
132.094046497661));
#97276=CARTESIAN_POINT('Ctrl Pts',(-94.318203817282,-4.70097636774123,132.250045317782));
#97277=CARTESIAN_POINT('Ctrl Pts',(-94.3200238219645,-4.69158585609541,
132.28058072659));
#97278=CARTESIAN_POINT('Ctrl Pts',(-94.3218438266471,-4.68189923651167,
132.31102004001));
#97279=CARTESIAN_POINT('Ctrl Pts',(-94.3236638313296,-4.67191843243465,
132.341358087693));
#97280=CARTESIAN_POINT('Ctrl Pts',(-94.3314381654491,-4.62928441812665,
132.470950127476));
#97281=CARTESIAN_POINT('Ctrl Pts',(-94.3392124995686,-4.58118675379454,
132.598972181592));
#97282=CARTESIAN_POINT('Ctrl Pts',(-94.3469868336881,-4.52775882311562,
132.724929049619));
#97283=CARTESIAN_POINT('Ctrl Pts',(-94.3547515866357,-4.47439673758627,
132.850730687063));
#97284=CARTESIAN_POINT('Ctrl Pts',(-94.3625163395831,-4.4157176074208,132.974471846052));
#97285=CARTESIAN_POINT('Ctrl Pts',(-94.3702810925306,-4.35190458292287,
133.095672373664));
#97286=CARTESIAN_POINT('Ctrl Pts',(-94.3780381334161,-4.28815493842031,
133.216752523204));
#97287=CARTESIAN_POINT('Ctrl Pts',(-94.3857951743015,-4.21928172790127,
133.335296719322));
#97288=CARTESIAN_POINT('Ctrl Pts',(-94.3935522151869,-4.14551604825105,
133.450845032066));
#97289=CARTESIAN_POINT('Ctrl Pts',(-94.4013034064275,-4.07180599587357,
133.566306208929));
#97290=CARTESIAN_POINT('Ctrl Pts',(-94.409054597668,-3.99321102751453,133.678775671053));
#97291=CARTESIAN_POINT('Ctrl Pts',(-94.4168057889085,-3.91000782088841,
133.787818662032));
#97292=CARTESIAN_POINT('Ctrl Pts',(-94.424553685686,-3.82683997784474,133.896815306832));
#97293=CARTESIAN_POINT('Ctrl Pts',(-94.4323015824634,-3.73906802875495,
134.002388066874));
#97294=CARTESIAN_POINT('Ctrl Pts',(-94.4400494792409,-3.64701143655703,
134.104131919357));
#97295=CARTESIAN_POINT('Ctrl Pts',(-94.4477957553253,-3.55497410061344,
134.205854489219));
#97296=CARTESIAN_POINT('Ctrl Pts',(-94.4555420314098,-3.45865416640367,
134.303749454879));
#97297=CARTESIAN_POINT('Ctrl Pts',(-94.4632883074943,-3.35841051293748,
134.397445905879));
#97298=CARTESIAN_POINT('Ctrl Pts',(-94.47103464076,-3.25816611949555,134.491143048525));
#97299=CARTESIAN_POINT('Ctrl Pts',(-94.4787809740257,-3.15399823462587,
134.580641347699));
#97300=CARTESIAN_POINT('Ctrl Pts',(-94.4865273072914,-3.04630132780064,
134.665607991504));
#97301=CARTESIAN_POINT('Ctrl Pts',(-94.4942753752947,-2.93858030299999,
134.750593662999));
#97302=CARTESIAN_POINT('Ctrl Pts',(-94.502023443298,-2.82732899052071,134.831045417611));
#97303=CARTESIAN_POINT('Ctrl Pts',(-94.5097715113014,-2.71297321364428,
134.906672088499));
#97304=CARTESIAN_POINT('Ctrl Pts',(-94.5175278140436,-2.59849589808718,
134.982379136313));
#97305=CARTESIAN_POINT('Ctrl Pts',(-94.5252841167858,-2.48090785372675,
135.053250640351));
#97306=CARTESIAN_POINT('Ctrl Pts',(-94.533040419528,-2.36066251329971,135.119039697266));
#97307=CARTESIAN_POINT('Ctrl Pts',(-94.5408008620426,-2.24035299431363,
135.184863867782));
#97308=CARTESIAN_POINT('Ctrl Pts',(-94.5485613045571,-2.1173837035878,135.245600012929));
#97309=CARTESIAN_POINT('Ctrl Pts',(-94.5563217470716,-1.99222980359294,
135.301048673477));
#97310=CARTESIAN_POINT('Ctrl Pts',(-94.5640946473374,-1.86687499544717,
135.356586345138));
#97311=CARTESIAN_POINT('Ctrl Pts',(-94.5718675476033,-1.73932893404993,
135.406819427243));
#97312=CARTESIAN_POINT('Ctrl Pts',(-94.5796404478691,-1.61008460208522,
135.451597499481));
#97313=CARTESIAN_POINT('Ctrl Pts',(-94.5871307836269,-1.48553862721053,
135.494747775977));
#97314=CARTESIAN_POINT('Ctrl Pts',(-94.5946211193847,-1.35941600579462,
135.532832674595));
#97315=CARTESIAN_POINT('Ctrl Pts',(-94.6021114551425,-1.23216652903071,
135.565762586234));
#97316=CARTESIAN_POINT('Ctrl Pts',(-94.6098857892615,-1.10009234960476,
135.599941045501));
#97317=CARTESIAN_POINT('Ctrl Pts',(-94.6176601233806,-0.966385807288509,
135.628674165663));
#97318=CARTESIAN_POINT('Ctrl Pts',(-94.6254344574997,-0.831535625359408,
135.65180649826));
#97319=CARTESIAN_POINT('Ctrl Pts',(-94.6331992104467,-0.696851634227995,
135.674910322325));
#97320=CARTESIAN_POINT('Ctrl Pts',(-94.6409639633938,-0.561027189474129,
135.692427027217));
#97321=CARTESIAN_POINT('Ctrl Pts',(-94.6487287163409,-0.424565254563363,
135.70425116809));
#97322=CARTESIAN_POINT('Ctrl Pts',(-94.6564857572259,-0.288238855569757,
135.71606356506));
#97323=CARTESIAN_POINT('Ctrl Pts',(-94.6642427981108,-0.151276613429885,
135.722194616066));
#97324=CARTESIAN_POINT('Ctrl Pts',(-94.6719998389958,-0.0141903937488982,
135.722590146088));
#97325=CARTESIAN_POINT('Ctrl Pts',(-94.679751030236,0.122792448147638,135.722985377838));
#97326=CARTESIAN_POINT('Ctrl Pts',(-94.6875022214762,0.259898692112635,
135.717653696532));
#97327=CARTESIAN_POINT('Ctrl Pts',(-94.6952534127164,0.39661301420797,135.70659288251));
#97328=CARTESIAN_POINT('Ctrl Pts',(-94.7030013094935,0.533269229069254,
135.69553676963));
#97329=CARTESIAN_POINT('Ctrl Pts',(-94.7107492062706,0.669533464494266,
135.678756398594));
#97330=CARTESIAN_POINT('Ctrl Pts',(-94.7184971030477,0.804892285807843,
135.656301617903));
#97331=CARTESIAN_POINT('Ctrl Pts',(-94.7262433791318,0.940222792973999,
135.633851534267));
#97332=CARTESIAN_POINT('Ctrl Pts',(-94.7339896552158,1.07464787729224,135.605729465855));
#97333=CARTESIAN_POINT('Ctrl Pts',(-94.7417359312999,1.20766149842017,135.57203686158));
#97334=CARTESIAN_POINT('Ctrl Pts',(-94.7494822645652,1.34067610142462,135.538344008593));
#97335=CARTESIAN_POINT('Ctrl Pts',(-94.7572285978306,1.47227884145251,135.499080633691));
#97336=CARTESIAN_POINT('Ctrl Pts',(-94.764974931096,1.60197649404298,135.454398722252));
#97337=CARTESIAN_POINT('Ctrl Pts',(-94.7727229990989,1.73170319152331,135.409706804609));
#97338=CARTESIAN_POINT('Ctrl Pts',(-94.780471067102,1.85952358304612,135.359594063137));
#97339=CARTESIAN_POINT('Ctrl Pts',(-94.788219135105,1.98496253381547,135.304261372233));
#97340=CARTESIAN_POINT('Ctrl Pts',(-94.7959754378469,2.11053480259426,135.248869873086));
#97341=CARTESIAN_POINT('Ctrl Pts',(-94.8037317405888,2.23372021634751,135.188247500172));
#97342=CARTESIAN_POINT('Ctrl Pts',(-94.8114880433307,2.35406595682623,135.122642282003));
#97343=CARTESIAN_POINT('Ctrl Pts',(-94.8192484858449,2.47447592945051,135.057002048354));
#97344=CARTESIAN_POINT('Ctrl Pts',(-94.827008928359,2.59204287382563,134.986373871417));
#97345=CARTESIAN_POINT('Ctrl Pts',(-94.8347693708731,2.70634214233155,134.911049706253));
#97346=CARTESIAN_POINT('Ctrl Pts',(-94.8425422711386,2.82082489417029,134.835604624052));
#97347=CARTESIAN_POINT('Ctrl Pts',(-94.8503151714041,2.93202917048863,134.755448718204));
#97348=CARTESIAN_POINT('Ctrl Pts',(-94.8580880716695,3.03956194923661,134.670915443151));
#97349=CARTESIAN_POINT('Ctrl Pts',(-94.8655784074316,3.14318564061895,134.589455165572));
#97350=CARTESIAN_POINT('Ctrl Pts',(-94.8730687431937,3.24339990209743,134.503930450129));
#97351=CARTESIAN_POINT('Ctrl Pts',(-94.8805590789558,3.33988621986936,134.414671282983));
#97352=CARTESIAN_POINT('Ctrl Pts',(-94.8883334130748,3.44003084570447,134.322027827387));
#97353=CARTESIAN_POINT('Ctrl Pts',(-94.8961077471939,3.5364764855459,134.225067679864));
#97354=CARTESIAN_POINT('Ctrl Pts',(-94.9038820813129,3.62882818933252,134.12411799346));
#97355=CARTESIAN_POINT('Ctrl Pts',(-94.9116468342599,3.72106607789793,134.023292718523));
#97356=CARTESIAN_POINT('Ctrl Pts',(-94.919411587207,3.80921980790795,133.918487973268));
#97357=CARTESIAN_POINT('Ctrl Pts',(-94.927176340154,3.89292880158878,133.810069919588));
#97358=CARTESIAN_POINT('Ctrl Pts',(-94.9349333810389,3.97655465431699,133.701759548248));
#97359=CARTESIAN_POINT('Ctrl Pts',(-94.9426904219239,4.05574431853306,133.589843317792));
#97360=CARTESIAN_POINT('Ctrl Pts',(-94.9504474628088,4.13017553939704,133.47472259233));
#97361=CARTESIAN_POINT('Ctrl Pts',(-94.9581986540489,4.20455063109848,133.359688680303));
#97362=CARTESIAN_POINT('Ctrl Pts',(-94.9659498452889,4.27417421048338,133.241455410226));
#97363=CARTESIAN_POINT('Ctrl Pts',(-94.973701036529,4.33876586491409,133.120455138944));
#97364=CARTESIAN_POINT('Ctrl Pts',(-94.981448933306,4.40333006616854,132.999506296005));
#97365=CARTESIAN_POINT('Ctrl Pts',(-94.9891968300829,4.46286641245744,132.875793135111));
#97366=CARTESIAN_POINT('Ctrl Pts',(-94.9969447268599,4.51713931875218,132.749774567728));
#97367=CARTESIAN_POINT('Ctrl Pts',(-95.004691002944,4.5714008723249,132.623782360712));
#97368=CARTESIAN_POINT('Ctrl Pts',(-95.012437279028,4.62040102130089,132.495486065263));
#97369=CARTESIAN_POINT('Ctrl Pts',(-95.020183555112,4.66395159035826,132.36536626307));
#97370=CARTESIAN_POINT('Ctrl Pts',(-95.0279298883773,4.70750248089598,132.235245500361));
#97371=CARTESIAN_POINT('Ctrl Pts',(-95.0356762216425,4.74560358715529,132.103301574798));
#97372=CARTESIAN_POINT('Ctrl Pts',(-95.0434225549078,4.7781161788708,131.970031601898));
#97373=CARTESIAN_POINT('Ctrl Pts',(-95.0511706229106,4.81063605155575,131.836731784111));
#97374=CARTESIAN_POINT('Ctrl Pts',(-95.0589186909136,4.83756482669407,131.702105707825));
#97375=CARTESIAN_POINT('Ctrl Pts',(-95.0666667589165,4.85881468364112,131.566661694919));
#97376=CARTESIAN_POINT('Ctrl Pts',(-95.0744230616583,4.8800871251891,131.431073730503));
#97377=CARTESIAN_POINT('Ctrl Pts',(-95.0821793644,4.89566853104698,131.294666479777));
#97378=CARTESIAN_POINT('Ctrl Pts',(-95.0899356671418,4.90552281530287,131.157954977028));
#97379=CARTESIAN_POINT('Ctrl Pts',(-95.0976961096558,4.91538235908697,131.021170507233));
#97380=CARTESIAN_POINT('Ctrl Pts',(-95.10545655217,4.91950867870449,130.884081852439));
#97381=CARTESIAN_POINT('Ctrl Pts',(-95.1132169946841,4.91791787180366,130.747204089556));
#97382=CARTESIAN_POINT('Ctrl Pts',(-95.1209898949494,4.91632451119835,130.610106598336));
#97383=CARTESIAN_POINT('Ctrl Pts',(-95.1287627952148,4.90899570514173,130.473221066174));
#97384=CARTESIAN_POINT('Ctrl Pts',(-95.1365356954802,4.8959995602815,130.337058393921));
#97385=CARTESIAN_POINT('Ctrl Pts',(-95.144026031243,4.88347585802091,130.205845577764));
#97386=CARTESIAN_POINT('Ctrl Pts',(-95.1515163670057,4.86568974893018,130.0753042836));
#97387=CARTESIAN_POINT('Ctrl Pts',(-95.1590067027684,4.84274669522234,129.945880851693));
#97388=CARTESIAN_POINT('Ctrl Pts',(-95.1667810368876,4.81893374866204,129.811550291041));
#97389=CARTESIAN_POINT('Ctrl Pts',(-95.1745553710066,4.78948965464658,129.677998514639));
#97390=CARTESIAN_POINT('Ctrl Pts',(-95.1823297051257,4.75447617614294,129.54573463937));
#97391=CARTESIAN_POINT('Ctrl Pts',(-95.1900944580729,4.71950584862231,129.413633767508));
#97392=CARTESIAN_POINT('Ctrl Pts',(-95.19785921102,4.67897989255844,129.282818012996));
#97393=CARTESIAN_POINT('Ctrl Pts',(-95.2056239639671,4.6330114692282,129.153788659577));
#97394=CARTESIAN_POINT('Ctrl Pts',(-95.2133810048521,4.58708870238405,129.02488745993));
#97395=CARTESIAN_POINT('Ctrl Pts',(-95.2211380457372,4.53573435589198,128.897769496389));
#97396=CARTESIAN_POINT('Ctrl Pts',(-95.2288950866223,4.47911192213214,128.772922838181));
#97397=CARTESIAN_POINT('Ctrl Pts',(-95.2366462778624,4.42253218778998,128.648170327809));
#97398=CARTESIAN_POINT('Ctrl Pts',(-95.2443974691026,4.36069243444075,128.525686068144));
#97399=CARTESIAN_POINT('Ctrl Pts',(-95.2521486603428,4.29380484626233,128.405939677715));
#97400=CARTESIAN_POINT('Ctrl Pts',(-95.2598965571199,4.22694568709327,128.286244182697));
#97401=CARTESIAN_POINT('Ctrl Pts',(-95.2676444538971,4.15504315051818,128.169284583081));
#97402=CARTESIAN_POINT('Ctrl Pts',(-95.2753923506743,4.07835599228737,128.055507136081));
#97403=CARTESIAN_POINT('Ctrl Pts',(-95.2831386267584,4.00168487535666,127.941753488869));
#97404=CARTESIAN_POINT('Ctrl Pts',(-95.2908849028425,3.92023134587071,127.831180994277));
#97405=CARTESIAN_POINT('Ctrl Pts',(-95.2986311789267,3.8342980174561,127.724207735673));
#97406=CARTESIAN_POINT('Ctrl Pts',(-95.3063775121921,3.74836405470131,127.617233687417));
#97407=CARTESIAN_POINT('Ctrl Pts',(-95.3141238454575,3.65795047188117,127.513859232965));
#97408=CARTESIAN_POINT('Ctrl Pts',(-95.3218701787229,3.56340051926233,127.414469793097));
#97409=CARTESIAN_POINT('Ctrl Pts',(-95.329618246726,3.46882939283728,127.315058095653));
#97410=CARTESIAN_POINT('Ctrl Pts',(-95.3373663147289,3.37012032278139,127.219633471809));
#97411=CARTESIAN_POINT('Ctrl Pts',(-95.345114382732,3.26765350548347,127.128544567952));
#97412=CARTESIAN_POINT('Ctrl Pts',(-95.3528706854739,3.16507778523262,127.037358853724));
#97413=CARTESIAN_POINT('Ctrl Pts',(-95.3606269882158,3.05873663240364,126.950518324737));
#97414=CARTESIAN_POINT('Ctrl Pts',(-95.3683832909577,2.94904385461191,126.868331729705));
#97415=CARTESIAN_POINT('Ctrl Pts',(-95.3761437334719,2.83929253048188,126.786101269212));
#97416=CARTESIAN_POINT('Ctrl Pts',(-95.3839041759861,2.72618633919327,126.708529913162));
#97417=CARTESIAN_POINT('Ctrl Pts',(-95.3916646185004,2.61016733071024,126.635882529799));
#97418=CARTESIAN_POINT('Ctrl Pts',(-95.3994375187658,2.49396207821512,126.563118526407));
#97419=CARTESIAN_POINT('Ctrl Pts',(-95.4072104190314,2.37483500451532,126.495294484757));
#97420=CARTESIAN_POINT('Ctrl Pts',(-95.4149833192969,2.25325275827421,126.432629259188));
#97421=CARTESIAN_POINT('Ctrl Pts',(-95.4224736550584,2.13609033293938,126.372242072416));
#97422=CARTESIAN_POINT('Ctrl Pts',(-95.42996399082,2.01664841864358,126.316645271589));
#97423=CARTESIAN_POINT('Ctrl Pts',(-95.4374543265815,1.89535953899379,126.265991386174));
#97424=CARTESIAN_POINT('Ctrl Pts',(-95.4452286607005,1.76947195460049,126.213416943295));
#97425=CARTESIAN_POINT('Ctrl Pts',(-95.4530029948194,1.64119581070522,126.166001096162));
#97426=CARTESIAN_POINT('Ctrl Pts',(-95.4607773289384,1.51099282615369,126.123967071953));
#97427=CARTESIAN_POINT('Ctrl Pts',(-95.4685420818854,1.38095030514368,126.081984850923));
#97428=CARTESIAN_POINT('Ctrl Pts',(-95.4763068348325,1.24898603682646,126.045371374849));
#97429=CARTESIAN_POINT('Ctrl Pts',(-95.4840715877795,1.11558293184436,126.01430239405));
#97430=CARTESIAN_POINT('Ctrl Pts',(-95.4918286286644,0.982312324706775,
125.9832642714));
#97431=CARTESIAN_POINT('Ctrl Pts',(-95.4995856695494,0.847606103134692,
125.957759773211));
#97432=CARTESIAN_POINT('Ctrl Pts',(-95.5073427104344,0.71196326521803,125.937915162053));
#97433=CARTESIAN_POINT('Ctrl Pts',(-95.5150939016744,0.576422716620774,
125.918085515871));
#97434=CARTESIAN_POINT('Ctrl Pts',(-95.5228450929144,0.439947342827352,
125.903907317563));
#97435=CARTESIAN_POINT('Ctrl Pts',(-95.5305962841545,0.303046937937487,
125.895455890857));
#97436=CARTESIAN_POINT('Ctrl Pts',(-95.5383441809315,0.166204719371452,
125.887008056233));
#97437=CARTESIAN_POINT('Ctrl Pts',(-95.5460920777085,0.0289382184125221,
125.884282176149));
#97438=CARTESIAN_POINT('Ctrl Pts',(-95.5538399744855,-0.108237252303732,
125.887301764988));
#97439=CARTESIAN_POINT('Ctrl Pts',(-95.5615862505695,-0.245384028868673,
125.890320722195));
#97440=CARTESIAN_POINT('Ctrl Pts',(-95.5693325266535,-0.382439422442771,
125.899082749224));
#97441=CARTESIAN_POINT('Ctrl Pts',(-95.5770788027375,-0.518888117590341,
125.913559232933));
#97442=CARTESIAN_POINT('Ctrl Pts',(-95.5848251360028,-0.655337819970996,
125.928035823505));
#97443=CARTESIAN_POINT('Ctrl Pts',(-95.5925714692681,-0.791180426205342,
125.948226913683));
#97444=CARTESIAN_POINT('Ctrl Pts',(-95.6003178025333,-0.925906135721069,
125.974052046643));
#97445=CARTESIAN_POINT('Ctrl Pts',(-95.6080658705362,-1.0606620161255,125.999882962962));
#97446=CARTESIAN_POINT('Ctrl Pts',(-95.6158139385392,-1.19430011819792,
126.031350359121));
#97447=CARTESIAN_POINT('Ctrl Pts',(-95.6235620065421,-1.32632161042376,
126.068322817018));
#97448=CARTESIAN_POINT('Ctrl Pts',(-95.6313183092839,-1.45848341666278,
126.105334569683));
#97449=CARTESIAN_POINT('Ctrl Pts',(-95.6390746120257,-1.58902480378018,
126.147862966179));
#97450=CARTESIAN_POINT('Ctrl Pts',(-95.6468309147674,-1.71746233961627,
126.19572674466));
#97451=CARTESIAN_POINT('Ctrl Pts',(-95.6545913572815,-1.8459684264324,126.24361606948));
#97452=CARTESIAN_POINT('Ctrl Pts',(-95.6623517997955,-1.97236806437471,
126.296846298812));
#97453=CARTESIAN_POINT('Ctrl Pts',(-95.6701122423096,-2.09619947348481,
126.355188691256));
#97454=CARTESIAN_POINT('Ctrl Pts',(-95.677885142575,-2.22022966776605,126.413624740089));
#97455=CARTESIAN_POINT('Ctrl Pts',(-95.6856580428404,-2.34168304805709,
126.477189169837));
#97456=CARTESIAN_POINT('Ctrl Pts',(-95.6934309431057,-2.4601232510035,126.545607671882));
#97457=CARTESIAN_POINT('Ctrl Pts',(-95.7009212788685,-2.57425785425245,
126.611538989049));
#97458=CARTESIAN_POINT('Ctrl Pts',(-95.7084116146312,-2.68559428959815,
126.681977425453));
#97459=CARTESIAN_POINT('Ctrl Pts',(-95.7159019503939,-2.79377044010429,
126.756641532637));
#97460=CARTESIAN_POINT('Ctrl Pts',(-95.7236359322541,-2.9054653510155,126.833734318442));
#97461=CARTESIAN_POINT('Ctrl Pts',(-95.7313699141143,-3.01415319167601,
126.915582540708));
#97462=CARTESIAN_POINT('Ctrl Pts',(-95.7391038959745,-3.11939900417275,
127.001922858014));
#97463=CARTESIAN_POINT('Ctrl Pts',(-95.7468256553064,-3.22447848968136,
127.088126725949));
#97464=CARTESIAN_POINT('Ctrl Pts',(-95.7545474146384,-3.32612647623596,
127.1788083035));
#97465=CARTESIAN_POINT('Ctrl Pts',(-95.7622691739704,-3.42393670427249,
127.273660898299));
#97466=CARTESIAN_POINT('Ctrl Pts',(-95.7699838766338,-3.52165754667375,
127.368426810348));
#97467=CARTESIAN_POINT('Ctrl Pts',(-95.7776985792971,-3.61554732379551,
127.467355885301));
#97468=CARTESIAN_POINT('Ctrl Pts',(-95.7854132819605,-3.70523244929159,
127.570100955879));
#97469=CARTESIAN_POINT('Ctrl Pts',(-95.7931226519618,-3.79485558141093,
127.672775005606));
#97470=CARTESIAN_POINT('Ctrl Pts',(-95.8008320219632,-3.88027958457348,
127.779259506873));
#97471=CARTESIAN_POINT('Ctrl Pts',(-95.8085413919645,-3.96116772555666,
127.889170518703));
#97472=CARTESIAN_POINT('Ctrl Pts',(-95.8162471491015,-4.04201795969688,
127.999030022618));
#97473=CARTESIAN_POINT('Ctrl Pts',(-95.8239529062385,-4.11833632781777,
128.112312523592));
#97474=CARTESIAN_POINT('Ctrl Pts',(-95.8316586633755,-4.18982669797117,
128.22860144725));
#97475=CARTESIAN_POINT('Ctrl Pts',(-95.8393640142852,-4.26131329934031,
128.344884240461));
#97476=CARTESIAN_POINT('Ctrl Pts',(-95.8470693651949,-4.32797219364736,
128.464172809372));
#97477=CARTESIAN_POINT('Ctrl Pts',(-95.8547747161047,-4.38955097814496,
128.586022213993));
#97478=CARTESIAN_POINT('Ctrl Pts',(-95.8624797057105,-4.45112687521296,
128.707865905095));
#97479=CARTESIAN_POINT('Ctrl Pts',(-95.8701846953162,-4.50762296300028,
128.832269837348));
#97480=CARTESIAN_POINT('Ctrl Pts',(-95.877889684922,-4.55883351165112,128.958765842013));
#97481=CARTESIAN_POINT('Ctrl Pts',(-95.8855986625547,-4.61007056637895,
129.085327319769));
#97482=CARTESIAN_POINT('Ctrl Pts',(-95.8933076401875,-4.65601647346959,
129.213982664105));
#97483=CARTESIAN_POINT('Ctrl Pts',(-95.9010166178202,-4.69651421639679,
129.344245116079));
#97484=CARTESIAN_POINT('Ctrl Pts',(-95.9056837601004,-4.72103221829949,
129.423108154227));
#97485=CARTESIAN_POINT('Ctrl Pts',(-95.9103509023805,-4.7435542697273,129.502559922525));
#97486=CARTESIAN_POINT('Ctrl Pts',(-95.9150180446607,-4.76405452823415,
129.582490119309));
#97487=CARTESIAN_POINT('Ctrl Pts',(-94.1652277315646,-4.76405452823406,
129.582490119308));
#97488=CARTESIAN_POINT('Ctrl Pts',(-94.1729478262758,-4.79804369541448,
129.715013366287));
#97489=CARTESIAN_POINT('Ctrl Pts',(-94.1806679209871,-4.82650721410582,
129.848987986936));
#97490=CARTESIAN_POINT('Ctrl Pts',(-94.1883880156982,-4.84933477376199,
129.983912377588));
#97491=CARTESIAN_POINT('Ctrl Pts',(-94.1961801070834,-4.87237522049178,
130.120095056867));
#97492=CARTESIAN_POINT('Ctrl Pts',(-94.2039721984684,-4.88967394969018,
130.257244916243));
#97493=CARTESIAN_POINT('Ctrl Pts',(-94.2117642898536,-4.90117065471659,
130.394837387645));
#97494=CARTESIAN_POINT('Ctrl Pts',(-94.2195563812387,-4.912667359743,130.532429859047));
#97495=CARTESIAN_POINT('Ctrl Pts',(-94.2273484726239,-4.9183620243331,130.670464531076));
#97496=CARTESIAN_POINT('Ctrl Pts',(-94.2351405640091,-4.91824832960088,
130.808414119523));
#97497=CARTESIAN_POINT('',(-93.8898594359371,-4.9182489755649,130.801186211347));
#97498=CARTESIAN_POINT('Ctrl Pts',(-93.8201028328085,-4.76405452823393,
129.582490119308));
#97499=CARTESIAN_POINT('Ctrl Pts',(-93.8288924822948,-4.80247123866298,
129.732276290216));
#97500=CARTESIAN_POINT('Ctrl Pts',(-93.8376821317811,-4.83386392063157,
129.884047727739));
#97501=CARTESIAN_POINT('Ctrl Pts',(-93.8464717812675,-4.85804604657392,
130.037176368596));
#97502=CARTESIAN_POINT('Ctrl Pts',(-93.8552077517182,-4.88208049049494,
130.189369841584));
#97503=CARTESIAN_POINT('Ctrl Pts',(-93.8639437221688,-4.8989920902913,130.342903811076));
#97504=CARTESIAN_POINT('Ctrl Pts',(-93.8726796926194,-4.90864545612675,
130.497142700533));
#97505=CARTESIAN_POINT('Ctrl Pts',(-93.8784062737253,-4.91497340591942,
130.59824898462));
#97506=CARTESIAN_POINT('Ctrl Pts',(-93.8841328548312,-4.91818344564875,
130.699657792874));
#97507=CARTESIAN_POINT('Ctrl Pts',(-93.8898594359371,-4.9182489755649,130.801186211347));
#97508=CARTESIAN_POINT('Ctrl Pts',(-93.8898594359916,-4.91824897556552,
130.801186212314));
#97509=CARTESIAN_POINT('Ctrl Pts',(-93.8976582558575,-4.91833821831731,
130.93945402557));
#97510=CARTESIAN_POINT('Ctrl Pts',(-93.9054570757235,-4.91259240001704,
131.077749479743));
#97511=CARTESIAN_POINT('Ctrl Pts',(-93.9132558955893,-4.90103119738631,
131.215549460734));
#97512=CARTESIAN_POINT('Ctrl Pts',(-93.9210552260816,-4.88946923778778,
131.353358464156));
#97513=CARTESIAN_POINT('Ctrl Pts',(-93.928854556574,-4.87209116707281,131.490671547624));
#97514=CARTESIAN_POINT('Ctrl Pts',(-93.9366538870663,-4.84896860855516,
131.626970182151));
#97515=CARTESIAN_POINT('Ctrl Pts',(-93.9444553313755,-4.82583978323616,
131.763305757074));
#97516=CARTESIAN_POINT('Ctrl Pts',(-93.9522567756846,-4.79696343420705,
131.89862595763));
#97517=CARTESIAN_POINT('Ctrl Pts',(-93.9600582199938,-4.76246236580466,
132.032422210807));
#97518=CARTESIAN_POINT('Ctrl Pts',(-93.967863382338,-4.72794485478284,132.166282228992));
#97519=CARTESIAN_POINT('Ctrl Pts',(-93.9756685446822,-4.68779738267569,
132.298616482816));
#97520=CARTESIAN_POINT('Ctrl Pts',(-93.9834737070264,-4.64219260075093,
132.428931613255));
#97521=CARTESIAN_POINT('Ctrl Pts',(-93.9912890127563,-4.59652855203957,
132.559416097842));
#97522=CARTESIAN_POINT('Ctrl Pts',(-93.9991043184861,-4.54539315719707,
132.68787585688));
#97523=CARTESIAN_POINT('Ctrl Pts',(-94.006919624216,-4.48900745015003,132.813836961044));
#97524=CARTESIAN_POINT('Ctrl Pts',(-94.0147406807408,-4.43258025238576,
132.939890752111));
#97525=CARTESIAN_POINT('Ctrl Pts',(-94.0225617372657,-4.37089521509931,
133.063441882653));
#97526=CARTESIAN_POINT('Ctrl Pts',(-94.0303827937905,-4.30421889949876,
133.184041841532));
#97527=CARTESIAN_POINT('Ctrl Pts',(-94.038216330487,-4.23743618754821,133.30483424349));
#97528=CARTESIAN_POINT('Ctrl Pts',(-94.0460498671836,-4.16564648951891,
133.422665742289));
#97529=CARTESIAN_POINT('Ctrl Pts',(-94.0538834038801,-4.08915953845766,
133.537116979107));
#97530=CARTESIAN_POINT('Ctrl Pts',(-94.0575240038123,-4.05361258187441,
133.590307661826));
#97531=CARTESIAN_POINT('Ctrl Pts',(-94.0611646037445,-4.01705164262998,
133.642768717421));
#97532=CARTESIAN_POINT('Ctrl Pts',(-94.0648052036766,-3.97951065453995,
133.694460618068));
#97533=CARTESIAN_POINT('Ctrl Pts',(-94.0725795377957,-3.89934359690934,
133.8048463002));
#97534=CARTESIAN_POINT('Ctrl Pts',(-94.0803538719147,-3.8144531787387,133.912068725817));
#97535=CARTESIAN_POINT('Ctrl Pts',(-94.0881282060338,-3.72511761616584,
134.015697069611));
#97536=CARTESIAN_POINT('Ctrl Pts',(-94.0958929589809,-3.63589215168971,
134.119197700732));
#97537=CARTESIAN_POINT('Ctrl Pts',(-94.103657711928,-3.54223269570981,134.219112769909));
#97538=CARTESIAN_POINT('Ctrl Pts',(-94.1114224648751,-3.44446025984409,
134.315040976251));
#97539=CARTESIAN_POINT('Ctrl Pts',(-94.1191795057601,-3.34678493294002,
134.410873905346));
#97540=CARTESIAN_POINT('Ctrl Pts',(-94.1269365466451,-3.24500503289072,
134.502727579765));
#97541=CARTESIAN_POINT('Ctrl Pts',(-94.1346935875301,-3.13948105341171,
134.590234595628));
#97542=CARTESIAN_POINT('Ctrl Pts',(-94.1424447787702,-3.03403665038606,
134.677675621771));
#97543=CARTESIAN_POINT('Ctrl Pts',(-94.1501959700104,-2.92485408754741,
134.76077626516));
#97544=CARTESIAN_POINT('Ctrl Pts',(-94.1579471612506,-2.81232957634721,
134.839207010739));
#97545=CARTESIAN_POINT('Ctrl Pts',(-94.1656950580277,-2.69985289106641,
134.917604421159));
#97546=CARTESIAN_POINT('Ctrl Pts',(-94.1734429548046,-2.58403740259514,
134.991335658353));
#97547=CARTESIAN_POINT('Ctrl Pts',(-94.1811908515817,-2.46531098567366,
135.060112584777));
#97548=CARTESIAN_POINT('Ctrl Pts',(-94.1889371276658,-2.34660940375914,
135.12887512455));
#97549=CARTESIAN_POINT('Ctrl Pts',(-94.19668340375,-2.2249984426239,135.192685219029));
#97550=CARTESIAN_POINT('Ctrl Pts',(-94.2044296798341,-2.10093309505414,
135.251299249097));
#97551=CARTESIAN_POINT('Ctrl Pts',(-94.2121760130994,-1.976866831662,135.309913711841));
#97552=CARTESIAN_POINT('Ctrl Pts',(-94.2199223463648,-1.8503464991821,135.363331866627));
#97553=CARTESIAN_POINT('Ctrl Pts',(-94.2276686796302,-1.72184934839801,
135.411357240521));
#97554=CARTESIAN_POINT('Ctrl Pts',(-94.2354167476332,-1.59332342156811,
135.459393369365));
#97555=CARTESIAN_POINT('Ctrl Pts',(-94.2431648156361,-1.46282016167545,
135.502034177335));
#97556=CARTESIAN_POINT('Ctrl Pts',(-94.2509128836391,-1.33083396029842,
135.539132421214));
#97557=CARTESIAN_POINT('Ctrl Pts',(-94.2586691863809,-1.19870748241608,
135.576270093548));
#97558=CARTESIAN_POINT('Ctrl Pts',(-94.2664254891228,-1.06509529162429,
135.607853328517));
#97559=CARTESIAN_POINT('Ctrl Pts',(-94.2741817918646,-0.930504555252162,
135.633785462737));
#97560=CARTESIAN_POINT('Ctrl Pts',(-94.2819422343788,-0.795841983751215,
135.659731437718));
#97561=CARTESIAN_POINT('Ctrl Pts',(-94.2897026768929,-0.660200212458831,
135.680020244181));
#97562=CARTESIAN_POINT('Ctrl Pts',(-94.2974631194071,-0.524092614363329,
135.694607032019));
#97563=CARTESIAN_POINT('Ctrl Pts',(-94.3052360196725,-0.3877665242683,135.709217235863));
#97564=CARTESIAN_POINT('Ctrl Pts',(-94.3130089199379,-0.250973503421118,
135.718107104329));
#97565=CARTESIAN_POINT('Ctrl Pts',(-94.3207818202033,-0.114228920699665,
135.721283925507));
#97566=CARTESIAN_POINT('Ctrl Pts',(-94.3282721559654,0.0175446520010466,
135.724345261234));
#97567=CARTESIAN_POINT('Ctrl Pts',(-94.3357624917274,0.149272939156129,
135.72210171085));
#97568=CARTESIAN_POINT('Ctrl Pts',(-94.3432528274895,0.28050026857667,135.714605281718));
#97569=CARTESIAN_POINT('Ctrl Pts',(-94.3510271616085,0.41670312207732,135.706824623196));
#97570=CARTESIAN_POINT('Ctrl Pts',(-94.3588014957276,0.552797730030421,
135.693360250267));
#97571=CARTESIAN_POINT('Ctrl Pts',(-94.3665758298467,0.688271244284175,
135.674213362444));
#97572=CARTESIAN_POINT('Ctrl Pts',(-94.3743405827937,0.823577799539594,
135.655090071448));
#97573=CARTESIAN_POINT('Ctrl Pts',(-94.3821053357407,0.958264400696356,
135.63029825401));
#97574=CARTESIAN_POINT('Ctrl Pts',(-94.3898700886878,1.09181990732962,135.599891073361));
#97575=CARTESIAN_POINT('Ctrl Pts',(-94.3976271295728,1.22524276475018,135.569514093553));
#97576=CARTESIAN_POINT('Ctrl Pts',(-94.4053841704578,1.35753638455871,135.53353293576));
#97577=CARTESIAN_POINT('Ctrl Pts',(-94.4131412113428,1.4881968038063,135.492052302782));
#97578=CARTESIAN_POINT('Ctrl Pts',(-94.4208924025829,1.6187586910166,135.450602950671));
#97579=CARTESIAN_POINT('Ctrl Pts',(-94.428643593823,1.74768945797974,135.403662495943));
#97580=CARTESIAN_POINT('Ctrl Pts',(-94.4363947850632,1.87449771237708,135.351386171573));
#97581=CARTESIAN_POINT('Ctrl Pts',(-94.4441426818402,2.00125206988272,135.299132066036));
#97582=CARTESIAN_POINT('Ctrl Pts',(-94.4518905786173,2.12588534838054,135.24154675021));
#97583=CARTESIAN_POINT('Ctrl Pts',(-94.4596384753943,2.24792385284434,135.178834461849));
#97584=CARTESIAN_POINT('Ctrl Pts',(-94.4673847514784,2.36993682948418,135.116135291546));
#97585=CARTESIAN_POINT('Ctrl Pts',(-94.4751310275626,2.48935576417221,135.048311460457));
#97586=CARTESIAN_POINT('Ctrl Pts',(-94.4828773036467,2.60572975853007,134.975614084812));
#97587=CARTESIAN_POINT('Ctrl Pts',(-94.490623636912,2.72210461193449,134.902916172532));
#97588=CARTESIAN_POINT('Ctrl Pts',(-94.4983699701774,2.835434148573,134.825344851047));
#97589=CARTESIAN_POINT('Ctrl Pts',(-94.5061163034428,2.94529510449609,134.743195446539));
#97590=CARTESIAN_POINT('Ctrl Pts',(-94.5138643714458,3.05518066301839,134.661027645242));
#97591=CARTESIAN_POINT('Ctrl Pts',(-94.5216124394487,3.16159578210479,134.574279954917));
#97592=CARTESIAN_POINT('Ctrl Pts',(-94.5293605074517,3.26414935114367,134.483288732646));
#97593=CARTESIAN_POINT('Ctrl Pts',(-94.5371168101935,3.36681191533599,134.392200803822));
#97594=CARTESIAN_POINT('Ctrl Pts',(-94.5448731129353,3.46560443818187,134.29686059358));
#97595=CARTESIAN_POINT('Ctrl Pts',(-94.5526294156772,3.56017145770785,134.197642547236));
#97596=CARTESIAN_POINT('Ctrl Pts',(-94.5603898581913,3.65478895049952,134.098371545233));
#97597=CARTESIAN_POINT('Ctrl Pts',(-94.5681503007055,3.74517618860425,133.995218876946));
#97598=CARTESIAN_POINT('Ctrl Pts',(-94.5759107432196,3.83101794771462,133.888592215029));
#97599=CARTESIAN_POINT('Ctrl Pts',(-94.583683643485,3.91699750763739,133.781794386529));
#97600=CARTESIAN_POINT('Ctrl Pts',(-94.5914565437505,3.99841677487503,133.671511734964));
#97601=CARTESIAN_POINT('Ctrl Pts',(-94.5992294440159,4.07500331163742,133.558181794158));
#97602=CARTESIAN_POINT('Ctrl Pts',(-94.606719779778,4.1488057348801,133.448971682159));
#97603=CARTESIAN_POINT('Ctrl Pts',(-94.6142101155402,4.21812052925243,133.33693224965));
#97604=CARTESIAN_POINT('Ctrl Pts',(-94.6217004513024,4.28274514807211,133.222474977799));
#97605=CARTESIAN_POINT('Ctrl Pts',(-94.6294747854214,4.34982002895534,133.103678023699));
#97606=CARTESIAN_POINT('Ctrl Pts',(-94.6372491195405,4.41205453057355,132.981899953175));
#97607=CARTESIAN_POINT('Ctrl Pts',(-94.6450234536596,4.46917245515842,132.857572888266));
#97608=CARTESIAN_POINT('Ctrl Pts',(-94.6527882066067,4.52621998700617,132.733399045353));
#97609=CARTESIAN_POINT('Ctrl Pts',(-94.6605529595537,4.57816332668305,132.606682810378));
#97610=CARTESIAN_POINT('Ctrl Pts',(-94.6683177125009,4.62477091803712,132.477882956281));
#97611=CARTESIAN_POINT('Ctrl Pts',(-94.6760747533859,4.67133221807454,132.349211028015));
#97612=CARTESIAN_POINT('Ctrl Pts',(-94.6838317942709,4.71256818394173,132.218459964242));
#97613=CARTESIAN_POINT('Ctrl Pts',(-94.691588835156,4.74829450078647,132.086110357687));
#97614=CARTESIAN_POINT('Ctrl Pts',(-94.6993400263961,4.78399387613743,131.953860557001));
#97615=CARTESIAN_POINT('Ctrl Pts',(-94.7070912176363,4.81419177100366,131.820014988882));
#97616=CARTESIAN_POINT('Ctrl Pts',(-94.7148424088764,4.8387531777343,131.68507098282));
#97617=CARTESIAN_POINT('Ctrl Pts',(-94.7225903056535,4.86330414521205,131.55018433156));
#97618=CARTESIAN_POINT('Ctrl Pts',(-94.7303382024306,4.88222331947136,131.414200554757));
#97619=CARTESIAN_POINT('Ctrl Pts',(-94.7380860992077,4.89542648778786,131.277628580949));
#97620=CARTESIAN_POINT('Ctrl Pts',(-94.7458323752918,4.90862689428618,131.141085175054));
#97621=CARTESIAN_POINT('Ctrl Pts',(-94.7535786513759,4.91611363548783,131.003954205787));
#97622=CARTESIAN_POINT('Ctrl Pts',(-94.76132492746,4.91785426100443,130.866750761183));
#97623=CARTESIAN_POINT('Ctrl Pts',(-94.7690712607254,4.91959489936993,130.729546303775));
#97624=CARTESIAN_POINT('Ctrl Pts',(-94.7768175939907,4.91558933245176,130.592269760894));
#97625=CARTESIAN_POINT('Ctrl Pts',(-94.7845639272561,4.90585724202649,130.455436867506));
#97626=CARTESIAN_POINT('Ctrl Pts',(-94.7923119952591,4.89612297216703,130.318573331339));
#97627=CARTESIAN_POINT('Ctrl Pts',(-94.800060063262,4.88065965467418,130.182154032268));
#97628=CARTESIAN_POINT('Ctrl Pts',(-94.8078081312649,4.85953887144842,130.046689831946));
#97629=CARTESIAN_POINT('Ctrl Pts',(-94.8155644340068,4.83839564080288,129.91108165866));
#97630=CARTESIAN_POINT('Ctrl Pts',(-94.8233207367487,4.81158299349032,129.77643099879));
#97631=CARTESIAN_POINT('Ctrl Pts',(-94.8310770394906,4.77922382508127,129.643239309401));
#97632=CARTESIAN_POINT('Ctrl Pts',(-94.8388374820048,4.74684738560964,129.509976531596));
#97633=CARTESIAN_POINT('Ctrl Pts',(-94.8465979245189,4.70891863437051,129.378174651425));
#97634=CARTESIAN_POINT('Ctrl Pts',(-94.8543583670331,4.66561017147632,129.248319233053));
#97635=CARTESIAN_POINT('Ctrl Pts',(-94.8621312672986,4.62223218599287,129.118255359236));
#97636=CARTESIAN_POINT('Ctrl Pts',(-94.8699041675641,4.57345737058193,128.990144556821));
#97637=CARTESIAN_POINT('Ctrl Pts',(-94.8776770678295,4.51950657556094,128.864452533155));
#97638=CARTESIAN_POINT('Ctrl Pts',(-94.8851674035915,4.46751702783325,128.743329731151));
#97639=CARTESIAN_POINT('Ctrl Pts',(-94.8926577393534,4.41072141960972,128.624453181565));
#97640=CARTESIAN_POINT('Ctrl Pts',(-94.9001480751154,4.34935646022077,128.508215708281));
#97641=CARTESIAN_POINT('Ctrl Pts',(-94.9079224092344,4.28566482974465,128.387571055867));
#97642=CARTESIAN_POINT('Ctrl Pts',(-94.9156967433535,4.21684875836493,128.269387385369));
#97643=CARTESIAN_POINT('Ctrl Pts',(-94.9234710774726,4.14312251095284,128.154130642312));
#97644=CARTESIAN_POINT('Ctrl Pts',(-94.9312358304197,4.06948712455159,128.039015942889));
#97645=CARTESIAN_POINT('Ctrl Pts',(-94.9390005833668,3.99095381115865,127.926821319887));
#97646=CARTESIAN_POINT('Ctrl Pts',(-94.9467653363139,3.9077833876865,127.817989566035));
#97647=CARTESIAN_POINT('Ctrl Pts',(-94.9545223771989,3.82469557025121,127.709265905415));
#97648=CARTESIAN_POINT('Ctrl Pts',(-94.962279418084,3.73698004403296,127.603898775727));
#97649=CARTESIAN_POINT('Ctrl Pts',(-94.970036458969,3.64494151862112,127.502303018382));
#97650=CARTESIAN_POINT('Ctrl Pts',(-94.9777876502091,3.55297240017737,127.400783875187));
#97651=CARTESIAN_POINT('Ctrl Pts',(-94.9855388414492,3.45668703281444,127.303030732059));
#97652=CARTESIAN_POINT('Ctrl Pts',(-94.9932900326893,3.35643085898491,127.209425993494));
#97653=CARTESIAN_POINT('Ctrl Pts',(-95.0010379294664,3.25621729670381,127.11586103944));
#97654=CARTESIAN_POINT('Ctrl Pts',(-95.0087858262434,3.15203656983306,127.026441249366));
#97655=CARTESIAN_POINT('Ctrl Pts',(-95.0165337230204,3.0442713353298,126.94151256213));
#97656=CARTESIAN_POINT('Ctrl Pts',(-95.0242799991045,2.93652864299044,126.856601640143));
#97657=CARTESIAN_POINT('Ctrl Pts',(-95.0320262751887,2.82520324128915,126.776180194236));
#97658=CARTESIAN_POINT('Ctrl Pts',(-95.0397725512728,2.71071094814917,126.700553943503));
#97659=CARTESIAN_POINT('Ctrl Pts',(-95.0475188845381,2.59621780985325,126.624927134514));
#97660=CARTESIAN_POINT('Ctrl Pts',(-95.0552652178034,2.47855805969385,126.554095806813));
#97661=CARTESIAN_POINT('Ctrl Pts',(-95.0630115510687,2.35817623858243,126.488322168909));
#97662=CARTESIAN_POINT('Ctrl Pts',(-95.0707596190717,2.23776745879667,126.422533801455));
#97663=CARTESIAN_POINT('Ctrl Pts',(-95.0785076870747,2.11463573807559,126.361805565031));
#97664=CARTESIAN_POINT('Ctrl Pts',(-95.0862557550777,1.98924957056218,126.306353368959));
#97665=CARTESIAN_POINT('Ctrl Pts',(-95.0940120578196,1.86373014113764,126.250842237634));
#97666=CARTESIAN_POINT('Ctrl Pts',(-95.1017683605614,1.73595183667613,126.200618506506));
#97667=CARTESIAN_POINT('Ctrl Pts',(-95.1095246633032,1.6064029752666,126.155849829845));
#97668=CARTESIAN_POINT('Ctrl Pts',(-95.1172851058174,1.4767849697291,126.111057258794));
#97669=CARTESIAN_POINT('Ctrl Pts',(-95.1250455483315,1.34539489861243,126.071725655737));
#97670=CARTESIAN_POINT('Ctrl Pts',(-95.1328059908457,1.21273457537751,126.037972266604));
#97671=CARTESIAN_POINT('Ctrl Pts',(-95.1405788911111,1.07986129401471,126.004164693535));
#97672=CARTESIAN_POINT('Ctrl Pts',(-95.1483517913766,0.945714068535662,
125.975953309129));
#97673=CARTESIAN_POINT('Ctrl Pts',(-95.156124691642,0.810804086712758,125.953404031956));
#97674=CARTESIAN_POINT('Ctrl Pts',(-95.163615027404,0.680798422546853,125.931674477807));
#97675=CARTESIAN_POINT('Ctrl Pts',(-95.171105363166,0.550084801065957,125.915202552769));
#97676=CARTESIAN_POINT('Ctrl Pts',(-95.178595698928,0.419121663302422,125.90400143748));
#97677=CARTESIAN_POINT('Ctrl Pts',(-95.1863700330471,0.283193018365383,
125.892375628501));
#97678=CARTESIAN_POINT('Ctrl Pts',(-95.1941443671662,0.146564981733707,
125.886391377625));
#97679=CARTESIAN_POINT('Ctrl Pts',(-95.2019187012853,0.00974538196894736,
125.886120272683));
#97680=CARTESIAN_POINT('Ctrl Pts',(-95.2096834542324,-0.12690559986702,
125.885849501855));
#97681=CARTESIAN_POINT('Ctrl Pts',(-95.2174482071795,-0.263747287887186,
125.891277868353));
#97682=CARTESIAN_POINT('Ctrl Pts',(-95.2252129601266,-0.400266170115626,
125.902425279808));
#97683=CARTESIAN_POINT('Ctrl Pts',(-95.2329700010116,-0.536649459865659,
125.913561619497));
#97684=CARTESIAN_POINT('Ctrl Pts',(-95.2407270418965,-0.672710194716023,
125.930405668606));
#97685=CARTESIAN_POINT('Ctrl Pts',(-95.2484840827815,-0.807934653862507,
125.952925298242));
#97686=CARTESIAN_POINT('Ctrl Pts',(-95.2562352740216,-0.943057139191905,
125.97542794565));
#97687=CARTESIAN_POINT('Ctrl Pts',(-95.2639864652617,-1.07734421997863,
126.003597590541));
#97688=CARTESIAN_POINT('Ctrl Pts',(-95.2717376565018,-1.2102874484048,126.037350301368));
#97689=CARTESIAN_POINT('Ctrl Pts',(-95.2794855532788,-1.34317417241305,
126.071088666394));
#97690=CARTESIAN_POINT('Ctrl Pts',(-95.287233450056,-1.47471780193109,126.110405281727));
#97691=CARTESIAN_POINT('Ctrl Pts',(-95.2949813468331,-1.60442045337004,
126.155165195635));
#97692=CARTESIAN_POINT('Ctrl Pts',(-95.3027276229172,-1.73409597381037,
126.199915746733));
#97693=CARTESIAN_POINT('Ctrl Pts',(-95.3104738990013,-1.86193091279937,
126.250107204168));
#97694=CARTESIAN_POINT('Ctrl Pts',(-95.3182201750854,-1.98744330045985,
126.305554977181));
#97695=CARTESIAN_POINT('Ctrl Pts',(-95.3259665083507,-2.11295661462409,
126.361003159498));
#97696=CARTESIAN_POINT('Ctrl Pts',(-95.3337128416161,-2.23614698562669,
126.42170757683));
#97697=CARTESIAN_POINT('Ctrl Pts',(-95.3414591748815,-2.35655352480187,
126.487435954424));
#97698=CARTESIAN_POINT('Ctrl Pts',(-95.3492072428845,-2.47698702818748,
126.553179051433));
#97699=CARTESIAN_POINT('Ctrl Pts',(-95.3569553108874,-2.5946351161138,126.62394816019));
#97700=CARTESIAN_POINT('Ctrl Pts',(-95.3647033788904,-2.70906290542555,
126.699465827569));
#97701=CARTESIAN_POINT('Ctrl Pts',(-95.3724596816323,-2.82361230995271,
126.775063756022));
#97702=CARTESIAN_POINT('Ctrl Pts',(-95.3802159843742,-2.93493425208004,
126.855420108978));
#97703=CARTESIAN_POINT('Ctrl Pts',(-95.387972287116,-3.04262373166821,126.940214671825));
#97704=CARTESIAN_POINT('Ctrl Pts',(-95.3957327296302,-3.15037068837468,
127.025054492083));
#97705=CARTESIAN_POINT('Ctrl Pts',(-95.4034931721443,-3.25448102277499,
127.114336987894));
#97706=CARTESIAN_POINT('Ctrl Pts',(-95.4112536146585,-3.35458485011532,
127.207703343669));
#97707=CARTESIAN_POINT('Ctrl Pts',(-95.419026514924,-3.45484937300583,127.301219579406));
#97708=CARTESIAN_POINT('Ctrl Pts',(-95.4267994151894,-3.55109426179414,
127.398832497076));
#97709=CARTESIAN_POINT('Ctrl Pts',(-95.4345723154549,-3.64298774784284,
127.500147650524));
#97710=CARTESIAN_POINT('Ctrl Pts',(-95.4420626512169,-3.73154067420819,
127.597779742948));
#97711=CARTESIAN_POINT('Ctrl Pts',(-95.4495529869789,-3.81605287652075,
127.698849336869));
#97712=CARTESIAN_POINT('Ctrl Pts',(-95.457043322741,-3.89626546695886,127.802977857323));
#97713=CARTESIAN_POINT('Ctrl Pts',(-95.4648303242939,-3.97965499529767,
127.911230541345));
#97714=CARTESIAN_POINT('Ctrl Pts',(-95.4726173258466,-4.05866526764973,
128.023137238951));
#97715=CARTESIAN_POINT('Ctrl Pts',(-95.4804043273994,-4.13295930852,128.13830915208));
#97716=CARTESIAN_POINT('Ctrl Pts',(-95.4881786918195,-4.20713278133153,
128.25329415851));
#97717=CARTESIAN_POINT('Ctrl Pts',(-95.4959530562395,-4.27660505651125,
128.371533503499));
#97718=CARTESIAN_POINT('Ctrl Pts',(-95.5037274206595,-4.34107973569718,
128.492605918032));
#97719=CARTESIAN_POINT('Ctrl Pts',(-95.511494515971,-4.40549413041293,128.613565128645));
#97720=CARTESIAN_POINT('Ctrl Pts',(-95.5192616112825,-4.46492004108336,
128.73735179959));
#97721=CARTESIAN_POINT('Ctrl Pts',(-95.527028706594,-4.51910448149372,128.863516021045));
#97722=CARTESIAN_POINT('Ctrl Pts',(-95.5347892209818,-4.57324301237752,
128.989573345767));
#97723=CARTESIAN_POINT('Ctrl Pts',(-95.5425497353695,-4.62214876099844,
129.118003854856));
#97724=CARTESIAN_POINT('Ctrl Pts',(-95.5503102497573,-4.66561506002151,
129.248333890867));
#97725=CARTESIAN_POINT('Ctrl Pts',(-95.556867867916,-4.70234399028569,129.358462494213));
#97726=CARTESIAN_POINT('Ctrl Pts',(-95.5634254860746,-4.73518976908424,
129.469946861467));
#97727=CARTESIAN_POINT('Ctrl Pts',(-95.5699831042333,-4.76405452823397,
129.582490119308));
#97728=CARTESIAN_POINT('Origin',(213.235140564004,0.,130.804360617566));
#97729=CARTESIAN_POINT('',(-97.6652146800015,-4.76405452823416,129.582490119309));
#97730=CARTESIAN_POINT('',(-97.3196997604543,-4.76048812747127,129.583439530431));
#97731=CARTESIAN_POINT('',(213.235140564004,-4.76405452823405,129.582490119308));
#97732=CARTESIAN_POINT('',(-95.9851405639689,-4.91824989715129,130.805366436304));
#97733=CARTESIAN_POINT('Ctrl Pts',(-95.9851405640092,-4.91824989715114,
130.805366437011));
#97734=CARTESIAN_POINT('Ctrl Pts',(-95.9882102340752,-4.91823887890383,
130.85924339672));
#97735=CARTESIAN_POINT('Ctrl Pts',(-95.9912799041412,-4.91734259694869,
130.913110294248));
#97736=CARTESIAN_POINT('Ctrl Pts',(-95.9943495742066,-4.91556186802578,
130.966947776071));
#97737=CARTESIAN_POINT('Ctrl Pts',(-96.0021239083257,-4.91105194307381,
131.103298120867));
#97738=CARTESIAN_POINT('Ctrl Pts',(-96.0098982424448,-4.90085734288855,
131.239676644761));
#97739=CARTESIAN_POINT('Ctrl Pts',(-96.0176725765639,-4.8849669596966,131.375570618505));
#97740=CARTESIAN_POINT('Ctrl Pts',(-96.025437329511,-4.86909615998181,131.511297115071));
#97741=CARTESIAN_POINT('Ctrl Pts',(-96.0332020824581,-4.84754358903086,
131.646539865074));
#97742=CARTESIAN_POINT('Ctrl Pts',(-96.0409668354052,-4.82035012880556,
131.780786599515));
#97743=CARTESIAN_POINT('Ctrl Pts',(-96.0487238762902,-4.79318367750824,
131.914899998206));
#97744=CARTESIAN_POINT('Ctrl Pts',(-96.0564809171752,-4.76038756350126,
132.048018969298));
#97745=CARTESIAN_POINT('Ctrl Pts',(-96.0642379580601,-4.72205436571241,
132.179637182391));
#97746=CARTESIAN_POINT('Ctrl Pts',(-96.0719891493003,-4.68375007528626,
132.311156141165));
#97747=CARTESIAN_POINT('Ctrl Pts',(-96.0797403405404,-4.63991712115529,
132.441176220737));
#97748=CARTESIAN_POINT('Ctrl Pts',(-96.0874915317805,-4.59069889953289,
132.569202445132));
#97749=CARTESIAN_POINT('Ctrl Pts',(-96.0952394285576,-4.54150159696756,
132.697174254968));
#97750=CARTESIAN_POINT('Ctrl Pts',(-96.1029873253346,-4.48692371932166,
132.823153530961));
#97751=CARTESIAN_POINT('Ctrl Pts',(-96.1107352221117,-4.4271580781607,132.946661813354));
#97752=CARTESIAN_POINT('Ctrl Pts',(-96.1184814981958,-4.36740493868348,
133.070144260478));
#97753=CARTESIAN_POINT('Ctrl Pts',(-96.1262277742798,-4.30246636433993,
133.191156390399));
#97754=CARTESIAN_POINT('Ctrl Pts',(-96.1339740503639,-4.23258257873011,
133.309241408488));
#97755=CARTESIAN_POINT('Ctrl Pts',(-96.1417203836292,-4.16269827725396,
133.427327298254));
#97756=CARTESIAN_POINT('Ctrl Pts',(-96.1494667168946,-4.08786889078945,
133.542485696614));
#97757=CARTESIAN_POINT('Ctrl Pts',(-96.1572130501599,-4.00837950330312,
133.654286374494));
#97758=CARTESIAN_POINT('Ctrl Pts',(-96.1649611181629,-3.92887231471971,
133.766112089359));
#97759=CARTESIAN_POINT('Ctrl Pts',(-96.1727091861658,-3.84470327502629,
133.874578268899));
#97760=CARTESIAN_POINT('Ctrl Pts',(-96.1804572541687,-3.75619925886632,
133.979285843487));
#97761=CARTESIAN_POINT('Ctrl Pts',(-96.1882135569105,-3.66760117958464,
134.084104702533));
#97762=CARTESIAN_POINT('Ctrl Pts',(-96.1959698596524,-3.5746591731151,134.185156677737));
#97763=CARTESIAN_POINT('Ctrl Pts',(-96.2037261623942,-3.47773904683619,
134.282077423836));
#97764=CARTESIAN_POINT('Ctrl Pts',(-96.2114866049084,-3.38076719136742,
134.379049899455));
#97765=CARTESIAN_POINT('Ctrl Pts',(-96.2192470474225,-3.27981327299003,
134.471886487885));
#97766=CARTESIAN_POINT('Ctrl Pts',(-96.2270074899367,-3.17527728244498,
134.560262272574));
#97767=CARTESIAN_POINT('Ctrl Pts',(-96.2347803902021,-3.07057348144764,
134.648779925918));
#97768=CARTESIAN_POINT('Ctrl Pts',(-96.2425532904675,-2.96227642647806,
134.732822225973));
#97769=CARTESIAN_POINT('Ctrl Pts',(-96.2503261907329,-2.85081698760548,
134.8121063138));
#97770=CARTESIAN_POINT('Ctrl Pts',(-96.2578165264951,-2.74340938008197,
134.888508225332));
#97771=CARTESIAN_POINT('Ctrl Pts',(-96.2653068622573,-2.63306557610413,
134.96049169621));
#97772=CARTESIAN_POINT('Ctrl Pts',(-96.2727971980195,-2.52019207778084,
135.027844363668));
#97773=CARTESIAN_POINT('Ctrl Pts',(-96.2805715321388,-2.40303894646081,
135.097750727985));
#97774=CARTESIAN_POINT('Ctrl Pts',(-96.2883458662582,-2.28278940144744,
135.16288964552));
#97775=CARTESIAN_POINT('Ctrl Pts',(-96.2961202003775,-2.15986881235654,
135.222974628306));
#97776=CARTESIAN_POINT('Ctrl Pts',(-96.3038849533248,-2.03709971190629,
135.282985561721));
#97777=CARTESIAN_POINT('Ctrl Pts',(-96.3116497062722,-1.91166646500117,
135.337954783245));
#97778=CARTESIAN_POINT('Ctrl Pts',(-96.3194144592195,-1.78402215575809,
135.387639794123));
#97779=CARTESIAN_POINT('Ctrl Pts',(-96.3271715001047,-1.65650462464206,
135.437275457149));
#97780=CARTESIAN_POINT('Ctrl Pts',(-96.3349285409899,-1.52678076342298,
135.481637213087));
#97781=CARTESIAN_POINT('Ctrl Pts',(-96.3426855818751,-1.39532660337702,
135.520529267265));
#97782=CARTESIAN_POINT('Ctrl Pts',(-96.3504367731155,-1.26397157393589,
135.559391992643));
#97783=CARTESIAN_POINT('Ctrl Pts',(-96.3581879643559,-1.13088921624073,
135.592793115844));
#97784=CARTESIAN_POINT('Ctrl Pts',(-96.3659391555963,-0.996573476752261,
135.62058573356));
#97785=CARTESIAN_POINT('Ctrl Pts',(-96.3736870523736,-0.862314825035884,
135.648366538673));
#97786=CARTESIAN_POINT('Ctrl Pts',(-96.3814349491509,-0.726824216213565,
135.670543500372));
#97787=CARTESIAN_POINT('Ctrl Pts',(-96.3891828459282,-0.590608411390184,
135.687020217302));
#97788=CARTESIAN_POINT('Ctrl Pts',(-96.3969291220126,-0.454421099976698,
135.703493487659));
#97789=CARTESIAN_POINT('Ctrl Pts',(-96.404675398097,-0.31750928218268,135.714268838013));
#97790=CARTESIAN_POINT('Ctrl Pts',(-96.4124216741813,-0.180387118989354,
135.71930146663));
#97791=CARTESIAN_POINT('Ctrl Pts',(-96.4201680074469,-0.0432639435915556,
135.724334132397));
#97792=CARTESIAN_POINT('Ctrl Pts',(-96.4279143407125,0.094069189601743,
135.723623977498));
#97793=CARTESIAN_POINT('Ctrl Pts',(-96.435660673978,0.231096221838379,135.717178301823));
#97794=CARTESIAN_POINT('Ctrl Pts',(-96.4434087419813,0.368153940328618,
135.710731182685));
#97795=CARTESIAN_POINT('Ctrl Pts',(-96.4511568099844,0.50490503099862,135.698546005271));
#97796=CARTESIAN_POINT('Ctrl Pts',(-96.4589048779876,0.64083706154235,135.680682071598));
#97797=CARTESIAN_POINT('Ctrl Pts',(-96.4666611807297,0.776913562265933,
135.662799151924));
#97798=CARTESIAN_POINT('Ctrl Pts',(-96.4744174834719,0.912168875681759,
135.639225470552));
#97799=CARTESIAN_POINT('Ctrl Pts',(-96.482173786214,1.04609873997669,135.610071854076));
#97800=CARTESIAN_POINT('Ctrl Pts',(-96.4899342287284,1.18010008667275,135.580902677437));
#97801=CARTESIAN_POINT('Ctrl Pts',(-96.4976946712429,1.31277419661058,135.546147730444));
#97802=CARTESIAN_POINT('Ctrl Pts',(-96.5054551137573,1.44363150352852,135.505967911303));
#97803=CARTESIAN_POINT('Ctrl Pts',(-96.5132280140229,1.57469887421212,135.465723591949));
#97804=CARTESIAN_POINT('Ctrl Pts',(-96.5210009142885,1.70394324496737,135.420037128494));
#97805=CARTESIAN_POINT('Ctrl Pts',(-96.5287738145542,1.83089374275992,135.369118131961));
#97806=CARTESIAN_POINT('Ctrl Pts',(-96.5362641503141,1.95322927014955,135.320050169225));
#97807=CARTESIAN_POINT('Ctrl Pts',(-96.5437544860739,2.07343452418635,135.266123626158));
#97808=CARTESIAN_POINT('Ctrl Pts',(-96.5512448218338,2.19111111374094,135.207565717234));
#97809=CARTESIAN_POINT('Ctrl Pts',(-96.5590191559527,2.31324944698682,135.146787567379));
#97810=CARTESIAN_POINT('Ctrl Pts',(-96.5667934900716,2.43305047947014,135.080827395553));
#97811=CARTESIAN_POINT('Ctrl Pts',(-96.5745678241904,2.55004325808241,135.009888223516));
#97812=CARTESIAN_POINT('Ctrl Pts',(-96.5823325771373,2.66689185355067,134.939036477669));
#97813=CARTESIAN_POINT('Ctrl Pts',(-96.5900973300841,2.78093875025133,134.86321814153));
#97814=CARTESIAN_POINT('Ctrl Pts',(-96.5978620830309,2.89173502408148,134.782683331097));
#97815=CARTESIAN_POINT('Ctrl Pts',(-96.6056191239157,3.00242125349081,134.702228508974));
#97816=CARTESIAN_POINT('Ctrl Pts',(-96.6133761648005,3.10986297081719,134.617066763246));
#97817=CARTESIAN_POINT('Ctrl Pts',(-96.6211332056853,3.21363814192348,134.527492760705));
#97818=CARTESIAN_POINT('Ctrl Pts',(-96.6288843969252,3.31733505536585,134.437986306616));
#97819=CARTESIAN_POINT('Ctrl Pts',(-96.6366355881651,3.41737063133081,134.344074472963));
#97820=CARTESIAN_POINT('Ctrl Pts',(-96.644386779405,3.51335428577712,134.246093426067));
#97821=CARTESIAN_POINT('Ctrl Pts',(-96.6521346761819,3.60929714460997,134.148154023729));
#97822=CARTESIAN_POINT('Ctrl Pts',(-96.6598825729588,3.7011912341784,134.046149126742));
#97823=CARTESIAN_POINT('Ctrl Pts',(-96.6676304697357,3.78868153253689,133.940452980287));
#97824=CARTESIAN_POINT('Ctrl Pts',(-96.6753767458196,3.87615352981104,133.834778943187));
#97825=CARTESIAN_POINT('Ctrl Pts',(-96.6831230219035,3.95922331901052,133.72541549341));
#97826=CARTESIAN_POINT('Ctrl Pts',(-96.6908692979874,4.03757529059656,133.612770992718));
#97827=CARTESIAN_POINT('Ctrl Pts',(-96.6986156312526,4.11592784055916,133.500125660511));
#97828=CARTESIAN_POINT('Ctrl Pts',(-96.7063619645176,4.18956228016758,133.384199550018));
#97829=CARTESIAN_POINT('Ctrl Pts',(-96.7141082977828,4.25820580866642,133.265430781852));
#97830=CARTESIAN_POINT('Ctrl Pts',(-96.7218563657855,4.32686470940744,133.146635416245));
#97831=CARTESIAN_POINT('Ctrl Pts',(-96.7296044337884,4.39053027938544,133.024996464649));
#97832=CARTESIAN_POINT('Ctrl Pts',(-96.7373525017912,4.44897542888738,132.900977105066));
#97833=CARTESIAN_POINT('Ctrl Pts',(-96.7451088045329,4.50748269458981,132.776825936231));
#97834=CARTESIAN_POINT('Ctrl Pts',(-96.7528651072745,4.56075828950776,132.650289659834));
#97835=CARTESIAN_POINT('Ctrl Pts',(-96.7606214100161,4.60862288936522,132.521852430099));
#97836=CARTESIAN_POINT('Ctrl Pts',(-96.7683818525301,4.65651303600081,132.393346649548));
#97837=CARTESIAN_POINT('Ctrl Pts',(-96.7761422950441,4.6989863119534,132.262938265555));
#97838=CARTESIAN_POINT('Ctrl Pts',(-96.783902737558,4.73591346291848,132.131126133491));
#97839=CARTESIAN_POINT('Ctrl Pts',(-96.7916756378232,4.77289989262452,131.999102404891));
#97840=CARTESIAN_POINT('Ctrl Pts',(-96.7994485380884,4.8043223163777,131.865670805942));
#97841=CARTESIAN_POINT('Ctrl Pts',(-96.8072214383537,4.83010256749374,131.731340795342));
#97842=CARTESIAN_POINT('Ctrl Pts',(-96.8147117741174,4.85494564155144,131.601894018952));
#97843=CARTESIAN_POINT('Ctrl Pts',(-96.8222021098811,4.87454958958725,131.47161332052));
#97844=CARTESIAN_POINT('Ctrl Pts',(-96.8296924456448,4.8888902334363,131.340956692758));
#97845=CARTESIAN_POINT('Ctrl Pts',(-96.8374667797639,4.90377460715241,131.205346179271));
#97846=CARTESIAN_POINT('Ctrl Pts',(-96.845241113883,4.91303583086735,131.068901093659));
#97847=CARTESIAN_POINT('Ctrl Pts',(-96.8530154480021,4.9165901508792,130.932127400329));
#97848=CARTESIAN_POINT('Ctrl Pts',(-96.8607802009493,4.92014009050929,130.795522268353));
#97849=CARTESIAN_POINT('Ctrl Pts',(-96.8685449538964,4.91799711044606,130.658589721529));
#97850=CARTESIAN_POINT('Ctrl Pts',(-96.8763097068435,4.91012898591992,130.521842646228));
#97851=CARTESIAN_POINT('Ctrl Pts',(-96.8840667477285,4.90226867612598,130.385231390049));
#97852=CARTESIAN_POINT('Ctrl Pts',(-96.8918237886136,4.88869456016397,130.248805626594));
#97853=CARTESIAN_POINT('Ctrl Pts',(-96.8995808294986,4.86942642979025,130.113079699733));
#97854=CARTESIAN_POINT('Ctrl Pts',(-96.9073320207387,4.8501728296635,129.977456124849));
#97855=CARTESIAN_POINT('Ctrl Pts',(-96.9150832119789,4.82523381660316,129.842531721617));
#97856=CARTESIAN_POINT('Ctrl Pts',(-96.9228344032191,4.79468109664022,129.708816805562));
#97857=CARTESIAN_POINT('Ctrl Pts',(-96.9305822999961,4.76414136239833,129.575158721913));
#97858=CARTESIAN_POINT('Ctrl Pts',(-96.9383301967732,4.72799275368204,129.442709483349));
#97859=CARTESIAN_POINT('Ctrl Pts',(-96.9460780935503,4.68635823552932,129.311970068552));
#97860=CARTESIAN_POINT('Ctrl Pts',(-96.9538243696344,4.64473242642025,129.181258001622));
#97861=CARTESIAN_POINT('Ctrl Pts',(-96.9615706457184,4.59762310894182,129.052255419351));
#97862=CARTESIAN_POINT('Ctrl Pts',(-96.9693169218025,4.54520325474541,128.92544858249));
#97863=CARTESIAN_POINT('Ctrl Pts',(-96.9770632550679,4.49278301359748,128.798640809571));
#97864=CARTESIAN_POINT('Ctrl Pts',(-96.9848095883333,4.43505230686832,128.674029175715));
#97865=CARTESIAN_POINT('Ctrl Pts',(-96.9925559215987,4.37223228236641,128.552080010818));
#97866=CARTESIAN_POINT('Ctrl Pts',(-97.0003039896016,4.30939818975567,128.430103536251));
#97867=CARTESIAN_POINT('Ctrl Pts',(-97.0080520576045,4.24147269047217,128.310791064589));
#97868=CARTESIAN_POINT('Ctrl Pts',(-97.0158001256075,4.16872272174816,128.194584011862));
#97869=CARTESIAN_POINT('Ctrl Pts',(-97.0235564283493,4.09589543349176,128.078253452896));
#97870=CARTESIAN_POINT('Ctrl Pts',(-97.0313127310912,4.01823364084334,127.965035237833));
#97871=CARTESIAN_POINT('Ctrl Pts',(-97.039069033833,3.93604774731314,127.855341934449));
#97872=CARTESIAN_POINT('Ctrl Pts',(-97.0468294763472,3.85381798869699,127.745590084447));
#97873=CARTESIAN_POINT('Ctrl Pts',(-97.0545899188613,3.76705956500141,127.63936719753));
#97874=CARTESIAN_POINT('Ctrl Pts',(-97.0623503613754,3.67612231227041,127.537051662519));
#97875=CARTESIAN_POINT('Ctrl Pts',(-97.0701232616408,3.5850390789883,127.434571881529));
#97876=CARTESIAN_POINT('Ctrl Pts',(-97.0778961619063,3.48976388338215,127.336012268014));
#97877=CARTESIAN_POINT('Ctrl Pts',(-97.0856690621717,3.39068309648188,127.241713960692));
#97878=CARTESIAN_POINT('Ctrl Pts',(-97.0931593979342,3.29520414574868,127.150843634359));
#97879=CARTESIAN_POINT('Ctrl Pts',(-97.1006497336967,3.19619171719632,127.063930377892));
#97880=CARTESIAN_POINT('Ctrl Pts',(-97.1081400694592,3.09401806417718,126.981242089316));
#97881=CARTESIAN_POINT('Ctrl Pts',(-97.1159144035785,2.98797046605325,126.89541864915));
#97882=CARTESIAN_POINT('Ctrl Pts',(-97.1236887376978,2.87818126883451,126.813875017716));
#97883=CARTESIAN_POINT('Ctrl Pts',(-97.131463071817,2.76503088378618,126.736955145498));
#97884=CARTESIAN_POINT('Ctrl Pts',(-97.1392278247643,2.65201994647519,126.660130070148));
#97885=CARTESIAN_POINT('Ctrl Pts',(-97.1469925777114,2.53565638362885,126.587917633646));
#97886=CARTESIAN_POINT('Ctrl Pts',(-97.1547573306587,2.41635428279995,126.520622175213));
#97887=CARTESIAN_POINT('Ctrl Pts',(-97.1625143715438,2.29717067449977,126.453393555578));
#97888=CARTESIAN_POINT('Ctrl Pts',(-97.170271412429,2.17505467468009,126.391072386244));
#97889=CARTESIAN_POINT('Ctrl Pts',(-97.1780284533142,2.0504497133336,126.333920031271));
#97890=CARTESIAN_POINT('Ctrl Pts',(-97.1857796445544,1.92593871755757,126.276810775334));
#97891=CARTESIAN_POINT('Ctrl Pts',(-97.1935308357946,1.79894285013012,126.224862737674));
#97892=CARTESIAN_POINT('Ctrl Pts',(-97.2012820270349,1.66993021281508,126.178291427981));
#97893=CARTESIAN_POINT('Ctrl Pts',(-97.2090299238122,1.54097240931225,126.131739912337));
#97894=CARTESIAN_POINT('Ctrl Pts',(-97.2167778205895,1.40999990775853,126.090560711937));
#97895=CARTESIAN_POINT('Ctrl Pts',(-97.2245257173667,1.27750066131269,126.054921164026));
#97896=CARTESIAN_POINT('Ctrl Pts',(-97.232271993451,1.14502913085285,126.019289071139));
#97897=CARTESIAN_POINT('Ctrl Pts',(-97.2400182695353,1.01103186803643,125.98919442736));
#97898=CARTESIAN_POINT('Ctrl Pts',(-97.2477645456196,0.87601147320753,125.964754542552));
#97899=CARTESIAN_POINT('Ctrl Pts',(-97.2555108788851,0.740990081688564,
125.940314477335));
#97900=CARTESIAN_POINT('Ctrl Pts',(-97.2632572121506,0.604945927800174,
125.92152932402));
#97901=CARTESIAN_POINT('Ctrl Pts',(-97.2710035454161,0.468390883882421,
125.90846508739));
#97902=CARTESIAN_POINT('Ctrl Pts',(-97.2787516134193,0.331805259409576,
125.895397925116));
#97903=CARTESIAN_POINT('Ctrl Pts',(-97.2864996814225,0.194708906357857,
125.888054266113));
#97904=CARTESIAN_POINT('Ctrl Pts',(-97.2942477494257,0.0576174866290085,
125.886448124675));
#97905=CARTESIAN_POINT('Ctrl Pts',(-97.3020040521677,-0.0796196354923194,
125.884840276211));
#97906=CARTESIAN_POINT('Ctrl Pts',(-97.3097603549097,-0.216851422255191,
125.888982131115));
#97907=CARTESIAN_POINT('Ctrl Pts',(-97.3175166576517,-0.353562988024938,
125.898835541083));
#97908=CARTESIAN_POINT('Ctrl Pts',(-97.3252771001661,-0.490347520873641,
125.908694210114));
#97909=CARTESIAN_POINT('Ctrl Pts',(-97.3330375426805,-0.626610891227336,
125.924270464082));
#97910=CARTESIAN_POINT('Ctrl Pts',(-97.3407979851948,-0.76184565492745,
125.945474504415));
#97911=CARTESIAN_POINT('Ctrl Pts',(-97.3485708854604,-0.897297509475828,
125.966712583357));
#97912=CARTESIAN_POINT('Ctrl Pts',(-97.356343785726,-1.03171707413186,125.993596425201));
#97913=CARTESIAN_POINT('Ctrl Pts',(-97.3641166859917,-1.1646084962526,126.025985358866));
#97914=CARTESIAN_POINT('Ctrl Pts',(-97.3716070217516,-1.29266898040746,
126.0571968732));
#97915=CARTESIAN_POINT('Ctrl Pts',(-97.3790973575117,-1.41931020068542,
126.093520095413));
#97916=CARTESIAN_POINT('Ctrl Pts',(-97.3865876932717,-1.54410555486253,
126.134786643643));
#97917=CARTESIAN_POINT('Ctrl Pts',(-97.3943620273906,-1.67363256285817,
126.177617825602));
#97918=CARTESIAN_POINT('Ctrl Pts',(-97.4021363615096,-1.80158127226142,
126.225910262007));
#97919=CARTESIAN_POINT('Ctrl Pts',(-97.4099106956286,-1.9274566862086,126.279529815725));
#97920=CARTESIAN_POINT('Ctrl Pts',(-97.4176754485756,-2.05317696995756,
126.333083288134));
#97921=CARTESIAN_POINT('Ctrl Pts',(-97.4254402015226,-2.17682868600184,
126.391950663325));
#97922=CARTESIAN_POINT('Ctrl Pts',(-97.4332049544696,-2.29793196069802,
126.455948060494));
#97923=CARTESIAN_POINT('Ctrl Pts',(-97.4409619953545,-2.41891495391452,
126.519881894546));
#97924=CARTESIAN_POINT('Ctrl Pts',(-97.4487190362394,-2.53735419945096,
126.588935429391));
#97925=CARTESIAN_POINT('Ctrl Pts',(-97.4564760771243,-2.65279011957886,
126.662876868477));
#97926=CARTESIAN_POINT('Ctrl Pts',(-97.4642272683644,-2.76813898858159,
126.736762547749));
#97927=CARTESIAN_POINT('Ctrl Pts',(-97.4719784596044,-2.8804887122988,126.815528584465));
#97928=CARTESIAN_POINT('Ctrl Pts',(-97.4797296508445,-2.98940495588678,
126.898897639606));
#97929=CARTESIAN_POINT('Ctrl Pts',(-97.4874775476214,-3.09827490716565,
126.982231260674));
#97930=CARTESIAN_POINT('Ctrl Pts',(-97.4952254443983,-3.20371397098678,
127.070163771886));
#97931=CARTESIAN_POINT('Ctrl Pts',(-97.5029733411752,-3.30531761118572,
127.162375094299));
#97932=CARTESIAN_POINT('Ctrl Pts',(-97.5107196172593,-3.40689999809344,
127.254567128092));
#97933=CARTESIAN_POINT('Ctrl Pts',(-97.5184658933432,-3.50464826784564,
127.351035930229));
#97934=CARTESIAN_POINT('Ctrl Pts',(-97.5262121694272,-3.59819205656837,
127.451422057653));
#97935=CARTESIAN_POINT('Ctrl Pts',(-97.5339585026925,-3.69173653580997,
127.551808926106));
#97936=CARTESIAN_POINT('Ctrl Pts',(-97.5417048359577,-3.78107620555669,
127.656112891517));
#97937=CARTESIAN_POINT('Ctrl Pts',(-97.549451169223,-3.86587885461105,127.76393897839));
#97938=CARTESIAN_POINT('Ctrl Pts',(-97.5571992372258,-3.95070049463058,
127.871789212166));
#97939=CARTESIAN_POINT('Ctrl Pts',(-97.5649473052287,-4.03098285052187,
127.983162829684));
#97940=CARTESIAN_POINT('Ctrl Pts',(-97.5726953732315,-4.10643540380995,
128.097633565047));
#97941=CARTESIAN_POINT('Ctrl Pts',(-97.5804516759733,-4.18196814896966,
128.212225961271));
#97942=CARTESIAN_POINT('Ctrl Pts',(-97.588207978715,-4.25266062195452,128.329921723821));
#97943=CARTESIAN_POINT('Ctrl Pts',(-97.5959642814567,-4.31826660975013,
128.450267044741));
#97944=CARTESIAN_POINT('Ctrl Pts',(-97.6037247239708,-4.38390761343679,
128.570676597582));
#97945=CARTESIAN_POINT('Ctrl Pts',(-97.611485166485,-4.44445654992704,128.693738175975));
#97946=CARTESIAN_POINT('Ctrl Pts',(-97.619245608999,-4.49971468333945,128.818976314455));
#97947=CARTESIAN_POINT('Ctrl Pts',(-97.6270185092643,-4.5550615220132,128.944415496313));
#97948=CARTESIAN_POINT('Ctrl Pts',(-97.6347914095296,-4.60510044255946,
129.072037856203));
#97949=CARTESIAN_POINT('Ctrl Pts',(-97.6425643097949,-4.6496817750774,129.201350183098));
#97950=CARTESIAN_POINT('Ctrl Pts',(-97.6500546455582,-4.69264246387257,
129.325961681215));
#97951=CARTESIAN_POINT('Ctrl Pts',(-97.6575449813215,-4.73053538126077,
129.452142115407));
#97952=CARTESIAN_POINT('Ctrl Pts',(-97.6650353170848,-4.7632716027491,129.57944155863));
#97953=CARTESIAN_POINT('Ctrl Pts',(-97.6650951047238,-4.76353290230253,
129.580457659028));
#97954=CARTESIAN_POINT('Ctrl Pts',(-97.6651548923626,-4.76379387748142,
129.58147384598));
#97955=CARTESIAN_POINT('Ctrl Pts',(-97.6652146800015,-4.76405452823416,
129.582490119309));
#97956=CARTESIAN_POINT('Ctrl Pts',(-95.9150180446607,-4.76405452823415,
129.582490119309));
#97957=CARTESIAN_POINT('Ctrl Pts',(-95.9227359398604,-4.79795511176593,
129.714667979986));
#97958=CARTESIAN_POINT('Ctrl Pts',(-95.9304538350601,-4.82632412144731,
129.84815437457));
#97959=CARTESIAN_POINT('Ctrl Pts',(-95.9381717302599,-4.84908613199551,
129.982444109039));
#97960=CARTESIAN_POINT('Ctrl Pts',(-95.9459998692114,-4.87217327904473,
130.118652061334));
#97961=CARTESIAN_POINT('Ctrl Pts',(-95.9538280081629,-4.88949196545971,
130.255686058514));
#97962=CARTESIAN_POINT('Ctrl Pts',(-95.9616561471144,-4.90101813305355,
130.393016088029));
#97963=CARTESIAN_POINT('Ctrl Pts',(-95.9694842860659,-4.9125443006474,130.530346117543));
#97964=CARTESIAN_POINT('Ctrl Pts',(-95.9773124250174,-4.9182779953861,130.667971759409));
#97965=CARTESIAN_POINT('Ctrl Pts',(-95.9851405639689,-4.91824989715129,
130.805366436304));
#97966=CARTESIAN_POINT('',(-95.6398613041516,-4.91378236373845,130.808074515593));
#97967=CARTESIAN_POINT('Ctrl Pts',(-95.5699831042333,-4.76405452823397,
129.582490119308));
#97968=CARTESIAN_POINT('Ctrl Pts',(-95.5777374979323,-4.79818715094222,
129.715572697213));
#97969=CARTESIAN_POINT('Ctrl Pts',(-95.5854918916312,-4.82675179822305,
129.850135990574));
#97970=CARTESIAN_POINT('Ctrl Pts',(-95.5932462853303,-4.84963274388358,
129.985675505968));
#97971=CARTESIAN_POINT('Ctrl Pts',(-95.6010151437738,-4.87255637077067,
130.121467851505));
#97972=CARTESIAN_POINT('Ctrl Pts',(-95.6087840022174,-4.88977498398199,
130.258239682372));
#97973=CARTESIAN_POINT('Ctrl Pts',(-95.616552860661,-4.90122382829593,130.395474267287));
#97974=CARTESIAN_POINT('Ctrl Pts',(-95.6243217191045,-4.91267267260987,
130.532708852202));
#97975=CARTESIAN_POINT('Ctrl Pts',(-95.6320905775481,-4.91835172324539,
130.67040579917));
#97976=CARTESIAN_POINT('Ctrl Pts',(-95.6398594359917,-4.91824862012079,
130.808044797249));
#97977=CARTESIAN_POINT('Ctrl Pts',(-95.639861537601,-4.91322425034186,130.808078229263));
#97978=CARTESIAN_POINT('Ctrl Pts',(-95.671738007252,-4.91712121886186,131.372252204815));
#97979=CARTESIAN_POINT('Ctrl Pts',(-95.7964303515077,-4.56637019745189,
133.574446779133));
#97980=CARTESIAN_POINT('Ctrl Pts',(-96.0139385703665,-1.31322884073256,
136.471556559328));
#97981=CARTESIAN_POINT('Ctrl Pts',(-96.29238619418,4.05814018332094,134.972475069326));
#97982=CARTESIAN_POINT('Ctrl Pts',(-96.5708338179925,5.70027663007168,129.643100021867));
#97983=CARTESIAN_POINT('Ctrl Pts',(-96.8492814418056,2.10413732778126,125.380866731122));
#97984=CARTESIAN_POINT('Ctrl Pts',(-97.0989034226261,-2.85314803968669,
126.027847816815));
#97985=CARTESIAN_POINT('Ctrl Pts',(-97.2557095288423,-4.46971273000384,
128.48961976286));
#97986=CARTESIAN_POINT('Ctrl Pts',(-97.3196997604543,-4.76048812747127,
129.583439530431));
#97987=CARTESIAN_POINT('Origin',(213.235140564004,0.,130.804360617566));
#97988=CARTESIAN_POINT('',(-99.4153986790351,-4.76405452823397,129.582490119308));
#97989=CARTESIAN_POINT('',(-99.0698920977623,-4.76405452823408,129.582490119308));
#97990=CARTESIAN_POINT('',(213.235140564004,-4.76405452823405,129.582490119308));
#97991=CARTESIAN_POINT('',(-97.7351405639562,-4.91824790420648,130.799820213553));
#97992=CARTESIAN_POINT('Ctrl Pts',(-97.7351405640093,-4.91824790420734,
130.799820214491));
#97993=CARTESIAN_POINT('Ctrl Pts',(-97.7428066318137,-4.91837292102423,
130.935240723974));
#97994=CARTESIAN_POINT('Ctrl Pts',(-97.750472699618,-4.91290066797459,131.070804378959));
#97995=CARTESIAN_POINT('Ctrl Pts',(-97.7581387674224,-4.9018225276731,131.206005945805));
#97996=CARTESIAN_POINT('Ctrl Pts',(-97.7658614413172,-4.89066258660654,
131.342205838301));
#97997=CARTESIAN_POINT('Ctrl Pts',(-97.773584115212,-4.87381359281784,131.478037863531));
#97998=CARTESIAN_POINT('Ctrl Pts',(-97.7813067891068,-4.85132026448249,
131.612985842204));
#97999=CARTESIAN_POINT('Ctrl Pts',(-97.7889660047495,-4.8290117668574,131.74682493515));
#98000=CARTESIAN_POINT('Ctrl Pts',(-97.7966252203921,-4.80115142974561,
131.879794056288));
#98001=CARTESIAN_POINT('Ctrl Pts',(-97.8042844360347,-4.76783479633275,
132.011396001214));
#98002=CARTESIAN_POINT('Ctrl Pts',(-97.8119430718726,-4.7345206849984,132.142987983836));
#98003=CARTESIAN_POINT('Ctrl Pts',(-97.8196017077106,-4.69575119701223,
132.273212607617));
#98004=CARTESIAN_POINT('Ctrl Pts',(-97.8272603435484,-4.6516725183478,132.401585036534));
#98005=CARTESIAN_POINT('Ctrl Pts',(-97.8349201488105,-4.6075871091537,132.529977067092));
#98006=CARTESIAN_POINT('Ctrl Pts',(-97.8425799540726,-4.55819102745045,
132.656515961451));
#98007=CARTESIAN_POINT('Ctrl Pts',(-97.8502397593348,-4.50367945960312,
132.780734668106));
#98008=CARTESIAN_POINT('Ctrl Pts',(-97.858010024465,-4.44838179597548,132.906744697319));
#98009=CARTESIAN_POINT('Ctrl Pts',(-97.8657802895951,-4.3878201249069,133.030366707881));
#98010=CARTESIAN_POINT('Ctrl Pts',(-97.8735505547254,-4.32224705533296,
133.151137866298));
#98011=CARTESIAN_POINT('Ctrl Pts',(-97.8812219175975,-4.25750861939675,
133.270371813296));
#98012=CARTESIAN_POINT('Ctrl Pts',(-97.8888932804697,-4.18788587560084,
133.38682674569));
#98013=CARTESIAN_POINT('Ctrl Pts',(-97.8965646433418,-4.11366578001135,
133.500086292197));
#98014=CARTESIAN_POINT('Ctrl Pts',(-97.9043843596011,-4.03801037197998,
133.615536119314));
#98015=CARTESIAN_POINT('Ctrl Pts',(-97.9122040758604,-3.95757823358253,
133.727665346258));
#98016=CARTESIAN_POINT('Ctrl Pts',(-97.9200237921197,-3.87271585389831,
133.836068878178));
#98017=CARTESIAN_POINT('Ctrl Pts',(-97.927843508379,-3.78785347421433,133.944472410098));
#98018=CARTESIAN_POINT('Ctrl Pts',(-97.9356632246383,-3.69856118665766,
134.049149962176));
#98019=CARTESIAN_POINT('Ctrl Pts',(-97.9434829408976,-3.60522374645677,
134.149737248154));
#98020=CARTESIAN_POINT('Ctrl Pts',(-97.9512572750166,-3.51242799506625,
134.249740770455));
#98021=CARTESIAN_POINT('Ctrl Pts',(-97.9590316091357,-3.41532118597507,
134.346038741776));
#98022=CARTESIAN_POINT('Ctrl Pts',(-97.9668059432548,-3.31423107289613,
134.438236710383));
#98023=CARTESIAN_POINT('Ctrl Pts',(-97.9745706962019,-3.2132655443466,134.530321053235));
#98024=CARTESIAN_POINT('Ctrl Pts',(-97.9823354491489,-3.10832676548148,
134.618315186184));
#98025=CARTESIAN_POINT('Ctrl Pts',(-97.990100202096,-2.99978144650823,134.70185908911));
#98026=CARTESIAN_POINT('Ctrl Pts',(-97.997857242981,-2.89134393627599,134.785320015054));
#98027=CARTESIAN_POINT('Ctrl Pts',(-98.005614283866,-2.77930732222756,134.864339270119));
#98028=CARTESIAN_POINT('Ctrl Pts',(-98.013371324751,-2.66407345842478,134.938595210646));
#98029=CARTESIAN_POINT('Ctrl Pts',(-98.0211225159912,-2.54892649337556,
135.01279515419));
#98030=CARTESIAN_POINT('Ctrl Pts',(-98.0288737072314,-2.43058740497435,
135.082238722042));
#98031=CARTESIAN_POINT('Ctrl Pts',(-98.0366248984715,-2.30948897630498,
135.146646159861));
#98032=CARTESIAN_POINT('Ctrl Pts',(-98.0443727952486,-2.18844201769804,
135.211026222802));
#98033=CARTESIAN_POINT('Ctrl Pts',(-98.0521206920256,-2.06463839587678,
135.270374229777));
#98034=CARTESIAN_POINT('Ctrl Pts',(-98.0598685888026,-1.9385373802953,135.324455294417));
#98035=CARTESIAN_POINT('Ctrl Pts',(-98.0676148648867,-1.81246274232786,
135.378525046464));
#98036=CARTESIAN_POINT('Ctrl Pts',(-98.0753611409709,-1.68409202555793,
135.427329893577));
#98037=CARTESIAN_POINT('Ctrl Pts',(-98.0831074170549,-1.55390609748732,
135.470682392014));
#98038=CARTESIAN_POINT('Ctrl Pts',(-98.0908537503203,-1.42371920841394,
135.51403521047));
#98039=CARTESIAN_POINT('Ctrl Pts',(-98.0986000835856,-1.29171745224094,
135.551935476415));
#98040=CARTESIAN_POINT('Ctrl Pts',(-98.1063464168509,-1.15839815503381,
135.584245216269));
#98041=CARTESIAN_POINT('Ctrl Pts',(-98.1140944848539,-1.02504900189462,
135.616562191665));
#98042=CARTESIAN_POINT('Ctrl Pts',(-98.1218425528568,-0.890382100491075,
135.643286057649));
#98043=CARTESIAN_POINT('Ctrl Pts',(-98.1295906208598,-0.754905905760631,
135.664329767257));
#98044=CARTESIAN_POINT('Ctrl Pts',(-98.1373469236016,-0.619285725317686,
135.68539584237));
#98045=CARTESIAN_POINT('Ctrl Pts',(-98.1451032263436,-0.482854920300665,
135.70076964157));
#98046=CARTESIAN_POINT('Ctrl Pts',(-98.1528595290854,-0.346128579316764,
135.710415862779));
#98047=CARTESIAN_POINT('Ctrl Pts',(-98.1606199715996,-0.209329263367929,
135.720067232467));
#98048=CARTESIAN_POINT('Ctrl Pts',(-98.1683804141137,-0.0722344877634435,
135.723984921709));
#98049=CARTESIAN_POINT('Ctrl Pts',(-98.1761408566278,0.0646406956810316,
135.722185811995));
#98050=CARTESIAN_POINT('Ctrl Pts',(-98.1839137568933,0.20173560332118,135.72038381419));
#98051=CARTESIAN_POINT('Ctrl Pts',(-98.1916866571587,0.338609823777876,
135.712846700142));
#98052=CARTESIAN_POINT('Ctrl Pts',(-98.1994595574241,0.474752560436986,
135.699643353921));
#98053=CARTESIAN_POINT('Ctrl Pts',(-98.2069498931862,0.605946165696418,
135.686919982593));
#98054=CARTESIAN_POINT('Ctrl Pts',(-98.2144402289483,0.736460241253026,
135.668935232472));
#98055=CARTESIAN_POINT('Ctrl Pts',(-98.2219305647104,0.865848607855436,
135.645795244903));
#98056=CARTESIAN_POINT('Ctrl Pts',(-98.2297048988295,1.00014277370338,135.621777897671));
#98057=CARTESIAN_POINT('Ctrl Pts',(-98.2374792329486,1.13364958655527,135.592130594683));
#98058=CARTESIAN_POINT('Ctrl Pts',(-98.2452535670676,1.2658600241094,135.556915873622));
#98059=CARTESIAN_POINT('Ctrl Pts',(-98.2530183200147,1.39790752411522,135.521744551557));
#98060=CARTESIAN_POINT('Ctrl Pts',(-98.2607830729618,1.52866145353691,135.481019563112));
#98061=CARTESIAN_POINT('Ctrl Pts',(-98.2685478259089,1.65762070142654,135.434854832302));
#98062=CARTESIAN_POINT('Ctrl Pts',(-98.2763048667939,1.78645186517316,135.388735952953));
#98063=CARTESIAN_POINT('Ctrl Pts',(-98.2840619076788,1.91349152894031,135.337188214028));
#98064=CARTESIAN_POINT('Ctrl Pts',(-98.2918189485638,2.03825187287204,135.280375850475));
#98065=CARTESIAN_POINT('Ctrl Pts',(-98.2995701398039,2.16291813405775,135.223606329568));
#98066=CARTESIAN_POINT('Ctrl Pts',(-98.3073213310441,2.2853081423093,135.161580247636));
#98067=CARTESIAN_POINT('Ctrl Pts',(-98.3150725222842,2.40495260254972,135.094510503291));
#98068=CARTESIAN_POINT('Ctrl Pts',(-98.3228204190612,2.52454621070309,135.027469265377));
#98069=CARTESIAN_POINT('Ctrl Pts',(-98.3305683158383,2.6413962514606,134.955388819464));
#98070=CARTESIAN_POINT('Ctrl Pts',(-98.3383162126154,2.75505686190805,134.87852860013));
#98071=CARTESIAN_POINT('Ctrl Pts',(-98.3460624886995,2.86869369700605,134.801684458298));
#98072=CARTESIAN_POINT('Ctrl Pts',(-98.3538087647836,2.9791421051503,134.720062750621));
#98073=CARTESIAN_POINT('Ctrl Pts',(-98.3615550408677,3.08598446398274,134.633966726627));
#98074=CARTESIAN_POINT('Ctrl Pts',(-98.369301374133,3.19282761150135,134.547870067092));
#98075=CARTESIAN_POINT('Ctrl Pts',(-98.3770477073983,3.29606435216587,134.457299270648));
#98076=CARTESIAN_POINT('Ctrl Pts',(-98.3847940406637,3.39530978800992,134.362598173709));
#98077=CARTESIAN_POINT('Ctrl Pts',(-98.3925421086667,3.49457744918081,134.267875869116));
#98078=CARTESIAN_POINT('Ctrl Pts',(-98.4002901766696,3.58985174412298,134.169021693331));
#98079=CARTESIAN_POINT('Ctrl Pts',(-98.4080382446726,3.68078460544728,134.066416372884));
#98080=CARTESIAN_POINT('Ctrl Pts',(-98.4157945474144,3.77181411129909,133.96370200228));
#98081=CARTESIAN_POINT('Ctrl Pts',(-98.4235508501563,3.85849270659342,133.857228816091));
#98082=CARTESIAN_POINT('Ctrl Pts',(-98.4313071528981,3.94051227272033,133.747411091316));
#98083=CARTESIAN_POINT('Ctrl Pts',(-98.4390675954123,4.02257561515924,133.637534753514));
#98084=CARTESIAN_POINT('Ctrl Pts',(-98.4468280379265,4.09997475301399,133.524310642803));
#98085=CARTESIAN_POINT('Ctrl Pts',(-98.4545884804407,4.17244549107215,133.408181211718));
#98086=CARTESIAN_POINT('Ctrl Pts',(-98.4623613807061,4.24503256559269,133.291865359361));
#98087=CARTESIAN_POINT('Ctrl Pts',(-98.4701342809715,4.31267523757678,133.172635206964));
#98088=CARTESIAN_POINT('Ctrl Pts',(-98.4779071812369,4.37515536309906,133.050957735708));
#98089=CARTESIAN_POINT('Ctrl Pts',(-98.485397516999,4.43536417868101,132.933703547019));
#98090=CARTESIAN_POINT('Ctrl Pts',(-98.4928878527611,4.49077914487141,132.81417716216));
#98091=CARTESIAN_POINT('Ctrl Pts',(-98.5003781885232,4.54124839060584,132.692811336362));
#98092=CARTESIAN_POINT('Ctrl Pts',(-98.5081525226422,4.59363119313158,132.566843888391));
#98093=CARTESIAN_POINT('Ctrl Pts',(-98.5159268567614,4.6408517709036,132.438495734188));
#98094=CARTESIAN_POINT('Ctrl Pts',(-98.5237011908804,4.68268759965953,132.308228931779));
#98095=CARTESIAN_POINT('Ctrl Pts',(-98.5314659438275,4.72447186949562,132.178122671562));
#98096=CARTESIAN_POINT('Ctrl Pts',(-98.5392306967745,4.76088447602025,132.046102836578));
#98097=CARTESIAN_POINT('Ctrl Pts',(-98.5469954497215,4.79175040402551,131.912652604373));
#98098=CARTESIAN_POINT('Ctrl Pts',(-98.5547524906065,4.82258567555586,131.779334916821));
#98099=CARTESIAN_POINT('Ctrl Pts',(-98.5625095314916,4.84788514427261,131.644590037731));
#98100=CARTESIAN_POINT('Ctrl Pts',(-98.5702665723765,4.86752330714199,131.508917156766));
#98101=CARTESIAN_POINT('Ctrl Pts',(-98.5780177636167,4.88714666072008,131.373346587775));
#98102=CARTESIAN_POINT('Ctrl Pts',(-98.5857689548568,4.90111715032316,131.236849795212));
#98103=CARTESIAN_POINT('Ctrl Pts',(-98.5935201460969,4.90936022813055,131.099936687216));
#98104=CARTESIAN_POINT('Ctrl Pts',(-98.601268042874,4.91759980240997,130.963081770944));
#98105=CARTESIAN_POINT('Ctrl Pts',(-98.6090159396511,4.92011678308943,130.825811280611));
#98106=CARTESIAN_POINT('Ctrl Pts',(-98.6167638364282,4.91688844003116,130.68864056404));
#98107=CARTESIAN_POINT('Ctrl Pts',(-98.6245101125123,4.91366077227266,130.551498540627));
#98108=CARTESIAN_POINT('Ctrl Pts',(-98.6322563885964,4.90469018041137,130.414456640073));
#98109=CARTESIAN_POINT('Ctrl Pts',(-98.6400026646805,4.89000606177802,130.278030133674));
#98110=CARTESIAN_POINT('Ctrl Pts',(-98.6477489979459,4.87532183474981,130.141602620205));
#98111=CARTESIAN_POINT('Ctrl Pts',(-98.6554953312112,4.85492403862992,130.005790898674));
#98112=CARTESIAN_POINT('Ctrl Pts',(-98.6632416644765,4.82889390597889,129.871104646623));
#98113=CARTESIAN_POINT('Ctrl Pts',(-98.6709897324795,4.8028579440601,129.73638823252));
#98114=CARTESIAN_POINT('Ctrl Pts',(-98.6787378004826,4.77118720989687,129.602798173217));
#98115=CARTESIAN_POINT('Ctrl Pts',(-98.6864858684856,4.73401388057493,129.470833099656));
#98116=CARTESIAN_POINT('Ctrl Pts',(-98.6942421712274,4.69680104299638,129.338727772044));
#98117=CARTESIAN_POINT('Ctrl Pts',(-98.7019984739692,4.65407403397733,129.208251257071));
#98118=CARTESIAN_POINT('Ctrl Pts',(-98.709754776711,4.60601485085524,129.079886710486));
#98119=CARTESIAN_POINT('Ctrl Pts',(-98.7175152192252,4.55793001709981,128.951453651876));
#98120=CARTESIAN_POINT('Ctrl Pts',(-98.7252756617395,4.50450749067418,128.825135167649));
#98121=CARTESIAN_POINT('Ctrl Pts',(-98.7330361042537,4.44597671546269,128.701392689122));
#98122=CARTESIAN_POINT('Ctrl Pts',(-98.7408090045191,4.38735198145487,128.577451568184));
#98123=CARTESIAN_POINT('Ctrl Pts',(-98.7485819047844,4.3236027939411,128.456095062774));
#98124=CARTESIAN_POINT('Ctrl Pts',(-98.7563548050498,4.2550041252953,128.337759118292));
#98125=CARTESIAN_POINT('Ctrl Pts',(-98.7638451408119,4.1888991910442,128.223724983462));
#98126=CARTESIAN_POINT('Ctrl Pts',(-98.771335476574,4.11829140111115,128.112495872362));
#98127=CARTESIAN_POINT('Ctrl Pts',(-98.7788258123361,4.04346275470753,128.004433473194));
#98128=CARTESIAN_POINT('Ctrl Pts',(-98.7866001464551,3.96579695743217,127.892273855316));
#98129=CARTESIAN_POINT('Ctrl Pts',(-98.7943744805743,3.88333789600536,127.783170533456));
#98130=CARTESIAN_POINT('Ctrl Pts',(-98.8021488146934,3.7963540331303,127.677560477225));
#98131=CARTESIAN_POINT('Ctrl Pts',(-98.8099135676405,3.70947737009226,127.57208057595));
#98132=CARTESIAN_POINT('Ctrl Pts',(-98.8176783205875,3.61808724717833,127.47008567325));
#98133=CARTESIAN_POINT('Ctrl Pts',(-98.8254430735346,3.52249557534673,127.371984183641));
#98134=CARTESIAN_POINT('Ctrl Pts',(-98.8332001144196,3.42699884651094,127.273980129814));
#98135=CARTESIAN_POINT('Ctrl Pts',(-98.8409571553047,3.32730914437406,127.17986207179));
#98136=CARTESIAN_POINT('Ctrl Pts',(-98.8487141961897,3.22377861388139,127.090005423029));
#98137=CARTESIAN_POINT('Ctrl Pts',(-98.8564653874299,3.12032615656697,127.000216535867));
#98138=CARTESIAN_POINT('Ctrl Pts',(-98.8642165786699,3.013038930072,126.914682916799));
#98139=CARTESIAN_POINT('Ctrl Pts',(-98.8719677699101,2.90230563963737,126.833742902823));
#98140=CARTESIAN_POINT('Ctrl Pts',(-98.8797156666871,2.79161941380553,126.752837290513));
#98141=CARTESIAN_POINT('Ctrl Pts',(-98.8874635634643,2.67749035212375,126.676521630339));
#98142=CARTESIAN_POINT('Ctrl Pts',(-98.8952114602414,2.56033974511689,126.605093603899));
#98143=CARTESIAN_POINT('Ctrl Pts',(-98.9029577363255,2.44321364349122,126.533680518661));
#98144=CARTESIAN_POINT('Ctrl Pts',(-98.9107040124095,2.32306758730672,126.46715323697));
#98145=CARTESIAN_POINT('Ctrl Pts',(-98.9184502884936,2.20035097887212,126.405765542741));
#98146=CARTESIAN_POINT('Ctrl Pts',(-98.926196621759,2.0776334645719,126.344377395362));
#98147=CARTESIAN_POINT('Ctrl Pts',(-98.9339429550244,1.95234570981431,126.28812908606));
#98148=CARTESIAN_POINT('Ctrl Pts',(-98.9416892882897,1.8249604289321,126.237227764743));
#98149=CARTESIAN_POINT('Ctrl Pts',(-98.9494373562927,1.6975466209993,126.186315044428));
#98150=CARTESIAN_POINT('Ctrl Pts',(-98.9571854242956,1.5680347152251,126.14075183987));
#98151=CARTESIAN_POINT('Ctrl Pts',(-98.9649334922986,1.43691566888555,126.100696468946));
#98152=CARTESIAN_POINT('Ctrl Pts',(-98.9726897950404,1.30565726766303,126.060598526697));
#98153=CARTESIAN_POINT('Ctrl Pts',(-98.9804460977824,1.17278868828855,126.026020226068));
#98154=CARTESIAN_POINT('Ctrl Pts',(-98.9882024005242,1.03881479738488,125.997069605027));
#98155=CARTESIAN_POINT('Ctrl Pts',(-98.9959628430384,0.904769400581384,
125.968103532169));
#98156=CARTESIAN_POINT('Ctrl Pts',(-99.0037232855526,0.769617901824807,
125.94477119043));
#98157=CARTESIAN_POINT('Ctrl Pts',(-99.0114837280667,0.63387253637551,125.927128957072));
#98158=CARTESIAN_POINT('Ctrl Pts',(-99.0192566283322,0.497909260415057,
125.909458402834));
#98159=CARTESIAN_POINT('Ctrl Pts',(-99.0270295285976,0.361350602407642,
125.897496244289));
#98160=CARTESIAN_POINT('Ctrl Pts',(-99.0348024288631,0.224711964847995,
125.891246778527));
#98161=CARTESIAN_POINT('Ctrl Pts',(-99.042292764625,0.093040485936713,125.885224496588));
#98162=CARTESIAN_POINT('Ctrl Pts',(-99.049783100387,-0.0387049505519755,
125.884506778503));
#98163=CARTESIAN_POINT('Ctrl Pts',(-99.057273436149,-0.170067618629719,
125.889051871659));
#98164=CARTESIAN_POINT('Ctrl Pts',(-99.065047770268,-0.306410942195046,
125.893769293402));
#98165=CARTESIAN_POINT('Ctrl Pts',(-99.0728221043871,-0.442773793718309,
125.90417142668));
#98166=CARTESIAN_POINT('Ctrl Pts',(-99.0805964385061,-0.578643427639874,
125.920268598966));
#98167=CARTESIAN_POINT('Ctrl Pts',(-99.0883611914533,-0.714345614381386,
125.936345932926));
#98168=CARTESIAN_POINT('Ctrl Pts',(-99.0961259444003,-0.84955540843205,
125.958104295363));
#98169=CARTESIAN_POINT('Ctrl Pts',(-99.1038906973475,-0.98376060360043,
125.985502024776));
#98170=CARTESIAN_POINT('Ctrl Pts',(-99.1116477382324,-1.11783250427664,
126.012872542378));
#98171=CARTESIAN_POINT('Ctrl Pts',(-99.1194047791175,-1.25090141111581,
126.045871202821));
#98172=CARTESIAN_POINT('Ctrl Pts',(-99.1271618200025,-1.38246113519507,
126.084404656736));
#98173=CARTESIAN_POINT('Ctrl Pts',(-99.1349130112426,-1.5139216490632,126.122909052273));
#98174=CARTESIAN_POINT('Ctrl Pts',(-99.1426642024828,-1.6438748717794,126.166939824075));
#98175=CARTESIAN_POINT('Ctrl Pts',(-99.1504153937229,-1.77182604616822,
126.216352822823));
#98176=CARTESIAN_POINT('Ctrl Pts',(-99.1581632905,-1.89972283789489,126.265744819729));
#98177=CARTESIAN_POINT('Ctrl Pts',(-99.165911187277,-2.02561890976725,126.320514353188));
#98178=CARTESIAN_POINT('Ctrl Pts',(-99.1736590840542,-2.14903609600899,
126.380467883723));
#98179=CARTESIAN_POINT('Ctrl Pts',(-99.1814053601383,-2.27242746603561,
126.440408873271));
#98180=CARTESIAN_POINT('Ctrl Pts',(-99.1891516362224,-2.3933406303705,126.505531532279));
#98181=CARTESIAN_POINT('Ctrl Pts',(-99.1968979123065,-2.51131916049412,
126.575594942261));
#98182=CARTESIAN_POINT('Ctrl Pts',(-99.2046442455719,-2.62929856150861,
126.645658869436));
#98183=CARTESIAN_POINT('Ctrl Pts',(-99.2123905788372,-2.74434294892905,
126.720663420728));
#98184=CARTESIAN_POINT('Ctrl Pts',(-99.2201369121026,-2.85602252802894,
126.800322857768));
#98185=CARTESIAN_POINT('Ctrl Pts',(-99.2278849801056,-2.96772711699608,
126.880000133986));
#98186=CARTESIAN_POINT('Ctrl Pts',(-99.2356330481085,-3.07606507998314,
126.964334143274));
#98187=CARTESIAN_POINT('Ctrl Pts',(-99.2433811161115,-3.18063784527585,
127.052997404053));
#98188=CARTESIAN_POINT('Ctrl Pts',(-99.2511374188534,-3.28532175174808,
127.1417548972));
#98189=CARTESIAN_POINT('Ctrl Pts',(-99.2588937215952,-3.38623216802364,
127.23485057995));
#98190=CARTESIAN_POINT('Ctrl Pts',(-99.2666500243371,-3.48300530595665,
127.331918090874));
#98191=CARTESIAN_POINT('Ctrl Pts',(-99.2744104668513,-3.57983009462716,
127.429037409652));
#98192=CARTESIAN_POINT('Ctrl Pts',(-99.2821709093654,-3.67251294087485,
127.530132492611));
#98193=CARTESIAN_POINT('Ctrl Pts',(-99.2899313518796,-3.76072953724353,
127.634802855006));
#98194=CARTESIAN_POINT('Ctrl Pts',(-99.2977042521451,-3.84908774672421,
127.739641243559));
#98195=CARTESIAN_POINT('Ctrl Pts',(-99.3054771524106,-3.93296513977772,
127.848066071197));
#98196=CARTESIAN_POINT('Ctrl Pts',(-99.313250052676,-4.01207951350237,127.959646037888));
#98197=CARTESIAN_POINT('Ctrl Pts',(-99.320740388438,-4.08831788046484,128.067169791736));
#98198=CARTESIAN_POINT('Ctrl Pts',(-99.3282307242,-4.1601333434996,128.177623014523));
#98199=CARTESIAN_POINT('Ctrl Pts',(-99.335721059962,-4.22731415871232,128.290598881432));
#98200=CARTESIAN_POINT('Ctrl Pts',(-99.3437732964471,-4.29953466104291,
128.41204983188));
#98201=CARTESIAN_POINT('Ctrl Pts',(-99.3518255329323,-4.36661414793408,
128.536777810003));
#98202=CARTESIAN_POINT('Ctrl Pts',(-99.3598777694174,-4.42825387018387,
128.664325402038));
#98203=CARTESIAN_POINT('Ctrl Pts',(-99.3679189691167,-4.48980910604086,
128.791698171157));
#98204=CARTESIAN_POINT('Ctrl Pts',(-99.3759601688161,-4.54593927038731,
128.921882544925));
#98205=CARTESIAN_POINT('Ctrl Pts',(-99.3840013685154,-4.59638979165394,
129.054393776257));
#98206=CARTESIAN_POINT('Ctrl Pts',(-99.3920295010243,-4.64675832931226,
129.18668967287));
#98207=CARTESIAN_POINT('Ctrl Pts',(-99.4000576335332,-4.69146549368572,
129.321304563779));
#98208=CARTESIAN_POINT('Ctrl Pts',(-99.4080857660421,-4.73030365966211,
129.457731362765));
#98209=CARTESIAN_POINT('Ctrl Pts',(-99.4105234037064,-4.74209636189924,
129.499155579824));
#98210=CARTESIAN_POINT('Ctrl Pts',(-99.4129610413707,-4.75334829840962,
129.540746691713));
#98211=CARTESIAN_POINT('Ctrl Pts',(-99.4153986790351,-4.76405452823397,
129.582490119308));
#98212=CARTESIAN_POINT('Ctrl Pts',(-97.6652146800015,-4.76405452823416,
129.582490119309));
#98213=CARTESIAN_POINT('Ctrl Pts',(-97.6753787325341,-4.80836582721425,
129.755259201514));
#98214=CARTESIAN_POINT('Ctrl Pts',(-97.6855427850666,-4.84329698735637,
129.93052638174));
#98215=CARTESIAN_POINT('Ctrl Pts',(-97.6957068375993,-4.86861814770353,
130.107409834259));
#98216=CARTESIAN_POINT('Ctrl Pts',(-97.7056546069463,-4.89340049332051,
130.280529343561));
#98217=CARTESIAN_POINT('Ctrl Pts',(-97.7156023762933,-4.908977520003,130.4551973254));
#98218=CARTESIAN_POINT('Ctrl Pts',(-97.7255501456403,-4.91517833945882,
130.63056489318));
#98219=CARTESIAN_POINT('Ctrl Pts',(-97.7287469517456,-4.91717102915664,
130.686920855184));
#98220=CARTESIAN_POINT('Ctrl Pts',(-97.7319437578509,-4.91819577127258,
130.743348874851));
#98221=CARTESIAN_POINT('Ctrl Pts',(-97.7351405639562,-4.91824790420648,
130.799820213553));
#98222=CARTESIAN_POINT('',(-97.3898584762948,-4.92178906768926,130.806090568707));
#98223=CARTESIAN_POINT('Ctrl Pts',(-97.3196997604543,-4.76048812747127,
129.583439530431));
#98224=CARTESIAN_POINT('Ctrl Pts',(-97.3430856516127,-4.86675500017061,
129.983187263592));
#98225=CARTESIAN_POINT('Ctrl Pts',(-97.366471542771,-4.92374838532847,130.394849645968));
#98226=CARTESIAN_POINT('Ctrl Pts',(-97.3898574339294,-4.92563332792477,
130.806073603889));
#98227=CARTESIAN_POINT('Ctrl Pts',(-97.3898594359918,-4.91824969023367,
130.806106188069));
#98228=CARTESIAN_POINT('Ctrl Pts',(-97.3952985204717,-4.91821579607926,
130.901605003017));
#98229=CARTESIAN_POINT('Ctrl Pts',(-97.4007376049514,-4.9154006230219,130.997051187051));
#98230=CARTESIAN_POINT('Ctrl Pts',(-97.4061766894311,-4.9098121045098,131.092333117831));
#98231=CARTESIAN_POINT('Ctrl Pts',(-97.4139510235502,-4.90182417744125,
131.228523972774));
#98232=CARTESIAN_POINT('Ctrl Pts',(-97.4217253576694,-4.88815270727774,
131.364597932649));
#98233=CARTESIAN_POINT('Ctrl Pts',(-97.4294996917885,-4.86879967399904,
131.500042151723));
#98234=CARTESIAN_POINT('Ctrl Pts',(-97.4372644447356,-4.84947049160423,
131.635319447902));
#98235=CARTESIAN_POINT('Ctrl Pts',(-97.4450291976826,-4.82447373279531,
131.769968164168));
#98236=CARTESIAN_POINT('Ctrl Pts',(-97.4527939506297,-4.79386333861176,
131.903477241594));
#98237=CARTESIAN_POINT('Ctrl Pts',(-97.4605509915147,-4.76328334710323,
132.036853715921));
#98238=CARTESIAN_POINT('Ctrl Pts',(-97.4683080323997,-4.72710090260625,
132.16909242534));
#98239=CARTESIAN_POINT('Ctrl Pts',(-97.4760650732847,-4.68542147474618,
132.299689566823));
#98240=CARTESIAN_POINT('Ctrl Pts',(-97.4838162645248,-4.64377347766694,
132.430188223987));
#98241=CARTESIAN_POINT('Ctrl Pts',(-97.4915674557649,-4.59663686661538,
132.559047406268));
#98242=CARTESIAN_POINT('Ctrl Pts',(-97.499318647005,-4.54416762220457,132.685775958156));
#98243=CARTESIAN_POINT('Ctrl Pts',(-97.5070665437821,-4.49172067862222,
132.812450647029));
#98244=CARTESIAN_POINT('Ctrl Pts',(-97.5148144405592,-4.43394575884481,
132.936996146156));
#98245=CARTESIAN_POINT('Ctrl Pts',(-97.5225623373363,-4.37104782127443,
133.058939071875));
#98246=CARTESIAN_POINT('Ctrl Pts',(-97.5303086134204,-4.30816304059667,
133.180856489761));
#98247=CARTESIAN_POINT('Ctrl Pts',(-97.5380548895045,-4.24015755275567,
133.300172069839));
#98248=CARTESIAN_POINT('Ctrl Pts',(-97.5458011655886,-4.16728315988435,
133.416435296407));
#98249=CARTESIAN_POINT('Ctrl Pts',(-97.5535474988539,-4.09440822907092,
133.532699381204));
#98250=CARTESIAN_POINT('Ctrl Pts',(-97.5612938321193,-4.01666452915023,
133.645910736262));
#98251=CARTESIAN_POINT('Ctrl Pts',(-97.5690401653846,-3.93434803009684,
133.755646547559));
#98252=CARTESIAN_POINT('Ctrl Pts',(-97.5767882333876,-3.85201309683413,
133.865406933429));
#98253=CARTESIAN_POINT('Ctrl Pts',(-97.5845363013905,-3.76510356126534,
133.971689914071));
#98254=CARTESIAN_POINT('Ctrl Pts',(-97.5922843693935,-3.67395637528701,
134.074104891204));
#98255=CARTESIAN_POINT('Ctrl Pts',(-97.6000406721353,-3.58271231699489,
134.176628716193));
#98256=CARTESIAN_POINT('Ctrl Pts',(-97.6077969748772,-3.4872218717525,134.275276033069));
#98257=CARTESIAN_POINT('Ctrl Pts',(-97.6155532776191,-3.3878600253956,134.369691950111));
#98258=CARTESIAN_POINT('Ctrl Pts',(-97.6233137201332,-3.2884451466293,134.464158259771));
#98259=CARTESIAN_POINT('Ctrl Pts',(-97.6310741626475,-3.18515504380116,
134.554388412408));
#98260=CARTESIAN_POINT('Ctrl Pts',(-97.6388346051616,-3.07839786881164,
134.640067804487));
#98261=CARTESIAN_POINT('Ctrl Pts',(-97.6466075054271,-2.97146931772736,
134.725884736732));
#98262=CARTESIAN_POINT('Ctrl Pts',(-97.6543804056925,-2.86106288760271,
134.807136078266));
#98263=CARTESIAN_POINT('Ctrl Pts',(-97.6621533059579,-2.74761652635889,
134.883550057465));
#98264=CARTESIAN_POINT('Ctrl Pts',(-97.66964364172,-2.63829422609949,134.957186196045));
#98265=CARTESIAN_POINT('Ctrl Pts',(-97.6771339774821,-2.52614943801408,
135.026330405208));
#98266=CARTESIAN_POINT('Ctrl Pts',(-97.6846243132442,-2.41159395103489,
135.090780764709));
#98267=CARTESIAN_POINT('Ctrl Pts',(-97.6923986473633,-2.29269505794933,
135.157674779179));
#98268=CARTESIAN_POINT('Ctrl Pts',(-97.7001729814824,-2.17082241812403,
135.219723883238));
#98269=CARTESIAN_POINT('Ctrl Pts',(-97.7079473156015,-2.04640857342569,
135.276652537053));
#98270=CARTESIAN_POINT('Ctrl Pts',(-97.7157120685486,-1.92214805767176,
135.33351103139));
#98271=CARTESIAN_POINT('Ctrl Pts',(-97.7234768214958,-1.79535292051091,
135.385261470379));
#98272=CARTESIAN_POINT('Ctrl Pts',(-97.7312415744429,-1.66648228674226,
135.43167299631));
#98273=CARTESIAN_POINT('Ctrl Pts',(-97.7389986153279,-1.53773964910417,
135.478038425659));
#98274=CARTESIAN_POINT('Ctrl Pts',(-97.7467556562129,-1.40692598261968,
135.519075362914));
#98275=CARTESIAN_POINT('Ctrl Pts',(-97.7545126970979,-1.27452215995131,
135.554600224817));
#98276=CARTESIAN_POINT('Ctrl Pts',(-97.762263888338,-1.1422181840354,135.590098297145));
#98277=CARTESIAN_POINT('Ctrl Pts',(-97.7700150795781,-1.00832681485096,
135.620092466873));
#98278=CARTESIAN_POINT('Ctrl Pts',(-97.7777662708182,-0.873345586771444,
135.644448483356));
#98279=CARTESIAN_POINT('Ctrl Pts',(-97.7855141675953,-0.738421729314418,
135.668794147883));
#98280=CARTESIAN_POINT('Ctrl Pts',(-97.7932620643724,-0.602409318216158,
135.687506356074));
#98281=CARTESIAN_POINT('Ctrl Pts',(-97.8010099611495,-0.465817409581646,
135.700501669806));
#98282=CARTESIAN_POINT('Ctrl Pts',(-97.8087562372336,-0.32925407302984,
135.713494265199));
#98283=CARTESIAN_POINT('Ctrl Pts',(-97.8165025133178,-0.192111869012933,
135.720772307739));
#98284=CARTESIAN_POINT('Ctrl Pts',(-97.8242487894019,-0.0549059343520972,
135.722304130954));
#98285=CARTESIAN_POINT('Ctrl Pts',(-97.8319951226672,0.0823010131315924,
135.723835965476));
#98286=CARTESIAN_POINT('Ctrl Pts',(-97.8397414559326,0.219571301257105,
135.719621491666));
#98287=CARTESIAN_POINT('Ctrl Pts',(-97.847487789198,0.356389225611277,135.70968117614));
#98288=CARTESIAN_POINT('Ctrl Pts',(-97.8552358572009,0.493237789390792,
135.699738634549));
#98289=CARTESIAN_POINT('Ctrl Pts',(-97.8629839252039,0.629633397953496,
135.684067728012));
#98290=CARTESIAN_POINT('Ctrl Pts',(-97.8707319932069,0.76506529917312,135.662740815791));
#98291=CARTESIAN_POINT('Ctrl Pts',(-97.8784882959488,0.900641139029206,
135.641391237073));
#98292=CARTESIAN_POINT('Ctrl Pts',(-97.8862445986906,1.03525083869141,135.614373705427));
#98293=CARTESIAN_POINT('Ctrl Pts',(-97.8940009014325,1.16839312870102,135.581811879411));
#98294=CARTESIAN_POINT('Ctrl Pts',(-97.9017613439467,1.30160648076001,135.549232674168));
#98295=CARTESIAN_POINT('Ctrl Pts',(-97.9095217864608,1.43335048720379,135.511103386825));
#98296=CARTESIAN_POINT('Ctrl Pts',(-97.917282228975,1.56313984709728,135.46759735624));
#98297=CARTESIAN_POINT('Ctrl Pts',(-97.9250551292404,1.69313755639307,135.424021485912));
#98298=CARTESIAN_POINT('Ctrl Pts',(-97.9328280295059,1.82117398349192,135.375051764149));
#98299=CARTESIAN_POINT('Ctrl Pts',(-97.9406009297713,1.94678375768187,135.320909749738));
#98300=CARTESIAN_POINT('Ctrl Pts',(-97.9480912655332,2.06782730018638,135.268735933928));
#98301=CARTESIAN_POINT('Ctrl Pts',(-97.9555816012951,2.18661727886674,135.211759481601));
#98302=CARTESIAN_POINT('Ctrl Pts',(-97.963071937057,2.30276123052712,135.150217699625));
#98303=CARTESIAN_POINT('Ctrl Pts',(-97.9708462711761,2.42330881541743,135.086342542279));
#98304=CARTESIAN_POINT('Ctrl Pts',(-97.9786206052953,2.54138762271405,135.017346695159));
#98305=CARTESIAN_POINT('Ctrl Pts',(-97.9863949394143,2.65653203350798,134.943445131978));
#98306=CARTESIAN_POINT('Ctrl Pts',(-97.9941596923614,2.77153453910637,134.869634645869));
#98307=CARTESIAN_POINT('Ctrl Pts',(-98.0019244453084,2.88360951785468,134.790930682299));
#98308=CARTESIAN_POINT('Ctrl Pts',(-98.0096891982555,2.99231457445502,134.707594731734));
#98309=CARTESIAN_POINT('Ctrl Pts',(-98.0174462391405,3.10091166366068,134.62434155161));
#98310=CARTESIAN_POINT('Ctrl Pts',(-98.0252032800256,3.20614518323624,134.53646577613));
#98311=CARTESIAN_POINT('Ctrl Pts',(-98.0329603209106,3.30760075596693,134.44427274585));
#98312=CARTESIAN_POINT('Ctrl Pts',(-98.0407115121507,3.40897982026089,134.352149239051));
#98313=CARTESIAN_POINT('Ctrl Pts',(-98.0484627033908,3.50658632025427,134.255715219542));
#98314=CARTESIAN_POINT('Ctrl Pts',(-98.0562138946309,3.60003837759656,134.15531671133));
#98315=CARTESIAN_POINT('Ctrl Pts',(-98.0639617914079,3.69345071532169,134.054960875162));
#98316=CARTESIAN_POINT('Ctrl Pts',(-98.0717096881851,3.78271185651674,133.950644187232));
#98317=CARTESIAN_POINT('Ctrl Pts',(-98.0794575849622,3.86747644506555,133.842749830515));
#98318=CARTESIAN_POINT('Ctrl Pts',(-98.0872038610463,3.95222330268974,133.734878042971));
#98319=CARTESIAN_POINT('Ctrl Pts',(-98.0949501371303,4.03247523715973,133.623430382432));
#98320=CARTESIAN_POINT('Ctrl Pts',(-98.1026964132144,4.10792716253893,133.508823131593));
#98321=CARTESIAN_POINT('Ctrl Pts',(-98.1104427464797,4.18337964488699,133.394215034749));
#98322=CARTESIAN_POINT('Ctrl Pts',(-98.118189079745,4.25403183245597,133.276447627614));
#98323=CARTESIAN_POINT('Ctrl Pts',(-98.1259354130104,4.31962219355627,133.155965849623));
#98324=CARTESIAN_POINT('Ctrl Pts',(-98.1336834810133,4.38522724316325,133.035457090572));
#98325=CARTESIAN_POINT('Ctrl Pts',(-98.1414315490163,4.4457680237467,132.912233094398));
#98326=CARTESIAN_POINT('Ctrl Pts',(-98.1491796170193,4.50102933920304,132.786762683277));
#98327=CARTESIAN_POINT('Ctrl Pts',(-98.1569359197612,4.55634938704299,132.66115892071));
#98328=CARTESIAN_POINT('Ctrl Pts',(-98.164692222503,4.60637860318453,132.533304332244));
#98329=CARTESIAN_POINT('Ctrl Pts',(-98.1724485252448,4.65095007669019,132.403687490546));
#98330=CARTESIAN_POINT('Ctrl Pts',(-98.180208967759,4.69554533933328,132.274001468436));
#98331=CARTESIAN_POINT('Ctrl Pts',(-98.1879694102731,4.734676943523,132.142551693463));
#98332=CARTESIAN_POINT('Ctrl Pts',(-98.1957298527873,4.76822840714074,132.009840156935));
#98333=CARTESIAN_POINT('Ctrl Pts',(-98.2035027530527,4.80183373054652,131.876915580066));
#98334=CARTESIAN_POINT('Ctrl Pts',(-98.2112756533181,4.8298409330431,131.742725577002));
#98335=CARTESIAN_POINT('Ctrl Pts',(-98.2190485535836,4.85218487407739,131.607781435242));
#98336=CARTESIAN_POINT('Ctrl Pts',(-98.2265388893457,4.8737165565744,131.477742852936));
#98337=CARTESIAN_POINT('Ctrl Pts',(-98.2340292251079,4.88998953865862,131.347004315352));
#98338=CARTESIAN_POINT('Ctrl Pts',(-98.24151956087,4.90099133737466,131.216024283049));
#98339=CARTESIAN_POINT('Ctrl Pts',(-98.2492938949891,4.91241027263277,131.080078103012));
#98340=CARTESIAN_POINT('Ctrl Pts',(-98.2570682291081,4.91818659196586,130.943441117583));
#98341=CARTESIAN_POINT('Ctrl Pts',(-98.2648425632272,4.9182494804533,130.806621263677));
#98342=CARTESIAN_POINT('Ctrl Pts',(-98.2726073161743,4.9183122914363,130.669970028014));
#98343=CARTESIAN_POINT('Ctrl Pts',(-98.2803720691214,4.91267568146981,130.533136759504));
#98344=CARTESIAN_POINT('Ctrl Pts',(-98.2881368220685,4.90132052442372,130.396634999824));
#98345=CARTESIAN_POINT('Ctrl Pts',(-98.2958938629535,4.8899766454797,130.260268815617));
#98346=CARTESIAN_POINT('Ctrl Pts',(-98.3036509038384,4.87292555459962,130.124233872098));
#98347=CARTESIAN_POINT('Ctrl Pts',(-98.3114079447234,4.85020016243341,129.989043840582));
#98348=CARTESIAN_POINT('Ctrl Pts',(-98.3191591359635,4.82749190766217,129.853955756921));
#98349=CARTESIAN_POINT('Ctrl Pts',(-98.3269103272037,4.79911793331346,129.71971170104));
#98350=CARTESIAN_POINT('Ctrl Pts',(-98.3346615184439,4.76516294460801,129.586819992439));
#98351=CARTESIAN_POINT('Ctrl Pts',(-98.342409415221,4.73122238767848,129.453984766359));
#98352=CARTESIAN_POINT('Ctrl Pts',(-98.350157311998,4.69170563086144,129.322501122362));
#98353=CARTESIAN_POINT('Ctrl Pts',(-98.3579052087751,4.64674838342874,129.192866738086));
#98354=CARTESIAN_POINT('Ctrl Pts',(-98.3656514848592,4.60180054008315,129.063259470528));
#98355=CARTESIAN_POINT('Ctrl Pts',(-98.3733977609433,4.55141459775355,128.935501062424));
#98356=CARTESIAN_POINT('Ctrl Pts',(-98.3811440370274,4.4957758804594,128.810073202177));
#98357=CARTESIAN_POINT('Ctrl Pts',(-98.3888903702928,4.44013675245279,128.684644416049));
#98358=CARTESIAN_POINT('Ctrl Pts',(-98.3966367035582,4.37924493064071,128.561546569488));
#98359=CARTESIAN_POINT('Ctrl Pts',(-98.4043830368235,4.3133333909033,128.441240197143));
#98360=CARTESIAN_POINT('Ctrl Pts',(-98.4121311048265,4.24740709073367,128.320906883021));
#98361=CARTESIAN_POINT('Ctrl Pts',(-98.4198791728294,4.17645902356311,128.203366629866));
#98362=CARTESIAN_POINT('Ctrl Pts',(-98.4276272408324,4.10076730401701,128.089053898095));
#98363=CARTESIAN_POINT('Ctrl Pts',(-98.4353835435742,4.02499513841053,127.974619673392));
#98364=CARTESIAN_POINT('Ctrl Pts',(-98.4431398463161,3.94446946546042,127.863420148863));
#98365=CARTESIAN_POINT('Ctrl Pts',(-98.450896149058,3.85951111574793,127.755859836868));
#98366=CARTESIAN_POINT('Ctrl Pts',(-98.4586565915721,3.77450742120614,127.648242116695));
#98367=CARTESIAN_POINT('Ctrl Pts',(-98.4664170340864,3.68506659057689,127.544267775613));
#98368=CARTESIAN_POINT('Ctrl Pts',(-98.4741774766005,3.59154800193454,127.444306151891));
#98369=CARTESIAN_POINT('Ctrl Pts',(-98.481950376866,3.49787928895151,127.344184060897));
#98370=CARTESIAN_POINT('Ctrl Pts',(-98.4897232771314,3.40012001597915,127.248087833803));
#98371=CARTESIAN_POINT('Ctrl Pts',(-98.4974961773969,3.29866513360926,127.156348638582));
#98372=CARTESIAN_POINT('Ctrl Pts',(-98.5049865131589,3.20089839176322,127.067944394185));
#98373=CARTESIAN_POINT('Ctrl Pts',(-98.5124768489209,3.09970030169355,126.983586100453));
#98374=CARTESIAN_POINT('Ctrl Pts',(-98.5199671846829,2.99544983191148,126.903532068783));
#98375=CARTESIAN_POINT('Ctrl Pts',(-98.527741518802,2.88724667388123,126.82044276417));
#98376=CARTESIAN_POINT('Ctrl Pts',(-98.535515852921,2.77541234997262,126.741727354952));
#98377=CARTESIAN_POINT('Ctrl Pts',(-98.5432901870401,2.66033592470592,126.66771997204));
#98378=CARTESIAN_POINT('Ctrl Pts',(-98.5510549399872,2.54540132084868,126.593803796613));
#98379=CARTESIAN_POINT('Ctrl Pts',(-98.5588196929343,2.42723289136294,126.524584312247));
#98380=CARTESIAN_POINT('Ctrl Pts',(-98.5665844458814,2.30625235526557,126.460355192117));
#98381=CARTESIAN_POINT('Ctrl Pts',(-98.5743414867664,2.18539197874218,126.396189865255));
#98382=CARTESIAN_POINT('Ctrl Pts',(-98.5820985276514,2.0617253969332,126.337005221114));
#98383=CARTESIAN_POINT('Ctrl Pts',(-98.5898555685364,1.93570256507375,126.283051222925));
#98384=CARTESIAN_POINT('Ctrl Pts',(-98.5976067597765,1.80977476801229,126.229137911867));
#98385=CARTESIAN_POINT('Ctrl Pts',(-98.6053579510166,1.68149461560239,126.180447548782));
#98386=CARTESIAN_POINT('Ctrl Pts',(-98.6131091422567,1.55133555667627,126.137183627876));
#98387=CARTESIAN_POINT('Ctrl Pts',(-98.6208570390338,1.42123181882212,126.093938095291));
#98388=CARTESIAN_POINT('Ctrl Pts',(-98.6286049358109,1.28925113300718,126.056114540726));
#98389=CARTESIAN_POINT('Ctrl Pts',(-98.636352832588,1.15588556370023,126.02386779505));
#98390=CARTESIAN_POINT('Ctrl Pts',(-98.6440991086721,1.02254789159534,125.991627794697));
#98391=CARTESIAN_POINT('Ctrl Pts',(-98.6518453847561,0.887826291977052,
125.96496237473));
#98392=CARTESIAN_POINT('Ctrl Pts',(-98.6595916608402,0.752226195100541,
125.94397598115));
#98393=CARTESIAN_POINT('Ctrl Pts',(-98.6673379941055,0.616625097255102,
125.922989432654));
#98394=CARTESIAN_POINT('Ctrl Pts',(-98.6750843273709,0.480145875576691,
125.907682053992));
#98395=CARTESIAN_POINT('Ctrl Pts',(-98.6828306606363,0.34330192006288,125.898106766186));
#98396=CARTESIAN_POINT('Ctrl Pts',(-98.6905787286392,0.206427319293855,
125.888529334061));
#98397=CARTESIAN_POINT('Ctrl Pts',(-98.6983267966421,0.0691882120934057,
125.884686574414));
#98398=CARTESIAN_POINT('Ctrl Pts',(-98.706074864645,-0.067899549938197,
125.886579338003));
#98399=CARTESIAN_POINT('Ctrl Pts',(-98.7138311673869,-0.205133010474839,
125.888474113244));
#98400=CARTESIAN_POINT('Ctrl Pts',(-98.7215874701289,-0.342214412973249,
125.896116583295));
#98401=CARTESIAN_POINT('Ctrl Pts',(-98.7293437728707,-0.478630012964187,
125.909455473113));
#98402=CARTESIAN_POINT('Ctrl Pts',(-98.7371042153849,-0.615118422068234,
125.922801482299));
#98403=CARTESIAN_POINT('Ctrl Pts',(-98.744864657899,-0.75093993359559,125.941849915134));
#98404=CARTESIAN_POINT('Ctrl Pts',(-98.7526251004132,-0.885589560172638,
125.966498053022));
#98405=CARTESIAN_POINT('Ctrl Pts',(-98.7603980006786,-1.0204553382839,125.99118575829));
#98406=CARTESIAN_POINT('Ctrl Pts',(-98.7681709009441,-1.15414509066939,
126.021491045303));
#98407=CARTESIAN_POINT('Ctrl Pts',(-98.7759438012095,-1.28616671589187,
126.057260635321));
#98408=CARTESIAN_POINT('Ctrl Pts',(-98.7834341369716,-1.41338902249583,
126.091729910644));
#98409=CARTESIAN_POINT('Ctrl Pts',(-98.7909244727336,-1.53906208374758,
126.131273011571));
#98410=CARTESIAN_POINT('Ctrl Pts',(-98.7984148084957,-1.66276373321742,
126.175710724779));
#98411=CARTESIAN_POINT('Ctrl Pts',(-98.8061892740224,-1.79115773849947,
126.221834086988));
#98412=CARTESIAN_POINT('Ctrl Pts',(-98.8139637395492,-1.91783453747899,
126.273376832534));
#98413=CARTESIAN_POINT('Ctrl Pts',(-98.8217382050759,-2.04230269266731,
126.330192228466));
#98414=CARTESIAN_POINT('Ctrl Pts',(-98.829503058786,-2.16661696395553,126.386937381734));
#98415=CARTESIAN_POINT('Ctrl Pts',(-98.8372679124961,-2.28872767236615,
126.448942054039));
#98416=CARTESIAN_POINT('Ctrl Pts',(-98.8450327662062,-2.40815977482729,
126.516010169969));
#98417=CARTESIAN_POINT('Ctrl Pts',(-98.8527898773389,-2.52747278781919,
126.583011410192));
#98418=CARTESIAN_POINT('Ctrl Pts',(-98.8605469884715,-2.64411217150775,
126.655065856078));
#98419=CARTESIAN_POINT('Ctrl Pts',(-98.8683040996042,-2.75762440141954,
126.731930050546));
#98420=CARTESIAN_POINT('Ctrl Pts',(-98.8760553306746,-2.87105058654408,
126.808735980251));
#98421=CARTESIAN_POINT('Ctrl Pts',(-98.883806561745,-2.98135401381862,126.890344183093));
#98422=CARTESIAN_POINT('Ctrl Pts',(-98.8915577928154,-3.08810756172547,
126.976466320473));
#98423=CARTESIAN_POINT('Ctrl Pts',(-98.8993055730249,-3.19481358277658,
127.062550116136));
#98424=CARTESIAN_POINT('Ctrl Pts',(-98.9070533532344,-3.29797256497424,
127.153143603344));
#98425=CARTESIAN_POINT('Ctrl Pts',(-98.9148011334439,-3.39718829094002,
127.247916497606));
#98426=CARTESIAN_POINT('Ctrl Pts',(-98.922547249637,-3.49638270801475,127.342669037178));
#98427=CARTESIAN_POINT('Ctrl Pts',(-98.9302933658301,-3.59163527116042,
127.44159892824));
#98428=CARTESIAN_POINT('Ctrl Pts',(-98.9380394820231,-3.68258493265018,
127.544337415759));
#98429=CARTESIAN_POINT('Ctrl Pts',(-98.9457856120448,-3.77353475650647,
127.647076086691));
#98430=CARTESIAN_POINT('Ctrl Pts',(-98.9535317420665,-3.86018140440898,
127.753623074815));
#98431=CARTESIAN_POINT('Ctrl Pts',(-98.9612778720882,-3.94220287772239,
127.86357508758));
#98432=CARTESIAN_POINT('Ctrl Pts',(-98.9690256934281,-4.02424225990282,
127.973551107667));
#98433=CARTESIAN_POINT('Ctrl Pts',(-98.976773514768,-4.10165422457565,128.086933318308));
#98434=CARTESIAN_POINT('Ctrl Pts',(-98.9845213361079,-4.17415925078712,
128.203288221117));
#98435=CARTESIAN_POINT('Ctrl Pts',(-98.9922767939493,-4.24673574028139,
128.319757807056));
#98436=CARTESIAN_POINT('Ctrl Pts',(-99.0000322517909,-4.31439542526681,
128.43920560458));
#98437=CARTESIAN_POINT('Ctrl Pts',(-99.0077877096324,-4.37690382517589,
128.56117182309));
#98438=CARTESIAN_POINT('Ctrl Pts',(-99.0155472893426,-4.4394454470335,128.683202864176));
#98439=CARTESIAN_POINT('Ctrl Pts',(-99.0233068690528,-4.49683016518702,
128.807754638531));
#98440=CARTESIAN_POINT('Ctrl Pts',(-99.0310664487631,-4.54887149333015,
128.934346927865));
#98441=CARTESIAN_POINT('Ctrl Pts',(-99.0388370862935,-4.6009869831765,129.061119618049));
#98442=CARTESIAN_POINT('Ctrl Pts',(-99.046607723824,-4.64774373928055,129.189938264582));
#98443=CARTESIAN_POINT('Ctrl Pts',(-99.0543783613544,-4.68900482500524,
129.320306436083));
#98444=CARTESIAN_POINT('Ctrl Pts',(-99.0595496068237,-4.71646347325353,
129.407064544871));
#98445=CARTESIAN_POINT('Ctrl Pts',(-99.064720852293,-4.74148929291332,129.494508609268));
#98446=CARTESIAN_POINT('Ctrl Pts',(-99.0698920977623,-4.76405452823408,
129.582490119308));
#98447=CARTESIAN_POINT('Origin',(213.235140564004,0.,130.804360617566));
#98448=CARTESIAN_POINT('',(-101.165045656948,-4.76405452823419,129.582490119309));
#98449=CARTESIAN_POINT('',(-100.820132980931,-4.76405452823394,129.582490119308));
#98450=CARTESIAN_POINT('',(213.235140564004,-4.76405452823405,129.582490119308));
#98451=CARTESIAN_POINT('',(-99.4851405640526,-4.91824989996933,130.805352560943));
#98452=CARTESIAN_POINT('Ctrl Pts',(-99.4851405640525,-4.91824989996933,
130.805352560944));
#98453=CARTESIAN_POINT('Ctrl Pts',(-99.4933901351786,-4.91822036007165,
130.951817169788));
#98454=CARTESIAN_POINT('Ctrl Pts',(-99.5016397063047,-4.9116440396768,131.098114664302));
#98455=CARTESIAN_POINT('Ctrl Pts',(-99.5098892774308,-4.89859101298216,
131.243665921461));
#98456=CARTESIAN_POINT('Ctrl Pts',(-99.5185792279595,-4.88484118835586,
131.396987009887));
#98457=CARTESIAN_POINT('Ctrl Pts',(-99.5272691784882,-4.86390433493261,
131.549479585931));
#98458=CARTESIAN_POINT('Ctrl Pts',(-99.5359591290169,-4.83592288046644,
131.700481678964));
#98459=CARTESIAN_POINT('Ctrl Pts',(-99.5442498456649,-4.80922695054012,
131.844546430823));
#98460=CARTESIAN_POINT('Ctrl Pts',(-99.5525405623128,-4.77611938693527,
131.987254339953));
#98461=CARTESIAN_POINT('Ctrl Pts',(-99.5608312789607,-4.73677468896852,
132.128048121642));
#98462=CARTESIAN_POINT('Ctrl Pts',(-99.5691354981031,-4.6973659131193,132.269071204047));
#98463=CARTESIAN_POINT('Ctrl Pts',(-99.5774397172456,-4.65169981408719,
132.408173642682));
#98464=CARTESIAN_POINT('Ctrl Pts',(-99.585743936388,-4.59999944278608,132.544816933843));
#98465=CARTESIAN_POINT('Ctrl Pts',(-99.5940676315148,-4.5481778179863,132.681780696147));
#98466=CARTESIAN_POINT('Ctrl Pts',(-99.6023913266416,-4.49029374540701,
132.816273497092));
#98467=CARTESIAN_POINT('Ctrl Pts',(-99.6107150217685,-4.42661743930218,
132.947778707572));
#98468=CARTESIAN_POINT('Ctrl Pts',(-99.6118662424373,-4.41781059587682,
132.965966725521));
#98469=CARTESIAN_POINT('Ctrl Pts',(-99.6130174631061,-4.40889302351978,
132.98409763851));
#98470=CARTESIAN_POINT('Ctrl Pts',(-99.6141686837749,-4.39986550271429,
133.002170122624));
#98471=CARTESIAN_POINT('Ctrl Pts',(-99.621943017894,-4.33890154948689,133.124215820442));
#98472=CARTESIAN_POINT('Ctrl Pts',(-99.629717352013,-4.2727591372625,133.243916334047));
#98473=CARTESIAN_POINT('Ctrl Pts',(-99.6374916861321,-4.20164200427695,
133.360801019843));
#98474=CARTESIAN_POINT('Ctrl Pts',(-99.6452564390792,-4.13061251680189,
133.47754165571));
#98475=CARTESIAN_POINT('Ctrl Pts',(-99.6530211920263,-4.05462070849437,
133.591473037749));
#98476=CARTESIAN_POINT('Ctrl Pts',(-99.6607859449734,-3.97391737824988,
133.702146623009));
#98477=CARTESIAN_POINT('Ctrl Pts',(-99.6685429858584,-3.89329420369071,
133.812710285705));
#98478=CARTESIAN_POINT('Ctrl Pts',(-99.6763000267434,-3.8079690485726,133.920022276938));
#98479=CARTESIAN_POINT('Ctrl Pts',(-99.6840570676283,-3.71823722160899,
134.023661011493));
#98480=CARTESIAN_POINT('Ctrl Pts',(-99.6918082588684,-3.62857306211422,
134.127221591272));
#98481=CARTESIAN_POINT('Ctrl Pts',(-99.6995594501086,-3.53450910008951,
134.227114133576));
#98482=CARTESIAN_POINT('Ctrl Pts',(-99.7073106413487,-3.43638209586812,
134.322948566402));
#98483=CARTESIAN_POINT('Ctrl Pts',(-99.7150585381258,-3.33829679824102,
134.418742267039));
#98484=CARTESIAN_POINT('Ctrl Pts',(-99.7228064349029,-3.23615217220895,
134.510481016108));
#98485=CARTESIAN_POINT('Ctrl Pts',(-99.7305543316799,-3.13032300280422,
134.597810361614));
#98486=CARTESIAN_POINT('Ctrl Pts',(-99.738300607764,-3.02451597058032,134.685121439703));
#98487=CARTESIAN_POINT('Ctrl Pts',(-99.746046883848,-2.9150262293628,134.768024700156));
#98488=CARTESIAN_POINT('Ctrl Pts',(-99.7537931599321,-2.80226262074539,
134.846205155258));
#98489=CARTESIAN_POINT('Ctrl Pts',(-99.7615394931974,-2.68949817973248,
134.924386187471));
#98490=CARTESIAN_POINT('Ctrl Pts',(-99.7692858264628,-2.57346014439362,
134.997844122007));
#98491=CARTESIAN_POINT('Ctrl Pts',(-99.7770321597281,-2.4545870499912,135.066306825171));
#98492=CARTESIAN_POINT('Ctrl Pts',(-99.7847802277311,-2.33568733478367,
135.134784860082));
#98493=CARTESIAN_POINT('Ctrl Pts',(-99.7925282957342,-2.21395163588035,
135.198265242559));
#98494=CARTESIAN_POINT('Ctrl Pts',(-99.8002763637371,-2.08984347633659,
135.256521588029));
#98495=CARTESIAN_POINT('Ctrl Pts',(-99.808032666479,-1.9656034131638,135.314839849036));
#98496=CARTESIAN_POINT('Ctrl Pts',(-99.8157889692208,-1.83898620690269,
135.367922815589));
#98497=CARTESIAN_POINT('Ctrl Pts',(-99.8235452719626,-1.71047628411891,
135.41559190042));
#98498=CARTESIAN_POINT('Ctrl Pts',(-99.8313057144768,-1.58189777171998,
135.463286427676));
#98499=CARTESIAN_POINT('Ctrl Pts',(-99.8390661569911,-1.45142490163688,
135.505561195083));
#98500=CARTESIAN_POINT('Ctrl Pts',(-99.8468265995052,-1.31955672536704,
135.542287707659));
#98501=CARTESIAN_POINT('Ctrl Pts',(-99.8545994997707,-1.18747686259395,
135.579073176894));
#98502=CARTESIAN_POINT('Ctrl Pts',(-99.862372400036,-1.05399759857168,135.610292504079));
#98503=CARTESIAN_POINT('Ctrl Pts',(-99.8701453003014,-0.9196285103657,135.635868297931));
#98504=CARTESIAN_POINT('Ctrl Pts',(-99.8776356360634,-0.790144076970954,
135.660514347254));
#98505=CARTESIAN_POINT('Ctrl Pts',(-99.8851259718256,-0.65983369555726,
135.679920007538));
#98506=CARTESIAN_POINT('Ctrl Pts',(-99.8926163075877,-0.52915539510297,
135.694061797631));
#98507=CARTESIAN_POINT('Ctrl Pts',(-99.9003906417068,-0.393522387168712,
135.708739777995));
#98508=CARTESIAN_POINT('Ctrl Pts',(-99.9081649758259,-0.257063365551851,
135.717793344791));
#98509=CARTESIAN_POINT('Ctrl Pts',(-99.9159393099449,-0.120284421534253,
135.721139514409));
#98510=CARTESIAN_POINT('Ctrl Pts',(-99.923704062892,0.0163259546591279,
135.724481560171));
#98511=CARTESIAN_POINT('Ctrl Pts',(-99.9314688158392,0.153255081665827,
135.722130194562));
#98512=CARTESIAN_POINT('Ctrl Pts',(-99.9392335687862,0.28999002467024,135.714053973377));
#98513=CARTESIAN_POINT('Ctrl Pts',(-99.9469906096713,0.426589160601637,
135.705985773608));
#98514=CARTESIAN_POINT('Ctrl Pts',(-99.9547476505562,0.562994108583869,
135.692204056576));
#98515=CARTESIAN_POINT('Ctrl Pts',(-99.9625046914412,0.69869055546209,135.672729396758));
#98516=CARTESIAN_POINT('Ctrl Pts',(-99.9702558826814,0.83428467259434,135.653269422932));
#98517=CARTESIAN_POINT('Ctrl Pts',(-99.9780070739216,0.969170966652728,
135.628125106777));
#98518=CARTESIAN_POINT('Ctrl Pts',(-99.9857582651617,1.10283923182938,135.597368930853));
#98519=CARTESIAN_POINT('Ctrl Pts',(-99.9935061619388,1.23645068442743,135.566625827125));
#98520=CARTESIAN_POINT('Ctrl Pts',(-100.001254058716,1.36884475758745,135.530275695073));
#98521=CARTESIAN_POINT('Ctrl Pts',(-100.009001955493,1.49952066034119,135.488442261999));
#98522=CARTESIAN_POINT('Ctrl Pts',(-100.016748231577,1.63016922851311,135.446617579576));
#98523=CARTESIAN_POINT('Ctrl Pts',(-100.024494507661,1.75909996903882,135.399311996679));
#98524=CARTESIAN_POINT('Ctrl Pts',(-100.032240783745,1.88582688496382,135.346699224765));
#98525=CARTESIAN_POINT('Ctrl Pts',(-100.039987117011,2.01255473635794,135.294086064475));
#98526=CARTESIAN_POINT('Ctrl Pts',(-100.047733450276,2.13707836960651,135.236165786902));
#98527=CARTESIAN_POINT('Ctrl Pts',(-100.055479783541,2.25893179190393,135.173160249276));
#98528=CARTESIAN_POINT('Ctrl Pts',(-100.063227851544,2.38081250243057,135.110140601995));
#98529=CARTESIAN_POINT('Ctrl Pts',(-100.070975919547,2.50002146488317,135.042033608097));
#98530=CARTESIAN_POINT('Ctrl Pts',(-100.07872398755,2.61611766997616,134.969106876264));
#98531=CARTESIAN_POINT('Ctrl Pts',(-100.086480290292,2.73233726349732,134.896102637032));
#98532=CARTESIAN_POINT('Ctrl Pts',(-100.094236593034,2.84543715942706,134.818268635465));
#98533=CARTESIAN_POINT('Ctrl Pts',(-100.101992895776,2.9550052628474,134.73591590257));
#98534=CARTESIAN_POINT('Ctrl Pts',(-100.10975333829,3.06463184606387,134.653519215542));
#98535=CARTESIAN_POINT('Ctrl Pts',(-100.117513780804,3.17072257842416,134.56659923916));
#98536=CARTESIAN_POINT('Ctrl Pts',(-100.125274223318,3.27289960393646,134.475506384905));
#98537=CARTESIAN_POINT('Ctrl Pts',(-100.133047123584,3.37524065308097,134.384267300314));
#98538=CARTESIAN_POINT('Ctrl Pts',(-100.140820023849,3.47365515983561,134.288842224081));
#98539=CARTESIAN_POINT('Ctrl Pts',(-100.148592924115,3.56780257387002,134.189618045944));
#98540=CARTESIAN_POINT('Ctrl Pts',(-100.156083259877,3.65852749226177,134.094000916611));
#98541=CARTESIAN_POINT('Ctrl Pts',(-100.163573595639,3.74528996801761,133.994856335539));
#98542=CARTESIAN_POINT('Ctrl Pts',(-100.171063931401,3.8278226699303,133.892556963343));
#98543=CARTESIAN_POINT('Ctrl Pts',(-100.17883826552,3.91348462432068,133.786378879357));
#98544=CARTESIAN_POINT('Ctrl Pts',(-100.186612599639,3.99486108085797,133.67646571375));
#98545=CARTESIAN_POINT('Ctrl Pts',(-100.194386933758,4.07160866837837,133.563198400779));
#98546=CARTESIAN_POINT('Ctrl Pts',(-100.202151686705,4.14826167135627,133.45007067965));
#98547=CARTESIAN_POINT('Ctrl Pts',(-100.209916439652,4.22029693870276,133.333597356518));
#98548=CARTESIAN_POINT('Ctrl Pts',(-100.217681192599,4.28741076171937,133.21419298161));
#98549=CARTESIAN_POINT('Ctrl Pts',(-100.225438233484,4.35445792634083,133.09490720081));
#98550=CARTESIAN_POINT('Ctrl Pts',(-100.233195274369,4.4165931837437,132.972696500191));
#98551=CARTESIAN_POINT('Ctrl Pts',(-100.240952315254,4.47355584499542,132.848004706983));
#98552=CARTESIAN_POINT('Ctrl Pts',(-100.248703506494,4.53047555026125,132.723406944825));
#98553=CARTESIAN_POINT('Ctrl Pts',(-100.256454697734,4.58223026167519,132.59633216839));
#98554=CARTESIAN_POINT('Ctrl Pts',(-100.264205888974,4.62860518216726,132.467248806866));
#98555=CARTESIAN_POINT('Ctrl Pts',(-100.271953785752,4.67496039208097,132.338220309215));
#98556=CARTESIAN_POINT('Ctrl Pts',(-100.279701682529,4.71594022694488,132.207185291596));
#98557=CARTESIAN_POINT('Ctrl Pts',(-100.287449579306,4.75137809228967,132.07463196126));
#98558=CARTESIAN_POINT('Ctrl Pts',(-100.29519585539,4.78680854479707,131.942106358223));
#98559=CARTESIAN_POINT('Ctrl Pts',(-100.302942131474,4.81669923270472,131.808063451651));
#98560=CARTESIAN_POINT('Ctrl Pts',(-100.310688407558,4.84093361115626,131.673006019832));
#98561=CARTESIAN_POINT('Ctrl Pts',(-100.318434740823,4.86516816850043,131.53794759105));
#98562=CARTESIAN_POINT('Ctrl Pts',(-100.326181074089,4.88374626402124,131.401875006896));
#98563=CARTESIAN_POINT('Ctrl Pts',(-100.333927407354,4.89660267199325,131.265300239565));
#98564=CARTESIAN_POINT('Ctrl Pts',(-100.341675475357,4.90946195906866,131.128694887262));
#98565=CARTESIAN_POINT('Ctrl Pts',(-100.34942354336,4.9165969722581,130.99158751717));
#98566=CARTESIAN_POINT('Ctrl Pts',(-100.357171611363,4.91799448203471,130.85449381192));
#98567=CARTESIAN_POINT('Ctrl Pts',(-100.364927914105,4.91939347710135,130.717254401848));
#98568=CARTESIAN_POINT('Ctrl Pts',(-100.372684216847,4.91504278357763,130.580029077198));
#98569=CARTESIAN_POINT('Ctrl Pts',(-100.380440519588,4.90498133329089,130.443332664953));
#98570=CARTESIAN_POINT('Ctrl Pts',(-100.388200962103,4.89491451290518,130.306563293717));
#98571=CARTESIAN_POINT('Ctrl Pts',(-100.395961404617,4.87913090732387,130.170323785564));
#98572=CARTESIAN_POINT('Ctrl Pts',(-100.403721847131,4.85772108725793,130.035121447405));
#98573=CARTESIAN_POINT('Ctrl Pts',(-100.411494747396,4.83627689824814,129.899702070451));
#98574=CARTESIAN_POINT('Ctrl Pts',(-100.419267647662,4.80918852384349,129.765323574084));
#98575=CARTESIAN_POINT('Ctrl Pts',(-100.427040547927,4.77659738956548,129.632481596295));
#98576=CARTESIAN_POINT('Ctrl Pts',(-100.434530883689,4.7451910251106,129.504468759007));
#98577=CARTESIAN_POINT('Ctrl Pts',(-100.442021219451,4.70867511857131,129.377882963102));
#98578=CARTESIAN_POINT('Ctrl Pts',(-100.449511555213,4.6672187008311,129.253150554063));
#98579=CARTESIAN_POINT('Ctrl Pts',(-100.457285889332,4.62419045041181,129.123688877823));
#98580=CARTESIAN_POINT('Ctrl Pts',(-100.465060223451,4.57570335377249,128.995813809448));
#98581=CARTESIAN_POINT('Ctrl Pts',(-100.47283455757,4.52189230119232,128.870020141094));
#98582=CARTESIAN_POINT('Ctrl Pts',(-100.480599310517,4.46814756592537,128.744381502194));
#98583=CARTESIAN_POINT('Ctrl Pts',(-100.488364063465,4.40909208203862,128.620819515459));
#98584=CARTESIAN_POINT('Ctrl Pts',(-100.496128816412,4.34491046040765,128.499813774141));
#98585=CARTESIAN_POINT('Ctrl Pts',(-100.503885857297,4.28079258486808,128.378928217431));
#98586=CARTESIAN_POINT('Ctrl Pts',(-100.511642898182,4.21155888561439,128.260594196769));
#98587=CARTESIAN_POINT('Ctrl Pts',(-100.519399939067,4.13744185832994,128.145270936596));
#98588=CARTESIAN_POINT('Ctrl Pts',(-100.527151130307,4.0633807232722,128.030034642591));
#98589=CARTESIAN_POINT('Ctrl Pts',(-100.534902321547,3.98444380061046,127.917804917471));
#98590=CARTESIAN_POINT('Ctrl Pts',(-100.542653512787,3.90090909002651,127.809015673516));
#98591=CARTESIAN_POINT('Ctrl Pts',(-100.550401409564,3.81740988392304,127.700272667891));
#98592=CARTESIAN_POINT('Ctrl Pts',(-100.558149306341,3.72931701422712,127.594967544479));
#98593=CARTESIAN_POINT('Ctrl Pts',(-100.565897203118,3.63695117514703,127.49350435187));
#98594=CARTESIAN_POINT('Ctrl Pts',(-100.573643479202,3.5446046570093,127.392062383174));
#98595=CARTESIAN_POINT('Ctrl Pts',(-100.581389755287,3.44798721035295,127.294461035707));
#98596=CARTESIAN_POINT('Ctrl Pts',(-100.589136031371,3.3474588414492,127.201070125904));
#98597=CARTESIAN_POINT('Ctrl Pts',(-100.596882364636,3.24692973046774,127.107678526709));
#98598=CARTESIAN_POINT('Ctrl Pts',(-100.604628697901,3.14248992606727,127.018497693296));
#98599=CARTESIAN_POINT('Ctrl Pts',(-100.612375031167,3.03453490885772,126.93385923539));
#98600=CARTESIAN_POINT('Ctrl Pts',(-100.62012309917,2.92655571587073,126.849201823289));
#98601=CARTESIAN_POINT('Ctrl Pts',(-100.627871167173,2.81506005124071,126.76908905205));
#98602=CARTESIAN_POINT('Ctrl Pts',(-100.635619235176,2.70047462248842,126.693810791108));
#98603=CARTESIAN_POINT('Ctrl Pts',(-100.643375537918,2.58576741097871,126.618452523534));
#98604=CARTESIAN_POINT('Ctrl Pts',(-100.651131840659,2.46796420280636,126.547939245325));
#98605=CARTESIAN_POINT('Ctrl Pts',(-100.658888143401,2.34751918009664,126.482516478593));
#98606=CARTESIAN_POINT('Ctrl Pts',(-100.666648585915,2.22700987225176,126.41705879376));
#98607=CARTESIAN_POINT('Ctrl Pts',(-100.67440902843,2.10385629118612,126.356697206158));
#98608=CARTESIAN_POINT('Ctrl Pts',(-100.682169470944,1.97853420425474,126.301629727862));
#98609=CARTESIAN_POINT('Ctrl Pts',(-100.689942371209,1.85301093918384,126.246473850361));
#98610=CARTESIAN_POINT('Ctrl Pts',(-100.697715271475,1.72531257635716,126.196629207267));
#98611=CARTESIAN_POINT('Ctrl Pts',(-100.70548817174,1.59593255400286,126.152244717723));
#98612=CARTESIAN_POINT('Ctrl Pts',(-100.712978507502,1.4712558213501,126.109473716172));
#98613=CARTESIAN_POINT('Ctrl Pts',(-100.720468843264,1.34501786672497,126.071772867811));
#98614=CARTESIAN_POINT('Ctrl Pts',(-100.727959179026,1.21766875197736,126.039230412319));
#98615=CARTESIAN_POINT('Ctrl Pts',(-100.735733513145,1.08549115683662,126.005454099735));
#98616=CARTESIAN_POINT('Ctrl Pts',(-100.743507847264,0.95169778010567,125.977128069385));
#98617=CARTESIAN_POINT('Ctrl Pts',(-100.751282181383,0.81677781592988,125.954406281502));
#98618=CARTESIAN_POINT('Ctrl Pts',(-100.759046934331,0.682024128552159,
125.931712496192));
#98619=CARTESIAN_POINT('Ctrl Pts',(-100.766811687278,0.546146998103354,
125.914609275325));
#98620=CARTESIAN_POINT('Ctrl Pts',(-100.774576440225,0.409649706657167,
125.903200532409));
#98621=CARTESIAN_POINT('Ctrl Pts',(-100.78233348111,0.273287986245119,125.891803120818));
#98622=CARTESIAN_POINT('Ctrl Pts',(-100.790090521995,0.136307717694797,
125.886088964163));
#98623=CARTESIAN_POINT('Ctrl Pts',(-100.79784756288,-0.000779070869449877,
125.88611067927));
#98624=CARTESIAN_POINT('Ctrl Pts',(-100.80559875412,-0.137762481220248,
125.886132378001));
#98625=CARTESIAN_POINT('Ctrl Pts',(-100.81334994536,-0.274851862314551,
125.891881338856));
#98626=CARTESIAN_POINT('Ctrl Pts',(-100.8211011366,-0.41153188584531,125.903358213013));
#98627=CARTESIAN_POINT('Ctrl Pts',(-100.828849033377,-0.548153816719824,
125.914830209193));
#98628=CARTESIAN_POINT('Ctrl Pts',(-100.836596930154,-0.684366347300932,
125.932025243963));
#98629=CARTESIAN_POINT('Ctrl Pts',(-100.844344826931,-0.819656197013348,
125.954891906336));
#98630=CARTESIAN_POINT('Ctrl Pts',(-100.852091103016,-0.954917747005717,
125.977753785497));
#98631=CARTESIAN_POINT('Ctrl Pts',(-100.8598373791,-1.08925661477345,126.006284867366));
#98632=CARTESIAN_POINT('Ctrl Pts',(-100.867583655184,-1.22216707109371,
126.040382163287));
#98633=CARTESIAN_POINT('Ctrl Pts',(-100.875329988449,-1.35507850852894,
126.074479710907));
#98634=CARTESIAN_POINT('Ctrl Pts',(-100.883076321715,-1.48656113477474,
126.114143457415));
#98635=CARTESIAN_POINT('Ctrl Pts',(-100.89082265498,-1.61612219024604,126.159219916931));
#98636=CARTESIAN_POINT('Ctrl Pts',(-100.898570722983,-1.74571226001758,
126.204306471008));
#98637=CARTESIAN_POINT('Ctrl Pts',(-100.906318790986,-1.87337953353842,
126.254808021665));
#98638=CARTESIAN_POINT('Ctrl Pts',(-100.914066858989,-1.99864948960598,
126.310522249289));
#98639=CARTESIAN_POINT('Ctrl Pts',(-100.921823161731,-2.12405258407306,
126.366295690657));
#98640=CARTESIAN_POINT('Ctrl Pts',(-100.929579464473,-2.24705291358996,
126.427292716799));
#98641=CARTESIAN_POINT('Ctrl Pts',(-100.937335767215,-2.36719841691857,
126.493263922125));
#98642=CARTESIAN_POINT('Ctrl Pts',(-100.945096209729,-2.48740804552015,
126.559270338271));
#98643=CARTESIAN_POINT('Ctrl Pts',(-100.952856652243,-2.60475947745769,
126.6302560214));
#98644=CARTESIAN_POINT('Ctrl Pts',(-100.960617094757,-2.71882895568887,
126.705927725324));
#98645=CARTESIAN_POINT('Ctrl Pts',(-100.968389995023,-2.83308154837312,
126.781720904186));
#98646=CARTESIAN_POINT('Ctrl Pts',(-100.976162895288,-2.94404134259594,
126.862214906322));
#98647=CARTESIAN_POINT('Ctrl Pts',(-100.983935795553,-3.05131633304839,
126.947075082611));
#98648=CARTESIAN_POINT('Ctrl Pts',(-100.991426131315,-3.15469160738822,
127.028850377742));
#98649=CARTESIAN_POINT('Ctrl Pts',(-100.998916467077,-3.25464509686574,
127.11467971478));
#98650=CARTESIAN_POINT('Ctrl Pts',(-101.00640680284,-3.35085929351795,127.204232139644));
#98651=CARTESIAN_POINT('Ctrl Pts',(-101.01406385016,-3.44921491869811,127.295777722733));
#98652=CARTESIAN_POINT('Ctrl Pts',(-101.021720897481,-3.54399429620978,
127.391522944431));
#98653=CARTESIAN_POINT('Ctrl Pts',(-101.029377944801,-3.6348092257146,127.491152964074));
#98654=CARTESIAN_POINT('Ctrl Pts',(-101.037026122495,-3.7255189587235,127.590667576161));
#98655=CARTESIAN_POINT('Ctrl Pts',(-101.044674300189,-3.81227310359175,
127.694057745953));
#98656=CARTESIAN_POINT('Ctrl Pts',(-101.052322477882,-3.89471732244525,
127.8009691944));
#98657=CARTESIAN_POINT('Ctrl Pts',(-101.059963570359,-3.97708516556853,
127.907781600852));
#98658=CARTESIAN_POINT('Ctrl Pts',(-101.067604662836,-4.055150776805,128.018108482406));
#98659=CARTESIAN_POINT('Ctrl Pts',(-101.075245755313,-4.12859782843107,
128.131560020145));
#98660=CARTESIAN_POINT('Ctrl Pts',(-101.082881533129,-4.20199379492717,
128.244932648161));
#98661=CARTESIAN_POINT('Ctrl Pts',(-101.090517310945,-4.27077737290134,
128.361425272055));
#98662=CARTESIAN_POINT('Ctrl Pts',(-101.09815308876,-4.33467393107329,128.48061687658));
#98663=CARTESIAN_POINT('Ctrl Pts',(-101.105785602063,-4.39854317164236,
128.599757523291));
#98664=CARTESIAN_POINT('Ctrl Pts',(-101.113418115366,-4.4575293583208,128.721594500147));
#98665=CARTESIAN_POINT('Ctrl Pts',(-101.121050628668,-4.51140270703491,
128.84568027676));
#98666=CARTESIAN_POINT('Ctrl Pts',(-101.128683508868,-4.56527864545375,
128.969772018207));
#98667=CARTESIAN_POINT('Ctrl Pts',(-101.136316389067,-4.61404108335767,
129.096112409849));
#98668=CARTESIAN_POINT('Ctrl Pts',(-101.143949269266,-4.65750759204066,
129.224232112481));
#98669=CARTESIAN_POINT('Ctrl Pts',(-101.150981398493,-4.69755303990952,
129.342268067705));
#98670=CARTESIAN_POINT('Ctrl Pts',(-101.158013527721,-4.73310382814636,
129.461813809409));
#98671=CARTESIAN_POINT('Ctrl Pts',(-101.165045656948,-4.76405452823419,
129.582490119309));
#98672=CARTESIAN_POINT('Ctrl Pts',(-99.4153986790351,-4.76405452823397,
129.582490119308));
#98673=CARTESIAN_POINT('Ctrl Pts',(-99.4234124993472,-4.79925163865272,
129.71972311864));
#98674=CARTESIAN_POINT('Ctrl Pts',(-99.4314263196594,-4.82854706849966,
129.858603556017));
#98675=CARTESIAN_POINT('Ctrl Pts',(-99.4394401399715,-4.85179721396206,
129.998602057518));
#98676=CARTESIAN_POINT('Ctrl Pts',(-99.4474441489718,-4.87501889429581,
130.138429159002));
#98677=CARTESIAN_POINT('Ctrl Pts',(-99.455448157972,-4.89220998763033,130.279371249564));
#98678=CARTESIAN_POINT('Ctrl Pts',(-99.4634521669723,-4.90327761995071,
130.420887483969));
#98679=CARTESIAN_POINT('Ctrl Pts',(-99.4706816326513,-4.91327424389314,
130.548709274227));
#98680=CARTESIAN_POINT('Ctrl Pts',(-99.4779110983303,-4.91827578707414,
130.676999116505));
#98681=CARTESIAN_POINT('Ctrl Pts',(-99.4851405640093,-4.91824989996949,
130.805352560176));
#98682=CARTESIAN_POINT('',(-99.1398594360355,-4.91824791462173,130.799831509598));
#98683=CARTESIAN_POINT('Ctrl Pts',(-99.0698920977623,-4.76405452823408,
129.582490119308));
#98684=CARTESIAN_POINT('Ctrl Pts',(-99.0722155426109,-4.77419310704967,
129.622020284236));
#98685=CARTESIAN_POINT('Ctrl Pts',(-99.0745389874596,-4.78383510064487,
129.661658926553));
#98686=CARTESIAN_POINT('Ctrl Pts',(-99.0768624323083,-4.79297865804362,
129.701392510122));
#98687=CARTESIAN_POINT('Ctrl Pts',(-99.0873847719171,-4.8343876961091,129.881336639384));
#98688=CARTESIAN_POINT('Ctrl Pts',(-99.0979071115259,-4.86567686657927,
130.063689892457));
#98689=CARTESIAN_POINT('Ctrl Pts',(-99.1084294511346,-4.88662244155525,
130.247490636162));
#98690=CARTESIAN_POINT('Ctrl Pts',(-99.1189061127537,-4.90747709076822,
130.43049349187));
#98691=CARTESIAN_POINT('Ctrl Pts',(-99.1293827743728,-4.91807764454407,
130.614931896228));
#98692=CARTESIAN_POINT('Ctrl Pts',(-99.1398594359919,-4.91824791462102,
130.799831508829));
#98693=CARTESIAN_POINT('Ctrl Pts',(-99.1398594360355,-4.91824791462173,
130.799831509599));
#98694=CARTESIAN_POINT('Ctrl Pts',(-99.1475138473507,-4.91837231655715,
130.934922031593));
#98695=CARTESIAN_POINT('Ctrl Pts',(-99.1551682586658,-4.91292669612711,
131.070175337922));
#98696=CARTESIAN_POINT('Ctrl Pts',(-99.162822669981,-4.90189763815913,131.205088215205));
#98697=CARTESIAN_POINT('Ctrl Pts',(-99.1708429777369,-4.8903413687717,131.346450202625));
#98698=CARTESIAN_POINT('Ctrl Pts',(-99.1788632854928,-4.87265462096077,
131.48743796528));
#98699=CARTESIAN_POINT('Ctrl Pts',(-99.1868835932486,-4.84888341719431,
131.627472195032));
#98700=CARTESIAN_POINT('Ctrl Pts',(-99.1945292598886,-4.82622260352458,
131.760965206953));
#98701=CARTESIAN_POINT('Ctrl Pts',(-99.2021749265287,-4.7980329603097,131.893591305512));
#98702=CARTESIAN_POINT('Ctrl Pts',(-99.2098205931686,-4.76440737574616,
132.02485454235));
#98703=CARTESIAN_POINT('Ctrl Pts',(-99.2174650551137,-4.73078708942197,
132.156097096602));
#98704=CARTESIAN_POINT('Ctrl Pts',(-99.2251095170586,-4.69173266446441,
132.285976826505));
#98705=CARTESIAN_POINT('Ctrl Pts',(-99.2327539790036,-4.64738770754741,
132.414009821038));
#98706=CARTESIAN_POINT('Ctrl Pts',(-99.2403989952572,-4.60303953512731,
132.542052099388));
#98707=CARTESIAN_POINT('Ctrl Pts',(-99.2480440115109,-4.55340019985477,
132.668246996029));
#98708=CARTESIAN_POINT('Ctrl Pts',(-99.2556890277645,-4.49866241804575,
132.792128086603));
#98709=CARTESIAN_POINT('Ctrl Pts',(-99.2633363575497,-4.44390807151249,
132.91604666602));
#98710=CARTESIAN_POINT('Ctrl Pts',(-99.2709836873348,-4.38405237314869,
133.03764967938));
#98711=CARTESIAN_POINT('Ctrl Pts',(-99.27863101712,-4.31933494023983,133.156493423452));
#98712=CARTESIAN_POINT('Ctrl Pts',(-99.2862865694172,-4.25454792227538,
133.275464949918));
#98713=CARTESIAN_POINT('Ctrl Pts',(-99.2939421217144,-4.18488892867429,
133.391670932161));
#98714=CARTESIAN_POINT('Ctrl Pts',(-99.3015976740116,-4.11064217079655,
133.504694672117));
#98715=CARTESIAN_POINT('Ctrl Pts',(-99.3092580406042,-4.0363487218619,133.617789488549));
#98716=CARTESIAN_POINT('Ctrl Pts',(-99.3169184071968,-3.95746199965463,
133.727697753534));
#98717=CARTESIAN_POINT('Ctrl Pts',(-99.3245787737895,-3.87430697435425,
133.834035275177));
#98718=CARTESIAN_POINT('Ctrl Pts',(-99.3322500063426,-3.79103399657552,
133.940523632854));
#98719=CARTESIAN_POINT('Ctrl Pts',(-99.3399212388958,-3.70348089295842,
134.043430834714));
#98720=CARTESIAN_POINT('Ctrl Pts',(-99.347592471449,-3.61201015730344,134.142408802664));
#98721=CARTESIAN_POINT('Ctrl Pts',(-99.3501649996731,-3.58133567995954,
134.175600811165));
#98722=CARTESIAN_POINT('Ctrl Pts',(-99.3527375278972,-3.55022091423936,
134.208351277801));
#98723=CARTESIAN_POINT('Ctrl Pts',(-99.3553100561213,-3.51868034615613,
134.240648103222));
#98724=CARTESIAN_POINT('Ctrl Pts',(-99.3630843902404,-3.42336286342179,
134.338251040852));
#98725=CARTESIAN_POINT('Ctrl Pts',(-99.3708587243596,-3.32383028739127,
134.43203962204));
#98726=CARTESIAN_POINT('Ctrl Pts',(-99.3786330584786,-3.22042033090212,
134.521627887324));
#98727=CARTESIAN_POINT('Ctrl Pts',(-99.3863978114257,-3.11713781794233,
134.611105743078));
#98728=CARTESIAN_POINT('Ctrl Pts',(-99.3941625643728,-3.00998772502323,
134.696393329106));
#98729=CARTESIAN_POINT('Ctrl Pts',(-99.4019273173199,-2.89934583014384,
134.777140100463));
#98730=CARTESIAN_POINT('Ctrl Pts',(-99.4096843582049,-2.78881382635423,
134.857806672988));
#98731=CARTESIAN_POINT('Ctrl Pts',(-99.4174413990899,-2.67479723605721,
134.933941176963));
#98732=CARTESIAN_POINT('Ctrl Pts',(-99.4251984399749,-2.55770599034775,
135.005232328228));
#98733=CARTESIAN_POINT('Ctrl Pts',(-99.432949631215,-2.44070304405735,135.076469718281));
#98734=CARTESIAN_POINT('Ctrl Pts',(-99.4407008224552,-2.32063039001773,
135.142870823028));
#98735=CARTESIAN_POINT('Ctrl Pts',(-99.4484520136953,-2.19792780931666,
135.204167023254));
#98736=CARTESIAN_POINT('Ctrl Pts',(-99.4561999104724,-2.07527738048576,
135.265437170959));
#98737=CARTESIAN_POINT('Ctrl Pts',(-99.4639478072495,-1.94999959721095,
135.321606555199));
#98738=CARTESIAN_POINT('Ctrl Pts',(-99.4716957040266,-1.82255957335685,
135.372452086009));
#98739=CARTESIAN_POINT('Ctrl Pts',(-99.4794419801107,-1.69514620720846,
135.423286981031));
#98740=CARTESIAN_POINT('Ctrl Pts',(-99.4871882561947,-1.56557186301867,
135.468800092917));
#98741=CARTESIAN_POINT('Ctrl Pts',(-99.4949345322788,-1.43432203499653,
135.508816310037));
#98742=CARTESIAN_POINT('Ctrl Pts',(-99.5026808655442,-1.30307123811817,
135.548832822548));
#98743=CARTESIAN_POINT('Ctrl Pts',(-99.5104271988096,-1.17014530669805,
135.583352245306));
#98744=CARTESIAN_POINT('Ctrl Pts',(-99.5181735320749,-1.03604492573959,
135.612249340732));
#98745=CARTESIAN_POINT('Ctrl Pts',(-99.5259216000778,-0.901914513931145,
135.641152907462));
#98746=CARTESIAN_POINT('Ctrl Pts',(-99.5336696680808,-0.766609511344383,
135.664431559092));
#98747=CARTESIAN_POINT('Ctrl Pts',(-99.5414177360837,-0.630640428654262,
135.682011252067));
#98748=CARTESIAN_POINT('Ctrl Pts',(-99.5491740388256,-0.494526836404078,
135.699609628948));
#98749=CARTESIAN_POINT('Ctrl Pts',(-99.5569303415675,-0.357748142510617,
135.711496897611));
#98750=CARTESIAN_POINT('Ctrl Pts',(-99.5646866443093,-0.220820168700871,
135.717650911818));
#98751=CARTESIAN_POINT('Ctrl Pts',(-99.5724470868235,-0.0838191123086806,
135.723808210609));
#98752=CARTESIAN_POINT('Ctrl Pts',(-99.5802075293377,0.0533309919872466,
135.724226156423));
#98753=CARTESIAN_POINT('Ctrl Pts',(-99.5879679718518,0.190115690891329,
135.718934768658));
#98754=CARTESIAN_POINT('Ctrl Pts',(-99.5957408721173,0.327119968737268,
135.713634886687));
#98755=CARTESIAN_POINT('Ctrl Pts',(-99.6035137723827,0.46375727909287,135.702607387757));
#98756=CARTESIAN_POINT('Ctrl Pts',(-99.6112866726481,0.599518749511796,
135.685934168326));
#98757=CARTESIAN_POINT('Ctrl Pts',(-99.6187770084102,0.730344948519594,
135.66986706242));
#98758=CARTESIAN_POINT('Ctrl Pts',(-99.6262673441724,0.860357576060504,
135.648557631752));
#98759=CARTESIAN_POINT('Ctrl Pts',(-99.6337576799345,0.989113306761833,
135.622123368977));
#98760=CARTESIAN_POINT('Ctrl Pts',(-99.6415320140535,1.12275085012585,135.594686843095));
#98761=CARTESIAN_POINT('Ctrl Pts',(-99.6493063481726,1.2554576282722,135.561642287017));
#98762=CARTESIAN_POINT('Ctrl Pts',(-99.6570806822917,1.38672638053822,135.523065207601));
#98763=CARTESIAN_POINT('Ctrl Pts',(-99.6648454352388,1.5178333557989,135.484535670988));
#98764=CARTESIAN_POINT('Ctrl Pts',(-99.6726101881859,1.64750545990355,135.440487286681));
#98765=CARTESIAN_POINT('Ctrl Pts',(-99.680374941133,1.77524465227443,135.391046729245));
#98766=CARTESIAN_POINT('Ctrl Pts',(-99.688131982018,1.90285697227898,135.341655276868));
#98767=CARTESIAN_POINT('Ctrl Pts',(-99.695889022903,2.02853983877989,135.286882449421));
#98768=CARTESIAN_POINT('Ctrl Pts',(-99.7036460637881,2.15180978182806,135.22690487685));
#98769=CARTESIAN_POINT('Ctrl Pts',(-99.7113972550282,2.27498676605311,135.166972533834));
#98770=CARTESIAN_POINT('Ctrl Pts',(-99.7191484462683,2.39575409849983,135.101843428409));
#98771=CARTESIAN_POINT('Ctrl Pts',(-99.7268996375084,2.51364806979434,135.031742365613));
#98772=CARTESIAN_POINT('Ctrl Pts',(-99.7346475342855,2.63149193300629,134.961671097638));
#98773=CARTESIAN_POINT('Ctrl Pts',(-99.7423954310626,2.74646452870675,134.886632274712));
#98774=CARTESIAN_POINT('Ctrl Pts',(-99.7501433278397,2.85812675958685,134.806896624729));
#98775=CARTESIAN_POINT('Ctrl Pts',(-99.7578896039238,2.96976563313541,134.727177653724));
#98776=CARTESIAN_POINT('Ctrl Pts',(-99.7656358800078,3.07809520122745,134.642764036915));
#98777=CARTESIAN_POINT('Ctrl Pts',(-99.773382156092,3.18270571601008,134.553969582215));
#98778=CARTESIAN_POINT('Ctrl Pts',(-99.7811284893573,3.28731700300333,134.465174472055));
#98779=CARTESIAN_POINT('Ctrl Pts',(-99.7888748226226,3.3882088838396,134.371998712478));
#98780=CARTESIAN_POINT('Ctrl Pts',(-99.7966211558879,3.48500536012169,134.274795849986));
#98781=CARTESIAN_POINT('Ctrl Pts',(-99.8043692238909,3.58182351330364,134.177571219587));
#98782=CARTESIAN_POINT('Ctrl Pts',(-99.812117291894,3.67454416111241,134.076317968692));
#98783=CARTESIAN_POINT('Ctrl Pts',(-99.819865359897,3.7628290651184,133.97142558204));
#98784=CARTESIAN_POINT('Ctrl Pts',(-99.8276216626388,3.85120779937109,133.866421714512));
#98785=CARTESIAN_POINT('Ctrl Pts',(-99.8353779653807,3.93514112021633,133.75777128464));
#98786=CARTESIAN_POINT('Ctrl Pts',(-99.8431342681226,4.01433158115551,133.645896297271));
#98787=CARTESIAN_POINT('Ctrl Pts',(-99.8508947106368,4.0935643084283,133.533961598853));
#98788=CARTESIAN_POINT('Ctrl Pts',(-99.8586551531509,4.16804891952822,133.418799241737));
#98789=CARTESIAN_POINT('Ctrl Pts',(-99.8664155956651,4.23753259605088,133.300858276268));
#98790=CARTESIAN_POINT('Ctrl Pts',(-99.8741884959306,4.30712781393937,133.182727981492));
#98791=CARTESIAN_POINT('Ctrl Pts',(-99.881961396196,4.37170587057351,133.061810509987));
#98792=CARTESIAN_POINT('Ctrl Pts',(-99.8897342964615,4.43106060977608,132.93857825759));
#98793=CARTESIAN_POINT('Ctrl Pts',(-99.8972246322234,4.48825765470259,132.819825807973));
#98794=CARTESIAN_POINT('Ctrl Pts',(-99.9047149679853,4.54060442808771,132.698924234489));
#98795=CARTESIAN_POINT('Ctrl Pts',(-99.9122053037473,4.58796015163464,132.576310026977));
#98796=CARTESIAN_POINT('Ctrl Pts',(-99.9199796378664,4.63711138183367,132.449046864519));
#98797=CARTESIAN_POINT('Ctrl Pts',(-99.9277539719854,4.68104131606582,132.319535503895));
#98798=CARTESIAN_POINT('Ctrl Pts',(-99.9355283061045,4.71953929361126,132.188243531168));
#98799=CARTESIAN_POINT('Ctrl Pts',(-99.9432930590516,4.75798982583993,132.057113364064));
#98800=CARTESIAN_POINT('Ctrl Pts',(-99.9510578119986,4.7910216122923,131.924207322716));
#98801=CARTESIAN_POINT('Ctrl Pts',(-99.9588225649457,4.81847202477224,131.790012893466));
#98802=CARTESIAN_POINT('Ctrl Pts',(-99.9665796058306,4.84589517311553,131.655951748015));
#98803=CARTESIAN_POINT('Ctrl Pts',(-99.9743366467156,4.86774790145498,131.520605141769));
#98804=CARTESIAN_POINT('Ctrl Pts',(-99.9820936876006,4.88391748625177,131.384475304489));
#98805=CARTESIAN_POINT('Ctrl Pts',(-99.9898448788407,4.9000748774389,131.248448123779));
#98806=CARTESIAN_POINT('Ctrl Pts',(-99.9975960700808,4.91055760958646,131.111639274334));
#98807=CARTESIAN_POINT('Ctrl Pts',(-100.005347261321,4.91530417129558,130.974560400598));
#98808=CARTESIAN_POINT('Ctrl Pts',(-100.013095158098,4.92004871558936,130.837539789041));
#98809=CARTESIAN_POINT('Ctrl Pts',(-100.020843054875,4.91906192499011,130.700249771369));
#98810=CARTESIAN_POINT('Ctrl Pts',(-100.028590951652,4.91233422772049,130.563206107623));
#98811=CARTESIAN_POINT('Ctrl Pts',(-100.036337227736,4.90560793774011,130.426191110458));
#98812=CARTESIAN_POINT('Ctrl Pts',(-100.04408350382,4.89314314885131,130.289422754967));
#98813=CARTESIAN_POINT('Ctrl Pts',(-100.051829779904,4.87498239781686,130.153415394467));
#98814=CARTESIAN_POINT('Ctrl Pts',(-100.05957611317,4.85682151272385,130.017407029991));
#98815=CARTESIAN_POINT('Ctrl Pts',(-100.067322446435,4.83296463333027,129.88216005924));
#98816=CARTESIAN_POINT('Ctrl Pts',(-100.075068779701,4.80350597200363,129.748181920836));
#98817=CARTESIAN_POINT('Ctrl Pts',(-100.082816847703,4.77404071361408,129.614173778957));
#98818=CARTESIAN_POINT('Ctrl Pts',(-100.090564915706,4.73897126096355,129.481435416614));
#98819=CARTESIAN_POINT('Ctrl Pts',(-100.098312983709,4.6984424724607,129.350461929391));
#98820=CARTESIAN_POINT('Ctrl Pts',(-100.106069286451,4.65787060947907,129.219349241987));
#98821=CARTESIAN_POINT('Ctrl Pts',(-100.113825589193,4.61182793579019,129.090005550765));
#98822=CARTESIAN_POINT('Ctrl Pts',(-100.121581891935,4.56050871892502,128.962909209815));
#98823=CARTESIAN_POINT('Ctrl Pts',(-100.129342334449,4.50916211144861,128.835745033721));
#98824=CARTESIAN_POINT('Ctrl Pts',(-100.137102776963,4.45253351052727,128.710830953871));
#98825=CARTESIAN_POINT('Ctrl Pts',(-100.144863219478,4.39086406041055,128.588622396229));
#98826=CARTESIAN_POINT('Ctrl Pts',(-100.152636119743,4.32909561301774,128.46621765856));
#98827=CARTESIAN_POINT('Ctrl Pts',(-100.160409020008,4.26227033669737,128.346527463646));
#98828=CARTESIAN_POINT('Ctrl Pts',(-100.168181920274,4.1906742389969,128.229980598006));
#98829=CARTESIAN_POINT('Ctrl Pts',(-100.175672256036,4.12168083978695,128.117670504495));
#98830=CARTESIAN_POINT('Ctrl Pts',(-100.183162591798,4.04825763155853,128.008279427853));
#98831=CARTESIAN_POINT('Ctrl Pts',(-100.19065292756,3.9706957514681,127.902161742269));
#98832=CARTESIAN_POINT('Ctrl Pts',(-100.198427261679,3.89019308912041,127.792020572384));
#98833=CARTESIAN_POINT('Ctrl Pts',(-100.206201595798,3.80497671597569,127.685057020646));
#98834=CARTESIAN_POINT('Ctrl Pts',(-100.213975929917,3.71532615816712,127.581701063574));
#98835=CARTESIAN_POINT('Ctrl Pts',(-100.221740682864,3.62578608665876,127.478472483481));
#98836=CARTESIAN_POINT('Ctrl Pts',(-100.229505435811,3.53182295740176,127.378842944271));
#98837=CARTESIAN_POINT('Ctrl Pts',(-100.237270188759,3.43375900194902,127.283212767925));
#98838=CARTESIAN_POINT('Ctrl Pts',(-100.245027229644,3.33579244499904,127.187677572817));
#98839=CARTESIAN_POINT('Ctrl Pts',(-100.252784270529,3.23373344539835,127.096134106863));
#98840=CARTESIAN_POINT('Ctrl Pts',(-100.260541311414,3.1279436134437,127.008948675021));
#98841=CARTESIAN_POINT('Ctrl Pts',(-100.268292502654,3.02223355842469,126.921828990391));
#98842=CARTESIAN_POINT('Ctrl Pts',(-100.276043693894,2.91279857153971,126.839061046082));
#98843=CARTESIAN_POINT('Ctrl Pts',(-100.283794885134,2.80003586533546,126.760973149695));
#98844=CARTESIAN_POINT('Ctrl Pts',(-100.291542781911,2.68732108628953,126.682918442747));
#98845=CARTESIAN_POINT('Ctrl Pts',(-100.299290678688,2.57128172174446,126.609540049579));
#98846=CARTESIAN_POINT('Ctrl Pts',(-100.307038575465,2.45234652145019,126.541124804099));
#98847=CARTESIAN_POINT('Ctrl Pts',(-100.314784851549,2.33343619983524,126.472723869612));
#98848=CARTESIAN_POINT('Ctrl Pts',(-100.322531127633,2.2116315860155,126.40928421263));
#98849=CARTESIAN_POINT('Ctrl Pts',(-100.330277403718,2.08738841216248,126.351048066299));
#98850=CARTESIAN_POINT('Ctrl Pts',(-100.338023736983,1.96314432117509,126.292811490083));
#98851=CARTESIAN_POINT('Ctrl Pts',(-100.345770070248,1.83646198824102,126.239778667097));
#98852=CARTESIAN_POINT('Ctrl Pts',(-100.353516403513,1.70781925992925,126.192144616779));
#98853=CARTESIAN_POINT('Ctrl Pts',(-100.361264471516,1.57914772297059,126.144499899146));
#98854=CARTESIAN_POINT('Ctrl Pts',(-100.369012539519,1.44851528360887,126.102256495718));
#98855=CARTESIAN_POINT('Ctrl Pts',(-100.376760607522,1.31641677929023,126.065560144271));
#98856=CARTESIAN_POINT('Ctrl Pts',(-100.384516910264,1.18417787910866,126.028824791505));
#98857=CARTESIAN_POINT('Ctrl Pts',(-100.392273213006,1.05047017869606,125.997648372375));
#98858=CARTESIAN_POINT('Ctrl Pts',(-100.400029515748,0.915801137242447,
125.972126006175));
#98859=CARTESIAN_POINT('Ctrl Pts',(-100.407789958262,0.781060218866975,
125.94659001792));
#98860=CARTESIAN_POINT('Ctrl Pts',(-100.415550400776,0.645357323710639,
125.926714152326));
#98861=CARTESIAN_POINT('Ctrl Pts',(-100.42331084329,0.509205958892165,125.912541696763));
#98862=CARTESIAN_POINT('Ctrl Pts',(-100.431083743556,0.372836031815564,
125.898346490316));
#98863=CARTESIAN_POINT('Ctrl Pts',(-100.438856643821,0.236016586882788,
125.889873013928));
#98864=CARTESIAN_POINT('Ctrl Pts',(-100.446629544087,0.0992629684021214,
125.887112410936));
#98865=CARTESIAN_POINT('Ctrl Pts',(-100.454119879849,-0.0325193115866818,
125.884452162817));
#98866=CARTESIAN_POINT('Ctrl Pts',(-100.461610215611,-0.164240159991098,
125.887096638402));
#98867=CARTESIAN_POINT('Ctrl Pts',(-100.469100551373,-0.295444065025355,
125.894992443662));
#98868=CARTESIAN_POINT('Ctrl Pts',(-100.476874885492,-0.431622605996199,
125.903187620778));
#98869=CARTESIAN_POINT('Ctrl Pts',(-100.484649219611,-0.567675602649322,
125.917066156513));
#98870=CARTESIAN_POINT('Ctrl Pts',(-100.49242355373,-0.703090212859308,
125.936625290427));
#98871=CARTESIAN_POINT('Ctrl Pts',(-100.500188306677,-0.838337936663458,
125.956160319455));
#98872=CARTESIAN_POINT('Ctrl Pts',(-100.507953059624,-0.972948456195941,
125.981361961743));
#98873=CARTESIAN_POINT('Ctrl Pts',(-100.515717812571,-1.10641079521007,
126.012175498568));
#98874=CARTESIAN_POINT('Ctrl Pts',(-100.523474853456,-1.23974057754796,
126.042958430955));
#98875=CARTESIAN_POINT('Ctrl Pts',(-100.531231894341,-1.37192407031433,
126.079342078358));
#98876=CARTESIAN_POINT('Ctrl Pts',(-100.538988935226,-1.50245763157392,
126.121220204571));
#98877=CARTESIAN_POINT('Ctrl Pts',(-100.546740126466,-1.63289275645972,
126.163066750164));
#98878=CARTESIAN_POINT('Ctrl Pts',(-100.554491317707,-1.76168005562612,
126.210399408372));
#98879=CARTESIAN_POINT('Ctrl Pts',(-100.562242508947,-1.88832861150635,
126.263061451307));
#98880=CARTESIAN_POINT('Ctrl Pts',(-100.569990405724,-2.01492333837238,
126.315701111469));
#98881=CARTESIAN_POINT('Ctrl Pts',(-100.577738302501,-2.13938076968501,
126.373665501392));
#98882=CARTESIAN_POINT('Ctrl Pts',(-100.585486199278,-2.26122783424161,
126.436748942503));
#98883=CARTESIAN_POINT('Ctrl Pts',(-100.593232475362,-2.38304941101935,
126.499819187917));
#98884=CARTESIAN_POINT('Ctrl Pts',(-100.600978751446,-2.50226136015605,
126.568006175011));
#98885=CARTESIAN_POINT('Ctrl Pts',(-100.60872502753,-2.61841354967332,126.641057416334));
#98886=CARTESIAN_POINT('Ctrl Pts',(-100.616471360796,-2.73456659659919,
126.714109196905));
#98887=CARTESIAN_POINT('Ctrl Pts',(-100.624217694061,-2.84765950788361,
126.79202509521));
#98888=CARTESIAN_POINT('Ctrl Pts',(-100.631964027326,-2.95726992040894,
126.874508498167));
#98889=CARTESIAN_POINT('Ctrl Pts',(-100.639712095329,-3.06690487942601,
126.95701037271));
#98890=CARTESIAN_POINT('Ctrl Pts',(-100.647460163332,-3.17305547547524,
127.044081552243));
#98891=CARTESIAN_POINT('Ctrl Pts',(-100.655208231335,-3.27533162351188,
127.135384490835));
#98892=CARTESIAN_POINT('Ctrl Pts',(-100.662964534077,-3.37771647185616,
127.226784467277));
#98893=CARTESIAN_POINT('Ctrl Pts',(-100.670720836819,-3.47621835429782,
127.322424926367));
#98894=CARTESIAN_POINT('Ctrl Pts',(-100.678477139561,-3.57048295019262,
127.421930342618));
#98895=CARTESIAN_POINT('Ctrl Pts',(-100.686237582075,-3.66479785794024,
127.521488867906));
#98896=CARTESIAN_POINT('Ctrl Pts',(-100.693998024589,-3.75487071613825,
127.624916166058));
#98897=CARTESIAN_POINT('Ctrl Pts',(-100.701758467103,-3.84038754275462,
127.731803606874));
#98898=CARTESIAN_POINT('Ctrl Pts',(-100.709531367369,-3.92604164857291,
127.838862632898));
#98899=CARTESIAN_POINT('Ctrl Pts',(-100.717304267634,-4.00712487622633,
127.949392585884));
#98900=CARTESIAN_POINT('Ctrl Pts',(-100.7250771679,-4.08336612088915,128.062955104827));
#98901=CARTESIAN_POINT('Ctrl Pts',(-100.732567503662,-4.15683580426816,
128.172389340159));
#98902=CARTESIAN_POINT('Ctrl Pts',(-100.740057839424,-4.22580926808501,
128.284639224097));
#98903=CARTESIAN_POINT('Ctrl Pts',(-100.747548175186,-4.29008521900273,
128.399292660897));
#98904=CARTESIAN_POINT('Ctrl Pts',(-100.755683650374,-4.3598972301696,128.523821149328));
#98905=CARTESIAN_POINT('Ctrl Pts',(-100.763819125561,-4.42437184426201,
128.651549076575));
#98906=CARTESIAN_POINT('Ctrl Pts',(-100.771954600749,-4.48321825173858,
128.782001309783));
#98907=CARTESIAN_POINT('Ctrl Pts',(-100.78007251136,-4.54193760919861,128.912171895238));
#98908=CARTESIAN_POINT('Ctrl Pts',(-100.788190421971,-4.59505284665445,
129.045054753809));
#98909=CARTESIAN_POINT('Ctrl Pts',(-100.796308332581,-4.6423186290701,129.180149791137));
#98910=CARTESIAN_POINT('Ctrl Pts',(-100.804249882031,-4.68855756496666,
129.312309896222));
#98911=CARTESIAN_POINT('Ctrl Pts',(-100.812191431481,-4.72919843798944,
129.44658675246));
#98912=CARTESIAN_POINT('Ctrl Pts',(-100.820132980931,-4.76405452823393,
129.582490119308));
#98913=CARTESIAN_POINT('Origin',(213.235140564004,0.,130.804360617566));
#98914=CARTESIAN_POINT('',(-102.915060258535,-4.76405452823397,129.582490119308));
#98915=CARTESIAN_POINT('',(-102.569791376202,-4.76405452823412,129.582490119309));
#98916=CARTESIAN_POINT('',(213.235140564004,-4.76405452823405,129.582490119308));
#98917=CARTESIAN_POINT('',(-101.235140563964,-4.91824820892467,130.808557986892));
#98918=CARTESIAN_POINT('Ctrl Pts',(-101.235140564009,-4.918248208924,130.808557987678));
#98919=CARTESIAN_POINT('Ctrl Pts',(-101.247006338631,-4.91806979539947,
131.017613175562));
#98920=CARTESIAN_POINT('Ctrl Pts',(-101.258872113253,-4.90455922343421,
131.226120353833));
#98921=CARTESIAN_POINT('Ctrl Pts',(-101.270737887874,-4.87794266429464,
131.432738232026));
#98922=CARTESIAN_POINT('Ctrl Pts',(-101.2754434008,-4.86738755372939,131.514674989427));
#98923=CARTESIAN_POINT('Ctrl Pts',(-101.280148913726,-4.85477182893646,
131.596315055863));
#98924=CARTESIAN_POINT('Ctrl Pts',(-101.284854426652,-4.84011134684747,
131.677576062126));
#98925=CARTESIAN_POINT('Ctrl Pts',(-101.292628760771,-4.81588965456829,
131.81183352215));
#98926=CARTESIAN_POINT('Ctrl Pts',(-101.30040309489,-4.78603921126845,131.945295062255));
#98927=CARTESIAN_POINT('Ctrl Pts',(-101.308177429009,-4.7506233292055,132.077451755902));
#98928=CARTESIAN_POINT('Ctrl Pts',(-101.315942181957,-4.71525109405207,
132.209445578234));
#98929=CARTESIAN_POINT('Ctrl Pts',(-101.323706934904,-4.67432716754392,
132.340137379745));
#98930=CARTESIAN_POINT('Ctrl Pts',(-101.331471687851,-4.62796623616901,
132.46902622344));
#98931=CARTESIAN_POINT('Ctrl Pts',(-101.339228728736,-4.58165135112484,
132.597787052918));
#98932=CARTESIAN_POINT('Ctrl Pts',(-101.346985769621,-4.52991033914884,
132.724748122692));
#98933=CARTESIAN_POINT('Ctrl Pts',(-101.354742810506,-4.47290817737871,
132.849421863406));
#98934=CARTESIAN_POINT('Ctrl Pts',(-101.362494001746,-4.41594900138195,
132.974001586684));
#98935=CARTESIAN_POINT('Ctrl Pts',(-101.370245192986,-4.35373673451711,
133.096297060072));
#98936=CARTESIAN_POINT('Ctrl Pts',(-101.377996384226,-4.28648498933653,
133.215839313033));
#98937=CARTESIAN_POINT('Ctrl Pts',(-101.385744281003,-4.21926182794175,
133.335330757348));
#98938=CARTESIAN_POINT('Ctrl Pts',(-101.39349217778,-4.14700363962606,133.452070968626));
#98939=CARTESIAN_POINT('Ctrl Pts',(-101.401240074557,-4.06997053719467,
133.565614479287));
#98940=CARTESIAN_POINT('Ctrl Pts',(-101.408986350641,-3.99295354842767,
133.679134239092));
#98941=CARTESIAN_POINT('Ctrl Pts',(-101.416732626726,-3.91116385159159,
133.789458304995));
#98942=CARTESIAN_POINT('Ctrl Pts',(-101.42447890281,-3.82490533141331,133.896169516613));
#98943=CARTESIAN_POINT('Ctrl Pts',(-101.432225236075,-3.7386461744941,134.002881515949));
#98944=CARTESIAN_POINT('Ctrl Pts',(-101.43997156934,-3.64791837418422,134.105980303733));
#98945=CARTESIAN_POINT('Ctrl Pts',(-101.447717902606,-3.55306635224864,
134.205081505704));
#98946=CARTESIAN_POINT('Ctrl Pts',(-101.455465970609,-3.45819308886053,
134.304204900702));
#98947=CARTESIAN_POINT('Ctrl Pts',(-101.463214038612,-3.35919403628882,
134.399328646091));
#98948=CARTESIAN_POINT('Ctrl Pts',(-101.470962106615,-3.25645045032094,
134.490105254285));
#98949=CARTESIAN_POINT('Ctrl Pts',(-101.478718409356,-3.1535976672471,134.580978340939));
#98950=CARTESIAN_POINT('Ctrl Pts',(-101.486474712098,-3.04699269428558,
134.667494801797));
#98951=CARTESIAN_POINT('Ctrl Pts',(-101.49423101484,-2.93705027685989,134.749347149064));
#98952=CARTESIAN_POINT('Ctrl Pts',(-101.501991457354,-2.82704917985571,
134.831243183393));
#98953=CARTESIAN_POINT('Ctrl Pts',(-101.509751899869,-2.71370741194373,
134.908469923798));
#98954=CARTESIAN_POINT('Ctrl Pts',(-101.517512342383,-2.59746782720842,
134.980763848711));
#98955=CARTESIAN_POINT('Ctrl Pts',(-101.525285242648,-2.48104164437242,
135.05317382625));
#98956=CARTESIAN_POINT('Ctrl Pts',(-101.533058142914,-2.3617086894097,135.120634971909));
#98957=CARTESIAN_POINT('Ctrl Pts',(-101.540831043179,-2.23993627493946,
135.182929852683));
#98958=CARTESIAN_POINT('Ctrl Pts',(-101.548321378941,-2.12259059446142,
135.242960157628));
#98959=CARTESIAN_POINT('Ctrl Pts',(-101.555811714703,-2.0029800158675,135.298193160838));
#98960=CARTESIAN_POINT('Ctrl Pts',(-101.563302050465,-1.88153752500862,
135.348477650003));
#98961=CARTESIAN_POINT('Ctrl Pts',(-101.571076384584,-1.75549050519735,
135.400668690858));
#98962=CARTESIAN_POINT('Ctrl Pts',(-101.578850718703,-1.62707063793868,
135.447693889908));
#98963=CARTESIAN_POINT('Ctrl Pts',(-101.586625052822,-1.49674031936641,
135.489331426321));
#98964=CARTESIAN_POINT('Ctrl Pts',(-101.594389805769,-1.36657062126383,
135.530917648191));
#98965=CARTESIAN_POINT('Ctrl Pts',(-101.602154558716,-1.23449552536829,
135.567129300836));
#98966=CARTESIAN_POINT('Ctrl Pts',(-101.609919311664,-1.10099847500883,
135.597792104562));
#98967=CARTESIAN_POINT('Ctrl Pts',(-101.617676352549,-0.967634015801769,
135.62842445356));
#98968=CARTESIAN_POINT('Ctrl Pts',(-101.625433393434,-0.832850791259232,
135.653518834212));
#98969=CARTESIAN_POINT('Ctrl Pts',(-101.633190434319,-0.697148181459653,
135.672950503312));
#98970=CARTESIAN_POINT('Ctrl Pts',(-101.640941625559,-0.561547906053921,
135.692367518839));
#98971=CARTESIAN_POINT('Ctrl Pts',(-101.648692816799,-0.425030010845373,
135.706130267382));
#98972=CARTESIAN_POINT('Ctrl Pts',(-101.656444008039,-0.288104516831927,
135.7141649772));
#98973=CARTESIAN_POINT('Ctrl Pts',(-101.664191904816,-0.151237219805858,
135.722196272052));
#98974=CARTESIAN_POINT('Ctrl Pts',(-101.671939801593,-0.0139630580134921,
135.724504347499));
#98975=CARTESIAN_POINT('Ctrl Pts',(-101.67968769837,0.123202586726795,135.721067257699));
#98976=CARTESIAN_POINT('Ctrl Pts',(-101.687433974454,0.260339539371152,
135.717630886864));
#98977=CARTESIAN_POINT('Ctrl Pts',(-101.695180250538,0.397367629518935,
135.708451750946));
#98978=CARTESIAN_POINT('Ctrl Pts',(-101.702926526622,0.533771631209913,
135.693560031398));
#98979=CARTESIAN_POINT('Ctrl Pts',(-101.710672859888,0.670176639804059,
135.678668201923));
#98980=CARTESIAN_POINT('Ctrl Pts',(-101.718419193153,0.805957162092814,
135.658063747102));
#98981=CARTESIAN_POINT('Ctrl Pts',(-101.726165526418,0.940603644748119,
135.631828675046));
#98982=CARTESIAN_POINT('Ctrl Pts',(-101.733913594421,1.07528028054982,135.605587727827));
#98983=CARTESIAN_POINT('Ctrl Pts',(-101.741661662424,1.2088219876912,135.573713729009));
#98984=CARTESIAN_POINT('Ctrl Pts',(-101.749409730427,1.34073033695971,135.536339614355));
#98985=CARTESIAN_POINT('Ctrl Pts',(-101.757166033169,1.47277887999138,135.498925778048));
#98986=CARTESIAN_POINT('Ctrl Pts',(-101.764922335911,1.60319022064089,135.456000255462));
#98987=CARTESIAN_POINT('Ctrl Pts',(-101.772678638653,1.73148148068647,135.407745779003));
#98988=CARTESIAN_POINT('Ctrl Pts',(-101.780439081167,1.85984121364067,135.359465547677));
#98989=CARTESIAN_POINT('Ctrl Pts',(-101.788199523681,1.98607825160179,135.305850847885));
#98990=CARTESIAN_POINT('Ctrl Pts',(-101.795959966195,2.10973151296049,135.247131825463));
#98991=CARTESIAN_POINT('Ctrl Pts',(-101.803732866461,2.23358327351175,135.188318542055));
#98992=CARTESIAN_POINT('Ctrl Pts',(-101.811505766726,2.35484262298096,135.124384744419));
#98993=CARTESIAN_POINT('Ctrl Pts',(-101.819278666992,2.47307403493597,135.055606068046));
#98994=CARTESIAN_POINT('Ctrl Pts',(-101.826769002754,2.58700743726043,134.989327669802));
#98995=CARTESIAN_POINT('Ctrl Pts',(-101.834259338516,2.69812896652249,134.918550689858));
#98996=CARTESIAN_POINT('Ctrl Pts',(-101.841749674278,2.80607736409552,134.843557677529));
#98997=CARTESIAN_POINT('Ctrl Pts',(-101.849524008397,2.91811865797165,134.765721282344));
#98998=CARTESIAN_POINT('Ctrl Pts',(-101.857298342516,3.02709636483782,134.68309627972));
#98999=CARTESIAN_POINT('Ctrl Pts',(-101.865072676635,3.13257392414164,134.595951797043));
#99000=CARTESIAN_POINT('Ctrl Pts',(-101.872837429582,3.23792149178041,134.508914712153));
#99001=CARTESIAN_POINT('Ctrl Pts',(-101.880602182529,3.33977719616249,134.417369476188));
#99002=CARTESIAN_POINT('Ctrl Pts',(-101.888366935476,3.43773309791964,134.321628621282));
#99003=CARTESIAN_POINT('Ctrl Pts',(-101.896123976361,3.53559170849424,134.225982857544));
#99004=CARTESIAN_POINT('Ctrl Pts',(-101.903881017247,3.62955794677515,134.126150039184));
#99005=CARTESIAN_POINT('Ctrl Pts',(-101.911638058132,3.71925693563923,134.022482882055));
#99006=CARTESIAN_POINT('Ctrl Pts',(-101.919389249372,3.80888828179817,133.918893901136));
#99007=CARTESIAN_POINT('Ctrl Pts',(-101.927140440612,3.8942585289241,133.81147663127));
#99008=CARTESIAN_POINT('Ctrl Pts',(-101.934891631852,3.9750299319547,133.70062029214));
#99009=CARTESIAN_POINT('Ctrl Pts',(-101.942639528629,4.05576700498424,133.589811069912));
#99010=CARTESIAN_POINT('Ctrl Pts',(-101.950387425406,4.1319088917817,133.475566000946));
#99011=CARTESIAN_POINT('Ctrl Pts',(-101.958135322183,4.20315855222879,133.358306828301));
#99012=CARTESIAN_POINT('Ctrl Pts',(-101.965881598267,4.27439330878288,133.241072183746));
#99013=CARTESIAN_POINT('Ctrl Pts',(-101.973627874351,4.34073767159088,133.120825023492));
#99014=CARTESIAN_POINT('Ctrl Pts',(-101.981374150435,4.40193854094643,132.998015135541));
#99015=CARTESIAN_POINT('Ctrl Pts',(-101.989120483701,4.46313986207299,132.875204341035));
#99016=CARTESIAN_POINT('Ctrl Pts',(-101.996866816966,4.51919743960488,132.749831131006));
#99017=CARTESIAN_POINT('Ctrl Pts',(-102.004613150232,4.56990484326638,132.622368534488));
#99018=CARTESIAN_POINT('Ctrl Pts',(-102.012361218234,4.62062360249929,132.494877393605));
#99019=CARTESIAN_POINT('Ctrl Pts',(-102.020109286237,4.66598965922242,132.365296298362));
#99020=CARTESIAN_POINT('Ctrl Pts',(-102.02785735424,4.70584544289486,132.2341164464));
#99021=CARTESIAN_POINT('Ctrl Pts',(-102.035613656982,4.74574358576852,132.102797174931));
#99022=CARTESIAN_POINT('Ctrl Pts',(-102.043369959724,4.78011964299761,131.969876127129));
#99023=CARTESIAN_POINT('Ctrl Pts',(-102.051126262466,4.80886634505797,131.835858333448));
#99024=CARTESIAN_POINT('Ctrl Pts',(-102.05888670498,4.83762839009877,131.701769010435));
#99025=CARTESIAN_POINT('Ctrl Pts',(-102.066647147494,4.86075502724483,131.56658216033));
#99026=CARTESIAN_POINT('Ctrl Pts',(-102.074407590008,4.87819065883584,131.430810103596));
#99027=CARTESIAN_POINT('Ctrl Pts',(-102.082180490274,4.89565427965054,131.294820093503));
#99028=CARTESIAN_POINT('Ctrl Pts',(-102.089953390539,4.9074086053125,131.158243389259));
#99029=CARTESIAN_POINT('Ctrl Pts',(-102.097726290805,4.91345012309112,131.021595399302));
#99030=CARTESIAN_POINT('Ctrl Pts',(-102.105216626567,4.91927201648083,130.889914907975));
#99031=CARTESIAN_POINT('Ctrl Pts',(-102.112706962329,4.91978923960662,130.7581685318));
#99032=CARTESIAN_POINT('Ctrl Pts',(-102.120197298091,4.91504424009559,130.626812932695));
#99033=CARTESIAN_POINT('Ctrl Pts',(-102.12797163221,4.91011933248587,130.490476946125));
#99034=CARTESIAN_POINT('Ctrl Pts',(-102.135745966329,4.89950969020642,130.354130082783));
#99035=CARTESIAN_POINT('Ctrl Pts',(-102.143520300448,4.88320576610674,130.218285103351));
#99036=CARTESIAN_POINT('Ctrl Pts',(-102.151285053395,4.86692193513642,130.082607540717));
#99037=CARTESIAN_POINT('Ctrl Pts',(-102.159049806342,4.84495783160567,129.947431015761));
#99038=CARTESIAN_POINT('Ctrl Pts',(-102.166814559289,4.8173558964575,129.813267670681));
#99039=CARTESIAN_POINT('Ctrl Pts',(-102.174571600174,4.78978137594045,129.679237578526));
#99040=CARTESIAN_POINT('Ctrl Pts',(-102.182328641059,4.7565802454855,129.546219044122));
#99041=CARTESIAN_POINT('Ctrl Pts',(-102.190085681944,4.71784662468719,129.414718113744));
#99042=CARTESIAN_POINT('Ctrl Pts',(-102.197836873184,4.67914221321358,129.283316349241));
#99043=CARTESIAN_POINT('Ctrl Pts',(-102.205588064425,4.63491372571621,129.153430284348));
#99044=CARTESIAN_POINT('Ctrl Pts',(-102.213339255665,4.58530606428086,129.025554456297));
#99045=CARTESIAN_POINT('Ctrl Pts',(-102.221087152442,4.53571948742489,128.897732978884));
#99046=CARTESIAN_POINT('Ctrl Pts',(-102.228835049219,4.48075842499837,128.771920402704));
#99047=CARTESIAN_POINT('Ctrl Pts',(-102.236582945996,4.42061714394063,128.648594598445));
#99048=CARTESIAN_POINT('Ctrl Pts',(-102.24432922208,4.36048844314255,128.525294591286));
#99049=CARTESIAN_POINT('Ctrl Pts',(-102.252075498164,4.29518185029251,128.404480672567));
#99050=CARTESIAN_POINT('Ctrl Pts',(-102.259821774248,4.22493897820357,128.286608903644));
#99051=CARTESIAN_POINT('Ctrl Pts',(-102.267568107513,4.15469558759761,128.168736264618));
#99052=CARTESIAN_POINT('Ctrl Pts',(-102.275314440779,4.07951604518537,128.053806154576));
#99053=CARTESIAN_POINT('Ctrl Pts',(-102.283060774044,3.99968674308219,127.942247932902));
#99054=CARTESIAN_POINT('Ctrl Pts',(-102.290808842047,3.91983956376019,127.830664728538));
#99055=CARTESIAN_POINT('Ctrl Pts',(-102.29855691005,3.83534078019137,127.72245523301));
#99056=CARTESIAN_POINT('Ctrl Pts',(-102.306304978053,3.7465184801358,127.618017519201));
#99057=CARTESIAN_POINT('Ctrl Pts',(-102.314061280795,3.65760177868286,127.513468807746));
#99058=CARTESIAN_POINT('Ctrl Pts',(-102.321817583537,3.56435263526141,127.412700184105));
#99059=CARTESIAN_POINT('Ctrl Pts',(-102.329573886279,3.46713796449722,127.316074878461));
#99060=CARTESIAN_POINT('Ctrl Pts',(-102.337334328793,3.36987140733617,127.219398000983));
#99061=CARTESIAN_POINT('Ctrl Pts',(-102.345094771307,3.26863539392902,127.126869111567));
#99062=CARTESIAN_POINT('Ctrl Pts',(-102.352855213821,3.16383090209819,127.038811907825));
#99063=CARTESIAN_POINT('Ctrl Pts',(-102.360628114087,3.05885816879296,126.950613346843));
#99064=CARTESIAN_POINT('Ctrl Pts',(-102.368401014352,2.95030581959511,126.866901055049));
#99065=CARTESIAN_POINT('Ctrl Pts',(-102.376173914617,2.8386055835034,126.787956578652));
#99066=CARTESIAN_POINT('Ctrl Pts',(-102.383664250379,2.73096593235044,126.711881932823));
#99067=CARTESIAN_POINT('Ctrl Pts',(-102.391154586141,2.62040354655705,126.640234643952));
#99068=CARTESIAN_POINT('Ctrl Pts',(-102.398644921903,2.50732557270838,126.573225836571));
#99069=CARTESIAN_POINT('Ctrl Pts',(-102.406419256022,2.3899602131111,126.503676369892));
#99070=CARTESIAN_POINT('Ctrl Pts',(-102.414193590142,2.26951296463109,126.438903752329));
#99071=CARTESIAN_POINT('Ctrl Pts',(-102.421967924261,2.14641006688465,126.379193175844));
#99072=CARTESIAN_POINT('Ctrl Pts',(-102.429732677208,2.02345888245767,126.319556187309));
#99073=CARTESIAN_POINT('Ctrl Pts',(-102.437497430155,1.8978589091528,126.264968996056));
#99074=CARTESIAN_POINT('Ctrl Pts',(-102.445262183102,1.77006396707104,126.215672720686));
#99075=CARTESIAN_POINT('Ctrl Pts',(-102.453019223987,1.64239595272735,126.166425407071));
#99076=CARTESIAN_POINT('Ctrl Pts',(-102.460776264872,1.5125376704593,126.122458691424));
#99077=CARTESIAN_POINT('Ctrl Pts',(-102.468533305757,1.38096574526973,126.083966918637));
#99078=CARTESIAN_POINT('Ctrl Pts',(-102.476284496997,1.24949303949224,126.045504172795));
#99079=CARTESIAN_POINT('Ctrl Pts',(-102.484035688237,1.11630963669997,126.012508261224));
#99080=CARTESIAN_POINT('Ctrl Pts',(-102.491786879477,0.981909928188809,
125.985124583149));
#99081=CARTESIAN_POINT('Ctrl Pts',(-102.499534776254,0.847567343139183,
125.957752543868));
#99082=CARTESIAN_POINT('Ctrl Pts',(-102.507282673032,0.712009862861705,
125.935988071697));
#99083=CARTESIAN_POINT('Ctrl Pts',(-102.515030569809,0.575744539526512,
125.919926025138));
#99084=CARTESIAN_POINT('Ctrl Pts',(-102.522776845893,0.43950771995942,125.903867338413));
#99085=CARTESIAN_POINT('Ctrl Pts',(-102.530523121977,0.302563739876156,
125.893508750446));
#99086=CARTESIAN_POINT('Ctrl Pts',(-102.538269398061,0.165426894237428,
125.888893497834));
#99087=CARTESIAN_POINT('Ctrl Pts',(-102.546015731326,0.0282890362854728,
125.884278211154));
#99088=CARTESIAN_POINT('Ctrl Pts',(-102.553762064592,-0.109041299318828,
125.885406357579));
#99089=CARTESIAN_POINT('Ctrl Pts',(-102.561508397857,-0.24604807843205,
125.892269066546));
#99090=CARTESIAN_POINT('Ctrl Pts',(-102.56925646586,-0.383085539263329,
125.899133312369));
#99091=CARTESIAN_POINT('Ctrl Pts',(-102.577004533863,-0.519798909019114,
125.911734656619));
#99092=CARTESIAN_POINT('Ctrl Pts',(-102.584752601866,-0.655675938261888,
125.930012237886));
#99093=CARTESIAN_POINT('Ctrl Pts',(-102.592508904608,-0.791697379228114,
125.948309244785));
#99094=CARTESIAN_POINT('Ctrl Pts',(-102.60026520735,-0.926880315969279,
125.97229448761));
#99095=CARTESIAN_POINT('Ctrl Pts',(-102.608021510092,-1.06072082632601,
126.001855605481));
#99096=CARTESIAN_POINT('Ctrl Pts',(-102.615781952606,-1.19463277139335,
126.031432501012));
#99097=CARTESIAN_POINT('Ctrl Pts',(-102.62354239512,-1.3272004846867,126.066591101371));
#99098=CARTESIAN_POINT('Ctrl Pts',(-102.631302837634,-1.45793489193086,
126.107169019026));
#99099=CARTESIAN_POINT('Ctrl Pts',(-102.6390757379,-1.58887916565159,126.147812075958));
#99100=CARTESIAN_POINT('Ctrl Pts',(-102.646848638165,-1.71798388387347,
126.193891703199));
#99101=CARTESIAN_POINT('Ctrl Pts',(-102.654621538431,-1.84477881372711,
126.245196857519));
#99102=CARTESIAN_POINT('Ctrl Pts',(-102.662111874193,-1.9669644285041,126.294636940251));
#99103=CARTESIAN_POINT('Ctrl Pts',(-102.669602209955,-2.08700499194705,
126.348929096992));
#99104=CARTESIAN_POINT('Ctrl Pts',(-102.677092545717,-2.20450280633424,
126.407844901756));
#99105=CARTESIAN_POINT('Ctrl Pts',(-102.684867679213,-2.32646812557258,
126.469000804729));
#99106=CARTESIAN_POINT('Ctrl Pts',(-102.69264281271,-2.44607989834717,126.535332656813));
#99107=CARTESIAN_POINT('Ctrl Pts',(-102.700417946207,-2.56286764750348,
126.606635938186));
#99108=CARTESIAN_POINT('Ctrl Pts',(-102.708183320531,-2.67950880731297,
126.677849721288));
#99109=CARTESIAN_POINT('Ctrl Pts',(-102.715948694856,-2.79333266624636,
126.754022314974));
#99110=CARTESIAN_POINT('Ctrl Pts',(-102.72371406918,-2.90389095927734,126.834902170986));
#99111=CARTESIAN_POINT('Ctrl Pts',(-102.73168682707,-3.01740184313235,126.917942019832));
#99112=CARTESIAN_POINT('Ctrl Pts',(-102.73965958496,-3.12746990584699,127.005943931496));
#99113=CARTESIAN_POINT('Ctrl Pts',(-102.74763234285,-3.23363833206806,127.098585907754));
#99114=CARTESIAN_POINT('Ctrl Pts',(-102.75538313854,-3.33685102105582,127.188648724197));
#99115=CARTESIAN_POINT('Ctrl Pts',(-102.763133934231,-3.43637799670921,
127.283096407964));
#99116=CARTESIAN_POINT('Ctrl Pts',(-102.770884729922,-3.53183068472812,
127.381590529331));
#99117=CARTESIAN_POINT('Ctrl Pts',(-102.778632020455,-3.6272402059904,127.480040108509));
#99118=CARTESIAN_POINT('Ctrl Pts',(-102.786379310989,-3.71857883439708,
127.582532204005));
#99119=CARTESIAN_POINT('Ctrl Pts',(-102.794126601522,-3.80549381601036,
127.688690564623));
#99120=CARTESIAN_POINT('Ctrl Pts',(-102.801872066229,-3.89238831412471,
127.794823906601));
#99121=CARTESIAN_POINT('Ctrl Pts',(-102.809617530937,-3.97486099342078,
127.904621491454));
#99122=CARTESIAN_POINT('Ctrl Pts',(-102.817362995644,-4.05259873568158,
128.017673238248));
#99123=CARTESIAN_POINT('Ctrl Pts',(-102.825504434218,-4.13431068937647,
128.136504565612));
#99124=CARTESIAN_POINT('Ctrl Pts',(-102.833645872793,-4.2107905216308,128.258931186203));
#99125=CARTESIAN_POINT('Ctrl Pts',(-102.841787311367,-4.28172584201632,
128.384441842832));
#99126=CARTESIAN_POINT('Ctrl Pts',(-102.849536903174,-4.34924705128524,
128.503911681915));
#99127=CARTESIAN_POINT('Ctrl Pts',(-102.857286494982,-4.41174482490943,
128.626175246942));
#99128=CARTESIAN_POINT('Ctrl Pts',(-102.865036086789,-4.46899709010937,
128.750766677398));
#99129=CARTESIAN_POINT('Ctrl Pts',(-102.872788327524,-4.52626892499603,
128.875400695082));
#99130=CARTESIAN_POINT('Ctrl Pts',(-102.880540568259,-4.57829152778495,
129.002363803426));
#99131=CARTESIAN_POINT('Ctrl Pts',(-102.888292808993,-4.6248912238265,129.131170780676));
#99132=CARTESIAN_POINT('Ctrl Pts',(-102.896051980615,-4.67153258229963,
129.26009291773));
#99133=CARTESIAN_POINT('Ctrl Pts',(-102.903811152236,-4.71274123686296,
129.390861842772));
#99134=CARTESIAN_POINT('Ctrl Pts',(-102.911570323857,-4.74839351052368,
129.522977719398));
#99135=CARTESIAN_POINT('Ctrl Pts',(-102.912733635416,-4.75373875922984,
129.542785494502));
#99136=CARTESIAN_POINT('Ctrl Pts',(-102.913896946976,-4.75895920425979,
129.562623528465));
#99137=CARTESIAN_POINT('Ctrl Pts',(-102.915060258535,-4.76405452823397,
129.582490119308));
#99138=CARTESIAN_POINT('Ctrl Pts',(-101.165045656948,-4.76405452823419,
129.582490119309));
#99139=CARTESIAN_POINT('Ctrl Pts',(-101.172682180364,-4.79766536477147,
129.713538260852));
#99140=CARTESIAN_POINT('Ctrl Pts',(-101.18031870378,-4.82585068438517,129.845919443598));
#99141=CARTESIAN_POINT('Ctrl Pts',(-101.187955227196,-4.84852456437522,
129.979137853005));
#99142=CARTESIAN_POINT('Ctrl Pts',(-101.195819449991,-4.8718745148893,130.116328455962));
#99143=CARTESIAN_POINT('Ctrl Pts',(-101.203683672785,-4.88937914754242,
130.254406536086));
#99144=CARTESIAN_POINT('Ctrl Pts',(-101.21154789558,-4.90100212544491,130.392825407791));
#99145=CARTESIAN_POINT('Ctrl Pts',(-101.219412118375,-4.9126251033474,130.531244279497));
#99146=CARTESIAN_POINT('Ctrl Pts',(-101.22727634117,-4.91836645518236,130.670003478117));
#99147=CARTESIAN_POINT('Ctrl Pts',(-101.235140563964,-4.91824820892467,
130.808557986892));
#99148=CARTESIAN_POINT('',(-100.889859436022,-4.918249990696,130.804663138373));
#99149=CARTESIAN_POINT('Ctrl Pts',(-100.820132980931,-4.76405452823393,
129.582490119308));
#99150=CARTESIAN_POINT('Ctrl Pts',(-100.82822748962,-4.79958196870859,129.721011070514));
#99151=CARTESIAN_POINT('Ctrl Pts',(-100.83632199831,-4.82909935154331,129.861221551865));
#99152=CARTESIAN_POINT('Ctrl Pts',(-100.844416506999,-4.85245675817816,
130.002583545986));
#99153=CARTESIAN_POINT('Ctrl Pts',(-100.852497712237,-4.87577577655068,
130.143713209463));
#99154=CARTESIAN_POINT('Ctrl Pts',(-100.860578917475,-4.8929549507117,130.285990279047));
#99155=CARTESIAN_POINT('Ctrl Pts',(-100.868660122712,-4.90389499969728,
130.42886508571));
#99156=CARTESIAN_POINT('Ctrl Pts',(-100.875726560472,-4.9134612924681,130.55379891662));
#99157=CARTESIAN_POINT('Ctrl Pts',(-100.882792998232,-4.91825770855033,
130.679189440182));
#99158=CARTESIAN_POINT('Ctrl Pts',(-100.889859435992,-4.91824999069603,
130.804663137836));
#99159=CARTESIAN_POINT('Ctrl Pts',(-100.889859436022,-4.91824999069599,
130.804663138372));
#99160=CARTESIAN_POINT('Ctrl Pts',(-100.898012385779,-4.91824108615426,
130.949429254983));
#99161=CARTESIAN_POINT('Ctrl Pts',(-100.906165335536,-4.91183621813621,
131.094059493338));
#99162=CARTESIAN_POINT('Ctrl Pts',(-100.914318285293,-4.89909698201659,
131.237986981266));
#99163=CARTESIAN_POINT('Ctrl Pts',(-100.922483363176,-4.88633879532363,
131.382128572174));
#99164=CARTESIAN_POINT('Ctrl Pts',(-100.93064844106,-4.86722746182756,131.52556500171));
#99165=CARTESIAN_POINT('Ctrl Pts',(-100.938813518944,-4.84187593075419,
131.667738016901));
#99166=CARTESIAN_POINT('Ctrl Pts',(-100.946999214543,-4.81646038428944,
131.810270034521));
#99167=CARTESIAN_POINT('Ctrl Pts',(-100.955184910142,-4.7847731895604,131.951531936429));
#99168=CARTESIAN_POINT('Ctrl Pts',(-100.963370605741,-4.74697807774749,
132.090977185112));
#99169=CARTESIAN_POINT('Ctrl Pts',(-100.971567362971,-4.70913189201404,
132.230610871274));
#99170=CARTESIAN_POINT('Ctrl Pts',(-100.979764120201,-4.66516141326116,
132.368422693961));
#99171=CARTESIAN_POINT('Ctrl Pts',(-100.987960877431,-4.61527916584051,
132.503884457898));
#99172=CARTESIAN_POINT('Ctrl Pts',(-100.996176610845,-4.56528143680963,
132.639659827246));
#99173=CARTESIAN_POINT('Ctrl Pts',(-101.004392344259,-4.50934469907841,
132.773073958039));
#99174=CARTESIAN_POINT('Ctrl Pts',(-101.012608077673,-4.44772897719346,
132.90362001267));
#99175=CARTESIAN_POINT('Ctrl Pts',(-101.017070651448,-4.41426091162266,
132.974529251136));
#99176=CARTESIAN_POINT('Ctrl Pts',(-101.021533225223,-4.37911811220072,
133.044592757345));
#99177=CARTESIAN_POINT('Ctrl Pts',(-101.025995798998,-4.34234763903753,
133.11373283621));
#99178=CARTESIAN_POINT('Ctrl Pts',(-101.033770133118,-4.27828910275458,
133.234183074393));
#99179=CARTESIAN_POINT('Ctrl Pts',(-101.041544467237,-4.20911363968645,
133.352156745023));
#99180=CARTESIAN_POINT('Ctrl Pts',(-101.049318801356,-4.13503693188983,
133.467188556883));
#99181=CARTESIAN_POINT('Ctrl Pts',(-101.057083554303,-4.06105151701534,
133.582078602316));
#99182=CARTESIAN_POINT('Ctrl Pts',(-101.06484830725,-3.98217708554418,133.694033677248));
#99183=CARTESIAN_POINT('Ctrl Pts',(-101.072613060197,-3.89867580088949,
133.80261178484));
#99184=CARTESIAN_POINT('Ctrl Pts',(-101.080370101082,-3.81525745088788,
133.911082051124));
#99185=CARTESIAN_POINT('Ctrl Pts',(-101.088127141967,-3.7272216296641,134.01618171687));
#99186=CARTESIAN_POINT('Ctrl Pts',(-101.095884182852,-3.63487430803071,
134.117496870019));
#99187=CARTESIAN_POINT('Ctrl Pts',(-101.103635374092,-3.54259662623079,
134.218735620623));
#99188=CARTESIAN_POINT('Ctrl Pts',(-101.111386565332,-3.446014177913,134.316195251428));
#99189=CARTESIAN_POINT('Ctrl Pts',(-101.119137756573,-3.34547356783761,
134.409494411117));
#99190=CARTESIAN_POINT('Ctrl Pts',(-101.12688565335,-3.24497569020364,134.502753916173));
#99191=CARTESIAN_POINT('Ctrl Pts',(-101.134633550127,-3.14052328280892,
134.591856201764));
#99192=CARTESIAN_POINT('Ctrl Pts',(-101.142381446904,-3.03250005375704,
134.676456495313));
#99193=CARTESIAN_POINT('Ctrl Pts',(-101.150127722988,-2.92449942083597,
134.761039092304));
#99194=CARTESIAN_POINT('Ctrl Pts',(-101.157873999072,-2.81292975956872,
134.841121329476));
#99195=CARTESIAN_POINT('Ctrl Pts',(-101.165620275156,-2.6982078164562,134.916398754757));
#99196=CARTESIAN_POINT('Ctrl Pts',(-101.173366608422,-2.58348502649221,
134.991676735719));
#99197=CARTESIAN_POINT('Ctrl Pts',(-101.181112941687,-2.46561023512771,
135.062149619528));
#99198=CARTESIAN_POINT('Ctrl Pts',(-101.188859274952,-2.34502877928759,
135.12755655192));
#99199=CARTESIAN_POINT('Ctrl Pts',(-101.196607342955,-2.22442032006698,
135.19297813174));
#99200=CARTESIAN_POINT('Ctrl Pts',(-101.204355410958,-2.1011043338218,135.253331316272));
#99201=CARTESIAN_POINT('Ctrl Pts',(-101.212103478961,-1.97554996967867,
135.30840162313));
#99202=CARTESIAN_POINT('Ctrl Pts',(-101.219859781703,-1.8498621648627,135.363530459365));
#99203=CARTESIAN_POINT('Ctrl Pts',(-101.227616084445,-1.72193158850011,
135.413365044655));
#99204=CARTESIAN_POINT('Ctrl Pts',(-101.235372387187,-1.59224706669994,
135.45773921178));
#99205=CARTESIAN_POINT('Ctrl Pts',(-101.243132829701,-1.46249332836542,
135.502137062733));
#99206=CARTESIAN_POINT('Ctrl Pts',(-101.250893272215,-1.33098415396787,
135.541068577429));
#99207=CARTESIAN_POINT('Ctrl Pts',(-101.258653714729,-1.19822171150016,
135.574418037827));
#99208=CARTESIAN_POINT('Ctrl Pts',(-101.266426614995,-1.06524614697407,
135.60782103374));
#99209=CARTESIAN_POINT('Ctrl Pts',(-101.27419951526,-0.93101367710583,135.635623989463));
#99210=CARTESIAN_POINT('Ctrl Pts',(-101.281972415526,-0.796035687933511,
135.657762542612));
#99211=CARTESIAN_POINT('Ctrl Pts',(-101.289462751288,-0.66596448865701,
135.679096303589));
#99212=CARTESIAN_POINT('Ctrl Pts',(-101.29695308705,-0.535201337759194,
135.695170305031));
#99213=CARTESIAN_POINT('Ctrl Pts',(-101.304443422812,-0.404204714266281,
135.705972761694));
#99214=CARTESIAN_POINT('Ctrl Pts',(-101.312217756931,-0.268241313977503,
135.717184796786));
#99215=CARTESIAN_POINT('Ctrl Pts',(-101.31999209105,-0.131595696195883,
135.722753171198));
#99216=CARTESIAN_POINT('Ctrl Pts',(-101.327766425169,0.00522409498051373,
135.722607843086));
#99217=CARTESIAN_POINT('Ctrl Pts',(-101.335531178116,0.141875267992222,
135.722462694077));
#99218=CARTESIAN_POINT('Ctrl Pts',(-101.343295931063,0.278699800091174,
135.716617853696));
#99219=CARTESIAN_POINT('Ctrl Pts',(-101.351060684011,0.415184121088017,
135.705054977358));
#99220=CARTESIAN_POINT('Ctrl Pts',(-101.358817724896,0.551532883932784,
135.693503585431));
#99221=CARTESIAN_POINT('Ctrl Pts',(-101.366574765781,0.687541721067824,
135.676245492269));
#99222=CARTESIAN_POINT('Ctrl Pts',(-101.374331806666,0.822697011857725,
135.653314390204));
#99223=CARTESIAN_POINT('Ctrl Pts',(-101.382082997906,0.957750380991672,
135.630400580661));
#99224=CARTESIAN_POINT('Ctrl Pts',(-101.389834189146,1.09195110106149,135.601822342568));
#99225=CARTESIAN_POINT('Ctrl Pts',(-101.397585380386,1.22479098206313,135.567665154624));
#99226=CARTESIAN_POINT('Ctrl Pts',(-101.405333277163,1.3575744025719,135.533522484395));
#99227=CARTESIAN_POINT('Ctrl Pts',(-101.41308117394,1.48899775653647,135.493805677614));
#99228=CARTESIAN_POINT('Ctrl Pts',(-101.420829070717,1.61856357342074,135.448651200776));
#99229=CARTESIAN_POINT('Ctrl Pts',(-101.428575346801,1.74810228792925,135.403506169281));
#99230=CARTESIAN_POINT('Ctrl Pts',(-101.436321622886,1.87578386926455,135.352925858749));
#99231=CARTESIAN_POINT('Ctrl Pts',(-101.44406789897,2.00112691161267,135.297096326031));
#99232=CARTESIAN_POINT('Ctrl Pts',(-101.451814232235,2.12647087921449,135.241266381193));
#99233=CARTESIAN_POINT('Ctrl Pts',(-101.459560565501,2.24947591624303,135.180187295925));
#99234=CARTESIAN_POINT('Ctrl Pts',(-101.467306898766,2.36968184313177,135.114092746693));
#99235=CARTESIAN_POINT('Ctrl Pts',(-101.475054966769,2.48991468930455,135.047983396045));
#99236=CARTESIAN_POINT('Ctrl Pts',(-101.482803034772,2.60734683546902,134.976856534775));
#99237=CARTESIAN_POINT('Ctrl Pts',(-101.490551102775,2.72154424495612,134.90099093836));
#99238=CARTESIAN_POINT('Ctrl Pts',(-101.498307405517,2.83586302480883,134.825044711086));
#99239=CARTESIAN_POINT('Ctrl Pts',(-101.506063708259,2.9469398742037,134.744349904637));
#99240=CARTESIAN_POINT('Ctrl Pts',(-101.513820011,3.05437076950047,134.659227964819));
#99241=CARTESIAN_POINT('Ctrl Pts',(-101.521580453515,3.16185900390074,134.57406059286));
#99242=CARTESIAN_POINT('Ctrl Pts',(-101.529340896029,3.26569711086327,134.484461634554));
#99243=CARTESIAN_POINT('Ctrl Pts',(-101.537101338543,3.36551629945877,134.39079102963));
#99244=CARTESIAN_POINT('Ctrl Pts',(-101.544874238808,3.46549572667732,134.296970056335));
#99245=CARTESIAN_POINT('Ctrl Pts',(-101.552647139074,3.56144306952175,134.199064654467));
#99246=CARTESIAN_POINT('Ctrl Pts',(-101.560420039339,3.65302776144976,134.097470278142));
#99247=CARTESIAN_POINT('Ctrl Pts',(-101.567910375101,3.74128311913701,133.999569113298));
#99248=CARTESIAN_POINT('Ctrl Pts',(-101.575400710863,3.82548730891585,133.898242761453));
#99249=CARTESIAN_POINT('Ctrl Pts',(-101.582891046625,3.90538259641576,133.793870583783));
#99250=CARTESIAN_POINT('Ctrl Pts',(-101.590665380744,3.98830713802593,133.685541103273));
#99251=CARTESIAN_POINT('Ctrl Pts',(-101.598439714863,4.06685226328891,133.573587117414));
#99252=CARTESIAN_POINT('Ctrl Pts',(-101.606214048982,4.14068443377205,133.458398198765));
#99253=CARTESIAN_POINT('Ctrl Pts',(-101.613978801929,4.21442561270363,133.343351240164));
#99254=CARTESIAN_POINT('Ctrl Pts',(-101.621743554876,4.28346518468094,133.225077607244));
#99255=CARTESIAN_POINT('Ctrl Pts',(-101.629508307824,4.34751011865313,133.103999465452));
#99256=CARTESIAN_POINT('Ctrl Pts',(-101.637265348709,4.41149144229402,132.983041580179));
#99257=CARTESIAN_POINT('Ctrl Pts',(-101.645022389594,4.47048781841425,132.85928507262));
#99258=CARTESIAN_POINT('Ctrl Pts',(-101.652779430479,4.52424996882774,132.733180277893));
#99259=CARTESIAN_POINT('Ctrl Pts',(-101.660530621719,4.57797157678532,132.607170579772));
#99260=CARTESIAN_POINT('Ctrl Pts',(-101.668281812959,4.62646666293253,132.478816477464));
#99261=CARTESIAN_POINT('Ctrl Pts',(-101.676033004199,4.6695324538088,132.348591728937));
#99262=CARTESIAN_POINT('Ctrl Pts',(-101.683780900976,4.7125799405752,132.218422329402));
#99263=CARTESIAN_POINT('Ctrl Pts',(-101.691528797753,4.75020259920362,132.086384235407));
#99264=CARTESIAN_POINT('Ctrl Pts',(-101.69927669453,4.78224634784539,131.952969746478));
#99265=CARTESIAN_POINT('Ctrl Pts',(-101.707022970614,4.81428339362574,131.819583164983));
#99266=CARTESIAN_POINT('Ctrl Pts',(-101.714769246698,4.84074375937369,131.68482114114));
#99267=CARTESIAN_POINT('Ctrl Pts',(-101.722515522782,4.8615237683873,131.549189263568));
#99268=CARTESIAN_POINT('Ctrl Pts',(-101.730261856048,4.88230393079419,131.413556384792));
#99269=CARTESIAN_POINT('Ctrl Pts',(-101.738008189313,4.89740359358778,131.27705402593));
#99270=CARTESIAN_POINT('Ctrl Pts',(-101.745754522578,4.90677061710056,131.140195656921));
#99271=CARTESIAN_POINT('Ctrl Pts',(-101.753502590581,4.91613973829328,131.00330663943));
#99272=CARTESIAN_POINT('Ctrl Pts',(-101.761250658584,4.9197736389307,130.866061843124));
#99273=CARTESIAN_POINT('Ctrl Pts',(-101.768998726587,4.9176722532963,130.728977120302));
#99274=CARTESIAN_POINT('Ctrl Pts',(-101.776755029329,4.91556863428424,130.591746702205));
#99275=CARTESIAN_POINT('Ctrl Pts',(-101.784511332071,4.90771755852357,130.454677088984));
#99276=CARTESIAN_POINT('Ctrl Pts',(-101.792267634813,4.89417108283057,130.31828194648));
#99277=CARTESIAN_POINT('Ctrl Pts',(-101.800028077327,4.88061737697558,130.181814005781));
#99278=CARTESIAN_POINT('Ctrl Pts',(-101.807788519841,4.86136226897875,130.046021640005));
#99279=CARTESIAN_POINT('Ctrl Pts',(-101.815548962355,4.83650924582193,129.91140967962));
#99280=CARTESIAN_POINT('Ctrl Pts',(-101.823321862621,4.81161632638598,129.776581628166));
#99281=CARTESIAN_POINT('Ctrl Pts',(-101.831094762886,4.7811076214212,129.642938150079));
#99282=CARTESIAN_POINT('Ctrl Pts',(-101.838867663151,4.74513715838434,129.510971112962));
#99283=CARTESIAN_POINT('Ctrl Pts',(-101.846357998914,4.71047431228261,129.383801410048));
#99284=CARTESIAN_POINT('Ctrl Pts',(-101.853848334676,4.67074000413977,129.258188672191));
#99285=CARTESIAN_POINT('Ctrl Pts',(-101.861338670438,4.62611408953649,129.1345547926));
#99286=CARTESIAN_POINT('Ctrl Pts',(-101.869113004557,4.57979616981786,129.006233296887));
#99287=CARTESIAN_POINT('Ctrl Pts',(-101.876887338676,4.52806166958869,128.879637194505));
#99288=CARTESIAN_POINT('Ctrl Pts',(-101.884661672795,4.47105806160708,128.755257674267));
#99289=CARTESIAN_POINT('Ctrl Pts',(-101.892426425742,4.41412470547775,128.631031440671));
#99290=CARTESIAN_POINT('Ctrl Pts',(-101.900191178689,4.35193532345734,128.509016705876));
#99291=CARTESIAN_POINT('Ctrl Pts',(-101.907955931636,4.28468670485385,128.389688195943));
#99292=CARTESIAN_POINT('Ctrl Pts',(-101.915712972521,4.2175048785264,128.270478204767));
#99293=CARTESIAN_POINT('Ctrl Pts',(-101.923470013406,4.14527400611062,128.153949467417));
#99294=CARTESIAN_POINT('Ctrl Pts',(-101.931227054291,4.06823822634483,128.04055512582));
#99295=CARTESIAN_POINT('Ctrl Pts',(-101.938978245531,3.99126053985992,127.927246295778));
#99296=CARTESIAN_POINT('Ctrl Pts',(-101.946729436771,3.90948537703234,127.817067478829));
#99297=CARTESIAN_POINT('Ctrl Pts',(-101.954480628012,3.82320171984922,127.710445351784));
#99298=CARTESIAN_POINT('Ctrl Pts',(-101.962228524789,3.73695473552198,127.603868541986));
#99299=CARTESIAN_POINT('Ctrl Pts',(-101.969976421566,3.6462033135042,127.500845718739));
#99300=CARTESIAN_POINT('Ctrl Pts',(-101.977724318343,3.55127835432622,127.401772615384));
#99301=CARTESIAN_POINT('Ctrl Pts',(-101.985470594427,3.45637325140336,127.302720235986));
#99302=CARTESIAN_POINT('Ctrl Pts',(-101.993216870511,3.3572966181027,127.207616215254));
#99303=CARTESIAN_POINT('Ctrl Pts',(-102.000963146595,3.25441778065853,127.11682106233));
#99304=CARTESIAN_POINT('Ctrl Pts',(-102.00870947986,3.15153818378629,127.026025239176));
#99305=CARTESIAN_POINT('Ctrl Pts',(-102.016455813126,3.04485661989751,126.939538606003));
#99306=CARTESIAN_POINT('Ctrl Pts',(-102.024202146391,2.93477690303093,126.857682572433));
#99307=CARTESIAN_POINT('Ctrl Pts',(-102.031950214394,2.82467253457515,126.775808207772));
#99308=CARTESIAN_POINT('Ctrl Pts',(-102.039698282397,2.71116881252626,126.698566739455));
#99309=CARTESIAN_POINT('Ctrl Pts',(-102.0474463504,2.59469970251056,126.626237053537));
#99310=CARTESIAN_POINT('Ctrl Pts',(-102.055202653141,2.47810680773858,126.553830494769));
#99311=CARTESIAN_POINT('Ctrl Pts',(-102.062958955883,2.3585425619003,126.486346353103));
#99312=CARTESIAN_POINT('Ctrl Pts',(-102.070715258625,2.23646726459749,126.4240184806));
#99313=CARTESIAN_POINT('Ctrl Pts',(-102.078475701139,2.11432681203256,126.361657341834));
#99314=CARTESIAN_POINT('Ctrl Pts',(-102.086236143653,1.98967299266106,126.30445811891));
#99315=CARTESIAN_POINT('Ctrl Pts',(-102.093996586168,1.86298647189528,126.252606618498));
#99316=CARTESIAN_POINT('Ctrl Pts',(-102.101769486433,1.73609658267967,126.200671881454));
#99317=CARTESIAN_POINT('Ctrl Pts',(-102.109542386698,1.60716783933513,126.154102154663));
#99318=CARTESIAN_POINT('Ctrl Pts',(-102.117315286964,1.47669731960939,126.113033716916));
#99319=CARTESIAN_POINT('Ctrl Pts',(-102.124805622726,1.35096973190967,126.073458220327));
#99320=CARTESIAN_POINT('Ctrl Pts',(-102.132295958488,1.22381081389744,126.038991066028));
#99321=CARTESIAN_POINT('Ctrl Pts',(-102.13978629425,1.09567273261236,126.009708980011));
#99322=CARTESIAN_POINT('Ctrl Pts',(-102.147560628369,0.962676257029962,
125.979316654803));
#99323=CARTESIAN_POINT('Ctrl Pts',(-102.155334962488,0.828203609648187,
125.954414069423));
#99324=CARTESIAN_POINT('Ctrl Pts',(-102.163109296607,0.692747754155644,
125.935142650416));
#99325=CARTESIAN_POINT('Ctrl Pts',(-102.170874049555,0.557458835899325,
125.915894981711));
#99326=CARTESIAN_POINT('Ctrl Pts',(-102.178638802502,0.421189503837876,
125.902264725568));
#99327=CARTESIAN_POINT('Ctrl Pts',(-102.186403555449,0.284445527877808,
125.894342918599));
#99328=CARTESIAN_POINT('Ctrl Pts',(-102.194160596334,0.147837367962416,
125.88642897968));
#99329=CARTESIAN_POINT('Ctrl Pts',(-102.201917637219,0.0107558900865783,
125.884212229418));
#99330=CARTESIAN_POINT('Ctrl Pts',(-102.209674678104,-0.12628570166064,
125.887732201257));
#99331=CARTESIAN_POINT('Ctrl Pts',(-102.217425869344,-0.263223949277679,
125.891249518658));
#99332=CARTESIAN_POINT('Ctrl Pts',(-102.225177060584,-0.400121981380527,
125.90049493731));
#99333=CARTESIAN_POINT('Ctrl Pts',(-102.232928251824,-0.536464620862973,
125.91545595772));
#99334=CARTESIAN_POINT('Ctrl Pts',(-102.240676148601,-0.672749311086765,
125.930410619297));
#99335=CARTESIAN_POINT('Ctrl Pts',(-102.248424045378,-0.808478690370066,
125.951076008417));
#99336=CARTESIAN_POINT('Ctrl Pts',(-102.256171942155,-0.943140957225522,
125.97738763263));
#99337=CARTESIAN_POINT('Ctrl Pts',(-102.26391821824,-1.07777505563737,126.003693753018));
#99338=CARTESIAN_POINT('Ctrl Pts',(-102.271664494324,-1.21134210214581,
126.035643684359));
#99339=CARTESIAN_POINT('Ctrl Pts',(-102.279410770408,-1.34333916034705,
126.07312156603));
#99340=CARTESIAN_POINT('Ctrl Pts',(-102.287157103673,-1.47533719292078,
126.110599724355));
#99341=CARTESIAN_POINT('Ctrl Pts',(-102.294903436938,-1.6057648379625,126.15360580765));
#99342=CARTESIAN_POINT('Ctrl Pts',(-102.302649770204,-1.7341334131014,126.20197380548));
#99343=CARTESIAN_POINT('Ctrl Pts',(-102.310397838207,-1.86253073549282,
126.250352634988));
#99344=CARTESIAN_POINT('Ctrl Pts',(-102.31814590621,-1.98886770463073,126.304095630587));
#99345=CARTESIAN_POINT('Ctrl Pts',(-102.325893974213,-2.11267511675619,
126.362988429431));
#99346=CARTESIAN_POINT('Ctrl Pts',(-102.333650276955,-2.2366141128724,126.421943820242));
#99347=CARTESIAN_POINT('Ctrl Pts',(-102.341406579696,-2.35801782790125,
126.486059779539));
#99348=CARTESIAN_POINT('Ctrl Pts',(-102.349162882438,-2.4764407123026,126.555075446981));
#99349=CARTESIAN_POINT('Ctrl Pts',(-102.356923324952,-2.59492680256331,
126.624127950163));
#99350=CARTESIAN_POINT('Ctrl Pts',(-102.364683767467,-2.71042856298488,
126.698085161621));
#99351=CARTESIAN_POINT('Ctrl Pts',(-102.372444209981,-2.82252985775665,
126.776643116974));
#99352=CARTESIAN_POINT('Ctrl Pts',(-102.380217110246,-2.93481110747836,
126.855327180531));
#99353=CARTESIAN_POINT('Ctrl Pts',(-102.387990010512,-3.04368067258819,
126.938626508899));
#99354=CARTESIAN_POINT('Ctrl Pts',(-102.395762910777,-3.14875521521399,
127.026196558507));
#99355=CARTESIAN_POINT('Ctrl Pts',(-102.403253246539,-3.2500100335474,127.110583216236));
#99356=CARTESIAN_POINT('Ctrl Pts',(-102.410743582301,-3.34774072783208,
127.198935276479));
#99357=CARTESIAN_POINT('Ctrl Pts',(-102.418233918063,-3.44163833898923,
127.290913790574));
#99358=CARTESIAN_POINT('Ctrl Pts',(-102.425895793646,-3.53768634499599,
127.384998749344));
#99359=CARTESIAN_POINT('Ctrl Pts',(-102.43355766923,-3.63004660103402,127.48319505752));
#99360=CARTESIAN_POINT('Ctrl Pts',(-102.441219544813,-3.71833879881601,
127.585177547326));
#99361=CARTESIAN_POINT('Ctrl Pts',(-102.448872484318,-3.80652802103169,
127.68704109452));
#99362=CARTESIAN_POINT('Ctrl Pts',(-102.456525423823,-3.89065835611075,
127.792681743424));
#99363=CARTESIAN_POINT('Ctrl Pts',(-102.464178363328,-3.97038438058634,
127.901735782542));
#99364=CARTESIAN_POINT('Ctrl Pts',(-102.471824148583,-4.05003587423122,
128.010687873919));
#99365=CARTESIAN_POINT('Ctrl Pts',(-102.479469933838,-4.12529100819736,
128.123046687155));
#99366=CARTESIAN_POINT('Ctrl Pts',(-102.487115719093,-4.19584328337776,
128.238413968893));
#99367=CARTESIAN_POINT('Ctrl Pts',(-102.49475589586,-4.266343805663,128.35369662415));
#99368=CARTESIAN_POINT('Ctrl Pts',(-102.502396072628,-4.33214812334253,
128.47198301457));
#99369=CARTESIAN_POINT('Ctrl Pts',(-102.510036249396,-4.39299225161995,
128.592844816197));
#99370=CARTESIAN_POINT('Ctrl Pts',(-102.517673120172,-4.4538100519486,128.713654319542));
#99371=CARTESIAN_POINT('Ctrl Pts',(-102.525309990948,-4.50967175179214,
128.837036657736));
#99372=CARTESIAN_POINT('Ctrl Pts',(-102.532946861724,-4.56035887464973,
128.962538151392));
#99373=CARTESIAN_POINT('Ctrl Pts',(-102.540583337081,-4.61104337304876,
129.088033146879));
#99374=CARTESIAN_POINT('Ctrl Pts',(-102.548219812438,-4.65655366963076,
129.215646708699));
#99375=CARTESIAN_POINT('Ctrl Pts',(-102.555856287795,-4.69671922554291,
129.344904698768));
#99376=CARTESIAN_POINT('Ctrl Pts',(-102.560501317264,-4.72115067881412,
129.423528297335));
#99377=CARTESIAN_POINT('Ctrl Pts',(-102.565146346733,-4.74360557052034,
129.502759943539));
#99378=CARTESIAN_POINT('Ctrl Pts',(-102.569791376202,-4.76405452823412,
129.582490119309));
#99379=CARTESIAN_POINT('Origin',(213.235140564004,0.,130.804360617566));
#99380=CARTESIAN_POINT('',(-104.665400201108,-4.76405452823405,129.582490119308));
#99381=CARTESIAN_POINT('',(-104.319770171817,-4.76405452823413,129.582490119309));
#99382=CARTESIAN_POINT('',(213.235140564004,-4.76405452823405,129.582490119308));
#99383=CARTESIAN_POINT('',(-102.985140564047,-4.91824910835199,130.801399081676));
#99384=CARTESIAN_POINT('Ctrl Pts',(-102.985140564047,-4.91824910835199,
130.801399081677));
#99385=CARTESIAN_POINT('Ctrl Pts',(-102.992809150511,-4.91833027429495,
130.936192088233));
#99386=CARTESIAN_POINT('Ctrl Pts',(-103.000477736976,-4.91286591839689,
131.071207562454));
#99387=CARTESIAN_POINT('Ctrl Pts',(-103.008146323441,-4.90182760008308,
131.205944035505));
#99388=CARTESIAN_POINT('Ctrl Pts',(-103.015806418068,-4.89080150509054,
131.340531307641));
#99389=CARTESIAN_POINT('Ctrl Pts',(-103.023466512696,-4.87421375603655,
131.474839795842));
#99390=CARTESIAN_POINT('Ctrl Pts',(-103.031126607324,-4.85208791853538,
131.608366770094));
#99391=CARTESIAN_POINT('Ctrl Pts',(-103.038780165911,-4.82998096009431,
131.741779811313));
#99392=CARTESIAN_POINT('Ctrl Pts',(-103.046433724498,-4.80234537868109,
131.87441227058));
#99393=CARTESIAN_POINT('Ctrl Pts',(-103.054087283084,-4.76925661605141,
132.005765791831));
#99394=CARTESIAN_POINT('Ctrl Pts',(-103.061736716309,-4.73618568867177,
132.137048511918));
#99395=CARTESIAN_POINT('Ctrl Pts',(-103.069386149533,-4.69766752323498,
132.267053276107));
#99396=CARTESIAN_POINT('Ctrl Pts',(-103.077035582757,-4.65382871039418,
132.395291601868));
#99397=CARTESIAN_POINT('Ctrl Pts',(-103.084682936707,-4.61000181385035,
132.523495069797));
#99398=CARTESIAN_POINT('Ctrl Pts',(-103.092330290657,-4.56085727503352,
132.649932673786));
#99399=CARTESIAN_POINT('Ctrl Pts',(-103.099977644607,-4.50657149761993,
132.774131263946));
#99400=CARTESIAN_POINT('Ctrl Pts',(-103.107624677276,-4.45228800086938,
132.898324636254));
#99401=CARTESIAN_POINT('Ctrl Pts',(-103.115271709944,-4.39286385612323,
133.020278813433));
#99402=CARTESIAN_POINT('Ctrl Pts',(-103.122918742612,-4.3285233274563,133.139541309968));
#99403=CARTESIAN_POINT('Ctrl Pts',(-103.130567211507,-4.26417071467739,
133.25882620578));
#99404=CARTESIAN_POINT('Ctrl Pts',(-103.138215680402,-4.19490007299654,
133.375418062055));
#99405=CARTESIAN_POINT('Ctrl Pts',(-103.145864149297,-4.12098098982155,
133.488890137618));
#99406=CARTESIAN_POINT('Ctrl Pts',(-103.153520399481,-4.04698670391944,
133.602477655758));
#99407=CARTESIAN_POINT('Ctrl Pts',(-103.161176649664,-3.96833475199176,
133.712938717368));
#99408=CARTESIAN_POINT('Ctrl Pts',(-103.168832899848,-3.88533752884895,
133.819876385958));
#99409=CARTESIAN_POINT('Ctrl Pts',(-103.176493173238,-3.80229669232332,
133.926870248156));
#99410=CARTESIAN_POINT('Ctrl Pts',(-103.184153446628,-3.71490629724936,
134.03033672405));
#99411=CARTESIAN_POINT('Ctrl Pts',(-103.191813720019,-3.62351733110619,
134.129913987108));
#99412=CARTESIAN_POINT('Ctrl Pts',(-103.199485883508,-3.53198651312275,
134.229645811691));
#99413=CARTESIAN_POINT('Ctrl Pts',(-103.207158046997,-3.43644501090141,
134.325476081341));
#99414=CARTESIAN_POINT('Ctrl Pts',(-103.214830210487,-3.33727923066267,
134.417081254301));
#99415=CARTESIAN_POINT('Ctrl Pts',(-103.221216071439,-3.25473942495501,
134.493328051933));
#99416=CARTESIAN_POINT('Ctrl Pts',(-103.22760193239,-3.16968944572114,134.566648390191));
#99417=CARTESIAN_POINT('Ctrl Pts',(-103.233987793342,-3.08236747520497,
134.636878564073));
#99418=CARTESIAN_POINT('Ctrl Pts',(-103.241762127461,-2.97605915125946,
134.722378834299));
#99419=CARTESIAN_POINT('Ctrl Pts',(-103.24953646158,-2.86602227181567,134.803587927477));
#99420=CARTESIAN_POINT('Ctrl Pts',(-103.257310795699,-2.75263829324372,
134.880163052556));
#99421=CARTESIAN_POINT('Ctrl Pts',(-103.265075548646,-2.63939405029195,
134.956643805637));
#99422=CARTESIAN_POINT('Ctrl Pts',(-103.272840301594,-2.52281123661999,
135.028501736997));
#99423=CARTESIAN_POINT('Ctrl Pts',(-103.280605054541,-2.40330486416648,
135.095433769165));
#99424=CARTESIAN_POINT('Ctrl Pts',(-103.288362095426,-2.28391718712685,
135.162299323495));
#99425=CARTESIAN_POINT('Ctrl Pts',(-103.296119136311,-2.16161206874099,
135.224248525064));
#99426=CARTESIAN_POINT('Ctrl Pts',(-103.303876177196,-2.03683373244994,
135.281021360671));
#99427=CARTESIAN_POINT('Ctrl Pts',(-103.311627368436,-1.91214949247241,
135.337751383441));
#99428=CARTESIAN_POINT('Ctrl Pts',(-103.319378559676,-1.78499610132625,
135.389312648746));
#99429=CARTESIAN_POINT('Ctrl Pts',(-103.327129750916,-1.65584231454443,
135.435491072635));
#99430=CARTESIAN_POINT('Ctrl Pts',(-103.334877647693,-1.52674342156781,
135.481649869461));
#99431=CARTESIAN_POINT('Ctrl Pts',(-103.34262554447,-1.39564619135186,135.52243024388));
#99432=CARTESIAN_POINT('Ctrl Pts',(-103.350373441247,-1.26303908411213,
135.557666344584));
#99433=CARTESIAN_POINT('Ctrl Pts',(-103.358119717331,-1.13045971542056,
135.592895074656));
#99434=CARTESIAN_POINT('Ctrl Pts',(-103.365865993416,-0.996371475529762,
135.622581737465));
#99435=CARTESIAN_POINT('Ctrl Pts',(-103.3736122695,-0.861277319506663,135.646610553433));
#99436=CARTESIAN_POINT('Ctrl Pts',(-103.381358602765,-0.726182166249009,
135.670639546776));
#99437=CARTESIAN_POINT('Ctrl Pts',(-103.38910493603,-0.59008146696587,135.689010541475));
#99438=CARTESIAN_POINT('Ctrl Pts',(-103.396851269296,-0.453487292522191,
135.701659091012));
#99439=CARTESIAN_POINT('Ctrl Pts',(-103.404599337299,-0.316862528760408,
135.714310473105));
#99440=CARTESIAN_POINT('Ctrl Pts',(-103.412347405302,-0.179744459160507,
135.721236823955));
#99441=CARTESIAN_POINT('Ctrl Pts',(-103.420095473305,-0.0426487858903845,
135.722425698831));
#99442=CARTESIAN_POINT('Ctrl Pts',(-103.427851776046,0.0945925942929355,
135.723615837258));
#99443=CARTESIAN_POINT('Ctrl Pts',(-103.435608078788,0.231811139023357,
135.719056315188));
#99444=CARTESIAN_POINT('Ctrl Pts',(-103.44336438153,0.368492081161458,135.708786847883));
#99445=CARTESIAN_POINT('Ctrl Pts',(-103.451124824044,0.505245974033762,
135.698511899454));
#99446=CARTESIAN_POINT('Ctrl Pts',(-103.458885266558,0.641461304463368,
135.68252097881));
#99447=CARTESIAN_POINT('Ctrl Pts',(-103.466645709073,0.776630903958121,
135.660905428593));
#99448=CARTESIAN_POINT('Ctrl Pts',(-103.474418609338,0.912017489693777,
135.639255179176));
#99449=CARTESIAN_POINT('Ctrl Pts',(-103.482191509604,1.04635460655848,135.611962334943));
#99450=CARTESIAN_POINT('Ctrl Pts',(-103.489964409869,1.17914683236046,135.579169075529));
#99451=CARTESIAN_POINT('Ctrl Pts',(-103.497454745631,1.30711172627074,135.547567933695));
#99452=CARTESIAN_POINT('Ctrl Pts',(-103.504945081393,1.43364180459688,135.510859427408));
#99453=CARTESIAN_POINT('Ctrl Pts',(-103.512435417155,1.55831097958705,135.469213236181));
#99454=CARTESIAN_POINT('Ctrl Pts',(-103.520209751274,1.68770702423953,135.425988016955));
#99455=CARTESIAN_POINT('Ctrl Pts',(-103.527984085393,1.81550815543012,135.377306372377));
#99456=CARTESIAN_POINT('Ctrl Pts',(-103.535758419512,1.94121978685523,135.32330394556));
#99457=CARTESIAN_POINT('Ctrl Pts',(-103.543523172459,2.06677648993011,135.269368071908));
#99458=CARTESIAN_POINT('Ctrl Pts',(-103.551287925407,2.19024846118948,135.210124616096));
#99459=CARTESIAN_POINT('Ctrl Pts',(-103.559052678354,2.31115638888255,135.145758918647));
#99460=CARTESIAN_POINT('Ctrl Pts',(-103.566809719239,2.43194422911701,135.081457150116));
#99461=CARTESIAN_POINT('Ctrl Pts',(-103.574566760124,2.55017275084561,135.012043446798));
#99462=CARTESIAN_POINT('Ctrl Pts',(-103.582323801009,2.66538308397759,134.93775100297));
#99463=CARTESIAN_POINT('Ctrl Pts',(-103.590074992249,2.7805065361013,134.863514583651));
#99464=CARTESIAN_POINT('Ctrl Pts',(-103.597826183489,2.8926160027019,134.78440695786));
#99465=CARTESIAN_POINT('Ctrl Pts',(-103.605577374729,3.00127799507205,134.700706785298));
#99466=CARTESIAN_POINT('Ctrl Pts',(-103.613325271506,3.10989380319664,134.617042187542));
#99467=CARTESIAN_POINT('Ctrl Pts',(-103.621073168283,3.21506474231533,134.528789163384));
#99468=CARTESIAN_POINT('Ctrl Pts',(-103.62882106506,3.31638725234764,134.436269021555));
#99469=CARTESIAN_POINT('Ctrl Pts',(-103.636567341144,3.41768856789512,134.343768232945));
#99470=CARTESIAN_POINT('Ctrl Pts',(-103.644313617229,3.5151427670346,134.247002365534));
#99471=CARTESIAN_POINT('Ctrl Pts',(-103.652059893313,3.60838058162866,134.146331987974));
#99472=CARTESIAN_POINT('Ctrl Pts',(-103.659806226578,3.70161908448321,134.045660867287));
#99473=CARTESIAN_POINT('Ctrl Pts',(-103.667552559843,3.79064087502338,133.941085465779));
#99474=CARTESIAN_POINT('Ctrl Pts',(-103.675298893109,3.87511494576002,133.833001768255));
#99475=CARTESIAN_POINT('Ctrl Pts',(-103.683046961112,3.95960793387923,133.724893866136));
#99476=CARTESIAN_POINT('Ctrl Pts',(-103.690795029115,4.03955093492755,133.613276412616));
#99477=CARTESIAN_POINT('Ctrl Pts',(-103.698543097118,4.11465472918241,133.498576555852));
#99478=CARTESIAN_POINT('Ctrl Pts',(-103.706299399859,4.18983834464345,133.383754794717));
#99479=CARTESIAN_POINT('Ctrl Pts',(-103.714055702601,4.26017226476969,133.265844413753));
#99480=CARTESIAN_POINT('Ctrl Pts',(-103.721812005343,4.3254116589225,133.145299968202));
#99481=CARTESIAN_POINT('Ctrl Pts',(-103.729572447857,4.39068587330446,133.024691184451));
#99482=CARTESIAN_POINT('Ctrl Pts',(-103.737332890372,4.4508599722224,132.901445885934));
#99483=CARTESIAN_POINT('Ctrl Pts',(-103.745093332886,4.50573666786875,132.776040140796));
#99484=CARTESIAN_POINT('Ctrl Pts',(-103.752866233151,4.56070145645852,132.650433083222));
#99485=CARTESIAN_POINT('Ctrl Pts',(-103.760639133417,4.61035170666361,132.522659013206));
#99486=CARTESIAN_POINT('Ctrl Pts',(-103.768412033682,4.65453925044116,132.393211595035));
#99487=CARTESIAN_POINT('Ctrl Pts',(-103.775902369444,4.69712046570032,132.268469916573));
#99488=CARTESIAN_POINT('Ctrl Pts',(-103.783392705206,4.73462915772616,132.142174733856));
#99489=CARTESIAN_POINT('Ctrl Pts',(-103.790883040968,4.76697777186086,132.0147762425));
#99490=CARTESIAN_POINT('Ctrl Pts',(-103.798657375087,4.80055289353287,131.882547398621));
#99491=CARTESIAN_POINT('Ctrl Pts',(-103.806431709206,4.82867528033846,131.748711069425));
#99492=CARTESIAN_POINT('Ctrl Pts',(-103.814206043325,4.85119171669166,131.613756682791));
#99493=CARTESIAN_POINT('Ctrl Pts',(-103.821970796272,4.87368040354941,131.478968615378));
#99494=CARTESIAN_POINT('Ctrl Pts',(-103.829735549219,4.89057682274961,131.343065614082));
#99495=CARTESIAN_POINT('Ctrl Pts',(-103.837500302166,4.90177782681263,131.206551118533));
#99496=CARTESIAN_POINT('Ctrl Pts',(-103.845257343052,4.91296770588052,131.070172211105));
#99497=CARTESIAN_POINT('Ctrl Pts',(-103.853014383937,4.91847339526769,130.933183405202));
#99498=CARTESIAN_POINT('Ctrl Pts',(-103.860771424822,4.91824305743001,130.796096808429));
#99499=CARTESIAN_POINT('Ctrl Pts',(-103.868522616062,4.91801289329189,130.659113589724));
#99500=CARTESIAN_POINT('Ctrl Pts',(-103.876273807302,4.91205531239327,130.522033116316));
#99501=CARTESIAN_POINT('Ctrl Pts',(-103.884024998542,4.90037044779738,130.385370716907));
#99502=CARTESIAN_POINT('Ctrl Pts',(-103.891772895319,4.88869054958068,130.248766402664));
#99503=CARTESIAN_POINT('Ctrl Pts',(-103.899520792096,4.87128824243807,130.11258019773));
#99504=CARTESIAN_POINT('Ctrl Pts',(-103.907268688873,4.84821571842312,129.977325303849));
#99505=CARTESIAN_POINT('Ctrl Pts',(-103.915014964957,4.82514802068279,129.842098702376));
#99506=CARTESIAN_POINT('Ctrl Pts',(-103.922761241041,4.79641253096411,129.70780340962));
#99507=CARTESIAN_POINT('Ctrl Pts',(-103.930507517126,4.7621130074377,129.574944997488));
#99508=CARTESIAN_POINT('Ctrl Pts',(-103.938253850391,4.72781323071985,129.442085604624));
#99509=CARTESIAN_POINT('Ctrl Pts',(-103.946000183656,4.68794943596679,129.310663492103));
#99510=CARTESIAN_POINT('Ctrl Pts',(-103.953746516922,4.6426758587771,129.181171185359));
#99511=CARTESIAN_POINT('Ctrl Pts',(-103.961494584925,4.59739214288389,129.051649879711));
#99512=CARTESIAN_POINT('Ctrl Pts',(-103.969242652928,4.54669636284973,128.924059608791));
#99513=CARTESIAN_POINT('Ctrl Pts',(-103.976990720931,4.49079156019326,128.798874585354));
#99514=CARTESIAN_POINT('Ctrl Pts',(-103.984747023672,4.43482734124717,128.673556513785));
#99515=CARTESIAN_POINT('Ctrl Pts',(-103.992503326414,4.37364320017627,128.55064915379));
#99516=CARTESIAN_POINT('Ctrl Pts',(-104.000259629156,4.30748923023899,128.430604186532));
#99517=CARTESIAN_POINT('Ctrl Pts',(-104.00802007167,4.24129995193592,128.31049514766));
#99518=CARTESIAN_POINT('Ctrl Pts',(-104.015780514185,4.17013576210445,128.193251879739));
#99519=CARTESIAN_POINT('Ctrl Pts',(-104.023540956699,4.09429055147871,128.07929769305));
#99520=CARTESIAN_POINT('Ctrl Pts',(-104.031313856964,4.01832358738785,127.965160576984));
#99521=CARTESIAN_POINT('Ctrl Pts',(-104.03908675723,3.93766081654446,127.85432340942));
#99522=CARTESIAN_POINT('Ctrl Pts',(-104.046859657495,3.85263748424759,127.747177685933));
#99523=CARTESIAN_POINT('Ctrl Pts',(-104.054349993257,3.77070496424125,127.643926979379));
#99524=CARTESIAN_POINT('Ctrl Pts',(-104.061840329019,3.68472361439727,127.544104223287));
#99525=CARTESIAN_POINT('Ctrl Pts',(-104.069330664781,3.59502487160512,127.448026421596));
#99526=CARTESIAN_POINT('Ctrl Pts',(-104.0771049989,3.50192517371625,127.348305800851));
#99527=CARTESIAN_POINT('Ctrl Pts',(-104.084879333019,3.40452571651778,127.252303835299));
#99528=CARTESIAN_POINT('Ctrl Pts',(-104.092653667138,3.30315545277988,127.160413977277));
#99529=CARTESIAN_POINT('Ctrl Pts',(-104.100418420085,3.20191011883204,127.068637365293));
#99530=CARTESIAN_POINT('Ctrl Pts',(-104.108183173032,3.09670400216443,126.980963037472));
#99531=CARTESIAN_POINT('Ctrl Pts',(-104.115947925979,2.98790490706331,126.897749896129));
#99532=CARTESIAN_POINT('Ctrl Pts',(-104.123704966864,2.87921387275754,126.814619403251));
#99533=CARTESIAN_POINT('Ctrl Pts',(-104.131462007749,2.76693727022471,126.735941515112));
#99534=CARTESIAN_POINT('Ctrl Pts',(-104.139219048634,2.65147793063793,126.662036650776));
#99535=CARTESIAN_POINT('Ctrl Pts',(-104.146970239874,2.53610565983744,126.588187518674));
#99536=CARTESIAN_POINT('Ctrl Pts',(-104.154721431115,2.41755575724214,126.519104455958));
#99537=CARTESIAN_POINT('Ctrl Pts',(-104.162472622355,2.29626185540724,126.45506589843));
#99538=CARTESIAN_POINT('Ctrl Pts',(-104.170220519132,2.17501950671576,126.391054558997));
#99539=CARTESIAN_POINT('Ctrl Pts',(-104.177968415909,2.05103582342604,126.332083642556));
#99540=CARTESIAN_POINT('Ctrl Pts',(-104.185716312686,1.92477078777817,126.27838663653));
#99541=CARTESIAN_POINT('Ctrl Pts',(-104.19346258877,1.79853216405381,126.22470086276));
#99542=CARTESIAN_POINT('Ctrl Pts',(-104.201208864854,1.67001349672181,126.176286958012));
#99543=CARTESIAN_POINT('Ctrl Pts',(-104.208955140938,1.5396962215709,126.133330901563));
#99544=CARTESIAN_POINT('Ctrl Pts',(-104.216701474203,1.40937798444764,126.090374528023));
#99545=CARTESIAN_POINT('Ctrl Pts',(-104.224447807469,1.27726148432534,126.052876205568));
#99546=CARTESIAN_POINT('Ctrl Pts',(-104.232194140734,1.14384446491003,126.020972393452));
#99547=CARTESIAN_POINT('Ctrl Pts',(-104.239942208737,1.01039756767809,125.989061436698));
#99548=CARTESIAN_POINT('Ctrl Pts',(-104.24769027674,0.875649951786629,125.962747574221));
#99549=CARTESIAN_POINT('Ctrl Pts',(-104.255438344743,0.740110334758956,
125.94211630502));
#99550=CARTESIAN_POINT('Ctrl Pts',(-104.263194647485,0.604426664613549,
125.921463108661));
#99551=CARTESIAN_POINT('Ctrl Pts',(-104.270950950227,0.467949698978643,
125.906504629113));
#99552=CARTESIAN_POINT('Ctrl Pts',(-104.278707252969,0.331194631522968,
125.897274600534));
#99553=CARTESIAN_POINT('Ctrl Pts',(-104.286467695483,0.194366573769804,
125.888039645611));
#99554=CARTESIAN_POINT('Ctrl Pts',(-104.294228137997,0.0572605090805218,
125.884539243853));
#99555=CARTESIAN_POINT('Ctrl Pts',(-104.301988580511,-0.0796085644963637,
125.886754946209));
#99556=CARTESIAN_POINT('Ctrl Pts',(-104.309761480777,-0.216697352460448,
125.888974205407));
#99557=CARTESIAN_POINT('Ctrl Pts',(-104.317534381042,-0.353547998542257,
125.896927882589));
#99558=CARTESIAN_POINT('Ctrl Pts',(-104.325307281307,-0.48964991815302,
125.910545539311));
#99559=CARTESIAN_POINT('Ctrl Pts',(-104.332797617069,-0.620804190168828,
125.923668159911));
#99560=CARTESIAN_POINT('Ctrl Pts',(-104.340287952832,-0.751262921802112,
125.942050066679));
#99561=CARTESIAN_POINT('Ctrl Pts',(-104.347778288594,-0.880580258925905,
125.965583760747));
#99562=CARTESIAN_POINT('Ctrl Pts',(-104.355552622713,-1.01480070218907,
125.990009741977));
#99563=CARTESIAN_POINT('Ctrl Pts',(-104.363326956832,-1.14821666045444,
126.020063256455));
#99564=CARTESIAN_POINT('Ctrl Pts',(-104.371101290951,-1.28031930412125,
126.055680217498));
#99565=CARTESIAN_POINT('Ctrl Pts',(-104.378866043898,-1.41225914308646,
126.091253283819));
#99566=CARTESIAN_POINT('Ctrl Pts',(-104.386630796845,-1.54288851400916,
126.132376053612));
#99567=CARTESIAN_POINT('Ctrl Pts',(-104.394395549792,-1.67170665500806,
126.178933078181));
#99568=CARTESIAN_POINT('Ctrl Pts',(-104.402152590677,-1.8003968520133,126.225443861657));
#99569=CARTESIAN_POINT('Ctrl Pts',(-104.409909631562,-1.92727903375607,
126.277378026853));
#99570=CARTESIAN_POINT('Ctrl Pts',(-104.417666672447,-2.05186588251464,
126.334569854826));
#99571=CARTESIAN_POINT('Ctrl Pts',(-104.425417863688,-2.17635877936091,
126.391718553997));
#99572=CARTESIAN_POINT('Ctrl Pts',(-104.433169054928,-2.29855943465286,
126.454116861713));
#99573=CARTESIAN_POINT('Ctrl Pts',(-104.440920246168,-2.41799920347746,
126.521550451976));
#99574=CARTESIAN_POINT('Ctrl Pts',(-104.448668142945,-2.53738820721431,
126.588955381164));
#99575=CARTESIAN_POINT('Ctrl Pts',(-104.456416039722,-2.65401831864758,
126.661391144535));
#99576=CARTESIAN_POINT('Ctrl Pts',(-104.464163936499,-2.7674444665579,126.738596951658));
#99577=CARTESIAN_POINT('Ctrl Pts',(-104.471910212583,-2.88084688816326,
126.81578660899));
#99578=CARTESIAN_POINT('Ctrl Pts',(-104.479656488667,-2.99104635631646,
126.897744105563));
#99579=CARTESIAN_POINT('Ctrl Pts',(-104.487402764751,-3.09762617358104,
126.984164922154));
#99580=CARTESIAN_POINT('Ctrl Pts',(-104.495149098017,-3.20420677759376,
127.070586376684));
#99581=CARTESIAN_POINT('Ctrl Pts',(-104.502895431282,-3.3071673737233,127.161470970737));
#99582=CARTESIAN_POINT('Ctrl Pts',(-104.510641764547,-3.4061241123059,127.256473697994));
#99583=CARTESIAN_POINT('Ctrl Pts',(-104.51838983255,-3.50510301156412,127.351497700454));
#99584=CARTESIAN_POINT('Ctrl Pts',(-104.526137900553,-3.60007598709598,
127.450641400534));
#99585=CARTESIAN_POINT('Ctrl Pts',(-104.533885968556,-3.69069613192513,
127.553523014072));
#99586=CARTESIAN_POINT('Ctrl Pts',(-104.541642271298,-3.78141258892249,
127.656513971412));
#99587=CARTESIAN_POINT('Ctrl Pts',(-104.54939857404,-3.86776671497381,127.763250484252));
#99588=CARTESIAN_POINT('Ctrl Pts',(-104.557154876782,-3.94945165381305,
127.873317339705));
#99589=CARTESIAN_POINT('Ctrl Pts',(-104.564915319296,-4.03118019036386,
127.983442941153));
#99590=CARTESIAN_POINT('Ctrl Pts',(-104.57267576181,-4.10823435446561,128.09690210377));
#99591=CARTESIAN_POINT('Ctrl Pts',(-104.580436204324,-4.18035129880294,
128.213251572949));
#99592=CARTESIAN_POINT('Ctrl Pts',(-104.58820910459,-4.25258401166136,128.329787816625));
#99593=CARTESIAN_POINT('Ctrl Pts',(-104.595982004855,-4.31986347475862,
128.449223297781));
#99594=CARTESIAN_POINT('Ctrl Pts',(-104.603754905121,-4.38197296650989,
128.571090373445));
#99595=CARTESIAN_POINT('Ctrl Pts',(-104.611245240883,-4.44182462179129,
128.688527273943));
#99596=CARTESIAN_POINT('Ctrl Pts',(-104.618735576645,-4.49687553410252,
128.808221769257));
#99597=CARTESIAN_POINT('Ctrl Pts',(-104.626225912407,-4.54697515024065,
128.92974064392));
#99598=CARTESIAN_POINT('Ctrl Pts',(-104.634929516994,-4.605189796778,129.070942890192));
#99599=CARTESIAN_POINT('Ctrl Pts',(-104.643633121581,-4.65687583065861,
129.214986364832));
#99600=CARTESIAN_POINT('Ctrl Pts',(-104.652336726168,-4.7017783882902,129.361286451105));
#99601=CARTESIAN_POINT('Ctrl Pts',(-104.656691217814,-4.72424354168428,
129.434481699951));
#99602=CARTESIAN_POINT('Ctrl Pts',(-104.661045709461,-4.74501143990967,
129.508241406951));
#99603=CARTESIAN_POINT('Ctrl Pts',(-104.665400201108,-4.76405452823405,
129.582490119308));
#99604=CARTESIAN_POINT('Ctrl Pts',(-102.915060258535,-4.76405452823397,
129.582490119308));
#99605=CARTESIAN_POINT('Ctrl Pts',(-102.92283380042,-4.7981027709504,129.715243700905));
#99606=CARTESIAN_POINT('Ctrl Pts',(-102.930607342304,-4.82655979954569,
129.849272768635));
#99607=CARTESIAN_POINT('Ctrl Pts',(-102.938380884189,-4.84936084534268,
129.984066490952));
#99608=CARTESIAN_POINT('Ctrl Pts',(-102.944100645969,-4.86613782451462,
130.083247532556));
#99609=CARTESIAN_POINT('Ctrl Pts',(-102.949820407749,-4.87985373792882,
130.182842392454));
#99610=CARTESIAN_POINT('Ctrl Pts',(-102.955540169529,-4.89050080230448,
130.282647128034));
#99611=CARTESIAN_POINT('Ctrl Pts',(-102.965406967689,-4.90886737756294,
130.454813945338));
#99612=CARTESIAN_POINT('Ctrl Pts',(-102.975273765849,-4.91814467604707,
130.627967458999));
#99613=CARTESIAN_POINT('Ctrl Pts',(-102.985140564009,-4.91824910835159,
130.80139908101));
#99614=CARTESIAN_POINT('',(-102.639859435943,-4.91824800921729,130.808785810233));
#99615=CARTESIAN_POINT('Ctrl Pts',(-102.569791376202,-4.76405452823412,
129.582490119309));
#99616=CARTESIAN_POINT('Ctrl Pts',(-102.577430973814,-4.79768656643153,
129.713620925803));
#99617=CARTESIAN_POINT('Ctrl Pts',(-102.585070571426,-4.82588986934994,
129.846100596011));
#99618=CARTESIAN_POINT('Ctrl Pts',(-102.592710169038,-4.84857485260586,
129.979433371575));
#99619=CARTESIAN_POINT('Ctrl Pts',(-102.600568380189,-4.871908985819,130.116581577134));
#99620=CARTESIAN_POINT('Ctrl Pts',(-102.60842659134,-4.88940415632356,130.254631994833));
#99621=CARTESIAN_POINT('Ctrl Pts',(-102.616284802491,-4.9010200776338,130.393039257641));
#99622=CARTESIAN_POINT('Ctrl Pts',(-102.624143013642,-4.91263599894403,
130.531446520449));
#99623=CARTESIAN_POINT('Ctrl Pts',(-102.632001224793,-4.91837269262525,
130.670210166371));
#99624=CARTESIAN_POINT('Ctrl Pts',(-102.639859435943,-4.91824800921729,
130.808785810233));
#99625=CARTESIAN_POINT('Ctrl Pts',(-102.639859435992,-4.91824800921652,
130.80878581109));
#99626=CARTESIAN_POINT('Ctrl Pts',(-102.650907811304,-4.91807270858805,
131.0036184127));
#99627=CARTESIAN_POINT('Ctrl Pts',(-102.661956186616,-4.90631686207873,
131.197951502016));
#99628=CARTESIAN_POINT('Ctrl Pts',(-102.673004561928,-4.88317768197775,
131.390670082554));
#99629=CARTESIAN_POINT('Ctrl Pts',(-102.680896888577,-4.86664837675505,
131.528337200658));
#99630=CARTESIAN_POINT('Ctrl Pts',(-102.688789215226,-4.84431127361759,
131.665181352765));
#99631=CARTESIAN_POINT('Ctrl Pts',(-102.696681541875,-4.81625191044857,
131.800804593713));
#99632=CARTESIAN_POINT('Ctrl Pts',(-102.704455875994,-4.78861204274581,
131.934400228606));
#99633=CARTESIAN_POINT('Ctrl Pts',(-102.712230210113,-4.7553655678073,132.067056564891));
#99634=CARTESIAN_POINT('Ctrl Pts',(-102.720004544232,-4.71658876436888,
132.198266457402));
#99635=CARTESIAN_POINT('Ctrl Pts',(-102.727769297179,-4.67785974987522,
132.329314645447));
#99636=CARTESIAN_POINT('Ctrl Pts',(-102.735534050127,-4.6336140777068,132.458919565251));
#99637=CARTESIAN_POINT('Ctrl Pts',(-102.743298803074,-4.58397918021763,
132.58658336959));
#99638=CARTESIAN_POINT('Ctrl Pts',(-102.751055843959,-4.53439358080839,
132.714120376438));
#99639=CARTESIAN_POINT('Ctrl Pts',(-102.758812884844,-4.47942954885954,
132.839719742481));
#99640=CARTESIAN_POINT('Ctrl Pts',(-102.766569925729,-4.41926444987399,
132.962898267129));
#99641=CARTESIAN_POINT('Ctrl Pts',(-102.774321116969,-4.35914472185735,
133.085983901894));
#99642=CARTESIAN_POINT('Ctrl Pts',(-102.782072308209,-4.29383190452954,
133.206651979083));
#99643=CARTESIAN_POINT('Ctrl Pts',(-102.789823499449,-4.22355150835399,
133.324439131974));
#99644=CARTESIAN_POINT('Ctrl Pts',(-102.797571396226,-4.15330098322189,
133.442176222183));
#99645=CARTESIAN_POINT('Ctrl Pts',(-102.805319293003,-4.07808727847184,
133.557034488432));
#99646=CARTESIAN_POINT('Ctrl Pts',(-102.81306718978,-3.99818178991451,133.668575245923));
#99647=CARTESIAN_POINT('Ctrl Pts',(-102.820813465864,-3.91829301586261,
133.780092671493));
#99648=CARTESIAN_POINT('Ctrl Pts',(-102.828559741948,-3.83371463764168,
133.888293650986));
#99649=CARTESIAN_POINT('Ctrl Pts',(-102.836306018033,-3.74476108636928,
133.992768914587));
#99650=CARTESIAN_POINT('Ctrl Pts',(-102.844052351298,-3.6558068784621,134.097244949401));
#99651=CARTESIAN_POINT('Ctrl Pts',(-102.851798684563,-3.56247768651339,
134.197994915762));
#99652=CARTESIAN_POINT('Ctrl Pts',(-102.859545017829,-3.46512762882175,
134.294643353746));
#99653=CARTESIAN_POINT('Ctrl Pts',(-102.867293085832,-3.36775577025954,
134.391313435478));
#99654=CARTESIAN_POINT('Ctrl Pts',(-102.875041153835,-3.26636153157214,
134.483879885707));
#99655=CARTESIAN_POINT('Ctrl Pts',(-102.882789221838,-3.16133491178896,
134.572005059124));
#99656=CARTESIAN_POINT('Ctrl Pts',(-102.89054552458,-3.05619666846459,134.660223893025));
#99657=CARTESIAN_POINT('Ctrl Pts',(-102.898301827321,-2.94741863218222,
134.743991769218));
#99658=CARTESIAN_POINT('Ctrl Pts',(-102.906058130063,-2.83542325996239,
134.82301188377));
#99659=CARTESIAN_POINT('Ctrl Pts',(-102.913818572577,-2.7233681124403,134.902074173737));
#99660=CARTESIAN_POINT('Ctrl Pts',(-102.921579015091,-2.60809253578269,
134.976383441081));
#99661=CARTESIAN_POINT('Ctrl Pts',(-102.929339457606,-2.49004596456064,
135.045687551071));
#99662=CARTESIAN_POINT('Ctrl Pts',(-102.937112357871,-2.37180989450277,
135.115102914171));
#99663=CARTESIAN_POINT('Ctrl Pts',(-102.944885258137,-2.25079428620926,
135.179496880217));
#99664=CARTESIAN_POINT('Ctrl Pts',(-102.952658158402,-2.12747184870504,
135.238664012178));
#99665=CARTESIAN_POINT('Ctrl Pts',(-102.960148494165,-2.00863249242518,
135.295680269864));
#99666=CARTESIAN_POINT('Ctrl Pts',(-102.967638829927,-1.88765139605412,
135.347842991023));
#99667=CARTESIAN_POINT('Ctrl Pts',(-102.97512916569,-1.76496526316726,135.395012061785));
#99668=CARTESIAN_POINT('Ctrl Pts',(-102.982903499809,-1.63762744827224,
135.443969562199));
#99669=CARTESIAN_POINT('Ctrl Pts',(-102.990677833928,-1.50804938373783,
135.487702351316));
#99670=CARTESIAN_POINT('Ctrl Pts',(-102.998452168047,-1.3766989756758,135.526000480249));
#99671=CARTESIAN_POINT('Ctrl Pts',(-103.006216920994,-1.24551044525223,
135.56425141016));
#99672=CARTESIAN_POINT('Ctrl Pts',(-103.013981673941,-1.11255428905039,
135.597080897992));
#99673=CARTESIAN_POINT('Ctrl Pts',(-103.021746426889,-0.978318240339559,
135.624327057607));
#99674=CARTESIAN_POINT('Ctrl Pts',(-103.029503467774,-0.84421551676507,
135.651546155952));
#99675=CARTESIAN_POINT('Ctrl Pts',(-103.037260508659,-0.708835811114473,
135.673192884491));
#99676=CARTESIAN_POINT('Ctrl Pts',(-103.045017549544,-0.57268152411455,
135.689155284124));
#99677=CARTESIAN_POINT('Ctrl Pts',(-103.052768740784,-0.436629912121395,
135.705105646388));
#99678=CARTESIAN_POINT('Ctrl Pts',(-103.060519932024,-0.299805268164579,
135.715380166616));
#99679=CARTESIAN_POINT('Ctrl Pts',(-103.068271123264,-0.162719329704358,
135.719918112117));
#99680=CARTESIAN_POINT('Ctrl Pts',(-103.076019020041,-0.0256916564250546,
135.724454128871));
#99681=CARTESIAN_POINT('Ctrl Pts',(-103.083766916818,0.111596700540384,
135.723258407377));
#99682=CARTESIAN_POINT('Ctrl Pts',(-103.091514813595,0.24862996718179,135.71632216077));
#99683=CARTESIAN_POINT('Ctrl Pts',(-103.09926108968,0.385634569417911,135.709387365077));
#99684=CARTESIAN_POINT('Ctrl Pts',(-103.107007365764,0.522383797246825,
135.696714452466));
#99685=CARTESIAN_POINT('Ctrl Pts',(-103.114753641848,0.658363362681601,
135.678346742411));
#99686=CARTESIAN_POINT('Ctrl Pts',(-103.122499975113,0.794343931886825,
135.659978896769));
#99687=CARTESIAN_POINT('Ctrl Pts',(-103.130246308379,0.92955443991439,135.635916222134));
#99688=CARTESIAN_POINT('Ctrl Pts',(-103.137992641644,1.06348759210629,135.606253703));
#99689=CARTESIAN_POINT('Ctrl Pts',(-103.145740709647,1.1974507376988,135.57658454115));
#99690=CARTESIAN_POINT('Ctrl Pts',(-103.15348877765,1.33013557659674,135.541313123917));
#99691=CARTESIAN_POINT('Ctrl Pts',(-103.161236845653,1.4610472342378,135.500585062993));
#99692=CARTESIAN_POINT('Ctrl Pts',(-103.168993148395,1.59209802634665,135.459813715801));
#99693=CARTESIAN_POINT('Ctrl Pts',(-103.176749451137,1.72137149867967,135.413574256348));
#99694=CARTESIAN_POINT('Ctrl Pts',(-103.184505753879,1.84838959334207,135.362061679914));
#99695=CARTESIAN_POINT('Ctrl Pts',(-103.192266196393,1.97547548138603,135.310521609666));
#99696=CARTESIAN_POINT('Ctrl Pts',(-103.200026638907,2.10030323749682,135.253702976353));
#99697=CARTESIAN_POINT('Ctrl Pts',(-103.207787081421,2.22241780321864,135.191847617027));
#99698=CARTESIAN_POINT('Ctrl Pts',(-103.215559981687,2.34472839808219,135.129892961986));
#99699=CARTESIAN_POINT('Ctrl Pts',(-103.223332881952,2.46431675770193,135.062885614945));
#99700=CARTESIAN_POINT('Ctrl Pts',(-103.231105782218,2.58075453130965,134.991112235661));
#99701=CARTESIAN_POINT('Ctrl Pts',(-103.238596117979,2.6929594985498,134.921947999505));
#99702=CARTESIAN_POINT('Ctrl Pts',(-103.246086453741,2.80223871088605,134.848358401708));
#99703=CARTESIAN_POINT('Ctrl Pts',(-103.253576789502,2.90823823760139,134.770635118386));
#99704=CARTESIAN_POINT('Ctrl Pts',(-103.261351123621,3.01825676859669,134.689964933148));
#99705=CARTESIAN_POINT('Ctrl Pts',(-103.26912545774,3.12509051165878,134.604585878365));
#99706=CARTESIAN_POINT('Ctrl Pts',(-103.276899791859,3.22830991615819,134.514778134199));
#99707=CARTESIAN_POINT('Ctrl Pts',(-103.284664544806,3.33140211196653,134.42508107005));
#99708=CARTESIAN_POINT('Ctrl Pts',(-103.292429297753,3.43088853991979,134.330966430403));
#99709=CARTESIAN_POINT('Ctrl Pts',(-103.3001940507,3.5263693688808,134.232757055658));
#99710=CARTESIAN_POINT('Ctrl Pts',(-103.307951091585,3.62175536493645,134.134645223848));
#99711=CARTESIAN_POINT('Ctrl Pts',(-103.31570813247,3.71314340846088,134.032447028859));
#99712=CARTESIAN_POINT('Ctrl Pts',(-103.323465173355,3.80016774522769,133.926524638022));
#99713=CARTESIAN_POINT('Ctrl Pts',(-103.331216364596,3.88712645626532,133.820682124084));
#99714=CARTESIAN_POINT('Ctrl Pts',(-103.338967555836,3.9697277633093,133.711121305202));
#99715=CARTESIAN_POINT('Ctrl Pts',(-103.346718747076,4.04764396362877,133.598239893089));
#99716=CARTESIAN_POINT('Ctrl Pts',(-103.354466643853,4.12552704748452,133.485406458589));
#99717=CARTESIAN_POINT('Ctrl Pts',(-103.36221454063,4.1987287635222,133.369255558992));
#99718=CARTESIAN_POINT('Ctrl Pts',(-103.369962437407,4.26696293065056,133.250216380066));
#99719=CARTESIAN_POINT('Ctrl Pts',(-103.377708713491,4.33518282466211,133.131202101569));
#99720=CARTESIAN_POINT('Ctrl Pts',(-103.385454989575,4.39843704229483,133.00930108444));
#99721=CARTESIAN_POINT('Ctrl Pts',(-103.393201265659,4.45648404422802,132.884969428958));
#99722=CARTESIAN_POINT('Ctrl Pts',(-103.400947598925,4.5145314746509,132.760636855688));
#99723=CARTESIAN_POINT('Ctrl Pts',(-103.40869393219,4.56737144727976,132.633873962522));
#99724=CARTESIAN_POINT('Ctrl Pts',(-103.416440265455,4.61480967010514,132.505158892261));
#99725=CARTESIAN_POINT('Ctrl Pts',(-103.424188333458,4.66225851639168,132.376414997152));
#99726=CARTESIAN_POINT('Ctrl Pts',(-103.431936401461,4.70430307056754,132.245718421791));
#99727=CARTESIAN_POINT('Ctrl Pts',(-103.439684469464,4.74079834808433,132.113564224841));
#99728=CARTESIAN_POINT('Ctrl Pts',(-103.447440772206,4.77733241321632,131.981269572837));
#99729=CARTESIAN_POINT('Ctrl Pts',(-103.455197074948,4.80830531588587,131.847514582053));
#99730=CARTESIAN_POINT('Ctrl Pts',(-103.462953377689,4.83362270917481,131.712806855848));
#99731=CARTESIAN_POINT('Ctrl Pts',(-103.470713820204,4.85895361511892,131.578027232074));
#99732=CARTESIAN_POINT('Ctrl Pts',(-103.478474262718,4.87862294099198,131.442294246375));
#99733=CARTESIAN_POINT('Ctrl Pts',(-103.486234705232,4.89258818094349,131.306121471153));
#99734=CARTESIAN_POINT('Ctrl Pts',(-103.494007605497,4.90657583913795,131.169730099303));
#99735=CARTESIAN_POINT('Ctrl Pts',(-103.501780505763,4.91484108980973,131.032897917616));
#99736=CARTESIAN_POINT('Ctrl Pts',(-103.509553406028,4.91739357387722,130.896140256327));
#99737=CARTESIAN_POINT('Ctrl Pts',(-103.51704374179,4.91985326871964,130.764354080491));
#99738=CARTESIAN_POINT('Ctrl Pts',(-103.524534077553,4.91700833948822,130.632637409056));
#99739=CARTESIAN_POINT('Ctrl Pts',(-103.532024413315,4.90891287336266,130.501445672021));
#99740=CARTESIAN_POINT('Ctrl Pts',(-103.539798747434,4.90051046517871,130.365279760408));
#99741=CARTESIAN_POINT('Ctrl Pts',(-103.547573081553,4.88642489601396,130.229248042071));
#99742=CARTESIAN_POINT('Ctrl Pts',(-103.555347415672,4.86665970676502,130.093863354341));
#99743=CARTESIAN_POINT('Ctrl Pts',(-103.563112168619,4.84691887634537,129.95864551614));
#99744=CARTESIAN_POINT('Ctrl Pts',(-103.570876921566,4.82151240894448,129.824073505093));
#99745=CARTESIAN_POINT('Ctrl Pts',(-103.578641674513,4.79049580083954,129.690658213582));
#99746=CARTESIAN_POINT('Ctrl Pts',(-103.586398715398,4.75950999886703,129.557375432021));
#99747=CARTESIAN_POINT('Ctrl Pts',(-103.594155756284,4.72292523282126,129.425247462038));
#99748=CARTESIAN_POINT('Ctrl Pts',(-103.601912797169,4.68084850524219,129.294777783313));
#99749=CARTESIAN_POINT('Ctrl Pts',(-103.609663988409,4.63880350805062,129.164406492787));
#99750=CARTESIAN_POINT('Ctrl Pts',(-103.617415179649,4.59127491230719,129.035691375002));
#99751=CARTESIAN_POINT('Ctrl Pts',(-103.625166370889,4.5384201928109,128.909123108443));
#99752=CARTESIAN_POINT('Ctrl Pts',(-103.632914267666,4.48558793798041,128.782608636774));
#99753=CARTESIAN_POINT('Ctrl Pts',(-103.640662164443,4.42743421215485,128.658239561515));
#99754=CARTESIAN_POINT('Ctrl Pts',(-103.64841006122,4.36416541360402,128.536488640315));
#99755=CARTESIAN_POINT('Ctrl Pts',(-103.656156337304,4.30090984952192,128.414763186782));
#99756=CARTESIAN_POINT('Ctrl Pts',(-103.663902613388,4.23254152109466,128.295655144678));
#99757=CARTESIAN_POINT('Ctrl Pts',(-103.671648889472,4.15931360050365,128.179614261217));
#99758=CARTESIAN_POINT('Ctrl Pts',(-103.679395222738,4.08608513936066,128.063572521169));
#99759=CARTESIAN_POINT('Ctrl Pts',(-103.687141556003,4.00799722312143,127.950598315578));
#99760=CARTESIAN_POINT('Ctrl Pts',(-103.694887889269,3.92534710729005,127.841113555678));
#99761=CARTESIAN_POINT('Ctrl Pts',(-103.702635957271,3.84267848253841,127.731604277425));
#99762=CARTESIAN_POINT('Ctrl Pts',(-103.710384025275,3.75544586069529,127.625586311809));
#99763=CARTESIAN_POINT('Ctrl Pts',(-103.718132093277,3.66398738094329,127.523449229737));
#99764=CARTESIAN_POINT('Ctrl Pts',(-103.725888396019,3.57243169803076,127.421203595158));
#99765=CARTESIAN_POINT('Ctrl Pts',(-103.733644698761,3.47664144659419,127.322847375278));
#99766=CARTESIAN_POINT('Ctrl Pts',(-103.741401001503,3.37699269090074,127.228734318845));
#99767=CARTESIAN_POINT('Ctrl Pts',(-103.749161444017,3.27729074966573,127.13457103144));
#99768=CARTESIAN_POINT('Ctrl Pts',(-103.756921886531,3.17372649572347,127.044655676286));
#99769=CARTESIAN_POINT('Ctrl Pts',(-103.764682329046,3.06670903662881,126.959301613187));
#99770=CARTESIAN_POINT('Ctrl Pts',(-103.772455229311,2.95951978360825,126.873810532167));
#99771=CARTESIAN_POINT('Ctrl Pts',(-103.780228129576,2.84886656374427,126.79289560618));
#99772=CARTESIAN_POINT('Ctrl Pts',(-103.788001029842,2.73518815010882,126.716827272625));
#99773=CARTESIAN_POINT('Ctrl Pts',(-103.795491365604,2.62564223314736,126.643524214599));
#99774=CARTESIAN_POINT('Ctrl Pts',(-103.802981701366,2.51328751332149,126.574721655867));
#99775=CARTESIAN_POINT('Ctrl Pts',(-103.810472037128,2.39853639223181,126.510620262393));
#99776=CARTESIAN_POINT('Ctrl Pts',(-103.818246371247,2.27943444750834,126.444088445102));
#99777=CARTESIAN_POINT('Ctrl Pts',(-103.826020705366,2.15737351606003,126.382410566844));
#99778=CARTESIAN_POINT('Ctrl Pts',(-103.833795039485,2.03278697639856,126.325860849666));
#99779=CARTESIAN_POINT('Ctrl Pts',(-103.841559792432,1.9083539785126,126.26938082496));
#99780=CARTESIAN_POINT('Ctrl Pts',(-103.84932454538,1.7814019181233,126.218016546457));
#99781=CARTESIAN_POINT('Ctrl Pts',(-103.857089298327,1.65239062055459,126.171997473381));
#99782=CARTESIAN_POINT('Ctrl Pts',(-103.864846339212,1.52350745882537,126.126024107097));
#99783=CARTESIAN_POINT('Ctrl Pts',(-103.872603380097,1.39256949593961,126.085385511725));
#99784=CARTESIAN_POINT('Ctrl Pts',(-103.880360420982,1.26005816109676,126.050263806062));
#99785=CARTESIAN_POINT('Ctrl Pts',(-103.888111612222,1.12764675408248,126.015168585951));
#99786=CARTESIAN_POINT('Ctrl Pts',(-103.895862803462,0.993664713138639,
125.985582074425));
#99787=CARTESIAN_POINT('Ctrl Pts',(-103.903613994702,0.858609978946894,
125.961637007184));
#99788=CARTESIAN_POINT('Ctrl Pts',(-103.911361891479,0.723612646619699,
125.937702117235));
#99789=CARTESIAN_POINT('Ctrl Pts',(-103.919109788256,0.587543911996632,
125.91940397071));
#99790=CARTESIAN_POINT('Ctrl Pts',(-103.926857685033,0.450913082781708,
125.906824455956));
#99791=CARTESIAN_POINT('Ctrl Pts',(-103.934603961118,0.314310833790836,
125.894247572565));
#99792=CARTESIAN_POINT('Ctrl Pts',(-103.942350237202,0.177147113149288,
125.88738697743));
#99793=CARTESIAN_POINT('Ctrl Pts',(-103.950096513286,0.0399371516740185,
125.886272768979));
#99794=CARTESIAN_POINT('Ctrl Pts',(-103.957842846551,-0.0972738226542039,
125.885158552304));
#99795=CARTESIAN_POINT('Ctrl Pts',(-103.965589179817,-0.23453064754495,
125.88979081013));
#99796=CARTESIAN_POINT('Ctrl Pts',(-103.973335513082,-0.371317683267096,
125.900147506312));
#99797=CARTESIAN_POINT('Ctrl Pts',(-103.981083581085,-0.508135351497291,
125.910506521805));
#99798=CARTESIAN_POINT('Ctrl Pts',(-103.988831649088,-0.644482631436312,
125.92659249707));
#99799=CARTESIAN_POINT('Ctrl Pts',(-103.996579717091,-0.779848993560361,
125.948331518627));
#99800=CARTESIAN_POINT('Ctrl Pts',(-104.004336019833,-0.91535922466514,
125.970093644675));
#99801=CARTESIAN_POINT('Ctrl Pts',(-104.012092322575,-1.0498860687521,125.997520756801));
#99802=CARTESIAN_POINT('Ctrl Pts',(-104.019848625317,-1.18292863505851,
126.030487671324));
#99803=CARTESIAN_POINT('Ctrl Pts',(-104.027609067831,-1.3160422101884,126.063472181283));
#99804=CARTESIAN_POINT('Ctrl Pts',(-104.035369510345,-1.44766955396821,
126.102002275452));
#99805=CARTESIAN_POINT('Ctrl Pts',(-104.043129952859,-1.57732589529462,
126.145903138686));
#99806=CARTESIAN_POINT('Ctrl Pts',(-104.050902853125,-1.70719037249047,
126.189874475483));
#99807=CARTESIAN_POINT('Ctrl Pts',(-104.05867575339,-1.83507715954553,126.239233669264));
#99808=CARTESIAN_POINT('Ctrl Pts',(-104.066448653655,-1.96052156225215,
126.293757745838));
#99809=CARTESIAN_POINT('Ctrl Pts',(-104.073938989417,-2.08140574494126,
126.346299734888));
#99810=CARTESIAN_POINT('Ctrl Pts',(-104.081429325179,-2.20002175667112,
126.403637479136));
#99811=CARTESIAN_POINT('Ctrl Pts',(-104.088919660941,-2.31597785834425,
126.465532478292));
#99812=CARTESIAN_POINT('Ctrl Pts',(-104.096694944032,-2.4363451616712,126.529782086809));
#99813=CARTESIAN_POINT('Ctrl Pts',(-104.104470227123,-2.55422750628298,
126.599146096603));
#99814=CARTESIAN_POINT('Ctrl Pts',(-104.112245510215,-2.66915976063969,
126.673408035572));
#99815=CARTESIAN_POINT('Ctrl Pts',(-104.120011002829,-2.78394729466695,
126.747576465436));
#99816=CARTESIAN_POINT('Ctrl Pts',(-104.127776495444,-2.8957918048788,126.826630341773));
#99817=CARTESIAN_POINT('Ctrl Pts',(-104.135541988059,-3.00425157186128,
126.910306745896));
#99818=CARTESIAN_POINT('Ctrl Pts',(-104.143298171535,-3.1125813191387,126.993882840183));
#99819=CARTESIAN_POINT('Ctrl Pts',(-104.15105435501,-3.21753409680233,127.082070188469));
#99820=CARTESIAN_POINT('Ctrl Pts',(-104.158810538486,-3.31869660073135,
127.174562285042));
#99821=CARTESIAN_POINT('Ctrl Pts',(-104.166561443349,-3.41979025667306,
127.266991434431));
#99822=CARTESIAN_POINT('Ctrl Pts',(-104.174312348213,-3.51709848335758,
127.363719241173));
#99823=CARTESIAN_POINT('Ctrl Pts',(-104.182063253076,-3.61024050260019,
127.464398555523));
#99824=CARTESIAN_POINT('Ctrl Pts',(-104.189810561528,-3.70333930404406,
127.565031154778));
#99825=CARTESIAN_POINT('Ctrl Pts',(-104.19755786998,-3.79227547989826,127.669611326847));
#99826=CARTESIAN_POINT('Ctrl Pts',(-104.205305178432,-3.87670492154576,
127.777754925745));
#99827=CARTESIAN_POINT('Ctrl Pts',(-104.213050569898,-3.96111347206215,
127.885871765706));
#99828=CARTESIAN_POINT('Ctrl Pts',(-104.220795961364,-4.04101726819991,
127.997549969224));
#99829=CARTESIAN_POINT('Ctrl Pts',(-104.22854135283,-4.11611259387954,128.112372471789));
#99830=CARTESIAN_POINT('Ctrl Pts',(-104.236289194533,-4.1912316757932,128.227231298188));
#99831=CARTESIAN_POINT('Ctrl Pts',(-104.244037036236,-4.26153902828456,
128.345236087324));
#99832=CARTESIAN_POINT('Ctrl Pts',(-104.251784877939,-4.32677432210976,
128.465940846004));
#99833=CARTESIAN_POINT('Ctrl Pts',(-104.259533727165,-4.39201809907846,
128.58666130103));
#99834=CARTESIAN_POINT('Ctrl Pts',(-104.26728257639,-4.45218832466746,128.710082077126));
#99835=CARTESIAN_POINT('Ctrl Pts',(-104.275031425616,-4.50707117204207,
128.8357335547));
#99836=CARTESIAN_POINT('Ctrl Pts',(-104.282787377523,-4.56200432563929,
128.961500205803));
#99837=CARTESIAN_POINT('Ctrl Pts',(-104.290543329429,-4.61164026750674,
129.089501282152));
#99838=CARTESIAN_POINT('Ctrl Pts',(-104.298299281335,-4.65581360460957,
129.219247769333));
#99839=CARTESIAN_POINT('Ctrl Pts',(-104.305456244829,-4.69657545626425,
129.338973998096));
#99840=CARTESIAN_POINT('Ctrl Pts',(-104.312613208323,-4.73268634054227,
129.460186031577));
#99841=CARTESIAN_POINT('Ctrl Pts',(-104.319770171817,-4.76405452823413,
129.582490119309));
#99842=CARTESIAN_POINT('Origin',(213.235140564004,0.,130.804360617566));
#99843=CARTESIAN_POINT('',(-106.415236531453,-4.76405452823412,129.582490119309));
#99844=CARTESIAN_POINT('',(-106.070096981463,-4.76405452823408,129.582490119308));
#99845=CARTESIAN_POINT('',(213.235140564004,-4.76405452823405,129.582490119308));
#99846=CARTESIAN_POINT('',(-104.735140563956,-4.91824921984811,130.801590425618));
#99847=CARTESIAN_POINT('Ctrl Pts',(-104.735140564009,-4.91824921984864,
130.80159042655));
#99848=CARTESIAN_POINT('Ctrl Pts',(-104.742974204282,-4.91832747923958,
130.940533620822));
#99849=CARTESIAN_POINT('Ctrl Pts',(-104.750807844555,-4.91251356494721,
131.07948295469));
#99850=CARTESIAN_POINT('Ctrl Pts',(-104.758641484828,-4.90083249721782,
131.217910973283));
#99851=CARTESIAN_POINT('Ctrl Pts',(-104.766476674903,-4.88914911851372,
131.356366378384));
#99852=CARTESIAN_POINT('Ctrl Pts',(-104.774311864978,-4.87159630597743,
131.49429988545));
#99853=CARTESIAN_POINT('Ctrl Pts',(-104.782147055053,-4.84825097285308,
131.631189237492));
#99854=CARTESIAN_POINT('Ctrl Pts',(-104.789985344041,-4.8248964063682,131.768132730923));
#99855=CARTESIAN_POINT('Ctrl Pts',(-104.797823633028,-4.79574482004112,
131.904030873771));
#99856=CARTESIAN_POINT('Ctrl Pts',(-104.805661922015,-4.7609241962113,132.038371906181));
#99857=CARTESIAN_POINT('Ctrl Pts',(-104.813912889865,-4.72427029786459,
132.179785873083));
#99858=CARTESIAN_POINT('Ctrl Pts',(-104.822163857716,-4.68133437221187,
132.319473861166));
#99859=CARTESIAN_POINT('Ctrl Pts',(-104.830414825566,-4.63232475084333,
132.456858867255));
#99860=CARTESIAN_POINT('Ctrl Pts',(-104.838268951371,-4.58567231698785,
132.587636145885));
#99861=CARTESIAN_POINT('Ctrl Pts',(-104.846123077176,-4.53351697905264,
132.71632647103));
#99862=CARTESIAN_POINT('Ctrl Pts',(-104.853977202981,-4.47608702524996,
132.842454826598));
#99863=CARTESIAN_POINT('Ctrl Pts',(-104.861837876973,-4.41860919061258,
132.968688338631));
#99864=CARTESIAN_POINT('Ctrl Pts',(-104.869698550966,-4.35584814706225,
133.092355288183));
#99865=CARTESIAN_POINT('Ctrl Pts',(-104.877559224958,-4.28807735207693,
133.213006644923));
#99866=CARTESIAN_POINT('Ctrl Pts',(-104.885432015159,-4.22020209720895,
133.333843970068));
#99867=CARTESIAN_POINT('Ctrl Pts',(-104.89330480536,-4.14730187255067,133.451656102214));
#99868=CARTESIAN_POINT('Ctrl Pts',(-104.901177595561,-4.0696927951611,133.566023814901));
#99869=CARTESIAN_POINT('Ctrl Pts',(-104.902342909114,-4.05820526565772,
133.582952278915));
#99870=CARTESIAN_POINT('Ctrl Pts',(-104.903508222666,-4.04661463849552,
133.599805339595));
#99871=CARTESIAN_POINT('Ctrl Pts',(-104.904673536219,-4.03492201057254,
133.616581702598));
#99872=CARTESIAN_POINT('Ctrl Pts',(-104.912447870338,-3.9569151977443,133.728504412989));
#99873=CARTESIAN_POINT('Ctrl Pts',(-104.920222204457,-3.87412444528042,
133.837356252472));
#99874=CARTESIAN_POINT('Ctrl Pts',(-104.927996538576,-3.7868195446258,133.942701070567));
#99875=CARTESIAN_POINT('Ctrl Pts',(-104.935761291523,-3.6996222394588,134.047916060588));
#99876=CARTESIAN_POINT('Ctrl Pts',(-104.94352604447,-3.60792210245885,134.149632330757));
#99877=CARTESIAN_POINT('Ctrl Pts',(-104.951290797418,-3.5120322862127,134.2474424178));
#99878=CARTESIAN_POINT('Ctrl Pts',(-104.959047838303,-3.41623770908385,
134.345155358485));
#99879=CARTESIAN_POINT('Ctrl Pts',(-104.966804879188,-3.31626200571,134.438969559399));
#99880=CARTESIAN_POINT('Ctrl Pts',(-104.974561920073,-3.21245846203479,
134.528510680628));
#99881=CARTESIAN_POINT('Ctrl Pts',(-104.982313111313,-3.10873319741892,
134.6179842782));
#99882=CARTESIAN_POINT('Ctrl Pts',(-104.990064302553,-3.00118613295721,
134.70319095567));
#99883=CARTESIAN_POINT('Ctrl Pts',(-104.997815493793,-2.89020700187156,
134.783793560692));
#99884=CARTESIAN_POINT('Ctrl Pts',(-105.00556339057,-2.77927503987724,134.864361907456));
#99885=CARTESIAN_POINT('Ctrl Pts',(-105.013311287347,-2.66491422821539,
134.940329844535));
#99886=CARTESIAN_POINT('Ctrl Pts',(-105.021059184124,-2.54754676149983,
135.011400973977));
#99887=CARTESIAN_POINT('Ctrl Pts',(-105.028805460208,-2.43020384552816,
135.082457236871));
#99888=CARTESIAN_POINT('Ctrl Pts',(-105.036551736292,-2.30985585969123,
135.148618527145));
#99889=CARTESIAN_POINT('Ctrl Pts',(-105.044298012377,-2.18695297664713,
135.209632429888));
#99890=CARTESIAN_POINT('Ctrl Pts',(-105.052044345642,-2.06404918636203,
135.270646783021));
#99891=CARTESIAN_POINT('Ctrl Pts',(-105.059790678907,-1.93859081142382,
135.326513498956));
#99892=CARTESIAN_POINT('Ctrl Pts',(-105.067537012173,-1.81105119446872,
135.377026867525));
#99893=CARTESIAN_POINT('Ctrl Pts',(-105.075285080176,-1.68348301590087,
135.427551548213));
#99894=CARTESIAN_POINT('Ctrl Pts',(-105.083033148178,-1.55383303129568,
135.472720352035));
#99895=CARTESIAN_POINT('Ctrl Pts',(-105.090781216181,-1.42259267752029,
135.512376456151));
#99896=CARTESIAN_POINT('Ctrl Pts',(-105.098537518923,-1.29121283993458,
135.552074707247));
#99897=CARTESIAN_POINT('Ctrl Pts',(-105.106293821665,-1.15823963154555,
135.586248441461));
#99898=CARTESIAN_POINT('Ctrl Pts',(-105.114050124407,-1.02417824546788,
135.614791157966));
#99899=CARTESIAN_POINT('Ctrl Pts',(-105.121810566921,-0.890045306791942,
135.643349108577));
#99900=CARTESIAN_POINT('Ctrl Pts',(-105.129571009435,-0.754823418425915,
135.66626998757));
#99901=CARTESIAN_POINT('Ctrl Pts',(-105.13733145195,-0.619024984850516,
135.683498977013));
#99902=CARTESIAN_POINT('Ctrl Pts',(-105.145104352215,-0.483008555573924,
135.70075562396));
#99903=CARTESIAN_POINT('Ctrl Pts',(-105.15287725248,-0.346414121401026,
135.712302089516));
#99904=CARTESIAN_POINT('Ctrl Pts',(-105.160650152746,-0.209757095518095,
135.71813564532));
#99905=CARTESIAN_POINT('Ctrl Pts',(-105.168140488508,-0.0780678967427983,
135.723757136677));
#99906=CARTESIAN_POINT('Ctrl Pts',(-105.17563082427,0.0536791139996607,
135.724073863646));
#99907=CARTESIAN_POINT('Ctrl Pts',(-105.183121160032,0.185027339917025,
135.719128968769));
#99908=CARTESIAN_POINT('Ctrl Pts',(-105.190895494151,0.321355673741123,
135.713996586699));
#99909=CARTESIAN_POINT('Ctrl Pts',(-105.19866982827,0.457686233126234,135.70317945999));
#99910=CARTESIAN_POINT('Ctrl Pts',(-105.20644416239,0.593506243454455,135.686668821836));
#99911=CARTESIAN_POINT('Ctrl Pts',(-105.214208915337,0.729158867757792,
135.670178531568));
#99912=CARTESIAN_POINT('Ctrl Pts',(-105.221973668284,0.864301810554518,
135.648008737812));
#99913=CARTESIAN_POINT('Ctrl Pts',(-105.229738421231,0.99842299482897,135.620202660854));
#99914=CARTESIAN_POINT('Ctrl Pts',(-105.237495462116,1.13241096805315,135.592424201283));
#99915=CARTESIAN_POINT('Ctrl Pts',(-105.245252503001,1.26537882195526,135.559020677709));
#99916=CARTESIAN_POINT('Ctrl Pts',(-105.253009543886,1.39682065408044,135.520086979733));
#99917=CARTESIAN_POINT('Ctrl Pts',(-105.260760735126,1.52816336489773,135.481182641961));
#99918=CARTESIAN_POINT('Ctrl Pts',(-105.268511926366,1.65798197115636,135.436756541199));
#99919=CARTESIAN_POINT('Ctrl Pts',(-105.276263117606,1.78578215671355,135.386954331967));
#99920=CARTESIAN_POINT('Ctrl Pts',(-105.284011014384,1.91352802378217,135.337173290002));
#99921=CARTESIAN_POINT('Ctrl Pts',(-105.291758911161,2.03925681289221,135.282020825895));
#99922=CARTESIAN_POINT('Ctrl Pts',(-105.299506807938,2.16249094954978,135.2216919336));
#99923=CARTESIAN_POINT('Ctrl Pts',(-105.307253084022,2.28569930828292,135.161375660808));
#99924=CARTESIAN_POINT('Ctrl Pts',(-105.314999360106,2.40641370158378,135.095885285364));
#99925=CARTESIAN_POINT('Ctrl Pts',(-105.32274563619,2.52417843631995,135.025463113848));
#99926=CARTESIAN_POINT('Ctrl Pts',(-105.330491969456,2.64194404036848,134.955040422491));
#99927=CARTESIAN_POINT('Ctrl Pts',(-105.338238302721,2.75675960685744,134.879686063073));
#99928=CARTESIAN_POINT('Ctrl Pts',(-105.345984635986,2.86819621274039,134.799687080788));
#99929=CARTESIAN_POINT('Ctrl Pts',(-105.353732703989,2.97965777407843,134.719670183286));
#99930=CARTESIAN_POINT('Ctrl Pts',(-105.361480771992,3.08773855153675,134.635006821134));
#99931=CARTESIAN_POINT('Ctrl Pts',(-105.369228839995,3.19204097198851,134.546025687511));
#99932=CARTESIAN_POINT('Ctrl Pts',(-105.376985142737,3.29645424629409,134.456949983681));
#99933=CARTESIAN_POINT('Ctrl Pts',(-105.384741445479,3.39708084392467,134.363547595549));
#99934=CARTESIAN_POINT('Ctrl Pts',(-105.392497748221,3.49355809349757,134.266185990091));
#99935=CARTESIAN_POINT('Ctrl Pts',(-105.400258190735,3.59008683588344,134.168772419813));
#99936=CARTESIAN_POINT('Ctrl Pts',(-105.408018633249,3.68246155417312,134.067395710417));
#99937=CARTESIAN_POINT('Ctrl Pts',(-105.415779075763,3.7703591613504,133.962457331874));
#99938=CARTESIAN_POINT('Ctrl Pts',(-105.423551976029,3.85839786956991,133.857350496929));
#99939=CARTESIAN_POINT('Ctrl Pts',(-105.431324876294,3.94194486623019,133.748670877576));
#99940=CARTESIAN_POINT('Ctrl Pts',(-105.43909777656,4.02071926246565,133.636850630777));
#99941=CARTESIAN_POINT('Ctrl Pts',(-105.446588112322,4.09663001097658,133.529095331608));
#99942=CARTESIAN_POINT('Ctrl Pts',(-105.454078448084,4.1681089597507,133.418424038867));
#99943=CARTESIAN_POINT('Ctrl Pts',(-105.461568783846,4.23494560410924,133.305244219963));
#99944=CARTESIAN_POINT('Ctrl Pts',(-105.469343117965,4.30431638015387,133.187773153823));
#99945=CARTESIAN_POINT('Ctrl Pts',(-105.477117452084,4.36890562250306,133.067227471921));
#99946=CARTESIAN_POINT('Ctrl Pts',(-105.484891786203,4.42842878818928,132.944033847393));
#99947=CARTESIAN_POINT('Ctrl Pts',(-105.49265653915,4.4878785968932,132.820992047997));
#99948=CARTESIAN_POINT('Ctrl Pts',(-105.500421292097,4.54227458315621,132.695309147722));
#99949=CARTESIAN_POINT('Ctrl Pts',(-105.508186045044,4.59137631929478,132.567439333086));
#99950=CARTESIAN_POINT('Ctrl Pts',(-105.515943085929,4.6404292868968,132.439696520552));
#99951=CARTESIAN_POINT('Ctrl Pts',(-105.523700126814,4.6841983294311,132.309771478801));
#99952=CARTESIAN_POINT('Ctrl Pts',(-105.531457167699,4.72248982757289,132.178141128045));
#99953=CARTESIAN_POINT('Ctrl Pts',(-105.539208358939,4.76075244979813,132.046610040759));
#99954=CARTESIAN_POINT('Ctrl Pts',(-105.546959550179,4.79354564069304,131.913376578031));
#99955=CARTESIAN_POINT('Ctrl Pts',(-105.554710741419,4.82072475358047,131.778935351856));
#99956=CARTESIAN_POINT('Ctrl Pts',(-105.562458638196,4.84789231461993,131.644551266789));
#99957=CARTESIAN_POINT('Ctrl Pts',(-105.570206534974,4.86945046617891,131.508960821663));
#99958=CARTESIAN_POINT('Ctrl Pts',(-105.577954431751,4.88530512151254,131.37267121242));
#99959=CARTESIAN_POINT('Ctrl Pts',(-105.585700707835,4.90115646039411,131.236410112025));
#99960=CARTESIAN_POINT('Ctrl Pts',(-105.593446983919,4.91130663094113,131.099450526513));
#99961=CARTESIAN_POINT('Ctrl Pts',(-105.601193260003,4.91571317927373,130.962306816047));
#99962=CARTESIAN_POINT('Ctrl Pts',(-105.608939593268,4.92011976013443,130.825162093218));
#99963=CARTESIAN_POINT('Ctrl Pts',(-105.616685926534,4.91878262162284,130.687833633488));
#99964=CARTESIAN_POINT('Ctrl Pts',(-105.624432259799,4.91171141960792,130.550837456902));
#99965=CARTESIAN_POINT('Ctrl Pts',(-105.632180327802,4.90463863404629,130.413810600971));
#99966=CARTESIAN_POINT('Ctrl Pts',(-105.639928395805,4.89182924991284,130.277116566627));
#99967=CARTESIAN_POINT('Ctrl Pts',(-105.647676463808,4.87334490810206,130.141267510095));
#99968=CARTESIAN_POINT('Ctrl Pts',(-105.65543276655,4.85484092091291,130.005274071569));
#99969=CARTESIAN_POINT('Ctrl Pts',(-105.663189069291,4.83064998044537,129.870127792824));
#99970=CARTESIAN_POINT('Ctrl Pts',(-105.670945372033,4.80088521433196,129.736332424442));
#99971=CARTESIAN_POINT('Ctrl Pts',(-105.678705814547,4.77110456186667,129.602465645442));
#99972=CARTESIAN_POINT('Ctrl Pts',(-105.686466257061,4.73574425672799,129.469951591065));
#99973=CARTESIAN_POINT('Ctrl Pts',(-105.694226699576,4.69496743054843,129.339279087893));
#99974=CARTESIAN_POINT('Ctrl Pts',(-105.701999599841,4.65412514578738,129.208396817617));
#99975=CARTESIAN_POINT('Ctrl Pts',(-105.709772500106,4.6078490965022,129.079362374245));
#99976=CARTESIAN_POINT('Ctrl Pts',(-105.717545400372,4.55635104129327,128.952645668929));
#99977=CARTESIAN_POINT('Ctrl Pts',(-105.725035736134,4.5067250701064,128.83053543503));
#99978=CARTESIAN_POINT('Ctrl Pts',(-105.732526071896,4.45225029493123,128.710577634012));
#99979=CARTESIAN_POINT('Ctrl Pts',(-105.740016407658,4.39315574671854,128.59316961551));
#99980=CARTESIAN_POINT('Ctrl Pts',(-105.747790741777,4.33182061074958,128.471310036302));
#99981=CARTESIAN_POINT('Ctrl Pts',(-105.755565075896,4.26531417770391,128.351811391892));
#99982=CARTESIAN_POINT('Ctrl Pts',(-105.763339410015,4.19384161735086,128.235143703587));
#99983=CARTESIAN_POINT('Ctrl Pts',(-105.771104162962,4.12245714054114,128.118619797782));
#99984=CARTESIAN_POINT('Ctrl Pts',(-105.77886891591,4.04611891628644,128.004920236391));
#99985=CARTESIAN_POINT('Ctrl Pts',(-105.786633668857,3.965079107531,127.894492796939));
#99986=CARTESIAN_POINT('Ctrl Pts',(-105.794390709742,3.88411978865586,127.784175035577));
#99987=CARTESIAN_POINT('Ctrl Pts',(-105.802147750627,3.79846840797045,127.677123241827));
#99988=CARTESIAN_POINT('Ctrl Pts',(-105.809904791512,3.70842155598071,127.573758100134));
#99989=CARTESIAN_POINT('Ctrl Pts',(-105.817655982752,3.6184426090219,127.470470906898));
#99990=CARTESIAN_POINT('Ctrl Pts',(-105.825407173992,3.52407504415699,127.370865125633));
#99991=CARTESIAN_POINT('Ctrl Pts',(-105.833158365232,3.4256568074044,127.275329801551));
#99992=CARTESIAN_POINT('Ctrl Pts',(-105.840906262009,3.3272804010285,127.179835082531));
#99993=CARTESIAN_POINT('Ctrl Pts',(-105.848654158786,3.22485702692788,127.088407651494));
#99994=CARTESIAN_POINT('Ctrl Pts',(-105.856402055563,3.11876254722884,127.001400818081));
#99995=CARTESIAN_POINT('Ctrl Pts',(-105.864148331647,3.01269026020783,126.914412184621));
#99996=CARTESIAN_POINT('Ctrl Pts',(-105.871894607732,2.90294869713193,126.831842557279));
#99997=CARTESIAN_POINT('Ctrl Pts',(-105.879640883816,2.78994765641538,126.754005677939));
#99998=CARTESIAN_POINT('Ctrl Pts',(-105.887387217081,2.67694578155067,126.676168224025));
#99999=CARTESIAN_POINT('Ctrl Pts',(-105.895133550346,2.56068470300772,126.603063809605));
#100000=CARTESIAN_POINT('Ctrl Pts',(-105.902879883612,2.44160378229905,
126.534963232365));
#100001=CARTESIAN_POINT('Ctrl Pts',(-105.910627951615,2.32249619424367,
126.466847404472));
#100002=CARTESIAN_POINT('Ctrl Pts',(-105.918376019618,2.20056784676347,
126.403737837624));
#100003=CARTESIAN_POINT('Ctrl Pts',(-105.926124087621,2.07628294980358,
126.34585950454));
#100004=CARTESIAN_POINT('Ctrl Pts',(-105.933880390363,1.95186596137635,
126.287919657675));
#100005=CARTESIAN_POINT('Ctrl Pts',(-105.941636693104,1.82508777530703,
126.23522231622));
#100006=CARTESIAN_POINT('Ctrl Pts',(-105.949392995846,1.69643335947566,
126.187944592189));
#100007=CARTESIAN_POINT('Ctrl Pts',(-105.957153438361,1.56771027690885,
126.140641634613));
#100008=CARTESIAN_POINT('Ctrl Pts',(-105.964913880875,1.43710934131709,
126.098764177556));
#100009=CARTESIAN_POINT('Ctrl Pts',(-105.972674323389,1.30512999298075,
126.062439196462));
#100010=CARTESIAN_POINT('Ctrl Pts',(-105.980447223654,1.17293877967788,
126.026055903285));
#100011=CARTESIAN_POINT('Ctrl Pts',(-105.98822012392,1.0393651130295,125.99524298567));
#100012=CARTESIAN_POINT('Ctrl Pts',(-105.995993024185,0.904918803293208,
125.970076283567));
#100013=CARTESIAN_POINT('Ctrl Pts',(-106.003483359947,0.775359955566745,
125.945824454477));
#100014=CARTESIAN_POINT('Ctrl Pts',(-106.010973695709,0.644991113588729,
125.926815504056));
#100015=CARTESIAN_POINT('Ctrl Pts',(-106.018464031471,0.514270375684464,
125.913071519261));
#100016=CARTESIAN_POINT('Ctrl Pts',(-106.02623836559,0.378593321269518,
125.898806427106));
#100017=CARTESIAN_POINT('Ctrl Pts',(-106.034012699709,0.242107375778195,
125.890168236567));
#100018=CARTESIAN_POINT('Ctrl Pts',(-106.041787033828,0.105318880721756,
125.887238390504));
#100019=CARTESIAN_POINT('Ctrl Pts',(-106.049551786775,-0.0313010347389233,
125.884312155215));
#100020=CARTESIAN_POINT('Ctrl Pts',(-106.057316539722,-0.168222370750725,
125.887080275094));
#100021=CARTESIAN_POINT('Ctrl Pts',(-106.06508129267,-0.304932099168563,
125.895572633002));
#100022=CARTESIAN_POINT('Ctrl Pts',(-106.072838333555,-0.441506045557609,
125.904056556182));
#100023=CARTESIAN_POINT('Ctrl Pts',(-106.08059537444,-0.577868414915769,
125.918253379118));
#100024=CARTESIAN_POINT('Ctrl Pts',(-106.088352415325,-0.71350495909208,
125.938140962038));
#100025=CARTESIAN_POINT('Ctrl Pts',(-106.096103606565,-0.849039218695514,
125.958013547576));
#100026=CARTESIAN_POINT('Ctrl Pts',(-106.103854797805,-0.98384835732093,
125.983568294745));
#100027=CARTESIAN_POINT('Ctrl Pts',(-106.111605989045,-1.1174223921357,
126.014731168428));
#100028=CARTESIAN_POINT('Ctrl Pts',(-106.119353885822,-1.25093965442192,
126.045880797057));
#100029=CARTESIAN_POINT('Ctrl Pts',(-106.127101782599,-1.38322247704346,
126.082633722755));
#100030=CARTESIAN_POINT('Ctrl Pts',(-106.134849679376,-1.513770447935,126.124864694557));
#100031=CARTESIAN_POINT('Ctrl Pts',(-106.14259595546,-1.64429111100569,
126.16708683255));
#100032=CARTESIAN_POINT('Ctrl Pts',(-106.150342231544,-1.77307727241129,
126.214784617155));
#100033=CARTESIAN_POINT('Ctrl Pts',(-106.158088507629,-1.89964346616637,
126.267782858511));
#100034=CARTESIAN_POINT('Ctrl Pts',(-106.165834840894,-2.0262105942045,
126.320781491088));
#100035=CARTESIAN_POINT('Ctrl Pts',(-106.173581174159,-2.15055736126741,
126.379080507483));
#100036=CARTESIAN_POINT('Ctrl Pts',(-106.181327507425,-2.27221845196502,
126.442456633175));
#100037=CARTESIAN_POINT('Ctrl Pts',(-106.189075575428,-2.39390678782019,
126.50584695151));
#100038=CARTESIAN_POINT('Ctrl Pts',(-106.196823643431,-2.51290790384352,
126.574316461017));
#100039=CARTESIAN_POINT('Ctrl Pts',(-106.204571711434,-2.62878160730095,
126.647596211972));
#100040=CARTESIAN_POINT('Ctrl Pts',(-106.212328014175,-2.74477846270917,
126.720953845517));
#100041=CARTESIAN_POINT('Ctrl Pts',(-106.220084316917,-2.85764093484098,
126.799131723742));
#100042=CARTESIAN_POINT('Ctrl Pts',(-106.227840619659,-2.96695787735862,
126.881817562802));
#100043=CARTESIAN_POINT('Ctrl Pts',(-106.235601062173,-3.07633316561995,
126.964547533783));
#100044=CARTESIAN_POINT('Ctrl Pts',(-106.243361504688,-3.18215885206609,
127.051790011254));
#100045=CARTESIAN_POINT('Ctrl Pts',(-106.251121947202,-3.28405814898742,
127.143193435291));
#100046=CARTESIAN_POINT('Ctrl Pts',(-106.258894847467,-3.38612102370636,
127.234743588218));
#100047=CARTESIAN_POINT('Ctrl Pts',(-106.266667747733,-3.4842446335043,
127.330467762354));
#100048=CARTESIAN_POINT('Ctrl Pts',(-106.274440647998,-3.57808960718752,
127.429978033235));
#100049=CARTESIAN_POINT('Ctrl Pts',(-106.28193098376,-3.66852307969486,
127.525870855117));
#100050=CARTESIAN_POINT('Ctrl Pts',(-106.289421319522,-3.7549833915705,
127.625279052087));
#100051=CARTESIAN_POINT('Ctrl Pts',(-106.296911655284,-3.83720434709623,
127.727829151592));
#100052=CARTESIAN_POINT('Ctrl Pts',(-106.304670430773,-3.92237194902209,
127.834054456276));
#100053=CARTESIAN_POINT('Ctrl Pts',(-106.312429206263,-4.00326690146727,
127.943995672536));
#100054=CARTESIAN_POINT('Ctrl Pts',(-106.320187981752,-4.07954613905818,
128.0572737311));
#100055=CARTESIAN_POINT('Ctrl Pts',(-106.328108694227,-4.15741743583502,
128.172916068324));
#100056=CARTESIAN_POINT('Ctrl Pts',(-106.336029406702,-4.23047789099962,
128.292035822503));
#100057=CARTESIAN_POINT('Ctrl Pts',(-106.343950119177,-4.29840385481742,
128.414191719059));
#100058=CARTESIAN_POINT('Ctrl Pts',(-106.351689422288,-4.36477409925469,
128.533549859278));
#100059=CARTESIAN_POINT('Ctrl Pts',(-106.359428725399,-4.42624226601099,
128.655806220943));
#100060=CARTESIAN_POINT('Ctrl Pts',(-106.36716802851,-4.48254895009903,
128.780518239201));
#100061=CARTESIAN_POINT('Ctrl Pts',(-106.375179445667,-4.54083537828252,
128.90961513442));
#100062=CARTESIAN_POINT('Ctrl Pts',(-106.383190862824,-4.59359046755274,
129.041343187705));
#100063=CARTESIAN_POINT('Ctrl Pts',(-106.391202279981,-4.64057775253825,
129.175182547143));
#100064=CARTESIAN_POINT('Ctrl Pts',(-106.399213697139,-4.68756503752376,
129.309021906581));
#100065=CARTESIAN_POINT('Ctrl Pts',(-106.407225114296,-4.72878432796288,
129.444972143751));
#100066=CARTESIAN_POINT('Ctrl Pts',(-106.415236531453,-4.76405452823412,
129.582490119309));
#100067=CARTESIAN_POINT('Ctrl Pts',(-104.665400201108,-4.76405452823405,
129.582490119308));
#100068=CARTESIAN_POINT('Ctrl Pts',(-104.674057866373,-4.80191628057872,
129.730112517068));
#100069=CARTESIAN_POINT('Ctrl Pts',(-104.682715531638,-4.8329568645889,
129.87966918857));
#100070=CARTESIAN_POINT('Ctrl Pts',(-104.691373196903,-4.85699517168876,
130.030551232322));
#100071=CARTESIAN_POINT('Ctrl Pts',(-104.699986564182,-4.8809104839014,
130.180661269963));
#100072=CARTESIAN_POINT('Ctrl Pts',(-104.708599931462,-4.8978948960219,
130.332082940685));
#100073=CARTESIAN_POINT('Ctrl Pts',(-104.717213298742,-4.90781816629195,
130.484198300741));
#100074=CARTESIAN_POINT('Ctrl Pts',(-104.723189053814,-4.91470270177198,
130.589732420529));
#100075=CARTESIAN_POINT('Ctrl Pts',(-104.729164808885,-4.9181895210244,
130.695600047087));
#100076=CARTESIAN_POINT('Ctrl Pts',(-104.735140563956,-4.91824921984811,
130.801590425618));
#100077=CARTESIAN_POINT('',(-104.389859436028,-4.9182494419762,130.802017755898));
#100078=CARTESIAN_POINT('Ctrl Pts',(-104.319770171817,-4.76405452823413,
129.582490119309));
#100079=CARTESIAN_POINT('Ctrl Pts',(-104.327703023973,-4.79882335101448,
129.718053231639));
#100080=CARTESIAN_POINT('Ctrl Pts',(-104.33563587613,-4.82776451325459,
129.85495775685));
#100081=CARTESIAN_POINT('Ctrl Pts',(-104.343568728286,-4.85080669696491,
129.992660271884));
#100082=CARTESIAN_POINT('Ctrl Pts',(-104.351501580442,-4.87384888067523,
130.130362786918));
#100083=CARTESIAN_POINT('Ctrl Pts',(-104.359434432598,-4.89099209668079,
130.268862857689));
#100084=CARTESIAN_POINT('Ctrl Pts',(-104.367367284754,-4.90222159891013,
130.407615790657));
#100085=CARTESIAN_POINT('Ctrl Pts',(-104.3748646685,-4.91283466541256,130.538751977723));
#100086=CARTESIAN_POINT('Ctrl Pts',(-104.382362052246,-4.91818670614076,
130.670319667333));
#100087=CARTESIAN_POINT('Ctrl Pts',(-104.389859435992,-4.9182494419759,
130.802017755259));
#100088=CARTESIAN_POINT('Ctrl Pts',(-104.389859436028,-4.9182494419762,
130.802017755897));
#100089=CARTESIAN_POINT('Ctrl Pts',(-104.397545371812,-4.91831375554012,
130.937027924903));
#100090=CARTESIAN_POINT('Ctrl Pts',(-104.405231307596,-4.91281465613365,
131.072264896961));
#100091=CARTESIAN_POINT('Ctrl Pts',(-104.41291724338,-4.90172242161412,
131.207225810832));
#100092=CARTESIAN_POINT('Ctrl Pts',(-104.420594276387,-4.89064303545788,
131.342030396702));
#100093=CARTESIAN_POINT('Ctrl Pts',(-104.428271309393,-4.87398343223574,
131.476559165036));
#100094=CARTESIAN_POINT('Ctrl Pts',(-104.4359483424,-4.85176588145133,131.610307820604));
#100095=CARTESIAN_POINT('Ctrl Pts',(-104.443618418405,-4.82956846442449,
131.743935271858));
#100096=CARTESIAN_POINT('Ctrl Pts',(-104.451288494411,-4.80182318464016,
131.876783624039));
#100097=CARTESIAN_POINT('Ctrl Pts',(-104.458958570417,-4.76860419642255,
132.008352760548));
#100098=CARTESIAN_POINT('Ctrl Pts',(-104.466744251173,-4.73488452570238,
132.141904930498));
#100099=CARTESIAN_POINT('Ctrl Pts',(-104.474529931929,-4.69552482911067,
132.274138591999));
#100100=CARTESIAN_POINT('Ctrl Pts',(-104.482315612685,-4.65065684970194,
132.404539960271));
#100101=CARTESIAN_POINT('Ctrl Pts',(-104.48997848367,-4.60649660883172,
132.532884403426));
#100102=CARTESIAN_POINT('Ctrl Pts',(-104.497641354654,-4.55700073228512,
132.659453546734));
#100103=CARTESIAN_POINT('Ctrl Pts',(-104.505304225638,-4.50234520281099,
132.783772332502));
#100104=CARTESIAN_POINT('Ctrl Pts',(-104.512966394213,-4.44769468328114,
132.908079722713));
#100105=CARTESIAN_POINT('Ctrl Pts',(-104.520628562788,-4.38788561240711,
133.030136799074));
#100106=CARTESIAN_POINT('Ctrl Pts',(-104.528290731363,-4.32314190563217,
133.149488999183));
#100107=CARTESIAN_POINT('Ctrl Pts',(-104.535953944915,-4.25838936902452,
133.268857476704));
#100108=CARTESIAN_POINT('Ctrl Pts',(-104.543617158466,-4.18870104925746,
133.385519992526));
#100109=CARTESIAN_POINT('Ctrl Pts',(-104.551280372018,-4.11434629046257,
133.499047550153));
#100110=CARTESIAN_POINT('Ctrl Pts',(-104.559158250064,-4.03790868136313,
133.615755279592));
#100111=CARTESIAN_POINT('Ctrl Pts',(-104.56703612811,-3.95653959196402,
133.729149450618));
#100112=CARTESIAN_POINT('Ctrl Pts',(-104.574914006155,-3.87057790563903,
133.838797919419));
#100113=CARTESIAN_POINT('Ctrl Pts',(-104.582588618686,-3.7868342082679,
133.945617231383));
#100114=CARTESIAN_POINT('Ctrl Pts',(-104.590263231216,-3.69873231707316,
134.048881501605));
#100115=CARTESIAN_POINT('Ctrl Pts',(-104.597937843746,-3.60662432917995,
134.148227243295));
#100116=CARTESIAN_POINT('Ctrl Pts',(-104.60591735455,-3.51085705994149,
134.251519809009));
#100117=CARTESIAN_POINT('Ctrl Pts',(-104.613896865353,-3.41075917559361,
134.350575735485));
#100118=CARTESIAN_POINT('Ctrl Pts',(-104.621876376157,-3.30676506649801,
134.445031964651));
#100119=CARTESIAN_POINT('Ctrl Pts',(-104.62985588696,-3.20277095740268,
134.539488193817));
#100120=CARTESIAN_POINT('Ctrl Pts',(-104.637835397764,-3.09488103853637,
134.629344477018));
#100121=CARTESIAN_POINT('Ctrl Pts',(-104.645814908567,-2.98356317691055,
134.714288216881));
#100122=CARTESIAN_POINT('Ctrl Pts',(-104.653589242686,-2.87510762480794,
134.797047803437));
#100123=CARTESIAN_POINT('Ctrl Pts',(-104.661363576805,-2.76303423627931,
134.875422462838));
#100124=CARTESIAN_POINT('Ctrl Pts',(-104.669137910924,-2.64773309102237,
134.949079249899));
#100125=CARTESIAN_POINT('Ctrl Pts',(-104.676902663871,-2.5325740441222,
135.022645261552));
#100126=CARTESIAN_POINT('Ctrl Pts',(-104.684667416819,-2.41419548168438,
135.091504761247));
#100127=CARTESIAN_POINT('Ctrl Pts',(-104.692432169766,-2.29302001461254,
135.155365360736));
#100128=CARTESIAN_POINT('Ctrl Pts',(-104.700189210651,-2.17196490072286,
135.219162532977));
#100129=CARTESIAN_POINT('Ctrl Pts',(-104.707946251535,-2.04811875403068,
135.277970504442));
#100130=CARTESIAN_POINT('Ctrl Pts',(-104.71570329242,-1.92193228848902,
135.331540682569));
#100131=CARTESIAN_POINT('Ctrl Pts',(-104.723454483661,-1.79584098114279,
135.385070463008));
#100132=CARTESIAN_POINT('Ctrl Pts',(-104.731205674901,-1.66741322620109,
135.433370159905));
#100133=CARTESIAN_POINT('Ctrl Pts',(-104.738956866141,-1.53712308966951,
135.476237721012));
#100134=CARTESIAN_POINT('Ctrl Pts',(-104.746704762918,-1.40688832992137,
135.519087062263));
#100135=CARTESIAN_POINT('Ctrl Pts',(-104.754452659695,-1.27479313354236,
135.556508737822));
#100136=CARTESIAN_POINT('Ctrl Pts',(-104.762200556472,-1.14133003397393,
135.588349415217));
#100137=CARTESIAN_POINT('Ctrl Pts',(-104.769946832556,-1.00789485200844,
135.620183432228));
#100138=CARTESIAN_POINT('Ctrl Pts',(-104.77769310864,-0.873092716044913,
135.646438682476));
#100139=CARTESIAN_POINT('Ctrl Pts',(-104.785439384725,-0.737429371895126,
135.667012258797));
#100140=CARTESIAN_POINT('Ctrl Pts',(-104.79318571799,-0.601765026309906,
135.687585986988));
#100141=CARTESIAN_POINT('Ctrl Pts',(-104.800932051255,-0.465239846398554,
135.702477898943));
#100142=CARTESIAN_POINT('Ctrl Pts',(-104.80867838452,-0.328367380854038,
135.711636636468));
#100143=CARTESIAN_POINT('Ctrl Pts',(-104.816426452523,-0.191464263670057,
135.720797425029));
#100144=CARTESIAN_POINT('Ctrl Pts',(-104.824174520526,-0.0542140961134072,
135.724222458242));
#100145=CARTESIAN_POINT('Ctrl Pts',(-104.831922588529,0.0828672700156155,
135.721912455428));
#100146=CARTESIAN_POINT('Ctrl Pts',(-104.839678891271,0.220094327852036,
135.719599997516));
#100147=CARTESIAN_POINT('Ctrl Pts',(-104.847435194013,0.357151834348657,
135.711540334229));
#100148=CARTESIAN_POINT('Ctrl Pts',(-104.855191496755,0.493526203479473,
135.697786304033));
#100149=CARTESIAN_POINT('Ctrl Pts',(-104.862951939269,0.629973359717618,
135.684024932898));
#100150=CARTESIAN_POINT('Ctrl Pts',(-104.870712381783,0.765736265252047,
135.664563194333));
#100151=CARTESIAN_POINT('Ctrl Pts',(-104.878472824297,0.900310247688287,
135.639505343467));
#100152=CARTESIAN_POINT('Ctrl Pts',(-104.886245724563,1.03510026022768,
135.614407267514));
#100153=CARTESIAN_POINT('Ctrl Pts',(-104.894018624828,1.16869715450211,
135.583695215254));
#100154=CARTESIAN_POINT('Ctrl Pts',(-104.901791525094,1.30060929788147,
135.547523962504));
#100155=CARTESIAN_POINT('Ctrl Pts',(-104.909281860856,1.42772610258021,
135.512667625902));
#100156=CARTESIAN_POINT('Ctrl Pts',(-104.916772196617,1.55327822612299,
135.472742202568));
#100157=CARTESIAN_POINT('Ctrl Pts',(-104.924262532379,1.67684404949931,
135.427928189924));
#100158=CARTESIAN_POINT('Ctrl Pts',(-104.932036866498,1.80509490862829,
135.381415040368));
#100159=CARTESIAN_POINT('Ctrl Pts',(-104.939811200617,1.93161213331215,
135.329487942329));
#100160=CARTESIAN_POINT('Ctrl Pts',(-104.947585534736,2.05590475973382,
135.2722951159));
#100161=CARTESIAN_POINT('Ctrl Pts',(-104.955350287684,2.1800442066011,135.215172774518));
#100162=CARTESIAN_POINT('Ctrl Pts',(-104.963115040631,2.30196415845116,
135.152797778857));
#100163=CARTESIAN_POINT('Ctrl Pts',(-104.970879793578,2.42119018925418,
135.085367640447));
#100164=CARTESIAN_POINT('Ctrl Pts',(-104.978636834463,2.54029780308294,
135.018004474602));
#100165=CARTESIAN_POINT('Ctrl Pts',(-104.986393875348,2.65671648240282,
134.945596348927));
#100166=CARTESIAN_POINT('Ctrl Pts',(-104.994150916233,2.76999345734827,
134.868388091482));
#100167=CARTESIAN_POINT('Ctrl Pts',(-105.001902107473,2.8831850092459,134.791238057386));
#100168=CARTESIAN_POINT('Ctrl Pts',(-105.009653298713,2.99323925073205,
134.709295315848));
#100169=CARTESIAN_POINT('Ctrl Pts',(-105.017404489953,3.09972994527334,
134.622849497853));
#100170=CARTESIAN_POINT('Ctrl Pts',(-105.02515238673,3.20617537842858,134.536440421636));
#100171=CARTESIAN_POINT('Ctrl Pts',(-105.032900283507,3.30905997416121,
134.445532321508));
#100172=CARTESIAN_POINT('Ctrl Pts',(-105.040648180284,3.40798850316221,
134.350456699853));
#100173=CARTESIAN_POINT('Ctrl Pts',(-105.048394456368,3.50689633844732,
134.25540096597));
#100174=CARTESIAN_POINT('Ctrl Pts',(-105.056140732452,3.60184947128084,
134.156179715268));
#100175=CARTESIAN_POINT('Ctrl Pts',(-105.063887008536,3.69248795498802,
134.05316282219));
#100176=CARTESIAN_POINT('Ctrl Pts',(-105.071633341802,3.78312710776778,
133.950145168664));
#100177=CARTESIAN_POINT('Ctrl Pts',(-105.079379675067,3.86945128961112,
133.843332110378));
#100178=CARTESIAN_POINT('Ctrl Pts',(-105.087126008332,3.95113970580277,
133.733127950033));
#100179=CARTESIAN_POINT('Ctrl Pts',(-105.094874076335,4.0328464155494,133.622899110231));
#100180=CARTESIAN_POINT('Ctrl Pts',(-105.102622144338,4.10991506107959,
133.509277971251));
#100181=CARTESIAN_POINT('Ctrl Pts',(-105.110370212341,4.1820674170817,133.392698922634));
#100182=CARTESIAN_POINT('Ctrl Pts',(-105.118126515083,4.2542964574661,133.275995972418));
#100183=CARTESIAN_POINT('Ctrl Pts',(-105.125882817825,4.32159856455811,
133.156329165658));
#100184=CARTESIAN_POINT('Ctrl Pts',(-105.133639120567,4.38374058706518,
133.034159157304));
#100185=CARTESIAN_POINT('Ctrl Pts',(-105.141399563081,4.44591577664072,
132.911923943138));
#100186=CARTESIAN_POINT('Ctrl Pts',(-105.149160005595,4.50292523143581,
132.787183220634));
#100187=CARTESIAN_POINT('Ctrl Pts',(-105.156920448109,4.55458387648579,
132.660417937412));
#100188=CARTESIAN_POINT('Ctrl Pts',(-105.164693348375,4.60632544857885,
132.533449159305));
#100189=CARTESIAN_POINT('Ctrl Pts',(-105.17246624864,4.65269891384318,132.404449694061));
#100190=CARTESIAN_POINT('Ctrl Pts',(-105.180239148906,4.69356875011187,
132.273916826247));
#100191=CARTESIAN_POINT('Ctrl Pts',(-105.187729484668,4.73295286488795,
132.148129156969));
#100192=CARTESIAN_POINT('Ctrl Pts',(-105.19521982043,4.76722646504752,132.020917933062));
#100193=CARTESIAN_POINT('Ctrl Pts',(-105.202710156192,4.79631351280986,
131.892735437808));
#100194=CARTESIAN_POINT('Ctrl Pts',(-105.210484490311,4.82650340482854,
131.759692864288));
#100195=CARTESIAN_POINT('Ctrl Pts',(-105.21825882443,4.85120131689324,131.625182475128));
#100196=CARTESIAN_POINT('Ctrl Pts',(-105.226033158549,4.87026657283051,
131.489697448672));
#100197=CARTESIAN_POINT('Ctrl Pts',(-105.233797911496,4.88930833254364,
131.354379395403));
#100198=CARTESIAN_POINT('Ctrl Pts',(-105.241562664443,4.90273119417715,
131.218089478209));
#100199=CARTESIAN_POINT('Ctrl Pts',(-105.249327417391,4.91044489091943,
131.081333604955));
#100200=CARTESIAN_POINT('Ctrl Pts',(-105.257084458276,4.91815092630938,
130.944713559562));
#100201=CARTESIAN_POINT('Ctrl Pts',(-105.26484149916,4.92015905933097,130.807628866907));
#100202=CARTESIAN_POINT('Ctrl Pts',(-105.272598540045,4.91643053759352,
130.67059279065));
#100203=CARTESIAN_POINT('Ctrl Pts',(-105.280349731286,4.9127048275633,130.533660054363));
#100204=CARTESIAN_POINT('Ctrl Pts',(-105.288100922526,4.9032510841166,130.396776250738));
#100205=CARTESIAN_POINT('Ctrl Pts',(-105.295852113766,4.88808259074364,
130.260456537264));
#100206=CARTESIAN_POINT('Ctrl Pts',(-105.303600010543,4.87292054438506,
130.124194763305));
#100207=CARTESIAN_POINT('Ctrl Pts',(-105.31134790732,4.85204862218518,129.988496990399));
#100208=CARTESIAN_POINT('Ctrl Pts',(-105.319095804097,4.82553209539436,
129.853874921293));
#100209=CARTESIAN_POINT('Ctrl Pts',(-105.326842080181,4.79902111528932,
129.719281012223));
#100210=CARTESIAN_POINT('Ctrl Pts',(-105.334588356266,4.7668679546381,129.585762742739));
#100211=CARTESIAN_POINT('Ctrl Pts',(-105.34233463235,4.72918923931268,129.453822872344));
#100212=CARTESIAN_POINT('Ctrl Pts',(-105.350080965615,4.6915102458515,129.321882027999));
#100213=CARTESIAN_POINT('Ctrl Pts',(-105.35782729888,4.64830572368379,129.191519981928));
#100214=CARTESIAN_POINT('Ctrl Pts',(-105.365573632146,4.59974242674365,
129.063225163296));
#100215=CARTESIAN_POINT('Ctrl Pts',(-105.373321700149,4.5511682543898,128.93490161393));
#100216=CARTESIAN_POINT('Ctrl Pts',(-105.381069768152,4.49723305766329,
128.808646578779));
#100217=CARTESIAN_POINT('Ctrl Pts',(-105.388817836155,4.43815191321042,
128.684928934834));
#100218=CARTESIAN_POINT('Ctrl Pts',(-105.396574138896,4.3790079766144,128.561079802306));
#100219=CARTESIAN_POINT('Ctrl Pts',(-105.404330441638,4.31470733577502,
128.439773801437));
#100220=CARTESIAN_POINT('Ctrl Pts',(-105.41208674438,4.24551152878097,128.321456084265));
#100221=CARTESIAN_POINT('Ctrl Pts',(-105.419847186894,4.17627878990128,
128.203075217364));
#100222=CARTESIAN_POINT('Ctrl Pts',(-105.427607629408,4.10214589006745,
128.087686140979));
#100223=CARTESIAN_POINT('Ctrl Pts',(-105.435368071923,4.02341742659575,
127.975704527854));
#100224=CARTESIAN_POINT('Ctrl Pts',(-105.443140972188,3.94456258120508,
127.863543151902));
#100225=CARTESIAN_POINT('Ctrl Pts',(-105.450913872453,3.8610976683509,127.754800480259));
#100226=CARTESIAN_POINT('Ctrl Pts',(-105.458686772719,3.77336781458023,
127.649859326016));
#100227=CARTESIAN_POINT('Ctrl Pts',(-105.466177108481,3.6888271619723,127.548733047061));
#100228=CARTESIAN_POINT('Ctrl Pts',(-105.473667444243,3.60032647455756,
127.451136922741));
#100229=CARTESIAN_POINT('Ctrl Pts',(-105.481157780005,3.50820517079095,
127.357379395955));
#100230=CARTESIAN_POINT('Ctrl Pts',(-105.488932114124,3.41259105979224,
127.260067024045));
#100231=CARTESIAN_POINT('Ctrl Pts',(-105.496706448243,3.31277348461028,
127.166581820203));
#100232=CARTESIAN_POINT('Ctrl Pts',(-105.504480782362,3.20909133124621,
127.077308714222));
#100233=CARTESIAN_POINT('Ctrl Pts',(-105.512245535309,3.10553695687011,
126.988145629365));
#100234=CARTESIAN_POINT('Ctrl Pts',(-105.520010288257,2.99812777418872,
126.903184566408));
#100235=CARTESIAN_POINT('Ctrl Pts',(-105.527775041204,2.88724062639873,
126.822774924934));
#100236=CARTESIAN_POINT('Ctrl Pts',(-105.535532082089,2.77646361328686,
126.742445147449));
#100237=CARTESIAN_POINT('Ctrl Pts',(-105.543289122974,2.66221582386565,
126.666658023405));
#100238=CARTESIAN_POINT('Ctrl Pts',(-105.551046163859,2.54490813477318,
126.59572358783));
#100239=CARTESIAN_POINT('Ctrl Pts',(-105.558797355099,2.42768890832237,
126.524842644465));
#100240=CARTESIAN_POINT('Ctrl Pts',(-105.566548546339,2.30741470832992,
126.45880730714));
#100241=CARTESIAN_POINT('Ctrl Pts',(-105.574299737579,2.18452613143105,
126.397884855282));
#100242=CARTESIAN_POINT('Ctrl Pts',(-105.582047634356,2.06168978545502,
126.336988297091));
#100243=CARTESIAN_POINT('Ctrl Pts',(-105.589795531133,1.93624162217422,
126.281200475503));
#100244=CARTESIAN_POINT('Ctrl Pts',(-105.59754342791,1.808647432308,126.230743063801));
#100245=CARTESIAN_POINT('Ctrl Pts',(-105.605289703994,1.68107993239568,
126.180296206702));
#100246=CARTESIAN_POINT('Ctrl Pts',(-105.613035980078,1.5513676621287,126.135177685362));
#100247=CARTESIAN_POINT('Ctrl Pts',(-105.620782256162,1.41999664644693,
126.095561132922));
#100248=CARTESIAN_POINT('Ctrl Pts',(-105.628528589428,1.288624661014,126.055944288043));
#100249=CARTESIAN_POINT('Ctrl Pts',(-105.636274922693,1.1555942800487,126.021829605987));
#100250=CARTESIAN_POINT('Ctrl Pts',(-105.644021255959,1.02140656741542,
125.993340799841));
#100251=CARTESIAN_POINT('Ctrl Pts',(-105.651769323961,0.887188804374838,
125.964845613825));
#100252=CARTESIAN_POINT('Ctrl Pts',(-105.659517391965,0.75181357630323,
125.941978891905));
#100253=CARTESIAN_POINT('Ctrl Pts',(-105.667265459967,0.615791616874018,
125.924813123475));
#100254=CARTESIAN_POINT('Ctrl Pts',(-105.675021762709,0.479625091687086,
125.907629111062));
#100255=CARTESIAN_POINT('Ctrl Pts',(-105.682778065451,0.342810850586459,
125.896158204755));
#100256=CARTESIAN_POINT('Ctrl Pts',(-105.690534368193,0.205864780315405,
125.890420980704));
#100257=CARTESIAN_POINT('Ctrl Pts',(-105.698294810707,0.0688456178032804,
125.884680694523));
#100258=CARTESIAN_POINT('Ctrl Pts',(-105.706055253221,-0.068305123305999,
125.884680188385));
#100259=CARTESIAN_POINT('Ctrl Pts',(-105.713815695736,-0.205073083468483,
125.890387877213));
#100260=CARTESIAN_POINT('Ctrl Pts',(-105.721588596001,-0.342060595702309,
125.896104728529));
#100261=CARTESIAN_POINT('Ctrl Pts',(-105.729361496266,-0.47866370924976,
125.907548053352));
#100262=CARTESIAN_POINT('Ctrl Pts',(-105.737134396532,-0.614373803286218,
125.924634406769));
#100263=CARTESIAN_POINT('Ctrl Pts',(-105.744624732294,-0.745150493571723,
125.941099628202));
#100264=CARTESIAN_POINT('Ctrl Pts',(-105.752115068056,-0.875097660325476,
125.962804673881));
#100265=CARTESIAN_POINT('Ctrl Pts',(-105.759605403818,-1.00377233783546,
125.989630702369));
#100266=CARTESIAN_POINT('Ctrl Pts',(-105.767379737937,-1.13732575485286,
126.01747384788));
#100267=CARTESIAN_POINT('Ctrl Pts',(-105.775154072056,-1.26993134204901,
126.050922164682));
#100268=CARTESIAN_POINT('Ctrl Pts',(-105.782928406175,-1.40108207092772,
126.089898602338));
#100269=CARTESIAN_POINT('Ctrl Pts',(-105.790693159122,-1.53207116825331,
126.128827005019));
#100270=CARTESIAN_POINT('Ctrl Pts',(-105.798457912069,-1.66160860359512,
126.173269862577));
#100271=CARTESIAN_POINT('Ctrl Pts',(-105.806222665016,-1.78919672423613,
126.223098985168));
#100272=CARTESIAN_POINT('Ctrl Pts',(-105.813979705901,-1.91665812255705,
126.272878616772));
#100273=CARTESIAN_POINT('Ctrl Pts',(-105.821736746786,-2.04217369725687,
126.328033725928));
#100274=CARTESIAN_POINT('Ctrl Pts',(-105.829493787671,-2.16526051822668,
126.388386211989));
#100275=CARTESIAN_POINT('Ctrl Pts',(-105.837244978912,-2.28825451846816,
126.448693185772));
#100276=CARTESIAN_POINT('Ctrl Pts',(-105.844996170152,-2.40882306093549,
126.514189563741));
#100277=CARTESIAN_POINT('Ctrl Pts',(-105.852747361392,-2.52650312263188,
126.584649130529));
#100278=CARTESIAN_POINT('Ctrl Pts',(-105.860495258169,-2.64413316716267,
126.655078750122));
#100279=CARTESIAN_POINT('Ctrl Pts',(-105.868243154946,-2.75887683795299,
126.730467162505));
#100280=CARTESIAN_POINT('Ctrl Pts',(-105.875991051723,-2.87029586373044,
126.810542304579));
#100281=CARTESIAN_POINT('Ctrl Pts',(-105.883737327807,-2.98169158304962,
126.890600696659));
#100282=CARTESIAN_POINT('Ctrl Pts',(-105.891483603891,-3.08976372335384,
126.975343640412));
#100283=CARTESIAN_POINT('Ctrl Pts',(-105.899229879975,-3.19410349381147,
127.064456082244));
#100284=CARTESIAN_POINT('Ctrl Pts',(-105.906976213241,-3.29844403448201,
127.153569181885));
#100285=CARTESIAN_POINT('Ctrl Pts',(-105.914722546506,-3.3990518530336,
127.247051590059));
#100286=CARTESIAN_POINT('Ctrl Pts',(-105.922468879771,-3.4955520288846,
127.344548617491));
#100287=CARTESIAN_POINT('Ctrl Pts',(-105.930216947774,-3.59207381528024,
127.442067478707));
#100288=CARTESIAN_POINT('Ctrl Pts',(-105.937965015777,-3.68448585354708,
127.543602470361));
#100289=CARTESIAN_POINT('Ctrl Pts',(-105.94571308378,-3.77245109227978,
127.648763080037));
#100290=CARTESIAN_POINT('Ctrl Pts',(-105.953469386522,-3.86050982151513,
127.754035455661));
#100291=CARTESIAN_POINT('Ctrl Pts',(-105.961225689264,-3.94411205905247,
127.862940846428));
#100292=CARTESIAN_POINT('Ctrl Pts',(-105.968981992006,-4.02296164420858,
127.975056344122));
#100293=CARTESIAN_POINT('Ctrl Pts',(-105.97674243452,-4.10185331376239,
128.087231681233));
#100294=CARTESIAN_POINT('Ctrl Pts',(-105.984502877034,-4.17598706525354,
128.202620210459));
#100295=CARTESIAN_POINT('Ctrl Pts',(-105.992263319548,-4.24511144820341,
128.320772114043));
#100296=CARTESIAN_POINT('Ctrl Pts',(-106.000036219814,-4.31434679574956,
128.439113685552));
#100297=CARTESIAN_POINT('Ctrl Pts',(-106.007809120079,-4.37855652207327,
128.560227150366));
#100298=CARTESIAN_POINT('Ctrl Pts',(-106.015582020345,-4.43753590976266,
128.683639487368));
#100299=CARTESIAN_POINT('Ctrl Pts',(-106.023072356107,-4.49437124815023,
128.802565475065));
#100300=CARTESIAN_POINT('Ctrl Pts',(-106.030562691869,-4.54634979626853,
128.923625814116));
#100301=CARTESIAN_POINT('Ctrl Pts',(-106.038053027631,-4.59333210499773,
129.046383588223));
#100302=CARTESIAN_POINT('Ctrl Pts',(-106.046937466579,-4.64905877290856,
129.19198907029));
#100303=CARTESIAN_POINT('Ctrl Pts',(-106.055821905528,-4.69790417122911,
129.340366392219));
#100304=CARTESIAN_POINT('Ctrl Pts',(-106.064706344476,-4.73961983046872,
129.490896904657));
#100305=CARTESIAN_POINT('Ctrl Pts',(-106.066503223472,-4.74805682827102,
129.521341721442));
#100306=CARTESIAN_POINT('Ctrl Pts',(-106.068300102468,-4.75620233512269,
129.551874537541));
#100307=CARTESIAN_POINT('Ctrl Pts',(-106.070096981463,-4.76405452823408,
129.582490119308));
#100308=CARTESIAN_POINT('Origin',(213.235140564004,0.,130.804360617566));
#100309=CARTESIAN_POINT('',(-108.165013787364,-4.76405452823416,129.582490119309));
#100310=CARTESIAN_POINT('',(-107.819991607676,-4.76405452823401,129.582490119308));
#100311=CARTESIAN_POINT('',(213.235140564004,-4.76405452823405,129.582490119308));
#100312=CARTESIAN_POINT('',(-106.48514056406,-4.91824839459279,130.808334480353));
#100313=CARTESIAN_POINT('Ctrl Pts',(-106.485140564059,-4.91824839459279,
130.808334480353));
#100314=CARTESIAN_POINT('Ctrl Pts',(-106.49424843149,-4.91811808858843,
130.969607612091));
#100315=CARTESIAN_POINT('Ctrl Pts',(-106.50335629892,-4.91005153646411,
131.130544562526));
#100316=CARTESIAN_POINT('Ctrl Pts',(-106.512464166351,-4.89417093461805,
131.290440780955));
#100317=CARTESIAN_POINT('Ctrl Pts',(-106.521632239911,-4.87818535654372,
131.451393968262));
#100318=CARTESIAN_POINT('Ctrl Pts',(-106.530800313471,-4.85428218621434,
131.611292547037));
#100319=CARTESIAN_POINT('Ctrl Pts',(-106.539968387031,-4.82263498104052,
131.769438283945));
#100320=CARTESIAN_POINT('Ctrl Pts',(-106.549204021272,-4.79075456365281,
131.928749416573));
#100321=CARTESIAN_POINT('Ctrl Pts',(-106.558439655513,-4.7510156272781,
132.086281709925));
#100322=CARTESIAN_POINT('Ctrl Pts',(-106.567675289754,-4.70364375126848,
132.24134305436));
#100323=CARTESIAN_POINT('Ctrl Pts',(-106.570236619535,-4.69050605074448,
132.284346407354));
#100324=CARTESIAN_POINT('Ctrl Pts',(-106.572797949316,-4.67678156078555,
132.327159843967));
#100325=CARTESIAN_POINT('Ctrl Pts',(-106.575359279097,-4.66247573275551,
132.369768904233));
#100326=CARTESIAN_POINT('Ctrl Pts',(-106.583133613216,-4.61905364483081,
132.499099017622));
#100327=CARTESIAN_POINT('Ctrl Pts',(-106.590907947335,-4.57017756505967,
132.626825915645));
#100328=CARTESIAN_POINT('Ctrl Pts',(-106.598682281454,-4.51598388907358,
132.752455218998));
#100329=CARTESIAN_POINT('Ctrl Pts',(-106.606447034401,-4.4618570019497,
132.877929695462));
#100330=CARTESIAN_POINT('Ctrl Pts',(-106.614211787348,-4.40242571141989,
133.001311365288));
#100331=CARTESIAN_POINT('Ctrl Pts',(-106.621976540295,-4.3378760872215,
133.122121199337));
#100332=CARTESIAN_POINT('Ctrl Pts',(-106.62973358118,-4.27339057462002,
133.242811043356));
#100333=CARTESIAN_POINT('Ctrl Pts',(-106.637490622065,-4.20379702799861,
133.360933792337));
#100334=CARTESIAN_POINT('Ctrl Pts',(-106.64524766295,-4.12932933968496,
133.476030931605));
#100335=CARTESIAN_POINT('Ctrl Pts',(-106.65299885419,-4.05491780803404,
133.591041275225));
#100336=CARTESIAN_POINT('Ctrl Pts',(-106.66075004543,-3.97563966232488,
133.703030223665));
#100337=CARTESIAN_POINT('Ctrl Pts',(-106.66850123667,-3.89177422163134,
133.811564712792));
#100338=CARTESIAN_POINT('Ctrl Pts',(-106.676249133448,-3.80794442598738,
133.920053071866));
#100339=CARTESIAN_POINT('Ctrl Pts',(-106.683997030225,-3.71953145175937,
134.02508958312));
#100340=CARTESIAN_POINT('Ctrl Pts',(-106.691744927002,-3.62685722145508,
134.126271175916));
#100341=CARTESIAN_POINT('Ctrl Pts',(-106.699491203086,-3.53420237660195,
134.227431603705));
#100342=CARTESIAN_POINT('Ctrl Pts',(-106.70723747917,-3.43728831254272,
134.324738428817));
#100343=CARTESIAN_POINT('Ctrl Pts',(-106.714983755254,-3.33647615947514,
134.417822932266));
#100344=CARTESIAN_POINT('Ctrl Pts',(-106.72273008852,-3.23566326223529,
134.510908122843));
#100345=CARTESIAN_POINT('Ctrl Pts',(-106.730476421785,-3.1309525058131,
134.599770664338));
#100346=CARTESIAN_POINT('Ctrl Pts',(-106.73822275505,-3.0227403782926,134.684080152267));
#100347=CARTESIAN_POINT('Ctrl Pts',(-106.745970823053,-2.91450401741658,
134.768408520721));
#100348=CARTESIAN_POINT('Ctrl Pts',(-106.753718891056,-2.8027650335091,
134.848181566432));
#100349=CARTESIAN_POINT('Ctrl Pts',(-106.761466959059,-2.68795101437728,
134.923110720062));
#100350=CARTESIAN_POINT('Ctrl Pts',(-106.769223261801,-2.57301496953946,
134.998119509287));
#100351=CARTESIAN_POINT('Ctrl Pts',(-106.776979564543,-2.45499768886047,
135.06827390844));
#100352=CARTESIAN_POINT('Ctrl Pts',(-106.784735867285,-2.33435409964669,
135.133329778921));
#100353=CARTESIAN_POINT('Ctrl Pts',(-106.792496309799,-2.21364611931651,
135.198420371679));
#100354=CARTESIAN_POINT('Ctrl Pts',(-106.800256752313,-2.09030938878064,
135.258406842552));
#100355=CARTESIAN_POINT('Ctrl Pts',(-106.808017194827,-1.96482027587102,
135.313092628456));
#100356=CARTESIAN_POINT('Ctrl Pts',(-106.815790095093,-1.83912971669696,
135.367866200838));
#100357=CARTESIAN_POINT('Ctrl Pts',(-106.823562995358,-1.71128023541256,
135.417321943166));
#100358=CARTESIAN_POINT('Ctrl Pts',(-106.831335895624,-1.58176572121906,
135.461312438841));
#100359=CARTESIAN_POINT('Ctrl Pts',(-106.838826231386,-1.45695938584211,
135.503703769193));
#100360=CARTESIAN_POINT('Ctrl Pts',(-106.846316567148,-1.33060726752646,
135.541020218017));
#100361=CARTESIAN_POINT('Ctrl Pts',(-106.85380690291,-1.20315969460859,
135.573174915876));
#100362=CARTESIAN_POINT('Ctrl Pts',(-106.861581237029,-1.07087990822838,
135.606548768878));
#100363=CARTESIAN_POINT('Ctrl Pts',(-106.869355571148,-0.93700093652646,
135.634467447008));
#100364=CARTESIAN_POINT('Ctrl Pts',(-106.877129905267,-0.802012439984278,
135.656778479685));
#100365=CARTESIAN_POINT('Ctrl Pts',(-106.884894658214,-0.667190304699816,
135.679062016008));
#100366=CARTESIAN_POINT('Ctrl Pts',(-106.892659411162,-0.531261747303075,
135.695751594409));
#100367=CARTESIAN_POINT('Ctrl Pts',(-106.900424164109,-0.39473036381357,
135.706744833678));
#100368=CARTESIAN_POINT('Ctrl Pts',(-106.908181204994,-0.258334585218901,
135.717727154307));
#100369=CARTESIAN_POINT('Ctrl Pts',(-106.915938245879,-0.121337559224111,
135.723024363676));
#100370=CARTESIAN_POINT('Ctrl Pts',(-106.923695286764,0.0157485282706149,
135.72258540364));
#100371=CARTESIAN_POINT('Ctrl Pts',(-106.931446478004,0.1527312380802,135.722146774629));
#100372=CARTESIAN_POINT('Ctrl Pts',(-106.939197669244,0.289802486326624,
135.715980587483));
#100373=CARTESIAN_POINT('Ctrl Pts',(-106.946948860484,0.426446945107832,
135.704087759511));
#100374=CARTESIAN_POINT('Ctrl Pts',(-106.954696757261,0.563033326349133,
135.692199986307));
#100375=CARTESIAN_POINT('Ctrl Pts',(-106.962444654038,0.699192890232504,
135.674590447095));
#100376=CARTESIAN_POINT('Ctrl Pts',(-106.970192550815,0.834412515037491,
135.651312114873));
#100377=CARTESIAN_POINT('Ctrl Pts',(-106.9779388269,0.969603854811967,135.628038651977));
#100378=CARTESIAN_POINT('Ctrl Pts',(-106.985685102984,1.10385526153267,
135.599098820959));
#100379=CARTESIAN_POINT('Ctrl Pts',(-106.993431379068,1.2366613217813,135.564597149264));
#100380=CARTESIAN_POINT('Ctrl Pts',(-107.001177712333,1.36946836237391,
135.530095222885));
#100381=CARTESIAN_POINT('Ctrl Pts',(-107.008924045599,1.50082965680052,
135.490031472211));
#100382=CARTESIAN_POINT('Ctrl Pts',(-107.016670378864,1.6302529149167,135.4445608822));
#100383=CARTESIAN_POINT('Ctrl Pts',(-107.024418446867,1.75970515647435,
135.399080109365));
#100384=CARTESIAN_POINT('Ctrl Pts',(-107.03216651487,1.88721812930065,135.348190217363));
#100385=CARTESIAN_POINT('Ctrl Pts',(-107.039914582873,2.01231793018225,
135.292094969148));
#100386=CARTESIAN_POINT('Ctrl Pts',(-107.047670885615,2.13755068862111,
135.235940102235));
#100387=CARTESIAN_POINT('Ctrl Pts',(-107.055427188357,2.26036479444397,
135.174568987935));
#100388=CARTESIAN_POINT('Ctrl Pts',(-107.063183491099,2.38030894761148,
135.108232406597));
#100389=CARTESIAN_POINT('Ctrl Pts',(-107.070943933613,2.50031711858497,
135.041860419429));
#100390=CARTESIAN_POINT('Ctrl Pts',(-107.078704376127,2.61745195095748,
134.970517887709));
#100391=CARTESIAN_POINT('Ctrl Pts',(-107.086464818641,2.73129058219,134.894499346037));
#100392=CARTESIAN_POINT('Ctrl Pts',(-107.094237718907,2.8453119572995,134.818358772653));
#100393=CARTESIAN_POINT('Ctrl Pts',(-107.102010619172,2.95602624151052,
134.737527419915));
#100394=CARTESIAN_POINT('Ctrl Pts',(-107.109783519438,3.06304244988668,
134.652341128521));
#100395=CARTESIAN_POINT('Ctrl Pts',(-107.117273855199,3.16616834952791,
134.570251573394));
#100396=CARTESIAN_POINT('Ctrl Pts',(-107.124764190961,3.26586014104743,
134.484118409874));
#100397=CARTESIAN_POINT('Ctrl Pts',(-107.132254526723,3.3618013252633,134.394273556894));
#100398=CARTESIAN_POINT('Ctrl Pts',(-107.140028860842,3.4613801486418,134.301022209004));
#100399=CARTESIAN_POINT('Ctrl Pts',(-107.147803194961,3.55723377763119,
134.203476765943));
#100400=CARTESIAN_POINT('Ctrl Pts',(-107.15557752908,3.64896926096127,134.101966778868));
#100401=CARTESIAN_POINT('Ctrl Pts',(-107.163342282027,3.74059168850678,
134.000581893781));
#100402=CARTESIAN_POINT('Ctrl Pts',(-107.171107034974,3.82810580900147,
133.895242473538));
#100403=CARTESIAN_POINT('Ctrl Pts',(-107.178871787922,3.91115328028357,
133.786316868189));
#100404=CARTESIAN_POINT('Ctrl Pts',(-107.186628828807,3.99411826764643,
133.677499449286));
#100405=CARTESIAN_POINT('Ctrl Pts',(-107.194385869692,4.07262519880145,
133.565103242415));
#100406=CARTESIAN_POINT('Ctrl Pts',(-107.202142910576,4.14635426809657,
133.449531565905));
#100407=CARTESIAN_POINT('Ctrl Pts',(-107.209894101817,4.22002773772709,
133.334047042895));
#100408=CARTESIAN_POINT('Ctrl Pts',(-107.217645293057,4.28893030767497,
133.215392144917));
#100409=CARTESIAN_POINT('Ctrl Pts',(-107.225396484297,4.35278420237677,
133.094000927754));
#100410=CARTESIAN_POINT('Ctrl Pts',(-107.233144381074,4.41661095746987,
132.972661305097));
#100411=CARTESIAN_POINT('Ctrl Pts',(-107.240892277851,4.47539312356383,
132.848588021683));
#100412=CARTESIAN_POINT('Ctrl Pts',(-107.248640174628,4.52889791351924,
132.722241414545));
#100413=CARTESIAN_POINT('Ctrl Pts',(-107.256386450712,4.58239151142601,
132.595921236394));
#100414=CARTESIAN_POINT('Ctrl Pts',(-107.264132726796,4.63060977657732,
132.467329040163));
#100415=CARTESIAN_POINT('Ctrl Pts',(-107.27187900288,4.67336746257489,132.336946544112));
#100416=CARTESIAN_POINT('Ctrl Pts',(-107.279625336146,4.71612546420004,
132.206563085606));
#100417=CARTESIAN_POINT('Ctrl Pts',(-107.287371669411,4.75342268440877,
132.074389672409));
#100418=CARTESIAN_POINT('Ctrl Pts',(-107.295118002677,4.78512342158928,
131.940924255317));
#100419=CARTESIAN_POINT('Ctrl Pts',(-107.30286607068,4.81683125793005,131.80742894957));
#100420=CARTESIAN_POINT('Ctrl Pts',(-107.310614138682,4.84294002700223,
131.672641444495));
#100421=CARTESIAN_POINT('Ctrl Pts',(-107.318362206685,4.86336500408786,
131.53707058714));
#100422=CARTESIAN_POINT('Ctrl Pts',(-107.326118509427,4.88381168908217,
131.401355643465));
#100423=CARTESIAN_POINT('Ctrl Pts',(-107.333874812169,4.89856245659972,
131.264856071609));
#100424=CARTESIAN_POINT('Ctrl Pts',(-107.341631114911,4.90758435655711,
131.128087115981));
#100425=CARTESIAN_POINT('Ctrl Pts',(-107.349391557425,4.91661107177417,
130.991245162643));
#100426=CARTESIAN_POINT('Ctrl Pts',(-107.357151999939,4.9199028173875,130.854133929705));
#100427=CARTESIAN_POINT('Ctrl Pts',(-107.364912442454,4.91747882616643,
130.717268386542));
#100428=CARTESIAN_POINT('Ctrl Pts',(-107.372685342719,4.91505094373946,
130.580183134658));
#100429=CARTESIAN_POINT('Ctrl Pts',(-107.380458242984,4.90688901238055,
130.44334475119));
#100430=CARTESIAN_POINT('Ctrl Pts',(-107.38823114325,4.89306424747406,130.307263712938));
#100431=CARTESIAN_POINT('Ctrl Pts',(-107.395721479012,4.87974204759436,
130.176129563193));
#100432=CARTESIAN_POINT('Ctrl Pts',(-107.403211814774,4.86116162613072,
130.045698956764));
#100433=CARTESIAN_POINT('Ctrl Pts',(-107.410702150536,4.83743116034206,
129.916417583666));
#100434=CARTESIAN_POINT('Ctrl Pts',(-107.418476484655,4.81280094673047,
129.782234468014));
#100435=CARTESIAN_POINT('Ctrl Pts',(-107.426250818774,4.78254443067672,
129.648864400575));
#100436=CARTESIAN_POINT('Ctrl Pts',(-107.434025152893,4.74672647314242,
129.516816112833));
#100437=CARTESIAN_POINT('Ctrl Pts',(-107.44178990584,4.71095265803954,129.384930562803));
#100438=CARTESIAN_POINT('Ctrl Pts',(-107.449554658787,4.66963114020049,
129.254363925003));
#100439=CARTESIAN_POINT('Ctrl Pts',(-107.457319411734,4.62287813026192,
129.125616785039));
#100440=CARTESIAN_POINT('Ctrl Pts',(-107.465076452619,4.57617155607191,
128.99699751855));
#100441=CARTESIAN_POINT('Ctrl Pts',(-107.472833493504,4.52404435793295,
128.870194518694));
#100442=CARTESIAN_POINT('Ctrl Pts',(-107.480590534389,4.46666299621196,
128.745694850432));
#100443=CARTESIAN_POINT('Ctrl Pts',(-107.48834172563,4.40932490622228,128.621289068338));
#100444=CARTESIAN_POINT('Ctrl Pts',(-107.49609291687,4.34674070216743,128.499183514154));
#100445=CARTESIAN_POINT('Ctrl Pts',(-107.50384410811,4.27912542299531,128.379846506084));
#100446=CARTESIAN_POINT('Ctrl Pts',(-107.511592004887,4.21153888212043,
128.260560219425));
#100447=CARTESIAN_POINT('Ctrl Pts',(-107.519339901664,4.13892571145353,
128.144040477949));
#100448=CARTESIAN_POINT('Ctrl Pts',(-107.527087798441,4.06154737844507,
128.03073195548));
#100449=CARTESIAN_POINT('Ctrl Pts',(-107.534834074525,3.984185231316,127.917447134711));
#100450=CARTESIAN_POINT('Ctrl Pts',(-107.542580350609,3.90206012481772,
127.807372519526));
#100451=CARTESIAN_POINT('Ctrl Pts',(-107.550326626693,3.81547721196221,
127.70092434345));
#100452=CARTESIAN_POINT('Ctrl Pts',(-107.558072959959,3.72889365997118,
127.594475381599));
#100453=CARTESIAN_POINT('Ctrl Pts',(-107.565819293224,3.63785248266103,
127.491653215577));
#100454=CARTESIAN_POINT('Ctrl Pts',(-107.573565626489,3.54269927010443,
127.392841169563));
#100455=CARTESIAN_POINT('Ctrl Pts',(-107.581313694492,3.44752474864576,
127.294006995277));
#100456=CARTESIAN_POINT('Ctrl Pts',(-107.589061762495,3.34823663067146,
127.199185009557));
#100457=CARTESIAN_POINT('Ctrl Pts',(-107.596809830498,3.24521722783572,
127.108721537967));
#100458=CARTESIAN_POINT('Ctrl Pts',(-107.60456613324,3.14208833475255,127.018161920723));
#100459=CARTESIAN_POINT('Ctrl Pts',(-107.612322435982,3.03522052923194,
126.931970329471));
#100460=CARTESIAN_POINT('Ctrl Pts',(-107.620078738724,2.92502949066337,
126.850452988239));
#100461=CARTESIAN_POINT('Ctrl Pts',(-107.627839181238,2.81477963981943,
126.768892138747));
#100462=CARTESIAN_POINT('Ctrl Pts',(-107.635599623752,2.70120334526599,
126.692010729404));
#100463=CARTESIAN_POINT('Ctrl Pts',(-107.643360066266,2.58474426110525,
126.620070932663));
#100464=CARTESIAN_POINT('Ctrl Pts',(-107.651132966531,2.46809822648417,
126.548015651774));
#100465=CARTESIAN_POINT('Ctrl Pts',(-107.658905866797,2.34856049574229,
126.480918027056));
#100466=CARTESIAN_POINT('Ctrl Pts',(-107.666678767062,2.22659904112551,
126.41899406817));
#100467=CARTESIAN_POINT('Ctrl Pts',(-107.674169102824,2.10907119258378,
126.359321201166));
#100468=CARTESIAN_POINT('Ctrl Pts',(-107.681659438587,1.98929305775323,
126.304452507247));
#100469=CARTESIAN_POINT('Ctrl Pts',(-107.689149774349,1.86769808071749,
126.254537880164));
#100470=CARTESIAN_POINT('Ctrl Pts',(-107.696924108468,1.7414927931721,126.202730724824));
#100471=CARTESIAN_POINT('Ctrl Pts',(-107.704698442587,1.61293039221567,
126.156096609493));
#100472=CARTESIAN_POINT('Ctrl Pts',(-107.712472776706,1.48247394698653,
126.114855946601));
#100473=CARTESIAN_POINT('Ctrl Pts',(-107.720237529653,1.35217827766691,
126.073666109139));
#100474=CARTESIAN_POINT('Ctrl Pts',(-107.7280022826,1.21999357771997,126.037856615385));
#100475=CARTESIAN_POINT('Ctrl Pts',(-107.735767035547,1.08640381868289,
126.007600272786));
#100476=CARTESIAN_POINT('Ctrl Pts',(-107.743524076432,0.952946742877412,
125.977373981214));
#100477=CARTESIAN_POINT('Ctrl Pts',(-107.751281117317,0.818087763978748,
125.952689950569));
#100478=CARTESIAN_POINT('Ctrl Pts',(-107.759038158202,0.682326639427653,
125.93367140354));
#100479=CARTESIAN_POINT('Ctrl Pts',(-107.766789349442,0.546667893396835,
125.914667198546));
#100480=CARTESIAN_POINT('Ctrl Pts',(-107.774540540683,0.410108741457273,
125.901320027264));
#100481=CARTESIAN_POINT('Ctrl Pts',(-107.782291731923,0.273159426780302,
125.893702108765));
#100482=CARTESIAN_POINT('Ctrl Pts',(-107.7900396287,0.136268319215125,125.886087428085));
#100483=CARTESIAN_POINT('Ctrl Pts',(-107.797787525477,-0.00101223172060871,
125.884197178658));
#100484=CARTESIAN_POINT('Ctrl Pts',(-107.805535422254,-0.138166779800137,
125.888051737577));
#100485=CARTESIAN_POINT('Ctrl Pts',(-107.813281698338,-0.275292638104918,
125.891905490206));
#100486=CARTESIAN_POINT('Ctrl Pts',(-107.821027974422,-0.41229215541587,
125.901501649977));
#100487=CARTESIAN_POINT('Ctrl Pts',(-107.828774250506,-0.548650200021222,
125.916808467408));
#100488=CARTESIAN_POINT('Ctrl Pts',(-107.836520583772,-0.685009251190497,
125.93211539783));
#100489=CARTESIAN_POINT('Ctrl Pts',(-107.844266917037,-0.820726431680461,
125.953133026416));
#100490=CARTESIAN_POINT('Ctrl Pts',(-107.852013250302,-0.95529244012774,
125.97977779453));
#100491=CARTESIAN_POINT('Ctrl Pts',(-107.859761318305,-1.08988858369941,
126.006428529555));
#100492=CARTESIAN_POINT('Ctrl Pts',(-107.867509386308,-1.22333265879628,
126.038708835755));
#100493=CARTESIAN_POINT('Ctrl Pts',(-107.875257454311,-1.35512664312525,
126.076484260935));
#100494=CARTESIAN_POINT('Ctrl Pts',(-107.883013757053,-1.4870606996693,
126.114299834286));
#100495=CARTESIAN_POINT('Ctrl Pts',(-107.890770059795,-1.61734078573751,
126.157622085306));
#100496=CARTESIAN_POINT('Ctrl Pts',(-107.898526362537,-1.74548458151935,
126.206266812718));
#100497=CARTESIAN_POINT('Ctrl Pts',(-107.906286805051,-1.87369677150367,
126.254937503287));
#100498=CARTESIAN_POINT('Ctrl Pts',(-107.914047247565,-1.99977004004005,
126.30893617686));
#100499=CARTESIAN_POINT('Ctrl Pts',(-107.921807690079,-2.12324400813961,
126.368031285291));
#100500=CARTESIAN_POINT('Ctrl Pts',(-107.929580590345,-2.24691618761394,
126.427221258437));
#100501=CARTESIAN_POINT('Ctrl Pts',(-107.93735349061,-2.36798038293016,
126.491523831684));
#100502=CARTESIAN_POINT('Ctrl Pts',(-107.945126390875,-2.48600190861309,
126.560662045227));
#100503=CARTESIAN_POINT('Ctrl Pts',(-107.952616726637,-2.59973305455787,
126.627286910558));
#100504=CARTESIAN_POINT('Ctrl Pts',(-107.960107062399,-2.71063864832953,
126.698401778377));
#100505=CARTESIAN_POINT('Ctrl Pts',(-107.967597398161,-2.8183582929577,
126.773723001132));
#100506=CARTESIAN_POINT('Ctrl Pts',(-107.975324751309,-2.9294865202445,
126.851427620291));
#100507=CARTESIAN_POINT('Ctrl Pts',(-107.983052104457,-3.03758561542063,
126.933862313187));
#100508=CARTESIAN_POINT('Ctrl Pts',(-107.990779457605,-3.1422226496235,
127.020761817126));
#100509=CARTESIAN_POINT('Ctrl Pts',(-107.998494604148,-3.24669439269638,
127.107524049234));
#100510=CARTESIAN_POINT('Ctrl Pts',(-108.006209750691,-3.34771466284118,
127.198736797226));
#100511=CARTESIAN_POINT('Ctrl Pts',(-108.013924897234,-3.44487945656981,
127.294091597647));
#100512=CARTESIAN_POINT('Ctrl Pts',(-108.021632994712,-3.54195547415997,
127.389359275658));
#100513=CARTESIAN_POINT('Ctrl Pts',(-108.02934109219,-3.63518274011879,
127.488761204126));
#100514=CARTESIAN_POINT('Ctrl Pts',(-108.037049189669,-3.72419014628851,
127.591948623941));
#100515=CARTESIAN_POINT('Ctrl Pts',(-108.044751967482,-3.8131361249043,
127.69506483001));
#100516=CARTESIAN_POINT('Ctrl Pts',(-108.052454745295,-3.89786777924379,
127.801961031591));
#100517=CARTESIAN_POINT('Ctrl Pts',(-108.060157523109,-3.97805106294793,
127.912251905384));
#100518=CARTESIAN_POINT('Ctrl Pts',(-108.067856706407,-4.05819692898108,
128.022491311746));
#100519=CARTESIAN_POINT('Ctrl Pts',(-108.075555889706,-4.13379841561625,
128.136121917994));
#100520=CARTESIAN_POINT('Ctrl Pts',(-108.083255073004,-4.20456226891132,
128.252726006312));
#100521=CARTESIAN_POINT('Ctrl Pts',(-108.090953828883,-4.27532219375253,
128.369323621357));
#100522=CARTESIAN_POINT('Ctrl Pts',(-108.098652584761,-4.34124480596481,
128.488894056327));
#100523=CARTESIAN_POINT('Ctrl Pts',(-108.10635134064,-4.4020807562358,128.610991501781));
#100524=CARTESIAN_POINT('Ctrl Pts',(-108.114049764063,-4.46291407942287,
128.733083674691));
#100525=CARTESIAN_POINT('Ctrl Pts',(-108.121748187485,-4.5186610060928,
128.857702283649));
#100526=CARTESIAN_POINT('Ctrl Pts',(-108.129446610908,-4.56911900262065,
128.984378584031));
#100527=CARTESIAN_POINT('Ctrl Pts',(-108.137148893038,-4.61960229038739,
129.11111837882));
#100528=CARTESIAN_POINT('Ctrl Pts',(-108.144851175168,-4.6647912115551,
129.23991755464));
#100529=CARTESIAN_POINT('Ctrl Pts',(-108.152553457298,-4.70453207169467,
129.370289123917));
#100530=CARTESIAN_POINT('Ctrl Pts',(-108.156706900654,-4.72596226714681,
129.440591784736));
#100531=CARTESIAN_POINT('Ctrl Pts',(-108.160860344009,-4.74580908471365,
129.511351411935));
#100532=CARTESIAN_POINT('Ctrl Pts',(-108.165013787364,-4.76405452823417,
129.582490119309));
#100533=CARTESIAN_POINT('Ctrl Pts',(-106.415236531453,-4.76405452823412,
129.582490119309));
#100534=CARTESIAN_POINT('Ctrl Pts',(-106.422964224241,-4.79807563422773,
129.715137895235));
#100535=CARTESIAN_POINT('Ctrl Pts',(-106.430691917029,-4.82656175502522,
129.849243845907));
#100536=CARTESIAN_POINT('Ctrl Pts',(-106.438419609817,-4.84940130922175,
129.984305738538));
#100537=CARTESIAN_POINT('Ctrl Pts',(-106.446206435515,-4.87241563347753,
130.120401135359));
#100538=CARTESIAN_POINT('Ctrl Pts',(-106.453993261214,-4.88969651031593,
130.257466773977));
#100539=CARTESIAN_POINT('Ctrl Pts',(-106.461780086913,-4.90118255664471,
130.394979854777));
#100540=CARTESIAN_POINT('Ctrl Pts',(-106.469566912612,-4.91266860297349,
130.532492935577));
#100541=CARTESIAN_POINT('Ctrl Pts',(-106.477353738311,-4.9183598004662,
130.670453051542));
#100542=CARTESIAN_POINT('Ctrl Pts',(-106.48514056401,-4.9182483945935,130.808334479476));
#100543=CARTESIAN_POINT('',(-106.139859435937,-4.91824889795569,130.801068162911));
#100544=CARTESIAN_POINT('Ctrl Pts',(-106.070096981463,-4.76405452823408,
129.582490119308));
#100545=CARTESIAN_POINT('Ctrl Pts',(-106.078931279564,-4.80265958447516,
129.733010647679));
#100546=CARTESIAN_POINT('Ctrl Pts',(-106.087765577665,-4.83417096701391,
129.885533426967));
#100547=CARTESIAN_POINT('Ctrl Pts',(-106.096599875766,-4.85840041307,130.039423699395));
#100548=CARTESIAN_POINT('Ctrl Pts',(-106.105377112359,-4.88247335900662,
130.192319981041));
#100549=CARTESIAN_POINT('Ctrl Pts',(-106.114154348953,-4.8993580463698,
130.346565977745));
#100550=CARTESIAN_POINT('Ctrl Pts',(-106.122931585546,-4.90891746033364,
130.501520015712));
#100551=CARTESIAN_POINT('Ctrl Pts',(-106.128574202343,-4.91506291502496,
130.601135224674));
#100552=CARTESIAN_POINT('Ctrl Pts',(-106.13421681914,-4.91818193725568,
130.70104267325));
#100553=CARTESIAN_POINT('Ctrl Pts',(-106.139859435937,-4.91824889795569,
130.801068162911));
#100554=CARTESIAN_POINT('Ctrl Pts',(-106.139859435992,-4.91824889795634,
130.801068163883));
#100555=CARTESIAN_POINT('Ctrl Pts',(-106.147648177268,-4.91834132659944,
130.939137554038));
#100556=CARTESIAN_POINT('Ctrl Pts',(-106.155436918545,-4.91261542175427,
131.077241192686));
#100557=CARTESIAN_POINT('Ctrl Pts',(-106.163225659822,-4.90108922495837,
131.214857233261));
#100558=CARTESIAN_POINT('Ctrl Pts',(-106.171014608845,-4.88956272072675,
131.352476944438));
#100559=CARTESIAN_POINT('Ctrl Pts',(-106.178803557869,-4.87223564783958,
131.48960864811));
#100560=CARTESIAN_POINT('Ctrl Pts',(-106.186592506893,-4.84917800910811,
131.625734891866));
#100561=CARTESIAN_POINT('Ctrl Pts',(-106.19438328114,-4.82611496716673,
131.761893034755));
#100562=CARTESIAN_POINT('Ctrl Pts',(-106.202174055386,-4.79731874994963,
131.89704486925));
#100563=CARTESIAN_POINT('Ctrl Pts',(-106.209964829633,-4.76291057467061,
132.030682728673));
#100564=CARTESIAN_POINT('Ctrl Pts',(-106.217759047408,-4.72848719095131,
132.164379656134));
#100565=CARTESIAN_POINT('Ctrl Pts',(-106.225553265183,-4.68844700662207,
132.296560903952));
#100566=CARTESIAN_POINT('Ctrl Pts',(-106.233347482957,-4.64296113357161,
132.426733871365));
#100567=CARTESIAN_POINT('Ctrl Pts',(-106.24115162473,-4.59741734557249,
132.557072581684));
#100568=CARTESIAN_POINT('Ctrl Pts',(-106.248955766503,-4.54641414880807,
132.68539754155));
#100569=CARTESIAN_POINT('Ctrl Pts',(-106.256759908277,-4.49017109703257,
132.811235447214));
#100570=CARTESIAN_POINT('Ctrl Pts',(-106.264569584085,-4.43388816245424,
132.937162586448));
#100571=CARTESIAN_POINT('Ctrl Pts',(-106.272379259894,-4.37235814057708,
133.060598813939));
#100572=CARTESIAN_POINT('Ctrl Pts',(-106.280188935702,-4.30584618069132,
133.181096137292));
#100573=CARTESIAN_POINT('Ctrl Pts',(-106.28801117471,-4.23922722494315,
133.301787301197));
#100574=CARTESIAN_POINT('Ctrl Pts',(-106.295833413718,-4.16761052345866,
133.419529790201));
#100575=CARTESIAN_POINT('Ctrl Pts',(-106.303655652726,-4.09130450084059,
133.533904635145));
#100576=CARTESIAN_POINT('Ctrl Pts',(-106.307937318965,-4.04953680228271,
133.59651010038));
#100577=CARTESIAN_POINT('Ctrl Pts',(-106.312218985205,-4.00636482728613,
133.658107142264));
#100578=CARTESIAN_POINT('Ctrl Pts',(-106.316500651445,-3.96184406440911,
133.718631482089));
#100579=CARTESIAN_POINT('Ctrl Pts',(-106.324274985564,-3.88100654310979,
133.828527119396));
#100580=CARTESIAN_POINT('Ctrl Pts',(-106.332049319683,-3.79546500442361,
133.935230806359));
#100581=CARTESIAN_POINT('Ctrl Pts',(-106.339823653802,-3.70550028188961,
134.038313419234));
#100582=CARTESIAN_POINT('Ctrl Pts',(-106.347588406749,-3.61564643283601,
134.141268992001));
#100583=CARTESIAN_POINT('Ctrl Pts',(-106.355353159696,-3.52138050076351,
134.24061207829));
#100584=CARTESIAN_POINT('Ctrl Pts',(-106.363117912643,-3.42302593417488,
134.335943338736));
#100585=CARTESIAN_POINT('Ctrl Pts',(-106.370874953528,-3.32476905472807,
134.43117991483));
#100586=CARTESIAN_POINT('Ctrl Pts',(-106.378631994413,-3.22243190103691,
134.522412324273));
#100587=CARTESIAN_POINT('Ctrl Pts',(-106.386389035298,-3.11637719662952,
134.60927536442));
#100588=CARTESIAN_POINT('Ctrl Pts',(-106.394140226538,-3.01040246889985,
134.696072900472));
#100589=CARTESIAN_POINT('Ctrl Pts',(-106.401891417778,-2.90071607175843,
134.77850737895));
#100590=CARTESIAN_POINT('Ctrl Pts',(-106.409642609019,-2.7877162151675,
134.85625170275));
#100591=CARTESIAN_POINT('Ctrl Pts',(-106.417390505796,-2.67476438653015,
134.933962983139));
#100592=CARTESIAN_POINT('Ctrl Pts',(-106.425138402573,-2.55850222088346,
135.006987852513));
#100593=CARTESIAN_POINT('Ctrl Pts',(-106.43288629935,-2.43935933901518,
135.075040783261));
#100594=CARTESIAN_POINT('Ctrl Pts',(-106.440632575434,-2.32024137926938,
135.143079478803));
#100595=CARTESIAN_POINT('Ctrl Pts',(-106.448378851518,-2.19824424114708,
135.206148110591));
#100596=CARTESIAN_POINT('Ctrl Pts',(-106.456125127602,-2.07382439198327,
135.264005833692));
#100597=CARTESIAN_POINT('Ctrl Pts',(-106.463871460867,-1.94940362438022,
135.321863983886));
#100598=CARTESIAN_POINT('Ctrl Pts',(-106.471617794133,-1.82256046455907,
135.374510983782));
#100599=CARTESIAN_POINT('Ctrl Pts',(-106.479364127398,-1.69377335044753,
135.421753269249));
#100600=CARTESIAN_POINT('Ctrl Pts',(-106.487112195401,-1.56495739535456,
135.469006134298));
#100601=CARTESIAN_POINT('Ctrl Pts',(-106.494860263404,-1.43419698668376,
135.510851741847));
#100602=CARTESIAN_POINT('Ctrl Pts',(-106.502608331407,-1.30198740316484,
135.547145860912));
#100603=CARTESIAN_POINT('Ctrl Pts',(-106.510364634149,-1.16963730572743,
135.583478553798));
#100604=CARTESIAN_POINT('Ctrl Pts',(-106.518120936891,-1.03583533434416,
135.614247868274));
#100605=CARTESIAN_POINT('Ctrl Pts',(-106.525877239633,-0.901089235364966,
135.639360230018));
#100606=CARTESIAN_POINT('Ctrl Pts',(-106.533637682147,-0.766271218335622,
135.664485994985));
#100607=CARTESIAN_POINT('Ctrl Pts',(-106.541398124661,-0.630508456447608,
135.683948735582));
#100608=CARTESIAN_POINT('Ctrl Pts',(-106.549158567175,-0.494314586192979,
135.697706727579));
#100609=CARTESIAN_POINT('Ctrl Pts',(-106.55693146744,-0.357902085447093,
135.711486805125));
#100610=CARTESIAN_POINT('Ctrl Pts',(-106.564704367706,-0.221057483905281,
135.719543810938));
#100611=CARTESIAN_POINT('Ctrl Pts',(-106.572477267971,-0.0842960965321487,
135.721888170169));
#100612=CARTESIAN_POINT('Ctrl Pts',(-106.579967603733,0.0474936699277105,
135.724147306037));
#100613=CARTESIAN_POINT('Ctrl Pts',(-106.587457939495,0.179205859333517,
135.721101929748));
#100614=CARTESIAN_POINT('Ctrl Pts',(-106.594948275257,0.310385124522492,
135.712806821506));
#100615=CARTESIAN_POINT('Ctrl Pts',(-106.602722609376,0.446538091423518,
135.704197201714));
#100616=CARTESIAN_POINT('Ctrl Pts',(-106.610496943495,0.582548216399707,
135.689904631742));
#100617=CARTESIAN_POINT('Ctrl Pts',(-106.618271277614,0.717902668102916,
135.669933432932));
#100618=CARTESIAN_POINT('Ctrl Pts',(-106.626036030561,0.853090307540641,
135.649986846841));
#100619=CARTESIAN_POINT('Ctrl Pts',(-106.633800783509,0.987623498436658,
135.624375613167));
#100620=CARTESIAN_POINT('Ctrl Pts',(-106.641565536456,1.12099143345606,
135.593156005617));
#100621=CARTESIAN_POINT('Ctrl Pts',(-106.649322577341,1.25422690556259,
135.561967405821));
#100622=CARTESIAN_POINT('Ctrl Pts',(-106.657079618226,1.3862990467572,135.525181605861));
#100623=CARTESIAN_POINT('Ctrl Pts',(-106.664836659111,1.5167045407839,135.482906374365));
#100624=CARTESIAN_POINT('Ctrl Pts',(-106.672587850351,1.64701169501333,
135.44066302295));
#100625=CARTESIAN_POINT('Ctrl Pts',(-106.680339041591,1.7756543333163,135.392938599746));
#100626=CARTESIAN_POINT('Ctrl Pts',(-106.688090232831,1.90214201742572,
135.339891326099));
#100627=CARTESIAN_POINT('Ctrl Pts',(-106.695838129608,2.0285759408947,135.286866598958));
#100628=CARTESIAN_POINT('Ctrl Pts',(-106.703586026385,2.15285637206435,
135.228523671913));
#100629=CARTESIAN_POINT('Ctrl Pts',(-106.711333923162,2.2745108679381,135.16506966245));
#100630=CARTESIAN_POINT('Ctrl Pts',(-106.719080199246,2.39613991631421,
135.101628926198));
#100631=CARTESIAN_POINT('Ctrl Pts',(-106.72682647533,2.51514377553532,135.033079414776));
#100632=CARTESIAN_POINT('Ctrl Pts',(-106.734572751414,2.631073084193,134.95967498451));
#100633=CARTESIAN_POINT('Ctrl Pts',(-106.74231908468,2.74700324861402,134.886270012391));
#100634=CARTESIAN_POINT('Ctrl Pts',(-106.750065417945,2.85985848686679,
134.808010259067));
#100635=CARTESIAN_POINT('Ctrl Pts',(-106.75781175121,2.96921734057817,134.725193621777));
#100636=CARTESIAN_POINT('Ctrl Pts',(-106.765559819213,3.07860068444704,
134.642358438275));
#100637=CARTESIAN_POINT('Ctrl Pts',(-106.773307887216,3.18448577409477,
134.554964576149));
#100638=CARTESIAN_POINT('Ctrl Pts',(-106.781055955219,3.28648355365717,
134.463350767053));
#100639=CARTESIAN_POINT('Ctrl Pts',(-106.788812257961,3.38858973767334,
134.37163958971));
#100640=CARTESIAN_POINT('Ctrl Pts',(-106.796568560703,3.48680006720204,
134.275699767773));
#100641=CARTESIAN_POINT('Ctrl Pts',(-106.804324863445,3.58076136621063,
134.175907903421));
#100642=CARTESIAN_POINT('Ctrl Pts',(-106.812085305959,3.67477281519387,
134.076062777145));
#100643=CARTESIAN_POINT('Ctrl Pts',(-106.819845748473,3.76453045906257,
133.972361807264));
#100644=CARTESIAN_POINT('Ctrl Pts',(-106.827606190987,3.84972156096882,
133.86521457774));
#100645=CARTESIAN_POINT('Ctrl Pts',(-106.835379091253,3.93504941919453,
133.757895345971));
#100646=CARTESIAN_POINT('Ctrl Pts',(-106.843151991518,4.01579585611967,
133.647119115499));
#100647=CARTESIAN_POINT('Ctrl Pts',(-106.850924891784,4.09169110239433,
133.533325070447));
#100648=CARTESIAN_POINT('Ctrl Pts',(-106.858415227546,4.16482736529955,
133.423667725561));
#100649=CARTESIAN_POINT('Ctrl Pts',(-106.865905563308,4.23345885960281,
133.311208430056));
#100650=CARTESIAN_POINT('Ctrl Pts',(-106.87339589907,4.2973855471772,133.196359890436));
#100651=CARTESIAN_POINT('Ctrl Pts',(-106.881170233189,4.36373603454005,
133.077156833531));
#100652=CARTESIAN_POINT('Ctrl Pts',(-106.888944567308,4.42522808541707,
132.955002180196));
#100653=CARTESIAN_POINT('Ctrl Pts',(-106.896718901427,4.48158813760678,
132.830329725761));
#100654=CARTESIAN_POINT('Ctrl Pts',(-106.904483654374,4.53787873106935,
132.705810918984));
#100655=CARTESIAN_POINT('Ctrl Pts',(-106.912248407321,4.58904975066781,
132.578780837915));
#100656=CARTESIAN_POINT('Ctrl Pts',(-106.920013160268,4.63487243722153,
132.449699656544));
#100657=CARTESIAN_POINT('Ctrl Pts',(-106.927770201154,4.68064961203698,
132.320746680422));
#100658=CARTESIAN_POINT('Ctrl Pts',(-106.935527242039,4.72108889506038,
132.189747024136));
#100659=CARTESIAN_POINT('Ctrl Pts',(-106.943284282924,4.75600890035877,
132.057182393482));
#100660=CARTESIAN_POINT('Ctrl Pts',(-106.951035474164,4.79090257220928,
131.924717730848));
#100661=CARTESIAN_POINT('Ctrl Pts',(-106.958786665404,4.82028515161546,
131.790690819419));
#100662=CARTESIAN_POINT('Ctrl Pts',(-106.966537856644,4.84402466081358,
131.655599801303));
#100663=CARTESIAN_POINT('Ctrl Pts',(-106.974285753421,4.86775408008712,
131.520566200473));
#100664=CARTESIAN_POINT('Ctrl Pts',(-106.982033650198,4.88584513197175,
131.384469776752));
#100665=CARTESIAN_POINT('Ctrl Pts',(-106.989781546975,4.89821670329584,
131.247819961873));
#100666=CARTESIAN_POINT('Ctrl Pts',(-106.997527823059,4.91058568675391,
131.111198731191));
#100667=CARTESIAN_POINT('Ctrl Pts',(-107.005274099143,4.91723753411131,
130.974024728725));
#100668=CARTESIAN_POINT('Ctrl Pts',(-107.013020375228,4.91814293106795,
130.836813230501));
#100669=CARTESIAN_POINT('Ctrl Pts',(-107.020766708493,4.91904833470803,
130.699600719413));
#100670=CARTESIAN_POINT('Ctrl Pts',(-107.028513041758,4.91420720072357,
130.562351102972));
#100671=CARTESIAN_POINT('Ctrl Pts',(-107.036259375023,4.90364234995155,
130.425579986776));
#100672=CARTESIAN_POINT('Ctrl Pts',(-107.044007443026,4.89307513325447,
130.288778241637));
#100673=CARTESIAN_POINT('Ctrl Pts',(-107.051755511029,4.87678167926728,
130.152455599702));
#100674=CARTESIAN_POINT('Ctrl Pts',(-107.059503579032,4.85483667832409,
130.017122477421));
#100675=CARTESIAN_POINT('Ctrl Pts',(-107.067259881774,4.83286835397271,
129.881645521486));
#100676=CARTESIAN_POINT('Ctrl Pts',(-107.075016184516,4.80523654665141,
129.747160572575));
#100677=CARTESIAN_POINT('Ctrl Pts',(-107.082772487258,4.77206720216523,
129.614168330362));
#100678=CARTESIAN_POINT('Ctrl Pts',(-107.090532929772,4.73888015420119,
129.481105106185));
#100679=CARTESIAN_POINT('Ctrl Pts',(-107.098293372286,4.70014979023972,
129.349536551073));
#100680=CARTESIAN_POINT('Ctrl Pts',(-107.1060538148,4.65605166296224,129.219947169527));
#100681=CARTESIAN_POINT('Ctrl Pts',(-107.113826715066,4.61188274545601,
129.090149759602));
#100682=CARTESIAN_POINT('Ctrl Pts',(-107.121599615331,4.56232898691303,
128.962338236928));
#100683=CARTESIAN_POINT('Ctrl Pts',(-107.129372515597,4.50761406845169,
128.836976955848));
#100684=CARTESIAN_POINT('Ctrl Pts',(-107.136862851359,4.45488817509484,
128.7161728731));
#100685=CARTESIAN_POINT('Ctrl Pts',(-107.144353187121,4.39736998386324,
128.597644257008));
#100686=CARTESIAN_POINT('Ctrl Pts',(-107.151843522883,4.33529859093212,
128.481782483259));
#100687=CARTESIAN_POINT('Ctrl Pts',(-107.159617857002,4.27087374227209,
128.361527775143));
#100688=CARTESIAN_POINT('Ctrl Pts',(-107.167392191121,4.20133952834792,
128.243765197274));
#100689=CARTESIAN_POINT('Ctrl Pts',(-107.17516652524,4.12691304640367,128.128959382251));
#100690=CARTESIAN_POINT('Ctrl Pts',(-107.182931278187,4.05257828844652,
128.014295055135));
#100691=CARTESIAN_POINT('Ctrl Pts',(-107.190696031134,3.9733634695789,127.902580565408));
#100692=CARTESIAN_POINT('Ctrl Pts',(-107.198460784081,3.88953209728597,
127.79425710993));
#100693=CARTESIAN_POINT('Ctrl Pts',(-107.206217824966,3.80578398749381,
127.686041242835));
#100694=CARTESIAN_POINT('Ctrl Pts',(-107.213974865851,3.71742868681588,
127.581210014661));
#100695=CARTESIAN_POINT('Ctrl Pts',(-107.221731906736,3.62477342445343,
127.480176404278));
#100696=CARTESIAN_POINT('Ctrl Pts',(-107.229483097976,3.53218803414521,
127.379218984126));
#100697=CARTESIAN_POINT('Ctrl Pts',(-107.237234289217,3.43530939959924,
127.282053768497));
#100698=CARTESIAN_POINT('Ctrl Pts',(-107.244985480457,3.33448528467254,
127.189061051997));
#100699=CARTESIAN_POINT('Ctrl Pts',(-107.252733377234,3.23370402268439,
127.096107859883));
#100700=CARTESIAN_POINT('Ctrl Pts',(-107.260481274011,3.12898090239863,
127.007323904205));
#100701=CARTESIAN_POINT('Ctrl Pts',(-107.268229170788,3.02070067951069,
126.92305278807));
#100702=CARTESIAN_POINT('Ctrl Pts',(-107.275975446872,2.91244310651083,
126.838799299636));
#100703=CARTESIAN_POINT('Ctrl Pts',(-107.283721722956,2.8006302192435,126.75905701307));
#100704=CARTESIAN_POINT('Ctrl Pts',(-107.29146799904,2.68567968892668,126.684129110601));
#100705=CARTESIAN_POINT('Ctrl Pts',(-107.299214332305,2.57072831007162,
126.609200655032));
#100706=CARTESIAN_POINT('Ctrl Pts',(-107.306960665571,2.45263956947877,
126.539086867966));
#100707=CARTESIAN_POINT('Ctrl Pts',(-107.314706998836,2.33185959596092,
126.474047247009));
#100708=CARTESIAN_POINT('Ctrl Pts',(-107.322455066839,2.21105257460493,
126.408993060879));
#100709=CARTESIAN_POINT('Ctrl Pts',(-107.330203134842,2.08755346521724,
126.349015487342));
#100710=CARTESIAN_POINT('Ctrl Pts',(-107.337951202845,1.96183206756199,
126.294327579862));
#100711=CARTESIAN_POINT('Ctrl Pts',(-107.345707505587,1.83597705170938,
126.239581549423));
#100712=CARTESIAN_POINT('Ctrl Pts',(-107.353463808329,1.70789538857726,
126.190136571632));
#100713=CARTESIAN_POINT('Ctrl Pts',(-107.361220111071,1.57807640776632,
126.14615732512));
#100714=CARTESIAN_POINT('Ctrl Pts',(-107.368980553585,1.44818813865619,
126.102154605561));
#100715=CARTESIAN_POINT('Ctrl Pts',(-107.376740996099,1.31656107926134,
126.063623539884));
#100716=CARTESIAN_POINT('Ctrl Pts',(-107.384501438613,1.18369774745451,
126.030678317164));
#100717=CARTESIAN_POINT('Ctrl Pts',(-107.392274338879,1.05062113163277,
125.997680207848));
#100718=CARTESIAN_POINT('Ctrl Pts',(-107.400047239144,0.916304660886786,
125.970285938371));
#100719=CARTESIAN_POINT('Ctrl Pts',(-107.407820139409,0.78125991478289,
125.948558314336));
#100720=CARTESIAN_POINT('Ctrl Pts',(-107.415310475171,0.651124385358525,
125.927620544164));
#100721=CARTESIAN_POINT('Ctrl Pts',(-107.422800810933,0.520312916416678,
125.911944615227));
#100722=CARTESIAN_POINT('Ctrl Pts',(-107.430291146695,0.389284020730129,
125.90154091726));
#100723=CARTESIAN_POINT('Ctrl Pts',(-107.438065480814,0.253287124636906,
125.890742759924));
#100724=CARTESIAN_POINT('Ctrl Pts',(-107.445839814933,0.116625191572592,
125.88559031356));
#100725=CARTESIAN_POINT('Ctrl Pts',(-107.453614149052,-0.0201935235346973,
125.88615207338));
#100726=CARTESIAN_POINT('Ctrl Pts',(-107.461378901999,-0.156843621803085,
125.88671314088));
#100727=CARTESIAN_POINT('Ctrl Pts',(-107.469143654947,-0.293649730455816,
125.892974400998));
#100728=CARTESIAN_POINT('Ctrl Pts',(-107.476908407894,-0.430098225847748,
125.904952635103));
#100729=CARTESIAN_POINT('Ctrl Pts',(-107.484665448779,-0.566411198670471,
125.916918972257));
#100730=CARTESIAN_POINT('Ctrl Pts',(-107.492422489664,-0.702366878122446,
125.934590949595));
#100731=CARTESIAN_POINT('Ctrl Pts',(-107.500179530549,-0.837451748495209,
125.957933311659));
#100732=CARTESIAN_POINT('Ctrl Pts',(-107.507930721789,-0.9724347503166,
125.981258071066));
#100733=CARTESIAN_POINT('Ctrl Pts',(-107.515681913029,-1.10654786645127,
126.010244637615));
#100734=CARTESIAN_POINT('Ctrl Pts',(-107.523433104269,-1.23928316941682,
126.044805986248));
#100735=CARTESIAN_POINT('Ctrl Pts',(-107.531181001046,-1.37196205633796,
126.079352645386));
#100736=CARTESIAN_POINT('Ctrl Pts',(-107.538928897823,-1.50326391726038,
126.119469275683));
#100737=CARTESIAN_POINT('Ctrl Pts',(-107.5466767946,-1.63269169930937,126.165017897147));
#100738=CARTESIAN_POINT('Ctrl Pts',(-107.554423070684,-1.76209240785649,
126.210556990821));
#100739=CARTESIAN_POINT('Ctrl Pts',(-107.562169346768,-1.88961944871283,
126.261525685881));
#100740=CARTESIAN_POINT('Ctrl Pts',(-107.569915622853,-2.01479198458728,
126.317736461105));
#100741=CARTESIAN_POINT('Ctrl Pts',(-107.577661956118,-2.13996544445746,
126.373947651263));
#100742=CARTESIAN_POINT('Ctrl Pts',(-107.585408289383,-2.26278400801027,
126.435400838638));
#100743=CARTESIAN_POINT('Ctrl Pts',(-107.593154622649,-2.38278820904152,
126.501860947217));
#100744=CARTESIAN_POINT('Ctrl Pts',(-107.600902690652,-2.50281928418105,
126.568335939076));
#100745=CARTESIAN_POINT('Ctrl Pts',(-107.608650758655,-2.62003440070854,
126.63981989395));
#100746=CARTESIAN_POINT('Ctrl Pts',(-107.616398826658,-2.73400037246204,
126.716032716593));
#100747=CARTESIAN_POINT('Ctrl Pts',(-107.624155129399,-2.84808746860638,
126.79232653913));
#100748=CARTESIAN_POINT('Ctrl Pts',(-107.631911432141,-2.95891819626775,
126.873359051527));
#100749=CARTESIAN_POINT('Ctrl Pts',(-107.639667734883,-3.06608951204773,
126.958807579756));
#100750=CARTESIAN_POINT('Ctrl Pts',(-107.647428177397,-3.17331802838582,
127.044301714437));
#100751=CARTESIAN_POINT('Ctrl Pts',(-107.655188619911,-3.27688294596889,
127.134216305205));
#100752=CARTESIAN_POINT('Ctrl Pts',(-107.662949062426,-3.37641657110857,
127.228190291527));
#100753=CARTESIAN_POINT('Ctrl Pts',(-107.670721962691,-3.47610997645951,
127.322315133234));
#100754=CARTESIAN_POINT('Ctrl Pts',(-107.678494862956,-3.5717588845171,
127.420512112318));
#100755=CARTESIAN_POINT('Ctrl Pts',(-107.686267763222,-3.66303393389649,
127.522384770363));
#100756=CARTESIAN_POINT('Ctrl Pts',(-107.693758098984,-3.75099090532443,
127.620554100688));
#100757=CARTESIAN_POINT('Ctrl Pts',(-107.701248434746,-3.83488630251744,
127.722136271789));
#100758=CARTESIAN_POINT('Ctrl Pts',(-107.708738770508,-3.91446354694372,
127.826751139789));
#100759=CARTESIAN_POINT('Ctrl Pts',(-107.716535406243,-3.99729491889724,
127.935643991076));
#100760=CARTESIAN_POINT('Ctrl Pts',(-107.724332041978,-4.0757128098723,
128.048171562633));
#100761=CARTESIAN_POINT('Ctrl Pts',(-107.732128677713,-4.1493821549345,
128.163941939627));
#100762=CARTESIAN_POINT('Ctrl Pts',(-107.739912552866,-4.22293092700115,
128.279522837793));
#100763=CARTESIAN_POINT('Ctrl Pts',(-107.747696428018,-4.29174642551336,
128.398335646724));
#100764=CARTESIAN_POINT('Ctrl Pts',(-107.755480303171,-4.35553438864326,
128.519956263725));
#100765=CARTESIAN_POINT('Ctrl Pts',(-107.763256838091,-4.4192621994103,
128.641462191887));
#100766=CARTESIAN_POINT('Ctrl Pts',(-107.771033373011,-4.47797172552326,
128.765770320832));
#100767=CARTESIAN_POINT('Ctrl Pts',(-107.778809907932,-4.5314123009601,
128.892428186436));
#100768=CARTESIAN_POINT('Ctrl Pts',(-107.786579663597,-4.58480628916007,
129.018975637061));
#100769=CARTESIAN_POINT('Ctrl Pts',(-107.794349419262,-4.63294032147407,
129.14786839028));
#100770=CARTESIAN_POINT('Ctrl Pts',(-107.802119174928,-4.67561020552408,
129.278630540357));
#100771=CARTESIAN_POINT('Ctrl Pts',(-107.808076652511,-4.70832743482112,
129.378892712207));
#100772=CARTESIAN_POINT('Ctrl Pts',(-107.814034130093,-4.73783315307493,
129.480253375528));
#100773=CARTESIAN_POINT('Ctrl Pts',(-107.819991607676,-4.76405452823401,
129.582490119308));
#100774=CARTESIAN_POINT('Origin',(213.235140564004,0.,130.804360617566));
#100775=CARTESIAN_POINT('',(-109.915204178194,-4.76405452823412,129.582490119309));
#100776=CARTESIAN_POINT('',(-109.569720587678,-4.76405452823413,129.582490119309));
#100777=CARTESIAN_POINT('',(213.235140564004,-4.76405452823405,129.582490119308));
#100778=CARTESIAN_POINT('',(-108.235140563964,-4.91824985693288,130.805546905785));
#100779=CARTESIAN_POINT('Ctrl Pts',(-108.23514056401,-4.91824985693268,
130.805546906598));
#100780=CARTESIAN_POINT('Ctrl Pts',(-108.238775383331,-4.91823446811159,
130.869347603656));
#100781=CARTESIAN_POINT('Ctrl Pts',(-108.242410202652,-4.9169776757414,
130.933131835064));
#100782=CARTESIAN_POINT('Ctrl Pts',(-108.246045021973,-4.91448107986788,
130.996867184001));
#100783=CARTESIAN_POINT('Ctrl Pts',(-108.253819356093,-4.90914123522478,
131.133187549347));
#100784=CARTESIAN_POINT('Ctrl Pts',(-108.261593690212,-4.89811664913808,
131.269501489038));
#100785=CARTESIAN_POINT('Ctrl Pts',(-108.269368024331,-4.88139933516864,
131.405296215709));
#100786=CARTESIAN_POINT('Ctrl Pts',(-108.277132777278,-4.8647026237946,
131.540923587515));
#100787=CARTESIAN_POINT('Ctrl Pts',(-108.284897530225,-4.84232719115706,
131.676032635167));
#100788=CARTESIAN_POINT('Ctrl Pts',(-108.292662283172,-4.81431703678716,
131.810111348016));
#100789=CARTESIAN_POINT('Ctrl Pts',(-108.300419324057,-4.78633470249745,
131.944056891998));
#100790=CARTESIAN_POINT('Ctrl Pts',(-108.308176364942,-4.75272886316572,
132.076973757449));
#100791=CARTESIAN_POINT('Ctrl Pts',(-108.315933405827,-4.71359517818133,
132.208356186906));
#100792=CARTESIAN_POINT('Ctrl Pts',(-108.323684597067,-4.67449100421316,
132.339639539851));
#100793=CARTESIAN_POINT('Ctrl Pts',(-108.331435788308,-4.62986739307658,
132.469390386819));
#100794=CARTESIAN_POINT('Ctrl Pts',(-108.339186979548,-4.57987075138741,
132.597114633901));
#100795=CARTESIAN_POINT('Ctrl Pts',(-108.346934876325,-4.52989535960474,
132.724784594771));
#100796=CARTESIAN_POINT('Ctrl Pts',(-108.354682773102,-4.4745516215501,
132.850429305628));
#100797=CARTESIAN_POINT('Ctrl Pts',(-108.362430669879,-4.41403525773697,
132.973571489278));
#100798=CARTESIAN_POINT('Ctrl Pts',(-108.370176945963,-4.35353155264258,
133.096687914239));
#100799=CARTESIAN_POINT('Ctrl Pts',(-108.377923222047,-4.28785754627787,
133.217302502551));
#100800=CARTESIAN_POINT('Ctrl Pts',(-108.385669498131,-4.21725623843067,
133.334959930361));
#100801=CARTESIAN_POINT('Ctrl Pts',(-108.393415831397,-4.14665440942056,
133.452618226691));
#100802=CARTESIAN_POINT('Ctrl Pts',(-108.401162164662,-4.07112540751411,
133.567318983718));
#100803=CARTESIAN_POINT('Ctrl Pts',(-108.408908497928,-3.99095693032238,
133.678633715727));
#100804=CARTESIAN_POINT('Ctrl Pts',(-108.416656565931,-3.91077049995615,
133.789973375898));
#100805=CARTESIAN_POINT('Ctrl Pts',(-108.424404633933,-3.82594275529821,
133.897925184976));
#100806=CARTESIAN_POINT('Ctrl Pts',(-108.432152701936,-3.73680299418588,
134.002092070509));
#100807=CARTESIAN_POINT('Ctrl Pts',(-108.439909004678,-3.64756849427478,
134.106369665848));
#100808=CARTESIAN_POINT('Ctrl Pts',(-108.44766530742,-3.55401307774977,
134.20685400442));
#100809=CARTESIAN_POINT('Ctrl Pts',(-108.455421610162,-3.45650476308482,
134.303182974484));
#100810=CARTESIAN_POINT('Ctrl Pts',(-108.463182052676,-3.35894440529616,
134.399563358221));
#100811=CARTESIAN_POINT('Ctrl Pts',(-108.47094249519,-3.25742723469645,
134.491783691448));
#100812=CARTESIAN_POINT('Ctrl Pts',(-108.478702937705,-3.152355212475,134.579521498493));
#100813=CARTESIAN_POINT('Ctrl Pts',(-108.48647583797,-3.04711451931563,
134.667400150055));
#100814=CARTESIAN_POINT('Ctrl Pts',(-108.494248738235,-2.93830788150435,
134.750781658089));
#100815=CARTESIAN_POINT('Ctrl Pts',(-108.502021638501,-2.82636788297,134.829385791725));
#100816=CARTESIAN_POINT('Ctrl Pts',(-108.509511974263,-2.71849718534192,
134.905132467112));
#100817=CARTESIAN_POINT('Ctrl Pts',(-108.517002310025,-2.60771724196288,
134.976442910247));
#100818=CARTESIAN_POINT('Ctrl Pts',(-108.524492645787,-2.49443584012262,
135.043107236793));
#100819=CARTESIAN_POINT('Ctrl Pts',(-108.532266979906,-2.37685933950062,
135.112299161542));
#100820=CARTESIAN_POINT('Ctrl Pts',(-108.540041314025,-2.25621550335653,
135.176704879091));
#100821=CARTESIAN_POINT('Ctrl Pts',(-108.547815648144,-2.13293143735857,
135.236040496125));
#100822=CARTESIAN_POINT('Ctrl Pts',(-108.555580401091,-2.00979930795374,
135.295302987315));
#100823=CARTESIAN_POINT('Ctrl Pts',(-108.563345154039,-1.88403377178589,
135.349507642609));
#100824=CARTESIAN_POINT('Ctrl Pts',(-108.571109906986,-1.75608938073606,
135.398414725798));
#100825=CARTESIAN_POINT('Ctrl Pts',(-108.578866947871,-1.62827206585947,
135.447273233783));
#100826=CARTESIAN_POINT('Ctrl Pts',(-108.586623988756,-1.49828056552746,
135.490844501837));
#100827=CARTESIAN_POINT('Ctrl Pts',(-108.594381029641,-1.36659209405418,
135.528935636652));
#100828=CARTESIAN_POINT('Ctrl Pts',(-108.602132220881,-1.2350029298811,
135.566998046645));
#100829=CARTESIAN_POINT('Ctrl Pts',(-108.609883412121,-1.10171971578006,
135.599588440916));
#100830=CARTESIAN_POINT('Ctrl Pts',(-108.617634603361,-0.967237283302234,
135.626562925671));
#100831=CARTESIAN_POINT('Ctrl Pts',(-108.625382500138,-0.832812009445832,
135.653525945549));
#100832=CARTESIAN_POINT('Ctrl Pts',(-108.633130396915,-0.697188913494261,
135.674877726568));
#100833=CARTESIAN_POINT('Ctrl Pts',(-108.640878293692,-0.560875333985677,
135.690524953958));
#100834=CARTESIAN_POINT('Ctrl Pts',(-108.648624569777,-0.424590268339345,
135.706168908285));
#100835=CARTESIAN_POINT('Ctrl Pts',(-108.656370845861,-0.287615394592241,
135.716110637903));
#100836=CARTESIAN_POINT('Ctrl Pts',(-108.664117121945,-0.150465136920227,
135.720308471752));
#100837=CARTESIAN_POINT('Ctrl Pts',(-108.67186345521,-0.0133138668359791,
135.724506336587));
#100838=CARTESIAN_POINT('Ctrl Pts',(-108.679609788475,0.124012398974345,
135.722960209086));
#100839=CARTESIAN_POINT('Ctrl Pts',(-108.687356121741,0.260997655756491,
135.715680530399));
#100840=CARTESIAN_POINT('Ctrl Pts',(-108.695104189744,0.398013589436917,
135.708399221479));
#100841=CARTESIAN_POINT('Ctrl Pts',(-108.702852257747,0.534687971788868,
135.695381827127));
#100842=CARTESIAN_POINT('Ctrl Pts',(-108.71060032575,0.670508740988721,
135.676690767582));
#100843=CARTESIAN_POINT('Ctrl Pts',(-108.718356628492,0.806473862118552,
135.657979842957));
#100844=CARTESIAN_POINT('Ctrl Pts',(-108.726112931234,0.941583169873703,
135.633583260871));
#100845=CARTESIAN_POINT('Ctrl Pts',(-108.733869233976,1.0753330864168,135.60361491545));
#100846=CARTESIAN_POINT('Ctrl Pts',(-108.74162967649,1.20915438931712,135.57363057502));
#100847=CARTESIAN_POINT('Ctrl Pts',(-108.749390119004,1.34161447788036,
135.538068646995));
#100848=CARTESIAN_POINT('Ctrl Pts',(-108.757150561518,1.47222477434846,
135.497093006728));
#100849=CARTESIAN_POINT('Ctrl Pts',(-108.764923461783,1.60304473805985,
135.456051588726));
#100850=CARTESIAN_POINT('Ctrl Pts',(-108.772696362049,1.73200860774313,
135.40957922457));
#100851=CARTESIAN_POINT('Ctrl Pts',(-108.780469262314,1.85864679505001,
135.357888387741));
#100852=CARTESIAN_POINT('Ctrl Pts',(-108.787959598076,1.98068136526252,
135.308076643032));
#100853=CARTESIAN_POINT('Ctrl Pts',(-108.795449933838,2.10055612603258,
135.253419375587));
#100854=CARTESIAN_POINT('Ctrl Pts',(-108.8029402696,2.21787407673078,135.194146220789));
#100855=CARTESIAN_POINT('Ctrl Pts',(-108.810714603719,2.33964017319065,
135.13262570631));
#100856=CARTESIAN_POINT('Ctrl Pts',(-108.818488937838,2.45903746775401,
135.065937493684));
#100857=CARTESIAN_POINT('Ctrl Pts',(-108.826263271957,2.57559625188908,
134.994287467734));
#100858=CARTESIAN_POINT('Ctrl Pts',(-108.834028024904,2.69201138773987,
134.922725744037));
#100859=CARTESIAN_POINT('Ctrl Pts',(-108.841792777851,2.80559464368708,
134.846214576803));
#100860=CARTESIAN_POINT('Ctrl Pts',(-108.849557530798,2.91589862647236,
134.765006810126));
#100861=CARTESIAN_POINT('Ctrl Pts',(-108.857314571683,3.02609305378692,
134.683879700147));
#100862=CARTESIAN_POINT('Ctrl Pts',(-108.865071612568,3.13301437675168,
134.598065504037));
#100863=CARTESIAN_POINT('Ctrl Pts',(-108.872828653453,3.23624236276918,
134.507861452171));
#100864=CARTESIAN_POINT('Ctrl Pts',(-108.880579844694,3.33939250375929,
134.417725423881));
#100865=CARTESIAN_POINT('Ctrl Pts',(-108.888331035934,3.43885455831209,
134.32320638525));
#100866=CARTESIAN_POINT('Ctrl Pts',(-108.896082227174,3.53423999596275,
134.224642873965));
#100867=CARTESIAN_POINT('Ctrl Pts',(-108.903830123951,3.62958489225804,
134.126121254801));
#100868=CARTESIAN_POINT('Ctrl Pts',(-108.911578020728,3.72085634648314,
134.023558862319));
#100869=CARTESIAN_POINT('Ctrl Pts',(-108.919325917505,3.80770162140692,
133.917332095886));
#100870=CARTESIAN_POINT('Ctrl Pts',(-108.927072193589,3.89452873017134,
133.811127549803));
#100871=CARTESIAN_POINT('Ctrl Pts',(-108.934818469673,3.97693125392143,
133.701260456889));
#100872=CARTESIAN_POINT('Ctrl Pts',(-108.942564745757,4.05459607477986,
133.588141092546));
#100873=CARTESIAN_POINT('Ctrl Pts',(-108.950311079023,4.13226146894226,
133.475020893181));
#100874=CARTESIAN_POINT('Ctrl Pts',(-108.958057412288,4.20518886913727,
133.358648696793));
#100875=CARTESIAN_POINT('Ctrl Pts',(-108.965803745553,4.27310814662839,
133.239464276493));
#100876=CARTESIAN_POINT('Ctrl Pts',(-108.973551813556,4.34104263417088,
133.120253165668));
#100877=CARTESIAN_POINT('Ctrl Pts',(-108.981299881559,4.40396657374991,
132.998228917361));
#100878=CARTESIAN_POINT('Ctrl Pts',(-108.989047949562,4.46165569935583,
132.873856083351));
#100879=CARTESIAN_POINT('Ctrl Pts',(-108.996804252304,4.51940613765103,
132.749351064413));
#100880=CARTESIAN_POINT('Ctrl Pts',(-109.004560555046,4.5719104832655,132.622492828768));
#100881=CARTESIAN_POINT('Ctrl Pts',(-109.012316857788,4.61899236242985,
132.493766613268));
#100882=CARTESIAN_POINT('Ctrl Pts',(-109.020077300302,4.66609937061072,
132.364971692712));
#100883=CARTESIAN_POINT('Ctrl Pts',(-109.027837742816,4.70777802678318,
132.234307177993));
#100884=CARTESIAN_POINT('Ctrl Pts',(-109.03559818533,4.74390211571169,132.102272702049));
#100885=CARTESIAN_POINT('Ctrl Pts',(-109.043371085596,4.7800841942347,131.970026272642));
#100886=CARTESIAN_POINT('Ctrl Pts',(-109.051143985861,4.81069379978623,
131.836405868655));
#100887=CARTESIAN_POINT('Ctrl Pts',(-109.058916886127,4.83565586834993,
131.701921415169));
#100888=CARTESIAN_POINT('Ctrl Pts',(-109.066407221889,4.85971050284589,
131.572325810311));
#100889=CARTESIAN_POINT('Ctrl Pts',(-109.073897557651,4.87852103207088,
131.441928190909));
#100890=CARTESIAN_POINT('Ctrl Pts',(-109.081387893413,4.89206606623963,
131.31118668837));
#100891=CARTESIAN_POINT('Ctrl Pts',(-109.089162227532,4.90612466449572,
131.175488082025));
#100892=CARTESIAN_POINT('Ctrl Pts',(-109.096936561651,4.91455513665716,
131.038989148726));
#100893=CARTESIAN_POINT('Ctrl Pts',(-109.10471089577,4.91727681052279,130.902196353342));
#100894=CARTESIAN_POINT('Ctrl Pts',(-109.112475648717,4.91999513016862,
130.765572142852));
#100895=CARTESIAN_POINT('Ctrl Pts',(-109.120240401664,4.91701864253065,
130.628655178));
#100896=CARTESIAN_POINT('Ctrl Pts',(-109.128005154612,4.90831824552124,
130.491958531812));
#100897=CARTESIAN_POINT('Ctrl Pts',(-109.135762195497,4.8996264898688,130.355397654661));
#100898=CARTESIAN_POINT('Ctrl Pts',(-109.143519236382,4.88522216305875,
130.219057048356));
#100899=CARTESIAN_POINT('Ctrl Pts',(-109.151276277267,4.86512818743791,
130.083450926761));
#100900=CARTESIAN_POINT('Ctrl Pts',(-109.159027468507,4.84504936484035,
129.947947066796));
#100901=CARTESIAN_POINT('Ctrl Pts',(-109.166778659747,4.81928949070307,
129.813176974253));
#100902=CARTESIAN_POINT('Ctrl Pts',(-109.174529850987,4.78792337616393,
129.679650518704));
#100903=CARTESIAN_POINT('Ctrl Pts',(-109.182277747764,4.75657059306024,
129.54618081546));
#100904=CARTESIAN_POINT('Ctrl Pts',(-109.190025644541,4.71961639798478,
129.413954077716));
#100905=CARTESIAN_POINT('Ctrl Pts',(-109.197773541318,4.67718680329669,
129.283470526347));
#100906=CARTESIAN_POINT('Ctrl Pts',(-109.205519817402,4.63476608396513,
129.153014269324));
#100907=CARTESIAN_POINT('Ctrl Pts',(-109.213266093487,4.58687236397928,
129.02430084496));
#100908=CARTESIAN_POINT('Ctrl Pts',(-109.221012369571,4.53368157179299,
128.897815452068));
#100909=CARTESIAN_POINT('Ctrl Pts',(-109.228758702836,4.48049038696428,
128.771329125489));
#100910=CARTESIAN_POINT('Ctrl Pts',(-109.236505036101,4.42200220346684,
128.647071223597));
#100911=CARTESIAN_POINT('Ctrl Pts',(-109.244251369367,4.35844100369424,
128.525506721456));
#100912=CARTESIAN_POINT('Ctrl Pts',(-109.25199943737,4.29486556983173,128.403914995787));
#100913=CARTESIAN_POINT('Ctrl Pts',(-109.259747505373,4.22621504017031,
128.285018216504));
#100914=CARTESIAN_POINT('Ctrl Pts',(-109.267495573375,4.15275903402116,
128.169256166533));
#100915=CARTESIAN_POINT('Ctrl Pts',(-109.275251876117,4.07922495795443,
128.053371083277));
#100916=CARTESIAN_POINT('Ctrl Pts',(-109.283008178859,4.00087541278862,
127.940627715261));
#100917=CARTESIAN_POINT('Ctrl Pts',(-109.290764481601,3.91802330770006,
127.831436733102));
#100918=CARTESIAN_POINT('Ctrl Pts',(-109.298524924115,3.83512698194838,
127.722187472428));
#100919=CARTESIAN_POINT('Ctrl Pts',(-109.306285366629,3.74772355682294,
127.616494676725));
#100920=CARTESIAN_POINT('Ctrl Pts',(-109.314045809144,3.65616516524623,
127.514734598253));
#100921=CARTESIAN_POINT('Ctrl Pts',(-109.321818709409,3.56445979601119,
127.412811165469));
#100922=CARTESIAN_POINT('Ctrl Pts',(-109.329591609675,3.46858640529162,
127.314833345195));
#100923=CARTESIAN_POINT('Ctrl Pts',(-109.33736450994,3.36893343356707,127.221139917875));
#100924=CARTESIAN_POINT('Ctrl Pts',(-109.344854845702,3.27290309837567,
127.130852482638));
#100925=CARTESIAN_POINT('Ctrl Pts',(-109.352345181464,3.17336343864022,
127.044543553235));
#100926=CARTESIAN_POINT('Ctrl Pts',(-109.359835517226,3.07068833158736,
126.962478756713));
#100927=CARTESIAN_POINT('Ctrl Pts',(-109.367609851345,2.96412026664301,
126.877302448488));
#100928=CARTESIAN_POINT('Ctrl Pts',(-109.375384185464,2.85383672433764,
126.796428645875));
#100929=CARTESIAN_POINT('Ctrl Pts',(-109.383158519583,2.74022020261252,
126.720198977315));
#100930=CARTESIAN_POINT('Ctrl Pts',(-109.39092327253,2.62674370309654,126.644063255009));
#100931=CARTESIAN_POINT('Ctrl Pts',(-109.398688025477,2.50994271860356,
126.572560494472));
#100932=CARTESIAN_POINT('Ctrl Pts',(-109.406452778424,2.39023318161349,
126.505992508619));
#100933=CARTESIAN_POINT('Ctrl Pts',(-109.414209819309,2.27064254182317,
126.439490639027));
#100934=CARTESIAN_POINT('Ctrl Pts',(-109.421966860194,2.14814943788668,
126.377913979112));
#100935=CARTESIAN_POINT('Ctrl Pts',(-109.429723901079,2.0231988825782,126.321521188807));
#100936=CARTESIAN_POINT('Ctrl Pts',(-109.437475092319,1.89834255345527,
126.265170924744));
#100937=CARTESIAN_POINT('Ctrl Pts',(-109.44522628356,1.77103281652043,126.213996909451));
#100938=CARTESIAN_POINT('Ctrl Pts',(-109.4529774748,1.6417390767333,126.168211799158));
#100939=CARTESIAN_POINT('Ctrl Pts',(-109.460725371577,1.51250029023479,
126.122446148758));
#100940=CARTESIAN_POINT('Ctrl Pts',(-109.468473268354,1.38127954582082,
126.082064978104));
#100941=CARTESIAN_POINT('Ctrl Pts',(-109.476221165131,1.24856580623878,
126.047232651031));
#100942=CARTESIAN_POINT('Ctrl Pts',(-109.483967441215,1.11587982751008,
126.012407610129));
#100943=CARTESIAN_POINT('Ctrl Pts',(-109.491713717299,0.981701852717511,
125.983129203305));
#100944=CARTESIAN_POINT('Ctrl Pts',(-109.499459993383,0.84653518699155,
125.959511678777));
#100945=CARTESIAN_POINT('Ctrl Pts',(-109.507206326648,0.711367523495783,
125.93589397991));
#100946=CARTESIAN_POINT('Ctrl Pts',(-109.514952659914,0.575211539633765,
125.917937314017));
#100947=CARTESIAN_POINT('Ctrl Pts',(-109.522698993179,0.438579500051587,
125.905704568747));
#100948=CARTESIAN_POINT('Ctrl Pts',(-109.530447061182,0.30191686267167,
125.893469084038));
#100949=CARTESIAN_POINT('Ctrl Pts',(-109.538195129185,0.164778346764372,
125.886960105508));
#100950=CARTESIAN_POINT('Ctrl Pts',(-109.545943197188,0.0276796899863722,
125.886188508208));
#100951=CARTESIAN_POINT('Ctrl Pts',(-109.55369949993,-0.109564676875734,
125.885416090846));
#100952=CARTESIAN_POINT('Ctrl Pts',(-109.561455802672,-0.24676870840196,
125.890393237846));
#100953=CARTESIAN_POINT('Ctrl Pts',(-109.569212105413,-0.383417760716848,
125.901078667355));
#100954=CARTESIAN_POINT('Ctrl Pts',(-109.576972547928,-0.520139746745752,
125.911769799999));
#100955=CARTESIAN_POINT('Ctrl Pts',(-109.584732990442,-0.656305775373332,
125.928175239184));
#100956=CARTESIAN_POINT('Ctrl Pts',(-109.592493432956,-0.791408958472185,
125.950202099043));
#100957=CARTESIAN_POINT('Ctrl Pts',(-109.600266333221,-0.926729021194078,
125.972264318373));
#100958=CARTESIAN_POINT('Ctrl Pts',(-109.608039233487,-1.06098244578844,
125.999965912161));
#100959=CARTESIAN_POINT('Ctrl Pts',(-109.615812133752,-1.19367424510417,
126.033163193536));
#100960=CARTESIAN_POINT('Ctrl Pts',(-109.623302469514,-1.32154236328789,
126.065153670114));
#100961=CARTESIAN_POINT('Ctrl Pts',(-109.630792805277,-1.44796012747283,
126.102247120405));
#100962=CARTESIAN_POINT('Ctrl Pts',(-109.638283141039,-1.57250196832677,
126.144272568815));
#100963=CARTESIAN_POINT('Ctrl Pts',(-109.646057503716,-1.70176632575835,
126.187891585102));
#100964=CARTESIAN_POINT('Ctrl Pts',(-109.653831866393,-1.82941915778745,
126.236962187181));
#100965=CARTESIAN_POINT('Ctrl Pts',(-109.661606229069,-1.9549662878274,
126.291347225612));
#100966=CARTESIAN_POINT('Ctrl Pts',(-109.669371003863,-2.08035858443769,
126.345665192641));
#100967=CARTESIAN_POINT('Ctrl Pts',(-109.677135778657,-2.20364999081397,
126.405284401296));
#100968=CARTESIAN_POINT('Ctrl Pts',(-109.68490055345,-2.32436175758185,
126.470018051226));
#100969=CARTESIAN_POINT('Ctrl Pts',(-109.692657609498,-2.44495352816216,
126.534687351246));
#100970=CARTESIAN_POINT('Ctrl Pts',(-109.700414665547,-2.56297041999857,
126.60446079129));
#100971=CARTESIAN_POINT('Ctrl Pts',(-109.708171721595,-2.67795427236633,
126.67910377979));
#100972=CARTESIAN_POINT('Ctrl Pts',(-109.715922921337,-2.79285131593833,
126.753690415439));
#100973=CARTESIAN_POINT('Ctrl Pts',(-109.723674121079,-2.90471955124832,
126.833139069955));
#100974=CARTESIAN_POINT('Ctrl Pts',(-109.73142532082,-3.01312633856167,
126.917169764216));
#100975=CARTESIAN_POINT('Ctrl Pts',(-109.739173191178,-3.12148656175295,
127.001164364653));
#100976=CARTESIAN_POINT('Ctrl Pts',(-109.746921061536,-3.22638798590924,
127.089736851114));
#100977=CARTESIAN_POINT('Ctrl Pts',(-109.754668931894,-3.32742803514063,
127.182564691032));
#100978=CARTESIAN_POINT('Ctrl Pts',(-109.762415172071,-3.42844682516336,
127.275372999621));
#100979=CARTESIAN_POINT('Ctrl Pts',(-109.770161412247,-3.52560556860359,
127.372434616387));
#100980=CARTESIAN_POINT('Ctrl Pts',(-109.777907652424,-3.6185361017395,
127.473387855308));
#100981=CARTESIAN_POINT('Ctrl Pts',(-109.785653940287,-3.71146720696074,
127.574341715702));
#100982=CARTESIAN_POINT('Ctrl Pts',(-109.793400228149,-3.8001697851892,
127.679186958386));
#100983=CARTESIAN_POINT('Ctrl Pts',(-109.801146516012,-3.88431404145138,
127.787526599944));
#100984=CARTESIAN_POINT('Ctrl Pts',(-109.808894529103,-3.96847703804494,
127.895890370549));
#100985=CARTESIAN_POINT('Ctrl Pts',(-109.816642542193,-4.04807945281788,
128.007749779919));
#100986=CARTESIAN_POINT('Ctrl Pts',(-109.824390555284,-4.1228333732546,
128.122676810911));
#100987=CARTESIAN_POINT('Ctrl Pts',(-109.832146669428,-4.19766545379882,
128.237724005622));
#100988=CARTESIAN_POINT('Ctrl Pts',(-109.839902783573,-4.26763870030987,
128.355844900542));
#100989=CARTESIAN_POINT('Ctrl Pts',(-109.847658897717,-4.3325096834453,
128.476584231108));
#100990=CARTESIAN_POINT('Ctrl Pts',(-109.855419147713,-4.39741525822069,
128.597387944411));
#100991=CARTESIAN_POINT('Ctrl Pts',(-109.863179397708,-4.45721297802206,
128.720812523861));
#100992=CARTESIAN_POINT('Ctrl Pts',(-109.870939647703,-4.51170701715605,
128.84638133937));
#100993=CARTESIAN_POINT('Ctrl Pts',(-109.878712038238,-4.56628630960457,
128.972146601277));
#100994=CARTESIAN_POINT('Ctrl Pts',(-109.886484428773,-4.61554520146936,
129.100062437227));
#100995=CARTESIAN_POINT('Ctrl Pts',(-109.894256819308,-4.65933705204792,
129.229634832576));
#100996=CARTESIAN_POINT('Ctrl Pts',(-109.90123927227,-4.69867817051366,
129.346038293219));
#100997=CARTESIAN_POINT('Ctrl Pts',(-109.908221725232,-4.73360767680117,
129.463778307667));
#100998=CARTESIAN_POINT('Ctrl Pts',(-109.915204178194,-4.76405452823412,
129.582490119309));
#100999=CARTESIAN_POINT('Ctrl Pts',(-108.165013787364,-4.76405452823417,
129.582490119309));
#101000=CARTESIAN_POINT('Ctrl Pts',(-108.172724877397,-4.79792817128851,
129.714562939473));
#101001=CARTESIAN_POINT('Ctrl Pts',(-108.180435967429,-4.82627913472933,
129.847942656428));
#101002=CARTESIAN_POINT('Ctrl Pts',(-108.188147057461,-4.84903199837822,
129.982124799078));
#101003=CARTESIAN_POINT('Ctrl Pts',(-108.195979308545,-4.87214236801854,
130.118415288206));
#101004=CARTESIAN_POINT('Ctrl Pts',(-108.203811559628,-4.88947718626042,
130.25553320641));
#101005=CARTESIAN_POINT('Ctrl Pts',(-108.211643810712,-4.90101233682553,
130.39294703395));
#101006=CARTESIAN_POINT('Ctrl Pts',(-108.219476061796,-4.91254748739063,
130.53036086149));
#101007=CARTESIAN_POINT('Ctrl Pts',(-108.22730831288,-4.91828301649803,
130.668070174626));
#101008=CARTESIAN_POINT('Ctrl Pts',(-108.235140563964,-4.91824985693288,
130.805546905785));
#101009=CARTESIAN_POINT('',(-107.889859436047,-4.918248694981,130.80794346806));
#101010=CARTESIAN_POINT('Ctrl Pts',(-107.819991607676,-4.76405452823401,
129.582490119308));
#101011=CARTESIAN_POINT('Ctrl Pts',(-107.827755149809,-4.7982251563202,
129.715720879604));
#101012=CARTESIAN_POINT('Ctrl Pts',(-107.835518691941,-4.82681644330726,
129.850439672405));
#101013=CARTESIAN_POINT('Ctrl Pts',(-107.843282234073,-4.84971133876424,
129.986141213517));
#101014=CARTESIAN_POINT('Ctrl Pts',(-107.851046301406,-4.87260778305285,
130.121851934792));
#101015=CARTESIAN_POINT('Ctrl Pts',(-107.858810368739,-4.88980699116055,
130.258545156335));
#101016=CARTESIAN_POINT('Ctrl Pts',(-107.866574436072,-4.90124315007472,
130.395705938961));
#101017=CARTESIAN_POINT('Ctrl Pts',(-107.874336102712,-4.91267577286425,
130.532824310702));
#101018=CARTESIAN_POINT('Ctrl Pts',(-107.882097769352,-4.91834888578083,
130.670409567373));
#101019=CARTESIAN_POINT('Ctrl Pts',(-107.889859435992,-4.91824869498171,
130.807943467089));
#101020=CARTESIAN_POINT('Ctrl Pts',(-107.889859436047,-4.918248694981,130.80794346806));
#101021=CARTESIAN_POINT('Ctrl Pts',(-107.89875976081,-4.91813380588136,
130.965653974093));
#101022=CARTESIAN_POINT('Ctrl Pts',(-107.907660085574,-4.91042916089496,
131.123058384268));
#101023=CARTESIAN_POINT('Ctrl Pts',(-107.916560410337,-4.89524667639518,
131.279484853679));
#101024=CARTESIAN_POINT('Ctrl Pts',(-107.925505275757,-4.87998821288942,
131.436694141453));
#101025=CARTESIAN_POINT('Ctrl Pts',(-107.934450141177,-4.85717698919893,
131.592915538265));
#101026=CARTESIAN_POINT('Ctrl Pts',(-107.943395006597,-4.82697604074685,
131.747485935091));
#101027=CARTESIAN_POINT('Ctrl Pts',(-107.952396337752,-4.79658444451355,
131.903032079524));
#101028=CARTESIAN_POINT('Ctrl Pts',(-107.961397668907,-4.75870961922783,
132.056906178003));
#101029=CARTESIAN_POINT('Ctrl Pts',(-107.970399000062,-4.71356615637689,
132.20845361732));
#101030=CARTESIAN_POINT('Ctrl Pts',(-107.975994798149,-4.68550211799258,
132.302665112971));
#101031=CARTESIAN_POINT('Ctrl Pts',(-107.981590596235,-4.6546299540778,
132.395977861219));
#101032=CARTESIAN_POINT('Ctrl Pts',(-107.987186394322,-4.62101034714682,
132.488239008087));
#101033=CARTESIAN_POINT('Ctrl Pts',(-107.994960728441,-4.57430207547727,
132.616418933607));
#101034=CARTESIAN_POINT('Ctrl Pts',(-108.00273506256,-4.52218249989022,
132.742856987582));
#101035=CARTESIAN_POINT('Ctrl Pts',(-108.010509396679,-4.46480058747047,
132.867062432328));
#101036=CARTESIAN_POINT('Ctrl Pts',(-108.018274149626,-4.4074893931294,
132.991114804965));
#101037=CARTESIAN_POINT('Ctrl Pts',(-108.026038902573,-4.34492892828445,
133.112939691508));
#101038=CARTESIAN_POINT('Ctrl Pts',(-108.03380365552,-4.27731742623493,
133.232062967058));
#101039=CARTESIAN_POINT('Ctrl Pts',(-108.041560696405,-4.2097730768824,
133.35106792769));
#101040=CARTESIAN_POINT('Ctrl Pts',(-108.04931773729,-4.13718786564272,
133.467376279358));
#101041=CARTESIAN_POINT('Ctrl Pts',(-108.057074778175,-4.05980730933153,
133.580535625306));
#101042=CARTESIAN_POINT('Ctrl Pts',(-108.064825969415,-3.98248510629969,
133.693609636911));
#101043=CARTESIAN_POINT('Ctrl Pts',(-108.072577160656,-3.90037497582993,
133.803539048052));
#101044=CARTESIAN_POINT('Ctrl Pts',(-108.080328351896,-3.81376719722825,
133.909898063459));
#101045=CARTESIAN_POINT('Ctrl Pts',(-108.088076248673,-3.7271962292427,
134.016211873448));
#101046=CARTESIAN_POINT('Ctrl Pts',(-108.09582414545,-3.63613166154339,
134.118958003389));
#101047=CARTESIAN_POINT('Ctrl Pts',(-108.103572042227,-3.54090559760411,
134.217741728921));
#101048=CARTESIAN_POINT('Ctrl Pts',(-108.111318318311,-3.44569945290483,
134.316504791027));
#101049=CARTESIAN_POINT('Ctrl Pts',(-108.119064594395,-3.3463338145956,
134.411306816053));
#101050=CARTESIAN_POINT('Ctrl Pts',(-108.126810870479,-3.24317910446583,
134.501788420628));
#101051=CARTESIAN_POINT('Ctrl Pts',(-108.134557203744,-3.14002363287128,
134.592270693118));
#101052=CARTESIAN_POINT('Ctrl Pts',(-108.14230353701,-3.03307932756264,
134.678432223707));
#101053=CARTESIAN_POINT('Ctrl Pts',(-108.150049870275,-2.92275097896852,
134.759952833333));
#101054=CARTESIAN_POINT('Ctrl Pts',(-108.157797938278,-2.81239792310586,
134.841491698935));
#101055=CARTESIAN_POINT('Ctrl Pts',(-108.165546006281,-2.69865963033845,
134.918387343188));
#101056=CARTESIAN_POINT('Ctrl Pts',(-108.173294074284,-2.58197091311574,
134.990362202172));
#101057=CARTESIAN_POINT('Ctrl Pts',(-108.181050377026,-2.46515817773561,
135.062413556893));
#101058=CARTESIAN_POINT('Ctrl Pts',(-108.188806679768,-2.34538908719667,
135.129533473541));
#101059=CARTESIAN_POINT('Ctrl Pts',(-108.19656298251,-2.22312465073385,
135.191489502133));
#101060=CARTESIAN_POINT('Ctrl Pts',(-108.204323425024,-2.10079495805999,
135.253478598523));
#101061=CARTESIAN_POINT('Ctrl Pts',(-108.212083867538,-1.9759676213175,
135.310298153157));
#101062=CARTESIAN_POINT('Ctrl Pts',(-108.219844310052,-1.84912386922385,
135.361763823205));
#101063=CARTESIAN_POINT('Ctrl Pts',(-108.227617210318,-1.72207649627869,
135.413312110516));
#101064=CARTESIAN_POINT('Ctrl Pts',(-108.235390110583,-1.59300660789415,
135.459489206854));
#101065=CARTESIAN_POINT('Ctrl Pts',(-108.243163010848,-1.4624116943013,
135.500160346991));
#101066=CARTESIAN_POINT('Ctrl Pts',(-108.25065334661,-1.33656423476664,
135.539352988741));
#101067=CARTESIAN_POINT('Ctrl Pts',(-108.258143682372,-1.20930099958607,
135.573432955384));
#101068=CARTESIAN_POINT('Ctrl Pts',(-108.265634018134,-1.08107438723236,
135.602324897526));
#101069=CARTESIAN_POINT('Ctrl Pts',(-108.273408352253,-0.94798602389743,
135.632312286436));
#101070=CARTESIAN_POINT('Ctrl Pts',(-108.281182686372,-0.813438204480298,
135.656805467986));
#101071=CARTESIAN_POINT('Ctrl Pts',(-108.288957020491,-0.677924320839947,
135.6756645167));
#101072=CARTESIAN_POINT('Ctrl Pts',(-108.296721773438,-0.542577445949959,
135.694500323321));
#101073=CARTESIAN_POINT('Ctrl Pts',(-108.304486526386,-0.406267259267573,
135.707715759358));
#101074=CARTESIAN_POINT('Ctrl Pts',(-108.312251279333,-0.269499805440736,
135.715221328008));
#101075=CARTESIAN_POINT('Ctrl Pts',(-108.320008320218,-0.132868190977123,
135.722719442023));
#101076=CARTESIAN_POINT('Ctrl Pts',(-108.327765361103,0.00421939897204796,
135.724518953153));
#101077=CARTESIAN_POINT('Ctrl Pts',(-108.335522401988,0.141249642368628,
135.720581890152));
#101078=CARTESIAN_POINT('Ctrl Pts',(-108.343273593228,0.278176550192536,
135.716647796122));
#101079=CARTESIAN_POINT('Ctrl Pts',(-108.351024784468,0.415045808318711,
135.706985749775));
#101080=CARTESIAN_POINT('Ctrl Pts',(-108.358775975708,0.551342280071368,
135.691609818569));
#101081=CARTESIAN_POINT('Ctrl Pts',(-108.366523872485,0.687580822187889,
135.676240422544));
#101082=CARTESIAN_POINT('Ctrl Pts',(-108.374271769262,0.823246674445855,
135.655162015603));
#101083=CARTESIAN_POINT('Ctrl Pts',(-108.382019666039,0.957828234021382,
135.628440647645));
#101084=CARTESIAN_POINT('Ctrl Pts',(-108.389765942123,1.09238164203589,
135.601724869222));
#101085=CARTESIAN_POINT('Ctrl Pts',(-108.397512218207,1.22585082527036,
135.569368553726));
#101086=CARTESIAN_POINT('Ctrl Pts',(-108.405258494291,1.35773320229044,
135.53148909201));
#101087=CARTESIAN_POINT('Ctrl Pts',(-108.413004827557,1.48961655283645,
135.493609350676));
#101088=CARTESIAN_POINT('Ctrl Pts',(-108.420751160822,1.6199126980223,135.450206489696));
#101089=CARTESIAN_POINT('Ctrl Pts',(-108.428497494087,1.74813346301937,
135.401448006117));
#101090=CARTESIAN_POINT('Ctrl Pts',(-108.43624556209,1.87638294216757,135.352678603414));
#101091=CARTESIAN_POINT('Ctrl Pts',(-108.443993630094,2.00255575092929,
135.298551330472));
#101092=CARTESIAN_POINT('Ctrl Pts',(-108.451741698097,2.12618334016567,
135.239281977241));
#101093=CARTESIAN_POINT('Ctrl Pts',(-108.459498000838,2.24994232227492,
135.179949631836));
#101094=CARTESIAN_POINT('Ctrl Pts',(-108.46725430358,2.37115032804475,135.115464458372));
#101095=CARTESIAN_POINT('Ctrl Pts',(-108.475010606322,2.48936260396792,
135.046088672082));
#101096=CARTESIAN_POINT('Ctrl Pts',(-108.482771048836,2.60763797334238,
134.976675857845));
#101097=CARTESIAN_POINT('Ctrl Pts',(-108.49053149135,2.72291409845608,134.902367441324));
#101098=CARTESIAN_POINT('Ctrl Pts',(-108.498291933864,2.83477577058887,
134.823468652066));
#101099=CARTESIAN_POINT('Ctrl Pts',(-108.50606483413,2.94681701300808,134.744443207467));
#101100=CARTESIAN_POINT('Ctrl Pts',(-108.513837734395,3.0554325393396,134.660812903429));
#101101=CARTESIAN_POINT('Ctrl Pts',(-108.521610634661,3.160240062159,134.572923448676));
#101102=CARTESIAN_POINT('Ctrl Pts',(-108.529100970423,3.26123756753083,
134.488228996982));
#101103=CARTESIAN_POINT('Ctrl Pts',(-108.536591306185,3.35869889585605,
134.399579887362));
#101104=CARTESIAN_POINT('Ctrl Pts',(-108.544081641947,3.45231612113009,
134.307316007274));
#101105=CARTESIAN_POINT('Ctrl Pts',(-108.551855976066,3.54948287195378,
134.211553914131));
#101106=CARTESIAN_POINT('Ctrl Pts',(-108.559630310185,3.64281606218321,
134.11159418597));
#101107=CARTESIAN_POINT('Ctrl Pts',(-108.567404644304,3.73193127820006,
134.007776294198));
#101108=CARTESIAN_POINT('Ctrl Pts',(-108.575169397251,3.82093666767763,
133.904086348699));
#101109=CARTESIAN_POINT('Ctrl Pts',(-108.582934150198,3.90573417375926,
133.796547994121));
#101110=CARTESIAN_POINT('Ctrl Pts',(-108.590698903146,3.9859749707582,133.685538604951));
#101111=CARTESIAN_POINT('Ctrl Pts',(-108.598455944031,4.06613607146636,
133.57463947187));
#101112=CARTESIAN_POINT('Ctrl Pts',(-108.606212984916,4.14174924206289,
133.460276479645));
#101113=CARTESIAN_POINT('Ctrl Pts',(-108.613970025801,4.212505073163,133.342860976257));
#101114=CARTESIAN_POINT('Ctrl Pts',(-108.621721217041,4.28320754674038,
133.225534016814));
#101115=CARTESIAN_POINT('Ctrl Pts',(-108.629472408281,4.34905977074026,
133.105159461555));
#101116=CARTESIAN_POINT('Ctrl Pts',(-108.637223599521,4.40979513655629,
132.982178313358));
#101117=CARTESIAN_POINT('Ctrl Pts',(-108.644971496298,4.47050468822176,
132.859249435429));
#101118=CARTESIAN_POINT('Ctrl Pts',(-108.652719393075,4.52610153445893,
132.733716517848));
#101119=CARTESIAN_POINT('Ctrl Pts',(-108.660467289852,4.57636471109577,
132.606045688142));
#101120=CARTESIAN_POINT('Ctrl Pts',(-108.668213565936,4.62661737375961,
132.478401564422));
#101121=CARTESIAN_POINT('Ctrl Pts',(-108.67595984202,4.67153844285894,132.348620781651));
#101122=CARTESIAN_POINT('Ctrl Pts',(-108.683706118104,4.71095502510017,
132.217189628446));
#101123=CARTESIAN_POINT('Ctrl Pts',(-108.69145245137,4.75037189830571,132.085757505046));
#101124=CARTESIAN_POINT('Ctrl Pts',(-108.699198784635,4.78428409126352,
131.952675361389));
#101125=CARTESIAN_POINT('Ctrl Pts',(-108.706945117901,4.81256865356381,
131.818444449029));
#101126=CARTESIAN_POINT('Ctrl Pts',(-108.714693185903,4.84085954999569,
131.684183476588));
#101127=CARTESIAN_POINT('Ctrl Pts',(-108.722441253906,4.86352022738405,
131.54877360602));
#101128=CARTESIAN_POINT('Ctrl Pts',(-108.730189321909,4.88047897366933,
131.412725680724));
#101129=CARTESIAN_POINT('Ctrl Pts',(-108.737945624651,4.897455743912,131.276533162074));
#101130=CARTESIAN_POINT('Ctrl Pts',(-108.745701927393,4.90871842895081,
131.139701622636));
#101131=CARTESIAN_POINT('Ctrl Pts',(-108.753458230135,4.91424723775195,
131.002746979868));
#101132=CARTESIAN_POINT('Ctrl Pts',(-108.761218672649,4.91977899744482,
130.865719240283));
#101133=CARTESIAN_POINT('Ctrl Pts',(-108.768979115163,4.91957078350195,
130.728568657222));
#101134=CARTESIAN_POINT('Ctrl Pts',(-108.776739557678,4.91365496373026,
130.591809541565));
#101135=CARTESIAN_POINT('Ctrl Pts',(-108.784512457943,4.90772964735949,
130.454830888035));
#101136=CARTESIAN_POINT('Ctrl Pts',(-108.792285358208,4.89607844910299,
130.318245347465));
#101137=CARTESIAN_POINT('Ctrl Pts',(-108.800058258474,4.87878558781025,
130.1825614131));
#101138=CARTESIAN_POINT('Ctrl Pts',(-108.807548594236,4.86212136558354,
130.051809931516));
#101139=CARTESIAN_POINT('Ctrl Pts',(-108.815038929998,4.84021858757171,
129.921895946623));
#101140=CARTESIAN_POINT('Ctrl Pts',(-108.82252926576,4.81319676919358,129.793262242765));
#101141=CARTESIAN_POINT('Ctrl Pts',(-108.830303599879,4.78515041035858,
129.659751352929));
#101142=CARTESIAN_POINT('Ctrl Pts',(-108.838077933998,4.7515003291591,129.527196821932));
#101143=CARTESIAN_POINT('Ctrl Pts',(-108.845852268117,4.7123243475531,129.396105560427));
#101144=CARTESIAN_POINT('Ctrl Pts',(-108.853617021064,4.67319664684327,
129.265175857186));
#101145=CARTESIAN_POINT('Ctrl Pts',(-108.861381774011,4.62855670682352,
129.135706206309));
#101146=CARTESIAN_POINT('Ctrl Pts',(-108.869146526959,4.57853347453332,
129.008194064855));
#101147=CARTESIAN_POINT('Ctrl Pts',(-108.876903567844,4.5285599260225,128.880808570257));
#101148=CARTESIAN_POINT('Ctrl Pts',(-108.884660608729,4.47321386739668,
128.755377077588));
#101149=CARTESIAN_POINT('Ctrl Pts',(-108.892417649614,4.41267413403358,
128.63238224536));
#101150=CARTESIAN_POINT('Ctrl Pts',(-108.900168840854,4.35218005415442,
128.509480164492));
#101151=CARTESIAN_POINT('Ctrl Pts',(-108.907920032094,4.28650026723182,
128.389011435979));
#101152=CARTESIAN_POINT('Ctrl Pts',(-108.915671223334,4.21586169301357,
128.27143873802));
#101153=CARTESIAN_POINT('Ctrl Pts',(-108.923419120111,4.14525314207361,
128.153916011595));
#101154=CARTESIAN_POINT('Ctrl Pts',(-108.931167016888,4.06969019665465,
128.039287202006));
#101155=CARTESIAN_POINT('Ctrl Pts',(-108.938914913665,3.98944558651591,
127.927990165985));
#101156=CARTESIAN_POINT('Ctrl Pts',(-108.946661189749,3.90921776181995,
127.816716410905));
#101157=CARTESIAN_POINT('Ctrl Pts',(-108.954407465834,3.82431044879798,
127.708773360081));
#101158=CARTESIAN_POINT('Ctrl Pts',(-108.962153741918,3.73503932278767,
127.604569324414));
#101159=CARTESIAN_POINT('Ctrl Pts',(-108.969900075183,3.64576753779807,
127.500364519537));
#101160=CARTESIAN_POINT('Ctrl Pts',(-108.977646408448,3.55213212990225,
127.3998990818));
#101161=CARTESIAN_POINT('Ctrl Pts',(-108.985392741714,3.4544883585294,127.303547391573));
#101162=CARTESIAN_POINT('Ctrl Pts',(-108.993140809717,3.35682272051084,
127.207174124054));
#101163=CARTESIAN_POINT('Ctrl Pts',(-109.00088887772,3.25514721104121,127.114916711772));
#101164=CARTESIAN_POINT('Ctrl Pts',(-109.008636945723,3.14985285501965,
127.027111611447));
#101165=CARTESIAN_POINT('Ctrl Pts',(-109.016393248464,3.04444659090363,
126.939213190818));
#101166=CARTESIAN_POINT('Ctrl Pts',(-109.024149551206,2.93541409787311,
126.855776785556));
#101167=CARTESIAN_POINT('Ctrl Pts',(-109.031905853948,2.8231787343609,126.777097912409));
#101168=CARTESIAN_POINT('Ctrl Pts',(-109.039666296463,2.71088346745585,
126.698377045977));
#101169=CARTESIAN_POINT('Ctrl Pts',(-109.047426738977,2.59538225289803,
126.624418982031));
#101170=CARTESIAN_POINT('Ctrl Pts',(-109.055187181491,2.47712529058811,
126.55547448621));
#101171=CARTESIAN_POINT('Ctrl Pts',(-109.062960081756,2.35867849170394,
126.486419314564));
#101172=CARTESIAN_POINT('Ctrl Pts',(-109.070732982022,2.23746745086413,
126.422393976671));
#101173=CARTESIAN_POINT('Ctrl Pts',(-109.078505882287,2.11396550018371,
126.363602469847));
#101174=CARTESIAN_POINT('Ctrl Pts',(-109.085996218049,1.99495315649417,
126.306948182384));
#101175=CARTESIAN_POINT('Ctrl Pts',(-109.093486553811,1.87381385512986,
126.255153927685));
#101176=CARTESIAN_POINT('Ctrl Pts',(-109.100976889573,1.75098472410171,
126.208358489796));
#101177=CARTESIAN_POINT('Ctrl Pts',(-109.108751223692,1.62349848923628,
126.159788788657));
#101178=CARTESIAN_POINT('Ctrl Pts',(-109.116525557811,1.49378791733207,
126.116450593162));
#101179=CARTESIAN_POINT('Ctrl Pts',(-109.12429989193,1.36232155134577,126.078552427083));
#101180=CARTESIAN_POINT('Ctrl Pts',(-109.132064644877,1.23101720590641,
126.040700967107));
#101181=CARTESIAN_POINT('Ctrl Pts',(-109.139829397824,1.09796174388108,
126.008276304143));
#101182=CARTESIAN_POINT('Ctrl Pts',(-109.147594150771,0.963643389005652,
125.981438839087));
#101183=CARTESIAN_POINT('Ctrl Pts',(-109.155351191656,0.829458441013838,
125.95462802938));
#101184=CARTESIAN_POINT('Ctrl Pts',(-109.163108232541,0.694013477237669,
125.933393450362));
#101185=CARTESIAN_POINT('Ctrl Pts',(-109.170865273426,0.557811236841828,
125.917845531479));
#101186=CARTESIAN_POINT('Ctrl Pts',(-109.178616464667,0.421711707614783,
125.902309337404));
#101187=CARTESIAN_POINT('Ctrl Pts',(-109.186367655907,0.28485642531544,
125.892451311916));
#101188=CARTESIAN_POINT('Ctrl Pts',(-109.194118847147,0.147757309883138,
125.888330629875));
#101189=CARTESIAN_POINT('Ctrl Pts',(-109.201866743924,0.0107164652323208,
125.884211699234));
#101190=CARTESIAN_POINT('Ctrl Pts',(-109.209614640701,-0.126567616457595,
125.885825273722));
#101191=CARTESIAN_POINT('Ctrl Pts',(-109.217362537478,-0.263579136821274,
125.893178570326));
#101192=CARTESIAN_POINT('Ctrl Pts',(-109.225108813562,-0.40056199732852,
125.900530328779));
#101193=CARTESIAN_POINT('Ctrl Pts',(-109.232855089646,-0.537272019757397,
125.913619400299));
#101194=CARTESIAN_POINT('Ctrl Pts',(-109.24060136573,-0.673195050352685,
125.932400900298));
#101195=CARTESIAN_POINT('Ctrl Pts',(-109.248347698996,-0.809119084301092,
125.951182538938));
#101196=CARTESIAN_POINT('Ctrl Pts',(-109.256094032261,-0.944255727538221,
125.975656636392));
#101197=CARTESIAN_POINT('Ctrl Pts',(-109.263840365526,-1.07809797685594,
126.005726664575));
#101198=CARTESIAN_POINT('Ctrl Pts',(-109.271588433529,-1.21197019921721,
126.035803426732));
#101199=CARTESIAN_POINT('Ctrl Pts',(-109.279336501532,-1.34454706946666,
126.071478527598));
#101200=CARTESIAN_POINT('Ctrl Pts',(-109.287084569535,-1.47533415852613,
126.112604849926));
#101201=CARTESIAN_POINT('Ctrl Pts',(-109.294840872277,-1.60626024966006,
126.153774881798));
#101202=CARTESIAN_POINT('Ctrl Pts',(-109.302597175019,-1.73539238619786,
126.200407591054));
#101203=CARTESIAN_POINT('Ctrl Pts',(-109.310353477761,-1.86225310595762,
126.252306528273));
#101204=CARTESIAN_POINT('Ctrl Pts',(-109.318113920275,-1.98918153510355,
126.304233165517));
#101205=CARTESIAN_POINT('Ctrl Pts',(-109.325874362789,-2.11383577664564,
126.3614314684));
#101206=CARTESIAN_POINT('Ctrl Pts',(-109.333634805303,-2.23576151030469,
126.423658215948));
#101207=CARTESIAN_POINT('Ctrl Pts',(-109.341407705569,-2.35788296997546,
126.485984855396));
#101208=CARTESIAN_POINT('Ctrl Pts',(-109.349180605834,-2.47726682835527,
126.553355877892));
#101209=CARTESIAN_POINT('Ctrl Pts',(-109.3569535061,-2.59348560915369,126.625483321256));
#101210=CARTESIAN_POINT('Ctrl Pts',(-109.364443841862,-2.70547954453265,
126.694988750376));
#101211=CARTESIAN_POINT('Ctrl Pts',(-109.371934177624,-2.81453426928065,
126.768910615648));
#101212=CARTESIAN_POINT('Ctrl Pts',(-109.379424513386,-2.92029674208176,
126.846956165063));
#101213=CARTESIAN_POINT('Ctrl Pts',(-109.387353516481,-3.03225313507579,
126.929572408523));
#101214=CARTESIAN_POINT('Ctrl Pts',(-109.395282519577,-3.14090019779782,
127.017090611809));
#101215=CARTESIAN_POINT('Ctrl Pts',(-109.403211522672,-3.24577532853165,
127.109211692395));
#101216=CARTESIAN_POINT('Ctrl Pts',(-109.410902197704,-3.34749814786704,
127.198563819747));
#101217=CARTESIAN_POINT('Ctrl Pts',(-109.418592872736,-3.44567216479411,
127.292245841371));
#101218=CARTESIAN_POINT('Ctrl Pts',(-109.426283547768,-3.53990365071903,
127.38994043163));
#101219=CARTESIAN_POINT('Ctrl Pts',(-109.43396725077,-3.63404971049636,
127.487546456243));
#101220=CARTESIAN_POINT('Ctrl Pts',(-109.441650953772,-3.72426007157515,
127.589157530773));
#101221=CARTESIAN_POINT('Ctrl Pts',(-109.449334656774,-3.81017496384986,
127.694416919144));
#101222=CARTESIAN_POINT('Ctrl Pts',(-109.457013135598,-3.89603144227701,
127.799604741276));
#101223=CARTESIAN_POINT('Ctrl Pts',(-109.464691614422,-3.97759800978754,
127.908435635457));
#101224=CARTESIAN_POINT('Ctrl Pts',(-109.472370093246,-4.05455294464068,
128.020517324274));
#101225=CARTESIAN_POINT('Ctrl Pts',(-109.480045091343,-4.1314729950906,
128.132548205396));
#101226=CARTESIAN_POINT('Ctrl Pts',(-109.48772008944,-4.20378534745559,
128.247826620486));
#101227=CARTESIAN_POINT('Ctrl Pts',(-109.495395087537,-4.27120996446139,
128.365929051582));
#101228=CARTESIAN_POINT('Ctrl Pts',(-109.503069587789,-4.33863020791451,
128.484023821868));
#101229=CARTESIAN_POINT('Ctrl Pts',(-109.510744088041,-4.40116314251367,
128.604941901142));
#101230=CARTESIAN_POINT('Ctrl Pts',(-109.518418588293,-4.45857344127018,
128.72823298871));
#101231=CARTESIAN_POINT('Ctrl Pts',(-109.526092904013,-4.51598235960552,
128.851521111764));
#101232=CARTESIAN_POINT('Ctrl Pts',(-109.533767219733,-4.56826872447677,
128.977181765286));
#101233=CARTESIAN_POINT('Ctrl Pts',(-109.541441535452,-4.6152446707871,
129.104743104338));
#101234=CARTESIAN_POINT('Ctrl Pts',(-109.549119155242,-4.66224084193589,
129.232359363146));
#101235=CARTESIAN_POINT('Ctrl Pts',(-109.556796775031,-4.70392189957251,
129.36187756421));
#101236=CARTESIAN_POINT('Ctrl Pts',(-109.564474394821,-4.7401493703113,
129.492809242424));
#101237=CARTESIAN_POINT('Ctrl Pts',(-109.566223125773,-4.74840089892985,
129.522631542127));
#101238=CARTESIAN_POINT('Ctrl Pts',(-109.567971856726,-4.75636970745135,
129.55252711971));
#101239=CARTESIAN_POINT('Ctrl Pts',(-109.569720587678,-4.76405452823413,
129.582490119309));
#101240=CARTESIAN_POINT('Origin',(213.235140564004,0.,130.804360617566));
#101241=CARTESIAN_POINT('',(-111.665402883959,-4.76405452823393,129.582490119308));
#101242=CARTESIAN_POINT('',(-111.319883193423,-4.764054528234,129.582490119308));
#101243=CARTESIAN_POINT('',(213.235140564004,-4.76405452823405,129.582490119308));
#101244=CARTESIAN_POINT('',(-109.985140563973,-4.91824789704149,130.799812458929));
#101245=CARTESIAN_POINT('Ctrl Pts',(-109.98514056401,-4.91824789704208,
130.799812459574));
#101246=CARTESIAN_POINT('Ctrl Pts',(-109.992803365887,-4.91837304686826,
130.935145900162));
#101247=CARTESIAN_POINT('Ctrl Pts',(-110.000466167764,-4.9129081225041,
131.070627357));
#101248=CARTESIAN_POINT('Ctrl Pts',(-110.008128969641,-4.90184331819967,
131.205752130084));
#101249=CARTESIAN_POINT('Ctrl Pts',(-110.015922695434,-4.89058946457277,
131.343185597122));
#101250=CARTESIAN_POINT('Ctrl Pts',(-110.023716421227,-4.87354257725691,
131.480249661262));
#101251=CARTESIAN_POINT('Ctrl Pts',(-110.031510147019,-4.85074769783324,
131.616413469581));
#101252=CARTESIAN_POINT('Ctrl Pts',(-110.039165636601,-4.82835712795713,
131.750162159719));
#101253=CARTESIAN_POINT('Ctrl Pts',(-110.046821126184,-4.80042086055033,
131.883041855564));
#101254=CARTESIAN_POINT('Ctrl Pts',(-110.054476615766,-4.76703376610004,
132.014555699097));
#101255=CARTESIAN_POINT('Ctrl Pts',(-110.062131371041,-4.73364987410669,
132.146056927953));
#101256=CARTESIAN_POINT('Ctrl Pts',(-110.069786126316,-4.69481629336717,
132.276192176238));
#101257=CARTESIAN_POINT('Ctrl Pts',(-110.077440881592,-4.65067855629213,
132.404476872263));
#101258=CARTESIAN_POINT('Ctrl Pts',(-110.085096654511,-4.60653495142652,
132.532778622803));
#101259=CARTESIAN_POINT('Ctrl Pts',(-110.09275242743,-4.55708591869811,
132.659228952612));
#101260=CARTESIAN_POINT('Ctrl Pts',(-110.100408200349,-4.50252601811771,
132.783361001263));
#101261=CARTESIAN_POINT('Ctrl Pts',(-110.108305716042,-4.44624330498246,
132.911412709767));
#101262=CARTESIAN_POINT('Ctrl Pts',(-110.116203231735,-4.38452180407454,
133.036996889814));
#101263=CARTESIAN_POINT('Ctrl Pts',(-110.124100747428,-4.3176269459999,
133.159627187973));
#101264=CARTESIAN_POINT('Ctrl Pts',(-110.131767916235,-4.25268321063482,
133.278680727521));
#101265=CARTESIAN_POINT('Ctrl Pts',(-110.139435085042,-4.1828639623609,
133.39494998521));
#101266=CARTESIAN_POINT('Ctrl Pts',(-110.14710225385,-4.10845633554988,
133.508019176145));
#101267=CARTESIAN_POINT('Ctrl Pts',(-110.155114942985,-4.03069553518883,
133.626183820822));
#101268=CARTESIAN_POINT('Ctrl Pts',(-110.163127632121,-3.94792346969235,
133.740852849937));
#101269=CARTESIAN_POINT('Ctrl Pts',(-110.171140321257,-3.86051427395563,
133.851590934277));
#101270=CARTESIAN_POINT('Ctrl Pts',(-110.179153010393,-3.77310507821891,
133.962329018618));
#101271=CARTESIAN_POINT('Ctrl Pts',(-110.187165699528,-3.68105913125749,
134.069135836365));
#101272=CARTESIAN_POINT('Ctrl Pts',(-110.195178388664,-3.58479269293473,
134.171621286297));
#101273=CARTESIAN_POINT('Ctrl Pts',(-110.202952722783,-3.49138991100893,
134.271058081689));
#101274=CARTESIAN_POINT('Ctrl Pts',(-110.210727056902,-3.39369870799688,
134.366763152123));
#101275=CARTESIAN_POINT('Ctrl Pts',(-110.218501391022,-3.29204923267864,
134.458344048306));
#101276=CARTESIAN_POINT('Ctrl Pts',(-110.226266143969,-3.19052503125433,
134.549812079218));
#101277=CARTESIAN_POINT('Ctrl Pts',(-110.234030896916,-3.08505255139815,
134.637165789708));
#101278=CARTESIAN_POINT('Ctrl Pts',(-110.241795649863,-2.97600068806793,
134.720047398594));
#101279=CARTESIAN_POINT('Ctrl Pts',(-110.249552690748,-2.86705713658573,
134.802846688298));
#101280=CARTESIAN_POINT('Ctrl Pts',(-110.257309731633,-2.75454158568171,
134.88118248065));
#101281=CARTESIAN_POINT('Ctrl Pts',(-110.265066772518,-2.63885783990856,
134.954735584151));
#101282=CARTESIAN_POINT('Ctrl Pts',(-110.272817963758,-2.52326133214814,
135.028233220684));
#101283=CARTESIAN_POINT('Ctrl Pts',(-110.280569154999,-2.40450171358722,
135.096955138288));
#101284=CARTESIAN_POINT('Ctrl Pts',(-110.288320346239,-2.28301346223526,
135.16062422228));
#101285=CARTESIAN_POINT('Ctrl Pts',(-110.296068243016,-2.16157684663075,
135.224266245213));
#101286=CARTESIAN_POINT('Ctrl Pts',(-110.303816139793,-2.03741425043942,
135.282859524822));
#101287=CARTESIAN_POINT('Ctrl Pts',(-110.31156403657,-1.9109863644262,135.336171974791));
#101288=CARTESIAN_POINT('Ctrl Pts',(-110.319310312654,-1.78458492440091,
135.389473272946));
#101289=CARTESIAN_POINT('Ctrl Pts',(-110.327056588738,-1.65591949708484,
135.437495786829));
#101290=CARTESIAN_POINT('Ctrl Pts',(-110.334802864823,-1.52547208209369,
135.48005500335));
#101291=CARTESIAN_POINT('Ctrl Pts',(-110.342549198088,-1.39502370416953,
135.522614534033));
#101292=CARTESIAN_POINT('Ctrl Pts',(-110.350295531353,-1.26279368400579,
135.559710565617));
#101293=CARTESIAN_POINT('Ctrl Pts',(-110.358041864619,-1.129280178338,135.591208154444));
#101294=CARTESIAN_POINT('Ctrl Pts',(-110.365789932622,-0.995736773246146,
135.622712796937));
#101295=CARTESIAN_POINT('Ctrl Pts',(-110.373538000625,-0.860909691149279,
135.648616412137));
#101296=CARTESIAN_POINT('Ctrl Pts',(-110.381286068628,-0.725307907443927,
135.668835049804));
#101297=CARTESIAN_POINT('Ctrl Pts',(-110.38904237137,-0.589562004549358,
135.68907517608));
#101298=CARTESIAN_POINT('Ctrl Pts',(-110.396798674112,-0.453040142598879,
135.703618197404));
#101299=CARTESIAN_POINT('Ctrl Pts',(-110.404554976854,-0.316257615550054,
135.712431947845));
#101300=CARTESIAN_POINT('Ctrl Pts',(-110.412315419368,-0.179402083547729,
135.72125040245));
#101301=CARTESIAN_POINT('Ctrl Pts',(-110.420075861882,-0.0422859999042523,
135.724333484295));
#101302=CARTESIAN_POINT('Ctrl Pts',(-110.427836304396,0.0945756958698464,
135.721701209822));
#101303=CARTESIAN_POINT('Ctrl Pts',(-110.435609204662,0.231657094187638,
135.719064709789));
#101304=CARTESIAN_POINT('Ctrl Pts',(-110.443382104927,0.368482898130376,
135.710694543155));
#101305=CARTESIAN_POINT('Ctrl Pts',(-110.451155005193,0.504542739864685,
135.696662702081));
#101306=CARTESIAN_POINT('Ctrl Pts',(-110.458645340954,0.635656463627944,
135.683140953775));
#101307=CARTESIAN_POINT('Ctrl Pts',(-110.466135676716,0.766058642772488,
135.664362060649));
#101308=CARTESIAN_POINT('Ctrl Pts',(-110.473626012477,0.895303752426226,
135.640434878099));
#101309=CARTESIAN_POINT('Ctrl Pts',(-110.481400346597,1.02944922970568,
135.615600489149));
#101310=CARTESIAN_POINT('Ctrl Pts',(-110.489174680716,1.16277309743821,
135.585141041592));
#101311=CARTESIAN_POINT('Ctrl Pts',(-110.496949014835,1.29476672343772,
135.549122170519));
#101312=CARTESIAN_POINT('Ctrl Pts',(-110.504713767782,1.4265976790898,135.513147689485));
#101313=CARTESIAN_POINT('Ctrl Pts',(-110.512478520729,1.55710128138099,
135.471627519299));
#101314=CARTESIAN_POINT('Ctrl Pts',(-110.520243273676,1.6857771221356,135.424678632268));
#101315=CARTESIAN_POINT('Ctrl Pts',(-110.528000314561,1.81432516023115,
135.377776375535));
#101316=CARTESIAN_POINT('Ctrl Pts',(-110.535757355446,1.9410486845304,135.325456265178));
#101317=CARTESIAN_POINT('Ctrl Pts',(-110.543514396331,2.06546088396031,
135.267885502601));
#101318=CARTESIAN_POINT('Ctrl Pts',(-110.551265587571,2.18977926318301,
135.210358154585));
#101319=CARTESIAN_POINT('Ctrl Pts',(-110.559016778812,2.31178943346622,
135.147588199133));
#101320=CARTESIAN_POINT('Ctrl Pts',(-110.566767970052,2.43102340440222,
135.079791387646));
#101321=CARTESIAN_POINT('Ctrl Pts',(-110.574515866829,2.55020669771975,
135.012023391613));
#101322=CARTESIAN_POINT('Ctrl Pts',(-110.582263763606,2.66661579938392,
134.939232981819));
#101323=CARTESIAN_POINT('Ctrl Pts',(-110.590011660383,2.77980643399327,
134.86168230213));
#101324=CARTESIAN_POINT('Ctrl Pts',(-110.597757936467,2.89297339156197,
134.784147844371));
#101325=CARTESIAN_POINT('Ctrl Pts',(-110.605504212551,3.00292289885171,
134.701855318145));
#101326=CARTESIAN_POINT('Ctrl Pts',(-110.613250488636,3.10923918720794,
134.615110509547));
#101327=CARTESIAN_POINT('Ctrl Pts',(-110.620996821901,3.215556260367,134.528365060618));
#101328=CARTESIAN_POINT('Ctrl Pts',(-110.628743155166,3.31823975814899,
134.437167510897));
#101329=CARTESIAN_POINT('Ctrl Pts',(-110.636489488432,3.41690688274867,
134.341864033412));
#101330=CARTESIAN_POINT('Ctrl Pts',(-110.644237556435,3.51559610316639,
134.246539213375));
#101331=CARTESIAN_POINT('Ctrl Pts',(-110.651985624438,3.61026687947045,
134.147106907453));
#101332=CARTESIAN_POINT('Ctrl Pts',(-110.659733692441,3.70057346831104,
134.043949953907));
#101333=CARTESIAN_POINT('Ctrl Pts',(-110.667489995183,3.79097603606927,
133.940683363922));
#101334=CARTESIAN_POINT('Ctrl Pts',(-110.675246297925,3.87700489290491,
133.833684513222));
#101335=CARTESIAN_POINT('Ctrl Pts',(-110.683002600667,3.95835444773843,
133.723369546735));
#101336=CARTESIAN_POINT('Ctrl Pts',(-110.690763043181,4.03974742127875,
133.612995701829));
#101337=CARTESIAN_POINT('Ctrl Pts',(-110.698523485695,4.11645589780784,
133.499302538377));
#101338=CARTESIAN_POINT('Ctrl Pts',(-110.706283928209,4.18821838034238,
133.382734108948));
#101339=CARTESIAN_POINT('Ctrl Pts',(-110.714056828475,4.26009606238465,
133.265978553528));
#101340=CARTESIAN_POINT('Ctrl Pts',(-110.72182972874,4.32701169332723,133.146338850045));
#101341=CARTESIAN_POINT('Ctrl Pts',(-110.729602629005,4.38874997593343,
133.024283298932));
#101342=CARTESIAN_POINT('Ctrl Pts',(-110.737092964767,4.44824391645371,
132.906664774549));
#101343=CARTESIAN_POINT('Ctrl Pts',(-110.744583300529,4.50293026489899,
132.786803277617));
#101344=CARTESIAN_POINT('Ctrl Pts',(-110.75207363629,4.55265978732259,132.665132479831));
#101345=CARTESIAN_POINT('Ctrl Pts',(-110.759847970409,4.60427481970683,
132.538848496758));
#101346=CARTESIAN_POINT('Ctrl Pts',(-110.767622304528,4.65071323094684,
132.410215275489));
#101347=CARTESIAN_POINT('Ctrl Pts',(-110.775396638647,4.69175531358146,
132.279696220058));
#101348=CARTESIAN_POINT('Ctrl Pts',(-110.783161391595,4.73274681551716,
132.149338017698));
#101349=CARTESIAN_POINT('Ctrl Pts',(-110.790926144542,4.76835510519319,
132.017098974865));
#101350=CARTESIAN_POINT('Ctrl Pts',(-110.798690897489,4.79840811188311,
131.88346332552));
#101351=CARTESIAN_POINT('Ctrl Pts',(-110.806447938374,4.82843126950303,
131.749960404987));
#101352=CARTESIAN_POINT('Ctrl Pts',(-110.814204979259,4.85291003915501,
131.615064017361));
#101353=CARTESIAN_POINT('Ctrl Pts',(-110.821962020144,4.87172195883974,
131.479274107029));
#101354=CARTESIAN_POINT('Ctrl Pts',(-110.829713211384,4.89051969230952,
131.343586596924));
#101355=CARTESIAN_POINT('Ctrl Pts',(-110.837464402624,4.90365902835306,
131.207007290996));
#101356=CARTESIAN_POINT('Ctrl Pts',(-110.845215593864,4.91106852448644,
131.070046541729));
#101357=CARTESIAN_POINT('Ctrl Pts',(-110.852963490641,4.91847487138633,
130.933144004435));
#101358=CARTESIAN_POINT('Ctrl Pts',(-110.860711387418,4.92015620099542,
130.79586073583));
#101359=CARTESIAN_POINT('Ctrl Pts',(-110.868459284195,4.91609292066558,
130.658712212557));
#101360=CARTESIAN_POINT('Ctrl Pts',(-110.876205560279,4.91203049028638,
130.521592377797));
#101361=CARTESIAN_POINT('Ctrl Pts',(-110.883951836363,4.90222585168377,
130.384607622852));
#101362=CARTESIAN_POINT('Ctrl Pts',(-110.891698112447,4.88671153824642,
130.248273030518));
#101363=CARTESIAN_POINT('Ctrl Pts',(-110.899444445713,4.87119711028592,
130.111937431792));
#101364=CARTESIAN_POINT('Ctrl Pts',(-110.907190778978,4.84997296759328,
129.976252393714));
#101365=CARTESIAN_POINT('Ctrl Pts',(-110.914937112243,4.82312344377584,
129.841727089893));
#101366=CARTESIAN_POINT('Ctrl Pts',(-110.922685180246,4.79626790719366,
129.707171660063));
#101367=CARTESIAN_POINT('Ctrl Pts',(-110.930433248249,4.76378455920772,
129.573776864623));
#101368=CARTESIAN_POINT('Ctrl Pts',(-110.938181316252,4.72580860976288,
129.442040520676));
#101369=CARTESIAN_POINT('Ctrl Pts',(-110.945937618994,4.6877922990271,129.310164165775));
#101370=CARTESIAN_POINT('Ctrl Pts',(-110.953693921736,4.64427183406049,
129.17995015966));
#101371=CARTESIAN_POINT('Ctrl Pts',(-110.961450224478,4.59543214993469,
129.051880541261));
#101372=CARTESIAN_POINT('Ctrl Pts',(-110.969210666992,4.54656639859894,
128.92374256825));
#101373=CARTESIAN_POINT('Ctrl Pts',(-110.976971109506,4.49237592550257,
128.797751622494));
#101374=CARTESIAN_POINT('Ctrl Pts',(-110.98473155202,4.43309297914226,128.674367730071));
#101375=CARTESIAN_POINT('Ctrl Pts',(-110.992504452286,4.37371486653356,
128.55078577087));
#101376=CARTESIAN_POINT('Ctrl Pts',(-111.000277352551,4.30922812865151,
128.429819573315));
#101377=CARTESIAN_POINT('Ctrl Pts',(-111.008050252817,4.23991038649881,
128.31190340089));
#101378=CARTESIAN_POINT('Ctrl Pts',(-111.015540588579,4.17311251887195,
128.198273778342));
#101379=CARTESIAN_POINT('Ctrl Pts',(-111.023030924341,4.10182895396599,
128.087476537716));
#101380=CARTESIAN_POINT('Ctrl Pts',(-111.030521260103,4.02634388746626,
127.9798716439));
#101381=CARTESIAN_POINT('Ctrl Pts',(-111.038295594222,3.94799678172954,
127.868186877832));
#101382=CARTESIAN_POINT('Ctrl Pts',(-111.046069928341,3.86487510519078,
127.759587529115));
#101383=CARTESIAN_POINT('Ctrl Pts',(-111.053844262461,3.77724997553727,
127.654508925057));
#101384=CARTESIAN_POINT('Ctrl Pts',(-111.061609015408,3.68973283602453,
127.549559820986));
#101385=CARTESIAN_POINT('Ctrl Pts',(-111.069373768355,3.59772353443533,
127.448123125633));
#101386=CARTESIAN_POINT('Ctrl Pts',(-111.077138521302,3.50153646208397,
127.350605347256));
#101387=CARTESIAN_POINT('Ctrl Pts',(-111.084895562187,3.40544492408886,
127.253184424911));
#101388=CARTESIAN_POINT('Ctrl Pts',(-111.092652603072,3.30518414563818,
127.159674950188));
#101389=CARTESIAN_POINT('Ctrl Pts',(-111.100409643957,3.20110855040108,
127.070450185988));
#101390=CARTESIAN_POINT('Ctrl Pts',(-111.108160835197,3.09711143938065,
126.981292706877));
#101391=CARTESIAN_POINT('Ctrl Pts',(-111.115912026437,2.98930553325379,
126.896413760349));
#101392=CARTESIAN_POINT('Ctrl Pts',(-111.123663217677,2.87808158961293,
126.816149310974));
#101393=CARTESIAN_POINT('Ctrl Pts',(-111.131411114454,2.76690491911467,
126.73591897613));
#101394=CARTESIAN_POINT('Ctrl Pts',(-111.139159011231,2.65231341689568,
126.660299465901));
#101395=CARTESIAN_POINT('Ctrl Pts',(-111.146906908009,2.53473017774764,
126.589585891852));
#101396=CARTESIAN_POINT('Ctrl Pts',(-111.154653184093,2.41717153447844,
126.518887109559));
#101397=CARTESIAN_POINT('Ctrl Pts',(-111.162399460177,2.2966227338761,126.45309242361));
#101398=CARTESIAN_POINT('Ctrl Pts',(-111.170145736261,2.17353471477774,
126.392452877579));
#101399=CARTESIAN_POINT('Ctrl Pts',(-111.177892069526,2.05044578707142,
126.331812883921));
#101400=CARTESIAN_POINT('Ctrl Pts',(-111.185638402792,1.92481795418158,
126.276328278894));
#101401=CARTESIAN_POINT('Ctrl Pts',(-111.193384736057,1.7971251826629,126.226203331022));
#101402=CARTESIAN_POINT('Ctrl Pts',(-111.20113280406,1.66940381523358,126.176067158015));
#101403=CARTESIAN_POINT('Ctrl Pts',(-111.208880872063,1.53961695285653,
126.131293173367));
#101404=CARTESIAN_POINT('Ctrl Pts',(-111.216628940066,1.40825650743737,
126.092036703428));
#101405=CARTESIAN_POINT('Ctrl Pts',(-111.224385242808,1.27675645057343,
126.052738511244));
#101406=CARTESIAN_POINT('Ctrl Pts',(-111.23214154555,1.1436798450156,126.018969660026));
#101407=CARTESIAN_POINT('Ctrl Pts',(-111.239897848291,1.00953220569041,
125.990835112474));
#101408=CARTESIAN_POINT('Ctrl Pts',(-111.247658290806,0.875312967731013,
125.962685548667));
#101409=CARTESIAN_POINT('Ctrl Pts',(-111.25541873332,0.740021942432409,
125.940176344755));
#101410=CARTESIAN_POINT('Ctrl Pts',(-111.263179175834,0.604171698748815,
125.923360758835));
#101411=CARTESIAN_POINT('Ctrl Pts',(-111.270952076099,0.468103376193841,
125.906518179043));
#101412=CARTESIAN_POINT('Ctrl Pts',(-111.278724976365,0.331474431247777,
125.895387513441));
#101413=CARTESIAN_POINT('Ctrl Pts',(-111.28649787663,0.194800283013736,
125.889969921637));
#101414=CARTESIAN_POINT('Ctrl Pts',(-111.293988212392,0.0630945843290355,
125.884749272941));
#101415=CARTESIAN_POINT('Ctrl Pts',(-111.301478548154,-0.0686527801770063,
125.88483354002));
#101416=CARTESIAN_POINT('Ctrl Pts',(-111.308968883916,-0.199985347138127,
125.890178190811));
#101417=CARTESIAN_POINT('Ctrl Pts',(-111.316743218035,-0.336297428291199,
125.895725485661));
#101418=CARTESIAN_POINT('Ctrl Pts',(-111.324517552154,-0.472594432587768,
125.906957505593));
#101419=CARTESIAN_POINT('Ctrl Pts',(-111.332291886273,-0.608363561101947,
125.923881456661));
#101420=CARTESIAN_POINT('Ctrl Pts',(-111.34005663922,-0.743965366299635,
125.940784550473));
#101421=CARTESIAN_POINT('Ctrl Pts',(-111.347821392167,-0.879040205896588,
125.963365570171));
#101422=CARTESIAN_POINT('Ctrl Pts',(-111.355586145114,-1.01307613679673,
125.991579737082));
#101423=CARTESIAN_POINT('Ctrl Pts',(-111.363343185999,-1.14697894132072,
126.019765881285));
#101424=CARTESIAN_POINT('Ctrl Pts',(-111.371100226884,-1.27984451048792,
126.053573958544));
#101425=CARTESIAN_POINT('Ctrl Pts',(-111.378857267769,-1.41116723299806,
126.092907539904));
#101426=CARTESIAN_POINT('Ctrl Pts',(-111.386608459009,-1.5423909240218,
126.132211459504));
#101427=CARTESIAN_POINT('Ctrl Pts',(-111.394359650249,-1.67207371119932,
126.177032477668));
#101428=CARTESIAN_POINT('Ctrl Pts',(-111.402110841489,-1.79972172399976,
126.227223436023));
#101429=CARTESIAN_POINT('Ctrl Pts',(-111.409858738266,-1.92731548298946,
126.277393061881));
#101430=CARTESIAN_POINT('Ctrl Pts',(-111.417606635044,-2.05287582460229,
126.332927945709));
#101431=CARTESIAN_POINT('Ctrl Pts',(-111.425354531821,-2.17592577005096,
126.393631640886));
#101432=CARTESIAN_POINT('Ctrl Pts',(-111.433100807905,-2.2989499761037,
126.454322638157));
#101433=CARTESIAN_POINT('Ctrl Pts',(-111.440847083989,-2.41946448008742,
126.520180123343));
#101434=CARTESIAN_POINT('Ctrl Pts',(-111.448593360073,-2.53701432847838,
126.59096040401));
#101435=CARTESIAN_POINT('Ctrl Pts',(-111.456339693338,-2.65456504459546,
126.661741207161));
#101436=CARTESIAN_POINT('Ctrl Pts',(-111.464086026603,-2.76915072651625,
126.737444676631));
#101437=CARTESIAN_POINT('Ctrl Pts',(-111.471832359868,-2.88034332684791,
126.81778246306));
#101438=CARTESIAN_POINT('Ctrl Pts',(-111.479580427871,-2.99156082799161,
126.89813824058));
#101439=CARTESIAN_POINT('Ctrl Pts',(-111.487328495874,-3.09938341867515,
126.983130171284));
#101440=CARTESIAN_POINT('Ctrl Pts',(-111.495076563877,-3.20341452804219,
127.07242835344));
#101441=CARTESIAN_POINT('Ctrl Pts',(-111.502832866619,-3.30755620291067,
127.161821442766));
#101442=CARTESIAN_POINT('Ctrl Pts',(-111.510589169361,-3.40789804970514,
127.255529671012));
#101443=CARTESIAN_POINT('Ctrl Pts',(-111.518345472102,-3.50407851716587,
127.353184469057));
#101444=CARTESIAN_POINT('Ctrl Pts',(-111.526105914617,-3.60031031903777,
127.450891388408));
#101445=CARTESIAN_POINT('Ctrl Pts',(-111.533866357131,-3.69237605362251,
127.552548785099));
#101446=CARTESIAN_POINT('Ctrl Pts',(-111.541626799645,-3.77995385733691,
127.657754207653));
#101447=CARTESIAN_POINT('Ctrl Pts',(-111.54939969991,-3.86767224871661,
127.763128515292));
#101448=CARTESIAN_POINT('Ctrl Pts',(-111.557172600175,-3.95088807501574,
127.872061919566));
#101449=CARTESIAN_POINT('Ctrl Pts',(-111.564945500441,-4.02932176400691,
127.984121410584));
#101450=CARTESIAN_POINT('Ctrl Pts',(-111.572435836203,-4.10490419084857,
128.092107256854));
#101451=CARTESIAN_POINT('Ctrl Pts',(-111.579926171966,-4.17604596319895,
128.202995594316));
#101452=CARTESIAN_POINT('Ctrl Pts',(-111.587416507729,-4.24253781754489,
128.316378316744));
#101453=CARTESIAN_POINT('Ctrl Pts',(-111.595487622467,-4.31418525800406,
128.438552407604));
#101454=CARTESIAN_POINT('Ctrl Pts',(-111.603558737205,-4.38064618870131,
128.563984957254));
#101455=CARTESIAN_POINT('Ctrl Pts',(-111.611629851943,-4.44162376095062,
128.692214451066));
#101456=CARTESIAN_POINT('Ctrl Pts',(-111.61968972964,-4.50251643693333,
128.820265416858));
#101457=CARTESIAN_POINT('Ctrl Pts',(-111.627749607336,-4.55794080676336,
128.951105260088));
#101458=CARTESIAN_POINT('Ctrl Pts',(-111.635809485033,-4.60764439350489,
129.084245445404));
#101459=CARTESIAN_POINT('Ctrl Pts',(-111.643856063879,-4.65726596900233,
129.217165948541));
#101460=CARTESIAN_POINT('Ctrl Pts',(-111.651902642724,-4.70118545278094,
129.35237890351));
#101461=CARTESIAN_POINT('Ctrl Pts',(-111.65994922157,-4.73919745996105,
129.489373736263));
#101462=CARTESIAN_POINT('Ctrl Pts',(-111.661767109033,-4.74778515326904,
129.520323683286));
#101463=CARTESIAN_POINT('Ctrl Pts',(-111.663584996496,-4.756071519496,129.551364489398));
#101464=CARTESIAN_POINT('Ctrl Pts',(-111.665402883959,-4.76405452823392,
129.582490119308));
#101465=CARTESIAN_POINT('Ctrl Pts',(-109.915204178194,-4.76405452823412,
129.582490119309));
#101466=CARTESIAN_POINT('Ctrl Pts',(-109.915713040413,-4.76627341212307,
129.591141513915));
#101467=CARTESIAN_POINT('Ctrl Pts',(-109.916221902632,-4.76846850299481,
129.599798068042));
#101468=CARTESIAN_POINT('Ctrl Pts',(-109.916730764851,-4.77063978033951,
129.60845963975));
#101469=CARTESIAN_POINT('Ctrl Pts',(-109.927005307824,-4.81448049310873,
129.783347236812));
#101470=CARTESIAN_POINT('Ctrl Pts',(-109.937279850797,-4.84872130166821,
129.960730603675));
#101471=CARTESIAN_POINT('Ctrl Pts',(-109.94755439377,-4.87313170538994,
130.139702476547));
#101472=CARTESIAN_POINT('Ctrl Pts',(-109.957592050043,-4.89697931035751,
130.314548029009));
#101473=CARTESIAN_POINT('Ctrl Pts',(-109.967629706315,-4.91144463375593,
130.490909983889));
#101474=CARTESIAN_POINT('Ctrl Pts',(-109.977667362588,-4.91635708443026,
130.667919857995));
#101475=CARTESIAN_POINT('Ctrl Pts',(-109.980158429716,-4.91757621806691,
130.711848785906));
#101476=CARTESIAN_POINT('Ctrl Pts',(-109.982649496845,-4.91820721261987,
130.755817495907));
#101477=CARTESIAN_POINT('Ctrl Pts',(-109.985140563974,-4.91824789704149,
130.799812458929));
#101478=CARTESIAN_POINT('',(-109.639859435959,-4.91824962741785,130.806275011501));
#101479=CARTESIAN_POINT('Ctrl Pts',(-109.569720587678,-4.76405452823413,
129.582490119309));
#101480=CARTESIAN_POINT('Ctrl Pts',(-109.577406436354,-4.79783008961758,
129.714180520527));
#101481=CARTESIAN_POINT('Ctrl Pts',(-109.585092285029,-4.8261157894635,
129.847173809154));
#101482=CARTESIAN_POINT('Ctrl Pts',(-109.592778133704,-4.84883573668985,
129.980968207412));
#101483=CARTESIAN_POINT('Ctrl Pts',(-109.600625017413,-4.87203171559869,
130.117565885619));
#101484=CARTESIAN_POINT('Ctrl Pts',(-109.608471901122,-4.88942606939395,
130.254998176776));
#101485=CARTESIAN_POINT('Ctrl Pts',(-109.616318784832,-4.90099394425744,
130.392727989059));
#101486=CARTESIAN_POINT('Ctrl Pts',(-109.624165668541,-4.91256181912092,
130.530457801341));
#101487=CARTESIAN_POINT('Ctrl Pts',(-109.63201255225,-4.91830326132474,
130.668484696905));
#101488=CARTESIAN_POINT('Ctrl Pts',(-109.63985943596,-4.91824962741785,
130.806275011501));
#101489=CARTESIAN_POINT('Ctrl Pts',(-109.639859435992,-4.91824962741763,
130.806275012075));
#101490=CARTESIAN_POINT('Ctrl Pts',(-109.645863669728,-4.91820858811826,
130.911708619347));
#101491=CARTESIAN_POINT('Ctrl Pts',(-109.651867903463,-4.91477752119081,
131.017072484126));
#101492=CARTESIAN_POINT('Ctrl Pts',(-109.657872137199,-4.90796816671738,
131.122215202225));
#101493=CARTESIAN_POINT('Ctrl Pts',(-109.665646471318,-4.89915135525686,
131.258354909087));
#101494=CARTESIAN_POINT('Ctrl Pts',(-109.673420805437,-4.88465181757774,
131.394343125707));
#101495=CARTESIAN_POINT('Ctrl Pts',(-109.681195139556,-4.86447465546066,
131.529667027906));
#101496=CARTESIAN_POINT('Ctrl Pts',(-109.688959892503,-4.8443223598926,
131.664824155491));
#101497=CARTESIAN_POINT('Ctrl Pts',(-109.69672464545,-4.81850641926187,
131.799318214662));
#101498=CARTESIAN_POINT('Ctrl Pts',(-109.704489398397,-4.78708388456926,
131.932638484316));
#101499=CARTESIAN_POINT('Ctrl Pts',(-109.712246439282,-4.7556925591811,
132.065826338398));
#101500=CARTESIAN_POINT('Ctrl Pts',(-109.720003480167,-4.7187058105029,
132.19784234493));
#101501=CARTESIAN_POINT('Ctrl Pts',(-109.727760521052,-4.67623217299796,
132.328183352243));
#101502=CARTESIAN_POINT('Ctrl Pts',(-109.735511712292,-4.63379056519351,
132.458426068389));
#101503=CARTESIAN_POINT('Ctrl Pts',(-109.743262903532,-4.58587042505701,
132.586995929277));
#101504=CARTESIAN_POINT('Ctrl Pts',(-109.751014094772,-4.53263072011456,
132.713402737995));
#101505=CARTESIAN_POINT('Ctrl Pts',(-109.75876199155,-4.47941364346685,
132.839755820448));
#101506=CARTESIAN_POINT('Ctrl Pts',(-109.766509888327,-4.42088165032147,
132.9639473197));
#101507=CARTESIAN_POINT('Ctrl Pts',(-109.774257785104,-4.35724257690382,
133.0855051085));
#101508=CARTESIAN_POINT('Ctrl Pts',(-109.782004061188,-4.29361681540843,
133.20703747003));
#101509=CARTESIAN_POINT('Ctrl Pts',(-109.789750337272,-4.22488627974989,
133.32593687076));
#101510=CARTESIAN_POINT('Ctrl Pts',(-109.797496613356,-4.15130550981274,
133.441754336126));
#101511=CARTESIAN_POINT('Ctrl Pts',(-109.805242946621,-4.07772419671917,
133.55757265643));
#101512=CARTESIAN_POINT('Ctrl Pts',(-109.812989279887,-3.99929278755774,
133.670308665976));
#101513=CARTESIAN_POINT('Ctrl Pts',(-109.820735613152,-3.91630982060835,
133.779541360228));
#101514=CARTESIAN_POINT('Ctrl Pts',(-109.828483681155,-3.83330827019899,
133.888798516384));
#101515=CARTESIAN_POINT('Ctrl Pts',(-109.836231749158,-3.74575337019301,
133.994550484837));
#101516=CARTESIAN_POINT('Ctrl Pts',(-109.843979817161,-3.65398444392659,
134.096408725666));
#101517=CARTESIAN_POINT('Ctrl Pts',(-109.851736119903,-3.56211798455314,
134.198375222645));
#101518=CARTESIAN_POINT('Ctrl Pts',(-109.859492422644,-3.46602881431032,
134.29643943437));
#101519=CARTESIAN_POINT('Ctrl Pts',(-109.867248725386,-3.36609407241288,
134.390248758343));
#101520=CARTESIAN_POINT('Ctrl Pts',(-109.8750091679,-3.26610599233444,134.484108151177));
#101521=CARTESIAN_POINT('Ctrl Pts',(-109.882769610414,-3.16226854668325,
134.573707875885));
#101522=CARTESIAN_POINT('Ctrl Pts',(-109.890530052929,-3.05499179487866,
134.658735819298));
#101523=CARTESIAN_POINT('Ctrl Pts',(-109.898302953194,-2.94754283290878,
134.743900257113));
#101524=CARTESIAN_POINT('Ctrl Pts',(-109.90607585346,-2.83664384838213,
134.82447801797));
#101525=CARTESIAN_POINT('Ctrl Pts',(-109.913848753725,-2.72273443545673,
134.900200001194));
#101526=CARTESIAN_POINT('Ctrl Pts',(-109.921339089487,-2.61296591660983,
134.973169299597));
#101527=CARTESIAN_POINT('Ctrl Pts',(-109.928829425249,-2.50040230588036,
135.041629570522));
#101528=CARTESIAN_POINT('Ctrl Pts',(-109.936319761011,-2.38545661371691,
135.105381404144));
#101529=CARTESIAN_POINT('Ctrl Pts',(-109.94409409513,-2.26615272069961,
135.171550407913));
#101530=CARTESIAN_POINT('Ctrl Pts',(-109.951868429249,-2.14390462838403,
135.232856488996));
#101531=CARTESIAN_POINT('Ctrl Pts',(-109.959642763369,-2.01914654791204,
135.289026745669));
#101532=CARTESIAN_POINT('Ctrl Pts',(-109.967407516316,-1.89454222062462,
135.345127777521));
#101533=CARTESIAN_POINT('Ctrl Pts',(-109.975172269263,-1.76743441307371,
135.396105419705));
#101534=CARTESIAN_POINT('Ctrl Pts',(-109.98293702221,-1.63828364684828,
135.441731613612));
#101535=CARTESIAN_POINT('Ctrl Pts',(-109.990694063095,-1.50926115498458,
135.48731249094));
#101536=CARTESIAN_POINT('Ctrl Pts',(-109.99845110398,-1.37820010868962,
135.527552367959));
#101537=CARTESIAN_POINT('Ctrl Pts',(-110.006208144865,-1.24558248923989,
135.562270592019));
#101538=CARTESIAN_POINT('Ctrl Pts',(-110.013959336105,-1.11306487776877,
135.596962634796));
#101539=CARTESIAN_POINT('Ctrl Pts',(-110.021710527345,-0.978993406257185,
135.626141214034));
#101540=CARTESIAN_POINT('Ctrl Pts',(-110.029461718585,-0.843866417082174,
135.649675110209));
#101541=CARTESIAN_POINT('Ctrl Pts',(-110.037209615362,-0.708796860482009,
135.673199003851));
#101542=CARTESIAN_POINT('Ctrl Pts',(-110.044957512139,-0.572673062856663,
135.691082919197));
#101543=CARTESIAN_POINT('Ctrl Pts',(-110.052705408916,-0.436004578791037,
135.703246518439));
#101544=CARTESIAN_POINT('Ctrl Pts',(-110.060451685001,-0.299364682826046,
135.715407573318));
#101545=CARTESIAN_POINT('Ctrl Pts',(-110.068197961085,-0.162180716226217,
135.721850657492));
#101546=CARTESIAN_POINT('Ctrl Pts',(-110.075944237169,-0.0249679990312448,
135.722547240858));
#101547=CARTESIAN_POINT('Ctrl Pts',(-110.083690570434,0.112245731037023,
135.723243829365));
#101548=CARTESIAN_POINT('Ctrl Pts',(-110.0914369037,0.249487821163756,135.718193830434));
#101549=CARTESIAN_POINT('Ctrl Pts',(-110.099183236965,0.386242701076687,
135.70742084954));
#101550=CARTESIAN_POINT('Ctrl Pts',(-110.106931304968,0.523028206296596,
135.696645456111));
#101551=CARTESIAN_POINT('Ctrl Pts',(-110.114679372971,0.659325894508578,
135.680144561137));
#101552=CARTESIAN_POINT('Ctrl Pts',(-110.122427440974,0.794625463520789,
135.657993631631));
#101553=CARTESIAN_POINT('Ctrl Pts',(-110.130183743716,0.930068830525216,
135.635819159854));
#101554=CARTESIAN_POINT('Ctrl Pts',(-110.137940046458,1.06451157279787,
135.607982721331));
#101555=CARTESIAN_POINT('Ctrl Pts',(-110.145696349199,1.19745318291215,
135.574611023701));
#101556=CARTESIAN_POINT('Ctrl Pts',(-110.153456791714,1.33046574796655,
135.541221514591));
#101557=CARTESIAN_POINT('Ctrl Pts',(-110.161217234228,1.46197520970428,
135.502290970535));
#101558=CARTESIAN_POINT('Ctrl Pts',(-110.168977676742,1.59149733134458,
135.457995681344));
#101559=CARTESIAN_POINT('Ctrl Pts',(-110.176750577007,1.72122737339297,
135.413629285422));
#101560=CARTESIAN_POINT('Ctrl Pts',(-110.184523477273,1.8489633356778,135.363881076881));
#101561=CARTESIAN_POINT('Ctrl Pts',(-110.192296377538,1.97424120480058,
135.308975443249));
#101562=CARTESIAN_POINT('Ctrl Pts',(-110.1997867133,2.09496490782483,135.256065767699));
#101563=CARTESIAN_POINT('Ctrl Pts',(-110.207277049062,2.21340585376656,
135.198367262696));
#101564=CARTESIAN_POINT('Ctrl Pts',(-110.214767384824,2.32917303125561,
135.136119619746));
#101565=CARTESIAN_POINT('Ctrl Pts',(-110.222541718943,2.44932955646568,
135.071511838495));
#101566=CARTESIAN_POINT('Ctrl Pts',(-110.230316053063,2.5669861787307,135.001798490493));
#101567=CARTESIAN_POINT('Ctrl Pts',(-110.238090387182,2.68167859637454,
134.927197379827));
#101568=CARTESIAN_POINT('Ctrl Pts',(-110.245855140129,2.79622966586399,
134.852688208361));
#101569=CARTESIAN_POINT('Ctrl Pts',(-110.253619893076,2.90782347475742,
134.773303470787));
#101570=CARTESIAN_POINT('Ctrl Pts',(-110.261384646023,3.01601922772018,
134.689307345711));
#101571=CARTESIAN_POINT('Ctrl Pts',(-110.269141686908,3.1241075191358,134.60539464677));
#101572=CARTESIAN_POINT('Ctrl Pts',(-110.276898727793,3.2288041641905,134.516879913122));
#101573=CARTESIAN_POINT('Ctrl Pts',(-110.284655768678,3.32969665204159,
134.424071002097));
#101574=CARTESIAN_POINT('Ctrl Pts',(-110.292406959918,3.43051305608263,
134.331332078994));
#101575=CARTESIAN_POINT('Ctrl Pts',(-110.300158151158,3.52753072640563,
134.234305687715));
#101576=CARTESIAN_POINT('Ctrl Pts',(-110.307909342398,3.62036989808175,
134.133340170457));
#101577=CARTESIAN_POINT('Ctrl Pts',(-110.315657239175,3.71316961063347,
134.032417566237));
#101578=CARTESIAN_POINT('Ctrl Pts',(-110.323405135953,3.80179409273827,
133.927559453152));
#101579=CARTESIAN_POINT('Ctrl Pts',(-110.33115303273,3.88590032722215,133.819151109357));
#101580=CARTESIAN_POINT('Ctrl Pts',(-110.338899308814,3.9699889684949,133.710765442251));
#101581=CARTESIAN_POINT('Ctrl Pts',(-110.346645584898,4.04956100254009,
133.598831330276));
#101582=CARTESIAN_POINT('Ctrl Pts',(-110.354391860982,4.12431388310457,
133.483766905558));
#101583=CARTESIAN_POINT('Ctrl Pts',(-110.362138194247,4.19906731547773,
133.36870163146));
#101584=CARTESIAN_POINT('Ctrl Pts',(-110.369884527512,4.26900131039169,
133.250506326364));
#101585=CARTESIAN_POINT('Ctrl Pts',(-110.377630860778,4.33385704947505,
133.129627513476));
#101586=CARTESIAN_POINT('Ctrl Pts',(-110.385378928781,4.3987273125514,133.008721630616));
#101587=CARTESIAN_POINT('Ctrl Pts',(-110.393126996784,4.45851687201439,
132.885131388582));
#101588=CARTESIAN_POINT('Ctrl Pts',(-110.400875064787,4.51301338960115,
132.759326910825));
#101589=CARTESIAN_POINT('Ctrl Pts',(-110.408631367528,4.5675678267354,132.633388726572));
#101590=CARTESIAN_POINT('Ctrl Pts',(-110.41638767027,4.616817828782,132.505231964918));
#101591=CARTESIAN_POINT('Ctrl Pts',(-110.424143973012,4.66059946197643,
132.375346205509));
#101592=CARTESIAN_POINT('Ctrl Pts',(-110.431904415526,4.70440446274684,
132.245391122159));
#101593=CARTESIAN_POINT('Ctrl Pts',(-110.439664858041,4.74273516982851,
132.113705577464));
#101594=CARTESIAN_POINT('Ctrl Pts',(-110.447425300555,4.77547815902452,
131.980792262491));
#101595=CARTESIAN_POINT('Ctrl Pts',(-110.45519820082,4.80827371017357,131.847665583264));
#101596=CARTESIAN_POINT('Ctrl Pts',(-110.462971101086,4.83546354112521,
131.71330757864));
#101597=CARTESIAN_POINT('Ctrl Pts',(-110.470744001351,4.85698562488538,
131.578229923171));
#101598=CARTESIAN_POINT('Ctrl Pts',(-110.478234337113,4.87772532669024,
131.448062680716));
#101599=CARTESIAN_POINT('Ctrl Pts',(-110.485724672875,4.89320216468743,
131.317227507154));
#101600=CARTESIAN_POINT('Ctrl Pts',(-110.493215008637,4.90340644693239,
131.186182930536));
#101601=CARTESIAN_POINT('Ctrl Pts',(-110.500989342756,4.91399762764009,
131.050169758967));
#101602=CARTESIAN_POINT('Ctrl Pts',(-110.508763676875,4.91894209183884,
130.913500143009));
#101603=CARTESIAN_POINT('Ctrl Pts',(-110.516538010995,4.91817211787623,
130.776682441238));
#101604=CARTESIAN_POINT('Ctrl Pts',(-110.524302763942,4.91740309283771,
130.640033355057));
#101605=CARTESIAN_POINT('Ctrl Pts',(-110.532067516889,4.91093364436117,
130.503236933395));
#101606=CARTESIAN_POINT('Ctrl Pts',(-110.539832269836,4.89874777274482,
130.366806824841));
#101607=CARTESIAN_POINT('Ctrl Pts',(-110.547589310721,4.88657400430795,
130.230512220595));
#101608=CARTESIAN_POINT('Ctrl Pts',(-110.555346351606,4.86869514603252,
130.094583592318));
#101609=CARTESIAN_POINT('Ctrl Pts',(-110.563103392491,4.8451472348218,129.959534401473));
#101610=CARTESIAN_POINT('Ctrl Pts',(-110.570854583731,4.82161708127407,
129.824587052272));
#101611=CARTESIAN_POINT('Ctrl Pts',(-110.578605774971,4.79242645095818,
129.690518204058));
#101612=CARTESIAN_POINT('Ctrl Pts',(-110.586356966211,4.75766314181056,
129.557835651287));
#101613=CARTESIAN_POINT('Ctrl Pts',(-110.594104862988,4.72291460799662,
129.42520949214));
#101614=CARTESIAN_POINT('Ctrl Pts',(-110.601852759766,4.68259820507299,
129.293968833945));
#101615=CARTESIAN_POINT('Ctrl Pts',(-110.609600656543,4.63685266930219,
129.164610519019));
#101616=CARTESIAN_POINT('Ctrl Pts',(-110.617346932627,4.59111670251143,
129.035279263064));
#101617=CARTESIAN_POINT('Ctrl Pts',(-110.625093208711,4.53995399202432,
128.90782993556));
#101618=CARTESIAN_POINT('Ctrl Pts',(-110.632839484795,4.48355279060068,
128.782743087864));
#101619=CARTESIAN_POINT('Ctrl Pts',(-110.64058581806,4.42715117283611,128.657655316806));
#101620=CARTESIAN_POINT('Ctrl Pts',(-110.648332151326,4.36551114767705,
128.534930416766));
#101621=CARTESIAN_POINT('Ctrl Pts',(-110.656078484591,4.2988684900923,128.41502749567));
#101622=CARTESIAN_POINT('Ctrl Pts',(-110.663826552594,4.23221090834635,
128.295097723145));
#101623=CARTESIAN_POINT('Ctrl Pts',(-110.671574620597,4.16054865479605,
128.177991528762));
#101624=CARTESIAN_POINT('Ctrl Pts',(-110.6793226886,4.08416248359781,128.064141671921));
#101625=CARTESIAN_POINT('Ctrl Pts',(-110.687078991342,4.00769512826792,
127.950170814098));
#101626=CARTESIAN_POINT('Ctrl Pts',(-110.694835294084,3.92649404420397,
127.839463532466));
#101627=CARTESIAN_POINT('Ctrl Pts',(-110.702591596826,3.84088251842448,
127.732422378903));
#101628=CARTESIAN_POINT('Ctrl Pts',(-110.71035203934,3.75522529919598,127.625324094253));
#101629=CARTESIAN_POINT('Ctrl Pts',(-110.718112481854,3.6651532043725,127.521896131297));
#101630=CARTESIAN_POINT('Ctrl Pts',(-110.725872924368,3.57102785363685,
127.422505633826));
#101631=CARTESIAN_POINT('Ctrl Pts',(-110.733645824634,3.47675140453215,
127.322955585904));
#101632=CARTESIAN_POINT('Ctrl Pts',(-110.741418724899,3.37840897780296,
127.227456227692));
#101633=CARTESIAN_POINT('Ctrl Pts',(-110.749191625164,3.27639753263701,
127.136336316852));
#101634=CARTESIAN_POINT('Ctrl Pts',(-110.756681960926,3.17809446045501,
127.048528844288));
#101635=CARTESIAN_POINT('Ctrl Pts',(-110.764172296688,3.07638473247442,
126.964788135019));
#101636=CARTESIAN_POINT('Ctrl Pts',(-110.77166263245,2.97164888259986,126.885370188764));
#101637=CARTESIAN_POINT('Ctrl Pts',(-110.779436966569,2.86294194114248,
126.802941086937));
#101638=CARTESIAN_POINT('Ctrl Pts',(-110.787211300689,2.75063052622654,
126.724907903406));
#101639=CARTESIAN_POINT('Ctrl Pts',(-110.794985634808,2.63510572911355,
126.651602394542));
#101640=CARTESIAN_POINT('Ctrl Pts',(-110.802750387755,2.51972330598856,
126.578387228167));
#101641=CARTESIAN_POINT('Ctrl Pts',(-110.810515140702,2.40113570724194,
126.509888351048));
#101642=CARTESIAN_POINT('Ctrl Pts',(-110.818279893649,2.27976643174905,
126.446396863796));
#101643=CARTESIAN_POINT('Ctrl Pts',(-110.826036934534,2.15851770193159,
126.382968437185));
#101644=CARTESIAN_POINT('Ctrl Pts',(-110.833793975419,2.03449313765044,
126.324537683183));
#101645=CARTESIAN_POINT('Ctrl Pts',(-110.841551016304,1.90814420740121,
126.271351821384));
#101646=CARTESIAN_POINT('Ctrl Pts',(-110.849302207544,1.78189055786297,
126.218206067458));
#101647=CARTESIAN_POINT('Ctrl Pts',(-110.857053398784,1.65331639012675,
126.17029748419));
#101648=CARTESIAN_POINT('Ctrl Pts',(-110.864804590024,1.52289638297982,
126.12782668));
#101649=CARTESIAN_POINT('Ctrl Pts',(-110.872552486801,1.39253180781518,
126.085373927034));
#101650=CARTESIAN_POINT('Ctrl Pts',(-110.880300383578,1.2603233245844,126.048354477148));
#101651=CARTESIAN_POINT('Ctrl Pts',(-110.888048280356,1.12676393113888,
126.016920163003));
#101652=CARTESIAN_POINT('Ctrl Pts',(-110.89579455644,0.993232475439257,
125.985492424239));
#101653=CARTESIAN_POINT('Ctrl Pts',(-110.903540832524,0.858351051920262,
125.959647586936));
#101654=CARTESIAN_POINT('Ctrl Pts',(-110.911287108608,0.722625717265087,
125.939487018463));
#101655=CARTESIAN_POINT('Ctrl Pts',(-110.919033441873,0.586899380716138,
125.91932630117));
#101656=CARTESIAN_POINT('Ctrl Pts',(-110.926779775139,0.450329507322539,
125.904849993878));
#101657=CARTESIAN_POINT('Ctrl Pts',(-110.934526108404,0.313429799715211,
125.896107891478));
#101658=CARTESIAN_POINT('Ctrl Pts',(-110.942274176407,0.176499434367747,
125.887363831345));
#101659=CARTESIAN_POINT('Ctrl Pts',(-110.95002224441,0.0392394779213967,
125.884356556295));
#101660=CARTESIAN_POINT('Ctrl Pts',(-110.957770312413,-0.0978342224023159,
125.887083776933));
#101661=CARTESIAN_POINT('Ctrl Pts',(-110.965526615155,-0.235053606286117,
125.889813896094));
#101662=CARTESIAN_POINT('Ctrl Pts',(-110.973282917897,-0.372085947099265,
125.898290677953));
#101663=CARTESIAN_POINT('Ctrl Pts',(-110.981039220638,-0.508417822016762,
125.912459721109));
#101664=CARTESIAN_POINT('Ctrl Pts',(-110.988799663153,-0.644822461360775,
125.92663632671));
#101665=CARTESIAN_POINT('Ctrl Pts',(-110.996560105667,-0.780525503212871,
125.946511190713));
#101666=CARTESIAN_POINT('Ctrl Pts',(-111.004320548181,-0.915022594832922,
125.971978522424));
#101667=CARTESIAN_POINT('Ctrl Pts',(-111.012093448446,-1.04973559312453,
125.997486736557));
#101668=CARTESIAN_POINT('Ctrl Pts',(-111.019866348712,-1.18323839166486,
126.028605269552));
#101669=CARTESIAN_POINT('Ctrl Pts',(-111.027639248977,-1.31503983118537,
126.065177849947));
#101670=CARTESIAN_POINT('Ctrl Pts',(-111.035129584739,-1.44204995639116,
126.100420924924));
#101671=CARTESIAN_POINT('Ctrl Pts',(-111.042619920501,-1.56747997913212,
126.140728300803));
#101672=CARTESIAN_POINT('Ctrl Pts',(-111.050110256263,-1.69090883172269,
126.185918197734));
#101673=CARTESIAN_POINT('Ctrl Pts',(-111.057884754316,-1.81902022814314,
126.23282247237));
#101674=CARTESIAN_POINT('Ctrl Pts',(-111.065659252369,-1.94538144609914,
126.285135622105));
#101675=CARTESIAN_POINT('Ctrl Pts',(-111.073433750422,-2.06950194428199,
126.342707923203));
#101676=CARTESIAN_POINT('Ctrl Pts',(-111.081198629165,-2.19346886939339,
126.40020899066));
#101677=CARTESIAN_POINT('Ctrl Pts',(-111.088963507908,-2.31520023982343,
126.462956099113));
#101678=CARTESIAN_POINT('Ctrl Pts',(-111.09672838665,-2.43422221038913,
126.530750282855));
#101679=CARTESIAN_POINT('Ctrl Pts',(-111.104485515354,-2.55312538644857,
126.598476801976));
#101680=CARTESIAN_POINT('Ctrl Pts',(-111.112242644058,-2.6693242067441,
126.671240179177));
#101681=CARTESIAN_POINT('Ctrl Pts',(-111.119999772762,-2.7823666343237,
126.748794199086));
#101682=CARTESIAN_POINT('Ctrl Pts',(-111.127751013966,-2.89532326504654,
126.826289357103));
#101683=CARTESIAN_POINT('Ctrl Pts',(-111.135502255169,-3.0051279504709,
126.908567700077));
#101684=CARTESIAN_POINT('Ctrl Pts',(-111.143253496373,-3.11135533081537,
126.995338293149));
#101685=CARTESIAN_POINT('Ctrl Pts',(-111.151001249663,-3.21753491081371,
127.082069841067));
#101686=CARTESIAN_POINT('Ctrl Pts',(-111.158749002952,-3.32014008624431,
127.173289370495));
#101687=CARTESIAN_POINT('Ctrl Pts',(-111.166496756242,-3.41877666201874,
127.268664194266));
#101688=CARTESIAN_POINT('Ctrl Pts',(-111.174242834922,-3.51739191834894,
127.364018403592));
#101689=CARTESIAN_POINT('Ctrl Pts',(-111.181988913601,-3.61204000067276,
127.463525848915));
#101690=CARTESIAN_POINT('Ctrl Pts',(-111.189734992281,-3.70236211807162,
127.566815589436));
#101691=CARTESIAN_POINT('Ctrl Pts',(-111.197481074189,-3.7926842731182,
127.67010537301));
#101692=CARTESIAN_POINT('Ctrl Pts',(-111.205227156097,-3.87868020250311,
127.777177160502));
#101693=CARTESIAN_POINT('Ctrl Pts',(-111.212973238005,-3.96003037444908,
127.887625714298));
#101694=CARTESIAN_POINT('Ctrl Pts',(-111.220721000616,-4.04139819731153,
127.998098232619));
#101695=CARTESIAN_POINT('Ctrl Pts',(-111.228468763227,-4.11811802552781,
128.111948660221));
#101696=CARTESIAN_POINT('Ctrl Pts',(-111.236216525838,-4.18991298812066,
128.228741815321));
#101697=CARTESIAN_POINT('Ctrl Pts',(-111.243971783412,-4.26177740309686,
128.345647952763));
#101698=CARTESIAN_POINT('Ctrl Pts',(-111.251727040985,-4.32870723333778,
128.465502169262));
#101699=CARTESIAN_POINT('Ctrl Pts',(-111.259482298559,-4.39047081830445,
128.587843291643));
#101700=CARTESIAN_POINT('Ctrl Pts',(-111.267241673625,-4.45226719535576,
128.710249368486));
#101701=CARTESIAN_POINT('Ctrl Pts',(-111.27500104869,-4.5088917005392,128.835144626436));
#101702=CARTESIAN_POINT('Ctrl Pts',(-111.282760423756,-4.56016078627259,
128.962047759813));
#101703=CARTESIAN_POINT('Ctrl Pts',(-111.290530533217,-4.61150079815912,
129.089126452222));
#101704=CARTESIAN_POINT('Ctrl Pts',(-111.298300642677,-4.6574704619042,
129.218218200255));
#101705=CARTESIAN_POINT('Ctrl Pts',(-111.306070752138,-4.69793588766045,
129.348825850571));
#101706=CARTESIAN_POINT('Ctrl Pts',(-111.310674899233,-4.72191351286471,
129.426216888217));
#101707=CARTESIAN_POINT('Ctrl Pts',(-111.315279046328,-4.74395950786869,
129.504139939888));
#101708=CARTESIAN_POINT('Ctrl Pts',(-111.319883193423,-4.764054528234,129.582490119308));
#101709=CARTESIAN_POINT('Origin',(213.235140564004,0.,130.804360617566));
#101710=CARTESIAN_POINT('',(-113.415051629673,-4.76405452823414,129.582490119309));
#101711=CARTESIAN_POINT('',(-113.070135781827,-4.76405452823415,129.582490119309));
#101712=CARTESIAN_POINT('',(213.235140564004,-4.76405452823405,129.582490119308));
#101713=CARTESIAN_POINT('',(-111.735140564046,-4.91824993013872,130.805189587063));
#101714=CARTESIAN_POINT('Ctrl Pts',(-111.735140564046,-4.91824993013872,
130.805189587062));
#101715=CARTESIAN_POINT('Ctrl Pts',(-111.743365975676,-4.91822531490536,
130.951230991851));
#101716=CARTESIAN_POINT('Ctrl Pts',(-111.751591387307,-4.91169166136951,
131.097112736765));
#101717=CARTESIAN_POINT('Ctrl Pts',(-111.759816798937,-4.89871700114936,
131.242258785123));
#101718=CARTESIAN_POINT('Ctrl Pts',(-111.768057245701,-4.88571862470098,
131.387670144231));
#101719=CARTESIAN_POINT('Ctrl Pts',(-111.776297692464,-4.86625575973969,
131.532342811153));
#101720=CARTESIAN_POINT('Ctrl Pts',(-111.784538139227,-4.84044768410444,
131.675709732415));
#101721=CARTESIAN_POINT('Ctrl Pts',(-111.792802012384,-4.81456623985632,
131.819484225023));
#101722=CARTESIAN_POINT('Ctrl Pts',(-111.801065885542,-4.78230356247516,
131.961945239414));
#101723=CARTESIAN_POINT('Ctrl Pts',(-111.809329758699,-4.74382963025624,
132.102537609198));
#101724=CARTESIAN_POINT('Ctrl Pts',(-111.817606503093,-4.70529577370621,
132.243348955916));
#101725=CARTESIAN_POINT('Ctrl Pts',(-111.825883247486,-4.66053144156212,
132.382285550338));
#101726=CARTESIAN_POINT('Ctrl Pts',(-111.83415999188,-4.60975528610488,
132.51881075237));
#101727=CARTESIAN_POINT('Ctrl Pts',(-111.842456281904,-4.55885922214883,
132.6556583603));
#101728=CARTESIAN_POINT('Ctrl Pts',(-111.850752571929,-4.5019230691995,
132.790082901989));
#101729=CARTESIAN_POINT('Ctrl Pts',(-111.859048861953,-4.43921281799391,
132.921569303326));
#101730=CARTESIAN_POINT('Ctrl Pts',(-111.861320618483,-4.42204099514086,
132.957573962022));
#101731=CARTESIAN_POINT('Ctrl Pts',(-111.863592375012,-4.40443647618341,
132.993358473109));
#101732=CARTESIAN_POINT('Ctrl Pts',(-111.865864131542,-4.38640529312948,
133.028912632446));
#101733=CARTESIAN_POINT('Ctrl Pts',(-111.873638465661,-4.32469954261759,
133.150584964156));
#101734=CARTESIAN_POINT('Ctrl Pts',(-111.881412799781,-4.25782970485521,
133.269880632356));
#101735=CARTESIAN_POINT('Ctrl Pts',(-111.8891871339,-4.18600237924457,133.386330242379));
#101736=CARTESIAN_POINT('Ctrl Pts',(-111.896951886847,-4.11426357439335,
133.502636338665));
#101737=CARTESIAN_POINT('Ctrl Pts',(-111.904716639795,-4.03757964137516,
133.616103026116));
#101738=CARTESIAN_POINT('Ctrl Pts',(-111.912481392742,-3.95620410484703,
133.726283296778));
#101739=CARTESIAN_POINT('Ctrl Pts',(-111.920238433627,-3.87490939164875,
133.836354134841));
#101740=CARTESIAN_POINT('Ctrl Pts',(-111.927995474512,-3.78893257885525,
133.943144739397));
#101741=CARTESIAN_POINT('Ctrl Pts',(-111.935752515398,-3.69857153601745,
134.04623533067));
#101742=CARTESIAN_POINT('Ctrl Pts',(-111.943503706638,-3.60827863514509,
134.149248180525));
#101743=CARTESIAN_POINT('Ctrl Pts',(-111.951254897879,-3.51360834164596,
134.248566278018));
#101744=CARTESIAN_POINT('Ctrl Pts',(-111.959006089119,-3.41489978409298,
134.34380160833));
#101745=CARTESIAN_POINT('Ctrl Pts',(-111.966753985896,-3.31623318030997,
134.438996461087));
#101746=CARTESIAN_POINT('Ctrl Pts',(-111.974501882674,-3.2135320069729,
134.53011172712));
#101747=CARTESIAN_POINT('Ctrl Pts',(-111.982249779451,-3.10717319982014,
134.616795242424));
#101748=CARTESIAN_POINT('Ctrl Pts',(-111.989996055535,-3.00083664063701,
134.703460625406));
#101749=CARTESIAN_POINT('Ctrl Pts',(-111.99774233162,-2.89084427232924,
134.785695854723));
#101750=CARTESIAN_POINT('Ctrl Pts',(-112.005488607704,-2.77760684633535,
134.863188437232));
#101751=CARTESIAN_POINT('Ctrl Pts',(-112.013234940969,-2.66436858444834,
134.940681591772));
#101752=CARTESIAN_POINT('Ctrl Pts',(-112.020981274235,-2.54788553972355,
135.013431808846));
#101753=CARTESIAN_POINT('Ctrl Pts',(-112.028727607501,-2.42859789585341,
135.081169629289));
#101754=CARTESIAN_POINT('Ctrl Pts',(-112.036475675504,-2.309283538343,135.148922619147));
#101755=CARTESIAN_POINT('Ctrl Pts',(-112.044223743507,-2.18716367180985,
135.211660785727));
#101756=CARTESIAN_POINT('Ctrl Pts',(-112.05197181151,-2.06270318878847,
135.269160570247));
#101757=CARTESIAN_POINT('Ctrl Pts',(-112.059728114252,-1.93811042768414,
135.326721466223));
#101758=CARTESIAN_POINT('Ctrl Pts',(-112.067484416994,-1.81117243625772,
135.379032694398));
#101759=CARTESIAN_POINT('Ctrl Pts',(-112.075240719736,-1.68237471921097,
135.425918619654));
#101760=CARTESIAN_POINT('Ctrl Pts',(-112.083001162251,-1.55350825894461,
135.472829569339));
#101761=CARTESIAN_POINT('Ctrl Pts',(-112.090761604765,-1.42278046770866,
135.514309328098));
#101762=CARTESIAN_POINT('Ctrl Pts',(-112.09852204728,-1.29069116993974,
135.550232441198));
#101763=CARTESIAN_POINT('Ctrl Pts',(-112.106294947545,-1.1583898307037,
135.586213221267));
#101764=CARTESIAN_POINT('Ctrl Pts',(-112.114067847811,-1.0247229988327,
135.616619443862));
#101765=CARTESIAN_POINT('Ctrl Pts',(-112.121840748076,-0.890200713053664,
135.641376821072));
#101766=CARTESIAN_POINT('Ctrl Pts',(-112.129331083836,-0.760568651250498,
135.665234205252));
#101767=CARTESIAN_POINT('Ctrl Pts',(-112.136821419595,-0.630142556467407,
135.683846269707));
#101768=CARTESIAN_POINT('Ctrl Pts',(-112.144311755355,-0.499380592132474,
135.697192321876));
#101769=CARTESIAN_POINT('Ctrl Pts',(-112.152086089474,-0.363660748130608,
135.711044393674));
#101770=CARTESIAN_POINT('Ctrl Pts',(-112.159860423593,-0.227149143152057,
135.719267127933));
#101771=CARTESIAN_POINT('Ctrl Pts',(-112.167634757712,-0.0903523642468036,
135.721780623298));
#101772=CARTESIAN_POINT('Ctrl Pts',(-112.175399510659,0.0462758248546998,
135.724291021005));
#101773=CARTESIAN_POINT('Ctrl Pts',(-112.183164263606,0.183188101452787,
135.721106172501));
#101774=CARTESIAN_POINT('Ctrl Pts',(-112.190929016553,0.319871348825531,
135.712197756541));
#101775=CARTESIAN_POINT('Ctrl Pts',(-112.198686057438,0.456418840470089,
135.703298188545));
#101776=CARTESIAN_POINT('Ctrl Pts',(-112.206443098323,0.592737367962033,
135.688686391221));
#101777=CARTESIAN_POINT('Ctrl Pts',(-112.214200139208,0.728312752918227,
135.668386069436));
#101778=CARTESIAN_POINT('Ctrl Pts',(-112.221951330449,0.863785899421818,
135.648101056281));
#101779=CARTESIAN_POINT('Ctrl Pts',(-112.229702521689,0.99851663376067,
135.622136114834));
#101780=CARTESIAN_POINT('Ctrl Pts',(-112.237453712929,1.13199520080176,
135.590566832081));
#101781=CARTESIAN_POINT('Ctrl Pts',(-112.245201609706,1.26541703589138,
135.559010967115));
#101782=CARTESIAN_POINT('Ctrl Pts',(-112.252949506483,1.39758738252528,
135.521855588246));
#101783=CARTESIAN_POINT('Ctrl Pts',(-112.26069740326,1.52800621217691,135.479227468937));
#101784=CARTESIAN_POINT('Ctrl Pts',(-112.268443679344,1.65839776102087,
135.436608266512));
#101785=CARTESIAN_POINT('Ctrl Pts',(-112.276189955428,1.78703815024909,
135.388518722065));
#101786=CARTESIAN_POINT('Ctrl Pts',(-112.283936231513,1.9134424493424,135.335135502236));
#101787=CARTESIAN_POINT('Ctrl Pts',(-112.291682564778,2.03984768152336,
135.281751888344));
#101788=CARTESIAN_POINT('Ctrl Pts',(-112.299428898043,2.16401643046852,
135.2230746732));
#101789=CARTESIAN_POINT('Ctrl Pts',(-112.307175231309,2.28548406251401,
135.159328546552));
#101790=CARTESIAN_POINT('Ctrl Pts',(-112.314923299312,2.40697889639366,
135.0955681444));
#101791=CARTESIAN_POINT('Ctrl Pts',(-112.322671367315,2.5257710635777,135.026736753576));
#101792=CARTESIAN_POINT('Ctrl Pts',(-112.330419435318,2.64142119196144,
134.953104662353));
#101793=CARTESIAN_POINT('Ctrl Pts',(-112.33817573806,2.75719423467773,134.879394314068));
#101794=CARTESIAN_POINT('Ctrl Pts',(-112.345932040801,2.86981823746912,
134.800873283415));
#101795=CARTESIAN_POINT('Ctrl Pts',(-112.353688343543,2.97888300638684,
134.71785510418));
#101796=CARTESIAN_POINT('Ctrl Pts',(-112.361448786057,3.0880059864559,134.634792615643));
#101797=CARTESIAN_POINT('Ctrl Pts',(-112.369209228572,3.1935656466337,134.547228445286));
#101798=CARTESIAN_POINT('Ctrl Pts',(-112.376969671086,3.29518627098337,
134.455515298215));
#101799=CARTESIAN_POINT('Ctrl Pts',(-112.384742571351,3.3969700257807,134.363654925058));
#101800=CARTESIAN_POINT('Ctrl Pts',(-112.392515471617,3.4948018296186,134.267632539794));
#101801=CARTESIAN_POINT('Ctrl Pts',(-112.400288371882,3.58834349358395,
134.167837098018));
#101802=CARTESIAN_POINT('Ctrl Pts',(-112.407778707644,3.67848468244187,
134.071669471926));
#101803=CARTESIAN_POINT('Ctrl Pts',(-112.415269043406,3.76464202947925,
133.971998579962));
#101804=CARTESIAN_POINT('Ctrl Pts',(-112.422759379167,3.84655047693288,
133.86919870316));
#101805=CARTESIAN_POINT('Ctrl Pts',(-112.430533713286,3.93156450807075,
133.762501137779));
#101806=CARTESIAN_POINT('Ctrl Pts',(-112.438308047405,4.01227038425401,
133.652094647021));
#101807=CARTESIAN_POINT('Ctrl Pts',(-112.446082381524,4.08832705953567,
133.538362248284));
#101808=CARTESIAN_POINT('Ctrl Pts',(-112.453847134471,4.16429000176242,
133.424770014564));
#101809=CARTESIAN_POINT('Ctrl Pts',(-112.461611887418,4.23561492828482,
133.307860350296));
#101810=CARTESIAN_POINT('Ctrl Pts',(-112.469376640365,4.30200065951633,
133.188049646785));
#101811=CARTESIAN_POINT('Ctrl Pts',(-112.47713368125,4.3683204555037,133.068357940955));
#101812=CARTESIAN_POINT('Ctrl Pts',(-112.484890722135,4.42971063046171,
132.94577126967));
#101813=CARTESIAN_POINT('Ctrl Pts',(-112.49264776302,4.48591320199007,132.820735038826));
#101814=CARTESIAN_POINT('Ctrl Pts',(-112.50039895426,4.54207339072213,132.695793098776));
#101815=CARTESIAN_POINT('Ctrl Pts',(-112.5081501455,4.59305360300879,132.568405631124));
#101816=CARTESIAN_POINT('Ctrl Pts',(-112.51590133674,4.6386418972212,132.439042363914));
#101817=CARTESIAN_POINT('Ctrl Pts',(-112.523649233517,4.6842108151924,132.309734079544));
#101818=CARTESIAN_POINT('Ctrl Pts',(-112.531397130294,4.72439224345059,
132.178452033814));
#101819=CARTESIAN_POINT('Ctrl Pts',(-112.539145027071,4.75902256246914,
132.045685439041));
#101820=CARTESIAN_POINT('Ctrl Pts',(-112.546891303156,4.7936456375715,131.912946616177));
#101821=CARTESIAN_POINT('Ctrl Pts',(-112.55463757924,4.82271981445595,131.77872424001));
#101822=CARTESIAN_POINT('Ctrl Pts',(-112.562383855324,4.84613161097958,
131.643521788954));
#101823=CARTESIAN_POINT('Ctrl Pts',(-112.570130188589,4.86954358032375,
131.508318339863));
#101824=CARTESIAN_POINT('Ctrl Pts',(-112.577876521854,4.88729301919419,
131.37213518668));
#101825=CARTESIAN_POINT('Ctrl Pts',(-112.585622855119,4.89931781959404,
131.235484689161));
#101826=CARTESIAN_POINT('Ctrl Pts',(-112.593370923122,4.91134531286457,
131.09880358971));
#101827=CARTESIAN_POINT('Ctrl Pts',(-112.601118991125,4.91764558238198,
130.96165532705));
#101828=CARTESIAN_POINT('Ctrl Pts',(-112.608867059128,4.91820853797107,
130.82455565479));
#101829=CARTESIAN_POINT('Ctrl Pts',(-112.61662336187,4.91877209187605,130.687310271368));
#101830=CARTESIAN_POINT('Ctrl Pts',(-112.624379664612,4.91358614946113,
130.550113973093));
#101831=CARTESIAN_POINT('Ctrl Pts',(-112.632135967354,4.9026927757303,130.41348134042));
#101832=CARTESIAN_POINT('Ctrl Pts',(-112.639896409868,4.89179358787791,
130.276775782798));
#101833=CARTESIAN_POINT('Ctrl Pts',(-112.647656852382,4.87518094617575,
130.140634878135));
#101834=CARTESIAN_POINT('Ctrl Pts',(-112.655417294896,4.85294850777792,
130.005565372615));
#101835=CARTESIAN_POINT('Ctrl Pts',(-112.663190195161,4.83068037989626,
129.870279041534));
#101836=CARTESIAN_POINT('Ctrl Pts',(-112.670963095427,4.80277450732906,
129.736067929514));
#101837=CARTESIAN_POINT('Ctrl Pts',(-112.678735995692,4.76937533006668,
129.603426804464));
#101838=CARTESIAN_POINT('Ctrl Pts',(-112.686226331455,4.73719029702189,
129.4756075184));
#101839=CARTESIAN_POINT('Ctrl Pts',(-112.693716667218,4.69990450336563,
129.349246350512));
#101840=CARTESIAN_POINT('Ctrl Pts',(-112.70120700298,4.65768957213563,129.224768609445));
#101841=CARTESIAN_POINT('Ctrl Pts',(-112.7089813371,4.61387404896124,129.095571257004));
#101842=CARTESIAN_POINT('Ctrl Pts',(-112.716755671219,4.56460943883901,
128.967993712577));
#101843=CARTESIAN_POINT('Ctrl Pts',(-112.724530005338,4.5100336414892,128.842529938038));
#101844=CARTESIAN_POINT('Ctrl Pts',(-112.732294758285,4.45552510393205,
128.717220786389));
#101845=CARTESIAN_POINT('Ctrl Pts',(-112.740059511232,4.39571855732209,
128.594020576463));
#101846=CARTESIAN_POINT('Ctrl Pts',(-112.747824264179,4.33080152853476,
128.473407768849));
#101847=CARTESIAN_POINT('Ctrl Pts',(-112.755581305064,4.26594897625558,
128.352914755576));
#101848=CARTESIAN_POINT('Ctrl Pts',(-112.763338345949,4.19599622697075,
128.235004372547));
#101849=CARTESIAN_POINT('Ctrl Pts',(-112.771095386834,4.12117856748556,
128.120134420429));
#101850=CARTESIAN_POINT('Ctrl Pts',(-112.778846578074,4.04641732857948,
128.005351092635));
#101851=CARTESIAN_POINT('Ctrl Pts',(-112.786597769314,3.96679869424462,
127.893603958326));
#101852=CARTESIAN_POINT('Ctrl Pts',(-112.794348960554,3.8826033003593,127.785325229476));
#101853=CARTESIAN_POINT('Ctrl Pts',(-112.802096857332,3.79844369176225,
127.677092521975));
#101854=CARTESIAN_POINT('Ctrl Pts',(-112.809844754109,3.7097114320475,127.572325595924));
#101855=CARTESIAN_POINT('Ctrl Pts',(-112.817592650886,3.61672966904007,
127.471426540272));
#101856=CARTESIAN_POINT('Ctrl Pts',(-112.82533892697,3.523767355813,127.370548590528));
#101857=CARTESIAN_POINT('Ctrl Pts',(-112.833085203054,3.42655757214922,
127.273537189209));
#101858=CARTESIAN_POINT('Ctrl Pts',(-112.840831479138,3.32546256882749,
127.180759954437));
#101859=CARTESIAN_POINT('Ctrl Pts',(-112.848577812404,3.22436681924528,
127.087982034805));
#101860=CARTESIAN_POINT('Ctrl Pts',(-112.856324145669,3.1193860808266,126.999438608439));
#101861=CARTESIAN_POINT('Ctrl Pts',(-112.864070478934,3.01091784545658,
126.915458871519));
#101862=CARTESIAN_POINT('Ctrl Pts',(-112.871818546937,2.90242531937718,
126.831460327919));
#101863=CARTESIAN_POINT('Ctrl Pts',(-112.87956661494,2.79044405132565,126.75202774674));
#101864=CARTESIAN_POINT('Ctrl Pts',(-112.887314682943,2.67540250543436,
126.677448394558));
#101865=CARTESIAN_POINT('Ctrl Pts',(-112.895070985685,2.56023869201925,
126.602789778552));
#101866=CARTESIAN_POINT('Ctrl Pts',(-112.902827288427,2.44200843212858,
126.532994908356));
#101867=CARTESIAN_POINT('Ctrl Pts',(-112.910583591169,2.32116739403544,
126.468306536795));
#101868=CARTESIAN_POINT('Ctrl Pts',(-112.918344033683,2.20026185944183,
126.403583639103));
#101869=CARTESIAN_POINT('Ctrl Pts',(-112.926104476197,2.07674312200999,
126.343972840666));
#101870=CARTESIAN_POINT('Ctrl Pts',(-112.933864918712,1.95108814563578,
126.289669253756));
#101871=CARTESIAN_POINT('Ctrl Pts',(-112.941637818977,1.82523145673838,
126.235278493908));
#101872=CARTESIAN_POINT('Ctrl Pts',(-112.949410719243,1.69723204137605,
126.186212110499));
#101873=CARTESIAN_POINT('Ctrl Pts',(-112.957183619508,1.5675842351478,126.142616016216));
#101874=CARTESIAN_POINT('Ctrl Pts',(-112.96467395527,1.44264945324328,126.100604749773));
#101875=CARTESIAN_POINT('Ctrl Pts',(-112.972164291032,1.31618434175386,
126.063673046184));
#101876=CARTESIAN_POINT('Ctrl Pts',(-112.979654626793,1.18863949133075,
126.031906403836));
#101877=CARTESIAN_POINT('Ctrl Pts',(-112.987428960912,1.05625873913458,
125.998935319588));
#101878=CARTESIAN_POINT('Ctrl Pts',(-112.995203295031,0.922295412699854,
125.971424252312));
#101879=CARTESIAN_POINT('Ctrl Pts',(-113.00297762915,0.787239634307942,
125.949524181529));
#101880=CARTESIAN_POINT('Ctrl Pts',(-113.010742382097,0.652350300092618,
125.927651100625));
#101881=CARTESIAN_POINT('Ctrl Pts',(-113.018507135045,0.516371574973577,
125.9113753193));
#101882=CARTESIAN_POINT('Ctrl Pts',(-113.026271887992,0.379807364250885,
125.900797685517));
#101883=CARTESIAN_POINT('Ctrl Pts',(-113.034028928876,0.243378791027502,
125.89023055759));
#101884=CARTESIAN_POINT('Ctrl Pts',(-113.041785969761,0.106366276712021,
125.885350344579));
#101885=CARTESIAN_POINT('Ctrl Pts',(-113.049543010646,-0.0307178397643694,
125.886206545476));
#101886=CARTESIAN_POINT('Ctrl Pts',(-113.057294201886,-0.167698580042352,
125.887062100704));
#101887=CARTESIAN_POINT('Ctrl Pts',(-113.065045393126,-0.304750425630313,
125.893645457017));
#101888=CARTESIAN_POINT('Ctrl Pts',(-113.072796584367,-0.441358053805133,
125.905954128631));
#101889=CARTESIAN_POINT('Ctrl Pts',(-113.080544481144,-0.577907620093665,
125.918257568732));
#101890=CARTESIAN_POINT('Ctrl Pts',(-113.08829237792,-0.714012955913745,
125.936281449252));
#101891=CARTESIAN_POINT('Ctrl Pts',(-113.096040274698,-0.849161103153265,
125.959971235674));
#101892=CARTESIAN_POINT('Ctrl Pts',(-113.103786550782,-0.984280980313839,
125.983656066702));
#101893=CARTESIAN_POINT('Ctrl Pts',(-113.111532826866,-1.11844368229896,
126.013004378774));
#101894=CARTESIAN_POINT('Ctrl Pts',(-113.11927910295,-1.25114411617696,
126.047910106622));
#101895=CARTESIAN_POINT('Ctrl Pts',(-113.127025436215,-1.3838455296196,
126.082816092137));
#101896=CARTESIAN_POINT('Ctrl Pts',(-113.13477176948,-1.51508427531289,
126.123279475832));
#101897=CARTESIAN_POINT('Ctrl Pts',(-113.142518102746,-1.64436853711358,
126.169143775103));
#101898=CARTESIAN_POINT('Ctrl Pts',(-113.150266170748,-1.77368175122813,
126.215018345366));
#101899=CARTESIAN_POINT('Ctrl Pts',(-113.158014238751,-1.90103924209585,
126.266296107275));
#101900=CARTESIAN_POINT('Ctrl Pts',(-113.165762306754,-2.02596772888285,
126.322771856421));
#101901=CARTESIAN_POINT('Ctrl Pts',(-113.173518609496,-2.15102899115244,
126.379307628665));
#101902=CARTESIAN_POINT('Ctrl Pts',(-113.181274912238,-2.2736557355464,
126.441052262588));
#101903=CARTESIAN_POINT('Ctrl Pts',(-113.18903121498,-2.39339742740489,
126.5077536054));
#101904=CARTESIAN_POINT('Ctrl Pts',(-113.196791657494,-2.51320302900968,
126.574490548727));
#101905=CARTESIAN_POINT('Ctrl Pts',(-113.204552100008,-2.63012017669485,
126.646189268129));
#101906=CARTESIAN_POINT('Ctrl Pts',(-113.212312542522,-2.7437269063421,
126.722553943321));
#101907=CARTESIAN_POINT('Ctrl Pts',(-113.220085442787,-2.85751600759731,
126.799041205868));
#101908=CARTESIAN_POINT('Ctrl Pts',(-113.227858343053,-2.96798375615356,
126.880209160397));
#101909=CARTESIAN_POINT('Ctrl Pts',(-113.235631243318,-3.07474019106907,
126.965720777737));
#101910=CARTESIAN_POINT('Ctrl Pts',(-113.243121579081,-3.17761576068258,
127.048123832404));
#101911=CARTESIAN_POINT('Ctrl Pts',(-113.250611914843,-3.27704493072714,
127.134560024491));
#101912=CARTESIAN_POINT('Ctrl Pts',(-113.258102250606,-3.37271221373376,
127.224696473288));
#101913=CARTESIAN_POINT('Ctrl Pts',(-113.265759968658,-3.47051731930888,
127.316847150235));
#101914=CARTESIAN_POINT('Ctrl Pts',(-113.27341768671,-3.56471992965631,
127.413176237924));
#101915=CARTESIAN_POINT('Ctrl Pts',(-113.281075404762,-3.6549337278169,
127.513366465677));
#101916=CARTESIAN_POINT('Ctrl Pts',(-113.288724239367,-3.74504287215535,
127.613440466307));
#101917=CARTESIAN_POINT('Ctrl Pts',(-113.296373073973,-3.83117213571676,
127.717366406469));
#101918=CARTESIAN_POINT('Ctrl Pts',(-113.304021908578,-3.912969308254,127.824787786578));
#101919=CARTESIAN_POINT('Ctrl Pts',(-113.311663643837,-3.99469055988334,
127.932109462401));
#101920=CARTESIAN_POINT('Ctrl Pts',(-113.319305379096,-4.07208747274599,
128.0429198084));
#101921=CARTESIAN_POINT('Ctrl Pts',(-113.326947114355,-4.14484606607501,
128.156827019849));
#101922=CARTESIAN_POINT('Ctrl Pts',(-113.334583466117,-4.21755340197961,
128.27065398524));
#101923=CARTESIAN_POINT('Ctrl Pts',(-113.342219817878,-4.28562870190555,
128.38757313751));
#101924=CARTESIAN_POINT('Ctrl Pts',(-113.34985616964,-4.34879987894162,
128.50716174167));
#101925=CARTESIAN_POINT('Ctrl Pts',(-113.357489249431,-4.41194398882871,
128.626699105333));
#101926=CARTESIAN_POINT('Ctrl Pts',(-113.365122329222,-4.47018796774985,
128.748903289383));
#101927=CARTESIAN_POINT('Ctrl Pts',(-113.372755409012,-4.52330473628331,
128.873325318765));
#101928=CARTESIAN_POINT('Ctrl Pts',(-113.38038866589,-4.57642273712397,
128.997750234733));
#101929=CARTESIAN_POINT('Ctrl Pts',(-113.388021922768,-4.62441312113937,
129.124392732159));
#101930=CARTESIAN_POINT('Ctrl Pts',(-113.395655179646,-4.66709630748311,
129.252782350389));
#101931=CARTESIAN_POINT('Ctrl Pts',(-113.402120662988,-4.70324960806195,
129.361530287379));
#101932=CARTESIAN_POINT('Ctrl Pts',(-113.40858614633,-4.73559611044108,
129.47153118025));
#101933=CARTESIAN_POINT('Ctrl Pts',(-113.415051629673,-4.76405452823414,
129.582490119309));
#101934=CARTESIAN_POINT('Ctrl Pts',(-111.665402883959,-4.76405452823392,
129.582490119308));
#101935=CARTESIAN_POINT('Ctrl Pts',(-111.673434994141,-4.7993264617604,
129.720014852801));
#101936=CARTESIAN_POINT('Ctrl Pts',(-111.681467104322,-4.82867233280825,
129.859196828031));
#101937=CARTESIAN_POINT('Ctrl Pts',(-111.689499214503,-4.8519470411507,
129.99950474701));
#101938=CARTESIAN_POINT('Ctrl Pts',(-111.697520736002,-4.87519106658524,
130.139627698904));
#101939=CARTESIAN_POINT('Ctrl Pts',(-111.705542257501,-4.89237982900867,
130.280873292029));
#101940=CARTESIAN_POINT('Ctrl Pts',(-111.713563779,-4.90341893425279,130.422698702108));
#101941=CARTESIAN_POINT('Ctrl Pts',(-111.72075604067,-4.91331682376556,
130.549862290824));
#101942=CARTESIAN_POINT('Ctrl Pts',(-111.72794830234,-4.91827145356775,
130.677491661371));
#101943=CARTESIAN_POINT('Ctrl Pts',(-111.73514056401,-4.91824993013883,
130.805189586421));
#101944=CARTESIAN_POINT('',(-111.389859436035,-4.91824793280489,130.799851298284));
#101945=CARTESIAN_POINT('Ctrl Pts',(-111.319883193423,-4.764054528234,129.582490119308));
#101946=CARTESIAN_POINT('Ctrl Pts',(-111.322774755641,-4.77667488993176,
129.631696718027));
#101947=CARTESIAN_POINT('Ctrl Pts',(-111.325666317859,-4.78852586105957,
129.681071769191));
#101948=CARTESIAN_POINT('Ctrl Pts',(-111.328557880076,-4.79960393518158,
129.730589167075));
#101949=CARTESIAN_POINT('Ctrl Pts',(-111.33921170086,-4.84042056212739,
129.913033618565));
#101950=CARTESIAN_POINT('Ctrl Pts',(-111.349865521643,-4.87084727414698,
130.097880784251));
#101951=CARTESIAN_POINT('Ctrl Pts',(-111.360519342427,-4.89065949885459,
130.284136888039));
#101952=CARTESIAN_POINT('Ctrl Pts',(-111.370299373615,-4.90884679329887,
130.455116909294));
#101953=CARTESIAN_POINT('Ctrl Pts',(-111.380079404804,-4.91808971405691,
130.627284475731));
#101954=CARTESIAN_POINT('Ctrl Pts',(-111.389859435992,-4.9182479328042,
130.799851297532));
#101955=CARTESIAN_POINT('Ctrl Pts',(-111.389859436035,-4.91824793280489,
130.799851298284));
#101956=CARTESIAN_POINT('Ctrl Pts',(-111.397511849573,-4.91837173149822,
130.934876704435));
#101957=CARTESIAN_POINT('Ctrl Pts',(-111.405164263111,-4.91293087685927,
131.070069265922));
#101958=CARTESIAN_POINT('Ctrl Pts',(-111.412816676649,-4.90191088279818,
131.204926167264));
#101959=CARTESIAN_POINT('Ctrl Pts',(-111.420463247981,-4.89089930190938,
131.33968011262));
#101960=CARTESIAN_POINT('Ctrl Pts',(-111.428109819313,-4.87431708776526,
131.47409850816));
#101961=CARTESIAN_POINT('Ctrl Pts',(-111.435756390646,-4.8522018223889,
131.6076790708));
#101962=CARTESIAN_POINT('Ctrl Pts',(-111.443399754411,-4.83009583387479,
131.741203599363));
#101963=CARTESIAN_POINT('Ctrl Pts',(-111.451043118177,-4.80246147333269,
131.87389059729));
#101964=CARTESIAN_POINT('Ctrl Pts',(-111.458686481942,-4.76938807451487,
132.005243816372));
#101965=CARTESIAN_POINT('Ctrl Pts',(-111.466328398073,-4.73632093972174,
132.136572157461));
#101966=CARTESIAN_POINT('Ctrl Pts',(-111.473970314203,-4.69781691292974,
132.266566831726));
#101967=CARTESIAN_POINT('Ctrl Pts',(-111.481612230333,-4.65401613678662,
132.394743232231));
#101968=CARTESIAN_POINT('Ctrl Pts',(-111.489254459609,-4.61021356580659,
132.522924885058));
#101969=CARTESIAN_POINT('Ctrl Pts',(-111.496896688884,-4.56111394432089,
132.64928773508));
#101970=CARTESIAN_POINT('Ctrl Pts',(-111.504538918159,-4.50690665855051,
132.773364282777));
#101971=CARTESIAN_POINT('Ctrl Pts',(-111.512183221394,-4.45268466192745,
132.897474502548));
#101972=CARTESIAN_POINT('Ctrl Pts',(-111.519827524629,-4.39335240615422,
133.019296817625));
#101973=CARTESIAN_POINT('Ctrl Pts',(-111.527471827863,-4.32914635320659,
133.138386091938));
#101974=CARTESIAN_POINT('Ctrl Pts',(-111.535124225635,-4.26487231259977,
133.257601469643));
#101975=CARTESIAN_POINT('Ctrl Pts',(-111.542776623407,-4.19571436395245,
133.374077675035));
#101976=CARTESIAN_POINT('Ctrl Pts',(-111.550429021179,-4.12195378371499,
133.487396224377));
#101977=CARTESIAN_POINT('Ctrl Pts',(-111.558086021216,-4.04814884277513,
133.600782925169));
#101978=CARTESIAN_POINT('Ctrl Pts',(-111.565743021253,-3.9697359927938,
133.711007862496));
#101979=CARTESIAN_POINT('Ctrl Pts',(-111.57340002129,-3.88703752267745,
133.817684755424));
#101980=CARTESIAN_POINT('Ctrl Pts',(-111.581068124949,-3.80421912927281,
133.924516343399));
#101981=CARTESIAN_POINT('Ctrl Pts',(-111.588736228609,-3.71710296951947,
134.027789310629));
#101982=CARTESIAN_POINT('Ctrl Pts',(-111.596404332269,-3.62604920045386,
134.12715315674));
#101983=CARTESIAN_POINT('Ctrl Pts',(-111.599938056142,-3.58408851606613,
134.172943408247));
#101984=CARTESIAN_POINT('Ctrl Pts',(-111.603471780016,-3.54129208983065,
134.217904034757));
#101985=CARTESIAN_POINT('Ctrl Pts',(-111.607005503889,-3.49769749589534,
134.262003642765));
#101986=CARTESIAN_POINT('Ctrl Pts',(-111.614779838008,-3.40178764238884,
134.359024547467));
#101987=CARTESIAN_POINT('Ctrl Pts',(-111.622554172128,-3.30168599275238,
134.452205507928));
#101988=CARTESIAN_POINT('Ctrl Pts',(-111.630328506247,-3.19773260301129,
134.541162627593));
#101989=CARTESIAN_POINT('Ctrl Pts',(-111.638093259194,-3.09390732653218,
134.630010115558));
#101990=CARTESIAN_POINT('Ctrl Pts',(-111.645858012141,-2.98624004911221,
134.714643868376));
#101991=CARTESIAN_POINT('Ctrl Pts',(-111.653622765088,-2.8751086756547,
134.794715635064));
#101992=CARTESIAN_POINT('Ctrl Pts',(-111.661379805973,-2.76408767944398,
134.874707873345));
#101993=CARTESIAN_POINT('Ctrl Pts',(-111.669136846858,-2.64960974927478,
134.950146915377));
#101994=CARTESIAN_POINT('Ctrl Pts',(-111.676893887743,-2.53208670352203,
135.020723978135));
#101995=CARTESIAN_POINT('Ctrl Pts',(-111.684645078983,-2.41465228281275,
135.09124781818));
#101996=CARTESIAN_POINT('Ctrl Pts',(-111.692396270223,-2.29417765107022,
135.156916776342));
#101997=CARTESIAN_POINT('Ctrl Pts',(-111.700147461463,-2.17110421639548,
135.217464915455));
#101998=CARTESIAN_POINT('Ctrl Pts',(-111.70789535824,-2.04808309121306,
135.277987319994));
#101999=CARTESIAN_POINT('Ctrl Pts',(-111.715643255017,-1.9224657100605,
135.33339306212));
#102000=CARTESIAN_POINT('Ctrl Pts',(-111.723391151794,-1.79471853619688,
135.383461887284));
#102001=CARTESIAN_POINT('Ctrl Pts',(-111.731137427878,-1.66699808428811,
135.433520239129));
#102002=CARTESIAN_POINT('Ctrl Pts',(-111.738883703962,-1.53714908958031,
135.478243751951));
#102003=CARTESIAN_POINT('Ctrl Pts',(-111.746629980046,-1.40565810324164,
135.517460272707));
#102004=CARTESIAN_POINT('Ctrl Pts',(-111.754376313312,-1.27416614626692,
135.55667708295));
#102005=CARTESIAN_POINT('Ctrl Pts',(-111.762122646577,-1.14103254813241,
135.59038670827));
#102006=CARTESIAN_POINT('Ctrl Pts',(-111.769868979842,-1.00675874692166,
135.618466961219));
#102007=CARTESIAN_POINT('Ctrl Pts',(-111.777617047845,-0.872454876023937,
135.646553502545));
#102008=CARTESIAN_POINT('Ctrl Pts',(-111.785365115848,-0.737010676565102,
135.669008082921));
#102009=CARTESIAN_POINT('Ctrl Pts',(-111.793113183851,-0.600937100485652,
135.685759767785));
#102010=CARTESIAN_POINT('Ctrl Pts',(-111.800869486593,-0.464718903790064,
135.70252925654));
#102011=CARTESIAN_POINT('Ctrl Pts',(-111.808625789335,-0.327870382910718,
135.713583694226));
#102012=CARTESIAN_POINT('Ctrl Pts',(-111.816382092077,-0.190907484828074,
135.718904074972));
#102013=CARTESIAN_POINT('Ctrl Pts',(-111.824142534591,-0.0538714855224776,
135.724227295366));
#102014=CARTESIAN_POINT('Ctrl Pts',(-111.831902977105,0.0832786218547538,
135.723810361824));
#102015=CARTESIAN_POINT('Ctrl Pts',(-111.839663419619,0.220028576276249,
135.717686424809));
#102016=CARTESIAN_POINT('Ctrl Pts',(-111.847436319885,0.356998053864299,
135.711552657107));
#102017=CARTESIAN_POINT('Ctrl Pts',(-111.85520922015,0.493565705130944,
135.6996936124));
#102018=CARTESIAN_POINT('Ctrl Pts',(-111.862982120415,0.629223165585064,
135.682194283282));
#102019=CARTESIAN_POINT('Ctrl Pts',(-111.870472456177,0.75994913565005,
135.665331098855));
#102020=CARTESIAN_POINT('Ctrl Pts',(-111.877962791939,0.889829637803004,
135.643230639237));
#102021=CARTESIAN_POINT('Ctrl Pts',(-111.885453127701,1.01842207009617,
135.61601309355));
#102022=CARTESIAN_POINT('Ctrl Pts',(-111.89322746182,1.15189012354551,135.587763586345));
#102023=CARTESIAN_POINT('Ctrl Pts',(-111.901001795939,1.28439329135057,
135.553911818681));
#102024=CARTESIAN_POINT('Ctrl Pts',(-111.908776130058,1.41542478187872,
135.514536383856));
#102025=CARTESIAN_POINT('Ctrl Pts',(-111.916540883005,1.54629478780541,
135.475209475735));
#102026=CARTESIAN_POINT('Ctrl Pts',(-111.924305635952,1.67569635436854,
135.430372556639));
#102027=CARTESIAN_POINT('Ctrl Pts',(-111.9320703889,1.803132221322,135.380155330502));
#102028=CARTESIAN_POINT('Ctrl Pts',(-111.939827429785,1.93044151717586,
135.329987980822));
#102029=CARTESIAN_POINT('Ctrl Pts',(-111.94758447067,2.05578863731693,135.274451100906));
#102030=CARTESIAN_POINT('Ctrl Pts',(-111.955341511555,2.17869119595031,
135.21372426045));
#102031=CARTESIAN_POINT('Ctrl Pts',(-111.963092702795,2.30150107280869,
135.153043214577));
#102032=CARTESIAN_POINT('Ctrl Pts',(-111.970843894035,2.42186970836619,
135.087180170813));
#102033=CARTESIAN_POINT('Ctrl Pts',(-111.978595085275,2.53933477029247,
135.016362752761));
#102034=CARTESIAN_POINT('Ctrl Pts',(-111.986342982052,2.65674990643348,
134.945575434001));
#102035=CARTESIAN_POINT('Ctrl Pts',(-111.994090878829,2.77126358934399,
134.869838130548));
#102036=CARTESIAN_POINT('Ctrl Pts',(-112.001838775606,2.88243837784815,
134.789424238188));
#102037=CARTESIAN_POINT('Ctrl Pts',(-112.00958505169,2.99358991098321,134.709027166682));
#102038=CARTESIAN_POINT('Ctrl Pts',(-112.017331327775,3.10140362233403,
134.623955681033));
#102039=CARTESIAN_POINT('Ctrl Pts',(-112.025077603859,3.20547168187723,
134.534526077594));
#102040=CARTESIAN_POINT('Ctrl Pts',(-112.032823937124,3.30954050962734,
134.445095814005));
#102041=CARTESIAN_POINT('Ctrl Pts',(-112.04057027039,3.40986333387604,134.351307623244));
#102042=CARTESIAN_POINT('Ctrl Pts',(-112.048316603655,3.50606631533044,
134.25351733407));
#102043=CARTESIAN_POINT('Ctrl Pts',(-112.056064671658,3.60229084077539,
134.155705145439));
#102044=CARTESIAN_POINT('Ctrl Pts',(-112.063812739661,3.69439341340803,
134.053889353632));
#102045=CARTESIAN_POINT('Ctrl Pts',(-112.071560807664,3.78203817196968,
133.948461495125));
#102046=CARTESIAN_POINT('Ctrl Pts',(-112.079317110406,3.86977608042383,
133.842921586634));
#102047=CARTESIAN_POINT('Ctrl Pts',(-112.087073413148,3.95304646017374,
133.733762243856));
#102048=CARTESIAN_POINT('Ctrl Pts',(-112.094829715889,4.0315544390951,133.621407274459));
#102049=CARTESIAN_POINT('Ctrl Pts',(-112.102590158404,4.11010432008863,
133.508992337832));
#102050=CARTESIAN_POINT('Ctrl Pts',(-112.110350600918,4.18388652520632,
133.393378705439));
#102051=CARTESIAN_POINT('Ctrl Pts',(-112.118111043432,4.25265097422479,
133.275016958283));
#102052=CARTESIAN_POINT('Ctrl Pts',(-112.125883943697,4.32152581004145,
133.156465206342));
#102053=CARTESIAN_POINT('Ctrl Pts',(-112.133656843963,4.38536661122429,
133.035156870198));
#102054=CARTESIAN_POINT('Ctrl Pts',(-112.141429744228,4.44397010102323,
132.911565591865));
#102055=CARTESIAN_POINT('Ctrl Pts',(-112.148920079991,4.50044320635454,
132.792467167808));
#102056=CARTESIAN_POINT('Ctrl Pts',(-112.156410415752,4.55205304768174,
132.671249184682));
#102057=CARTESIAN_POINT('Ctrl Pts',(-112.163900751514,4.59866150635386,
132.548348981197));
#102058=CARTESIAN_POINT('Ctrl Pts',(-112.171675085634,4.64703713890294,
132.420788979141));
#102059=CARTESIAN_POINT('Ctrl Pts',(-112.179449419753,4.69017788680332,
132.291012604084));
#102060=CARTESIAN_POINT('Ctrl Pts',(-112.187223753872,4.72787593956728,
132.159488715777));
#102061=CARTESIAN_POINT('Ctrl Pts',(-112.194988506819,4.76552753285039,
132.028126918907));
#102062=CARTESIAN_POINT('Ctrl Pts',(-112.202753259766,4.7977496705034,131.895022266141));
#102063=CARTESIAN_POINT('Ctrl Pts',(-112.210518012713,4.82438269481104,
131.76066322475));
#102064=CARTESIAN_POINT('Ctrl Pts',(-112.218275053598,4.85098926682348,
131.626437630654));
#102065=CARTESIAN_POINT('Ctrl Pts',(-112.226032094483,4.87201769707431,
131.490960508307));
#102066=CARTESIAN_POINT('Ctrl Pts',(-112.233789135368,4.88735832132833,
131.354734764345));
#102067=CARTESIAN_POINT('Ctrl Pts',(-112.241540326608,4.90268737709833,
131.218611749276));
#102068=CARTESIAN_POINT('Ctrl Pts',(-112.249291517848,4.91233712072752,
131.081741623216));
#102069=CARTESIAN_POINT('Ctrl Pts',(-112.257042709088,4.91624915648167,
130.944636395565));
#102070=CARTESIAN_POINT('Ctrl Pts',(-112.264790605866,4.92015952951625,
130.807589441294));
#102071=CARTESIAN_POINT('Ctrl Pts',(-112.272538502643,4.91833703389468,
130.670307974163));
#102072=CARTESIAN_POINT('Ctrl Pts',(-112.28028639942,4.91077523759472,130.533307802922));
#102073=CARTESIAN_POINT('Ctrl Pts',(-112.288032675504,4.90321502305955,
130.396336289164));
#102074=CARTESIAN_POINT('Ctrl Pts',(-112.295778951588,4.88991791731495,
130.259646344382));
#102075=CARTESIAN_POINT('Ctrl Pts',(-112.303525227672,4.87092958735024,
130.123752053429));
#102076=CARTESIAN_POINT('Ctrl Pts',(-112.311271560937,4.85194111721796,
129.987856759336));
#102077=CARTESIAN_POINT('Ctrl Pts',(-112.319017894203,4.82726139313845,
129.852757517995));
#102078=CARTESIAN_POINT('Ctrl Pts',(-112.326764227468,4.79698771465657,
129.718961185129));
#102079=CARTESIAN_POINT('Ctrl Pts',(-112.334512295471,4.76670725659434,
129.585134889502));
#102080=CARTESIAN_POINT('Ctrl Pts',(-112.342260363474,4.73083043761234,
129.452612464206));
#102081=CARTESIAN_POINT('Ctrl Pts',(-112.350008431477,4.6895051272227,129.321888113857));
#102082=CARTESIAN_POINT('Ctrl Pts',(-112.357764734218,4.64813589580133,
129.191024828114));
#102083=CARTESIAN_POINT('Ctrl Pts',(-112.36552103696,4.60130672341606,129.061963808154));
#102084=CARTESIAN_POINT('Ctrl Pts',(-112.373277339702,4.54921478587561,
128.935182216645));
#102085=CARTESIAN_POINT('Ctrl Pts',(-112.381037782216,4.49709504529965,
128.808332957983));
#102086=CARTESIAN_POINT('Ctrl Pts',(-112.38879822473,4.43970710611637,128.683765906868));
#102087=CARTESIAN_POINT('Ctrl Pts',(-112.396558667245,4.3772948804146,128.561935012915));
#102088=CARTESIAN_POINT('Ctrl Pts',(-112.40433156751,4.31478246506725,128.439908545194));
#102089=CARTESIAN_POINT('Ctrl Pts',(-112.412104467775,4.24722983867589,
128.320627352286));
#102090=CARTESIAN_POINT('Ctrl Pts',(-112.419877368041,4.17492561363418,
128.204518471758));
#102091=CARTESIAN_POINT('Ctrl Pts',(-112.427367703803,4.1052498292953,128.092630441496));
#102092=CARTESIAN_POINT('Ctrl Pts',(-112.434858039565,4.03116208689624,
127.983688339525));
#102093=CARTESIAN_POINT('Ctrl Pts',(-112.442348375327,3.9529556753756,127.878044761235));
#102094=CARTESIAN_POINT('Ctrl Pts',(-112.450122709446,3.87178404399286,
127.768395674565));
#102095=CARTESIAN_POINT('Ctrl Pts',(-112.457897043565,3.78591813221081,
127.661952840864));
#102096=CARTESIAN_POINT('Ctrl Pts',(-112.465671377684,3.69564007837278,
127.55914452713));
#102097=CARTESIAN_POINT('Ctrl Pts',(-112.473436130632,3.60547328416748,
127.456462915454));
#102098=CARTESIAN_POINT('Ctrl Pts',(-112.481200883579,3.51090542254593,
127.357407202385));
#102099=CARTESIAN_POINT('Ctrl Pts',(-112.488965636526,3.41226115596433,
127.262375740975));
#102100=CARTESIAN_POINT('Ctrl Pts',(-112.496722677411,3.31371486425921,
127.167438666153));
#102101=CARTESIAN_POINT('Ctrl Pts',(-112.504479718296,3.21110050451521,
127.076518158385));
#102102=CARTESIAN_POINT('Ctrl Pts',(-112.512236759181,3.10478191013158,
126.989978314621));
#102103=CARTESIAN_POINT('Ctrl Pts',(-112.519987950421,2.99854349142686,
126.903503731226));
#102104=CARTESIAN_POINT('Ctrl Pts',(-112.527739141661,2.88860670014902,
126.821403482242));
#102105=CARTESIAN_POINT('Ctrl Pts',(-112.535490332901,2.77537073998687,
126.744003451241));
#102106=CARTESIAN_POINT('Ctrl Pts',(-112.543238229678,2.66218290812861,
126.666636317318));
#102107=CARTESIAN_POINT('Ctrl Pts',(-112.550986126455,2.54569901841734,
126.59396564823));
#102108=CARTESIAN_POINT('Ctrl Pts',(-112.558734023232,2.42634955869867,
126.526275662647));
#102109=CARTESIAN_POINT('Ctrl Pts',(-112.566480299317,2.30702506431409,
126.45859983635));
#102110=CARTESIAN_POINT('Ctrl Pts',(-112.574226575401,2.18483653205361,
126.395902814015));
#102111=CARTESIAN_POINT('Ctrl Pts',(-112.581972851485,2.06024116018702,
126.338424050129));
#102112=CARTESIAN_POINT('Ctrl Pts',(-112.58971918475,1.93564486858553,126.280944861948));
#102113=CARTESIAN_POINT('Ctrl Pts',(-112.597465518016,1.80864205693524,
126.228684172855));
#102114=CARTESIAN_POINT('Ctrl Pts',(-112.605211851281,1.6797117500904,126.181834089886));
#102115=CARTESIAN_POINT('Ctrl Pts',(-112.612959919284,1.55075257019676,
126.134973515165));
#102116=CARTESIAN_POINT('Ctrl Pts',(-112.620707987287,1.41986540356366,
126.093526091145));
#102117=CARTESIAN_POINT('Ctrl Pts',(-112.62845605529,1.28754596561625,126.057634540687));
#102118=CARTESIAN_POINT('Ctrl Pts',(-112.636212358032,1.1550858969961,126.021704844261));
#102119=CARTESIAN_POINT('Ctrl Pts',(-112.643968660774,1.02119089416524,
125.991342919481));
#102120=CARTESIAN_POINT('Ctrl Pts',(-112.651724963516,0.886368985929803,
125.966640794831));
#102121=CARTESIAN_POINT('Ctrl Pts',(-112.65948540603,0.751475119182901,
125.941925485913));
#102122=CARTESIAN_POINT('Ctrl Pts',(-112.667245848544,0.615653748251519,
125.922876050613));
#102123=CARTESIAN_POINT('Ctrl Pts',(-112.675006291058,0.479418634242783,
125.909532649635));
#102124=CARTESIAN_POINT('Ctrl Pts',(-112.682779191323,0.342964823534284,
125.896167828645));
#102125=CARTESIAN_POINT('Ctrl Pts',(-112.690552091589,0.206096333093022,
125.888527368046));
#102126=CARTESIAN_POINT('Ctrl Pts',(-112.698324991854,0.0693284437661364,
125.886599274294));
#102127=CARTESIAN_POINT('Ctrl Pts',(-112.705815327616,-0.0624675882854512,
125.884741271605));
#102128=CARTESIAN_POINT('Ctrl Pts',(-112.713305663378,-0.194169898531983,
125.888187520386));
#102129=CARTESIAN_POINT('Ctrl Pts',(-112.72079599914,-0.325323308651908,
125.896881854765));
#102130=CARTESIAN_POINT('Ctrl Pts',(-112.728570333259,-0.461449440179959,
125.905905837474));
#102131=CARTESIAN_POINT('Ctrl Pts',(-112.736344667379,-0.597415433499299,
125.920612309279));
#102132=CARTESIAN_POINT('Ctrl Pts',(-112.744119001498,-0.732708472789882,
125.940995387974));
#102133=CARTESIAN_POINT('Ctrl Pts',(-112.751883754445,-0.867834775501393,
125.961353346347));
#102134=CARTESIAN_POINT('Ctrl Pts',(-112.759648507392,-1.00228939146386,
125.987373934146));
#102135=CARTESIAN_POINT('Ctrl Pts',(-112.767413260339,-1.1355616869862,
126.018999323207));
#102136=CARTESIAN_POINT('Ctrl Pts',(-112.775170301224,-1.26870161458509,
126.050593301486));
#102137=CARTESIAN_POINT('Ctrl Pts',(-112.782927342109,-1.40066118070857,
126.087780913222));
#102138=CARTESIAN_POINT('Ctrl Pts',(-112.790684382994,-1.53093739944265,
126.130452858368));
#102139=CARTESIAN_POINT('Ctrl Pts',(-112.798435574234,-1.66111537586696,
126.173092624269));
#102140=CARTESIAN_POINT('Ctrl Pts',(-112.806186765474,-1.78961216157762,
126.221208370356));
#102141=CARTESIAN_POINT('Ctrl Pts',(-112.813937956714,-1.91593780215059,
126.274640383292));
#102142=CARTESIAN_POINT('Ctrl Pts',(-112.821685853491,-2.04220975095664,
126.328049686197));
#102143=CARTESIAN_POINT('Ctrl Pts',(-112.829433750268,-2.16631203066705,
126.386770609884));
#102144=CARTESIAN_POINT('Ctrl Pts',(-112.837181647045,-2.28777283086798,
126.45059459987));
#102145=CARTESIAN_POINT('Ctrl Pts',(-112.844927923129,-2.40920822408822,
126.514405239254));
#102146=CARTESIAN_POINT('Ctrl Pts',(-112.852674199213,-2.52800289095891,
126.583316639971));
#102147=CARTESIAN_POINT('Ctrl Pts',(-112.860420475298,-2.64370824480431,
126.657073579169));
#102148=CARTESIAN_POINT('Ctrl Pts',(-112.868166808563,-2.7594144527605,
126.730831062825));
#102149=CARTESIAN_POINT('Ctrl Pts',(-112.875913141828,-2.87203097250722,
126.809433946179));
#102150=CARTESIAN_POINT('Ctrl Pts',(-112.883659475094,-2.98113725432025,
126.892583050602));
#102151=CARTESIAN_POINT('Ctrl Pts',(-112.891407543096,-3.09026796972756,
126.975750775689));
#102152=CARTESIAN_POINT('Ctrl Pts',(-112.899155611099,-3.19588657206786,
127.063466510801));
#102153=CARTESIAN_POINT('Ctrl Pts',(-112.906903679102,-3.29760503826166,
127.155390341703));
#102154=CARTESIAN_POINT('Ctrl Pts',(-112.914659981844,-3.39943161205249,
127.247411870347));
#102155=CARTESIAN_POINT('Ctrl Pts',(-112.922416284586,-3.49734947886164,
127.343650166357));
#102156=CARTESIAN_POINT('Ctrl Pts',(-112.930172587328,-3.59100661053982,
127.443727554353));
#102157=CARTESIAN_POINT('Ctrl Pts',(-112.937933029842,-3.68471372984914,
127.543858356665));
#102158=CARTESIAN_POINT('Ctrl Pts',(-112.945693472356,-3.77415532788571,
127.647832037602));
#102159=CARTESIAN_POINT('Ctrl Pts',(-112.95345391487,-3.85901991588287,
127.755238063237));
#102160=CARTESIAN_POINT('Ctrl Pts',(-112.961226815136,-3.94402073605061,
127.862816506559));
#102161=CARTESIAN_POINT('Ctrl Pts',(-112.968999715401,-4.02442963422371,
127.973837988302));
#102162=CARTESIAN_POINT('Ctrl Pts',(-112.976772615666,-4.09997817902724,
128.08786250529));
#102163=CARTESIAN_POINT('Ctrl Pts',(-112.984262951429,-4.17278034393452,
128.197741943879));
#102164=CARTESIAN_POINT('Ctrl Pts',(-112.991753287191,-4.2410692329316,
128.310409609142));
#102165=CARTESIAN_POINT('Ctrl Pts',(-112.999243622953,-4.30464606495475,
128.425452187641));
#102166=CARTESIAN_POINT('Ctrl Pts',(-113.007400604759,-4.37388128731284,
128.550733650235));
#102167=CARTESIAN_POINT('Ctrl Pts',(-113.015557586564,-4.43772995529178,
128.679196150845));
#102168=CARTESIAN_POINT('Ctrl Pts',(-113.023714568369,-4.4959031403072,
128.810360112181));
#102169=CARTESIAN_POINT('Ctrl Pts',(-113.031853641808,-4.55394860814338,
128.941236107659));
#102170=CARTESIAN_POINT('Ctrl Pts',(-113.039992715246,-4.60634329976436,
129.074801434836));
#102171=CARTESIAN_POINT('Ctrl Pts',(-113.048131788685,-4.65284395117964,
129.210551899912));
#102172=CARTESIAN_POINT('Ctrl Pts',(-113.055466453066,-4.69474880364021,
129.332885739058));
#102173=CARTESIAN_POINT('Ctrl Pts',(-113.062801117447,-4.7318675628499,
129.456993629781));
#102174=CARTESIAN_POINT('Ctrl Pts',(-113.070135781827,-4.76405452823415,
129.582490119309));
#102175=CARTESIAN_POINT('Origin',(213.235140564004,0.,130.804360617566));
#102176=CARTESIAN_POINT('',(-115.165057694931,-4.76405452823392,129.582490119308));
#102177=CARTESIAN_POINT('',(-114.819798430105,-4.76405452823404,129.582490119308));
#102178=CARTESIAN_POINT('',(213.235140564004,-4.76405452823405,129.582490119308));
#102179=CARTESIAN_POINT('',(-113.48514056397,-4.91824815323073,130.80862274644));
#102180=CARTESIAN_POINT('Ctrl Pts',(-113.48514056401,-4.91824815323012,
130.808622747144));
#102181=CARTESIAN_POINT('Ctrl Pts',(-113.496784765158,-4.91807033148742,
131.013818633735));
#102182=CARTESIAN_POINT('Ctrl Pts',(-113.508428966306,-4.90504783934739,
131.218479327865));
#102183=CARTESIAN_POINT('Ctrl Pts',(-113.520073167454,-4.87939893910603,
131.421328246823));
#102184=CARTESIAN_POINT('Ctrl Pts',(-113.525565403109,-4.86730108862862,
131.517006262955));
#102185=CARTESIAN_POINT('Ctrl Pts',(-113.531057638764,-4.85239479824405,
131.612281762984));
#102186=CARTESIAN_POINT('Ctrl Pts',(-113.536549874419,-4.83470616053732,
131.707023015012));
#102187=CARTESIAN_POINT('Ctrl Pts',(-113.544324208538,-4.80966765376402,
131.841130543242));
#102188=CARTESIAN_POINT('Ctrl Pts',(-113.552098542657,-4.77900534524811,
131.974407902494));
#102189=CARTESIAN_POINT('Ctrl Pts',(-113.559872876776,-4.74278564405443,
132.106346561058));
#102190=CARTESIAN_POINT('Ctrl Pts',(-113.567637629724,-4.70661058040543,
132.238122617017));
#102191=CARTESIAN_POINT('Ctrl Pts',(-113.575402382671,-4.66489185403184,
132.368562881557));
#102192=CARTESIAN_POINT('Ctrl Pts',(-113.583167135618,-4.61774719864245,
132.497167125094));
#102193=CARTESIAN_POINT('Ctrl Pts',(-113.590924176503,-4.57064936798941,
132.625643637084));
#102194=CARTESIAN_POINT('Ctrl Pts',(-113.598681217388,-4.51813646658613,
132.752287392338));
#102195=CARTESIAN_POINT('Ctrl Pts',(-113.606438258273,-4.4603764364867,
132.876611834802));
#102196=CARTESIAN_POINT('Ctrl Pts',(-113.614189449513,-4.40265996367536,
133.000842523235));
#102197=CARTESIAN_POINT('Ctrl Pts',(-113.621940640754,-4.33970440220091,
133.122757027046));
#102198=CARTESIAN_POINT('Ctrl Pts',(-113.629691831994,-4.27172621541472,
133.241887684706));
#102199=CARTESIAN_POINT('Ctrl Pts',(-113.637439728771,-4.2037769211712,
133.360967708658));
#102200=CARTESIAN_POINT('Ctrl Pts',(-113.645187625548,-4.13080944083047,
133.47726590091));
#102201=CARTESIAN_POINT('Ctrl Pts',(-113.652935522325,-4.05308659406606,
133.590338385514));
#102202=CARTESIAN_POINT('Ctrl Pts',(-113.66068179841,-3.97538000524546,
133.703387217792));
#102203=CARTESIAN_POINT('Ctrl Pts',(-113.668428074494,-3.89292024987878,
133.813211362547));
#102204=CARTESIAN_POINT('Ctrl Pts',(-113.676174350578,-3.80601374643623,
133.919395516959));
#102205=CARTESIAN_POINT('Ctrl Pts',(-113.683920683843,-3.71910660146973,
134.025580455199));
#102206=CARTESIAN_POINT('Ctrl Pts',(-113.691667017109,-3.62775289055038,
134.128125046929));
#102207=CARTESIAN_POINT('Ctrl Pts',(-113.699413350374,-3.53229936885708,
134.226647021605));
#102208=CARTESIAN_POINT('Ctrl Pts',(-113.707161418377,-3.43682447100954,
134.325191059594));
#102209=CARTESIAN_POINT('Ctrl Pts',(-113.71490948638,-3.33724820742209,
134.419710407228));
#102210=CARTESIAN_POINT('Ctrl Pts',(-113.722657554383,-3.23395394207395,
134.509859904173));
#102211=CARTESIAN_POINT('Ctrl Pts',(-113.730413857125,-3.13054989435124,
134.600105213076));
#102212=CARTESIAN_POINT('Ctrl Pts',(-113.738170159867,-3.023420246278,134.685971136255));
#102213=CARTESIAN_POINT('Ctrl Pts',(-113.745926462609,-2.91298160735896,
134.767152716287));
#102214=CARTESIAN_POINT('Ctrl Pts',(-113.753686905123,-2.80248402401307,
134.848377625373));
#102215=CARTESIAN_POINT('Ctrl Pts',(-113.761447347638,-2.6886742549717,
134.924912991434));
#102216=CARTESIAN_POINT('Ctrl Pts',(-113.769207790152,-2.57199675024481,
134.996497993563));
#102217=CARTESIAN_POINT('Ctrl Pts',(-113.776980690417,-2.45513194442919,
135.068197910292));
#102218=CARTESIAN_POINT('Ctrl Pts',(-113.784753590683,-2.33539054528691,
135.134931392485));
#102219=CARTESIAN_POINT('Ctrl Pts',(-113.792526490948,-2.21324118035538,
135.196483855828));
#102220=CARTESIAN_POINT('Ctrl Pts',(-113.80001682671,-2.09553225252669,
135.255798732081));
#102221=CARTESIAN_POINT('Ctrl Pts',(-113.807507162471,-1.97558767108321,
135.310302608404));
#102222=CARTESIAN_POINT('Ctrl Pts',(-113.814997498232,-1.85384133432574,
135.359846910998));
#102223=CARTESIAN_POINT('Ctrl Pts',(-113.822771832351,-1.7274789481942,
135.411269700888));
#102224=CARTESIAN_POINT('Ctrl Pts',(-113.83054616647,-1.5987752045239,135.457512300488));
#102225=CARTESIAN_POINT('Ctrl Pts',(-113.83832050059,-1.46819384116792,
135.498355707812));
#102226=CARTESIAN_POINT('Ctrl Pts',(-113.846085253537,-1.33777340767224,
135.539148779288));
#102227=CARTESIAN_POINT('Ctrl Pts',(-113.853850006484,-1.20548032821458,
135.574555782418));
#102228=CARTESIAN_POINT('Ctrl Pts',(-113.861614759431,-1.07179909805683,
135.604405383597));
#102229=CARTESIAN_POINT('Ctrl Pts',(-113.869371800316,-0.938250641981456,
135.634225337732));
#102230=CARTESIAN_POINT('Ctrl Pts',(-113.877128841201,-0.803317158042228,
135.6584987897));
#102231=CARTESIAN_POINT('Ctrl Pts',(-113.884885882086,-0.667498776412525,
135.677104038473));
#102232=CARTESIAN_POINT('Ctrl Pts',(-113.892637073326,-0.531782816481107,
135.695695256883));
#102233=CARTESIAN_POINT('Ctrl Pts',(-113.900388264566,-0.395183672876246,
135.708626727257));
#102234=CARTESIAN_POINT('Ctrl Pts',(-113.908139455806,-0.25821180621588,
135.715827783865));
#102235=CARTESIAN_POINT('Ctrl Pts',(-113.915887352583,-0.121298156252501,
135.723025779831));
#102236=CARTESIAN_POINT('Ctrl Pts',(-113.92363524936,0.0159875120779447,
135.724498185728));
#102237=CARTESIAN_POINT('Ctrl Pts',(-113.931383146137,0.153129692915351,
135.720226193398));
#102238=CARTESIAN_POINT('Ctrl Pts',(-113.939129422221,0.29024318656497,
135.715955094676));
#102239=CARTESIAN_POINT('Ctrl Pts',(-113.946875698306,0.427212861893932,
135.705941999949));
#102240=CARTESIAN_POINT('Ctrl Pts',(-113.95462197439,0.563523686211019,
135.690220226435));
#102241=CARTESIAN_POINT('Ctrl Pts',(-113.962368307655,0.699835516743832,
135.674498336867));
#102242=CARTESIAN_POINT('Ctrl Pts',(-113.97011464092,0.835488098169624,
135.653067729221));
#102243=CARTESIAN_POINT('Ctrl Pts',(-113.977860974186,0.969972385807809,
135.626013511882));
#102244=CARTESIAN_POINT('Ctrl Pts',(-113.985609042189,1.10448679026958,
135.59895323594));
#102245=CARTESIAN_POINT('Ctrl Pts',(-113.993357110192,1.23783199711468,
135.566266921398));
#102246=CARTESIAN_POINT('Ctrl Pts',(-114.001105178195,1.36951039558305,
135.528090535638));
#102247=CARTESIAN_POINT('Ctrl Pts',(-114.008861480937,1.50132874342048,
135.489873575561));
#102248=CARTESIAN_POINT('Ctrl Pts',(-114.016617783678,1.63147636801053,
135.44615499744));
#102249=CARTESIAN_POINT('Ctrl Pts',(-114.02437408642,1.75947151242207,135.397120469711));
#102250=CARTESIAN_POINT('Ctrl Pts',(-114.032134528935,1.88753497169604,
135.348059770779));
#102251=CARTESIAN_POINT('Ctrl Pts',(-114.039894971449,2.01344330288188,
135.293677623662));
#102252=CARTESIAN_POINT('Ctrl Pts',(-114.047655413963,2.13673683387609,
135.234206976669));
#102253=CARTESIAN_POINT('Ctrl Pts',(-114.055428314228,2.26022828659174,
135.174640862114));
#102254=CARTESIAN_POINT('Ctrl Pts',(-114.063201214494,2.38109620623323,
135.109970108946));
#102255=CARTESIAN_POINT('Ctrl Pts',(-114.070974114759,2.49890675230919,
135.04047299872));
#102256=CARTESIAN_POINT('Ctrl Pts',(-114.078464450521,2.61243458828842,
134.973502283503));
#102257=CARTESIAN_POINT('Ctrl Pts',(-114.085954786283,2.72312321915914,
134.902050186605));
#102258=CARTESIAN_POINT('Ctrl Pts',(-114.093445122045,2.83061311294589,
134.826401451188));
#102259=CARTESIAN_POINT('Ctrl Pts',(-114.101219456164,2.94217851872625,
134.747884470974));
#102260=CARTESIAN_POINT('Ctrl Pts',(-114.108993790284,3.05065124464519,
134.664597620967));
#102261=CARTESIAN_POINT('Ctrl Pts',(-114.116768124403,3.15559637649354,
134.576812681034));
#102262=CARTESIAN_POINT('Ctrl Pts',(-114.12453287735,3.2604121728461,134.489135928194));
#102263=CARTESIAN_POINT('Ctrl Pts',(-114.132297630297,3.36170872824294,
134.396972363767));
#102264=CARTESIAN_POINT('Ctrl Pts',(-114.140062383244,3.45908001334582,
134.300636997341));
#102265=CARTESIAN_POINT('Ctrl Pts',(-114.147819424129,3.55635458791564,
134.204397312559));
#102266=CARTESIAN_POINT('Ctrl Pts',(-114.155576465014,3.64971137451852,
134.103994344706));
#102267=CARTESIAN_POINT('Ctrl Pts',(-114.163333505899,3.7387776500584,133.999783085085));
#102268=CARTESIAN_POINT('Ctrl Pts',(-114.171084697139,3.82777676002694,
133.895650411985));
#102269=CARTESIAN_POINT('Ctrl Pts',(-114.178835888379,3.91249154602938,
133.787715459388));
#102270=CARTESIAN_POINT('Ctrl Pts',(-114.186587079619,3.9925866385517,133.676369495714));
#102271=CARTESIAN_POINT('Ctrl Pts',(-114.194334976396,4.0726476885232,133.565070857044));
#102272=CARTESIAN_POINT('Ctrl Pts',(-114.202082873173,4.14809272242647,
133.450364407498));
#102273=CARTESIAN_POINT('Ctrl Pts',(-114.209830769951,4.21862727291639,
133.332673690488));
#102274=CARTESIAN_POINT('Ctrl Pts',(-114.217577046035,4.28914706909891,
133.215007591838));
#102275=CARTESIAN_POINT('Ctrl Pts',(-114.225323322119,4.35475822410486,
133.094358802517));
#102276=CARTESIAN_POINT('Ctrl Pts',(-114.233069598203,4.41521038090453,
132.971178642886));
#102277=CARTESIAN_POINT('Ctrl Pts',(-114.240815931468,4.4756629839482,132.847997573968));
#102278=CARTESIAN_POINT('Ctrl Pts',(-114.248562264733,4.53095634054831,
132.722285448429));
#102279=CARTESIAN_POINT('Ctrl Pts',(-114.256308597999,4.58088690371579,
132.594516543139));
#102280=CARTESIAN_POINT('Ctrl Pts',(-114.264056666002,4.63082864848676,
132.466719024889));
#102281=CARTESIAN_POINT('Ctrl Pts',(-114.271804734005,4.67540506777575,
132.33686417442));
#102282=CARTESIAN_POINT('Ctrl Pts',(-114.279552802008,4.71446158402071,
132.205444139449));
#102283=CARTESIAN_POINT('Ctrl Pts',(-114.287309104749,4.75355960999586,
132.073884429702));
#102284=CARTESIAN_POINT('Ctrl Pts',(-114.295065407491,4.78712590217075,
131.940756587802));
#102285=CARTESIAN_POINT('Ctrl Pts',(-114.302821710233,4.8150562672724,131.806566287826));
#102286=CARTESIAN_POINT('Ctrl Pts',(-114.310582152747,4.84300153965094,
131.672304366446));
#102287=CARTESIAN_POINT('Ctrl Pts',(-114.318342595262,4.86530482758688,
131.536979242635));
#102288=CARTESIAN_POINT('Ctrl Pts',(-114.326103037776,4.88191365309006,
131.401103565805));
#102289=CARTESIAN_POINT('Ctrl Pts',(-114.333875938041,4.8985491405544,131.265009769275));
#102290=CARTESIAN_POINT('Ctrl Pts',(-114.341648838307,4.9094718672722,131.128364043565));
#102291=CARTESIAN_POINT('Ctrl Pts',(-114.349421738572,4.91468145801539,
130.991681808945));
#102292=CARTESIAN_POINT('Ctrl Pts',(-114.356912074334,4.91970166701294,
130.859968317834));
#102293=CARTESIAN_POINT('Ctrl Pts',(-114.364402410096,4.91941690296997,
130.728221234129));
#102294=CARTESIAN_POINT('Ctrl Pts',(-114.371892745858,4.91387239255782,
130.596896952897));
#102295=CARTESIAN_POINT('Ctrl Pts',(-114.379667079977,4.90811766034822,
130.460593471627));
#102296=CARTESIAN_POINT('Ctrl Pts',(-114.387441414096,4.89667823258385,
130.324313718381));
#102297=CARTESIAN_POINT('Ctrl Pts',(-114.395215748216,4.8795476836109,130.188570502456));
#102298=CARTESIAN_POINT('Ctrl Pts',(-114.402980501163,4.86243824650862,
130.052994577913));
#102299=CARTESIAN_POINT('Ctrl Pts',(-114.41074525411,4.83965169204675,129.917954259197));
#102300=CARTESIAN_POINT('Ctrl Pts',(-114.418510007057,4.8112335779369,129.783961420667));
#102301=CARTESIAN_POINT('Ctrl Pts',(-114.426267047942,4.78284368909862,
129.650101665712));
#102302=CARTESIAN_POINT('Ctrl Pts',(-114.434024088827,4.74883345220964,
129.517287700539));
#102303=CARTESIAN_POINT('Ctrl Pts',(-114.441781129712,4.70930006556798,
129.386024989112));
#102304=CARTESIAN_POINT('Ctrl Pts',(-114.449532320952,4.66979649136065,
129.254861263917));
#102305=CARTESIAN_POINT('Ctrl Pts',(-114.457283512192,4.62477816997164,
129.125246836869));
#102306=CARTESIAN_POINT('Ctrl Pts',(-114.465034703432,4.57439301119051,
128.997675353977));
#102307=CARTESIAN_POINT('Ctrl Pts',(-114.472782600209,4.524029267446,128.870158092368));
#102308=CARTESIAN_POINT('Ctrl Pts',(-114.480530496986,4.46830336645975,
128.74468241079));
#102309=CARTESIAN_POINT('Ctrl Pts',(-114.488278393764,4.40741248050626,
128.621724988521));
#102310=CARTESIAN_POINT('Ctrl Pts',(-114.496024669848,4.34653433161346,
128.498793286294));
#102311=CARTESIAN_POINT('Ctrl Pts',(-114.503770945932,4.28049352012902,
128.378379145744));
#102312=CARTESIAN_POINT('Ctrl Pts',(-114.511517222016,4.20953443056437,
128.260937149012));
#102313=CARTESIAN_POINT('Ctrl Pts',(-114.519263555281,4.13857481719575,
128.143494285349));
#102314=CARTESIAN_POINT('Ctrl Pts',(-114.527009888547,4.06269705548542,
128.029023943909));
#102315=CARTESIAN_POINT('Ctrl Pts',(-114.534756221812,3.98219014587498,
127.91795373277));
#102316=CARTESIAN_POINT('Ctrl Pts',(-114.542504289815,3.90166520730044,
127.806858648228));
#102317=CARTESIAN_POINT('Ctrl Pts',(-114.550252357818,3.81650928738582,
127.699165525651));
#102318=CARTESIAN_POINT('Ctrl Pts',(-114.558000425821,3.72705289099508,
127.595270433382));
#102319=CARTESIAN_POINT('Ctrl Pts',(-114.565756728563,3.6375014192816,127.491264920172));
#102320=CARTESIAN_POINT('Ctrl Pts',(-114.573513031304,3.54364059633716,
127.391065797543));
#102321=CARTESIAN_POINT('Ctrl Pts',(-114.581269334046,3.44583954107468,
127.295034055437));
#102322=CARTESIAN_POINT('Ctrl Pts',(-114.58902977656,3.34798628644428,127.198951058298));
#102323=CARTESIAN_POINT('Ctrl Pts',(-114.596790219075,3.24618889909328,
127.107040135576));
#102324=CARTESIAN_POINT('Ctrl Pts',(-114.604550661589,3.14085031985415,
127.019622538019));
#102325=CARTESIAN_POINT('Ctrl Pts',(-114.612323561854,3.03534264177611,
126.932064609974));
#102326=CARTESIAN_POINT('Ctrl Pts',(-114.62009646212,2.92628272332133,126.849014658135));
#102327=CARTESIAN_POINT('Ctrl Pts',(-114.627869362385,2.81410399934133,
126.770751595438));
#102328=CARTESIAN_POINT('Ctrl Pts',(-114.635359698147,2.70600325453947,
126.695333592203));
#102329=CARTESIAN_POINT('Ctrl Pts',(-114.642850033909,2.59500677982708,
126.624360655414));
#102330=CARTESIAN_POINT('Ctrl Pts',(-114.650340369671,2.4815229994208,126.558041427274));
#102331=CARTESIAN_POINT('Ctrl Pts',(-114.65811470379,2.36373644698727,126.48920768544));
#102332=CARTESIAN_POINT('Ctrl Pts',(-114.665889037909,2.24289714080766,
126.425169464552));
#102333=CARTESIAN_POINT('Ctrl Pts',(-114.673663372028,2.11943304864548,
126.366209356646));
#102334=CARTESIAN_POINT('Ctrl Pts',(-114.681428124975,1.99612111494292,
126.307321911803));
#102335=CARTESIAN_POINT('Ctrl Pts',(-114.689192877922,1.87019118098777,
126.253500294611));
#102336=CARTESIAN_POINT('Ctrl Pts',(-114.696957630869,1.74209852623014,
126.204982856672));
#102337=CARTESIAN_POINT('Ctrl Pts',(-114.704714671754,1.614133094903,126.156513606936));
#102338=CARTESIAN_POINT('Ctrl Pts',(-114.71247171264,1.48400958073074,126.113338190113));
#102339=CARTESIAN_POINT('Ctrl Pts',(-114.720228753525,1.35220578291796,
126.075648046142));
#102340=CARTESIAN_POINT('Ctrl Pts',(-114.727979944765,1.22050137937422,
126.037986324602));
#102341=CARTESIAN_POINT('Ctrl Pts',(-114.735731136005,1.08711958868282,
126.005801749544));
#102342=CARTESIAN_POINT('Ctrl Pts',(-114.743482327245,0.952555678066113,
125.979236707998));
#102343=CARTESIAN_POINT('Ctrl Pts',(-114.751230224022,0.818048960700843,
125.952682957304));
#102344=CARTESIAN_POINT('Ctrl Pts',(-114.758978120799,0.682361505469531,
125.931744065236));
#102345=CARTESIAN_POINT('Ctrl Pts',(-114.766726017576,0.54600093257844,
125.91651180197));
#102346=CARTESIAN_POINT('Ctrl Pts',(-114.77447229366,0.409668883379975,
125.901282724965));
#102347=CARTESIAN_POINT('Ctrl Pts',(-114.782218569744,0.272664384886409,
125.891757945794));
#102348=CARTESIAN_POINT('Ctrl Pts',(-114.789964845828,0.135501985723202,
125.887977569596));
#102349=CARTESIAN_POINT('Ctrl Pts',(-114.797711179094,-0.00166142594186416,
125.884197165493));
#102350=CARTESIAN_POINT('Ctrl Pts',(-114.805457512359,-0.138982349785618,
125.886161259748));
#102351=CARTESIAN_POINT('Ctrl Pts',(-114.813203845624,-0.275944815223184,
125.893857840716));
#102352=CARTESIAN_POINT('Ctrl Pts',(-114.820951913627,-0.41293795245544,
125.90155614528));
#102353=CARTESIAN_POINT('Ctrl Pts',(-114.82869998163,-0.549572081270348,
125.914989469142));
#102354=CARTESIAN_POINT('Ctrl Pts',(-114.836448049633,-0.685335332201852,
125.934093833812));
#102355=CARTESIAN_POINT('Ctrl Pts',(-114.844204352375,-0.821242873931864,
125.953218502828));
#102356=CARTESIAN_POINT('Ctrl Pts',(-114.851960655117,-0.956277301065753,
125.978026198168));
#102357=CARTESIAN_POINT('Ctrl Pts',(-114.859716957859,-1.08993538475321,
126.008401493516));
#102358=CARTESIAN_POINT('Ctrl Pts',(-114.867477400373,-1.22366480578431,
126.038793001073));
#102359=CARTESIAN_POINT('Ctrl Pts',(-114.875237842887,-1.35601604252535,
126.074757927323));
#102360=CARTESIAN_POINT('Ctrl Pts',(-114.882998285401,-1.48650101826154,
126.116130910608));
#102361=CARTESIAN_POINT('Ctrl Pts',(-114.890771185667,-1.6171954600647,
126.157570309478));
#102362=CARTESIAN_POINT('Ctrl Pts',(-114.898544085932,-1.74601728650515,
126.204434980034));
#102363=CARTESIAN_POINT('Ctrl Pts',(-114.906316986197,-1.87249755810587,
126.256511020516));
#102364=CARTESIAN_POINT('Ctrl Pts',(-114.913807321959,-1.99437995324829,
126.306693965754));
#102365=CARTESIAN_POINT('Ctrl Pts',(-114.921297657721,-2.11408780084788,
126.361715837568));
#102366=CARTESIAN_POINT('Ctrl Pts',(-114.928787993483,-2.23122480104518,
126.421345793304));
#102367=CARTESIAN_POINT('Ctrl Pts',(-114.936563162424,-2.3528161414993,
126.483243282884));
#102368=CARTESIAN_POINT('Ctrl Pts',(-114.944338331365,-2.47202244986505,
126.550302346067));
#102369=CARTESIAN_POINT('Ctrl Pts',(-114.952113500305,-2.58837449630025,
126.622315599946));
#102370=CARTESIAN_POINT('Ctrl Pts',(-114.959878902606,-2.70458038917816,
126.694238395654));
#102371=CARTESIAN_POINT('Ctrl Pts',(-114.967644304906,-2.81793882506746,
126.771102794938));
#102372=CARTESIAN_POINT('Ctrl Pts',(-114.975409707207,-2.92800307381476,
126.852654522443));
#102373=CARTESIAN_POINT('Ctrl Pts',(-114.983311706695,-3.04000340601512,
126.93564078434));
#102374=CARTESIAN_POINT('Ctrl Pts',(-114.991213706184,-3.14859219035022,
127.023480673468));
#102375=CARTESIAN_POINT('Ctrl Pts',(-114.999115705672,-3.25332644318739,
127.11585819564));
#102376=CARTESIAN_POINT('Ctrl Pts',(-115.006866536838,-3.3560570890443,
127.206468499893));
#102377=CARTESIAN_POINT('Ctrl Pts',(-115.014617368004,-3.45507904201751,
127.301444117669));
#102378=CARTESIAN_POINT('Ctrl Pts',(-115.02236819917,-3.55000548578644,
127.400444620749));
#102379=CARTESIAN_POINT('Ctrl Pts',(-115.03011549927,-3.6448886836772,127.499400021921));
#102380=CARTESIAN_POINT('Ctrl Pts',(-115.03786279937,-3.73567981501322,
127.602376378269));
#102381=CARTESIAN_POINT('Ctrl Pts',(-115.04561009947,-3.82202807819197,
127.708995625839));
#102382=CARTESIAN_POINT('Ctrl Pts',(-115.053355547864,-3.90835570299911,
127.815589390005));
#102383=CARTESIAN_POINT('Ctrl Pts',(-115.061100996257,-3.99024232785089,
127.925824008542));
#102384=CARTESIAN_POINT('Ctrl Pts',(-115.068846444651,-4.0673769604366,
128.039287793171));
#102385=CARTESIAN_POINT('Ctrl Pts',(-115.076864048841,-4.14722191220701,
128.156738413051));
#102386=CARTESIAN_POINT('Ctrl Pts',(-115.084881653031,-4.22197453572727,
128.27764893658));
#102387=CARTESIAN_POINT('Ctrl Pts',(-115.092899257221,-4.29133860411453,
128.401529777216));
#102388=CARTESIAN_POINT('Ctrl Pts',(-115.100648655071,-4.35838229318922,
128.521266533652));
#102389=CARTESIAN_POINT('Ctrl Pts',(-115.108398052922,-4.42039199947249,
128.643777695005));
#102390=CARTESIAN_POINT('Ctrl Pts',(-115.116147450772,-4.47714731123146,
128.768596629272));
#102391=CARTESIAN_POINT('Ctrl Pts',(-115.124299158132,-4.53684907148763,
128.899895530787));
#102392=CARTESIAN_POINT('Ctrl Pts',(-115.132450865492,-4.59073607669625,
129.033747784281));
#102393=CARTESIAN_POINT('Ctrl Pts',(-115.140602572852,-4.6386098775966,
129.169588013819));
#102394=CARTESIAN_POINT('Ctrl Pts',(-115.148754280212,-4.68648367849696,
129.305428243356));
#102395=CARTESIAN_POINT('Ctrl Pts',(-115.156905987572,-4.72834416606678,
129.443255959199));
#102396=CARTESIAN_POINT('Ctrl Pts',(-115.165057694931,-4.76405452823392,
129.582490119308));
#102397=CARTESIAN_POINT('Ctrl Pts',(-113.415051629673,-4.76405452823414,
129.582490119309));
#102398=CARTESIAN_POINT('Ctrl Pts',(-113.422688410304,-4.79766851844642,
129.713550556983));
#102399=CARTESIAN_POINT('Ctrl Pts',(-113.430325190934,-4.82585680892114,
129.845947543374));
#102400=CARTESIAN_POINT('Ctrl Pts',(-113.437961971565,-4.84853264300647,
129.979185319705));
#102401=CARTESIAN_POINT('Ctrl Pts',(-113.445825070299,-4.87188048169826,
130.116371634339));
#102402=CARTESIAN_POINT('Ctrl Pts',(-113.453688169033,-4.88938398938119,
130.254448891163));
#102403=CARTESIAN_POINT('Ctrl Pts',(-113.461551267768,-4.90100592036944,
130.392870604317));
#102404=CARTESIAN_POINT('Ctrl Pts',(-113.469414366502,-4.91262785135766,
130.53129231747));
#102405=CARTESIAN_POINT('Ctrl Pts',(-113.477277465236,-4.91836823271671,
130.670058022627));
#102406=CARTESIAN_POINT('Ctrl Pts',(-113.48514056397,-4.91824815323073,
130.808622746439));
#102407=CARTESIAN_POINT('',(-113.139859436022,-4.91824999810658,130.804497089607));
#102408=CARTESIAN_POINT('Ctrl Pts',(-113.070135781827,-4.76405452823415,
129.582490119309));
#102409=CARTESIAN_POINT('Ctrl Pts',(-113.078251155085,-4.79966750581325,
129.721344578387));
#102410=CARTESIAN_POINT('Ctrl Pts',(-113.086366528344,-4.82924206252691,
129.861899006423));
#102411=CARTESIAN_POINT('Ctrl Pts',(-113.094481901602,-4.85262675814392,
130.003613086414));
#102412=CARTESIAN_POINT('Ctrl Pts',(-113.102583039655,-4.87597043458281,
130.145078585231));
#102413=CARTESIAN_POINT('Ctrl Pts',(-113.110684177708,-4.89314584612007,
130.28769935033));
#102414=CARTESIAN_POINT('Ctrl Pts',(-113.118785315761,-4.90405217150556,
130.430923391715));
#102415=CARTESIAN_POINT('Ctrl Pts',(-113.125810022504,-4.91350932888095,
130.5551166696));
#102416=CARTESIAN_POINT('Ctrl Pts',(-113.132834729248,-4.91825345922004,
130.679763201676));
#102417=CARTESIAN_POINT('Ctrl Pts',(-113.139859435992,-4.9182499981066,
130.80449708907));
#102418=CARTESIAN_POINT('Ctrl Pts',(-113.139859436022,-4.91824999810658,
130.804497089606));
#102419=CARTESIAN_POINT('Ctrl Pts',(-113.147991076814,-4.91824599158461,
130.948886201333));
#102420=CARTESIAN_POINT('Ctrl Pts',(-113.156122717607,-4.91187926007567,
131.093146870426));
#102421=CARTESIAN_POINT('Ctrl Pts',(-113.164254358399,-4.89920940978586,
131.236714895405));
#102422=CARTESIAN_POINT('Ctrl Pts',(-113.172397316585,-4.88652192594669,
131.380482734414));
#102423=CARTESIAN_POINT('Ctrl Pts',(-113.180540274771,-4.86751384528746,
131.523555677082));
#102424=CARTESIAN_POINT('Ctrl Pts',(-113.188683232958,-4.8422961614743,
131.665378008256));
#102425=CARTESIAN_POINT('Ctrl Pts',(-113.196846014214,-4.8170170881869,
131.807545589154));
#102426=CARTESIAN_POINT('Ctrl Pts',(-113.205008795471,-4.78549824440557,
131.948456145151));
#102427=CARTESIAN_POINT('Ctrl Pts',(-113.213171576728,-4.74790143450914,
132.087565601458));
#102428=CARTESIAN_POINT('Ctrl Pts',(-113.221344900657,-4.71025606630158,
132.226854725144));
#102429=CARTESIAN_POINT('Ctrl Pts',(-113.229518224587,-4.66651716453983,
132.364337792287));
#102430=CARTESIAN_POINT('Ctrl Pts',(-113.237691548517,-4.61689536894023,
132.499488994639));
#102431=CARTESIAN_POINT('Ctrl Pts',(-113.24588368943,-4.56715933187323,
132.634951347998));
#102432=CARTESIAN_POINT('Ctrl Pts',(-113.254075830343,-4.51151344663191,
132.76807079685));
#102433=CARTESIAN_POINT('Ctrl Pts',(-113.262267971257,-4.45021591031225,
132.898342808059));
#102434=CARTESIAN_POINT('Ctrl Pts',(-113.267409063093,-4.41174778984284,
132.980096818447));
#102435=CARTESIAN_POINT('Ctrl Pts',(-113.272550154929,-4.37105475365047,
133.060729916846));
#102436=CARTESIAN_POINT('Ctrl Pts',(-113.277691246765,-4.3282093812174,
133.140123151481));
#102437=CARTESIAN_POINT('Ctrl Pts',(-113.285465580885,-4.263418817003,133.260181215507));
#102438=CARTESIAN_POINT('Ctrl Pts',(-113.293239915004,-4.19352649637786,
133.37773160968));
#102439=CARTESIAN_POINT('Ctrl Pts',(-113.301014249123,-4.11875092976229,
133.492310364321));
#102440=CARTESIAN_POINT('Ctrl Pts',(-113.30877900207,-4.04406751734969,
133.606747910888));
#102441=CARTESIAN_POINT('Ctrl Pts',(-113.316543755017,-3.96451304492104,
133.718220780501));
#102442=CARTESIAN_POINT('Ctrl Pts',(-113.324308507964,-3.88035236159243,
133.826288580371));
#102443=CARTESIAN_POINT('Ctrl Pts',(-113.332065548849,-3.79627526784095,
133.934249045779));
#102444=CARTESIAN_POINT('Ctrl Pts',(-113.339822589734,-3.70760130622051,
134.038810865241));
#102445=CARTESIAN_POINT('Ctrl Pts',(-113.347579630619,-3.61463896147492,
134.139561996896));
#102446=CARTESIAN_POINT('Ctrl Pts',(-113.355330821859,-3.52174672035651,
134.24023715134));
#102447=CARTESIAN_POINT('Ctrl Pts',(-113.363082013099,-3.42457279705244,
134.337107051668));
#102448=CARTESIAN_POINT('Ctrl Pts',(-113.37083320434,-3.32346611129491,
134.429792463509));
#102449=CARTESIAN_POINT('Ctrl Pts',(-113.378581101117,-3.22240239857606,
134.522438481576));
#102450=CARTESIAN_POINT('Ctrl Pts',(-113.386328997894,-3.11740953553958,
134.610903284857));
#102451=CARTESIAN_POINT('Ctrl Pts',(-113.394076894671,-3.00887332190837,
134.694844442903));
#102452=CARTESIAN_POINT('Ctrl Pts',(-113.401823170755,-2.90035981171328,
134.778768042268));
#102453=CARTESIAN_POINT('Ctrl Pts',(-113.409569446839,-2.78830473426541,
134.858169639506));
#102454=CARTESIAN_POINT('Ctrl Pts',(-113.417315722924,-2.67312668163051,
134.932747325041));
#102455=CARTESIAN_POINT('Ctrl Pts',(-113.425062056189,-2.55794777877723,
135.007325561091));
#102456=CARTESIAN_POINT('Ctrl Pts',(-113.432808389454,-2.43964618291295,
135.077079601889));
#102457=CARTESIAN_POINT('Ctrl Pts',(-113.44055472272,-2.31866881060544,
135.141751308895));
#102458=CARTESIAN_POINT('Ctrl Pts',(-113.448302790723,-2.19766434625469,
135.20643749868));
#102459=CARTESIAN_POINT('Ctrl Pts',(-113.456050858726,-2.07398325780427,
135.266038905598));
#102460=CARTESIAN_POINT('Ctrl Pts',(-113.463798926729,-1.94809599130373,
135.32034390708));
#102461=CARTESIAN_POINT('Ctrl Pts',(-113.471555229471,-1.82207493031777,
135.374706624563));
#102462=CARTESIAN_POINT('Ctrl Pts',(-113.479311532213,-1.69384336694674,
135.423761536804));
#102463=CARTESIAN_POINT('Ctrl Pts',(-113.487067834955,-1.56389112974991,
135.467345455284));
#102464=CARTESIAN_POINT('Ctrl Pts',(-113.494828277469,-1.4338695331313,
135.510952635814));
#102465=CARTESIAN_POINT('Ctrl Pts',(-113.502588719983,-1.30212580811419,
135.549082895527));
#102466=CARTESIAN_POINT('Ctrl Pts',(-113.510349162498,-1.16916281779595,
135.581623575368));
#102467=CARTESIAN_POINT('Ctrl Pts',(-113.518122062763,-1.03598638348176,
135.614216492396));
#102468=CARTESIAN_POINT('Ctrl Pts',(-113.525894963029,-0.901587156147086,
135.641201821851));
#102469=CARTESIAN_POINT('Ctrl Pts',(-113.533667863294,-0.766476904147307,
135.662518315491));
#102470=CARTESIAN_POINT('Ctrl Pts',(-113.541158199056,-0.636278250133563,
135.683059900894));
#102471=CARTESIAN_POINT('Ctrl Pts',(-113.548648534818,-0.505419674967997,
135.698337612106));
#102472=CARTESIAN_POINT('Ctrl Pts',(-113.55613887058,-0.374359720922348,
135.708342454997));
#102473=CARTESIAN_POINT('Ctrl Pts',(-113.563913204699,-0.238330588880613,
135.718726634547));
#102474=CARTESIAN_POINT('Ctrl Pts',(-113.571687538818,-0.101653606550363,
135.723463105129));
#102475=CARTESIAN_POINT('Ctrl Pts',(-113.579461872937,0.0351627650186293,
135.722484918807));
#102476=CARTESIAN_POINT('Ctrl Pts',(-113.587226625884,0.171810522637293,
135.721507938012));
#102477=CARTESIAN_POINT('Ctrl Pts',(-113.594991378831,0.308596940492108,
135.71483031616));
#102478=CARTESIAN_POINT('Ctrl Pts',(-113.602756131778,0.445008346240295,
135.702436835254));
#102479=CARTESIAN_POINT('Ctrl Pts',(-113.610513172663,0.581284266257229,
135.690055663727));
#102480=CARTESIAN_POINT('Ctrl Pts',(-113.618270213548,0.717185528552299,
135.671969965922));
#102481=CARTESIAN_POINT('Ctrl Pts',(-113.626027254433,0.852198727101079,
135.648216560101));
#102482=CARTESIAN_POINT('Ctrl Pts',(-113.633778445673,0.987110111146399,
135.624481066907));
#102483=CARTESIAN_POINT('Ctrl Pts',(-113.641529636914,1.12113438094086,
135.595086440429));
#102484=CARTESIAN_POINT('Ctrl Pts',(-113.649280828154,1.25376387622911,
135.560121251278));
#102485=CARTESIAN_POINT('Ctrl Pts',(-113.657028724931,1.38633700044403,
135.525170923265));
#102486=CARTESIAN_POINT('Ctrl Pts',(-113.664776621708,1.5175161519623,135.484654841086));
#102487=CARTESIAN_POINT('Ctrl Pts',(-113.672524518485,1.64680470017511,
135.438712496953));
#102488=CARTESIAN_POINT('Ctrl Pts',(-113.680270794569,1.77606620401078,
135.392779762968));
#102489=CARTESIAN_POINT('Ctrl Pts',(-113.688017070653,1.90343752299542,
135.341423155546));
#102490=CARTESIAN_POINT('Ctrl Pts',(-113.695763346737,2.02843839281524,
135.284831658545));
#102491=CARTESIAN_POINT('Ctrl Pts',(-113.703509680003,2.15344018536291,
135.228239743799));
#102492=CARTESIAN_POINT('Ctrl Pts',(-113.711256013268,2.2760711376646,135.166413023612));
#102493=CARTESIAN_POINT('Ctrl Pts',(-113.719002346533,2.39587250113482,
135.099587971363));
#102494=CARTESIAN_POINT('Ctrl Pts',(-113.726750414536,2.51570069328991,
135.032747954107));
#102495=CARTESIAN_POINT('Ctrl Pts',(-113.734498482539,2.63269769431587,
134.960907567848));
#102496=CARTESIAN_POINT('Ctrl Pts',(-113.742246550542,2.7464311725708,134.884348225002));
#102497=CARTESIAN_POINT('Ctrl Pts',(-113.750002853284,2.86028552811971,
134.807707513976));
#102498=CARTESIAN_POINT('Ctrl Pts',(-113.757759156026,2.97086910732701,
134.726338046304));
#102499=CARTESIAN_POINT('Ctrl Pts',(-113.765515458768,3.07777985076991,
134.640563721247));
#102500=CARTESIAN_POINT('Ctrl Pts',(-113.773275901282,3.1847476556956,134.554743615851));
#102501=CARTESIAN_POINT('Ctrl Pts',(-113.781036343796,3.28803842448805,
134.464514225576));
#102502=CARTESIAN_POINT('Ctrl Pts',(-113.78879678631,3.38728556410607,134.370237728418));
#102503=CARTESIAN_POINT('Ctrl Pts',(-113.796569686576,3.48669202404362,
134.275809890257));
#102504=CARTESIAN_POINT('Ctrl Pts',(-113.804342586841,3.58204161123619,
134.17732224364));
#102505=CARTESIAN_POINT('Ctrl Pts',(-113.812115487107,3.67300617250755,
134.075172247609));
#102506=CARTESIAN_POINT('Ctrl Pts',(-113.819605822868,3.76066394284882,
133.976735661235));
#102507=CARTESIAN_POINT('Ctrl Pts',(-113.82709615863,3.84424977025502,133.87489861193));
#102508=CARTESIAN_POINT('Ctrl Pts',(-113.834586494392,3.92350823441002,
133.770042022744));
#102509=CARTESIAN_POINT('Ctrl Pts',(-113.842360828511,4.00577180732484,
133.661209764107));
#102510=CARTESIAN_POINT('Ctrl Pts',(-113.85013516263,4.08363398164012,133.548779726024));
#102511=CARTESIAN_POINT('Ctrl Pts',(-113.857909496749,4.15676359654165,
133.433143504182));
#102512=CARTESIAN_POINT('Ctrl Pts',(-113.865674249696,4.22980308572859,
133.317649793649));
#102513=CARTESIAN_POINT('Ctrl Pts',(-113.873439002643,4.29812141338876,
133.198958088594));
#102514=CARTESIAN_POINT('Ctrl Pts',(-113.881203755591,4.36142812374139,
133.07749233041));
#102515=CARTESIAN_POINT('Ctrl Pts',(-113.888960796476,4.42467195697684,
132.956147213729));
#102516=CARTESIAN_POINT('Ctrl Pts',(-113.89671783736,4.482913899043,132.832033871406));
#102517=CARTESIAN_POINT('Ctrl Pts',(-113.904474878245,4.53590741769,132.705604147639));
#102518=CARTESIAN_POINT('Ctrl Pts',(-113.912226069486,4.58886097351228,
132.579269765511));
#102519=CARTESIAN_POINT('Ctrl Pts',(-113.919977260726,4.63657383330587,
132.450622837954));
#102520=CARTESIAN_POINT('Ctrl Pts',(-113.927728451966,4.67884611126632,
132.320138348498));
#102521=CARTESIAN_POINT('Ctrl Pts',(-113.935476348743,4.72110042238105,
132.18970931843));
#102522=CARTESIAN_POINT('Ctrl Pts',(-113.94322424552,4.75791863059376,132.057444650994));
#102523=CARTESIAN_POINT('Ctrl Pts',(-113.950972142297,4.7891496536775,131.923837574533));
#102524=CARTESIAN_POINT('Ctrl Pts',(-113.958718418381,4.82037414390447,
131.790258445793));
#102525=CARTESIAN_POINT('Ctrl Pts',(-113.966464694465,4.84601368471408,
131.655337847022));
#102526=CARTESIAN_POINT('Ctrl Pts',(-113.974210970549,4.86596767898667,
131.519581988581));
#102527=CARTESIAN_POINT('Ctrl Pts',(-113.981957303814,4.88592182055509,
131.383825128022));
#102528=CARTESIAN_POINT('Ctrl Pts',(-113.98970363708,4.90019027498468,131.2472333823));
#102529=CARTESIAN_POINT('Ctrl Pts',(-113.997449970345,4.90872402921118,
131.110320529229));
#102530=CARTESIAN_POINT('Ctrl Pts',(-114.005198038348,4.91725969451279,
130.973377015474));
#102531=CARTESIAN_POINT('Ctrl Pts',(-114.012946106351,4.9200580797928,130.836112641412));
#102532=CARTESIAN_POINT('Ctrl Pts',(-114.020694174354,4.9171222594753,130.699043250183));
#102533=CARTESIAN_POINT('Ctrl Pts',(-114.028450477096,4.91418331893304,
130.561828179974));
#102534=CARTESIAN_POINT('Ctrl Pts',(-114.036206779838,4.90549800699418,
130.424808898062));
#102535=CARTESIAN_POINT('Ctrl Pts',(-114.043963082579,4.89112150634027,
130.288498743887));
#102536=CARTESIAN_POINT('Ctrl Pts',(-114.051723525094,4.87673733251505,
130.152115836878));
#102537=CARTESIAN_POINT('Ctrl Pts',(-114.059483967608,4.8566559745981,130.016443198328));
#102538=CARTESIAN_POINT('Ctrl Pts',(-114.067244410122,4.83098399070024,
129.881985019397));
#102539=CARTESIAN_POINT('Ctrl Pts',(-114.075017310387,4.80527079585478,
129.747310996261));
#102540=CARTESIAN_POINT('Ctrl Pts',(-114.082790210653,4.77394913036231,
129.613855709424));
#102541=CARTESIAN_POINT('Ctrl Pts',(-114.090563110918,4.73717601296352,
129.48211007977));
#102542=CARTESIAN_POINT('Ctrl Pts',(-114.09805344668,4.70173969100659,129.355153735595));
#102543=CARTESIAN_POINT('Ctrl Pts',(-114.105543782443,4.66124147865892,
129.229785199059));
#102544=CARTESIAN_POINT('Ctrl Pts',(-114.113034118205,4.6158637963526,129.106425260722));
#102545=CARTESIAN_POINT('Ctrl Pts',(-114.120808452324,4.56876560543119,
128.978388092834));
#102546=CARTESIAN_POINT('Ctrl Pts',(-114.128582786443,4.51626143731483,
128.85210925857));
#102547=CARTESIAN_POINT('Ctrl Pts',(-114.136357120562,4.45850175203502,
128.728079039937));
#102548=CARTESIAN_POINT('Ctrl Pts',(-114.144121873509,4.40081325040534,
128.604201677464));
#102549=CARTESIAN_POINT('Ctrl Pts',(-114.151886626456,4.33788228228746,
128.48256776774));
#102550=CARTESIAN_POINT('Ctrl Pts',(-114.159651379404,4.26990852313562,
128.363650830116));
#102551=CARTESIAN_POINT('Ctrl Pts',(-114.167408420289,4.20200227647944,
128.244852002471));
#102552=CARTESIAN_POINT('Ctrl Pts',(-114.175165461174,4.12906339883511,
128.12876511395));
#102553=CARTESIAN_POINT('Ctrl Pts',(-114.182922502059,4.05133878282114,
128.015841811944));
#102554=CARTESIAN_POINT('Ctrl Pts',(-114.190673693299,3.97367277954483,
127.903003666278));
#102555=CARTESIAN_POINT('Ctrl Pts',(-114.198424884539,3.89122844209005,
127.793324679314));
#102556=CARTESIAN_POINT('Ctrl Pts',(-114.206176075779,3.80429734439262,
127.687229760841));
#102557=CARTESIAN_POINT('Ctrl Pts',(-114.213923972556,3.71740319473054,
127.581179935538));
#102558=CARTESIAN_POINT('Ctrl Pts',(-114.221671869333,3.62602632495959,
127.478711450729));
#102559=CARTESIAN_POINT('Ctrl Pts',(-114.22941976611,3.53050003842044,127.380218018139));
#102560=CARTESIAN_POINT('Ctrl Pts',(-114.237166042194,3.43499373392113,
127.281745188251));
#102561=CARTESIAN_POINT('Ctrl Pts',(-114.244912318278,3.33534001111267,
127.187246037164));
#102562=CARTESIAN_POINT('Ctrl Pts',(-114.252658594362,3.23191038390806,
127.097078819147));
#102563=CARTESIAN_POINT('Ctrl Pts',(-114.260404927628,3.12847999320959,
127.006910935537));
#102564=CARTESIAN_POINT('Ctrl Pts',(-114.268151260893,3.0212739371987,126.92107530572));
#102565=CARTESIAN_POINT('Ctrl Pts',(-114.275897594158,2.91069797894401,
126.839890875233));
#102566=CARTESIAN_POINT('Ctrl Pts',(-114.283645662161,2.80009725797,126.758688264057));
#102567=CARTESIAN_POINT('Ctrl Pts',(-114.291393730164,2.68612544814,126.682139156217));
#102568=CARTESIAN_POINT('Ctrl Pts',(-114.299141798167,2.56921820469855,
126.610519790932));
#102569=CARTESIAN_POINT('Ctrl Pts',(-114.306898100909,2.4521867108477,126.538824307733));
#102570=CARTESIAN_POINT('Ctrl Pts',(-114.314654403651,2.33221388513286,
126.472069237892));
#102571=CARTESIAN_POINT('Ctrl Pts',(-114.322410706393,2.20976144215135,
126.410485627164));
#102572=CARTESIAN_POINT('Ctrl Pts',(-114.330171148907,2.08724364261372,
126.348869147408));
#102573=CARTESIAN_POINT('Ctrl Pts',(-114.337931591421,1.96224394488322,
126.292429787433));
#102574=CARTESIAN_POINT('Ctrl Pts',(-114.345692033935,1.83524413652449,
126.241350424519));
#102575=CARTESIAN_POINT('Ctrl Pts',(-114.353464934201,1.70804045679922,
126.190189064477));
#102576=CARTESIAN_POINT('Ctrl Pts',(-114.361237834466,1.57883061906044,
126.144405026371));
#102577=CARTESIAN_POINT('Ctrl Pts',(-114.369010734731,1.44811252141387,
126.104131560613));
#102578=CARTESIAN_POINT('Ctrl Pts',(-114.376501070493,1.32214635587791,
126.065322136779));
#102579=CARTESIAN_POINT('Ctrl Pts',(-114.383991406255,1.19477998247819,
126.031629673504));
#102580=CARTESIAN_POINT('Ctrl Pts',(-114.391481742017,1.06646602692964,
126.003128142888));
#102581=CARTESIAN_POINT('Ctrl Pts',(-114.399256076136,0.9332870087542,125.973545968075));
#102582=CARTESIAN_POINT('Ctrl Pts',(-114.407030410255,0.798665263733949,
125.949462417255));
#102583=CARTESIAN_POINT('Ctrl Pts',(-114.414804744374,0.66309460732753,
125.931015913543));
#102584=CARTESIAN_POINT('Ctrl Pts',(-114.422569497321,0.527691029639202,
125.912592143497));
#102585=CARTESIAN_POINT('Ctrl Pts',(-114.430334250269,0.391341251095219,
125.899791649993));
#102586=CARTESIAN_POINT('Ctrl Pts',(-114.438099003216,0.25455158639704,
125.892702389191));
#102587=CARTESIAN_POINT('Ctrl Pts',(-114.445856044101,0.117897783122235,
125.885620169543));
#102588=CARTESIAN_POINT('Ctrl Pts',(-114.453613084986,-0.0191946489391239,
125.884237914216));
#102589=CARTESIAN_POINT('Ctrl Pts',(-114.461370125871,-0.156212274555154,
125.888592031904));
#102590=CARTESIAN_POINT('Ctrl Pts',(-114.469121317111,-0.293126574114052,
125.892942866119));
#102591=CARTESIAN_POINT('Ctrl Pts',(-114.476872508351,-0.429965790325719,
125.903021450652));
#102592=CARTESIAN_POINT('Ctrl Pts',(-114.484623699591,-0.566214831716947,
125.918812150214));
#102593=CARTESIAN_POINT('Ctrl Pts',(-114.492371596368,-0.702405963631207,
125.934596138308));
#102594=CARTESIAN_POINT('Ctrl Pts',(-114.500119493145,-0.83800703207415,
125.956087367802));
#102595=CARTESIAN_POINT('Ctrl Pts',(-114.507867389922,-0.97250663762478,
125.983218231961));
#102596=CARTESIAN_POINT('Ctrl Pts',(-114.515613666006,-1.1069781087574,
126.010343420928));
#102597=CARTESIAN_POINT('Ctrl Pts',(-114.52335994209,-1.24034819227746,
126.043105820834));
#102598=CARTESIAN_POINT('Ctrl Pts',(-114.531106218175,-1.37211466637587,
126.081386511686));
#102599=CARTESIAN_POINT('Ctrl Pts',(-114.53885255144,-1.50388211314428,
126.119667485117));
#102600=CARTESIAN_POINT('Ctrl Pts',(-114.546598884705,-1.63404555142804,
126.163466721703));
#102601=CARTESIAN_POINT('Ctrl Pts',(-114.554345217971,-1.7621173184631,
126.212615239339));
#102602=CARTESIAN_POINT('Ctrl Pts',(-114.562093285973,-1.89021776628258,
126.261774763444));
#102603=CARTESIAN_POINT('Ctrl Pts',(-114.569841353977,-2.01622524582059,
126.316285812299));
#102604=CARTESIAN_POINT('Ctrl Pts',(-114.57758942198,-2.13967186689895,
126.375931170855));
#102605=CARTESIAN_POINT('Ctrl Pts',(-114.585345724721,-2.26324968851539,
126.435639921207));
#102606=CARTESIAN_POINT('Ctrl Pts',(-114.593102027463,-2.38426086217223,
126.500493711455));
#102607=CARTESIAN_POINT('Ctrl Pts',(-114.600858330205,-2.50226143451527,
126.570228973907));
#102608=CARTESIAN_POINT('Ctrl Pts',(-114.608618772719,-2.62032498731669,
126.640001456167));
#102609=CARTESIAN_POINT('Ctrl Pts',(-114.616379215234,-2.73537440922031,
126.714660389368));
#102610=CARTESIAN_POINT('Ctrl Pts',(-114.624139657748,-2.84699542244294,
126.793899281624));
#102611=CARTESIAN_POINT('Ctrl Pts',(-114.631912558013,-2.95879561962494,
126.873265375183));
#102612=CARTESIAN_POINT('Ctrl Pts',(-114.639685458279,-3.0671561009788,
126.957225880151));
#102613=CARTESIAN_POINT('Ctrl Pts',(-114.647458358544,-3.17169563306927,
127.045433925853));
#102614=CARTESIAN_POINT('Ctrl Pts',(-114.654948694306,-3.27243488985076,
127.130435386913));
#102615=CARTESIAN_POINT('Ctrl Pts',(-114.662439030068,-3.36962594934654,
127.219380724676));
#102616=CARTESIAN_POINT('Ctrl Pts',(-114.66992936583,-3.46296192147884,
127.311929116035));
#102617=CARTESIAN_POINT('Ctrl Pts',(-114.677593179188,-3.55845957241312,
127.406620945676));
#102618=CARTESIAN_POINT('Ctrl Pts',(-114.685256992546,-3.65024229607719,
127.505403328312));
#102619=CARTESIAN_POINT('Ctrl Pts',(-114.692920805904,-3.7379316658509,
127.607948578431));
#102620=CARTESIAN_POINT('Ctrl Pts',(-114.700575663818,-3.82551856741475,
127.710374000704));
#102621=CARTESIAN_POINT('Ctrl Pts',(-114.708230521732,-3.90902136515567,
127.816553246285));
#102622=CARTESIAN_POINT('Ctrl Pts',(-114.715885379645,-3.98809676030264,
127.92612030568));
#102623=CARTESIAN_POINT('Ctrl Pts',(-114.723533062815,-4.06709803967039,
128.035584670072));
#102624=CARTESIAN_POINT('Ctrl Pts',(-114.731180745984,-4.141679934057,128.148430209594));
#102625=CARTESIAN_POINT('Ctrl Pts',(-114.738828429153,-4.21153828487946,
128.264256616251));
#102626=CARTESIAN_POINT('Ctrl Pts',(-114.746470431731,-4.28134474589961,
128.379996988679));
#102627=CARTESIAN_POINT('Ctrl Pts',(-114.754112434309,-4.34643443729279,
128.498713478947));
#102628=CARTESIAN_POINT('Ctrl Pts',(-114.761754436886,-4.4065459059208,
128.61997598076));
#102629=CARTESIAN_POINT('Ctrl Pts',(-114.769393119383,-4.46663125901525,
128.741185799866));
#102630=CARTESIAN_POINT('Ctrl Pts',(-114.777031801879,-4.52174251339146,
128.864939069701));
#102631=CARTESIAN_POINT('Ctrl Pts',(-114.784670484375,-4.57166387757908,
128.990780607492));
#102632=CARTESIAN_POINT('Ctrl Pts',(-114.792308603226,-4.6215815581549,
129.116612859653));
#102633=CARTESIAN_POINT('Ctrl Pts',(-114.799946722077,-4.66630995621222,
129.244532701114));
#102634=CARTESIAN_POINT('Ctrl Pts',(-114.807584840927,-4.70568134977687,
129.374064810097));
#102635=CARTESIAN_POINT('Ctrl Pts',(-114.81165603732,-4.72666670999266,
129.443106764685));
#102636=CARTESIAN_POINT('Ctrl Pts',(-114.815727233713,-4.74613097435518,
129.512606454762));
#102637=CARTESIAN_POINT('Ctrl Pts',(-114.819798430105,-4.76405452823403,
129.582490119308));
#102638=CARTESIAN_POINT('Origin',(213.235140564004,0.,130.804360617566));
#102639=CARTESIAN_POINT('',(-116.915395520338,-4.76405452823393,129.582490119308));
#102640=CARTESIAN_POINT('',(-116.569768711529,-4.764054528234,129.582490119308));
#102641=CARTESIAN_POINT('',(213.235140564004,-4.76405452823405,129.582490119308));
#102642=CARTESIAN_POINT('',(-115.235140564048,-4.91824919069818,130.8015391469));
#102643=CARTESIAN_POINT('Ctrl Pts',(-115.235140564048,-4.91824919069818,
130.801539146901));
#102644=CARTESIAN_POINT('Ctrl Pts',(-115.242812832889,-4.91832654221255,
130.936374510484));
#102645=CARTESIAN_POINT('Ctrl Pts',(-115.25048510173,-4.91285488430728,
131.07143367892));
#102646=CARTESIAN_POINT('Ctrl Pts',(-115.258157370572,-4.90180540092902,
131.20621491196));
#102647=CARTESIAN_POINT('Ctrl Pts',(-115.265821042731,-4.89076829835908,
131.34084512431));
#102648=CARTESIAN_POINT('Ctrl Pts',(-115.273484714891,-4.87416583295605,
131.47519762382));
#102649=CARTESIAN_POINT('Ctrl Pts',(-115.281148387051,-4.85202119112362,
131.608769359057));
#102650=CARTESIAN_POINT('Ctrl Pts',(-115.28880541639,-4.82989574411947,
131.742225315202));
#102651=CARTESIAN_POINT('Ctrl Pts',(-115.29646244573,-4.80223774232766,
131.874901459221));
#102652=CARTESIAN_POINT('Ctrl Pts',(-115.30411947507,-4.76912225105761,
132.006299058988));
#102653=CARTESIAN_POINT('Ctrl Pts',(-115.311772234452,-4.73602522670474,
132.137623384631));
#102654=CARTESIAN_POINT('Ctrl Pts',(-115.319424993835,-4.69747686328041,
132.267670195588));
#102655=CARTESIAN_POINT('Ctrl Pts',(-115.327077753217,-4.6536033832788,
132.395950581607));
#102656=CARTESIAN_POINT('Ctrl Pts',(-115.334728333214,-4.60974239775475,
132.524194435389));
#102657=CARTESIAN_POINT('Ctrl Pts',(-115.342378913211,-4.56055944039268,
132.650672484618));
#102658=CARTESIAN_POINT('Ctrl Pts',(-115.350029493208,-4.50623056509855,
132.774911088037));
#102659=CARTESIAN_POINT('Ctrl Pts',(-115.357679649845,-4.45190469620125,
132.899142816464));
#102660=CARTESIAN_POINT('Ctrl Pts',(-115.365329806482,-4.39243363660449,
133.021134977492));
#102661=CARTESIAN_POINT('Ctrl Pts',(-115.372979963118,-4.3280413287019,
133.140434528971));
#102662=CARTESIAN_POINT('Ctrl Pts',(-115.380631451853,-4.26363780836859,
133.259754853707));
#102663=CARTESIAN_POINT('Ctrl Pts',(-115.388282940587,-4.19431152675196,
133.376381283243));
#102664=CARTESIAN_POINT('Ctrl Pts',(-115.395934429322,-4.12033178794101,
133.489886454303));
#102665=CARTESIAN_POINT('Ctrl Pts',(-115.403593655997,-4.04627723351424,
133.603506412999));
#102666=CARTESIAN_POINT('Ctrl Pts',(-115.411252882673,-3.96756004269017,
133.713998471985));
#102667=CARTESIAN_POINT('Ctrl Pts',(-115.418912109348,-3.88449238319413,
133.820964997893));
#102668=CARTESIAN_POINT('Ctrl Pts',(-115.42657526174,-3.80138214758843,
133.927986349211));
#102669=CARTESIAN_POINT('Ctrl Pts',(-115.434238414132,-3.71391726219272,
134.031478262712));
#102670=CARTESIAN_POINT('Ctrl Pts',(-115.441901566524,-3.62244855016294,
134.131078153505));
#102671=CARTESIAN_POINT('Ctrl Pts',(-115.449576772241,-3.53083596755705,
134.230834704355));
#102672=CARTESIAN_POINT('Ctrl Pts',(-115.457251977958,-3.43520726163659,
134.326686719321));
#102673=CARTESIAN_POINT('Ctrl Pts',(-115.464927183675,-3.33594878756641,
134.41830980775));
#102674=CARTESIAN_POINT('Ctrl Pts',(-115.471845869486,-3.24647389640542,
134.500901908242));
#102675=CARTESIAN_POINT('Ctrl Pts',(-115.478764555298,-3.1540501305834,
134.58005806291));
#102676=CARTESIAN_POINT('Ctrl Pts',(-115.485683241109,-3.05898074154688,
134.655570802085));
#102677=CARTESIAN_POINT('Ctrl Pts',(-115.493457575228,-2.95215392283586,
134.740422359248));
#102678=CARTESIAN_POINT('Ctrl Pts',(-115.501231909347,-2.84162473932073,
134.820960122092));
#102679=CARTESIAN_POINT('Ctrl Pts',(-115.509006243466,-2.72777672697051,
134.896843627952));
#102680=CARTESIAN_POINT('Ctrl Pts',(-115.516770996413,-2.61406902212063,
134.972633614173));
#102681=CARTESIAN_POINT('Ctrl Pts',(-115.52453574936,-2.49705094883447,
135.043780541496));
#102682=CARTESIAN_POINT('Ctrl Pts',(-115.532300502307,-2.37713935628005,
135.109983864359));
#102683=CARTESIAN_POINT('Ctrl Pts',(-115.540057543192,-2.25734686160982,
135.176121433149));
#102684=CARTESIAN_POINT('Ctrl Pts',(-115.547814584077,-2.13466690688147,
135.237324980973));
#102685=CARTESIAN_POINT('Ctrl Pts',(-115.555571624962,-2.00954529007976,
135.293337203562));
#102686=CARTESIAN_POINT('Ctrl Pts',(-115.563322816202,-1.88451802846241,
135.349307186898));
#102687=CARTESIAN_POINT('Ctrl Pts',(-115.571074007442,-1.75705312511785,
135.40009347811));
#102688=CARTESIAN_POINT('Ctrl Pts',(-115.578825198683,-1.62762063008387,
135.445484850661));
#102689=CARTESIAN_POINT('Ctrl Pts',(-115.58657309546,-1.49824314731317,
135.490856930668));
#102690=CARTESIAN_POINT('Ctrl Pts',(-115.594320992237,-1.36690010431146,
135.530838523472));
#102691=CARTESIAN_POINT('Ctrl Pts',(-115.602068889014,-1.23408096182825,
135.565266754233));
#102692=CARTESIAN_POINT('Ctrl Pts',(-115.609815165098,-1.10128960224641,
135.59968778335));
#102693=CARTESIAN_POINT('Ctrl Pts',(-115.617561441182,-0.96702313555767,
135.62855766296));
#102694=CARTESIAN_POINT('Ctrl Pts',(-115.625307717266,-0.831785212293523,
135.651763677258));
#102695=CARTESIAN_POINT('Ctrl Pts',(-115.633054050531,-0.696546290733931,
135.674969862858));
#102696=CARTESIAN_POINT('Ctrl Pts',(-115.640800383796,-0.560336283622972,
135.692512033598));
#102697=CARTESIAN_POINT('Ctrl Pts',(-115.648546717062,-0.423667644642334,
135.704328861278));
#102698=CARTESIAN_POINT('Ctrl Pts',(-115.656294785065,-0.286968399667777,
135.716148335254));
#102699=CARTESIAN_POINT('Ctrl Pts',(-115.664042853068,-0.149810707885037,
135.722239881167));
#102700=CARTESIAN_POINT('Ctrl Pts',(-115.671790921071,-0.0127103376618529,
135.722594193741));
#102701=CARTESIAN_POINT('Ctrl Pts',(-115.679547223812,0.124535744466881,
135.722948882883));
#102702=CARTESIAN_POINT('Ctrl Pts',(-115.687303526554,0.261723991750434,
135.717554157062));
#102703=CARTESIAN_POINT('Ctrl Pts',(-115.695059829296,0.398339888344879,
135.706452864337));
#102704=CARTESIAN_POINT('Ctrl Pts',(-115.70282027181,0.535028700956762,
135.695345646518));
#102705=CARTESIAN_POINT('Ctrl Pts',(-115.710580714325,0.671144166359014,
135.678525840771));
#102706=CARTESIAN_POINT('Ctrl Pts',(-115.718341156839,0.806179681484734,
135.656087875323));
#102707=CARTESIAN_POINT('Ctrl Pts',(-115.726114057104,0.941431967607224,
135.633613890461));
#102708=CARTESIAN_POINT('Ctrl Pts',(-115.73388695737,1.0756004562268,135.605503803742));
#102709=CARTESIAN_POINT('Ctrl Pts',(-115.741659857635,1.20819059981851,
135.571902807941));
#102710=CARTESIAN_POINT('Ctrl Pts',(-115.749150193397,1.33596075772162,
135.539523292973));
#102711=CARTESIAN_POINT('Ctrl Pts',(-115.75664052916,1.46226503664722,135.502045242308));
#102712=CARTESIAN_POINT('Ctrl Pts',(-115.764130864922,1.58667838962518,
135.459640926033));
#102713=CARTESIAN_POINT('Ctrl Pts',(-115.771905199041,1.715808912691,135.415628837219));
#102714=CARTESIAN_POINT('Ctrl Pts',(-115.77967953316,1.84331133703511,135.366170132839));
#102715=CARTESIAN_POINT('Ctrl Pts',(-115.787453867279,1.96869191121559,
135.31140346418));
#102716=CARTESIAN_POINT('Ctrl Pts',(-115.795218620226,2.09391796504398,
135.256704290545));
#102717=CARTESIAN_POINT('Ctrl Pts',(-115.802983373173,2.21702701692301,
135.196710323443));
#102718=CARTESIAN_POINT('Ctrl Pts',(-115.810748126121,2.3375408922028,135.131609817668));
#102719=CARTESIAN_POINT('Ctrl Pts',(-115.818505167006,2.45793507140303,
135.066573970632));
#102720=CARTESIAN_POINT('Ctrl Pts',(-115.826262207891,2.57573886171761,
134.99644186282));
#102721=CARTESIAN_POINT('Ctrl Pts',(-115.834019248776,2.69049482107732,
134.921449477459));
#102722=CARTESIAN_POINT('Ctrl Pts',(-115.841770440016,2.80516424207525,
134.84651364444));
#102723=CARTESIAN_POINT('Ctrl Pts',(-115.849521631256,2.91679008097579,
134.766725042186));
#102724=CARTESIAN_POINT('Ctrl Pts',(-115.857272822496,3.02494055338384,
134.682364964004));
#102725=CARTESIAN_POINT('Ctrl Pts',(-115.865020719273,3.13304505895596,
134.598040741106));
#102726=CARTESIAN_POINT('Ctrl Pts',(-115.87276861605,3.23767682829374,134.509149146715));
#102727=CARTESIAN_POINT('Ctrl Pts',(-115.880516512828,3.33843426469115,
134.416013940192));
#102728=CARTESIAN_POINT('Ctrl Pts',(-115.888262788912,3.43917062480496,
134.322898215547));
#102729=CARTESIAN_POINT('Ctrl Pts',(-115.896009064996,3.53603397704364,
134.225540909612));
#102730=CARTESIAN_POINT('Ctrl Pts',(-115.90375534108,3.62865725499519,134.124304832198));
#102731=CARTESIAN_POINT('Ctrl Pts',(-115.911501674345,3.72128121667087,
134.023068007483));
#102732=CARTESIAN_POINT('Ctrl Pts',(-115.919248007611,3.80966477769252,
133.917952642608));
#102733=CARTESIAN_POINT('Ctrl Pts',(-115.926994340876,3.8934793471757,133.809356729979));
#102734=CARTESIAN_POINT('Ctrl Pts',(-115.934742408879,3.9773126863507,133.700736498048));
#102735=CARTESIAN_POINT('Ctrl Pts',(-115.942490476882,4.05657475911999,
133.588634476802));
#102736=CARTESIAN_POINT('Ctrl Pts',(-115.950238544885,4.13097895129165,
133.473479567048));
#102737=CARTESIAN_POINT('Ctrl Pts',(-115.957994847627,4.20546222112427,
133.358202269286));
#102738=CARTESIAN_POINT('Ctrl Pts',(-115.965751150369,4.2750770841701,133.239865930393));
#102739=CARTESIAN_POINT('Ctrl Pts',(-115.973507453111,4.33958148133343,
133.118926587541));
#102740=CARTESIAN_POINT('Ctrl Pts',(-115.981267895625,4.40412030643554,
132.997922695722));
#102741=CARTESIAN_POINT('Ctrl Pts',(-115.989028338139,4.46354306135324,
132.874313383835));
#102742=CARTESIAN_POINT('Ctrl Pts',(-115.996788780653,4.51765535989615,
132.748575912152));
#102743=CARTESIAN_POINT('Ctrl Pts',(-116.004561680919,4.57185452430455,
132.622636595517));
#102744=CARTESIAN_POINT('Ctrl Pts',(-116.012334581184,4.62072605757451,
132.494562657693));
#102745=CARTESIAN_POINT('Ctrl Pts',(-116.02010748145,4.66412479948301,132.36484865576));
#102746=CARTESIAN_POINT('Ctrl Pts',(-116.027597817212,4.70594588780654,
132.239850084533));
#102747=CARTESIAN_POINT('Ctrl Pts',(-116.035088152973,4.74268509025783,
132.113328915723));
#102748=CARTESIAN_POINT('Ctrl Pts',(-116.042578488735,4.77425759426975,
131.985735869574));
#102749=CARTESIAN_POINT('Ctrl Pts',(-116.050352822854,4.80702717936878,
131.853305094294));
#102750=CARTESIAN_POINT('Ctrl Pts',(-116.058127156973,4.83433434540856,
131.719300055825));
#102751=CARTESIAN_POINT('Ctrl Pts',(-116.065901491092,4.85602885892827,
131.584211105644));
#102752=CARTESIAN_POINT('Ctrl Pts',(-116.073666244039,4.87769663589896,
131.449288640522));
#102753=CARTESIAN_POINT('Ctrl Pts',(-116.081430996986,4.89376546190486,
131.313285303894));
#102754=CARTESIAN_POINT('Ctrl Pts',(-116.089195749933,4.90413525595736,
131.176705153951));
#102755=CARTESIAN_POINT('Ctrl Pts',(-116.096952790818,4.91449475058421,
131.040260657339));
#102756=CARTESIAN_POINT('Ctrl Pts',(-116.104709831703,4.9191664482201,130.903240874827));
#102757=CARTESIAN_POINT('Ctrl Pts',(-116.112466872588,4.91810162962566,
130.766158220083));
#102758=CARTESIAN_POINT('Ctrl Pts',(-116.120218063829,4.9170376140192,130.629178940435));
#102759=CARTESIAN_POINT('Ctrl Pts',(-116.127969255069,4.91024569575109,
130.492137272298));
#102760=CARTESIAN_POINT('Ctrl Pts',(-116.135720446309,4.89772914483416,
130.355548534014));
#102761=CARTESIAN_POINT('Ctrl Pts',(-116.143468343086,4.88521791378525,
130.219017849588));
#102762=CARTESIAN_POINT('Ctrl Pts',(-116.151216239863,4.86698692498344,
130.082940100653));
#102763=CARTESIAN_POINT('Ctrl Pts',(-116.15896413664,4.84309149351998,129.947828161734));
#102764=CARTESIAN_POINT('Ctrl Pts',(-116.166710412724,4.81920106046559,
129.812744485319));
#102765=CARTESIAN_POINT('Ctrl Pts',(-116.174456688808,4.78964860958437,
129.678626601826));
#102766=CARTESIAN_POINT('Ctrl Pts',(-116.182202964892,4.75454097468424,
129.545979442187));
#102767=CARTESIAN_POINT('Ctrl Pts',(-116.189949298158,4.71943308062757,
129.413331303377));
#102768=CARTESIAN_POINT('Ctrl Pts',(-116.197695631423,4.67877002075748,
129.282154288037));
#102769=CARTESIAN_POINT('Ctrl Pts',(-116.205441964689,4.63270902595703,
129.1529399736));
#102770=CARTESIAN_POINT('Ctrl Pts',(-116.213190032692,4.58663771611622,
129.023696722514));
#102771=CARTESIAN_POINT('Ctrl Pts',(-116.220938100695,4.53516619716396,
128.896417415148));
#102772=CARTESIAN_POINT('Ctrl Pts',(-116.228686168698,4.47850039352463,
128.771575019501));
#102773=CARTESIAN_POINT('Ctrl Pts',(-116.236442471439,4.42177436479494,
128.646599939871));
#102774=CARTESIAN_POINT('Ctrl Pts',(-116.244198774181,4.35984318533914,
128.524067302298));
#102775=CARTESIAN_POINT('Ctrl Pts',(-116.251955076923,4.29295969329342,
128.404427257187));
#102776=CARTESIAN_POINT('Ctrl Pts',(-116.259715519437,4.22604050351418,
128.284723356582));
#102777=CARTESIAN_POINT('Ctrl Pts',(-116.267475961951,4.15416393914136,
128.16791545753));
#102778=CARTESIAN_POINT('Ctrl Pts',(-116.275236404466,4.07762646227381,
128.054425073473));
#102779=CARTESIAN_POINT('Ctrl Pts',(-116.283009304731,4.00096612065349,
127.940752504576));
#102780=CARTESIAN_POINT('Ctrl Pts',(-116.290782204996,3.91963014700623,
127.830408407749));
#102781=CARTESIAN_POINT('Ctrl Pts',(-116.298555105262,3.83395616356444,
127.72378223058));
#102782=CARTESIAN_POINT('Ctrl Pts',(-116.306045441024,3.75139664522004,
127.621032183526));
#102783=CARTESIAN_POINT('Ctrl Pts',(-116.313535776786,3.66480923896074,
127.521734669797));
#102784=CARTESIAN_POINT('Ctrl Pts',(-116.321026112548,3.57452730522823,
127.426204669911));
#102785=CARTESIAN_POINT('Ctrl Pts',(-116.328800446667,3.48082230453882,
127.327052621044));
#102786=CARTESIAN_POINT('Ctrl Pts',(-116.336574780786,3.38284026071406,
127.231645332329));
#102787=CARTESIAN_POINT('Ctrl Pts',(-116.344349114905,3.28091251548542,
127.140374246381));
#102788=CARTESIAN_POINT('Ctrl Pts',(-116.352113867852,3.17911038709295,
127.049215643889));
#102789=CARTESIAN_POINT('Ctrl Pts',(-116.359878620799,3.07337252113294,
126.962183359964));
#102790=CARTESIAN_POINT('Ctrl Pts',(-116.367643373746,2.96406889981733,
126.879634051341));
#102791=CARTESIAN_POINT('Ctrl Pts',(-116.375400414631,2.85487384039962,
126.797166731854));
#102792=CARTESIAN_POINT('Ctrl Pts',(-116.383157455516,2.74212038345597,
126.719173760982));
#102793=CARTESIAN_POINT('Ctrl Pts',(-116.390914496401,2.62621330317779,
126.645973099704));
#102794=CARTESIAN_POINT('Ctrl Pts',(-116.398665687641,2.51039362933032,
126.572827639613));
#102795=CARTESIAN_POINT('Ctrl Pts',(-116.406416878881,2.39142539497933,
126.504467503753));
#102796=CARTESIAN_POINT('Ctrl Pts',(-116.414168070121,2.26974391956358,
126.441168483119));
#102797=CARTESIAN_POINT('Ctrl Pts',(-116.421915966899,2.14811416202067,
126.377896366257));
#102798=CARTESIAN_POINT('Ctrl Pts',(-116.429663863676,2.02377380315551,
126.319681266281));
#102799=CARTESIAN_POINT('Ctrl Pts',(-116.437411760453,1.89718423799002,
126.266753866246));
#102800=CARTESIAN_POINT('Ctrl Pts',(-116.445158036537,1.77062115263295,
126.213837537483));
#102801=CARTESIAN_POINT('Ctrl Pts',(-116.452904312621,1.64181015727526,
126.166206859339));
#102802=CARTESIAN_POINT('Ctrl Pts',(-116.460650588705,1.51123381089445,
126.124044877009));
#102803=CARTESIAN_POINT('Ctrl Pts',(-116.46839692197,1.38065650062817,126.081882583448));
#102804=CARTESIAN_POINT('Ctrl Pts',(-116.476143255236,1.24831418538666,
126.045189186386));
#102805=CARTESIAN_POINT('Ctrl Pts',(-116.483889588501,1.11470543032008,
126.014098112638));
#102806=CARTESIAN_POINT('Ctrl Pts',(-116.491637656504,0.981066754499727,
125.983000076261));
#102807=CARTESIAN_POINT('Ctrl Pts',(-116.499385724507,0.846161455220684,
125.957506948303));
#102808=CARTESIAN_POINT('Ctrl Pts',(-116.50713379251,0.710498761037574,
125.937701129471));
#102809=CARTESIAN_POINT('Ctrl Pts',(-116.514890095251,0.574691882928494,
125.91787426078));
#102810=CARTESIAN_POINT('Ctrl Pts',(-116.522646397993,0.438126389385423,
125.903746832403));
#102811=CARTESIAN_POINT('Ctrl Pts',(-116.530402700735,0.30131766988116,
125.895349441747));
#102812=CARTESIAN_POINT('Ctrl Pts',(-116.538163143249,0.164435931443695,
125.88694756915));
#102813=CARTESIAN_POINT('Ctrl Pts',(-116.545923585763,0.0273110990737119,
125.884281835777));
#102814=CARTESIAN_POINT('Ctrl Pts',(-116.553684028278,-0.109541951026601,
125.88733065798));
#102815=CARTESIAN_POINT('Ctrl Pts',(-116.561456928543,-0.246614689792179,
125.890384374423));
#102816=CARTESIAN_POINT('Ctrl Pts',(-116.569229828808,-0.383414384057801,
125.899170952967));
#102817=CARTESIAN_POINT('Ctrl Pts',(-116.577002729074,-0.519430887473454,
125.9136168484));
#102818=CARTESIAN_POINT('Ctrl Pts',(-116.584493064836,-0.650502848391687,
125.927537599148));
#102819=CARTESIAN_POINT('Ctrl Pts',(-116.591983400599,-0.780847267046429,
125.94671330467));
#102820=CARTESIAN_POINT('Ctrl Pts',(-116.599473736361,-0.91001895194746,
125.971033754049));
#102821=CARTESIAN_POINT('Ctrl Pts',(-116.60724807048,-1.04408822053579,
125.996276320657));
#102822=CARTESIAN_POINT('Ctrl Pts',(-116.615022404599,-1.17731876263939,
126.027141419119));
#102823=CARTESIAN_POINT('Ctrl Pts',(-116.622796738718,-1.30920214819879,
126.063561866548));
#102824=CARTESIAN_POINT('Ctrl Pts',(-116.630561491665,-1.4409229992726,
126.099937429032));
#102825=CARTESIAN_POINT('Ctrl Pts',(-116.638326244612,-1.57129962396362,
126.141854614973));
#102826=CARTESIAN_POINT('Ctrl Pts',(-116.646090997559,-1.69983197243749,
126.189194929535));
#102827=CARTESIAN_POINT('Ctrl Pts',(-116.653848038444,-1.82823666077086,
126.236488225029));
#102828=CARTESIAN_POINT('Ctrl Pts',(-116.66160507933,-1.95480035367621,
126.28919379586));
#102829=CARTESIAN_POINT('Ctrl Pts',(-116.669362120215,-2.07903675123895,
126.347142959711));
#102830=CARTESIAN_POINT('Ctrl Pts',(-116.677113311455,-2.20317946116737,
126.405048423646));
#102831=CARTESIAN_POINT('Ctrl Pts',(-116.684864502695,-2.32499801615418,
126.468189445339));
#102832=CARTESIAN_POINT('Ctrl Pts',(-116.692615693935,-2.44402508463241,
126.536348849988));
#102833=CARTESIAN_POINT('Ctrl Pts',(-116.700363590712,-2.56300156343187,
126.604479285071));
#102834=CARTESIAN_POINT('Ctrl Pts',(-116.708111487489,-2.67918857692805,
126.677623666967));
#102835=CARTESIAN_POINT('Ctrl Pts',(-116.715859384266,-2.79214264965307,
126.755518500801));
#102836=CARTESIAN_POINT('Ctrl Pts',(-116.72360566035,-2.90507309482109,
126.833397040716));
#102837=CARTESIAN_POINT('Ctrl Pts',(-116.731351936434,-3.01477162268949,
126.916023834247));
#102838=CARTESIAN_POINT('Ctrl Pts',(-116.739098212518,-3.12082339723724,
127.003091831258));
#102839=CARTESIAN_POINT('Ctrl Pts',(-116.746844545784,-3.22687595463467,
127.090160470986));
#102840=CARTESIAN_POINT('Ctrl Pts',(-116.754590879049,-3.32928140282224,
127.18167013153));
#102841=CARTESIAN_POINT('Ctrl Pts',(-116.762337212314,-3.42765799939943,
127.277273476361));
#102842=CARTESIAN_POINT('Ctrl Pts',(-116.770085280317,-3.52605662673347,
127.372898230899));
#102843=CARTESIAN_POINT('Ctrl Pts',(-116.77783334832,-3.62042432679295,
127.472618221534));
#102844=CARTESIAN_POINT('Ctrl Pts',(-116.785581416323,-3.71041652305749,
127.576049559455));
#102845=CARTESIAN_POINT('Ctrl Pts',(-116.793337719065,-3.80050436409951,
127.679590825433));
#102846=CARTESIAN_POINT('Ctrl Pts',(-116.801094021807,-3.88620715475995,
127.786851022769));
#102847=CARTESIAN_POINT('Ctrl Pts',(-116.808850324549,-3.96722057197679,
127.897413078345));
#102848=CARTESIAN_POINT('Ctrl Pts',(-116.816610767063,-4.04827722849366,
128.008034144219));
#102849=CARTESIAN_POINT('Ctrl Pts',(-116.824371209577,-4.12463930683379,
128.121960255267));
#102850=CARTESIAN_POINT('Ctrl Pts',(-116.832131652091,-4.19604666276836,
128.238746565069));
#102851=CARTESIAN_POINT('Ctrl Pts',(-116.839904552357,-4.26756864812992,
128.355720350623));
#102852=CARTESIAN_POINT('Ctrl Pts',(-116.847677452622,-4.33411982702114,
128.475563168104));
#102853=CARTESIAN_POINT('Ctrl Pts',(-116.855450352887,-4.39548632854803,
128.597806063958));
#102854=CARTESIAN_POINT('Ctrl Pts',(-116.862940688649,-4.45462200317053,
128.715605122634));
#102855=CARTESIAN_POINT('Ctrl Pts',(-116.870431024411,-4.5089432811492,
128.835632510814));
#102856=CARTESIAN_POINT('Ctrl Pts',(-116.877921360173,-4.55830224917604,
128.957454104594));
#102857=CARTESIAN_POINT('Ctrl Pts',(-116.886665625701,-4.61592422185459,
129.099669406678));
#102858=CARTESIAN_POINT('Ctrl Pts',(-116.895409891229,-4.66693782596252,
129.244709120248));
#102859=CARTESIAN_POINT('Ctrl Pts',(-116.904154156758,-4.71108977676246,
129.391981002241));
#102860=CARTESIAN_POINT('Ctrl Pts',(-116.907901277951,-4.73000991477147,
129.455090429609));
#102861=CARTESIAN_POINT('Ctrl Pts',(-116.911648399145,-4.7476706039676,
129.518609447254));
#102862=CARTESIAN_POINT('Ctrl Pts',(-116.915395520338,-4.76405452823392,
129.582490119308));
#102863=CARTESIAN_POINT('Ctrl Pts',(-115.165057694931,-4.76405452823392,
129.582490119308));
#102864=CARTESIAN_POINT('Ctrl Pts',(-115.17283102114,-4.79810730784155,
129.715261390175));
#102865=CARTESIAN_POINT('Ctrl Pts',(-115.180604347349,-4.82656804915046,
129.849311089595));
#102866=CARTESIAN_POINT('Ctrl Pts',(-115.188377673557,-4.8493713020677,
129.984128310727));
#102867=CARTESIAN_POINT('Ctrl Pts',(-115.194663654803,-4.8678113901763,
130.093149661552));
#102868=CARTESIAN_POINT('Ctrl Pts',(-115.200949636049,-4.88255285482992,
130.202672705539));
#102869=CARTESIAN_POINT('Ctrl Pts',(-115.207235617295,-4.89358601074035,
130.31242666063));
#102870=CARTESIAN_POINT('Ctrl Pts',(-115.2165372662,-4.9099122673069,130.474834519684));
#102871=CARTESIAN_POINT('Ctrl Pts',(-115.225838915105,-4.91815541181523,
130.638068439213));
#102872=CARTESIAN_POINT('Ctrl Pts',(-115.23514056401,-4.9182491906978,130.801539146235));
#102873=CARTESIAN_POINT('',(-114.889859435954,-4.91824797553828,130.808823084782));
#102874=CARTESIAN_POINT('Ctrl Pts',(-114.819798430105,-4.76405452823403,
129.582490119308));
#102875=CARTESIAN_POINT('Ctrl Pts',(-114.827439539859,-4.79769472368095,
129.713652730795));
#102876=CARTESIAN_POINT('Ctrl Pts',(-114.835080649612,-4.82590446010578,
129.846168403197));
#102877=CARTESIAN_POINT('Ctrl Pts',(-114.842721759365,-4.84859321787777,
129.979541322175));
#102878=CARTESIAN_POINT('Ctrl Pts',(-114.850578038796,-4.87192087927397,
130.116669953217));
#102879=CARTESIAN_POINT('Ctrl Pts',(-114.858434318228,-4.88941194984212,
130.254704374717));
#102880=CARTESIAN_POINT('Ctrl Pts',(-114.866290597659,-4.90102515160505,
130.393099720039));
#102881=CARTESIAN_POINT('Ctrl Pts',(-114.874146877091,-4.91263835336799,
130.531495065361));
#102882=CARTESIAN_POINT('Ctrl Pts',(-114.882003156522,-4.9183737060733,
130.670250873629));
#102883=CARTESIAN_POINT('Ctrl Pts',(-114.889859435954,-4.91824797553828,
130.808823084782));
#102884=CARTESIAN_POINT('Ctrl Pts',(-114.889859435992,-4.91824797553766,
130.808823085458));
#102885=CARTESIAN_POINT('Ctrl Pts',(-114.900749617536,-4.91807369093242,
131.000908480268));
#102886=CARTESIAN_POINT('Ctrl Pts',(-114.911639799079,-4.90664298984596,
131.19250429803));
#102887=CARTESIAN_POINT('Ctrl Pts',(-114.922529980623,-4.88414751305809,
131.382535446825));
#102888=CARTESIAN_POINT('Ctrl Pts',(-114.931145650296,-4.8663504179064,
131.532876889631));
#102889=CARTESIAN_POINT('Ctrl Pts',(-114.93976131997,-4.84162875804521,
131.682239922326));
#102890=CARTESIAN_POINT('Ctrl Pts',(-114.948376989643,-4.8100970391455,
131.830104024322));
#102891=CARTESIAN_POINT('Ctrl Pts',(-114.956151323762,-4.78164444899655,
131.963528932277));
#102892=CARTESIAN_POINT('Ctrl Pts',(-114.963925657881,-4.74759107326653,
132.095980430018));
#102893=CARTESIAN_POINT('Ctrl Pts',(-114.971699992,-4.7080162764146,132.226951846105));
#102894=CARTESIAN_POINT('Ctrl Pts',(-114.979464744948,-4.66849025196288,
132.357761851627));
#102895=CARTESIAN_POINT('Ctrl Pts',(-114.987229497895,-4.62345645763071,
132.487095034187));
#102896=CARTESIAN_POINT('Ctrl Pts',(-114.994994250842,-4.57304535394844,
132.614454331502));
#102897=CARTESIAN_POINT('Ctrl Pts',(-115.002751291727,-4.52268431928502,
132.741687133768));
#102898=CARTESIAN_POINT('Ctrl Pts',(-115.010508332612,-4.46695674670145,
132.866949591082));
#102899=CARTESIAN_POINT('Ctrl Pts',(-115.018265373497,-4.40604293979356,
132.989759591483));
#102900=CARTESIAN_POINT('Ctrl Pts',(-115.026016564737,-4.34517506846139,
133.112476979906));
#102901=CARTESIAN_POINT('Ctrl Pts',(-115.033767755977,-4.27912892039318,
133.232745243738));
#102902=CARTESIAN_POINT('Ctrl Pts',(-115.041518947217,-4.2081328225189,
133.350102397586));
#102903=CARTESIAN_POINT('Ctrl Pts',(-115.049266843994,-4.13716689988001,
133.467409671513));
#102904=CARTESIAN_POINT('Ctrl Pts',(-115.057014740772,-4.06125541379793,
133.581807962536));
#102905=CARTESIAN_POINT('Ctrl Pts',(-115.064762637549,-3.9806724254539,
133.692860246046));
#102906=CARTESIAN_POINT('Ctrl Pts',(-115.072508913633,-3.90010629333387,
133.803889299813));
#102907=CARTESIAN_POINT('Ctrl Pts',(-115.080255189717,-3.81487083208093,
133.911573421998));
#102908=CARTESIAN_POINT('Ctrl Pts',(-115.088001465801,-3.72528295832849,
134.015505264399));
#102909=CARTESIAN_POINT('Ctrl Pts',(-115.095747799066,-3.63569442325884,
134.119437874002));
#102910=CARTESIAN_POINT('Ctrl Pts',(-115.103494132331,-3.54175366684228,
134.219617852418));
#102911=CARTESIAN_POINT('Ctrl Pts',(-115.111240465597,-3.44381708634754,
134.315671902297));
#102912=CARTESIAN_POINT('Ctrl Pts',(-115.1189885336,-3.34585857363477,134.411747462815));
#102913=CARTESIAN_POINT('Ctrl Pts',(-115.126736601603,-3.24390273529196,
134.503694982491));
#102914=CARTESIAN_POINT('Ctrl Pts',(-115.134484669606,-3.13834161846558,
134.591179196308));
#102915=CARTESIAN_POINT('Ctrl Pts',(-115.142240972347,-3.0326683100279,
134.678756389389));
#102916=CARTESIAN_POINT('Ctrl Pts',(-115.149997275089,-2.92338237031208,
134.761860550775));
#102917=CARTESIAN_POINT('Ctrl Pts',(-115.157753577831,-2.8109080552413,
134.840197453648));
#102918=CARTESIAN_POINT('Ctrl Pts',(-115.165514020345,-2.69837370924173,
134.918576167286));
#102919=CARTESIAN_POINT('Ctrl Pts',(-115.173274462859,-2.58264792677154,
134.992182342697));
#102920=CARTESIAN_POINT('Ctrl Pts',(-115.181034905374,-2.46418166889047,
135.060766585657));
#102921=CARTESIAN_POINT('Ctrl Pts',(-115.188807805639,-2.34552523845531,
135.129460926133));
#102922=CARTESIAN_POINT('Ctrl Pts',(-115.196580705904,-2.22411988795204,
135.193117042752));
#102923=CARTESIAN_POINT('Ctrl Pts',(-115.20435360617,-2.10043956820091,
135.251532379803));
#102924=CARTESIAN_POINT('Ctrl Pts',(-115.211843941932,-1.98125533960332,
135.307824172213));
#102925=CARTESIAN_POINT('Ctrl Pts',(-115.219334277694,-1.85995895545075,
135.359249480642));
#102926=CARTESIAN_POINT('Ctrl Pts',(-115.226824613456,-1.73698796414032,
135.405670852155));
#102927=CARTESIAN_POINT('Ctrl Pts',(-115.234598947575,-1.60935449031939,
135.453852304077));
#102928=CARTESIAN_POINT('Ctrl Pts',(-115.242373281694,-1.47951261266629,
135.496795504471));
#102929=CARTESIAN_POINT('Ctrl Pts',(-115.250147615813,-1.34793150664207,
135.534293356612));
#102930=CARTESIAN_POINT('Ctrl Pts',(-115.257912368761,-1.21651256257163,
135.571744996002));
#102931=CARTESIAN_POINT('Ctrl Pts',(-115.265677121708,-1.08335902732966,
135.60376453372));
#102932=CARTESIAN_POINT('Ctrl Pts',(-115.273441874655,-0.948959610595738,
135.630193055598));
#102933=CARTESIAN_POINT('Ctrl Pts',(-115.28119891554,-0.814693681257212,
135.656595328295));
#102934=CARTESIAN_POINT('Ctrl Pts',(-115.288955956425,-0.679184714098721,
135.677417561077));
#102935=CARTESIAN_POINT('Ctrl Pts',(-115.29671299731,-0.54293578206554,
135.692550855175));
#102936=CARTESIAN_POINT('Ctrl Pts',(-115.30446418855,-0.406789596411682,
135.707672737137));
#102937=CARTESIAN_POINT('Ctrl Pts',(-115.31221537979,-0.269904943578103,
135.71711417656));
#102938=CARTESIAN_POINT('Ctrl Pts',(-115.31996657103,-0.132793921240878,
135.720817556967));
#102939=CARTESIAN_POINT('Ctrl Pts',(-115.327714467807,0.00425882525448443,
135.724519363338));
#102940=CARTESIAN_POINT('Ctrl Pts',(-115.335462364584,0.141537359888569,
135.722487950804));
#102941=CARTESIAN_POINT('Ctrl Pts',(-115.343210261361,0.278525864719153,
135.714717672321));
#102942=CARTESIAN_POINT('Ctrl Pts',(-115.350956537445,0.415485714507284,
135.706949019213));
#102943=CARTESIAN_POINT('Ctrl Pts',(-115.35870281353,0.552155265073385,
135.693443910039));
#102944=CARTESIAN_POINT('Ctrl Pts',(-115.366449089614,0.688020501657005,
135.674248794085));
#102945=CARTESIAN_POINT('Ctrl Pts',(-115.374195422879,0.823886741167122,
135.655053536437));
#102946=CARTESIAN_POINT('Ctrl Pts',(-115.381941756144,0.95894826772659,
135.630168242889));
#102947=CARTESIAN_POINT('Ctrl Pts',(-115.38968808941,1.09269837427396,135.599690984221));
#102948=CARTESIAN_POINT('Ctrl Pts',(-115.397436157413,1.22647843323052,
135.569206900382));
#102949=CARTESIAN_POINT('Ctrl Pts',(-115.405184225416,1.35894610665796,
135.533128446372));
#102950=CARTESIAN_POINT('Ctrl Pts',(-115.412932293419,1.48960741554254,
135.491604243628));
#102951=CARTESIAN_POINT('Ctrl Pts',(-115.420688596161,1.62040759282092,
135.450035908467));
#102952=CARTESIAN_POINT('Ctrl Pts',(-115.428444898902,1.74939719730176,
135.403010381407));
#102953=CARTESIAN_POINT('Ctrl Pts',(-115.436201201644,1.87609936693917,
135.350725564188));
#102954=CARTESIAN_POINT('Ctrl Pts',(-115.443961644158,2.00286916133944,
135.298412840987));
#102955=CARTESIAN_POINT('Ctrl Pts',(-115.451722086673,2.12734873353291,
135.240835398411));
#102956=CARTESIAN_POINT('Ctrl Pts',(-115.459482529187,2.24908450562575,
135.1782378391));
#102957=CARTESIAN_POINT('Ctrl Pts',(-115.467255429452,2.37101569878714,
135.11553979263));
#102958=CARTESIAN_POINT('Ctrl Pts',(-115.475028329718,2.49019394997115,
135.047805718793));
#102959=CARTESIAN_POINT('Ctrl Pts',(-115.482801229983,2.60619266132521,
134.975324879527));
#102960=CARTESIAN_POINT('Ctrl Pts',(-115.490291565745,2.71797452733748,
134.905478901337));
#102961=CARTESIAN_POINT('Ctrl Pts',(-115.497781901507,2.8268037542206,134.831225453398));
#102962=CARTESIAN_POINT('Ctrl Pts',(-115.505272237269,2.93232819333034,
134.752858360898));
#102963=CARTESIAN_POINT('Ctrl Pts',(-115.513046571388,3.04185362362315,
134.671519956267));
#102964=CARTESIAN_POINT('Ctrl Pts',(-115.520820905507,3.14816566076399,
134.585492156043));
#102965=CARTESIAN_POINT('Ctrl Pts',(-115.528595239626,3.25083646761813,
134.495057749993));
#102966=CARTESIAN_POINT('Ctrl Pts',(-115.536359992573,3.35338074187878,
134.404734796266));
#102967=CARTESIAN_POINT('Ctrl Pts',(-115.54412474552,3.4522924240549,134.31001629822));
#102968=CARTESIAN_POINT('Ctrl Pts',(-115.551889498467,3.54717365563843,
134.21122752416));
#102969=CARTESIAN_POINT('Ctrl Pts',(-115.559646539352,3.64196064984516,
134.112536868503));
#102970=CARTESIAN_POINT('Ctrl Pts',(-115.567403580237,3.73272489074091,
134.009784262049));
#102971=CARTESIAN_POINT('Ctrl Pts',(-115.575160621122,3.81910283549119,
133.903334091871));
#102972=CARTESIAN_POINT('Ctrl Pts',(-115.582911812363,3.90541564196153,
133.796964196593));
#102973=CARTESIAN_POINT('Ctrl Pts',(-115.590663003603,3.9873484907932,133.686902590017));
#102974=CARTESIAN_POINT('Ctrl Pts',(-115.598414194843,4.06457610631102,
133.573548971309));
#102975=CARTESIAN_POINT('Ctrl Pts',(-115.60616209162,4.14177089803202,133.460243530913));
#102976=CARTESIAN_POINT('Ctrl Pts',(-115.613909988397,4.21426421431816,
133.3436491837));
#102977=CARTESIAN_POINT('Ctrl Pts',(-115.621657885174,4.28177249195604,
133.224196849551));
#102978=CARTESIAN_POINT('Ctrl Pts',(-115.629404161258,4.34926664831774,
133.104769502255));
#102979=CARTESIAN_POINT('Ctrl Pts',(-115.637150437342,4.41177764790559,
132.982485697291));
#102980=CARTESIAN_POINT('Ctrl Pts',(-115.644896713427,4.46906673228595,
132.85780299681));
#102981=CARTESIAN_POINT('Ctrl Pts',(-115.652643046692,4.52635623956123,
132.733119375949));
#102982=CARTESIAN_POINT('Ctrl Pts',(-115.660389379957,4.57842359147752,
132.606037179494));
#102983=CARTESIAN_POINT('Ctrl Pts',(-115.668135713223,4.62507741021612,
132.477035724097));
#102984=CARTESIAN_POINT('Ctrl Pts',(-115.675883781226,4.67174167675389,
132.348005379719));
#102985=CARTESIAN_POINT('Ctrl Pts',(-115.683631849229,4.71298986479103,
132.217055288728));
#102986=CARTESIAN_POINT('Ctrl Pts',(-115.691379917232,4.74868000602797,
132.084681383175));
#102987=CARTESIAN_POINT('Ctrl Pts',(-115.699136219973,4.78440807917179,
131.95216678906));
#102988=CARTESIAN_POINT('Ctrl Pts',(-115.706892522715,4.81456620339192,
131.818225735596));
#102989=CARTESIAN_POINT('Ctrl Pts',(-115.714648825457,4.83906312344394,
131.683366391054));
#102990=CARTESIAN_POINT('Ctrl Pts',(-115.722409267971,4.86357311823978,
131.548435068019));
#102991=CARTESIAN_POINT('Ctrl Pts',(-115.730169710485,4.88241583447588,
131.412584864368));
#102992=CARTESIAN_POINT('Ctrl Pts',(-115.737930153,4.89555189335025,131.276329601732));
#102993=CARTESIAN_POINT('Ctrl Pts',(-115.745703053265,4.90870903939248,
131.139855610052));
#102994=CARTESIAN_POINT('Ctrl Pts',(-115.75347595353,4.91614120060038,131.002975650622));
#102995=CARTESIAN_POINT('Ctrl Pts',(-115.761248853796,4.9178611546751,130.86620498544));
#102996=CARTESIAN_POINT('Ctrl Pts',(-115.768739189558,4.9195185840869,130.734406278441));
#102997=CARTESIAN_POINT('Ctrl Pts',(-115.77622952532,4.91587191080067,130.602709365307));
#102998=CARTESIAN_POINT('Ctrl Pts',(-115.783719861082,4.90697799332566,
130.471569338357));
#102999=CARTESIAN_POINT('Ctrl Pts',(-115.791494195201,4.89774686026636,
130.335457097426));
#103000=CARTESIAN_POINT('Ctrl Pts',(-115.79926852932,4.88283348839464,130.199513642299));
#103001=CARTESIAN_POINT('Ctrl Pts',(-115.807042863439,4.86224454032789,
130.064251779251));
#103002=CARTESIAN_POINT('Ctrl Pts',(-115.814807616386,4.84168096629954,
129.929156614361));
#103003=CARTESIAN_POINT('Ctrl Pts',(-115.822572369333,4.81545579159429,
129.794741753));
#103004=CARTESIAN_POINT('Ctrl Pts',(-115.830337122281,4.78362762140805,
129.661517740263));
#103005=CARTESIAN_POINT('Ctrl Pts',(-115.838094163166,4.75183106340914,
129.528426047494));
#103006=CARTESIAN_POINT('Ctrl Pts',(-115.845851204051,4.71444267473866,
129.396523227391));
#103007=CARTESIAN_POINT('Ctrl Pts',(-115.853608244936,4.67157252077776,
129.266312098951));
#103008=CARTESIAN_POINT('Ctrl Pts',(-115.861359436176,4.62873469553339,
129.136199163735));
#103009=CARTESIAN_POINT('Ctrl Pts',(-115.869110627416,4.58042345492907,
129.007775750796));
#103010=CARTESIAN_POINT('Ctrl Pts',(-115.876861818656,4.5267992577454,128.881531570933));
#103011=CARTESIAN_POINT('Ctrl Pts',(-115.884609715433,4.47319785227607,
128.755341048215));
#103012=CARTESIAN_POINT('Ctrl Pts',(-115.89235761221,4.4142881340431,128.631328275462));
#103013=CARTESIAN_POINT('Ctrl Pts',(-115.900105508987,4.35027937530218,
128.509964745159));
#103014=CARTESIAN_POINT('Ctrl Pts',(-115.907851785071,4.28628400581372,
128.388626601489));
#103015=CARTESIAN_POINT('Ctrl Pts',(-115.915598061155,4.21719189963404,
128.269936943602));
#103016=CARTESIAN_POINT('Ctrl Pts',(-115.92334433724,4.14325896199284,128.154343969247));
#103017=CARTESIAN_POINT('Ctrl Pts',(-115.931090670505,4.06932547859537,
128.038750141612));
#103018=CARTESIAN_POINT('Ctrl Pts',(-115.93883700377,3.99055130308902,127.926253372481));
#103019=CARTESIAN_POINT('Ctrl Pts',(-115.946583337036,3.90723625376387,
127.817273755794));
#103020=CARTESIAN_POINT('Ctrl Pts',(-115.954331405039,3.8239025466112,127.708269733877));
#103021=CARTESIAN_POINT('Ctrl Pts',(-115.962079473041,3.73602617953833,
127.602784742258));
#103022=CARTESIAN_POINT('Ctrl Pts',(-115.969827541044,3.64394765689159,
127.501206286274));
#103023=CARTESIAN_POINT('Ctrl Pts',(-115.977583843786,3.55177127209536,
127.399519871498));
#103024=CARTESIAN_POINT('Ctrl Pts',(-115.985340146528,3.45538407320305,
127.301748576381));
#103025=CARTESIAN_POINT('Ctrl Pts',(-115.99309644927,3.35516427088326,127.208243853904));
#103026=CARTESIAN_POINT('Ctrl Pts',(-116.000856891784,3.25489097823714,
127.114689225142));
#103027=CARTESIAN_POINT('Ctrl Pts',(-116.008617334298,3.15078130281278,
127.02540596092));
#103028=CARTESIAN_POINT('Ctrl Pts',(-116.016377776813,3.04324625209531,
126.940704924882));
#103029=CARTESIAN_POINT('Ctrl Pts',(-116.024150677078,2.93553857656792,
126.855867919222));
#103030=CARTESIAN_POINT('Ctrl Pts',(-116.031923577343,2.82439485473092,
126.775628069957));
#103031=CARTESIAN_POINT('Ctrl Pts',(-116.039696477609,2.71025549775606,
126.700253138542));
#103032=CARTESIAN_POINT('Ctrl Pts',(-116.047186813371,2.60026539390663,
126.627618275741));
#103033=CARTESIAN_POINT('Ctrl Pts',(-116.054677149133,2.48749393504998,
126.559500926831));
#103034=CARTESIAN_POINT('Ctrl Pts',(-116.062167484895,2.37235473665656,
126.496099243652));
#103035=CARTESIAN_POINT('Ctrl Pts',(-116.069941819014,2.25285000056076,
126.430293666384));
#103036=CARTESIAN_POINT('Ctrl Pts',(-116.077716153133,2.1304158798679,126.369359950409));
#103037=CARTESIAN_POINT('Ctrl Pts',(-116.085490487252,2.0054874143276,126.313569674595));
#103038=CARTESIAN_POINT('Ctrl Pts',(-116.093255240199,1.8807129119559,126.257848155309));
#103039=CARTESIAN_POINT('Ctrl Pts',(-116.101019993146,1.75345053475243,
126.207257621693));
#103040=CARTESIAN_POINT('Ctrl Pts',(-116.108784746093,1.62416149630504,
126.16202472963));
#103041=CARTESIAN_POINT('Ctrl Pts',(-116.116541786978,1.49500086955328,
126.116836763513));
#103042=CARTESIAN_POINT('Ctrl Pts',(-116.124298827863,1.36381795398044,
126.076995977624));
#103043=CARTESIAN_POINT('Ctrl Pts',(-116.132055868748,1.23109527847499,
126.042681556792));
#103044=CARTESIAN_POINT('Ctrl Pts',(-116.139807059989,1.0984726901714,126.008393012731));
#103045=CARTESIAN_POINT('Ctrl Pts',(-116.147558251229,0.964313030111163,
125.979622636087));
#103046=CARTESIAN_POINT('Ctrl Pts',(-116.155309442469,0.829115037750144,
125.956500128992));
#103047=CARTESIAN_POINT('Ctrl Pts',(-116.163057339246,0.693974508142587,
125.93338744958));
#103048=CARTESIAN_POINT('Ctrl Pts',(-116.170805236023,0.557796908546889,
125.915917931086));
#103049=CARTESIAN_POINT('Ctrl Pts',(-116.1785531328,0.421092035708382,125.904170360039));
#103050=CARTESIAN_POINT('Ctrl Pts',(-116.186299408884,0.284415758582256,
125.89242524633));
#103051=CARTESIAN_POINT('Ctrl Pts',(-116.194045684968,0.147212816877323,
125.886399732805));
#103052=CARTESIAN_POINT('Ctrl Pts',(-116.201791961052,0.00999861508217229,
125.886120780978));
#103053=CARTESIAN_POINT('Ctrl Pts',(-116.209538294318,-0.127216599596859,
125.885841827092));
#103054=CARTESIAN_POINT('Ctrl Pts',(-116.217284627583,-0.264442683567566,
125.891309520345));
#103055=CARTESIAN_POINT('Ctrl Pts',(-116.225030960848,-0.40116414079272,
125.902498686152));
#103056=CARTESIAN_POINT('Ctrl Pts',(-116.232779028851,-0.537916215840074,
125.913690357696));
#103057=CARTESIAN_POINT('Ctrl Pts',(-116.240527096854,-0.67416304968182,
125.930606019518));
#103058=CARTESIAN_POINT('Ctrl Pts',(-116.248275164857,-0.809394572185431,
125.953168651769));
#103059=CARTESIAN_POINT('Ctrl Pts',(-116.256031467599,-0.944769820360988,
125.975755263854));
#103060=CARTESIAN_POINT('Ctrl Pts',(-116.263787770341,-1.07912721536045,
126.004000770901));
#103061=CARTESIAN_POINT('Ctrl Pts',(-116.271544073083,-1.21196663773001,
126.037776942487));
#103062=CARTESIAN_POINT('Ctrl Pts',(-116.279304515597,-1.34487696049901,
126.071571141433));
#103063=CARTESIAN_POINT('Ctrl Pts',(-116.287064958111,-1.47626732190926,
126.110901774729));
#103064=CARTESIAN_POINT('Ctrl Pts',(-116.294825400625,-1.60565402398851,
126.155591079532));
#103065=CARTESIAN_POINT('Ctrl Pts',(-116.302598300891,-1.73524842908835,
126.200352123575));
#103066=CARTESIAN_POINT('Ctrl Pts',(-116.310371201156,-1.86283238327472,
126.250488886015));
#103067=CARTESIAN_POINT('Ctrl Pts',(-116.318144101422,-1.98794255825685,
126.305775568068));
#103068=CARTESIAN_POINT('Ctrl Pts',(-116.325634437184,-2.10850466324555,
126.359052439969));
#103069=CARTESIAN_POINT('Ctrl Pts',(-116.333124772946,-2.22676944617571,
126.417111171214));
#103070=CARTESIAN_POINT('Ctrl Pts',(-116.340615108708,-2.3423466270268,
126.479710881303));
#103071=CARTESIAN_POINT('Ctrl Pts',(-116.348390427865,-2.46232115113111,
126.544692310784));
#103072=CARTESIAN_POINT('Ctrl Pts',(-116.356165747023,-2.57977960639145,
126.614772967477));
#103073=CARTESIAN_POINT('Ctrl Pts',(-116.36394106618,-2.69425818120466,
126.68973354874));
#103074=CARTESIAN_POINT('Ctrl Pts',(-116.371706587397,-2.80859249772535,
126.764599669661));
#103075=CARTESIAN_POINT('Ctrl Pts',(-116.379472108614,-2.91995408184397,
126.844333266275));
#103076=CARTESIAN_POINT('Ctrl Pts',(-116.387237629831,-3.02790281808886,
126.928668732662));
#103077=CARTESIAN_POINT('Ctrl Pts',(-116.394993822415,-3.13572187673097,
127.012902887802));
#103078=CARTESIAN_POINT('Ctrl Pts',(-116.402750014998,-3.24013594675893,
127.101727663325));
#103079=CARTESIAN_POINT('Ctrl Pts',(-116.410506207582,-3.3407335963119,
127.194834041826));
#103080=CARTESIAN_POINT('Ctrl Pts',(-116.418257110972,-3.44126264513647,
127.287876928134));
#103081=CARTESIAN_POINT('Ctrl Pts',(-116.426008014362,-3.53798016537562,
127.385195344403));
#103082=CARTESIAN_POINT('Ctrl Pts',(-116.433758917752,-3.63050749963723,
127.486439829244));
#103083=CARTESIAN_POINT('Ctrl Pts',(-116.441506214166,-3.72299177520397,
127.587637198761));
#103084=CARTESIAN_POINT('Ctrl Pts',(-116.449253510581,-3.81128948195976,
127.692756713233));
#103085=CARTESIAN_POINT('Ctrl Pts',(-116.457000806996,-3.89505885799039,
127.801412140604));
#103086=CARTESIAN_POINT('Ctrl Pts',(-116.464746175871,-3.97880739205941,
127.910040534321));
#103087=CARTESIAN_POINT('Ctrl Pts',(-116.472491544745,-4.0580296001001,
128.022202780125));
#103088=CARTESIAN_POINT('Ctrl Pts',(-116.48023691362,-4.13242431335157,
128.137479975895));
#103089=CARTESIAN_POINT('Ctrl Pts',(-116.487984623368,-4.20684151083047,
128.252792011757));
#103090=CARTESIAN_POINT('Ctrl Pts',(-116.495732333116,-4.27642808098253,
128.371220553363));
#103091=CARTESIAN_POINT('Ctrl Pts',(-116.503480042864,-4.34092642726801,
128.492318054042));
#103092=CARTESIAN_POINT('Ctrl Pts',(-116.511228755889,-4.405433125659,128.613431236039));
#103093=CARTESIAN_POINT('Ctrl Pts',(-116.518977468914,-4.46485011097761,
128.737213716634));
#103094=CARTESIAN_POINT('Ctrl Pts',(-116.526726181939,-4.51896642917555,
128.863194608569));
#103095=CARTESIAN_POINT('Ctrl Pts',(-116.534481725635,-4.57313045216502,
128.989286555587));
#103096=CARTESIAN_POINT('Ctrl Pts',(-116.54223726933,-4.62198432500997,
129.117580423228));
#103097=CARTESIAN_POINT('Ctrl Pts',(-116.549992813026,-4.66536565734462,
129.247586277538));
#103098=CARTESIAN_POINT('Ctrl Pts',(-116.556584779194,-4.70223841395482,
129.358087130461));
#103099=CARTESIAN_POINT('Ctrl Pts',(-116.563176745361,-4.73515835422674,
129.469824375414));
#103100=CARTESIAN_POINT('Ctrl Pts',(-116.569768711529,-4.764054528234,129.582490119308));
#103101=CARTESIAN_POINT('Origin',(213.235140564004,0.,130.804360617566));
#103102=CARTESIAN_POINT('',(-118.665245282749,-4.764054528234,129.582490119308));
#103103=CARTESIAN_POINT('',(-118.320090776197,-4.76405452823413,129.582490119309));
#103104=CARTESIAN_POINT('',(213.235140564004,-4.76405452823405,129.582490119308));
#103105=CARTESIAN_POINT('',(-116.985140563956,-4.91824914438459,130.801459538413));
#103106=CARTESIAN_POINT('Ctrl Pts',(-116.98514056401,-4.91824914438515,
130.801459539365));
#103107=CARTESIAN_POINT('Ctrl Pts',(-116.992962856645,-4.91833097250967,
130.940184204984));
#103108=CARTESIAN_POINT('Ctrl Pts',(-117.00078514928,-4.91253913636687,
131.07892180876));
#103109=CARTESIAN_POINT('Ctrl Pts',(-117.008607441915,-4.90089696268117,
131.217146304918));
#103110=CARTESIAN_POINT('Ctrl Pts',(-117.016430946283,-4.88925298553342,
131.355392213111));
#103111=CARTESIAN_POINT('Ctrl Pts',(-117.024254450651,-4.87175689745055,
131.493124476448));
#103112=CARTESIAN_POINT('Ctrl Pts',(-117.032077955019,-4.84848393605076,
131.629822054798));
#103113=CARTESIAN_POINT('Ctrl Pts',(-117.039904238686,-4.82520270693484,
131.766568194943));
#103114=CARTESIAN_POINT('Ctrl Pts',(-117.047730522353,-4.79614058131351,
131.90227854341));
#103115=CARTESIAN_POINT('Ctrl Pts',(-117.055556806019,-4.7614239018093,
132.036442388302));
#103116=CARTESIAN_POINT('Ctrl Pts',(-117.063387438058,-4.7266879333254,
132.170680776143));
#103117=CARTESIAN_POINT('Ctrl Pts',(-117.071218070097,-4.68629124943694,
132.303370581688));
#103118=CARTESIAN_POINT('Ctrl Pts',(-117.079048702135,-4.64040993340714,
132.434016628028));
#103119=CARTESIAN_POINT('Ctrl Pts',(-117.086889979928,-4.59446624166729,
132.564840287843));
#103120=CARTESIAN_POINT('Ctrl Pts',(-117.094731257722,-4.54302315428032,
132.693614281432));
#103121=CARTESIAN_POINT('Ctrl Pts',(-117.102572535515,-4.48630500709428,
132.819863146917));
#103122=CARTESIAN_POINT('Ctrl Pts',(-117.110420056086,-4.42954170415399,
132.94621252455));
#103123=CARTESIAN_POINT('Ctrl Pts',(-117.118267576657,-4.36749514211798,
133.070032429201));
#103124=CARTESIAN_POINT('Ctrl Pts',(-117.126115097229,-4.3004350362841,
133.190873043932));
#103125=CARTESIAN_POINT('Ctrl Pts',(-117.133974930124,-4.23326971686555,
133.311903250882));
#103126=CARTESIAN_POINT('Ctrl Pts',(-117.14183476302,-4.1610753444807,133.429944511274));
#103127=CARTESIAN_POINT('Ctrl Pts',(-117.149694595916,-4.0841645832594,
133.544576433765));
#103128=CARTESIAN_POINT('Ctrl Pts',(-117.151919391939,-4.06239430417253,
133.577024025042));
#103129=CARTESIAN_POINT('Ctrl Pts',(-117.154144187963,-4.0402463801263,
133.609198660703));
#103130=CARTESIAN_POINT('Ctrl Pts',(-117.156368983986,-4.01772846487362,
133.641091314168));
#103131=CARTESIAN_POINT('Ctrl Pts',(-117.164143318105,-3.9390417920256,
133.75253710128));
#103132=CARTESIAN_POINT('Ctrl Pts',(-117.171917652224,-3.85558996144009,
133.860882953182));
#103133=CARTESIAN_POINT('Ctrl Pts',(-117.179691986343,-3.76764541453514,
133.965694369771));
#103134=CARTESIAN_POINT('Ctrl Pts',(-117.18745673929,-3.67980925142443,
134.070376615657));
#103135=CARTESIAN_POINT('Ctrl Pts',(-117.195221492237,-3.58749163760855,
134.171532796498));
#103136=CARTESIAN_POINT('Ctrl Pts',(-117.202986245185,-3.4910082002169,
134.268757362819));
#103137=CARTESIAN_POINT('Ctrl Pts',(-117.21074328607,-3.39462059153519,
134.36588536433));
#103138=CARTESIAN_POINT('Ctrl Pts',(-117.218500326955,-3.29407566681059,
134.459089246602));
#103139=CARTESIAN_POINT('Ctrl Pts',(-117.22625736784,-3.1897289841545,134.547996827208));
#103140=CARTESIAN_POINT('Ctrl Pts',(-117.23400855908,-3.08546099014392,
134.636837361916));
#103141=CARTESIAN_POINT('Ctrl Pts',(-117.24175975032,-2.97739724105038,
134.721387791196));
#103142=CARTESIAN_POINT('Ctrl Pts',(-117.24951094156,-2.86592951521695,
134.801313341368));
#103143=CARTESIAN_POINT('Ctrl Pts',(-117.257258838337,-2.75450916614035,
134.881204921049));
#103144=CARTESIAN_POINT('Ctrl Pts',(-117.265006735114,-2.63968803492435,
134.956475303899));
#103145=CARTESIAN_POINT('Ctrl Pts',(-117.272754631891,-2.52189011261899,
135.026830667475));
#103146=CARTESIAN_POINT('Ctrl Pts',(-117.280500907975,-2.40411683109921,
135.097171314225));
#103147=CARTESIAN_POINT('Ctrl Pts',(-117.28824718406,-2.28336833247884,
135.162598786336));
#103148=CARTESIAN_POINT('Ctrl Pts',(-117.295993460144,-2.16009631759652,
135.222863413899));
#103149=CARTESIAN_POINT('Ctrl Pts',(-117.303739793409,-2.03682339274835,
135.283128486323));
#103150=CARTESIAN_POINT('Ctrl Pts',(-117.311486126674,-1.9110272657063,
135.33823046644));
#103151=CARTESIAN_POINT('Ctrl Pts',(-117.31923245994,-1.78318252255282,
135.387966529265));
#103152=CARTESIAN_POINT('Ctrl Pts',(-117.326980527943,-1.65530914945569,
135.437713730137));
#103153=CARTESIAN_POINT('Ctrl Pts',(-117.334728595946,-1.52538661163492,
135.48209248083));
#103154=CARTESIAN_POINT('Ctrl Pts',(-117.342476663949,-1.39390729147759,
135.520948952927));
#103155=CARTESIAN_POINT('Ctrl Pts',(-117.350232966691,-1.26228823353399,
135.559846722145));
#103156=CARTESIAN_POINT('Ctrl Pts',(-117.357989269432,-1.12910946361085,
135.593210377538));
#103157=CARTESIAN_POINT('Ctrl Pts',(-117.365745572174,-0.994876813763548,
135.620936495504));
#103158=CARTESIAN_POINT('Ctrl Pts',(-117.373506014688,-0.860572519909357,
135.648677411734));
#103159=CARTESIAN_POINT('Ctrl Pts',(-117.381266457203,-0.725213610995721,
135.670774732041));
#103160=CARTESIAN_POINT('Ctrl Pts',(-117.389026899717,-0.589312815702003,
135.687176758662));
#103161=CARTESIAN_POINT('Ctrl Pts',(-117.396799799982,-0.453193860386973,
135.703605115272));
#103162=CARTESIAN_POINT('Ctrl Pts',(-117.404572700248,-0.316531670379598,
135.714319877809));
#103163=CARTESIAN_POINT('Ctrl Pts',(-117.412345600513,-0.179841665925045,
135.719321455426));
#103164=CARTESIAN_POINT('Ctrl Pts',(-117.419835936275,-0.0481206874296885,
135.724141213099));
#103165=CARTESIAN_POINT('Ctrl Pts',(-117.427326272038,0.0836258103552183,
135.723655952752));
#103166=CARTESIAN_POINT('Ctrl Pts',(-117.4348166078,0.214941501717956,135.717911595559));
#103167=CARTESIAN_POINT('Ctrl Pts',(-117.442590941919,0.351236067427596,
135.711949439318));
#103168=CARTESIAN_POINT('Ctrl Pts',(-117.450365276038,0.487498254002862,
135.700302630215));
#103169=CARTESIAN_POINT('Ctrl Pts',(-117.458139610157,0.623215242960326,
135.682965523012));
#103170=CARTESIAN_POINT('Ctrl Pts',(-117.465904363104,0.758764972858276,
135.665649782244));
#103171=CARTESIAN_POINT('Ctrl Pts',(-117.473669116051,0.893770457943031,
135.642657745792));
#103172=CARTESIAN_POINT('Ctrl Pts',(-117.481433868999,1.02771989378069,
135.614035750299));
#103173=CARTESIAN_POINT('Ctrl Pts',(-117.489190909884,1.16153628915069,
135.585442182575));
#103174=CARTESIAN_POINT('Ctrl Pts',(-117.496947950769,1.29429834273785,
135.551229864823));
#103175=CARTESIAN_POINT('Ctrl Pts',(-117.504704991654,1.42550073908048,
135.511496764458));
#103176=CARTESIAN_POINT('Ctrl Pts',(-117.512456182894,1.55660419467524,
135.471793627134));
#103177=CARTESIAN_POINT('Ctrl Pts',(-117.520207374134,1.68614996141089,
135.426578106781));
#103178=CARTESIAN_POINT('Ctrl Pts',(-117.527958565374,1.81364461894353,
135.375998864265));
#103179=CARTESIAN_POINT('Ctrl Pts',(-117.535706462151,1.94108508784587,
135.325441119275));
#103180=CARTESIAN_POINT('Ctrl Pts',(-117.543454358928,2.06647581879019,
135.269524330191));
#103181=CARTESIAN_POINT('Ctrl Pts',(-117.551202255706,2.18934043311451,
135.208446394482));
#103182=CARTESIAN_POINT('Ctrl Pts',(-117.55894853179,2.31217934681017,135.14738123496));
#103183=CARTESIAN_POINT('Ctrl Pts',(-117.566694807874,2.43249284504949,
135.081157250125));
#103184=CARTESIAN_POINT('Ctrl Pts',(-117.574441083958,2.54982671813193,
135.010019516003));
#103185=CARTESIAN_POINT('Ctrl Pts',(-117.582187417223,2.6671614573462,134.938881256758));
#103186=CARTESIAN_POINT('Ctrl Pts',(-117.589933750489,2.78151619319496,
134.862829378539));
#103187=CARTESIAN_POINT('Ctrl Pts',(-117.597680083754,2.89246375790431,
134.7821535322));
#103188=CARTESIAN_POINT('Ctrl Pts',(-117.605428151757,3.00343616855138,
134.701459619064));
#103189=CARTESIAN_POINT('Ctrl Pts',(-117.61317621976,3.11099957360763,134.616139907158));
#103190=CARTESIAN_POINT('Ctrl Pts',(-117.620924287763,3.21475840816102,
134.526525503712));
#103191=CARTESIAN_POINT('Ctrl Pts',(-117.628680590505,3.31862751883867,
134.436815857011));
#103192=CARTESIAN_POINT('Ctrl Pts',(-117.636436893247,3.41868368524422,
134.342802656748));
#103193=CARTESIAN_POINT('Ctrl Pts',(-117.644193195989,3.51456647959025,
134.244855570773));
#103194=CARTESIAN_POINT('Ctrl Pts',(-117.651953638503,3.6105004494706,134.146856207489));
#103195=CARTESIAN_POINT('Ctrl Pts',(-117.659714081017,3.70225634746651,
134.044919065239));
#103196=CARTESIAN_POINT('Ctrl Pts',(-117.667474523531,3.78951353640945,
133.939447573277));
#103197=CARTESIAN_POINT('Ctrl Pts',(-117.675247423797,3.87691079833841,
133.833806769113));
#103198=CARTESIAN_POINT('Ctrl Pts',(-117.683020324062,3.95979468337634,
133.724620589058));
#103199=CARTESIAN_POINT('Ctrl Pts',(-117.690793224328,4.03788693852398,
133.61232289192));
#103200=CARTESIAN_POINT('Ctrl Pts',(-117.69828356009,4.11314034349131,133.504107498939));
#103201=CARTESIAN_POINT('Ctrl Pts',(-117.705773895851,4.18394428035254,
133.393003144034));
#103202=CARTESIAN_POINT('Ctrl Pts',(-117.713264231613,4.25009072869888,
133.279418568469));
#103203=CARTESIAN_POINT('Ctrl Pts',(-117.721038565732,4.3187451397413,133.161527399194));
#103204=CARTESIAN_POINT('Ctrl Pts',(-117.728812899851,4.38259938962026,
133.040590777674));
#103205=CARTESIAN_POINT('Ctrl Pts',(-117.73658723397,4.44137153792066,132.917037101235));
#103206=CARTESIAN_POINT('Ctrl Pts',(-117.744351986917,4.50007125480122,
132.793635693659));
#103207=CARTESIAN_POINT('Ctrl Pts',(-117.752116739864,4.55370116574578,
132.66762399819));
#103208=CARTESIAN_POINT('Ctrl Pts',(-117.759881492811,4.60202361228762,
132.53945765648));
#103209=CARTESIAN_POINT('Ctrl Pts',(-117.767638533696,4.6502980642942,132.411418611388));
#103210=CARTESIAN_POINT('Ctrl Pts',(-117.775395574581,4.69327540528332,
132.281229542262));
#103211=CARTESIAN_POINT('Ctrl Pts',(-117.783152615466,4.73076492266621,
132.149368539093));
#103212=CARTESIAN_POINT('Ctrl Pts',(-117.790903806706,4.76822616891236,
132.017606973333));
#103213=CARTESIAN_POINT('Ctrl Pts',(-117.798654997946,4.8002077223216,131.884176357652));
#103214=CARTESIAN_POINT('Ctrl Pts',(-117.806406189187,4.82656794974035,
131.749572175387));
#103215=CARTESIAN_POINT('Ctrl Pts',(-117.814154085964,4.8529169733593,131.615025203491));
#103216=CARTESIAN_POINT('Ctrl Pts',(-117.821901982741,4.87364934797108,
131.479306039955));
#103217=CARTESIAN_POINT('Ctrl Pts',(-117.829649879518,4.88867407601971,
131.342922444057));
#103218=CARTESIAN_POINT('Ctrl Pts',(-117.837396155602,4.90369566121912,
131.206567376666));
#103219=CARTESIAN_POINT('Ctrl Pts',(-117.845142431686,4.91301193183634,
131.069548541729));
#103220=CARTESIAN_POINT('Ctrl Pts',(-117.85288870777,4.91658356583436,130.932380548309));
#103221=CARTESIAN_POINT('Ctrl Pts',(-117.860635041035,4.92015522619736,
130.795211542347));
#103222=CARTESIAN_POINT('Ctrl Pts',(-117.868381374301,4.91798215514722,
130.657893766536));
#103223=CARTESIAN_POINT('Ctrl Pts',(-117.876127707566,4.9100771495345,130.520943172586));
#103224=CARTESIAN_POINT('Ctrl Pts',(-117.883875775569,4.90217037365058,
130.383961909499));
#103225=CARTESIAN_POINT('Ctrl Pts',(-117.891623843572,4.8885291314603,130.247348382138));
#103226=CARTESIAN_POINT('Ctrl Pts',(-117.899371911575,4.86921818035638,
130.11161436201));
#103227=CARTESIAN_POINT('Ctrl Pts',(-117.907128214316,4.84988670534375,
129.97573608215));
#103228=CARTESIAN_POINT('Ctrl Pts',(-117.914884517058,4.82487353932085,
129.840739564473));
#103229=CARTESIAN_POINT('Ctrl Pts',(-117.9226408198,4.79429487429698,129.707127861589));
#103230=CARTESIAN_POINT('Ctrl Pts',(-117.930401262314,4.76369988851896,
129.573444846116));
#103231=CARTESIAN_POINT('Ctrl Pts',(-117.938161704828,4.72753358786435,
129.441148495131));
#103232=CARTESIAN_POINT('Ctrl Pts',(-117.945922147342,4.68596207656938,
129.310726633133));
#103233=CARTESIAN_POINT('Ctrl Pts',(-117.953695047608,4.64432383099382,
129.180095406383));
#103234=CARTESIAN_POINT('Ctrl Pts',(-117.961467947873,4.59726316981607,
129.051345049167));
#103235=CARTESIAN_POINT('Ctrl Pts',(-117.969240848139,4.5449947081957,128.924944174897));
#103236=CARTESIAN_POINT('Ctrl Pts',(-117.976731183901,4.49462633680913,
128.803138290786));
#103237=CARTESIAN_POINT('Ctrl Pts',(-117.984221519663,4.43942235374094,
128.683514315722));
#103238=CARTESIAN_POINT('Ctrl Pts',(-117.991711855426,4.37961420447853,
128.566468197804));
#103239=CARTESIAN_POINT('Ctrl Pts',(-117.999486189545,4.31753841106076,
128.444984240753));
#103240=CARTESIAN_POINT('Ctrl Pts',(-118.007260523664,4.25030578805859,
128.325892653909));
#103241=CARTESIAN_POINT('Ctrl Pts',(-118.015034857783,4.17812436259317,
128.209662200947));
#103242=CARTESIAN_POINT('Ctrl Pts',(-118.02279961073,4.10603189428359,128.09357499163));
#103243=CARTESIAN_POINT('Ctrl Pts',(-118.030564363677,4.02900296289648,
127.980342229266));
#103244=CARTESIAN_POINT('Ctrl Pts',(-118.038329116625,3.94729245245299,
127.870410148095));
#103245=CARTESIAN_POINT('Ctrl Pts',(-118.04608615751,3.86566309804061,127.760587253018));
#103246=CARTESIAN_POINT('Ctrl Pts',(-118.053843198395,3.7793616496228,127.654058826954));
#103247=CARTESIAN_POINT('Ctrl Pts',(-118.06160023928,3.68868725303599,127.551243741124));
#103248=CARTESIAN_POINT('Ctrl Pts',(-118.06935143052,3.59808123471687,127.44850618895));
#103249=CARTESIAN_POINT('Ctrl Pts',(-118.07710262176,3.50310908960216,127.349476695302));
#103250=CARTESIAN_POINT('Ctrl Pts',(-118.084853813,3.40411112567754,127.254542241009));
#103251=CARTESIAN_POINT('Ctrl Pts',(-118.092601709777,3.30515523852858,
127.159648136393));
#103252=CARTESIAN_POINT('Ctrl Pts',(-118.100349606554,3.20217721737219,
127.068845879444));
#103253=CARTESIAN_POINT('Ctrl Pts',(-118.108097503331,3.09555506806689,
126.982486485276));
#103254=CARTESIAN_POINT('Ctrl Pts',(-118.115843779416,2.98895522181642,
126.896145155632));
#103255=CARTESIAN_POINT('Ctrl Pts',(-118.1235900555,2.8787130672387,126.814245086156));
#103256=CARTESIAN_POINT('Ctrl Pts',(-118.131336331584,2.76524030499126,
126.737097518361));
#103257=CARTESIAN_POINT('Ctrl Pts',(-118.139082664849,2.65176670511382,
126.659949381081));
#103258=CARTESIAN_POINT('Ctrl Pts',(-118.146828998115,2.5350627732984,126.587554035301));
#103259=CARTESIAN_POINT('Ctrl Pts',(-118.15457533138,2.41556951133955,126.52017959917));
#103260=CARTESIAN_POINT('Ctrl Pts',(-118.162323399383,2.29604948969368,
126.452790075001));
#103261=CARTESIAN_POINT('Ctrl Pts',(-118.170071467386,2.17373923541706,
126.390423889886));
#103262=CARTESIAN_POINT('Ctrl Pts',(-118.177819535389,2.04910431932686,
126.333303186598));
#103263=CARTESIAN_POINT('Ctrl Pts',(-118.185575838131,1.92433693976416,
126.276121774746));
#103264=CARTESIAN_POINT('Ctrl Pts',(-118.193332140873,1.7972403189253,126.224197144454));
#103265=CARTESIAN_POINT('Ctrl Pts',(-118.201088443615,1.66830049383609,
126.177703452315));
#103266=CARTESIAN_POINT('Ctrl Pts',(-118.208848886129,1.53929184967992,
126.131184945093));
#103267=CARTESIAN_POINT('Ctrl Pts',(-118.216609328643,1.40843841385262,
126.090103268892));
#103268=CARTESIAN_POINT('Ctrl Pts',(-118.224369771157,1.27624039031671,
126.054582356571));
#103269=CARTESIAN_POINT('Ctrl Pts',(-118.232142671423,1.14383015077744,
126.019004422927));
#103270=CARTESIAN_POINT('Ctrl Pts',(-118.239915571688,1.01007139196343,
125.989005177026));
#103271=CARTESIAN_POINT('Ctrl Pts',(-118.247688471954,0.875474376345938,
125.964657354053));
#103272=CARTESIAN_POINT('Ctrl Pts',(-118.255178807715,0.745770301289418,
125.941194635775));
#103273=CARTESIAN_POINT('Ctrl Pts',(-118.262669143476,0.615288161879356,
125.922979629691));
#103274=CARTESIAN_POINT('Ctrl Pts',(-118.270159479238,0.484486182403032,
125.910031633777));
#103275=CARTESIAN_POINT('Ctrl Pts',(-118.277933813357,0.348724806104517,
125.89659271066));
#103276=CARTESIAN_POINT('Ctrl Pts',(-118.285708147476,0.212188806263716,
125.888785508856));
#103277=CARTESIAN_POINT('Ctrl Pts',(-118.293482481595,0.0753850107763749,
125.886688387471));
#103278=CARTESIAN_POINT('Ctrl Pts',(-118.301247234542,-0.0612501862595348,
125.884593850601));
#103279=CARTESIAN_POINT('Ctrl Pts',(-118.309011987489,-0.198152135105806,
125.888195398227));
#103280=CARTESIAN_POINT('Ctrl Pts',(-118.316776740436,-0.334807635217108,
125.897519789711));
#103281=CARTESIAN_POINT('Ctrl Pts',(-118.324533781321,-0.471327407158824,
125.906834920079));
#103282=CARTESIAN_POINT('Ctrl Pts',(-118.332290822206,-0.607600829947365,
125.921861556428));
#103283=CARTESIAN_POINT('Ctrl Pts',(-118.340047863091,-0.74311379973069,
125.942574429019));
#103284=CARTESIAN_POINT('Ctrl Pts',(-118.347799054331,-0.878524578128811,
125.963271681871));
#103285=CARTESIAN_POINT('Ctrl Pts',(-118.355550245572,-1.01317566005314,
125.98964657706));
#103286=CARTESIAN_POINT('Ctrl Pts',(-118.363301436812,-1.14655752279258,
126.021621976429));
#103287=CARTESIAN_POINT('Ctrl Pts',(-118.371049333589,-1.27988269468283,
126.0535837854));
#103288=CARTESIAN_POINT('Ctrl Pts',(-118.378797230366,-1.41193934092004,
126.091141273238));
#103289=CARTESIAN_POINT('Ctrl Pts',(-118.386545127143,-1.54222782114858,
126.134166145151));
#103290=CARTESIAN_POINT('Ctrl Pts',(-118.394291403227,-1.67248904783576,
126.177182017188));
#103291=CARTESIAN_POINT('Ctrl Pts',(-118.402037679311,-1.80098247317908,
126.225662875982));
#103292=CARTESIAN_POINT('Ctrl Pts',(-118.409783955395,-1.92722370661806,
126.279430579748));
#103293=CARTESIAN_POINT('Ctrl Pts',(-118.417530288661,-2.05346587194097,
126.333198680415));
#103294=CARTESIAN_POINT('Ctrl Pts',(-118.425276621926,-2.17745545248608,
126.392253550729));
#103295=CARTESIAN_POINT('Ctrl Pts',(-118.433022955191,-2.29872850061997,
126.456369087798));
#103296=CARTESIAN_POINT('Ctrl Pts',(-118.440771023194,-2.42002870701197,
126.520498983097));
#103297=CARTESIAN_POINT('Ctrl Pts',(-118.448519091197,-2.53861082488183,
126.589691617592));
#103298=CARTESIAN_POINT('Ctrl Pts',(-118.4562671592,-2.65403630682452,126.663675366963));
#103299=CARTESIAN_POINT('Ctrl Pts',(-118.464023461942,-2.76958446434316,
126.737737747145));
#103300=CARTESIAN_POINT('Ctrl Pts',(-118.471779764684,-2.88196895446078,
126.816601202816));
#103301=CARTESIAN_POINT('Ctrl Pts',(-118.479536067426,-2.99078053941757,
126.899950953156));
#103302=CARTESIAN_POINT('Ctrl Pts',(-118.48729650994,-3.09965020039379,
126.983345189767));
#103303=CARTESIAN_POINT('Ctrl Pts',(-118.495056952454,-3.20494285641292,
127.071230241827));
#103304=CARTESIAN_POINT('Ctrl Pts',(-118.502817394969,-3.30628386679137,
127.163252262313));
#103305=CARTESIAN_POINT('Ctrl Pts',(-118.510590295234,-3.40778755875631,
127.255422004715));
#103306=CARTESIAN_POINT('Ctrl Pts',(-118.5183631955,-3.50532665033385,127.351741711568));
#103307=CARTESIAN_POINT('Ctrl Pts',(-118.526136095765,-3.59856413802438,
127.451821399745));
#103308=CARTESIAN_POINT('Ctrl Pts',(-118.533626431528,-3.68841220819517,
127.548262939182));
#103309=CARTESIAN_POINT('Ctrl Pts',(-118.54111676729,-3.77426579226086,
127.64819560282));
#103310=CARTESIAN_POINT('Ctrl Pts',(-118.548607103053,-3.85586097286858,
127.751244304615));
#103311=CARTESIAN_POINT('Ctrl Pts',(-118.55637431177,-3.94047223972398,
127.858102101139));
#103312=CARTESIAN_POINT('Ctrl Pts',(-118.564141520487,-4.02077788700481,
127.968656369638));
#103313=CARTESIAN_POINT('Ctrl Pts',(-118.571908729203,-4.09643675520393,
128.082525028645));
#103314=CARTESIAN_POINT('Ctrl Pts',(-118.579686775332,-4.17220118852415,
128.196552566037));
#103315=CARTESIAN_POINT('Ctrl Pts',(-118.587464821461,-4.24330557771578,
128.313903478333));
#103316=CARTESIAN_POINT('Ctrl Pts',(-118.59524286759,-4.30944618965557,
128.434158811609));
#103317=CARTESIAN_POINT('Ctrl Pts',(-118.602990553207,-4.37532863099839,
128.553944745067));
#103318=CARTESIAN_POINT('Ctrl Pts',(-118.610738238824,-4.43628575567785,
128.6766121405));
#103319=CARTESIAN_POINT('Ctrl Pts',(-118.618485924442,-4.49205961804044,
128.801716502784));
#103320=CARTESIAN_POINT('Ctrl Pts',(-118.626279150826,-4.54816131823912,
128.92755622643));
#103321=CARTESIAN_POINT('Ctrl Pts',(-118.634072377211,-4.59901839116217,
129.055861332303));
#103322=CARTESIAN_POINT('Ctrl Pts',(-118.641865603595,-4.64441475660832,
129.186153390077));
#103323=CARTESIAN_POINT('Ctrl Pts',(-118.64965882998,-4.68981112205447,
129.316445447851));
#103324=CARTESIAN_POINT('Ctrl Pts',(-118.657452056364,-4.72974661527674,
129.448724087383));
#103325=CARTESIAN_POINT('Ctrl Pts',(-118.665245282749,-4.764054528234,129.582490119308));
#103326=CARTESIAN_POINT('Ctrl Pts',(-116.915395520338,-4.76405452823392,
129.582490119308));
#103327=CARTESIAN_POINT('Ctrl Pts',(-116.924092892827,-4.80208294653435,
129.730762345099));
#103328=CARTESIAN_POINT('Ctrl Pts',(-116.932790265316,-4.83322964626429,
129.880984325762));
#103329=CARTESIAN_POINT('Ctrl Pts',(-116.941487637805,-4.85731183919284,
130.032541494107));
#103330=CARTESIAN_POINT('Ctrl Pts',(-116.950137985105,-4.88126382387196,
130.183279219071));
#103331=CARTESIAN_POINT('Ctrl Pts',(-116.958788332406,-4.89822739411557,
130.335337530523));
#103332=CARTESIAN_POINT('Ctrl Pts',(-116.967438679707,-4.90807070138259,
130.488093242186));
#103333=CARTESIAN_POINT('Ctrl Pts',(-116.97333930779,-4.91478507865219,
130.592291907367));
#103334=CARTESIAN_POINT('Ctrl Pts',(-116.979239935873,-4.91818741855684,
130.696814686071));
#103335=CARTESIAN_POINT('Ctrl Pts',(-116.985140563957,-4.91824914438459,
130.801459538414));
#103336=CARTESIAN_POINT('',(-116.639859436028,-4.91824951514326,130.802176746446));
#103337=CARTESIAN_POINT('Ctrl Pts',(-116.569768711529,-4.764054528234,129.582490119308));
#103338=CARTESIAN_POINT('Ctrl Pts',(-116.57753385721,-4.79809338630334,
129.715207110309));
#103339=CARTESIAN_POINT('Ctrl Pts',(-116.585299002891,-4.82654756773742,
129.849212355614));
#103340=CARTESIAN_POINT('Ctrl Pts',(-116.593064148572,-4.84934893978864,
129.983996111587));
#103341=CARTESIAN_POINT('Ctrl Pts',(-116.60083993049,-4.87218154381213,
130.118964486385));
#103342=CARTESIAN_POINT('Ctrl Pts',(-116.608615712409,-4.88934583784685,
130.254713114104));
#103343=CARTESIAN_POINT('Ctrl Pts',(-116.616391494328,-4.90082561797627,
130.39072874659));
#103344=CARTESIAN_POINT('Ctrl Pts',(-116.617281907059,-4.90214017932632,
130.406304035615));
#103345=CARTESIAN_POINT('Ctrl Pts',(-116.618172319789,-4.90338025709753,
130.421882828062));
#103346=CARTESIAN_POINT('Ctrl Pts',(-116.619062732521,-4.90454587046754,
130.437464355688));
#103347=CARTESIAN_POINT('Ctrl Pts',(-116.625994967011,-4.9136206567155,
130.558773047115));
#103348=CARTESIAN_POINT('Ctrl Pts',(-116.632927201502,-4.91819545210003,
130.680422555685));
#103349=CARTESIAN_POINT('Ctrl Pts',(-116.639859435993,-4.91824951514299,
130.802176745828));
#103350=CARTESIAN_POINT('Ctrl Pts',(-116.639859436028,-4.91824951514326,
130.802176746446));
#103351=CARTESIAN_POINT('Ctrl Pts',(-116.647550252922,-4.91830949419432,
130.937254286567));
#103352=CARTESIAN_POINT('Ctrl Pts',(-116.655241069817,-4.91280050443035,
131.072559157636));
#103353=CARTESIAN_POINT('Ctrl Pts',(-116.662931886711,-4.9016926349703,
131.207588065513));
#103354=CARTESIAN_POINT('Ctrl Pts',(-116.670613714433,-4.8905977485991,
131.342459149038));
#103355=CARTESIAN_POINT('Ctrl Pts',(-116.678295542154,-4.87391703091717,
131.477054516098));
#103356=CARTESIAN_POINT('Ctrl Pts',(-116.685977369876,-4.85167255973251,
131.610869412086));
#103357=CARTESIAN_POINT('Ctrl Pts',(-116.69365215102,-4.82944849350706,
131.744561559034));
#103358=CARTESIAN_POINT('Ctrl Pts',(-116.701326932164,-4.80167089195159,
131.877474267016));
#103359=CARTESIAN_POINT('Ctrl Pts',(-116.709001713309,-4.76841371866942,
132.009106927004));
#103360=CARTESIAN_POINT('Ctrl Pts',(-116.716856240102,-4.73437765253562,
132.14382246289));
#103361=CARTESIAN_POINT('Ctrl Pts',(-116.724710766894,-4.69460219268531,
132.277196824325));
#103362=CARTESIAN_POINT('Ctrl Pts',(-116.732565293687,-4.64922239386322,
132.408702911125));
#103363=CARTESIAN_POINT('Ctrl Pts',(-116.740232642522,-4.60492402213343,
132.537075131121));
#103364=CARTESIAN_POINT('Ctrl Pts',(-116.747899991357,-4.55528555475067,
132.663666720708));
#103365=CARTESIAN_POINT('Ctrl Pts',(-116.755567340191,-4.500483211658,132.788002199124));
#103366=CARTESIAN_POINT('Ctrl Pts',(-116.76323391152,-4.44568642578892,
132.912325069318));
#103367=CARTESIAN_POINT('Ctrl Pts',(-116.770900482848,-4.38572696672752,
133.034391917382));
#103368=CARTESIAN_POINT('Ctrl Pts',(-116.778567054177,-4.32082899001699,
133.153747750741));
#103369=CARTESIAN_POINT('Ctrl Pts',(-116.786234592332,-4.25592282905808,
133.273118636));
#103370=CARTESIAN_POINT('Ctrl Pts',(-116.793902130488,-4.1860771030835,
133.389777475395));
#103371=CARTESIAN_POINT('Ctrl Pts',(-116.801569668643,-4.11156140404656,
133.503294830039));
#103372=CARTESIAN_POINT('Ctrl Pts',(-116.809564725951,-4.03386276440252,
133.621661082328));
#103373=CARTESIAN_POINT('Ctrl Pts',(-116.817559783258,-3.95108662217911,
133.736611128411));
#103374=CARTESIAN_POINT('Ctrl Pts',(-116.825554840566,-3.8635872492604,
133.847693762303));
#103375=CARTESIAN_POINT('Ctrl Pts',(-116.833233736856,-3.77954800047656,
133.954383682399));
#103376=CARTESIAN_POINT('Ctrl Pts',(-116.840912633146,-3.69115225753485,
134.057505957197));
#103377=CARTESIAN_POINT('Ctrl Pts',(-116.848591529437,-3.59875294848772,
134.15669715769));
#103378=CARTESIAN_POINT('Ctrl Pts',(-116.856275636906,-3.50629093390068,
134.255955672948));
#103379=CARTESIAN_POINT('Ctrl Pts',(-116.863959744375,-3.40982022794286,
134.351277523349));
#103380=CARTESIAN_POINT('Ctrl Pts',(-116.871643851844,-3.30972829668614,
134.442338306422));
#103381=CARTESIAN_POINT('Ctrl Pts',(-116.879338453627,-3.20949966821425,
134.533523452721));
#103382=CARTESIAN_POINT('Ctrl Pts',(-116.88703305541,-3.10564025306591,
134.620435667313));
#103383=CARTESIAN_POINT('Ctrl Pts',(-116.894727657192,-2.99856814818128,
134.70279262585));
#103384=CARTESIAN_POINT('Ctrl Pts',(-116.895655223573,-2.98566085452607,
134.712720565994));
#103385=CARTESIAN_POINT('Ctrl Pts',(-116.896582789953,-2.97270690586817,
134.722582364275));
#103386=CARTESIAN_POINT('Ctrl Pts',(-116.897510356333,-2.9597070593381,
134.732377570865));
#103387=CARTESIAN_POINT('Ctrl Pts',(-116.905284690452,-2.85074973557279,
134.814475424349));
#103388=CARTESIAN_POINT('Ctrl Pts',(-116.913059024572,-2.7382013347078,
134.892166409122));
#103389=CARTESIAN_POINT('Ctrl Pts',(-116.920833358691,-2.62245395594538,
134.965119960696));
#103390=CARTESIAN_POINT('Ctrl Pts',(-116.928598111638,-2.50684922548233,
135.037983603538));
#103391=CARTESIAN_POINT('Ctrl Pts',(-116.936362864585,-2.38805368900595,
135.106121223517));
#103392=CARTESIAN_POINT('Ctrl Pts',(-116.944127617532,-2.26649172944012,
135.169243010355));
#103393=CARTESIAN_POINT('Ctrl Pts',(-116.951884658417,-2.14505050692625,
135.232302103744));
#103394=CARTESIAN_POINT('Ctrl Pts',(-116.959641699302,-2.02084867400246,
135.290355098988));
#103395=CARTESIAN_POINT('Ctrl Pts',(-116.967398740187,-1.8943384495246,
135.343156151753));
#103396=CARTESIAN_POINT('Ctrl Pts',(-116.975149931427,-1.76792362739129,
135.395917386832));
#103397=CARTESIAN_POINT('Ctrl Pts',(-116.982901122667,-1.63920423795447,
135.443434412651));
#103398=CARTESIAN_POINT('Ctrl Pts',(-116.990652313907,-1.50865556838574,
135.48550806648));
#103399=CARTESIAN_POINT('Ctrl Pts',(-116.998400210684,-1.3781623854839,
135.527563837885));
#103400=CARTESIAN_POINT('Ctrl Pts',(-117.006148107461,-1.24584184016237,
135.564180719154));
#103401=CARTESIAN_POINT('Ctrl Pts',(-117.013896004239,-1.11218739011541,
135.595208378847));
#103402=CARTESIAN_POINT('Ctrl Pts',(-117.021642280323,-0.978560897698143,
135.626229548222));
#103403=CARTESIAN_POINT('Ctrl Pts',(-117.029388556407,-0.843601436146065,
135.651663733157));
#103404=CARTESIAN_POINT('Ctrl Pts',(-117.037134832491,-0.707815368325756,
135.671411107017));
#103405=CARTESIAN_POINT('Ctrl Pts',(-117.044881165756,-0.572028298163726,
135.691158626647));
#103406=CARTESIAN_POINT('Ctrl Pts',(-117.052627499022,-0.435414996452943,
135.705219195169));
#103407=CARTESIAN_POINT('Ctrl Pts',(-117.060373832287,-0.298489315003407,
135.713544581457));
#103408=CARTESIAN_POINT('Ctrl Pts',(-117.06812190029,-0.161532969996699,
135.721871832159));
#103409=CARTESIAN_POINT('Ctrl Pts',(-117.075869968293,-0.0242644962181748,
135.724461321187));
#103410=CARTESIAN_POINT('Ctrl Pts',(-117.083618036296,0.112800268468153,
135.721316907989));
#103411=CARTESIAN_POINT('Ctrl Pts',(-117.091374339038,0.250010707217295,
135.718169152871));
#103412=CARTESIAN_POINT('Ctrl Pts',(-117.09913064178,0.387016612897677,
135.709275330968));
#103413=CARTESIAN_POINT('Ctrl Pts',(-117.106886944522,0.523304730641585,
135.694691406111));
#103414=CARTESIAN_POINT('Ctrl Pts',(-117.114647387036,0.659665589457489,
135.680099697374));
#103415=CARTESIAN_POINT('Ctrl Pts',(-117.12240782955,0.795307510492773,
135.65981189205));
#103416=CARTESIAN_POINT('Ctrl Pts',(-117.130168272064,0.929726465333926,
135.633935315421));
#103417=CARTESIAN_POINT('Ctrl Pts',(-117.137941172329,1.06436120141491,
135.608017199413));
#103418=CARTESIAN_POINT('Ctrl Pts',(-117.145714072595,1.19776866746943,
135.576492473962));
#103419=CARTESIAN_POINT('Ctrl Pts',(-117.15348697286,1.32945818214053,135.539518904724));
#103420=CARTESIAN_POINT('Ctrl Pts',(-117.160977308622,1.45636045124926,
135.503889417858));
#103421=CARTESIAN_POINT('Ctrl Pts',(-117.168467644385,1.58166721122214,
135.463200462837));
#103422=CARTESIAN_POINT('Ctrl Pts',(-117.175957980147,1.70495794959927,
135.417635100252));
#103423=CARTESIAN_POINT('Ctrl Pts',(-117.183732314266,1.8329232937934,135.370342113096));
#103424=CARTESIAN_POINT('Ctrl Pts',(-117.191506648385,1.95912207942153,
135.317645830889));
#103425=CARTESIAN_POINT('Ctrl Pts',(-117.199280982504,2.08306425402082,
135.259697459615));
#103426=CARTESIAN_POINT('Ctrl Pts',(-117.207045735451,2.20685368096696,
135.20182050453));
#103427=CARTESIAN_POINT('Ctrl Pts',(-117.214810488398,2.32839167962045,
135.13870450318));
#103428=CARTESIAN_POINT('Ctrl Pts',(-117.222575241345,2.44720503505027,
135.070549851405));
#103429=CARTESIAN_POINT('Ctrl Pts',(-117.23033228223,2.5659003833805,135.002462891791));
#103430=CARTESIAN_POINT('Ctrl Pts',(-117.238089323115,2.68187613691915,
134.929347434126));
#103431=CARTESIAN_POINT('Ctrl Pts',(-117.245846364,2.79468102452733,134.851451058073));
#103432=CARTESIAN_POINT('Ctrl Pts',(-117.25359755524,2.90740084509273,134.773613424284));
#103433=CARTESIAN_POINT('Ctrl Pts',(-117.26134874648,3.0169542388032,134.69100226955));
#103434=CARTESIAN_POINT('Ctrl Pts',(-117.269099937721,3.12291674008852,
134.603909814112));
#103435=CARTESIAN_POINT('Ctrl Pts',(-117.276847834498,3.22883420448401,
134.516854375291));
#103436=CARTESIAN_POINT('Ctrl Pts',(-117.284595731275,3.3311635105954,134.425321671742));
#103437=CARTESIAN_POINT('Ctrl Pts',(-117.292343628052,3.42951145438546,
134.329645605583));
#103438=CARTESIAN_POINT('Ctrl Pts',(-117.300089904136,3.52783882590582,
134.233989552794));
#103439=CARTESIAN_POINT('Ctrl Pts',(-117.30783618022,3.62218621156281,134.134192133762));
#103440=CARTESIAN_POINT('Ctrl Pts',(-117.315582456304,3.71219592288139,
134.030625407171));
#103441=CARTESIAN_POINT('Ctrl Pts',(-117.323328789569,3.80220629863084,
133.927057916074));
#103442=CARTESIAN_POINT('Ctrl Pts',(-117.331075122835,3.88787867968421,
133.819721356989));
#103443=CARTESIAN_POINT('Ctrl Pts',(-117.3388214561,3.96889473837512,133.709021977897));
#103444=CARTESIAN_POINT('Ctrl Pts',(-117.346569524103,4.04992894005076,
133.598297808446));
#103445=CARTESIAN_POINT('Ctrl Pts',(-117.354317592106,4.12630451355463,
133.484209635882));
#103446=CARTESIAN_POINT('Ctrl Pts',(-117.362065660109,4.19774588298238,
133.367193535336));
#103447=CARTESIAN_POINT('Ctrl Pts',(-117.369821962851,4.26926318114782,
133.250053068685));
#103448=CARTESIAN_POINT('Ctrl Pts',(-117.377578265593,4.33583559546947,
133.129978792044));
#103449=CARTESIAN_POINT('Ctrl Pts',(-117.385334568335,4.39723278311197,
133.007432771088));
#103450=CARTESIAN_POINT('Ctrl Pts',(-117.393095010849,4.45866274028231,
132.884821343631));
#103451=CARTESIAN_POINT('Ctrl Pts',(-117.400855453363,4.51491180664084,
132.75973589955));
#103452=CARTESIAN_POINT('Ctrl Pts',(-117.408615895877,4.56579783831658,
132.63265850416));
#103453=CARTESIAN_POINT('Ctrl Pts',(-117.416388796143,4.61676555676768,
132.505377112854));
#103454=CARTESIAN_POINT('Ctrl Pts',(-117.424161696408,4.66235290647963,
132.376097749226));
#103455=CARTESIAN_POINT('Ctrl Pts',(-117.431934596673,4.70242739490873,
132.245318513589));
#103456=CARTESIAN_POINT('Ctrl Pts',(-117.439424932435,4.74104507474156,
132.119293432582));
#103457=CARTESIAN_POINT('Ctrl Pts',(-117.446915268197,4.77454366906303,
131.991875932476));
#103458=CARTESIAN_POINT('Ctrl Pts',(-117.454405603959,4.80284989467795,
131.863518751034));
#103459=CARTESIAN_POINT('Ctrl Pts',(-117.462179938078,4.83222935944075,
131.730294868044));
#103460=CARTESIAN_POINT('Ctrl Pts',(-117.469954272197,4.85610801099285,
131.595636627849));
#103461=CARTESIAN_POINT('Ctrl Pts',(-117.477728606316,4.87434817788376,
131.460038055992));
#103462=CARTESIAN_POINT('Ctrl Pts',(-117.485493359264,4.8925658653992,131.324606597257));
#103463=CARTESIAN_POINT('Ctrl Pts',(-117.493258112211,4.90515884292857,
131.188237496431));
#103464=CARTESIAN_POINT('Ctrl Pts',(-117.501022865158,4.91203992493745,
131.051437201484));
#103465=CARTESIAN_POINT('Ctrl Pts',(-117.508779906043,4.91891417255864,
130.914772778519));
#103466=CARTESIAN_POINT('Ctrl Pts',(-117.516536946928,4.92008779494067,
130.777678401651));
#103467=CARTESIAN_POINT('Ctrl Pts',(-117.524293987813,4.91552516479242,
130.640667560925));
#103468=CARTESIAN_POINT('Ctrl Pts',(-117.532045179053,4.91096597535903,
130.503760041139));
#103469=CARTESIAN_POINT('Ctrl Pts',(-117.539796370293,4.90067915650337,
130.366936321274));
#103470=CARTESIAN_POINT('Ctrl Pts',(-117.547547561533,4.88468112737937,
130.230711468413));
#103471=CARTESIAN_POINT('Ctrl Pts',(-117.55529545831,4.86868989784457,130.094544514749));
#103472=CARTESIAN_POINT('Ctrl Pts',(-117.563043355088,4.84699233149375,
129.958976309323));
#103473=CARTESIAN_POINT('Ctrl Pts',(-117.570791251865,4.81965681324779,
129.824518148077));
#103474=CARTESIAN_POINT('Ctrl Pts',(-117.578537527949,4.79232701300297,
129.69008811258));
#103475=CARTESIAN_POINT('Ctrl Pts',(-117.586283804033,4.75936168447198,
129.556768042296));
#103476=CARTESIAN_POINT('Ctrl Pts',(-117.594030080117,4.72088051180578,
129.425059977476));
#103477=CARTESIAN_POINT('Ctrl Pts',(-117.601776413382,4.68239905508025,
129.293350940417));
#103478=CARTESIAN_POINT('Ctrl Pts',(-117.609522746648,4.63840178261667,
129.163254307842));
#103479=CARTESIAN_POINT('Ctrl Pts',(-117.617269079913,4.5890584184665,129.035257484789));
#103480=CARTESIAN_POINT('Ctrl Pts',(-117.625017147916,4.53970400421199,
128.907231997735));
#103481=CARTESIAN_POINT('Ctrl Pts',(-117.632765215919,4.48500125654532,
128.781307620648));
#103482=CARTESIAN_POINT('Ctrl Pts',(-117.640513283922,4.42516810231528,
128.657951912601));
#103483=CARTESIAN_POINT('Ctrl Pts',(-117.648269586664,4.36527135669697,
128.534465100639));
#103484=CARTESIAN_POINT('Ctrl Pts',(-117.656025889406,4.30023348314129,
128.41355276354));
#103485=CARTESIAN_POINT('Ctrl Pts',(-117.663782192148,4.23031872465806,
128.295658453038));
#103486=CARTESIAN_POINT('Ctrl Pts',(-117.671542634662,4.16036665056294,
128.177701218793));
#103487=CARTESIAN_POINT('Ctrl Pts',(-117.679303077176,4.0855327181803,128.062765548301));
#103488=CARTESIAN_POINT('Ctrl Pts',(-117.68706351969,4.00612404950091,127.951265252439));
#103489=CARTESIAN_POINT('Ctrl Pts',(-117.694836419956,3.9265879069772,127.839585966403));
#103490=CARTESIAN_POINT('Ctrl Pts',(-117.702609320221,3.84246259302732,
127.731353384125));
#103491=CARTESIAN_POINT('Ctrl Pts',(-117.710382220487,3.75409555809586,
127.626948210719));
#103492=CARTESIAN_POINT('Ctrl Pts',(-117.717872556249,3.66894088746801,
127.526338428348));
#103493=CARTESIAN_POINT('Ctrl Pts',(-117.725362892011,3.57984774445693,
127.429282841063));
#103494=CARTESIAN_POINT('Ctrl Pts',(-117.732853227773,3.48715741880841,
127.336087819912));
#103495=CARTESIAN_POINT('Ctrl Pts',(-117.740627561892,3.39095271128988,
127.239359281207));
#103496=CARTESIAN_POINT('Ctrl Pts',(-117.748401896011,3.29056791452693,
127.146483427342));
#103497=CARTESIAN_POINT('Ctrl Pts',(-117.75617623013,3.1863442514188,127.057843118081));
#103498=CARTESIAN_POINT('Ctrl Pts',(-117.763940983077,3.08224903466071,
126.969312050079));
#103499=CARTESIAN_POINT('Ctrl Pts',(-117.771705736024,2.974324659918,126.885006391435));
#103500=CARTESIAN_POINT('Ctrl Pts',(-117.779470488971,2.86295009029976,
126.805273241307));
#103501=CARTESIAN_POINT('Ctrl Pts',(-117.787227529856,2.75168613947388,
126.725619283268));
#103502=CARTESIAN_POINT('Ctrl Pts',(-117.794984570741,2.63697912906497,
126.650529022105));
#103503=CARTESIAN_POINT('Ctrl Pts',(-117.802741611626,2.51924181536975,
126.580309985981));
#103504=CARTESIAN_POINT('Ctrl Pts',(-117.810492802866,2.4015932882988,126.510143902578));
#103505=CARTESIAN_POINT('Ctrl Pts',(-117.818243994106,2.2809193408671,126.444841931928));
#103506=CARTESIAN_POINT('Ctrl Pts',(-117.825995185346,2.15766218855235,
126.384668666469));
#103507=CARTESIAN_POINT('Ctrl Pts',(-117.833743082123,2.03445742381516,
126.324520976253));
#103508=CARTESIAN_POINT('Ctrl Pts',(-117.8414909789,1.90867198849386,126.269497826861));
#103509=CARTESIAN_POINT('Ctrl Pts',(-117.849238875677,1.78077301406596,
126.219818052067));
#103510=CARTESIAN_POINT('Ctrl Pts',(-117.856985151762,1.65290079334634,
126.170148669211));
#103511=CARTESIAN_POINT('Ctrl Pts',(-117.864731427846,1.52291627710181,
126.125820579218));
#103512=CARTESIAN_POINT('Ctrl Pts',(-117.87247770393,1.39130653822156,126.087004453442));
#103513=CARTESIAN_POINT('Ctrl Pts',(-117.880224037195,1.2596958278283,126.048188041134));
#103514=CARTESIAN_POINT('Ctrl Pts',(-117.88797037046,1.12646024585573,126.014883784831));
#103515=CARTESIAN_POINT('Ctrl Pts',(-117.895716703726,0.992101599961341,
125.987212345211));
#103516=CARTESIAN_POINT('Ctrl Pts',(-117.903464771729,0.857712865380334,
125.959534708764));
#103517=CARTESIAN_POINT('Ctrl Pts',(-117.911212839732,0.722200949271972,
125.937492477949));
#103518=CARTESIAN_POINT('Ctrl Pts',(-117.918960907734,0.586077017110458,
125.921155031835));
#103519=CARTESIAN_POINT('Ctrl Pts',(-117.926717210476,0.44980841081339,
125.904800222089));
#103520=CARTESIAN_POINT('Ctrl Pts',(-117.934473513218,0.312926877901743,
125.894162355429));
#103521=CARTESIAN_POINT('Ctrl Pts',(-117.94222981596,0.175948420813479,
125.889258867275));
#103522=CARTESIAN_POINT('Ctrl Pts',(-117.949990258474,0.0388968541975787,
125.884352761981));
#103523=CARTESIAN_POINT('Ctrl Pts',(-117.957750700988,-0.0982513489073537,
125.885187131341));
#103524=CARTESIAN_POINT('Ctrl Pts',(-117.965511143502,-0.234982030754595,
125.891727259811));
#103525=CARTESIAN_POINT('Ctrl Pts',(-117.973284043768,-0.371932204829973,
125.898277887077));
#103526=CARTESIAN_POINT('Ctrl Pts',(-117.981056944033,-0.508463128671392,
125.910552541806));
#103527=CARTESIAN_POINT('Ctrl Pts',(-117.988829844299,-0.644066698830658,
125.928464684514));
#103528=CARTESIAN_POINT('Ctrl Pts',(-117.996320180061,-0.774740737653156,
125.945725675717));
#103529=CARTESIAN_POINT('Ctrl Pts',(-118.003810515823,-0.904553372015585,
125.968221344539));
#103530=CARTESIAN_POINT('Ctrl Pts',(-118.011300851585,-1.03306236783459,
125.995830155287));
#103531=CARTESIAN_POINT('Ctrl Pts',(-118.019075185704,-1.16644382128672,
126.024485762485));
#103532=CARTESIAN_POINT('Ctrl Pts',(-118.026849519823,-1.29884334221009,
126.058740667415));
#103533=CARTESIAN_POINT('Ctrl Pts',(-118.034623853942,-1.42975438053048,
126.09851473464));
#103534=CARTESIAN_POINT('Ctrl Pts',(-118.042388606889,-1.56050408269493,
126.138239783881));
#103535=CARTESIAN_POINT('Ctrl Pts',(-118.050153359837,-1.68976858171951,
126.183470349152));
#103536=CARTESIAN_POINT('Ctrl Pts',(-118.057918112784,-1.81705101443552,
126.234075213629));
#103537=CARTESIAN_POINT('Ctrl Pts',(-118.065675153668,-1.94420702844499,
126.284629816641));
#103538=CARTESIAN_POINT('Ctrl Pts',(-118.073432194553,-2.06938453282734,
126.340547952829));
#103539=CARTESIAN_POINT('Ctrl Pts',(-118.081189235438,-2.19210169057048,
126.401648585114));
#103540=CARTESIAN_POINT('Ctrl Pts',(-118.088940426678,-2.31472630635053,
126.462703140937));
#103541=CARTESIAN_POINT('Ctrl Pts',(-118.096691617918,-2.43489391991838,
126.528932240348));
#103542=CARTESIAN_POINT('Ctrl Pts',(-118.104442809159,-2.55214289389311,
126.60010685362));
#103543=CARTESIAN_POINT('Ctrl Pts',(-118.112190705936,-2.66934203392666,
126.671251215783));
#103544=CARTESIAN_POINT('Ctrl Pts',(-118.119938602713,-2.7836246681184,
126.747336708686));
#103545=CARTESIAN_POINT('Ctrl Pts',(-118.12768649949,-2.89455418944136,
126.828088606387));
#103546=CARTESIAN_POINT('Ctrl Pts',(-118.135432775574,-3.00546050670013,
126.908823612532));
#103547=CARTESIAN_POINT('Ctrl Pts',(-118.143179051658,-3.11301479032648,
126.994222851986));
#103548=CARTESIAN_POINT('Ctrl Pts',(-118.150925327742,-3.21681017488339,
127.083968788569));
#103549=CARTESIAN_POINT('Ctrl Pts',(-118.158671661007,-3.32060632563383,
127.173715387636));
#103550=CARTESIAN_POINT('Ctrl Pts',(-118.166417994273,-3.42064322620289,
127.267808492144));
#103551=CARTESIAN_POINT('Ctrl Pts',(-118.174164327538,-3.5165481220496,
127.365891137142));
#103552=CARTESIAN_POINT('Ctrl Pts',(-118.181912395541,-3.61247449513265,
127.463995747068));
#103553=CARTESIAN_POINT('Ctrl Pts',(-118.189660463544,-3.70426674890516,
127.56609139582));
#103554=CARTESIAN_POINT('Ctrl Pts',(-118.197408531547,-3.79159021536647,
127.671785526489));
#103555=CARTESIAN_POINT('Ctrl Pts',(-118.205164834289,-3.87900649024745,
127.777591990138));
#103556=CARTESIAN_POINT('Ctrl Pts',(-118.212921137031,-3.96194424080455,
127.887004273689));
#103557=CARTESIAN_POINT('Ctrl Pts',(-118.220677439772,-4.04010988620406,
127.999597673947));
#103558=CARTESIAN_POINT('Ctrl Pts',(-118.228437882287,-4.11831725096182,
128.112251168693));
#103559=CARTESIAN_POINT('Ctrl Pts',(-118.236198324801,-4.19174722619774,
128.228088833223));
#103560=CARTESIAN_POINT('Ctrl Pts',(-118.243958767315,-4.26015110426036,
128.346659327464));
#103561=CARTESIAN_POINT('Ctrl Pts',(-118.25173166758,-4.32866479030085,
128.465420161589));
#103562=CARTESIAN_POINT('Ctrl Pts',(-118.259504567846,-4.39213607493075,
128.58692224528));
#103563=CARTESIAN_POINT('Ctrl Pts',(-118.267277468111,-4.45036312394494,
128.710691320009));
#103564=CARTESIAN_POINT('Ctrl Pts',(-118.274767803873,-4.50647347306347,
128.82996107712));
#103565=CARTESIAN_POINT('Ctrl Pts',(-118.282258139635,-4.5577141294953,
128.951335581379));
#103566=CARTESIAN_POINT('Ctrl Pts',(-118.289748475398,-4.60394830633779,
129.074377075717));
#103567=CARTESIAN_POINT('Ctrl Pts',(-118.298680373519,-4.65908054211458,
129.221098681668));
#103568=CARTESIAN_POINT('Ctrl Pts',(-118.30761227164,-4.70723965118029,
129.37057606111));
#103569=CARTESIAN_POINT('Ctrl Pts',(-118.316544169762,-4.74817859164396,
129.522181564409));
#103570=CARTESIAN_POINT('Ctrl Pts',(-118.317726371907,-4.75359716030281,
129.542247663321));
#103571=CARTESIAN_POINT('Ctrl Pts',(-118.318908574052,-4.75888930957911,
129.562351010166));
#103572=CARTESIAN_POINT('Ctrl Pts',(-118.320090776197,-4.76405452823413,
129.582490119309));
#103573=CARTESIAN_POINT('Origin',(213.235140564004,0.,130.804360617566));
#103574=CARTESIAN_POINT('',(-120.415010068595,-4.76405452823409,129.582490119308));
#103575=CARTESIAN_POINT('',(-120.07000000496,-4.76405452823398,129.582490119308));
#103576=CARTESIAN_POINT('',(213.235140564004,-4.76405452823405,129.582490119308));
#103577=CARTESIAN_POINT('',(-118.735140564061,-4.91824846256215,130.808249448373));
#103578=CARTESIAN_POINT('Ctrl Pts',(-118.735140564061,-4.91824846256215,
130.808249448372));
#103579=CARTESIAN_POINT('Ctrl Pts',(-118.744195936264,-4.91812165730422,
130.968621497431));
#103580=CARTESIAN_POINT('Ctrl Pts',(-118.753251308467,-4.91014697441995,
131.128664503842));
#103581=CARTESIAN_POINT('Ctrl Pts',(-118.76230668067,-4.8944441109897,131.287682360195));
#103582=CARTESIAN_POINT('Ctrl Pts',(-118.771417983749,-4.87864425818275,
131.447682396827));
#103583=CARTESIAN_POINT('Ctrl Pts',(-118.780529286828,-4.85502057080147,
131.606644491328));
#103584=CARTESIAN_POINT('Ctrl Pts',(-118.789640589907,-4.82374402601055,
131.763879577268));
#103585=CARTESIAN_POINT('Ctrl Pts',(-118.798816522011,-4.79224562792691,
131.922229975714));
#103586=CARTESIAN_POINT('Ctrl Pts',(-118.807992454115,-4.75298549464554,
132.078828692096));
#103587=CARTESIAN_POINT('Ctrl Pts',(-118.817168386218,-4.70618648829651,
132.232993460488));
#103588=CARTESIAN_POINT('Ctrl Pts',(-118.820463833101,-4.68937907975926,
132.288360239541));
#103589=CARTESIAN_POINT('Ctrl Pts',(-118.823759279983,-4.67159973789066,
132.343413290778));
#103590=CARTESIAN_POINT('Ctrl Pts',(-118.827054726866,-4.65286026331153,
132.398121714028));
#103591=CARTESIAN_POINT('Ctrl Pts',(-118.834829060985,-4.60865171078849,
132.527185108655));
#103592=CARTESIAN_POINT('Ctrl Pts',(-118.842603395104,-4.55899902669587,
132.654612117623));
#103593=CARTESIAN_POINT('Ctrl Pts',(-118.850377729223,-4.50404161356523,
132.779909201067));
#103594=CARTESIAN_POINT('Ctrl Pts',(-118.85814248217,-4.44915193053458,
132.905051867054));
#103595=CARTESIAN_POINT('Ctrl Pts',(-118.865907235117,-4.38897068188437,
133.028069475768));
#103596=CARTESIAN_POINT('Ctrl Pts',(-118.873671988064,-4.32368684989084,
133.148484139606));
#103597=CARTESIAN_POINT('Ctrl Pts',(-118.881429028949,-4.25846785871959,
133.268779205902));
#103598=CARTESIAN_POINT('Ctrl Pts',(-118.889186069834,-4.18815655480457,
133.386476130671));
#103599=CARTESIAN_POINT('Ctrl Pts',(-118.896943110719,-4.11298961724899,
133.501117831499));
#103600=CARTESIAN_POINT('Ctrl Pts',(-118.904694301959,-4.03787936366583,
133.615673080129));
#103601=CARTESIAN_POINT('Ctrl Pts',(-118.912445493199,-3.95792097828162,
133.727177365098));
#103602=CARTESIAN_POINT('Ctrl Pts',(-118.920196684439,-3.87339641117935,
133.83519933059));
#103603=CARTESIAN_POINT('Ctrl Pts',(-118.927944581216,-3.78890776927276,
133.943175383865));
#103604=CARTESIAN_POINT('Ctrl Pts',(-118.935692477993,-3.69985704607525,
134.047671754166));
#103605=CARTESIAN_POINT('Ctrl Pts',(-118.94344037477,-3.60656861173551,
134.148287337957));
#103606=CARTESIAN_POINT('Ctrl Pts',(-118.951186650855,-3.51329969132516,
134.248881875137));
#103607=CARTESIAN_POINT('Ctrl Pts',(-118.958932926939,-3.41579508859549,
134.345596953963));
#103608=CARTESIAN_POINT('Ctrl Pts',(-118.966679203023,-3.31441817155045,
134.438066060581));
#103609=CARTESIAN_POINT('Ctrl Pts',(-118.974425536288,-3.21304050616417,
134.530535849785));
#103610=CARTESIAN_POINT('Ctrl Pts',(-118.982171869553,-3.10779075827736,
134.618759340768));
#103611=CARTESIAN_POINT('Ctrl Pts',(-118.989918202819,-2.99906741989393,
134.702408548702));
#103612=CARTESIAN_POINT('Ctrl Pts',(-118.997666270822,-2.89031973367286,
134.786076489296));
#103613=CARTESIAN_POINT('Ctrl Pts',(-119.005414338824,-2.77809721885831,
134.865167870087));
#103614=CARTESIAN_POINT('Ctrl Pts',(-119.013162406827,-2.66282921193867,
134.939396729929));
#103615=CARTESIAN_POINT('Ctrl Pts',(-119.020918709569,-2.54743869680942,
135.013704481087));
#103616=CARTESIAN_POINT('Ctrl Pts',(-119.028675012311,-2.42899655297738,
135.083139175756));
#103617=CARTESIAN_POINT('Ctrl Pts',(-119.036431315053,-2.30795918546113,
135.147459449132));
#103618=CARTESIAN_POINT('Ctrl Pts',(-119.044191757567,-2.18685721665748,
135.211814052174));
#103619=CARTESIAN_POINT('Ctrl Pts',(-119.051952200081,-2.06315761659144,
135.27104862595));
#103620=CARTESIAN_POINT('Ctrl Pts',(-119.059712642595,-1.93733794080425,
135.324969510804));
#103621=CARTESIAN_POINT('Ctrl Pts',(-119.067485542861,-1.81131628810374,
135.378976954249));
#103622=CARTESIAN_POINT('Ctrl Pts',(-119.075258443126,-1.68316812443365,
135.427653524195));
#103623=CARTESIAN_POINT('Ctrl Pts',(-119.083031343392,-1.55338822721128,
135.470854813219));
#103624=CARTESIAN_POINT('Ctrl Pts',(-119.090521679153,-1.42832615615053,
135.512485626568));
#103625=CARTESIAN_POINT('Ctrl Pts',(-119.098012014915,-1.30174922303526,
135.549032242796));
#103626=CARTESIAN_POINT('Ctrl Pts',(-119.105502350677,-1.17410827665724,
135.580410535352));
#103627=CARTESIAN_POINT('Ctrl Pts',(-119.113276684796,-1.04162778500035,
135.612978545408));
#103628=CARTESIAN_POINT('Ctrl Pts',(-119.121051018915,-0.90758134484875,
135.64008174697));
#103629=CARTESIAN_POINT('Ctrl Pts',(-119.128825353034,-0.772459535743308,
135.661570652981));
#103630=CARTESIAN_POINT('Ctrl Pts',(-119.136590105981,-0.637504252191772,
135.683033075837));
#103631=CARTESIAN_POINT('Ctrl Pts',(-119.144354858928,-0.501476619037,135.698894909309));
#103632=CARTESIAN_POINT('Ctrl Pts',(-119.152119611875,-0.36488084619152,
135.709056839615));
#103633=CARTESIAN_POINT('Ctrl Pts',(-119.15987665276,-0.228420742192922,
135.719208676949));
#103634=CARTESIAN_POINT('Ctrl Pts',(-119.167633693645,-0.0913940088197629,
135.723671848391));
#103635=CARTESIAN_POINT('Ctrl Pts',(-119.17539073453,0.0456868667119894,
135.722398414565));
#103636=CARTESIAN_POINT('Ctrl Pts',(-119.18314192577,0.182664368488983,
135.721125941045));
#103637=CARTESIAN_POINT('Ctrl Pts',(-119.19089311701,0.319695541790409,
135.714125476552));
#103638=CARTESIAN_POINT('Ctrl Pts',(-119.198644308251,0.456265073845951,
135.701401075321));
#103639=CARTESIAN_POINT('Ctrl Pts',(-119.206392205028,0.592776560207071,
135.6886820823));
#103640=CARTESIAN_POINT('Ctrl Pts',(-119.214140101805,0.728826407104518,
135.67024402744));
#103641=CARTESIAN_POINT('Ctrl Pts',(-119.221887998582,0.86390182478649,
135.646143006277));
#103642=CARTESIAN_POINT('Ctrl Pts',(-119.229634274666,0.998948987602972,
135.622047026527));
#103643=CARTESIAN_POINT('Ctrl Pts',(-119.23738055075,1.13302174198946,135.59229050528));
#103644=CARTESIAN_POINT('Ctrl Pts',(-119.245126826834,1.26561532018001,
135.556981044638));
#103645=CARTESIAN_POINT('Ctrl Pts',(-119.252873160099,1.39820987714642,
135.52167132335));
#103646=CARTESIAN_POINT('Ctrl Pts',(-119.260619493364,1.52932485833007,
135.480808681481));
#103647=CARTESIAN_POINT('Ctrl Pts',(-119.26836582663,1.658468926145,135.434551097828));
#103648=CARTESIAN_POINT('Ctrl Pts',(-119.276113894633,1.78764191487831,
135.388283155111));
#103649=CARTESIAN_POINT('Ctrl Pts',(-119.283861962636,1.91484274396684,
135.336617998323));
#103650=CARTESIAN_POINT('Ctrl Pts',(-119.291610030639,2.0395987593405,135.279762271429));
#103651=CARTESIAN_POINT('Ctrl Pts',(-119.29936633338,2.1644873668921,135.222846117591));
#103652=CARTESIAN_POINT('Ctrl Pts',(-119.307122636122,2.2869256138614,135.160728536035));
#103653=CARTESIAN_POINT('Ctrl Pts',(-119.314878938864,2.40646373514178,
135.093663049658));
#103654=CARTESIAN_POINT('Ctrl Pts',(-119.322639381378,2.5260656575167,135.026561768411));
#103655=CARTESIAN_POINT('Ctrl Pts',(-119.330399823892,2.64276403741153,
134.954507525532));
#103656=CARTESIAN_POINT('Ctrl Pts',(-119.338160266406,2.75613781303765,
134.87779742425));
#103657=CARTESIAN_POINT('Ctrl Pts',(-119.345933166672,2.86969358631325,
134.800964181102));
#103658=CARTESIAN_POINT('Ctrl Pts',(-119.353706066937,2.97991377585785,
134.71946037671));
#103659=CARTESIAN_POINT('Ctrl Pts',(-119.361478967203,3.0864094483368,134.633624225587));
#103660=CARTESIAN_POINT('Ctrl Pts',(-119.368969302965,3.18903373488107,
134.550908434761));
#103661=CARTESIAN_POINT('Ctrl Pts',(-119.376459638728,3.28819936233715,
134.464170014852));
#103662=CARTESIAN_POINT('Ctrl Pts',(-119.38394997449,3.38359185787179,134.373742805262));
#103663=CARTESIAN_POINT('Ctrl Pts',(-119.391724308609,3.4826011888631,134.279887020541));
#103664=CARTESIAN_POINT('Ctrl Pts',(-119.399498642728,3.57785925510838,
134.181759896525));
#103665=CARTESIAN_POINT('Ctrl Pts',(-119.407272976847,3.66897511868935,
134.07969337027));
#103666=CARTESIAN_POINT('Ctrl Pts',(-119.415037729794,3.75997869011147,
133.977752631888));
#103667=CARTESIAN_POINT('Ctrl Pts',(-119.422802482742,3.84684995822226,
133.87188244005));
#103668=CARTESIAN_POINT('Ctrl Pts',(-119.430567235689,3.9292328297505,133.76245331931));
#103669=CARTESIAN_POINT('Ctrl Pts',(-119.438324276574,4.01153387744935,
133.653132885116));
#103670=CARTESIAN_POINT('Ctrl Pts',(-119.446081317459,4.08935516643966,
133.540260866713));
#103671=CARTESIAN_POINT('Ctrl Pts',(-119.453838358344,4.16237935210778,
133.424242521707));
#103672=CARTESIAN_POINT('Ctrl Pts',(-119.461589549584,4.23534846966934,
133.308311667038));
#103673=CARTESIAN_POINT('Ctrl Pts',(-119.469340740824,4.30352747696971,
133.18923953796));
#103674=CARTESIAN_POINT('Ctrl Pts',(-119.477091932064,4.36664124581274,
133.067461873115));
#103675=CARTESIAN_POINT('Ctrl Pts',(-119.484839828841,4.42972818962049,
132.945735967026));
#103676=CARTESIAN_POINT('Ctrl Pts',(-119.492587725618,4.4877539973247,132.821307158672));
#103677=CARTESIAN_POINT('Ctrl Pts',(-119.500335622395,4.54048868830118,
132.694637193602));
#103678=CARTESIAN_POINT('Ctrl Pts',(-119.508081898479,4.59321234831713,
132.567993725157));
#103679=CARTESIAN_POINT('Ctrl Pts',(-119.515828174563,4.64064694289837,
132.439110393176));
#103680=CARTESIAN_POINT('Ctrl Pts',(-119.523574450647,4.68261016143461,
132.30847003464));
#103681=CARTESIAN_POINT('Ctrl Pts',(-119.531320783913,4.72457368973386,
132.177828711746));
#103682=CARTESIAN_POINT('Ctrl Pts',(-119.539067117178,4.76106564183005,
132.04543070865));
#103683=CARTESIAN_POINT('Ctrl Pts',(-119.546813450444,4.79195334979348,
131.911774792978));
#103684=CARTESIAN_POINT('Ctrl Pts',(-119.554561518446,4.8228479748449,131.77808894599));
#103685=CARTESIAN_POINT('Ctrl Pts',(-119.56230958645,4.84813577038141,131.643145006728));
#103686=CARTESIAN_POINT('Ctrl Pts',(-119.570057654452,4.8677351107512,131.507452328554));
#103687=CARTESIAN_POINT('Ctrl Pts',(-119.577813957194,4.8873552815332,131.371615434587));
#103688=CARTESIAN_POINT('Ctrl Pts',(-119.585570259936,4.90127486411613,
131.235028599643));
#103689=CARTESIAN_POINT('Ctrl Pts',(-119.593326562678,4.90946404546602,
131.098207259161));
#103690=CARTESIAN_POINT('Ctrl Pts',(-119.601087005192,4.91765759762857,
130.96131289301));
#103691=CARTESIAN_POINT('Ctrl Pts',(-119.608847447706,4.92011464726175,
130.824184162635));
#103692=CARTESIAN_POINT('Ctrl Pts',(-119.616607890221,4.91685756154329,
130.687335910796));
#103693=CARTESIAN_POINT('Ctrl Pts',(-119.624380790486,4.91359524726167,
130.550267977994));
#103694=CARTESIAN_POINT('Ctrl Pts',(-119.632153690751,4.90460049304488,
130.413481813817));
#103695=CARTESIAN_POINT('Ctrl Pts',(-119.639926591017,4.88994762037499,
130.277487452099));
#103696=CARTESIAN_POINT('Ctrl Pts',(-119.647416926779,4.87582741653501,
130.146436827979));
#103697=CARTESIAN_POINT('Ctrl Pts',(-119.654907262541,4.85645337120164,
130.016121742427));
#103698=CARTESIAN_POINT('Ctrl Pts',(-119.662397598303,4.83193637267114,
129.886987218694));
#103699=CARTESIAN_POINT('Ctrl Pts',(-119.670171932422,4.80648980468948,
129.752956520244));
#103700=CARTESIAN_POINT('Ctrl Pts',(-119.677946266541,4.77542198776316,
129.619773103844));
#103701=CARTESIAN_POINT('Ctrl Pts',(-119.68572060066,4.73880087844502,129.487945296724));
#103702=CARTESIAN_POINT('Ctrl Pts',(-119.693485353608,4.70222490137129,
129.356279955594));
#103703=CARTESIAN_POINT('Ctrl Pts',(-119.701250106555,4.66010935294053,
129.225967272698));
#103704=CARTESIAN_POINT('Ctrl Pts',(-119.709014859502,4.61257348884296,
129.097507116962));
#103705=CARTESIAN_POINT('Ctrl Pts',(-119.716771900387,4.56508483803575,
128.969174549664));
#103706=CARTESIAN_POINT('Ctrl Pts',(-119.724528941272,4.51218671984167,
128.842691212224));
#103707=CARTESIAN_POINT('Ctrl Pts',(-119.732285982157,4.45404855644619,
128.718543147287));
#103708=CARTESIAN_POINT('Ctrl Pts',(-119.740037173397,4.3959542354919,128.594488703372));
#103709=CARTESIAN_POINT('Ctrl Pts',(-119.747788364637,4.33262789981089,
128.472766379335));
#103710=CARTESIAN_POINT('Ctrl Pts',(-119.755539555877,4.26428743515272,
128.353843175698));
#103711=CARTESIAN_POINT('Ctrl Pts',(-119.763287452654,4.19597601701498,
128.234970517595));
#103712=CARTESIAN_POINT('Ctrl Pts',(-119.771035349432,4.12265490296274,
128.118894951939));
#103713=CARTESIAN_POINT('Ctrl Pts',(-119.778783246209,4.04458826245784,
128.00605955269));
#103714=CARTESIAN_POINT('Ctrl Pts',(-119.786529522293,3.96653795181122,
127.893247756173));
#103715=CARTESIAN_POINT('Ctrl Pts',(-119.794275798377,3.88374431147446,
127.783675099248));
#103716=CARTESIAN_POINT('Ctrl Pts',(-119.802022074461,3.7965150225374,127.677755950176));
#103717=CARTESIAN_POINT('Ctrl Pts',(-119.809768407726,3.70928508969366,
127.571836019232));
#103718=CARTESIAN_POINT('Ctrl Pts',(-119.817514740992,3.61761969145584,
127.469569951754));
#103719=CARTESIAN_POINT('Ctrl Pts',(-119.825261074257,3.5218667448967,127.371338961111));
#103720=CARTESIAN_POINT('Ctrl Pts',(-119.83300914226,3.42609235512896,127.273085972318));
#103721=CARTESIAN_POINT('Ctrl Pts',(-119.840757210263,3.32622886839154,
127.178870138385));
#103722=CARTESIAN_POINT('Ctrl Pts',(-119.848505278266,3.22266069743728,
127.089035451219));
#103723=CARTESIAN_POINT('Ctrl Pts',(-119.856261581008,3.11898245299859,
126.999105286678));
#103724=CARTESIAN_POINT('Ctrl Pts',(-119.86401788375,3.01159195480981,126.913565827022));
#103725=CARTESIAN_POINT('Ctrl Pts',(-119.871774186492,2.90090673863142,
126.832720760245));
#103726=CARTESIAN_POINT('Ctrl Pts',(-119.879534629006,2.79016244642049,
126.751832544022));
#103727=CARTESIAN_POINT('Ctrl Pts',(-119.88729507152,2.6761202572117,126.675643930255));
#103728=CARTESIAN_POINT('Ctrl Pts',(-119.895055514034,2.5592254128055,126.604414385892));
#103729=CARTESIAN_POINT('Ctrl Pts',(-119.9028284143,2.44214291841763,126.533070497541));
#103730=CARTESIAN_POINT('Ctrl Pts',(-119.910601314565,2.32219896014561,
126.466701776083));
#103731=CARTESIAN_POINT('Ctrl Pts',(-119.918374214831,2.19986281647702,
126.405521378496));
#103732=CARTESIAN_POINT('Ctrl Pts',(-119.925864550593,2.08197389978224,
126.346565042468));
#103733=CARTESIAN_POINT('Ctrl Pts',(-119.933354886354,1.96186398285667,
126.292426488647));
#103734=CARTESIAN_POINT('Ctrl Pts',(-119.940845222116,1.83996741419893,
126.243252969507));
#103735=CARTESIAN_POINT('Ctrl Pts',(-119.948619556235,1.71344910008603,
126.19221502144));
#103736=CARTESIAN_POINT('Ctrl Pts',(-119.956393890354,1.58460520599674,
126.146364365957));
#103737=CARTESIAN_POINT('Ctrl Pts',(-119.964168224473,1.45390013420282,
126.105918592568));
#103738=CARTESIAN_POINT('Ctrl Pts',(-119.97193297742,1.32335614472843,126.065522664981));
#103739=CARTESIAN_POINT('Ctrl Pts',(-119.979697730367,1.19095591130534,
126.03051848048));
#103740=CARTESIAN_POINT('Ctrl Pts',(-119.987462483314,1.05718444843186,
126.001075897242));
#103741=CARTESIAN_POINT('Ctrl Pts',(-119.995219524199,0.923545849260778,
125.971662556793));
#103742=CARTESIAN_POINT('Ctrl Pts',(-120.002976565084,0.788539110285869,
125.947799908369));
#103743=CARTESIAN_POINT('Ctrl Pts',(-120.010733605969,0.652664729780009,
125.929608130208));
#103744=CARTESIAN_POINT('Ctrl Pts',(-120.01848479721,0.516892813201622,
125.911430070609));
#103745=CARTESIAN_POINT('Ctrl Pts',(-120.02623598845,0.380254943366777,
125.898914420937));
#103746=CARTESIAN_POINT('Ctrl Pts',(-120.03398717969,0.243261793611174,
125.89213029293));
#103747=CARTESIAN_POINT('Ctrl Pts',(-120.041735076467,0.106326869598815,
125.885349048359));
#103748=CARTESIAN_POINT('Ctrl Pts',(-120.049482973244,-0.030962644330799,
125.884294499632));
#103749=CARTESIAN_POINT('Ctrl Pts',(-120.057230870021,-0.168091187459792,
125.888983885799));
#103750=CARTESIAN_POINT('Ctrl Pts',(-120.064977146105,-0.305191046253711,
125.893672291047));
#103751=CARTESIAN_POINT('Ctrl Pts',(-120.072723422189,-0.44212961073246,
125.90410222797));
#103752=CARTESIAN_POINT('Ctrl Pts',(-120.080469698273,-0.578391951996569,
125.920238811922));
#103753=CARTESIAN_POINT('Ctrl Pts',(-120.088216031538,-0.714655299118141,
125.936375514991));
#103754=CARTESIAN_POINT('Ctrl Pts',(-120.095962364804,-0.850242024812184,
125.958218903167));
#103755=CARTESIAN_POINT('Ctrl Pts',(-120.103708698069,-0.984643345796628,
125.985682319103));
#103756=CARTESIAN_POINT('Ctrl Pts',(-120.111456766072,-1.11907476502522,
126.013151885281));
#103757=CARTESIAN_POINT('Ctrl Pts',(-120.119204834075,-1.25231986832657,
126.046243905363));
#103758=CARTESIAN_POINT('Ctrl Pts',(-120.126952902078,-1.38388146108346,
126.084820898041));
#103759=CARTESIAN_POINT('Ctrl Pts',(-120.13470920482,-1.5155828790669,126.123438890807));
#103760=CARTESIAN_POINT('Ctrl Pts',(-120.142465507562,-1.6455968365088,
126.167553391028));
#103761=CARTESIAN_POINT('Ctrl Pts',(-120.150221810304,-1.77344214382034,
126.216977264823));
#103762=CARTESIAN_POINT('Ctrl Pts',(-120.157982252818,-1.90135568602173,
126.266427517628));
#103763=CARTESIAN_POINT('Ctrl Pts',(-120.165742695332,-2.02709791345964,
126.3211926345));
#103764=CARTESIAN_POINT('Ctrl Pts',(-120.173503137846,-2.15020986517425,
126.381038269126));
#103765=CARTESIAN_POINT('Ctrl Pts',(-120.181276038112,-2.27351944712311,
126.440979973278));
#103766=CARTESIAN_POINT('Ctrl Pts',(-120.189048938377,-2.39418997138583,
126.506018307266));
#103767=CARTESIAN_POINT('Ctrl Pts',(-120.196821838643,-2.51178844647387,
126.575873670364));
#103768=CARTESIAN_POINT('Ctrl Pts',(-120.204312174405,-2.62511192078391,
126.64318961506));
#103769=CARTESIAN_POINT('Ctrl Pts',(-120.211802510167,-2.73558256335194,
126.714978279117));
#103770=CARTESIAN_POINT('Ctrl Pts',(-120.219292845929,-2.842841710528,126.790953826399));
#103771=CARTESIAN_POINT('Ctrl Pts',(-120.22701389374,-2.95340457842834,
126.869269518991));
#103772=CARTESIAN_POINT('Ctrl Pts',(-120.23473494155,-3.06091610256276,
126.952290169606));
#103773=CARTESIAN_POINT('Ctrl Pts',(-120.24245598936,-3.1649453704542,127.03974857055));
#103774=CARTESIAN_POINT('Ctrl Pts',(-120.250164846145,-3.2688103829921,
127.127068880446));
#103775=CARTESIAN_POINT('Ctrl Pts',(-120.257873702929,-3.36920378652162,
127.218812735198));
#103776=CARTESIAN_POINT('Ctrl Pts',(-120.265582559714,-3.46572382234608,
127.314669879159));
#103777=CARTESIAN_POINT('Ctrl Pts',(-120.273284374497,-3.5621556876001,
127.410439458098));
#103778=CARTESIAN_POINT('Ctrl Pts',(-120.280986189279,-3.65472094208111,
127.510314576008));
#103779=CARTESIAN_POINT('Ctrl Pts',(-120.288688004062,-3.74305094511466,
127.613944863346));
#103780=CARTESIAN_POINT('Ctrl Pts',(-120.296384511242,-3.831320076708,127.717503735257));
#103781=CARTESIAN_POINT('Ctrl Pts',(-120.304081018422,-3.91535950621426,
127.824812327972));
#103782=CARTESIAN_POINT('Ctrl Pts',(-120.311777525602,-3.99483786329218,
127.935483919535));
#103783=CARTESIAN_POINT('Ctrl Pts',(-120.319470455286,-4.07427927717795,
128.046104068641));
#103784=CARTESIAN_POINT('Ctrl Pts',(-120.327163384969,-4.14916360644363,
128.160083784069));
#103785=CARTESIAN_POINT('Ctrl Pts',(-120.334856314653,-4.21920046350886,
128.277004190145));
#103786=CARTESIAN_POINT('Ctrl Pts',(-120.342548792745,-4.28923320925824,
128.393917732739));
#103787=CARTESIAN_POINT('Ctrl Pts',(-120.350241270836,-4.35441883727088,
128.513771286775));
#103788=CARTESIAN_POINT('Ctrl Pts',(-120.357933748928,-4.41451103866694,
128.636118160647));
#103789=CARTESIAN_POINT('Ctrl Pts',(-120.365625921623,-4.47460085435652,
128.758460177254));
#103790=CARTESIAN_POINT('Ctrl Pts',(-120.373318094317,-4.5295974759841,
128.883294957802));
#103791=CARTESIAN_POINT('Ctrl Pts',(-120.381010267012,-4.57930155123303,
129.010153169868));
#103792=CARTESIAN_POINT('Ctrl Pts',(-120.388706168035,-4.62902971760968,
129.137072868992));
#103793=CARTESIAN_POINT('Ctrl Pts',(-120.396402069058,-4.67346007517859,
129.266017586356));
#103794=CARTESIAN_POINT('Ctrl Pts',(-120.404097970081,-4.71244223394075,
129.396500093838));
#103795=CARTESIAN_POINT('Ctrl Pts',(-120.407735336252,-4.73086663741748,
129.458170930981));
#103796=CARTESIAN_POINT('Ctrl Pts',(-120.411372702423,-4.748074716149,129.520185074516));
#103797=CARTESIAN_POINT('Ctrl Pts',(-120.415010068595,-4.76405452823409,
129.582490119308));
#103798=CARTESIAN_POINT('Ctrl Pts',(-118.665245282749,-4.764054528234,129.582490119308));
#103799=CARTESIAN_POINT('Ctrl Pts',(-118.672980934985,-4.79810898405142,
129.715267925692));
#103800=CARTESIAN_POINT('Ctrl Pts',(-118.680716587222,-4.82661864926354,
129.849510832222));
#103801=CARTESIAN_POINT('Ctrl Pts',(-118.688452239458,-4.84947065823497,
129.984715940027));
#103802=CARTESIAN_POINT('Ctrl Pts',(-118.696233626883,-4.87245777422998,
130.120720415613));
#103803=CARTESIAN_POINT('Ctrl Pts',(-118.704015014309,-4.88972001690422,
130.257698118956));
#103804=CARTESIAN_POINT('Ctrl Pts',(-118.711796401734,-4.9011949353849,
130.395128082377));
#103805=CARTESIAN_POINT('Ctrl Pts',(-118.719577789159,-4.91266985386559,
130.532558045797));
#103806=CARTESIAN_POINT('Ctrl Pts',(-118.727359176585,-4.91835742778128,
130.670439866815));
#103807=CARTESIAN_POINT('Ctrl Pts',(-118.73514056401,-4.91824846256287,
130.808249447467));
#103808=CARTESIAN_POINT('',(-118.389859435938,-4.91824882054746,130.800954493157));
#103809=CARTESIAN_POINT('Ctrl Pts',(-118.320090776197,-4.76405452823413,
129.582490119309));
#103810=CARTESIAN_POINT('Ctrl Pts',(-118.328971454939,-4.8028555469181,
129.73377470227));
#103811=CARTESIAN_POINT('Ctrl Pts',(-118.337852133682,-4.83449000944879,
129.887079065182));
#103812=CARTESIAN_POINT('Ctrl Pts',(-118.346732812425,-4.85876789631629,
130.041761383219));
#103813=CARTESIAN_POINT('Ctrl Pts',(-118.355552800387,-4.88287986749901,
130.195386598435));
#103814=CARTESIAN_POINT('Ctrl Pts',(-118.36437278835,-4.89973538446453,
130.350370840933));
#103815=CARTESIAN_POINT('Ctrl Pts',(-118.373192776313,-4.90919580011069,
130.506066033848));
#103816=CARTESIAN_POINT('Ctrl Pts',(-118.378748329521,-4.91515474730177,
130.604135660721));
#103817=CARTESIAN_POINT('Ctrl Pts',(-118.38430388273,-4.91818062704774,
130.702486980166));
#103818=CARTESIAN_POINT('Ctrl Pts',(-118.389859435938,-4.91824882054746,
130.800954493156));
#103819=CARTESIAN_POINT('Ctrl Pts',(-118.389859435993,-4.91824882054814,
130.800954494129));
#103820=CARTESIAN_POINT('Ctrl Pts',(-118.3976384828,-4.91834430703793,130.938831563033));
#103821=CARTESIAN_POINT('Ctrl Pts',(-118.405417529606,-4.91263765077987,
131.076749423057));
#103822=CARTESIAN_POINT('Ctrl Pts',(-118.413196576413,-4.90114527712532,
131.214187452964));
#103823=CARTESIAN_POINT('Ctrl Pts',(-118.420975537861,-4.8896530295752,
131.351623974779));
#103824=CARTESIAN_POINT('Ctrl Pts',(-118.428754499309,-4.87237522228776,
131.488580292133));
#103825=CARTESIAN_POINT('Ctrl Pts',(-118.436533460757,-4.84938025557986,
131.62453998776));
#103826=CARTESIAN_POINT('Ctrl Pts',(-118.444313967514,-4.82638072086928,
131.760526692091));
#103827=CARTESIAN_POINT('Ctrl Pts',(-118.452094474271,-4.79766182998921,
131.895515999847));
#103828=CARTESIAN_POINT('Ctrl Pts',(-118.459874981027,-4.7633432302008,
132.029001109221));
#103829=CARTESIAN_POINT('Ctrl Pts',(-118.467658664403,-4.72901061884117,
132.162540717791));
#103830=CARTESIAN_POINT('Ctrl Pts',(-118.475442347779,-4.68907384333215,
132.294574531751));
#103831=CARTESIAN_POINT('Ctrl Pts',(-118.483226031155,-4.6437024928228,
132.424610666371));
#103832=CARTESIAN_POINT('Ctrl Pts',(-118.491019424938,-4.59827454002439,
132.554809025451));
#103833=CARTESIAN_POINT('Ctrl Pts',(-118.498812818721,-4.54739859933736,
132.683004363148));
#103834=CARTESIAN_POINT('Ctrl Pts',(-118.506606212504,-4.49129276080419,
132.808723957694));
#103835=CARTESIAN_POINT('Ctrl Pts',(-118.514404928122,-4.43514860956972,
132.934529401723));
#103836=CARTESIAN_POINT('Ctrl Pts',(-118.522203643739,-4.37376761644027,
133.057855389245));
#103837=CARTESIAN_POINT('Ctrl Pts',(-118.530002359356,-4.30741353561459,
133.178254401143));
#103838=CARTESIAN_POINT('Ctrl Pts',(-118.537813725445,-4.24095182035202,
133.298848714967));
#103839=CARTESIAN_POINT('Ctrl Pts',(-118.545625091533,-4.1695011036118,
133.416506239816));
#103840=CARTESIAN_POINT('Ctrl Pts',(-118.553436457621,-4.09336851931609,
133.530808348144));
#103841=CARTESIAN_POINT('Ctrl Pts',(-118.558356338151,-4.04541746761306,
133.602799944868));
#103842=CARTESIAN_POINT('Ctrl Pts',(-118.563276218681,-3.99560997945149,
133.673461107767));
#103843=CARTESIAN_POINT('Ctrl Pts',(-118.568196099211,-3.94403066670205,
133.742694356714));
#103844=CARTESIAN_POINT('Ctrl Pts',(-118.57597043333,-3.86252567719863,
133.852095876973));
#103845=CARTESIAN_POINT('Ctrl Pts',(-118.583744767449,-3.77633618777062,
133.958276871339));
#103846=CARTESIAN_POINT('Ctrl Pts',(-118.591519101568,-3.68574563895189,
134.060809933531));
#103847=CARTESIAN_POINT('Ctrl Pts',(-118.599283854515,-3.59526673488852,
134.163216632887));
#103848=CARTESIAN_POINT('Ctrl Pts',(-118.607048607462,-3.50039781978248,
134.261984055095));
#103849=CARTESIAN_POINT('Ctrl Pts',(-118.614813360409,-3.40146476703581,
134.35671483711));
#103850=CARTESIAN_POINT('Ctrl Pts',(-118.622570401294,-3.30262997599211,
134.451351531177));
#103851=CARTESIAN_POINT('Ctrl Pts',(-118.630327442179,-3.19973936080105,
134.541959294994));
#103852=CARTESIAN_POINT('Ctrl Pts',(-118.638084483064,-3.09315786136248,
134.628175140682));
#103853=CARTESIAN_POINT('Ctrl Pts',(-118.645835674304,-2.98665673586157,
134.71432597033));
#103854=CARTESIAN_POINT('Ctrl Pts',(-118.653586865544,-2.87647056888741,
134.796091229255));
#103855=CARTESIAN_POINT('Ctrl Pts',(-118.661338056784,-2.76299955415722,
134.873146250433));
#103856=CARTESIAN_POINT('Ctrl Pts',(-118.669085953561,-2.64957676763507,
134.950168521172));
#103857=CARTESIAN_POINT('Ctrl Pts',(-118.676833850338,-2.53287223295046,
135.022484316764));
#103858=CARTESIAN_POINT('Ctrl Pts',(-118.684581747116,-2.41331730101888,
135.08981073011));
#103859=CARTESIAN_POINT('Ctrl Pts',(-118.6923280232,-2.29378737740143,135.157123060222));
#103860=CARTESIAN_POINT('Ctrl Pts',(-118.700074299284,-2.17140858294072,
135.219447892289));
#103861=CARTESIAN_POINT('Ctrl Pts',(-118.707820575368,-2.0466388426059,
135.276547164484));
#103862=CARTESIAN_POINT('Ctrl Pts',(-118.715566908633,-1.92186818124938,
135.333646858173));
#103863=CARTESIAN_POINT('Ctrl Pts',(-118.723313241899,-1.79470689430702,
135.385520752327));
#103864=CARTESIAN_POINT('Ctrl Pts',(-118.731059575164,-1.66563458912202,
135.431978198786));
#103865=CARTESIAN_POINT('Ctrl Pts',(-118.738807643167,-1.53653337908936,
135.478446049069));
#103866=CARTESIAN_POINT('Ctrl Pts',(-118.74655571117,-1.40552066701626,
135.519494905595));
#103867=CARTESIAN_POINT('Ctrl Pts',(-118.754303779173,-1.27309260043101,
135.554983554953));
#103868=CARTESIAN_POINT('Ctrl Pts',(-118.762060081915,-1.14052378772014,
135.59050992207));
#103869=CARTESIAN_POINT('Ctrl Pts',(-118.769816384657,-1.00653699382671,
135.620464175886));
#103870=CARTESIAN_POINT('Ctrl Pts',(-118.777572687398,-0.871640525306763,
135.644755834606));
#103871=CARTESIAN_POINT('Ctrl Pts',(-118.785333129913,-0.736672058479913,
135.669060458516));
#103872=CARTESIAN_POINT('Ctrl Pts',(-118.793093572427,-0.600793336735016,
135.687696412048));
#103873=CARTESIAN_POINT('Ctrl Pts',(-118.800854014941,-0.464518241034863,
135.700625098397));
#103874=CARTESIAN_POINT('Ctrl Pts',(-118.808626915206,-0.328024384453529,
135.71357453902));
#103875=CARTESIAN_POINT('Ctrl Pts',(-118.816399815472,-0.191133273044126,
135.720798383625));
#103876=CARTESIAN_POINT('Ctrl Pts',(-118.824172715737,-0.0543601487628199,
135.722310194039));
#103877=CARTESIAN_POINT('Ctrl Pts',(-118.831663051499,0.0774409279438527,
135.723767046336));
#103878=CARTESIAN_POINT('Ctrl Pts',(-118.839153387262,0.209132138962692,
135.719919956989));
#103879=CARTESIAN_POINT('Ctrl Pts',(-118.846643723024,0.34025847903006,
135.710826477016));
#103880=CARTESIAN_POINT('Ctrl Pts',(-118.854418057143,0.476356514132803,
135.701388214986));
#103881=CARTESIAN_POINT('Ctrl Pts',(-118.862192391262,0.612277116226453,
135.686267977587));
#103882=CARTESIAN_POINT('Ctrl Pts',(-118.869966725381,0.7475074897697,135.665473207832));
#103883=CARTESIAN_POINT('Ctrl Pts',(-118.877731478328,0.882571203962706,
135.644704065772));
#103884=CARTESIAN_POINT('Ctrl Pts',(-118.885496231275,1.01694599942176,
135.618274364898));
#103885=CARTESIAN_POINT('Ctrl Pts',(-118.893260984222,1.15012142083002,
135.586243487299));
#103886=CARTESIAN_POINT('Ctrl Pts',(-118.901018025107,1.28316457053266,
135.55424442322));
#103887=CARTESIAN_POINT('Ctrl Pts',(-118.908775065992,1.41501033913111,
135.516655344206));
#103888=CARTESIAN_POINT('Ctrl Pts',(-118.916532106877,1.5451560757129,135.473587080717));
#103889=CARTESIAN_POINT('Ctrl Pts',(-118.924283298117,1.67520366838288,
135.43055129534));
#103890=CARTESIAN_POINT('Ctrl Pts',(-118.932034489357,1.80355341112631,
135.382044672106));
#103891=CARTESIAN_POINT('Ctrl Pts',(-118.939785680598,1.92971583790101,
135.328228414867));
#103892=CARTESIAN_POINT('Ctrl Pts',(-118.947533577375,2.05582464227867,
135.274435030973));
#103893=CARTESIAN_POINT('Ctrl Pts',(-118.955281474152,2.17974762086387,
135.215336654626));
#103894=CARTESIAN_POINT('Ctrl Pts',(-118.963029370929,2.30101360019626,
135.151143275373));
#103895=CARTESIAN_POINT('Ctrl Pts',(-118.970775647013,2.42225421329996,
135.086963323991));
#103896=CARTESIAN_POINT('Ctrl Pts',(-118.978521923097,2.5408385873228,135.017690672364));
#103897=CARTESIAN_POINT('Ctrl Pts',(-118.986268199181,2.65631891447749,
134.943581907506));
#103898=CARTESIAN_POINT('Ctrl Pts',(-118.994014532446,2.77180009408156,
134.869472595594));
#103899=CARTESIAN_POINT('Ctrl Pts',(-119.001760865712,2.88417685205744,
134.790527310374));
#103900=CARTESIAN_POINT('Ctrl Pts',(-119.009507198977,2.99302955122568,
134.707046509101));
#103901=CARTESIAN_POINT('Ctrl Pts',(-119.01725526698,3.10190662720103,134.623547012882));
#103902=CARTESIAN_POINT('Ctrl Pts',(-119.025003334983,3.2072577637991,134.535510217368));
#103903=CARTESIAN_POINT('Ctrl Pts',(-119.032751402986,3.30869597431968,
134.443277216228));
#103904=CARTESIAN_POINT('Ctrl Pts',(-119.040507705728,3.41024199457768,
134.350946188757));
#103905=CARTESIAN_POINT('Ctrl Pts',(-119.04826400847,3.50786649156947,134.254410310212));
#103906=CARTESIAN_POINT('Ctrl Pts',(-119.056020311212,3.60121858829027,
134.154048325674));
#103907=CARTESIAN_POINT('Ctrl Pts',(-119.063780753726,3.69462050983586,
134.053632774924));
#103908=CARTESIAN_POINT('Ctrl Pts',(-119.07154119624,3.78374523346562,133.949387346127));
#103909=CARTESIAN_POINT('Ctrl Pts',(-119.079301638754,3.86828252137975,
133.841723519375));
#103910=CARTESIAN_POINT('Ctrl Pts',(-119.08707453902,3.95295551605331,133.733886861091));
#103911=CARTESIAN_POINT('Ctrl Pts',(-119.094847439285,4.03302613057707,
133.622621156565));
#103912=CARTESIAN_POINT('Ctrl Pts',(-119.10262033955,4.10822727403774,133.508367223947));
#103913=CARTESIAN_POINT('Ctrl Pts',(-119.110110675312,4.18069466651276,
133.398266709569));
#103914=CARTESIAN_POINT('Ctrl Pts',(-119.117601011074,4.24864031758024,
133.285391718292));
#103915=CARTESIAN_POINT('Ctrl Pts',(-119.125091346836,4.31186670508116,
133.17015616666));
#103916=CARTESIAN_POINT('Ctrl Pts',(-119.132865680955,4.37749034028207,
133.050551424062));
#103917=CARTESIAN_POINT('Ctrl Pts',(-119.140640015075,4.43823766180747,
132.928024714402));
#103918=CARTESIAN_POINT('Ctrl Pts',(-119.148414349194,4.49383775315963,
132.803011490224));
#103919=CARTESIAN_POINT('Ctrl Pts',(-119.156179102141,4.54936932236817,
132.678152333672));
#103920=CARTESIAN_POINT('Ctrl Pts',(-119.163943855088,4.59976612572708,
132.550813113657));
#103921=CARTESIAN_POINT('Ctrl Pts',(-119.171708608035,4.64480220950378,
132.421455388162));
#103922=CARTESIAN_POINT('Ctrl Pts',(-119.17946564892,4.68979356280718,132.292226142584));
#103923=CARTESIAN_POINT('Ctrl Pts',(-119.187222689805,4.72943466449426,
132.160982748025));
#103924=CARTESIAN_POINT('Ctrl Pts',(-119.19497973069,4.76354706427261,132.028208005503));
#103925=CARTESIAN_POINT('Ctrl Pts',(-119.20273092193,4.79763373962507,131.895533389447));
#103926=CARTESIAN_POINT('Ctrl Pts',(-119.21048211317,4.82619991478906,131.761330101125));
#103927=CARTESIAN_POINT('Ctrl Pts',(-119.21823330441,4.84911664677847,131.626097076801));
#103928=CARTESIAN_POINT('Ctrl Pts',(-119.225981201188,4.87202363854537,
131.49092153012));
#103929=CARTESIAN_POINT('Ctrl Pts',(-119.233729097965,4.88928589768466,
131.354717502583));
#103930=CARTESIAN_POINT('Ctrl Pts',(-119.241476994742,4.90082541358308,
131.217994910243));
#103931=CARTESIAN_POINT('Ctrl Pts',(-119.249223270826,4.91236251566357,
131.081300917321));
#103932=CARTESIAN_POINT('Ctrl Pts',(-119.25696954691,4.91817922268991,130.944088964689));
#103933=CARTESIAN_POINT('Ctrl Pts',(-119.264715822994,4.91824935753657,
130.806874497268));
#103934=CARTESIAN_POINT('Ctrl Pts',(-119.27246215626,4.91831949290093,130.669659016961));
#103935=CARTESIAN_POINT('Ctrl Pts',(-119.280208489525,4.91264297123998,
130.532441412794));
#103936=CARTESIAN_POINT('Ctrl Pts',(-119.28795482279,4.90124575160549,130.395737141895));
#103937=CARTESIAN_POINT('Ctrl Pts',(-119.295702890793,4.8898459796427,130.259002257023));
#103938=CARTESIAN_POINT('Ctrl Pts',(-119.303450958796,4.87272299292091,
130.12278132371));
#103939=CARTESIAN_POINT('Ctrl Pts',(-119.311199026799,4.84995458744018,
129.987584294288));
#103940=CARTESIAN_POINT('Ctrl Pts',(-119.318955329541,4.82716198342713,
129.852243575853));
#103941=CARTESIAN_POINT('Ctrl Pts',(-119.326711632283,4.79871204000369,
129.717929321291));
#103942=CARTESIAN_POINT('Ctrl Pts',(-119.334467935025,4.76473374854247,
129.585141454331));
#103943=CARTESIAN_POINT('Ctrl Pts',(-119.342228377539,4.73073732184402,
129.452282714488));
#103944=CARTESIAN_POINT('Ctrl Pts',(-119.349988820053,4.69120678032778,
129.320952359754));
#103945=CARTESIAN_POINT('Ctrl Pts',(-119.357749262568,4.64632062273903,
129.191633817017));
#103946=CARTESIAN_POINT('Ctrl Pts',(-119.365522162833,4.60136240990531,
129.062107680674));
#103947=CARTESIAN_POINT('Ctrl Pts',(-119.373295063098,4.55103154446283,
128.934600173846));
#103948=CARTESIAN_POINT('Ctrl Pts',(-119.381067963364,4.49555453004237,
128.809574280658));
#103949=CARTESIAN_POINT('Ctrl Pts',(-119.388558299126,4.44209424483472,
128.689093393609));
#103950=CARTESIAN_POINT('Ctrl Pts',(-119.396048634888,4.38385560195401,
128.570917103135));
#103951=CARTESIAN_POINT('Ctrl Pts',(-119.40353897065,4.32108007556043,128.455435322225));
#103952=CARTESIAN_POINT('Ctrl Pts',(-119.411313304769,4.25592439600279,
128.33557501449));
#103953=CARTESIAN_POINT('Ctrl Pts',(-119.419087638888,4.18567461614985,
128.218237892985));
#103954=CARTESIAN_POINT('Ctrl Pts',(-119.426861973007,4.11055065757387,
128.103887260168));
#103955=CARTESIAN_POINT('Ctrl Pts',(-119.434626725954,4.03551928256342,
127.989677554287));
#103956=CARTESIAN_POINT('Ctrl Pts',(-119.442391478901,3.95562589355626,
127.878447337458));
#103957=CARTESIAN_POINT('Ctrl Pts',(-119.450156231848,3.87113667884586,
127.770636194321));
#103958=CARTESIAN_POINT('Ctrl Pts',(-119.457913272733,3.7867313800146,127.662932130731));
#103959=CARTESIAN_POINT('Ctrl Pts',(-119.465670313618,3.69773957891601,
127.558640688631));
#103960=CARTESIAN_POINT('Ctrl Pts',(-119.473427354503,3.60447101297868,
127.458172969048));
#103961=CARTESIAN_POINT('Ctrl Pts',(-119.481178545743,3.51127278159232,
127.357781012953));
#103962=CARTESIAN_POINT('Ctrl Pts',(-119.488929736983,3.4138044697374,127.261207325317));
#103963=CARTESIAN_POINT('Ctrl Pts',(-119.496680928223,3.31241614978891,
127.168830076762));
#103964=CARTESIAN_POINT('Ctrl Pts',(-119.504428825,3.21107092258088,127.076492091002));
#103965=CARTESIAN_POINT('Ctrl Pts',(-119.512176721777,3.10580928943434,
126.988347259643));
#103966=CARTESIAN_POINT('Ctrl Pts',(-119.519924618554,2.99701809052568,
126.904736837307));
#103967=CARTESIAN_POINT('Ctrl Pts',(-119.527670894638,2.88824964839057,
126.821143904469));
#103968=CARTESIAN_POINT('Ctrl Pts',(-119.535417170723,2.77595341882597,
126.742083732124));
#103969=CARTESIAN_POINT('Ctrl Pts',(-119.543163446807,2.66054891086765,
126.667856954401));
#103970=CARTESIAN_POINT('Ctrl Pts',(-119.550909780072,2.5451435510193,126.593629628752));
#103971=CARTESIAN_POINT('Ctrl Pts',(-119.558656113337,2.42663019581498,
126.524235980414));
#103972=CARTESIAN_POINT('Ctrl Pts',(-119.566402446603,2.30545654543727,
126.45993278647));
#103973=CARTESIAN_POINT('Ctrl Pts',(-119.574150514605,2.18425575906088,
126.395615192272));
#103974=CARTESIAN_POINT('Ctrl Pts',(-119.581898582608,2.06039383731272,
126.336390504112));
#103975=CARTESIAN_POINT('Ctrl Pts',(-119.589646650611,1.93434186816958,
126.282468911704));
#103976=CARTESIAN_POINT('Ctrl Pts',(-119.597402953353,1.80815592949342,
126.228490010785));
#103977=CARTESIAN_POINT('Ctrl Pts',(-119.605159256095,1.67977565380446,
126.179825618532));
#103978=CARTESIAN_POINT('Ctrl Pts',(-119.612915558837,1.54969136408282,
126.136637431838));
#103979=CARTESIAN_POINT('Ctrl Pts',(-119.620676001351,1.41953764445899,
126.093426194307));
#103980=CARTESIAN_POINT('Ctrl Pts',(-119.628436443865,1.28767847427642,
126.055697093792));
#103981=CARTESIAN_POINT('Ctrl Pts',(-119.636196886379,1.1546170571987,126.023561258282));
#103982=CARTESIAN_POINT('Ctrl Pts',(-119.643969786645,1.02134203812164,
125.991373835477));
#103983=CARTESIAN_POINT('Ctrl Pts',(-119.65174268691,0.886861299255647,
125.964797696033));
#103984=CARTESIAN_POINT('Ctrl Pts',(-119.659515587175,0.751686793004185,
125.94389253026));
#103985=CARTESIAN_POINT('Ctrl Pts',(-119.667005922938,0.621426220534238,
125.923747319919));
#103986=CARTESIAN_POINT('Ctrl Pts',(-119.6744962587,0.490521751391431,125.90886796796));
#103987=CARTESIAN_POINT('Ctrl Pts',(-119.681986594462,0.359431953098699,
125.899262072828));
#103988=CARTESIAN_POINT('Ctrl Pts',(-119.689760928581,0.223371845264233,
125.889291967263));
#103989=CARTESIAN_POINT('Ctrl Pts',(-119.6975352627,0.0866810798254277,
125.884971516338));
#103990=CARTESIAN_POINT('Ctrl Pts',(-119.70530959682,-0.0501316807566252,
125.886366120102));
#103991=CARTESIAN_POINT('Ctrl Pts',(-119.713074349767,-0.186775831837826,
125.887759005142));
#103992=CARTESIAN_POINT('Ctrl Pts',(-119.720839102714,-0.323541291722485,
125.894852926867));
#103993=CARTESIAN_POINT('Ctrl Pts',(-119.728603855661,-0.45991434412875,
125.907661539762));
#103994=CARTESIAN_POINT('Ctrl Pts',(-119.736360896546,-0.596151948897583,
125.920457430963));
#103995=CARTESIAN_POINT('Ctrl Pts',(-119.744117937431,-0.731997535064224,
125.938956681691));
#103996=CARTESIAN_POINT('Ctrl Pts',(-119.751874978316,-0.866937811044434,
125.963120911222));
#103997=CARTESIAN_POINT('Ctrl Pts',(-119.759626169556,-1.00177632751303,
125.98726691832));
#103998=CARTESIAN_POINT('Ctrl Pts',(-119.767377360796,-1.13571050938475,
126.017069332419));
#103999=CARTESIAN_POINT('Ctrl Pts',(-119.775128552036,-1.26823296833418,
126.052438038175));
#104000=CARTESIAN_POINT('Ctrl Pts',(-119.782876448813,-1.40069910170322,
126.087791711287));
#104001=CARTESIAN_POINT('Ctrl Pts',(-119.79062434559,-1.53175432859126,
126.128706870011));
#104002=CARTESIAN_POINT('Ctrl Pts',(-119.798372242368,-1.66090244525615,
126.175042511209));
#104003=CARTESIAN_POINT('Ctrl Pts',(-119.806118518452,-1.79002354691951,
126.22136845999));
#104004=CARTESIAN_POINT('Ctrl Pts',(-119.813864794536,-1.91723796408203,
126.273112504014));
#104005=CARTESIAN_POINT('Ctrl Pts',(-119.82161107062,-2.04206600985632,
126.330084198536));
#104006=CARTESIAN_POINT('Ctrl Pts',(-119.829357403885,-2.16689497708273,
126.38705631361));
#104007=CARTESIAN_POINT('Ctrl Pts',(-119.837103737151,-2.28933718209762,
126.449255993856));
#104008=CARTESIAN_POINT('Ctrl Pts',(-119.844850070416,-2.40893459818407,
126.516445370716));
#104009=CARTESIAN_POINT('Ctrl Pts',(-119.852598138419,-2.52855879728214,
126.58364979417));
#104010=CARTESIAN_POINT('Ctrl Pts',(-119.860346206422,-2.64533659896179,
126.655845946296));
#104011=CARTESIAN_POINT('Ctrl Pts',(-119.868094274425,-2.75883653010626,
126.732751100108));
#104012=CARTESIAN_POINT('Ctrl Pts',(-119.875850577167,-2.87245709032837,
126.809737989634));
#104013=CARTESIAN_POINT('Ctrl Pts',(-119.883606879909,-2.98279249665029,
126.891443658783));
#104014=CARTESIAN_POINT('Ctrl Pts',(-119.891363182651,-3.08944167734946,
126.977542986066));
#104015=CARTESIAN_POINT('Ctrl Pts',(-119.899123625165,-3.19614777992781,
127.063688267153));
#104016=CARTESIAN_POINT('Ctrl Pts',(-119.906884067679,-3.29916344305824,
127.154231621061));
#104017=CARTESIAN_POINT('Ctrl Pts',(-119.914644510193,-3.39812317774284,
127.24880975569));
#104018=CARTESIAN_POINT('Ctrl Pts',(-119.922417410459,-3.49724177137852,
127.343539715537));
#104019=CARTESIAN_POINT('Ctrl Pts',(-119.930190310724,-3.5922911544,127.44231711731));
#104020=CARTESIAN_POINT('Ctrl Pts',(-119.93796321099,-3.68294438487962,
127.544743505023));
#104021=CARTESIAN_POINT('Ctrl Pts',(-119.945453546751,-3.77030214208787,
127.643446435544));
#104022=CARTESIAN_POINT('Ctrl Pts',(-119.952943882513,-3.85357762538255,
127.745537419654));
#104023=CARTESIAN_POINT('Ctrl Pts',(-119.960434218275,-3.9325165750294,
127.850634758652));
#104024=CARTESIAN_POINT('Ctrl Pts',(-119.96824087687,-4.01478917926819,
127.960170441817));
#104025=CARTESIAN_POINT('Ctrl Pts',(-119.976047535465,-4.09261365977126,
128.073321594936));
#104026=CARTESIAN_POINT('Ctrl Pts',(-119.983854194061,-4.16565686347,128.189693151458));
#104027=CARTESIAN_POINT('Ctrl Pts',(-119.991647965675,-4.23857948980098,
128.305872605562));
#104028=CARTESIAN_POINT('Ctrl Pts',(-119.99944173729,-4.30673635587862,
128.42526155029));
#104029=CARTESIAN_POINT('Ctrl Pts',(-120.007235508904,-4.36983533622441,
128.547433016427));
#104030=CARTESIAN_POINT('Ctrl Pts',(-120.015021864543,-4.43287427625572,
128.669488233248));
#104031=CARTESIAN_POINT('Ctrl Pts',(-120.022808220182,-4.49086472713496,
128.794320364123));
#104032=CARTESIAN_POINT('Ctrl Pts',(-120.030594575821,-4.54355834120615,
128.921474359037));
#104033=CARTESIAN_POINT('Ctrl Pts',(-120.038373959203,-4.59620477101535,
129.048514494473));
#104034=CARTESIAN_POINT('Ctrl Pts',(-120.046153342584,-4.64356366066462,
129.17787199853));
#104035=CARTESIAN_POINT('Ctrl Pts',(-120.053932725966,-4.68543328799281,
129.309068684107));
#104036=CARTESIAN_POINT('Ctrl Pts',(-120.059288485631,-4.71425866530427,
129.399391770436));
#104037=CARTESIAN_POINT('Ctrl Pts',(-120.064644245295,-4.74048325069915,
129.490586065944));
#104038=CARTESIAN_POINT('Ctrl Pts',(-120.07000000496,-4.76405452823399,
129.582490119308));
#104039=CARTESIAN_POINT('Origin',(213.235140564004,0.,130.804360617566));
#104040=CARTESIAN_POINT('',(-122.165194063467,-4.76405452823402,129.582490119308));
#104041=CARTESIAN_POINT('',(-121.81971904495,-4.76405452823411,129.582490119308));
#104042=CARTESIAN_POINT('',(213.235140564004,-4.76405452823405,129.582490119308));
#104043=CARTESIAN_POINT('',(-120.485140563958,-4.91824981073044,130.805725077145));
#104044=CARTESIAN_POINT('Ctrl Pts',(-120.48514056401,-4.91824981073019,
130.805725078055));
#104045=CARTESIAN_POINT('Ctrl Pts',(-120.489340532587,-4.91822935689092,
130.879451720875));
#104046=CARTESIAN_POINT('Ctrl Pts',(-120.493540501165,-4.91655120048444,
130.953153330112));
#104047=CARTESIAN_POINT('Ctrl Pts',(-120.497740469743,-4.91321818380445,
131.026779458569));
#104048=CARTESIAN_POINT('Ctrl Pts',(-120.505514803862,-4.90704861733907,
131.163064793063));
#104049=CARTESIAN_POINT('Ctrl Pts',(-120.513289137981,-4.89519445387011,
131.299309097387));
#104050=CARTESIAN_POINT('Ctrl Pts',(-120.5210634721,-4.87765082858863,131.434999545058));
#104051=CARTESIAN_POINT('Ctrl Pts',(-120.528828225047,-4.86012882425739,
131.57052276638));
#104052=CARTESIAN_POINT('Ctrl Pts',(-120.536592977994,-4.83693135906257,
131.705493105164));
#104053=CARTESIAN_POINT('Ctrl Pts',(-120.544357730941,-4.80810554847421,
131.839398828084));
#104054=CARTESIAN_POINT('Ctrl Pts',(-120.552114771826,-4.77930836808731,
131.973171553952));
#104055=CARTESIAN_POINT('Ctrl Pts',(-120.559871812711,-4.74489404870721,
132.105881388477));
#104056=CARTESIAN_POINT('Ctrl Pts',(-120.567628853596,-4.70496132664014,
132.237023165873));
#104057=CARTESIAN_POINT('Ctrl Pts',(-120.575380044836,-4.66505871814947,
132.368066048234));
#104058=CARTESIAN_POINT('Ctrl Pts',(-120.583131236076,-4.61964610355175,
132.497542854631));
#104059=CARTESIAN_POINT('Ctrl Pts',(-120.590882427316,-4.5688728944401,
132.624960391528));
#104060=CARTESIAN_POINT('Ctrl Pts',(-120.598630324094,-4.51812126529666,
132.752323772573));
#104061=CARTESIAN_POINT('Ctrl Pts',(-120.606378220871,-4.46201371761603,
132.877629262481));
#104062=CARTESIAN_POINT('Ctrl Pts',(-120.614126117648,-4.40074887360715,
133.000400784308));
#104063=CARTESIAN_POINT('Ctrl Pts',(-120.621872393732,-4.33949684488292,
133.123146624979));
#104064=CARTESIAN_POINT('Ctrl Pts',(-120.629618669816,-4.27308984007193,
133.243359202265));
#104065=CARTESIAN_POINT('Ctrl Pts',(-120.6373649459,-4.20177362614531,133.360584679954));
#104066=CARTESIAN_POINT('Ctrl Pts',(-120.645111279165,-4.1304568857785,
133.477811022975));
#104067=CARTESIAN_POINT('Ctrl Pts',(-120.65285761243,-4.05423106718569,
133.592049888389));
#104068=CARTESIAN_POINT('Ctrl Pts',(-120.660603945695,-3.97338647096173,
133.702874549718));
#104069=CARTESIAN_POINT('Ctrl Pts',(-120.668352013698,-3.89252377015109,
133.813724029461));
#104070=CARTESIAN_POINT('Ctrl Pts',(-120.676100081701,-3.80704046385279,
133.921157467882));
#104071=CARTESIAN_POINT('Ctrl Pts',(-120.683848149704,-3.71726826089569,
134.024779804417));
#104072=CARTESIAN_POINT('Ctrl Pts',(-120.691604452446,-3.62740064697311,
134.128512272004));
#104073=CARTESIAN_POINT('Ctrl Pts',(-120.699360755188,-3.53323528712383,
134.228425250459));
#104074=CARTESIAN_POINT('Ctrl Pts',(-120.70711705793,-3.43514239728022,
134.324158874982));
#104075=CARTESIAN_POINT('Ctrl Pts',(-120.714877500444,-3.33699715230778,
134.419943595423));
#104076=CARTESIAN_POINT('Ctrl Pts',(-120.722637942958,-3.23492049124312,
134.511544256189));
#104077=CARTESIAN_POINT('Ctrl Pts',(-120.730398385472,-3.12931633082908,
134.598640834433));
#104078=CARTESIAN_POINT('Ctrl Pts',(-120.738171285737,-3.02354264524165,
134.685877227836));
#104079=CARTESIAN_POINT('Ctrl Pts',(-120.745944186003,-2.91423045646014,
134.768594854116));
#104080=CARTESIAN_POINT('Ctrl Pts',(-120.753717086268,-2.80181404624344,
134.846516120855));
#104081=CARTESIAN_POINT('Ctrl Pts',(-120.76120742203,-2.69348425569646,
134.921604753278));
#104082=CARTESIAN_POINT('Ctrl Pts',(-120.768697757792,-2.58227227790492,
134.992239526238));
#104083=CARTESIAN_POINT('Ctrl Pts',(-120.776188093554,-2.46858717022877,
135.058213041603));
#104084=CARTESIAN_POINT('Ctrl Pts',(-120.783962427673,-2.35059165714305,
135.126687962853));
#104085=CARTESIAN_POINT('Ctrl Pts',(-120.791736761792,-2.22955800036758,
135.190358093839));
#104086=CARTESIAN_POINT('Ctrl Pts',(-120.799511095911,-2.1059150257965,
135.248942146419));
#104087=CARTESIAN_POINT('Ctrl Pts',(-120.807275848858,-1.98242443014161,
135.30745399939));
#104088=CARTESIAN_POINT('Ctrl Pts',(-120.815040601805,-1.85633126499734,
135.360892079882));
#104089=CARTESIAN_POINT('Ctrl Pts',(-120.822805354752,-1.72809153316525,
135.409019423113));
#104090=CARTESIAN_POINT('Ctrl Pts',(-120.830562395637,-1.59997917084234,
135.457098965588));
#104091=CARTESIAN_POINT('Ctrl Pts',(-120.838319436522,-1.46972484827676,
135.499878131209));
#104092=CARTESIAN_POINT('Ctrl Pts',(-120.846076477407,-1.33780694513731,
135.53716693518));
#104093=CARTESIAN_POINT('Ctrl Pts',(-120.853827668647,-1.20598852231497,
135.574427619373));
#104094=CARTESIAN_POINT('Ctrl Pts',(-120.861578859888,-1.07250939066434,
135.606206077065));
#104095=CARTESIAN_POINT('Ctrl Pts',(-120.869330051128,-0.937865248490862,
135.632361429307));
#104096=CARTESIAN_POINT('Ctrl Pts',(-120.877077947905,-0.803278333669372,
135.658505664827));
#104097=CARTESIAN_POINT('Ctrl Pts',(-120.884825844682,-0.667527776149154,
135.679031473968));
#104098=CARTESIAN_POINT('Ctrl Pts',(-120.892573741459,-0.531121473102041,
135.693848632002));
#104099=CARTESIAN_POINT('Ctrl Pts',(-120.900320017543,-0.394743703313317,
135.708662690605));
#104100=CARTESIAN_POINT('Ctrl Pts',(-120.908066293627,-0.257710849264619,
135.717770431093));
#104101=CARTESIAN_POINT('Ctrl Pts',(-120.915812569711,-0.120537579264298,
135.721133314619));
#104102=CARTESIAN_POINT('Ctrl Pts',(-120.923558902976,0.0166367033181279,
135.724496222969));
#104103=CARTESIAN_POINT('Ctrl Pts',(-120.931305236242,0.153951013072703,
135.722114180156));
#104104=CARTESIAN_POINT('Ctrl Pts',(-120.939051569507,0.290889418363816,
135.714000768207));
#104105=CARTESIAN_POINT('Ctrl Pts',(-120.94679963751,0.427858490061144,
135.705885539315));
#104106=CARTESIAN_POINT('Ctrl Pts',(-120.954547705513,0.564451099578084,
135.692036410388));
#104107=CARTESIAN_POINT('Ctrl Pts',(-120.962295773516,0.700155574548042,
135.672518917573));
#104108=CARTESIAN_POINT('Ctrl Pts',(-120.970052076257,0.836004277849088,
135.652980681335));
#104109=CARTESIAN_POINT('Ctrl Pts',(-120.977808378999,0.970962573421003,
135.627762102557));
#104110=CARTESIAN_POINT('Ctrl Pts',(-120.985564681741,1.10452758606241,
135.596980138676));
#104111=CARTESIAN_POINT('Ctrl Pts',(-120.993325124255,1.23816388637263,
135.566181745534));
#104112=CARTESIAN_POINT('Ctrl Pts',(-121.001085566769,1.37040504520718,
135.529814154234));
#104113=CARTESIAN_POINT('Ctrl Pts',(-121.008846009284,1.50076349141599,
135.488044211206));
#104114=CARTESIAN_POINT('Ctrl Pts',(-121.016618909549,1.63133120057534,
135.446207215357));
#104115=CARTESIAN_POINT('Ctrl Pts',(-121.024391809814,1.76000979038505,
135.398950672549));
#104116=CARTESIAN_POINT('Ctrl Pts',(-121.03216471008,1.88633097458358,135.346489910841));
#104117=CARTESIAN_POINT('Ctrl Pts',(-121.039655045842,2.00806006555982,
135.295936229959));
#104118=CARTESIAN_POINT('Ctrl Pts',(-121.047145381605,2.12759989103735,
135.240550263489));
#104119=CARTESIAN_POINT('Ctrl Pts',(-121.054635717367,2.24455485559791,
135.180564059216));
#104120=CARTESIAN_POINT('Ctrl Pts',(-121.062410051486,2.3659442031808,135.118303459779));
#104121=CARTESIAN_POINT('Ctrl Pts',(-121.070184385605,2.48493333551021,
135.05088967751));
#104122=CARTESIAN_POINT('Ctrl Pts',(-121.077958719724,2.60105380603633,
134.978531452667));
#104123=CARTESIAN_POINT('Ctrl Pts',(-121.085723472671,2.71703116846052,
134.906262402868));
#104124=CARTESIAN_POINT('Ctrl Pts',(-121.093488225619,2.83014657478166,
134.829061239692));
#104125=CARTESIAN_POINT('Ctrl Pts',(-121.101252978566,2.93995417916434,
134.747183525955));
#104126=CARTESIAN_POINT('Ctrl Pts',(-121.109010019451,3.04965272108634,
134.665387134317));
#104127=CARTESIAN_POINT('Ctrl Pts',(-121.116767060336,3.15604968767794,
134.578923667706));
#104128=CARTESIAN_POINT('Ctrl Pts',(-121.124524101221,3.25872666345328,
134.48809290906));
#104129=CARTESIAN_POINT('Ctrl Pts',(-121.132275292461,3.36132620972233,
134.397330646597));
#104130=CARTESIAN_POINT('Ctrl Pts',(-121.140026483701,3.46021105725778,
134.302207905428));
#104131=CARTESIAN_POINT('Ctrl Pts',(-121.147777674941,3.55499474356835,
134.203065582064));
#104132=CARTESIAN_POINT('Ctrl Pts',(-121.155525571718,3.64973814428392,
134.103965396831));
#104133=CARTESIAN_POINT('Ctrl Pts',(-121.163273468495,3.74038358106666,
134.000849309345));
#104134=CARTESIAN_POINT('Ctrl Pts',(-121.171021365272,3.8265806144706,133.89409585921));
#104135=CARTESIAN_POINT('Ctrl Pts',(-121.178767641356,3.91275961731335,
133.787364739596));
#104136=CARTESIAN_POINT('Ctrl Pts',(-121.18651391744,3.99449182215695,133.676998074714));
#104137=CARTESIAN_POINT('Ctrl Pts',(-121.194260193524,4.07146661438827,
133.563408038402));
#104138=CARTESIAN_POINT('Ctrl Pts',(-121.20200652679,4.14844197483012,133.449817163594));
#104139=CARTESIAN_POINT('Ctrl Pts',(-121.209752860055,4.22065963325971,
133.333003193528));
#104140=CARTESIAN_POINT('Ctrl Pts',(-121.21749919332,4.28785214296914,133.213407537519));
#104141=CARTESIAN_POINT('Ctrl Pts',(-121.225247261323,4.35505969997514,
133.093785098892));
#104142=CARTESIAN_POINT('Ctrl Pts',(-121.232995329326,4.41723967748522,
132.971380075532));
#104143=CARTESIAN_POINT('Ctrl Pts',(-121.240743397329,4.47417064150337,
132.846658375781));
#104144=CARTESIAN_POINT('Ctrl Pts',(-121.248499700071,4.53116211242765,
132.721804120323));
#104145=CARTESIAN_POINT('Ctrl Pts',(-121.256256002813,4.58289326317113,
132.594628626213));
#104146=CARTESIAN_POINT('Ctrl Pts',(-121.264012305555,4.62919067700666,
132.46561819495));
#104147=CARTESIAN_POINT('Ctrl Pts',(-121.271772748069,4.67551280116594,
132.336538906935));
#104148=CARTESIAN_POINT('Ctrl Pts',(-121.279533190583,4.71639529314128,
132.205623103317));
#104149=CARTESIAN_POINT('Ctrl Pts',(-121.287293633098,4.75171498144312,
132.073371176084));
#104150=CARTESIAN_POINT('Ctrl Pts',(-121.295066533363,4.78709136804415,
131.940906946316));
#104151=CARTESIAN_POINT('Ctrl Pts',(-121.302839433628,4.81688702114547,
131.807102688647));
#104152=CARTESIAN_POINT('Ctrl Pts',(-121.310612333894,4.84102998218019,
131.67246877565));
#104153=CARTESIAN_POINT('Ctrl Pts',(-121.318102669656,4.86429528576891,
131.542729144513));
#104154=CARTESIAN_POINT('Ctrl Pts',(-121.325593005418,4.88231169915768,
131.412219436047));
#104155=CARTESIAN_POINT('Ctrl Pts',(-121.33308334118,4.89506062173344,131.281397903378));
#104156=CARTESIAN_POINT('Ctrl Pts',(-121.340857675299,4.90829292358355,
131.145616232536));
#104157=CARTESIAN_POINT('Ctrl Pts',(-121.348632009418,4.91589233179786,
131.00906850957));
#104158=CARTESIAN_POINT('Ctrl Pts',(-121.356406343537,4.91778125866527,
130.872261681038));
#104159=CARTESIAN_POINT('Ctrl Pts',(-121.364171096484,4.91966785759914,
130.735623454695));
#104160=CARTESIAN_POINT('Ctrl Pts',(-121.371935849431,4.91585797268189,
130.598727145322));
#104161=CARTESIAN_POINT('Ctrl Pts',(-121.379700602379,4.90632562558624,
130.462085993593));
#104162=CARTESIAN_POINT('Ctrl Pts',(-121.387457643264,4.8968027461521,130.325580555782));
#104163=CARTESIAN_POINT('Ctrl Pts',(-121.395214684149,4.88156874225225,
130.189330158779));
#104164=CARTESIAN_POINT('Ctrl Pts',(-121.402971725034,4.86064966597449,
130.053848867383));
#104165=CARTESIAN_POINT('Ctrl Pts',(-121.410722916274,4.83974636493486,
129.918469743484));
#104166=CARTESIAN_POINT('Ctrl Pts',(-121.418474107514,4.81316658426278,
129.783858955584));
#104167=CARTESIAN_POINT('Ctrl Pts',(-121.426225298754,4.78098823743087,
129.650525908412));
#104168=CARTESIAN_POINT('Ctrl Pts',(-121.433973195531,4.7488235672547,129.517249531343));
#104169=CARTESIAN_POINT('Ctrl Pts',(-121.441721092308,4.71106515517172,
129.385250194128));
#104170=CARTESIAN_POINT('Ctrl Pts',(-121.449468989085,4.66784205619279,
129.255027341302));
#104171=CARTESIAN_POINT('Ctrl Pts',(-121.457215265169,4.6246279985545,129.124831728291));
#104172=CARTESIAN_POINT('Ctrl Pts',(-121.464961541253,4.57595165078101,
128.996412231355));
#104173=CARTESIAN_POINT('Ctrl Pts',(-121.472707817338,4.52199189160953,
128.870252969394));
#104174=CARTESIAN_POINT('Ctrl Pts',(-121.480454150603,4.46803173411928,
128.744092776154));
#104175=CARTESIAN_POINT('Ctrl Pts',(-121.488200483868,4.408788241155,128.620193210646));
#104176=CARTESIAN_POINT('Ctrl Pts',(-121.495946817134,4.34448822139555,
128.499017875878));
#104177=CARTESIAN_POINT('Ctrl Pts',(-121.503694885137,4.28017380209259,
128.377815404733));
#104178=CARTESIAN_POINT('Ctrl Pts',(-121.51144295314,4.21080078592403,128.259338723591));
#104179=CARTESIAN_POINT('Ctrl Pts',(-121.519191021143,4.13664146428917,
128.144025965981));
#104180=CARTESIAN_POINT('Ctrl Pts',(-121.526947323884,4.06240332524467,
128.0285906526));
#104181=CARTESIAN_POINT('Ctrl Pts',(-121.534703626626,3.98336893083296,
127.916326309377));
#104182=CARTESIAN_POINT('Ctrl Pts',(-121.542459929368,3.89985368430151,
127.807641694554));
#104183=CARTESIAN_POINT('Ctrl Pts',(-121.550220371882,3.81629386316838,
127.698899071479));
#104184=CARTESIAN_POINT('Ctrl Pts',(-121.557980814396,3.72824867537933,
127.593740283476));
#104185=CARTESIAN_POINT('Ctrl Pts',(-121.565741256911,3.63607253768694,
127.4925394323));
#104186=CARTESIAN_POINT('Ctrl Pts',(-121.573514157176,3.54374843067531,
127.391176124533));
#104187=CARTESIAN_POINT('Ctrl Pts',(-121.581287057442,3.44728039746618,
127.293783728102));
#104188=CARTESIAN_POINT('Ctrl Pts',(-121.589059957707,3.34705893359493,
127.200698652628));
#104189=CARTESIAN_POINT('Ctrl Pts',(-121.596550293469,3.2504807723783,127.110997454115));
#104190=CARTESIAN_POINT('Ctrl Pts',(-121.604040629231,3.15041756993152,
127.025296049977));
#104191=CARTESIAN_POINT('Ctrl Pts',(-121.611530964993,3.0472448135014,126.943857786446));
#104192=CARTESIAN_POINT('Ctrl Pts',(-121.619305299112,2.9401602306518,126.859331766399));
#104193=CARTESIAN_POINT('Ctrl Pts',(-121.627079633231,2.8293864298532,126.779130789415));
#104194=CARTESIAN_POINT('Ctrl Pts',(-121.63485396735,2.71530798154935,126.703594149229));
#104195=CARTESIAN_POINT('Ctrl Pts',(-121.642618720297,2.60137012473755,
126.628150601202));
#104196=CARTESIAN_POINT('Ctrl Pts',(-121.650383473245,2.48413604669699,
126.55736016619));
#104197=CARTESIAN_POINT('Ctrl Pts',(-121.658148226192,2.36402350942219,
126.491522119616));
#104198=CARTESIAN_POINT('Ctrl Pts',(-121.665905267077,2.2440302696127,126.425749464318));
#104199=CARTESIAN_POINT('Ctrl Pts',(-121.673662307962,2.12116460058219,
126.364919595567));
#104200=CARTESIAN_POINT('Ctrl Pts',(-121.681419348847,1.99587308139619,
126.309288459585));
#104201=CARTESIAN_POINT('Ctrl Pts',(-121.689170540087,1.87067604551961,
126.253699275475));
#104202=CARTESIAN_POINT('Ctrl Pts',(-121.696921731327,1.74305715658251,
126.203301178822));
#104203=CARTESIAN_POINT('Ctrl Pts',(-121.704672922567,1.61348710534638,
126.158303964513));
#104204=CARTESIAN_POINT('Ctrl Pts',(-121.712420819345,1.48397212483824,
126.11332587522));
#104205=CARTESIAN_POINT('Ctrl Pts',(-121.720168716122,1.35250799999222,
126.073744230652));
#104206=CARTESIAN_POINT('Ctrl Pts',(-121.727916612899,1.21958468502567,
126.039720415142));
#104207=CARTESIAN_POINT('Ctrl Pts',(-121.735662888983,1.08668917475112,
126.005703716682));
#104208=CARTESIAN_POINT('Ctrl Pts',(-121.743409165067,0.952335459991848,
125.977242631735));
#104209=CARTESIAN_POINT('Ctrl Pts',(-121.751155441151,0.817027532014618,
125.954448342645));
#104210=CARTESIAN_POINT('Ctrl Pts',(-121.758901774417,0.681718605225186,
125.931653885292));
#104211=CARTESIAN_POINT('Ctrl Pts',(-121.766648107682,0.545455836695285,
125.914526372214));
#104212=CARTESIAN_POINT('Ctrl Pts',(-121.774394440947,0.408751864394905,
125.903125571595));
#104213=CARTESIAN_POINT('Ctrl Pts',(-121.78214250895,0.272017278187582,
125.891722217845));
#104214=CARTESIAN_POINT('Ctrl Pts',(-121.789890576953,0.134841681138283,
125.886048160983));
#104215=CARTESIAN_POINT('Ctrl Pts',(-121.797638644956,-0.00225913245219713,
125.886111136417));
#104216=CARTESIAN_POINT('Ctrl Pts',(-121.805394947698,-0.139505658418695,
125.886174178783));
#104217=CARTESIAN_POINT('Ctrl Pts',(-121.81315125044,-0.276676850566443,
125.891986433451));
#104218=CARTESIAN_POINT('Ctrl Pts',(-121.820907553182,-0.413258325849479,
125.903503486551));
#104219=CARTESIAN_POINT('Ctrl Pts',(-121.828667995696,-0.549912698778263,
125.91502668665));
#104220=CARTESIAN_POINT('Ctrl Pts',(-121.83642843821,-0.685976340000499,
125.932260703145));
#104221=CARTESIAN_POINT('Ctrl Pts',(-121.844188880725,-0.820942936202866,
125.955109566321));
#104222=CARTESIAN_POINT('Ctrl Pts',(-121.85196178099,-0.956126192767228,
125.977995108521));
#104223=CARTESIAN_POINT('Ctrl Pts',(-121.859734681256,-1.09020850249341,
126.006513427764));
#104224=CARTESIAN_POINT('Ctrl Pts',(-121.867507581521,-1.22269576206403,
126.040517826716));
#104225=CARTESIAN_POINT('Ctrl Pts',(-121.874997917283,-1.35036677602753,
126.073286080113));
#104226=CARTESIAN_POINT('Ctrl Pts',(-121.882488253044,-1.47655639961478,
126.111148383958));
#104227=CARTESIAN_POINT('Ctrl Pts',(-121.889978588806,-1.60084011215543,
126.153931175266));
#104228=CARTESIAN_POINT('Ctrl Pts',(-121.897752983536,-1.72983708512919,
126.198336435306));
#104229=CARTESIAN_POINT('Ctrl Pts',(-121.905527378266,-1.85718936363839,
126.248183415226));
#104230=CARTESIAN_POINT('Ctrl Pts',(-121.913301772997,-1.98240360904195,
126.303331958097));
#104231=CARTESIAN_POINT('Ctrl Pts',(-121.921066572345,-2.10746331142232,
126.358412435051));
#104232=CARTESIAN_POINT('Ctrl Pts',(-121.928831371694,-2.23038987682462,
126.418781299487));
#104233=CARTESIAN_POINT('Ctrl Pts',(-121.936596171042,-2.35070569741676,
126.484248838152));
#104234=CARTESIAN_POINT('Ctrl Pts',(-121.944353244179,-2.47090180010097,
126.549651234621));
#104235=CARTESIAN_POINT('Ctrl Pts',(-121.952110317315,-2.58849198649592,
126.620142023403));
#104236=CARTESIAN_POINT('Ctrl Pts',(-121.959867390452,-2.7030195295595,
126.695483826359));
#104237=CARTESIAN_POINT('Ctrl Pts',(-121.967618599839,-2.81746049862763,
126.770768676719));
#104238=CARTESIAN_POINT('Ctrl Pts',(-121.975369809226,-2.92884310721815,
126.850897028237));
#104239=CARTESIAN_POINT('Ctrl Pts',(-121.983121018613,-3.03673642659321,
126.935586271872));
#104240=CARTESIAN_POINT('Ctrl Pts',(-121.990868860044,-3.14458286555112,
127.020238717426));
#104241=CARTESIAN_POINT('Ctrl Pts',(-121.998616701476,-3.24894272423925,
127.10944787217));
#104242=CARTESIAN_POINT('Ctrl Pts',(-122.006364542907,-3.34941540234577,
127.202888762195));
#104243=CARTESIAN_POINT('Ctrl Pts',(-122.014110743557,-3.44986680307331,
127.296309863982));
#104244=CARTESIAN_POINT('Ctrl Pts',(-122.021856944206,-3.546432374632,127.393960652319));
#104245=CARTESIAN_POINT('Ctrl Pts',(-122.029603144855,-3.63874616757133,
127.495477212173));
#104246=CARTESIAN_POINT('Ctrl Pts',(-122.037349382583,-3.73106040238364,
127.59699425795));
#104247=CARTESIAN_POINT('Ctrl Pts',(-122.045095620311,-3.81912255501641,
127.702376822868));
#104248=CARTESIAN_POINT('Ctrl Pts',(-122.052841858038,-3.90260525945919,
127.811225931097));
#104249=CARTESIAN_POINT('Ctrl Pts',(-122.060589810369,-3.98610644251257,
127.920099132704));
#104250=CARTESIAN_POINT('Ctrl Pts',(-122.0683377627,-4.0650259226125,128.032440094219));
#104251=CARTESIAN_POINT('Ctrl Pts',(-122.076085715031,-4.13907840437813,
128.147819064172));
#104252=CARTESIAN_POINT('Ctrl Pts',(-122.083841620825,-4.21320690282966,
128.263316473462));
#104253=CARTESIAN_POINT('Ctrl Pts',(-122.091597526618,-4.28245821230543,
128.381857790778));
#104254=CARTESIAN_POINT('Ctrl Pts',(-122.099353432412,-4.34659169747729,
128.502986315563));
#104255=CARTESIAN_POINT('Ctrl Pts',(-122.107113469675,-4.41075934571951,
128.624179363931));
#104256=CARTESIAN_POINT('Ctrl Pts',(-122.114873506939,-4.46980356933109,
128.747962013255));
#104257=CARTESIAN_POINT('Ctrl Pts',(-122.122633544202,-4.52353146089156,
128.873856490447));
#104258=CARTESIAN_POINT('Ctrl Pts',(-122.130405374641,-4.57734100443896,
128.999942293483));
#104259=CARTESIAN_POINT('Ctrl Pts',(-122.13817720508,-4.62581793532609,
129.128145971041));
#104260=CARTESIAN_POINT('Ctrl Pts',(-122.145949035519,-4.66881864859992,
129.257972733177));
#104261=CARTESIAN_POINT('Ctrl Pts',(-122.152364044835,-4.70431221455001,
129.36513408919));
#104262=CARTESIAN_POINT('Ctrl Pts',(-122.158779054151,-4.73607565219564,
129.473400906273));
#104263=CARTESIAN_POINT('Ctrl Pts',(-122.165194063467,-4.76405452823402,
129.582490119308));
#104264=CARTESIAN_POINT('Ctrl Pts',(-120.415010068595,-4.76405452823409,
129.582490119308));
#104265=CARTESIAN_POINT('Ctrl Pts',(-120.422714657118,-4.79790261253537,
129.714463286283));
#104266=CARTESIAN_POINT('Ctrl Pts',(-120.430419245642,-4.82623649557487,
129.847741980942));
#104267=CARTESIAN_POINT('Ctrl Pts',(-120.438123834165,-4.8489807157756,
129.981822423598));
#104268=CARTESIAN_POINT('Ctrl Pts',(-120.445959955797,-4.87211322640586,
130.118191894069));
#104269=CARTESIAN_POINT('Ctrl Pts',(-120.453796077429,-4.88946342946171,
130.255390308165));
#104270=CARTESIAN_POINT('Ctrl Pts',(-120.461632199062,-4.90100710441625,
130.392884707018));
#104271=CARTESIAN_POINT('Ctrl Pts',(-120.469468320694,-4.91255077937079,
130.530379105871));
#104272=CARTESIAN_POINT('Ctrl Pts',(-120.477304442326,-4.918287972603,130.66816906213));
#104273=CARTESIAN_POINT('Ctrl Pts',(-120.485140563958,-4.91824981073044,
130.805725077146));
#104274=CARTESIAN_POINT('',(-120.139859436048,-4.91824877114872,130.807837339308));
#104275=CARTESIAN_POINT('Ctrl Pts',(-120.07000000496,-4.76405452823399,
129.582490119308));
#104276=CARTESIAN_POINT('Ctrl Pts',(-120.077773079977,-4.79826467207663,
129.715874950939));
#104277=CARTESIAN_POINT('Ctrl Pts',(-120.085546154993,-4.82688359845568,
129.850755253548));
#104278=CARTESIAN_POINT('Ctrl Pts',(-120.09331923001,-4.84979292098213,
129.986624910817));
#104279=CARTESIAN_POINT('Ctrl Pts',(-120.101092419275,-4.87270258022868,
130.122496565093));
#104280=CARTESIAN_POINT('Ctrl Pts',(-120.10886560854,-4.88990239253311,
130.25935722365));
#104281=CARTESIAN_POINT('Ctrl Pts',(-120.116638797805,-4.90132518231807,
130.396690996825));
#104282=CARTESIAN_POINT('Ctrl Pts',(-120.124379010535,-4.91269951270971,
130.533442153017));
#104283=CARTESIAN_POINT('Ctrl Pts',(-120.132119223264,-4.91834574066988,
130.670662035112));
#104284=CARTESIAN_POINT('Ctrl Pts',(-120.139859435993,-4.91824877114942,
130.807837338329));
#104285=CARTESIAN_POINT('Ctrl Pts',(-120.139859436048,-4.91824877114872,
130.807837339307));
#104286=CARTESIAN_POINT('Ctrl Pts',(-120.148714778364,-4.91813783123406,
130.964775437756));
#104287=CARTESIAN_POINT('Ctrl Pts',(-120.15757012068,-4.91051123559427,
131.121414678335));
#104288=CARTESIAN_POINT('Ctrl Pts',(-120.166425462996,-4.89547851881717,
131.277090069049));
#104289=CARTESIAN_POINT('Ctrl Pts',(-120.175322363441,-4.8803752534876,
131.433496044503));
#104290=CARTESIAN_POINT('Ctrl Pts',(-120.184219263886,-4.8577963009599,
131.58892895109));
#104291=CARTESIAN_POINT('Ctrl Pts',(-120.193116164331,-4.82790228850742,
131.742732907824));
#104292=CARTESIAN_POINT('Ctrl Pts',(-120.20206730258,-4.79782603443221,
131.897474493213));
#104293=CARTESIAN_POINT('Ctrl Pts',(-120.211018440828,-4.7603453501292,
132.050567057875));
#104294=CARTESIAN_POINT('Ctrl Pts',(-120.219969579077,-4.71567234460993,
132.201363624285));
#104295=CARTESIAN_POINT('Ctrl Pts',(-120.226273666747,-4.6842101399758,
132.307566293556));
#104296=CARTESIAN_POINT('Ctrl Pts',(-120.232577754417,-4.64918150738479,
132.412630567728));
#104297=CARTESIAN_POINT('Ctrl Pts',(-120.238881842088,-4.61067448482932,
132.516337211286));
#104298=CARTESIAN_POINT('Ctrl Pts',(-120.246656176207,-4.56318681096764,
132.644230435423));
#104299=CARTESIAN_POINT('Ctrl Pts',(-120.254430510326,-4.51029853671385,
132.770348880144));
#104300=CARTESIAN_POINT('Ctrl Pts',(-120.262204844445,-4.45216161365228,
132.894202723664));
#104301=CARTESIAN_POINT('Ctrl Pts',(-120.269969597392,-4.39409633915254,
133.017903928391));
#104302=CARTESIAN_POINT('Ctrl Pts',(-120.277734350339,-4.33079545074578,
133.139345734496));
#104303=CARTESIAN_POINT('Ctrl Pts',(-120.285499103286,-4.26246006419136,
133.258055232565));
#104304=CARTESIAN_POINT('Ctrl Pts',(-120.293256144171,-4.19419254930622,
133.376646826686));
#104305=CARTESIAN_POINT('Ctrl Pts',(-120.301013185056,-4.12090068095356,
133.492511176647));
#104306=CARTESIAN_POINT('Ctrl Pts',(-120.308770225941,-4.0428327252676,
133.605197388605));
#104307=CARTESIAN_POINT('Ctrl Pts',(-120.316521417181,-3.9648236412342,
133.717798623015));
#104308=CARTESIAN_POINT('Ctrl Pts',(-120.324272608422,-3.88204586054762,
133.82722616975));
#104309=CARTESIAN_POINT('Ctrl Pts',(-120.332023799662,-3.79479224907234,
133.933056008441));
#104310=CARTESIAN_POINT('Ctrl Pts',(-120.339771696439,-3.70757572270962,
134.038840866627));
#104311=CARTESIAN_POINT('Ctrl Pts',(-120.347519593216,-3.61588739737021,
134.14103075705));
#104312=CARTESIAN_POINT('Ctrl Pts',(-120.355267489993,-3.52006177317402,
134.239232984269));
#104313=CARTESIAN_POINT('Ctrl Pts',(-120.363013766077,-3.42425619363265,
134.337414669699));
#104314=CARTESIAN_POINT('Ctrl Pts',(-120.370760042161,-3.32431530950407,
134.43161007142));
#104315=CARTESIAN_POINT('Ctrl Pts',(-120.378506318245,-3.22061172338323,
134.521462067581));
#104316=CARTESIAN_POINT('Ctrl Pts',(-120.386252651511,-3.11690737174593,
134.61131472701));
#104317=CARTESIAN_POINT('Ctrl Pts',(-120.393998984776,-3.00944055817514,
134.696823660885));
#104318=CARTESIAN_POINT('Ctrl Pts',(-120.401745318041,-2.89861801462052,
134.777671160151));
#104319=CARTESIAN_POINT('Ctrl Pts',(-120.409493386044,-2.78777065312581,
134.858536764653));
#104320=CARTESIAN_POINT('Ctrl Pts',(-120.417241454047,-2.67356638205318,
134.934738626938));
#104321=CARTESIAN_POINT('Ctrl Pts',(-120.42498952205,-2.55644169540641,
135.006001835053));
#104322=CARTESIAN_POINT('Ctrl Pts',(-120.432745824792,-2.43919252724871,
135.077340782554));
#104323=CARTESIAN_POINT('Ctrl Pts',(-120.440502127534,-2.31901707776987,
135.143730387177));
#104324=CARTESIAN_POINT('Ctrl Pts',(-120.448258430276,-2.19637776265242,
135.20494100954));
#104325=CARTESIAN_POINT('Ctrl Pts',(-120.45601887279,-2.07367299123988,
135.266184301855));
#104326=CARTESIAN_POINT('Ctrl Pts',(-120.463779315304,-1.94850209050223,
135.322242944326));
#104327=CARTESIAN_POINT('Ctrl Pts',(-120.471539757819,-1.82134740238802,
135.372935526913));
#104328=CARTESIAN_POINT('Ctrl Pts',(-120.479312658084,-1.69398859428018,
135.423709485734));
#104329=CARTESIAN_POINT('Ctrl Pts',(-120.487085558349,-1.56464000416947,
135.469100041473));
#104330=CARTESIAN_POINT('Ctrl Pts',(-120.494858458615,-1.4337999334238,
135.508975459762));
#104331=CARTESIAN_POINT('Ctrl Pts',(-120.502348794377,-1.30771622881598,
135.547401306157));
#104332=CARTESIAN_POINT('Ctrl Pts',(-120.509839130139,-1.18024789709782,
135.580705953943));
#104333=CARTESIAN_POINT('Ctrl Pts',(-120.517329465901,-1.05184778703333,
135.608816809));
#104334=CARTESIAN_POINT('Ctrl Pts',(-120.52510380002,-0.918579347769554,
135.637993495671));
#104335=CARTESIAN_POINT('Ctrl Pts',(-120.532878134139,-0.783884924263575,
135.661667192654));
#104336=CARTESIAN_POINT('Ctrl Pts',(-120.540652468258,-0.648258750999061,
135.679700980479));
#104337=CARTESIAN_POINT('Ctrl Pts',(-120.548417221205,-0.512799724871836,
135.697712543273));
#104338=CARTESIAN_POINT('Ctrl Pts',(-120.556181974152,-0.376411617591162,
135.710097975663));
#104339=CARTESIAN_POINT('Ctrl Pts',(-120.563946727099,-0.239601009221587,
135.716770862942));
#104340=CARTESIAN_POINT('Ctrl Pts',(-120.571703767984,-0.102926283076566,
135.723437122616));
#104341=CARTESIAN_POINT('Ctrl Pts',(-120.579460808869,0.0341697210926163,
135.724402109335));
#104342=CARTESIAN_POINT('Ctrl Pts',(-120.587217849755,0.171173459616725,
135.719630977294));
#104343=CARTESIAN_POINT('Ctrl Pts',(-120.594969040995,0.308073882555693,
135.714863443201));
#104344=CARTESIAN_POINT('Ctrl Pts',(-120.602720232235,0.444881789193491,
135.704368413847));
#104345=CARTESIAN_POINT('Ctrl Pts',(-120.610471423475,0.581082138031221,
135.688163092212));
#104346=CARTESIAN_POINT('Ctrl Pts',(-120.618219320252,0.717224598087617,
135.671964658271));
#104347=CARTESIAN_POINT('Ctrl Pts',(-120.625967217029,0.8527596265262,135.650060805315));
#104348=CARTESIAN_POINT('Ctrl Pts',(-120.633715113806,0.987176032066382,
135.62252069629));
#104349=CARTESIAN_POINT('Ctrl Pts',(-120.64146138989,1.12156432059221,135.594986348063));
#104350=CARTESIAN_POINT('Ctrl Pts',(-120.649207665974,1.25483406887601,
135.561818167253));
#104351=CARTESIAN_POINT('Ctrl Pts',(-120.656953942059,1.38648341938654,
135.523136601894));
#104352=CARTESIAN_POINT('Ctrl Pts',(-120.664700275324,1.51813374170249,
135.484454750995));
#104353=CARTESIAN_POINT('Ctrl Pts',(-120.672446608589,1.64816326726858,
135.440259544551));
#104354=CARTESIAN_POINT('Ctrl Pts',(-120.680192941855,1.77608484990299,
135.390721448164));
#104355=CARTESIAN_POINT('Ctrl Pts',(-120.687941009858,1.90403507968906,
135.341172258064));
#104356=CARTESIAN_POINT('Ctrl Pts',(-120.695689077861,2.02987606268763,
135.286277938276));
#104357=CARTESIAN_POINT('Ctrl Pts',(-120.703437145864,2.15314057201565,
135.226257126943));
#104358=CARTESIAN_POINT('Ctrl Pts',(-120.711193448606,2.27653608833087,
135.166172524777));
#104359=CARTESIAN_POINT('Ctrl Pts',(-120.718949751347,2.3973493088434,135.10095071854));
#104360=CARTESIAN_POINT('Ctrl Pts',(-120.726706054089,2.51513708446478,
135.030856625946));
#104361=CARTESIAN_POINT('Ctrl Pts',(-120.734466496603,2.63298772696853,
134.960725122023));
#104362=CARTESIAN_POINT('Ctrl Pts',(-120.742226939118,2.74780937985991,
134.885716363772));
#104363=CARTESIAN_POINT('Ctrl Pts',(-120.749987381632,2.85918870013053,
134.806138102578));
#104364=CARTESIAN_POINT('Ctrl Pts',(-120.757760281897,2.97074681637384,
134.726432095293));
#104365=CARTESIAN_POINT('Ctrl Pts',(-120.765533182163,3.0788512489136,134.642142167193));
#104366=CARTESIAN_POINT('Ctrl Pts',(-120.773306082428,3.1831218218354,134.553616347688));
#104367=CARTESIAN_POINT('Ctrl Pts',(-120.78079641819,3.28360189678864,134.468308664706));
#104368=CARTESIAN_POINT('Ctrl Pts',(-120.788286753952,3.38052178708731,
134.379067922782));
#104369=CARTESIAN_POINT('Ctrl Pts',(-120.795777089714,3.47357564142344,
134.28623587751));
#104370=CARTESIAN_POINT('Ctrl Pts',(-120.803551423833,3.5701576609308,134.189884077025));
#104371=CARTESIAN_POINT('Ctrl Pts',(-120.811325757952,3.6628806386751,134.089358055266));
#104372=CARTESIAN_POINT('Ctrl Pts',(-120.819100092071,3.75136223461914,
133.984999617386));
#104373=CARTESIAN_POINT('Ctrl Pts',(-120.826864845018,3.83973478490401,
133.880769791953));
#104374=CARTESIAN_POINT('Ctrl Pts',(-120.834629597965,3.9238761033969,133.772717243323));
#104375=CARTESIAN_POINT('Ctrl Pts',(-120.842394350913,4.0034396680596,133.661221462393));
#104376=CARTESIAN_POINT('Ctrl Pts',(-120.850151391798,4.08292420906822,
133.549836420644));
#104377=CARTESIAN_POINT('Ctrl Pts',(-120.857908432682,4.15783981873404,
133.435015268469));
#104378=CARTESIAN_POINT('Ctrl Pts',(-120.865665473567,4.22787959739684,
133.317171229692));
#104379=CARTESIAN_POINT('Ctrl Pts',(-120.873416664808,4.29786655851782,
133.199416058022));
#104380=CARTESIAN_POINT('Ctrl Pts',(-120.881167856048,4.36298480834441,
133.078642871845));
#104381=CARTESIAN_POINT('Ctrl Pts',(-120.888919047288,4.42297042771961,
132.955294288793));
#104382=CARTESIAN_POINT('Ctrl Pts',(-120.896666944065,4.48293055160648,
132.831998132179));
#104383=CARTESIAN_POINT('Ctrl Pts',(-120.904414840842,4.53776221326313,
132.706129106648));
#104384=CARTESIAN_POINT('Ctrl Pts',(-120.912162737619,4.58724729006206,
132.578154676164));
#104385=CARTESIAN_POINT('Ctrl Pts',(-120.919909013703,4.63672201564956,
132.450207015173));
#104386=CARTESIAN_POINT('Ctrl Pts',(-120.927655289787,4.68085224000453,
132.320155189641));
#104387=CARTESIAN_POINT('Ctrl Pts',(-120.935401565872,4.71946803321353,
132.188486531627));
#104388=CARTESIAN_POINT('Ctrl Pts',(-120.943147899137,4.75808411147559,
132.056816901665));
#104389=CARTESIAN_POINT('Ctrl Pts',(-120.950894232402,4.79118556733727,
131.923530790568));
#104390=CARTESIAN_POINT('Ctrl Pts',(-120.958640565668,4.81865250392724,
131.789130189037));
#104391=CARTESIAN_POINT('Ctrl Pts',(-120.966388633671,4.84612559154718,
131.654699489424));
#104392=CARTESIAN_POINT('Ctrl Pts',(-120.974136701674,4.86796157076954,
131.519154185713));
#104393=CARTESIAN_POINT('Ctrl Pts',(-120.981884769677,4.88409184051216,
131.383005548368));
#104394=CARTESIAN_POINT('Ctrl Pts',(-120.989641072418,4.90023925369744,
131.246712210631));
#104395=CARTESIAN_POINT('Ctrl Pts',(-120.99739737516,4.91066879764671,131.109814647203));
#104396=CARTESIAN_POINT('Ctrl Pts',(-121.005153677902,4.91536382222885,
130.972828886459));
#104397=CARTESIAN_POINT('Ctrl Pts',(-121.012914120416,4.92006135268698,
130.83577001229));
#104398=CARTESIAN_POINT('Ctrl Pts',(-121.02067456293,4.91901826807467,130.698623237768));
#104399=CARTESIAN_POINT('Ctrl Pts',(-121.028435005445,4.91227006635546,
130.561902667216));
#104400=CARTESIAN_POINT('Ctrl Pts',(-121.03620790571,4.90551103182378,130.424962620665));
#104401=CARTESIAN_POINT('Ctrl Pts',(-121.043980805976,4.89302861448386,
130.288450534859));
#104402=CARTESIAN_POINT('Ctrl Pts',(-121.051753706241,4.87491012696753,
130.152874380958));
#104403=CARTESIAN_POINT('Ctrl Pts',(-121.059244042003,4.85745029211018,
130.022226761748));
#104404=CARTESIAN_POINT('Ctrl Pts',(-121.066734377765,4.83475709660615,
129.892448512288));
#104405=CARTESIAN_POINT('Ctrl Pts',(-121.074224713527,4.80695274901388,
129.763981681193));
#104406=CARTESIAN_POINT('Ctrl Pts',(-121.081999047646,4.77809419113173,
129.630643991151));
#104407=CARTESIAN_POINT('Ctrl Pts',(-121.089773381765,4.74363783633687,
129.498296753679));
#104408=CARTESIAN_POINT('Ctrl Pts',(-121.097547715884,4.7036645908544,129.367446396312));
#104409=CARTESIAN_POINT('Ctrl Pts',(-121.105312468831,4.66374060882447,
129.236757300315));
#104410=CARTESIAN_POINT('Ctrl Pts',(-121.113077221778,4.61831337736683,
129.107561784197));
#104411=CARTESIAN_POINT('Ctrl Pts',(-121.120841974725,4.56751486929416,
128.980356510861));
#104412=CARTESIAN_POINT('Ctrl Pts',(-121.12859901561,4.51676681501585,128.853277579595));
#104413=CARTESIAN_POINT('Ctrl Pts',(-121.136356056495,4.46065824472712,
128.72818531805));
#104414=CARTESIAN_POINT('Ctrl Pts',(-121.14411309738,4.39937092857163,128.605561287173));
#104415=CARTESIAN_POINT('Ctrl Pts',(-121.151864288621,4.33812982965792,
128.48302972803));
#104416=CARTESIAN_POINT('Ctrl Pts',(-121.159615479861,4.2717179322864,128.362963043029));
#104417=CARTESIAN_POINT('Ctrl Pts',(-121.167366671101,4.20036496845406,
128.245822520472));
#104418=CARTESIAN_POINT('Ctrl Pts',(-121.175114567878,4.12904233153485,
128.128731785761));
#104419=CARTESIAN_POINT('Ctrl Pts',(-121.182862464655,4.05278300802332,
128.014565073075));
#104420=CARTESIAN_POINT('Ctrl Pts',(-121.190610361432,3.97186238798385,
127.903758570849));
#104421=CARTESIAN_POINT('Ctrl Pts',(-121.198356637516,3.89095869479341,
127.792975246954));
#104422=CARTESIAN_POINT('Ctrl Pts',(-121.2061029136,3.80539587491923,127.685551050979));
#104423=CARTESIAN_POINT('Ctrl Pts',(-121.213849189684,3.71549208335456,
127.581892364653));
#104424=CARTESIAN_POINT('Ctrl Pts',(-121.22159552295,3.62558762814065,127.478232913143));
#104425=CARTESIAN_POINT('Ctrl Pts',(-121.229341856215,3.53134239345751,
127.378339322103));
#104426=CARTESIAN_POINT('Ctrl Pts',(-121.23708818948,3.43311391111179,127.282583802401));
#104427=CARTESIAN_POINT('Ctrl Pts',(-121.244836257483,3.33486343117865,
127.186806838915));
#104428=CARTESIAN_POINT('Ctrl Pts',(-121.252584325486,3.23262820846716,
127.095170063634));
#104429=CARTESIAN_POINT('Ctrl Pts',(-121.260332393489,3.12680130873923,
127.008007546767));
#104430=CARTESIAN_POINT('Ctrl Pts',(-121.268088696231,3.02086193492277,
126.920752392539));
#104431=CARTESIAN_POINT('Ctrl Pts',(-121.275844998973,2.91132356093146,
126.837981244893));
#104432=CARTESIAN_POINT('Ctrl Pts',(-121.283601301715,2.79861133624859,
126.759987037996));
#104433=CARTESIAN_POINT('Ctrl Pts',(-121.291361744229,2.68583895365771,
126.681951203243));
#104434=CARTESIAN_POINT('Ctrl Pts',(-121.299122186743,2.56988967534342,
126.608697598245));
#104435=CARTESIAN_POINT('Ctrl Pts',(-121.306882629257,2.4512152193469,126.5404742435));
#104436=CARTESIAN_POINT('Ctrl Pts',(-121.314655529523,2.33235025657818,
126.472141370571));
#104437=CARTESIAN_POINT('Ctrl Pts',(-121.322428429788,2.21075172109453,
126.408855064928));
#104438=CARTESIAN_POINT('Ctrl Pts',(-121.330201330053,2.08689417803081,
126.350816438802));
#104439=CARTESIAN_POINT('Ctrl Pts',(-121.337691665816,1.96753916863208,
126.294887662925));
#104440=CARTESIAN_POINT('Ctrl Pts',(-121.345182001578,1.84608682536492,
126.243831777163));
#104441=CARTESIAN_POINT('Ctrl Pts',(-121.35267233734,1.72297511295921,126.197784902067));
#104442=CARTESIAN_POINT('Ctrl Pts',(-121.360446671459,1.59519558256207,
126.149992145708));
#104443=CARTESIAN_POINT('Ctrl Pts',(-121.368221005578,1.46522360199772,
126.107444338237));
#104444=CARTESIAN_POINT('Ctrl Pts',(-121.375995339697,1.3335289748852,126.070347147408));
#104445=CARTESIAN_POINT('Ctrl Pts',(-121.383760092644,1.20199664963107,
126.033295675551));
#104446=CARTESIAN_POINT('Ctrl Pts',(-121.391524845591,1.06874627468884,
126.001681559704));
#104447=CARTESIAN_POINT('Ctrl Pts',(-121.399289598539,0.934267041154496,
125.975662225834));
#104448=CARTESIAN_POINT('Ctrl Pts',(-121.407046639424,0.799921374290355,
125.949668734734));
#104449=CARTESIAN_POINT('Ctrl Pts',(-121.414803680308,0.664349659085967,
125.929259041081));
#104450=CARTESIAN_POINT('Ctrl Pts',(-121.422560721193,0.528055297606805,
125.914540511962));
#104451=CARTESIAN_POINT('Ctrl Pts',(-121.430311912434,0.391863716766036,
125.8998330822));
#104452=CARTESIAN_POINT('Ctrl Pts',(-121.438063103674,0.254950961479189,
125.890808316306));
#104453=CARTESIAN_POINT('Ctrl Pts',(-121.445814294914,0.117829302415059,
125.887522271841));
#104454=CARTESIAN_POINT('Ctrl Pts',(-121.453562191691,-0.0192340762863155,
125.884237624032));
#104455=CARTESIAN_POINT('Ctrl Pts',(-121.461310088468,-0.156505792134369,
125.886686855795));
#104456=CARTESIAN_POINT('Ctrl Pts',(-121.469057985245,-0.293470012388454,
125.894874044173));
#104457=CARTESIAN_POINT('Ctrl Pts',(-121.476804261329,-0.430405582680269,
125.903059519967));
#104458=CARTESIAN_POINT('Ctrl Pts',(-121.484550537413,-0.567033395295687,
125.916980541686));
#104459=CARTESIAN_POINT('Ctrl Pts',(-121.492296813497,-0.702839579230788,
125.936589095774));
#104460=CARTESIAN_POINT('Ctrl Pts',(-121.500043146763,-0.838646765656474,
125.956197794608));
#104461=CARTESIAN_POINT('Ctrl Pts',(-121.507789480028,-0.973631924346888,
125.981494053717));
#104462=CARTESIAN_POINT('Ctrl Pts',(-121.515535813294,-1.10728864908134,
126.012378260533));
#104463=CARTESIAN_POINT('Ctrl Pts',(-121.523283881297,-1.24097530531204,
126.043269383653));
#104464=CARTESIAN_POINT('Ctrl Pts',(-121.531031949299,-1.37333255475409,
126.07975085658));
#104465=CARTESIAN_POINT('Ctrl Pts',(-121.538780017302,-1.50386687303437,
126.121672555065));
#104466=CARTESIAN_POINT('Ctrl Pts',(-121.546536320044,-1.63453992474168,
126.16363880843));
#104467=CARTESIAN_POINT('Ctrl Pts',(-121.554292622786,-1.76338580222295,
126.211056717657));
#104468=CARTESIAN_POINT('Ctrl Pts',(-121.562048925528,-1.88992824798591,
126.263726930517));
#104469=CARTESIAN_POINT('Ctrl Pts',(-121.569809368042,-2.0165382332623,
126.316425255056));
#104470=CARTESIAN_POINT('Ctrl Pts',(-121.577569810556,-2.14084198294527,
126.374381303935));
#104471=CARTESIAN_POINT('Ctrl Pts',(-121.58533025307,-2.2623866657282,126.437349095113));
#104472=CARTESIAN_POINT('Ctrl Pts',(-121.593103153336,-2.3841264628265,
126.50041796778));
#104473=CARTESIAN_POINT('Ctrl Pts',(-121.600876053601,-2.50309800276387,
126.568514465478));
#104474=CARTESIAN_POINT('Ctrl Pts',(-121.608648953867,-2.61887557007755,
126.641348029193));
#104475=CARTESIAN_POINT('Ctrl Pts',(-121.616139289629,-2.7304443311911,
126.711533909409));
#104476=CARTESIAN_POINT('Ctrl Pts',(-121.623629625391,-2.83904705203017,
126.786118252141));
#104477=CARTESIAN_POINT('Ctrl Pts',(-121.631119961152,-2.94433247988447,
126.864806161743));
#104478=CARTESIAN_POINT('Ctrl Pts',(-121.638978256311,-3.05479000732286,
126.947359579732));
#104479=CARTESIAN_POINT('Ctrl Pts',(-121.646836551469,-3.16196897788224,
127.034708896594));
#104480=CARTESIAN_POINT('Ctrl Pts',(-121.654694846627,-3.26542016347724,
127.126560430164));
#104481=CARTESIAN_POINT('Ctrl Pts',(-121.662380624164,-3.36660022638171,
127.216395494799));
#104482=CARTESIAN_POINT('Ctrl Pts',(-121.670066401701,-3.46421413479997,
127.310536894367));
#104483=CARTESIAN_POINT('Ctrl Pts',(-121.677752179238,-3.55787009888527,
127.408665781165));
#104484=CARTESIAN_POINT('Ctrl Pts',(-121.685430974352,-3.65144097781133,
127.506705519215));
#104485=CARTESIAN_POINT('Ctrl Pts',(-121.693109769465,-3.74106078866552,
127.608725254032));
#104486=CARTESIAN_POINT('Ctrl Pts',(-121.700788564579,-3.82637188746135,
127.714366889199));
#104487=CARTESIAN_POINT('Ctrl Pts',(-121.708462128761,-3.91162487082498,
127.819936559413));
#104488=CARTESIAN_POINT('Ctrl Pts',(-121.716135692944,-3.99257473035327,
127.929122912813));
#104489=CARTESIAN_POINT('Ctrl Pts',(-121.723809257126,-4.06890204433508,
128.041532498391));
#104490=CARTESIAN_POINT('Ctrl Pts',(-121.731801739445,-4.14840156931981,
128.158613896791));
#104491=CARTESIAN_POINT('Ctrl Pts',(-121.739794221763,-4.22288572883434,
128.279191893274));
#104492=CARTESIAN_POINT('Ctrl Pts',(-121.747786704082,-4.29204148410264,
128.402785517503));
#104493=CARTESIAN_POINT('Ctrl Pts',(-121.755456199217,-4.35840256035367,
128.521384553691));
#104494=CARTESIAN_POINT('Ctrl Pts',(-121.763125694352,-4.41985729000343,
128.642759856617));
#104495=CARTESIAN_POINT('Ctrl Pts',(-121.770795189487,-4.47617489732447,
128.766459405274));
#104496=CARTESIAN_POINT('Ctrl Pts',(-121.778464572672,-4.53249168258754,
128.890157148311));
#104497=CARTESIAN_POINT('Ctrl Pts',(-121.786133955856,-4.58367133513182,
129.016178703345));
#104498=CARTESIAN_POINT('Ctrl Pts',(-121.793803339041,-4.62953074956426,
129.144050977367));
#104499=CARTESIAN_POINT('Ctrl Pts',(-121.80147589271,-4.675409122048,129.271976113143));
#104500=CARTESIAN_POINT('Ctrl Pts',(-121.809148446379,-4.71596273961054,
129.401753116337));
#104501=CARTESIAN_POINT('Ctrl Pts',(-121.816821000049,-4.75105805935766,
129.532892812581));
#104502=CARTESIAN_POINT('Ctrl Pts',(-121.817787015016,-4.75547674518463,
129.549403991887));
#104503=CARTESIAN_POINT('Ctrl Pts',(-121.818753029983,-4.75980897126095,
129.565936757105));
#104504=CARTESIAN_POINT('Ctrl Pts',(-121.81971904495,-4.76405452823411,
129.582490119308));
#104505=CARTESIAN_POINT('Origin',(213.235140564004,0.,130.804360617566));
#104506=CARTESIAN_POINT('',(-123.915406765754,-4.76405452823402,129.582490119308));
#104507=CARTESIAN_POINT('',(-123.5698746576,-4.76405452823401,129.582490119308));
#104508=CARTESIAN_POINT('',(213.235140564004,-4.76405452823405,129.582490119308));
#104509=CARTESIAN_POINT('',(-122.235140563971,-4.91824789589999,130.799811224715));
#104510=CARTESIAN_POINT('Ctrl Pts',(-122.23514056401,-4.91824789590063,
130.799811225407));
#104511=CARTESIAN_POINT('Ctrl Pts',(-122.242800405751,-4.91837300399556,
130.935062837746));
#104512=CARTESIAN_POINT('Ctrl Pts',(-122.250460247491,-4.91291479637063,
131.070467222207));
#104513=CARTESIAN_POINT('Ctrl Pts',(-122.258120089232,-4.90186230610599,
131.205520179931));
#104514=CARTESIAN_POINT('Ctrl Pts',(-122.265984828699,-4.89051416611397,
131.344185750667));
#104515=CARTESIAN_POINT('Ctrl Pts',(-122.273849568165,-4.87326819136258,
131.482480401144));
#104516=CARTESIAN_POINT('Ctrl Pts',(-122.281714307632,-4.85016973800614,
131.619858364362));
#104517=CARTESIAN_POINT('Ctrl Pts',(-122.289366382498,-4.82769587283603,
131.753521591725));
#104518=CARTESIAN_POINT('Ctrl Pts',(-122.297018457364,-4.79968204027882,
131.886316648974));
#104519=CARTESIAN_POINT('Ctrl Pts',(-122.30467053223,-4.76622246247628,
132.017746994895));
#104520=CARTESIAN_POINT('Ctrl Pts',(-122.312321721774,-4.73276675584337,
132.149162134731));
#104521=CARTESIAN_POINT('Ctrl Pts',(-122.319972911319,-4.69386665576557,
132.279212488126));
#104522=CARTESIAN_POINT('Ctrl Pts',(-122.327624100864,-4.64966706477045,
132.40741372002));
#104523=CARTESIAN_POINT('Ctrl Pts',(-122.335276159506,-4.60546245315207,
132.535629514268));
#104524=CARTESIAN_POINT('Ctrl Pts',(-122.342928218147,-4.55595728469253,
132.661995389799));
#104525=CARTESIAN_POINT('Ctrl Pts',(-122.350580276789,-4.50134551602286,
132.786044650877));
#104526=CARTESIAN_POINT('Ctrl Pts',(-122.358604740093,-4.44407594267695,
132.916131048533));
#104527=CARTESIAN_POINT('Ctrl Pts',(-122.366629203397,-4.38119041985976,
133.043669224295));
#104528=CARTESIAN_POINT('Ctrl Pts',(-122.3746536667,-4.31296759164002,133.168148597898));
#104529=CARTESIAN_POINT('Ctrl Pts',(-122.382316960419,-4.24781537507506,
133.28702533342));
#104530=CARTESIAN_POINT('Ctrl Pts',(-122.389980254138,-4.17779608753363,
133.403112291733));
#104531=CARTESIAN_POINT('Ctrl Pts',(-122.397643547857,-4.10319706125064,
133.515994246773));
#104532=CARTESIAN_POINT('Ctrl Pts',(-122.405312002117,-4.0285477992074,
133.628952217695));
#104533=CARTESIAN_POINT('Ctrl Pts',(-122.412980456377,-3.94931289385773,
133.738700565194));
#104534=CARTESIAN_POINT('Ctrl Pts',(-122.420648910638,-3.86582016351056,
133.844856880661));
#104535=CARTESIAN_POINT('Ctrl Pts',(-122.428327883103,-3.78221291287369,
133.951158802242));
#104536=CARTESIAN_POINT('Ctrl Pts',(-122.436006855568,-3.69433644631845,
134.053858560136));
#104537=CARTESIAN_POINT('Ctrl Pts',(-122.443685828033,-3.60255570892061,
134.152610223946));
#104538=CARTESIAN_POINT('Ctrl Pts',(-122.444748497499,-3.58985445394045,
134.166276164069));
#104539=CARTESIAN_POINT('Ctrl Pts',(-122.445811166966,-3.57707848019253,
134.1798665576));
#104540=CARTESIAN_POINT('Ctrl Pts',(-122.446873836433,-3.56422880358217,
134.193380549377));
#104541=CARTESIAN_POINT('Ctrl Pts',(-122.454648170552,-3.47022245219701,
134.29224693319));
#104542=CARTESIAN_POINT('Ctrl Pts',(-122.462422504671,-3.37195047524916,
134.387355556349));
#104543=CARTESIAN_POINT('Ctrl Pts',(-122.47019683879,-3.26974540435205,
134.478315986541));
#104544=CARTESIAN_POINT('Ctrl Pts',(-122.477961591737,-3.16766629207076,
134.569164316131));
#104545=CARTESIAN_POINT('Ctrl Pts',(-122.485726344684,-3.06166401954631,
134.655874367237));
#104546=CARTESIAN_POINT('Ctrl Pts',(-122.493491097631,-2.95210965281732,
134.738090610873));
#104547=CARTESIAN_POINT('Ctrl Pts',(-122.501248138516,-2.84266409702982,
134.820225196177));
#104548=CARTESIAN_POINT('Ctrl Pts',(-122.509005179401,-2.72967377857668,
134.897874623053));
#104549=CARTESIAN_POINT('Ctrl Pts',(-122.516762220286,-2.61354443753827,
134.970722163989));
#104550=CARTESIAN_POINT('Ctrl Pts',(-122.524513411526,-2.49750267053945,
135.043514770027));
#104551=CARTESIAN_POINT('Ctrl Pts',(-122.532264602766,-2.3783269225019,
135.111512490866));
#104552=CARTESIAN_POINT('Ctrl Pts',(-122.540015794007,-2.25645335026092,
135.174440861749));
#104553=CARTESIAN_POINT('Ctrl Pts',(-122.547763690784,-2.13463157753873,
135.237342486395));
#104554=CARTESIAN_POINT('Ctrl Pts',(-122.555511587561,-2.01011460786944,
135.295178867441));
#104555=CARTESIAN_POINT('Ctrl Pts',(-122.563259484338,-1.88336453625771,
135.347720727228));
#104556=CARTESIAN_POINT('Ctrl Pts',(-122.571005760422,-1.75664097802889,
135.40025159639));
#104557=CARTESIAN_POINT('Ctrl Pts',(-122.578752036506,-1.6276856079139,
135.447489997551));
#104558=CARTESIAN_POINT('Ctrl Pts',(-122.58649831259,-1.49698153978166,
135.489254355107));
#104559=CARTESIAN_POINT('Ctrl Pts',(-122.594244645855,-1.36627650682186,
135.531019020959));
#104560=CARTESIAN_POINT('Ctrl Pts',(-122.601990979121,-1.23382312250193,
135.567309443575));
#104561=CARTESIAN_POINT('Ctrl Pts',(-122.609737312386,-1.10012035576805,
135.597993714219));
#104562=CARTESIAN_POINT('Ctrl Pts',(-122.617485380389,-0.966387647226413,
135.628684856393));
#104563=CARTESIAN_POINT('Ctrl Pts',(-122.625233448392,-0.831405380506198,
135.653767260942));
#104564=CARTESIAN_POINT('Ctrl Pts',(-122.632981516395,-0.695683032602759,
135.673160077458));
#104565=CARTESIAN_POINT('Ctrl Pts',(-122.640737819137,-0.559816437372668,
135.692573504891));
#104566=CARTESIAN_POINT('Ctrl Pts',(-122.648494121879,-0.423208577358247,
135.706285209443));
#104567=CARTESIAN_POINT('Ctrl Pts',(-122.656250424621,-0.286374932773004,
135.714266162521));
#104568=CARTESIAN_POINT('Ctrl Pts',(-122.664010867135,-0.149468255951664,
135.722251375273));
#104569=CARTESIAN_POINT('Ctrl Pts',(-122.671771309649,-0.0123359451584667,
135.724499735477));
#104570=CARTESIAN_POINT('Ctrl Pts',(-122.679531752163,0.124507191482485,
135.721034393786));
#104571=CARTESIAN_POINT('Ctrl Pts',(-122.687304652429,0.261570000874363,
135.717563489221));
#104572=CARTESIAN_POINT('Ctrl Pts',(-122.695077552694,0.398342318170785,
135.708360580163));
#104573=CARTESIAN_POINT('Ctrl Pts',(-122.70285045296,0.534314223231023,
135.693500764192));
#104574=CARTESIAN_POINT('Ctrl Pts',(-122.710340788721,0.665343207046069,
135.679181139962));
#104575=CARTESIAN_POINT('Ctrl Pts',(-122.717831124483,0.795628657692951,
135.659608799687));
#104576=CARTESIAN_POINT('Ctrl Pts',(-122.725321460245,0.924725721187771,
135.634895308785));
#104577=CARTESIAN_POINT('Ctrl Pts',(-122.733095794364,1.0587175390868,135.609244798364));
#104578=CARTESIAN_POINT('Ctrl Pts',(-122.740870128483,1.19185352133314,
135.577974334926));
#104579=CARTESIAN_POINT('Ctrl Pts',(-122.748644462602,1.32362544470394,
135.541152648533));
#104580=CARTESIAN_POINT('Ctrl Pts',(-122.756409215549,1.45523497095563,
135.504376341578));
#104581=CARTESIAN_POINT('Ctrl Pts',(-122.764173968496,1.58548341025536,
135.462062528197));
#104582=CARTESIAN_POINT('Ctrl Pts',(-122.771938721444,1.71387107574249,
135.414331224656));
#104583=CARTESIAN_POINT('Ctrl Pts',(-122.779695762329,1.8421312247903,135.366647328519));
#104584=CARTESIAN_POINT('Ctrl Pts',(-122.787452803213,1.96853391383312,
135.313556785472));
#104585=CARTESIAN_POINT('Ctrl Pts',(-122.795209844098,2.0925933586198,135.255229757179));
#104586=CARTESIAN_POINT('Ctrl Pts',(-122.802961035338,2.21655924921363,
135.196946713752));
#104587=CARTESIAN_POINT('Ctrl Pts',(-122.810712226579,2.33818506039435,
135.133435210747));
#104588=CARTESIAN_POINT('Ctrl Pts',(-122.818463417819,2.45700412376505,
135.064913844355));
#104589=CARTESIAN_POINT('Ctrl Pts',(-122.826211314596,2.57577268586469,
134.996421601372));
#104590=CARTESIAN_POINT('Ctrl Pts',(-122.833959211373,2.69173653485233,
134.922923924974));
#104591=CARTESIAN_POINT('Ctrl Pts',(-122.84170710815,2.80445299930199,134.8446856586));
#104592=CARTESIAN_POINT('Ctrl Pts',(-122.849453384234,2.91714588589718,
134.766463757985));
#104593=CARTESIAN_POINT('Ctrl Pts',(-122.857199660318,3.02659241811215,
134.683503462592));
#104594=CARTESIAN_POINT('Ctrl Pts',(-122.864945936402,3.13237869640231,
134.596113083752));
#104595=CARTESIAN_POINT('Ctrl Pts',(-122.872692269667,3.23816575558289,
134.508722059816));
#104596=CARTESIAN_POINT('Ctrl Pts',(-122.880438602933,3.34029220550706,
134.41690113618));
#104597=CARTESIAN_POINT('Ctrl Pts',(-122.888184936198,3.43837736271539,
134.320998809656));
#104598=CARTESIAN_POINT('Ctrl Pts',(-122.895933004201,3.53648448541448,
134.225075006471));
#104599=CARTESIAN_POINT('Ctrl Pts',(-122.903681072204,3.63054823502001,
134.125068254915));
#104600=CARTESIAN_POINT('Ctrl Pts',(-122.911429140207,3.72022520503315,
134.021363490791));
#104601=CARTESIAN_POINT('Ctrl Pts',(-122.919185442949,3.80999748479707,
133.917548508009));
#104602=CARTESIAN_POINT('Ctrl Pts',(-122.926941745691,3.89537341534292,
133.810027957682));
#104603=CARTESIAN_POINT('Ctrl Pts',(-122.934698048432,3.97604994444538,
133.699219837248));
#104604=CARTESIAN_POINT('Ctrl Pts',(-122.942458490946,4.05676953304054,
133.588352575183));
#104605=CARTESIAN_POINT('Ctrl Pts',(-122.950218933461,4.13278450578335,
133.474194571934));
#104606=CARTESIAN_POINT('Ctrl Pts',(-122.957979375975,4.20383607360944,
133.35719146365));
#104607=CARTESIAN_POINT('Ctrl Pts',(-122.96575227624,4.27500169972006,133.24000053159));
#104608=CARTESIAN_POINT('Ctrl Pts',(-122.973525176505,4.3411878100385,133.119955710316));
#104609=CARTESIAN_POINT('Ctrl Pts',(-122.981298076771,4.40218196199473,
132.997526602162));
#104610=CARTESIAN_POINT('Ctrl Pts',(-122.988788412533,4.46095882289482,
132.879548100464));
#104611=CARTESIAN_POINT('Ctrl Pts',(-122.996278748296,4.51491452718198,
132.759355932951));
#104612=CARTESIAN_POINT('Ctrl Pts',(-123.003769084058,4.56390248355713,
132.637384671713));
#104613=CARTESIAN_POINT('Ctrl Pts',(-123.011543418177,4.61474783318588,
132.510788833037));
#104614=CARTESIAN_POINT('Ctrl Pts',(-123.019317752296,4.66040235710147,
132.381875311254));
#104615=CARTESIAN_POINT('Ctrl Pts',(-123.027092086415,4.7006491727853,132.251108839232));
#104616=CARTESIAN_POINT('Ctrl Pts',(-123.034856839362,4.74084638786554,
132.1205035252));
#104617=CARTESIAN_POINT('Ctrl Pts',(-123.042621592309,4.77564904121475,
131.988050174685));
#104618=CARTESIAN_POINT('Ctrl Pts',(-123.050386345256,4.80488801296413,
131.854234060117));
#104619=CARTESIAN_POINT('Ctrl Pts',(-123.058143386141,4.83409794415466,
131.7205508536));
#104620=CARTESIAN_POINT('Ctrl Pts',(-123.065900427026,4.85775510767214,
131.585507956072));
#104621=CARTESIAN_POINT('Ctrl Pts',(-123.073657467911,4.87574008708958,
131.449606048118));
#104622=CARTESIAN_POINT('Ctrl Pts',(-123.081408659151,4.89371150389416,
131.313806624849));
#104623=CARTESIAN_POINT('Ctrl Pts',(-123.089159850391,4.90601919949514,
131.17714986655));
#104624=CARTESIAN_POINT('Ctrl Pts',(-123.096911041632,4.91259483939269,
131.040146551142));
#104625=CARTESIAN_POINT('Ctrl Pts',(-123.104658938409,4.91916768446787,
130.903201465798));
#104626=CARTESIAN_POINT('Ctrl Pts',(-123.112406835186,4.92001330070399,
130.765910506004));
#104627=CARTESIAN_POINT('Ctrl Pts',(-123.120154731963,4.91511523366853,
130.628789258115));
#104628=CARTESIAN_POINT('Ctrl Pts',(-123.127901008047,4.91021819120311,
130.491696693035));
#104629=CARTESIAN_POINT('Ctrl Pts',(-123.135647284131,4.89957986917322,
130.354774159717));
#104630=CARTESIAN_POINT('Ctrl Pts',(-123.143393560215,4.88323593581998,
130.218536533377));
#104631=CARTESIAN_POINT('Ctrl Pts',(-123.15113989348,4.86689188181951,130.08229790136));
#104632=CARTESIAN_POINT('Ctrl Pts',(-123.158886226746,4.84484217902196,
129.946744574592));
#104633=CARTESIAN_POINT('Ctrl Pts',(-123.166632560011,4.81717425895649,
129.812385203885));
#104634=CARTESIAN_POINT('Ctrl Pts',(-123.174380628014,4.78950014285218,
129.67799574433));
#104635=CARTESIAN_POINT('Ctrl Pts',(-123.182128696017,4.75620538472538,
129.544801155745));
#104636=CARTESIAN_POINT('Ctrl Pts',(-123.18987676402,4.71742822236983,129.41329842295));
#104637=CARTESIAN_POINT('Ctrl Pts',(-123.197633066762,4.67860984718462,
129.281655927486));
#104638=CARTESIAN_POINT('Ctrl Pts',(-123.205389369504,4.63429753893669,
129.151709255358));
#104639=CARTESIAN_POINT('Ctrl Pts',(-123.213145672245,4.58467916357902,
129.023939310812));
#104640=CARTESIAN_POINT('Ctrl Pts',(-123.22090611476,4.53503430540045,128.896101171599));
#104641=CARTESIAN_POINT('Ctrl Pts',(-123.228666557274,4.48007789368029,
128.770442432954));
#104642=CARTESIAN_POINT('Ctrl Pts',(-123.236426999788,4.42004497292152,
128.647421698669));
#104643=CARTESIAN_POINT('Ctrl Pts',(-123.244199900053,4.35991568198887,
128.524203480581));
#104644=CARTESIAN_POINT('Ctrl Pts',(-123.251972800319,4.29469378331742,
128.403632073326));
#104645=CARTESIAN_POINT('Ctrl Pts',(-123.259745700584,4.22465953625129,
128.286140042386));
#104646=CARTESIAN_POINT('Ctrl Pts',(-123.267236036346,4.15717121047164,
128.172919142715));
#104647=CARTESIAN_POINT('Ctrl Pts',(-123.274726372108,4.08521451203541,
128.062557878201));
#104648=CARTESIAN_POINT('Ctrl Pts',(-123.28221670787,4.0090758225709,127.955414477082));
#104649=CARTESIAN_POINT('Ctrl Pts',(-123.289991041989,3.93005031155317,
127.844208701344));
#104650=CARTESIAN_POINT('Ctrl Pts',(-123.297765376108,3.84626910000627,
127.736117349959));
#104651=CARTESIAN_POINT('Ctrl Pts',(-123.305539710228,3.75800595055514,
127.631574091798));
#104652=CARTESIAN_POINT('Ctrl Pts',(-123.313304463175,3.66985157754765,
127.52715967386));
#104653=CARTESIAN_POINT('Ctrl Pts',(-123.321069216122,3.57722650672185,
127.426284944628));
#104654=CARTESIAN_POINT('Ctrl Pts',(-123.328833969069,3.48044759809827,
127.32935449104));
#104655=CARTESIAN_POINT('Ctrl Pts',(-123.336591009954,3.38376481165134,
127.232520310145));
#104656=CARTESIAN_POINT('Ctrl Pts',(-123.344348050839,3.2829366720871,127.139622883753));
#104657=CARTESIAN_POINT('Ctrl Pts',(-123.352105091724,3.17831986866529,
127.051033310369));
#104658=CARTESIAN_POINT('Ctrl Pts',(-123.359856282964,3.07378195758859,
126.962510543073));
#104659=CARTESIAN_POINT('Ctrl Pts',(-123.367607474204,2.96546136661579,
126.878289414304));
#104660=CARTESIAN_POINT('Ctrl Pts',(-123.375358665444,2.85375089121121,
126.798703503757));
#104661=CARTESIAN_POINT('Ctrl Pts',(-123.383106562221,2.74208789573849,
126.719151419344));
#104662=CARTESIAN_POINT('Ctrl Pts',(-123.390854458998,2.6270381992121,126.644230861169));
#104663=CARTESIAN_POINT('Ctrl Pts',(-123.398602355775,2.50902668501259,
126.574234359829));
#104664=CARTESIAN_POINT('Ctrl Pts',(-123.40634863186,2.39103985627782,126.504252500249));
#104665=CARTESIAN_POINT('Ctrl Pts',(-123.414094907944,2.27009277823699,
126.439192848089));
#104666=CARTESIAN_POINT('Ctrl Pts',(-123.421841184028,2.14663790954584,
126.379303697277));
#104667=CARTESIAN_POINT('Ctrl Pts',(-123.429587517293,2.02318212953872,
126.319414104377));
#104668=CARTESIAN_POINT('Ctrl Pts',(-123.437333850559,1.89721887370198,
126.264695259628));
#104669=CARTESIAN_POINT('Ctrl Pts',(-123.445080183824,1.76922334324927,
126.215348542598));
#104670=CARTESIAN_POINT('Ctrl Pts',(-123.452828251827,1.6411991490855,126.165990774714));
#104671=CARTESIAN_POINT('Ctrl Pts',(-123.46057631983,1.51114213940536,126.122007669094));
#104672=CARTESIAN_POINT('Ctrl Pts',(-123.468324387833,1.37954516251603,
126.083551554802));
#104673=CARTESIAN_POINT('Ctrl Pts',(-123.476080690575,1.24780832279347,
126.045054568893));
#104674=CARTESIAN_POINT('Ctrl Pts',(-123.483836993317,1.11452862225466,
126.012096418403));
#104675=CARTESIAN_POINT('Ctrl Pts',(-123.491593296058,0.980212205397892,
125.984778986876));
#104676=CARTESIAN_POINT('Ctrl Pts',(-123.499353738573,0.845824099825262,
125.957446975212));
#104677=CARTESIAN_POINT('Ctrl Pts',(-123.507114181087,0.710398561242755,
125.935761743216));
#104678=CARTESIAN_POINT('Ctrl Pts',(-123.514874623601,0.574448473305037,
125.919773427842));
#104679=CARTESIAN_POINT('Ctrl Pts',(-123.522647523867,0.438280146216711,
125.903759446604));
#104680=CARTESIAN_POINT('Ctrl Pts',(-123.530420424132,0.301585977167221,
125.893460686395));
#104681=CARTESIAN_POINT('Ctrl Pts',(-123.538193324397,0.164881382769034,
125.8888751693));
#104682=CARTESIAN_POINT('Ctrl Pts',(-123.545683660159,0.033146344718272,
125.884456347301));
#104683=CARTESIAN_POINT('Ctrl Pts',(-123.553173995921,-0.0985980658538286,
125.885342596421));
#104684=CARTESIAN_POINT('Ctrl Pts',(-123.560664331683,-0.229895665117554,
125.8914866068));
#104685=CARTESIAN_POINT('Ctrl Pts',(-123.568438665802,-0.366171452767279,
125.8978635692));
#104686=CARTESIAN_POINT('Ctrl Pts',(-123.576212999921,-0.502397559304757,
125.90992505958));
#104687=CARTESIAN_POINT('Ctrl Pts',(-123.58398733404,-0.638061151439749,
125.927675162308));
#104688=CARTESIAN_POINT('Ctrl Pts',(-123.591752086988,-0.77355755032167,
125.945403389622));
#104689=CARTESIAN_POINT('Ctrl Pts',(-123.599516839935,-0.908492430219827,
125.968806229833));
#104690=CARTESIAN_POINT('Ctrl Pts',(-123.607281592882,-1.04235413010378,
125.997835788757));
#104691=CARTESIAN_POINT('Ctrl Pts',(-123.615038633767,-1.17608287666028,
126.026836515114));
#104692=CARTESIAN_POINT('Ctrl Pts',(-123.622795674652,-1.30874018477532,
126.06145275642));
#104693=CARTESIAN_POINT('Ctrl Pts',(-123.630552715537,-1.43982103950688,
126.101585007706));
#104694=CARTESIAN_POINT('Ctrl Pts',(-123.638303906777,-1.57080304514604,
126.14168699495));
#104695=CARTESIAN_POINT('Ctrl Pts',(-123.646055098017,-1.70021059134348,
126.187296598619));
#104696=CARTESIAN_POINT('Ctrl Pts',(-123.653806289257,-1.82755071251333,
126.238263656737));
#104697=CARTESIAN_POINT('Ctrl Pts',(-123.661554186035,-1.95483671073461,
126.289209052496));
#104698=CARTESIAN_POINT('Ctrl Pts',(-123.669302082812,-2.08005666940539,
126.34550722883));
#104699=CARTESIAN_POINT('Ctrl Pts',(-123.677049979589,-2.20273481440205,
126.406958839252));
#104700=CARTESIAN_POINT('Ctrl Pts',(-123.684796255673,-2.32538729777607,
126.468397595322));
#104701=CARTESIAN_POINT('Ctrl Pts',(-123.692542531757,-2.44549867570165,
126.534987466314));
#104702=CARTESIAN_POINT('Ctrl Pts',(-123.700288807841,-2.56261548650922,
126.60648199488));
#104703=CARTESIAN_POINT('Ctrl Pts',(-123.708035141107,-2.67973316184601,
126.677977051202));
#104704=CARTESIAN_POINT('Ctrl Pts',(-123.715781474372,-2.79385589225454,
126.754376633633));
#104705=CARTESIAN_POINT('Ctrl Pts',(-123.723527807637,-2.90455739353712,
126.83538979251));
#104706=CARTESIAN_POINT('Ctrl Pts',(-123.73127587564,-3.01528368565291,
126.916421093721));
#104707=CARTESIAN_POINT('Ctrl Pts',(-123.739023943643,-3.12258690862798,
127.002067796436));
#104708=CARTESIAN_POINT('Ctrl Pts',(-123.746772011646,-3.22607250715903,
127.091997590995));
#104709=CARTESIAN_POINT('Ctrl Pts',(-123.754528314388,-3.32966809141612,
127.18202296401));
#104710=CARTESIAN_POINT('Ctrl Pts',(-123.76228461713,-3.42943765052578,
127.276340265363));
#104711=CARTESIAN_POINT('Ctrl Pts',(-123.770040919872,-3.52502188351182,
127.374578731897));
#104712=CARTESIAN_POINT('Ctrl Pts',(-123.777801362386,-3.62065713268125,
127.472869631259));
#104713=CARTESIAN_POINT('Ctrl Pts',(-123.7855618049,-3.71210234407415,127.575085574734));
#104714=CARTESIAN_POINT('Ctrl Pts',(-123.793322247414,-3.79903810990706,
127.680822159027));
#104715=CARTESIAN_POINT('Ctrl Pts',(-123.80109514768,-3.88611343274884,
127.786728481071));
#104716=CARTESIAN_POINT('Ctrl Pts',(-123.808868047945,-3.96866460870062,
127.896166425418));
#104717=CARTESIAN_POINT('Ctrl Pts',(-123.816640948211,-4.04641470656897,
128.008701288363));
#104718=CARTESIAN_POINT('Ctrl Pts',(-123.824131283973,-4.12133839254038,
128.117145225583));
#104719=CARTESIAN_POINT('Ctrl Pts',(-123.831621619735,-4.19180383800849,
128.228464568694));
#104720=CARTESIAN_POINT('Ctrl Pts',(-123.839111955497,-4.25760426759582,
128.342249945186));
#104721=CARTESIAN_POINT('Ctrl Pts',(-123.847202547063,-4.32867777051783,
128.465153782429));
#104722=CARTESIAN_POINT('Ctrl Pts',(-123.85529313863,-4.39451845037392,
128.591297548042));
#104723=CARTESIAN_POINT('Ctrl Pts',(-123.863383730196,-4.45483135510529,
128.720215550621));
#104724=CARTESIAN_POINT('Ctrl Pts',(-123.871462872162,-4.51505890654167,
128.848951111708));
#104725=CARTESIAN_POINT('Ctrl Pts',(-123.879542014128,-4.56977411494359,
128.980452780504));
#104726=CARTESIAN_POINT('Ctrl Pts',(-123.887621156094,-4.61872659268647,
129.114228159884));
#104727=CARTESIAN_POINT('Ctrl Pts',(-123.895686767567,-4.66759708757046,
129.247779499776));
#104728=CARTESIAN_POINT('Ctrl Pts',(-123.903752379041,-4.71072396876428,
129.383596637296));
#104729=CARTESIAN_POINT('Ctrl Pts',(-123.911817990514,-4.74790408347292,
129.521165434969));
#104730=CARTESIAN_POINT('Ctrl Pts',(-123.913014248927,-4.75341848559683,
129.541569074818));
#104731=CARTESIAN_POINT('Ctrl Pts',(-123.914210507341,-4.75880215823508,
129.562011208398));
#104732=CARTESIAN_POINT('Ctrl Pts',(-123.915406765754,-4.76405452823402,
129.582490119308));
#104733=CARTESIAN_POINT('Ctrl Pts',(-122.165194063467,-4.76405452823402,
129.582490119308));
#104734=CARTESIAN_POINT('Ctrl Pts',(-122.166271446518,-4.76875350298938,
129.600811350562));
#104735=CARTESIAN_POINT('Ctrl Pts',(-122.167348829569,-4.77334578412048,
129.619155771924));
#104736=CARTESIAN_POINT('Ctrl Pts',(-122.16842621262,-4.77783118013098,
129.63752203547));
#104737=CARTESIAN_POINT('Ctrl Pts',(-122.178817676348,-4.82109325846368,
129.814666423688));
#104738=CARTESIAN_POINT('Ctrl Pts',(-122.189209140076,-4.854519516994,129.994300071186));
#104739=CARTESIAN_POINT('Ctrl Pts',(-122.199600603804,-4.87787888710515,
130.175488114404));
#104740=CARTESIAN_POINT('Ctrl Pts',(-122.209731485858,-4.90065248567181,
130.352132593329));
#104741=CARTESIAN_POINT('Ctrl Pts',(-122.219862367913,-4.91385781485816,
130.530254837794));
#104742=CARTESIAN_POINT('Ctrl Pts',(-122.229993249967,-4.91732476503059,
130.708965556285));
#104743=CARTESIAN_POINT('Ctrl Pts',(-122.231709021302,-4.91791192947415,
130.739232094412));
#104744=CARTESIAN_POINT('Ctrl Pts',(-122.233424792636,-4.91821987222497,
130.769515450041));
#104745=CARTESIAN_POINT('Ctrl Pts',(-122.235140563971,-4.91824789589999,
130.799811224715));
#104746=CARTESIAN_POINT('',(-121.889859435959,-4.91824956029332,130.806440322977));
#104747=CARTESIAN_POINT('Ctrl Pts',(-121.81971904495,-4.76405452823411,
129.582490119308));
#104748=CARTESIAN_POINT('Ctrl Pts',(-121.82739965095,-4.79781016501553,
129.714102834806));
#104749=CARTESIAN_POINT('Ctrl Pts',(-121.835080256949,-4.8260827257844,
129.847018133833));
#104750=CARTESIAN_POINT('Ctrl Pts',(-121.842760862948,-4.84879609593379,
129.980734802916));
#104751=CARTESIAN_POINT('Ctrl Pts',(-121.850610625117,-4.87200970091906,
130.11739642185));
#104752=CARTESIAN_POINT('Ctrl Pts',(-121.858460387285,-4.88941633854078,
130.254894678313));
#104753=CARTESIAN_POINT('Ctrl Pts',(-121.866310149453,-4.90099086532254,
130.392691332186));
#104754=CARTESIAN_POINT('Ctrl Pts',(-121.874159911622,-4.91256539210432,
130.53048798606));
#104755=CARTESIAN_POINT('Ctrl Pts',(-121.88200967379,-4.918307854094,130.668582596542));
#104756=CARTESIAN_POINT('Ctrl Pts',(-121.889859435959,-4.91824956029332,
130.806440322977));
#104757=CARTESIAN_POINT('Ctrl Pts',(-121.889859435993,-4.91824956029306,
130.80644032358));
#104758=CARTESIAN_POINT('Ctrl Pts',(-121.896428818984,-4.91820077481326,
130.921811997752));
#104759=CARTESIAN_POINT('Ctrl Pts',(-121.902998201974,-4.91409278695161,
131.037093702136));
#104760=CARTESIAN_POINT('Ctrl Pts',(-121.909567584965,-4.90594236236138,
131.152085508375));
#104761=CARTESIAN_POINT('Ctrl Pts',(-121.917341919084,-4.8962969932197,
131.28816902245));
#104762=CARTESIAN_POINT('Ctrl Pts',(-121.925116253203,-4.8809699253112,
131.424066456723));
#104763=CARTESIAN_POINT('Ctrl Pts',(-121.932890587322,-4.85996938202834,
131.559265027572));
#104764=CARTESIAN_POINT('Ctrl Pts',(-121.940655340269,-4.8389947200382,
131.694296978266));
#104765=CARTESIAN_POINT('Ctrl Pts',(-121.948420093217,-4.81236055420518,
131.828631396617));
#104766=CARTESIAN_POINT('Ctrl Pts',(-121.956184846164,-4.78012704337739,
131.961757918268));
#104767=CARTESIAN_POINT('Ctrl Pts',(-121.963941887049,-4.74792554732696,
132.094752216781));
#104768=CARTESIAN_POINT('Ctrl Pts',(-121.971698927934,-4.71013586502534,
132.226540628525));
#104769=CARTESIAN_POINT('Ctrl Pts',(-121.979455968819,-4.66686959175194,
132.356620671836));
#104770=CARTESIAN_POINT('Ctrl Pts',(-121.987207160059,-4.62363594591171,
132.486602620773));
#104771=CARTESIAN_POINT('Ctrl Pts',(-121.994958351299,-4.57493405238862,
132.614878396067));
#104772=CARTESIAN_POINT('Ctrl Pts',(-122.002709542539,-4.52092585973126,
132.740958777565));
#104773=CARTESIAN_POINT('Ctrl Pts',(-122.010457439316,-4.46694062199641,
132.866985571539));
#104774=CARTESIAN_POINT('Ctrl Pts',(-122.018205336093,-4.40765372440739,
132.990818468955));
#104775=CARTESIAN_POINT('Ctrl Pts',(-122.02595323287,-4.34327587331147,
133.111986616468));
#104776=CARTESIAN_POINT('Ctrl Pts',(-122.033699508955,-4.27891148867419,
133.233129418217));
#104777=CARTESIAN_POINT('Ctrl Pts',(-122.041445785039,-4.20945845203306,
133.351608233738));
#104778=CARTESIAN_POINT('Ctrl Pts',(-122.049192061123,-4.1351740315922,
133.466975646245));
#104779=CARTESIAN_POINT('Ctrl Pts',(-122.056938394388,-4.06088906280073,
133.582343910367));
#104780=CARTESIAN_POINT('Ctrl Pts',(-122.064684727654,-3.98177285070284,
133.694600396927));
#104781=CARTESIAN_POINT('Ctrl Pts',(-122.072431060919,-3.89812649082136,
133.803325926478));
#104782=CARTESIAN_POINT('Ctrl Pts',(-122.080179128922,-3.81446139891765,
133.912075804357));
#104783=CARTESIAN_POINT('Ctrl Pts',(-122.087927196925,-3.72626437885274,
134.017292841944));
#104784=CARTESIAN_POINT('Ctrl Pts',(-122.095675264928,-3.63387711282874,
134.118590572074));
#104785=CARTESIAN_POINT('Ctrl Pts',(-122.10343156767,-3.54139165651886,
134.219995962638));
#104786=CARTESIAN_POINT('Ctrl Pts',(-122.111187870412,-3.44470732189457,
134.317473435408));
#104787=CARTESIAN_POINT('Ctrl Pts',(-122.118944173154,-3.34420338757461,
134.410672690173));
#104788=CARTESIAN_POINT('Ctrl Pts',(-122.126704615668,-3.24364581127851,
134.503921688187));
#104789=CARTESIAN_POINT('Ctrl Pts',(-122.134465058182,-3.13926487053839,
134.592887664816));
#104790=CARTESIAN_POINT('Ctrl Pts',(-122.142225500696,-3.03147251709762,
134.677261008821));
#104791=CARTESIAN_POINT('Ctrl Pts',(-122.149998400962,-2.92350712580204,
134.761769796408));
#104792=CARTESIAN_POINT('Ctrl Pts',(-122.157771301227,-2.8121196962751,
134.84167099075));
#104793=CARTESIAN_POINT('Ctrl Pts',(-122.165544201493,-2.69775145262236,
134.916698172093));
#104794=CARTESIAN_POINT('Ctrl Pts',(-122.173034537255,-2.58754078270355,
134.988997926412));
#104795=CARTESIAN_POINT('Ctrl Pts',(-122.180524873017,-2.47456252041896,
135.056771722278));
#104796=CARTESIAN_POINT('Ctrl Pts',(-122.188015208779,-2.35923088242923,
135.119822667671));
#104797=CARTESIAN_POINT('Ctrl Pts',(-122.195789542898,-2.23952641032965,
135.185264208823));
#104798=CARTESIAN_POINT('Ctrl Pts',(-122.203563877017,-2.11690739547165,
135.245824995209));
#104799=CARTESIAN_POINT('Ctrl Pts',(-122.211338211136,-1.99180970218241,
135.301234773332));
#104800=CARTESIAN_POINT('Ctrl Pts',(-122.219102964083,-1.86686618061986,
135.356576263854));
#104801=CARTESIAN_POINT('Ctrl Pts',(-122.22686771703,-1.73945041270459,
135.406779220239));
#104802=CARTESIAN_POINT('Ctrl Pts',(-122.234632469977,-1.61002429975069,
135.451618391427));
#104803=CARTESIAN_POINT('Ctrl Pts',(-122.242389510862,-1.48072673463677,
135.496413027718));
#104804=CARTESIAN_POINT('Ctrl Pts',(-122.250146551747,-1.34942316504612,
135.535854353397));
#104805=CARTESIAN_POINT('Ctrl Pts',(-122.257903592633,-1.21659666300919,
135.569764653118));
#104806=CARTESIAN_POINT('Ctrl Pts',(-122.265654783873,-1.08387032647049,
135.603649380818));
#104807=CARTESIAN_POINT('Ctrl Pts',(-122.273405975113,-0.949623720698228,
135.632011288344));
#104808=CARTESIAN_POINT('Ctrl Pts',(-122.281157166353,-0.814355977606796,
135.654722192154));
#104809=CARTESIAN_POINT('Ctrl Pts',(-122.28890506313,-0.679145726914747,
135.677423443224));
#104810=CARTESIAN_POINT('Ctrl Pts',(-122.296652959907,-0.542915586878875,
135.69447840303));
#104811=CARTESIAN_POINT('Ctrl Pts',(-122.304400856684,-0.406175591682259,
135.705809837054));
#104812=CARTESIAN_POINT('Ctrl Pts',(-122.312147132769,-0.269464199544866,
135.717138900787));
#104813=CARTESIAN_POINT('Ctrl Pts',(-122.319893408853,-0.132243553763652,
135.722746787843));
#104814=CARTESIAN_POINT('Ctrl Pts',(-122.327639684937,0.00497086149853406,
135.722608105547));
#104815=CARTESIAN_POINT('Ctrl Pts',(-122.335386018202,0.14218628964655,
135.722469422228));
#104816=CARTESIAN_POINT('Ctrl Pts',(-122.343132351467,0.279395096218759,
135.716584085305));
#104817=CARTESIAN_POINT('Ctrl Pts',(-122.350878684733,0.416081864188433,
135.704978838239));
#104818=CARTESIAN_POINT('Ctrl Pts',(-122.358626752736,0.552799242211888,
135.693370992259));
#104819=CARTESIAN_POINT('Ctrl Pts',(-122.366374820739,0.688993959512517,
135.676040720293));
#104820=CARTESIAN_POINT('Ctrl Pts',(-122.374122888742,0.824156182742329,
135.653066594314));
#104821=CARTESIAN_POINT('Ctrl Pts',(-122.381879191484,0.959462057991624,
135.630068051159));
#104822=CARTESIAN_POINT('Ctrl Pts',(-122.389635494226,1.09373286104974,
135.601413737249));
#104823=CARTESIAN_POINT('Ctrl Pts',(-122.397391796968,1.22646886506869,
135.567233404605));
#104824=CARTESIAN_POINT('Ctrl Pts',(-122.405152239482,1.35927571428996,
135.533034828888));
#104825=CARTESIAN_POINT('Ctrl Pts',(-122.412912681996,1.49054575819109,
135.493304470704));
#104826=CARTESIAN_POINT('Ctrl Pts',(-122.42067312451,1.61979584208923,135.448221564284));
#104827=CARTESIAN_POINT('Ctrl Pts',(-122.428446024776,1.74925340969599,
135.40306628678));
#104828=CARTESIAN_POINT('Ctrl Pts',(-122.436218925041,1.87668417386388,
135.3525414349));
#104829=CARTESIAN_POINT('Ctrl Pts',(-122.443991825306,2.00162549570208,
135.296874216594));
#104830=CARTESIAN_POINT('Ctrl Pts',(-122.451482161068,2.1220248857792,135.243230641893));
#104831=CARTESIAN_POINT('Ctrl Pts',(-122.45897249683,2.24011241010403,135.184812222256));
#104832=CARTESIAN_POINT('Ctrl Pts',(-122.466462832592,2.35549852362121,
135.121861024945));
#104833=CARTESIAN_POINT('Ctrl Pts',(-122.474237166711,2.47525953670711,
135.056523013852));
#104834=CARTESIAN_POINT('Ctrl Pts',(-122.48201150083,2.59248961413143,134.986094748223));
#104835=CARTESIAN_POINT('Ctrl Pts',(-122.489785834949,2.70672578865574,
134.910796854442));
#104836=CARTESIAN_POINT('Ctrl Pts',(-122.497550587896,2.82082117730422,
134.835591758586));
#104837=CARTESIAN_POINT('Ctrl Pts',(-122.505315340843,2.9319296811931,134.755529188638));
#104838=CARTESIAN_POINT('Ctrl Pts',(-122.51308009379,3.03961212128482,134.670876001557));
#104839=CARTESIAN_POINT('Ctrl Pts',(-122.520837134675,3.14718760965899,
134.586306893215));
#104840=CARTESIAN_POINT('Ctrl Pts',(-122.52859417556,3.25134350062011,134.497156481345));
#104841=CARTESIAN_POINT('Ctrl Pts',(-122.536351216445,3.35166916498331,
134.403735128644));
#104842=CARTESIAN_POINT('Ctrl Pts',(-122.544102407686,3.45191917298246,
134.310384225712));
#104843=CARTESIAN_POINT('Ctrl Pts',(-122.551853598926,3.54834441860959,
134.212769058011));
#104844=CARTESIAN_POINT('Ctrl Pts',(-122.559604790166,3.64056726442985,
134.111240273021));
#104845=CARTESIAN_POINT('Ctrl Pts',(-122.567352686943,3.73275091308064,
134.009754640473));
#104846=CARTESIAN_POINT('Ctrl Pts',(-122.57510058372,3.82073545208235,133.904358987789));
#104847=CARTESIAN_POINT('Ctrl Pts',(-122.582848480497,3.90418021591382,
133.795440674028));
#104848=CARTESIAN_POINT('Ctrl Pts',(-122.590594756581,3.98760752489955,
133.686545143631));
#104849=CARTESIAN_POINT('Ctrl Pts',(-122.598341032665,4.0664967099489,133.574128727979));
#104850=CARTESIAN_POINT('Ctrl Pts',(-122.606087308749,4.14054777570314,
133.458611393137));
#104851=CARTESIAN_POINT('Ctrl Pts',(-122.613833642014,4.21459938808562,
133.343093205572));
#104852=CARTESIAN_POINT('Ctrl Pts',(-122.62157997528,4.28381259891479,133.224474382284));
#104853=CARTESIAN_POINT('Ctrl Pts',(-122.629326308545,4.34793131272805,
133.103203013708));
#104854=CARTESIAN_POINT('Ctrl Pts',(-122.637074376548,4.41206438548262,
132.98190448725));
#104855=CARTESIAN_POINT('Ctrl Pts',(-122.644822444551,4.47110050830124,
132.857952579038));
#104856=CARTESIAN_POINT('Ctrl Pts',(-122.652570512554,4.52483020863011,
132.731818696376));
#104857=CARTESIAN_POINT('Ctrl Pts',(-122.660326815296,4.57861701352396,
132.605550757122));
#104858=CARTESIAN_POINT('Ctrl Pts',(-122.668083118038,4.62708597649866,
132.477096571174));
#104859=CARTESIAN_POINT('Ctrl Pts',(-122.675839420779,4.6700761470373,132.346946707019));
#104860=CARTESIAN_POINT('Ctrl Pts',(-122.683599863294,4.71308926272436,
132.216727377963));
#104861=CARTESIAN_POINT('Ctrl Pts',(-122.691360305808,4.75061765233928,
132.084810943202));
#104862=CARTESIAN_POINT('Ctrl Pts',(-122.699120748322,4.78255095380984,
131.951700774935));
#104863=CARTESIAN_POINT('Ctrl Pts',(-122.706893648587,4.81453551745083,
131.81837692641));
#104864=CARTESIAN_POINT('Ctrl Pts',(-122.714666548853,4.84090696932823,
131.68385589891));
#104865=CARTESIAN_POINT('Ctrl Pts',(-122.722439449118,4.86160639830543,
131.548649735084));
#104866=CARTESIAN_POINT('Ctrl Pts',(-122.72992978488,4.8815533509006,131.418358655877));
#104867=CARTESIAN_POINT('Ctrl Pts',(-122.737420120642,4.89623347131066,
131.287431694483));
#104868=CARTESIAN_POINT('Ctrl Pts',(-122.744910456404,4.90563985896102,
131.156327429457));
#104869=CARTESIAN_POINT('Ctrl Pts',(-122.752684790523,4.91540289265817,
131.020252306375));
#104870=CARTESIAN_POINT('Ctrl Pts',(-122.760459124642,4.91951531850364,
130.88355512423));
#104871=CARTESIAN_POINT('Ctrl Pts',(-122.768233458761,4.91791251062267,
130.746744644425));
#104872=CARTESIAN_POINT('Ctrl Pts',(-122.775998211708,4.91631167805917,
130.610102771309));
#104873=CARTESIAN_POINT('Ctrl Pts',(-122.783762964656,4.90900963080041,
130.473348265537));
#104874=CARTESIAN_POINT('Ctrl Pts',(-122.791527717603,4.89599349616577,
130.336994863576));
#104875=CARTESIAN_POINT('Ctrl Pts',(-122.799284758488,4.88299028933954,
130.200776889737));
#104876=CARTESIAN_POINT('Ctrl Pts',(-122.807041799373,4.86428432617648,
130.064959613588));
#104877=CARTESIAN_POINT('Ctrl Pts',(-122.814798840258,4.83991476849779,
129.93005626771));
#104878=CARTESIAN_POINT('Ctrl Pts',(-122.822550031498,4.81556358809209,
129.795254653495));
#104879=CARTESIAN_POINT('Ctrl Pts',(-122.830301222738,4.78555738347861,
129.661365980918));
#104880=CARTESIAN_POINT('Ctrl Pts',(-122.838052413978,4.74998704205606,
129.528897500577));
#104881=CARTESIAN_POINT('Ctrl Pts',(-122.845800310755,4.71443181897753,
129.396485322874));
#104882=CARTESIAN_POINT('Ctrl Pts',(-122.853548207532,4.67331726388662,
129.265492513652));
#104883=CARTESIAN_POINT('Ctrl Pts',(-122.861296104309,4.62678513489556,
129.136415061497));
#104884=CARTESIAN_POINT('Ctrl Pts',(-122.869042380393,4.58026273942278,
129.007364609563));
#104885=CARTESIAN_POINT('Ctrl Pts',(-122.876788656478,4.52832515663125,
128.880229085339));
#104886=CARTESIAN_POINT('Ctrl Pts',(-122.884534932562,4.47116356104546,
128.755487885335));
#104887=CARTESIAN_POINT('Ctrl Pts',(-122.892281265827,4.41400154350568,
128.63074576452));
#104888=CARTESIAN_POINT('Ctrl Pts',(-122.900027599092,4.35161559909351,
128.508398358616));
#104889=CARTESIAN_POINT('Ctrl Pts',(-122.907773932358,4.28424429312964,
128.388903331815));
#104890=CARTESIAN_POINT('Ctrl Pts',(-122.915522000361,4.21685789982901,
128.269381544932));
#104891=CARTESIAN_POINT('Ctrl Pts',(-122.923270068364,4.1444841153706,128.152713748733));
#104892=CARTESIAN_POINT('Ctrl Pts',(-122.931018136367,4.06740632303842,
128.039330985572));
#104893=CARTESIAN_POINT('Ctrl Pts',(-122.938774439108,3.99024661151119,
127.92582771786));
#104894=CARTESIAN_POINT('Ctrl Pts',(-122.94653074185,3.90837312526953,127.815616781425));
#104895=CARTESIAN_POINT('Ctrl Pts',(-122.954287044592,3.82211159578972,
127.709098752743));
#104896=CARTESIAN_POINT('Ctrl Pts',(-122.962047487106,3.73580402593434,
127.602523872182));
#104897=CARTESIAN_POINT('Ctrl Pts',(-122.969807929621,3.64510400457132,
127.499646119913));
#104898=CARTESIAN_POINT('Ctrl Pts',(-122.977568372135,3.55037537959195,
127.400830431643));
#104899=CARTESIAN_POINT('Ctrl Pts',(-122.9853412724,3.45549468781415,127.301856115658));
#104900=CARTESIAN_POINT('Ctrl Pts',(-122.993114172666,3.356572751443,127.206957165093));
#104901=CARTESIAN_POINT('Ctrl Pts',(-123.000887072931,3.25400852355268,
127.116459915114));
#104902=CARTESIAN_POINT('Ctrl Pts',(-123.008377408693,3.15517276369015,
127.029252468121));
#104903=CARTESIAN_POINT('Ctrl Pts',(-123.015867744455,3.0529551666889,126.946132446355));
#104904=CARTESIAN_POINT('Ctrl Pts',(-123.023358080217,2.9477378177461,126.867353528376));
#104905=CARTESIAN_POINT('Ctrl Pts',(-123.031132414336,2.83853112103815,
126.785587683778));
#104906=CARTESIAN_POINT('Ctrl Pts',(-123.038906748455,2.7257467768566,126.708239617481));
#104907=CARTESIAN_POINT('Ctrl Pts',(-123.046681082574,2.60977788871213,
126.635638699029));
#104908=CARTESIAN_POINT('Ctrl Pts',(-123.054445835521,2.49395192185787,
126.56312725472));
#104909=CARTESIAN_POINT('Ctrl Pts',(-123.062210588468,2.37494954815781,
126.4953515231));
#104910=CARTESIAN_POINT('Ctrl Pts',(-123.069975341416,2.25319603065291,
126.432600021427));
#104911=CARTESIAN_POINT('Ctrl Pts',(-123.077732382301,2.13156344045803,
126.369910845431));
#104912=CARTESIAN_POINT('Ctrl Pts',(-123.085489423185,2.00718548948093,
126.312236146741));
#104913=CARTESIAN_POINT('Ctrl Pts',(-123.09324646407,1.88051514274842,126.259820392153));
#104914=CARTESIAN_POINT('Ctrl Pts',(-123.100997655311,1.75394031910989,
126.207444164694));
#104915=CARTESIAN_POINT('Ctrl Pts',(-123.108748846551,1.62507690041153,
126.160319136515));
#104916=CARTESIAN_POINT('Ctrl Pts',(-123.116500037791,1.49440077780628,
126.118643022811));
#104917=CARTESIAN_POINT('Ctrl Pts',(-123.124247934568,1.36378019603886,
126.076984622568));
#104918=CARTESIAN_POINT('Ctrl Pts',(-123.131995831345,1.23134881442666,
126.040770649129));
#104919=CARTESIAN_POINT('Ctrl Pts',(-123.139743728122,1.09760054593546,
126.010149931326));
#104920=CARTESIAN_POINT('Ctrl Pts',(-123.147490004206,0.963880254698756,
125.979535618716));
#104921=CARTESIAN_POINT('Ctrl Pts',(-123.15523628029,0.828844005360271,
125.954512321767));
#104922=CARTESIAN_POINT('Ctrl Pts',(-123.162982556374,0.692998462279085,
125.935178325458));
#104923=CARTESIAN_POINT('Ctrl Pts',(-123.170728889639,0.557151916416775,
125.91584418643));
#104924=CARTESIAN_POINT('Ctrl Pts',(-123.178475222905,0.420496451955711,
125.902199486933));
#104925=CARTESIAN_POINT('Ctrl Pts',(-123.18622155617,0.283546065124721,
125.894290893881));
#104926=CARTESIAN_POINT('Ctrl Pts',(-123.193969624173,0.146565009204334,
125.886380529754));
#104927=CARTESIAN_POINT('Ctrl Pts',(-123.201717692176,0.00928928973071805,
125.884208850735));
#104928=CARTESIAN_POINT('Ctrl Pts',(-123.209465760179,-0.127765269568259,
125.887770427364));
#104929=CARTESIAN_POINT('Ctrl Pts',(-123.217222062921,-0.264965492084016,
125.891335789279));
#104930=CARTESIAN_POINT('Ctrl Pts',(-123.224978365663,-0.401943693427651,
125.900646568836));
#104931=CARTESIAN_POINT('Ctrl Pts',(-123.232734668404,-0.538186791443481,
125.91564524029));
#104932=CARTESIAN_POINT('Ctrl Pts',(-123.240495110918,-0.674502606502924,
125.930651916987));
#104933=CARTESIAN_POINT('Ctrl Pts',(-123.248255553433,-0.810082150153177,
125.951352475687));
#104934=CARTESIAN_POINT('Ctrl Pts',(-123.256015995947,-0.944421722976589,
125.977638057519));
#104935=CARTESIAN_POINT('Ctrl Pts',(-123.263788896212,-1.0789769496084,
126.0039658353));
#104936=CARTESIAN_POINT('Ctrl Pts',(-123.271561796477,-1.21228784730783,
126.035896461167));
#104937=CARTESIAN_POINT('Ctrl Pts',(-123.279334696743,-1.34386421717513,
126.073270676728));
#104938=CARTESIAN_POINT('Ctrl Pts',(-123.286825032505,-1.47065745458151,
126.109286245416));
#104939=CARTESIAN_POINT('Ctrl Pts',(-123.294315368268,-1.59583979096157,
126.150356402643));
#104940=CARTESIAN_POINT('Ctrl Pts',(-123.30180570403,-1.71899127297666,
126.196296808771));
#104941=CARTESIAN_POINT('Ctrl Pts',(-123.309580234757,-1.846815313366,126.243980265212));
#104942=CARTESIAN_POINT('Ctrl Pts',(-123.317354765484,-1.972856267363,126.297061888114));
#104943=CARTESIAN_POINT('Ctrl Pts',(-123.325129296211,-2.09662450801239,
126.35538896842));
#104944=CARTESIAN_POINT('Ctrl Pts',(-123.332894200136,-2.22023949280895,
126.4136438253));
#104945=CARTESIAN_POINT('Ctrl Pts',(-123.340659104061,-2.34158701345982,
126.477131050741));
#104946=CARTESIAN_POINT('Ctrl Pts',(-123.348424007986,-2.4601944402295,
126.545648796045));
#104947=CARTESIAN_POINT('Ctrl Pts',(-123.356181154412,-2.57868337267675,
126.614098088942));
#104948=CARTESIAN_POINT('Ctrl Pts',(-123.363938300838,-2.69443732272807,
126.68756770569));
#104949=CARTESIAN_POINT('Ctrl Pts',(-123.371695447264,-2.80700575770333,
126.765808681696));
#104950=CARTESIAN_POINT('Ctrl Pts',(-123.379446698754,-2.91948864786013,
126.843990199558));
#104951=CARTESIAN_POINT('Ctrl Pts',(-123.387197950244,-3.02879052179509,
126.926935636976));
#104952=CARTESIAN_POINT('Ctrl Pts',(-123.394949201734,-3.13448779722124,
127.01435147357));
#104953=CARTESIAN_POINT('Ctrl Pts',(-123.402696928731,-3.24013701210768,
127.101727562193));
#104954=CARTESIAN_POINT('Ctrl Pts',(-123.410444655728,-3.34218458896928,
127.193569756934));
#104955=CARTESIAN_POINT('Ctrl Pts',(-123.418192382725,-3.44023836948567,
127.289542980246));
#104956=CARTESIAN_POINT('Ctrl Pts',(-123.425938424521,-3.53827082241121,
127.385495328506));
#104957=CARTESIAN_POINT('Ctrl Pts',(-123.433684466316,-3.63231092807136,
127.48557664442));
#104958=CARTESIAN_POINT('Ctrl Pts',(-123.441430508112,-3.72200216550812,
127.589413815136));
#104959=CARTESIAN_POINT('Ctrl Pts',(-123.449176542539,-3.8116933176219,
127.693250887072));
#104960=CARTESIAN_POINT('Ctrl Pts',(-123.456922576966,-3.89703535446943,
127.800843510671));
#104961=CARTESIAN_POINT('Ctrl Pts',(-123.464668611393,-3.97771122281371,
127.911784518238));
#104962=CARTESIAN_POINT('Ctrl Pts',(-123.472416315909,-4.05840448534014,
128.022749445326));
#104963=CARTESIAN_POINT('Ctrl Pts',(-123.480164020426,-4.13442934805928,
128.137063876537));
#104964=CARTESIAN_POINT('Ctrl Pts',(-123.487911724943,-4.20551160005577,
128.254290962773));
#104965=CARTESIAN_POINT('Ctrl Pts',(-123.495666784776,-4.27666133429309,
128.371629339046));
#104966=CARTESIAN_POINT('Ctrl Pts',(-123.503421844609,-4.34285888487681,
128.491885557472));
#104967=CARTESIAN_POINT('Ctrl Pts',(-123.511176904442,-4.40387541924184,
128.614597079122));
#104968=CARTESIAN_POINT('Ctrl Pts',(-123.518936077391,-4.46492431546065,
128.737373684317));
#104969=CARTESIAN_POINT('Ctrl Pts',(-123.526695250341,-4.5207865611397,
128.862607830896));
#104970=CARTESIAN_POINT('Ctrl Pts',(-123.53445442329,-4.57128155361596,
128.989817143281));
#104971=CARTESIAN_POINT('Ctrl Pts',(-123.542224014698,-4.62184434712703,
129.117197263158));
#104972=CARTESIAN_POINT('Ctrl Pts',(-123.549993606105,-4.66702536594817,
129.246557476954));
#104973=CARTESIAN_POINT('Ctrl Pts',(-123.557763197513,-4.70669377031537,
129.377399926105));
#104974=CARTESIAN_POINT('Ctrl Pts',(-123.561800350875,-4.72730584933898,
129.445386903262));
#104975=CARTESIAN_POINT('Ctrl Pts',(-123.565837504238,-4.74643039414011,
129.51377388796));
#104976=CARTESIAN_POINT('Ctrl Pts',(-123.5698746576,-4.76405452823401,129.582490119308));
#104977=CARTESIAN_POINT('Origin',(213.235140564004,0.,130.804360617566));
#104978=CARTESIAN_POINT('',(-125.665057882386,-4.76405452823409,129.582490119308));
#104979=CARTESIAN_POINT('',(-125.320138230236,-4.76405452823398,129.582490119308));
#104980=CARTESIAN_POINT('',(213.235140564004,-4.76405452823405,129.582490119308));
#104981=CARTESIAN_POINT('',(-123.985140564039,-4.9182499550531,130.805025538748));
#104982=CARTESIAN_POINT('Ctrl Pts',(-123.985140564039,-4.9182499550531,
130.805025538749));
#104983=CARTESIAN_POINT('Ctrl Pts',(-123.993342529297,-4.91823026668018,
130.950655339306));
#104984=CARTESIAN_POINT('Ctrl Pts',(-124.001544494556,-4.91173814329656,
131.09613293352));
#104985=CARTESIAN_POINT('Ctrl Pts',(-124.009746459814,-4.89883958656253,
131.240885264783));
#104986=CARTESIAN_POINT('Ctrl Pts',(-124.01796249326,-4.88591890594608,
131.385885878363));
#104987=CARTESIAN_POINT('Ctrl Pts',(-124.026178526706,-4.86656988110953,
131.530158430338));
#104988=CARTESIAN_POINT('Ctrl Pts',(-124.034394560152,-4.84090979353874,
131.673138744202));
#104989=CARTESIAN_POINT('Ctrl Pts',(-124.042633092738,-4.81517943728027,
131.816510601508));
#104990=CARTESIAN_POINT('Ctrl Pts',(-124.050871625323,-4.78310351118545,
131.958582830783));
#104991=CARTESIAN_POINT('Ctrl Pts',(-124.059110157909,-4.74485002077881,
132.09880310096));
#104992=CARTESIAN_POINT('Ctrl Pts',(-124.06736096834,-4.7065395213777,132.239232340738));
#104993=CARTESIAN_POINT('Ctrl Pts',(-124.075611778772,-4.66203317409171,
132.377803810291));
#104994=CARTESIAN_POINT('Ctrl Pts',(-124.083862589203,-4.61154769293278,
132.513983657393));
#104995=CARTESIAN_POINT('Ctrl Pts',(-124.092132757458,-4.56094376413327,
132.650483005888));
#104996=CARTESIAN_POINT('Ctrl Pts',(-124.100402925713,-4.50433277511573,
132.784579220322));
#104997=CARTESIAN_POINT('Ctrl Pts',(-124.108673093967,-4.44197882532874,
132.915759958721));
#104998=CARTESIAN_POINT('Ctrl Pts',(-124.111635255748,-4.41964524259493,
132.962745528748));
#104999=CARTESIAN_POINT('Ctrl Pts',(-124.114597417529,-4.39657531659368,
133.009357330806));
#105000=CARTESIAN_POINT('Ctrl Pts',(-124.11755957931,-4.37278254367277,
133.055572710695));
#105001=CARTESIAN_POINT('Ctrl Pts',(-124.125333913429,-4.31033728240945,
133.176867167677));
#105002=CARTESIAN_POINT('Ctrl Pts',(-124.133108247548,-4.24274249699988,
133.295753569918));
#105003=CARTESIAN_POINT('Ctrl Pts',(-124.140882581667,-4.17020764035701,
133.411763789077));
#105004=CARTESIAN_POINT('Ctrl Pts',(-124.148647334614,-4.09776217644232,
133.52763103601));
#105005=CARTESIAN_POINT('Ctrl Pts',(-124.156412087561,-4.02038896027019,
133.640628824317));
#105006=CARTESIAN_POINT('Ctrl Pts',(-124.164176840508,-3.93834423286467,
133.750311697601));
#105007=CARTESIAN_POINT('Ctrl Pts',(-124.171933881393,-3.85638099343926,
133.85988563231));
#105008=CARTESIAN_POINT('Ctrl Pts',(-124.179690922278,-3.76975570887975,
133.966150893017));
#105009=CARTESIAN_POINT('Ctrl Pts',(-124.187447963163,-3.67876879853684,
134.068689520941));
#105010=CARTESIAN_POINT('Ctrl Pts',(-124.195199154403,-3.58785050213043,
134.171150823689));
#105011=CARTESIAN_POINT('Ctrl Pts',(-124.202950345644,-3.4925773852067,
134.269890796098));
#105012=CARTESIAN_POINT('Ctrl Pts',(-124.210701536884,-3.39329093201159,
134.364523494911));
#105013=CARTESIAN_POINT('Ctrl Pts',(-124.218449433661,-3.29404667820778,
134.459115972303));
#105014=CARTESIAN_POINT('Ctrl Pts',(-124.226197330438,-3.1907927632036,
134.549604378988));
#105015=CARTESIAN_POINT('Ctrl Pts',(-124.233945227215,-3.0839082594759,
134.635638851999));
#105016=CARTESIAN_POINT('Ctrl Pts',(-124.241691503299,-2.97704611368223,
134.721655328452));
#105017=CARTESIAN_POINT('Ctrl Pts',(-124.249437779383,-2.86655519410049,
134.803219479374));
#105018=CARTESIAN_POINT('Ctrl Pts',(-124.257184055467,-2.75284814679336,
134.880021317771));
#105019=CARTESIAN_POINT('Ctrl Pts',(-124.264930388732,-2.6391402601268,
134.956823723101));
#105020=CARTESIAN_POINT('Ctrl Pts',(-124.272676721998,-2.52221652234742,
135.028863526926));
#105021=CARTESIAN_POINT('Ctrl Pts',(-124.280423055263,-2.40251874926647,
135.095873954598));
#105022=CARTESIAN_POINT('Ctrl Pts',(-124.288171123266,-2.28279417069933,
135.16289938879));
#105023=CARTESIAN_POINT('Ctrl Pts',(-124.295919191269,-2.16029466174176,
135.224893014688));
#105024=CARTESIAN_POINT('Ctrl Pts',(-124.303667259272,-2.0354864671806,
135.281634107585));
#105025=CARTESIAN_POINT('Ctrl Pts',(-124.311423562014,-1.91054562498486,
135.338435505591));
#105026=CARTESIAN_POINT('Ctrl Pts',(-124.319179864756,-1.7832915521367,
135.389973056977));
#105027=CARTESIAN_POINT('Ctrl Pts',(-124.326936167498,-1.65421081348336,
135.436074085286));
#105028=CARTESIAN_POINT('Ctrl Pts',(-124.334696610012,-1.52506118055326,
135.482199719101));
#105029=CARTESIAN_POINT('Ctrl Pts',(-124.342457052526,-1.39408331234045,
135.522882932168));
#105030=CARTESIAN_POINT('Ctrl Pts',(-124.35021749504,-1.26177778769949,
135.558001314649));
#105031=CARTESIAN_POINT('Ctrl Pts',(-124.357990395306,-1.12925987448485,
135.593176072277));
#105032=CARTESIAN_POINT('Ctrl Pts',(-124.365763295571,-0.995410427848216,
135.622768063572));
#105033=CARTESIAN_POINT('Ctrl Pts',(-124.373536195836,-0.860739929278256,
135.646706106753));
#105034=CARTESIAN_POINT('Ctrl Pts',(-124.381026531598,-0.730965042547292,
135.669773941767));
#105035=CARTESIAN_POINT('Ctrl Pts',(-124.38851686736,-0.600428067297373,
135.687591720733));
#105036=CARTESIAN_POINT('Ctrl Pts',(-124.396007203122,-0.469587284429826,
135.700141540443));
#105037=CARTESIAN_POINT('Ctrl Pts',(-124.403781537241,-0.333785633510681,
135.713167190381));
#105038=CARTESIAN_POINT('Ctrl Pts',(-124.41155587136,-0.197226503659713,
135.720558787405));
#105039=CARTESIAN_POINT('Ctrl Pts',(-124.419330205479,-0.0604169589232291,
135.722239515381));
#105040=CARTESIAN_POINT('Ctrl Pts',(-124.427094958426,0.0762239802763863,
135.72391817201));
#105041=CARTESIAN_POINT('Ctrl Pts',(-124.434859711373,0.213114333128947,
135.719899958625));
#105042=CARTESIAN_POINT('Ctrl Pts',(-124.442624464321,0.349740820019951,
135.710159677996));
#105043=CARTESIAN_POINT('Ctrl Pts',(-124.450381505205,0.486231607558078,
135.70042907155));
#105044=CARTESIAN_POINT('Ctrl Pts',(-124.45813854609,0.622458663224571,
135.684987735381));
#105045=CARTESIAN_POINT('Ctrl Pts',(-124.465895586975,0.757907962461091,
135.663862503864));
#105046=CARTESIAN_POINT('Ctrl Pts',(-124.473646778216,0.893255118327599,
135.64275320305));
#105047=CARTESIAN_POINT('Ctrl Pts',(-124.481397969456,1.02782530044893,
135.615968598452));
#105048=CARTESIAN_POINT('Ctrl Pts',(-124.489149160696,1.16110922325608,
135.583587378682));
#105049=CARTESIAN_POINT('Ctrl Pts',(-124.496897057473,1.29433649684039,
135.551219921794));
#105050=CARTESIAN_POINT('Ctrl Pts',(-124.50464495425,1.42627821932577,135.513260672914));
#105051=CARTESIAN_POINT('Ctrl Pts',(-124.512392851027,1.55643514315609,
135.469839446973));
#105052=CARTESIAN_POINT('Ctrl Pts',(-124.520139127111,1.6865648409638,135.426427303817));
#105053=CARTESIAN_POINT('Ctrl Pts',(-124.527885403195,1.8149101120762,135.377555579797));
#105054=CARTESIAN_POINT('Ctrl Pts',(-124.535631679279,1.94098711037878,
135.323403890189));
#105055=CARTESIAN_POINT('Ctrl Pts',(-124.543378012545,2.06706503935294,
135.269251800847));
#105056=CARTESIAN_POINT('Ctrl Pts',(-124.55112434581,2.19087430287492,135.209819822439));
#105057=CARTESIAN_POINT('Ctrl Pts',(-124.558870679075,2.31195164363967,
135.145335468907));
#105058=CARTESIAN_POINT('Ctrl Pts',(-124.566618747078,2.43305609883556,
135.08083667455));
#105059=CARTESIAN_POINT('Ctrl Pts',(-124.574366815081,2.55142706886271,
135.011283437375));
#105060=CARTESIAN_POINT('Ctrl Pts',(-124.582114883084,2.66662683507841,
134.936948715228));
#105061=CARTESIAN_POINT('Ctrl Pts',(-124.589871185826,2.78194903697639,
134.862534989255));
#105062=CARTESIAN_POINT('Ctrl Pts',(-124.597627488568,2.89409297330497,
134.783329839145));
#105063=CARTESIAN_POINT('Ctrl Pts',(-124.605383791309,3.00265036628445,
134.699649289841));
#105064=CARTESIAN_POINT('Ctrl Pts',(-124.613144233824,3.11126569961346,
134.615924077708));
#105065=CARTESIAN_POINT('Ctrl Pts',(-124.620904676338,3.21629037605639,
134.5277189581));
#105066=CARTESIAN_POINT('Ctrl Pts',(-124.628665118852,3.31735083365361,
134.435388916679));
#105067=CARTESIAN_POINT('Ctrl Pts',(-124.636438019117,3.41857352246909,
134.342910658878));
#105068=CARTESIAN_POINT('Ctrl Pts',(-124.644210919383,3.5158189981967,134.24629452273));
#105069=CARTESIAN_POINT('Ctrl Pts',(-124.651983819648,3.6087514458723,134.145931515275));
#105070=CARTESIAN_POINT('Ctrl Pts',(-124.65947415541,3.6983055649957,134.049216955936));
#105071=CARTESIAN_POINT('Ctrl Pts',(-124.666964491173,3.78385459073554,
133.949023446409));
#105072=CARTESIAN_POINT('Ctrl Pts',(-124.674454826935,3.86513574859431,
133.845726874273));
#105073=CARTESIAN_POINT('Ctrl Pts',(-124.682229161054,3.94949870625497,
133.738513781213));
#105074=CARTESIAN_POINT('Ctrl Pts',(-124.690003495173,4.02953101149955,
133.627618056455));
#105075=CARTESIAN_POINT('Ctrl Pts',(-124.697777829292,4.10489395623549,
133.513424786345));
#105076=CARTESIAN_POINT('Ctrl Pts',(-124.705542582239,4.18016402287743,
133.399372249235));
#105077=CARTESIAN_POINT('Ctrl Pts',(-124.713307335186,4.25077596560525,
133.282030575958));
#105078=CARTESIAN_POINT('Ctrl Pts',(-124.721072088134,4.31643114510465,
133.161817983473));
#105079=CARTESIAN_POINT('Ctrl Pts',(-124.728829129019,4.38202111495419,
133.04172478783));
#105080=CARTESIAN_POINT('Ctrl Pts',(-124.736586169904,4.44266393263232,
132.918766688371));
#105081=CARTESIAN_POINT('Ctrl Pts',(-124.744343210789,4.49810433183068,
132.793390653153));
#105082=CARTESIAN_POINT('Ctrl Pts',(-124.752094402029,4.55350292299267,
132.668109164978));
#105083=CARTESIAN_POINT('Ctrl Pts',(-124.759845593269,4.60370674706152,
132.540413726498));
#105084=CARTESIAN_POINT('Ctrl Pts',(-124.767596784509,4.6485067257031,132.410775347202));
#105085=CARTESIAN_POINT('Ctrl Pts',(-124.775344681286,4.69328766315874,
132.281192067676));
#105086=CARTESIAN_POINT('Ctrl Pts',(-124.783092578063,4.73266919587337,
132.149667858539));
#105087=CARTESIAN_POINT('Ctrl Pts',(-124.79084047484,4.76649068532607,132.016692919041));
#105088=CARTESIAN_POINT('Ctrl Pts',(-124.798586750924,4.80030510005229,
131.883745795034));
#105089=CARTESIAN_POINT('Ctrl Pts',(-124.806333027008,4.8285616885587,131.749348922928));
#105090=CARTESIAN_POINT('Ctrl Pts',(-124.814079303092,4.85115003562096,
131.614006462609));
#105091=CARTESIAN_POINT('Ctrl Pts',(-124.821825636358,4.87373854942531,
131.478663003221));
#105092=CARTESIAN_POINT('Ctrl Pts',(-124.829571969623,4.8906586739325,131.342374327323));
#105093=CARTESIAN_POINT('Ctrl Pts',(-124.837318302888,4.90185142117565,
131.205653163246));
#105094=CARTESIAN_POINT('Ctrl Pts',(-124.845066370891,4.91304667495692,
131.068901381413));
#105095=CARTESIAN_POINT('Ctrl Pts',(-124.852814438894,4.91851196734212,
130.931717308263));
#105096=CARTESIAN_POINT('Ctrl Pts',(-124.860562506897,4.91824034788161,
130.794616749271));
#105097=CARTESIAN_POINT('Ctrl Pts',(-124.868318809639,4.91796843974071,
130.657370478174));
#105098=CARTESIAN_POINT('Ctrl Pts',(-124.876075112381,4.91194744059989,
130.520208290131));
#105099=CARTESIAN_POINT('Ctrl Pts',(-124.883831415123,4.90022254708108,
130.383644500002));
#105100=CARTESIAN_POINT('Ctrl Pts',(-124.891591857637,4.88849139563357,
130.247007821666));
#105101=CARTESIAN_POINT('Ctrl Pts',(-124.899352300151,4.87105033339611,
130.110970565243));
#105102=CARTESIAN_POINT('Ctrl Pts',(-124.907112742666,4.8479961004954,129.97603889741));
#105103=CARTESIAN_POINT('Ctrl Pts',(-124.914885642931,4.82490485889337,
129.840890625286));
#105104=CARTESIAN_POINT('Ctrl Pts',(-124.922658543196,4.79618252222367,
129.706851870852));
#105105=CARTESIAN_POINT('Ctrl Pts',(-124.930431443462,4.76197653959325,
129.574416513607));
#105106=CARTESIAN_POINT('Ctrl Pts',(-124.937921779224,4.72901403059102,
129.446795515182));
#105107=CARTESIAN_POINT('Ctrl Pts',(-124.945412114986,4.69095973146277,
129.320663657695));
#105108=CARTESIAN_POINT('Ctrl Pts',(-124.952902450748,4.64798785104083,
129.196445197192));
#105109=CARTESIAN_POINT('Ctrl Pts',(-124.960676784867,4.60338667871175,
129.067516956004));
#105110=CARTESIAN_POINT('Ctrl Pts',(-124.968451118986,4.55334638062493,
128.940241662958));
#105111=CARTESIAN_POINT('Ctrl Pts',(-124.976225453105,4.49800786083179,
128.815112431342));
#105112=CARTESIAN_POINT('Ctrl Pts',(-124.983990206052,4.44273754081855,
128.690137410321));
#105113=CARTESIAN_POINT('Ctrl Pts',(-124.991754959,4.38218214763921,128.567303542434));
#105114=CARTESIAN_POINT('Ctrl Pts',(-124.999519711947,4.31653211722015,
128.447088137875));
#105115=CARTESIAN_POINT('Ctrl Pts',(-125.007276752832,4.2509472913368,128.326992132951));
#105116=CARTESIAN_POINT('Ctrl Pts',(-125.015033793717,4.18027808414597,
128.209509756769));
#105117=CARTESIAN_POINT('Ctrl Pts',(-125.022790834602,4.10476256485621,
128.095097369254));
#105118=CARTESIAN_POINT('Ctrl Pts',(-125.030542025842,4.02930399240708,
127.98077126101));
#105119=CARTESIAN_POINT('Ctrl Pts',(-125.038293217082,3.94900659669696,
127.869510858342));
#105120=CARTESIAN_POINT('Ctrl Pts',(-125.046044408322,3.86415363940161,
127.761746656907));
#105121=CARTESIAN_POINT('Ctrl Pts',(-125.053792305099,3.77933674687652,
127.654028258131));
#105122=CARTESIAN_POINT('Ctrl Pts',(-125.061540201876,3.68996838514976,
127.549803411619));
#105123=CARTESIAN_POINT('Ctrl Pts',(-125.069288098653,3.5963741436887,127.449472231776));
#105124=CARTESIAN_POINT('Ctrl Pts',(-125.077034374737,3.5027994801253,127.349162039053));
#105125=CARTESIAN_POINT('Ctrl Pts',(-125.084780650822,3.4050009615987,127.252744178675));
#105126=CARTESIAN_POINT('Ctrl Pts',(-125.092526926906,3.30334306997183,
127.16058405683));
#105127=CARTESIAN_POINT('Ctrl Pts',(-125.100273260171,3.20168442792936,
127.06842325468));
#105128=CARTESIAN_POINT('Ctrl Pts',(-125.108019593436,3.09616664559266,
126.98052051637));
#105129=CARTESIAN_POINT('Ctrl Pts',(-125.115765926702,2.98718921139284,
126.897202612335));
#105130=CARTESIAN_POINT('Ctrl Pts',(-125.123513994705,2.87818737245238,
126.813866049834));
#105131=CARTESIAN_POINT('Ctrl Pts',(-125.131262062708,2.76572465048735,
126.73511660212));
#105132=CARTESIAN_POINT('Ctrl Pts',(-125.139010130711,2.65023125036484,
126.661238922263));
#105133=CARTESIAN_POINT('Ctrl Pts',(-125.146766433453,2.53461510248213,
126.587282724328));
#105134=CARTESIAN_POINT('Ctrl Pts',(-125.154522736195,2.41596217193923,
126.518208848419));
#105135=CARTESIAN_POINT('Ctrl Pts',(-125.162279038937,2.29472959627212,
126.454257269082));
#105136=CARTESIAN_POINT('Ctrl Pts',(-125.170039481451,2.17343231512914,
126.390271556861));
#105137=CARTESIAN_POINT('Ctrl Pts',(-125.177799923965,2.04955299836367,
126.331413756487));
#105138=CARTESIAN_POINT('Ctrl Pts',(-125.185560366479,1.92356978873832,
126.277876073203));
#105139=CARTESIAN_POINT('Ctrl Pts',(-125.193333266745,1.79738433968062,
126.224252446478));
#105140=CARTESIAN_POINT('Ctrl Pts',(-125.20110616701,1.66908861484836,126.175966140927));
#105141=CARTESIAN_POINT('Ctrl Pts',(-125.208879067276,1.53917782889359,
126.133160057374));
#105142=CARTESIAN_POINT('Ctrl Pts',(-125.216369403037,1.41398962723766,
126.09191008278));
#105143=CARTESIAN_POINT('Ctrl Pts',(-125.223859738799,1.28730204509113,
126.055748892478));
#105144=CARTESIAN_POINT('Ctrl Pts',(-125.231350074561,1.15956618520974,
126.024759240399));
#105145=CARTESIAN_POINT('Ctrl Pts',(-125.23912440868,1.02698718137328,125.992594606241));
#105146=CARTESIAN_POINT('Ctrl Pts',(-125.246898742799,0.892858869292728,
125.965899521473));
#105147=CARTESIAN_POINT('Ctrl Pts',(-125.254673076918,0.757672281223806,
125.944821979304));
#105148=CARTESIAN_POINT('Ctrl Pts',(-125.262437829865,0.62265229854234,
125.923770413321));
#105149=CARTESIAN_POINT('Ctrl Pts',(-125.270202582812,0.486577017492259,
125.908322674644));
#105150=CARTESIAN_POINT('Ctrl Pts',(-125.27796733576,0.349950947927619,
125.898576541952));
#105151=CARTESIAN_POINT('Ctrl Pts',(-125.285724376645,0.213460577301733,
125.888840089257));
#105152=CARTESIAN_POINT('Ctrl Pts',(-125.29348141753,0.0764208942680485,
125.88479400073));
#105153=CARTESIAN_POINT('Ctrl Pts',(-125.301238458415,-0.0606554704202938,
125.886484655689));
#105154=CARTESIAN_POINT('Ctrl Pts',(-125.308989649655,-0.197628464755912,
125.888174035712));
#105155=CARTESIAN_POINT('Ctrl Pts',(-125.316740840895,-0.33463769633316,
125.895591543535));
#105156=CARTESIAN_POINT('Ctrl Pts',(-125.324492032135,-0.471167867108309,
125.908731556505));
#105157=CARTESIAN_POINT('Ctrl Pts',(-125.332239928912,-0.607640008919003,
125.921865984619));
#105158=CARTESIAN_POINT('Ctrl Pts',(-125.339987825689,-0.743633106547314,
125.94071804301));
#105159=CARTESIAN_POINT('Ctrl Pts',(-125.347735722466,-0.87863454335215,
125.965230075648));
#105160=CARTESIAN_POINT('Ctrl Pts',(-125.35548199855,-1.01360774076633,
125.989736980896));
#105161=CARTESIAN_POINT('Ctrl Pts',(-125.363228274634,-1.1475893055227,
126.019901435659));
#105162=CARTESIAN_POINT('Ctrl Pts',(-125.370974550718,-1.28007479969716,
126.055614301992));
#105163=CARTESIAN_POINT('Ctrl Pts',(-125.378720883984,-1.41256127184962,
126.091327431949));
#105164=CARTESIAN_POINT('Ctrl Pts',(-125.386467217249,-1.54355127389247,
126.132588953447));
#105165=CARTESIAN_POINT('Ctrl Pts',(-125.394213550514,-1.67255395134867,
126.179239392957));
#105166=CARTESIAN_POINT('Ctrl Pts',(-125.401961618517,-1.80158551805987,
126.225900279509));
#105167=CARTESIAN_POINT('Ctrl Pts',(-125.40970968652,-1.92862850699809,
126.277952352556));
#105168=CARTESIAN_POINT('Ctrl Pts',(-125.417457754523,-2.05321089523569,
126.335187530497));
#105169=CARTESIAN_POINT('Ctrl Pts',(-125.425214057265,-2.17792569111822,
126.392483538665));
#105170=CARTESIAN_POINT('Ctrl Pts',(-125.432970360007,-2.30017430641158,
126.454973492404));
#105171=CARTESIAN_POINT('Ctrl Pts',(-125.440726662749,-2.41950774972887,
126.522402501061));
#105172=CARTESIAN_POINT('Ctrl Pts',(-125.448487105263,-2.53890488489792,
126.589867498611));
#105173=CARTESIAN_POINT('Ctrl Pts',(-125.456247547777,-2.65538341592438,
126.662276597465));
#105174=CARTESIAN_POINT('Ctrl Pts',(-125.464007990292,-2.76852318724998,
126.739331414207));
#105175=CARTESIAN_POINT('Ctrl Pts',(-125.471780890557,-2.88184458058059,
126.816509926182));
#105176=CARTESIAN_POINT('Ctrl Pts',(-125.479553790822,-2.99181619004853,
126.898348825397));
#105177=CARTESIAN_POINT('Ctrl Pts',(-125.487326691088,-3.09805011352928,
126.984508715128));
#105178=CARTESIAN_POINT('Ctrl Pts',(-125.49481702685,-3.20042216630728,
127.067536475845));
#105179=CARTESIAN_POINT('Ctrl Pts',(-125.502307362612,-3.29932333251835,
127.154576320044));
#105180=CARTESIAN_POINT('Ctrl Pts',(-125.509797698375,-3.39444015687818,
127.245293452722));
#105181=CARTESIAN_POINT('Ctrl Pts',(-125.517456387707,-3.49169483693849,
127.338049553169));
#105182=CARTESIAN_POINT('Ctrl Pts',(-125.52511507704,-3.58532055949805,
127.434962945229));
#105183=CARTESIAN_POINT('Ctrl Pts',(-125.532773766373,-3.67493289018205,
127.53571390751));
#105184=CARTESIAN_POINT('Ctrl Pts',(-125.54042355721,-3.76444110187399,
127.636347809019));
#105185=CARTESIAN_POINT('Ctrl Pts',(-125.548073348046,-3.84994492627025,
127.740810119028));
#105186=CARTESIAN_POINT('Ctrl Pts',(-125.555723138882,-3.93109427974338,
127.848742099173));
#105187=CARTESIAN_POINT('Ctrl Pts',(-125.563365814823,-4.01216815805833,
127.956573694251));
#105188=CARTESIAN_POINT('Ctrl Pts',(-125.571008490764,-4.08889537772311,
128.067868222531));
#105189=CARTESIAN_POINT('Ctrl Pts',(-125.578651166705,-4.16096430315406,
128.182231877329));
#105190=CARTESIAN_POINT('Ctrl Pts',(-125.586288389527,-4.23298180675273,
128.296513932622));
#105191=CARTESIAN_POINT('Ctrl Pts',(-125.593925612349,-4.30034741386355,
128.413860418107));
#105192=CARTESIAN_POINT('Ctrl Pts',(-125.601562835171,-4.36279157873713,
128.533846864469));
#105193=CARTESIAN_POINT('Ctrl Pts',(-125.609196777083,-4.42520891793052,
128.653781765295));
#105194=CARTESIAN_POINT('Ctrl Pts',(-125.616830718995,-4.48270883483468,
128.776354013667));
#105195=CARTESIAN_POINT('Ctrl Pts',(-125.624464660907,-4.53506694985962,
128.901113176272));
#105196=CARTESIAN_POINT('Ctrl Pts',(-125.632098594968,-4.58742501104085,
129.025872210579));
#105197=CARTESIAN_POINT('Ctrl Pts',(-125.63973252903,-4.63464111484539,
129.152817786874));
#105198=CARTESIAN_POINT('Ctrl Pts',(-125.647366463091,-4.67653852076034,
129.281478308803));
#105199=CARTESIAN_POINT('Ctrl Pts',(-125.653263602856,-4.70890385906255,
129.380867309802));
#105200=CARTESIAN_POINT('Ctrl Pts',(-125.659160742621,-4.73809625624943,
129.481279210812));
#105201=CARTESIAN_POINT('Ctrl Pts',(-125.665057882386,-4.76405452823409,
129.582490119308));
#105202=CARTESIAN_POINT('Ctrl Pts',(-123.915406765754,-4.76405452823402,
129.582490119308));
#105203=CARTESIAN_POINT('Ctrl Pts',(-123.923457752182,-4.79940371290318,
129.720316053834));
#105204=CARTESIAN_POINT('Ctrl Pts',(-123.931508738609,-4.82880155768346,
129.859809178845));
#105205=CARTESIAN_POINT('Ctrl Pts',(-123.939559725037,-4.8521014597191,
130.000436188847));
#105206=CARTESIAN_POINT('Ctrl Pts',(-123.947599312199,-4.87536837178949,
130.140864087274));
#105207=CARTESIAN_POINT('Ctrl Pts',(-123.955638899361,-4.8925544991057,
130.282422329576));
#105208=CARTESIAN_POINT('Ctrl Pts',(-123.963678486524,-4.90356392212458,
130.424566036064));
#105209=CARTESIAN_POINT('Ctrl Pts',(-123.970832512353,-4.91336065609192,
130.551052599003));
#105210=CARTESIAN_POINT('Ctrl Pts',(-123.977986538181,-4.91826712789107,
130.678002401489));
#105211=CARTESIAN_POINT('Ctrl Pts',(-123.98514056401,-4.91824995505317,
130.805025538236));
#105212=CARTESIAN_POINT('',(-123.639859436025,-4.91824795694567,130.7998777056));
#105213=CARTESIAN_POINT('Ctrl Pts',(-123.5698746576,-4.76405452823401,129.582490119308));
#105214=CARTESIAN_POINT('Ctrl Pts',(-123.573334214347,-4.77915717273279,
129.641375100994));
#105215=CARTESIAN_POINT('Ctrl Pts',(-123.576793771095,-4.79315808372837,
129.700501843481));
#105216=CARTESIAN_POINT('Ctrl Pts',(-123.580253327842,-4.8060513612251,
129.759825612999));
#105217=CARTESIAN_POINT('Ctrl Pts',(-123.59104783843,-4.84628097172893,
129.944927666523));
#105218=CARTESIAN_POINT('Ctrl Pts',(-123.601842349019,-4.87582893446835,
130.13242751813));
#105219=CARTESIAN_POINT('Ctrl Pts',(-123.612636859607,-4.89446950845077,
130.321296136005));
#105220=CARTESIAN_POINT('Ctrl Pts',(-123.621711051736,-4.91013933880728,
130.480064809361));
#105221=CARTESIAN_POINT('Ctrl Pts',(-123.630785243864,-4.91810204906405,
130.639800716198));
#105222=CARTESIAN_POINT('Ctrl Pts',(-123.639859435993,-4.91824795694516,
130.799877705041));
#105223=CARTESIAN_POINT('Ctrl Pts',(-123.639859436025,-4.91824795694567,
130.7998777056));
#105224=CARTESIAN_POINT('Ctrl Pts',(-123.647510149338,-4.9183709760766,
130.934843235573));
#105225=CARTESIAN_POINT('Ctrl Pts',(-123.655160862651,-4.91293427663035,
131.069980165572));
#105226=CARTESIAN_POINT('Ctrl Pts',(-123.662811575964,-4.90192233098187,
131.204786045731));
#105227=CARTESIAN_POINT('Ctrl Pts',(-123.670456272973,-4.89091904481468,
131.339485918375));
#105228=CARTESIAN_POINT('Ctrl Pts',(-123.678100969983,-4.87434926666466,
131.47385485943));
#105229=CARTESIAN_POINT('Ctrl Pts',(-123.685745666992,-4.85224953570836,
131.607390819811));
#105230=CARTESIAN_POINT('Ctrl Pts',(-123.693386929821,-4.83015973248057,
131.74086679264));
#105231=CARTESIAN_POINT('Ctrl Pts',(-123.701028192649,-4.80254498058789,
131.873510132164));
#105232=CARTESIAN_POINT('Ctrl Pts',(-123.708669455477,-4.76949358225916,
132.004824707528));
#105233=CARTESIAN_POINT('Ctrl Pts',(-123.716309116396,-4.73644911280605,
132.136111754183));
#105234=CARTESIAN_POINT('Ctrl Pts',(-123.723948777315,-4.69797036103166,
132.266070200052));
#105235=CARTESIAN_POINT('Ctrl Pts',(-123.731588438233,-4.65419646501906,
132.394215430907));
#105236=CARTESIAN_POINT('Ctrl Pts',(-123.739228259569,-4.61042164984267,
132.522363352555));
#105237=CARTESIAN_POINT('Ctrl Pts',(-123.746868080906,-4.56135159979542,
132.648697602335));
#105238=CARTESIAN_POINT('Ctrl Pts',(-123.754507902242,-4.50717473717055,
132.772750556351));
#105239=CARTESIAN_POINT('Ctrl Pts',(-123.76214964624,-4.45298424022255,
132.896834729932));
#105240=CARTESIAN_POINT('Ctrl Pts',(-123.769791390238,-4.39368453665895,
133.018636097276));
#105241=CARTESIAN_POINT('Ctrl Pts',(-123.777433134236,-4.32951117748467,
133.137709289868));
#105242=CARTESIAN_POINT('Ctrl Pts',(-123.785082886883,-4.26527056377848,
133.256907272746));
#105243=CARTESIAN_POINT('Ctrl Pts',(-123.79273263953,-4.19614628908974,
133.373371018123));
#105244=CARTESIAN_POINT('Ctrl Pts',(-123.800382392177,-4.12241878867837,
133.486681700742));
#105245=CARTESIAN_POINT('Ctrl Pts',(-123.808036614016,-4.04864821467418,
133.600058582516));
#105246=CARTESIAN_POINT('Ctrl Pts',(-123.815690835855,-3.97026929430983,
133.71027840705));
#105247=CARTESIAN_POINT('Ctrl Pts',(-123.823345057694,-3.88760355211351,
133.816954464087));
#105248=CARTESIAN_POINT('Ctrl Pts',(-123.831010526621,-3.80481634114609,
133.923787270573));
#105249=CARTESIAN_POINT('Ctrl Pts',(-123.838675995549,-3.71772999235346,
134.027065607486));
#105250=CARTESIAN_POINT('Ctrl Pts',(-123.846341464476,-3.62670402139129,
134.126438431785));
#105251=CARTESIAN_POINT('Ctrl Pts',(-123.850461293536,-3.5777818427361,
134.179846651576));
#105252=CARTESIAN_POINT('Ctrl Pts',(-123.854581122595,-3.52772228186842,
134.232127407389));
#105253=CARTESIAN_POINT('Ctrl Pts',(-123.858700951655,-3.47658503718195,
134.28323105806));
#105254=CARTESIAN_POINT('Ctrl Pts',(-123.866475285774,-3.38008636687777,
134.37966633469));
#105255=CARTESIAN_POINT('Ctrl Pts',(-123.874249619893,-3.27941935293837,
134.47223622157));
#105256=CARTESIAN_POINT('Ctrl Pts',(-123.882023954012,-3.17492638197591,
134.560558899278));
#105257=CARTESIAN_POINT('Ctrl Pts',(-123.889788706959,-3.07056218926165,
134.648772727178));
#105258=CARTESIAN_POINT('Ctrl Pts',(-123.897553459906,-2.96238171699174,
134.732749510652));
#105259=CARTESIAN_POINT('Ctrl Pts',(-123.905318212853,-2.85076498297038,
134.812143305583));
#105260=CARTESIAN_POINT('Ctrl Pts',(-123.913075253739,-2.73925910826277,
134.891458245478));
#105261=CARTESIAN_POINT('Ctrl Pts',(-123.920832294624,-2.6243240802436,
134.966199030146));
#105262=CARTESIAN_POINT('Ctrl Pts',(-123.928589335509,-2.50637358930765,
135.036059389138));
#105263=CARTESIAN_POINT('Ctrl Pts',(-123.936340526749,-2.38851204575459,
135.105867065889));
#105264=CARTESIAN_POINT('Ctrl Pts',(-123.944091717989,-2.26763990054034,
135.17080144408));
#105265=CARTESIAN_POINT('Ctrl Pts',(-123.951842909229,-2.14420017242268,
135.230599278448));
#105266=CARTESIAN_POINT('Ctrl Pts',(-123.959590806006,-2.02081290948184,
135.29037169714));
#105267=CARTESIAN_POINT('Ctrl Pts',(-123.967338702783,-1.89486058524985,
135.345011744073));
#105268=CARTESIAN_POINT('Ctrl Pts',(-123.975086599561,-1.76681099509527,
135.394302008271));
#105269=CARTESIAN_POINT('Ctrl Pts',(-123.982832875645,-1.63878819015452,
135.443581962009));
#105270=CARTESIAN_POINT('Ctrl Pts',(-123.990579151729,-1.50866935653103,
135.487514218523));
#105271=CARTESIAN_POINT('Ctrl Pts',(-123.998325427813,-1.37694208432276,
135.525929589732));
#105272=CARTESIAN_POINT('Ctrl Pts',(-124.006071761078,-1.24521383973352,
135.564345244515));
#105273=CARTESIAN_POINT('Ctrl Pts',(-124.013818094344,-1.11187750819803,
135.597243823274));
#105274=CARTESIAN_POINT('Ctrl Pts',(-124.021564427609,-0.977435262299058,
135.624506193222));
#105275=CARTESIAN_POINT('Ctrl Pts',(-124.029312495612,-0.842962908991819,
135.651774668388));
#105276=CARTESIAN_POINT('Ctrl Pts',(-124.037060563615,-0.707384531595962,
135.673404345446));
#105277=CARTESIAN_POINT('Ctrl Pts',(-124.044808631618,-0.571211504384053,
135.689327401461));
#105278=CARTESIAN_POINT('Ctrl Pts',(-124.05256493436,-0.434893750858157,
135.705267380689));
#105279=CARTESIAN_POINT('Ctrl Pts',(-124.060321237102,-0.29798047396495,
135.715488577774));
#105280=CARTESIAN_POINT('Ctrl Pts',(-124.068077539844,-0.160987726819701,
135.719975127911));
#105281=CARTESIAN_POINT('Ctrl Pts',(-124.075837982358,-0.0239218625201553,
135.724464072655));
#105282=CARTESIAN_POINT('Ctrl Pts',(-124.083598424872,0.113223165790601,
135.723212275206));
#105283=CARTESIAN_POINT('Ctrl Pts',(-124.091358867386,0.249933308409536,
135.716256015867));
#105284=CARTESIAN_POINT('Ctrl Pts',(-124.099131767652,0.386862910285958,
135.709288589722));
#105285=CARTESIAN_POINT('Ctrl Pts',(-124.106904667917,0.523355841899727,
135.696598438681));
#105286=CARTESIAN_POINT('Ctrl Pts',(-124.114677568183,0.658904265552558,
135.678273648318));
#105287=CARTESIAN_POINT('Ctrl Pts',(-124.122167903944,0.789525162573133,
135.660615010244));
#105288=CARTESIAN_POINT('Ctrl Pts',(-124.129658239706,0.919268726565691,
135.637724340616));
#105289=CARTESIAN_POINT('Ctrl Pts',(-124.137148575468,1.04769309540822,
135.609724520574));
#105290=CARTESIAN_POINT('Ctrl Pts',(-124.144922909587,1.18098671323608,
135.580663078844));
#105291=CARTESIAN_POINT('Ctrl Pts',(-124.152697243706,1.3132813607472,135.546005353983));
#105292=CARTESIAN_POINT('Ctrl Pts',(-124.160471577825,1.44407073411834,
135.50583302282));
#105293=CARTESIAN_POINT('Ctrl Pts',(-124.168236330772,1.57469892127578,
135.465710200464));
#105294=CARTESIAN_POINT('Ctrl Pts',(-124.17600108372,1.7038251552757,135.420086408028));
#105295=CARTESIAN_POINT('Ctrl Pts',(-124.183765836667,1.83095297462968,
135.369094374007));
#105296=CARTESIAN_POINT('Ctrl Pts',(-124.191522877552,1.9579545288413,135.318152985994));
#105297=CARTESIAN_POINT('Ctrl Pts',(-124.199279918437,2.08296125784006,
135.26185411155));
#105298=CARTESIAN_POINT('Ctrl Pts',(-124.207036959322,2.20549187786027,
135.200380253463));
#105299=CARTESIAN_POINT('Ctrl Pts',(-124.214788150562,2.32793009658628,
135.138952753291));
#105300=CARTESIAN_POINT('Ctrl Pts',(-124.222539341802,2.44789557494999,
135.072358211768));
#105301=CARTESIAN_POINT('Ctrl Pts',(-124.230290533042,2.56492737479648,
135.000827062627));
#105302=CARTESIAN_POINT('Ctrl Pts',(-124.238038429819,2.68190943300691,
134.929326316131));
#105303=CARTESIAN_POINT('Ctrl Pts',(-124.245786326597,2.79595995978222,
134.852893338624));
#105304=CARTESIAN_POINT('Ctrl Pts',(-124.253534223374,2.90664318628904,
134.771804183655));
#105305=CARTESIAN_POINT('Ctrl Pts',(-124.261280499458,3.01730326025094,
134.690731990789));
#105306=CARTESIAN_POINT('Ctrl Pts',(-124.269026775542,3.124597119785,134.605005788655));
#105307=CARTESIAN_POINT('Ctrl Pts',(-124.276773051626,3.22811886780967,
134.514944350322));
#105308=CARTESIAN_POINT('Ctrl Pts',(-124.284519384892,3.33164138000795,
134.424882247176));
#105309=CARTESIAN_POINT('Ctrl Pts',(-124.292265718157,3.43139143016995,
134.330485100586));
#105310=CARTESIAN_POINT('Ctrl Pts',(-124.300012051422,3.52699735195981,
134.232111008386));
#105311=CARTESIAN_POINT('Ctrl Pts',(-124.307760119425,3.62262468403336,
134.13371488599));
#105312=CARTESIAN_POINT('Ctrl Pts',(-124.315508187428,3.71410576859588,
134.031340326092));
#105313=CARTESIAN_POINT('Ctrl Pts',(-124.323256255431,3.80110713400509,
133.925380902395));
#105314=CARTESIAN_POINT('Ctrl Pts',(-124.331012558173,3.88820096550067,
133.819308863763));
#105315=CARTESIAN_POINT('Ctrl Pts',(-124.338768860915,3.9708053185411,133.709644653017));
#105316=CARTESIAN_POINT('Ctrl Pts',(-124.346525163657,4.04862790630293,
133.596813864946));
#105317=CARTESIAN_POINT('Ctrl Pts',(-124.354285606171,4.12649203032326,
133.483922855686));
#105318=CARTESIAN_POINT('Ctrl Pts',(-124.362046048686,4.19956909543263,
133.367862232121));
#105319=CARTESIAN_POINT('Ctrl Pts',(-124.3698064912,4.26761176885554,133.249084089214));
#105320=CARTESIAN_POINT('Ctrl Pts',(-124.377579391465,4.33576367041838,
133.130115273087));
#105321=CARTESIAN_POINT('Ctrl Pts',(-124.385352291731,4.39886485050586,
133.008420567427));
#105322=CARTESIAN_POINT('Ctrl Pts',(-124.393125191996,4.45671491932755,
132.884474842877));
#105323=CARTESIAN_POINT('Ctrl Pts',(-124.400615527759,4.51246199243284,
132.765034857614));
#105324=CARTESIAN_POINT('Ctrl Pts',(-124.408105863521,4.56333298928115,
132.64350495662));
#105325=CARTESIAN_POINT('Ctrl Pts',(-124.415596199283,4.60919245598536,
132.520323311271));
#105326=CARTESIAN_POINT('Ctrl Pts',(-124.423370533402,4.65679069830721,
132.392471196401));
#105327=CARTESIAN_POINT('Ctrl Pts',(-124.431144867521,4.69914066127909,
132.262434615822));
#105328=CARTESIAN_POINT('Ctrl Pts',(-124.43891920164,4.73603739234594,132.130683685601));
#105329=CARTESIAN_POINT('Ctrl Pts',(-124.446683954587,4.7728886514894,131.999095126625));
#105330=CARTESIAN_POINT('Ctrl Pts',(-124.454448707534,4.80429994633945,
131.865796794682));
#105331=CARTESIAN_POINT('Ctrl Pts',(-124.462213460481,4.83011459557783,
131.731278119875));
#105332=CARTESIAN_POINT('Ctrl Pts',(-124.469970501366,4.8559036053426,131.596893050912));
#105333=CARTESIAN_POINT('Ctrl Pts',(-124.477727542251,4.87610695828812,
131.461290432618));
#105334=CARTESIAN_POINT('Ctrl Pts',(-124.485484583136,4.89061805354644,
131.32497382987));
#105335=CARTESIAN_POINT('Ctrl Pts',(-124.493235774377,4.90511820587501,
131.188760024532));
#105336=CARTESIAN_POINT('Ctrl Pts',(-124.500986965617,4.91393460341063,
131.05183369363));
#105337=CARTESIAN_POINT('Ctrl Pts',(-124.508738156857,4.91701196824753,
130.914707192549));
#105338=CARTESIAN_POINT('Ctrl Pts',(-124.516486053634,4.92008802512227,
130.77763897389));
#105339=CARTESIAN_POINT('Ctrl Pts',(-124.524233950411,4.91742989201127,
130.640371144314));
#105340=CARTESIAN_POINT('Ctrl Pts',(-124.531981847188,4.90903427688573,
130.503419542169));
#105341=CARTESIAN_POINT('Ctrl Pts',(-124.539728123272,4.90064041794189,
130.366496587347));
#105342=CARTESIAN_POINT('Ctrl Pts',(-124.547474399356,4.88651148807015,
130.22989011837));
#105343=CARTESIAN_POINT('Ctrl Pts',(-124.555220675441,4.86669628279414,
130.094113932577));
#105344=CARTESIAN_POINT('Ctrl Pts',(-124.562967008706,4.84688093124675,
129.958336744515));
#105345=CARTESIAN_POINT('Ctrl Pts',(-124.570713341971,4.82137927699687,
129.823390238736));
#105346=CARTESIAN_POINT('Ctrl Pts',(-124.578459675237,4.79029170316129,
129.689780669279));
#105347=CARTESIAN_POINT('Ctrl Pts',(-124.58620774324,4.75919716747914,129.556141178885));
#105348=CARTESIAN_POINT('Ctrl Pts',(-124.593955811243,4.72251431159356,
129.423839601302));
#105349=CARTESIAN_POINT('Ctrl Pts',(-124.601703879246,4.68039401064077,
129.293369231867));
#105350=CARTESIAN_POINT('Ctrl Pts',(-124.609460181988,4.63822894373095,
129.16276019697));
#105351=CARTESIAN_POINT('Ctrl Pts',(-124.617216484729,4.59061500792062,
129.033986630676));
#105352=CARTESIAN_POINT('Ctrl Pts',(-124.624972787471,4.53775227998991,
128.907524486545));
#105353=CARTESIAN_POINT('Ctrl Pts',(-124.632733229985,4.48486133762936,
128.780994845759));
#105354=CARTESIAN_POINT('Ctrl Pts',(-124.6404936725,4.42671618671405,128.656779439258));
#105355=CARTESIAN_POINT('Ctrl Pts',(-124.648254115014,4.36356349813381,
128.53533072348));
#105356=CARTESIAN_POINT('Ctrl Pts',(-124.656027015279,4.30030943125177,
128.413687047443));
#105357=CARTESIAN_POINT('Ctrl Pts',(-124.663799915545,4.23203195797615,
128.294819276551));
#105358=CARTESIAN_POINT('Ctrl Pts',(-124.67157281581,4.15902228485217,128.179152683591));
#105359=CARTESIAN_POINT('Ctrl Pts',(-124.679063151572,4.08866669725028,
128.067690862639));
#105360=CARTESIAN_POINT('Ctrl Pts',(-124.686553487333,4.01391716603381,
127.959201772237));
#105361=CARTESIAN_POINT('Ctrl Pts',(-124.694043823095,3.93506912105555,
127.854036215909));
#105362=CARTESIAN_POINT('Ctrl Pts',(-124.701818157214,3.85323152848279,
127.744883275543));
#105363=CARTESIAN_POINT('Ctrl Pts',(-124.709592491333,3.76671925985676,
127.638965104158));
#105364=CARTESIAN_POINT('Ctrl Pts',(-124.717366825452,3.67581705527618,
127.536708243362));
#105365=CARTESIAN_POINT('Ctrl Pts',(-124.725131578399,3.58502687953833,
127.434577405007));
#105366=CARTESIAN_POINT('Ctrl Pts',(-124.732896331346,3.48985778979982,
127.336099188628));
#105367=CARTESIAN_POINT('Ctrl Pts',(-124.740661084293,3.39063686738969,
127.24166996358));
#105368=CARTESIAN_POINT('Ctrl Pts',(-124.748418125178,3.29151449259873,
127.14733452697));
#105369=CARTESIAN_POINT('Ctrl Pts',(-124.756175166063,3.18834857512451,
127.057040346483));
#105370=CARTESIAN_POINT('Ctrl Pts',(-124.763932206948,3.0815051579867,126.971149297563));
#105371=CARTESIAN_POINT('Ctrl Pts',(-124.771683398188,2.97474231230074,
126.885323019751));
#105372=CARTESIAN_POINT('Ctrl Pts',(-124.779434589428,2.86430779037907,
126.803893508347));
#105373=CARTESIAN_POINT('Ctrl Pts',(-124.787185780668,2.75060277226001,
126.727184210819));
#105374=CARTESIAN_POINT('Ctrl Pts',(-124.794933677446,2.63694608180668,
126.650507516789));
#105375=CARTESIAN_POINT('Ctrl Pts',(-124.802681574222,2.5200219832831,126.578547264618));
#105376=CARTESIAN_POINT('Ctrl Pts',(-124.810429471,2.40026268667866,126.511585047211));
#105377=CARTESIAN_POINT('Ctrl Pts',(-124.818175747084,2.28052844113769,
126.444636836856));
#105378=CARTESIAN_POINT('Ctrl Pts',(-124.825922023168,2.15796051817767,
126.382684772428));
#105379=CARTESIAN_POINT('Ctrl Pts',(-124.833668299252,2.033017565225,126.325965520884));
#105380=CARTESIAN_POINT('Ctrl Pts',(-124.841414632517,1.90807368997165,
126.269245850651));
#105381=CARTESIAN_POINT('Ctrl Pts',(-124.849160965782,1.78075510574187,
126.21775923199));
#105382=CARTESIAN_POINT('Ctrl Pts',(-124.856907299048,1.65154199792476,
126.171694852416));
#105383=CARTESIAN_POINT('Ctrl Pts',(-124.864655367051,1.52229995372822,
126.125620157045));
#105384=CARTESIAN_POINT('Ctrl Pts',(-124.872403435054,1.39116290989811,
126.084970248283));
#105385=CARTESIAN_POINT('Ctrl Pts',(-124.880151503057,1.25862744146967,
126.049884828788));
#105386=CARTESIAN_POINT('Ctrl Pts',(-124.887907805798,1.12595111276801,
126.01476212009));
#105387=CARTESIAN_POINT('Ctrl Pts',(-124.89566410854,0.991873769047962,
125.985215814733));
#105388=CARTESIAN_POINT('Ctrl Pts',(-124.903420411282,0.856903989906555,
125.961334846978));
#105389=CARTESIAN_POINT('Ctrl Pts',(-124.911180853796,0.721862173330159,
125.937441133231));
#105390=CARTESIAN_POINT('Ctrl Pts',(-124.91894129631,0.585927359534623,
125.919218834108));
#105391=CARTESIAN_POINT('Ctrl Pts',(-124.926701738824,0.449613544577908,
125.906704982159));
#105392=CARTESIAN_POINT('Ctrl Pts',(-124.93447463909,0.313080906584052,
125.894171041864));
#105393=CARTESIAN_POINT('Ctrl Pts',(-124.942247539355,0.176168442346944,
125.887363880175));
#105394=CARTESIAN_POINT('Ctrl Pts',(-124.950020439621,0.0393913501586266,
125.886268367106));
#105395=CARTESIAN_POINT('Ctrl Pts',(-124.957510775383,-0.0924135502116431,
125.885212678697));
#105396=CARTESIAN_POINT('Ctrl Pts',(-124.965001111145,-0.224092442029103,
125.889460572971));
#105397=CARTESIAN_POINT('Ctrl Pts',(-124.972491446907,-0.355190497303149,
125.898953114297));
#105398=CARTESIAN_POINT('Ctrl Pts',(-124.980265781026,-0.491259175185668,
125.908805568213));
#105399=CARTESIAN_POINT('Ctrl Pts',(-124.988040115145,-0.627133126902452,
125.924339431135));
#105400=CARTESIAN_POINT('Ctrl Pts',(-124.995814449264,-0.762299581941407,
125.94554569931));
#105401=CARTESIAN_POINT('Ctrl Pts',(-125.003579202212,-0.897299456404333,
125.966725832654));
#105402=CARTESIAN_POINT('Ctrl Pts',(-125.011343955159,-1.03159318653046,
125.993564401762));
#105403=CARTESIAN_POINT('Ctrl Pts',(-125.019108708106,-1.164670500106,126.026000471168));
#105404=CARTESIAN_POINT('Ctrl Pts',(-125.026865748991,-1.29761563941764,
126.058404324613));
#105405=CARTESIAN_POINT('Ctrl Pts',(-125.034622789876,-1.4293463890887,
126.096394522683));
#105406=CARTESIAN_POINT('Ctrl Pts',(-125.042379830761,-1.55936043786478,
126.139858705537));
#105407=CARTESIAN_POINT('Ctrl Pts',(-125.050131022001,-1.68927644203549,
126.183290111713));
#105408=CARTESIAN_POINT('Ctrl Pts',(-125.057882213241,-1.81747795279544,
126.232187162733));
#105409=CARTESIAN_POINT('Ctrl Pts',(-125.065633404481,-1.94347599701874,
126.286387165728));
#105410=CARTESIAN_POINT('Ctrl Pts',(-125.073381301258,-2.0694204887123,
126.340564132276));
#105411=CARTESIAN_POINT('Ctrl Pts',(-125.081129198035,-2.19316301816585,
126.400039413801));
#105412=CARTESIAN_POINT('Ctrl Pts',(-125.088877094812,-2.31423305323739,
126.464601587642));
#105413=CARTESIAN_POINT('Ctrl Pts',(-125.096623370896,-2.43527776306756,
126.529150256469));
#105414=CARTESIAN_POINT('Ctrl Pts',(-125.104369646981,-2.5536507456927,
126.598783517273));
#105415=CARTESIAN_POINT('Ctrl Pts',(-125.112115923065,-2.6689049763623,
126.673243421256));
#105416=CARTESIAN_POINT('Ctrl Pts',(-125.11986225633,-2.78416005781261,
126.747703874885));
#105417=CARTESIAN_POINT('Ctrl Pts',(-125.127608589595,-2.89629601297496,
126.826990830631));
#105418=CARTESIAN_POINT('Ctrl Pts',(-125.135354922861,-3.00489412110217,
126.910802555399));
#105419=CARTESIAN_POINT('Ctrl Pts',(-125.143102990864,-3.11351654902287,
126.994633049222));
#105420=CARTESIAN_POINT('Ctrl Pts',(-125.150851058867,-3.21859924391988,
127.082990089576));
#105421=CARTESIAN_POINT('Ctrl Pts',(-125.15859912687,-3.31975625905732,
127.175531406519));
#105422=CARTESIAN_POINT('Ctrl Pts',(-125.166355429612,-3.42102078507409,
127.268171077474));
#105423=CARTESIAN_POINT('Ctrl Pts',(-125.174111732354,-3.51835100786864,
127.365003644259));
#105424=CARTESIAN_POINT('Ctrl Pts',(-125.181868035095,-3.61139720483113,
127.465649295598));
#105425=CARTESIAN_POINT('Ctrl Pts',(-125.18962847761,-3.70449306335076,
127.566348664551));
#105426=CARTESIAN_POINT('Ctrl Pts',(-125.197388920124,-3.79330008693485,
127.670864875492));
#105427=CARTESIAN_POINT('Ctrl Pts',(-125.205149362638,-3.87750929162449,
127.778785505977));
#105428=CARTESIAN_POINT('Ctrl Pts',(-125.212922262904,-3.96185367640501,
127.886879380239));
#105429=CARTESIAN_POINT('Ctrl Pts',(-125.220695163169,-4.0415852655164,
127.998388276798));
#105430=CARTESIAN_POINT('Ctrl Pts',(-125.228468063434,-4.11643831098136,
128.112870566612));
#105431=CARTESIAN_POINT('Ctrl Pts',(-125.235958399196,-4.18857025970044,
128.223191136828));
#105432=CARTESIAN_POINT('Ctrl Pts',(-125.243448734959,-4.25617204340296,
128.336272408467));
#105433=CARTESIAN_POINT('Ctrl Pts',(-125.250939070721,-4.31904740066438,
128.451699865712));
#105434=CARTESIAN_POINT('Ctrl Pts',(-125.259118235739,-4.38770492670435,
128.577742308995));
#105435=CARTESIAN_POINT('Ctrl Pts',(-125.267297400758,-4.45092577115809,
128.706947432853));
#105436=CARTESIAN_POINT('Ctrl Pts',(-125.275476565776,-4.50842288035711,
128.838831122907));
#105437=CARTESIAN_POINT('Ctrl Pts',(-125.283637476055,-4.56579166414356,
128.970420467226));
#105438=CARTESIAN_POINT('Ctrl Pts',(-125.291798386335,-4.61746205009728,
129.104676156598));
#105439=CARTESIAN_POINT('Ctrl Pts',(-125.299959296614,-4.66319283653817,
129.241089805531));
#105440=CARTESIAN_POINT('Ctrl Pts',(-125.306685607822,-4.70088464919518,
129.353523421911));
#105441=CARTESIAN_POINT('Ctrl Pts',(-125.313411919029,-4.73454230683632,
129.467422415989));
#105442=CARTESIAN_POINT('Ctrl Pts',(-125.320138230236,-4.76405452823398,
129.582490119308));
#105443=CARTESIAN_POINT('Origin',(213.235140564004,0.,130.804360617566));
#105444=CARTESIAN_POINT('',(-127.415055402248,-4.76405452823392,129.582490119308));
#105445=CARTESIAN_POINT('',(-127.069805705487,-4.76405452823416,129.582490119309));
#105446=CARTESIAN_POINT('',(213.235140564004,-4.76405452823405,129.582490119308));
#105447=CARTESIAN_POINT('',(-125.735140563975,-4.91824810239634,130.808681008151));
#105448=CARTESIAN_POINT('Ctrl Pts',(-125.73514056401,-4.91824810239579,
130.808681008773));
#105449=CARTESIAN_POINT('Ctrl Pts',(-125.74658130245,-4.91807096085325,
131.010335445559));
#105450=CARTESIAN_POINT('Ctrl Pts',(-125.75802204089,-4.90548850143151,
131.211466635464));
#105451=CARTESIAN_POINT('Ctrl Pts',(-125.76946277933,-4.88071177055635,
131.410855197305));
#105452=CARTESIAN_POINT('Ctrl Pts',(-125.775723626949,-4.86715291355413,
131.519968906111));
#105453=CARTESIAN_POINT('Ctrl Pts',(-125.781984474568,-4.84994295193747,
131.628561430318));
#105454=CARTESIAN_POINT('Ctrl Pts',(-125.788245322187,-4.82912182240563,
131.736436519446));
#105455=CARTESIAN_POINT('Ctrl Pts',(-125.796019656307,-4.80326742894898,
131.870389146474));
#105456=CARTESIAN_POINT('Ctrl Pts',(-125.803793990425,-4.77179439142009,
132.003477386229));
#105457=CARTESIAN_POINT('Ctrl Pts',(-125.811568324545,-4.73477221323026,
132.135193120672));
#105458=CARTESIAN_POINT('Ctrl Pts',(-125.819333077492,-4.69779566156628,
132.266746527243));
#105459=CARTESIAN_POINT('Ctrl Pts',(-125.827097830439,-4.65528368123059,
132.396930421297));
#105460=CARTESIAN_POINT('Ctrl Pts',(-125.834862583386,-4.6073570487901,
132.525245299195));
#105461=CARTESIAN_POINT('Ctrl Pts',(-125.842619624271,-4.55947801775672,
132.653432732947));
#105462=CARTESIAN_POINT('Ctrl Pts',(-125.850376665156,-4.5061951728124,
132.779754480848));
#105463=CARTESIAN_POINT('Ctrl Pts',(-125.858133706041,-4.44767941470448,
132.903725018168));
#105464=CARTESIAN_POINT('Ctrl Pts',(-125.865884897281,-4.38920778378469,
133.027602068341));
#105465=CARTESIAN_POINT('Ctrl Pts',(-125.873636088521,-4.32551126054325,
133.149131084986));
#105466=CARTESIAN_POINT('Ctrl Pts',(-125.881387279761,-4.25680915110943,
133.267845732912));
#105467=CARTESIAN_POINT('Ctrl Pts',(-125.889135176538,-4.18813624190508,
133.386509923945));
#105468=CARTESIAN_POINT('Ctrl Pts',(-125.896883073315,-4.11446217337812,
133.502361787696));
#105469=CARTESIAN_POINT('Ctrl Pts',(-125.904630970092,-4.03605246233152,
133.614959056299));
#105470=CARTESIAN_POINT('Ctrl Pts',(-125.912377246176,-3.95765915290595,
133.727532771981));
#105471=CARTESIAN_POINT('Ctrl Pts',(-125.92012352226,-3.87453239458777,
133.836852926011));
#105472=CARTESIAN_POINT('Ctrl Pts',(-125.927869798344,-3.7869811282361,
133.942506088522));
#105473=CARTESIAN_POINT('Ctrl Pts',(-125.93561613161,-3.69942921560099,
134.048160030941));
#105474=CARTESIAN_POINT('Ctrl Pts',(-125.943362464875,-3.60745297922013,
134.150146626789));
#105475=CARTESIAN_POINT('Ctrl Pts',(-125.95110879814,-3.51140149483713,
134.248085723401));
#105476=CARTESIAN_POINT('Ctrl Pts',(-125.958856866143,-3.4153285003903,
134.346046752794));
#105477=CARTESIAN_POINT('Ctrl Pts',(-125.966604934146,-3.31517871562495,
134.439958200223));
#105478=CARTESIAN_POINT('Ctrl Pts',(-125.974353002149,-3.21133759850637,
134.529477245394));
#105479=CARTESIAN_POINT('Ctrl Pts',(-125.982109304891,-3.10738611781265,
134.619091432471));
#105480=CARTESIAN_POINT('Ctrl Pts',(-125.989865607633,-2.9997357643591,
134.704303636179));
#105481=CARTESIAN_POINT('Ctrl Pts',(-125.997621910375,-2.88880499629402,
134.784811440763));
#105482=CARTESIAN_POINT('Ctrl Pts',(-126.005382352889,-2.77781502113796,
134.865362214786));
#105483=CARTESIAN_POINT('Ctrl Pts',(-126.013142795403,-2.66354146823299,
134.941203370456));
#105484=CARTESIAN_POINT('Ctrl Pts',(-126.020903237917,-2.54643036704537,
135.012076797192));
#105485=CARTESIAN_POINT('Ctrl Pts',(-126.028676138183,-2.42913126872149,
135.083063996245));
#105486=CARTESIAN_POINT('Ctrl Pts',(-126.036449038448,-2.30898586246423,
135.149067342137));
#105487=CARTESIAN_POINT('Ctrl Pts',(-126.044221938713,-2.18646407336403,
135.209875107201));
#105488=CARTESIAN_POINT('Ctrl Pts',(-126.051712274475,-2.06839625991271,
135.268472356839));
#105489=CARTESIAN_POINT('Ctrl Pts',(-126.059202610237,-1.94812212018979,
135.322245086625));
#105490=CARTESIAN_POINT('Ctrl Pts',(-126.066692945999,-1.82607644886793,
135.371047366774));
#105491=CARTESIAN_POINT('Ctrl Pts',(-126.074467280118,-1.699403378822,135.421700000208));
#105492=CARTESIAN_POINT('Ctrl Pts',(-126.082241614237,-1.5704205279059,
135.467158286821));
#105493=CARTESIAN_POINT('Ctrl Pts',(-126.090015948356,-1.43959295850791,
135.507206051589));
#105494=CARTESIAN_POINT('Ctrl Pts',(-126.097780701303,-1.3089266223968,
135.547204461067));
#105495=CARTESIAN_POINT('Ctrl Pts',(-126.10554545425,-1.17642046154627,
135.581805502663));
#105496=CARTESIAN_POINT('Ctrl Pts',(-126.113310207198,-1.04256000519791,
135.610840795208));
#105497=CARTESIAN_POINT('Ctrl Pts',(-126.121067248083,-0.908832500941903,
135.63984724949));
#105498=CARTESIAN_POINT('Ctrl Pts',(-126.128824288968,-0.773753757616368,
135.663298873311));
#105499=CARTESIAN_POINT('Ctrl Pts',(-126.136581329852,-0.637824636957127,
135.681077012333));
#105500=CARTESIAN_POINT('Ctrl Pts',(-126.144332521093,-0.501998021504966,
135.698841744722));
#105501=CARTESIAN_POINT('Ctrl Pts',(-126.152083712333,-0.365322691235412,
135.710941457748));
#105502=CARTESIAN_POINT('Ctrl Pts',(-126.159834903573,-0.228309527471113,
135.717308594307));
#105503=CARTESIAN_POINT('Ctrl Pts',(-126.16758280035,-0.0913545979565474,
135.723673024664));
#105504=CARTESIAN_POINT('Ctrl Pts',(-126.175330697127,0.0459374897405901,
135.724309706451));
#105505=CARTESIAN_POINT('Ctrl Pts',(-126.183078593904,0.183051124820735,
135.71920296989));
#105506=CARTESIAN_POINT('Ctrl Pts',(-126.190824869988,0.32013607868425,
135.714097301549));
#105507=CARTESIAN_POINT('Ctrl Pts',(-126.198571146072,0.457042263732288,
135.703250619051));
#105508=CARTESIAN_POINT('Ctrl Pts',(-126.206317422156,0.593254859627366,
135.686699374149));
#105509=CARTESIAN_POINT('Ctrl Pts',(-126.214063755422,0.729468461012698,
135.670148007069));
#105510=CARTESIAN_POINT('Ctrl Pts',(-126.221810088687,0.864988074918127,
135.647892040717));
#105511=CARTESIAN_POINT('Ctrl Pts',(-126.229556421952,0.999305184173385,
135.6200196806));
#105512=CARTESIAN_POINT('Ctrl Pts',(-126.237304489955,1.13365237281416,
135.592141078662));
#105513=CARTESIAN_POINT('Ctrl Pts',(-126.245052557958,1.266796138207,135.5586436596));
#105514=CARTESIAN_POINT('Ctrl Pts',(-126.252800625961,1.39823970648345,
135.519666417375));
#105515=CARTESIAN_POINT('Ctrl Pts',(-126.260556928703,1.52982297454865,
135.480647749673));
#105516=CARTESIAN_POINT('Ctrl Pts',(-126.268313231445,1.65970206041054,
135.436137736024));
#105517=CARTESIAN_POINT('Ctrl Pts',(-126.276069534186,1.78739634628032,
135.386324974019));
#105518=CARTESIAN_POINT('Ctrl Pts',(-126.2838299767,1.91515878643526,135.336485625443));
#105519=CARTESIAN_POINT('Ctrl Pts',(-126.291590419215,2.04073374526613,
135.281338046152));
#105520=CARTESIAN_POINT('Ctrl Pts',(-126.299350861729,2.16366297720856,
135.221117978295));
#105521=CARTESIAN_POINT('Ctrl Pts',(-126.307123761994,2.28678954606724,
135.160801239839));
#105522=CARTESIAN_POINT('Ctrl Pts',(-126.31489666226,2.40726155707568,135.095395927537));
#105523=CARTESIAN_POINT('Ctrl Pts',(-126.322669562525,2.52464687175936,
135.0251829587));
#105524=CARTESIAN_POINT('Ctrl Pts',(-126.330159898287,2.63776493458266,
134.957522408133));
#105525=CARTESIAN_POINT('Ctrl Pts',(-126.33765023405,2.74801656545889,134.885397841961));
#105526=CARTESIAN_POINT('Ctrl Pts',(-126.345140569812,2.85504397238631,
134.809096186644));
#105527=CARTESIAN_POINT('Ctrl Pts',(-126.352914903931,2.96612935597375,
134.729901530877));
#105528=CARTESIAN_POINT('Ctrl Pts',(-126.36068923805,3.07409308144867,134.645955919712));
#105529=CARTESIAN_POINT('Ctrl Pts',(-126.368463572169,3.17850189706106,
134.557533775426));
#105530=CARTESIAN_POINT('Ctrl Pts',(-126.376228325116,3.28278203813949,
134.46922060353));
#105531=CARTESIAN_POINT('Ctrl Pts',(-126.383993078063,3.38351569096996,
134.376442125797));
#105532=CARTESIAN_POINT('Ctrl Pts',(-126.391757831011,3.48029875128976,
134.279515817592));
#105533=CARTESIAN_POINT('Ctrl Pts',(-126.399514871896,3.57698568530965,
134.182685777963));
#105534=CARTESIAN_POINT('Ctrl Pts',(-126.40727191278,3.66972956086441,134.081716381088));
#105535=CARTESIAN_POINT('Ctrl Pts',(-126.415028953665,3.75815982269649,
133.97696488056));
#105536=CARTESIAN_POINT('Ctrl Pts',(-126.422780144906,3.84652339858035,
133.872292373954));
#105537=CARTESIAN_POINT('Ctrl Pts',(-126.430531336146,3.93057958432218,
133.763843738194));
#105538=CARTESIAN_POINT('Ctrl Pts',(-126.438282527386,4.00999539838349,
133.652012275941));
#105539=CARTESIAN_POINT('Ctrl Pts',(-126.446030424163,4.08937745860524,
133.540228345042));
#105540=CARTESIAN_POINT('Ctrl Pts',(-126.45377832094,4.16412284397078,133.425064765406));
#105541=CARTESIAN_POINT('Ctrl Pts',(-126.461526217717,4.23393967081978,
133.306946865102));
#105542=CARTESIAN_POINT('Ctrl Pts',(-126.469272493801,4.30374189349386,
133.188853672517));
#105543=CARTESIAN_POINT('Ctrl Pts',(-126.477018769885,4.36861740945242,
133.067807724816));
#105544=CARTESIAN_POINT('Ctrl Pts',(-126.484765045969,4.42831861361938,
132.944261857991));
#105545=CARTESIAN_POINT('Ctrl Pts',(-126.492511379235,4.48802025848699,
132.820715079179));
#105546=CARTESIAN_POINT('Ctrl Pts',(-126.5002577125,4.54254734523984,132.694668696439));
#105547=CARTESIAN_POINT('Ctrl Pts',(-126.508004045766,4.59169921771805,
132.5665982169));
#105548=CARTESIAN_POINT('Ctrl Pts',(-126.515752113769,4.64086209741724,
132.438499056866));
#105549=CARTESIAN_POINT('Ctrl Pts',(-126.523500181772,4.68464722747635,
132.30837526299));
#105550=CARTESIAN_POINT('Ctrl Pts',(-126.531248249775,4.72290302904014,
132.176719914829));
#105551=CARTESIAN_POINT('Ctrl Pts',(-126.539004552516,4.76119948932512,
132.044924641796));
#105552=CARTESIAN_POINT('Ctrl Pts',(-126.546760855258,4.79395477263454,
131.911594938899));
#105553=CARTESIAN_POINT('Ctrl Pts',(-126.554517158,4.82106776580748,131.777237105098));
#105554=CARTESIAN_POINT('Ctrl Pts',(-126.562277600514,4.84819523000124,
131.642807560475));
#105555=CARTESIAN_POINT('Ctrl Pts',(-126.570038043028,4.86967434227033,
131.507349177482));
#105556=CARTESIAN_POINT('Ctrl Pts',(-126.577798485543,4.88545574623936,
131.371374915478));
#105557=CARTESIAN_POINT('Ctrl Pts',(-126.585571385808,4.90126248391906,
131.235182375518));
#105558=CARTESIAN_POINT('Ctrl Pts',(-126.593344286073,4.91135320694685,
131.098472691798));
#105559=CARTESIAN_POINT('Ctrl Pts',(-126.601117186339,4.91573067761112,
130.961761277326));
#105560=CARTESIAN_POINT('Ctrl Pts',(-126.608607522101,4.91994901619056,
130.830019667125));
#105561=CARTESIAN_POINT('Ctrl Pts',(-126.616097857863,4.91886227553077,
130.698276757829));
#105562=CARTESIAN_POINT('Ctrl Pts',(-126.623588193625,4.91251845967148,
130.566988660741));
#105563=CARTESIAN_POINT('Ctrl Pts',(-126.631362527744,4.9059341161057,130.430722735548));
#105564=CARTESIAN_POINT('Ctrl Pts',(-126.639136861863,4.89366532674861,
130.294515142293));
#105565=CARTESIAN_POINT('Ctrl Pts',(-126.646911195982,4.87570878768121,
130.158878719889));
#105566=CARTESIAN_POINT('Ctrl Pts',(-126.654675948929,4.85777437844344,
130.023409457254));
#105567=CARTESIAN_POINT('Ctrl Pts',(-126.662440701877,4.8341662174146,129.888510348748));
#105568=CARTESIAN_POINT('Ctrl Pts',(-126.670205454824,4.80493297738675,
129.754692981921));
#105569=CARTESIAN_POINT('Ctrl Pts',(-126.677962495709,4.77572877222501,
129.621008524389));
#105570=CARTESIAN_POINT('Ctrl Pts',(-126.685719536594,4.74091068916384,
129.488404049916));
#105571=CARTESIAN_POINT('Ctrl Pts',(-126.693476577479,4.70057900160301,
129.357384421428));
#105572=CARTESIAN_POINT('Ctrl Pts',(-126.701227768719,4.66027772848145,
129.226463595862));
#105573=CARTESIAN_POINT('Ctrl Pts',(-126.708978959959,4.61447124137126,
129.097125609569));
#105574=CARTESIAN_POINT('Ctrl Pts',(-126.716730151199,4.56331045228496,
128.969863199043));
#105575=CARTESIAN_POINT('Ctrl Pts',(-126.724478047976,4.51217140789884,
128.842654878437));
#105576=CARTESIAN_POINT('Ctrl Pts',(-126.732225944753,4.45568273329646,
128.717520741009));
#105577=CARTESIAN_POINT('Ctrl Pts',(-126.73997384153,4.39404449878123,128.594936256962));
#105578=CARTESIAN_POINT('Ctrl Pts',(-126.747720117614,4.33241915765589,
128.472377414946));
#105579=CARTESIAN_POINT('Ctrl Pts',(-126.755466393698,4.26564657470359,
128.352367514556));
#105580=CARTESIAN_POINT('Ctrl Pts',(-126.763212669783,4.1939738970784,128.23535964187));
#105581=CARTESIAN_POINT('Ctrl Pts',(-126.770959003048,4.12230069038169,
128.118350905459));
#105582=CARTESIAN_POINT('Ctrl Pts',(-126.778705336313,4.04572752105165,
128.004344574361));
#105583=CARTESIAN_POINT('Ctrl Pts',(-126.786451669579,3.9645459871471,127.893766489506));
#105584=CARTESIAN_POINT('Ctrl Pts',(-126.794199737582,3.88334627320102,
127.783163641456));
#105585=CARTESIAN_POINT('Ctrl Pts',(-126.801947805585,3.79753637242429,
127.675990882438));
#105586=CARTESIAN_POINT('Ctrl Pts',(-126.809695873588,3.70744919453781,
127.572642261579));
#105587=CARTESIAN_POINT('Ctrl Pts',(-126.817452176329,3.6172662709265,127.469183800577));
#105588=CARTESIAN_POINT('Ctrl Pts',(-126.825208479071,3.52279724650639,
127.369557891876));
#105589=CARTESIAN_POINT('Ctrl Pts',(-126.832964781813,3.42441343079969,
127.274123271797));
#105590=CARTESIAN_POINT('Ctrl Pts',(-126.840725224327,3.32597710468828,
127.178637715389));
#105591=CARTESIAN_POINT('Ctrl Pts',(-126.848485666841,3.22362211553307,
127.087348165154));
#105592=CARTESIAN_POINT('Ctrl Pts',(-126.856246109356,3.11775335224545,
127.000573413073));
#105593=CARTESIAN_POINT('Ctrl Pts',(-126.864019009621,3.01171463902042,
126.913659362457));
#105594=CARTESIAN_POINT('Ctrl Pts',(-126.871791909887,2.90215119256412,
126.83127482802));
#105595=CARTESIAN_POINT('Ctrl Pts',(-126.879564810152,2.78949813751974,
126.753696079089));
#105596=CARTESIAN_POINT('Ctrl Pts',(-126.887055145914,2.68094030478244,
126.678937513092));
#105597=CARTESIAN_POINT('Ctrl Pts',(-126.894545481676,2.56951385416692,
126.608641558313));
#105598=CARTESIAN_POINT('Ctrl Pts',(-126.902035817438,2.45562847238693,
126.543014366896));
#105599=CARTESIAN_POINT('Ctrl Pts',(-126.909810151557,2.33742509174123,
126.474898900568));
#105600=CARTESIAN_POINT('Ctrl Pts',(-126.917584485676,2.21619820560702,
126.411597449315));
#105601=CARTESIAN_POINT('Ctrl Pts',(-126.925358819795,2.09237749403648,
126.353389994775));
#105602=CARTESIAN_POINT('Ctrl Pts',(-126.933123572742,1.96870938042711,
126.29525427572));
#105603=CARTESIAN_POINT('Ctrl Pts',(-126.940888325689,1.84245415220137,
126.24220022697));
#105604=CARTESIAN_POINT('Ctrl Pts',(-126.948653078637,1.71406853128797,
126.194463424293));
#105605=CARTESIAN_POINT('Ctrl Pts',(-126.956410119522,1.58581042478318,
126.146774034481));
#105606=CARTESIAN_POINT('Ctrl Pts',(-126.964167160407,1.45542650048104,
126.104391516362));
#105607=CARTESIAN_POINT('Ctrl Pts',(-126.971924201292,1.32339571408289,
126.06750439783));
#105608=CARTESIAN_POINT('Ctrl Pts',(-126.979675392532,1.19146449312764,
126.030645096161));
#105609=CARTESIAN_POINT('Ctrl Pts',(-126.987426583772,1.05788925704805,
125.999273050227));
#105610=CARTESIAN_POINT('Ctrl Pts',(-126.995177775012,0.923166130640588,
125.973527629588));
#105611=CARTESIAN_POINT('Ctrl Pts',(-127.002925671789,0.788500265155893,
125.947793151439));
#105612=CARTESIAN_POINT('Ctrl Pts',(-127.010673568566,0.652687862919644,
125.927680615374));
#105613=CARTESIAN_POINT('Ctrl Pts',(-127.018421465344,0.516237093364168,
125.913278699837));
#105614=CARTESIAN_POINT('Ctrl Pts',(-127.026167741428,0.379814866368144,
125.898879796871));
#105615=CARTESIAN_POINT('Ctrl Pts',(-127.033914017512,0.242754926215932,
125.890189179441));
#105616=CARTESIAN_POINT('Ctrl Pts',(-127.041660293596,0.105572056130962,
125.88724381974));
#105617=CARTESIAN_POINT('Ctrl Pts',(-127.049406626861,-0.0316118266066049,
125.884298438297));
#105618=CARTESIAN_POINT('Ctrl Pts',(-127.057152960127,-0.168918250212538,
125.887098407602));
#105619=CARTESIAN_POINT('Ctrl Pts',(-127.064899293392,-0.30583132677999,
125.895628575372));
#105620=CARTESIAN_POINT('Ctrl Pts',(-127.072647361395,-0.442775064082211,
125.904160653415));
#105621=CARTESIAN_POINT('Ctrl Pts',(-127.080395429398,-0.579324888928421,
125.918425459112));
#105622=CARTESIAN_POINT('Ctrl Pts',(-127.088143497401,-0.714969330791542,
125.938355899265));
#105623=CARTESIAN_POINT('Ctrl Pts',(-127.095899800143,-0.850757937181479,
125.958307521727));
#105624=CARTESIAN_POINT('Ctrl Pts',(-127.103656102885,-0.985638850957818,
125.983936750323));
#105625=CARTESIAN_POINT('Ctrl Pts',(-127.111412405627,-1.11910955522665,
126.015125097579));
#105626=CARTESIAN_POINT('Ctrl Pts',(-127.119172848141,-1.25265149682872,
126.046330090996));
#105627=CARTESIAN_POINT('Ctrl Pts',(-127.126933290655,-1.38478135269379,
126.083100010443));
#105628=CARTESIAN_POINT('Ctrl Pts',(-127.134693733169,-1.51501206175335,
126.125266526266));
#105629=CARTESIAN_POINT('Ctrl Pts',(-127.142466633435,-1.64545182870879,
126.167500731523));
#105630=CARTESIAN_POINT('Ctrl Pts',(-127.1502395337,-1.7739859898281,126.215148708808));
#105631=CARTESIAN_POINT('Ctrl Pts',(-127.158012433966,-1.90014691640336,
126.267993705754));
#105632=CARTESIAN_POINT('Ctrl Pts',(-127.165502769727,-2.02172157551332,
126.318917653951));
#105633=CARTESIAN_POINT('Ctrl Pts',(-127.172993105489,-2.14109227145035,
126.374667201982));
#105634=CARTESIAN_POINT('Ctrl Pts',(-127.180483441251,-2.25786411690229,
126.435009099079));
#105635=CARTESIAN_POINT('Ctrl Pts',(-127.188258645785,-2.37907697184334,
126.497645889578));
#105636=CARTESIAN_POINT('Ctrl Pts',(-127.196033850318,-2.49787339678363,
126.565429686841));
#105637=CARTESIAN_POINT('Ctrl Pts',(-127.203809054852,-2.61378542659004,
126.638150252469));
#105638=CARTESIAN_POINT('Ctrl Pts',(-127.211574485278,-2.72955174490323,
126.710779402027));
#105639=CARTESIAN_POINT('Ctrl Pts',(-127.219339915704,-2.84244055508795,
126.788332764952));
#105640=CARTESIAN_POINT('Ctrl Pts',(-127.22710534613,-2.95200667842948,
126.870553348138));
#105641=CARTESIAN_POINT('Ctrl Pts',(-127.234936598468,-3.06250151420178,
126.953470855476));
#105642=CARTESIAN_POINT('Ctrl Pts',(-127.242767850806,-3.1696167021075,
127.041134914113));
#105643=CARTESIAN_POINT('Ctrl Pts',(-127.250599103144,-3.27292279347026,
127.13323552429));
#105644=CARTESIAN_POINT('Ctrl Pts',(-127.25834997073,-3.37516848807113,
127.224390757601));
#105645=CARTESIAN_POINT('Ctrl Pts',(-127.266100838315,-3.47368261274716,
127.319891630404));
#105646=CARTESIAN_POINT('Ctrl Pts',(-127.273851705901,-3.56808011938389,
127.419395724963));
#105647=CARTESIAN_POINT('Ctrl Pts',(-127.281599016516,-3.66243430582419,
127.518854155847));
#105648=CARTESIAN_POINT('Ctrl Pts',(-127.289346327131,-3.75267536492801,
127.622311869915));
#105649=CARTESIAN_POINT('Ctrl Pts',(-127.297093637747,-3.83845445671201,
127.729389000421));
#105650=CARTESIAN_POINT('Ctrl Pts',(-127.304839070779,-3.92421275968017,
127.836440180469));
#105651=CARTESIAN_POINT('Ctrl Pts',(-127.31258450381,-4.00551100395607,
127.947108725872));
#105652=CARTESIAN_POINT('Ctrl Pts',(-127.320329936842,-4.08204033137633,
128.060981351858));
#105653=CARTESIAN_POINT('Ctrl Pts',(-127.328223725626,-4.16003549884399,
128.17703509012));
#105654=CARTESIAN_POINT('Ctrl Pts',(-127.33611751441,-4.23307693528564,
128.296416576218));
#105655=CARTESIAN_POINT('Ctrl Pts',(-127.344011303193,-4.3008839601664,
128.41865732007));
#105656=CARTESIAN_POINT('Ctrl Pts',(-127.351760510745,-4.3674490436303,
128.538659124183));
#105657=CARTESIAN_POINT('Ctrl Pts',(-127.359509718296,-4.4289696688949,
128.661415971348));
#105658=CARTESIAN_POINT('Ctrl Pts',(-127.367258925848,-4.48522708801597,
128.786460463587));
#105659=CARTESIAN_POINT('Ctrl Pts',(-127.375225005248,-4.54305894560785,
128.915004491749));
#105660=CARTESIAN_POINT('Ctrl Pts',(-127.383191084648,-4.59532849085163,
129.045965689352));
#105661=CARTESIAN_POINT('Ctrl Pts',(-127.391157164048,-4.64185173657047,
129.178815934022));
#105662=CARTESIAN_POINT('Ctrl Pts',(-127.399123243448,-4.68837498228919,
129.311666178692));
#105663=CARTESIAN_POINT('Ctrl Pts',(-127.407089322848,-4.72915183134664,
129.446405033867));
#105664=CARTESIAN_POINT('Ctrl Pts',(-127.415055402248,-4.76405452823392,
129.582490119308));
#105665=CARTESIAN_POINT('Ctrl Pts',(-125.665057882386,-4.76405452823409,
129.582490119308));
#105666=CARTESIAN_POINT('Ctrl Pts',(-125.672695217592,-4.79767286397123,
129.713567500118));
#105667=CARTESIAN_POINT('Ctrl Pts',(-125.680332552798,-4.82586495161931,
129.845985106168));
#105668=CARTESIAN_POINT('Ctrl Pts',(-125.687969888004,-4.84854317541177,
129.979247207986));
#105669=CARTESIAN_POINT('Ctrl Pts',(-125.695831667332,-4.87188786124959,
130.116425583573));
#105670=CARTESIAN_POINT('Ctrl Pts',(-125.703693446661,-4.88938953514324,
130.254498400782));
#105671=CARTESIAN_POINT('Ctrl Pts',(-125.711555225989,-4.90101002084738,
130.392919445521));
#105672=CARTESIAN_POINT('Ctrl Pts',(-125.719417005318,-4.91263050655152,
130.53134049026));
#105673=CARTESIAN_POINT('Ctrl Pts',(-125.727278784646,-4.9183698294618,
130.670109298731));
#105674=CARTESIAN_POINT('Ctrl Pts',(-125.735140563975,-4.91824810239634,
130.808681008151));
#105675=CARTESIAN_POINT('',(-125.389859435955,-4.91824999990999,130.804330862985));
#105676=CARTESIAN_POINT('Ctrl Pts',(-125.320138230236,-4.76405452823398,
129.582490119308));
#105677=CARTESIAN_POINT('Ctrl Pts',(-125.328275130921,-4.79975582231666,
129.721688923094));
#105678=CARTESIAN_POINT('Ctrl Pts',(-125.336412031606,-4.82938928728266,
129.862598298068));
#105679=CARTESIAN_POINT('Ctrl Pts',(-125.344548932291,-4.85280195543081,
130.004675527129));
#105680=CARTESIAN_POINT('Ctrl Pts',(-125.352670622673,-4.87617085829199,
130.146487171309));
#105681=CARTESIAN_POINT('Ctrl Pts',(-125.360792313054,-4.89334209898037,
130.289461990503));
#105682=CARTESIAN_POINT('Ctrl Pts',(-125.368914003435,-4.90421331179742,
130.433045583008));
#105683=CARTESIAN_POINT('Ctrl Pts',(-125.375895814266,-4.9135587494866,
130.556477212902));
#105684=CARTESIAN_POINT('Ctrl Pts',(-125.382877625097,-4.91824924988505,
130.680358369937));
#105685=CARTESIAN_POINT('Ctrl Pts',(-125.389859435927,-4.91824999990999,
130.804330862496));
#105686=CARTESIAN_POINT('Ctrl Pts',(-125.389859435993,-4.91824999991,130.804330863662));
#105687=CARTESIAN_POINT('Ctrl Pts',(-125.397970397523,-4.91825087120044,
130.948353115535));
#105688=CARTESIAN_POINT('Ctrl Pts',(-125.406081359054,-4.91192127880867,
131.092254350031));
#105689=CARTESIAN_POINT('Ctrl Pts',(-125.414192320584,-4.89931885277626,
131.235472947859));
#105690=CARTESIAN_POINT('Ctrl Pts',(-125.422313830718,-4.88670003682647,
131.378877806729));
#105691=CARTESIAN_POINT('Ctrl Pts',(-125.430435340851,-4.86779213784465,
131.521597925211));
#105692=CARTESIAN_POINT('Ctrl Pts',(-125.438556850985,-4.84270420667647,
131.663080029911));
#105693=CARTESIAN_POINT('Ctrl Pts',(-125.446697426043,-4.81755738258036,
131.804894258266));
#105694=CARTESIAN_POINT('Ctrl Pts',(-125.4548380011,-4.78620157904461,131.945464332473));
#105695=CARTESIAN_POINT('Ctrl Pts',(-125.462978576158,-4.74879668757742,
132.084248535531));
#105696=CARTESIAN_POINT('Ctrl Pts',(-125.471129195619,-4.71134564337744,
132.223203980103));
#105697=CARTESIAN_POINT('Ctrl Pts',(-125.479279815079,-4.66783071693721,
132.360368838192));
#105698=CARTESIAN_POINT('Ctrl Pts',(-125.48743043454,-4.61846067915778,
132.495219576076));
#105699=CARTESIAN_POINT('Ctrl Pts',(-125.49559972164,-4.56897756750725,
132.630379167176));
#105700=CARTESIAN_POINT('Ctrl Pts',(-125.50376900874,-4.51361265832525,
132.763213731274));
#105701=CARTESIAN_POINT('Ctrl Pts',(-125.511938295841,-4.4526223398104,
132.893220919626));
#105702=CARTESIAN_POINT('Ctrl Pts',(-125.517754428738,-4.40920021575162,
132.985779679748));
#105703=CARTESIAN_POINT('Ctrl Pts',(-125.523570561636,-4.36292768914718,
133.076905826833));
#105704=CARTESIAN_POINT('Ctrl Pts',(-125.529386694533,-4.31391074000627,
133.166426914214));
#105705=CARTESIAN_POINT('Ctrl Pts',(-125.537161028653,-4.24839054869866,
133.286088355288));
#105706=CARTESIAN_POINT('Ctrl Pts',(-125.544935362771,-4.17778396040222,
133.40321111713));
#105707=CARTESIAN_POINT('Ctrl Pts',(-125.552709696891,-4.10231230580387,
133.517332568794));
#105708=CARTESIAN_POINT('Ctrl Pts',(-125.560474449838,-4.02693366327493,
133.631313375968));
#105709=CARTESIAN_POINT('Ctrl Pts',(-125.568239202785,-3.94670209780952,
133.742299909592));
#105710=CARTESIAN_POINT('Ctrl Pts',(-125.576003955732,-3.8618851344126,
133.849853397249));
#105711=CARTESIAN_POINT('Ctrl Pts',(-125.583760996617,-3.77715241241943,
133.957300061266));
#105712=CARTESIAN_POINT('Ctrl Pts',(-125.591518037502,-3.68784359624918,
134.061320159865));
#105713=CARTESIAN_POINT('Ctrl Pts',(-125.599275078387,-3.59426967314588,
134.161503536657));
#105714=CARTESIAN_POINT('Ctrl Pts',(-125.607026269627,-3.50076631486576,
134.261611364385));
#105715=CARTESIAN_POINT('Ctrl Pts',(-125.614777460867,-3.40300451739153,
134.357887944686));
#105716=CARTESIAN_POINT('Ctrl Pts',(-125.622528652107,-3.30133550249796,
134.449956174186));
#105717=CARTESIAN_POINT('Ctrl Pts',(-125.630276548884,-3.19970969964768,
134.541985272233));
#105718=CARTESIAN_POINT('Ctrl Pts',(-125.638024445661,-3.094180271519,134.629809315108));
#105719=CARTESIAN_POINT('Ctrl Pts',(-125.645772342439,-2.98513509515818,
134.71308822718));
#105720=CARTESIAN_POINT('Ctrl Pts',(-125.653518618523,-2.87611272869752,
134.796349719098));
#105721=CARTESIAN_POINT('Ctrl Pts',(-125.661264894607,-2.76357638731155,
134.875067734147));
#105722=CARTESIAN_POINT('Ctrl Pts',(-125.669011170691,-2.64794649311978,
134.948942916432));
#105723=CARTESIAN_POINT('Ctrl Pts',(-125.676757503956,-2.53231574537487,
135.022818644047));
#105724=CARTESIAN_POINT('Ctrl Pts',(-125.684503837221,-2.41359172872102,
135.091851257071));
#105725=CARTESIAN_POINT('Ctrl Pts',(-125.692250170487,-2.29222292280824,
135.155785342257));
#105726=CARTESIAN_POINT('Ctrl Pts',(-125.69999823849,-2.17082693719273,
135.219733745038));
#105727=CARTESIAN_POINT('Ctrl Pts',(-125.707746306493,-2.04678532958573,
135.278581165789));
#105728=CARTESIAN_POINT('Ctrl Pts',(-125.715494374496,-1.92056982552717,
135.332118849603));
#105729=CARTESIAN_POINT('Ctrl Pts',(-125.723250677238,-1.79422017812874,
135.385713433903));
#105730=CARTESIAN_POINT('Ctrl Pts',(-125.731006979979,-1.66569237941779,
135.433986855347));
#105731=CARTESIAN_POINT('Ctrl Pts',(-125.738763282721,-1.53547724225302,
135.476778910166));
#105732=CARTESIAN_POINT('Ctrl Pts',(-125.746523725235,-1.40519260534884,
135.519593804393));
#105733=CARTESIAN_POINT('Ctrl Pts',(-125.75428416775,-1.27321921152475,
135.556921396193));
#105734=CARTESIAN_POINT('Ctrl Pts',(-125.762044610264,-1.14006060034891,
135.588652089668));
#105735=CARTESIAN_POINT('Ctrl Pts',(-125.769817510529,-1.00668823114914,
135.62043372007));
#105736=CARTESIAN_POINT('Ctrl Pts',(-125.777590410795,-0.872127226561587,
135.646600423305));
#105737=CARTESIAN_POINT('Ctrl Pts',(-125.78536331106,-0.736889718295181,
135.667094067548));
#105738=CARTESIAN_POINT('Ctrl Pts',(-125.792853646822,-0.60656843409772,
135.686842716201));
#105739=CARTESIAN_POINT('Ctrl Pts',(-125.800343982584,-0.475619283671478,
135.701323571064));
#105740=CARTESIAN_POINT('Ctrl Pts',(-125.807834318346,-0.344500855542329,
135.710530429449));
#105741=CARTESIAN_POINT('Ctrl Pts',(-125.815608652465,-0.208411032357867,
135.720086368667));
#105742=CARTESIAN_POINT('Ctrl Pts',(-125.823382986584,-0.071707750095534,
135.723990759909));
#105743=CARTESIAN_POINT('Ctrl Pts',(-125.831157320703,0.0651001320843933,
135.722179751624));
#105744=CARTESIAN_POINT('Ctrl Pts',(-125.83892207365,0.201739410776776,
135.720370975244));
#105745=CARTESIAN_POINT('Ctrl Pts',(-125.846686826597,0.338482645716124,
135.712860819362));
#105746=CARTESIAN_POINT('Ctrl Pts',(-125.854451579544,0.474816081440552,
135.699637193134));
#105747=CARTESIAN_POINT('Ctrl Pts',(-125.862208620429,0.611014108874283,
135.686426700798));
#105748=CARTESIAN_POINT('Ctrl Pts',(-125.869965661314,0.74680276045711,
135.667514068522));
#105749=CARTESIAN_POINT('Ctrl Pts',(-125.877722702199,0.881668863800053,
135.642939239135));
#105750=CARTESIAN_POINT('Ctrl Pts',(-125.88547389344,1.01643326356554,135.618382941818));
#105751=CARTESIAN_POINT('Ctrl Pts',(-125.89322508468,1.15027611676581,135.588173016184));
#105752=CARTESIAN_POINT('Ctrl Pts',(-125.90097627592,1.28269031170572,135.552401121475));
#105753=CARTESIAN_POINT('Ctrl Pts',(-125.908724172697,1.4150482270807,135.516644430775));
#105754=CARTESIAN_POINT('Ctrl Pts',(-125.916472069474,1.54597831526078,
135.475330574537));
#105755=CARTESIAN_POINT('Ctrl Pts',(-125.924219966251,1.67498480396725,
135.42860206552));
#105756=CARTESIAN_POINT('Ctrl Pts',(-125.931966242335,1.80396430729735,
135.3818833311));
#105757=CARTESIAN_POINT('Ctrl Pts',(-125.939712518419,1.9310206441401,135.329752329826));
#105758=CARTESIAN_POINT('Ctrl Pts',(-125.947458794503,2.05567470947828,
135.272400965561));
#105759=CARTESIAN_POINT('Ctrl Pts',(-125.955205127769,2.18032969498462,
135.215049177941));
#105760=CARTESIAN_POINT('Ctrl Pts',(-125.962951461034,2.30258201842463,
135.152477113846));
#105761=CARTESIAN_POINT('Ctrl Pts',(-125.970697794299,2.42197437919295,
135.084924034808));
#105762=CARTESIAN_POINT('Ctrl Pts',(-125.978445862302,2.5413934770525,135.017355827727));
#105763=CARTESIAN_POINT('Ctrl Pts',(-125.986193930305,2.65795099757296,
134.944804578551));
#105764=CARTESIAN_POINT('Ctrl Pts',(-125.993941998308,2.7712163301598,134.867554326209));
#105765=CARTESIAN_POINT('Ctrl Pts',(-126.00169830105,2.88460204248983,134.79022197138));
#105766=CARTESIAN_POINT('Ctrl Pts',(-126.009454603792,2.99468825379429,
134.708180857663));
#105767=CARTESIAN_POINT('Ctrl Pts',(-126.017210906534,3.10107488376638,
134.621757325766));
#105768=CARTESIAN_POINT('Ctrl Pts',(-126.024971349048,3.20751829548612,
134.535287667027));
#105769=CARTESIAN_POINT('Ctrl Pts',(-126.032731791562,3.31025789863104,
134.444431188268));
#105770=CARTESIAN_POINT('Ctrl Pts',(-126.040492234076,3.40892931163234,
134.349552292327));
#105771=CARTESIAN_POINT('Ctrl Pts',(-126.048265134342,3.50775912074542,
134.254521088359));
#105772=CARTESIAN_POINT('Ctrl Pts',(-126.056038034607,3.60250741907165,
134.15545484649));
#105773=CARTESIAN_POINT('Ctrl Pts',(-126.063810934873,3.69284847896071,
134.052753015959));
#105774=CARTESIAN_POINT('Ctrl Pts',(-126.071301270635,3.77990541376911,
133.953784655656));
#105775=CARTESIAN_POINT('Ctrl Pts',(-126.078791606397,3.86286978150277,
133.851440682495));
#105776=CARTESIAN_POINT('Ctrl Pts',(-126.086281942159,3.94148848536463,
133.746103567288));
#105777=CARTESIAN_POINT('Ctrl Pts',(-126.094056276278,4.02308804127756,
133.636772563343));
#105778=CARTESIAN_POINT('Ctrl Pts',(-126.101830610397,4.10026437943399,
133.523870639173));
#105779=CARTESIAN_POINT('Ctrl Pts',(-126.109604944516,4.17268872890944,
133.40779139908));
#105780=CARTESIAN_POINT('Ctrl Pts',(-126.117369697463,4.2450238218469,133.291855216275));
#105781=CARTESIAN_POINT('Ctrl Pts',(-126.12513445041,4.3126183736294,133.172749837251));
#105782=CARTESIAN_POINT('Ctrl Pts',(-126.132899203357,4.37518451450922,
133.050900963631));
#105783=CARTESIAN_POINT('Ctrl Pts',(-126.140656244242,4.4376885138159,132.92917311203));
#105784=CARTESIAN_POINT('Ctrl Pts',(-126.148413285128,4.49517386365152,
132.804707534007));
#105785=CARTESIAN_POINT('Ctrl Pts',(-126.156170326013,4.54739678683776,
132.6779575661));
#105786=CARTESIAN_POINT('Ctrl Pts',(-126.163921517253,4.5995803283116,132.55130318133));
#105787=CARTESIAN_POINT('Ctrl Pts',(-126.171672708493,4.64650919373422,
132.422368195582));
#105788=CARTESIAN_POINT('Ctrl Pts',(-126.179423899733,4.68798639236415,
132.291628800346));
#105789=CARTESIAN_POINT('Ctrl Pts',(-126.18717179651,4.72944596207806,132.160944972841));
#105790=CARTESIAN_POINT('Ctrl Pts',(-126.194919693287,4.76545835556264,
132.028458633078));
#105791=CARTESIAN_POINT('Ctrl Pts',(-126.202667590064,4.79587549581106,
131.894663919945));
#105792=CARTESIAN_POINT('Ctrl Pts',(-126.210413866148,4.82628627344947,
131.760897193782));
#105793=CARTESIAN_POINT('Ctrl Pts',(-126.218160142232,4.85110403923783,
131.625823019614));
#105794=CARTESIAN_POINT('Ctrl Pts',(-126.225906418317,4.87023127936647,
131.489948210788));
#105795=CARTESIAN_POINT('Ctrl Pts',(-126.233652751582,4.88935866068808,
131.354072398965));
#105796=CARTESIAN_POINT('Ctrl Pts',(-126.241399084847,4.90279537803046,
131.217396327839));
#105797=CARTESIAN_POINT('Ctrl Pts',(-126.249145418113,4.91049554674885,
131.080434064061));
#105798=CARTESIAN_POINT('Ctrl Pts',(-126.256893486116,4.91819743986666,
130.943441128534));
#105799=CARTESIAN_POINT('Ctrl Pts',(-126.264641554119,4.92016020609354,
130.806162263096));
#105800=CARTESIAN_POINT('Ctrl Pts',(-126.272389622122,4.91639005988022,
130.669113282616));
#105801=CARTESIAN_POINT('Ctrl Pts',(-126.280145924864,4.91261590671065,
130.53191864485));
#105802=CARTESIAN_POINT('Ctrl Pts',(-126.287902227605,4.90309668043032,
130.394954771546));
#105803=CARTESIAN_POINT('Ctrl Pts',(-126.295658530347,4.88789068754124,
130.258734656721));
#105804=CARTESIAN_POINT('Ctrl Pts',(-126.303418972862,4.87267657875587,
130.12244183712));
#105805=CARTESIAN_POINT('Ctrl Pts',(-126.311179415376,4.85176971504005,
129.986893953194));
#105806=CARTESIAN_POINT('Ctrl Pts',(-126.31893985789,4.82527972168502,129.852594538114));
#105807=CARTESIAN_POINT('Ctrl Pts',(-126.326712758155,4.79874720424106,
129.718079533691));
#105808=CARTESIAN_POINT('Ctrl Pts',(-126.334485658421,4.76661373885582,
129.58481738334));
#105809=CARTESIAN_POINT('Ctrl Pts',(-126.342258558686,4.72903932973555,
129.453298043029));
#105810=CARTESIAN_POINT('Ctrl Pts',(-126.349748894448,4.69283084503144,
129.326559762017));
#105811=CARTESIAN_POINT('Ctrl Pts',(-126.35723923021,4.65157022915798,129.20144007239));
#105812=CARTESIAN_POINT('Ctrl Pts',(-126.364729565972,4.60544246063901,
129.078358646465));
#105813=CARTESIAN_POINT('Ctrl Pts',(-126.372503900091,4.55756574375593,
128.950610550866));
#105814=CARTESIAN_POINT('Ctrl Pts',(-126.38027823421,4.50429385331401,128.824653664031));
#105815=CARTESIAN_POINT('Ctrl Pts',(-126.388052568329,4.4457802310428,128.700977342989));
#105816=CARTESIAN_POINT('Ctrl Pts',(-126.395817321276,4.38733872158137,
128.57745344196));
#105817=CARTESIAN_POINT('Ctrl Pts',(-126.403582074223,4.32366849929613,
128.456204864495));
#105818=CARTESIAN_POINT('Ctrl Pts',(-126.411346827171,4.25497211838848,
128.337703905691));
#105819=CARTESIAN_POINT('Ctrl Pts',(-126.419103868056,4.18634396769479,
128.219320643711));
#105820=CARTESIAN_POINT('Ctrl Pts',(-126.426860908941,4.11269978759912,
128.103679905662));
#105821=CARTESIAN_POINT('Ctrl Pts',(-126.434617949826,4.03428921545152,
127.991231827661));
#105822=CARTESIAN_POINT('Ctrl Pts',(-126.442369141066,3.95593777332664,
127.878868547632));
#105823=CARTESIAN_POINT('Ctrl Pts',(-126.450120332306,3.87282731625049,
127.769693454848));
#105824=CARTESIAN_POINT('Ctrl Pts',(-126.457871523546,3.78525199930314,
127.664129676334));
#105825=CARTESIAN_POINT('Ctrl Pts',(-126.465619420323,3.69771390420153,
127.558610765241));
#105826=CARTESIAN_POINT('Ctrl Pts',(-126.4733673171,3.60571497268157,127.456700415878));
#105827=CARTESIAN_POINT('Ctrl Pts',(-126.481115213877,3.50959089854363,
127.358790303763));
#105828=CARTESIAN_POINT('Ctrl Pts',(-126.488861489961,3.41348693148979,
127.260900672333));
#105829=CARTESIAN_POINT('Ctrl Pts',(-126.496607766045,3.3132598118796,127.167009892592));
#105830=CARTESIAN_POINT('Ctrl Pts',(-126.50435404213,3.2092832275382,127.077473950663));
#105831=CARTESIAN_POINT('Ctrl Pts',(-126.512100375395,3.10530587566542,
126.9879373478));
#105832=CARTESIAN_POINT('Ctrl Pts',(-126.51984670866,2.99757930009304,126.90275590201));
#105833=CARTESIAN_POINT('Ctrl Pts',(-126.527593041925,2.88651119788386,
126.822246082926));
#105834=CARTESIAN_POINT('Ctrl Pts',(-126.535341109928,2.77541822274283,
126.741718234226));
#105835=CARTESIAN_POINT('Ctrl Pts',(-126.543089177931,2.66098254839991,
126.66586432342));
#105836=CARTESIAN_POINT('Ctrl Pts',(-126.550837245934,2.54364150357446,
126.594957932648));
#105837=CARTESIAN_POINT('Ctrl Pts',(-126.558593548676,2.42617574729036,
126.523976181721));
#105838=CARTESIAN_POINT('Ctrl Pts',(-126.566349851418,2.30579878733667,
126.45795265734));
#105839=CARTESIAN_POINT('Ctrl Pts',(-126.57410615416,2.18297373619734,126.397115590389));
#105840=CARTESIAN_POINT('Ctrl Pts',(-126.581866596674,2.06008312963003,
126.336246052865));
#105841=CARTESIAN_POINT('Ctrl Pts',(-126.589627039188,1.93474218545123,
126.280568647219));
#105842=CARTESIAN_POINT('Ctrl Pts',(-126.597387481703,1.80743379552507,
126.230263314568));
#105843=CARTESIAN_POINT('Ctrl Pts',(-126.605160381968,1.6799210388695,126.179877227331));
#105844=CARTESIAN_POINT('Ctrl Pts',(-126.612933282233,1.55043489465477,
126.134880574453));
#105845=CARTESIAN_POINT('Ctrl Pts',(-126.620706182499,1.41947406289477,
126.095403573032));
#105846=CARTESIAN_POINT('Ctrl Pts',(-126.628196518261,1.29327398723969,
126.057361660049));
#105847=CARTESIAN_POINT('Ctrl Pts',(-126.635686854023,1.16570487805469,
126.024445136282));
#105848=CARTESIAN_POINT('Ctrl Pts',(-126.643177189785,1.03721980295778,
125.9967252172));
#105849=CARTESIAN_POINT('Ctrl Pts',(-126.650951523904,0.903863177186204,
125.96795428896));
#105850=CARTESIAN_POINT('Ctrl Pts',(-126.658725858023,0.769097322985132,
125.944690665125));
#105851=CARTESIAN_POINT('Ctrl Pts',(-126.666500192142,0.633416889284741,
125.927069760249));
#105852=CARTESIAN_POINT('Ctrl Pts',(-126.674264945089,0.497903669593145,
125.909470571563));
#105853=CARTESIAN_POINT('Ctrl Pts',(-126.682029698036,0.361478497057188,
125.897500315025));
#105854=CARTESIAN_POINT('Ctrl Pts',(-126.689794450983,0.224648212411595,
125.891243863085));
#105855=CARTESIAN_POINT('Ctrl Pts',(-126.697551491868,0.0879538295340525,
125.884993625142));
#105856=CARTESIAN_POINT('Ctrl Pts',(-126.705308532753,-0.0491444767026139,
125.88444591597));
#105857=CARTESIAN_POINT('Ctrl Pts',(-126.713065573638,-0.186133058949208,
125.889634018164));
#105858=CARTESIAN_POINT('Ctrl Pts',(-126.720816764879,-0.323018337041245,
125.89481820797));
#105859=CARTESIAN_POINT('Ctrl Pts',(-126.728567956119,-0.459793666735248,
125.90572958492));
#105860=CARTESIAN_POINT('Ctrl Pts',(-126.736319147359,-0.59594406127791,
125.922349378504));
#105861=CARTESIAN_POINT('Ctrl Pts',(-126.744067044136,-0.732036588270405,
125.938962108232));
#105862=CARTESIAN_POINT('Ctrl Pts',(-126.751814940913,-0.867504321125767,
125.961278381736));
#105863=CARTESIAN_POINT('Ctrl Pts',(-126.75956283769,-1.00183628143945,
125.989227480498));
#105864=CARTESIAN_POINT('Ctrl Pts',(-126.767309113774,-1.13614014240291,
126.017170732911));
#105865=CARTESIAN_POINT('Ctrl Pts',(-126.775055389858,-1.26930832085694,
126.050744387359));
#105866=CARTESIAN_POINT('Ctrl Pts',(-126.782801665942,-1.40083932819723,
126.089826468885));
#105867=CARTESIAN_POINT('Ctrl Pts',(-126.790547999208,-1.53237130647008,
126.128908838907));
#105868=CARTESIAN_POINT('Ctrl Pts',(-126.798294332473,-1.6622657147427,
126.17349960579));
#105869=CARTESIAN_POINT('Ctrl Pts',(-126.806040665739,-1.79003592792838,
126.223426822015));
#105870=CARTESIAN_POINT('Ctrl Pts',(-126.813788733742,-1.91783475436689,
126.273365219093));
#105871=CARTESIAN_POINT('Ctrl Pts',(-126.821536801744,-2.04350807505169,
126.328642301279));
#105872=CARTESIAN_POINT('Ctrl Pts',(-126.829284869747,-2.16658933072317,
126.389038009364));
#105873=CARTESIAN_POINT('Ctrl Pts',(-126.837041172489,-2.28980139861769,
126.449497906727));
#105874=CARTESIAN_POINT('Ctrl Pts',(-126.844797475231,-2.41041554678848,
126.515087124747));
#105875=CARTESIAN_POINT('Ctrl Pts',(-126.852553777973,-2.52798943451812,
126.585539398142));
#105876=CARTESIAN_POINT('Ctrl Pts',(-126.860314220487,-2.64562607497205,
126.656029274037));
#105877=CARTESIAN_POINT('Ctrl Pts',(-126.868074663001,-2.76021889515922,
126.731387162467));
#105878=CARTESIAN_POINT('Ctrl Pts',(-126.875835105515,-2.87135549067515,
126.811304055398));
#105879=CARTESIAN_POINT('Ctrl Pts',(-126.883608005781,-2.98267049252045,
126.891349238021));
#105880=CARTESIAN_POINT('Ctrl Pts',(-126.891380906046,-3.09051787478126,
126.975967808403));
#105881=CARTESIAN_POINT('Ctrl Pts',(-126.899153806312,-3.19451852258594,
127.064810581618));
#105882=CARTESIAN_POINT('Ctrl Pts',(-126.906644142074,-3.29473848488082,
127.150423696246));
#105883=CARTESIAN_POINT('Ctrl Pts',(-126.914134477836,-3.39138630813309,
127.239959015622));
#105884=CARTESIAN_POINT('Ctrl Pts',(-126.921624813598,-3.48415718263795,
127.333073854826));
#105885=CARTESIAN_POINT('Ctrl Pts',(-126.929290870202,-3.57910443169735,
127.428373137885));
#105886=CARTESIAN_POINT('Ctrl Pts',(-126.936956926805,-3.6703093423292,
127.527742271385));
#105887=CARTESIAN_POINT('Ctrl Pts',(-126.944622983409,-3.75739536974699,
127.630851030704));
#105888=CARTESIAN_POINT('Ctrl Pts',(-126.95228006372,-3.84437942691375,
127.733839058531));
#105889=CARTESIAN_POINT('Ctrl Pts',(-126.95993714403,-3.9272539318922,127.840557702724));
#105890=CARTESIAN_POINT('Ctrl Pts',(-126.967594224341,-4.005677710359,127.950638636848));
#105891=CARTESIAN_POINT('Ctrl Pts',(-126.975244107721,-4.08402777790123,
128.060616105319));
#105892=CARTESIAN_POINT('Ctrl Pts',(-126.982893991101,-4.15793520554822,
128.17394925367));
#105893=CARTESIAN_POINT('Ctrl Pts',(-126.990543874482,-4.22709817404826,
128.290235702321));
#105894=CARTESIAN_POINT('Ctrl Pts',(-126.998188004376,-4.29620912499887,
128.406434691797));
#105895=CARTESIAN_POINT('Ctrl Pts',(-127.005832134269,-4.36058251228523,
128.525582216926));
#105896=CARTESIAN_POINT('Ctrl Pts',(-127.013476264163,-4.41995941163802,
128.647246373495));
#105897=CARTESIAN_POINT('Ctrl Pts',(-127.021117058123,-4.47931039863054,
128.76885743525));
#105898=CARTESIAN_POINT('Ctrl Pts',(-127.028757852082,-4.53366905933335,
128.892982582333));
#105899=CARTESIAN_POINT('Ctrl Pts',(-127.036398646042,-4.58282228281413,
129.019165113807));
#105900=CARTESIAN_POINT('Ctrl Pts',(-127.044038713696,-4.63197083396903,
129.14533565083));
#105901=CARTESIAN_POINT('Ctrl Pts',(-127.051678781349,-4.67591478172896,
129.273562809888));
#105902=CARTESIAN_POINT('Ctrl Pts',(-127.059318849003,-4.71448921379823,
129.403370069604));
#105903=CARTESIAN_POINT('Ctrl Pts',(-127.062814467831,-4.7321384699489,
129.462761782042));
#105904=CARTESIAN_POINT('Ctrl Pts',(-127.066310086659,-4.74866434615969,
129.522484032979));
#105905=CARTESIAN_POINT('Ctrl Pts',(-127.069805705487,-4.76405452823416,
129.582490119309));
#105906=CARTESIAN_POINT('Origin',(213.235140564004,0.,130.804360617566));
#105907=CARTESIAN_POINT('',(-129.165390467031,-4.76405452823393,129.582490119308));
#105908=CARTESIAN_POINT('',(-128.819767501811,-4.76405452823396,129.582490119308));
#105909=CARTESIAN_POINT('',(213.235140564004,-4.76405452823405,129.582490119308));
#105910=CARTESIAN_POINT('',(-127.485140564048,-4.91824927169589,130.801684059538));
#105911=CARTESIAN_POINT('Ctrl Pts',(-127.485140564048,-4.91824927169589,
130.801684059538));
#105912=CARTESIAN_POINT('Ctrl Pts',(-127.492816800484,-4.91832267662926,
130.936567651182));
#105913=CARTESIAN_POINT('Ctrl Pts',(-127.500493036919,-4.91284309997266,
131.071676197592));
#105914=CARTESIAN_POINT('Ctrl Pts',(-127.508169273355,-4.90178139325122,
131.206507649479));
#105915=CARTESIAN_POINT('Ctrl Pts',(-127.515836812447,-4.89073221968645,
131.341186334369));
#105916=CARTESIAN_POINT('Ctrl Pts',(-127.523504351538,-4.87411352755219,
131.475588152765));
#105917=CARTESIAN_POINT('Ctrl Pts',(-127.531171890629,-4.85194816724617,
131.609209699603));
#105918=CARTESIAN_POINT('Ctrl Pts',(-127.538832684027,-4.82980230742348,
131.742713689826));
#105919=CARTESIAN_POINT('Ctrl Pts',(-127.546493477426,-4.80211955205956,
131.875438380367));
#105920=CARTESIAN_POINT('Ctrl Pts',(-127.554154270824,-4.76897463277987,
132.006884635789));
#105921=CARTESIAN_POINT('Ctrl Pts',(-127.561810653954,-4.73584879481185,
132.138255218467));
#105922=CARTESIAN_POINT('Ctrl Pts',(-127.569467037084,-4.69726714482858,
132.268348441846));
#105923=CARTESIAN_POINT('Ctrl Pts',(-127.577123420214,-4.65335557905117,
132.396674945019));
#105924=CARTESIAN_POINT('Ctrl Pts',(-127.58477752692,-4.60945706921822,
132.524963293696));
#105925=CARTESIAN_POINT('Ctrl Pts',(-127.592431633627,-4.56023192387332,
132.651485587176));
#105926=CARTESIAN_POINT('Ctrl Pts',(-127.600085740334,-4.50585588773273,
132.775767673829));
#105927=CARTESIAN_POINT('Ctrl Pts',(-127.607739324453,-4.45148356414024,
132.900041275068));
#105928=CARTESIAN_POINT('Ctrl Pts',(-127.615392908572,-4.39196120994408,
133.022074605982));
#105929=CARTESIAN_POINT('Ctrl Pts',(-127.623046492691,-4.32751248485484,
133.141414052112));
#105930=CARTESIAN_POINT('Ctrl Pts',(-127.63070130741,-4.26305339721827,
133.260772686531));
#105931=CARTESIAN_POINT('Ctrl Pts',(-127.63835612213,-4.19366655447161,
133.377436221861));
#105932=CARTESIAN_POINT('Ctrl Pts',(-127.646010936849,-4.11962101464151,
133.490976659769));
#105933=CARTESIAN_POINT('Ctrl Pts',(-127.653673447881,-4.04550102786041,
133.604631253635));
#105934=CARTESIAN_POINT('Ctrl Pts',(-127.661335958913,-3.96671320802992,
133.7151561416));
#105935=CARTESIAN_POINT('Ctrl Pts',(-127.668998469945,-3.88356953119964,
133.822152982663));
#105936=CARTESIAN_POINT('Ctrl Pts',(-127.676664811165,-3.80038429411459,
133.92920330724));
#105937=CARTESIAN_POINT('Ctrl Pts',(-127.684331152385,-3.71283912305295,
134.032721766762));
#105938=CARTESIAN_POINT('Ctrl Pts',(-127.691997493605,-3.62128471047743,
134.13234500878));
#105939=CARTESIAN_POINT('Ctrl Pts',(-127.6996760532,-3.52958438134226,134.232127027205));
#105940=CARTESIAN_POINT('Ctrl Pts',(-127.707354612795,-3.4338623282698,
134.328001141216));
#105941=CARTESIAN_POINT('Ctrl Pts',(-127.71503317239,-3.33450488740009,
134.419642102929));
#105942=CARTESIAN_POINT('Ctrl Pts',(-127.722481677886,-3.23812425308863,
134.508537448274));
#105943=CARTESIAN_POINT('Ctrl Pts',(-127.729930183381,-3.13832324827053,
134.593449509662));
#105944=CARTESIAN_POINT('Ctrl Pts',(-127.737378688877,-3.03548065620261,
134.674120332112));
#105945=CARTESIAN_POINT('Ctrl Pts',(-127.745153022996,-2.92813930123221,
134.758320032005));
#105946=CARTESIAN_POINT('Ctrl Pts',(-127.752927357115,-2.81712190934436,
134.838183480158));
#105947=CARTESIAN_POINT('Ctrl Pts',(-127.760701691234,-2.70281408189493,
134.913372554907));
#105948=CARTESIAN_POINT('Ctrl Pts',(-127.768466444181,-2.58864712862715,
134.988468965841));
#105949=CARTESIAN_POINT('Ctrl Pts',(-127.776231197129,-2.47119813187394,
135.058902252749));
#105950=CARTESIAN_POINT('Ctrl Pts',(-127.783995950076,-2.35088576258619,
135.124374413119));
#105951=CARTESIAN_POINT('Ctrl Pts',(-127.791752990961,-2.23069288924006,
135.189781545616));
#105952=CARTESIAN_POINT('Ctrl Pts',(-127.799510031846,-2.10764264411985,
135.250237171774));
#105953=CARTESIAN_POINT('Ctrl Pts',(-127.807267072731,-1.98218238323482,
135.30548670579));
#105954=CARTESIAN_POINT('Ctrl Pts',(-127.815018263971,-1.85681673290829,
135.360694575703));
#105955=CARTESIAN_POINT('Ctrl Pts',(-127.822769455211,-1.72904504062368,
135.410704010917));
#105956=CARTESIAN_POINT('Ctrl Pts',(-127.830520646451,-1.59933863350574,
135.455306650136));
#105957=CARTESIAN_POINT('Ctrl Pts',(-127.838268543228,-1.46968735507068,
135.499890332043));
#105958=CARTESIAN_POINT('Ctrl Pts',(-127.846016440005,-1.33810336624751,
135.539071661697));
#105959=CARTESIAN_POINT('Ctrl Pts',(-127.853764336782,-1.20507711018253,
135.572690746764));
#105960=CARTESIAN_POINT('Ctrl Pts',(-127.861510612866,-1.07207868034261,
135.606302799442));
#105961=CARTESIAN_POINT('Ctrl Pts',(-127.869256888951,-0.937638962148778,
135.634354826067));
#105962=CARTESIAN_POINT('Ctrl Pts',(-127.877003165035,-0.802262282934139,
135.656737178786));
#105963=CARTESIAN_POINT('Ctrl Pts',(-127.8847494983,-0.666884604399793,
135.679119696728));
#105964=CARTESIAN_POINT('Ctrl Pts',(-127.892495831565,-0.530570336772146,
135.695832393477));
#105965=CARTESIAN_POINT('Ctrl Pts',(-127.900242164831,-0.393832297560471,
135.706817061421));
#105966=CARTESIAN_POINT('Ctrl Pts',(-127.907990232834,-0.257063636812804,
135.717804189306));
#105967=CARTESIAN_POINT('Ctrl Pts',(-127.915738300837,-0.11987140527484,
135.723060704555));
#105968=CARTESIAN_POINT('Ctrl Pts',(-127.92348636884,0.0172285815978464,
135.722580441697));
#105969=CARTESIAN_POINT('Ctrl Pts',(-127.931242671582,0.154474279967905,
135.72209966841));
#105970=CARTESIAN_POINT('Ctrl Pts',(-127.938998974323,0.291627146243551,
135.71586993874));
#105971=CARTESIAN_POINT('Ctrl Pts',(-127.946755277065,0.428172934941949,
135.703937231957));
#105972=CARTESIAN_POINT('Ctrl Pts',(-127.95451571958,0.564791602239091,
135.691998156329));
#105973=CARTESIAN_POINT('Ctrl Pts',(-127.962276162094,0.70080215880525,
135.674350088741));
#105974=CARTESIAN_POINT('Ctrl Pts',(-127.970036604608,0.835698585771106,
135.651090539507));
#105975=CARTESIAN_POINT('Ctrl Pts',(-127.977809504873,0.97081156045707,
135.62779365198));
#105976=CARTESIAN_POINT('Ctrl Pts',(-127.985582405139,1.10480644916865,
135.598867364404));
#105977=CARTESIAN_POINT('Ctrl Pts',(-127.993355305404,1.23718959737333,
135.564459877314));
#105978=CARTESIAN_POINT('Ctrl Pts',(-128.000845641166,1.36476028468559,
135.531303189047));
#105979=CARTESIAN_POINT('Ctrl Pts',(-128.008335976928,1.49083408394592,
135.49305698277));
#105980=CARTESIAN_POINT('Ctrl Pts',(-128.01582631269,1.61498700471631,135.449896112759));
#105981=CARTESIAN_POINT('Ctrl Pts',(-128.023600646809,1.74384722121518,
135.405098785242));
#105982=CARTESIAN_POINT('Ctrl Pts',(-128.031374980928,1.87104621406241,
135.354864853771));
#105983=CARTESIAN_POINT('Ctrl Pts',(-128.039149315047,1.99609108497388,
135.299335972669));
#105984=CARTESIAN_POINT('Ctrl Pts',(-128.046914067994,2.12098184925719,
135.243875525951));
#105985=CARTESIAN_POINT('Ctrl Pts',(-128.054678820941,2.24372341990366,
135.183133270658));
#105986=CARTESIAN_POINT('Ctrl Pts',(-128.062443573888,2.36383877708325,
135.117300368879));
#105987=CARTESIAN_POINT('Ctrl Pts',(-128.070200614773,2.48383483399644,
135.051532853267));
#105988=CARTESIAN_POINT('Ctrl Pts',(-128.077957655658,2.60120952763215,
134.980684939733));
#105989=CARTESIAN_POINT('Ctrl Pts',(-128.085714696543,2.71550686089337,
134.904995391713));
#105990=CARTESIAN_POINT('Ctrl Pts',(-128.093465887783,2.82971800164694,
134.829362921769));
#105991=CARTESIAN_POINT('Ctrl Pts',(-128.101217079024,2.94085607651002,
134.748896299649));
#105992=CARTESIAN_POINT('Ctrl Pts',(-128.108968270264,3.04849102139965,
134.663879441843));
#105993=CARTESIAN_POINT('Ctrl Pts',(-128.116716167041,3.1560802185666,134.578898718469));
#105994=CARTESIAN_POINT('Ctrl Pts',(-128.124464063818,3.26016894095434,
134.489371847755));
#105995=CARTESIAN_POINT('Ctrl Pts',(-128.132211960595,3.36035757011268,
134.395625027699));
#105996=CARTESIAN_POINT('Ctrl Pts',(-128.139958236679,3.46052524196961,
134.301897817456));
#105997=CARTESIAN_POINT('Ctrl Pts',(-128.147704512763,3.55679415800012,
134.203952680609));
#105998=CARTESIAN_POINT('Ctrl Pts',(-128.155450788847,3.6487994671194,134.102154654684));
#105999=CARTESIAN_POINT('Ctrl Pts',(-128.163197122113,3.74080545540084,
134.000355877309));
#106000=CARTESIAN_POINT('Ctrl Pts',(-128.170943455378,3.8285475118183,133.894704444157));
#106001=CARTESIAN_POINT('Ctrl Pts',(-128.178689788643,3.91169947426812,
133.785600340485));
#106002=CARTESIAN_POINT('Ctrl Pts',(-128.186437856646,3.99487005802305,
133.676471803706));
#106003=CARTESIAN_POINT('Ctrl Pts',(-128.194185924649,4.07344826542758,
133.563889368719));
#106004=CARTESIAN_POINT('Ctrl Pts',(-128.201933992652,4.147150098441,133.448283673084));
#106005=CARTESIAN_POINT('Ctrl Pts',(-128.209690295394,4.22093026263992,
133.33255511034));
#106006=CARTESIAN_POINT('Ctrl Pts',(-128.217446598136,4.28982348900082,
133.213797198516));
#106007=CARTESIAN_POINT('Ctrl Pts',(-128.225202900878,4.3535904989405,133.092467439818));
#106008=CARTESIAN_POINT('Ctrl Pts',(-128.232963343392,4.41739154325355,
132.971072923774));
#106009=CARTESIAN_POINT('Ctrl Pts',(-128.240723785906,4.47606075223969,
132.847104178907));
#106010=CARTESIAN_POINT('Ctrl Pts',(-128.24848422842,4.52940664852883,132.721039639928));
#106011=CARTESIAN_POINT('Ctrl Pts',(-128.256257128686,4.58283818038637,
132.59477273096));
#106012=CARTESIAN_POINT('Ctrl Pts',(-128.264030028951,4.63092918576915,
132.466403671156));
#106013=CARTESIAN_POINT('Ctrl Pts',(-128.271802929216,4.67353751765295,
132.336427892065));
#106014=CARTESIAN_POINT('Ctrl Pts',(-128.279293264978,4.71459692935002,
132.211177059929));
#106015=CARTESIAN_POINT('Ctrl Pts',(-128.286783600741,4.75056528084611,
132.084434593302));
#106016=CARTESIAN_POINT('Ctrl Pts',(-128.294273936503,4.78136050480752,
131.956651720355));
#106017=CARTESIAN_POINT('Ctrl Pts',(-128.302048270622,4.81332333904467,
131.824023920945));
#106018=CARTESIAN_POINT('Ctrl Pts',(-128.309822604741,4.83981427244164,
131.689855138807));
#106019=CARTESIAN_POINT('Ctrl Pts',(-128.31759693886,4.86068605922972,131.55463663085));
#106020=CARTESIAN_POINT('Ctrl Pts',(-128.325361691807,4.88153212340584,
131.419584767621));
#106021=CARTESIAN_POINT('Ctrl Pts',(-128.333126444754,4.89677276078116,
131.283486135315));
#106022=CARTESIAN_POINT('Ctrl Pts',(-128.340891197702,4.9063109605666,131.146845392007));
#106023=CARTESIAN_POINT('Ctrl Pts',(-128.348648238587,4.9158396868776,131.010340362211));
#106024=CARTESIAN_POINT('Ctrl Pts',(-128.356405279472,4.91967721965075,
130.873294680408));
#106025=CARTESIAN_POINT('Ctrl Pts',(-128.364162320357,4.91777795975678,
130.736221047341));
#106026=CARTESIAN_POINT('Ctrl Pts',(-128.371913511597,4.91588013210946,
130.599250782566));
#106027=CARTESIAN_POINT('Ctrl Pts',(-128.379664702837,4.90825412814875,
130.462252997827));
#106028=CARTESIAN_POINT('Ctrl Pts',(-128.387415894077,4.89490635471592,
130.325742982014));
#106029=CARTESIAN_POINT('Ctrl Pts',(-128.395163790854,4.88156425444292,
130.189290986599));
#106030=CARTESIAN_POINT('Ctrl Pts',(-128.402911687631,4.86250525953779,
130.053326736073));
#106031=CARTESIAN_POINT('Ctrl Pts',(-128.410659584408,4.8377878060797,129.918362758739));
#106032=CARTESIAN_POINT('Ctrl Pts',(-128.418405860492,4.81307552298004,
129.783427012959));
#106033=CARTESIAN_POINT('Ctrl Pts',(-128.426152136577,4.78270720601328,
129.649491508516));
#106034=CARTESIAN_POINT('Ctrl Pts',(-128.433898412661,4.74679276066588,
129.517060516661));
#106035=CARTESIAN_POINT('Ctrl Pts',(-128.441644745926,4.71087805020616,
129.38462854723));
#106036=CARTESIAN_POINT('Ctrl Pts',(-128.449391079191,4.66941723200348,
129.253701489883));
#106037=CARTESIAN_POINT('Ctrl Pts',(-128.457137412457,4.62257052639916,
129.124769955837));
#106038=CARTESIAN_POINT('Ctrl Pts',(-128.46488548046,4.57571332979974,128.995809548468));
#106039=CARTESIAN_POINT('Ctrl Pts',(-128.472633548463,4.52346797922504,
128.868845921037));
#106040=CARTESIAN_POINT('Ctrl Pts',(-128.480381616466,4.46604327437459,
128.744350779261));
#106041=CARTESIAN_POINT('Ctrl Pts',(-128.488137919208,4.40855753786471,
128.619723322567));
#106042=CARTESIAN_POINT('Ctrl Pts',(-128.495894221949,4.34588161490612,
128.497569947907));
#106043=CARTESIAN_POINT('Ctrl Pts',(-128.503650524691,4.27827107914381,
128.378339258249));
#106044=CARTESIAN_POINT('Ctrl Pts',(-128.511410967205,4.21062445760285,
128.259044931582));
#106045=CARTESIAN_POINT('Ctrl Pts',(-128.51917140972,4.1380381821004,128.142676729758));
#106046=CARTESIAN_POINT('Ctrl Pts',(-128.526931852234,4.0608112751145,128.02965435376));
#106047=CARTESIAN_POINT('Ctrl Pts',(-128.534704752499,3.98346039664162,
127.916450544211));
#106048=CARTESIAN_POINT('Ctrl Pts',(-128.542477652765,3.90145423412465,
127.806603606962));
#106049=CARTESIAN_POINT('Ctrl Pts',(-128.55025055303,3.81513277421867,127.700500927183));
#106050=CARTESIAN_POINT('Ctrl Pts',(-128.557740888792,3.73194931681184,
127.598255347073));
#106051=CARTESIAN_POINT('Ctrl Pts',(-128.565231224554,3.64475906266799,
127.499486755217));
#106052=CARTESIAN_POINT('Ctrl Pts',(-128.572721560316,3.5538972834282,127.404508097038));
#106053=CARTESIAN_POINT('Ctrl Pts',(-128.580495894435,3.4595904522105,127.305928294164));
#106054=CARTESIAN_POINT('Ctrl Pts',(-128.588270228554,3.36102945251901,
127.211119217635));
#106055=CARTESIAN_POINT('Ctrl Pts',(-128.596044562673,3.25854800276854,
127.120470285844));
#106056=CARTESIAN_POINT('Ctrl Pts',(-128.60380931562,3.15619285224613,127.029933070761));
#106057=CARTESIAN_POINT('Ctrl Pts',(-128.611574068567,3.04992715514856,
126.943546055744));
#106058=CARTESIAN_POINT('Ctrl Pts',(-128.619338821514,2.94012305790365,
126.861663638735));
#106059=CARTESIAN_POINT('Ctrl Pts',(-128.627095862399,2.83042801963579,
126.779862548496));
#106060=CARTESIAN_POINT('Ctrl Pts',(-128.634852903284,2.71720188640079,
126.702557384949));
#106061=CARTESIAN_POINT('Ctrl Pts',(-128.642609944169,2.60085136040926,
126.630063639205));
#106062=CARTESIAN_POINT('Ctrl Pts',(-128.650361135409,2.48458857525494,
126.557624561558));
#106063=CARTESIAN_POINT('Ctrl Pts',(-128.65811232665,2.36520641755945,126.489989885662));
#106064=CARTESIAN_POINT('Ctrl Pts',(-128.66586351789,2.24314187751414,126.427432747491));
#106065=CARTESIAN_POINT('Ctrl Pts',(-128.673611414667,2.12112921815404,
126.364902197771));
#106066=CARTESIAN_POINT('Ctrl Pts',(-128.681359311444,1.99643679118995,
126.307445071443));
#106067=CARTESIAN_POINT('Ctrl Pts',(-128.689107208221,1.86952738732846,
126.255289238644));
#106068=CARTESIAN_POINT('Ctrl Pts',(-128.696853484305,1.74264453017841,
126.203144315721));
#106069=CARTESIAN_POINT('Ctrl Pts',(-128.704599760389,1.61354597993184,
126.156298629153));
#106070=CARTESIAN_POINT('Ctrl Pts',(-128.712346036473,1.48271540087359,
126.114932283269));
#106071=CARTESIAN_POINT('Ctrl Pts',(-128.720092369739,1.35188385605355,
126.073565632027));
#106072=CARTESIAN_POINT('Ctrl Pts',(-128.727838703004,1.21932062968495,
126.037678520046));
#106073=CARTESIAN_POINT('Ctrl Pts',(-128.735585036269,1.0855250898876,126.007401336759));
#106074=CARTESIAN_POINT('Ctrl Pts',(-128.743333104272,0.951699587506616,
125.977117373106));
#106075=CARTESIAN_POINT('Ctrl Pts',(-128.751081172275,0.816641603802916,
125.952445924325));
#106076=CARTESIAN_POINT('Ctrl Pts',(-128.758829240278,0.680860859492816,
125.933466289775));
#106077=CARTESIAN_POINT('Ctrl Pts',(-128.76658554302,0.544935805792407,
125.914466483443));
#106078=CARTESIAN_POINT('Ctrl Pts',(-128.774341845762,0.408286844824283,
125.901170629737));
#106079=CARTESIAN_POINT('Ctrl Pts',(-128.782098148504,0.271429542767353,
125.893606188172));
#106080=CARTESIAN_POINT('Ctrl Pts',(-128.789858591018,0.134499195847249,
125.886037709237));
#106081=CARTESIAN_POINT('Ctrl Pts',(-128.797619033532,-0.00263932299382713,
125.88420674303));
#106082=CARTESIAN_POINT('Ctrl Pts',(-128.805379476046,-0.139471278478966,
125.888088572105));
#106083=CARTESIAN_POINT('Ctrl Pts',(-128.813152376312,-0.276522888766048,
125.891976632637));
#106084=CARTESIAN_POINT('Ctrl Pts',(-128.820925276577,-0.413266562053272,
125.901595786954));
#106085=CARTESIAN_POINT('Ctrl Pts',(-128.828698176843,-0.549192609133013,
125.916869385802));
#106086=CARTESIAN_POINT('Ctrl Pts',(-128.836188512605,-0.680177402022141,
125.931587750859));
#106087=CARTESIAN_POINT('Ctrl Pts',(-128.843678848366,-0.810402677726295,
125.951556544572));
#106088=CARTESIAN_POINT('Ctrl Pts',(-128.851169184128,-0.939423923888862,
125.976662848057));
#106089=CARTESIAN_POINT('Ctrl Pts',(-128.858943518247,-1.07333704981692,
126.00272106467));
#106090=CARTESIAN_POINT('Ctrl Pts',(-128.866717852367,-1.20637723885266,
126.034396603398));
#106091=CARTESIAN_POINT('Ctrl Pts',(-128.874492186486,-1.33803647931793,
126.071619187642));
#106092=CARTESIAN_POINT('Ctrl Pts',(-128.882256939433,-1.46953346153604,
126.108795898378));
#106093=CARTESIAN_POINT('Ctrl Pts',(-128.89002169238,-1.5996525088419,126.151505947211));
#106094=CARTESIAN_POINT('Ctrl Pts',(-128.897786445327,-1.72789430197759,
126.199627797554));
#106095=CARTESIAN_POINT('Ctrl Pts',(-128.905543486212,-1.85600872355644,
126.247701852597));
#106096=CARTESIAN_POINT('Ctrl Pts',(-128.913300527097,-1.98224923776051,
126.301176876037));
#106097=CARTESIAN_POINT('Ctrl Pts',(-128.921057567982,-2.10613058050234,
126.359881228439));
#106098=CARTESIAN_POINT('Ctrl Pts',(-128.928808759222,-2.2299185033608,
126.418541311433));
#106099=CARTESIAN_POINT('Ctrl Pts',(-128.936559950462,-2.3513504440127,
126.48242270739));
#106100=CARTESIAN_POINT('Ctrl Pts',(-128.944311141702,-2.46996040155432,
126.551305400754));
#106101=CARTESIAN_POINT('Ctrl Pts',(-128.952059038479,-2.58851994669915,
126.620158817135));
#106102=CARTESIAN_POINT('Ctrl Pts',(-128.959806935257,-2.70425955690565,
126.694009107164));
#106103=CARTESIAN_POINT('Ctrl Pts',(-128.967554832034,-2.8167373688906,
126.772590081289));
#106104=CARTESIAN_POINT('Ctrl Pts',(-128.975301108118,-2.92919165294203,
126.851154617968));
#106105=CARTESIAN_POINT('Ctrl Pts',(-128.983047384202,-3.03838517560633,
126.934447646691));
#106106=CARTESIAN_POINT('Ctrl Pts',(-128.990793660286,-3.14390497764968,
127.022159597788));
#106107=CARTESIAN_POINT('Ctrl Pts',(-128.998539993551,-3.24942555861639,
127.109872196355));
#106108=CARTESIAN_POINT('Ctrl Pts',(-129.006286326817,-3.35127206419146,
127.202003532466));
#106109=CARTESIAN_POINT('Ctrl Pts',(-129.014032660082,-3.4490648733832,
127.298203952257));
#106110=CARTESIAN_POINT('Ctrl Pts',(-129.021780728085,-3.5468795825961,
127.394425915463));
#106111=CARTESIAN_POINT('Ctrl Pts',(-129.029528796088,-3.64063851035369,
127.494718501493));
#106112=CARTESIAN_POINT('Ctrl Pts',(-129.037276864091,-3.72999942335993,
127.598695731113));
#106113=CARTESIAN_POINT('Ctrl Pts',(-129.045033166833,-3.81945531020804,
127.702783468971));
#106114=CARTESIAN_POINT('Ctrl Pts',(-129.052789469575,-3.90450358972869,
127.810563376235));
#106115=CARTESIAN_POINT('Ctrl Pts',(-129.060545772316,-3.98484248334066,
127.921616535018));
#106116=CARTESIAN_POINT('Ctrl Pts',(-129.068306214831,-4.0652242562391,
128.032728966216));
#106117=CARTESIAN_POINT('Ctrl Pts',(-129.076066657345,-4.14089141919241,
128.147117804122));
#106118=CARTESIAN_POINT('Ctrl Pts',(-129.083827099859,-4.21158654069804,
128.264336626988));
#106119=CARTESIAN_POINT('Ctrl Pts',(-129.091600000125,-4.28239514828893,
128.381743619915));
#106120=CARTESIAN_POINT('Ctrl Pts',(-129.09937290039,-4.34821557689528,
128.501989332903));
#106121=CARTESIAN_POINT('Ctrl Pts',(-129.107145800655,-4.40883681423906,
128.624603519192));
#106122=CARTESIAN_POINT('Ctrl Pts',(-129.114636136417,-4.46725431690987,
128.742760370964));
#106123=CARTESIAN_POINT('Ctrl Pts',(-129.12212647218,-4.52084394766207,
128.863116204355));
#106124=CARTESIAN_POINT('Ctrl Pts',(-129.129616807942,-4.56946043856356,
128.985236003115));
#106125=CARTESIAN_POINT('Ctrl Pts',(-129.13840322465,-4.62648922359083,
129.128486649591));
#106126=CARTESIAN_POINT('Ctrl Pts',(-129.147189641358,-4.67682727565074,
129.274545048183));
#106127=CARTESIAN_POINT('Ctrl Pts',(-129.155976058067,-4.72022285708224,
129.422811037573));
#106128=CARTESIAN_POINT('Ctrl Pts',(-129.159114194388,-4.73572192283395,
129.475765376298));
#106129=CARTESIAN_POINT('Ctrl Pts',(-129.16225233071,-4.75033582251471,
129.529001093919));
#106130=CARTESIAN_POINT('Ctrl Pts',(-129.165390467031,-4.76405452823393,
129.582490119308));
#106131=CARTESIAN_POINT('Ctrl Pts',(-127.415055402248,-4.76405452823392,
129.582490119308));
#106132=CARTESIAN_POINT('Ctrl Pts',(-127.422828522679,-4.79811179187028,
129.715278873335));
#106133=CARTESIAN_POINT('Ctrl Pts',(-127.43060164311,-4.82657620982016,
129.849348992912));
#106134=CARTESIAN_POINT('Ctrl Pts',(-127.438374763542,-4.84938165098749,
129.984189497881));
#106135=CARTESIAN_POINT('Ctrl Pts',(-127.445226864049,-4.869484925649,130.103053048338));
#106136=CARTESIAN_POINT('Ctrl Pts',(-127.452078964557,-4.88519157307536,
130.222514965625));
#106137=CARTESIAN_POINT('Ctrl Pts',(-127.458931065065,-4.89648988555254,
130.342224422076));
#106138=CARTESIAN_POINT('Ctrl Pts',(-127.467667564714,-4.91089535185762,
130.494855228206));
#106139=CARTESIAN_POINT('Ctrl Pts',(-127.476404064362,-4.91816572784717,
130.648169968883));
#106140=CARTESIAN_POINT('Ctrl Pts',(-127.48514056401,-4.91824927169553,
130.801684058878));
#106141=CARTESIAN_POINT('',(-127.139859435937,-4.91824794762588,130.808853742736));
#106142=CARTESIAN_POINT('Ctrl Pts',(-127.069805705487,-4.76405452823416,
129.582490119309));
#106143=CARTESIAN_POINT('Ctrl Pts',(-127.077448630367,-4.79770407965101,
129.71368920958));
#106144=CARTESIAN_POINT('Ctrl Pts',(-127.085091555248,-4.82592107650535,
129.846245715456));
#106145=CARTESIAN_POINT('Ctrl Pts',(-127.092734480128,-4.84861404133926,
129.979663739539));
#106146=CARTESIAN_POINT('Ctrl Pts',(-127.10058863943,-4.87193419214756,
130.116769158109));
#106147=CARTESIAN_POINT('Ctrl Pts',(-127.108442798731,-4.88942045119155,
130.254783960365));
#106148=CARTESIAN_POINT('Ctrl Pts',(-127.116296958033,-4.90103053263342,
130.39316385117));
#106149=CARTESIAN_POINT('Ctrl Pts',(-127.124151117334,-4.91264061407527,
130.531543741973));
#106150=CARTESIAN_POINT('Ctrl Pts',(-127.132005276636,-4.91837453580464,
130.67028826175));
#106151=CARTESIAN_POINT('Ctrl Pts',(-127.139859435937,-4.91824794762588,
130.808853742736));
#106152=CARTESIAN_POINT('Ctrl Pts',(-127.139859435993,-4.91824794762498,
130.808853743724));
#106153=CARTESIAN_POINT('Ctrl Pts',(-127.150602464173,-4.9180747985178,
130.998385533179));
#106154=CARTESIAN_POINT('Ctrl Pts',(-127.161345492353,-4.90694239374391,
131.187437242374));
#106155=CARTESIAN_POINT('Ctrl Pts',(-127.172088520534,-4.88503717887384,
131.374969786367));
#106156=CARTESIAN_POINT('Ctrl Pts',(-127.181416492826,-4.86601728672331,
131.537800819189));
#106157=CARTESIAN_POINT('Ctrl Pts',(-127.190744465118,-4.83887641295327,
131.699487419958));
#106158=CARTESIAN_POINT('Ctrl Pts',(-127.200072437411,-4.80376392792892,
131.859365445626));
#106159=CARTESIAN_POINT('Ctrl Pts',(-127.20784677153,-4.77449966965511,
131.992614682534));
#106160=CARTESIAN_POINT('Ctrl Pts',(-127.215621105649,-4.73964065499407,
132.124856433692));
#106161=CARTESIAN_POINT('Ctrl Pts',(-127.223395439768,-4.69926933118736,
132.255584520161));
#106162=CARTESIAN_POINT('Ctrl Pts',(-127.231160192715,-4.65894776142927,
132.386151495946));
#106163=CARTESIAN_POINT('Ctrl Pts',(-127.238924945662,-4.6131275136775,
132.515208148773));
#106164=CARTESIAN_POINT('Ctrl Pts',(-127.246689698609,-4.56194207180448,
132.642258219719));
#106165=CARTESIAN_POINT('Ctrl Pts',(-127.254446739494,-4.51080746803392,
132.769182102743));
#106166=CARTESIAN_POINT('Ctrl Pts',(-127.262203780379,-4.45431841982171,
132.894103009682));
#106167=CARTESIAN_POINT('Ctrl Pts',(-127.269960821264,-4.39265816217544,
133.016539935066));
#106168=CARTESIAN_POINT('Ctrl Pts',(-127.277712012504,-4.33104440300919,
133.138884529811));
#106169=CARTESIAN_POINT('Ctrl Pts',(-127.285463203744,-4.26426737156493,
133.258748523701));
#106170=CARTESIAN_POINT('Ctrl Pts',(-127.293214394985,-4.19255820277847,
133.375671329793));
#106171=CARTESIAN_POINT('Ctrl Pts',(-127.300962291762,-4.12087951230154,
133.492544440575));
#106172=CARTESIAN_POINT('Ctrl Pts',(-127.308710188539,-4.04427305781589,
133.6064785173));
#106173=CARTESIAN_POINT('Ctrl Pts',(-127.316458085316,-3.96301555571786,
133.717038211746));
#106174=CARTESIAN_POINT('Ctrl Pts',(-127.3242043614,-3.88177505093734,133.827574779488));
#106175=CARTESIAN_POINT('Ctrl Pts',(-127.331950637484,-3.79588566508369,
133.93473805409));
#106176=CARTESIAN_POINT('Ctrl Pts',(-127.339696913568,-3.70566678856273,
134.03812262406));
#106177=CARTESIAN_POINT('Ctrl Pts',(-127.347443246834,-3.61544724606663,
134.141507957191));
#106178=CARTESIAN_POINT('Ctrl Pts',(-127.355189580099,-3.52089840619136,
134.241114235455));
#106179=CARTESIAN_POINT('Ctrl Pts',(-127.362935913364,-3.42237893196932,
134.336570337913));
#106180=CARTESIAN_POINT('Ctrl Pts',(-127.370683981367,-3.32383739499426,
134.432047817102));
#106181=CARTESIAN_POINT('Ctrl Pts',(-127.37843204937,-3.22132373500662,
134.523372999078));
#106182=CARTESIAN_POINT('Ctrl Pts',(-127.386180117373,-3.11523203274245,
134.610213011534));
#106183=CARTESIAN_POINT('Ctrl Pts',(-127.393936420115,-3.00902757495447,
134.69714531859));
#106184=CARTESIAN_POINT('Ctrl Pts',(-127.401692722857,-2.89923778143554,
134.779582685715));
#106185=CARTESIAN_POINT('Ctrl Pts',(-127.409449025599,-2.78628869129055,
134.857233474107));
#106186=CARTESIAN_POINT('Ctrl Pts',(-127.417209468113,-2.67327931681531,
134.934925707063));
#106187=CARTESIAN_POINT('Ctrl Pts',(-127.424969910627,-2.55710761679417,
135.007826063037));
#106188=CARTESIAN_POINT('Ctrl Pts',(-127.432730353141,-2.43822606206505,
135.075687897554));
#106189=CARTESIAN_POINT('Ctrl Pts',(-127.440503253407,-2.31915366811048,
135.143658669911));
#106190=CARTESIAN_POINT('Ctrl Pts',(-127.448276153672,-2.19736307411755,
135.206574578302));
#106191=CARTESIAN_POINT('Ctrl Pts',(-127.456049053938,-2.07332945513943,
135.264235955841));
#106192=CARTESIAN_POINT('Ctrl Pts',(-127.4635393897,-1.95380477063333,135.319801197065));
#106193=CARTESIAN_POINT('Ctrl Pts',(-127.471029725462,-1.83219759337493,
135.370487187184));
#106194=CARTESIAN_POINT('Ctrl Pts',(-127.478520061224,-1.7089463003696,
135.416159139288));
#106195=CARTESIAN_POINT('Ctrl Pts',(-127.486294395343,-1.58102189712837,
135.463562757337));
#106196=CARTESIAN_POINT('Ctrl Pts',(-127.494068729462,-1.45092101769544,
135.50571477773));
#106197=CARTESIAN_POINT('Ctrl Pts',(-127.501843063581,-1.31911408949564,
135.542410963583));
#106198=CARTESIAN_POINT('Ctrl Pts',(-127.509607816528,-1.18746960155492,
135.579061924667));
#106199=CARTESIAN_POINT('Ctrl Pts',(-127.517372569475,-1.05412362132532,
135.610270325774));
#106200=CARTESIAN_POINT('Ctrl Pts',(-127.525137322422,-0.919565816787381,
135.635880230596));
#106201=CARTESIAN_POINT('Ctrl Pts',(-127.532894363307,-0.785141656957844,
135.6614646993));
#106202=CARTESIAN_POINT('Ctrl Pts',(-127.540651404192,-0.649508449625715,
135.681461664749));
#106203=CARTESIAN_POINT('Ctrl Pts',(-127.548408445077,-0.513169921313215,
135.69576529254));
#106204=CARTESIAN_POINT('Ctrl Pts',(-127.556159636317,-0.376934206945661,
135.710058133854));
#106205=CARTESIAN_POINT('Ctrl Pts',(-127.563910827557,-0.239994617546514,
135.718666142614));
#106206=CARTESIAN_POINT('Ctrl Pts',(-127.571662018797,-0.102863592031699,
135.721534820697));
#106207=CARTESIAN_POINT('Ctrl Pts',(-127.579409915575,0.0342091491393702,
135.724402279514));
#106208=CARTESIAN_POINT('Ctrl Pts',(-127.587157812352,0.171472774535073,
135.721535251213));
#106209=CARTESIAN_POINT('Ctrl Pts',(-127.594905709129,0.308411441394956,
135.712931228784));
#106210=CARTESIAN_POINT('Ctrl Pts',(-127.602651985213,0.445321463637787,
135.704329006132));
#106211=CARTESIAN_POINT('Ctrl Pts',(-127.610398261297,0.581906272600894,
135.689992200831));
#106212=CARTESIAN_POINT('Ctrl Pts',(-127.618144537381,0.717652145797315,
135.66997039026));
#106213=CARTESIAN_POINT('Ctrl Pts',(-127.625890870646,0.853399021038751,
135.649948431892));
#106214=CARTESIAN_POINT('Ctrl Pts',(-127.633637203911,0.988306561375466,
135.624241441564));
#106215=CARTESIAN_POINT('Ctrl Pts',(-127.641383537177,1.12186866611881,
135.592950572707));
#106216=CARTESIAN_POINT('Ctrl Pts',(-127.64913160518,1.25546068116927,135.561652696478));
#106217=CARTESIAN_POINT('Ctrl Pts',(-127.656879673183,1.38770628048699,
135.524768542592));
#106218=CARTESIAN_POINT('Ctrl Pts',(-127.664627741186,1.51811239891141,
135.482449736723));
#106219=CARTESIAN_POINT('Ctrl Pts',(-127.672384043927,1.64865711451052,
135.440085953923));
#106220=CARTESIAN_POINT('Ctrl Pts',(-127.680140346669,1.77735807138181,
135.392276101802));
#106221=CARTESIAN_POINT('Ctrl Pts',(-127.687896649411,1.90373962099859,
135.339220981231));
#106222=CARTESIAN_POINT('Ctrl Pts',(-127.695657091925,2.03018862425402,
135.286137543544));
#106223=CARTESIAN_POINT('Ctrl Pts',(-127.70341753444,2.15431539989403,135.227803425258));
#106224=CARTESIAN_POINT('Ctrl Pts',(-127.711177976954,2.27566786739423,
135.164465985537));
#106225=CARTESIAN_POINT('Ctrl Pts',(-127.718950877219,2.39721514064843,
135.101026870935));
#106226=CARTESIAN_POINT('Ctrl Pts',(-127.726723777485,2.51597886720291,
135.032568580212));
#106227=CARTESIAN_POINT('Ctrl Pts',(-127.73449667775,2.6315342179285,134.959382966768));
#106228=CARTESIAN_POINT('Ctrl Pts',(-127.741987013512,2.74288884059012,
134.888857834716));
#106229=CARTESIAN_POINT('Ctrl Pts',(-127.749477349274,2.85126404930867,
134.813943288126));
#106230=CARTESIAN_POINT('Ctrl Pts',(-127.756967685036,2.95630949056174,
134.734935290373));
#106231=CARTESIAN_POINT('Ctrl Pts',(-127.764742019155,3.06533776164671,
134.652931680373));
#106232=CARTESIAN_POINT('Ctrl Pts',(-127.772516353274,3.17112415343445,
134.566258322499));
#106233=CARTESIAN_POINT('Ctrl Pts',(-127.780290687394,3.27324255813862,
134.475200605646));
#106234=CARTESIAN_POINT('Ctrl Pts',(-127.788055440341,3.37523511103529,
134.384255109292));
#106235=CARTESIAN_POINT('Ctrl Pts',(-127.795820193288,3.47356838222508,
134.288936262676));
#106236=CARTESIAN_POINT('Ctrl Pts',(-127.803584946235,3.56784650057182,
134.189571749956));
#106237=CARTESIAN_POINT('Ctrl Pts',(-127.81134198712,3.66203098056234,134.090305927471));
#106238=CARTESIAN_POINT('Ctrl Pts',(-127.819099028005,3.75216805552674,
133.987002717089));
#106239=CARTESIAN_POINT('Ctrl Pts',(-127.82685606889,3.8378964074937,133.880028712118));
#106240=CARTESIAN_POINT('Ctrl Pts',(-127.83460726013,3.92356011104369,133.773135377077));
#106241=CARTESIAN_POINT('Ctrl Pts',(-127.84235845137,4.00482146561099,133.662577061182));
#106242=CARTESIAN_POINT('Ctrl Pts',(-127.85010964261,4.08135763462926,133.548755436238));
#106243=CARTESIAN_POINT('Ctrl Pts',(-127.857857539388,4.15786127373392,
133.434982188521));
#106244=CARTESIAN_POINT('Ctrl Pts',(-127.865605436165,4.22964350400189,
133.31794871414));
#106245=CARTESIAN_POINT('Ctrl Pts',(-127.873353332942,4.29642339060513,
133.198087651119));
#106246=CARTESIAN_POINT('Ctrl Pts',(-127.881099609026,4.36318930829571,
133.078251660448));
#106247=CARTESIAN_POINT('Ctrl Pts',(-127.88884588511,4.42495477347024,132.955589598923));
#106248=CARTESIAN_POINT('Ctrl Pts',(-127.896592161194,4.48148381742939,
132.830560473606));
#106249=CARTESIAN_POINT('Ctrl Pts',(-127.904338494459,4.53801327867318,
132.705530425353));
#106250=CARTESIAN_POINT('Ctrl Pts',(-127.912084827725,4.58930608050198,
132.578133634687));
#106251=CARTESIAN_POINT('Ctrl Pts',(-127.91983116099,4.63517376637939,132.448850574351));
#106252=CARTESIAN_POINT('Ctrl Pts',(-127.927579228993,4.68105172400696,
132.319538561972));
#106253=CARTESIAN_POINT('Ctrl Pts',(-127.935327296996,4.72150201743878,
132.188339807754));
#106254=CARTESIAN_POINT('Ctrl Pts',(-127.943075364999,4.75638569988476,
132.055751098764));
#106255=CARTESIAN_POINT('Ctrl Pts',(-127.950831667741,4.79130645712362,
131.923021472915));
#106256=CARTESIAN_POINT('Ctrl Pts',(-127.958587970483,4.82064868537411,
131.788899320007));
#106257=CARTESIAN_POINT('Ctrl Pts',(-127.966344273225,4.84432422444705,
131.65389335439));
#106258=CARTESIAN_POINT('Ctrl Pts',(-127.974104715739,4.86801239986804,
131.518815332024));
#106259=CARTESIAN_POINT('Ctrl Pts',(-127.981865158253,4.88602780824374,
131.382852944402));
#106260=CARTESIAN_POINT('Ctrl Pts',(-127.989625600767,4.89833419927982,
131.246520243341));
#106261=CARTESIAN_POINT('Ctrl Pts',(-127.997398501033,4.91066034562731,
131.109968688926));
#106262=CARTESIAN_POINT('Ctrl Pts',(-128.005171401298,4.91725914197024,
130.97304602389));
#106263=CARTESIAN_POINT('Ctrl Pts',(-128.012944301564,4.91814650231906,
130.836267422902));
#106264=CARTESIAN_POINT('Ctrl Pts',(-128.020434637326,4.91900160488408,
130.704461068586));
#106265=CARTESIAN_POINT('Ctrl Pts',(-128.027924973088,4.91455332267198,
130.572788793826));
#106266=CARTESIAN_POINT('Ctrl Pts',(-128.03541530885,4.90486128341468,130.441705336397));
#106267=CARTESIAN_POINT('Ctrl Pts',(-128.043189642969,4.89480176754306,
130.305651809837));
#106268=CARTESIAN_POINT('Ctrl Pts',(-128.050963977088,4.87906114558482,
130.169801655355));
#106269=CARTESIAN_POINT('Ctrl Pts',(-128.058738311207,4.85764920163124,
130.034667629166));
#106270=CARTESIAN_POINT('Ctrl Pts',(-128.066503064154,4.83626364598499,
129.899700143588));
#106271=CARTESIAN_POINT('Ctrl Pts',(-128.074267817101,4.80922073575887,
129.765447412705));
#106272=CARTESIAN_POINT('Ctrl Pts',(-128.082032570048,4.77658218289587,
129.632419615407));
#106273=CARTESIAN_POINT('Ctrl Pts',(-128.089789610933,4.74397604710368,
129.499523943192));
#106274=CARTESIAN_POINT('Ctrl Pts',(-128.097546651818,4.70578542124897,
129.367851160677));
#106275=CARTESIAN_POINT('Ctrl Pts',(-128.105303692703,4.66212342947555,
129.237903407542));
#106276=CARTESIAN_POINT('Ctrl Pts',(-128.113054883943,4.61849436354972,
129.108053649019));
#106277=CARTESIAN_POINT('Ctrl Pts',(-128.120806075183,4.56940226827529,
128.979926699702));
#106278=CARTESIAN_POINT('Ctrl Pts',(-128.128557266424,4.51501058046856,
128.85401128456));
#106279=CARTESIAN_POINT('Ctrl Pts',(-128.136305163201,4.46064201058017,
128.728149386829));
#106280=CARTESIAN_POINT('Ctrl Pts',(-128.144053059978,4.40097848286103,
128.604497511921));
#106281=CARTESIAN_POINT('Ctrl Pts',(-128.151800956755,4.33623213579808,
128.483525869685));
#106282=CARTESIAN_POINT('Ctrl Pts',(-128.159547232839,4.27149933227517,
128.362579532109));
#106283=CARTESIAN_POINT('Ctrl Pts',(-128.167293508923,4.20168600857646,
128.244312656527));
#106284=CARTESIAN_POINT('Ctrl Pts',(-128.175039785007,4.12705079349721,
128.129171874618));
#106285=CARTESIAN_POINT('Ctrl Pts',(-128.182786118272,4.05241502747766,
128.014030242767));
#106286=CARTESIAN_POINT('Ctrl Pts',(-128.190532451538,3.9729575117102,127.902015078706));
#106287=CARTESIAN_POINT('Ctrl Pts',(-128.198278784803,3.88898061616103,
127.793544643511));
#106288=CARTESIAN_POINT('Ctrl Pts',(-128.206026852806,3.80498491456847,
127.685049917115));
#106289=CARTESIAN_POINT('Ctrl Pts',(-128.213774920809,3.7164680585569,127.580101808277));
#106290=CARTESIAN_POINT('Ctrl Pts',(-128.221522988812,3.62377290501891,
127.479085742409));
#106291=CARTESIAN_POINT('Ctrl Pts',(-128.229279291554,3.53097923396852,
127.377962315464));
#106292=CARTESIAN_POINT('Ctrl Pts',(-128.237035594296,3.43399865928326,
127.280779568059));
#106293=CARTESIAN_POINT('Ctrl Pts',(-128.244791897037,3.33321152401844,
127.187886644391));
#106294=CARTESIAN_POINT('Ctrl Pts',(-128.252552339552,3.23237059562488,
127.094944140973));
#106295=CARTESIAN_POINT('Ctrl Pts',(-128.260312782066,3.1277193565407,127.006296276107));
#106296=CARTESIAN_POINT('Ctrl Pts',(-128.26807322458,3.01967069895121,126.922251405759));
#106297=CARTESIAN_POINT('Ctrl Pts',(-128.275846124845,2.91144859206446,
126.838071619124));
#106298=CARTESIAN_POINT('Ctrl Pts',(-128.283619025111,2.79981848672589,
126.758509819899));
#106299=CARTESIAN_POINT('Ctrl Pts',(-128.291391925376,2.68522241588744,
126.683831083669));
#106300=CARTESIAN_POINT('Ctrl Pts',(-128.298882261138,2.57479220087435,
126.611867107606));
#106301=CARTESIAN_POINT('Ctrl Pts',(-128.3063725969,2.46160818177543,126.544437492631));
#106302=CARTESIAN_POINT('Ctrl Pts',(-128.313862932662,2.34608517260426,
126.48173786912));
#106303=CARTESIAN_POINT('Ctrl Pts',(-128.321637266781,2.22618207342741,
126.416660970325));
#106304=CARTESIAN_POINT('Ctrl Pts',(-128.3294116009,2.1033793003307,126.356473674554));
#106305=CARTESIAN_POINT('Ctrl Pts',(-128.337185935019,1.9781135381811,126.301444907433));
#106306=CARTESIAN_POINT('Ctrl Pts',(-128.344950687966,1.85300215488837,
126.246483958349));
#106307=CARTESIAN_POINT('Ctrl Pts',(-128.352715440914,1.72543417662455,
126.19666904427));
#106308=CARTESIAN_POINT('Ctrl Pts',(-128.360480193861,1.59587218815095,
126.152224009341));
#106309=CARTESIAN_POINT('Ctrl Pts',(-128.368237234746,1.46643888247081,
126.107823117847));
#106310=CARTESIAN_POINT('Ctrl Pts',(-128.375994275631,1.33501587524167,
126.068781617758));
#106311=CARTESIAN_POINT('Ctrl Pts',(-128.383751316516,1.20208677716079,
126.035275753289));
#106312=CARTESIAN_POINT('Ctrl Pts',(-128.391502507756,1.06925792194662,
126.001795155853));
#106313=CARTESIAN_POINT('Ctrl Pts',(-128.399253698996,0.934925614105497,
125.973841980187));
#106314=CARTESIAN_POINT('Ctrl Pts',(-128.407004890236,0.799589373386491,
125.951542890053));
#106315=CARTESIAN_POINT('Ctrl Pts',(-128.414752787013,0.664310654180187,
125.929253277626));
#106316=CARTESIAN_POINT('Ctrl Pts',(-128.42250068379,0.528029235722478,
125.912613034503));
#106317=CARTESIAN_POINT('Ctrl Pts',(-128.430248580567,0.3912553849093,125.901697842473));
#106318=CARTESIAN_POINT('Ctrl Pts',(-128.437994856651,0.254510144237209,
125.890784933667));
#106319=CARTESIAN_POINT('Ctrl Pts',(-128.445741132736,0.117273065573916,
125.88559472503));
#106320=CARTESIAN_POINT('Ctrl Pts',(-128.45348740882,-0.019940292018846,
125.886151040163));
#106321=CARTESIAN_POINT('Ctrl Pts',(-128.461233742085,-0.15715466248963,
125.886707359404));
#106322=CARTESIAN_POINT('Ctrl Pts',(-128.46898007535,-0.294344920578484,
125.893010285475));
#106323=CARTESIAN_POINT('Ctrl Pts',(-128.476726408616,-0.430995733043958,
125.90503150629));
#106324=CARTESIAN_POINT('Ctrl Pts',(-128.484474476619,-0.567677147511227,
125.917055419173));
#106325=CARTESIAN_POINT('Ctrl Pts',(-128.492222544622,-0.703818486580345,
125.934800140736));
#106326=CARTESIAN_POINT('Ctrl Pts',(-128.499970612625,-0.83891015841089,
125.958185547615));
#106327=CARTESIAN_POINT('Ctrl Pts',(-128.507726915366,-0.974145407278053,
125.981595808782));
#106328=CARTESIAN_POINT('Ctrl Pts',(-128.515483218108,-1.10832837452776,
126.010658664105));
#106329=CARTESIAN_POINT('Ctrl Pts',(-128.52323952085,-1.24095973054725,
126.045242841165));
#106330=CARTESIAN_POINT('Ctrl Pts',(-128.530999963364,-1.3736618759149,
126.079845476841));
#106331=CARTESIAN_POINT('Ctrl Pts',(-128.538760405879,-1.50481038623784,
126.119975191855));
#106332=CARTESIAN_POINT('Ctrl Pts',(-128.546520848393,-1.63392265459852,
126.165451282249));
#106333=CARTESIAN_POINT('Ctrl Pts',(-128.554293748658,-1.76324218543442,
126.2110003749));
#106334=CARTESIAN_POINT('Ctrl Pts',(-128.562066648924,-1.89051857908216,
126.261912848164));
#106335=CARTESIAN_POINT('Ctrl Pts',(-128.569839549189,-2.01528989033665,
126.317960087029));
#106336=CARTESIAN_POINT('Ctrl Pts',(-128.577329884951,-2.13552545014673,
126.371969867585));
#106337=CARTESIAN_POINT('Ctrl Pts',(-128.584820220713,-2.25343462192729,
126.430747434437));
#106338=CARTESIAN_POINT('Ctrl Pts',(-128.592310556475,-2.36862859919677,
126.494049535803));
#106339=CARTESIAN_POINT('Ctrl Pts',(-128.600085911847,-2.48820589699215,
126.559760386366));
#106340=CARTESIAN_POINT('Ctrl Pts',(-128.607861267219,-2.60523610837478,
126.630555101034));
#106341=CARTESIAN_POINT('Ctrl Pts',(-128.615636622592,-2.71925675887713,
126.70621155466));
#106342=CARTESIAN_POINT('Ctrl Pts',(-128.62340217256,-2.83313361935999,
126.781772598876));
#106343=CARTESIAN_POINT('Ctrl Pts',(-128.631167722529,-2.94400814846235,
126.86218296753));
#106344=CARTESIAN_POINT('Ctrl Pts',(-128.638933272497,-3.05144185097819,
126.947174377235));
#106345=CARTESIAN_POINT('Ctrl Pts',(-128.646689474804,-3.15874623181723,
127.032063479831));
#106346=CARTESIAN_POINT('Ctrl Pts',(-128.65444567711,-3.2626177305517,127.12152239966));
#106347=CARTESIAN_POINT('Ctrl Pts',(-128.662201879417,-3.36264680274936,
127.215239618984));
#106348=CARTESIAN_POINT('Ctrl Pts',(-128.669952781949,-3.46260752558305,
127.308892801803));
#106349=CARTESIAN_POINT('Ctrl Pts',(-128.677703684481,-3.55873076114183,
127.406798229367));
#106350=CARTESIAN_POINT('Ctrl Pts',(-128.685454587013,-3.6506399867753,
127.508604141511));
#106351=CARTESIAN_POINT('Ctrl Pts',(-128.693201872009,-3.74250631611235,
127.610362538332));
#106352=CARTESIAN_POINT('Ctrl Pts',(-128.700949157004,-3.83016228799984,
127.716017507579));
#106353=CARTESIAN_POINT('Ctrl Pts',(-128.708696442,-3.9132684998003,127.825180745358));
#106354=CARTESIAN_POINT('Ctrl Pts',(-128.716441788902,-3.99635392140223,
127.934316674403));
#106355=CARTESIAN_POINT('Ctrl Pts',(-128.724187135804,-4.07489161252377,
128.046958813855));
#106356=CARTESIAN_POINT('Ctrl Pts',(-128.731932482706,-4.14858296278212,
128.162686439433));
#106357=CARTESIAN_POINT('Ctrl Pts',(-128.739680062984,-4.22229556199313,
128.278447435153));
#106358=CARTESIAN_POINT('Ctrl Pts',(-128.747427643263,-4.29115881307777,
128.397295367957));
#106359=CARTESIAN_POINT('Ctrl Pts',(-128.755175223541,-4.35491786124421,
128.518781153991));
#106360=CARTESIAN_POINT('Ctrl Pts',(-128.76292380285,-4.41868513097717,
128.640282605307));
#106361=CARTESIAN_POINT('Ctrl Pts',(-128.770672382159,-4.47734671218335,
128.764422237434));
#106362=CARTESIAN_POINT('Ctrl Pts',(-128.778420961468,-4.5306945309502,
128.890727912547));
#106363=CARTESIAN_POINT('Ctrl Pts',(-128.786176106855,-4.58408755618451,
129.017140617966));
#106364=CARTESIAN_POINT('Ctrl Pts',(-128.793931252241,-4.63215767846045,
129.145722669742));
#106365=CARTESIAN_POINT('Ctrl Pts',(-128.801686397627,-4.6747455146166,
129.2759832309));
#106366=CARTESIAN_POINT('Ctrl Pts',(-128.807713432355,-4.70784332964267,
129.377217300238));
#106367=CARTESIAN_POINT('Ctrl Pts',(-128.813740467083,-4.7376308916783,
129.479464761412));
#106368=CARTESIAN_POINT('Ctrl Pts',(-128.819767501811,-4.76405452823396,
129.582490119308));
#106369=CARTESIAN_POINT('Origin',(213.235140564004,0.,130.804360617566));
#106370=CARTESIAN_POINT('',(-130.915253971501,-4.76405452823413,129.582490119309));
#106371=CARTESIAN_POINT('',(-130.570084224261,-4.7640545282341,129.582490119308));
#106372=CARTESIAN_POINT('',(213.235140564004,-4.76405452823405,129.582490119308));
#106373=CARTESIAN_POINT('',(-129.235140563955,-4.9182490677973,130.801332481017));
#106374=CARTESIAN_POINT('Ctrl Pts',(-129.23514056401,-4.9182490677979,130.801332481984));
#106375=CARTESIAN_POINT('Ctrl Pts',(-129.24295191385,-4.91833434911582,
130.939845025767));
#106376=CARTESIAN_POINT('Ctrl Pts',(-129.250763263691,-4.91256390560037,
131.078377249122));
#106377=CARTESIAN_POINT('Ctrl Pts',(-129.258574613531,-4.9009593883557,
131.216404469829));
#106378=CARTESIAN_POINT('Ctrl Pts',(-129.266386848761,-4.88935355577846,
131.354447335453));
#106379=CARTESIAN_POINT('Ctrl Pts',(-129.274199083992,-4.87191236406227,
131.491984703982));
#106380=CARTESIAN_POINT('Ctrl Pts',(-129.282011319222,-4.84870939208773,
131.628496706801));
#106381=CARTESIAN_POINT('Ctrl Pts',(-129.289826024435,-4.82549908406397,
131.765051870418));
#106382=CARTESIAN_POINT('Ctrl Pts',(-129.297640729648,-4.7965234321486,
131.900580646536));
#106383=CARTESIAN_POINT('Ctrl Pts',(-129.305455434861,-4.76190715537071,
132.034573325243));
#106384=CARTESIAN_POINT('Ctrl Pts',(-129.31327419593,-4.72727291264148,
132.168635546551));
#106385=CARTESIAN_POINT('Ctrl Pts',(-129.321092956999,-4.68699231094,132.301159713808));
#106386=CARTESIAN_POINT('Ctrl Pts',(-129.328911718067,-4.64123985866449,
132.431651506388));
#106387=CARTESIAN_POINT('Ctrl Pts',(-129.336740892029,-4.59542647404768,
132.562317085729));
#106388=CARTESIAN_POINT('Ctrl Pts',(-129.344570065991,-4.54412681293921,
132.690944525078));
#106389=CARTESIAN_POINT('Ctrl Pts',(-129.352399239954,-4.4875636956581,
132.817059089745));
#106390=CARTESIAN_POINT('Ctrl Pts',(-129.360234429384,-4.43095711866616,
132.943270553288));
#106391=CARTESIAN_POINT('Ctrl Pts',(-129.368069618814,-4.36907919709057,
133.066964954525));
#106392=CARTESIAN_POINT('Ctrl Pts',(-129.375904808245,-4.30219819776465,
133.187693101642));
#106393=CARTESIAN_POINT('Ctrl Pts',(-129.383752384201,-4.23521146733595,
133.308612105956));
#106394=CARTESIAN_POINT('Ctrl Pts',(-129.391599960157,-4.16320606284185,
133.426555167243));
#106395=CARTESIAN_POINT('Ctrl Pts',(-129.399447536114,-4.08649330094691,
133.541102396364));
#106396=CARTESIAN_POINT('Ctrl Pts',(-129.40231983466,-4.05841559188692,
133.583027933829));
#106397=CARTESIAN_POINT('Ctrl Pts',(-129.405192133207,-4.02970765191056,
133.624498877993));
#106398=CARTESIAN_POINT('Ctrl Pts',(-129.408064431754,-4.00038604074756,
133.665495809669));
#106399=CARTESIAN_POINT('Ctrl Pts',(-129.415838765873,-3.92102242364362,
133.776460543836));
#106400=CARTESIAN_POINT('Ctrl Pts',(-129.423613099992,-3.83691260727512,
133.884296393359));
#106401=CARTESIAN_POINT('Ctrl Pts',(-129.431387434111,-3.74833167293782,
133.988570524615));
#106402=CARTESIAN_POINT('Ctrl Pts',(-129.439152187058,-3.65985990668539,
134.092716147324));
#106403=CARTESIAN_POINT('Ctrl Pts',(-129.446916940005,-3.56692823691752,
134.193308490456));
#106404=CARTESIAN_POINT('Ctrl Pts',(-129.454681692952,-3.46985475361051,
134.289943933361));
#106405=CARTESIAN_POINT('Ctrl Pts',(-129.462438733837,-3.37287768505588,
134.386483396581));
#106406=CARTESIAN_POINT('Ctrl Pts',(-129.470195774722,-3.27176726471152,
134.479073506505));
#106407=CARTESIAN_POINT('Ctrl Pts',(-129.477952815607,-3.1668813096812,
134.567344251983));
#106408=CARTESIAN_POINT('Ctrl Pts',(-129.485704006847,-3.06207444996532,
134.655548431806));
#106409=CARTESIAN_POINT('Ctrl Pts',(-129.493455198087,-2.95349802058249,
134.739439479849));
#106410=CARTESIAN_POINT('Ctrl Pts',(-129.501206389327,-2.84154583047943,
134.818685013499));
#106411=CARTESIAN_POINT('Ctrl Pts',(-129.508954286104,-2.72964122304344,
134.897896865684));
#106412=CARTESIAN_POINT('Ctrl Pts',(-129.516702182881,-2.61436402701347,
134.972466905131));
#106413=CARTESIAN_POINT('Ctrl Pts',(-129.524450079658,-2.49614001416456,
135.042103895796));
#106414=CARTESIAN_POINT('Ctrl Pts',(-129.532196355742,-2.37794073123053,
135.111726319904));
#106415=CARTESIAN_POINT('Ctrl Pts',(-129.539942631826,-2.25679619420837,
135.176417549411));
#106416=CARTESIAN_POINT('Ctrl Pts',(-129.54768890791,-2.13315961537935,
135.235930668667));
#106417=CARTESIAN_POINT('Ctrl Pts',(-129.555435241176,-2.00952212389335,
135.295444227235));
#106418=CARTESIAN_POINT('Ctrl Pts',(-129.563181574441,-1.88339290617092,
135.349779429709));
#106419=CARTESIAN_POINT('Ctrl Pts',(-129.570927907706,-1.75524777415475,
135.398736343802));
#106420=CARTESIAN_POINT('Ctrl Pts',(-129.578675975709,-1.62707394492495,
135.447704221456));
#106421=CARTESIAN_POINT('Ctrl Pts',(-129.586424043712,-1.49688366821777,
135.49129127455));
#106422=CARTESIAN_POINT('Ctrl Pts',(-129.594172111715,-1.36517025369483,
135.529346674786));
#106423=CARTESIAN_POINT('Ctrl Pts',(-129.601928414457,-1.23331685258735,
135.567442520755));
#106424=CARTESIAN_POINT('Ctrl Pts',(-129.609684717199,-1.09993745611978,
135.599994861024));
#106425=CARTESIAN_POINT('Ctrl Pts',(-129.61744101994,-0.965538516544453,
135.62690335305));
#106426=CARTESIAN_POINT('Ctrl Pts',(-129.625201462454,-0.831067844208397,
135.653826206948));
#106427=CARTESIAN_POINT('Ctrl Pts',(-129.632961904969,-0.695576930522671,
135.675099149746));
#106428=CARTESIAN_POINT('Ctrl Pts',(-129.640722347483,-0.55957880936594,
135.690673605762));
#106429=CARTESIAN_POINT('Ctrl Pts',(-129.648495247748,-0.42336237195178,
135.706273063277));
#106430=CARTESIAN_POINT('Ctrl Pts',(-129.656268148013,-0.286637490178972,
135.716155725754));
#106431=CARTESIAN_POINT('Ctrl Pts',(-129.664041048279,-0.149919572252493,
135.72032513985));
#106432=CARTESIAN_POINT('Ctrl Pts',(-129.671531384042,-0.0181716949980125,
135.724342985242));
#106433=CARTESIAN_POINT('Ctrl Pts',(-129.679021719805,0.113569407922806,
135.72305575556));
#106434=CARTESIAN_POINT('Ctrl Pts',(-129.686512055567,0.244847698787995,
135.716512148911));
#106435=CARTESIAN_POINT('Ctrl Pts',(-129.694286389686,0.381103445936596,
135.709720439429));
#106436=CARTESIAN_POINT('Ctrl Pts',(-129.702060723806,0.517292210455308,
135.697244379508));
#106437=CARTESIAN_POINT('Ctrl Pts',(-129.709835057925,0.652901148997882,
135.679081445689));
#106438=CARTESIAN_POINT('Ctrl Pts',(-129.717599810872,0.788342961643788,
135.660940896062));
#106439=CARTESIAN_POINT('Ctrl Pts',(-129.725364563819,0.923205986337173,
135.637127468892));
#106440=CARTESIAN_POINT('Ctrl Pts',(-129.733129316766,1.05697871019101,
135.607690615464));
#106441=CARTESIAN_POINT('Ctrl Pts',(-129.740886357651,1.19061856908893,
135.578282999133));
#106442=CARTESIAN_POINT('Ctrl Pts',(-129.748643398536,1.32316990281239,
135.543263154954));
#106443=CARTESIAN_POINT('Ctrl Pts',(-129.756400439421,1.45412800161747,
135.502732124526));
#106444=CARTESIAN_POINT('Ctrl Pts',(-129.764151630661,1.58498734390241,
135.462231658863));
#106445=CARTESIAN_POINT('Ctrl Pts',(-129.771902821901,1.71425547074857,
135.416228394398));
#106446=CARTESIAN_POINT('Ctrl Pts',(-129.779654013141,1.84143987589486,
135.36487399283));
#106447=CARTESIAN_POINT('Ctrl Pts',(-129.787401909918,1.96857022427568,
135.313541418253));
#106448=CARTESIAN_POINT('Ctrl Pts',(-129.795149806695,2.09361825065299,
135.256862376209));
#106449=CARTESIAN_POINT('Ctrl Pts',(-129.802897703472,2.21610878984904,
135.195037660353));
#106450=CARTESIAN_POINT('Ctrl Pts',(-129.810643979556,2.33857370666522,
135.133225876894));
#106451=CARTESIAN_POINT('Ctrl Pts',(-129.81839025564,2.45848185158128,135.066270736625));
#106452=CARTESIAN_POINT('Ctrl Pts',(-129.826136531724,2.57538051515948,
134.994420075931));
#106453=CARTESIAN_POINT('Ctrl Pts',(-129.83388286499,2.6922800416569,134.922568884853));
#106454=CARTESIAN_POINT('Ctrl Pts',(-129.841629198255,2.80616970940809,
134.845822305965));
#106455=CARTESIAN_POINT('Ctrl Pts',(-129.84937553152,2.91662412174053,134.764472585046));
#106456=CARTESIAN_POINT('Ctrl Pts',(-129.857123599523,3.02710326957233,
134.683104646422));
#106457=CARTESIAN_POINT('Ctrl Pts',(-129.864871667527,3.13414531642431,
134.597131746317));
#106458=CARTESIAN_POINT('Ctrl Pts',(-129.872619735529,3.237356720257,134.506887393743));
#106459=CARTESIAN_POINT('Ctrl Pts',(-129.880376038271,3.34067781839835,
134.416547128396));
#106460=CARTESIAN_POINT('Ctrl Pts',(-129.888132341013,3.44015984596066,
134.321926599697));
#106461=CARTESIAN_POINT('Ctrl Pts',(-129.895888643755,3.53544463210754,
134.223397662671));
#106462=CARTESIAN_POINT('Ctrl Pts',(-129.903649086269,3.63078027461376,
134.124816137786));
#106463=CARTESIAN_POINT('Ctrl Pts',(-129.911409528783,3.72191395226734,
134.022322340001));
#106464=CARTESIAN_POINT('Ctrl Pts',(-129.919169971297,3.80852748962882,
133.916321642907));
#106465=CARTESIAN_POINT('Ctrl Pts',(-129.926942871563,3.89528006672966,
133.810150784084));
#106466=CARTESIAN_POINT('Ctrl Pts',(-129.934715771828,3.97749776885261,
133.700462089264));
#106467=CARTESIAN_POINT('Ctrl Pts',(-129.942488672093,4.05490498917549,
133.58769110302));
#106468=CARTESIAN_POINT('Ctrl Pts',(-129.949979007856,4.12949826206492,
133.479019626177));
#106469=CARTESIAN_POINT('Ctrl Pts',(-129.957469343618,4.19962456335478,
133.367486326111));
#106470=CARTESIAN_POINT('Ctrl Pts',(-129.96495967938,4.26507836461446,133.253501202791));
#106471=CARTESIAN_POINT('Ctrl Pts',(-129.972734013499,4.33301386664132,
133.135194298879));
#106472=CARTESIAN_POINT('Ctrl Pts',(-129.980508347618,4.3961307579083,133.013871219091));
#106473=CARTESIAN_POINT('Ctrl Pts',(-129.988282681737,4.45414971100009,
132.889962069066));
#106474=CARTESIAN_POINT('Ctrl Pts',(-129.996047434684,4.51209716091734,
132.766205625994));
#106475=CARTESIAN_POINT('Ctrl Pts',(-130.003812187631,4.56495900926703,
132.63986980474));
#106476=CARTESIAN_POINT('Ctrl Pts',(-130.011576940578,4.61250037560581,
132.511411685208));
#106477=CARTESIAN_POINT('Ctrl Pts',(-130.019333981463,4.65999452318945,
132.38308115209));
#106478=CARTESIAN_POINT('Ctrl Pts',(-130.027091022348,4.70217857009222,
132.252632879793));
#106479=CARTESIAN_POINT('Ctrl Pts',(-130.034848063233,4.73886471752829,
132.120546110369));
#106480=CARTESIAN_POINT('Ctrl Pts',(-130.042599254474,4.77552319965514,
131.988558948606));
#106481=CARTESIAN_POINT('Ctrl Pts',(-130.050350445714,4.80669193049044,
131.854936124291));
#106482=CARTESIAN_POINT('Ctrl Pts',(-130.058101636954,4.83223229565244,
131.720173973744));
#106483=CARTESIAN_POINT('Ctrl Pts',(-130.065849533731,4.85776180547798,
131.585469100705));
#106484=CARTESIAN_POINT('Ctrl Pts',(-130.073597430508,4.87766763489656,
131.449626247881));
#106485=CARTESIAN_POINT('Ctrl Pts',(-130.081345327285,4.89186187891301,
131.31315371907));
#106486=CARTESIAN_POINT('Ctrl Pts',(-130.089091603369,4.90605315379964,
131.176709737369));
#106487=CARTESIAN_POINT('Ctrl Pts',(-130.096837879453,4.91453517926879,
131.039636730289));
#106488=CARTESIAN_POINT('Ctrl Pts',(-130.104584155537,4.91727176658343,
130.902449536723));
#106489=CARTESIAN_POINT('Ctrl Pts',(-130.112330488803,4.92000837409894,
130.765261330473));
#106490=CARTESIAN_POINT('Ctrl Pts',(-130.120076822068,4.91699945103348,
130.627959326942));
#106491=CARTESIAN_POINT('Ctrl Pts',(-130.127823155333,4.90826093474502,
130.491059390381));
#106492=CARTESIAN_POINT('Ctrl Pts',(-130.135571223336,4.89952046152641,
130.354128796027));
#106493=CARTESIAN_POINT('Ctrl Pts',(-130.143319291339,4.88504786675941,
130.21760083791));
#106494=CARTESIAN_POINT('Ctrl Pts',(-130.151067359342,4.86491102193539,
130.081986883858));
#106495=CARTESIAN_POINT('Ctrl Pts',(-130.158823662084,4.8447527754331,129.946228797682));
#106496=CARTESIAN_POINT('Ctrl Pts',(-130.166579964826,4.81891831072572,
129.811387043419));
#106497=CARTESIAN_POINT('Ctrl Pts',(-130.174336267568,4.78752687989382,
129.677963957062));
#106498=CARTESIAN_POINT('Ctrl Pts',(-130.182096710082,4.75611869451001,
129.544469658787));
#106499=CARTESIAN_POINT('Ctrl Pts',(-130.189857152596,4.71914773849338,
129.412395913483));
#106500=CARTESIAN_POINT('Ctrl Pts',(-130.197617595111,4.6767830825288,129.282229525487));
#106501=CARTESIAN_POINT('Ctrl Pts',(-130.205390495376,4.63435041905762,
129.15185418285));
#106502=CARTESIAN_POINT('Ctrl Pts',(-130.213163395641,4.5865068898357,129.023392682682));
#106503=CARTESIAN_POINT('Ctrl Pts',(-130.220936295907,4.53346995862913,
128.897312323288));
#106504=CARTESIAN_POINT('Ctrl Pts',(-130.228426631669,4.48236105346576,
128.775815302541));
#106505=CARTESIAN_POINT('Ctrl Pts',(-130.23591696743,4.42642990811386,128.656529586155));
#106506=CARTESIAN_POINT('Ctrl Pts',(-130.243407303192,4.36591037402112,
128.539849706019));
#106507=CARTESIAN_POINT('Ctrl Pts',(-130.251181637311,4.30309622339669,
128.41874587276));
#106508=CARTESIAN_POINT('Ctrl Pts',(-130.25895597143,4.23513990176855,128.300065756467));
#106509=CARTESIAN_POINT('Ctrl Pts',(-130.266730305549,4.1622522859011,128.184276845812));
#106510=CARTESIAN_POINT('Ctrl Pts',(-130.274495058497,4.08945449750606,
128.06863063464));
#106511=CARTESIAN_POINT('Ctrl Pts',(-130.282259811444,4.01173771332357,
127.955868867186));
#106512=CARTESIAN_POINT('Ctrl Pts',(-130.290024564391,3.92935952900686,
127.846436217872));
#106513=CARTESIAN_POINT('Ctrl Pts',(-130.297781605276,3.84706316386393,
127.737112258609));
#106514=CARTESIAN_POINT('Ctrl Pts',(-130.305538646161,3.76011484564662,
127.631111147682));
#106515=CARTESIAN_POINT('Ctrl Pts',(-130.313295687046,3.66881626443692,
127.528849927566));
#106516=CARTESIAN_POINT('Ctrl Pts',(-130.321046878286,3.57758653219737,
127.426665823432));
#106517=CARTESIAN_POINT('Ctrl Pts',(-130.328798069526,3.4820133260612,127.328216286974));
#106518=CARTESIAN_POINT('Ctrl Pts',(-130.336549260766,3.38243930337109,
127.233886220303));
#106519=CARTESIAN_POINT('Ctrl Pts',(-130.344297157543,3.28290760229726,
127.139596246427));
#106520=CARTESIAN_POINT('Ctrl Pts',(-130.352045054321,3.17937874997502,
127.049422528277));
#106521=CARTESIAN_POINT('Ctrl Pts',(-130.359792951098,3.07223288198794,
126.963713773435));
#106522=CARTESIAN_POINT('Ctrl Pts',(-130.367539227182,2.96510942660635,
126.878022947017));
#106523=CARTESIAN_POINT('Ctrl Pts',(-130.375285503266,2.8543707655923,126.796795470245));
#106524=CARTESIAN_POINT('Ctrl Pts',(-130.38303177935,2.74043048659089,126.720340072727));
#106525=CARTESIAN_POINT('Ctrl Pts',(-130.390778112615,2.626489366509,126.643884110834));
#106526=CARTESIAN_POINT('Ctrl Pts',(-130.398524445881,2.50934690593064,
126.57220051633));
#106527=CARTESIAN_POINT('Ctrl Pts',(-130.406270779146,2.38944573059084,
126.505554717893));
#106528=CARTESIAN_POINT('Ctrl Pts',(-130.414018847149,2.26951770421335,
126.438893994592));
#106529=CARTESIAN_POINT('Ctrl Pts',(-130.421766915152,2.14683007539228,
126.377273502211));
#106530=CARTESIAN_POINT('Ctrl Pts',(-130.429514983155,2.02184975856494,
126.320912545346));
#106531=CARTESIAN_POINT('Ctrl Pts',(-130.437271285897,1.8967366111701,126.264491687386));
#106532=CARTESIAN_POINT('Ctrl Pts',(-130.445027588639,1.76932626517598,
126.213341692342));
#106533=CARTESIAN_POINT('Ctrl Pts',(-130.452783891381,1.64010580874387,
126.167633754937));
#106534=CARTESIAN_POINT('Ctrl Pts',(-130.460544333895,1.5108163834634,126.121901421829));
#106535=CARTESIAN_POINT('Ctrl Pts',(-130.468304776409,1.37971529622514,
126.081617048781));
#106536=CARTESIAN_POINT('Ctrl Pts',(-130.476065218923,1.24730349613843,
126.046901521471));
#106537=CARTESIAN_POINT('Ctrl Pts',(-130.483838119188,1.11467913687526,
126.012130265714));
#106538=CARTESIAN_POINT('Ctrl Pts',(-130.491611019454,0.980740242377996,
125.98294580316));
#106539=CARTESIAN_POINT('Ctrl Pts',(-130.499383919719,0.845997508423659,
125.959417761531));
#106540=CARTESIAN_POINT('Ctrl Pts',(-130.506874255481,0.716153012244307,
125.93674502348));
#106541=CARTESIAN_POINT('Ctrl Pts',(-130.514364591243,0.585562410440587,
125.919324636694));
#106542=CARTESIAN_POINT('Ctrl Pts',(-130.521854927005,0.454684036282337,
125.90717310945));
#106543=CARTESIAN_POINT('Ctrl Pts',(-130.529629261125,0.318843368788455,
125.894560853357));
#106544=CARTESIAN_POINT('Ctrl Pts',(-130.537403595244,0.182262373990399,
125.887584929587));
#106545=CARTESIAN_POINT('Ctrl Pts',(-130.545177929363,0.0454483473876703,
125.88632061059));
#106546=CARTESIAN_POINT('Ctrl Pts',(-130.55294268231,-0.0911970681546911,
125.885057849753));
#106547=CARTESIAN_POINT('Ctrl Pts',(-130.560707435257,-0.228074556882044,
125.889492691671));
#106548=CARTESIAN_POINT('Ctrl Pts',(-130.568472188204,-0.364670764865625,
125.899648771213));
#106549=CARTESIAN_POINT('Ctrl Pts',(-130.576229229089,-0.501131303569768,
125.909794763594));
#106550=CARTESIAN_POINT('Ctrl Pts',(-130.583986269974,-0.637310730126963,
125.925650656538));
#106551=CARTESIAN_POINT('Ctrl Pts',(-130.591743310859,-0.772695104034419,
125.947188051278));
#106552=CARTESIAN_POINT('Ctrl Pts',(-130.599494502099,-0.907977383532191,
125.968709204501));
#106553=CARTESIAN_POINT('Ctrl Pts',(-130.607245693339,-1.04246541921117,
125.995903270378));
#106554=CARTESIAN_POINT('Ctrl Pts',(-130.61499688458,-1.17565016736236,
126.028690010575));
#106555=CARTESIAN_POINT('Ctrl Pts',(-130.622744781357,-1.30877830844295,
126.061462815532));
#106556=CARTESIAN_POINT('Ctrl Pts',(-130.630492678134,-1.44060388488783,
126.099823473805));
#106557=CARTESIAN_POINT('Ctrl Pts',(-130.638240574911,-1.57062804656535,
126.143640651526));
#106558=CARTESIAN_POINT('Ctrl Pts',(-130.645986850995,-1.70062500999159,
126.187448663639));
#106559=CARTESIAN_POINT('Ctrl Pts',(-130.653733127079,-1.8288209379017,
126.236710800146));
#106560=CARTESIAN_POINT('Ctrl Pts',(-130.661479403163,-1.95473253310938,
126.291245973941));
#106561=CARTESIAN_POINT('Ctrl Pts',(-130.669225736429,-2.08064505776769,
126.345781550302));
#106562=CARTESIAN_POINT('Ctrl Pts',(-130.676972069694,-2.20427285731595,
126.405590086236));
#106563=CARTESIAN_POINT('Ctrl Pts',(-130.684718402959,-2.32515336906907,
126.470442658859));
#106564=CARTESIAN_POINT('Ctrl Pts',(-130.692466470962,-2.44606095117516,
126.535309754765));
#106565=CARTESIAN_POINT('Ctrl Pts',(-130.700214538966,-2.56421967678846,
126.605222950291));
#106566=CARTESIAN_POINT('Ctrl Pts',(-130.707962606969,-2.67919266008354,
126.679907956587));
#106567=CARTESIAN_POINT('Ctrl Pts',(-130.71571890971,-2.79428783803299,
126.754672338996));
#106568=CARTESIAN_POINT('Ctrl Pts',(-130.723475212452,-2.9061901816876,
126.834218449801));
#106569=CARTESIAN_POINT('Ctrl Pts',(-130.731231515194,-3.01449237702997,
126.918229022866));
#106570=CARTESIAN_POINT('Ctrl Pts',(-130.738991957708,-3.12285237651492,
127.002284434903));
#106571=CARTESIAN_POINT('Ctrl Pts',(-130.746752400223,-3.22760810044807,
127.09080880494));
#106572=CARTESIAN_POINT('Ctrl Pts',(-130.754512842737,-3.32838706905434,
127.183446011965));
#106573=CARTESIAN_POINT('Ctrl Pts',(-130.762285743002,-3.42932781700776,
127.27623192846));
#106574=CARTESIAN_POINT('Ctrl Pts',(-130.770058643268,-3.52627877601712,
127.373143598867));
#106575=CARTESIAN_POINT('Ctrl Pts',(-130.777831543533,-3.61890532276465,
127.473788995852));
#106576=CARTESIAN_POINT('Ctrl Pts',(-130.785321879295,-3.70816466122221,
127.570775679142));
#106577=CARTESIAN_POINT('Ctrl Pts',(-130.792812215057,-3.79340833612041,
127.67122910638));
#106578=CARTESIAN_POINT('Ctrl Pts',(-130.800302550818,-3.87437471825148,
127.774772591931));
#106579=CARTESIAN_POINT('Ctrl Pts',(-130.808078562731,-3.95842910139558,
127.88226515338));
#106580=CARTESIAN_POINT('Ctrl Pts',(-130.815854574644,-4.03814451413704,
127.993434794596));
#106581=CARTESIAN_POINT('Ctrl Pts',(-130.823630586557,-4.11318170437701,
128.107896390235));
#106582=CARTESIAN_POINT('Ctrl Pts',(-130.83139410495,-4.18809833427191,
128.222174083339));
#106583=CARTESIAN_POINT('Ctrl Pts',(-130.839157623342,-4.25835149809897,
128.3397328746));
#106584=CARTESIAN_POINT('Ctrl Pts',(-130.846921141734,-4.3236422494969,
128.460154832899));
#106585=CARTESIAN_POINT('Ctrl Pts',(-130.854677470153,-4.38887253362138,
128.58046526564));
#106586=CARTESIAN_POINT('Ctrl Pts',(-130.862433798571,-4.44914936042055,
128.703633251401));
#106587=CARTESIAN_POINT('Ctrl Pts',(-130.87019012699,-4.50421697454002,
128.82921188677));
#106588=CARTESIAN_POINT('Ctrl Pts',(-130.877940118031,-4.55923959517303,
128.954687916992));
#106589=CARTESIAN_POINT('Ctrl Pts',(-130.885690109072,-4.60906131881629,
129.082570320442));
#106590=CARTESIAN_POINT('Ctrl Pts',(-130.893440100113,-4.65347252061787,
129.212388079375));
#106591=CARTESIAN_POINT('Ctrl Pts',(-130.900711390576,-4.69514053628081,
129.334187269515));
#106592=CARTESIAN_POINT('Ctrl Pts',(-130.907982681038,-4.7320460761973,
129.457689650613));
#106593=CARTESIAN_POINT('Ctrl Pts',(-130.915253971501,-4.76405452823413,
129.582490119309));
#106594=CARTESIAN_POINT('Ctrl Pts',(-129.165390467031,-4.76405452823393,
129.582490119308));
#106595=CARTESIAN_POINT('Ctrl Pts',(-129.174129006297,-4.80225600717498,
129.731437105911));
#106596=CARTESIAN_POINT('Ctrl Pts',(-129.182867545563,-4.83351255353467,
129.882349764501));
#106597=CARTESIAN_POINT('Ctrl Pts',(-129.191606084828,-4.85763968390153,
130.034607563733));
#106598=CARTESIAN_POINT('Ctrl Pts',(-129.200294685767,-4.88162893441413,
130.185995251897));
#106599=CARTESIAN_POINT('Ctrl Pts',(-129.208983286706,-4.898569928941,130.338712557988));
#106600=CARTESIAN_POINT('Ctrl Pts',(-129.217671887645,-4.90832920715419,
130.492130803652));
#106601=CARTESIAN_POINT('Ctrl Pts',(-129.223494779748,-4.91486964150533,
130.594948034814));
#106602=CARTESIAN_POINT('Ctrl Pts',(-129.229317671852,-4.91818549567706,
130.698079699626));
#106603=CARTESIAN_POINT('Ctrl Pts',(-129.235140563955,-4.9182490677973,
130.801332481017));
#106604=CARTESIAN_POINT('',(-128.889859436027,-4.91824958478679,130.802339666168));
#106605=CARTESIAN_POINT('Ctrl Pts',(-128.819767501811,-4.76405452823396,
129.582490119308));
#106606=CARTESIAN_POINT('Ctrl Pts',(-128.827532201341,-4.79809640912882,
129.715218896259));
#106607=CARTESIAN_POINT('Ctrl Pts',(-128.835296900871,-4.82655328367222,
129.849238742757));
#106608=CARTESIAN_POINT('Ctrl Pts',(-128.843061600402,-4.84935634828604,
129.984039905992));
#106609=CARTESIAN_POINT('Ctrl Pts',(-128.850837082564,-4.8721910789097,
130.119028264019));
#106610=CARTESIAN_POINT('Ctrl Pts',(-128.858612564726,-4.88935628061214,
130.254799718294));
#106611=CARTESIAN_POINT('Ctrl Pts',(-128.866388046888,-4.90083508009763,
130.390840871744));
#106612=CARTESIAN_POINT('Ctrl Pts',(-128.867844758022,-4.90298559561034,
130.416327736571));
#106613=CARTESIAN_POINT('Ctrl Pts',(-128.869301469155,-4.90493667231859,
130.441824072901));
#106614=CARTESIAN_POINT('Ctrl Pts',(-128.870758180288,-4.90668840227637,
130.467326516225));
#106615=CARTESIAN_POINT('Ctrl Pts',(-128.877125265523,-4.91434497446415,
130.578794209867));
#106616=CARTESIAN_POINT('Ctrl Pts',(-128.883492350758,-4.91820363946887,
130.690525757813));
#106617=CARTESIAN_POINT('Ctrl Pts',(-128.889859435993,-4.91824958478655,
130.802339665574));
#106618=CARTESIAN_POINT('Ctrl Pts',(-128.889859436027,-4.91824958478679,
130.802339666168));
#106619=CARTESIAN_POINT('Ctrl Pts',(-128.897555421386,-4.91830511952132,
130.937490707074));
#106620=CARTESIAN_POINT('Ctrl Pts',(-128.905251406744,-4.91278562112983,
131.072869404203));
#106621=CARTESIAN_POINT('Ctrl Pts',(-128.912947392103,-4.90166103705458,
131.20797199045));
#106622=CARTESIAN_POINT('Ctrl Pts',(-128.920634306705,-4.89054956480244,
131.342915340072));
#106623=CARTESIAN_POINT('Ctrl Pts',(-128.928321221307,-4.87384617933464,
131.477582831837));
#106624=CARTESIAN_POINT('Ctrl Pts',(-128.936008135908,-4.85157281406662,
131.611469217638));
#106625=CARTESIAN_POINT('Ctrl Pts',(-128.943687918832,-4.82932011332853,
131.745231387847));
#106626=CARTESIAN_POINT('Ctrl Pts',(-128.951367701755,-4.80150777839274,
131.878213502192));
#106627=CARTESIAN_POINT('Ctrl Pts',(-128.959047484678,-4.76820962903876,
132.009914430567));
#106628=CARTESIAN_POINT('Ctrl Pts',(-128.966970747988,-4.73385579278136,
132.145790814575));
#106629=CARTESIAN_POINT('Ctrl Pts',(-128.974894011297,-4.69366255280835,
132.280302995556));
#106630=CARTESIAN_POINT('Ctrl Pts',(-128.982817274606,-4.64776835386384,
132.412910396504));
#106631=CARTESIAN_POINT('Ctrl Pts',(-128.990489405404,-4.60332879867177,
132.541314727527));
#106632=CARTESIAN_POINT('Ctrl Pts',(-128.998161536201,-4.55354433661832,
132.667932788518));
#106633=CARTESIAN_POINT('Ctrl Pts',(-129.005833666998,-4.49859146641576,
132.792288654692));
#106634=CARTESIAN_POINT('Ctrl Pts',(-129.013504948196,-4.4436446816015,
132.916630749907));
#106635=CARTESIAN_POINT('Ctrl Pts',(-129.021176229395,-4.38353078813123,
133.038710783194));
#106636=CARTESIAN_POINT('Ctrl Pts',(-129.028847510593,-4.31847422177379,
133.158073314217));
#106637=CARTESIAN_POINT('Ctrl Pts',(-129.036519683198,-4.253410095812,133.277449715223));
#106638=CARTESIAN_POINT('Ctrl Pts',(-129.044191855803,-4.18340234600604,
133.394107635336));
#106639=CARTESIAN_POINT('Ctrl Pts',(-129.051864028408,-4.10872085066102,
133.507617178428));
#106640=CARTESIAN_POINT('Ctrl Pts',(-129.059538833809,-4.03401372747844,
133.62116567366));
#106641=CARTESIAN_POINT('Ctrl Pts',(-129.067213639211,-3.95462988835823,
133.731563309756));
#106642=CARTESIAN_POINT('Ctrl Pts',(-129.074888444613,-3.87088161302354,
133.838410485392));
#106643=CARTESIAN_POINT('Ctrl Pts',(-129.082571689898,-3.78704124079564,
133.945375159483));
#106644=CARTESIAN_POINT('Ctrl Pts',(-129.090254935184,-3.69882709964671,
134.048781266191));
#106645=CARTESIAN_POINT('Ctrl Pts',(-129.097938180469,-3.60659088887542,
134.148263310944));
#106646=CARTESIAN_POINT('Ctrl Pts',(-129.105626493196,-3.51429384422726,
134.247810968523));
#106647=CARTESIAN_POINT('Ctrl Pts',(-129.113314805924,-3.4179697312889,
134.343429131395));
#106648=CARTESIAN_POINT('Ctrl Pts',(-129.121003118651,-3.31800499906879,
134.43479115521));
#106649=CARTESIAN_POINT('Ctrl Pts',(-129.128702134705,-3.21790110039125,
134.526280369173));
#106650=CARTESIAN_POINT('Ctrl Pts',(-129.13640115076,-3.11414677331246,
134.613501365509));
#106651=CARTESIAN_POINT('Ctrl Pts',(-129.144100166814,-3.00715939119916,
134.696169381935));
#106652=CARTESIAN_POINT('Ctrl Pts',(-129.14580204591,-2.98350966922823,
134.714443271489));
#106653=CARTESIAN_POINT('Ctrl Pts',(-129.147503925006,-2.9597020700224,
134.732494859633));
#106654=CARTESIAN_POINT('Ctrl Pts',(-129.149205804101,-2.93574126871814,
134.750321370747));
#106655=CARTESIAN_POINT('Ctrl Pts',(-129.15698013822,-2.82628621074341,
134.831754448992));
#106656=CARTESIAN_POINT('Ctrl Pts',(-129.164754472339,-2.713266968064,134.90875888027));
#106657=CARTESIAN_POINT('Ctrl Pts',(-129.172528806458,-2.59707764485735,
134.981006493036));
#106658=CARTESIAN_POINT('Ctrl Pts',(-129.180293559406,-2.4810315146071,
135.053165067076));
#106659=CARTESIAN_POINT('Ctrl Pts',(-129.188058312353,-2.36182340610435,
135.120578282474));
#106660=CARTESIAN_POINT('Ctrl Pts',(-129.1958230653,-2.23987945856755,135.18295891766));
#106661=CARTESIAN_POINT('Ctrl Pts',(-129.203580106185,-2.11805662747856,
135.24527759552));
#106662=CARTESIAN_POINT('Ctrl Pts',(-129.21133714707,-1.99350371066769,
135.302573463366));
#106663=CARTESIAN_POINT('Ctrl Pts',(-129.219094187955,-1.86667441513644,
135.354603434205));
#106664=CARTESIAN_POINT('Ctrl Pts',(-129.226845379195,-1.73994076256337,
135.406594168838));
#106665=CARTESIAN_POINT('Ctrl Pts',(-129.234596570435,-1.61093450837533,
135.453326762818));
#106666=CARTESIAN_POINT('Ctrl Pts',(-129.242347761675,-1.48013214329801,
135.494604950314));
#106667=CARTESIAN_POINT('Ctrl Pts',(-129.250095658452,-1.3493853727153,
135.53586559348));
#106668=CARTESIAN_POINT('Ctrl Pts',(-129.257843555229,-1.21684438163768,
135.571676323606));
#106669=CARTESIAN_POINT('Ctrl Pts',(-129.265591452006,-1.08300353372696,
135.601889815855));
#106670=CARTESIAN_POINT('Ctrl Pts',(-129.27333772809,-0.949190682436344,
135.632096988092));
#106671=CARTESIAN_POINT('Ctrl Pts',(-129.281084004174,-0.814078896267816,
135.656709165243));
#106672=CARTESIAN_POINT('Ctrl Pts',(-129.288830280258,-0.678175136379287,
135.675629604893));
#106673=CARTESIAN_POINT('Ctrl Pts',(-129.296576613524,-0.54227037327989,
135.69455018421));
#106674=CARTESIAN_POINT('Ctrl Pts',(-129.304322946789,-0.405574012025448,
135.707778888279));
#106675=CARTESIAN_POINT('Ctrl Pts',(-129.312069280054,-0.268600188502013,
135.715270614831));
#106676=CARTESIAN_POINT('Ctrl Pts',(-129.319817348057,-0.13159569064107,
135.722764019103));
#106677=CARTESIAN_POINT('Ctrl Pts',(-129.32756541606,0.00568600282480028,
135.724517867993));
#106678=CARTESIAN_POINT('Ctrl Pts',(-129.335313484063,0.14272908708239,
135.720539160927));
#106679=CARTESIAN_POINT('Ctrl Pts',(-129.343069786805,0.279917822361323,
135.716556225244));
#106680=CARTESIAN_POINT('Ctrl Pts',(-129.350826089547,0.416867050421558,
135.706828574287));
#106681=CARTESIAN_POINT('Ctrl Pts',(-129.358582392288,0.553063866572545,
135.69141529518));
#106682=CARTESIAN_POINT('Ctrl Pts',(-129.366342834802,0.689333375065119,
135.675993789543));
#106683=CARTESIAN_POINT('Ctrl Pts',(-129.374103277317,0.82484928534065,
135.654880669232));
#106684=CARTESIAN_POINT('Ctrl Pts',(-129.381863719831,0.959108231643547,
135.628186325704));
#106685=CARTESIAN_POINT('Ctrl Pts',(-129.389636620096,1.093582702326,135.601449130046));
#106686=CARTESIAN_POINT('Ctrl Pts',(-129.397409520362,1.22679579669742,
135.569112899564));
#106687=CARTESIAN_POINT('Ctrl Pts',(-129.405182420627,1.3582578028564,135.531338383907));
#106688=CARTESIAN_POINT('Ctrl Pts',(-129.412672756389,1.4849408339594,135.494937067042));
#106689=CARTESIAN_POINT('Ctrl Pts',(-129.420163092151,1.60999758706895,
135.453486088079));
#106690=CARTESIAN_POINT('Ctrl Pts',(-129.427653427913,1.73300867185807,
135.407171063996));
#106691=CARTESIAN_POINT('Ctrl Pts',(-129.435427762032,1.86068375931449,
135.359099991698));
#106692=CARTESIAN_POINT('Ctrl Pts',(-129.443202096151,1.98655942954455,
135.305636478004));
#106693=CARTESIAN_POINT('Ctrl Pts',(-129.45097643027,2.11014655959868,135.246934709184));
#106694=CARTESIAN_POINT('Ctrl Pts',(-129.458741183217,2.23358137956032,
135.188305285047));
#106695=CARTESIAN_POINT('Ctrl Pts',(-129.466505936165,2.35473292138145,
135.124450616796));
#106696=CARTESIAN_POINT('Ctrl Pts',(-129.474270689112,2.47312919876496,
135.055573977151));
#106697=CARTESIAN_POINT('Ctrl Pts',(-129.482027729997,2.591407883297,134.986765746756));
#106698=CARTESIAN_POINT('Ctrl Pts',(-129.489784770882,2.70693641353036,
134.912945666421));
#106699=CARTESIAN_POINT('Ctrl Pts',(-129.497541811767,2.81926503377483,
134.834364058239));
#106700=CARTESIAN_POINT('Ctrl Pts',(-129.505293003007,2.93150894613283,
134.755841709059));
#106701=CARTESIAN_POINT('Ctrl Pts',(-129.513044194247,3.04055743252559,
134.672565202317));
#106702=CARTESIAN_POINT('Ctrl Pts',(-129.520795385487,3.14598781407482,
134.584829336679));
#106703=CARTESIAN_POINT('Ctrl Pts',(-129.528543282264,3.2513733848993,134.497130761125));
#106704=CARTESIAN_POINT('Ctrl Pts',(-129.536291179041,3.35314360953878,
134.404976845935));
#106705=CARTESIAN_POINT('Ctrl Pts',(-129.544039075818,3.45090732379814,
134.308703880584));
#106706=CARTESIAN_POINT('Ctrl Pts',(-129.551785351902,3.54865058799602,
134.212451053461));
#106707=CARTESIAN_POINT('Ctrl Pts',(-129.559531627987,3.64238873039872,
134.112081164129));
#106708=CARTESIAN_POINT('Ctrl Pts',(-129.567277904071,3.7317663339851,134.007968441729));
#106709=CARTESIAN_POINT('Ctrl Pts',(-129.575024237336,3.82114459733677,
133.903854950792));
#106710=CARTESIAN_POINT('Ctrl Pts',(-129.582770570601,3.9061620029787,133.795998868305));
#106711=CARTESIAN_POINT('Ctrl Pts',(-129.590516903867,3.98650270208916,
133.684808372471));
#106712=CARTESIAN_POINT('Ctrl Pts',(-129.59826497187,4.06686139294246,133.573592976296));
#106713=CARTESIAN_POINT('Ctrl Pts',(-129.606013039873,4.14254106429578,
133.459041997728));
#106714=CARTESIAN_POINT('Ctrl Pts',(-129.613761107876,4.21326879986361,
133.341593181324));
#106715=CARTESIAN_POINT('Ctrl Pts',(-129.621517410618,4.28407170571019,
133.224019538922));
#106716=CARTESIAN_POINT('Ctrl Pts',(-129.62927371336,4.3499119603961,133.103542241798));
#106717=CARTESIAN_POINT('Ctrl Pts',(-129.637030016102,4.41056203807861,
132.980624749228));
#106718=CARTESIAN_POINT('Ctrl Pts',(-129.644790458616,4.47124448653372,
132.857641651892));
#106719=CARTESIAN_POINT('Ctrl Pts',(-129.65255090113,4.52673108012555,132.732216121322));
#106720=CARTESIAN_POINT('Ctrl Pts',(-129.660311343644,4.57684261282624,
132.604831322665));
#106721=CARTESIAN_POINT('Ctrl Pts',(-129.66808424391,4.62703458900791,132.477242034619));
#106722=CARTESIAN_POINT('Ctrl Pts',(-129.675857144175,4.67183413391158,
132.347687563101));
#106723=CARTESIAN_POINT('Ctrl Pts',(-129.683630044441,4.71111178952633,
132.216666805716));
#106724=CARTESIAN_POINT('Ctrl Pts',(-129.691120380203,4.74896160342472,
132.090408982884));
#106725=CARTESIAN_POINT('Ctrl Pts',(-129.698610715965,4.78168395060627,
131.962789928077));
#106726=CARTESIAN_POINT('Ctrl Pts',(-129.706101051727,4.80920830517683,
131.834262816767));
#106727=CARTESIAN_POINT('Ctrl Pts',(-129.713875385846,4.83777625401698,
131.700862560965));
#106728=CARTESIAN_POINT('Ctrl Pts',(-129.721649719965,4.86083476022433,
131.566061459546));
#106729=CARTESIAN_POINT('Ctrl Pts',(-129.729424054084,4.87824916217283,
131.430354366944));
#106730=CARTESIAN_POINT('Ctrl Pts',(-129.737188807031,4.89564210242735,
131.294814521205));
#106731=CARTESIAN_POINT('Ctrl Pts',(-129.744953559978,4.9074047292151,131.158371289954));
#106732=CARTESIAN_POINT('Ctrl Pts',(-129.752718312925,4.91345294150957,
131.0215316425));
#106733=CARTESIAN_POINT('Ctrl Pts',(-129.76047535381,4.91949514663432,130.884827906114));
#106734=CARTESIAN_POINT('Ctrl Pts',(-129.768232394695,4.91983421488778,
130.747728925114));
#106735=CARTESIAN_POINT('Ctrl Pts',(-129.77598943558,4.91443764539859,130.610748396905));
#106736=CARTESIAN_POINT('Ctrl Pts',(-129.78374062682,4.90904514550445,130.473871166779));
#106737=CARTESIAN_POINT('Ctrl Pts',(-129.79149181806,4.89792563242171,130.337112600728));
#106738=CARTESIAN_POINT('Ctrl Pts',(-129.799243009301,4.88109866035963,
130.200987656343));
#106739=CARTESIAN_POINT('Ctrl Pts',(-129.806990906078,4.86427884020948,
130.064920568689));
#106740=CARTESIAN_POINT('Ctrl Pts',(-129.814738802855,4.84175643371894,
129.929486954272));
#106741=CARTESIAN_POINT('Ctrl Pts',(-129.822486699632,4.81360293694544,
129.795197683283));
#106742=CARTESIAN_POINT('Ctrl Pts',(-129.830232975716,4.78545532927654,
129.660936502714));
#106743=CARTESIAN_POINT('Ctrl Pts',(-129.8379792518,4.75167905440802,129.527819571854));
#106744=CARTESIAN_POINT('Ctrl Pts',(-129.845725527884,4.71239685033488,
129.396348193099));
#106745=CARTESIAN_POINT('Ctrl Pts',(-129.853471861149,4.6731143562896,129.264875843853));
#106746=CARTESIAN_POINT('Ctrl Pts',(-129.861218194415,4.62832596386533,
129.135049445553));
#106747=CARTESIAN_POINT('Ctrl Pts',(-129.86896452768,4.57820436094176,129.007355361048));
#106748=CARTESIAN_POINT('Ctrl Pts',(-129.876712595683,4.52807153363267,
128.879632680338));
#106749=CARTESIAN_POINT('Ctrl Pts',(-129.884460663686,4.47260326205642,
128.75404362749));
#106750=CARTESIAN_POINT('Ctrl Pts',(-129.892208731689,4.41202031518889,
128.631054426331));
#106751=CARTESIAN_POINT('Ctrl Pts',(-129.899965034431,4.3513729800444,128.507934510785));
#106752=CARTESIAN_POINT('Ctrl Pts',(-129.907721337173,4.28560028377494,
128.387420317908));
#106753=CARTESIAN_POINT('Ctrl Pts',(-129.915477639915,4.21496916451982,
128.269953782694));
#106754=CARTESIAN_POINT('Ctrl Pts',(-129.923238082429,4.14430034730951,
128.152424552052));
#106755=CARTESIAN_POINT('Ctrl Pts',(-129.930998524943,4.06876815537738,
128.03794654644));
#106756=CARTESIAN_POINT('Ctrl Pts',(-129.938758967457,3.98868222400822,
127.926931699525));
#106757=CARTESIAN_POINT('Ctrl Pts',(-129.946531867723,3.90846773159255,
127.815738641722));
#106758=CARTESIAN_POINT('Ctrl Pts',(-129.954304767988,3.82368513384148,
127.708020159406));
#106759=CARTESIAN_POINT('Ctrl Pts',(-129.962077668253,3.73468419222225,
127.60415483561));
#106760=CARTESIAN_POINT('Ctrl Pts',(-129.969568004015,3.64891865901144,
127.504065277955));
#106761=CARTESIAN_POINT('Ctrl Pts',(-129.977058339777,3.55923636178248,
127.407553824135));
#106762=CARTESIAN_POINT('Ctrl Pts',(-129.984548675539,3.46598044892533,
127.314924761992));
#106763=CARTESIAN_POINT('Ctrl Pts',(-129.992323009658,3.36918870978726,
127.218783640803));
#106764=CARTESIAN_POINT('Ctrl Pts',(-130.000097343777,3.26824041123828,
127.126520578463));
#106765=CARTESIAN_POINT('Ctrl Pts',(-130.007871677896,3.16347910043161,
127.038516350521));
#106766=CARTESIAN_POINT('Ctrl Pts',(-130.015636430844,3.05884689857715,
126.950620579925));
#106767=CARTESIAN_POINT('Ctrl Pts',(-130.023401183791,2.95041133094954,
126.866973449571));
#106768=CARTESIAN_POINT('Ctrl Pts',(-130.031165936738,2.83855346652765,
126.787919745331));
#106769=CARTESIAN_POINT('Ctrl Pts',(-130.038922977623,2.72680670091393,
126.708944558344));
#106770=CARTESIAN_POINT('Ctrl Pts',(-130.046680018508,2.61164472002733,
126.63455394256));
#106771=CARTESIAN_POINT('Ctrl Pts',(-130.054437059393,2.49348214452833,
126.565052907878));
#106772=CARTESIAN_POINT('Ctrl Pts',(-130.062188250633,2.3754086763462,126.495604284467));
#106773=CARTESIAN_POINT('Ctrl Pts',(-130.069939441873,2.25433945309223,
126.43103810028));
#106774=CARTESIAN_POINT('Ctrl Pts',(-130.077690633113,2.1307182927002,126.371616250963));
#106775=CARTESIAN_POINT('Ctrl Pts',(-130.08543852989,2.00714967459955,126.312219657517));
#106776=CARTESIAN_POINT('Ctrl Pts',(-130.093186426667,1.88103162826315,
126.257963219223));
#106777=CARTESIAN_POINT('Ctrl Pts',(-130.100934323444,1.75283260861695,
126.20906292224));
#106778=CARTESIAN_POINT('Ctrl Pts',(-130.108680599528,1.62466040544201,
126.160172854144));
#106779=CARTESIAN_POINT('Ctrl Pts',(-130.116426875613,1.49440845984381,
126.116636838093));
#106780=CARTESIAN_POINT('Ctrl Pts',(-130.124173151697,1.36256487461217,
126.078622577326));
#106781=CARTESIAN_POINT('Ctrl Pts',(-130.131919484962,1.23072031614095,
126.040608035946));
#106782=CARTESIAN_POINT('Ctrl Pts',(-130.139665818228,1.09728447025367,
126.008115439498));
#106783=CARTESIAN_POINT('Ctrl Pts',(-130.147412151493,0.962759869806269,
125.981262391779));
#106784=CARTESIAN_POINT('Ctrl Pts',(-130.155160219496,0.82820514350751,
125.954403330506));
#106785=CARTESIAN_POINT('Ctrl Pts',(-130.162908287499,0.69256156080494,
125.933186407578));
#106786=CARTESIAN_POINT('Ctrl Pts',(-130.170656355502,0.556340700032145,
125.917677889172));
#106787=CARTESIAN_POINT('Ctrl Pts',(-130.178412658244,0.419975062107657,
125.902152888127));
#106788=CARTESIAN_POINT('Ctrl Pts',(-130.186168960985,0.283031309579939,
125.892348455305));
#106789=CARTESIAN_POINT('Ctrl Pts',(-130.193925263727,0.146025541460958,
125.888278884749));
#106790=CARTESIAN_POINT('Ctrl Pts',(-130.201685706242,0.00894664923799438,
125.88420714214));
#106791=CARTESIAN_POINT('Ctrl Pts',(-130.209446148756,-0.12819393378499,
125.885876356081));
#106792=CARTESIAN_POINT('Ctrl Pts',(-130.21720659127,-0.264882270710789,
125.893248681847));
#106793=CARTESIAN_POINT('Ctrl Pts',(-130.224979491535,-0.40179003188927,
125.900632842325));
#106794=CARTESIAN_POINT('Ctrl Pts',(-130.232752391801,-0.538243706821677,
125.913738372119));
#106795=CARTESIAN_POINT('Ctrl Pts',(-130.240525292066,-0.673735728264205,
125.932475640377));
#106796=CARTESIAN_POINT('Ctrl Pts',(-130.248015627828,-0.804302273444213,
125.950531761738));
#106797=CARTESIAN_POINT('Ctrl Pts',(-130.25550596359,-0.933975565155572,
125.973817220118));
#106798=CARTESIAN_POINT('Ctrl Pts',(-130.262996299352,-1.06231411733078,
126.002207790071));
#106799=CARTESIAN_POINT('Ctrl Pts',(-130.270770633471,-1.19551866471845,
126.031674797112));
#106800=CARTESIAN_POINT('Ctrl Pts',(-130.27854496759,-1.32770721325576,
126.066735020841));
#106801=CARTESIAN_POINT('Ctrl Pts',(-130.28631930171,-1.45837371006082,
126.107305243792));
#106802=CARTESIAN_POINT('Ctrl Pts',(-130.294084054657,-1.58887917208691,
126.147825467569));
#106803=CARTESIAN_POINT('Ctrl Pts',(-130.301848807604,-1.71786594485178,
126.193842064517));
#106804=CARTESIAN_POINT('Ctrl Pts',(-130.309613560551,-1.84483797314648,
126.245220795699));
#106805=CARTESIAN_POINT('Ctrl Pts',(-130.317370601436,-1.97168389103233,
126.2965484968));
#106806=CARTESIAN_POINT('Ctrl Pts',(-130.325127642321,-2.09651868659945,
126.353227587953));
#106807=CARTESIAN_POINT('Ctrl Pts',(-130.332884683206,-2.21886163378716,
126.415074102356));
#106808=CARTESIAN_POINT('Ctrl Pts',(-130.340635874446,-2.34111232120587,
126.47687397782));
#106809=CARTESIAN_POINT('Ctrl Pts',(-130.348387065686,-2.46087455301941,
126.543833344531));
#106810=CARTESIAN_POINT('Ctrl Pts',(-130.356138256926,-2.57768809456893,
126.615720366886));
#106811=CARTESIAN_POINT('Ctrl Pts',(-130.363886153703,-2.69445198724798,
126.687576835339));
#106812=CARTESIAN_POINT('Ctrl Pts',(-130.37163405048,-2.80826935005605,
126.764356589385));
#106813=CARTESIAN_POINT('Ctrl Pts',(-130.379381947257,-2.91870525639027,
126.845782250422));
#106814=CARTESIAN_POINT('Ctrl Pts',(-130.387128223341,-3.02911806191362,
126.927190878966));
#106815=CARTESIAN_POINT('Ctrl Pts',(-130.394874499425,-3.13615050339798,
127.013243249622));
#106816=CARTESIAN_POINT('Ctrl Pts',(-130.402620775509,-3.23939765587746,
127.103619355387));
#106817=CARTESIAN_POINT('Ctrl Pts',(-130.410367108774,-3.34264557050411,
127.193996128287));
#106818=CARTESIAN_POINT('Ctrl Pts',(-130.41811344204,-3.44210784618725,
127.288696442476));
#106819=CARTESIAN_POINT('Ctrl Pts',(-130.425859775305,-3.53741390823919,
127.387361070552));
#106820=CARTESIAN_POINT('Ctrl Pts',(-130.433607843308,-3.63274131342305,
127.486047793887));
#106821=CARTESIAN_POINT('Ctrl Pts',(-130.441355911311,-3.72391038130586,
127.588700316546));
#106822=CARTESIAN_POINT('Ctrl Pts',(-130.449103979314,-3.81058883969292,
127.694924051674));
#106823=CARTESIAN_POINT('Ctrl Pts',(-130.456860282056,-3.89735942097691,
127.801260682651));
#106824=CARTESIAN_POINT('Ctrl Pts',(-130.464616584798,-3.97962961126454,
127.911175804674));
#106825=CARTESIAN_POINT('Ctrl Pts',(-130.47237288754,-4.05710842045033,
128.024242935307));
#106826=CARTESIAN_POINT('Ctrl Pts',(-130.480133330054,-4.13462858240921,
128.137370413271));
#106827=CARTESIAN_POINT('Ctrl Pts',(-130.487893772568,-4.20735206041497,
128.253652920698));
#106828=CARTESIAN_POINT('Ctrl Pts',(-130.495654215082,-4.27503289885926,
128.372637611924));
#106829=CARTESIAN_POINT('Ctrl Pts',(-130.503427115348,-4.34282238459404,
128.491813307938));
#106830=CARTESIAN_POINT('Ctrl Pts',(-130.511200015613,-4.4055528755781,
128.613699508202));
#106831=CARTESIAN_POINT('Ctrl Pts',(-130.518972915878,-4.46302542829209,
128.737820734351));
#106832=CARTESIAN_POINT('Ctrl Pts',(-130.526463251641,-4.51840870895248,
128.857429841292));
#106833=CARTESIAN_POINT('Ctrl Pts',(-130.533953587403,-4.56890957495682,
128.979114013185));
#106834=CARTESIAN_POINT('Ctrl Pts',(-130.541443923165,-4.61439390668836,
129.102434668408));
#106835=CARTESIAN_POINT('Ctrl Pts',(-130.55042514124,-4.66893147553119,
129.250301163703));
#106836=CARTESIAN_POINT('Ctrl Pts',(-130.559406359316,-4.71640066332549,
129.400907585557));
#106837=CARTESIAN_POINT('Ctrl Pts',(-130.568387577391,-4.7565558117372,
129.553616889887));
#106838=CARTESIAN_POINT('Ctrl Pts',(-130.568953126347,-4.7590843888292,
129.563233022909));
#106839=CARTESIAN_POINT('Ctrl Pts',(-130.569518675304,-4.76158397936226,
129.572857486753));
#106840=CARTESIAN_POINT('Ctrl Pts',(-130.570084224261,-4.7640545282341,
129.582490119308));
#106841=CARTESIAN_POINT('Origin',(213.235140564004,0.,130.804360617566));
#106842=CARTESIAN_POINT('',(-132.66500688127,-4.76405452823412,129.582490119309));
#106843=CARTESIAN_POINT('',(-132.320008282756,-4.76405452823417,129.582490119309));
#106844=CARTESIAN_POINT('',(213.235140564004,-4.76405452823405,129.582490119308));
#106845=CARTESIAN_POINT('',(-130.985140564062,-4.91824853312603,130.808159157235));
#106846=CARTESIAN_POINT('Ctrl Pts',(-130.985140564062,-4.91824853312603,
130.808159157235));
#106847=CARTESIAN_POINT('Ctrl Pts',(-130.994145389984,-4.91812534212975,
130.967663595687));
#106848=CARTESIAN_POINT('Ctrl Pts',(-131.003150215905,-4.9102388911086,
131.126846153038));
#106849=CARTESIAN_POINT('Ctrl Pts',(-131.012155041827,-4.89470640897744,
131.285018741824));
#106850=CARTESIAN_POINT('Ctrl Pts',(-131.021211888168,-4.87908419648849,
131.444105085595));
#106851=CARTESIAN_POINT('Ctrl Pts',(-131.03026873451,-4.85572746516266,
131.602169652566));
#106852=CARTESIAN_POINT('Ctrl Pts',(-131.039325580852,-4.82480465905455,
131.758532019603));
#106853=CARTESIAN_POINT('Ctrl Pts',(-131.048444313205,-4.79367055543172,
131.915962820709));
#106854=CARTESIAN_POINT('Ctrl Pts',(-131.057563045558,-4.7548667042909,
132.071667976947));
#106855=CARTESIAN_POINT('Ctrl Pts',(-131.06668177791,-4.70861331502907,
132.224974467995));
#106856=CARTESIAN_POINT('Ctrl Pts',(-131.070704576817,-4.68820827663491,
132.292606805556));
#106857=CARTESIAN_POINT('Ctrl Pts',(-131.074727375724,-4.66635402911844,
132.359772602815));
#106858=CARTESIAN_POINT('Ctrl Pts',(-131.078750174631,-4.64307238043769,
132.426415466366));
#106859=CARTESIAN_POINT('Ctrl Pts',(-131.08652450875,-4.59807900148245,
132.555207359738));
#106860=CARTESIAN_POINT('Ctrl Pts',(-131.094298842869,-4.5476515529689,
132.682329757796));
#106861=CARTESIAN_POINT('Ctrl Pts',(-131.102073176988,-4.49193243916302,
132.807289978401));
#106862=CARTESIAN_POINT('Ctrl Pts',(-131.109837929935,-4.4362819941853,
132.932096196702));
#106863=CARTESIAN_POINT('Ctrl Pts',(-131.117602682882,-4.37535301745541,
133.054745185841));
#106864=CARTESIAN_POINT('Ctrl Pts',(-131.125367435829,-4.30933739678566,
133.174760217457));
#106865=CARTESIAN_POINT('Ctrl Pts',(-131.133124476713,-4.24338734376119,
133.294656048452));
#106866=CARTESIAN_POINT('Ctrl Pts',(-131.140881517598,-4.17236088796681,
133.411922787704));
#106867=CARTESIAN_POINT('Ctrl Pts',(-131.148638558483,-4.09649748651096,
133.526104802002));
#106868=CARTESIAN_POINT('Ctrl Pts',(-131.156389749723,-4.02069129423618,
133.640200710754));
#106869=CARTESIAN_POINT('Ctrl Pts',(-131.164140940963,-3.94005563206689,
133.751216200419));
#106870=CARTESIAN_POINT('Ctrl Pts',(-131.171892132203,-3.85487507064748,
133.858721639482));
#106871=CARTESIAN_POINT('Ctrl Pts',(-131.17964002898,-3.76973071323882,
133.966181385866));
#106872=CARTESIAN_POINT('Ctrl Pts',(-131.187387925757,-3.68004554088208,
134.070133743063));
#106873=CARTESIAN_POINT('Ctrl Pts',(-131.195135822534,-3.58614635934712,
134.170179589502));
#106874=CARTESIAN_POINT('Ctrl Pts',(-131.202882098618,-3.49226681949672,
134.270204508506));
#106875=CARTESIAN_POINT('Ctrl Pts',(-131.210628374702,-3.39417529116859,
134.366324257233));
#106876=CARTESIAN_POINT('Ctrl Pts',(-131.218374650786,-3.29223736670814,
134.458174540544));
#106877=CARTESIAN_POINT('Ctrl Pts',(-131.226120984051,-3.19029868976522,
134.550025501874));
#106878=CARTESIAN_POINT('Ctrl Pts',(-131.233867317316,-3.08451385048509,
134.637606673191));
#106879=CARTESIAN_POINT('Ctrl Pts',(-131.241613650581,-2.97528333002523,
134.720592501479));
#106880=CARTESIAN_POINT('Ctrl Pts',(-131.249361718584,-2.86602834814781,
134.803596913867));
#106881=CARTESIAN_POINT('Ctrl Pts',(-131.257109786587,-2.753326460876,134.882003698979));
#106882=CARTESIAN_POINT('Ctrl Pts',(-131.26485785459,-2.6376087374702,134.955529514458));
#106883=CARTESIAN_POINT('Ctrl Pts',(-131.272614157332,-2.52176802789076,
135.029133474049));
#106884=CARTESIAN_POINT('Ctrl Pts',(-131.280370460073,-2.40290540982616,
135.097845891307));
#106885=CARTESIAN_POINT('Ctrl Pts',(-131.288126762815,-2.28147874909492,
135.161428184167));
#106886=CARTESIAN_POINT('Ctrl Pts',(-131.295887205329,-2.15998727929876,
135.225044412812));
#106887=CARTESIAN_POINT('Ctrl Pts',(-131.303647647843,-2.0359293934397,
135.283524894534));
#106888=CARTESIAN_POINT('Ctrl Pts',(-131.311408090357,-1.90978381707225,
135.336678880282));
#106889=CARTESIAN_POINT('Ctrl Pts',(-131.319180990623,-1.78343574062694,
135.389918193527));
#106890=CARTESIAN_POINT('Ctrl Pts',(-131.326953890888,-1.65499364315145,
135.437813787365));
#106891=CARTESIAN_POINT('Ctrl Pts',(-131.334726791153,-1.52495317194495,
135.480224268901));
#106892=CARTESIAN_POINT('Ctrl Pts',(-131.342217126917,-1.39963999938695,
135.521093022618));
#106893=CARTESIAN_POINT('Ctrl Pts',(-131.349707462681,-1.27284294179143,
135.556868452013));
#106894=CARTESIAN_POINT('Ctrl Pts',(-131.357197798445,-1.14501335169955,
135.58746917654));
#106895=CARTESIAN_POINT('Ctrl Pts',(-131.364972132564,-1.01233706387723,
135.619230136831));
#106896=CARTESIAN_POINT('Ctrl Pts',(-131.372746466683,-0.878128122414002,
135.645516857505));
#106897=CARTESIAN_POINT('Ctrl Pts',(-131.380520800802,-0.742878007731576,
135.666182840573));
#106898=CARTESIAN_POINT('Ctrl Pts',(-131.388285553749,-0.607794576728214,
135.686823354664));
#106899=CARTESIAN_POINT('Ctrl Pts',(-131.396050306696,-0.471672908366999,
135.701856855441));
#106900=CARTESIAN_POINT('Ctrl Pts',(-131.403815059643,-0.335017807769798,
135.71118710023));
#106901=CARTESIAN_POINT('Ctrl Pts',(-131.411572100528,-0.198498434945009,
135.720508078089));
#106902=CARTESIAN_POINT('Ctrl Pts',(-131.419329141413,-0.0614470717679311,
135.72413704622));
#106903=CARTESIAN_POINT('Ctrl Pts',(-131.427086182298,0.0756235122200777,
135.72202918579));
#106904=CARTESIAN_POINT('Ctrl Pts',(-131.434837373538,0.212590730214261,
135.719922914914));
#106905=CARTESIAN_POINT('Ctrl Pts',(-131.442588564779,0.349576750831591,
135.712088432477));
#106906=CARTESIAN_POINT('Ctrl Pts',(-131.450339756019,0.486066295528583,
135.698532929495));
#106907=CARTESIAN_POINT('Ctrl Pts',(-131.458087652796,0.622497828528287,
135.684983187963));
#106908=CARTESIAN_POINT('Ctrl Pts',(-131.465835549573,0.758432917064726,
135.665717300684));
#106909=CARTESIAN_POINT('Ctrl Pts',(-131.47358344635,0.893359122356336,
135.64079448365));
#106910=CARTESIAN_POINT('Ctrl Pts',(-131.481329722434,1.02825710399447,
135.615876879932));
#106911=CARTESIAN_POINT('Ctrl Pts',(-131.489075998518,1.16214623793336,
135.585304771093));
#106912=CARTESIAN_POINT('Ctrl Pts',(-131.496822274602,1.29452242076377,
135.549188829908));
#106913=CARTESIAN_POINT('Ctrl Pts',(-131.504568607867,1.42689958076527,
135.513072622124));
#106914=CARTESIAN_POINT('Ctrl Pts',(-131.512314941133,1.55776339019342,
135.471412603239));
#106915=CARTESIAN_POINT('Ctrl Pts',(-131.520061274398,1.68662348222734,
135.424369740035));
#106916=CARTESIAN_POINT('Ctrl Pts',(-131.527809342401,1.81551243158525,
135.377316341909));
#106917=CARTESIAN_POINT('Ctrl Pts',(-131.535557410404,1.94239640346392,
135.324877834806));
#106918=CARTESIAN_POINT('Ctrl Pts',(-131.543305478407,2.06680401045092,
135.26726373604));
#106919=CARTESIAN_POINT('Ctrl Pts',(-131.551061781149,2.19134383932326,
135.209588404324));
#106920=CARTESIAN_POINT('Ctrl Pts',(-131.558818083891,2.31340169044591,
135.146726657301));
#106921=CARTESIAN_POINT('Ctrl Pts',(-131.566574386632,2.43252935031116,
135.078934751018));
#106922=CARTESIAN_POINT('Ctrl Pts',(-131.574334829147,2.55172059219534,
135.011106662153));
#106923=CARTESIAN_POINT('Ctrl Pts',(-131.582095271661,2.66797819531203,
134.93834337811));
#106924=CARTESIAN_POINT('Ctrl Pts',(-131.589855714175,2.78088291422556,
134.860944559736));
#106925=CARTESIAN_POINT('Ctrl Pts',(-131.59762861444,2.8939688778171,134.783421493906));
#106926=CARTESIAN_POINT('Ctrl Pts',(-131.605401514706,3.00369088844627,
134.701248258012));
#106927=CARTESIAN_POINT('Ctrl Pts',(-131.613174414971,3.10966207879219,
134.614765427848));
#106928=CARTESIAN_POINT('Ctrl Pts',(-131.620664750733,3.21178094944371,
134.531426466398));
#106929=CARTESIAN_POINT('Ctrl Pts',(-131.628155086495,3.31041673820338,
134.444086004235));
#106930=CARTESIAN_POINT('Ctrl Pts',(-131.635645422257,3.40525701023964,
134.353079788861));
#106931=CARTESIAN_POINT('Ctrl Pts',(-131.643419756376,3.50369318001663,
134.25862304517));
#106932=CARTESIAN_POINT('Ctrl Pts',(-131.651194090495,3.59835215369516,
134.159917876335));
#106933=CARTESIAN_POINT('Ctrl Pts',(-131.658968424614,3.68884502119521,
134.057298593013));
#106934=CARTESIAN_POINT('Ctrl Pts',(-131.666733177562,3.7792263643234,133.954805778786));
#106935=CARTESIAN_POINT('Ctrl Pts',(-131.674497930509,3.86545156100374,
133.848408738411));
#106936=CARTESIAN_POINT('Ctrl Pts',(-131.682262683456,3.94716678005073,
133.738480157217));
#106937=CARTESIAN_POINT('Ctrl Pts',(-131.690019724341,4.02880083839017,
133.62866075864));
#106938=CARTESIAN_POINT('Ctrl Pts',(-131.697776765226,4.10593360151946,
133.51531711122));
#106939=CARTESIAN_POINT('Ctrl Pts',(-131.705533806111,4.17825019762267,
133.39885639682));
#106940=CARTESIAN_POINT('Ctrl Pts',(-131.713284997351,4.25051225921813,
133.282483506351));
#106941=CARTESIAN_POINT('Ctrl Pts',(-131.721036188591,4.31796517747307,
133.162998558434));
#106942=CARTESIAN_POINT('Ctrl Pts',(-131.728787379831,4.38033648175365,
133.040838958422));
#106943=CARTESIAN_POINT('Ctrl Pts',(-131.736535276609,4.44268127656636,
132.918731279498));
#106944=CARTESIAN_POINT('Ctrl Pts',(-131.744283173386,4.49994857571334,
132.79395155696));
#106945=CARTESIAN_POINT('Ctrl Pts',(-131.752031070163,4.55191121360761,
132.666962927758));
#106946=CARTESIAN_POINT('Ctrl Pts',(-131.759777346247,4.60386298203822,
132.54000086184));
#106947=CARTESIAN_POINT('Ctrl Pts',(-131.767523622331,4.6505121483431,132.410831169927));
#106948=CARTESIAN_POINT('Ctrl Pts',(-131.775269898415,4.69167934445549,
132.279937789831));
#106949=CARTESIAN_POINT('Ctrl Pts',(-131.783016231681,4.73284684445472,
132.14904344351));
#106950=CARTESIAN_POINT('Ctrl Pts',(-131.790762564946,4.7685321762155,132.016425756573));
#106951=CARTESIAN_POINT('Ctrl Pts',(-131.798508898211,4.79860571040627,
131.882584294989));
#106952=CARTESIAN_POINT('Ctrl Pts',(-131.806256966214,4.82868597935646,
131.748712860539));
#106953=CARTESIAN_POINT('Ctrl Pts',(-131.814005034217,4.8531518643085,131.613617487485));
#106954=CARTESIAN_POINT('Ctrl Pts',(-131.82175310222,4.87192484170143,131.477808016635));
#106955=CARTESIAN_POINT('Ctrl Pts',(-131.829509404962,4.89071777123815,
131.341854205862));
#106956=CARTESIAN_POINT('Ctrl Pts',(-131.837265707704,4.90380565309088,
131.205185169105));
#106957=CARTESIAN_POINT('Ctrl Pts',(-131.845022010446,4.91116181237985,
131.068316513734));
#106958=CARTESIAN_POINT('Ctrl Pts',(-131.85278245296,4.91852189787253,130.93137480744));
#106959=CARTESIAN_POINT('Ctrl Pts',(-131.860542895475,4.92014416047835,
130.794233660985));
#106960=CARTESIAN_POINT('Ctrl Pts',(-131.868303337989,4.91605410095466,
130.657407771432));
#106961=CARTESIAN_POINT('Ctrl Pts',(-131.876076238254,4.91195747570431,
130.520362236814));
#106962=CARTESIAN_POINT('Ctrl Pts',(-131.88384913852,4.90213023193319,130.383633360589));
#106963=CARTESIAN_POINT('Ctrl Pts',(-131.891622038785,4.88664979446709,
130.247730714727));
#106964=CARTESIAN_POINT('Ctrl Pts',(-131.899112374547,4.87173210989633,
130.116768472365));
#106965=CARTESIAN_POINT('Ctrl Pts',(-131.906602710309,4.85156515860612,
129.986573736567));
#106966=CARTESIAN_POINT('Ctrl Pts',(-131.91409304607,4.82626253582105,129.857590847331));
#106967=CARTESIAN_POINT('Ctrl Pts',(-131.921867380189,4.80000055640159,
129.723717532642));
#106968=CARTESIAN_POINT('Ctrl Pts',(-131.929641714309,4.76812258983259,
129.590725702443));
#106969=CARTESIAN_POINT('Ctrl Pts',(-131.937416048428,4.73069968573992,
129.459123260874));
#106970=CARTESIAN_POINT('Ctrl Pts',(-131.945180801375,4.69332290203206,
129.327683007553));
#106971=CARTESIAN_POINT('Ctrl Pts',(-131.952945554322,4.65041488361725,
129.197629108347));
#106972=CARTESIAN_POINT('Ctrl Pts',(-131.960710307269,4.60209792682021,
129.069460696978));
#106973=CARTESIAN_POINT('Ctrl Pts',(-131.968467348154,4.55382895910582,
128.941419584282));
#106974=CARTESIAN_POINT('Ctrl Pts',(-131.976224389039,4.50016188101653,
128.815260596145));
#106975=CARTESIAN_POINT('Ctrl Pts',(-131.983981429924,4.44126907027835,
128.691468734887));
#106976=CARTESIAN_POINT('Ctrl Pts',(-131.991732621164,4.38242067106679,
128.567770226035));
#106977=CARTESIAN_POINT('Ctrl Pts',(-131.999483812404,4.31835455034131,
128.44643564261));
#106978=CARTESIAN_POINT('Ctrl Pts',(-132.007235003644,4.24929143257928,
128.327930650152));
#106979=CARTESIAN_POINT('Ctrl Pts',(-132.014982900421,4.1802576684847,128.209476025476));
#106980=CARTESIAN_POINT('Ctrl Pts',(-132.022730797198,4.10623132798939,
128.093848936864));
#106981=CARTESIAN_POINT('Ctrl Pts',(-132.030478693975,4.02747927277771,
127.981490841993));
#106982=CARTESIAN_POINT('Ctrl Pts',(-132.03822497006,3.94874369079828,127.869156250012));
#106983=CARTESIAN_POINT('Ctrl Pts',(-132.045971246144,3.86528458457376,
127.760089611603));
#106984=CARTESIAN_POINT('Ctrl Pts',(-132.053717522228,3.77741215187059,
127.654703414409));
#106985=CARTESIAN_POINT('Ctrl Pts',(-132.061463855493,3.68953907051297,
127.549316439277));
#106986=CARTESIAN_POINT('Ctrl Pts',(-132.069210188758,3.5972528480442,127.447610259849));
#106987=CARTESIAN_POINT('Ctrl Pts',(-132.076956522024,3.50090371564495,
127.349963964562));
#106988=CARTESIAN_POINT('Ctrl Pts',(-132.084704590027,3.40453300652541,
127.252295802065));
#106989=CARTESIAN_POINT('Ctrl Pts',(-132.092452658029,3.30409785150523,
127.158689611121));
#106990=CARTESIAN_POINT('Ctrl Pts',(-132.100200726032,3.19998475019136,
127.069487037237));
#106991=CARTESIAN_POINT('Ctrl Pts',(-132.107957028774,3.09576099623459,
126.980189657795));
#106992=CARTESIAN_POINT('Ctrl Pts',(-132.115713331516,2.98785178477408,
126.89530549943));
#106993=CARTESIAN_POINT('Ctrl Pts',(-132.123469634258,2.87667649246938,
126.815135702852));
#106994=CARTESIAN_POINT('Ctrl Pts',(-132.131230076772,2.76544186256376,
126.73492311724));
#106995=CARTESIAN_POINT('Ctrl Pts',(-132.138990519286,2.65093800457677,
126.659430122247));
#106996=CARTESIAN_POINT('Ctrl Pts',(-132.1467509618,2.5336117315085,126.588913469699));
#106997=CARTESIAN_POINT('Ctrl Pts',(-132.154523862066,2.41609711589096,
126.51828361756));
#106998=CARTESIAN_POINT('Ctrl Pts',(-132.162296762331,2.2957513746586,126.452646258678));
#106999=CARTESIAN_POINT('Ctrl Pts',(-132.170069662597,2.17304507515138,
126.392211689452));
#107000=CARTESIAN_POINT('Ctrl Pts',(-132.177559998359,2.05479945870645,
126.33397406904));
#107001=CARTESIAN_POINT('Ctrl Pts',(-132.185050334121,1.93436221038816,
126.280567661433));
#107002=CARTESIAN_POINT('Ctrl Pts',(-132.192540669883,1.81216856701536,
126.232137072373));
#107003=CARTESIAN_POINT('Ctrl Pts',(-132.200315004003,1.68534191451682,
126.181870222809));
#107004=CARTESIAN_POINT('Ctrl Pts',(-132.208089338122,1.55622130165177,
126.136804726185));
#107005=CARTESIAN_POINT('Ctrl Pts',(-132.215863672241,1.4252724466168,126.097155341034));
#107006=CARTESIAN_POINT('Ctrl Pts',(-132.223628425188,1.29448497434277,
126.057554820206));
#107007=CARTESIAN_POINT('Ctrl Pts',(-132.231393178135,1.16187411358247,
126.023357242052));
#107008=CARTESIAN_POINT('Ctrl Pts',(-132.239157931082,1.02792590382294,
125.99472950918));
#107009=CARTESIAN_POINT('Ctrl Pts',(-132.246914971967,0.894110733314049,
125.966130209777));
#107010=CARTESIAN_POINT('Ctrl Pts',(-132.254672012852,0.758961236987637,
125.943089827811));
#107011=CARTESIAN_POINT('Ctrl Pts',(-132.262429053737,0.622978635402561,
125.925725492623));
#107012=CARTESIAN_POINT('Ctrl Pts',(-132.270180244977,0.487098579354945,
125.908374252014));
#107013=CARTESIAN_POINT('Ctrl Pts',(-132.277931436217,0.3503870547914,125.896690587724));
#107014=CARTESIAN_POINT('Ctrl Pts',(-132.285682627457,0.213355146288797,
125.890740501597));
#107015=CARTESIAN_POINT('Ctrl Pts',(-132.293430524235,0.0763814800025666,
125.884792944416));
#107016=CARTESIAN_POINT('Ctrl Pts',(-132.301178421012,-0.0609119096081409,
125.884574135466));
#107017=CARTESIAN_POINT('Ctrl Pts',(-132.308926317789,-0.198009366438615,
125.890098175113));
#107018=CARTESIAN_POINT('Ctrl Pts',(-132.316672593873,-0.335078145436599,
125.89562105925));
#107019=CARTESIAN_POINT('Ctrl Pts',(-132.324418869957,-0.471950682774863,
125.906884386841));
#107020=CARTESIAN_POINT('Ctrl Pts',(-132.332165146041,-0.608112271447121,
125.923850139366));
#107021=CARTESIAN_POINT('Ctrl Pts',(-132.339911479307,-0.744274865233481,
125.940816017129));
#107022=CARTESIAN_POINT('Ctrl Pts',(-132.347657812572,-0.879726111916518,
125.963484355482));
#107023=CARTESIAN_POINT('Ctrl Pts',(-132.355404145837,-1.01395776514861,
125.991765401573));
#107024=CARTESIAN_POINT('Ctrl Pts',(-132.36315221384,-1.14821947862856,
126.020052781009));
#107025=CARTESIAN_POINT('Ctrl Pts',(-132.370900281843,-1.28126067268819,
126.053955288736));
#107026=CARTESIAN_POINT('Ctrl Pts',(-132.378648349846,-1.41258499880986,
126.09333241943));
#107027=CARTESIAN_POINT('Ctrl Pts',(-132.386404652588,-1.5440488979883,
126.132751400606));
#107028=CARTESIAN_POINT('Ctrl Pts',(-132.39416095533,-1.67379190908892,
126.177656515349));
#107029=CARTESIAN_POINT('Ctrl Pts',(-132.401917258072,-1.8013339905753,
126.227857704107));
#107030=CARTESIAN_POINT('Ctrl Pts',(-132.409677700586,-1.92894414511079,
126.278085686751));
#107031=CARTESIAN_POINT('Ctrl Pts',(-132.4174381431,-2.05435067202608,126.333615217581));
#107032=CARTESIAN_POINT('Ctrl Pts',(-132.425198585614,-2.17709604539738,
126.3942091608));
#107033=CARTESIAN_POINT('Ctrl Pts',(-132.43297148588,-2.30003846053883,
126.454900374796));
#107034=CARTESIAN_POINT('Ctrl Pts',(-132.440744386145,-2.42031084225733,
126.520672059507));
#107035=CARTESIAN_POINT('Ctrl Pts',(-132.448517286411,-2.53748190909566,
126.591241983643));
#107036=CARTESIAN_POINT('Ctrl Pts',(-132.456007622173,-2.65039351251482,
126.659246513279));
#107037=CARTESIAN_POINT('Ctrl Pts',(-132.463497957934,-2.76042511033644,
126.73170631341));
#107038=CARTESIAN_POINT('Ctrl Pts',(-132.470988293696,-2.86721978552152,
126.808333369909));
#107039=CARTESIAN_POINT('Ctrl Pts',(-132.479072401512,-2.98248026192425,
126.89103478758));
#107040=CARTESIAN_POINT('Ctrl Pts',(-132.487156509327,-3.09436571278089,
126.978875139808));
#107041=CARTESIAN_POINT('Ctrl Pts',(-132.495240617143,-3.20238339056155,
127.071543493415));
#107042=CARTESIAN_POINT('Ctrl Pts',(-132.502943127705,-3.30530226830804,
127.159837587047));
#107043=CARTESIAN_POINT('Ctrl Pts',(-132.510645638266,-3.40470975968766,
127.252514062167));
#107044=CARTESIAN_POINT('Ctrl Pts',(-132.518348148828,-3.50020783643636,
127.349258858681));
#107045=CARTESIAN_POINT('Ctrl Pts',(-132.526043707272,-3.59561971870363,
127.445916335452));
#107046=CARTESIAN_POINT('Ctrl Pts',(-132.533739265715,-3.68712892603642,
127.546634550249));
#107047=CARTESIAN_POINT('Ctrl Pts',(-132.541434824159,-3.77437097888463,
127.651059684218));
#107048=CARTESIAN_POINT('Ctrl Pts',(-132.549125169276,-3.86155392993868,
127.75541407578));
#107049=CARTESIAN_POINT('Ctrl Pts',(-132.556815514393,-3.94447522285435,
127.863470087221));
#107050=CARTESIAN_POINT('Ctrl Pts',(-132.564505859511,-4.02280804413306,
127.97483795419));
#107051=CARTESIAN_POINT('Ctrl Pts',(-132.572192725819,-4.10110543073162,
128.086155442726));
#107052=CARTESIAN_POINT('Ctrl Pts',(-132.579879592127,-4.17481824789527,
128.200781480837));
#107053=CARTESIAN_POINT('Ctrl Pts',(-132.587566458435,-4.24366101930423,
128.318294605623));
#107054=CARTESIAN_POINT('Ctrl Pts',(-132.595252924575,-4.31250020685146,
128.435801612835));
#107055=CARTESIAN_POINT('Ctrl Pts',(-132.602939390716,-4.37646964477829,
128.556195069042));
#107056=CARTESIAN_POINT('Ctrl Pts',(-132.610625856856,-4.43532825009467,
128.679026202371));
#107057=CARTESIAN_POINT('Ctrl Pts',(-132.618312117137,-4.49418527906035,
128.801854046037));
#107058=CARTESIAN_POINT('Ctrl Pts',(-132.625998377419,-4.54793158141725,
128.927119075682));
#107059=CARTESIAN_POINT('Ctrl Pts',(-132.6336846377,-4.59637328421861,129.054350419132));
#107060=CARTESIAN_POINT('Ctrl Pts',(-132.641374478885,-4.64483755521738,
129.181641037586));
#107061=CARTESIAN_POINT('Ctrl Pts',(-132.649064320069,-4.68799215692162,
129.310899424951));
#107062=CARTESIAN_POINT('Ctrl Pts',(-132.656754161253,-4.72569239232696,
129.441637433789));
#107063=CARTESIAN_POINT('Ctrl Pts',(-132.659505067925,-4.73917899453737,
129.488406678066));
#107064=CARTESIAN_POINT('Ctrl Pts',(-132.662255974597,-4.7519680557209,
129.535365146417));
#107065=CARTESIAN_POINT('Ctrl Pts',(-132.66500688127,-4.76405452823412,
129.582490119309));
#107066=CARTESIAN_POINT('Ctrl Pts',(-130.915253971501,-4.76405452823413,
129.582490119309));
#107067=CARTESIAN_POINT('Ctrl Pts',(-130.92299794964,-4.7981437664688,129.715403541809));
#107068=CARTESIAN_POINT('Ctrl Pts',(-130.93074192778,-4.82667793081882,
129.849789113317));
#107069=CARTESIAN_POINT('Ctrl Pts',(-130.938485905919,-4.84954285845313,
129.985143230955));
#107070=CARTESIAN_POINT('Ctrl Pts',(-130.946261682268,-4.87250167371655,
130.121053137677));
#107071=CARTESIAN_POINT('Ctrl Pts',(-130.954037458616,-4.8897444930153,
130.257939177433));
#107072=CARTESIAN_POINT('Ctrl Pts',(-130.961813234965,-4.90120780769012,
130.395282277468));
#107073=CARTESIAN_POINT('Ctrl Pts',(-130.969589011313,-4.91267112236497,
130.532625377503));
#107074=CARTESIAN_POINT('Ctrl Pts',(-130.977364787662,-4.91835491001948,
130.67042514003));
#107075=CARTESIAN_POINT('Ctrl Pts',(-130.98514056401,-4.91824853312675,
130.808159156306));
#107076=CARTESIAN_POINT('',(-130.639859435939,-4.91824874376019,130.800845364896));
#107077=CARTESIAN_POINT('Ctrl Pts',(-130.570084224261,-4.7640545282341,
129.582490119308));
#107078=CARTESIAN_POINT('Ctrl Pts',(-130.579013117024,-4.80305957932508,
129.734570221528));
#107079=CARTESIAN_POINT('Ctrl Pts',(-130.587942009788,-4.83482173916823,
129.888688219058));
#107080=CARTESIAN_POINT('Ctrl Pts',(-130.596870902552,-4.85914920758507,
130.044194819253));
#107081=CARTESIAN_POINT('Ctrl Pts',(-130.605735204511,-4.88330069329145,
130.19857649874));
#107082=CARTESIAN_POINT('Ctrl Pts',(-130.61459950647,-4.90012458017203,
130.354326617327));
#107083=CARTESIAN_POINT('Ctrl Pts',(-130.62346380843,-4.90948058058899,
130.510790368189));
#107084=CARTESIAN_POINT('Ctrl Pts',(-130.628929017599,-4.9152489422156,
130.607256748715));
#107085=CARTESIAN_POINT('Ctrl Pts',(-130.634394226769,-4.91817952055531,
130.703994022351));
#107086=CARTESIAN_POINT('Ctrl Pts',(-130.639859435938,-4.91824874376019,
130.800845364897));
#107087=CARTESIAN_POINT('Ctrl Pts',(-130.639859435993,-4.91824874376088,
130.800845365864));
#107088=CARTESIAN_POINT('Ctrl Pts',(-130.647629166547,-4.91834715637149,
130.938536131584));
#107089=CARTESIAN_POINT('Ctrl Pts',(-130.655398897101,-4.91265908930728,
131.076274163644));
#107090=CARTESIAN_POINT('Ctrl Pts',(-130.663168627655,-4.90119937108808,
131.213540024851));
#107091=CARTESIAN_POINT('Ctrl Pts',(-130.67093798899,-4.88974019743642,
131.350799363162));
#107092=CARTESIAN_POINT('Ctrl Pts',(-130.678707350325,-4.87250994982521,
131.487586189239));
#107093=CARTESIAN_POINT('Ctrl Pts',(-130.68647671166,-4.84957544445324,
131.623385080605));
#107094=CARTESIAN_POINT('Ctrl Pts',(-130.694247346629,-4.82663717942049,
131.759206233527));
#107095=CARTESIAN_POINT('Ctrl Pts',(-130.702017981599,-4.79799285950334,
131.894038747379));
#107096=CARTESIAN_POINT('Ctrl Pts',(-130.709788616568,-4.76376057953252,
132.027376645013));
#107097=CARTESIAN_POINT('Ctrl Pts',(-130.71756216849,-4.72951544939281,
132.160764595244));
#107098=CARTESIAN_POINT('Ctrl Pts',(-130.725335720413,-4.68967827999649,
132.292656437506));
#107099=CARTESIAN_POINT('Ctrl Pts',(-130.733109272335,-4.64441715469809,
132.422560962284));
#107100=CARTESIAN_POINT('Ctrl Pts',(-130.740892326663,-4.59910070210849,
132.552624282617));
#107101=CARTESIAN_POINT('Ctrl Pts',(-130.748675380992,-4.54834717913024,
132.680695067481));
#107102=CARTESIAN_POINT('Ctrl Pts',(-130.75645843532,-4.49237322879146,
132.806301135098));
#107103=CARTESIAN_POINT('Ctrl Pts',(-130.764246603688,-4.43636249944749,
132.931989735147));
#107104=CARTESIAN_POINT('Ctrl Pts',(-130.772034772055,-4.37512468040176,
133.055210045001));
#107105=CARTESIAN_POINT('Ctrl Pts',(-130.779822940423,-4.30892214772164,
133.175514975126));
#107106=CARTESIAN_POINT('Ctrl Pts',(-130.787623850887,-4.2426113021474,
133.296016734203));
#107107=CARTESIAN_POINT('Ctrl Pts',(-130.795424761352,-4.17131971689215,
133.413593254228));
#107108=CARTESIAN_POINT('Ctrl Pts',(-130.803225671816,-4.09535325298106,
133.527826203138));
#107109=CARTESIAN_POINT('Ctrl Pts',(-130.808780963536,-4.04125496920386,
133.60917534286));
#107110=CARTESIAN_POINT('Ctrl Pts',(-130.814336255257,-3.98478678623946,
133.688829483076));
#107111=CARTESIAN_POINT('Ctrl Pts',(-130.819891546978,-3.92607112147604,
133.766648350318));
#107112=CARTESIAN_POINT('Ctrl Pts',(-130.827665881097,-3.84390168396533,
133.875551699615));
#107113=CARTESIAN_POINT('Ctrl Pts',(-130.835440215216,-3.75706743757816,
133.981206066808));
#107114=CARTESIAN_POINT('Ctrl Pts',(-130.843214549335,-3.66585441934026,
134.083185778916));
#107115=CARTESIAN_POINT('Ctrl Pts',(-130.850979302282,-3.5747538129954,
134.185039810144));
#107116=CARTESIAN_POINT('Ctrl Pts',(-130.858744055229,-3.47928543025752,
134.283227908407));
#107117=CARTESIAN_POINT('Ctrl Pts',(-130.866508808176,-3.37977755735265,
134.377354701708));
#107118=CARTESIAN_POINT('Ctrl Pts',(-130.874265849061,-3.28036851706996,
134.471388006951));
#107119=CARTESIAN_POINT('Ctrl Pts',(-130.882022889946,-3.17692825302688,
134.561367767638));
#107120=CARTESIAN_POINT('Ctrl Pts',(-130.889779930831,-3.06982390797201,
134.646933224108));
#107121=CARTESIAN_POINT('Ctrl Pts',(-130.897531122071,-2.96280033113704,
134.732434155001));
#107122=CARTESIAN_POINT('Ctrl Pts',(-130.905282313312,-2.85211847731784,
134.813527164532));
#107123=CARTESIAN_POINT('Ctrl Pts',(-130.913033504552,-2.73818050915732,
134.889890027786));
#107124=CARTESIAN_POINT('Ctrl Pts',(-130.920781401329,-2.62429096767219,
134.966220434786));
#107125=CARTESIAN_POINT('Ctrl Pts',(-130.928529298106,-2.50714838847784,
135.037824476906));
#107126=CARTESIAN_POINT('Ctrl Pts',(-130.936277194883,-2.38718583663365,
135.104421878045));
#107127=CARTESIAN_POINT('Ctrl Pts',(-130.944023470967,-2.26724837836954,
135.171005348444));
#107128=CARTESIAN_POINT('Ctrl Pts',(-130.951769747052,-2.14449246236137,
135.232584071319));
#107129=CARTESIAN_POINT('Ctrl Pts',(-130.959516023136,-2.01937745424393,
135.288922776773));
#107130=CARTESIAN_POINT('Ctrl Pts',(-130.967262356401,-1.89426152255575,
135.345261898107));
#107131=CARTESIAN_POINT('Ctrl Pts',(-130.975008689667,-1.76678682049953,
135.396360764311));
#107132=CARTESIAN_POINT('Ctrl Pts',(-130.982755022932,-1.63743410706188,
135.442031650264));
#107133=CARTESIAN_POINT('Ctrl Pts',(-130.990503090935,-1.5080524259811,
135.487712763896));
#107134=CARTESIAN_POINT('Ctrl Pts',(-130.998251158938,-1.37679226522868,
135.527963348317));
#107135=CARTESIAN_POINT('Ctrl Pts',(-131.005999226941,-1.24415062274655,
135.562645212924));
#107136=CARTESIAN_POINT('Ctrl Pts',(-131.013755529683,-1.11136800714816,
135.597363937829));
#107137=CARTESIAN_POINT('Ctrl Pts',(-131.021511832425,-0.977201355674347,
135.626502021016));
#107138=CARTESIAN_POINT('Ctrl Pts',(-131.029268135167,-0.842159516251782,
135.649972076576));
#107139=CARTESIAN_POINT('Ctrl Pts',(-131.037028577681,-0.707045600933118,
135.67345465881));
#107140=CARTESIAN_POINT('Ctrl Pts',(-131.044789020195,-0.571055954366869,
135.691263134715));
#107141=CARTESIAN_POINT('Ctrl Pts',(-131.05254946271,-0.434704682944541,
135.703362036338));
#107142=CARTESIAN_POINT('Ctrl Pts',(-131.060322362975,-0.298134528357001,
135.715480360191));
#107143=CARTESIAN_POINT('Ctrl Pts',(-131.068095263241,-0.161201979629705,
135.721870775904));
#107144=CARTESIAN_POINT('Ctrl Pts',(-131.075868163506,-0.02442218661788,
135.722549981478));
#107145=CARTESIAN_POINT('Ctrl Pts',(-131.083358499268,0.107385316386014,
135.723204496219));
#107146=CARTESIAN_POINT('Ctrl Pts',(-131.09084883503,0.239050669139419,
135.71855583637));
#107147=CARTESIAN_POINT('Ctrl Pts',(-131.098339170792,0.370119225138331,
135.708664321629));
#107148=CARTESIAN_POINT('Ctrl Pts',(-131.106113504911,0.506157285279768,
135.698397767099));
#107149=CARTESIAN_POINT('Ctrl Pts',(-131.11388783903,0.641983327902732,
135.682450422559));
#107150=CARTESIAN_POINT('Ctrl Pts',(-131.121662173149,0.777084612274554,
135.660832852416));
#107151=CARTESIAN_POINT('Ctrl Pts',(-131.129426926096,0.912019396387003,
135.639241923996));
#107152=CARTESIAN_POINT('Ctrl Pts',(-131.137191679043,1.0462308171014,135.611994735283));
#107153=CARTESIAN_POINT('Ctrl Pts',(-131.14495643199,1.17920879003412,135.579153774553));
#107154=CARTESIAN_POINT('Ctrl Pts',(-131.152713472875,1.31205468736982,
135.546345431928));
#107155=CARTESIAN_POINT('Ctrl Pts',(-131.16047051376,1.44366919777849,135.507954466737));
#107156=CARTESIAN_POINT('Ctrl Pts',(-131.168227554645,1.57355035431707,
135.464094767164));
#107157=CARTESIAN_POINT('Ctrl Pts',(-131.175978745885,1.70333356646536,
135.420268142532));
#107158=CARTESIAN_POINT('Ctrl Pts',(-131.183729937125,1.83138565760149,
135.370981116699));
#107159=CARTESIAN_POINT('Ctrl Pts',(-131.191481128366,1.95721815204557,
135.31639787005));
#107160=CARTESIAN_POINT('Ctrl Pts',(-131.199229025143,2.08299716432264,
135.261837822737));
#107161=CARTESIAN_POINT('Ctrl Pts',(-131.20697692192,2.20655809831076,135.201986187003));
#107162=CARTESIAN_POINT('Ctrl Pts',(-131.214724818697,2.32743106754529,
135.137055816668));
#107163=CARTESIAN_POINT('Ctrl Pts',(-131.222471094781,2.44827875276039,
135.072139028368));
#107164=CARTESIAN_POINT('Ctrl Pts',(-131.230217370865,2.56643924739674,
135.00214580346));
#107165=CARTESIAN_POINT('Ctrl Pts',(-131.237963646949,2.68146631388185,
134.927335450137));
#107166=CARTESIAN_POINT('Ctrl Pts',(-131.245709980214,2.79649422947079,
134.852524544582));
#107167=CARTESIAN_POINT('Ctrl Pts',(-131.25345631348,2.90838834300716,134.772896652813));
#107168=CARTESIAN_POINT('Ctrl Pts',(-131.261202646745,3.01673085405499,
134.688754780971));
#107169=CARTESIAN_POINT('Ctrl Pts',(-131.268950714748,3.12509762765683,
134.604594066139));
#107170=CARTESIAN_POINT('Ctrl Pts',(-131.276698782751,3.22991090738022,
134.515917599473));
#107171=CARTESIAN_POINT('Ctrl Pts',(-131.284446850754,3.33078579002894,
134.423068824018));
#107172=CARTESIAN_POINT('Ctrl Pts',(-131.292203153496,3.4317678837035,134.330121367779));
#107173=CARTESIAN_POINT('Ctrl Pts',(-131.299959456238,3.52880293064662,
134.232993009798));
#107174=CARTESIAN_POINT('Ctrl Pts',(-131.307715758979,3.62154236588328,
134.132064624026));
#107175=CARTESIAN_POINT('Ctrl Pts',(-131.315476201494,3.71433129894887,
134.031082369736));
#107176=CARTESIAN_POINT('Ctrl Pts',(-131.323236644008,3.80281979979047,
133.926296344877));
#107177=CARTESIAN_POINT('Ctrl Pts',(-131.330997086522,3.8867001411524,133.81811991042));
#107178=CARTESIAN_POINT('Ctrl Pts',(-131.338769986787,3.97071513468482,
133.709769821548));
#107179=CARTESIAN_POINT('Ctrl Pts',(-131.346542887053,4.05010695976115,
133.59801876596));
#107180=CARTESIAN_POINT('Ctrl Pts',(-131.354315787318,4.12461121380186,
133.483309179498));
#107181=CARTESIAN_POINT('Ctrl Pts',(-131.36180612308,4.19640705054329,133.37276957544));
#107182=CARTESIAN_POINT('Ctrl Pts',(-131.369296458842,4.26366434062614,
133.259483071011));
#107183=CARTESIAN_POINT('Ctrl Pts',(-131.376786794604,4.32618808517848,
133.14386477746));
#107184=CARTESIAN_POINT('Ctrl Pts',(-131.384561128723,4.39108243650947,
133.023862781166));
#107185=CARTESIAN_POINT('Ctrl Pts',(-131.392335462842,4.45108277766888,
132.900968555455));
#107186=CARTESIAN_POINT('Ctrl Pts',(-131.400109796961,4.50592084790166,
132.775619193944));
#107187=CARTESIAN_POINT('Ctrl Pts',(-131.407874549909,4.56069133511359,
132.65042431432));
#107188=CARTESIAN_POINT('Ctrl Pts',(-131.415639302856,4.61031205476097,
132.522780673959));
#107189=CARTESIAN_POINT('Ctrl Pts',(-131.423404055803,4.65455986693211,
132.393151197739));
#107190=CARTESIAN_POINT('Ctrl Pts',(-131.431161096688,4.69876373155253,
132.263650471341));
#107191=CARTESIAN_POINT('Ctrl Pts',(-131.438918137573,4.73760518298785,
132.13216820178));
#107192=CARTESIAN_POINT('Ctrl Pts',(-131.446675178458,4.77090871319876,
131.999188267407));
#107193=CARTESIAN_POINT('Ctrl Pts',(-131.454426369698,4.80418712895843,
131.866308614236));
#107194=CARTESIAN_POINT('Ctrl Pts',(-131.462177560938,4.83193584134976,
131.731933921975));
#107195=CARTESIAN_POINT('Ctrl Pts',(-131.469928752178,4.85402894694235,
131.596563902554));
#107196=CARTESIAN_POINT('Ctrl Pts',(-131.477676648955,4.87611266237567,
131.461251419003));
#107197=CARTESIAN_POINT('Ctrl Pts',(-131.485424545732,4.8925454891103,131.324944834739));
#107198=CARTESIAN_POINT('Ctrl Pts',(-131.49317244251,4.90325252198212,131.188154531244));
#107199=CARTESIAN_POINT('Ctrl Pts',(-131.500918718594,4.9139573151735,131.05139284133));
#107200=CARTESIAN_POINT('Ctrl Pts',(-131.508664994678,4.91893866632863,
130.914148022971));
#107201=CARTESIAN_POINT('Ctrl Pts',(-131.516411270762,4.91817353646652,
130.776935670886));
#107202=CARTESIAN_POINT('Ctrl Pts',(-131.524157604027,4.91740840095639,
130.63972230593));
#107203=CARTESIAN_POINT('Ctrl Pts',(-131.531903937293,4.91089670196464,
130.502541798686));
#107204=CARTESIAN_POINT('Ctrl Pts',(-131.539650270558,4.89866753579594,
130.365909438711));
#107205=CARTESIAN_POINT('Ctrl Pts',(-131.547398338561,4.88643563099029,
130.229246480868));
#107206=CARTESIAN_POINT('Ctrl Pts',(-131.555146406564,4.86848374603258,
130.093132303893));
#107207=CARTESIAN_POINT('Ctrl Pts',(-131.562894474567,4.84489277970605,
129.958076377105));
#107208=CARTESIAN_POINT('Ctrl Pts',(-131.570650777309,4.82127674061974,
129.822876911271));
#107209=CARTESIAN_POINT('Ctrl Pts',(-131.578407080051,4.79200971531739,
129.688738328121));
#107210=CARTESIAN_POINT('Ctrl Pts',(-131.586163382793,4.7572237359593,129.556159756917));
#107211=CARTESIAN_POINT('Ctrl Pts',(-131.593923825307,4.72241919027664,
129.423510424537));
#107212=CARTESIAN_POINT('Ctrl Pts',(-131.601684267821,4.68208993602448,
129.292423136677));
#107213=CARTESIAN_POINT('Ctrl Pts',(-131.609444710335,4.63641741139761,
129.163380224694));
#107214=CARTESIAN_POINT('Ctrl Pts',(-131.617217610601,4.59067156917959,
129.034130161574));
#107215=CARTESIAN_POINT('Ctrl Pts',(-131.624990510866,4.53956546186643,
128.906931395427));
#107216=CARTESIAN_POINT('Ctrl Pts',(-131.632763411131,4.48332840720811,
128.782245523013));
#107217=CARTESIAN_POINT('Ctrl Pts',(-131.640253746893,4.42913571113982,
128.662092296126));
#107218=CARTESIAN_POINT('Ctrl Pts',(-131.647744082655,4.37017877466386,
128.544272710335));
#107219=CARTESIAN_POINT('Ctrl Pts',(-131.655234418417,4.30670144097751,
128.429175201481));
#107220=CARTESIAN_POINT('Ctrl Pts',(-131.663008752536,4.2408173448901,128.309713735595));
#107221=CARTESIAN_POINT('Ctrl Pts',(-131.670783086655,4.16985460224,128.192806418424));
#107222=CARTESIAN_POINT('Ctrl Pts',(-131.678557420775,4.09403595077842,
128.078915205118));
#107223=CARTESIAN_POINT('Ctrl Pts',(-131.686322173722,4.01831073902906,
127.965164352554));
#107224=CARTESIAN_POINT('Ctrl Pts',(-131.694086926669,3.93774174036037,
127.854422530299));
#107225=CARTESIAN_POINT('Ctrl Pts',(-131.701851679616,3.85259781401043,
127.747127694483));
#107226=CARTESIAN_POINT('Ctrl Pts',(-131.709608720501,3.767538453808,127.639939425411));
#107227=CARTESIAN_POINT('Ctrl Pts',(-131.717365761386,3.67791344991105,
127.53619163394));
#107228=CARTESIAN_POINT('Ctrl Pts',(-131.725122802271,3.58403503649811,
127.436293528024));
#107229=CARTESIAN_POINT('Ctrl Pts',(-131.732873993511,3.49022741752687,
127.336470756047));
#107230=CARTESIAN_POINT('Ctrl Pts',(-131.740625184751,3.39217304008557,
127.240492174976));
#107231=CARTESIAN_POINT('Ctrl Pts',(-131.748376375991,3.29022427209507,
127.148733817438));
#107232=CARTESIAN_POINT('Ctrl Pts',(-131.756124272768,3.18831883505097,
127.05701445965));
#107233=CARTESIAN_POINT('Ctrl Pts',(-131.763872169546,3.08252258955126,
126.969512018848));
#107234=CARTESIAN_POINT('Ctrl Pts',(-131.771620066323,2.97322444591885,
126.886565388526));
#107235=CARTESIAN_POINT('Ctrl Pts',(-131.779366342407,2.86394916510189,
126.80363610885));
#107236=CARTESIAN_POINT('Ctrl Pts',(-131.787112618491,2.75117375441684,
126.72526098033));
#107237=CARTESIAN_POINT('Ctrl Pts',(-131.794858894575,2.6353195451722,126.651738077853));
#107238=CARTESIAN_POINT('Ctrl Pts',(-131.80260522784,2.51946448071794,126.578214632646));
#107239=CARTESIAN_POINT('Ctrl Pts',(-131.810351561106,2.4005309024574,126.509543694443));
#107240=CARTESIAN_POINT('Ctrl Pts',(-131.818097894371,2.27896806535331,
126.445979310292));
#107241=CARTESIAN_POINT('Ctrl Pts',(-131.825845962374,2.15737800509455,
126.382400691337));
#107242=CARTESIAN_POINT('Ctrl Pts',(-131.833594030377,2.03315786073327,
126.323931083147));
#107243=CARTESIAN_POINT('Ctrl Pts',(-131.84134209838,1.90677999100253,126.270777803895));
#107244=CARTESIAN_POINT('Ctrl Pts',(-131.849098401122,1.7802678053681,126.217568032705));
#107245=CARTESIAN_POINT('Ctrl Pts',(-131.856854703864,1.65159367429952,
126.169686029268));
#107246=CARTESIAN_POINT('Ctrl Pts',(-131.864611006606,1.52124889598726,
126.127290502744));
#107247=CARTESIAN_POINT('Ctrl Pts',(-131.87237144912,1.39083454874222,126.084872348452));
#107248=CARTESIAN_POINT('Ctrl Pts',(-131.880131891634,1.25874815386053,
126.047946611165));
#107249=CARTESIAN_POINT('Ctrl Pts',(-131.887892334148,1.12549358215017,
126.016621353671));
#107250=CARTESIAN_POINT('Ctrl Pts',(-131.895665234413,0.992025098371515,
125.985245810094));
#107251=CARTESIAN_POINT('Ctrl Pts',(-131.903438134679,0.857385074617616,
125.959488785472));
#107252=CARTESIAN_POINT('Ctrl Pts',(-131.911211034944,0.722085817158509,
125.93940685261));
#107253=CARTESIAN_POINT('Ctrl Pts',(-131.918701370706,0.591705028507405,
125.920054948591));
#107254=CARTESIAN_POINT('Ctrl Pts',(-131.926191706468,0.460712409888022,
125.905972724972));
#107255=CARTESIAN_POINT('Ctrl Pts',(-131.93368204223,0.329566566580926,
125.897164988626));
#107256=CARTESIAN_POINT('Ctrl Pts',(-131.941456376349,0.193448288762958,
125.888023304278));
#107257=CARTESIAN_POINT('Ctrl Pts',(-131.949230710468,0.0567337560766165,
125.884535008888));
#107258=CARTESIAN_POINT('Ctrl Pts',(-131.957005044587,-0.0800679803326742,
125.886762404919));
#107259=CARTESIAN_POINT('Ctrl Pts',(-131.964769797534,-0.216701120827791,
125.888987055884));
#107260=CARTESIAN_POINT('Ctrl Pts',(-131.972534550481,-0.353420864050336,
125.896913376348));
#107261=CARTESIAN_POINT('Ctrl Pts',(-131.980299303428,-0.489713420117738,
125.910551893407));
#107262=CARTESIAN_POINT('Ctrl Pts',(-131.988056344313,-0.625870608496693,
125.924176864498));
#107263=CARTESIAN_POINT('Ctrl Pts',(-131.995813385198,-0.761601067568436,
125.943502703118));
#107264=CARTESIAN_POINT('Ctrl Pts',(-132.003570426083,-0.896391748893166,
125.968487904703));
#107265=CARTESIAN_POINT('Ctrl Pts',(-132.011321617323,-1.03108078351677,
125.993454264752));
#107266=CARTESIAN_POINT('Ctrl Pts',(-132.019072808563,-1.16483106814385,
126.024071422061));
#107267=CARTESIAN_POINT('Ctrl Pts',(-132.026823999803,-1.29713577240741,
126.060246174338));
#107268=CARTESIAN_POINT('Ctrl Pts',(-132.03457189658,-1.4293842436425,126.096405551381));
#107269=CARTESIAN_POINT('Ctrl Pts',(-132.042319793357,-1.56018798019597,
126.138117722406));
#107270=CARTESIAN_POINT('Ctrl Pts',(-132.050067690134,-1.68905164584534,
126.185238666354));
#107271=CARTESIAN_POINT('Ctrl Pts',(-132.057813966218,-1.81788835599383,
126.232349753617));
#107272=CARTESIAN_POINT('Ctrl Pts',(-132.065560242303,-1.94478543548438,
126.284867229208));
#107273=CARTESIAN_POINT('Ctrl Pts',(-132.073306518387,-2.06926436560832,
126.342597731921));
#107274=CARTESIAN_POINT('Ctrl Pts',(-132.081052851652,-2.19374421460728,
126.400328660787));
#107275=CARTESIAN_POINT('Ctrl Pts',(-132.088799184917,-2.31580552394301,
126.463272529071));
#107276=CARTESIAN_POINT('Ctrl Pts',(-132.096545518183,-2.43499172335814,
126.531188684484));
#107277=CARTESIAN_POINT('Ctrl Pts',(-132.104293586185,-2.55420461369674,
126.59912004925));
#107278=CARTESIAN_POINT('Ctrl Pts',(-132.112041654188,-2.67054077328484,
126.672025723372));
#107279=CARTESIAN_POINT('Ctrl Pts',(-132.119789722191,-2.78357045803926,
126.749620358606));
#107280=CARTESIAN_POINT('Ctrl Pts',(-132.127546024933,-2.89672027208725,
126.827297462342));
#107281=CARTESIAN_POINT('Ctrl Pts',(-132.135302327675,-3.00655626855044,
126.909673260609));
#107282=CARTESIAN_POINT('Ctrl Pts',(-132.143058630417,-3.11267936224403,
126.996420196504));
#107283=CARTESIAN_POINT('Ctrl Pts',(-132.150819072931,-3.21885909702832,
127.08321343185));
#107284=CARTESIAN_POINT('Ctrl Pts',(-132.158579515445,-3.32132168842245,
127.17438219378));
#107285=CARTESIAN_POINT('Ctrl Pts',(-132.166339957959,-3.41970386566228,
127.269560972088));
#107286=CARTESIAN_POINT('Ctrl Pts',(-132.174112858225,-3.51824397470698,
127.36489253982));
#107287=CARTESIAN_POINT('Ctrl Pts',(-132.18188575849,-3.61269031060273,
127.464246704048));
#107288=CARTESIAN_POINT('Ctrl Pts',(-132.189658658755,-3.70271836299404,
127.567223025982));
#107289=CARTESIAN_POINT('Ctrl Pts',(-132.197148994518,-3.78947366891736,
127.666455899235));
#107290=CARTESIAN_POINT('Ctrl Pts',(-132.20463933028,-3.87212615251791,
127.769051913344));
#107291=CARTESIAN_POINT('Ctrl Pts',(-132.212129666042,-3.95042388228051,
127.87462782893));
#107292=CARTESIAN_POINT('Ctrl Pts',(-132.21994674266,-4.0321370887297,127.98480914086));
#107293=CARTESIAN_POINT('Ctrl Pts',(-132.227763819277,-4.10936709823398,
128.098586714222));
#107294=CARTESIAN_POINT('Ctrl Pts',(-132.235580895894,-4.18178267079426,
128.215562294648));
#107295=CARTESIAN_POINT('Ctrl Pts',(-132.243384955992,-4.25407766135055,
128.332343094456));
#107296=CARTESIAN_POINT('Ctrl Pts',(-132.251189016089,-4.32157398171214,
128.452310969956));
#107297=CARTESIAN_POINT('Ctrl Pts',(-132.258993076186,-4.38398164243891,
128.575036051412));
#107298=CARTESIAN_POINT('Ctrl Pts',(-132.266789639672,-4.44632935411981,
128.697643242669));
#107299=CARTESIAN_POINT('Ctrl Pts',(-132.274586203158,-4.50359795612399,
128.82300203038));
#107300=CARTESIAN_POINT('Ctrl Pts',(-132.282382766644,-4.55554141719004,
128.950654745868));
#107301=CARTESIAN_POINT('Ctrl Pts',(-132.290172170143,-4.60743717589171,
129.078190231272));
#107302=CARTESIAN_POINT('Ctrl Pts',(-132.297961573642,-4.65401738723624,
129.2080150941));
#107303=CARTESIAN_POINT('Ctrl Pts',(-132.305750977141,-4.69508279439975,
129.339648831503));
#107304=CARTESIAN_POINT('Ctrl Pts',(-132.310503412346,-4.7201374326307,
129.41996060478));
#107305=CARTESIAN_POINT('Ctrl Pts',(-132.315255847551,-4.74314014747024,
129.50094526613));
#107306=CARTESIAN_POINT('Ctrl Pts',(-132.320008282756,-4.76405452823418,
129.582490119309));
#107307=CARTESIAN_POINT('Origin',(213.235140564004,0.,130.804360617566));
#107308=CARTESIAN_POINT('',(-134.415184333433,-4.76405452823396,129.582490119308));
#107309=CARTESIAN_POINT('',(-134.069717999649,-4.76405452823413,129.582490119309));
#107310=CARTESIAN_POINT('',(213.235140564004,-4.76405452823405,129.582490119308));
#107311=CARTESIAN_POINT('',(-132.735140563954,-4.9182497588907,130.805900640808));
#107312=CARTESIAN_POINT('Ctrl Pts',(-132.73514056401,-4.91824975889039,
130.805900641798));
#107313=CARTESIAN_POINT('Ctrl Pts',(-132.739905681843,-4.91822356444062,
130.88955571917));
#107314=CARTESIAN_POINT('Ctrl Pts',(-132.744670799676,-4.91606315597891,
130.973174771754));
#107315=CARTESIAN_POINT('Ctrl Pts',(-132.749435917509,-4.91177322663725,
131.056683491261));
#107316=CARTESIAN_POINT('Ctrl Pts',(-132.757210251628,-4.90477416696683,
131.192928744802));
#107317=CARTESIAN_POINT('Ctrl Pts',(-132.764984585747,-4.89209086537747,
131.329098365177));
#107318=CARTESIAN_POINT('Ctrl Pts',(-132.772758919866,-4.8737215788707,
131.464679505794));
#107319=CARTESIAN_POINT('Ctrl Pts',(-132.780523672813,-4.85537493086784,
131.600093554771));
#107320=CARTESIAN_POINT('Ctrl Pts',(-132.78828842576,-4.83135629270741,
131.734920183313));
#107321=CARTESIAN_POINT('Ctrl Pts',(-132.796053178707,-4.80171589405253,
131.86864795438));
#107322=CARTESIAN_POINT('Ctrl Pts',(-132.803810219592,-4.77210493465952,
132.00224290514));
#107323=CARTESIAN_POINT('Ctrl Pts',(-132.811567260477,-4.73688341046714,
132.13474079113));
#107324=CARTESIAN_POINT('Ctrl Pts',(-132.819324301362,-4.69615313103981,
132.265637056959));
#107325=CARTESIAN_POINT('Ctrl Pts',(-132.827075492602,-4.65545356663297,
132.396434612896));
#107326=CARTESIAN_POINT('Ctrl Pts',(-132.834826683842,-4.60925363135559,
132.525632580914));
#107327=CARTESIAN_POINT('Ctrl Pts',(-132.842577875082,-4.55770573624154,
132.652738686125));
#107328=CARTESIAN_POINT('Ctrl Pts',(-132.850325771859,-4.50617975035794,
132.779790767851));
#107329=CARTESIAN_POINT('Ctrl Pts',(-132.858073668637,-4.4493104721373,
132.904752393572));
#107330=CARTESIAN_POINT('Ctrl Pts',(-132.865821565414,-4.38729941812407,
133.027148704233));
#107331=CARTESIAN_POINT('Ctrl Pts',(-132.873567841498,-4.32530133548654,
133.149519412224));
#107332=CARTESIAN_POINT('Ctrl Pts',(-132.881314117582,-4.25816379296523,
133.269325523963));
#107333=CARTESIAN_POINT('Ctrl Pts',(-132.889060393666,-4.18613531560761,
133.3861147077));
#107334=CARTESIAN_POINT('Ctrl Pts',(-132.896806726931,-4.11410630655223,
133.502904753548));
#107335=CARTESIAN_POINT('Ctrl Pts',(-132.904553060197,-4.03718649584882,
133.616677494188));
#107336=CARTESIAN_POINT('Ctrl Pts',(-132.912299393462,-3.95566877631886,
133.727007978189));
#107337=CARTESIAN_POINT('Ctrl Pts',(-132.920047461465,-3.87413280146092,
133.837363169937));
#107338=CARTESIAN_POINT('Ctrl Pts',(-132.927795529468,-3.78799710113754,
133.944274256717));
#107339=CARTESIAN_POINT('Ctrl Pts',(-132.935543597471,-3.69759578287759,
134.04734820449));
#107340=CARTESIAN_POINT('Ctrl Pts',(-132.943299900212,-3.60709838502069,
134.150531700482));
#107341=CARTESIAN_POINT('Ctrl Pts',(-132.951056202954,-3.51232657117879,
134.249869616509));
#107342=CARTESIAN_POINT('Ctrl Pts',(-132.958812505696,-3.41365274102419,
134.345004348048));
#107343=CARTESIAN_POINT('Ctrl Pts',(-132.96657294821,-3.31492624567543,
134.440189855857));
#107344=CARTESIAN_POINT('Ctrl Pts',(-132.974333390724,-3.21229387663329,
134.531167449867));
#107345=CARTESIAN_POINT('Ctrl Pts',(-132.982093833239,-3.10616149122688,
134.617619571915));
#107346=CARTESIAN_POINT('Ctrl Pts',(-132.989866733504,-2.99985873269342,
134.704210474584));
#107347=CARTESIAN_POINT('Ctrl Pts',(-132.997639633769,-2.89004504354419,
134.786261153979));
#107348=CARTESIAN_POINT('Ctrl Pts',(-133.005412534035,-2.7771563872757,
134.863496666421));
#107349=CARTESIAN_POINT('Ctrl Pts',(-133.012902869797,-2.66837151800949,
134.937924473443));
#107350=CARTESIAN_POINT('Ctrl Pts',(-133.020393205559,-2.55673162680563,
135.007880958831));
#107351=CARTESIAN_POINT('Ctrl Pts',(-133.027883541321,-2.44264702593649,
135.073161218342));
#107352=CARTESIAN_POINT('Ctrl Pts',(-133.03565787544,-2.32423687275231,
135.140916598732));
#107353=CARTESIAN_POINT('Ctrl Pts',(-133.043432209559,-2.20281788029023,
135.203848783836));
#107354=CARTESIAN_POINT('Ctrl Pts',(-133.051206543678,-2.07882057878,135.26167910111));
#107355=CARTESIAN_POINT('Ctrl Pts',(-133.058971296626,-1.95497609286226,
135.319438147686));
#107356=CARTESIAN_POINT('Ctrl Pts',(-133.066736049573,-1.8285599711679,
135.372107673208));
#107357=CARTESIAN_POINT('Ctrl Pts',(-133.07450080252,-1.7000296505217,135.419453493105));
#107358=CARTESIAN_POINT('Ctrl Pts',(-133.082257843405,-1.57162698800194,
135.466752288465));
#107359=CARTESIAN_POINT('Ctrl Pts',(-133.09001488429,-1.44111466982342,
135.508737766455));
#107360=CARTESIAN_POINT('Ctrl Pts',(-133.097771925175,-1.30897222328307,
135.545222857831));
#107361=CARTESIAN_POINT('Ctrl Pts',(-133.105523116415,-1.17692942638939,
135.581680435516));
#107362=CARTESIAN_POINT('Ctrl Pts',(-133.113274307655,-1.04325932330527,
135.612645779067));
#107363=CARTESIAN_POINT('Ctrl Pts',(-133.121025498895,-0.908458460722157,
135.637981029601));
#107364=CARTESIAN_POINT('Ctrl Pts',(-133.128773395672,-0.773714892101393,
135.663305511978));
#107365=CARTESIAN_POINT('Ctrl Pts',(-133.136521292449,-0.637841903297591,
135.683004588649));
#107366=CARTESIAN_POINT('Ctrl Pts',(-133.144269189227,-0.501347931295957,
135.696991128271));
#107367=CARTESIAN_POINT('Ctrl Pts',(-133.152015465311,-0.364882510890796,
135.710974742212));
#107368=CARTESIAN_POINT('Ctrl Pts',(-133.159761741395,-0.227796754340897,
135.719248156076));
#107369=CARTESIAN_POINT('Ctrl Pts',(-133.167508017479,-0.0906055550158913,
135.721775964667));
#107370=CARTESIAN_POINT('Ctrl Pts',(-133.175254350744,0.046586657023196,
135.724303791917));
#107371=CARTESIAN_POINT('Ctrl Pts',(-133.18300068401,0.183883922491684,
135.721085922059));
#107372=CARTESIAN_POINT('Ctrl Pts',(-133.190747017275,0.32077040199062,
135.712139077491));
#107373=CARTESIAN_POINT('Ctrl Pts',(-133.198495085278,0.45768753626735,
135.703190229339));
#107374=CARTESIAN_POINT('Ctrl Pts',(-133.206243153281,0.594193311461642,
135.688509879021));
#107375=CARTESIAN_POINT('Ctrl Pts',(-133.213991221284,0.729776463624133,
135.668166676163));
#107376=CARTESIAN_POINT('Ctrl Pts',(-133.221747524026,0.865503715174387,
135.647801852306));
#107377=CARTESIAN_POINT('Ctrl Pts',(-133.229503826768,1.00030599763536,
135.621762211319));
#107378=CARTESIAN_POINT('Ctrl Pts',(-133.23726012951,1.13368115707588,135.590167769614));
#107379=CARTESIAN_POINT('Ctrl Pts',(-133.245020572024,1.26712750285521,
135.558556465003));
#107380=CARTESIAN_POINT('Ctrl Pts',(-133.252781014538,1.39914483171764,
135.521384558041));
#107381=CARTESIAN_POINT('Ctrl Pts',(-133.260541457052,1.52924659718825,
135.47882186005));
#107382=CARTESIAN_POINT('Ctrl Pts',(-133.268314357318,1.65955721356232,
135.436190836638));
#107383=CARTESIAN_POINT('Ctrl Pts',(-133.276087257583,1.78794575526713,
135.388151866283));
#107384=CARTESIAN_POINT('Ctrl Pts',(-133.283860157848,1.91394525548041,
135.334923123649));
#107385=CARTESIAN_POINT('Ctrl Pts',(-133.29135049361,2.03536435648632,135.283629379885));
#107386=CARTESIAN_POINT('Ctrl Pts',(-133.298840829372,2.15456481706185,
135.227516766744));
#107387=CARTESIAN_POINT('Ctrl Pts',(-133.306331165134,2.27115246165902,
135.166819735816));
#107388=CARTESIAN_POINT('Ctrl Pts',(-133.314105499253,2.392160562238,135.10382135851));
#107389=CARTESIAN_POINT('Ctrl Pts',(-133.321879833373,2.51073712314737,
135.035684504641));
#107390=CARTESIAN_POINT('Ctrl Pts',(-133.329654167492,2.62641497717776,
134.962620762165));
#107391=CARTESIAN_POINT('Ctrl Pts',(-133.337418920439,2.7419502685915,134.889647064221));
#107392=CARTESIAN_POINT('Ctrl Pts',(-133.345183673386,2.85459363375357,
134.811758765819));
#107393=CARTESIAN_POINT('Ctrl Pts',(-133.352948426333,2.96390079077247,
134.729214139031));
#107394=CARTESIAN_POINT('Ctrl Pts',(-133.360705467218,3.07309938238206,
134.646751496731));
#107395=CARTESIAN_POINT('Ctrl Pts',(-133.368462508103,3.17896805002177,
134.559641963552));
#107396=CARTESIAN_POINT('Ctrl Pts',(-133.376219548988,3.28109021082183,
134.468187863896));
#107397=CARTESIAN_POINT('Ctrl Pts',(-133.383970740228,3.38313536050617,
134.376802730487));
#107398=CARTESIAN_POINT('Ctrl Pts',(-133.391721931468,3.48143933681013,
134.281079811588));
#107399=CARTESIAN_POINT('Ctrl Pts',(-133.399473122708,3.57561775953648,
134.1813623499));
#107400=CARTESIAN_POINT('Ctrl Pts',(-133.407221019485,3.66975615392075,
134.081687270793));
#107401=CARTESIAN_POINT('Ctrl Pts',(-133.414968916262,3.75977221436109,
133.978021309307));
#107402=CARTESIAN_POINT('Ctrl Pts',(-133.42271681304,3.84531781218241,133.870745131258));
#107403=CARTESIAN_POINT('Ctrl Pts',(-133.430463089124,3.93084551570882,
133.763491393074));
#107404=CARTESIAN_POINT('Ctrl Pts',(-133.438209365208,4.01190437302902,
133.652629245901));
#107405=CARTESIAN_POINT('Ctrl Pts',(-133.445955641292,4.08818628430396,
133.538572746741));
#107406=CARTESIAN_POINT('Ctrl Pts',(-133.453701974557,4.16446875867476,
133.424515405642));
#107407=CARTESIAN_POINT('Ctrl Pts',(-133.461448307823,4.23597399928683,
133.307263990484));
#107408=CARTESIAN_POINT('Ctrl Pts',(-133.469194641088,4.30243725137123,
133.187261530427));
#107409=CARTESIAN_POINT('Ctrl Pts',(-133.476942709091,4.36891538744003,
133.067232196651));
#107410=CARTESIAN_POINT('Ctrl Pts',(-133.484690777094,4.43034909877924,
132.944450934001));
#107411=CARTESIAN_POINT('Ctrl Pts',(-133.492438845097,4.48651979161184,
132.819384990117));
#107412=CARTESIAN_POINT('Ctrl Pts',(-133.500195147839,4.54275018332516,
132.69418612466));
#107413=CARTESIAN_POINT('Ctrl Pts',(-133.50795145058,4.59370622228072,132.56669808462));
#107414=CARTESIAN_POINT('Ctrl Pts',(-133.515707753322,4.63921745521967,
132.437408218123));
#107415=CARTESIAN_POINT('Ctrl Pts',(-133.523468195836,4.68475297887408,
132.308049345731));
#107416=CARTESIAN_POINT('Ctrl Pts',(-133.531228638351,4.72483779173659,
132.176887104347));
#107417=CARTESIAN_POINT('Ctrl Pts',(-133.538989080865,4.75935177062778,
132.044422626468));
#107418=CARTESIAN_POINT('Ctrl Pts',(-133.54676198113,4.79392115442189,131.911745504849));
#107419=CARTESIAN_POINT('Ctrl Pts',(-133.554534881396,4.82290175098418,
131.777762351667));
#107420=CARTESIAN_POINT('Ctrl Pts',(-133.562307781661,4.84622470986369,
131.642983968068));
#107421=CARTESIAN_POINT('Ctrl Pts',(-133.569798117423,4.86869982044101,
131.513105118198));
#107422=CARTESIAN_POINT('Ctrl Pts',(-133.577288453185,4.88592145038888,
131.382488156753));
#107423=CARTESIAN_POINT('Ctrl Pts',(-133.584778788947,4.8978737889557,131.251591441594));
#107424=CARTESIAN_POINT('Ctrl Pts',(-133.592553123066,4.91027930407208,
131.115731737695));
#107425=CARTESIAN_POINT('Ctrl Pts',(-133.600327457186,4.91704736674041,
130.979140284887));
#107426=CARTESIAN_POINT('Ctrl Pts',(-133.608101791305,4.91810347661472,
130.842324492635));
#107427=CARTESIAN_POINT('Ctrl Pts',(-133.615866544252,4.91915828492799,
130.705677313619));
#107428=CARTESIAN_POINT('Ctrl Pts',(-133.623631297199,4.91451514390814,
130.568806732468));
#107429=CARTESIAN_POINT('Ctrl Pts',(-133.631396050146,4.90415119995085,
130.432226138485));
#107430=CARTESIAN_POINT('Ctrl Pts',(-133.639153091031,4.89379754960881,
130.295781198274));
#107431=CARTESIAN_POINT('Ctrl Pts',(-133.646910131916,4.87773443312074,
130.15962605938));
#107432=CARTESIAN_POINT('Ctrl Pts',(-133.654667172801,4.85599103135013,
130.024274618495));
#107433=CARTESIAN_POINT('Ctrl Pts',(-133.662418364041,4.8342640264479,129.889025247183));
#107434=CARTESIAN_POINT('Ctrl Pts',(-133.670169555281,4.80686532416455,
129.754578751978));
#107435=CARTESIAN_POINT('Ctrl Pts',(-133.677920746521,4.77387593742032,
129.62144405389));
#107436=CARTESIAN_POINT('Ctrl Pts',(-133.685668643298,4.74090057204552,
129.4883659416));
#107437=CARTESIAN_POINT('Ctrl Pts',(-133.693416540075,4.70233934210709,
129.356598896199));
#107438=CARTESIAN_POINT('Ctrl Pts',(-133.701164436853,4.65832434048542,
129.226641567373));
#107439=CARTESIAN_POINT('Ctrl Pts',(-133.708910712937,4.61431854585323,
129.096711422819));
#107440=CARTESIAN_POINT('Ctrl Pts',(-133.716656989021,4.56486137401212,
128.968590611944));
#107441=CARTESIAN_POINT('Ctrl Pts',(-133.724403265105,4.51013464735419,
128.842762155792));
#107442=CARTESIAN_POINT('Ctrl Pts',(-133.73214959837,4.45540751671593,128.716932770802));
#107443=CARTESIAN_POINT('Ctrl Pts',(-133.739895931636,4.39541090957425,
128.593396132823));
#107444=CARTESIAN_POINT('Ctrl Pts',(-133.747642264901,4.33037445248886,
128.472614455624));
#107445=CARTESIAN_POINT('Ctrl Pts',(-133.755390332904,4.26532343093993,
128.351805730205));
#107446=CARTESIAN_POINT('Ctrl Pts',(-133.763138400907,4.19523049890691,
128.233753537401));
#107447=CARTESIAN_POINT('Ctrl Pts',(-133.77088646891,4.12037060978731,128.11889434511));
#107448=CARTESIAN_POINT('Ctrl Pts',(-133.778642771652,4.0454311586868,128.003913079102));
#107449=CARTESIAN_POINT('Ctrl Pts',(-133.786399074394,3.96571484367799,
127.892131920668));
#107450=CARTESIAN_POINT('Ctrl Pts',(-133.794155377135,3.8815395503921,127.78395770053));
#107451=CARTESIAN_POINT('Ctrl Pts',(-133.80191581965,3.79731933021748,127.675725744552));
#107452=CARTESIAN_POINT('Ctrl Pts',(-133.809676262164,3.70863564231168,
127.571104860946));
#107453=CARTESIAN_POINT('Ctrl Pts',(-133.817436704678,3.61584517412433,
127.4704669871));
#107454=CARTESIAN_POINT('Ctrl Pts',(-133.825209604943,3.5229057504399,127.369667560404));
#107455=CARTESIAN_POINT('Ctrl Pts',(-133.832982505209,3.4258466493997,127.272864196728));
#107456=CARTESIAN_POINT('Ctrl Pts',(-133.840755405474,3.32506040712498,
127.180390922402));
#107457=CARTESIAN_POINT('Ctrl Pts',(-133.848245741236,3.2279379986219,127.091279284523));
#107458=CARTESIAN_POINT('Ctrl Pts',(-133.855736076998,3.12735496134202,
127.006188581348));
#107459=CARTESIAN_POINT('Ctrl Pts',(-133.86322641276,3.02368837863848,126.925379868531));
#107460=CARTESIAN_POINT('Ctrl Pts',(-133.871000746879,2.9160912459434,126.841507268806));
#107461=CARTESIAN_POINT('Ctrl Pts',(-133.878775080999,2.80483129141674,
126.761982089327));
#107462=CARTESIAN_POINT('Ctrl Pts',(-133.886549415118,2.69029514375431,
126.687141276555));
#107463=CARTESIAN_POINT('Ctrl Pts',(-133.894314168065,2.57590015165748,
126.612392698397));
#107464=CARTESIAN_POINT('Ctrl Pts',(-133.902078921012,2.45823732422291,
126.542317212076));
#107465=CARTESIAN_POINT('Ctrl Pts',(-133.909843673959,2.33772623747939,
126.477211544435));
#107466=CARTESIAN_POINT('Ctrl Pts',(-133.917600714844,2.21733484404613,
126.412170540661));
#107467=CARTESIAN_POINT('Ctrl Pts',(-133.925357755729,2.09410116275597,
126.352089717147));
#107468=CARTESIAN_POINT('Ctrl Pts',(-133.933114796614,1.96847332241768,
126.297222296921));
#107469=CARTESIAN_POINT('Ctrl Pts',(-133.940865987854,1.84294021901086,
126.242396252642));
#107470=CARTESIAN_POINT('Ctrl Pts',(-133.948617179094,1.71501690703762,
126.192775942148));
#107471=CARTESIAN_POINT('Ctrl Pts',(-133.956368370334,1.58517534561964,
126.148568291212));
#107472=CARTESIAN_POINT('Ctrl Pts',(-133.964116267111,1.45538897032874,
126.104379429706));
#107473=CARTESIAN_POINT('Ctrl Pts',(-133.971864163888,1.32368633650381,
126.065598777936));
#107474=CARTESIAN_POINT('Ctrl Pts',(-133.979612060666,1.19055837167676,
126.032384734755));
#107475=CARTESIAN_POINT('Ctrl Pts',(-133.98735833675,1.05745825435041,125.999177639236));
#107476=CARTESIAN_POINT('Ctrl Pts',(-133.995104612834,0.922933778152838,
125.971534930803));
#107477=CARTESIAN_POINT('Ctrl Pts',(-134.002850888918,0.787489601811479,
125.949564721801));
#107478=CARTESIAN_POINT('Ctrl Pts',(-134.010597222183,0.652044425651795,
125.927594350619));
#107479=CARTESIAN_POINT('Ctrl Pts',(-134.018343555449,0.515679921722393,
125.911296625022));
#107480=CARTESIAN_POINT('Ctrl Pts',(-134.026089888714,0.378909082321167,
125.900728191513));
#107481=CARTESIAN_POINT('Ctrl Pts',(-134.033837956717,0.242107614038945,
125.890157391277));
#107482=CARTESIAN_POINT('Ctrl Pts',(-134.04158602472,0.104900018941983,
125.885318466336));
#107483=CARTESIAN_POINT('Ctrl Pts',(-134.049334092723,-0.0321978711377765,
125.886216012169));
#107484=CARTESIAN_POINT('Ctrl Pts',(-134.057090395465,-0.169441470486786,
125.887114511925));
#107485=CARTESIAN_POINT('Ctrl Pts',(-134.064846698207,-0.306574740325703,
125.893761658885));
#107486=CARTESIAN_POINT('Ctrl Pts',(-134.072603000948,-0.443083577498728,
125.906109908808));
#107487=CARTESIAN_POINT('Ctrl Pts',(-134.080363443463,-0.579665273548354,
125.918464749363));
#107488=CARTESIAN_POINT('Ctrl Pts',(-134.088123885977,-0.715621485476006,
125.936526704555));
#107489=CARTESIAN_POINT('Ctrl Pts',(-134.095884328491,-0.850446493544069,
125.960196724373));
#107490=CARTESIAN_POINT('Ctrl Pts',(-134.103657228756,-0.985487934684285,
125.983904741408));
#107491=CARTESIAN_POINT('Ctrl Pts',(-134.111430129022,-1.11939416107169,
126.013238729349));
#107492=CARTESIAN_POINT('Ctrl Pts',(-134.119203029287,-1.25167197153181,
126.048048985831));
#107493=CARTESIAN_POINT('Ctrl Pts',(-134.126693365049,-1.37914115039364,
126.081593801808));
#107494=CARTESIAN_POINT('Ctrl Pts',(-134.134183700811,-1.50509795739489,
126.120223556209));
#107495=CARTESIAN_POINT('Ctrl Pts',(-134.141674036573,-1.62911893625768,
126.163762105087));
#107496=CARTESIAN_POINT('Ctrl Pts',(-134.149448463505,-1.75784374496744,
126.208951970763));
#107497=CARTESIAN_POINT('Ctrl Pts',(-134.157222890436,-1.88489075048452,
126.259573488805));
#107498=CARTESIAN_POINT('Ctrl Pts',(-134.164997317368,-2.0097674703886,
126.315483499904));
#107499=CARTESIAN_POINT('Ctrl Pts',(-134.172762141421,-2.13448994407502,
126.371324451632));
#107500=CARTESIAN_POINT('Ctrl Pts',(-134.180526965474,-2.25704711259141,
126.432440740749));
#107501=CARTESIAN_POINT('Ctrl Pts',(-134.188291789527,-2.37696252734415,
126.49863974806));
#107502=CARTESIAN_POINT('Ctrl Pts',(-134.196048879903,-2.49675850769784,
126.564772821907));
#107503=CARTESIAN_POINT('Ctrl Pts',(-134.203805970279,-2.61391763040504,
126.635978351813));
#107504=CARTESIAN_POINT('Ctrl Pts',(-134.211563060655,-2.7279846190288,
126.712016181813));
#107505=CARTESIAN_POINT('Ctrl Pts',(-134.219314279841,-2.84196527257224,
126.78799646026));
#107506=CARTESIAN_POINT('Ctrl Pts',(-134.227065499026,-2.9528581264867,
126.86880154271));
#107507=CARTESIAN_POINT('Ctrl Pts',(-134.234816718212,-3.0602339789941,
126.954146200639));
#107508=CARTESIAN_POINT('Ctrl Pts',(-134.242564531346,-3.16756264825349,
127.039453356299));
#107509=CARTESIAN_POINT('Ctrl Pts',(-134.25031234448,-3.27137708505586,
127.12929587644));
#107510=CARTESIAN_POINT('Ctrl Pts',(-134.258060157614,-3.37127867937868,
127.223346357825));
#107511=CARTESIAN_POINT('Ctrl Pts',(-134.265806319367,-3.47115898052738,
127.317376793151));
#107512=CARTESIAN_POINT('Ctrl Pts',(-134.273552481121,-3.56712781376811,
127.41561313775));
#107513=CARTESIAN_POINT('Ctrl Pts',(-134.281298642874,-3.6588214573347,
127.517689261034));
#107514=CARTESIAN_POINT('Ctrl Pts',(-134.2890448311,-3.75051541426831,127.619765733168));
#107515=CARTESIAN_POINT('Ctrl Pts',(-134.296791019327,-3.83793389123298,
127.725681719254));
#107516=CARTESIAN_POINT('Ctrl Pts',(-134.304537207553,-3.92075196314873,
127.835036265804));
#107517=CARTESIAN_POINT('Ctrl Pts',(-134.312285099761,-4.00358825311694,
127.944414867815));
#107518=CARTESIAN_POINT('Ctrl Pts',(-134.320032991969,-4.08182188855919,
128.057233223704));
#107519=CARTESIAN_POINT('Ctrl Pts',(-134.327780884177,-4.15517020162144,
128.173059863555));
#107520=CARTESIAN_POINT('Ctrl Pts',(-134.335536584154,-4.22859242984516,
128.289003225175));
#107521=CARTESIAN_POINT('Ctrl Pts',(-134.343292284131,-4.29711929348696,
128.40796059487));
#107522=CARTESIAN_POINT('Ctrl Pts',(-134.351047984108,-4.36051295948724,
128.52947385277));
#107523=CARTESIAN_POINT('Ctrl Pts',(-134.358807811175,-4.42394035956292,
128.651051772294));
#107524=CARTESIAN_POINT('Ctrl Pts',(-134.366567638243,-4.48222895318106,
128.775187936481));
#107525=CARTESIAN_POINT('Ctrl Pts',(-134.37432746531,-4.53518875771006,
128.901403446624));
#107526=CARTESIAN_POINT('Ctrl Pts',(-134.382098745693,-4.58822672962043,
129.027805247785));
#107527=CARTESIAN_POINT('Ctrl Pts',(-134.389870026076,-4.63592006366403,
129.156292159856));
#107528=CARTESIAN_POINT('Ctrl Pts',(-134.397641306458,-4.67812819418134,
129.286368634285));
#107529=CARTESIAN_POINT('Ctrl Pts',(-134.403488982117,-4.70988865645254,
129.384247618922));
#107530=CARTESIAN_POINT('Ctrl Pts',(-134.409336657775,-4.73854434489769,
129.483026301651));
#107531=CARTESIAN_POINT('Ctrl Pts',(-134.415184333433,-4.76405452823397,
129.582490119308));
#107532=CARTESIAN_POINT('Ctrl Pts',(-132.66500688127,-4.76405452823412,
129.582490119309));
#107533=CARTESIAN_POINT('Ctrl Pts',(-132.672705270541,-4.79787842028983,
129.714368961085));
#107534=CARTESIAN_POINT('Ctrl Pts',(-132.680403659813,-4.82619617847106,
129.847552223936));
#107535=CARTESIAN_POINT('Ctrl Pts',(-132.688102049085,-4.84893225451799,
129.981536788551));
#107536=CARTESIAN_POINT('Ctrl Pts',(-132.695941801563,-4.87208582628908,
130.117981671415));
#107537=CARTESIAN_POINT('Ctrl Pts',(-132.703781554041,-4.88945067006474,
130.255257139546));
#107538=CARTESIAN_POINT('Ctrl Pts',(-132.71162130652,-4.90100241562209,
130.392828863546));
#107539=CARTESIAN_POINT('Ctrl Pts',(-132.719461058998,-4.91255416117943,
130.530400587546));
#107540=CARTESIAN_POINT('Ctrl Pts',(-132.727300811476,-4.91829285496466,
130.668268136608));
#107541=CARTESIAN_POINT('Ctrl Pts',(-132.735140563954,-4.9182497588907,
130.805900640808));
#107542=CARTESIAN_POINT('',(-132.389859436048,-4.9182488482065,130.807726566983));
#107543=CARTESIAN_POINT('Ctrl Pts',(-132.320008282756,-4.76405452823418,
129.582490119309));
#107544=CARTESIAN_POINT('Ctrl Pts',(-132.327791281343,-4.79830572555041,
129.71603501781));
#107545=CARTESIAN_POINT('Ctrl Pts',(-132.33557427993,-4.826953306866,129.851082946797));
#107546=CARTESIAN_POINT('Ctrl Pts',(-132.343357278516,-4.84987753848702,
129.987126915263));
#107547=CARTESIAN_POINT('Ctrl Pts',(-132.351139968801,-4.87280086202732,
130.12316549472));
#107548=CARTESIAN_POINT('Ctrl Pts',(-132.358922659086,-4.89000121271092,
130.2601996569));
#107549=CARTESIAN_POINT('Ctrl Pts',(-132.366705349371,-4.90141004073329,
130.397712520191));
#107550=CARTESIAN_POINT('Ctrl Pts',(-132.374423378245,-4.91272408007915,
130.534082876794));
#107551=CARTESIAN_POINT('Ctrl Pts',(-132.382141407119,-4.91834247332233,
130.670923633975));
#107552=CARTESIAN_POINT('Ctrl Pts',(-132.389859435993,-4.91824884820717,
130.807726566));
#107553=CARTESIAN_POINT('Ctrl Pts',(-132.389859436049,-4.9182488482065,
130.807726566983));
#107554=CARTESIAN_POINT('Ctrl Pts',(-132.398671358528,-4.91814195336178,
130.963918886508));
#107555=CARTESIAN_POINT('Ctrl Pts',(-132.407483281008,-4.91059060283849,
131.119819610132));
#107556=CARTESIAN_POINT('Ctrl Pts',(-132.416295203488,-4.89570197311823,
131.274770282546));
#107557=CARTESIAN_POINT('Ctrl Pts',(-132.425145933195,-4.88074777468338,
131.430403349283));
#107558=CARTESIAN_POINT('Ctrl Pts',(-132.433996662901,-4.85839163980709,
131.585077814765));
#107559=CARTESIAN_POINT('Ctrl Pts',(-132.442847392608,-4.82879182031729,
131.73814464963));
#107560=CARTESIAN_POINT('Ctrl Pts',(-132.451750270414,-4.79901760002992,
131.892113347362));
#107561=CARTESIAN_POINT('Ctrl Pts',(-132.460653148219,-4.76191417788455,
132.044455252463));
#107562=CARTESIAN_POINT('Ctrl Pts',(-132.469556026025,-4.71769122469761,
132.194530596709));
#107563=CARTESIAN_POINT('Ctrl Pts',(-132.476563113968,-4.68288516211224,
132.312648710673));
#107564=CARTESIAN_POINT('Ctrl Pts',(-132.483570201912,-4.64366980231781,
132.429363166074));
#107565=CARTESIAN_POINT('Ctrl Pts',(-132.490577289855,-4.60016777226407,
132.544371976587));
#107566=CARTESIAN_POINT('Ctrl Pts',(-132.498351623974,-4.55190245588252,
132.671973760211));
#107567=CARTESIAN_POINT('Ctrl Pts',(-132.506125958093,-4.49824744275542,
132.797767922314));
#107568=CARTESIAN_POINT('Ctrl Pts',(-132.513900292213,-4.43935766333605,
132.921265575158));
#107569=CARTESIAN_POINT('Ctrl Pts',(-132.52166504516,-4.38054046030684,
133.044611028183));
#107570=CARTESIAN_POINT('Ctrl Pts',(-132.529429798107,-4.31650149397504,
133.165665253779));
#107571=CARTESIAN_POINT('Ctrl Pts',(-132.537194551054,-4.24744475510768,
133.283956575541));
#107572=CARTESIAN_POINT('Ctrl Pts',(-132.544951591939,-4.1784566043667,
133.402130408696));
#107573=CARTESIAN_POINT('Ctrl Pts',(-132.552708632824,-4.10446079475703,
133.517546463555));
#107574=CARTESIAN_POINT('Ctrl Pts',(-132.560465673709,-4.02570833253192,
133.629755365895));
#107575=CARTESIAN_POINT('Ctrl Pts',(-132.568216864949,-3.94701525815128,
133.741879650628));
#107576=CARTESIAN_POINT('Ctrl Pts',(-132.57596805619,-3.863572894608,133.850801278078));
#107577=CARTESIAN_POINT('Ctrl Pts',(-132.58371924743,-3.77567668347278,
133.95609801849));
#107578=CARTESIAN_POINT('Ctrl Pts',(-132.591467144207,-3.68781783057211,
134.061350004977));
#107579=CARTESIAN_POINT('Ctrl Pts',(-132.599215040984,-3.59550914513596,
134.162979869197));
#107580=CARTESIAN_POINT('Ctrl Pts',(-132.606962937761,-3.49908751153531,
134.260596959184));
#107581=CARTESIAN_POINT('Ctrl Pts',(-132.614709213846,-3.4026860472618,
134.358193629779));
#107582=CARTESIAN_POINT('Ctrl Pts',(-132.62245548993,-3.30217362065905,
134.451778917749));
#107583=CARTESIAN_POINT('Ctrl Pts',(-132.630201766014,-3.19792500132062,
134.540997975998));
#107584=CARTESIAN_POINT('Ctrl Pts',(-132.637948099279,-3.09367561244242,
134.630217692841));
#107585=CARTESIAN_POINT('Ctrl Pts',(-132.645694432545,-2.98569027283076,
134.715070861438));
#107586=CARTESIAN_POINT('Ctrl Pts',(-132.65344076581,-2.87437764088469,
134.795242254508));
#107587=CARTESIAN_POINT('Ctrl Pts',(-132.661188833813,-2.76304008124663,
134.875431601406));
#107588=CARTESIAN_POINT('Ctrl Pts',(-132.668936901816,-2.64837406374902,
134.950936858034));
#107589=CARTESIAN_POINT('Ctrl Pts',(-132.676684969819,-2.53081774777548,
135.021485774595));
#107590=CARTESIAN_POINT('Ctrl Pts',(-132.684441272561,-2.41313649155023,
135.092109671384));
#107591=CARTESIAN_POINT('Ctrl Pts',(-132.692197575303,-2.29255913627593,
135.15776650389));
#107592=CARTESIAN_POINT('Ctrl Pts',(-132.699953878045,-2.16954948694773,
135.218229451841));
#107593=CARTESIAN_POINT('Ctrl Pts',(-132.707714320559,-2.04647418366593,
135.278724670688));
#107594=CARTESIAN_POINT('Ctrl Pts',(-132.715474763074,-1.92096435718586,
135.334020323721));
#107595=CARTESIAN_POINT('Ctrl Pts',(-132.723235205588,-1.7935034448138,
135.383937940414));
#107596=CARTESIAN_POINT('Ctrl Pts',(-132.731008105853,-1.66583792086975,
135.433935689297));
#107597=CARTESIAN_POINT('Ctrl Pts',(-132.738781006119,-1.53621542209145,
135.478538022471));
#107598=CARTESIAN_POINT('Ctrl Pts',(-132.746553906385,-1.40513504251891,
135.517616241313));
#107599=CARTESIAN_POINT('Ctrl Pts',(-132.754044242146,-1.27881976492886,
135.555273868464));
#107600=CARTESIAN_POINT('Ctrl Pts',(-132.761534577907,-1.15115106007221,
135.587801963274));
#107601=CARTESIAN_POINT('Ctrl Pts',(-132.769024913668,-1.02258221022359,
135.615130689585));
#107602=CARTESIAN_POINT('Ctrl Pts',(-132.776799247787,-0.889138633341971,
135.643495592864));
#107603=CARTESIAN_POINT('Ctrl Pts',(-132.784573581907,-0.754302596898488,
135.66634892804));
#107604=CARTESIAN_POINT('Ctrl Pts',(-132.792347916026,-0.618569159687465,
135.68355678673));
#107605=CARTESIAN_POINT('Ctrl Pts',(-132.800112668973,-0.483003001806959,
135.700743438271));
#107606=CARTESIAN_POINT('Ctrl Pts',(-132.80787742192,-0.346542027839381,
135.712298408067));
#107607=CARTESIAN_POINT('Ctrl Pts',(-132.815642174867,-0.209693334494366,
135.718138366709));
#107608=CARTESIAN_POINT('Ctrl Pts',(-132.823399215752,-0.0729805612011811,
135.723972525021));
#107609=CARTESIAN_POINT('Ctrl Pts',(-132.831156256637,0.0641187770441665,
135.724102951571));
#107610=CARTESIAN_POINT('Ctrl Pts',(-132.838913297522,0.201090933970913,
135.718497927285));
#107611=CARTESIAN_POINT('Ctrl Pts',(-132.846664488762,0.33795979912882,
135.712897129792));
#107612=CARTESIAN_POINT('Ctrl Pts',(-132.854415680002,0.474701284810364,
135.701569506328));
#107613=CARTESIAN_POINT('Ctrl Pts',(-132.862166871242,0.610800463778589,
135.684535394759));
#107614=CARTESIAN_POINT('Ctrl Pts',(-132.86991476802,0.746841796965374,
135.667508523141));
#107615=CARTESIAN_POINT('Ctrl Pts',(-132.877662664797,0.882240979283709,
135.644780035825));
#107616=CARTESIAN_POINT('Ctrl Pts',(-132.885410561574,1.01648724993869,
135.616422206242));
#107617=CARTESIAN_POINT('Ctrl Pts',(-132.893156837658,1.15070543916787,
135.588070308506));
#107618=CARTESIAN_POINT('Ctrl Pts',(-132.900903113742,1.28377081414098,
135.554091491442));
#107619=CARTESIAN_POINT('Ctrl Pts',(-132.908649389826,1.4151822598264,135.514609255799));
#107620=CARTESIAN_POINT('Ctrl Pts',(-132.916395723091,1.54659467556108,
135.475126728707));
#107621=CARTESIAN_POINT('Ctrl Pts',(-132.924142056357,1.67635276321543,
135.430140814469));
#107622=CARTESIAN_POINT('Ctrl Pts',(-132.931888389622,1.80397042330583,
135.379824940926));
#107623=CARTESIAN_POINT('Ctrl Pts',(-132.939636457625,1.93161666248619,
135.329497799492));
#107624=CARTESIAN_POINT('Ctrl Pts',(-132.947384525628,2.05712115663699,
135.273838466987));
#107625=CARTESIAN_POINT('Ctrl Pts',(-132.955132593631,2.18001801844423,
135.213068421646));
#107626=CARTESIAN_POINT('Ctrl Pts',(-132.962888896373,2.30304549649886,
135.152233789178));
#107627=CARTESIAN_POINT('Ctrl Pts',(-132.970645199115,2.42345945497546,
135.086277766985));
#107628=CARTESIAN_POINT('Ctrl Pts',(-132.978401501857,2.54081836562543,
135.01546796545));
#107629=CARTESIAN_POINT('Ctrl Pts',(-132.986161944371,2.65823991425993,
134.944620370591));
#107630=CARTESIAN_POINT('Ctrl Pts',(-132.993922386885,2.7726028401708,134.868914050087));
#107631=CARTESIAN_POINT('Ctrl Pts',(-133.001682829399,2.88349568137793,
134.788659265757));
#107632=CARTESIAN_POINT('Ctrl Pts',(-133.009455729665,2.99456653761808,
134.708275649323));
#107633=CARTESIAN_POINT('Ctrl Pts',(-133.01722862993,3.10215587051635,134.623329220555));
#107634=CARTESIAN_POINT('Ctrl Pts',(-133.025001530196,3.20588562975594,
134.534170316656));
#107635=CARTESIAN_POINT('Ctrl Pts',(-133.032491865957,3.30584455096627,
134.448252563492));
#107636=CARTESIAN_POINT('Ctrl Pts',(-133.039982201719,3.40221941183791,
134.358423496111));
#107637=CARTESIAN_POINT('Ctrl Pts',(-133.047472537481,3.49470644709292,
134.265026725579));
#107638=CARTESIAN_POINT('Ctrl Pts',(-133.0552468716,3.59070015640142,134.168088788104));
#107639=CARTESIAN_POINT('Ctrl Pts',(-133.063021205719,3.68280948577632,
134.067000197776));
#107640=CARTESIAN_POINT('Ctrl Pts',(-133.070795539838,3.77065418292927,
133.962105080827));
#107641=CARTESIAN_POINT('Ctrl Pts',(-133.078560292785,3.85839061934412,
133.857339237735));
#107642=CARTESIAN_POINT('Ctrl Pts',(-133.086325045733,3.94187263236082,
133.748776498982));
#107643=CARTESIAN_POINT('Ctrl Pts',(-133.09408979868,4.02075601643018,133.636798457809));
#107644=CARTESIAN_POINT('Ctrl Pts',(-133.101846839565,4.09956105241042,
133.524931634806));
#107645=CARTESIAN_POINT('Ctrl Pts',(-133.10960388045,4.17377632512013,133.409656577421));
#107646=CARTESIAN_POINT('Ctrl Pts',(-133.117360921335,4.24309745599594,
133.291388370009));
#107647=CARTESIAN_POINT('Ctrl Pts',(-133.125112112575,4.31236631126763,
133.173209349572));
#107648=CARTESIAN_POINT('Ctrl Pts',(-133.132863303815,4.37674817393998,
133.052042007774));
#107649=CARTESIAN_POINT('Ctrl Pts',(-133.140614495055,4.43598182408496,
132.928330560594));
#107650=CARTESIAN_POINT('Ctrl Pts',(-133.148362391832,4.4951902983486,132.80467169408));
#107651=CARTESIAN_POINT('Ctrl Pts',(-133.156110288609,4.54925474361721,
132.678471224723));
#107652=CARTESIAN_POINT('Ctrl Pts',(-133.163858185386,4.59795988689043,
132.550197935602));
#107653=CARTESIAN_POINT('Ctrl Pts',(-133.17160446147,4.6466548420975,132.421951478488));
#107654=CARTESIAN_POINT('Ctrl Pts',(-133.179350737554,4.68999258644652,
132.291633429314));
#107655=CARTESIAN_POINT('Ctrl Pts',(-133.187097013639,4.727806159701,132.159732145522));
#107656=CARTESIAN_POINT('Ctrl Pts',(-133.194843346904,4.76562001208673,
132.027829888064));
#107657=CARTESIAN_POINT('Ctrl Pts',(-133.202589680169,4.79790950426581,
131.894344748493));
#107658=CARTESIAN_POINT('Ctrl Pts',(-133.210336013434,4.82455779734822,
131.759779438056));
#107659=CARTESIAN_POINT('Ctrl Pts',(-133.218084081437,4.85121205813113,
131.62518399265));
#107660=CARTESIAN_POINT('Ctrl Pts',(-133.225832149441,4.8722225300475,131.489508278476));
#107661=CARTESIAN_POINT('Ctrl Pts',(-133.233580217444,4.88752372553465,
131.35326397412));
#107662=CARTESIAN_POINT('Ctrl Pts',(-133.241336520185,4.90284118331442,
131.216874867696));
#107663=CARTESIAN_POINT('Ctrl Pts',(-133.249092822927,4.91243719970382,
131.079916353069));
#107664=CARTESIAN_POINT('Ctrl Pts',(-133.256849125669,4.91629826609137,
130.942904550407));
#107665=CARTESIAN_POINT('Ctrl Pts',(-133.264609568183,4.92016139324633,
130.80581962042));
#107666=CARTESIAN_POINT('Ctrl Pts',(-133.272370010697,4.91828347661674,
130.668681736463));
#107667=CARTESIAN_POINT('Ctrl Pts',(-133.280130453212,4.9107031430074,130.532004777245));
#107668=CARTESIAN_POINT('Ctrl Pts',(-133.287903353477,4.90311064077362,
130.395108412038));
#107669=CARTESIAN_POINT('Ctrl Pts',(-133.295676253742,4.88979746689118,
130.258674839502));
#107670=CARTESIAN_POINT('Ctrl Pts',(-133.303449154008,4.87085402453883,
130.12321148989));
#107671=CARTESIAN_POINT('Ctrl Pts',(-133.31093948977,4.85259922403123,129.992672574245));
#107672=CARTESIAN_POINT('Ctrl Pts',(-133.318429825532,4.8291164519392,129.863034869194));
#107673=CARTESIAN_POINT('Ctrl Pts',(-133.325920161294,4.80053060543232,
129.734739671245));
#107674=CARTESIAN_POINT('Ctrl Pts',(-133.333694495413,4.77086091786727,
129.601580121875));
#107675=CARTESIAN_POINT('Ctrl Pts',(-133.341468829533,4.73559956626961,
129.469445082101));
#107676=CARTESIAN_POINT('Ctrl Pts',(-133.349243163652,4.69483053813357,
129.338840477579));
#107677=CARTESIAN_POINT('Ctrl Pts',(-133.357007916599,4.65411175418109,
129.208396831559));
#107678=CARTESIAN_POINT('Ctrl Pts',(-133.364772669546,4.60789891460797,
129.079480237585));
#107679=CARTESIAN_POINT('Ctrl Pts',(-133.372537422493,4.55632701310982,
128.952586546005));
#107680=CARTESIAN_POINT('Ctrl Pts',(-133.380294463378,4.50480633355128,
128.825818887028));
#107681=CARTESIAN_POINT('Ctrl Pts',(-133.388051504263,4.44793733072271,
128.701070491945));
#107682=CARTESIAN_POINT('Ctrl Pts',(-133.395808545148,4.38590470279817,
128.578821806295));
#107683=CARTESIAN_POINT('Ctrl Pts',(-133.403559736388,4.3239188541608,128.45666530933));
#107684=CARTESIAN_POINT('Ctrl Pts',(-133.411310927628,4.25677730725702,
128.337005116955));
#107685=CARTESIAN_POINT('Ctrl Pts',(-133.419062118868,4.18471259782026,
128.220301110483));
#107686=CARTESIAN_POINT('Ctrl Pts',(-133.426810015645,4.11267851780731,
128.103646706327));
#107687=CARTESIAN_POINT('Ctrl Pts',(-133.434557912422,4.03572564201934,
127.989946321033));
#107688=CARTESIAN_POINT('Ctrl Pts',(-133.442305809199,3.95413201062122,
127.879634458576));
#107689=CARTESIAN_POINT('Ctrl Pts',(-133.450052085284,3.87255544685205,
127.769345670983));
#107690=CARTESIAN_POINT('Ctrl Pts',(-133.457798361368,3.78634029068704,
127.6624443105));
#107691=CARTESIAN_POINT('Ctrl Pts',(-133.465544637452,3.69580716498571,
127.559334814627));
#107692=CARTESIAN_POINT('Ctrl Pts',(-133.473290970717,3.6052733709893,127.456224557623));
#107693=CARTESIAN_POINT('Ctrl Pts',(-133.481037303983,3.51042180180978,
127.356906514873));
#107694=CARTESIAN_POINT('Ctrl Pts',(-133.488783637248,3.41161224838277,
127.261750713952));
#107695=CARTESIAN_POINT('Ctrl Pts',(-133.496531705251,3.31278056724151,
127.166573603549));
#107696=CARTESIAN_POINT('Ctrl Pts',(-133.504279773254,3.20998941965065,
127.075560860904));
#107697=CARTESIAN_POINT('Ctrl Pts',(-133.512027841257,3.1036338976697,126.989044157332));
#107698=CARTESIAN_POINT('Ctrl Pts',(-133.519784143999,2.9971653397742,126.902435502777));
#107699=CARTESIAN_POINT('Ctrl Pts',(-133.527540446741,2.88712514380574,
126.820332679862));
#107700=CARTESIAN_POINT('Ctrl Pts',(-133.535296749483,2.77394023454401,
126.743026029321));
#107701=CARTESIAN_POINT('Ctrl Pts',(-133.543057191997,2.66069491508827,
126.665678117892));
#107702=CARTESIAN_POINT('Ctrl Pts',(-133.550817634511,2.5443018695595,126.593131686281));
#107703=CARTESIAN_POINT('Ctrl Pts',(-133.558578077025,2.42521431740076,
126.525632000655));
#107704=CARTESIAN_POINT('Ctrl Pts',(-133.56635097729,2.3059355953312,126.458023958541));
#107705=CARTESIAN_POINT('Ctrl Pts',(-133.574123877556,2.18395407108092,
126.395479030246));
#107706=CARTESIAN_POINT('Ctrl Pts',(-133.581896777821,2.05974552521942,
126.338195435462));
#107707=CARTESIAN_POINT('Ctrl Pts',(-133.589387113583,1.94005227286277,
126.282994243637));
#107708=CARTESIAN_POINT('Ctrl Pts',(-133.596877449345,1.81829138816176,
126.232678618709));
#107709=CARTESIAN_POINT('Ctrl Pts',(-133.604367785107,1.69490165633622,
126.187382012694));
#107710=CARTESIAN_POINT('Ctrl Pts',(-133.612142119226,1.56683356532517,
126.140367972094));
#107711=CARTESIAN_POINT('Ctrl Pts',(-133.619916453345,1.43660499226052,
126.098612129271));
#107712=CARTESIAN_POINT('Ctrl Pts',(-133.627690787465,1.30468698401493,
126.062317288342));
#107713=CARTESIAN_POINT('Ctrl Pts',(-133.635455540412,1.17293155292466,
126.02606717756));
#107714=CARTESIAN_POINT('Ctrl Pts',(-133.643220293359,1.03949120270712,
125.995264780303));
#107715=CARTESIAN_POINT('Ctrl Pts',(-133.650985046306,0.904856073691232,
125.970064541775));
#107716=CARTESIAN_POINT('Ctrl Pts',(-133.658742087191,0.77035466618351,
125.94488933248));
#107717=CARTESIAN_POINT('Ctrl Pts',(-133.666499128076,0.634661223211319,
125.925305280483));
#107718=CARTESIAN_POINT('Ctrl Pts',(-133.674256168961,0.498279791087177,
125.911416686527));
#107719=CARTESIAN_POINT('Ctrl Pts',(-133.682007360201,0.362001205261707,
125.897538566068));
#107720=CARTESIAN_POINT('Ctrl Pts',(-133.689758551441,0.225036050339748,
125.889347394184));
#107721=CARTESIAN_POINT('Ctrl Pts',(-133.697509742681,0.0878969287371864,
125.88689610906));
#107722=CARTESIAN_POINT('Ctrl Pts',(-133.705257639458,-0.0491839050802019,
125.884445865797));
#107723=CARTESIAN_POINT('Ctrl Pts',(-133.713005536235,-0.186438168431842,
125.887730664078));
#107724=CARTESIAN_POINT('Ctrl Pts',(-133.720753433012,-0.323350013316159,
125.89675144085));
#107725=CARTESIAN_POINT('Ctrl Pts',(-133.728499709096,-0.460233219194004,
125.90577033067));
#107726=CARTESIAN_POINT('Ctrl Pts',(-133.73624598518,-0.596773759201507,
125.920522786739));
#107727=CARTESIAN_POINT('Ctrl Pts',(-133.743992261264,-0.732458064127735,
125.940957668314));
#107728=CARTESIAN_POINT('Ctrl Pts',(-133.75173859453,-0.868143370644494,
125.961392700734));
#107729=CARTESIAN_POINT('Ctrl Pts',(-133.759484927795,-1.00297204286255,
125.987510184136));
#107730=CARTESIAN_POINT('Ctrl Pts',(-133.76723126106,-1.13643829031373,
126.019207425158));
#107731=CARTESIAN_POINT('Ctrl Pts',(-133.774979329063,-1.26993442660582,
126.050911764558));
#107732=CARTESIAN_POINT('Ctrl Pts',(-133.782727397066,-1.40206715069408,
126.088198257713));
#107733=CARTESIAN_POINT('Ctrl Pts',(-133.790475465069,-1.53234386119818,
126.130913778931));
#107734=CARTESIAN_POINT('Ctrl Pts',(-133.798231767811,-1.6627590313407,
126.173674698713));
#107735=CARTESIAN_POINT('Ctrl Pts',(-133.805988070553,-1.7913138753339,
126.221876050823));
#107736=CARTESIAN_POINT('Ctrl Pts',(-133.813744373295,-1.91753335802306,
126.27531558761));
#107737=CARTESIAN_POINT('Ctrl Pts',(-133.821504815809,-2.04382020785053,
126.328783646687));
#107738=CARTESIAN_POINT('Ctrl Pts',(-133.829265258323,-2.1677688595534,
126.387495293981));
#107739=CARTESIAN_POINT('Ctrl Pts',(-133.837025700837,-2.2889279875775,
126.451201795494));
#107740=CARTESIAN_POINT('Ctrl Pts',(-133.844798601102,-2.4102816109899,
126.515010564339));
#107741=CARTESIAN_POINT('Ctrl Pts',(-133.852571501368,-2.52883642395021,
126.583830013898));
#107742=CARTESIAN_POINT('Ctrl Pts',(-133.860344401633,-2.64416848759839,
126.657366999089));
#107743=CARTESIAN_POINT('Ctrl Pts',(-133.867834737396,-2.75530794023309,
126.728230729642));
#107744=CARTESIAN_POINT('Ctrl Pts',(-133.875325073158,-2.86345463285709,
126.80347478609));
#107745=CARTESIAN_POINT('Ctrl Pts',(-133.88281540892,-2.96825911438144,
126.882802140074));
#107746=CARTESIAN_POINT('Ctrl Pts',(-133.890603016867,-3.07722301654917,
126.965277792956));
#107747=CARTESIAN_POINT('Ctrl Pts',(-133.898390624814,-3.18293962587666,
127.052444551435));
#107748=CARTESIAN_POINT('Ctrl Pts',(-133.906178232761,-3.28497285252097,
127.144014128407));
#107749=CARTESIAN_POINT('Ctrl Pts',(-133.913859423379,-3.38561179948952,
127.234332411028));
#107750=CARTESIAN_POINT('Ctrl Pts',(-133.921540613997,-3.48266705776343,
127.328933697929));
#107751=CARTESIAN_POINT('Ctrl Pts',(-133.929221804614,-3.57574876308413,
127.427497599053));
#107752=CARTESIAN_POINT('Ctrl Pts',(-133.936896001566,-3.66874571821173,
127.525971758486));
#107753=CARTESIAN_POINT('Ctrl Pts',(-133.944570198517,-3.7577760417264,
127.628401069164));
#107754=CARTESIAN_POINT('Ctrl Pts',(-133.952244395468,-3.84248420284421,
127.734426055822));
#107755=CARTESIAN_POINT('Ctrl Pts',(-133.959913353601,-3.92713453762649,
127.840378664134));
#107756=CARTESIAN_POINT('Ctrl Pts',(-133.967582311734,-4.0074683300128,
127.949921754922));
#107757=CARTESIAN_POINT('Ctrl Pts',(-133.975251269866,-4.08316844507548,
128.062660686567));
#107758=CARTESIAN_POINT('Ctrl Pts',(-133.983123497348,-4.1608750273593,
128.17838781672));
#107759=CARTESIAN_POINT('Ctrl Pts',(-133.99099572483,-4.23369857512685,
128.297482249238));
#107760=CARTESIAN_POINT('Ctrl Pts',(-133.998867952312,-4.30134172047524,
128.419482745179));
#107761=CARTESIAN_POINT('Ctrl Pts',(-134.006532799929,-4.36720292718514,
128.538269354533));
#107762=CARTESIAN_POINT('Ctrl Pts',(-134.014197647547,-4.42815306647365,
128.659810455679));
#107763=CARTESIAN_POINT('Ctrl Pts',(-134.021862495164,-4.48396325040901,
128.783653654278));
#107764=CARTESIAN_POINT('Ctrl Pts',(-134.029838412578,-4.54203843209047,
128.912522899127));
#107765=CARTESIAN_POINT('Ctrl Pts',(-134.037814329992,-4.59454745370409,
129.043884623148));
#107766=CARTESIAN_POINT('Ctrl Pts',(-134.045790247406,-4.64128732456252,
129.177205113825));
#107767=CARTESIAN_POINT('Ctrl Pts',(-134.05376616482,-4.68802719542096,
129.310525604502));
#107768=CARTESIAN_POINT('Ctrl Pts',(-134.061742082235,-4.72899778085758,
129.445804393348));
#107769=CARTESIAN_POINT('Ctrl Pts',(-134.069717999649,-4.76405452823413,
129.582490119309));
#107770=CARTESIAN_POINT('Origin',(213.235140564004,0.,130.804360617566));
#107771=CARTESIAN_POINT('',(-136.165410316754,-4.76405452823394,129.582490119308));
#107772=CARTESIAN_POINT('',(-135.819866485249,-4.76405452823408,129.582490119308));
#107773=CARTESIAN_POINT('',(213.235140564004,-4.76405452823405,129.582490119308));
#107774=CARTESIAN_POINT('',(-134.485140563972,-4.91824790082115,130.799816547985));
#107775=CARTESIAN_POINT('Ctrl Pts',(-134.48514056401,-4.91824790082178,
130.799816548665));
#107776=CARTESIAN_POINT('Ctrl Pts',(-134.492797749234,-4.9183727917618,
130.934991568447));
#107777=CARTESIAN_POINT('Ctrl Pts',(-134.500454934458,-4.91292068941301,
131.070323998656));
#107778=CARTESIAN_POINT('Ctrl Pts',(-134.508112119682,-4.90187949338597,
131.205310109176));
#107779=CARTESIAN_POINT('Ctrl Pts',(-134.51604783487,-4.89043667406738,
131.345206336851));
#107780=CARTESIAN_POINT('Ctrl Pts',(-134.523983550059,-4.87299040046864,
131.484730136805));
#107781=CARTESIAN_POINT('Ctrl Pts',(-134.531919265247,-4.84958633597631,
131.623320587535));
#107782=CARTESIAN_POINT('Ctrl Pts',(-134.539568234451,-4.82702794466393,
131.75690326591));
#107783=CARTESIAN_POINT('Ctrl Pts',(-134.547217203656,-4.79893490755988,
131.889618442244));
#107784=CARTESIAN_POINT('Ctrl Pts',(-134.55486617286,-4.76540082329047,
132.020969862921));
#107785=CARTESIAN_POINT('Ctrl Pts',(-134.562514109117,-4.73187126759849,
132.152303545374));
#107786=CARTESIAN_POINT('Ctrl Pts',(-134.570162045374,-4.69290222506853,
132.28227344903));
#107787=CARTESIAN_POINT('Ctrl Pts',(-134.577809981631,-4.64863799249533,
132.410395448206));
#107788=CARTESIAN_POINT('Ctrl Pts',(-134.585458641586,-4.60436957134925,
132.538529571129));
#107789=CARTESIAN_POINT('Ctrl Pts',(-134.593107301541,-4.55480509528288,
132.66481506206));
#107790=CARTESIAN_POINT('Ctrl Pts',(-134.600755961495,-4.50013794097112,
132.788785364119));
#107791=CARTESIAN_POINT('Ctrl Pts',(-134.608407102135,-4.44545305649669,
132.912795873386));
#107792=CARTESIAN_POINT('Ctrl Pts',(-134.616058242775,-4.38566236507843,
133.034489333225));
#107793=CARTESIAN_POINT('Ctrl Pts',(-134.623709383415,-4.32100610677341,
133.153421980691));
#107794=CARTESIAN_POINT('Ctrl Pts',(-134.631368842986,-4.25627954901759,
133.272483941236));
#107795=CARTESIAN_POINT('Ctrl Pts',(-134.639028302557,-4.18667705819371,
133.388778745395));
#107796=CARTESIAN_POINT('Ctrl Pts',(-134.646687762129,-4.11248341754616,
133.5018897097));
#107797=CARTESIAN_POINT('Ctrl Pts',(-134.654352181613,-4.03824173251984,
133.615073919446));
#107798=CARTESIAN_POINT('Ctrl Pts',(-134.662016601097,-3.95940321316816,
133.725069860044));
#107799=CARTESIAN_POINT('Ctrl Pts',(-134.669681020581,-3.87629334941419,
133.831493408143));
#107800=CARTESIAN_POINT('Ctrl Pts',(-134.677356166266,-3.79306717507348,
133.938065893862));
#107801=CARTESIAN_POINT('Ctrl Pts',(-134.685031311951,-3.70555798788263,
134.041055707016));
#107802=CARTESIAN_POINT('Ctrl Pts',(-134.692706457636,-3.61412870578418,
134.140114919149));
#107803=CARTESIAN_POINT('Ctrl Pts',(-134.694660733157,-3.59084862547951,
134.165337761989));
#107804=CARTESIAN_POINT('Ctrl Pts',(-134.696615008678,-3.56731456141368,
134.190305973104));
#107805=CARTESIAN_POINT('Ctrl Pts',(-134.698569284199,-3.54353284044415,
134.215014231053));
#107806=CARTESIAN_POINT('Ctrl Pts',(-134.706343618318,-3.44892640303954,
134.313306539758));
#107807=CARTESIAN_POINT('Ctrl Pts',(-134.714117952437,-3.35007729366011,
134.407815191358));
#107808=CARTESIAN_POINT('Ctrl Pts',(-134.721892286556,-3.24732041443052,
134.498151784988));
#107809=CARTESIAN_POINT('Ctrl Pts',(-134.729657039504,-3.14469017387093,
134.58837704684));
#107810=CARTESIAN_POINT('Ctrl Pts',(-134.737421792451,-3.03816203663097,
134.674440225489));
#107811=CARTESIAN_POINT('Ctrl Pts',(-134.745186545398,-2.9281092260801,
134.755988057324));
#107812=CARTESIAN_POINT('Ctrl Pts',(-134.752943586283,-2.81816572153215,
134.837454894702));
#107813=CARTESIAN_POINT('Ctrl Pts',(-134.760700627168,-2.70470482242719,
134.914415078776));
#107814=CARTESIAN_POINT('Ctrl Pts',(-134.768457668053,-2.58813418933842,
134.986554357755));
#107815=CARTESIAN_POINT('Ctrl Pts',(-134.776208859293,-2.4716514630707,
135.058639235943));
#107816=CARTESIAN_POINT('Ctrl Pts',(-134.783960050533,-2.35206400165679,
135.125910240338));
#107817=CARTESIAN_POINT('Ctrl Pts',(-134.791711241773,-2.22980962459591,
135.188095566278));
#107818=CARTESIAN_POINT('Ctrl Pts',(-134.79945913855,-2.10760720890669,
135.250254461795));
#107819=CARTESIAN_POINT('Ctrl Pts',(-134.807207035327,-1.98274047978162,
135.307331801131));
#107820=CARTESIAN_POINT('Ctrl Pts',(-134.814954932104,-1.85567291934199,
135.359101123777));
#107821=CARTESIAN_POINT('Ctrl Pts',(-134.822701208188,-1.72863193869674,
135.410859617397));
#107822=CARTESIAN_POINT('Ctrl Pts',(-134.830447484273,-1.59939140427053,
135.4573121554));
#107823=CARTESIAN_POINT('Ctrl Pts',(-134.838193760357,-1.46843552628352,
135.498280106399));
#107824=CARTESIAN_POINT('Ctrl Pts',(-134.845940093622,-1.33747868160979,
135.539248359814));
#107825=CARTESIAN_POINT('Ctrl Pts',(-134.853686426887,-1.20480684124116,
135.574731828708));
#107826=CARTESIAN_POINT('Ctrl Pts',(-134.861432760153,-1.07091976784501,
135.604601644154));
#107827=CARTESIAN_POINT('Ctrl Pts',(-134.869180828156,-0.937002711367266,
135.634478148738));
#107828=CARTESIAN_POINT('Ctrl Pts',(-134.876928896159,-0.801870261840225,
135.658738413198));
#107829=CARTESIAN_POINT('Ctrl Pts',(-134.884676964162,-0.666032378979198,
135.677304689957));
#107830=CARTESIAN_POINT('Ctrl Pts',(-134.892433266904,-0.53005012599959,
135.695890699176));
#107831=CARTESIAN_POINT('Ctrl Pts',(-134.900189569645,-0.393361329975081,
135.708770578864));
#107832=CARTESIAN_POINT('Ctrl Pts',(-134.907945872387,-0.256481638273815,
135.715918438841));
#107833=CARTESIAN_POINT('Ctrl Pts',(-134.915706314901,-0.11952888975972,
135.723070113846));
#107834=CARTESIAN_POINT('Ctrl Pts',(-134.923466757416,0.0176145666959897,
135.724483669094));
#107835=CARTESIAN_POINT('Ctrl Pts',(-134.93122719993,0.154434073432016,
135.720185388595));
#107836=CARTESIAN_POINT('Ctrl Pts',(-134.939000100195,0.291473214986519,
135.715880208115));
#107837=CARTESIAN_POINT('Ctrl Pts',(-134.946773000461,0.428186977489429,
135.705844897649));
#107838=CARTESIAN_POINT('Ctrl Pts',(-134.954545900726,0.564065907387949,
135.690157657418));
#107839=CARTESIAN_POINT('Ctrl Pts',(-134.962036236488,0.695005295926288,
135.675040687882));
#107840=CARTESIAN_POINT('Ctrl Pts',(-134.96952657225,0.825169190298912,
135.654675625719));
#107841=CARTESIAN_POINT('Ctrl Pts',(-134.977016908012,0.954113423894353,
135.629176742233));
#107842=CARTESIAN_POINT('Ctrl Pts',(-134.984791242131,1.08794661729813,
135.602711060829));
#107843=CARTESIAN_POINT('Ctrl Pts',(-134.99256557625,1.22088978065673,135.570630740247));
#107844=CARTESIAN_POINT('Ctrl Pts',(-135.000339910369,1.35243511854286,
135.533007602977));
#107845=CARTESIAN_POINT('Ctrl Pts',(-135.008104663316,1.48381833855659,
135.49543083286));
#107846=CARTESIAN_POINT('Ctrl Pts',(-135.015869416263,1.61380678846277,
135.452324944236));
#107847=CARTESIAN_POINT('Ctrl Pts',(-135.023634169211,1.74190152123189,
135.403812992885));
#107848=CARTESIAN_POINT('Ctrl Pts',(-135.031391210096,1.86986902850694,
135.355349224288));
#107849=CARTESIAN_POINT('Ctrl Pts',(-135.039148250981,1.99594619839706,
135.30149021584));
#107850=CARTESIAN_POINT('Ctrl Pts',(-135.046905291866,2.11964829147391,
135.242409083159));
#107851=CARTESIAN_POINT('Ctrl Pts',(-135.054656483106,2.24325709984027,
135.183372504019));
#107852=CARTESIAN_POINT('Ctrl Pts',(-135.062407674346,2.36449404503223,
135.1191218069));
#107853=CARTESIAN_POINT('Ctrl Pts',(-135.070158865586,2.48289379795623,
135.049878424686));
#107854=CARTESIAN_POINT('Ctrl Pts',(-135.077906762363,2.60124322782633,
134.980664472757));
#107855=CARTESIAN_POINT('Ctrl Pts',(-135.08565465914,2.71675752705532,134.906462253237));
#107856=CARTESIAN_POINT('Ctrl Pts',(-135.093402555917,2.82899564459609,
134.827539299325));
#107857=CARTESIAN_POINT('Ctrl Pts',(-135.101148832001,2.94121028434255,
134.748632854393));
#107858=CARTESIAN_POINT('Ctrl Pts',(-135.108895108086,3.05014978590222,
134.665007863955));
#107859=CARTESIAN_POINT('Ctrl Pts',(-135.11664138417,3.15540213417772,134.576975153154));
#107860=CARTESIAN_POINT('Ctrl Pts',(-135.124387717435,3.26065525940142,
134.488941792516));
#107861=CARTESIAN_POINT('Ctrl Pts',(-135.1321340507,3.3622208771345,134.396500897421));
#107862=CARTESIAN_POINT('Ctrl Pts',(-135.139880383966,3.45972043236972,
134.300003275554));
#107863=CARTESIAN_POINT('Ctrl Pts',(-135.147628451969,3.55724182195499,
134.203484043712));
#107864=CARTESIAN_POINT('Ctrl Pts',(-135.155376519972,3.65069505929536,
134.102906552306));
#107865=CARTESIAN_POINT('Ctrl Pts',(-135.163124587975,3.73973908746803,
133.99865782042));
#107866=CARTESIAN_POINT('Ctrl Pts',(-135.170880890716,3.82887775269336,
133.894298291742));
#107867=CARTESIAN_POINT('Ctrl Pts',(-135.178637193458,3.91359759331332,
133.786260025999));
#107868=CARTESIAN_POINT('Ctrl Pts',(-135.1863934962,3.99359810718647,133.67496285765));
#107869=CARTESIAN_POINT('Ctrl Pts',(-135.194153938714,4.07364131974264,
133.563606286651));
#107870=CARTESIAN_POINT('Ctrl Pts',(-135.201914381228,4.14895997193643,
133.44898767377));
#107871=CARTESIAN_POINT('Ctrl Pts',(-135.209674823743,4.21929799221194,
133.331554222222));
#107872=CARTESIAN_POINT('Ctrl Pts',(-135.217447724008,4.28974892532192,
133.213932256073));
#107873=CARTESIAN_POINT('Ctrl Pts',(-135.225220624274,4.3552030624649,133.093486765312));
#107874=CARTESIAN_POINT('Ctrl Pts',(-135.232993524539,4.41545082360962,
132.970688636769));
#107875=CARTESIAN_POINT('Ctrl Pts',(-135.240483860301,4.47350842688144,
132.85235452951));
#107876=CARTESIAN_POINT('Ctrl Pts',(-135.247974196063,4.52673148765348,
132.731836145199));
#107877=CARTESIAN_POINT('Ctrl Pts',(-135.255464531825,4.57497606270637,
132.609568940216));
#107878=CARTESIAN_POINT('Ctrl Pts',(-135.263238865944,4.62504984548622,
132.482665936993));
#107879=CARTESIAN_POINT('Ctrl Pts',(-135.271013200063,4.66991879033201,
132.353476891634));
#107880=CARTESIAN_POINT('Ctrl Pts',(-135.278787534182,4.70936884770434,
132.222467848622));
#107881=CARTESIAN_POINT('Ctrl Pts',(-135.286552287129,4.74877028640672,
132.091620262546));
#107882=CARTESIAN_POINT('Ctrl Pts',(-135.294317040076,4.78276601380415,
131.958957512455));
#107883=CARTESIAN_POINT('Ctrl Pts',(-135.302081793023,4.81118986715228,
131.824965891269));
#107884=CARTESIAN_POINT('Ctrl Pts',(-135.309838833908,4.83958548952856,
131.691107352451));
#107885=CARTESIAN_POINT('Ctrl Pts',(-135.317595874794,4.86242017028661,
131.555922949086));
#107886=CARTESIAN_POINT('Ctrl Pts',(-135.325352915679,4.87957754299677,
131.419914079405));
#107887=CARTESIAN_POINT('Ctrl Pts',(-135.333104106919,4.89672197719873,
131.284007775069));
#107888=CARTESIAN_POINT('Ctrl Pts',(-135.340855298159,4.90819757629105,
131.147278628267));
#107889=CARTESIAN_POINT('Ctrl Pts',(-135.348606489399,4.91393911629018,
131.010237823427));
#107890=CARTESIAN_POINT('Ctrl Pts',(-135.356354386176,4.91967821598163,
130.873255264585));
#107891=CARTESIAN_POINT('Ctrl Pts',(-135.364102282953,4.91968808751038,
130.735961700969));
#107892=CARTESIAN_POINT('Ctrl Pts',(-135.37185017973,4.91395541526928,130.598872809544));
#107893=CARTESIAN_POINT('Ctrl Pts',(-135.379596455814,4.90822394217959,
130.461812594159));
#107894=CARTESIAN_POINT('Ctrl Pts',(-135.387342731898,4.89675233092962,
130.324957356184));
#107895=CARTESIAN_POINT('Ctrl Pts',(-135.395089007983,4.87957938329119,
130.188821744172));
#107896=CARTESIAN_POINT('Ctrl Pts',(-135.402835341248,4.86240630888604,
130.052685127238));
#107897=CARTESIAN_POINT('Ctrl Pts',(-135.410581674513,4.83953186304386,
129.917268534758));
#107898=CARTESIAN_POINT('Ctrl Pts',(-135.418328007778,4.81104657197576,
129.783080075903));
#107899=CARTESIAN_POINT('Ctrl Pts',(-135.426076075781,4.78255490182426,
129.648861566472));
#107900=CARTESIAN_POINT('Ctrl Pts',(-135.433824143784,4.74844996730653,
129.515872120318));
#107901=CARTESIAN_POINT('Ctrl Pts',(-135.441572211787,4.70887302894273,
129.384607871559));
#107902=CARTESIAN_POINT('Ctrl Pts',(-135.449328514529,4.6692540277377,129.253204113592));
#107903=CARTESIAN_POINT('Ctrl Pts',(-135.457084817271,4.62415151821778,
129.123529590673));
#107904=CARTESIAN_POINT('Ctrl Pts',(-135.464841120013,4.57375629025588,
128.996064054542));
#107905=CARTESIAN_POINT('Ctrl Pts',(-135.472601562527,4.52333416484358,
128.868530486217));
#107906=CARTESIAN_POINT('Ctrl Pts',(-135.480362005041,4.46761385093035,
128.743208611014));
#107907=CARTESIAN_POINT('Ctrl Pts',(-135.488122447555,4.40683318031578,
128.620555593447));
#107908=CARTESIAN_POINT('Ctrl Pts',(-135.495895347821,4.34595493917273,
128.497705682367));
#107909=CARTESIAN_POINT('Ctrl Pts',(-135.503668248086,4.2800002965339,128.37753353323));
#107910=CARTESIAN_POINT('Ctrl Pts',(-135.511441148352,4.20925213969972,
128.260469997486));
#107911=CARTESIAN_POINT('Ctrl Pts',(-135.518931484114,4.14107585656954,
128.147662016129));
#107912=CARTESIAN_POINT('Ctrl Pts',(-135.526421819876,4.06844869098213,
128.037740817199));
#107913=CARTESIAN_POINT('Ctrl Pts',(-135.533912155638,3.99165919989679,
127.931062879012));
#107914=CARTESIAN_POINT('Ctrl Pts',(-135.541686489757,3.91195821191808,
127.820340214376));
#107915=CARTESIAN_POINT('Ctrl Pts',(-135.549460823876,3.82752056990735,
127.712760865688));
#107916=CARTESIAN_POINT('Ctrl Pts',(-135.557235157995,3.73862267128287,
127.608756827315));
#107917=CARTESIAN_POINT('Ctrl Pts',(-135.564999910942,3.6498343313739,127.504880964624));
#107918=CARTESIAN_POINT('Ctrl Pts',(-135.57276466389,3.55659692356819,127.404571939464));
#107919=CARTESIAN_POINT('Ctrl Pts',(-135.580529416837,3.45922976485109,
127.308232402459));
#107920=CARTESIAN_POINT('Ctrl Pts',(-135.588286457722,3.3619593125684,127.21198855124));
#107921=CARTESIAN_POINT('Ctrl Pts',(-135.596043498607,3.26056754811422,
127.119706615525));
#107922=CARTESIAN_POINT('Ctrl Pts',(-135.603800539492,3.15541341312163,
127.031755515678));
#107923=CARTESIAN_POINT('Ctrl Pts',(-135.611551730732,3.0503385756795,126.943870740438));
#107924=CARTESIAN_POINT('Ctrl Pts',(-135.619302921972,2.9415073137202,126.860310550274));
#107925=CARTESIAN_POINT('Ctrl Pts',(-135.627054113212,2.82931444602472,
126.78140612764));
#107926=CARTESIAN_POINT('Ctrl Pts',(-135.634802009989,2.71716926329162,
126.702535241491));
#107927=CARTESIAN_POINT('Ctrl Pts',(-135.642549906766,2.60166563566736,
126.628316411577));
#107928=CARTESIAN_POINT('Ctrl Pts',(-135.650297803543,2.48323021937723,
126.559039576694));
#107929=CARTESIAN_POINT('Ctrl Pts',(-135.658044079628,2.364819577223,126.489777233031));
#107930=CARTESIAN_POINT('Ctrl Pts',(-135.665790355711,2.24347870348298,
126.425455025468));
#107931=CARTESIAN_POINT('Ctrl Pts',(-135.673536631796,2.11966155986546,
126.36631848909));
#107932=CARTESIAN_POINT('Ctrl Pts',(-135.681282965061,1.99584350225775,
126.307181516179));
#107933=CARTESIAN_POINT('Ctrl Pts',(-135.689029298326,1.86954949108976,
126.253230459335));
#107934=CARTESIAN_POINT('Ctrl Pts',(-135.696775631592,1.74125594462539,
126.204663801709));
#107935=CARTESIAN_POINT('Ctrl Pts',(-135.704523699595,1.6129336677103,126.156086267917));
#107936=CARTESIAN_POINT('Ctrl Pts',(-135.712271767598,1.48261133003691,
126.112895671134));
#107937=CARTESIAN_POINT('Ctrl Pts',(-135.720019835601,1.3507826980513,126.075241337494));
#107938=CARTESIAN_POINT('Ctrl Pts',(-135.727776138343,1.21881395702702,
126.037546984381));
#107939=CARTESIAN_POINT('Ctrl Pts',(-135.735532441084,1.08533610023545,
126.005400755895));
#107940=CARTESIAN_POINT('Ctrl Pts',(-135.743288743826,0.950855882991227,
125.978901452649));
#107941=CARTESIAN_POINT('Ctrl Pts',(-135.75104918634,0.816303889606305,
125.952388005927));
#107942=CARTESIAN_POINT('Ctrl Pts',(-135.758809628855,0.680748855983335,
125.9315275494));
#107943=CARTESIAN_POINT('Ctrl Pts',(-135.766570071369,0.54470396147231,
125.916367097024));
#107944=CARTESIAN_POINT('Ctrl Pts',(-135.774342971634,0.408440675619118,
125.901182307745));
#107945=CARTESIAN_POINT('Ctrl Pts',(-135.7821158719,0.271686347719986,125.891715834554));
#107946=CARTESIAN_POINT('Ctrl Pts',(-135.789888772165,0.134956372797775,
125.887962562085));
#107947=CARTESIAN_POINT('Ctrl Pts',(-135.797379107927,0.00319687686786632,
125.884345730524));
#107948=CARTESIAN_POINT('Ctrl Pts',(-135.804869443689,-0.128539697936056,
125.886033928844));
#107949=CARTESIAN_POINT('Ctrl Pts',(-135.812359779451,-0.259797464224848,
125.892977071142));
#107950=CARTESIAN_POINT('Ctrl Pts',(-135.82013411357,-0.39603190861952,
125.900183464791));
#107951=CARTESIAN_POINT('Ctrl Pts',(-135.827908447689,-0.532182069487139,
125.913073978675));
#107952=CARTESIAN_POINT('Ctrl Pts',(-135.835682781808,-0.667735098176365,
125.931649575326));
#107953=CARTESIAN_POINT('Ctrl Pts',(-135.843447534755,-0.803121069871718,
125.950202279215));
#107954=CARTESIAN_POINT('Ctrl Pts',(-135.851212287702,-0.937910990007601,
125.974426072739));
#107955=CARTESIAN_POINT('Ctrl Pts',(-135.858977040649,-1.07159349857896,
126.004269947974));
#107956=CARTESIAN_POINT('Ctrl Pts',(-135.866734081534,-1.2051432317993,
126.034084181851));
#107957=CARTESIAN_POINT('Ctrl Pts',(-135.874491122419,-1.33758736319606,
126.069507304486));
#107958=CARTESIAN_POINT('Ctrl Pts',(-135.882248163304,-1.46842149289897,
126.110436738582));
#107959=CARTESIAN_POINT('Ctrl Pts',(-135.889999354544,-1.59915695956568,
126.151335307474));
#107960=CARTESIAN_POINT('Ctrl Pts',(-135.897750545784,-1.72828446953734,
126.197731806567));
#107961=CARTESIAN_POINT('Ctrl Pts',(-135.905501737025,-1.85531198044017,
126.249473075844));
#107962=CARTESIAN_POINT('Ctrl Pts',(-135.913249633802,-1.9822855012628,
126.301192353702));
#107963=CARTESIAN_POINT('Ctrl Pts',(-135.920997530579,-2.10716043691919,
126.358251736391));
#107964=CARTESIAN_POINT('Ctrl Pts',(-135.928745427356,-2.22946223557937,
126.420448984945));
#107965=CARTESIAN_POINT('Ctrl Pts',(-135.93649170344,-2.3517384513398,126.482633223177));
#107966=CARTESIAN_POINT('Ctrl Pts',(-135.944237979524,-2.47144225243399,
126.549953012461));
#107967=CARTESIAN_POINT('Ctrl Pts',(-135.951984255608,-2.58812168584984,
126.622159139668));
#107968=CARTESIAN_POINT('Ctrl Pts',(-135.959730588873,-2.70480198056661,
126.694365799883));
#107969=CARTESIAN_POINT('Ctrl Pts',(-135.967476922138,-2.81845753060206,
126.771458664259));
#107970=CARTESIAN_POINT('Ctrl Pts',(-135.975223255404,-2.92866383074969,
126.853144193608));
#107971=CARTESIAN_POINT('Ctrl Pts',(-135.982971323407,-3.03889481083367,
126.934848015864));
#107972=CARTESIAN_POINT('Ctrl Pts',(-135.99071939141,-3.14567468993953,
127.021146316918));
#107973=CARTESIAN_POINT('Ctrl Pts',(-135.998467459413,-3.24861094293739,
127.111704391497));
#107974=CARTESIAN_POINT('Ctrl Pts',(-136.006223762154,-3.35165659781059,
127.202358712275));
#107975=CARTESIAN_POINT('Ctrl Pts',(-136.013980064896,-3.45085017223776,
127.297281591771));
#107976=CARTESIAN_POINT('Ctrl Pts',(-136.021736367638,-3.5458346288403,
127.39610008653));
#107977=CARTESIAN_POINT('Ctrl Pts',(-136.029496810152,-3.64086978150725,
127.494971323695));
#107978=CARTESIAN_POINT('Ctrl Pts',(-136.037257252666,-3.73169108117181,
127.597742026302));
#107979=CARTESIAN_POINT('Ctrl Pts',(-136.045017695181,-3.81798158768606,
127.704005854222));
#107980=CARTESIAN_POINT('Ctrl Pts',(-136.052790595446,-3.90441061538187,
127.810440266272));
#107981=CARTESIAN_POINT('Ctrl Pts',(-136.060563495711,-3.98629408202232,
127.920378695426));
#107982=CARTESIAN_POINT('Ctrl Pts',(-136.068336395977,-4.06335770770966,
128.033384760274));
#107983=CARTESIAN_POINT('Ctrl Pts',(-136.075826731739,-4.13761987649234,
128.14228277002));
#107984=CARTESIAN_POINT('Ctrl Pts',(-136.083317067501,-4.20740638396089,
128.254028993808));
#107985=CARTESIAN_POINT('Ctrl Pts',(-136.090807403263,-4.27251295053554,
128.36821280801));
#107986=CARTESIAN_POINT('Ctrl Pts',(-136.098918087298,-4.34301163134893,
128.491853305351));
#107987=CARTESIAN_POINT('Ctrl Pts',(-136.107028771333,-4.40823032391749,
128.618715240005));
#107988=CARTESIAN_POINT('Ctrl Pts',(-136.115139455368,-4.46787596845634,
128.748328664266));
#107989=CARTESIAN_POINT('Ctrl Pts',(-136.123517932265,-4.52949095095091,
128.882221573441));
#107990=CARTESIAN_POINT('Ctrl Pts',(-136.131896409163,-4.58515829912374,
129.019050525924));
#107991=CARTESIAN_POINT('Ctrl Pts',(-136.140274886061,-4.6346039730973,
129.158265518536));
#107992=CARTESIAN_POINT('Ctrl Pts',(-136.148653362959,-4.68404964707086,
129.297480511148));
#107993=CARTESIAN_POINT('Ctrl Pts',(-136.157031839857,-4.72727343413117,
129.439081191632));
#107994=CARTESIAN_POINT('Ctrl Pts',(-136.165410316754,-4.76405452823394,
129.582490119308));
#107995=CARTESIAN_POINT('Ctrl Pts',(-134.415184333433,-4.76405452823397,
129.582490119308));
#107996=CARTESIAN_POINT('Ctrl Pts',(-134.416830109084,-4.77123413959544,
129.61048331504));
#107997=CARTESIAN_POINT('Ctrl Pts',(-134.418475884735,-4.77816469915982,
129.638530767353));
#107998=CARTESIAN_POINT('Ctrl Pts',(-134.420121660386,-4.7848455356183,
129.666627668771));
#107999=CARTESIAN_POINT('Ctrl Pts',(-134.430958144317,-4.82883499242778,
129.851629567725));
#108000=CARTESIAN_POINT('Ctrl Pts',(-134.441794628249,-4.86211074913044,
130.03926938264));
#108001=CARTESIAN_POINT('Ctrl Pts',(-134.452631112179,-4.88441983383602,
130.228490884615));
#108002=CARTESIAN_POINT('Ctrl Pts',(-134.462854396381,-4.90546652339598,
130.407004986053));
#108003=CARTESIAN_POINT('Ctrl Pts',(-134.473077680582,-4.91675286075667,
130.586927132526));
#108004=CARTESIAN_POINT('Ctrl Pts',(-134.483300964783,-4.91811071544171,
130.767346388444));
#108005=CARTESIAN_POINT('Ctrl Pts',(-134.483914164512,-4.91819216051448,
130.778168061478));
#108006=CARTESIAN_POINT('Ctrl Pts',(-134.484527364242,-4.91823789935196,
130.788991514613));
#108007=CARTESIAN_POINT('Ctrl Pts',(-134.485140563972,-4.91824790082115,
130.799816547985));
#108008=CARTESIAN_POINT('',(-134.139859435957,-4.91824948933185,130.806601864317));
#108009=CARTESIAN_POINT('Ctrl Pts',(-134.069717999649,-4.76405452823413,
129.582490119309));
#108010=CARTESIAN_POINT('Ctrl Pts',(-134.077393660297,-4.79779154961053,
129.714030253624));
#108011=CARTESIAN_POINT('Ctrl Pts',(-134.085069320945,-4.82605188755225,
129.846872908459));
#108012=CARTESIAN_POINT('Ctrl Pts',(-134.092744981594,-4.84875916336053,
129.980517405403));
#108013=CARTESIAN_POINT('Ctrl Pts',(-134.100597390654,-4.87198932249181,
130.117239351146));
#108014=CARTESIAN_POINT('Ctrl Pts',(-134.108449799715,-4.88940751121968,
130.254800071525));
#108015=CARTESIAN_POINT('Ctrl Pts',(-134.116302208776,-4.90098825429152,
130.392660248612));
#108016=CARTESIAN_POINT('Ctrl Pts',(-134.124154617836,-4.91256899736335,
130.5305204257));
#108017=CARTESIAN_POINT('Ctrl Pts',(-134.132007026897,-4.91831234051333,
130.668679615899));
#108018=CARTESIAN_POINT('Ctrl Pts',(-134.139859435957,-4.91824948933185,
130.806601864317));
#108019=CARTESIAN_POINT('Ctrl Pts',(-134.139859435993,-4.91824948933156,
130.806601864944));
#108020=CARTESIAN_POINT('Ctrl Pts',(-134.14699396824,-4.9181923840658,130.931915093187));
#108021=CARTESIAN_POINT('Ctrl Pts',(-134.154128500486,-4.91334639594518,
131.057114832502));
#108022=CARTESIAN_POINT('Ctrl Pts',(-134.161263032733,-4.90373476650503,
131.181942929479));
#108023=CARTESIAN_POINT('Ctrl Pts',(-134.169037366852,-4.89326119709418,
131.317965208143));
#108024=CARTESIAN_POINT('Ctrl Pts',(-134.176811700971,-4.87710716690586,
131.453766824337));
#108025=CARTESIAN_POINT('Ctrl Pts',(-134.18458603509,-4.85528402063956,
131.588835054002));
#108026=CARTESIAN_POINT('Ctrl Pts',(-134.192350788037,-4.83348776945065,
131.723736824146));
#108027=CARTESIAN_POINT('Ctrl Pts',(-134.200115540984,-4.80603636535375,
131.857906623863));
#108028=CARTESIAN_POINT('Ctrl Pts',(-134.207880293932,-4.77299307281504,
131.990834464458));
#108029=CARTESIAN_POINT('Ctrl Pts',(-134.215637334817,-4.7399825993404,
132.123630279248));
#108030=CARTESIAN_POINT('Ctrl Pts',(-134.223394375701,-4.7013913837258,
132.255186212736));
#108031=CARTESIAN_POINT('Ctrl Pts',(-134.231151416586,-4.65733407793156,
132.385000471877));
#108032=CARTESIAN_POINT('Ctrl Pts',(-134.238902607827,-4.61330999609415,
132.514716837077));
#108033=CARTESIAN_POINT('Ctrl Pts',(-134.246653799067,-4.56382815385111,
132.642693773468));
#108034=CARTESIAN_POINT('Ctrl Pts',(-134.254404990307,-4.5090534747724,
132.768443055791));
#108035=CARTESIAN_POINT('Ctrl Pts',(-134.262152887084,-4.45430207639353,
132.894138891314));
#108036=CARTESIAN_POINT('Ctrl Pts',(-134.269900783861,-4.39426247125905,
133.01760859822));
#108037=CARTESIAN_POINT('Ctrl Pts',(-134.277648680638,-4.3291482280303,
133.138382614515));
#108038=CARTESIAN_POINT('Ctrl Pts',(-134.285394956722,-4.26404760529753,
133.25913136749));
#108039=CARTESIAN_POINT('Ctrl Pts',(-134.293141232806,-4.19387464128219,
133.377185207525));
#108040=CARTESIAN_POINT('Ctrl Pts',(-134.30088750889,-4.11888932297478,
133.492098292188));
#108041=CARTESIAN_POINT('Ctrl Pts',(-134.308633842156,-4.04390345114269,
133.607012225114));
#108042=CARTESIAN_POINT('Ctrl Pts',(-134.316380175421,-3.96410536778918,
133.718785028983));
#108043=CARTESIAN_POINT('Ctrl Pts',(-134.324126508686,-3.87979871452275,
133.826999364967));
#108044=CARTESIAN_POINT('Ctrl Pts',(-134.331874576689,-3.79547318136574,
133.935237934801));
#108045=CARTESIAN_POINT('Ctrl Pts',(-134.339622644693,-3.70663730941524,
134.039916142666));
#108046=CARTESIAN_POINT('Ctrl Pts',(-134.347370712696,-3.61363512707809,
134.140649608473));
#108047=CARTESIAN_POINT('Ctrl Pts',(-134.355127015437,-3.5205341009152,
134.241490135006));
#108048=CARTESIAN_POINT('Ctrl Pts',(-134.362883318179,-3.42325818458389,
134.338377256757));
#108049=CARTESIAN_POINT('Ctrl Pts',(-134.370639620921,-3.32218878205257,
134.430962988781));
#108050=CARTESIAN_POINT('Ctrl Pts',(-134.378400063435,-3.2210654357377,
134.523598136598));
#108051=CARTESIAN_POINT('Ctrl Pts',(-134.386160505949,-3.11614486778376,
134.61192706848));
#108052=CARTESIAN_POINT('Ctrl Pts',(-134.393920948464,-3.00784090699308,
134.695642686591));
#108053=CARTESIAN_POINT('Ctrl Pts',(-134.401693848729,-2.89936308706975,
134.779492692445));
#108054=CARTESIAN_POINT('Ctrl Pts',(-134.409466748994,-2.78749134004539,
134.858714359504));
#108055=CARTESIAN_POINT('Ctrl Pts',(-134.41723964926,-2.67266850362333,
134.933043958807));
#108056=CARTESIAN_POINT('Ctrl Pts',(-134.424729985022,-2.56201976652617,
135.00467148995));
#108057=CARTESIAN_POINT('Ctrl Pts',(-134.432220320784,-2.44863103913397,
135.071756299375));
#108058=CARTESIAN_POINT('Ctrl Pts',(-134.439710656546,-2.33291772897051,
135.134104020166));
#108059=CARTESIAN_POINT('Ctrl Pts',(-134.447484990665,-2.2128171134824,
135.198815673739));
#108060=CARTESIAN_POINT('Ctrl Pts',(-134.455259324784,-2.08983171977518,
135.258628921328));
#108061=CARTESIAN_POINT('Ctrl Pts',(-134.463033658903,-1.96439904921026,
135.313276167669));
#108062=CARTESIAN_POINT('Ctrl Pts',(-134.47079841185,-1.83912096320156,
135.367856066163));
#108063=CARTESIAN_POINT('Ctrl Pts',(-134.478563164797,-1.71140195636095,
135.417282476459));
#108064=CARTESIAN_POINT('Ctrl Pts',(-134.486327917745,-1.58170529261166,
135.461332963396));
#108065=CARTESIAN_POINT('Ctrl Pts',(-134.49408495863,-1.45213744541721,
135.505339698768));
#108066=CARTESIAN_POINT('Ctrl Pts',(-134.501841999515,-1.32059621803381,
135.543981011594));
#108067=CARTESIAN_POINT('Ctrl Pts',(-134.5095990404,-1.18756575534543,135.577082130417));
#108068=CARTESIAN_POINT('Ctrl Pts',(-134.51735023164,-1.0546356119636,135.610158287429));
#108069=CARTESIAN_POINT('Ctrl Pts',(-134.52510142288,-0.920218846489242,
135.637702472281));
#108070=CARTESIAN_POINT('Ctrl Pts',(-134.53285261412,-0.78481536187858,
135.659589542165));
#108071=CARTESIAN_POINT('Ctrl Pts',(-134.540600510897,-0.649469427360699,
135.68146730946));
#108072=CARTESIAN_POINT('Ctrl Pts',(-134.548348407674,-0.513137992972702,
135.697692681748));
#108073=CARTESIAN_POINT('Ctrl Pts',(-134.556096304451,-0.376331553596354,
135.708191530665));
#108074=CARTESIAN_POINT('Ctrl Pts',(-134.563842580535,-0.239553731177918,
135.71868818345));
#108075=CARTESIAN_POINT('Ctrl Pts',(-134.57158885662,-0.102301490977237,
135.723460665586));
#108076=CARTESIAN_POINT('Ctrl Pts',(-134.579335132704,0.0349095378211423,
135.722486722768));
#108077=CARTESIAN_POINT('Ctrl Pts',(-134.587081465969,0.172121579479979,
135.72151277276));
#108078=CARTESIAN_POINT('Ctrl Pts',(-134.594827799234,0.309292018174121,
135.714792315929));
#108079=CARTESIAN_POINT('Ctrl Pts',(-134.6025741325,0.44590560922136,135.702355232729));
#108080=CARTESIAN_POINT('Ctrl Pts',(-134.610322200503,0.582549793934916,
135.68991536433));
#108081=CARTESIAN_POINT('Ctrl Pts',(-134.618070268506,0.718636493578164,
135.671756357554));
#108082=CARTESIAN_POINT('Ctrl Pts',(-134.625818336509,0.853656362539028,
135.647959886415));
#108083=CARTESIAN_POINT('Ctrl Pts',(-134.63357463925,0.988819732223933,
135.624138124104));
#108084=CARTESIAN_POINT('Ctrl Pts',(-134.641330941992,1.12291362061326,
135.594666996603));
#108085=CARTESIAN_POINT('Ctrl Pts',(-134.649087244734,1.25543909995521,
135.55967929551));
#108086=CARTESIAN_POINT('Ctrl Pts',(-134.656847687248,1.38803531213538,
135.524672920428));
#108087=CARTESIAN_POINT('Ctrl Pts',(-134.664608129763,1.5190610739389,135.484144220339));
#108088=CARTESIAN_POINT('Ctrl Pts',(-134.672368572277,1.6480343306843,135.438275367255));
#108089=CARTESIAN_POINT('Ctrl Pts',(-134.680141472542,1.77721462675114,
135.392332881416));
#108090=CARTESIAN_POINT('Ctrl Pts',(-134.687914372808,1.90433547080781,
135.341033258414));
#108091=CARTESIAN_POINT('Ctrl Pts',(-134.695687273073,2.0289356156144,135.284606518205));
#108092=CARTESIAN_POINT('Ctrl Pts',(-134.703177608835,2.14900623130743,
135.230231032133));
#108093=CARTESIAN_POINT('Ctrl Pts',(-134.710667944597,2.2667359582452,135.171094862575));
#108094=CARTESIAN_POINT('Ctrl Pts',(-134.718158280359,2.38173673212182,
135.107442443579));
#108095=CARTESIAN_POINT('Ctrl Pts',(-134.725932614478,2.50109779529455,
135.041376623769));
#108096=CARTESIAN_POINT('Ctrl Pts',(-134.733706948597,2.61789698387393,
134.970236050257));
#108097=CARTESIAN_POINT('Ctrl Pts',(-134.741481282716,2.73167268221469,
134.894244163554));
#108098=CARTESIAN_POINT('Ctrl Pts',(-134.749246035663,2.84530816217566,
134.818345930059));
#108099=CARTESIAN_POINT('Ctrl Pts',(-134.75701078861,2.95592724389358,134.737608494486));
#108100=CARTESIAN_POINT('Ctrl Pts',(-134.764775541557,3.06309238090191,
134.652301382256));
#108101=CARTESIAN_POINT('Ctrl Pts',(-134.772532582442,3.1701510799854,134.567078998252));
#108102=CARTESIAN_POINT('Ctrl Pts',(-134.780289623327,3.27376235731816,
134.477296211662));
#108103=CARTESIAN_POINT('Ctrl Pts',(-134.788046664212,3.37351748058916,
134.383265879047));
#108104=CARTESIAN_POINT('Ctrl Pts',(-134.795797855453,3.47319737774557,
134.289306455438));
#108105=CARTESIAN_POINT('Ctrl Pts',(-134.803549046693,3.56902662560396,
134.191106128481));
#108106=CARTESIAN_POINT('Ctrl Pts',(-134.811300237933,3.66062972821697,
134.089017837946));
#108107=CARTESIAN_POINT('Ctrl Pts',(-134.81904813471,3.7521938970679,133.986972937658));
#108108=CARTESIAN_POINT('Ctrl Pts',(-134.826796031487,3.83953523266718,
133.881043650849));
#108109=CARTESIAN_POINT('Ctrl Pts',(-134.834543928264,3.92231543376989,
133.771619403131));
#108110=CARTESIAN_POINT('Ctrl Pts',(-134.842290204348,4.00507831903908,
133.662218044606));
#108111=CARTESIAN_POINT('Ctrl Pts',(-134.850036480432,4.08328173182491,
133.549323490909));
#108112=CARTESIAN_POINT('Ctrl Pts',(-134.857782756516,4.15662823877952,
133.43335752648));
#108113=CARTESIAN_POINT('Ctrl Pts',(-134.865529089782,4.22997528716148,
133.317390706017));
#108114=CARTESIAN_POINT('Ctrl Pts',(-134.873275423047,4.2984651491848,133.198352760001));
#108115=CARTESIAN_POINT('Ctrl Pts',(-134.881021756312,4.36184446178538,
133.076693329493));
#108116=CARTESIAN_POINT('Ctrl Pts',(-134.888769824315,4.42523796774349,
132.955006654199));
#108117=CARTESIAN_POINT('Ctrl Pts',(-134.896517892318,4.48351846631249,
132.830697672892));
#108118=CARTESIAN_POINT('Ctrl Pts',(-134.904265960321,4.53647935840965,
132.704239059263));
#108119=CARTESIAN_POINT('Ctrl Pts',(-134.912022263063,4.58949653797325,
132.577646043913));
#108120=CARTESIAN_POINT('Ctrl Pts',(-134.919778565805,4.63718266584084,
132.448899193589));
#108121=CARTESIAN_POINT('Ctrl Pts',(-134.927534868547,4.67937978070716,
132.318490047439));
#108122=CARTESIAN_POINT('Ctrl Pts',(-134.935295311061,4.72159941744422,
132.188011298002));
#108123=CARTESIAN_POINT('Ctrl Pts',(-134.943055753575,4.75832409896428,
132.055868861388));
#108124=CARTESIAN_POINT('Ctrl Pts',(-134.95081619609,4.78944652940935,131.922566772275));
#108125=CARTESIAN_POINT('Ctrl Pts',(-134.958589096355,4.82061892034268,
131.789050694814));
#108126=CARTESIAN_POINT('Ctrl Pts',(-134.96636199662,4.84617101594217,131.654371629164));
#108127=CARTESIAN_POINT('Ctrl Pts',(-134.974134896886,4.86604702311163,
131.519041967096));
#108128=CARTESIAN_POINT('Ctrl Pts',(-134.981625232648,4.88520048735589,
131.388631879119));
#108129=CARTESIAN_POINT('Ctrl Pts',(-134.98911556841,4.89908334620185,131.257617981438));
#108130=CARTESIAN_POINT('Ctrl Pts',(-134.996605904172,4.90769149070061,
131.126458886119));
#108131=CARTESIAN_POINT('Ctrl Pts',(-135.004380238291,4.9166260156144,130.990326853836));
#108132=CARTESIAN_POINT('Ctrl Pts',(-135.01215457241,4.91990625071914,130.853607170871));
#108133=CARTESIAN_POINT('Ctrl Pts',(-135.019928906529,4.91747066831249,
130.716808982594));
#108134=CARTESIAN_POINT('Ctrl Pts',(-135.027693659476,4.91503808754349,
130.580179385857));
#108135=CARTESIAN_POINT('Ctrl Pts',(-135.035458412423,4.90690371208257,
130.443471863464));
#108136=CARTESIAN_POINT('Ctrl Pts',(-135.043223165371,4.89305779674734,
130.307200220722));
#108137=CARTESIAN_POINT('Ctrl Pts',(-135.050980206256,4.87922563337041,
130.171063924897));
#108138=CARTESIAN_POINT('Ctrl Pts',(-135.058737247141,4.85969325847608,
130.035363033634));
#108139=CARTESIAN_POINT('Ctrl Pts',(-135.066494288026,4.83450295735238,
129.900610531618));
#108140=CARTESIAN_POINT('Ctrl Pts',(-135.074245479266,4.80933165243068,
129.765959647511));
#108141=CARTESIAN_POINT('Ctrl Pts',(-135.081996670506,4.77851098541058,
129.632256111866));
#108142=CARTESIAN_POINT('Ctrl Pts',(-135.089747861746,4.74213492978522,
129.500006612623));
#108143=CARTESIAN_POINT('Ctrl Pts',(-135.097495758523,4.70577433495381,
129.367813322945));
#108144=CARTESIAN_POINT('Ctrl Pts',(-135.1052436553,4.66386315121035,129.237073216683));
#108145=CARTESIAN_POINT('Ctrl Pts',(-135.112991552077,4.61654615326392,
129.108281410311));
#108146=CARTESIAN_POINT('Ctrl Pts',(-135.120737828161,4.56923905301355,
128.979516544408));
#108147=CARTESIAN_POINT('Ctrl Pts',(-135.128484104246,4.51652852248383,
128.852699534519));
#108148=CARTESIAN_POINT('Ctrl Pts',(-135.13623038033,4.45860865087981,128.728308604537));
#108149=CARTESIAN_POINT('Ctrl Pts',(-135.143976713595,4.40068835172437,
128.60391675633));
#108150=CARTESIAN_POINT('Ctrl Pts',(-135.15172304686,4.33755879979319,128.481951378191));
#108151=CARTESIAN_POINT('Ctrl Pts',(-135.159469380126,4.26946134191871,
128.362868673618));
#108152=CARTESIAN_POINT('Ctrl Pts',(-135.167217448129,4.20134863409078,
128.2437593013));
#108153=CARTESIAN_POINT('Ctrl Pts',(-135.174965516132,4.12826600056123,
128.127534226452));
#108154=CARTESIAN_POINT('Ctrl Pts',(-135.182713584135,4.05049944324079,
128.01462275841));
#108155=CARTESIAN_POINT('Ctrl Pts',(-135.190469886876,3.97265023469769,
127.901591286716));
#108156=CARTESIAN_POINT('Ctrl Pts',(-135.198226189618,3.89010738013041,
127.791880779383));
#108157=CARTESIAN_POINT('Ctrl Pts',(-135.20598249236,3.80319904340295,127.685889822648));
#108158=CARTESIAN_POINT('Ctrl Pts',(-135.213742934874,3.71624432107941,
127.579842295347));
#108159=CARTESIAN_POINT('Ctrl Pts',(-135.221503377388,3.62491973409948,
127.477518565939));
#108160=CARTESIAN_POINT('Ctrl Pts',(-135.229263819903,3.5295913450804,127.379281348522));
#108161=CARTESIAN_POINT('Ctrl Pts',(-135.237036720168,3.43410992646841,
127.280886432003));
#108162=CARTESIAN_POINT('Ctrl Pts',(-135.244809620433,3.334612146044,127.1865914056));
#108163=CARTESIAN_POINT('Ctrl Pts',(-135.252582520699,3.23149893598448,
127.096720169892));
#108164=CARTESIAN_POINT('Ctrl Pts',(-135.260072856461,3.1321341508374,127.010115979974));
#108165=CARTESIAN_POINT('Ctrl Pts',(-135.267563192223,3.02941247252673,
126.927619725755));
#108166=CARTESIAN_POINT('Ctrl Pts',(-135.275053527985,2.92371752338386,
126.849482755235));
#108167=CARTESIAN_POINT('Ctrl Pts',(-135.282827862104,2.81401511811908,
126.768383197728));
#108168=CARTESIAN_POINT('Ctrl Pts',(-135.290602196223,2.70076202393668,
126.691723114827));
#108169=CARTESIAN_POINT('Ctrl Pts',(-135.298376530342,2.58435334202991,
126.619829477039));
#108170=CARTESIAN_POINT('Ctrl Pts',(-135.306141283289,2.46808812341954,
126.548024441735));
#108171=CARTESIAN_POINT('Ctrl Pts',(-135.313906036236,2.3486753844421,126.480974367067));
#108172=CARTESIAN_POINT('Ctrl Pts',(-135.321670789183,2.22654213654588,
126.418965176253));
#108173=CARTESIAN_POINT('Ctrl Pts',(-135.329427830068,2.10453019311325,
126.357017573842));
#108174=CARTESIAN_POINT('Ctrl Pts',(-135.337184870953,1.97980346431021,
126.30010106762));
#108175=CARTESIAN_POINT('Ctrl Pts',(-135.344941911838,1.85281639490994,
126.248457362529));
#108176=CARTESIAN_POINT('Ctrl Pts',(-135.352693103078,1.72592508744669,
126.196852602358));
#108177=CARTESIAN_POINT('Ctrl Pts',(-135.360444294318,1.59677719286645,
126.150512875502));
#108178=CARTESIAN_POINT('Ctrl Pts',(-135.368195485558,1.46584979705351,
126.109632996609));
#108179=CARTESIAN_POINT('Ctrl Pts',(-135.375943382336,1.33497804887622,
126.068770492755));
#108180=CARTESIAN_POINT('Ctrl Pts',(-135.383691279113,1.20232867617534,
126.033363337685));
#108181=CARTESIAN_POINT('Ctrl Pts',(-135.39143917589,1.06839648872893,126.003557350885));
#108182=CARTESIAN_POINT('Ctrl Pts',(-135.399185451974,0.934492317008893,
125.973757598855));
#108183=CARTESIAN_POINT('Ctrl Pts',(-135.406931728058,0.79930624566797,
125.949556769507));
#108184=CARTESIAN_POINT('Ctrl Pts',(-135.414678004142,0.663345527966497,
125.931050061791));
#108185=CARTESIAN_POINT('Ctrl Pts',(-135.422424337407,0.527383806634076,
125.912543217463));
#108186=CARTESIAN_POINT('Ctrl Pts',(-135.430170670673,0.390647814923571,
125.89973063137));
#108187=CARTESIAN_POINT('Ctrl Pts',(-135.437917003938,0.253651823615402,
125.892655840722));
#108188=CARTESIAN_POINT('Ctrl Pts',(-135.445665071941,0.116625153004655,
125.885579465723));
#108189=CARTESIAN_POINT('Ctrl Pts',(-135.453413139944,-0.0206612426947995,
125.884243463208));
#108190=CARTESIAN_POINT('Ctrl Pts',(-135.461161207947,-0.157691582362782,
125.888639263853));
#108191=CARTESIAN_POINT('Ctrl Pts',(-135.468917510688,-0.294867559506259,
125.893039736406));
#108192=CARTESIAN_POINT('Ctrl Pts',(-135.47667381343,-0.431786545603219,
125.903184168647));
#108193=CARTESIAN_POINT('Ctrl Pts',(-135.484430116172,-0.567935818179739,
125.919011912619));
#108194=CARTESIAN_POINT('Ctrl Pts',(-135.492190558686,-0.70415775772241,
125.934848104334));
#108195=CARTESIAN_POINT('Ctrl Pts',(-135.4999510012,-0.839608779221424,
125.956373590666));
#108196=CARTESIAN_POINT('Ctrl Pts',(-135.507711443714,-0.973785855246366,
125.983476448596));
#108197=CARTESIAN_POINT('Ctrl Pts',(-135.51548434398,-1.10817832422542,
126.010622814441));
#108198=CARTESIAN_POINT('Ctrl Pts',(-135.523257244245,-1.24129238120005,
126.04336434998));
#108199=CARTESIAN_POINT('Ctrl Pts',(-135.531030144511,-1.37263880580378,
126.081538815793));
#108200=CARTESIAN_POINT('Ctrl Pts',(-135.538520480273,-1.49921045703433,
126.118325543619));
#108201=CARTESIAN_POINT('Ctrl Pts',(-135.546010816035,-1.62414046836977,
126.160156960324));
#108202=CARTESIAN_POINT('Ctrl Pts',(-135.553501151797,-1.74701001637993,
126.206846173307));
#108203=CARTESIAN_POINT('Ctrl Pts',(-135.561275715347,-1.87454196416161,
126.25530705209));
#108204=CARTESIAN_POINT('Ctrl Pts',(-135.569050278896,-2.00025798307386,
126.309155188687));
#108205=CARTESIAN_POINT('Ctrl Pts',(-135.576824842445,-2.12366937865501,
126.368234894295));
#108206=CARTESIAN_POINT('Ctrl Pts',(-135.584589771702,-2.24692784198943,
126.427241387928));
#108207=CARTESIAN_POINT('Ctrl Pts',(-135.592354700959,-2.36788701523326,
126.491466383794));
#108208=CARTESIAN_POINT('Ctrl Pts',(-135.600119630216,-2.48607550161256,
126.560705157614));
#108209=CARTESIAN_POINT('Ctrl Pts',(-135.607876794515,-2.60414579906952,
126.629874692404));
#108210=CARTESIAN_POINT('Ctrl Pts',(-135.615633958814,-2.71945058845976,
126.70404783078));
#108211=CARTESIAN_POINT('Ctrl Pts',(-135.623391123114,-2.83154085807021,
126.782972868097));
#108212=CARTESIAN_POINT('Ctrl Pts',(-135.631142385043,-2.94354583900826,
126.861837851926));
#108213=CARTESIAN_POINT('Ctrl Pts',(-135.638893646972,-3.05234085040114,
126.945447313396));
#108214=CARTESIAN_POINT('Ctrl Pts',(-135.646644908901,-3.15750410314911,
127.033505157449));
#108215=CARTESIAN_POINT('Ctrl Pts',(-135.654392610232,-3.26261904840245,
127.121522551499));
#108216=CARTESIAN_POINT('Ctrl Pts',(-135.662140311563,-3.36410525542632,
127.21398401172));
#108217=CARTESIAN_POINT('Ctrl Pts',(-135.669888012895,-3.46157261707227,
127.310552082567));
#108218=CARTESIAN_POINT('Ctrl Pts',(-135.677634018436,-3.55901864539654,
127.407099016925));
#108219=CARTESIAN_POINT('Ctrl Pts',(-135.685380023977,-3.65244730093421,
127.507750498632));
#108220=CARTESIAN_POINT('Ctrl Pts',(-135.693126029518,-3.74150434575747,
127.612131256574));
#108221=CARTESIAN_POINT('Ctrl Pts',(-135.700872017095,-3.83056118404747,
127.716511772446));
#108222=CARTESIAN_POINT('Ctrl Pts',(-135.708618004672,-3.91524617840537,
127.824621249715));
#108223=CARTESIAN_POINT('Ctrl Pts',(-135.716363992249,-3.99524476572642,
127.936050605654));
#108224=CARTESIAN_POINT('Ctrl Pts',(-135.724111639306,-4.07526049172812,
128.047503833916));
#108225=CARTESIAN_POINT('Ctrl Pts',(-135.731859286362,-4.15058758548289,
128.1622780383));
#108226=CARTESIAN_POINT('Ctrl Pts',(-135.739606933419,-4.22095450612584,
128.279934718532));
#108227=CARTESIAN_POINT('Ctrl Pts',(-135.747361798037,-4.29138697925732,
128.397701005494));
#108228=CARTESIAN_POINT('Ctrl Pts',(-135.755116662654,-4.35684985172949,
128.518354794396));
#108229=CARTESIAN_POINT('Ctrl Pts',(-135.762871527272,-4.41711712679915,
128.641432197429));
#108230=CARTESIAN_POINT('Ctrl Pts',(-135.770630500632,-4.47741633314267,
128.764574810283));
#108231=CARTESIAN_POINT('Ctrl Pts',(-135.778389473992,-4.53251430027346,
128.890143238351));
#108232=CARTESIAN_POINT('Ctrl Pts',(-135.786148447351,-4.58223337654167,
129.017654053687));
#108233=CARTESIAN_POINT('Ctrl Pts',(-135.793917530715,-4.63201723716028,
129.145331016626));
#108234=CARTESIAN_POINT('Ctrl Pts',(-135.801686614079,-4.67640808468846,
129.274955051779));
#108235=CARTESIAN_POINT('Ctrl Pts',(-135.809455697443,-4.7152781326607,
129.406027612108));
#108236=CARTESIAN_POINT('Ctrl Pts',(-135.812925960045,-4.73264044781501,
129.464574570995));
#108237=CARTESIAN_POINT('Ctrl Pts',(-135.816396222647,-4.74890193738055,
129.523410397543));
#108238=CARTESIAN_POINT('Ctrl Pts',(-135.819866485249,-4.76405452823408,
129.582490119308));
#108239=CARTESIAN_POINT('Origin',(213.235140564004,0.,130.804360617566));
#108240=CARTESIAN_POINT('',(-137.915064401336,-4.76405452823416,129.582490119309));
#108241=CARTESIAN_POINT('',(-137.570140320276,-4.76405452823416,129.582490119309));
#108242=CARTESIAN_POINT('',(213.235140564004,-4.76405452823405,129.582490119308));
#108243=CARTESIAN_POINT('',(-136.235140564053,-4.91824997458325,130.804860629426));
#108244=CARTESIAN_POINT('Ctrl Pts',(-136.235140564053,-4.91824997458325,
130.804860629426));
#108245=CARTESIAN_POINT('Ctrl Pts',(-136.243319774442,-4.91823520989426,
130.950090047185));
#108246=CARTESIAN_POINT('Ctrl Pts',(-136.251498984831,-4.91178351684229,
131.095174708989));
#108247=CARTESIAN_POINT('Ctrl Pts',(-136.259678195219,-4.89895887980969,
131.239544436697));
#108248=CARTESIAN_POINT('Ctrl Pts',(-136.267870559774,-4.88611361763175,
131.384146346152));
#108249=CARTESIAN_POINT('Ctrl Pts',(-136.276062924329,-4.86687497963747,
131.528030706833));
#108250=CARTESIAN_POINT('Ctrl Pts',(-136.284255288883,-4.84135826379696,
131.670636107272));
#108251=CARTESIAN_POINT('Ctrl Pts',(-136.292469269702,-4.81577421989171,
131.81361778441));
#108252=CARTESIAN_POINT('Ctrl Pts',(-136.30068325052,-4.78387902838337,
131.955313435641));
#108253=CARTESIAN_POINT('Ctrl Pts',(-136.308897231338,-4.7458387367286,
132.0951734419));
#108254=CARTESIAN_POINT('Ctrl Pts',(-136.317122921387,-4.70774421770548,
132.235232822028));
#108255=CARTESIAN_POINT('Ctrl Pts',(-136.325348611436,-4.66348720906491,
132.373451028176));
#108256=CARTESIAN_POINT('Ctrl Pts',(-136.333574301485,-4.61328250394212,
132.509296863096));
#108257=CARTESIAN_POINT('Ctrl Pts',(-136.341819169943,-4.56296074525599,
132.645459426079));
#108258=CARTESIAN_POINT('Ctrl Pts',(-136.3500640384,-4.506663686799,132.779238261702));
#108259=CARTESIAN_POINT('Ctrl Pts',(-136.358308906858,-4.44465355757561,
132.910123618388));
#108260=CARTESIAN_POINT('Ctrl Pts',(-136.361957613597,-4.41721142461937,
132.968045983737));
#108261=CARTESIAN_POINT('Ctrl Pts',(-136.365606320337,-4.38865100754711,
133.025402033596));
#108262=CARTESIAN_POINT('Ctrl Pts',(-136.369255027076,-4.35899775916615,
133.082149369423));
#108263=CARTESIAN_POINT('Ctrl Pts',(-136.377029361195,-4.29581530108187,
133.203061457071));
#108264=CARTESIAN_POINT('Ctrl Pts',(-136.384803695314,-4.22749807277276,
133.321534187978));
#108265=CARTESIAN_POINT('Ctrl Pts',(-136.392578029434,-4.15425837290117,
133.437100717477));
#108266=CARTESIAN_POINT('Ctrl Pts',(-136.400342782381,-4.08110893441424,
133.552524821557));
#108267=CARTESIAN_POINT('Ctrl Pts',(-136.408107535328,-4.0030493021788,
133.665049523549));
#108268=CARTESIAN_POINT('Ctrl Pts',(-136.415872288275,-3.92033842409087,
133.774230935121));
#108269=CARTESIAN_POINT('Ctrl Pts',(-136.42362932916,-3.83770969561308,
133.883303906177));
#108270=CARTESIAN_POINT('Ctrl Pts',(-136.431386370045,-3.75043914921582,
133.989039885342));
#108271=CARTESIAN_POINT('Ctrl Pts',(-136.43914341093,-3.65882974291745,
134.091022750314));
#108272=CARTESIAN_POINT('Ctrl Pts',(-136.44689460217,-3.56728941998486,
134.192928709216));
#108273=CARTESIAN_POINT('Ctrl Pts',(-136.45464579341,-3.47141701001369,
134.291086897698));
#108274=CARTESIAN_POINT('Ctrl Pts',(-136.46239698465,-3.37155634026913,
134.385113458365));
#108275=CARTESIAN_POINT('Ctrl Pts',(-136.470144881427,-3.27173811397295,
134.479100055236));
#108276=CARTESIAN_POINT('Ctrl Pts',(-136.477892778205,-3.16793528340938,
134.568958249493));
#108277=CARTESIAN_POINT('Ctrl Pts',(-136.485640674982,-3.06052904374713,
134.654340492173));
#108278=CARTESIAN_POINT('Ctrl Pts',(-136.493386951066,-2.9531452711551,
134.739704874728));
#108279=CARTESIAN_POINT('Ctrl Pts',(-136.50113322715,-2.84215989457701,
134.820594924868));
#108280=CARTESIAN_POINT('Ctrl Pts',(-136.508879503234,-2.72798743940898,
134.896703173233));
#108281=CARTESIAN_POINT('Ctrl Pts',(-136.516625836499,-2.61381414144566,
134.972811983413));
#108282=CARTESIAN_POINT('Ctrl Pts',(-136.524372169765,-2.49645404325894,
135.044138704529));
#108283=CARTESIAN_POINT('Ctrl Pts',(-136.53211850303,-2.37635057640724,
135.110419256334));
#108284=CARTESIAN_POINT('Ctrl Pts',(-136.539866571033,-2.25622021321672,
135.176714651209));
#108285=CARTESIAN_POINT('Ctrl Pts',(-136.547614639036,-2.13334560109405,
135.237961439228));
#108286=CARTESIAN_POINT('Ctrl Pts',(-136.555362707039,-2.0081943198016,
135.29394173794));
#108287=CARTESIAN_POINT('Ctrl Pts',(-136.563119009781,-1.88291002623824,
135.349981533179));
#108288=CARTESIAN_POINT('Ctrl Pts',(-136.570875312523,-1.75534458740969,
135.400743498033));
#108289=CARTESIAN_POINT('Ctrl Pts',(-136.578631615265,-1.6259856102789,
135.446057921103));
#108290=CARTESIAN_POINT('Ctrl Pts',(-136.586392057779,-1.49655759036708,
135.491396529845));
#108291=CARTESIAN_POINT('Ctrl Pts',(-136.594152500293,-1.36533449860536,
135.531281689686));
#108292=CARTESIAN_POINT('Ctrl Pts',(-136.601912942807,-1.23281764971714,
135.565594040225));
#108293=CARTESIAN_POINT('Ctrl Pts',(-136.609685843072,-1.1000880730188,
135.599961471995));
#108294=CARTESIAN_POINT('Ctrl Pts',(-136.617458743338,-0.966060971451945,
135.628738135447));
#108295=CARTESIAN_POINT('Ctrl Pts',(-136.625231643603,-0.831247250350906,
135.651855957562));
#108296=CARTESIAN_POINT('Ctrl Pts',(-136.632721979365,-0.701334347588259,
135.674133388613));
#108297=CARTESIAN_POINT('Ctrl Pts',(-136.640212315127,-0.570691329007694,
135.691156221838));
#108298=CARTESIAN_POINT('Ctrl Pts',(-136.647702650889,-0.439776576001578,
135.702909344046));
#108299=CARTESIAN_POINT('Ctrl Pts',(-136.655476985008,-0.303898150343225,
135.715108089455));
#108300=CARTESIAN_POINT('Ctrl Pts',(-136.663251319127,-0.167296555866609,
135.721668275347));
#108301=CARTESIAN_POINT('Ctrl Pts',(-136.671025653246,-0.0304793148249454,
135.722516173653));
#108302=CARTESIAN_POINT('Ctrl Pts',(-136.678790406194,0.106169311194472,
135.723363027));
#108303=CARTESIAN_POINT('Ctrl Pts',(-136.686555159141,0.243032667781021,
135.718511597631));
#108304=CARTESIAN_POINT('Ctrl Pts',(-136.694319912088,0.379597331447376,
135.707939813262));
#108305=CARTESIAN_POINT('Ctrl Pts',(-136.702076952973,0.516026357164553,
135.697378528937));
#108306=CARTESIAN_POINT('Ctrl Pts',(-136.709833993858,0.652156893063687,
135.681108226106));
#108307=CARTESIAN_POINT('Ctrl Pts',(-136.717591034743,0.787475087458587,
135.659158867662));
#108308=CARTESIAN_POINT('Ctrl Pts',(-136.725342225983,0.922691237350655,
135.637226061399));
#108309=CARTESIAN_POINT('Ctrl Pts',(-136.733093417223,1.05709588070808,
135.609622786164));
#108310=CARTESIAN_POINT('Ctrl Pts',(-136.740844608463,1.19018022039763,
135.576430829274));
#108311=CARTESIAN_POINT('Ctrl Pts',(-136.74859250524,1.32320799569249,135.543252979851));
#108312=CARTESIAN_POINT('Ctrl Pts',(-136.756340402017,1.45491620488167,
135.504491267554));
#108313=CARTESIAN_POINT('Ctrl Pts',(-136.764088298794,1.58480639987929,
135.460278543969));
#108314=CARTESIAN_POINT('Ctrl Pts',(-136.771834574878,1.71466942464822,
135.416075068733));
#108315=CARTESIAN_POINT('Ctrl Pts',(-136.779580850963,1.84271482176478,
135.366422976098));
#108316=CARTESIAN_POINT('Ctrl Pts',(-136.787327127047,1.96845984744815,
135.311504823323));
#108317=CARTESIAN_POINT('Ctrl Pts',(-136.795073460312,2.09420580135291,
135.256586265153));
#108318=CARTESIAN_POINT('Ctrl Pts',(-136.802819793577,2.2176509916552,135.196401725753));
#108319=CARTESIAN_POINT('Ctrl Pts',(-136.810566126843,2.33833355457501,
135.131181534827));
#108320=CARTESIAN_POINT('Ctrl Pts',(-136.818314194846,2.45904314351786,
135.065946738291));
#108321=CARTESIAN_POINT('Ctrl Pts',(-136.826062262849,2.57698853010902,
134.995674232083));
#108322=CARTESIAN_POINT('Ctrl Pts',(-136.833810330851,2.6917336653876,134.920639633512));
#108323=CARTESIAN_POINT('Ctrl Pts',(-136.841566633593,2.8066007531616,134.845525287277));
#108324=CARTESIAN_POINT('Ctrl Pts',(-136.849322936335,2.91826046749335,
134.765638952683));
#108325=CARTESIAN_POINT('Ctrl Pts',(-136.857079239077,3.02630646190114,
134.681299134122));
#108326=CARTESIAN_POINT('Ctrl Pts',(-136.864839681591,3.13441012370934,
134.59691430086));
#108327=CARTESIAN_POINT('Ctrl Pts',(-136.872600124105,3.23889592468964,
134.508071500474));
#108328=CARTESIAN_POINT('Ctrl Pts',(-136.88036056662,3.33939247070211,134.415127986024));
#108329=CARTESIAN_POINT('Ctrl Pts',(-136.888133466885,3.4400503426919,134.322035270393));
#108330=CARTESIAN_POINT('Ctrl Pts',(-136.895906367151,3.53670588684236,
134.224828963505));
#108331=CARTESIAN_POINT('Ctrl Pts',(-136.903679267416,3.62902567458206,
134.123902109357));
#108332=CARTESIAN_POINT('Ctrl Pts',(-136.911169603178,3.71798940549767,
134.026644200578));
#108333=CARTESIAN_POINT('Ctrl Pts',(-136.91865993894,3.80292693987788,133.925931786206));
#108334=CARTESIAN_POINT('Ctrl Pts',(-136.926150274702,3.88357779622821,
133.822142346443));
#108335=CARTESIAN_POINT('Ctrl Pts',(-136.933924608821,3.96728655431049,
133.714417698524));
#108336=CARTESIAN_POINT('Ctrl Pts',(-136.94169894294,4.04664232298926,133.603036849049));
#108337=CARTESIAN_POINT('Ctrl Pts',(-136.949473277059,4.12130874457731,
133.488386939041));
#108338=CARTESIAN_POINT('Ctrl Pts',(-136.957238030006,4.19588314647388,
133.3738783248));
#108339=CARTESIAN_POINT('Ctrl Pts',(-136.965002782953,4.26577948885518,
133.256108990656));
#108340=CARTESIAN_POINT('Ctrl Pts',(-136.972767535901,4.33070168374531,
133.135498963719));
#108341=CARTESIAN_POINT('Ctrl Pts',(-136.980524576786,4.39555939699623,
133.015008728361));
#108342=CARTESIAN_POINT('Ctrl Pts',(-136.988281617671,4.45545261025234,
132.891683756988));
#108343=CARTESIAN_POINT('Ctrl Pts',(-136.996038658556,4.51012878275617,
132.765972563251));
#108344=CARTESIAN_POINT('Ctrl Pts',(-137.003789849796,4.56476372353308,
132.640356169303));
#108345=CARTESIAN_POINT('Ctrl Pts',(-137.011541041036,4.61418929906316,
132.512357491797));
#108346=CARTESIAN_POINT('Ctrl Pts',(-137.019292232276,4.65819930205446,
132.382448804214));
#108347=CARTESIAN_POINT('Ctrl Pts',(-137.027040129053,4.70219059962042,
132.252595331289));
#108348=CARTESIAN_POINT('Ctrl Pts',(-137.03478802583,4.7407707774944,132.120833832424));
#108349=CARTESIAN_POINT('Ctrl Pts',(-137.042535922607,4.7737821841137,131.987655475638));
#108350=CARTESIAN_POINT('Ctrl Pts',(-137.050282198691,4.80678668545838,
131.854504976892));
#108351=CARTESIAN_POINT('Ctrl Pts',(-137.058028474775,4.83422463852874,
131.719938588975));
#108352=CARTESIAN_POINT('Ctrl Pts',(-137.065774750859,4.85598869911049,
131.584461134558));
#108353=CARTESIAN_POINT('Ctrl Pts',(-137.073521084125,4.87775292034962,
131.448982680077));
#108354=CARTESIAN_POINT('Ctrl Pts',(-137.08126741739,4.89384310351253,131.312593531691));
#108355=CARTESIAN_POINT('Ctrl Pts',(-137.089013750656,4.90420338284815,
131.175806767312));
#108356=CARTESIAN_POINT('Ctrl Pts',(-137.096761818659,4.91456598229647,
131.038989370485));
#108357=CARTESIAN_POINT('Ctrl Pts',(-137.104509886662,4.91919609503168,
130.901774570252));
#108358=CARTESIAN_POINT('Ctrl Pts',(-137.112257954664,4.91808991058727,
130.764678204841));
#108359=CARTESIAN_POINT('Ctrl Pts',(-137.120014257406,4.91698255047687,
130.627436131782));
#108360=CARTESIAN_POINT('Ctrl Pts',(-137.127770560148,4.9101267177213,130.490313136567));
#108361=CARTESIAN_POINT('Ctrl Pts',(-137.13552686289,4.89757073888565,130.353823249403));
#108362=CARTESIAN_POINT('Ctrl Pts',(-137.143287305404,4.88500805854603,
130.217260513477));
#108363=CARTESIAN_POINT('Ctrl Pts',(-137.151047747918,4.86673922205921,
130.081331946206));
#108364=CARTESIAN_POINT('Ctrl Pts',(-137.158808190433,4.84286404893974,
129.946543116003));
#108365=CARTESIAN_POINT('Ctrl Pts',(-137.166581090698,4.81895054927284,
129.811537910805));
#108366=CARTESIAN_POINT('Ctrl Pts',(-137.174353990963,4.78941281281852,
129.677676480815));
#108367=CARTESIAN_POINT('Ctrl Pts',(-137.182126891229,4.75440129233651,
129.545451798815));
#108368=CARTESIAN_POINT('Ctrl Pts',(-137.189617226991,4.72066252881273,
129.41803381706));
#108369=CARTESIAN_POINT('Ctrl Pts',(-137.197107562753,4.68184113432559,
129.292135943824));
#108370=CARTESIAN_POINT('Ctrl Pts',(-137.204597898515,4.63811389704672,
129.168181366835));
#108371=CARTESIAN_POINT('Ctrl Pts',(-137.212372232634,4.59272872827575,
129.039527014384));
#108372=CARTESIAN_POINT('Ctrl Pts',(-137.220146566753,4.54191459648595,
128.912558688953));
#108373=CARTESIAN_POINT('Ctrl Pts',(-137.227920900872,4.48581540483866,
128.787768636968));
#108374=CARTESIAN_POINT('Ctrl Pts',(-137.235685653819,4.42978535043149,
128.66313237757));
#108375=CARTESIAN_POINT('Ctrl Pts',(-137.243450406766,4.36848335458528,
128.540669403377));
#108376=CARTESIAN_POINT('Ctrl Pts',(-137.251215159714,4.30210275522069,
128.4208558565));
#108377=CARTESIAN_POINT('Ctrl Pts',(-137.258972200599,4.23578808600318,
128.301161310128));
#108378=CARTESIAN_POINT('Ctrl Pts',(-137.266729241484,4.16440503958002,
128.184111294144));
#108379=CARTESIAN_POINT('Ctrl Pts',(-137.274486282369,4.08819445874128,
128.070160710826));
#108380=CARTESIAN_POINT('Ctrl Pts',(-137.282237473609,4.01204134889428,
127.956296058529));
#108381=CARTESIAN_POINT('Ctrl Pts',(-137.289988664849,3.93106816725847,
127.845526510297));
#108382=CARTESIAN_POINT('Ctrl Pts',(-137.297739856089,3.84556079081068,
127.738280829518));
#108383=CARTESIAN_POINT('Ctrl Pts',(-137.305487752866,3.76008975727898,
127.631080731014));
#108384=CARTESIAN_POINT('Ctrl Pts',(-137.313235649643,3.67008860511802,
127.527401826131));
#108385=CARTESIAN_POINT('Ctrl Pts',(-137.32098354642,3.57588535337274,127.427642239905));
#108386=CARTESIAN_POINT('Ctrl Pts',(-137.328729822504,3.48170180691693,
127.327903521234));
#108387=CARTESIAN_POINT('Ctrl Pts',(-137.336476098589,3.38331817748795,
127.232082774597));
#108388=CARTESIAN_POINT('Ctrl Pts',(-137.344222374673,3.28110116452691,
127.140543180706));
#108389=CARTESIAN_POINT('Ctrl Pts',(-137.351968707938,3.17888339702297,
127.04900291109));
#108390=CARTESIAN_POINT('Ctrl Pts',(-137.359715041203,3.07283248076893,
126.961744118105));
#108391=CARTESIAN_POINT('Ctrl Pts',(-137.367461374469,2.96334988593871,
126.879091134332));
#108392=CARTESIAN_POINT('Ctrl Pts',(-137.375209442472,2.85384277324062,
126.796419640997));
#108393=CARTESIAN_POINT('Ctrl Pts',(-137.382957510475,2.74090276470982,
126.718356244837));
#108394=CARTESIAN_POINT('Ctrl Pts',(-137.390705578478,2.62496179000672,
126.64518297487));
#108395=CARTESIAN_POINT('Ctrl Pts',(-137.398461881219,2.50889759185583,
126.57193193548));
#108396=CARTESIAN_POINT('Ctrl Pts',(-137.406218183961,2.38982638738926,
126.503581613416));
#108397=CARTESIAN_POINT('Ctrl Pts',(-137.413974486703,2.26820676646648,
126.440369196051));
#108398=CARTESIAN_POINT('Ctrl Pts',(-137.421734929217,2.14652223349011,
126.377123040316));
#108399=CARTESIAN_POINT('Ctrl Pts',(-137.429495371731,2.02228692778529,
126.319020419003));
#108400=CARTESIAN_POINT('Ctrl Pts',(-137.437255814246,1.89598015326364,
126.266250623204));
#108401=CARTESIAN_POINT('Ctrl Pts',(-137.445028714511,1.76947061989453,
126.213396116644));
#108402=CARTESIAN_POINT('Ctrl Pts',(-137.452801614777,1.64088333963832,
126.165891678218));
#108403=CARTESIAN_POINT('Ctrl Pts',(-137.460574515042,1.51071438784972,
126.123877191589));
#108404=CARTESIAN_POINT('Ctrl Pts',(-137.468064850804,1.3852774053348,126.083390037377));
#108405=CARTESIAN_POINT('Ctrl Pts',(-137.475555186566,1.25837204698359,
126.048000700328));
#108406=CARTESIAN_POINT('Ctrl Pts',(-137.483045522328,1.13044991094067,
126.017789186849));
#108407=CARTESIAN_POINT('Ctrl Pts',(-137.490819856447,0.997677568228408,
125.986432194654));
#108408=CARTESIAN_POINT('Ctrl Pts',(-137.498594190566,0.863389240676738,
125.96055408159));
#108409=CARTESIAN_POINT('Ctrl Pts',(-137.506368524685,0.728076852320345,
125.940299849071));
#108410=CARTESIAN_POINT('Ctrl Pts',(-137.514133277632,0.592931224389387,
125.920070578083));
#108411=CARTESIAN_POINT('Ctrl Pts',(-137.521898030579,0.456764429729424,
125.905451454475));
#108412=CARTESIAN_POINT('Ctrl Pts',(-137.529662783526,0.320081564053693,
125.896537184021));
#108413=CARTESIAN_POINT('Ctrl Pts',(-137.537419824411,0.183534453726671,
125.887631767347));
#108414=CARTESIAN_POINT('Ctrl Pts',(-137.545176865296,0.0464726800311459,
125.884419953231));
#108415=CARTESIAN_POINT('Ctrl Pts',(-137.552933906181,-0.0905908534535143,
125.886944999605));
#108416=CARTESIAN_POINT('Ctrl Pts',(-137.560685097422,-0.227551026261189,
125.889468141822));
#108417=CARTESIAN_POINT('Ctrl Pts',(-137.568436288662,-0.364512566899337,
125.897719526295));
#108418=CARTESIAN_POINT('Ctrl Pts',(-137.576187479902,-0.500960221098191,
125.911690393713));
#108419=CARTESIAN_POINT('Ctrl Pts',(-137.583935376679,-0.637349881404335,
125.925655323139));
#108420=CARTESIAN_POINT('Ctrl Pts',(-137.591683273456,-0.773225701565315,
125.94533486083));
#108421=CARTESIAN_POINT('Ctrl Pts',(-137.599431170233,-0.908075425406258,
125.97066823138));
#108422=CARTESIAN_POINT('Ctrl Pts',(-137.607177446317,-1.04289694159163,
125.995996302735));
#108423=CARTESIAN_POINT('Ctrl Pts',(-137.614923722401,-1.17669240438214,
126.026975782433));
#108424=CARTESIAN_POINT('Ctrl Pts',(-137.622669998485,-1.30895804955339,
126.063494463896));
#108425=CARTESIAN_POINT('Ctrl Pts',(-137.630416331751,-1.44122467107977,
126.100013414932));
#108426=CARTESIAN_POINT('Ctrl Pts',(-137.638162665016,-1.57196107558851,
126.142071545272));
#108427=CARTESIAN_POINT('Ctrl Pts',(-137.645908998281,-1.70067738845764,
126.18950639637));
#108428=CARTESIAN_POINT('Ctrl Pts',(-137.653657066284,-1.82942252645239,
126.236951870174));
#108429=CARTESIAN_POINT('Ctrl Pts',(-137.661405134287,-1.9561463058355,
126.28977632555));
#108430=CARTESIAN_POINT('Ctrl Pts',(-137.66915320229,-2.08037797907659,
126.347768811413));
#108431=CARTESIAN_POINT('Ctrl Pts',(-137.676909505032,-2.20474168721854,
126.40582293238));
#108432=CARTESIAN_POINT('Ctrl Pts',(-137.684665807774,-2.32660764344301,
126.469055890344));
#108433=CARTESIAN_POINT('Ctrl Pts',(-137.692422110516,-2.44552841627364,
126.537210066238));
#108434=CARTESIAN_POINT('Ctrl Pts',(-137.70018255303,-2.56451266070136,
126.605400618068));
#108435=CARTESIAN_POINT('Ctrl Pts',(-137.707942995544,-2.68054825891351,
126.678517413229));
#108436=CARTESIAN_POINT('Ctrl Pts',(-137.715703438058,-2.79321687948089,
126.756259516224));
#108437=CARTESIAN_POINT('Ctrl Pts',(-137.723476338324,-2.90606636572026,
126.834126417745));
#108438=CARTESIAN_POINT('Ctrl Pts',(-137.731249238589,-3.01553776106076,
126.916633229076));
#108439=CARTESIAN_POINT('Ctrl Pts',(-137.739022138855,-3.12124523656904,
127.003438198508));
#108440=CARTESIAN_POINT('Ctrl Pts',(-137.746512474617,-3.22310997908124,
127.087087588653));
#108441=CARTESIAN_POINT('Ctrl Pts',(-137.754002810378,-3.32147947664331,
127.174727859672));
#108442=CARTESIAN_POINT('Ctrl Pts',(-137.761493146141,-3.41604231777075,
127.266022314676));
#108443=CARTESIAN_POINT('Ctrl Pts',(-137.769153108236,-3.5127466313919,
127.359384226218));
#108444=CARTESIAN_POINT('Ctrl Pts',(-137.776813070331,-3.60579530623451,
127.456882415243));
#108445=CARTESIAN_POINT('Ctrl Pts',(-137.784473032426,-3.69480578996644,
127.558194688823));
#108446=CARTESIAN_POINT('Ctrl Pts',(-137.792124079689,-3.78371268133452,
127.659389052946));
#108447=CARTESIAN_POINT('Ctrl Pts',(-137.799775126951,-3.86859046105256,
127.764388377782));
#108448=CARTESIAN_POINT('Ctrl Pts',(-137.807426174214,-3.94909117130883,
127.872831667821));
#108449=CARTESIAN_POINT('Ctrl Pts',(-137.815070089553,-4.02951684283165,
127.981173872453));
#108450=CARTESIAN_POINT('Ctrl Pts',(-137.822714004892,-4.10557331916048,
128.092953337223));
#108451=CARTESIAN_POINT('Ctrl Pts',(-137.830357920231,-4.17695130828101,
128.207774237191));
#108452=CARTESIAN_POINT('Ctrl Pts',(-137.837996312052,-4.2482777194334,
128.322512167201));
#108453=CARTESIAN_POINT('Ctrl Pts',(-137.845634703873,-4.31493215704285,
128.440286818867));
#108454=CARTESIAN_POINT('Ctrl Pts',(-137.853273095694,-4.37664761343337,
128.560671973764));
#108455=CARTESIAN_POINT('Ctrl Pts',(-137.860908196125,-4.43833647657792,
128.681005254588));
#108456=CARTESIAN_POINT('Ctrl Pts',(-137.868543296556,-4.49509040858418,
128.803946442666));
#108457=CARTESIAN_POINT('Ctrl Pts',(-137.876178396987,-4.54668772496982,
128.929043632598));
#108458=CARTESIAN_POINT('Ctrl Pts',(-137.883813309681,-4.59828377264686,
129.054137746559));
#108459=CARTESIAN_POINT('Ctrl Pts',(-137.891448222375,-4.64472329467837,
129.181387387688));
#108460=CARTESIAN_POINT('Ctrl Pts',(-137.899083135069,-4.68583238345119,
129.310319809321));
#108461=CARTESIAN_POINT('Ctrl Pts',(-137.904410223825,-4.71451532631305,
129.400279509065));
#108462=CARTESIAN_POINT('Ctrl Pts',(-137.909737312581,-4.74060428684821,
129.491057984052));
#108463=CARTESIAN_POINT('Ctrl Pts',(-137.915064401336,-4.76405452823416,
129.582490119309));
#108464=CARTESIAN_POINT('Ctrl Pts',(-136.165410316754,-4.76405452823394,
129.582490119308));
#108465=CARTESIAN_POINT('Ctrl Pts',(-136.173480782487,-4.79948346874215,
129.72062702064));
#108466=CARTESIAN_POINT('Ctrl Pts',(-136.181551248219,-4.82893486395653,
129.860441210009));
#108467=CARTESIAN_POINT('Ctrl Pts',(-136.189621713952,-4.8522606023129,
130.001397287306));
#108468=CARTESIAN_POINT('Ctrl Pts',(-136.197679934484,-4.8755509488655,
130.142139493995));
#108469=CARTESIAN_POINT('Ctrl Pts',(-136.205738155016,-4.89273411466211,
130.284019797074));
#108470=CARTESIAN_POINT('Ctrl Pts',(-136.213796375548,-4.90371264983407,
130.42649118197));
#108471=CARTESIAN_POINT('Ctrl Pts',(-136.220911105036,-4.91340577098946,
130.552281405652));
#108472=CARTESIAN_POINT('Ctrl Pts',(-136.228025834523,-4.91826281770671,
130.678532050252));
#108473=CARTESIAN_POINT('Ctrl Pts',(-136.23514056401,-4.91824997458333,
130.804860628664));
#108474=CARTESIAN_POINT('',(-135.889859436035,-4.91824798693904,130.799910733292));
#108475=CARTESIAN_POINT('Ctrl Pts',(-135.819866485249,-4.76405452823408,
129.582490119308));
#108476=CARTESIAN_POINT('Ctrl Pts',(-135.823893915369,-4.78163994115519,
129.651055377392));
#108477=CARTESIAN_POINT('Ctrl Pts',(-135.827921345489,-4.79773171155441,
129.719949130419));
#108478=CARTESIAN_POINT('Ctrl Pts',(-135.83194877561,-4.81232069727367,
129.789100764577));
#108479=CARTESIAN_POINT('Ctrl Pts',(-135.842894248747,-4.85196964126975,
129.977036329305));
#108480=CARTESIAN_POINT('Ctrl Pts',(-135.853839721884,-4.88062061044695,
130.167366481324));
#108481=CARTESIAN_POINT('Ctrl Pts',(-135.86478519502,-4.8980463227066,130.359023348611));
#108482=CARTESIAN_POINT('Ctrl Pts',(-135.873143275345,-4.91135278291635,
130.505374581804));
#108483=CARTESIAN_POINT('Ctrl Pts',(-135.881501355669,-4.91811461337833,
130.652499228452));
#108484=CARTESIAN_POINT('Ctrl Pts',(-135.889859435993,-4.91824798693837,
130.799910732551));
#108485=CARTESIAN_POINT('Ctrl Pts',(-135.889859436035,-4.91824798693904,
130.799910733292));
#108486=CARTESIAN_POINT('Ctrl Pts',(-135.897508745035,-4.9183700503033,
130.934821634027));
#108487=CARTESIAN_POINT('Ctrl Pts',(-135.905158054034,-4.9129368955204,
131.069908050386));
#108488=CARTESIAN_POINT('Ctrl Pts',(-135.912807363034,-4.90193198336201,
131.204667865805));
#108489=CARTESIAN_POINT('Ctrl Pts',(-135.92045048546,-4.89093597170746,
131.33931869078));
#108490=CARTESIAN_POINT('Ctrl Pts',(-135.928093607885,-4.87437719946991,
131.473643040524));
#108491=CARTESIAN_POINT('Ctrl Pts',(-135.935736730311,-4.85229119251697,
131.60713907114));
#108492=CARTESIAN_POINT('Ctrl Pts',(-135.943376195721,-4.83021575308755,
131.740571227717));
#108493=CARTESIAN_POINT('Ctrl Pts',(-135.95101566113,-4.80261840252355,
131.873175456455));
#108494=CARTESIAN_POINT('Ctrl Pts',(-135.95865512654,-4.76958644040095,
132.004455717982));
#108495=CARTESIAN_POINT('Ctrl Pts',(-135.966292838885,-4.73656205828356,
132.135705853988));
#108496=CARTESIAN_POINT('Ctrl Pts',(-135.973930551229,-4.69810564212933,
132.265632236171));
#108497=CARTESIAN_POINT('Ctrl Pts',(-135.981568263573,-4.65435535336774,
132.393750219607));
#108498=CARTESIAN_POINT('Ctrl Pts',(-135.98920598653,-4.61060500381579,
132.521868381062));
#108499=CARTESIAN_POINT('Ctrl Pts',(-135.996843709487,-4.56156089749562,
132.648177757406));
#108500=CARTESIAN_POINT('Ctrl Pts',(-136.004481432444,-4.50741051960844,
132.772210578875));
#108501=CARTESIAN_POINT('Ctrl Pts',(-136.012120929491,-4.45324756367058,
132.89627221069));
#108502=CARTESIAN_POINT('Ctrl Pts',(-136.019760426539,-4.39397613931752,
133.018055867051));
#108503=CARTESIAN_POINT('Ctrl Pts',(-136.027399923586,-4.32983091234054,
133.13711592686));
#108504=CARTESIAN_POINT('Ctrl Pts',(-136.035047345095,-4.26561914742068,
133.256299487853));
#108505=CARTESIAN_POINT('Ctrl Pts',(-136.042694766605,-4.19652367769785,
133.372753456631));
#108506=CARTESIAN_POINT('Ctrl Pts',(-136.050342188114,-4.1228241219153,
133.486058647221));
#108507=CARTESIAN_POINT('Ctrl Pts',(-136.057993947771,-4.04908275863514,
133.59942811237));
#108508=CARTESIAN_POINT('Ctrl Pts',(-136.065645707428,-3.97073234307121,
133.7096449157));
#108509=CARTESIAN_POINT('Ctrl Pts',(-136.073297467085,-3.88809365920726,
133.816321898813));
#108510=CARTESIAN_POINT('Ctrl Pts',(-136.080960620258,-3.80533192585335,
133.923157724586));
#108511=CARTESIAN_POINT('Ctrl Pts',(-136.08862377343,-3.71826943466092,
134.026442899304));
#108512=CARTESIAN_POINT('Ctrl Pts',(-136.096286926603,-3.62726508325272,
134.125825818094));
#108513=CARTESIAN_POINT('Ctrl Pts',(-136.100990084209,-3.57141238163821,
134.186820753202));
#108514=CARTESIAN_POINT('Ctrl Pts',(-136.105693241816,-3.51407559081868,
134.246346564863));
#108515=CARTESIAN_POINT('Ctrl Pts',(-136.110396399423,-3.45534375231488,
134.304329562548));
#108516=CARTESIAN_POINT('Ctrl Pts',(-136.118170733542,-3.35825984100745,
134.400175637659));
#108517=CARTESIAN_POINT('Ctrl Pts',(-136.125945067661,-3.2570311930191,
134.492131020747));
#108518=CARTESIAN_POINT('Ctrl Pts',(-136.13371940178,-3.15200251286159,
134.579815983666));
#108519=CARTESIAN_POINT('Ctrl Pts',(-136.141484154727,-3.04710327116569,
134.667392882705));
#108520=CARTESIAN_POINT('Ctrl Pts',(-136.149248907674,-2.938413612713,134.750709585043));
#108521=CARTESIAN_POINT('Ctrl Pts',(-136.157013660621,-2.82631565412691,
134.829422466251));
#108522=CARTESIAN_POINT('Ctrl Pts',(-136.164770701506,-2.71432903281359,
134.908057168715));
#108523=CARTESIAN_POINT('Ctrl Pts',(-136.172527742391,-2.59894116590414,
134.982096926471));
#108524=CARTESIAN_POINT('Ctrl Pts',(-136.180284783276,-2.48056760048377,
135.051237992995));
#108525=CARTESIAN_POINT('Ctrl Pts',(-136.188035974517,-2.36228330148941,
135.120326919704));
#108526=CARTESIAN_POINT('Ctrl Pts',(-136.195787165757,-2.24101812176485,
135.184524311755));
#108527=CARTESIAN_POINT('Ctrl Pts',(-136.203538356997,-2.1172166743084,
135.243569625546));
#108528=CARTESIAN_POINT('Ctrl Pts',(-136.211286253774,-1.99346784577013,
135.302589843503));
#108529=CARTESIAN_POINT('Ctrl Pts',(-136.219034150551,-1.86718524566903,
135.356462170535));
#108530=CARTESIAN_POINT('Ctrl Pts',(-136.226782047328,-1.73883798414876,
135.404972047298));
#108531=CARTESIAN_POINT('Ctrl Pts',(-136.234528323412,-1.61051757010912,
135.453471776841));
#108532=CARTESIAN_POINT('Ctrl Pts',(-136.242274599496,-1.48013371917215,
135.496611149119));
#108533=CARTESIAN_POINT('Ctrl Pts',(-136.25002087558,-1.3481750422978,135.534223947286));
#108534=CARTESIAN_POINT('Ctrl Pts',(-136.257767208846,-1.2162153913343,
135.571837023101));
#108535=CARTESIAN_POINT('Ctrl Pts',(-136.265513542111,-1.08268126722637,
135.603923336231));
#108536=CARTESIAN_POINT('Ctrl Pts',(-136.273259875376,-0.948075558447773,
135.630366812959));
#108537=CARTESIAN_POINT('Ctrl Pts',(-136.281007943379,-0.813439705654168,
135.656816211521));
#108538=CARTESIAN_POINT('Ctrl Pts',(-136.288756011382,-0.677732174228575,
135.677620183767));
#108539=CARTESIAN_POINT('Ctrl Pts',(-136.296504079385,-0.541464741826425,
135.692714020897));
#108540=CARTESIAN_POINT('Ctrl Pts',(-136.304260382127,-0.405052482775329,
135.707823899937));
#108541=CARTESIAN_POINT('Ctrl Pts',(-136.312016684869,-0.268079523240667,
135.71721147767));
#108542=CARTESIAN_POINT('Ctrl Pts',(-136.319772987611,-0.131062003350017,
135.720864030946));
#108543=CARTESIAN_POINT('Ctrl Pts',(-136.327533430125,0.00602864691651589,
135.7245185337));
#108544=CARTESIAN_POINT('Ctrl Pts',(-136.335293872639,0.143163514200399,
135.722431918731));
#108545=CARTESIAN_POINT('Ctrl Pts',(-136.343054315153,0.279828779171258,
135.714643594834));
#108546=CARTESIAN_POINT('Ctrl Pts',(-136.350827215419,0.416713431358021,
135.706842768428));
#108547=CARTESIAN_POINT('Ctrl Pts',(-136.358600115684,0.553126585521877,
135.69332198129));
#108548=CARTESIAN_POINT('Ctrl Pts',(-136.36637301595,0.68856094957552,135.674172408716));
#108549=CARTESIAN_POINT('Ctrl Pts',(-136.373863351712,0.819071933359431,
135.655718971339));
#108550=CARTESIAN_POINT('Ctrl Pts',(-136.381353687474,0.948673751509082,
135.632038939921));
#108551=CARTESIAN_POINT('Ctrl Pts',(-136.388844023236,1.07692529810143,
135.603257883065));
#108552=CARTESIAN_POINT('Ctrl Pts',(-136.396618357355,1.21003954106235,
135.57338558369));
#108553=CARTESIAN_POINT('Ctrl Pts',(-136.404392691474,1.34212076605131,
135.537923185887));
#108554=CARTESIAN_POINT('Ctrl Pts',(-136.412167025593,1.47266317581575,
135.496955446986));
#108555=CARTESIAN_POINT('Ctrl Pts',(-136.41993177854,1.60304470372636,135.456038197161));
#108556=CARTESIAN_POINT('Ctrl Pts',(-136.427696531487,1.73189082034094,
135.409629221991));
#108557=CARTESIAN_POINT('Ctrl Pts',(-136.435461284435,1.8587058813254,135.357864269615));
#108558=CARTESIAN_POINT('Ctrl Pts',(-136.44321832532,1.98539498780385,135.30615073092));
#108559=CARTESIAN_POINT('Ctrl Pts',(-136.450975366204,2.11005669348842,
135.249091948123));
#108560=CARTESIAN_POINT('Ctrl Pts',(-136.458732407089,2.23221083447676,
135.186873350342));
#108561=CARTESIAN_POINT('Ctrl Pts',(-136.46648359833,2.35427285807766,135.124701672089));
#108562=CARTESIAN_POINT('Ctrl Pts',(-136.47423478957,2.47383073388311,135.057378100491));
#108563=CARTESIAN_POINT('Ctrl Pts',(-136.48198598081,2.59042493499383,134.985135870873));
#108564=CARTESIAN_POINT('Ctrl Pts',(-136.489733877587,2.70696958045836,
134.912924346129));
#108565=CARTESIAN_POINT('Ctrl Pts',(-136.497481774364,2.82055272491218,
134.83579852682));
#108566=CARTESIAN_POINT('Ctrl Pts',(-136.505229671141,2.93074028801205,
134.75403711403));
#108567=CARTESIAN_POINT('Ctrl Pts',(-136.512975947225,3.04090480224909,
134.672292803965));
#108568=CARTESIAN_POINT('Ctrl Pts',(-136.520722223309,3.14767483415114,
134.585915061963));
#108569=CARTESIAN_POINT('Ctrl Pts',(-136.528468499394,3.2506464346191,134.495225125997));
#108570=CARTESIAN_POINT('Ctrl Pts',(-136.536214832659,3.35361879520044,
134.404534520579));
#108571=CARTESIAN_POINT('Ctrl Pts',(-136.543961165924,3.45279237500059,
134.309531916081));
#108572=CARTESIAN_POINT('Ctrl Pts',(-136.55170749919,3.54779769441297,134.210577666143));
#108573=CARTESIAN_POINT('Ctrl Pts',(-136.559455567193,3.64282428960779,
134.111601256087));
#108574=CARTESIAN_POINT('Ctrl Pts',(-136.567203635196,3.7336804962337,134.008671721625));
#108575=CARTESIAN_POINT('Ctrl Pts',(-136.574951703199,3.8200352446217,133.902184659107));
#108576=CARTESIAN_POINT('Ctrl Pts',(-136.582708005941,3.9064817718638,133.795584420871));
#108577=CARTESIAN_POINT('Ctrl Pts',(-136.590464308682,3.9884170372592,133.685419405807));
#108578=CARTESIAN_POINT('Ctrl Pts',(-136.598220611424,4.06555135011611,
133.57211698005));
#108579=CARTESIAN_POINT('Ctrl Pts',(-136.605981053939,4.14272683187848,
133.458754081376));
#108580=CARTESIAN_POINT('Ctrl Pts',(-136.613741496453,4.21509604908112,
133.342250767308));
#108581=CARTESIAN_POINT('Ctrl Pts',(-136.621501938967,4.28241442556141,
133.22306063002));
#108582=CARTESIAN_POINT('Ctrl Pts',(-136.629274839232,4.34984086747569,
133.103679158142));
#108583=CARTESIAN_POINT('Ctrl Pts',(-136.637047739498,4.41220008822957,
132.98160259241));
#108584=CARTESIAN_POINT('Ctrl Pts',(-136.644820639763,4.46929459241776,
132.8573070145));
#108585=CARTESIAN_POINT('Ctrl Pts',(-136.652310975525,4.52431356756571,
132.73752989393));
#108586=CARTESIAN_POINT('Ctrl Pts',(-136.659801311287,4.57444383488916,
132.615692578412));
#108587=CARTESIAN_POINT('Ctrl Pts',(-136.667291647049,4.61955261028419,
132.492234055747));
#108588=CARTESIAN_POINT('Ctrl Pts',(-136.675065981168,4.66637169860943,
132.364094565669));
#108589=CARTESIAN_POINT('Ctrl Pts',(-136.682840315287,4.70792930736034,
132.233802598122));
#108590=CARTESIAN_POINT('Ctrl Pts',(-136.690614649406,4.74402334950908,
132.101829508065));
#108591=CARTESIAN_POINT('Ctrl Pts',(-136.698379402353,4.78007290897649,
131.970019063048));
#108592=CARTESIAN_POINT('Ctrl Pts',(-136.706144155301,4.81067219706714,
131.836531991347));
#108593=CARTESIAN_POINT('Ctrl Pts',(-136.713908908248,4.83566751466568,
131.701858667763));
#108594=CARTESIAN_POINT('Ctrl Pts',(-136.721665949133,4.86063800656254,
131.567319103622));
#108595=CARTESIAN_POINT('Ctrl Pts',(-136.729422990018,4.88001553356104,
131.431596014186));
#108596=CARTESIAN_POINT('Ctrl Pts',(-136.737180030903,4.89369656211065,
131.295193603913));
#108597=CARTESIAN_POINT('Ctrl Pts',(-136.744931222143,4.90736727369014,
131.158894055759));
#108598=CARTESIAN_POINT('Ctrl Pts',(-136.752682413383,4.91534999843821,
131.021916593871));
#108599=CARTESIAN_POINT('Ctrl Pts',(-136.760433604623,4.91759257832591,
130.884773900635));
#108600=CARTESIAN_POINT('Ctrl Pts',(-136.7681815014,4.91983420505734,130.747689496701));
#108601=CARTESIAN_POINT('Ctrl Pts',(-136.775929398177,4.916340532956,130.610440391191));
#108602=CARTESIAN_POINT('Ctrl Pts',(-136.783677294954,4.90711141010853,
130.473542432935));
#108603=CARTESIAN_POINT('Ctrl Pts',(-136.791423571038,4.89788421779461,
130.33667311078));
#108604=CARTESIAN_POINT('Ctrl Pts',(-136.799169847122,4.88292398734956,
130.200155179611));
#108605=CARTESIAN_POINT('Ctrl Pts',(-136.806916123206,4.86228264102318,
130.064502130215));
#108606=CARTESIAN_POINT('Ctrl Pts',(-136.814662456472,4.8416411423271,129.92884807946));
#108607=CARTESIAN_POINT('Ctrl Pts',(-136.822408789737,4.81531850288144,
129.794059309735));
#108608=CARTESIAN_POINT('Ctrl Pts',(-136.830155123002,4.78341818565514,
129.66064145464));
#108609=CARTESIAN_POINT('Ctrl Pts',(-136.837903191005,4.75151072457403,
129.527193721542));
#108610=CARTESIAN_POINT('Ctrl Pts',(-136.845651259008,4.71402319108318,
129.395117894156));
#108611=CARTESIAN_POINT('Ctrl Pts',(-136.853399327011,4.6711094603522,129.264906340262));
#108612=CARTESIAN_POINT('Ctrl Pts',(-136.861155629753,4.62815012039746,
129.134556395979));
#108613=CARTESIAN_POINT('Ctrl Pts',(-136.868911932495,4.57975318551552,
129.006075055103));
#108614=CARTESIAN_POINT('Ctrl Pts',(-136.876668235237,4.52612162604393,
128.879937044452));
#108615=CARTESIAN_POINT('Ctrl Pts',(-136.884428677751,4.4724614417941,128.753731710146));
#108616=CARTESIAN_POINT('Ctrl Pts',(-136.892189120265,4.41356123373883,
128.629872551106));
#108617=CARTESIAN_POINT('Ctrl Pts',(-136.899949562779,4.34967042242846,
128.508810513832));
#108618=CARTESIAN_POINT('Ctrl Pts',(-136.907722463045,4.28567704791581,
128.387554137029));
#108619=CARTESIAN_POINT('Ctrl Pts',(-136.91549536331,4.21667725780417,128.26910419284));
#108620=CARTESIAN_POINT('Ctrl Pts',(-136.923268263576,4.14296484199955,
128.153884173518));
#108621=CARTESIAN_POINT('Ctrl Pts',(-136.930758599338,4.07193205817919,
128.042852692118));
#108622=CARTESIAN_POINT('Ctrl Pts',(-136.9382489351,3.99652350800793,127.934820633374));
#108623=CARTESIAN_POINT('Ctrl Pts',(-136.945739270862,3.91703675130559,
127.830136995943));
#108624=CARTESIAN_POINT('Ctrl Pts',(-136.953513604981,3.83453623006422,
127.721484246582));
#108625=CARTESIAN_POINT('Ctrl Pts',(-136.9612879391,3.74738081033742,127.61609466235));
#108626=CARTESIAN_POINT('Ctrl Pts',(-136.969062273219,3.65585782342812,
127.514393043656));
#108627=CARTESIAN_POINT('Ctrl Pts',(-136.976827026166,3.5644476304208,127.412816763118));
#108628=CARTESIAN_POINT('Ctrl Pts',(-136.984591779113,3.46868083909066,
127.314919692574));
#108629=CARTESIAN_POINT('Ctrl Pts',(-136.99235653206,3.36888693751949,127.221096202998));
#108630=CARTESIAN_POINT('Ctrl Pts',(-137.000113572945,3.2691921526582,127.127365900235));
#108631=CARTESIAN_POINT('Ctrl Pts',(-137.00787061383,3.1654785003042,127.037701392911));
#108632=CARTESIAN_POINT('Ctrl Pts',(-137.015627654715,3.05811421953378,
126.952462321559));
#108633=CARTESIAN_POINT('Ctrl Pts',(-137.023378845955,2.95083090300311,
126.867287529654));
#108634=CARTESIAN_POINT('Ctrl Pts',(-137.031130037196,2.83990274262951,
126.78653177323));
#108635=CARTESIAN_POINT('Ctrl Pts',(-137.038881228436,2.72573287993491,
126.710516051667));
#108636=CARTESIAN_POINT('Ctrl Pts',(-137.046629125213,2.61161154247706,
126.634532638813));
#108637=CARTESIAN_POINT('Ctrl Pts',(-137.05437702199,2.49425156780679,126.563285470074));
#108638=CARTESIAN_POINT('Ctrl Pts',(-137.062124918767,2.37408687204156,
126.497053502152));
#108639=CARTESIAN_POINT('Ctrl Pts',(-137.069871194851,2.25394731214024,
126.430835388529));
#108640=CARTESIAN_POINT('Ctrl Pts',(-137.077617470935,2.13100454027969,
126.369630577666));
#108641=CARTESIAN_POINT('Ctrl Pts',(-137.085363747019,2.00571863604758,
126.313672940215));
#108642=CARTESIAN_POINT('Ctrl Pts',(-137.093110080284,1.88043180698355,
126.257714889698));
#108643=CARTESIAN_POINT('Ctrl Pts',(-137.10085641355,1.75280216801121,126.207004249324));
#108644=CARTESIAN_POINT('Ctrl Pts',(-137.108602746815,1.62331104726103,
126.16172728008));
#108645=CARTESIAN_POINT('Ctrl Pts',(-137.116350814818,1.49379092787166,
126.116440171371));
#108646=CARTESIAN_POINT('Ctrl Pts',(-137.124098882821,1.36240886617453,
126.076589284166));
#108647=CARTESIAN_POINT('Ctrl Pts',(-137.131846950824,1.22966227841419,
126.042311295736));
#108648=CARTESIAN_POINT('Ctrl Pts',(-137.139603253566,1.09677460600084,
126.007996876252));
#108649=CARTESIAN_POINT('Ctrl Pts',(-137.147359556308,0.962519889676573,
125.979267285165));
#108650=CARTESIAN_POINT('Ctrl Pts',(-137.155115859049,0.827407240983745,
125.956208359224));
#108651=CARTESIAN_POINT('Ctrl Pts',(-137.162876301564,0.692222478602147,
125.93313712604));
#108652=CARTESIAN_POINT('Ctrl Pts',(-137.170636744078,0.556179259057161,
125.915742638328));
#108653=CARTESIAN_POINT('Ctrl Pts',(-137.178397186592,0.419791794311216,
125.904058799113));
#108654=CARTESIAN_POINT('Ctrl Pts',(-137.186170086857,0.283185388298951,
125.892356203963));
#108655=CARTESIAN_POINT('Ctrl Pts',(-137.193942987123,0.146234023607563,
125.886382593425));
#108656=CARTESIAN_POINT('Ctrl Pts',(-137.201715887388,0.00945279688317982,
125.886119701636));
#108657=CARTESIAN_POINT('Ctrl Pts',(-137.20920622315,-0.12235608772347,
125.885866366625));
#108658=CARTESIAN_POINT('Ctrl Pts',(-137.216696558913,-0.254006681698812,
125.890915748984));
#108659=CARTESIAN_POINT('Ctrl Pts',(-137.224186894675,-0.385044524237053,
125.901206145509));
#108660=CARTESIAN_POINT('Ctrl Pts',(-137.231961228794,-0.521050706398806,
125.911886705545));
#108661=CARTESIAN_POINT('Ctrl Pts',(-137.239735562913,-0.656827581653451,
125.928247383969));
#108662=CARTESIAN_POINT('Ctrl Pts',(-137.247509897032,-0.79186244379773,
125.950276055818));
#108663=CARTESIAN_POINT('Ctrl Pts',(-137.255274649979,-0.926730887542094,
125.972277579297));
#108664=CARTESIAN_POINT('Ctrl Pts',(-137.263039402926,-1.06085875552832,
125.999933135201));
#108665=CARTESIAN_POINT('Ctrl Pts',(-137.270804155873,-1.19373615592827,
126.033178683021));
#108666=CARTESIAN_POINT('Ctrl Pts',(-137.278561196758,-1.32648158062163,
126.066391210894));
#108667=CARTESIAN_POINT('Ctrl Pts',(-137.286318237643,-1.45797863250889,
126.105182587557));
#108668=CARTESIAN_POINT('Ctrl Pts',(-137.294075278528,-1.58772569360855,
126.149437397538));
#108669=CARTESIAN_POINT('Ctrl Pts',(-137.301826469769,-1.71737491144033,
126.193658834623));
#108670=CARTESIAN_POINT('Ctrl Pts',(-137.309577661009,-1.84527639669542,
126.243335378678));
#108671=CARTESIAN_POINT('Ctrl Pts',(-137.317328852249,-1.97094217566513,
126.29830136333));
#108672=CARTESIAN_POINT('Ctrl Pts',(-137.325076749026,-2.09655454332602,
126.353243985972));
#108673=CARTESIAN_POINT('Ctrl Pts',(-137.332824645803,-2.21993273719704,
126.413471421457));
#108674=CARTESIAN_POINT('Ctrl Pts',(-137.34057254258,-2.34060752084383,
126.478769386778));
#108675=CARTESIAN_POINT('Ctrl Pts',(-137.348318818664,-2.46125706192766,
126.544053693172));
#108676=CARTESIAN_POINT('Ctrl Pts',(-137.356065094748,-2.57920397395281,
126.614406233777));
#108677=CARTESIAN_POINT('Ctrl Pts',(-137.363811370832,-2.69400281065868,
126.689566343406));
#108678=CARTESIAN_POINT('Ctrl Pts',(-137.371557704098,-2.80880249478363,
126.764727007849));
#108679=CARTESIAN_POINT('Ctrl Pts',(-137.379304037363,-2.9204537301225,
126.844695097978));
#108680=CARTESIAN_POINT('Ctrl Pts',(-137.387050370628,-3.028539640421,126.929166337417));
#108681=CARTESIAN_POINT('Ctrl Pts',(-137.394798438631,-3.13664975580955,
127.013656493604));
#108682=CARTESIAN_POINT('Ctrl Pts',(-137.402546506634,-3.24119264938395,
127.102651565097));
#108683=CARTESIAN_POINT('Ctrl Pts',(-137.410294574637,-3.34178446505332,
127.195806938926));
#108684=CARTESIAN_POINT('Ctrl Pts',(-137.418050877379,-3.44248319090131,
127.289061319394));
#108685=CARTESIAN_POINT('Ctrl Pts',(-137.425807180121,-3.53922216307358,
127.386484568788));
#108686=CARTESIAN_POINT('Ctrl Pts',(-137.433563482863,-3.63165397745896,
127.487694754006));
#108687=CARTESIAN_POINT('Ctrl Pts',(-137.441323925377,-3.724135125487,127.588958958147));
#108688=CARTESIAN_POINT('Ctrl Pts',(-137.449084367891,-3.81230428384118,
127.694013826203));
#108689=CARTESIAN_POINT('Ctrl Pts',(-137.456844810405,-3.8958549848198,
127.802445062499));
#108690=CARTESIAN_POINT('Ctrl Pts',(-137.464617710671,-3.97953980880069,
127.911050362241));
#108691=CARTESIAN_POINT('Ctrl Pts',(-137.472390610936,-4.0585911343669,
128.023042541611));
#108692=CARTESIAN_POINT('Ctrl Pts',(-137.480163511202,-4.13274590678611,
128.137978362066));
#108693=CARTESIAN_POINT('Ctrl Pts',(-137.487653846963,-4.20420496644208,
128.248735975941));
#108694=CARTESIAN_POINT('Ctrl Pts',(-137.495144182725,-4.27111713984203,
128.362226663688));
#108695=CARTESIAN_POINT('Ctrl Pts',(-137.502634518487,-4.33328869247314,
128.478034722472));
#108696=CARTESIAN_POINT('Ctrl Pts',(-137.510836564675,-4.40136760942104,
128.604846534019));
#108697=CARTESIAN_POINT('Ctrl Pts',(-137.519038610863,-4.46395870610563,
128.734802713715));
#108698=CARTESIAN_POINT('Ctrl Pts',(-137.527240657051,-4.52077679713304,
128.867414512739));
#108699=CARTESIAN_POINT('Ctrl Pts',(-137.535424098946,-4.57746601051898,
128.999725515035));
#108700=CARTESIAN_POINT('Ctrl Pts',(-137.543607540842,-4.62840819793778,
129.134679827183));
#108701=CARTESIAN_POINT('Ctrl Pts',(-137.551790982737,-4.67336421070967,
129.27176477503));
#108702=CARTESIAN_POINT('Ctrl Pts',(-137.557907428584,-4.70696511129607,
129.374224433271));
#108703=CARTESIAN_POINT('Ctrl Pts',(-137.56402387443,-4.73722283313247,
129.477873747335));
#108704=CARTESIAN_POINT('Ctrl Pts',(-137.570140320276,-4.76405452823416,
129.582490119309));
#108705=CARTESIAN_POINT('Origin',(213.235140564004,0.,130.804360617566));
#108706=CARTESIAN_POINT('',(-139.665053375618,-4.76405452823406,129.582490119308));
#108707=CARTESIAN_POINT('',(-139.319813188101,-4.76405452823411,129.582490119308));
#108708=CARTESIAN_POINT('',(213.235140564004,-4.76405452823405,129.582490119308));
#108709=CARTESIAN_POINT('',(-137.985140563981,-4.91824805669077,130.808732728893));
#108710=CARTESIAN_POINT('Ctrl Pts',(-137.985140564011,-4.9182480566903,
130.808732729428));
#108711=CARTESIAN_POINT('Ctrl Pts',(-137.996393910965,-4.91807169202414,
131.007127739449));
#108712=CARTESIAN_POINT('Ctrl Pts',(-138.007647257918,-4.90588761893176,
131.205010702));
#108713=CARTESIAN_POINT('Ctrl Pts',(-138.018900604872,-4.88190026809492,
131.401213057349));
#108714=CARTESIAN_POINT('Ctrl Pts',(-138.025913993233,-4.86695070616923,
131.523491639974));
#108715=CARTESIAN_POINT('Ctrl Pts',(-138.032927381593,-4.84741748905136,
131.645118254441));
#108716=CARTESIAN_POINT('Ctrl Pts',(-138.039940769954,-4.82335853939743,
131.765815485421));
#108717=CARTESIAN_POINT('Ctrl Pts',(-138.047715104073,-4.79668921730225,
131.899608247586));
#108718=CARTESIAN_POINT('Ctrl Pts',(-138.055489438192,-4.76440661700594,
132.032502436212));
#108719=CARTESIAN_POINT('Ctrl Pts',(-138.063263772311,-4.72658333369079,
132.163990365761));
#108720=CARTESIAN_POINT('Ctrl Pts',(-138.071028525258,-4.68880666419196,
132.295316248188));
#108721=CARTESIAN_POINT('Ctrl Pts',(-138.078793278205,-4.64550300519149,
132.425238947745));
#108722=CARTESIAN_POINT('Ctrl Pts',(-138.086558031152,-4.59679617163898,
132.553259705251));
#108723=CARTESIAN_POINT('Ctrl Pts',(-138.094315072037,-4.54813771440021,
132.681153310736));
#108724=CARTESIAN_POINT('Ctrl Pts',(-138.102072112922,-4.49408690032992,
132.807148370388));
#108725=CARTESIAN_POINT('Ctrl Pts',(-138.109829153807,-4.43481758253591,
132.930760408793));
#108726=CARTESIAN_POINT('Ctrl Pts',(-138.117580345047,-4.37559296019541,
133.054279230399));
#108727=CARTESIAN_POINT('Ctrl Pts',(-138.125331536288,-4.31115783548495,
133.175418256576));
#108728=CARTESIAN_POINT('Ctrl Pts',(-138.133082727528,-4.24173434918522,
133.293712495755));
#108729=CARTESIAN_POINT('Ctrl Pts',(-138.140830624305,-4.172340369719,133.411956456726));
#108730=CARTESIAN_POINT('Ctrl Pts',(-138.148578521082,-4.09796244302441,
133.527357699045));
#108731=CARTESIAN_POINT('Ctrl Pts',(-138.156326417859,-4.01886877319504,
133.639475579316));
#108732=CARTESIAN_POINT('Ctrl Pts',(-138.164072693943,-3.93979164805634,
133.751570006943));
#108733=CARTESIAN_POINT('Ctrl Pts',(-138.171818970027,-3.8560009670781,
133.860382119352));
#108734=CARTESIAN_POINT('Ctrl Pts',(-138.179565246112,-3.76780818206042,
133.965500374948));
#108735=CARTESIAN_POINT('Ctrl Pts',(-138.187311579377,-3.67961474602376,
134.070619406502));
#108736=CARTESIAN_POINT('Ctrl Pts',(-138.195057912642,-3.58701939239329,
134.172044227318));
#108737=CARTESIAN_POINT('Ctrl Pts',(-138.202804245908,-3.49037350454223,
134.269396816697));
#108738=CARTESIAN_POINT('Ctrl Pts',(-138.210552313911,-3.39370597351482,
134.366771207514));
#108739=CARTESIAN_POINT('Ctrl Pts',(-138.218300381914,-3.29298637865716,
134.460071274816));
#108740=CARTESIAN_POINT('Ctrl Pts',(-138.226048449916,-3.18860225763736,
134.548956551053));
#108741=CARTESIAN_POINT('Ctrl Pts',(-138.233804752658,-3.08410719593141,
134.63793629562));
#108742=CARTESIAN_POINT('Ctrl Pts',(-138.2415610554,-2.97594012611937,134.722491622287));
#108743=CARTESIAN_POINT('Ctrl Pts',(-138.249317358142,-2.86452133948699,
134.802322668177));
#108744=CARTESIAN_POINT('Ctrl Pts',(-138.257077800656,-2.75304308529314,
134.8821963223));
#108745=CARTESIAN_POINT('Ctrl Pts',(-138.264838243171,-2.6383099829711,
134.957340457259));
#108746=CARTESIAN_POINT('Ctrl Pts',(-138.272598685685,-2.52076962491561,
135.027499682362));
#108747=CARTESIAN_POINT('Ctrl Pts',(-138.28037158595,-2.40304058064295,
135.097771533281));
#108748=CARTESIAN_POINT('Ctrl Pts',(-138.288144486216,-2.28249561930117,
135.163042297096));
#108749=CARTESIAN_POINT('Ctrl Pts',(-138.295917386481,-2.1596059461205,
135.223103110627));
#108750=CARTESIAN_POINT('Ctrl Pts',(-138.303407722243,-2.04118362210135,
135.280980562302));
#108751=CARTESIAN_POINT('Ctrl Pts',(-138.310898058005,-1.9205843809104,
135.334020152977));
#108752=CARTESIAN_POINT('Ctrl Pts',(-138.318388393767,-1.79824389748059,
135.382078602291));
#108753=CARTESIAN_POINT('Ctrl Pts',(-138.326162727886,-1.67126483743606,
135.431959202318));
#108754=CARTESIAN_POINT('Ctrl Pts',(-138.333937062005,-1.54200765877966,
135.476631491471));
#108755=CARTESIAN_POINT('Ctrl Pts',(-138.341711396124,-1.41093873120191,
135.515882129699));
#108756=CARTESIAN_POINT('Ctrl Pts',(-138.349476149071,-1.28003133436342,
135.555084395024));
#108757=CARTESIAN_POINT('Ctrl Pts',(-138.357240902018,-1.14731700218345,
135.588878192932));
#108758=CARTESIAN_POINT('Ctrl Pts',(-138.365005654965,-1.01328227989185,
135.617098100928));
#108759=CARTESIAN_POINT('Ctrl Pts',(-138.37276269585,-0.879380682775994,
135.645289980513));
#108760=CARTESIAN_POINT('Ctrl Pts',(-138.380519736736,-0.744161685455616,
135.66791890718));
#108761=CARTESIAN_POINT('Ctrl Pts',(-138.388276777621,-0.60812686266937,
135.684869277675));
#108762=CARTESIAN_POINT('Ctrl Pts',(-138.396027968861,-0.472194624800999,
135.701806865764));
#108763=CARTESIAN_POINT('Ctrl Pts',(-138.403779160101,-0.335448172420758,
135.713074373082));
#108764=CARTESIAN_POINT('Ctrl Pts',(-138.411530351341,-0.198398788625114,
135.718607353656));
#108765=CARTESIAN_POINT('Ctrl Pts',(-138.419278248118,-0.0614076544733079,
135.724137982566));
#108766=CARTESIAN_POINT('Ctrl Pts',(-138.427026144895,0.0758857651830259,
135.723938916651));
#108767=CARTESIAN_POINT('Ctrl Pts',(-138.434774041672,0.212965773710997,
135.717997625092));
#108768=CARTESIAN_POINT('Ctrl Pts',(-138.442520317756,0.350017108055913,
135.712057576323));
#108769=CARTESIAN_POINT('Ctrl Pts',(-138.45026659384,0.486854729714837,
135.700377707982));
#108770=CARTESIAN_POINT('Ctrl Pts',(-138.458012869925,0.622964049780873,
135.682997605002));
#108771=CARTESIAN_POINT('Ctrl Pts',(-138.46575920319,0.759074374575175,
135.665617373727));
#108772=CARTESIAN_POINT('Ctrl Pts',(-138.473505536455,0.894455999232597,
135.642536873371));
#108773=CARTESIAN_POINT('Ctrl Pts',(-138.481251869721,1.02860095293648,
135.613847403297));
#108774=CARTESIAN_POINT('Ctrl Pts',(-138.488999937724,1.16277594747246,
135.585151508415));
#108775=CARTESIAN_POINT('Ctrl Pts',(-138.496748005726,1.29571333772249,
135.550844226091));
#108776=CARTESIAN_POINT('Ctrl Pts',(-138.504496073729,1.42691720511787,
135.511067571715));
#108777=CARTESIAN_POINT('Ctrl Pts',(-138.512252376471,1.55826051754504,
135.471248642238));
#108778=CARTESIAN_POINT('Ctrl Pts',(-138.520008679213,1.68786625196201,
135.425948842396));
#108779=CARTESIAN_POINT('Ctrl Pts',(-138.527764981955,1.81525494753177,
135.375359691944));
#108780=CARTESIAN_POINT('Ctrl Pts',(-138.535525424469,1.94271163428396,
135.324743540538));
#108781=CARTESIAN_POINT('Ctrl Pts',(-138.543285866983,2.067948567534,135.268832572587));
#108782=CARTESIAN_POINT('Ctrl Pts',(-138.551046309498,2.1905089452371,135.207865315342));
#108783=CARTESIAN_POINT('Ctrl Pts',(-138.558819209763,2.31326606773889,
135.146800188043));
#108784=CARTESIAN_POINT('Ctrl Pts',(-138.566592110028,2.43333770597991,
135.080662740224));
#108785=CARTESIAN_POINT('Ctrl Pts',(-138.574365010294,2.55029343951556,
135.009736514542));
#108786=CARTESIAN_POINT('Ctrl Pts',(-138.581855346056,2.66299753754316,
134.941388635815));
#108787=CARTESIAN_POINT('Ctrl Pts',(-138.589345681818,2.77280808300221,
134.868594272977));
#108788=CARTESIAN_POINT('Ctrl Pts',(-138.59683601758,2.87936903712286,134.791642525151));
#108789=CARTESIAN_POINT('Ctrl Pts',(-138.604610351699,2.98997028220766,
134.711773128418));
#108790=CARTESIAN_POINT('Ctrl Pts',(-138.612384685818,3.09742100660305,
134.62717186673));
#108791=CARTESIAN_POINT('Ctrl Pts',(-138.620159019937,3.20128963707245,
134.538115794606));
#108792=CARTESIAN_POINT('Ctrl Pts',(-138.627923772884,3.3050302587378,134.449169476132));
#108793=CARTESIAN_POINT('Ctrl Pts',(-138.635688525831,3.40519727627937,
134.355779523033));
#108794=CARTESIAN_POINT('Ctrl Pts',(-138.643453278778,3.50138852548422,
134.25826586469));
#108795=CARTESIAN_POINT('Ctrl Pts',(-138.651210319663,3.5974842361843,134.160849058286));
#108796=CARTESIAN_POINT('Ctrl Pts',(-138.658967360548,3.68961176403253,
134.059316973845));
#108797=CARTESIAN_POINT('Ctrl Pts',(-138.666724401433,3.77740273534095,
133.954029114017));
#108798=CARTESIAN_POINT('Ctrl Pts',(-138.674475592673,3.8651275027951,133.848820652584));
#108799=CARTESIAN_POINT('Ctrl Pts',(-138.682226783913,3.94852197354323,
133.739862352265));
#108800=CARTESIAN_POINT('Ctrl Pts',(-138.689977975154,4.02725556636115,
133.627549535388));
#108801=CARTESIAN_POINT('Ctrl Pts',(-138.697725871931,4.10595569530195,
133.515284454454));
#108802=CARTESIAN_POINT('Ctrl Pts',(-138.705473768708,4.17999866241224,
133.399668012156));
#108803=CARTESIAN_POINT('Ctrl Pts',(-138.713221665485,4.24909517853229,
133.281127305462));
#108804=CARTESIAN_POINT('Ctrl Pts',(-138.720967941569,4.31817724115053,
133.162611394929));
#108805=CARTESIAN_POINT('Ctrl Pts',(-138.728714217653,4.38231471407525,
133.04117277425));
#108806=CARTESIAN_POINT('Ctrl Pts',(-138.736460493737,4.44126275335914,
132.917265778269));
#108807=CARTESIAN_POINT('Ctrl Pts',(-138.744206827003,4.50021122778415,
132.793357867635));
#108808=CARTESIAN_POINT('Ctrl Pts',(-138.751953160268,4.5539700241684,132.666981898389));
#108809=CARTESIAN_POINT('Ctrl Pts',(-138.759699493533,4.60234138461656,
132.538614590301));
#108810=CARTESIAN_POINT('Ctrl Pts',(-138.767447561536,4.65072357749543,
132.410218535244));
#108811=CARTESIAN_POINT('Ctrl Pts',(-138.775195629539,4.69371579585063,
132.279830619747));
#108812=CARTESIAN_POINT('Ctrl Pts',(-138.782943697542,4.7311694651505,132.147944836931));
#108813=CARTESIAN_POINT('Ctrl Pts',(-138.790700000284,4.76866294065585,
132.015918884336));
#108814=CARTESIAN_POINT('Ctrl Pts',(-138.798456303026,4.80060600134069,
131.882392261023));
#108815=CARTESIAN_POINT('Ctrl Pts',(-138.806212605767,4.82690061790301,
131.747871872076));
#108816=CARTESIAN_POINT('Ctrl Pts',(-138.813973048282,4.85320926869389,
131.613279685548));
#108817=CARTESIAN_POINT('Ctrl Pts',(-138.821733490796,4.87386340937981,
131.477693062832));
#108818=CARTESIAN_POINT('Ctrl Pts',(-138.82949393331,4.88881680702904,131.341625254231));
#108819=CARTESIAN_POINT('Ctrl Pts',(-138.837266833575,4.90379420919969,
131.205339017504));
#108820=CARTESIAN_POINT('Ctrl Pts',(-138.845039733841,4.9130525546221,131.068570441603));
#108821=CARTESIAN_POINT('Ctrl Pts',(-138.852812634106,4.91659774299873,
130.93183491317));
#108822=CARTESIAN_POINT('Ctrl Pts',(-138.860302969868,4.92001405484807,
130.800070065612));
#108823=CARTESIAN_POINT('Ctrl Pts',(-138.86779330563,4.91812537784109,130.668336212506));
#108824=CARTESIAN_POINT('Ctrl Pts',(-138.875283641392,4.91098249160705,
130.537089164491));
#108825=CARTESIAN_POINT('Ctrl Pts',(-138.883057975511,4.9035687806704,130.400865844758));
#108826=CARTESIAN_POINT('Ctrl Pts',(-138.89083230963,4.89047108434516,130.264735458718));
#108827=CARTESIAN_POINT('Ctrl Pts',(-138.898606643749,4.87168922056954,
130.129210855893));
#108828=CARTESIAN_POINT('Ctrl Pts',(-138.906371396697,4.85293050376244,
129.993853275029));
#108829=CARTESIAN_POINT('Ctrl Pts',(-138.914136149644,4.82850161097577,
129.859100375468));
#108830=CARTESIAN_POINT('Ctrl Pts',(-138.921900902591,4.79845432827841,
129.725463438996));
#108831=CARTESIAN_POINT('Ctrl Pts',(-138.929657943476,4.76843688896581,
129.591959232614));
#108832=CARTESIAN_POINT('Ctrl Pts',(-138.937414984361,4.73281224992935,
129.459569162548));
#108833=CARTESIAN_POINT('Ctrl Pts',(-138.945172025246,4.6916837559549,129.328797471981));
#108834=CARTESIAN_POINT('Ctrl Pts',(-138.952923216486,4.65058627729763,
129.198124397363));
#108835=CARTESIAN_POINT('Ctrl Pts',(-138.960674407726,4.60399332184252,
129.069067644491));
#108836=CARTESIAN_POINT('Ctrl Pts',(-138.968425598966,4.55205879823291,
128.942119022087));
#108837=CARTESIAN_POINT('Ctrl Pts',(-138.976173495743,4.50014634818131,
128.815224356235));
#108838=CARTESIAN_POINT('Ctrl Pts',(-138.98392139252,4.44289699317143,128.690436399849));
#108839=CARTESIAN_POINT('Ctrl Pts',(-138.991669289297,4.38051369412193,
128.568229396436));
#108840=CARTESIAN_POINT('Ctrl Pts',(-138.999415565381,4.31814344431375,
128.446047956095));
#108841=CARTESIAN_POINT('Ctrl Pts',(-139.007161841465,4.25064156417624,
128.326446742875));
#108842=CARTESIAN_POINT('Ctrl Pts',(-139.01490811755,4.17825795434795,128.209877330006));
#108843=CARTESIAN_POINT('Ctrl Pts',(-139.022654450815,4.1058738102002,128.093307056648));
#108844=CARTESIAN_POINT('Ctrl Pts',(-139.03040078408,4.02860807069741,127.979768960439));
#108845=CARTESIAN_POINT('Ctrl Pts',(-139.038147117346,3.94675492071036,
127.869687099379));
#108846=CARTESIAN_POINT('Ctrl Pts',(-139.045895185349,3.86488344027801,
127.759580586249));
#108847=CARTESIAN_POINT('Ctrl Pts',(-139.053643253352,3.77842273835661,
127.652932162116));
#108848=CARTESIAN_POINT('Ctrl Pts',(-139.061391321355,3.6877081171879,127.55013384229));
#108849=CARTESIAN_POINT('Ctrl Pts',(-139.069147624096,3.59689708344042,
127.447226267186));
#108850=CARTESIAN_POINT('Ctrl Pts',(-139.076903926838,3.50182335812934,
127.348177264087));
#108851=CARTESIAN_POINT('Ctrl Pts',(-139.08466022958,3.4028604276272,127.253343302403));
#108852=CARTESIAN_POINT('Ctrl Pts',(-139.092420672094,3.30384467762906,
127.158458724977));
#108853=CARTESIAN_POINT('Ctrl Pts',(-139.100181114608,3.20093587947142,
127.067793929997));
#108854=CARTESIAN_POINT('Ctrl Pts',(-139.107941557123,3.09454085514129,
126.981665238862));
#108855=CARTESIAN_POINT('Ctrl Pts',(-139.115714457388,2.9879750360728,126.895398286307));
#108856=CARTESIAN_POINT('Ctrl Pts',(-139.123487357653,2.87791212152879,
126.813682222061));
#108857=CARTESIAN_POINT('Ctrl Pts',(-139.131260257919,2.76478890982042,
126.736790661605));
#108858=CARTESIAN_POINT('Ctrl Pts',(-139.138750593681,2.65577801179751,
126.662694303051));
#108859=CARTESIAN_POINT('Ctrl Pts',(-139.146240929443,2.54392571422631,
126.593077935124));
#108860=CARTESIAN_POINT('Ctrl Pts',(-139.153731265205,2.42964295113666,
126.52814521227));
#108861=CARTESIAN_POINT('Ctrl Pts',(-139.161505599324,2.31102712234946,
126.460750545493));
#108862=CARTESIAN_POINT('Ctrl Pts',(-139.169279933443,2.18941714836848,
126.398188209533));
#108863=CARTESIAN_POINT('Ctrl Pts',(-139.177054267562,2.0652444056126,126.340735565259));
#108864=CARTESIAN_POINT('Ctrl Pts',(-139.184819020509,1.94122469466454,
126.283353726233));
#108865=CARTESIAN_POINT('Ctrl Pts',(-139.192583773456,1.81464885060286,
126.231069211861));
#108866=CARTESIAN_POINT('Ctrl Pts',(-139.200348526404,1.68597502091083,
126.184114813351));
#108867=CARTESIAN_POINT('Ctrl Pts',(-139.208105567289,1.55742899188043,
126.137207050612));
#108868=CARTESIAN_POINT('Ctrl Pts',(-139.215862608174,1.42678948887343,
126.095619001698));
#108869=CARTESIAN_POINT('Ctrl Pts',(-139.223619649059,1.29453660634004,
126.05953627547));
#108870=CARTESIAN_POINT('Ctrl Pts',(-139.231370840299,1.16238345673433,
126.023480759507));
#108871=CARTESIAN_POINT('Ctrl Pts',(-139.239122031539,1.02861972494722,
125.992922405199));
#108872=CARTESIAN_POINT('Ctrl Pts',(-139.246873222779,0.893742374965194,
125.967997559472));
#108873=CARTESIAN_POINT('Ctrl Pts',(-139.254621119556,0.758922351454701,
125.94308330747));
#108874=CARTESIAN_POINT('Ctrl Pts',(-139.262369016333,0.622990034792487,
125.923797872684));
#108875=CARTESIAN_POINT('Ctrl Pts',(-139.27011691311,0.486454124806543,
125.910226838545));
#108876=CARTESIAN_POINT('Ctrl Pts',(-139.277863189194,0.349946775189595,
125.896658643173));
#108877=CARTESIAN_POINT('Ctrl Pts',(-139.285609465278,0.212836472186074,
125.888802509518));
#108878=CARTESIAN_POINT('Ctrl Pts',(-139.293355741362,0.075638214541899,
125.886692275455));
#108879=CARTESIAN_POINT('Ctrl Pts',(-139.301102074628,-0.0615610558684601,
125.884582025815));
#108880=CARTESIAN_POINT('Ctrl Pts',(-139.308848407893,-0.198847891296058,
125.888217766415));
#108881=CARTESIAN_POINT('Ctrl Pts',(-139.316594741158,-0.335706505628503,
125.897581204898));
#108882=CARTESIAN_POINT('Ctrl Pts',(-139.324342809161,-0.472595768498903,
125.906946740259));
#108883=CARTESIAN_POINT('Ctrl Pts',(-139.332090877164,-0.609056229471209,
125.922042499203));
#108884=CARTESIAN_POINT('Ctrl Pts',(-139.339838945167,-0.744576835910049,
125.942798276309));
#108885=CARTESIAN_POINT('Ctrl Pts',(-139.347595247909,-0.880241475262313,
125.963576112902));
#108886=CARTESIAN_POINT('Ctrl Pts',(-139.355351550651,-1.0149638776184,
125.990025925053));
#108887=CARTESIAN_POINT('Ctrl Pts',(-139.363107853393,-1.14824225666175,
126.022026168522));
#108888=CARTESIAN_POINT('Ctrl Pts',(-139.370868295907,-1.28159177038893,
126.054043491484));
#108889=CARTESIAN_POINT('Ctrl Pts',(-139.378628738421,-1.41349534925753,
126.091617041605));
#108890=CARTESIAN_POINT('Ctrl Pts',(-139.386389180935,-1.54346696589354,
126.134575527469));
#108891=CARTESIAN_POINT('Ctrl Pts',(-139.394162081201,-1.67364722450692,
126.177602974108));
#108892=CARTESIAN_POINT('Ctrl Pts',(-139.401934981466,-1.8018889574237,
126.226032492506));
#108893=CARTESIAN_POINT('Ctrl Pts',(-139.409707881732,-1.92772586403322,
126.279644487726));
#108894=CARTESIAN_POINT('Ctrl Pts',(-139.417198217494,-2.04898828212412,
126.331307551878));
#108895=CARTESIAN_POINT('Ctrl Pts',(-139.424688553256,-2.16801740308042,
126.387782710308));
#108896=CARTESIAN_POINT('Ctrl Pts',(-139.432178889018,-2.28441976676988,
126.448834312779));
#108897=CARTESIAN_POINT('Ctrl Pts',(-139.439954129292,-2.40524964342127,
126.512208091129));
#108898=CARTESIAN_POINT('Ctrl Pts',(-139.447729369567,-2.52363178103368,
126.580714118607));
#108899=CARTESIAN_POINT('Ctrl Pts',(-139.455504609842,-2.6390994965336,
126.654139309022));
#108900=CARTESIAN_POINT('Ctrl Pts',(-139.463270068542,-2.75442194887057,
126.727472127509));
#108901=CARTESIAN_POINT('Ctrl Pts',(-139.471035527243,-2.86683694802424,
126.80571158659));
#108902=CARTESIAN_POINT('Ctrl Pts',(-139.478800985943,-2.97590088322747,
126.888597984859));
#108903=CARTESIAN_POINT('Ctrl Pts',(-139.48656150218,-3.08489540275135,
126.971431628606));
#108904=CARTESIAN_POINT('Ctrl Pts',(-139.494322018416,-3.19054278141714,
127.058906106823));
#108905=CARTESIAN_POINT('Ctrl Pts',(-139.502082534653,-3.29242681219755,
127.150717401703));
#108906=CARTESIAN_POINT('Ctrl Pts',(-139.509833439601,-3.39418466107156,
127.242414989615));
#108907=CARTESIAN_POINT('Ctrl Pts',(-139.51758434455,-3.49218816612692,
127.338438423298));
#108908=CARTESIAN_POINT('Ctrl Pts',(-139.525335249499,-3.58605405763608,
127.438443304528));
#108909=CARTESIAN_POINT('Ctrl Pts',(-139.533082571577,-3.67987655945166,
127.538401958304));
#108910=CARTESIAN_POINT('Ctrl Pts',(-139.540829893654,-3.76956498665699,
127.642338113013));
#108911=CARTESIAN_POINT('Ctrl Pts',(-139.548577215732,-3.85477247012094,
127.749870109135));
#108912=CARTESIAN_POINT('Ctrl Pts',(-139.556322634353,-3.93995901877257,
127.857375685485));
#108913=CARTESIAN_POINT('Ctrl Pts',(-139.564068052974,-4.02066657293211,
127.968475038309));
#108914=CARTESIAN_POINT('Ctrl Pts',(-139.571813471595,-4.09658841676912,
128.082753297232));
#108915=CARTESIAN_POINT('Ctrl Pts',(-139.579583463597,-4.17275113285114,
128.197394119279));
#108916=CARTESIAN_POINT('Ctrl Pts',(-139.587353455599,-4.24409748231012,
128.315233736527));
#108917=CARTESIAN_POINT('Ctrl Pts',(-139.595123447601,-4.31036172877056,
128.435824185579));
#108918=CARTESIAN_POINT('Ctrl Pts',(-139.602872468509,-4.37644712900863,
128.55608916279));
#108919=CARTESIAN_POINT('Ctrl Pts',(-139.610621489417,-4.43747766755824,
128.679089780643));
#108920=CARTESIAN_POINT('Ctrl Pts',(-139.618370510325,-4.49323626298589,
128.804357880696));
#108921=CARTESIAN_POINT('Ctrl Pts',(-139.626150987874,-4.54922120676266,
128.930134498358));
#108922=CARTESIAN_POINT('Ctrl Pts',(-139.633931465423,-4.59989115241724,
129.058196684052));
#108923=CARTESIAN_POINT('Ctrl Pts',(-139.641711942971,-4.64507580615303,
129.188051916361));
#108924=CARTESIAN_POINT('Ctrl Pts',(-139.64949242052,-4.69026045988882,
129.317907148669));
#108925=CARTESIAN_POINT('Ctrl Pts',(-139.657272898069,-4.7299597353934,
129.449555039483));
#108926=CARTESIAN_POINT('Ctrl Pts',(-139.665053375618,-4.76405452823406,
129.582490119308));
#108927=CARTESIAN_POINT('Ctrl Pts',(-137.915064401336,-4.76405452823416,
129.582490119309));
#108928=CARTESIAN_POINT('Ctrl Pts',(-137.922702589614,-4.79767840181093,
129.713589092071));
#108929=CARTESIAN_POINT('Ctrl Pts',(-137.930340777891,-4.82587511235423,
129.84603213272));
#108930=CARTESIAN_POINT('Ctrl Pts',(-137.937978966169,-4.84855616045776,
129.979323514529));
#108931=CARTESIAN_POINT('Ctrl Pts',(-137.945839232471,-4.87189665320671,
130.116490303137));
#108932=CARTESIAN_POINT('Ctrl Pts',(-137.953699498773,-4.88939578415974,
130.2545550626));
#108933=CARTESIAN_POINT('Ctrl Pts',(-137.961559765075,-4.90101442601767,
130.392971922453));
#108934=CARTESIAN_POINT('Ctrl Pts',(-137.969420031377,-4.91263306787557,
130.531388782306));
#108935=CARTESIAN_POINT('Ctrl Pts',(-137.977280297679,-4.91837124431475,
130.67015727946));
#108936=CARTESIAN_POINT('Ctrl Pts',(-137.985140563981,-4.91824805669077,
130.808732728894));
#108937=CARTESIAN_POINT('',(-137.639859435963,-4.91824999609688,130.804164676221));
#108938=CARTESIAN_POINT('Ctrl Pts',(-137.570140320276,-4.76405452823416,
129.582490119309));
#108939=CARTESIAN_POINT('Ctrl Pts',(-137.578299432275,-4.79984701474554,
129.72204448099));
#108940=CARTESIAN_POINT('Ctrl Pts',(-137.586458544274,-4.82954117751263,
129.86332018502));
#108941=CARTESIAN_POINT('Ctrl Pts',(-137.594617656273,-4.85298251559954,
130.005772008966));
#108942=CARTESIAN_POINT('Ctrl Pts',(-137.602760536601,-4.87637721968048,
130.147940440421));
#108943=CARTESIAN_POINT('Ctrl Pts',(-137.610903416929,-4.89354385174692,
130.291280003989));
#108944=CARTESIAN_POINT('Ctrl Pts',(-137.619046297257,-4.90437849770947,
130.435233791523));
#108945=CARTESIAN_POINT('Ctrl Pts',(-137.625984010159,-4.91360958794428,
130.557882044816));
#108946=CARTESIAN_POINT('Ctrl Pts',(-137.632921723061,-4.91824508829574,
130.680975806247));
#108947=CARTESIAN_POINT('Ctrl Pts',(-137.639859435962,-4.91824999609688,
130.80416467622));
#108948=CARTESIAN_POINT('Ctrl Pts',(-137.639859435993,-4.9182499960969,
130.804164676763));
#108949=CARTESIAN_POINT('Ctrl Pts',(-137.647950330633,-4.91825571965343,
130.947829913684));
#108950=CARTESIAN_POINT('Ctrl Pts',(-137.656041225272,-4.91196229675644,
131.091381545826));
#108951=CARTESIAN_POINT('Ctrl Pts',(-137.664132119912,-4.89942539442703,
131.234260451183));
#108952=CARTESIAN_POINT('Ctrl Pts',(-137.672232833425,-4.88687327767845,
131.377312750213));
#108953=CARTESIAN_POINT('Ctrl Pts',(-137.680333546939,-4.86806259391348,
131.519690357764));
#108954=CARTESIAN_POINT('Ctrl Pts',(-137.688434260452,-4.84310046393196,
131.660842350449));
#108955=CARTESIAN_POINT('Ctrl Pts',(-137.69655331512,-4.81808181617694,
131.802313931099));
#108956=CARTESIAN_POINT('Ctrl Pts',(-137.704672369788,-4.78688393570534,
131.94255401557));
#108957=CARTESIAN_POINT('Ctrl Pts',(-137.712791424457,-4.7496648149431,
132.081023144701));
#108958=CARTESIAN_POINT('Ctrl Pts',(-137.720920044814,-4.71240184344443,
132.219655415067));
#108959=CARTESIAN_POINT('Ctrl Pts',(-137.729048665171,-4.66910357720709,
132.356512245095));
#108960=CARTESIAN_POINT('Ctrl Pts',(-137.737177285528,-4.61997693377902,
132.491072268634));
#108961=CARTESIAN_POINT('Ctrl Pts',(-137.745324434336,-4.57073831063017,
132.625939009523));
#108962=CARTESIAN_POINT('Ctrl Pts',(-137.753471583145,-4.51564487449885,
132.75849816283));
#108963=CARTESIAN_POINT('Ctrl Pts',(-137.761618731954,-4.45495122267971,
132.888249450024));
#108964=CARTESIAN_POINT('Ctrl Pts',(-137.768106535402,-4.40661916285855,
132.991574044715));
#108965=CARTESIAN_POINT('Ctrl Pts',(-137.774594338851,-4.3547367290656,
133.093118493441));
#108966=CARTESIAN_POINT('Ctrl Pts',(-137.7810821423,-4.29945224525747,133.19264314969));
#108967=CARTESIAN_POINT('Ctrl Pts',(-137.788856476419,-4.23320485473174,
133.311903533714));
#108968=CARTESIAN_POINT('Ctrl Pts',(-137.796630810538,-4.16188661511739,
133.4285943232));
#108969=CARTESIAN_POINT('Ctrl Pts',(-137.804405144657,-4.08572166916645,
133.542254243075));
#108970=CARTESIAN_POINT('Ctrl Pts',(-137.812169897604,-4.00965058970434,
133.655774087257));
#108971=CARTESIAN_POINT('Ctrl Pts',(-137.819934650552,-3.92874490421212,
133.766270172248));
#108972=CARTESIAN_POINT('Ctrl Pts',(-137.827699403499,-3.84327480367038,
133.873305362258));
#108973=CARTESIAN_POINT('Ctrl Pts',(-137.835456444384,-3.75788959323741,
133.980234243409));
#108974=CARTESIAN_POINT('Ctrl Pts',(-137.843213485269,-3.66794923188803,
134.083708766644));
#108975=CARTESIAN_POINT('Ctrl Pts',(-137.850970526154,-3.57376719784275,
134.183320676241));
#108976=CARTESIAN_POINT('Ctrl Pts',(-137.858721717394,-3.47965618720185,
134.282857467723));
#108977=CARTESIAN_POINT('Ctrl Pts',(-137.866472908634,-3.38131013815635,
134.378537160432));
#108978=CARTESIAN_POINT('Ctrl Pts',(-137.874224099874,-3.27908256150896,
134.469984795971));
#108979=CARTESIAN_POINT('Ctrl Pts',(-137.881971996651,-3.1768984343088,
134.561393563825));
#108980=CARTESIAN_POINT('Ctrl Pts',(-137.889719893428,-3.07083635151974,
134.648573591943));
#108981=CARTESIAN_POINT('Ctrl Pts',(-137.897467790205,-2.96128625313847,
134.73118717211));
#108982=CARTESIAN_POINT('Ctrl Pts',(-137.90521406629,-2.85175907027616,
134.813783471297));
#108983=CARTESIAN_POINT('Ctrl Pts',(-137.912960342374,-2.73874563502764,
134.891814987232));
#108984=CARTESIAN_POINT('Ctrl Pts',(-137.920706618458,-2.62266818398729,
134.964984928796));
#108985=CARTESIAN_POINT('Ctrl Pts',(-137.928452951723,-2.50658987608973,
135.038155410484));
#108986=CARTESIAN_POINT('Ctrl Pts',(-137.936199284989,-2.38744783800748,
135.106464037707));
#108987=CARTESIAN_POINT('Ctrl Pts',(-137.943945618254,-2.26569209585419,
135.169658131973));
#108988=CARTESIAN_POINT('Ctrl Pts',(-137.951693686257,-2.14390908734681,
135.232866378117));
#108989=CARTESIAN_POINT('Ctrl Pts',(-137.95944175426,-2.01951155699064,
135.29095763209));
#108990=CARTESIAN_POINT('Ctrl Pts',(-137.967189822263,-1.892972492336,135.343726014376));
#108991=CARTESIAN_POINT('Ctrl Pts',(-137.974946125005,-1.76629894045744,
135.396550479528));
#108992=CARTESIAN_POINT('Ctrl Pts',(-137.982702427747,-1.63747966905109,
135.444040621386));
#108993=CARTESIAN_POINT('Ctrl Pts',(-137.990458730488,-1.50700645708785,
135.486039226868));
#108994=CARTESIAN_POINT('Ctrl Pts',(-137.998219173003,-1.3764636076429,
135.52806024827));
#108995=CARTESIAN_POINT('Ctrl Pts',(-138.005979615517,-1.24426543533416,
135.56458378897));
#108996=CARTESIAN_POINT('Ctrl Pts',(-138.013740058031,-1.11091613754168,
135.595503320288));
#108997=CARTESIAN_POINT('Ctrl Pts',(-138.021512958296,-0.977352775617833,
135.626472486383));
#108998=CARTESIAN_POINT('Ctrl Pts',(-138.029285858562,-0.842634979984229,
135.651819593783));
#108999=CARTESIAN_POINT('Ctrl Pts',(-138.037058758827,-0.707275226726109,
135.671489629228));
#109000=CARTESIAN_POINT('Ctrl Pts',(-138.044549094589,-0.576836141448093,
135.690444609339));
#109001=CARTESIAN_POINT('Ctrl Pts',(-138.052039430351,-0.44580126813016,
135.704128071259));
#109002=CARTESIAN_POINT('Ctrl Pts',(-138.059529766114,-0.314629224559155,
135.712536603974));
#109003=CARTESIAN_POINT('Ctrl Pts',(-138.067304100233,-0.178483753088626,
135.721263948763));
#109004=CARTESIAN_POINT('Ctrl Pts',(-138.075078434352,-0.04175923648286,
135.724336115985));
#109005=CARTESIAN_POINT('Ctrl Pts',(-138.082852768471,0.0950350868433429,
135.721692352844));
#109006=CARTESIAN_POINT('Ctrl Pts',(-138.090617521418,0.231660823391335,
135.719051847904));
#109007=CARTESIAN_POINT('Ctrl Pts',(-138.098382274365,0.368355808344941,
135.710709436285));
#109008=CARTESIAN_POINT('Ctrl Pts',(-138.106147027312,0.504606222160545,
135.69665615474));
#109009=CARTESIAN_POINT('Ctrl Pts',(-138.113904068197,0.640721310144724,
135.682616831113));
#109010=CARTESIAN_POINT('Ctrl Pts',(-138.121661109082,0.776392319318485,
135.662877965181));
#109011=CARTESIAN_POINT('Ctrl Pts',(-138.129418149967,0.911106329944074,
135.637482622858));
#109012=CARTESIAN_POINT('Ctrl Pts',(-138.137169341207,1.04571875168615,
135.61210643136));
#109013=CARTESIAN_POINT('Ctrl Pts',(-138.144920532447,1.17937522869683,
135.581082326009));
#109014=CARTESIAN_POINT('Ctrl Pts',(-138.152671723688,1.31156921663241,
135.544505051281));
#109015=CARTESIAN_POINT('Ctrl Pts',(-138.160419620465,1.44370701859692,
135.507943322871));
#109016=CARTESIAN_POINT('Ctrl Pts',(-138.168167517242,1.57438319177689,
135.465833223474));
#109017=CARTESIAN_POINT('Ctrl Pts',(-138.175915414019,1.70310284059474,
135.418320281115));
#109018=CARTESIAN_POINT('Ctrl Pts',(-138.183661690103,1.83179556403693,
135.370817277439));
#109019=CARTESIAN_POINT('Ctrl Pts',(-138.191407966187,1.95853221061903,
135.317913814046));
#109020=CARTESIAN_POINT('Ctrl Pts',(-138.199154242271,2.08283485237382,
135.259804707692));
#109021=CARTESIAN_POINT('Ctrl Pts',(-138.206900575537,2.20713841170265,
135.201695172389));
#109022=CARTESIAN_POINT('Ctrl Pts',(-138.214646908802,2.32900757617628,
135.138380083017));
#109023=CARTESIAN_POINT('Ctrl Pts',(-138.222393242067,2.44798651011493,
135.070101480393));
#109024=CARTESIAN_POINT('Ctrl Pts',(-138.23014131007,2.56699208856074,135.00180758725));
#109025=CARTESIAN_POINT('Ctrl Pts',(-138.237889378073,2.68310580949424,
134.92854816357));
#109026=CARTESIAN_POINT('Ctrl Pts',(-138.245637446076,2.7958987993247,134.850609864268));
#109027=CARTESIAN_POINT('Ctrl Pts',(-138.253393748818,2.90881166688716,
134.772588731214));
#109028=CARTESIAN_POINT('Ctrl Pts',(-138.26115005156,3.01839643100426,134.689879011513));
#109029=CARTESIAN_POINT('Ctrl Pts',(-138.268906354302,3.12425500531025,
134.602809475231));
#109030=CARTESIAN_POINT('Ctrl Pts',(-138.276666796816,3.23017007952469,
134.515693467315));
#109031=CARTESIAN_POINT('Ctrl Pts',(-138.28442723933,3.33235470996866,134.424213266789));
#109032=CARTESIAN_POINT('Ctrl Pts',(-138.292187681844,3.430446740048,134.328735487836));
#109033=CARTESIAN_POINT('Ctrl Pts',(-138.29996058211,3.52869623616224,134.233104439477));
#109034=CARTESIAN_POINT('Ctrl Pts',(-138.307733482375,3.62283973468952,
134.13346327329));
#109035=CARTESIAN_POINT('Ctrl Pts',(-138.315506382641,3.71255394557539,
134.030213413912));
#109036=CARTESIAN_POINT('Ctrl Pts',(-138.322996718403,3.79900681891668,
133.930716946995));
#109037=CARTESIAN_POINT('Ctrl Pts',(-138.330487054164,3.88134665269578,
133.827869842381));
#109038=CARTESIAN_POINT('Ctrl Pts',(-138.337977389926,3.95932268301334,
133.722056104466));
#109039=CARTESIAN_POINT('Ctrl Pts',(-138.345751724045,4.04025519822242,
133.612230406514));
#109040=CARTESIAN_POINT('Ctrl Pts',(-138.353526058164,4.11674284042205,
133.49886077988));
#109041=CARTESIAN_POINT('Ctrl Pts',(-138.361300392283,4.1884592407602,133.382342822895));
#109042=CARTESIAN_POINT('Ctrl Pts',(-138.36906514523,4.2600872570448,133.265968463877));
#109043=CARTESIAN_POINT('Ctrl Pts',(-138.376829898178,4.32695552820875,
133.146453824377));
#109044=CARTESIAN_POINT('Ctrl Pts',(-138.384594651125,4.3887787812045,133.024226350476));
#109045=CARTESIAN_POINT('Ctrl Pts',(-138.39235169201,4.45054063047365,132.902120274626));
#109046=CARTESIAN_POINT('Ctrl Pts',(-138.400108732895,4.5072672579379,132.777307073021));
#109047=CARTESIAN_POINT('Ctrl Pts',(-138.40786577378,4.55871765052375,132.650241557742));
#109048=CARTESIAN_POINT('Ctrl Pts',(-138.41561696502,4.6101292439684,132.523271863556));
#109049=CARTESIAN_POINT('Ctrl Pts',(-138.42336815626,4.65627237605335,132.39405359735));
#109050=CARTESIAN_POINT('Ctrl Pts',(-138.4311193475,4.69695295839971,132.263064140932));
#109051=CARTESIAN_POINT('Ctrl Pts',(-138.438867244277,4.73761625041343,
132.132130358527));
#109052=CARTESIAN_POINT('Ctrl Pts',(-138.446615141054,4.77282149471763,
131.999427255769));
#109053=CARTESIAN_POINT('Ctrl Pts',(-138.454363037831,4.80242362501266,
131.865449863775));
#109054=CARTESIAN_POINT('Ctrl Pts',(-138.462109313915,4.83201956318009,
131.731500496964));
#109055=CARTESIAN_POINT('Ctrl Pts',(-138.46985559,4.85601463431594,131.596277752624));
#109056=CARTESIAN_POINT('Ctrl Pts',(-138.477601866084,4.87431441153392,
131.460289028304));
#109057=CARTESIAN_POINT('Ctrl Pts',(-138.485348199349,4.89261432383673,
131.324299300145));
#109058=CARTESIAN_POINT('Ctrl Pts',(-138.493094532614,4.90521880618959,
131.187543968198));
#109059=CARTESIAN_POINT('Ctrl Pts',(-138.50084086588,4.91208510406753,131.050537368901));
#109060=CARTESIAN_POINT('Ctrl Pts',(-138.508588933883,4.91895293960527,
130.913500087926));
#109061=CARTESIAN_POINT('Ctrl Pts',(-138.516337001886,4.92008001404833,
130.776211818033));
#109062=CARTESIAN_POINT('Ctrl Pts',(-138.524085069889,4.91547568164379,
130.639188326704));
#109063=CARTESIAN_POINT('Ctrl Pts',(-138.53184137263,4.91086645569998,130.502019205178));
#109064=CARTESIAN_POINT('Ctrl Pts',(-138.539597675372,4.90051366781708,
130.365115815729));
#109065=CARTESIAN_POINT('Ctrl Pts',(-138.547353978114,4.88447874615702,
130.228990787943));
#109066=CARTESIAN_POINT('Ctrl Pts',(-138.555114420628,4.86843526617642,
130.09279310613));
#109067=CARTESIAN_POINT('Ctrl Pts',(-138.562874863143,4.84670367137383,
129.957374999607));
#109068=CARTESIAN_POINT('Ctrl Pts',(-138.570635305657,4.81939665015872,
129.823239324892));
#109069=CARTESIAN_POINT('Ctrl Pts',(-138.578408205922,4.79204579328902,
129.688888323684));
#109070=CARTESIAN_POINT('Ctrl Pts',(-138.586181106188,4.75910171872897,
129.555824247897));
#109071=CARTESIAN_POINT('Ctrl Pts',(-138.593954006453,4.72072741022136,
129.424536070428));
#109072=CARTESIAN_POINT('Ctrl Pts',(-138.601444342215,4.68374810448736,
129.298020548906));
#109073=CARTESIAN_POINT('Ctrl Pts',(-138.608934677977,4.64172661401346,
129.173154342537));
#109074=CARTESIAN_POINT('Ctrl Pts',(-138.616425013739,4.59485046856075,
129.050355989845));
#109075=CARTESIAN_POINT('Ctrl Pts',(-138.624199347858,4.54619699980529,
128.922901700287));
#109076=CARTESIAN_POINT('Ctrl Pts',(-138.631973681977,4.49215936104726,
128.797271428259));
#109077=CARTESIAN_POINT('Ctrl Pts',(-138.639748016096,4.43289397002839,
128.67395358768));
#109078=CARTESIAN_POINT('Ctrl Pts',(-138.647512769043,4.3737016183071,128.550787725319));
#109079=CARTESIAN_POINT('Ctrl Pts',(-138.65527752199,4.30929450117831,128.429928973024));
#109080=CARTESIAN_POINT('Ctrl Pts',(-138.663042274938,4.23987804408487,
128.311848384138));
#109081=CARTESIAN_POINT('Ctrl Pts',(-138.670799315822,4.1705305323954,128.193885074558));
#109082=CARTESIAN_POINT('Ctrl Pts',(-138.678556356707,4.09618377876101,
128.078694772092));
#109083=CARTESIAN_POINT('Ctrl Pts',(-138.686313397592,4.01709015601284,
127.966726084902));
#109084=CARTESIAN_POINT('Ctrl Pts',(-138.694064588833,3.93805617838074,
127.854841834171));
#109085=CARTESIAN_POINT('Ctrl Pts',(-138.701815780073,3.85428268137157,
127.746174681091));
#109086=CARTESIAN_POINT('Ctrl Pts',(-138.709566971313,3.76606639030969,
127.64114595424));
#109087=CARTESIAN_POINT('Ctrl Pts',(-138.71731486809,3.67788759352464,127.5361618674));
#109088=CARTESIAN_POINT('Ctrl Pts',(-138.725062764867,3.5852700093097,127.434813429808));
#109089=CARTESIAN_POINT('Ctrl Pts',(-138.732810661644,3.48855170948563,
127.337490266263));
#109090=CARTESIAN_POINT('Ctrl Pts',(-138.740556937728,3.39185364104515,
127.240187460626));
#109091=CARTESIAN_POINT('Ctrl Pts',(-138.748303213812,3.29105683858605,
127.146908531388));
#109092=CARTESIAN_POINT('Ctrl Pts',(-138.756049489896,3.18653714999846,
127.058007183334));
#109093=CARTESIAN_POINT('Ctrl Pts',(-138.763795823162,3.08201668987014,
126.96910517903));
#109094=CARTESIAN_POINT('Ctrl Pts',(-138.771542156427,2.97377358658391,
126.884581073697));
#109095=CARTESIAN_POINT('Ctrl Pts',(-138.779288489692,2.86221745608935,
126.804748849337));
#109096=CARTESIAN_POINT('Ctrl Pts',(-138.787036557695,2.750636343373,126.724898747104));
#109097=CARTESIAN_POINT('Ctrl Pts',(-138.794784625698,2.63574104497385,
126.649742844125));
#109098=CARTESIAN_POINT('Ctrl Pts',(-138.802532693701,2.51797054688072,
126.57955205533));
#109099=CARTESIAN_POINT('Ctrl Pts',(-138.810288996443,2.40007488090058,
126.50928666693));
#109100=CARTESIAN_POINT('Ctrl Pts',(-138.818045299185,2.27929824732104,
126.443997134534));
#109101=CARTESIAN_POINT('Ctrl Pts',(-138.825801601927,2.15610513935181,
126.383908865702));
#109102=CARTESIAN_POINT('Ctrl Pts',(-138.833562044441,2.03284627951158,
126.323788525951));
#109103=CARTESIAN_POINT('Ctrl Pts',(-138.841322486955,1.90716873343941,
126.268875137782));
#109104=CARTESIAN_POINT('Ctrl Pts',(-138.849082929469,1.77955647940521,
126.219345699476));
#109105=CARTESIAN_POINT('Ctrl Pts',(-138.856855829735,1.65173937085196,
126.169736752119));
#109106=CARTESIAN_POINT('Ctrl Pts',(-138.86462873,1.5219817183185,126.125529151837));
#109107=CARTESIAN_POINT('Ctrl Pts',(-138.872401630265,1.39078300524743,
126.086850077587));
#109108=CARTESIAN_POINT('Ctrl Pts',(-138.879891966028,1.26435369586256,
126.049577085112));
#109109=CARTESIAN_POINT('Ctrl Pts',(-138.88738230179,1.13658657801167,126.017437720587));
#109110=CARTESIAN_POINT('Ctrl Pts',(-138.894872637552,1.00793514442725,
125.990500440211));
#109111=CARTESIAN_POINT('Ctrl Pts',(-138.902646971671,0.87440585263892,
125.962541824662));
#109112=CARTESIAN_POINT('Ctrl Pts',(-138.91042130579,0.739500883055925,
125.940098989853));
#109113=CARTESIAN_POINT('Ctrl Pts',(-138.918195639909,0.603715699750552,
125.923304336762));
#109114=CARTESIAN_POINT('Ctrl Pts',(-138.925960392856,0.468097859548501,
125.90653038158));
#109115=CARTESIAN_POINT('Ctrl Pts',(-138.933725145803,0.331602348306135,
125.89539080557));
#109116=CARTESIAN_POINT('Ctrl Pts',(-138.94148989875,0.194736514010293,
125.889967394328));
#109117=CARTESIAN_POINT('Ctrl Pts',(-138.949246939635,0.0580066167901712,
125.884549369693));
#109118=CARTESIAN_POINT('Ctrl Pts',(-138.957003980521,-0.0790924833940932,
125.884836226973));
#109119=CARTESIAN_POINT('Ctrl Pts',(-138.964761021406,-0.216046946109414,
125.890858121426));
#109120=CARTESIAN_POINT('Ctrl Pts',(-138.972512212646,-0.352898130398864,
125.896875474721));
#109121=CARTESIAN_POINT('Ctrl Pts',(-138.980263403886,-0.489604505313652,
125.908619239761));
#109122=CARTESIAN_POINT('Ctrl Pts',(-138.988014595126,-0.625651207903403,
125.926067511515));
#109123=CARTESIAN_POINT('Ctrl Pts',(-138.995762491903,-0.761640087015575,
125.943508367287));
#109124=CARTESIAN_POINT('Ctrl Pts',(-139.00351038868,-0.896969464476789,
125.966648857862));
#109125=CARTESIAN_POINT('Ctrl Pts',(-139.011258285457,-1.03112880183341,
125.995415155562));
#109126=CARTESIAN_POINT('Ctrl Pts',(-139.019004561541,-1.1652600759488,
126.024175435973));
#109127=CARTESIAN_POINT('Ctrl Pts',(-139.026750837625,-1.29822141474103,
126.058559100878));
#109128=CARTESIAN_POINT('Ctrl Pts',(-139.03449711371,-1.42951208139341,
126.098441124879));
#109129=CARTESIAN_POINT('Ctrl Pts',(-139.042243446975,-1.56080371720383,
126.13832344328));
#109130=CARTESIAN_POINT('Ctrl Pts',(-139.04998978024,-1.69042428217927,
126.18370408813));
#109131=CARTESIAN_POINT('Ctrl Pts',(-139.057736113506,-1.81788820694238,
126.234408152872));
#109132=CARTESIAN_POINT('Ctrl Pts',(-139.065484181509,-1.94538067636714,
126.285123572438));
#109133=CARTESIAN_POINT('Ctrl Pts',(-139.073232249512,-2.07071518132734,
126.34116463964));
#109134=CARTESIAN_POINT('Ctrl Pts',(-139.080980317515,-2.1934265107705,
126.402308459271));
#109135=CARTESIAN_POINT('Ctrl Pts',(-139.088736620256,-2.31626825927505,
126.463517263281));
#109136=CARTESIAN_POINT('Ctrl Pts',(-139.096492922998,-2.43648091255858,
126.529839478638));
#109137=CARTESIAN_POINT('Ctrl Pts',(-139.10424922574,-2.55362375893157,
126.601006152342));
#109138=CARTESIAN_POINT('Ctrl Pts',(-139.112009668254,-2.67082912796878,
126.672210809842));
#109139=CARTESIAN_POINT('Ctrl Pts',(-139.119770110768,-2.78496110016019,
126.748264861086));
#109140=CARTESIAN_POINT('Ctrl Pts',(-139.127530553283,-2.89560915976181,
126.828856793344));
#109141=CARTESIAN_POINT('Ctrl Pts',(-139.135303453548,-3.00643484145187,
126.909578098926));
#109142=CARTESIAN_POINT('Ctrl Pts',(-139.143076353813,-3.11376512829503,
126.994851599148));
#109143=CARTESIAN_POINT('Ctrl Pts',(-139.150849254079,-3.21722303803153,
127.084325807775));
#109144=CARTESIAN_POINT('Ctrl Pts',(-139.158339589841,-3.31691999215239,
127.170547403544));
#109145=CARTESIAN_POINT('Ctrl Pts',(-139.165829925603,-3.41302099784068,
127.260669386768));
#109146=CARTESIAN_POINT('Ctrl Pts',(-139.173320261364,-3.50522333705938,
127.354347223413));
#109147=CARTESIAN_POINT('Ctrl Pts',(-139.180988868259,-3.59962010600881,
127.450254606853));
#109148=CARTESIAN_POINT('Ctrl Pts',(-139.188657475154,-3.69024688647966,
127.550211228781));
#109149=CARTESIAN_POINT('Ctrl Pts',(-139.196326082049,-3.77672901587722,
127.653884303875));
#109150=CARTESIAN_POINT('Ctrl Pts',(-139.203985690251,-3.86310966319121,
127.757435724243));
#109151=CARTESIAN_POINT('Ctrl Pts',(-139.211645298452,-3.94535507353085,
127.864694621992));
#109152=CARTESIAN_POINT('Ctrl Pts',(-139.219304906653,-4.02312619691822,
127.975290334563));
#109153=CARTESIAN_POINT('Ctrl Pts',(-139.226957293971,-4.10082400374231,
128.085781786103));
#109154=CARTESIAN_POINT('Ctrl Pts',(-139.23460968129,-4.1740556816684,128.199603469983));
#109155=CARTESIAN_POINT('Ctrl Pts',(-139.242262068609,-4.24252174968882,
128.316350917843));
#109156=CARTESIAN_POINT('Ctrl Pts',(-139.249908628741,-4.31093568174997,
128.433009464143));
#109157=CARTESIAN_POINT('Ctrl Pts',(-139.257555188873,-4.3745910227568,
128.552588995038));
#109158=CARTESIAN_POINT('Ctrl Pts',(-139.265201749005,-4.43323137458916,
128.674655792512));
#109159=CARTESIAN_POINT('Ctrl Pts',(-139.272844955505,-4.49184600791408,
128.796669053885));
#109160=CARTESIAN_POINT('Ctrl Pts',(-139.280488162006,-4.54544985390176,
128.921167049584));
#109161=CARTESIAN_POINT('Ctrl Pts',(-139.288131368507,-4.59383247771545,
129.047691545377));
#109162=CARTESIAN_POINT('Ctrl Pts',(-139.29577369175,-4.64220951038032,
129.17420141986));
#109163=CARTESIAN_POINT('Ctrl Pts',(-139.303416014994,-4.6853663742553,
129.302736954155));
#109164=CARTESIAN_POINT('Ctrl Pts',(-139.311058338237,-4.72314095957784,
129.432820410916));
#109165=CARTESIAN_POINT('Ctrl Pts',(-139.313976621525,-4.73756549221534,
129.482493836888));
#109166=CARTESIAN_POINT('Ctrl Pts',(-139.316894904813,-4.75120571705062,
129.532392799512));
#109167=CARTESIAN_POINT('Ctrl Pts',(-139.319813188101,-4.76405452823411,
129.582490119308));
#109168=CARTESIAN_POINT('Origin',(213.235140564004,0.,130.804360617566));
#109169=CARTESIAN_POINT('',(-141.415385046285,-4.76405452823413,129.582490119309));
#109170=CARTESIAN_POINT('',(-141.069766537825,-4.76405452823392,129.582490119308));
#109171=CARTESIAN_POINT('',(213.235140564004,-4.76405452823405,129.582490119308));
#109172=CARTESIAN_POINT('',(-139.735140564048,-4.91824935081372,130.801833619268));
#109173=CARTESIAN_POINT('Ctrl Pts',(-139.735140564048,-4.91824935081372,
130.801833619268));
#109174=CARTESIAN_POINT('Ctrl Pts',(-139.742821053676,-4.91831868187791,
130.936771368003));
#109175=CARTESIAN_POINT('Ctrl Pts',(-139.750501543305,-4.9128305693135,
131.071935030579));
#109176=CARTESIAN_POINT('Ctrl Pts',(-139.758182032933,-4.90175557619006,
131.206822210503));
#109177=CARTESIAN_POINT('Ctrl Pts',(-139.765853728862,-4.89069326326819,
131.341554952713));
#109178=CARTESIAN_POINT('Ctrl Pts',(-139.773525424791,-4.87405682454765,
131.476011445941));
#109179=CARTESIAN_POINT('Ctrl Pts',(-139.78119712072,-4.85186881855777,
131.609687898866));
#109180=CARTESIAN_POINT('Ctrl Pts',(-139.788861972103,-4.82970060830019,
131.74324508811));
#109181=CARTESIAN_POINT('Ctrl Pts',(-139.796526823485,-4.8019907490666,
131.876023228245));
#109182=CARTESIAN_POINT('Ctrl Pts',(-139.804191674868,-4.76881368250428,
132.007522752966));
#109183=CARTESIAN_POINT('Ctrl Pts',(-139.811895110775,-4.73546960404813,
132.139684240511));
#109184=CARTESIAN_POINT('Ctrl Pts',(-139.819598546683,-4.69660315285988,
132.27055379557));
#109185=CARTESIAN_POINT('Ctrl Pts',(-139.82730198259,-4.65234222047004,
132.399633298374));
#109186=CARTESIAN_POINT('Ctrl Pts',(-139.834959909155,-4.60834276697728,
132.52795024232));
#109187=CARTESIAN_POINT('Ctrl Pts',(-139.84261783572,-4.55901254032337,
132.654497847047));
#109188=CARTESIAN_POINT('Ctrl Pts',(-139.850275762285,-4.5045272934658,
132.778801532084));
#109189=CARTESIAN_POINT('Ctrl Pts',(-139.85793307981,-4.45004637985369,
132.903095331171));
#109190=CARTESIAN_POINT('Ctrl Pts',(-139.865590397335,-4.3904114222263,
133.025145198277));
#109191=CARTESIAN_POINT('Ctrl Pts',(-139.873247714861,-4.32584610092109,
133.144497060948));
#109192=CARTESIAN_POINT('Ctrl Pts',(-139.880906174034,-4.26127115341642,
133.263866718077));
#109193=CARTESIAN_POINT('Ctrl Pts',(-139.888564633207,-4.19176457141299,
133.380537218349));
#109194=CARTESIAN_POINT('Ctrl Pts',(-139.89622309238,-4.11759545269744,
133.494080073276));
#109195=CARTESIAN_POINT('Ctrl Pts',(-139.903960679402,-4.04266001236714,
133.608796062594));
#109196=CARTESIAN_POINT('Ctrl Pts',(-139.911698266424,-3.96296536702992,
133.720319057401));
#109197=CARTESIAN_POINT('Ctrl Pts',(-139.919435853446,-3.87883256599563,
133.828239085275));
#109198=CARTESIAN_POINT('Ctrl Pts',(-139.927105762205,-3.79543564836133,
133.935215170285));
#109199=CARTESIAN_POINT('Ctrl Pts',(-139.934775670964,-3.707678215686,134.038650802036));
#109200=CARTESIAN_POINT('Ctrl Pts',(-139.942445579722,-3.61591141374249,
134.138182405015));
#109201=CARTESIAN_POINT('Ctrl Pts',(-139.950217005876,-3.5229300045667,
134.239031388596));
#109202=CARTESIAN_POINT('Ctrl Pts',(-139.957988432029,-3.42583264137427,
134.335871962731));
#109203=CARTESIAN_POINT('Ctrl Pts',(-139.965759858183,-3.32501996462775,
134.428367419067));
#109204=CARTESIAN_POINT('Ctrl Pts',(-139.973531284336,-3.22420728788096,
134.520862875403));
#109205=CARTESIAN_POINT('Ctrl Pts',(-139.981302710489,-3.11967966202699,
134.609012993809));
#109206=CARTESIAN_POINT('Ctrl Pts',(-139.989074136643,-3.01186809004675,
134.692526466737));
#109207=CARTESIAN_POINT('Ctrl Pts',(-139.996848470762,-2.90401617639166,
134.77607118931));
#109208=CARTESIAN_POINT('Ctrl Pts',(-140.004622804881,-2.79251468992268,
134.855257363404));
#109209=CARTESIAN_POINT('Ctrl Pts',(-140.012397139,-2.6777512830939,134.929749220884));
#109210=CARTESIAN_POINT('Ctrl Pts',(-140.020161891947,-2.56312931190734,
135.004149273808));
#109211=CARTESIAN_POINT('Ctrl Pts',(-140.027926644894,-2.44525374380347,
135.073866310372));
#109212=CARTESIAN_POINT('Ctrl Pts',(-140.035691397842,-2.32454505600209,
135.138604882154));
#109213=CARTESIAN_POINT('Ctrl Pts',(-140.043448438727,-2.20395625777112,
135.203279154674));
#109214=CARTESIAN_POINT('Ctrl Pts',(-140.051205479612,-2.08054028193099,
135.262984618963));
#109215=CARTESIAN_POINT('Ctrl Pts',(-140.058962520497,-1.95474602593855,
135.317469417116));
#109216=CARTESIAN_POINT('Ctrl Pts',(-140.066713711737,-1.82904663237326,
135.371913127859));
#109217=CARTESIAN_POINT('Ctrl Pts',(-140.074464902977,-1.70097288577576,
135.421143853958));
#109218=CARTESIAN_POINT('Ctrl Pts',(-140.082216094217,-1.57099737289253,
135.464956107079));
#109219=CARTESIAN_POINT('Ctrl Pts',(-140.089963990994,-1.44107710306931,
135.508749738823));
#109220=CARTESIAN_POINT('Ctrl Pts',(-140.097711887771,-1.30925704431813,
135.547129353451));
#109221=CARTESIAN_POINT('Ctrl Pts',(-140.105459784548,-1.17602860400855,
135.579938047056));
#109222=CARTESIAN_POINT('Ctrl Pts',(-140.113206060632,-1.04282803221661,
135.61273987779));
#109223=CARTESIAN_POINT('Ctrl Pts',(-140.120952336717,-0.908220044231184,
135.639973011953));
#109224=CARTESIAN_POINT('Ctrl Pts',(-140.128698612801,-0.772709625498943,
135.661530873709));
#109225=CARTESIAN_POINT('Ctrl Pts',(-140.136444946066,-0.63719820645939,
135.683088894601));
#109226=CARTESIAN_POINT('Ctrl Pts',(-140.144191279331,-0.500784729490214,
135.698971498066));
#109227=CARTESIAN_POINT('Ctrl Pts',(-140.151937612597,-0.363982356925633,
135.709123599235));
#109228=CARTESIAN_POINT('Ctrl Pts',(-140.1596856806,-0.227149348418796,
135.719277973896));
#109229=CARTESIAN_POINT('Ctrl Pts',(-140.167433748603,-0.089927660835064,
135.723699263702));
#109230=CARTESIAN_POINT('Ctrl Pts',(-140.175181816606,0.0471668623958541,
135.722384443209));
#109231=CARTESIAN_POINT('Ctrl Pts',(-140.182938119348,0.184407091317694,
135.721068225309));
#109232=CARTESIAN_POINT('Ctrl Pts',(-140.190694422089,0.321519494335863,
135.714003722636));
#109233=CARTESIAN_POINT('Ctrl Pts',(-140.198450724831,0.457990115384167,
135.701240043967));
#109234=CARTESIAN_POINT('Ctrl Pts',(-140.206211167346,0.594533574912346,
135.688469552938));
#109235=CARTESIAN_POINT('Ctrl Pts',(-140.21397160986,0.730434182721979,
135.669993877467));
#109236=CARTESIAN_POINT('Ctrl Pts',(-140.221732052374,0.865186522892068,
135.64591360634));
#109237=CARTESIAN_POINT('Ctrl Pts',(-140.229504952639,1.00015517948135,
135.621794679424));
#109238=CARTESIAN_POINT('Ctrl Pts',(-140.237277852905,1.13397150305589,
135.592053262865));
#109239=CARTESIAN_POINT('Ctrl Pts',(-140.24505075317,1.26614275036817,135.556840559469));
#109240=CARTESIAN_POINT('Ctrl Pts',(-140.252541088933,1.39350923992966,
135.522907926534));
#109241=CARTESIAN_POINT('Ctrl Pts',(-140.260031424695,1.51934788783213,
135.483894981868));
#109242=CARTESIAN_POINT('Ctrl Pts',(-140.267521760458,1.64323577588066,
135.439979157455));
#109243=CARTESIAN_POINT('Ctrl Pts',(-140.275296094577,1.77182091085091,
135.394398251216));
#109244=CARTESIAN_POINT('Ctrl Pts',(-140.283070428696,1.89871175879676,
135.34339095409));
#109245=CARTESIAN_POINT('Ctrl Pts',(-140.290844762815,2.02341629285639,
135.287101918188));
#109246=CARTESIAN_POINT('Ctrl Pts',(-140.298609515762,2.14796713972295,
135.230882253492));
#109247=CARTESIAN_POINT('Ctrl Pts',(-140.306374268709,2.27033668090424,
135.169393960832));
#109248=CARTESIAN_POINT('Ctrl Pts',(-140.314139021656,2.3900490690662,135.102831102512));
#109249=CARTESIAN_POINT('Ctrl Pts',(-140.321896062541,2.50964255719625,
135.036334355362));
#109250=CARTESIAN_POINT('Ctrl Pts',(-140.329653103427,2.62658380479242,
134.9647732614));
#109251=CARTESIAN_POINT('Ctrl Pts',(-140.337410144312,2.74041827662706,
134.888389355421));
#109252=CARTESIAN_POINT('Ctrl Pts',(-140.345161335552,2.85416690500176,
134.81206305114));
#109253=CARTESIAN_POINT('Ctrl Pts',(-140.352912526792,2.96481309756629,
134.730921390873));
#109254=CARTESIAN_POINT('Ctrl Pts',(-140.360663718032,3.07192852648603,
134.645250903771));
#109255=CARTESIAN_POINT('Ctrl Pts',(-140.368411614809,3.17899842849065,
134.559616828911));
#109256=CARTESIAN_POINT('Ctrl Pts',(-140.376159511586,3.28254024688251,
134.469457999325));
#109257=CARTESIAN_POINT('Ctrl Pts',(-140.383907408363,3.38215635627519,
134.375103039557));
#109258=CARTESIAN_POINT('Ctrl Pts',(-140.391653684448,3.48175162812526,
134.280767816812));
#109259=CARTESIAN_POINT('Ctrl Pts',(-140.399399960532,3.57742254066734,
134.182238478445));
#109260=CARTESIAN_POINT('Ctrl Pts',(-140.407146236616,3.66880647166351,
134.079882276169));
#109261=CARTESIAN_POINT('Ctrl Pts',(-140.414892569881,3.76019107723546,
133.977525318324));
#109262=CARTESIAN_POINT('Ctrl Pts',(-140.422638903146,3.8472883777349,133.871341731845));
#109263=CARTESIAN_POINT('Ctrl Pts',(-140.430385236412,3.92977465192497,
133.761733480021));
#109264=CARTESIAN_POINT('Ctrl Pts',(-140.438133304415,4.01227939834366,
133.652100682191));
#109265=CARTESIAN_POINT('Ctrl Pts',(-140.445881372418,4.09017082863923,
133.539042005242));
#109266=CARTESIAN_POINT('Ctrl Pts',(-140.453629440421,4.16316757144591,
133.422989807536));
#109267=CARTESIAN_POINT('Ctrl Pts',(-140.461385743163,4.23624189605981,
133.306814268172));
#109268=CARTESIAN_POINT('Ctrl Pts',(-140.469142045905,4.30441093287157,
133.187639184032));
#109269=CARTESIAN_POINT('Ctrl Pts',(-140.476898348647,4.36743819267706,
133.065923505404));
#109270=CARTESIAN_POINT('Ctrl Pts',(-140.484658791161,4.43049909202883,
132.944142863453));
#109271=CARTESIAN_POINT('Ctrl Pts',(-140.492419233675,4.48841258107316,
132.819819279311));
#109272=CARTESIAN_POINT('Ctrl Pts',(-140.500179676189,4.5409900983555,132.693432344404));
#109273=CARTESIAN_POINT('Ctrl Pts',(-140.507952576455,4.59365201773618,
132.566842521968));
#109274=CARTESIAN_POINT('Ctrl Pts',(-140.51572547672,4.64096071320081,132.438183096945));
#109275=CARTESIAN_POINT('Ctrl Pts',(-140.523498376985,4.68277705619129,
132.307950356992));
#109276=CARTESIAN_POINT('Ctrl Pts',(-140.530988712747,4.72307326978234,
132.182451905182));
#109277=CARTESIAN_POINT('Ctrl Pts',(-140.538479048509,4.75826943749636,
132.055492837246));
#109278=CARTESIAN_POINT('Ctrl Pts',(-140.54596938427,4.78828624027411,131.927524872562));
#109279=CARTESIAN_POINT('Ctrl Pts',(-140.553743718389,4.81944113925448,
131.794704963594));
#109280=CARTESIAN_POINT('Ctrl Pts',(-140.561518052508,4.84511485837714,
131.660377409464));
#109281=CARTESIAN_POINT('Ctrl Pts',(-140.569292386627,4.86516314502173,
131.525034354303));
#109282=CARTESIAN_POINT('Ctrl Pts',(-140.577057139574,4.88518672394474,
131.389858097362));
#109283=CARTESIAN_POINT('Ctrl Pts',(-140.584821892521,4.89959860794207,
131.253669212564));
#109284=CARTESIAN_POINT('Ctrl Pts',(-140.592586645469,4.90830486001895,
131.116972939163));
#109285=CARTESIAN_POINT('Ctrl Pts',(-140.600343686353,4.91700246492351,
130.980412434428));
#109286=CARTESIAN_POINT('Ctrl Pts',(-140.608100727239,4.92000569063275,
130.843345931615));
#109287=CARTESIAN_POINT('Ctrl Pts',(-140.615857768123,4.91727205981716,
130.70628639954));
#109288=CARTESIAN_POINT('Ctrl Pts',(-140.623608959364,4.91454049045383,
130.569330225123));
#109289=CARTESIAN_POINT('Ctrl Pts',(-140.631360150604,4.90608068338522,
130.432381400288));
#109290=CARTESIAN_POINT('Ctrl Pts',(-140.639111341844,4.89190218204362,
130.295955165376));
#109291=CARTESIAN_POINT('Ctrl Pts',(-140.646859238621,4.8777297069433,130.159586915253));
#109292=CARTESIAN_POINT('Ctrl Pts',(-140.654607135398,4.85784341217327,
130.023741201341));
#109293=CARTESIAN_POINT('Ctrl Pts',(-140.662355032175,4.83230485263528,
129.888930186732));
#109294=CARTESIAN_POINT('Ctrl Pts',(-140.670101308259,4.8067716352134,129.754147371681));
#109295=CARTESIAN_POINT('Ctrl Pts',(-140.677847584343,4.77558857747059,
129.620399209318));
#109296=CARTESIAN_POINT('Ctrl Pts',(-140.685593860427,4.73886865249923,
129.488189292525));
#109297=CARTESIAN_POINT('Ctrl Pts',(-140.693340193692,4.70214845646967,
129.355978399788));
#109298=CARTESIAN_POINT('Ctrl Pts',(-140.701086526958,4.65989141628072,
129.225306151985));
#109299=CARTESIAN_POINT('Ctrl Pts',(-140.708832860223,4.6122607357949,129.096662175936));
#109300=CARTESIAN_POINT('Ctrl Pts',(-140.716580928226,4.56461938874837,
128.967989390961));
#109301=CARTESIAN_POINT('Ctrl Pts',(-140.724328996229,4.51160214252286,
128.84134614815));
#109302=CARTESIAN_POINT('Ctrl Pts',(-140.732077064232,4.45342066435591,
128.717202873459));
#109303=CARTESIAN_POINT('Ctrl Pts',(-140.739833366974,4.39517735022184,
128.592927657818));
#109304=CARTESIAN_POINT('Ctrl Pts',(-140.747589669715,4.33175900624082,
128.47115807251));
#109305=CARTESIAN_POINT('Ctrl Pts',(-140.755345972457,4.26342393209622,
128.352341156442));
#109306=CARTESIAN_POINT('Ctrl Pts',(-140.763106414971,4.19505238546502,
128.233460824209));
#109307=CARTESIAN_POINT('Ctrl Pts',(-140.770866857486,4.12175908854517,
128.11753663168));
#109308=CARTESIAN_POINT('Ctrl Pts',(-140.7786273,4.04384561311353,128.004986451828));
#109309=CARTESIAN_POINT('Ctrl Pts',(-140.786400200265,3.96580706405408,
127.892255596435));
#109310=CARTESIAN_POINT('Ctrl Pts',(-140.794173100531,3.88313375143666,
127.782909889182));
#109311=CARTESIAN_POINT('Ctrl Pts',(-140.801946000796,3.79616801374068,
127.677334638468));
#109312=CARTESIAN_POINT('Ctrl Pts',(-140.809436336558,3.71236369966012,
127.575597314042));
#109313=CARTESIAN_POINT('Ctrl Pts',(-140.816926672321,3.6245738284932,127.477361303959));
#109314=CARTESIAN_POINT('Ctrl Pts',(-140.824417008083,3.53313557065684,
127.38293750695));
#109315=CARTESIAN_POINT('Ctrl Pts',(-140.832191342202,3.43823040348566,
127.28493360298));
#109316=CARTESIAN_POINT('Ctrl Pts',(-140.839965676321,3.33909410014207,
127.190726251824));
#109317=CARTESIAN_POINT('Ctrl Pts',(-140.84774001044,3.23606274335815,127.10070283322));
#109318=CARTESIAN_POINT('Ctrl Pts',(-140.855504763387,3.13315836351357,
127.010790360434));
#109319=CARTESIAN_POINT('Ctrl Pts',(-140.863269516334,3.02636877299296,
126.925051815429));
#109320=CARTESIAN_POINT('Ctrl Pts',(-140.871034269281,2.91606826864997,
126.843839324217));
#109321=CARTESIAN_POINT('Ctrl Pts',(-140.878791310166,2.80587731632346,
126.762707494396));
#109322=CARTESIAN_POINT('Ctrl Pts',(-140.886548351051,2.69218270243471,
126.686093002745));
#109323=CARTESIAN_POINT('Ctrl Pts',(-140.894305391936,2.57539304214305,
126.614308858819));
#109324=CARTESIAN_POINT('Ctrl Pts',(-140.902056583176,2.45869145384224,
126.542578847873));
#109325=CARTESIAN_POINT('Ctrl Pts',(-140.909807774417,2.3388997965521,126.475672138169));
#109326=CARTESIAN_POINT('Ctrl Pts',(-140.917558965657,2.21645671502376,
126.413859200538));
#109327=CARTESIAN_POINT('Ctrl Pts',(-140.925306862434,2.09406567507118,
126.352072535054));
#109328=CARTESIAN_POINT('Ctrl Pts',(-140.933054759211,1.96902580053268,
126.295375511467));
#109329=CARTESIAN_POINT('Ctrl Pts',(-140.940802655988,1.84180126065065,
126.243993178558));
#109330=CARTESIAN_POINT('Ctrl Pts',(-140.948548932072,1.71460333339936,
126.192621593725));
#109331=CARTESIAN_POINT('Ctrl Pts',(-140.956295208156,1.58522201205899,
126.146562634616));
#109332=CARTESIAN_POINT('Ctrl Pts',(-140.96404148424,1.45414204829938,126.105993458023));
#109333=CARTESIAN_POINT('Ctrl Pts',(-140.971787817506,1.32306111693744,
126.065423981958));
#109334=CARTESIAN_POINT('Ctrl Pts',(-140.979534150771,1.19028189162174,
126.030344484867));
#109335=CARTESIAN_POINT('Ctrl Pts',(-140.987280484036,1.05630452493746,
126.000882313972));
#109336=CARTESIAN_POINT('Ctrl Pts',(-140.995028552039,0.922297154951022,
125.971413545229));
#109337=CARTESIAN_POINT('Ctrl Pts',(-141.002776620042,0.787091491447936,
125.947564689833));
#109338=CARTESIAN_POINT('Ctrl Pts',(-141.010524688045,0.65119772841829,
125.929411942862));
#109339=CARTESIAN_POINT('Ctrl Pts',(-141.018280990787,0.515159535880326,
125.911239902935));
#109340=CARTESIAN_POINT('Ctrl Pts',(-141.026037293529,0.37843217106558,
125.898776116581));
#109341=CARTESIAN_POINT('Ctrl Pts',(-141.033793596271,0.241531357754565,
125.89204490441));
#109342=CARTESIAN_POINT('Ctrl Pts',(-141.041554038785,0.104557476357109,
125.885310099588));
#109343=CARTESIAN_POINT('Ctrl Pts',(-141.049314481299,-0.0325896472359078,
125.884313968394));
#109344=CARTESIAN_POINT('Ctrl Pts',(-141.057074923813,-0.16939543774653,
125.889028660498));
#109345=CARTESIAN_POINT('Ctrl Pts',(-141.064847824079,-0.306420841057127,
125.893750921045));
#109346=CARTESIAN_POINT('Ctrl Pts',(-141.072620724344,-0.443103426278679,
125.904202294694));
#109347=CARTESIAN_POINT('Ctrl Pts',(-141.08039362461,-0.578933980232691,
125.920303030986));
#109348=CARTESIAN_POINT('Ctrl Pts',(-141.087883960372,-0.709826751410281,
125.935818464958));
#109349=CARTESIAN_POINT('Ctrl Pts',(-141.095374296134,-0.839928058625539,
125.956579606911));
#109350=CARTESIAN_POINT('Ctrl Pts',(-141.102864631895,-0.968794085126929,
125.98247083418));
#109351=CARTESIAN_POINT('Ctrl Pts',(-141.110638966015,-1.10254610619467,
126.009343735201));
#109352=CARTESIAN_POINT('Ctrl Pts',(-141.118413300134,-1.23539101230949,
126.041828540447));
#109353=CARTESIAN_POINT('Ctrl Pts',(-141.126187634253,-1.36682122899911,
126.07985188221));
#109354=CARTESIAN_POINT('Ctrl Pts',(-141.1339523872,-1.49808946969184,126.117828363601));
#109355=CARTESIAN_POINT('Ctrl Pts',(-141.141717140147,-1.62794611800273,
126.161329692689));
#109356=CARTESIAN_POINT('Ctrl Pts',(-141.149481893094,-1.7558926037528,
126.210231295639));
#109357=CARTESIAN_POINT('Ctrl Pts',(-141.157238933979,-1.88371201125019,
126.259084328829));
#109358=CARTESIAN_POINT('Ctrl Pts',(-141.164995974864,-2.00962466886434,
126.313326823342));
#109359=CARTESIAN_POINT('Ctrl Pts',(-141.172753015749,-2.13314636631659,
126.372784188983));
#109360=CARTESIAN_POINT('Ctrl Pts',(-141.180504206989,-2.25657491509577,
126.432196717363));
#109361=CARTESIAN_POINT('Ctrl Pts',(-141.188255398229,-2.37761574170534,
126.496816120435));
#109362=CARTESIAN_POINT('Ctrl Pts',(-141.196006589469,-2.49580419317262,
126.566419550038));
#109363=CARTESIAN_POINT('Ctrl Pts',(-141.203754486246,-2.61394241139541,
126.635993396327));
#109364=CARTESIAN_POINT('Ctrl Pts',(-141.211502383024,-2.72923032953855,
126.710546857939));
#109365=CARTESIAN_POINT('Ctrl Pts',(-141.219250279801,-2.8412277128769,
126.789811060507));
#109366=CARTESIAN_POINT('Ctrl Pts',(-141.226996555885,-2.95320166877703,
126.869058682713));
#109367=CARTESIAN_POINT('Ctrl Pts',(-141.234742831969,-3.0618861400312,
126.953014860175));
#109368=CARTESIAN_POINT('Ctrl Pts',(-141.242489108053,-3.16687005949524,
127.041367515158));
#109369=CARTESIAN_POINT('Ctrl Pts',(-141.250235441318,-3.27185475392629,
127.129720822339));
#109370=CARTESIAN_POINT('Ctrl Pts',(-141.257981774584,-3.37313854292823,
127.222470420057));
#109371=CARTESIAN_POINT('Ctrl Pts',(-141.265728107849,-3.47034394098518,
127.319264350062));
#109372=CARTESIAN_POINT('Ctrl Pts',(-141.273476175852,-3.56757110751745,
127.416079956397));
#109373=CARTESIAN_POINT('Ctrl Pts',(-141.281224243855,-3.6607177887021,
127.516941421444));
#109374=CARTESIAN_POINT('Ctrl Pts',(-141.288972311858,-3.74944410714905,
127.621460689848));
#109375=CARTESIAN_POINT('Ctrl Pts',(-141.2967286146,-3.83826472498297,127.726091042575));
#109376=CARTESIAN_POINT('Ctrl Pts',(-141.304484917342,-3.92265534186903,
127.834386665945));
#109377=CARTESIAN_POINT('Ctrl Pts',(-141.312241220084,-4.00231673488935,
127.945926812818));
#109378=CARTESIAN_POINT('Ctrl Pts',(-141.320001662598,-4.08202064559369,
128.057526492027));
#109379=CARTESIAN_POINT('Ctrl Pts',(-141.327762105112,-4.15699008928609,
128.172373818071));
#109380=CARTESIAN_POINT('Ctrl Pts',(-141.335522547626,-4.22697035672952,
128.290020810414));
#109381=CARTESIAN_POINT('Ctrl Pts',(-141.343295447892,-4.29706296271081,
128.407856660153));
#109382=CARTESIAN_POINT('Ctrl Pts',(-141.351068348157,-4.36215020203226,
128.528500812897));
#109383=CARTESIAN_POINT('Ctrl Pts',(-141.358841248423,-4.42202392885086,
128.651481746108));
#109384=CARTESIAN_POINT('Ctrl Pts',(-141.366331584185,-4.47972109488809,
128.769992012629));
#109385=CARTESIAN_POINT('Ctrl Pts',(-141.373821919947,-4.53257709263054,
128.8906718314));
#109386=CARTESIAN_POINT('Ctrl Pts',(-141.381312255709,-4.580449304905,129.013085309944));
#109387=CARTESIAN_POINT('Ctrl Pts',(-141.390142391297,-4.63688444194875,
129.15739494406));
#109388=CARTESIAN_POINT('Ctrl Pts',(-141.398972526884,-4.68654370990747,
129.304495840899));
#109389=CARTESIAN_POINT('Ctrl Pts',(-141.407802662471,-4.7291768839033,
129.453779608054));
#109390=CARTESIAN_POINT('Ctrl Pts',(-141.410330123743,-4.74137983312049,
129.496509296201));
#109391=CARTESIAN_POINT('Ctrl Pts',(-141.412857585014,-4.75300743572739,
129.539417673288));
#109392=CARTESIAN_POINT('Ctrl Pts',(-141.415385046285,-4.76405452823413,
129.582490119309));
#109393=CARTESIAN_POINT('Ctrl Pts',(-139.665053375618,-4.76405452823406,
129.582490119308));
#109394=CARTESIAN_POINT('Ctrl Pts',(-139.672826300165,-4.79811622310555,
129.715296150654));
#109395=CARTESIAN_POINT('Ctrl Pts',(-139.680599224713,-4.82658428168376,
129.849386479152));
#109396=CARTESIAN_POINT('Ctrl Pts',(-139.68837214926,-4.84939189227845,
129.98425005331));
#109397=CARTESIAN_POINT('Ctrl Pts',(-139.69579027045,-4.8711584253778,130.112957637062));
#109398=CARTESIAN_POINT('Ctrl Pts',(-139.70320839164,-4.88776983181743,
130.242369144826));
#109399=CARTESIAN_POINT('Ctrl Pts',(-139.71062651283,-4.89921231912583,
130.372039308092));
#109400=CARTESIAN_POINT('Ctrl Pts',(-139.718797863224,-4.9118166660722,
130.514876060481));
#109401=CARTESIAN_POINT('Ctrl Pts',(-139.726969213617,-4.91817558877562,
130.658271986534));
#109402=CARTESIAN_POINT('Ctrl Pts',(-139.735140564011,-4.91824935081338,
130.80183361861));
#109403=CARTESIAN_POINT('',(-139.389859435958,-4.91824792560688,130.808877780788));
#109404=CARTESIAN_POINT('Ctrl Pts',(-139.319813188101,-4.76405452823411,
129.582490119308));
#109405=CARTESIAN_POINT('Ctrl Pts',(-139.327458232781,-4.79771463792605,
129.713730376134));
#109406=CARTESIAN_POINT('Ctrl Pts',(-139.33510327746,-4.8259397234975,129.846332558212));
#109407=CARTESIAN_POINT('Ctrl Pts',(-139.34274832214,-4.84863732766595,
129.979800657791));
#109408=CARTESIAN_POINT('Ctrl Pts',(-139.350600174443,-4.87194892923586,
130.116879229458));
#109409=CARTESIAN_POINT('Ctrl Pts',(-139.358452026746,-4.88942966397046,
130.254870788241));
#109410=CARTESIAN_POINT('Ctrl Pts',(-139.366303879049,-4.90103622311378,
130.39323168131));
#109411=CARTESIAN_POINT('Ctrl Pts',(-139.374155731352,-4.91264278225707,
130.53159257438));
#109412=CARTESIAN_POINT('Ctrl Pts',(-139.382007583655,-4.91837518180347,
130.670322343648));
#109413=CARTESIAN_POINT('Ctrl Pts',(-139.389859435958,-4.91824792560688,
130.808877780788));
#109414=CARTESIAN_POINT('Ctrl Pts',(-139.389859435993,-4.91824792560632,
130.808877781408));
#109415=CARTESIAN_POINT('Ctrl Pts',(-139.400465185153,-4.91807603654967,
130.996029061678));
#109416=CARTESIAN_POINT('Ctrl Pts',(-139.411070934312,-4.90721832858287,
131.182709389041));
#109417=CARTESIAN_POINT('Ctrl Pts',(-139.421676683472,-4.88585637864041,
131.367912309781));
#109418=CARTESIAN_POINT('Ctrl Pts',(-139.43170708404,-4.86565328769117,
131.543068204345));
#109419=CARTESIAN_POINT('Ctrl Pts',(-139.441737484609,-4.83605519733954,
131.716903404704));
#109420=CARTESIAN_POINT('Ctrl Pts',(-139.451767885177,-4.79725281147905,
131.888587773312));
#109421=CARTESIAN_POINT('Ctrl Pts',(-139.459542219296,-4.76717796947889,
132.021656401574));
#109422=CARTESIAN_POINT('Ctrl Pts',(-139.467316553416,-4.73151460760105,
132.153683505883));
#109423=CARTESIAN_POINT('Ctrl Pts',(-139.475090887535,-4.69034825281445,
132.284163418557));
#109424=CARTESIAN_POINT('Ctrl Pts',(-139.482855640482,-4.64923263188098,
132.4144825264));
#109425=CARTESIAN_POINT('Ctrl Pts',(-139.490620393429,-4.60262762859607,
132.543257867254));
#109426=CARTESIAN_POINT('Ctrl Pts',(-139.498385146376,-4.55066974522794,
132.669994003944));
#109427=CARTESIAN_POINT('Ctrl Pts',(-139.506142187261,-4.49876346716205,
132.796604264516));
#109428=CARTESIAN_POINT('Ctrl Pts',(-139.513899228146,-4.44151503654386,
132.921178992091));
#109429=CARTESIAN_POINT('Ctrl Pts',(-139.521656269031,-4.37911061300287,
133.043238305513));
#109430=CARTESIAN_POINT('Ctrl Pts',(-139.529407460271,-4.31675324912303,
133.165205573057));
#109431=CARTESIAN_POINT('Ctrl Pts',(-139.537158651511,-4.24924780875008,
133.284660855401));
#109432=CARTESIAN_POINT('Ctrl Pts',(-139.544909842751,-4.17682822626087,
133.401144981122));
#109433=CARTESIAN_POINT('Ctrl Pts',(-139.552657739529,-4.10443942402598,
133.517579597983));
#109434=CARTESIAN_POINT('Ctrl Pts',(-139.560405636305,-4.02714083981685,
133.631045238542));
#109435=CARTESIAN_POINT('Ctrl Pts',(-139.568153533083,-3.94521183499113,
133.741108247095));
#109436=CARTESIAN_POINT('Ctrl Pts',(-139.575899809167,-3.86329996794725,
133.85114823284));
#109437=CARTESIAN_POINT('Ctrl Pts',(-139.583646085251,-3.77675984015605,
133.957786688885));
#109438=CARTESIAN_POINT('Ctrl Pts',(-139.591392361335,-3.6859133039606,
134.060620155469));
#109439=CARTESIAN_POINT('Ctrl Pts',(-139.599138694601,-3.59506609715677,
134.163454381147));
#109440=CARTESIAN_POINT('Ctrl Pts',(-139.606885027866,-3.49991267736521,
134.262483268314));
#109441=CARTESIAN_POINT('Ctrl Pts',(-139.614631361131,-3.40081396009166,
134.357337886188));
#109442=CARTESIAN_POINT('Ctrl Pts',(-139.622379429134,-3.30169305034735,
134.452213746097));
#109443=CARTESIAN_POINT('Ctrl Pts',(-139.630127497137,-3.19862536739638,
134.542913206283));
#109444=CARTESIAN_POINT('Ctrl Pts',(-139.63787556514,-3.09200701096162,
134.629105799492));
#109445=CARTESIAN_POINT('Ctrl Pts',(-139.645631867882,-2.98527533926872,
134.715389999215));
#109446=CARTESIAN_POINT('Ctrl Pts',(-139.653388170624,-2.87498576024801,
134.797157517331));
#109447=CARTESIAN_POINT('Ctrl Pts',(-139.661144473366,-2.76156608039902,
134.874119313864));
#109448=CARTESIAN_POINT('Ctrl Pts',(-139.66890491588,-2.64808586505189,
134.951122187224));
#109449=CARTESIAN_POINT('Ctrl Pts',(-139.676665358394,-2.53147255226469,
135.023314022413));
#109450=CARTESIAN_POINT('Ctrl Pts',(-139.684425800908,-2.41218010588707,
135.090450933841));
#109451=CARTESIAN_POINT('Ctrl Pts',(-139.692198701174,-2.29269616068424,
135.157695619399));
#109452=CARTESIAN_POINT('Ctrl Pts',(-139.699971601439,-2.17052483619671,
135.21986898819));
#109453=CARTESIAN_POINT('Ctrl Pts',(-139.707744501705,-2.04614251410275,
135.276774269553));
#109454=CARTESIAN_POINT('Ctrl Pts',(-139.715234837467,-1.92628180271707,
135.331610900603));
#109455=CARTESIAN_POINT('Ctrl Pts',(-139.722725173229,-1.80436833854923,
135.381555694223));
#109456=CARTESIAN_POINT('Ctrl Pts',(-139.730215508991,-1.68084131096866,
135.426476534529));
#109457=CARTESIAN_POINT('Ctrl Pts',(-139.73798984311,-1.55263071859196,
135.473100562148));
#109458=CARTESIAN_POINT('Ctrl Pts',(-139.745764177229,-1.42227565831415,
135.514459840581));
#109459=CARTESIAN_POINT('Ctrl Pts',(-139.753538511348,-1.290247792092,135.550353000356));
#109460=CARTESIAN_POINT('Ctrl Pts',(-139.761303264295,-1.1583826384153,
135.58620192502));
#109461=CARTESIAN_POINT('Ctrl Pts',(-139.769068017242,-1.0248491543818,
135.616598033078));
#109462=CARTESIAN_POINT('Ctrl Pts',(-139.776832770189,-0.890137948128198,
135.641388371859));
#109463=CARTESIAN_POINT('Ctrl Pts',(-139.784589811075,-0.755560538943744,
135.666154088527));
#109464=CARTESIAN_POINT('Ctrl Pts',(-139.79234685196,-0.619808117375787,
135.685325045648));
#109465=CARTESIAN_POINT('Ctrl Pts',(-139.800103892845,-0.483385044857731,
135.698798477107));
#109466=CARTESIAN_POINT('Ctrl Pts',(-139.807855084085,-0.347064850039692,
135.712261748146));
#109467=CARTESIAN_POINT('Ctrl Pts',(-139.815606275325,-0.210075398420547,
135.720036007271));
#109468=CARTESIAN_POINT('Ctrl Pts',(-139.823357466565,-0.072929451167475,
135.722069876728));
#109469=CARTESIAN_POINT('Ctrl Pts',(-139.831105363342,0.0641582053993405,
135.724102881737));
#109470=CARTESIAN_POINT('Ctrl Pts',(-139.838853260119,0.201401835203392,
135.720400343907));
#109471=CARTESIAN_POINT('Ctrl Pts',(-139.846601156896,0.338285589780728,
135.710962896358));
#109472=CARTESIAN_POINT('Ctrl Pts',(-139.854347432981,0.475140711227478,
135.70152742292));
#109473=CARTESIAN_POINT('Ctrl Pts',(-139.862093709065,0.611635717387672,
135.686359452747));
#109474=CARTESIAN_POINT('Ctrl Pts',(-139.869839985149,0.747257197084021,
135.665511689473));
#109475=CARTESIAN_POINT('Ctrl Pts',(-139.877586318414,0.88287967790751,
135.644663772307));
#109476=CARTESIAN_POINT('Ctrl Pts',(-139.885332651679,1.01762823297403,
135.618136037779));
#109477=CARTESIAN_POINT('Ctrl Pts',(-139.893078984945,1.15099738672146,
135.586032718229));
#109478=CARTESIAN_POINT('Ctrl Pts',(-139.900827052948,1.28439640756597,
135.553922209363));
#109479=CARTESIAN_POINT('Ctrl Pts',(-139.908575120951,1.416415032366,135.516233722356));
#109480=CARTESIAN_POINT('Ctrl Pts',(-139.916323188954,1.54656112808484,
135.473121881499));
#109481=CARTESIAN_POINT('Ctrl Pts',(-139.924079491696,1.67684554462315,
135.429964220864));
#109482=CARTESIAN_POINT('Ctrl Pts',(-139.931835794438,1.80525308482444,
135.381371815295));
#109483=CARTESIAN_POINT('Ctrl Pts',(-139.93959209718,1.93130933130658,135.327548357347));
#109484=CARTESIAN_POINT('Ctrl Pts',(-139.947352539694,2.05743285780295,
135.2736961722));
#109485=CARTESIAN_POINT('Ctrl Pts',(-139.955112982208,2.18120223732624,
135.214607539794));
#109486=CARTESIAN_POINT('Ctrl Pts',(-139.962873424722,2.3021669034735,135.150532566655));
#109487=CARTESIAN_POINT('Ctrl Pts',(-139.970646324988,2.4233257528416,135.086354734681));
#109488=CARTESIAN_POINT('Ctrl Pts',(-139.978419225253,2.54167055393297,
135.017174763819));
#109489=CARTESIAN_POINT('Ctrl Pts',(-139.986192125519,2.65677826208401,
134.943287088116));
#109490=CARTESIAN_POINT('Ctrl Pts',(-139.99368246128,2.76770151510152,134.872085415539));
#109491=CARTESIAN_POINT('Ctrl Pts',(-140.001172797042,2.87561868976568,
134.796512546289));
#109492=CARTESIAN_POINT('Ctrl Pts',(-140.008663132804,2.98018124065842,
134.716866570958));
#109493=CARTESIAN_POINT('Ctrl Pts',(-140.016437466923,3.08870831245255,
134.634200794262));
#109494=CARTESIAN_POINT('Ctrl Pts',(-140.024211801042,3.19396513893323,
134.546885090453));
#109495=CARTESIAN_POINT('Ctrl Pts',(-140.031986135161,3.29552735745211,
134.455207436974));
#109496=CARTESIAN_POINT('Ctrl Pts',(-140.039750888109,3.39696440961326,
134.363642768011));
#109497=CARTESIAN_POINT('Ctrl Pts',(-140.047515641056,3.4947156260412,134.2677271049));
#109498=CARTESIAN_POINT('Ctrl Pts',(-140.055280394003,3.5883871376408,134.167790535509));
#109499=CARTESIAN_POINT('Ctrl Pts',(-140.063037434888,3.68196561337455,
134.067953224527));
#109500=CARTESIAN_POINT('Ctrl Pts',(-140.070794475773,3.77147218234516,
133.964103238155));
#109501=CARTESIAN_POINT('Ctrl Pts',(-140.078551516658,3.85654776483319,
133.856609362354));
#109502=CARTESIAN_POINT('Ctrl Pts',(-140.086302707898,3.94155919116279,
133.749196548521));
#109503=CARTESIAN_POINT('Ctrl Pts',(-140.094053899138,4.02214604029632,
133.638145620085));
#109504=CARTESIAN_POINT('Ctrl Pts',(-140.101805090378,4.09798792673915,
133.523860206608));
#109505=CARTESIAN_POINT('Ctrl Pts',(-140.109552987155,4.1737975783572,133.40962336748));
#109506=CARTESIAN_POINT('Ctrl Pts',(-140.117300883932,4.24486606269023,
133.292155102648));
#109507=CARTESIAN_POINT('Ctrl Pts',(-140.125048780709,4.31091508370574,
133.17188975225));
#109508=CARTESIAN_POINT('Ctrl Pts',(-140.132795056793,4.37695028868971,
133.051649558771));
#109509=CARTESIAN_POINT('Ctrl Pts',(-140.140541332877,4.43796793070903,
132.928613785973));
#109510=CARTESIAN_POINT('Ctrl Pts',(-140.148287608962,4.49373483954257,
132.803242868821));
#109511=CARTESIAN_POINT('Ctrl Pts',(-140.156033942227,4.54950216003483,
132.677871026209));
#109512=CARTESIAN_POINT('Ctrl Pts',(-140.163780275492,4.60001851110245,
132.550164362067));
#109513=CARTESIAN_POINT('Ctrl Pts',(-140.171526608758,4.64509836447465,
132.420604487424));
#109514=CARTESIAN_POINT('Ctrl Pts',(-140.179274676761,4.69018831316752,
132.291015598746));
#109515=CARTESIAN_POINT('Ctrl Pts',(-140.187022744764,4.72983921309355,
132.159573042921));
#109516=CARTESIAN_POINT('Ctrl Pts',(-140.194770812767,4.76391514412091,
132.026774443615));
#109517=CARTESIAN_POINT('Ctrl Pts',(-140.202527115508,4.79802729145323,
131.893834704378));
#109518=CARTESIAN_POINT('Ctrl Pts',(-140.21028341825,4.82655253644694,131.759536421971));
#109519=CARTESIAN_POINT('Ctrl Pts',(-140.218039720992,4.84940581723492,
131.624388837976));
#109520=CARTESIAN_POINT('Ctrl Pts',(-140.225800163506,4.87227129550696,
131.489169121646));
#109521=CARTESIAN_POINT('Ctrl Pts',(-140.233560606021,4.88945872845459,
131.353099588187));
#109522=CARTESIAN_POINT('Ctrl Pts',(-140.241321048535,4.90093499563448,
131.21669450056));
#109523=CARTESIAN_POINT('Ctrl Pts',(-140.2490939488,4.91242968553726,131.080070443378));
#109524=CARTESIAN_POINT('Ctrl Pts',(-140.256866849066,4.91819487249433,
130.943110146455));
#109525=CARTESIAN_POINT('Ctrl Pts',(-140.264639749331,4.91824960623573,
130.806328678044));
#109526=CARTESIAN_POINT('Ctrl Pts',(-140.272130085093,4.91830235026777,
130.674519560543));
#109527=CARTESIAN_POINT('Ctrl Pts',(-140.279620420855,4.91305262396251,
130.542876803322));
#109528=CARTESIAN_POINT('Ctrl Pts',(-140.287110756617,4.902562822065,130.411854772761));
#109529=CARTESIAN_POINT('Ctrl Pts',(-140.294885090736,4.89167529614016,
130.275865002087));
#109530=CARTESIAN_POINT('Ctrl Pts',(-140.302659424855,4.87510800737002,
130.140113182227));
#109531=CARTESIAN_POINT('Ctrl Pts',(-140.310433758974,4.85287386095722,
130.00511200034));
#109532=CARTESIAN_POINT('Ctrl Pts',(-140.318198511921,4.83066711614275,
129.870277195344));
#109533=CARTESIAN_POINT('Ctrl Pts',(-140.325963264868,4.80280747248079,
129.736191569723));
#109534=CARTESIAN_POINT('Ctrl Pts',(-140.333728017815,4.76935974637463,
129.603364917257));
#109535=CARTESIAN_POINT('Ctrl Pts',(-140.3414850587,4.73594524102158,129.470670190094));
#109536=CARTESIAN_POINT('Ctrl Pts',(-140.349242099585,4.69695379315036,
129.33923232435));
#109537=CARTESIAN_POINT('Ctrl Pts',(-140.35699914047,4.65250158147564,129.209552761783));
#109538=CARTESIAN_POINT('Ctrl Pts',(-140.36475033171,4.60808289155947,129.079970991583));
#109539=CARTESIAN_POINT('Ctrl Pts',(-140.372501522951,4.55821176074062,
128.952145253679));
#109540=CARTESIAN_POINT('Ctrl Pts',(-140.380252714191,4.50305459781487,
128.8265632691));
#109541=CARTESIAN_POINT('Ctrl Pts',(-140.388000610968,4.44792087815481,
128.701034660215));
#109542=CARTESIAN_POINT('Ctrl Pts',(-140.395748507745,4.38750575180352,
128.577748265118));
#109543=CARTESIAN_POINT('Ctrl Pts',(-140.403496404522,4.32202421561829,
128.457172993598));
#109544=CARTESIAN_POINT('Ctrl Pts',(-140.411242680606,4.25655637675882,
128.336622943825));
#109545=CARTESIAN_POINT('Ctrl Pts',(-140.41898895669,4.1860244224995,128.218783232972));
#109546=CARTESIAN_POINT('Ctrl Pts',(-140.426735232774,4.11068969561761,
128.104098910093));
#109547=CARTESIAN_POINT('Ctrl Pts',(-140.434481566039,4.03535441263177,
127.989413740641));
#109548=CARTESIAN_POINT('Ctrl Pts',(-140.442227899305,3.95521650093072,
127.877884332413));
#109549=CARTESIAN_POINT('Ctrl Pts',(-140.44997423257,3.87058087095232,127.769927098123));
#109550=CARTESIAN_POINT('Ctrl Pts',(-140.457722300573,3.78592628741152,
127.661945687559));
#109551=CARTESIAN_POINT('Ctrl Pts',(-140.465470368576,3.69677222248597,
127.557538350393));
#109552=CARTESIAN_POINT('Ctrl Pts',(-140.473218436579,3.60346387290977,
127.457088417829));
#109553=CARTESIAN_POINT('Ctrl Pts',(-140.480974739321,3.51005635410912,
127.35653172588));
#109554=CARTESIAN_POINT('Ctrl Pts',(-140.488731042063,3.4124859972821,127.259941127331));
#109555=CARTESIAN_POINT('Ctrl Pts',(-140.496487344805,3.31113526377693,
127.167663444653));
#109556=CARTESIAN_POINT('Ctrl Pts',(-140.504247787319,3.20973043633369,
127.075336510597));
#109557=CARTESIAN_POINT('Ctrl Pts',(-140.512008229833,3.10454151147988,
126.987327329967));
#109558=CARTESIAN_POINT('Ctrl Pts',(-140.519768672347,2.99598325080118,
126.903941739622));
#109559=CARTESIAN_POINT('Ctrl Pts',(-140.527541572612,2.88725072276509,
126.820422291325));
#109560=CARTESIAN_POINT('Ctrl Pts',(-140.535314472878,2.77513837041962,
126.741541490332));
#109561=CARTESIAN_POINT('Ctrl Pts',(-140.543087373143,2.66008983211715,
126.667561716536));
#109562=CARTESIAN_POINT('Ctrl Pts',(-140.550577708905,2.54922359797177,
126.596271293861));
#109563=CARTESIAN_POINT('Ctrl Pts',(-140.558068044667,2.43563121270508,
126.52953191145));
#109564=CARTESIAN_POINT('Ctrl Pts',(-140.565558380429,2.31972867350278,
126.467536670963));
#109565=CARTESIAN_POINT('Ctrl Pts',(-140.573332714548,2.1994316542993,126.40319086209));
#109566=CARTESIAN_POINT('Ctrl Pts',(-140.581107048667,2.07626477930166,
126.343752216786));
#109567=CARTESIAN_POINT('Ctrl Pts',(-140.588881382787,1.9506663623127,126.28948699747));
#109568=CARTESIAN_POINT('Ctrl Pts',(-140.596646135734,1.82522273414763,
126.235288655186));
#109569=CARTESIAN_POINT('Ctrl Pts',(-140.604410888681,1.69735388190218,
126.186251206554));
#109570=CARTESIAN_POINT('Ctrl Pts',(-140.612175641628,1.5675237443699,126.142595675687));
#109571=CARTESIAN_POINT('Ctrl Pts',(-140.619932682513,1.43782255596051,
126.098983504108));
#109572=CARTESIAN_POINT('Ctrl Pts',(-140.627689723398,1.30616432700333,
126.060742736514));
#109573=CARTESIAN_POINT('Ctrl Pts',(-140.635446764283,1.17303373208401,
126.028046669981));
#109574=CARTESIAN_POINT('Ctrl Pts',(-140.643197955523,1.04000353198211,
125.995375259806));
#109575=CARTESIAN_POINT('Ctrl Pts',(-140.650949146763,0.905503554093948,
125.968240320934));
#109576=CARTESIAN_POINT('Ctrl Pts',(-140.658700338003,0.770034079951911,
125.94676547406));
#109577=CARTESIAN_POINT('Ctrl Pts',(-140.66644823478,0.634622183949966,
125.925299754569));
#109578=CARTESIAN_POINT('Ctrl Pts',(-140.674196131557,0.498241996588744,
125.909489403426));
#109579=CARTESIAN_POINT('Ctrl Pts',(-140.681944028334,0.36140423600666,
125.89940699488));
#109580=CARTESIAN_POINT('Ctrl Pts',(-140.689690304418,0.224595098934209,
125.889326695358));
#109581=CARTESIAN_POINT('Ctrl Pts',(-140.697436580502,0.0873289686834048,
125.884971983933));
#109582=CARTESIAN_POINT('Ctrl Pts',(-140.705182856587,-0.0498784602151125,
125.886363545413));
#109583=CARTESIAN_POINT('Ctrl Pts',(-140.712929189852,-0.187086901947514,
125.887755117165));
#109584=CARTESIAN_POINT('Ctrl Pts',(-140.720675523117,-0.324236250517871,
125.894893042498));
#109585=CARTESIAN_POINT('Ctrl Pts',(-140.728421856382,-0.460811354576384,
125.907745872868));
#109586=CARTESIAN_POINT('Ctrl Pts',(-140.736169924385,-0.597417043682692,
125.920601581541));
#109587=CARTESIAN_POINT('Ctrl Pts',(-140.743917992388,-0.733447843211009,
125.939174705307));
#109588=CARTESIAN_POINT('Ctrl Pts',(-140.751666060391,-0.868394658496127,
125.963382020258));
#109589=CARTESIAN_POINT('Ctrl Pts',(-140.759422363133,-1.00348489686223,
125.987615063031));
#109590=CARTESIAN_POINT('Ctrl Pts',(-140.767178665875,-1.13748846416222,
126.017494189693));
#109591=CARTESIAN_POINT('Ctrl Pts',(-140.774934968617,-1.26990683912721,
126.052885090697));
#109592=CARTESIAN_POINT('Ctrl Pts',(-140.782695411131,-1.40239588976633,
126.08829488089));
#109593=CARTESIAN_POINT('Ctrl Pts',(-140.790455853645,-1.5332976892453,
126.1292221906));
#109594=CARTESIAN_POINT('Ctrl Pts',(-140.798216296159,-1.66213073958446,
126.17548338145));
#109595=CARTESIAN_POINT('Ctrl Pts',(-140.805989196425,-1.79117060417328,
126.221818834871));
#109596=CARTESIAN_POINT('Ctrl Pts',(-140.81376209669,-1.91813472100845,
126.273505132378));
#109597=CARTESIAN_POINT('Ctrl Pts',(-140.821534996955,-2.04256254508814,
126.330310851202));
#109598=CARTESIAN_POINT('Ctrl Pts',(-140.829025332718,-2.16246710435282,
126.385051539064));
#109599=CARTESIAN_POINT('Ctrl Pts',(-140.83651566848,-2.28001629582192,
126.444545763501));
#109600=CARTESIAN_POINT('Ctrl Pts',(-140.844006004242,-2.39482280096016,
126.508547910464));
#109601=CARTESIAN_POINT('Ctrl Pts',(-140.851781395978,-2.51399844001437,
126.574985755218));
#109602=CARTESIAN_POINT('Ctrl Pts',(-140.859556787713,-2.63059606879468,
126.646491912489));
#109603=CARTESIAN_POINT('Ctrl Pts',(-140.867332179448,-2.74415456711921,
126.722841442766));
#109604=CARTESIAN_POINT('Ctrl Pts',(-140.875097758318,-2.85756974992467,
126.79909461678));
#109605=CARTESIAN_POINT('Ctrl Pts',(-140.882863337187,-2.96795311307466,
126.880178784166));
#109606=CARTESIAN_POINT('Ctrl Pts',(-140.890628916056,-3.0748677978928,
126.965822993941));
#109607=CARTESIAN_POINT('Ctrl Pts',(-140.8983851287,-3.18165353069318,127.05136390646));
#109608=CARTESIAN_POINT('Ctrl Pts',(-140.906141341344,-3.28497861443026,
127.141453664288));
#109609=CARTESIAN_POINT('Ctrl Pts',(-140.913897553988,-3.38443540720065,
127.235778260805));
#109610=CARTESIAN_POINT('Ctrl Pts',(-140.921648456278,-3.4838241060778,
127.330038277228));
#109611=CARTESIAN_POINT('Ctrl Pts',(-140.929399358569,-3.57934950058017,
127.428527096211));
#109612=CARTESIAN_POINT('Ctrl Pts',(-140.937150260859,-3.67063721667059,
127.53089067176));
#109613=CARTESIAN_POINT('Ctrl Pts',(-140.944897535052,-3.76188220215985,
127.633206332242));
#109614=CARTESIAN_POINT('Ctrl Pts',(-140.952644809245,-3.84889319701488,
127.739392848883));
#109615=CARTESIAN_POINT('Ctrl Pts',(-140.960392083438,-3.93133317036314,
127.849059860265));
#109616=CARTESIAN_POINT('Ctrl Pts',(-140.968137408987,-4.01375240787563,
127.958699287491));
#109617=CARTESIAN_POINT('Ctrl Pts',(-140.975882734536,-4.09160267843705,
128.071817154245));
#109618=CARTESIAN_POINT('Ctrl Pts',(-140.983628060084,-4.16458794100919,
128.187990929601));
#109619=CARTESIAN_POINT('Ctrl Pts',(-140.991375513376,-4.23759325359433,
128.304196619424));
#109620=CARTESIAN_POINT('Ctrl Pts',(-140.999122966667,-4.30573067500899,
128.423459567046));
#109621=CARTESIAN_POINT('Ctrl Pts',(-141.006870419959,-4.36874810115888,
128.54532916778));
#109622=CARTESIAN_POINT('Ctrl Pts',(-141.014618868035,-4.43177361884299,
128.667214416759));
#109623=CARTESIAN_POINT('Ctrl Pts',(-141.022367316111,-4.48967765933981,
128.791706634542));
#109624=CARTESIAN_POINT('Ctrl Pts',(-141.030115764188,-4.54225503612316,
128.918332449878));
#109625=CARTESIAN_POINT('Ctrl Pts',(-141.037870521161,-4.59487522215801,
129.045061365762));
#109626=CARTESIAN_POINT('Ctrl Pts',(-141.045625278135,-4.64215993836921,
129.173926985059));
#109627=CARTESIAN_POINT('Ctrl Pts',(-141.053380035108,-4.6839528132572,
129.304437584314));
#109628=CARTESIAN_POINT('Ctrl Pts',(-141.058842202681,-4.71339018785739,
129.396364483573));
#109629=CARTESIAN_POINT('Ctrl Pts',(-141.064304370253,-4.74010393889211,
129.489107134965));
#109630=CARTESIAN_POINT('Ctrl Pts',(-141.069766537825,-4.76405452823392,
129.582490119308));
#109631=CARTESIAN_POINT('Origin',(213.235140564004,0.,130.804360617566));
#109632=CARTESIAN_POINT('',(-143.165347877338,-4.75725076560214,129.584194750691));
#109633=CARTESIAN_POINT('',(-142.820077333605,-4.76405452823405,129.582490119308));
#109634=CARTESIAN_POINT('',(213.235140564004,-4.76405452823405,129.582490119308));
#109635=CARTESIAN_POINT('',(-141.485140564011,-4.91265574211895,130.801213014533));
#109636=CARTESIAN_POINT('Ctrl Pts',(-141.485140564011,-4.91219653301638,
130.801213308754));
#109637=CARTESIAN_POINT('Ctrl Pts',(-141.543347002514,-4.9061844889293,
131.831936216524));
#109638=CARTESIAN_POINT('Ctrl Pts',(-141.694369315622,-4.08506870756113,
134.515011964414));
#109639=CARTESIAN_POINT('Ctrl Pts',(-141.938207503334,0.324971199359551,
136.612636915233));
#109640=CARTESIAN_POINT('Ctrl Pts',(-142.216655127147,5.06232221927725,
133.670468357807));
#109641=CARTESIAN_POINT('Ctrl Pts',(-142.49510275096,5.14764642786865,128.094486804246));
#109642=CARTESIAN_POINT('Ctrl Pts',(-142.773550374773,0.502535045756554,
125.00874690043));
#109643=CARTESIAN_POINT('Ctrl Pts',(-142.996965416899,-3.59504696289219,
126.806148866277));
#109644=CARTESIAN_POINT('Ctrl Pts',(-143.127564584421,-4.59411981166379,
128.934973156602));
#109645=CARTESIAN_POINT('Ctrl Pts',(-143.165347877338,-4.75725076560214,
129.584194750691));
#109646=CARTESIAN_POINT('Ctrl Pts',(-141.415385046285,-4.76405452823413,
129.582490119309));
#109647=CARTESIAN_POINT('Ctrl Pts',(-141.424166289759,-4.80243581228232,
129.732138163295));
#109648=CARTESIAN_POINT('Ctrl Pts',(-141.432947533233,-4.83380612295216,
129.88376826295));
#109649=CARTESIAN_POINT('Ctrl Pts',(-141.441728776707,-4.85797926450059,
130.036753603409));
#109650=CARTESIAN_POINT('Ctrl Pts',(-141.450456965926,-4.88200635748487,
130.188814641612));
#109651=CARTESIAN_POINT('Ctrl Pts',(-141.459185155146,-4.89892289552827,
130.342214411613));
#109652=CARTESIAN_POINT('Ctrl Pts',(-141.467913344365,-4.908593800916,130.496318477415));
#109653=CARTESIAN_POINT('Ctrl Pts',(-141.473655750914,-4.91495643456568,
130.597705852775));
#109654=CARTESIAN_POINT('Ctrl Pts',(-141.479398157462,-4.91818375838515,
130.699397701661));
#109655=CARTESIAN_POINT('Ctrl Pts',(-141.485140564011,-4.91824899049676,
130.801209430865));
#109656=CARTESIAN_POINT('',(-141.139859436025,-4.91824965042212,130.802506265195));
#109657=CARTESIAN_POINT('Ctrl Pts',(-141.069766537825,-4.76405452823392,
129.582490119308));
#109658=CARTESIAN_POINT('Ctrl Pts',(-141.077530799274,-4.79809937124775,
129.715230445516));
#109659=CARTESIAN_POINT('Ctrl Pts',(-141.085295060724,-4.82655889760429,
129.849264650235));
#109660=CARTESIAN_POINT('Ctrl Pts',(-141.093059322173,-4.84936363347628,
129.984082973827));
#109661=CARTESIAN_POINT('Ctrl Pts',(-141.100834514477,-4.87220047481901,
130.119091100351));
#109662=CARTESIAN_POINT('Ctrl Pts',(-141.108609706782,-4.88936658559759,
130.254885163094));
#109663=CARTESIAN_POINT('Ctrl Pts',(-141.116384899086,-4.90084442332398,
130.390951618058));
#109664=CARTESIAN_POINT('Ctrl Pts',(-141.118407808742,-4.90383066827534,
130.426352690444));
#109665=CARTESIAN_POINT('Ctrl Pts',(-141.120430718398,-4.90643214275736,
130.46177221019));
#109666=CARTESIAN_POINT('Ctrl Pts',(-141.122453628054,-4.90864911493995,
130.497201165653));
#109667=CARTESIAN_POINT('Ctrl Pts',(-141.128255564034,-4.91500764441522,
130.598815457145));
#109668=CARTESIAN_POINT('Ctrl Pts',(-141.134057500014,-4.91821123919876,
130.700629226373));
#109669=CARTESIAN_POINT('Ctrl Pts',(-141.139859435993,-4.91824965042191,
130.802506264632));
#109670=CARTESIAN_POINT('Ctrl Pts',(-141.139859436025,-4.91824965042212,
130.802506265195));
#109671=CARTESIAN_POINT('Ctrl Pts',(-141.147560877912,-4.91830063714692,
130.937737004134));
#109672=CARTESIAN_POINT('Ctrl Pts',(-141.155262319799,-4.91277001159415,
131.073195518115));
#109673=CARTESIAN_POINT('Ctrl Pts',(-141.162963761685,-4.9016276276267,
131.208377526354));
#109674=CARTESIAN_POINT('Ctrl Pts',(-141.170656056235,-4.89049847795258,
131.343398973051));
#109675=CARTESIAN_POINT('Ctrl Pts',(-141.178348350785,-4.87377085989654,
131.478144173562));
#109676=CARTESIAN_POINT('Ctrl Pts',(-141.186040645335,-4.85146661083934,
131.612107351642));
#109677=CARTESIAN_POINT('Ctrl Pts',(-141.193725727755,-4.82918327376654,
131.745944928727));
#109678=CARTESIAN_POINT('Ctrl Pts',(-141.201410810175,-4.80133377254601,
131.879001551044));
#109679=CARTESIAN_POINT('Ctrl Pts',(-141.209095892594,-4.76799183109079,
132.010775538375));
#109680=CARTESIAN_POINT('Ctrl Pts',(-141.217087782564,-4.73331879664153,
132.147810270093));
#109681=CARTESIAN_POINT('Ctrl Pts',(-141.225079672534,-4.69270571207718,
132.283457393));
#109682=CARTESIAN_POINT('Ctrl Pts',(-141.233071562504,-4.64629449388461,
132.417162694263));
#109683=CARTESIAN_POINT('Ctrl Pts',(-141.240748780933,-4.60171066440629,
132.545603501982));
#109684=CARTESIAN_POINT('Ctrl Pts',(-141.248425999362,-4.55177676325002,
132.67225208524));
#109685=CARTESIAN_POINT('Ctrl Pts',(-141.256103217791,-4.49666961042024,
132.796632054199));
#109686=CARTESIAN_POINT('Ctrl Pts',(-141.263779517625,-4.44156905127304,
132.920997140842));
#109687=CARTESIAN_POINT('Ctrl Pts',(-141.271455817459,-4.38129663284183,
133.043093788377));
#109688=CARTESIAN_POINT('Ctrl Pts',(-141.279132117293,-4.31607711216116,
133.162466091114));
#109689=CARTESIAN_POINT('Ctrl Pts',(-141.286809235918,-4.25085063485896,
133.281851126665));
#109690=CARTESIAN_POINT('Ctrl Pts',(-141.294486354542,-4.18067619718312,
133.398510889518));
#109691=CARTESIAN_POINT('Ctrl Pts',(-141.302163473167,-4.10582400319464,
133.512015011556));
#109692=CARTESIAN_POINT('Ctrl Pts',(-141.309843148281,-4.03094688333255,
133.625556930606));
#109693=CARTESIAN_POINT('Ctrl Pts',(-141.317522823396,-3.95138912850936,
133.735940786137));
#109694=CARTESIAN_POINT('Ctrl Pts',(-141.325202498511,-3.86746335458778,
133.842766492926));
#109695=CARTESIAN_POINT('Ctrl Pts',(-141.332890594324,-3.78344555676406,
133.9497093332));
#109696=CARTESIAN_POINT('Ctrl Pts',(-141.340578690138,-3.69505042649711,
134.053085923735));
#109697=CARTESIAN_POINT('Ctrl Pts',(-141.348266785951,-3.60263002539251,
134.152530261213));
#109698=CARTESIAN_POINT('Ctrl Pts',(-141.355959873652,-3.51014961563883,
134.252039167989));
#109699=CARTESIAN_POINT('Ctrl Pts',(-141.363652961353,-3.41363901397913,
134.347610458735));
#109700=CARTESIAN_POINT('Ctrl Pts',(-141.371346049054,-3.31348505945223,
134.438916962333));
#109701=CARTESIAN_POINT('Ctrl Pts',(-141.379049968107,-3.21319009486476,
134.530352019373));
#109702=CARTESIAN_POINT('Ctrl Pts',(-141.386753887161,-3.10924184473051,
134.617510051455));
#109703=CARTESIAN_POINT('Ctrl Pts',(-141.394457806214,-3.00205814321372,
134.70010572823));
#109704=CARTESIAN_POINT('Ctrl Pts',(-141.396605621432,-2.97217584776836,
134.723133001789));
#109705=CARTESIAN_POINT('Ctrl Pts',(-141.39875343665,-2.9420422295363,134.745805926892));
#109706=CARTESIAN_POINT('Ctrl Pts',(-141.400901251868,-2.91166669313975,
134.768118951592));
#109707=CARTESIAN_POINT('Ctrl Pts',(-141.408675585987,-2.80171795685258,
134.848884237067));
#109708=CARTESIAN_POINT('Ctrl Pts',(-141.416449920106,-2.68823206032786,
134.925199261423));
#109709=CARTESIAN_POINT('Ctrl Pts',(-141.424224254225,-2.57160509811455,
134.996738258219));
#109710=CARTESIAN_POINT('Ctrl Pts',(-141.431989007172,-2.45512186820923,
135.068189089596));
#109711=CARTESIAN_POINT('Ctrl Pts',(-141.439753760119,-2.3355056049805,
135.134875402391));
#109712=CARTESIAN_POINT('Ctrl Pts',(-141.447518513066,-2.21318418815064,
135.196512574389));
#109713=CARTESIAN_POINT('Ctrl Pts',(-141.455275553951,-2.09098426267641,
135.258088527477));
#109714=CARTESIAN_POINT('Ctrl Pts',(-141.463032594836,-1.96608487733265,
135.314625144808));
#109715=CARTESIAN_POINT('Ctrl Pts',(-141.470789635721,-1.83894121045427,
135.365882105731));
#109716=CARTESIAN_POINT('Ctrl Pts',(-141.478540826961,-1.7118934236036,
135.417100413382));
#109717=CARTESIAN_POINT('Ctrl Pts',(-141.486292018202,-1.58260508503859,
135.46304684383));
#109718=CARTESIAN_POINT('Ctrl Pts',(-141.494043209442,-1.45155387138247,
135.503528035415));
#109719=CARTESIAN_POINT('Ctrl Pts',(-141.501791106219,-1.3205583579886,
135.543992021414));
#109720=CARTESIAN_POINT('Ctrl Pts',(-141.509539002996,-1.18780183251011,
135.578995273419));
#109721=CARTESIAN_POINT('Ctrl Pts',(-141.517286899773,-1.0537795462575,
135.608393478651));
#109722=CARTESIAN_POINT('Ctrl Pts',(-141.525033175857,-0.91978529457762,
135.637785534414));
#109723=CARTESIAN_POINT('Ctrl Pts',(-141.532779451941,-0.784526190409212,
135.661574791766));
#109724=CARTESIAN_POINT('Ctrl Pts',(-141.540525728025,-0.64850977441591,
135.679667596105));
#109725=CARTESIAN_POINT('Ctrl Pts',(-141.548272061291,-0.512492354380508,
135.697760534));
#109726=CARTESIAN_POINT('Ctrl Pts',(-141.556018394556,-0.375717998916713,
135.710156883422));
#109727=CARTESIAN_POINT('Ctrl Pts',(-141.563764727821,-0.238701108935161,
135.716814672628));
#109728=CARTESIAN_POINT('Ctrl Pts',(-141.571512795824,-0.101653534971293,
135.723473952799));
#109729=CARTESIAN_POINT('Ctrl Pts',(-141.579260863827,0.0356362911590168,
135.724392096561));
#109730=CARTESIAN_POINT('Ctrl Pts',(-141.58700893183,0.172652616806735,
135.719579243061));
#109731=CARTESIAN_POINT('Ctrl Pts',(-141.594765234572,0.309814565036055,
135.714761274402));
#109732=CARTESIAN_POINT('Ctrl Pts',(-141.602521537314,0.446702040771774,
135.704200154854));
#109733=CARTESIAN_POINT('Ctrl Pts',(-141.610277840056,0.582802508506382,
135.687958092643));
#109734=CARTESIAN_POINT('Ctrl Pts',(-141.61803828257,0.718975617158156,
135.671707361554));
#109735=CARTESIAN_POINT('Ctrl Pts',(-141.625798725084,0.854360495081336,
135.649769708611));
#109736=CARTESIAN_POINT('Ctrl Pts',(-141.633559167598,0.988454457830667,
135.622258587355));
#109737=CARTESIAN_POINT('Ctrl Pts',(-141.641332067863,1.12276368011367,
135.594703302804));
#109738=CARTESIAN_POINT('Ctrl Pts',(-141.649104968129,1.25577746654187,
135.561556765521));
#109739=CARTESIAN_POINT('Ctrl Pts',(-141.656877868395,1.38700709281581,
135.522982703194));
#109740=CARTESIAN_POINT('Ctrl Pts',(-141.664368204157,1.51346619163076,
135.485810905194));
#109741=CARTESIAN_POINT('Ctrl Pts',(-141.671858539919,1.63826830385689,
135.443599438269));
#109742=CARTESIAN_POINT('Ctrl Pts',(-141.679348875681,1.76099517684078,
135.396536468907));
#109743=CARTESIAN_POINT('Ctrl Pts',(-141.6871232098,1.88837527651317,135.347689092759));
#109744=CARTESIAN_POINT('Ctrl Pts',(-141.694897543919,2.01392316697685,
135.293460328688));
#109745=CARTESIAN_POINT('Ctrl Pts',(-141.702671878038,2.13715067292015,
135.234007337536));
#109746=CARTESIAN_POINT('Ctrl Pts',(-141.710436630986,2.2602263119752,135.174627616882));
#109747=CARTESIAN_POINT('Ctrl Pts',(-141.718201383933,2.38098690764954,
135.110036647888));
#109748=CARTESIAN_POINT('Ctrl Pts',(-141.72596613688,2.4989617197696,135.040440572622));
#109749=CARTESIAN_POINT('Ctrl Pts',(-141.733723177765,2.61681935764311,
134.970913621159));
#109750=CARTESIAN_POINT('Ctrl Pts',(-141.74148021865,2.73189638361879,134.896391653585));
#109751=CARTESIAN_POINT('Ctrl Pts',(-141.749237259535,2.84374457412099,
134.817127725144));
#109752=CARTESIAN_POINT('Ctrl Pts',(-141.756988450775,2.95550841903283,
134.737923570248));
#109753=CARTESIAN_POINT('Ctrl Pts',(-141.764739642015,3.06404795727677,
134.653984797337));
#109754=CARTESIAN_POINT('Ctrl Pts',(-141.772490833255,3.16894231232893,
134.565608772585));
#109755=CARTESIAN_POINT('Ctrl Pts',(-141.780238730032,3.2737920844819,134.47727031));
#109756=CARTESIAN_POINT('Ctrl Pts',(-141.78798662681,3.37499945651688,134.384498597965));
#109757=CARTESIAN_POINT('Ctrl Pts',(-141.795734523587,3.4721753185756,134.287632300851));
#109758=CARTESIAN_POINT('Ctrl Pts',(-141.803480799671,3.56933085353912,
134.190786266078));
#109759=CARTESIAN_POINT('Ctrl Pts',(-141.811227075755,3.66245627918677,
134.089847625687));
#109760=CARTESIAN_POINT('Ctrl Pts',(-141.818973351839,3.75119846312152,
133.985192765413));
#109761=CARTESIAN_POINT('Ctrl Pts',(-141.826719685104,3.83994130213079,
133.8805371326));
#109762=CARTESIAN_POINT('Ctrl Pts',(-141.83446601837,3.92430058200984,133.772165523357));
#109763=CARTESIAN_POINT('Ctrl Pts',(-141.842212351635,4.00396294448545,
133.660488030986));
#109764=CARTESIAN_POINT('Ctrl Pts',(-141.849960419638,4.08364314679447,
133.548785529215));
#109765=CARTESIAN_POINT('Ctrl Pts',(-141.857708487641,4.15862411165816,
133.433775989372));
#109766=CARTESIAN_POINT('Ctrl Pts',(-141.865456555644,4.22863559252291,
133.315898809222));
#109767=CARTESIAN_POINT('Ctrl Pts',(-141.873212858386,4.29872148242296,
133.197896347803));
#109768=CARTESIAN_POINT('Ctrl Pts',(-141.880969161128,4.36382713773829,
133.077020494525));
#109769=CARTESIAN_POINT('Ctrl Pts',(-141.88872546387,4.42372785804987,132.953736085095));
#109770=CARTESIAN_POINT('Ctrl Pts',(-141.896485906384,4.48366054917929,
132.830385875063));
#109771=CARTESIAN_POINT('Ctrl Pts',(-141.904246348898,4.53838261392825,
132.704624905693));
#109772=CARTESIAN_POINT('Ctrl Pts',(-141.912006791412,4.58771779075253,
132.576937424058));
#109773=CARTESIAN_POINT('Ctrl Pts',(-141.919779691678,4.63713216478255,
132.449044967141));
#109774=CARTESIAN_POINT('Ctrl Pts',(-141.927552591943,4.68114224481423,
132.319220188421));
#109775=CARTESIAN_POINT('Ctrl Pts',(-141.935325492209,4.71962161216651,
132.187962764309));
#109776=CARTESIAN_POINT('Ctrl Pts',(-141.94281582797,4.75670215759062,132.061476878184));
#109777=CARTESIAN_POINT('Ctrl Pts',(-141.950306163732,4.7886470450928,131.933660997651));
#109778=CARTESIAN_POINT('Ctrl Pts',(-141.957796499494,4.81538850869332,
131.804968719094));
#109779=CARTESIAN_POINT('Ctrl Pts',(-141.965570833613,4.84314388301496,
131.671397033678));
#109780=CARTESIAN_POINT('Ctrl Pts',(-141.973345167732,4.86538138943614,
131.536458066138));
#109781=CARTESIAN_POINT('Ctrl Pts',(-141.981119501851,4.88196938114517,
131.400647481467));
#109782=CARTESIAN_POINT('Ctrl Pts',(-141.988884254798,4.89853692963693,
131.265004271204));
#109783=CARTESIAN_POINT('Ctrl Pts',(-141.996649007745,4.90946876981461,
131.128491965482));
#109784=CARTESIAN_POINT('Ctrl Pts',(-142.004413760693,4.91468388827595,
130.991618036166));
#109785=CARTESIAN_POINT('Ctrl Pts',(-142.012170801578,4.91989382700812,
130.854880051966));
#109786=CARTESIAN_POINT('Ctrl Pts',(-142.019927842462,4.91939832856881,
130.717781547088));
#109787=CARTESIAN_POINT('Ctrl Pts',(-142.027684883347,4.91316801971071,
130.580836407262));
#109788=CARTESIAN_POINT('Ctrl Pts',(-142.035436074588,4.90694240917697,
130.443994538831));
#109789=CARTESIAN_POINT('Ctrl Pts',(-142.043187265828,4.89499061390475,
130.307306194231));
#109790=CARTESIAN_POINT('Ctrl Pts',(-142.050938457068,4.87733532243406,
130.17128620248));
#109791=CARTESIAN_POINT('Ctrl Pts',(-142.058686353845,4.85968753493327,
130.035324022854));
#109792=CARTESIAN_POINT('Ctrl Pts',(-142.066434250622,4.83634112287924,
129.900030017989));
#109793=CARTESIAN_POINT('Ctrl Pts',(-142.074182147399,4.80737069081658,
129.765914613395));
#109794=CARTESIAN_POINT('Ctrl Pts',(-142.081928423483,4.77840631874378,
129.631827262853));
#109795=CARTESIAN_POINT('Ctrl Pts',(-142.089674699567,4.74382034913029,
129.498918404113));
#109796=CARTESIAN_POINT('Ctrl Pts',(-142.097420975652,4.70373856926707,
129.367688583144));
#109797=CARTESIAN_POINT('Ctrl Pts',(-142.105167308917,4.66365649352931,
129.236457793467));
#109798=CARTESIAN_POINT('Ctrl Pts',(-142.112913642182,4.61807864079469,
129.106906440207));
#109799=CARTESIAN_POINT('Ctrl Pts',(-142.120659975447,4.56718065637211,
128.979519826001));
#109800=CARTESIAN_POINT('Ctrl Pts',(-142.12840804345,4.51627127369888,128.852104684446));
#109801=CARTESIAN_POINT('Ctrl Pts',(-142.136156111453,4.46003953361033,
128.726855609585));
#109802=CARTESIAN_POINT('Ctrl Pts',(-142.143904179456,4.39870903902877,
128.604237472725));
#109803=CARTESIAN_POINT('Ctrl Pts',(-142.151660482198,4.33731336166748,
128.481489015849));
#109804=CARTESIAN_POINT('Ctrl Pts',(-142.15941678494,4.27080827991578,128.361377432891));
#109805=CARTESIAN_POINT('Ctrl Pts',(-142.167173087682,4.19946341715095,
128.24434302573));
#109806=CARTESIAN_POINT('Ctrl Pts',(-142.174933530196,4.12808047548452,
128.127246153781));
#109807=CARTESIAN_POINT('Ctrl Pts',(-142.18269397271,4.05185282287614,128.013230055072));
#109808=CARTESIAN_POINT('Ctrl Pts',(-142.190454415225,3.97109259643092,
127.9027047708));
#109809=CARTESIAN_POINT('Ctrl Pts',(-142.19822731549,3.89020272650088,127.79200206153));
#109810=CARTESIAN_POINT('Ctrl Pts',(-142.206000215755,3.80476598659904,
127.684801670725));
#109811=CARTESIAN_POINT('Ctrl Pts',(-142.213773116021,3.71513443625474,
127.581480045306));
#109812=CARTESIAN_POINT('Ctrl Pts',(-142.221263451783,3.62876121853347,
127.481914421221));
#109813=CARTESIAN_POINT('Ctrl Pts',(-142.228753787545,3.53849309029612,
127.385950677131));
#109814=CARTESIAN_POINT('Ctrl Pts',(-142.236244123307,3.44467504586145,
127.2938910064));
#109815=CARTESIAN_POINT('Ctrl Pts',(-142.244018457426,3.34729986175733,
127.198340865273));
#109816=CARTESIAN_POINT('Ctrl Pts',(-142.251792791545,3.24579180209864,
127.1066940133));
#109817=CARTESIAN_POINT('Ctrl Pts',(-142.259567125664,3.14049672556235,
127.019329127706));
#109818=CARTESIAN_POINT('Ctrl Pts',(-142.267331878611,3.03533141579711,
126.932071911526));
#109819=CARTESIAN_POINT('Ctrl Pts',(-142.275096631558,2.92638867340537,
126.849086409037));
#109820=CARTESIAN_POINT('Ctrl Pts',(-142.282861384505,2.81405165911513,
126.770715080049));
#109821=CARTESIAN_POINT('Ctrl Pts',(-142.29061842539,2.70182621953176,126.69242159057));
#109822=CARTESIAN_POINT('Ctrl Pts',(-142.298375466275,2.58621353553775,
126.618733376737));
#109823=CARTESIAN_POINT('Ctrl Pts',(-142.30613250716,2.46763007679345,126.549952918884));
#109824=CARTESIAN_POINT('Ctrl Pts',(-142.313883698401,2.34913604275702,
126.481224328909));
#109825=CARTESIAN_POINT('Ctrl Pts',(-142.321634889641,2.22767602994654,
126.417396323709));
#109826=CARTESIAN_POINT('Ctrl Pts',(-142.329386080881,2.10369544230599,
126.358728092433));
#109827=CARTESIAN_POINT('Ctrl Pts',(-142.337133977658,1.97976754972299,
126.30008479672));
#109828=CARTESIAN_POINT('Ctrl Pts',(-142.344881874435,1.85332156572261,
126.246597080017));
#109829=CARTESIAN_POINT('Ctrl Pts',(-142.352629771212,1.72482725132048,
126.198478072863));
#109830=CARTESIAN_POINT('Ctrl Pts',(-142.360376047296,1.5963598151589,126.150369131167));
#109831=CARTESIAN_POINT('Ctrl Pts',(-142.36812232338,1.46584526674136,126.1076268023));
#109832=CARTESIAN_POINT('Ctrl Pts',(-142.375868599464,1.33377272067146,
126.070415815174));
#109833=CARTESIAN_POINT('Ctrl Pts',(-142.383614932729,1.2016991996722,126.033204553365));
#109834=CARTESIAN_POINT('Ctrl Pts',(-142.391361265995,1.06806803438588,
126.001524820798));
#109835=CARTESIAN_POINT('Ctrl Pts',(-142.39910759926,0.933382464245367,
125.975491160028));
#109836=CARTESIAN_POINT('Ctrl Pts',(-142.406855667263,0.798666732205084,
125.949451669201));
#109837=CARTESIAN_POINT('Ctrl Pts',(-142.414603735266,0.662896509232523,
125.929060840363));
#109838=CARTESIAN_POINT('Ctrl Pts',(-142.422351803269,0.52658376756393,
125.914381824336));
#109839=CARTESIAN_POINT('Ctrl Pts',(-142.430108106011,0.390126151091534,
125.899687207277));
#109840=CARTESIAN_POINT('Ctrl Pts',(-142.437864408752,0.253125253449516,
125.890716571599));
#109841=CARTESIAN_POINT('Ctrl Pts',(-142.445620711494,0.116097251099588,
125.887481069439));
#109842=CARTESIAN_POINT('Ctrl Pts',(-142.453381154008,-0.0210038872214008,
125.884243840395));
#109843=CARTESIAN_POINT('Ctrl Pts',(-142.461141596523,-0.158131768367437,
125.886747837062));
#109844=CARTESIAN_POINT('Ctrl Pts',(-142.468902039037,-0.294772695334932,
125.89495208694));
#109845=CARTESIAN_POINT('Ctrl Pts',(-142.476674939302,-0.431632970448808,
125.903169507007));
#109846=CARTESIAN_POINT('Ctrl Pts',(-142.484447839568,-0.568004340130829,
125.917105426235));
#109847=CARTESIAN_POINT('Ctrl Pts',(-142.492220739833,-0.703379792149672,
125.936667125727));
#109848=CARTESIAN_POINT('Ctrl Pts',(-142.499711075595,-0.833834005502211,
125.955517708169));
#109849=CARTESIAN_POINT('Ctrl Pts',(-142.507201411357,-0.963363149477259,
125.979592093257));
#109850=CARTESIAN_POINT('Ctrl Pts',(-142.51469174712,-1.09152650238254,
126.008763370393));
#109851=CARTESIAN_POINT('Ctrl Pts',(-142.522466081239,-1.22454920776332,
126.039040685367));
#109852=CARTESIAN_POINT('Ctrl Pts',(-142.530240415358,-1.35652188562031,
126.074904928725));
#109853=CARTESIAN_POINT('Ctrl Pts',(-142.538014749477,-1.48693899901593,
126.116269804057));
#109854=CARTESIAN_POINT('Ctrl Pts',(-142.545779502424,-1.61719538497429,
126.157583700877));
#109855=CARTESIAN_POINT('Ctrl Pts',(-142.553544255371,-1.74589965182567,
126.204384624342));
#109856=CARTESIAN_POINT('Ctrl Pts',(-142.561309008318,-1.87255657070242,
126.256535318369));
#109857=CARTESIAN_POINT('Ctrl Pts',(-142.569066049203,-1.99908769214247,
126.308634215592));
#109858=CARTESIAN_POINT('Ctrl Pts',(-142.576823090088,-2.12357515309508,
126.366072161446));
#109859=CARTESIAN_POINT('Ctrl Pts',(-142.584580130973,-2.2455393562644,
126.428662266221));
#109860=CARTESIAN_POINT('Ctrl Pts',(-142.592331322213,-2.36741158527987,
126.49120517131));
#109861=CARTESIAN_POINT('Ctrl Pts',(-142.600082513453,-2.48676399750776,
126.558892324118));
#109862=CARTESIAN_POINT('Ctrl Pts',(-142.607833704693,-2.6031377780654,
126.631489091757));
#109863=CARTESIAN_POINT('Ctrl Pts',(-142.615581601471,-2.71946209666113,
126.704055003832));
#109864=CARTESIAN_POINT('Ctrl Pts',(-142.623329498248,-2.83280997054145,
126.78152617392));
#109865=CARTESIAN_POINT('Ctrl Pts',(-142.631077395025,-2.94274816964395,
126.863622581036));
#109866=CARTESIAN_POINT('Ctrl Pts',(-142.638823671109,-3.05266337204549,
126.945701815353));
#109867=CARTESIAN_POINT('Ctrl Pts',(-142.646569947193,-3.15917000526206,
127.032404128509));
#109868=CARTESIAN_POINT('Ctrl Pts',(-142.654316223277,-3.26186509980353,
127.123407054536));
#109869=CARTESIAN_POINT('Ctrl Pts',(-142.662062556542,-3.36456095241727,
127.214410652326));
#109870=CARTESIAN_POINT('Ctrl Pts',(-142.669808889807,-3.46344491760358,
127.309714667041));
#109871=CARTESIAN_POINT('Ctrl Pts',(-142.677555223073,-3.55814861425983,
127.408957622141));
#109872=CARTESIAN_POINT('Ctrl Pts',(-142.685303291076,-3.65287351915166,
127.508222802012));
#109873=CARTESIAN_POINT('Ctrl Pts',(-142.693051359079,-3.74341602284071,
127.611428394751));
#109874=CARTESIAN_POINT('Ctrl Pts',(-142.700799427082,-3.82944626125069,
127.718177798177));
#109875=CARTESIAN_POINT('Ctrl Pts',(-142.708555729824,-3.91556793362217,
127.82504065614));
#109876=CARTESIAN_POINT('Ctrl Pts',(-142.716312032565,-3.99716751508839,
127.93545454369));
#109877=CARTESIAN_POINT('Ctrl Pts',(-142.724068335307,-4.07395661705488,
128.048991214953));
#109878=CARTESIAN_POINT('Ctrl Pts',(-142.731828777821,-4.15078670367695,
128.162588484156));
#109879=CARTESIAN_POINT('Ctrl Pts',(-142.739589220335,-4.22280098965747,
128.27931152559));
#109880=CARTESIAN_POINT('Ctrl Pts',(-142.74734966285,-4.28975628054519,
128.398706004779));
#109881=CARTESIAN_POINT('Ctrl Pts',(-142.755122563115,-4.35681905401003,
128.518292146585));
#109882=CARTESIAN_POINT('Ctrl Pts',(-142.76289546338,-4.41880642684689,
128.640557946883));
#109883=CARTESIAN_POINT('Ctrl Pts',(-142.770668363646,-4.47552235359413,
128.765026725095));
#109884=CARTESIAN_POINT('Ctrl Pts',(-142.778158699408,-4.53017651354393,
128.884970749698));
#109885=CARTESIAN_POINT('Ctrl Pts',(-142.785649035169,-4.57993571778879,
129.006960080163));
#109886=CARTESIAN_POINT('Ctrl Pts',(-142.793139370931,-4.62466851896773,
129.130555326569));
#109887=CARTESIAN_POINT('Ctrl Pts',(-142.802118691822,-4.67829364191574,
129.278719763172));
#109888=CARTESIAN_POINT('Ctrl Pts',(-142.811098012714,-4.72483570086139,
129.429576506611));
#109889=CARTESIAN_POINT('Ctrl Pts',(-142.820077333605,-4.76405452823405,
129.582490119308));
#109890=CARTESIAN_POINT('Origin',(213.235140564004,0.,130.804360617566));
#109891=CARTESIAN_POINT('',(-144.915004217899,-4.7640545282341,129.582490119308));
#109892=CARTESIAN_POINT('',(-144.570016427913,-4.76405452823402,129.582490119308));
#109893=CARTESIAN_POINT('',(213.235140564004,-4.76405452823405,129.582490119308));
#109894=CARTESIAN_POINT('',(-143.235140564011,-4.91565778800209,130.808061793682));
#109895=CARTESIAN_POINT('Ctrl Pts',(-143.235140564011,-4.91824860589129,
130.808063744402));
#109896=CARTESIAN_POINT('Ctrl Pts',(-143.244096688567,-4.91812913868428,
130.966732202243));
#109897=CARTESIAN_POINT('Ctrl Pts',(-143.253052813123,-4.91032750956385,
131.125085964154));
#109898=CARTESIAN_POINT('Ctrl Pts',(-143.262008937679,-4.89495850831957,
131.282444568698));
#109899=CARTESIAN_POINT('Ctrl Pts',(-143.271013498197,-4.8795063893897,
131.440654190352));
#109900=CARTESIAN_POINT('Ctrl Pts',(-143.280018058714,-4.8564049360629,
131.597857740923));
#109901=CARTESIAN_POINT('Ctrl Pts',(-143.289022619231,-4.82582010225577,
131.753382958275));
#109902=CARTESIAN_POINT('Ctrl Pts',(-143.298086497441,-4.79503379034313,
131.909932700604));
#109903=CARTESIAN_POINT('Ctrl Pts',(-143.307150375652,-4.75666526286325,
132.064781806234));
#109904=CARTESIAN_POINT('Ctrl Pts',(-143.316214253862,-4.71093213517195,
132.217265950667));
#109905=CARTESIAN_POINT('Ctrl Pts',(-143.320958043375,-4.68699664900692,
132.297072041212));
#109906=CARTESIAN_POINT('Ctrl Pts',(-143.325701832887,-4.66104464757951,
132.376230686379));
#109907=CARTESIAN_POINT('Ctrl Pts',(-143.3304456224,-4.63311244679749,132.4546491129));
#109908=CARTESIAN_POINT('Ctrl Pts',(-143.338219956519,-4.58733590865378,
132.583164732589));
#109909=CARTESIAN_POINT('Ctrl Pts',(-143.345994290638,-4.53613556432417,
132.709977809174));
#109910=CARTESIAN_POINT('Ctrl Pts',(-143.353768624757,-4.47965681453224,
132.834596536496));
#109911=CARTESIAN_POINT('Ctrl Pts',(-143.361533377704,-4.42324766975178,
132.959061682375));
#109912=CARTESIAN_POINT('Ctrl Pts',(-143.369298130651,-4.36157322268416,
133.081337507139));
#109913=CARTESIAN_POINT('Ctrl Pts',(-143.377062883598,-4.29482825956732,
133.200948459336));
#109914=CARTESIAN_POINT('Ctrl Pts',(-143.384819924483,-4.22814958848879,
133.32044061225));
#109915=CARTESIAN_POINT('Ctrl Pts',(-143.392576965368,-4.15641061272182,
133.437272820626));
#109916=CARTESIAN_POINT('Ctrl Pts',(-143.400334006253,-4.07985355850699,
133.55099091734));
#109917=CARTESIAN_POINT('Ctrl Pts',(-143.408085197493,-4.00335423656216,
133.664623258353));
#109918=CARTESIAN_POINT('Ctrl Pts',(-143.415836388733,-3.92204428558689,
133.775145838996));
#109919=CARTESIAN_POINT('Ctrl Pts',(-143.423587579973,-3.83621088624211,
133.88213076798));
#109920=CARTESIAN_POINT('Ctrl Pts',(-143.43133547675,-3.75041396838162,
133.989070225515));
#109921=CARTESIAN_POINT('Ctrl Pts',(-143.439083373527,-3.6600976701772,
134.092474717616));
#109922=CARTESIAN_POINT('Ctrl Pts',(-143.446831270304,-3.56559122091009,
134.191947119468));
#109923=CARTESIAN_POINT('Ctrl Pts',(-143.454577546388,-3.47110454035511,
134.291398713838));
#109924=CARTESIAN_POINT('Ctrl Pts',(-143.462323822473,-3.37242972124061,
134.386919570714));
#109925=CARTESIAN_POINT('Ctrl Pts',(-143.470070098557,-3.26993456670635,
134.478147627173));
#109926=CARTESIAN_POINT('Ctrl Pts',(-143.477816431822,-3.167438655576,134.569376357057));
#109927=CARTESIAN_POINT('Ctrl Pts',(-143.485562765087,-3.06112264479254,
134.656311963356));
#109928=CARTESIAN_POINT('Ctrl Pts',(-143.493309098353,-2.95138898982712,
134.738631336928));
#109929=CARTESIAN_POINT('Ctrl Pts',(-143.501057166356,-2.84163076077066,
134.820969145352));
#109930=CARTESIAN_POINT('Ctrl Pts',(-143.508805234359,-2.72845367724512,
134.898688429391));
#109931=CARTESIAN_POINT('Ctrl Pts',(-143.516553302362,-2.61229052530956,
134.971508475979));
#109932=CARTESIAN_POINT('Ctrl Pts',(-143.524309605103,-2.4960039137936,
135.04440591658));
#109933=CARTESIAN_POINT('Ctrl Pts',(-143.532065907845,-2.37672522598798,
135.112393510263));
#109934=CARTESIAN_POINT('Ctrl Pts',(-143.539822210587,-2.25491377154477,
135.17523546654));
#109935=CARTESIAN_POINT('Ctrl Pts',(-143.547582653101,-2.13303730266066,
135.238110963463));
#109936=CARTESIAN_POINT('Ctrl Pts',(-143.555343095615,-2.00862572801258,
135.295835186113));
#109937=CARTESIAN_POINT('Ctrl Pts',(-143.56310353813,-1.88215892542903,
135.348220303112));
#109938=CARTESIAN_POINT('Ctrl Pts',(-143.570876438395,-1.75548910710677,
135.400689513351));
#109939=CARTESIAN_POINT('Ctrl Pts',(-143.57864933866,-1.62675783528844,
135.44780235629));
#109940=CARTESIAN_POINT('Ctrl Pts',(-143.586422238926,-1.49646160878872,
135.489420458798));
#109941=CARTESIAN_POINT('Ctrl Pts',(-143.593912574688,-1.37090197831902,
135.529525638449));
#109942=CARTESIAN_POINT('Ctrl Pts',(-143.60140291045,-1.24388949481631,
135.56452855532));
#109943=CARTESIAN_POINT('Ctrl Pts',(-143.608893246212,-1.1158759978454,
135.594350577882));
#109944=CARTESIAN_POINT('Ctrl Pts',(-143.616667580331,-0.983008830228136,
135.625303311494));
#109945=CARTESIAN_POINT('Ctrl Pts',(-143.62444191445,-0.848642360616826,
135.650772577217));
#109946=CARTESIAN_POINT('Ctrl Pts',(-143.632216248569,-0.713268952102007,
135.670614871555));
#109947=CARTESIAN_POINT('Ctrl Pts',(-143.639981001516,-0.578062379214514,
135.690432712039));
#109948=CARTESIAN_POINT('Ctrl Pts',(-143.647745754463,-0.441851719686798,
135.704637323049));
#109949=CARTESIAN_POINT('Ctrl Pts',(-143.65551050741,-0.305142355144324,
135.713135536586));
#109950=CARTESIAN_POINT('Ctrl Pts',(-143.663267548295,-0.168568772269607,
135.721625309577));
#109951=CARTESIAN_POINT('Ctrl Pts',(-143.67102458918,-0.0314978577779321,
135.724419939924));
#109952=CARTESIAN_POINT('Ctrl Pts',(-143.678781630065,0.105557355464807,
135.721477730998));
#109953=CARTESIAN_POINT('Ctrl Pts',(-143.686532821305,0.24250921430492,
135.718537740815));
#109954=CARTESIAN_POINT('Ctrl Pts',(-143.694284012545,0.379445006170189,
135.709869530744));
#109955=CARTESIAN_POINT('Ctrl Pts',(-143.702035203785,0.515849505837805,
135.695483428315));
#109956=CARTESIAN_POINT('Ctrl Pts',(-143.709783100562,0.652196029954167,
135.681103440363));
#109957=CARTESIAN_POINT('Ctrl Pts',(-143.717530997339,0.788011323003643,
135.66101043457));
#109958=CARTESIAN_POINT('Ctrl Pts',(-143.725278894116,0.92278331616353,
135.63526674519));
#109959=CARTESIAN_POINT('Ctrl Pts',(-143.733025170201,1.0575271179278,135.609528440834));
#109960=CARTESIAN_POINT('Ctrl Pts',(-143.740771446285,1.19122767010683,
135.578141877266));
#109961=CARTESIAN_POINT('Ctrl Pts',(-143.748517722369,1.32338155232788,
135.541220793828));
#109962=CARTESIAN_POINT('Ctrl Pts',(-143.756264055634,1.45553641007868,
135.504299437848));
#109963=CARTESIAN_POINT('Ctrl Pts',(-143.764010388899,1.58614419854334,
135.461843585675));
#109964=CARTESIAN_POINT('Ctrl Pts',(-143.771756722165,1.71471553983686,
135.414017186112));
#109965=CARTESIAN_POINT('Ctrl Pts',(-143.779504790168,1.84331567379099,
135.366180076159));
#109966=CARTESIAN_POINT('Ctrl Pts',(-143.78725285817,1.96987808672668,135.31297016187));
#109967=CARTESIAN_POINT('Ctrl Pts',(-143.795000926173,2.09393267535656,
135.254599826145));
#109968=CARTESIAN_POINT('Ctrl Pts',(-143.802757228915,2.21811911067933,
135.196167453733));
#109969=CARTESIAN_POINT('Ctrl Pts',(-143.810513531657,2.33979204305571,
135.132563870609));
#109970=CARTESIAN_POINT('Ctrl Pts',(-143.818269834399,2.45850482718562,
135.064048056476));
#109971=CARTESIAN_POINT('Ctrl Pts',(-143.826030276913,2.57728097190311,
134.995495673389));
#109972=CARTESIAN_POINT('Ctrl Pts',(-143.833790719427,2.69309349027285,
134.922026044454));
#109973=CARTESIAN_POINT('Ctrl Pts',(-143.841551161941,2.80552496874744,
134.84394137703));
#109974=CARTESIAN_POINT('Ctrl Pts',(-143.849324062206,2.91813693221248,
134.765731361167));
#109975=CARTESIAN_POINT('Ctrl Pts',(-143.857096962472,3.02735669813637,
134.682891738731));
#109976=CARTESIAN_POINT('Ctrl Pts',(-143.864869862737,3.13279947954752,
134.59576543418));
#109977=CARTESIAN_POINT('Ctrl Pts',(-143.8723601985,3.23440915026375,134.511806390255));
#109978=CARTESIAN_POINT('Ctrl Pts',(-143.879850534262,3.33251144535074,
134.423867122263));
#109979=CARTESIAN_POINT('Ctrl Pts',(-143.887340870024,3.42679597955594,
134.332285273366));
#109980=CARTESIAN_POINT('Ctrl Pts',(-143.895115204143,3.52465534052926,
134.237231070835));
#109981=CARTESIAN_POINT('Ctrl Pts',(-143.902889538262,3.61871171401717,
134.137951514739));
#109982=CARTESIAN_POINT('Ctrl Pts',(-143.910663872381,3.70857823218911,
134.034783276946));
#109983=CARTESIAN_POINT('Ctrl Pts',(-143.918428625328,3.79833399790901,
133.931742184785));
#109984=CARTESIAN_POINT('Ctrl Pts',(-143.926193378276,3.88390992805215,
133.824822238455));
#109985=CARTESIAN_POINT('Ctrl Pts',(-143.933958131223,3.96495446663007,
133.714398270252));
#109986=CARTESIAN_POINT('Ctrl Pts',(-143.941715172108,4.04591851062975,
133.604083976691));
#109987=CARTESIAN_POINT('Ctrl Pts',(-143.949472212993,4.12235988971488,
133.490272900244));
#109988=CARTESIAN_POINT('Ctrl Pts',(-143.957229253878,4.19396621653495,
133.373374131945));
#109989=CARTESIAN_POINT('Ctrl Pts',(-143.964980445118,4.26551854446704,
133.256563517917));
#109990=CARTESIAN_POINT('Ctrl Pts',(-143.972731636358,4.33224287418394,
133.136670178721));
#109991=CARTESIAN_POINT('Ctrl Pts',(-143.980482827598,4.39386940271056,
133.014133170211));
#109992=CARTESIAN_POINT('Ctrl Pts',(-143.988230724375,4.45546973831852,
132.891648243199));
#109993=CARTESIAN_POINT('Ctrl Pts',(-143.995978621152,4.51197640684717,
132.766522230237));
#109994=CARTESIAN_POINT('Ctrl Pts',(-144.003726517929,4.56316506616442,
132.639219642515));
#109995=CARTESIAN_POINT('Ctrl Pts',(-144.011472794013,4.61434301791764,
132.51194368375));
#109996=CARTESIAN_POINT('Ctrl Pts',(-144.019219070097,4.6602050273441,132.382492418337));
#109997=CARTESIAN_POINT('Ctrl Pts',(-144.026965346182,4.70057467556714,
132.251350866986));
#109998=CARTESIAN_POINT('Ctrl Pts',(-144.034711679447,4.7409446217897,132.120208347578));
#109999=CARTESIAN_POINT('Ctrl Pts',(-144.042458012712,4.77582201088228,
131.987375890996));
#110000=CARTESIAN_POINT('Ctrl Pts',(-144.050204345977,4.8050802569149,131.853353843048));
#110001=CARTESIAN_POINT('Ctrl Pts',(-144.05795241398,4.83434505512889,131.719301781791));
#110002=CARTESIAN_POINT('Ctrl Pts',(-144.065700481983,4.85798812290462,
131.584059980956));
#110003=CARTESIAN_POINT('Ctrl Pts',(-144.073448549986,4.87593404168169,
131.448138749899));
#110004=CARTESIAN_POINT('Ctrl Pts',(-144.081204852728,4.89389903359476,
131.31207306014));
#110005=CARTESIAN_POINT('Ctrl Pts',(-144.08896115547,4.90615472974164,131.175326885892));
#110006=CARTESIAN_POINT('Ctrl Pts',(-144.096717458212,4.91267759438521,
131.038415987352));
#110007=CARTESIAN_POINT('Ctrl Pts',(-144.104477900726,4.91920394047805,
130.901432015342));
#110008=CARTESIAN_POINT('Ctrl Pts',(-144.11223834324,4.91999135594377,130.764283534621));
#110009=CARTESIAN_POINT('Ctrl Pts',(-144.119998785755,4.91506847417433,
130.627485077489));
#110010=CARTESIAN_POINT('Ctrl Pts',(-144.12777168602,4.91013768975805,130.490467019329));
#110011=CARTESIAN_POINT('Ctrl Pts',(-144.135544586285,4.89947832058561,
130.353800497595));
#110012=CARTESIAN_POINT('Ctrl Pts',(-144.143317486551,4.88317089195754,
130.217994603511));
#110013=CARTESIAN_POINT('Ctrl Pts',(-144.150807822313,4.8674562794359,130.08712559575));
#110014=CARTESIAN_POINT('Ctrl Pts',(-144.158298158075,4.84649716948137,
129.95705603411));
#110015=CARTESIAN_POINT('Ctrl Pts',(-144.165788493837,4.82040986003761,
129.828229558869));
#110016=CARTESIAN_POINT('Ctrl Pts',(-144.173562827956,4.79333344232742,
129.694518588665));
#110017=CARTESIAN_POINT('Ctrl Pts',(-144.181337162075,4.76064650736517,
129.561723272727));
#110018=CARTESIAN_POINT('Ctrl Pts',(-144.189111496194,4.72242319521703,
129.430351073285));
#110019=CARTESIAN_POINT('Ctrl Pts',(-144.196876249141,4.68424698988499,
129.299140778337));
#110020=CARTESIAN_POINT('Ctrl Pts',(-144.204641002089,4.6405480914579,129.169350482015));
#110021=CARTESIAN_POINT('Ctrl Pts',(-144.212405755036,4.59145183236326,
129.04147856434));
#110022=CARTESIAN_POINT('Ctrl Pts',(-144.220162795921,4.54240433636529,
128.913733650855));
#110023=CARTESIAN_POINT('Ctrl Pts',(-144.227919836806,4.48797028703326,
128.787903686889));
#110024=CARTESIAN_POINT('Ctrl Pts',(-144.235676877691,4.4283250112462,128.664472616461));
#110025=CARTESIAN_POINT('Ctrl Pts',(-144.243428068931,4.36872471442565,
128.541134626365));
#110026=CARTESIAN_POINT('Ctrl Pts',(-144.251179260171,4.30392118264851,
128.42019227965));
#110027=CARTESIAN_POINT('Ctrl Pts',(-144.258930451411,4.23413797094092,
128.302109889614));
#110028=CARTESIAN_POINT('Ctrl Pts',(-144.266678348188,4.16438441895973,
128.184077687744));
#110029=CARTESIAN_POINT('Ctrl Pts',(-144.274426244965,4.08965559509321,
128.068903360779));
#110030=CARTESIAN_POINT('Ctrl Pts',(-144.282174141742,4.01022104335957,
127.957026733755));
#110031=CARTESIAN_POINT('Ctrl Pts',(-144.289920417827,3.93080310762173,
127.84517350891));
#110032=CARTESIAN_POINT('Ctrl Pts',(-144.297666693911,3.84668162811568,
127.736616930521));
#110033=CARTESIAN_POINT('Ctrl Pts',(-144.305412969995,3.75816930778995,
127.631767590327));
#110034=CARTESIAN_POINT('Ctrl Pts',(-144.31315930326,3.66965633408651,127.526917476159));
#110035=CARTESIAN_POINT('Ctrl Pts',(-144.320905636525,3.57675270708537,
127.425774953541));
#110036=CARTESIAN_POINT('Ctrl Pts',(-144.328651969791,3.47981095909716,
127.32871697193));
#110037=CARTESIAN_POINT('Ctrl Pts',(-144.336400037794,3.38284750167649,
127.231637254858));
#110038=CARTESIAN_POINT('Ctrl Pts',(-144.344148105797,3.28184440003372,
127.138644175515));
#110039=CARTESIAN_POINT('Ctrl Pts',(-144.3518961738,3.17719022630799,127.050077020346));
#110040=CARTESIAN_POINT('Ctrl Pts',(-144.359652476542,3.07242482488117,
126.961415734951));
#110041=CARTESIAN_POINT('Ctrl Pts',(-144.367408779284,2.96400089876291,
126.877190023291));
#110042=CARTESIAN_POINT('Ctrl Pts',(-144.375165082025,2.85233964997165,
126.797698467634));
#110043=CARTESIAN_POINT('Ctrl Pts',(-144.38292552454,2.74061880420985,126.718164484939));
#110044=CARTESIAN_POINT('Ctrl Pts',(-144.390685967054,2.62565752042557,
126.64336990614));
#110045=CARTESIAN_POINT('Ctrl Pts',(-144.398446409568,2.50790416626174,
126.573568758428));
#110046=CARTESIAN_POINT('Ctrl Pts',(-144.406219309834,2.38996178395983,
126.503655559717));
#110047=CARTESIAN_POINT('Ctrl Pts',(-144.413992210099,2.26921871922076,
126.438751995629));
#110048=CARTESIAN_POINT('Ctrl Pts',(-144.421765110364,2.14614681079986,
126.379065494188));
#110049=CARTESIAN_POINT('Ctrl Pts',(-144.429255446126,2.02754887625214,
126.321548747417));
#110050=CARTESIAN_POINT('Ctrl Pts',(-144.436745781888,1.90678875940073,
126.268876465024));
#110051=CARTESIAN_POINT('Ctrl Pts',(-144.44423611765,1.78430256925667,126.221190600662));
#110052=CARTESIAN_POINT('Ctrl Pts',(-144.452010451769,1.65717227798209,
126.171696712259));
#110053=CARTESIAN_POINT('Ctrl Pts',(-144.459784785888,1.52777973095445,
126.127418044414));
#110054=CARTESIAN_POINT('Ctrl Pts',(-144.467559120007,1.39659194503779,
126.088566516722));
#110055=CARTESIAN_POINT('Ctrl Pts',(-144.475323872955,1.26556583634267,
126.049762870066));
#110056=CARTESIAN_POINT('Ctrl Pts',(-144.483088625902,1.13274926219005,
126.016373165463));
#110057=CARTESIAN_POINT('Ctrl Pts',(-144.490853378849,0.998629269045308,
125.988561343769));
#110058=CARTESIAN_POINT('Ctrl Pts',(-144.498610419734,0.86464248576852,
125.960777145168));
#110059=CARTESIAN_POINT('Ctrl Pts',(-144.506367460619,0.729355240104424,
125.938559883432));
#110060=CARTESIAN_POINT('Ctrl Pts',(-144.514124501504,0.593269456324948,
125.922023634656));
#110061=CARTESIAN_POINT('Ctrl Pts',(-144.521875692744,0.457286295893428,
125.905499855994));
#110062=CARTESIAN_POINT('Ctrl Pts',(-144.529626883984,0.320506182496859,
125.894648610029));
#110063=CARTESIAN_POINT('Ctrl Pts',(-144.537378075224,0.183440593014859,
125.889532786265));
#110064=CARTESIAN_POINT('Ctrl Pts',(-144.545125972001,0.0464332600652932,
125.884419136862));
#110065=CARTESIAN_POINT('Ctrl Pts',(-144.552873868778,-0.0908589177685185,
125.885036075798));
#110066=CARTESIAN_POINT('Ctrl Pts',(-144.560621765556,-0.227920208102862,
125.891394564229));
#110067=CARTESIAN_POINT('Ctrl Pts',(-144.56836804164,-0.364952828170341,
125.897751722602));
#110068=CARTESIAN_POINT('Ctrl Pts',(-144.576114317724,-0.501754266505367,
125.909848023494));
#110069=CARTESIAN_POINT('Ctrl Pts',(-144.583860593808,-0.637810057067511,
125.927642315921));
#110070=CARTESIAN_POINT('Ctrl Pts',(-144.591606927073,-0.773866851962038,
125.945436739701));
#110071=CARTESIAN_POINT('Ctrl Pts',(-144.599353260339,-0.909177600436715,
125.968929188245));
#110072=CARTESIAN_POINT('Ctrl Pts',(-144.607099593604,-1.04323461191162,
125.998026816527));
#110073=CARTESIAN_POINT('Ctrl Pts',(-144.614847661607,-1.17732164452531,
126.027130961021));
#110074=CARTESIAN_POINT('Ctrl Pts',(-144.62259572961,-1.3101539994524,126.061842700123));
#110075=CARTESIAN_POINT('Ctrl Pts',(-144.630343797613,-1.44123619266726,
126.102018509696));
#110076=CARTESIAN_POINT('Ctrl Pts',(-144.638100100355,-1.57245770159679,
126.142237018598));
#110077=CARTESIAN_POINT('Ctrl Pts',(-144.645856403097,-1.70192495868042,
126.187931083887));
#110078=CARTESIAN_POINT('Ctrl Pts',(-144.653612705838,-1.82915908822223,
126.238907727384));
#110079=CARTESIAN_POINT('Ctrl Pts',(-144.661373148353,-1.95646112645026,
126.28991157865));
#110080=CARTESIAN_POINT('Ctrl Pts',(-144.669133590867,-2.08152730585766,
126.34620346577));
#110081=CARTESIAN_POINT('Ctrl Pts',(-144.676894033381,-2.20390155251043,
126.40754347225));
#110082=CARTESIAN_POINT('Ctrl Pts',(-144.684666933646,-2.32647224516746,
126.468981947154));
#110083=CARTESIAN_POINT('Ctrl Pts',(-144.692439833912,-2.44634202760384,
126.535484545392));
#110084=CARTESIAN_POINT('Ctrl Pts',(-144.700212734177,-2.56308134437499,
126.606766415572));
#110085=CARTESIAN_POINT('Ctrl Pts',(-144.70770306994,-2.6755768929348,126.675457010223));
#110086=CARTESIAN_POINT('Ctrl Pts',(-144.715193405702,-2.78516536876059,
126.748585261411));
#110087=CARTESIAN_POINT('Ctrl Pts',(-144.722683741464,-2.89149161464991,
126.825860987692));
#110088=CARTESIAN_POINT('Ctrl Pts',(-144.730697094649,-3.00524215777342,
126.908532540338));
#110089=CARTESIAN_POINT('Ctrl Pts',(-144.738710447833,-3.11564733037586,
126.996234191182));
#110090=CARTESIAN_POINT('Ctrl Pts',(-144.746723801018,-3.22222827438724,
127.088660412996));
#110091=CARTESIAN_POINT('Ctrl Pts',(-144.754420725515,-3.32460058470019,
127.177436938185));
#110092=CARTESIAN_POINT('Ctrl Pts',(-144.762117650012,-3.4234445500382,
127.270571761214));
#110093=CARTESIAN_POINT('Ctrl Pts',(-144.769814574509,-3.51836411176413,
127.36774934488));
#110094=CARTESIAN_POINT('Ctrl Pts',(-144.777504538288,-3.61319783293093,
127.464839045944));
#110095=CARTESIAN_POINT('Ctrl Pts',(-144.785194502067,-3.70411393179018,
127.565963954223));
#110096=CARTESIAN_POINT('Ctrl Pts',(-144.792884465846,-3.79075008511641,
127.670768931547));
#110097=CARTESIAN_POINT('Ctrl Pts',(-144.800569212024,-3.87732745624877,
127.775502799221));
#110098=CARTESIAN_POINT('Ctrl Pts',(-144.808253958201,-3.95963040542177,
127.883911463481));
#110099=CARTESIAN_POINT('Ctrl Pts',(-144.815938704378,-4.03733444998907,
127.995604024084));
#110100=CARTESIAN_POINT('Ctrl Pts',(-144.823619971739,-4.11500331862091,
128.107246022449));
#110101=CARTESIAN_POINT('Ctrl Pts',(-144.831301239099,-4.18807719852429,
128.22216863258));
#110102=CARTESIAN_POINT('Ctrl Pts',(-144.83898250646,-4.25627310309848,
128.339949463895));
#110103=CARTESIAN_POINT('Ctrl Pts',(-144.846663330622,-4.32446507286651,
128.457723499424));
#110104=CARTESIAN_POINT('Ctrl Pts',(-144.854344154785,-4.38777942079224,
128.578355087569));
#110105=CARTESIAN_POINT('Ctrl Pts',(-144.862024978947,-4.44597769891592,
128.701394768285));
#110106=CARTESIAN_POINT('Ctrl Pts',(-144.869705608028,-4.50417449889121,
128.824431323979));
#110107=CARTESIAN_POINT('Ctrl Pts',(-144.877386237109,-4.55725532290773,
128.949875487892));
#110108=CARTESIAN_POINT('Ctrl Pts',(-144.88506686619,-4.60502904888281,
129.077255953266));
#110109=CARTESIAN_POINT('Ctrl Pts',(-144.892750950078,-4.65282426384832,
129.204693715357));
#110110=CARTESIAN_POINT('Ctrl Pts',(-144.900435033965,-4.69530748152023,
129.334069142459));
#110111=CARTESIAN_POINT('Ctrl Pts',(-144.908119117852,-4.73233685550399,
129.46489395186));
#110112=CARTESIAN_POINT('Ctrl Pts',(-144.910414151201,-4.7433965536316,
129.503967874638));
#110113=CARTESIAN_POINT('Ctrl Pts',(-144.91270918455,-4.75397007818319,
129.543171001613));
#110114=CARTESIAN_POINT('Ctrl Pts',(-144.915004217899,-4.7640545282341,
129.582490119308));
#110115=CARTESIAN_POINT('Ctrl Pts',(-143.165347877338,-4.75725076560214,
129.584194750691));
#110116=CARTESIAN_POINT('Ctrl Pts',(-143.188612106229,-4.85769505085557,
129.983938621581));
#110117=CARTESIAN_POINT('Ctrl Pts',(-143.21187633512,-4.91040493875306,
130.396321313897));
#110118=CARTESIAN_POINT('Ctrl Pts',(-143.235140564011,-4.91326838458752,
130.808059994614));
#110119=CARTESIAN_POINT('',(-142.889859435939,-4.91824866801256,130.80074093627));
#110120=CARTESIAN_POINT('Ctrl Pts',(-142.820077333605,-4.76405452823405,
129.582490119308));
#110121=CARTESIAN_POINT('Ctrl Pts',(-142.829056384281,-4.80327217539394,
129.735399130374));
#110122=CARTESIAN_POINT('Ctrl Pts',(-142.838035434958,-4.83516690740692,
129.890364784401));
#110123=CARTESIAN_POINT('Ctrl Pts',(-142.847014485634,-4.85954511673974,
130.046729888998));
#110124=CARTESIAN_POINT('Ctrl Pts',(-142.855924747846,-4.88373656472607,
130.201897081267));
#110125=CARTESIAN_POINT('Ctrl Pts',(-142.864835010057,-4.90052613806173,
130.358442230497));
#110126=CARTESIAN_POINT('Ctrl Pts',(-142.873745272269,-4.90977189919264,
130.515703449981));
#110127=CARTESIAN_POINT('Ctrl Pts',(-142.879116660159,-4.91534553644312,
130.610505487213));
#110128=CARTESIAN_POINT('Ctrl Pts',(-142.884488048049,-4.91817862317039,
130.705567377168));
#110129=CARTESIAN_POINT('Ctrl Pts',(-142.889859435939,-4.91824866801256,
130.800740936271));
#110130=CARTESIAN_POINT('Ctrl Pts',(-142.889859435993,-4.91824866801326,
130.800740937229));
#110131=CARTESIAN_POINT('Ctrl Pts',(-142.89762022287,-4.91834987145624,
130.938251339318));
#110132=CARTESIAN_POINT('Ctrl Pts',(-142.905381009747,-4.91267973923835,
131.075815413098));
#110133=CARTESIAN_POINT('Ctrl Pts',(-142.913141796625,-4.90125152276576,
131.212914864988));
#110134=CARTESIAN_POINT('Ctrl Pts',(-142.920901939177,-4.88982425510002,
131.350002934445));
#110135=CARTESIAN_POINT('Ctrl Pts',(-142.928662081729,-4.87263988591247,
131.486626071592));
#110136=CARTESIAN_POINT('Ctrl Pts',(-142.936422224281,-4.84976366603659,
131.622269809403));
#110137=CARTESIAN_POINT('Ctrl Pts',(-142.944183376621,-4.82688446939635,
131.757931197833));
#110138=CARTESIAN_POINT('Ctrl Pts',(-142.95194452896,-4.79831201220062,
131.892612550079));
#110139=CARTESIAN_POINT('Ctrl Pts',(-142.959705681299,-4.76416285473462,
132.025808674614));
#110140=CARTESIAN_POINT('Ctrl Pts',(-142.967469497837,-4.73000197476788,
132.159050521849));
#110141=CARTESIAN_POINT('Ctrl Pts',(-142.975233314374,-4.69026068064949,
132.290805750421));
#110142=CARTESIAN_POINT('Ctrl Pts',(-142.982997130911,-4.64510556720512,
132.420583786568));
#110143=CARTESIAN_POINT('Ctrl Pts',(-142.990770247241,-4.599896365257,132.550517275758));
#110144=CARTESIAN_POINT('Ctrl Pts',(-142.998543363572,-4.54926051948765,
132.678468474795));
#110145=CARTESIAN_POINT('Ctrl Pts',(-143.006316479902,-4.4934132428636,
132.803965701416));
#110146=CARTESIAN_POINT('Ctrl Pts',(-143.014094506739,-4.43753068587032,
132.929542208331));
#110147=CARTESIAN_POINT('Ctrl Pts',(-143.021872533576,-4.37643031110508,
133.052661306647));
#110148=CARTESIAN_POINT('Ctrl Pts',(-143.029650560413,-4.31037313362153,
133.17287629441));
#110149=CARTESIAN_POINT('Ctrl Pts',(-143.037441425418,-4.24420692422634,
133.293289705272));
#110150=CARTESIAN_POINT('Ctrl Pts',(-143.045232290423,-4.17306776748978,
133.410789096853));
#110151=CARTESIAN_POINT('Ctrl Pts',(-143.053023155428,-4.09726026937177,
133.524956388262));
#110152=CARTESIAN_POINT('Ctrl Pts',(-143.059211101867,-4.03704965890129,
133.615634520137));
#110153=CARTESIAN_POINT('Ctrl Pts',(-143.065399048306,-3.97389493110227,
133.704211170842));
#110154=CARTESIAN_POINT('Ctrl Pts',(-143.071586994745,-3.90796609425353,
133.790492575244));
#110155=CARTESIAN_POINT('Ctrl Pts',(-143.079361328864,-3.82513525355506,
133.898893718126));
#110156=CARTESIAN_POINT('Ctrl Pts',(-143.087135662983,-3.73765946788447,
134.004017543083));
#110157=CARTESIAN_POINT('Ctrl Pts',(-143.094909997102,-3.64582736016016,
134.105440126213));
#110158=CARTESIAN_POINT('Ctrl Pts',(-143.102674750049,-3.55410842730135,
134.206737715073));
#110159=CARTESIAN_POINT('Ctrl Pts',(-143.110439502996,-3.45804411454878,
134.304342850995));
#110160=CARTESIAN_POINT('Ctrl Pts',(-143.118204255943,-3.35796510878766,
134.397862167679));
#110161=CARTESIAN_POINT('Ctrl Pts',(-143.125961296828,-3.25798550290592,
134.491288599659));
#110162=CARTESIAN_POINT('Ctrl Pts',(-143.133718337713,-3.1539994230293,
134.580637022982));
#110163=CARTESIAN_POINT('Ctrl Pts',(-143.141475378598,-3.04637620115051,
134.665548919574));
#110164=CARTESIAN_POINT('Ctrl Pts',(-143.149226569839,-2.9388341387798,
134.750396783445));
#110165=CARTESIAN_POINT('Ctrl Pts',(-143.156977761079,-2.82766069947265,
134.830814538652));
#110166=CARTESIAN_POINT('Ctrl Pts',(-143.164728952319,-2.71325999989535,
134.906482414328));
#110167=CARTESIAN_POINT('Ctrl Pts',(-143.172476849096,-2.5989079236679,
134.982118129137));
#110168=CARTESIAN_POINT('Ctrl Pts',(-143.180224745873,-2.48133164072702,
135.053007764472));
#110169=CARTESIAN_POINT('Ctrl Pts',(-143.18797264265,-2.36096591422859,
135.118873685613));
#110170=CARTESIAN_POINT('Ctrl Pts',(-143.195718918734,-2.24062536564535,
135.184725829024));
#110171=CARTESIAN_POINT('Ctrl Pts',(-143.203465194818,-2.11749687685625,
135.245556160885));
#110172=CARTESIAN_POINT('Ctrl Pts',(-143.211211470902,-1.99204123713972,
135.301132211947));
#110173=CARTESIAN_POINT('Ctrl Pts',(-143.218957804168,-1.86658467133833,
135.35670867326));
#110174=CARTESIAN_POINT('Ctrl Pts',(-143.226704137433,-1.73880127779179,
135.407030618027));
#110175=CARTESIAN_POINT('Ctrl Pts',(-143.234450470698,-1.60917294931547,
135.451913251124));
#110176=CARTESIAN_POINT('Ctrl Pts',(-143.242198538701,-1.4795155914736,
135.496805935375));
#110177=CARTESIAN_POINT('Ctrl Pts',(-143.249946606704,-1.34801284593662,
135.536256756192));
#110178=CARTESIAN_POINT('Ctrl Pts',(-143.257694674707,-1.2151625426437,
135.570130550898));
#110179=CARTESIAN_POINT('Ctrl Pts',(-143.265450977449,-1.08217104446732,
135.604040347077));
#110180=CARTESIAN_POINT('Ctrl Pts',(-143.273207280191,-0.947829507008607,
135.632361179915));
#110181=CARTESIAN_POINT('Ctrl Pts',(-143.280963582933,-0.812647300709287,
135.655008762624));
#110182=CARTESIAN_POINT('Ctrl Pts',(-143.288724025447,-0.677392943596207,
135.677668433028));
#110183=CARTESIAN_POINT('Ctrl Pts',(-143.296484467961,-0.541297411356543,
135.694648771407));
#110184=CARTESIAN_POINT('Ctrl Pts',(-143.304244910475,-0.404875016760093,
135.705917439975));
#110185=CARTESIAN_POINT('Ctrl Pts',(-143.312017810741,-0.268233624824826,
135.71720419801));
#110186=CARTESIAN_POINT('Ctrl Pts',(-143.319790711006,-0.131264712866735,
135.722760948034));
#110187=CARTESIAN_POINT('Ctrl Pts',(-143.327563611272,0.00551668044895405,
135.722607523602));
#110188=CARTESIAN_POINT('Ctrl Pts',(-143.335053947034,0.137325725590153,
135.722459676535));
#110189=CARTESIAN_POINT('Ctrl Pts',(-143.342544282796,0.268960341185616,
135.717009618442));
#110190=CARTESIAN_POINT('Ctrl Pts',(-143.350034618558,0.399966256337925,
135.706320435464));
#110191=CARTESIAN_POINT('Ctrl Pts',(-143.357808952677,0.535939300577972,
135.695225968866));
#110192=CARTESIAN_POINT('Ctrl Pts',(-143.365583286796,0.671665750646524,
135.67845210812));
#110193=CARTESIAN_POINT('Ctrl Pts',(-143.373357620916,0.806632939619369,
135.656012538636));
#110194=CARTESIAN_POINT('Ctrl Pts',(-143.381122373863,0.941433793593803,
135.633600623916));
#110195=CARTESIAN_POINT('Ctrl Pts',(-143.38888712681,1.07547686631057,135.605536957018));
#110196=CARTESIAN_POINT('Ctrl Pts',(-143.396651879757,1.20825246322059,
135.57188713009));
#110197=CARTESIAN_POINT('Ctrl Pts',(-143.404408920642,1.34089618553632,
135.538270724644));
#110198=CARTESIAN_POINT('Ctrl Pts',(-143.412165961527,1.47227456073164,
135.499079295868));
#110199=CARTESIAN_POINT('Ctrl Pts',(-143.419923002412,1.60188632443349,
135.454429785449));
#110200=CARTESIAN_POINT('Ctrl Pts',(-143.427674193652,1.73140034689592,
135.409813945573));
#110201=CARTESIAN_POINT('Ctrl Pts',(-143.435425384892,1.85915004140789,
135.359748343491));
#110202=CARTESIAN_POINT('Ctrl Pts',(-143.443176576132,1.98464794075242,
135.304400130033));
#110203=CARTESIAN_POINT('Ctrl Pts',(-143.450924472909,2.11009250014213,
135.249075441043));
#110204=CARTESIAN_POINT('Ctrl Pts',(-143.458672369687,2.23328681093808,
135.188472763745));
#110205=CARTESIAN_POINT('Ctrl Pts',(-143.466420266464,2.35376229108314,
135.122807808348));
#110206=CARTESIAN_POINT('Ctrl Pts',(-143.474166542548,2.47421257035523,
135.057156588645));
#110207=CARTESIAN_POINT('Ctrl Pts',(-143.481912818632,2.59194480712546,
134.986445384079));
#110208=CARTESIAN_POINT('Ctrl Pts',(-143.489659094716,2.70651435057165,
134.910936214417));
#110209=CARTESIAN_POINT('Ctrl Pts',(-143.497405427982,2.82108473974403,
134.835426487363));
#110210=CARTESIAN_POINT('Ctrl Pts',(-143.505151761247,2.93249206256358,
134.755118939686));
#110211=CARTESIAN_POINT('Ctrl Pts',(-143.512898094512,3.04032037081962,
134.670319115181));
#110212=CARTESIAN_POINT('Ctrl Pts',(-143.520646162515,3.1481728264778,134.585500300343));
#110213=CARTESIAN_POINT('Ctrl Pts',(-143.528394230519,3.25244436543236,
134.496187448462));
#110214=CARTESIAN_POINT('Ctrl Pts',(-143.536142298522,3.35275218225372,
134.402726339236));
#110215=CARTESIAN_POINT('Ctrl Pts',(-143.543898601263,3.45316660741635,
134.309165898432));
#110216=CARTESIAN_POINT('Ctrl Pts',(-143.551654904005,3.54960860864155,
134.211448660141));
#110217=CARTESIAN_POINT('Ctrl Pts',(-143.559411206747,3.64173194590026,
134.109957613074));
#110218=CARTESIAN_POINT('Ctrl Pts',(-143.567171649262,3.7339044521581,134.008412397178));
#110219=CARTESIAN_POINT('Ctrl Pts',(-143.574932091776,3.82175345123784,
133.903089659139));
#110220=CARTESIAN_POINT('Ctrl Pts',(-143.58269253429,3.90497373783085,133.794404625495));
#110221=CARTESIAN_POINT('Ctrl Pts',(-143.590465434555,3.98832761701562,
133.685545120986));
#110222=CARTESIAN_POINT('Ctrl Pts',(-143.598238334821,4.06703771075116,
133.573312855313));
#110223=CARTESIAN_POINT('Ctrl Pts',(-143.606011235086,4.14084231458924,
133.458151865612));
#110224=CARTESIAN_POINT('Ctrl Pts',(-143.613501570848,4.21196393517264,
133.347177267964));
#110225=CARTESIAN_POINT('Ctrl Pts',(-143.62099190661,4.27853037202427,133.233483448261));
#110226=CARTESIAN_POINT('Ctrl Pts',(-143.628482242372,4.34034915678514,
133.117486697073));
#110227=CARTESIAN_POINT('Ctrl Pts',(-143.636256576491,4.40451181956171,
132.997091893803));
#110228=CARTESIAN_POINT('Ctrl Pts',(-143.64403091061,4.46376295702004,132.873834705931));
#110229=CARTESIAN_POINT('Ctrl Pts',(-143.651805244729,4.51783697408825,
132.748153851956));
#110230=CARTESIAN_POINT('Ctrl Pts',(-143.659569997676,4.57184434976315,
132.622627888402));
#110231=CARTESIAN_POINT('Ctrl Pts',(-143.667334750623,4.62068714698513,
132.494684557577));
#110232=CARTESIAN_POINT('Ctrl Pts',(-143.67509950357,4.66414504793186,132.364788134099));
#110233=CARTESIAN_POINT('Ctrl Pts',(-143.682856544455,4.70755978587884,
132.23502072558));
#110234=CARTESIAN_POINT('Ctrl Pts',(-143.69061358534,4.74560014777814,132.103304453141));
#110235=CARTESIAN_POINT('Ctrl Pts',(-143.698370626225,4.77809357434708,
131.970124254537));
#110236=CARTESIAN_POINT('Ctrl Pts',(-143.706121817465,4.81056249737024,
131.837044488156));
#110237=CARTESIAN_POINT('Ctrl Pts',(-143.713873008705,4.83749271875037,
131.702503371258));
#110238=CARTESIAN_POINT('Ctrl Pts',(-143.721624199946,4.85876137927811,
131.567001372926));
#110239=CARTESIAN_POINT('Ctrl Pts',(-143.729372096723,4.88002100005774,
131.431556966557));
#110240=CARTESIAN_POINT('Ctrl Pts',(-143.7371199935,4.89562378546336,131.295152876458));
#110241=CARTESIAN_POINT('Ctrl Pts',(-143.744867890277,4.9054979385556,131.158299930622));
#110242=CARTESIAN_POINT('Ctrl Pts',(-143.752614166361,4.91537002618787,
131.021475611472));
#110243=CARTESIAN_POINT('Ctrl Pts',(-143.760360442445,4.91951583688607,
130.884203013044));
#110244=CARTESIAN_POINT('Ctrl Pts',(-143.768106718529,4.91791547066745,
130.746997860748));
#110245=CARTESIAN_POINT('Ctrl Pts',(-143.775853051794,4.91631509263529,
130.609791695636));
#110246=CARTESIAN_POINT('Ctrl Pts',(-143.78359938506,4.90896845760624,130.472653368588));
#110247=CARTESIAN_POINT('Ctrl Pts',(-143.791345718325,4.89590779805969,
130.336097982501));
#110248=CARTESIAN_POINT('Ctrl Pts',(-143.799093786328,4.882844213669,130.199512015781));
#110249=CARTESIAN_POINT('Ctrl Pts',(-143.806841854331,4.86406409568915,
130.063509638907));
#110250=CARTESIAN_POINT('Ctrl Pts',(-143.814589922334,4.83965144268885,
129.9285998193));
#110251=CARTESIAN_POINT('Ctrl Pts',(-143.822346225076,4.81521284363039,
129.793546615931));
#110252=CARTESIAN_POINT('Ctrl Pts',(-143.830102527817,4.7851298209496,129.659588674749));
#110253=CARTESIAN_POINT('Ctrl Pts',(-143.837858830559,4.749537442702,129.527224312048));
#110254=CARTESIAN_POINT('Ctrl Pts',(-143.845619273073,4.71392606773046,
129.394789302502));
#110255=CARTESIAN_POINT('Ctrl Pts',(-143.853379715588,4.67279959515783,
129.263949939003));
#110256=CARTESIAN_POINT('Ctrl Pts',(-143.861140158102,4.62634239590514,
129.135187439507));
#110257=CARTESIAN_POINT('Ctrl Pts',(-143.868913058367,4.57981061943194,
129.006218239017));
#110258=CARTESIAN_POINT('Ctrl Pts',(-143.876685958633,4.5279311640038,128.87933292695));
#110259=CARTESIAN_POINT('Ctrl Pts',(-143.884458858898,4.47093615299246,
128.754991695589));
#110260=CARTESIAN_POINT('Ctrl Pts',(-143.89194919466,4.41601305419331,128.635170581185));
#110261=CARTESIAN_POINT('Ctrl Pts',(-143.899439530422,4.35634000879247,
128.517712065923));
#110262=CARTESIAN_POINT('Ctrl Pts',(-143.906929866184,4.29216321998859,
128.403003094106));
#110263=CARTESIAN_POINT('Ctrl Pts',(-143.914704200303,4.22555314873118,
128.283944896758));
#110264=CARTESIAN_POINT('Ctrl Pts',(-143.922478534422,4.15388007283489,
128.167471715966));
#110265=CARTESIAN_POINT('Ctrl Pts',(-143.930252868541,4.0773695379762,128.054044142452));
#110266=CARTESIAN_POINT('Ctrl Pts',(-143.938017621488,4.00095329551399,
127.940756358286));
#110267=CARTESIAN_POINT('Ctrl Pts',(-143.945782374435,3.91971167269818,
127.830507034183));
#110268=CARTESIAN_POINT('Ctrl Pts',(-143.953547127382,3.83391618974878,
127.723732481539));
#110269=CARTESIAN_POINT('Ctrl Pts',(-143.961304168267,3.74820592008233,
127.617063978885));
#110270=CARTESIAN_POINT('Ctrl Pts',(-143.969061209152,3.65795103447589,
127.513863682459));
#110271=CARTESIAN_POINT('Ctrl Pts',(-143.976818250037,3.56346625228798,
127.414538891973));
#110272=CARTESIAN_POINT('Ctrl Pts',(-143.984569441277,3.46905272180943,
127.315289003083));
#110273=CARTESIAN_POINT('Ctrl Pts',(-143.992320632517,3.37041591222463,
127.2199090851));
#110274=CARTESIAN_POINT('Ctrl Pts',(-144.000071823758,3.26791047394323,
127.12877301872));
#110275=CARTESIAN_POINT('Ctrl Pts',(-144.007819720535,3.16544860320739,
127.037675687598));
#110276=CARTESIAN_POINT('Ctrl Pts',(-144.015567617312,3.05912166567425,
126.950818879789));
#110277=CARTESIAN_POINT('Ctrl Pts',(-144.023315514089,2.94932062740195,
126.868539115099));
#110278=CARTESIAN_POINT('Ctrl Pts',(-144.031061790173,2.83954255713982,
126.786276561562));
#110279=CARTESIAN_POINT('Ctrl Pts',(-144.038808066257,2.72629214426961,
126.708589381085));
#110280=CARTESIAN_POINT('Ctrl Pts',(-144.046554342341,2.60999252675999,
126.635773078272));
#110281=CARTESIAN_POINT('Ctrl Pts',(-144.054300675606,2.49369205075284,
126.562956237945));
#110282=CARTESIAN_POINT('Ctrl Pts',(-144.062047008872,2.37434265656461,
126.495010554504));
#110283=CARTESIAN_POINT('Ctrl Pts',(-144.069793342137,2.25239513729084,
126.432187335546));
#110284=CARTESIAN_POINT('Ctrl Pts',(-144.07754141014,2.13042030871615,126.369350047764));
#110285=CARTESIAN_POINT('Ctrl Pts',(-144.085289478143,2.00584654476699,
126.311637686158));
#110286=CARTESIAN_POINT('Ctrl Pts',(-144.093037546146,1.87914745742925,
126.259254689676));
#110287=CARTESIAN_POINT('Ctrl Pts',(-144.100793848887,1.75231371279358,
126.206816019923));
#110288=CARTESIAN_POINT('Ctrl Pts',(-144.108550151629,1.62335049441414,
126.159718179586));
#110289=CARTESIAN_POINT('Ctrl Pts',(-144.116306454371,1.49275005748649,
126.118116884215));
#110290=CARTESIAN_POINT('Ctrl Pts',(-144.124066896885,1.36207991517334,
126.07649338498));
#110291=CARTESIAN_POINT('Ctrl Pts',(-144.131827339399,1.22977119010396,
126.040372379217));
#110292=CARTESIAN_POINT('Ctrl Pts',(-144.139587781913,1.09632840155966,
126.009858860508));
#110293=CARTESIAN_POINT('Ctrl Pts',(-144.147360682179,0.962671398804334,
125.97929635879));
#110294=CARTESIAN_POINT('Ctrl Pts',(-144.155133582444,0.827877079299284,
125.954359403425));
#110295=CARTESIAN_POINT('Ctrl Pts',(-144.16290648271,0.692458084197433,
125.935101447617));
#110296=CARTESIAN_POINT('Ctrl Pts',(-144.170396818472,0.561961910660792,
125.91654356701));
#110297=CARTESIAN_POINT('Ctrl Pts',(-144.177887154234,0.430885996531902,
125.90325899355));
#110298=CARTESIAN_POINT('Ctrl Pts',(-144.185377489997,0.299688967855314,
125.895249742362));
#110299=CARTESIAN_POINT('Ctrl Pts',(-144.193151824116,0.163517563965948,
125.886936817981));
#110300=CARTESIAN_POINT('Ctrl Pts',(-144.200926158235,0.0267843300386512,
125.884280807386));
#110301=CARTESIAN_POINT('Ctrl Pts',(-144.208700492354,-0.110001312959909,
125.887340913147));
#110302=CARTESIAN_POINT('Ctrl Pts',(-144.216465245301,-0.246618379877987,
125.890397247601));
#110303=CARTESIAN_POINT('Ctrl Pts',(-144.224229998248,-0.383287340238361,
125.899155673091));
#110304=CARTESIAN_POINT('Ctrl Pts',(-144.231994751195,-0.519494349596362,
125.913623588933));
#110305=CARTESIAN_POINT('Ctrl Pts',(-144.23975179208,-0.655566076232488,
125.928077135038));
#110306=CARTESIAN_POINT('Ctrl Pts',(-144.247508832965,-0.791176378668927,
125.948228845424));
#110307=CARTESIAN_POINT('Ctrl Pts',(-144.25526587385,-0.92581247062156,
125.974034093226));
#110308=CARTESIAN_POINT('Ctrl Pts',(-144.263017065091,-1.06034703245085,
125.99981988109));
#110309=CARTESIAN_POINT('Ctrl Pts',(-144.270768256331,-1.19390846366965,
126.03125064708));
#110310=CARTESIAN_POINT('Ctrl Pts',(-144.278519447571,-1.32599051065011,
126.068230105411));
#110311=CARTESIAN_POINT('Ctrl Pts',(-144.286267344348,-1.4580164192363,
126.105193846485));
#110312=CARTESIAN_POINT('Ctrl Pts',(-144.294015241125,-1.58856381847538,
126.147701484151));
#110313=CARTESIAN_POINT('Ctrl Pts',(-144.301763137902,-1.71713825801937,
126.195605984767));
#110314=CARTESIAN_POINT('Ctrl Pts',(-144.309509413986,-1.84568580256271,
126.243500464794));
#110315=CARTESIAN_POINT('Ctrl Pts',(-144.31725569007,-1.97226084216465,
126.296789425898));
#110316=CARTESIAN_POINT('Ctrl Pts',(-144.325001966154,-2.09638604402693,
126.355276597578));
#110317=CARTESIAN_POINT('Ctrl Pts',(-144.33274829942,-2.22051216215275,
126.413764200997));
#110318=CARTESIAN_POINT('Ctrl Pts',(-144.340494632685,-2.3421880527834,
126.477449924913));
#110319=CARTESIAN_POINT('Ctrl Pts',(-144.34824096595,-2.46095861903949,
126.546090342222));
#110320=CARTESIAN_POINT('Ctrl Pts',(-144.355989033953,-2.57975578313991,
126.614746131077));
#110321=CARTESIAN_POINT('Ctrl Pts',(-144.363737101956,-2.69564598975608,
126.688358625649));
#110322=CARTESIAN_POINT('Ctrl Pts',(-144.371485169959,-2.80820123976273,
126.766639867007));
#110323=CARTESIAN_POINT('Ctrl Pts',(-144.379241472701,-2.92087611482929,
126.8450043066));
#110324=CARTESIAN_POINT('Ctrl Pts',(-144.386997775443,-3.03020863142111,
126.928047181521));
#110325=CARTESIAN_POINT('Ctrl Pts',(-144.394754078185,-3.13580170567935,
127.015438511589));
#110326=CARTESIAN_POINT('Ctrl Pts',(-144.402514520699,-3.24145113814037,
127.102876485042));
#110327=CARTESIAN_POINT('Ctrl Pts',(-144.410274963213,-3.34335686100905,
127.194667276701));
#110328=CARTESIAN_POINT('Ctrl Pts',(-144.418035405727,-3.44115783521619,
127.290443171804));
#110329=CARTESIAN_POINT('Ctrl Pts',(-144.425808305993,-3.53911580822975,
127.386372814876));
#110330=CARTESIAN_POINT('Ctrl Pts',(-144.433581206258,-3.63295559725585,
127.486300059957));
#110331=CARTESIAN_POINT('Ctrl Pts',(-144.441354106524,-3.72235513553601,
127.589822500286));
#110332=CARTESIAN_POINT('Ctrl Pts',(-144.448844442285,-3.80850477541293,
127.689581639148));
#110333=CARTESIAN_POINT('Ctrl Pts',(-144.456334778047,-3.89053119659048,
127.79267888151));
#110334=CARTESIAN_POINT('Ctrl Pts',(-144.463825113809,-3.96818480510813,
127.898729461516));
#110335=CARTESIAN_POINT('Ctrl Pts',(-144.471653010412,-4.04933796534868,
128.009559336355));
#110336=CARTESIAN_POINT('Ctrl Pts',(-144.479480907015,-4.12597241173223,
128.12396630478));
#110337=CARTESIAN_POINT('Ctrl Pts',(-144.487308803618,-4.19775881841822,
128.24154888728));
#110338=CARTESIAN_POINT('Ctrl Pts',(-144.495123550815,-4.26942463733033,
128.358933952973));
#110339=CARTESIAN_POINT('Ctrl Pts',(-144.502938298012,-4.33625843984316,
128.479483682202));
#110340=CARTESIAN_POINT('Ctrl Pts',(-144.510753045208,-4.39797237210572,
128.602765269484));
#110341=CARTESIAN_POINT('Ctrl Pts',(-144.518560209974,-4.45962642506256,
128.725927240084));
#110342=CARTESIAN_POINT('Ctrl Pts',(-144.52636737474,-4.51617031912051,
128.851815454922));
#110343=CARTESIAN_POINT('Ctrl Pts',(-144.534174539506,-4.56736033728549,
128.979969592623));
#110344=CARTESIAN_POINT('Ctrl Pts',(-144.541974361762,-4.61850221208431,
129.108003203476));
#110345=CARTESIAN_POINT('Ctrl Pts',(-144.549774184018,-4.66430009660497,
129.238298138185));
#110346=CARTESIAN_POINT('Ctrl Pts',(-144.557574006274,-4.70455719433246,
129.370371542379));
#110347=CARTESIAN_POINT('Ctrl Pts',(-144.561721480154,-4.72596348486209,
129.440600193251));
#110348=CARTESIAN_POINT('Ctrl Pts',(-144.565868954034,-4.74580393375321,
129.511331328419));
#110349=CARTESIAN_POINT('Ctrl Pts',(-144.570016427913,-4.76405452823402,
129.582490119308));
#110350=CARTESIAN_POINT('Origin',(213.235140564004,0.,130.804360617566));
#110351=CARTESIAN_POINT('',(-146.665174983012,-4.76405452823419,129.582490119309));
#110352=CARTESIAN_POINT('',(-146.319717442688,-4.76405452823404,129.582490119308));
#110353=CARTESIAN_POINT('',(213.235140564004,-4.76405452823405,129.582490119308));
#110354=CARTESIAN_POINT('',(-144.985140563981,-4.91824970179615,130.806073300273));
#110355=CARTESIAN_POINT('Ctrl Pts',(-144.985140564011,-4.91824970179597,
130.806073300807));
#110356=CARTESIAN_POINT('Ctrl Pts',(-144.990470831099,-4.91821711222921,
130.899659565425));
#110357=CARTESIAN_POINT('Ctrl Pts',(-144.995801098188,-4.91551352483608,
130.993196152259));
#110358=CARTESIAN_POINT('Ctrl Pts',(-145.001131365277,-4.91014626190504,
131.086578174072));
#110359=CARTESIAN_POINT('Ctrl Pts',(-145.008905699396,-4.90231796838136,
131.222778298041));
#110360=CARTESIAN_POINT('Ctrl Pts',(-145.016680033515,-4.88880599865511,
131.358868188652));
#110361=CARTESIAN_POINT('Ctrl Pts',(-145.024454367634,-4.86961173160291,
131.494334998203));
#110362=CARTESIAN_POINT('Ctrl Pts',(-145.032219120581,-4.85044111976941,
131.629634857018));
#110363=CARTESIAN_POINT('Ctrl Pts',(-145.039983873528,-4.82560219866211,
131.764312779267));
#110364=CARTESIAN_POINT('Ctrl Pts',(-145.047748626475,-4.79514831027588,
131.897857643149));
#110365=CARTESIAN_POINT('Ctrl Pts',(-145.05550566736,-4.76472466912101,
132.031269868389));
#110366=CARTESIAN_POINT('Ctrl Pts',(-145.063262708245,-4.72869724526217,
132.163550896085));
#110367=CARTESIAN_POINT('Ctrl Pts',(-145.07101974913,-4.68717091774936,
132.294196799938));
#110368=CARTESIAN_POINT('Ctrl Pts',(-145.07877094037,-4.6456759055631,132.424744182699));
#110369=CARTESIAN_POINT('Ctrl Pts',(-145.08652213161,-4.59869036156111,
132.553658524858));
#110370=CARTESIAN_POINT('Ctrl Pts',(-145.094273322851,-4.5463696905704,
132.680448488419));
#110371=CARTESIAN_POINT('Ctrl Pts',(-145.102021219628,-4.49407125726064,
132.807184562863));
#110372=CARTESIAN_POINT('Ctrl Pts',(-145.109769116405,-4.43644235581175,
132.931797693896));
#110373=CARTESIAN_POINT('Ctrl Pts',(-145.117517013182,-4.37368738963638,
133.05381425795));
#110374=CARTESIAN_POINT('Ctrl Pts',(-145.125263289266,-4.31094555044709,
133.175805298769));
#110375=CARTESIAN_POINT('Ctrl Pts',(-145.13300956535,-4.24307995802164,
133.2952005055));
#110376=CARTESIAN_POINT('Ctrl Pts',(-145.140755841434,-4.17034188627465,
133.411549067618));
#110377=CARTESIAN_POINT('Ctrl Pts',(-145.148502174699,-4.09760327759184,
133.527898488594));
#110378=CARTESIAN_POINT('Ctrl Pts',(-145.156248507965,-4.01999232506947,
133.641200888568));
#110379=CARTESIAN_POINT('Ctrl Pts',(-145.16399484123,-3.93780450290235,
133.751033106904));
#110380=CARTESIAN_POINT('Ctrl Pts',(-145.171742909233,-3.85559827534241,
133.860889921404));
#110381=CARTESIAN_POINT('Ctrl Pts',(-145.179490977236,-3.7688133727838,
133.967274694913));
#110382=CARTESIAN_POINT('Ctrl Pts',(-145.187239045239,-3.67778628907491,
134.069796434481));
#110383=CARTESIAN_POINT('Ctrl Pts',(-145.194995347981,-3.58666246069784,
134.172427135375));
#110384=CARTESIAN_POINT('Ctrl Pts',(-145.202751650723,-3.49128770466755,
134.271186307969));
#110385=CARTESIAN_POINT('Ctrl Pts',(-145.210507953464,-3.39203659059686,
134.365718621271));
#110386=CARTESIAN_POINT('Ctrl Pts',(-145.218268395979,-3.29273250321821,
134.460301389314));
#110387=CARTESIAN_POINT('Ctrl Pts',(-145.226028838493,-3.18954822927861,
134.550652545359));
#110388=CARTESIAN_POINT('Ctrl Pts',(-145.233789281007,-3.08289155165424,
134.636457007695));
#110389=CARTESIAN_POINT('Ctrl Pts',(-145.241562181272,-2.9760636592624,
134.722399210971));
#110390=CARTESIAN_POINT('Ctrl Pts',(-145.249335081538,-2.86575253893195,
134.803779903063));
#110391=CARTESIAN_POINT('Ctrl Pts',(-145.257107981803,-2.75239581974219,
134.880326799217));
#110392=CARTESIAN_POINT('Ctrl Pts',(-145.264598317565,-2.64315990282333,
134.954091022887));
#110393=CARTESIAN_POINT('Ctrl Pts',(-145.272088653327,-2.53109623506778,
135.023366628437));
#110394=CARTESIAN_POINT('Ctrl Pts',(-145.279578989089,-2.41661636845603,
135.087951213107));
#110395=CARTESIAN_POINT('Ctrl Pts',(-145.287353323208,-2.29779596290646,
135.154984541936));
#110396=CARTESIAN_POINT('Ctrl Pts',(-145.295127657327,-2.17599613398452,
135.217176449182));
#110397=CARTESIAN_POINT('Ctrl Pts',(-145.302901991446,-2.05164910030208,
135.274250888225));
#110398=CARTESIAN_POINT('Ctrl Pts',(-145.310666744393,-1.92745531322579,
135.331254988122));
#110399=CARTESIAN_POINT('Ctrl Pts',(-145.31843149734,-1.80072091937854,
135.383154006986));
#110400=CARTESIAN_POINT('Ctrl Pts',(-145.326196250287,-1.67190477265788,
135.429716549131));
#110401=CARTESIAN_POINT('Ctrl Pts',(-145.333953291172,-1.54321656795012,
135.476232844702));
#110402=CARTESIAN_POINT('Ctrl Pts',(-145.341710332057,-1.41245109034158,
135.517423079274));
#110403=CARTESIAN_POINT('Ctrl Pts',(-145.349467372942,-1.28008899698821,
135.553103106088));
#110404=CARTESIAN_POINT('Ctrl Pts',(-145.357218564183,-1.14782671891888,
135.588756226315));
#110405=CARTESIAN_POINT('Ctrl Pts',(-145.364969755423,-1.01397059759738,
135.618907308292));
#110406=CARTESIAN_POINT('Ctrl Pts',(-145.372720946663,-0.87901800970143,
135.643421518311));
#110407=CARTESIAN_POINT('Ctrl Pts',(-145.38046884344,-0.744122780255502,
135.667925309137));
#110408=CARTESIAN_POINT('Ctrl Pts',(-145.388216740217,-0.608132394993289,
135.686796923381));
#110409=CARTESIAN_POINT('Ctrl Pts',(-145.395964636994,-0.471555811873031,
135.699952326317));
#110410=CARTESIAN_POINT('Ctrl Pts',(-145.403710913078,-0.335007797629711,
135.713104977425));
#110411=CARTESIAN_POINT('Ctrl Pts',(-145.411457189162,-0.197874218343641,
135.720543758093));
#110412=CARTESIAN_POINT('Ctrl Pts',(-145.419203465246,-0.0606701733661577,
135.72223639808));
#110413=CARTESIAN_POINT('Ctrl Pts',(-145.426949798512,0.0765348844206047,
135.723929050561));
#110414=CARTESIAN_POINT('Ctrl Pts',(-145.434696131777,0.21381001800127,
135.719875472899));
#110415=CARTESIAN_POINT('Ctrl Pts',(-145.442442465042,0.350639499328176,
135.710095527242));
#110416=CARTESIAN_POINT('Ctrl Pts',(-145.450190533045,0.487499622668529,
135.700313391433));
#110417=CARTESIAN_POINT('Ctrl Pts',(-145.457938601048,0.623913505267511,
135.684802363709));
#110418=CARTESIAN_POINT('Ctrl Pts',(-145.465686669051,0.759370310538065,
135.663634204634));
#110419=CARTESIAN_POINT('Ctrl Pts',(-145.473442971793,0.894971080913033,
135.642443547787));
#110420=CARTESIAN_POINT('Ctrl Pts',(-145.481199274535,1.0296123551137,135.6155838095));
#110421=CARTESIAN_POINT('Ctrl Pts',(-145.488955577277,1.16279271908662,
135.583178060714));
#110422=CARTESIAN_POINT('Ctrl Pts',(-145.496716019791,1.29604416543013,
135.550755016005));
#110423=CARTESIAN_POINT('Ctrl Pts',(-145.504476462305,1.42783277236835,
135.512780170801));
#110424=CARTESIAN_POINT('Ctrl Pts',(-145.512236904819,1.55767303613065,
135.469426295026));
#110425=CARTESIAN_POINT('Ctrl Pts',(-145.520009805084,1.68772173101102,
135.42600282376));
#110426=CARTESIAN_POINT('Ctrl Pts',(-145.52778270535,1.81581546712574,135.377183205962));
#110427=CARTESIAN_POINT('Ctrl Pts',(-145.535555605615,1.94148861439546,
135.323188454812));
#110428=CARTESIAN_POINT('Ctrl Pts',(-145.543045941377,2.06259322621445,
135.27115654887));
#110429=CARTESIAN_POINT('Ctrl Pts',(-145.55053627714,2.18144990488352,135.214319368328));
#110430=CARTESIAN_POINT('Ctrl Pts',(-145.558026612902,2.29766590933114,
135.152913759888));
#110431=CARTESIAN_POINT('Ctrl Pts',(-145.565800947021,2.41828827890691,
135.089179939142));
#110432=CARTESIAN_POINT('Ctrl Pts',(-145.57357528114,2.53644787449853,135.020322538508));
#110433=CARTESIAN_POINT('Ctrl Pts',(-145.581349615259,2.65167882554812,
134.946555985802));
#110434=CARTESIAN_POINT('Ctrl Pts',(-145.589114368206,2.76676776474871,
134.872880343781));
#110435=CARTESIAN_POINT('Ctrl Pts',(-145.596879121153,2.87893491471041,
134.794307796333));
#110436=CARTESIAN_POINT('Ctrl Pts',(-145.604643874101,2.98773757394863,
134.711099315216));
#110437=CARTESIAN_POINT('Ctrl Pts',(-145.612400914986,3.09643216885185,
134.627973477936));
#110438=CARTESIAN_POINT('Ctrl Pts',(-145.620157955871,3.20176861453724,
134.540221106066));
#110439=CARTESIAN_POINT('Ctrl Pts',(-145.627914996756,3.30333217618779,
134.448147054264));
#110440=CARTESIAN_POINT('Ctrl Pts',(-145.635666187996,3.40481914796659,
134.35614243622));
#110441=CARTESIAN_POINT('Ctrl Pts',(-145.643417379236,3.50253861034877,
134.259822886639));
#110442=CARTESIAN_POINT('Ctrl Pts',(-145.651168570476,3.59610827967456,
134.159533981694));
#110443=CARTESIAN_POINT('Ctrl Pts',(-145.658916467253,3.6896381793947,134.059287702209));
#110444=CARTESIAN_POINT('Ctrl Pts',(-145.66666436403,3.77902152791442,133.955075708104));
#110445=CARTESIAN_POINT('Ctrl Pts',(-145.674412260807,3.86391252022951,
133.8472807773));
#110446=CARTESIAN_POINT('Ctrl Pts',(-145.682158536891,3.94878575517905,
133.739508394871));
#110447=CARTESIAN_POINT('Ctrl Pts',(-145.689904812975,4.02916826131005,
133.628154873446));
#110448=CARTESIAN_POINT('Ctrl Pts',(-145.69765108906,4.10475446497433,133.513636137843));
#110449=CARTESIAN_POINT('Ctrl Pts',(-145.705397422325,4.18034122659889,
133.399116556889));
#110450=CARTESIAN_POINT('Ctrl Pts',(-145.71314375559,4.25113139974043,133.281432041433));
#110451=CARTESIAN_POINT('Ctrl Pts',(-145.720890088856,4.31686293137953,
133.161027224064));
#110452=CARTESIAN_POINT('Ctrl Pts',(-145.728638156859,4.3826091831393,133.040595442871));
#110453=CARTESIAN_POINT('Ctrl Pts',(-145.736386224862,4.44329435185884,
132.917442490635));
#110454=CARTESIAN_POINT('Ctrl Pts',(-145.744134292865,4.49870269208018,
132.792036936983));
#110455=CARTESIAN_POINT('Ctrl Pts',(-145.751890595606,4.55416992094495,
132.666498100816));
#110456=CARTESIAN_POINT('Ctrl Pts',(-145.759646898348,4.60434895991805,
132.538702238961));
#110457=CARTESIAN_POINT('Ctrl Pts',(-145.76740320109,4.64907232552509,132.409137728113));
#110458=CARTESIAN_POINT('Ctrl Pts',(-145.775163643604,4.69381956133894,
132.279504064785));
#110459=CARTESIAN_POINT('Ctrl Pts',(-145.782924086118,4.73310520973102,
132.1481002459));
#110460=CARTESIAN_POINT('Ctrl Pts',(-145.790684528633,4.76681220028328,
132.015428125895));
#110461=CARTESIAN_POINT('Ctrl Pts',(-145.798457428898,4.80057330028914,
131.882543028825));
#110462=CARTESIAN_POINT('Ctrl Pts',(-145.806230329163,4.82873776642562,
131.748385944923));
#110463=CARTESIAN_POINT('Ctrl Pts',(-145.814003229429,4.851239858909,131.613468084985));
#110464=CARTESIAN_POINT('Ctrl Pts',(-145.821493565191,4.87292394365119,
131.483454829093));
#110465=CARTESIAN_POINT('Ctrl Pts',(-145.828983900953,4.88935015200417,
131.352735454729));
#110466=CARTESIAN_POINT('Ctrl Pts',(-145.836474236715,4.90050546366366,
131.221768407506));
#110467=CARTESIAN_POINT('Ctrl Pts',(-145.844248570834,4.91208373235536,
131.085835704881));
#110468=CARTESIAN_POINT('Ctrl Pts',(-145.852022904953,4.91802019868463,
130.949205583677));
#110469=CARTESIAN_POINT('Ctrl Pts',(-145.859797239072,4.91824345243122,
130.812385897464));
#110470=CARTESIAN_POINT('Ctrl Pts',(-145.867561992019,4.91846643103752,
130.675734829286));
#110471=CARTESIAN_POINT('Ctrl Pts',(-145.875326744966,4.9129902059683,130.538895048148));
#110472=CARTESIAN_POINT('Ctrl Pts',(-145.883091497913,4.90179504918907,
130.402380072955));
#110473=CARTESIAN_POINT('Ctrl Pts',(-145.890848538798,4.89061101159739,
130.266000686361));
#110474=CARTESIAN_POINT('Ctrl Pts',(-145.898605579683,4.87371937774573,
130.129945850856));
#110475=CARTESIAN_POINT('Ctrl Pts',(-145.906362620568,4.85115245619196,
129.994729275977));
#110476=CARTESIAN_POINT('Ctrl Pts',(-145.914113811808,4.82860255252925,
129.859614668969));
#110477=CARTESIAN_POINT('Ctrl Pts',(-145.921865003049,4.80038594390358,
129.725337448424));
#110478=CARTESIAN_POINT('Ctrl Pts',(-145.929616194289,4.76658673968084,
129.592406032774));
#110479=CARTESIAN_POINT('Ctrl Pts',(-145.937364091066,4.73280190102157,
129.459531116522));
#110480=CARTESIAN_POINT('Ctrl Pts',(-145.945111987843,4.69343928212807,
129.328001245611));
#110481=CARTESIAN_POINT('Ctrl Pts',(-145.95285988462,4.64863400885555,129.198314256401));
#110482=CARTESIAN_POINT('Ctrl Pts',(-145.960606160704,4.60383810788032,
129.068654394914));
#110483=CARTESIAN_POINT('Ctrl Pts',(-145.968352436788,4.5536019446252,128.940837017663));
#110484=CARTESIAN_POINT('Ctrl Pts',(-145.976098712872,4.49811027839977,
128.815344029939));
#110485=CARTESIAN_POINT('Ctrl Pts',(-145.983845046137,4.44261820254738,
128.689850115854));
#110486=CARTESIAN_POINT('Ctrl Pts',(-145.991591379403,4.38187070442459,
128.5666809831));
#110487=CARTESIAN_POINT('Ctrl Pts',(-145.999337712668,4.31610021996306,
128.446297439079));
#110488=CARTESIAN_POINT('Ctrl Pts',(-146.007085780671,4.25031500665764,
128.325886935999));
#110489=CARTESIAN_POINT('Ctrl Pts',(-146.014833848674,4.17950475607948,
128.208263606));
#110490=CARTESIAN_POINT('Ctrl Pts',(-146.022581916677,4.10394707343582,
128.093862235176));
#110491=CARTESIAN_POINT('Ctrl Pts',(-146.030338219419,4.02830908718779,
127.979339277214));
#110492=CARTESIAN_POINT('Ctrl Pts',(-146.038094522161,3.94791380549875,
127.868045445662));
#110493=CARTESIAN_POINT('Ctrl Pts',(-146.045850824902,3.86308158460433,
127.760385628643));
#110494=CARTESIAN_POINT('Ctrl Pts',(-146.053611267417,3.77820408619936,
127.652668350338));
#110495=CARTESIAN_POINT('Ctrl Pts',(-146.061371709931,3.6888851843834,127.548589247894));
#110496=CARTESIAN_POINT('Ctrl Pts',(-146.069132152445,3.59548382408594,
127.448518080551));
#110497=CARTESIAN_POINT('Ctrl Pts',(-146.07690505271,3.50193252763315,127.348286270087));
#110498=CARTESIAN_POINT('Ctrl Pts',(-146.084677952976,3.40428595532249,
127.252075526249));
#110499=CARTESIAN_POINT('Ctrl Pts',(-146.092450853241,3.30293866931551,
127.160217479702));
#110500=CARTESIAN_POINT('Ctrl Pts',(-146.099941189003,3.20527561243356,
127.071698704524));
#110501=CARTESIAN_POINT('Ctrl Pts',(-146.107431524765,3.10417646746311,
126.98722185538));
#110502=CARTESIAN_POINT('Ctrl Pts',(-146.114921860527,3.00001989989066,
126.907045687674));
#110503=CARTESIAN_POINT('Ctrl Pts',(-146.122696194646,2.89191420440055,
126.8238296162));
#110504=CARTESIAN_POINT('Ctrl Pts',(-146.130470528765,2.78017221892343,
126.744983181061));
#110505=CARTESIAN_POINT('Ctrl Pts',(-146.138244862885,2.66518261608051,
126.670840968956));
#110506=CARTESIAN_POINT('Ctrl Pts',(-146.146009615832,2.55033472764619,
126.596790130502));
#110507=CARTESIAN_POINT('Ctrl Pts',(-146.153774368779,2.43224751085592,
126.527432189544));
#110508=CARTESIAN_POINT('Ctrl Pts',(-146.161539121726,2.31134234022524,
126.46306131335));
#110509=CARTESIAN_POINT('Ctrl Pts',(-146.169296162611,2.1905572543145,126.398754371219));
#110510=CARTESIAN_POINT('Ctrl Pts',(-146.177053203496,2.06696012723298,
126.339424819259));
#110511=CARTESIAN_POINT('Ctrl Pts',(-146.184810244381,1.94100062092707,
126.28532314792));
#110512=CARTESIAN_POINT('Ctrl Pts',(-146.192561435621,1.81513610166486,
126.231262275073));
#110513=CARTESIAN_POINT('Ctrl Pts',(-146.200312626861,1.68691310690037,
126.182421589437));
#110514=CARTESIAN_POINT('Ctrl Pts',(-146.208063818101,1.5568048466269,126.139005140004));
#110515=CARTESIAN_POINT('Ctrl Pts',(-146.215811714879,1.42675188583462,
126.09560714372));
#110516=CARTESIAN_POINT('Ctrl Pts',(-146.223559611656,1.29481562331984,
126.057628921779));
#110517=CARTESIAN_POINT('Ctrl Pts',(-146.231307508433,1.1614879417375,126.025225881686));
#110518=CARTESIAN_POINT('Ctrl Pts',(-146.239053784517,1.02818814943193,
125.99282961961));
#110519=CARTESIAN_POINT('Ctrl Pts',(-146.246800060601,0.893497896648766,
125.966006312002));
#110520=CARTESIAN_POINT('Ctrl Pts',(-146.254546336685,0.757922490875799,
125.944860997201));
#110521=CARTESIAN_POINT('Ctrl Pts',(-146.262292669951,0.622346084316169,
125.923715526311));
#110522=CARTESIAN_POINT('Ctrl Pts',(-146.270039003216,0.485884898023598,
125.908248192114));
#110523=CARTESIAN_POINT('Ctrl Pts',(-146.277785336482,0.349052259614766,
125.898512517333));
#110524=CARTESIAN_POINT('Ctrl Pts',(-146.285533404485,0.212188978485107,
125.888774662316));
#110525=CARTESIAN_POINT('Ctrl Pts',(-146.293281472487,0.0749544696171083,
125.884771048604));
#110526=CARTESIAN_POINT('Ctrl Pts',(-146.30102954049,-0.0621354167404537,
125.886503131578));
#110527=CARTESIAN_POINT('Ctrl Pts',(-146.308785843232,-0.19937100386044,
125.888237055431));
#110528=CARTESIAN_POINT('Ctrl Pts',(-146.316542145974,-0.336461269867287,
125.895718848371));
#110529=CARTESIAN_POINT('Ctrl Pts',(-146.324298448716,-0.472892410545639,
125.908897837547));
#110530=CARTESIAN_POINT('Ctrl Pts',(-146.33205889123,-0.609396368632005,
125.922083860747));
#110531=CARTESIAN_POINT('Ctrl Pts',(-146.339819333744,-0.745240113358501,
125.940973085343));
#110532=CARTESIAN_POINT('Ctrl Pts',(-146.347579776259,-0.879918537302853,
125.965463384703));
#110533=CARTESIAN_POINT('Ctrl Pts',(-146.355352676524,-1.01481315900914,
125.989992998065));
#110534=CARTESIAN_POINT('Ctrl Pts',(-146.36312557679,-1.14853834011378,
126.020141567723));
#110535=CARTESIAN_POINT('Ctrl Pts',(-146.370898477055,-1.28060179986094,
126.055756391828));
#110536=CARTESIAN_POINT('Ctrl Pts',(-146.378388812817,-1.40786442019636,
126.090076527369));
#110537=CARTESIAN_POINT('Ctrl Pts',(-146.385879148579,-1.53358374322851,
126.129472300885));
#110538=CARTESIAN_POINT('Ctrl Pts',(-146.393369484341,-1.65733739276342,
126.173764993994));
#110539=CARTESIAN_POINT('Ctrl Pts',(-146.401143943622,-1.78578526743254,
126.219737798146));
#110540=CARTESIAN_POINT('Ctrl Pts',(-146.408918402903,-1.912522291739,126.271131985916));
#110541=CARTESIAN_POINT('Ctrl Pts',(-146.416692862184,-2.03705685772722,
126.327801400836));
#110542=CARTESIAN_POINT('Ctrl Pts',(-146.424457711091,-2.16143748070047,
126.384400764037));
#110543=CARTESIAN_POINT('Ctrl Pts',(-146.432222559998,-2.28362071005336,
126.446262219059));
#110544=CARTESIAN_POINT('Ctrl Pts',(-146.439987408906,-2.40313127408453,
126.51319024784));
#110545=CARTESIAN_POINT('Ctrl Pts',(-146.447744516672,-2.5225226924516,
126.580051552942));
#110546=CARTESIAN_POINT('Ctrl Pts',(-146.455501624439,-2.63924640914733,
126.651969189893));
#110547=CARTESIAN_POINT('Ctrl Pts',(-146.463258732206,-2.75284861520924,
126.728700233746));
#110548=CARTESIAN_POINT('Ctrl Pts',(-146.471009961343,-2.8663647292182,
126.805373127909));
#110549=CARTESIAN_POINT('Ctrl Pts',(-146.478761190479,-2.97676371859975,
126.88685195016));
#110550=CARTESIAN_POINT('Ctrl Pts',(-146.486512419616,-3.08361812443508,
126.972848863029));
#110551=CARTESIAN_POINT('Ctrl Pts',(-146.494260205081,-3.19042505760531,
127.05880756968));
#110552=CARTESIAN_POINT('Ctrl Pts',(-146.502007990546,-3.29369023618939,
127.149280129012));
#110553=CARTESIAN_POINT('Ctrl Pts',(-146.509755776011,-3.39301705509289,
127.243936720563));
#110554=CARTESIAN_POINT('Ctrl Pts',(-146.5175018995,-3.49232256741227,127.33857300734));
#110555=CARTESIAN_POINT('Ctrl Pts',(-146.525248022988,-3.58769111786824,
127.437391271333));
#110556=CARTESIAN_POINT('Ctrl Pts',(-146.532994146476,-3.67876122571081,
127.540023179937));
#110557=CARTESIAN_POINT('Ctrl Pts',(-146.540740285835,-3.76983152013388,
127.642655298809));
#110558=CARTESIAN_POINT('Ctrl Pts',(-146.548486425193,-3.85660309504985,
127.749100785359));
#110559=CARTESIAN_POINT('Ctrl Pts',(-146.556232564552,-3.93875347818782,
127.858956723265));
#110560=CARTESIAN_POINT('Ctrl Pts',(-146.563980397272,-4.02092181999879,
127.96883667648));
#110561=CARTESIAN_POINT('Ctrl Pts',(-146.571728229993,-4.09846672603568,
128.082128251392));
#110562=CARTESIAN_POINT('Ctrl Pts',(-146.579476062714,-4.17110816626757,
128.19839827559));
#110563=CARTESIAN_POINT('Ctrl Pts',(-146.587231559407,-4.24382146168303,
128.314783311329));
#110564=CARTESIAN_POINT('Ctrl Pts',(-146.5949870561,-4.31162139687108,128.434152348484));
#110565=CARTESIAN_POINT('Ctrl Pts',(-146.602742552792,-4.37427294919856,
128.556045864599));
#110566=CARTESIAN_POINT('Ctrl Pts',(-146.610502172197,-4.43695780619945,
128.678004177571));
#110567=CARTESIAN_POINT('Ctrl Pts',(-146.618261791601,-4.49448866327323,
128.802489288919));
#110568=CARTESIAN_POINT('Ctrl Pts',(-146.626021411005,-4.5466784689929,
128.92902119173));
#110569=CARTESIAN_POINT('Ctrl Pts',(-146.633792151364,-4.59894307225455,
129.055734437911));
#110570=CARTESIAN_POINT('Ctrl Pts',(-146.641562891723,-4.64585119962519,
129.184499968273));
#110571=CARTESIAN_POINT('Ctrl Pts',(-146.649333632082,-4.6872653282045,
129.314821492363));
#110572=CARTESIAN_POINT('Ctrl Pts',(-146.654614082392,-4.7154074662754,
129.403378862766));
#110573=CARTESIAN_POINT('Ctrl Pts',(-146.659894532702,-4.74101374047461,
129.492654437527));
#110574=CARTESIAN_POINT('Ctrl Pts',(-146.665174983012,-4.76405452823419,
129.582490119309));
#110575=CARTESIAN_POINT('Ctrl Pts',(-144.915004217899,-4.7640545282341,
129.582490119308));
#110576=CARTESIAN_POINT('Ctrl Pts',(-144.922696708858,-4.79785557992013,
129.71427990683));
#110577=CARTESIAN_POINT('Ctrl Pts',(-144.930389199817,-4.82615815883693,
129.84737326594));
#110578=CARTESIAN_POINT('Ctrl Pts',(-144.938081690777,-4.84888658593865,
129.981267707133));
#110579=CARTESIAN_POINT('Ctrl Pts',(-144.945924836311,-4.87206014083276,
130.117784421165));
#110580=CARTESIAN_POINT('Ctrl Pts',(-144.953767981845,-4.88943888408906,
130.255133485846));
#110581=CARTESIAN_POINT('Ctrl Pts',(-144.961611127379,-4.90099825108423,
130.392779270358));
#110582=CARTESIAN_POINT('Ctrl Pts',(-144.969454272913,-4.91255761807938,
130.53042505487));
#110583=CARTESIAN_POINT('Ctrl Pts',(-144.977297418447,-4.91829765523471,
130.668367125102));
#110584=CARTESIAN_POINT('Ctrl Pts',(-144.985140563981,-4.91824970179615,
130.806073300273));
#110585=CARTESIAN_POINT('',(-144.639859436048,-4.91824892573493,130.807611310912));
#110586=CARTESIAN_POINT('Ctrl Pts',(-144.570016427913,-4.76405452823402,
129.582490119308));
#110587=CARTESIAN_POINT('Ctrl Pts',(-144.577809747297,-4.79834834559403,
129.716201192713));
#110588=CARTESIAN_POINT('Ctrl Pts',(-144.585603066681,-4.82702561414829,
129.851422976877));
#110589=CARTESIAN_POINT('Ctrl Pts',(-144.593396386065,-4.84996524191635,
129.987647562262));
#110590=CARTESIAN_POINT('Ctrl Pts',(-144.601188962403,-4.87290268252795,
130.123859159448));
#110591=CARTESIAN_POINT('Ctrl Pts',(-144.60898153874,-4.89010349849468,
130.261072990475));
#110592=CARTESIAN_POINT('Ctrl Pts',(-144.616774115077,-4.90149775451951,
130.398771139226));
#110593=CARTESIAN_POINT('Ctrl Pts',(-144.624469222049,-4.91274949145216,
130.5347469627));
#110594=CARTESIAN_POINT('Ctrl Pts',(-144.632164329021,-4.91833908962852,
130.671194688538));
#110595=CARTESIAN_POINT('Ctrl Pts',(-144.639859435993,-4.91824892573558,
130.807611309931));
#110596=CARTESIAN_POINT('Ctrl Pts',(-144.639859436049,-4.91824892573493,
130.807611310912));
#110597=CARTESIAN_POINT('Ctrl Pts',(-144.648629426068,-4.91814616736096,
130.963083146767));
#110598=CARTESIAN_POINT('Ctrl Pts',(-144.657399416086,-4.91066741602864,
131.118270672276));
#110599=CARTESIAN_POINT('Ctrl Pts',(-144.666169406105,-4.89591751247246,
131.272521672723));
#110600=CARTESIAN_POINT('Ctrl Pts',(-144.674975661587,-4.88110661545087,
131.427410528395));
#110601=CARTESIAN_POINT('Ctrl Pts',(-144.683781917069,-4.85896441776539,
131.58135492203));
#110602=CARTESIAN_POINT('Ctrl Pts',(-144.692588172551,-4.8296468260347,
131.733712326163));
#110603=CARTESIAN_POINT('Ctrl Pts',(-144.70144461531,-4.80016215192807,
131.886938022526));
#110604=CARTESIAN_POINT('Ctrl Pts',(-144.710301058068,-4.76342016027957,
132.038558415203));
#110605=CARTESIAN_POINT('Ctrl Pts',(-144.719157500827,-4.71962812449032,
132.18794054985));
#110606=CARTESIAN_POINT('Ctrl Pts',(-144.726862579758,-4.68152918324244,
132.317902563921));
#110607=CARTESIAN_POINT('Ctrl Pts',(-144.73456765869,-4.63809490151152,
132.446170711984));
#110608=CARTESIAN_POINT('Ctrl Pts',(-144.742272737621,-4.58949059879999,
132.572342265103));
#110609=CARTESIAN_POINT('Ctrl Pts',(-144.75004707174,-4.54044942838947,
132.699647879879));
#110610=CARTESIAN_POINT('Ctrl Pts',(-144.757821405859,-4.48602966459737,
132.825113098012));
#110611=CARTESIAN_POINT('Ctrl Pts',(-144.765595739979,-4.42638921100489,
132.948249983928));
#110612=CARTESIAN_POINT('Ctrl Pts',(-144.773360492926,-4.36682225894124,
133.071235114637));
#110613=CARTESIAN_POINT('Ctrl Pts',(-144.781125245873,-4.30204758767397,
133.191897274012));
#110614=CARTESIAN_POINT('Ctrl Pts',(-144.78888999882,-4.23227205541874,
133.30976603614));
#110615=CARTESIAN_POINT('Ctrl Pts',(-144.796647039705,-4.16256582520581,
133.427517729352));
#110616=CARTESIAN_POINT('Ctrl Pts',(-144.80440408059,-4.08786881628386,
133.542481212322));
#110617=CARTESIAN_POINT('Ctrl Pts',(-144.812161121475,-4.008434765724,133.654208647099));
#110618=CARTESIAN_POINT('Ctrl Pts',(-144.819912312715,-3.92906061699948,
133.76585182735));
#110619=CARTESIAN_POINT('Ctrl Pts',(-144.827663503955,-3.84495676258961,
133.874263499383));
#110620=CARTESIAN_POINT('Ctrl Pts',(-144.835414695195,-3.75642120882361,
133.979023239704));
#110621=CARTESIAN_POINT('Ctrl Pts',(-144.843162591972,-3.66792328502985,
134.083738454341));
#110622=CARTESIAN_POINT('Ctrl Pts',(-144.85091048875,-3.57499766003207,
134.184804526426));
#110623=CARTESIAN_POINT('Ctrl Pts',(-144.858658385527,-3.47798358996898,
134.281832861942));
#110624=CARTESIAN_POINT('Ctrl Pts',(-144.866404661611,-3.3809898131577,
134.378840901223));
#110625=CARTESIAN_POINT('Ctrl Pts',(-144.874150937695,-3.27990956860844,
134.471812607605));
#110626=CARTESIAN_POINT('Ctrl Pts',(-144.881897213779,-3.17511977902612,
134.560395421896));
#110627=CARTESIAN_POINT('Ctrl Pts',(-144.889643547044,-3.07032921590952,
134.648978890085));
#110628=CARTESIAN_POINT('Ctrl Pts',(-144.89738988031,-2.96182935169657,
134.733173149137));
#110629=CARTESIAN_POINT('Ctrl Pts',(-144.905136213575,-2.85003075609275,
134.812665465232));
#110630=CARTESIAN_POINT('Ctrl Pts',(-144.912884281578,-2.73820712396876,
134.892175583081));
#110631=CARTESIAN_POINT('Ctrl Pts',(-144.920632349581,-2.62308360904085,
134.966981436177));
#110632=CARTESIAN_POINT('Ctrl Pts',(-144.928380417584,-2.50510001983634,
135.036813446968));
#110633=CARTESIAN_POINT('Ctrl Pts',(-144.936136720326,-2.38699103626904,
135.106719676052));
#110634=CARTESIAN_POINT('Ctrl Pts',(-144.943893023068,-2.26601624324084,
135.171641303504));
#110635=CARTESIAN_POINT('Ctrl Pts',(-144.951649325809,-2.14264081787303,
135.231354336568));
#110636=CARTESIAN_POINT('Ctrl Pts',(-144.959409768324,-2.0191995433256,
135.291099240276));
#110637=CARTESIAN_POINT('Ctrl Pts',(-144.967170210838,-1.89335544191891,
135.345629854871));
#110638=CARTESIAN_POINT('Ctrl Pts',(-144.974930653352,-1.765593028403,135.394770655956));
#110639=CARTESIAN_POINT('Ctrl Pts',(-144.982703553617,-1.63762551931871,
135.443990342218));
#110640=CARTESIAN_POINT('Ctrl Pts',(-144.990476453883,-1.50773391508519,
135.487802800074));
#110641=CARTESIAN_POINT('Ctrl Pts',(-144.998249354148,-1.37641808392046,
135.526082371414));
#110642=CARTESIAN_POINT('Ctrl Pts',(-145.005739689911,-1.24987591397607,
135.562970383916));
#110643=CARTESIAN_POINT('Ctrl Pts',(-145.013230025673,-1.1220115667598,
135.594720720418));
#110644=CARTESIAN_POINT('Ctrl Pts',(-145.020720361436,-0.993278741260765,
135.621266305314));
#110645=CARTESIAN_POINT('Ctrl Pts',(-145.028494695555,-0.859664971561687,
135.648818374129));
#110646=CARTESIAN_POINT('Ctrl Pts',(-145.036269029674,-0.724692318579218,
135.670850500661));
#110647=CARTESIAN_POINT('Ctrl Pts',(-145.044043363793,-0.588856647073741,
135.687231792571));
#110648=CARTESIAN_POINT('Ctrl Pts',(-145.05180811674,-0.453188380893411,
135.703592896003));
#110649=CARTESIAN_POINT('Ctrl Pts',(-145.059572869687,-0.316659596850146,
135.714316975031));
#110650=CARTESIAN_POINT('Ctrl Pts',(-145.067337622635,-0.179777889508018,
135.719323788633));
#110651=CARTESIAN_POINT('Ctrl Pts',(-145.07509466352,-0.0430321350073147,
135.724325629397));
#110652=CARTESIAN_POINT('Ctrl Pts',(-145.082851704405,0.0940654570492294,
135.723621490945));
#110653=CARTESIAN_POINT('Ctrl Pts',(-145.09060874529,0.231000956826365,
135.717182782111));
#110654=CARTESIAN_POINT('Ctrl Pts',(-145.09835993653,0.36783319247773,135.710748928757));
#110655=CARTESIAN_POINT('Ctrl Pts',(-145.10611112777,0.5045031901976,135.698589130933));
#110656=CARTESIAN_POINT('Ctrl Pts',(-145.11386231901,0.640496156091784,
135.680726860634));
#110657=CARTESIAN_POINT('Ctrl Pts',(-145.121610215787,0.776431321347918,
135.662872182276));
#110658=CARTESIAN_POINT('Ctrl Pts',(-145.129358112564,0.911689640280075,
135.639319902812));
#110659=CARTESIAN_POINT('Ctrl Pts',(-145.137106009342,1.04576080150545,
135.610145403481));
#110660=CARTESIAN_POINT('Ctrl Pts',(-145.144852285426,1.17980391793451,
135.580977006826));
#110661=CARTESIAN_POINT('Ctrl Pts',(-145.15259856151,1.31265998881138,135.546188812605));
#110662=CARTESIAN_POINT('Ctrl Pts',(-145.160344837594,1.44382866017305,
135.505907369707));
#110663=CARTESIAN_POINT('Ctrl Pts',(-145.16809117086,1.57499829979187,135.46562562946));
#110664=CARTESIAN_POINT('Ctrl Pts',(-145.175837504125,1.70448014130158,
135.419850674397));
#110665=CARTESIAN_POINT('Ctrl Pts',(-145.18358383739,1.83178914992934,135.368758888171));
#110666=CARTESIAN_POINT('Ctrl Pts',(-145.191331905393,1.95912666852671,
135.317655660294));
#110667=CARTESIAN_POINT('Ctrl Pts',(-145.199079973396,2.08429002321555,
135.261233377549));
#110668=CARTESIAN_POINT('Ctrl Pts',(-145.206828041399,2.20681468351453,
135.199716350055));
#110669=CARTESIAN_POINT('Ctrl Pts',(-145.214584344141,2.32946956448071,
135.138133941532));
#110670=CARTESIAN_POINT('Ctrl Pts',(-145.222340646883,2.44947979893839,
135.071446147409));
#110671=CARTESIAN_POINT('Ctrl Pts',(-145.230096949625,2.56640549583982,
134.999923260815));
#110672=CARTESIAN_POINT('Ctrl Pts',(-145.237857392139,2.68339359950625,
134.928362200302));
#110673=CARTESIAN_POINT('Ctrl Pts',(-145.245617834653,2.79729356067612,
134.85196112287));
#110674=CARTESIAN_POINT('Ctrl Pts',(-145.253378277168,2.90769581364454,
134.771032789275));
#110675=CARTESIAN_POINT('Ctrl Pts',(-145.261151177433,3.01827529411048,
134.689974542335));
#110676=CARTESIAN_POINT('Ctrl Pts',(-145.268924077699,3.1253455406053,134.604374760621));
#110677=CARTESIAN_POINT('Ctrl Pts',(-145.276696977964,3.22853064241857,
134.514586076142));
#110678=CARTESIAN_POINT('Ctrl Pts',(-145.284187313725,3.32796470586329,
134.428061436517));
#110679=CARTESIAN_POINT('Ctrl Pts',(-145.291677649487,3.42379096609442,
134.337647372335));
#110680=CARTESIAN_POINT('Ctrl Pts',(-145.299167985248,3.51570775512027,
134.243689337402));
#110681=CARTESIAN_POINT('Ctrl Pts',(-145.306942319367,3.61110959714906,
134.146168855007));
#110682=CARTESIAN_POINT('Ctrl Pts',(-145.314716653486,3.70260186501073,
134.044521441985));
#110683=CARTESIAN_POINT('Ctrl Pts',(-145.322490987605,3.78980640825618,
133.939093532894));
#110684=CARTESIAN_POINT('Ctrl Pts',(-145.330255740553,3.87690347969578,
133.833795554279));
#110685=CARTESIAN_POINT('Ctrl Pts',(-145.3380204935,3.95972309378019,133.724726648233));
#110686=CARTESIAN_POINT('Ctrl Pts',(-145.345785246447,4.03792337420397,
133.612270496205));
#110687=CARTESIAN_POINT('Ctrl Pts',(-145.353542287332,4.1160459850068,133.499926037213));
#110688=CARTESIAN_POINT('Ctrl Pts',(-145.361299328217,4.18955817068668,
133.384201346178));
#110689=CARTESIAN_POINT('Ctrl Pts',(-145.369056369102,4.25815808505595,
133.265513352601));
#110690=CARTESIAN_POINT('Ctrl Pts',(-145.376807560342,4.32670626769607,
133.146914862565));
#110691=CARTESIAN_POINT('Ctrl Pts',(-145.384558751582,4.39034935752116,
133.025357855044));
#110692=CARTESIAN_POINT('Ctrl Pts',(-145.392309942822,4.44882884351171,
132.90128812791));
#110693=CARTESIAN_POINT('Ctrl Pts',(-145.400057839599,4.50728347416081,
132.77727113372));
#110694=CARTESIAN_POINT('Ctrl Pts',(-145.407805736377,4.56057869966388,
132.650743896941));
#110695=CARTESIAN_POINT('Ctrl Pts',(-145.415553633154,4.60850210462471,
132.522176502395));
#110696=CARTESIAN_POINT('Ctrl Pts',(-145.423299909238,4.65641548504234,
132.393636001376));
#110697=CARTESIAN_POINT('Ctrl Pts',(-145.431046185322,4.69895914348969,
132.263056557542));
#110698=CARTESIAN_POINT('Ctrl Pts',(-145.438792461406,4.73596909559401,
132.130927535621));
#110699=CARTESIAN_POINT('Ctrl Pts',(-145.446538794672,4.77297932089734,
131.998797538354));
#110700=CARTESIAN_POINT('Ctrl Pts',(-145.454285127937,4.80445565289487,
131.865118316649));
#110701=CARTESIAN_POINT('Ctrl Pts',(-145.462031461202,4.83028431500737,
131.730393283671));
#110702=CARTESIAN_POINT('Ctrl Pts',(-145.469779529205,4.8561187612697,131.595638079956));
#110703=CARTESIAN_POINT('Ctrl Pts',(-145.477527597208,4.87630294732916,
131.459836982832));
#110704=CARTESIAN_POINT('Ctrl Pts',(-145.485275665211,4.8907745015692,131.323502060046));
#110705=CARTESIAN_POINT('Ctrl Pts',(-145.493031967953,4.90526143634928,
131.187022238883));
#110706=CARTESIAN_POINT('Ctrl Pts',(-145.500788270695,4.91402356959464,
131.050007848104));
#110707=CARTESIAN_POINT('Ctrl Pts',(-145.508544573437,4.91705053471405,
130.912975080545));
#110708=CARTESIAN_POINT('Ctrl Pts',(-145.516305015951,4.92007911541589,
130.775869174473));
#110709=CARTESIAN_POINT('Ctrl Pts',(-145.524065458466,4.91736643635554,
130.638745262774));
#110710=CARTESIAN_POINT('Ctrl Pts',(-145.53182590098,4.90895425174767,130.502116979505));
#110711=CARTESIAN_POINT('Ctrl Pts',(-145.539598801245,4.90052856315427,
130.365269368386));
#110712=CARTESIAN_POINT('Ctrl Pts',(-145.547371701511,4.88638512605326,
130.228919364716));
#110713=CARTESIAN_POINT('Ctrl Pts',(-145.555144601776,4.86661743082042,
130.093573839035));
#110714=CARTESIAN_POINT('Ctrl Pts',(-145.562634937539,4.84756834110051,
129.963148464123));
#110715=CARTESIAN_POINT('Ctrl Pts',(-145.570125273301,4.82329686258288,
129.833656107256));
#110716=CARTESIAN_POINT('Ctrl Pts',(-145.577615609063,4.79393057642016,
129.705537296479));
#110717=CARTESIAN_POINT('Ctrl Pts',(-145.585389943182,4.76345085859289,
129.572560822056));
#110718=CARTESIAN_POINT('Ctrl Pts',(-145.593164277301,4.72738581681424,
129.440642876293));
#110719=CARTESIAN_POINT('Ctrl Pts',(-145.60093861142,4.68582251673542,129.310288864217));
#110720=CARTESIAN_POINT('Ctrl Pts',(-145.608703364367,4.64431043970944,
129.180095501811));
#110721=CARTESIAN_POINT('Ctrl Pts',(-145.616468117315,4.59731370445418,
129.051462607035));
#110722=CARTESIAN_POINT('Ctrl Pts',(-145.624232870262,4.54497032054591,
128.924885199303));
#110723=CARTESIAN_POINT('Ctrl Pts',(-145.631989911147,4.49267892482445,
128.798433510036));
#110724=CARTESIAN_POINT('Ctrl Pts',(-145.639746952032,4.43505159675745,
128.674033604014));
#110725=CARTESIAN_POINT('Ctrl Pts',(-145.647503992917,4.3722759557053,128.552164793562));
#110726=CARTESIAN_POINT('Ctrl Pts',(-145.655255184157,4.3095476542523,128.430387885328));
#110727=CARTESIAN_POINT('Ctrl Pts',(-145.663006375397,4.2416789457706,128.311138619633));
#110728=CARTESIAN_POINT('Ctrl Pts',(-145.670757566637,4.16890516111337,
128.194875453756));
#110729=CARTESIAN_POINT('Ctrl Pts',(-145.678505463414,4.09616230725602,
128.078661702827));
#110730=CARTESIAN_POINT('Ctrl Pts',(-145.686253360191,4.01851873070883,
127.965431858135));
#110731=CARTESIAN_POINT('Ctrl Pts',(-145.694001256968,3.93625511143424,
127.855618723095));
#110732=CARTESIAN_POINT('Ctrl Pts',(-145.701747533053,3.85400869993541,
127.745828558596));
#110733=CARTESIAN_POINT('Ctrl Pts',(-145.709493809137,3.76714440221338,
127.639453994874));
#110734=CARTESIAN_POINT('Ctrl Pts',(-145.717240085221,3.67598529711315,
127.536897510214));
#110735=CARTESIAN_POINT('Ctrl Pts',(-145.724986418486,3.58482551909723,
127.434340268505));
#110736=CARTESIAN_POINT('Ctrl Pts',(-145.732732751752,3.48937113018113,
127.335601454312));
#110737=CARTESIAN_POINT('Ctrl Pts',(-145.740479085017,3.38998416709723,
127.241048898206));
#110738=CARTESIAN_POINT('Ctrl Pts',(-145.74822715302,3.29057494699219,127.14647516771));
#110739=CARTESIAN_POINT('Ctrl Pts',(-145.755975221023,3.18723168348585,
127.056089830211));
#110740=CARTESIAN_POINT('Ctrl Pts',(-145.763723289026,3.08035148029499,
126.970222145843));
#110741=CARTESIAN_POINT('Ctrl Pts',(-145.771479591768,2.97335768355186,
126.884263200278));
#110742=CARTESIAN_POINT('Ctrl Pts',(-145.77923589451,2.86281974318605,126.802831744444));
#110743=CARTESIAN_POINT('Ctrl Pts',(-145.786992197251,2.74916634345377,
126.726215514885));
#110744=CARTESIAN_POINT('Ctrl Pts',(-145.794752639766,2.63545228348002,
126.649558392937));
#110745=CARTESIAN_POINT('Ctrl Pts',(-145.80251308228,2.51861978372378,126.577721822948));
#110746=CARTESIAN_POINT('Ctrl Pts',(-145.810273524794,2.39912354823579,
126.510948307666));
#110747=CARTESIAN_POINT('Ctrl Pts',(-145.818046425059,2.27943548678222,
126.44406760161));
#110748=CARTESIAN_POINT('Ctrl Pts',(-145.825819325325,2.15707549383549,
126.382266368289));
#110749=CARTESIAN_POINT('Ctrl Pts',(-145.83359222559,2.03252054776953,126.32573992751));
#110750=CARTESIAN_POINT('Ctrl Pts',(-145.841082561352,1.91249348773579,
126.271268365239));
#110751=CARTESIAN_POINT('Ctrl Pts',(-145.848572897114,1.79042857349879,
126.221694865612));
#110752=CARTESIAN_POINT('Ctrl Pts',(-145.856063232875,1.66676539450888,
126.17715020716));
#110753=CARTESIAN_POINT('Ctrl Pts',(-145.863837566994,1.53841348849389,
126.130916624442));
#110754=CARTESIAN_POINT('Ctrl Pts',(-145.871611901113,1.40793314859634,
126.089954293546));
#110755=CARTESIAN_POINT('Ctrl Pts',(-145.879386235232,1.27579664748769,
126.054463147435));
#110756=CARTESIAN_POINT('Ctrl Pts',(-145.887150988179,1.14382299280727,
126.019015740989));
#110757=CARTESIAN_POINT('Ctrl Pts',(-145.894915741126,1.0101976119957,125.989026203716));
#110758=CARTESIAN_POINT('Ctrl Pts',(-145.902680494073,0.875411576452517,
125.964645994335));
#110759=CARTESIAN_POINT('Ctrl Pts',(-145.910437534958,0.740759412299987,
125.940289999722));
#110760=CARTESIAN_POINT('Ctrl Pts',(-145.918194575843,0.604949269730058,
125.921532315073));
#110761=CARTESIAN_POINT('Ctrl Pts',(-145.925951616728,0.468485820624661,
125.908474170928));
#110762=CARTESIAN_POINT('Ctrl Pts',(-145.933702807968,0.332125279667952,
125.895425874031));
#110763=CARTESIAN_POINT('Ctrl Pts',(-145.941453999208,0.195112800405398,
125.888068599684));
#110764=CARTESIAN_POINT('Ctrl Pts',(-145.949205190448,0.0579612980052955,
125.886452164734));
#110765=CARTESIAN_POINT('Ctrl Pts',(-145.956953087225,-0.0791319113478376,
125.884836416813));
#110766=CARTESIAN_POINT('Ctrl Pts',(-145.964700984002,-0.216363636196324,
125.888956659892));
#110767=CARTESIAN_POINT('Ctrl Pts',(-145.97244888078,-0.353218032392594,
125.89881069079));
#110768=CARTESIAN_POINT('Ctrl Pts',(-145.980195156864,-0.49004380159942,
125.908662660437));
#110769=CARTESIAN_POINT('Ctrl Pts',(-145.987941432948,-0.626492009439593,
125.924246004199));
#110770=CARTESIAN_POINT('Ctrl Pts',(-145.995687709032,-0.76204940752565,
125.945506456039));
#110771=CARTESIAN_POINT('Ctrl Pts',(-146.003434042297,-0.89760780626544,
125.966767064818));
#110772=CARTESIAN_POINT('Ctrl Pts',(-146.011180375562,-1.03227499588601,
125.99370480472));
#110773=CARTESIAN_POINT('Ctrl Pts',(-146.018926708828,-1.16554582041393,
126.026213905397));
#110774=CARTESIAN_POINT('Ctrl Pts',(-146.026674776831,-1.29884649001916,
126.058730286261));
#110775=CARTESIAN_POINT('Ctrl Pts',(-146.034422844833,-1.43074979252714,
126.096820417978));
#110776=CARTESIAN_POINT('Ctrl Pts',(-146.042170912836,-1.56076406780385,
126.14032817909));
#110777=CARTESIAN_POINT('Ctrl Pts',(-146.049927215578,-1.69091652379934,
126.183882180769));
#110778=CARTESIAN_POINT('Ctrl Pts',(-146.05768351832,-1.81917557065732,
126.232865189642));
#110779=CARTESIAN_POINT('Ctrl Pts',(-146.065439821062,-1.94506741316322,
126.287072070135));
#110780=CARTESIAN_POINT('Ctrl Pts',(-146.073200263576,-2.07102644793634,
126.341307882472));
#110781=CARTESIAN_POINT('Ctrl Pts',(-146.08096070609,-2.19461540869649,
126.400772952599));
#110782=CARTESIAN_POINT('Ctrl Pts',(-146.088721148604,-2.31538449236595,
126.465215803779));
#110783=CARTESIAN_POINT('Ctrl Pts',(-146.09649404887,-2.43634744528957,
126.529762104345));
#110784=CARTESIAN_POINT('Ctrl Pts',(-146.104266949135,-2.55448113818088,
126.599301955636));
#110785=CARTESIAN_POINT('Ctrl Pts',(-146.1120398494,-2.6693634244918,126.673539637363));
#110786=CARTESIAN_POINT('Ctrl Pts',(-146.119530185163,-2.78006945032958,
126.745078592369));
#110787=CARTESIAN_POINT('Ctrl Pts',(-146.127020520925,-2.88775610731852,
126.820979574334));
#110788=CARTESIAN_POINT('Ctrl Pts',(-146.134510856687,-2.99207575894011,
126.900943433192));
#110789=CARTESIAN_POINT('Ctrl Pts',(-146.142227797771,-3.09955139567316,
126.983326440736));
#110790=CARTESIAN_POINT('Ctrl Pts',(-146.149944738854,-3.20381148190246,
127.07029702923));
#110791=CARTESIAN_POINT('Ctrl Pts',(-146.157661679937,-3.30443283070756,
127.161572299554));
#110792=CARTESIAN_POINT('Ctrl Pts',(-146.165338592275,-3.40453224389806,
127.252374113551));
#110793=CARTESIAN_POINT('Ctrl Pts',(-146.173015504613,-3.5010302502149,
127.347435823624));
#110794=CARTESIAN_POINT('Ctrl Pts',(-146.18069241695,-3.59353889837519,
127.446435477191));
#110795=CARTESIAN_POINT('Ctrl Pts',(-146.18836232351,-3.68596312521306,
127.545344785889));
#110796=CARTESIAN_POINT('Ctrl Pts',(-146.196032230069,-3.77440496146833,
127.648184601815));
#110797=CARTESIAN_POINT('Ctrl Pts',(-146.203702136628,-3.85851097715001,
127.754594052448));
#110798=CARTESIAN_POINT('Ctrl Pts',(-146.211366795343,-3.9425594464631,
127.860930696428));
#110799=CARTESIAN_POINT('Ctrl Pts',(-146.219031454058,-4.02227774844276,
127.97083180432));
#110800=CARTESIAN_POINT('Ctrl Pts',(-146.226696112773,-4.09735102217618,
128.083901526976));
#110801=CARTESIAN_POINT('Ctrl Pts',(-146.234447890266,-4.17327760094385,
128.198256433543));
#110802=CARTESIAN_POINT('Ctrl Pts',(-146.242199667759,-4.24445262150303,
128.315852125728));
#110803=CARTESIAN_POINT('Ctrl Pts',(-146.249951445252,-4.31059385348899,
128.43624666491));
#110804=CARTESIAN_POINT('Ctrl Pts',(-146.257611948836,-4.37595630038468,
128.555223609209));
#110805=CARTESIAN_POINT('Ctrl Pts',(-146.265272452421,-4.43640268564307,
128.676933474641));
#110806=CARTESIAN_POINT('Ctrl Pts',(-146.272932956006,-4.49170598713918,
128.800923474155));
#110807=CARTESIAN_POINT('Ctrl Pts',(-146.280730370453,-4.54799768614846,
128.927129460851));
#110808=CARTESIAN_POINT('Ctrl Pts',(-146.2885277849,-4.5989605040081,129.055697485442));
#110809=CARTESIAN_POINT('Ctrl Pts',(-146.296325199347,-4.64440591072963,
129.186128001753));
#110810=CARTESIAN_POINT('Ctrl Pts',(-146.304122613794,-4.68985131745129,
129.316558518066));
#110811=CARTESIAN_POINT('Ctrl Pts',(-146.311920028241,-4.72977919261785,
129.448851105942));
#110812=CARTESIAN_POINT('Ctrl Pts',(-146.319717442688,-4.76405452823404,
129.582490119308));
#110813=CARTESIAN_POINT('Origin',(213.235140564004,0.,130.804360617566));
#110814=CARTESIAN_POINT('',(-148.415413529701,-4.76405452823396,129.582490119308));
#110815=CARTESIAN_POINT('',(-148.069858671336,-4.76405452823417,129.582490119309));
#110816=CARTESIAN_POINT('',(213.235140564004,-4.76405452823405,129.582490119308));
#110817=CARTESIAN_POINT('',(-146.735140564047,-4.91824791181105,130.799828458446));
#110818=CARTESIAN_POINT('Ctrl Pts',(-146.735140564047,-4.91824791181105,
130.799828458447));
#110819=CARTESIAN_POINT('Ctrl Pts',(-146.742795394334,-4.91837240966069,
130.934932119401));
#110820=CARTESIAN_POINT('Ctrl Pts',(-146.750450224622,-4.91292580148298,
131.070197708801));
#110821=CARTESIAN_POINT('Ctrl Pts',(-146.758105054909,-4.90189488163458,
131.205121932946));
#110822=CARTESIAN_POINT('Ctrl Pts',(-146.76611170812,-4.89035697073346,
131.346247396458));
#110823=CARTESIAN_POINT('Ctrl Pts',(-146.774118361331,-4.87270916905005,
131.486998925891));
#110824=CARTESIAN_POINT('Ctrl Pts',(-146.782125014542,-4.8489974415009,
131.626800204902));
#110825=CARTESIAN_POINT('Ctrl Pts',(-146.789771185002,-4.82635328470157,
131.760307224841));
#110826=CARTESIAN_POINT('Ctrl Pts',(-146.797417355461,-4.79817939812983,
131.892947251875));
#110827=CARTESIAN_POINT('Ctrl Pts',(-146.805063525921,-4.76456878221447,
132.024224291116));
#110828=CARTESIAN_POINT('Ctrl Pts',(-146.812708519105,-4.73096334130619,
132.155481117707));
#110829=CARTESIAN_POINT('Ctrl Pts',(-146.820353512288,-4.69192293508799,
132.285374984212));
#110830=CARTESIAN_POINT('Ctrl Pts',(-146.827998505472,-4.6475912792535,
132.413421947506));
#110831=CARTESIAN_POINT('Ctrl Pts',(-146.835644080023,-4.6032562521943,
132.541478648199));
#110832=CARTESIAN_POINT('Ctrl Pts',(-146.843289654574,-4.55362930726439,
132.667687786376));
#110833=CARTESIAN_POINT('Ctrl Pts',(-146.850935229125,-4.49890326506744,
132.791582918685));
#110834=CARTESIAN_POINT('Ctrl Pts',(-146.858583143927,-4.44416047165521,
132.915515974329));
#110835=CARTESIAN_POINT('Ctrl Pts',(-146.866231058729,-4.38431563998919,
133.037133248047));
#110836=CARTESIAN_POINT('Ctrl Pts',(-146.873878973531,-4.3196084856433,
133.155991029272));
#110837=CARTESIAN_POINT('Ctrl Pts',(-146.881535126221,-4.25483163252887,
133.274976837158));
#110838=CARTESIAN_POINT('Ctrl Pts',(-146.88919127891,-4.18518219572135,
133.391196866629));
#110839=CARTESIAN_POINT('Ctrl Pts',(-146.896847431599,-4.11094447671507,
133.504234424222));
#110840=CARTESIAN_POINT('Ctrl Pts',(-146.904508421899,-4.03665984992233,
133.617343405636));
#110841=CARTESIAN_POINT('Ctrl Pts',(-146.912169412199,-3.9577814038534,
133.727265586795));
#110842=CARTESIAN_POINT('Ctrl Pts',(-146.919830402499,-3.87463419044237,
133.833616789096));
#110843=CARTESIAN_POINT('Ctrl Pts',(-146.927502235942,-3.79136929288242,
133.940118517798));
#110844=CARTESIAN_POINT('Ctrl Pts',(-146.935174069385,-3.70382383045527,
134.043038876829));
#110845=CARTESIAN_POINT('Ctrl Pts',(-146.942845902827,-3.61236036328028,
134.142029814521));
#110846=CARTESIAN_POINT('Ctrl Pts',(-146.945318845874,-3.58287797855105,
134.173938608271));
#110847=CARTESIAN_POINT('Ctrl Pts',(-146.94779178892,-3.55298876082955,
134.205439431177));
#110848=CARTESIAN_POINT('Ctrl Pts',(-146.950264731966,-3.52270557038244,
134.236521529717));
#110849=CARTESIAN_POINT('Ctrl Pts',(-146.958039066085,-3.42750255263486,
134.334236121055));
#110850=CARTESIAN_POINT('Ctrl Pts',(-146.965813400204,-3.3280799737141,
134.428141299042));
#110851=CARTESIAN_POINT('Ctrl Pts',(-146.973587734323,-3.22477509384618,
134.517850708654));
#110852=CARTESIAN_POINT('Ctrl Pts',(-146.98135248727,-3.12159752801007,
134.607449559436));
#110853=CARTESIAN_POINT('Ctrl Pts',(-146.989117240217,-3.01454747349441,
134.692862676526));
#110854=CARTESIAN_POINT('Ctrl Pts',(-146.996881993164,-2.90400029716957,
134.773739074773));
#110855=CARTESIAN_POINT('Ctrl Pts',(-147.004639034049,-2.793562917859,134.854535145441));
#110856=CARTESIAN_POINT('Ctrl Pts',(-147.012396074934,-2.67963564243843,
134.930803234923));
#110857=CARTESIAN_POINT('Ctrl Pts',(-147.020153115819,-2.56262803686791,
135.002231578798));
#110858=CARTESIAN_POINT('Ctrl Pts',(-147.027904307059,-2.44570866764246,
135.073606058004));
#110859=CARTESIAN_POINT('Ctrl Pts',(-147.035655498299,-2.32571392421053,
135.140147853202));
#110860=CARTESIAN_POINT('Ctrl Pts',(-147.043406689539,-2.20308327251162,
135.201587829899));
#110861=CARTESIAN_POINT('Ctrl Pts',(-147.051154586316,-2.08050474211114,
135.263001692966));
#110862=CARTESIAN_POINT('Ctrl Pts',(-147.058902483094,-1.95529288051316,
135.319317875569));
#110863=CARTESIAN_POINT('Ctrl Pts',(-147.066650379871,-1.82791253978112,
135.370312742743));
#110864=CARTESIAN_POINT('Ctrl Pts',(-147.074396655955,-1.70055884427036,
135.42129694289));
#110865=CARTESIAN_POINT('Ctrl Pts',(-147.082142932039,-1.57103793458912,
135.46696189642));
#110866=CARTESIAN_POINT('Ctrl Pts',(-147.089889208123,-1.43983509936622,
135.507131922779));
#110867=CARTESIAN_POINT('Ctrl Pts',(-147.097635541388,-1.30863129563363,
135.547302245664));
#110868=CARTESIAN_POINT('Ctrl Pts',(-147.105381874654,-1.17574591542118,
135.581977445982));
#110869=CARTESIAN_POINT('Ctrl Pts',(-147.113128207919,-1.04167949659853,
135.611031699392));
#110870=CARTESIAN_POINT('Ctrl Pts',(-147.120876275922,-0.907583054531121,
135.640092459301));
#110871=CARTESIAN_POINT('Ctrl Pts',(-147.128624343925,-0.772305429580536,
135.6635296847));
#110872=CARTESIAN_POINT('Ctrl Pts',(-147.136372411928,-0.636357045285282,
135.681268733721));
#110873=CARTESIAN_POINT('Ctrl Pts',(-147.144128714669,-0.500264173429578,
135.699026636014));
#110874=CARTESIAN_POINT('Ctrl Pts',(-147.151885017411,-0.363499506449614,
135.71107421357));
#110875=CARTESIAN_POINT('Ctrl Pts',(-147.159641320153,-0.226578839760653,
135.71738871558));
#110876=CARTESIAN_POINT('Ctrl Pts',(-147.167401762667,-0.0895850943892772,
135.723706587829));
#110877=CARTESIAN_POINT('Ctrl Pts',(-147.175162205181,0.0475644258267302,
135.724285285743));
#110878=CARTESIAN_POINT('Ctrl Pts',(-147.182922647695,0.184355232759708,
135.71915422571));
#110879=CARTESIAN_POINT('Ctrl Pts',(-147.190695547961,0.321365628439695,
135.714014928844));
#110880=CARTESIAN_POINT('Ctrl Pts',(-147.198468448226,0.458015770169014,
135.703147588835));
#110881=CARTESIAN_POINT('Ctrl Pts',(-147.206241348492,0.593796689860795,
135.686633505639));
#110882=CARTESIAN_POINT('Ctrl Pts',(-147.213731684254,0.724641631120937,
135.670719750962));
#110883=CARTESIAN_POINT('Ctrl Pts',(-147.221222020017,0.854679145953966,
135.649562721546));
#110884=CARTESIAN_POINT('Ctrl Pts',(-147.228712355779,0.983465771579554,
135.623279390344));
#110885=CARTESIAN_POINT('Ctrl Pts',(-147.236486689898,1.11713538124924,
135.595999518653));
#110886=CARTESIAN_POINT('Ctrl Pts',(-147.244261024017,1.24988079946168,
135.563110529677));
#110887=CARTESIAN_POINT('Ctrl Pts',(-147.252035358137,1.3811946774017,135.524687335667));
#110888=CARTESIAN_POINT('Ctrl Pts',(-147.259800111084,1.51234672272302,
135.48631149481));
#110889=CARTESIAN_POINT('Ctrl Pts',(-147.267564864031,1.64207036646498,
135.442415128249));
#110890=CARTESIAN_POINT('Ctrl Pts',(-147.275329616978,1.76986741991784,
135.393124326716));
#110891=CARTESIAN_POINT('Ctrl Pts',(-147.283086657863,1.89753754353559,
135.343882481503));
#110892=CARTESIAN_POINT('Ctrl Pts',(-147.290843698748,2.0232845224357,135.28925700342));
#110893=CARTESIAN_POINT('Ctrl Pts',(-147.298600739633,2.14662467997481,
135.229423955624));
#110894=CARTESIAN_POINT('Ctrl Pts',(-147.306351930873,2.26987182574184,
135.169636028395));
#110895=CARTESIAN_POINT('Ctrl Pts',(-147.314103122113,2.39071541246357,
135.104648517996));
#110896=CARTESIAN_POINT('Ctrl Pts',(-147.321854313353,2.50869146759271,
135.0346856858));
#110897=CARTESIAN_POINT('Ctrl Pts',(-147.32960221013,2.62661737975114,134.964752589674));
#110898=CARTESIAN_POINT('Ctrl Pts',(-147.337350106907,2.74167784879623,
134.889848576623));
#110899=CARTESIAN_POINT('Ctrl Pts',(-147.345098003684,2.85343346040303,
134.810243859693));
#110900=CARTESIAN_POINT('Ctrl Pts',(-147.352844279768,2.96516569514506,
134.730655794353));
#110901=CARTESIAN_POINT('Ctrl Pts',(-147.360590555852,3.0735941292553,134.646369207626));
#110902=CARTESIAN_POINT('Ctrl Pts',(-147.368336831937,3.1783086473509,134.55769742695));
#110903=CARTESIAN_POINT('Ctrl Pts',(-147.376083165202,3.28302393842515,
134.469024991718));
#110904=CARTESIAN_POINT('Ctrl Pts',(-147.383829498467,3.38402496041651,
134.375967550597));
#110905=CARTESIAN_POINT('Ctrl Pts',(-147.391575831732,3.48093530079744,
134.278878209141));
#110906=CARTESIAN_POINT('Ctrl Pts',(-147.399323899735,3.57786734357729,
134.181767125199));
#110907=CARTESIAN_POINT('Ctrl Pts',(-147.407071967738,3.67070660570791,
134.080622620881));
#110908=CARTESIAN_POINT('Ctrl Pts',(-147.414820035741,3.75911439248049,
133.97583378421));
#110909=CARTESIAN_POINT('Ctrl Pts',(-147.422576338483,3.84761614010079,
133.870933576718));
#110910=CARTESIAN_POINT('Ctrl Pts',(-147.430332641225,3.9316767514697,133.762381598958));
#110911=CARTESIAN_POINT('Ctrl Pts',(-147.438088943967,4.0109982856649,133.650599506854));
#110912=CARTESIAN_POINT('Ctrl Pts',(-147.445849386481,4.09036215615144,
133.538757753281));
#110913=CARTESIAN_POINT('Ctrl Pts',(-147.453609828995,4.16498169683597,
133.423682778004));
#110914=CARTESIAN_POINT('Ctrl Pts',(-147.461370271509,4.23460356315992,
133.305823334732));
#110915=CARTESIAN_POINT('Ctrl Pts',(-147.469143171775,4.30433719268442,
133.18777469302));
#110916=CARTESIAN_POINT('Ctrl Pts',(-147.47691607204,4.3690569312253,133.066932995924));
#110917=CARTESIAN_POINT('Ctrl Pts',(-147.484688972305,4.42855606905609,
132.943770397325));
#110918=CARTESIAN_POINT('Ctrl Pts',(-147.492179308068,4.4858922633597,132.825085069407));
#110919=CARTESIAN_POINT('Ctrl Pts',(-147.49966964383,4.53838070842162,132.70424493414));
#110920=CARTESIAN_POINT('Ctrl Pts',(-147.507159979592,4.58588011443595,
132.581686316058));
#110921=CARTESIAN_POINT('Ctrl Pts',(-147.514934313711,4.6351804748647,132.454480850725));
#110922=CARTESIAN_POINT('Ctrl Pts',(-147.52270864783,4.67926217800561,132.325021068937));
#110923=CARTESIAN_POINT('Ctrl Pts',(-147.53048298195,4.71791401523017,132.193774309522));
#110924=CARTESIAN_POINT('Ctrl Pts',(-147.538247734897,4.75651821751966,
132.062689300008));
#110925=CARTESIAN_POINT('Ctrl Pts',(-147.546012487844,4.78970575924094,
131.929822066209));
#110926=CARTESIAN_POINT('Ctrl Pts',(-147.553777240791,4.81731344093131,
131.795659903515));
#110927=CARTESIAN_POINT('Ctrl Pts',(-147.561534281676,4.84489370228309,
131.661630992572));
#110928=CARTESIAN_POINT('Ctrl Pts',(-147.569291322561,4.86690505413417,
131.526310092678));
#110929=CARTESIAN_POINT('Ctrl Pts',(-147.577048363446,4.88323418436421,
131.390199301127));
#110930=CARTESIAN_POINT('Ctrl Pts',(-147.584799554686,4.89955100067006,
131.254191151784));
#110931=CARTESIAN_POINT('Ctrl Pts',(-147.592550745926,4.91019407802103,
131.117394683028));
#110932=CARTESIAN_POINT('Ctrl Pts',(-147.600301937166,4.91510130536675,
130.980321466854));
#110933=CARTESIAN_POINT('Ctrl Pts',(-147.608049833943,4.92000644700997,
130.843306510452));
#110934=CARTESIAN_POINT('Ctrl Pts',(-147.61579773072,4.91918057346542,130.706015430476));
#110935=CARTESIAN_POINT('Ctrl Pts',(-147.623545627498,4.91261350844471,
130.568963975393));
#110936=CARTESIAN_POINT('Ctrl Pts',(-147.631291903582,4.90604781711242,
130.431941188519));
#110937=CARTESIAN_POINT('Ctrl Pts',(-147.639038179666,4.89374334172696,
130.295158317108));
#110938=CARTESIAN_POINT('Ctrl Pts',(-147.64678445575,4.87574201615306,130.15912976398));
#110939=CARTESIAN_POINT('Ctrl Pts',(-147.654530789015,4.85774055769745,
130.023100206719));
#110940=CARTESIAN_POINT('Ctrl Pts',(-147.662277122281,4.83404221643115,
129.887825366439));
#110941=CARTESIAN_POINT('Ctrl Pts',(-147.670023455546,4.80474060989277,
129.753812791835));
#110942=CARTESIAN_POINT('Ctrl Pts',(-147.677771523549,4.7754324414628,129.619770206045));
#110943=CARTESIAN_POINT('Ctrl Pts',(-147.685519591552,4.74051859432432,
129.486990830293));
#110944=CARTESIAN_POINT('Ctrl Pts',(-147.693267659555,4.70014334648945,
129.355969929612));
#110945=CARTESIAN_POINT('Ctrl Pts',(-147.701023962297,4.65972518736077,
129.224809778359));
#110946=CARTESIAN_POINT('Ctrl Pts',(-147.708780265039,4.61383414785842,
129.095412209785));
#110947=CARTESIAN_POINT('Ctrl Pts',(-147.716536567781,4.56266393470546,
128.968255805351));
#110948=CARTESIAN_POINT('Ctrl Pts',(-147.724297010295,4.51146641046904,
128.841031533716));
#110949=CARTESIAN_POINT('Ctrl Pts',(-147.732057452809,4.45498425909858,
128.716051165803));
#110950=CARTESIAN_POINT('Ctrl Pts',(-147.739817895323,4.39345809087738,
128.593770409906));
#110951=CARTESIAN_POINT('Ctrl Pts',(-147.747590795589,4.33183315538891,
128.471293358083));
#110952=CARTESIAN_POINT('Ctrl Pts',(-147.755363695854,4.2651482127556,128.351524920088));
#110953=CARTESIAN_POINT('Ctrl Pts',(-147.76313659612,4.19368876775168,128.234894217371));
#110954=CARTESIAN_POINT('Ctrl Pts',(-147.770626931882,4.12482705357146,
128.122503334476));
#110955=CARTESIAN_POINT('Ctrl Pts',(-147.778117267643,4.05153211206293,
128.013026274307));
#110956=CARTESIAN_POINT('Ctrl Pts',(-147.785607603405,3.97409466482375,
127.906817752047));
#110957=CARTESIAN_POINT('Ctrl Pts',(-147.793381937524,3.89372115323352,
127.796582301381));
#110958=CARTESIAN_POINT('Ctrl Pts',(-147.801156271643,3.80863020962687,
127.689518941783));
#110959=CARTESIAN_POINT('Ctrl Pts',(-147.808930605762,3.71910085597341,
127.586057977105));
#110960=CARTESIAN_POINT('Ctrl Pts',(-147.816695358709,3.62968183924686,
127.48272451882));
#110961=CARTESIAN_POINT('Ctrl Pts',(-147.824460111656,3.53583554940689,
127.382984914718));
#110962=CARTESIAN_POINT('Ctrl Pts',(-147.832224864604,3.43788374857132,
127.287239864193));
#110963=CARTESIAN_POINT('Ctrl Pts',(-147.839981905489,3.34002923484521,
127.191589909001));
#110964=CARTESIAN_POINT('Ctrl Pts',(-147.847738946374,3.23807760261019,
127.099926883506));
#110965=CARTESIAN_POINT('Ctrl Pts',(-147.855495987258,3.13239003257192,
127.012617516254));
#110966=CARTESIAN_POINT('Ctrl Pts',(-147.863247178499,3.02678216235249,
126.925373989676));
#110967=CARTESIAN_POINT('Ctrl Pts',(-147.870998369739,2.9174442621906,126.842477834471));
#110968=CARTESIAN_POINT('Ctrl Pts',(-147.878749560979,2.80477315955378,
126.764257823583));
#110969=CARTESIAN_POINT('Ctrl Pts',(-147.886497457756,2.69214994514103,
126.686071058287));
#110970=CARTESIAN_POINT('Ctrl Pts',(-147.894245354533,2.57619666644804,
126.612556706841));
#110971=CARTESIAN_POINT('Ctrl Pts',(-147.90199325131,2.45734173673487,126.544002105492));
#110972=CARTESIAN_POINT('Ctrl Pts',(-147.909739527394,2.33851166891046,
126.475461844287));
#110973=CARTESIAN_POINT('Ctrl Pts',(-147.917485803478,2.21678149580125,
126.411879464805));
#110974=CARTESIAN_POINT('Ctrl Pts',(-147.925232079562,2.09260666534645,
126.353497734186));
#110975=CARTESIAN_POINT('Ctrl Pts',(-147.932978412827,1.96843091826176,
126.295115572607));
#110976=CARTESIAN_POINT('Ctrl Pts',(-147.940724746093,1.84181083163353,
126.241934302843));
#110977=CARTESIAN_POINT('Ctrl Pts',(-147.948471079358,1.71322402312201,
126.194149504277));
#110978=CARTESIAN_POINT('Ctrl Pts',(-147.956219147361,1.5846084184868,126.146354004636));
#110979=CARTESIAN_POINT('Ctrl Pts',(-147.963967215364,1.45402558196438,
126.103957517135));
#110980=CARTESIAN_POINT('Ctrl Pts',(-147.971715283367,1.32197017984307,
126.067106359443));
#110981=CARTESIAN_POINT('Ctrl Pts',(-147.979471586109,1.18977442766799,
126.030216035902));
#110982=CARTESIAN_POINT('Ctrl Pts',(-147.98722788885,1.0561033606954,125.998882920611));
#110983=CARTESIAN_POINT('Ctrl Pts',(-147.994984191592,0.921464326278293,
125.973202727588));
#110984=CARTESIAN_POINT('Ctrl Pts',(-148.002744634106,0.786753430954979,
125.947508828273));
#110985=CARTESIAN_POINT('Ctrl Pts',(-148.010505076621,0.65107392533345,
125.927473920206));
#110986=CARTESIAN_POINT('Ctrl Pts',(-148.018265519135,0.514939265442972,
125.913141892605));
#110987=CARTESIAN_POINT('Ctrl Pts',(-148.0260384194,0.378586070110599,125.898786857962));
#110988=CARTESIAN_POINT('Ctrl Pts',(-148.033811319665,0.241776650843219,
125.890153022571));
#110989=CARTESIAN_POINT('Ctrl Pts',(-148.041584219931,0.105026361975948,
125.887232133807));
#110990=CARTESIAN_POINT('Ctrl Pts',(-148.049074555693,-0.0267527094392925,
125.884417426707));
#110991=CARTESIAN_POINT('Ctrl Pts',(-148.056564891455,-0.158476566930597,
125.886907511672));
#110992=CARTESIAN_POINT('Ctrl Pts',(-148.064055227217,-0.289689636442435,
125.894649528608));
#110993=CARTESIAN_POINT('Ctrl Pts',(-148.071829561336,-0.425877689364814,
125.902685086469));
#110994=CARTESIAN_POINT('Ctrl Pts',(-148.079603895455,-0.561946859468491,
125.916404146196));
#110995=CARTESIAN_POINT('Ctrl Pts',(-148.087378229574,-0.697384301744843,
125.935804548444));
#110996=CARTESIAN_POINT('Ctrl Pts',(-148.095142982522,-0.832654829477982,
125.955181041431));
#110997=CARTESIAN_POINT('Ctrl Pts',(-148.102907735469,-0.967294795162843,
125.980224890647));
#110998=CARTESIAN_POINT('Ctrl Pts',(-148.110672488416,-1.1007931587684,
126.010881976317));
#110999=CARTESIAN_POINT('Ctrl Pts',(-148.118429529301,-1.23415892991759,
126.041508612938));
#111000=CARTESIAN_POINT('Ctrl Pts',(-148.126186570186,-1.36638497682959,
126.077737304284));
#111001=CARTESIAN_POINT('Ctrl Pts',(-148.133943611071,-1.49696753339659,
126.119462404535));
#111002=CARTESIAN_POINT('Ctrl Pts',(-148.141694802311,-1.62745161664102,
126.161156039564));
#111003=CARTESIAN_POINT('Ctrl Pts',(-148.149445993551,-1.75629430552048,
126.208337714841));
#111004=CARTESIAN_POINT('Ctrl Pts',(-148.157197184791,-1.88300449910607,
126.260851277986));
#111005=CARTESIAN_POINT('Ctrl Pts',(-148.164945081568,-2.00966083747979,
126.313342521467));
#111006=CARTESIAN_POINT('Ctrl Pts',(-148.172692978346,-2.13418612283538,
126.371160996155));
#111007=CARTESIAN_POINT('Ctrl Pts',(-148.180440875123,-2.25610704322118,
126.434101578101));
#111008=CARTESIAN_POINT('Ctrl Pts',(-148.188187151207,-2.37800246037876,
126.497028994234));
#111009=CARTESIAN_POINT('Ctrl Pts',(-148.195933427291,-2.49729424897409,
126.565076207252));
#111010=CARTESIAN_POINT('Ctrl Pts',(-148.203679703375,-2.61353198139975,
126.637991257476));
#111011=CARTESIAN_POINT('Ctrl Pts',(-148.211426036641,-2.7297705718661,
126.710906845941));
#111012=CARTESIAN_POINT('Ctrl Pts',(-148.219172369906,-2.84295472998101,
126.788690135557));
#111013=CARTESIAN_POINT('Ctrl Pts',(-148.226918703171,-2.95266174525944,
126.871045008492));
#111014=CARTESIAN_POINT('Ctrl Pts',(-148.234666771174,-3.06239332866343,
126.953418324231));
#111015=CARTESIAN_POINT('Ctrl Pts',(-148.242414839177,-3.16864590713363,
127.04036502581));
#111016=CARTESIAN_POINT('Ctrl Pts',(-148.25016290718,-3.27102900025871,
127.131548024747));
#111017=CARTESIAN_POINT('Ctrl Pts',(-148.257919209922,-3.3735209073534,
127.222827934061));
#111018=CARTESIAN_POINT('Ctrl Pts',(-148.265675512664,-3.47213482144369,
127.318352874299));
#111019=CARTESIAN_POINT('Ctrl Pts',(-148.273431815406,-3.56651598197871,
127.417747735527));
#111020=CARTESIAN_POINT('Ctrl Pts',(-148.28119225792,-3.66094751658086,
127.517195646786));
#111021=CARTESIAN_POINT('Ctrl Pts',(-148.288952700435,-3.75114153910059,
127.62051730032));
#111022=CARTESIAN_POINT('Ctrl Pts',(-148.296713142949,-3.83678358876981,
127.727304434223));
#111023=CARTESIAN_POINT('Ctrl Pts',(-148.304486043214,-3.92256311866011,
127.834262992315));
#111024=CARTESIAN_POINT('Ctrl Pts',(-148.31225894348,-4.00377584176706,
127.944697832467));
#111025=CARTESIAN_POINT('Ctrl Pts',(-148.320031843745,-4.08015013965218,
128.058170911738));
#111026=CARTESIAN_POINT('Ctrl Pts',(-148.327522179507,-4.15374803943145,
128.167518958752));
#111027=CARTESIAN_POINT('Ctrl Pts',(-148.335012515269,-4.22285302293328,
128.279687922415));
#111028=CARTESIAN_POINT('Ctrl Pts',(-148.342502851031,-4.28726331394532,
128.394265943202));
#111029=CARTESIAN_POINT('Ctrl Pts',(-148.350634261164,-4.35718627997413,
128.518650337826));
#111030=CARTESIAN_POINT('Ctrl Pts',(-148.358765671297,-4.42178120596168,
128.646237719128));
#111031=CARTESIAN_POINT('Ctrl Pts',(-148.36689708143,-4.4807569195496,128.776553799743));
#111032=CARTESIAN_POINT('Ctrl Pts',(-148.375010992932,-4.5396057185882,
128.906589442775));
#111033=CARTESIAN_POINT('Ctrl Pts',(-148.383124904435,-4.59285927356076,
129.039341771286));
#111034=CARTESIAN_POINT('Ctrl Pts',(-148.391238815937,-4.64027184970223,
129.174311470037));
#111035=CARTESIAN_POINT('Ctrl Pts',(-148.399297053858,-4.68735910458748,
129.308355074584));
#111036=CARTESIAN_POINT('Ctrl Pts',(-148.40735529178,-4.728685140066,129.444585411646));
#111037=CARTESIAN_POINT('Ctrl Pts',(-148.415413529701,-4.76405452823396,
129.582490119308));
#111038=CARTESIAN_POINT('Ctrl Pts',(-146.665174983012,-4.76405452823419,
129.582490119309));
#111039=CARTESIAN_POINT('Ctrl Pts',(-146.667389024726,-4.77371530756762,
129.620157351307));
#111040=CARTESIAN_POINT('Ctrl Pts',(-146.66960306644,-4.78292519609886,
129.657923035737));
#111041=CARTESIAN_POINT('Ctrl Pts',(-146.671817108154,-4.79168258690122,
129.695775461212));
#111042=CARTESIAN_POINT('Ctrl Pts',(-146.682371017463,-4.83342737776348,
129.876210663977));
#111043=CARTESIAN_POINT('Ctrl Pts',(-146.692924926773,-4.86499443715233,
130.059082143305));
#111044=CARTESIAN_POINT('Ctrl Pts',(-146.703478836082,-4.88615669536868,
130.243418721463));
#111045=CARTESIAN_POINT('Ctrl Pts',(-146.714032745392,-4.90731895358504,
130.427755299621));
#111046=CARTESIAN_POINT('Ctrl Pts',(-146.724586654701,-4.91807626343323,
130.613557602484));
#111047=CARTESIAN_POINT('Ctrl Pts',(-146.735140564011,-4.91824791181047,
130.799828457817));
#111048=CARTESIAN_POINT('',(-146.389859435956,-4.91824941502472,130.806759389969));
#111049=CARTESIAN_POINT('Ctrl Pts',(-146.319717442688,-4.76405452823404,
129.582490119308));
#111050=CARTESIAN_POINT('Ctrl Pts',(-146.327388454375,-4.79777423132902,
129.713962729908));
#111051=CARTESIAN_POINT('Ctrl Pts',(-146.335059466061,-4.82602325428672,
129.846738034062));
#111052=CARTESIAN_POINT('Ctrl Pts',(-146.342730477747,-4.84872491478903,
129.980315859556));
#111053=CARTESIAN_POINT('Ctrl Pts',(-146.350585304115,-4.87197055810291,
130.117094509988));
#111054=CARTESIAN_POINT('Ctrl Pts',(-146.358440130483,-4.88939956768438,
130.254714181017));
#111055=CARTESIAN_POINT('Ctrl Pts',(-146.366294956852,-4.90098609526096,
130.392634547759));
#111056=CARTESIAN_POINT('Ctrl Pts',(-146.37414978322,-4.9125726228375,130.530554914501));
#111057=CARTESIAN_POINT('Ctrl Pts',(-146.382004609588,-4.91831671374134,
130.668775530728));
#111058=CARTESIAN_POINT('Ctrl Pts',(-146.389859435956,-4.91824941502472,
130.80675938997));
#111059=CARTESIAN_POINT('Ctrl Pts',(-146.389859435993,-4.9182494150244,
130.806759390615));
#111060=CARTESIAN_POINT('Ctrl Pts',(-146.397559117496,-4.91818344554288,
130.942017857041));
#111061=CARTESIAN_POINT('Ctrl Pts',(-146.405258798998,-4.912538321635,131.077135866295));
#111062=CARTESIAN_POINT('Ctrl Pts',(-146.4129584805,-4.90134546095345,131.211786359132));
#111063=CARTESIAN_POINT('Ctrl Pts',(-146.420732814619,-4.89004407937541,
131.347742362028));
#111064=CARTESIAN_POINT('Ctrl Pts',(-146.428507148739,-4.87306368550077,
131.483443127966));
#111065=CARTESIAN_POINT('Ctrl Pts',(-146.436281482858,-4.85041874491575,
131.618376011444));
#111066=CARTESIAN_POINT('Ctrl Pts',(-146.444046235805,-4.82780171219616,
131.753142602202));
#111067=CARTESIAN_POINT('Ctrl Pts',(-146.451810988752,-4.79953408705723,
131.887142811575));
#111068=CARTESIAN_POINT('Ctrl Pts',(-146.459575741699,-4.76568223723894,
132.019867045424));
#111069=CARTESIAN_POINT('Ctrl Pts',(-146.467332782584,-4.73186400955512,
132.152459455694));
#111070=CARTESIAN_POINT('Ctrl Pts',(-146.475089823469,-4.69247269063897,
132.283778036072));
#111071=CARTESIAN_POINT('Ctrl Pts',(-146.482846864354,-4.64762598488324,
132.413321700731));
#111072=CARTESIAN_POINT('Ctrl Pts',(-146.490598055594,-4.60281309837712,
132.542767675504));
#111073=CARTESIAN_POINT('Ctrl Pts',(-146.498349246834,-4.55255314098193,
132.670441030761));
#111074=CARTESIAN_POINT('Ctrl Pts',(-146.506100438074,-4.49701400517767,
132.795854554222));
#111075=CARTESIAN_POINT('Ctrl Pts',(-146.513848334852,-4.44149847498761,
132.92121477359));
#111076=CARTESIAN_POINT('Ctrl Pts',(-146.521596231629,-4.38070838709689,
133.04431671477));
#111077=CARTESIAN_POINT('Ctrl Pts',(-146.529344128406,-4.31486016456706,
133.164692124523));
#111078=CARTESIAN_POINT('Ctrl Pts',(-146.53709040449,-4.24902571606586,
133.285042354334));
#111079=CARTESIAN_POINT('Ctrl Pts',(-146.544836680574,-4.17813542496078,
133.402666844356));
#111080=CARTESIAN_POINT('Ctrl Pts',(-146.552582956658,-4.10245198739481,
133.51712134303));
#111081=CARTESIAN_POINT('Ctrl Pts',(-146.560329289923,-4.02676799115099,
133.631576686581));
#111082=CARTESIAN_POINT('Ctrl Pts',(-146.568075623189,-3.94629099348904,
133.742861665976));
#111083=CARTESIAN_POINT('Ctrl Pts',(-146.575821956454,-3.86132717085156,
133.850560798471));
#111084=CARTESIAN_POINT('Ctrl Pts',(-146.583570024457,-3.77634432115522,
133.958284049439));
#111085=CARTESIAN_POINT('Ctrl Pts',(-146.59131809246,-3.6868728891654,134.062419548692));
#111086=CARTESIAN_POINT('Ctrl Pts',(-146.599066160463,-3.59325923674562,
134.16258501746));
#111087=CARTESIAN_POINT('Ctrl Pts',(-146.606822463205,-3.4995460906219,
134.26285694328));
#111088=CARTESIAN_POINT('Ctrl Pts',(-146.614578765947,-3.40168219717782,
134.359150123825));
#111089=CARTESIAN_POINT('Ctrl Pts',(-146.622335068689,-3.30005107159837,
134.451118902309));
#111090=CARTESIAN_POINT('Ctrl Pts',(-146.630095511203,-3.19836570242715,
134.5431367673));
#111091=CARTESIAN_POINT('Ctrl Pts',(-146.637855953717,-3.09290939512924,
134.630825381373));
#111092=CARTESIAN_POINT('Ctrl Pts',(-146.645616396231,-2.98409784023135,
134.713880171479));
#111093=CARTESIAN_POINT('Ctrl Pts',(-146.653389296496,-2.8751116113657,
134.797068288507));
#111094=CARTESIAN_POINT('Ctrl Pts',(-146.661162196762,-2.76275969229254,
134.875607492694));
#111095=CARTESIAN_POINT('Ctrl Pts',(-146.668935097027,-2.64748651790352,
134.949236755645));
#111096=CARTESIAN_POINT('Ctrl Pts',(-146.676425432789,-2.53640381375977,
135.020189409427));
#111097=CARTESIAN_POINT('Ctrl Pts',(-146.683915768551,-2.42260882292317,
135.086582746558));
#111098=CARTESIAN_POINT('Ctrl Pts',(-146.691406104313,-2.30651812838755,
135.148224932427));
#111099=CARTESIAN_POINT('Ctrl Pts',(-146.699180438432,-2.18602581988309,
135.212204300508));
#111100=CARTESIAN_POINT('Ctrl Pts',(-146.706954772551,-2.06267860459535,
135.271267792897));
#111101=CARTESIAN_POINT('Ctrl Pts',(-146.71472910667,-1.93691560470815,
135.325150482483));
#111102=CARTESIAN_POINT('Ctrl Pts',(-146.722493859618,-1.81130759647854,
135.37896676647));
#111103=CARTESIAN_POINT('Ctrl Pts',(-146.730258612565,-1.68329008338702,
135.427614799163));
#111104=CARTESIAN_POINT('Ctrl Pts',(-146.738023365512,-1.55332767479957,
135.470874969542));
#111105=CARTESIAN_POINT('Ctrl Pts',(-146.745780406397,-1.42349434670848,
135.51409217331));
#111106=CARTESIAN_POINT('Ctrl Pts',(-146.753537447282,-1.29172033584053,
135.551932041415));
#111107=CARTESIAN_POINT('Ctrl Pts',(-146.761294488167,-1.15849084199306,
135.584222752766));
#111108=CARTESIAN_POINT('Ctrl Pts',(-146.769045679407,-1.02536181754346,
135.61648911344));
#111109=CARTESIAN_POINT('Ctrl Pts',(-146.776796870647,-0.890779873229676,
135.643214554959));
#111110=CARTESIAN_POINT('Ctrl Pts',(-146.784548061887,-0.75524566452571,
135.664276979883));
#111111=CARTESIAN_POINT('Ctrl Pts',(-146.792295958664,-0.619769061475753,
135.685330452715));
#111112=CARTESIAN_POINT('Ctrl Pts',(-146.800043855441,-0.483341384547462,
135.700725636247));
#111113=CARTESIAN_POINT('Ctrl Pts',(-146.807791752218,-0.34647357040469,
135.710391511019));
#111114=CARTESIAN_POINT('Ctrl Pts',(-146.815538028302,-0.209634386058108,
135.720055363897));
#111115=CARTESIAN_POINT('Ctrl Pts',(-146.823284304386,-0.0723556373705812,
135.723992264268));
#111116=CARTESIAN_POINT('Ctrl Pts',(-146.831030580471,0.0648469205584715,
135.722183097017));
#111117=CARTESIAN_POINT('Ctrl Pts',(-146.838776913736,0.202050491285826,
135.720373916412));
#111118=CARTESIAN_POINT('Ctrl Pts',(-146.846523247001,0.339177479201213,
135.712818588701));
#111119=CARTESIAN_POINT('Ctrl Pts',(-146.854269580267,0.475712831059523,
135.699550130227));
#111120=CARTESIAN_POINT('Ctrl Pts',(-146.86201764827,0.612278759063397,
135.686278700373));
#111121=CARTESIAN_POINT('Ctrl Pts',(-146.869765716273,0.748252398307283,
135.667291631675));
#111122=CARTESIAN_POINT('Ctrl Pts',(-146.877513784276,0.883124909789015,
135.642673697164));
#111123=CARTESIAN_POINT('Ctrl Pts',(-146.885270087018,1.01814076538077,
135.61802959842));
#111124=CARTESIAN_POINT('Ctrl Pts',(-146.893026389759,1.15205277020258,
135.587742749392));
#111125=CARTESIAN_POINT('Ctrl Pts',(-146.900782692501,1.28436281408676,
135.551948976332));
#111126=CARTESIAN_POINT('Ctrl Pts',(-146.908543135016,1.41674347582515,
135.516136099058));
#111127=CARTESIAN_POINT('Ctrl Pts',(-146.91630357753,1.54752010032395,135.474810558871));
#111128=CARTESIAN_POINT('Ctrl Pts',(-146.924064020044,1.67621175076582,
135.42815745881));
#111129=CARTESIAN_POINT('Ctrl Pts',(-146.931836920309,1.80510998846968,
135.381429467051));
#111130=CARTESIAN_POINT('Ctrl Pts',(-146.939609820575,1.9319162019058,135.329356973853));
#111131=CARTESIAN_POINT('Ctrl Pts',(-146.94738272084,2.05617055257688,135.272172802653));
#111132=CARTESIAN_POINT('Ctrl Pts',(-146.954873056602,2.17590794462324,
135.217067420115));
#111133=CARTESIAN_POINT('Ctrl Pts',(-146.962363392364,2.29327551165393,
135.157215691949));
#111134=CARTESIAN_POINT('Ctrl Pts',(-146.969853728126,2.4078866844924,135.092864409933));
#111135=CARTESIAN_POINT('Ctrl Pts',(-146.977628062245,2.52684337478388,
135.0260732295));
#111136=CARTESIAN_POINT('Ctrl Pts',(-146.985402396365,2.64320734648145,
134.954222984246));
#111137=CARTESIAN_POINT('Ctrl Pts',(-146.993176730484,2.75651835263832,
134.877539920527));
#111138=CARTESIAN_POINT('Ctrl Pts',(-147.000941483431,2.869689713107,134.800951361831));
#111139=CARTESIAN_POINT('Ctrl Pts',(-147.008706236378,2.97981527362293,
134.719542052387));
#111140=CARTESIAN_POINT('Ctrl Pts',(-147.016470989325,3.08645913650406,
134.633584176095));
#111141=CARTESIAN_POINT('Ctrl Pts',(-147.02422803021,3.19299707919715,134.547711674376));
#111142=CARTESIAN_POINT('Ctrl Pts',(-147.031985071095,3.29605990354734,
134.45729984));
#111143=CARTESIAN_POINT('Ctrl Pts',(-147.03974211198,3.39524078926313,134.362664011801));
#111144=CARTESIAN_POINT('Ctrl Pts',(-147.04749330322,3.49434688190162,134.268099549216));
#111145=CARTESIAN_POINT('Ctrl Pts',(-147.05524449446,3.58957658100332,134.169317701852));
#111146=CARTESIAN_POINT('Ctrl Pts',(-147.0629956857,3.68055654602248,134.066673688691));
#111147=CARTESIAN_POINT('Ctrl Pts',(-147.070743582477,3.77149784212941,
133.964073301973));
#111148=CARTESIAN_POINT('Ctrl Pts',(-147.078491479254,3.85819273786076,
133.857614306289));
#111149=CARTESIAN_POINT('Ctrl Pts',(-147.086239376031,3.94030530878379,
133.747688179369));
#111150=CARTESIAN_POINT('Ctrl Pts',(-147.093985652115,4.02240070352712,
133.637785046625));
#111151=CARTESIAN_POINT('Ctrl Pts',(-147.101731928199,4.0999154461931,133.524416538233));
#111152=CARTESIAN_POINT('Ctrl Pts',(-147.109478204283,4.17255467646619,
133.408006241379));
#111153=CARTESIAN_POINT('Ctrl Pts',(-147.117224537549,4.24519444294548,
133.291595085211));
#111154=CARTESIAN_POINT('Ctrl Pts',(-147.124970870814,4.31295841824567,
133.172142427463));
#111155=CARTESIAN_POINT('Ctrl Pts',(-147.132717204079,4.37559598108965,
133.050099443158));
#111156=CARTESIAN_POINT('Ctrl Pts',(-147.140465272082,4.43824757118162,
132.928029128173));
#111157=CARTESIAN_POINT('Ctrl Pts',(-147.148213340085,4.49577028589568,
132.803367680087));
#111158=CARTESIAN_POINT('Ctrl Pts',(-147.155961408088,4.54796040727584,
132.676589021461));
#111159=CARTESIAN_POINT('Ctrl Pts',(-147.16371771083,4.60020599693814,132.549675620967));
#111160=CARTESIAN_POINT('Ctrl Pts',(-147.171474013572,4.64710752267168,
132.420640877029));
#111161=CARTESIAN_POINT('Ctrl Pts',(-147.179230316314,4.68851001823618,
132.289977281244));
#111162=CARTESIAN_POINT('Ctrl Pts',(-147.186990758828,4.72993461155915,
132.159243946364));
#111163=CARTESIAN_POINT('Ctrl Pts',(-147.194751201342,4.76585422413791,
132.026880404484));
#111164=CARTESIAN_POINT('Ctrl Pts',(-147.202511643856,4.79616463030452,
131.893391334082));
#111165=CARTESIAN_POINT('Ctrl Pts',(-147.210284544122,4.82652369342594,
131.759687975174));
#111166=CARTESIAN_POINT('Ctrl Pts',(-147.218057444387,4.85125548590539,
131.624855861958));
#111167=CARTESIAN_POINT('Ctrl Pts',(-147.225830344652,4.87030733475456,
131.489407716338));
#111168=CARTESIAN_POINT('Ctrl Pts',(-147.233320680415,4.88866660091003,
131.35888345198));
#111169=CARTESIAN_POINT('Ctrl Pts',(-147.240811016177,4.90175168375792,
131.227787472777));
#111170=CARTESIAN_POINT('Ctrl Pts',(-147.248301351939,4.9095612661273,131.096578407309));
#111171=CARTESIAN_POINT('Ctrl Pts',(-147.256075686058,4.91766695118562,
130.960394510249));
#111172=CARTESIAN_POINT('Ctrl Pts',(-147.263850020177,4.92011487399926,
130.82365739266));
#111173=CARTESIAN_POINT('Ctrl Pts',(-147.271624354297,4.91684660731822,
130.686876565017));
#111174=CARTESIAN_POINT('Ctrl Pts',(-147.279389107244,4.91358236848378,
130.55026430752));
#111175=CARTESIAN_POINT('Ctrl Pts',(-147.287153860191,4.90461596624286,
130.413608834252));
#111176=CARTESIAN_POINT('Ctrl Pts',(-147.294918613138,4.88994078327235,
130.277424000325));
#111177=CARTESIAN_POINT('Ctrl Pts',(-147.302675654023,4.87528017590045,
130.141374427094));
#111178=CARTESIAN_POINT('Ctrl Pts',(-147.310432694908,4.85492211305399,
130.005794949164));
#111179=CARTESIAN_POINT('Ctrl Pts',(-147.318189735793,4.82891200192094,
129.871198284312));
#111180=CARTESIAN_POINT('Ctrl Pts',(-147.325940927033,4.80292150521505,
129.736703119852));
#111181=CARTESIAN_POINT('Ctrl Pts',(-147.333692118273,4.77128751785934,
129.603189675571));
#111182=CARTESIAN_POINT('Ctrl Pts',(-147.341443309513,4.73410709595915,
129.471164057981));
#111183=CARTESIAN_POINT('Ctrl Pts',(-147.34919120629,4.69694247673003,129.3391945548));
#111184=CARTESIAN_POINT('Ctrl Pts',(-147.356939103068,4.65423621736833,
129.208711996121));
#111185=CARTESIAN_POINT('Ctrl Pts',(-147.364686999845,4.60613610381531,
129.080210607959));
#111186=CARTESIAN_POINT('Ctrl Pts',(-147.372433275929,4.55804605176913,
128.951736099517));
#111187=CARTESIAN_POINT('Ctrl Pts',(-147.380179552013,4.50456452670903,
128.825242303214));
#111188=CARTESIAN_POINT('Ctrl Pts',(-147.387925828097,4.44588852532864,
128.701206252606));
#111189=CARTESIAN_POINT('Ctrl Pts',(-147.395672161362,4.38721209081541,
128.577169286392));
#111190=CARTESIAN_POINT('Ctrl Pts',(-147.403418494628,4.32334127065386,
128.45559045549));
#111191=CARTESIAN_POINT('Ctrl Pts',(-147.411164827893,4.254520184245,128.336924485798));
#111192=CARTESIAN_POINT('Ctrl Pts',(-147.418912895896,4.18568368583092,
128.218231941686));
#111193=CARTESIAN_POINT('Ctrl Pts',(-147.426660963899,4.11189491133377,
128.102453894953));
#111194=CARTESIAN_POINT('Ctrl Pts',(-147.434409031902,4.0334424706931,127.990017906006));
#111195=CARTESIAN_POINT('Ctrl Pts',(-147.442165334644,3.95490664986482,
127.877462418752));
#111196=CARTESIAN_POINT('Ctrl Pts',(-147.449921637386,3.87169748562741,
127.768256405885));
#111197=CARTESIAN_POINT('Ctrl Pts',(-147.457677940128,3.78414556207228,
127.662796448629));
#111198=CARTESIAN_POINT('Ctrl Pts',(-147.465438382642,3.69654690941941,
127.557280204219));
#111199=CARTESIAN_POINT('Ctrl Pts',(-147.473198825156,3.60460114088831,
127.455514289314));
#111200=CARTESIAN_POINT('Ctrl Pts',(-147.48095926767,3.5086765202576,127.357859182967));
#111201=CARTESIAN_POINT('Ctrl Pts',(-147.488732167936,3.41259791291007,
127.260047311974));
#111202=CARTESIAN_POINT('Ctrl Pts',(-147.496505068201,3.31252797535881,
127.166359703869));
#111203=CARTESIAN_POINT('Ctrl Pts',(-147.504277968467,3.20886960402755,
127.077117812643));
#111204=CARTESIAN_POINT('Ctrl Pts',(-147.511768304229,3.10897947559666,
126.991120088953));
#111205=CARTESIAN_POINT('Ctrl Pts',(-147.51925863999,3.00575752236836,126.909250659213));
#111206=CARTESIAN_POINT('Ctrl Pts',(-147.526748975752,2.89958888959299,
126.831758531546));
#111207=CARTESIAN_POINT('Ctrl Pts',(-147.534523309871,2.78939484083403,
126.751328266304));
#111208=CARTESIAN_POINT('Ctrl Pts',(-147.54229764399,2.67567719328548,126.675359007466));
#111209=CARTESIAN_POINT('Ctrl Pts',(-147.550071978109,2.55883303118256,
126.604175314388));
#111210=CARTESIAN_POINT('Ctrl Pts',(-147.557836731056,2.44213286906676,
126.533079348851));
#111211=CARTESIAN_POINT('Ctrl Pts',(-147.565601484004,2.32231418969519,
126.466757415701));
#111212=CARTESIAN_POINT('Ctrl Pts',(-147.573366236951,2.19980573710036,
126.40549283352));
#111213=CARTESIAN_POINT('Ctrl Pts',(-147.581123277836,2.07741896162737,
126.344289100185));
#111214=CARTESIAN_POINT('Ctrl Pts',(-147.588880318721,1.95234807679316,
126.288132895494));
#111215=CARTESIAN_POINT('Ctrl Pts',(-147.596637359606,1.82504899027767,
126.237263153576));
#111216=CARTESIAN_POINT('Ctrl Pts',(-147.604388550846,1.69784590099373,
126.186431772926));
#111217=CARTESIAN_POINT('Ctrl Pts',(-147.612139742086,1.56841831615429,
126.140879064528));
#111218=CARTESIAN_POINT('Ctrl Pts',(-147.619890933326,1.43724449869644,
126.100796935264));
#111219=CARTESIAN_POINT('Ctrl Pts',(-147.627638830103,1.30612643361,126.060731841975));
#111220=CARTESIAN_POINT('Ctrl Pts',(-147.63538672688,1.1732639851917,126.0261328173));
#111221=CARTESIAN_POINT('Ctrl Pts',(-147.643134623657,1.03915284169651,
125.997142665975));
#111222=CARTESIAN_POINT('Ctrl Pts',(-147.650880899741,0.905069751361432,
125.968158578766));
#111223=CARTESIAN_POINT('Ctrl Pts',(-147.658627175825,0.769738867387632,
125.94478111379));
#111224=CARTESIAN_POINT('Ctrl Pts',(-147.666373451909,0.633668013140237,
125.927102380439));
#111225=CARTESIAN_POINT('Ctrl Pts',(-147.674119785175,0.497596154449264,
125.909423516588));
#111226=CARTESIAN_POINT('Ctrl Pts',(-147.68186611844,0.360784702291752,
125.897443518675));
#111227=CARTESIAN_POINT('Ctrl Pts',(-147.689612451705,0.223748182943215,
125.891202792589));
#111228=CARTESIAN_POINT('Ctrl Pts',(-147.697360519708,0.0866809752161283,
125.884960668936));
#111229=CARTESIAN_POINT('Ctrl Pts',(-147.705108587711,-0.0506110095109376,
125.884460392432));
#111230=CARTESIAN_POINT('Ctrl Pts',(-147.712856655714,-0.187612051837948,
125.889690254204));
#111231=CARTESIAN_POINT('Ctrl Pts',(-147.720612958456,-0.324758700503263,
125.894925674336));
#111232=CARTESIAN_POINT('Ctrl Pts',(-147.728369261198,-0.461613397770562,
125.905903383354));
#111233=CARTESIAN_POINT('Ctrl Pts',(-147.73612556394,-0.5976637998468,125.922559613341));
#111234=CARTESIAN_POINT('Ctrl Pts',(-147.743886006454,-0.733786816119395,
125.939224733259));
#111235=CARTESIAN_POINT('Ctrl Pts',(-147.751646448968,-0.869104296280502,
125.961574349587));
#111236=CARTESIAN_POINT('Ctrl Pts',(-147.759406891482,-1.00311390352681,
125.989493479311));
#111237=CARTESIAN_POINT('Ctrl Pts',(-147.767179791747,-1.13733863489112,
126.0174574273));
#111238=CARTESIAN_POINT('Ctrl Pts',(-147.774952692013,-1.27025091855097,
126.051008659262));
#111239=CARTESIAN_POINT('Ctrl Pts',(-147.782725592278,-1.40136253080141,
126.089981960758));
#111240=CARTESIAN_POINT('Ctrl Pts',(-147.79021592804,-1.52770790569526,
126.127538484577));
#111241=CARTESIAN_POINT('Ctrl Pts',(-147.797706263802,-1.65238096265682,
126.17012961068));
#111242=CARTESIAN_POINT('Ctrl Pts',(-147.805196599564,-1.77496402368408,
126.217565900432));
#111243=CARTESIAN_POINT('Ctrl Pts',(-147.812971196084,-1.90219915304758,
126.266802413312));
#111244=CARTESIAN_POINT('Ctrl Pts',(-147.820745792604,-2.02758557772969,
126.321415075754));
#111245=CARTESIAN_POINT('Ctrl Pts',(-147.828520389124,-2.15063555386864,
126.381245224889));
#111246=CARTESIAN_POINT('Ctrl Pts',(-147.836285343862,-2.27353292775047,
126.441001174776));
#111247=CARTESIAN_POINT('Ctrl Pts',(-147.8440502986,-2.39409927029319,126.505961567184));
#111248=CARTESIAN_POINT('Ctrl Pts',(-147.851815253339,-2.51186443515346,
126.575918809771));
#111249=CARTESIAN_POINT('Ctrl Pts',(-147.859572435662,-2.62951172170435,
126.645806027903));
#111250=CARTESIAN_POINT('Ctrl Pts',(-147.867329617985,-2.74436307660795,
126.720679943931));
#111251=CARTESIAN_POINT('Ctrl Pts',(-147.875086800309,-2.85597102575763,
126.800286122438));
#111252=CARTESIAN_POINT('Ctrl Pts',(-147.883202294935,-2.97273426191766,
126.883569392955));
#111253=CARTESIAN_POINT('Ctrl Pts',(-147.891317789561,-3.08594690877269,
126.972032362944));
#111254=CARTESIAN_POINT('Ctrl Pts',(-147.899433284187,-3.19512775469468,
127.065331105289));
#111255=CARTESIAN_POINT('Ctrl Pts',(-147.907180842681,-3.29935861542577,
127.154399917109));
#111256=CARTESIAN_POINT('Ctrl Pts',(-147.914928401174,-3.39991488835662,
127.247875374623));
#111257=CARTESIAN_POINT('Ctrl Pts',(-147.922675959667,-3.49641013770257,
127.345415805709));
#111258=CARTESIAN_POINT('Ctrl Pts',(-147.93042189067,-3.59288511677337,
127.442935746965));
#111259=CARTESIAN_POINT('Ctrl Pts',(-147.938167821672,-3.68530049487148,
127.544518685051));
#111260=CARTESIAN_POINT('Ctrl Pts',(-147.945913752675,-3.77330612332224,
127.649785533312));
#111261=CARTESIAN_POINT('Ctrl Pts',(-147.953659733964,-3.86131232310902,
127.755053064968));
#111262=CARTESIAN_POINT('Ctrl Pts',(-147.961405715253,-3.94490846597896,
127.864004254169));
#111263=CARTESIAN_POINT('Ctrl Pts',(-147.969151696543,-4.02378445040055,
127.976226646338));
#111264=CARTESIAN_POINT('Ctrl Pts',(-147.976899405556,-4.1026780279326,
128.088474069458));
#111265=CARTESIAN_POINT('Ctrl Pts',(-147.984647114569,-4.17684912795344,
128.203993827306));
#111266=CARTESIAN_POINT('Ctrl Pts',(-147.992394823582,-4.24603099350536,
128.322344528841));
#111267=CARTESIAN_POINT('Ctrl Pts',(-148.000149654562,-4.3152764534664,
128.440804022512));
#111268=CARTESIAN_POINT('Ctrl Pts',(-148.007904485542,-4.37952332477647,
128.562099317812));
#111269=CARTESIAN_POINT('Ctrl Pts',(-148.015659316523,-4.43855068430019,
128.685764175249));
#111270=CARTESIAN_POINT('Ctrl Pts',(-148.02341832273,-4.49760982435684,
128.80949561427));
#111271=CARTESIAN_POINT('Ctrl Pts',(-148.031177328938,-4.55144370020625,
128.9355987984));
#111272=CARTESIAN_POINT('Ctrl Pts',(-148.038936335146,-4.59987993991676,
129.063588489787));
#111273=CARTESIAN_POINT('Ctrl Pts',(-148.046705067216,-4.64837689413137,
129.1917386154));
#111274=CARTESIAN_POINT('Ctrl Pts',(-148.054473799287,-4.69146258125346,
129.321779599376));
#111275=CARTESIAN_POINT('Ctrl Pts',(-148.062242531358,-4.72901466968156,
129.453211729976));
#111276=CARTESIAN_POINT('Ctrl Pts',(-148.064781244684,-4.74128616861459,
129.49616191778));
#111277=CARTESIAN_POINT('Ctrl Pts',(-148.06731995801,-4.75296714721703,
129.539260588997));
#111278=CARTESIAN_POINT('Ctrl Pts',(-148.069858671336,-4.76405452823417,
129.582490119309));
#111279=CARTESIAN_POINT('Origin',(213.235140564004,0.,130.804360617566));
#111280=CARTESIAN_POINT('',(-150.165071172634,-4.76405452823414,129.582490119309));
#111281=CARTESIAN_POINT('',(-149.820142046519,-4.76405452823404,129.582490119308));
#111282=CARTESIAN_POINT('',(213.235140564004,-4.76405452823405,129.582490119308));
#111283=CARTESIAN_POINT('',(-148.485140564067,-4.91824998862805,130.804695072583));
#111284=CARTESIAN_POINT('Ctrl Pts',(-148.485140564067,-4.91824998862805,
130.804695072582));
#111285=CARTESIAN_POINT('Ctrl Pts',(-148.493297690597,-4.91824013910216,
130.949534971136));
#111286=CARTESIAN_POINT('Ctrl Pts',(-148.501454817127,-4.911827811054,131.094237558735));
#111287=CARTESIAN_POINT('Ctrl Pts',(-148.509611943658,-4.89907498434783,
131.238235438496));
#111288=CARTESIAN_POINT('Ctrl Pts',(-148.517781359492,-4.88630294458163,
131.382450261526));
#111289=CARTESIAN_POINT('Ctrl Pts',(-148.525950775326,-4.86717136828516,
131.525957933976));
#111290=CARTESIAN_POINT('Ctrl Pts',(-148.53412019116,-4.84179358268159,
131.668199702815));
#111291=CARTESIAN_POINT('Ctrl Pts',(-148.542310382095,-4.81635126051228,
131.810803197275));
#111292=CARTESIAN_POINT('Ctrl Pts',(-148.550500573029,-4.78463102363235,
131.952134029516));
#111293=CARTESIAN_POINT('Ctrl Pts',(-148.558690763964,-4.74679697583506,
132.091645175348));
#111294=CARTESIAN_POINT('Ctrl Pts',(-148.566892118927,-4.70891135654272,
132.23134648847));
#111295=CARTESIAN_POINT('Ctrl Pts',(-148.57509347389,-4.66489539047846,
132.369222854717));
#111296=CARTESIAN_POINT('Ctrl Pts',(-148.583294828853,-4.6149619667238,
132.504745605794));
#111297=CARTESIAN_POINT('Ctrl Pts',(-148.591515191756,-4.56491281434578,
132.640582452326));
#111298=CARTESIAN_POINT('Ctrl Pts',(-148.599735554659,-4.50891890724185,
132.774054476094));
#111299=CARTESIAN_POINT('Ctrl Pts',(-148.607955917562,-4.44724062400924,
132.904654381462));
#111300=CARTESIAN_POINT('Ctrl Pts',(-148.612287436656,-4.41474076181952,
132.973470806045));
#111301=CARTESIAN_POINT('Ctrl Pts',(-148.61661895575,-4.38066338322728,
133.04149023043));
#111302=CARTESIAN_POINT('Ctrl Pts',(-148.620950474844,-4.3450514503867,
133.108641623865));
#111303=CARTESIAN_POINT('Ctrl Pts',(-148.628724808963,-4.28113413673123,
133.229166861735));
#111304=CARTESIAN_POINT('Ctrl Pts',(-148.636499143082,-4.21209699704326,
133.347221531257));
#111305=CARTESIAN_POINT('Ctrl Pts',(-148.644273477201,-4.13815516786773,
133.462340088734));
#111306=CARTESIAN_POINT('Ctrl Pts',(-148.652038230148,-4.06430446538848,
133.577316772877));
#111307=CARTESIAN_POINT('Ctrl Pts',(-148.659802983095,-3.98556130961877,
133.689364218908));
#111308=CARTESIAN_POINT('Ctrl Pts',(-148.667567736042,-3.90218734573117,
133.79804012301));
#111309=CARTESIAN_POINT('Ctrl Pts',(-148.675324776927,-3.81889619003987,
133.906608088672));
#111310=CARTESIAN_POINT('Ctrl Pts',(-148.683081817812,-3.73098361564808,
134.011810868207));
#111311=CARTESIAN_POINT('Ctrl Pts',(-148.690838858697,-3.6387551080156,
134.113234191215));
#111312=CARTESIAN_POINT('Ctrl Pts',(-148.698590049937,-3.5465961506183,
134.214581030106));
#111313=CARTESIAN_POINT('Ctrl Pts',(-148.706341241177,-3.45012800018831,
134.312153797371));
#111314=CARTESIAN_POINT('Ctrl Pts',(-148.714092432417,-3.34969681426941,
134.405570735703));
#111315=CARTESIAN_POINT('Ctrl Pts',(-148.721840329194,-3.24930831428347,
134.498947969344));
#111316=CARTESIAN_POINT('Ctrl Pts',(-148.729588225971,-3.14496041461418,
134.588172621444));
#111317=CARTESIAN_POINT('Ctrl Pts',(-148.737336122748,-3.03703641899676,
134.672899469922));
#111318=CARTESIAN_POINT('Ctrl Pts',(-148.745082398832,-2.92913499875266,
134.757608595369));
#111319=CARTESIAN_POINT('Ctrl Pts',(-148.752828674916,-2.81765927778328,
134.837821547315));
#111320=CARTESIAN_POINT('Ctrl Pts',(-148.760574951,-2.70302564545779,134.91323338543));
#111321=CARTESIAN_POINT('Ctrl Pts',(-148.768321284265,-2.58839116693302,
134.988645780219));
#111322=CARTESIAN_POINT('Ctrl Pts',(-148.77606761753,-2.47059905716237,
135.059256775587));
#111323=CARTESIAN_POINT('Ctrl Pts',(-148.783813950796,-2.35009434701988,
135.124804995475));
#111324=CARTESIAN_POINT('Ctrl Pts',(-148.791562018799,-2.22956265068292,
135.190367894432));
#111325=CARTESIAN_POINT('Ctrl Pts',(-148.799310086801,-2.1063174885613,
135.25086557505));
#111326=CARTESIAN_POINT('Ctrl Pts',(-148.807058154804,-1.98082775806655,
135.306083005205));
#111327=CARTESIAN_POINT('Ctrl Pts',(-148.814814457546,-1.85520465559305,
135.361359121102));
#111328=CARTESIAN_POINT('Ctrl Pts',(-148.822570760288,-1.72733257777028,
135.411343618422));
#111329=CARTESIAN_POINT('Ctrl Pts',(-148.83032706303,-1.59770015560841,
135.455869757111));
#111330=CARTESIAN_POINT('Ctrl Pts',(-148.838087505544,-1.46799854471932,
135.500419660741));
#111331=CARTESIAN_POINT('Ctrl Pts',(-148.845847948058,-1.33653509193017,
135.539505289398));
#111332=CARTESIAN_POINT('Ctrl Pts',(-148.853608390572,-1.2038118292568,
135.573010336537));
#111333=CARTESIAN_POINT('Ctrl Pts',(-148.861381290837,-1.07087550741994,
135.606569168952));
#111334=CARTESIAN_POINT('Ctrl Pts',(-148.869154191103,-0.936675717348273,
135.634529438231));
#111335=CARTESIAN_POINT('Ctrl Pts',(-148.876927091368,-0.801723769290029,
135.656826182643));
#111336=CARTESIAN_POINT('Ctrl Pts',(-148.884417427131,-0.67167766445254,
135.678312384235));
#111337=CARTESIAN_POINT('Ctrl Pts',(-148.891907762893,-0.540933443552698,
135.694539640934));
#111338=CARTESIAN_POINT('Ctrl Pts',(-148.899398098656,-0.409949571488562,
135.705495630125));
#111339=CARTESIAN_POINT('Ctrl Pts',(-148.907172432775,-0.273999406117406,
135.716867018976));
#111340=CARTESIAN_POINT('Ctrl Pts',(-148.914946766894,-0.137360408838824,
135.722595550645));
#111341=CARTESIAN_POINT('Ctrl Pts',(-148.922721101013,-0.000540541306493031,
135.722610587862));
#111342=CARTESIAN_POINT('Ctrl Pts',(-148.93048585396,0.136110707967047,
135.722625606546));
#111343=CARTESIAN_POINT('Ctrl Pts',(-148.938250606908,0.272941996765018,
135.716941140966));
#111344=CARTESIAN_POINT('Ctrl Pts',(-148.946015359855,0.409439776752363,
135.705538244597));
#111345=CARTESIAN_POINT('Ctrl Pts',(-148.95377240074,0.545801985220342,
135.694146673746));
#111346=CARTESIAN_POINT('Ctrl Pts',(-148.961529441625,0.681830956984554,
135.677048007156));
#111347=CARTESIAN_POINT('Ctrl Pts',(-148.96928648251,0.817013032271916,
135.654275335125));
#111348=CARTESIAN_POINT('Ctrl Pts',(-148.97703767375,0.952093165704557,
135.631519836144));
#111349=CARTESIAN_POINT('Ctrl Pts',(-148.98478886499,1.08632728988379,135.603098913121));
#111350=CARTESIAN_POINT('Ctrl Pts',(-148.99254005623,1.21920711496585,135.569097449052));
#111351=CARTESIAN_POINT('Ctrl Pts',(-149.000287953007,1.35203046257774,
135.535110436512));
#111352=CARTESIAN_POINT('Ctrl Pts',(-149.008035849784,1.48350027797426,
135.495547697126));
#111353=CARTESIAN_POINT('Ctrl Pts',(-149.015783746561,1.61311893100992,
135.450545114217));
#111354=CARTESIAN_POINT('Ctrl Pts',(-149.023530022645,1.74271047061762,
135.405551944877));
#111355=CARTESIAN_POINT('Ctrl Pts',(-149.031276298729,1.87045124896878,
135.355121323505));
#111356=CARTESIAN_POINT('Ctrl Pts',(-149.039022574814,1.99585964250455,
135.299438742574));
#111357=CARTESIAN_POINT('Ctrl Pts',(-149.046768908079,2.12126896177642,
135.243755750606));
#111358=CARTESIAN_POINT('Ctrl Pts',(-149.054515241344,2.24434550455125,
135.182820880375));
#111359=CARTESIAN_POINT('Ctrl Pts',(-149.06226157461,2.36462881768856,135.116867268814));
#111360=CARTESIAN_POINT('Ctrl Pts',(-149.070009642613,2.4849390674397,135.050898887399));
#111361=CARTESIAN_POINT('Ctrl Pts',(-149.077757710616,2.60245450008479,
134.979909716133));
#111362=CARTESIAN_POINT('Ctrl Pts',(-149.085505778619,2.71674075250271,
134.904178021572));
#111363=CARTESIAN_POINT('Ctrl Pts',(-149.09326208136,2.83114846970988,134.828365838465));
#111364=CARTESIAN_POINT('Ctrl Pts',(-149.101018384102,2.94231982445245,
134.747801279607));
#111365=CARTESIAN_POINT('Ctrl Pts',(-149.108774686844,3.04985041660397,
134.662805317032));
#111366=CARTESIAN_POINT('Ctrl Pts',(-149.116535129358,3.1574384010705,134.577763989553));
#111367=CARTESIAN_POINT('Ctrl Pts',(-149.124295571873,3.26138145482849,
134.488286800491));
#111368=CARTESIAN_POINT('Ctrl Pts',(-149.132056014387,3.36131036531989,
134.394733257069));
#111369=CARTESIAN_POINT('Ctrl Pts',(-149.139828914652,3.4613996905694,134.301029533195));
#111370=CARTESIAN_POINT('Ctrl Pts',(-149.147601814918,3.55746172153592,
134.203236657583));
#111371=CARTESIAN_POINT('Ctrl Pts',(-149.155374715183,3.64916542839605,
134.101749696625));
#111372=CARTESIAN_POINT('Ctrl Pts',(-149.162865050945,3.73753547452559,
134.003952042327));
#111373=CARTESIAN_POINT('Ctrl Pts',(-149.170355386707,3.82185837015966,
133.902724455042));
#111374=CARTESIAN_POINT('Ctrl Pts',(-149.177845722469,3.901875936459,133.7984459936));
#111375=CARTESIAN_POINT('Ctrl Pts',(-149.185620056589,3.98492739310433,
133.6902137826));
#111376=CARTESIAN_POINT('Ctrl Pts',(-149.193394390708,4.0636036846603,133.578351935666));
#111377=CARTESIAN_POINT('Ctrl Pts',(-149.201168724827,4.13757081630893,
133.463249634153));
#111378=CARTESIAN_POINT('Ctrl Pts',(-149.208933477774,4.21144679007823,
133.348289185941));
#111379=CARTESIAN_POINT('Ctrl Pts',(-149.216698230721,4.28062494207831,
133.230096554915));
#111380=CARTESIAN_POINT('Ctrl Pts',(-149.224462983668,4.34481174664333,
133.109093562775));
#111381=CARTESIAN_POINT('Ctrl Pts',(-149.232220024553,4.40893479996935,
132.988210752512));
#111382=CARTESIAN_POINT('Ctrl Pts',(-149.239977065438,4.46807618943849,
132.864523479076));
#111383=CARTESIAN_POINT('Ctrl Pts',(-149.247734106323,4.5219861092022,132.738481785095));
#111384=CARTESIAN_POINT('Ctrl Pts',(-149.255485297563,4.57585537507598,
132.612535140136));
#111385=CARTESIAN_POINT('Ctrl Pts',(-149.263236488803,4.62450087058421,
132.484237966642));
#111386=CARTESIAN_POINT('Ctrl Pts',(-149.270987680043,4.66771926711822,
132.354063784587));
#111387=CARTESIAN_POINT('Ctrl Pts',(-149.278735576821,4.71091929468086,
132.223944930031));
#111388=CARTESIAN_POINT('Ctrl Pts',(-149.286483473598,4.74869668811154,
132.091951023907));
#111389=CARTESIAN_POINT('Ctrl Pts',(-149.294231370375,4.78089678864764,
131.958574184805));
#111390=CARTESIAN_POINT('Ctrl Pts',(-149.301977646459,4.81309015361685,
131.825225245262));
#111391=CARTESIAN_POINT('Ctrl Pts',(-149.309723922543,4.83970845452769,
131.69049432794));
#111392=CARTESIAN_POINT('Ctrl Pts',(-149.317470198627,4.8606474221536,131.554886899592));
#111393=CARTESIAN_POINT('Ctrl Pts',(-149.325216531893,4.88158654434618,
131.41927847022));
#111394=CARTESIAN_POINT('Ctrl Pts',(-149.332962865158,4.89684618993705,
131.282793903298));
#111395=CARTESIAN_POINT('Ctrl Pts',(-149.340709198423,4.90637361746105,
131.145946607299));
#111396=CARTESIAN_POINT('Ctrl Pts',(-149.348457266426,4.91590317858639,
131.009068665298));
#111397=CARTESIAN_POINT('Ctrl Pts',(-149.356205334429,4.91969794010098,
130.871828222526));
#111398=CARTESIAN_POINT('Ctrl Pts',(-149.363953402432,4.91775723166259,
130.734741130852));
#111399=CARTESIAN_POINT('Ctrl Pts',(-149.371709705174,4.91581446061618,
130.597508341386));
#111400=CARTESIAN_POINT('Ctrl Pts',(-149.379466007916,4.90812404829113,
130.460429620142));
#111401=CARTESIAN_POINT('Ctrl Pts',(-149.387222310658,4.8947374494049,130.324018693627));
#111402=CARTESIAN_POINT('Ctrl Pts',(-149.394982753172,4.88134370568778,
130.187534960493));
#111403=CARTESIAN_POINT('Ctrl Pts',(-149.402743195686,4.86224777190991,
130.051720119256));
#111404=CARTESIAN_POINT('Ctrl Pts',(-149.4105036382,4.83755254327486,129.917079121334));
#111405=CARTESIAN_POINT('Ctrl Pts',(-149.418276538466,4.81281767166647,
129.78222198573));
#111406=CARTESIAN_POINT('Ctrl Pts',(-149.426049438731,4.78246562995908,
129.648542840468));
#111407=CARTESIAN_POINT('Ctrl Pts',(-149.433822338997,4.74664986899012,
129.516533733347));
#111408=CARTESIAN_POINT('Ctrl Pts',(-149.441312674759,4.71213610114734,
129.389323489784));
#111409=CARTESIAN_POINT('Ctrl Pts',(-149.44880301052,4.67254904984274,129.263664265993));
#111410=CARTESIAN_POINT('Ctrl Pts',(-149.456293346282,4.62806807603627,
129.139978165702));
#111411=CARTESIAN_POINT('Ctrl Pts',(-149.464067680402,4.58190059258752,
129.011602469322));
#111412=CARTESIAN_POINT('Ctrl Pts',(-149.471842014521,4.53031451003106,
128.884945816362));
#111413=CARTESIAN_POINT('Ctrl Pts',(-149.47961634864,4.47345672530577,128.760499568151));
#111414=CARTESIAN_POINT('Ctrl Pts',(-149.487381101587,4.41666901271879,
128.636206688818));
#111415=CARTESIAN_POINT('Ctrl Pts',(-149.495145854534,4.3546226857735,128.514119146229));
#111416=CARTESIAN_POINT('Ctrl Pts',(-149.502910607481,4.28751397722068,
128.394711896769));
#111417=CARTESIAN_POINT('Ctrl Pts',(-149.510667648366,4.22047192198326,
128.275423244273));
#111418=CARTESIAN_POINT('Ctrl Pts',(-149.518424689251,4.14837768145254,
128.15880992582));
#111419=CARTESIAN_POINT('Ctrl Pts',(-149.526181730136,4.07147486307564,
128.045325369179));
#111420=CARTESIAN_POINT('Ctrl Pts',(-149.533932921376,3.99463003771219,
127.931926392124));
#111421=CARTESIAN_POINT('Ctrl Pts',(-149.541684112616,3.91298407064164,
127.821651802935));
#111422=CARTESIAN_POINT('Ctrl Pts',(-149.549435303856,3.82682544354861,
127.71492861684));
#111423=CARTESIAN_POINT('Ctrl Pts',(-149.557183200633,3.74070343617058,
127.608250790946));
#111424=CARTESIAN_POINT('Ctrl Pts',(-149.56493109741,3.65007282860089,127.505121669552));
#111425=CARTESIAN_POINT('Ctrl Pts',(-149.572678994188,3.55526405730715,
127.405937373572));
#111426=CARTESIAN_POINT('Ctrl Pts',(-149.580425270272,3.46047511796452,
127.306773824808));
#111427=CARTESIAN_POINT('Ctrl Pts',(-149.588171546356,3.36151002327435,
127.211553742584));
#111428=CARTESIAN_POINT('Ctrl Pts',(-149.59591782244,3.25873767666774,127.120638068681));
#111429=CARTESIAN_POINT('Ctrl Pts',(-149.603664155705,3.15596457141888,
127.029721723658));
#111430=CARTESIAN_POINT('Ctrl Pts',(-149.611410488971,3.04938445100277,
126.943110109404));
#111431=CARTESIAN_POINT('Ctrl Pts',(-149.619156822236,2.93940075245949,
126.861125108629));
#111432=CARTESIAN_POINT('Ctrl Pts',(-149.626904890239,2.82939242382964,
126.779121747882));
#111433=CARTESIAN_POINT('Ctrl Pts',(-149.634652958242,2.71597931376613,
126.701747295944));
#111434=CARTESIAN_POINT('Ctrl Pts',(-149.642401026245,2.59959506071738,
126.629281147329));
#111435=CARTESIAN_POINT('Ctrl Pts',(-149.650157328987,2.48308711309935,
126.556737980829));
#111436=CARTESIAN_POINT('Ctrl Pts',(-149.657913631729,2.36360204693584,
126.489113745355));
#111437=CARTESIAN_POINT('Ctrl Pts',(-149.66566993447,2.24159988741659,126.426642832323));
#111438=CARTESIAN_POINT('Ctrl Pts',(-149.673430376985,2.11953261167139,
126.364138576683));
#111439=CARTESIAN_POINT('Ctrl Pts',(-149.681190819499,1.99494592061158,
126.306793287445));
#111440=CARTESIAN_POINT('Ctrl Pts',(-149.688951262013,1.868320261537,126.254793334535));
#111441=CARTESIAN_POINT('Ctrl Pts',(-149.696724162278,1.74149133171317,
126.202709906684));
#111442=CARTESIAN_POINT('Ctrl Pts',(-149.704497062544,1.61261726088133,
126.155989095678));
#111443=CARTESIAN_POINT('Ctrl Pts',(-149.712269962809,1.48219496671664,
126.114767762835));
#111444=CARTESIAN_POINT('Ctrl Pts',(-149.719760298571,1.35651385145912,
126.075044929273));
#111445=CARTESIAN_POINT('Ctrl Pts',(-149.727250634333,1.22939541943093,
126.040428756842));
#111446=CARTESIAN_POINT('Ctrl Pts',(-149.734740970095,1.10129174743127,
126.010996501463));
#111447=CARTESIAN_POINT('Ctrl Pts',(-149.742515304215,0.968330985770924,
125.980448313176));
#111448=CARTESIAN_POINT('Ctrl Pts',(-149.750289638334,0.833887618851214,
125.955388130739));
#111449=CARTESIAN_POINT('Ctrl Pts',(-149.758063972453,0.69845444425737,
125.935957958398));
#111450=CARTESIAN_POINT('Ctrl Pts',(-149.7658287254,0.56318817894757,125.916551732007));
#111451=CARTESIAN_POINT('Ctrl Pts',(-149.773593478347,0.42693491638807,
125.902761765186));
#111452=CARTESIAN_POINT('Ctrl Pts',(-149.781358231294,0.290200319434784,
125.894679687292));
#111453=CARTESIAN_POINT('Ctrl Pts',(-149.789115272179,0.15360152921044,
125.886605636631));
#111454=CARTESIAN_POINT('Ctrl Pts',(-149.796872313064,0.0165227437279239,
125.884228215942));
#111455=CARTESIAN_POINT('Ctrl Pts',(-149.804629353949,-0.120522879613008,
125.887587560164));
#111456=CARTESIAN_POINT('Ctrl Pts',(-149.812380545189,-0.257465155783134,
125.890944371079));
#111457=CARTESIAN_POINT('Ctrl Pts',(-149.820131736429,-0.394373930321906,
125.900029326446));
#111458=CARTESIAN_POINT('Ctrl Pts',(-149.827882927669,-0.530734011826448,
125.914830530616));
#111459=CARTESIAN_POINT('Ctrl Pts',(-149.835630824446,-0.667036136659012,
125.929625443879));
#111460=CARTESIAN_POINT('Ctrl Pts',(-149.843378721224,-0.802789644424176,
125.950131731637));
#111461=CARTESIAN_POINT('Ctrl Pts',(-149.851126618001,-0.937482658395131,
125.976285501362));
#111462=CARTESIAN_POINT('Ctrl Pts',(-149.858872894085,-1.07214749749121,
126.002433800282));
#111463=CARTESIAN_POINT('Ctrl Pts',(-149.866619170169,-1.20575190047616,
126.034227156961));
#111464=CARTESIAN_POINT('Ctrl Pts',(-149.874365446253,-1.33779279549247,
126.071550300341));
#111465=CARTESIAN_POINT('Ctrl Pts',(-149.882111779518,-1.46983466520449,
126.108873719233));
#111466=CARTESIAN_POINT('Ctrl Pts',(-149.889858112784,-1.60031262769362,
126.151726899934));
#111467=CARTESIAN_POINT('Ctrl Pts',(-149.897604446049,-1.7287378063454,
126.199944404905));
#111468=CARTESIAN_POINT('Ctrl Pts',(-149.905352514052,-1.85719174492533,
126.248172707852));
#111469=CARTESIAN_POINT('Ctrl Pts',(-149.913100582055,-1.98359161895713,
126.301767588127));
#111470=CARTESIAN_POINT('Ctrl Pts',(-149.920848650058,-2.10746797375143,
126.360515232979));
#111471=CARTESIAN_POINT('Ctrl Pts',(-149.9286049528,-2.23147598580992,126.419325315528));
#111472=CARTESIAN_POINT('Ctrl Pts',(-149.936361255542,-2.35295476717775,
126.483298934598));
#111473=CARTESIAN_POINT('Ctrl Pts',(-149.944117558284,-2.47145846286881,
126.552175752251));
#111474=CARTESIAN_POINT('Ctrl Pts',(-149.951878000798,-2.59002540755066,
126.621089331536));
#111475=CARTESIAN_POINT('Ctrl Pts',(-149.959638443312,-2.70561377320711,
126.694911113634));
#111476=CARTESIAN_POINT('Ctrl Pts',(-149.967398885826,-2.81780706803946,
126.773337622121));
#111477=CARTESIAN_POINT('Ctrl Pts',(-149.975171786092,-2.93018046550842,
126.851890027802));
#111478=CARTESIAN_POINT('Ctrl Pts',(-149.982944686357,-3.03914759021873,
126.935061693928));
#111479=CARTESIAN_POINT('Ctrl Pts',(-149.990717586623,-3.1443247007252,
127.022508526472));
#111480=CARTESIAN_POINT('Ctrl Pts',(-149.998207922385,-3.24567835833818,
127.106776446387));
#111481=CARTESIAN_POINT('Ctrl Pts',(-150.005698258146,-3.34351254213525,
127.195013896687));
#111482=CARTESIAN_POINT('Ctrl Pts',(-150.013188593908,-3.43751789597122,
127.286882291069));
#111483=CARTESIAN_POINT('Ctrl Pts',(-150.02085013133,-3.53367186812148,
127.380850460693));
#111484=CARTESIAN_POINT('Ctrl Pts',(-150.028511668752,-3.62614329675247,
127.478933995053));
#111485=CARTESIAN_POINT('Ctrl Pts',(-150.036173206173,-3.71455151127092,
127.580808208714));
#111486=CARTESIAN_POINT('Ctrl Pts',(-150.043825811081,-3.80285665148715,
127.682563648192));
#111487=CARTESIAN_POINT('Ctrl Pts',(-150.051478415988,-3.88710773373148,
127.788100680055));
#111488=CARTESIAN_POINT('Ctrl Pts',(-150.059131020896,-3.96695892539313,
127.897056033119));
#111489=CARTESIAN_POINT('Ctrl Pts',(-150.066776475311,-4.04673550516101,
128.005909579748));
#111490=CARTESIAN_POINT('Ctrl Pts',(-150.074421929726,-4.12212013268671,
128.118174773394));
#111491=CARTESIAN_POINT('Ctrl Pts',(-150.082067384141,-4.19280585805743,
128.233453754387));
#111492=CARTESIAN_POINT('Ctrl Pts',(-150.089707243863,-4.26343985792733,
128.348648377994));
#111493=CARTESIAN_POINT('Ctrl Pts',(-150.097347103585,-4.32938158696644,
128.46685205875));
#111494=CARTESIAN_POINT('Ctrl Pts',(-150.104986963306,-4.39036657259015,
128.587636814116));
#111495=CARTESIAN_POINT('Ctrl Pts',(-150.112623519553,-4.45132518831032,
128.708369342161));
#111496=CARTESIAN_POINT('Ctrl Pts',(-150.1202600758,-4.50733114304092,128.83168036537));
#111497=CARTESIAN_POINT('Ctrl Pts',(-150.127896632047,-4.55816544276777,
128.957116492157));
#111498=CARTESIAN_POINT('Ctrl Pts',(-150.135532825893,-4.60899733009657,
129.082546666234));
#111499=CARTESIAN_POINT('Ctrl Pts',(-150.143169019738,-4.65465789211696,
129.210101372672));
#111500=CARTESIAN_POINT('Ctrl Pts',(-150.150805213584,-4.69497604676473,
129.339306699512));
#111501=CARTESIAN_POINT('Ctrl Pts',(-150.155560533267,-4.72008354380697,
129.419767285812));
#111502=CARTESIAN_POINT('Ctrl Pts',(-150.160315852951,-4.74312022574812,
129.500867591638));
#111503=CARTESIAN_POINT('Ctrl Pts',(-150.165071172634,-4.76405452823413,
129.582490119309));
#111504=CARTESIAN_POINT('Ctrl Pts',(-148.415413529701,-4.76405452823396,
129.582490119308));
#111505=CARTESIAN_POINT('Ctrl Pts',(-148.423504095412,-4.79956581021559,
129.720948068795));
#111506=CARTESIAN_POINT('Ctrl Pts',(-148.431594661122,-4.82907237912164,
129.861093556804));
#111507=CARTESIAN_POINT('Ctrl Pts',(-148.439685226832,-4.85242460871388,
130.002388997589));
#111508=CARTESIAN_POINT('Ctrl Pts',(-148.447762663752,-4.87573894397912,
130.143455154245));
#111509=CARTESIAN_POINT('Ctrl Pts',(-148.455840100671,-4.89291879809602,
130.285667209157));
#111510=CARTESIAN_POINT('Ctrl Pts',(-148.46391753759,-4.90386518617971,
130.428475930096));
#111511=CARTESIAN_POINT('Ctrl Pts',(-148.47099187973,-4.91345219939669,
130.55354998052));
#111512=CARTESIAN_POINT('Ctrl Pts',(-148.478066221871,-4.91825853069369,
130.679081352824));
#111513=CARTESIAN_POINT('Ctrl Pts',(-148.485140564011,-4.91824998862812,
130.804695071591));
#111514=CARTESIAN_POINT('',(-148.139859436045,-4.9182480226444,130.7999503733));
#111515=CARTESIAN_POINT('Ctrl Pts',(-148.069858671336,-4.76405452823417,
129.582490119309));
#111516=CARTESIAN_POINT('Ctrl Pts',(-148.074453855349,-4.78412318091859,
129.660737491541));
#111517=CARTESIAN_POINT('Ctrl Pts',(-148.079049039363,-4.80224668583714,
129.739413610789));
#111518=CARTESIAN_POINT('Ctrl Pts',(-148.083644223377,-4.81841171100897,
129.818413536982));
#111519=CARTESIAN_POINT('Ctrl Pts',(-148.094752159043,-4.85748741703195,
130.009380012998));
#111520=CARTESIAN_POINT('Ctrl Pts',(-148.105860094709,-4.88522080271822,
130.202739816459));
#111521=CARTESIAN_POINT('Ctrl Pts',(-148.116968030375,-4.90138261484219,
130.397382085672));
#111522=CARTESIAN_POINT('Ctrl Pts',(-148.124598498914,-4.91248478563783,
130.531089351929));
#111523=CARTESIAN_POINT('Ctrl Pts',(-148.132228967454,-4.91812737123165,
130.665401488351));
#111524=CARTESIAN_POINT('Ctrl Pts',(-148.139859435993,-4.91824802264357,
130.79995037238));
#111525=CARTESIAN_POINT('Ctrl Pts',(-148.139859436045,-4.9182480226444,
130.799950373301));
#111526=CARTESIAN_POINT('Ctrl Pts',(-148.147507635122,-4.91836895438269,
130.934811901826));
#111527=CARTESIAN_POINT('Ctrl Pts',(-148.155155834198,-4.91293873375263,
131.069852929669));
#111528=CARTESIAN_POINT('Ctrl Pts',(-148.162804033275,-4.90193984041586,
131.204571641207));
#111529=CARTESIAN_POINT('Ctrl Pts',(-148.170445879266,-4.89095008346705,
131.339178446721));
#111530=CARTESIAN_POINT('Ctrl Pts',(-148.178087725256,-4.87440088783354,
131.473463068676));
#111531=CARTESIAN_POINT('Ctrl Pts',(-148.185729571247,-4.85232679620336,
131.606923839591));
#111532=CARTESIAN_POINT('Ctrl Pts',(-148.193367541118,-4.83026390105813,
131.740316916145));
#111533=CARTESIAN_POINT('Ctrl Pts',(-148.20100551099,-4.80268174754368,
131.872886575743));
#111534=CARTESIAN_POINT('Ctrl Pts',(-148.208643480861,-4.76966666205955,
132.004136844759));
#111535=CARTESIAN_POINT('Ctrl Pts',(-148.216279549579,-4.73665979430195,
132.135354444503));
#111536=CARTESIAN_POINT('Ctrl Pts',(-148.223915618296,-4.69822278116591,
132.265252915777));
#111537=CARTESIAN_POINT('Ctrl Pts',(-148.231551687014,-4.65449283594518,
132.393347559814));
#111538=CARTESIAN_POINT('Ctrl Pts',(-148.239187619417,-4.61076367136765,
132.521439917175));
#111539=CARTESIAN_POINT('Ctrl Pts',(-148.24682355182,-4.56174189304386,
132.647728129766));
#111540=CARTESIAN_POINT('Ctrl Pts',(-148.254459484222,-4.50761407650963,
132.771744260822));
#111541=CARTESIAN_POINT('Ctrl Pts',(-148.262097044832,-4.45347471832187,
132.895786835791));
#111542=CARTESIAN_POINT('Ctrl Pts',(-148.269734605442,-4.39422731869069,
133.017555996583));
#111543=CARTESIAN_POINT('Ctrl Pts',(-148.277372166051,-4.33010568450893,
133.136605849844));
#111544=CARTESIAN_POINT('Ctrl Pts',(-148.285017568631,-4.26591821256074,
133.255777939173));
#111545=CARTESIAN_POINT('Ctrl Pts',(-148.292662971211,-4.19684670479271,
133.372224790697));
#111546=CARTESIAN_POINT('Ctrl Pts',(-148.300308373791,-4.12316998861898,
133.485526839092));
#111547=CARTESIAN_POINT('Ctrl Pts',(-148.307957985488,-4.04945271029629,
133.598891265058));
#111548=CARTESIAN_POINT('Ctrl Pts',(-148.315607597185,-3.97112540938517,
133.709107113066));
#111549=CARTESIAN_POINT('Ctrl Pts',(-148.323257208882,-3.88850815360802,
133.815786758421));
#111550=CARTESIAN_POINT('Ctrl Pts',(-148.330918363464,-3.80576623248856,
133.922627378071));
#111551=CARTESIAN_POINT('Ctrl Pts',(-148.338579518046,-3.71872168967319,
134.025920832434));
#111552=CARTESIAN_POINT('Ctrl Pts',(-148.346240672628,-3.62773282847055,
134.125314936393));
#111553=CARTESIAN_POINT('Ctrl Pts',(-148.351524397482,-3.56497987103348,
134.193864799451));
#111554=CARTESIAN_POINT('Ctrl Pts',(-148.356808122337,-3.50035154979511,
134.260560695635));
#111555=CARTESIAN_POINT('Ctrl Pts',(-148.362091847191,-3.43397442841546,
134.325298374398));
#111556=CARTESIAN_POINT('Ctrl Pts',(-148.36986618131,-3.3363088735842,134.42055169638));
#111557=CARTESIAN_POINT('Ctrl Pts',(-148.377640515429,-3.23452234261106,
134.511889168235));
#111558=CARTESIAN_POINT('Ctrl Pts',(-148.385414849548,-3.12896184513419,
134.598933167168));
#111559=CARTESIAN_POINT('Ctrl Pts',(-148.393179602495,-3.02353144153626,
134.685869892152));
#111560=CARTESIAN_POINT('Ctrl Pts',(-148.400944355442,-2.91433662443569,
134.768523426024));
#111561=CARTESIAN_POINT('Ctrl Pts',(-148.408709108389,-2.80176159511557,
134.846552476773));
#111562=CARTESIAN_POINT('Ctrl Pts',(-148.416466149274,-2.6892983769016,
134.924504027968));
#111563=CARTESIAN_POINT('Ctrl Pts',(-148.424223190159,-2.57346194684135,
134.997840015242));
#111564=CARTESIAN_POINT('Ctrl Pts',(-148.431980231044,-2.45466969331219,
135.066259227251));
#111565=CARTESIAN_POINT('Ctrl Pts',(-148.439731422285,-2.33596702194565,
135.1346268438));
#111566=CARTESIAN_POINT('Ctrl Pts',(-148.447482613525,-2.2143133012376,
135.198084870854));
#111567=CARTESIAN_POINT('Ctrl Pts',(-148.455233804765,-2.09015472195155,
135.256375476122));
#111568=CARTESIAN_POINT('Ctrl Pts',(-148.462981701542,-1.96604891337324,
135.314641306328));
#111569=CARTESIAN_POINT('Ctrl Pts',(-148.470729598319,-1.83944071685019,
135.3677439172));
#111570=CARTESIAN_POINT('Ctrl Pts',(-148.478477495096,-1.71080053991821,
135.415471608977));
#111571=CARTESIAN_POINT('Ctrl Pts',(-148.48622377118,-1.58218727173843,
135.463189317151));
#111572=CARTESIAN_POINT('Ctrl Pts',(-148.493970047264,-1.45154323490816,
135.505534206648));
#111573=CARTESIAN_POINT('Ctrl Pts',(-148.501716323348,-1.31935804314362,
135.542343038016));
#111574=CARTESIAN_POINT('Ctrl Pts',(-148.509462656614,-1.18717187561784,
135.579152141098));
#111575=CARTESIAN_POINT('Ctrl Pts',(-148.517208989879,-1.05344490709213,
135.610424999627));
#111576=CARTESIAN_POINT('Ctrl Pts',(-148.524955323144,-0.918680723296531,
135.636048603265));
#111577=CARTESIAN_POINT('Ctrl Pts',(-148.532703391147,-0.783886359996543,
135.66167794513));
#111578=CARTESIAN_POINT('Ctrl Pts',(-148.54045145915,-0.648054703232639,
135.681655441664));
#111579=CARTESIAN_POINT('Ctrl Pts',(-148.548199527153,-0.51169791507903,
135.695919500602));
#111580=CARTESIAN_POINT('Ctrl Pts',(-148.555955829895,-0.37519620530812,
135.710198719551));
#111581=CARTESIAN_POINT('Ctrl Pts',(-148.563712132637,-0.23816863871437,
135.718752330071));
#111582=CARTESIAN_POINT('Ctrl Pts',(-148.571468435379,-0.101131423311902,
135.72157075114));
#111583=CARTESIAN_POINT('Ctrl Pts',(-148.579228877893,0.035978932978537,
135.724390676485));
#111584=CARTESIAN_POINT('Ctrl Pts',(-148.586989320407,0.173098557653976,
135.721469321314));
#111585=CARTESIAN_POINT('Ctrl Pts',(-148.594749762921,0.309713880796437,
135.712849221458));
#111586=CARTESIAN_POINT('Ctrl Pts',(-148.602522663187,0.446548510983743,
135.704215283853));
#111587=CARTESIAN_POINT('Ctrl Pts',(-148.610295563452,0.582876832859398,
135.689864361635));
#111588=CARTESIAN_POINT('Ctrl Pts',(-148.618068463718,0.718192118744943,
135.669890716442));
#111589=CARTESIAN_POINT('Ctrl Pts',(-148.62555879948,0.848588353145884,
135.650643163564));
#111590=CARTESIAN_POINT('Ctrl Pts',(-148.633049135241,0.978043622995952,
135.62617464783));
#111591=CARTESIAN_POINT('Ctrl Pts',(-148.640539471003,1.10611759491657,
135.596613420655));
#111592=CARTESIAN_POINT('Ctrl Pts',(-148.648313805122,1.23904753041373,
135.565931370566));
#111593=CARTESIAN_POINT('Ctrl Pts',(-148.656088139241,1.37091043856259,
135.529665613894));
#111594=CARTESIAN_POINT('Ctrl Pts',(-148.663862473361,1.50120104742373,
135.487903985329));
#111595=CARTESIAN_POINT('Ctrl Pts',(-148.671627226308,1.63133108475315,
135.446193824239));
#111596=CARTESIAN_POINT('Ctrl Pts',(-148.679391979255,1.75989230954324,
135.399001386037));
#111597=CARTESIAN_POINT('Ctrl Pts',(-148.687156732202,1.88638991298052,
135.346465433475));
#111598=CARTESIAN_POINT('Ctrl Pts',(-148.694913773087,2.0127618772151,135.293981660362));
#111599=CARTESIAN_POINT('Ctrl Pts',(-148.702670813972,2.13707394020085,
135.236165083547));
#111600=CARTESIAN_POINT('Ctrl Pts',(-148.710427854857,2.2588470756914,135.173204051604));
#111601=CARTESIAN_POINT('Ctrl Pts',(-148.718179046097,2.38052838111338,
135.110290499066));
#111602=CARTESIAN_POINT('Ctrl Pts',(-148.725930237337,2.49967422409891,
135.042240392093));
#111603=CARTESIAN_POINT('Ctrl Pts',(-148.733681428577,2.61582650603231,
134.969289758961));
#111604=CARTESIAN_POINT('Ctrl Pts',(-148.741429325354,2.73192942014727,
134.896370131793));
#111605=CARTESIAN_POINT('Ctrl Pts',(-148.749177222131,2.84504097341543,
134.818554328608));
#111606=CARTESIAN_POINT('Ctrl Pts',(-148.756925118908,2.95472879006864,
134.736123687696));
#111607=CARTESIAN_POINT('Ctrl Pts',(-148.764671394993,3.0643936623952,134.653710289497));
#111608=CARTESIAN_POINT('Ctrl Pts',(-148.772417671077,3.17063591026333,
134.566684208386));
#111609=CARTESIAN_POINT('Ctrl Pts',(-148.780163947161,3.27305354752491,
134.475369135335));
#111610=CARTESIAN_POINT('Ctrl Pts',(-148.787910280426,3.37547194081008,
134.384053388218));
#111611=CARTESIAN_POINT('Ctrl Pts',(-148.795656613691,3.47406537533444,
134.28844884617));
#111612=CARTESIAN_POINT('Ctrl Pts',(-148.803402946957,3.56846657191188,
134.188918105281));
#111613=CARTESIAN_POINT('Ctrl Pts',(-148.81115101496,3.66288890898238,134.089365075173));
#111614=CARTESIAN_POINT('Ctrl Pts',(-148.818899082963,3.75311687096139,
133.98588438024));
#111615=CARTESIAN_POINT('Ctrl Pts',(-148.826647150966,3.83882180242114,
133.878873624817));
#111616=CARTESIAN_POINT('Ctrl Pts',(-148.834403453707,3.92461782210253,
133.771749137089));
#111617=CARTESIAN_POINT('Ctrl Pts',(-148.842159756449,4.0058809637121,133.661087399912));
#111618=CARTESIAN_POINT('Ctrl Pts',(-148.849916059191,4.08232414342432,
133.54731753493));
#111619=CARTESIAN_POINT('Ctrl Pts',(-148.857676501705,4.15880812316321,
133.433486947546));
#111620=CARTESIAN_POINT('Ctrl Pts',(-148.86543694422,4.23046681079151,133.31654526005));
#111621=CARTESIAN_POINT('Ctrl Pts',(-148.873197386734,4.2970583958223,133.196947545014));
#111622=CARTESIAN_POINT('Ctrl Pts',(-148.880970286999,4.36375687957711,
133.077157841108));
#111623=CARTESIAN_POINT('Ctrl Pts',(-148.888743187265,4.42537183025414,
132.954703938896));
#111624=CARTESIAN_POINT('Ctrl Pts',(-148.89651608753,4.48170865415154,132.830063113443));
#111625=CARTESIAN_POINT('Ctrl Pts',(-148.904006423292,4.53599749259683,
132.709953295946));
#111626=CARTESIAN_POINT('Ctrl Pts',(-148.911496759054,4.58538517280245,
132.587813080622));
#111627=CARTESIAN_POINT('Ctrl Pts',(-148.918987094816,4.62974158536802,
132.464082255436));
#111628=CARTESIAN_POINT('Ctrl Pts',(-148.926761428936,4.67577978479752,
132.335660138407));
#111629=CARTESIAN_POINT('Ctrl Pts',(-148.934535763055,4.71654349939442,
132.205117611908));
#111630=CARTESIAN_POINT('Ctrl Pts',(-148.942310097174,4.75183351514652,
132.072927252328));
#111631=CARTESIAN_POINT('Ctrl Pts',(-148.950074850121,4.78708003910796,
131.940899805552));
#111632=CARTESIAN_POINT('Ctrl Pts',(-148.957839603068,4.81686618657105,
131.807228940505));
#111633=CARTESIAN_POINT('Ctrl Pts',(-148.965604356015,4.84104124631871,
131.672405958514));
#111634=CARTESIAN_POINT('Ctrl Pts',(-148.9733613969,4.86519229505628,131.537716884608));
#111635=CARTESIAN_POINT('Ctrl Pts',(-148.981118437785,4.88374327806583,
131.4018783533));
#111636=CARTESIAN_POINT('Ctrl Pts',(-148.98887547867,4.89659373295067,131.265395189944));
#111637=CARTESIAN_POINT('Ctrl Pts',(-148.99662666991,4.90943449720761,131.129014949603));
#111638=CARTESIAN_POINT('Ctrl Pts',(-149.00437786115,4.91658325336494,130.991991432478));
#111639=CARTESIAN_POINT('Ctrl Pts',(-149.01212905239,4.91799096520328,130.854837628956));
#111640=CARTESIAN_POINT('Ctrl Pts',(-149.019876949168,4.91939807872653,
130.717742119461));
#111641=CARTESIAN_POINT('Ctrl Pts',(-149.027624845945,4.91506899709357,
130.580516823833));
#111642=CARTESIAN_POINT('Ctrl Pts',(-149.035372742722,4.90500670851211,
130.443677582269));
#111643=CARTESIAN_POINT('Ctrl Pts',(-149.043119018806,4.89494652474449,
130.306866964524));
#111644=CARTESIAN_POINT('Ctrl Pts',(-149.05086529489,4.87915554808234,130.170442629885));
#111645=CARTESIAN_POINT('Ctrl Pts',(-149.058611570974,4.85768882557762,
130.03491774356));
#111646=CARTESIAN_POINT('Ctrl Pts',(-149.066357904239,4.83622194461039,
129.899391856821));
#111647=CARTESIAN_POINT('Ctrl Pts',(-149.074104237505,4.80907929536316,
129.764765817797));
#111648=CARTESIAN_POINT('Ctrl Pts',(-149.08185057077,4.77636741682319,129.631544620911));
#111649=CARTESIAN_POINT('Ctrl Pts',(-149.089598638773,4.74364821268478,
129.498293590062));
#111650=CARTESIAN_POINT('Ctrl Pts',(-149.097346706776,4.70535739070186,
129.366448406991));
#111651=CARTESIAN_POINT('Ctrl Pts',(-149.105094774779,4.66165182037551,
129.236500493674));
#111652=CARTESIAN_POINT('Ctrl Pts',(-149.112851077521,4.61789979924897,
129.106414470169));
#111653=CARTESIAN_POINT('Ctrl Pts',(-149.120607380263,4.56872165866055,
128.978230115633));
#111654=CARTESIAN_POINT('Ctrl Pts',(-149.128363683005,4.51432325498414,
128.852420912552));
#111655=CARTESIAN_POINT('Ctrl Pts',(-149.136124125519,4.45989581724178,
128.726544561311));
#111656=CARTESIAN_POINT('Ctrl Pts',(-149.143884568033,4.40024273461425,
128.603046239379));
#111657=CARTESIAN_POINT('Ctrl Pts',(-149.151645010547,4.33561616807006,
128.482375366607));
#111658=CARTESIAN_POINT('Ctrl Pts',(-149.159417910813,4.27088585722397,
128.361510782238));
#111659=CARTESIAN_POINT('Ctrl Pts',(-149.167190811078,4.20116630708807,
128.243483053959));
#111660=CARTESIAN_POINT('Ctrl Pts',(-149.174963711343,4.12675388004265,
128.128713877794));
#111661=CARTESIAN_POINT('Ctrl Pts',(-149.182454047105,4.05504653215453,
128.018116850269));
#111662=CARTESIAN_POINT('Ctrl Pts',(-149.189944382867,3.97898175732552,
127.910545826359));
#111663=CARTESIAN_POINT('Ctrl Pts',(-149.197434718629,3.89885923431622,
127.806347986924));
#111664=CARTESIAN_POINT('Ctrl Pts',(-149.205209052748,3.81569884149349,
127.698199454736));
#111665=CARTESIAN_POINT('Ctrl Pts',(-149.212983386868,3.72790350024213,
127.593342362906));
#111666=CARTESIAN_POINT('Ctrl Pts',(-149.220757720987,3.63576312242217,
127.492199754906));
#111667=CARTESIAN_POINT('Ctrl Pts',(-149.228522473934,3.54373629938355,
127.391181796132));
#111668=CARTESIAN_POINT('Ctrl Pts',(-149.236287226881,3.4473753551353,127.293869499034));
#111669=CARTESIAN_POINT('Ctrl Pts',(-149.244051979828,3.34701217230263,
127.200655221594));
#111670=CARTESIAN_POINT('Ctrl Pts',(-149.251809020713,3.24674867159775,
127.107533525888));
#111671=CARTESIAN_POINT('Ctrl Pts',(-149.259566061598,3.14249112751129,
127.018502014279));
#111672=CARTESIAN_POINT('Ctrl Pts',(-149.267323102483,3.03460996153094,
126.93391807906));
#111673=CARTESIAN_POINT('Ctrl Pts',(-149.275074293723,2.92681014957661,
126.849397929244));
#111674=CARTESIAN_POINT('Ctrl Pts',(-149.282825484963,2.81539246123304,
126.769318920234));
#111675=CARTESIAN_POINT('Ctrl Pts',(-149.290576676203,2.70076198456721,
126.693999591425));
#111676=CARTESIAN_POINT('Ctrl Pts',(-149.29832457298,2.58618022891199,126.61871227534));
#111677=CARTESIAN_POINT('Ctrl Pts',(-149.306072469758,2.46838872691099,
126.548180830123));
#111678=CARTESIAN_POINT('Ctrl Pts',(-149.313820366535,2.34782308473086,
126.482681565935));
#111679=CARTESIAN_POINT('Ctrl Pts',(-149.321566642619,2.22728266228398,
126.417196002782));
#111680=CARTESIAN_POINT('Ctrl Pts',(-149.329312918703,2.10396959721172,
126.356740713449));
#111681=CARTESIAN_POINT('Ctrl Pts',(-149.337059194787,1.97834538421457,
126.301546763623));
#111682=CARTESIAN_POINT('Ctrl Pts',(-149.344805528052,1.8527202438882,126.246352406369));
#111683=CARTESIAN_POINT('Ctrl Pts',(-149.352551861318,1.72478427953526,
126.196419623384));
#111684=CARTESIAN_POINT('Ctrl Pts',(-149.360298194583,1.59501994419185,
126.151931742222));
#111685=CARTESIAN_POINT('Ctrl Pts',(-149.368046262586,1.46522654902508,
126.107433898309));
#111686=CARTESIAN_POINT('Ctrl Pts',(-149.375794330589,1.3336043378713,126.068383509348));
#111687=CARTESIAN_POINT('Ctrl Pts',(-149.383542398592,1.20065154975243,
126.034914222168));
#111688=CARTESIAN_POINT('Ctrl Pts',(-149.391298701334,1.06755745782838,
126.001409363431));
#111689=CARTESIAN_POINT('Ctrl Pts',(-149.399055004076,0.933130343757175,
125.973497551202));
#111690=CARTESIAN_POINT('Ctrl Pts',(-149.406811306818,0.797879832161182,
125.951261521532));
#111691=CARTESIAN_POINT('Ctrl Pts',(-149.414571749332,0.662557133294468,
125.929013623823));
#111692=CARTESIAN_POINT('Ctrl Pts',(-149.422332191846,0.526410549130532,
125.912447592082));
#111693=CARTESIAN_POINT('Ctrl Pts',(-149.43009263436,0.38995448848199,125.901594198552));
#111694=CARTESIAN_POINT('Ctrl Pts',(-149.437865534626,0.253279376451267,
125.890723382191));
#111695=CARTESIAN_POINT('Ctrl Pts',(-149.445638434891,0.116294186088119,
125.885583544159));
#111696=CARTESIAN_POINT('Ctrl Pts',(-149.453411335157,-0.0204861066943495,
125.886153283391));
#111697=CARTESIAN_POINT('Ctrl Pts',(-149.460901670918,-0.152294091303552,
125.886702311167));
#111698=CARTESIAN_POINT('Ctrl Pts',(-149.46839200668,-0.283911509068489,
125.892552994506));
#111699=CARTESIAN_POINT('Ctrl Pts',(-149.475882342442,-0.414884283208473,
125.903640864913));
#111700=CARTESIAN_POINT('Ctrl Pts',(-149.483656676561,-0.55082292988965,
125.915149135296));
#111701=CARTESIAN_POINT('Ctrl Pts',(-149.491431010681,-0.686497697419421,
125.932336022973));
#111702=CARTESIAN_POINT('Ctrl Pts',(-149.4992053448,-0.82139596290188,125.955186282215));
#111703=CARTESIAN_POINT('Ctrl Pts',(-149.506970097747,-0.956127978328336,
125.978008380554));
#111704=CARTESIAN_POINT('Ctrl Pts',(-149.514734850694,-1.09008501401763,
126.006479898467));
#111705=CARTESIAN_POINT('Ctrl Pts',(-149.522499603641,-1.2227575774215,
126.040533692776));
#111706=CARTESIAN_POINT('Ctrl Pts',(-149.530256644526,-1.35529836856504,
126.074553664375));
#111707=CARTESIAN_POINT('Ctrl Pts',(-149.538013685411,-1.48655684999594,
126.114144782202));
#111708=CARTESIAN_POINT('Ctrl Pts',(-149.545770726296,-1.6160321155932,
126.159188579431));
#111709=CARTESIAN_POINT('Ctrl Pts',(-149.553521917536,-1.74540974288462,
126.204198408782));
#111710=CARTESIAN_POINT('Ctrl Pts',(-149.561273108776,-1.87300646319637,
126.254652605089));
#111711=CARTESIAN_POINT('Ctrl Pts',(-149.569024300016,-1.99833532031902,
126.310382534613));
#111712=CARTESIAN_POINT('Ctrl Pts',(-149.576772196793,-2.123610909335,126.36608877743));
#111713=CARTESIAN_POINT('Ctrl Pts',(-149.58452009357,-2.24662019579938,
126.427066135125));
#111714=CARTESIAN_POINT('Ctrl Pts',(-149.592267990347,-2.36689525637319,
126.493097472285));
#111715=CARTESIAN_POINT('Ctrl Pts',(-149.600014266431,-2.48714515799717,
126.559114997113));
#111716=CARTESIAN_POINT('Ctrl Pts',(-149.607760542515,-2.60466162885577,
126.630184210578));
#111717=CARTESIAN_POINT('Ctrl Pts',(-149.615506818599,-2.71900081768446,
126.706041740766));
#111718=CARTESIAN_POINT('Ctrl Pts',(-149.623253151865,-2.83334085053892,
126.781899830918));
#111719=CARTESIAN_POINT('Ctrl Pts',(-149.63099948513,-2.94450322877614,
126.862546092183));
#111720=CARTESIAN_POINT('Ctrl Pts',(-149.638745818395,-3.05207293608227,
126.947673716178));
#111721=CARTESIAN_POINT('Ctrl Pts',(-149.646493886398,-3.15966673287837,
127.032820403915));
#111722=CARTESIAN_POINT('Ctrl Pts',(-149.654241954401,-3.26366595125462,
127.122450208801));
#111723=CARTESIAN_POINT('Ctrl Pts',(-149.661990022404,-3.36368883998906,
127.216216187609));
#111724=CARTESIAN_POINT('Ctrl Pts',(-149.669746325146,-3.46381803424008,
127.310081822015));
#111725=CARTESIAN_POINT('Ctrl Pts',(-149.677502627888,-3.55996217109209,
127.408092143962));
#111726=CARTESIAN_POINT('Ctrl Pts',(-149.685258930629,-3.65177617780567,
127.509863112678));
#111727=CARTESIAN_POINT('Ctrl Pts',(-149.693019373143,-3.74363918841935,
127.611688399625));
#111728=CARTESIAN_POINT('Ctrl Pts',(-149.700779815658,-3.83116721440323,
127.717278031949));
#111729=CARTESIAN_POINT('Ctrl Pts',(-149.708540258172,-3.91405631566911,
127.826215856096));
#111730=CARTESIAN_POINT('Ctrl Pts',(-149.716313158437,-3.99707847787888,
127.93532855691));
#111731=CARTESIAN_POINT('Ctrl Pts',(-149.724086058703,-4.07544661062439,
128.047799869179));
#111732=CARTESIAN_POINT('Ctrl Pts',(-149.731858958968,-4.14890036216591,
128.163184961287));
#111733=CARTESIAN_POINT('Ctrl Pts',(-149.73934929473,-4.21968388482365,
128.274375514665));
#111734=CARTESIAN_POINT('Ctrl Pts',(-149.746839630493,-4.28590396847165,
128.388271413092));
#111735=CARTESIAN_POINT('Ctrl Pts',(-149.754329966255,-4.34736941268764,
128.504455782116));
#111736=CARTESIAN_POINT('Ctrl Pts',(-149.762555614144,-4.41486880356576,
128.632045751385));
#111737=CARTESIAN_POINT('Ctrl Pts',(-149.770781262032,-4.47682817998231,
128.762761823252));
#111738=CARTESIAN_POINT('Ctrl Pts',(-149.779006909921,-4.53296421753863,
128.896110512099));
#111739=CARTESIAN_POINT('Ctrl Pts',(-149.787213600141,-4.58897087825169,
129.029151871944));
#111740=CARTESIAN_POINT('Ctrl Pts',(-149.795420290362,-4.63918083480873,
129.164813454452));
#111741=CARTESIAN_POINT('Ctrl Pts',(-149.803626980582,-4.68335698160947,
129.302578194806));
#111742=CARTESIAN_POINT('Ctrl Pts',(-149.809132002562,-4.71299020189066,
129.394990349183));
#111743=CARTESIAN_POINT('Ctrl Pts',(-149.81463702454,-4.73990931628902,
129.488348304389));
#111744=CARTESIAN_POINT('Ctrl Pts',(-149.820142046519,-4.76405452823404,
129.582490119308));
#111745=CARTESIAN_POINT('Origin',(213.235140564004,0.,130.804360617566));
#111746=CARTESIAN_POINT('',(-151.915051610183,-4.76405452823401,129.582490119308));
#111747=CARTESIAN_POINT('',(-151.569820863616,-4.76405452823393,129.582490119308));
#111748=CARTESIAN_POINT('',(213.235140564004,-4.76405452823405,129.582490119308));
#111749=CARTESIAN_POINT('',(-150.23514056396,-4.91824801635102,130.808777874548));
#111750=CARTESIAN_POINT('Ctrl Pts',(-150.235140564011,-4.91824801635022,
130.808777875439));
#111751=CARTESIAN_POINT('Ctrl Pts',(-150.246220776016,-4.91807253331176,
131.004163594484));
#111752=CARTESIAN_POINT('Ctrl Pts',(-150.257300988021,-4.90625068833561,
131.199047831327));
#111753=CARTESIAN_POINT('Ctrl Pts',(-150.268381200027,-4.88298081443509,
131.392307407981));
#111754=CARTESIAN_POINT('Ctrl Pts',(-150.276132872591,-4.86670130254354,
131.527511044654));
#111755=CARTESIAN_POINT('Ctrl Pts',(-150.283884545156,-4.84481967606861,
131.661920399415));
#111756=CARTESIAN_POINT('Ctrl Pts',(-150.291636217721,-4.81741652506013,
131.795158824356));
#111757=CARTESIAN_POINT('Ctrl Pts',(-150.29941055184,-4.78993326256789,
131.928786763915));
#111758=CARTESIAN_POINT('Ctrl Pts',(-150.307184885959,-4.75684229574795,
132.061481976966));
#111759=CARTESIAN_POINT('Ctrl Pts',(-150.314959220078,-4.71821930886351,
132.192737229285));
#111760=CARTESIAN_POINT('Ctrl Pts',(-150.322723973025,-4.67964392135857,
132.323830721235));
#111761=CARTESIAN_POINT('Ctrl Pts',(-150.330488725972,-4.63555018832687,
132.45348741196));
#111762=CARTESIAN_POINT('Ctrl Pts',(-150.338253478919,-4.58606495851269,
132.581209305216));
#111763=CARTESIAN_POINT('Ctrl Pts',(-150.346010519803,-4.53662887812639,
132.708804343286));
#111764=CARTESIAN_POINT('Ctrl Pts',(-150.353767560688,-4.48181209780396,
132.834468045893));
#111765=CARTESIAN_POINT('Ctrl Pts',(-150.361524601573,-4.42179141657143,
132.957717004891));
#111766=CARTESIAN_POINT('Ctrl Pts',(-150.369275792813,-4.36181599740159,
133.080873020891));
#111767=CARTESIAN_POINT('Ctrl Pts',(-150.377026984053,-4.29664465889072,
133.201617567748));
#111768=CARTESIAN_POINT('Ctrl Pts',(-150.384778175293,-4.22650236823941,
133.319487014741));
#111769=CARTESIAN_POINT('Ctrl Pts',(-150.39252607207,-4.15638988993283,
133.437306364074));
#111770=CARTESIAN_POINT('Ctrl Pts',(-150.400273968847,-4.08131086117433,
133.552252708723));
#111771=CARTESIAN_POINT('Ctrl Pts',(-150.408021865624,-4.00153616340971,
133.663887046089));
#111772=CARTESIAN_POINT('Ctrl Pts',(-150.415768141708,-3.92177815279212,
133.775498031959));
#111773=CARTESIAN_POINT('Ctrl Pts',(-150.423514417792,-3.83732665405074,
133.883798070673));
#111774=CARTESIAN_POINT('Ctrl Pts',(-150.431260693876,-3.74849561838572,
133.988377524155));
#111775=CARTESIAN_POINT('Ctrl Pts',(-150.439007027141,-3.6596639269903,
134.092957749618));
#111776=CARTESIAN_POINT('Ctrl Pts',(-150.446753360406,-3.56645288726782,
134.193817037067));
#111777=CARTESIAN_POINT('Ctrl Pts',(-150.454499693671,-3.46921617720046,
134.290579511777));
#111778=CARTESIAN_POINT('Ctrl Pts',(-150.462247761674,-3.3719576916462,
134.387363655771));
#111779=CARTESIAN_POINT('Ctrl Pts',(-150.469995829677,-3.27067201890082,
134.480048885677));
#111780=CARTESIAN_POINT('Ctrl Pts',(-150.47774389768,-3.16574876197482,
134.568297099304));
#111781=CARTESIAN_POINT('Ctrl Pts',(-150.485500200422,-3.06071399136262,
134.656639104181));
#111782=CARTESIAN_POINT('Ctrl Pts',(-150.493256503163,-2.95203421336577,
134.740534420578));
#111783=CARTESIAN_POINT('Ctrl Pts',(-150.501012805905,-2.84013153683342,
134.819685749605));
#111784=CARTESIAN_POINT('Ctrl Pts',(-150.508773248419,-2.72816913447328,
134.898879324079));
#111785=CARTESIAN_POINT('Ctrl Pts',(-150.516533690933,-2.61298073421539,
134.973323653833));
#111786=CARTESIAN_POINT('Ctrl Pts',(-150.524294133447,-2.49501547479722,
135.042766077526));
#111787=CARTESIAN_POINT('Ctrl Pts',(-150.532067033712,-2.37686084707217,
135.112319976364));
#111788=CARTESIAN_POINT('Ctrl Pts',(-150.539839933978,-2.25592079748713,
135.176855739468));
#111789=CARTESIAN_POINT('Ctrl Pts',(-150.547612834243,-2.13266779395145,
135.236167375892));
#111790=CARTESIAN_POINT('Ctrl Pts',(-150.555103170006,-2.01389534752485,
135.293322884946));
#111791=CARTESIAN_POINT('Ctrl Pts',(-150.56259350577,-1.89297547369181,
135.345627371121));
#111792=CARTESIAN_POINT('Ctrl Pts',(-150.570083841533,-1.77034471150173,
135.392940208786));
#111793=CARTESIAN_POINT('Ctrl Pts',(-150.577858175652,-1.64306436671462,
135.442046927061));
#111794=CARTESIAN_POINT('Ctrl Pts',(-150.585632509772,-1.51353764999049,
135.485931563407));
#111795=CARTESIAN_POINT('Ctrl Pts',(-150.593406843891,-1.38223222104053,
135.524383620647));
#111796=CARTESIAN_POINT('Ctrl Pts',(-150.601171596838,-1.25108861429664,
135.562788289164));
#111797=CARTESIAN_POINT('Ctrl Pts',(-150.608936349785,-1.11817102856585,
135.595773591143));
#111798=CARTESIAN_POINT('Ctrl Pts',(-150.616701102732,-0.983967007037161,
135.623177068891));
#111799=CARTESIAN_POINT('Ctrl Pts',(-150.624458143617,-0.849896278834962,
135.650553329119));
#111800=CARTESIAN_POINT('Ctrl Pts',(-150.632215184502,-0.714542038109991,
135.672358720107));
#111801=CARTESIAN_POINT('Ctrl Pts',(-150.639972225387,-0.578406554017688,
135.688480693974));
#111802=CARTESIAN_POINT('Ctrl Pts',(-150.647723416627,-0.442373730752734,
135.704590510135));
#111803=CARTESIAN_POINT('Ctrl Pts',(-150.655474607867,-0.305561223452434,
135.715025394223));
#111804=CARTESIAN_POINT('Ctrl Pts',(-150.663225799107,-0.16848069804129,
135.719724013785));
#111805=CARTESIAN_POINT('Ctrl Pts',(-150.670973695884,-0.0314584355100012,
135.724420636308));
#111806=CARTESIAN_POINT('Ctrl Pts',(-150.678721592662,0.105831228646485,
135.723385830068));
#111807=CARTESIAN_POINT('Ctrl Pts',(-150.686469489439,0.242872531071293,
135.716610203667));
#111808=CARTESIAN_POINT('Ctrl Pts',(-150.694215765523,0.379885167409903,
135.709835994582));
#111809=CARTESIAN_POINT('Ctrl Pts',(-150.701962041607,0.516649155111232,
135.697323373199));
#111810=CARTESIAN_POINT('Ctrl Pts',(-150.709708317691,0.652650155767247,
135.679115056169));
#111811=CARTESIAN_POINT('Ctrl Pts',(-150.717454650956,0.78865216035157,
135.660906604729));
#111812=CARTESIAN_POINT('Ctrl Pts',(-150.725200984222,0.92389077914432,
135.637002425626));
#111813=CARTESIAN_POINT('Ctrl Pts',(-150.732947317487,1.05785860650549,
135.607496908693));
#111814=CARTESIAN_POINT('Ctrl Pts',(-150.74069538549,1.19185643503291,135.577984784204));
#111815=CARTESIAN_POINT('Ctrl Pts',(-150.748443453493,1.32458252409625,
135.542868909889));
#111816=CARTESIAN_POINT('Ctrl Pts',(-150.756191521496,1.45554182880302,
135.502294317301));
#111817=CARTESIAN_POINT('Ctrl Pts',(-150.763947824238,1.58664031861709,
135.461676601553));
#111818=CARTESIAN_POINT('Ctrl Pts',(-150.77170412698,1.71596789900071,135.41558869412));
#111819=CARTESIAN_POINT('Ctrl Pts',(-150.779460429722,1.84304628383524,
135.36422502982));
#111820=CARTESIAN_POINT('Ctrl Pts',(-150.787220872236,1.97019249423002,
135.312833951186));
#111821=CARTESIAN_POINT('Ctrl Pts',(-150.79498131475,2.09508676119838,135.256161666376));
#111822=CARTESIAN_POINT('Ctrl Pts',(-150.802741757264,2.2172737431421,135.194449478907));
#111823=CARTESIAN_POINT('Ctrl Pts',(-150.81051465753,2.33965687047648,135.132638225556));
#111824=CARTESIAN_POINT('Ctrl Pts',(-150.818287557795,2.4593236866512,135.065771092969));
#111825=CARTESIAN_POINT('Ctrl Pts',(-150.82606045806,2.57584550520097,134.994134238639));
#111826=CARTESIAN_POINT('Ctrl Pts',(-150.833550793822,2.68813146214445,
134.925101564406));
#111827=CARTESIAN_POINT('Ctrl Pts',(-150.841041129584,2.79749685311942,
134.851640102322));
#111828=CARTESIAN_POINT('Ctrl Pts',(-150.848531465346,2.90358740578101,
134.774041113461));
#111829=CARTESIAN_POINT('Ctrl Pts',(-150.856305799465,3.01370041399339,
134.693499935351));
#111830=CARTESIAN_POINT('Ctrl Pts',(-150.864080133584,3.12063415568315,
134.608246158071));
#111831=CARTESIAN_POINT('Ctrl Pts',(-150.871854467704,3.22395875211928,
134.518559458115));
#111832=CARTESIAN_POINT('Ctrl Pts',(-150.879619220651,3.32715601022469,
134.428983289001));
#111833=CARTESIAN_POINT('Ctrl Pts',(-150.887383973598,3.42675268075169,
134.334985321135));
#111834=CARTESIAN_POINT('Ctrl Pts',(-150.895148726545,3.52234855443948,
134.236887926057));
#111835=CARTESIAN_POINT('Ctrl Pts',(-150.90290576743,3.61784948095785,134.138887962696));
#111836=CARTESIAN_POINT('Ctrl Pts',(-150.910662808315,3.70935724728015,
134.036796952998));
#111837=CARTESIAN_POINT('Ctrl Pts',(-150.9184198492,3.79650567493816,133.93097663535));
#111838=CARTESIAN_POINT('Ctrl Pts',(-150.92617104044,3.88358838328908,133.825236117626));
#111839=CARTESIAN_POINT('Ctrl Pts',(-150.93392223168,3.96631804883071,133.715772190239));
#111840=CARTESIAN_POINT('Ctrl Pts',(-150.94167342292,4.04436650290299,133.602982180532));
#111841=CARTESIAN_POINT('Ctrl Pts',(-150.949421319697,4.12238178430039,
133.490240109587));
#111842=CARTESIAN_POINT('Ctrl Pts',(-150.957169216474,4.19571958946585,
133.374175088837));
#111843=CARTESIAN_POINT('Ctrl Pts',(-150.964917113252,4.26409323445996,
133.255215968323));
#111844=CARTESIAN_POINT('Ctrl Pts',(-150.972663389336,4.33245257716132,
133.136281731492));
#111845=CARTESIAN_POINT('Ctrl Pts',(-150.98040966542,4.39584963041472,133.014454937787));
#111846=CARTESIAN_POINT('Ctrl Pts',(-150.988155941504,4.45404232047442,
132.890191404069));
#111847=CARTESIAN_POINT('Ctrl Pts',(-150.995902274769,4.51223544009941,
132.765926953066));
#111848=CARTESIAN_POINT('Ctrl Pts',(-151.003648608035,4.56522395406307,
132.639226080222));
#111849=CARTESIAN_POINT('Ctrl Pts',(-151.0113949413,4.6128130100626,132.510566700282));
#111850=CARTESIAN_POINT('Ctrl Pts',(-151.019143009303,4.66041272330121,
132.381878507967));
#111851=CARTESIAN_POINT('Ctrl Pts',(-151.026891077306,4.70261043686,132.251231302419));
#111852=CARTESIAN_POINT('Ctrl Pts',(-151.034639145309,4.73926058603645,
132.119119972027));
#111853=CARTESIAN_POINT('Ctrl Pts',(-151.042395448051,4.77594968742764,
131.986868232139));
#111854=CARTESIAN_POINT('Ctrl Pts',(-151.050151750793,4.80707934182604,
131.853149636288));
#111855=CARTESIAN_POINT('Ctrl Pts',(-151.057908053534,4.83255460742102,
131.718471676898));
#111856=CARTESIAN_POINT('Ctrl Pts',(-151.065668496049,4.8580434699323,131.583721835827));
#111857=CARTESIAN_POINT('Ctrl Pts',(-151.073428938563,4.87787187368826,
131.4480119976));
#111858=CARTESIAN_POINT('Ctrl Pts',(-151.081189381077,4.89199671091405,
131.311855684445));
#111859=CARTESIAN_POINT('Ctrl Pts',(-151.088962281342,4.90614422258249,
131.175480801088));
#111860=CARTESIAN_POINT('Ctrl Pts',(-151.096735181608,4.91456984732813,
131.038658401016));
#111861=CARTESIAN_POINT('Ctrl Pts',(-151.104508081873,4.91728262204888,
130.901903825408));
#111862=CARTESIAN_POINT('Ctrl Pts',(-151.111998417635,4.91989678057545,
130.770120623087));
#111863=CARTESIAN_POINT('Ctrl Pts',(-151.119488753397,4.91720623720689,
130.638400707617));
#111864=CARTESIAN_POINT('Ctrl Pts',(-151.126979089159,4.90926454528036,
130.507199572082));
#111865=CARTESIAN_POINT('Ctrl Pts',(-151.134753423278,4.9010217416906,130.371023905615));
#111866=CARTESIAN_POINT('Ctrl Pts',(-151.142527757397,4.8870956237371,130.234975771151));
#111867=CARTESIAN_POINT('Ctrl Pts',(-151.150302091517,4.86748913122206,
130.099568009819));
#111868=CARTESIAN_POINT('Ctrl Pts',(-151.158066844464,4.84790680195676,
129.964327126451));
#111869=CARTESIAN_POINT('Ctrl Pts',(-151.165831597411,4.82265808263384,
129.829725429153));
#111870=CARTESIAN_POINT('Ctrl Pts',(-151.173596350358,4.79179787068005,
129.696273875002));
#111871=CARTESIAN_POINT('Ctrl Pts',(-151.181353391243,4.76096830952383,
129.562954866816));
#111872=CARTESIAN_POINT('Ctrl Pts',(-151.189110432128,4.72453843459616,
129.430784106922));
#111873=CARTESIAN_POINT('Ctrl Pts',(-151.196867473013,4.68261465823956,
129.300265200067));
#111874=CARTESIAN_POINT('Ctrl Pts',(-151.204618664253,4.64072249692876,
129.169844718536));
#111875=CARTESIAN_POINT('Ctrl Pts',(-151.212369855493,4.59334479964782,
129.041073981332));
#111876=CARTESIAN_POINT('Ctrl Pts',(-151.220121046733,4.54063846596778,
128.914443851178));
#111877=CARTESIAN_POINT('Ctrl Pts',(-151.22786894351,4.48795453388548,128.787867542207));
#111878=CARTESIAN_POINT('Ctrl Pts',(-151.235616840287,4.42994661986385,
128.663430390926));
#111879=CARTESIAN_POINT('Ctrl Pts',(-151.243364737065,4.36682056791596,
128.541605396574));
#111880=CARTESIAN_POINT('Ctrl Pts',(-151.251111013149,4.30370772057747,
128.419805885385));
#111881=CARTESIAN_POINT('Ctrl Pts',(-151.258857289233,4.23547904456171,
128.300617791202));
#111882=CARTESIAN_POINT('Ctrl Pts',(-151.266603565317,4.16238718473159,
128.184491157673));
#111883=CARTESIAN_POINT('Ctrl Pts',(-151.274349898582,4.08929478535387,
128.068363666922));
#111884=CARTESIAN_POINT('Ctrl Pts',(-151.282096231848,4.0113393387887,127.955298012799));
#111885=CARTESIAN_POINT('Ctrl Pts',(-151.289842565113,3.9288176058177,127.845716454657));
#111886=CARTESIAN_POINT('Ctrl Pts',(-151.297590633116,3.84627739267689,
127.736110356485));
#111887=CARTESIAN_POINT('Ctrl Pts',(-151.305338701119,3.75916909344392,
127.629990219133));
#111888=CARTESIAN_POINT('Ctrl Pts',(-151.313086769122,3.66783039045661,
127.527746009568));
#111889=CARTESIAN_POINT('Ctrl Pts',(-151.320843071864,3.5763946116087,127.425393133641));
#111890=CARTESIAN_POINT('Ctrl Pts',(-151.328599374606,3.48071970839796,
127.326924706442));
#111891=CARTESIAN_POINT('Ctrl Pts',(-151.336355677347,3.38118133020755,
127.232694917258));
#111892=CARTESIAN_POINT('Ctrl Pts',(-151.344116119862,3.28158982538766,
127.138414834798));
#111893=CARTESIAN_POINT('Ctrl Pts',(-151.351876562376,3.17813103155089,
127.04837815469));
#111894=CARTESIAN_POINT('Ctrl Pts',(-151.35963700489,3.07121368868493,126.962898716032));
#111895=CARTESIAN_POINT('Ctrl Pts',(-151.367409905155,2.96412471260853,
126.877282058191));
#111896=CARTESIAN_POINT('Ctrl Pts',(-151.375182805421,2.85356640839853,
126.796237492155));
#111897=CARTESIAN_POINT('Ctrl Pts',(-151.382955705686,2.73997723184831,
126.72003596942));
#111898=CARTESIAN_POINT('Ctrl Pts',(-151.390446041448,2.63051730797986,
126.646604563977));
#111899=CARTESIAN_POINT('Ctrl Pts',(-151.39793637721,2.51824330818223,126.577670362564));
#111900=CARTESIAN_POINT('Ctrl Pts',(-151.405426712972,2.403567398574,126.513434514379));
#111901=CARTESIAN_POINT('Ctrl Pts',(-151.413201047091,2.2845435169978,126.446763144486));
#111902=CARTESIAN_POINT('Ctrl Pts',(-151.42097538121,2.16255496147165,126.38494224209));
#111903=CARTESIAN_POINT('Ctrl Pts',(-151.42874971533,2.03803478879638,126.32824653701));
#111904=CARTESIAN_POINT('Ctrl Pts',(-151.436514468277,1.91366807610524,
126.271620704318));
#111905=CARTESIAN_POINT('Ctrl Pts',(-151.444279221224,1.78677630652166,
126.220107661746));
#111906=CARTESIAN_POINT('Ctrl Pts',(-151.452043974171,1.65781903610666,
126.173937407316));
#111907=CARTESIAN_POINT('Ctrl Pts',(-151.459801015056,1.52898984787061,
126.127813009833));
#111908=CARTESIAN_POINT('Ctrl Pts',(-151.467558055941,1.39809960705316,
126.087020971184));
#111909=CARTESIAN_POINT('Ctrl Pts',(-151.475315096826,1.26562952906329,
126.05174397432));
#111910=CARTESIAN_POINT('Ctrl Pts',(-151.483066288066,1.13325934778988,
126.016493580113));
#111911=CARTESIAN_POINT('Ctrl Pts',(-151.490817479306,0.999312076958704,
125.986750049783));
#111912=CARTESIAN_POINT('Ctrl Pts',(-151.498568670546,0.86428550133109,
125.962646702568));
#111913=CARTESIAN_POINT('Ctrl Pts',(-151.506316567323,0.729316315599885,
125.938553599918));
#111914=CARTESIAN_POINT('Ctrl Pts',(-151.514064464101,0.593269121533218,
125.92009598104));
#111915=CARTESIAN_POINT('Ctrl Pts',(-151.521812360878,0.456653130504683,
125.907356331178));
#111916=CARTESIAN_POINT('Ctrl Pts',(-151.529558636962,0.32006571659637,
125.894619346177));
#111917=CARTESIAN_POINT('Ctrl Pts',(-151.537304913046,0.182910131413754,
125.887597987408));
#111918=CARTESIAN_POINT('Ctrl Pts',(-151.54505118913,0.0457015701417753,
125.886322957179));
#111919=CARTESIAN_POINT('Ctrl Pts',(-151.552797522395,-0.0915080039728203,
125.885047917537));
#111920=CARTESIAN_POINT('Ctrl Pts',(-151.56054385566,-0.228770164008777,
125.88951929471));
#111921=CARTESIAN_POINT('Ctrl Pts',(-151.568290188926,-0.365569244760797,
125.899715656941));
#111922=CARTESIAN_POINT('Ctrl Pts',(-151.576038256929,-0.502398960718268,
125.909914302577));
#111923=CARTESIAN_POINT('Ctrl Pts',(-151.583786324932,-0.63876500122497,
125.925840455389));
#111924=CARTESIAN_POINT('Ctrl Pts',(-151.591534392935,-0.774156750474476,
125.947420800336));
#111925=CARTESIAN_POINT('Ctrl Pts',(-151.599290695677,-0.909692395686082,
125.96902408113));
#111926=CARTESIAN_POINT('Ctrl Pts',(-151.607046998418,-1.04425129443386,
125.996293496729));
#111927=CARTESIAN_POINT('Ctrl Pts',(-151.61480330116,-1.1773324095725,126.029104450629));
#111928=CARTESIAN_POINT('Ctrl Pts',(-151.622563743675,-1.31048455410964,
126.061932916723));
#111929=CARTESIAN_POINT('Ctrl Pts',(-151.630324186189,-1.44215696824627,
126.100308705217));
#111930=CARTESIAN_POINT('Ctrl Pts',(-151.638084628703,-1.5718646763128,
126.14405756928));
#111931=CARTESIAN_POINT('Ctrl Pts',(-151.645857528968,-1.70178060270723,
126.187876662905));
#111932=CARTESIAN_POINT('Ctrl Pts',(-151.653630429234,-1.82972515537736,
126.237085927844));
#111933=CARTESIAN_POINT('Ctrl Pts',(-151.661403329499,-1.95523337908873,
126.291462934724));
#111934=CARTESIAN_POINT('Ctrl Pts',(-151.668893665261,-2.07617906273273,
126.343863200438));
#111935=CARTESIAN_POINT('Ctrl Pts',(-151.676384001023,-2.19486219803625,
126.401061876557));
#111936=CARTESIAN_POINT('Ctrl Pts',(-151.683874336785,-2.31089076662683,
126.46282092211));
#111937=CARTESIAN_POINT('Ctrl Pts',(-151.691649612949,-2.43133318634517,
126.526929347959));
#111938=CARTESIAN_POINT('Ctrl Pts',(-151.699424889113,-2.5492966480185,
126.596155075043));
#111939=CARTESIAN_POINT('Ctrl Pts',(-151.707200165277,-2.66431576793663,
126.670282177185));
#111940=CARTESIAN_POINT('Ctrl Pts',(-151.714965652402,-2.77919007927822,
126.744315953624));
#111941=CARTESIAN_POINT('Ctrl Pts',(-151.722731139526,-2.89112709957447,
126.823238615968));
#111942=CARTESIAN_POINT('Ctrl Pts',(-151.730496626651,-2.99968480245734,
126.906787764057));
#111943=CARTESIAN_POINT('Ctrl Pts',(-151.738252808443,-3.10811242135966,
126.990236795753));
#111944=CARTESIAN_POINT('Ctrl Pts',(-151.746008990236,-3.21316847992648,
127.078301034847));
#111945=CARTESIAN_POINT('Ctrl Pts',(-151.753765172028,-3.31443931528753,
127.170674460538));
#111946=CARTESIAN_POINT('Ctrl Pts',(-151.761516077246,-3.41564125552377,
127.262985044063));
#111947=CARTESIAN_POINT('Ctrl Pts',(-151.769266982464,-3.51306280789825,
127.359598719844));
#111948=CARTESIAN_POINT('Ctrl Pts',(-151.777017887682,-3.60632278748346,
127.460168784705));
#111949=CARTESIAN_POINT('Ctrl Pts',(-151.784765198523,-3.69953951901311,
127.560692211557));
#111950=CARTESIAN_POINT('Ctrl Pts',(-151.792512509363,-3.7885982528057,
127.665168090575));
#111951=CARTESIAN_POINT('Ctrl Pts',(-151.800259820204,-3.87315442984602,
127.773212679067));
#111952=CARTESIAN_POINT('Ctrl Pts',(-151.808005216091,-3.95768970658522,
127.881230561475));
#111953=CARTESIAN_POINT('Ctrl Pts',(-151.815750611978,-4.03772440161672,
127.992815089638));
#111954=CARTESIAN_POINT('Ctrl Pts',(-151.823496007865,-4.11295430966178,
128.107549554637));
#111955=CARTESIAN_POINT('Ctrl Pts',(-151.831243875261,-4.1882082231111,
128.222320630704));
#111956=CARTESIAN_POINT('Ctrl Pts',(-151.838991742656,-4.25865406613801,
128.340243328434));
#111957=CARTESIAN_POINT('Ctrl Pts',(-151.846739610052,-4.32403098437282,
128.460871955617));
#111958=CARTESIAN_POINT('Ctrl Pts',(-151.854488485788,-4.38941641103889,
128.581516281925));
#111959=CARTESIAN_POINT('Ctrl Pts',(-151.862237361525,-4.44973141953418,
128.704866891528));
#111960=CARTESIAN_POINT('Ctrl Pts',(-151.869986237261,-4.50476163073174,
128.830454410882));
#111961=CARTESIAN_POINT('Ctrl Pts',(-151.877742268904,-4.55984266105212,
128.956157907394));
#111962=CARTESIAN_POINT('Ctrl Pts',(-151.885498300547,-4.60962899216592,
129.08410207972));
#111963=CARTESIAN_POINT('Ctrl Pts',(-151.89325433219,-4.65395465341272,
129.213798092395));
#111964=CARTESIAN_POINT('Ctrl Pts',(-151.900520091521,-4.69547841216282,
129.335295793494));
#111965=CARTESIAN_POINT('Ctrl Pts',(-151.907785850852,-4.73221042479218,
129.45833044329));
#111966=CARTESIAN_POINT('Ctrl Pts',(-151.915051610183,-4.76405452823401,
129.582490119308));
#111967=CARTESIAN_POINT('Ctrl Pts',(-150.165071172634,-4.76405452823413,
129.582490119309));
#111968=CARTESIAN_POINT('Ctrl Pts',(-150.172710513743,-4.79768513315927,
129.713615337496));
#111969=CARTESIAN_POINT('Ctrl Pts',(-150.180349854851,-4.82588729218672,
129.84608862954));
#111970=CARTESIAN_POINT('Ctrl Pts',(-150.18798919596,-4.84857159836929,
129.979414244772));
#111971=CARTESIAN_POINT('Ctrl Pts',(-150.195847757293,-4.87190685842699,
130.116565801391));
#111972=CARTESIAN_POINT('Ctrl Pts',(-150.203706318627,-4.88940273674939,
130.254618883265));
#111973=CARTESIAN_POINT('Ctrl Pts',(-150.21156487996,-4.90101913576986,
130.393028035198));
#111974=CARTESIAN_POINT('Ctrl Pts',(-150.219423441294,-4.9126355347903,
130.531437187131));
#111975=CARTESIAN_POINT('Ctrl Pts',(-150.227282002627,-4.91837247641928,
130.670201946933));
#111976=CARTESIAN_POINT('Ctrl Pts',(-150.23514056396,-4.91824801635102,
130.808777874548));
#111977=CARTESIAN_POINT('',(-149.889859435963,-4.91824998668701,130.803998742957));
#111978=CARTESIAN_POINT('Ctrl Pts',(-149.820142046519,-4.76405452823404,
129.582490119308));
#111979=CARTESIAN_POINT('Ctrl Pts',(-149.828324075985,-4.79994118524423,
129.722411650335));
#111980=CARTESIAN_POINT('Ctrl Pts',(-149.836506105451,-4.82969789362151,
129.86406546982));
#111981=CARTESIAN_POINT('Ctrl Pts',(-149.844688134917,-4.8531686134343,
130.006903739687));
#111982=CARTESIAN_POINT('Ctrl Pts',(-149.85285286192,-4.87658969993171,
130.149439950779));
#111983=CARTESIAN_POINT('Ctrl Pts',(-149.861017588924,-4.89375125390065,
130.293155299377));
#111984=CARTESIAN_POINT('Ctrl Pts',(-149.869182315927,-4.90454780912303,
130.437490271904));
#111985=CARTESIAN_POINT('Ctrl Pts',(-149.876074689272,-4.91366187863253,
130.559332743429));
#111986=CARTESIAN_POINT('Ctrl Pts',(-149.882967062617,-4.9182409820493,
130.681616409001));
#111987=CARTESIAN_POINT('Ctrl Pts',(-149.889859435963,-4.91824998668701,
130.803998742957));
#111988=CARTESIAN_POINT('Ctrl Pts',(-149.889859435993,-4.91824998668705,
130.803998743496));
#111989=CARTESIAN_POINT('Ctrl Pts',(-149.897930859643,-4.91826053169582,
130.947316526095));
#111990=CARTESIAN_POINT('Ctrl Pts',(-149.906002283294,-4.91200233468265,
131.090528101548));
#111991=CARTESIAN_POINT('Ctrl Pts',(-149.914073706944,-4.89952911294758,
131.23307676361));
#111992=CARTESIAN_POINT('Ctrl Pts',(-149.922154256147,-4.88704178898657,
131.375786591207));
#111993=CARTESIAN_POINT('Ctrl Pts',(-149.93023480535,-4.86832545243638,
131.517831670927));
#111994=CARTESIAN_POINT('Ctrl Pts',(-149.938315354553,-4.84348530688792,
131.658663341699));
#111995=CARTESIAN_POINT('Ctrl Pts',(-149.946413553537,-4.81859090473859,
131.799802621287));
#111996=CARTESIAN_POINT('Ctrl Pts',(-149.954511752521,-4.78754601215525,
131.939722856525));
#111997=CARTESIAN_POINT('Ctrl Pts',(-149.962609951505,-4.75050673616793,
132.077886750837));
#111998=CARTESIAN_POINT('Ctrl Pts',(-149.970717255956,-4.71342581389545,
132.216205994107));
#111999=CARTESIAN_POINT('Ctrl Pts',(-149.978824560407,-4.67033716232297,
132.352764631252));
#112000=CARTESIAN_POINT('Ctrl Pts',(-149.986931864858,-4.62144586080497,
132.487043361921));
#112001=CARTESIAN_POINT('Ctrl Pts',(-149.995057568965,-4.57244359970468,
132.621626840293));
#112002=CARTESIAN_POINT('Ctrl Pts',(-150.003183273071,-4.51761248540803,
132.753919749579));
#112003=CARTESIAN_POINT('Ctrl Pts',(-150.011308977178,-4.45720534180436,
132.883423772809));
#112004=CARTESIAN_POINT('Ctrl Pts',(-150.018465181474,-4.4040055384498,
132.997476319552));
#112005=CARTESIAN_POINT('Ctrl Pts',(-150.025621385771,-4.3464816776517,
133.109366018076));
#112006=CARTESIAN_POINT('Ctrl Pts',(-150.032777590067,-4.28483443271258,
133.218770886501));
#112007=CARTESIAN_POINT('Ctrl Pts',(-150.040551924186,-4.21786229778898,
133.337625794238));
#112008=CARTESIAN_POINT('Ctrl Pts',(-150.048326258306,-4.14583504957903,
133.453880287348));
#112009=CARTESIAN_POINT('Ctrl Pts',(-150.056100592425,-4.06897963459425,
133.567074463725));
#112010=CARTESIAN_POINT('Ctrl Pts',(-150.063865345372,-3.99221893703967,
133.680129138396));
#112011=CARTESIAN_POINT('Ctrl Pts',(-150.071630098319,-3.91064212950941,
133.790130680279));
#112012=CARTESIAN_POINT('Ctrl Pts',(-150.079394851266,-3.82452205894767,
133.896643606415));
#112013=CARTESIAN_POINT('Ctrl Pts',(-150.087151892151,-3.73848752405432,
134.00305074241));
#112014=CARTESIAN_POINT('Ctrl Pts',(-150.094908933036,-3.647918950298,134.105975855995));
#112015=CARTESIAN_POINT('Ctrl Pts',(-150.102665973921,-3.55313229525969,
134.205012607241));
#112016=CARTESIAN_POINT('Ctrl Pts',(-150.110417165162,-3.4584171195754,
134.303974674103));
#112017=CARTESIAN_POINT('Ctrl Pts',(-150.118168356402,-3.35949046320697,
134.399053933775));
#112018=CARTESIAN_POINT('Ctrl Pts',(-150.125919547642,-3.25670811288556,
134.489877586726));
#112019=CARTESIAN_POINT('Ctrl Pts',(-150.133667444419,-3.1539694478047,
134.580662637202));
#112020=CARTESIAN_POINT('Ctrl Pts',(-150.141415341196,-3.04737864052349,
134.667195420074));
#112021=CARTESIAN_POINT('Ctrl Pts',(-150.149163237973,-2.9373276795397,
134.74914060706));
#112022=CARTESIAN_POINT('Ctrl Pts',(-150.156909514057,-2.82729973884452,
134.831068652879));
#112023=CARTESIAN_POINT('Ctrl Pts',(-150.164655790142,-2.7138133974866,
134.908410778214));
#112024=CARTESIAN_POINT('Ctrl Pts',(-150.172402066226,-2.59729269088903,
134.980872767716));
#112025=CARTESIAN_POINT('Ctrl Pts',(-150.180148399491,-2.48077112416191,
135.053335292117));
#112026=CARTESIAN_POINT('Ctrl Pts',(-150.187894732757,-2.361215479502,135.120917402338));
#112027=CARTESIAN_POINT('Ctrl Pts',(-150.195641066022,-2.2390773128107,
135.183369164002));
#112028=CARTESIAN_POINT('Ctrl Pts',(-150.203389134025,-2.11691179412432,
135.245834911304));
#112029=CARTESIAN_POINT('Ctrl Pts',(-150.211137202028,-1.99216295061391,
135.303167845905));
#112030=CARTESIAN_POINT('Ctrl Pts',(-150.218885270031,-1.86530501431347,
135.355164971312));
#112031=CARTESIAN_POINT('Ctrl Pts',(-150.226641572773,-1.73831225188818,
135.407217359884));
#112032=CARTESIAN_POINT('Ctrl Pts',(-150.234397875515,-1.60920628123026,
135.453922462391));
#112033=CARTESIAN_POINT('Ctrl Pts',(-150.242154178257,-1.47847982919974,
135.495126062262));
#112034=CARTESIAN_POINT('Ctrl Pts',(-150.249914620771,-1.34768360452567,
135.536351653734));
#112035=CARTESIAN_POINT('Ctrl Pts',(-150.257675063286,-1.21526555238251,
135.572069789939));
#112036=CARTESIAN_POINT('Ctrl Pts',(-150.2654355058,-1.08173050927903,135.602177013365));
#112037=CARTESIAN_POINT('Ctrl Pts',(-150.273208406065,-0.947981103869675,
135.632332567578));
#112038=CARTESIAN_POINT('Ctrl Pts',(-150.280981306331,-0.813111509206581,
135.656859139894));
#112039=CARTESIAN_POINT('Ctrl Pts',(-150.288754206596,-0.677634526761312,
135.67570483766));
#112040=CARTESIAN_POINT('Ctrl Pts',(-150.296244542358,-0.547082473887059,
135.693865446841));
#112041=CARTESIAN_POINT('Ctrl Pts',(-150.303734878119,-0.415966733239075,
135.70675100877));
#112042=CARTESIAN_POINT('Ctrl Pts',(-150.31122521388,-0.284745934870738,
135.714360904233));
#112043=CARTESIAN_POINT('Ctrl Pts',(-150.318999548,-0.148549860035717,135.722259331197));
#112044=CARTESIAN_POINT('Ctrl Pts',(-150.326773882119,-0.0118091754647882,
135.72449916056));
#112045=CARTESIAN_POINT('Ctrl Pts',(-150.334548216238,0.12496652004272,
135.721022740528));
#112046=CARTESIAN_POINT('Ctrl Pts',(-150.342312969185,0.261573651729139,
135.717550604873));
#112047=CARTESIAN_POINT('Ctrl Pts',(-150.350077722132,0.398215321413812,
135.708376246648));
#112048=CARTESIAN_POINT('Ctrl Pts',(-150.357842475079,0.534377664511189,
135.693493830537));
#112049=CARTESIAN_POINT('Ctrl Pts',(-150.365599515964,0.67040476925022,
135.678626195851));
#112050=CARTESIAN_POINT('Ctrl Pts',(-150.373356556849,0.805953108674859,
135.658061827693));
#112051=CARTESIAN_POINT('Ctrl Pts',(-150.381113597734,0.940510034705003,
135.631846913468));
#112052=CARTESIAN_POINT('Ctrl Pts',(-150.388864788974,1.07496549030998,
135.605651768113));
#112053=CARTESIAN_POINT('Ctrl Pts',(-150.396615980214,1.20843063844032,
135.573814632655));
#112054=CARTESIAN_POINT('Ctrl Pts',(-150.404367171454,1.34039952087395,
135.536433333294));
#112055=CARTESIAN_POINT('Ctrl Pts',(-150.412115068232,1.4723123130127,135.499067921983));
#112056=CARTESIAN_POINT('Ctrl Pts',(-150.419862965009,1.6027297289385,135.456163139832));
#112057=CARTESIAN_POINT('Ctrl Pts',(-150.427610861786,1.73115776811343,
135.40786752474));
#112058=CARTESIAN_POINT('Ctrl Pts',(-150.43535713787,1.85955894291115,135.35958201205));
#112059=CARTESIAN_POINT('Ctrl Pts',(-150.443103413954,1.98597120295921,
135.305908046896));
#112060=CARTESIAN_POINT('Ctrl Pts',(-150.450849690038,2.1099178150502,135.247043351707));
#112061=CARTESIAN_POINT('Ctrl Pts',(-150.458596023303,2.23386534208677,
135.188178221992));
#112062=CARTESIAN_POINT('Ctrl Pts',(-150.466342356569,2.35534683168672,
135.124122453508));
#112063=CARTESIAN_POINT('Ctrl Pts',(-150.474088689834,2.47390792998701,
135.055120857388));
#112064=CARTESIAN_POINT('Ctrl Pts',(-150.481836757837,2.59249557922307,
134.986103808838));
#112065=CARTESIAN_POINT('Ctrl Pts',(-150.48958482584,2.7081611979325,134.912138925309));
#112066=CARTESIAN_POINT('Ctrl Pts',(-150.497332893843,2.82047766542043,
134.83351546708));
#112067=CARTESIAN_POINT('Ctrl Pts',(-150.505089196585,2.93291350418674,
134.754808446904));
#112068=CARTESIAN_POINT('Ctrl Pts',(-150.512845499327,3.04199276041207,
134.671433186061));
#112069=CARTESIAN_POINT('Ctrl Pts',(-150.520601802069,3.14731935642298,
134.583720871787));
#112070=CARTESIAN_POINT('Ctrl Pts',(-150.528362244583,3.25270216840951,
134.49596174281));
#112071=CARTESIAN_POINT('Ctrl Pts',(-150.536122687097,3.35432803966295,
134.403861210352));
#112072=CARTESIAN_POINT('Ctrl Pts',(-150.543883129611,3.45183705198367,
134.307788086353));
#112073=CARTESIAN_POINT('Ctrl Pts',(-150.551656029877,3.54950259442742,
134.211560737246));
#112074=CARTESIAN_POINT('Ctrl Pts',(-150.559428930142,3.64303780463344,
134.111348338984));
#112075=CARTESIAN_POINT('Ctrl Pts',(-150.567201830407,3.7321218421228,134.007554276721));
#112076=CARTESIAN_POINT('Ctrl Pts',(-150.574692166169,3.81796745045954,
133.907533390064));
#112077=CARTESIAN_POINT('Ctrl Pts',(-150.582182501931,3.89967969915637,
133.804186965027));
#112078=CARTESIAN_POINT('Ctrl Pts',(-150.589672837693,3.97701016650376,
133.697900525365));
#112079=CARTESIAN_POINT('Ctrl Pts',(-150.597447171812,4.05727264202506,
133.587584203037));
#112080=CARTESIAN_POINT('Ctrl Pts',(-150.605221505931,4.13306875399035,
133.473751074893));
#112081=CARTESIAN_POINT('Ctrl Pts',(-150.612995840051,4.20407454771377,
133.35679871863));
#112082=CARTESIAN_POINT('Ctrl Pts',(-150.620760592998,4.2749928331424,133.239990495695));
#112083=CARTESIAN_POINT('Ctrl Pts',(-150.628525345945,4.34113234585888,
133.12007102438));
#112084=CARTESIAN_POINT('Ctrl Pts',(-150.636290098892,4.40221042008673,
132.997469479383));
#112085=CARTESIAN_POINT('Ctrl Pts',(-150.644047139777,4.46322783071036,
132.874989703969));
#112086=CARTESIAN_POINT('Ctrl Pts',(-150.651804180662,4.51919363377727,
132.749833503781));
#112087=CARTESIAN_POINT('Ctrl Pts',(-150.659561221547,4.56986958924957,
132.622457149588));
#112088=CARTESIAN_POINT('Ctrl Pts',(-150.667312412787,4.62050732958944,
132.495176850896));
#112089=CARTESIAN_POINT('Ctrl Pts',(-150.675063604027,4.66586301848597,
132.365680092465));
#112090=CARTESIAN_POINT('Ctrl Pts',(-150.682814795267,4.7057454771148,132.234445428727));
#112091=CARTESIAN_POINT('Ctrl Pts',(-150.690562692044,4.74561098463498,
132.103266543222));
#112092=CARTESIAN_POINT('Ctrl Pts',(-150.698310588821,4.78000777521548,
131.970351594831));
#112093=CARTESIAN_POINT('Ctrl Pts',(-150.706058485598,4.8087937986393,131.836196488559));
#112094=CARTESIAN_POINT('Ctrl Pts',(-150.713804761682,4.83757380064758,
131.702069444644));
#112095=CARTESIAN_POINT('Ctrl Pts',(-150.721551037766,4.86074528798491,
131.566703140859));
#112096=CARTESIAN_POINT('Ctrl Pts',(-150.72929731385,4.87821692418744,131.430605540157));
#112097=CARTESIAN_POINT('Ctrl Pts',(-150.737043647116,4.89568868936159,
131.294506934814));
#112098=CARTESIAN_POINT('Ctrl Pts',(-150.744789980381,4.9074604696614,131.157677409564));
#112099=CARTESIAN_POINT('Ctrl Pts',(-150.752536313647,4.9134926422659,131.020631551579));
#112100=CARTESIAN_POINT('Ctrl Pts',(-150.760284381649,4.91952616573362,
130.883555003124));
#112101=CARTESIAN_POINT('Ctrl Pts',(-150.768032449652,4.91981750662894,
130.746262416044));
#112102=CARTESIAN_POINT('Ctrl Pts',(-150.775780517655,4.91437915864869,
130.609269491321));
#112103=CARTESIAN_POINT('Ctrl Pts',(-150.783536820397,4.90893503072747,
130.472130968888));
#112104=CARTESIAN_POINT('Ctrl Pts',(-150.791293123139,4.89774906486869,
130.335293136301));
#112105=CARTESIAN_POINT('Ctrl Pts',(-150.799049425881,4.8808858086179,130.199268239716));
#112106=CARTESIAN_POINT('Ctrl Pts',(-150.806809868395,4.86401355193951,
130.063170742548));
#112107=CARTESIAN_POINT('Ctrl Pts',(-150.814570310909,4.84145803132284,
129.927887431394));
#112108=CARTESIAN_POINT('Ctrl Pts',(-150.822330753423,4.81333499411985,
129.793920467492));
#112109=CARTESIAN_POINT('Ctrl Pts',(-150.830103653689,4.78516681132089,
129.659738447927));
#112110=CARTESIAN_POINT('Ctrl Pts',(-150.837876553954,4.75141334834129,
129.526877377441));
#112111=CARTESIAN_POINT('Ctrl Pts',(-150.84564945422,4.71224056242093,129.395825227746));
#112112=CARTESIAN_POINT('Ctrl Pts',(-150.853139789982,4.6744918059379,129.269537153789));
#112113=CARTESIAN_POINT('Ctrl Pts',(-150.860630125744,4.63171099798405,
129.144929057636));
#112114=CARTESIAN_POINT('Ctrl Pts',(-150.868120461506,4.58408821260883,
129.022418328511));
#112115=CARTESIAN_POINT('Ctrl Pts',(-150.875894795626,4.53465979485293,
128.895262567859));
#112116=CARTESIAN_POINT('Ctrl Pts',(-150.883669129745,4.47985841016305,
128.769963565914));
#112117=CARTESIAN_POINT('Ctrl Pts',(-150.891443463864,4.41984344649703,
128.647008775386));
#112118=CARTESIAN_POINT('Ctrl Pts',(-150.899208216811,4.35990244591004,
128.524205515648));
#112119=CARTESIAN_POINT('Ctrl Pts',(-150.906972969758,4.29476082056689,
128.403741066989));
#112120=CARTESIAN_POINT('Ctrl Pts',(-150.914737722705,4.22462685953976,
128.28608522354));
#112121=CARTESIAN_POINT('Ctrl Pts',(-150.92249476359,4.15456255655145,128.168546237534));
#112122=CARTESIAN_POINT('Ctrl Pts',(-150.930251804475,4.07951598432393,
128.053810639068));
#112123=CARTESIAN_POINT('Ctrl Pts',(-150.93800884536,3.99974224181769,127.94232549173));
#112124=CARTESIAN_POINT('Ctrl Pts',(-150.9457600366,3.9200286573109,127.830924416208));
#112125=CARTESIAN_POINT('Ctrl Pts',(-150.95351122784,3.83559522462584,127.722769229533));
#112126=CARTESIAN_POINT('Ctrl Pts',(-150.96126241908,3.74674122833586,127.618279446223));
#112127=CARTESIAN_POINT('Ctrl Pts',(-150.969010315857,3.65792499736493,
127.513834073858));
#112128=CARTESIAN_POINT('Ctrl Pts',(-150.976758212634,3.56469219243346,
127.413051303542));
#112129=CARTESIAN_POINT('Ctrl Pts',(-150.984506109412,3.46738325085526,
127.316318694912));
#112130=CARTESIAN_POINT('Ctrl Pts',(-150.992252385496,3.3700946642099,127.21960632066));
#112131=CARTESIAN_POINT('Ctrl Pts',(-150.99999866158,3.2687319139637,127.126942698411));
#112132=CARTESIAN_POINT('Ctrl Pts',(-151.007744937664,3.16367299414463,
127.038679238503));
#112133=CARTESIAN_POINT('Ctrl Pts',(-151.015491270929,3.05861329880433,
126.950415127055));
#112134=CARTESIAN_POINT('Ctrl Pts',(-151.023237604195,2.9498576787917,126.86655149425));
#112135=CARTESIAN_POINT('Ctrl Pts',(-151.03098393746,2.83781765376463,126.787399822826));
#112136=CARTESIAN_POINT('Ctrl Pts',(-151.038732005463,2.72575253815063,
126.708230425933));
#112137=CARTESIAN_POINT('Ctrl Pts',(-151.046480073466,2.61040187318124,
126.633775315712));
#112138=CARTESIAN_POINT('Ctrl Pts',(-151.054228141469,2.49220628584793,
126.564302729839));
#112139=CARTESIAN_POINT('Ctrl Pts',(-151.061984444211,2.37388507883801,
126.494756307675));
#112140=CARTESIAN_POINT('Ctrl Pts',(-151.069740746953,2.25271324705414,
126.430203186592));
#112141=CARTESIAN_POINT('Ctrl Pts',(-151.077497049695,2.12915664721986,
126.370865942471));
#112142=CARTESIAN_POINT('Ctrl Pts',(-151.085257492209,2.00553410150769,
126.311497028276));
#112143=CARTESIAN_POINT('Ctrl Pts',(-151.093017934723,1.8795246105684,126.257349692419));
#112144=CARTESIAN_POINT('Ctrl Pts',(-151.100778377237,1.75161322114368,
126.20859798379));
#112145=CARTESIAN_POINT('Ctrl Pts',(-151.108551277503,1.62349649700157,
126.15976801459));
#112146=CARTESIAN_POINT('Ctrl Pts',(-151.116324177768,1.49347214436577,
126.116351105033));
#112147=CARTESIAN_POINT('Ctrl Pts',(-151.124097078034,1.362040411599,126.078471391222));
#112148=CARTESIAN_POINT('Ctrl Pts',(-151.131587413796,1.23538655337593,
126.041968700422));
#112149=CARTESIAN_POINT('Ctrl Pts',(-151.139077749557,1.10742616132385,
126.010607686078));
#112150=CARTESIAN_POINT('Ctrl Pts',(-151.146568085319,0.978613136485346,
125.984454042579));
#112151=CARTESIAN_POINT('Ctrl Pts',(-151.154342419439,0.844916126655815,
125.957308775738));
#112152=CARTESIAN_POINT('Ctrl Pts',(-151.162116753558,0.709877040642642,
125.935687561584));
#112153=CARTESIAN_POINT('Ctrl Pts',(-151.169891087677,0.573992139300663,
125.91971978261));
#112154=CARTESIAN_POINT('Ctrl Pts',(-151.177655840624,0.438274703954835,
125.903771682496));
#112155=CARTESIAN_POINT('Ctrl Pts',(-151.185420593571,0.301713911895122,
125.893463199796));
#112156=CARTESIAN_POINT('Ctrl Pts',(-151.193185346518,0.164817599560541,
125.888873030218));
#112157=CARTESIAN_POINT('Ctrl Pts',(-151.200942387404,0.0280572545732683,
125.88428741966));
#112158=CARTESIAN_POINT('Ctrl Pts',(-151.208699428289,-0.10903755930222,
125.885408832761));
#112159=CARTESIAN_POINT('Ctrl Pts',(-151.216456469174,-0.24595282758949,
125.89226429633));
#112160=CARTESIAN_POINT('Ctrl Pts',(-151.224207660414,-0.382764847007342,
125.89911459014));
#112161=CARTESIAN_POINT('Ctrl Pts',(-151.231958851654,-0.519397201439868,
125.911690308102));
#112162=CARTESIAN_POINT('Ctrl Pts',(-151.239710042894,-0.655335170818045,
125.929966411473));
#112163=CARTESIAN_POINT('Ctrl Pts',(-151.247457939671,-0.791215362933158,
125.948234747013));
#112164=CARTESIAN_POINT('Ctrl Pts',(-151.255205836449,-0.92640137032155,
125.972198597181));
#112165=CARTESIAN_POINT('Ctrl Pts',(-151.262953733226,-1.06038311339868,
126.001781027875));
#112166=CARTESIAN_POINT('Ctrl Pts',(-151.27070000931,-1.19433683038348,
126.031357270562));
#112167=CARTESIAN_POINT('Ctrl Pts',(-151.278446285394,-1.32708640258374,
126.066549671827));
#112168=CARTESIAN_POINT('Ctrl Pts',(-151.286192561478,-1.45813186352537,
126.10723016046));
#112169=CARTESIAN_POINT('Ctrl Pts',(-151.293938894744,-1.58917829181429,
126.147910949387));
#112170=CARTESIAN_POINT('Ctrl Pts',(-151.301685228009,-1.71852021035558,
126.19407979061));
#112171=CARTESIAN_POINT('Ctrl Pts',(-151.309431561275,-1.84567312347419,
126.245558825013));
#112172=CARTESIAN_POINT('Ctrl Pts',(-151.317179629278,-1.97285451160694,
126.297049387789));
#112173=CARTESIAN_POINT('Ctrl Pts',(-151.324927697281,-2.09784555652837,
126.353852363388));
#112174=CARTESIAN_POINT('Ctrl Pts',(-151.332675765284,-2.22018241263168,
126.415742028859));
#112175=CARTESIAN_POINT('Ctrl Pts',(-151.340432068026,-2.34264928980066,
126.477697471404));
#112176=CARTESIAN_POINT('Ctrl Pts',(-151.348188370768,-2.46245599367338,
126.544750226506));
#112177=CARTESIAN_POINT('Ctrl Pts',(-151.35594467351,-2.57916345791894,
126.616628663413));
#112178=CARTESIAN_POINT('Ctrl Pts',(-151.363705116024,-2.69593321245216,
126.688545464005));
#112179=CARTESIAN_POINT('Ctrl Pts',(-151.371465558538,-2.8096001074463,
126.765292859855));
#112180=CARTESIAN_POINT('Ctrl Pts',(-151.379226001052,-2.91975553102968,
126.846556845078));
#112181=CARTESIAN_POINT('Ctrl Pts',(-151.386998901318,-3.03008778587843,
126.927951282464));
#112182=CARTESIAN_POINT('Ctrl Pts',(-151.394771801583,-3.13689700014094,
127.013876552687));
#112183=CARTESIAN_POINT('Ctrl Pts',(-151.402544701849,-3.23980833813851,
127.103978881227));
#112184=CARTESIAN_POINT('Ctrl Pts',(-151.41003503761,-3.33897858977014,
127.190805763161));
#112185=CARTESIAN_POINT('Ctrl Pts',(-151.417525373371,-3.43452921682893,
127.281511070724));
#112186=CARTESIAN_POINT('Ctrl Pts',(-151.425015709133,-3.52615960416304,
127.375748433537));
#112187=CARTESIAN_POINT('Ctrl Pts',(-151.432687175097,-3.62000578411265,
127.472264630465));
#112188=CARTESIAN_POINT('Ctrl Pts',(-151.440358641061,-3.71005408140359,
127.572809541388));
#112189=CARTESIAN_POINT('Ctrl Pts',(-151.448030107026,-3.79593171616864,
127.677047798438));
#112190=CARTESIAN_POINT('Ctrl Pts',(-151.455692550273,-3.88170834681902,
127.781163456711));
#112191=CARTESIAN_POINT('Ctrl Pts',(-151.46335499352,-3.96332381434113,
127.888963517903));
#112192=CARTESIAN_POINT('Ctrl Pts',(-151.471017436767,-4.04044119313304,
128.000074963904));
#112193=CARTESIAN_POINT('Ctrl Pts',(-151.478672633333,-4.1174856389195,
128.111081327343));
#112194=CARTESIAN_POINT('Ctrl Pts',(-151.486327829899,-4.19004022802817,
128.225392519584));
#112195=CARTESIAN_POINT('Ctrl Pts',(-151.493983026465,-4.2578078167015,
128.342601966005));
#112196=CARTESIAN_POINT('Ctrl Pts',(-151.501632321317,-4.32552316047735,
128.459721050712));
#112197=CARTESIAN_POINT('Ctrl Pts',(-151.509281616169,-4.38845864790343,
128.579733596101));
#112198=CARTESIAN_POINT('Ctrl Pts',(-151.516930911021,-4.4463604043477,
128.702204054141));
#112199=CARTESIAN_POINT('Ctrl Pts',(-151.524576832615,-4.50423662673283,
128.824620504012));
#112200=CARTESIAN_POINT('Ctrl Pts',(-151.532222754209,-4.5570833629016,
128.949492347286));
#112201=CARTESIAN_POINT('Ctrl Pts',(-151.539868675803,-4.60469284971006,
129.07635980092));
#112202=CARTESIAN_POINT('Ctrl Pts',(-151.547513563034,-4.65229589576303,
129.203210091541));
#112203=CARTESIAN_POINT('Ctrl Pts',(-151.555158450265,-4.69466295854988,
129.332055080029));
#112204=CARTESIAN_POINT('Ctrl Pts',(-151.562803337496,-4.73163472374242,
129.462415796206));
#112205=CARTESIAN_POINT('Ctrl Pts',(-151.565142512869,-4.74294730953171,
129.502303445));
#112206=CARTESIAN_POINT('Ctrl Pts',(-151.567481688242,-4.75375512073537,
129.542332885786));
#112207=CARTESIAN_POINT('Ctrl Pts',(-151.569820863616,-4.76405452823393,
129.582490119308));
#112208=CARTESIAN_POINT('Origin',(213.235140564004,0.,130.804360617566));
#112209=CARTESIAN_POINT('',(-153.665379263862,-4.76405452823391,129.582490119308));
#112210=CARTESIAN_POINT('',(-153.319765814746,-4.76405452823394,129.582490119308));
#112211=CARTESIAN_POINT('',(213.235140564004,-4.76405452823405,129.582490119308));
#112212=CARTESIAN_POINT('',(-151.985140564048,-4.91824942752548,130.801987614138));
#112213=CARTESIAN_POINT('Ctrl Pts',(-151.985140564047,-4.91824942752548,
130.801987614138));
#112214=CARTESIAN_POINT('Ctrl Pts',(-151.992825592928,-4.91831456258477,
130.936985509313));
#112215=CARTESIAN_POINT('Ctrl Pts',(-152.000510621809,-4.91281729657113,
131.07221008295));
#112216=CARTESIAN_POINT('Ctrl Pts',(-152.00819565069,-4.90172794900123,
131.207158552616));
#112217=CARTESIAN_POINT('Ctrl Pts',(-152.015871793966,-4.89065142318675,
131.341950991797));
#112218=CARTESIAN_POINT('Ctrl Pts',(-152.023547937242,-4.87399570806901,
131.476467566512));
#112219=CARTESIAN_POINT('Ctrl Pts',(-152.031224080518,-4.85178311540639,
131.610204066108));
#112220=CARTESIAN_POINT('Ctrl Pts',(-152.038893284541,-4.82959060298433,
131.743819667566));
#112221=CARTESIAN_POINT('Ctrl Pts',(-152.046562488563,-4.80185127147943,
131.876656204003));
#112222=CARTESIAN_POINT('Ctrl Pts',(-152.054231692586,-4.76863931723582,
132.008213650379));
#112223=CARTESIAN_POINT('Ctrl Pts',(-152.062004104746,-4.73498041388242,
132.141541528061));
#112224=CARTESIAN_POINT('Ctrl Pts',(-152.069776516905,-4.69570054335466,
132.27355522112));
#112225=CARTESIAN_POINT('Ctrl Pts',(-152.077548929064,-4.65093081976605,
132.40374348988));
#112226=CARTESIAN_POINT('Ctrl Pts',(-152.085210972649,-4.60679682810612,
132.532083079833));
#112227=CARTESIAN_POINT('Ctrl Pts',(-152.092873016234,-4.55732801938075,
132.658648361305));
#112228=CARTESIAN_POINT('Ctrl Pts',(-152.100535059819,-4.50270033536339,
132.782964355665));
#112229=CARTESIAN_POINT('Ctrl Pts',(-152.108196415792,-4.4480775537778,
132.907269193581));
#112230=CARTESIAN_POINT('Ctrl Pts',(-152.115857771765,-4.38829697860385,
133.029324779174));
#112231=CARTESIAN_POINT('Ctrl Pts',(-152.123519127738,-4.32358248358636,
133.148676630847));
#112232=CARTESIAN_POINT('Ctrl Pts',(-152.131181544043,-4.25885903208279,
133.268045000816));
#112233=CARTESIAN_POINT('Ctrl Pts',(-152.138843960347,-4.18920049385073,
133.384708540768));
#112234=CARTESIAN_POINT('Ctrl Pts',(-152.146506376652,-4.11487616965667,
133.498238337674));
#112235=CARTESIAN_POINT('Ctrl Pts',(-152.154361643965,-4.03868121871575,
133.614625501625));
#112236=CARTESIAN_POINT('Ctrl Pts',(-152.162216911279,-3.95758274152315,
133.727718709357));
#112237=CARTESIAN_POINT('Ctrl Pts',(-152.170072178592,-3.87191670395517,
133.837089438304));
#112238=CARTESIAN_POINT('Ctrl Pts',(-152.177746001913,-3.78822941354097,
133.943933879998));
#112239=CARTESIAN_POINT('Ctrl Pts',(-152.185419825234,-3.70018357625764,
134.047225667719));
#112240=CARTESIAN_POINT('Ctrl Pts',(-152.193093648556,-3.60813113273665,
134.146601301819));
#112241=CARTESIAN_POINT('Ctrl Pts',(-152.201039637865,-3.51281388323865,
134.249501472061));
#112242=CARTESIAN_POINT('Ctrl Pts',(-152.208985627174,-3.41320092224242,
134.348202239315));
#112243=CARTESIAN_POINT('Ctrl Pts',(-152.216931616484,-3.30972107970913,
134.442344872209));
#112244=CARTESIAN_POINT('Ctrl Pts',(-152.224877605793,-3.2062412371761,
134.536487505102));
#112245=CARTESIAN_POINT('Ctrl Pts',(-152.232823595102,-3.09889491960027,
134.626071759748));
#112246=CARTESIAN_POINT('Ctrl Pts',(-152.240769584411,-2.98814391797463,
134.710788523975));
#112247=CARTESIAN_POINT('Ctrl Pts',(-152.24854391853,-2.87978544212651,
134.793675173447));
#112248=CARTESIAN_POINT('Ctrl Pts',(-152.256318252649,-2.76780399280436,
134.872181139208));
#112249=CARTESIAN_POINT('Ctrl Pts',(-152.264092586769,-2.65258925919592,
134.945973019095));
#112250=CARTESIAN_POINT('Ctrl Pts',(-152.271857339716,-2.53751651744961,
135.019673957085));
#112251=CARTESIAN_POINT('Ctrl Pts',(-152.279622092663,-2.41921874591742,
135.088672159913));
#112252=CARTESIAN_POINT('Ctrl Pts',(-152.28738684561,-2.29811821250707,
135.152674744195));
#112253=CARTESIAN_POINT('Ctrl Pts',(-152.295143886495,-2.17713795785372,
135.216613760208));
#112254=CARTESIAN_POINT('Ctrl Pts',(-152.30290092738,-2.05336082451832,
135.275566850218));
#112255=CARTESIAN_POINT('Ctrl Pts',(-152.310657968265,-1.92723723477123,
135.329284893552));
#112256=CARTESIAN_POINT('Ctrl Pts',(-152.318409159505,-1.80120875580408,
135.382962427693));
#112257=CARTESIAN_POINT('Ctrl Pts',(-152.326160350745,-1.67283770071316,
135.431412620412));
#112258=CARTESIAN_POINT('Ctrl Pts',(-152.333911541985,-1.54259789835482,
135.474432863955));
#112259=CARTESIAN_POINT('Ctrl Pts',(-152.341659438762,-1.41241345138656,
135.517434822746));
#112260=CARTESIAN_POINT('Ctrl Pts',(-152.349407335539,-1.28036220734792,
135.555011300176));
#112261=CARTESIAN_POINT('Ctrl Pts',(-152.357155232316,-1.14693651962243,
135.58700838658));
#112262=CARTESIAN_POINT('Ctrl Pts',(-152.364901508401,-1.01353874167486,
135.618998779884));
#112263=CARTESIAN_POINT('Ctrl Pts',(-152.372647784485,-0.878767471846586,
135.64541201245));
#112264=CARTESIAN_POINT('Ctrl Pts',(-152.380394060569,-0.743128334985456,
135.666144584408));
#112265=CARTESIAN_POINT('Ctrl Pts',(-152.388140393834,-0.607488196866845,
135.686877309409));
#112266=CARTESIAN_POINT('Ctrl Pts',(-152.395886727099,-0.47098056540843,
135.701929231052));
#112267=CARTESIAN_POINT('Ctrl Pts',(-152.403633060365,-0.334118928753958,
135.711248389255));
#112268=CARTESIAN_POINT('Ctrl Pts',(-152.411381128368,-0.197226642884703,
135.720569634418));
#112269=CARTESIAN_POINT('Ctrl Pts',(-152.419129196371,-0.059980584054659,
135.724155534947));
#112270=CARTESIAN_POINT('Ctrl Pts',(-152.426877264374,0.077103395447118,
135.722006205539));
#112271=CARTESIAN_POINT('Ctrl Pts',(-152.434633567116,0.214333069433443,
135.719854591798));
#112272=CARTESIAN_POINT('Ctrl Pts',(-152.442389869858,0.351399928443426,
135.7119555779));
#112273=CARTESIAN_POINT('Ctrl Pts',(-152.450146172599,0.48779032487234,
135.698361400306));
#112274=CARTESIAN_POINT('Ctrl Pts',(-152.457906615114,0.624253516962835,
135.684759967091));
#112275=CARTESIAN_POINT('Ctrl Pts',(-152.465667057628,0.760039140168273,
135.665457368357));
#112276=CARTESIAN_POINT('Ctrl Pts',(-152.473427500142,0.894642400244366,
135.64055726764));
#112277=CARTESIAN_POINT('Ctrl Pts',(-152.481200400407,1.02946173742268,
135.61561719507));
#112278=CARTESIAN_POINT('Ctrl Pts',(-152.488973300673,1.16309453724599,
135.585061751607));
#112279=CARTESIAN_POINT('Ctrl Pts',(-152.496746200938,1.29504898601056,
135.549045136724));
#112280=CARTESIAN_POINT('Ctrl Pts',(-152.5042365367,1.42220655818827,135.514337816511));
#112281=CARTESIAN_POINT('Ctrl Pts',(-152.511726872462,1.54780539171509,
135.4745595791));
#112282=CARTESIAN_POINT('Ctrl Pts',(-152.519217208224,1.6714236563107,135.429890427612));
#112283=CARTESIAN_POINT('Ctrl Pts',(-152.526991542343,1.79972894498233,
135.383527631668));
#112284=CARTESIAN_POINT('Ctrl Pts',(-152.534765876462,1.92630694603927,
135.331748858983));
#112285=CARTESIAN_POINT('Ctrl Pts',(-152.542540210581,2.05066652227431,
135.274701754093));
#112286=CARTESIAN_POINT('Ctrl Pts',(-152.550304963528,2.17487283644597,
135.217724954661));
#112287=CARTESIAN_POINT('Ctrl Pts',(-152.558069716475,2.2968658137131,135.155492903108));
#112288=CARTESIAN_POINT('Ctrl Pts',(-152.565834469423,2.41617079687032,
135.088202554759));
#112289=CARTESIAN_POINT('Ctrl Pts',(-152.573591510307,2.53535728463604,
135.020979040133));
#112290=CARTESIAN_POINT('Ctrl Pts',(-152.581348551192,2.65186075289129,
134.948707417466));
#112291=CARTESIAN_POINT('Ctrl Pts',(-152.589105592077,2.76522814512081,
134.871631983965));
#112292=CARTESIAN_POINT('Ctrl Pts',(-152.596856783317,2.87851004611781,
134.794614673648));
#112293=CARTESIAN_POINT('Ctrl Pts',(-152.604607974558,2.98866025634705,
134.71280098197));
#112294=CARTESIAN_POINT('Ctrl Pts',(-152.612359165798,3.09525220009408,
134.626480040126));
#112295=CARTESIAN_POINT('Ctrl Pts',(-152.620107062575,3.20179883942202,
134.540195786985));
#112296=CARTESIAN_POINT('Ctrl Pts',(-152.627854959352,3.30478991703817,
134.449408339397));
#112297=CARTESIAN_POINT('Ctrl Pts',(-152.635602856129,3.40382981535404,
134.354448736276));
#112298=CARTESIAN_POINT('Ctrl Pts',(-152.643349132213,3.50284899665824,
134.259508996657));
#112299=CARTESIAN_POINT('Ctrl Pts',(-152.651095408297,3.59791836059156,
134.160399107811));
#112300=CARTESIAN_POINT('Ctrl Pts',(-152.658841684381,3.68867752720004,
134.057488522034));
#112301=CARTESIAN_POINT('Ctrl Pts',(-152.666588017647,3.77943736377219,
133.954577176595));
#112302=CARTESIAN_POINT('Ctrl Pts',(-152.674334350912,3.8658866809311,133.847865371464));
#112303=CARTESIAN_POINT('Ctrl Pts',(-152.682080684177,3.94770421030237,
133.737757033065));
#112304=CARTESIAN_POINT('Ctrl Pts',(-152.68982875218,4.02954006214171,133.627624036667));
#112305=CARTESIAN_POINT('Ctrl Pts',(-152.697576820183,4.10674182903347,
133.51409330719));
#112306=CARTESIAN_POINT('Ctrl Pts',(-152.705324888186,4.17903077671307,
133.397598907771));
#112307=CARTESIAN_POINT('Ctrl Pts',(-152.713081190928,4.25139655394662,
133.280980696717));
#112308=CARTESIAN_POINT('Ctrl Pts',(-152.72083749367,4.31883887518129,133.161392856341));
#112309=CARTESIAN_POINT('Ctrl Pts',(-152.728593796412,4.38112404935522,
133.039295768004));
#112310=CARTESIAN_POINT('Ctrl Pts',(-152.736354238926,4.44344246700198,
132.917133512774));
#112311=CARTESIAN_POINT('Ctrl Pts',(-152.74411468144,4.50059809010008,132.792459696215));
#112312=CARTESIAN_POINT('Ctrl Pts',(-152.751875123954,4.55240528009769,
132.665755048695));
#112313=CARTESIAN_POINT('Ctrl Pts',(-152.75964802422,4.60429563559604,132.538847003626));
#112314=CARTESIAN_POINT('Ctrl Pts',(-152.767420924485,4.65082026810285,
132.409901980907));
#112315=CARTESIAN_POINT('Ctrl Pts',(-152.775193824751,4.69184307268158,
132.279417105918));
#112316=CARTESIAN_POINT('Ctrl Pts',(-152.782684160513,4.73137459498434,
132.153675684804));
#112317=CARTESIAN_POINT('Ctrl Pts',(-152.790174496275,4.76579727471635,
132.026504720053));
#112318=CARTESIAN_POINT('Ctrl Pts',(-152.797664832037,4.79503454403202,
131.89835640551));
#112319=CARTESIAN_POINT('Ctrl Pts',(-152.805439166156,4.82538035329972,
131.765349308674));
#112320=CARTESIAN_POINT('Ctrl Pts',(-152.813213500275,4.85023590679922,
131.630867960106));
#112321=CARTESIAN_POINT('Ctrl Pts',(-152.820987834394,4.86945995040386,
131.495405372928));
#112322=CARTESIAN_POINT('Ctrl Pts',(-152.828752587341,4.88866030209292,
131.360109731281));
#112323=CARTESIAN_POINT('Ctrl Pts',(-152.836517340288,4.90224289867473,
131.223835640518));
#112324=CARTESIAN_POINT('Ctrl Pts',(-152.844282093236,4.91011688042973,
131.087088902354));
#112325=CARTESIAN_POINT('Ctrl Pts',(-152.852039134121,4.91798304163505,
130.950477982978));
#112326=CARTESIAN_POINT('Ctrl Pts',(-152.859796175006,4.92015184899466,
130.813395738201));
#112327=CARTESIAN_POINT('Ctrl Pts',(-152.867553215891,4.91658394855288,
130.676355385906));
#112328=CARTESIAN_POINT('Ctrl Pts',(-152.875304407131,4.91301873869258,
130.539418376808));
#112329=CARTESIAN_POINT('Ctrl Pts',(-152.883055598371,4.90372544199692,
130.402523586564));
#112330=CARTESIAN_POINT('Ctrl Pts',(-152.890806789611,4.8887167381356,130.266186187875));
#112331=CARTESIAN_POINT('Ctrl Pts',(-152.898554686388,4.87371441337377,
130.129906736218));
#112332=CARTESIAN_POINT('Ctrl Pts',(-152.906302583165,4.85300155563226,
129.994184592733));
#112333=CARTESIAN_POINT('Ctrl Pts',(-152.914050479942,4.82664283635449,
129.85953153632));
#112334=CARTESIAN_POINT('Ctrl Pts',(-152.921796756026,4.80028963075256,
129.724906646424));
#112335=CARTESIAN_POINT('Ctrl Pts',(-152.92954303211,4.7682929877327,129.591350782228));
#112336=CARTESIAN_POINT('Ctrl Pts',(-152.937289308194,4.73076894380699,
129.459366839584));
#112337=CARTESIAN_POINT('Ctrl Pts',(-152.94503564146,4.69324462288736,129.327381922664));
#112338=CARTESIAN_POINT('Ctrl Pts',(-152.952781974725,4.65019292656167,
129.196969326513));
#112339=CARTESIAN_POINT('Ctrl Pts',(-152.960528307991,4.60178003616608,
129.06861767541));
#112340=CARTESIAN_POINT('Ctrl Pts',(-152.968276375994,4.55335630403916,
128.940237280845));
#112341=CARTESIAN_POINT('Ctrl Pts',(-152.976024443997,4.49956912673542,
128.813919115466));
#112342=CARTESIAN_POINT('Ctrl Pts',(-152.983772512,4.44063303118699,128.690132308033));
#112343=CARTESIAN_POINT('Ctrl Pts',(-152.991528814741,4.38163429765495,
128.566213938508));
#112344=CARTESIAN_POINT('Ctrl Pts',(-152.999285117483,4.31747588264024,
128.444832654769));
#112345=CARTESIAN_POINT('Ctrl Pts',(-153.007041420225,4.24841880229327,
128.326433915095));
#112346=CARTESIAN_POINT('Ctrl Pts',(-153.014801862739,4.17932486410306,
128.207971982448));
#112347=CARTESIAN_POINT('Ctrl Pts',(-153.022562305254,4.1053272616742,128.092496094826));
#112348=CARTESIAN_POINT('Ctrl Pts',(-153.030322747768,4.02673010490752,
127.980422281707));
#112349=CARTESIAN_POINT('Ctrl Pts',(-153.038095648033,3.94800677700748,
127.868168557755));
#112350=CARTESIAN_POINT('Ctrl Pts',(-153.045868548299,3.86466937777846,
127.759328132344));
#112351=CARTESIAN_POINT('Ctrl Pts',(-153.053641448564,3.77706258483867,
127.654284222824));
#112352=CARTESIAN_POINT('Ctrl Pts',(-153.061131784326,3.69264051949069,
127.553058924005));
#112353=CARTESIAN_POINT('Ctrl Pts',(-153.068622120088,3.60425428439401,
127.455359135876));
#112354=CARTESIAN_POINT('Ctrl Pts',(-153.07611245585,3.51224293624735,127.361493698953));
#112355=CARTESIAN_POINT('Ctrl Pts',(-153.083886789969,3.41674294986907,
127.264069325459));
#112356=CARTESIAN_POINT('Ctrl Pts',(-153.091661124088,3.31703501640613,
127.170467190563));
#112357=CARTESIAN_POINT('Ctrl Pts',(-153.099435458207,3.21345757045418,
127.081072620998));
#112358=CARTESIAN_POINT('Ctrl Pts',(-153.107200211154,3.11000777444794,
126.99178822225));
#112359=CARTESIAN_POINT('Ctrl Pts',(-153.114964964101,3.00269824763277,
126.90670132433));
#112360=CARTESIAN_POINT('Ctrl Pts',(-153.122729717049,2.89190542341845,
126.826161768275));
#112361=CARTESIAN_POINT('Ctrl Pts',(-153.130486757934,2.78122264019844,
126.745702205241));
#112362=CARTESIAN_POINT('Ctrl Pts',(-153.138243798819,2.66706375865052,
126.669781224464));
#112363=CARTESIAN_POINT('Ctrl Pts',(-153.146000839704,2.5498392917413,126.598709342342));
#112364=CARTESIAN_POINT('Ctrl Pts',(-153.153752030944,2.43270322471429,
126.527691056079));
#112365=CARTESIAN_POINT('Ctrl Pts',(-153.161503222184,2.31250650675344,
126.46151479182));
#112366=CARTESIAN_POINT('Ctrl Pts',(-153.169254413424,2.18968942091553,
126.40044834523));
#112367=CARTESIAN_POINT('Ctrl Pts',(-153.177002310201,2.06692453561584,
126.339407853509));
#112368=CARTESIAN_POINT('Ctrl Pts',(-153.184750206978,1.94154184690188,
126.283473033594));
#112369=CARTESIAN_POINT('Ctrl Pts',(-153.192498103755,1.81400688535183,
126.232866104565));
#112370=CARTESIAN_POINT('Ctrl Pts',(-153.20024437984,1.68649860136605,126.182269761415));
#112371=CARTESIAN_POINT('Ctrl Pts',(-153.207990655924,1.55683930320513,
126.136999236498));
#112372=CARTESIAN_POINT('Ctrl Pts',(-153.215736932008,1.42551481196126,
126.097228732503));
#112373=CARTESIAN_POINT('Ctrl Pts',(-153.223483265273,1.29418935131037,
126.057457934931));
#112374=CARTESIAN_POINT('Ctrl Pts',(-153.231229598538,1.16119904723143,
126.023187352613));
#112375=CARTESIAN_POINT('Ctrl Pts',(-153.238975931804,1.02704481824168,
125.994541285842));
#112376=CARTESIAN_POINT('Ctrl Pts',(-153.246723999807,0.8928605463416,125.965888803984));
#112377=CARTESIAN_POINT('Ctrl Pts',(-153.25447206781,0.757512213134137,
125.942863425702));
#112378=CARTESIAN_POINT('Ctrl Pts',(-153.262220135813,0.621510466977741,
125.925538238965));
#112379=CARTESIAN_POINT('Ctrl Pts',(-153.269976438555,0.485364176547275,
125.908194638814));
#112380=CARTESIAN_POINT('Ctrl Pts',(-153.277732741296,0.348563474368509,
125.896563381663));
#112381=CARTESIAN_POINT('Ctrl Pts',(-153.285489044038,0.211624222713222,
125.890665648313));
#112382=CARTESIAN_POINT('Ctrl Pts',(-153.293249486553,0.074611882456538,
125.884764767166));
#112383=CARTESIAN_POINT('Ctrl Pts',(-153.301009929067,-0.0625387638507193,
125.884603507895));
#112384=CARTESIAN_POINT('Ctrl Pts',(-153.308770371581,-0.199313319997331,
125.890150888325));
#112385=CARTESIAN_POINT('Ctrl Pts',(-153.316543271846,-0.336307438803744,
125.895707173901));
#112386=CARTESIAN_POINT('Ctrl Pts',(-153.324316172112,-0.47292387113516,
125.906990379601));
#112387=CARTESIAN_POINT('Ctrl Pts',(-153.332089072377,-0.608653898711304,
125.923917656719));
#112388=CARTESIAN_POINT('Ctrl Pts',(-153.339579408139,-0.739449797899905,
125.940229584676));
#112389=CARTESIAN_POINT('Ctrl Pts',(-153.347069743901,-0.869422315676756,
125.961782305557));
#112390=CARTESIAN_POINT('Ctrl Pts',(-153.354560079663,-0.998128347341169,
125.988457497202));
#112391=CARTESIAN_POINT('Ctrl Pts',(-153.362334413782,-1.13171430731719,
126.016144086846));
#112392=CARTESIAN_POINT('Ctrl Pts',(-153.370108747901,-1.26435900789317,
126.049436954873));
#112393=CARTESIAN_POINT('Ctrl Pts',(-153.37788308202,-1.39555533061107,
126.088259645184));
#112394=CARTESIAN_POINT('Ctrl Pts',(-153.385647834967,-1.52658996558657,
126.127034489999));
#112395=CARTESIAN_POINT('Ctrl Pts',(-153.393412587914,-1.65617940301768,
126.171325487383));
#112396=CARTESIAN_POINT('Ctrl Pts',(-153.401177340861,-1.78382584027905,
126.221005030875));
#112397=CARTESIAN_POINT('Ctrl Pts',(-153.408934381746,-1.91134549729944,
126.270635231944));
#112398=CARTESIAN_POINT('Ctrl Pts',(-153.416691422632,-2.03692563258346,
126.325643187554));
#112399=CARTESIAN_POINT('Ctrl Pts',(-153.424448463517,-2.16008310760382,
126.38585136322));
#112400=CARTESIAN_POINT('Ctrl Pts',(-153.432199654757,-2.28314770861475,
126.446014135432));
#112401=CARTESIAN_POINT('Ctrl Pts',(-153.439950845997,-2.40379293597087,
126.511369151123));
#112402=CARTESIAN_POINT('Ctrl Pts',(-153.447702037237,-2.52155550184845,
126.581690737786));
#112403=CARTESIAN_POINT('Ctrl Pts',(-153.455449934014,-2.63926801549364,
126.651982435899));
#112404=CARTESIAN_POINT('Ctrl Pts',(-153.463197830791,-2.75409996953678,
126.727236306488));
#112405=CARTESIAN_POINT('Ctrl Pts',(-153.470945727568,-2.86561277412387,
126.807180800335));
#112406=CARTESIAN_POINT('Ctrl Pts',(-153.478692003652,-2.97710225263617,
126.887108571517));
#112407=CARTESIAN_POINT('Ctrl Pts',(-153.486438279736,-3.08527364513676,
126.97172478669));
#112408=CARTESIAN_POINT('Ctrl Pts',(-153.494184555821,-3.18971779180335,
127.060714871618));
#112409=CARTESIAN_POINT('Ctrl Pts',(-153.501930889086,-3.29416270945276,
127.149705613451));
#112410=CARTESIAN_POINT('Ctrl Pts',(-153.509677222351,-3.39488002877393,
127.243070035905));
#112411=CARTESIAN_POINT('Ctrl Pts',(-153.517423555617,-3.49149441371472,
127.340453889391));
#112412=CARTESIAN_POINT('Ctrl Pts',(-153.52517162362,-3.58813043477726,
127.437859551315));
#112413=CARTESIAN_POINT('Ctrl Pts',(-153.532919691623,-3.68066141780383,
127.539286157918));
#112414=CARTESIAN_POINT('Ctrl Pts',(-153.540667759626,-3.76874985390454,
127.644343592106));
#112415=CARTESIAN_POINT('Ctrl Pts',(-153.548424062367,-3.85693191144352,
127.749512682586));
#112416=CARTESIAN_POINT('Ctrl Pts',(-153.556180365109,-3.94066173856956,
127.858320009126));
#112417=CARTESIAN_POINT('Ctrl Pts',(-153.563936667851,-4.01964267911597,
127.970343010929));
#112418=CARTESIAN_POINT('Ctrl Pts',(-153.571697110365,-4.09866577416863,
128.082425802781));
#112419=CARTESIAN_POINT('Ctrl Pts',(-153.579457552879,-4.17293472057995,
128.197727361253));
#112420=CARTESIAN_POINT('Ctrl Pts',(-153.587217995394,-4.24219754081677,
128.31579816362));
#112421=CARTESIAN_POINT('Ctrl Pts',(-153.594990895659,-4.31157154788131,
128.434058503721));
#112422=CARTESIAN_POINT('Ctrl Pts',(-153.602763795924,-4.37592318608638,
128.555096625708));
#112423=CARTESIAN_POINT('Ctrl Pts',(-153.61053669619,-4.43504718373698,
128.678439748736));
#112424=CARTESIAN_POINT('Ctrl Pts',(-153.618027031952,-4.49202187514845,
128.797299038559));
#112425=CARTESIAN_POINT('Ctrl Pts',(-153.625517367714,-4.5441422812807,
128.91829837087));
#112426=CARTESIAN_POINT('Ctrl Pts',(-153.633007703476,-4.59126844100411,
129.041000993116));
#112427=CARTESIAN_POINT('Ctrl Pts',(-153.641883209428,-4.64710953069987,
129.186394722947));
#112428=CARTESIAN_POINT('Ctrl Pts',(-153.650758715381,-4.69608666589014,
129.334563409874));
#112429=CARTESIAN_POINT('Ctrl Pts',(-153.659634221333,-4.73795109743712,
129.484890094669));
#112430=CARTESIAN_POINT('Ctrl Pts',(-153.661549235509,-4.74698393233495,
129.517325173191));
#112431=CARTESIAN_POINT('Ctrl Pts',(-153.663464249686,-4.75568581355614,
129.549860627792));
#112432=CARTESIAN_POINT('Ctrl Pts',(-153.665379263862,-4.76405452823391,
129.582490119308));
#112433=CARTESIAN_POINT('Ctrl Pts',(-151.915051610183,-4.76405452823401,
129.582490119308));
#112434=CARTESIAN_POINT('Ctrl Pts',(-151.922930001919,-4.79858365450474,
129.717118658585));
#112435=CARTESIAN_POINT('Ctrl Pts',(-151.930808393655,-4.82736512749261,
129.853069661433));
#112436=CARTESIAN_POINT('Ctrl Pts',(-151.938686785391,-4.85032903477576,
129.989810854254));
#112437=CARTESIAN_POINT('Ctrl Pts',(-151.946565177126,-4.87329294205884,
130.126552047075));
#112438=CARTESIAN_POINT('Ctrl Pts',(-151.954443568862,-4.89043929396322,
130.264083010487));
#112439=CARTESIAN_POINT('Ctrl Pts',(-151.962321960598,-4.90175321058763,
130.401870213961));
#112440=CARTESIAN_POINT('Ctrl Pts',(-151.969928161735,-4.91267624264595,
130.534897006605));
#112441=CARTESIAN_POINT('Ctrl Pts',(-151.977534362873,-4.91818496055907,
130.668374433924));
#112442=CARTESIAN_POINT('Ctrl Pts',(-151.985140564011,-4.91824942752517,
130.801987613495));
#112443=CARTESIAN_POINT('',(-151.639859435965,-4.91824790957522,130.808895202333));
#112444=CARTESIAN_POINT('Ctrl Pts',(-151.569820863616,-4.76405452823393,
129.582490119308));
#112445=CARTESIAN_POINT('Ctrl Pts',(-151.577468334592,-4.7977264028668,
129.713776247459));
#112446=CARTESIAN_POINT('Ctrl Pts',(-151.585115805568,-4.82596040729268,
129.846428963026));
#112447=CARTESIAN_POINT('Ctrl Pts',(-151.592763276544,-4.84866308297735,
129.979952120356));
#112448=CARTESIAN_POINT('Ctrl Pts',(-151.600612636447,-4.87196509651644,
130.117000213853));
#112449=CARTESIAN_POINT('Ctrl Pts',(-151.608461996351,-4.88943959269887,
130.254964903359));
#112450=CARTESIAN_POINT('Ctrl Pts',(-151.616311356255,-4.90104222611252,
130.393303248867));
#112451=CARTESIAN_POINT('Ctrl Pts',(-151.624160716158,-4.91264485952617,
130.531641594374));
#112452=CARTESIAN_POINT('Ctrl Pts',(-151.632010076062,-4.91837564423588,
130.670353139465));
#112453=CARTESIAN_POINT('Ctrl Pts',(-151.639859435965,-4.91824790957522,
130.808895202333));
#112454=CARTESIAN_POINT('Ctrl Pts',(-151.639859435994,-4.91824790957475,
130.80889520284));
#112455=CARTESIAN_POINT('Ctrl Pts',(-151.650460085486,-4.91807540244884,
130.995997828581));
#112456=CARTESIAN_POINT('Ctrl Pts',(-151.661060734978,-4.90722241257785,
131.182627316781));
#112457=CARTESIAN_POINT('Ctrl Pts',(-151.67166138447,-4.88587253895692,
131.367772186108));
#112458=CARTESIAN_POINT('Ctrl Pts',(-151.682262033962,-4.86452266533604,
131.552917055434));
#112459=CARTESIAN_POINT('Ctrl Pts',(-151.692862683455,-4.83267605973099,
131.736577937587));
#112460=CARTESIAN_POINT('Ctrl Pts',(-151.703463332947,-4.79056393105034,
131.917769924613));
#112461=CARTESIAN_POINT('Ctrl Pts',(-151.711237667066,-4.759679619757,132.050653013322));
#112462=CARTESIAN_POINT('Ctrl Pts',(-151.719012001185,-4.72321323218033,
132.182460578467));
#112463=CARTESIAN_POINT('Ctrl Pts',(-151.726786335304,-4.68125337184728,
132.312687482363));
#112464=CARTESIAN_POINT('Ctrl Pts',(-151.734551088251,-4.63934522329203,
132.442753893239));
#112465=CARTESIAN_POINT('Ctrl Pts',(-151.742315841198,-4.59195719143878,
132.5712431503));
#112466=CARTESIAN_POINT('Ctrl Pts',(-151.750080594145,-4.53922879189337,
132.697660656479));
#112467=CARTESIAN_POINT('Ctrl Pts',(-151.75783763503,-4.48655276293787,
132.823952603007));
#112468=CARTESIAN_POINT('Ctrl Pts',(-151.765594675915,-4.42854707127498,
132.948176535053));
#112469=CARTESIAN_POINT('Ctrl Pts',(-151.7733517168,-4.36540079425787,133.069853713559));
#112470=CARTESIAN_POINT('Ctrl Pts',(-151.78110290804,-4.30230213633922,
133.191439134359));
#112471=CARTESIAN_POINT('Ctrl Pts',(-151.78885409928,-4.23407078847632,
133.310481278696));
#112472=CARTESIAN_POINT('Ctrl Pts',(-151.79660529052,-4.16094347581855,
133.426522407682));
#112473=CARTESIAN_POINT('Ctrl Pts',(-151.804353187297,-4.0878472442195,
133.542514216092));
#112474=CARTESIAN_POINT('Ctrl Pts',(-151.812101084074,-4.00985939461461,
133.655507215972));
#112475=CARTESIAN_POINT('Ctrl Pts',(-151.819848980851,-3.92726192297093,
133.765069460205));
#112476=CARTESIAN_POINT('Ctrl Pts',(-151.827595256935,-3.84468172893774,
133.874608786379));
#112477=CARTESIAN_POINT('Ctrl Pts',(-151.83534153302,-3.75749406598494,
133.980718472339));
#112478=CARTESIAN_POINT('Ctrl Pts',(-151.843087809104,-3.6660232364665,
134.082997025005));
#112479=CARTESIAN_POINT('Ctrl Pts',(-151.850834142369,-3.57455173173131,
134.185276332669));
#112480=CARTESIAN_POINT('Ctrl Pts',(-151.858580475634,-3.47879725796815,
134.283724159185));
#112481=CARTESIAN_POINT('Ctrl Pts',(-151.8663268089,-3.37912296978222,134.377973777603));
#112482=CARTESIAN_POINT('Ctrl Pts',(-151.874074876903,-3.27942636023042,
134.472244502569));
#112483=CARTESIAN_POINT('Ctrl Pts',(-151.881822944905,-3.17580847352705,
134.562314880064));
#112484=CARTESIAN_POINT('Ctrl Pts',(-151.889571012908,-3.06866741370414,
134.647856860126));
#112485=CARTESIAN_POINT('Ctrl Pts',(-151.89732731565,-2.96141248308801,
134.733489755222));
#112486=CARTESIAN_POINT('Ctrl Pts',(-151.905083618392,-2.8506272053868,
134.814584394403));
#112487=CARTESIAN_POINT('Ctrl Pts',(-151.912839921134,-2.73674113864215,
134.890854347228));
#112488=CARTESIAN_POINT('Ctrl Pts',(-151.920600363648,-2.62279428747433,
134.967165007622));
#112489=CARTESIAN_POINT('Ctrl Pts',(-151.928360806162,-2.50574368307037,
135.038645646929));
#112490=CARTESIAN_POINT('Ctrl Pts',(-151.936121248676,-2.38604476546982,
135.105055147485));
#112491=CARTESIAN_POINT('Ctrl Pts',(-151.943894148942,-2.26615369654069,
135.171571254466));
#112492=CARTESIAN_POINT('Ctrl Pts',(-151.951667049207,-2.14360616866237,
135.2329997798));
#112493=CARTESIAN_POINT('Ctrl Pts',(-151.959439949473,-2.01887975248573,
135.289146856341));
#112494=CARTESIAN_POINT('Ctrl Pts',(-151.966930285235,-1.89868745570637,
135.343252845223));
#112495=CARTESIAN_POINT('Ctrl Pts',(-151.974420620996,-1.77647222218059,
135.392454591621));
#112496=CARTESIAN_POINT('Ctrl Pts',(-151.981910956758,-1.65267403736753,
135.436622655568));
#112497=CARTESIAN_POINT('Ctrl Pts',(-151.989685290877,-1.52418200674763,
135.482465365085));
#112498=CARTESIAN_POINT('Ctrl Pts',(-151.997459624996,-1.39357759598124,
135.523030368974));
#112499=CARTESIAN_POINT('Ctrl Pts',(-152.005233959115,-1.26133368407946,
135.558119172637));
#112500=CARTESIAN_POINT('Ctrl Pts',(-152.012998712062,-1.12925275098013,
135.593164732484));
#112501=CARTESIAN_POINT('Ctrl Pts',(-152.020763465009,-0.995536711276644,
135.622747421154));
#112502=CARTESIAN_POINT('Ctrl Pts',(-152.028528217957,-0.860677095082207,
135.646717275279));
#112503=CARTESIAN_POINT('Ctrl Pts',(-152.036285258841,-0.725951423359762,
135.670663322208));
#112504=CARTESIAN_POINT('Ctrl Pts',(-152.044042299727,-0.590084817913392,
135.689007560615));
#112505=CARTESIAN_POINT('Ctrl Pts',(-152.051799340611,-0.453582256398363,
135.701650296478));
#112506=CARTESIAN_POINT('Ctrl Pts',(-152.059550531852,-0.317182632526622,
135.714283498356));
#112507=CARTESIAN_POINT('Ctrl Pts',(-152.067301723092,-0.180148394883785,
135.721223719768));
#112508=CARTESIAN_POINT('Ctrl Pts',(-152.075052914332,-0.0429926078877076,
135.722422705235));
#112509=CARTESIAN_POINT('Ctrl Pts',(-152.082800811109,0.0941048842399591,
135.723621181101));
#112510=CARTESIAN_POINT('Ctrl Pts',(-152.090548707886,0.231323432837869,
135.719083270942));
#112511=CARTESIAN_POINT('Ctrl Pts',(-152.098296604663,0.368147202853541,
135.708812747981));
#112512=CARTESIAN_POINT('Ctrl Pts',(-152.106042880747,0.504942352286105,
135.698544373392));
#112513=CARTESIAN_POINT('Ctrl Pts',(-152.113789156831,0.641342497769553,
135.682545800402));
#112514=CARTESIAN_POINT('Ctrl Pts',(-152.121535432915,0.776834558460905,
135.660872856949));
#112515=CARTESIAN_POINT('Ctrl Pts',(-152.12928176618,0.912327619323686,
135.639199753512));
#112516=CARTESIAN_POINT('Ctrl Pts',(-152.137028099446,1.04691219596097,
135.611852257782));
#112517=CARTESIAN_POINT('Ctrl Pts',(-152.144774432711,1.18008345666775,
135.578937677139));
#112518=CARTESIAN_POINT('Ctrl Pts',(-152.152522500714,1.3132845401552,135.546015725504));
#112519=CARTESIAN_POINT('Ctrl Pts',(-152.160270568717,1.4450712984376,135.507524301937));
#112520=CARTESIAN_POINT('Ctrl Pts',(-152.16801863672,1.57495254883828,135.463621023618));
#112521=CARTESIAN_POINT('Ctrl Pts',(-152.175774939462,1.70497183857732,
135.419671084373));
#112522=CARTESIAN_POINT('Ctrl Pts',(-152.183531242204,1.83308120391858,
135.370297925966));
#112523=CARTESIAN_POINT('Ctrl Pts',(-152.191287544945,1.95880747620422,
135.315708125093));
#112524=CARTESIAN_POINT('Ctrl Pts',(-152.19904798746,2.08460085238727,135.261089187998));
#112525=CARTESIAN_POINT('Ctrl Pts',(-152.206808429974,2.20800824947343,
135.201248231026));
#112526=CARTESIAN_POINT('Ctrl Pts',(-152.214568872488,2.32858063187714,
135.136438098792));
#112527=CARTESIAN_POINT('Ctrl Pts',(-152.222341772753,2.44934656777267,
135.071523927581));
#112528=CARTESIAN_POINT('Ctrl Pts',(-152.230114673019,2.56726805809014,
135.001624840069));
#112529=CARTESIAN_POINT('Ctrl Pts',(-152.237887573284,2.68192385830763,
134.927037840044));
#112530=CARTESIAN_POINT('Ctrl Pts',(-152.245377909046,2.79241163139165,
134.85516226534));
#112531=CARTESIAN_POINT('Ctrl Pts',(-152.252868244809,2.89986677310276,
134.778933873803));
#112532=CARTESIAN_POINT('Ctrl Pts',(-152.260358580571,3.00394255904258,
134.698652872196));
#112533=CARTESIAN_POINT('Ctrl Pts',(-152.26813291469,3.11196441003506,134.615327992016));
#112534=CARTESIAN_POINT('Ctrl Pts',(-152.275907248809,3.21668777087802,
134.527373177787));
#112535=CARTESIAN_POINT('Ctrl Pts',(-152.283681582928,3.31769003978603,
134.435078984832));
#112536=CARTESIAN_POINT('Ctrl Pts',(-152.291446335875,3.41856783242444,
134.342898536222));
#112537=CARTESIAN_POINT('Ctrl Pts',(-152.299211088822,3.5157333718833,134.246389610807));
#112538=CARTESIAN_POINT('Ctrl Pts',(-152.306975841769,3.60879480570351,
134.145884687931));
#112539=CARTESIAN_POINT('Ctrl Pts',(-152.314732882654,3.70176380959571,
134.045479587961));
#112540=CARTESIAN_POINT('Ctrl Pts',(-152.322489923539,3.79063655587374,
133.941086673798));
#112541=CARTESIAN_POINT('Ctrl Pts',(-152.330246964424,3.8750562163759,133.833076910391));
#112542=CARTESIAN_POINT('Ctrl Pts',(-152.337998155665,3.9594122153555,133.725148597988));
#112543=CARTESIAN_POINT('Ctrl Pts',(-152.345749346905,4.03932157287999,
133.613609172044));
#112544=CARTESIAN_POINT('Ctrl Pts',(-152.353500538145,4.11446636639845,
133.498864204922));
#112545=CARTESIAN_POINT('Ctrl Pts',(-152.361248434922,4.18957922137501,
133.384168007472));
#112546=CARTESIAN_POINT('Ctrl Pts',(-152.368996331699,4.25993132630397,
133.266269305019));
#112547=CARTESIAN_POINT('Ctrl Pts',(-152.376744228476,4.32524703426072,
133.145604123722));
#112548=CARTESIAN_POINT('Ctrl Pts',(-152.38449050456,4.39054907957941,133.02496418298));
#112549=CARTESIAN_POINT('Ctrl Pts',(-152.392236780644,4.45081663741246,
132.901559258044));
#112550=CARTESIAN_POINT('Ctrl Pts',(-152.399983056729,4.50581934465717,
132.775851194722));
#112551=CARTESIAN_POINT('Ctrl Pts',(-152.407729389994,4.56082245791946,
132.650142203451));
#112552=CARTESIAN_POINT('Ctrl Pts',(-152.415475723259,4.61056048632403,
132.52213039805));
#112553=CARTESIAN_POINT('Ctrl Pts',(-152.423222056525,4.65485083674059,
132.39229850999));
#112554=CARTESIAN_POINT('Ctrl Pts',(-152.430970124527,4.69915110567397,
132.262437546978));
#112555=CARTESIAN_POINT('Ctrl Pts',(-152.438718192531,4.73800114281547,
132.130756060197));
#112556=CARTESIAN_POINT('Ctrl Pts',(-152.446466260534,4.77126805972803,
131.997752491478));
#112557=CARTESIAN_POINT('Ctrl Pts',(-152.454222563275,4.80457033311571,
131.864607564984));
#112558=CARTESIAN_POINT('Ctrl Pts',(-152.461978866017,4.83227753783932,
131.73013812955));
#112559=CARTESIAN_POINT('Ctrl Pts',(-152.469735168759,4.85430771350575,
131.594853935121));
#112560=CARTESIAN_POINT('Ctrl Pts',(-152.477495611273,4.8763496473403,131.459497535443));
#112561=CARTESIAN_POINT('Ctrl Pts',(-152.485256053787,4.89270846797341,
131.323325898254));
#112562=CARTESIAN_POINT('Ctrl Pts',(-152.493016496302,4.90335418604,131.186853478603));
#112563=CARTESIAN_POINT('Ctrl Pts',(-152.500789396567,4.9140169935583,131.050161981308));
#112564=CARTESIAN_POINT('Ctrl Pts',(-152.508562296832,4.91894835749858,
130.913169127612));
#112565=CARTESIAN_POINT('Ctrl Pts',(-152.516335197098,4.91817046260457,
130.776389860265));
#112566=CARTESIAN_POINT('Ctrl Pts',(-152.52382553286,4.91742084614935,130.644582863812));
#112567=CARTESIAN_POINT('Ctrl Pts',(-152.531315868622,4.91136987028146,
130.5129745022));
#112568=CARTESIAN_POINT('Ctrl Pts',(-152.538806204384,4.90008269444702,
130.382018753573));
#112569=CARTESIAN_POINT('Ctrl Pts',(-152.546580538503,4.88836756191021,
130.246097777935));
#112570=CARTESIAN_POINT('Ctrl Pts',(-152.554354872622,4.87097422023509,
130.110449323031));
#112571=CARTESIAN_POINT('Ctrl Pts',(-152.562129206741,4.84791869525746,
129.975585987963));
#112572=CARTESIAN_POINT('Ctrl Pts',(-152.569893959688,4.82489158415382,
129.840888859902));
#112573=CARTESIAN_POINT('Ctrl Pts',(-152.577658712635,4.79621623940532,
129.706975308136));
#112574=CARTESIAN_POINT('Ctrl Pts',(-152.585423465583,4.76196057947378,
129.574354722443));
#112575=CARTESIAN_POINT('Ctrl Pts',(-152.593180506468,4.72773894274661,
129.441865857385));
#112576=CARTESIAN_POINT('Ctrl Pts',(-152.600937547353,4.68794811770129,
129.31066777889));
#112577=CARTESIAN_POINT('Ctrl Pts',(-152.608694588238,4.64270733331829,
129.181261212214));
#112578=CARTESIAN_POINT('Ctrl Pts',(-152.616445779478,4.59750066536264,
129.051952232037));
#112579=CARTESIAN_POINT('Ctrl Pts',(-152.624196970718,4.54685234699244,
128.924432442177));
#112580=CARTESIAN_POINT('Ctrl Pts',(-152.631948161958,4.49093175281661,
128.799188541647));
#112581=CARTESIAN_POINT('Ctrl Pts',(-152.639696058735,4.43503492638511,
128.673997873117));
#112582=CARTESIAN_POINT('Ctrl Pts',(-152.647443955512,4.37387044010636,
128.551081526253));
#112583=CARTESIAN_POINT('Ctrl Pts',(-152.655191852289,4.30765614124125,
128.43090709341));
#112584=CARTESIAN_POINT('Ctrl Pts',(-152.662938128373,4.24145569298004,
128.310757798468));
#112585=CARTESIAN_POINT('Ctrl Pts',(-152.670684404457,4.1702077217476,128.193349618936));
#112586=CARTESIAN_POINT('Ctrl Pts',(-152.678430680542,4.09417627461906,
128.079126004758));
#112587=CARTESIAN_POINT('Ctrl Pts',(-152.686177013807,4.01814426624353,
127.964901547407));
#112588=CARTESIAN_POINT('Ctrl Pts',(-152.693923347072,3.93732892814867,
127.853862027775));
#112589=CARTESIAN_POINT('Ctrl Pts',(-152.701669680338,3.85203769994542,
127.746421994784));
#112590=CARTESIAN_POINT('Ctrl Pts',(-152.709417748341,3.76672737136311,
127.638957901344));
#112591=CARTESIAN_POINT('Ctrl Pts',(-152.717165816344,3.67693940116022,
127.535095204702));
#112592=CARTESIAN_POINT('Ctrl Pts',(-152.724913884347,3.58302131312101,
127.43521512765));
#112593=CARTESIAN_POINT('Ctrl Pts',(-152.732670187088,3.48900340782032,
127.335228896864));
#112594=CARTESIAN_POINT('Ctrl Pts',(-152.74042648983,3.39084688435725,127.239234026371));
#112595=CARTESIAN_POINT('Ctrl Pts',(-152.748182792572,3.28893630820075,
127.147575004066));
#112596=CARTESIAN_POINT('Ctrl Pts',(-152.755943235086,3.18697133930101,
127.055867060581));
#112597=CARTESIAN_POINT('Ctrl Pts',(-152.7637036776,3.0812486264919,126.968499825399));
#112598=CARTESIAN_POINT('Ctrl Pts',(-152.771464120114,2.97218478539028,
126.885776604942));
#112599=CARTESIAN_POINT('Ctrl Pts',(-152.77923702038,2.86294586532869,126.802920589827));
#112600=CARTESIAN_POINT('Ctrl Pts',(-152.787009920645,2.75035542034077,
126.724723710022));
#112601=CARTESIAN_POINT('Ctrl Pts',(-152.794782820911,2.63485867774022,
126.651445640007));
#112602=CARTESIAN_POINT('Ctrl Pts',(-152.802273156673,2.52356053265162,
126.580831412413));
#112603=CARTESIAN_POINT('Ctrl Pts',(-152.809763492435,2.4095639904248,126.514784735619));
#112604=CARTESIAN_POINT('Ctrl Pts',(-152.817253828197,2.29328621600259,
126.453496175413));
#112605=CARTESIAN_POINT('Ctrl Pts',(-152.825028162316,2.17259973442148,
126.389883840819));
#112606=CARTESIAN_POINT('Ctrl Pts',(-152.832802496435,2.04907332151543,
126.331196048502));
#112607=CARTESIAN_POINT('Ctrl Pts',(-152.840576830554,1.92314690378126,
126.277696387807));
#112608=CARTESIAN_POINT('Ctrl Pts',(-152.848341583501,1.79737567910258,
126.224262660663));
#112609=CARTESIAN_POINT('Ctrl Pts',(-152.856106336448,1.66921069110178,
126.176004494578));
#112610=CARTESIAN_POINT('Ctrl Pts',(-152.863871089395,1.5391172154132,126.133140085444));
#112611=CARTESIAN_POINT('Ctrl Pts',(-152.87162813028,1.40915295039868,126.090318249845));
#112612=CARTESIAN_POINT('Ctrl Pts',(-152.879385171165,1.27726437835644,
126.052879631773));
#112613=CARTESIAN_POINT('Ctrl Pts',(-152.88714221205,1.1439372198007,126.020994574741));
#112614=CARTESIAN_POINT('Ctrl Pts',(-152.89489340329,1.01071060429254,125.989133562478));
#112615=CARTESIAN_POINT('Ctrl Pts',(-152.902644594531,0.876047940301947,
125.962817865894));
#112616=CARTESIAN_POINT('Ctrl Pts',(-152.910395785771,0.740450252606506,
125.942168058039));
#112617=CARTESIAN_POINT('Ctrl Pts',(-152.918143682548,0.604910197545337,
125.921527026904));
#112618=CARTESIAN_POINT('Ctrl Pts',(-152.925891579325,0.468436294897397,
125.9065471536));
#112619=CARTESIAN_POINT('Ctrl Pts',(-152.933639476102,0.331539695118737,
125.897297902146));
#112620=CARTESIAN_POINT('Ctrl Pts',(-152.941385752186,0.194671731157229,
125.888050585437));
#112621=CARTESIAN_POINT('Ctrl Pts',(-152.94913202827,0.0573816357642553,
125.884531532591));
#112622=CARTESIAN_POINT('Ctrl Pts',(-152.956878304354,-0.0798147801698766,
125.886758288853));
#112623=CARTESIAN_POINT('Ctrl Pts',(-152.96462463762,-0.217012208856598,
125.888985061552));
#112624=CARTESIAN_POINT('Ctrl Pts',(-152.972370970885,-0.354115565790877,
125.896957721648));
#112625=CARTESIAN_POINT('Ctrl Pts',(-152.98011730415,-0.490609900603677,
125.910641685309));
#112626=CARTESIAN_POINT('Ctrl Pts',(-152.987865372153,-0.627134802376186,
125.924328713399));
#112627=CARTESIAN_POINT('Ctrl Pts',(-152.995613440156,-0.763050021693598,
125.943729551136));
#112628=CARTESIAN_POINT('Ctrl Pts',(-153.003361508159,-0.897846979930605,
125.968757877149));
#112629=CARTESIAN_POINT('Ctrl Pts',(-153.011117810901,-1.03278720197911,
125.993812803565));
#112630=CARTESIAN_POINT('Ctrl Pts',(-153.018874113643,-1.1666064037798,
126.024507094385));
#112631=CARTESIAN_POINT('Ctrl Pts',(-153.026630416385,-1.29880689088056,
126.060703407912));
#112632=CARTESIAN_POINT('Ctrl Pts',(-153.034390858899,-1.43107793736177,
126.096919040501));
#112633=CARTESIAN_POINT('Ctrl Pts',(-153.042151301413,-1.56172817538354,
126.138642428332));
#112634=CARTESIAN_POINT('Ctrl Pts',(-153.049911743928,-1.69027723374617,
126.185687005415));
#112635=CARTESIAN_POINT('Ctrl Pts',(-153.057684644193,-1.81903265046933,
126.23280710263));
#112636=CARTESIAN_POINT('Ctrl Pts',(-153.065457544459,-1.9456797857909,
126.285265309126));
#112637=CARTESIAN_POINT('Ctrl Pts',(-153.073230444724,-2.06975951197796,
126.342827402955));
#112638=CARTESIAN_POINT('Ctrl Pts',(-153.080720780486,-2.18932862757646,
126.398296969681));
#112639=CARTESIAN_POINT('Ctrl Pts',(-153.088211116248,-2.30651348289287,
126.458505647118));
#112640=CARTESIAN_POINT('Ctrl Pts',(-153.095701452009,-2.42092826169051,
126.523205468048));
#112641=CARTESIAN_POINT('Ctrl Pts',(-153.103476880256,-2.53969782439262,
126.590367853182));
#112642=CARTESIAN_POINT('Ctrl Pts',(-153.111252308503,-2.65585854781134,
126.66258281134));
#112643=CARTESIAN_POINT('Ctrl Pts',(-153.11902773675,-2.76895068315104,
126.739622596884));
#112644=CARTESIAN_POINT('Ctrl Pts',(-153.12679334467,-2.88189998368885,
126.816565081564));
#112645=CARTESIAN_POINT('Ctrl Pts',(-153.13455895259,-2.99178808809088,
126.898320049418));
#112646=CARTESIAN_POINT('Ctrl Pts',(-153.14232456051,-3.09817979041436,
126.98461389183));
#112647=CARTESIAN_POINT('Ctrl Pts',(-153.150080784105,-3.20444292402153,
127.070803452722));
#112648=CARTESIAN_POINT('Ctrl Pts',(-153.157837007701,-3.30721776915533,
127.16152071899));
#112649=CARTESIAN_POINT('Ctrl Pts',(-153.165593231296,-3.40609860147247,
127.256449206673));
#112650=CARTESIAN_POINT('Ctrl Pts',(-153.17334413396,-3.50491159947248,
127.351312571429));
#112651=CARTESIAN_POINT('Ctrl Pts',(-153.181095036625,-3.59983561853296,
127.450381140445));
#112652=CARTESIAN_POINT('Ctrl Pts',(-153.188845939289,-3.6904984470236,
127.553298594932));
#112653=CARTESIAN_POINT('Ctrl Pts',(-153.196593203296,-3.7811187139077,
127.656167734885));
#112654=CARTESIAN_POINT('Ctrl Pts',(-153.204340467304,-3.86748151329224,
127.762881871938));
#112655=CARTESIAN_POINT('Ctrl Pts',(-153.212087731312,-3.94925219847171,
127.873048601528));
#112656=CARTESIAN_POINT('Ctrl Pts',(-153.219833036126,-4.0310022047831,
127.983187471217));
#112657=CARTESIAN_POINT('Ctrl Pts',(-153.227578340939,-4.1081621764316,
128.096776881375));
#112658=CARTESIAN_POINT('Ctrl Pts',(-153.235323645753,-4.1804386525967,
128.213392510009));
#112659=CARTESIAN_POINT('Ctrl Pts',(-153.243070974539,-4.25273401576939,
128.330038612186));
#112660=CARTESIAN_POINT('Ctrl Pts',(-153.250818303326,-4.32014312312706,
128.449712183301));
#112661=CARTESIAN_POINT('Ctrl Pts',(-153.258565632113,-4.38241663012796,
128.571961114234));
#112662=CARTESIAN_POINT('Ctrl Pts',(-153.266313951439,-4.444698099145,128.694225675376));
#112663=CARTESIAN_POINT('Ctrl Pts',(-153.274062270765,-4.50184248965709,
128.819065900196));
#112664=CARTESIAN_POINT('Ctrl Pts',(-153.28181059009,-4.55364750967603,
128.946007201199));
#112665=CARTESIAN_POINT('Ctrl Pts',(-153.289564968543,-4.60549304082644,
129.073047769334));
#112666=CARTESIAN_POINT('Ctrl Pts',(-153.297319346996,-4.65199072157926,
129.202192330231));
#112667=CARTESIAN_POINT('Ctrl Pts',(-153.305073725448,-4.69298719647638,
129.332948290511));
#112668=CARTESIAN_POINT('Ctrl Pts',(-153.309971088547,-4.71887897163126,
129.415528657049));
#112669=CARTESIAN_POINT('Ctrl Pts',(-153.314868451647,-4.74257748189,129.498751441572));
#112670=CARTESIAN_POINT('Ctrl Pts',(-153.319765814746,-4.76405452823394,
129.582490119308));
#112671=CARTESIAN_POINT('Origin',(213.235140564004,0.,130.804360617566));
#112672=CARTESIAN_POINT('',(-155.415271106226,-4.76405452823407,129.582490119308));
#112673=CARTESIAN_POINT('',(-155.070070112882,-4.76405452823396,129.582490119308));
#112674=CARTESIAN_POINT('',(213.235140564004,-4.76405452823405,129.582490119308));
#112675=CARTESIAN_POINT('',(-153.735140563956,-4.91824891289641,130.801090557425));
#112676=CARTESIAN_POINT('Ctrl Pts',(-153.735140564011,-4.91824891289706,
130.801090558408));
#112677=CARTESIAN_POINT('Ctrl Pts',(-153.742931215836,-4.9183407379463,
130.939197677182));
#112678=CARTESIAN_POINT('Ctrl Pts',(-153.75072186766,-4.91261105069972,
131.077337777159));
#112679=CARTESIAN_POINT('Ctrl Pts',(-153.758512519485,-4.9010782060776,
131.214988771023));
#112680=CARTESIAN_POINT('Ctrl Pts',(-153.766303436599,-4.88954496873651,
131.352644452208));
#112681=CARTESIAN_POINT('Ctrl Pts',(-153.774094353712,-4.87220821190394,
131.489810610838));
#112682=CARTESIAN_POINT('Ctrl Pts',(-153.781885270826,-4.84913824902427,
131.625969590466));
#112683=CARTESIAN_POINT('Ctrl Pts',(-153.789678068041,-4.82606271890851,
131.762161427936));
#112684=CARTESIAN_POINT('Ctrl Pts',(-153.797470865256,-4.79725129229373,
131.897345223374));
#112685=CARTESIAN_POINT('Ctrl Pts',(-153.805263662471,-4.76282549066431,
132.031013138852));
#112686=CARTESIAN_POINT('Ctrl Pts',(-153.813059955468,-4.72838424591735,
132.164741016605));
#112687=CARTESIAN_POINT('Ctrl Pts',(-153.820856248465,-4.68832370769074,
132.296951288505));
#112688=CARTESIAN_POINT('Ctrl Pts',(-153.828652541462,-4.64281528299066,
132.42715121112));
#112689=CARTESIAN_POINT('Ctrl Pts',(-153.836458800242,-4.59724868614392,
132.557517564656));
#112690=CARTESIAN_POINT('Ctrl Pts',(-153.844265059022,-4.54622042260291,
132.685868073745));
#112691=CARTESIAN_POINT('Ctrl Pts',(-153.852071317802,-4.489950329851,132.811729317624));
#112692=CARTESIAN_POINT('Ctrl Pts',(-153.859883151995,-4.43364004768217,
132.937680454548));
#112693=CARTESIAN_POINT('Ctrl Pts',(-153.867694986188,-4.3720806477439,
133.061138440512));
#112694=CARTESIAN_POINT('Ctrl Pts',(-153.875506820381,-4.30553754988166,
133.181655186831));
#112695=CARTESIAN_POINT('Ctrl Pts',(-153.88333120146,-4.23888757459962,
133.302365499716));
#112696=CARTESIAN_POINT('Ctrl Pts',(-153.891155582539,-4.16723811338279,
133.42012481001));
#112697=CARTESIAN_POINT('Ctrl Pts',(-153.898979963618,-4.09089784138924,
133.534514077322));
#112698=CARTESIAN_POINT('Ctrl Pts',(-153.903138418175,-4.05032497706778,
133.595308990691));
#112699=CARTESIAN_POINT('Ctrl Pts',(-153.907296872732,-4.00842781287545,
133.655152541907));
#112700=CARTESIAN_POINT('Ctrl Pts',(-153.911455327288,-3.96525713331834,
133.713985838994));
#112701=CARTESIAN_POINT('Ctrl Pts',(-153.919229661407,-3.88454847522001,
133.823976149735));
#112702=CARTESIAN_POINT('Ctrl Pts',(-153.927003995526,-3.7991320617101,
133.930780025861));
#112703=CARTESIAN_POINT('Ctrl Pts',(-153.934778329645,-3.70928822316274,
134.033968014759));
#112704=CARTESIAN_POINT('Ctrl Pts',(-153.942543082592,-3.61955510911731,
134.137028833683));
#112705=CARTESIAN_POINT('Ctrl Pts',(-153.95030783554,-3.5254056809212,134.236482339973));
#112706=CARTESIAN_POINT('Ctrl Pts',(-153.958072588487,-3.42716291879298,
134.331928815426));
#112707=CARTESIAN_POINT('Ctrl Pts',(-153.965829629372,-3.32901773276055,
134.427280492094));
#112708=CARTESIAN_POINT('Ctrl Pts',(-153.973586670257,-3.22678758203929,
134.518632787314));
#112709=CARTESIAN_POINT('Ctrl Pts',(-153.981343711142,-3.12083476185748,
134.605620073547));
#112710=CARTESIAN_POINT('Ctrl Pts',(-153.989094902382,-3.01496184152142,
134.69254176199));
#112711=CARTESIAN_POINT('Ctrl Pts',(-153.996846093622,-2.90537214042314,
134.775104746269));
#112712=CARTESIAN_POINT('Ctrl Pts',(-154.004597284862,-2.79246348486383,
134.852981462768));
#112713=CARTESIAN_POINT('Ctrl Pts',(-154.012345181639,-2.67960281849553,
134.930825079585));
#112714=CARTESIAN_POINT('Ctrl Pts',(-154.020093078417,-2.56342632449215,
135.003986168622));
#112715=CARTESIAN_POINT('Ctrl Pts',(-154.027840975194,-2.44436328868205,
135.07217869891));
#112716=CARTESIAN_POINT('Ctrl Pts',(-154.035587251278,-2.32532515829235,
135.14035696479));
#112717=CARTESIAN_POINT('Ctrl Pts',(-154.043333527362,-2.20340202613747,
135.203568544989));
#112718=CARTESIAN_POINT('Ctrl Pts',(-154.051079803446,-2.0790500769467,
135.261572059718));
#112719=CARTESIAN_POINT('Ctrl Pts',(-154.058826136711,-1.95469720981792,
135.319576002615));
#112720=CARTESIAN_POINT('Ctrl Pts',(-154.066572469977,-1.82791584419325,
135.372371638059));
#112721=CARTESIAN_POINT('Ctrl Pts',(-154.074318803242,-1.69918419079703,
135.419764841277));
#112722=CARTESIAN_POINT('Ctrl Pts',(-154.082066871245,-1.57042370883941,
135.467168657874));
#112723=CARTESIAN_POINT('Ctrl Pts',(-154.089814939248,-1.43971243684242,
135.509167499762));
#112724=CARTESIAN_POINT('Ctrl Pts',(-154.097563007251,-1.30754548414376,
135.545616555542));
#112725=CARTESIAN_POINT('Ctrl Pts',(-154.105319309993,-1.17523806283514,
135.582104349813));
#112726=CARTESIAN_POINT('Ctrl Pts',(-154.113075612735,-1.04147224779288,
135.613030471224));
#112727=CARTESIAN_POINT('Ctrl Pts',(-154.120831915477,-0.906755675340532,
135.638300750391));
#112728=CARTESIAN_POINT('Ctrl Pts',(-154.128592357991,-0.771967200597233,
135.663584517067));
#112729=CARTESIAN_POINT('Ctrl Pts',(-154.136352800505,-0.636227344065018,
135.68320637059));
#112730=CARTESIAN_POINT('Ctrl Pts',(-154.144113243019,-0.500049692978532,
135.697123984729));
#112731=CARTESIAN_POINT('Ctrl Pts',(-154.151886143285,-0.363653437437238,
135.711063940657));
#112732=CARTESIAN_POINT('Ctrl Pts',(-154.15965904355,-0.226818373436666,
135.719281335245));
#112733=CARTESIAN_POINT('Ctrl Pts',(-154.167431943816,-0.0900598278066852,
135.72178598964));
#112734=CARTESIAN_POINT('Ctrl Pts',(-154.174922279578,0.0417272002145433,
135.724199593539));
#112735=CARTESIAN_POINT('Ctrl Pts',(-154.18241261534,0.173442868605299,
135.721308597997));
#112736=CARTESIAN_POINT('Ctrl Pts',(-154.189902951102,0.304631766308209,
135.713167249473));
#112737=CARTESIAN_POINT('Ctrl Pts',(-154.197677285221,0.440794730942865,
135.704717219245));
#112738=CARTESIAN_POINT('Ctrl Pts',(-154.20545161934,0.576821514684844,
135.690584075317));
#112739=CARTESIAN_POINT('Ctrl Pts',(-154.213225953459,0.712199281473261,
135.670771537943));
#112740=CARTESIAN_POINT('Ctrl Pts',(-154.220990706406,0.847410207262435,
135.650983417752));
#112741=CARTESIAN_POINT('Ctrl Pts',(-154.228755459353,0.981973324441182,
135.625529886797));
#112742=CARTESIAN_POINT('Ctrl Pts',(-154.2365202123,1.11537776006755,135.594466620031));
#112743=CARTESIAN_POINT('Ctrl Pts',(-154.244277253185,1.24864969652815,
135.563434205739));
#112744=CARTESIAN_POINT('Ctrl Pts',(-154.25203429407,1.38076486330313,135.526803231599));
#112745=CARTESIAN_POINT('Ctrl Pts',(-154.259791334955,1.51121981816764,
135.484680876232));
#112746=CARTESIAN_POINT('Ctrl Pts',(-154.267542526195,1.64157639593607,
135.44259028566));
#112747=CARTESIAN_POINT('Ctrl Pts',(-154.275293717435,1.77027488323562,
135.3950166761));
#112748=CARTESIAN_POINT('Ctrl Pts',(-154.283044908676,1.89682465668628,
135.342117693952));
#112749=CARTESIAN_POINT('Ctrl Pts',(-154.290792805453,2.02332064310723,
135.289241195281));
#112750=CARTESIAN_POINT('Ctrl Pts',(-154.29854070223,2.14766937212164,135.231043976271));
#112751=CARTESIAN_POINT('Ctrl Pts',(-154.306288599007,2.26939815829694,
135.167732600519));
#112752=CARTESIAN_POINT('Ctrl Pts',(-154.314034875091,2.39110148143435,
135.104434468142));
#112753=CARTESIAN_POINT('Ctrl Pts',(-154.321781151175,2.51018560516876,
135.036024487144));
#112754=CARTESIAN_POINT('Ctrl Pts',(-154.329527427259,2.6262008708577,134.962755986985));
#112755=CARTESIAN_POINT('Ctrl Pts',(-154.337273760524,2.74221699294514,
134.889486945975));
#112756=CARTESIAN_POINT('Ctrl Pts',(-154.34502009379,2.85516388122118,134.811359523002));
#112757=CARTESIAN_POINT('Ctrl Pts',(-154.352766427055,2.96461972843958,
134.728671121113));
#112758=CARTESIAN_POINT('Ctrl Pts',(-154.360514495058,3.0741000875359,134.645964201729));
#112759=CARTESIAN_POINT('Ctrl Pts',(-154.368262563061,3.18008753799965,
134.558694506582));
#112760=CARTESIAN_POINT('Ctrl Pts',(-154.376010631064,3.28219262720959,
134.467200311081));
#112761=CARTESIAN_POINT('Ctrl Pts',(-154.383766933806,3.38440623492354,
134.375608874461));
#112762=CARTESIAN_POINT('Ctrl Pts',(-154.391523236548,3.4827289471818,134.279784229856));
#112763=CARTESIAN_POINT('Ctrl Pts',(-154.399279539289,3.57680714678234,
134.180102565231));
#112764=CARTESIAN_POINT('Ctrl Pts',(-154.407039981804,3.67093555875065,
134.080367697501));
#112765=CARTESIAN_POINT('Ctrl Pts',(-154.414800424318,3.76081468792545,
133.976772002967));
#112766=CARTESIAN_POINT('Ctrl Pts',(-154.422560866832,3.84613131760403,
133.869724698755));
#112767=CARTESIAN_POINT('Ctrl Pts',(-154.430333767097,3.93158490511063,
133.762505552707));
#112768=CARTESIAN_POINT('Ctrl Pts',(-154.438106667363,4.01246112638024,
133.651824040489));
#112769=CARTESIAN_POINT('Ctrl Pts',(-154.445879567628,4.08848969748455,
133.538119029727));
#112770=CARTESIAN_POINT('Ctrl Pts',(-154.45336990339,4.16175443852481,133.428547482513));
#112771=CARTESIAN_POINT('Ctrl Pts',(-154.460860239152,4.2305176981983,133.316168706606));
#112772=CARTESIAN_POINT('Ctrl Pts',(-154.468350574914,4.29457895478601,
133.201395173764));
#112773=CARTESIAN_POINT('Ctrl Pts',(-154.476124909033,4.36106911338816,
133.08226996754));
#112774=CARTESIAN_POINT('Ctrl Pts',(-154.483899243152,4.42270429838098,
132.960187472385));
#112775=CARTESIAN_POINT('Ctrl Pts',(-154.491673577271,4.47921043930333,
132.835581162691));
#112776=CARTESIAN_POINT('Ctrl Pts',(-154.499438330219,4.53564694145726,
132.711128419136));
#112777=CARTESIAN_POINT('Ctrl Pts',(-154.507203083166,4.58696681670537,
132.584158402409));
#112778=CARTESIAN_POINT('Ctrl Pts',(-154.514967836113,4.63294076665846,
132.455131018056));
#112779=CARTESIAN_POINT('Ctrl Pts',(-154.522724876998,4.67886905463621,
132.326231785521));
#112780=CARTESIAN_POINT('Ctrl Pts',(-154.530481917883,4.71946185338369,
132.195279617733));
#112781=CARTESIAN_POINT('Ctrl Pts',(-154.538238958768,4.75453721248953,
132.062756007558));
#112782=CARTESIAN_POINT('Ctrl Pts',(-154.545990150008,4.78958612099428,
131.930332334467));
#112783=CARTESIAN_POINT('Ctrl Pts',(-154.553741341248,4.81912577193774,
131.796339954154));
#112784=CARTESIAN_POINT('Ctrl Pts',(-154.561492532488,4.84302360377905,
131.661276853694));
#112785=CARTESIAN_POINT('Ctrl Pts',(-154.569240429265,4.86691127840429,
131.526271158654));
#112786=CARTESIAN_POINT('Ctrl Pts',(-154.576988326042,4.88516183523863,
131.390196032773));
#112787=CARTESIAN_POINT('Ctrl Pts',(-154.584736222819,4.89769356406585,
131.253560812366));
#112788=CARTESIAN_POINT('Ctrl Pts',(-154.592482498903,4.91022267152555,
131.1169541731));
#112789=CARTESIAN_POINT('Ctrl Pts',(-154.600228774988,4.91703529471044,
130.979788061429));
#112790=CARTESIAN_POINT('Ctrl Pts',(-154.607975051072,4.91810151539024,
130.842577718663));
#112791=CARTESIAN_POINT('Ctrl Pts',(-154.615721384337,4.91916774394063,
130.705366363042));
#112792=CARTESIAN_POINT('Ctrl Pts',(-154.623467717602,4.91448748230462,
130.568111166628));
#112793=CARTESIAN_POINT('Ctrl Pts',(-154.631214050868,4.90408294696689,
130.431327761415));
#112794=CARTESIAN_POINT('Ctrl Pts',(-154.638962118871,4.8936760816056,130.294513724506));
#112795=CARTESIAN_POINT('Ctrl Pts',(-154.646710186874,4.87754242133503,
130.158172078802));
#112796=CARTESIAN_POINT('Ctrl Pts',(-154.654458254877,4.8557560581835,130.022813327945));
#112797=CARTESIAN_POINT('Ctrl Pts',(-154.662214557618,4.83394654022603,
129.887310716197));
#112798=CARTESIAN_POINT('Ctrl Pts',(-154.66997086036,4.80647238046654,129.752793472675));
#112799=CARTESIAN_POINT('Ctrl Pts',(-154.677727163102,4.77345893775802,
129.619762444328));
#112800=CARTESIAN_POINT('Ctrl Pts',(-154.685487605616,4.74042787478112,
129.486660413317));
#112801=CARTESIAN_POINT('Ctrl Pts',(-154.69324804813,4.70185174772653,129.355046553072));
#112802=CARTESIAN_POINT('Ctrl Pts',(-154.701008490645,4.6579055412718,129.225405573529));
#112803=CARTESIAN_POINT('Ctrl Pts',(-154.70878139091,4.61388878846499,129.095556482776));
#112804=CARTESIAN_POINT('Ctrl Pts',(-154.716554291175,4.56448487067994,
128.967686966388));
#112805=CARTESIAN_POINT('Ctrl Pts',(-154.724327191441,4.50991692461591,
128.842261640561));
#112806=CARTESIAN_POINT('Ctrl Pts',(-154.731817527203,4.45733266083968,
128.721395841255));
#112807=CARTESIAN_POINT('Ctrl Pts',(-154.739307862965,4.39995343542685,
128.602799890034));
#112808=CARTESIAN_POINT('Ctrl Pts',(-154.746798198727,4.33801788566053,
128.486865442557));
#112809=CARTESIAN_POINT('Ctrl Pts',(-154.754572532846,4.27373403069983,
128.366535305267));
#112810=CARTESIAN_POINT('Ctrl Pts',(-154.762346866965,4.20433789298146,
128.248691307871));
#112811=CARTESIAN_POINT('Ctrl Pts',(-154.770121201084,4.13004602500871,
128.133798337107));
#112812=CARTESIAN_POINT('Ctrl Pts',(-154.777885954031,4.05584571512399,
128.019046961662));
#112813=CARTESIAN_POINT('Ctrl Pts',(-154.785650706979,3.97676189020346,
127.907239701706));
#112814=CARTESIAN_POINT('Ctrl Pts',(-154.793415459926,3.89305754042848,
127.79881806265));
#112815=CARTESIAN_POINT('Ctrl Pts',(-154.801172500811,3.80943632699348,
127.690504109493));
#112816=CARTESIAN_POINT('Ctrl Pts',(-154.808929541696,3.72120395873303,
127.585569392886));
#112817=CARTESIAN_POINT('Ctrl Pts',(-154.816686582581,3.62866718058855,
127.484427251515));
#112818=CARTESIAN_POINT('Ctrl Pts',(-154.824437773821,3.53620018514767,
127.383361382219));
#112819=CARTESIAN_POINT('Ctrl Pts',(-154.832188965061,3.4394355036097,127.286082682769));
#112820=CARTESIAN_POINT('Ctrl Pts',(-154.839940156301,3.33872045385295,
127.19297185512));
#112821=CARTESIAN_POINT('Ctrl Pts',(-154.847688053078,3.23804821067969,
127.099900602057));
#112822=CARTESIAN_POINT('Ctrl Pts',(-154.855435949855,3.1334292251925,127.010993962352));
#112823=CARTESIAN_POINT('Ctrl Pts',(-154.863183846632,3.02524785008844,
126.926595989841));
#112824=CARTESIAN_POINT('Ctrl Pts',(-154.870930122716,2.91708910419564,
126.842215671567));
#112825=CARTESIAN_POINT('Ctrl Pts',(-154.8786763988,2.80536975893898,126.762342384911));
#112826=CARTESIAN_POINT('Ctrl Pts',(-154.886422674885,2.69050712989239,
126.687279801442));
#112827=CARTESIAN_POINT('Ctrl Pts',(-154.89416900815,2.57564365295612,126.612216663878));
#112828=CARTESIAN_POINT('Ctrl Pts',(-154.901915341415,2.45763717320808,
126.541964514238));
#112829=CARTESIAN_POINT('Ctrl Pts',(-154.909661674681,2.33693351499983,
126.476783372852));
#112830=CARTESIAN_POINT('Ctrl Pts',(-154.917409742684,2.21620282604407,
126.4115876346));
#112831=CARTESIAN_POINT('Ctrl Pts',(-154.925157810687,2.09277410065448,
126.351465350082));
#112832=CARTESIAN_POINT('Ctrl Pts',(-154.93290587869,1.96711688855453,126.296630123264));
#112833=CARTESIAN_POINT('Ctrl Pts',(-154.940662181432,1.84132612647439,
126.241736616914));
#112834=CARTESIAN_POINT('Ctrl Pts',(-154.948418484173,1.71330250532879,
126.192141549738));
#112835=CARTESIAN_POINT('Ctrl Pts',(-154.956174786915,1.58353516136397,
126.148010173793));
#112836=CARTESIAN_POINT('Ctrl Pts',(-154.963935229429,1.45369855666011,
126.103855243604));
#112837=CARTESIAN_POINT('Ctrl Pts',(-154.971695671944,1.32211674959033,
126.065169925518));
#112838=CARTESIAN_POINT('Ctrl Pts',(-154.979456114458,1.1892921238422,126.03206899753));
#112839=CARTESIAN_POINT('Ctrl Pts',(-154.987229014723,1.05625427621356,
125.998914932993));
#112840=CARTESIAN_POINT('Ctrl Pts',(-154.995001914989,0.921970006302803,
125.971363251223));
#112841=CARTESIAN_POINT('Ctrl Pts',(-155.002774815254,0.786950819710978,
125.949477357398));
#112842=CARTESIAN_POINT('Ctrl Pts',(-155.010265151016,0.656839920646407,
125.928387070941));
#112843=CARTESIAN_POINT('Ctrl Pts',(-155.017755486778,0.52604691517257,
125.912557829843));
#112844=CARTESIAN_POINT('Ctrl Pts',(-155.02524582254,0.395030303569576,
125.90200056125));
#112845=CARTESIAN_POINT('Ctrl Pts',(-155.033020156659,0.259046157314284,
125.891043010609));
#112846=CARTESIAN_POINT('Ctrl Pts',(-155.040794490778,0.122390357258395,
125.88573038758));
#112847=CARTESIAN_POINT('Ctrl Pts',(-155.048568824897,-0.0144289223016949,
125.886131783046));
#112848=CARTESIAN_POINT('Ctrl Pts',(-155.056333577844,-0.151079584327988,
125.886532683828));
#112849=CARTESIAN_POINT('Ctrl Pts',(-155.064098330791,-0.287892937775208,
125.892633590454));
#112850=CARTESIAN_POINT('Ctrl Pts',(-155.071863083738,-0.42435537902032,
125.904451886294));
#112851=CARTESIAN_POINT('Ctrl Pts',(-155.079620124623,-0.560682283845004,
125.916258444036));
#112852=CARTESIAN_POINT('Ctrl Pts',(-155.087377165508,-0.696658583073169,
125.933771056825));
#112853=CARTESIAN_POINT('Ctrl Pts',(-155.095134206393,-0.831770720026451,
125.956955071111));
#112854=CARTESIAN_POINT('Ctrl Pts',(-155.102885397633,-0.966780967865318,
125.980121602151));
#112855=CARTESIAN_POINT('Ctrl Pts',(-155.110636588873,-1.10092796676746,
126.008950956029));
#112856=CARTESIAN_POINT('Ctrl Pts',(-155.118387780114,-1.23370368759815,
126.043356703085));
#112857=CARTESIAN_POINT('Ctrl Pts',(-155.126135676891,-1.36642297520611,
126.07774782678));
#112858=CARTESIAN_POINT('Ctrl Pts',(-155.133883573668,-1.49777176627361,
126.117710531808));
#112859=CARTESIAN_POINT('Ctrl Pts',(-155.141631470445,-1.62725284654226,
126.163107420861));
#112860=CARTESIAN_POINT('Ctrl Pts',(-155.149377746529,-1.75670684216055,
126.208494813865));
#112861=CARTESIAN_POINT('Ctrl Pts',(-155.157124022613,-1.8842935353613,
126.259314000634));
#112862=CARTESIAN_POINT('Ctrl Pts',(-155.164870298697,-2.0095318693918,
126.315378023659));
#112863=CARTESIAN_POINT('Ctrl Pts',(-155.172616631963,-2.13477112790305,
126.371442460536));
#112864=CARTESIAN_POINT('Ctrl Pts',(-155.180362965228,-2.25766163581166,
126.432751651181));
#112865=CARTESIAN_POINT('Ctrl Pts',(-155.188109298493,-2.37774365169854,
126.499071058279));
#112866=CARTESIAN_POINT('Ctrl Pts',(-155.195857366496,-2.49785255912045,
126.565405317149));
#112867=CARTESIAN_POINT('Ctrl Pts',(-155.203605434499,-2.61515138082445,
126.636751836151));
#112868=CARTESIAN_POINT('Ctrl Pts',(-155.211353502502,-2.72920660264905,
126.712831027968));
#112869=CARTESIAN_POINT('Ctrl Pts',(-155.219109805244,-2.84338304372052,
126.788991077655));
#112870=CARTESIAN_POINT('Ctrl Pts',(-155.226866107986,-2.95430867272093,
126.869893630706));
#112871=CARTESIAN_POINT('Ctrl Pts',(-155.234622410728,-3.06158006832547,
126.955216485719));
#112872=CARTESIAN_POINT('Ctrl Pts',(-155.242382853242,-3.16890871790373,
127.040584880108));
#112873=CARTESIAN_POINT('Ctrl Pts',(-155.250143295756,-3.27257895241974,
127.130378021619));
#112874=CARTESIAN_POINT('Ctrl Pts',(-155.25790373827,-3.37222265524193,
127.224235280937));
#112875=CARTESIAN_POINT('Ctrl Pts',(-155.265676638536,-3.47202631498211,
127.31824320826));
#112876=CARTESIAN_POINT('Ctrl Pts',(-155.273449538801,-3.56779025312211,
127.41632801068));
#112877=CARTESIAN_POINT('Ctrl Pts',(-155.281222439066,-3.65918464381807,
127.518093616097));
#112878=CARTESIAN_POINT('Ctrl Pts',(-155.288712774828,-3.74725661820291,
127.616159785424));
#112879=CARTESIAN_POINT('Ctrl Pts',(-155.29620311059,-3.83127102130242,
127.717643553716));
#112880=CARTESIAN_POINT('Ctrl Pts',(-155.303693446352,-3.91097082919788,
127.822165078091));
#112881=CARTESIAN_POINT('Ctrl Pts',(-155.311488197042,-3.9939097190257,
127.930934464414));
#112882=CARTESIAN_POINT('Ctrl Pts',(-155.319282947731,-4.0724417498631,
128.043342282481));
#112883=CARTESIAN_POINT('Ctrl Pts',(-155.32707769842,-4.14623148879997,
128.158997220264));
#112884=CARTESIAN_POINT('Ctrl Pts',(-155.334859712521,-4.21990065562333,
128.274463178381));
#112885=CARTESIAN_POINT('Ctrl Pts',(-155.342641726622,-4.28884275654833,
128.393165364981));
#112886=CARTESIAN_POINT('Ctrl Pts',(-155.350423740722,-4.35276311837608,
128.514680225501));
#112887=CARTESIAN_POINT('Ctrl Pts',(-155.358198428636,-4.41662330394175,
128.636080688826));
#112888=CARTESIAN_POINT('Ctrl Pts',(-155.365973116549,-4.47547097388064,
128.760288218568));
#112889=CARTESIAN_POINT('Ctrl Pts',(-155.373747804463,-4.52905501556395,
128.886850844841));
#112890=CARTESIAN_POINT('Ctrl Pts',(-155.381515750894,-4.5825925941757,
129.013303727837));
#112891=CARTESIAN_POINT('Ctrl Pts',(-155.389283697325,-4.63087548063379,
129.142107285863));
#112892=CARTESIAN_POINT('Ctrl Pts',(-155.397051643756,-4.67369900638074,
129.272786048616));
#112893=CARTESIAN_POINT('Ctrl Pts',(-155.403124797913,-4.70717939604278,
129.374953626394));
#112894=CARTESIAN_POINT('Ctrl Pts',(-155.409197952069,-4.73732365996748,
129.478266869634));
#112895=CARTESIAN_POINT('Ctrl Pts',(-155.415271106226,-4.76405452823407,
129.582490119308));
#112896=CARTESIAN_POINT('Ctrl Pts',(-153.665379263862,-4.76405452823391,
129.582490119308));
#112897=CARTESIAN_POINT('Ctrl Pts',(-153.674204833383,-4.80262274046709,
129.732866993451));
#112898=CARTESIAN_POINT('Ctrl Pts',(-153.683030402904,-4.83411093424905,
129.885242807117));
#112899=CARTESIAN_POINT('Ctrl Pts',(-153.691855972424,-4.8583311825113,
130.038984119666));
#112900=CARTESIAN_POINT('Ctrl Pts',(-153.700625150211,-4.88239667341757,
130.191743088896));
#112901=CARTESIAN_POINT('Ctrl Pts',(-153.709394327997,-4.89928671230653,
130.345849991077));
#112902=CARTESIAN_POINT('Ctrl Pts',(-153.718163505784,-4.90886459777685,
130.500664349573));
#112903=CARTESIAN_POINT('Ctrl Pts',(-153.723822525174,-4.91504550104034,
130.600570803521));
#112904=CARTESIAN_POINT('Ctrl Pts',(-153.729481544565,-4.91818221245824,
130.700771498029));
#112905=CARTESIAN_POINT('Ctrl Pts',(-153.735140563956,-4.91824891289641,
130.801090557425));
#112906=CARTESIAN_POINT('',(-153.389859436024,-4.91824971158563,130.802676281535));
#112907=CARTESIAN_POINT('Ctrl Pts',(-153.319765814746,-4.76405452823394,
129.582490119308));
#112908=CARTESIAN_POINT('Ctrl Pts',(-153.32752964618,-4.79810227272907,
129.715241758348));
#112909=CARTESIAN_POINT('Ctrl Pts',(-153.335293477613,-4.82656440966018,
129.849290078614));
#112910=CARTESIAN_POINT('Ctrl Pts',(-153.343057309047,-4.84937079552965,
129.984125315982));
#112911=CARTESIAN_POINT('Ctrl Pts',(-153.350832221389,-4.87220973175494,
130.119152996598));
#112912=CARTESIAN_POINT('Ctrl Pts',(-153.358607133731,-4.88937675304912,
130.254969450077));
#112913=CARTESIAN_POINT('Ctrl Pts',(-153.366382046073,-4.90085364791497,
130.391060987493));
#112914=CARTESIAN_POINT('Ctrl Pts',(-153.36897105599,-4.90467540092215,
130.436378841185));
#112915=CARTESIAN_POINT('Ctrl Pts',(-153.371560065907,-4.90786662768838,
130.481727209334));
#112916=CARTESIAN_POINT('Ctrl Pts',(-153.374149075824,-4.91042793580915,
130.527087197049));
#112917=CARTESIAN_POINT('Ctrl Pts',(-153.379385862547,-4.91560869014808,
130.6188367805));
#112918=CARTESIAN_POINT('Ctrl Pts',(-153.38462264927,-4.91821822404875,
130.710732917615));
#112919=CARTESIAN_POINT('Ctrl Pts',(-153.389859435994,-4.91824971158545,
130.802676281007));
#112920=CARTESIAN_POINT('Ctrl Pts',(-153.389859436024,-4.91824971158563,
130.802676281536));
#112921=CARTESIAN_POINT('Ctrl Pts',(-153.397566623283,-4.91829605303094,
130.937992985503));
#112922=CARTESIAN_POINT('Ctrl Pts',(-153.405273810541,-4.9127536815725,
131.073537372969));
#112923=CARTESIAN_POINT('Ctrl Pts',(-153.412980997799,-4.90159240666056,
131.208804608086));
#112924=CARTESIAN_POINT('Ctrl Pts',(-153.420678966356,-4.89044448194448,
131.3439100477));
#112925=CARTESIAN_POINT('Ctrl Pts',(-153.428376934913,-4.87369105456227,
131.47873860129));
#112926=CARTESIAN_POINT('Ctrl Pts',(-153.43607490347,-4.85135391530499,
131.6127839293));
#112927=CARTESIAN_POINT('Ctrl Pts',(-153.443765584287,-4.82903792283001,
131.746702355323));
#112928=CARTESIAN_POINT('Ctrl Pts',(-153.451456265104,-4.80114880013807,
131.879838640546));
#112929=CARTESIAN_POINT('Ctrl Pts',(-153.459146945921,-4.76776022432417,
132.011690525194));
#112930=CARTESIAN_POINT('Ctrl Pts',(-153.467207352325,-4.73276650962672,
132.149881122463));
#112931=CARTESIAN_POINT('Ctrl Pts',(-153.47526775873,-4.69173146770541,
132.286660312855));
#112932=CARTESIAN_POINT('Ctrl Pts',(-153.483328165135,-4.64480057212113,
132.42146009123));
#112933=CARTESIAN_POINT('Ctrl Pts',(-153.491010778568,-4.6000693376497,
132.549941775163));
#112934=CARTESIAN_POINT('Ctrl Pts',(-153.498693392001,-4.54998251046827,
132.67662495948));
#112935=CARTESIAN_POINT('Ctrl Pts',(-153.506376005433,-4.49471727537261,
132.801032768162));
#112936=CARTESIAN_POINT('Ctrl Pts',(-153.514057634474,-4.43945912154896,
132.925424636162));
#112937=CARTESIAN_POINT('Ctrl Pts',(-153.521739263514,-4.37902404088357,
133.04754134441));
#112938=CARTESIAN_POINT('Ctrl Pts',(-153.529420892554,-4.31363715365821,
133.166926504283));
#112939=CARTESIAN_POINT('Ctrl Pts',(-153.537103270656,-4.2482438903378,
133.286323305805));
#112940=CARTESIAN_POINT('Ctrl Pts',(-153.544785648758,-4.1778980514845,
133.402987679917));
#112941=CARTESIAN_POINT('Ctrl Pts',(-153.55246802686,-4.10287020721939,
133.516488771841));
#112942=CARTESIAN_POINT('Ctrl Pts',(-153.560152887725,-4.02781811572429,
133.630026544641));
#112943=CARTESIAN_POINT('Ctrl Pts',(-153.567837748591,-3.9480812287841,
133.740398669932));
#112944=CARTESIAN_POINT('Ctrl Pts',(-153.575522609456,-3.86397253698667,
133.847204566229));
#112945=CARTESIAN_POINT('Ctrl Pts',(-153.583215873473,-3.77977187499904,
133.954127251389));
#112946=CARTESIAN_POINT('Ctrl Pts',(-153.590909137491,-3.69119011225881,
134.057475610537));
#112947=CARTESIAN_POINT('Ctrl Pts',(-153.598602401508,-3.59857970956993,
134.156883121051));
#112948=CARTESIAN_POINT('Ctrl Pts',(-153.606300583607,-3.50591010372204,
134.256354179918));
#112949=CARTESIAN_POINT('Ctrl Pts',(-153.613998765706,-3.40920701263355,
134.351879095128));
#112950=CARTESIAN_POINT('Ctrl Pts',(-153.621696947805,-3.30885770073661,
134.443130159427));
#112951=CARTESIAN_POINT('Ctrl Pts',(-153.629406090281,-3.2083655153262,
134.534511143503));
#112952=CARTESIAN_POINT('Ctrl Pts',(-153.637115232758,-3.10421705191336,
134.621605877482));
#112953=CARTESIAN_POINT('Ctrl Pts',(-153.644824375234,-2.99683063954928,
134.704128454291));
#112954=CARTESIAN_POINT('Ctrl Pts',(-153.647415150035,-2.96074179932616,
134.731861423703));
#112955=CARTESIAN_POINT('Ctrl Pts',(-153.650005924835,-2.92428748844057,
134.75907838895));
#112956=CARTESIAN_POINT('Ctrl Pts',(-153.652596699636,-2.887484224653,134.785769653935));
#112957=CARTESIAN_POINT('Ctrl Pts',(-153.660371033755,-2.77704588424454,
134.86586415385));
#112958=CARTESIAN_POINT('Ctrl Pts',(-153.668145367874,-2.66309753913652,
134.941486943402));
#112959=CARTESIAN_POINT('Ctrl Pts',(-153.675919701993,-2.54603725957195,
135.012314673324));
#112960=CARTESIAN_POINT('Ctrl Pts',(-153.68368445494,-2.42912124634028,
135.083055114399));
#112961=CARTESIAN_POINT('Ctrl Pts',(-153.691449207887,-2.30910126081001,
135.149012053506));
#112962=CARTESIAN_POINT('Ctrl Pts',(-153.699213960834,-2.18640690735201,
135.209903478325));
#112963=CARTESIAN_POINT('Ctrl Pts',(-153.706971001719,-2.06383441565523,
135.270734424923));
#112964=CARTESIAN_POINT('Ctrl Pts',(-153.714728042604,-1.93859318997076,
135.326509696751));
#112965=CARTESIAN_POINT('Ctrl Pts',(-153.722485083489,-1.81113986310011,
135.376991748413));
#112966=CARTESIAN_POINT('Ctrl Pts',(-153.730236274729,-1.68378264977487,
135.427435731167));
#112967=CARTESIAN_POINT('Ctrl Pts',(-153.737987465969,-1.55421701766041,
135.47259429552));
#112968=CARTESIAN_POINT('Ctrl Pts',(-153.74573865721,-1.42292181157704,
135.512276991148));
#112969=CARTESIAN_POINT('Ctrl Pts',(-153.753486553987,-1.2916824094585,
135.551942820571));
#112970=CARTESIAN_POINT('Ctrl Pts',(-153.761234450764,-1.15871526892059,
135.586137297395));
#112971=CARTESIAN_POINT('Ctrl Pts',(-153.768982347541,-1.02451651057077,
135.61471912625));
#112972=CARTESIAN_POINT('Ctrl Pts',(-153.776728623625,-0.890345823708212,
135.643294976403));
#112973=CARTESIAN_POINT('Ctrl Pts',(-153.784474899709,-0.754944413616102,
135.666260432437));
#112974=CARTESIAN_POINT('Ctrl Pts',(-153.792221175793,-0.618820381656688,
135.683524931026));
#112975=CARTESIAN_POINT('Ctrl Pts',(-153.799967509058,-0.482695344860406,
135.700789557059));
#112976=CARTESIAN_POINT('Ctrl Pts',(-153.807713842324,-0.345848063410923,
135.712353092482));
#112977=CARTESIAN_POINT('Ctrl Pts',(-153.815460175589,-0.208793184182127,
135.718176697634));
#112978=CARTESIAN_POINT('Ctrl Pts',(-153.823208243592,-0.0717076124639604,
135.724001606943));
#112979=CARTESIAN_POINT('Ctrl Pts',(-153.830956311595,0.0655852590054131,
135.724084011554));
#112980=CARTESIAN_POINT('Ctrl Pts',(-153.838704379598,0.202569748852529,
135.71843718996));
#112981=CARTESIAN_POINT('Ctrl Pts',(-153.84646068234,0.339699827445778,
135.712784366856));
#112982=CARTESIAN_POINT('Ctrl Pts',(-153.854216985082,0.476520478441192,
135.701390170063));
#112983=CARTESIAN_POINT('Ctrl Pts',(-153.861973287824,0.612519554506488,
135.684319926602));
#112984=CARTESIAN_POINT('Ctrl Pts',(-153.869733730338,0.748591217373533,
135.667240572238));
#112985=CARTESIAN_POINT('Ctrl Pts',(-153.877494172852,0.883840046208596,
135.64447919957));
#112986=CARTESIAN_POINT('Ctrl Pts',(-153.885254615366,1.0177640565039,135.616152320018));
#112987=CARTESIAN_POINT('Ctrl Pts',(-153.893027515632,1.15190305350974,
135.587779967645));
#112988=CARTESIAN_POINT('Ctrl Pts',(-153.900800415897,1.28471260311983,
135.553824351819));
#112989=CARTESIAN_POINT('Ctrl Pts',(-153.908573316162,1.41570498674655,
135.514452172196));
#112990=CARTESIAN_POINT('Ctrl Pts',(-153.916063651924,1.54193546727675,
135.476511270477));
#112991=CARTESIAN_POINT('Ctrl Pts',(-153.923553987686,1.66647831402322,
135.433540879754));
#112992=CARTESIAN_POINT('Ctrl Pts',(-153.931044323448,1.78891642750466,
135.385731709052));
#112993=CARTESIAN_POINT('Ctrl Pts',(-153.938818657567,1.91599681927462,
135.336109839112));
#112994=CARTESIAN_POINT('Ctrl Pts',(-153.946592991686,2.04121227774682,
135.28111783413));
#112995=CARTESIAN_POINT('Ctrl Pts',(-153.954367325805,2.164075593337,135.220915823699));
#112996=CARTESIAN_POINT('Ctrl Pts',(-153.962132078752,2.28678749087133,
135.160788006867));
#112997=CARTESIAN_POINT('Ctrl Pts',(-153.9698968317,2.40715266556961,135.095463130572));
#112998=CARTESIAN_POINT('Ctrl Pts',(-153.977661584647,2.52470164082529,
135.025150198594));
#112999=CARTESIAN_POINT('Ctrl Pts',(-153.985418625532,2.64213386478127,
134.954907102411));
#113000=CARTESIAN_POINT('Ctrl Pts',(-153.993175666416,2.75675512227696,
134.879686009037));
#113001=CARTESIAN_POINT('Ctrl Pts',(-154.000932707301,2.86811873846036,
134.799742697492));
#113002=CARTESIAN_POINT('Ctrl Pts',(-154.008683898542,2.97939837447466,
134.719859671819));
#113003=CARTESIAN_POINT('Ctrl Pts',(-154.016435089782,3.08742494259636,
134.635261743125));
#113004=CARTESIAN_POINT('Ctrl Pts',(-154.024186281022,3.19177938425175,
134.546248834064));
#113005=CARTESIAN_POINT('Ctrl Pts',(-154.031934177799,3.29608947248583,
134.457273757864));
#113006=CARTESIAN_POINT('Ctrl Pts',(-154.039682074576,3.3967302416395,134.363887686674));
#113007=CARTESIAN_POINT('Ctrl Pts',(-154.047429971353,3.49331465060994,
134.266431647215));
#113008=CARTESIAN_POINT('Ctrl Pts',(-154.055176247437,3.58987885620415,
134.168995993458));
#113009=CARTESIAN_POINT('Ctrl Pts',(-154.062922523521,3.68238811429914,
134.067492342329));
#113010=CARTESIAN_POINT('Ctrl Pts',(-154.070668799605,3.77049159020739,
133.962299222206));
#113011=CARTESIAN_POINT('Ctrl Pts',(-154.078415132871,3.85859571647536,
133.857105325571));
#113012=CARTESIAN_POINT('Ctrl Pts',(-154.086161466136,3.94229374462713,
133.748222205323));
#113013=CARTESIAN_POINT('Ctrl Pts',(-154.093907799401,4.02127481854961,
133.636061854667));
#113014=CARTESIAN_POINT('Ctrl Pts',(-154.101655867404,4.1002735797363,133.523876386477));
#113015=CARTESIAN_POINT('Ctrl Pts',(-154.109403935407,4.17455305966423,
133.408412547079));
#113016=CARTESIAN_POINT('Ctrl Pts',(-154.11715200341,4.24384569152576,133.290111371165));
#113017=CARTESIAN_POINT('Ctrl Pts',(-154.124908306152,4.31321196842056,
133.171684463354));
#113018=CARTESIAN_POINT('Ctrl Pts',(-154.132664608894,4.37758061185115,
133.050414533025));
#113019=CARTESIAN_POINT('Ctrl Pts',(-154.140420911636,4.43672975514852,
132.926767775083));
#113020=CARTESIAN_POINT('Ctrl Pts',(-154.14818135415,4.49591046812495,132.803055023143));
#113021=CARTESIAN_POINT('Ctrl Pts',(-154.155941796664,4.54986597628541,
132.676963275094));
#113022=CARTESIAN_POINT('Ctrl Pts',(-154.163702239178,4.59842296910078,
132.548977841987));
#113023=CARTESIAN_POINT('Ctrl Pts',(-154.171475139444,4.64705790991157,
132.420786955302));
#113024=CARTESIAN_POINT('Ctrl Pts',(-154.179248039709,4.69027689426186,
132.290696680087));
#113025=CARTESIAN_POINT('Ctrl Pts',(-154.187020939975,4.72795654748498,
132.15920745304));
#113026=CARTESIAN_POINT('Ctrl Pts',(-154.194511275737,4.76426645040473,
132.032498190596));
#113027=CARTESIAN_POINT('Ctrl Pts',(-154.202001611499,4.79543269450047,
131.904490220591));
#113028=CARTESIAN_POINT('Ctrl Pts',(-154.209491947261,4.82139027621796,
131.77563754352));
#113029=CARTESIAN_POINT('Ctrl Pts',(-154.21726628138,4.84833204753548,131.641899378036));
#113030=CARTESIAN_POINT('Ctrl Pts',(-154.225040615499,4.86974773015148,
131.50682754459));
#113031=CARTESIAN_POINT('Ctrl Pts',(-154.232814949618,4.88550869694688,
131.37091850036));
#113032=CARTESIAN_POINT('Ctrl Pts',(-154.240579702565,4.90125023975931,
131.235176951881));
#113033=CARTESIAN_POINT('Ctrl Pts',(-154.248344455512,4.91135088824354,
131.098600630203));
#113034=CARTESIAN_POINT('Ctrl Pts',(-154.256109208459,4.91573271962358,
130.961697490937));
#113035=CARTESIAN_POINT('Ctrl Pts',(-154.263866249344,4.92011019890692,
130.824930325799));
#113036=CARTESIAN_POINT('Ctrl Pts',(-154.27162329023,4.91878015213563,130.687837377279));
#113037=CARTESIAN_POINT('Ctrl Pts',(-154.279380331115,4.9117163347749,130.550932700388));
#113038=CARTESIAN_POINT('Ctrl Pts',(-154.287131522355,4.90465784429375,
130.414131264377));
#113039=CARTESIAN_POINT('Ctrl Pts',(-154.294882713595,4.89187420971017,
130.277518206265));
#113040=CARTESIAN_POINT('Ctrl Pts',(-154.302633904835,4.87339125305414,
130.141608207419));
#113041=CARTESIAN_POINT('Ctrl Pts',(-154.310381801612,4.85491615214787,
130.005755973949));
#113042=CARTESIAN_POINT('Ctrl Pts',(-154.318129698389,4.83074659964008,
129.870606592006));
#113043=CARTESIAN_POINT('Ctrl Pts',(-154.325877595166,4.8009603057981,129.736670023503));
#113044=CARTESIAN_POINT('Ctrl Pts',(-154.33362387125,4.77118024260667,129.602761471642));
#113045=CARTESIAN_POINT('Ctrl Pts',(-154.341370147335,4.73578585984384,
129.470065610009));
#113046=CARTESIAN_POINT('Ctrl Pts',(-154.349116423419,4.69490598943539,
129.339082209596));
#113047=CARTESIAN_POINT('Ctrl Pts',(-154.356862756684,4.65402581726097,
129.208097842293));
#113048=CARTESIAN_POINT('Ctrl Pts',(-154.364609089949,4.60766019311983,
129.078826334645));
#113049=CARTESIAN_POINT('Ctrl Pts',(-154.372355423215,4.55598771324147,
128.951751911095));
#113050=CARTESIAN_POINT('Ctrl Pts',(-154.380103491218,4.50430366166957,
128.824649030109));
#113051=CARTESIAN_POINT('Ctrl Pts',(-154.387851559221,4.44731053675606,
128.699744574386));
#113052=CARTESIAN_POINT('Ctrl Pts',(-154.395599627224,4.38523476708398,
128.577502045483));
#113053=CARTESIAN_POINT('Ctrl Pts',(-154.403355929965,4.32309302254526,
128.455129595767));
#113054=CARTESIAN_POINT('Ctrl Pts',(-154.411112232707,4.25585801968156,
128.335425073508));
#113055=CARTESIAN_POINT('Ctrl Pts',(-154.418868535449,4.18380205711718,
128.218827131153));
#113056=CARTESIAN_POINT('Ctrl Pts',(-154.426628977963,4.11170763611583,
128.102166956966));
#113057=CARTESIAN_POINT('Ctrl Pts',(-154.434389420477,4.03478734747495,
127.988616990068));
#113058=CARTESIAN_POINT('Ctrl Pts',(-154.442149862992,3.95335581855366,
127.878585363995));
#113059=CARTESIAN_POINT('Ctrl Pts',(-154.449922763257,3.87179356851299,
127.768377105388));
#113060=CARTESIAN_POINT('Ctrl Pts',(-154.457695663523,3.78570585235007,
127.661698778443));
#113061=CARTESIAN_POINT('Ctrl Pts',(-154.465468563788,3.69544701461065,
127.558924680022));
#113062=CARTESIAN_POINT('Ctrl Pts',(-154.47295889955,3.60846931297158,127.45988667895));
#113063=CARTESIAN_POINT('Ctrl Pts',(-154.480449235312,3.51761869864603,
127.364474200564));
#113064=CARTESIAN_POINT('Ctrl Pts',(-154.487939571074,3.42324199909756,
127.272987332551));
#113065=CARTESIAN_POINT('Ctrl Pts',(-154.495713905193,3.32528697829986,
127.17803171213));
#113066=CARTESIAN_POINT('Ctrl Pts',(-154.503488239312,3.22322291894911,
127.087004466531));
#113067=CARTESIAN_POINT('Ctrl Pts',(-154.511262573431,3.11739797843007,
127.000282160623));
#113068=CARTESIAN_POINT('Ctrl Pts',(-154.519027326378,3.01170345769294,
126.913666732206));
#113069=CARTESIAN_POINT('Ctrl Pts',(-154.526792079326,2.90225757745008,
126.831345932642));
#113070=CARTESIAN_POINT('Ctrl Pts',(-154.534556832273,2.78944557598048,
126.753659882984));
#113071=CARTESIAN_POINT('Ctrl Pts',(-154.542313873158,2.6767456209805,126.676050992205));
#113072=CARTESIAN_POINT('Ctrl Pts',(-154.550070914043,2.56068651794759,
126.603067910866));
#113073=CARTESIAN_POINT('Ctrl Pts',(-154.557827954928,2.44168657010954,
126.535010578526));
#113074=CARTESIAN_POINT('Ctrl Pts',(-154.565579146168,2.32277636105768,
126.467004568751));
#113075=CARTESIAN_POINT('Ctrl Pts',(-154.573330337408,2.20093005943492,
126.403917107708));
#113076=CARTESIAN_POINT('Ctrl Pts',(-154.581081528648,2.07659463869087,
126.346004668445));
#113077=CARTESIAN_POINT('Ctrl Pts',(-154.588829425425,1.95231206381791,
126.288116843514));
#113078=CARTESIAN_POINT('Ctrl Pts',(-154.596577322203,1.8255428276547,126.235399830409));
#113079=CARTESIAN_POINT('Ctrl Pts',(-154.60432521898,1.69675797989939,126.188063896151));
#113080=CARTESIAN_POINT('Ctrl Pts',(-154.612071495064,1.56800007115794,
126.14073786355));
#113081=CARTESIAN_POINT('Ctrl Pts',(-154.619817771148,1.43722775618427,
126.0987908057));
#113082=CARTESIAN_POINT('Ctrl Pts',(-154.627564047232,1.30493114327146,
126.062384471082));
#113083=CARTESIAN_POINT('Ctrl Pts',(-154.635310380497,1.17263355377529,
126.025977867721));
#113084=CARTESIAN_POINT('Ctrl Pts',(-154.643056713763,1.03881202084012,
125.995112172938));
#113085=CARTESIAN_POINT('Ctrl Pts',(-154.650803047028,0.903970471827993,
125.969898863807));
#113086=CARTESIAN_POINT('Ctrl Pts',(-154.658551115031,0.769098725986079,
125.944679908329));
#113087=CARTESIAN_POINT('Ctrl Pts',(-154.666299183034,0.63320689375795,
125.925115929169));
#113088=CARTESIAN_POINT('Ctrl Pts',(-154.674047251037,0.4968073223112,125.91126695946));
#113089=CARTESIAN_POINT('Ctrl Pts',(-154.681803553779,0.360262783776184,
125.897403270901));
#113090=CARTESIAN_POINT('Ctrl Pts',(-154.689559856521,0.22320981763661,
125.889266764778));
#113091=CARTESIAN_POINT('Ctrl Pts',(-154.697316159263,0.0861646586768549,
125.886865450909));
#113092=CARTESIAN_POINT('Ctrl Pts',(-154.705076601777,-0.0509536454105864,
125.884462855386));
#113093=CARTESIAN_POINT('Ctrl Pts',(-154.712837044291,-0.188063743357137,
125.887801541996));
#113094=CARTESIAN_POINT('Ctrl Pts',(-154.720597486805,-0.324652197088056,
125.896837411974));
#113095=CARTESIAN_POINT('Ctrl Pts',(-154.728370387071,-0.461459914730657,
125.905887787133));
#113096=CARTESIAN_POINT('Ctrl Pts',(-154.736143287336,-0.597743925872199,
125.920653579395));
#113097=CARTESIAN_POINT('Ctrl Pts',(-154.743916187602,-0.732997792081342,
125.941038985255));
#113098=CARTESIAN_POINT('Ctrl Pts',(-154.751406523364,-0.863334839565459,
125.960683330264));
#113099=CARTESIAN_POINT('Ctrl Pts',(-154.758896859125,-0.992715036042196,
125.985545749971));
#113100=CARTESIAN_POINT('Ctrl Pts',(-154.766387194887,-1.12069844052577,
126.015496653336));
#113101=CARTESIAN_POINT('Ctrl Pts',(-154.774161529006,-1.25353437469434,
126.046583154306));
#113102=CARTESIAN_POINT('Ctrl Pts',(-154.781935863125,-1.38528629157488,
126.083250088331));
#113103=CARTESIAN_POINT('Ctrl Pts',(-154.789710197244,-1.51544918890696,
126.125408083254));
#113104=CARTESIAN_POINT('Ctrl Pts',(-154.797474950192,-1.64545167210001,
126.167514122216));
#113105=CARTESIAN_POINT('Ctrl Pts',(-154.805239703139,-1.77386866385468,
126.215097637971));
#113106=CARTESIAN_POINT('Ctrl Pts',(-154.813004456086,-1.90020577999547,
126.268018362382));
#113107=CARTESIAN_POINT('Ctrl Pts',(-154.820761496971,-2.02641741633215,
126.320886525183));
#113108=CARTESIAN_POINT('Ctrl Pts',(-154.828518537856,-2.15055292974125,
126.379081197354));
#113109=CARTESIAN_POINT('Ctrl Pts',(-154.836275578741,-2.27213386946351,
126.442412573201));
#113110=CARTESIAN_POINT('Ctrl Pts',(-154.844026769981,-2.39362312405253,
126.505696190365));
#113111=CARTESIAN_POINT('Ctrl Pts',(-154.851777961221,-2.51256129404445,
126.574108621096));
#113112=CARTESIAN_POINT('Ctrl Pts',(-154.859529152461,-2.62849100133433,
126.647412443917));
#113113=CARTESIAN_POINT('Ctrl Pts',(-154.867277049238,-2.74437143540687,
126.720685110659));
#113114=CARTESIAN_POINT('Ctrl Pts',(-154.875024946015,-2.85724562021281,
126.798844826066));
#113115=CARTESIAN_POINT('Ctrl Pts',(-154.882772842792,-2.96668203828371,
126.881608937148));
#113116=CARTESIAN_POINT('Ctrl Pts',(-154.890519118876,-3.07609556461512,
126.964355735762));
#113117=CARTESIAN_POINT('Ctrl Pts',(-154.89826539496,-3.18207244292137,
127.051704778632));
#113118=CARTESIAN_POINT('Ctrl Pts',(-154.906011671044,-3.2842116741203,
127.143331152774));
#113119=CARTESIAN_POINT('Ctrl Pts',(-154.91375800431,-3.38635165928769,
127.234958203282));
#113120=CARTESIAN_POINT('Ctrl Pts',(-154.921504337575,-3.48465364979472,
127.330862386996));
#113121=CARTESIAN_POINT('Ctrl Pts',(-154.929250670841,-3.57875147177427,
127.430679991636));
#113122=CARTESIAN_POINT('Ctrl Pts',(-154.936998738843,-3.67287036630849,
127.530519949736));
#113123=CARTESIAN_POINT('Ctrl Pts',(-154.944746806846,-3.76278295071859,
127.634274788234));
#113124=CARTESIAN_POINT('Ctrl Pts',(-154.952494874849,-3.84816178126991,
127.74154590432));
#113125=CARTESIAN_POINT('Ctrl Pts',(-154.960251177591,-3.93363135345848,
127.848931029426));
#113126=CARTESIAN_POINT('Ctrl Pts',(-154.968007480333,-4.01455730240066,
127.959839591076));
#113127=CARTESIAN_POINT('Ctrl Pts',(-154.975763783075,-4.09065385169935,
128.073841595827));
#113128=CARTESIAN_POINT('Ctrl Pts',(-154.983524225589,-4.16679101601782,
128.187904446881));
#113129=CARTESIAN_POINT('Ctrl Pts',(-154.991284668103,-4.23809344145754,
128.305063697107));
#113130=CARTESIAN_POINT('Ctrl Pts',(-154.999045110617,-4.30432070373601,
128.424863540054));
#113131=CARTESIAN_POINT('Ctrl Pts',(-155.006818010883,-4.3706542798951,
128.544855696343));
#113132=CARTESIAN_POINT('Ctrl Pts',(-155.014590911148,-4.4318962376198,
128.667496566072));
#113133=CARTESIAN_POINT('Ctrl Pts',(-155.022363811414,-4.4878534367707,
128.79230828411));
#113134=CARTESIAN_POINT('Ctrl Pts',(-155.029854147176,-4.54177645078616,
128.912582781819));
#113135=CARTESIAN_POINT('Ctrl Pts',(-155.037344482938,-4.59079214943105,
129.03487275051));
#113136=CARTESIAN_POINT('Ctrl Pts',(-155.0448348187,-4.63477176247094,129.158738008247));
#113137=CARTESIAN_POINT('Ctrl Pts',(-155.053246583428,-4.68416155879476,
129.297840638497));
#113138=CARTESIAN_POINT('Ctrl Pts',(-155.061658348155,-4.72732056080959,
129.439264937836));
#113139=CARTESIAN_POINT('Ctrl Pts',(-155.070070112883,-4.76405452823396,
129.582490119308));
#113140=CARTESIAN_POINT('Origin',(213.235140564004,0.,130.804360617566));
#113141=CARTESIAN_POINT('',(-157.165002070592,-4.7640545282341,129.582490119308));
#113142=CARTESIAN_POINT('',(-156.820024427474,-4.76405452823416,129.582490119309));
#113143=CARTESIAN_POINT('',(213.235140564004,-4.76405452823405,129.582490119308));
#113144=CARTESIAN_POINT('',(-155.485140564065,-4.91824868045241,130.807963356535));
#113145=CARTESIAN_POINT('Ctrl Pts',(-155.485140564065,-4.91824868045242,
130.807963356535));
#113146=CARTESIAN_POINT('Ctrl Pts',(-155.494049736137,-4.91813304233005,
130.96582576278));
#113147=CARTESIAN_POINT('Ctrl Pts',(-155.502958908209,-4.91041303307629,
131.123380682287));
#113148=CARTESIAN_POINT('Ctrl Pts',(-155.511868080281,-4.89520103050853,
131.279954912536));
#113149=CARTESIAN_POINT('Ctrl Pts',(-155.52082239596,-4.8799119473028,131.437322519036));
#113150=CARTESIAN_POINT('Ctrl Pts',(-155.529776711638,-4.85705486365668,
131.59369933755));
#113151=CARTESIAN_POINT('Ctrl Pts',(-155.538731027317,-4.82679328265685,
131.748420821684));
#113152=CARTESIAN_POINT('Ctrl Pts',(-155.547742254425,-4.79633936648892,
131.904125677527));
#113153=CARTESIAN_POINT('Ctrl Pts',(-155.556753481532,-4.75838661846912,
132.058153957194));
#113154=CARTESIAN_POINT('Ctrl Pts',(-155.56576470864,-4.71315011348257,
132.209849525484));
#113155=CARTESIAN_POINT('Ctrl Pts',(-155.571223495815,-4.68574691408184,
132.301743094787));
#113156=CARTESIAN_POINT('Ctrl Pts',(-155.57668228299,-4.65567176233512,
132.392781059726));
#113157=CARTESIAN_POINT('Ctrl Pts',(-155.582141070166,-4.62298083148197,
132.482821607357));
#113158=CARTESIAN_POINT('Ctrl Pts',(-155.589915404285,-4.5764228304176,
132.61105619117));
#113159=CARTESIAN_POINT('Ctrl Pts',(-155.597689738404,-4.52445148752097,
132.737555247174));
#113160=CARTESIAN_POINT('Ctrl Pts',(-155.605464072523,-4.4672151945854,
132.861827863421));
#113161=CARTESIAN_POINT('Ctrl Pts',(-155.61322882547,-4.41004944026551,
132.985947324774));
#113162=CARTESIAN_POINT('Ctrl Pts',(-155.620993578417,-4.3476318082313,
133.107845454187));
#113163=CARTESIAN_POINT('Ctrl Pts',(-155.628758331364,-4.28015997592845,
133.227047894736));
#113164=CARTESIAN_POINT('Ctrl Pts',(-155.636515372249,-4.21275515760082,
133.34613194174));
#113165=CARTESIAN_POINT('Ctrl Pts',(-155.644272413134,-4.14030632017784,
133.462525289979));
#113166=CARTESIAN_POINT('Ctrl Pts',(-155.652029454019,-4.0630584500564,
133.575775255242));
#113167=CARTESIAN_POINT('Ctrl Pts',(-155.659780645259,-3.98586883315461,
133.688939817825));
#113168=CARTESIAN_POINT('Ctrl Pts',(-155.667531836499,-3.90388760634622,
133.798965393991));
#113169=CARTESIAN_POINT('Ctrl Pts',(-155.675283027739,-3.81740454966709,
133.905425848528));
#113170=CARTESIAN_POINT('Ctrl Pts',(-155.683030924516,-3.73095825059394,
134.011841054532));
#113171=CARTESIAN_POINT('Ctrl Pts',(-155.690778821293,-3.64001417324846,
134.114693849845));
#113172=CARTESIAN_POINT('Ctrl Pts',(-155.69852671807,-3.54490395822348,
134.213589121124));
#113173=CARTESIAN_POINT('Ctrl Pts',(-155.706272994155,-3.44981363820514,
134.312463705643));
#113174=CARTESIAN_POINT('Ctrl Pts',(-155.714019270239,-3.35055918473857,
134.407382131109));
#113175=CARTESIAN_POINT('Ctrl Pts',(-155.721765546323,-3.24751059812876,
134.497984580227));
#113176=CARTESIAN_POINT('Ctrl Pts',(-155.729511879588,-3.14446125083784,
134.588587698151));
#113177=CARTESIAN_POINT('Ctrl Pts',(-155.737258212854,-3.0376180081332,
134.674874518001));
#113178=CARTESIAN_POINT('Ctrl Pts',(-155.745004546119,-2.92738528488649,
134.756524386482));
#113179=CARTESIAN_POINT('Ctrl Pts',(-155.752752614122,-2.81712787578586,
134.838192539884));
#113180=CARTESIAN_POINT('Ctrl Pts',(-155.760500682125,-2.70347978982842,
134.915221442934));
#113181=CARTESIAN_POINT('Ctrl Pts',(-155.768248750128,-2.58687551383483,
134.987333022259));
#113182=CARTESIAN_POINT('Ctrl Pts',(-155.77600505287,-2.47014730942894,
135.059521242629));
#113183=CARTESIAN_POINT('Ctrl Pts',(-155.783761355611,-2.3504569718014,
135.126781493431));
#113184=CARTESIAN_POINT('Ctrl Pts',(-155.791517658353,-2.22826523741797,
135.188880784496));
#113185=CARTESIAN_POINT('Ctrl Pts',(-155.799278100868,-2.10600828562643,
135.251013219822));
#113186=CARTESIAN_POINT('Ctrl Pts',(-155.807038543382,-1.98124763230917,
135.30797904441));
#113187=CARTESIAN_POINT('Ctrl Pts',(-155.814798985896,-1.85446428978654,
135.359593351511));
#113188=CARTESIAN_POINT('Ctrl Pts',(-155.822571886161,-1.7274774233872,
135.41129051448));
#113189=CARTESIAN_POINT('Ctrl Pts',(-155.830344786427,-1.59846174741381,
135.457618860738));
#113190=CARTESIAN_POINT('Ctrl Pts',(-155.838117686692,-1.4679145937986,
135.498443042046));
#113191=CARTESIAN_POINT('Ctrl Pts',(-155.845608022454,-1.34211315804398,
135.537783161534));
#113192=CARTESIAN_POINT('Ctrl Pts',(-155.853098358217,-1.21488995509605,
135.572012268845));
#113193=CARTESIAN_POINT('Ctrl Pts',(-155.860588693979,-1.0866972948005,
135.601054484384));
#113194=CARTESIAN_POINT('Ctrl Pts',(-155.868363028098,-0.953644170828582,
135.631197844353));
#113195=CARTESIAN_POINT('Ctrl Pts',(-155.876137362217,-0.819125152066657,
135.65584871135));
#113196=CARTESIAN_POINT('Ctrl Pts',(-155.883911696336,-0.683633466029421,
135.674866581696));
#113197=CARTESIAN_POINT('Ctrl Pts',(-155.891676449283,-0.548308761385986,
135.693861014216));
#113198=CARTESIAN_POINT('Ctrl Pts',(-155.89944120223,-0.412014158026778,
135.707236209101));
#113199=CARTESIAN_POINT('Ctrl Pts',(-155.907205955177,-0.275255595353761,
135.714902076481));
#113200=CARTESIAN_POINT('Ctrl Pts',(-155.914962996062,-0.138632863213149,
135.722560330014));
#113201=CARTESIAN_POINT('Ctrl Pts',(-155.922720036947,-0.00154747661975313,
135.724520519021));
#113202=CARTESIAN_POINT('Ctrl Pts',(-155.930477077832,0.135487287246631,
135.720744070623));
#113203=CARTESIAN_POINT('Ctrl Pts',(-155.938228269072,0.272418712131794,
135.716970470074));
#113204=CARTESIAN_POINT('Ctrl Pts',(-155.945979460312,0.409299201039463,
135.707468853573));
#113205=CARTESIAN_POINT('Ctrl Pts',(-155.953730651553,0.545613601159354,
135.69225268478));
#113206=CARTESIAN_POINT('Ctrl Pts',(-155.96147854833,0.681870064023075,
135.677042983264));
#113207=CARTESIAN_POINT('Ctrl Pts',(-155.969226445107,0.817560528901214,
135.656123603509));
#113208=CARTESIAN_POINT('Ctrl Pts',(-155.976974341884,0.952173315904815,
135.629559995724));
#113209=CARTESIAN_POINT('Ctrl Pts',(-155.984720617968,1.08675794481492,
135.603001944474));
#113210=CARTESIAN_POINT('Ctrl Pts',(-155.992466894052,1.22026496091177,
135.570802089215));
#113211=CARTESIAN_POINT('Ctrl Pts',(-156.000213170136,1.35219164551349,
135.533077231649));
#113212=CARTESIAN_POINT('Ctrl Pts',(-156.007959503401,1.48411930396821,
135.495352095606));
#113213=CARTESIAN_POINT('Ctrl Pts',(-156.015705836667,1.61446623175116,
135.452101983362));
#113214=CARTESIAN_POINT('Ctrl Pts',(-156.023452169932,1.74274405804727,
135.403493819664));
#113215=CARTESIAN_POINT('Ctrl Pts',(-156.031200237935,1.87105061127299,
135.354874770505));
#113216=CARTESIAN_POINT('Ctrl Pts',(-156.038948305938,1.99728677544951,
135.300895420741));
#113217=CARTESIAN_POINT('Ctrl Pts',(-156.046696373941,2.12098374883439,
135.241771010991));
#113218=CARTESIAN_POINT('Ctrl Pts',(-156.054452676683,2.24481218883476,
135.182583763115));
#113219=CARTESIAN_POINT('Ctrl Pts',(-156.062208979425,2.36609569383071,
135.118240700744));
#113220=CARTESIAN_POINT('Ctrl Pts',(-156.069965282167,2.48438920328042,
135.049003517637));
#113221=CARTESIAN_POINT('Ctrl Pts',(-156.077725724681,2.60274584953787,
134.979729380561));
#113222=CARTESIAN_POINT('Ctrl Pts',(-156.085486167195,2.7181089916855,134.905556129177));
#113223=CARTESIAN_POINT('Ctrl Pts',(-156.093246609709,2.83006306353161,
134.826788506159));
#113224=CARTESIAN_POINT('Ctrl Pts',(-156.101019509974,2.94219685399266,
134.747894438361));
#113225=CARTESIAN_POINT('Ctrl Pts',(-156.10879241024,3.05091032803284,134.664391499036));
#113226=CARTESIAN_POINT('Ctrl Pts',(-156.116565310505,3.1558207932883,134.576624948594));
#113227=CARTESIAN_POINT('Ctrl Pts',(-156.124055646267,3.25691749887792,
134.492048933333));
#113228=CARTESIAN_POINT('Ctrl Pts',(-156.131545982029,3.35448266506848,
134.40351411814));
#113229=CARTESIAN_POINT('Ctrl Pts',(-156.139036317791,3.44820796768794,
134.311360029324));
#113230=CARTESIAN_POINT('Ctrl Pts',(-156.14681065191,3.54548689364354,134.215711890222));
#113231=CARTESIAN_POINT('Ctrl Pts',(-156.15458498603,3.63893718164784,134.115861625704));
#113232=CARTESIAN_POINT('Ctrl Pts',(-156.162359320149,3.72817402045526,
134.012148256376));
#113233=CARTESIAN_POINT('Ctrl Pts',(-156.170124073096,3.81730088283418,
133.908562704507));
#113234=CARTESIAN_POINT('Ctrl Pts',(-156.177888826043,3.90222437539272,
133.80112381418));
#113235=CARTESIAN_POINT('Ctrl Pts',(-156.18565357899,3.98259523036654,133.690208550767));
#113236=CARTESIAN_POINT('Ctrl Pts',(-156.193410619875,4.06288625987417,
133.579403449958));
#113237=CARTESIAN_POINT('Ctrl Pts',(-156.20116766076,4.13863342235182,133.465129161796));
#113238=CARTESIAN_POINT('Ctrl Pts',(-156.208924701645,4.20952682649004,
133.347796671325));
#113239=CARTESIAN_POINT('Ctrl Pts',(-156.216675892885,4.28036676936083,
133.230552662198));
#113240=CARTESIAN_POINT('Ctrl Pts',(-156.224427084125,4.34636003804496,
133.110255374414));
#113241=CARTESIAN_POINT('Ctrl Pts',(-156.232178275365,4.40723950722377,
132.98734549806));
#113242=CARTESIAN_POINT('Ctrl Pts',(-156.239926172142,4.46809310100409,
132.864487861683));
#113243=CARTESIAN_POINT('Ctrl Pts',(-156.24767406892,4.52383704503914,132.739020194886));
#113244=CARTESIAN_POINT('Ctrl Pts',(-156.255421965697,4.57424982896484,
132.611408365888));
#113245=CARTESIAN_POINT('Ctrl Pts',(-156.263168241781,4.62465206762291,
132.483823230534));
#113246=CARTESIAN_POINT('Ctrl Pts',(-156.270914517865,4.66972522073733,
132.354095188484));
#113247=CARTESIAN_POINT('Ctrl Pts',(-156.278660793949,4.70929582515879,
132.222710325375));
#113248=CARTESIAN_POINT('Ctrl Pts',(-156.286407127214,4.74886672168152,
132.091324492413));
#113249=CARTESIAN_POINT('Ctrl Pts',(-156.29415346048,4.78293487571136,131.958282188342));
#113250=CARTESIAN_POINT('Ctrl Pts',(-156.301899793745,4.81137674941061,
131.824084520263));
#113251=CARTESIAN_POINT('Ctrl Pts',(-156.309647861748,4.83982499247024,
131.689856799547));
#113252=CARTESIAN_POINT('Ctrl Pts',(-156.317395929751,4.86264436696675,
131.554473582365));
#113253=CARTESIAN_POINT('Ctrl Pts',(-156.325143997754,4.87976256213496,
131.418445627712));
#113254=CARTESIAN_POINT('Ctrl Pts',(-156.332900300496,4.89689895072467,
131.28227310093));
#113255=CARTESIAN_POINT('Ctrl Pts',(-156.340656603238,4.908322007026,131.145454856372));
#113256=CARTESIAN_POINT('Ctrl Pts',(-156.34841290598,4.91401133531657,131.008506787945));
#113257=CARTESIAN_POINT('Ctrl Pts',(-156.356173348494,4.91970370017297,
130.871485626209));
#113258=CARTESIAN_POINT('Ctrl Pts',(-156.363933791008,4.91965623932011,
130.734334893311));
#113259=CARTESIAN_POINT('Ctrl Pts',(-156.371694233522,4.91390071772362,
130.597568937716));
#113260=CARTESIAN_POINT('Ctrl Pts',(-156.379467133788,4.90813595685291,
130.460583433267));
#113261=CARTESIAN_POINT('Ctrl Pts',(-156.387240034053,4.89664485726546,
130.323984330253));
#113262=CARTESIAN_POINT('Ctrl Pts',(-156.395012934318,4.8795110417526,130.188280220285));
#113263=CARTESIAN_POINT('Ctrl Pts',(-156.402503270081,4.86300008359107,
130.057509296531));
#113264=CARTESIAN_POINT('Ctrl Pts',(-156.409993605843,4.84124959162055,
129.92756972883));
#113265=CARTESIAN_POINT('Ctrl Pts',(-156.417483941605,4.81437856219427,
129.798904441304));
#113266=CARTESIAN_POINT('Ctrl Pts',(-156.425258275724,4.78648870952013,
129.665360770294));
#113267=CARTESIAN_POINT('Ctrl Pts',(-156.433032609843,4.75299401739126,
129.532766889396));
#113268=CARTESIAN_POINT('Ctrl Pts',(-156.440806943962,4.71397171356682,
129.401629800127));
#113269=CARTESIAN_POINT('Ctrl Pts',(-156.448571696909,4.67499750124431,
129.270654325601));
#113270=CARTESIAN_POINT('Ctrl Pts',(-156.456336449856,4.63050934208417,
129.141132441591));
#113271=CARTESIAN_POINT('Ctrl Pts',(-156.464101202803,4.58063559997242,
129.01356175595));
#113272=CARTESIAN_POINT('Ctrl Pts',(-156.471858243688,4.53081139316444,
128.886117775313));
#113273=CARTESIAN_POINT('Ctrl Pts',(-156.479615284573,4.47561238966402,
128.760621498193));
#113274=CARTESIAN_POINT('Ctrl Pts',(-156.487372325458,4.41521685900641,
128.637555792381));
#113275=CARTESIAN_POINT('Ctrl Pts',(-156.495123516698,4.35486687308819,
128.514582891375));
#113276=CARTESIAN_POINT('Ctrl Pts',(-156.502874707938,4.2893283315785,128.394037262933));
#113277=CARTESIAN_POINT('Ctrl Pts',(-156.510625899179,4.21882761176835,
128.276381850907));
#113278=CARTESIAN_POINT('Ctrl Pts',(-156.518373795956,4.14835685664489,
128.158776445569));
#113279=CARTESIAN_POINT('Ctrl Pts',(-156.526121692733,4.07292831851209,
128.04405914808));
#113280=CARTESIAN_POINT('Ctrl Pts',(-156.53386958951,3.99281421373397,127.932668134534));
#113281=CARTESIAN_POINT('Ctrl Pts',(-156.541615865594,3.91271686709952,
127.821300421586));
#113282=CARTESIAN_POINT('Ctrl Pts',(-156.549362141678,3.82793613146532,
127.713257925821));
#113283=CARTESIAN_POINT('Ctrl Pts',(-156.557108417762,3.73878720337472,
127.60894932786));
#113284=CARTESIAN_POINT('Ctrl Pts',(-156.564854751027,3.64963761720686,
127.504639959916));
#113285=CARTESIAN_POINT('Ctrl Pts',(-156.572601084293,3.55612002825205,
127.404064841981));
#113286=CARTESIAN_POINT('Ctrl Pts',(-156.580347417558,3.45858925688764,
127.307598770565));
#113287=CARTESIAN_POINT('Ctrl Pts',(-156.588095485561,3.36103664418335,
127.211111096242));
#113288=CARTESIAN_POINT('Ctrl Pts',(-156.595843553564,3.25946933862601,
127.118734574394));
#113289=CARTESIAN_POINT('Ctrl Pts',(-156.603591621567,3.15427797048833,
127.030806119829));
#113290=CARTESIAN_POINT('Ctrl Pts',(-156.611347924309,3.04897480371294,
126.942784213856));
#113291=CARTESIAN_POINT('Ctrl Pts',(-156.61910422705,2.94004018062642,126.859220069917));
#113292=CARTESIAN_POINT('Ctrl Pts',(-156.626860529792,2.82789711299831,
126.780409700768));
#113293=CARTESIAN_POINT('Ctrl Pts',(-156.634620972306,2.71569419123814,
126.701557268153));
#113294=CARTESIAN_POINT('Ctrl Pts',(-156.642381414821,2.60027974159002,
126.627463877088));
#113295=CARTESIAN_POINT('Ctrl Pts',(-156.650141857335,2.48210366972528,
126.558380820719));
#113296=CARTESIAN_POINT('Ctrl Pts',(-156.6579147576,2.36373789113881,126.489186866094));
#113297=CARTESIAN_POINT('Ctrl Pts',(-156.665687657866,2.24260197707321,
126.425019501825));
#113298=CARTESIAN_POINT('Ctrl Pts',(-156.673460558131,2.11916902021499,
126.366083279875));
#113299=CARTESIAN_POINT('Ctrl Pts',(-156.680950893893,2.00022316224708,
126.309289538045));
#113300=CARTESIAN_POINT('Ctrl Pts',(-156.688441229655,1.87914465166531,
126.257353332653));
#113301=CARTESIAN_POINT('Ctrl Pts',(-156.695931565417,1.75637045351285,
126.210413960004));
#113302=CARTESIAN_POINT('Ctrl Pts',(-156.703705899536,1.62894123432155,
126.161694866774));
#113303=CARTESIAN_POINT('Ctrl Pts',(-156.711480233655,1.49928154781937,
126.11820466847));
#113304=CARTESIAN_POINT('Ctrl Pts',(-156.719254567774,1.36785969223231,
126.080152437895));
#113305=CARTESIAN_POINT('Ctrl Pts',(-156.727019320721,1.23659980233676,
126.042147103294));
#113306=CARTESIAN_POINT('Ctrl Pts',(-156.734784073668,1.10358243635882,
126.00956650951));
#113307=CARTESIAN_POINT('Ctrl Pts',(-156.742548826616,0.969295629694564,
125.98257162957));
#113308=CARTESIAN_POINT('Ctrl Pts',(-156.750305867501,0.835142198579437,
125.955603561326));
#113309=CARTESIAN_POINT('Ctrl Pts',(-156.758062908386,0.699722216696345,
125.934210243088));
#113310=CARTESIAN_POINT('Ctrl Pts',(-156.765819949271,0.563538293431292,
125.918502693482));
#113311=CARTESIAN_POINT('Ctrl Pts',(-156.773571140511,0.427457067522315,
125.902806989061));
#113312=CARTESIAN_POINT('Ctrl Pts',(-156.781322331751,0.290613433730575,
125.892788563518));
#113313=CARTESIAN_POINT('Ctrl Pts',(-156.789073522991,0.153519242285463,
125.888507191685));
#113314=CARTESIAN_POINT('Ctrl Pts',(-156.796821419768,0.0164833195286367,
125.884227639549));
#113315=CARTESIAN_POINT('Ctrl Pts',(-156.804569316545,-0.120802559117167,
125.885680303509));
#113316=CARTESIAN_POINT('Ctrl Pts',(-156.812317213322,-0.257822604099873,
125.892873005109));
#113317=CARTESIAN_POINT('Ctrl Pts',(-156.820063489406,-0.39481398744298,
125.900064202152));
#113318=CARTESIAN_POINT('Ctrl Pts',(-156.82780976549,-0.531539257547418,
125.912993028111));
#113319=CARTESIAN_POINT('Ctrl Pts',(-156.835556041575,-0.667484208402331,
125.931615201065));
#113320=CARTESIAN_POINT('Ctrl Pts',(-156.84330237484,-0.803430162771434,
125.950237511484));
#113321=CARTESIAN_POINT('Ctrl Pts',(-156.851048708105,-0.938595399049157,
125.974553199699));
#113322=CARTESIAN_POINT('Ctrl Pts',(-156.858795041371,-1.07247280123594,
126.004466331948));
#113323=CARTESIAN_POINT('Ctrl Pts',(-156.866543109374,-1.20638018433889,
126.034386163035));
#113324=CARTESIAN_POINT('Ctrl Pts',(-156.874291177376,-1.33899877798152,
126.069905847255));
#113325=CARTESIAN_POINT('Ctrl Pts',(-156.882039245379,-1.4698339809905,
126.11087884698));
#113326=CARTESIAN_POINT('Ctrl Pts',(-156.889795548121,-1.60080823721038,
126.151895393296));
#113327=CARTESIAN_POINT('Ctrl Pts',(-156.897551850863,-1.72999494282071,
126.198376715921));
#113328=CARTESIAN_POINT('Ctrl Pts',(-156.905308153605,-1.85691640571096,
126.250126925198));
#113329=CARTESIAN_POINT('Ctrl Pts',(-156.913068596119,-1.98390561040783,
126.30190475512));
#113330=CARTESIAN_POINT('Ctrl Pts',(-156.920829038633,-2.10862680793417,
126.358956912614));
#113331=CARTESIAN_POINT('Ctrl Pts',(-156.928589481148,-2.23062539324579,
126.421040709379));
#113332=CARTESIAN_POINT('Ctrl Pts',(-156.936362381413,-2.35281982151674,
126.483224168566));
#113333=CARTESIAN_POINT('Ctrl Pts',(-156.944135281679,-2.47228256285254,
126.550455216054));
#113334=CARTESIAN_POINT('Ctrl Pts',(-156.951908181944,-2.58858580373855,
126.622446390901));
#113335=CARTESIAN_POINT('Ctrl Pts',(-156.959398517706,-2.70066112886722,
126.691820505207));
#113336=CARTESIAN_POINT('Ctrl Pts',(-156.966888853468,-2.80980242184844,
126.765614497653));
#113337=CARTESIAN_POINT('Ctrl Pts',(-156.97437918923,-2.91565629847685,
126.843536030229));
#113338=CARTESIAN_POINT('Ctrl Pts',(-156.982321809287,-3.02790188403022,
126.926162650338));
#113339=CARTESIAN_POINT('Ctrl Pts',(-156.990264429343,-3.13683227136789,
127.013711797369));
#113340=CARTESIAN_POINT('Ctrl Pts',(-156.9982070494,-3.24198225670693,127.105883348514));
#113341=CARTESIAN_POINT('Ctrl Pts',(-157.005898703257,-3.34380977515242,
127.195142517634));
#113342=CARTESIAN_POINT('Ctrl Pts',(-157.013590357115,-3.44209181150377,
127.288736144081));
#113343=CARTESIAN_POINT('Ctrl Pts',(-157.021282010972,-3.53643426231045,
127.38634719295));
#113344=CARTESIAN_POINT('Ctrl Pts',(-157.028966694705,-3.63069122062843,
127.483869787348));
#113345=CARTESIAN_POINT('Ctrl Pts',(-157.036651378438,-3.72101541736759,
127.585402279919));
#113346=CARTESIAN_POINT('Ctrl Pts',(-157.044336062171,-3.80704667151909,
127.690588194383));
#113347=CARTESIAN_POINT('Ctrl Pts',(-157.052015522896,-3.89301945327776,
127.79570261771));
#113348=CARTESIAN_POINT('Ctrl Pts',(-157.059694983622,-3.97470484465933,
127.904465216283));
#113349=CARTESIAN_POINT('Ctrl Pts',(-157.067374444348,-4.05178067949858,
128.016483936695));
#113350=CARTESIAN_POINT('Ctrl Pts',(-157.075050424794,-4.12882158408524,
128.128451890973));
#113351=CARTESIAN_POINT('Ctrl Pts',(-157.082726405239,-4.2012568635084,
128.243672702675));
#113352=CARTESIAN_POINT('Ctrl Pts',(-157.090402385685,-4.26880600572468,
128.36172303741));
#113353=CARTESIAN_POINT('Ctrl Pts',(-157.098077877342,-4.33635084657299,
128.479765854982));
#113354=CARTESIAN_POINT('Ctrl Pts',(-157.105753369,-4.39900996460309,128.600637494883));
#113355=CARTESIAN_POINT('Ctrl Pts',(-157.113428860657,-4.4565475304664,
128.723887793616));
#113356=CARTESIAN_POINT('Ctrl Pts',(-157.121104166245,-4.51408370150439,
128.847135104516));
#113357=CARTESIAN_POINT('Ctrl Pts',(-157.128779471834,-4.5664984043857,
128.972760595479));
#113358=CARTESIAN_POINT('Ctrl Pts',(-157.136454777422,-4.61360324984863,
129.100292509923));
#113359=CARTESIAN_POINT('Ctrl Pts',(-157.144133411417,-4.66072852239329,
129.227879728759));
#113360=CARTESIAN_POINT('Ctrl Pts',(-157.151812045412,-4.70253920954631,
129.357374644865));
#113361=CARTESIAN_POINT('Ctrl Pts',(-157.159490679407,-4.73889629523923,
129.488288824134));
#113362=CARTESIAN_POINT('Ctrl Pts',(-157.161327809802,-4.74759480948431,
129.519610334963));
#113363=CARTESIAN_POINT('Ctrl Pts',(-157.163164940197,-4.75598137804317,
129.551013029241));
#113364=CARTESIAN_POINT('Ctrl Pts',(-157.165002070592,-4.7640545282341,
129.582490119308));
#113365=CARTESIAN_POINT('Ctrl Pts',(-155.415271106226,-4.76405452823407,
129.582490119308));
#113366=CARTESIAN_POINT('Ctrl Pts',(-155.423032857163,-4.79821772193378,
129.715691893045));
#113367=CARTESIAN_POINT('Ctrl Pts',(-155.4307946081,-4.82680380230719,129.850380280961));
#113368=CARTESIAN_POINT('Ctrl Pts',(-155.438556359037,-4.84969597482323,
129.986050154304));
#113369=CARTESIAN_POINT('Ctrl Pts',(-155.446320393199,-4.87259488138504,
130.121759936797));
#113370=CARTESIAN_POINT('Ctrl Pts',(-155.454084427362,-4.88979645416441,
130.258451400986));
#113371=CARTESIAN_POINT('Ctrl Pts',(-155.461848461524,-4.90123510417065,
130.395609451029));
#113372=CARTESIAN_POINT('Ctrl Pts',(-155.469612495686,-4.91267375417689,
130.532767501072));
#113373=CARTESIAN_POINT('Ctrl Pts',(-155.477376529849,-4.9183494550353,
130.670391749014));
#113374=CARTESIAN_POINT('Ctrl Pts',(-155.485140564011,-4.91824868045312,
130.807963355574));
#113375=CARTESIAN_POINT('',(-155.139859435941,-4.91824859371983,130.80064136053));
#113376=CARTESIAN_POINT('Ctrl Pts',(-155.070070112883,-4.76405452823396,
129.582490119308));
#113377=CARTESIAN_POINT('Ctrl Pts',(-155.079101386156,-4.80349387407437,
129.736263530164));
#113378=CARTESIAN_POINT('Ctrl Pts',(-155.088132659429,-4.83552633251772,
129.892113014839));
#113379=CARTESIAN_POINT('Ctrl Pts',(-155.097163932702,-4.85995645887181,
130.049373014774));
#113380=CARTESIAN_POINT('Ctrl Pts',(-155.106121891946,-4.88418826645835,
130.205356410203));
#113381=CARTESIAN_POINT('Ctrl Pts',(-155.11507985119,-4.90094059396684,
130.36272739353));
#113382=CARTESIAN_POINT('Ctrl Pts',(-155.124037810435,-4.91006984325492,
130.520816622993));
#113383=CARTESIAN_POINT('Ctrl Pts',(-155.129311685603,-4.91544456307824,
130.613889480205));
#113384=CARTESIAN_POINT('Ctrl Pts',(-155.134585560772,-4.91817794015085,
130.707210921886));
#113385=CARTESIAN_POINT('Ctrl Pts',(-155.139859435941,-4.91824859371983,
130.80064136053));
#113386=CARTESIAN_POINT('Ctrl Pts',(-155.139859435994,-4.91824859372054,
130.800641361475));
#113387=CARTESIAN_POINT('Ctrl Pts',(-155.147611646378,-4.91835244926784,
130.937977266002));
#113388=CARTESIAN_POINT('Ctrl Pts',(-155.155363856762,-4.91269960219612,
131.075373175227));
#113389=CARTESIAN_POINT('Ctrl Pts',(-155.163116067145,-4.90130174688514,
131.21231189956));
#113390=CARTESIAN_POINT('Ctrl Pts',(-155.170867366393,-4.88990523119227,
131.349234529147));
#113391=CARTESIAN_POINT('Ctrl Pts',(-155.17861866564,-4.87276508230385,
131.485699692495));
#113392=CARTESIAN_POINT('Ctrl Pts',(-155.186369964887,-4.84994500482501,
131.621193839633));
#113393=CARTESIAN_POINT('Ctrl Pts',(-155.194122017518,-4.82712270936145,
131.75670115605));
#113394=CARTESIAN_POINT('Ctrl Pts',(-155.201874070149,-4.79861945097126,
131.891236884105));
#113395=CARTESIAN_POINT('Ctrl Pts',(-155.209626122779,-4.76455027365204,
132.02429657996));
#113396=CARTESIAN_POINT('Ctrl Pts',(-155.217380593448,-4.73047046939316,
132.157397780116));
#113397=CARTESIAN_POINT('Ctrl Pts',(-155.225135064118,-4.69082138744712,
132.289021654418));
#113398=CARTESIAN_POINT('Ctrl Pts',(-155.232889534787,-4.64576815171044,
132.418678226667));
#113399=CARTESIAN_POINT('Ctrl Pts',(-155.240653107835,-4.60066203143611,
132.548486992821));
#113400=CARTESIAN_POINT('Ctrl Pts',(-155.248416680883,-4.55013921478554,
132.676323475793));
#113401=CARTESIAN_POINT('Ctrl Pts',(-155.256180253931,-4.49441350188924,
132.801716453799));
#113402=CARTESIAN_POINT('Ctrl Pts',(-155.263948538074,-4.43865397348732,
132.927185522837));
#113403=CARTESIAN_POINT('Ctrl Pts',(-155.271716822217,-4.37768543129941,
133.050207783983));
#113404=CARTESIAN_POINT('Ctrl Pts',(-155.27948510636,-4.31176754666298,
133.17033688246));
#113405=CARTESIAN_POINT('Ctrl Pts',(-155.287266329264,-4.24573986998919,
133.290666066522));
#113406=CARTESIAN_POINT('Ctrl Pts',(-155.295047552168,-4.17474658127562,
133.408092126304));
#113407=CARTESIAN_POINT('Ctrl Pts',(-155.302828775072,-4.09909104932332,
133.522197189521));
#113408=CARTESIAN_POINT('Ctrl Pts',(-155.309646664219,-4.03280185074966,
133.622175776661));
#113409=CARTESIAN_POINT('Ctrl Pts',(-155.316464553366,-3.96293409402055,
133.719605105171));
#113410=CARTESIAN_POINT('Ctrl Pts',(-155.323282442513,-3.88971625588467,
133.814226147985));
#113411=CARTESIAN_POINT('Ctrl Pts',(-155.331056776633,-3.80622708132492,
133.922121067607));
#113412=CARTESIAN_POINT('Ctrl Pts',(-155.338831110752,-3.71811299781759,
134.026710454927));
#113413=CARTESIAN_POINT('Ctrl Pts',(-155.346605444871,-3.62566520347868,
134.127572150825));
#113414=CARTESIAN_POINT('Ctrl Pts',(-155.354370197818,-3.53333134278399,
134.228309543697));
#113415=CARTESIAN_POINT('Ctrl Pts',(-155.362134950765,-3.43667465971446,
134.325328100484));
#113416=CARTESIAN_POINT('Ctrl Pts',(-155.369899703712,-3.33602822956078,
134.418236475156));
#113417=CARTESIAN_POINT('Ctrl Pts',(-155.377656744597,-3.23548176286012,
134.511052571922));
#113418=CARTESIAN_POINT('Ctrl Pts',(-155.385413785482,-3.13095372039143,
134.599766347042));
#113419=CARTESIAN_POINT('Ctrl Pts',(-155.393170826367,-3.02281560970584,
134.684021537314));
#113420=CARTESIAN_POINT('Ctrl Pts',(-155.400922017607,-2.91475904681087,
134.768213190091));
#113421=CARTESIAN_POINT('Ctrl Pts',(-155.408673208847,-2.80309814158936,
134.847952711063));
#113422=CARTESIAN_POINT('Ctrl Pts',(-155.416424400087,-2.68823894975632,
134.922922795258));
#113423=CARTESIAN_POINT('Ctrl Pts',(-155.424172296864,-2.57342857614361,
134.997861015167));
#113424=CARTESIAN_POINT('Ctrl Pts',(-155.431920193641,-2.45542294628743,
135.068033616874));
#113425=CARTESIAN_POINT('Ctrl Pts',(-155.439668090418,-2.3346585053298,
135.133165617331));
#113426=CARTESIAN_POINT('Ctrl Pts',(-155.447414366502,-2.21391932568985,
135.198283993578));
#113427=CARTESIAN_POINT('Ctrl Pts',(-155.455160642586,-2.09042282669038,
135.258363680333));
#113428=CARTESIAN_POINT('Ctrl Pts',(-155.46290691867,-1.96463120417875,
135.313175017613));
#113429=CARTESIAN_POINT('Ctrl Pts',(-155.470653251936,-1.83883865310245,
135.367986759496));
#113430=CARTESIAN_POINT('Ctrl Pts',(-155.478399585201,-1.71075130312537,
135.417529918128));
#113431=CARTESIAN_POINT('Ctrl Pts',(-155.486145918466,-1.58085216303489,
135.461622635225));
#113432=CARTESIAN_POINT('Ctrl Pts',(-155.493893986469,-1.45092393293247,
135.50572522658));
#113433=CARTESIAN_POINT('Ctrl Pts',(-155.501642054472,-1.31918347549303,
135.544374821926));
#113434=CARTESIAN_POINT('Ctrl Pts',(-155.509390122475,-1.18612943420565,
135.577439291526));
#113435=CARTESIAN_POINT('Ctrl Pts',(-155.517146425217,-1.05293398149965,
135.610538902437));
#113436=CARTESIAN_POINT('Ctrl Pts',(-155.524902727959,-0.918422536130609,
135.638041435486));
#113437=CARTESIAN_POINT('Ctrl Pts',(-155.532659030701,-0.783104972180423,
135.659865706127));
#113438=CARTESIAN_POINT('Ctrl Pts',(-155.540419473215,-0.647715185171655,
135.681701625039));
#113439=CARTESIAN_POINT('Ctrl Pts',(-155.548179915729,-0.511518810327363,
135.697853196678));
#113440=CARTESIAN_POINT('Ctrl Pts',(-155.555940358243,-0.375030347737595,
135.708291214625));
#113441=CARTESIAN_POINT('Ctrl Pts',(-155.563713258509,-0.238322781751173,
135.718745988606));
#113442=CARTESIAN_POINT('Ctrl Pts',(-155.571486158774,-0.101322581995252,
135.723468867033));
#113443=CARTESIAN_POINT('Ctrl Pts',(-155.57925905904,0.0354553431398876,
135.722482818279));
#113444=CARTESIAN_POINT('Ctrl Pts',(-155.586749394801,0.167261046172449,
135.72153261488));
#113445=CARTESIAN_POINT('Ctrl Pts',(-155.594239730563,0.298860046827601,
135.715281360497));
#113446=CARTESIAN_POINT('Ctrl Pts',(-155.601730066325,0.429798466647812,
135.703794905376));
#113447=CARTESIAN_POINT('Ctrl Pts',(-155.609504400444,0.565701456453974,
135.691872937818));
#113448=CARTESIAN_POINT('Ctrl Pts',(-155.617278734563,0.701323284573325,
135.674273182427));
#113449=CARTESIAN_POINT('Ctrl Pts',(-155.625053068683,0.836151376887149,
135.651012445109));
#113450=CARTESIAN_POINT('Ctrl Pts',(-155.63281782163,0.970813305627494,
135.627780374571));
#113451=CARTESIAN_POINT('Ctrl Pts',(-155.640582574577,1.10468306333046,
135.598901269399));
#113452=CARTESIAN_POINT('Ctrl Pts',(-155.648347327524,1.23725136416848,
135.564443823179));
#113453=CARTESIAN_POINT('Ctrl Pts',(-155.656104368409,1.36968799630085,
135.530020600582));
#113454=CARTESIAN_POINT('Ctrl Pts',(-155.663861409294,1.50082536800743,
135.490030160472));
#113455=CARTESIAN_POINT('Ctrl Pts',(-155.671618450179,1.63016293605966,
135.444592493712));
#113456=CARTESIAN_POINT('Ctrl Pts',(-155.679369641419,1.7594029696459,135.399189091849));
#113457=CARTESIAN_POINT('Ctrl Pts',(-155.687120832659,1.88684553372126,
135.348346768717));
#113458=CARTESIAN_POINT('Ctrl Pts',(-155.694872023899,2.01200418759494,
135.2922356394));
#113459=CARTESIAN_POINT('Ctrl Pts',(-155.702619920676,2.13710964570217,
135.23614835881));
#113460=CARTESIAN_POINT('Ctrl Pts',(-155.710367817453,2.25993276829467,
135.174796885603));
#113461=CARTESIAN_POINT('Ctrl Pts',(-155.71811571423,2.38000629508634,135.108399778383));
#113462=CARTESIAN_POINT('Ctrl Pts',(-155.725861990314,2.50005470508436,
135.042016560008));
#113463=CARTESIAN_POINT('Ctrl Pts',(-155.733608266399,2.61735432137557,
134.970589996017));
#113464=CARTESIAN_POINT('Ctrl Pts',(-155.741354542483,2.73146209636484,
134.894384808035));
#113465=CARTESIAN_POINT('Ctrl Pts',(-155.749100875748,2.84557071367193,
134.818179057524));
#113466=CARTESIAN_POINT('Ctrl Pts',(-155.756847209013,2.95648711753465,
134.737194829766));
#113467=CARTESIAN_POINT('Ctrl Pts',(-155.764593542279,3.06379722738064,
134.651740194888));
#113468=CARTESIAN_POINT('Ctrl Pts',(-155.772341610282,3.17113136858155,
134.566266423037));
#113469=CARTESIAN_POINT('Ctrl Pts',(-155.780089678285,3.27485730294596,
134.476320495464));
#113470=CARTESIAN_POINT('Ctrl Pts',(-155.787837746288,3.37459433699599,
134.382250515706));
#113471=CARTESIAN_POINT('Ctrl Pts',(-155.79559404903,3.47443737275283,134.288080557254));
#113472=CARTESIAN_POINT('Ctrl Pts',(-155.803350351771,3.57028275456598,
134.189778059603));
#113473=CARTESIAN_POINT('Ctrl Pts',(-155.811106654513,3.66178658018239,
134.087728112029));
#113474=CARTESIAN_POINT('Ctrl Pts',(-155.818867097028,3.75333924414566,
133.985623697325));
#113475=CARTESIAN_POINT('Ctrl Pts',(-155.826627539542,3.84054548618603,
133.879768148882));
#113476=CARTESIAN_POINT('Ctrl Pts',(-155.834387982056,3.92310263425139,
133.770578543415));
#113477=CARTESIAN_POINT('Ctrl Pts',(-155.842160882321,4.0057923103799,133.661213657101));
#113478=CARTESIAN_POINT('Ctrl Pts',(-155.849933782587,4.08381775614332,
133.548504340151));
#113479=CARTESIAN_POINT('Ctrl Pts',(-155.857706682852,4.1569199749223,133.432896214546));
#113480=CARTESIAN_POINT('Ctrl Pts',(-155.865197018614,4.22736474391726,
133.321490735503));
#113481=CARTESIAN_POINT('Ctrl Pts',(-155.872687354377,4.29323786090048,
133.207393813481));
#113482=CARTESIAN_POINT('Ctrl Pts',(-155.880177690139,4.35434939515777,
133.091022902948));
#113483=CARTESIAN_POINT('Ctrl Pts',(-155.887952024258,4.41777799180917,
132.970239753976));
#113484=CARTESIAN_POINT('Ctrl Pts',(-155.895726358377,4.476277729994,132.846624171282));
#113485=CARTESIAN_POINT('Ctrl Pts',(-155.903500692496,4.52958569016528,
132.720616481993));
#113486=CARTESIAN_POINT('Ctrl Pts',(-155.911265445443,4.58282795303991,
132.594764085919));
#113487=CARTESIAN_POINT('Ctrl Pts',(-155.91903019839,4.63089101794859,132.466525805617));
#113488=CARTESIAN_POINT('Ctrl Pts',(-155.926794951337,4.67355739732234,
132.336367248241));
#113489=CARTESIAN_POINT('Ctrl Pts',(-155.934551992222,4.71618139984661,
132.20633796618));
#113490=CARTESIAN_POINT('Ctrl Pts',(-155.942309033107,4.75341926261015,
132.074392571659));
#113491=CARTESIAN_POINT('Ctrl Pts',(-155.950066073992,4.78510138148113,
131.941017043865));
#113492=CARTESIAN_POINT('Ctrl Pts',(-155.957817265233,4.81675960861986,
131.807742095594));
#113493=CARTESIAN_POINT('Ctrl Pts',(-155.965568456473,4.84287034107949,
131.67303953953));
#113494=CARTESIAN_POINT('Ctrl Pts',(-155.973319647713,4.86331376842432,
131.537410583363));
#113495=CARTESIAN_POINT('Ctrl Pts',(-155.98106754449,4.88374850676721,131.401839273119));
#113496=CARTESIAN_POINT('Ctrl Pts',(-155.988815441267,4.89852067267687,
131.265342731688));
#113497=CARTESIAN_POINT('Ctrl Pts',(-155.996563338044,4.90756158009912,
131.128432214648));
#113498=CARTESIAN_POINT('Ctrl Pts',(-156.004309614128,4.91660059635842,
130.991550336336));
#113499=CARTESIAN_POINT('Ctrl Pts',(-156.012055890213,4.91991071297508,
130.854255044524));
#113500=CARTESIAN_POINT('Ctrl Pts',(-156.019802166297,4.91747516970204,
130.717062176206));
#113501=CARTESIAN_POINT('Ctrl Pts',(-156.027548499562,4.91503960845036,
130.579868295161));
#113502=CARTESIAN_POINT('Ctrl Pts',(-156.035294832827,4.90685830961618,
130.442777230022));
#113503=CARTESIAN_POINT('Ctrl Pts',(-156.043041166093,4.89296664065922,
130.306303877931));
#113504=CARTESIAN_POINT('Ctrl Pts',(-156.050789234096,4.87907186075926,
130.169799963578));
#113505=CARTESIAN_POINT('Ctrl Pts',(-156.058537302099,4.85946420566122,
130.033914426421));
#113506=CARTESIAN_POINT('Ctrl Pts',(-156.066285370102,4.8342307706067,129.899155713128));
#113507=CARTESIAN_POINT('Ctrl Pts',(-156.074041672843,4.80897051715722,
129.764253776671));
#113508=CARTESIAN_POINT('Ctrl Pts',(-156.081797975585,4.77807261183529,
129.630481441317));
#113509=CARTESIAN_POINT('Ctrl Pts',(-156.089554278327,4.74167515358669,
129.49833619193));
#113510=CARTESIAN_POINT('Ctrl Pts',(-156.097314720841,4.70525826891872,
129.366120412644));
#113511=CARTESIAN_POINT('Ctrl Pts',(-156.105075163356,4.66333610198203,
129.235533821808));
#113512=CARTESIAN_POINT('Ctrl Pts',(-156.11283560587,4.61609594959198,129.107056506141));
#113513=CARTESIAN_POINT('Ctrl Pts',(-156.120608506135,4.56877996311553,
128.978372947281));
#113514=CARTESIAN_POINT('Ctrl Pts',(-156.128381406401,4.51612908198456,
128.851805791076));
#113515=CARTESIAN_POINT('Ctrl Pts',(-156.136154306666,4.45837822659115,
128.72781380828));
#113516=CARTESIAN_POINT('Ctrl Pts',(-156.143644642428,4.40272676025738,
128.608329246376));
#113517=CARTESIAN_POINT('Ctrl Pts',(-156.15113497819,4.34233981713904,128.491236154113));
#113518=CARTESIAN_POINT('Ctrl Pts',(-156.158625313952,4.27746595131303,
128.376919969917));
#113519=CARTESIAN_POINT('Ctrl Pts',(-156.166399648071,4.21013237314557,
128.258269452851));
#113520=CARTESIAN_POINT('Ctrl Pts',(-156.17417398219,4.13775161987442,128.142234724393));
#113521=CARTESIAN_POINT('Ctrl Pts',(-156.181948316309,4.06055203674368,
128.02927499377));
#113522=CARTESIAN_POINT('Ctrl Pts',(-156.189713069256,3.98344759520005,
127.916454475921));
#113523=CARTESIAN_POINT('Ctrl Pts',(-156.197477822203,3.90153635867472,
127.8067017353));
#113524=CARTESIAN_POINT('Ctrl Pts',(-156.20524257515,3.81509249830841,127.700451422398));
#113525=CARTESIAN_POINT('Ctrl Pts',(-156.212999616035,3.72873449520216,
127.594306638803));
#113526=CARTESIAN_POINT('Ctrl Pts',(-156.22075665692,3.63785307231276,127.491657661544));
#113527=CARTESIAN_POINT('Ctrl Pts',(-156.228513697805,3.54276542251666,
127.392909867002));
#113528=CARTESIAN_POINT('Ctrl Pts',(-156.236264889045,3.44774947905759,
127.294236538941));
#113529=CARTESIAN_POINT('Ctrl Pts',(-156.244016080286,3.34853389235116,
127.199458818384));
#113530=CARTESIAN_POINT('Ctrl Pts',(-156.251767271526,3.2454755821541,127.108948420241));
#113531=CARTESIAN_POINT('Ctrl Pts',(-156.259515168303,3.14246107448762,
127.018476491431));
#113532=CARTESIAN_POINT('Ctrl Pts',(-156.26726306508,3.03560738490353,126.932268535125));
#113533=CARTESIAN_POINT('Ctrl Pts',(-156.275010961857,2.92530752070788,
126.850658684973));
#113534=CARTESIAN_POINT('Ctrl Pts',(-156.282757237941,2.81503072886603,
126.769065905842));
#113535=CARTESIAN_POINT('Ctrl Pts',(-156.290503514025,2.701309510345,126.692069552137));
#113536=CARTESIAN_POINT('Ctrl Pts',(-156.298249790109,2.58456879409407,
126.619962547222));
#113537=CARTESIAN_POINT('Ctrl Pts',(-156.305996123374,2.46782721609016,
126.547855010031));
#113538=CARTESIAN_POINT('Ctrl Pts',(-156.31374245664,2.34806642850909,126.480637099103));
#113539=CARTESIAN_POINT('Ctrl Pts',(-156.321488789905,2.22573874587498,
126.418557373278));
#113540=CARTESIAN_POINT('Ctrl Pts',(-156.329236857908,2.10338366880434,
126.356463745127));
#113541=CARTESIAN_POINT('Ctrl Pts',(-156.336984925911,1.9784609013917,126.299510768657));
#113542=CARTESIAN_POINT('Ctrl Pts',(-156.344732993914,1.85144529132593,
126.247899996017));
#113543=CARTESIAN_POINT('Ctrl Pts',(-156.352489296656,1.72429468755811,
126.196234370834));
#113544=CARTESIAN_POINT('Ctrl Pts',(-156.360245599398,1.59504716064527,
126.149922438825));
#113545=CARTESIAN_POINT('Ctrl Pts',(-156.36800190214,1.46419590454737,126.109116916159));
#113546=CARTESIAN_POINT('Ctrl Pts',(-156.375762344654,1.33327480919353,
126.068289614356));
#113547=CARTESIAN_POINT('Ctrl Pts',(-156.383522787168,1.20074865668212,
126.032974678594));
#113548=CARTESIAN_POINT('Ctrl Pts',(-156.391283229682,1.06712259607261,
126.00327402936));
#113549=CARTESIAN_POINT('Ctrl Pts',(-156.399056129948,0.933282027048574,
125.973525702007));
#113550=CARTESIAN_POINT('Ctrl Pts',(-156.406829030213,0.798338406644024,
125.949409739949));
#113551=CARTESIAN_POINT('Ctrl Pts',(-156.414601930479,0.66280469189865,
125.930976474807));
#113552=CARTESIAN_POINT('Ctrl Pts',(-156.42209226624,0.532197969074568,
125.913213305283));
#113553=CARTESIAN_POINT('Ctrl Pts',(-156.429582602002,0.401043616516894,
125.90072687425));
#113554=CARTESIAN_POINT('Ctrl Pts',(-156.437072937764,0.269800264039454,
125.893516405007));
#113555=CARTESIAN_POINT('Ctrl Pts',(-156.444847271883,0.133580779960928,
125.886032548631));
#113556=CARTESIAN_POINT('Ctrl Pts',(-156.452621606003,-0.00316608850629907,
125.88420892125));
#113557=CARTESIAN_POINT('Ctrl Pts',(-156.460395940122,-0.139930569451091,
125.888101623348));
#113558=CARTESIAN_POINT('Ctrl Pts',(-156.468160693069,-0.276526500396111,
125.891989528038));
#113559=CARTESIAN_POINT('Ctrl Pts',(-156.475925446016,-0.413139613575392,
125.901579734008));
#113560=CARTESIAN_POINT('Ctrl Pts',(-156.483690198963,-0.54925602902288,
125.91687651252));
#113561=CARTESIAN_POINT('Ctrl Pts',(-156.491447239848,-0.685237251727639,
125.932158098055));
#113562=CARTESIAN_POINT('Ctrl Pts',(-156.499204280733,-0.82072237243852,
125.953134933479));
#113563=CARTESIAN_POINT('Ctrl Pts',(-156.506961321618,-0.955198886028568,
125.979759271275));
#113564=CARTESIAN_POINT('Ctrl Pts',(-156.514712512858,-1.08957398983383,
126.006363531452));
#113565=CARTESIAN_POINT('Ctrl Pts',(-156.522463704098,-1.22294161847439,
126.038606741444));
#113566=CARTESIAN_POINT('Ctrl Pts',(-156.530214895338,-1.35479611382101,
126.07638953554));
#113567=CARTESIAN_POINT('Ctrl Pts',(-156.537962792116,-1.48659456748996,
126.114156270941));
#113568=CARTESIAN_POINT('Ctrl Pts',(-156.545710688892,-1.61688079193306,
126.157457800112));
#113569=CARTESIAN_POINT('Ctrl Pts',(-156.55345858567,-1.74516124099885,
126.206144082276));
#113570=CARTESIAN_POINT('Ctrl Pts',(-156.561204861754,-1.87341485655976,
126.254820180319));
#113571=CARTESIAN_POINT('Ctrl Pts',(-156.568951137838,-1.9996631659878,
126.308878652295));
#113572=CARTESIAN_POINT('Ctrl Pts',(-156.576697413922,-2.12343004008279,
126.368120325678));
#113573=CARTESIAN_POINT('Ctrl Pts',(-156.584443747187,-2.24719782779657,
126.427362436369));
#113574=CARTESIAN_POINT('Ctrl Pts',(-156.592190080453,-2.36848379097736,
126.491787656018));
#113575=CARTESIAN_POINT('Ctrl Pts',(-156.599936413718,-2.48683432298753,
126.561149791728));
#113576=CARTESIAN_POINT('Ctrl Pts',(-156.607684481721,-2.60521135877859,
126.630527460607));
#113577=CARTESIAN_POINT('Ctrl Pts',(-156.615432549724,-2.72065131807,126.704844047891));
#113578=CARTESIAN_POINT('Ctrl Pts',(-156.623180617727,-2.83272796255406,
126.783808994634));
#113579=CARTESIAN_POINT('Ctrl Pts',(-156.630936920469,-2.94492372342975,
126.862857866261));
#113580=CARTESIAN_POINT('Ctrl Pts',(-156.638693223211,-3.05374870879315,
126.94656474065));
#113581=CARTESIAN_POINT('Ctrl Pts',(-156.646449525952,-3.15880785082546,
127.034597226574));
#113582=CARTESIAN_POINT('Ctrl Pts',(-156.654209968467,-3.26392306608571,
127.122676698086));
#113583=CARTESIAN_POINT('Ctrl Pts',(-156.661970410981,-3.36526814427592,
127.215086118136));
#113584=CARTESIAN_POINT('Ctrl Pts',(-156.669730853495,-3.46248429140025,
127.311455581023));
#113585=CARTESIAN_POINT('Ctrl Pts',(-156.677503753761,-3.55985649851412,
127.407979744727));
#113586=CARTESIAN_POINT('Ctrl Pts',(-156.685276654026,-3.65308626340284,
127.508476367818));
#113587=CARTESIAN_POINT('Ctrl Pts',(-156.693049554291,-3.74185397483924,
127.612541090481));
#113588=CARTESIAN_POINT('Ctrl Pts',(-156.700539890054,-3.8273947563728,
127.712822798352));
#113589=CARTESIAN_POINT('Ctrl Pts',(-156.708030225816,-3.90879207561689,
127.816417448674));
#113590=CARTESIAN_POINT('Ctrl Pts',(-156.715520561578,-3.98579868541431,
127.922938763368));
#113591=CARTESIAN_POINT('Ctrl Pts',(-156.723359687267,-4.06639113311023,
128.03442027782));
#113592=CARTESIAN_POINT('Ctrl Pts',(-156.731198812957,-4.14242889248428,
128.149459757647));
#113593=CARTESIAN_POINT('Ctrl Pts',(-156.739037938646,-4.21358455281497,
128.267652459583));
#113594=CARTESIAN_POINT('Ctrl Pts',(-156.746863778478,-4.28461961755481,
128.385644846903));
#113595=CARTESIAN_POINT('Ctrl Pts',(-156.75468961831,-4.3507888698194,128.506779485963));
#113596=CARTESIAN_POINT('Ctrl Pts',(-156.762515458141,-4.41180659074676,
128.630620598994));
#113597=CARTESIAN_POINT('Ctrl Pts',(-156.770333624224,-4.47276447980175,
128.754340277701));
#113598=CARTESIAN_POINT('Ctrl Pts',(-156.778151790307,-4.52858071880324,
128.880760810003));
#113599=CARTESIAN_POINT('Ctrl Pts',(-156.78596995639,-4.57901390273034,
129.00941918646));
#113600=CARTESIAN_POINT('Ctrl Pts',(-156.793780602572,-4.62939857751095,
129.137953812886));
#113601=CARTESIAN_POINT('Ctrl Pts',(-156.801591248754,-4.67441037000992,
129.268721641938));
#113602=CARTESIAN_POINT('Ctrl Pts',(-156.809401894936,-4.71385493883423,
129.401237430484));
#113603=CARTESIAN_POINT('Ctrl Pts',(-156.812942739115,-4.73173656715076,
129.461311558493));
#113604=CARTESIAN_POINT('Ctrl Pts',(-156.816483583295,-4.74847470512542,
129.521744625465));
#113605=CARTESIAN_POINT('Ctrl Pts',(-156.820024427474,-4.76405452823416,
129.582490119309));
#113606=CARTESIAN_POINT('Origin',(213.235140564004,0.,130.804360617566));
#113607=CARTESIAN_POINT('',(-158.915166007136,-4.76405452823407,129.582490119308));
#113608=CARTESIAN_POINT('',(-158.569717364632,-4.76405452823396,129.582490119308));
#113609=CARTESIAN_POINT('',(213.235140564004,-4.76405452823405,129.582490119308));
#113610=CARTESIAN_POINT('',(-157.235140563979,-4.91824963986197,130.806242769961));
#113611=CARTESIAN_POINT('Ctrl Pts',(-157.235140564011,-4.91824963986175,
130.80624277053));
#113612=CARTESIAN_POINT('Ctrl Pts',(-157.241035980355,-4.91821002387229,
130.9097632227));
#113613=CARTESIAN_POINT('Ctrl Pts',(-157.246931396699,-4.91490228748288,
131.01321746358));
#113614=CARTESIAN_POINT('Ctrl Pts',(-157.252826813043,-4.90833734989934,
131.116462399174));
#113615=CARTESIAN_POINT('Ctrl Pts',(-157.260601147162,-4.89968011260356,
131.252612346627));
#113616=CARTESIAN_POINT('Ctrl Pts',(-157.268375481281,-4.88533997543229,
131.388617464613));
#113617=CARTESIAN_POINT('Ctrl Pts',(-157.2761498154,-4.8653214390861,131.523964923327));
#113618=CARTESIAN_POINT('Ctrl Pts',(-157.283914568347,-4.84532757379684,
131.659145578394));
#113619=CARTESIAN_POINT('Ctrl Pts',(-157.291679321294,-4.8196692901588,
131.79366980381));
#113620=CARTESIAN_POINT('Ctrl Pts',(-157.299444074241,-4.78840304052204,
131.927026811953));
#113621=CARTESIAN_POINT('Ctrl Pts',(-157.307201115126,-4.75716784496519,
132.060251368035));
#113622=CARTESIAN_POINT('Ctrl Pts',(-157.314958156011,-4.72033585644996,
132.192310635716));
#113623=CARTESIAN_POINT('Ctrl Pts',(-157.322715196896,-4.6780150196256,
132.322701336462));
#113624=CARTESIAN_POINT('Ctrl Pts',(-157.330466388137,-4.63572609727343,
132.452993708566));
#113625=CARTESIAN_POINT('Ctrl Pts',(-157.338217579377,-4.58795668561397,
132.5816196479));
#113626=CARTESIAN_POINT('Ctrl Pts',(-157.345968770617,-4.53486517750881,
132.708088771562));
#113627=CARTESIAN_POINT('Ctrl Pts',(-157.353716667394,-4.48179623471093,
132.834504142473));
#113628=CARTESIAN_POINT('Ctrl Pts',(-157.361464564171,-4.42340984549422,
132.958764161234));
#113629=CARTESIAN_POINT('Ctrl Pts',(-157.369212460948,-4.35991329256529,
133.080396457313));
#113630=CARTESIAN_POINT('Ctrl Pts',(-157.376958737032,-4.29643002174622,
133.202003310538));
#113631=CARTESIAN_POINT('Ctrl Pts',(-157.384705013117,-4.2278388942011,
133.32098318803));
#113632=CARTESIAN_POINT('Ctrl Pts',(-157.392451289201,-4.15439392340065,
133.436886817191));
#113633=CARTESIAN_POINT('Ctrl Pts',(-157.400197622466,-4.0809484104462,
133.552791301926));
#113634=CARTESIAN_POINT('Ctrl Pts',(-157.407943955731,-4.00264919200707,
133.665619162773));
#113635=CARTESIAN_POINT('Ctrl Pts',(-157.415690288997,-3.91979431270252,
133.774949045572));
#113636=CARTESIAN_POINT('Ctrl Pts',(-157.423438357,-3.83692087862234,133.88430341204));
#113637=CARTESIAN_POINT('Ctrl Pts',(-157.431186425003,-3.74948998967467,
133.990157930152));
#113638=CARTESIAN_POINT('Ctrl Pts',(-157.438934493006,-3.65784051355853,
134.092123662536));
#113639=CARTESIAN_POINT('Ctrl Pts',(-157.446690795747,-3.5660936312884,
134.194197765313));
#113640=CARTESIAN_POINT('Ctrl Pts',(-157.454447098489,-3.47011946721651,
134.292374534919));
#113641=CARTESIAN_POINT('Ctrl Pts',(-157.462203401231,-3.37029474701639,
134.386300927054));
#113642=CARTESIAN_POINT('Ctrl Pts',(-157.469963843745,-3.27041674735744,
134.480277450532));
#113643=CARTESIAN_POINT('Ctrl Pts',(-157.47772428626,-3.16668439205171,
134.569998820617));
#113644=CARTESIAN_POINT('Ctrl Pts',(-157.485484728774,-3.05950737441191,
134.655152443726));
#113645=CARTESIAN_POINT('Ctrl Pts',(-157.493257629039,-2.95215830670866,
134.74044276299));
#113646=CARTESIAN_POINT('Ctrl Pts',(-157.501030529305,-2.84135384281622,
134.821150452186));
#113647=CARTESIAN_POINT('Ctrl Pts',(-157.50880342957,-2.72753326118023,
134.897005895581));
#113648=CARTESIAN_POINT('Ctrl Pts',(-157.516293765332,-2.61785034438345,
134.970103802539));
#113649=CARTESIAN_POINT('Ctrl Pts',(-157.523784101094,-2.50536705263417,
135.038695961219));
#113650=CARTESIAN_POINT('Ctrl Pts',(-157.531274436856,-2.39049616237082,
135.102582477846));
#113651=CARTESIAN_POINT('Ctrl Pts',(-157.539048770975,-2.27126990738872,
135.168891271169));
#113652=CARTESIAN_POINT('Ctrl Pts',(-157.546823105094,-2.1490937553434,
135.230340596014));
#113653=CARTESIAN_POINT('Ctrl Pts',(-157.554597439213,-2.02440159721285,
135.286657041912));
#113654=CARTESIAN_POINT('Ctrl Pts',(-157.56236219216,-1.89986311102314,
135.342904082823));
#113655=CARTESIAN_POINT('Ctrl Pts',(-157.570126945108,-1.77281514121128,
135.394030671892));
#113656=CARTESIAN_POINT('Ctrl Pts',(-157.577891698055,-1.64371794174452,
135.439808210894));
#113657=CARTESIAN_POINT('Ctrl Pts',(-157.58564873894,-1.51474896343656,
135.485540282998));
#113658=CARTESIAN_POINT('Ctrl Pts',(-157.593405779825,-1.38373517195991,
135.525933747832));
#113659=CARTESIAN_POINT('Ctrl Pts',(-157.60116282071,-1.25115833651864,
135.560807387946));
#113660=CARTESIAN_POINT('Ctrl Pts',(-157.60891401195,-1.1186814783001,135.595654729577));
#113661=CARTESIAN_POINT('Ctrl Pts',(-157.61666520319,-0.984644298828111,
135.624990432721));
#113662=CARTESIAN_POINT('Ctrl Pts',(-157.62441639443,-0.849544986336227,
135.648682693842));
#113663=CARTESIAN_POINT('Ctrl Pts',(-157.632164291207,-0.714503094655859,
135.67236488512));
#113664=CARTESIAN_POINT('Ctrl Pts',(-157.639912187984,-0.578400352107374,
135.690408337643));
#113665=CARTESIAN_POINT('Ctrl Pts',(-157.647660084761,-0.441746218762442,
135.702732116412));
#113666=CARTESIAN_POINT('Ctrl Pts',(-157.655406360845,-0.305120670516284,
135.715053317313));
#113667=CARTESIAN_POINT('Ctrl Pts',(-157.66315263693,-0.167944350027724,
135.721657189137));
#113668=CARTESIAN_POINT('Ctrl Pts',(-157.670898913014,-0.0307325435426136,
135.722514597798));
#113669=CARTESIAN_POINT('Ctrl Pts',(-157.678645246279,0.106480275808695,
135.723372012787));
#113670=CARTESIAN_POINT('Ctrl Pts',(-157.686391579544,0.243728190721681,
135.718482877527));
#113671=CARTESIAN_POINT('Ctrl Pts',(-157.69413791281,0.380495603610463,
135.707870193179));
#113672=CARTESIAN_POINT('Ctrl Pts',(-157.701885980813,0.517293644612896,
135.697255132195));
#113673=CARTESIAN_POINT('Ctrl Pts',(-157.709634048816,0.653610579750593,
135.680914001831));
#113674=CARTESIAN_POINT('Ctrl Pts',(-157.717382116819,0.788936018728041,
135.658921670932));
#113675=CARTESIAN_POINT('Ctrl Pts',(-157.725138419561,0.924405283192612,
135.636905966321));
#113676=CARTESIAN_POINT('Ctrl Pts',(-157.732894722302,1.05888055995229,
135.60922712603));
#113677=CARTESIAN_POINT('Ctrl Pts',(-157.740651025044,1.19186119341141,
135.576011270971));
#113678=CARTESIAN_POINT('Ctrl Pts',(-157.748411467559,1.32491280263895,
135.54277768761));
#113679=CARTESIAN_POINT('Ctrl Pts',(-157.756171910073,1.45646780417877,
135.504001311335));
#113680=CARTESIAN_POINT('Ctrl Pts',(-157.763932352587,1.58604175495508,
135.459857864267));
#113681=CARTESIAN_POINT('Ctrl Pts',(-157.771705252852,1.71582370933987,
135.415643554219));
#113682=CARTESIAN_POINT('Ctrl Pts',(-157.779478153118,1.84361789330427,
135.366045098006));
#113683=CARTESIAN_POINT('Ctrl Pts',(-157.787251053383,1.96896003076597,
135.311286339136));
#113684=CARTESIAN_POINT('Ctrl Pts',(-157.794741389145,2.08974566581144,
135.25851819908));
#113685=CARTESIAN_POINT('Ctrl Pts',(-157.802231724907,2.20825415828578,
135.200958557263));
#113686=CARTESIAN_POINT('Ctrl Pts',(-157.809722060669,2.32409421614721,
135.138846646725));
#113687=CARTESIAN_POINT('Ctrl Pts',(-157.817496394788,2.44432638501281,
135.074379744219));
#113688=CARTESIAN_POINT('Ctrl Pts',(-157.825270728907,2.56206463683875,
135.004804348357));
#113689=CARTESIAN_POINT('Ctrl Pts',(-157.833045063026,2.67684441498163,
134.93033771887));
#113690=CARTESIAN_POINT('Ctrl Pts',(-157.840809815973,2.79148273730613,
134.855962862848));
#113691=CARTESIAN_POINT('Ctrl Pts',(-157.84857456892,2.90316951567248,134.776708977889));
#113692=CARTESIAN_POINT('Ctrl Pts',(-157.856339321867,3.0114636454075,134.692839725764));
#113693=CARTESIAN_POINT('Ctrl Pts',(-157.864096362752,3.11965021588619,
134.609053773762));
#113694=CARTESIAN_POINT('Ctrl Pts',(-157.871853403638,3.22445053633657,
134.520661814898));
#113695=CARTESIAN_POINT('Ctrl Pts',(-157.879610444523,3.32545173536253,
134.427971222788));
#113696=CARTESIAN_POINT('Ctrl Pts',(-157.887361635763,3.42637676859849,
134.335350529374));
#113697=CARTESIAN_POINT('Ctrl Pts',(-157.895112827003,3.52350809602809,
134.238437918268));
#113698=CARTESIAN_POINT('Ctrl Pts',(-157.902864018243,3.61646554469464,
134.137581286309));
#113699=CARTESIAN_POINT('Ctrl Pts',(-157.91061191502,3.70938348396591,134.036767521109));
#113700=CARTESIAN_POINT('Ctrl Pts',(-157.918359811797,3.79813080843224,
133.932013355998));
#113701=CARTESIAN_POINT('Ctrl Pts',(-157.926107708574,3.88236404957427,
133.823703666819));
#113702=CARTESIAN_POINT('Ctrl Pts',(-157.933853984658,3.9665796709381,133.715416633692));
#113703=CARTESIAN_POINT('Ctrl Pts',(-157.941600260742,4.04628284727668,
133.60357586426));
#113704=CARTESIAN_POINT('Ctrl Pts',(-157.949346536826,4.12117054245583,
133.488599135748));
#113705=CARTESIAN_POINT('Ctrl Pts',(-157.957092870092,4.19605879043883,
133.373621558505));
#113706=CARTESIAN_POINT('Ctrl Pts',(-157.964839203357,4.26613127295388,
133.255508303594));
#113707=CARTESIAN_POINT('Ctrl Pts',(-157.972585536622,4.33112864844156,
133.134705590558));
#113708=CARTESIAN_POINT('Ctrl Pts',(-157.980333604625,4.39614057964091,
133.013875824591));
#113709=CARTESIAN_POINT('Ctrl Pts',(-157.988081672628,4.45607495702969,
132.890355746248));
#113710=CARTESIAN_POINT('Ctrl Pts',(-157.995829740631,4.5107188914635,132.764615229777));
#113711=CARTESIAN_POINT('Ctrl Pts',(-158.003586043373,4.56542090212102,
132.638741074789));
#113712=CARTESIAN_POINT('Ctrl Pts',(-158.011342346115,4.61482108170882,
132.510642126643));
#113713=CARTESIAN_POINT('Ctrl Pts',(-158.019098648857,4.65875492274316,
132.380807772505));
#113714=CARTESIAN_POINT('Ctrl Pts',(-158.026859091371,4.70271221259141,
132.250904121863));
#113715=CARTESIAN_POINT('Ctrl Pts',(-158.034619533885,4.74119724076914,
132.119263594695));
#113716=CARTESIAN_POINT('Ctrl Pts',(-158.042379976399,4.77409599395775,
131.986388748778));
#113717=CARTESIAN_POINT('Ctrl Pts',(-158.050152876665,4.8070475591456,131.853300600363));
#113718=CARTESIAN_POINT('Ctrl Pts',(-158.05792577693,4.83439485121186,131.718974556981));
#113719=CARTESIAN_POINT('Ctrl Pts',(-158.065698677196,4.85607524347601,
131.583922220135));
#113720=CARTESIAN_POINT('Ctrl Pts',(-158.073189012958,4.87696749887192,
131.453779375908));
#113721=CARTESIAN_POINT('Ctrl Pts',(-158.08067934872,4.8925976769512,131.322962432477));
#113722=CARTESIAN_POINT('Ctrl Pts',(-158.088169684482,4.90295554833941,
131.19192990622));
#113723=CARTESIAN_POINT('Ctrl Pts',(-158.095944018601,4.91370614156943,
131.055929241905));
#113724=CARTESIAN_POINT('Ctrl Pts',(-158.10371835272,4.91881079158172,130.919265515186));
#113725=CARTESIAN_POINT('Ctrl Pts',(-158.111492686839,4.9182011809279,130.782447004915));
#113726=CARTESIAN_POINT('Ctrl Pts',(-158.119257439786,4.91759232156474,
130.645797111231));
#113727=CARTESIAN_POINT('Ctrl Pts',(-158.127022192733,4.91128321536974,
130.508993200753));
#113728=CARTESIAN_POINT('Ctrl Pts',(-158.134786945681,4.89925726060928,
130.372548902964));
#113729=CARTESIAN_POINT('Ctrl Pts',(-158.142543986566,4.88724325019662,
130.236240123575));
#113730=CARTESIAN_POINT('Ctrl Pts',(-158.150301027451,4.86952372490714,
130.100290633021));
#113731=CARTESIAN_POINT('Ctrl Pts',(-158.158058068336,4.84613411979584,
129.965213934649));
#113732=CARTESIAN_POINT('Ctrl Pts',(-158.165809259576,4.82276215296767,
129.830239098666));
#113733=CARTESIAN_POINT('Ctrl Pts',(-158.173560450816,4.79372868357652,
129.696136128472));
#113734=CARTESIAN_POINT('Ctrl Pts',(-158.181311642056,4.75912091431727,
129.563412921082));
#113735=CARTESIAN_POINT('Ctrl Pts',(-158.189059538833,4.72452785428319,
129.430746124597));
#113736=CARTESIAN_POINT('Ctrl Pts',(-158.19680743561,4.684365305031,129.299458302063));
#113737=CARTESIAN_POINT('Ctrl Pts',(-158.204555332387,4.63877142038355,
129.170046458069));
#113738=CARTESIAN_POINT('Ctrl Pts',(-158.212301608471,4.59318707299387,
129.040661684242));
#113739=CARTESIAN_POINT('Ctrl Pts',(-158.220047884555,4.54217377984429,
128.913152476936));
#113740=CARTESIAN_POINT('Ctrl Pts',(-158.22779416064,4.48591923031548,128.787999607829));
#113741=CARTESIAN_POINT('Ctrl Pts',(-158.235540493905,4.42966426552828,
128.662845814872));
#113742=CARTESIAN_POINT('Ctrl Pts',(-158.24328682717,4.36816812744529,128.54004875142));
#113743=CARTESIAN_POINT('Ctrl Pts',(-158.251033160436,4.30166605275713,
128.420067801434));
#113744=CARTESIAN_POINT('Ctrl Pts',(-158.258781228439,4.23514908539053,
128.300059982547));
#113745=CARTESIAN_POINT('Ctrl Pts',(-158.266529296442,4.16362414016712,
128.18286987393));
#113746=CARTESIAN_POINT('Ctrl Pts',(-158.274277364444,4.08737146381713,
128.068930563758));
#113747=CARTESIAN_POINT('Ctrl Pts',(-158.282033667186,4.01103774521519,
127.954870157532));
#113748=CARTESIAN_POINT('Ctrl Pts',(-158.289789969928,3.9299664759229,127.844067776896));
#113749=CARTESIAN_POINT('Ctrl Pts',(-158.29754627267,3.84448047090935,127.73692635237));
#113750=CARTESIAN_POINT('Ctrl Pts',(-158.305306715184,3.75894883944098,
127.629727743241));
#113751=CARTESIAN_POINT('Ctrl Pts',(-158.313067157698,3.66899803345964,
127.526194278649));
#113752=CARTESIAN_POINT('Ctrl Pts',(-158.320827600213,3.57498924207386,
127.426693525984));
#113753=CARTESIAN_POINT('Ctrl Pts',(-158.328600500478,3.48082953943043,
127.327033045877));
#113754=CARTESIAN_POINT('Ctrl Pts',(-158.336373400744,3.38259911417897,
127.231418487003));
#113755=CARTESIAN_POINT('Ctrl Pts',(-158.344146301009,3.2806945399007,127.140179072068));
#113756=CARTESIAN_POINT('Ctrl Pts',(-158.351636636771,3.18249445357985,
127.052256439685));
#113757=CARTESIAN_POINT('Ctrl Pts',(-158.359126972533,3.08088294718426,
126.968396574892));
#113758=CARTESIAN_POINT('Ctrl Pts',(-158.366617308295,2.97624025430221,
126.888855923255));
#113759=CARTESIAN_POINT('Ctrl Pts',(-158.374391642414,2.86763000191393,
126.806299463635));
#113760=CARTESIAN_POINT('Ctrl Pts',(-158.382165976533,2.7554101261273,126.72813469452));
#113761=CARTESIAN_POINT('Ctrl Pts',(-158.389940310652,2.63997132908655,
126.654693830449));
#113762=CARTESIAN_POINT('Ctrl Pts',(-158.397705063599,2.52467480004641,
126.58134347568));
#113763=CARTESIAN_POINT('Ctrl Pts',(-158.405469816546,2.40616756966668,
126.51270565017));
#113764=CARTESIAN_POINT('Ctrl Pts',(-158.413234569493,2.28487279533544,
126.449071950711));
#113765=CARTESIAN_POINT('Ctrl Pts',(-158.420991610378,2.16369849268403,
126.385501453139));
#113766=CARTESIAN_POINT('Ctrl Pts',(-158.428748651263,2.0397424997492,126.326925371213));
#113767=CARTESIAN_POINT('Ctrl Pts',(-158.436505692148,1.91345599495261,
126.273591453519));
#113768=CARTESIAN_POINT('Ctrl Pts',(-158.444256883389,1.78726472379148,
126.220297755347));
#113769=CARTESIAN_POINT('Ctrl Pts',(-158.452008074629,1.6587467975864,126.17223850438));
#113770=CARTESIAN_POINT('Ctrl Pts',(-158.459759265869,1.52837665966729,
126.129614865262));
#113771=CARTESIAN_POINT('Ctrl Pts',(-158.467507162646,1.39806193253436,
126.087009342328));
#113772=CARTESIAN_POINT('Ctrl Pts',(-158.475255059423,1.2658969302769,126.049834957513));
#113773=CARTESIAN_POINT('Ctrl Pts',(-158.4830029562,1.13237447244599,126.018244121214));
#113774=CARTESIAN_POINT('Ctrl Pts',(-158.490749232284,0.998879944634847,
125.986659893037));
#113775=CARTESIAN_POINT('Ctrl Pts',(-158.498495508368,0.864028906263758,
125.9606569802));
#113776=CARTESIAN_POINT('Ctrl Pts',(-158.506241784452,0.728327294856539,
125.940337343149));
#113777=CARTESIAN_POINT('Ctrl Pts',(-158.513988117718,0.592624681731036,
125.920017556103));
#113778=CARTESIAN_POINT('Ctrl Pts',(-158.521734450983,0.456071869695214,
125.905381186453));
#113779=CARTESIAN_POINT('Ctrl Pts',(-158.529480784248,0.319182502662992,
125.896478631159));
#113780=CARTESIAN_POINT('Ctrl Pts',(-158.537228852251,0.18226248020596,
125.887574082201));
#113781=CARTESIAN_POINT('Ctrl Pts',(-158.544976920254,0.0450061428429854,
125.884405928074));
#113782=CARTESIAN_POINT('Ctrl Pts',(-158.552724988257,-0.0920706598753649,
125.886972484005));
#113783=CARTESIAN_POINT('Ctrl Pts',(-158.560481290999,-0.229293149450692,
125.889541767702));
#113784=CARTESIAN_POINT('Ctrl Pts',(-158.568237593741,-0.366335331694764,
125.897857929382));
#113785=CARTESIAN_POINT('Ctrl Pts',(-158.575993896483,-0.502683720371866,
125.911867169459));
#113786=CARTESIAN_POINT('Ctrl Pts',(-158.583754338997,-0.639104882289376,
125.925883886688));
#113787=CARTESIAN_POINT('Ctrl Pts',(-158.591514781511,-0.77483112607358,
125.945599680742));
#113788=CARTESIAN_POINT('Ctrl Pts',(-158.599275224025,-0.90935797533449,
125.970909352145));
#113789=CARTESIAN_POINT('Ctrl Pts',(-158.60704812429,-1.04410077903657,
125.99625965288));
#113790=CARTESIAN_POINT('Ctrl Pts',(-158.614821024556,-1.1776399596222,
126.027221687087));
#113791=CARTESIAN_POINT('Ctrl Pts',(-158.622593924821,-1.30948417499589,
126.063639759096));
#113792=CARTESIAN_POINT('Ctrl Pts',(-158.630084260583,-1.43653552104805,
126.098733942456));
#113793=CARTESIAN_POINT('Ctrl Pts',(-158.637574596346,-1.56201270154158,
126.138894275263));
#113794=CARTESIAN_POINT('Ctrl Pts',(-158.645064932108,-1.68549443601759,
126.183939471323));
#113795=CARTESIAN_POINT('Ctrl Pts',(-158.652839423886,-1.8136606170759,
126.230693517809));
#113796=CARTESIAN_POINT('Ctrl Pts',(-158.660613915665,-1.94008296338148,
126.282858478307));
#113797=CARTESIAN_POINT('Ctrl Pts',(-158.668388407444,-2.06427075965575,
126.340285204524));
#113798=CARTESIAN_POINT('Ctrl Pts',(-158.676153281355,-2.18830492251237,
126.397640887816));
#113799=CARTESIAN_POINT('Ctrl Pts',(-158.683918155266,-2.31010968422649,
126.460245222378));
#113800=CARTESIAN_POINT('Ctrl Pts',(-158.691683029177,-2.42921096759975,
126.527899798455));
#113801=CARTESIAN_POINT('Ctrl Pts',(-158.699440154486,-2.54819339926752,
126.595486861726));
#113802=CARTESIAN_POINT('Ctrl Pts',(-158.707197279795,-2.66447738371206,
126.668113945272));
#113803=CARTESIAN_POINT('Ctrl Pts',(-158.714954405103,-2.77761059626085,
126.745535364116));
#113804=CARTESIAN_POINT('Ctrl Pts',(-158.722705644344,-2.89065796389446,
126.822898035976));
#113805=CARTESIAN_POINT('Ctrl Pts',(-158.730456883585,-3.00055899713958,
126.905047581949));
#113806=CARTESIAN_POINT('Ctrl Pts',(-158.738208122826,-3.10688799577204,
126.991693566245));
#113807=CARTESIAN_POINT('Ctrl Pts',(-158.74595588125,-3.21316924568295,
127.078300640789));
#113808=CARTESIAN_POINT('Ctrl Pts',(-158.753703639674,-3.31588134994253,
127.169399889908));
#113809=CARTESIAN_POINT('Ctrl Pts',(-158.761451398098,-3.41462972295018,
127.264659088108));
#113810=CARTESIAN_POINT('Ctrl Pts',(-158.769197483952,-3.51335677835895,
127.359897721946));
#113811=CARTESIAN_POINT('Ctrl Pts',(-158.776943569805,-3.60812152366368,
127.459294247038));
#113812=CARTESIAN_POINT('Ctrl Pts',(-158.784689655659,-3.69856473238077,
127.562478142384));
#113813=CARTESIAN_POINT('Ctrl Pts',(-158.792435746782,-3.78900800262413,
127.665662107924));
#113814=CARTESIAN_POINT('Ctrl Pts',(-158.800181837905,-3.87512947292165,
127.772633154739));
#113815=CARTESIAN_POINT('Ctrl Pts',(-158.807927929028,-3.95660913560079,
127.882986418566));
#113816=CARTESIAN_POINT('Ctrl Pts',(-158.815675702898,-4.03810649877011,
127.993363655332));
#113817=CARTESIAN_POINT('Ctrl Pts',(-158.823423476768,-4.11495981599913,
128.107124256495));
#113818=CARTESIAN_POINT('Ctrl Pts',(-158.831171250637,-4.18689170528051,
128.223833363156));
#113819=CARTESIAN_POINT('Ctrl Pts',(-158.838926546575,-4.2588934309567,
128.340655778995));
#113820=CARTESIAN_POINT('Ctrl Pts',(-158.846681842513,-4.32596398133885,
128.460432083946));
#113821=CARTESIAN_POINT('Ctrl Pts',(-158.854437138451,-4.38787115228131,
128.582701369734));
#113822=CARTESIAN_POINT('Ctrl Pts',(-158.862196552724,-4.44981119810611,
128.705035584808));
#113823=CARTESIAN_POINT('Ctrl Pts',(-158.869955966996,-4.50658223941287,
128.829865063082));
#113824=CARTESIAN_POINT('Ctrl Pts',(-158.877715381269,-4.55800016229432,
128.95670870689));
#113825=CARTESIAN_POINT('Ctrl Pts',(-158.885485591628,-4.60948962567612,
129.083728835029));
#113826=CARTESIAN_POINT('Ctrl Pts',(-158.893255801988,-4.65561096263242,
129.212768358475));
#113827=CARTESIAN_POINT('Ctrl Pts',(-158.901026012348,-4.69622969640936,
129.343330261597));
#113828=CARTESIAN_POINT('Ctrl Pts',(-158.905739343944,-4.72086861253178,
129.422527801271));
#113829=CARTESIAN_POINT('Ctrl Pts',(-158.91045267554,-4.74348382451808,
129.502285257724));
#113830=CARTESIAN_POINT('Ctrl Pts',(-158.915166007136,-4.76405452823407,
129.582490119308));
#113831=CARTESIAN_POINT('Ctrl Pts',(-157.165002070592,-4.7640545282341,
129.582490119308));
#113832=CARTESIAN_POINT('Ctrl Pts',(-157.172688962945,-4.79783407738971,
129.71419606879));
#113833=CARTESIAN_POINT('Ctrl Pts',(-157.180375855299,-4.82612241304179,
129.847204992258));
#113834=CARTESIAN_POINT('Ctrl Pts',(-157.188062747653,-4.84884368240038,
129.98101499989));
#113835=CARTESIAN_POINT('Ctrl Pts',(-157.195909050374,-4.87203614424156,
130.117599952386));
#113836=CARTESIAN_POINT('Ctrl Pts',(-157.203755353095,-4.88942804849412,
130.255019141227));
#113837=CARTESIAN_POINT('Ctrl Pts',(-157.211601655816,-4.90099459220552,
130.392735703752));
#113838=CARTESIAN_POINT('Ctrl Pts',(-157.219447958537,-4.91256113591689,
130.530452266277));
#113839=CARTESIAN_POINT('Ctrl Pts',(-157.227294261258,-4.91830236539209,
130.668465765227));
#113840=CARTESIAN_POINT('Ctrl Pts',(-157.235140563979,-4.91824963986197,
130.806242769962));
#113841=CARTESIAN_POINT('',(-156.889859436049,-4.91824900331411,130.807491735542));
#113842=CARTESIAN_POINT('Ctrl Pts',(-156.820024427474,-4.76405452823416,
129.582490119309));
#113843=CARTESIAN_POINT('Ctrl Pts',(-156.827828471748,-4.7983925626546,
129.716373594362));
#113844=CARTESIAN_POINT('Ctrl Pts',(-156.835632516021,-4.8271005684515,
129.851775581074));
#113845=CARTESIAN_POINT('Ctrl Pts',(-156.843436560295,-4.85005608473303,
129.988187206186));
#113846=CARTESIAN_POINT('Ctrl Pts',(-156.851239413947,-4.87300809881336,
130.1245780197));
#113847=CARTESIAN_POINT('Ctrl Pts',(-156.859042267599,-4.89020929928041,
130.261977789153));
#113848=CARTESIAN_POINT('Ctrl Pts',(-156.866845121251,-4.90158835447094,
130.399867520202));
#113849=CARTESIAN_POINT('Ctrl Pts',(-156.874516559498,-4.91277576398896,
130.535434916946));
#113850=CARTESIAN_POINT('Ctrl Pts',(-156.882187997746,-4.91833559564134,
130.671475538436));
#113851=CARTESIAN_POINT('Ctrl Pts',(-156.889859435994,-4.91824900331473,
130.807491734567));
#113852=CARTESIAN_POINT('Ctrl Pts',(-156.889859436049,-4.91824900331411,
130.807491735541));
#113853=CARTESIAN_POINT('Ctrl Pts',(-156.898588911057,-4.91815046823347,
130.962267143557));
#113854=CARTESIAN_POINT('Ctrl Pts',(-156.907318386066,-4.91074181595013,
131.116765549781));
#113855=CARTESIAN_POINT('Ctrl Pts',(-156.916047861075,-4.8961255726307,
131.270340702475));
#113856=CARTESIAN_POINT('Ctrl Pts',(-156.92481124902,-4.88145254700271,
131.424512475758));
#113857=CARTESIAN_POINT('Ctrl Pts',(-156.933574636966,-4.8595159309414,
131.577753621313));
#113858=CARTESIAN_POINT('Ctrl Pts',(-156.942338024912,-4.83046931390519,
131.729427788057));
#113859=CARTESIAN_POINT('Ctrl Pts',(-156.951149759663,-4.80126244935518,
131.881938727224));
#113860=CARTESIAN_POINT('Ctrl Pts',(-156.959961494414,-4.76486701429897,
132.032865164884));
#113861=CARTESIAN_POINT('Ctrl Pts',(-156.968773229165,-4.72148792238269,
132.181580593203));
#113862=CARTESIAN_POINT('Ctrl Pts',(-156.977171547907,-4.68014402689176,
132.323318809812));
#113863=CARTESIAN_POINT('Ctrl Pts',(-156.985569866649,-4.63245684193933,
132.463048641733));
#113864=CARTESIAN_POINT('Ctrl Pts',(-156.993968185391,-4.57864336005564,
132.600247040455));
#113865=CARTESIAN_POINT('Ctrl Pts',(-157.00174251951,-4.52882815285295,
132.727251769029));
#113866=CARTESIAN_POINT('Ctrl Pts',(-157.009516853629,-4.47364565493833,
132.852383394033));
#113867=CARTESIAN_POINT('Ctrl Pts',(-157.017291187748,-4.41325673716972,
132.975154950138));
#113868=CARTESIAN_POINT('Ctrl Pts',(-157.025055940695,-4.35294224334497,
133.097775201272));
#113869=CARTESIAN_POINT('Ctrl Pts',(-157.032820693642,-4.28743426738942,
133.218040823248));
#113870=CARTESIAN_POINT('Ctrl Pts',(-157.040585446589,-4.21694252730218,
133.335482658071));
#113871=CARTESIAN_POINT('Ctrl Pts',(-157.048342487474,-4.14652080060495,
133.452807848008));
#113872=CARTESIAN_POINT('Ctrl Pts',(-157.056099528359,-4.0711253602934,
133.567314499075));
#113873=CARTESIAN_POINT('Ctrl Pts',(-157.063856569244,-3.99101266485418,
133.67855632619));
#113874=CARTESIAN_POINT('Ctrl Pts',(-157.071607760484,-3.91096038302167,
133.789714264978));
#113875=CARTESIAN_POINT('Ctrl Pts',(-157.079358951724,-3.82619815424202,
133.897611964361));
#113876=CARTESIAN_POINT('Ctrl Pts',(-157.087110142965,-3.73702653856023,
134.001830822681));
#113877=CARTESIAN_POINT('Ctrl Pts',(-157.094858039742,-3.64789282319396,
134.106005385206));
#113878=CARTESIAN_POINT('Ctrl Pts',(-157.102605936519,-3.55435370202516,
134.206503920116));
#113879=CARTESIAN_POINT('Ctrl Pts',(-157.110353833296,-3.45675079038899,
134.302939905741));
#113880=CARTESIAN_POINT('Ctrl Pts',(-157.11810010938,-3.35916829517786,
134.399355719037));
#113881=CARTESIAN_POINT('Ctrl Pts',(-157.125846385464,-3.25752397824553,
134.491710398729));
#113882=CARTESIAN_POINT('Ctrl Pts',(-157.133592661548,-3.15219690144129,
134.579653686593));
#113883=CARTESIAN_POINT('Ctrl Pts',(-157.141338994814,-3.04686904713664,
134.667597623634));
#113884=CARTESIAN_POINT('Ctrl Pts',(-157.149085328079,-2.93785867882222,
134.751129853291));
#113885=CARTESIAN_POINT('Ctrl Pts',(-157.156831661344,-2.82557826229612,
134.829940146794));
#113886=CARTESIAN_POINT('Ctrl Pts',(-157.164579729347,-2.71327270134939,
134.908768089316));
#113887=CARTESIAN_POINT('Ctrl Pts',(-157.17232779735,-2.5976959549327,134.98287176692));
#113888=CARTESIAN_POINT('Ctrl Pts',(-157.180075865353,-2.47928946441981,
135.05198428429));
#113889=CARTESIAN_POINT('Ctrl Pts',(-157.187832168095,-2.36075713007959,
135.121170255266));
#113890=CARTESIAN_POINT('Ctrl Pts',(-157.195588470837,-2.23938938206019,
135.185354271969));
#113891=CARTESIAN_POINT('Ctrl Pts',(-157.203344773579,-2.11565275237175,
135.244315177455));
#113892=CARTESIAN_POINT('Ctrl Pts',(-157.211105216093,-1.99185008071841,
135.303307552152));
#113893=CARTESIAN_POINT('Ctrl Pts',(-157.218865658607,-1.86567636758244,
135.357071107657));
#113894=CARTESIAN_POINT('Ctrl Pts',(-157.226626101121,-1.73761718720378,
135.405433272201));
#113895=CARTESIAN_POINT('Ctrl Pts',(-157.234399001387,-1.60935243486022,
135.453873071986));
#113896=CARTESIAN_POINT('Ctrl Pts',(-157.242171901652,-1.47919653835052,
135.496894031036));
#113897=CARTESIAN_POINT('Ctrl Pts',(-157.249944801917,-1.34765012154788,
135.534373536406));
#113898=CARTESIAN_POINT('Ctrl Pts',(-157.257435137679,-1.22088574834322,
135.57049056735));
#113899=CARTESIAN_POINT('Ctrl Pts',(-157.264925473441,-1.09283049685582,
135.601461969015));
#113900=CARTESIAN_POINT('Ctrl Pts',(-157.272415809203,-0.963938465976928,
135.627223428834));
#113901=CARTESIAN_POINT('Ctrl Pts',(-157.280190143322,-0.830159454569675,
135.653961642232));
#113902=CARTESIAN_POINT('Ctrl Pts',(-157.287964477441,-0.695055186511383,
135.675171743711));
#113903=CARTESIAN_POINT('Ctrl Pts',(-157.29573881156,-0.559122314154034,
135.690725861826));
#113904=CARTESIAN_POINT('Ctrl Pts',(-157.303503564507,-0.423356966913566,
135.706260810881));
#113905=CARTESIAN_POINT('Ctrl Pts',(-157.311268317455,-0.286765431921058,
135.716153601756));
#113906=CARTESIAN_POINT('Ctrl Pts',(-157.319033070402,-0.149855782785903,
135.720327084789));
#113907=CARTESIAN_POINT('Ctrl Pts',(-157.326790111287,-0.0130821142439842,
135.72449642266));
#113908=CARTESIAN_POINT('Ctrl Pts',(-157.334547152171,0.124008651420045,
135.722957745299));
#113909=CARTESIAN_POINT('Ctrl Pts',(-157.342304193056,0.260902419850325,
135.715685590505));
#113910=CARTESIAN_POINT('Ctrl Pts',(-157.350055384297,0.397692955625139,
135.7084189197));
#113911=CARTESIAN_POINT('Ctrl Pts',(-157.357806575537,0.534286401025188,
135.695427398101));
#113912=CARTESIAN_POINT('Ctrl Pts',(-157.365557766777,0.670168114574924,
135.676737630966));
#113913=CARTESIAN_POINT('Ctrl Pts',(-157.373305663554,0.805992074771452,
135.65805580748));
#113914=CARTESIAN_POINT('Ctrl Pts',(-157.381053560331,0.941104518269342,
135.633680608608));
#113915=CARTESIAN_POINT('Ctrl Pts',(-157.388801457108,1.07499560200768,
135.603690520601));
#113916=CARTESIAN_POINT('Ctrl Pts',(-157.396547733192,1.20885867861767,
135.573706705874));
#113917=CARTESIAN_POINT('Ctrl Pts',(-157.404294009276,1.34150052236585,
135.538110423585));
#113918=CARTESIAN_POINT('Ctrl Pts',(-157.41204028536,1.47242155889865,135.497031266076));
#113919=CARTESIAN_POINT('Ctrl Pts',(-157.419786618626,1.60334356186061,
135.455951805331));
#113920=CARTESIAN_POINT('Ctrl Pts',(-157.427532951891,1.73254435922677,
135.409389505652));
#113921=CARTESIAN_POINT('Ctrl Pts',(-157.435279285156,1.85953999890823,
135.357523699969));
#113922=CARTESIAN_POINT('Ctrl Pts',(-157.443027353159,1.9865640783825,135.305646279299));
#113923=CARTESIAN_POINT('Ctrl Pts',(-157.450775421162,2.11138165563383,
135.248463137064));
#113924=CARTESIAN_POINT('Ctrl Pts',(-157.458523489165,2.23352957422692,
135.186201406955));
#113925=CARTESIAN_POINT('Ctrl Pts',(-157.466279791907,2.35580731308164,
135.123873504339));
#113926=CARTESIAN_POINT('Ctrl Pts',(-157.474036094649,2.47540937649589,
135.056456409427));
#113927=CARTESIAN_POINT('Ctrl Pts',(-157.481792397391,2.59189752692306,
134.984223088082));
#113928=CARTESIAN_POINT('Ctrl Pts',(-157.489552839905,2.70844785058351,
134.911951213639));
#113929=CARTESIAN_POINT('Ctrl Pts',(-157.497313282419,2.82188062640686,
134.834858210351));
#113930=CARTESIAN_POINT('Ctrl Pts',(-157.505073724933,2.93178820014002,
134.753259326323));
#113931=CARTESIAN_POINT('Ctrl Pts',(-157.512846625199,3.04187220726768,
134.671529452521));
#113932=CARTESIAN_POINT('Ctrl Pts',(-157.520619525464,3.14841939983107,
134.585279489793));
#113933=CARTESIAN_POINT('Ctrl Pts',(-157.528392425729,3.25105602065565,
134.49486435189));
#113934=CARTESIAN_POINT('Ctrl Pts',(-157.535882761492,3.34996154178944,
134.407736031989));
#113935=CARTESIAN_POINT('Ctrl Pts',(-157.543373097254,3.44523565052182,
134.316740321315));
#113936=CARTESIAN_POINT('Ctrl Pts',(-157.550863433016,3.53657878732559,
134.222224503612));
#113937=CARTESIAN_POINT('Ctrl Pts',(-157.558637767135,3.63138522692268,
134.124125089955));
#113938=CARTESIAN_POINT('Ctrl Pts',(-157.566412101254,3.72225704298993,
134.021922620821));
#113939=CARTESIAN_POINT('Ctrl Pts',(-157.574186435373,3.80881820092998,
133.915965826259));
#113940=CARTESIAN_POINT('Ctrl Pts',(-157.58195118832,3.89527267997883,133.810139613977));
#113941=CARTESIAN_POINT('Ctrl Pts',(-157.589715941267,3.97742682621833,
133.700568582227));
#113942=CARTESIAN_POINT('Ctrl Pts',(-157.597480694215,4.05494110525508,
133.587638486449));
#113943=CARTESIAN_POINT('Ctrl Pts',(-157.6052377351,4.13237839601712,133.474820554434));
#113944=CARTESIAN_POINT('Ctrl Pts',(-157.612994775985,4.2051847706449,133.35865051797));
#113945=CARTESIAN_POINT('Ctrl Pts',(-157.62075181687,4.27306092651146,133.239547136258));
#113946=CARTESIAN_POINT('Ctrl Pts',(-157.62850300811,4.3408858964408,133.120533571333));
#113947=CARTESIAN_POINT('Ctrl Pts',(-157.63625419935,4.40378785509949,132.998591402431));
#113948=CARTESIAN_POINT('Ctrl Pts',(-157.64400539059,4.46151100995585,132.874167992793));
#113949=CARTESIAN_POINT('Ctrl Pts',(-157.651753287367,4.51920963093165,
132.749797466422));
#113950=CARTESIAN_POINT('Ctrl Pts',(-157.659501184144,4.57173366179417,
132.622948150736));
#113951=CARTESIAN_POINT('Ctrl Pts',(-157.667249080921,4.6188735526225,132.494091414878));
#113952=CARTESIAN_POINT('Ctrl Pts',(-157.674995357005,4.66600358280189,
132.365261633071));
#113953=CARTESIAN_POINT('Ctrl Pts',(-157.682741633089,4.70775157887593,
132.234425633249));
#113954=CARTESIAN_POINT('Ctrl Pts',(-157.690487909174,4.74395653841211,
132.10207376929));
#113955=CARTESIAN_POINT('Ctrl Pts',(-157.698234242439,4.78016176520513,
131.969720928339));
#113956=CARTESIAN_POINT('Ctrl Pts',(-157.705980575704,4.81082377065371,
131.835852578034));
#113957=CARTESIAN_POINT('Ctrl Pts',(-157.71372690897,4.83583184470548,131.700972814802));
#113958=CARTESIAN_POINT('Ctrl Pts',(-157.721474976973,4.860845519142,131.566062846182));
#113959=CARTESIAN_POINT('Ctrl Pts',(-157.729223044976,4.8802026714119,131.430141398269));
#113960=CARTESIAN_POINT('Ctrl Pts',(-157.736971112979,4.89384404815594,
131.293720908996));
#113961=CARTESIAN_POINT('Ctrl Pts',(-157.74472741572,4.90749992311754,131.157155430404));
#113962=CARTESIAN_POINT('Ctrl Pts',(-157.752483718462,4.91542784853478,
131.020090240593));
#113963=CARTESIAN_POINT('Ctrl Pts',(-157.760240021204,4.9176206002208,130.883041585939));
#113964=CARTESIAN_POINT('Ctrl Pts',(-157.768000463718,4.91981452224442,
130.745919784291));
#113965=CARTESIAN_POINT('Ctrl Pts',(-157.775760906232,4.91626718127279,
130.608814926029));
#113966=CARTESIAN_POINT('Ctrl Pts',(-157.783521348747,4.90702345738327,
130.472240381521));
#113967=CARTESIAN_POINT('Ctrl Pts',(-157.791294249012,4.89776489464754,
130.335446595431));
#113968=CARTESIAN_POINT('Ctrl Pts',(-157.799067149277,4.88279171841866,
130.199185213126));
#113969=CARTESIAN_POINT('Ctrl Pts',(-157.806840049543,4.86220050280511,
130.063962526657));
#113970=CARTESIAN_POINT('Ctrl Pts',(-157.814330385305,4.84235782974526,
129.933655525446));
#113971=CARTESIAN_POINT('Ctrl Pts',(-157.821820721067,4.81729854419249,
129.804313315156));
#113972=CARTESIAN_POINT('Ctrl Pts',(-157.829311056829,4.7871529065549,129.676375639048));
#113973=CARTESIAN_POINT('Ctrl Pts',(-157.837085390948,4.75586428790367,
129.543587167064));
#113974=CARTESIAN_POINT('Ctrl Pts',(-157.844859725067,4.71899689234862,
129.411891203582));
#113975=CARTESIAN_POINT('Ctrl Pts',(-157.852634059186,4.67664086047165,
129.281792614268));
#113976=CARTESIAN_POINT('Ctrl Pts',(-157.860398812133,4.63433702861861,
129.151854359839));
#113977=CARTESIAN_POINT('Ctrl Pts',(-157.86816356508,4.58655813916371,129.023509930799));
#113978=CARTESIAN_POINT('Ctrl Pts',(-157.875928318028,4.53344521244988,
128.897253497288));
#113979=CARTESIAN_POINT('Ctrl Pts',(-157.883685358913,4.48038503824348,
128.771122463446));
#113980=CARTESIAN_POINT('Ctrl Pts',(-157.891442399798,4.42200152034097,
128.647075656168));
#113981=CARTESIAN_POINT('Ctrl Pts',(-157.899199440683,4.35848519233676,
128.525591236808));
#113982=CARTESIAN_POINT('Ctrl Pts',(-157.906950631923,4.29501676248966,
128.404198429793));
#113983=CARTESIAN_POINT('Ctrl Pts',(-157.914701823163,4.22642340733128,
128.285364509603));
#113984=CARTESIAN_POINT('Ctrl Pts',(-157.922453014403,4.15294324411424,
128.169546492496));
#113985=CARTESIAN_POINT('Ctrl Pts',(-157.93020091118,4.07949431192661,128.053777701137));
#113986=CARTESIAN_POINT('Ctrl Pts',(-157.937948807957,4.00116291173236,
127.941022592819));
#113987=CARTESIAN_POINT('Ctrl Pts',(-157.945696704734,3.91823235289083,
127.831712254362));
#113988=CARTESIAN_POINT('Ctrl Pts',(-157.953442980819,3.83531914133443,
127.722424781271));
#113989=CARTESIAN_POINT('Ctrl Pts',(-157.961189256903,3.74780892084494,
127.616580956058));
#113990=CARTESIAN_POINT('Ctrl Pts',(-157.968935532987,3.65602721428102,
127.514581282879));
#113991=CARTESIAN_POINT('Ctrl Pts',(-157.976681866252,3.56424483020552,
127.412580856761));
#113992=CARTESIAN_POINT('Ctrl Pts',(-157.984428199517,3.4681911586511,127.314424929928));
#113993=CARTESIAN_POINT('Ctrl Pts',(-157.992174532783,3.36823046873152,
127.220479122314));
#113994=CARTESIAN_POINT('Ctrl Pts',(-157.999922600786,3.26824739330839,
127.126512276188));
#113995=CARTESIAN_POINT('Ctrl Pts',(-158.007670668789,3.1643558433096,127.036757693097));
#113996=CARTESIAN_POINT('Ctrl Pts',(-158.015418736792,3.05695491939445,
126.951542209791));
#113997=CARTESIAN_POINT('Ctrl Pts',(-158.023175039534,2.94943984849941,
126.866236158455));
#113998=CARTESIAN_POINT('Ctrl Pts',(-158.030931342275,2.83840825976152,
126.785479087175));
#113999=CARTESIAN_POINT('Ctrl Pts',(-158.038687645017,2.72429058102847,
126.709556117639));
#114000=CARTESIAN_POINT('Ctrl Pts',(-158.046448087532,2.61011199425426,
126.633592625729));
#114001=CARTESIAN_POINT('Ctrl Pts',(-158.054208530046,2.49284436954304,
126.562468579292));
#114002=CARTESIAN_POINT('Ctrl Pts',(-158.06196897256,2.37294387870398,126.496423708671));
#114003=CARTESIAN_POINT('Ctrl Pts',(-158.069741872825,2.25285091295277,
126.430272816961));
#114004=CARTESIAN_POINT('Ctrl Pts',(-158.077514773091,2.13011698540537,
126.36921756868));
#114005=CARTESIAN_POINT('Ctrl Pts',(-158.085287673356,2.00522025456549,
126.313450376515));
#114006=CARTESIAN_POINT('Ctrl Pts',(-158.092778009118,1.88486383448922,
126.259710462255));
#114007=CARTESIAN_POINT('Ctrl Pts',(-158.10026834488,1.76249941386373,126.210880924886));
#114008=CARTESIAN_POINT('Ctrl Pts',(-158.107758680642,1.63856737008093,
126.167089864612));
#114009=CARTESIAN_POINT('Ctrl Pts',(-158.115533014761,1.50993640518813,
126.121638452977));
#114010=CARTESIAN_POINT('Ctrl Pts',(-158.12330734888,1.37920913345374,126.081471151881));
#114011=CARTESIAN_POINT('Ctrl Pts',(-158.131081682999,1.24685903584777,
126.046785015726));
#114012=CARTESIAN_POINT('Ctrl Pts',(-158.138846435946,1.11467204790863,
126.012141627133));
#114013=CARTESIAN_POINT('Ctrl Pts',(-158.146611188894,0.980866588039771,
125.982966061117));
#114014=CARTESIAN_POINT('Ctrl Pts',(-158.154375941841,0.845934640514557,
125.9594067843));
#114015=CARTESIAN_POINT('Ctrl Pts',(-158.162132982726,0.711136709301832,
125.935870906889));
#114016=CARTESIAN_POINT('Ctrl Pts',(-158.169890023611,0.57521489962812,
125.917940284662));
#114017=CARTESIAN_POINT('Ctrl Pts',(-158.177647064496,0.43867449024398,
125.905713074202));
#114018=CARTESIAN_POINT('Ctrl Pts',(-158.185398255736,0.302237047044501,
125.893495084376));
#114019=CARTESIAN_POINT('Ctrl Pts',(-158.193149446976,0.165182320487663,
125.886971980192));
#114020=CARTESIAN_POINT('Ctrl Pts',(-158.200900638216,0.0280235194879294,
125.886190455315));
#114021=CARTESIAN_POINT('Ctrl Pts',(-158.208648534993,-0.109076985362361,
125.885409262607));
#114022=CARTESIAN_POINT('Ctrl Pts',(-158.21639643177,-0.246281086536319,
125.890364797808));
#114023=CARTESIAN_POINT('Ctrl Pts',(-158.224144328547,-0.383072962855172,
125.901051717687));
#114024=CARTESIAN_POINT('Ctrl Pts',(-158.231890604631,-0.51983622526239,
125.911736402093));
#114025=CARTESIAN_POINT('Ctrl Pts',(-158.239636880715,-0.656187044797271,
125.928150056102));
#114026=CARTESIAN_POINT('Ctrl Pts',(-158.2473831568,-0.791612512914426,
125.950235290394));
#114027=CARTESIAN_POINT('Ctrl Pts',(-158.255129490065,-0.927038980711439,
125.972320687713));
#114028=CARTESIAN_POINT('Ctrl Pts',(-158.26287582333,-1.06153969759273,
126.000077685928));
#114029=CARTESIAN_POINT('Ctrl Pts',(-158.270622156596,-1.1946101607984,
126.033397441622));
#114030=CARTESIAN_POINT('Ctrl Pts',(-158.278370224598,-1.32771042421147,
126.066724659044));
#114031=CARTESIAN_POINT('Ctrl Pts',(-158.286118292601,-1.45937941741378,
126.105617017881));
#114032=CARTESIAN_POINT('Ctrl Pts',(-158.293866360604,-1.58912643973627,
126.149915406692));
#114033=CARTESIAN_POINT('Ctrl Pts',(-158.301622663346,-1.71901135873827,
126.194260876357));
#114034=CARTESIAN_POINT('Ctrl Pts',(-158.309378966088,-1.8469698557755,
126.244023726912));
#114035=CARTESIAN_POINT('Ctrl Pts',(-158.31713526883,-1.97252939313016,
126.298995942455));
#114036=CARTESIAN_POINT('Ctrl Pts',(-158.324895711344,-2.09815594539077,
126.353997498325));
#114037=CARTESIAN_POINT('Ctrl Pts',(-158.332656153858,-2.22138063557395,
126.414213787785));
#114038=CARTESIAN_POINT('Ctrl Pts',(-158.340416596372,-2.34175519974607,
126.47939060068));
#114039=CARTESIAN_POINT('Ctrl Pts',(-158.348189496638,-2.46232299985494,
126.544672041181));
#114040=CARTESIAN_POINT('Ctrl Pts',(-158.355962396903,-2.5800311951905,
126.614929717379));
#114041=CARTESIAN_POINT('Ctrl Pts',(-158.363735297169,-2.69445944715936,
126.689865344739));
#114042=CARTESIAN_POINT('Ctrl Pts',(-158.371225632931,-2.80472794394272,
126.762076873294));
#114043=CARTESIAN_POINT('Ctrl Pts',(-158.378715968693,-2.91195057492315,
126.838631968233));
#114044=CARTESIAN_POINT('Ctrl Pts',(-158.386206304455,-3.01578153103443,
126.919229368873));
#114045=CARTESIAN_POINT('Ctrl Pts',(-158.393887986589,-3.12226492854991,
127.001885691924));
#114046=CARTESIAN_POINT('Ctrl Pts',(-158.401569668722,-3.22553542916593,
127.089068988183));
#114047=CARTESIAN_POINT('Ctrl Pts',(-158.409251350856,-3.32517684946278,
127.180497763884));
#114048=CARTESIAN_POINT('Ctrl Pts',(-158.416924255383,-3.42470441277153,
127.271822066916));
#114049=CARTESIAN_POINT('Ctrl Pts',(-158.42459715991,-3.52061084737626,
127.367381937551));
#114050=CARTESIAN_POINT('Ctrl Pts',(-158.432270064437,-3.61251025297089,
127.466853653576));
#114051=CARTESIAN_POINT('Ctrl Pts',(-158.439935958313,-3.70432569105768,
127.566234483354));
#114052=CARTESIAN_POINT('Ctrl Pts',(-158.447601852189,-3.79214110987175,
127.669519759237));
#114053=CARTESIAN_POINT('Ctrl Pts',(-158.455267746065,-3.87560533796325,
127.776347023334));
#114054=CARTESIAN_POINT('Ctrl Pts',(-158.46292839003,-3.9590124064113,127.883101127846));
#114055=CARTESIAN_POINT('Ctrl Pts',(-158.470589033995,-4.03807396514902,
127.993392081312));
#114056=CARTESIAN_POINT('Ctrl Pts',(-158.47824967796,-4.11247760218458,
128.106822659718));
#114057=CARTESIAN_POINT('Ctrl Pts',(-158.485907859796,-4.18685732591744,
128.220216781576));
#114058=CARTESIAN_POINT('Ctrl Pts',(-158.493566041633,-4.25658188049758,
128.336748190372));
#114059=CARTESIAN_POINT('Ctrl Pts',(-158.50122422347,-4.32138107082593,
128.455989117312));
#114060=CARTESIAN_POINT('Ctrl Pts',(-158.508880677199,-4.38616563888634,
128.575203136928));
#114061=CARTESIAN_POINT('Ctrl Pts',(-158.516537130928,-4.44602686532444,
128.697125104533));
#114062=CARTESIAN_POINT('Ctrl Pts',(-158.524193584657,-4.50073995299582,
128.821301632562));
#114063=CARTESIAN_POINT('Ctrl Pts',(-158.531853047558,-4.55547454424035,
128.945526964984));
#114064=CARTESIAN_POINT('Ctrl Pts',(-158.539512510459,-4.60505678905809,
129.072008262286));
#114065=CARTESIAN_POINT('Ctrl Pts',(-158.547171973361,-4.64930959280485,
129.200271040032));
#114066=CARTESIAN_POINT('Ctrl Pts',(-158.554687103784,-4.69272851082307,
129.326116874877));
#114067=CARTESIAN_POINT('Ctrl Pts',(-158.562202234208,-4.73101699474162,
129.453677277636));
#114068=CARTESIAN_POINT('Ctrl Pts',(-158.569717364632,-4.76405452823396,
129.582490119308));
#114069=CARTESIAN_POINT('Origin',(213.235140564004,0.,130.804360617566));
#114070=CARTESIAN_POINT('',(-160.665416397755,-4.76405452823408,129.582490119308));
#114071=CARTESIAN_POINT('',(-160.319851210837,-4.76405452823417,129.582490119309));
#114072=CARTESIAN_POINT('',(213.235140564004,-4.76405452823405,129.582490119308));
#114073=CARTESIAN_POINT('',(-158.98514056405,-4.91824792883793,130.799846973648));
#114074=CARTESIAN_POINT('Ctrl Pts',(-158.985140564049,-4.91824792883793,
130.799846973648));
#114075=CARTESIAN_POINT('Ctrl Pts',(-158.992793339069,-4.9183718573925,
130.934884510481));
#114076=CARTESIAN_POINT('Ctrl Pts',(-159.000446114088,-4.91293013258963,
131.070088370763));
#114077=CARTESIAN_POINT('Ctrl Pts',(-159.008098889108,-4.90190847227337,
131.204955664908));
#114078=CARTESIAN_POINT('Ctrl Pts',(-159.015745855889,-4.890895177083,131.339720598622));
#114079=CARTESIAN_POINT('Ctrl Pts',(-159.023392822671,-4.87431040414284,
131.474149074946));
#114080=CARTESIAN_POINT('Ctrl Pts',(-159.031039789452,-4.85219193961457,
131.607738762426));
#114081=CARTESIAN_POINT('Ctrl Pts',(-159.03868359274,-4.83008262533319,
131.741273184831));
#114082=CARTESIAN_POINT('Ctrl Pts',(-159.046327396027,-4.80244423546131,
131.873969111832));
#114083=CARTESIAN_POINT('Ctrl Pts',(-159.053971199314,-4.76936630563182,
132.00533026964));
#114084=CARTESIAN_POINT('Ctrl Pts',(-159.061613585034,-4.73629451020871,
132.136667066108));
#114085=CARTESIAN_POINT('Ctrl Pts',(-159.069255970754,-4.69778527864374,
132.266669195356));
#114086=CARTESIAN_POINT('Ctrl Pts',(-159.076898356474,-4.65397895016428,
132.394852049145));
#114087=CARTESIAN_POINT('Ctrl Pts',(-159.084541085085,-4.61017065622125,
132.52304065413));
#114088=CARTESIAN_POINT('Ctrl Pts',(-159.092183813697,-4.56106492320184,
132.649409440511));
#114089=CARTESIAN_POINT('Ctrl Pts',(-159.099826542309,-4.50685132596009,
132.773490930215));
#114090=CARTESIAN_POINT('Ctrl Pts',(-159.107471374328,-4.4526228082238,
132.897606569233));
#114091=CARTESIAN_POINT('Ctrl Pts',(-159.115116206347,-4.3932837923077,
133.019433291276));
#114092=CARTESIAN_POINT('Ctrl Pts',(-159.122761038366,-4.329070918503,133.138526002682));
#114093=CARTESIAN_POINT('Ctrl Pts',(-159.130413981656,-4.26478991396683,
133.257745073071));
#114094=CARTESIAN_POINT('Ctrl Pts',(-159.138066924946,-4.19562492009736,
133.374223987828));
#114095=CARTESIAN_POINT('Ctrl Pts',(-159.145719868236,-4.12185737810384,
133.48754432672));
#114096=CARTESIAN_POINT('Ctrl Pts',(-159.153377439648,-4.04804522514282,
133.600933196159));
#114097=CARTESIAN_POINT('Ctrl Pts',(-159.16103501106,-3.96962521613434,
133.711159360329));
#114098=CARTESIAN_POINT('Ctrl Pts',(-159.168692582472,-3.88691978986297,
133.817836618743));
#114099=CARTESIAN_POINT('Ctrl Pts',(-159.176361230224,-3.80409473383051,
133.92466818112));
#114100=CARTESIAN_POINT('Ctrl Pts',(-159.184029877976,-3.71697214657841,
134.027940285255));
#114101=CARTESIAN_POINT('Ctrl Pts',(-159.191698525729,-3.62591231128936,
134.127302532999));
#114102=CARTESIAN_POINT('Ctrl Pts',(-159.195119077063,-3.58529565354169,
134.171622428778));
#114103=CARTESIAN_POINT('Ctrl Pts',(-159.198539628398,-3.54389611784006,
134.215164962064));
#114104=CARTESIAN_POINT('Ctrl Pts',(-159.201960179733,-3.50174776517832,
134.257901648388));
#114105=CARTESIAN_POINT('Ctrl Pts',(-159.209734513852,-3.4059516948696,
134.35503490151));
#114106=CARTESIAN_POINT('Ctrl Pts',(-159.217508847971,-3.30595933054666,
134.448333126196));
#114107=CARTESIAN_POINT('Ctrl Pts',(-159.22528318209,-3.20211027803959,
134.537412027575));
#114108=CARTESIAN_POINT('Ctrl Pts',(-159.233047935037,-3.09838921020848,
134.62638114717));
#114109=CARTESIAN_POINT('Ctrl Pts',(-159.240812687984,-2.99082120519507,
134.711141037687));
#114110=CARTESIAN_POINT('Ctrl Pts',(-159.248577440931,-2.8797837594613,
134.791343005443));
#114111=CARTESIAN_POINT('Ctrl Pts',(-159.256334481816,-2.76885659768368,
134.871465315474));
#114112=CARTESIAN_POINT('Ctrl Pts',(-159.264091522701,-2.65446716756238,
134.947038484225));
#114113=CARTESIAN_POINT('Ctrl Pts',(-159.271848563586,-2.53702692526766,
135.017753246193));
#114114=CARTESIAN_POINT('Ctrl Pts',(-159.279599754827,-2.41967524557337,
135.088414681609));
#114115=CARTESIAN_POINT('Ctrl Pts',(-159.287350946067,-2.29927766657136,
135.15422480188));
#114116=CARTESIAN_POINT('Ctrl Pts',(-159.295102137307,-2.17627528435696,
135.214917152653));
#114117=CARTESIAN_POINT('Ctrl Pts',(-159.302850034084,-2.05332518143635,
135.275583707557));
#114118=CARTESIAN_POINT('Ctrl Pts',(-159.310597930861,-1.92777282713566,
135.331136646611));
#114119=CARTESIAN_POINT('Ctrl Pts',(-159.318345827638,-1.80008442623519,
135.38135516868));
#114120=CARTESIAN_POINT('Ctrl Pts',(-159.326092103722,-1.6724227349952,
135.431563186116));
#114121=CARTESIAN_POINT('Ctrl Pts',(-159.333838379806,-1.5426262495021,
135.47643886304));
#114122=CARTESIAN_POINT('Ctrl Pts',(-159.34158465589,-1.41118131881087,
135.515809476244));
#114123=CARTESIAN_POINT('Ctrl Pts',(-159.349330989156,-1.27973541782321,
135.555180380073));
#114124=CARTESIAN_POINT('Ctrl Pts',(-159.357077322421,-1.14664142188218,
135.589046026913));
#114125=CARTESIAN_POINT('Ctrl Pts',(-159.364823655686,-1.01240062551212,
135.617283641671));
#114126=CARTESIAN_POINT('Ctrl Pts',(-159.372571723689,-0.878129766847015,
135.645527580047));
#114127=CARTESIAN_POINT('Ctrl Pts',(-159.380319791692,-0.742711979234038,
135.668140897909));
#114128=CARTESIAN_POINT('Ctrl Pts',(-159.388067859695,-0.606658131120976,
135.685052061864));
#114129=CARTESIAN_POINT('Ctrl Pts',(-159.395824162437,-0.470459683358521,
135.701981199205));
#114130=CARTESIAN_POINT('Ctrl Pts',(-159.403580465179,-0.333624213286068,
135.713196028202));
#114131=CARTESIAN_POINT('Ctrl Pts',(-159.411336767921,-0.196667645253042,
135.718676938257));
#114132=CARTESIAN_POINT('Ctrl Pts',(-159.419097210435,-0.0596379793756009,
135.724160773639));
#114133=CARTESIAN_POINT('Ctrl Pts',(-159.426857652949,0.0775125224771561,
135.723904592773));
#114134=CARTESIAN_POINT('Ctrl Pts',(-159.434618095463,0.214269560775753,
135.717940943339));
#114135=CARTESIAN_POINT('Ctrl Pts',(-159.442390995729,0.351246133612573,
135.711967720526));
#114136=CARTESIAN_POINT('Ctrl Pts',(-159.450163895994,0.487827590948962,
135.700268753663));
#114137=CARTESIAN_POINT('Ctrl Pts',(-159.457936796259,0.623505469023936,
135.682928439437));
#114138=CARTESIAN_POINT('Ctrl Pts',(-159.465427132022,0.754251114482975,
135.66621848931));
#114139=CARTESIAN_POINT('Ctrl Pts',(-159.472917467784,0.884157431173136,
135.644270276624));
#114140=CARTESIAN_POINT('Ctrl Pts',(-159.480407803546,1.01278167657808,
135.617203471648));
#114141=CARTESIAN_POINT('Ctrl Pts',(-159.488182137665,1.14628274933811,
135.589110420536));
#114142=CARTESIAN_POINT('Ctrl Pts',(-159.495956471784,1.27882550347499,
135.555413981878));
#114143=CARTESIAN_POINT('Ctrl Pts',(-159.503730805903,1.40990305558572,
135.516192154914));
#114144=CARTESIAN_POINT('Ctrl Pts',(-159.51149555885,1.54081906632821,135.477018665347));
#114145=CARTESIAN_POINT('Ctrl Pts',(-159.519260311798,1.67027309694941,
135.432333447445));
#114146=CARTESIAN_POINT('Ctrl Pts',(-159.527025064745,1.79776773551994,
135.382265622219));
#114147=CARTESIAN_POINT('Ctrl Pts',(-159.53478210563,1.92513574461842,135.332247525062));
#114148=CARTESIAN_POINT('Ctrl Pts',(-159.542539146515,2.0505478729293,135.276857601511));
#114149=CARTESIAN_POINT('Ctrl Pts',(-159.5502961874,2.17352152451703,135.216274855735));
#114150=CARTESIAN_POINT('Ctrl Pts',(-159.55804737864,2.29640244071768,135.15573779588));
#114151=CARTESIAN_POINT('Ctrl Pts',(-159.56579856988,2.41684819106677,135.090015880336));
#114152=CARTESIAN_POINT('Ctrl Pts',(-159.57354976112,2.534396176756,135.019336190656));
#114153=CARTESIAN_POINT('Ctrl Pts',(-159.581297657897,2.65189420141546,
134.948686541729));
#114154=CARTESIAN_POINT('Ctrl Pts',(-159.589045554674,2.76649657666931,
134.873083510743));
#114155=CARTESIAN_POINT('Ctrl Pts',(-159.596793451451,2.87776554119744,
134.792799980575));
#114156=CARTESIAN_POINT('Ctrl Pts',(-159.604539727536,2.98901123065688,
134.71253324399));
#114157=CARTESIAN_POINT('Ctrl Pts',(-159.61228600362,3.09692457946296,134.627588184244));
#114158=CARTESIAN_POINT('Ctrl Pts',(-159.620032279704,3.20109738714437,
134.538280619456));
#114159=CARTESIAN_POINT('Ctrl Pts',(-159.627778612969,3.30527096380593,
134.448972395421));
#114160=CARTESIAN_POINT('Ctrl Pts',(-159.635524946235,3.40570364742586,
134.355301856549));
#114161=CARTESIAN_POINT('Ctrl Pts',(-159.6432712795,3.50202118190441,134.257624393184));
#114162=CARTESIAN_POINT('Ctrl Pts',(-159.651019347503,3.59836028602659,
134.159925055628));
#114163=CARTESIAN_POINT('Ctrl Pts',(-159.658767415506,3.69058213275458,
134.058217286343));
#114164=CARTESIAN_POINT('Ctrl Pts',(-159.666515483509,3.77835040214406,
133.952892227875));
#114165=CARTESIAN_POINT('Ctrl Pts',(-159.674271786251,3.86621195269483,
133.847455228682));
#114166=CARTESIAN_POINT('Ctrl Pts',(-159.682028088993,3.94961021991599,
133.738393561338));
#114167=CARTESIAN_POINT('Ctrl Pts',(-159.689784391734,4.02824983514469,
133.626130687603));
#114168=CARTESIAN_POINT('Ctrl Pts',(-159.697544834249,4.10693142270382,
133.513807895792));
#114169=CARTESIAN_POINT('Ctrl Pts',(-159.705305276763,4.18084908682414,
133.398280822264));
#114170=CARTESIAN_POINT('Ctrl Pts',(-159.713065719277,4.24975221933218,
133.279999754593));
#114171=CARTESIAN_POINT('Ctrl Pts',(-159.720838619542,4.31876596126544,
133.161528811652));
#114172=CARTESIAN_POINT('Ctrl Pts',(-159.728611519808,4.38274890298996,
133.040295386055));
#114173=CARTESIAN_POINT('Ctrl Pts',(-159.736384420073,4.44149721274379,
132.916772881233));
#114174=CARTESIAN_POINT('Ctrl Pts',(-159.743874755835,4.4981098734592,132.797740730597));
#114175=CARTESIAN_POINT('Ctrl Pts',(-159.751365091597,4.54986175782703,
132.67658332216));
#114176=CARTESIAN_POINT('Ctrl Pts',(-159.758855427359,4.59661423469048,
132.553737832446));
#114177=CARTESIAN_POINT('Ctrl Pts',(-159.766629761478,4.64513934592479,
132.426234618649));
#114178=CARTESIAN_POINT('Ctrl Pts',(-159.774404095597,4.68843217389684,
132.296508897613));
#114179=CARTESIAN_POINT('Ctrl Pts',(-159.782178429716,4.72628435871543,
132.165029285193));
#114180=CARTESIAN_POINT('Ctrl Pts',(-159.789943182663,4.76408989409937,
132.033711709644));
#114181=CARTESIAN_POINT('Ctrl Pts',(-159.79770793561,4.79646802036818,131.90064491558));
#114182=CARTESIAN_POINT('Ctrl Pts',(-159.805472688558,4.8232585073882,131.766317182805));
#114183=CARTESIAN_POINT('Ctrl Pts',(-159.813229729443,4.85002238571876,
131.632122866229));
#114184=CARTESIAN_POINT('Ctrl Pts',(-159.820986770328,4.87120959302418,
131.496670484172));
#114185=CARTESIAN_POINT('Ctrl Pts',(-159.828743811213,4.88670987569229,
131.360462814389));
#114186=CARTESIAN_POINT('Ctrl Pts',(-159.836495002453,4.90219846947669,
131.22435785987));
#114187=CARTESIAN_POINT('Ctrl Pts',(-159.844246193693,4.91200863070341,
131.087499138202));
#114188=CARTESIAN_POINT('Ctrl Pts',(-159.851997384933,4.91608136355676,
130.950398589991));
#114189=CARTESIAN_POINT('Ctrl Pts',(-159.85974528171,4.92015236539,130.81335631317));
#114190=CARTESIAN_POINT('Ctrl Pts',(-159.867493178487,4.91849077737537,
130.676072804206));
#114191=CARTESIAN_POINT('Ctrl Pts',(-159.875241075264,4.91108956292033,
130.539063863958));
#114192=CARTESIAN_POINT('Ctrl Pts',(-159.882987351348,4.9036898966398,130.402083583027));
#114193=CARTESIAN_POINT('Ctrl Pts',(-159.890733627432,4.89055301306605,
130.26537814672));
#114194=CARTESIAN_POINT('Ctrl Pts',(-159.898479903516,4.87172397660285,
130.129461693065));
#114195=CARTESIAN_POINT('Ctrl Pts',(-159.906226236782,4.85289480114806,
129.993544236105));
#114196=CARTESIAN_POINT('Ctrl Pts',(-159.913972570047,4.8283734426092,129.858416160685));
#114197=CARTESIAN_POINT('Ctrl Pts',(-159.921718903312,4.79825660638337,
129.724584436222));
#114198=CARTESIAN_POINT('Ctrl Pts',(-159.929466971315,4.76813302570067,
129.590722741071));
#114199=CARTESIAN_POINT('Ctrl Pts',(-159.937215039318,4.73241155968775,
129.45815835591));
#114200=CARTESIAN_POINT('Ctrl Pts',(-159.944963107321,4.69123949850245,
129.327385658337));
#114201=CARTESIAN_POINT('Ctrl Pts',(-159.952719410063,4.65002367916073,
129.196473973984));
#114202=CARTESIAN_POINT('Ctrl Pts',(-159.960475712805,4.60334581018625,
129.067358154631));
#114203=CARTESIAN_POINT('Ctrl Pts',(-159.968232015547,4.5514025079743,128.940515593723));
#114204=CARTESIAN_POINT('Ctrl Pts',(-159.975992458061,4.49943148205784,
128.81360533312));
#114205=CARTESIAN_POINT('Ctrl Pts',(-159.983752900575,4.44218958619812,
128.688971103691));
#114206=CARTESIAN_POINT('Ctrl Pts',(-159.991513343089,4.37992020024621,
128.567067140622));
#114207=CARTESIAN_POINT('Ctrl Pts',(-159.999286243355,4.31755085394812,
128.44496748649));
#114208=CARTESIAN_POINT('Ctrl Pts',(-160.00705914362,4.25013808235659,128.3256071977));
#114209=CARTESIAN_POINT('Ctrl Pts',(-160.014832043886,4.17796999714021,
128.209413649804));
#114210=CARTESIAN_POINT('Ctrl Pts',(-160.022322379648,4.10842540360111,
128.097444030047));
#114211=CARTESIAN_POINT('Ctrl Pts',(-160.02981271541,4.03446540213675,127.988415165342));
#114212=CARTESIAN_POINT('Ctrl Pts',(-160.037303051172,3.95638286821043,
127.882679994597));
#114213=CARTESIAN_POINT('Ctrl Pts',(-160.045077385291,3.87533981127865,
127.772935842717));
#114214=CARTESIAN_POINT('Ctrl Pts',(-160.05285171941,3.78959871915223,127.66639243948));
#114215=CARTESIAN_POINT('Ctrl Pts',(-160.060626053529,3.69944122801285,
127.563478382282));
#114216=CARTESIAN_POINT('Ctrl Pts',(-160.068390806476,3.60939484792321,
127.460691157461));
#114217=CARTESIAN_POINT('Ctrl Pts',(-160.076155559423,3.51494315355772,
127.361524670306));
#114218=CARTESIAN_POINT('Ctrl Pts',(-160.083920312371,3.41641034024362,
127.266377654128));
#114219=CARTESIAN_POINT('Ctrl Pts',(-160.091677353256,3.31797539110931,
127.171325139309));
#114220=CARTESIAN_POINT('Ctrl Pts',(-160.09943439414,3.21546766894891,127.08028442064));
#114221=CARTESIAN_POINT('Ctrl Pts',(-160.107191435025,3.109250580157,126.993620021265));
#114222=CARTESIAN_POINT('Ctrl Pts',(-160.114942626265,3.00311359049814,
126.907020976189));
#114223=CARTESIAN_POINT('Ctrl Pts',(-160.122693817506,2.89327310368915,
126.82479192769));
#114224=CARTESIAN_POINT('Ctrl Pts',(-160.130445008746,2.78012794117947,
126.74725922702));
#114225=CARTESIAN_POINT('Ctrl Pts',(-160.138192905523,2.66703086838164,
126.669759479815));
#114226=CARTESIAN_POINT('Ctrl Pts',(-160.1459408023,2.55063223531128,126.596952330939));
#114227=CARTESIAN_POINT('Ctrl Pts',(-160.153688699077,2.43136219638818,
126.52912250344));
#114228=CARTESIAN_POINT('Ctrl Pts',(-160.161434975161,2.31211710618605,
126.461306864479));
#114229=CARTESIAN_POINT('Ctrl Pts',(-160.169181251245,2.19000214446463,
126.398466669145));
#114230=CARTESIAN_POINT('Ctrl Pts',(-160.176927527329,2.06547422851724,
126.340841907643));
#114231=CARTESIAN_POINT('Ctrl Pts',(-160.184673860595,1.94094539333288,
126.283216720768));
#114232=CARTESIAN_POINT('Ctrl Pts',(-160.19242019386,1.81400392319758,126.230807208736));
#114233=CARTESIAN_POINT('Ctrl Pts',(-160.200166527125,1.68512861746968,
126.183806039911));
#114234=CARTESIAN_POINT('Ctrl Pts',(-160.207914595128,1.55622445101008,
126.136794345501));
#114235=CARTESIAN_POINT('Ctrl Pts',(-160.215662663131,1.42538595443084,
126.095193538298));
#114236=CARTESIAN_POINT('Ctrl Pts',(-160.223410731134,1.29310867553237,
126.059146922087));
#114237=CARTESIAN_POINT('Ctrl Pts',(-160.231167033876,1.16069081076868,
126.023061995104));
#114238=CARTESIAN_POINT('Ctrl Pts',(-160.238923336618,1.02683148684558,
125.992543154068));
#114239=CARTESIAN_POINT('Ctrl Pts',(-160.24667963936,0.89203862435452,125.967683022857));
#114240=CARTESIAN_POINT('Ctrl Pts',(-160.254440081874,0.757173818853848,
125.942809623046));
#114241=CARTESIAN_POINT('Ctrl Pts',(-160.262200524388,0.621374868887031,
125.92360100584));
#114242=CARTESIAN_POINT('Ctrl Pts',(-160.269960966902,0.485155488136284,
125.910097934094));
#114243=CARTESIAN_POINT('Ctrl Pts',(-160.277733867168,0.348717435942938,
125.896573186017));
#114244=CARTESIAN_POINT('Ctrl Pts',(-160.285506767433,0.211857994831101,
125.888772308358));
#114245=CARTESIAN_POINT('Ctrl Pts',(-160.293279667699,0.0750924593514712,
125.886683911534));
#114246=CARTESIAN_POINT('Ctrl Pts',(-160.300770003461,-0.0567013044233523,
125.884671433195));
#114247=CARTESIAN_POINT('Ctrl Pts',(-160.308260339223,-0.18840756352225,
125.887963312532));
#114248=CARTESIAN_POINT('Ctrl Pts',(-160.315750674985,-0.319571074104795,
125.896503917224));
#114249=CARTESIAN_POINT('Ctrl Pts',(-160.323525009104,-0.455707689056029,
125.905368341538));
#114250=CARTESIAN_POINT('Ctrl Pts',(-160.331299343223,-0.591690826302174,
125.919915438741));
#114251=CARTESIAN_POINT('Ctrl Pts',(-160.339073677342,-0.727007663480937,
125.940139927698));
#114252=CARTESIAN_POINT('Ctrl Pts',(-160.346838430289,-0.862157734751858,
125.96033949178));
#114253=CARTESIAN_POINT('Ctrl Pts',(-160.354603183236,-0.996642756851381,
125.986202468677));
#114254=CARTESIAN_POINT('Ctrl Pts',(-160.362367936183,-1.12995202865933,
126.017671628773));
#114255=CARTESIAN_POINT('Ctrl Pts',(-160.370124977068,-1.26312889581919,
126.049109533256));
#114256=CARTESIAN_POINT('Ctrl Pts',(-160.377882017953,-1.39513195856115,
126.086142450845));
#114257=CARTESIAN_POINT('Ctrl Pts',(-160.385639058839,-1.52545810320711,
126.128661671113));
#114258=CARTESIAN_POINT('Ctrl Pts',(-160.393390250079,-1.65568596789307,
126.171148827306));
#114259=CARTESIAN_POINT('Ctrl Pts',(-160.401141441319,-1.78423906136659,
126.219113930433));
#114260=CARTESIAN_POINT('Ctrl Pts',(-160.408892632559,-1.91062724234163,
126.272397841536));
#114261=CARTESIAN_POINT('Ctrl Pts',(-160.416640529336,-2.03696170496875,
126.325659105556));
#114262=CARTESIAN_POINT('Ctrl Pts',(-160.424388426113,-2.16113272569281,
126.384234529758));
#114263=CARTESIAN_POINT('Ctrl Pts',(-160.43213632289,-2.28266824997923,
126.447916112808));
#114264=CARTESIAN_POINT('Ctrl Pts',(-160.439882598974,-2.40417835165429,
126.511584375044));
#114265=CARTESIAN_POINT('Ctrl Pts',(-160.447628875058,-2.52305370734948,
126.580356490281));
#114266=CARTESIAN_POINT('Ctrl Pts',(-160.455375151142,-2.63884543155285,
126.653977761627));
#114267=CARTESIAN_POINT('Ctrl Pts',(-160.463121484408,-2.75463801050396,
126.727599576428));
#114268=CARTESIAN_POINT('Ctrl Pts',(-160.470867817673,-2.86734658261668,
126.806070408995));
#114269=CARTESIAN_POINT('Ctrl Pts',(-160.478614150939,-2.97655024779111,
126.889091573825));
#114270=CARTESIAN_POINT('Ctrl Pts',(-160.486362218942,-3.08577836836934,
126.97213133067));
#114271=CARTESIAN_POINT('Ctrl Pts',(-160.494110286945,-3.19149970897399,
127.059723210931));
#114272=CARTESIAN_POINT('Ctrl Pts',(-160.501858354948,-3.29332584838174,
127.151527755405));
#114273=CARTESIAN_POINT('Ctrl Pts',(-160.509614657689,-3.39526020982207,
127.243429870842));
#114274=CARTESIAN_POINT('Ctrl Pts',(-160.517370960431,-3.49329080940013,
127.339553332108));
#114275=CARTESIAN_POINT('Ctrl Pts',(-160.525127263173,-3.58706517653859,
127.439520876692));
#114276=CARTESIAN_POINT('Ctrl Pts',(-160.532887705687,-3.68088959388028,
127.539541776965));
#114277=CARTESIAN_POINT('Ctrl Pts',(-160.540648148201,-3.77045299708215,
127.643410552802));
#114278=CARTESIAN_POINT('Ctrl Pts',(-160.548408590715,-3.85544341640844,
127.750717035651));
#114279=CARTESIAN_POINT('Ctrl Pts',(-160.556181490981,-3.94057026990094,
127.858195776392));
#114280=CARTESIAN_POINT('Ctrl Pts',(-160.563954391246,-4.02110924010688,
127.969122935338));
#114281=CARTESIAN_POINT('Ctrl Pts',(-160.571727291512,-4.096791380112,128.083058824244));
#114282=CARTESIAN_POINT('Ctrl Pts',(-160.579217627274,-4.16972228369511,
128.192852856598));
#114283=CARTESIAN_POINT('Ctrl Pts',(-160.586707963036,-4.23814318252366,
128.305440403681));
#114284=CARTESIAN_POINT('Ctrl Pts',(-160.594198298797,-4.3018548112296,
128.420408385326));
#114285=CARTESIAN_POINT('Ctrl Pts',(-160.602351087627,-4.37120116249653,
128.545544254579));
#114286=CARTESIAN_POINT('Ctrl Pts',(-160.610503876457,-4.43517049859319,
128.67386470153));
#114287=CARTESIAN_POINT('Ctrl Pts',(-160.618656665287,-4.49347352921566,
128.804891011711));
#114288=CARTESIAN_POINT('Ctrl Pts',(-160.626791612129,-4.55164896644803,
128.935630577088));
#114289=CARTESIAN_POINT('Ctrl Pts',(-160.634926558971,-4.60418268476158,
129.069063894864));
#114290=CARTESIAN_POINT('Ctrl Pts',(-160.643061505813,-4.65083102205554,
129.204687567601));
#114291=CARTESIAN_POINT('Ctrl Pts',(-160.650513136461,-4.6935610099174,
129.328919174256));
#114292=CARTESIAN_POINT('Ctrl Pts',(-160.657964767108,-4.73135320081311,
129.454988140006));
#114293=CARTESIAN_POINT('Ctrl Pts',(-160.665416397755,-4.76405452823407,
129.582490119308));
#114294=CARTESIAN_POINT('Ctrl Pts',(-158.915166007136,-4.76405452823407,
129.582490119308));
#114295=CARTESIAN_POINT('Ctrl Pts',(-158.917948190064,-4.77619699254554,
129.629833403371));
#114296=CARTESIAN_POINT('Ctrl Pts',(-158.920730372992,-4.78762722131158,
129.67733255829));
#114297=CARTESIAN_POINT('Ctrl Pts',(-158.92351255592,-4.79834208061758,
129.724964332657));
#114298=CARTESIAN_POINT('Ctrl Pts',(-158.934140375005,-4.839272382174,129.906915661448));
#114299=CARTESIAN_POINT('Ctrl Pts',(-158.944768194091,-4.86986636907114,
130.091270828495));
#114300=CARTESIAN_POINT('Ctrl Pts',(-158.955396013176,-4.88989965536501,
130.277042475491));
#114301=CARTESIAN_POINT('Ctrl Pts',(-158.965310863454,-4.90858900570155,
130.450351604227));
#114302=CARTESIAN_POINT('Ctrl Pts',(-158.975225713733,-4.91808736835487,
130.624893840766));
#114303=CARTESIAN_POINT('Ctrl Pts',(-158.985140564011,-4.9182479288373,
130.799846972967));
#114304=CARTESIAN_POINT('',(-158.639859435957,-4.91824933787898,130.806912666353));
#114305=CARTESIAN_POINT('Ctrl Pts',(-158.569717364632,-4.76405452823396,
129.582490119308));
#114306=CARTESIAN_POINT('Ctrl Pts',(-158.577384022907,-4.79775819872745,
129.713900219037));
#114307=CARTESIAN_POINT('Ctrl Pts',(-158.585050681181,-4.82599680652233,
129.846613416711));
#114308=CARTESIAN_POINT('Ctrl Pts',(-158.592717339456,-4.84869332716268,
129.980130017777));
#114309=CARTESIAN_POINT('Ctrl Pts',(-158.600574355539,-4.87195338667268,
130.116961743467));
#114310=CARTESIAN_POINT('Ctrl Pts',(-158.608431371623,-4.88939248921531,
130.25463684083));
#114311=CARTESIAN_POINT('Ctrl Pts',(-158.616288387706,-4.90098437315832,
130.392614049204));
#114312=CARTESIAN_POINT('Ctrl Pts',(-158.62414540379,-4.91257625710132,
130.530591257578));
#114313=CARTESIAN_POINT('Ctrl Pts',(-158.632002419873,-4.91832096728769,
130.66887012827));
#114314=CARTESIAN_POINT('Ctrl Pts',(-158.639859435957,-4.91824933787898,
130.806912666354));
#114315=CARTESIAN_POINT('Ctrl Pts',(-158.639859435994,-4.91824933787863,
130.806912667012));
#114316=CARTESIAN_POINT('Ctrl Pts',(-158.648124266752,-4.91817399056016,
130.952120237231));
#114317=CARTESIAN_POINT('Ctrl Pts',(-158.65638909751,-4.91166853530904,
131.09715679426));
#114318=CARTESIAN_POINT('Ctrl Pts',(-158.664653928268,-4.89877453424325,
131.241614691475));
#114319=CARTESIAN_POINT('Ctrl Pts',(-158.672428262387,-4.88664575927484,
131.377499380703));
#114320=CARTESIAN_POINT('Ctrl Pts',(-158.680202596506,-4.86883963092858,
131.513094267943));
#114321=CARTESIAN_POINT('Ctrl Pts',(-158.687976930625,-4.84537373514135,
131.647886805246));
#114322=CARTESIAN_POINT('Ctrl Pts',(-158.695741683572,-4.82193675897347,
131.782513222794));
#114323=CARTESIAN_POINT('Ctrl Pts',(-158.70350643652,-4.79285396025964,
131.916338876396));
#114324=CARTESIAN_POINT('Ctrl Pts',(-158.711271189467,-4.75819480755438,
132.048854585355));
#114325=CARTESIAN_POINT('Ctrl Pts',(-158.719028230352,-4.72357007880828,
132.181238677843));
#114326=CARTESIAN_POINT('Ctrl Pts',(-158.726785271237,-4.68338011625046,
132.312315039052));
#114327=CARTESIAN_POINT('Ctrl Pts',(-158.734542312122,-4.63774567234452,
132.44158330894));
#114328=CARTESIAN_POINT('Ctrl Pts',(-158.742293503362,-4.59214564172766,
132.57075409662));
#114329=CARTESIAN_POINT('Ctrl Pts',(-158.750044694602,-4.54110943158147,
132.698119139758));
#114330=CARTESIAN_POINT('Ctrl Pts',(-158.757795885842,-4.48480789707475,
132.823192257113));
#114331=CARTESIAN_POINT('Ctrl Pts',(-158.765543782619,-4.42853029222216,
132.948212215057));
#114332=CARTESIAN_POINT('Ctrl Pts',(-158.773291679396,-4.3669919741746,
133.070941828923));
#114333=CARTESIAN_POINT('Ctrl Pts',(-158.781039576173,-4.30041221237417,
133.190914171577));
#114334=CARTESIAN_POINT('Ctrl Pts',(-158.788785852257,-4.23384637762462,
133.310861418603));
#114335=CARTESIAN_POINT('Ctrl Pts',(-158.796532128341,-4.16224138629604,
133.428052199992));
#114336=CARTESIAN_POINT('Ctrl Pts',(-158.804278404425,-4.08586263394959,
133.542043871523));
#114337=CARTESIAN_POINT('Ctrl Pts',(-158.812024737691,-4.00948331779265,
133.656036384514));
#114338=CARTESIAN_POINT('Ctrl Pts',(-158.819771070956,-3.92833038792729,
133.766829415728));
#114339=CARTESIAN_POINT('Ctrl Pts',(-158.827517404221,-3.84271254428478,
133.874009353903));
#114340=CARTESIAN_POINT('Ctrl Pts',(-158.835265472224,-3.75707552711993,
133.981213294282));
#114341=CARTESIAN_POINT('Ctrl Pts',(-158.843013540227,-3.6669718504877,
134.084802226143));
#114342=CARTESIAN_POINT('Ctrl Pts',(-158.85076160823,-3.57275019687367,
134.184395986203));
#114343=CARTESIAN_POINT('Ctrl Pts',(-158.858517910972,-3.47842840336455,
134.284095595697));
#114344=CARTESIAN_POINT('Ctrl Pts',(-158.866274213714,-3.37998015919058,
134.379791266856));
#114345=CARTESIAN_POINT('Ctrl Pts',(-158.874030516456,-3.2777910765421,
134.471139683864));
#114346=CARTESIAN_POINT('Ctrl Pts',(-158.88179095897,-3.17554745250336,
134.562536856273));
#114347=CARTESIAN_POINT('Ctrl Pts',(-158.889551401484,-3.0695593135838,
134.649581903205));
#114348=CARTESIAN_POINT('Ctrl Pts',(-158.897311843998,-2.96024419663096,
134.731972787678));
#114349=CARTESIAN_POINT('Ctrl Pts',(-158.905084744263,-2.85075359734785,
134.814495933313));
#114350=CARTESIAN_POINT('Ctrl Pts',(-158.912857644529,-2.73792566946765,
134.892349764331));
#114351=CARTESIAN_POINT('Ctrl Pts',(-158.920630544794,-2.6222064286016,
134.965275962571));
#114352=CARTESIAN_POINT('Ctrl Pts',(-158.928120880556,-2.51069387362021,
135.035551109816));
#114353=CARTESIAN_POINT('Ctrl Pts',(-158.935611216318,-2.39649683605287,
135.101250514425));
#114354=CARTESIAN_POINT('Ctrl Pts',(-158.94310155208,-2.28003305892684,
135.162184881198));
#114355=CARTESIAN_POINT('Ctrl Pts',(-158.950875886199,-2.15915352229284,
135.225429593008));
#114356=CARTESIAN_POINT('Ctrl Pts',(-158.958650220318,-2.03544905610099,
135.283741141578));
#114357=CARTESIAN_POINT('Ctrl Pts',(-158.966424554437,-1.90936038708572,
135.336857277766));
#114358=CARTESIAN_POINT('Ctrl Pts',(-158.974189307384,-1.78342711108648,
135.389907953064));
#114359=CARTESIAN_POINT('Ctrl Pts',(-158.981954060332,-1.65511583548042,
135.437775805484));
#114360=CARTESIAN_POINT('Ctrl Pts',(-158.989718813279,-1.52489249786003,
135.480244056283));
#114361=CARTESIAN_POINT('Ctrl Pts',(-158.997475854164,-1.39479849989403,
135.522670127017));
#114362=CARTESIAN_POINT('Ctrl Pts',(-159.005232895049,-1.26279658847597,
135.559707148231));
#114363=CARTESIAN_POINT('Ctrl Pts',(-159.012989935934,-1.12937300033731,
135.591186255565));
#114364=CARTESIAN_POINT('Ctrl Pts',(-159.020741127174,-0.996050027964171,
135.622641624261));
#114365=CARTESIAN_POINT('Ctrl Pts',(-159.028492318414,-0.861307891793686,
135.648547332125));
#114366=CARTESIAN_POINT('Ctrl Pts',(-159.036243509654,-0.725647981265623,
135.668784331613));
#114367=CARTESIAN_POINT('Ctrl Pts',(-159.043991406431,-0.590045729818567,
135.689012729837));
#114368=CARTESIAN_POINT('Ctrl Pts',(-159.051739303208,-0.453526865727344,
135.703577154141));
#114369=CARTESIAN_POINT('Ctrl Pts',(-159.059487199985,-0.316602748504965,
135.712409696593));
#114370=CARTESIAN_POINT('Ctrl Pts',(-159.067233476069,-0.179707272856166,
135.721240391468));
#114371=CARTESIAN_POINT('Ctrl Pts',(-159.074979752153,-0.0424071025959459,
135.724341564189));
#114372=CARTESIAN_POINT('Ctrl Pts',(-159.082726028237,0.0947819003729015,
135.721697239546));
#114373=CARTESIAN_POINT('Ctrl Pts',(-159.090472361503,0.231971916039617,
135.719052895382));
#114374=CARTESIAN_POINT('Ctrl Pts',(-159.098218694768,0.369050371884892,
135.710662976758));
#114375=CARTESIAN_POINT('Ctrl Pts',(-159.105965028033,0.505502425186202,
135.696563634677));
#114376=CARTESIAN_POINT('Ctrl Pts',(-159.113713096036,0.641985035978571,
135.682461135147));
#114377=CARTESIAN_POINT('Ctrl Pts',(-159.121461164039,0.777840576268759,
135.662646708099));
#114378=CARTESIAN_POINT('Ctrl Pts',(-159.129209232042,0.912560732519729,
135.637208222443));
#114379=CARTESIAN_POINT('Ctrl Pts',(-159.136965534784,1.04742407095614,
135.611742700462));
#114380=CARTESIAN_POINT('Ctrl Pts',(-159.144721837526,1.18114923005184,
135.580641252197));
#114381=CARTESIAN_POINT('Ctrl Pts',(-159.152478140268,1.31323893568091,
135.544042733522));
#114382=CARTESIAN_POINT('Ctrl Pts',(-159.160238582782,1.44539914156338,
135.507424681115));
#114383=CARTESIAN_POINT('Ctrl Pts',(-159.167999025296,1.57592178278154,
135.465303832163));
#114384=CARTESIAN_POINT('Ctrl Pts',(-159.17575946781,1.70432705820341,135.417868213872));
#114385=CARTESIAN_POINT('Ctrl Pts',(-159.183532368076,1.83293846117232,
135.370356447717));
#114386=CARTESIAN_POINT('Ctrl Pts',(-159.191305268341,1.95942534513667,
135.317513013889));
#114387=CARTESIAN_POINT('Ctrl Pts',(-159.199078168607,2.08332929738123,
135.259573530679));
#114388=CARTESIAN_POINT('Ctrl Pts',(-159.206568504369,2.20272902886848,
135.203740293625));
#114389=CARTESIAN_POINT('Ctrl Pts',(-159.214058840131,2.31973008689436,
135.143175224679));
#114390=CARTESIAN_POINT('Ctrl Pts',(-159.221549175893,2.43394741173613,
135.078127464202));
#114391=CARTESIAN_POINT('Ctrl Pts',(-159.229323510012,2.55249532116304,
135.010613398117));
#114392=CARTESIAN_POINT('Ctrl Pts',(-159.237097844131,2.66841976406962,
134.938056143557));
#114393=CARTESIAN_POINT('Ctrl Pts',(-159.24487217825,2.78126187926213,134.860684744342));
#114394=CARTESIAN_POINT('Ctrl Pts',(-159.252636931197,2.89396492663266,
134.783408698461));
#114395=CARTESIAN_POINT('Ctrl Pts',(-159.260401684144,3.00359288520396,
134.701330531799));
#114396=CARTESIAN_POINT('Ctrl Pts',(-159.268166437092,3.10971152223076,
134.614725076644));
#114397=CARTESIAN_POINT('Ctrl Pts',(-159.275923477977,3.21572476073126,
134.528205639248));
#114398=CARTESIAN_POINT('Ctrl Pts',(-159.283680518862,3.31823531306843,
134.437168107329));
#114399=CARTESIAN_POINT('Ctrl Pts',(-159.291437559747,3.41683828604519,
134.34193029031));
#114400=CARTESIAN_POINT('Ctrl Pts',(-159.299188750987,3.51536690175314,
134.246764292869));
#114401=CARTESIAN_POINT('Ctrl Pts',(-159.306939942227,3.60999352332669,
134.147404585496));
#114402=CARTESIAN_POINT('Ctrl Pts',(-159.314691133467,3.70034697945598,
134.04420865322));
#114403=CARTESIAN_POINT('Ctrl Pts',(-159.322439030244,3.79066203295604,
133.941056581968));
#114404=CARTESIAN_POINT('Ctrl Pts',(-159.330186927021,3.87670727630846,
133.834071822285));
#114405=CARTESIAN_POINT('Ctrl Pts',(-159.337934823798,3.95814917434049,
133.723647889516));
#114406=CARTESIAN_POINT('Ctrl Pts',(-159.345681099882,4.03957403648313,
133.613247055053));
#114407=CARTESIAN_POINT('Ctrl Pts',(-159.353427375966,4.11639723669211,
133.499408792876));
#114408=CARTESIAN_POINT('Ctrl Pts',(-159.36117365205,4.18832649861039,133.382558477223));
#114409=CARTESIAN_POINT('Ctrl Pts',(-159.368919985316,4.26025629149425,
133.265707299007));
#114410=CARTESIAN_POINT('Ctrl Pts',(-159.376666318581,4.32729186905267,
133.145844355888));
#114411=CARTESIAN_POINT('Ctrl Pts',(-159.384412651847,4.3891853610824,133.023422340133));
#114412=CARTESIAN_POINT('Ctrl Pts',(-159.39216071985,4.45109271373045,132.900972908815));
#114413=CARTESIAN_POINT('Ctrl Pts',(-159.399908787853,4.50785551306411,
132.775963613326));
#114414=CARTESIAN_POINT('Ctrl Pts',(-159.407656855855,4.55927292980295,
132.648869607532));
#114415=CARTESIAN_POINT('Ctrl Pts',(-159.415413158597,4.61074499358424,
132.521640524716));
#114416=CARTESIAN_POINT('Ctrl Pts',(-159.423169461339,4.65686017923022,
132.392322668593));
#114417=CARTESIAN_POINT('Ctrl Pts',(-159.430925764081,4.69746652130789,
132.26140946496));
#114418=CARTESIAN_POINT('Ctrl Pts',(-159.438686206595,4.73809453621296,
132.130426389008));
#114419=CARTESIAN_POINT('Ctrl Pts',(-159.446446649109,4.77320774883561,
131.99784664664));
#114420=CARTESIAN_POINT('Ctrl Pts',(-159.454207091624,4.80270500756011,
131.864175541436));
#114421=CARTESIAN_POINT('Ctrl Pts',(-159.461979991889,4.83224961790295,
131.730289855507));
#114422=CARTESIAN_POINT('Ctrl Pts',(-159.469752892154,4.85616019081624,
131.595309690976));
#114423=CARTESIAN_POINT('Ctrl Pts',(-159.47752579242,4.87438717537133,131.459748080885));
#114424=CARTESIAN_POINT('Ctrl Pts',(-159.485016128182,4.89195156312684,
131.32911447678));
#114425=CARTESIAN_POINT('Ctrl Pts',(-159.492506463944,4.90423838510301,
131.197941273873));
#114426=CARTESIAN_POINT('Ctrl Pts',(-159.499996799706,4.91124911595562,
131.066687100265));
#114427=CARTESIAN_POINT('Ctrl Pts',(-159.507771133825,4.91852566079937,
130.930456384771));
#114428=CARTESIAN_POINT('Ctrl Pts',(-159.515545467944,4.92014118061332,
130.793706899404));
#114429=CARTESIAN_POINT('Ctrl Pts',(-159.523319802063,4.91604035076487,
130.65694850086));
#114430=CARTESIAN_POINT('Ctrl Pts',(-159.53108455501,4.9119445748227,130.52035864482));
#114431=CARTESIAN_POINT('Ctrl Pts',(-159.538849307957,4.90214647805531,
130.383760284498));
#114432=CARTESIAN_POINT('Ctrl Pts',(-159.546614060904,4.88664257124409,
130.247667305764));
#114433=CARTESIAN_POINT('Ctrl Pts',(-159.554371101789,4.87115406313168,
130.111709496495));
#114434=CARTESIAN_POINT('Ctrl Pts',(-159.562128142674,4.84997106670892,
129.976256455847));
#114435=CARTESIAN_POINT('Ctrl Pts',(-159.569885183559,4.82314210938111,
129.841820615688));
#114436=CARTESIAN_POINT('Ctrl Pts',(-159.5776363748,4.79633338397869,129.707486154643));
#114437=CARTESIAN_POINT('Ctrl Pts',(-159.58538756604,4.76388724849662,129.574167749116));
#114438=CARTESIAN_POINT('Ctrl Pts',(-159.59313875728,4.72590383805602,129.442370905436));
#114439=CARTESIAN_POINT('Ctrl Pts',(-159.600886654057,4.68793657157814,
129.31063007893));
#114440=CARTESIAN_POINT('Ctrl Pts',(-159.608634550834,4.64443681909469,
129.180409902913));
#114441=CARTESIAN_POINT('Ctrl Pts',(-159.616382447611,4.59555537230282,
129.052203694628));
#114442=CARTESIAN_POINT('Ctrl Pts',(-159.624128723695,4.54668415045573,
128.924024304318));
#114443=CARTESIAN_POINT('Ctrl Pts',(-159.631874999779,4.49243361264322,
128.797858408875));
#114444=CARTESIAN_POINT('Ctrl Pts',(-159.639621275863,4.43300365574765,
128.674181833842));
#114445=CARTESIAN_POINT('Ctrl Pts',(-159.647367609129,4.37357326015372,
128.550504345857));
#114446=CARTESIAN_POINT('Ctrl Pts',(-159.655113942394,4.30896353851874,
128.42931656734));
#114447=CARTESIAN_POINT('Ctrl Pts',(-159.66286027566,4.23942137376638,128.311071729741));
#114448=CARTESIAN_POINT('Ctrl Pts',(-159.670608343663,4.16986363552848,
128.19280041203));
#114449=CARTESIAN_POINT('Ctrl Pts',(-159.678356411666,4.09537145433454,
128.077473683611));
#114450=CARTESIAN_POINT('Ctrl Pts',(-159.686104479669,4.01623603745836,
127.965517340116));
#114451=CARTESIAN_POINT('Ctrl Pts',(-159.69386078241,3.93701651451929,127.853442008088));
#114452=CARTESIAN_POINT('Ctrl Pts',(-159.701617085152,3.85314412395863,
127.744744536355));
#114453=CARTESIAN_POINT('Ctrl Pts',(-159.709373387894,3.76495185784531,
127.639819486437));
#114454=CARTESIAN_POINT('Ctrl Pts',(-159.717133830408,3.67671252086414,
127.534838434861));
#114455=CARTESIAN_POINT('Ctrl Pts',(-159.724894272922,3.58414897786692,
127.433634105433));
#114456=CARTESIAN_POINT('Ctrl Pts',(-159.732654715437,3.48763168014751,
127.336564728802));
#114457=CARTESIAN_POINT('Ctrl Pts',(-159.740427615702,3.39095944429339,
127.239339527789));
#114458=CARTESIAN_POINT('Ctrl Pts',(-159.748200515967,3.29032105774447,
127.146262809612));
#114459=CARTESIAN_POINT('Ctrl Pts',(-159.755973416233,3.18612136624142,
127.05765356976));
#114460=CARTESIAN_POINT('Ctrl Pts',(-159.763463751995,3.08570959598768,
126.97226549897));
#114461=CARTESIAN_POINT('Ctrl Pts',(-159.770954087757,2.98199119276438,
126.891025927406));
#114462=CARTESIAN_POINT('Ctrl Pts',(-159.778444423519,2.87535281046917,
126.814181514089));
#114463=CARTESIAN_POINT('Ctrl Pts',(-159.786218757638,2.76467120149735,
126.734423521485));
#114464=CARTESIAN_POINT('Ctrl Pts',(-159.793993091757,2.65049321443222,
126.659147901778));
#114465=CARTESIAN_POINT('Ctrl Pts',(-159.801767425876,2.53321790183688,
126.588676791149));
#114466=CARTESIAN_POINT('Ctrl Pts',(-159.809532178823,2.41608712058281,
126.518292529865));
#114467=CARTESIAN_POINT('Ctrl Pts',(-159.81729693177,2.29586694074203,126.452701195817));
#114468=CARTESIAN_POINT('Ctrl Pts',(-159.825061684718,2.17298782304402,
126.392183492449));
#114469=CARTESIAN_POINT('Ctrl Pts',(-159.832818725603,2.050230750618,126.331725896118));
#114470=CARTESIAN_POINT('Ctrl Pts',(-159.840575766488,1.9248203443006,126.276332073847));
#114471=CARTESIAN_POINT('Ctrl Pts',(-159.848332807373,1.79721395778471,
126.226238180098));
#114472=CARTESIAN_POINT('Ctrl Pts',(-159.856083998613,1.6697038002377,126.176182062545));
#114473=CARTESIAN_POINT('Ctrl Pts',(-159.863835189853,1.54000132112621,
126.131418060579));
#114474=CARTESIAN_POINT('Ctrl Pts',(-159.871586381093,1.40858594271787,
126.092135166203));
#114475=CARTESIAN_POINT('Ctrl Pts',(-159.87933427787,1.27722641935079,126.052868968104));
#114476=CARTESIAN_POINT('Ctrl Pts',(-159.887082174647,1.14415581848234,
126.019079355904));
#114477=CARTESIAN_POINT('Ctrl Pts',(-159.894830071424,1.00987068847651,
125.990906114295));
#114478=CARTESIAN_POINT('Ctrl Pts',(-159.902576347508,0.875613648025022,
125.962738765922));
#114479=CARTESIAN_POINT('Ctrl Pts',(-159.910322623593,0.740142966154415,
125.940185531579));
#114480=CARTESIAN_POINT('Ctrl Pts',(-159.918068899677,0.603967017517046,
125.923335427685));
#114481=CARTESIAN_POINT('Ctrl Pts',(-159.925815232942,0.467790063659945,
125.906485199408));
#114482=CARTESIAN_POINT('Ctrl Pts',(-159.933561566207,0.330908220653752,
125.895338233598));
#114483=CARTESIAN_POINT('Ctrl Pts',(-159.941307899473,0.193836251203119,
125.889931803327));
#114484=CARTESIAN_POINT('Ctrl Pts',(-159.949055967476,0.056733585435131,
125.884524162324));
#114485=CARTESIAN_POINT('Ctrl Pts',(-159.956804035479,-0.0805589009149116,
125.884859630369));
#114486=CARTESIAN_POINT('Ctrl Pts',(-159.964552103482,-0.217525569277293,
125.890923359474));
#114487=CARTESIAN_POINT('Ctrl Pts',(-159.972308406224,-0.354637807444547,
125.896993533182));
#114488=CARTESIAN_POINT('Ctrl Pts',(-159.980064708966,-0.49142314468065,
125.908804112196));
#114489=CARTESIAN_POINT('Ctrl Pts',(-159.987821011707,-0.627369634858531,
125.926288210994));
#114490=CARTESIAN_POINT('Ctrl Pts',(-159.995581454222,-0.763388683771491,
125.943781641583));
#114491=CARTESIAN_POINT('Ctrl Pts',(-160.003341896736,-0.89856760835459,
125.966954559733));
#114492=CARTESIAN_POINT('Ctrl Pts',(-160.01110233925,-1.0324047810459,125.995688926696));
#114493=CARTESIAN_POINT('Ctrl Pts',(-160.018875239515,-1.16645680104831,
126.024469420615));
#114494=CARTESIAN_POINT('Ctrl Pts',(-160.026648139781,-1.29916238627948,
126.058829105746));
#114495=CARTESIAN_POINT('Ctrl Pts',(-160.034421040046,-1.43003432778728,
126.098599798756));
#114496=CARTESIAN_POINT('Ctrl Pts',(-160.041911375808,-1.55614874457298,
126.136924726897));
#114497=CARTESIAN_POINT('Ctrl Pts',(-160.04940171157,-1.68056022735749,
126.180273984169));
#114498=CARTESIAN_POINT('Ctrl Pts',(-160.056892047332,-1.80285225904415,
126.228455592922));
#114499=CARTESIAN_POINT('Ctrl Pts',(-160.06466667697,-1.92978585512154,
126.278465922945));
#114500=CARTESIAN_POINT('Ctrl Pts',(-160.072441306609,-2.05483803858265,
126.333841095074));
#114501=CARTESIAN_POINT('Ctrl Pts',(-160.080215936247,-2.17752203423722,
126.394419478173));
#114502=CARTESIAN_POINT('Ctrl Pts',(-160.087980916616,-2.3000537640038,
126.454922676067));
#114503=CARTESIAN_POINT('Ctrl Pts',(-160.095745896986,-2.42022280705301,
126.520616063905));
#114504=CARTESIAN_POINT('Ctrl Pts',(-160.103510877355,-2.53756028489532,
126.591289188902));
#114505=CARTESIAN_POINT('Ctrl Pts',(-160.111268077854,-2.65478020025133,
126.661891505251));
#114506=CARTESIAN_POINT('Ctrl Pts',(-160.119025278352,-2.76917386359483,
126.737463429008));
#114507=CARTESIAN_POINT('Ctrl Pts',(-160.126782478851,-2.88029535500852,
126.817747803357));
#114508=CARTESIAN_POINT('Ctrl Pts',(-160.13482700935,-2.99553283365445,
126.901005945026));
#114509=CARTESIAN_POINT('Ctrl Pts',(-160.14287153985,-3.10725067608075,
126.989332189158));
#114510=CARTESIAN_POINT('Ctrl Pts',(-160.150916070349,-3.21498207941223,
127.082388923483));
#114511=CARTESIAN_POINT('Ctrl Pts',(-160.158663626693,-3.31873643988849,
127.17201034917));
#114512=CARTESIAN_POINT('Ctrl Pts',(-160.166411183037,-3.4187931316515,
127.266018933222));
#114513=CARTESIAN_POINT('Ctrl Pts',(-160.17415873938,-3.51476749411372,
127.36407101859));
#114514=CARTESIAN_POINT('Ctrl Pts',(-160.181904642276,-3.61072137416904,
127.462102178133));
#114515=CARTESIAN_POINT('Ctrl Pts',(-160.189650545172,-3.70259438520297,
127.564174842764));
#114516=CARTESIAN_POINT('Ctrl Pts',(-160.197396448068,-3.79003834556156,
127.669908129224));
#114517=CARTESIAN_POINT('Ctrl Pts',(-160.205142375296,-3.87748258060947,
127.775641747827));
#114518=CARTESIAN_POINT('Ctrl Pts',(-160.212888302524,-3.96049748866926,
127.885035709547));
#114519=CARTESIAN_POINT('Ctrl Pts',(-160.220634229753,-4.03877510595296,
127.997675970864));
#114520=CARTESIAN_POINT('Ctrl Pts',(-160.228381858733,-4.11706992054616,
128.110340978839));
#114521=CARTESIAN_POINT('Ctrl Pts',(-160.236129487714,-4.19062515107944,
128.226253384234));
#114522=CARTESIAN_POINT('Ctrl Pts',(-160.243877116694,-4.259176325971,128.344970431608));
#114523=CARTESIAN_POINT('Ctrl Pts',(-160.251631726085,-4.32778926367754,
128.463794439934));
#114524=CARTESIAN_POINT('Ctrl Pts',(-160.259386335477,-4.39138894912225,
128.58542779636));
#114525=CARTESIAN_POINT('Ctrl Pts',(-160.267140944868,-4.44975688027795,
128.709403155249));
#114526=CARTESIAN_POINT('Ctrl Pts',(-160.274899711305,-4.50815610097031,
128.833444974118));
#114527=CARTESIAN_POINT('Ctrl Pts',(-160.282658477742,-4.56131782802171,
128.959830937214));
#114528=CARTESIAN_POINT('Ctrl Pts',(-160.290417244178,-4.60907220310745,
129.088074951063));
#114529=CARTESIAN_POINT('Ctrl Pts',(-160.298185461519,-4.65688474748967,
129.216475178119));
#114530=CARTESIAN_POINT('Ctrl Pts',(-160.305953678859,-4.69927667010316,
129.346737603508));
#114531=CARTESIAN_POINT('Ctrl Pts',(-160.313721896199,-4.7361282332075,
129.478361967071));
#114532=CARTESIAN_POINT('Ctrl Pts',(-160.315765001078,-4.74582049657902,
129.512980254337));
#114533=CARTESIAN_POINT('Ctrl Pts',(-160.317808105958,-4.75512979050262,
129.547692702345));
#114534=CARTESIAN_POINT('Ctrl Pts',(-160.319851210837,-4.76405452823417,
129.582490119309));
#114535=CARTESIAN_POINT('Origin',(213.235140564004,0.,130.804360617566));
#114536=CARTESIAN_POINT('',(-162.415078182266,-4.764054528234,129.582490119308));
#114537=CARTESIAN_POINT('',(-162.070143404005,-4.764054528234,129.582490119308));
#114538=CARTESIAN_POINT('',(213.235140564004,-4.76405452823405,129.582490119308));
#114539=CARTESIAN_POINT('',(-160.735140564062,-4.91824999711478,130.80452908244));
#114540=CARTESIAN_POINT('Ctrl Pts',(-160.735140564062,-4.91824999711478,
130.804529082441));
#114541=CARTESIAN_POINT('Ctrl Pts',(-160.743276258315,-4.91824504889373,
130.948989986876));
#114542=CARTESIAN_POINT('Ctrl Pts',(-160.751411952569,-4.91187105275536,
131.093321017711));
#114543=CARTESIAN_POINT('Ctrl Pts',(-160.759547646822,-4.89918799690607,
131.236957466227));
#114544=CARTESIAN_POINT('Ctrl Pts',(-160.767694811219,-4.88648705979481,
131.380796421221));
#114545=CARTESIAN_POINT('Ctrl Pts',(-160.775841975617,-4.86745934026142,
131.523938511925));
#114546=CARTESIAN_POINT('Ctrl Pts',(-160.783989140014,-4.84221620751817,
131.665827542148));
#114547=CARTESIAN_POINT('Ctrl Pts',(-160.792156277582,-4.81691119000347,
131.80806442025));
#114548=CARTESIAN_POINT('Ctrl Pts',(-160.800323415151,-4.78536034987918,
131.949041770207));
#114549=CARTESIAN_POINT('Ctrl Pts',(-160.808490552719,-4.74772586143461,
132.088215051357));
#114550=CARTESIAN_POINT('Ctrl Pts',(-160.816668331239,-4.71004233906773,
132.227569661181));
#114551=CARTESIAN_POINT('Ctrl Pts',(-160.82484610976,-4.66625944808496,
132.3651151975));
#114552=CARTESIAN_POINT('Ctrl Pts',(-160.83302388828,-4.6165881898404,132.500325401377));
#114553=CARTESIAN_POINT('Ctrl Pts',(-160.841220513682,-4.56680245694882,
132.635847216855));
#114554=CARTESIAN_POINT('Ctrl Pts',(-160.849417139084,-4.51110134880628,
132.769022633757));
#114555=CARTESIAN_POINT('Ctrl Pts',(-160.857613764485,-4.44974341291696,
132.899346684752));
#114556=CARTESIAN_POINT('Ctrl Pts',(-160.86262448386,-4.41223439144694,
132.979015721136));
#114557=CARTESIAN_POINT('Ctrl Pts',(-160.867635203235,-4.37261226985345,
133.057619691176));
#114558=CARTESIAN_POINT('Ctrl Pts',(-160.87264592261,-4.33094413413395,
133.135048492317));
#114559=CARTESIAN_POINT('Ctrl Pts',(-160.88042025673,-4.2662943333858,133.255182414305));
#114560=CARTESIAN_POINT('Ctrl Pts',(-160.888194590849,-4.19653984051435,
133.372814647883));
#114561=CARTESIAN_POINT('Ctrl Pts',(-160.895968924968,-4.12189862197519,
133.48748096758));
#114562=CARTESIAN_POINT('Ctrl Pts',(-160.903733677915,-4.047349392067,133.602005971286));
#114563=CARTESIAN_POINT('Ctrl Pts',(-160.911498430862,-3.96792563061788,
133.713572009399));
#114564=CARTESIAN_POINT('Ctrl Pts',(-160.919263183809,-3.88389167038163,
133.821738379007));
#114565=CARTESIAN_POINT('Ctrl Pts',(-160.927020224694,-3.79994117385935,
133.929797316252));
#114566=CARTESIAN_POINT('Ctrl Pts',(-160.934777265579,-3.71138982910379,
134.034462997831));
#114567=CARTESIAN_POINT('Ctrl Pts',(-160.942534306464,-3.61854563769635,
134.135323020597));
#114568=CARTESIAN_POINT('Ctrl Pts',(-160.950285497704,-3.525771460816,134.236106984036));
#114569=CARTESIAN_POINT('Ctrl Pts',(-160.958036688944,-3.42871114458747,
134.333090714492));
#114570=CARTESIAN_POINT('Ctrl Pts',(-160.965787880184,-3.32771316400612,
134.425894568891));
#114571=CARTESIAN_POINT('Ctrl Pts',(-160.973535776962,-3.22675811026059,
134.518658979176));
#114572=CARTESIAN_POINT('Ctrl Pts',(-160.981283673739,-3.12186900813265,
134.607246782868));
#114573=CARTESIAN_POINT('Ctrl Pts',(-160.989031570516,-3.01343125572059,
134.69131509756));
#114574=CARTESIAN_POINT('Ctrl Pts',(-160.9967778466,-2.90501618614869,134.775365826973));
#114575=CARTESIAN_POINT('Ctrl Pts',(-161.004524122684,-2.79305425155926,
134.854898708405));
#114576=CARTESIAN_POINT('Ctrl Pts',(-161.012270398768,-2.67796368986509,
134.929611341857));
#114577=CARTESIAN_POINT('Ctrl Pts',(-161.020016732033,-2.56287227859838,
135.004324526821));
#114578=CARTESIAN_POINT('Ctrl Pts',(-161.027763065299,-2.44465252207039,
135.074217179926));
#114579=CARTESIAN_POINT('Ctrl Pts',(-161.035509398564,-2.32375103398009,
135.139030638984));
#114580=CARTESIAN_POINT('Ctrl Pts',(-161.043257466567,-2.20282247083997,
135.203858612565));
#114581=CARTESIAN_POINT('Ctrl Pts',(-161.05100553457,-2.07921132561113,
135.263604944019));
#114582=CARTESIAN_POINT('Ctrl Pts',(-161.058753602573,-1.95338779597909,
135.318057459515));
#114583=CARTESIAN_POINT('Ctrl Pts',(-161.066509905315,-1.82743053960226,
135.372567847792));
#114584=CARTESIAN_POINT('Ctrl Pts',(-161.074266208057,-1.69925656112866,
135.421773025383));
#114585=CARTESIAN_POINT('Ctrl Pts',(-161.082022510799,-1.56935549750932,
135.465509229758));
#114586=CARTESIAN_POINT('Ctrl Pts',(-161.089782953313,-1.43938510178109,
135.509268777462));
#114587=CARTESIAN_POINT('Ctrl Pts',(-161.097543395827,-1.30768615938835,
135.547553426601));
#114588=CARTESIAN_POINT('Ctrl Pts',(-161.105303838341,-1.17476140103643,
135.580249928797));
#114589=CARTESIAN_POINT('Ctrl Pts',(-161.113076738607,-1.0416232600619,
135.612998918322));
#114590=CARTESIAN_POINT('Ctrl Pts',(-161.120849638872,-0.90725575430458,
135.640141757349));
#114591=CARTESIAN_POINT('Ctrl Pts',(-161.128622539138,-0.772170579979823,
135.661616597841));
#114592=CARTESIAN_POINT('Ctrl Pts',(-161.1361128749,-0.641996092000425,
135.682310773789));
#114593=CARTESIAN_POINT('Ctrl Pts',(-161.143603210662,-0.511155513583549,
135.69774185265));
#114594=CARTESIAN_POINT('Ctrl Pts',(-161.151093546424,-0.380107376144063,
135.707900302844));
#114595=CARTESIAN_POINT('Ctrl Pts',(-161.158867880543,-0.244090508743276,
135.718443913766));
#114596=CARTESIAN_POINT('Ctrl Pts',(-161.166642214662,-0.10741917187084,
135.723340578939));
#114597=CARTESIAN_POINT('Ctrl Pts',(-161.174416548781,0.0293982522418081,
135.72252275451));
#114598=CARTESIAN_POINT('Ctrl Pts',(-161.182181301728,0.166047061106961,
135.721705937975));
#114599=CARTESIAN_POINT('Ctrl Pts',(-161.189946054675,0.302841211782387,
135.715188646823));
#114600=CARTESIAN_POINT('Ctrl Pts',(-161.197710807622,0.439267050115026,
135.702955060994));
#114601=CARTESIAN_POINT('Ctrl Pts',(-161.205467848507,0.575557388381766,
135.690733625735));
#114602=CARTESIAN_POINT('Ctrl Pts',(-161.213224889392,0.711479755407197,
135.672807228983));
#114603=CARTESIAN_POINT('Ctrl Pts',(-161.220981930277,0.84652070236521,
135.649212087216));
#114604=CARTESIAN_POINT('Ctrl Pts',(-161.228733121517,0.98145981389484,
135.625634738729));
#114605=CARTESIAN_POINT('Ctrl Pts',(-161.236484312758,1.11551844480146,
135.596397221066));
#114606=CARTESIAN_POINT('Ctrl Pts',(-161.244235503998,1.24818883136562,
135.561587509754));
#114607=CARTESIAN_POINT('Ctrl Pts',(-161.251983400775,1.3808028294762,135.526792593498));
#114608=CARTESIAN_POINT('Ctrl Pts',(-161.259731297552,1.51202937941735,
135.486430293037));
#114609=CARTESIAN_POINT('Ctrl Pts',(-161.267479194329,1.64137168742383,
135.44063951839));
#114610=CARTESIAN_POINT('Ctrl Pts',(-161.275225470413,1.77068693980813,
135.394858322186));
#114611=CARTESIAN_POINT('Ctrl Pts',(-161.282971746497,1.89811836591234,
135.343651040801));
#114612=CARTESIAN_POINT('Ctrl Pts',(-161.290718022581,2.02318548024631,
135.287206095052));
#114613=CARTESIAN_POINT('Ctrl Pts',(-161.298464355846,2.14825351779714,
135.23076073264));
#114614=CARTESIAN_POINT('Ctrl Pts',(-161.306210689112,2.27095685239821,
135.169077789542));
#114615=CARTESIAN_POINT('Ctrl Pts',(-161.313957022377,2.39083645861087,
135.102393201281));
#114616=CARTESIAN_POINT('Ctrl Pts',(-161.32170509038,2.51074291102999,135.035693679469));
#114617=CARTESIAN_POINT('Ctrl Pts',(-161.329453158383,2.62782403515164,
134.963990473675));
#114618=CARTESIAN_POINT('Ctrl Pts',(-161.337201226386,2.74164716978996,
134.887564489391));
#114619=CARTESIAN_POINT('Ctrl Pts',(-161.344957529128,2.85559127701044,
134.811057278661));
#114620=CARTESIAN_POINT('Ctrl Pts',(-161.35271383187,2.96627015266854,134.729817480887));
#114621=CARTESIAN_POINT('Ctrl Pts',(-161.360470134612,3.07328135797828,
134.644168523855));
#114622=CARTESIAN_POINT('Ctrl Pts',(-161.368230577126,3.18034967839033,
134.558473853397));
#114623=CARTESIAN_POINT('Ctrl Pts',(-161.37599101964,3.28374613327749,134.468365591269));
#114624=CARTESIAN_POINT('Ctrl Pts',(-161.383751462154,3.38310370534486,
134.374205485537));
#114625=CARTESIAN_POINT('Ctrl Pts',(-161.391524362419,3.48262077500746,
134.279894225645));
#114626=CARTESIAN_POINT('Ctrl Pts',(-161.399297262685,3.57808573317624,
134.181518405061));
#114627=CARTESIAN_POINT('Ctrl Pts',(-161.40707016295,3.66916996104227,134.079475097929));
#114628=CARTESIAN_POINT('Ctrl Pts',(-161.414560498712,3.75694304780076,
133.98114132204));
#114629=CARTESIAN_POINT('Ctrl Pts',(-161.422050834474,3.84064818007237,
133.879402312868));
#114630=CARTESIAN_POINT('Ctrl Pts',(-161.429541170237,3.92002949123998,
133.774638693826));
#114631=CARTESIAN_POINT('Ctrl Pts',(-161.437315504356,4.00242056894595,
133.665902930328));
#114632=CARTESIAN_POINT('Ctrl Pts',(-161.445089838475,4.0804144680001,133.553564231017));
#114633=CARTESIAN_POINT('Ctrl Pts',(-161.452864172594,4.15367956882995,
133.438013803159));
#114634=CARTESIAN_POINT('Ctrl Pts',(-161.460628925541,4.22685437697091,
133.322605780876));
#114635=CARTESIAN_POINT('Ctrl Pts',(-161.468393678488,4.29531177516819,
133.203994232639));
#114636=CARTESIAN_POINT('Ctrl Pts',(-161.476158431435,4.3587608109427,133.082602759106));
#114637=CARTESIAN_POINT('Ctrl Pts',(-161.48391547232,4.42214682824041,132.961331853296));
#114638=CARTESIAN_POINT('Ctrl Pts',(-161.491672513205,4.48053420241659,
132.837286861075));
#114639=CARTESIAN_POINT('Ctrl Pts',(-161.49942955409,4.53367587178823,132.710919337371));
#114640=CARTESIAN_POINT('Ctrl Pts',(-161.50718074533,4.58677746661368,132.5846471084));
#114641=CARTESIAN_POINT('Ctrl Pts',(-161.51493193657,4.63464107952358,132.456056193017));
#114642=CARTESIAN_POINT('Ctrl Pts',(-161.522683127811,4.67706626812691,
132.325621340141));
#114643=CARTESIAN_POINT('Ctrl Pts',(-161.530431024588,4.7194734248933,132.195241925557));
#114644=CARTESIAN_POINT('Ctrl Pts',(-161.538178921365,4.75644663402547,
132.063020503258));
#114645=CARTESIAN_POINT('Ctrl Pts',(-161.545926818142,4.78783423529182,
131.929450124169));
#114646=CARTESIAN_POINT('Ctrl Pts',(-161.553673094226,4.81921527094861,
131.795907685123));
#114647=CARTESIAN_POINT('Ctrl Pts',(-161.56141937031,4.84501293334906,131.6610172309));
#114648=CARTESIAN_POINT('Ctrl Pts',(-161.569165646394,4.86512603211808,
131.525284853604));
#114649=CARTESIAN_POINT('Ctrl Pts',(-161.57691197966,4.88523927935745,131.389551474362));
#114650=CARTESIAN_POINT('Ctrl Pts',(-161.584658312925,4.89966782192467,
131.252976546389));
#114651=CARTESIAN_POINT('Ctrl Pts',(-161.59240464619,4.90836204459488,131.116073789698));
#114652=CARTESIAN_POINT('Ctrl Pts',(-161.600152714193,4.91705821427597,
130.979140374584));
#114653=CARTESIAN_POINT('Ctrl Pts',(-161.607900782196,4.92001748395377,
130.84187937477));
#114654=CARTESIAN_POINT('Ctrl Pts',(-161.615648850199,4.91724232343523,
130.704806636645));
#114655=CARTESIAN_POINT('Ctrl Pts',(-161.623405152941,4.91446421344307,
130.567588215983));
#114656=CARTESIAN_POINT('Ctrl Pts',(-161.631161455683,4.90593950651972,
130.430558848213));
#114657=CARTESIAN_POINT('Ctrl Pts',(-161.638917758425,4.89172278362837,
130.294231937103));
#114658=CARTESIAN_POINT('Ctrl Pts',(-161.646678200939,4.87749847284395,
130.157832264216));
#114659=CARTESIAN_POINT('Ctrl Pts',(-161.654438643453,4.85757614938197,
130.022136181682));
#114660=CARTESIAN_POINT('Ctrl Pts',(-161.662199085967,4.83206178032218,
129.887648005212));
#114661=CARTESIAN_POINT('Ctrl Pts',(-161.669971986233,4.80650645333211,
129.752943936381));
#114662=CARTESIAN_POINT('Ctrl Pts',(-161.677744886498,4.77534123107775,
129.619452029376));
#114663=CARTESIAN_POINT('Ctrl Pts',(-161.685517786764,4.73872255678805,
129.487663388782));
#114664=CARTESIAN_POINT('Ctrl Pts',(-161.693008122525,4.70343506354793,
129.360665597236));
#114665=CARTESIAN_POINT('Ctrl Pts',(-161.700498458287,4.66308382234028,
129.235249679244));
#114666=CARTESIAN_POINT('Ctrl Pts',(-161.707988794048,4.61785076026705,
129.111836638888));
#114667=CARTESIAN_POINT('Ctrl Pts',(-161.715763128167,4.5709026728938,128.983744355587));
#114668=CARTESIAN_POINT('Ctrl Pts',(-161.723537462287,4.5185465511121,128.857404068408));
#114669=CARTESIAN_POINT('Ctrl Pts',(-161.731311796406,4.46093228019504,
128.73330623537));
#114670=CARTESIAN_POINT('Ctrl Pts',(-161.739076549353,4.4033890137179,128.609361341821));
#114671=CARTESIAN_POINT('Ctrl Pts',(-161.7468413023,4.34060065482306,128.487653754832));
#114672=CARTESIAN_POINT('Ctrl Pts',(-161.754606055247,4.27276632381988,
128.368657227469));
#114673=CARTESIAN_POINT('Ctrl Pts',(-161.762363096132,4.20499936683054,
128.249778889134));
#114674=CARTESIAN_POINT('Ctrl Pts',(-161.770120137017,4.13219660367083,
128.133606589359));
#114675=CARTESIAN_POINT('Ctrl Pts',(-161.777877177902,4.05460439741788,
128.020592264606));
#114676=CARTESIAN_POINT('Ctrl Pts',(-161.785628369142,3.97707070405115,
127.907663164835));
#114677=CARTESIAN_POINT('Ctrl Pts',(-161.793379560382,3.89475497696704,
127.797887620953));
#114678=CARTESIAN_POINT('Ctrl Pts',(-161.801130751623,3.80794829186819,
127.691690884209));
#114679=CARTESIAN_POINT('Ctrl Pts',(-161.8088786484,3.72117850192603,127.58553928391));
#114680=CARTESIAN_POINT('Ctrl Pts',(-161.816626545177,3.62992179729761,
127.482963767491));
#114681=CARTESIAN_POINT('Ctrl Pts',(-161.824374441954,3.53451101962872,
127.384358437066));
#114682=CARTESIAN_POINT('Ctrl Pts',(-161.832120718038,3.43912019983797,
127.285773732751));
#114683=CARTESIAN_POINT('Ctrl Pts',(-161.839866994122,3.33957730707423,
127.191157843355));
#114684=CARTESIAN_POINT('Ctrl Pts',(-161.847613270206,3.23625343508876,
127.100869458352));
#114685=CARTESIAN_POINT('Ctrl Pts',(-161.855359603472,3.13292880038979,
127.01058040686));
#114686=CARTESIAN_POINT('Ctrl Pts',(-161.863105936737,3.02582342517673,
126.924619180763));
#114687=CARTESIAN_POINT('Ctrl Pts',(-161.870852270003,2.9153426984063,126.843305200969));
#114688=CARTESIAN_POINT('Ctrl Pts',(-161.878600338006,2.80483723024298,
126.761973011474));
#114689=CARTESIAN_POINT('Ctrl Pts',(-161.886348406009,2.69095522121042,
126.685290370897));
#114690=CARTESIAN_POINT('Ctrl Pts',(-161.894096474012,2.57413200247644,
126.613534028893));
#114691=CARTESIAN_POINT('Ctrl Pts',(-161.901852776754,2.45718462263553,
126.541701423395));
#114692=CARTESIAN_POINT('Ctrl Pts',(-161.909609079496,2.33729012233755,
126.474805780354));
#114693=CARTESIAN_POINT('Ctrl Pts',(-161.917365382237,2.21490994505608,
126.413078686536));
#114694=CARTESIAN_POINT('Ctrl Pts',(-161.925125824752,2.09246444978919,
126.351318647109));
#114695=CARTESIAN_POINT('Ctrl Pts',(-161.932886267266,1.96753098997938,
126.294732814897));
#114696=CARTESIAN_POINT('Ctrl Pts',(-161.94064670978,1.84059113851152,126.243504631752));
#114697=CARTESIAN_POINT('Ctrl Pts',(-161.948419610046,1.7134475119249,126.192194212581));
#114698=CARTESIAN_POINT('Ctrl Pts',(-161.956192510311,1.58429142599279,
126.146258760251));
#114699=CARTESIAN_POINT('Ctrl Pts',(-161.963965410577,1.45362062229731,
126.105832108667));
#114700=CARTESIAN_POINT('Ctrl Pts',(-161.971455746339,1.32770003145424,
126.066875067697));
#114701=CARTESIAN_POINT('Ctrl Pts',(-161.978946082101,1.20037323616632,
126.0330333426));
#114702=CARTESIAN_POINT('Ctrl Pts',(-161.986436417863,1.07209277513557,
126.004381435944));
#114703=CARTESIAN_POINT('Ctrl Pts',(-161.994210751982,0.938948521436942,
125.974643183539));
#114704=CARTESIAN_POINT('Ctrl Pts',(-162.001985086101,0.80435509699749,
125.950401860344));
#114705=CARTESIAN_POINT('Ctrl Pts',(-162.00975942022,0.668806154692202,
125.931796468173));
#114706=CARTESIAN_POINT('Ctrl Pts',(-162.017524173168,0.533424264343947,
125.913214005486));
#114707=CARTESIAN_POINT('Ctrl Pts',(-162.025288926115,0.397089582798854,
125.900253706443));
#114708=CARTESIAN_POINT('Ctrl Pts',(-162.033053679062,0.260308321317996,
125.893004120594));
#114709=CARTESIAN_POINT('Ctrl Pts',(-162.040810719947,0.123662912914318,
125.885761735135));
#114710=CARTESIAN_POINT('Ctrl Pts',(-162.048567760832,-0.0134278048507813,
125.884218795969));
#114711=CARTESIAN_POINT('Ctrl Pts',(-162.056324801717,-0.150450439772387,
125.888412313559));
#114712=CARTESIAN_POINT('Ctrl Pts',(-162.064075992957,-0.287369744858932,
125.892602668784));
#114713=CARTESIAN_POINT('Ctrl Pts',(-162.071827184198,-0.424220680093688,
125.902520858399));
#114714=CARTESIAN_POINT('Ctrl Pts',(-162.079578375438,-0.560488136031272,
125.918151850857));
#114715=CARTESIAN_POINT('Ctrl Pts',(-162.087326272215,-0.696697674664843,
125.933776199726));
#114716=CARTESIAN_POINT('Ctrl Pts',(-162.095074168992,-0.83232383963796,
125.955108477684));
#114717=CARTESIAN_POINT('Ctrl Pts',(-162.102822065769,-0.96685515263966,
125.982081677447));
#114718=CARTESIAN_POINT('Ctrl Pts',(-162.110568341853,-1.10135832459084,
126.009049234999));
#114719=CARTESIAN_POINT('Ctrl Pts',(-162.118314617937,-1.23476671700946,
126.041655290543));
#114720=CARTESIAN_POINT('Ctrl Pts',(-162.126060894021,-1.3665779690464,
126.079781512818));
#114721=CARTESIAN_POINT('Ctrl Pts',(-162.133807227287,-1.49839019408388,
126.117908016533));
#114722=CARTESIAN_POINT('Ctrl Pts',(-162.141553560552,-1.62860487964437,
126.161554659657));
#114723=CARTESIAN_POINT('Ctrl Pts',(-162.149299893818,-1.75673416523639,
126.210553031784));
#114724=CARTESIAN_POINT('Ctrl Pts',(-162.157047961821,-1.88489214449372,
126.259562376756));
#114725=CARTESIAN_POINT('Ctrl Pts',(-162.164796029824,-2.01096342938053,
126.313925695952));
#114726=CARTESIAN_POINT('Ctrl Pts',(-162.172544097827,-2.13447987544425,
126.37342632288));
#114727=CARTESIAN_POINT('Ctrl Pts',(-162.180300400569,-2.25812759625655,
126.432990187782));
#114728=CARTESIAN_POINT('Ctrl Pts',(-162.18805670331,-2.37921470132656,
126.497702097391));
#114729=CARTESIAN_POINT('Ctrl Pts',(-162.195813006052,-2.49729692867975,
126.567299004548));
#114730=CARTESIAN_POINT('Ctrl Pts',(-162.203573448567,-2.61544218007338,
126.636933057671));
#114731=CARTESIAN_POINT('Ctrl Pts',(-162.211333891081,-2.73057903000413,
126.711457091212));
#114732=CARTESIAN_POINT('Ctrl Pts',(-162.219094333595,-2.84229284173704,
126.790565099069));
#114733=CARTESIAN_POINT('Ctrl Pts',(-162.22686723386,-2.95418598639803,
126.869800098122));
#114734=CARTESIAN_POINT('Ctrl Pts',(-162.234640134126,-3.06264480266123,
126.953633537088));
#114735=CARTESIAN_POINT('Ctrl Pts',(-162.242413034391,-3.16728765078931,
127.04171899237));
#114736=CARTESIAN_POINT('Ctrl Pts',(-162.249903370153,-3.26812646780143,
127.126602319473));
#114737=CARTESIAN_POINT('Ctrl Pts',(-162.257393705915,-3.36542171254754,
127.215433679379));
#114738=CARTESIAN_POINT('Ctrl Pts',(-162.264884041676,-3.45886609568509,
127.307872608918));
#114739=CARTESIAN_POINT('Ctrl Pts',(-162.272547458222,-3.55446971809865,
127.402447544503));
#114740=CARTESIAN_POINT('Ctrl Pts',(-162.280210874769,-3.64636366415717,
127.501117029956));
#114741=CARTESIAN_POINT('Ctrl Pts',(-162.287874291315,-3.7341691449257,
127.603553866201));
#114742=CARTESIAN_POINT('Ctrl Pts',(-162.29552875626,-3.82187206051309,
127.705871046445));
#114743=CARTESIAN_POINT('Ctrl Pts',(-162.303183221204,-3.90549574552366,
127.811946526502));
#114744=CARTESIAN_POINT('Ctrl Pts',(-162.310837686149,-3.98469649210809,
127.921414740814));
#114745=CARTESIAN_POINT('Ctrl Pts',(-162.318484980424,-4.06382304378054,
128.030780405783));
#114746=CARTESIAN_POINT('Ctrl Pts',(-162.326132274699,-4.13853466162266,
128.143532160693));
#114747=CARTESIAN_POINT('Ctrl Pts',(-162.333779568974,-4.20852673648843,
128.259270094468));
#114748=CARTESIAN_POINT('Ctrl Pts',(-162.341421196602,-4.278466947207,128.374922266402));
#114749=CARTESIAN_POINT('Ctrl Pts',(-162.34906282423,-4.34369436568951,
128.493555870933));
#114750=CARTESIAN_POINT('Ctrl Pts',(-162.356704451859,-4.40394705155555,
128.614741146152));
#114751=CARTESIAN_POINT('Ctrl Pts',(-162.364342762253,-4.46417358170449,
128.73587381479));
#114752=CARTESIAN_POINT('Ctrl Pts',(-162.371981072647,-4.51942949633178,
128.859555590372));
#114753=CARTESIAN_POINT('Ctrl Pts',(-162.379619383041,-4.5694984873254,
128.985331580736));
#114754=CARTESIAN_POINT('Ctrl Pts',(-162.387257161753,-4.61956399315277,
129.111098816175));
#114755=CARTESIAN_POINT('Ctrl Pts',(-162.394894940465,-4.66444313873443,
129.238959604522));
#114756=CARTESIAN_POINT('Ctrl Pts',(-162.402532719178,-4.70396766027824,
129.368438853139));
#114757=CARTESIAN_POINT('Ctrl Pts',(-162.406714540207,-4.72560804573572,
129.439331067373));
#114758=CARTESIAN_POINT('Ctrl Pts',(-162.410896361237,-4.74564409874225,
129.510708134137));
#114759=CARTESIAN_POINT('Ctrl Pts',(-162.415078182266,-4.764054528234,129.582490119308));
#114760=CARTESIAN_POINT('Ctrl Pts',(-160.665416397755,-4.76405452823407,
129.582490119308));
#114761=CARTESIAN_POINT('Ctrl Pts',(-160.673527702719,-4.79965082279286,
129.721279531544));
#114762=CARTESIAN_POINT('Ctrl Pts',(-160.681639007684,-4.82921423771951,
129.861766890241));
#114763=CARTESIAN_POINT('Ctrl Pts',(-160.689750312649,-4.85259362622729,
130.003412328849));
#114764=CARTESIAN_POINT('Ctrl Pts',(-160.697847565096,-4.87593251086433,
130.144812372308));
#114765=CARTESIAN_POINT('Ctrl Pts',(-160.705944817544,-4.89310867773608,
130.287366164819));
#114766=CARTESIAN_POINT('Ctrl Pts',(-160.714042069992,-4.90402160249942,
130.430522170213));
#114767=CARTESIAN_POINT('Ctrl Pts',(-160.721074901332,-4.91349997306731,
130.554859659711));
#114768=CARTESIAN_POINT('Ctrl Pts',(-160.728107732671,-4.91825427453916,
130.679651087786));
#114769=CARTESIAN_POINT('Ctrl Pts',(-160.735140564011,-4.91824999711482,
130.804529081534));
#114770=CARTESIAN_POINT('',(-160.389859436025,-4.91824806388654,130.799996608369));
#114771=CARTESIAN_POINT('Ctrl Pts',(-160.319851210837,-4.76405452823417,
129.582490119309));
#114772=CARTESIAN_POINT('Ctrl Pts',(-160.32501403094,-4.78660687776802,
129.670421387862));
#114773=CARTESIAN_POINT('Ctrl Pts',(-160.330176851042,-4.80670294628824,
129.758895265214));
#114774=CARTESIAN_POINT('Ctrl Pts',(-160.335339671145,-4.82432417672621,
129.847762844019));
#114775=CARTESIAN_POINT('Ctrl Pts',(-160.346622984336,-4.86283527296383,
130.041982418629));
#114776=CARTESIAN_POINT('Ctrl Pts',(-160.357906297526,-4.88962764439993,
130.238596295259));
#114777=CARTESIAN_POINT('Ctrl Pts',(-160.369189610716,-4.90446956815478,
130.436445793804));
#114778=CARTESIAN_POINT('Ctrl Pts',(-160.376079552476,-4.91353250813849,
130.557258847472));
#114779=CARTESIAN_POINT('Ctrl Pts',(-160.382969494235,-4.91814028738697,
130.678532269095));
#114780=CARTESIAN_POINT('Ctrl Pts',(-160.389859435994,-4.91824806388606,
130.79999660782));
#114781=CARTESIAN_POINT('Ctrl Pts',(-160.389859436025,-4.91824806388654,
130.79999660837));
#114782=CARTESIAN_POINT('Ctrl Pts',(-160.397506818166,-4.91836768869606,
130.934814034577));
#114783=CARTESIAN_POINT('Ctrl Pts',(-160.405154200306,-4.91293979166222,
131.069814809062));
#114784=CARTESIAN_POINT('Ctrl Pts',(-160.412801582447,-4.90194590240347,
131.204497384697));
#114785=CARTESIAN_POINT('Ctrl Pts',(-160.420442448689,-4.89096138041009,
131.339065204998));
#114786=CARTESIAN_POINT('Ctrl Pts',(-160.428083314932,-4.87442033222005,
131.473314965856));
#114787=CARTESIAN_POINT('Ctrl Pts',(-160.435724181175,-4.85235634807507,
131.606745147449));
#114788=CARTESIAN_POINT('Ctrl Pts',(-160.443360955889,-4.83030417874477,
131.740103879894));
#114789=CARTESIAN_POINT('Ctrl Pts',(-160.450997730604,-4.80273501982829,
131.872643508878));
#114790=CARTESIAN_POINT('Ctrl Pts',(-160.458634505318,-4.76973425464364,
132.003868100902));
#114791=CARTESIAN_POINT('Ctrl Pts',(-160.466269233813,-4.73674233177829,
132.135057532234));
#114792=CARTESIAN_POINT('Ctrl Pts',(-160.473903962308,-4.69832179405056,
132.264932236198));
#114793=CARTESIAN_POINT('Ctrl Pts',(-160.481538690803,-4.65460893575638,
132.393007437245));
#114794=CARTESIAN_POINT('Ctrl Pts',(-160.489173138895,-4.61089768292314,
132.52107793442));
#114795=CARTESIAN_POINT('Ctrl Pts',(-160.496807586986,-4.56189462645772,
132.647348678373));
#114796=CARTESIAN_POINT('Ctrl Pts',(-160.504442035077,-4.50778546026211,
132.771351544528));
#114797=CARTESIAN_POINT('Ctrl Pts',(-160.512077968147,-4.45366576927798,
132.895378530513));
#114798=CARTESIAN_POINT('Ctrl Pts',(-160.519713901216,-4.39443815542719,
133.01713639209));
#114799=CARTESIAN_POINT('Ctrl Pts',(-160.527349834286,-4.33033559359262,
133.136178944401));
#114800=CARTESIAN_POINT('Ctrl Pts',(-160.534993528525,-4.26616787785568,
133.255342491671));
#114801=CARTESIAN_POINT('Ctrl Pts',(-160.542637222764,-4.19711551150681,
133.371784863109));
#114802=CARTESIAN_POINT('Ctrl Pts',(-160.550280917003,-4.1234565563492,
133.485086095939));
#114803=CARTESIAN_POINT('Ctrl Pts',(-160.55792869333,-4.04975826388435,
133.598447836896));
#114804=CARTESIAN_POINT('Ctrl Pts',(-160.565576469658,-3.97144871812164,
133.708664771202));
#114805=CARTESIAN_POINT('Ctrl Pts',(-160.573224245985,-3.88884729527296,
133.815348790334));
#114806=CARTESIAN_POINT('Ctrl Pts',(-160.580883717483,-3.80611955626038,
133.922195953339));
#114807=CARTESIAN_POINT('Ctrl Pts',(-160.588543188981,-3.71908709232117,
134.025499103716));
#114808=CARTESIAN_POINT('Ctrl Pts',(-160.59620266048,-3.62810763655974,
134.124905458407));
#114809=CARTESIAN_POINT('Ctrl Pts',(-160.602064205306,-3.55848401326856,
134.200977913819));
#114810=CARTESIAN_POINT('Ctrl Pts',(-160.607925750132,-3.48654968589756,
134.274768999458));
#114811=CARTESIAN_POINT('Ctrl Pts',(-160.613787294958,-3.41247785733266,
134.346136716604));
#114812=CARTESIAN_POINT('Ctrl Pts',(-160.621561629077,-3.31423427801122,
134.440793755808));
#114813=CARTESIAN_POINT('Ctrl Pts',(-160.629335963196,-3.21189363579122,
134.531509931887));
#114814=CARTESIAN_POINT('Ctrl Pts',(-160.637110297315,-3.1058052325787,
134.617909741386));
#114815=CARTESIAN_POINT('Ctrl Pts',(-160.644875050262,-2.99984757384174,
134.704203070841));
#114816=CARTESIAN_POINT('Ctrl Pts',(-160.652639803209,-2.89015164434804,
134.78619037349));
#114817=CARTESIAN_POINT('Ctrl Pts',(-160.660404556156,-2.77710371580365,
134.863532702384));
#114818=CARTESIAN_POINT('Ctrl Pts',(-160.668161597041,-2.6641680680556,
134.940798213788));
#114819=CARTESIAN_POINT('Ctrl Pts',(-160.675918637926,-2.54788736720672,
135.013427713087));
#114820=CARTESIAN_POINT('Ctrl Pts',(-160.683675678811,-2.4286808274601,
135.081122535282));
#114821=CARTESIAN_POINT('Ctrl Pts',(-160.691426870051,-2.30956418229223,
135.148766308285));
#114822=CARTESIAN_POINT('Ctrl Pts',(-160.699178061292,-2.18752642852371,
135.211482618882));
#114823=CARTESIAN_POINT('Ctrl Pts',(-160.706929252532,-2.06301531814953,
135.269016355647));
#114824=CARTESIAN_POINT('Ctrl Pts',(-160.714677149309,-1.93855712831887,
135.326525639039));
#114825=CARTESIAN_POINT('Ctrl Pts',(-160.722425046086,-1.81162802688853,
135.378856566015));
#114826=CARTESIAN_POINT('Ctrl Pts',(-160.730172942863,-1.68269970135527,
135.425800304239));
#114827=CARTESIAN_POINT('Ctrl Pts',(-160.737919218947,-1.55379834484835,
135.472734222846));
#114828=CARTESIAN_POINT('Ctrl Pts',(-160.745665495031,-1.42289896318864,
135.514283060457));
#114829=CARTESIAN_POINT('Ctrl Pts',(-160.753411771115,-1.29049215470584,
135.550286561061));
#114830=CARTESIAN_POINT('Ctrl Pts',(-160.761158104381,-1.15808436882588,
135.586290327436));
#114831=CARTESIAN_POINT('Ctrl Pts',(-160.768904437646,-1.02416951118544,
135.616748572538));
#114832=CARTESIAN_POINT('Ctrl Pts',(-160.776650770911,-0.889251846110277,
135.641551353591));
#114833=CARTESIAN_POINT('Ctrl Pts',(-160.784398838914,-0.754303967159656,
135.666359689056));
#114834=CARTESIAN_POINT('Ctrl Pts',(-160.792146906917,-0.618353218350478,
135.685509969605));
#114835=CARTESIAN_POINT('Ctrl Pts',(-160.79989497492,-0.481912127197375,
135.698943721791));
#114836=CARTESIAN_POINT('Ctrl Pts',(-160.807651277662,-0.345326024828738,
135.712391751528));
#114837=CARTESIAN_POINT('Ctrl Pts',(-160.815407580404,-0.208248928783801,
135.720111077879));
#114838=CARTESIAN_POINT('Ctrl Pts',(-160.823163883146,-0.0711970958349331,
135.722095262303));
#114839=CARTESIAN_POINT('Ctrl Pts',(-160.83092432566,0.0659278858037303,
135.724080505746));
#114840=CARTESIAN_POINT('Ctrl Pts',(-160.838684768174,0.203027186851613,
135.720324518627));
#114841=CARTESIAN_POINT('Ctrl Pts',(-160.846445210688,0.33958750583367,
135.710872962234));
#114842=CARTESIAN_POINT('Ctrl Pts',(-160.854218110954,0.476367043563012,
135.701406233364));
#114843=CARTESIAN_POINT('Ctrl Pts',(-160.861991011219,0.612605481453423,
135.686225707845));
#114844=CARTESIAN_POINT('Ctrl Pts',(-160.869763911485,0.747796675012283,
135.665428730166));
#114845=CARTESIAN_POINT('Ctrl Pts',(-160.877254247247,0.878073328159212,
135.64538777501));
#114846=CARTESIAN_POINT('Ctrl Pts',(-160.884744583009,1.00737725270633,
135.62013168165));
#114847=CARTESIAN_POINT('Ctrl Pts',(-160.892234918771,1.13526890413614,
135.589791379556));
#114848=CARTESIAN_POINT('Ctrl Pts',(-160.90000925289,1.26800960640155,135.558300715687));
#114849=CARTESIAN_POINT('Ctrl Pts',(-160.907783587009,1.3996493114814,135.521232943986));
#114850=CARTESIAN_POINT('Ctrl Pts',(-160.915557921128,1.5296832914725,135.478678973251));
#114851=CARTESIAN_POINT('Ctrl Pts',(-160.923322674075,1.65955701620473,
135.436177446481));
#114852=CARTESIAN_POINT('Ctrl Pts',(-160.931087427022,1.78782858528725,
135.38820329398));
#114853=CARTESIAN_POINT('Ctrl Pts',(-160.938852179969,1.91400404376249,
135.334898287971));
#114854=CARTESIAN_POINT('Ctrl Pts',(-160.946609220854,2.04005418299362,
135.281646225246));
#114855=CARTESIAN_POINT('Ctrl Pts',(-160.954366261739,2.16401199685134,
135.223073996826));
#114856=CARTESIAN_POINT('Ctrl Pts',(-160.962123302624,2.28539961449579,
135.159372863767));
#114857=CARTESIAN_POINT('Ctrl Pts',(-160.969874493865,2.40669569279335,
135.095719768228));
#114858=CARTESIAN_POINT('Ctrl Pts',(-160.977625685105,2.52542508796596,
135.026945647503));
#114859=CARTESIAN_POINT('Ctrl Pts',(-160.985376876345,2.64113114665654,
134.953289314068));
#114860=CARTESIAN_POINT('Ctrl Pts',(-160.993124773122,2.75678802718578,
134.879664286541));
#114861=CARTESIAN_POINT('Ctrl Pts',(-161.000872669899,2.86942379787809,
134.801161382973));
#114862=CARTESIAN_POINT('Ctrl Pts',(-161.008620566676,2.97860780356227,
134.718064568436));
#114863=CARTESIAN_POINT('Ctrl Pts',(-161.01636684276,3.08776897030619,134.634985135962));
#114864=CARTESIAN_POINT('Ctrl Pts',(-161.024113118844,3.19347949729487,
134.547313940524));
#114865=CARTESIAN_POINT('Ctrl Pts',(-161.031859394928,3.29533937622689,
134.455377114103));
#114866=CARTESIAN_POINT('Ctrl Pts',(-161.039605728194,3.39720000706553,
134.363439609026));
#114867=CARTESIAN_POINT('Ctrl Pts',(-161.047352061459,3.49520964289892,
134.267236672088));
#114868=CARTESIAN_POINT('Ctrl Pts',(-161.055098394724,3.5890032185711,134.167133128395));
#114869=CARTESIAN_POINT('Ctrl Pts',(-161.062846462727,3.68281779866359,
134.067007167208));
#114870=CARTESIAN_POINT('Ctrl Pts',(-161.07059453073,3.77241417256607,133.962979146318));
#114871=CARTESIAN_POINT('Ctrl Pts',(-161.078342598733,3.8574661112704,133.855448663313));
#114872=CARTESIAN_POINT('Ctrl Pts',(-161.086098901475,3.94260844418767,
133.747803895631));
#114873=CARTESIAN_POINT('Ctrl Pts',(-161.093855204217,4.02319645077549,
133.636649536951));
#114874=CARTESIAN_POINT('Ctrl Pts',(-161.101611506959,4.09894566471257,
133.522416448529));
#114875=CARTESIAN_POINT('Ctrl Pts',(-161.109371949473,4.1747353082859,133.408122390469));
#114876=CARTESIAN_POINT('Ctrl Pts',(-161.117132391987,4.24568081100074,
133.290746662861));
#114877=CARTESIAN_POINT('Ctrl Pts',(-161.124892834501,4.31154313700627,
133.170745801815));
#114878=CARTESIAN_POINT('Ctrl Pts',(-161.132665734767,4.37751119106466,
133.050552304734));
#114879=CARTESIAN_POINT('Ctrl Pts',(-161.140438635032,4.4383795885001,132.927725603616));
#114880=CARTESIAN_POINT('Ctrl Pts',(-161.148211535297,4.49395664452488,
132.802744149231));
#114881=CARTESIAN_POINT('Ctrl Pts',(-161.155701871059,4.54751333457375,
132.682306085521));
#114882=CARTESIAN_POINT('Ctrl Pts',(-161.163192206822,4.59615659758214,
132.559867496345));
#114883=CARTESIAN_POINT('Ctrl Pts',(-161.170682542584,4.63975900367446,
132.435868953531));
#114884=CARTESIAN_POINT('Ctrl Pts',(-161.178456876703,4.68501460824573,
132.307168968279));
#114885=CARTESIAN_POINT('Ctrl Pts',(-161.186231210822,4.72498291817413,
132.17638072013));
#114886=CARTESIAN_POINT('Ctrl Pts',(-161.194005544941,4.75946759984504,
132.043977989389));
#114887=CARTESIAN_POINT('Ctrl Pts',(-161.201770297888,4.79390978222777,
131.91173843318));
#114888=CARTESIAN_POINT('Ctrl Pts',(-161.209535050835,4.82288168532676,
131.777888728011));
#114889=CARTESIAN_POINT('Ctrl Pts',(-161.217299803782,4.84623559140791,
131.642921083526));
#114890=CARTESIAN_POINT('Ctrl Pts',(-161.225056844667,4.86956630206036,
131.508087490808));
#114891=CARTESIAN_POINT('Ctrl Pts',(-161.232813885552,4.88729005366754,
131.372138551175));
#114892=CARTESIAN_POINT('Ctrl Pts',(-161.240570926437,4.89930945870933,
131.235579692169));
#114893=CARTESIAN_POINT('Ctrl Pts',(-161.248322117677,4.91131979982429,
131.099123813261));
#114894=CARTESIAN_POINT('Ctrl Pts',(-161.256073308917,4.91763432249103,
130.962059318357));
#114895=CARTESIAN_POINT('Ctrl Pts',(-161.263824500158,4.9182071141168,130.824899486837));
#114896=CARTESIAN_POINT('Ctrl Pts',(-161.271572396935,4.91877966229084,
130.687797951904));
#114897=CARTESIAN_POINT('Ctrl Pts',(-161.279320293712,4.91361533154206,
130.550601551091));
#114898=CARTESIAN_POINT('Ctrl Pts',(-161.287068190489,4.90272025008849,
130.413826096848));
#114899=CARTESIAN_POINT('Ctrl Pts',(-161.294814466573,4.89182744765106,
130.277079253081));
#114900=CARTESIAN_POINT('Ctrl Pts',(-161.302560742657,4.87520630991227,
130.140753570225));
#114901=CARTESIAN_POINT('Ctrl Pts',(-161.310307018741,4.8529150066865,130.005361868896));
#114902=CARTESIAN_POINT('Ctrl Pts',(-161.318053352006,4.83062353891148,
129.869969168135));
#114903=CARTESIAN_POINT('Ctrl Pts',(-161.325799685272,4.80266188564376,
129.73551084843));
#114904=CARTESIAN_POINT('Ctrl Pts',(-161.333546018537,4.7691396579411,129.602491246314));
#114905=CARTESIAN_POINT('Ctrl Pts',(-161.34129408654,4.73560992316792,129.46944185538));
#114906=CARTESIAN_POINT('Ctrl Pts',(-161.349042154543,4.6965172315739,129.337832202198));
#114907=CARTESIAN_POINT('Ctrl Pts',(-161.356790222546,4.65202144117872,
129.208152744727));
#114908=CARTESIAN_POINT('Ctrl Pts',(-161.364546525288,4.60747836012794,
129.078335462385));
#114909=CARTESIAN_POINT('Ctrl Pts',(-161.37230282803,4.55752083614748,128.950452844109));
#114910=CARTESIAN_POINT('Ctrl Pts',(-161.380059130772,4.50235760401946,
128.824977110504));
#114911=CARTESIAN_POINT('Ctrl Pts',(-161.387819573286,4.44716492961338,
128.699434406722));
#114912=CARTESIAN_POINT('Ctrl Pts',(-161.3955800158,4.38676118288056,128.576301498173));
#114913=CARTESIAN_POINT('Ctrl Pts',(-161.403340458314,4.32140125586376,
128.456026261406));
#114914=CARTESIAN_POINT('Ctrl Pts',(-161.41111335858,4.2559364072899,128.335557948153));
#114915=CARTESIAN_POINT('Ctrl Pts',(-161.418886258845,4.18549968061349,
128.217956809345));
#114916=CARTESIAN_POINT('Ctrl Pts',(-161.42665915911,4.11038999970731,128.103642729151));
#114917=CARTESIAN_POINT('Ctrl Pts',(-161.434149494872,4.03801074489255,
127.993484253712));
#114918=CARTESIAN_POINT('Ctrl Pts',(-161.441639830634,3.96129256401282,
127.886378250718));
#114919=CARTESIAN_POINT('Ctrl Pts',(-161.449130166396,3.88053724366479,
127.782670070367));
#114920=CARTESIAN_POINT('Ctrl Pts',(-161.456904500515,3.79672006080012,
127.675029762836));
#114921=CARTESIAN_POINT('Ctrl Pts',(-161.464678834634,3.70828805131338,
127.570709048927));
#114922=CARTESIAN_POINT('Ctrl Pts',(-161.472453168754,3.61553369687891,
127.470129199498));
#114923=CARTESIAN_POINT('Ctrl Pts',(-161.480217921701,3.52289365389632,
127.369673305744));
#114924=CARTESIAN_POINT('Ctrl Pts',(-161.487982674648,3.42594212741971,
127.272949388035));
#114925=CARTESIAN_POINT('Ctrl Pts',(-161.495747427595,3.32501338231965,
127.18034777682));
#114926=CARTESIAN_POINT('Ctrl Pts',(-161.50350446848,3.22418488107207,127.08783813883));
#114927=CARTESIAN_POINT('Ctrl Pts',(-161.511261509365,3.11938730855479,
126.999442922031));
#114928=CARTESIAN_POINT('Ctrl Pts',(-161.51901855025,3.01099325494078,126.915517257234));
#114929=CARTESIAN_POINT('Ctrl Pts',(-161.52676974149,2.90268094212622,126.831654881434));
#114930=CARTESIAN_POINT('Ctrl Pts',(-161.53452093273,2.79077785443798,126.752255587196));
#114931=CARTESIAN_POINT('Ctrl Pts',(-161.54227212397,2.67569101147737,126.677635442127));
#114932=CARTESIAN_POINT('Ctrl Pts',(-161.550020020747,2.5606530834949,126.603047012611));
#114933=CARTESIAN_POINT('Ctrl Pts',(-161.557767917524,2.44243441897169,
126.533233904484));
#114934=CARTESIAN_POINT('Ctrl Pts',(-161.565515814302,2.32147229798197,
126.468469771131));
#114935=CARTESIAN_POINT('Ctrl Pts',(-161.573262090386,2.20053547966033,
126.403719185038));
#114936=CARTESIAN_POINT('Ctrl Pts',(-161.58100836647,2.07685669078846,126.344015657429));
#114937=CARTESIAN_POINT('Ctrl Pts',(-161.588754642554,1.95089882407887,
126.289587440461));
#114938=CARTESIAN_POINT('Ctrl Pts',(-161.596500975819,1.82494002757676,
126.235158821716));
#114939=CARTESIAN_POINT('Ctrl Pts',(-161.604247309085,1.69670247855829,
126.186005746397));
#114940=CARTESIAN_POINT('Ctrl Pts',(-161.61199364235,1.56666973708766,126.142308601834));
#114941=CARTESIAN_POINT('Ctrl Pts',(-161.619741710353,1.43660787568599,
126.098601671598));
#114942=CARTESIAN_POINT('Ctrl Pts',(-161.627489778356,1.3047503923855,126.060353227909));
#114943=CARTESIAN_POINT('Ctrl Pts',(-161.635237846359,1.17159633052308,
126.027693882194));
#114944=CARTESIAN_POINT('Ctrl Pts',(-161.642994149101,1.03830075093933,
125.994999825739));
#114945=CARTESIAN_POINT('Ctrl Pts',(-161.650750451843,0.903706220367848,
125.967906826649));
#114946=CARTESIAN_POINT('Ctrl Pts',(-161.658506754585,0.768322857626625,
125.946494517214));
#114947=CARTESIAN_POINT('Ctrl Pts',(-161.666267197099,0.632867236708392,
125.925070779384));
#114948=CARTESIAN_POINT('Ctrl Pts',(-161.674027639613,0.496622332888463,
125.909333817474));
#114949=CARTESIAN_POINT('Ctrl Pts',(-161.681788082127,0.360102732768053,
125.899311271805));
#114950=CARTESIAN_POINT('Ctrl Pts',(-161.689560982393,0.223363979265889,
125.889272637055));
#114951=CARTESIAN_POINT('Ctrl Pts',(-161.697333882658,0.0863500392680675,
125.884966761986));
#114952=CARTESIAN_POINT('Ctrl Pts',(-161.705106782924,-0.0504242511279812,
125.886369111128));
#114953=CARTESIAN_POINT('Ctrl Pts',(-161.712597118686,-0.182226451554115,
125.887720481346));
#114954=CARTESIAN_POINT('Ctrl Pts',(-161.720087454448,-0.313805815984554,
125.894372248864));
#114955=CARTESIAN_POINT('Ctrl Pts',(-161.72757779021,-0.444708668489591,
125.906257182289));
#114956=CARTESIAN_POINT('Ctrl Pts',(-161.735352124329,-0.580574742435354,
125.918592736578));
#114957=CARTESIAN_POINT('Ctrl Pts',(-161.743126458448,-0.716142374763522,
125.936605196641));
#114958=CARTESIAN_POINT('Ctrl Pts',(-161.750900792567,-0.850899044880972,
125.960276196551));
#114959=CARTESIAN_POINT('Ctrl Pts',(-161.758665545514,-0.985489639445686,
125.983918024069));
#114960=CARTESIAN_POINT('Ctrl Pts',(-161.766430298461,-1.11927087901136,
126.013204448969));
#114961=CARTESIAN_POINT('Ctrl Pts',(-161.774195051408,-1.25173368918903,
126.04806522789));
#114962=CARTESIAN_POINT('Ctrl Pts',(-161.781952092293,-1.38406493543623,
126.082891382595));
#114963=CARTESIAN_POINT('Ctrl Pts',(-161.789709133178,-1.51507998258062,
126.123280774522));
#114964=CARTESIAN_POINT('Ctrl Pts',(-161.797466174063,-1.64427865492304,
126.169111889885));
#114965=CARTESIAN_POINT('Ctrl Pts',(-161.805217365304,-1.7733798975418,
126.214908443648));
#114966=CARTESIAN_POINT('Ctrl Pts',(-161.812968556544,-1.90066712476996,
126.26613842261));
#114967=CARTESIAN_POINT('Ctrl Pts',(-161.820719747784,-2.02565441594169,
126.322630231914));
#114968=CARTESIAN_POINT('Ctrl Pts',(-161.828467644561,-2.15058858418035,
126.379098030692));
#114969=CARTESIAN_POINT('Ctrl Pts',(-161.836215541338,-2.27322440508434,
126.44082305106));
#114970=CARTESIAN_POINT('Ctrl Pts',(-161.843963438115,-2.3930952857491,
126.507585313245));
#114971=CARTESIAN_POINT('Ctrl Pts',(-161.851709714199,-2.51294109200942,
126.574333610204));
#114972=CARTESIAN_POINT('Ctrl Pts',(-161.859455990283,-2.6300227670859,
126.646116863035));
#114973=CARTESIAN_POINT('Ctrl Pts',(-161.867202266367,-2.74389807115714,
126.722669002855));
#114974=CARTESIAN_POINT('Ctrl Pts',(-161.874948599633,-2.85777421583017,
126.799221707766));
#114975=CARTESIAN_POINT('Ctrl Pts',(-161.882694932898,-2.96844361780387,
126.880543151792));
#114976=CARTESIAN_POINT('Ctrl Pts',(-161.890441266163,-3.07549313608341,
126.966324005911));
#114977=CARTESIAN_POINT('Ctrl Pts',(-161.898189334166,-3.18256662736019,
127.052124070058));
#114978=CARTESIAN_POINT('Ctrl Pts',(-161.905937402169,-3.28601831680974,
127.142385287072));
#114979=CARTESIAN_POINT('Ctrl Pts',(-161.913685470172,-3.38546857222495,
127.236758396329));
#114980=CARTESIAN_POINT('Ctrl Pts',(-161.921441772914,-3.48502452455496,
127.331231806448));
#114981=CARTESIAN_POINT('Ctrl Pts',(-161.929198075656,-3.58057026343033,
127.429825569142));
#114982=CARTESIAN_POINT('Ctrl Pts',(-161.936954378398,-3.67176306027024,
127.532153550198));
#114983=CARTESIAN_POINT('Ctrl Pts',(-161.944714820912,-3.76300452945184,
127.634536146778));
#114984=CARTESIAN_POINT('Ctrl Pts',(-161.952475263426,-3.84988817968207,
127.740656630709));
#114985=CARTESIAN_POINT('Ctrl Pts',(-161.96023570594,-3.93211260974882,
127.850097005978));
#114986=CARTESIAN_POINT('Ctrl Pts',(-161.968008606206,-4.01446903377025,
127.959713064653));
#114987=CARTESIAN_POINT('Ctrl Pts',(-161.975781506471,-4.09215106973453,
128.072659342158));
#114988=CARTESIAN_POINT('Ctrl Pts',(-161.983554406737,-4.16490107854198,
128.188489430283));
#114989=CARTESIAN_POINT('Ctrl Pts',(-161.991044742499,-4.23500644128207,
128.300108802944));
#114990=CARTESIAN_POINT('Ctrl Pts',(-161.99853507826,-4.30053198135975,
128.414405691581));
#114991=CARTESIAN_POINT('Ctrl Pts',(-162.006025414022,-4.36128903952838,
128.530962065576));
#114992=CARTESIAN_POINT('Ctrl Pts',(-162.014275408015,-4.42820798426658,
128.659339406174));
#114993=CARTESIAN_POINT('Ctrl Pts',(-162.022525402008,-4.48953361810604,
128.790824632779));
#114994=CARTESIAN_POINT('Ctrl Pts',(-162.030775396001,-4.5449844696847,
128.924919415287));
#114995=CARTESIAN_POINT('Ctrl Pts',(-162.039006074437,-4.60030549521436,
129.058700244171));
#114996=CARTESIAN_POINT('Ctrl Pts',(-162.047236752872,-4.64977904220322,
129.195078152985));
#114997=CARTESIAN_POINT('Ctrl Pts',(-162.055467431307,-4.69317003756102,
129.333531578881));
#114998=CARTESIAN_POINT('Ctrl Pts',(-162.060359422207,-4.71895993520688,
129.415822838925));
#114999=CARTESIAN_POINT('Ctrl Pts',(-162.065251413106,-4.74260194298077,
129.498846814994));
#115000=CARTESIAN_POINT('Ctrl Pts',(-162.070143404005,-4.764054528234,129.582490119308));
#115001=CARTESIAN_POINT('Origin',(213.235140564004,0.,130.804360617566));
#115002=CARTESIAN_POINT('',(-164.165050101093,-4.76405452823413,129.582490119309));
#115003=CARTESIAN_POINT('',(-163.819828717623,-4.76405452823398,129.582490119308));
#115004=CARTESIAN_POINT('',(213.235140564004,-4.76405452823405,129.582490119308));
#115005=CARTESIAN_POINT('',(-162.485140563971,-4.91824798157934,130.808816421734));
#115006=CARTESIAN_POINT('Ctrl Pts',(-162.485140564011,-4.91824798157869,
130.808816422445));
#115007=CARTESIAN_POINT('Ctrl Pts',(-162.496060307999,-4.918073492229,131.001415047217));
#115008=CARTESIAN_POINT('Ctrl Pts',(-162.506980051987,-4.90658238243364,
131.193522218363));
#115009=CARTESIAN_POINT('Ctrl Pts',(-162.517899795976,-4.88396733481339,
131.384055481245));
#115010=CARTESIAN_POINT('Ctrl Pts',(-162.526377085813,-4.86641066740618,
131.531971558301));
#115011=CARTESIAN_POINT('Ctrl Pts',(-162.534854375651,-4.8421507266267,
131.678939988927));
#115012=CARTESIAN_POINT('Ctrl Pts',(-162.543331665489,-4.8112959995807,
131.824465448904));
#115013=CARTESIAN_POINT('Ctrl Pts',(-162.551105999608,-4.78299981509265,
131.95792361423));
#115014=CARTESIAN_POINT('Ctrl Pts',(-162.558880333727,-4.74910170794549,
132.090414934641));
#115015=CARTESIAN_POINT('Ctrl Pts',(-162.566654667846,-4.70968044867888,
132.221432646022));
#115016=CARTESIAN_POINT('Ctrl Pts',(-162.574419420793,-4.67030777259114,
132.352288889783));
#115017=CARTESIAN_POINT('Ctrl Pts',(-162.58218417374,-4.62542559943551,
132.481674767203));
#115018=CARTESIAN_POINT('Ctrl Pts',(-162.589948926687,-4.57516380705058,
132.60909306343));
#115019=CARTESIAN_POINT('Ctrl Pts',(-162.597705967572,-4.52495193538641,
132.736384806009));
#115020=CARTESIAN_POINT('Ctrl Pts',(-162.605463008457,-4.46937122006502,
132.861712495059));
#115021=CARTESIAN_POINT('Ctrl Pts',(-162.613220049342,-4.40860139947938,
132.984593807619));
#115022=CARTESIAN_POINT('Ctrl Pts',(-162.620971240582,-4.34787740588808,
133.107382454425));
#115023=CARTESIAN_POINT('Ctrl Pts',(-162.628722431823,-4.28197226852108,
133.227728047732));
#115024=CARTESIAN_POINT('Ctrl Pts',(-162.636473623063,-4.21111377266266,
133.345168334846));
#115025=CARTESIAN_POINT('Ctrl Pts',(-162.64422151984,-4.14028539355529,
133.462558706706));
#115026=CARTESIAN_POINT('Ctrl Pts',(-162.651969416617,-4.06450804480952,
133.577045894308));
#115027=CARTESIAN_POINT('Ctrl Pts',(-162.659717313394,-3.98405527518577,
133.688192552122));
#115028=CARTESIAN_POINT('Ctrl Pts',(-162.667463589478,-3.90361933454707,
133.799315960451));
#115029=CARTESIAN_POINT('Ctrl Pts',(-162.675209865562,-3.81851014741903,
133.907099912374));
#115030=CARTESIAN_POINT('Ctrl Pts',(-162.682956141646,-3.72904415276827,
134.011136688514));
#115031=CARTESIAN_POINT('Ctrl Pts',(-162.690702474912,-3.63957749769998,
134.11517423263));
#115032=CARTESIAN_POINT('Ctrl Pts',(-162.698448808177,-3.54575422584954,
134.215464249335));
#115033=CARTESIAN_POINT('Ctrl Pts',(-162.706195141442,-3.44793029670246,
134.311633023807));
#115034=CARTESIAN_POINT('Ctrl Pts',(-162.713943209445,-3.35008446056483,
134.40782333461));
#115035=CARTESIAN_POINT('Ctrl Pts',(-162.721691277448,-3.24823646310393,
134.499890292635));
#115036=CARTESIAN_POINT('Ctrl Pts',(-162.729439345451,-3.14277795823583,
134.58749817358));
#115037=CARTESIAN_POINT('Ctrl Pts',(-162.737195648193,-3.03720737081365,
134.675199165225));
#115038=CARTESIAN_POINT('Ctrl Pts',(-162.744951950935,-2.9280189117952,
134.75843136258));
#115039=CARTESIAN_POINT('Ctrl Pts',(-162.752708253677,-2.81563649195168,
134.836900041761));
#115040=CARTESIAN_POINT('Ctrl Pts',(-162.760468696191,-2.70319409022693,
134.91541060204));
#115041=CARTESIAN_POINT('Ctrl Pts',(-162.768229138705,-2.58755466037525,
134.989152368025));
#115042=CARTESIAN_POINT('Ctrl Pts',(-162.775989581219,-2.46916887083393,
135.057875417094));
#115043=CARTESIAN_POINT('Ctrl Pts',(-162.783762481485,-2.35059303791345,
135.126708786503));
#115044=CARTESIAN_POINT('Ctrl Pts',(-162.79153538175,-2.22926238155688,
135.1905071575));
#115045=CARTESIAN_POINT('Ctrl Pts',(-162.799308282015,-2.10565061484523,
135.249067418999));
#115046=CARTESIAN_POINT('Ctrl Pts',(-162.806798617777,-1.98653244721482,
135.305498867487));
#115047=CARTESIAN_POINT('Ctrl Pts',(-162.814288953539,-1.86529642151892,
135.357066310976));
#115048=CARTESIAN_POINT('Ctrl Pts',(-162.821779289301,-1.74237992474672,
135.403631783777));
#115049=CARTESIAN_POINT('Ctrl Pts',(-162.82955362342,-1.61480301163777,
135.451962800634));
#115050=CARTESIAN_POINT('Ctrl Pts',(-162.837327957539,-1.48501155650677,
135.495058158009));
#115051=CARTESIAN_POINT('Ctrl Pts',(-162.845102291658,-1.35347449175632,
135.532710209407));
#115052=CARTESIAN_POINT('Ctrl Pts',(-162.852867044605,-1.22209953468272,
135.570315858017));
#115053=CARTESIAN_POINT('Ctrl Pts',(-162.860631797552,-1.08898362071227,
135.602491441784));
#115054=CARTESIAN_POINT('Ctrl Pts',(-162.8683965505,-0.954615272926989,
135.629077473838));
#115055=CARTESIAN_POINT('Ctrl Pts',(-162.876153591384,-0.820380381678994,
135.65563710027));
#115056=CARTESIAN_POINT('Ctrl Pts',(-162.883910632269,-0.684895913150993,
135.676618147574));
#115057=CARTESIAN_POINT('Ctrl Pts',(-162.891667673154,-0.548664812303447,
135.691911127406));
#115058=CARTESIAN_POINT('Ctrl Pts',(-162.899418864395,-0.412536444388588,
135.707192574684));
#115059=CARTESIAN_POINT('Ctrl Pts',(-162.907170055635,-0.275662951806377,
135.716794448873));
#115060=CARTESIAN_POINT('Ctrl Pts',(-162.914921246875,-0.138556364349379,
135.720658533315));
#115061=CARTESIAN_POINT('Ctrl Pts',(-162.922669143652,-0.00150805084967565,
135.724520975418));
#115062=CARTESIAN_POINT('Ctrl Pts',(-162.930417040429,0.13577277048724,
135.722650467196));
#115063=CARTESIAN_POINT('Ctrl Pts',(-162.938164937206,0.272770288692314,
135.715040757028));
#115064=CARTESIAN_POINT('Ctrl Pts',(-162.94591121329,0.409739149969904,
135.707432638647));
#115065=CARTESIAN_POINT('Ctrl Pts',(-162.953657489374,0.546424435872705,
135.694087727883));
#115066=CARTESIAN_POINT('Ctrl Pts',(-162.961403765458,0.682312077550561,
135.675051871518));
#115067=CARTESIAN_POINT('Ctrl Pts',(-162.969150098724,0.818200722320303,
135.656015874635));
#115068=CARTESIAN_POINT('Ctrl Pts',(-162.976896431989,0.953291323931337,
135.631288902564));
#115069=CARTESIAN_POINT('Ctrl Pts',(-162.984642765254,1.08707706072241,
135.600968432111));
#115070=CARTESIAN_POINT('Ctrl Pts',(-162.992390833257,1.22089275790145,
135.570641171598));
#115071=CARTESIAN_POINT('Ctrl Pts',(-163.00013890126,1.3534026275631,135.534718006523));
#115072=CARTESIAN_POINT('Ctrl Pts',(-163.007886969263,1.48411251683514,
135.49334697923));
#115073=CARTESIAN_POINT('Ctrl Pts',(-163.015643272005,1.61496132613314,
135.451931982318));
#115074=CARTESIAN_POINT('Ctrl Pts',(-163.023399574747,1.74400596020215,
135.405057675098));
#115075=CARTESIAN_POINT('Ctrl Pts',(-163.031155877489,1.87076932536499,
135.35292140025));
#115076=CARTESIAN_POINT('Ctrl Pts',(-163.038916320003,1.9976003479526,135.300757298703));
#115077=CARTESIAN_POINT('Ctrl Pts',(-163.046676762517,2.12214732063613,
135.243325797048));
#115078=CARTESIAN_POINT('Ctrl Pts',(-163.054437205031,2.24395637913678,
135.180870966124));
#115079=CARTESIAN_POINT('Ctrl Pts',(-163.062210105296,2.36596097635184,
135.11831587716));
#115080=CARTESIAN_POINT('Ctrl Pts',(-163.069983005562,2.48521853616227,
135.050721537591));
#115081=CARTESIAN_POINT('Ctrl Pts',(-163.077755905827,2.60130212196725,
134.978376709144));
#115082=CARTESIAN_POINT('Ctrl Pts',(-163.08524624159,2.71316577703477,134.908661797434));
#115083=CARTESIAN_POINT('Ctrl Pts',(-163.092736577352,2.82208196095618,
134.834535958241));
#115084=CARTESIAN_POINT('Ctrl Pts',(-163.100226913114,2.92769818093926,
134.756292603801));
#115085=CARTESIAN_POINT('Ctrl Pts',(-163.108001247233,3.03731887200142,
134.675082628798));
#115086=CARTESIAN_POINT('Ctrl Pts',(-163.115775581352,3.14373166851665,
134.589179495035));
#115087=CARTESIAN_POINT('Ctrl Pts',(-163.123549915471,3.2465084021888,134.49886549062));
#115088=CARTESIAN_POINT('Ctrl Pts',(-163.131314668418,3.34915847272184,
134.408662790144));
#115089=CARTESIAN_POINT('Ctrl Pts',(-163.139079421365,3.44818110564297,
134.31406029064));
#115090=CARTESIAN_POINT('Ctrl Pts',(-163.146844174313,3.5431780614734,134.215382793864));
#115091=CARTESIAN_POINT('Ctrl Pts',(-163.154601215198,3.63808066498807,
134.116803304968));
#115092=CARTESIAN_POINT('Ctrl Pts',(-163.162358256083,3.72896527893046,
134.014157153034));
#115093=CARTESIAN_POINT('Ctrl Pts',(-163.170115296968,3.81546793362102,
133.907808298776));
#115094=CARTESIAN_POINT('Ctrl Pts',(-163.177866488208,3.90190535598691,
133.801539643017));
#115095=CARTESIAN_POINT('Ctrl Pts',(-163.185617679448,3.98396715074385,
133.691574144787));
#115096=CARTESIAN_POINT('Ctrl Pts',(-163.193368870688,4.06132757395633,
133.578311121725));
#115097=CARTESIAN_POINT('Ctrl Pts',(-163.201116767465,4.13865511692518,
133.465096238469));
#115098=CARTESIAN_POINT('Ctrl Pts',(-163.208864664242,4.21128504258629,
133.348586940099));
#115099=CARTESIAN_POINT('Ctrl Pts',(-163.216612561019,4.27893328284376,
133.229213813838));
#115100=CARTESIAN_POINT('Ctrl Pts',(-163.224358837103,4.34656737254769,
133.109865657862));
#115101=CARTESIAN_POINT('Ctrl Pts',(-163.232105113188,4.40922165692871,
132.987655205467));
#115102=CARTESIAN_POINT('Ctrl Pts',(-163.239851389272,4.46665684141273,
132.863039738644));
#115103=CARTESIAN_POINT('Ctrl Pts',(-163.247597722537,4.52409244987031,
132.738423351937));
#115104=CARTESIAN_POINT('Ctrl Pts',(-163.255344055802,4.57630871790457,
132.611402270442));
#115105=CARTESIAN_POINT('Ctrl Pts',(-163.263090389068,4.62311370602557,
132.482455586171));
#115106=CARTESIAN_POINT('Ctrl Pts',(-163.270838457071,4.66992917579907,
132.353480025185));
#115107=CARTESIAN_POINT('Ctrl Pts',(-163.278586525074,4.71133082090973,
132.222578370769));
#115108=CARTESIAN_POINT('Ctrl Pts',(-163.286334593077,4.74717609187807,
132.090246388232));
#115109=CARTESIAN_POINT('Ctrl Pts',(-163.294090895818,4.783059459627,131.957773761689));
#115110=CARTESIAN_POINT('Ctrl Pts',(-163.30184719856,4.81337455421823,131.823868148292));
#115111=CARTESIAN_POINT('Ctrl Pts',(-163.309603501302,4.83802952485061,
131.689037609001));
#115112=CARTESIAN_POINT('Ctrl Pts',(-163.317363943816,4.86269765458316,
131.554135106591));
#115113=CARTESIAN_POINT('Ctrl Pts',(-163.325124386331,4.88169958666042,
131.418307081631));
#115114=CARTESIAN_POINT('Ctrl Pts',(-163.332884828845,4.89499534006176,
131.282067309244));
#115115=CARTESIAN_POINT('Ctrl Pts',(-163.34065772911,4.90831243698681,131.145608832679));
#115116=CARTESIAN_POINT('Ctrl Pts',(-163.348430629376,4.9159050288411,131.008737678439));
#115117=CARTESIAN_POINT('Ctrl Pts',(-163.356203529641,4.91778528938313,
130.871969123147));
#115118=CARTESIAN_POINT('Ctrl Pts',(-163.363693865403,4.91959719771836,
130.740172449339));
#115119=CARTESIAN_POINT('Ctrl Pts',(-163.371184201165,4.91610488768731,
130.608471352435));
#115120=CARTESIAN_POINT('Ctrl Pts',(-163.378674536927,4.90736468435062,
130.477320991086));
#115121=CARTESIAN_POINT('Ctrl Pts',(-163.386448871046,4.89829309354788,
130.341198023923));
#115122=CARTESIAN_POINT('Ctrl Pts',(-163.394223205165,4.88353907000355,
130.205237182349));
#115123=CARTESIAN_POINT('Ctrl Pts',(-163.401997539284,4.86310867527487,
130.069951280094));
#115124=CARTESIAN_POINT('Ctrl Pts',(-163.409762292231,4.84270345918178,
129.934832105623));
#115125=CARTESIAN_POINT('Ctrl Pts',(-163.417527045178,4.81663584892317,
129.800386598303));
#115126=CARTESIAN_POINT('Ctrl Pts',(-163.425291798126,4.78496385124945,
129.66712537157));
#115127=CARTESIAN_POINT('Ctrl Pts',(-163.433048839011,4.75332331065031,
129.533996501766));
#115128=CARTESIAN_POINT('Ctrl Pts',(-163.440805879896,4.71608954975383,
129.402049949678));
#115129=CARTESIAN_POINT('Ctrl Pts',(-163.448562920781,4.67337204451598,
129.271788662963));
#115130=CARTESIAN_POINT('Ctrl Pts',(-163.456314112021,4.63068675288106,
129.141625607297));
#115131=CARTESIAN_POINT('Ctrl Pts',(-163.464065303261,4.58252606937225,
129.013145657407));
#115132=CARTESIAN_POINT('Ctrl Pts',(-163.471816494501,4.52904987867432,
128.886838711829));
#115133=CARTESIAN_POINT('Ctrl Pts',(-163.479564391278,4.47559641678404,
128.760585450073));
#115134=CARTESIAN_POINT('Ctrl Pts',(-163.487312288055,4.41683209325552,
128.636503714961));
#115135=CARTESIAN_POINT('Ctrl Pts',(-163.495060184832,4.35296562756867,
128.51506524394));
#115136=CARTESIAN_POINT('Ctrl Pts',(-163.502806460916,4.28911252136964,
128.393652175229));
#115137=CARTESIAN_POINT('Ctrl Pts',(-163.510552737,4.22015957771432,128.274881616642));
#115138=CARTESIAN_POINT('Ctrl Pts',(-163.518299013084,4.14636217632811,
128.159202065567));
#115139=CARTESIAN_POINT('Ctrl Pts',(-163.52604534635,4.07256423018615,128.043521660571));
#115140=CARTESIAN_POINT('Ctrl Pts',(-163.533791679615,3.99392196522635,
127.930932638221));
#115141=CARTESIAN_POINT('Ctrl Pts',(-163.541538012881,3.91073470714457,
127.821855443583));
#115142=CARTESIAN_POINT('Ctrl Pts',(-163.549286080884,3.82752881985325,
127.712753821863));
#115143=CARTESIAN_POINT('Ctrl Pts',(-163.557034148887,3.73977615113876,
127.607165903613));
#115144=CARTESIAN_POINT('Ctrl Pts',(-163.564782216889,3.64781675092208,
127.505479593007));
#115145=CARTESIAN_POINT('Ctrl Pts',(-163.572538519631,3.5557596151604,127.40368520898));
#115146=CARTESIAN_POINT('Ctrl Pts',(-163.580294822373,3.459487079319,127.305801006465));
#115147=CARTESIAN_POINT('Ctrl Pts',(-163.588051125115,3.35937694187183,
127.212178881501));
#115148=CARTESIAN_POINT('Ctrl Pts',(-163.595811567629,3.25921337263006,
127.11850678759));
#115149=CARTESIAN_POINT('Ctrl Pts',(-163.603572010143,3.15520841681785,
127.029101558696));
#115150=CARTESIAN_POINT('Ctrl Pts',(-163.611332452658,3.04777271727758,
126.944274539987));
#115151=CARTESIAN_POINT('Ctrl Pts',(-163.619105352923,2.9401645524147,126.859311349417));
#115152=CARTESIAN_POINT('Ctrl Pts',(-163.626878253189,2.82911495531737,
126.778941284727));
#115153=CARTESIAN_POINT('Ctrl Pts',(-163.634651153454,2.71506402301407,
126.703432623388));
#115154=CARTESIAN_POINT('Ctrl Pts',(-163.642141489216,2.60515912937695,
126.630668892083));
#115155=CARTESIAN_POINT('Ctrl Pts',(-163.649631824978,2.49246758770634,
126.562419411565));
#115156=CARTESIAN_POINT('Ctrl Pts',(-163.65712216074,2.3774027809366,126.498882818332));
#115157=CARTESIAN_POINT('Ctrl Pts',(-163.664896494859,2.25797525704483,
126.432937215856));
#115158=CARTESIAN_POINT('Ctrl Pts',(-163.672670828978,2.13561264030401,
126.37186003782));
#115159=CARTESIAN_POINT('Ctrl Pts',(-163.680445163097,2.01074965184982,
126.315923372813));
#115160=CARTESIAN_POINT('Ctrl Pts',(-163.688209916044,1.88604054586957,
126.260055644747));
#115161=CARTESIAN_POINT('Ctrl Pts',(-163.695974668992,1.75883755278497,
126.20931598281));
#115162=CARTESIAN_POINT('Ctrl Pts',(-163.703739421939,1.62960162020577,
126.163931583315));
#115163=CARTESIAN_POINT('Ctrl Pts',(-163.711496462824,1.50049404657672,
126.118592260245));
#115164=CARTESIAN_POINT('Ctrl Pts',(-163.719253503709,1.36935791813451,
126.078597743425));
#115165=CARTESIAN_POINT('Ctrl Pts',(-163.727010544594,1.23667555341529,
126.044127783126));
#115166=CARTESIAN_POINT('Ctrl Pts',(-163.734761735834,1.10409324549961,
126.009683816892));
#115167=CARTESIAN_POINT('Ctrl Pts',(-163.742512927074,0.969967399089417,
125.980756212697));
#115168=CARTESIAN_POINT('Ctrl Pts',(-163.750264118314,0.834796601275304,
125.957475257152));
#115169=CARTESIAN_POINT('Ctrl Pts',(-163.758012015091,0.699683254655876,
125.934204196634));
#115170=CARTESIAN_POINT('Ctrl Pts',(-163.765759911868,0.56352622446324,
125.916575077618));
#115171=CARTESIAN_POINT('Ctrl Pts',(-163.773507808645,0.426835214747577,
125.904667284106));
#115172=CARTESIAN_POINT('Ctrl Pts',(-163.78125408473,0.290172797844429,
125.892761981448));
#115173=CARTESIAN_POINT('Ctrl Pts',(-163.789000360814,0.152977012833045,
125.886575657746));
#115174=CARTESIAN_POINT('Ctrl Pts',(-163.796746636898,0.0157632322466415,
125.886135878597));
#115175=CARTESIAN_POINT('Ctrl Pts',(-163.804492970163,-0.121451561220533,
125.885696096201));
#115176=CARTESIAN_POINT('Ctrl Pts',(-163.812239303428,-0.258683959564604,
125.891002944257));
#115177=CARTESIAN_POINT('Ctrl Pts',(-163.819985636694,-0.395418437595522,
125.902031852407));
#115178=CARTESIAN_POINT('Ctrl Pts',(-163.827733704697,-0.532183536364932,
125.913063230403));
#115179=CARTESIAN_POINT('Ctrl Pts',(-163.8354817727,-0.668450103312558,
125.929819186935));
#115180=CARTESIAN_POINT('Ctrl Pts',(-163.843229840703,-0.803707978381973,
125.952223300055));
#115181=CARTESIAN_POINT('Ctrl Pts',(-163.850986143445,-0.939109607130786,
125.974651224532));
#115182=CARTESIAN_POINT('Ctrl Pts',(-163.858742446186,-1.07350001614181,
126.002739233102));
#115183=CARTESIAN_POINT('Ctrl Pts',(-163.866498748928,-1.20637893600707,
126.036359681612));
#115184=CARTESIAN_POINT('Ctrl Pts',(-163.874259191443,-1.33932877735277,
126.069998074368));
#115185=CARTESIAN_POINT('Ctrl Pts',(-163.882019633957,-1.47076514758795,
126.109174679205));
#115186=CARTESIAN_POINT('Ctrl Pts',(-163.889780076471,-1.60020414071843,
126.153712300339));
#115187=CARTESIAN_POINT('Ctrl Pts',(-163.897552976736,-1.72985092081172,
126.198321417216));
#115188=CARTESIAN_POINT('Ctrl Pts',(-163.905325877002,-1.857493552203,126.248308605229));
#115189=CARTESIAN_POINT('Ctrl Pts',(-163.913098777267,-1.98266844226304,
126.303448608811));
#115190=CARTESIAN_POINT('Ctrl Pts',(-163.920589113029,-2.10329290976984,
126.356584134372));
#115191=CARTESIAN_POINT('Ctrl Pts',(-163.928079448791,-2.22162566156996,
126.414504208663));
#115192=CARTESIAN_POINT('Ctrl Pts',(-163.935569784553,-2.33727613557715,
126.476968408792));
#115193=CARTESIAN_POINT('Ctrl Pts',(-163.943345096754,-2.45732663401265,
126.541809114584));
#115194=CARTESIAN_POINT('Ctrl Pts',(-163.951120408956,-2.57486704658424,
126.611751984011));
#115195=CARTESIAN_POINT('Ctrl Pts',(-163.958895721157,-2.68943330620135,
126.686578258821));
#115196=CARTESIAN_POINT('Ctrl Pts',(-163.966661236855,-2.80385521807688,
126.761310256276));
#115197=CARTESIAN_POINT('Ctrl Pts',(-163.974426752554,-2.91531010934181,
126.840913203683));
#115198=CARTESIAN_POINT('Ctrl Pts',(-163.982192268252,-3.02335755442061,
126.925122011779));
#115199=CARTESIAN_POINT('Ctrl Pts',(-163.989948459034,-3.13127525494891,
127.00922970102));
#115200=CARTESIAN_POINT('Ctrl Pts',(-163.997704649816,-3.23579335209254,
127.097931996773));
#115201=CARTESIAN_POINT('Ctrl Pts',(-164.005460840598,-3.3365000523127,
127.19092036437));
#115202=CARTESIAN_POINT('Ctrl Pts',(-164.013211744224,-3.43713810387628,
127.28384534466));
#115203=CARTESIAN_POINT('Ctrl Pts',(-164.02096264785,-3.53396964127995,
127.381050320298));
#115204=CARTESIAN_POINT('Ctrl Pts',(-164.028713551475,-3.62661559769413,
127.482186273998));
#115205=CARTESIAN_POINT('Ctrl Pts',(-164.03646085016,-3.71921846452278,
127.583275189419));
#115206=CARTESIAN_POINT('Ctrl Pts',(-164.044208148844,-3.80763936072918,
127.688291157111));
#115207=CARTESIAN_POINT('Ctrl Pts',(-164.051955447529,-3.89153607157014,
127.796848345576));
#115208=CARTESIAN_POINT('Ctrl Pts',(-164.059700820705,-3.97541193078043,
127.905378553313));
#115209=CARTESIAN_POINT('Ctrl Pts',(-164.067446193881,-4.0547656045305,
128.017447920521));
#115210=CARTESIAN_POINT('Ctrl Pts',(-164.075191567058,-4.1292954327201,
128.132637897706));
#115211=CARTESIAN_POINT('Ctrl Pts',(-164.08293930202,-4.20384798718999,
128.247862999615));
#115212=CARTESIAN_POINT('Ctrl Pts',(-164.090687036983,-4.27357353930711,
128.366210287816));
#115213=CARTESIAN_POINT('Ctrl Pts',(-164.098434771945,-4.33821396565373,
128.487232513488));
#115214=CARTESIAN_POINT('Ctrl Pts',(-164.106183511002,-4.40286276929815,
128.608270423451));
#115215=CARTESIAN_POINT('Ctrl Pts',(-164.113932250058,-4.46242495728391,
128.731983612716));
#115216=CARTESIAN_POINT('Ctrl Pts',(-164.121680989115,-4.51668902184401,
128.857901436783));
#115217=CARTESIAN_POINT('Ctrl Pts',(-164.12943661064,-4.57100128401486,
128.983931101685));
#115218=CARTESIAN_POINT('Ctrl Pts',(-164.137192232166,-4.62000587286779,
129.112168951298));
#115219=CARTESIAN_POINT('Ctrl Pts',(-164.144947853691,-4.66353981952929,
129.242125227439));
#115220=CARTESIAN_POINT('Ctrl Pts',(-164.151648602825,-4.70115254398312,
129.354405642619));
#115221=CARTESIAN_POINT('Ctrl Pts',(-164.158349351959,-4.73468233602094,
129.467968387655));
#115222=CARTESIAN_POINT('Ctrl Pts',(-164.165050101093,-4.76405452823413,
129.582490119309));
#115223=CARTESIAN_POINT('Ctrl Pts',(-162.415078182266,-4.764054528234,129.582490119308));
#115224=CARTESIAN_POINT('Ctrl Pts',(-162.422718977359,-4.7976930599468,
129.71364624392));
#115225=CARTESIAN_POINT('Ctrl Pts',(-162.430359772452,-4.82590149337616,
129.846154608971));
#115226=CARTESIAN_POINT('Ctrl Pts',(-162.438000567544,-4.8485894907432,
129.979519412997));
#115227=CARTESIAN_POINT('Ctrl Pts',(-162.445857233615,-4.87191847901874,
130.116652095938));
#115228=CARTESIAN_POINT('Ctrl Pts',(-162.453713899686,-4.88941039429629,
130.254689879039));
#115229=CARTESIAN_POINT('Ctrl Pts',(-162.461570565758,-4.90102415081955,
130.393087793782));
#115230=CARTESIAN_POINT('Ctrl Pts',(-162.469427231829,-4.91263790734284,
130.531485708525));
#115231=CARTESIAN_POINT('Ctrl Pts',(-162.4772838979,-4.9183735252126,130.670243293803));
#115232=CARTESIAN_POINT('Ctrl Pts',(-162.485140563971,-4.91824798157934,
130.808816421733));
#115233=CARTESIAN_POINT('',(-162.139859435949,-4.91824997172906,130.803833277931));
#115234=CARTESIAN_POINT('Ctrl Pts',(-162.070143404005,-4.764054528234,129.582490119308));
#115235=CARTESIAN_POINT('Ctrl Pts',(-162.07834908068,-4.80003844195155,
129.722790852761));
#115236=CARTESIAN_POINT('Ctrl Pts',(-162.086554757355,-4.8298596052829,
129.864835002293));
#115237=CARTESIAN_POINT('Ctrl Pts',(-162.09476043403,-4.85336043351166,
130.008071998456));
#115238=CARTESIAN_POINT('Ctrl Pts',(-162.102947684613,-4.87680848993161,
130.150987351684));
#115239=CARTESIAN_POINT('Ctrl Pts',(-162.111134935197,-4.89396446228111,
130.295089896159));
#115240=CARTESIAN_POINT('Ctrl Pts',(-162.119322185781,-4.90472132866419,
130.439817409364));
#115241=CARTESIAN_POINT('Ctrl Pts',(-162.126167935837,-4.91371565684435,
130.560830974476));
#115242=CARTESIAN_POINT('Ctrl Pts',(-162.133013685893,-4.91823693878644,
130.682281121578));
#115243=CARTESIAN_POINT('Ctrl Pts',(-162.139859435949,-4.91824997172906,
130.803833277932));
#115244=CARTESIAN_POINT('Ctrl Pts',(-162.139859435994,-4.91824997172915,
130.803833278737));
#115245=CARTESIAN_POINT('Ctrl Pts',(-162.147911968904,-4.9182653021222,
130.946812898396));
#115246=CARTESIAN_POINT('Ctrl Pts',(-162.155964501813,-4.91204141168342,
131.089693691258));
#115247=CARTESIAN_POINT('Ctrl Pts',(-162.164017034723,-4.89963008146219,
131.231921288501));
#115248=CARTESIAN_POINT('Ctrl Pts',(-162.172078033823,-4.88720570234165,
131.374298419563));
#115249=CARTESIAN_POINT('Ctrl Pts',(-162.180139032924,-4.86858093756128,
131.516020642525));
#115250=CARTESIAN_POINT('Ctrl Pts',(-162.188200032025,-4.84385908642783,
131.656541474738));
#115251=CARTESIAN_POINT('Ctrl Pts',(-162.196278020079,-4.81908513277144,
131.797358461549));
#115252=CARTESIAN_POINT('Ctrl Pts',(-162.204356008134,-4.78818846408692,
131.936968655778));
#115253=CARTESIAN_POINT('Ctrl Pts',(-162.212433996188,-4.75132331563071,
132.074836832552));
#115254=CARTESIAN_POINT('Ctrl Pts',(-162.220520646977,-4.71441863344631,
132.212852857449));
#115255=CARTESIAN_POINT('Ctrl Pts',(-162.228607297766,-4.67153280467116,
132.349122809565));
#115256=CARTESIAN_POINT('Ctrl Pts',(-162.236693948555,-4.62286908537536,
132.483129357441));
#115257=CARTESIAN_POINT('Ctrl Pts',(-162.244798880779,-4.5740953523452,
132.617438852994));
#115258=CARTESIAN_POINT('Ctrl Pts',(-162.252903813003,-4.51951774017395,
132.749474392978));
#115259=CARTESIAN_POINT('Ctrl Pts',(-162.261008745228,-4.45938731641086,
132.878739518523));
#115260=CARTESIAN_POINT('Ctrl Pts',(-162.268830176097,-4.40136018681003,
133.00348309629));
#115261=CARTESIAN_POINT('Ctrl Pts',(-162.276651606966,-4.33816233291167,
133.125646591769));
#115262=CARTESIAN_POINT('Ctrl Pts',(-162.284473037835,-4.27005784405416,
133.244809156448));
#115263=CARTESIAN_POINT('Ctrl Pts',(-162.292247371954,-4.20236344641148,
133.363254183683));
#115264=CARTESIAN_POINT('Ctrl Pts',(-162.300021706073,-4.12962985860404,
133.479068072561));
#115265=CARTESIAN_POINT('Ctrl Pts',(-162.307796040192,-4.05208682249319,
133.591792310985));
#115266=CARTESIAN_POINT('Ctrl Pts',(-162.315560793139,-3.97463935124413,
133.70437762686));
#115267=CARTESIAN_POINT('Ctrl Pts',(-162.323325546086,-3.89239444453671,
133.813880549487));
#115268=CARTESIAN_POINT('Ctrl Pts',(-162.331090299033,-3.80562759516828,
133.91986726487));
#115269=CARTESIAN_POINT('Ctrl Pts',(-162.338847339918,-3.71894692385783,
134.025748712753));
#115270=CARTESIAN_POINT('Ctrl Pts',(-162.346604380804,-3.62775349374845,
134.128120602758));
#115271=CARTESIAN_POINT('Ctrl Pts',(-162.354361421689,-3.53236573007361,
134.226578525809));
#115272=CARTESIAN_POINT('Ctrl Pts',(-162.362112612929,-3.43704989905323,
134.324962200975));
#115273=CARTESIAN_POINT('Ctrl Pts',(-162.369863804169,-3.33754630112714,
134.419437504412));
#115274=CARTESIAN_POINT('Ctrl Pts',(-162.377614995409,-3.23421298577117,
134.509633809271));
#115275=CARTESIAN_POINT('Ctrl Pts',(-162.385362892186,-3.13092358983087,
134.599791778295));
#115276=CARTESIAN_POINT('Ctrl Pts',(-162.393110788963,-3.02380800782137,
134.685674109416));
#115277=CARTESIAN_POINT('Ctrl Pts',(-162.40085868574,-2.91326026221623,
134.766947866712));
#115278=CARTESIAN_POINT('Ctrl Pts',(-162.408604961824,-2.80273564081633,
134.848204623289));
#115279=CARTESIAN_POINT('Ctrl Pts',(-162.416351237908,-2.6887805986295,
134.924854492082));
#115280=CARTESIAN_POINT('Ctrl Pts',(-162.424097513992,-2.57182095419476,
134.996605844418));
#115281=CARTESIAN_POINT('Ctrl Pts',(-162.431843847258,-2.45486044639033,
135.068357726407));
#115282=CARTESIAN_POINT('Ctrl Pts',(-162.439590180523,-2.3348956253339,
135.135210815344));
#115283=CARTESIAN_POINT('Ctrl Pts',(-162.447336513788,-2.21237955998207,
135.196917930234));
#115284=CARTESIAN_POINT('Ctrl Pts',(-162.455084581791,-2.08983605800738,
135.258638864004));
#115285=CARTESIAN_POINT('Ctrl Pts',(-162.462832649794,-1.96474052395948,
135.31521135474));
#115286=CARTESIAN_POINT('Ctrl Pts',(-162.470580717797,-1.83756841678319,
135.366435296497));
#115287=CARTESIAN_POINT('Ctrl Pts',(-162.478337020539,-1.71026114957786,
135.417713679668));
#115288=CARTESIAN_POINT('Ctrl Pts',(-162.486093323281,-1.58087326374077,
135.46363201215));
#115289=CARTESIAN_POINT('Ctrl Pts',(-162.493849626023,-1.4498984157629,
135.504039079596));
#115290=CARTESIAN_POINT('Ctrl Pts',(-162.501610068537,-1.3188536625651,
135.54446771351));
#115291=CARTESIAN_POINT('Ctrl Pts',(-162.509370511051,-1.18622063739033,
135.579379121673));
#115292=CARTESIAN_POINT('Ctrl Pts',(-162.517130953565,-1.05250479716914,
135.608672921573));
#115293=CARTESIAN_POINT('Ctrl Pts',(-162.524903853831,-0.918574304410121,
135.638013746482));
#115294=CARTESIAN_POINT('Ctrl Pts',(-162.532676754096,-0.783557908362372,
135.661718874874));
#115295=CARTESIAN_POINT('Ctrl Pts',(-162.540449654362,-0.647968716881717,
135.679739536629));
#115296=CARTESIAN_POINT('Ctrl Pts',(-162.547939990124,-0.517308534038841,
135.697105101938));
#115297=CARTESIAN_POINT('Ctrl Pts',(-162.555430325886,-0.386116784575783,
135.709192286401));
#115298=CARTESIAN_POINT('Ctrl Pts',(-162.562920661648,-0.254852093818049,
135.716003262626));
#115299=CARTESIAN_POINT('Ctrl Pts',(-162.570694995767,-0.118610462414162,
135.723072479086));
#115300=CARTESIAN_POINT('Ctrl Pts',(-162.578469329886,0.0181413231455887,
135.724479887591));
#115301=CARTESIAN_POINT('Ctrl Pts',(-162.586243664005,0.154893322560722,
135.720170939489));
#115302=CARTESIAN_POINT('Ctrl Pts',(-162.594008416952,0.291476787357712,
135.715867301781));
#115303=CARTESIAN_POINT('Ctrl Pts',(-162.601773169899,0.428060078465787,
135.705861336908));
#115304=CARTESIAN_POINT('Ctrl Pts',(-162.609537922847,0.564129305298895,
135.690150337704));
#115305=CARTESIAN_POINT('Ctrl Pts',(-162.617294963732,0.700063386258412,
135.674454942885));
#115306=CARTESIAN_POINT('Ctrl Pts',(-162.625052004617,0.835484033140381,
135.653065834522));
#115307=CARTESIAN_POINT('Ctrl Pts',(-162.632809045502,0.96987888851874,
135.626032319798));
#115308=CARTESIAN_POINT('Ctrl Pts',(-162.640560236742,1.10417239569067,
135.599019191258));
#115309=CARTESIAN_POINT('Ctrl Pts',(-162.648311427982,1.23744126934094,
135.56637020543));
#115310=CARTESIAN_POINT('Ctrl Pts',(-162.656062619222,1.36918015611753,
135.528186266613));
#115311=CARTESIAN_POINT('Ctrl Pts',(-162.663810515999,1.50086305035318,
135.490018556989));
#115312=CARTESIAN_POINT('Ctrl Pts',(-162.671558412776,1.63101687635918,
135.446320681937));
#115313=CARTESIAN_POINT('Ctrl Pts',(-162.679306309553,1.75914854694267,
135.397244183725));
#115314=CARTESIAN_POINT('Ctrl Pts',(-162.687052585637,1.88725341514287,
135.348177951258));
#115315=CARTESIAN_POINT('Ctrl Pts',(-162.694798861721,2.01333660440385,
135.293735473251));
#115316=CARTESIAN_POINT('Ctrl Pts',(-162.702545137805,2.13692259394351,
135.234117370481));
#115317=CARTESIAN_POINT('Ctrl Pts',(-162.710291471071,2.26050949576669,
135.174498827623));
#115318=CARTESIAN_POINT('Ctrl Pts',(-162.718037804336,2.38159880895178,
135.109704753637));
#115319=CARTESIAN_POINT('Ctrl Pts',(-162.725784137601,2.4997376782887,135.039982720899));
#115320=CARTESIAN_POINT('Ctrl Pts',(-162.733532205604,2.61790300400614,
134.970245074396));
#115321=CARTESIAN_POINT('Ctrl Pts',(-162.741280273607,2.73311623445955,
134.895577471814));
#115322=CARTESIAN_POINT('Ctrl Pts',(-162.74902834161,2.84495201767705,134.81627176808));
#115323=CARTESIAN_POINT('Ctrl Pts',(-162.756784644352,2.95690666129596,
134.736881777299));
#115324=CARTESIAN_POINT('Ctrl Pts',(-162.764540947094,3.06547636765766,
134.652844064813));
#115325=CARTESIAN_POINT('Ctrl Pts',(-162.772297249836,3.17026708245786,
134.564492222761));
#115326=CARTESIAN_POINT('Ctrl Pts',(-162.78005769235,3.27511372721801,134.47609322467));
#115327=CARTESIAN_POINT('Ctrl Pts',(-162.787818134864,3.37617707349728,
134.383375773098));
#115328=CARTESIAN_POINT('Ctrl Pts',(-162.795578577378,3.47309945482742,
134.286710864077));
#115329=CARTESIAN_POINT('Ctrl Pts',(-162.803351477644,3.57017742456843,
134.189890779963));
#115330=CARTESIAN_POINT('Ctrl Pts',(-162.811124377909,3.6631008804719,134.089110863031));
#115331=CARTESIAN_POINT('Ctrl Pts',(-162.818897278174,3.75155144352328,
133.98477644401));
#115332=CARTESIAN_POINT('Ctrl Pts',(-162.826387613937,3.83678660581494,
133.884234843923));
#115333=CARTESIAN_POINT('Ctrl Pts',(-162.833877949699,3.91786824155212,
133.780392928005));
#115334=CARTESIAN_POINT('Ctrl Pts',(-162.841368285461,3.99455028042045,
133.673637725078));
#115335=CARTESIAN_POINT('Ctrl Pts',(-162.84914261958,4.07413974209891,133.562834866186));
#115336=CARTESIAN_POINT('Ctrl Pts',(-162.856916953699,4.14924151517748,
133.448542454658));
#115337=CARTESIAN_POINT('Ctrl Pts',(-162.864691287818,4.21953407114073,
133.331160032831));
#115338=CARTESIAN_POINT('Ctrl Pts',(-162.872456040765,4.2897399978106,133.213922274349));
#115339=CARTESIAN_POINT('Ctrl Pts',(-162.880220793712,4.35514830125592,
133.093602414877));
#115340=CARTESIAN_POINT('Ctrl Pts',(-162.887985546659,4.41547893344559,
132.970631341829));
#115341=CARTESIAN_POINT('Ctrl Pts',(-162.895742587544,4.47574964440102,
132.847782405384));
#115342=CARTESIAN_POINT('Ctrl Pts',(-162.903499628429,4.53095254923703,
132.722287844322));
#115343=CARTESIAN_POINT('Ctrl Pts',(-162.911256669314,4.58085218977948,
132.594605371194));
#115344=CARTESIAN_POINT('Ctrl Pts',(-162.919007860554,4.6307142006149,132.467019184412));
#115345=CARTESIAN_POINT('Ctrl Pts',(-162.926759051794,4.67528076565155,
132.337248732303));
#115346=CARTESIAN_POINT('Ctrl Pts',(-162.934510243035,4.71436362270386,
132.205773724193));
#115347=CARTESIAN_POINT('Ctrl Pts',(-162.942258139812,4.75342986849929,
132.074354596469));
#115348=CARTESIAN_POINT('Ctrl Pts',(-162.950006036589,4.78701693077016,
131.941232727657));
#115349=CARTESIAN_POINT('Ctrl Pts',(-162.957753933366,4.81498578064584,
131.806904878274));
#115350=CARTESIAN_POINT('Ctrl Pts',(-162.96550020945,4.84294878004108,131.672605127381));
#115351=CARTESIAN_POINT('Ctrl Pts',(-162.973246485534,4.86529582495158,
131.5371002802));
#115352=CARTESIAN_POINT('Ctrl Pts',(-162.980992761618,4.88193867272042,
131.400898846263));
#115353=CARTESIAN_POINT('Ctrl Pts',(-162.988739094883,4.89858164334296,
131.264696406918));
#115354=CARTESIAN_POINT('Ctrl Pts',(-162.996485428149,4.90952028538173,
131.127797758634));
#115355=CARTESIAN_POINT('Ctrl Pts',(-163.004231761414,4.91471810918807,
130.990717720245));
#115356=CARTESIAN_POINT('Ctrl Pts',(-163.011979829417,4.91991709701101,
130.853606983731));
#115357=CARTESIAN_POINT('Ctrl Pts',(-163.01972789742,4.91937269356245,130.716315166889));
#115358=CARTESIAN_POINT('Ctrl Pts',(-163.027475965423,4.91310053152602,
130.579357885096));
#115359=CARTESIAN_POINT('Ctrl Pts',(-163.035232268164,4.90682170336112,
130.442255043474));
#115360=CARTESIAN_POINT('Ctrl Pts',(-163.042988570906,4.89480297402604,
130.305487838324));
#115361=CARTESIAN_POINT('Ctrl Pts',(-163.050744873648,4.8771120080582,130.169568113393));
#115362=CARTESIAN_POINT('Ctrl Pts',(-163.058505316162,4.8594115998891,130.033575844011));
#115363=CARTESIAN_POINT('Ctrl Pts',(-163.066265758677,4.83603298926077,
129.8984323412));
#115364=CARTESIAN_POINT('Ctrl Pts',(-163.074026201191,4.80709497817862,
129.764639052304));
#115365=CARTESIAN_POINT('Ctrl Pts',(-163.081799101456,4.7781105132321,129.630630986545));
#115366=CARTESIAN_POINT('Ctrl Pts',(-163.089572001722,4.74354891257918,
129.497977844576));
#115367=CARTESIAN_POINT('Ctrl Pts',(-163.097344901987,4.70357910080727,
129.36716657884));
#115368=CARTESIAN_POINT('Ctrl Pts',(-163.104835237749,4.66506229237082,
129.241110632107));
#115369=CARTESIAN_POINT('Ctrl Pts',(-163.112325573511,4.62152375219774,
129.116765263576));
#115370=CARTESIAN_POINT('Ctrl Pts',(-163.119815909273,4.57315609158251,
128.994546697705));
#115371=CARTESIAN_POINT('Ctrl Pts',(-163.127590243392,4.52295455641437,
128.867694177763));
#115372=CARTESIAN_POINT('Ctrl Pts',(-163.135364577511,4.46739145647812,
128.742731088901));
#115373=CARTESIAN_POINT('Ctrl Pts',(-163.143138911631,4.4066291440415,128.620143904558));
#115374=CARTESIAN_POINT('Ctrl Pts',(-163.150903664578,4.3459417157248,128.497707797964));
#115375=CARTESIAN_POINT('Ctrl Pts',(-163.158668417525,4.28006799601437,
128.377642116796));
#115376=CARTESIAN_POINT('Ctrl Pts',(-163.166433170472,4.20921912989351,
128.260415378564));
#115377=CARTESIAN_POINT('Ctrl Pts',(-163.174190211357,4.13844063186508,
128.143305071582));
#115378=CARTESIAN_POINT('Ctrl Pts',(-163.181947252242,4.06269702192301,
128.029028428687));
#115379=CARTESIAN_POINT('Ctrl Pts',(-163.189704293127,3.98224611570434,
127.918030952324));
#115380=CARTESIAN_POINT('Ctrl Pts',(-163.197455484367,3.90185587813976,
127.807117180021));
#115381=CARTESIAN_POINT('Ctrl Pts',(-163.205206675607,3.81676563849148,
127.69947796748));
#115382=CARTESIAN_POINT('Ctrl Pts',(-163.212957866847,3.72727722949177,
127.595530999619));
#115383=CARTESIAN_POINT('Ctrl Pts',(-163.220705763624,3.63782685545318,
127.491628211993));
#115384=CARTESIAN_POINT('Ctrl Pts',(-163.228453660401,3.54398228458119,
127.391414843494));
#115385=CARTESIAN_POINT('Ctrl Pts',(-163.236201557179,3.44608630706758,
127.295276374243));
#115386=CARTESIAN_POINT('Ctrl Pts',(-163.243947833263,3.34821080728209,
127.199158015087));
#115387=CARTESIAN_POINT('Ctrl Pts',(-163.251694109347,3.24628586528319,
127.107113133511));
#115388=CARTESIAN_POINT('Ctrl Pts',(-163.259440385431,3.14069160722997,
127.019490832385));
#115389=CARTESIAN_POINT('Ctrl Pts',(-163.267186718696,3.03509656970406,
126.931867884451));
#115390=CARTESIAN_POINT('Ctrl Pts',(-163.274933051962,2.92583246294526,
126.848667831773));
#115391=CARTESIAN_POINT('Ctrl Pts',(-163.282679385227,2.8133126950708,126.770199646279));
#115392=CARTESIAN_POINT('Ctrl Pts',(-163.29042745323,2.70076772917464,126.691713888379));
#115393=CARTESIAN_POINT('Ctrl Pts',(-163.298175521233,2.58496597199776,
126.617962329877));
#115394=CARTESIAN_POINT('Ctrl Pts',(-163.305923589236,2.46634967520674,
126.549210521258));
#115395=CARTESIAN_POINT('Ctrl Pts',(-163.313679891978,2.34760731160378,
126.480385642399));
#115396=CARTESIAN_POINT('Ctrl Pts',(-163.32143619472,2.2260447716833,126.416571324669));
#115397=CARTESIAN_POINT('Ctrl Pts',(-163.329192497461,2.10212925842015,
126.357987304022));
#115398=CARTESIAN_POINT('Ctrl Pts',(-163.336952939976,1.97814760771621,
126.29937201532));
#115399=CARTESIAN_POINT('Ctrl Pts',(-163.34471338249,1.85181084123913,126.245992738225));
#115400=CARTESIAN_POINT('Ctrl Pts',(-163.352473825004,1.72360505622879,
126.198020565785));
#115401=CARTESIAN_POINT('Ctrl Pts',(-163.36024672527,1.59519346391078,126.149971384155));
#115402=CARTESIAN_POINT('Ctrl Pts',(-163.368019625535,1.46490722927346,
126.107346774152));
#115403=CARTESIAN_POINT('Ctrl Pts',(-163.3757925258,1.33324734706282,126.070267824427));
#115404=CARTESIAN_POINT('Ctrl Pts',(-163.383282861563,1.2063736332007,126.03453678792));
#115405=CARTESIAN_POINT('Ctrl Pts',(-163.390773197325,1.07822470856052,
126.003955285848));
#115406=CARTESIAN_POINT('Ctrl Pts',(-163.398263533087,0.949254865675583,
125.978586248359));
#115407=CARTESIAN_POINT('Ctrl Pts',(-163.406037867206,0.815395091999074,
125.952255336104));
#115408=CARTESIAN_POINT('Ctrl Pts',(-163.413812201325,0.680226893481132,
125.931456543786));
#115409=CARTESIAN_POINT('Ctrl Pts',(-163.421586535444,0.544247309369959,
125.916316230621));
#115410=CARTESIAN_POINT('Ctrl Pts',(-163.429351288391,0.408435307944097,
125.901194576539));
#115411=CARTESIAN_POINT('Ctrl Pts',(-163.437116041338,0.271814295381725,
125.891717569133));
#115412=CARTESIAN_POINT('Ctrl Pts',(-163.444880794285,0.134892577755928,
125.887960811309));
#115413=CARTESIAN_POINT('Ctrl Pts',(-163.45263783517,-0.00189314729040985,
125.884207784749));
#115414=CARTESIAN_POINT('Ctrl Pts',(-163.460394876055,-0.138978594755176,
125.886163712117));
#115415=CARTESIAN_POINT('Ctrl Pts',(-163.46815191694,-0.275849595165583,
125.893852490768));
#115416=CARTESIAN_POINT('Ctrl Pts',(-163.475903108181,-0.412617380089693,
125.901535471252));
#115417=CARTESIAN_POINT('Ctrl Pts',(-163.483654299421,-0.549170651075375,
125.914942676137));
#115418=CARTESIAN_POINT('Ctrl Pts',(-163.491405490661,-0.684994850008131,
125.934045933897));
#115419=CARTESIAN_POINT('Ctrl Pts',(-163.499153387438,-0.820761320032926,
125.953141072263));
#115420=CARTESIAN_POINT('Ctrl Pts',(-163.506901284215,-0.955798947978522,
125.977927394033));
#115421=CARTESIAN_POINT('Ctrl Pts',(-163.514649180992,-1.08959813203073,
126.00832486153));
#115422=CARTESIAN_POINT('Ctrl Pts',(-163.522395457076,-1.22336932817801,
126.038715970533));
#115423=CARTESIAN_POINT('Ctrl Pts',(-163.53014173316,-1.35590221469952,
126.074715804088));
#115424=CARTESIAN_POINT('Ctrl Pts',(-163.537888009244,-1.48669761399013,
126.116193249921));
#115425=CARTESIAN_POINT('Ctrl Pts',(-163.54563434251,-1.61749397878356,
126.157671001931));
#115426=CARTESIAN_POINT('Ctrl Pts',(-163.553380675775,-1.74655245807792,
126.204626328721));
#115427=CARTESIAN_POINT('Ctrl Pts',(-163.56112700904,-1.87338964785375,
126.256878425208));
#115428=CARTESIAN_POINT('Ctrl Pts',(-163.568875077043,-2.00025524193726,
126.309142223189));
#115429=CARTESIAN_POINT('Ctrl Pts',(-163.576623145046,-2.12489819522684,
126.366705002326));
#115430=CARTESIAN_POINT('Ctrl Pts',(-163.584371213049,-2.24685604474934,
126.429338220289));
#115431=CARTESIAN_POINT('Ctrl Pts',(-163.592127515791,-2.36894351252647,
126.492038005583));
#115432=CARTESIAN_POINT('Ctrl Pts',(-163.599883818533,-2.4883398275059,
126.559818815763));
#115433=CARTESIAN_POINT('Ctrl Pts',(-163.607640121275,-2.60460758498512,
126.632406352388));
#115434=CARTESIAN_POINT('Ctrl Pts',(-163.615400563789,-2.72093739806726,
126.705032631166));
#115435=CARTESIAN_POINT('Ctrl Pts',(-163.623161006303,-2.83413500389475,
126.782470527716));
#115436=CARTESIAN_POINT('Ctrl Pts',(-163.630921448817,-2.9437937096095,
126.864403554632));
#115437=CARTESIAN_POINT('Ctrl Pts',(-163.638694349083,-3.05362844921401,
126.946468107717));
#115438=CARTESIAN_POINT('Ctrl Pts',(-163.646467249348,-3.15991263304063,
127.033041963945));
#115439=CARTESIAN_POINT('Ctrl Pts',(-163.654240149614,-3.26227358588143,
127.123769073621));
#115440=CARTESIAN_POINT('Ctrl Pts',(-163.661730485376,-3.36091346025397,
127.211198024331));
#115441=CARTESIAN_POINT('Ctrl Pts',(-163.669220821137,-3.45591016803856,
127.302483295131));
#115442=CARTESIAN_POINT('Ctrl Pts',(-163.676711156899,-3.5469652081078,
127.397276692129));
#115443=CARTESIAN_POINT('Ctrl Pts',(-163.684385792604,-3.64026066025408,
127.494402483591));
#115444=CARTESIAN_POINT('Ctrl Pts',(-163.69206042831,-3.72973008599226,
127.595536548972));
#115445=CARTESIAN_POINT('Ctrl Pts',(-163.699735064015,-3.81500258888229,
127.70034091574));
#115446=CARTESIAN_POINT('Ctrl Pts',(-163.707400651281,-3.9001745550129,
127.805021717572));
#115447=CARTESIAN_POINT('Ctrl Pts',(-163.715066238548,-3.98115918533349,
127.913363909036));
#115448=CARTESIAN_POINT('Ctrl Pts',(-163.722731825814,-4.05762167876876,
128.024992096753));
#115449=CARTESIAN_POINT('Ctrl Pts',(-163.730390138672,-4.13401161163089,
128.136514352726));
#115450=CARTESIAN_POINT('Ctrl Pts',(-163.73804845153,-4.20588771635221,
128.251316074298));
#115451=CARTESIAN_POINT('Ctrl Pts',(-163.745706764389,-4.27295518551259,
128.368988562807));
#115452=CARTESIAN_POINT('Ctrl Pts',(-163.753359100149,-4.33997031039783,
128.486569211245));
#115453=CARTESIAN_POINT('Ctrl Pts',(-163.761011435909,-4.40218407095881,
128.607015819636));
#115454=CARTESIAN_POINT('Ctrl Pts',(-163.768663771669,-4.45934511343825,
128.72989099336));
#115455=CARTESIAN_POINT('Ctrl Pts',(-163.776312712522,-4.51648079681339,
128.852711654356));
#115456=CARTESIAN_POINT('Ctrl Pts',(-163.783961653376,-4.5685680526837,
128.977958373579));
#115457=CARTESIAN_POINT('Ctrl Pts',(-163.79161059423,-4.61540178522491,
129.105169803254));
#115458=CARTESIAN_POINT('Ctrl Pts',(-163.799258355588,-4.66222829582559,
129.23236161644));
#115459=CARTESIAN_POINT('Ctrl Pts',(-163.806906116946,-4.70380275481576,
129.361517161017));
#115460=CARTESIAN_POINT('Ctrl Pts',(-163.814553878304,-4.73996863624117,
129.492156216586));
#115461=CARTESIAN_POINT('Ctrl Pts',(-163.816312158077,-4.74828345345535,
129.522191150764));
#115462=CARTESIAN_POINT('Ctrl Pts',(-163.81807043785,-4.756312593584,129.552304433608));
#115463=CARTESIAN_POINT('Ctrl Pts',(-163.819828717624,-4.76405452823398,
129.582490119308));
#115464=CARTESIAN_POINT('Origin',(213.235140564004,0.,130.804360617566));
#115465=CARTESIAN_POINT('',(-165.915373126199,-4.76405452823409,129.582490119308));
#115466=CARTESIAN_POINT('',(-165.569765327751,-4.76405452823417,129.582490119309));
#115467=CARTESIAN_POINT('',(213.235140564004,-4.76405452823405,129.582490119308));
#115468=CARTESIAN_POINT('',(-164.235140564046,-4.91824950131384,130.802145820462));
#115469=CARTESIAN_POINT('Ctrl Pts',(-164.235140564046,-4.91824950131383,
130.802145820462));
#115470=CARTESIAN_POINT('Ctrl Pts',(-164.242830418784,-4.91831032367823,
130.937209914078));
#115471=CARTESIAN_POINT('Ctrl Pts',(-164.250520273522,-4.91280328631858,
131.072501252631));
#115472=CARTESIAN_POINT('Ctrl Pts',(-164.25821012826,-4.90169851106774,
131.207516628431));
#115473=CARTESIAN_POINT('Ctrl Pts',(-164.265891010091,-4.89060669342265,
131.342374461554));
#115474=CARTESIAN_POINT('Ctrl Pts',(-164.273571891923,-4.87393016165421,
131.476956577464));
#115475=CARTESIAN_POINT('Ctrl Pts',(-164.281252773754,-4.85169102683561,
131.610758312641));
#115476=CARTESIAN_POINT('Ctrl Pts',(-164.288926625913,-4.82947224564739,
131.744437590219));
#115477=CARTESIAN_POINT('Ctrl Pts',(-164.296600478073,-4.8017010543568,
131.877337515657));
#115478=CARTESIAN_POINT('Ctrl Pts',(-164.304274330232,-4.76845144967642,
132.008957576959));
#115479=CARTESIAN_POINT('Ctrl Pts',(-164.31211560948,-4.73447640953122,
132.143449307301));
#115480=CARTESIAN_POINT('Ctrl Pts',(-164.319956888727,-4.69478115867656,
132.276604255187));
#115481=CARTESIAN_POINT('Ctrl Pts',(-164.327798167975,-4.64950010821961,
132.407897896885));
#115482=CARTESIAN_POINT('Ctrl Pts',(-164.335464631022,-4.60522856921845,
132.536264432563));
#115483=CARTESIAN_POINT('Ctrl Pts',(-164.343131094069,-4.55561782055014,
132.662851388063));
#115484=CARTESIAN_POINT('Ctrl Pts',(-164.350797557115,-4.50084403328383,
132.787183365709));
#115485=CARTESIAN_POINT('Ctrl Pts',(-164.358463256884,-4.44607569932835,
132.911502964789));
#115486=CARTESIAN_POINT('Ctrl Pts',(-164.366128956653,-4.38614551016219,
133.033567666439));
#115487=CARTESIAN_POINT('Ctrl Pts',(-164.373794656422,-4.32127757200678,
133.152922562283));
#115488=CARTESIAN_POINT('Ctrl Pts',(-164.381461337856,-4.25640132690476,
133.272292742637));
#115489=CARTESIAN_POINT('Ctrl Pts',(-164.389128019289,-4.18658626648107,
133.388952075709));
#115490=CARTESIAN_POINT('Ctrl Pts',(-164.396794700723,-4.11210193200325,
133.502471208946));
#115491=CARTESIAN_POINT('Ctrl Pts',(-164.404767228344,-4.03464620110701,
133.620518950087));
#115492=CARTESIAN_POINT('Ctrl Pts',(-164.412739755965,-3.95214119226765,
133.7351703593));
#115493=CARTESIAN_POINT('Ctrl Pts',(-164.420712283587,-3.86493818351943,
133.845977934073));
#115494=CARTESIAN_POINT('Ctrl Pts',(-164.428390330897,-3.7809561820072,
133.952692622542));
#115495=CARTESIAN_POINT('Ctrl Pts',(-164.436068378207,-3.69261737648841,
134.055842119024));
#115496=CARTESIAN_POINT('Ctrl Pts',(-164.443746425517,-3.60027453263862,
134.155062984553));
#115497=CARTESIAN_POINT('Ctrl Pts',(-164.451429694675,-3.50786888632366,
134.254351330298));
#115498=CARTESIAN_POINT('Ctrl Pts',(-164.459112963834,-3.41145406407904,
134.34970544625));
#115499=CARTESIAN_POINT('Ctrl Pts',(-164.466796232992,-3.31141737594062,
134.440800913352));
#115500=CARTESIAN_POINT('Ctrl Pts',(-164.474489977799,-3.21124429413058,
134.532020583339));
#115501=CARTESIAN_POINT('Ctrl Pts',(-164.482183722607,-3.10743979991024,
134.618969766111));
#115502=CARTESIAN_POINT('Ctrl Pts',(-164.489877467415,-3.00042183492989,
134.701366118585));
#115503=CARTESIAN_POINT('Ctrl Pts',(-164.490739989003,-2.98842438668954,
134.710603315108));
#115504=CARTESIAN_POINT('Ctrl Pts',(-164.491602510591,-2.9763865785575,
134.719783338642));
#115505=CARTESIAN_POINT('Ctrl Pts',(-164.492465032179,-2.96430901914137,
134.728905827082));
#115506=CARTESIAN_POINT('Ctrl Pts',(-164.500239366298,-2.85544799636351,
134.811131332058));
#115507=CARTESIAN_POINT('Ctrl Pts',(-164.508013700417,-2.74299073370207,
134.888954180419));
#115508=CARTESIAN_POINT('Ctrl Pts',(-164.515788034536,-2.62732894263834,
134.962043348328));
#115509=CARTESIAN_POINT('Ctrl Pts',(-164.523552787484,-2.5118096943948,
135.035042440369));
#115510=CARTESIAN_POINT('Ctrl Pts',(-164.531317540431,-2.39309410300142,
135.103319252709));
#115511=CARTESIAN_POINT('Ctrl Pts',(-164.539082293378,-2.27160621140658,
135.166583477852));
#115512=CARTESIAN_POINT('Ctrl Pts',(-164.546839334263,-2.15023898329835,
135.229784868075));
#115513=CARTESIAN_POINT('Ctrl Pts',(-164.554596375148,-2.0261052790745,
135.287983399277));
#115514=CARTESIAN_POINT('Ctrl Pts',(-164.562353416033,-1.89965702912835,
135.340932697252));
#115515=CARTESIAN_POINT('Ctrl Pts',(-164.570104607273,-1.77330413479162,
135.393842065749));
#115516=CARTESIAN_POINT('Ctrl Pts',(-164.577855798513,-1.64464052804457,
135.44150992975));
#115517=CARTESIAN_POINT('Ctrl Pts',(-164.585606989753,-1.51414126229552,
135.483736569583));
#115518=CARTESIAN_POINT('Ctrl Pts',(-164.59335488653,-1.38369746221506,
135.525945261968));
#115519=CARTESIAN_POINT('Ctrl Pts',(-164.601102783307,-1.25141992609663,
135.562717209789));
#115520=CARTESIAN_POINT('Ctrl Pts',(-164.608850680084,-1.1178019350934,
135.59390150333));
#115521=CARTESIAN_POINT('Ctrl Pts',(-164.616596956168,-0.984211894093428,
135.625079273788));
#115522=CARTESIAN_POINT('Ctrl Pts',(-164.624343232252,-0.849282336420786,
135.650671626007));
#115523=CARTESIAN_POINT('Ctrl Pts',(-164.632089508336,-0.713519507588329,
135.670578139912));
#115524=CARTESIAN_POINT('Ctrl Pts',(-164.639835841602,-0.577755676586065,
135.690484800763));
#115525=CARTESIAN_POINT('Ctrl Pts',(-164.647582174867,-0.441158948979083,
135.704705482831));
#115526=CARTESIAN_POINT('Ctrl Pts',(-164.655328508132,-0.304243119693164,
135.713191352743));
#115527=CARTESIAN_POINT('Ctrl Pts',(-164.663076576135,-0.167296629056397,
135.721679123007));
#115528=CARTESIAN_POINT('Ctrl Pts',(-164.670824644138,-0.0300312846841078,
135.724429501382));
#115529=CARTESIAN_POINT('Ctrl Pts',(-164.678572712141,0.107037071390386,
135.721445742703));
#115530=CARTESIAN_POINT('Ctrl Pts',(-164.686329014883,0.244251105345036,
135.718458812851));
#115531=CARTESIAN_POINT('Ctrl Pts',(-164.694085317625,0.381267341283862,
135.709725580428));
#115532=CARTESIAN_POINT('Ctrl Pts',(-164.701841620367,0.517572459097017,
135.695301407648));
#115533=CARTESIAN_POINT('Ctrl Pts',(-164.709602062881,0.653950327055988,
135.680869536252));
#115534=CARTESIAN_POINT('Ctrl Pts',(-164.717362505395,0.789615934071009,
135.660740729522));
#115535=CARTESIAN_POINT('Ctrl Pts',(-164.725122947909,0.924065126279789,
135.635021721897));
#115536=CARTESIAN_POINT('Ctrl Pts',(-164.732895848174,1.05873014826737,
135.609261427837));
#115537=CARTESIAN_POINT('Ctrl Pts',(-164.74066874844,1.19217447252728,135.577893089714));
#115538=CARTESIAN_POINT('Ctrl Pts',(-164.748441648705,1.32390723312391,
135.541073897952));
#115539=CARTESIAN_POINT('Ctrl Pts',(-164.755931984467,1.45085117605698,
135.505593176552));
#115540=CARTESIAN_POINT('Ctrl Pts',(-164.763422320229,1.57620554110669,
135.465051120391));
#115541=CARTESIAN_POINT('Ctrl Pts',(-164.770912655991,1.69954960153836,
135.419630297055));
#115542=CARTESIAN_POINT('Ctrl Pts',(-164.77868699011,1.82757028951183,135.372487329397));
#115543=CARTESIAN_POINT('Ctrl Pts',(-164.786461324229,1.95383075328559,
135.319938999833));
#115544=CARTESIAN_POINT('Ctrl Pts',(-164.794235658348,2.07784076350627,
135.262135939855));
#115545=CARTESIAN_POINT('Ctrl Pts',(-164.802000411295,2.20169794247211,
135.204404116984));
#115546=CARTESIAN_POINT('Ctrl Pts',(-164.809765164243,2.32330983533017,
135.141430612568));
#115547=CARTESIAN_POINT('Ctrl Pts',(-164.81752991719,2.44220299259232,135.073415267658));
#115548=CARTESIAN_POINT('Ctrl Pts',(-164.825286958075,2.56097806349458,
135.005467476548));
#115549=CARTESIAN_POINT('Ctrl Pts',(-164.83304399896,2.67703943533007,134.932488003229));
#115550=CARTESIAN_POINT('Ctrl Pts',(-164.840801039845,2.789935547084,134.854723898263));
#115551=CARTESIAN_POINT('Ctrl Pts',(-164.848552231085,2.90274652300201,
134.777018435813));
#115552=CARTESIAN_POINT('Ctrl Pts',(-164.856303422325,3.01239666924048,
134.694535744359));
#115553=CARTESIAN_POINT('Ctrl Pts',(-164.864054613565,3.11846117801212,
134.607567546426));
#115554=CARTESIAN_POINT('Ctrl Pts',(-164.871802510342,3.2244806065383,134.520636312297));
#115555=CARTESIAN_POINT('Ctrl Pts',(-164.879550407119,3.32691712700626,
134.429223610869));
#115556=CARTESIAN_POINT('Ctrl Pts',(-164.887298303896,3.42537714428523,
134.333662883157));
#115557=CARTESIAN_POINT('Ctrl Pts',(-164.89504457998,3.52381656585087,134.23812214469));
#115558=CARTESIAN_POINT('Ctrl Pts',(-164.902790856064,3.61828085834464,
134.138435377919));
#115559=CARTESIAN_POINT('Ctrl Pts',(-164.910537132148,3.70841189745059,
134.03497422203));
#115560=CARTESIAN_POINT('Ctrl Pts',(-164.918283465414,3.79854360188352,
133.931512302413));
#115561=CARTESIAN_POINT('Ctrl Pts',(-164.926029798679,3.88434173229034,
133.824276232875));
#115562=CARTESIAN_POINT('Ctrl Pts',(-164.933776131944,3.96548748506379,
133.713671888005));
#115563=CARTESIAN_POINT('Ctrl Pts',(-164.941524199947,4.04665140986583,
133.603042774059));
#115564=CARTESIAN_POINT('Ctrl Pts',(-164.94927226795,4.1231606526135,133.489044198976));
#115565=CARTESIAN_POINT('Ctrl Pts',(-164.957020335953,4.19473912647206,
133.372111914585));
#115566=CARTESIAN_POINT('Ctrl Pts',(-164.964776638695,4.26639367478452,
133.255055353171));
#115567=CARTESIAN_POINT('Ctrl Pts',(-164.972532941437,4.33310678134179,
133.135059187929));
#115568=CARTESIAN_POINT('Ctrl Pts',(-164.980289244179,4.39464756188375,
133.012585214234));
#115569=CARTESIAN_POINT('Ctrl Pts',(-164.988049686693,4.45622118859342,
132.890045872491));
#115570=CARTESIAN_POINT('Ctrl Pts',(-164.995810129207,4.51261682782236,
132.765026443349));
#115571=CARTESIAN_POINT('Ctrl Pts',(-165.003570571721,4.56365177080036,
132.638008778302));
#115572=CARTESIAN_POINT('Ctrl Pts',(-165.011343471987,4.61476863959937,
132.510787213223));
#115573=CARTESIAN_POINT('Ctrl Pts',(-165.019116372252,4.66050748516016,
132.381561370914));
#115574=CARTESIAN_POINT('Ctrl Pts',(-165.026889272517,4.70073523121121,
132.250829196053));
#115575=CARTESIAN_POINT('Ctrl Pts',(-165.03437960828,4.7395005973667,132.124849465039));
#115576=CARTESIAN_POINT('Ctrl Pts',(-165.041869944042,4.77314851356853,
131.997471315848));
#115577=CARTESIAN_POINT('Ctrl Pts',(-165.049360279804,4.80160516602204,
131.86914740004));
#115578=CARTESIAN_POINT('Ctrl Pts',(-165.057134613923,4.83114076110182,
131.735958043963));
#115579=CARTESIAN_POINT('Ctrl Pts',(-165.064908948042,4.8551772279464,131.601327884214));
#115580=CARTESIAN_POINT('Ctrl Pts',(-165.072683282161,4.87357631615702,
131.465750784633));
#115581=CARTESIAN_POINT('Ctrl Pts',(-165.080448035108,4.89195272913579,
131.330340771711));
#115582=CARTESIAN_POINT('Ctrl Pts',(-165.088212788056,4.90470553499386,
131.193986524671));
#115583=CARTESIAN_POINT('Ctrl Pts',(-165.095977541003,4.91174695465368,
131.057194388946));
#115584=CARTESIAN_POINT('Ctrl Pts',(-165.103734581888,4.91878138067624,
130.920538117098));
#115585=CARTESIAN_POINT('Ctrl Pts',(-165.111491622773,4.92011568932038,
130.783445209992));
#115586=CARTESIAN_POINT('Ctrl Pts',(-165.119248663658,4.91571365146245,
130.64642911556));
#115587=CARTESIAN_POINT('Ctrl Pts',(-165.126999854898,4.91131493321552,
130.509516346032));
#115588=CARTESIAN_POINT('Ctrl Pts',(-165.134751046138,4.90118849125952,
130.372680663065));
#115589=CARTESIAN_POINT('Ctrl Pts',(-165.142502237378,4.8853501410317,130.236437152633));
#115590=CARTESIAN_POINT('Ctrl Pts',(-165.150250134155,4.86951852252524,
130.100251549327));
#115591=CARTESIAN_POINT('Ctrl Pts',(-165.157998030932,4.84797986933509,
129.964658005503));
#115592=CARTESIAN_POINT('Ctrl Pts',(-165.165745927709,4.82080196704985,
129.830167896905));
#115593=CARTESIAN_POINT('Ctrl Pts',(-165.173492203793,4.79362974979589,
129.695705920739));
#115594=CARTESIAN_POINT('Ctrl Pts',(-165.181238479878,4.76082070714668,
129.562347303671));
#115595=CARTESIAN_POINT('Ctrl Pts',(-165.188984755962,4.72249393473421,
129.43059422589));
#115596=CARTESIAN_POINT('Ctrl Pts',(-165.196731089227,4.68416687940215,
129.298840175537));
#115597=CARTESIAN_POINT('Ctrl Pts',(-165.204477422492,4.64032212223626,
129.168692063524));
#115598=CARTESIAN_POINT('Ctrl Pts',(-165.212223755758,4.59112881588843,
129.040637493485));
#115599=CARTESIAN_POINT('Ctrl Pts',(-165.219971823761,4.54192449304066,
128.912554246512));
#115600=CARTESIAN_POINT('Ctrl Pts',(-165.227719891764,4.48736937776267,
128.786565839331));
#115601=CARTESIAN_POINT('Ctrl Pts',(-165.235467959767,4.42768084873182,
128.663140086123));
#115602=CARTESIAN_POINT('Ctrl Pts',(-165.243224262508,4.36792888202211,
128.539583154555));
#115603=CARTESIAN_POINT('Ctrl Pts',(-165.25098056525,4.30303277338795,128.418594670212));
#115604=CARTESIAN_POINT('Ctrl Pts',(-165.258736867992,4.23325624577473,
128.300618494242));
#115605=CARTESIAN_POINT('Ctrl Pts',(-165.266497310506,4.1634424763278,128.182579350833));
#115606=CARTESIAN_POINT('Ctrl Pts',(-165.27425775302,4.08874331039939,128.067556047122));
#115607=CARTESIAN_POINT('Ctrl Pts',(-165.282018195535,4.00946538474539,
127.955962753673));
#115608=CARTESIAN_POINT('Ctrl Pts',(-165.2897910958,3.93006019512716,127.844190320763));
#115609=CARTESIAN_POINT('Ctrl Pts',(-165.297563996066,3.84606179738503,
127.735859210317));
#115610=CARTESIAN_POINT('Ctrl Pts',(-165.305336896331,3.75781719550393,
127.631350534431));
#115611=CARTESIAN_POINT('Ctrl Pts',(-165.312827232093,3.67278050717643,
127.530641012156));
#115612=CARTESIAN_POINT('Ctrl Pts',(-165.320317567855,3.58380118333138,
127.433481066278));
#115613=CARTESIAN_POINT('Ctrl Pts',(-165.327807903617,3.49122015438542,
127.340177467657));
#115614=CARTESIAN_POINT('Ctrl Pts',(-165.335582237736,3.39512888758716,
127.243336234735));
#115615=CARTESIAN_POINT('Ctrl Pts',(-165.343356571855,3.294853018719,127.150342784561));
#115616=CARTESIAN_POINT('Ctrl Pts',(-165.351130905974,3.19073332169938,
127.061580376582));
#115617=CARTESIAN_POINT('Ctrl Pts',(-165.358895658921,3.0867419429006,126.972927360338));
#115618=CARTESIAN_POINT('Ctrl Pts',(-165.366660411868,2.97891645618367,
126.888495262429));
#115619=CARTESIAN_POINT('Ctrl Pts',(-165.374425164816,2.86763541756558,
126.808631625952));
#115620=CARTESIAN_POINT('Ctrl Pts',(-165.382182205701,2.75646490484384,
126.728847311165));
#115621=CARTESIAN_POINT('Ctrl Pts',(-165.389939246586,2.64184598583662,
126.653622654542));
#115622=CARTESIAN_POINT('Ctrl Pts',(-165.397696287471,2.52419105610616,
126.58326566782));
#115623=CARTESIAN_POINT('Ctrl Pts',(-165.405447478711,2.40662485087423,
126.512961737849));
#115624=CARTESIAN_POINT('Ctrl Pts',(-165.413198669951,2.28602752617753,
126.447518371222));
#115625=CARTESIAN_POINT('Ctrl Pts',(-165.420949861191,2.16284098706366,
126.387200678513));
#115626=CARTESIAN_POINT('Ctrl Pts',(-165.428697757968,2.03970680551417,
126.326908622432));
#115627=CARTESIAN_POINT('Ctrl Pts',(-165.436445654745,1.91398594872568,
126.271738078873));
#115628=CARTESIAN_POINT('Ctrl Pts',(-165.444193551522,1.78614529136175,
126.221908428983));
#115629=CARTESIAN_POINT('Ctrl Pts',(-165.451939827606,1.65833137550742,
126.172089202382));
#115630=CARTESIAN_POINT('Ctrl Pts',(-165.459686103691,1.52839890509849,
126.127608789172));
#115631=CARTESIAN_POINT('Ctrl Pts',(-165.467432379775,1.39683475264722,
126.088638431485));
#115632=CARTESIAN_POINT('Ctrl Pts',(-165.47517871304,1.26526962901908,126.049667786127));
#115633=CARTESIAN_POINT('Ctrl Pts',(-165.482925046305,1.13207317417998,
126.016207388491));
#115634=CARTESIAN_POINT('Ctrl Pts',(-165.490671379571,0.997747054017446,
125.988378487336));
#115635=CARTESIAN_POINT('Ctrl Pts',(-165.498419447574,0.863390852452566,
125.960543354091));
#115636=CARTESIAN_POINT('Ctrl Pts',(-165.506167515577,0.72790486492431,
125.938342306136));
#115637=CARTESIAN_POINT('Ctrl Pts',(-165.51391558358,0.591800175237199,
125.921845321626));
#115638=CARTESIAN_POINT('Ctrl Pts',(-165.521671886321,0.455550831865665,
125.905330803924));
#115639=CARTESIAN_POINT('Ctrl Pts',(-165.529428189063,0.318681861523744,
125.894532506976));
#115640=CARTESIAN_POINT('Ctrl Pts',(-165.537184491805,0.181709245859055,
125.889468470991));
#115641=CARTESIAN_POINT('Ctrl Pts',(-165.544944934319,0.0446635237848468,
125.884401732176));
#115642=CARTESIAN_POINT('Ctrl Pts',(-165.552705376834,-0.0924855630699909,
125.885075350806));
#115643=CARTESIAN_POINT('Ctrl Pts',(-165.560465819348,-0.229223816622113,
125.891455213999));
#115644=CARTESIAN_POINT('Ctrl Pts',(-165.568238719613,-0.366181574557515,
125.897845318716));
#115645=CARTESIAN_POINT('Ctrl Pts',(-165.576011619879,-0.5027267916273,
125.909959938364));
#115646=CARTESIAN_POINT('Ctrl Pts',(-165.583784520144,-0.638351263300149,
125.927713129061));
#115647=CARTESIAN_POINT('Ctrl Pts',(-165.591274855906,-0.769045443809156,
125.944820946559));
#115648=CARTESIAN_POINT('Ctrl Pts',(-165.598765191668,-0.898884355967715,
125.967164447724));
#115649=CARTESIAN_POINT('Ctrl Pts',(-165.60625552743,-1.02742562354542,
125.994622615285));
#115650=CARTESIAN_POINT('Ctrl Pts',(-165.614029861549,-1.16084057235355,
126.023121867616));
#115651=CARTESIAN_POINT('Ctrl Pts',(-165.621804195668,-1.2932801521932,
126.057221564745));
#115652=CARTESIAN_POINT('Ctrl Pts',(-165.629578529787,-1.42423771941209,
126.096842165015));
#115653=CARTESIAN_POINT('Ctrl Pts',(-165.637343282734,-1.55503389313304,
126.136413936437));
#115654=CARTESIAN_POINT('Ctrl Pts',(-165.645108035681,-1.68435131769941,
126.1814929609));
#115655=CARTESIAN_POINT('Ctrl Pts',(-165.652872788628,-1.81169297648574,
126.231948604038));
#115656=CARTESIAN_POINT('Ctrl Pts',(-165.660629829513,-1.93890815774136,
126.282354133921));
#115657=CARTESIAN_POINT('Ctrl Pts',(-165.668386870398,-2.06415111727719,
126.338125512288));
#115658=CARTESIAN_POINT('Ctrl Pts',(-165.676143911283,-2.18693980622018,
126.399082266943));
#115659=CARTESIAN_POINT('Ctrl Pts',(-165.683895102523,-2.30963589925718,
126.459993053634));
#115660=CARTESIAN_POINT('Ctrl Pts',(-165.691646293764,-2.42988105680503,
126.52608126019));
#115661=CARTESIAN_POINT('Ctrl Pts',(-165.699397485004,-2.54721337335625,
126.597118398119));
#115662=CARTESIAN_POINT('Ctrl Pts',(-165.707145381781,-2.6644958205438,
126.668125343371));
#115663=CARTESIAN_POINT('Ctrl Pts',(-165.714893278558,-2.77886755534712,
126.744076834378));
#115664=CARTESIAN_POINT('Ctrl Pts',(-165.722641175335,-2.8898916490354,
126.824698657131));
#115665=CARTESIAN_POINT('Ctrl Pts',(-165.730387451419,-3.00089251887698,
126.905303615537));
#115666=CARTESIAN_POINT('Ctrl Pts',(-165.738133727503,-3.10854682429395,
126.990576732936));
#115667=CARTESIAN_POINT('Ctrl Pts',(-165.745880003587,-3.2124473279475,
127.08020095025));
#115668=CARTESIAN_POINT('Ctrl Pts',(-165.753626336853,-3.31634859857054,
127.169825829149));
#115669=CARTESIAN_POINT('Ctrl Pts',(-165.761372670118,-3.41649571609377,
127.263801616686));
#115670=CARTESIAN_POINT('Ctrl Pts',(-165.769119003383,-3.51251550783692,
127.361771785059));
#115671=CARTESIAN_POINT('Ctrl Pts',(-165.776867071386,-3.60855680254629,
127.45976389317));
#115672=CARTESIAN_POINT('Ctrl Pts',(-165.784615139389,-3.70046865864504,
127.56175188293));
#115673=CARTESIAN_POINT('Ctrl Pts',(-165.792363207392,-3.78791594825001,
127.667343589959));
#115674=CARTESIAN_POINT('Ctrl Pts',(-165.800119510134,-3.87545617787537,
127.773047521112));
#115675=CARTESIAN_POINT('Ctrl Pts',(-165.807875812876,-3.95852211260176,
127.882362518928));
#115676=CARTESIAN_POINT('Ctrl Pts',(-165.815632115618,-4.03681967400637,
127.994864224606));
#115677=CARTESIAN_POINT('Ctrl Pts',(-165.823392558132,-4.11515902517722,
128.107425975832));
#115678=CARTESIAN_POINT('Ctrl Pts',(-165.831153000646,-4.18872472224408,
128.22317749419));
#115679=CARTESIAN_POINT('Ctrl Pts',(-165.83891344316,-4.25726752871479,
128.341667731425));
#115680=CARTESIAN_POINT('Ctrl Pts',(-165.846686343426,-4.32592036618321,
128.460348179707));
#115681=CARTESIAN_POINT('Ctrl Pts',(-165.854459243691,-4.38953401869827,
128.581775785825));
#115682=CARTESIAN_POINT('Ctrl Pts',(-165.862232143956,-4.44790609631937,
128.705476528145));
#115683=CARTESIAN_POINT('Ctrl Pts',(-165.869722479719,-4.50415620189013,
128.824680436902));
#115684=CARTESIAN_POINT('Ctrl Pts',(-165.877212815481,-4.55553908507402,
128.945994799085));
#115685=CARTESIAN_POINT('Ctrl Pts',(-165.884703151243,-4.60191744597129,
129.06898201825));
#115686=CARTESIAN_POINT('Ctrl Pts',(-165.893625769841,-4.65716415835103,
129.215486538723));
#115687=CARTESIAN_POINT('Ctrl Pts',(-165.902548388439,-4.70545568793346,
129.364749909709));
#115688=CARTESIAN_POINT('Ctrl Pts',(-165.911471007037,-4.74654472126346,
129.516146244278));
#115689=CARTESIAN_POINT('Ctrl Pts',(-165.912771713424,-4.75253452879746,
129.538216242813));
#115690=CARTESIAN_POINT('Ctrl Pts',(-165.914072419812,-4.75837135876387,
129.560331527798));
#115691=CARTESIAN_POINT('Ctrl Pts',(-165.915373126199,-4.76405452823409,
129.582490119308));
#115692=CARTESIAN_POINT('Ctrl Pts',(-164.165050101093,-4.76405452823413,
129.582490119309));
#115693=CARTESIAN_POINT('Ctrl Pts',(-164.173211318972,-4.79982856714151,
129.721972554062));
#115694=CARTESIAN_POINT('Ctrl Pts',(-164.181372536851,-4.82943340149729,
129.862877416774));
#115695=CARTESIAN_POINT('Ctrl Pts',(-164.189533754729,-4.85279162353424,
130.004612831664));
#115696=CARTESIAN_POINT('Ctrl Pts',(-164.197694972608,-4.8761498455712,
130.146348246553));
#115697=CARTESIAN_POINT('Ctrl Pts',(-164.205856190487,-4.89326146842792,
130.288913713304));
#115698=CARTESIAN_POINT('Ctrl Pts',(-164.214017408366,-4.90411246578154,
130.431716034262));
#115699=CARTESIAN_POINT('Ctrl Pts',(-164.221058460247,-4.91347411210312,
130.554918057001));
#115700=CARTESIAN_POINT('Ctrl Pts',(-164.228099512129,-4.91819381059395,
130.678477256128));
#115701=CARTESIAN_POINT('Ctrl Pts',(-164.235140564011,-4.91824950131355,
130.802145819838));
#115702=CARTESIAN_POINT('',(-163.889859436036,-4.91824789958789,130.80890602176));
#115703=CARTESIAN_POINT('Ctrl Pts',(-163.819828717624,-4.76405452823398,
129.582490119308));
#115704=CARTESIAN_POINT('Ctrl Pts',(-163.827478923358,-4.79773937961931,
129.71382684362));
#115705=CARTESIAN_POINT('Ctrl Pts',(-163.835129129092,-4.82598313537643,
129.846534967663));
#115706=CARTESIAN_POINT('Ctrl Pts',(-163.842779334826,-4.84869131485123,
129.98011818006));
#115707=CARTESIAN_POINT('Ctrl Pts',(-163.850626018354,-4.87198270125662,
130.117132167493));
#115708=CARTESIAN_POINT('Ctrl Pts',(-163.858472701882,-4.88945024297251,
130.255066360533));
#115709=CARTESIAN_POINT('Ctrl Pts',(-163.86631938541,-4.90104854551911,
130.393378602187));
#115710=CARTESIAN_POINT('Ctrl Pts',(-163.874166068938,-4.9126468480657,
130.531690843841));
#115711=CARTESIAN_POINT('Ctrl Pts',(-163.882012752466,-4.91837592354709,
130.670380679545));
#115712=CARTESIAN_POINT('Ctrl Pts',(-163.889859435994,-4.91824789958858,
130.808906021016));
#115713=CARTESIAN_POINT('Ctrl Pts',(-163.889859436036,-4.91824789958789,
130.80890602176));
#115714=CARTESIAN_POINT('Ctrl Pts',(-163.900065351294,-4.91808138313789,
130.989081237333));
#115715=CARTESIAN_POINT('Ctrl Pts',(-163.910271266553,-4.90801070907263,
131.168816066842));
#115716=CARTESIAN_POINT('Ctrl Pts',(-163.920477181811,-4.88820076612934,
131.347201600279));
#115717=CARTESIAN_POINT('Ctrl Pts',(-163.930965019466,-4.86784360459338,
131.530514754195));
#115718=CARTESIAN_POINT('Ctrl Pts',(-163.94145285712,-4.83720162180321,
131.712403451349));
#115719=CARTESIAN_POINT('Ctrl Pts',(-163.951940694775,-4.79650129041414,
131.891907597496));
#115720=CARTESIAN_POINT('Ctrl Pts',(-163.953013390087,-4.79233846332531,
131.91026726919));
#115721=CARTESIAN_POINT('Ctrl Pts',(-163.9540860854,-4.78807045466479,131.928602014415));
#115722=CARTESIAN_POINT('Ctrl Pts',(-163.955158780712,-4.78369753452532,
131.946910818072));
#115723=CARTESIAN_POINT('Ctrl Pts',(-163.962933114831,-4.75200489836948,
132.079603443196));
#115724=CARTESIAN_POINT('Ctrl Pts',(-163.97070744895,-4.71473683637041,
132.211186585001));
#115725=CARTESIAN_POINT('Ctrl Pts',(-163.978481783069,-4.67198502532995,
132.341155654516));
#115726=CARTESIAN_POINT('Ctrl Pts',(-163.986246536016,-4.62928590207575,
132.470964548768));
#115727=CARTESIAN_POINT('Ctrl Pts',(-163.994011288963,-4.581116597636,132.59916296082));
#115728=CARTESIAN_POINT('Ctrl Pts',(-164.001776041911,-4.52761963578437,
132.725257152041));
#115729=CARTESIAN_POINT('Ctrl Pts',(-164.009533082796,-4.47417580786943,
132.851226104734));
#115730=CARTESIAN_POINT('Ctrl Pts',(-164.017290123681,-4.41541500458449,
132.97509463809));
#115731=CARTESIAN_POINT('Ctrl Pts',(-164.025047164566,-4.35152921400009,
133.096385172889));
#115732=CARTESIAN_POINT('Ctrl Pts',(-164.032798355806,-4.28769160018724,
133.217584241552));
#115733=CARTESIAN_POINT('Ctrl Pts',(-164.040549547046,-4.21873687317269,
133.336208836734));
#115734=CARTESIAN_POINT('Ctrl Pts',(-164.048300738286,-4.14490454010639,
133.451802669039));
#115735=CARTESIAN_POINT('Ctrl Pts',(-164.056048635063,-4.07110358775109,
133.567347370881));
#115736=CARTESIAN_POINT('Ctrl Pts',(-164.06379653184,-3.99242936261894,
133.679863543087));
#115737=CARTESIAN_POINT('Ctrl Pts',(-164.071544428617,-3.90916648483699,
133.788920963132));
#115738=CARTESIAN_POINT('Ctrl Pts',(-164.079290704701,-3.82592102385414,
133.897955570716));
#115739=CARTESIAN_POINT('Ctrl Pts',(-164.087036980786,-3.73808905651081,
134.003532554659));
#115740=CARTESIAN_POINT('Ctrl Pts',(-164.09478325687,-3.64599732315475,
134.10525240344));
#115741=CARTESIAN_POINT('Ctrl Pts',(-164.102529590135,-3.55390490999855,
134.206973003093));
#115742=CARTESIAN_POINT('Ctrl Pts',(-164.1102759234,-3.45755293048111,134.30483612094));
#115743=CARTESIAN_POINT('Ctrl Pts',(-164.118022256666,-3.35730676485025,
134.398477247448));
#115744=CARTESIAN_POINT('Ctrl Pts',(-164.125770324669,-3.25703814978579,
134.492139344236));
#115745=CARTESIAN_POINT('Ctrl Pts',(-164.133518392672,-3.15287389892922,
134.581577301449));
#115746=CARTESIAN_POINT('Ctrl Pts',(-164.141266460675,-3.04521410586984,
134.666465498575));
#115747=CARTESIAN_POINT('Ctrl Pts',(-164.149022763416,-2.93743989070108,
134.751443915887));
#115748=CARTESIAN_POINT('Ctrl Pts',(-164.156779066158,-2.82616301950824,
134.831862671143));
#115749=CARTESIAN_POINT('Ctrl Pts',(-164.1645353689,-2.71181478595766,134.907437954049));
#115750=CARTESIAN_POINT('Ctrl Pts',(-164.172295811414,-2.59740552131156,
134.98305357376));
#115751=CARTESIAN_POINT('Ctrl Pts',(-164.180056253929,-2.47992196264395,
135.053820368444));
#115752=CARTESIAN_POINT('Ctrl Pts',(-164.187816696443,-2.3598210093078,
135.1194999973));
#115753=CARTESIAN_POINT('Ctrl Pts',(-164.195589596708,-2.23952725925961,
135.185285060926));
#115754=CARTESIAN_POINT('Ctrl Pts',(-164.203362496974,-2.11660806903376,
135.245966466546));
#115755=CARTESIAN_POINT('Ctrl Pts',(-164.211135397239,-1.9915421805572,
135.301353257716));
#115756=CARTESIAN_POINT('Ctrl Pts',(-164.218625733001,-1.87102275214975,
135.354726599515));
#115757=CARTESIAN_POINT('Ctrl Pts',(-164.226116068763,-1.74851027799214,
135.403183475504));
#115758=CARTESIAN_POINT('Ctrl Pts',(-164.233606404525,-1.62444552332945,
135.446597126431));
#115759=CARTESIAN_POINT('Ctrl Pts',(-164.241380738644,-1.49567681578414,
135.491656819128));
#115760=CARTESIAN_POINT('Ctrl Pts',(-164.249155072763,-1.36482789412201,
135.531426045324));
#115761=CARTESIAN_POINT('Ctrl Pts',(-164.256929406882,-1.23237283688576,
135.565709192645));
#115762=CARTESIAN_POINT('Ctrl Pts',(-164.264694159829,-1.10008101866971,
135.599950089051));
#115763=CARTESIAN_POINT('Ctrl Pts',(-164.272458912777,-0.966187378191674,
135.628718262135));
#115764=CARTESIAN_POINT('Ctrl Pts',(-164.280223665724,-0.831184349327498,
135.651866743393));
#115765=CARTESIAN_POINT('Ctrl Pts',(-164.287980706609,-0.696315407374798,
135.674992233254));
#115766=CARTESIAN_POINT('Ctrl Pts',(-164.295737747494,-0.560339652635501,
135.692509073194));
#115767=CARTESIAN_POINT('Ctrl Pts',(-164.303494788379,-0.423762660274618,
135.70432064498));
#115768=CARTESIAN_POINT('Ctrl Pts',(-164.311245979619,-0.287288661686275,
135.716123309569));
#115769=CARTESIAN_POINT('Ctrl Pts',(-164.318997170859,-0.150214715872734,
135.722229236095));
#115770=CARTESIAN_POINT('Ctrl Pts',(-164.326748362099,-0.0130541714907547,
135.722593293142));
#115771=CARTESIAN_POINT('Ctrl Pts',(-164.334496258876,0.124048076001172,
135.722957195456));
#115772=CARTESIAN_POINT('Ctrl Pts',(-164.342244155653,0.261236458710503,
135.717584081121));
#115773=CARTESIAN_POINT('Ctrl Pts',(-164.34999205243,0.39799517411068,135.706480863325));
#115774=CARTESIAN_POINT('Ctrl Pts',(-164.357738328514,0.534725282535772,
135.695379968084));
#115775=CARTESIAN_POINT('Ctrl Pts',(-164.365484604598,0.671025512986141,
135.67855138511));
#115776=CARTESIAN_POINT('Ctrl Pts',(-164.373230880682,0.806383133965511,
135.656054064576));
#115777=CARTESIAN_POINT('Ctrl Pts',(-164.380977213948,0.941741754124274,
135.633556577971));
#115778=CARTESIAN_POINT('Ctrl Pts',(-164.388723547213,1.07615736525315,
135.605390334409));
#115779=CARTESIAN_POINT('Ctrl Pts',(-164.396469880478,1.20912579821097,
135.571665712334));
#115780=CARTESIAN_POINT('Ctrl Pts',(-164.404217948481,1.34212400852723,
135.537933537864));
#115781=CARTESIAN_POINT('Ctrl Pts',(-164.411966016484,1.47367401688612,
135.49864060405));
#115782=CARTESIAN_POINT('Ctrl Pts',(-164.419714084487,1.60328560917197,
135.453947515122));
#115783=CARTESIAN_POINT('Ctrl Pts',(-164.427470387229,1.73303495420068,
135.409206925846));
#115784=CARTESIAN_POINT('Ctrl Pts',(-164.435226689971,1.86084139754372,
135.35905484414));
#115785=CARTESIAN_POINT('Ctrl Pts',(-164.442982992713,1.98623303680093,
135.303700723184));
#115786=CARTESIAN_POINT('Ctrl Pts',(-164.450743435227,2.11169160135148,
135.248317058066));
#115787=CARTESIAN_POINT('Ctrl Pts',(-164.458503877741,2.2347324430946,135.187725993954));
#115788=CARTESIAN_POINT('Ctrl Pts',(-164.466264320256,2.35490807390126,
135.122183104188));
#115789=CARTESIAN_POINT('Ctrl Pts',(-164.474037220521,2.47527662129917,
135.056534999156));
#115790=CARTESIAN_POINT('Ctrl Pts',(-164.481810120786,2.59277043121956,
134.98591938513));
#115791=CARTESIAN_POINT('Ctrl Pts',(-164.489583021052,2.70697007489154,
134.910635824629));
#115792=CARTESIAN_POINT('Ctrl Pts',(-164.497073356814,2.81701827386481,
134.83808901118));
#115793=CARTESIAN_POINT('Ctrl Pts',(-164.504563692576,2.92400740082148,
134.761207922034));
#115794=CARTESIAN_POINT('Ctrl Pts',(-164.512054028338,3.02759256523099,
134.680294869002));
#115795=CARTESIAN_POINT('Ctrl Pts',(-164.519828362457,3.13510519263266,
134.596313972972));
#115796=CARTESIAN_POINT('Ctrl Pts',(-164.527602696576,3.23929120727552,
134.50772330752));
#115797=CARTESIAN_POINT('Ctrl Pts',(-164.535377030695,3.33972978389667,
134.414815995085));
#115798=CARTESIAN_POINT('Ctrl Pts',(-164.543141783642,3.44004457894859,
134.322023182608));
#115799=CARTESIAN_POINT('Ctrl Pts',(-164.550906536589,3.53662084093353,
134.224924571063));
#115800=CARTESIAN_POINT('Ctrl Pts',(-164.558671289536,3.62906874854865,
134.123855018948));
#115801=CARTESIAN_POINT('Ctrl Pts',(-164.566428330421,3.72142483559863,
134.022885850538));
#115802=CARTESIAN_POINT('Ctrl Pts',(-164.574185371307,3.80966046597174,
133.917953876902));
#115803=CARTESIAN_POINT('Ctrl Pts',(-164.581942412192,3.89342107628641,
133.809432228232));
#115804=CARTESIAN_POINT('Ctrl Pts',(-164.589693603432,3.9771185220734,133.700992416581));
#115805=CARTESIAN_POINT('Ctrl Pts',(-164.597444794672,4.05634742691817,
133.588968626264));
#115806=CARTESIAN_POINT('Ctrl Pts',(-164.605195985912,4.13079234299426,
133.473768357414));
#115807=CARTESIAN_POINT('Ctrl Pts',(-164.612943882689,4.20520561799523,
133.358617051751));
#115808=CARTESIAN_POINT('Ctrl Pts',(-164.620691779466,4.27483873659731,
133.240292280456));
#115809=CARTESIAN_POINT('Ctrl Pts',(-164.628439676243,4.33941871119797,
133.119231739552));
#115810=CARTESIAN_POINT('Ctrl Pts',(-164.636185952327,4.40398517705996,
132.998196521904));
#115811=CARTESIAN_POINT('Ctrl Pts',(-164.643932228411,4.46350041747012,
132.874427017644));
#115812=CARTESIAN_POINT('Ctrl Pts',(-164.651678504496,4.51773688498037,
132.748386466311));
#115813=CARTESIAN_POINT('Ctrl Pts',(-164.659424837761,4.57197375285197,
132.622344984575));
#115814=CARTESIAN_POINT('Ctrl Pts',(-164.667171171026,4.62093161553248,
132.49403278144));
#115815=CARTESIAN_POINT('Ctrl Pts',(-164.674917504292,4.66443082179806,
132.363933690929));
#115816=CARTESIAN_POINT('Ctrl Pts',(-164.682665572295,4.70793976940923,
132.23380546563));
#115817=CARTESIAN_POINT('Ctrl Pts',(-164.690413640298,4.74598750416377,
132.101889927398));
#115818=CARTESIAN_POINT('Ctrl Pts',(-164.6981617083,4.77844417424365,131.968686317762));
#115819=CARTESIAN_POINT('Ctrl Pts',(-164.705918011042,4.81093533965878,
131.835341137744));
#115820=CARTESIAN_POINT('Ctrl Pts',(-164.713674313784,4.8378234774116,131.700705532098));
#115821=CARTESIAN_POINT('Ctrl Pts',(-164.721430616526,4.85902973162015,
131.565289740239));
#115822=CARTESIAN_POINT('Ctrl Pts',(-164.72919105904,4.88024730424508,131.429801672894));
#115823=CARTESIAN_POINT('Ctrl Pts',(-164.736951501554,4.89577690638137,
131.293532977866));
#115824=CARTESIAN_POINT('Ctrl Pts',(-164.744711944069,4.90559168085346,
131.156998283225));
#115825=CARTESIAN_POINT('Ctrl Pts',(-164.752484844334,4.91542221087285,
131.020244410971));
#115826=CARTESIAN_POINT('Ctrl Pts',(-164.760257744599,4.91951956906265,
130.883224076824));
#115827=CARTESIAN_POINT('Ctrl Pts',(-164.768030644865,4.91790907435823,
130.746452078947));
#115828=CARTESIAN_POINT('Ctrl Pts',(-164.775520980627,4.91635712519291,
130.614652087701));
#115829=CARTESIAN_POINT('Ctrl Pts',(-164.783011316389,4.90950512398354,
130.483082998495));
#115830=CARTESIAN_POINT('Ctrl Pts',(-164.790501652151,4.89742099246282,
130.352198384419));
#115831=CARTESIAN_POINT('Ctrl Pts',(-164.79827598627,4.88487868742258,130.216351240418));
#115832=CARTESIAN_POINT('Ctrl Pts',(-164.806050320389,4.86665993735916,
130.080811176974));
#115833=CARTESIAN_POINT('Ctrl Pts',(-164.813824654508,4.84278388814765,
129.946090686136));
#115834=CARTESIAN_POINT('Ctrl Pts',(-164.821589407455,4.81893726403294,
129.811536226262));
#115835=CARTESIAN_POINT('Ctrl Pts',(-164.829354160402,4.78944728077334,
129.677799710566));
#115836=CARTESIAN_POINT('Ctrl Pts',(-164.83711891335,4.7543849563725,129.54539010595));
#115837=CARTESIAN_POINT('Ctrl Pts',(-164.844875954235,4.71935745636655,
129.413112012419));
#115838=CARTESIAN_POINT('Ctrl Pts',(-164.852632995119,4.67876872861081,
129.282158582768));
#115839=CARTESIAN_POINT('Ctrl Pts',(-164.860390036004,4.63274104793342,
129.153029807191));
#115840=CARTESIAN_POINT('Ctrl Pts',(-164.868141227245,4.58674807708801,
129.023998408629));
#115841=CARTESIAN_POINT('Ctrl Pts',(-164.875892418485,4.53532444795852,
128.896789292105));
#115842=CARTESIAN_POINT('Ctrl Pts',(-164.883643609725,4.47864249469079,
128.771888116584));
#115843=CARTESIAN_POINT('Ctrl Pts',(-164.891391506502,4.42198463276531,
128.647040027394));
#115844=CARTESIAN_POINT('Ctrl Pts',(-164.899139403279,4.36007305303164,
128.524498283474));
#115845=CARTESIAN_POINT('Ctrl Pts',(-164.906887300056,4.29312844508182,
128.404729142416));
#115846=CARTESIAN_POINT('Ctrl Pts',(-164.91463357614,4.22619784050083,128.284985054481));
#115847=CARTESIAN_POINT('Ctrl Pts',(-164.922379852224,4.15423649241504,
128.168012756874));
#115848=CARTESIAN_POINT('Ctrl Pts',(-164.930126128309,4.07751114241307,
128.054254083994));
#115849=CARTESIAN_POINT('Ctrl Pts',(-164.937872461574,4.00078522604189,
127.940494571373));
#115850=CARTESIAN_POINT('Ctrl Pts',(-164.945618794839,3.91929545619527,
127.829949054947));
#115851=CARTESIAN_POINT('Ctrl Pts',(-164.953365128105,3.83335179026499,
127.723030204486));
#115852=CARTESIAN_POINT('Ctrl Pts',(-164.961113196108,3.74738887784674,
127.61608741029));
#115853=CARTESIAN_POINT('Ctrl Pts',(-164.968861264111,3.65697032949276,
127.512773202843));
#115854=CARTESIAN_POINT('Ctrl Pts',(-164.976609332114,3.56244598315982,
127.413466682397));
#115855=CARTESIAN_POINT('Ctrl Pts',(-164.984365634855,3.46782117522687,
127.314054617799));
#115856=CARTESIAN_POINT('Ctrl Pts',(-164.992121937597,3.36908212235354,
127.218659032487));
#115857=CARTESIAN_POINT('Ctrl Pts',(-164.999878240339,3.26661547987926,
127.127622067014));
#115858=CARTESIAN_POINT('Ctrl Pts',(-165.007638682853,3.1640941478724,127.036536512372));
#115859=CARTESIAN_POINT('Ctrl Pts',(-165.015399125367,3.05784156470194,
126.949814460063));
#115860=CARTESIAN_POINT('Ctrl Pts',(-165.023159567882,2.9482761845781,126.867756674832));
#115861=CARTESIAN_POINT('Ctrl Pts',(-165.030932468147,2.83853492037933,
126.785567163159));
#115862=CARTESIAN_POINT('Ctrl Pts',(-165.038705368412,2.72547055482927,
126.708057102157));
#115863=CARTESIAN_POINT('Ctrl Pts',(-165.046478268678,2.60952988770485,
126.635483451269));
#115864=CARTESIAN_POINT('Ctrl Pts',(-165.05396860444,2.49780395586702,126.565548035392));
#115865=CARTESIAN_POINT('Ctrl Pts',(-165.061458940202,2.38340748086415,
126.500196511599));
#115866=CARTESIAN_POINT('Ctrl Pts',(-165.068949275964,2.26675877993803,
126.439616902745));
#115867=CARTESIAN_POINT('Ctrl Pts',(-165.076723610083,2.1456873080622,126.376740399608));
#115868=CARTESIAN_POINT('Ctrl Pts',(-165.084497944202,2.02180593456538,
126.318805634976));
#115869=CARTESIAN_POINT('Ctrl Pts',(-165.092272278321,1.89555618233674,
126.266073515354));
#115870=CARTESIAN_POINT('Ctrl Pts',(-165.100037031268,1.76946202164446,
126.213406383356));
#115871=CARTESIAN_POINT('Ctrl Pts',(-165.107801784216,1.64100564709012,
126.165929288042));
#115872=CARTESIAN_POINT('Ctrl Pts',(-165.115566537163,1.51065365390793,
126.123857588998));
#115873=CARTESIAN_POINT('Ctrl Pts',(-165.123323578048,1.38043112816301,
126.081827676158));
#115874=CARTESIAN_POINT('Ctrl Pts',(-165.131080618933,1.24831710021635,
126.045192594909));
#115875=CARTESIAN_POINT('Ctrl Pts',(-165.138837659818,1.11479831851221,
126.01411972889));
#115876=CARTESIAN_POINT('Ctrl Pts',(-165.146588851058,0.981380224359805,
125.983070295161));
#115877=CARTESIAN_POINT('Ctrl Pts',(-165.154340042298,0.846559864242099,
125.957574816004));
#115878=CARTESIAN_POINT('Ctrl Pts',(-165.162091233538,0.71083898761624,
125.937750812354));
#115879=CARTESIAN_POINT('Ctrl Pts',(-165.169839130315,0.575175795983603,
125.917935234435));
#115880=CARTESIAN_POINT('Ctrl Pts',(-165.177587027092,0.438613235140789,
125.903786394055));
#115881=CARTESIAN_POINT('Ctrl Pts',(-165.185334923869,0.301662868920606,
125.895370642427));
#115882=CARTESIAN_POINT('Ctrl Pts',(-165.193081199953,0.164741149764728,
125.886956651193));
#115883=CARTESIAN_POINT('Ctrl Pts',(-165.200827476037,0.0274321765665248,
125.884273387325));
#115884=CARTESIAN_POINT('Ctrl Pts',(-165.208573752121,-0.109748142537605,
125.887335255855));
#115885=CARTESIAN_POINT('Ctrl Pts',(-165.216320085387,-0.246929474275501,
125.890397146987));
#115886=CARTESIAN_POINT('Ctrl Pts',(-165.224066418652,-0.383981759156418,
125.899204246416));
#115887=CARTESIAN_POINT('Ctrl Pts',(-165.231812751917,-0.520390266873772,
125.913718836302));
#115888=CARTESIAN_POINT('Ctrl Pts',(-165.23956081992,-0.656829322330825,
125.92823667663));
#115889=CARTESIAN_POINT('Ctrl Pts',(-165.247308887923,-0.79262392504769,
125.948464509432));
#115890=CARTESIAN_POINT('Ctrl Pts',(-165.255056955926,-0.927266031284532,
125.974312919072));
#115891=CARTESIAN_POINT('Ctrl Pts',(-165.262813258668,-1.06205123675433,
126.00018880071));
#115892=CARTESIAN_POINT('Ctrl Pts',(-165.27056956141,-1.19568111433443,
126.0316971183));
#115893=CARTESIAN_POINT('Ctrl Pts',(-165.278325864152,-1.32765881483179,
126.06869750308));
#115894=CARTESIAN_POINT('Ctrl Pts',(-165.286086306666,-1.45970695580167,
126.10571763608));
#115895=CARTESIAN_POINT('Ctrl Pts',(-165.29384674918,-1.59010079107251,
126.148235555954));
#115896=CARTESIAN_POINT('Ctrl Pts',(-165.301607191694,-1.71836109402489,
126.196061776015));
#115897=CARTESIAN_POINT('Ctrl Pts',(-165.30938009196,-1.84682729180199,
126.24396477097));
#115898=CARTESIAN_POINT('Ctrl Pts',(-165.317152992225,-1.97315275265275,
126.297192942596));
#115899=CARTESIAN_POINT('Ctrl Pts',(-165.324925892491,-2.09687978312631,
126.355509278443));
#115900=CARTESIAN_POINT('Ctrl Pts',(-165.332416228253,-2.21610902439291,
126.411705668592));
#115901=CARTESIAN_POINT('Ctrl Pts',(-165.339906564015,-2.33292520124008,
126.472626567979));
#115902=CARTESIAN_POINT('Ctrl Pts',(-165.347396899777,-2.44694401402623,
126.538021665406));
#115903=CARTESIAN_POINT('Ctrl Pts',(-165.355172364684,-2.56530309774718,
126.605906110281));
#115904=CARTESIAN_POINT('Ctrl Pts',(-165.362947829591,-2.68102260916758,
126.678827201352));
#115905=CARTESIAN_POINT('Ctrl Pts',(-165.370723294498,-2.79364418792851,
126.756554395209));
#115906=CARTESIAN_POINT('Ctrl Pts',(-165.378488931618,-2.90612341881161,
126.834183345894));
#115907=CARTESIAN_POINT('Ctrl Pts',(-165.386254568737,-3.01551218996034,
126.916606091101));
#115908=CARTESIAN_POINT('Ctrl Pts',(-165.394020205857,-3.12137696430902,
127.003546374646));
#115909=CARTESIAN_POINT('Ctrl Pts',(-165.401776441018,-3.22711356679057,
127.090381398453));
#115910=CARTESIAN_POINT('Ctrl Pts',(-165.409532676179,-3.32933436994994,
127.181722820468));
#115911=CARTESIAN_POINT('Ctrl Pts',(-165.41728891134,-3.42763558196576,
127.277251691017));
#115912=CARTESIAN_POINT('Ctrl Pts',(-165.425039814993,-3.5258692233466,
127.372714896593));
#115913=CARTESIAN_POINT('Ctrl Pts',(-165.432790718646,-3.62018835469884,
127.472359552875));
#115914=CARTESIAN_POINT('Ctrl Pts',(-165.440541622299,-3.71022294051425,
127.575827081395));
#115915=CARTESIAN_POINT('Ctrl Pts',(-165.448288876738,-3.80021513701893,
127.679245896222));
#115916=CARTESIAN_POINT('Ctrl Pts',(-165.456036131177,-3.88592654633809,
127.786483707236));
#115917=CARTESIAN_POINT('Ctrl Pts',(-165.463783385616,-3.96702491824877,
127.897146081194));
#115918=CARTESIAN_POINT('Ctrl Pts',(-165.471528670312,-4.04810267087022,
128.007780319204));
#115919=CARTESIAN_POINT('Ctrl Pts',(-165.479273955009,-4.12456949064734,
128.121837071464));
#115920=CARTESIAN_POINT('Ctrl Pts',(-165.487019239706,-4.19613450775678,
128.238890240557));
#115921=CARTESIAN_POINT('Ctrl Pts',(-165.494766446468,-4.26771728439569,
128.355972457489));
#115922=CARTESIAN_POINT('Ctrl Pts',(-165.502513653229,-4.33439561961306,
128.476052245975));
#115923=CARTESIAN_POINT('Ctrl Pts',(-165.510260859991,-4.39592293717988,
128.598676008907));
#115924=CARTESIAN_POINT('Ctrl Pts',(-165.518009053047,-4.45745808776662,
128.721315383025));
#115925=CARTESIAN_POINT('Ctrl Pts',(-165.525757246103,-4.51384074641663,
128.846499023675));
#115926=CARTESIAN_POINT('Ctrl Pts',(-165.533505439158,-4.56487152273224,
128.973751144345));
#115927=CARTESIAN_POINT('Ctrl Pts',(-165.541259448977,-4.61594060913102,
129.101098796372));
#115928=CARTESIAN_POINT('Ctrl Pts',(-165.549013458795,-4.66164965118814,
129.230517663771));
#115929=CARTESIAN_POINT('Ctrl Pts',(-165.556767468614,-4.70184831378861,
129.361514299823));
#115930=CARTESIAN_POINT('Ctrl Pts',(-165.561100088326,-4.72430966244096,
129.434709797492));
#115931=CARTESIAN_POINT('Ctrl Pts',(-165.565432708038,-4.74505150669632,
129.508397626744));
#115932=CARTESIAN_POINT('Ctrl Pts',(-165.569765327751,-4.76405452823417,
129.582490119309));
#115933=CARTESIAN_POINT('Origin',(213.235140564004,0.,130.804360617566));
#115934=CARTESIAN_POINT('',(-167.665279524992,-4.76405452823393,129.582490119308));
#115935=CARTESIAN_POINT('',(-167.320062571459,-4.76405452823401,129.582490119308));
#115936=CARTESIAN_POINT('',(213.235140564004,-4.76405452823405,129.582490119308));
#115937=CARTESIAN_POINT('',(-165.985140563955,-4.91824883541683,130.800976031773));
#115938=CARTESIAN_POINT('Ctrl Pts',(-165.985140564011,-4.91824883541751,
130.800976032755));
#115939=CARTESIAN_POINT('Ctrl Pts',(-165.992921447872,-4.91834374325779,
130.938889662065));
#115940=CARTESIAN_POINT('Ctrl Pts',(-166.000702331733,-4.91263343217728,
131.076842827902));
#115941=CARTESIAN_POINT('Ctrl Pts',(-166.008483215594,-4.90113463722454,
131.214314676331));
#115942=CARTESIAN_POINT('Ctrl Pts',(-166.016264069799,-4.8896358860991,
131.35178600079));
#115943=CARTESIAN_POINT('Ctrl Pts',(-166.024044924003,-4.87234872630466,
131.48877562691));
#115944=CARTESIAN_POINT('Ctrl Pts',(-166.031825778208,-4.84934186529542,
131.624766941282));
#115945=CARTESIAN_POINT('Ctrl Pts',(-166.039608230963,-4.82633027760143,
131.760786194627));
#115946=CARTESIAN_POINT('Ctrl Pts',(-166.047390683719,-4.79759671352023,
131.895806347448));
#115947=CARTESIAN_POINT('Ctrl Pts',(-166.055173136475,-4.76326112125045,
132.029320434574));
#115948=CARTESIAN_POINT('Ctrl Pts',(-166.062958816668,-4.72891128976911,
132.162889890931));
#115949=CARTESIAN_POINT('Ctrl Pts',(-166.070744496861,-4.68895490117725,
132.29495166481));
#115950=CARTESIAN_POINT('Ctrl Pts',(-166.078530177055,-4.64356183651419,
132.425013736827));
#115951=CARTESIAN_POINT('Ctrl Pts',(-166.086325608341,-4.598111919788,132.555238703708));
#115952=CARTESIAN_POINT('Ctrl Pts',(-166.094121039627,-4.54721185565204,
132.683458602351));
#115953=CARTESIAN_POINT('Ctrl Pts',(-166.101916470914,-4.4910800146906,
132.80920060224));
#115954=CARTESIAN_POINT('Ctrl Pts',(-166.109717264546,-4.43490956158325,
132.935029097928));
#115955=CARTESIAN_POINT('Ctrl Pts',(-166.117518058177,-4.37350033261783,
133.058375954042));
#115956=CARTESIAN_POINT('Ctrl Pts',(-166.125318851809,-4.30711634929883,
133.178793563788));
#115957=CARTESIAN_POINT('Ctrl Pts',(-166.133132278773,-4.2406248575752,
133.299406189024));
#115958=CARTESIAN_POINT('Ctrl Pts',(-166.140945705736,-4.16914271861626,
133.417079763003));
#115959=CARTESIAN_POINT('Ctrl Pts',(-166.1487591327,-4.0929773134785,133.531395596045));
#115960=CARTESIAN_POINT('Ctrl Pts',(-166.153556346819,-4.04621399712678,
133.601582151935));
#115961=CARTESIAN_POINT('Ctrl Pts',(-166.158353560937,-3.99768608866018,
133.670503604081));
#115962=CARTESIAN_POINT('Ctrl Pts',(-166.163150775056,-3.94747195171253,
133.738069576025));
#115963=CARTESIAN_POINT('Ctrl Pts',(-166.170925109175,-3.86609524671875,
133.84756655239));
#115964=CARTESIAN_POINT('Ctrl Pts',(-166.178699443294,-3.78003027026917,
133.953848495734));
#115965=CARTESIAN_POINT('Ctrl Pts',(-166.186473777413,-3.68955996174399,
134.056487667851));
#115966=CARTESIAN_POINT('Ctrl Pts',(-166.19423853036,-3.5992011497885,134.159000346362));
#115967=CARTESIAN_POINT('Ctrl Pts',(-166.202003283307,-3.5044480642423,
134.257878895716));
#115968=CARTESIAN_POINT('Ctrl Pts',(-166.209768036254,-3.405626112538,134.352725571189));
#115969=CARTESIAN_POINT('Ctrl Pts',(-166.217525077139,-3.30690231218927,
134.447478043607));
#115970=CARTESIAN_POINT('Ctrl Pts',(-166.225282118024,-3.20411796820674,
134.538206342336));
#115971=CARTESIAN_POINT('Ctrl Pts',(-166.233039158909,-3.09763759478476,
134.624547052006));
#115972=CARTESIAN_POINT('Ctrl Pts',(-166.240790350149,-2.99123751904083,
134.710822651474));
#115973=CARTESIAN_POINT('Ctrl Pts',(-166.248541541389,-2.88114726406746,
134.792717002435));
#115974=CARTESIAN_POINT('Ctrl Pts',(-166.256292732629,-2.76776664276774,
134.869904969025));
#115975=CARTESIAN_POINT('Ctrl Pts',(-166.264040629406,-2.65443421125675,
134.94706012867));
#115976=CARTESIAN_POINT('Ctrl Pts',(-166.271788526183,-2.53781451742097,
135.019512662908));
#115977=CARTESIAN_POINT('Ctrl Pts',(-166.27953642296,-2.41833858028677,
135.086979159252));
#115978=CARTESIAN_POINT('Ctrl Pts',(-166.287282699044,-2.29888763494301,
135.15443154306));
#115979=CARTESIAN_POINT('Ctrl Pts',(-166.295028975128,-2.17658197491196,
135.216899771384));
#115980=CARTESIAN_POINT('Ctrl Pts',(-166.302775251212,-2.05187924581811,
135.274145245832));
#115981=CARTESIAN_POINT('Ctrl Pts',(-166.310521584478,-1.92717559619688,
135.331391142853));
#115982=CARTESIAN_POINT('Ctrl Pts',(-166.318267917743,-1.80007519751998,
135.383414045958));
#115983=CARTESIAN_POINT('Ctrl Pts',(-166.326014251008,-1.67105743334419,
135.430022744977));
#115984=CARTESIAN_POINT('Ctrl Pts',(-166.333762319011,-1.54201077653484,
135.476641881691));
#115985=CARTESIAN_POINT('Ctrl Pts',(-166.341510387014,-1.41104626744494,
135.517844268825));
#115986=CARTESIAN_POINT('Ctrl Pts',(-166.349258455017,-1.27865988774699,
135.553488111534));
#115987=CARTESIAN_POINT('Ctrl Pts',(-166.357014757759,-1.14613280622909,
135.589169836944));
#115988=CARTESIAN_POINT('Ctrl Pts',(-166.364771060501,-1.01218121347949,
135.619281114883));
#115989=CARTESIAN_POINT('Ctrl Pts',(-166.372527363242,-0.877313309652195,
135.643730867837));
#115990=CARTESIAN_POINT('Ctrl Pts',(-166.380287805757,-0.74237342276383,
135.66819367036));
#115991=CARTESIAN_POINT('Ctrl Pts',(-166.388048248271,-0.606516637385834,
135.686988873302));
#115992=CARTESIAN_POINT('Ctrl Pts',(-166.395808690785,-0.470256788889064,
135.700077277566));
#115993=CARTESIAN_POINT('Ctrl Pts',(-166.40358159105,-0.333778203986905,
135.713186692499));
#115994=CARTESIAN_POINT('Ctrl Pts',(-166.411354491316,-0.196895653610697,
135.720570980964));
#115995=CARTESIAN_POINT('Ctrl Pts',(-166.419127391581,-0.0601243952583667,
135.722243100871));
#115996=CARTESIAN_POINT('Ctrl Pts',(-166.426617727343,0.0716748833546202,
135.723854435007));
#115997=CARTESIAN_POINT('Ctrl Pts',(-166.434108063106,0.203370513056851,
135.72016170237));
#115998=CARTESIAN_POINT('Ctrl Pts',(-166.441598398868,0.334507421442165,
135.711221920629));
#115999=CARTESIAN_POINT('Ctrl Pts',(-166.449372732987,0.470616425560006,
135.701943184347));
#116000=CARTESIAN_POINT('Ctrl Pts',(-166.457147067106,0.606554656582134,
135.686982268632));
#116001=CARTESIAN_POINT('Ctrl Pts',(-166.464921401225,0.741809310595588,
135.666346015448));
#116002=CARTESIAN_POINT('Ctrl Pts',(-166.472686154172,0.876897275335291,
135.645735194601));
#116003=CARTESIAN_POINT('Ctrl Pts',(-166.48045090712,1.01130295650361,135.619463011353));
#116004=CARTESIAN_POINT('Ctrl Pts',(-166.488215660067,1.14451582953313,
135.587588249453));
#116005=CARTESIAN_POINT('Ctrl Pts',(-166.495972700952,1.27759639365991,
135.555745146016));
#116006=CARTESIAN_POINT('Ctrl Pts',(-166.503729741837,1.4094861295105,135.518310628044));
#116007=CARTESIAN_POINT('Ctrl Pts',(-166.511486782722,1.5396822566143,135.475394936768));
#116008=CARTESIAN_POINT('Ctrl Pts',(-166.519237973962,1.66978020180605,
135.432511608549));
#116009=CARTESIAN_POINT('Ctrl Pts',(-166.526989165202,1.79818671055663,
135.384155456197));
#116010=CARTESIAN_POINT('Ctrl Pts',(-166.534740356442,1.92441212821454,
135.330487109753));
#116011=CARTESIAN_POINT('Ctrl Pts',(-166.542488253219,2.05058389670226,
135.276841573789));
#116012=CARTESIAN_POINT('Ctrl Pts',(-166.550236149997,2.17457605883224,
135.21788848703));
#116013=CARTESIAN_POINT('Ctrl Pts',(-166.557984046774,2.29591719534093,
135.153837286619));
#116014=CARTESIAN_POINT('Ctrl Pts',(-166.565730322858,2.41723294989967,
135.089799484338));
#116015=CARTESIAN_POINT('Ctrl Pts',(-166.573476598942,2.53589843630963,
135.020665871958));
#116016=CARTESIAN_POINT('Ctrl Pts',(-166.581222875026,2.65146554634782,
134.946692511443));
#116017=CARTESIAN_POINT('Ctrl Pts',(-166.588969208291,2.767033509476,134.872718604874));
#116018=CARTESIAN_POINT('Ctrl Pts',(-166.596715541557,2.87950272130864,
134.793905089655));
#116019=CARTESIAN_POINT('Ctrl Pts',(-166.604461874822,2.98845319279131,
134.710551930981));
#116020=CARTESIAN_POINT('Ctrl Pts',(-166.612209942825,3.09742806297681,
134.627180105944));
#116021=CARTESIAN_POINT('Ctrl Pts',(-166.619958010828,3.2028823143341,134.539266852009));
#116022=CARTESIAN_POINT('Ctrl Pts',(-166.627706078831,3.30442856063603,
134.447152809025));
#116023=CARTESIAN_POINT('Ctrl Pts',(-166.635462381573,3.40608273149709,
134.35494086614));
#116024=CARTESIAN_POINT('Ctrl Pts',(-166.643218684315,3.5038203102532,134.258519478687));
#116025=CARTESIAN_POINT('Ctrl Pts',(-166.650974987057,3.59728997621696,
134.158266980229));
#116026=CARTESIAN_POINT('Ctrl Pts',(-166.658735429571,3.69080952975576,
134.057960973993));
#116027=CARTESIAN_POINT('Ctrl Pts',(-166.666495872085,3.78005637728183,
133.953820079078));
#116028=CARTESIAN_POINT('Ctrl Pts',(-166.674256314599,3.86471979891645,
133.846255411664));
#116029=CARTESIAN_POINT('Ctrl Pts',(-166.682029214865,3.9495191297913,133.738518071898));
#116030=CARTESIAN_POINT('Ctrl Pts',(-166.68980211513,4.02972010283157,133.627346293837));
#116031=CARTESIAN_POINT('Ctrl Pts',(-166.697575015395,4.10505511062848,
133.513180582274));
#116032=CARTESIAN_POINT('Ctrl Pts',(-166.705065351157,4.17765150113475,
133.403165081893));
#116033=CARTESIAN_POINT('Ctrl Pts',(-166.712555686919,4.24572940527844,
133.290369806626));
#116034=CARTESIAN_POINT('Ctrl Pts',(-166.720046022681,4.30909081588839,
133.17520844122));
#116035=CARTESIAN_POINT('Ctrl Pts',(-166.727820356801,4.37485459364,133.055680697643));
#116036=CARTESIAN_POINT('Ctrl Pts',(-166.73559469092,4.43574548587656,132.933225273528));
#116037=CARTESIAN_POINT('Ctrl Pts',(-166.743369025039,4.49149206589649,
132.808277303581));
#116038=CARTESIAN_POINT('Ctrl Pts',(-166.751133777986,4.54716994323846,
132.683483320841));
#116039=CARTESIAN_POINT('Ctrl Pts',(-166.758898530933,4.59771596511764,
132.556203257928));
#116040=CARTESIAN_POINT('Ctrl Pts',(-166.76666328388,4.64290363696878,132.426898407672));
#116041=CARTESIAN_POINT('Ctrl Pts',(-166.774420324765,4.68804642778731,
132.297721984816));
#116042=CARTESIAN_POINT('Ctrl Pts',(-166.78217736565,4.72784133143026,132.166525143382));
#116043=CARTESIAN_POINT('Ctrl Pts',(-166.789934406535,4.76210933184111,
132.033790474895));
#116044=CARTESIAN_POINT('Ctrl Pts',(-166.797685597775,4.79635149048652,
131.901155902653));
#116045=CARTESIAN_POINT('Ctrl Pts',(-166.805436789015,4.82507494447826,
131.766986188669));
#116046=CARTESIAN_POINT('Ctrl Pts',(-166.813187980256,4.84815016612017,
131.631780117728));
#116047=CARTESIAN_POINT('Ctrl Pts',(-166.820935877033,4.87121558017724,
131.496631512975));
#116048=CARTESIAN_POINT('Ctrl Pts',(-166.82868377381,4.88863747095705,131.360447811932));
#116049=CARTESIAN_POINT('Ctrl Pts',(-166.836431670587,4.90033723023199,
131.223738838868));
#116050=CARTESIAN_POINT('Ctrl Pts',(-166.844177946671,4.9120345421695,131.087058462374));
#116051=CARTESIAN_POINT('Ctrl Pts',(-166.851924222755,4.91801207007805,
130.949853421701));
#116052=CARTESIAN_POINT('Ctrl Pts',(-166.859670498839,4.91824303270179,
130.812639130737));
#116053=CARTESIAN_POINT('Ctrl Pts',(-166.867416832105,4.91847399703044,
130.675423826888));
#116054=CARTESIAN_POINT('Ctrl Pts',(-166.87516316537,4.91295831077049,130.538199663577));
#116055=CARTESIAN_POINT('Ctrl Pts',(-166.882909498635,4.90172132879331,
130.401482128003));
#116056=CARTESIAN_POINT('Ctrl Pts',(-166.890657566638,4.89048183037195,
130.264733975485));
#116057=CARTESIAN_POINT('Ctrl Pts',(-166.898405634641,4.87351851872493,
130.128493066046));
#116058=CARTESIAN_POINT('Ctrl Pts',(-166.906153702644,4.85090859208839,
129.993269442849));
#116059=CARTESIAN_POINT('Ctrl Pts',(-166.913910005386,4.82827463535267,
129.857902102377));
#116060=CARTESIAN_POINT('Ctrl Pts',(-166.921666308128,4.79998213998362,
129.723554594155));
#116061=CARTESIAN_POINT('Ctrl Pts',(-166.92942261087,4.76615951130919,129.590726992761));
#116062=CARTESIAN_POINT('Ctrl Pts',(-166.937183053384,4.73231883047954,
129.457828497277));
#116063=CARTESIAN_POINT('Ctrl Pts',(-166.944943495898,4.69294224722724,
129.326451899367));
#116064=CARTESIAN_POINT('Ctrl Pts',(-166.952703938412,4.64820769355471,
129.197080834803));
#116065=CARTESIAN_POINT('Ctrl Pts',(-166.960476838678,4.60340132800528,
129.067502092321));
#116066=CARTESIAN_POINT('Ctrl Pts',(-166.968249738943,4.55321994752032,
128.939935680729));
#116067=CARTESIAN_POINT('Ctrl Pts',(-166.976022639209,4.49788951291557,
128.814844849319));
#116068=CARTESIAN_POINT('Ctrl Pts',(-166.983512974971,4.44457047897841,
128.694301384717));
#116069=CARTESIAN_POINT('Ctrl Pts',(-166.991003310732,4.38647038945388,
128.576056914437));
#116070=CARTESIAN_POINT('Ctrl Pts',(-166.998493646494,4.32383026132284,
128.460501634229));
#116071=CARTESIAN_POINT('Ctrl Pts',(-167.006267980613,4.25881511369365,
128.340565040449));
#116072=CARTESIAN_POINT('Ctrl Pts',(-167.014042314732,4.18870291186473,
128.223145660416));
#116073=CARTESIAN_POINT('Ctrl Pts',(-167.021816648852,4.1137130342247,128.10870705404));
#116074=CARTESIAN_POINT('Ctrl Pts',(-167.029581401799,4.03881557490723,
127.994409483019));
#116075=CARTESIAN_POINT('Ctrl Pts',(-167.037346154746,3.95905261270079,
127.883085700282));
#116076=CARTESIAN_POINT('Ctrl Pts',(-167.045110907693,3.87468982048289,
127.775175602162));
#116077=CARTESIAN_POINT('Ctrl Pts',(-167.052867948578,3.79041081857929,
127.667372681873));
#116078=CARTESIAN_POINT('Ctrl Pts',(-167.060624989463,3.70154131765627,
127.562977004932));
#116079=CARTESIAN_POINT('Ctrl Pts',(-167.068382030348,3.6083905730819,127.462400035124));
#116080=CARTESIAN_POINT('Ctrl Pts',(-167.076133221588,3.51531007420823,
127.361898911192));
#116081=CARTESIAN_POINT('Ctrl Pts',(-167.083884412828,3.41795502244142,
127.265211048172));
#116082=CARTESIAN_POINT('Ctrl Pts',(-167.091635604068,3.31667504666567,
127.172715026746));
#116083=CARTESIAN_POINT('Ctrl Pts',(-167.099383500845,3.21543811758177,
127.080258318596));
#116084=CARTESIAN_POINT('Ctrl Pts',(-167.107131397622,3.11027987049151,
126.991990171584));
#116085=CARTESIAN_POINT('Ctrl Pts',(-167.1148792944,3.00158674532412,126.908252293508));
#116086=CARTESIAN_POINT('Ctrl Pts',(-167.122625570484,2.89291635641537,
126.824531931591));
#116087=CARTESIAN_POINT('Ctrl Pts',(-167.130371846568,2.78071286969311,
126.745340192166));
#116088=CARTESIAN_POINT('Ctrl Pts',(-167.138118122652,2.66539544153446,
126.670978200858));
#116089=CARTESIAN_POINT('Ctrl Pts',(-167.145864455917,2.55007716212859,
126.596615660627));
#116090=CARTESIAN_POINT('Ctrl Pts',(-167.153610789183,2.43164522399254,
126.527083151533));
#116091=CARTESIAN_POINT('Ctrl Pts',(-167.161357122448,2.31054702603529,
126.462637975229));
#116092=CARTESIAN_POINT('Ctrl Pts',(-167.169105190451,2.18942170897608,
126.398178366875));
#116093=CARTESIAN_POINT('Ctrl Pts',(-167.176853258454,2.06562928902431,
126.338808541968));
#116094=CARTESIAN_POINT('Ctrl Pts',(-167.184601326457,1.93964060747172,
126.284739242235));
#116095=CARTESIAN_POINT('Ctrl Pts',(-167.192357629199,1.81351802364926,
126.230612477007));
#116096=CARTESIAN_POINT('Ctrl Pts',(-167.200113931941,1.68519487523416,
126.181797644832));
#116097=CARTESIAN_POINT('Ctrl Pts',(-167.207870234683,1.5551612953463,126.138457017195));
#116098=CARTESIAN_POINT('Ctrl Pts',(-167.215630677197,1.42505831262161,
126.095093257359));
#116099=CARTESIAN_POINT('Ctrl Pts',(-167.223391119711,1.29324345494687,
126.05720963183));
#116100=CARTESIAN_POINT('Ctrl Pts',(-167.231151562225,1.16021979538792,
126.024917858322));
#116101=CARTESIAN_POINT('Ctrl Pts',(-167.23892446249,1.02698259444135,125.992574247193));
#116102=CARTESIAN_POINT('Ctrl Pts',(-167.246697362756,0.892533097600021,
125.965840502357));
#116103=CARTESIAN_POINT('Ctrl Pts',(-167.254470263021,0.757383186953273,
125.944776914138));
#116104=CARTESIAN_POINT('Ctrl Pts',(-167.261960598783,0.62714631598135,
125.924479040408));
#116105=CARTESIAN_POINT('Ctrl Pts',(-167.269450934545,0.496259376714351,
125.909446266736));
#116106=CARTESIAN_POINT('Ctrl Pts',(-167.276941270307,0.365180927454096,
125.899686729047));
#116107=CARTESIAN_POINT('Ctrl Pts',(-167.284715604427,0.229132598948755,
125.889557155519));
#116108=CARTESIAN_POINT('Ctrl Pts',(-167.292489938545,0.0924469913636022,
125.885076493563));
#116109=CARTESIAN_POINT('Ctrl Pts',(-167.300264272665,-0.0443673098444563,
125.886310739381));
#116110=CARTESIAN_POINT('Ctrl Pts',(-167.308029025612,-0.181012999652978,
125.887543464101));
#116111=CARTESIAN_POINT('Ctrl Pts',(-167.315793778559,-0.317786680314714,
125.894477079405));
#116112=CARTESIAN_POINT('Ctrl Pts',(-167.323558531506,-0.454174651904994,
125.907125841892));
#116113=CARTESIAN_POINT('Ctrl Pts',(-167.331315572391,-0.590427161039898,
125.91976204145));
#116114=CARTESIAN_POINT('Ctrl Pts',(-167.339072613276,-0.726294336697561,
125.938102056099));
#116115=CARTESIAN_POINT('Ctrl Pts',(-167.346829654161,-0.861262842660616,
125.962108106766));
#116116=CARTESIAN_POINT('Ctrl Pts',(-167.354580845401,-0.996129567823606,
125.986096054283));
#116117=CARTESIAN_POINT('Ctrl Pts',(-167.362332036641,-1.13009858883394,
126.015741464878));
#116118=CARTESIAN_POINT('Ctrl Pts',(-167.370083227881,-1.26266241209136,
126.050954817974));
#116119=CARTESIAN_POINT('Ctrl Pts',(-167.377831124658,-1.3951698921871,
126.086153204456));
#116120=CARTESIAN_POINT('Ctrl Pts',(-167.385579021436,-1.52627298533755,
126.12691472644));
#116121=CARTESIAN_POINT('Ctrl Pts',(-167.393326918213,-1.6554753228729,
126.173098962481));
#116122=CARTESIAN_POINT('Ctrl Pts',(-167.401073194297,-1.78465063406488,
126.219273537776));
#116123=CARTESIAN_POINT('Ctrl Pts',(-167.408819470381,-1.9119256125657,
126.270868439399));
#116124=CARTESIAN_POINT('Ctrl Pts',(-167.416565746465,-2.03682034859898,
126.327693784974));
#116125=CARTESIAN_POINT('Ctrl Pts',(-167.42431207973,-2.16171600657666,
126.38451955002));
#116126=CARTESIAN_POINT('Ctrl Pts',(-167.432058412996,-2.28423103116377,
126.44657567415));
#116127=CARTESIAN_POINT('Ctrl Pts',(-167.439804746261,-2.40390711715438,
126.513624825817));
#116128=CARTESIAN_POINT('Ctrl Pts',(-167.447552814264,-2.52361000377451,
126.580688992677));
#116129=CARTESIAN_POINT('Ctrl Pts',(-167.455300882267,-2.64047234569105,
126.652748221015));
#116130=CARTESIAN_POINT('Ctrl Pts',(-167.46304895027,-2.75406233870187,
126.729520289769));
#116131=CARTESIAN_POINT('Ctrl Pts',(-167.470805253012,-2.86777305650915,
126.80637395279));
#116132=CARTESIAN_POINT('Ctrl Pts',(-167.478561555754,-2.97820415351134,
126.887950242693));
#116133=CARTESIAN_POINT('Ctrl Pts',(-167.486317858496,-3.08495417718945,
126.973924508304));
#116134=CARTESIAN_POINT('Ctrl Pts',(-167.49407830101,-3.19176117656938,
127.059944660968));
#116135=CARTESIAN_POINT('Ctrl Pts',(-167.501838743524,-3.29488289397738,
127.150367208963));
#116136=CARTESIAN_POINT('Ctrl Pts',(-167.509599186038,-3.39395341485524,
127.244829288824));
#116137=CARTESIAN_POINT('Ctrl Pts',(-167.517372086303,-3.49318297252828,
127.339443007602));
#116138=CARTESIAN_POINT('Ctrl Pts',(-167.525144986569,-3.588348066352,127.438108935011));
#116139=CARTESIAN_POINT('Ctrl Pts',(-167.532917886834,-3.67912128759667,
127.540428998544));
#116140=CARTESIAN_POINT('Ctrl Pts',(-167.540408222596,-3.76659467360441,
127.639029470038));
#116141=CARTESIAN_POINT('Ctrl Pts',(-167.547898558358,-3.84998975960928,
127.741022777588));
#116142=CARTESIAN_POINT('Ctrl Pts',(-167.55538889412,-3.92905183866609,
127.846027520774));
#116143=CARTESIAN_POINT('Ctrl Pts',(-167.563193592337,-4.01143207996082,
127.955439215786));
#116144=CARTESIAN_POINT('Ctrl Pts',(-167.570998290554,-4.08937090091598,
128.068470084042));
#116145=CARTESIAN_POINT('Ctrl Pts',(-167.578802988771,-4.16253478024338,
128.184725668615));
#116146=CARTESIAN_POINT('Ctrl Pts',(-167.586594824583,-4.23557808303929,
128.300789660078));
#116147=CARTESIAN_POINT('Ctrl Pts',(-167.594386660396,-4.30386191328346,
128.4200674586));
#116148=CARTESIAN_POINT('Ctrl Pts',(-167.602178496208,-4.36709373417131,
128.542132649508));
#116149=CARTESIAN_POINT('Ctrl Pts',(-167.609962931,-4.430265494763,128.664081897662));
#116150=CARTESIAN_POINT('Ctrl Pts',(-167.617747365792,-4.48839461392436,
128.78881293102));
#116151=CARTESIAN_POINT('Ctrl Pts',(-167.625531800584,-4.54123229775526,
128.915871199983));
#116152=CARTESIAN_POINT('Ctrl Pts',(-167.633309299869,-4.59402290608838,
129.042816266949));
#116153=CARTESIAN_POINT('Ctrl Pts',(-167.641086799154,-4.64153131800097,
129.17208408541));
#116154=CARTESIAN_POINT('Ctrl Pts',(-167.648864298439,-4.68355533607567,
129.303196910165));
#116155=CARTESIAN_POINT('Ctrl Pts',(-167.654336040623,-4.7131206994435,
129.395439358262));
#116156=CARTESIAN_POINT('Ctrl Pts',(-167.659807782807,-4.73997245841085,
129.488594494564));
#116157=CARTESIAN_POINT('Ctrl Pts',(-167.665279524992,-4.76405452823393,
129.582490119308));
#116158=CARTESIAN_POINT('Ctrl Pts',(-165.915373126199,-4.76405452823409,
129.582490119308));
#116159=CARTESIAN_POINT('Ctrl Pts',(-165.924244735256,-4.80281720230029,
129.733625197187));
#116160=CARTESIAN_POINT('Ctrl Pts',(-165.933116344314,-4.83442761491979,
129.886776635631));
#116161=CARTESIAN_POINT('Ctrl Pts',(-165.941987953371,-4.85869608661611,
130.041304000793));
#116162=CARTESIAN_POINT('Ctrl Pts',(-165.95079959072,-4.88280050445183,
130.194786767385));
#116163=CARTESIAN_POINT('Ctrl Pts',(-165.959611228069,-4.89966182275025,
130.349626760674));
#116164=CARTESIAN_POINT('Ctrl Pts',(-165.968422865418,-4.90914170930784,
130.505177161416));
#116165=CARTESIAN_POINT('Ctrl Pts',(-165.973995431597,-4.91513688286347,
130.603548765699));
#116166=CARTESIAN_POINT('Ctrl Pts',(-165.979567997776,-4.91818086365629,
130.702204113299));
#116167=CARTESIAN_POINT('Ctrl Pts',(-165.985140563956,-4.91824883541683,
130.800976031772));
#116168=CARTESIAN_POINT('',(-165.63985943605,-4.91824976783883,130.802849441434));
#116169=CARTESIAN_POINT('Ctrl Pts',(-165.569765327751,-4.76405452823417,
129.582490119309));
#116170=CARTESIAN_POINT('Ctrl Pts',(-165.577528737229,-4.79810511363771,
129.715252835007));
#116171=CARTESIAN_POINT('Ctrl Pts',(-165.585292146708,-4.8265698199595,
129.849315028426));
#116172=CARTESIAN_POINT('Ctrl Pts',(-165.593055556187,-4.84937783460778,
129.984166933297));
#116173=CARTESIAN_POINT('Ctrl Pts',(-165.600830198457,-4.87221884992079,
130.119213953901));
#116174=CARTESIAN_POINT('Ctrl Pts',(-165.608604840728,-4.88938678319999,
130.255052580719));
#116175=CARTESIAN_POINT('Ctrl Pts',(-165.616379482998,-4.90086275411845,
130.391168981888));
#116176=CARTESIAN_POINT('Ctrl Pts',(-165.619534496529,-4.90551979713908,
130.446406132675));
#116177=CARTESIAN_POINT('Ctrl Pts',(-165.622689510059,-4.90924008483265,
130.50168903927));
#116178=CARTESIAN_POINT('Ctrl Pts',(-165.625844523589,-4.91202479896185,
130.556983502853));
#116179=CARTESIAN_POINT('Ctrl Pts',(-165.630516161058,-4.91614813305812,
130.638858171651));
#116180=CARTESIAN_POINT('Ctrl Pts',(-165.635187798526,-4.91822456870397,
130.720836791468));
#116181=CARTESIAN_POINT('Ctrl Pts',(-165.639859435994,-4.91824976783853,
130.802849440458));
#116182=CARTESIAN_POINT('Ctrl Pts',(-165.63985943605,-4.91824976783883,
130.802849441434));
#116183=CARTESIAN_POINT('Ctrl Pts',(-165.647572658369,-4.91829137346489,
130.9382584493));
#116184=CARTESIAN_POINT('Ctrl Pts',(-165.655285880688,-4.91273663719269,
131.073894834778));
#116185=CARTESIAN_POINT('Ctrl Pts',(-165.662999103007,-4.90155537433178,
131.209253164866));
#116186=CARTESIAN_POINT('Ctrl Pts',(-165.670703040709,-4.89038757066458,
131.344448560409));
#116187=CARTESIAN_POINT('Ctrl Pts',(-165.67840697841,-4.87360674481668,
131.479366173904));
#116188=CARTESIAN_POINT('Ctrl Pts',(-165.686110916112,-4.85123469155569,
131.613499066749));
#116189=CARTESIAN_POINT('Ctrl Pts',(-165.693807495515,-4.82888400661853,
131.747503844617));
#116190=CARTESIAN_POINT('Ctrl Pts',(-165.701504074918,-4.80095278398878,
131.880725003266));
#116191=CARTESIAN_POINT('Ctrl Pts',(-165.709200654322,-4.76751470411547,
132.012659673488));
#116192=CARTESIAN_POINT('Ctrl Pts',(-165.716891794583,-4.73410025479962,
132.144501106007));
#116193=CARTESIAN_POINT('Ctrl Pts',(-165.724582934844,-4.6951867898392,
132.275057475282));
#116194=CARTESIAN_POINT('Ctrl Pts',(-165.732274075106,-4.65089917305424,
132.403835514082));
#116195=CARTESIAN_POINT('Ctrl Pts',(-165.739962504378,-4.60662716685935,
132.532568160933));
#116196=CARTESIAN_POINT('Ctrl Pts',(-165.747650933651,-4.55698490298903,
132.659523347808));
#116197=CARTESIAN_POINT('Ctrl Pts',(-165.755339362923,-4.50214718436271,
132.784222681659));
#116198=CARTESIAN_POINT('Ctrl Pts',(-165.763026646874,-4.44731763474355,
132.908903439432));
#116199=CARTESIAN_POINT('Ctrl Pts',(-165.770713930825,-4.38729432942435,
133.031328648556));
#116200=CARTESIAN_POINT('Ctrl Pts',(-165.778401214776,-4.32230012797284,
133.151040115543));
#116201=CARTESIAN_POINT('Ctrl Pts',(-165.786089082622,-4.2573009898167,
133.270760675344));
#116202=CARTESIAN_POINT('Ctrl Pts',(-165.793776950469,-4.18733039434107,
133.387766733588));
#116203=CARTESIAN_POINT('Ctrl Pts',(-165.801464818316,-4.11265680816186,
133.501625350732));
#116204=CARTESIAN_POINT('Ctrl Pts',(-165.809154999391,-4.03796075319266,
133.615518227183));
#116205=CARTESIAN_POINT('Ctrl Pts',(-165.816845180466,-3.9585591108194,
133.726261446517));
#116206=CARTESIAN_POINT('Ctrl Pts',(-165.824535361542,-3.87476296104074,
133.833452075123));
#116207=CARTESIAN_POINT('Ctrl Pts',(-165.832233884725,-3.79087591139023,
133.94075898132));
#116208=CARTESIAN_POINT('Ctrl Pts',(-165.839932407907,-3.70258508251573,
134.04450528975));
#116209=CARTESIAN_POINT('Ctrl Pts',(-165.84763093109,-3.61024126495735,
134.14432185556));
#116210=CARTESIAN_POINT('Ctrl Pts',(-165.855334211813,-3.51784038068537,
134.244200106098));
#116211=CARTESIAN_POINT('Ctrl Pts',(-165.863037492536,-3.4213818015299,
134.340143498591));
#116212=CARTESIAN_POINT('Ctrl Pts',(-165.870740773259,-3.32125138849588,
134.431821475648));
#116213=CARTESIAN_POINT('Ctrl Pts',(-165.878455261322,-3.22097529783983,
134.523632833055));
#116214=CARTESIAN_POINT('Ctrl Pts',(-165.886169749385,-3.11701701183142,
134.611166131248));
#116215=CARTESIAN_POINT('Ctrl Pts',(-165.893884237449,-3.00979381929446,
134.694132362519));
#116216=CARTESIAN_POINT('Ctrl Pts',(-165.897353540766,-2.96157418701721,
134.731443331058));
#116217=CARTESIAN_POINT('Ctrl Pts',(-165.900822844084,-2.91269462428702,
134.767831246968));
#116218=CARTESIAN_POINT('Ctrl Pts',(-165.904292147402,-2.86319475940396,
134.803272823682));
#116219=CARTESIAN_POINT('Ctrl Pts',(-165.912066481521,-2.75227090720901,
134.882693570107));
#116220=CARTESIAN_POINT('Ctrl Pts',(-165.91984081564,-2.63786433591703,
134.957621322623));
#116221=CARTESIAN_POINT('Ctrl Pts',(-165.927615149759,-2.52037507671445,
135.027735161124));
#116222=CARTESIAN_POINT('Ctrl Pts',(-165.935379902706,-2.40303061252321,
135.097762590586));
#116223=CARTESIAN_POINT('Ctrl Pts',(-165.943144655653,-2.282611352077,135.162987711945));
#116224=CARTESIAN_POINT('Ctrl Pts',(-165.9509094086,-2.15954860847618,135.223131133233));
#116225=CARTESIAN_POINT('Ctrl Pts',(-165.958666449485,-2.03660809252719,
135.283214819227));
#116226=CARTESIAN_POINT('Ctrl Pts',(-165.96642349037,-1.91102966736331,
135.33822667878));
#116227=CARTESIAN_POINT('Ctrl Pts',(-165.974180531255,-1.78327140333194,
135.387931950551));
#116228=CARTESIAN_POINT('Ctrl Pts',(-165.981931722495,-1.65560948280146,
135.437599739189));
#116229=CARTESIAN_POINT('Ctrl Pts',(-165.989682913735,-1.52577135824068,
135.481968764081));
#116230=CARTESIAN_POINT('Ctrl Pts',(-165.997434104975,-1.39423702492319,
135.520851493295));
#116231=CARTESIAN_POINT('Ctrl Pts',(-166.005182001752,-1.26275859720598,
135.559717696311));
#116232=CARTESIAN_POINT('Ctrl Pts',(-166.012929898529,-1.12958576875664,
135.593102130866));
#116233=CARTESIAN_POINT('Ctrl Pts',(-166.020677795306,-0.99521551109569,
135.620866524235));
#116234=CARTESIAN_POINT('Ctrl Pts',(-166.02842407139,-0.860873360795957,
135.648625109891));
#116235=CARTESIAN_POINT('Ctrl Pts',(-166.036170347474,-0.725334662130575,
135.670765913614));
#116236=CARTESIAN_POINT('Ctrl Pts',(-166.043916623558,-0.589108058332495,
135.687201466714));
#116237=CARTESIAN_POINT('Ctrl Pts',(-166.051662956824,-0.452880448940758,
135.703637141138));
#116238=CARTESIAN_POINT('Ctrl Pts',(-166.059409290089,-0.315965312434059,
135.714367434072));
#116239=CARTESIAN_POINT('Ctrl Pts',(-166.067155623354,-0.178877522579107,
135.719356639377));
#116240=CARTESIAN_POINT('Ctrl Pts',(-166.074903691357,-0.0417590328643031,
135.72434696198));
#116241=CARTESIAN_POINT('Ctrl Pts',(-166.08265175936,0.0955317965049134,
135.723593624388));
#116242=CARTESIAN_POINT('Ctrl Pts',(-166.090399827363,0.232479374539408,
135.717113043947));
#116243=CARTESIAN_POINT('Ctrl Pts',(-166.098156130105,0.369572502089724,
135.710625575868));
#116244=CARTESIAN_POINT('Ctrl Pts',(-166.105912432846,0.506321258403937,
135.698398724047));
#116245=CARTESIAN_POINT('Ctrl Pts',(-166.113668735588,0.642213903302813,
135.680500931883));
#116246=CARTESIAN_POINT('Ctrl Pts',(-166.121429178102,0.77817907819792,
135.662593587128));
#116247=CARTESIAN_POINT('Ctrl Pts',(-166.129189620616,0.913286846248104,
135.639009338167));
#116248=CARTESIAN_POINT('Ctrl Pts',(-166.13695006313,1.0470359414843,135.609867749986));
#116249=CARTESIAN_POINT('Ctrl Pts',(-166.144722963396,1.18099974264222,
135.580679381141));
#116250=CARTESIAN_POINT('Ctrl Pts',(-166.152495863661,1.31360013412663,
135.545915945011));
#116251=CARTESIAN_POINT('Ctrl Pts',(-166.160268763926,1.44435042113434,
135.505747107046));
#116252=CARTESIAN_POINT('Ctrl Pts',(-166.167759099689,1.57034760588446,
135.467038507517));
#116253=CARTESIAN_POINT('Ctrl Pts',(-166.175249435452,1.69462657219126,
135.423310785273));
#116254=CARTESIAN_POINT('Ctrl Pts',(-166.182739771215,1.81677138920114,
135.37475718481));
#116255=CARTESIAN_POINT('Ctrl Pts',(-166.190514105334,1.94354736406204,
135.324362659833));
#116256=CARTESIAN_POINT('Ctrl Pts',(-166.198288439453,2.0684257506417,135.268609451688));
#116257=CARTESIAN_POINT('Ctrl Pts',(-166.206062773573,2.190920323137,135.207660652786));
#116258=CARTESIAN_POINT('Ctrl Pts',(-166.21382752652,2.31326393201936,135.146786967831));
#116259=CARTESIAN_POINT('Ctrl Pts',(-166.221592279467,2.4332292255688,135.080730604871));
#116260=CARTESIAN_POINT('Ctrl Pts',(-166.229357032414,2.5503480081424,135.00970342165));
#116261=CARTESIAN_POINT('Ctrl Pts',(-166.237114073299,2.66735046668975,
134.938746783629));
#116262=CARTESIAN_POINT('Ctrl Pts',(-166.244871114185,2.78151170837552,
134.862829351798));
#116263=CARTESIAN_POINT('Ctrl Pts',(-166.25262815507,2.89238662362302,134.782209619475));
#116264=CARTESIAN_POINT('Ctrl Pts',(-166.26037934631,3.00317792723491,134.701650683118));
#116265=CARTESIAN_POINT('Ctrl Pts',(-166.26813053755,3.11068752227287,134.616396733443));
#116266=CARTESIAN_POINT('Ctrl Pts',(-166.275881728791,3.21449818364169,
134.526750238477));
#116267=CARTESIAN_POINT('Ctrl Pts',(-166.283629625568,3.31826472271004,
134.437141845663));
#116268=CARTESIAN_POINT('Ctrl Pts',(-166.291377522345,3.41833515970329,
134.343144875771));
#116269=CARTESIAN_POINT('Ctrl Pts',(-166.299125419122,3.51432453661603,
134.245102705232));
#116270=CARTESIAN_POINT('Ctrl Pts',(-166.306871695207,3.6102938346204,134.147081043002));
#116271=CARTESIAN_POINT('Ctrl Pts',(-166.314617971291,3.70218349719951,
134.045016142387));
#116272=CARTESIAN_POINT('Ctrl Pts',(-166.322364247375,3.78964500037565,
133.939288660381));
#116273=CARTESIAN_POINT('Ctrl Pts',(-166.330110580641,3.87710714917261,
133.833560397919));
#116274=CARTESIAN_POINT('Ctrl Pts',(-166.337856913906,3.9601408241367,133.724169801366));
#116275=CARTESIAN_POINT('Ctrl Pts',(-166.345603247172,4.03843768283384,
133.611530748564));
#116276=CARTESIAN_POINT('Ctrl Pts',(-166.353351315175,4.11675207556993,
133.498866471027));
#116277=CARTESIAN_POINT('Ctrl Pts',(-166.361099383178,4.19032731810833,
133.382952610625));
#116278=CARTESIAN_POINT('Ctrl Pts',(-166.368847451181,4.25889853330216,
133.264231822637));
#116279=CARTESIAN_POINT('Ctrl Pts',(-166.376603753923,4.32754262679921,
133.145384856783));
#116280=CARTESIAN_POINT('Ctrl Pts',(-166.384360056665,4.39117187314136,
133.023725343098));
#116281=CARTESIAN_POINT('Ctrl Pts',(-166.392116359407,4.44956724763099,
132.899720818417));
#116282=CARTESIAN_POINT('Ctrl Pts',(-166.399876801921,4.50799378949023,
132.775650108787));
#116283=CARTESIAN_POINT('Ctrl Pts',(-166.407637244436,4.56118074171969,
132.64923225443));
#116284=CARTESIAN_POINT('Ctrl Pts',(-166.41539768695,4.6089577512274,132.520953612396));
#116285=CARTESIAN_POINT('Ctrl Pts',(-166.423170587216,4.65681145663234,
132.392469046098));
#116286=CARTESIAN_POINT('Ctrl Pts',(-166.430943487481,4.69923774380455,
132.262118094926));
#116287=CARTESIAN_POINT('Ctrl Pts',(-166.438716387747,4.7361162866634,132.130401937323));
#116288=CARTESIAN_POINT('Ctrl Pts',(-166.446206723507,4.77165420159061,
132.003473993847));
#116289=CARTESIAN_POINT('Ctrl Pts',(-166.453697059268,4.8020406473944,131.875278677785));
#116290=CARTESIAN_POINT('Ctrl Pts',(-166.461187395029,4.82721338535474,
131.746270376912));
#116291=CARTESIAN_POINT('Ctrl Pts',(-166.468961729148,4.85334055533075,
131.612370687077));
#116292=CARTESIAN_POINT('Ctrl Pts',(-166.476736063267,4.87393362057539,
131.47717099286));
#116293=CARTESIAN_POINT('Ctrl Pts',(-166.484510397386,4.88886697842848,
131.341168525231));
#116294=CARTESIAN_POINT('Ctrl Pts',(-166.492275150333,4.90378193225261,
131.205333668489));
#116295=CARTESIAN_POINT('Ctrl Pts',(-166.50003990328,4.91305101475983,131.068698391739));
#116296=CARTESIAN_POINT('Ctrl Pts',(-166.507804656227,4.91659939668784,
130.931771115519));
#116297=CARTESIAN_POINT('Ctrl Pts',(-166.515561697112,4.92014425431291,
130.794979837401));
#116298=CARTESIAN_POINT('Ctrl Pts',(-166.523318737997,4.91797970849462,
130.657897525268));
#116299=CARTESIAN_POINT('Ctrl Pts',(-166.531075778882,4.91008264438322,
130.521038384364));
#116300=CARTESIAN_POINT('Ctrl Pts',(-166.538826970123,4.90219153550928,
130.384282450003));
#116301=CARTESIAN_POINT('Ctrl Pts',(-166.546578161363,4.88857653531634,
130.247749740626));
#116302=CARTESIAN_POINT('Ctrl Pts',(-166.554329352603,4.86926659836753,
130.111954770882));
#116303=CARTESIAN_POINT('Ctrl Pts',(-166.56207724938,4.84996486865707,129.976217517622));
#116304=CARTESIAN_POINT('Ctrl Pts',(-166.569825146157,4.82497307130679,
129.84121776661));
#116305=CARTESIAN_POINT('Ctrl Pts',(-166.577573042934,4.79437201942716,
129.707464997266));
#116306=CARTESIAN_POINT('Ctrl Pts',(-166.585319319018,4.76377736862789,
129.573740206117));
#116307=CARTESIAN_POINT('Ctrl Pts',(-166.593065595103,4.72757588426715,
129.441262258685));
#116308=CARTESIAN_POINT('Ctrl Pts',(-166.600811871187,4.68589943813165,
129.310530132465));
#116309=CARTESIAN_POINT('Ctrl Pts',(-166.608558204452,4.64422268435015,
129.17979704121));
#116310=CARTESIAN_POINT('Ctrl Pts',(-166.616304537717,4.59707100689755,
129.050810169378));
#116311=CARTESIAN_POINT('Ctrl Pts',(-166.624050870983,4.54462594630597,
128.924052645275));
#116312=CARTESIAN_POINT('Ctrl Pts',(-166.631798938986,4.49216914100678,
128.797266734702));
#116313=CARTESIAN_POINT('Ctrl Pts',(-166.639547006989,4.43441674316936,
128.672711526498));
#116314=CARTESIAN_POINT('Ctrl Pts',(-166.647295074992,4.37159799864712,
128.550849135296));
#116315=CARTESIAN_POINT('Ctrl Pts',(-166.655051377734,4.3087124896154,128.428857227293));
#116316=CARTESIAN_POINT('Ctrl Pts',(-166.662807680476,4.2407500570566,128.309564201428));
#116317=CARTESIAN_POINT('Ctrl Pts',(-166.670563983218,4.16798566475193,
128.193407044459));
#116318=CARTESIAN_POINT('Ctrl Pts',(-166.678324425732,4.09518243590039,
128.077187890918));
#116319=CARTESIAN_POINT('Ctrl Pts',(-166.686084868246,4.01757236153604,
127.964108263468));
#116320=CARTESIAN_POINT('Ctrl Pts',(-166.69384531076,3.93547254761333,127.854574372856));
#116321=CARTESIAN_POINT('Ctrl Pts',(-166.701618211026,3.85324093978062,
127.744864648718));
#116322=CARTESIAN_POINT('Ctrl Pts',(-166.709391111291,3.76650543736798,
127.638712338639));
#116323=CARTESIAN_POINT('Ctrl Pts',(-166.717164011557,3.67562265680721,
127.536489575547));
#116324=CARTESIAN_POINT('Ctrl Pts',(-166.724654347318,3.58804369424514,
127.437982867383));
#116325=CARTESIAN_POINT('Ctrl Pts',(-166.73214468308,3.49661396033875,127.343125190251));
#116326=CARTESIAN_POINT('Ctrl Pts',(-166.739635018841,3.40168210284458,
127.252214515041));
#116327=CARTESIAN_POINT('Ctrl Pts',(-166.74740935296,3.30315087511524,127.157856933943));
#116328=CARTESIAN_POINT('Ctrl Pts',(-166.755183687079,3.20053459809648,
127.067452667768));
#116329=CARTESIAN_POINT('Ctrl Pts',(-166.762958021198,3.0941837149797,126.981376155074));
#116330=CARTESIAN_POINT('Ctrl Pts',(-166.770722774145,2.98796389982179,
126.89540572399));
#116331=CARTESIAN_POINT('Ctrl Pts',(-166.778487527092,2.878018937287,126.813752677777));
#116332=CARTESIAN_POINT('Ctrl Pts',(-166.786252280039,2.76473612893011,
126.736754786135));
#116333=CARTESIAN_POINT('Ctrl Pts',(-166.794009320924,2.65156583465549,
126.659833369885));
#116334=CARTESIAN_POINT('Ctrl Pts',(-166.801766361809,2.53506461320026,
126.587558125455));
#116335=CARTESIAN_POINT('Ctrl Pts',(-166.809523402694,2.41565258585925,
126.52022644052));
#116336=CARTESIAN_POINT('Ctrl Pts',(-166.817274593934,2.29633060805678,
126.452945530932));
#116337=CARTESIAN_POINT('Ctrl Pts',(-166.825025785174,2.17410253268466,
126.390600951777));
#116338=CARTESIAN_POINT('Ctrl Pts',(-166.832776976414,2.04941688613532,
126.333446450494));
#116339=CARTESIAN_POINT('Ctrl Pts',(-166.840524873191,1.92478423431202,
126.276316241399));
#116340=CARTESIAN_POINT('Ctrl Pts',(-166.848272769968,1.79769644346981,
126.22437188534));
#116341=CARTESIAN_POINT('Ctrl Pts',(-166.856020666745,1.66862583453439,
126.177820778029));
#116342=CARTESIAN_POINT('Ctrl Pts',(-166.863766942829,1.53958222438827,
126.131279408206));
#116343=CARTESIAN_POINT('Ctrl Pts',(-166.871513218913,1.40855698867826,
126.090129175737));
#116344=CARTESIAN_POINT('Ctrl Pts',(-166.879259494997,1.27604121122577,
126.054528842676));
#116345=CARTESIAN_POINT('Ctrl Pts',(-166.887005828262,1.1435244555721,126.018928246822));
#116346=CARTESIAN_POINT('Ctrl Pts',(-166.894752161527,1.00951751379776,
125.988877733562));
#116347=CARTESIAN_POINT('Ctrl Pts',(-166.902498494793,0.874524982520793,
125.964485710355));
#116348=CARTESIAN_POINT('Ctrl Pts',(-166.910246562795,0.739502220601866,
125.940088224724));
#116349=CARTESIAN_POINT('Ctrl Pts',(-166.917994630798,0.603493814642456,
125.921351820191));
#116350=CARTESIAN_POINT('Ctrl Pts',(-166.925742698801,0.46701246775624,
125.908333409976));
#116351=CARTESIAN_POINT('Ctrl Pts',(-166.933499001543,0.330386066870588,
125.89530116364));
#116352=CARTESIAN_POINT('Ctrl Pts',(-166.941255304285,0.193286110785362,
125.887999088571));
#116353=CARTESIAN_POINT('Ctrl Pts',(-166.949011607026,0.0562288734783581,
125.886432051972));
#116354=CARTESIAN_POINT('Ctrl Pts',(-166.95677204954,-0.0809015154032844,
125.884864178998));
#116355=CARTESIAN_POINT('Ctrl Pts',(-166.964532492055,-0.217988749482219,
125.88903743183));
#116356=CARTESIAN_POINT('Ctrl Pts',(-166.972292934569,-0.354519668638239,
125.898904587078));
#116357=CARTESIAN_POINT('Ctrl Pts',(-166.980065834834,-0.491269759345966,
125.90878758196));
#116358=CARTESIAN_POINT('Ctrl Pts',(-166.987838735099,-0.627461361889623,
125.924382700102));
#116359=CARTESIAN_POINT('Ctrl Pts',(-166.995611635364,-0.762588630404179,
125.945591056939));
#116360=CARTESIAN_POINT('Ctrl Pts',(-167.003101971128,-0.892803682366956,
125.966028436587));
#116361=CARTESIAN_POINT('Ctrl Pts',(-167.010592306891,-1.02203013714848,
125.991677969634));
#116362=CARTESIAN_POINT('Ctrl Pts',(-167.018082642654,-1.14982885077125,
126.022407389393));
#116363=CARTESIAN_POINT('Ctrl Pts',(-167.025856976774,-1.28247309144524,
126.054301924437));
#116364=CARTESIAN_POINT('Ctrl Pts',(-167.033631310893,-1.41399936523554,
126.091770190424));
#116365=CARTESIAN_POINT('Ctrl Pts',(-167.041405645012,-1.5439032232719,
126.134719742759));
#116366=CARTESIAN_POINT('Ctrl Pts',(-167.049170397959,-1.67364698641273,
126.177616363609));
#116367=CARTESIAN_POINT('Ctrl Pts',(-167.056935150907,-1.80177194453462,
126.22598070843));
#116368=CARTESIAN_POINT('Ctrl Pts',(-167.064699903854,-1.92778457647381,
126.279669502229));
#116369=CARTESIAN_POINT('Ctrl Pts',(-167.072456944739,-2.05367205089085,
126.333304971561));
#116370=CARTESIAN_POINT('Ctrl Pts',(-167.080213985624,-2.17745101687157,
126.392254213625));
#116371=CARTESIAN_POINT('Ctrl Pts',(-167.087971026509,-2.29864418792239,
126.45632451378));
#116372=CARTESIAN_POINT('Ctrl Pts',(-167.09572221775,-2.41974596626035,
126.520346498022));
#116373=CARTESIAN_POINT('Ctrl Pts',(-167.10347340899,-2.53826548672278,
126.589481671631));
#116374=CARTESIAN_POINT('Ctrl Pts',(-167.11122460023,-2.65374682493084,
126.663489833338));
#116375=CARTESIAN_POINT('Ctrl Pts',(-167.118972497007,-2.76917908048912,
126.737466539603));
#116376=CARTESIAN_POINT('Ctrl Pts',(-167.126720393785,-2.88157539362716,
126.816311904094));
#116377=CARTESIAN_POINT('Ctrl Pts',(-167.134468290562,-2.99050597546051,
126.89974065229));
#116378=CARTESIAN_POINT('Ctrl Pts',(-167.142214566646,-3.09941377136441,
126.98315194899));
#116379=CARTESIAN_POINT('Ctrl Pts',(-167.14996084273,-3.20485696774908,
127.071144484825));
#116380=CARTESIAN_POINT('Ctrl Pts',(-167.157707118815,-3.30643655079946,
127.163390911837));
#116381=CARTESIAN_POINT('Ctrl Pts',(-167.16545345208,-3.40801688368738,
127.255638019791));
#116382=CARTESIAN_POINT('Ctrl Pts',(-167.173199785346,-3.50573325690008,
127.352138818744));
#116383=CARTESIAN_POINT('Ctrl Pts',(-167.180946118611,-3.59922171737467,
127.452527374149));
#116384=CARTESIAN_POINT('Ctrl Pts',(-167.188694186614,-3.69273111394165,
127.552938410874));
#116385=CARTESIAN_POINT('Ctrl Pts',(-167.196442254618,-3.78201044732934,
127.657238650459));
#116386=CARTESIAN_POINT('Ctrl Pts',(-167.204190322621,-3.86673470627826,
127.765027504239));
#116387=CARTESIAN_POINT('Ctrl Pts',(-167.211946625363,-3.9515490111777,
127.872930917296));
#116388=CARTESIAN_POINT('Ctrl Pts',(-167.219702928105,-4.03179832885506,
127.984330043291));
#116389=CARTESIAN_POINT('Ctrl Pts',(-167.227459230847,-4.10719950570012,
128.098793157147));
#116390=CARTESIAN_POINT('Ctrl Pts',(-167.235219673361,-4.18264092642375,
128.213317363414));
#116391=CARTESIAN_POINT('Ctrl Pts',(-167.242980115875,-4.25322884918431,
128.330908481056));
#116392=CARTESIAN_POINT('Ctrl Pts',(-167.25074055839,-4.31872562877702,
128.451109248535));
#116393=CARTESIAN_POINT('Ctrl Pts',(-167.258513458655,-4.38432754961469,
128.571502972957));
#116394=CARTESIAN_POINT('Ctrl Pts',(-167.266286358921,-4.44482182288314,
128.694514367618));
#116395=CARTESIAN_POINT('Ctrl Pts',(-167.274059259186,-4.50001822092207,
128.819664400542));
#116396=CARTESIAN_POINT('Ctrl Pts',(-167.281549594947,-4.5532080908484,
128.940264914507));
#116397=CARTESIAN_POINT('Ctrl Pts',(-167.289039930707,-4.60147846758377,
129.062850989889));
#116398=CARTESIAN_POINT('Ctrl Pts',(-167.296530266468,-4.644703262792,129.186981669048));
#116399=CARTESIAN_POINT('Ctrl Pts',(-167.304374368132,-4.68996954975881,
129.316974996191));
#116400=CARTESIAN_POINT('Ctrl Pts',(-167.312218469795,-4.72980493418321,
129.448951471914));
#116401=CARTESIAN_POINT('Ctrl Pts',(-167.320062571459,-4.76405452823401,
129.582490119308));
#116402=CARTESIAN_POINT('Origin',(213.235140564004,0.,130.804360617566));
#116403=CARTESIAN_POINT('',(-169.415000431073,-4.76405452823411,129.582490119308));
#116404=CARTESIAN_POINT('',(-169.070032268681,-4.7640545282341,129.582490119308));
#116405=CARTESIAN_POINT('',(213.235140564004,-4.76405452823405,129.582490119308));
#116406=CARTESIAN_POINT('',(-167.735140564067,-4.91824875640079,130.807858139837));
#116407=CARTESIAN_POINT('Ctrl Pts',(-167.735140564067,-4.91824875640079,
130.807858139838));
#116408=CARTESIAN_POINT('Ctrl Pts',(-167.744004443693,-4.91813704849458,
130.964942849568));
#116409=CARTESIAN_POINT('Ctrl Pts',(-167.752868323319,-4.91049564785334,
131.121727305909));
#116410=CARTESIAN_POINT('Ctrl Pts',(-167.761732202945,-4.89543454578459,
131.277545222598));
#116411=CARTESIAN_POINT('Ctrl Pts',(-167.770638196226,-4.88030188610434,
131.434103454164));
#116412=CARTESIAN_POINT('Ctrl Pts',(-167.779544189507,-4.85767896409776,
131.589685791336));
#116413=CARTESIAN_POINT('Ctrl Pts',(-167.788450182788,-4.82772686809456,
131.743634991526));
#116414=CARTESIAN_POINT('Ctrl Pts',(-167.797410831803,-4.79759095724287,
131.898528971972));
#116415=CARTESIAN_POINT('Ctrl Pts',(-167.806371480818,-4.76003572865256,
132.051769562129));
#116416=CARTESIAN_POINT('Ctrl Pts',(-167.815332129834,-4.71527376576907,
132.202708348408));
#116417=CARTESIAN_POINT('Ctrl Pts',(-167.8215002592,-4.68446153584179,132.306608184075));
#116418=CARTESIAN_POINT('Ctrl Pts',(-167.827668388567,-4.65023550546441,
132.409417780665));
#116419=CARTESIAN_POINT('Ctrl Pts',(-167.833836517933,-4.61267790990394,
132.510931905847));
#116420=CARTESIAN_POINT('Ctrl Pts',(-167.841610852052,-4.56534017114263,
132.638880702002));
#116421=CARTESIAN_POINT('Ctrl Pts',(-167.849385186171,-4.51259975549616,
132.765061049956));
#116422=CARTESIAN_POINT('Ctrl Pts',(-167.85715952029,-4.45460804032886,
132.888982950157));
#116423=CARTESIAN_POINT('Ctrl Pts',(-167.864924273237,-4.3966877947678,
133.012752127691));
#116424=CARTESIAN_POINT('Ctrl Pts',(-167.872689026184,-4.33352929067561,
133.134268044771));
#116425=CARTESIAN_POINT('Ctrl Pts',(-167.880453779131,-4.26533308938072,
133.253057556579));
#116426=CARTESIAN_POINT('Ctrl Pts',(-167.888210820016,-4.19720462151417,
133.371729084971));
#116427=CARTESIAN_POINT('Ctrl Pts',(-167.895967860901,-4.12404860705336,
133.487679260074));
#116428=CARTESIAN_POINT('Ctrl Pts',(-167.903724901786,-4.04611278347342,
133.600456897366));
#116429=CARTESIAN_POINT('Ctrl Pts',(-167.911476093026,-3.96823573190462,
133.713149488164));
#116430=CARTESIAN_POINT('Ctrl Pts',(-167.919227284266,-3.88558626710797,
133.822673982814));
#116431=CARTESIAN_POINT('Ctrl Pts',(-167.926978475507,-3.79845675775636,
133.928606017972));
#116432=CARTESIAN_POINT('Ctrl Pts',(-167.934726372284,-3.71136428077037,
134.034493029188));
#116433=CARTESIAN_POINT('Ctrl Pts',(-167.942474269061,-3.6197957942505,
134.136790316466));
#116434=CARTESIAN_POINT('Ctrl Pts',(-167.950222165838,-3.52408533781213,
134.235104792569));
#116435=CARTESIAN_POINT('Ctrl Pts',(-167.957968441922,-3.42839490193797,
134.333398703403));
#116436=CARTESIAN_POINT('Ctrl Pts',(-167.965714718006,-3.32856449203041,
134.42771118022));
#116437=CARTESIAN_POINT('Ctrl Pts',(-167.97346099409,-3.2249662918492,134.517684664688));
#116438=CARTESIAN_POINT('Ctrl Pts',(-167.981207327355,-3.12136732692946,
134.607658813321));
#116439=CARTESIAN_POINT('Ctrl Pts',(-167.98895366062,-3.01400081141961,
134.693293649332));
#116440=CARTESIAN_POINT('Ctrl Pts',(-167.996699993886,-2.90327310460602,
134.774270987155));
#116441=CARTESIAN_POINT('Ctrl Pts',(-168.004448061889,-2.79252060109037,
134.855266459292));
#116442=CARTESIAN_POINT('Ctrl Pts',(-168.012196129892,-2.678405723973,134.931602127018));
#116443=CARTESIAN_POINT('Ctrl Pts',(-168.019944197895,-2.56136464473602,
135.003002566958));
#116444=CARTESIAN_POINT('Ctrl Pts',(-168.027700500637,-2.44419917284739,
135.074478892136));
#116445=CARTESIAN_POINT('Ctrl Pts',(-168.035456803378,-2.32410162056808,
135.141009307704));
#116446=CARTESIAN_POINT('Ctrl Pts',(-168.04321310612,-2.20153413410475,
135.202363632444));
#116447=CARTESIAN_POINT('Ctrl Pts',(-168.050973548634,-2.07890122968346,
135.263750703834));
#116448=CARTESIAN_POINT('Ctrl Pts',(-168.058733991148,-1.95379612075027,
135.319956019468));
#116449=CARTESIAN_POINT('Ctrl Pts',(-168.066494433663,-1.82670093629337,
135.370797604085));
#116450=CARTESIAN_POINT('Ctrl Pts',(-168.074267333928,-1.69940172736305,
135.421720804126));
#116451=CARTESIAN_POINT('Ctrl Pts',(-168.082040234193,-1.57010642795901,
135.467262936989));
#116452=CARTESIAN_POINT('Ctrl Pts',(-168.089813134459,-1.43931318470221,
135.507291684342));
#116453=CARTESIAN_POINT('Ctrl Pts',(-168.097303470221,-1.31327460527724,
135.545865285904));
#116454=CARTESIAN_POINT('Ctrl Pts',(-168.104793805984,-1.18584539718265,
135.579319315285));
#116455=CARTESIAN_POINT('Ctrl Pts',(-168.112284141746,-1.0574783237846,
135.607580647632));
#116456=CARTESIAN_POINT('Ctrl Pts',(-168.120058475865,-0.924244173791153,
135.636913516983));
#116457=CARTESIAN_POINT('Ctrl Pts',(-168.127832809984,-0.789577590530997,
135.660745071809));
#116458=CARTESIAN_POINT('Ctrl Pts',(-168.135607144103,-0.653972647666248,
135.678937813447));
#116459=CARTESIAN_POINT('Ctrl Pts',(-168.14337189705,-0.518534825774218,
135.697108134158));
#116460=CARTESIAN_POINT('Ctrl Pts',(-168.151136649998,-0.382161329030799,
135.709653417296));
#116461=CARTESIAN_POINT('Ctrl Pts',(-168.158901402945,-0.245358635866684,
135.716486654457));
#116462=CARTESIAN_POINT('Ctrl Pts',(-168.16665844383,-0.108691817066,135.723313104751));
#116463=CARTESIAN_POINT('Ctrl Pts',(-168.174415484715,0.0284029618794884,
135.724438779783));
#116464=CARTESIAN_POINT('Ctrl Pts',(-168.1821725256,0.165412198495755,135.719828231851));
#116465=CARTESIAN_POINT('Ctrl Pts',(-168.18992371684,0.302318115381099,
135.71522116077));
#116466=CARTESIAN_POINT('Ctrl Pts',(-168.19767490808,0.439138229173773,
135.704886489924));
#116467=CARTESIAN_POINT('Ctrl Pts',(-168.20542609932,0.575357478565201,
135.688840818607));
#116468=CARTESIAN_POINT('Ctrl Pts',(-168.213173996097,0.711518831141686,
135.672801967128));
#116469=CARTESIAN_POINT('Ctrl Pts',(-168.220921892874,0.847079439787187,
135.651056988588));
#116470=CARTESIAN_POINT('Ctrl Pts',(-168.228669789651,0.981528032506999,
135.623674446723));
#116471=CARTESIAN_POINT('Ctrl Pts',(-168.236416065735,1.11594850147996,
135.596297632696));
#116472=CARTESIAN_POINT('Ctrl Pts',(-168.244162341819,1.24925703434299,
135.563285678925));
#116473=CARTESIAN_POINT('Ctrl Pts',(-168.251908617903,1.38095163273355,
135.524758445138));
#116474=CARTESIAN_POINT('Ctrl Pts',(-168.259654951168,1.51264720326353,
135.486230926952));
#116475=CARTESIAN_POINT('Ctrl Pts',(-168.267401284434,1.64272844031071,
135.442188157287));
#116476=CARTESIAN_POINT('Ctrl Pts',(-168.275147617699,1.77070799822673,
135.392800030647));
#116477=CARTESIAN_POINT('Ctrl Pts',(-168.282895685702,1.89871621627722,
135.343400843879));
#116478=CARTESIAN_POINT('Ctrl Pts',(-168.290643753705,2.02462145396681,
135.288654058866));
#116479=CARTESIAN_POINT('Ctrl Pts',(-168.298391821708,2.14795622846961,
135.228777765969));
#116480=CARTESIAN_POINT('Ctrl Pts',(-168.30614812445,2.27142208463862,135.168837835834));
#116481=CARTESIAN_POINT('Ctrl Pts',(-168.313904427192,2.39231166804874,
135.103757678471));
#116482=CARTESIAN_POINT('Ctrl Pts',(-168.321660729933,2.51018151940827,
135.033801692001));
#116483=CARTESIAN_POINT('Ctrl Pts',(-168.329421172448,2.62811428145648,
134.963808367915));
#116484=CARTESIAN_POINT('Ctrl Pts',(-168.337181614962,2.74302377255823,
134.8889342426));
#116485=CARTESIAN_POINT('Ctrl Pts',(-168.344942057476,2.85449628927647,
134.809486582752));
#116486=CARTESIAN_POINT('Ctrl Pts',(-168.352714957741,2.96614775157461,
134.729911386468));
#116487=CARTESIAN_POINT('Ctrl Pts',(-168.360487858007,3.07435090531329,
134.645748224486));
#116488=CARTESIAN_POINT('Ctrl Pts',(-168.368260758272,3.17872516691717,
134.557344680376));
#116489=CARTESIAN_POINT('Ctrl Pts',(-168.375751094034,3.27930516120885,
134.47215482777));
#116490=CARTESIAN_POINT('Ctrl Pts',(-168.383241429796,3.37632958319387,
134.383027746063));
#116491=CARTESIAN_POINT('Ctrl Pts',(-168.390731765558,3.46949218120573,
134.29030483213));
#116492=CARTESIAN_POINT('Ctrl Pts',(-168.398506099677,3.56618706743725,
134.194066300733));
#116493=CARTESIAN_POINT('Ctrl Pts',(-168.406280433796,3.65902780712314,
134.093649027781));
#116494=CARTESIAN_POINT('Ctrl Pts',(-168.414054767915,3.74763165986214,
133.989394370056));
#116495=CARTESIAN_POINT('Ctrl Pts',(-168.421819520862,3.8361263162714,133.885268196878));
#116496=CARTESIAN_POINT('Ctrl Pts',(-168.42958427381,3.92039422437408,133.777314343742));
#116497=CARTESIAN_POINT('Ctrl Pts',(-168.437349026757,4.00008841757219,
133.665911895126));
#116498=CARTESIAN_POINT('Ctrl Pts',(-168.445106067642,4.07970345737412,
133.554620092993));
#116499=CARTESIAN_POINT('Ctrl Pts',(-168.452863108527,4.15475359640531,
133.439886827591));
#116500=CARTESIAN_POINT('Ctrl Pts',(-168.460620149412,4.2249314508805,133.322124962746));
#116501=CARTESIAN_POINT('Ctrl Pts',(-168.468371340652,4.29505638368982,
133.20445190304));
#116502=CARTESIAN_POINT('Ctrl Pts',(-168.476122531892,4.36031614593633,
133.083755124329));
#116503=CARTESIAN_POINT('Ctrl Pts',(-168.483873723132,4.42044629985622,
132.960476934602));
#116504=CARTESIAN_POINT('Ctrl Pts',(-168.491621619909,4.48055089685675,
132.837251141394));
#116505=CARTESIAN_POINT('Ctrl Pts',(-168.499369516686,4.53553005078597,
132.711446470012));
#116506=CARTESIAN_POINT('Ctrl Pts',(-168.507117413463,4.58516509125597,
132.583530128441));
#116507=CARTESIAN_POINT('Ctrl Pts',(-168.514863689547,4.63478974914537,
132.455640544211));
#116508=CARTESIAN_POINT('Ctrl Pts',(-168.522609965632,4.67907237574544,
132.325640532646));
#116509=CARTESIAN_POINT('Ctrl Pts',(-168.530356241716,4.71784247006198,
132.194017226293));
#116510=CARTESIAN_POINT('Ctrl Pts',(-168.538102574981,4.75661285057061,
132.062392948328));
#116511=CARTESIAN_POINT('Ctrl Pts',(-168.545848908246,4.78987050712963,
131.929145726699));
#116512=CARTESIAN_POINT('Ctrl Pts',(-168.553595241512,4.81749495457136,
131.794777411234));
#116513=CARTESIAN_POINT('Ctrl Pts',(-168.561343309515,4.84512558831652,
131.660379004917));
#116514=CARTESIAN_POINT('Ctrl Pts',(-168.569091377518,4.86712042395351,
131.524859388063));
#116515=CARTESIAN_POINT('Ctrl Pts',(-168.576839445521,4.88341026119186,
131.38872975038));
#116516=CARTESIAN_POINT('Ctrl Pts',(-168.584595748263,4.8997174114631,131.252455432499));
#116517=CARTESIAN_POINT('Ctrl Pts',(-168.592352051005,4.91030740463335,
131.115570187479));
#116518=CARTESIAN_POINT('Ctrl Pts',(-168.600108353747,4.91516298575077,
130.978590023826));
#116519=CARTESIAN_POINT('Ctrl Pts',(-168.607868796261,4.92002115843803,
130.841536749735));
#116520=CARTESIAN_POINT('Ctrl Pts',(-168.615629238775,4.91913882302528,
130.704388846829));
#116521=CARTESIAN_POINT('Ctrl Pts',(-168.623389681289,4.91255087487469,
130.567660460684));
#116522=CARTESIAN_POINT('Ctrl Pts',(-168.631162581554,4.90595235116488,
130.430712585995));
#116523=CARTESIAN_POINT('Ctrl Pts',(-168.63893548182,4.89362994696933,130.294185963431));
#116524=CARTESIAN_POINT('Ctrl Pts',(-168.646708382085,4.87567037947153,
130.158588666144));
#116525=CARTESIAN_POINT('Ctrl Pts',(-168.654198717847,4.85836368748974,
130.027920672162));
#116526=CARTESIAN_POINT('Ctrl Pts',(-168.66168905361,4.83582261947571,129.898115913359));
#116527=CARTESIAN_POINT('Ctrl Pts',(-168.669179389372,4.80816886578278,
129.769616581286));
#116528=CARTESIAN_POINT('Ctrl Pts',(-168.676953723491,4.77946661161336,
129.636245157981));
#116529=CARTESIAN_POINT('Ctrl Pts',(-168.68472805761,4.74516540347589,129.503857625438));
#116530=CARTESIAN_POINT('Ctrl Pts',(-168.692502391729,4.70534555396082,
129.372960505675));
#116531=CARTESIAN_POINT('Ctrl Pts',(-168.700267144676,4.66557477885148,
129.242224704914));
#116532=CARTESIAN_POINT('Ctrl Pts',(-168.708031897623,4.62029900748321,
129.112976032696));
#116533=CARTESIAN_POINT('Ctrl Pts',(-168.71579665057,4.56964963044401,128.985711306268));
#116534=CARTESIAN_POINT('Ctrl Pts',(-168.723553691455,4.51905055908011,
128.858572980962));
#116535=CARTESIAN_POINT('Ctrl Pts',(-168.73131073234,4.46308864683044,128.733415040999));
#116536=CARTESIAN_POINT('Ctrl Pts',(-168.739067773225,4.40194509928063,
128.610719260047));
#116537=CARTESIAN_POINT('Ctrl Pts',(-168.746818964465,4.34084766055557,
128.488116004937));
#116538=CARTESIAN_POINT('Ctrl Pts',(-168.754570155705,4.27457653786798,
128.367971561631));
#116539=CARTESIAN_POINT('Ctrl Pts',(-168.762321346945,4.20336092238527,
128.250747487379));
#116540=CARTESIAN_POINT('Ctrl Pts',(-168.770069243723,4.13217557543898,
128.133573236486));
#116541=CARTESIAN_POINT('Ctrl Pts',(-168.7778171405,4.0560501180718,128.019317219363));
#116542=CARTESIAN_POINT('Ctrl Pts',(-168.785565037277,3.97525942890647,
127.908415946929));
#116543=CARTESIAN_POINT('Ctrl Pts',(-168.793311313361,3.89448563941166,
127.79753787265));
#116544=CARTESIAN_POINT('Ctrl Pts',(-168.801057589445,3.80904878923027,
127.690013463064));
#116545=CARTESIAN_POINT('Ctrl Pts',(-168.808803865529,3.7192665568207,127.586249472528));
#116546=CARTESIAN_POINT('Ctrl Pts',(-168.816550198794,3.62948366165896,
127.48248471603));
#116547=CARTESIAN_POINT('Ctrl Pts',(-168.82429653206,3.53535557607895,127.382480729627));
#116548=CARTESIAN_POINT('Ctrl Pts',(-168.832042865325,3.43723939537676,
127.286610142991));
#116549=CARTESIAN_POINT('Ctrl Pts',(-168.839790933328,3.33910124223633,
127.190718086803));
#116550=CARTESIAN_POINT('Ctrl Pts',(-168.847539001331,3.23697349637781,
127.098961545496));
#116551=CARTESIAN_POINT('Ctrl Pts',(-168.855287069334,3.1312488317325,127.011675049756));
#116552=CARTESIAN_POINT('Ctrl Pts',(-168.863043372076,3.02541180165561,
126.92429578489));
#116553=CARTESIAN_POINT('Ctrl Pts',(-168.870799674817,2.91597051821281,
126.841396305171));
#116554=CARTESIAN_POINT('Ctrl Pts',(-168.878555977559,2.8033497872499,126.763270042879));
#116555=CARTESIAN_POINT('Ctrl Pts',(-168.886316420073,2.69066894721163,
126.685102082248));
#116556=CARTESIAN_POINT('Ctrl Pts',(-168.894076862588,2.57480560842427,
126.611712624476));
#116557=CARTESIAN_POINT('Ctrl Pts',(-168.901837305102,2.45621119791615,
126.543350219347));
#116558=CARTESIAN_POINT('Ctrl Pts',(-168.909610205367,2.33742640913197,
126.474878072817));
#116559=CARTESIAN_POINT('Ctrl Pts',(-168.917383105633,2.21590213447506,
126.411449286111));
#116560=CARTESIAN_POINT('Ctrl Pts',(-168.925156005898,2.09211270303249,
126.353265527556));
#116561=CARTESIAN_POINT('Ctrl Pts',(-168.93264634166,1.97282332922927,126.297196895181));
#116562=CARTESIAN_POINT('Ctrl Pts',(-168.940136677422,1.85143091152834,
126.245998691306));
#116563=CARTESIAN_POINT('Ctrl Pts',(-168.947627013184,1.72837325481305,
126.199807549727));
#116564=CARTESIAN_POINT('Ctrl Pts',(-168.955401347303,1.60064982964137,
126.151865056975));
#116565=CARTESIAN_POINT('Ctrl Pts',(-168.963175681422,1.47072780825174,
126.109164939757));
#116566=CARTESIAN_POINT('Ctrl Pts',(-168.970950015542,1.33907675287918,
126.071913416339));
#116567=CARTESIAN_POINT('Ctrl Pts',(-168.978714768489,1.20758794566637,
126.034707802095));
#116568=CARTESIAN_POINT('Ctrl Pts',(-168.986479521436,1.07437471687023,
126.002937526415));
#116569=CARTESIAN_POINT('Ctrl Pts',(-168.994244274383,0.93992607273314,
125.976760588535));
#116570=CARTESIAN_POINT('Ctrl Pts',(-169.002001315268,0.805610964884803,
125.950609649959));
#116571=CARTESIAN_POINT('Ctrl Pts',(-169.009758356153,0.670063264820346,
125.930041067956));
#116572=CARTESIAN_POINT('Ctrl Pts',(-169.017515397038,0.533786248415471,
125.915162799569));
#116573=CARTESIAN_POINT('Ctrl Pts',(-169.025266588278,0.397611999568561,
125.900295751001));
#116574=CARTESIAN_POINT('Ctrl Pts',(-169.033017779518,0.260709916172463,
125.891110517115));
#116575=CARTESIAN_POINT('Ctrl Pts',(-169.040768970758,0.12359220283955,
125.887663755861));
#116576=CARTESIAN_POINT('Ctrl Pts',(-169.048516867535,-0.0134672318076487,
125.884218459573));
#116577=CARTESIAN_POINT('Ctrl Pts',(-169.056264764312,-0.150741724086354,
125.886506794728));
#116578=CARTESIAN_POINT('Ctrl Pts',(-169.064012661089,-0.287715446388911,
125.894533442969));
#116579=CARTESIAN_POINT('Ctrl Pts',(-169.071758937174,-0.424660516741201,
125.902558412209));
#116580=CARTESIAN_POINT('Ctrl Pts',(-169.079505213258,-0.561304552209544,
125.916319284153));
#116581=CARTESIAN_POINT('Ctrl Pts',(-169.087251489342,-0.697133625866751,
125.935768647583));
#116582=CARTESIAN_POINT('Ctrl Pts',(-169.094997822607,-0.832963702183509,
125.955218154584));
#116583=CARTESIAN_POINT('Ctrl Pts',(-169.102744155873,-0.967978417667158,
125.980356181444));
#116584=CARTESIAN_POINT('Ctrl Pts',(-169.110490489138,-1.10167124968987,
126.011083709218));
#116585=CARTESIAN_POINT('Ctrl Pts',(-169.118238557141,-1.23539402129518,
126.041818118208));
#116586=CARTESIAN_POINT('Ctrl Pts',(-169.125986625144,-1.367793939423,126.078144431352));
#116587=CARTESIAN_POINT('Ctrl Pts',(-169.133734693147,-1.49837730407996,
126.119913102958));
#116588=CARTESIAN_POINT('Ctrl Pts',(-169.141490995889,-1.62909945429102,
126.161726166805));
#116589=CARTESIAN_POINT('Ctrl Pts',(-169.149247298631,-1.75800082136722,
126.208993024383));
#116590=CARTESIAN_POINT('Ctrl Pts',(-169.157003601373,-1.88460491448449,
126.261514881818));
#116591=CARTESIAN_POINT('Ctrl Pts',(-169.164764043887,-2.01127658001824,
126.31406477175));
#116592=CARTESIAN_POINT('Ctrl Pts',(-169.172524486401,-2.13564817407344,
126.371875085529));
#116593=CARTESIAN_POINT('Ctrl Pts',(-169.180284928915,-2.25726657734122,
126.434700372041));
#116594=CARTESIAN_POINT('Ctrl Pts',(-169.188057829181,-2.3790802132667,
126.497626511281));
#116595=CARTESIAN_POINT('Ctrl Pts',(-169.195830729446,-2.49813148676619,
126.565583516747));
#116596=CARTESIAN_POINT('Ctrl Pts',(-169.203603629711,-2.61399434210779,
126.638281328603));
#116597=CARTESIAN_POINT('Ctrl Pts',(-169.211093965474,-2.72564529081649,
126.708336391882));
#116598=CARTESIAN_POINT('Ctrl Pts',(-169.218584301236,-2.83433535668576,
126.782793391126));
#116599=CARTESIAN_POINT('Ctrl Pts',(-169.226074636998,-2.93971294160209,
126.861357842589));
#116600=CARTESIAN_POINT('Ctrl Pts',(-169.233946545084,-3.05045866638537,
126.943924520563));
#116601=CARTESIAN_POINT('Ctrl Pts',(-169.24181845317,-3.1579198704667,127.031307420539));
#116602=CARTESIAN_POINT('Ctrl Pts',(-169.249690361257,-3.2616447690163,
127.123211820893));
#116603=CARTESIAN_POINT('Ctrl Pts',(-169.257377057583,-3.36292920829519,
127.21295387692));
#116604=CARTESIAN_POINT('Ctrl Pts',(-169.265063753909,-3.46065084826931,
127.307006786171));
#116605=CARTESIAN_POINT('Ctrl Pts',(-169.272750450235,-3.55441752683353,
127.40505199559));
#116606=CARTESIAN_POINT('Ctrl Pts',(-169.280430166204,-3.64809905504815,
127.503008169288));
#116607=CARTESIAN_POINT('Ctrl Pts',(-169.288109882173,-3.73783248956393,
127.604949147311));
#116608=CARTESIAN_POINT('Ctrl Pts',(-169.295789598142,-3.82325977803816,
127.710517096614));
#116609=CARTESIAN_POINT('Ctrl Pts',(-169.303464084568,-3.90862889435205,
127.816013158868));
#116610=CARTESIAN_POINT('Ctrl Pts',(-169.311138570994,-3.9896974468948,
127.925130970572));
#116611=CARTESIAN_POINT('Ctrl Pts',(-169.318813057421,-4.06614557213797,
128.037477308013));
#116612=CARTESIAN_POINT('Ctrl Pts',(-169.326828671892,-4.14599178789105,
128.15481739804));
#116613=CARTESIAN_POINT('Ctrl Pts',(-169.334844286363,-4.22079706390486,
128.275679301211));
#116614=CARTESIAN_POINT('Ctrl Pts',(-169.342859900834,-4.29024528215741,
128.399578198837));
#116615=CARTESIAN_POINT('Ctrl Pts',(-169.350530325816,-4.35670273843905,
128.518141436017));
#116616=CARTESIAN_POINT('Ctrl Pts',(-169.358200750799,-4.41825472573536,
128.639485156536));
#116617=CARTESIAN_POINT('Ctrl Pts',(-169.365871175782,-4.47467010225927,
128.763157409052));
#116618=CARTESIAN_POINT('Ctrl Pts',(-169.373541492086,-4.5310846794608,
128.886827909315));
#116619=CARTESIAN_POINT('Ctrl Pts',(-169.381211808389,-4.58236263087159,
129.012826509912));
#116620=CARTESIAN_POINT('Ctrl Pts',(-169.388882124693,-4.62832047033365,
129.140680153537));
#116621=CARTESIAN_POINT('Ctrl Pts',(-169.396555634837,-4.67429744616276,
129.268587034092));
#116622=CARTESIAN_POINT('Ctrl Pts',(-169.404229144981,-4.71494976119077,
129.398350120979));
#116623=CARTESIAN_POINT('Ctrl Pts',(-169.411902655125,-4.75014347914318,
129.529480234921));
#116624=CARTESIAN_POINT('Ctrl Pts',(-169.412935247108,-4.75487934973022,
129.547125862772));
#116625=CARTESIAN_POINT('Ctrl Pts',(-169.41396783909,-4.75951645143451,
129.564796226742));
#116626=CARTESIAN_POINT('Ctrl Pts',(-169.415000431073,-4.76405452823411,
129.582490119308));
#116627=CARTESIAN_POINT('Ctrl Pts',(-167.665279524992,-4.76405452823393,
129.582490119308));
#116628=CARTESIAN_POINT('Ctrl Pts',(-167.673050734313,-4.79825694479428,
129.715844822382));
#116629=CARTESIAN_POINT('Ctrl Pts',(-167.680821943635,-4.8268704708693,
129.850693554765));
#116630=CARTESIAN_POINT('Ctrl Pts',(-167.688593152957,-4.84977697819716,
129.986530363633));
#116631=CARTESIAN_POINT('Ctrl Pts',(-167.696364556538,-4.87268405812648,
130.122370568057));
#116632=CARTESIAN_POINT('Ctrl Pts',(-167.70413596012,-4.88988375899316,
130.259198518599));
#116633=CARTESIAN_POINT('Ctrl Pts',(-167.711907363701,-4.90130916849556,
130.396498511798));
#116634=CARTESIAN_POINT('Ctrl Pts',(-167.719651763805,-4.91269487786053,
130.533321425502));
#116635=CARTESIAN_POINT('Ctrl Pts',(-167.727396163908,-4.91834635593093,
130.670612723358));
#116636=CARTESIAN_POINT('Ctrl Pts',(-167.735140564012,-4.91824875640148,
130.807858138868));
#116637=CARTESIAN_POINT('',(-167.389859435942,-4.91824852129168,130.800546785874));
#116638=CARTESIAN_POINT('Ctrl Pts',(-167.320062571459,-4.76405452823401,
129.582490119308));
#116639=CARTESIAN_POINT('Ctrl Pts',(-167.329148264296,-4.8037252648817,
129.73716571941));
#116640=CARTESIAN_POINT('Ctrl Pts',(-167.338233957133,-4.83590090763201,
129.893937563884));
#116641=CARTESIAN_POINT('Ctrl Pts',(-167.34731964997,-4.86038414129069,
130.052131223305));
#116642=CARTESIAN_POINT('Ctrl Pts',(-167.356327141138,-4.88465664476358,
130.208963290556));
#116643=CARTESIAN_POINT('Ctrl Pts',(-167.365334632306,-4.90136851684252,
130.367192697347));
#116644=CARTESIAN_POINT('Ctrl Pts',(-167.374342123475,-4.9103744866449,
130.526142243969));
#116645=CARTESIAN_POINT('Ctrl Pts',(-167.379514560964,-4.915546050509,130.617417003885));
#116646=CARTESIAN_POINT('Ctrl Pts',(-167.384686998453,-4.91817747662585,
130.708928866947));
#116647=CARTESIAN_POINT('Ctrl Pts',(-167.389859435942,-4.91824852129168,
130.800546785875));
#116648=CARTESIAN_POINT('Ctrl Pts',(-167.389859435994,-4.9182485212924,
130.800546786799));
#116649=CARTESIAN_POINT('Ctrl Pts',(-167.397603431916,-4.91835488690249,
130.937713991253));
#116650=CARTESIAN_POINT('Ctrl Pts',(-167.405347427839,-4.91271867954416,
131.074947458596));
#116651=CARTESIAN_POINT('Ctrl Pts',(-167.413091423761,-4.90135005703395,
131.21173106435));
#116652=CARTESIAN_POINT('Ctrl Pts',(-167.420834249603,-4.88998315226744,
131.348494002765));
#116653=CARTESIAN_POINT('Ctrl Pts',(-167.428577075445,-4.87288558719664,
131.484806825541));
#116654=CARTESIAN_POINT('Ctrl Pts',(-167.436319901287,-4.85011953972756,
131.620156862258));
#116655=CARTESIAN_POINT('Ctrl Pts',(-167.44406323119,-4.82735201017931,
131.755515710318));
#116656=CARTESIAN_POINT('Ctrl Pts',(-167.451806561093,-4.79891532830318,
131.88991126219));
#116657=CARTESIAN_POINT('Ctrl Pts',(-167.459549890996,-4.76492304045049,
132.022839784841));
#116658=CARTESIAN_POINT('Ctrl Pts',(-167.467295399081,-4.73092119064166,
132.155805699995));
#116659=CARTESIAN_POINT('Ctrl Pts',(-167.475040907166,-4.69136072150968,
132.287303386235));
#116660=CARTESIAN_POINT('Ctrl Pts',(-167.482786415251,-4.64640530396952,
132.416843427938));
#116661=CARTESIAN_POINT('Ctrl Pts',(-167.490540833312,-4.60139817236386,
132.546532484878));
#116662=CARTESIAN_POINT('Ctrl Pts',(-167.498295251373,-4.5509838239062,
132.674259029234));
#116663=CARTESIAN_POINT('Ctrl Pts',(-167.506049669435,-4.49537466340656,
132.799552262021));
#116664=CARTESIAN_POINT('Ctrl Pts',(-167.513808603169,-4.43973311971965,
132.924918457503));
#116665=CARTESIAN_POINT('Ctrl Pts',(-167.521567536903,-4.37889091000552,
133.047848168369));
#116666=CARTESIAN_POINT('Ctrl Pts',(-167.529326470637,-4.31310637938491,
133.167895348136));
#116667=CARTESIAN_POINT('Ctrl Pts',(-167.537098448307,-4.24721125506443,
133.288144345284));
#116668=CARTESIAN_POINT('Ctrl Pts',(-167.544870425977,-4.17635740882347,
133.405500793338));
#116669=CARTESIAN_POINT('Ctrl Pts',(-167.552642403647,-4.10084699031093,
133.519546987699));
#116670=CARTESIAN_POINT('Ctrl Pts',(-167.560087565858,-4.02851182179512,
133.628797483859));
#116671=CARTESIAN_POINT('Ctrl Pts',(-167.567532728069,-3.95190395140043,
133.735010250059));
#116672=CARTESIAN_POINT('Ctrl Pts',(-167.57497789028,-3.87132228266898,
133.837848189027));
#116673=CARTESIAN_POINT('Ctrl Pts',(-167.582752224399,-3.78717786797176,
133.945232887301));
#116674=CARTESIAN_POINT('Ctrl Pts',(-167.590526558518,-3.69842875172925,
134.049283961385));
#116675=CARTESIAN_POINT('Ctrl Pts',(-167.598300892637,-3.60536869646458,
134.149581032584));
#116676=CARTESIAN_POINT('Ctrl Pts',(-167.606065645584,-3.512423329401,134.249754496607));
#116677=CARTESIAN_POINT('Ctrl Pts',(-167.613830398531,-3.41517785766535,
134.346182879199));
#116678=CARTESIAN_POINT('Ctrl Pts',(-167.621595151478,-3.3139677326115,
134.438476869106));
#116679=CARTESIAN_POINT('Ctrl Pts',(-167.629352192362,-3.21285813088094,
134.530679191322));
#116680=CARTESIAN_POINT('Ctrl Pts',(-167.637109233247,-3.10779199914807,
134.618755030917));
#116681=CARTESIAN_POINT('Ctrl Pts',(-167.644866274132,-2.99914300675604,
134.702350392761));
#116682=CARTESIAN_POINT('Ctrl Pts',(-167.652617465372,-2.8905759474145,
134.785882714693));
#116683=CARTESIAN_POINT('Ctrl Pts',(-167.660368656612,-2.77843171391658,
134.864941046652));
#116684=CARTESIAN_POINT('Ctrl Pts',(-167.668119847852,-2.66311828597941,
134.939210561322));
#116685=CARTESIAN_POINT('Ctrl Pts',(-167.675867744629,-2.54785386932473,
135.013448509468));
#116686=CARTESIAN_POINT('Ctrl Pts',(-167.683615641406,-2.42942326529795,
135.082901477276));
#116687=CARTESIAN_POINT('Ctrl Pts',(-167.691363538183,-2.30826458485462,
135.147297143559));
#116688=CARTESIAN_POINT('Ctrl Pts',(-167.699109814267,-2.1871312481957,
135.211679339657));
#116689=CARTESIAN_POINT('Ctrl Pts',(-167.706856090351,-2.06327131519712,
135.271006155033));
#116690=CARTESIAN_POINT('Ctrl Pts',(-167.714602366435,-1.93714837114832,
135.325050747475));
#116691=CARTESIAN_POINT('Ctrl Pts',(-167.7223486997,-1.81102449608876,135.379095738862));
#116692=CARTESIAN_POINT('Ctrl Pts',(-167.730095032966,-1.68263793600738,
135.42785827552));
#116693=CARTESIAN_POINT('Ctrl Pts',(-167.737841366231,-1.55247279776552,
135.471159442746));
#116694=CARTESIAN_POINT('Ctrl Pts',(-167.745589434234,-1.42227850994327,
135.514470306968));
#116695=CARTESIAN_POINT('Ctrl Pts',(-167.753337502237,-1.2903052222948,
135.552317244671));
#116696=CARTESIAN_POINT('Ctrl Pts',(-167.76108557024,-1.15705237338171,
135.584571163949));
#116697=CARTESIAN_POINT('Ctrl Pts',(-167.768841872981,-1.02365790175525,
135.616859363076));
#116698=CARTESIAN_POINT('Ctrl Pts',(-167.776598175723,-0.888981532849623,
135.643542577221));
#116699=CARTESIAN_POINT('Ctrl Pts',(-167.784354478465,-0.753533625493269,
135.664542727091));
#116700=CARTESIAN_POINT('Ctrl Pts',(-167.792114920979,-0.618013425510501,
135.685554085374));
#116701=CARTESIAN_POINT('Ctrl Pts',(-167.799875363493,-0.481721254871638,
135.700876291772));
#116702=CARTESIAN_POINT('Ctrl Pts',(-167.807635806007,-0.345171781921969,
135.710483272317));
#116703=CARTESIAN_POINT('Ctrl Pts',(-167.815408706272,-0.208403107636025,
135.720105674841));
#116704=CARTESIAN_POINT('Ctrl Pts',(-167.823181606538,-0.071376696677498,
135.723994506665));
#116705=CARTESIAN_POINT('Ctrl Pts',(-167.830954506803,0.0653926919184216,
135.722175870129));
#116706=CARTESIAN_POINT('Ctrl Pts',(-167.838444842567,0.197190168765343,
135.720423345612));
#116707=CARTESIAN_POINT('Ctrl Pts',(-167.84593517833,0.328748678062574,
135.713371126581));
#116708=CARTESIAN_POINT('Ctrl Pts',(-167.853425514094,0.459614750610761,
135.701087824949));
#116709=CARTESIAN_POINT('Ctrl Pts',(-167.861199848213,0.595442650048543,
135.688338798204));
#116710=CARTESIAN_POINT('Ctrl Pts',(-167.868974182332,0.730954830702724,
135.669913800335));
#116711=CARTESIAN_POINT('Ctrl Pts',(-167.876748516451,0.865638830253724,
135.645832757118));
#116712=CARTESIAN_POINT('Ctrl Pts',(-167.884513269398,1.00015684381233,
135.621781391635));
#116713=CARTESIAN_POINT('Ctrl Pts',(-167.892278022345,1.13384832590805,
135.592087918313));
#116714=CARTESIAN_POINT('Ctrl Pts',(-167.900042775292,1.26620441830655,
135.556824129636));
#116715=CARTESIAN_POINT('Ctrl Pts',(-167.907799816177,1.39842905276819,
135.521595365452));
#116716=CARTESIAN_POINT('Ctrl Pts',(-167.915556857062,1.52932056164317,
135.48080739587));
#116717=CARTESIAN_POINT('Ctrl Pts',(-167.923313897947,1.6583791413953,135.434583256477));
#116718=CARTESIAN_POINT('Ctrl Pts',(-167.931065089187,1.78734039706799,
135.388393975068));
#116719=CARTESIAN_POINT('Ctrl Pts',(-167.938816280427,1.91447110827526,
135.336776814866));
#116720=CARTESIAN_POINT('Ctrl Pts',(-167.946567471667,2.03928587887777,
135.279904848909));
#116721=CARTESIAN_POINT('Ctrl Pts',(-167.954315368444,2.16404759987373,
135.223057055054));
#116722=CARTESIAN_POINT('Ctrl Pts',(-167.962063265221,2.28649498300679,
135.16095905934));
#116723=CARTESIAN_POINT('Ctrl Pts',(-167.969811161998,2.40616210707633,
135.093832260667));
#116724=CARTESIAN_POINT('Ctrl Pts',(-167.977557438082,2.52580419936324,
135.026719503474));
#116725=CARTESIAN_POINT('Ctrl Pts',(-167.985303714166,2.64266684859592,
134.954580226794));
#116726=CARTESIAN_POINT('Ctrl Pts',(-167.99304999025,2.75630862682354,134.877681844304));
#116727=CARTESIAN_POINT('Ctrl Pts',(-168.000796323516,2.86995124392879,
134.800782894169));
#116728=CARTESIAN_POINT('Ctrl Pts',(-168.008542656781,2.98037261878673,
134.719124987229));
#116729=CARTESIAN_POINT('Ctrl Pts',(-168.016288990046,3.08716055380728,
134.633018708532));
#116730=CARTESIAN_POINT('Ctrl Pts',(-168.024037058049,3.19397240324561,
134.54689314693));
#116731=CARTESIAN_POINT('Ctrl Pts',(-168.031785126052,3.29714888941794,
134.456317476643));
#116732=CARTESIAN_POINT('Ctrl Pts',(-168.039533194055,3.39631144490481,
134.36164211215));
#116733=CARTESIAN_POINT('Ctrl Pts',(-168.047289496796,3.49557939153557,
134.266866125552));
#116734=CARTESIAN_POINT('Ctrl Pts',(-168.055045799538,3.5908246023509,134.167982011176));
#116735=CARTESIAN_POINT('Ctrl Pts',(-168.06280210228,3.68170552561717,134.065376944594));
#116736=CARTESIAN_POINT('Ctrl Pts',(-168.070562544794,3.77263495476857,
133.962717114597));
#116737=CARTESIAN_POINT('Ctrl Pts',(-168.078322987308,3.85919520831048,
133.856332678266));
#116738=CARTESIAN_POINT('Ctrl Pts',(-168.086083429822,3.94108615866295,
133.746642547038));
#116739=CARTESIAN_POINT('Ctrl Pts',(-168.093856330088,4.02310856763886,
133.636776331473));
#116740=CARTESIAN_POINT('Ctrl Pts',(-168.101629230353,4.10044647416858,
133.523594139733));
#116741=CARTESIAN_POINT('Ctrl Pts',(-168.109402130618,4.17284359905884,
133.407543162124));
#116742=CARTESIAN_POINT('Ctrl Pts',(-168.116892466381,4.24260890610805,
133.295710929857));
#116743=CARTESIAN_POINT('Ctrl Pts',(-168.124382802143,4.30778626226982,
133.181215133421));
#116744=CARTESIAN_POINT('Ctrl Pts',(-168.131873137906,4.36818828151273,
133.064474375711));
#116745=CARTESIAN_POINT('Ctrl Pts',(-168.139647472025,4.43088046166951,
132.943307356698));
#116746=CARTESIAN_POINT('Ctrl Pts',(-168.147421806144,4.48862663285195,
132.819337959803));
#116747=CARTESIAN_POINT('Ctrl Pts',(-168.155196140263,4.54116656078055,
132.693008104459));
#116748=CARTESIAN_POINT('Ctrl Pts',(-168.16296089321,4.59364173794374,132.566833939371));
#116749=CARTESIAN_POINT('Ctrl Pts',(-168.170725646157,4.64092328954491,
132.438305461509));
#116750=CARTESIAN_POINT('Ctrl Pts',(-168.178490399105,4.68279656632752,
132.307889593306));
#116751=CARTESIAN_POINT('Ctrl Pts',(-168.18624743999,4.7246282539812,132.177603255983));
#116752=CARTESIAN_POINT('Ctrl Pts',(-168.194004480875,4.76106223774635,
132.045433628664));
#116753=CARTESIAN_POINT('Ctrl Pts',(-168.20176152176,4.79193187492677,131.911867713959));
#116754=CARTESIAN_POINT('Ctrl Pts',(-168.209512713,4.82277823307345,131.77840252235));
#116755=CARTESIAN_POINT('Ctrl Pts',(-168.21726390424,4.84806850906943,131.643543518573));
#116756=CARTESIAN_POINT('Ctrl Pts',(-168.22501509548,4.86768594569225,131.507792630351));
#116757=CARTESIAN_POINT('Ctrl Pts',(-168.232762992257,4.88729504438133,
131.372099439876));
#116758=CARTESIAN_POINT('Ctrl Pts',(-168.240510889034,4.90123604340663,
131.235515505043));
#116759=CARTESIAN_POINT('Ctrl Pts',(-168.248258785811,4.90944337014437,
131.098552490067));
#116760=CARTESIAN_POINT('Ctrl Pts',(-168.256005061896,4.91764898008629,
130.961618124801));
#116761=CARTESIAN_POINT('Ctrl Pts',(-168.26375133798,4.92012327996341,130.824305227132));
#116762=CARTESIAN_POINT('Ctrl Pts',(-168.271497614064,4.9168526498854,130.687129726522));
#116763=CARTESIAN_POINT('Ctrl Pts',(-168.279243947329,4.91358199566433,
130.549953213314));
#116764=CARTESIAN_POINT('Ctrl Pts',(-168.286990280595,4.90456633618552,
130.412914490042));
#116765=CARTESIAN_POINT('Ctrl Pts',(-168.29473661386,4.88984417257847,130.276528229018));
#116766=CARTESIAN_POINT('Ctrl Pts',(-168.302484681863,4.87511871204496,
130.140111425236));
#116767=CARTESIAN_POINT('Ctrl Pts',(-168.310232749866,4.85468424639725,
130.004347763085));
#116768=CARTESIAN_POINT('Ctrl Pts',(-168.317980817869,4.82863096432243,
129.86974514964));
#116769=CARTESIAN_POINT('Ctrl Pts',(-168.325737120611,4.80254999250934,
129.734999478936));
#116770=CARTESIAN_POINT('Ctrl Pts',(-168.333493423353,4.77083834947892,
129.601417706392));
#116771=CARTESIAN_POINT('Ctrl Pts',(-168.341249726095,4.73363715994987,
129.469496467009));
#116772=CARTESIAN_POINT('Ctrl Pts',(-168.349010168609,4.69641611502586,
129.337504817289));
#116773=CARTESIAN_POINT('Ctrl Pts',(-168.356770611123,4.65369980716572,
129.207175838048));
#116774=CARTESIAN_POINT('Ctrl Pts',(-168.364531053637,4.60567845213877,
129.078988466984));
#116775=CARTESIAN_POINT('Ctrl Pts',(-168.372303953903,4.55758000896946,
128.950595318172));
#116776=CARTESIAN_POINT('Ctrl Pts',(-168.380076854168,4.50415965313248,
128.824351007819));
#116777=CARTESIAN_POINT('Ctrl Pts',(-168.387849754434,4.44565509333515,
128.700712868155));
#116778=CARTESIAN_POINT('Ctrl Pts',(-168.395340090195,4.38927732165513,
128.581569286303));
#116779=CARTESIAN_POINT('Ctrl Pts',(-168.402830425957,4.32817871848307,
128.464845955974));
#116780=CARTESIAN_POINT('Ctrl Pts',(-168.410320761718,4.26261017956376,
128.350926795434));
#116781=CARTESIAN_POINT('Ctrl Pts',(-168.418095095837,4.1945555895575,128.23268835529));
#116782=CARTESIAN_POINT('Ctrl Pts',(-168.425869429956,4.12146984100777,
128.117096378876));
#116783=CARTESIAN_POINT('Ctrl Pts',(-168.433643764076,4.04358407026487,
128.004608676911));
#116784=CARTESIAN_POINT('Ctrl Pts',(-168.441408517023,3.96579428677336,
127.892259605985));
#116785=CARTESIAN_POINT('Ctrl Pts',(-168.449173269969,3.88321647178963,
127.783007515774));
#116786=CARTESIAN_POINT('Ctrl Pts',(-168.456938022917,3.79612743721554,
127.677285379757));
#116787=CARTESIAN_POINT('Ctrl Pts',(-168.464695063802,3.70912490069856,
127.571668248456));
#116788=CARTESIAN_POINT('Ctrl Pts',(-168.472452104687,3.6176203081724,127.469574394062));
#116789=CARTESIAN_POINT('Ctrl Pts',(-168.480209145572,3.52193331427772,
127.371407254603));
#116790=CARTESIAN_POINT('Ctrl Pts',(-168.487960336812,3.42631847868961,
127.273314143747));
#116791=CARTESIAN_POINT('Ctrl Pts',(-168.495711528052,3.32652779133241,
127.179142132638));
#116792=CARTESIAN_POINT('Ctrl Pts',(-168.503462719292,3.2229204280841,127.089260756628));
#116793=CARTESIAN_POINT('Ctrl Pts',(-168.511210616069,3.11935710072857,
126.999417582601));
#116794=CARTESIAN_POINT('Ctrl Pts',(-168.518958512846,3.01198061859749,
126.913861672267));
#116795=CARTESIAN_POINT('Ctrl Pts',(-168.526706409623,2.90118601568176,
126.832924760736));
#116796=CARTESIAN_POINT('Ctrl Pts',(-168.534452685707,2.79041458860849,
126.752004779463));
#116797=CARTESIAN_POINT('Ctrl Pts',(-168.542198961791,2.6762267784195,126.675702105657));
#116798=CARTESIAN_POINT('Ctrl Pts',(-168.549945237875,2.55904928929877,
126.604307070593));
#116799=CARTESIAN_POINT('Ctrl Pts',(-168.557691571141,2.44187093520091,
126.532911508508));
#116800=CARTESIAN_POINT('Ctrl Pts',(-168.565437904406,2.32170319200777,
126.466423860879));
#116801=CARTESIAN_POINT('Ctrl Pts',(-168.573184237671,2.19899987891132,
126.405089928571));
#116802=CARTESIAN_POINT('Ctrl Pts',(-168.580932305674,2.07626908725818,
126.343742260955));
#116803=CARTESIAN_POINT('Ctrl Pts',(-168.588680373677,1.95100194544226,
126.287550780033));
#116804=CARTESIAN_POINT('Ctrl Pts',(-168.59642844168,1.82367451925975,126.236714143691));
#116805=CARTESIAN_POINT('Ctrl Pts',(-168.604184744422,1.69621176797366,
126.185823477567));
#116806=CARTESIAN_POINT('Ctrl Pts',(-168.611941047164,1.56668472184361,
126.140299169992));
#116807=CARTESIAN_POINT('Ctrl Pts',(-168.619697349906,1.43558749531847,
126.100290932093));
#116808=CARTESIAN_POINT('Ctrl Pts',(-168.62745779242,1.30442029825626,126.060261340593));
#116809=CARTESIAN_POINT('Ctrl Pts',(-168.635218234934,1.17168162911119,
126.025753783441));
#116810=CARTESIAN_POINT('Ctrl Pts',(-168.642978677448,1.03787724800241,
125.99686710425));
#116811=CARTESIAN_POINT('Ctrl Pts',(-168.650751577714,0.903858072222484,
125.967934053596));
#116812=CARTESIAN_POINT('Ctrl Pts',(-168.658524477979,0.768770151305243,
125.94463997847));
#116813=CARTESIAN_POINT('Ctrl Pts',(-168.666297378245,0.633126739169326,
125.927032087044));
#116814=CARTESIAN_POINT('Ctrl Pts',(-168.673787714007,0.502414306726015,
125.910064286822));
#116815=CARTESIAN_POINT('Ctrl Pts',(-168.681278049769,0.37118637570029,
125.898376460903));
#116816=CARTESIAN_POINT('Ctrl Pts',(-168.688768385531,0.239901562680689,
125.891965040791));
#116817=CARTESIAN_POINT('Ctrl Pts',(-168.69654271965,0.103639046074826,
125.885310529736));
#116818=CARTESIAN_POINT('Ctrl Pts',(-168.70431705377,-0.033116389728072,
125.884319353145));
#116819=CARTESIAN_POINT('Ctrl Pts',(-168.712091387889,-0.169854640762195,
125.889044507333));
#116820=CARTESIAN_POINT('Ctrl Pts',(-168.719856140836,-0.306424374122569,
125.893763838192));
#116821=CARTESIAN_POINT('Ctrl Pts',(-168.727620893783,-0.442976577872466,
125.904185469273));
#116822=CARTESIAN_POINT('Ctrl Pts',(-168.73538564673,-0.578997355566437,
125.920310543627));
#116823=CARTESIAN_POINT('Ctrl Pts',(-168.743142687615,-0.714883035507554,
125.936419602329));
#116824=CARTESIAN_POINT('Ctrl Pts',(-168.7508997285,-0.850237954043831,
125.958220785486));
#116825=CARTESIAN_POINT('Ctrl Pts',(-168.758656769386,-0.984549906196488,
125.985663226703));
#116826=CARTESIAN_POINT('Ctrl Pts',(-168.766407960626,-1.11876057266032,
126.013084973362));
#116827=CARTESIAN_POINT('Ctrl Pts',(-168.774159151866,-1.25192945673756,
126.046139432572));
#116828=CARTESIAN_POINT('Ctrl Pts',(-168.781910343106,-1.38355151453494,
126.084724162379));
#116829=CARTESIAN_POINT('Ctrl Pts',(-168.789658239883,-1.51511762944608,
126.123292492647));
#116830=CARTESIAN_POINT('Ctrl Pts',(-168.797406136661,-1.64513785128884,
126.167386308769));
#116831=CARTESIAN_POINT('Ctrl Pts',(-168.805154033438,-1.77311955639681,
126.216852568393));
#116832=CARTESIAN_POINT('Ctrl Pts',(-168.812900309522,-1.90107449049138,
126.266308480742));
#116833=CARTESIAN_POINT('Ctrl Pts',(-168.820646585606,-2.02699139156891,
126.321134460434));
#116834=CARTESIAN_POINT('Ctrl Pts',(-168.82839286169,-2.15039535167048,
126.381128440299));
#116835=CARTESIAN_POINT('Ctrl Pts',(-168.836139194956,-2.27380022271188,
126.441122863025));
#116836=CARTESIAN_POINT('Ctrl Pts',(-168.843885528221,-2.39469176414734,
126.506285191108));
#116837=CARTESIAN_POINT('Ctrl Pts',(-168.851631861486,-2.51261787638955,
126.576366474979));
#116838=CARTESIAN_POINT('Ctrl Pts',(-168.859379929489,-2.63057039736744,
126.646463453069));
#116839=CARTESIAN_POINT('Ctrl Pts',(-168.867127997493,-2.74555583166465,
126.721481379239));
#116840=CARTESIAN_POINT('Ctrl Pts',(-168.874876065496,-2.85714971758546,
126.801127105291));
#116841=CARTESIAN_POINT('Ctrl Pts',(-168.882632368238,-2.96886220681607,
126.880857479769));
#116842=CARTESIAN_POINT('Ctrl Pts',(-168.89038867098,-3.07717562840205,
126.96522525184));
#116843=CARTESIAN_POINT('Ctrl Pts',(-168.898144973721,-3.18169694520404,
127.053895631544));
#116844=CARTESIAN_POINT('Ctrl Pts',(-168.905905416236,-3.28627404817961,
127.142613337299));
#116845=CARTESIAN_POINT('Ctrl Pts',(-168.91366585875,-3.38705472631127,
127.235637961473));
#116846=CARTESIAN_POINT('Ctrl Pts',(-168.921426301264,-3.48368244397181,
127.332597421139));
#116847=CARTESIAN_POINT('Ctrl Pts',(-168.92919920153,-3.58046527702294,
127.429712528738));
#116848=CARTESIAN_POINT('Ctrl Pts',(-168.936972101795,-3.67308156311091,
127.530774805901));
#116849=CARTESIAN_POINT('Ctrl Pts',(-168.944745002061,-3.76121415838317,
127.635377954742));
#116850=CARTESIAN_POINT('Ctrl Pts',(-168.952235337822,-3.84614291181632,
127.736178515633));
#116851=CARTESIAN_POINT('Ctrl Pts',(-168.959725673583,-3.92690811290851,
127.840266735162));
#116852=CARTESIAN_POINT('Ctrl Pts',(-168.967216009345,-4.00326487046784,
127.947254837344));
#116853=CARTESIAN_POINT('Ctrl Pts',(-168.975066780707,-4.08329592176035,
128.059391216194));
#116854=CARTESIAN_POINT('Ctrl Pts',(-168.982917552068,-4.15873583823605,
128.175066470889));
#116855=CARTESIAN_POINT('Ctrl Pts',(-168.99076832343,-4.22925912511095,
128.293872554427));
#116856=CARTESIAN_POINT('Ctrl Pts',(-168.998605668683,-4.29966180557835,
128.412475460041));
#116857=CARTESIAN_POINT('Ctrl Pts',(-169.006443013935,-4.36516441340019,
128.534198203532));
#116858=CARTESIAN_POINT('Ctrl Pts',(-169.014280359188,-4.42548336394001,
128.65860199694));
#116859=CARTESIAN_POINT('Ctrl Pts',(-169.022109933543,-4.48574250692737,
128.782882441279));
#116860=CARTESIAN_POINT('Ctrl Pts',(-169.029939507897,-4.54082805295072,
128.909838306252));
#116861=CARTESIAN_POINT('Ctrl Pts',(-169.037769082251,-4.59050090648996,
129.039003857584));
#116862=CARTESIAN_POINT('Ctrl Pts',(-169.045590964355,-4.64012495839209,
129.16804250881));
#116863=CARTESIAN_POINT('Ctrl Pts',(-169.053412846459,-4.68434677298601,
129.29928616832));
#116864=CARTESIAN_POINT('Ctrl Pts',(-169.061234728562,-4.72297445864585,
129.43224716545));
#116865=CARTESIAN_POINT('Ctrl Pts',(-169.064167241935,-4.73745642133288,
129.482095769278));
#116866=CARTESIAN_POINT('Ctrl Pts',(-169.067099755308,-4.75115256260494,
129.532185551135));
#116867=CARTESIAN_POINT('Ctrl Pts',(-169.070032268681,-4.76405452823411,
129.582490119308));
#116868=CARTESIAN_POINT('Origin',(213.235140564004,0.,130.804360617566));
#116869=CARTESIAN_POINT('',(-171.165157400749,-4.76405452823416,129.582490119309));
#116870=CARTESIAN_POINT('',(-170.819717755703,-4.76405452823413,129.582490119309));
#116871=CARTESIAN_POINT('',(213.235140564004,-4.76405452823405,129.582490119308));
#116872=CARTESIAN_POINT('',(-169.485140563978,-4.91824957353103,130.806408778158));
#116873=CARTESIAN_POINT('Ctrl Pts',(-169.485140564012,-4.91824957353078,
130.806408778756));
#116874=CARTESIAN_POINT('Ctrl Pts',(-169.491601129611,-4.91820232501163,
130.919866650305));
#116875=CARTESIAN_POINT('Ctrl Pts',(-169.498061695211,-4.91422942216106,
131.033238697484));
#116876=CARTESIAN_POINT('Ctrl Pts',(-169.504522260811,-4.9063465576463,
131.146335059261));
#116877=CARTESIAN_POINT('Ctrl Pts',(-169.51229659493,-4.89686069737473,
131.282429785109));
#116878=CARTESIAN_POINT('Ctrl Pts',(-169.520070929049,-4.8816929241367,
131.41834509075));
#116879=CARTESIAN_POINT('Ctrl Pts',(-169.527845263168,-4.86085086028999,
131.553568183277));
#116880=CARTESIAN_POINT('Ctrl Pts',(-169.535610016115,-4.84003448242426,
131.688624625427));
#116881=CARTESIAN_POINT('Ctrl Pts',(-169.543374769062,-4.81355778703188,
131.822990169166));
#116882=CARTESIAN_POINT('Ctrl Pts',(-169.551139522009,-4.78148033472624,
131.956154379976));
#116883=CARTESIAN_POINT('Ctrl Pts',(-169.558896562894,-4.74943474219844,
132.089186330215));
#116884=CARTESIAN_POINT('Ctrl Pts',(-169.566653603779,-4.7117995538491,
132.221018944375));
#116885=CARTESIAN_POINT('Ctrl Pts',(-169.574410644664,-4.66868577592679,
132.351149610337));
#116886=CARTESIAN_POINT('Ctrl Pts',(-169.582161835904,-4.62560451043985,
132.481182143752));
#116887=CARTESIAN_POINT('Ctrl Pts',(-169.589913027145,-4.57705300123568,
132.609514913977));
#116888=CARTESIAN_POINT('Ctrl Pts',(-169.597664218385,-4.52319262334111,
132.735658511381));
#116889=CARTESIAN_POINT('Ctrl Pts',(-169.605412115162,-4.46935513754385,
132.86174849439));
#116890=CARTESIAN_POINT('Ctrl Pts',(-169.613160011939,-4.41021342408801,
132.985650796377));
#116891=CARTESIAN_POINT('Ctrl Pts',(-169.620907908716,-4.34597763729324,
133.106894317351));
#116892=CARTESIAN_POINT('Ctrl Pts',(-169.6286541848,-4.2817552872403,133.228112476795));
#116893=CARTESIAN_POINT('Ctrl Pts',(-169.636400460884,-4.21244116624499,
133.346672616203));
#116894=CARTESIAN_POINT('Ctrl Pts',(-169.644146736968,-4.13829201792157,
133.462127017554));
#116895=CARTESIAN_POINT('Ctrl Pts',(-169.651893070234,-4.06414232224607,
133.577582271164));
#116896=CARTESIAN_POINT('Ctrl Pts',(-169.659639403499,-3.98515773929668,
133.689931412005));
#116897=CARTESIAN_POINT('Ctrl Pts',(-169.667385736764,-3.90163887307296,
133.798754908007));
#116898=CARTESIAN_POINT('Ctrl Pts',(-169.675133804767,-3.81810130337812,
133.907602774276));
#116899=CARTESIAN_POINT('Ctrl Pts',(-169.68288187277,-3.73002766782518,
134.012923114513));
#116900=CARTESIAN_POINT('Ctrl Pts',(-169.690629940773,-3.6377591954069,
134.114329061333));
#116901=CARTESIAN_POINT('Ctrl Pts',(-169.698386243515,-3.545392658958,134.2158427836));
#116902=CARTESIAN_POINT('Ctrl Pts',(-169.706142546257,-3.44882264320227,
134.31343351224));
#116903=CARTESIAN_POINT('Ctrl Pts',(-169.713898848999,-3.34842801591426,
134.406750502731));
#116904=CARTESIAN_POINT('Ctrl Pts',(-169.721659291513,-3.24797980499085,
134.50011729931));
#116905=CARTESIAN_POINT('Ctrl Pts',(-169.729419734027,-3.1437032121594,
134.589205558775));
#116906=CARTESIAN_POINT('Ctrl Pts',(-169.737180176541,-3.03600982598779,
134.673705187258));
#116907=CARTESIAN_POINT('Ctrl Pts',(-169.744953076807,-2.92814356083214,
134.758340462046));
#116908=CARTESIAN_POINT('Ctrl Pts',(-169.752725977072,-2.81684985927771,
134.838372157694));
#116909=CARTESIAN_POINT('Ctrl Pts',(-169.760498877338,-2.70256963285882,
134.913533337476));
#116910=CARTESIAN_POINT('Ctrl Pts',(-169.7679892131,-2.59244378052787,134.985962219051));
#116911=CARTESIAN_POINT('Ctrl Pts',(-169.775479548861,-2.47954503289768,
135.053868389152));
#116912=CARTESIAN_POINT('Ctrl Pts',(-169.782969884623,-2.36428737556901,
135.117054470395));
#116913=CARTESIAN_POINT('Ctrl Pts',(-169.790744218742,-2.24465968912837,
135.182636271114));
#116914=CARTESIAN_POINT('Ctrl Pts',(-169.798518552862,-2.1221117412432,
135.24334073653));
#116915=CARTESIAN_POINT('Ctrl Pts',(-169.806292886981,-1.99707907917962,
135.298897102456));
#116916=CARTESIAN_POINT('Ctrl Pts',(-169.814057639928,-1.87220050869754,
135.354385000126));
#116917=CARTESIAN_POINT('Ctrl Pts',(-169.821822392875,-1.74484367073196,
135.404737264885));
#116918=CARTESIAN_POINT('Ctrl Pts',(-169.829587145822,-1.61547020226498,
135.449728104439));
#116919=CARTESIAN_POINT('Ctrl Pts',(-169.837344186707,-1.48622522935037,
135.494674258457));
#116920=CARTESIAN_POINT('Ctrl Pts',(-169.845101227592,-1.35496797877043,
135.534269456759));
#116921=CARTESIAN_POINT('Ctrl Pts',(-169.852858268477,-1.22218131392522,
135.568335417918));
#116922=CARTESIAN_POINT('Ctrl Pts',(-169.860609459717,-1.08949478453673,
135.602375689671));
#116923=CARTESIAN_POINT('Ctrl Pts',(-169.868360650957,-0.955281513711783,
135.630894926937));
#116924=CARTESIAN_POINT('Ctrl Pts',(-169.876111842197,-0.820040482779182,
135.653764361234));
#116925=CARTESIAN_POINT('Ctrl Pts',(-169.883859738974,-0.684856932892583,
135.676624075412));
#116926=CARTESIAN_POINT('Ctrl Pts',(-169.891607635751,-0.548646876396235,
135.693838697607));
#116927=CARTESIAN_POINT('Ctrl Pts',(-169.899355532528,-0.411920256597,135.705330395549));
#116928=CARTESIAN_POINT('Ctrl Pts',(-169.907101808613,-0.275222237059142,
135.716819689676));
#116929=CARTESIAN_POINT('Ctrl Pts',(-169.914848084697,-0.138008258488271,
135.722588407947));
#116930=CARTESIAN_POINT('Ctrl Pts',(-169.922594360781,-0.000793774930625052,
135.722610553511));
#116931=CARTESIAN_POINT('Ctrl Pts',(-169.930340694046,0.136421721512981,
135.722632699238));
#116932=CARTESIAN_POINT('Ctrl Pts',(-169.938087027311,0.273637331985599,
135.716908187549));
#116933=CARTESIAN_POINT('Ctrl Pts',(-169.945833360577,0.410337608468786,
135.705463157768));
#116934=CARTESIAN_POINT('Ctrl Pts',(-169.95358142858,0.547068498030891,
135.694015564953));
#116935=CARTESIAN_POINT('Ctrl Pts',(-169.961329496583,0.683283434432496,
135.676844937477));
#116936=CARTESIAN_POINT('Ctrl Pts',(-169.969077564586,0.818472492582324,
135.654029249688));
#116937=CARTESIAN_POINT('Ctrl Pts',(-169.976833867327,0.953805231272109,
135.631189313114));
#116938=CARTESIAN_POINT('Ctrl Pts',(-169.984590170069,1.08810952755903,
135.60269239647));
#116939=CARTESIAN_POINT('Ctrl Pts',(-169.992346472811,1.22088550285722,
135.568667665964));
#116940=CARTESIAN_POINT('Ctrl Pts',(-170.000106915325,1.35373234469159,
135.534624775435));
#116941=CARTESIAN_POINT('Ctrl Pts',(-170.00786735784,1.48504886601324,135.495048304962));
#116942=CARTESIAN_POINT('Ctrl Pts',(-170.015627800354,1.61435170239241,
135.450116922355));
#116943=CARTESIAN_POINT('Ctrl Pts',(-170.023400700619,1.74386210716315,
135.405113411903));
#116944=CARTESIAN_POINT('Ctrl Pts',(-170.031173600884,1.87135200351641,
135.354737955165));
#116945=CARTESIAN_POINT('Ctrl Pts',(-170.03894650115,1.99635848657079,135.299217217681));
#116946=CARTESIAN_POINT('Ctrl Pts',(-170.046436836912,2.11682066909617,
135.245714798852));
#116947=CARTESIAN_POINT('Ctrl Pts',(-170.053927172674,2.23497658400925,
135.18743482865));
#116948=CARTESIAN_POINT('Ctrl Pts',(-170.061417508436,2.35043640279736,
135.124618917588));
#116949=CARTESIAN_POINT('Ctrl Pts',(-170.069191842555,2.47027391570589,
135.059421322166));
#116950=CARTESIAN_POINT('Ctrl Pts',(-170.076966176675,2.58758646093225,
134.989130509218));
#116951=CARTESIAN_POINT('Ctrl Pts',(-170.084740510794,2.70191081296185,
134.913966562337));
#116952=CARTESIAN_POINT('Ctrl Pts',(-170.092505263741,2.81609427044503,
134.838895248304));
#116953=CARTESIAN_POINT('Ctrl Pts',(-170.100270016688,2.92729653862137,
134.758962962614));
#116954=CARTESIAN_POINT('Ctrl Pts',(-170.108034769635,3.03507812597438,
134.674436047287));
#116955=CARTESIAN_POINT('Ctrl Pts',(-170.11579181052,3.14275266313536,134.589993085284));
#116956=CARTESIAN_POINT('Ctrl Pts',(-170.123548851405,3.24701297493629,
134.500964814821));
#116957=CARTESIAN_POINT('Ctrl Pts',(-170.13130589229,3.34744806870106,134.407661117087));
#116958=CARTESIAN_POINT('Ctrl Pts',(-170.13905708353,3.44780742358021,134.314427780397));
#116959=CARTESIAN_POINT('Ctrl Pts',(-170.14680827477,3.54434701682041,134.216925698898));
#116960=CARTESIAN_POINT('Ctrl Pts',(-170.15455946601,3.63668880025547,134.115505077205));
#116961=CARTESIAN_POINT('Ctrl Pts',(-170.162307362787,3.7289913359694,134.014127561981));
#116962=CARTESIAN_POINT('Ctrl Pts',(-170.170055259564,3.81709934781756,
133.908835107568));
#116963=CARTESIAN_POINT('Ctrl Pts',(-170.177803156342,3.90067171649274,
133.80001467347));
#116964=CARTESIAN_POINT('Ctrl Pts',(-170.185549432426,3.98422660363,133.691217002261));
#116965=CARTESIAN_POINT('Ctrl Pts',(-170.19329570851,4.0632474967456,133.578893129122));
#116966=CARTESIAN_POINT('Ctrl Pts',(-170.201041984594,4.13743390844848,
133.463462668207));
#116967=CARTESIAN_POINT('Ctrl Pts',(-170.208788317859,4.2116208677787,133.34803135521));
#116968=CARTESIAN_POINT('Ctrl Pts',(-170.216534651124,4.28097306310594,
133.229493737574));
#116969=CARTESIAN_POINT('Ctrl Pts',(-170.22428098439,4.3452338739408,133.108297605258));
#116970=CARTESIAN_POINT('Ctrl Pts',(-170.232029052393,4.40950907553861,
132.98707433191));
#116971=CARTESIAN_POINT('Ctrl Pts',(-170.239777120396,4.46869044070612,
132.863191704541));
#116972=CARTESIAN_POINT('Ctrl Pts',(-170.247525188399,4.5225679445012,132.737120884612));
#116973=CARTESIAN_POINT('Ctrl Pts',(-170.255281491141,4.57650270994852,
132.610916075114));
#116974=CARTESIAN_POINT('Ctrl Pts',(-170.263037793882,4.62512219960934,
132.482518787431));
#116975=CARTESIAN_POINT('Ctrl Pts',(-170.270794096624,4.66826488808641,
132.352419401062));
#116976=CARTESIAN_POINT('Ctrl Pts',(-170.278554539138,4.71143060311533,
132.222250576734));
#116977=CARTESIAN_POINT('Ctrl Pts',(-170.286314981653,4.74911358500167,
132.09037821927));
#116978=CARTESIAN_POINT('Ctrl Pts',(-170.294075424167,4.78120288175106,
131.957305571168));
#116979=CARTESIAN_POINT('Ctrl Pts',(-170.301848324432,4.81334369108835,
131.824019303037));
#116980=CARTESIAN_POINT('Ctrl Pts',(-170.309621224698,4.83987279572024,
131.689529277677));
#116981=CARTESIAN_POINT('Ctrl Pts',(-170.317394124963,4.86073068439009,
131.554347468337));
#116982=CARTESIAN_POINT('Ctrl Pts',(-170.324884460725,4.88083033626898,
131.424079858267));
#116983=CARTESIAN_POINT('Ctrl Pts',(-170.332374796487,4.89566390489223,
131.293170193242));
#116984=CARTESIAN_POINT('Ctrl Pts',(-170.339865132249,4.90522395219424,
131.162077043412));
#116985=CARTESIAN_POINT('Ctrl Pts',(-170.347639466368,4.91514647159538,
131.026013456962));
#116986=CARTESIAN_POINT('Ctrl Pts',(-170.355413800488,4.91941911613601,
130.889321188852));
#116987=CARTESIAN_POINT('Ctrl Pts',(-170.363188134607,4.91797666367118,
130.752508924385));
#116988=CARTESIAN_POINT('Ctrl Pts',(-170.370952887554,4.91653598890009,
130.615865268807));
#116989=CARTESIAN_POINT('Ctrl Pts',(-170.378717640501,4.90939423536557,
130.479102298308));
#116990=CARTESIAN_POINT('Ctrl Pts',(-170.386482393448,4.89653792825003,
130.342733733915));
#116991=CARTESIAN_POINT('Ctrl Pts',(-170.394239434333,4.88369439019996,
130.206500612703));
#116992=CARTESIAN_POINT('Ctrl Pts',(-170.401996475218,4.86514763007612,
130.070661504758));
#116993=CARTESIAN_POINT('Ctrl Pts',(-170.409753516103,4.84093620811762,
129.935729688209));
#116994=CARTESIAN_POINT('Ctrl Pts',(-170.417504707343,4.81674304418079,
129.800899624792));
#116995=CARTESIAN_POINT('Ctrl Pts',(-170.425255898583,4.78689378987004,
129.666975874185));
#116996=CARTESIAN_POINT('Ctrl Pts',(-170.433007089823,4.75147873797787,
129.534465793164));
#116997=CARTESIAN_POINT('Ctrl Pts',(-170.4407549866,4.71607873842743,129.402012032461));
#116998=CARTESIAN_POINT('Ctrl Pts',(-170.448502883378,4.67511774705443,
129.270971123223));
#116999=CARTESIAN_POINT('Ctrl Pts',(-170.456250780155,4.62873694053004,
129.141839219847));
#117000=CARTESIAN_POINT('Ctrl Pts',(-170.463997056239,4.58236583587065,
129.012734328082));
#117001=CARTESIAN_POINT('Ctrl Pts',(-170.471743332323,4.53057730314291,
128.885538015621));
#117002=CARTESIAN_POINT('Ctrl Pts',(-170.479489608407,4.4735619548437,128.760729902717));
#117003=CARTESIAN_POINT('Ctrl Pts',(-170.487235941672,4.41654618567006,
128.635920868507));
#117004=CARTESIAN_POINT('Ctrl Pts',(-170.494982274938,4.35430368638885,
128.513500424648));
#117005=CARTESIAN_POINT('Ctrl Pts',(-170.502728608203,4.28707248573286,
128.393926514635));
#117006=CARTESIAN_POINT('Ctrl Pts',(-170.510476676206,4.21982622911553,
128.274325826874));
#117007=CARTESIAN_POINT('Ctrl Pts',(-170.518224744209,4.1475892396298,128.157573282161));
#117008=CARTESIAN_POINT('Ctrl Pts',(-170.525972812212,4.07064439514418,
128.044100254705));
#117009=CARTESIAN_POINT('Ctrl Pts',(-170.533729114954,3.9936177727623,127.930506626765));
#117010=CARTESIAN_POINT('Ctrl Pts',(-170.541485417696,3.91187351999241,
127.820199802867));
#117011=CARTESIAN_POINT('Ctrl Pts',(-170.549241720438,3.82573689857504,
127.713580741001));
#117012=CARTESIAN_POINT('Ctrl Pts',(-170.557002162952,3.73955430344929,
127.606904773331));
#117013=CARTESIAN_POINT('Ctrl Pts',(-170.564762605466,3.64897492646274,
127.503920783061));
#117014=CARTESIAN_POINT('Ctrl Pts',(-170.57252304798,3.55436218751893,127.404994132111));
#117015=CARTESIAN_POINT('Ctrl Pts',(-170.580295948246,3.45959756780724,
127.305908675318));
#117016=CARTESIAN_POINT('Ctrl Pts',(-170.588068848511,3.3607869295795,127.21089384444));
#117017=CARTESIAN_POINT('Ctrl Pts',(-170.595841748776,3.25832884314138,
127.120276442028));
#117018=CARTESIAN_POINT('Ctrl Pts',(-170.603332084538,3.15959536622248,
127.032953210445));
#117019=CARTESIAN_POINT('Ctrl Pts',(-170.6108224203,3.05747526365405,126.949713437462));
#117020=CARTESIAN_POINT('Ctrl Pts',(-170.618312756062,2.95235032303649,
126.870811249302));
#117021=CARTESIAN_POINT('Ctrl Pts',(-170.626087090181,2.8432395383423,126.788917460696));
#117022=CARTESIAN_POINT('Ctrl Pts',(-170.633861424301,2.73054593059434,
126.711437254028));
#117023=CARTESIAN_POINT('Ctrl Pts',(-170.64163575842,2.6146622169822,126.63870045937));
#117024=CARTESIAN_POINT('Ctrl Pts',(-170.649400511367,2.49892131969058,
126.56605330631));
#117025=CARTESIAN_POINT('Ctrl Pts',(-170.657165264314,2.37999846704939,
126.498138139648));
#117026=CARTESIAN_POINT('Ctrl Pts',(-170.664930017261,2.25831858363902,
126.435243974892));
#117027=CARTESIAN_POINT('Ctrl Pts',(-170.672687058146,2.13675955440424,
126.372412277508));
#117028=CARTESIAN_POINT('Ctrl Pts',(-170.680444099031,2.01244928884994,
126.314591836172));
#117029=CARTESIAN_POINT('Ctrl Pts',(-170.688201139916,1.88584046515444,
126.262027648432));
#117030=CARTESIAN_POINT('Ctrl Pts',(-170.695952331156,1.75932711815759,
126.209503099754));
#117031=CARTESIAN_POINT('Ctrl Pts',(-170.703703522396,1.63051902279014,
126.162227064307));
#117032=CARTESIAN_POINT('Ctrl Pts',(-170.711454713636,1.499891838138,126.12039781494));
#117033=CARTESIAN_POINT('Ctrl Pts',(-170.719202610413,1.3693201735241,126.078586344119));
#117034=CARTESIAN_POINT('Ctrl Pts',(-170.72695050719,1.23693132894627,126.042217173942));
#117035=CARTESIAN_POINT('Ctrl Pts',(-170.734698403968,1.10321904259012,
126.011439712046));
#117036=CARTESIAN_POINT('Ctrl Pts',(-170.742444680052,0.96953472596176,
125.980668688133));
#117037=CARTESIAN_POINT('Ctrl Pts',(-170.750190956136,0.834527898957105,
125.955487133616));
#117038=CARTESIAN_POINT('Ctrl Pts',(-170.75793723222,0.698705110388279,
125.935993927267));
#117039=CARTESIAN_POINT('Ctrl Pts',(-170.765683565485,0.562881319206298,
125.916500577022));
#117040=CARTESIAN_POINT('Ctrl Pts',(-170.773429898751,0.426241941441041,
125.902695714275));
#117041=CARTESIAN_POINT('Ctrl Pts',(-170.781176232016,0.289300918270411,
125.894626608357));
#117042=CARTESIAN_POINT('Ctrl Pts',(-170.788924300019,0.152329228107311,
125.886555695418));
#117043=CARTESIAN_POINT('Ctrl Pts',(-170.796672368022,0.0150561483329293,
125.884223118273));
#117044=CARTESIAN_POINT('Ctrl Pts',(-170.804420436025,-0.12200249131536,
125.887624052057));
#117045=CARTESIAN_POINT('Ctrl Pts',(-170.812176738767,-0.259206798517073,
125.891028600394));
#117046=CARTESIAN_POINT('Ctrl Pts',(-170.819933041509,-0.396195818850764,
125.900178822656));
#117047=CARTESIAN_POINT('Ctrl Pts',(-170.82768934425,-0.532456403087785,
125.915017794516));
#117048=CARTESIAN_POINT('Ctrl Pts',(-170.835449786765,-0.66878971370134,
125.929864686382));
#117049=CARTESIAN_POINT('Ctrl Pts',(-170.843210229279,-0.804393427158591,
125.950406319318));
#117050=CARTESIAN_POINT('Ctrl Pts',(-170.850970671793,-0.93876371679538,
125.976534424907));
#117051=CARTESIAN_POINT('Ctrl Pts',(-170.858743572058,-1.07334970954993,
126.00270447365));
#117052=CARTESIAN_POINT('Ctrl Pts',(-170.866516472324,-1.20669794127393,
126.034478825098));
#117053=CARTESIAN_POINT('Ctrl Pts',(-170.874289372589,-1.33831802673905,
126.071698795525));
#117054=CARTESIAN_POINT('Ctrl Pts',(-170.881779708351,-1.46515339056616,
126.107565726276));
#117055=CARTESIAN_POINT('Ctrl Pts',(-170.889270044113,-1.59038377891071,
126.148489130217));
#117056=CARTESIAN_POINT('Ctrl Pts',(-170.896760379875,-1.71358902265974,
126.194285160058));
#117057=CARTESIAN_POINT('Ctrl Pts',(-170.904534904299,-1.84146876091866,
126.241818723818));
#117058=CARTESIAN_POINT('Ctrl Pts',(-170.912309428724,-1.96757174403429,
126.294752531509));
#117059=CARTESIAN_POINT('Ctrl Pts',(-170.920083953148,-2.09140816758484,
126.352934448454));
#117060=CARTESIAN_POINT('Ctrl Pts',(-170.927848852212,-2.21509127370658,
126.411044332457));
#117061=CARTESIAN_POINT('Ctrl Pts',(-170.935613751277,-2.33651305327552,
126.474389232686));
#117062=CARTESIAN_POINT('Ctrl Pts',(-170.943378650342,-2.45520064116338,
126.542767854979));
#117063=CARTESIAN_POINT('Ctrl Pts',(-170.951135793343,-2.57376967652441,
126.611078176462));
#117064=CARTESIAN_POINT('Ctrl Pts',(-170.958892936345,-2.68960961872044,
126.684412019881));
#117065=CARTESIAN_POINT('Ctrl Pts',(-170.966650079347,-2.80226964412983,
126.762520949285));
#117066=CARTESIAN_POINT('Ctrl Pts',(-170.974401328845,-2.91484407587179,
126.840570535282));
#117067=CARTESIAN_POINT('Ctrl Pts',(-170.982152578342,-3.02424307978171,
126.923387764059));
#117068=CARTESIAN_POINT('Ctrl Pts',(-170.98990382784,-3.13004273010074,
127.01067961223));
#117069=CARTESIAN_POINT('Ctrl Pts',(-170.997651559851,-3.23579436894872,
127.0979318477));
#117070=CARTESIAN_POINT('Ctrl Pts',(-171.005399291861,-3.3379496031451,
127.189654414129));
#117071=CARTESIAN_POINT('Ctrl Pts',(-171.013147023872,-3.43611588107539,
127.28551269327));
#117072=CARTESIAN_POINT('Ctrl Pts',(-171.02089307272,-3.53426083279562,
127.381350147604));
#117073=CARTESIAN_POINT('Ctrl Pts',(-171.028639121569,-3.62841827281185,
127.481321254211));
#117074=CARTESIAN_POINT('Ctrl Pts',(-171.036385170418,-3.71823124207505,
127.585053317391));
#117075=CARTESIAN_POINT('Ctrl Pts',(-171.044131213938,-3.80804414955658,
127.688785309215));
#117076=CARTESIAN_POINT('Ctrl Pts',(-171.051877257458,-3.89351233659524,
127.796277956744));
#117077=CARTESIAN_POINT('Ctrl Pts',(-171.059623300978,-3.97431827181639,
127.907124462744));
#117078=CARTESIAN_POINT('Ctrl Pts',(-171.067371016631,-4.05514165055738,
128.017994897101));
#117079=CARTESIAN_POINT('Ctrl Pts',(-171.075118732284,-4.13130054502534,
128.132220314472));
#117080=CARTESIAN_POINT('Ctrl Pts',(-171.082866447937,-4.20252023134042,
128.249364185538));
#117081=CARTESIAN_POINT('Ctrl Pts',(-171.090621545648,-4.27380777608902,
128.366619671806));
#117082=CARTESIAN_POINT('Ctrl Pts',(-171.098376643359,-4.34014651166784,
128.486798830294));
#117083=CARTESIAN_POINT('Ctrl Pts',(-171.10613174107,-4.40130706038281,
128.609439383734));
#117084=CARTESIAN_POINT('Ctrl Pts',(-171.11389095274,-4.4625000538186,128.732144996083));
#117085=CARTESIAN_POINT('Ctrl Pts',(-171.12165016441,-4.51850922753885,
128.857314248682));
#117086=CARTESIAN_POINT('Ctrl Pts',(-171.12940937608,-4.56915341137043,
128.984464970596));
#117087=CARTESIAN_POINT('Ctrl Pts',(-171.137179066458,-4.61986598947558,
129.11178740781));
#117088=CARTESIAN_POINT('Ctrl Pts',(-171.144948756837,-4.66519897841355,
129.241096290292));
#117089=CARTESIAN_POINT('Ctrl Pts',(-171.152718447215,-4.7050209508857,
129.371893893964));
#117090=CARTESIAN_POINT('Ctrl Pts',(-171.15686476506,-4.72627206219556,
129.441694415187));
#117091=CARTESIAN_POINT('Ctrl Pts',(-171.161011082905,-4.74595458264735,
129.511918706171));
#117092=CARTESIAN_POINT('Ctrl Pts',(-171.165157400749,-4.76405452823416,
129.582490119309));
#117093=CARTESIAN_POINT('Ctrl Pts',(-169.415000431073,-4.76405452823411,
129.582490119308));
#117094=CARTESIAN_POINT('Ctrl Pts',(-169.422682023387,-4.79781389926835,
129.714117394601));
#117095=CARTESIAN_POINT('Ctrl Pts',(-169.4303636157,-4.82608891842596,129.847047293059));
#117096=CARTESIAN_POINT('Ctrl Pts',(-169.438045208014,-4.84880351732504,
129.980778494838));
#117097=CARTESIAN_POINT('Ctrl Pts',(-169.445894434008,-4.87201381186302,
130.117428082886));
#117098=CARTESIAN_POINT('Ctrl Pts',(-169.453743660002,-4.8894181413164,
130.254913909779));
#117099=CARTESIAN_POINT('Ctrl Pts',(-169.461592885996,-4.90099142128198,
130.392697951029));
#117100=CARTESIAN_POINT('Ctrl Pts',(-169.46944211199,-4.91256470124756,
130.530481992279));
#117101=CARTESIAN_POINT('Ctrl Pts',(-169.477291337984,-4.91830697782338,
130.668563807642));
#117102=CARTESIAN_POINT('Ctrl Pts',(-169.485140563978,-4.91824957353103,
130.806408778157));
#117103=CARTESIAN_POINT('',(-169.139859436048,-4.91824908052575,130.80736800973));
#117104=CARTESIAN_POINT('Ctrl Pts',(-169.070032268681,-4.76405452823411,
129.582490119308));
#117105=CARTESIAN_POINT('Ctrl Pts',(-169.07784744914,-4.7984384088299,129.716552347903));
#117106=CARTESIAN_POINT('Ctrl Pts',(-169.085662629598,-4.82717822054996,
129.852141009683));
#117107=CARTESIAN_POINT('Ctrl Pts',(-169.093477810057,-4.85015012331475,
129.988746221046));
#117108=CARTESIAN_POINT('Ctrl Pts',(-169.101291338807,-4.87311717105495,
130.125322561416));
#117109=CARTESIAN_POINT('Ctrl Pts',(-169.109104867557,-4.89031866711784,
130.262914649134));
#117110=CARTESIAN_POINT('Ctrl Pts',(-169.116918396307,-4.90168187298647,
130.401002366707));
#117111=CARTESIAN_POINT('Ctrl Pts',(-169.124565409536,-4.91280291552475,
130.536147272018));
#117112=CARTESIAN_POINT('Ctrl Pts',(-169.132212422765,-4.91833199756882,
130.671766538623));
#117113=CARTESIAN_POINT('Ctrl Pts',(-169.139859435994,-4.91824908052634,
130.807368008766));
#117114=CARTESIAN_POINT('Ctrl Pts',(-169.139859436048,-4.91824908052575,
130.80736800973));
#117115=CARTESIAN_POINT('Ctrl Pts',(-169.148676452474,-4.91815347703479,
130.963716685191));
#117116=CARTESIAN_POINT('Ctrl Pts',(-169.1574934689,-4.91059820509904,131.119787728976));
#117117=CARTESIAN_POINT('Ctrl Pts',(-169.166310485326,-4.8956883266556,
131.274912283962));
#117118=CARTESIAN_POINT('Ctrl Pts',(-169.175032969929,-4.88093830477915,
131.428373667855));
#117119=CARTESIAN_POINT('Ctrl Pts',(-169.183755454533,-4.85899077049318,
131.58090858986));
#117120=CARTESIAN_POINT('Ctrl Pts',(-169.192477939136,-4.82999775806313,
131.731886746365));
#117121=CARTESIAN_POINT('Ctrl Pts',(-169.201342221473,-4.80053341852537,
131.885319290734));
#117122=CARTESIAN_POINT('Ctrl Pts',(-169.21020650381,-4.76379268072122,
132.037143802021));
#117123=CARTESIAN_POINT('Ctrl Pts',(-169.219070786147,-4.71998581934507,
132.186719806663));
#117124=CARTESIAN_POINT('Ctrl Pts',(-169.227935068484,-4.67617895796892,
132.336295811305));
#117125=CARTESIAN_POINT('Ctrl Pts',(-169.23679935082,-4.62530612193387,
132.483623132286));
#117126=CARTESIAN_POINT('Ctrl Pts',(-169.245663633157,-4.56762645801148,
132.628085268541));
#117127=CARTESIAN_POINT('Ctrl Pts',(-169.253437967276,-4.5170390599407,
132.7547844047));
#117128=CARTESIAN_POINT('Ctrl Pts',(-169.261212301395,-4.46109587271497,
132.879577799772));
#117129=CARTESIAN_POINT('Ctrl Pts',(-169.268986635513,-4.39996072850778,
133.001979476715));
#117130=CARTESIAN_POINT('Ctrl Pts',(-169.27675138846,-4.33890092790203,
133.124230304532));
#117131=CARTESIAN_POINT('Ctrl Pts',(-169.284516141407,-4.27266207468507,
133.244094932616));
#117132=CARTESIAN_POINT('Ctrl Pts',(-169.292280894354,-4.20145673886827,
133.361105488279));
#117133=CARTESIAN_POINT('Ctrl Pts',(-169.300037935238,-4.13032212519483,
133.477999827409));
#117134=CARTESIAN_POINT('Ctrl Pts',(-169.307794976123,-4.05423104730491,
133.592045403484));
#117135=CARTESIAN_POINT('Ctrl Pts',(-169.315552017007,-3.97344267559748,
133.702797500826));
#117136=CARTESIAN_POINT('Ctrl Pts',(-169.323303208247,-3.8927152270295,
133.81346607915));
#117137=CARTESIAN_POINT('Ctrl Pts',(-169.331054399487,-3.80729776478171,
133.92084580769));
#117138=CARTESIAN_POINT('Ctrl Pts',(-169.338805590727,-3.71749339147748,
134.024519922138));
#117139=CARTESIAN_POINT('Ctrl Pts',(-169.346553487504,-3.62772718742788,
134.128149972322));
#117140=CARTESIAN_POINT('Ctrl Pts',(-169.354301384281,-3.53357803622146,
134.228077246044));
#117141=CARTESIAN_POINT('Ctrl Pts',(-169.362049281057,-3.4353898997311,
134.323917308305));
#117142=CARTESIAN_POINT('Ctrl Pts',(-169.369795557141,-3.3372223020822,
134.419737322891));
#117143=CARTESIAN_POINT('Ctrl Pts',(-169.377541833225,-3.23501767924139,
134.511471553657));
#117144=CARTESIAN_POINT('Ctrl Pts',(-169.385288109309,-3.12915721815602,
134.598772056322));
#117145=CARTESIAN_POINT('Ctrl Pts',(-169.393034442574,-3.02329597563264,
134.68607320342));
#117146=CARTESIAN_POINT('Ctrl Pts',(-169.400780775839,-2.91377914264312,
134.768940308365));
#117147=CARTESIAN_POINT('Ctrl Pts',(-169.408527109104,-2.80102106579407,
134.847065658931));
#117148=CARTESIAN_POINT('Ctrl Pts',(-169.416275177106,-2.68823773755567,
134.925208505128));
#117149=CARTESIAN_POINT('Ctrl Pts',(-169.424023245109,-2.57221204239635,
134.998607261303));
#117150=CARTESIAN_POINT('Ctrl Pts',(-169.431771313112,-2.45338703817852,
135.066997724264));
#117151=CARTESIAN_POINT('Ctrl Pts',(-169.439527615853,-2.33443574533233,
135.135460873422));
#117152=CARTESIAN_POINT('Ctrl Pts',(-169.447283918595,-2.21267953965608,
135.198904901014));
#117153=CARTESIAN_POINT('Ctrl Pts',(-169.455040221336,-2.08858629076118,
135.257111494108));
#117154=CARTESIAN_POINT('Ctrl Pts',(-169.46280066385,-1.96442680956263,
135.315349153813));
#117155=CARTESIAN_POINT('Ctrl Pts',(-169.470561106364,-1.83792816011793,
135.368343658001));
#117156=CARTESIAN_POINT('Ctrl Pts',(-169.478321548878,-1.70957695816374,
135.415925393932));
#117157=CARTESIAN_POINT('Ctrl Pts',(-169.486094449143,-1.58101971546569,
135.463583512288));
#117158=CARTESIAN_POINT('Ctrl Pts',(-169.493867349408,-1.4506043496616,
135.505811378378));
#117159=CARTESIAN_POINT('Ctrl Pts',(-169.501640249673,-1.31883222172905,
135.542489428967));
#117160=CARTESIAN_POINT('Ctrl Pts',(-169.509130585439,-1.19185034249337,
135.57783414005));
#117161=CARTESIAN_POINT('Ctrl Pts',(-169.516620921205,-1.06360893179644,
135.608025459242));
#117162=CARTESIAN_POINT('Ctrl Pts',(-169.524111256971,-0.934562471605686,
135.633001839397));
#117163=CARTESIAN_POINT('Ctrl Pts',(-169.53188559109,-0.800623175719458,
135.658925206584));
#117164=CARTESIAN_POINT('Ctrl Pts',(-169.539659925209,-0.665392298922433,
135.679312497063));
#117165=CARTESIAN_POINT('Ctrl Pts',(-169.547434259328,-0.529367262754573,
135.69403886502));
#117166=CARTESIAN_POINT('Ctrl Pts',(-169.555199012275,-0.393509865286883,
135.708747084044));
#117167=CARTESIAN_POINT('Ctrl Pts',(-169.562963765222,-0.256860640792767,
135.717808220187));
#117168=CARTESIAN_POINT('Ctrl Pts',(-169.570728518169,-0.119928123100087,
135.721148218001));
#117169=CARTESIAN_POINT('Ctrl Pts',(-169.578485559054,0.0168683912856093,
135.724484898482));
#117170=CARTESIAN_POINT('Ctrl Pts',(-169.586242599939,0.153947250609493,
135.722111739227));
#117171=CARTESIAN_POINT('Ctrl Pts',(-169.593999640824,0.290794215045046,
135.714006407946));
#117172=CARTESIAN_POINT('Ctrl Pts',(-169.601750832064,0.427537982120017,
135.705907188958));
#117173=CARTESIAN_POINT('Ctrl Pts',(-169.609502023304,0.564049813680169,
135.69208442499));
#117174=CARTESIAN_POINT('Ctrl Pts',(-169.617253214545,0.699815239738818,
135.672567853575));
#117175=CARTESIAN_POINT('Ctrl Pts',(-169.625001111322,0.835522961869916,
135.653059577223));
#117176=CARTESIAN_POINT('Ctrl Pts',(-169.632749008099,0.970484523293181,
135.627862362174));
#117177=CARTESIAN_POINT('Ctrl Pts',(-169.640496904876,1.10419056816201,
135.597057796784));
#117178=CARTESIAN_POINT('Ctrl Pts',(-169.64824318096,1.23786864460862,135.566259675045));
#117179=CARTESIAN_POINT('Ctrl Pts',(-169.655989457044,1.370291346137,135.529856623721));
#117180=CARTESIAN_POINT('Ctrl Pts',(-169.663735733128,1.50095989651487,
135.487981273806));
#117181=CARTESIAN_POINT('Ctrl Pts',(-169.671482066393,1.63162941145847,
135.446105614775));
#117182=CARTESIAN_POINT('Ctrl Pts',(-169.679228399659,1.76054437709941,
135.398757695863));
#117183=CARTESIAN_POINT('Ctrl Pts',(-169.686974732924,1.88722194196574,
135.346119792628));
#117184=CARTESIAN_POINT('Ctrl Pts',(-169.694722800927,2.01392787539423,
135.293470101501));
#117185=CARTESIAN_POINT('Ctrl Pts',(-169.70247086893,2.13839505004803,135.235528218716));
#117186=CARTESIAN_POINT('Ctrl Pts',(-169.710218936933,2.26016170070031,
135.172524093123));
#117187=CARTESIAN_POINT('Ctrl Pts',(-169.717975239675,2.38205776639778,
135.109453005995));
#117188=CARTESIAN_POINT('Ctrl Pts',(-169.725731542417,2.50124722687086,
135.041309108458));
#117189=CARTESIAN_POINT('Ctrl Pts',(-169.733487845158,2.61729351431315,
134.968368028995));
#117190=CARTESIAN_POINT('Ctrl Pts',(-169.741248287673,2.73340173915345,
134.895388018681));
#117191=CARTESIAN_POINT('Ctrl Pts',(-169.749008730187,2.8463631263379,134.817605946245));
#117192=CARTESIAN_POINT('Ctrl Pts',(-169.756769172701,2.95577194817097,
134.735339535457));
#117193=CARTESIAN_POINT('Ctrl Pts',(-169.764542072966,3.06535640275742,
134.652941063324));
#117194=CARTESIAN_POINT('Ctrl Pts',(-169.772314973232,3.17137659324432,
134.566044115605));
#117195=CARTESIAN_POINT('Ctrl Pts',(-169.780087873497,3.27346092984274,
134.475005874642));
#117196=CARTESIAN_POINT('Ctrl Pts',(-169.787578209259,3.37183424367197,
134.387277103048));
#117197=CARTESIAN_POINT('Ctrl Pts',(-169.795068545021,3.46655267047621,
134.295703117773));
#117198=CARTESIAN_POINT('Ctrl Pts',(-169.802558880783,3.55731877029311,
134.20063301963));
#117199=CARTESIAN_POINT('Ctrl Pts',(-169.810333214902,3.65152629437217,
134.10195830982));
#117200=CARTESIAN_POINT('Ctrl Pts',(-169.818107549022,3.7417742913575,133.999204571723));
#117201=CARTESIAN_POINT('Ctrl Pts',(-169.825881883141,3.82768885643758,
133.892722817957));
#117202=CARTESIAN_POINT('Ctrl Pts',(-169.833646636088,3.91349753949483,
133.786372293435));
#117203=CARTESIAN_POINT('Ctrl Pts',(-169.841411389035,3.99498317363881,
133.676303196176));
#117204=CARTESIAN_POINT('Ctrl Pts',(-169.849176141982,4.07180857896975,
133.562903341311));
#117205=CARTESIAN_POINT('Ctrl Pts',(-169.856933182867,4.14855768022506,
133.449616116782));
#117206=CARTESIAN_POINT('Ctrl Pts',(-169.864690223752,4.22065554593491,
133.333005039611));
#117207=CARTESIAN_POINT('Ctrl Pts',(-169.872447264637,4.28780542812384,
133.213490683181));
#117208=CARTESIAN_POINT('Ctrl Pts',(-169.880198455878,4.35490467206418,
133.094066453458));
#117209=CARTESIAN_POINT('Ctrl Pts',(-169.887949647118,4.4170631687021,132.971743641784));
#117210=CARTESIAN_POINT('Ctrl Pts',(-169.895700838358,4.47402785347217,
132.846971160194));
#117211=CARTESIAN_POINT('Ctrl Pts',(-169.903448735135,4.53096832673171,
132.722251710237));
#117212=CARTESIAN_POINT('Ctrl Pts',(-169.911196631912,4.58271921665689,
132.59508501609));
#117213=CARTESIAN_POINT('Ctrl Pts',(-169.91894452869,4.62907384656703,132.465943713751));
#117214=CARTESIAN_POINT('Ctrl Pts',(-169.926690804774,4.67541878008789,
132.33682942499));
#117215=CARTESIAN_POINT('Ctrl Pts',(-169.934437080858,4.71636956680141,
132.205741717352));
#117216=CARTESIAN_POINT('Ctrl Pts',(-169.942183356942,4.75176819218133,
132.073171915701));
#117217=CARTESIAN_POINT('Ctrl Pts',(-169.949929690208,4.78716707886581,
131.940601135449));
#117218=CARTESIAN_POINT('Ctrl Pts',(-169.957676023473,4.81701362157322,
131.806548617083));
#117219=CARTESIAN_POINT('Ctrl Pts',(-169.965422356738,4.84120018088043,
131.671519121614));
#117220=CARTESIAN_POINT('Ctrl Pts',(-169.973170424742,4.86539215659986,
131.536459387227));
#117221=CARTESIAN_POINT('Ctrl Pts',(-169.980918492745,4.88392155779328,
131.400422625142));
#117222=CARTESIAN_POINT('Ctrl Pts',(-169.988666560748,4.89673225155445,
131.263921624492));
#117223=CARTESIAN_POINT('Ctrl Pts',(-169.99642286349,4.90955656067341,131.127275548954));
#117224=CARTESIAN_POINT('Ctrl Pts',(-170.004179166231,4.91664998448954,
130.990164639109));
#117225=CARTESIAN_POINT('Ctrl Pts',(-170.011935468973,4.91800844148806,
130.853105175747));
#117226=CARTESIAN_POINT('Ctrl Pts',(-170.019695911488,4.91936762353597,
130.715972559621));
#117227=CARTESIAN_POINT('Ctrl Pts',(-170.027456354002,4.91498575210007,
130.578891835265));
#117228=CARTESIAN_POINT('Ctrl Pts',(-170.035216796516,4.90491083145732,
130.442376090338));
#117229=CARTESIAN_POINT('Ctrl Pts',(-170.042989696782,4.89481973765754,
130.305641198217));
#117230=CARTESIAN_POINT('Ctrl Pts',(-170.050762597047,4.87901737713606,
130.169473486494));
#117231=CARTESIAN_POINT('Ctrl Pts',(-170.058535497313,4.85760340415545,
130.034378649961));
#117232=CARTESIAN_POINT('Ctrl Pts',(-170.066025833074,4.83696788303354,
129.904194851033));
#117233=CARTESIAN_POINT('Ctrl Pts',(-170.073516168835,4.81112171902776,
129.775007580153));
#117234=CARTESIAN_POINT('Ctrl Pts',(-170.081006504596,4.78019784697474,
129.647255779499));
#117235=CARTESIAN_POINT('Ctrl Pts',(-170.088780838715,4.74810148691061,
129.514660230481));
#117236=CARTESIAN_POINT('Ctrl Pts',(-170.096555172834,4.71043310371388,
129.383191129323));
#117237=CARTESIAN_POINT('Ctrl Pts',(-170.104329506954,4.66728590955701,
129.253352783624));
#117238=CARTESIAN_POINT('Ctrl Pts',(-170.112094259901,4.62419189046075,
129.123674452082));
#117239=CARTESIAN_POINT('Ctrl Pts',(-170.119859012848,4.57563261727034,
128.995623244629));
#117240=CARTESIAN_POINT('Ctrl Pts',(-170.127623765795,4.52175211586984,
128.869692463818));
#117241=CARTESIAN_POINT('Ctrl Pts',(-170.13538080668,4.46792512934291,128.743886759234));
#117242=CARTESIAN_POINT('Ctrl Pts',(-170.143137847565,4.40878758502785,
128.620197647302));
#117243=CARTESIAN_POINT('Ctrl Pts',(-170.15089488845,4.34453292369278,128.499102120683));
#117244=CARTESIAN_POINT('Ctrl Pts',(-170.15864607969,4.28032671729774,128.378097913144));
#117245=CARTESIAN_POINT('Ctrl Pts',(-170.16639727093,4.21101125721489,128.259683741894));
#117246=CARTESIAN_POINT('Ctrl Pts',(-170.17414846217,4.13682743827276,128.144315165237));
#117247=CARTESIAN_POINT('Ctrl Pts',(-170.181896358947,4.06267514943249,
128.028995623304));
#117248=CARTESIAN_POINT('Ctrl Pts',(-170.189644255724,3.98365882819056,
127.916719429544));
#117249=CARTESIAN_POINT('Ctrl Pts',(-170.197392152501,3.90006440280503,
127.807915938205));
#117250=CARTESIAN_POINT('Ctrl Pts',(-170.205138428585,3.81648746357121,
127.69913520621));
#117251=CARTESIAN_POINT('Ctrl Pts',(-170.212884704669,3.72833456303836,
127.593826041589));
#117252=CARTESIAN_POINT('Ctrl Pts',(-170.220630980753,3.63593365601639,
127.492386959527));
#117253=CARTESIAN_POINT('Ctrl Pts',(-170.228377314018,3.54353206691204,
127.390947128664));
#117254=CARTESIAN_POINT('Ctrl Pts',(-170.236123647284,3.44688267202423,
127.293377726395));
#117255=CARTESIAN_POINT('Ctrl Pts',(-170.243869980549,3.34635195934998,
127.200042148472));
#117256=CARTESIAN_POINT('Ctrl Pts',(-170.251618048552,3.24579873351952,
127.106685668693));
#117257=CARTESIAN_POINT('Ctrl Pts',(-170.259366116555,3.14136274676912,
127.017565165899));
#117258=CARTESIAN_POINT('Ctrl Pts',(-170.267114184558,3.03344508191169,
126.933005041347));
#117259=CARTESIAN_POINT('Ctrl Pts',(-170.2748704873,2.92541272087567,126.848355045287));
#117260=CARTESIAN_POINT('Ctrl Pts',(-170.282626790041,2.81389159808249,
126.768275351043));
#117261=CARTESIAN_POINT('Ctrl Pts',(-170.290383092783,2.69931386902168,
126.693048454885));
#117262=CARTESIAN_POINT('Ctrl Pts',(-170.298143535297,2.58467498637699,
126.617781407868));
#117263=CARTESIAN_POINT('Ctrl Pts',(-170.305903977811,2.46697658210621,
126.54737252051));
#117264=CARTESIAN_POINT('Ctrl Pts',(-170.313664420326,2.34667627887336,
126.482058741867));
#117265=CARTESIAN_POINT('Ctrl Pts',(-170.321437320591,2.22618285891401,
126.416640115748));
#117266=CARTESIAN_POINT('Ctrl Pts',(-170.329210220856,2.10307954471726,
126.356333114932));
#117267=CARTESIAN_POINT('Ctrl Pts',(-170.336983121122,1.97784565719827,
126.301327237854));
#117268=CARTESIAN_POINT('Ctrl Pts',(-170.344473456884,1.85716433692691,
126.248320962955));
#117269=CARTESIAN_POINT('Ctrl Pts',(-170.351963792647,1.73450494416747,
126.20023719724));
#117270=CARTESIAN_POINT('Ctrl Pts',(-170.359454128409,1.61030862793508,
126.157201357836));
#117271=CARTESIAN_POINT('Ctrl Pts',(-170.367228462528,1.48140337063193,
126.112533801503));
#117272=CARTESIAN_POINT('Ctrl Pts',(-170.375002796648,1.35043401120753,
126.073163018622));
#117273=CARTESIAN_POINT('Ctrl Pts',(-170.382777130767,1.21787522138547,
126.03928317773));
#117274=CARTESIAN_POINT('Ctrl Pts',(-170.390541883714,1.08547979842475,
126.005445090714));
#117275=CARTESIAN_POINT('Ctrl Pts',(-170.398306636661,0.951499217708815,
125.977084577066));
#117276=CARTESIAN_POINT('Ctrl Pts',(-170.406071389608,0.816426358154165,
125.95434710581));
#117277=CARTESIAN_POINT('Ctrl Pts',(-170.413828430493,0.681487654867818,
125.931632217732));
#117278=CARTESIAN_POINT('Ctrl Pts',(-170.421585471378,0.545459214722609,
125.914529322353));
#117279=CARTESIAN_POINT('Ctrl Pts',(-170.429342512263,0.408846904614433,
125.903133498661));
#117280=CARTESIAN_POINT('Ctrl Pts',(-170.437093703504,0.272337614911812,
125.891746268649));
#117281=CARTESIAN_POINT('Ctrl Pts',(-170.444844894744,0.13524571967397,
125.886057576345));
#117282=CARTESIAN_POINT('Ctrl Pts',(-170.452596085984,-0.00191529745561372,
125.8861109905));
#117283=CARTESIAN_POINT('Ctrl Pts',(-170.460343982761,-0.139018017493842,
125.886164381952));
#117284=CARTESIAN_POINT('Ctrl Pts',(-170.468091879538,-0.276189410845267,
125.891955025647));
#117285=CARTESIAN_POINT('Ctrl Pts',(-170.475839776315,-0.412913698413853,
125.9034744385));
#117286=CARTESIAN_POINT('Ctrl Pts',(-170.483586052399,-0.549609386208914,
125.91499144174));
#117287=CARTESIAN_POINT('Ctrl Pts',(-170.491332328484,-0.685857764909187,
125.932234797782));
#117288=CARTESIAN_POINT('Ctrl Pts',(-170.499078604568,-0.821146284817372,
125.955143996149));
#117289=CARTESIAN_POINT('Ctrl Pts',(-170.506824937833,-0.956435803394493,
125.978053363625));
#117290=CARTESIAN_POINT('Ctrl Pts',(-170.514571271099,-1.09076506356346,
126.006628591608));
#117291=CARTESIAN_POINT('Ctrl Pts',(-170.522317604364,-1.22363023447237,
126.040757767644));
#117292=CARTESIAN_POINT('Ctrl Pts',(-170.530065672367,-1.35652515961528,
126.074894586673));
#117293=CARTESIAN_POINT('Ctrl Pts',(-170.53781374037,-1.48795496447013,
126.114587731459));
#117294=CARTESIAN_POINT('Ctrl Pts',(-170.545561808373,-1.61742992601593,
126.159675106476));
#117295=CARTESIAN_POINT('Ctrl Pts',(-170.553318111115,-1.74704249509145,
126.204810400892));
#117296=CARTESIAN_POINT('Ctrl Pts',(-170.561074413857,-1.87469570075918,
126.255351249148));
#117297=CARTESIAN_POINT('Ctrl Pts',(-170.568830716599,-1.9999182803082,
126.311086762726));
#117298=CARTESIAN_POINT('Ctrl Pts',(-170.576591159113,-2.12520769491864,
126.366852024026));
#117299=CARTESIAN_POINT('Ctrl Pts',(-170.584351601627,-2.24806354838907,
126.427817301484));
#117300=CARTESIAN_POINT('Ctrl Pts',(-170.592112044142,-2.36803913254049,
126.493725660943));
#117301=CARTESIAN_POINT('Ctrl Pts',(-170.599884944407,-2.48820731215019,
126.559739822352));
#117302=CARTESIAN_POINT('Ctrl Pts',(-170.607657844673,-2.60548564820929,
126.630712720034));
#117303=CARTESIAN_POINT('Ctrl Pts',(-170.615430744938,-2.71945562565491,
126.70634351626));
#117304=CARTESIAN_POINT('Ctrl Pts',(-170.622921080699,-2.82928250733776,
126.779224942535));
#117305=CARTESIAN_POINT('Ctrl Pts',(-170.630411416461,-2.93603713912964,
126.856431313667));
#117306=CARTESIAN_POINT('Ctrl Pts',(-170.637901752222,-3.03937555223074,
126.937659269517));
#117307=CARTESIAN_POINT('Ctrl Pts',(-170.645579700367,-3.14530230938036,
127.020921763056));
#117308=CARTESIAN_POINT('Ctrl Pts',(-170.653257648512,-3.24799267487159,
127.108687882989));
#117309=CARTESIAN_POINT('Ctrl Pts',(-170.660935596657,-3.34703240044547,
127.200674008985));
#117310=CARTESIAN_POINT('Ctrl Pts',(-170.668604766083,-3.44595888717891,
127.292554960999));
#117311=CARTESIAN_POINT('Ctrl Pts',(-170.676273935508,-3.54124274087295,
127.388646057355));
#117312=CARTESIAN_POINT('Ctrl Pts',(-170.683943104934,-3.63250023729922,
127.488621621728));
#117313=CARTESIAN_POINT('Ctrl Pts',(-170.691605265208,-3.72367432995388,
127.588505814549));
#117314=CARTESIAN_POINT('Ctrl Pts',(-170.699267425482,-3.81082911358242,
127.6922671221));
#117315=CARTESIAN_POINT('Ctrl Pts',(-170.706929585756,-3.89361581775241,
127.799541334107));
#117316=CARTESIAN_POINT('Ctrl Pts',(-170.714586500158,-3.97634584228935,
127.906742101192));
#117317=CARTESIAN_POINT('Ctrl Pts',(-170.72224341456,-4.05471349128369,
128.017450672705));
#117318=CARTESIAN_POINT('Ctrl Pts',(-170.729900328962,-4.12840895911293,
128.131268301761));
#117319=CARTESIAN_POINT('Ctrl Pts',(-170.737554734118,-4.20208027622,128.245048631672));
#117320=CARTESIAN_POINT('Ctrl Pts',(-170.745209139275,-4.27108223460267,
128.361935659724));
#117321=CARTESIAN_POINT('Ctrl Pts',(-170.752863544432,-4.33514743436608,
128.481500358142));
#117322=CARTESIAN_POINT('Ctrl Pts',(-170.760516233525,-4.39919827116487,
128.601038251001));
#117323=CARTESIAN_POINT('Ctrl Pts',(-170.768168922618,-4.45831436466268,
128.723252264694));
#117324=CARTESIAN_POINT('Ctrl Pts',(-170.775821611711,-4.51227386738844,
128.847688031725));
#117325=CARTESIAN_POINT('Ctrl Pts',(-170.783477132258,-4.56625333483635,
128.972169839311));
#117326=CARTESIAN_POINT('Ctrl Pts',(-170.791132652804,-4.61507223721576,
129.098874675109));
#117327=CARTESIAN_POINT('Ctrl Pts',(-170.79878817335,-4.65855657066248,
129.227327409153));
#117328=CARTESIAN_POINT('Ctrl Pts',(-170.805764700801,-4.69818413669539,
129.3443872511));
#117329=CARTESIAN_POINT('Ctrl Pts',(-170.812741228252,-4.73338195825923,
129.462898234498));
#117330=CARTESIAN_POINT('Ctrl Pts',(-170.819717755703,-4.76405452823413,
129.582490119309));
#117331=CARTESIAN_POINT('Origin',(213.235140564004,0.,130.804360617566));
#117332=CARTESIAN_POINT('',(-172.915418914505,-4.76405452823406,129.582490119308));
#117333=CARTESIAN_POINT('',(-172.569844098739,-4.76405452823414,129.582490119309));
#117334=CARTESIAN_POINT('',(213.235140564004,-4.76405452823405,129.582490119308));
#117335=CARTESIAN_POINT('',(-171.235140564042,-4.91824795183872,130.799872106209));
#117336=CARTESIAN_POINT('Ctrl Pts',(-171.235140564042,-4.91824795183872,
130.799872106209));
#117337=CARTESIAN_POINT('Ctrl Pts',(-171.242791581675,-4.91837113477668,
130.934848757505));
#117338=CARTESIAN_POINT('Ctrl Pts',(-171.250442599308,-4.9129336827261,
131.069996001476));
#117339=CARTESIAN_POINT('Ctrl Pts',(-171.258093616941,-4.901920266296,131.20481132037));
#117340=CARTESIAN_POINT('Ctrl Pts',(-171.265738651492,-4.89091546233709,
131.339521213935));
#117341=CARTESIAN_POINT('Ctrl Pts',(-171.273383686044,-4.87434340088689,
131.473899299186));
#117342=CARTESIAN_POINT('Ctrl Pts',(-171.281028720596,-4.85224081964007,
131.607443484223));
#117343=CARTESIAN_POINT('Ctrl Pts',(-171.288670364304,-4.83014804166853,
131.740928437699));
#117344=CARTESIAN_POINT('Ctrl Pts',(-171.296312008013,-4.80252968590728,
131.873579829738));
#117345=CARTESIAN_POINT('Ctrl Pts',(-171.303953651722,-4.76947425097537,
132.004901508907));
#117346=CARTESIAN_POINT('Ctrl Pts',(-171.311593722981,-4.73642561798132,
132.136196165534));
#117347=CARTESIAN_POINT('Ctrl Pts',(-171.319233794241,-4.69794222833499,
132.266161262883));
#117348=CARTESIAN_POINT('Ctrl Pts',(-171.326873865501,-4.65416341139346,
132.394312189956));
#117349=CARTESIAN_POINT('Ctrl Pts',(-171.334514126357,-4.6103835080371,
132.522466297222));
#117350=CARTESIAN_POINT('Ctrl Pts',(-171.342154387212,-4.56130804653507,
132.648805763594));
#117351=CARTESIAN_POINT('Ctrl Pts',(-171.349794648068,-4.50712563271322,
132.772862990803));
#117352=CARTESIAN_POINT('Ctrl Pts',(-171.357436860504,-4.45292937887392,
132.896951906416));
#117353=CARTESIAN_POINT('Ctrl Pts',(-171.36507907294,-4.39362374029316,
133.018757054857));
#117354=CARTESIAN_POINT('Ctrl Pts',(-171.372721285377,-4.32944444139462,
133.137833113949));
#117355=CARTESIAN_POINT('Ctrl Pts',(-171.380371522867,-4.26519774809284,
133.257034214294));
#117356=CARTESIAN_POINT('Ctrl Pts',(-171.388021760357,-4.19606736896836,
133.373500149427));
#117357=CARTESIAN_POINT('Ctrl Pts',(-171.395671997848,-4.12233389934677,
133.486812161359));
#117358=CARTESIAN_POINT('Ctrl Pts',(-171.403326729994,-4.04855710994649,
133.600190746196));
#117359=CARTESIAN_POINT('Ctrl Pts',(-171.410981462141,-3.97017207940516,
133.710411391769));
#117360=CARTESIAN_POINT('Ctrl Pts',(-171.418636194287,-3.88750047758997,
133.817087471968));
#117361=CARTESIAN_POINT('Ctrl Pts',(-171.426302145668,-3.80470770732213,
133.923919903022));
#117362=CARTESIAN_POINT('Ctrl Pts',(-171.433968097048,-3.71761608277086,
134.027197091071));
#117363=CARTESIAN_POINT('Ctrl Pts',(-171.441634048429,-3.62658524128344,
134.126568099077));
#117364=CARTESIAN_POINT('Ctrl Pts',(-171.445641241453,-3.57900104268049,
134.178511920566));
#117365=CARTESIAN_POINT('Ctrl Pts',(-171.449648434477,-3.53034106028268,
134.229389052183));
#117366=CARTESIAN_POINT('Ctrl Pts',(-171.453655627501,-3.48066020141234,
134.279153794836));
#117367=CARTESIAN_POINT('Ctrl Pts',(-171.46142996162,-3.38427462830093,
134.375702110435));
#117368=CARTESIAN_POINT('Ctrl Pts',(-171.469204295739,-3.28371618382948,
134.468389924618));
#117369=CARTESIAN_POINT('Ctrl Pts',(-171.476978629858,-3.17932680684791,
134.556835016913));
#117370=CARTESIAN_POINT('Ctrl Pts',(-171.484743382805,-3.0750660804445,
134.645171108537));
#117371=CARTESIAN_POINT('Ctrl Pts',(-171.492508135752,-2.96698411090576,
134.729274631671));
#117372=CARTESIAN_POINT('Ctrl Pts',(-171.500272888699,-2.8554605102969,
134.808799197022));
#117373=CARTESIAN_POINT('Ctrl Pts',(-171.508029929584,-2.74404767650008,
134.888244777453));
#117374=CARTESIAN_POINT('Ctrl Pts',(-171.515786970469,-2.62920033042157,
134.963120225079));
#117375=CARTESIAN_POINT('Ctrl Pts',(-171.523544011354,-2.5113318031952,
135.033118784778));
#117376=CARTESIAN_POINT('Ctrl Pts',(-171.531295202594,-2.39355216154161,
135.103064558019));
#117377=CARTESIAN_POINT('Ctrl Pts',(-171.539046393834,-2.27275620834601,
135.168140564745));
#117378=CARTESIAN_POINT('Ctrl Pts',(-171.546797585075,-2.14938665351449,
135.228083040616));
#117379=CARTESIAN_POINT('Ctrl Pts',(-171.554545481852,-2.02606953403527,
135.288000039336));
#117380=CARTESIAN_POINT('Ctrl Pts',(-171.562293378629,-1.90018133942075,
135.342787676306));
#117381=CARTESIAN_POINT('Ctrl Pts',(-171.570041275406,-1.77218960989272,
135.392227992402));
#117382=CARTESIAN_POINT('Ctrl Pts',(-171.57778755149,-1.64422465347533,
135.441657966651));
#117383=CARTESIAN_POINT('Ctrl Pts',(-171.585533827574,-1.51415740182784,
135.485742704085));
#117384=CARTESIAN_POINT('Ctrl Pts',(-171.593280103658,-1.38247524640949,
135.52431244524));
#117385=CARTESIAN_POINT('Ctrl Pts',(-171.601026436923,-1.25079211894321,
135.562882471109));
#117386=CARTESIAN_POINT('Ctrl Pts',(-171.608772770189,-1.1174944391208,
135.595937309567));
#117387=CARTESIAN_POINT('Ctrl Pts',(-171.616519103454,-0.983084239545638,
135.623357239318));
#117388=CARTESIAN_POINT('Ctrl Pts',(-171.624267171457,-0.848643939738398,
135.650783309572));
#117389=CARTESIAN_POINT('Ctrl Pts',(-171.63201523946,-0.713091007418455,
135.672571881952));
#117390=CARTESIAN_POINT('Ctrl Pts',(-171.639763307463,-0.576936737012451,
135.688654534192));
#117391=CARTESIAN_POINT('Ctrl Pts',(-171.647519610205,-0.440637760227788,
135.704754279266));
#117392=CARTESIAN_POINT('Ctrl Pts',(-171.655275912947,-0.303736557552501,
135.715135944132));
#117393=CARTESIAN_POINT('Ctrl Pts',(-171.663032215688,-0.16674916315239,
135.719783059136));
#117394=CARTESIAN_POINT('Ctrl Pts',(-171.670792658203,-0.0296886544549024,
135.724432654445));
#117395=CARTESIAN_POINT('Ctrl Pts',(-171.678553100717,0.107457746870967,
135.723341604292));
#117396=CARTESIAN_POINT('Ctrl Pts',(-171.686313543231,0.244175948951485,
135.716545586442));
#117397=CARTESIAN_POINT('Ctrl Pts',(-171.694086443496,0.381113623227256,
135.709738659021));
#117398=CARTESIAN_POINT('Ctrl Pts',(-171.701859343762,0.517621335093968,
135.697208498816));
#117399=CARTESIAN_POINT('Ctrl Pts',(-171.709632244027,0.653191143957876,
135.679042596111));
#117400=CARTESIAN_POINT('Ctrl Pts',(-171.717122579789,0.78383264878984,
135.661537069727));
#117401=CARTESIAN_POINT('Ctrl Pts',(-171.724612915551,0.913602953612798,
135.638798487069));
#117402=CARTESIAN_POINT('Ctrl Pts',(-171.732103251313,1.04206005258033,
135.61094921129));
#117403=CARTESIAN_POINT('Ctrl Pts',(-171.739877585432,1.17538764149908,
135.582044021755));
#117404=CARTESIAN_POINT('Ctrl Pts',(-171.747651919551,1.3077228201397,135.547541382049));
#117405=CARTESIAN_POINT('Ctrl Pts',(-171.755426253671,1.43855918929407,
135.507522375511));
#117406=CARTESIAN_POINT('Ctrl Pts',(-171.763191006618,1.56923431431592,
135.467552688822));
#117407=CARTESIAN_POINT('Ctrl Pts',(-171.770955759565,1.69841393484881,
135.422080275406));
#117408=CARTESIAN_POINT('Ctrl Pts',(-171.778720512512,1.8256014341755,135.371237281768));
#117409=CARTESIAN_POINT('Ctrl Pts',(-171.786477553397,1.95266260908517,
135.320444786109));
#117410=CARTESIAN_POINT('Ctrl Pts',(-171.794234594282,2.07773523961322,
135.264292469583));
#117411=CARTESIAN_POINT('Ctrl Pts',(-171.801991635167,2.2003378284147,135.202962270745));
#117412=CARTESIAN_POINT('Ctrl Pts',(-171.809742826407,2.32284796165042,
135.141678321486));
#117413=CARTESIAN_POINT('Ctrl Pts',(-171.817494017647,2.4428914124644,135.075224436149));
#117414=CARTESIAN_POINT('Ctrl Pts',(-171.825245208887,2.56000697292905,
135.003830508047));
#117415=CARTESIAN_POINT('Ctrl Pts',(-171.832993105664,2.67707275615617,
134.932466924269));
#117416=CARTESIAN_POINT('Ctrl Pts',(-171.840741002442,2.79121279098485,
134.856167676845));
#117417=CARTESIAN_POINT('Ctrl Pts',(-171.848488899219,2.90199098532122,
134.775208308376));
#117418=CARTESIAN_POINT('Ctrl Pts',(-171.856235175303,3.01274600724743,
134.694265874862));
#117419=CARTESIAN_POINT('Ctrl Pts',(-171.863981451387,3.12014027197992,
134.608665489768));
#117420=CARTESIAN_POINT('Ctrl Pts',(-171.871727727471,3.22376750908492,
134.518725450195));
#117421=CARTESIAN_POINT('Ctrl Pts',(-171.879474060736,3.32739551114279,
134.428784746705));
#117422=CARTESIAN_POINT('Ctrl Pts',(-171.887220394002,3.42725613482055,
134.33450458108));
#117423=CARTESIAN_POINT('Ctrl Pts',(-171.894966727267,3.52297729431445,
134.236242615282));
#117424=CARTESIAN_POINT('Ctrl Pts',(-171.90271479527,3.61871988989795,134.137958644398));
#117425=CARTESIAN_POINT('Ctrl Pts',(-171.910462863273,3.71032090390886,
134.035691378966));
#117426=CARTESIAN_POINT('Ctrl Pts',(-171.918210931276,3.79744640362981,
133.929834001561));
#117427=CARTESIAN_POINT('Ctrl Pts',(-171.925967234018,3.88466450136878,
133.823864117675));
#117428=CARTESIAN_POINT('Ctrl Pts',(-171.93372353676,3.96739733408864,133.714296802067));
#117429=CARTESIAN_POINT('Ctrl Pts',(-171.941479839502,4.04535211633096,
133.601557306645));
#117430=CARTESIAN_POINT('Ctrl Pts',(-171.949240282016,4.12334850538773,
133.48875763876));
#117431=CARTESIAN_POINT('Ctrl Pts',(-171.95700072453,4.19656155389788,133.37278274788));
#117432=CARTESIAN_POINT('Ctrl Pts',(-171.964761167044,4.26474339935941,
133.254084438759));
#117433=CARTESIAN_POINT('Ctrl Pts',(-171.97253406731,4.33303469637237,133.135195584575));
#117434=CARTESIAN_POINT('Ctrl Pts',(-171.980306967575,4.39627847036963,
133.013574922825));
#117435=CARTESIAN_POINT('Ctrl Pts',(-171.98807986784,4.45427377510685,132.889697088953));
#117436=CARTESIAN_POINT('Ctrl Pts',(-171.995570203603,4.510160804436,132.77032252637));
#117437=CARTESIAN_POINT('Ctrl Pts',(-172.003060539365,4.56117421042881,
132.648852334288));
#117438=CARTESIAN_POINT('Ctrl Pts',(-172.010550875127,4.60717802571458,
132.525724525016));
#117439=CARTESIAN_POINT('Ctrl Pts',(-172.018325209246,4.65492608963912,
132.397928287433));
#117440=CARTESIAN_POINT('Ctrl Pts',(-172.026099543365,4.69742843821103,
132.267941434181));
#117441=CARTESIAN_POINT('Ctrl Pts',(-172.033873877484,4.73447956799728,
132.136233840781));
#117442=CARTESIAN_POINT('Ctrl Pts',(-172.041638630431,4.77148503557721,
132.004688565219));
#117443=CARTESIAN_POINT('Ctrl Pts',(-172.049403383378,4.80305254660979,
131.87142714173));
#117444=CARTESIAN_POINT('Ctrl Pts',(-172.057168136325,4.82902484622783,
131.73693881644));
#117445=CARTESIAN_POINT('Ctrl Pts',(-172.06492517721,4.85497134979189,131.602584066849));
#117446=CARTESIAN_POINT('Ctrl Pts',(-172.072682218095,4.8753336274519,131.467005221865));
#117447=CARTESIAN_POINT('Ctrl Pts',(-172.08043925898,4.89000448818936,131.330705721075));
#117448=CARTESIAN_POINT('Ctrl Pts',(-172.08819045022,4.9046642855166,131.194509004799));
#117449=CARTESIAN_POINT('Ctrl Pts',(-172.09594164146,4.91364116709979,131.05759310157));
#117450=CARTESIAN_POINT('Ctrl Pts',(-172.103692832701,4.91687925454406,
130.920470301634));
#117451=CARTESIAN_POINT('Ctrl Pts',(-172.111440729478,4.92011596571478,
130.783405782545));
#117452=CARTESIAN_POINT('Ctrl Pts',(-172.119188626255,4.91761872480073,
130.646134931685));
#117453=CARTESIAN_POINT('Ctrl Pts',(-172.126936523032,4.90938363516595,
130.509173583188));
#117454=CARTESIAN_POINT('Ctrl Pts',(-172.134682799116,4.90115026813439,
130.372240884053));
#117455=CARTESIAN_POINT('Ctrl Pts',(-172.1424290752,4.88718146316421,130.235617948521));
#117456=CARTESIAN_POINT('Ctrl Pts',(-172.150175351284,4.86752541352832,
130.099818630772));
#117457=CARTESIAN_POINT('Ctrl Pts',(-172.157921684549,4.84786921879592,
129.964018310583));
#117458=CARTESIAN_POINT('Ctrl Pts',(-172.165668017815,4.82252575163184,
129.829042007242));
#117459=CARTESIAN_POINT('Ctrl Pts',(-172.17341435108,4.79159480170818,129.6953960921));
#117460=CARTESIAN_POINT('Ctrl Pts',(-172.181162419083,4.76065692501263,
129.561720247881));
#117461=CARTESIAN_POINT('Ctrl Pts',(-172.188910487086,4.72412916379682,
129.429375765534));
#117462=CARTESIAN_POINT('Ctrl Pts',(-172.196658555089,4.68216181490638,
129.298856116898));
#117463=CARTESIAN_POINT('Ctrl Pts',(-172.204414857831,4.64014986261829,
129.168197750426));
#117464=CARTESIAN_POINT('Ctrl Pts',(-172.212171160573,4.59268689383651,
129.039368464727));
#117465=CARTESIAN_POINT('Ctrl Pts',(-172.219927463315,4.53997242734291,
128.912844447541));
#117466=CARTESIAN_POINT('Ctrl Pts',(-172.227687905829,4.48722982555134,
128.786252900678));
#117467=CARTESIAN_POINT('Ctrl Pts',(-172.235448348343,4.4292303063213,128.661969428099));
#117468=CARTESIAN_POINT('Ctrl Pts',(-172.243208790857,4.36622001005309,
128.540446775055));
#117469=CARTESIAN_POINT('Ctrl Pts',(-172.250981691122,4.30310856406351,
128.41872904306));
#117470=CARTESIAN_POINT('Ctrl Pts',(-172.258754591388,4.23497046151783,
128.299781326414));
#117471=CARTESIAN_POINT('Ctrl Pts',(-172.266527491653,4.16209641030288,
128.184029238934));
#117472=CARTESIAN_POINT('Ctrl Pts',(-172.274017827415,4.09187151440884,
128.072485031397));
#117473=CARTESIAN_POINT('Ctrl Pts',(-172.281508163177,4.01724919360767,
127.963908402267));
#117474=CARTESIAN_POINT('Ctrl Pts',(-172.288998498939,3.93852446637565,
127.858650501098));
#117475=CARTESIAN_POINT('Ctrl Pts',(-172.296772833058,3.85681486718197,
127.749401714613));
#117476=CARTESIAN_POINT('Ctrl Pts',(-172.304547167177,3.7704268037028,127.643382215742));
#117477=CARTESIAN_POINT('Ctrl Pts',(-172.312321501296,3.67964451589573,
127.541018879541));
#117478=CARTESIAN_POINT('Ctrl Pts',(-172.320086254243,3.58897410914518,
127.438781697003));
#117479=CARTESIAN_POINT('Ctrl Pts',(-172.32785100719,3.49392051019693,127.340192001446));
#117480=CARTESIAN_POINT('Ctrl Pts',(-172.335615760138,3.39481033557449,
127.245646545324));
#117481=CARTESIAN_POINT('Ctrl Pts',(-172.343372801023,3.29579859857468,
127.151194993081));
#117482=CARTESIAN_POINT('Ctrl Pts',(-172.351129841908,3.19273858494966,
127.060779954786));
#117483=CARTESIAN_POINT('Ctrl Pts',(-172.358886882793,3.08599591331679,
126.974763734669));
#117484=CARTESIAN_POINT('Ctrl Pts',(-172.366638074033,2.9793337371628,126.888812380054));
#117485=CARTESIAN_POINT('Ctrl Pts',(-172.374389265273,2.86899473388537,
126.807253485288));
#117486=CARTESIAN_POINT('Ctrl Pts',(-172.382140456513,2.75537970413742,
126.730410967837));
#117487=CARTESIAN_POINT('Ctrl Pts',(-172.38988835329,2.64181296380805,126.653601110506));
#117488=CARTESIAN_POINT('Ctrl Pts',(-172.397636250067,2.52497328955437,
126.581503862096));
#117489=CARTESIAN_POINT('Ctrl Pts',(-172.405384146844,2.40529256101639,
126.514401321906));
#117490=CARTESIAN_POINT('Ctrl Pts',(-172.413130422928,2.28563686710681,
126.447312818121));
#117491=CARTESIAN_POINT('Ctrl Pts',(-172.420876699012,2.16314164178756,
126.385217135504));
#117492=CARTESIAN_POINT('Ctrl Pts',(-172.428622975096,2.03826525477484,
126.328351478425));
#117493=CARTESIAN_POINT('Ctrl Pts',(-172.436369308362,1.91338794595283,
126.271485401576));
#117494=CARTESIAN_POINT('Ctrl Pts',(-172.444115641627,1.78612979617358,
126.21984958933));
#117495=CARTESIAN_POINT('Ctrl Pts',(-172.451861974893,1.65697076875139,
126.173633791893));
#117496=CARTESIAN_POINT('Ctrl Pts',(-172.459610042896,1.52778281706,126.127407644749));
#117497=CARTESIAN_POINT('Ctrl Pts',(-172.467358110899,1.39669350869382,
126.086604059378));
#117498=CARTESIAN_POINT('Ctrl Pts',(-172.475106178902,1.26419925460279,
126.051363320369));
#117499=CARTESIAN_POINT('Ctrl Pts',(-172.482862481644,1.13156418404234,
126.016085127083));
#117500=CARTESIAN_POINT('Ctrl Pts',(-172.490618784385,0.9975215633744,125.98638169119));
#117501=CARTESIAN_POINT('Ctrl Pts',(-172.498375087127,0.862579867607632,
125.962342542992));
#117502=CARTESIAN_POINT('Ctrl Pts',(-172.506135529641,0.727566149394817,
125.938290564378));
#117503=CARTESIAN_POINT('Ctrl Pts',(-172.513895972155,0.591652787162964,
125.919908949816));
#117504=CARTESIAN_POINT('Ctrl Pts',(-172.52165641467,0.455353733211432,
125.907235334285));
#117505=CARTESIAN_POINT('Ctrl Pts',(-172.529429314935,0.318835879918437,
125.894541373941));
#117506=CARTESIAN_POINT('Ctrl Pts',(-172.5372022152,0.181931488338155,125.887573743077));
#117507=CARTESIAN_POINT('Ctrl Pts',(-172.544975115466,0.0451557741424795,
125.88631791558));
#117508=CARTESIAN_POINT('Ctrl Pts',(-172.552465451228,-0.0866477983238361,
125.885107740575));
#117509=CARTESIAN_POINT('Ctrl Pts',(-172.55995578699,-0.218331578604747,
125.889201292303));
#117510=CARTESIAN_POINT('Ctrl Pts',(-172.567446122752,-0.349440669944215,
125.898540168274));
#117511=CARTESIAN_POINT('Ctrl Pts',(-172.575220456871,-0.485520802332531,
125.908233130567));
#117512=CARTESIAN_POINT('Ctrl Pts',(-172.58299479099,-0.621412867816529,
125.923607726199));
#117513=CARTESIAN_POINT('Ctrl Pts',(-172.590769125109,-0.756604085683117,
125.944655552438));
#117514=CARTESIAN_POINT('Ctrl Pts',(-172.598533878056,-0.891628692456069,
125.965677439113));
#117515=CARTESIAN_POINT('Ctrl Pts',(-172.606298631003,-1.0259537875782,
125.99235858533));
#117516=CARTESIAN_POINT('Ctrl Pts',(-172.61406338395,-1.15906902776432,
126.024638653751));
#117517=CARTESIAN_POINT('Ctrl Pts',(-172.621820424835,-1.29205205601728,
126.056886661152));
#117518=CARTESIAN_POINT('Ctrl Pts',(-172.62957746572,-1.4238272431674,126.094722432717));
#117519=CARTESIAN_POINT('Ctrl Pts',(-172.637334506605,-1.55389214660935,
126.138034197436));
#117520=CARTESIAN_POINT('Ctrl Pts',(-172.645085697846,-1.68385896709709,
126.181313300416));
#117521=CARTESIAN_POINT('Ctrl Pts',(-172.652836889086,-1.81211770158416,
126.230060054029));
#117522=CARTESIAN_POINT('Ctrl Pts',(-172.660588080326,-1.93817918658972,
126.284112338636));
#117523=CARTESIAN_POINT('Ctrl Pts',(-172.668335977103,-2.06418709210015,
126.33814164958));
#117524=CARTESIAN_POINT('Ctrl Pts',(-172.67608387388,-2.18799924698974,
126.397471852762));
#117525=CARTESIAN_POINT('Ctrl Pts',(-172.683831770657,-2.30914487163311,
126.461892077172));
#117526=CARTESIAN_POINT('Ctrl Pts',(-172.691578046741,-2.4302651552234,
126.52629882626));
#117527=CARTESIAN_POINT('Ctrl Pts',(-172.699324322825,-2.54871967304773,
126.59579329534));
#117528=CARTESIAN_POINT('Ctrl Pts',(-172.707070598909,-2.66406109832322,
126.670118059745));
#117529=CARTESIAN_POINT('Ctrl Pts',(-172.714816932175,-2.77940337502339,
126.744443372798));
#117530=CARTESIAN_POINT('Ctrl Pts',(-172.72256326544,-2.89163218467719,
126.823598840552));
#117531=CARTESIAN_POINT('Ctrl Pts',(-172.730309598705,-3.00032845316646,
126.907283220898));
#117532=CARTESIAN_POINT('Ctrl Pts',(-172.738057666708,-3.10904906343157,
126.990986341781));
#117533=CARTESIAN_POINT('Ctrl Pts',(-172.745805734712,-3.21423524862831,
127.079220154976));
#117534=CARTESIAN_POINT('Ctrl Pts',(-172.753553802715,-3.31550066111441,
127.171642843137));
#117535=CARTESIAN_POINT('Ctrl Pts',(-172.761310105456,-3.41687369968555,
127.264163759232));
#117536=CARTESIAN_POINT('Ctrl Pts',(-172.769066408198,-3.51431735219186,
127.360882179636));
#117537=CARTESIAN_POINT('Ctrl Pts',(-172.77682271094,-3.60748145109045,
127.461418703243));
#117538=CARTESIAN_POINT('Ctrl Pts',(-172.784583153454,-3.70069527447399,
127.562008886219));
#117539=CARTESIAN_POINT('Ctrl Pts',(-172.792343595968,-3.78962473955368,
127.666420935465));
#117540=CARTESIAN_POINT('Ctrl Pts',(-172.800104038482,-3.87396037918624,
127.77424279098));
#117541=CARTESIAN_POINT('Ctrl Pts',(-172.807876938748,-3.95843140187404,
127.882237731708));
#117542=CARTESIAN_POINT('Ctrl Pts',(-172.815649839013,-4.03829363477777,
127.993653099002));
#117543=CARTESIAN_POINT('Ctrl Pts',(-172.823422739279,-4.11328081247327,
128.108047575607));
#117544=CARTESIAN_POINT('Ctrl Pts',(-172.830913075041,-4.18554201737741,
128.218283524843));
#117545=CARTESIAN_POINT('Ctrl Pts',(-172.838403410803,-4.25327629616988,
128.331285483371));
#117546=CARTESIAN_POINT('Ctrl Pts',(-172.845893746565,-4.31628690171076,
128.446639165693));
#117547=CARTESIAN_POINT('Ctrl Pts',(-172.854068586708,-4.38505573183823,
128.572534445006));
#117548=CARTESIAN_POINT('Ctrl Pts',(-172.862243426851,-4.44839760949704,
128.701595936106));
#117549=CARTESIAN_POINT('Ctrl Pts',(-172.870418266993,-4.50602512050778,
128.833340405632));
#117550=CARTESIAN_POINT('Ctrl Pts',(-172.878574919318,-4.5635244187734,
128.96479176307));
#117551=CARTESIAN_POINT('Ctrl Pts',(-172.886731571643,-4.6153345655119,
129.098913895225));
#117552=CARTESIAN_POINT('Ctrl Pts',(-172.894888223968,-4.6612139626585,
129.235199231087));
#117553=CARTESIAN_POINT('Ctrl Pts',(-172.90173178748,-4.69970752052794,
129.349544836937));
#117554=CARTESIAN_POINT('Ctrl Pts',(-172.908575350993,-4.73402685051016,
129.465412659596));
#117555=CARTESIAN_POINT('Ctrl Pts',(-172.915418914505,-4.76405452823406,
129.582490119308));
#117556=CARTESIAN_POINT('Ctrl Pts',(-171.165157400749,-4.76405452823416,
129.582490119309));
#117557=CARTESIAN_POINT('Ctrl Pts',(-171.168507601729,-4.77867918020337,
129.639511415377));
#117558=CARTESIAN_POINT('Ctrl Pts',(-171.171857802708,-4.79227071959931,
129.696759316179));
#117559=CARTESIAN_POINT('Ctrl Pts',(-171.175208003688,-4.80482377000955,
129.754193201555));
#117560=CARTESIAN_POINT('Ctrl Pts',(-171.185974661452,-4.84516594604442,
129.938770482654));
#117561=CARTESIAN_POINT('Ctrl Pts',(-171.196741319217,-4.87488446168539,
130.125746382853));
#117562=CARTESIAN_POINT('Ctrl Pts',(-171.207507976981,-4.89375382829365,
130.31409892157));
#117563=CARTESIAN_POINT('Ctrl Pts',(-171.216718839325,-4.90989654798845,
130.47523428448));
#117564=CARTESIAN_POINT('Ctrl Pts',(-171.225929701668,-4.9180996550663,
130.637377204443));
#117565=CARTESIAN_POINT('Ctrl Pts',(-171.235140564012,-4.91824795183824,
130.799872105685));
#117566=CARTESIAN_POINT('',(-170.889859435956,-4.91824925841368,130.807061471733));
#117567=CARTESIAN_POINT('Ctrl Pts',(-170.819717755703,-4.76405452823413,
129.582490119309));
#117568=CARTESIAN_POINT('Ctrl Pts',(-170.827380355377,-4.79774344099872,
129.713842678877));
#117569=CARTESIAN_POINT('Ctrl Pts',(-170.835042955051,-4.82597252582046,
129.846498967558));
#117570=CARTESIAN_POINT('Ctrl Pts',(-170.842705554725,-4.84866437856723,
129.979959740254));
#117571=CARTESIAN_POINT('Ctrl Pts',(-170.85056453493,-4.87193778826417,
130.116840905317));
#117572=CARTESIAN_POINT('Ctrl Pts',(-170.858423515135,-4.88938625812206,
130.254567894436));
#117573=CARTESIAN_POINT('Ctrl Pts',(-170.866282495341,-4.90098307374099,
130.392598582643));
#117574=CARTESIAN_POINT('Ctrl Pts',(-170.874141475546,-4.91257988935995,
130.530629270849));
#117575=CARTESIAN_POINT('Ctrl Pts',(-170.882000455751,-4.91832509500793,
130.668963207153));
#117576=CARTESIAN_POINT('Ctrl Pts',(-170.889859435956,-4.91824925841368,
130.807061471733));
#117577=CARTESIAN_POINT('Ctrl Pts',(-170.889859435994,-4.91824925841332,
130.807061472394));
#117578=CARTESIAN_POINT('Ctrl Pts',(-170.898689416008,-4.91816405196695,
130.962222178274));
#117579=CARTESIAN_POINT('Ctrl Pts',(-170.907519396022,-4.91073700608355,
131.117177606773));
#117580=CARTESIAN_POINT('Ctrl Pts',(-170.916349376036,-4.8960220816411,
131.271426821206));
#117581=CARTESIAN_POINT('Ctrl Pts',(-170.924123710155,-4.88306636271859,
131.407235161509));
#117582=CARTESIAN_POINT('Ctrl Pts',(-170.931898044274,-4.86443515971341,
131.542719145533));
#117583=CARTESIAN_POINT('Ctrl Pts',(-170.939672378393,-4.84014917826146,
131.677366341874));
#117584=CARTESIAN_POINT('Ctrl Pts',(-170.94743713134,-4.81589312711116,
131.81184759758));
#117585=CARTESIAN_POINT('Ctrl Pts',(-170.955201884287,-4.78599623249637,
131.945493736452));
#117586=CARTESIAN_POINT('Ctrl Pts',(-170.962966637234,-4.75053106121194,
132.077796010101));
#117587=CARTESIAN_POINT('Ctrl Pts',(-170.970723678119,-4.71510111443569,
132.209966879267));
#117588=CARTESIAN_POINT('Ctrl Pts',(-170.978480719004,-4.6741139974901,
132.340796164225));
#117589=CARTESIAN_POINT('Ctrl Pts',(-170.986237759889,-4.62769350643511,
132.469784249258));
#117590=CARTESIAN_POINT('Ctrl Pts',(-170.993988951129,-4.58130802143347,
132.598675063373));
#117591=CARTESIAN_POINT('Ctrl Pts',(-171.001740142369,-4.52949744970189,
132.725727074835));
#117592=CARTESIAN_POINT('Ctrl Pts',(-171.009491333609,-4.47243560276683,
132.850455151453));
#117593=CARTESIAN_POINT('Ctrl Pts',(-171.017239230386,-4.41539800863882,
132.975130215313));
#117594=CARTESIAN_POINT('Ctrl Pts',(-171.024987127163,-4.35311374075912,
133.097482954075));
#117595=CARTESIAN_POINT('Ctrl Pts',(-171.03273502394,-4.2858049068253,133.217047784012));
#117596=CARTESIAN_POINT('Ctrl Pts',(-171.040481300024,-4.21851015244852,
133.336587603563));
#117597=CARTESIAN_POINT('Ctrl Pts',(-171.048227576109,-4.14619311424533,
133.453340333772));
#117598=CARTESIAN_POINT('Ctrl Pts',(-171.055973852193,-4.0691218773607,
133.566864954157));
#117599=CARTESIAN_POINT('Ctrl Pts',(-171.063720185458,-3.99205007155381,
133.680390412555));
#117600=CARTESIAN_POINT('Ctrl Pts',(-171.071466518723,-3.91022421663621,
133.790687390113));
#117601=CARTESIAN_POINT('Ctrl Pts',(-171.079212851989,-3.82395552458879,
133.897344162376));
#117602=CARTESIAN_POINT('Ctrl Pts',(-171.086960919992,-3.73766751326605,
134.004024819684));
#117603=CARTESIAN_POINT('Ctrl Pts',(-171.094708987995,-3.64693493081568,
134.107063345628));
#117604=CARTESIAN_POINT('Ctrl Pts',(-171.102457055998,-3.5521087674248,
134.206081706498));
#117605=CARTESIAN_POINT('Ctrl Pts',(-171.11021335874,-3.45718182165889,
134.30520530526));
#117606=CARTESIAN_POINT('Ctrl Pts',(-171.117969661481,-3.35815287479082,
134.400299920994));
#117607=CARTESIAN_POINT('Ctrl Pts',(-171.125725964223,-3.25540962172723,
134.491024591576));
#117608=CARTESIAN_POINT('Ctrl Pts',(-171.133486406737,-3.15261153149595,
134.581797684647));
#117609=CARTESIAN_POINT('Ctrl Pts',(-171.141246849251,-3.0460954883841,
134.668195938951));
#117610=CARTESIAN_POINT('Ctrl Pts',(-171.149007291766,-2.93628086008807,
134.749919864768));
#117611=CARTESIAN_POINT('Ctrl Pts',(-171.156780192031,-2.82628994760182,
134.831774981085));
#117612=CARTESIAN_POINT('Ctrl Pts',(-171.164553092297,-2.71299019179485,
134.90894055403));
#117613=CARTESIAN_POINT('Ctrl Pts',(-171.172325992562,-2.59682917247071,
134.981160985252));
#117614=CARTESIAN_POINT('Ctrl Pts',(-171.179816328324,-2.48489089879221,
135.050756021887));
#117615=CARTESIAN_POINT('Ctrl Pts',(-171.187306664086,-2.37029604610925,
135.115759059456));
#117616=CARTESIAN_POINT('Ctrl Pts',(-171.194796999848,-2.25346350200287,
135.175983349189));
#117617=CARTESIAN_POINT('Ctrl Pts',(-171.202571333967,-2.132201216475,135.238491061172));
#117618=CARTESIAN_POINT('Ctrl Pts',(-171.210345668086,-2.00814408329354,
135.296048505166));
#117619=CARTESIAN_POINT('Ctrl Pts',(-171.218120002205,-1.88173441741219,
135.348396119719));
#117620=CARTESIAN_POINT('Ctrl Pts',(-171.225884755152,-1.75548054014683,
135.400679220515));
#117621=CARTESIAN_POINT('Ctrl Pts',(-171.233649508099,-1.6268802566474,
135.447765118901));
#117622=CARTESIAN_POINT('Ctrl Pts',(-171.241414261046,-1.49640081546734,
135.489439876444));
#117623=CARTESIAN_POINT('Ctrl Pts',(-171.249171301931,-1.36605096830771,
135.53107324203));
#117624=CARTESIAN_POINT('Ctrl Pts',(-171.256928342816,-1.23382604771927,
135.567306043932));
#117625=CARTESIAN_POINT('Ctrl Pts',(-171.264685383701,-1.10021330934991,
135.597972380781));
#117626=CARTESIAN_POINT('Ctrl Pts',(-171.272436574942,-0.966701329385724,
135.628615591906));
#117627=CARTESIAN_POINT('Ctrl Pts',(-171.280187766182,-0.831803994278676,
135.65370060617));
#117628=CARTESIAN_POINT('Ctrl Pts',(-171.287938957422,-0.696023408855133,
135.673111430334));
#117629=CARTESIAN_POINT('Ctrl Pts',(-171.295686854199,-0.560300533802645,
135.692514004379));
#117630=CARTESIAN_POINT('Ctrl Pts',(-171.303434750976,-0.423695541305577,
135.706247129763));
#117631=CARTESIAN_POINT('Ctrl Pts',(-171.311182647753,-0.28672019477748,
135.714246012604));
#117632=CARTESIAN_POINT('Ctrl Pts',(-171.318928923837,-0.14977350053903,
135.722243222251));
#117633=CARTESIAN_POINT('Ctrl Pts',(-171.326675199921,-0.0124569964147891,
135.724508552408));
#117634=CARTESIAN_POINT('Ctrl Pts',(-171.334421476005,0.124713368004535,
135.721029168357));
#117635=CARTESIAN_POINT('Ctrl Pts',(-171.34216780927,0.261884744984515,
135.717549758623));
#117636=CARTESIAN_POINT('Ctrl Pts',(-171.349914142536,0.398909589267479,
135.708325559976));
#117637=CARTESIAN_POINT('Ctrl Pts',(-171.357660475801,0.535273287731169,
135.693395856746));
#117638=CARTESIAN_POINT('Ctrl Pts',(-171.365408543804,0.671667523899464,
135.678462810112));
#117639=CARTESIAN_POINT('Ctrl Pts',(-171.373156611807,0.807399931059714,
135.657821758945));
#117640=CARTESIAN_POINT('Ctrl Pts',(-171.38090467981,0.941962739975745,
135.631563664776));
#117641=CARTESIAN_POINT('Ctrl Pts',(-171.388660982552,1.07666856384623,
135.605277663193));
#117642=CARTESIAN_POINT('Ctrl Pts',(-171.396417285294,1.21020192198088,
135.573362768167));
#117643=CARTESIAN_POINT('Ctrl Pts',(-171.404173588035,1.34206639472225,
135.535960860048));
#117644=CARTESIAN_POINT('Ctrl Pts',(-171.41193403055,1.47400124750345,135.498538989405));
#117645=CARTESIAN_POINT('Ctrl Pts',(-171.419694473064,1.60426506887617,
135.45562439249));
#117646=CARTESIAN_POINT('Ctrl Pts',(-171.427454915578,1.73237921117304,
135.407408013715));
#117647=CARTESIAN_POINT('Ctrl Pts',(-171.435227815843,1.86069901366456,
135.359114233728));
#117648=CARTESIAN_POINT('Ctrl Pts',(-171.443000716109,1.98686188113952,
135.305501817403));
#117649=CARTESIAN_POINT('Ctrl Pts',(-171.450773616374,2.11041084365142,
135.246809169153));
#117650=CARTESIAN_POINT('Ctrl Pts',(-171.458263952136,2.22946849017897,
135.190250146503));
#117651=CARTESIAN_POINT('Ctrl Pts',(-171.465754287899,2.34609870368315,
135.128973981037));
#117652=CARTESIAN_POINT('Ctrl Pts',(-171.473244623661,2.45991794816356,
135.063232152469));
#117653=CARTESIAN_POINT('Ctrl Pts',(-171.48101895778,2.57805268388956,134.99499770249));
#117654=CARTESIAN_POINT('Ctrl Pts',(-171.488793291899,2.69353330238229,
134.921736127261));
#117655=CARTESIAN_POINT('Ctrl Pts',(-171.496567626018,2.8059023452044,134.843679259574));
#117656=CARTESIAN_POINT('Ctrl Pts',(-171.504332378965,2.91813290322363,
134.765718590001));
#117657=CARTESIAN_POINT('Ctrl Pts',(-171.512097131912,3.02725919754571,
134.682974607558));
#117658=CARTESIAN_POINT('Ctrl Pts',(-171.519861884859,3.13284867645284,
134.595724782738));
#117659=CARTESIAN_POINT('Ctrl Pts',(-171.527618925744,3.23833328240096,
134.508561615673));
#117660=CARTESIAN_POINT('Ctrl Pts',(-171.535375966629,3.34028776415866,
134.416901759641));
#117661=CARTESIAN_POINT('Ctrl Pts',(-171.543133007514,3.43830917062676,
134.321065482874));
#117662=CARTESIAN_POINT('Ctrl Pts',(-171.550884198754,3.53625665838989,
134.22530147699));
#117663=CARTESIAN_POINT('Ctrl Pts',(-171.558635389994,3.63027669601083,
134.125367591418));
#117664=CARTESIAN_POINT('Ctrl Pts',(-171.566386581235,3.72000029516956,
134.021623563991));
#117665=CARTESIAN_POINT('Ctrl Pts',(-171.574134478012,3.80968575940506,
133.917923630543));
#117666=CARTESIAN_POINT('Ctrl Pts',(-171.581882374789,3.89507816194029,
133.810417071221));
#117667=CARTESIAN_POINT('Ctrl Pts',(-171.589630271566,3.97584636922172,
133.699499424402));
#117668=CARTESIAN_POINT('Ctrl Pts',(-171.59737654765,4.05659768153535,133.588604979163));
#117669=CARTESIAN_POINT('Ctrl Pts',(-171.605122823734,4.1327264925753,133.474301181521));
#117670=CARTESIAN_POINT('Ctrl Pts',(-171.612869099818,4.20394312077346,
133.357015177));
#117671=CARTESIAN_POINT('Ctrl Pts',(-171.620615433083,4.27516027467669,
133.239728306701));
#117672=CARTESIAN_POINT('Ctrl Pts',(-171.628361766349,4.34146497046516,
133.119459519778));
#117673=CARTESIAN_POINT('Ctrl Pts',(-171.636108099614,4.40261209819438,
132.996663008965));
#117674=CARTESIAN_POINT('Ctrl Pts',(-171.643856167617,4.4637729193988,132.873838998725));
#117675=CARTESIAN_POINT('Ctrl Pts',(-171.65160423562,4.51977369998571,132.748486488098));
#117676=CARTESIAN_POINT('Ctrl Pts',(-171.659352303623,4.57041650679202,
132.621081844652));
#117677=CARTESIAN_POINT('Ctrl Pts',(-171.667108606365,4.62111313737612,
132.493541794034));
#117678=CARTESIAN_POINT('Ctrl Pts',(-171.674864909107,4.66644027411946,
132.363945617647));
#117679=CARTESIAN_POINT('Ctrl Pts',(-171.682621211849,4.70624895802751,
132.232787657203));
#117680=CARTESIAN_POINT('Ctrl Pts',(-171.690381654363,4.74607888902877,
132.101559693805));
#117681=CARTESIAN_POINT('Ctrl Pts',(-171.698142096877,4.78038440056246,
131.968768663741));
#117682=CARTESIAN_POINT('Ctrl Pts',(-171.705902539391,4.80906741881327,
131.834920476967));
#117683=CARTESIAN_POINT('Ctrl Pts',(-171.713675439656,4.83779648159133,
131.700857425201));
#117684=CARTESIAN_POINT('Ctrl Pts',(-171.721448339922,4.8608849489236,131.565734211096));
#117685=CARTESIAN_POINT('Ctrl Pts',(-171.729221240187,4.87828639377724,
131.430064159819));
#117686=CARTESIAN_POINT('Ctrl Pts',(-171.736711575949,4.89505525227881,
131.299326056639));
#117687=CARTESIAN_POINT('Ctrl Pts',(-171.744201911711,4.90654335809107,
131.168080490695));
#117688=CARTESIAN_POINT('Ctrl Pts',(-171.751692247473,4.91275497764192,
131.036786072615));
#117689=CARTESIAN_POINT('Ctrl Pts',(-171.759466581592,4.91920211263604,
130.900513586766));
#117690=CARTESIAN_POINT('Ctrl Pts',(-171.767240915711,4.91998516958657,
130.763756800922));
#117691=CARTESIAN_POINT('Ctrl Pts',(-171.775015249831,4.91505192852834,
130.62702589911));
#117692=CARTESIAN_POINT('Ctrl Pts',(-171.782780002778,4.91012476724883,
130.490463505914));
#117693=CARTESIAN_POINT('Ctrl Pts',(-171.790544755725,4.89949533902691,
130.353927320239));
#117694=CARTESIAN_POINT('Ctrl Pts',(-171.798309508672,4.88316328287778,
130.217931239674));
#117695=CARTESIAN_POINT('Ctrl Pts',(-171.806066549557,4.86684744795705,
130.082070232334));
#117696=CARTESIAN_POINT('Ctrl Pts',(-171.813823590442,4.84484030290152,
129.946748648228));
#117697=CARTESIAN_POINT('Ctrl Pts',(-171.821580631327,4.81719349353562,
129.812478614333));
#117698=CARTESIAN_POINT('Ctrl Pts',(-171.829331822567,4.78956753284368,
129.678309834514));
#117699=CARTESIAN_POINT('Ctrl Pts',(-171.837083013807,4.75631045153859,
129.545191407905));
#117700=CARTESIAN_POINT('Ctrl Pts',(-171.844834205047,4.71752546004666,
129.413628221916));
#117701=CARTESIAN_POINT('Ctrl Pts',(-171.852582101825,4.67875695321079,
129.28212095379));
#117702=CARTESIAN_POINT('Ctrl Pts',(-171.860329998602,4.63446531950464,
129.152167985791));
#117703=CARTESIAN_POINT('Ctrl Pts',(-171.868077895379,4.58480435079363,
129.024261708111));
#117704=CARTESIAN_POINT('Ctrl Pts',(-171.875824171463,4.5351537700867,128.896382185667));
#117705=CARTESIAN_POINT('Ctrl Pts',(-171.883570447547,4.4801362297954,128.770548866208));
#117706=CARTESIAN_POINT('Ctrl Pts',(-171.891316723631,4.4199545195836,128.647236349631));
#117707=CARTESIAN_POINT('Ctrl Pts',(-171.899063056896,4.359772365124,128.52392292279));
#117708=CARTESIAN_POINT('Ctrl Pts',(-171.906809390162,4.29442613615247,
128.403130687316));
#117709=CARTESIAN_POINT('Ctrl Pts',(-171.914555723427,4.22416546996696,
128.285311363415));
#117710=CARTESIAN_POINT('Ctrl Pts',(-171.92230379143,4.15388906939252,128.167465654693));
#117711=CARTESIAN_POINT('Ctrl Pts',(-171.930051859433,4.07869624183661,
128.052594518062));
#117712=CARTESIAN_POINT('Ctrl Pts',(-171.937799927436,3.99888078111654,
127.941121968603));
#117713=CARTESIAN_POINT('Ctrl Pts',(-171.945556230178,3.91898049157488,
127.829530944792));
#117714=CARTESIAN_POINT('Ctrl Pts',(-171.95331253292,3.83444798261287,127.721346042018));
#117715=CARTESIAN_POINT('Ctrl Pts',(-171.961068835662,3.74561864193781,
127.616959787475));
#117716=CARTESIAN_POINT('Ctrl Pts',(-171.968829278176,3.65674189036904,
127.512517818844));
#117717=CARTESIAN_POINT('Ctrl Pts',(-171.97658972069,3.56356400288141,127.411878825057));
#117718=CARTESIAN_POINT('Ctrl Pts',(-171.984350163204,3.46645760455681,
127.315398775082));
#117719=CARTESIAN_POINT('Ctrl Pts',(-171.99212306347,3.36919532242091,127.218763846766));
#117720=CARTESIAN_POINT('Ctrl Pts',(-171.999895963735,3.2679922160663,127.126301467508));
#117721=CARTESIAN_POINT('Ctrl Pts',(-172.007668864001,3.16325506554889,
127.038328162478));
#117722=CARTESIAN_POINT('Ctrl Pts',(-172.015159199763,3.06232537427002,
126.953552908677));
#117723=CARTESIAN_POINT('Ctrl Pts',(-172.022649535525,2.95811436437813,
126.872946205653));
#117724=CARTESIAN_POINT('Ctrl Pts',(-172.030139871287,2.85101018409053,
126.796752354186));
#117725=CARTESIAN_POINT('Ctrl Pts',(-172.037914205406,2.73984511625326,
126.717669589681));
#117726=CARTESIAN_POINT('Ctrl Pts',(-172.045688539525,2.62521102057852,
126.643090398473));
#117727=CARTESIAN_POINT('Ctrl Pts',(-172.053462873644,2.50750890317026,
126.573334481624));
#117728=CARTESIAN_POINT('Ctrl Pts',(-172.061227626591,2.38995184310237,
126.503664532709));
#117729=CARTESIAN_POINT('Ctrl Pts',(-172.068992379538,2.26933461759565,
126.438806228274));
#117730=CARTESIAN_POINT('Ctrl Pts',(-172.076757132485,2.14608938812568,
126.379037646225));
#117731=CARTESIAN_POINT('Ctrl Pts',(-172.08451417337,2.02296656755508,126.319328427175));
#117732=CARTESIAN_POINT('Ctrl Pts',(-172.092271214255,1.8972212868832,126.264699039963));
#117733=CARTESIAN_POINT('Ctrl Pts',(-172.10002825514,1.76931232886848,126.215382850632));
#117734=CARTESIAN_POINT('Ctrl Pts',(-172.10777944638,1.64149982799416,126.166103851024));
#117735=CARTESIAN_POINT('Ctrl Pts',(-172.115530637621,1.51152726078365,
126.122130214235));
#117736=CARTESIAN_POINT('Ctrl Pts',(-172.123281828861,1.37987519106998,
126.083648010388));
#117737=CARTESIAN_POINT('Ctrl Pts',(-172.131029725638,1.24827907699768,
126.045182162504));
#117738=CARTESIAN_POINT('Ctrl Pts',(-172.138777622415,1.11500525465913,
126.012203214865));
#117739=CARTESIAN_POINT('Ctrl Pts',(-172.146525519192,0.980551114127505,
125.984847926942));
#117740=CARTESIAN_POINT('Ctrl Pts',(-172.154271795276,0.846125098503584,
125.957498361156));
#117741=CARTESIAN_POINT('Ctrl Pts',(-172.16201807136,0.710519638652083,
125.935770193164));
#117742=CARTESIAN_POINT('Ctrl Pts',(-172.169764347444,0.57424364167457,
125.919749343115));
#117743=CARTESIAN_POINT('Ctrl Pts',(-172.17751068071,0.437966638738791,
125.903728374803));
#117744=CARTESIAN_POINT('Ctrl Pts',(-172.185257013975,0.301019477091297,
125.89341485415));
#117745=CARTESIAN_POINT('Ctrl Pts',(-172.19300334724,0.163917136791152,
125.888842920032));
#117746=CARTESIAN_POINT('Ctrl Pts',(-172.200751415243,0.0267840933723109,
125.884269962061));
#117747=CARTESIAN_POINT('Ctrl Pts',(-172.208499483246,-0.110503807176791,
125.885441162223));
#117748=CARTESIAN_POINT('Ctrl Pts',(-172.216247551249,-0.247431026223936,
125.892338533967));
#117749=CARTESIAN_POINT('Ctrl Pts',(-172.224003853991,-0.384503773148752,
125.89924323632));
#117750=CARTESIAN_POINT('Ctrl Pts',(-172.231760156733,-0.521214681722725,
125.911886247683));
#117751=CARTESIAN_POINT('Ctrl Pts',(-172.239516459475,-0.657052222455101,
125.930197567414));
#117752=CARTESIAN_POINT('Ctrl Pts',(-172.247276901989,-0.792962263772955,
125.948518660447));
#117753=CARTESIAN_POINT('Ctrl Pts',(-172.255037344503,-0.927997623673685,
125.97251402174));
#117754=CARTESIAN_POINT('Ctrl Pts',(-172.262797787017,-1.06165740242473,
126.002062561179));
#117755=CARTESIAN_POINT('Ctrl Pts',(-172.270570687283,-1.19553174371839,
126.031658534557));
#117756=CARTESIAN_POINT('Ctrl Pts',(-172.278343587548,-1.32802571306665,
126.066825399646));
#117757=CARTESIAN_POINT('Ctrl Pts',(-172.286116487814,-1.45865313432394,
126.107392010451));
#117758=CARTESIAN_POINT('Ctrl Pts',(-172.293606823576,-1.58453191978578,
126.146483922771));
#117759=CARTESIAN_POINT('Ctrl Pts',(-172.301097159337,-1.70867721828038,
126.190589704889));
#117760=CARTESIAN_POINT('Ctrl Pts',(-172.308587495099,-1.83067368905062,
126.239514847256));
#117761=CARTESIAN_POINT('Ctrl Pts',(-172.316362158004,-1.95730104808944,
126.290297148821));
#117762=CARTESIAN_POINT('Ctrl Pts',(-172.324136820909,-2.08201435566358,
126.346432786249));
#117763=CARTESIAN_POINT('Ctrl Pts',(-172.331911483814,-2.20432782329072,
126.40775716604));
#117764=CARTESIAN_POINT('Ctrl Pts',(-172.339676489964,-2.32648936777396,
126.46900537603));
#117765=CARTESIAN_POINT('Ctrl Pts',(-172.347441496114,-2.44625665720255,
126.53542933104));
#117766=CARTESIAN_POINT('Ctrl Pts',(-172.355206502264,-2.56316209831764,
126.606815725579));
#117767=CARTESIAN_POINT('Ctrl Pts',(-172.362963721089,-2.67995029797483,
126.67813052854));
#117768=CARTESIAN_POINT('Ctrl Pts',(-172.370720939913,-2.79388202959112,
126.75439766425));
#117769=CARTESIAN_POINT('Ctrl Pts',(-172.378478158738,-2.90451294396446,
126.835357263972));
#117770=CARTESIAN_POINT('Ctrl Pts',(-172.386451739572,-3.0182295424432,
126.918574964437));
#117771=CARTESIAN_POINT('Ctrl Pts',(-172.394425320405,-3.12845811514606,
127.006750549142));
#117772=CARTESIAN_POINT('Ctrl Pts',(-172.402398901239,-3.23474596164022,
127.099552710784));
#117773=CARTESIAN_POINT('Ctrl Pts',(-172.410146456388,-3.33802088537537,
127.189724225987));
#117774=CARTESIAN_POINT('Ctrl Pts',(-172.417894011538,-3.43757516142897,
127.284263291409));
#117775=CARTESIAN_POINT('Ctrl Pts',(-172.425641566688,-3.53302591456912,
127.382824274126));
#117776=CARTESIAN_POINT('Ctrl Pts',(-172.433387442438,-3.62845597731616,
127.48136389226));
#117777=CARTESIAN_POINT('Ctrl Pts',(-172.441133318188,-3.71978401533456,
127.583923412318));
#117778=CARTESIAN_POINT('Ctrl Pts',(-172.448879193938,-3.80666382319468,
127.690120164473));
#117779=CARTESIAN_POINT('Ctrl Pts',(-172.456625068071,-3.8935436129223,
127.796316894464));
#117780=CARTESIAN_POINT('Ctrl Pts',(-172.464370942205,-3.9759749273941,
127.90615055208));
#117781=CARTESIAN_POINT('Ctrl Pts',(-172.472116816338,-4.05365194871594,
128.01920551575));
#117782=CARTESIAN_POINT('Ctrl Pts',(-172.480260756539,-4.13532084826993,
128.138070455663));
#117783=CARTESIAN_POINT('Ctrl Pts',(-172.488404696739,-4.21173357218008,
128.260496177886));
#117784=CARTESIAN_POINT('Ctrl Pts',(-172.496548636939,-4.2825869625209,
128.385966114813));
#117785=CARTESIAN_POINT('Ctrl Pts',(-172.504303202507,-4.35005274046332,
128.505437136064));
#117786=CARTESIAN_POINT('Ctrl Pts',(-172.512057768075,-4.41247830169827,
128.627667653528));
#117787=CARTESIAN_POINT('Ctrl Pts',(-172.519812333643,-4.46965001415215,
128.752188155639));
#117788=CARTESIAN_POINT('Ctrl Pts',(-172.527571115191,-4.52685280956229,
128.876776356708));
#117789=CARTESIAN_POINT('Ctrl Pts',(-172.53532989674,-4.5787959173205,129.003656661905));
#117790=CARTESIAN_POINT('Ctrl Pts',(-172.543088678288,-4.62531453699467,
129.132341330487));
#117791=CARTESIAN_POINT('Ctrl Pts',(-172.55085655863,-4.67188770947539,
129.261176908744));
#117792=CARTESIAN_POINT('Ctrl Pts',(-172.558624438972,-4.71302357995576,
129.391820702198));
#117793=CARTESIAN_POINT('Ctrl Pts',(-172.566392319314,-4.748607623431,129.523771416771));
#117794=CARTESIAN_POINT('Ctrl Pts',(-172.567542912456,-4.75387839931574,
129.543316206413));
#117795=CARTESIAN_POINT('Ctrl Pts',(-172.568693505597,-4.75902745959226,
129.56288965497));
#117796=CARTESIAN_POINT('Ctrl Pts',(-172.569844098739,-4.76405452823414,
129.582490119309));
#117797=CARTESIAN_POINT('Origin',(213.235140564004,0.,130.804360617566));
#117798=CARTESIAN_POINT('',(-174.665085416107,-4.76405452823406,129.582490119308));
#117799=CARTESIAN_POINT('',(-174.32014438825,-4.76405452823397,129.582490119308));
#117800=CARTESIAN_POINT('',(213.235140564004,-4.76405452823405,129.582490119308));
#117801=CARTESIAN_POINT('',(-172.985140564014,-4.91824999999948,130.804362873451));
#117802=CARTESIAN_POINT('Ctrl Pts',(-172.985140564016,-4.91824999999948,
130.804362873489));
#117803=CARTESIAN_POINT('Ctrl Pts',(-172.993255459135,-4.91824993390674,
130.948454988518));
#117804=CARTESIAN_POINT('Ctrl Pts',(-173.001370354255,-4.91191326672245,
131.092424657378));
#117805=CARTESIAN_POINT('Ctrl Pts',(-173.009485249374,-4.89929800797417,
131.235709770295));
#117806=CARTESIAN_POINT('Ctrl Pts',(-173.017610838002,-4.88666612530449,
131.379183699035));
#117807=CARTESIAN_POINT('Ctrl Pts',(-173.02573642663,-4.86773917045749,
131.521970940276));
#117808=CARTESIAN_POINT('Ctrl Pts',(-173.033862015258,-4.84262656737017,
131.663517757733));
#117809=CARTESIAN_POINT('Ctrl Pts',(-173.042006812052,-4.81745460032891,
131.805399179243));
#117810=CARTESIAN_POINT('Ctrl Pts',(-173.050151608847,-4.78606780760041,
131.946033985146));
#117811=CARTESIAN_POINT('Ctrl Pts',(-173.058296405642,-4.74862644793337,
132.084880012377));
#117812=CARTESIAN_POINT('Ctrl Pts',(-173.066451341225,-4.71113848059374,
132.22389887762));
#117813=CARTESIAN_POINT('Ctrl Pts',(-173.074606276808,-4.66758100579246,
132.361124203243));
#117814=CARTESIAN_POINT('Ctrl Pts',(-173.082761212391,-4.61816315305185,
132.496032026054));
#117815=CARTESIAN_POINT('Ctrl Pts',(-173.090934843589,-4.56863200731042,
132.631249132073));
#117816=CARTESIAN_POINT('Ctrl Pts',(-173.099108474786,-4.51321374718174,
132.764137803449));
#117817=CARTESIAN_POINT('Ctrl Pts',(-173.107282105984,-4.45216510774585,
132.894195279895));
#117818=CARTESIAN_POINT('Ctrl Pts',(-173.112968527449,-4.40969337330281,
132.984676683788));
#117819=CARTESIAN_POINT('Ctrl Pts',(-173.118654948913,-4.36449748628318,
133.073788297874));
#117820=CARTESIAN_POINT('Ctrl Pts',(-173.124341370377,-4.3166763331456,
133.161368996287));
#117821=CARTESIAN_POINT('Ctrl Pts',(-173.132115704497,-4.25129644092726,
133.281107150784));
#117822=CARTESIAN_POINT('Ctrl Pts',(-173.139890038616,-4.18082717965119,
133.398312589513));
#117823=CARTESIAN_POINT('Ctrl Pts',(-173.147664372735,-4.10548933760674,
133.512522422425));
#117824=CARTESIAN_POINT('Ctrl Pts',(-173.155429125682,-4.03024434271947,
133.626591501925));
#117825=CARTESIAN_POINT('Ctrl Pts',(-173.163193878629,-3.95014291866849,
133.737671997999));
#117826=CARTESIAN_POINT('Ctrl Pts',(-173.170958631576,-3.86545207599381,
133.845324824967));
#117827=CARTESIAN_POINT('Ctrl Pts',(-173.178715672461,-3.78084534945801,
133.95287072963));
#117828=CARTESIAN_POINT('Ctrl Pts',(-173.186472713346,-3.69165851564237,
134.056995434827));
#117829=CARTESIAN_POINT('Ctrl Pts',(-173.194229754231,-3.59820208083672,
134.157288419944));
#117830=CARTESIAN_POINT('Ctrl Pts',(-173.201980945471,-3.50481612225568,
134.257505773342));
#117831=CARTESIAN_POINT('Ctrl Pts',(-173.209732136711,-3.40716723683549,
134.353896873221));
#117832=CARTESIAN_POINT('Ctrl Pts',(-173.217483327951,-3.30560620411024,
134.446084204804));
#117833=CARTESIAN_POINT('Ctrl Pts',(-173.225231224729,-3.204088337533,134.538232354313));
#117834=CARTESIAN_POINT('Ctrl Pts',(-173.232979121506,-3.09866191965195,
134.626180026942));
#117835=CARTESIAN_POINT('Ctrl Pts',(-173.240727018283,-2.98971442864739,
134.709586692666));
#117836=CARTESIAN_POINT('Ctrl Pts',(-173.248473294367,-2.88078972710931,
134.792975911513));
#117837=CARTESIAN_POINT('Ctrl Pts',(-173.256219570451,-2.76834572769189,
134.87182577531));
#117838=CARTESIAN_POINT('Ctrl Pts',(-173.263965846535,-2.65280250135353,
134.945836435594));
#117839=CARTESIAN_POINT('Ctrl Pts',(-173.2717121798,-2.53725842210117,135.019847642209));
#117840=CARTESIAN_POINT('Ctrl Pts',(-173.279458513066,-2.41861539949418,
135.089019363152));
#117841=CARTESIAN_POINT('Ctrl Pts',(-173.287204846331,-2.29732161350698,
135.153095659692));
#117842=CARTESIAN_POINT('Ctrl Pts',(-173.294952914334,-2.17600066461723,
135.217186305674));
#117843=CARTESIAN_POINT('Ctrl Pts',(-173.302700982337,-2.05202811673876,
135.276179074041));
#117844=CARTESIAN_POINT('Ctrl Pts',(-173.31044905034,-1.92587545040774,
135.32986465712));
#117845=CARTESIAN_POINT('Ctrl Pts',(-173.318205353082,-1.79958870752221,
135.383607297875));
#117846=CARTESIAN_POINT('Ctrl Pts',(-173.325961655824,-1.67111757793391,
135.432031332421));
#117847=CARTESIAN_POINT('Ctrl Pts',(-173.333717958566,-1.54095268639101,
135.47497598182));
#117848=CARTESIAN_POINT('Ctrl Pts',(-173.34147840108,-1.41071832192595,
135.517943552072));
#117849=CARTESIAN_POINT('Ctrl Pts',(-173.349238843594,-1.27878877008387,
135.555425803042));
#117850=CARTESIAN_POINT('Ctrl Pts',(-173.356999286108,-1.1456674416307,
135.587312548716));
#117851=CARTESIAN_POINT('Ctrl Pts',(-173.364772186374,-1.01233241500313,
135.619250481824));
#117852=CARTESIAN_POINT('Ctrl Pts',(-173.372545086639,-0.877802172599358,
135.645574884811));
#117853=CARTESIAN_POINT('Ctrl Pts',(-173.380317986905,-0.742588777640731,
135.666227025626));
#117854=CARTESIAN_POINT('Ctrl Pts',(-173.387808322667,-0.61229073017047,
135.686128409103));
#117855=CARTESIAN_POINT('Ctrl Pts',(-173.395298658429,-0.481358642569659,
135.700762738324));
#117856=CARTESIAN_POINT('Ctrl Pts',(-173.402788994191,-0.350251095779065,
135.710123273097));
#117857=CARTESIAN_POINT('Ctrl Pts',(-173.41056332831,-0.214172566503198,
135.719838715392));
#117858=CARTESIAN_POINT('Ctrl Pts',(-173.418337662429,-0.0774739544430357,
135.723903332622));
#117859=CARTESIAN_POINT('Ctrl Pts',(-173.426111996548,0.0593359564305044,
135.722252676851));
#117860=CARTESIAN_POINT('Ctrl Pts',(-173.433876749495,0.195977261315946,
135.720604055365));
#117861=CARTESIAN_POINT('Ctrl Pts',(-173.441641502442,0.332729204911828,
135.713254180141));
#117862=CARTESIAN_POINT('Ctrl Pts',(-173.449406255389,0.469078046280734,
135.700190358172));
#117863=CARTESIAN_POINT('Ctrl Pts',(-173.457163296274,0.60529146405821,
135.687139511375));
#117864=CARTESIAN_POINT('Ctrl Pts',(-173.464920337159,0.741102189692165,
135.668386048729));
#117865=CARTESIAN_POINT('Ctrl Pts',(-173.472677378044,0.87599700432949,
135.643969311552));
#117866=CARTESIAN_POINT('Ctrl Pts',(-173.480428569285,1.01079009373758,
135.619570987226));
#117867=CARTESIAN_POINT('Ctrl Pts',(-173.488179760525,1.14466826377962,
135.58951795833));
#117868=CARTESIAN_POINT('Ctrl Pts',(-173.495930951765,1.27712429567584,
135.553901289662));
#117869=CARTESIAN_POINT('Ctrl Pts',(-173.503678848542,1.4095240302253,135.518299759028));
#117870=CARTESIAN_POINT('Ctrl Pts',(-173.511426745319,1.54050245206364,
135.477139393131));
#117871=CARTESIAN_POINT('Ctrl Pts',(-173.519174642096,1.66956362221481,
135.43056212354));
#117872=CARTESIAN_POINT('Ctrl Pts',(-173.52692091818,1.79859779555143,135.38399459691));
#117873=CARTESIAN_POINT('Ctrl Pts',(-173.534667194264,1.92571514739029,
135.332012553018));
#117874=CARTESIAN_POINT('Ctrl Pts',(-173.542413470348,2.05043634811453,
135.27480733404));
#117875=CARTESIAN_POINT('Ctrl Pts',(-173.550159803614,2.17515846950252,
135.217601692786));
#117876=CARTESIAN_POINT('Ctrl Pts',(-173.557906136879,2.29748404911297,
135.155172962504));
#117877=CARTESIAN_POINT('Ctrl Pts',(-173.565652470144,2.41695550621841,
135.087759868565));
#117878=CARTESIAN_POINT('Ctrl Pts',(-173.573400538147,2.53645371812814,
135.020331677931));
#117879=CARTESIAN_POINT('Ctrl Pts',(-173.58114860615,2.65309619524257,134.947917094597));
#117880=CARTESIAN_POINT('Ctrl Pts',(-173.588896674153,2.7664519943435,134.870799652581));
#117881=CARTESIAN_POINT('Ctrl Pts',(-173.596652976895,2.87992826933682,
134.79360024923));
#117882=CARTESIAN_POINT('Ctrl Pts',(-173.604409279637,2.99011056466431,
134.71168822291));
#117883=CARTESIAN_POINT('Ctrl Pts',(-173.612165582379,3.09659841779299,
134.625389445175));
#117884=CARTESIAN_POINT('Ctrl Pts',(-173.619926024893,3.20314310669517,
134.539044607184));
#117885=CARTESIAN_POINT('Ctrl Pts',(-173.627686467407,3.30598913131837,
134.448308610985));
#117886=CARTESIAN_POINT('Ctrl Pts',(-173.635446909922,3.40477168323083,
134.353545432079));
#117887=CARTESIAN_POINT('Ctrl Pts',(-173.643219810187,3.50371280966513,
134.258630130905));
#117888=CARTESIAN_POINT('Ctrl Pts',(-173.650992710452,3.59857715754723,
134.159675010701));
#117889=CARTESIAN_POINT('Ctrl Pts',(-173.658765610718,3.68903853125977,
134.057079138647));
#117890=CARTESIAN_POINT('Ctrl Pts',(-173.66625594648,3.77621140617964,133.958212884965));
#117891=CARTESIAN_POINT('Ctrl Pts',(-173.673746282242,3.8592956733611,133.855966223884));
#117892=CARTESIAN_POINT('Ctrl Pts',(-173.681236618004,3.9380377878904,133.7507213293));
#117893=CARTESIAN_POINT('Ctrl Pts',(-173.689010952123,4.01976543362488,
133.641486042549));
#117894=CARTESIAN_POINT('Ctrl Pts',(-173.696785286242,4.09707405008418,
133.528674653613));
#117895=CARTESIAN_POINT('Ctrl Pts',(-173.704559620361,4.16963440522962,
133.412680381173));
#117896=CARTESIAN_POINT('Ctrl Pts',(-173.712324373308,4.24210533622226,
133.296829061308));
#117897=CARTESIAN_POINT('Ctrl Pts',(-173.720089126255,4.30983944390217,
133.177802991055));
#117898=CARTESIAN_POINT('Ctrl Pts',(-173.727853879203,4.3725483597584,133.056027534335));
#117899=CARTESIAN_POINT('Ctrl Pts',(-173.735610920088,4.43519499223536,
132.934373026716));
#117900=CARTESIAN_POINT('Ctrl Pts',(-173.743367960973,4.49282618755274,
132.809974912242));
#117901=CARTESIAN_POINT('Ctrl Pts',(-173.751125001858,4.54519763734802,
132.683286241412));
#117902=CARTESIAN_POINT('Ctrl Pts',(-173.758876193098,4.5975295934257,132.556693107494));
#117903=CARTESIAN_POINT('Ctrl Pts',(-173.766627384338,4.64460955013321,
132.427813215206));
#117904=CARTESIAN_POINT('Ctrl Pts',(-173.774378575578,4.68623995872471,
132.297122524821));
#117905=CARTESIAN_POINT('Ctrl Pts',(-173.782126472355,4.72785267328208,
132.166487381466));
#117906=CARTESIAN_POINT('Ctrl Pts',(-173.789874369132,4.76402032805993,
132.034043342506));
#117907=CARTESIAN_POINT('Ctrl Pts',(-173.797622265909,4.79459426697746,
131.900284372928));
#117908=CARTESIAN_POINT('Ctrl Pts',(-173.805368541993,4.82516181048598,
131.766553382844));
#117909=CARTESIAN_POINT('Ctrl Pts',(-173.813114818077,4.85013787843416,
131.631508390135));
#117910=CARTESIAN_POINT('Ctrl Pts',(-173.820861094162,4.86942436304803,
131.495656093505));
#117911=CARTESIAN_POINT('Ctrl Pts',(-173.828607427427,4.88871099003036,
131.359802794044));
#117912=CARTESIAN_POINT('Ctrl Pts',(-173.836353760692,4.90230789491901,
131.223142565854));
#117913=CARTESIAN_POINT('Ctrl Pts',(-173.844100093958,4.91016859056788,
131.086189421453));
#117914=CARTESIAN_POINT('Ctrl Pts',(-173.851848161961,4.91803104656503,
130.949205607346));
#117915=CARTESIAN_POINT('Ctrl Pts',(-173.859596229964,4.92015471474935,
130.811929136746));
#117916=CARTESIAN_POINT('Ctrl Pts',(-173.867344297966,4.9165452049854,130.674875831452));
#117917=CARTESIAN_POINT('Ctrl Pts',(-173.875100600708,4.91293185899151,
130.537676864273));
#117918=CARTESIAN_POINT('Ctrl Pts',(-173.88285690345,4.90357317335622,130.400701927651));
#117919=CARTESIAN_POINT('Ctrl Pts',(-173.890613206192,4.88852685326589,
130.264464083591));
#117920=CARTESIAN_POINT('Ctrl Pts',(-173.898373648706,4.87347250250149,
130.128153525291));
#117921=CARTESIAN_POINT('Ctrl Pts',(-173.90613409122,4.8527245275847,129.992581229729));
#117922=CARTESIAN_POINT('Ctrl Pts',(-173.913894533735,4.82639196354484,
129.85825085822));
#117923=CARTESIAN_POINT('Ctrl Pts',(-173.921667434,4.80001712813549,129.723704847673));
#117924=CARTESIAN_POINT('Ctrl Pts',(-173.929440334266,4.76803988017331,
129.590405125518));
#117925=CARTESIAN_POINT('Ctrl Pts',(-173.937213234531,4.73061964948173,
129.458841834926));
#117926=CARTESIAN_POINT('Ctrl Pts',(-173.944703570293,4.69455973843176,
129.332061201335));
#117927=CARTESIAN_POINT('Ctrl Pts',(-173.952193906055,4.65344580254648,
129.20689323646));
#117928=CARTESIAN_POINT('Ctrl Pts',(-173.959684241817,4.60746232832853,
129.083757829142));
#117929=CARTESIAN_POINT('Ctrl Pts',(-173.967458575936,4.55973537670931,
128.955953705429));
#117930=CARTESIAN_POINT('Ctrl Pts',(-173.975232910055,4.50661115577776,
128.829934465618));
#117931=CARTESIAN_POINT('Ctrl Pts',(-173.983007244174,4.44824253358713,
128.706189646247));
#117932=CARTESIAN_POINT('Ctrl Pts',(-173.990771997121,4.38994584550663,
128.582597331306));
#117933=CARTESIAN_POINT('Ctrl Pts',(-173.998536750068,4.32641778130796,
128.46127420984));
#117934=CARTESIAN_POINT('Ctrl Pts',(-174.006301503015,4.25786034148059,
128.342692814034));
#117935=CARTESIAN_POINT('Ctrl Pts',(-174.0140585439,4.18937099386895,128.224229194942));
#117936=CARTESIAN_POINT('Ctrl Pts',(-174.021815584785,4.11586240581359,
128.108502218655));
#117937=CARTESIAN_POINT('Ctrl Pts',(-174.02957262567,4.03758368689263,127.995962313579));
#117938=CARTESIAN_POINT('Ctrl Pts',(-174.03732381691,3.95936399856264,127.883507275721));
#117939=CARTESIAN_POINT('Ctrl Pts',(-174.04507500815,3.87638156170514,127.774234844921));
#117940=CARTESIAN_POINT('Ctrl Pts',(-174.05282619939,3.78893003525486,127.668568492689));
#117941=CARTESIAN_POINT('Ctrl Pts',(-174.060574096167,3.70151567803604,
127.562947051474));
#117942=CARTESIAN_POINT('Ctrl Pts',(-174.068321992945,3.60963625790074,
127.460928941005));
#117943=CARTESIAN_POINT('Ctrl Pts',(-174.076069889722,3.51362700933943,
127.362906229994));
#117944=CARTESIAN_POINT('Ctrl Pts',(-174.083816165806,3.41763784384346,
127.264904023221));
#117945=CARTESIAN_POINT('Ctrl Pts',(-174.09156244189,3.31752084160577,127.170895832681));
#117946=CARTESIAN_POINT('Ctrl Pts',(-174.099308717974,3.21364927294672,
127.081238082249));
#117947=CARTESIAN_POINT('Ctrl Pts',(-174.107055051239,3.1097769375312,126.991579669983));
#117948=CARTESIAN_POINT('Ctrl Pts',(-174.114801384505,3.00215027635157,
126.906272017367));
#117949=CARTESIAN_POINT('Ctrl Pts',(-174.12254771777,2.89117661525938,126.825632071676));
#117950=CARTESIAN_POINT('Ctrl Pts',(-174.130295785773,2.78017810238507,
126.744974067229));
#117951=CARTESIAN_POINT('Ctrl Pts',(-174.138043853776,2.66583141432503,
126.668986079516));
#117952=CARTESIAN_POINT('Ctrl Pts',(-174.145791921779,2.54857355883509,
126.597942203082));
#117953=CARTESIAN_POINT('Ctrl Pts',(-174.153548224521,2.4311910803011,126.526822820371));
#117954=CARTESIAN_POINT('Ctrl Pts',(-174.161304527262,2.31089158860516,
126.460658248605));
#117955=CARTESIAN_POINT('Ctrl Pts',(-174.169060830004,2.18813792840575,
126.399677261322));
#117956=CARTESIAN_POINT('Ctrl Pts',(-174.176821272518,2.06531875088184,
126.33866372665));
#117957=CARTESIAN_POINT('Ctrl Pts',(-174.184581715032,1.9400431517792,126.282839448272));
#117958=CARTESIAN_POINT('Ctrl Pts',(-174.192342157547,1.81279381172291,
126.232384933173));
#117959=CARTESIAN_POINT('Ctrl Pts',(-174.200115057812,1.6853401997293,126.181849424008));
#117960=CARTESIAN_POINT('Ctrl Pts',(-174.207887958077,1.55590688462521,
126.136701032509));
#117961=CARTESIAN_POINT('Ctrl Pts',(-174.215660858343,1.42499241345572,
126.097070560209));
#117962=CARTESIAN_POINT('Ctrl Pts',(-174.223151194105,1.29883701306407,
126.058880755399));
#117963=CARTESIAN_POINT('Ctrl Pts',(-174.230641529867,1.17130657266092,
126.025814731653));
#117964=CARTESIAN_POINT('Ctrl Pts',(-174.238131865629,1.04285407608206,
125.997944235427));
#117965=CARTESIAN_POINT('Ctrl Pts',(-174.245906199748,0.909531264055936,
125.969017020865));
#117966=CARTESIAN_POINT('Ctrl Pts',(-174.253680533868,0.774792769507084,
125.945595455182));
#117967=CARTESIAN_POINT('Ctrl Pts',(-174.261454867987,0.639133082307737,
125.927815532611));
#117968=CARTESIAN_POINT('Ctrl Pts',(-174.269219620934,0.50364058354861,
125.910057522205));
#117969=CARTESIAN_POINT('Ctrl Pts',(-174.276984373881,0.367229534951522,
125.89792737119));
#117970=CARTESIAN_POINT('Ctrl Pts',(-174.284749126828,0.230406677424843,
125.891510546019));
#117971=CARTESIAN_POINT('Ctrl Pts',(-174.292506167713,0.093719714288753,
125.88510009413));
#117972=CARTESIAN_POINT('Ctrl Pts',(-174.300263208598,-0.0433778558109409,
125.884391693661));
#117973=CARTESIAN_POINT('Ctrl Pts',(-174.308020249483,-0.180372424888108,
125.889419229224));
#117974=CARTESIAN_POINT('Ctrl Pts',(-174.315771440723,-0.317263685294886,
125.894442973483));
#117975=CARTESIAN_POINT('Ctrl Pts',(-174.323522631963,-0.454051710162949,
125.905194029822));
#117976=CARTESIAN_POINT('Ctrl Pts',(-174.331273823203,-0.59022149109199,
125.921654231354));
#117977=CARTESIAN_POINT('Ctrl Pts',(-174.339021719981,-0.726333396231504,
125.938107436862));
#117978=CARTESIAN_POINT('Ctrl Pts',(-174.346769616758,-0.861827192734683,
125.960264914543));
#117979=CARTESIAN_POINT('Ctrl Pts',(-174.354517513535,-0.996191819659431,
125.988056544841));
#117980=CARTESIAN_POINT('Ctrl Pts',(-174.362263789619,-1.13052834040079,
126.01584236173));
#117981=CARTESIAN_POINT('Ctrl Pts',(-174.370010065703,-1.26373577875568,
126.049259907909));
#117982=CARTESIAN_POINT('Ctrl Pts',(-174.377756341787,-1.39531250349853,
126.088187796297));
#117983=CARTESIAN_POINT('Ctrl Pts',(-174.385502675053,-1.52689019951104,
126.127115972041));
#117984=CARTESIAN_POINT('Ctrl Pts',(-174.393249008318,-1.65683678298991,
126.171554460243));
#117985=CARTESIAN_POINT('Ctrl Pts',(-174.400995341583,-1.78466542764453,
126.221331883871));
#117986=CARTESIAN_POINT('Ctrl Pts',(-174.408743409586,-1.91252269863765,
126.271120454809));
#117987=CARTESIAN_POINT('Ctrl Pts',(-174.416491477589,-2.03826072276117,
126.326250198472));
#117988=CARTESIAN_POINT('Ctrl Pts',(-174.424239545592,-2.16141268314659,
126.386501602655));
#117989=CARTESIAN_POINT('Ctrl Pts',(-174.431995848334,-2.2846955309012,
126.446817042747));
#117990=CARTESIAN_POINT('Ctrl Pts',(-174.439752151076,-2.40538647274651,
126.512264844971));
#117991=CARTESIAN_POINT('Ctrl Pts',(-174.447508453818,-2.52304285618185,
126.582579262691));
#117992=CARTESIAN_POINT('Ctrl Pts',(-174.455268896332,-2.6407620363716,
126.652931209333));
#117993=CARTESIAN_POINT('Ctrl Pts',(-174.463029338846,-2.75544310413847,
126.728154732801));
#117994=CARTESIAN_POINT('Ctrl Pts',(-174.47078978136,-2.86667329317578,
126.807941308648));
#117995=CARTESIAN_POINT('Ctrl Pts',(-174.478562681626,-2.97808203878708,
126.88785596499));
#117996=CARTESIAN_POINT('Ctrl Pts',(-174.486335581891,-3.08602852762187,
126.972348070314));
#117997=CARTESIAN_POINT('Ctrl Pts',(-174.494108482157,-3.19013323579247,
127.061068884293));
#117998=CARTESIAN_POINT('Ctrl Pts',(-174.501598817919,-3.29045347559684,
127.146564473209));
#117999=CARTESIAN_POINT('Ctrl Pts',(-174.509089153681,-3.38720617599272,
127.235986451051));
#118000=CARTESIAN_POINT('Ctrl Pts',(-174.516579489443,-3.4800861258268,
127.328992490399));
#118001=CARTESIAN_POINT('Ctrl Pts',(-174.5242450903,-3.57513935784502,127.424174762279));
#118002=CARTESIAN_POINT('Ctrl Pts',(-174.531910691157,-3.6664555477646,
127.523430863656));
#118003=CARTESIAN_POINT('Ctrl Pts',(-174.539576292015,-3.75365778843685,
127.626431060479));
#118004=CARTESIAN_POINT('Ctrl Pts',(-174.547232920712,-3.84075796372669,
127.729310701288));
#118005=CARTESIAN_POINT('Ctrl Pts',(-174.554889549409,-3.92375350504564,
127.835925421485));
#118006=CARTESIAN_POINT('Ctrl Pts',(-174.562546178106,-4.00230282902814,
127.945907342235));
#118007=CARTESIAN_POINT('Ctrl Pts',(-174.570195614279,-4.08077836493951,
128.055785947597));
#118008=CARTESIAN_POINT('Ctrl Pts',(-174.577845050453,-4.15481575665894,
128.169025138031));
#118009=CARTESIAN_POINT('Ctrl Pts',(-174.585494486626,-4.22411273459277,
128.285222934161));
#118010=CARTESIAN_POINT('Ctrl Pts',(-174.593138183411,-4.29335771885319,
128.401333546831));
#118011=CARTESIAN_POINT('Ctrl Pts',(-174.600781880196,-4.35786916126707,
128.520398003458));
#118012=CARTESIAN_POINT('Ctrl Pts',(-174.608425576981,-4.41738765085419,
128.641984747237));
#118013=CARTESIAN_POINT('Ctrl Pts',(-174.616065941024,-4.4768801896829,
128.763518477772));
#118014=CARTESIAN_POINT('Ctrl Pts',(-174.623706305068,-4.53138392989183,
128.887571946581));
#118015=CARTESIAN_POINT('Ctrl Pts',(-174.631346669112,-4.58068524476776,
129.01368874621));
#118016=CARTESIAN_POINT('Ctrl Pts',(-174.63898633773,-4.62998207223927,
129.13979406669));
#118017=CARTESIAN_POINT('Ctrl Pts',(-174.646626006347,-4.67407726516443,
129.267961971298));
#118018=CARTESIAN_POINT('Ctrl Pts',(-174.654265674965,-4.71280537081142,
129.397716170895));
#118019=CARTESIAN_POINT('Ctrl Pts',(-174.657872255346,-4.73108836618704,
129.458971308257));
#118020=CARTESIAN_POINT('Ctrl Pts',(-174.661478835727,-4.74817593400007,
129.520579721381));
#118021=CARTESIAN_POINT('Ctrl Pts',(-174.665085416107,-4.76405452823406,
129.582490119308));
#118022=CARTESIAN_POINT('Ctrl Pts',(-172.915418914505,-4.76405452823406,
129.582490119308));
#118023=CARTESIAN_POINT('Ctrl Pts',(-172.923551617668,-4.7997385967966,
129.721621761052));
#118024=CARTESIAN_POINT('Ctrl Pts',(-172.93168432083,-4.82936058183097,
129.86246191961));
#118025=CARTESIAN_POINT('Ctrl Pts',(-172.939817023993,-4.85276781019348,
130.004468348038));
#118026=CARTESIAN_POINT('Ctrl Pts',(-172.947934708106,-4.87613181131613,
130.146212526454));
#118027=CARTESIAN_POINT('Ctrl Pts',(-172.95605239222,-4.89330388817451,
130.289118353323));
#118028=CARTESIAN_POINT('Ctrl Pts',(-172.964170076333,-4.90418197276099,
130.432631898543));
#118029=CARTESIAN_POINT('Ctrl Pts',(-172.971160238893,-4.9135491245905,
130.556211850233));
#118030=CARTESIAN_POINT('Ctrl Pts',(-172.978150401452,-4.91825005692981,
130.680242069289));
#118031=CARTESIAN_POINT('Ctrl Pts',(-172.985140564012,-4.91824999999948,
130.804362873413));
#118032=CARTESIAN_POINT('',(-172.63985943603,-4.91824811045768,130.800049413617));
#118033=CARTESIAN_POINT('Ctrl Pts',(-172.569844098739,-4.76405452823414,
129.582490119309));
#118034=CARTESIAN_POINT('Ctrl Pts',(-172.575574438797,-4.78909101747142,
129.680107010863));
#118035=CARTESIAN_POINT('Ctrl Pts',(-172.581304778855,-4.81110043102754,
129.778394074122));
#118036=CARTESIAN_POINT('Ctrl Pts',(-172.587035118913,-4.83005787533671,
129.877147598137));
#118037=CARTESIAN_POINT('Ctrl Pts',(-172.598508350551,-4.86801428763181,
130.074870952193));
#118038=CARTESIAN_POINT('Ctrl Pts',(-172.609981582189,-4.89383874355218,
130.27499214093));
#118039=CARTESIAN_POINT('Ctrl Pts',(-172.621454813827,-4.90729647054678,
130.476299018687));
#118040=CARTESIAN_POINT('Ctrl Pts',(-172.627589687883,-4.91449247798305,
130.583940211727));
#118041=CARTESIAN_POINT('Ctrl Pts',(-172.633724561938,-4.91815332714998,
130.69192004631));
#118042=CARTESIAN_POINT('Ctrl Pts',(-172.639859435994,-4.91824811045712,
130.800049412982));
#118043=CARTESIAN_POINT('Ctrl Pts',(-172.63985943603,-4.91824811045768,
130.800049413617));
#118044=CARTESIAN_POINT('Ctrl Pts',(-172.647506292934,-4.91836625375992,
130.934828023003));
#118045=CARTESIAN_POINT('Ctrl Pts',(-172.655153149837,-4.91294006961445,
131.069793692025));
#118046=CARTESIAN_POINT('Ctrl Pts',(-172.66280000674,-4.90195016924981,
131.204445109507));
#118047=CARTESIAN_POINT('Ctrl Pts',(-172.670440188586,-4.8909698621364,
131.338978987718));
#118048=CARTESIAN_POINT('Ctrl Pts',(-172.678080370431,-4.87443553171941,
131.473198760116));
#118049=CARTESIAN_POINT('Ctrl Pts',(-172.685720552277,-4.85237984714444,
131.606603025773));
#118050=CARTESIAN_POINT('Ctrl Pts',(-172.693356430854,-4.83033658524968,
131.739932152592));
#118051=CARTESIAN_POINT('Ctrl Pts',(-172.700992309431,-4.80277821907229,
131.872446289167));
#118052=CARTESIAN_POINT('Ctrl Pts',(-172.708628188008,-4.76978921957538,
132.00364951659));
#118053=CARTESIAN_POINT('Ctrl Pts',(-172.716261878284,-4.73680967410985,
132.134815143618));
#118054=CARTESIAN_POINT('Ctrl Pts',(-172.723895568561,-4.69840268736267,
132.264670217367));
#118055=CARTESIAN_POINT('Ctrl Pts',(-172.731529258838,-4.65470366440352,
132.392729862763));
#118056=CARTESIAN_POINT('Ctrl Pts',(-172.739162527427,-4.61100705539324,
132.520782434102));
#118057=CARTESIAN_POINT('Ctrl Pts',(-172.746795796016,-4.56201912185757,
132.64703939245));
#118058=CARTESIAN_POINT('Ctrl Pts',(-172.754429064605,-4.50792470471584,
132.771032404904));
#118059=CARTESIAN_POINT('Ctrl Pts',(-172.762063677571,-4.45382076042516,
132.8950472551));
#118060=CARTESIAN_POINT('Ctrl Pts',(-172.769698290537,-4.39460870601867,
133.016796996958));
#118061=CARTESIAN_POINT('Ctrl Pts',(-172.777332903503,-4.33052071184678,
133.135835135284));
#118062=CARTESIAN_POINT('Ctrl Pts',(-172.784975198528,-4.26636823139755,
133.254993051525));
#118063=CARTESIAN_POINT('Ctrl Pts',(-172.792617493553,-4.19733020493732,
133.3714335597));
#118064=CARTESIAN_POINT('Ctrl Pts',(-172.800259788578,-4.1236839549241,
133.484736281984));
#118065=CARTESIAN_POINT('Ctrl Pts',(-172.807906040652,-4.04999957215319,
133.598097670461));
#118066=CARTESIAN_POINT('Ctrl Pts',(-172.815552292726,-3.9717024487071,
133.708317709803));
#118067=CARTESIAN_POINT('Ctrl Pts',(-172.8231985448,-3.88911129452465,133.815007790733));
#118068=CARTESIAN_POINT('Ctrl Pts',(-172.830856647217,-3.80639213860581,
133.921863222491));
#118069=CARTESIAN_POINT('Ctrl Pts',(-172.838514749634,-3.71936591941276,
134.025177460536));
#118070=CARTESIAN_POINT('Ctrl Pts',(-172.846172852051,-3.62838982436676,
134.124597106874));
#118071=CARTESIAN_POINT('Ctrl Pts',(-172.852609482276,-3.5519244741784,
134.208159256568));
#118072=CARTESIAN_POINT('Ctrl Pts',(-172.859046112501,-3.47266951968559,
134.288970687063));
#118073=CARTESIAN_POINT('Ctrl Pts',(-172.865482742726,-3.39085483562696,
134.366843816994));
#118074=CARTESIAN_POINT('Ctrl Pts',(-172.873257076845,-3.29203687226701,
134.46090106587));
#118075=CARTESIAN_POINT('Ctrl Pts',(-172.881031410964,-3.18914591107,134.550992584651));
#118076=CARTESIAN_POINT('Ctrl Pts',(-172.888805745083,-3.08253353326629,
134.63674500314));
#118077=CARTESIAN_POINT('Ctrl Pts',(-172.89657049803,-2.97605254569001,
134.722391739436));
#118078=CARTESIAN_POINT('Ctrl Pts',(-172.904335250977,-2.86585956862587,
134.803709772791));
#118079=CARTESIAN_POINT('Ctrl Pts',(-172.912100003924,-2.75234292988948,
134.880362513884));
#118080=CARTESIAN_POINT('Ctrl Pts',(-172.919857044809,-2.63893903747898,
134.956939122393));
#118081=CARTESIAN_POINT('Ctrl Pts',(-172.927614085694,-2.52221837466528,
135.028859442406));
#118082=CARTESIAN_POINT('Ctrl Pts',(-172.935371126579,-2.40260196594303,
135.09582736633));
#118083=CARTESIAN_POINT('Ctrl Pts',(-172.943122317819,-2.28307576088459,
135.162744789222));
#118084=CARTESIAN_POINT('Ctrl Pts',(-172.950873509059,-2.16065849620911,
135.224717059385));
#118085=CARTESIAN_POINT('Ctrl Pts',(-172.958624700299,-2.03579946855144,
135.281491795714));
#118086=CARTESIAN_POINT('Ctrl Pts',(-172.966372597076,-1.91099350931176,
135.338242401265));
#118087=CARTESIAN_POINT('Ctrl Pts',(-172.974120493853,-1.78374820637798,
135.389799705203));
#118088=CARTESIAN_POINT('Ctrl Pts',(-172.981868390631,-1.65453650972927,
135.435957750356));
#118089=CARTESIAN_POINT('Ctrl Pts',(-172.989614666715,-1.52535184138201,
135.482106140242));
#118090=CARTESIAN_POINT('Ctrl Pts',(-172.997360942799,-1.39420196541725,
135.52285738636));
#118091=CARTESIAN_POINT('Ctrl Pts',(-173.005107218883,-1.26157844659884,
135.558054222078));
#118092=CARTESIAN_POINT('Ctrl Pts',(-173.012853552148,-1.12895394878356,
135.593251317611));
#118093=CARTESIAN_POINT('Ctrl Pts',(-173.020599885413,-0.994856164292337,
135.622893820644));
#118094=CARTESIAN_POINT('Ctrl Pts',(-173.028346218679,-0.859790017360974,
135.646874860038));
#118095=CARTESIAN_POINT('Ctrl Pts',(-173.036094286682,-0.724693623302305,
135.67086126982));
#118096=CARTESIAN_POINT('Ctrl Pts',(-173.043842354685,-0.588628820152166,
135.689183624763));
#118097=CARTESIAN_POINT('Ctrl Pts',(-173.051590422688,-0.452108481873687,
135.701786572404));
#118098=CARTESIAN_POINT('Ctrl Pts',(-173.05934672543,-0.315443048155258,
135.714402914607));
#118099=CARTESIAN_POINT('Ctrl Pts',(-173.067103028172,-0.178321502101017,
135.721287670746));
#118100=CARTESIAN_POINT('Ctrl Pts',(-173.074859330913,-0.04126013011152,
135.722437545));
#118101=CARTESIAN_POINT('Ctrl Pts',(-173.082619773428,0.0958743956590458,
135.723588032978));
#118102=CARTESIAN_POINT('Ctrl Pts',(-173.090380215942,0.232948292814648,
135.71899755309));
#118103=CARTESIAN_POINT('Ctrl Pts',(-173.098140658456,0.36944854734374,
135.70871489039));
#118104=CARTESIAN_POINT('Ctrl Pts',(-173.105913558721,0.506167924199327,
135.698415721047));
#118105=CARTESIAN_POINT('Ctrl Pts',(-173.113686458987,0.642311429739336,
135.682406154748));
#118106=CARTESIAN_POINT('Ctrl Pts',(-173.121459359252,0.77737352141237,
135.660786615222));
#118107=CARTESIAN_POINT('Ctrl Pts',(-173.128949695014,0.907525765851477,
135.639953000414));
#118108=CARTESIAN_POINT('Ctrl Pts',(-173.136440030776,1.03667355368672,
135.6139102653));
#118109=CARTESIAN_POINT('Ctrl Pts',(-173.143930366538,1.16437814554918,
135.58279201256));
#118110=CARTESIAN_POINT('Ctrl Pts',(-173.151704700657,1.29692469582728,
135.550493901809));
#118111=CARTESIAN_POINT('Ctrl Pts',(-173.159479034776,1.42833631988041,
135.51262548864));
#118112=CARTESIAN_POINT('Ctrl Pts',(-173.167253368895,1.55810885254449,
135.469280752587));
#118113=CARTESIAN_POINT('Ctrl Pts',(-173.175018121842,1.68772145216052,
135.425989435047));
#118114=CARTESIAN_POINT('Ctrl Pts',(-173.182782874789,1.81569861238495,
135.377235345948));
#118115=CARTESIAN_POINT('Ctrl Pts',(-173.190547627736,1.94154725041979,
135.323163261728));
#118116=CARTESIAN_POINT('Ctrl Pts',(-173.198304668621,2.06727089381284,
135.269144882665));
#118117=CARTESIAN_POINT('Ctrl Pts',(-173.206061709506,2.19086986523984,
135.209819173058));
#118118=CARTESIAN_POINT('Ctrl Pts',(-173.213818750391,2.31186746697507,
135.145380299351));
#118119=CARTESIAN_POINT('Ctrl Pts',(-173.221569941631,2.43277382347777,
135.0809900195));
#118120=CARTESIAN_POINT('Ctrl Pts',(-173.229321132872,2.55108237127638,
135.011494433471));
#118121=CARTESIAN_POINT('Ctrl Pts',(-173.237072324112,2.66633791919391,
134.937135129098));
#118122=CARTESIAN_POINT('Ctrl Pts',(-173.244820220889,2.78154448042919,
134.862807429412));
#118123=CARTESIAN_POINT('Ctrl Pts',(-173.252568117666,2.89370029478576,
134.783620334415));
#118124=CARTESIAN_POINT('Ctrl Pts',(-173.260316014443,3.00237644364744,
134.699860425438));
#118125=CARTESIAN_POINT('Ctrl Pts',(-173.268062290527,3.11102985980157,
134.616118037228));
#118126=CARTESIAN_POINT('Ctrl Pts',(-173.275808566611,3.21620474876837,
134.527804976152));
#118127=CARTESIAN_POINT('Ctrl Pts',(-173.283554842695,3.31750309491557,
134.435249803113));
#118128=CARTESIAN_POINT('Ctrl Pts',(-173.291301175961,3.41880218882429,
134.342693946853));
#118129=CARTESIAN_POINT('Ctrl Pts',(-173.299047509226,3.51622439418338,
134.245896179862));
#118130=CARTESIAN_POINT('Ctrl Pts',(-173.306793842491,3.60940687339464,
134.145223542738));
#118131=CARTESIAN_POINT('Ctrl Pts',(-173.314541910494,3.70261022017591,
134.044528360676));
#118132=CARTESIAN_POINT('Ctrl Pts',(-173.322289978497,3.79157168597577,
133.939956868626));
#118133=CARTESIAN_POINT('Ctrl Pts',(-173.3300380465,3.87596748029428,133.831910642619));
#118134=CARTESIAN_POINT('Ctrl Pts',(-173.337794349242,3.96045297146721,
133.723749583799));
#118135=CARTESIAN_POINT('Ctrl Pts',(-173.345550651984,4.04036285681526,
133.612106722482));
#118136=CARTESIAN_POINT('Ctrl Pts',(-173.353306954726,4.11541529806242,
133.49741464357));
#118137=CARTESIAN_POINT('Ctrl Pts',(-173.36106739724,4.19050779705725,133.382661350041));
#118138=CARTESIAN_POINT('Ctrl Pts',(-173.368827839754,4.2607374859471,133.264855931722));
#118139=CARTESIAN_POINT('Ctrl Pts',(-173.376588282268,4.32586811237478,
133.144456371342));
#118140=CARTESIAN_POINT('Ctrl Pts',(-173.384361182534,4.39110329226603,
133.023863534898));
#118141=CARTESIAN_POINT('Ctrl Pts',(-173.392134082799,4.45122288095881,
132.900668586264));
#118142=CARTESIAN_POINT('Ctrl Pts',(-173.399906983064,4.50603810968254,
132.775351134182));
#118143=CARTESIAN_POINT('Ctrl Pts',(-173.407397318827,4.55886066677196,
132.654589287136));
#118144=CARTESIAN_POINT('Ctrl Pts',(-173.414887654589,4.60675771008897,
132.531856861114));
#118145=CARTESIAN_POINT('Ctrl Pts',(-173.422377990351,4.64960449400472,
132.407595195484));
#118146=CARTESIAN_POINT('Ctrl Pts',(-173.43015232447,4.69407582675482,132.278622111035));
#118147=CARTESIAN_POINT('Ctrl Pts',(-173.437926658589,4.7332472509744,132.147592987642));
#118148=CARTESIAN_POINT('Ctrl Pts',(-173.445700992708,4.76692532072162,
132.014982791972));
#118149=CARTESIAN_POINT('Ctrl Pts',(-173.453465745655,4.80056188525778,
131.882536026516));
#118150=CARTESIAN_POINT('Ctrl Pts',(-173.461230498602,4.82871847042807,
131.748512441074));
#118151=CARTESIAN_POINT('Ctrl Pts',(-173.46899525155,4.85125035745506,131.613405135372));
#118152=CARTESIAN_POINT('Ctrl Pts',(-173.476752292435,4.87375986549426,
131.47843202015));
#118153=CARTESIAN_POINT('Ctrl Pts',(-173.48450933332,4.89065572893891,131.342377709829));
#118154=CARTESIAN_POINT('Ctrl Pts',(-173.492266374205,4.90184363875416,
131.205748215413));
#118155=CARTESIAN_POINT('Ctrl Pts',(-173.500017565445,4.91302311167957,
131.069221754361));
#118156=CARTESIAN_POINT('Ctrl Pts',(-173.507768756685,4.91850316686881,
130.932121360653));
#118157=CARTESIAN_POINT('Ctrl Pts',(-173.515519947925,4.91824101705704,
130.794960583642));
#118158=CARTESIAN_POINT('Ctrl Pts',(-173.523267844702,4.91797897866593,
130.657858103621));
#118159=CARTESIAN_POINT('Ctrl Pts',(-173.531015741479,4.91197959016753,
130.520695681487));
#118160=CARTESIAN_POINT('Ctrl Pts',(-173.538763638256,4.90025211956312,
130.383989082829));
#118161=CARTESIAN_POINT('Ctrl Pts',(-173.54650991434,4.88852710209275,130.247311080245));
#118162=CARTESIAN_POINT('Ctrl Pts',(-173.554256190424,4.87107641917985,
130.111089100772));
#118163=CARTESIAN_POINT('Ctrl Pts',(-173.562002466509,4.84796136124566,
129.975835601426));
#118164=CARTESIAN_POINT('Ctrl Pts',(-173.569748799774,4.82484613268134,
129.840581103671));
#118165=CARTESIAN_POINT('Ctrl Pts',(-173.577495133039,4.79606651152239,
129.706295485686));
#118166=CARTESIAN_POINT('Ctrl Pts',(-173.585241466305,4.76173517683534,
129.573482407429));
#118167=CARTESIAN_POINT('Ctrl Pts',(-173.592989534308,4.72739615388388,
129.440639586605));
#118168=CARTESIAN_POINT('Ctrl Pts',(-173.60073760231,4.68750304127259,129.309270340154));
#118169=CARTESIAN_POINT('Ctrl Pts',(-173.608485670313,4.64221867961617,
129.179864143848));
#118170=CARTESIAN_POINT('Ctrl Pts',(-173.616241973055,4.59688618920134,
129.050320413097));
#118171=CARTESIAN_POINT('Ctrl Pts',(-173.623998275797,4.54615113302321,
128.922744269818));
#118172=CARTESIAN_POINT('Ctrl Pts',(-173.631754578539,4.49022511653739,
128.797606655239));
#118173=CARTESIAN_POINT('Ctrl Pts',(-173.639515021053,4.43426925065267,
128.672402250947));
#118174=CARTESIAN_POINT('Ctrl Pts',(-173.647275463567,4.37311707809791,
128.549639318517));
#118175=CARTESIAN_POINT('Ctrl Pts',(-173.655035906082,4.30702621254498,
128.429764174599));
#118176=CARTESIAN_POINT('Ctrl Pts',(-173.662808806347,4.24082925206739,
128.309696596459));
#118177=CARTESIAN_POINT('Ctrl Pts',(-173.670581706612,4.16967795890928,
128.192526404875));
#118178=CARTESIAN_POINT('Ctrl Pts',(-173.678354606878,4.09387380735918,
128.078671656602));
#118179=CARTESIAN_POINT('Ctrl Pts',(-173.68584494264,4.02082532765747,127.968955815213));
#118180=CARTESIAN_POINT('Ctrl Pts',(-173.693335278402,3.94345658354716,
127.862318801987));
#118181=CARTESIAN_POINT('Ctrl Pts',(-173.700825614164,3.86207145827823,
127.759104123664));
#118182=CARTESIAN_POINT('Ctrl Pts',(-173.708599948283,3.77760059124767,
127.65197602944));
#118183=CARTESIAN_POINT('Ctrl Pts',(-173.716374282402,3.68853519040565,
127.548195559094));
#118184=CARTESIAN_POINT('Ctrl Pts',(-173.724148616521,3.59517029640279,
127.448182195258));
#118185=CARTESIAN_POINT('Ctrl Pts',(-173.731913369468,3.50192046628777,
127.348292088956));
#118186=CARTESIAN_POINT('Ctrl Pts',(-173.739678122415,3.404381950158,127.252160134777));
#118187=CARTESIAN_POINT('Ctrl Pts',(-173.747442875362,3.30289138274313,
127.160174621174));
#118188=CARTESIAN_POINT('Ctrl Pts',(-173.755199916247,3.2015016171903,127.068280468879));
#118189=CARTESIAN_POINT('Ctrl Pts',(-173.762956957132,3.09616789955506,
126.980524822408));
#118190=CARTESIAN_POINT('Ctrl Pts',(-173.770713998017,2.98726497488921,
126.897260537929));
#118191=CARTESIAN_POINT('Ctrl Pts',(-173.778465189257,2.87844417476644,
126.814059043695));
#118192=CARTESIAN_POINT('Ctrl Pts',(-173.786216380497,2.76605983434295,
126.735342406399));
#118193=CARTESIAN_POINT('Ctrl Pts',(-173.793967571738,2.6505208896722,126.661424210148));
#118194=CARTESIAN_POINT('Ctrl Pts',(-173.801715468515,2.53503105213456,
126.587537431101));
#118195=CARTESIAN_POINT('Ctrl Pts',(-173.809463365292,2.41638960572452,
126.518445247014));
#118196=CARTESIAN_POINT('Ctrl Pts',(-173.817211262069,2.29503548822038,
126.454418644354));
#118197=CARTESIAN_POINT('Ctrl Pts',(-173.824957538153,2.17370675538154,
126.390405434679));
#118198=CARTESIAN_POINT('Ctrl Pts',(-173.832703814237,2.04966682567235,
126.331455881131));
#118199=CARTESIAN_POINT('Ctrl Pts',(-173.840450090321,1.92337997266463,
126.277795413877));
#118200=CARTESIAN_POINT('Ctrl Pts',(-173.848196423587,1.79709218743656,
126.224134550513));
#118201=CARTESIAN_POINT('Ctrl Pts',(-173.855942756852,1.66855780564238,
126.175763004246));
#118202=CARTESIAN_POINT('Ctrl Pts',(-173.863689090117,1.53826147645589,
126.132858215495));
#118203=CARTESIAN_POINT('Ctrl Pts',(-173.87143715812,1.40793596830971,126.089943818514));
#118204=CARTESIAN_POINT('Ctrl Pts',(-173.879185226123,1.27584809889036,
126.052498737407));
#118205=CARTESIAN_POINT('Ctrl Pts',(-173.886933294126,1.14249769735741,
126.020650543363));
#118206=CARTESIAN_POINT('Ctrl Pts',(-173.894689596868,1.00900556943065,
125.988768500679));
#118207=CARTESIAN_POINT('Ctrl Pts',(-173.90244589961,0.874248609808633,
125.96249531867));
#118208=CARTESIAN_POINT('Ctrl Pts',(-173.910202202352,0.738737412602422,
125.941907522911));
#118209=CARTESIAN_POINT('Ctrl Pts',(-173.917962644866,0.60315388898973,
125.921308738825));
#118210=CARTESIAN_POINT('Ctrl Pts',(-173.92572308738,0.46681571411805,125.906401429885));
#118211=CARTESIAN_POINT('Ctrl Pts',(-173.933483529894,0.330237633308961,
125.897210103465));
#118212=CARTESIAN_POINT('Ctrl Pts',(-173.94125643016,0.193440305240098,
125.888004022311));
#118213=CARTESIAN_POINT('Ctrl Pts',(-173.949029330425,0.0564026927094663,
125.884532269762));
#118214=CARTESIAN_POINT('Ctrl Pts',(-173.95680223069,-0.0803605270785853,
125.886767176849));
#118215=CARTESIAN_POINT('Ctrl Pts',(-173.964292566452,-0.212152059340465,
125.888920839433));
#118216=CARTESIAN_POINT('Ctrl Pts',(-173.971782902214,-0.343688494712483,
125.896373444647));
#118217=CARTESIAN_POINT('Ctrl Pts',(-173.979273237976,-0.47451657492709,
125.90905500069));
#118218=CARTESIAN_POINT('Ctrl Pts',(-173.987047572095,-0.610305041568332,
125.922217381785));
#118219=CARTESIAN_POINT('Ctrl Pts',(-173.994821906215,-0.745760515184663,
125.941054746775));
#118220=CARTESIAN_POINT('Ctrl Pts',(-174.002596240334,-0.880370596477415,
125.965545610216));
#118221=CARTESIAN_POINT('Ctrl Pts',(-174.010360993281,-1.01481478287542,
125.990006290856));
#118222=CARTESIAN_POINT('Ctrl Pts',(-174.018125746228,-1.14841526900349,
126.020106537523));
#118223=CARTESIAN_POINT('Ctrl Pts',(-174.025890499175,-1.28066341749588,
126.055773009278));
#118224=CARTESIAN_POINT('Ctrl Pts',(-174.03364754006,-1.41278021526318,
126.09140405659));
#118225=CARTESIAN_POINT('Ctrl Pts',(-174.041404580945,-1.54354697330977,
126.132590225974));
#118226=CARTESIAN_POINT('Ctrl Pts',(-174.04916162183,-1.67246426489251,
126.179206961183));
#118227=CARTESIAN_POINT('Ctrl Pts',(-174.05691281307,-1.80128433894267,
126.225788542348));
#118228=CARTESIAN_POINT('Ctrl Pts',(-174.06466400431,-1.92825735641036,
126.277792405618));
#118229=CARTESIAN_POINT('Ctrl Pts',(-174.072415195551,-2.05289845017935,
126.335044001376));
#118230=CARTESIAN_POINT('Ctrl Pts',(-174.080163092328,-2.1774865681584,
126.392271263679));
#118231=CARTESIAN_POINT('Ctrl Pts',(-174.087910989105,-2.29974437918586,
126.454741659475));
#118232=CARTESIAN_POINT('Ctrl Pts',(-174.095658885882,-2.41920663808135,
126.522232372784));
#118233=CARTESIAN_POINT('Ctrl Pts',(-174.103405161966,-2.5386439080476,
126.58970896849));
#118234=CARTESIAN_POINT('Ctrl Pts',(-174.11115143805,-2.65528644883749,
126.662203600732));
#118235=CARTESIAN_POINT('Ctrl Pts',(-174.118897714134,-2.76869364846007,
126.739447513516));
#118236=CARTESIAN_POINT('Ctrl Pts',(-174.1266440474,-2.882101685229,126.816691996497));
#118237=CARTESIAN_POINT('Ctrl Pts',(-174.134390380665,-2.99227401004361,
126.898685609886));
#118238=CARTESIAN_POINT('Ctrl Pts',(-174.14213671393,-3.09879937253713,
126.985116515487));
#118239=CARTESIAN_POINT('Ctrl Pts',(-174.149884781933,-3.20534859064743,
127.071566776691));
#118240=CARTESIAN_POINT('Ctrl Pts',(-174.157632849936,-3.30824891773031,
127.162456061171));
#118241=CARTESIAN_POINT('Ctrl Pts',(-174.165380917939,-3.40712285466095,
127.257432803845));
#118242=CARTESIAN_POINT('Ctrl Pts',(-174.173137220681,-3.50610187598796,
127.352510488931));
#118243=CARTESIAN_POINT('Ctrl Pts',(-174.180893523423,-3.60104567640467,
127.451684038943));
#118244=CARTESIAN_POINT('Ctrl Pts',(-174.188649826165,-3.69161388418876,
127.554565240536));
#118245=CARTESIAN_POINT('Ctrl Pts',(-174.196410268679,-3.78223043095229,
127.657501352925));
#118246=CARTESIAN_POINT('Ctrl Pts',(-174.204170711193,-3.86846648592348,
127.764148756128));
#118247=CARTESIAN_POINT('Ctrl Pts',(-174.211931153708,-3.95002319793488,
127.874087627165));
#118248=CARTESIAN_POINT('Ctrl Pts',(-174.219704053973,-4.03171083202067,
127.984202981836));
#118249=CARTESIAN_POINT('Ctrl Pts',(-174.227476954239,-4.10870389266763,
128.097620039311));
#118250=CARTESIAN_POINT('Ctrl Pts',(-174.235249854504,-4.18074746296302,
128.213890831325));
#118251=CARTESIAN_POINT('Ctrl Pts',(-174.242740190266,-4.25017206801078,
128.32593488718));
#118252=CARTESIAN_POINT('Ctrl Pts',(-174.250230526028,-4.31500063644984,
128.440628530722));
#118253=CARTESIAN_POINT('Ctrl Pts',(-174.25772086179,-4.37504705720004,
128.557552590656));
#118254=CARTESIAN_POINT('Ctrl Pts',(-174.265995971559,-4.44138463387784,
128.686726964323));
#118255=CARTESIAN_POINT('Ctrl Pts',(-174.274271081328,-4.50207445138269,
128.818991058705));
#118256=CARTESIAN_POINT('Ctrl Pts',(-174.282546191098,-4.55683688270711,
128.953841585808));
#118257=CARTESIAN_POINT('Ctrl Pts',(-174.290801622159,-4.61146908568318,
129.088371430263));
#118258=CARTESIAN_POINT('Ctrl Pts',(-174.29905705322,-4.66020189058618,
129.22547515269));
#118259=CARTESIAN_POINT('Ctrl Pts',(-174.307312484282,-4.70280224557678,
129.364626579107));
#118260=CARTESIAN_POINT('Ctrl Pts',(-174.311589785604,-4.72487432798964,
129.436723672016));
#118261=CARTESIAN_POINT('Ctrl Pts',(-174.315867086927,-4.74530091292852,
129.509370057858));
#118262=CARTESIAN_POINT('Ctrl Pts',(-174.32014438825,-4.76405452823397,
129.582490119308));
#118263=CARTESIAN_POINT('Origin',(213.235140564004,0.,130.804360617566));
#118264=CARTESIAN_POINT('',(-176.415048843504,-4.76405452823411,129.582490119309));
#118265=CARTESIAN_POINT('',(-176.069836735653,-4.76405452823418,129.582490119309));
#118266=CARTESIAN_POINT('',(213.235140564004,-4.76405452823405,129.582490119308));
#118267=CARTESIAN_POINT('',(-174.735140563982,-4.91824795254522,130.808848354713));
#118268=CARTESIAN_POINT('Ctrl Pts',(-174.735140564012,-4.91824795254474,
130.808848355242));
#118269=CARTESIAN_POINT('Ctrl Pts',(-174.745911124724,-4.91807457526139,
130.998857783261));
#118270=CARTESIAN_POINT('Ctrl Pts',(-174.756681685436,-4.90688666222565,
131.188385333141));
#118271=CARTESIAN_POINT('Ctrl Pts',(-174.767452246148,-4.88487163251762,
131.376385264172));
#118272=CARTESIAN_POINT('Ctrl Pts',(-174.776643868517,-4.86608395331184,
131.536824856658));
#118273=CARTESIAN_POINT('Ctrl Pts',(-174.785835490886,-4.83941174830359,
131.696152789862));
#118274=CARTESIAN_POINT('Ctrl Pts',(-174.795027113255,-4.80499718976505,
131.853734273062));
#118275=CARTESIAN_POINT('Ctrl Pts',(-174.802801447374,-4.77588913180794,
131.987017718812));
#118276=CARTESIAN_POINT('Ctrl Pts',(-174.810575781493,-4.74118514044176,
132.119300237066));
#118277=CARTESIAN_POINT('Ctrl Pts',(-174.818350115612,-4.70096706956376,
132.250075552599));
#118278=CARTESIAN_POINT('Ctrl Pts',(-174.826114868559,-4.66079856386371,
132.380689699243));
#118279=CARTESIAN_POINT('Ctrl Pts',(-174.833879621506,-4.61512961371124,
132.509799968916));
#118280=CARTESIAN_POINT('Ctrl Pts',(-174.841644374453,-4.56409312122651,
132.636909946581));
#118281=CARTESIAN_POINT('Ctrl Pts',(-174.849401415338,-4.51310731890562,
132.763893676824));
#118282=CARTESIAN_POINT('Ctrl Pts',(-174.857158456223,-4.45676472815101,
132.888880708253));
#118283=CARTESIAN_POINT('Ctrl Pts',(-174.864915497108,-4.3952480200623,
133.011389820961));
#118284=CARTESIAN_POINT('Ctrl Pts',(-174.872666688349,-4.33377770220161,
133.133806548594));
#118285=CARTESIAN_POINT('Ctrl Pts',(-174.880417879589,-4.26714120811986,
133.253748728899));
#118286=CARTESIAN_POINT('Ctrl Pts',(-174.888169070829,-4.19556913274437,
133.370755504341));
#118287=CARTESIAN_POINT('Ctrl Pts',(-174.895916967606,-4.12402747741026,
133.487712548781));
#118288=CARTESIAN_POINT('Ctrl Pts',(-174.903664864383,-4.04755461663727,
133.601736336972));
#118289=CARTESIAN_POINT('Ctrl Pts',(-174.91141276116,-3.96642675636401,
133.712391196652));
#118290=CARTESIAN_POINT('Ctrl Pts',(-174.919159037244,-3.88531586629019,
133.823022909721));
#118291=CARTESIAN_POINT('Ctrl Pts',(-174.926905313328,-3.79955214453047,
133.930286780879));
#118292=CARTESIAN_POINT('Ctrl Pts',(-174.934651589413,-3.70945450609213,
134.033777024555));
#118293=CARTESIAN_POINT('Ctrl Pts',(-174.942397922678,-3.61935620257362,
134.137268032174));
#118294=CARTESIAN_POINT('Ctrl Pts',(-174.950144255943,-3.52492417525399,
134.236985061852));
#118295=CARTESIAN_POINT('Ctrl Pts',(-174.957890589209,-3.42651665193184,
134.332556572517));
#118296=CARTESIAN_POINT('Ctrl Pts',(-174.965638657212,-3.32808709092703,
134.42814948576));
#118297=CARTESIAN_POINT('Ctrl Pts',(-174.973386725215,-3.22568054276838,
134.51959476033));
#118298=CARTESIAN_POINT('Ctrl Pts',(-174.981134793218,-3.11969069776469,
134.606559062253));
#118299=CARTESIAN_POINT('Ctrl Pts',(-174.98889109596,-3.01358820549229,
134.693615790871));
#118300=CARTESIAN_POINT('Ctrl Pts',(-174.996647398702,-2.90389511147362,
134.776181784986));
#118301=CARTESIAN_POINT('Ctrl Pts',(-175.004403701443,-2.79103711269373,
134.853964906637));
#118302=CARTESIAN_POINT('Ctrl Pts',(-175.012164143958,-2.67811887820181,
134.931789543483));
#118303=CARTESIAN_POINT('Ctrl Pts',(-175.019924586472,-2.56203270382088,
135.004826013173));
#118304=CARTESIAN_POINT('Ctrl Pts',(-175.027685028986,-2.44323077098833,
135.072827141061));
#118305=CARTESIAN_POINT('Ctrl Pts',(-175.035457929251,-2.32423812674647,
135.140937430396));
#118306=CARTESIAN_POINT('Ctrl Pts',(-175.043230829517,-2.20252135957344,
135.203996045214));
#118307=CARTESIAN_POINT('Ctrl Pts',(-175.051003729782,-2.07855541016828,
135.261802761819));
#118308=CARTESIAN_POINT('Ctrl Pts',(-175.058494065544,-1.9590959352747,
135.317508058668));
#118309=CARTESIAN_POINT('Ctrl Pts',(-175.065984401307,-1.83754825013354,
135.368336548634));
#118310=CARTESIAN_POINT('Ctrl Pts',(-175.073474737069,-1.71435057346656,
135.414152931082));
#118311=CARTESIAN_POINT('Ctrl Pts',(-175.081249071188,-1.58648181944417,
135.461706455597));
#118312=CARTESIAN_POINT('Ctrl Pts',(-175.089023405307,-1.4564304353754,
135.504010937089));
#118313=CARTESIAN_POINT('Ctrl Pts',(-175.096797739426,-1.32466660897776,
135.540861587434));
#118314=CARTESIAN_POINT('Ctrl Pts',(-175.104562492373,-1.19306516972009,
135.577666822646));
#118315=CARTESIAN_POINT('Ctrl Pts',(-175.11232724532,-1.05975586016739,
135.609031495923));
#118316=CARTESIAN_POINT('Ctrl Pts',(-175.120091998267,-0.925228165192352,
135.634799097128));
#118317=CARTESIAN_POINT('Ctrl Pts',(-175.127849039152,-0.790834085020836,
135.660541105589));
#118318=CARTESIAN_POINT('Ctrl Pts',(-175.135606080037,-0.655224409115649,
135.680697031747));
#118319=CARTESIAN_POINT('Ctrl Pts',(-175.143363120922,-0.518902739605467,
135.695160450858));
#118320=CARTESIAN_POINT('Ctrl Pts',(-175.151114312162,-0.382683871326505,
135.709612962992));
#118321=CARTESIAN_POINT('Ctrl Pts',(-175.158865503402,-0.245754465359081,
135.718381471483));
#118322=CARTESIAN_POINT('Ctrl Pts',(-175.166616694642,-0.108626896390376,
135.721410877618));
#118323=CARTESIAN_POINT('Ctrl Pts',(-175.17436459142,0.0284423897037063,
135.724438996175));
#118324=CARTESIAN_POINT('Ctrl Pts',(-175.182112488197,0.165709281231323,
135.721732855286));
#118325=CARTESIAN_POINT('Ctrl Pts',(-175.189860384974,0.302657938724789,
135.71328934333));
#118326=CARTESIAN_POINT('Ctrl Pts',(-175.197606661058,0.439577949511379,
135.704847597574));
#118327=CARTESIAN_POINT('Ctrl Pts',(-175.205352937142,0.576179468693615,
135.690670891929));
#118328=CARTESIAN_POINT('Ctrl Pts',(-175.213099213226,0.711948716028222,
135.67080820161));
#118329=CARTESIAN_POINT('Ctrl Pts',(-175.220845546492,0.847718965580385,
135.650945364669));
#118330=CARTESIAN_POINT('Ctrl Pts',(-175.228591879757,0.982656544178437,
135.625396515895));
#118331=CARTESIAN_POINT('Ctrl Pts',(-175.236338213022,1.11625523292035,
135.594262215457));
#118332=CARTESIAN_POINT('Ctrl Pts',(-175.244086281025,1.24988384016211,
135.563120942708));
#118333=CARTESIAN_POINT('Ctrl Pts',(-175.251834349028,1.38217258022104,
135.526391818018));
#118334=CARTESIAN_POINT('Ctrl Pts',(-175.259582417031,1.51262821055619,
135.484225889038));
#118335=CARTESIAN_POINT('Ctrl Pts',(-175.267338719773,1.64322249068787,
135.442015145607));
#118336=CARTESIAN_POINT('Ctrl Pts',(-175.275095022515,1.77197939664634,
135.394356175545));
#118337=CARTESIAN_POINT('Ctrl Pts',(-175.282851325257,1.89842304487477,
135.341449222078));
#118338=CARTESIAN_POINT('Ctrl Pts',(-175.290611767771,2.02493417988575,
135.288514030576));
#118339=CARTESIAN_POINT('Ctrl Pts',(-175.298372210285,2.14912924315125,
135.23032544022));
#118340=CARTESIAN_POINT('Ctrl Pts',(-175.306132652799,2.27055586452998,
135.167130280125));
#118341=CARTESIAN_POINT('Ctrl Pts',(-175.313905553065,2.39217741070076,
135.10383367355));
#118342=CARTESIAN_POINT('Ctrl Pts',(-175.32167845333,2.51102129501437,135.035514631731));
#118343=CARTESIAN_POINT('Ctrl Pts',(-175.329451353595,2.62666234655475,
134.96246450993));
#118344=CARTESIAN_POINT('Ctrl Pts',(-175.336941689357,2.73809955458783,
134.89206994406));
#118345=CARTESIAN_POINT('Ctrl Pts',(-175.344432025119,2.84656249551728,
134.817282474524));
#118346=CARTESIAN_POINT('Ctrl Pts',(-175.351922360881,2.95170046916539,
134.738397653847));
#118347=CARTESIAN_POINT('Ctrl Pts',(-175.359696695,3.06082478104204,134.656521891216));
#118348=CARTESIAN_POINT('Ctrl Pts',(-175.367471029119,3.16671268921718,
134.569972584143));
#118349=CARTESIAN_POINT('Ctrl Pts',(-175.375245363238,3.26893775169545,
134.479034621888));
#118350=CARTESIAN_POINT('Ctrl Pts',(-175.383010116185,3.37103683092005,
134.388208732544));
#118351=CARTESIAN_POINT('Ctrl Pts',(-175.390774869133,3.46948175691526,
134.293005206933));
#118352=CARTESIAN_POINT('Ctrl Pts',(-175.39853962208,3.56387627474123,134.193751264989));
#118353=CARTESIAN_POINT('Ctrl Pts',(-175.406296662965,3.65817703860136,
134.094595903459));
#118354=CARTESIAN_POINT('Ctrl Pts',(-175.41405370385,3.74843513240106,133.991398412879));
#118355=CARTESIAN_POINT('Ctrl Pts',(-175.421810744735,3.83428880873651,
133.884524962808));
#118356=CARTESIAN_POINT('Ctrl Pts',(-175.429561935975,3.92007774214691,
133.777732106836));
#118357=CARTESIAN_POINT('Ctrl Pts',(-175.437313127215,4.0014686252892,133.667269112576));
#118358=CARTESIAN_POINT('Ctrl Pts',(-175.445064318455,4.07813815102295,
133.553537273161));
#118359=CARTESIAN_POINT('Ctrl Pts',(-175.452812215232,4.15477509016293,
133.439853772813));
#118360=CARTESIAN_POINT('Ctrl Pts',(-175.460560112009,4.22669444499128,
133.322904514119));
#118361=CARTESIAN_POINT('Ctrl Pts',(-175.468308008786,4.29361477378184,
133.203121805526));
#118362=CARTESIAN_POINT('Ctrl Pts',(-175.47605428487,4.36052110428226,133.083364152893));
#118363=CARTESIAN_POINT('Ctrl Pts',(-175.483800560955,4.42243029811331,
132.960774570363));
#118364=CARTESIAN_POINT('Ctrl Pts',(-175.491546837039,4.47910584873974,
132.835811788105));
#118365=CARTESIAN_POINT('Ctrl Pts',(-175.499293170304,4.53578181773229,
132.7108480834));
#118366=CARTESIAN_POINT('Ctrl Pts',(-175.507039503569,4.58722390494409,
132.583511500068));
#118367=CARTESIAN_POINT('Ctrl Pts',(-175.514785836835,4.63324309081047,
132.454282289633));
#118368=CARTESIAN_POINT('Ctrl Pts',(-175.522533904838,4.67927258235439,
132.325024139213));
#118369=CARTESIAN_POINT('Ctrl Pts',(-175.530281972841,4.7198766248637,132.193872886536));
#118370=CARTESIAN_POINT('Ctrl Pts',(-175.538030040843,4.75491568936418,
132.061325155466));
#118371=CARTESIAN_POINT('Ctrl Pts',(-175.545786343585,4.78999199379943,
131.92863655109));
#118372=CARTESIAN_POINT('Ctrl Pts',(-175.553542646327,4.81949140524646,
131.794548882068));
#118373=CARTESIAN_POINT('Ctrl Pts',(-175.561298949069,4.84332516731719,
131.65957075907));
#118374=CARTESIAN_POINT('Ctrl Pts',(-175.569059391583,4.86717165018437,
131.524520594184));
#118375=CARTESIAN_POINT('Ctrl Pts',(-175.576819834097,4.8853464064593,131.388579415649));
#118376=CARTESIAN_POINT('Ctrl Pts',(-175.584580276612,4.89781258335714,
131.252261232444));
#118377=CARTESIAN_POINT('Ctrl Pts',(-175.592353176877,4.91029877206883,
131.11572421919));
#118378=CARTESIAN_POINT('Ctrl Pts',(-175.600126077143,4.91705804968544,
130.978809382595));
#118379=CARTESIAN_POINT('Ctrl Pts',(-175.607898977408,4.91810572637498,
130.842031915627));
#118380=CARTESIAN_POINT('Ctrl Pts',(-175.61538931317,4.91911531737791,130.710226654106));
#118381=CARTESIAN_POINT('Ctrl Pts',(-175.622879648932,4.91482137009318,
130.578549256001));
#118382=CARTESIAN_POINT('Ctrl Pts',(-175.630369984694,4.90528297921777,
130.447454528662));
#118383=CARTESIAN_POINT('Ctrl Pts',(-175.638144318813,4.89538293735313,
130.311389304891));
#118384=CARTESIAN_POINT('Ctrl Pts',(-175.645918652932,4.87980155493366,
130.175520794284));
#118385=CARTESIAN_POINT('Ctrl Pts',(-175.653692987051,4.85854801504704,
130.040361764175));
#118386=CARTESIAN_POINT('Ctrl Pts',(-175.661457739998,4.8373206682489,129.905369305491));
#118387=CARTESIAN_POINT('Ctrl Pts',(-175.669222492945,4.81043513299945,
129.771084970078));
#118388=CARTESIAN_POINT('Ctrl Pts',(-175.676987245893,4.77795252322328,
129.638019008806));
#118389=CARTESIAN_POINT('Ctrl Pts',(-175.684744286778,4.74550217563306,
129.505085210523));
#118390=CARTESIAN_POINT('Ctrl Pts',(-175.692501327663,4.70746590847843,
129.37336775557));
#118391=CARTESIAN_POINT('Ctrl Pts',(-175.700258368548,4.66395625727218,
129.243368915874));
#118392=CARTESIAN_POINT('Ctrl Pts',(-175.708009559788,4.6204794170323,129.113468109314));
#118393=CARTESIAN_POINT('Ctrl Pts',(-175.715760751028,4.57153753190743,
128.98528370761));
#118394=CARTESIAN_POINT('Ctrl Pts',(-175.723511942268,4.51729346577151,
128.859304626959));
#118395=CARTESIAN_POINT('Ctrl Pts',(-175.731259839045,4.46307245481078,
128.733379090777));
#118396=CARTESIAN_POINT('Ctrl Pts',(-175.739007735822,4.40355389930882,
128.609657369729));
#118397=CARTESIAN_POINT('Ctrl Pts',(-175.746755632599,4.33894938647817,
128.488609921986));
#118398=CARTESIAN_POINT('Ctrl Pts',(-175.754501908683,4.27435838751889,
128.367587794759));
#118399=CARTESIAN_POINT('Ctrl Pts',(-175.762248184767,4.20468373130066,
128.249239172855));
#118400=CARTESIAN_POINT('Ctrl Pts',(-175.769994460852,4.13018352294818,
128.134010990782));
#118401=CARTESIAN_POINT('Ctrl Pts',(-175.777740794117,4.05568276465198,
128.01878195812));
#118402=CARTESIAN_POINT('Ctrl Pts',(-175.785487127382,3.97635659541556,
127.906673739573));
#118403=CARTESIAN_POINT('Ctrl Pts',(-175.793233460648,3.89250689475741,
127.798104950334));
#118404=CARTESIAN_POINT('Ctrl Pts',(-175.800981528651,3.80863841654029,
127.689511847867));
#118405=CARTESIAN_POINT('Ctrl Pts',(-175.808729596654,3.72024463005167,
127.584460061318));
#118406=CARTESIAN_POINT('Ctrl Pts',(-175.816477664657,3.627667940195,127.483335417695));
#118407=CARTESIAN_POINT('Ctrl Pts',(-175.824233967398,3.53499285873054,
127.382103297596));
#118408=CARTESIAN_POINT('Ctrl Pts',(-175.83199027014,3.43812625767265,127.284806946899));
#118409=CARTESIAN_POINT('Ctrl Pts',(-175.839746572882,3.33744807058666,
127.191795955358));
#118410=CARTESIAN_POINT('Ctrl Pts',(-175.847507015396,3.23671614852086,
127.098735321049));
#118411=CARTESIAN_POINT('Ctrl Pts',(-175.855267457911,3.13216888467507,
127.009964856313));
#118412=CARTESIAN_POINT('Ctrl Pts',(-175.863027900425,3.02421880952979,
126.92579340085));
#118413=CARTESIAN_POINT('Ctrl Pts',(-175.87080080069,2.91609544334053,126.841486825893));
#118414=CARTESIAN_POINT('Ctrl Pts',(-175.878573700956,2.80455866833949,
126.761794240691));
#118415=CARTESIAN_POINT('Ctrl Pts',(-175.886346601221,2.6900502064823,126.686981238749));
#118416=CARTESIAN_POINT('Ctrl Pts',(-175.893836936983,2.57970441564334,
126.614887877871));
#118417=CARTESIAN_POINT('Ctrl Pts',(-175.901327272745,2.46659950792686,
126.547325647257));
#118418=CARTESIAN_POINT('Ctrl Pts',(-175.908817608507,2.35115006776496,
126.484490663349));
#118419=CARTESIAN_POINT('Ctrl Pts',(-175.916591942626,2.23132332698904,
126.419273271927));
#118420=CARTESIAN_POINT('Ctrl Pts',(-175.924366276745,2.10859118322595,
126.358942081489));
#118421=CARTESIAN_POINT('Ctrl Pts',(-175.932140610864,1.98339000583746,
126.30376652931));
#118422=CARTESIAN_POINT('Ctrl Pts',(-175.939905363811,1.8583431277109,126.248658976068));
#118423=CARTESIAN_POINT('Ctrl Pts',(-175.947670116758,1.73083362468,126.198694574944));
#118424=CARTESIAN_POINT('Ctrl Pts',(-175.955434869705,1.60132381882267,
126.15409771212));
#118425=CARTESIAN_POINT('Ctrl Pts',(-175.96319191059,1.47194264393028,126.109545143528));
#118426=CARTESIAN_POINT('Ctrl Pts',(-175.970948951475,1.34056548716186,
126.070349630549));
#118427=CARTESIAN_POINT('Ctrl Pts',(-175.97870599236,1.20767575230822,126.036687984112));
#118428=CARTESIAN_POINT('Ctrl Pts',(-175.986457183601,1.07488623063718,
126.003051722185));
#118429=CARTESIAN_POINT('Ctrl Pts',(-175.994208374841,0.940586778731302,
125.974941116047));
#118430=CARTESIAN_POINT('Ctrl Pts',(-176.001959566081,0.805276767535073,
125.952483414857));
#118431=CARTESIAN_POINT('Ctrl Pts',(-176.009707462858,0.670024266702931,
125.930035258788));
#118432=CARTESIAN_POINT('Ctrl Pts',(-176.017455359635,0.533762445733919,
125.913235292888));
#118433=CARTESIAN_POINT('Ctrl Pts',(-176.025203256412,0.397001482467536,
125.902159796973));
#118434=CARTESIAN_POINT('Ctrl Pts',(-176.032949532496,0.260269126646816,
125.891086617814));
#118435=CARTESIAN_POINT('Ctrl Pts',(-176.04069580858,0.123038225648086,
125.885735558414));
#118436=CARTESIAN_POINT('Ctrl Pts',(-176.048442084664,-0.0141756897444903,
125.886131046641));
#118437=CARTESIAN_POINT('Ctrl Pts',(-176.05618841793,-0.151390618019207,
125.886526537788));
#118438=CARTESIAN_POINT('Ctrl Pts',(-176.063934751195,-0.288588169473994,
125.89266866008));
#118439=CARTESIAN_POINT('Ctrl Pts',(-176.07168108446,-0.425252978037041,
125.904529705466));
#118440=CARTESIAN_POINT('Ctrl Pts',(-176.079429152463,-0.561948391736213,
125.916393407051));
#118441=CARTESIAN_POINT('Ctrl Pts',(-176.087177220466,-0.698110435715874,
125.933978546404));
#118442=CARTESIAN_POINT('Ctrl Pts',(-176.094925288469,-0.833229424573775,
125.957205597503));
#118443=CARTESIAN_POINT('Ctrl Pts',(-176.102681591211,-0.968492019501155,
125.980457334588));
#118444=CARTESIAN_POINT('Ctrl Pts',(-176.110437893953,-1.10270895888793,
126.009362895315));
#118445=CARTESIAN_POINT('Ctrl Pts',(-176.118194196695,-1.23538075960113,
126.043791592617));
#118446=CARTESIAN_POINT('Ctrl Pts',(-176.125954639209,-1.36812337124905,
126.07823866555));
#118447=CARTESIAN_POINT('Ctrl Pts',(-176.133715081723,-1.49931882715872,
126.118214635027));
#118448=CARTESIAN_POINT('Ctrl Pts',(-176.141475524237,-1.62848430894264,
126.163539362871));
#118449=CARTESIAN_POINT('Ctrl Pts',(-176.149248424503,-1.75785713862469,
126.208936849992));
#118450=CARTESIAN_POINT('Ctrl Pts',(-176.157021324768,-1.88519311889149,
126.259700108784));
#118451=CARTESIAN_POINT('Ctrl Pts',(-176.164794225033,-2.01003003689772,
126.315601065834));
#118452=CARTESIAN_POINT('Ctrl Pts',(-176.172284560796,-2.13032881849257,
126.36946988229));
#118453=CARTESIAN_POINT('Ctrl Pts',(-176.179774896558,-2.24830680193459,
126.428109208505));
#118454=CARTESIAN_POINT('Ctrl Pts',(-176.18726523232,-2.36357489589605,
126.49127624858));
#118455=CARTESIAN_POINT('Ctrl Pts',(-176.195040580708,-2.48322902315794,
126.556846839645));
#118456=CARTESIAN_POINT('Ctrl Pts',(-176.202815929095,-2.60034202907575,
126.627504267593));
#118457=CARTESIAN_POINT('Ctrl Pts',(-176.210591277483,-2.71445118038675,
126.703026950111));
#118458=CARTESIAN_POINT('Ctrl Pts',(-176.218356821904,-2.82841645102932,
126.778454405788));
#118459=CARTESIAN_POINT('Ctrl Pts',(-176.226122366324,-2.93938508089296,
126.858734694858));
#118460=CARTESIAN_POINT('Ctrl Pts',(-176.233887910745,-3.04691826152936,
126.943600048707));
#118461=CARTESIAN_POINT('Ctrl Pts',(-176.241644111132,-3.15432205088633,
127.028363286756));
#118462=CARTESIAN_POINT('Ctrl Pts',(-176.249400311519,-3.25829831912221,
127.117700360751));
#118463=CARTESIAN_POINT('Ctrl Pts',(-176.257156511905,-3.35843715721145,
127.211300233498));
#118464=CARTESIAN_POINT('Ctrl Pts',(-176.264907414555,-3.4585075972185,
127.304836174488));
#118465=CARTESIAN_POINT('Ctrl Pts',(-176.272658317204,-3.55474553722263,
127.402628855934));
#118466=CARTESIAN_POINT('Ctrl Pts',(-176.280409219854,-3.64677404245612,
127.504326959288));
#118467=CARTESIAN_POINT('Ctrl Pts',(-176.288156507,-3.73875961986784,127.605977624318));
#118468=CARTESIAN_POINT('Ctrl Pts',(-176.295903794146,-3.8265394081865,
127.711529796871));
#118469=CARTESIAN_POINT('Ctrl Pts',(-176.303651081292,-3.90977354953123,
127.82059557087));
#118470=CARTESIAN_POINT('Ctrl Pts',(-176.311396432377,-3.9929868905086,
127.929634089128));
#118471=CARTESIAN_POINT('Ctrl Pts',(-176.319141783462,-4.07165660931931,
128.042184150169));
#118472=CARTESIAN_POINT('Ctrl Pts',(-176.326887134546,-4.14548360211894,
128.157825379361));
#118473=CARTESIAN_POINT('Ctrl Pts',(-176.334634739561,-4.21933207888202,
128.273500260633));
#118474=CARTESIAN_POINT('Ctrl Pts',(-176.342382344575,-4.28833479834117,
128.392267780956));
#118475=CARTESIAN_POINT('Ctrl Pts',(-176.350129949589,-4.35223637709258,
128.513679151187));
#118476=CARTESIAN_POINT('Ctrl Pts',(-176.357878554451,-4.41614620250603,
128.635106189866));
#118477=CARTESIAN_POINT('Ctrl Pts',(-176.365627159314,-4.47495340090362,
128.759177408328));
#118478=CARTESIAN_POINT('Ctrl Pts',(-176.373375764176,-4.52844934324666,
128.885420908209));
#118479=CARTESIAN_POINT('Ctrl Pts',(-176.381130985486,-4.58199096517854,
129.011772206007));
#118480=CARTESIAN_POINT('Ctrl Pts',(-176.388886206796,-4.63021212521479,
129.140299127584));
#118481=CARTESIAN_POINT('Ctrl Pts',(-176.396641428105,-4.67295286081902,
129.270511008555));
#118482=CARTESIAN_POINT('Ctrl Pts',(-176.402777233238,-4.70676863659504,
129.373532533759));
#118483=CARTESIAN_POINT('Ctrl Pts',(-176.408913038371,-4.73715477371064,
129.477608384682));
#118484=CARTESIAN_POINT('Ctrl Pts',(-176.415048843504,-4.76405452823412,
129.582490119309));
#118485=CARTESIAN_POINT('Ctrl Pts',(-174.665085416107,-4.76405452823406,
129.582490119308));
#118486=CARTESIAN_POINT('Ctrl Pts',(-174.672727967862,-4.79770218485229,
129.713681821788));
#118487=CARTESIAN_POINT('Ctrl Pts',(-174.680370519616,-4.82591771939868,
129.846230089272));
#118488=CARTESIAN_POINT('Ctrl Pts',(-174.68801307137,-4.84860984056921,
129.979639042466));
#118489=CARTESIAN_POINT('Ctrl Pts',(-174.695867653472,-4.87193151826708,
130.116749213218));
#118490=CARTESIAN_POINT('Ctrl Pts',(-174.703722235574,-4.88941875912728,
130.254768074855));
#118491=CARTESIAN_POINT('Ctrl Pts',(-174.711576817676,-4.90102947258295,
130.393151216685));
#118492=CARTESIAN_POINT('Ctrl Pts',(-174.719431399778,-4.91264018603865,
130.531534358515));
#118493=CARTESIAN_POINT('Ctrl Pts',(-174.72728598188,-4.91837439034014,
130.670281320698));
#118494=CARTESIAN_POINT('Ctrl Pts',(-174.735140563982,-4.91824795254522,
130.808848354713));
#118495=CARTESIAN_POINT('',(-174.389859435964,-4.91824995130059,130.803668496368));
#118496=CARTESIAN_POINT('Ctrl Pts',(-174.32014438825,-4.76405452823397,
129.582490119308));
#118497=CARTESIAN_POINT('Ctrl Pts',(-174.328374466888,-4.80013889944959,
129.723182535021));
#118498=CARTESIAN_POINT('Ctrl Pts',(-174.336604545527,-4.83002649212231,
129.865629683102));
#118499=CARTESIAN_POINT('Ctrl Pts',(-174.344834624166,-4.85355817089815,
130.00927814121));
#118500=CARTESIAN_POINT('Ctrl Pts',(-174.353045096558,-4.8770337909267,
130.152584390304));
#118501=CARTESIAN_POINT('Ctrl Pts',(-174.36125556895,-4.89418364153536,
130.297085932918));
#118502=CARTESIAN_POINT('Ctrl Pts',(-174.369466041342,-4.90489914177198,
130.442217729268));
#118503=CARTESIAN_POINT('Ctrl Pts',(-174.376263839549,-4.91377095874204,
130.562378496879));
#118504=CARTESIAN_POINT('Ctrl Pts',(-174.383061637757,-4.91823296612448,
130.682970933855));
#118505=CARTESIAN_POINT('Ctrl Pts',(-174.389859435964,-4.91824995130059,
130.803668496368));
#118506=CARTESIAN_POINT('Ctrl Pts',(-174.389859435994,-4.91824995130066,
130.803668496902));
#118507=CARTESIAN_POINT('Ctrl Pts',(-174.397893643521,-4.91827002578954,
130.946318989852));
#118508=CARTESIAN_POINT('Ctrl Pts',(-174.405927851049,-4.91207954534012,
131.088878016736));
#118509=CARTESIAN_POINT('Ctrl Pts',(-174.413962058576,-4.8997283684063,
131.23079347082));
#118510=CARTESIAN_POINT('Ctrl Pts',(-174.422004104632,-4.88736514111757,
131.372847383903));
#118511=CARTESIAN_POINT('Ctrl Pts',(-174.430046150687,-4.86882925974451,
131.514256126069));
#118512=CARTESIAN_POINT('Ctrl Pts',(-174.438088196743,-4.84422213234544,
131.654475312766));
#118513=CARTESIAN_POINT('Ctrl Pts',(-174.446261554148,-4.81921321725763,
131.796984012661));
#118514=CARTESIAN_POINT('Ctrl Pts',(-174.454434911553,-4.78793315202345,
131.93826360489));
#118515=CARTESIAN_POINT('Ctrl Pts',(-174.462608268958,-4.75054129509018,
132.077757832163));
#118516=CARTESIAN_POINT('Ctrl Pts',(-174.470675033247,-4.71363708531844,
132.215432840773));
#118517=CARTESIAN_POINT('Ctrl Pts',(-174.478741797536,-4.67077971865268,
132.351368467718));
#118518=CARTESIAN_POINT('Ctrl Pts',(-174.486808561825,-4.62217132855038,
132.485049545365));
#118519=CARTESIAN_POINT('Ctrl Pts',(-174.495035215788,-4.57259948155753,
132.621380288124));
#118520=CARTESIAN_POINT('Ctrl Pts',(-174.503261869751,-4.51704640646669,
132.755365819133));
#118521=CARTESIAN_POINT('Ctrl Pts',(-174.511488523714,-4.45577587641786,
132.886485590192));
#118522=CARTESIAN_POINT('Ctrl Pts',(-174.519715177677,-4.39450534636902,
133.017605361251));
#118523=CARTESIAN_POINT('Ctrl Pts',(-174.52794183164,-4.32751759405783,
133.145859069558));
#118524=CARTESIAN_POINT('Ctrl Pts',(-174.536168485603,-4.25512302683112,
133.270756994678));
#118525=CARTESIAN_POINT('Ctrl Pts',(-174.543942819722,-4.1867088749093,
133.388787752388));
#118526=CARTESIAN_POINT('Ctrl Pts',(-174.551717153841,-4.11327164267325,
133.504156745509));
#118527=CARTESIAN_POINT('Ctrl Pts',(-174.55949148796,-4.03504385882099,
133.616406868944));
#118528=CARTESIAN_POINT('Ctrl Pts',(-174.567256240907,-3.95691248372091,
133.728518654134));
#118529=CARTESIAN_POINT('Ctrl Pts',(-174.575020993854,-3.87400252545046,
133.837518899834));
#118530=CARTESIAN_POINT('Ctrl Pts',(-174.582785746801,-3.78659211245163,
133.942975477089));
#118531=CARTESIAN_POINT('Ctrl Pts',(-174.590542787686,-3.69926851670726,
134.048327313385));
#118532=CARTESIAN_POINT('Ctrl Pts',(-174.598299828571,-3.60745360944987,
134.150142186383));
#118533=CARTESIAN_POINT('Ctrl Pts',(-174.606056869456,-3.51146827176608,
134.248017632845));
#118534=CARTESIAN_POINT('Ctrl Pts',(-174.613808060696,-3.4155553173717,
134.345819270672));
#118535=CARTESIAN_POINT('Ctrl Pts',(-174.621559251936,-3.31547846502927,
134.439687117057));
#118536=CARTESIAN_POINT('Ctrl Pts',(-174.629310443176,-3.21159801369159,
134.529252731568));
#118537=CARTESIAN_POINT('Ctrl Pts',(-174.637058339954,-3.10776171431726,
134.618780278303));
#118538=CARTESIAN_POINT('Ctrl Pts',(-174.64480623673,-3.0001253267856,134.704008975273));
#118539=CARTESIAN_POINT('Ctrl Pts',(-174.652554133508,-2.88908489294528,
134.784608291249));
#118540=CARTESIAN_POINT('Ctrl Pts',(-174.660300409592,-2.77806768636997,
134.865190747585));
#118541=CARTESIAN_POINT('Ctrl Pts',(-174.668046685676,-2.66364816599903,
134.941145519547));
#118542=CARTESIAN_POINT('Ctrl Pts',(-174.67579296176,-2.54625391770853,
135.012183575944));
#118543=CARTESIAN_POINT('Ctrl Pts',(-174.683539295025,-2.42885880284051,
135.083222156728));
#118544=CARTESIAN_POINT('Ctrl Pts',(-174.691285628291,-2.30848925072723,
135.149343747116));
#118545=CARTESIAN_POINT('Ctrl Pts',(-174.699031961556,-2.18559982659186,
135.210303928652));
#118546=CARTESIAN_POINT('Ctrl Pts',(-174.706780029559,-2.06268288222183,
135.271277761798));
#118547=CARTESIAN_POINT('Ctrl Pts',(-174.714528097562,-1.93724529309587,
135.327087712354));
#118548=CARTESIAN_POINT('Ctrl Pts',(-174.722276165565,-1.80976372745136,
135.377536572338));
#118549=CARTESIAN_POINT('Ctrl Pts',(-174.730032468307,-1.68214667288201,
135.42803904997));
#118550=CARTESIAN_POINT('Ctrl Pts',(-174.737788771048,-1.55248166637986,
135.473168910906));
#118551=CARTESIAN_POINT('Ctrl Pts',(-174.74554507379,-1.42126327577423,
135.512777948627));
#118552=CARTESIAN_POINT('Ctrl Pts',(-174.753305516304,-1.28997484996227,
135.552408126885));
#118553=CARTESIAN_POINT('Ctrl Pts',(-174.761065958818,-1.15713176651945,
135.58651151335));
#118554=CARTESIAN_POINT('Ctrl Pts',(-174.768826401333,-1.02324008406824,
135.614990804231));
#118555=CARTESIAN_POINT('Ctrl Pts',(-174.776599301598,-0.889133466802005,
135.643515812598));
#118556=CARTESIAN_POINT('Ctrl Pts',(-174.784372201863,-0.753975272450605,
135.666398618665));
#118557=CARTESIAN_POINT('Ctrl Pts',(-174.792145102129,-0.618278896240742,
135.683593576645));
#118558=CARTESIAN_POINT('Ctrl Pts',(-174.799635437891,-0.487515425104283,
135.700163454591));
#118559=CARTESIAN_POINT('Ctrl Pts',(-174.807125773653,-0.356252528198735,
135.711451813691));
#118560=CARTESIAN_POINT('Ctrl Pts',(-174.814616109415,-0.224948809127052,
135.717463618295));
#118561=CARTESIAN_POINT('Ctrl Pts',(-174.822390443534,-0.0886666696388036,
135.723703362298));
#118562=CARTESIAN_POINT('Ctrl Pts',(-174.830164777653,0.0480911495213038,
135.724278297794));
#118563=CARTESIAN_POINT('Ctrl Pts',(-174.837939111772,0.184814385447683,
135.719136981291));
#118564=CARTESIAN_POINT('Ctrl Pts',(-174.845703864719,0.321369122205461,
135.714002001002));
#118565=CARTESIAN_POINT('Ctrl Pts',(-174.853468617666,0.45788897359358,
135.703164800257));
#118566=CARTESIAN_POINT('Ctrl Pts',(-174.861233370613,0.593860042067909,
135.686625800136));
#118567=CARTESIAN_POINT('Ctrl Pts',(-174.868990411498,0.729696062159804,
135.670103226783));
#118568=CARTESIAN_POINT('Ctrl Pts',(-174.876747452383,0.864983998436506,
135.647890170797));
#118569=CARTESIAN_POINT('Ctrl Pts',(-174.884504493268,0.999211803111557,
135.620039057311));
#118570=CARTESIAN_POINT('Ctrl Pts',(-174.892255684508,1.13333838555514,
135.592208946566));
#118571=CARTESIAN_POINT('Ctrl Pts',(-174.900006875749,1.2664060463982,135.558749320188));
#118572=CARTESIAN_POINT('Ctrl Pts',(-174.907758066989,1.39791005588486,
135.519764156836));
#118573=CARTESIAN_POINT('Ctrl Pts',(-174.915505963766,1.52935817265969,
135.480795563218));
#118574=CARTESIAN_POINT('Ctrl Pts',(-174.923253860543,1.65924358584838,
135.436306214505));
#118575=CARTESIAN_POINT('Ctrl Pts',(-174.93100175732,1.7870741398746,135.38645065172));
#118576=CARTESIAN_POINT('Ctrl Pts',(-174.938748033404,1.91487795450462,
135.336605517643));
#118577=CARTESIAN_POINT('Ctrl Pts',(-174.946494309488,2.04062740091991,
135.28139654417));
#118578=CARTESIAN_POINT('Ctrl Pts',(-174.954240585572,2.16384818838424,
135.221027242989));
#118579=CARTESIAN_POINT('Ctrl Pts',(-174.961986918838,2.28706988543627,
135.160657496176));
#118580=CARTESIAN_POINT('Ctrl Pts',(-174.969733252103,2.40776253519777,
135.095127517655));
#118581=CARTESIAN_POINT('Ctrl Pts',(-174.977479585368,2.52547479789236,
135.024687631876));
#118582=CARTESIAN_POINT('Ctrl Pts',(-174.985227653371,2.64321342143187,
134.954231971573));
#118583=CARTESIAN_POINT('Ctrl Pts',(-174.992975721374,2.75796999436092,
134.878864416774));
#118584=CARTESIAN_POINT('Ctrl Pts',(-175.000723789377,2.86932094919215,
134.798879406235));
#118585=CARTESIAN_POINT('Ctrl Pts',(-175.008480092119,2.98079024914342,
134.718809386675));
#118586=CARTESIAN_POINT('Ctrl Pts',(-175.016236394861,3.08884638255133,
134.634112336595));
#118587=CARTESIAN_POINT('Ctrl Pts',(-175.023992697603,3.19309733308253,
134.545124240673));
#118588=CARTESIAN_POINT('Ctrl Pts',(-175.031753140117,3.29740392548496,
134.456088649125));
#118589=CARTESIAN_POINT('Ctrl Pts',(-175.039513582631,3.39790100185022,
134.36275771412));
#118590=CARTESIAN_POINT('Ctrl Pts',(-175.047274025145,3.49423316069496,
134.265504602031));
#118591=CARTESIAN_POINT('Ctrl Pts',(-175.055046925411,3.59071996047304,
134.168095370613));
#118592=CARTESIAN_POINT('Ctrl Pts',(-175.062819825676,3.68302821876085,
134.066751669449));
#118593=CARTESIAN_POINT('Ctrl Pts',(-175.070592725941,3.77084202980583,
133.961880759822));
#118594=CARTESIAN_POINT('Ctrl Pts',(-175.078083061704,3.85546358763205,
133.86082217191));
#118595=CARTESIAN_POINT('Ctrl Pts',(-175.085573397466,3.93591160589967,
133.75648861301));
#118596=CARTESIAN_POINT('Ctrl Pts',(-175.093063733228,4.01194237480773,
133.649268602672));
#118597=CARTESIAN_POINT('Ctrl Pts',(-175.100838067347,4.09085587342609,
133.537983313057));
#118598=CARTESIAN_POINT('Ctrl Pts',(-175.108612401466,4.16526052469369,
133.423235853293));
#118599=CARTESIAN_POINT('Ctrl Pts',(-175.116386735585,4.23483723817989,
133.305427715551));
#118600=CARTESIAN_POINT('Ctrl Pts',(-175.124151488532,4.30432820458459,
133.187764765811));
#118601=CARTESIAN_POINT('Ctrl Pts',(-175.13191624148,4.36900287503006,133.067048976679));
#118602=CARTESIAN_POINT('Ctrl Pts',(-175.139680994427,4.42858382960782,
132.943712932318));
#118603=CARTESIAN_POINT('Ctrl Pts',(-175.147438035312,4.4881056075417,132.820499387055));
#118604=CARTESIAN_POINT('Ctrl Pts',(-175.155195076197,4.54254356858293,
132.694671115367));
#118605=CARTESIAN_POINT('Ctrl Pts',(-175.162952117082,4.59166504514604,
132.566687254624));
#118606=CARTESIAN_POINT('Ctrl Pts',(-175.170703308322,4.64074947882176,
132.438799907505));
#118607=CARTESIAN_POINT('Ctrl Pts',(-175.178454499562,4.68452526856802,
132.308760570411));
#118608=CARTESIAN_POINT('Ctrl Pts',(-175.186205690802,4.72280707581413,
132.177050089785));
#118609=CARTESIAN_POINT('Ctrl Pts',(-175.193953587579,4.7610726122708,132.045395589626));
#118610=CARTESIAN_POINT('Ctrl Pts',(-175.201701484356,4.79384870165117,
131.912071733273));
#118611=CARTESIAN_POINT('Ctrl Pts',(-175.209449381133,4.8209993415828,131.777576118346));
#118612=CARTESIAN_POINT('Ctrl Pts',(-175.217195657217,4.84814430218586,
131.643108637002));
#118613=CARTESIAN_POINT('Ctrl Pts',(-175.224941933301,4.86966607659167,
131.507470267607));
#118614=CARTESIAN_POINT('Ctrl Pts',(-175.232688209386,4.88547951922007,
131.371170047429));
#118615=CARTESIAN_POINT('Ctrl Pts',(-175.240434542651,4.90129307857973,
131.234868821113));
#118616=CARTESIAN_POINT('Ctrl Pts',(-175.248180875916,4.91139817702218,
131.097906122625));
#118617=CARTESIAN_POINT('Ctrl Pts',(-175.255927209182,4.91576145942318,
130.960796983382));
#118618=CARTESIAN_POINT('Ctrl Pts',(-175.263675277185,4.92012571895103,
130.823657139497));
#118619=CARTESIAN_POINT('Ctrl Pts',(-175.271423345188,4.91874559133168,
130.686371180292));
#118620=CARTESIAN_POINT('Ctrl Pts',(-175.279171413191,4.91163984765625,
130.54945461643));
#118621=CARTESIAN_POINT('Ctrl Pts',(-175.286927715933,4.90452655191191,
130.412392536015));
#118622=CARTESIAN_POINT('Ctrl Pts',(-175.294684018674,4.89167550445891,
130.275701026261));
#118623=CARTESIAN_POINT('Ctrl Pts',(-175.302440321416,4.87315748431916,
130.139891509538));
#118624=CARTESIAN_POINT('Ctrl Pts',(-175.310200763931,4.85462958055448,
130.004009507186));
#118625=CARTESIAN_POINT('Ctrl Pts',(-175.317961206445,4.83042874621755,
129.869010820509));
#118626=CARTESIAN_POINT('Ctrl Pts',(-175.325721648959,4.80067683356496,
129.735396164381));
#118627=CARTESIAN_POINT('Ctrl Pts',(-175.333494549224,4.77087716050093,
129.601567018145));
#118628=CARTESIAN_POINT('Ctrl Pts',(-175.34126744949,4.73550870286761,129.469126720205));
#118629=CARTESIAN_POINT('Ctrl Pts',(-175.349040349755,4.69474334634035,
129.338561185688));
#118630=CARTESIAN_POINT('Ctrl Pts',(-175.356530685517,4.65545991320492,
129.212742037227));
#118631=CARTESIAN_POINT('Ctrl Pts',(-175.364021021279,4.61116525414913,
129.088664003982));
#118632=CARTESIAN_POINT('Ctrl Pts',(-175.371511357041,4.56205451057522,
128.966742130219));
#118633=CARTESIAN_POINT('Ctrl Pts',(-175.37928569116,4.51108171823132,128.840197551553));
#118634=CARTESIAN_POINT('Ctrl Pts',(-175.387060025279,4.45475896195995,
128.715575006328));
#118635=CARTESIAN_POINT('Ctrl Pts',(-175.394834359398,4.39325155232275,
128.593359970684));
#118636=CARTESIAN_POINT('Ctrl Pts',(-175.402599112345,4.33181994507102,
128.471295554149));
#118637=CARTESIAN_POINT('Ctrl Pts',(-175.410363865292,4.26521657196787,
128.351633089548));
#118638=CARTESIAN_POINT('Ctrl Pts',(-175.41812861824,4.19365542608364,128.234839800414));
#118639=CARTESIAN_POINT('Ctrl Pts',(-175.425885659125,4.12216535573814,
128.11816251202));
#118640=CARTESIAN_POINT('Ctrl Pts',(-175.43364270001,4.0457275147886,128.004349059259));
#118641=CARTESIAN_POINT('Ctrl Pts',(-175.441399740895,3.96460242599515,
127.893843366923));
#118642=CARTESIAN_POINT('Ctrl Pts',(-175.449150932135,3.88353851426233,
127.783421007788));
#118643=CARTESIAN_POINT('Ctrl Pts',(-175.456902123375,3.79779462070068,
127.676301757994));
#118644=CARTESIAN_POINT('Ctrl Pts',(-175.464653314615,3.70767511501683,
127.572901457375));
#118645=CARTESIAN_POINT('Ctrl Pts',(-175.472401211392,3.61759391252703,
127.469545104642));
#118646=CARTESIAN_POINT('Ctrl Pts',(-175.480149108169,3.52314105315951,
127.369904851404));
#118647=CARTESIAN_POINT('Ctrl Pts',(-175.487897004946,3.4246616672819,127.274364083977));
#118648=CARTESIAN_POINT('Ctrl Pts',(-175.495643281031,3.32620288116857,
127.178843301619));
#118649=CARTESIAN_POINT('Ctrl Pts',(-175.503389557114,3.22371952428284,
127.087420571474));
#118650=CARTESIAN_POINT('Ctrl Pts',(-175.511135833199,3.11759384082915,
127.000442676006));
#118651=CARTESIAN_POINT('Ctrl Pts',(-175.518882166464,3.01146737397992,
126.913464138487));
#118652=CARTESIAN_POINT('Ctrl Pts',(-175.526628499729,2.90169882929591,
126.830930748944));
#118653=CARTESIAN_POINT('Ctrl Pts',(-175.534374832995,2.78870348803471,
126.753148957047));
#118654=CARTESIAN_POINT('Ctrl Pts',(-175.542122900998,2.67568284225044,
126.675349746458));
#118655=CARTESIAN_POINT('Ctrl Pts',(-175.549870969001,2.5594342839417,126.602304472565));
#118656=CARTESIAN_POINT('Ctrl Pts',(-175.557619037004,2.44040167306233,
126.534275988824));
#118657=CARTESIAN_POINT('Ctrl Pts',(-175.565375339746,2.32124255290746,
126.466175203601));
#118658=CARTESIAN_POINT('Ctrl Pts',(-175.573131642488,2.19929380939415,
126.403102053886));
#118659=CARTESIAN_POINT('Ctrl Pts',(-175.580887945229,2.07502397443618,
126.345273427567));
#118660=CARTESIAN_POINT('Ctrl Pts',(-175.588648387744,1.95068781292527,
126.287413936368));
#118661=CARTESIAN_POINT('Ctrl Pts',(-175.596408830258,1.82402845236486,
126.234804696024));
#118662=CARTESIAN_POINT('Ctrl Pts',(-175.604169272772,1.69553302248052,
126.187613837399));
#118663=CARTESIAN_POINT('Ctrl Pts',(-175.611942173037,1.56683132032519,
126.14034722382));
#118664=CARTESIAN_POINT('Ctrl Pts',(-175.619715073303,1.43628803149051,
126.098516492843));
#118665=CARTESIAN_POINT('Ctrl Pts',(-175.627487973568,1.30440487854117,
126.062239681177));
#118666=CARTESIAN_POINT('Ctrl Pts',(-175.63497830933,1.17731601039659,126.027281622992));
#118667=CARTESIAN_POINT('Ctrl Pts',(-175.642468645092,1.04898330177843,
125.997480766402));
#118668=CARTESIAN_POINT('Ctrl Pts',(-175.649958980854,0.91986141987662,
125.972897274983));
#118669=CARTESIAN_POINT('Ctrl Pts',(-175.657733314973,0.785843842575069,
125.947381693015));
#118670=CARTESIAN_POINT('Ctrl Pts',(-175.665507649092,0.650551540258417,
125.92740609324));
#118671=CARTESIAN_POINT('Ctrl Pts',(-175.673281983211,0.514482312150306,
125.913093806914));
#118672=CARTESIAN_POINT('Ctrl Pts',(-175.681046736158,0.378580777205721,
125.898799159202));
#118673=CARTESIAN_POINT('Ctrl Pts',(-175.688811489106,0.241904606680187,
125.890153978265));
#118674=CARTESIAN_POINT('Ctrl Pts',(-175.696576242053,0.10496255744539,
125.887230771402));
#118675=CARTESIAN_POINT('Ctrl Pts',(-175.704333282938,-0.0318434790163065,
125.88431046791));
#118676=CARTESIAN_POINT('Ctrl Pts',(-175.712090323823,-0.168914480320329,
125.887100837067));
#118677=CARTESIAN_POINT('Ctrl Pts',(-175.719847364708,-0.305736141050252,
125.895622645892));
#118678=CARTESIAN_POINT('Ctrl Pts',(-175.727598555948,-0.442454623501687,
125.904138028354));
#118679=CARTESIAN_POINT('Ctrl Pts',(-175.735349747188,-0.578923751010477,
125.918376223353));
#118680=CARTESIAN_POINT('Ctrl Pts',(-175.743100938428,-0.71462914648377,
125.938305927625));
#118681=CARTESIAN_POINT('Ctrl Pts',(-175.750848835205,-0.850276863543373,
125.958227161241));
#118682=CARTESIAN_POINT('Ctrl Pts',(-175.758596731982,-0.985161108178815,
125.983835036147));
#118683=CARTESIAN_POINT('Ctrl Pts',(-175.766344628759,-1.11877277522967,
126.01504641406));
#118684=CARTESIAN_POINT('Ctrl Pts',(-175.774090904844,-1.25235649360048,
126.046251263226));
#118685=CARTESIAN_POINT('Ctrl Pts',(-175.781837180928,-1.38466778339019,
126.083057195085));
#118686=CARTESIAN_POINT('Ctrl Pts',(-175.789583457012,-1.51520827435996,
126.125330061157));
#118687=CARTESIAN_POINT('Ctrl Pts',(-175.797329790277,-1.6457497289498,
126.167603239277));
#118688=CARTESIAN_POINT('Ctrl Pts',(-175.805076123543,-1.7745199866872,
126.215343311688));
#118689=CARTESIAN_POINT('Ctrl Pts',(-175.812822456808,-1.90103675312087,
126.26836653404));
#118690=CARTESIAN_POINT('Ctrl Pts',(-175.820570524811,-2.02758185210666,
126.321401630574));
#118691=CARTESIAN_POINT('Ctrl Pts',(-175.828318592814,-2.15187209507656,
126.379722080241));
#118692=CARTESIAN_POINT('Ctrl Pts',(-175.836066660817,-2.27344641882782,
126.443096529802));
#118693=CARTESIAN_POINT('Ctrl Pts',(-175.843822963559,-2.39514995321728,
126.506538334483));
#118694=CARTESIAN_POINT('Ctrl Pts',(-175.8515792663,-2.51413145502923,126.5750446881));
#118695=CARTESIAN_POINT('Ctrl Pts',(-175.859335569042,-2.62995519739772,
126.648338634686));
#118696=CARTESIAN_POINT('Ctrl Pts',(-175.867096011556,-2.7458407583849,
126.721671700458));
#118697=CARTESIAN_POINT('Ctrl Pts',(-175.874856454071,-2.85856488046691,
126.799797228219));
#118698=CARTESIAN_POINT('Ctrl Pts',(-175.882616896585,-2.96772280486939,
126.882396260773));
#118699=CARTESIAN_POINT('Ctrl Pts',(-175.89038979685,-3.07705595926301,
126.965127888626));
#118700=CARTESIAN_POINT('Ctrl Pts',(-175.898162697116,-3.18281117425422,
127.052347122836));
#118701=CARTESIAN_POINT('Ctrl Pts',(-175.905935597381,-3.28461794891542,
127.143695651721));
#118702=CARTESIAN_POINT('Ctrl Pts',(-175.913425933143,-3.3827237908819,
127.231723431489));
#118703=CARTESIAN_POINT('Ctrl Pts',(-175.920916268905,-3.47716305924487,
127.323585282909));
#118704=CARTESIAN_POINT('Ctrl Pts',(-175.928406604667,-3.56763937796251,
127.418931201478));
#118705=CARTESIAN_POINT('Ctrl Pts',(-175.936084722842,-3.66038393431042,
127.516667438349));
#118706=CARTESIAN_POINT('Ctrl Pts',(-175.943762841017,-3.74927406527692,
127.618391590541));
#118707=CARTESIAN_POINT('Ctrl Pts',(-175.951440959192,-3.83394075869912,
127.723763058441));
#118708=CARTESIAN_POINT('Ctrl Pts',(-175.959110001431,-3.91850737167146,
127.829009971768));
#118709=CARTESIAN_POINT('Ctrl Pts',(-175.966779043669,-3.99886022424331,
127.937895319341));
#118710=CARTESIAN_POINT('Ctrl Pts',(-175.974448085908,-4.07466664012404,
128.050041312482));
#118711=CARTESIAN_POINT('Ctrl Pts',(-175.982397140053,-4.15324089824724,
128.166281977736));
#118712=CARTESIAN_POINT('Ctrl Pts',(-175.990346194199,-4.22693008600737,
128.286025634363));
#118713=CARTESIAN_POINT('Ctrl Pts',(-175.998295248344,-4.29540845154183,
128.408812810295));
#118714=CARTESIAN_POINT('Ctrl Pts',(-176.005950776368,-4.36135819056651,
128.527065957038));
#118715=CARTESIAN_POINT('Ctrl Pts',(-176.013606304392,-4.42247486355655,
128.648141468741));
#118716=CARTESIAN_POINT('Ctrl Pts',(-176.021261832416,-4.47851132733826,
128.771599108337));
#118717=CARTESIAN_POINT('Ctrl Pts',(-176.02891400081,-4.53452319950553,
128.89500256852));
#118718=CARTESIAN_POINT('Ctrl Pts',(-176.036566169204,-4.58545913263066,
129.020785711845));
#118719=CARTESIAN_POINT('Ctrl Pts',(-176.044218337598,-4.63111848361476,
129.14848482113));
#118720=CARTESIAN_POINT('Ctrl Pts',(-176.051869221783,-4.67677017191847,
129.276162499593));
#118721=CARTESIAN_POINT('Ctrl Pts',(-176.059520105969,-4.71714690477684,
129.405755126607));
#118722=CARTESIAN_POINT('Ctrl Pts',(-176.067170990154,-4.75209680438599,
129.53678063025));
#118723=CARTESIAN_POINT('Ctrl Pts',(-176.068059571987,-4.75615592292799,
129.551998071709));
#118724=CARTESIAN_POINT('Ctrl Pts',(-176.06894815382,-4.76014189558664,
129.567234823998));
#118725=CARTESIAN_POINT('Ctrl Pts',(-176.069836735653,-4.76405452823418,
129.582490119309));
#118726=CARTESIAN_POINT('Origin',(213.235140564004,0.,130.804360617566));
#118727=CARTESIAN_POINT('',(-178.165366640417,-4.76405452823403,129.582490119308));
#118728=CARTESIAN_POINT('',(-177.819765072025,-4.76405452823413,129.582490119309));
#118729=CARTESIAN_POINT('',(213.235140564004,-4.76405452823405,129.582490119308));
#118730=CARTESIAN_POINT('',(-176.485140564046,-4.91824957167407,130.802308002684));
#118731=CARTESIAN_POINT('Ctrl Pts',(-176.485140564046,-4.91824957167407,
130.802308002684));
#118732=CARTESIAN_POINT('Ctrl Pts',(-176.492835531866,-4.91830597039888,
130.937444411655));
#118733=CARTESIAN_POINT('Ctrl Pts',(-176.500530499686,-4.91278854347934,
131.072808430149));
#118734=CARTESIAN_POINT('Ctrl Pts',(-176.508225467506,-4.9016672619306,
131.207896385272));
#118735=CARTESIAN_POINT('Ctrl Pts',(-176.515911379896,-4.89055906789569,
131.342825369014));
#118736=CARTESIAN_POINT('Ctrl Pts',(-176.523597292285,-4.87386016830611,
131.477478541179));
#118737=CARTESIAN_POINT('Ctrl Pts',(-176.531283204674,-4.85159252065345,
131.611350751359));
#118738=CARTESIAN_POINT('Ctrl Pts',(-176.538962001415,-4.82934548847746,
131.745099022115));
#118739=CARTESIAN_POINT('Ctrl Pts',(-176.546640798155,-4.80154002977729,
131.878067377553));
#118740=CARTESIAN_POINT('Ctrl Pts',(-176.554319594896,-4.76824998833037,
132.009754790145));
#118741=CARTESIAN_POINT('Ctrl Pts',(-176.562229631773,-4.73395744688536,
132.145407852077));
#118742=CARTESIAN_POINT('Ctrl Pts',(-176.57013966865,-4.69384480792713,
132.279701173914));
#118743=CARTESIAN_POINT('Ctrl Pts',(-176.578049705527,-4.64804985722182,
132.412096785997));
#118744=CARTESIAN_POINT('Ctrl Pts',(-176.585720891864,-4.60363772544528,
132.540494595797));
#118745=CARTESIAN_POINT('Ctrl Pts',(-176.593392078201,-4.55388164059911,
132.667107245745));
#118746=CARTESIAN_POINT('Ctrl Pts',(-176.601063264538,-4.49895804444373,
132.791458898184));
#118747=CARTESIAN_POINT('Ctrl Pts',(-176.608733614919,-4.44404043350099,
132.915796999597));
#118748=CARTESIAN_POINT('Ctrl Pts',(-176.6164039653,-4.3839565923831,133.037874228065));
#118749=CARTESIAN_POINT('Ctrl Pts',(-176.624074315681,-4.31893089974082,
133.157235230835));
#118750=CARTESIAN_POINT('Ctrl Pts',(-176.631745571775,-4.25389752888149,
133.27661032772));
#118751=CARTESIAN_POINT('Ctrl Pts',(-176.63941682787,-4.1839213372524,133.393268210303));
#118752=CARTESIAN_POINT('Ctrl Pts',(-176.647088083964,-4.10927214498694,
133.506779071643));
#118753=CARTESIAN_POINT('Ctrl Pts',(-176.654761987838,-4.03459718710628,
133.620329111935));
#118754=CARTESIAN_POINT('Ctrl Pts',(-176.662435891712,-3.95524624017119,
133.730729637202));
#118755=CARTESIAN_POINT('Ctrl Pts',(-176.670109795586,-3.87153152354035,
133.83758113786));
#118756=CARTESIAN_POINT('Ctrl Pts',(-176.677792143222,-3.78772469380698,
133.944550209522));
#118757=CARTESIAN_POINT('Ctrl Pts',(-176.685474490857,-3.6995447577288,
134.047962148294));
#118758=CARTESIAN_POINT('Ctrl Pts',(-176.693156838493,-3.60734334901101,
134.14745155633));
#118759=CARTESIAN_POINT('Ctrl Pts',(-176.700844268316,-3.51508094528171,
134.247006780688));
#118760=CARTESIAN_POINT('Ctrl Pts',(-176.70853169814,-3.41879205509594,
134.342634027913));
#118761=CARTESIAN_POINT('Ctrl Pts',(-176.716219127963,-3.31886305635952,
134.434006753986));
#118762=CARTESIAN_POINT('Ctrl Pts',(-176.723917236586,-3.21879524377401,
134.525506408178));
#118763=CARTESIAN_POINT('Ctrl Pts',(-176.731615345209,-3.11507753719144,
134.612739493057));
#118764=CARTESIAN_POINT('Ctrl Pts',(-176.739313453832,-3.00812722510926,
134.695421354699));
#118765=CARTESIAN_POINT('Ctrl Pts',(-176.740929129203,-2.98568054454804,
134.71277458444));
#118766=CARTESIAN_POINT('Ctrl Pts',(-176.742544804574,-2.96309156194695,
134.729927493467));
#118767=CARTESIAN_POINT('Ctrl Pts',(-176.744160479945,-2.94036427676275,
134.746877704712));
#118768=CARTESIAN_POINT('Ctrl Pts',(-176.751934814064,-2.83100474094054,
134.828439018296));
#118769=CARTESIAN_POINT('Ctrl Pts',(-176.759709148183,-2.71807583208517,
134.905575865503));
#118770=CARTESIAN_POINT('Ctrl Pts',(-176.767483482302,-2.6019712694565,
134.977959613088));
#118771=CARTESIAN_POINT('Ctrl Pts',(-176.77524823525,-2.48600979532471,
135.050254154173));
#118772=CARTESIAN_POINT('Ctrl Pts',(-176.783012988197,-2.36688078312081,
135.117807046001));
#118773=CARTESIAN_POINT('Ctrl Pts',(-176.790777741144,-2.24501003512077,
135.180330567726));
#118774=CARTESIAN_POINT('Ctrl Pts',(-176.798534782029,-2.12326033086506,
135.242791990209));
#118775=CARTESIAN_POINT('Ctrl Pts',(-176.806291822914,-1.99877465557294,
135.300233806037));
#118776=CARTESIAN_POINT('Ctrl Pts',(-176.814048863799,-1.87200643101424,
135.352412396596));
#118777=CARTESIAN_POINT('Ctrl Pts',(-176.821800055039,-1.7453338033603,
135.404551638875));
#118778=CARTESIAN_POINT('Ctrl Pts',(-176.829551246279,-1.61638241263376,
135.451435407808));
#118779=CARTESIAN_POINT('Ctrl Pts',(-176.837302437519,-1.48562851919162,
135.492866879209));
#118780=CARTESIAN_POINT('Ctrl Pts',(-176.845050334296,-1.354930199642,135.534280741129));
#118781=CARTESIAN_POINT('Ctrl Pts',(-176.852798231074,-1.22243127303657,
135.570246796745));
#118782=CARTESIAN_POINT('Ctrl Pts',(-176.860546127851,-1.08862593001943,
135.600617141876));
#118783=CARTESIAN_POINT('Ctrl Pts',(-176.868292403935,-0.954848576195554,
135.630981134187));
#118784=CARTESIAN_POINT('Ctrl Pts',(-176.876038680019,-0.819765730543298,
135.655751657723));
#118785=CARTESIAN_POINT('Ctrl Pts',(-176.883784956103,-0.683884240481451,
135.674831375934));
#118786=CARTESIAN_POINT('Ctrl Pts',(-176.891531289368,-0.548001747373497,
135.693911234988));
#118787=CARTESIAN_POINT('Ctrl Pts',(-176.899277622634,-0.411320985259188,
135.707300150528));
#118788=CARTESIAN_POINT('Ctrl Pts',(-176.907023955899,-0.274356036807478,
135.714952417702));
#118789=CARTESIAN_POINT('Ctrl Pts',(-176.914772023902,-0.137360416005398,
135.722606398549));
#118790=CARTESIAN_POINT('Ctrl Pts',(-176.922520091905,-8.08725082983852E-5,
135.724521152855));
#118791=CARTESIAN_POINT('Ctrl Pts',(-176.930268159908,0.13696678102096,
135.720703075471));
#118792=CARTESIAN_POINT('Ctrl Pts',(-176.93802446265,0.274160090427464,
135.716880940189));
#118793=CARTESIAN_POINT('Ctrl Pts',(-176.945780765392,0.411120626108149,
135.707313812855));
#118794=CARTESIAN_POINT('Ctrl Pts',(-176.953537068133,0.547335414469305,
135.692060179381));
#118795=CARTESIAN_POINT('Ctrl Pts',(-176.961297510648,0.683622904764729,
135.676798404584));
#118796=CARTESIAN_POINT('Ctrl Pts',(-176.969057953162,0.819163468450381,
135.655844135738));
#118797=CARTESIAN_POINT('Ctrl Pts',(-176.976818395676,0.953453610727624,
135.629307174233));
#118798=CARTESIAN_POINT('Ctrl Pts',(-176.984591295941,1.0879593274626,135.602727613241));
#118799=CARTESIAN_POINT('Ctrl Pts',(-176.992364196207,1.22121023133064,
135.570547542823));
#118800=CARTESIAN_POINT('Ctrl Pts',(-177.000137096472,1.3527164223535,135.532927138531));
#118801=CARTESIAN_POINT('Ctrl Pts',(-177.007627432234,1.47944203209141,
135.496674330695));
#118802=CARTESIAN_POINT('Ctrl Pts',(-177.015117767997,1.60454728361578,
135.455369958083));
#118803=CARTESIAN_POINT('Ctrl Pts',(-177.022608103759,1.72761256932774,
135.409199145984));
#118804=CARTESIAN_POINT('Ctrl Pts',(-177.030382437878,1.85534391274966,
135.361277753511));
#118805=CARTESIAN_POINT('Ctrl Pts',(-177.038156771997,1.98128216061258,
135.307961814266));
#118806=CARTESIAN_POINT('Ctrl Pts',(-177.045931106116,2.1049380095826,135.249404941115));
#118807=CARTESIAN_POINT('Ctrl Pts',(-177.053695859063,2.22844146377053,
135.190920234077));
#118808=CARTESIAN_POINT('Ctrl Pts',(-177.06146061201,2.34966776584726,135.127207610304));
#118809=CARTESIAN_POINT('Ctrl Pts',(-177.069225364957,2.46814469158579,
135.058469789167));
#118810=CARTESIAN_POINT('Ctrl Pts',(-177.076982405842,2.58650394437144,
134.989800239402));
#118811=CARTESIAN_POINT('Ctrl Pts',(-177.084739446727,2.70211891909105,
134.916115619711));
#118812=CARTESIAN_POINT('Ctrl Pts',(-177.092496487612,2.81453956696313,
134.837665724857));
#118813=CARTESIAN_POINT('Ctrl Pts',(-177.100247678852,2.92687543754998,
134.759274989679));
#118814=CARTESIAN_POINT('Ctrl Pts',(-177.107998870092,3.03602145667123,
134.676126354876));
#118815=CARTESIAN_POINT('Ctrl Pts',(-177.115750061333,3.14155460020808,
134.588514123492));
#118816=CARTESIAN_POINT('Ctrl Pts',(-177.12349795811,3.24704288934388,134.500939129644));
#118817=CARTESIAN_POINT('Ctrl Pts',(-177.131245854887,3.34892105684096,
134.408904561705));
#118818=CARTESIAN_POINT('Ctrl Pts',(-177.138993751664,3.44679754461108,
134.312746250441));
#118819=CARTESIAN_POINT('Ctrl Pts',(-177.146740027748,3.54465355872992,
134.216608053422));
#118820=CARTESIAN_POINT('Ctrl Pts',(-177.154486303832,3.63850927937571,
134.116348102655));
#118821=CARTESIAN_POINT('Ctrl Pts',(-177.162232579916,3.7280088511409,134.012340210443));
#118822=CARTESIAN_POINT('Ctrl Pts',(-177.169978913182,3.81750908357147,
133.908331550469));
#118823=CARTESIAN_POINT('Ctrl Pts',(-177.177725246447,3.90265284794519,
133.800575190193));
#118824=CARTESIAN_POINT('Ctrl Pts',(-177.185471579712,3.9831238172353,133.689478937336));
#118825=CARTESIAN_POINT('Ctrl Pts',(-177.193219647715,4.06361280744114,
133.578357805243));
#118826=CARTESIAN_POINT('Ctrl Pts',(-177.200967715718,4.13942669096672,
133.463895608813));
#118827=CARTESIAN_POINT('Ctrl Pts',(-177.208715783721,4.2102920386376,133.346529772419));
#118828=CARTESIAN_POINT('Ctrl Pts',(-177.216472086463,4.2812327028432,133.229039198217));
#118829=CARTESIAN_POINT('Ctrl Pts',(-177.224228389205,4.34721412264418,
133.108639154611));
#118830=CARTESIAN_POINT('Ctrl Pts',(-177.231984691947,4.40800822913771,
132.985792833876));
#118831=CARTESIAN_POINT('Ctrl Pts',(-177.239745134461,4.46883478327634,
132.862880946361));
#118832=CARTESIAN_POINT('Ctrl Pts',(-177.247505576975,4.52446834887442,
132.737520537276));
#118833=CARTESIAN_POINT('Ctrl Pts',(-177.255266019489,4.57472915371374,
132.610194561389));
#118834=CARTESIAN_POINT('Ctrl Pts',(-177.263038919755,4.62507064165893,
132.482664190541));
#118835=CARTESIAN_POINT('Ctrl Pts',(-177.27081182002,4.6700220054038,132.353162317152));
#118836=CARTESIAN_POINT('Ctrl Pts',(-177.278584720286,4.70945320227301,
132.222187686746));
#118837=CARTESIAN_POINT('Ctrl Pts',(-177.286075056047,4.74745097581429,
132.095974314063));
#118838=CARTESIAN_POINT('Ctrl Pts',(-177.293565391809,4.78032288164842,
131.968393700483));
#118839=CARTESIAN_POINT('Ctrl Pts',(-177.301055727571,4.80799786276686,
131.839898938503));
#118840=CARTESIAN_POINT('Ctrl Pts',(-177.30883006169,4.83672214920632,131.706532258567));
#118841=CARTESIAN_POINT('Ctrl Pts',(-177.316604395809,4.8599386387158,131.571758276407));
#118842=CARTESIAN_POINT('Ctrl Pts',(-177.324378729928,4.8775120897474,131.436071688284));
#118843=CARTESIAN_POINT('Ctrl Pts',(-177.332143482875,4.89506388307123,
131.300552321754));
#118844=CARTESIAN_POINT('Ctrl Pts',(-177.339908235822,4.9069864256457,131.164122971094));
#118845=CARTESIAN_POINT('Ctrl Pts',(-177.34767298877,4.91319502228795,131.02729050669));
#118846=CARTESIAN_POINT('Ctrl Pts',(-177.355430029654,4.91939745246448,
130.890593946219));
#118847=CARTESIAN_POINT('Ctrl Pts',(-177.363187070539,4.91989721294986,
130.753495456812));
#118848=CARTESIAN_POINT('Ctrl Pts',(-177.370944111424,4.91466120079501,
130.616508697426));
#118849=CARTESIAN_POINT('Ctrl Pts',(-177.378695302665,4.90942913715766,
130.479625240822));
#118850=CARTESIAN_POINT('Ctrl Pts',(-177.386446493905,4.89846992518054,
130.34285373563));
#118851=CARTESIAN_POINT('Ctrl Pts',(-177.394197685145,4.88180251548238,
130.206709162009));
#118852=CARTESIAN_POINT('Ctrl Pts',(-177.401945581922,4.8651421898779,130.070622453462));
#118853=CARTESIAN_POINT('Ctrl Pts',(-177.409693478699,4.84277853936195,
129.935162533768));
#118854=CARTESIAN_POINT('Ctrl Pts',(-177.417441375476,4.81478246115655,
129.800840356565));
#118855=CARTESIAN_POINT('Ctrl Pts',(-177.42518765156,4.7867922391272,129.666546276666));
#118856=CARTESIAN_POINT('Ctrl Pts',(-177.432933927644,4.75317201259992,
129.53338984838));
#118857=CARTESIAN_POINT('Ctrl Pts',(-177.440680203728,4.71404393191347,
129.40187251762));
#118858=CARTESIAN_POINT('Ctrl Pts',(-177.448426536994,4.67491556239246,
129.270354216029));
#118859=CARTESIAN_POINT('Ctrl Pts',(-177.456172870259,4.63027936907037,
129.140475410841));
#118860=CARTESIAN_POINT('Ctrl Pts',(-177.463919203524,4.58030746964681,
129.012722666975));
#118861=CARTESIAN_POINT('Ctrl Pts',(-177.471667271527,4.53032437936306,
128.884941313769));
#118862=CARTESIAN_POINT('Ctrl Pts',(-177.47941533953,4.47500334767135,128.759287333333));
#118863=CARTESIAN_POINT('Ctrl Pts',(-177.487163407533,4.41456459693924,
128.636227207937));
#118864=CARTESIAN_POINT('Ctrl Pts',(-177.494919710275,4.35406161118338,
128.513036292774));
#118865=CARTESIAN_POINT('Ctrl Pts',(-177.502676013017,4.28843021367941,
128.392445091101));
#118866=CARTESIAN_POINT('Ctrl Pts',(-177.510432315759,4.2179368243953,128.274895850484));
#118867=CARTESIAN_POINT('Ctrl Pts',(-177.518192758273,4.14740581066662,
128.157283870298));
#118868=CARTESIAN_POINT('Ctrl Pts',(-177.525953200787,4.07200784924379,
128.042717412727));
#118869=CARTESIAN_POINT('Ctrl Pts',(-177.533713643301,3.99205209237518,
127.931608774078));
#118870=CARTESIAN_POINT('Ctrl Pts',(-177.541486543566,3.91196798342773,
127.820321773979));
#118871=CARTESIAN_POINT('Ctrl Pts',(-177.549259443832,3.82731169976449,
127.712503992746));
#118872=CARTESIAN_POINT('Ctrl Pts',(-177.557032344097,3.73843255887875,
127.608534423103));
#118873=CARTESIAN_POINT('Ctrl Pts',(-177.56452267986,3.65278439863484,127.508344409197));
#118874=CARTESIAN_POINT('Ctrl Pts',(-177.572013015622,3.56321528320005,
127.411727905865));
#118875=CARTESIAN_POINT('Ctrl Pts',(-177.579503351384,3.4700680040757,127.318989602941));
#118876=CARTESIAN_POINT('Ctrl Pts',(-177.587277685503,3.37338901755469,
127.222735099077));
#118877=CARTESIAN_POINT('Ctrl Pts',(-177.595052019622,3.27254892904052,
127.130353779533));
#118878=CARTESIAN_POINT('Ctrl Pts',(-177.602826353741,3.16789083914688,
127.042226822265));
#118879=CARTESIAN_POINT('Ctrl Pts',(-177.610591106688,3.06336173099519,
126.954208473595));
#118880=CARTESIAN_POINT('Ctrl Pts',(-177.618355859635,2.95502427989044,
126.870434304359));
#118881=CARTESIAN_POINT('Ctrl Pts',(-177.626120612582,2.84325915042936,
126.791249546838));
#118882=CARTESIAN_POINT('Ctrl Pts',(-177.633877653467,2.73160502767108,
126.712143436735));
#118883=CARTESIAN_POINT('Ctrl Pts',(-177.641634694352,2.61653031845178,
126.637617891744));
#118884=CARTESIAN_POINT('Ctrl Pts',(-177.649391735237,2.49844928564784,
126.567978407526));
#118885=CARTESIAN_POINT('Ctrl Pts',(-177.657142926478,2.38045729866815,
126.498391438984));
#118886=CARTESIAN_POINT('Ctrl Pts',(-177.664894117718,2.25946383601194,
126.433683395015));
#118887=CARTESIAN_POINT('Ctrl Pts',(-177.672645308958,2.13591240834263,
126.374116691281));
#118888=CARTESIAN_POINT('Ctrl Pts',(-177.680393205735,2.01241349332643,
126.314575304985));
#118889=CARTESIAN_POINT('Ctrl Pts',(-177.688141102512,1.88635912709672,
126.260171082148));
#118890=CARTESIAN_POINT('Ctrl Pts',(-177.695888999289,1.75821751110227,
126.211120557853));
#118891=CARTESIAN_POINT('Ctrl Pts',(-177.703635275373,1.63010269957183,
126.16208029387));
#118892=CARTESIAN_POINT('Ctrl Pts',(-177.711381551457,1.49990187161117,
126.118391640607));
#118893=CARTESIAN_POINT('Ctrl Pts',(-177.719127827541,1.36810293311139,
126.080222873288));
#118894=CARTESIAN_POINT('Ctrl Pts',(-177.726874160807,1.23630302170124,
126.042053824216));
#118895=CARTESIAN_POINT('Ctrl Pts',(-177.734620494072,1.10290535174681,
126.00940485115));
#118896=CARTESIAN_POINT('Ctrl Pts',(-177.742366827337,0.968412317916519,
125.982394146819));
#118897=CARTESIAN_POINT('Ctrl Pts',(-177.75011489534,0.833889165303631,
125.955377393628));
#118898=CARTESIAN_POINT('Ctrl Pts',(-177.757862963343,0.698270543936001,
125.934001498669));
#118899=CARTESIAN_POINT('Ctrl Pts',(-177.765611031346,0.562067954125812,
125.918333327687));
#118900=CARTESIAN_POINT('Ctrl Pts',(-177.773367334088,0.425720606582898,
125.902648504386));
#118901=CARTESIAN_POINT('Ctrl Pts',(-177.78112363683,0.288788439808046,
125.892683567776));
#118902=CARTESIAN_POINT('Ctrl Pts',(-177.788879939572,0.151787535704795,
125.888453416804));
#118903=CARTESIAN_POINT('Ctrl Pts',(-177.796640382086,0.0147135100936332,
125.884221008073));
#118904=CARTESIAN_POINT('Ctrl Pts',(-177.8044008246,-0.122428935197982,
125.885729479641));
#118905=CARTESIAN_POINT('Ctrl Pts',(-177.812161267115,-0.259125819268372,
125.892941589191));
#118906=CARTESIAN_POINT('Ctrl Pts',(-177.81993416738,-0.396042141312451,
125.900165276259));
#118907=CARTESIAN_POINT('Ctrl Pts',(-177.827707067645,-0.532511083387111,
125.913110860943));
#118908=CARTESIAN_POINT('Ctrl Pts',(-177.835479967911,-0.668024973541733,
125.931689307368));
#118909=CARTESIAN_POINT('Ctrl Pts',(-177.842970303673,-0.798612592451449,
125.94959238047));
#118910=CARTESIAN_POINT('Ctrl Pts',(-177.850460639435,-0.928313087764289,
125.972725833973));
#118911=CARTESIAN_POINT('Ctrl Pts',(-177.857950975197,-1.05668482811248,
126.000965959979));
#118912=CARTESIAN_POINT('Ctrl Pts',(-177.865725309316,-1.18992382201241,
126.030276818945));
#118913=CARTESIAN_POINT('Ctrl Pts',(-177.873499643435,-1.32215337351811,
126.065182081599));
#118914=CARTESIAN_POINT('Ctrl Pts',(-177.881273977554,-1.45286733255685,
126.105599123673));
#118915=CARTESIAN_POINT('Ctrl Pts',(-177.889038730501,-1.58342019832367,
126.145966355356));
#118916=CARTESIAN_POINT('Ctrl Pts',(-177.896803483448,-1.71246081812129,
126.191831736476));
#118917=CARTESIAN_POINT('Ctrl Pts',(-177.904568236396,-1.83949297974126,
126.24306160961));
#118918=CARTESIAN_POINT('Ctrl Pts',(-177.912325277281,-1.96639897122747,
126.294240600511));
#118919=CARTESIAN_POINT('Ctrl Pts',(-177.920082318166,-2.09130011409183,
126.350773335007));
#118920=CARTESIAN_POINT('Ctrl Pts',(-177.927839359051,-2.21371546697803,
126.412476409875));
#118921=CARTESIAN_POINT('Ctrl Pts',(-177.935590550291,-2.33603850549387,
126.474132953975));
#118922=CARTESIAN_POINT('Ctrl Pts',(-177.943341741531,-2.45587913750643,
126.540951902473));
#118923=CARTESIAN_POINT('Ctrl Pts',(-177.951092932771,-2.5727768569406,
126.612701959363));
#118924=CARTESIAN_POINT('Ctrl Pts',(-177.958840829548,-2.68962489172614,
126.684421520565));
#118925=CARTESIAN_POINT('Ctrl Pts',(-177.966588726325,-2.80353216920274,
126.761067817579));
#118926=CARTESIAN_POINT('Ctrl Pts',(-177.974336623102,-2.9140634379534,
126.842363981767));
#118927=CARTESIAN_POINT('Ctrl Pts',(-177.982082899186,-3.02457158594541,
126.92364314055));
#118928=CARTESIAN_POINT('Ctrl Pts',(-177.989829175271,-3.13170481510814,
127.009570000349));
#118929=CARTESIAN_POINT('Ctrl Pts',(-177.997575451355,-3.23505782567653,
127.09982502899));
#118930=CARTESIAN_POINT('Ctrl Pts',(-178.00532178462,-3.33841159917322,
127.190080723872));
#118931=CARTESIAN_POINT('Ctrl Pts',(-178.013068117885,-3.43798480391004,
127.284664394185));
#118932=CARTESIAN_POINT('Ctrl Pts',(-178.020814451151,-3.53340644440668,
127.383217247123));
#118933=CARTESIAN_POINT('Ctrl Pts',(-178.028562519154,-3.62884945391797,
127.481792170289));
#118934=CARTESIAN_POINT('Ctrl Pts',(-178.036310587157,-3.72013877726179,
127.584337764003));
#118935=CARTESIAN_POINT('Ctrl Pts',(-178.04405865516,-3.80694167998,127.690459831136));
#118936=CARTESIAN_POINT('Ctrl Pts',(-178.051814957901,-3.89383683785631,
127.796694686064));
#118937=CARTESIAN_POINT('Ctrl Pts',(-178.059571260643,-3.97623580214425,
127.906513304447));
#118938=CARTESIAN_POINT('Ctrl Pts',(-178.067327563385,-4.05384708306206,
128.019489545209));
#118939=CARTESIAN_POINT('Ctrl Pts',(-178.075088005899,-4.13149978745754,
128.132526084793));
#118940=CARTESIAN_POINT('Ctrl Pts',(-178.082848448413,-4.2043595091759,
128.248723273822));
#118941=CARTESIAN_POINT('Ctrl Pts',(-178.090608890927,-4.2721797620015,
128.367628555224));
#118942=CARTESIAN_POINT('Ctrl Pts',(-178.098381791193,-4.34010888591755,
128.48672471394));
#118943=CARTESIAN_POINT('Ctrl Pts',(-178.106154691458,-4.40298219551518,
128.608537304644));
#118944=CARTESIAN_POINT('Ctrl Pts',(-178.113927591724,-4.46060019010785,
128.73259108248));
#118945=CARTESIAN_POINT('Ctrl Pts',(-178.121417927486,-4.51612362546549,
128.852135193018));
#118946=CARTESIAN_POINT('Ctrl Pts',(-178.128908263248,-4.56676708168597,
128.973760089716));
#118947=CARTESIAN_POINT('Ctrl Pts',(-178.13639859901,-4.61239592518718,
129.097027348454));
#118948=CARTESIAN_POINT('Ctrl Pts',(-178.145370171086,-4.66704800905346,
129.244671076535));
#118949=CARTESIAN_POINT('Ctrl Pts',(-178.154341743163,-4.71465032755617,
129.395057764512));
#118950=CARTESIAN_POINT('Ctrl Pts',(-178.163313315239,-4.75495695955518,
129.547552209225));
#118951=CARTESIAN_POINT('Ctrl Pts',(-178.163997756965,-4.75803195472055,
129.559186018774));
#118952=CARTESIAN_POINT('Ctrl Pts',(-178.164682198691,-4.7610645102698,
129.570832084646));
#118953=CARTESIAN_POINT('Ctrl Pts',(-178.165366640417,-4.76405452823403,
129.582490119308));
#118954=CARTESIAN_POINT('Ctrl Pts',(-176.415048843504,-4.76405452823412,
129.582490119309));
#118955=CARTESIAN_POINT('Ctrl Pts',(-176.422813628312,-4.79809583181618,
129.715216645326));
#118956=CARTESIAN_POINT('Ctrl Pts',(-176.430578413119,-4.82655219102321,
129.849233699315));
#118957=CARTESIAN_POINT('Ctrl Pts',(-176.438343197927,-4.84935493139779,
129.984031530048));
#118958=CARTESIAN_POINT('Ctrl Pts',(-176.446118737036,-4.87218925378811,
130.119016057079));
#118959=CARTESIAN_POINT('Ctrl Pts',(-176.453894276145,-4.88935428061385,
130.254783133149));
#118960=CARTESIAN_POINT('Ctrl Pts',(-176.461669815255,-4.90083326745112,
130.390819389701));
#118961=CARTESIAN_POINT('Ctrl Pts',(-176.463017495547,-4.90282284066517,
130.41439761102));
#118962=CARTESIAN_POINT('Ctrl Pts',(-176.464365175839,-4.90464172672215,
130.437983923485));
#118963=CARTESIAN_POINT('Ctrl Pts',(-176.465712856132,-4.90628999728232,
130.461575663014));
#118964=CARTESIAN_POINT('Ctrl Pts',(-176.472188758758,-4.9142103027958,
130.574939202458));
#118965=CARTESIAN_POINT('Ctrl Pts',(-176.478664661385,-4.91820210782924,
130.688580401629));
#118966=CARTESIAN_POINT('Ctrl Pts',(-176.485140564012,-4.91824957167382,
130.802308002086));
#118967=CARTESIAN_POINT('',(-176.139859436039,-4.91824789567076,130.808910258228));
#118968=CARTESIAN_POINT('Ctrl Pts',(-176.069836735653,-4.76405452823418,
129.582490119309));
#118969=CARTESIAN_POINT('Ctrl Pts',(-176.077489986718,-4.79775357413248,
129.713882187812));
#118970=CARTESIAN_POINT('Ctrl Pts',(-176.085143237783,-4.82600791653814,
129.846650616237));
#118971=CARTESIAN_POINT('Ctrl Pts',(-176.092796488848,-4.84872203235654,
129.980298899343));
#118972=CARTESIAN_POINT('Ctrl Pts',(-176.100640313373,-4.87200175194107,
130.117275155806));
#118973=CARTESIAN_POINT('Ctrl Pts',(-176.108484137897,-4.88946162133592,
130.255175223402));
#118974=CARTESIAN_POINT('Ctrl Pts',(-176.116327962421,-4.90105518591459,
130.393457798009));
#118975=CARTESIAN_POINT('Ctrl Pts',(-176.124171786946,-4.91264875049327,
130.531740372616));
#118976=CARTESIAN_POINT('Ctrl Pts',(-176.13201561147,-4.91837602037099,
130.670405001707));
#118977=CARTESIAN_POINT('Ctrl Pts',(-176.139859435994,-4.91824789567149,
130.808910257436));
#118978=CARTESIAN_POINT('Ctrl Pts',(-176.139859436039,-4.91824789567076,
130.808910258228));
#118979=CARTESIAN_POINT('Ctrl Pts',(-176.149963599637,-4.91808284950663,
130.987328293797));
#118980=CARTESIAN_POINT('Ctrl Pts',(-176.160067763234,-4.9082057749942,
131.165313191804));
#118981=CARTESIAN_POINT('Ctrl Pts',(-176.170171926832,-4.88877810967605,
131.341977262446));
#118982=CARTESIAN_POINT('Ctrl Pts',(-176.180533275005,-4.8688559456477,
131.523138021375));
#118983=CARTESIAN_POINT('Ctrl Pts',(-176.190894623179,-4.8388907778309,
131.702910210726));
#118984=CARTESIAN_POINT('Ctrl Pts',(-176.201255971352,-4.7991043982783,
131.880362493459));
#118985=CARTESIAN_POINT('Ctrl Pts',(-176.203122057061,-4.79193884481255,
131.91232176781));
#118986=CARTESIAN_POINT('Ctrl Pts',(-176.204988142771,-4.78445485148977,
131.944205850854));
#118987=CARTESIAN_POINT('Ctrl Pts',(-176.20685422848,-4.77665387632276,
131.976009373939));
#118988=CARTESIAN_POINT('Ctrl Pts',(-176.214628562599,-4.74415408968602,
132.108506618505));
#118989=CARTESIAN_POINT('Ctrl Pts',(-176.222402896718,-4.70608573424566,
132.239860461107));
#118990=CARTESIAN_POINT('Ctrl Pts',(-176.230177230837,-4.66254355668122,
132.369566880188));
#118991=CARTESIAN_POINT('Ctrl Pts',(-176.237941983785,-4.61905504095927,
132.499113447699));
#118992=CARTESIAN_POINT('Ctrl Pts',(-176.245706736732,-4.57010624886383,
132.627016264303));
#118993=CARTESIAN_POINT('Ctrl Pts',(-176.253471489679,-4.51584270705513,
132.7527824681));
#118994=CARTESIAN_POINT('Ctrl Pts',(-176.261228530564,-4.46163306056114,
132.87842375913));
#118995=CARTESIAN_POINT('Ctrl Pts',(-176.268985571449,-4.40211932305708,
133.0019323038));
#118996=CARTESIAN_POINT('Ctrl Pts',(-176.276742612334,-4.33749638621665,
133.122831700426));
#118997=CARTESIAN_POINT('Ctrl Pts',(-176.284493803574,-4.27292218203551,
133.243639925876));
#118998=CARTESIAN_POINT('Ctrl Pts',(-176.292244994814,-4.20324663101173,
133.361842576224));
#118999=CARTESIAN_POINT('Ctrl Pts',(-176.299996186054,-4.12871201342084,
133.476984828475));
#119000=CARTESIAN_POINT('Ctrl Pts',(-176.307744082831,-4.05420907503059,
133.592078142196));
#119001=CARTESIAN_POINT('Ctrl Pts',(-176.315491979608,-3.97485138967346,
133.7041133174));
#119002=CARTESIAN_POINT('Ctrl Pts',(-176.323239876385,-3.89092619108978,
133.812661872093));
#119003=CARTESIAN_POINT('Ctrl Pts',(-176.330986152469,-3.80701854784865,
133.921187720769));
#119004=CARTESIAN_POINT('Ctrl Pts',(-176.338732428553,-3.71854553076091,
134.026228090499));
#119005=CARTESIAN_POINT('Ctrl Pts',(-176.346478704637,-3.62583630606058,
134.127385466127));
#119006=CARTESIAN_POINT('Ctrl Pts',(-176.354225037903,-3.53312639700193,
134.228543588475));
#119007=CARTESIAN_POINT('Ctrl Pts',(-176.361971371168,-3.43618048208862,
134.325818371297));
#119008=CARTESIAN_POINT('Ctrl Pts',(-176.369717704433,-3.33536615367179,
134.418847535988));
#119009=CARTESIAN_POINT('Ctrl Pts',(-176.377465772436,-3.23452924858498,
134.511897533915));
#119010=CARTESIAN_POINT('Ctrl Pts',(-176.385213840439,-3.12982249341971,
134.600699756689));
#119011=CARTESIAN_POINT('Ctrl Pts',(-176.392961908442,-3.02164795649696,
134.684931025315));
#119012=CARTESIAN_POINT('Ctrl Pts',(-176.400718211184,-2.91335845038894,
134.769251815936));
#119013=CARTESIAN_POINT('Ctrl Pts',(-176.408474513926,-2.80159410911006,
134.84899170732));
#119014=CARTESIAN_POINT('Ctrl Pts',(-176.416230816668,-2.68678794596961,
134.923869519837));
#119015=CARTESIAN_POINT('Ctrl Pts',(-176.423991259182,-2.57192050732314,
134.998787296898));
#119016=CARTESIAN_POINT('Ctrl Pts',(-176.431751701696,-2.45400834778893,
135.06883762467));
#119017=CARTESIAN_POINT('Ctrl Pts',(-176.43951214421,-2.33350980910276,
135.133784948042));
#119018=CARTESIAN_POINT('Ctrl Pts',(-176.447285044476,-2.21281783546493,
135.198836530624));
#119019=CARTESIAN_POINT('Ctrl Pts',(-176.455057944741,-2.08953153770764,
135.258768567959));
#119020=CARTESIAN_POINT('Ctrl Pts',(-176.462830845006,-1.96413081129394,
135.313393021378));
#119021=CARTESIAN_POINT('Ctrl Pts',(-176.470321180768,-1.84328871715109,
135.366031738325));
#119022=CARTESIAN_POINT('Ctrl Pts',(-176.47781151653,-1.72048354210743,
135.413741948317));
#119023=CARTESIAN_POINT('Ctrl Pts',(-176.485301852292,-1.59615681486123,
135.456399577514));
#119024=CARTESIAN_POINT('Ctrl Pts',(-176.493076186411,-1.46711620196301,
135.500674583687));
#119025=CARTESIAN_POINT('Ctrl Pts',(-176.50085052053,-1.33602761806071,
135.539646558526));
#119026=CARTESIAN_POINT('Ctrl Pts',(-176.508624854649,-1.20336632366152,
135.573122779131));
#119027=CARTESIAN_POINT('Ctrl Pts',(-176.516389607596,-1.0708685224514,
135.606557743286));
#119028=CARTESIAN_POINT('Ctrl Pts',(-176.524154360544,-0.936802242677544,
135.63451033477));
#119029=CARTESIAN_POINT('Ctrl Pts',(-176.531919113491,-0.801660803731147,
135.656836585385));
#119030=CARTESIAN_POINT('Ctrl Pts',(-176.539676154376,-0.666653589167438,
135.679140661254));
#119031=CARTESIAN_POINT('Ctrl Pts',(-176.547433195261,-0.5305737237678,
135.695829453633));
#119032=CARTESIAN_POINT('Ctrl Pts',(-176.555190236145,-0.393927361472714,
135.706809423661));
#119033=CARTESIAN_POINT('Ctrl Pts',(-176.562941427386,-0.257384045261832,
135.717781113608));
#119034=CARTESIAN_POINT('Ctrl Pts',(-176.570692618626,-0.12027547060289,
135.723052518991));
#119035=CARTESIAN_POINT('Ctrl Pts',(-176.578443809866,0.0168847486307748,
135.722581634129));
#119036=CARTESIAN_POINT('Ctrl Pts',(-176.586191706643,0.15398667111221,
135.722110949406));
#119037=CARTESIAN_POINT('Ctrl Pts',(-176.59393960342,0.291139804366465,
135.715902829998));
#119038=CARTESIAN_POINT('Ctrl Pts',(-176.601687500197,0.427828397506153,
135.703967328802));
#119039=CARTESIAN_POINT('Ctrl Pts',(-176.609433776281,0.564488398338821,
135.692034324256));
#119040=CARTESIAN_POINT('Ctrl Pts',(-176.617180052365,0.700683663100474,
135.674376354887));
#119041=CARTESIAN_POINT('Ctrl Pts',(-176.624926328449,0.835901828640993,
135.651055490918));
#119042=CARTESIAN_POINT('Ctrl Pts',(-176.632672661715,0.97112099233111,
135.627734454799));
#119043=CARTESIAN_POINT('Ctrl Pts',(-176.64041899498,1.10536265713054,135.598750507116));
#119044=CARTESIAN_POINT('Ctrl Pts',(-176.648165328245,1.23812333514411,
135.564217093288));
#119045=CARTESIAN_POINT('Ctrl Pts',(-176.655913396248,1.37091374399085,
135.529675945941));
#119046=CARTESIAN_POINT('Ctrl Pts',(-176.663661464251,1.5022221277916,135.489582957896));
#119047=CARTESIAN_POINT('Ctrl Pts',(-176.671409532254,1.63155925915677,
135.444101714476));
#119048=CARTESIAN_POINT('Ctrl Pts',(-176.679165834996,1.76103385156445,
135.39857213305));
#119049=CARTESIAN_POINT('Ctrl Pts',(-176.686922137738,1.88853263699357,
135.34764298645));
#119050=CARTESIAN_POINT('Ctrl Pts',(-176.69467844048,2.01358499678816,135.291526596579));
#119051=CARTESIAN_POINT('Ctrl Pts',(-176.702438882994,2.13870410079277,
135.2353802557));
#119052=CARTESIAN_POINT('Ctrl Pts',(-176.710199325508,2.26137382786905,
135.174041329674));
#119053=CARTESIAN_POINT('Ctrl Pts',(-176.717959768022,2.38114825392634,
135.107768111091));
#119054=CARTESIAN_POINT('Ctrl Pts',(-176.725732668288,2.50111495252507,
135.041388504854));
#119055=CARTESIAN_POINT('Ctrl Pts',(-176.733505568553,2.61817672827134,
134.970058981002));
#119056=CARTESIAN_POINT('Ctrl Pts',(-176.741278468819,2.73191598368738,
134.894081649687));
#119057=CARTESIAN_POINT('Ctrl Pts',(-176.748768804581,2.84152053067899,
134.820866285739));
#119058=CARTESIAN_POINT('Ctrl Pts',(-176.756259140343,2.94803967836508,
134.743335347838));
#119059=CARTESIAN_POINT('Ctrl Pts',(-176.763749476105,3.05113038286288,
134.66179324164));
#119060=CARTESIAN_POINT('Ctrl Pts',(-176.771523810224,3.15812980275411,
134.577159441702));
#119061=CARTESIAN_POINT('Ctrl Pts',(-176.779298144343,3.26177461054604,
134.487936207787));
#119062=CARTESIAN_POINT('Ctrl Pts',(-176.787072478462,3.3616457730922,134.394419218585));
#119063=CARTESIAN_POINT('Ctrl Pts',(-176.794837231409,3.461393853356,134.301017480714));
#119064=CARTESIAN_POINT('Ctrl Pts',(-176.802601984356,3.55737725919811,
134.203332781063));
#119065=CARTESIAN_POINT('Ctrl Pts',(-176.810366737304,3.64920821491691,
134.10170234488));
#119066=CARTESIAN_POINT('Ctrl Pts',(-176.818123778189,3.7409479628359,134.000172849478));
#119067=CARTESIAN_POINT('Ctrl Pts',(-176.825880819074,3.82854320770035,
133.894705704663));
#119068=CARTESIAN_POINT('Ctrl Pts',(-176.833637859959,3.91164166404732,
133.785676192038));
#119069=CARTESIAN_POINT('Ctrl Pts',(-176.841389051199,3.99467745520205,
133.676728899417));
#119070=CARTESIAN_POINT('Ctrl Pts',(-176.849140242439,4.0732229715109,133.56422489581));
#119071=CARTESIAN_POINT('Ctrl Pts',(-176.856891433679,4.14696525156086,
133.44857359402));
#119072=CARTESIAN_POINT('Ctrl Pts',(-176.864639330456,4.22067618917455,
133.332971447118));
#119073=CARTESIAN_POINT('Ctrl Pts',(-176.872387227233,4.28958774116858,
133.21422499155));
#119074=CARTESIAN_POINT('Ctrl Pts',(-176.88013512401,4.35342958937816,133.092773576983));
#119075=CARTESIAN_POINT('Ctrl Pts',(-176.887881400094,4.41725808324937,
132.971347567433));
#119076=CARTESIAN_POINT('Ctrl Pts',(-176.895627676178,4.47601880087756,
132.847218070175));
#119077=CARTESIAN_POINT('Ctrl Pts',(-176.903373952263,4.52948701890115,
132.720849701309));
#119078=CARTESIAN_POINT('Ctrl Pts',(-176.911120285528,4.58295563161505,
132.59448039962));
#119079=CARTESIAN_POINT('Ctrl Pts',(-176.918866618793,4.63113151441993,
132.465872553408));
#119080=CARTESIAN_POINT('Ctrl Pts',(-176.926612952059,4.67383796465551,
132.335511081317));
#119081=CARTESIAN_POINT('Ctrl Pts',(-176.934361020062,4.71655397870447,
132.205120415679));
#119082=CARTESIAN_POINT('Ctrl Pts',(-176.942109088065,4.75379800119929,
132.072975714176));
#119083=CARTESIAN_POINT('Ctrl Pts',(-176.949857156068,4.78544322175271,
131.939576999531));
#119084=CARTESIAN_POINT('Ctrl Pts',(-176.957613458809,4.81712207522315,
131.806036507144));
#119085=CARTESIAN_POINT('Ctrl Pts',(-176.965369761551,4.84319014965535,
131.671239720258));
#119086=CARTESIAN_POINT('Ctrl Pts',(-176.973126064293,4.86357169660049,
131.535697348851));
#119087=CARTESIAN_POINT('Ctrl Pts',(-176.980886506807,4.88396412179092,
131.400082634399));
#119088=CARTESIAN_POINT('Ctrl Pts',(-176.988646949322,4.89866392997535,
131.263721931019));
#119089=CARTESIAN_POINT('Ctrl Pts',(-176.996407391836,4.90764739716295,
131.127130020731));
#119090=CARTESIAN_POINT('Ctrl Pts',(-177.004180292101,4.9166452854096,130.990318840983));
#119091=CARTESIAN_POINT('Ctrl Pts',(-177.011953192367,4.91990848601988,
130.853276103724));
#119092=CARTESIAN_POINT('Ctrl Pts',(-177.019726092632,4.9174654511826,130.716516443453));
#119093=CARTESIAN_POINT('Ctrl Pts',(-177.027216428394,4.91511122681529,
130.584728341311));
#119094=CARTESIAN_POINT('Ctrl Pts',(-177.034706764156,4.90745845416787,
130.453203399852));
#119095=CARTESIAN_POINT('Ctrl Pts',(-177.042197099918,4.89457781474275,
130.322394770303));
#119096=CARTESIAN_POINT('Ctrl Pts',(-177.049971434037,4.88120880195881,
130.186626491806));
#119097=CARTESIAN_POINT('Ctrl Pts',(-177.057745768156,4.86216531860959,
130.051199842308));
#119098=CARTESIAN_POINT('Ctrl Pts',(-177.065520102275,4.83746962990001,
129.916627187816));
#119099=CARTESIAN_POINT('Ctrl Pts',(-177.073284855222,4.81280437641963,
129.782220382095));
#119100=CARTESIAN_POINT('Ctrl Pts',(-177.081049608169,4.78250084741113,
129.648665858125));
#119101=CARTESIAN_POINT('Ctrl Pts',(-177.088814361117,4.74663315778832,
129.516472141073));
#119102=CARTESIAN_POINT('Ctrl Pts',(-177.096571402002,4.71080109246049,
129.384409720683));
#119103=CARTESIAN_POINT('Ctrl Pts',(-177.104328442886,4.66941596602455,
129.253705792402));
#119104=CARTESIAN_POINT('Ctrl Pts',(-177.112085483771,4.62260309462542,
129.124859592839));
#119105=CARTESIAN_POINT('Ctrl Pts',(-177.119836675012,4.57582552517671,
128.996110557197));
#119106=CARTESIAN_POINT('Ctrl Pts',(-177.127587866252,4.52362849080941,
128.86921682779));
#119107=CARTESIAN_POINT('Ctrl Pts',(-177.135339057492,4.46618727882041,
128.744663005536));
#119108=CARTESIAN_POINT('Ctrl Pts',(-177.143086954269,4.40877048087887,
128.620162121979));
#119109=CARTESIAN_POINT('Ctrl Pts',(-177.150834851046,4.34611410184664,
128.497999521832));
#119110=CARTESIAN_POINT('Ctrl Pts',(-177.158582747823,4.27844166546919,
128.378640110649));
#119111=CARTESIAN_POINT('Ctrl Pts',(-177.166329023907,4.21078338470659,
128.259305666881));
#119112=CARTESIAN_POINT('Ctrl Pts',(-177.174075299991,4.13811132632168,
128.142773585651));
#119113=CARTESIAN_POINT('Ctrl Pts',(-177.181821576076,4.06069491653235,
128.029484069438));
#119114=CARTESIAN_POINT('Ctrl Pts',(-177.189567909341,3.98327793527256,
127.916193716948));
#119115=CARTESIAN_POINT('Ctrl Pts',(-177.197314242606,3.90111675330759,
127.806146300033));
#119116=CARTESIAN_POINT('Ctrl Pts',(-177.205060575872,3.81452383432444,
127.699752594019));
#119117=CARTESIAN_POINT('Ctrl Pts',(-177.212808643875,3.72791152345761,
127.593335061873));
#119118=CARTESIAN_POINT('Ctrl Pts',(-177.220556711878,3.6368657474451,127.490573171966));
#119119=CARTESIAN_POINT('Ctrl Pts',(-177.228304779881,3.54173864545286,
127.391843887965));
#119120=CARTESIAN_POINT('Ctrl Pts',(-177.236061082622,3.44651044124447,
127.293009673306));
#119121=CARTESIAN_POINT('Ctrl Pts',(-177.243817385364,3.34719251777253,
127.198216908093));
#119122=CARTESIAN_POINT('Ctrl Pts',(-177.251573688106,3.24417360591931,
127.107805372861));
#119123=CARTESIAN_POINT('Ctrl Pts',(-177.25933413062,3.14109970977099,127.01734558227));
#119124=CARTESIAN_POINT('Ctrl Pts',(-177.267094573134,3.03432119346774,
126.931271926352));
#119125=CARTESIAN_POINT('Ctrl Pts',(-177.274855015649,2.92425833430713,
126.849882617028));
#119126=CARTESIAN_POINT('Ctrl Pts',(-177.282627915914,2.81401879247408,
126.76836265436));
#119127=CARTESIAN_POINT('Ctrl Pts',(-177.29040081618,2.70048469600353,126.691542284325));
#119128=CARTESIAN_POINT('Ctrl Pts',(-177.298173716445,2.58410440057933,
126.619675741807));
#119129=CARTESIAN_POINT('Ctrl Pts',(-177.305664052207,2.47195482203776,
126.550421729131));
#119130=CARTESIAN_POINT('Ctrl Pts',(-177.313154387969,2.35716265326231,
126.485767779962));
#119131=CARTESIAN_POINT('Ctrl Pts',(-177.320644723731,2.24014734829281,
126.425899367259));
#119132=CARTESIAN_POINT('Ctrl Pts',(-177.32841905785,2.11869537246986,126.363761025492));
#119133=CARTESIAN_POINT('Ctrl Pts',(-177.336193391969,1.99446362885182,
126.30658143534));
#119134=CARTESIAN_POINT('Ctrl Pts',(-177.343967726088,1.86789522035938,
126.254618810797));
#119135=CARTESIAN_POINT('Ctrl Pts',(-177.351732479035,1.74148279611867,
126.202720225545));
#119136=CARTESIAN_POINT('Ctrl Pts',(-177.359497231982,1.61273979500866,
126.156025960285));
#119137=CARTESIAN_POINT('Ctrl Pts',(-177.36726198493,1.48213411457354,126.114748530312));
#119138=CARTESIAN_POINT('Ctrl Pts',(-177.375019025815,1.3516581535411,126.073512097665));
#119139=CARTESIAN_POINT('Ctrl Pts',(-177.3827760667,1.21932356522319,126.037681910766));
#119140=CARTESIAN_POINT('Ctrl Pts',(-177.390533107585,1.08561810795748,
126.007422387176));
#119141=CARTESIAN_POINT('Ctrl Pts',(-177.398284298825,0.952013479016992,
125.977185682529));
#119142=CARTESIAN_POINT('Ctrl Pts',(-177.406035490065,0.817040418589824,
125.952511365542));
#119143=CARTESIAN_POINT('Ctrl Pts',(-177.413786681305,0.681201382220152,
125.933513900684));
#119144=CARTESIAN_POINT('Ctrl Pts',(-177.421534578082,0.545420081064746,
125.914524510255));
#119145=CARTESIAN_POINT('Ctrl Pts',(-177.429282474859,0.408773922402197,
125.901207227089));
#119146=CARTESIAN_POINT('Ctrl Pts',(-177.437030371636,0.271774864485895,
125.893625287136));
#119147=CARTESIAN_POINT('Ctrl Pts',(-177.44477664772,0.134804463819151,
125.886044933161));
#119148=CARTESIAN_POINT('Ctrl Pts',(-177.452522923805,-0.00251829915094726,
125.884197557701));
#119149=CARTESIAN_POINT('Ctrl Pts',(-177.460269199889,-0.139677438159066,
125.88809442504));
#119150=CARTESIAN_POINT('Ctrl Pts',(-177.468015533154,-0.276837589644604,
125.891991321146));
#119151=CARTESIAN_POINT('Ctrl Pts',(-177.47576186642,-0.41383372395051,
125.901632533558));
#119152=CARTESIAN_POINT('Ctrl Pts',(-177.483508199685,-0.550151349906157,
125.916977211827));
#119153=CARTESIAN_POINT('Ctrl Pts',(-177.491256267688,-0.686499503249163,
125.932325326429));
#119154=CARTESIAN_POINT('Ctrl Pts',(-177.499004335691,-0.82216845744731,
125.953379404746));
#119155=CARTESIAN_POINT('Ctrl Pts',(-177.506752403694,-0.956650722471993,
125.980046940192));
#119156=CARTESIAN_POINT('Ctrl Pts',(-177.514508706436,-1.09127591684812,
126.006742818213));
#119157=CARTESIAN_POINT('Ctrl Pts',(-177.522265009177,-1.22471151850379,
126.03906399502));
#119158=CARTESIAN_POINT('Ctrl Pts',(-177.530021311919,-1.3564615419159,
126.076867079992));
#119159=CARTESIAN_POINT('Ctrl Pts',(-177.537781754434,-1.48828188428242,
126.114690341609));
#119160=CARTESIAN_POINT('Ctrl Pts',(-177.545542196948,-1.61841448501119,
126.15800121801));
#119161=CARTESIAN_POINT('Ctrl Pts',(-177.553302639462,-1.746381279821,126.20660730883));
#119162=CARTESIAN_POINT('Ctrl Pts',(-177.561075539727,-1.8745534982902,
126.255291426463));
#119163=CARTESIAN_POINT('Ctrl Pts',(-177.568848439993,-2.0005526036341,
126.30928759083));
#119164=CARTESIAN_POINT('Ctrl Pts',(-177.576621340258,-2.12392235364388,
126.368356007763));
#119165=CARTESIAN_POINT('Ctrl Pts',(-177.58411167602,-2.24280730248949,
126.425277138956));
#119166=CARTESIAN_POINT('Ctrl Pts',(-177.591602011782,-2.35925047219554,
126.486908002843));
#119167=CARTESIAN_POINT('Ctrl Pts',(-177.599092347544,-2.47286909395594,
126.552995953525));
#119168=CARTESIAN_POINT('Ctrl Pts',(-177.60686784926,-2.59081331121292,
126.621599950762));
#119169=CARTESIAN_POINT('Ctrl Pts',(-177.614643350975,-2.70608732028164,
126.695224480623));
#119170=CARTESIAN_POINT('Ctrl Pts',(-177.622418852691,-2.8182341662396,
126.773636210373));
#119171=CARTESIAN_POINT('Ctrl Pts',(-177.63018451916,-2.93023915743989,
126.851948756978));
#119172=CARTESIAN_POINT('Ctrl Pts',(-177.637950185629,-3.03912453927194,
126.935036231687));
#119173=CARTESIAN_POINT('Ctrl Pts',(-177.645715852098,-3.14445845962935,
127.022619740911));
#119174=CARTESIAN_POINT('Ctrl Pts',(-177.653472099438,-3.24966461842309,
127.110097018391));
#119175=CARTESIAN_POINT('Ctrl Pts',(-177.661228346779,-3.35132759661482,
127.202059220451));
#119176=CARTESIAN_POINT('Ctrl Pts',(-177.66898459412,-3.44904554979687,
127.298184943427));
#119177=CARTESIAN_POINT('Ctrl Pts',(-177.676735499376,-3.54669620013157,
127.394244460198));
#119178=CARTESIAN_POINT('Ctrl Pts',(-177.684486404633,-3.64040695375948,
127.494461519737));
#119179=CARTESIAN_POINT('Ctrl Pts',(-177.69223730989,-3.72980996493064,
127.598475297096));
#119180=CARTESIAN_POINT('Ctrl Pts',(-177.699984555376,-3.81917076239027,
127.70243996193));
#119181=CARTESIAN_POINT('Ctrl Pts',(-177.707731800862,-3.90422761101185,
127.810197481142));
#119182=CARTESIAN_POINT('Ctrl Pts',(-177.715479046349,-3.9846506692834,
127.921351407335));
#119183=CARTESIAN_POINT('Ctrl Pts',(-177.723224311547,-4.06505317046089,
128.032476921257));
#119184=CARTESIAN_POINT('Ctrl Pts',(-177.730969576744,-4.14082401090818,
128.146996797071));
#119185=CARTESIAN_POINT('Ctrl Pts',(-177.738714841942,-4.21167492248432,
128.264483177646));
#119186=CARTESIAN_POINT('Ctrl Pts',(-177.746461929158,-4.28254250122873,
128.381997196048));
#119187=CARTESIAN_POINT('Ctrl Pts',(-177.754209016374,-4.34848763261502,
128.502478781148));
#119188=CARTESIAN_POINT('Ctrl Pts',(-177.76195610359,-4.40926651739199,
128.625472864352));
#119189=CARTESIAN_POINT('Ctrl Pts',(-177.769704172855,-4.47005310672187,
128.748482538734));
#119190=CARTESIAN_POINT('Ctrl Pts',(-177.77745224212,-4.52567197910536,
128.874004991591));
#119191=CARTESIAN_POINT('Ctrl Pts',(-177.785200311385,-4.57592665268824,
129.001563254655));
#119192=CARTESIAN_POINT('Ctrl Pts',(-177.792953962452,-4.62621753033989,
129.12921341222));
#119193=CARTESIAN_POINT('Ctrl Pts',(-177.800707613519,-4.67113635666925,
129.258901942004));
#119194=CARTESIAN_POINT('Ctrl Pts',(-177.808461264585,-4.71053582112806,
129.390134560541));
#119195=CARTESIAN_POINT('Ctrl Pts',(-177.812229200399,-4.7296822402637,
129.453907882165));
#119196=CARTESIAN_POINT('Ctrl Pts',(-177.815997136212,-4.74752599936461,
129.518045636102));
#119197=CARTESIAN_POINT('Ctrl Pts',(-177.819765072025,-4.76405452823413,
129.582490119309));
#119198=CARTESIAN_POINT('Origin',(213.235140564004,0.,130.804360617566));
#119199=CARTESIAN_POINT('',(-179.915287826822,-4.76405452823417,129.582490119309));
#119200=CARTESIAN_POINT('',(-179.570054719422,-4.76405452823393,129.582490119308));
#119201=CARTESIAN_POINT('',(213.235140564004,-4.76405452823405,129.582490119308));
#119202=CARTESIAN_POINT('',(-178.235140563957,-4.91824875847738,130.800866016629));
#119203=CARTESIAN_POINT('Ctrl Pts',(-178.235140564012,-4.91824875847807,
130.800866017606));
#119204=CARTESIAN_POINT('Ctrl Pts',(-178.242912059243,-4.91834661808309,
130.938592191243));
#119205=CARTESIAN_POINT('Ctrl Pts',(-178.250683554473,-4.91265502275465,
131.076364389796));
#119206=CARTESIAN_POINT('Ctrl Pts',(-178.258455049704,-4.90118910695513,
131.213662951256));
#119207=CARTESIAN_POINT('Ctrl Pts',(-178.266226229677,-4.8897236562809,
131.350955943075));
#119208=CARTESIAN_POINT('Ctrl Pts',(-178.27399740965,-4.87248438266389,
131.487774950232));
#119209=CARTESIAN_POINT('Ctrl Pts',(-178.281768589622,-4.84953840587296,
131.623604361798));
#119210=CARTESIAN_POINT('Ctrl Pts',(-178.289541094918,-4.82658851579851,
131.759456938165));
#119211=CARTESIAN_POINT('Ctrl Pts',(-178.297313600214,-4.79793004946218,
131.894319201245));
#119212=CARTESIAN_POINT('Ctrl Pts',(-178.30508610551,-4.76368139923051,
132.027685018175));
#119213=CARTESIAN_POINT('Ctrl Pts',(-178.31286157721,-4.72941967788061,
132.161101734639));
#119214=CARTESIAN_POINT('Ctrl Pts',(-178.32063704891,-4.68956362187731,
132.293020493378));
#119215=CARTESIAN_POINT('Ctrl Pts',(-178.328412520609,-4.64428160317825,
132.422949957973));
#119216=CARTESIAN_POINT('Ctrl Pts',(-178.33619753434,-4.59894401455087,
132.553038871534));
#119217=CARTESIAN_POINT('Ctrl Pts',(-178.34398254807,-4.54816729194925,
132.68113324938));
#119218=CARTESIAN_POINT('Ctrl Pts',(-178.351767561801,-4.49216835570908,
132.806760808953));
#119219=CARTESIAN_POINT('Ctrl Pts',(-178.359557729245,-4.43613234792204,
132.932471534533));
#119220=CARTESIAN_POINT('Ctrl Pts',(-178.36734789669,-4.37486741040936,
133.055711842143));
#119221=CARTESIAN_POINT('Ctrl Pts',(-178.375138064134,-4.30863618326705,
133.176034562851));
#119222=CARTESIAN_POINT('Ctrl Pts',(-178.38294095569,-4.24229677699919,
133.296553813311));
#119223=CARTESIAN_POINT('Ctrl Pts',(-178.390743847245,-4.17097507715918,
133.414145626664));
#119224=CARTESIAN_POINT('Ctrl Pts',(-178.398546738801,-4.09497718847947,
133.528391617451));
#119225=CARTESIAN_POINT('Ctrl Pts',(-178.403979900142,-4.04205978115932,
133.607941217238));
#119226=CARTESIAN_POINT('Ctrl Pts',(-178.409413061482,-3.98687607958372,
133.685869291158));
#119227=CARTESIAN_POINT('Ctrl Pts',(-178.414846222822,-3.92954049509117,
133.76204460338));
#119228=CARTESIAN_POINT('Ctrl Pts',(-178.422620556941,-3.84749875864512,
133.871044187919));
#119229=CARTESIAN_POINT('Ctrl Pts',(-178.430394891061,-3.76078840842461,
133.976800260166));
#119230=CARTESIAN_POINT('Ctrl Pts',(-178.43816922518,-3.66969498233147,
134.078886812171));
#119231=CARTESIAN_POINT('Ctrl Pts',(-178.445933978127,-3.57871382074449,
134.180847551624));
#119232=CARTESIAN_POINT('Ctrl Pts',(-178.453698731074,-3.48336058895814,
134.279147480063));
#119233=CARTESIAN_POINT('Ctrl Pts',(-178.461463484021,-3.38396310956101,
134.373390840978));
#119234=CARTESIAN_POINT('Ctrl Pts',(-178.469220524906,-3.28466435314195,
134.467540598059));
#119235=CARTESIAN_POINT('Ctrl Pts',(-178.476977565791,-3.18132962460898,
134.557641538328));
#119236=CARTESIAN_POINT('Ctrl Pts',(-178.484734606676,-3.07432564361539,
134.643332472049));
#119237=CARTESIAN_POINT('Ctrl Pts',(-178.492485797916,-2.96740235515608,
134.728958785569));
#119238=CARTESIAN_POINT('Ctrl Pts',(-178.500236989156,-2.856815625741,134.81018146859));
#119239=CARTESIAN_POINT('Ctrl Pts',(-178.507988180396,-2.74296724005992,
134.886677825042));
#119240=CARTESIAN_POINT('Ctrl Pts',(-178.515736077173,-2.6291672429796,
134.963141668503));
#119241=CARTESIAN_POINT('Ctrl Pts',(-178.523483973951,-2.51210867069543,
135.034882963187));
#119242=CARTESIAN_POINT('Ctrl Pts',(-178.531231870728,-2.39222425946025,
135.101620925594));
#119243=CARTESIAN_POINT('Ctrl Pts',(-178.538978146812,-2.27236492545981,
135.168344927857));
#119244=CARTESIAN_POINT('Ctrl Pts',(-178.546724422896,-2.14968126963242,
135.230067489522));
#119245=CARTESIAN_POINT('Ctrl Pts',(-178.55447069898,-2.0246323815396,135.286552802437));
#119246=CARTESIAN_POINT('Ctrl Pts',(-178.562217032245,-1.89958257036413,
135.343038532314));
#119247=CARTESIAN_POINT('Ctrl Pts',(-178.569963365511,-1.77216784838562,
135.394286775354));
#119248=CARTESIAN_POINT('Ctrl Pts',(-178.577709698776,-1.64286875422958,
135.440109243072));
#119249=CARTESIAN_POINT('Ctrl Pts',(-178.585457766779,-1.51354070443772,
135.485941972413));
#119250=CARTESIAN_POINT('Ctrl Pts',(-178.593205834782,-1.38232781119079,
135.526346378023));
#119251=CARTESIAN_POINT('Ctrl Pts',(-178.600953902785,-1.24972691011741,
135.561183686866));
#119252=CARTESIAN_POINT('Ctrl Pts',(-178.608710205527,-1.11698507922857,
135.596058021216));
#119253=CARTESIAN_POINT('Ctrl Pts',(-178.616466508269,-0.982852672395769,
135.625353339897));
#119254=CARTESIAN_POINT('Ctrl Pts',(-178.62422281101,-0.847838434771901,
135.648981660643));
#119255=CARTESIAN_POINT('Ctrl Pts',(-178.631983253525,-0.712752135984214,
135.672622592535));
#119256=CARTESIAN_POINT('Ctrl Pts',(-178.639743696039,-0.576783455982213,
135.690590448432));
#119257=CARTESIAN_POINT('Ctrl Pts',(-178.647504138553,-0.440446459232609,
135.702849157825));
#119258=CARTESIAN_POINT('Ctrl Pts',(-178.655277038818,-0.303890602232393,
135.715127545987));
#119259=CARTESIAN_POINT('Ctrl Pts',(-178.663049939084,-0.166965637712462,
135.721678454702));
#119260=CARTESIAN_POINT('Ctrl Pts',(-178.670822839349,-0.03018673474577,
135.722517978158));
#119261=CARTESIAN_POINT('Ctrl Pts',(-178.678313175112,0.101619910576147,
135.723326982821));
#119262=CARTESIAN_POINT('Ctrl Pts',(-178.685803510874,0.233290621547758,
135.718832649925));
#119263=CARTESIAN_POINT('Ctrl Pts',(-178.693293846636,0.364370681277128,
135.709094766236));
#119264=CARTESIAN_POINT('Ctrl Pts',(-178.701068180755,0.500420681308806,
135.698987667727));
#119265=CARTESIAN_POINT('Ctrl Pts',(-178.708842514874,0.63626532236978,
135.683199534606));
#119266=CARTESIAN_POINT('Ctrl Pts',(-178.716616848993,0.77139185169714,
135.661740330295));
#119267=CARTESIAN_POINT('Ctrl Pts',(-178.72438160194,0.906351849653709,
135.640307572536));
#119268=CARTESIAN_POINT('Ctrl Pts',(-178.732146354887,1.04059511436018,
135.61321771052));
#119269=CARTESIAN_POINT('Ctrl Pts',(-178.739911107835,1.17361148854135,
135.580532634617));
#119270=CARTESIAN_POINT('Ctrl Pts',(-178.74766814872,1.30649574898521,135.547880021992));
#119271=CARTESIAN_POINT('Ctrl Pts',(-178.755425189605,1.43815516668883,
135.509643347339));
#119272=CARTESIAN_POINT('Ctrl Pts',(-178.76318223049,1.56808764156665,135.465935910411));
#119273=CARTESIAN_POINT('Ctrl Pts',(-178.77093342173,1.6979221333539,135.422261433602));
#119274=CARTESIAN_POINT('Ctrl Pts',(-178.77868461297,1.82603190540451,135.373124530313));
#119275=CARTESIAN_POINT('Ctrl Pts',(-178.78643580421,1.95192828993981,135.318688808275));
#119276=CARTESIAN_POINT('Ctrl Pts',(-178.794183700987,2.07777116515346,
135.264276222872));
#119277=CARTESIAN_POINT('Ctrl Pts',(-178.801931597764,2.20140216582424,
135.204569452893));
#119278=CARTESIAN_POINT('Ctrl Pts',(-178.809679494541,2.32235115632627,
135.139780801263));
#119279=CARTESIAN_POINT('Ctrl Pts',(-178.817425770625,2.44327484690683,
135.075005702023));
#119280=CARTESIAN_POINT('Ctrl Pts',(-178.82517204671,2.56151729879949,135.005151020031));
#119281=CARTESIAN_POINT('Ctrl Pts',(-178.832918322794,2.6766319708055,134.93047554027));
#119282=CARTESIAN_POINT('Ctrl Pts',(-178.840664656059,2.79174749256172,
134.855799509272));
#119283=CARTESIAN_POINT('Ctrl Pts',(-178.848410989325,2.90373486036354,
134.77630282227));
#119284=CARTESIAN_POINT('Ctrl Pts',(-178.85615732259,3.01217591891128,134.692287995493));
#119285=CARTESIAN_POINT('Ctrl Pts',(-178.863905390593,3.12064126208234,
134.608254354177));
#119286=CARTESIAN_POINT('Ctrl Pts',(-178.871653458596,3.22555840668735,
134.519700799111));
#119287=CARTESIAN_POINT('Ctrl Pts',(-178.879401526599,3.32654204724801,
134.426970321963));
#119288=CARTESIAN_POINT('Ctrl Pts',(-178.887157829341,3.42763301442343,
134.334141289761));
#119289=CARTESIAN_POINT('Ctrl Pts',(-178.894914132082,3.52478183797542,
134.23712673239));
#119290=CARTESIAN_POINT('Ctrl Pts',(-178.902670434824,3.61763950674951,
134.136307114991));
#119291=CARTESIAN_POINT('Ctrl Pts',(-178.910430877338,3.71054673645731,
134.035433687128));
#119292=CARTESIAN_POINT('Ctrl Pts',(-178.918191319852,3.79915799525986,
133.93075145081));
#119293=CARTESIAN_POINT('Ctrl Pts',(-178.925951762367,3.88316507161623,
133.822673406042));
#119294=CARTESIAN_POINT('Ctrl Pts',(-178.933724662632,3.96730700358959,
133.714421864802));
#119295=CARTESIAN_POINT('Ctrl Pts',(-178.941497562898,4.04682975652453,
133.60276394041));
#119296=CARTESIAN_POINT('Ctrl Pts',(-178.949270463163,4.12146840944813,
133.488141758498));
#119297=CARTESIAN_POINT('Ctrl Pts',(-178.956760798925,4.19339375933312,
133.377686381616));
#119298=CARTESIAN_POINT('Ctrl Pts',(-178.964251134687,4.26078378529405,
133.264478786661));
#119299=CARTESIAN_POINT('Ctrl Pts',(-178.971741470449,4.32344300204487,
133.14893385604));
#119300=CARTESIAN_POINT('Ctrl Pts',(-178.979515804568,4.38847796204466,
133.029008004254));
#119301=CARTESIAN_POINT('Ctrl Pts',(-178.987290138687,4.44862230519032,
132.906184188811));
#119302=CARTESIAN_POINT('Ctrl Pts',(-178.995064472806,4.50360725859762,
132.780899188606));
#119303=CARTESIAN_POINT('Ctrl Pts',(-179.002829225753,4.55852444796399,
132.655768590966));
#119304=CARTESIAN_POINT('Ctrl Pts',(-179.0105939787,4.60829474347329,132.528183198275));
#119305=CARTESIAN_POINT('Ctrl Pts',(-179.018358731647,4.65269446277708,
132.398605673554));
#119306=CARTESIAN_POINT('Ctrl Pts',(-179.026115772532,4.69705008365385,
132.269156847057));
#119307=CARTESIAN_POINT('Ctrl Pts',(-179.033872813417,4.73604561757761,
132.137720193522));
#119308=CARTESIAN_POINT('Ctrl Pts',(-179.041629854302,4.76950498948021,
132.004779385256));
#119309=CARTESIAN_POINT('Ctrl Pts',(-179.049381045542,4.80293912941014,
131.871938828688));
#119310=CARTESIAN_POINT('Ctrl Pts',(-179.057132236782,4.83084532209175,
131.737596752741));
#119311=CARTESIAN_POINT('Ctrl Pts',(-179.064883428023,4.85309707847332,
131.602252721433));
#119312=CARTESIAN_POINT('Ctrl Pts',(-179.0726313248,4.87533937726481,131.466966214949));
#119313=CARTESIAN_POINT('Ctrl Pts',(-179.080379221577,4.89193195641557,
131.330678985081));
#119314=CARTESIAN_POINT('Ctrl Pts',(-179.088127118354,4.90279931259945,
131.193901325162));
#119315=CARTESIAN_POINT('Ctrl Pts',(-179.095873394438,4.91366439556669,
131.057152276181));
#119316=CARTESIAN_POINT('Ctrl Pts',(-179.103619670522,4.91880660669958,
130.919913390691));
#119317=CARTESIAN_POINT('Ctrl Pts',(-179.111365946606,4.91820230270907,
130.782700236056));
#119318=CARTESIAN_POINT('Ctrl Pts',(-179.119112279871,4.91759799425773,
130.645486068543));
#119319=CARTESIAN_POINT('Ctrl Pts',(-179.126858613137,4.91124708775985,
130.508298023225));
#119320=CARTESIAN_POINT('Ctrl Pts',(-179.134604946402,4.89917807553393,
130.371651423409));
#119321=CARTESIAN_POINT('Ctrl Pts',(-179.142353014405,4.88710636053639,
130.234974222535));
#119322=CARTESIAN_POINT('Ctrl Pts',(-179.150101082408,4.86931402609475,
130.098839097816));
#119323=CARTESIAN_POINT('Ctrl Pts',(-179.157849150411,4.84588137379236,
129.963755613041));
#119324=CARTESIAN_POINT('Ctrl Pts',(-179.165605453153,4.82242381698827,
129.828528559931));
#119325=CARTESIAN_POINT('Ctrl Pts',(-179.173361755895,4.79331403439889,
129.694355765308));
#119326=CARTESIAN_POINT('Ctrl Pts',(-179.181118058636,4.75868347306896,
129.561736512842));
#119327=CARTESIAN_POINT('Ctrl Pts',(-179.188878501151,4.72403442836585,
129.429046477489));
#119328=CARTESIAN_POINT('Ctrl Pts',(-179.196638943665,4.68385884803004,
129.297912010122));
#119329=CARTESIAN_POINT('Ctrl Pts',(-179.204399386179,4.63833760479553,
129.16881565443));
#119330=CARTESIAN_POINT('Ctrl Pts',(-179.212172286444,4.59274328682007,
129.039512061807));
#119331=CARTESIAN_POINT('Ctrl Pts',(-179.21994518671,4.54178630312496,128.912253482031));
#119332=CARTESIAN_POINT('Ctrl Pts',(-179.227718086975,4.48569543026932,
128.787501780324));
#119333=CARTESIAN_POINT('Ctrl Pts',(-179.235208422737,4.43164360192636,
128.667285117205));
#119334=CARTESIAN_POINT('Ctrl Pts',(-179.242698758499,4.37282480120875,
128.549396509455));
#119335=CARTESIAN_POINT('Ctrl Pts',(-179.250189094261,4.30948241586416,
128.434224678457));
#119336=CARTESIAN_POINT('Ctrl Pts',(-179.25796342838,4.24373838472681,128.314686072481));
#119337=CARTESIAN_POINT('Ctrl Pts',(-179.265737762499,4.17291271682093,
128.197695660831));
#119338=CARTESIAN_POINT('Ctrl Pts',(-179.273512096618,4.09722760829128,
128.083715659407));
#119339=CARTESIAN_POINT('Ctrl Pts',(-179.281276849565,4.02163577489393,
127.969876128149));
#119340=CARTESIAN_POINT('Ctrl Pts',(-179.289041602512,3.94119663104747,
127.859039947773));
#119341=CARTESIAN_POINT('Ctrl Pts',(-179.29680635546,3.85617852248092,127.751645389239));
#119342=CARTESIAN_POINT('Ctrl Pts',(-179.304563396344,3.77124485509857,
127.644357496495));
#119343=CARTESIAN_POINT('Ctrl Pts',(-179.31232043723,3.6817415146055,127.540504727641));
#119344=CARTESIAN_POINT('Ctrl Pts',(-179.320077478115,3.58798025533687,
127.440496656314));
#119345=CARTESIAN_POINT('Ctrl Pts',(-179.327828669355,3.49428970216282,
127.340564001851));
#119346=CARTESIAN_POINT('Ctrl Pts',(-179.335579860595,3.39634788769476,
127.244470558066));
#119347=CARTESIAN_POINT('Ctrl Pts',(-179.343331051835,3.29450673886711,
127.152592770336));
#119348=CARTESIAN_POINT('Ctrl Pts',(-179.351078948612,3.19270887524427,
127.060754033117));
#119349=CARTESIAN_POINT('Ctrl Pts',(-179.358826845389,3.08701526322851,
126.973127649607));
#119350=CARTESIAN_POINT('Ctrl Pts',(-179.366574742166,2.97781441566159,
126.890052968903));
#119351=CARTESIAN_POINT('Ctrl Pts',(-179.37432101825,2.86863641055788,126.806995665632));
#119352=CARTESIAN_POINT('Ctrl Pts',(-179.382067294334,2.75595294011129,
126.728488407918));
#119353=CARTESIAN_POINT('Ctrl Pts',(-179.389813570418,2.64018498597006,
126.654829764282));
#119354=CARTESIAN_POINT('Ctrl Pts',(-179.397559903684,2.52441617725656,
126.581170576914));
#119355=CARTESIAN_POINT('Ctrl Pts',(-179.405306236949,2.40556316927225,
126.512360284919));
#119356=CARTESIAN_POINT('Ctrl Pts',(-179.413052570214,2.28407491890505,
126.448653461738));
#119357=CARTESIAN_POINT('Ctrl Pts',(-179.420800638217,2.16255946208602,
126.384932371855));
#119358=CARTESIAN_POINT('Ctrl Pts',(-179.42854870622,2.03840793474619,126.326317206531));
#119359=CARTESIAN_POINT('Ctrl Pts',(-179.436296774223,1.9120924522984,126.273015837441));
#119360=CARTESIAN_POINT('Ctrl Pts',(-179.444053076965,1.78564272025286,
126.219657819023));
#119361=CARTESIAN_POINT('Ctrl Pts',(-179.451809379707,1.65702479963027,
126.1716250307));
#119362=CARTESIAN_POINT('Ctrl Pts',(-179.459565682449,1.52672980226203,
126.129076757373));
#119363=CARTESIAN_POINT('Ctrl Pts',(-179.467326124963,1.39636526253059,
126.08650577475));
#119364=CARTESIAN_POINT('Ctrl Pts',(-179.475086567477,1.26432223869915,
126.049425245569));
#119365=CARTESIAN_POINT('Ctrl Pts',(-179.482847009991,1.13110447457022,
126.017943823125));
#119366=CARTESIAN_POINT('Ctrl Pts',(-179.490619910257,0.997672857459797,
125.986411863907));
#119367=CARTESIAN_POINT('Ctrl Pts',(-179.498392810522,0.863063115764055,
125.960497046634));
#119368=CARTESIAN_POINT('Ctrl Pts',(-179.506165710787,0.727787489092654,
125.940256544541));
#119369=CARTESIAN_POINT('Ctrl Pts',(-179.51365604655,0.597429472185839,
125.920751835681));
#119370=CARTESIAN_POINT('Ctrl Pts',(-179.521146382312,0.466453449186646,
125.906516086481));
#119371=CARTESIAN_POINT('Ctrl Pts',(-179.528636718074,0.335318019426584,
125.897554641338));
#119372=CARTESIAN_POINT('Ctrl Pts',(-179.536411052193,0.199210549992686,
125.888253420279));
#119373=CARTESIAN_POINT('Ctrl Pts',(-179.544185386312,0.0625001998143731,
125.884604885428));
#119374=CARTESIAN_POINT('Ctrl Pts',(-179.551959720431,-0.074304053336741,
125.886671935862));
#119375=CARTESIAN_POINT('Ctrl Pts',(-179.559724473378,-0.210939707472022,
125.888736438841));
#119376=CARTESIAN_POINT('Ctrl Pts',(-179.567489226326,-0.347668647150042,
125.896502505897));
#119377=CARTESIAN_POINT('Ctrl Pts',(-179.575253979273,-0.483977095179842,
125.909981266326));
#119378=CARTESIAN_POINT('Ctrl Pts',(-179.583011020158,-0.620150159737818,
125.923446639461));
#119379=CARTESIAN_POINT('Ctrl Pts',(-179.590768061043,-0.75590317721648,
125.942613376373));
#119380=CARTESIAN_POINT('Ctrl Pts',(-179.598525101928,-0.890723050881356,
125.967440573868));
#119381=CARTESIAN_POINT('Ctrl Pts',(-179.606276293168,-1.0254412558302,
125.99224904898));
#119382=CARTESIAN_POINT('Ctrl Pts',(-179.614027484408,-1.15922733467526,
126.02270941777));
#119383=CARTESIAN_POINT('Ctrl Pts',(-179.621778675648,-1.29157434815609,
126.058729072062));
#119384=CARTESIAN_POINT('Ctrl Pts',(-179.629526572425,-1.42386511062591,
126.09473341704));
#119385=CARTESIAN_POINT('Ctrl Pts',(-179.637274469202,-1.55471764778564,
126.136292245547));
#119386=CARTESIAN_POINT('Ctrl Pts',(-179.645022365979,-1.68363645494728,
126.183262117201));
#119387=CARTESIAN_POINT('Ctrl Pts',(-179.652768642063,-1.81252829507363,
126.230222163771));
#119388=CARTESIAN_POINT('Ctrl Pts',(-179.660514918148,-1.9394868426528,
126.282590868379));
#119389=CARTESIAN_POINT('Ctrl Pts',(-179.668261194232,-2.06403335266789,
126.340175430819));
#119390=CARTESIAN_POINT('Ctrl Pts',(-179.676007527497,-2.18858078205719,
126.397760418335));
#119391=CARTESIAN_POINT('Ctrl Pts',(-179.683753860762,-2.31071578348326,
126.460561176436));
#119392=CARTESIAN_POINT('Ctrl Pts',(-179.691500194028,-2.429981504936,126.528337588141));
#119393=CARTESIAN_POINT('Ctrl Pts',(-179.699248262031,-2.54927393512061,
126.596129177904));
#119394=CARTESIAN_POINT('Ctrl Pts',(-179.706996330034,-2.66569546687332,
126.668898445397));
#119395=CARTESIAN_POINT('Ctrl Pts',(-179.714744398037,-2.77881602195207,
126.746360546269));
#119396=CARTESIAN_POINT('Ctrl Pts',(-179.722500700779,-2.89205680290245,
126.823904974785));
#119397=CARTESIAN_POINT('Ctrl Pts',(-179.73025700352,-3.00198927584127,
126.906151978699));
#119398=CARTESIAN_POINT('Ctrl Pts',(-179.738013306262,-3.10821397193136,
126.992774469098));
#119399=CARTESIAN_POINT('Ctrl Pts',(-179.745773748776,-3.21449536334011,
127.079443192529));
#119400=CARTESIAN_POINT('Ctrl Pts',(-179.753534191291,-3.31706474242677,
127.170491796366));
#119401=CARTESIAN_POINT('Ctrl Pts',(-179.761294633805,-3.41555841026557,
127.265555196444));
#119402=CARTESIAN_POINT('Ctrl Pts',(-179.76906753407,-3.51421018888385,
127.36077120073));
#119403=CARTESIAN_POINT('Ctrl Pts',(-179.776840434336,-3.60877291201382,
127.460014597025));
#119404=CARTESIAN_POINT('Ctrl Pts',(-179.784613334601,-3.69892160017226,
127.562885327165));
#119405=CARTESIAN_POINT('Ctrl Pts',(-179.792103670363,-3.78579315644455,
127.662016447149));
#119406=CARTESIAN_POINT('Ctrl Pts',(-179.799594006125,-3.86856583511938,
127.764515514558));
#119407=CARTESIAN_POINT('Ctrl Pts',(-179.807084341887,-3.94698725566329,
127.869999585564));
#119408=CARTESIAN_POINT('Ctrl Pts',(-179.81489938152,-4.02880822192404,
127.980056360295));
#119409=CARTESIAN_POINT('Ctrl Pts',(-179.822714421154,-4.10615277853036,
128.093713091792));
#119410=CARTESIAN_POINT('Ctrl Pts',(-179.830529460787,-4.17868931704032,
128.210572142352));
#119411=CARTESIAN_POINT('Ctrl Pts',(-179.838331509096,-4.25110527449914,
128.327236932372));
#119412=CARTESIAN_POINT('Ctrl Pts',(-179.846133557405,-4.31872893195353,
128.447093113703));
#119413=CARTESIAN_POINT('Ctrl Pts',(-179.853935605714,-4.38126988870761,
128.569711377796));
#119414=CARTESIAN_POINT('Ctrl Pts',(-179.861730173332,-4.44375088049264,
128.692212074126));
#119415=CARTESIAN_POINT('Ctrl Pts',(-179.86952474095,-4.50115869139553,
128.817469244293));
#119416=CARTESIAN_POINT('Ctrl Pts',(-179.877319308568,-4.55324684430206,
128.945025726441));
#119417=CARTESIAN_POINT('Ctrl Pts',(-179.885106751938,-4.60528738855242,
129.072465621758));
#119418=CARTESIAN_POINT('Ctrl Pts',(-179.892894195309,-4.65201781159595,
129.202200288788));
#119419=CARTESIAN_POINT('Ctrl Pts',(-179.900681638679,-4.6932383823034,
129.333749673307));
#119420=CARTESIAN_POINT('Ctrl Pts',(-179.90555036806,-4.71900958783941,
129.415994682738));
#119421=CARTESIAN_POINT('Ctrl Pts',(-179.910419097441,-4.74262803915595,
129.498948563585));
#119422=CARTESIAN_POINT('Ctrl Pts',(-179.915287826822,-4.76405452823417,
129.582490119309));
#119423=CARTESIAN_POINT('Ctrl Pts',(-178.165366640417,-4.76405452823403,
129.582490119308));
#119424=CARTESIAN_POINT('Ctrl Pts',(-178.174286102188,-4.80301964378508,
129.734414513464));
#119425=CARTESIAN_POINT('Ctrl Pts',(-178.18320556396,-4.83475684527663,
129.888373267217));
#119426=CARTESIAN_POINT('Ctrl Pts',(-178.192125025732,-4.85907467737619,
130.043718558394));
#119427=CARTESIAN_POINT('Ctrl Pts',(-178.200980669897,-4.88321851850083,
130.197952373904));
#119428=CARTESIAN_POINT('Ctrl Pts',(-178.209836314062,-4.90004869699476,
130.353552808266));
#119429=CARTESIAN_POINT('Ctrl Pts',(-178.218691958226,-4.9094252417917,
130.509866376946));
#119430=CARTESIAN_POINT('Ctrl Pts',(-178.224174826803,-4.91523061990645,
130.606646095947));
#119431=CARTESIAN_POINT('Ctrl Pts',(-178.22965769538,-4.91817971751586,
130.70369880656));
#119432=CARTESIAN_POINT('Ctrl Pts',(-178.235140563957,-4.91824875847738,
130.80086601663));
#119433=CARTESIAN_POINT('',(-177.889859436045,-4.91824981877161,130.80302545727));
#119434=CARTESIAN_POINT('Ctrl Pts',(-177.819765072025,-4.76405452823413,
129.582490119309));
#119435=CARTESIAN_POINT('Ctrl Pts',(-177.827528067606,-4.79810789403879,
129.715263675749));
#119436=CARTESIAN_POINT('Ctrl Pts',(-177.835291063188,-4.8265751286225,
129.849339500209));
#119437=CARTESIAN_POINT('Ctrl Pts',(-177.843054058769,-4.84938475087311,
129.984207826618));
#119438=CARTESIAN_POINT('Ctrl Pts',(-177.850828440854,-4.87222782952149,
130.119273973418));
#119439=CARTESIAN_POINT('Ctrl Pts',(-177.85860282294,-4.88939667628533,
130.255134556517));
#119440=CARTESIAN_POINT('Ctrl Pts',(-177.866377205026,-4.90087174218351,
130.391275603111));
#119441=CARTESIAN_POINT('Ctrl Pts',(-177.870098127136,-4.90636386052159,
130.456434508968));
#119442=CARTESIAN_POINT('Ctrl Pts',(-177.873819049247,-4.91055247038315,
130.521657668791));
#119443=CARTESIAN_POINT('Ctrl Pts',(-177.877539971357,-4.91343964523087,
130.586888975338));
#119444=CARTESIAN_POINT('Ctrl Pts',(-177.88164645957,-4.91662599235856,
130.658879622671));
#119445=CARTESIAN_POINT('Ctrl Pts',(-177.885752947782,-4.91823024989552,
130.730940811616));
#119446=CARTESIAN_POINT('Ctrl Pts',(-177.889859435994,-4.91824981877137,
130.803025456376));
#119447=CARTESIAN_POINT('Ctrl Pts',(-177.889859436045,-4.91824981877161,
130.80302545727));
#119448=CARTESIAN_POINT('Ctrl Pts',(-177.897578984021,-4.91828660513675,
130.938533181825));
#119449=CARTESIAN_POINT('Ctrl Pts',(-177.905298531998,-4.91271888509105,
131.074267759702));
#119450=CARTESIAN_POINT('Ctrl Pts',(-177.913018079974,-4.90151653121722,
131.209723117934));
#119451=CARTESIAN_POINT('Ctrl Pts',(-177.920728283118,-4.89032773825667,
131.345014501845));
#119452=CARTESIAN_POINT('Ctrl Pts',(-177.928438486262,-4.87351791200395,
131.480026946718));
#119453=CARTESIAN_POINT('Ctrl Pts',(-177.936148689406,-4.85110890292581,
131.614252878582));
#119454=CARTESIAN_POINT('Ctrl Pts',(-177.943851468977,-4.82872146979285,
131.748349574418));
#119455=CARTESIAN_POINT('Ctrl Pts',(-177.951554248548,-4.80074564454809,
131.881660874833));
#119456=CARTESIAN_POINT('Ctrl Pts',(-177.959257028118,-4.76725516232351,
132.013683270872));
#119457=CARTESIAN_POINT('Ctrl Pts',(-177.966954298254,-4.73378863426308,
132.145611237511));
#119458=CARTESIAN_POINT('Ctrl Pts',(-177.974651568389,-4.69481539576988,
132.276251751023));
#119459=CARTESIAN_POINT('Ctrl Pts',(-177.982348838524,-4.65046036686952,
132.405110891243));
#119460=CARTESIAN_POINT('Ctrl Pts',(-177.990043303124,-4.60612150469107,
132.533923064299));
#119461=CARTESIAN_POINT('Ctrl Pts',(-177.997737767723,-4.55640488027498,
132.660954780006));
#119462=CARTESIAN_POINT('Ctrl Pts',(-178.005432232323,-4.5014853573474,
132.785726974424));
#119463=CARTESIAN_POINT('Ctrl Pts',(-178.013125478951,-4.44657452773564,
132.910479418413));
#119464=CARTESIAN_POINT('Ctrl Pts',(-178.020818725579,-4.38646259723445,
133.03297268916));
#119465=CARTESIAN_POINT('Ctrl Pts',(-178.028511972207,-4.32137249872143,
133.152747891802));
#119466=CARTESIAN_POINT('Ctrl Pts',(-178.036205725472,-4.25627811371228,
133.272530982217));
#119467=CARTESIAN_POINT('Ctrl Pts',(-178.043899478737,-4.18620509819149,
133.389595299688));
#119468=CARTESIAN_POINT('Ctrl Pts',(-178.051593232003,-4.11142201299136,
133.503507166679));
#119469=CARTESIAN_POINT('Ctrl Pts',(-178.059289216561,-4.03661723967682,
133.617452069665));
#119470=CARTESIAN_POINT('Ctrl Pts',(-178.06698520112,-3.95709989735997,
133.72824237193));
#119471=CARTESIAN_POINT('Ctrl Pts',(-178.074681185679,-3.87318119104158,
133.835474360708));
#119472=CARTESIAN_POINT('Ctrl Pts',(-178.082385491664,-3.78917174605771,
133.942822296072));
#119473=CARTESIAN_POINT('Ctrl Pts',(-178.09008979765,-3.70075168025727,
134.046603923423));
#119474=CARTESIAN_POINT('Ctrl Pts',(-178.097794103635,-3.60827196007457,
134.146449264601));
#119475=CARTESIAN_POINT('Ctrl Pts',(-178.105503084718,-3.5157361216954,
134.246355193554));
#119476=CARTESIAN_POINT('Ctrl Pts',(-178.113212065802,-3.41913600421425,
134.342319800581));
#119477=CARTESIAN_POINT('Ctrl Pts',(-178.120921046885,-3.31885770099228,
134.434011650801));
#119478=CARTESIAN_POINT('Ctrl Pts',(-178.128641384245,-3.21843167550299,
134.525838574388));
#119479=CARTESIAN_POINT('Ctrl Pts',(-178.136361721606,-3.11431694878514,
134.61337991927));
#119480=CARTESIAN_POINT('Ctrl Pts',(-178.144082058966,-3.00693114976664,
134.696345730983));
#119481=CARTESIAN_POINT('Ctrl Pts',(-178.148050571034,-2.9517312511805,
134.738992937919));
#119482=CARTESIAN_POINT('Ctrl Pts',(-178.152019083102,-2.89566748822361,
134.780431866513));
#119483=CARTESIAN_POINT('Ctrl Pts',(-178.15598759517,-2.83879919740751,
134.820627812275));
#119484=CARTESIAN_POINT('Ctrl Pts',(-178.163761929289,-2.72739394374767,
134.899371862246));
#119485=CARTESIAN_POINT('Ctrl Pts',(-178.171536263408,-2.61253338564665,
134.973601801254));
#119486=CARTESIAN_POINT('Ctrl Pts',(-178.179310597527,-2.49461950041102,
135.04299915024));
#119487=CARTESIAN_POINT('Ctrl Pts',(-178.187075350474,-2.37685093350067,
135.112310973196));
#119488=CARTESIAN_POINT('Ctrl Pts',(-178.194840103421,-2.25603686031665,
135.176801859868));
#119489=CARTESIAN_POINT('Ctrl Pts',(-178.202604856368,-2.13261028670629,
135.236195048988));
#119490=CARTESIAN_POINT('Ctrl Pts',(-178.210361897253,-2.00930630210852,
135.295529247955));
#119491=CARTESIAN_POINT('Ctrl Pts',(-178.218118938138,-1.88339533081727,
135.349775656748));
#119492=CARTESIAN_POINT('Ctrl Pts',(-178.225875979023,-1.75533686375186,
135.39870230678));
#119493=CARTESIAN_POINT('Ctrl Pts',(-178.233627170264,-1.6273749665728,
135.447592060845));
#119494=CARTESIAN_POINT('Ctrl Pts',(-178.241378361504,-1.49726916076229,
135.491169902165));
#119495=CARTESIAN_POINT('Ctrl Pts',(-178.249129552744,-1.36550057426087,
135.529251224151));
#119496=CARTESIAN_POINT('Ctrl Pts',(-178.256877449521,-1.23378799292357,
135.567316360559));
#119497=CARTESIAN_POINT('Ctrl Pts',(-178.264625346298,-1.10041441132796,
135.599889515772));
#119498=CARTESIAN_POINT('Ctrl Pts',(-178.272373243075,-0.965877633492174,
135.626835444833));
#119499=CARTESIAN_POINT('Ctrl Pts',(-178.280119519159,-0.831368997850033,
135.653775737386));
#119500=CARTESIAN_POINT('Ctrl Pts',(-178.287865795243,-0.695698033044637,
135.675091068361));
#119501=CARTESIAN_POINT('Ctrl Pts',(-178.295612071327,-0.559373905331694,
135.690697066945));
#119502=CARTESIAN_POINT('Ctrl Pts',(-178.303358404593,-0.423048771305566,
135.706303180729));
#119503=CARTESIAN_POINT('Ctrl Pts',(-178.311104737858,-0.286070853179251,
135.716199833558));
#119504=CARTESIAN_POINT('Ctrl Pts',(-178.318851071123,-0.148955232533464,
135.720354454137));
#119505=CARTESIAN_POINT('Ctrl Pts',(-178.326599139126,-0.01180890579494,
135.724510005114));
#119506=CARTESIAN_POINT('Ctrl Pts',(-178.334347207129,0.125474794115099,
135.722920953233));
#119507=CARTESIAN_POINT('Ctrl Pts',(-178.342095275132,0.262380385697254,
135.715606854083));
#119508=CARTESIAN_POINT('Ctrl Pts',(-178.349851577874,0.399431482171527,
135.708284981421));
#119509=CARTESIAN_POINT('Ctrl Pts',(-178.357607880616,0.536103276532238,
135.695225927641));
#119510=CARTESIAN_POINT('Ctrl Pts',(-178.365364183358,0.671884454715865,
135.676501249979));
#119511=CARTESIAN_POINT('Ctrl Pts',(-178.373124625872,0.807738103402582,
135.657766578393));
#119512=CARTESIAN_POINT('Ctrl Pts',(-178.380885068386,0.942699804202917,
135.63336032706));
#119513=CARTESIAN_POINT('Ctrl Pts',(-178.3886455109,1.0762690282611,135.603405110098));
#119514=CARTESIAN_POINT('Ctrl Pts',(-178.396418411166,1.21005266949546,
135.573401806363));
#119515=CARTESIAN_POINT('Ctrl Pts',(-178.404191311431,1.34243898930015,
135.537831838098));
#119516=CARTESIAN_POINT('Ctrl Pts',(-178.411964211697,1.47294233469106,
135.496867830259));
#119517=CARTESIAN_POINT('Ctrl Pts',(-178.419454547459,1.59870155475822,
135.457392967287));
#119518=CARTESIAN_POINT('Ctrl Pts',(-178.426944883221,1.72271203539251,
135.412909533879));
#119519=CARTESIAN_POINT('Ctrl Pts',(-178.434435218983,1.8445590297808,135.363613302837));
#119520=CARTESIAN_POINT('Ctrl Pts',(-178.442209553102,1.97102588999646,
135.312447990212));
#119521=CARTESIAN_POINT('Ctrl Pts',(-178.449983887221,2.09556257726352,
135.255935644863));
#119522=CARTESIAN_POINT('Ctrl Pts',(-178.45775822134,2.21768386757729,135.194242315971));
#119523=CARTESIAN_POINT('Ctrl Pts',(-178.465522974287,2.33965465431505,
135.132625018593));
#119524=CARTESIAN_POINT('Ctrl Pts',(-178.473287727234,2.45921562135268,
135.065839616714));
#119525=CARTESIAN_POINT('Ctrl Pts',(-178.481052480181,2.57589987136006,
134.994100814192));
#119526=CARTESIAN_POINT('Ctrl Pts',(-178.488809521066,2.69246822892538,
134.922433263661));
#119527=CARTESIAN_POINT('Ctrl Pts',(-178.496566561951,2.80616522451045,
134.845822306524));
#119528=CARTESIAN_POINT('Ctrl Pts',(-178.504323602836,2.91654733030766,
134.76452914082));
#119529=CARTESIAN_POINT('Ctrl Pts',(-178.512074794076,3.02684619610039,
134.683297278925));
#119530=CARTESIAN_POINT('Ctrl Pts',(-178.519825985316,3.13383483424316,
134.59739046739));
#119531=CARTESIAN_POINT('Ctrl Pts',(-178.527577176556,3.23709786857969,
134.507113708408));
#119532=CARTESIAN_POINT('Ctrl Pts',(-178.535325073334,3.34031701337215,
134.416875319456));
#119533=CARTESIAN_POINT('Ctrl Pts',(-178.543072970111,3.43981341005556,
134.322270933959));
#119534=CARTESIAN_POINT('Ctrl Pts',(-178.550820866888,3.53520419798672,
134.223646265335));
#119535=CARTESIAN_POINT('Ctrl Pts',(-178.558567142972,3.63057503222116,
134.125042226865));
#119536=CARTESIAN_POINT('Ctrl Pts',(-178.566313419056,3.72184169427708,
134.022419858821));
#119537=CARTESIAN_POINT('Ctrl Pts',(-178.57405969514,3.80865798380126,133.916161932709));
#119538=CARTESIAN_POINT('Ctrl Pts',(-178.581806028405,3.89547491418369,
133.809903222225));
#119539=CARTESIAN_POINT('Ctrl Pts',(-178.589552361671,3.97784115911567,
133.700009202882));
#119540=CARTESIAN_POINT('Ctrl Pts',(-178.597298694936,4.05545090126791,
133.586895621821));
#119541=CARTESIAN_POINT('Ctrl Pts',(-178.605046762939,4.1330780235839,133.473756709758));
#119542=CARTESIAN_POINT('Ctrl Pts',(-178.612794830942,4.20594630237465,
133.357397123591));
#119543=CARTESIAN_POINT('Ctrl Pts',(-178.620542898945,4.27379355996916,
133.238261122777));
#119544=CARTESIAN_POINT('Ctrl Pts',(-178.628299201687,4.34171292643635,
133.118998502804));
#119545=CARTESIAN_POINT('Ctrl Pts',(-178.636055504429,4.40460041788537,
132.996953913909));
#119546=CARTESIAN_POINT('Ctrl Pts',(-178.643811807171,4.46223985970607,
132.872596217528));
#119547=CARTESIAN_POINT('Ctrl Pts',(-178.651572249685,4.51991006543252,
132.7481721477));
#119548=CARTESIAN_POINT('Ctrl Pts',(-178.659332692199,4.57232649087066,
132.621432871501));
#119549=CARTESIAN_POINT('Ctrl Pts',(-178.667093134713,4.6193217466782,132.492865773959));
#119550=CARTESIAN_POINT('Ctrl Pts',(-178.674866034979,4.66639244344228,
132.364092289099));
#119551=CARTESIAN_POINT('Ctrl Pts',(-178.682638935244,4.70802446131689,
132.233485492179));
#119552=CARTESIAN_POINT('Ctrl Pts',(-178.69041183551,4.7441005272662,132.101547284817));
#119553=CARTESIAN_POINT('Ctrl Pts',(-178.697902171271,4.77886513734783,
131.974405363625));
#119554=CARTESIAN_POINT('Ctrl Pts',(-178.705392507033,4.80847065889238,
131.846027451783));
#119555=CARTESIAN_POINT('Ctrl Pts',(-178.712882842795,4.83285762032032,
131.716868307513));
#119556=CARTESIAN_POINT('Ctrl Pts',(-178.720657176914,4.85816922080323,
131.58281205503));
#119557=CARTESIAN_POINT('Ctrl Pts',(-178.728431511034,4.87793890559331,
131.447489509917));
#119558=CARTESIAN_POINT('Ctrl Pts',(-178.736205845153,4.89204410114357,
131.311398658512));
#119559=CARTESIAN_POINT('Ctrl Pts',(-178.7439705981,4.90613191330093,131.175475526918));
#119560=CARTESIAN_POINT('Ctrl Pts',(-178.751735351047,4.91456908636255,
131.038786358168));
#119561=CARTESIAN_POINT('Ctrl Pts',(-178.759500103994,4.91728388735268,
130.901840018886));
#119562=CARTESIAN_POINT('Ctrl Pts',(-178.767257144879,4.9199959919642,130.765029696639));
#119563=CARTESIAN_POINT('Ctrl Pts',(-178.775014185764,4.91699702730776,
130.627963100528));
#119564=CARTESIAN_POINT('Ctrl Pts',(-178.782771226649,4.90826700907514,
130.491154566979));
#119565=CARTESIAN_POINT('Ctrl Pts',(-178.790522417889,4.89954357421716,
130.354449201808));
#119566=CARTESIAN_POINT('Ctrl Pts',(-178.798273609129,4.88509771292451,
130.218001900438));
#119567=CARTESIAN_POINT('Ctrl Pts',(-178.806024800369,4.86496151122054,
130.082326991727));
#119568=CARTESIAN_POINT('Ctrl Pts',(-178.813772697147,4.84483386793941,
129.946709748471));
#119569=CARTESIAN_POINT('Ctrl Pts',(-178.821520593924,4.81902075182776,
129.811864630855));
#119570=CARTESIAN_POINT('Ctrl Pts',(-178.829268490701,4.78760607584458,
129.678300616928));
#119571=CARTESIAN_POINT('Ctrl Pts',(-178.837014766785,4.75619797113449,
129.544764541714));
#119572=CARTESIAN_POINT('Ctrl Pts',(-178.844761042869,4.71919072663617,
129.412509417502));
#119573=CARTESIAN_POINT('Ctrl Pts',(-178.852507318953,4.67671924911073,
129.282033409802));
#119574=CARTESIAN_POINT('Ctrl Pts',(-178.860253652219,4.63424745807043,
129.151556438958));
#119575=CARTESIAN_POINT('Ctrl Pts',(-178.867999985484,4.58631147452994,
129.022858982598));
#119576=CARTESIAN_POINT('Ctrl Pts',(-178.875746318749,4.53309577659699,
128.896423054987));
#119577=CARTESIAN_POINT('Ctrl Pts',(-178.883494386752,4.47986816137724,
128.769958812926));
#119578=CARTESIAN_POINT('Ctrl Pts',(-178.891242454755,4.42135863065274,
128.645757467678));
#119579=CARTESIAN_POINT('Ctrl Pts',(-178.898990522758,4.35779923905243,
128.524279729831));
#119580=CARTESIAN_POINT('Ctrl Pts',(-178.9067468255,4.29417229577462,128.402672883999));
#119581=CARTESIAN_POINT('Ctrl Pts',(-178.914503128242,4.22548495189499,
128.283795774974));
#119582=CARTESIAN_POINT('Ctrl Pts',(-178.922259430984,4.15201482616275,
128.168083707637));
#119583=CARTESIAN_POINT('Ctrl Pts',(-178.930019873498,4.07850548721226,
128.052309881286));
#119584=CARTESIAN_POINT('Ctrl Pts',(-178.937780316012,4.00020850299509,
127.93970478349));
#119585=CARTESIAN_POINT('Ctrl Pts',(-178.945540758526,3.91744344631057,
127.830672687157));
#119586=CARTESIAN_POINT('Ctrl Pts',(-178.953313658792,3.83454552780952,
127.721465562824));
#119587=CARTESIAN_POINT('Ctrl Pts',(-178.961086559057,3.74716545316439,
127.615843203123));
#119588=CARTESIAN_POINT('Ctrl Pts',(-178.968859459323,3.65566209747847,
127.514175563263));
#119589=CARTESIAN_POINT('Ctrl Pts',(-178.976349795085,3.56748511925551,
127.416203798198));
#119590=CARTESIAN_POINT('Ctrl Pts',(-178.983840130847,3.47547965372134,
127.321904437295));
#119591=CARTESIAN_POINT('Ctrl Pts',(-178.991330466609,3.37999615600626,
127.231573323606));
#119592=CARTESIAN_POINT('Ctrl Pts',(-178.999104800728,3.28089237245302,
127.137817278285));
#119593=CARTESIAN_POINT('Ctrl Pts',(-179.006879134847,3.17772768024682,
127.048039341494));
#119594=CARTESIAN_POINT('Ctrl Pts',(-179.014653468966,3.07085479539997,
126.962611811609));
#119595=CARTESIAN_POINT('Ctrl Pts',(-179.022418221913,2.9641136218319,126.87728956352));
#119596=CARTESIAN_POINT('Ctrl Pts',(-179.03018297486,2.85367365105237,126.796307296342));
#119597=CARTESIAN_POINT('Ctrl Pts',(-179.037947727807,2.73992423354038,
126.720000415899));
#119598=CARTESIAN_POINT('Ctrl Pts',(-179.045704768692,2.62628779355376,
126.643769324527));
#119599=CARTESIAN_POINT('Ctrl Pts',(-179.053461809577,2.50934877066748,
126.572204595192));
#119600=CARTESIAN_POINT('Ctrl Pts',(-179.061218850462,2.38952908867568,
126.50560105266));
#119601=CARTESIAN_POINT('Ctrl Pts',(-179.068970041702,2.26979976363732,
126.439047736377));
#119602=CARTESIAN_POINT('Ctrl Pts',(-179.076721232943,2.14719444371695,
126.377448349309));
#119603=CARTESIAN_POINT('Ctrl Pts',(-179.084472424183,2.02216319162956,
126.321053903887));
#119604=CARTESIAN_POINT('Ctrl Pts',(-179.09222032096,1.89718508116047,126.264683427609));
#119605=CARTESIAN_POINT('Ctrl Pts',(-179.099968217737,1.76978344491984,
126.213513653413));
#119606=CARTESIAN_POINT('Ctrl Pts',(-179.107716114514,1.64043185755897,
126.167749098018));
#119607=CARTESIAN_POINT('Ctrl Pts',(-179.115462390598,1.51110732776167,
126.121994115581));
#119608=CARTESIAN_POINT('Ctrl Pts',(-179.123208666682,1.37983402649866,
126.08164223333));
#119609=CARTESIAN_POINT('Ctrl Pts',(-179.130954942766,1.24710399492245,
126.046849221011));
#119610=CARTESIAN_POINT('Ctrl Pts',(-179.138701276032,1.11437298356347,
126.012055951859));
#119611=CARTESIAN_POINT('Ctrl Pts',(-179.146447609297,0.980185598621585,
125.982821733656));
#119612=CARTESIAN_POINT('Ctrl Pts',(-179.154193942562,0.845047087272823,
125.959251900231));
#119613=CARTESIAN_POINT('Ctrl Pts',(-179.161942010565,0.709878312591245,
125.935676788506));
#119614=CARTESIAN_POINT('Ctrl Pts',(-179.169690078568,0.573758372738378,
125.917768652887));
#119615=CARTESIAN_POINT('Ctrl Pts',(-179.177438146571,0.437200307775627,
125.905581284571));
#119616=CARTESIAN_POINT('Ctrl Pts',(-179.185194449313,0.300497107276185,
125.893380963375));
#119617=CARTESIAN_POINT('Ctrl Pts',(-179.192950752055,0.163355241530021,
125.886913589944));
#119618=CARTESIAN_POINT('Ctrl Pts',(-179.200707054797,0.0262910045776176,
125.886180888685));
#119619=CARTESIAN_POINT('Ctrl Pts',(-179.208467497311,-0.110846387685345,
125.885447796361));
#119620=CARTESIAN_POINT('Ctrl Pts',(-179.216227939825,-0.247905678082787,
125.890455460777));
#119621=CARTESIAN_POINT('Ctrl Pts',(-179.223988382339,-0.384374003464339,
125.901153535669));
#119622=CARTESIAN_POINT('Ctrl Pts',(-179.231761282605,-0.52106139991651,
125.911868784061));
#119623=CARTESIAN_POINT('Ctrl Pts',(-179.23953418287,-0.657155547236459,
125.928292650204));
#119624=CARTESIAN_POINT('Ctrl Pts',(-179.247307083135,-0.792151210869699,
125.950323172138));
#119625=CARTESIAN_POINT('Ctrl Pts',(-179.254797418897,-0.922239442095216,
125.971552829108));
#119626=CARTESIAN_POINT('Ctrl Pts',(-179.262287754659,-1.05130736659908,
125.997988525034));
#119627=CARTESIAN_POINT('Ctrl Pts',(-179.269778090421,-1.17891665368521,
126.029495322486));
#119628=CARTESIAN_POINT('Ctrl Pts',(-179.27755242454,-1.31136428567816,
126.062196709739));
#119629=CARTESIAN_POINT('Ctrl Pts',(-179.285326758659,-1.44266004261855,
126.100464919285));
#119630=CARTESIAN_POINT('Ctrl Pts',(-179.293101092779,-1.57230004771894,
126.144204437518));
#119631=CARTESIAN_POINT('Ctrl Pts',(-179.300865845726,-1.70178028309931,
126.187890050703));
#119632=CARTESIAN_POINT('Ctrl Pts',(-179.308630598673,-1.8296084598658,
126.237033432431));
#119633=CARTESIAN_POINT('Ctrl Pts',(-179.31639535162,-1.95529193815402,
126.291488306156));
#119634=CARTESIAN_POINT('Ctrl Pts',(-179.324152392505,-2.08085058584013,
126.345889094533));
#119635=CARTESIAN_POINT('Ctrl Pts',(-179.33190943339,-2.20426841771294,
126.405590722102));
#119636=CARTESIAN_POINT('Ctrl Pts',(-179.339666474275,-2.32506932923065,
126.470397572411));
#119637=CARTESIAN_POINT('Ctrl Pts',(-179.347417665515,-2.44577914384112,
126.53515555137));
#119638=CARTESIAN_POINT('Ctrl Pts',(-179.355168856755,-2.56387562298451,
126.605010906023));
#119639=CARTESIAN_POINT('Ctrl Pts',(-179.362920047995,-2.67890431290246,
126.679720664211));
#119640=CARTESIAN_POINT('Ctrl Pts',(-179.370667944772,-2.79388411255856,
126.754398668759));
#119641=CARTESIAN_POINT('Ctrl Pts',(-179.378415841549,-2.90579838913901,
126.833926760686));
#119642=CARTESIAN_POINT('Ctrl Pts',(-179.386163738326,-3.01421909826937,
126.918017054507));
#119643=CARTESIAN_POINT('Ctrl Pts',(-179.393910014411,-3.12261712812466,
127.002089758452));
#119644=CARTESIAN_POINT('Ctrl Pts',(-179.401656290495,-3.22752273534894,
127.090722526651));
#119645=CARTESIAN_POINT('Ctrl Pts',(-179.409402566579,-3.32853890617992,
127.183585588301));
#119646=CARTESIAN_POINT('Ctrl Pts',(-179.417148899844,-3.42955582268919,
127.276449335445));
#119647=CARTESIAN_POINT('Ctrl Pts',(-179.424895233109,-3.52668295768921,
127.373543173757));
#119648=CARTESIAN_POINT('Ctrl Pts',(-179.432641566375,-3.61955859240775,
127.474498959985));
#119649=CARTESIAN_POINT('Ctrl Pts',(-179.440389634378,-3.71245502598061,
127.575477354561));
#119650=CARTESIAN_POINT('Ctrl Pts',(-179.448137702381,-3.80109780006598,
127.680319130344));
#119651=CARTESIAN_POINT('Ctrl Pts',(-179.455885770384,-3.88516434792299,
127.788621727654));
#119652=CARTESIAN_POINT('Ctrl Pts',(-179.463642073126,-3.96932024270782,
127.897039430254));
#119653=CARTESIAN_POINT('Ctrl Pts',(-179.471398375867,-4.04888995545252,
128.008924992652));
#119654=CARTESIAN_POINT('Ctrl Pts',(-179.479154678609,-4.12359296582618,
128.123844974133));
#119655=CARTESIAN_POINT('Ctrl Pts',(-179.486915121123,-4.19833584744553,
128.238826291868));
#119656=CARTESIAN_POINT('Ctrl Pts',(-179.494675563638,-4.26820665186612,
128.356844919536));
#119657=CARTESIAN_POINT('Ctrl Pts',(-179.502436006152,-4.33297052176697,
128.477442157456));
#119658=CARTESIAN_POINT('Ctrl Pts',(-179.510208906417,-4.39783835638142,
128.59823298877));
#119659=CARTESIAN_POINT('Ctrl Pts',(-179.517981806683,-4.45758270355803,
128.721610350122));
#119660=CARTESIAN_POINT('Ctrl Pts',(-179.525754706948,-4.5120162551646,
128.847094060443));
#119661=CARTESIAN_POINT('Ctrl Pts',(-179.53324504271,-4.56447101006087,
128.968016121821));
#119662=CARTESIAN_POINT('Ctrl Pts',(-179.540735378472,-4.6119942762349,
129.090893761478));
#119663=CARTESIAN_POINT('Ctrl Pts',(-179.548225714234,-4.65446265192088,
129.215285262407));
#119664=CARTESIAN_POINT('Ctrl Pts',(-179.555502049297,-4.69571769586986,
129.336122868151));
#119665=CARTESIAN_POINT('Ctrl Pts',(-179.562778384359,-4.73228882758073,
129.458636134573));
#119666=CARTESIAN_POINT('Ctrl Pts',(-179.570054719422,-4.76405452823393,
129.582490119308));
#119667=CARTESIAN_POINT('Origin',(213.235140564004,0.,130.804360617566));
#119668=CARTESIAN_POINT('',(-181.664999290689,-4.76405452823418,129.582490119309));
#119669=CARTESIAN_POINT('',(-181.320039938991,-4.76405452823418,129.582490119309));
#119670=CARTESIAN_POINT('',(213.235140564004,-4.76405452823405,129.582490119308));
#119671=CARTESIAN_POINT('',(-179.985140564067,-4.91824883331974,130.807748249335));
#119672=CARTESIAN_POINT('Ctrl Pts',(-179.985140564067,-4.91824883331974,
130.807748249336));
#119673=CARTESIAN_POINT('Ctrl Pts',(-179.993960729007,-4.91814115236676,
130.964082159672));
#119674=CARTESIAN_POINT('Ctrl Pts',(-180.002780893947,-4.91057552406498,
131.120123073993));
#119675=CARTESIAN_POINT('Ctrl Pts',(-180.011601058887,-4.89565957716396,
131.27521130199));
#119676=CARTESIAN_POINT('Ctrl Pts',(-180.020460543816,-4.88067713548981,
131.43099090792));
#119677=CARTESIAN_POINT('Ctrl Pts',(-180.029320028745,-4.85827880522494,
131.585809153203));
#119678=CARTESIAN_POINT('Ctrl Pts',(-180.038179513674,-4.82862329315814,
131.739015717199));
#119679=CARTESIAN_POINT('Ctrl Pts',(-180.047091538771,-4.79879191244734,
131.893130855312));
#119680=CARTESIAN_POINT('Ctrl Pts',(-180.056003563869,-4.7616171115927,
132.045614980022));
#119681=CARTESIAN_POINT('Ctrl Pts',(-180.064915588966,-4.71730902760369,
132.195826966634));
#119682=CARTESIAN_POINT('Ctrl Pts',(-180.071787714544,-4.68314275069523,
132.311656491802));
#119683=CARTESIAN_POINT('Ctrl Pts',(-180.078659840122,-4.64473597477464,
132.426135393135));
#119684=CARTESIAN_POINT('Ctrl Pts',(-180.0855319657,-4.60220406385651,132.538978966691));
#119685=CARTESIAN_POINT('Ctrl Pts',(-180.093306299819,-4.55408834151546,
132.666637234001));
#119686=CARTESIAN_POINT('Ctrl Pts',(-180.101080633938,-4.50058080743443,
132.792494198247));
#119687=CARTESIAN_POINT('Ctrl Pts',(-180.108854968057,-4.44183581893942,
132.916060790433));
#119688=CARTESIAN_POINT('Ctrl Pts',(-180.116619721004,-4.3831632283927,
133.039475097838));
#119689=CARTESIAN_POINT('Ctrl Pts',(-180.124384473951,-4.31926619260353,
133.160604299769));
#119690=CARTESIAN_POINT('Ctrl Pts',(-180.132149226898,-4.25034814935119,
133.27897648105));
#119691=CARTESIAN_POINT('Ctrl Pts',(-180.139906267783,-4.1814985564708,
133.397231093413));
#119692=CARTESIAN_POINT('Ctrl Pts',(-180.147663308668,-4.10763807579476,
133.512733798804));
#119693=CARTESIAN_POINT('Ctrl Pts',(-180.155420349553,-4.02901718669648,
133.62503492911));
#119694=CARTESIAN_POINT('Ctrl Pts',(-180.163171540793,-3.95045558622215,
133.73725137226));
#119695=CARTESIAN_POINT('Ctrl Pts',(-180.170922732034,-3.8671409460421,
133.846270726925));
#119696=CARTESIAN_POINT('Ctrl Pts',(-180.178673923274,-3.77936821263246,
133.951670417354));
#119697=CARTESIAN_POINT('Ctrl Pts',(-180.186421820051,-3.69163278497605,
134.057025310104));
#119698=CARTESIAN_POINT('Ctrl Pts',(-180.194169716828,-3.5994432823843,
134.158763298683));
#119699=CARTESIAN_POINT('Ctrl Pts',(-180.201917613605,-3.50313613111719,
134.256493336533));
#119700=CARTESIAN_POINT('Ctrl Pts',(-180.209663889689,-3.40684912522998,
134.354202931366));
#119701=CARTESIAN_POINT('Ctrl Pts',(-180.217410165773,-3.30644645813239,
134.447905964751));
#119702=CARTESIAN_POINT('Ctrl Pts',(-180.225156441857,-3.20230248324751,
134.537247150571));
#119703=CARTESIAN_POINT('Ctrl Pts',(-180.232902775123,-3.0981577395956,
134.626588995887));
#119704=CARTESIAN_POINT('Ctrl Pts',(-180.240649108388,-2.99027192978512,
134.711568674828));
#119705=CARTESIAN_POINT('Ctrl Pts',(-180.248395441653,-2.8790533424594,
134.79187048135));
#119706=CARTESIAN_POINT('Ctrl Pts',(-180.256143509656,-2.76780984850203,
134.872190270904));
#119707=CARTESIAN_POINT('Ctrl Pts',(-180.263891577659,-2.65323240879196,
134.947829874661));
#119708=CARTESIAN_POINT('Ctrl Pts',(-180.271639645662,-2.53575886331033,
135.018516529447));
#119709=CARTESIAN_POINT('Ctrl Pts',(-180.279395948404,-2.41816046554677,
135.089278310851));
#119710=CARTESIAN_POINT('Ctrl Pts',(-180.287152251146,-2.29766014887279,
135.155076425877));
#119711=CARTESIAN_POINT('Ctrl Pts',(-180.294908553888,-2.17472145211095,
135.215683510784));
#119712=CARTESIAN_POINT('Ctrl Pts',(-180.302668996402,-2.05171713926471,
135.276322943517));
#119713=CARTESIAN_POINT('Ctrl Pts',(-180.310429438916,-1.92627221052881,
135.331765667491));
#119714=CARTESIAN_POINT('Ctrl Pts',(-180.31818988143,-1.79886989369378,
135.381832645669));
#119715=CARTESIAN_POINT('Ctrl Pts',(-180.325962781696,-1.67126305934953,
135.431979995805));
#119716=CARTESIAN_POINT('Ctrl Pts',(-180.333735681961,-1.54169292759772,
135.476734227691));
#119717=CARTESIAN_POINT('Ctrl Pts',(-180.341508582227,-1.41065844128908,
135.515966057808));
#119718=CARTESIAN_POINT('Ctrl Pts',(-180.348998917989,-1.28438738861264,
135.553771712082));
#119719=CARTESIAN_POINT('Ctrl Pts',(-180.356489253751,-1.15675689732088,
135.586449423876));
#119720=CARTESIAN_POINT('Ctrl Pts',(-180.363979589513,-1.02822016752291,
135.613928825794));
#119721=CARTESIAN_POINT('Ctrl Pts',(-180.371753923632,-0.894809928547707,
135.642450117588));
#119722=CARTESIAN_POINT('Ctrl Pts',(-180.379528257751,-0.760000770908441,
135.665461477155));
#119723=CARTESIAN_POINT('Ctrl Pts',(-180.38730259187,-0.624287596106585,
135.682828415948));
#119724=CARTESIAN_POINT('Ctrl Pts',(-180.395067344817,-0.488741675663636,
135.700173951541));
#119725=CARTESIAN_POINT('Ctrl Pts',(-180.402832097764,-0.352294338905479,
135.711888858062));
#119726=CARTESIAN_POINT('Ctrl Pts',(-180.410596850712,-0.215452584523784,
135.717889211797));
#119727=CARTESIAN_POINT('Ctrl Pts',(-180.418353891597,-0.0787467433016716,
135.723883605896));
#119728=CARTESIAN_POINT('Ctrl Pts',(-180.426110932482,0.0583523478990269,
135.72417472524));
#119729=CARTESIAN_POINT('Ctrl Pts',(-180.433867973367,0.195330980338071,
135.718730248619));
#119730=CARTESIAN_POINT('Ctrl Pts',(-180.441619164607,0.332206316124668,
135.713289877721));
#119731=CARTESIAN_POINT('Ctrl Pts',(-180.449370355847,0.468960984882857,
135.702122535486));
#119732=CARTESIAN_POINT('Ctrl Pts',(-180.457121547087,0.605080035891566,
135.685247956223));
#119733=CARTESIAN_POINT('Ctrl Pts',(-180.464869443864,0.741141232672686,
135.668380549107));
#119734=CARTESIAN_POINT('Ctrl Pts',(-180.472617340641,0.876566961838184,
135.645810777549));
#119735=CARTESIAN_POINT('Ctrl Pts',(-180.480365237418,1.01084637823296,
135.617610316274));
#119736=CARTESIAN_POINT('Ctrl Pts',(-180.488111513502,1.14509770626855,
135.589415753928));
#119737=CARTESIAN_POINT('Ctrl Pts',(-180.495857789587,1.27820281610075,
135.555592924915));
#119738=CARTESIAN_POINT('Ctrl Pts',(-180.503604065671,1.40966044828803,
135.516264742549));
#119739=CARTESIAN_POINT('Ctrl Pts',(-180.511350398936,1.54111905086551,
135.476936269871));
#119740=CARTESIAN_POINT('Ctrl Pts',(-180.519096732201,1.67092977696887,
135.432102474804));
#119741=CARTESIAN_POINT('Ctrl Pts',(-180.526843065467,1.7986063241752,135.381936215318));
#119742=CARTESIAN_POINT('Ctrl Pts',(-180.53459113347,1.9263114636592,135.331758721446));
#119743=CARTESIAN_POINT('Ctrl Pts',(-180.542339201473,2.05188110939729,
135.276246529846));
#119744=CARTESIAN_POINT('Ctrl Pts',(-180.550087269476,2.17484911480286,
135.215620572538));
#119745=CARTESIAN_POINT('Ctrl Pts',(-180.557843572218,2.29794781206775,
135.154930181241));
#119746=CARTESIAN_POINT('Ctrl Pts',(-180.56559987496,2.41843899428399,135.089115340456));
#119747=CARTESIAN_POINT('Ctrl Pts',(-180.573356177701,2.53588081984257,
135.018443142868));
#119748=CARTESIAN_POINT('Ctrl Pts',(-180.581116620216,2.65338532763989,
134.9477332254));
#119749=CARTESIAN_POINT('Ctrl Pts',(-180.58887706273,2.76783690968252,134.87216100064));
#119750=CARTESIAN_POINT('Ctrl Pts',(-180.596637505244,2.87882374061796,
134.792036247924));
#119751=CARTESIAN_POINT('Ctrl Pts',(-180.604410405509,2.98998873746736,
134.711782871843));
#119752=CARTESIAN_POINT('Ctrl Pts',(-180.612183305775,3.09767756139703,
134.6269626059));
#119753=CARTESIAN_POINT('Ctrl Pts',(-180.61995620604,3.2015117517228,134.537925343948));
#119754=CARTESIAN_POINT('Ctrl Pts',(-180.627446541802,3.30157130768515,
134.452124810741));
#119755=CARTESIAN_POINT('Ctrl Pts',(-180.634936877564,3.39805139018646,
134.362408765159));
#119756=CARTESIAN_POINT('Ctrl Pts',(-180.642427213326,3.49064783141407,
134.269120461992));
#119757=CARTESIAN_POINT('Ctrl Pts',(-180.650201547445,3.58675509485719,
134.172295104453));
#119758=CARTESIAN_POINT('Ctrl Pts',(-180.657975881564,3.67898284597718,
134.071314544067));
#119759=CARTESIAN_POINT('Ctrl Pts',(-180.665750215683,3.76695042939966,
133.966522461138));
#119760=CARTESIAN_POINT('Ctrl Pts',(-180.67351496863,3.85480960063723,133.861859525086));
#119761=CARTESIAN_POINT('Ctrl Pts',(-180.681279721577,3.93841880170574,
133.75339470941));
#119762=CARTESIAN_POINT('Ctrl Pts',(-180.689044474525,4.01743338003051,
133.64150920365));
#119763=CARTESIAN_POINT('Ctrl Pts',(-180.69680151541,4.09636947996217,133.529734824151));
#119764=CARTESIAN_POINT('Ctrl Pts',(-180.704558556295,4.17071981453642,
133.414546832993));
#119765=CARTESIAN_POINT('Ctrl Pts',(-180.71231559718,4.24017951888239,133.296359957484));
#119766=CARTESIAN_POINT('Ctrl Pts',(-180.72006678842,4.30958684312489,133.178262207617));
#119767=CARTESIAN_POINT('Ctrl Pts',(-180.72781797966,4.37411068070913,133.057170410442));
#119768=CARTESIAN_POINT('Ctrl Pts',(-180.7355691709,4.433489291225,132.933528475461));
#119769=CARTESIAN_POINT('Ctrl Pts',(-180.743317067677,4.4928426642475,132.8099390916));
#119770=CARTESIAN_POINT('Ctrl Pts',(-180.751064964454,4.5470549907979,132.683802077373));
#119771=CARTESIAN_POINT('Ctrl Pts',(-180.758812861231,4.59591044856734,
132.555585963217));
#119772=CARTESIAN_POINT('Ctrl Pts',(-180.766559137315,4.64475568682821,
132.427396669107));
#119773=CARTESIAN_POINT('Ctrl Pts',(-180.774305413399,4.68824614600501,
132.297129505223));
#119774=CARTESIAN_POINT('Ctrl Pts',(-180.782051689483,4.72621429357663,
132.165272632978));
#119775=CARTESIAN_POINT('Ctrl Pts',(-180.789798022749,4.76418272142055,
132.033414787394));
#119776=CARTESIAN_POINT('Ctrl Pts',(-180.797544356014,4.79662864813414,
131.899967585733));
#119777=CARTESIAN_POINT('Ctrl Pts',(-180.80529068928,4.82343464568437,131.765433601949));
#119778=CARTESIAN_POINT('Ctrl Pts',(-180.813038757283,4.85024664625185,
131.630869490213));
#119779=CARTESIAN_POINT('Ctrl Pts',(-180.820786825286,4.87141612800267,
131.495218495417));
#119780=CARTESIAN_POINT('Ctrl Pts',(-180.828534893288,4.88687700368533,
131.358992219038));
#119781=CARTESIAN_POINT('Ctrl Pts',(-180.83629119603,4.90235431137068,131.222621159752));
#119782=CARTESIAN_POINT('Ctrl Pts',(-180.844047498772,4.91211084899382,
131.085673986604));
#119783=CARTESIAN_POINT('Ctrl Pts',(-180.851803801514,4.91613250301284,
130.948666803576));
#119784=CARTESIAN_POINT('Ctrl Pts',(-180.859564244028,4.92015630350971,
130.811586495688));
#119785=CARTESIAN_POINT('Ctrl Pts',(-180.867324686542,4.91843912623242,
130.674446504842));
#119786=CARTESIAN_POINT('Ctrl Pts',(-180.875085129057,4.91101899564668,
130.537760754668));
#119787=CARTESIAN_POINT('Ctrl Pts',(-180.882858029322,4.90358695360859,
130.400855584392));
#119788=CARTESIAN_POINT('Ctrl Pts',(-180.890630929587,4.89043370141627,
130.264406501322));
#119789=CARTESIAN_POINT('Ctrl Pts',(-180.898403829853,4.871649047432,130.128921041323));
#119790=CARTESIAN_POINT('Ctrl Pts',(-180.905894165615,4.85354726293575,
129.998360819063));
#119791=CARTESIAN_POINT('Ctrl Pts',(-180.913384501377,4.83021645414565,
129.86869567912));
#119792=CARTESIAN_POINT('Ctrl Pts',(-180.920874837139,4.80178100090587,
129.74036706409));
#119793=CARTESIAN_POINT('Ctrl Pts',(-180.928649171258,4.77226740881377,
129.607172830616));
#119794=CARTESIAN_POINT('Ctrl Pts',(-180.936423505377,4.73716095571161,
129.474996552097));
#119795=CARTESIAN_POINT('Ctrl Pts',(-180.944197839496,4.69654503604511,
129.344344252281));
#119796=CARTESIAN_POINT('Ctrl Pts',(-180.951962592443,4.65597917186976,
129.213852969748));
#119797=CARTESIAN_POINT('Ctrl Pts',(-180.95972734539,4.60991746600389,129.08488229868));
#119798=CARTESIAN_POINT('Ctrl Pts',(-180.967492098337,4.55849433086872,
128.957928247308));
#119799=CARTESIAN_POINT('Ctrl Pts',(-180.975249139222,4.5071222699163,128.831100288489));
#119800=CARTESIAN_POINT('Ctrl Pts',(-180.983006180107,4.45039952260687,
128.706285323457));
#119801=CARTESIAN_POINT('Ctrl Pts',(-180.990763220992,4.38851022386175,
128.583964013902));
#119802=CARTESIAN_POINT('Ctrl Pts',(-180.998514412233,4.32666759631816,
128.461734947799));
#119803=CARTESIAN_POINT('Ctrl Pts',(-181.006265603473,4.2596663481538,128.341996141624));
#119804=CARTESIAN_POINT('Ctrl Pts',(-181.014016794713,4.18773847591968,
128.225207748928));
#119805=CARTESIAN_POINT('Ctrl Pts',(-181.02176469149,4.11584117494989,128.108468994414));
#119806=CARTESIAN_POINT('Ctrl Pts',(-181.029512588267,4.03902161920529,
127.994678491457));
#119807=CARTESIAN_POINT('Ctrl Pts',(-181.037260485044,3.95755733938158,
127.884271069623));
#119808=CARTESIAN_POINT('Ctrl Pts',(-181.045006761128,3.87611010012927,
127.773886742641));
#119809=CARTESIAN_POINT('Ctrl Pts',(-181.052753037212,3.79002030129498,
127.666884403591));
#119810=CARTESIAN_POINT('Ctrl Pts',(-181.060499313296,3.6996080914805,127.563668865493));
#119811=CARTESIAN_POINT('Ctrl Pts',(-181.068245646562,3.6091952142635,127.460452565482));
#119812=CARTESIAN_POINT('Ctrl Pts',(-181.075991979827,3.51446012000957,
127.361023416295));
#119813=CARTESIAN_POINT('Ctrl Pts',(-181.083738313092,3.41576216570124,
127.26575186696));
#119814=CARTESIAN_POINT('Ctrl Pts',(-181.091486381095,3.3170421086705,127.170458982223));
#119815=CARTESIAN_POINT('Ctrl Pts',(-181.099234449098,3.2143577068925,127.079325821528));
#119816=CARTESIAN_POINT('Ctrl Pts',(-181.106982517101,3.10810366340641,
126.992684519047));
#119817=CARTESIAN_POINT('Ctrl Pts',(-181.114738819843,3.00173669185833,
126.905951133159));
#119818=CARTESIAN_POINT('Ctrl Pts',(-181.122495122585,2.89179280344652,
126.82371938953));
#119819=CARTESIAN_POINT('Ctrl Pts',(-181.130251425327,2.77869858235167,
126.746280129092));
#119820=CARTESIAN_POINT('Ctrl Pts',(-181.138011867841,2.66554399946583,
126.668799536988));
#119821=CARTESIAN_POINT('Ctrl Pts',(-181.145772310355,2.54923606489846,
126.596116731981));
#119822=CARTESIAN_POINT('Ctrl Pts',(-181.153532752869,2.43022771030707,
126.528477511288));
#119823=CARTESIAN_POINT('Ctrl Pts',(-181.161305653134,2.31102831293982,
126.460729710112));
#119824=CARTESIAN_POINT('Ctrl Pts',(-181.1690785534,2.18912018081892,126.398041851348));
#119825=CARTESIAN_POINT('Ctrl Pts',(-181.176851453665,2.06497886185556,
126.340612712208));
#119826=CARTESIAN_POINT('Ctrl Pts',(-181.184341789427,1.94535039252626,
126.285271266929));
#119827=CARTESIAN_POINT('Ctrl Pts',(-181.19183212519,1.82364856594436,126.23481296174));
#119828=CARTESIAN_POINT('Ctrl Pts',(-181.199322460952,1.70031201061043,
126.189371762859));
#119829=CARTESIAN_POINT('Ctrl Pts',(-181.207096795071,1.57229911229676,
126.142207647111));
#119830=CARTESIAN_POINT('Ctrl Pts',(-181.21487112919,1.44211957032787,126.100299193248));
#119831=CARTESIAN_POINT('Ctrl Pts',(-181.222645463309,1.31024419354801,
126.063849757355));
#119832=CARTESIAN_POINT('Ctrl Pts',(-181.230410216256,1.17853134138399,
126.027445242135));
#119833=CARTESIAN_POINT('Ctrl Pts',(-181.238174969203,1.04512718603475,
125.996486461819));
#119834=CARTESIAN_POINT('Ctrl Pts',(-181.24593972215,0.910521686468727,
125.971128435995));
#119835=CARTESIAN_POINT('Ctrl Pts',(-181.253696763035,0.776049878982477,
125.94579559612));
#119836=CARTESIAN_POINT('Ctrl Pts',(-181.26145380392,0.640379483506111,
125.926052512528));
#119837=CARTESIAN_POINT('Ctrl Pts',(-181.269210844805,0.504014423755966,
125.91200407668));
#119838=CARTESIAN_POINT('Ctrl Pts',(-181.276962036045,0.36775219795833,
125.897966234867));
#119839=CARTESIAN_POINT('Ctrl Pts',(-181.284713227285,0.230796737915274,
125.889614533002));
#119840=CARTESIAN_POINT('Ctrl Pts',(-181.292464418526,0.0936605836422182,
125.887002510048));
#119841=CARTESIAN_POINT('Ctrl Pts',(-181.300212315303,-0.0434172841072315,
125.884391597274));
#119842=CARTESIAN_POINT('Ctrl Pts',(-181.30796021208,-0.180675303261666,
125.887515518829));
#119843=CARTESIAN_POINT('Ctrl Pts',(-181.315708108857,-0.317597627272033,
125.89637581628));
#119844=CARTESIAN_POINT('Ctrl Pts',(-181.323454384941,-0.454491310083921,
125.905234260348));
#119845=CARTESIAN_POINT('Ctrl Pts',(-181.331200661025,-0.591049047521525,
125.919826668363));
#119846=CARTESIAN_POINT('Ctrl Pts',(-181.338946937109,-0.726757210785079,
125.940102501566));
#119847=CARTESIAN_POINT('Ctrl Pts',(-181.346693270374,-0.862466375815651,
125.96037848444));
#119848=CARTESIAN_POINT('Ctrl Pts',(-181.35443960364,-0.997325567484876,
125.986337918446));
#119849=CARTESIAN_POINT('Ctrl Pts',(-181.362185936905,-1.13082887530605,
126.017878703125));
#119850=CARTESIAN_POINT('Ctrl Pts',(-181.369934004908,-1.26436208026681,
126.049426551144));
#119851=CARTESIAN_POINT('Ctrl Pts',(-181.377682072911,-1.39653841675175,
126.086558147126));
#119852=CARTESIAN_POINT('Ctrl Pts',(-181.385430140914,-1.52686510424168,
126.12912094286));
#119853=CARTESIAN_POINT('Ctrl Pts',(-181.393186443656,-1.65733030448651,
126.171728974839));
#119854=CARTESIAN_POINT('Ctrl Pts',(-181.400942746398,-1.78594155654096,
126.21977961588));
#119855=CARTESIAN_POINT('Ctrl Pts',(-181.408699049139,-1.91222358852397,
126.273071175256));
#119856=CARTESIAN_POINT('Ctrl Pts',(-181.416459491654,-2.03857302102973,
126.326391177942));
#119857=CARTESIAN_POINT('Ctrl Pts',(-181.424219934168,-2.16259040297888,
126.384957505823));
#119858=CARTESIAN_POINT('Ctrl Pts',(-181.431980376682,-2.28382411758841,
126.448521954068));
#119859=CARTESIAN_POINT('Ctrl Pts',(-181.439753276947,-2.40525244731925,
126.512188441609));
#119860=CARTESIAN_POINT('Ctrl Pts',(-181.447526177213,-2.52388784149363,
126.580868886882));
#119861=CARTESIAN_POINT('Ctrl Pts',(-181.455299077478,-2.63930601795003,
126.654270641901));
#119862=CARTESIAN_POINT('Ctrl Pts',(-181.46278941324,-2.75052845296859,
126.725004058236));
#119863=CARTESIAN_POINT('Ctrl Pts',(-181.470279749002,-2.85876326417252,
126.800121305243));
#119864=CARTESIAN_POINT('Ctrl Pts',(-181.477770084764,-2.96366065256876,
126.879325764356));
#119865=CARTESIAN_POINT('Ctrl Pts',(-181.485571301677,-3.07291173377017,
126.961817549197));
#119866=CARTESIAN_POINT('Ctrl Pts',(-181.493372518591,-3.17890946479242,
127.049020518601));
#119867=CARTESIAN_POINT('Ctrl Pts',(-181.501173735504,-3.28121524436916,
127.140645347158));
#119868=CARTESIAN_POINT('Ctrl Pts',(-181.508855785267,-3.38195825643629,
127.230870564611));
#119869=CARTESIAN_POINT('Ctrl Pts',(-181.516537835029,-3.47912097019819,
127.325383261093));
#119870=CARTESIAN_POINT('Ctrl Pts',(-181.524219884791,-3.57231315162841,
127.423863345092));
#119871=CARTESIAN_POINT('Ctrl Pts',(-181.531894943118,-3.66542051884068,
127.522253802353));
#119872=CARTESIAN_POINT('Ctrl Pts',(-181.539570001446,-3.75456426629303,
127.624604178921));
#119873=CARTESIAN_POINT('Ctrl Pts',(-181.547245059773,-3.83938845729224,
127.730555266456));
#119874=CARTESIAN_POINT('Ctrl Pts',(-181.554914880889,-3.92415476700669,
127.836434056396));
#119875=CARTESIAN_POINT('Ctrl Pts',(-181.562584702005,-4.00460713403721,
127.945908359317));
#119876=CARTESIAN_POINT('Ctrl Pts',(-181.570254523121,-4.08042798415152,
128.058583764169));
#119877=CARTESIAN_POINT('Ctrl Pts',(-181.578149920418,-4.15847879212069,
128.174573051728));
#119878=CARTESIAN_POINT('Ctrl Pts',(-181.586045317716,-4.2316211508202,
128.293954320808));
#119879=CARTESIAN_POINT('Ctrl Pts',(-181.593940715013,-4.29955471667743,
128.416262566648));
#119880=CARTESIAN_POINT('Ctrl Pts',(-181.60160643385,-4.36551208345984,
128.535012844653));
#119881=CARTESIAN_POINT('Ctrl Pts',(-181.609272152686,-4.42655931303819,
128.656521791086));
#119882=CARTESIAN_POINT('Ctrl Pts',(-181.616937871523,-4.48246715571917,
128.780337084996));
#119883=CARTESIAN_POINT('Ctrl Pts',(-181.624948108051,-4.54088764480406,
128.909716965876));
#119884=CARTESIAN_POINT('Ctrl Pts',(-181.632958344578,-4.59369582612956,
129.041614905708));
#119885=CARTESIAN_POINT('Ctrl Pts',(-181.640968581106,-4.6406858403334,
129.175490458889));
#119886=CARTESIAN_POINT('Ctrl Pts',(-181.648978817634,-4.68767585453736,
129.30936601207));
#119887=CARTESIAN_POINT('Ctrl Pts',(-181.656989054161,-4.72884756406629,
129.445218700358));
#119888=CARTESIAN_POINT('Ctrl Pts',(-181.664999290689,-4.76405452823418,
129.582490119309));
#119889=CARTESIAN_POINT('Ctrl Pts',(-179.915287826822,-4.76405452823417,
129.582490119309));
#119890=CARTESIAN_POINT('Ctrl Pts',(-179.92306888399,-4.79829769999019,
129.716003726273));
#119891=CARTESIAN_POINT('Ctrl Pts',(-179.930849941158,-4.82693968418732,
129.851018898772));
#119892=CARTESIAN_POINT('Ctrl Pts',(-179.938630998326,-4.84986100741504,
129.987028817588));
#119893=CARTESIAN_POINT('Ctrl Pts',(-179.946411829481,-4.87278166485761,
130.123034785786));
#119894=CARTESIAN_POINT('Ctrl Pts',(-179.954192660636,-4.88998191732996,
130.260035064349));
#119895=CARTESIAN_POINT('Ctrl Pts',(-179.961973491791,-4.90139348051783,
130.397512965935));
#119896=CARTESIAN_POINT('Ctrl Pts',(-179.969695849198,-4.91271928463228,
130.533957706923));
#119897=CARTESIAN_POINT('Ctrl Pts',(-179.977418206605,-4.91834311166686,
130.670872539273));
#119898=CARTESIAN_POINT('Ctrl Pts',(-179.985140564012,-4.91824883332041,
130.807748248363));
#119899=CARTESIAN_POINT('',(-179.639859435944,-4.91824845113006,130.800457355239));
#119900=CARTESIAN_POINT('Ctrl Pts',(-179.570054719422,-4.76405452823393,
129.582490119308));
#119901=CARTESIAN_POINT('Ctrl Pts',(-179.579197174056,-4.80396699441805,
129.738108219203));
#119902=CARTESIAN_POINT('Ctrl Pts',(-179.58833962869,-4.8362916101084,129.895843536568));
#119903=CARTESIAN_POINT('Ctrl Pts',(-179.597482083324,-4.86082915223956,
130.055012223801));
#119904=CARTESIAN_POINT('Ctrl Pts',(-179.606541047858,-4.88514261430456,
130.212727361621));
#119905=CARTESIAN_POINT('Ctrl Pts',(-179.615600012392,-4.90181051144224,
130.371849719594));
#119906=CARTESIAN_POINT('Ctrl Pts',(-179.624658976926,-4.91068588618086,
130.53169380667));
#119907=CARTESIAN_POINT('Ctrl Pts',(-179.629725796599,-4.91565002122716,
130.621097089119));
#119908=CARTESIAN_POINT('Ctrl Pts',(-179.634792616271,-4.91817723760474,
130.710725797053));
#119909=CARTESIAN_POINT('Ctrl Pts',(-179.639859435944,-4.91824845113006,
130.800457355239));
#119910=CARTESIAN_POINT('Ctrl Pts',(-179.639859435995,-4.91824845113077,
130.80045735614));
#119911=CARTESIAN_POINT('Ctrl Pts',(-179.647643348581,-4.91835785303648,
130.938307654795));
#119912=CARTESIAN_POINT('Ctrl Pts',(-179.655427261166,-4.91266728495612,
131.076231294055));
#119913=CARTESIAN_POINT('Ctrl Pts',(-179.663211173751,-4.90118571413701,
131.213703576513));
#119914=CARTESIAN_POINT('Ctrl Pts',(-179.670945887216,-4.88977671391655,
131.350306949481));
#119915=CARTESIAN_POINT('Ctrl Pts',(-179.67868060068,-4.87264975986795,
131.486464261715));
#119916=CARTESIAN_POINT('Ctrl Pts',(-179.686415314144,-4.84986584312386,
131.62166372303));
#119917=CARTESIAN_POINT('Ctrl Pts',(-179.694150299485,-4.82708112551935,
131.75686793664));
#119918=CARTESIAN_POINT('Ctrl Pts',(-179.701885284826,-4.79863911424742,
131.891113845955));
#119919=CARTESIAN_POINT('Ctrl Pts',(-179.709620270168,-4.76465219127589,
132.023898463912));
#119920=CARTESIAN_POINT('Ctrl Pts',(-179.717357210254,-4.73065667930619,
132.156716638506));
#119921=CARTESIAN_POINT('Ctrl Pts',(-179.725094150341,-4.69111356423603,
132.288072407442));
#119922=CARTESIAN_POINT('Ctrl Pts',(-179.732831090427,-4.64618538712646,
132.417476983782));
#119923=CARTESIAN_POINT('Ctrl Pts',(-179.740651277729,-4.6007737959558,
132.54827391556));
#119924=CARTESIAN_POINT('Ctrl Pts',(-179.748471465031,-4.54986071193366,
132.677077031875));
#119925=CARTESIAN_POINT('Ctrl Pts',(-179.756291652332,-4.4936638437746,
132.803402468467));
#119926=CARTESIAN_POINT('Ctrl Pts',(-179.764041702127,-4.43797099273028,
132.928594920532));
#119927=CARTESIAN_POINT('Ctrl Pts',(-179.771791751921,-4.37708898469712,
133.051353633612));
#119928=CARTESIAN_POINT('Ctrl Pts',(-179.779541801716,-4.31127556038019,
133.171233259887));
#119929=CARTESIAN_POINT('Ctrl Pts',(-179.787397057771,-4.24456872447766,
133.292740241798));
#119930=CARTESIAN_POINT('Ctrl Pts',(-179.795252313826,-4.17279583022991,
133.41128904481));
#119931=CARTESIAN_POINT('Ctrl Pts',(-179.803107569882,-4.09626958239033,
133.526447789367));
#119932=CARTESIAN_POINT('Ctrl Pts',(-179.810962825937,-4.01974333455076,
133.641606533924));
#119933=CARTESIAN_POINT('Ctrl Pts',(-179.818818081992,-3.93846402808792,
133.753374925537));
#119934=CARTESIAN_POINT('Ctrl Pts',(-179.826673338047,-3.85278485618213,
133.861357823072));
#119935=CARTESIAN_POINT('Ctrl Pts',(-179.834447672166,-3.76798831934649,
133.968228320824));
#119936=CARTESIAN_POINT('Ctrl Pts',(-179.842222006285,-3.67860745899652,
134.071737226023));
#119937=CARTESIAN_POINT('Ctrl Pts',(-179.849996340404,-3.58493859117706,
134.171465955982));
#119938=CARTESIAN_POINT('Ctrl Pts',(-179.857761093352,-3.491385161866,134.271071779194));
#119939=CARTESIAN_POINT('Ctrl Pts',(-179.865525846299,-3.39355450492741,
134.366906414405));
#119940=CARTESIAN_POINT('Ctrl Pts',(-179.873290599246,-3.29178443534814,
134.458582599562));
#119941=CARTESIAN_POINT('Ctrl Pts',(-179.881047640131,-3.19011544523642,
134.550167730639));
#119942=CARTESIAN_POINT('Ctrl Pts',(-179.888804681016,-3.08451511749853,
134.637602371029));
#119943=CARTESIAN_POINT('Ctrl Pts',(-179.896561721901,-2.97535926942331,
134.720534806792));
#119944=CARTESIAN_POINT('Ctrl Pts',(-179.904312913141,-2.86628573662238,
134.803404702559));
#119945=CARTESIAN_POINT('Ctrl Pts',(-179.912064104381,-2.75366233038859,
134.881778915971));
#119946=CARTESIAN_POINT('Ctrl Pts',(-179.919815295621,-2.63789893932337,
134.955345109035));
#119947=CARTESIAN_POINT('Ctrl Pts',(-179.927563192398,-2.52218475078761,
135.028880034504));
#119948=CARTESIAN_POINT('Ctrl Pts',(-179.935311089175,-2.40333356107528,
135.097610794808));
#119949=CARTESIAN_POINT('Ctrl Pts',(-179.943058985952,-2.28178513072117,
135.161267740712));
#119950=CARTESIAN_POINT('Ctrl Pts',(-179.950805262036,-2.16026212567808,
135.224911370955));
#119951=CARTESIAN_POINT('Ctrl Pts',(-179.958551538121,-2.03604334835015,
135.283483116575));
#119952=CARTESIAN_POINT('Ctrl Pts',(-179.966297814205,-1.9095937562906,
135.336758961538));
#119953=CARTESIAN_POINT('Ctrl Pts',(-179.97404414747,-1.78314323080907,
135.39003519977));
#119954=CARTESIAN_POINT('Ctrl Pts',(-179.981790480735,-1.65446221802928,
135.438015307539));
#119955=CARTESIAN_POINT('Ctrl Pts',(-179.989536814001,-1.5240359049478,
135.480523320352));
#119956=CARTESIAN_POINT('Ctrl Pts',(-179.997284882004,-1.393580383798,135.52304085254));
#119957=CARTESIAN_POINT('Ctrl Pts',(-180.005032950007,-1.26137915625431,
135.560083730166));
#119958=CARTESIAN_POINT('Ctrl Pts',(-180.01278101801,-1.12793243744398,
135.59152590394));
#119959=CARTESIAN_POINT('Ctrl Pts',(-180.020537320752,-0.994343889872685,
135.62300149483));
#119960=CARTESIAN_POINT('Ctrl Pts',(-180.028293623494,-0.859507587907298,
135.648864401312));
#119961=CARTESIAN_POINT('Ctrl Pts',(-180.036049926235,-0.723934356211346,
135.66903965224));
#119962=CARTESIAN_POINT('Ctrl Pts',(-180.04381036875,-0.588288764999606,
135.689225671307));
#119963=CARTESIAN_POINT('Ctrl Pts',(-180.051570811264,-0.45190584891694,
135.703717944691));
#119964=CARTESIAN_POINT('Ctrl Pts',(-180.059331253778,-0.315300425492684,
135.71249353184));
#119965=CARTESIAN_POINT('Ctrl Pts',(-180.067104154043,-0.178475710915488,
135.721283206341));
#119966=CARTESIAN_POINT('Ctrl Pts',(-180.074877054309,-0.0414281663132729,
135.724337847456));
#119967=CARTESIAN_POINT('Ctrl Pts',(-180.082649954574,0.0953276177084138,
135.721686690525));
#119968=CARTESIAN_POINT('Ctrl Pts',(-180.090140290336,0.227111984512766,
135.719131909827));
#119969=CARTESIAN_POINT('Ctrl Pts',(-180.097630626098,0.358625127450248,
135.71127898747));
#119970=CARTESIAN_POINT('Ctrl Pts',(-180.10512096186,0.489414003383709,
135.698199294494));
#119971=CARTESIAN_POINT('Ctrl Pts',(-180.112895295979,0.625161779301939,
135.684623680983));
#119972=CARTESIAN_POINT('Ctrl Pts',(-180.120669630098,0.76055929103879,
135.665374123379));
#119973=CARTESIAN_POINT('Ctrl Pts',(-180.128443964217,0.895094207063287,
135.640473666594));
#119974=CARTESIAN_POINT('Ctrl Pts',(-180.136208717164,1.02946332082715,
135.615603897398));
#119975=CARTESIAN_POINT('Ctrl Pts',(-180.143973470111,1.16297157332996,
135.58509715623));
#119976=CARTESIAN_POINT('Ctrl Pts',(-180.151738223059,1.29511055278657,
135.549028331807));
#119977=CARTESIAN_POINT('Ctrl Pts',(-180.159495263944,1.42711828994595,
135.512995331449));
#119978=CARTESIAN_POINT('Ctrl Pts',(-180.167252304829,1.55775908575723,
135.471411343807));
#119979=CARTESIAN_POINT('Ctrl Pts',(-180.175009345714,1.68653389489693,
135.424402444635));
#119980=CARTESIAN_POINT('Ctrl Pts',(-180.182760536954,1.81521159395151,
135.377428995238));
#119981=CARTESIAN_POINT('Ctrl Pts',(-180.190511728194,1.94202574141753,
135.325038910659));
#119982=CARTESIAN_POINT('Ctrl Pts',(-180.198262919434,2.06649200369359,
135.267408215472));
#119983=CARTESIAN_POINT('Ctrl Pts',(-180.206010816211,2.19090536448777,
135.209802014867));
#119984=CARTESIAN_POINT('Ctrl Pts',(-180.213758712988,2.31297247082939,
135.146959797708));
#119985=CARTESIAN_POINT('Ctrl Pts',(-180.221506609765,2.43222875786826,
135.079105794989));
#119986=CARTESIAN_POINT('Ctrl Pts',(-180.229252885849,2.55146009906276,
135.011265985864));
#119987=CARTESIAN_POINT('Ctrl Pts',(-180.236999161933,2.6678814508488,134.938416669642));
#119988=CARTESIAN_POINT('Ctrl Pts',(-180.244745438018,2.78105302127715,
134.860827942141));
#119989=CARTESIAN_POINT('Ctrl Pts',(-180.252491771283,2.89422542711247,
134.783238641898));
#119990=CARTESIAN_POINT('Ctrl Pts',(-180.260238104548,3.00414768126175,
134.700910081639));
#119991=CARTESIAN_POINT('Ctrl Pts',(-180.267984437814,3.11040948439129,
134.61415534982));
#119992=CARTESIAN_POINT('Ctrl Pts',(-180.275732505817,3.21669508411531,
134.52738118988));
#119993=CARTESIAN_POINT('Ctrl Pts',(-180.28348057382,3.31931829885344,134.436179133193));
#119994=CARTESIAN_POINT('Ctrl Pts',(-180.291228641823,3.41790270127258,
134.340901892192));
#119995=CARTESIAN_POINT('Ctrl Pts',(-180.298984944565,3.51659188036738,
134.245523389406));
#119996=CARTESIAN_POINT('Ctrl Pts',(-180.306741247306,3.61123339083883,
134.146061322491));
#119997=CARTESIAN_POINT('Ctrl Pts',(-180.314497550048,3.70148804412907,
134.042904938966));
#119998=CARTESIAN_POINT('Ctrl Pts',(-180.322257992563,3.79179086904529,
133.939693497773));
#119999=CARTESIAN_POINT('Ctrl Pts',(-180.330018435077,3.87770192656671,
133.832784115665));
#120000=CARTESIAN_POINT('Ctrl Pts',(-180.337778877591,3.95892364470687,
133.722597523282));
#120001=CARTESIAN_POINT('Ctrl Pts',(-180.345551777856,4.04027574715952,
133.612234049598));
#120002=CARTESIAN_POINT('Ctrl Pts',(-180.353324678122,4.1169232486707,133.498583177072));
#120003=CARTESIAN_POINT('Ctrl Pts',(-180.361097578387,4.18861259696973,
133.38209364777));
#120004=CARTESIAN_POINT('Ctrl Pts',(-180.368587914149,4.25769585688294,
133.269838806279));
#120005=CARTESIAN_POINT('Ctrl Pts',(-180.376078249911,4.32217503704249,
133.154948378128));
#120006=CARTESIAN_POINT('Ctrl Pts',(-180.383568585673,4.3818653030435,133.037842099129));
#120007=CARTESIAN_POINT('Ctrl Pts',(-180.391342919792,4.44381874362301,
132.916295699966));
#120008=CARTESIAN_POINT('Ctrl Pts',(-180.399117253911,4.50080920799675,
132.791977082604));
#120009=CARTESIAN_POINT('Ctrl Pts',(-180.40689158803,4.5525791567958,132.665329742406));
#120010=CARTESIAN_POINT('Ctrl Pts',(-180.414656340977,4.60428530375948,
132.538838483737));
#120011=CARTESIAN_POINT('Ctrl Pts',(-180.422421093925,4.65078359001705,
132.410024570987));
#120012=CARTESIAN_POINT('Ctrl Pts',(-180.430185846872,4.69186221257831,
132.27935622457));
#120013=CARTESIAN_POINT('Ctrl Pts',(-180.437942887757,4.73290003527265,
132.148817659796));
#120014=CARTESIAN_POINT('Ctrl Pts',(-180.445699928642,4.76852878996476,
132.016428697274));
#120015=CARTESIAN_POINT('Ctrl Pts',(-180.453456969527,4.79858480156904,
131.882677344994));
#120016=CARTESIAN_POINT('Ctrl Pts',(-180.461208160767,4.8286181477013,131.749026855648));
#120017=CARTESIAN_POINT('Ctrl Pts',(-180.468959352007,4.85308703009387,
131.614016401407));
#120018=CARTESIAN_POINT('Ctrl Pts',(-180.476710543247,4.87187774906408,
131.478148611429));
#120019=CARTESIAN_POINT('Ctrl Pts',(-180.484458440024,4.89066048147738,
131.342338568887));
#120020=CARTESIAN_POINT('Ctrl Pts',(-180.492206336801,4.90376979703001,
131.205672301821));
#120021=CARTESIAN_POINT('Ctrl Pts',(-180.499954233578,4.91114323895842,
131.068661864126));
#120022=CARTESIAN_POINT('Ctrl Pts',(-180.507700509662,4.91851513852172,
130.93168008606));
#120023=CARTESIAN_POINT('Ctrl Pts',(-180.515446785746,4.92015352997405,
130.794354670717));
#120024=CARTESIAN_POINT('Ctrl Pts',(-180.523193061831,4.91604793428645,
130.657201620906));
#120025=CARTESIAN_POINT('Ctrl Pts',(-180.530939395096,4.91194230829228,
130.520047558662));
#120026=CARTESIAN_POINT('Ctrl Pts',(-180.538685728361,4.9020926222485,130.38306625528));
#120027=CARTESIAN_POINT('Ctrl Pts',(-180.546432061627,4.88654050952772,
130.246772139166));
#120028=CARTESIAN_POINT('Ctrl Pts',(-180.55418012963,4.8709849140191,130.110447500929));
#120029=CARTESIAN_POINT('Ctrl Pts',(-180.561928197633,4.84972439502942,
129.974810744557));
#120030=CARTESIAN_POINT('Ctrl Pts',(-180.569676265636,4.82285223134933,
129.84036921871));
#120031=CARTESIAN_POINT('Ctrl Pts',(-180.577432568377,4.795951507614,129.70578480681));
#120032=CARTESIAN_POINT('Ctrl Pts',(-180.585188871119,4.76342730196317,
129.572398547));
#120033=CARTESIAN_POINT('Ctrl Pts',(-180.592945173861,4.72542375965904,
129.440706206012));
#120034=CARTESIAN_POINT('Ctrl Pts',(-180.600705616375,4.68739993372011,
129.308943576857));
#120035=CARTESIAN_POINT('Ctrl Pts',(-180.608466058889,4.64389106780674,
129.178877038601));
#120036=CARTESIAN_POINT('Ctrl Pts',(-180.616226501404,4.59509028959371,
129.050984362171));
#120037=CARTESIAN_POINT('Ctrl Pts',(-180.623999401669,4.54621117203903,
128.922886381063));
#120038=CARTESIAN_POINT('Ctrl Pts',(-180.631772301934,4.49202332100907,
128.796969594594));
#120039=CARTESIAN_POINT('Ctrl Pts',(-180.6395452022,4.43276722471806,128.67368987952));
#120040=CARTESIAN_POINT('Ctrl Pts',(-180.647035537962,4.37566523678433,
128.554891692612));
#120041=CARTESIAN_POINT('Ctrl Pts',(-180.654525873724,4.31385723758189,
128.438542449427));
#120042=CARTESIAN_POINT('Ctrl Pts',(-180.662016209486,4.24759645522655,
128.325024533844));
#120043=CARTESIAN_POINT('Ctrl Pts',(-180.669790543605,4.17882337516859,
128.207202551989));
#120044=CARTESIAN_POINT('Ctrl Pts',(-180.677564877724,4.10503533955871,
128.092057610922));
#120045=CARTESIAN_POINT('Ctrl Pts',(-180.685339211843,4.02646626728858,
127.980046105886));
#120046=CARTESIAN_POINT('Ctrl Pts',(-180.69310396479,3.94799402437853,127.86817264502));
#120047=CARTESIAN_POINT('Ctrl Pts',(-180.700868717737,3.86475269088806,
127.759425253595));
#120048=CARTESIAN_POINT('Ctrl Pts',(-180.708633470684,3.77702170922281,
127.654235212037));
#120049=CARTESIAN_POINT('Ctrl Pts',(-180.71639051157,3.68937786320486,127.54914964671));
#120050=CARTESIAN_POINT('Ctrl Pts',(-180.724147552455,3.59725349177691,
127.447614698306));
#120051=CARTESIAN_POINT('Ctrl Pts',(-180.73190459334,3.50097069949896,127.350031851547));
#120052=CARTESIAN_POINT('Ctrl Pts',(-180.73965578458,3.40476051482377,127.252522592771));
#120053=CARTESIAN_POINT('Ctrl Pts',(-180.74740697582,3.30439842459542,127.158959780689));
#120054=CARTESIAN_POINT('Ctrl Pts',(-180.75515816706,3.20024584750376,127.0697107574));
#120055=CARTESIAN_POINT('Ctrl Pts',(-180.762906063837,3.09613753803588,
126.980499667328));
#120056=CARTESIAN_POINT('Ctrl Pts',(-180.770653960614,2.98824224223235,
126.89559897327));
#120057=CARTESIAN_POINT('Ctrl Pts',(-180.778401857391,2.87695700613077,
126.815337999508));
#120058=CARTESIAN_POINT('Ctrl Pts',(-180.786148133475,2.76569504850156,
126.735093814613));
#120059=CARTESIAN_POINT('Ctrl Pts',(-180.793894409559,2.65104487791537,
126.659487648129));
#120060=CARTESIAN_POINT('Ctrl Pts',(-180.801640685643,2.53343495797927,
126.588807228485));
#120061=CARTESIAN_POINT('Ctrl Pts',(-180.809387018909,2.41582416987298,
126.518126287095));
#120062=CARTESIAN_POINT('Ctrl Pts',(-180.817133352174,2.29525392392618,
126.452371366488));
#120063=CARTESIAN_POINT('Ctrl Pts',(-180.82487968544,2.17217952718222,126.39178550045));
#120064=CARTESIAN_POINT('Ctrl Pts',(-180.832627753443,2.04907756878062,
126.331186066628));
#120065=CARTESIAN_POINT('Ctrl Pts',(-180.840375821446,1.92347069438084,
126.275758163452));
#120066=CARTESIAN_POINT('Ctrl Pts',(-180.848123889449,1.79583617024562,
126.225697547178));
#120067=CARTESIAN_POINT('Ctrl Pts',(-180.855880192191,1.66806599461945,
126.175583725885));
#120068=CARTESIAN_POINT('Ctrl Pts',(-180.863636494932,1.53826422894359,
126.130848729665));
#120069=CARTESIAN_POINT('Ctrl Pts',(-180.871392797674,1.40692588984619,
126.091639259053));
#120070=CARTESIAN_POINT('Ctrl Pts',(-180.879153240188,1.2755174515227,126.052408861167));
#120071=CARTESIAN_POINT('Ctrl Pts',(-180.886913682703,1.14257118442251,
126.018709961316));
#120072=CARTESIAN_POINT('Ctrl Pts',(-180.894674125217,1.00859344098332,
125.990638322574));
#120073=CARTESIAN_POINT('Ctrl Pts',(-180.902447025482,0.874400624576381,
125.962521620745));
#120074=CARTESIAN_POINT('Ctrl Pts',(-180.910219925748,0.739173408878079,
125.940050295721));
#120075=CARTESIAN_POINT('Ctrl Pts',(-180.917992826013,0.603425325667191,
125.923268430479));
#120076=CARTESIAN_POINT('Ctrl Pts',(-180.925483161775,0.472612027210911,
125.907096628309));
#120077=CARTESIAN_POINT('Ctrl Pts',(-180.932973497537,0.341315380425482,
125.896207840602));
#120078=CARTESIAN_POINT('Ctrl Pts',(-180.940463833299,0.20999397167983,
125.890595707199));
#120079=CARTESIAN_POINT('Ctrl Pts',(-180.948238167418,0.0736934718059715,
125.884770788052));
#120080=CARTESIAN_POINT('Ctrl Pts',(-180.956012501537,-0.0630654638079416,
125.884612098978));
#120081=CARTESIAN_POINT('Ctrl Pts',(-180.963786835656,-0.199772418043521,
125.890169530165));
#120082=CARTESIAN_POINT('Ctrl Pts',(-180.971551588603,-0.336310893175113,
125.895720112316));
#120083=CARTESIAN_POINT('Ctrl Pts',(-180.97931634155,-0.472797127501037,
125.90697278233));
#120084=CARTESIAN_POINT('Ctrl Pts',(-180.987081094497,-0.608717227139118,
125.923925555004));
#120085=CARTESIAN_POINT('Ctrl Pts',(-180.994838135382,-0.744502329018101,
125.940861489945));
#120086=CARTESIAN_POINT('Ctrl Pts',(-181.002595176267,-0.87972202974887,
125.963486212983));
#120087=CARTESIAN_POINT('Ctrl Pts',(-181.010352217152,-1.01386444348082,
125.99174574073));
#120088=CARTESIAN_POINT('Ctrl Pts',(-181.018103408392,-1.14790569937564,
126.019983957747));
#120089=CARTESIAN_POINT('Ctrl Pts',(-181.025854599632,-1.28087090426565,
126.053848441329));
#120090=CARTESIAN_POINT('Ctrl Pts',(-181.033605790873,-1.41225564720813,
126.093233677074));
#120091=CARTESIAN_POINT('Ctrl Pts',(-181.04135368765,-1.54358454812987,
126.132602173044));
#120092=CARTESIAN_POINT('Ctrl Pts',(-181.049101584427,-1.67333394942435,
126.177486642203));
#120093=CARTESIAN_POINT('Ctrl Pts',(-181.056849481204,-1.80101216816459,
126.227731046296));
#120094=CARTESIAN_POINT('Ctrl Pts',(-181.064595757288,-1.92866367937423,
126.277964940342));
#120095=CARTESIAN_POINT('Ctrl Pts',(-181.072342033372,-2.05424450620277,
126.333556396151));
#120096=CARTESIAN_POINT('Ctrl Pts',(-181.080088309456,-2.17728097953044,
126.394300459396));
#120097=CARTESIAN_POINT('Ctrl Pts',(-181.087834642722,-2.3003183610849,
126.455044971041));
#120098=CARTESIAN_POINT('Ctrl Pts',(-181.095580975987,-2.42081100109293,
126.520941992941));
#120099=CARTESIAN_POINT('Ctrl Pts',(-181.103327309252,-2.53830832377024,
126.591739828084));
#120100=CARTESIAN_POINT('Ctrl Pts',(-181.111075377255,-2.65583195915813,
126.662553517911));
#120101=CARTESIAN_POINT('Ctrl Pts',(-181.118823445258,-2.77035860763099,
126.738270003146));
#120102=CARTESIAN_POINT('Ctrl Pts',(-181.126571513261,-2.88146559983368,
126.818593557203));
#120103=CARTESIAN_POINT('Ctrl Pts',(-181.134327816003,-2.99269067787002,
126.89900248009));
#120104=CARTESIAN_POINT('Ctrl Pts',(-181.142084118745,-3.1004885220833,
126.984028023559));
#120105=CARTESIAN_POINT('Ctrl Pts',(-181.149840421487,-3.20446814057772,
127.073333011326));
#120106=CARTESIAN_POINT('Ctrl Pts',(-181.157600864001,-3.30850325612586,
127.162685663855));
#120107=CARTESIAN_POINT('Ctrl Pts',(-181.165361306515,-3.40871579973424,
127.25632204509));
#120108=CARTESIAN_POINT('Ctrl Pts',(-181.173121749029,-3.5047515073558,
127.353867908664));
#120109=CARTESIAN_POINT('Ctrl Pts',(-181.180894649295,-3.60094138002062,
127.451570361518));
#120110=CARTESIAN_POINT('Ctrl Pts',(-181.18866754956,-3.69294075537735,
127.55319454785));
#120111=CARTESIAN_POINT('Ctrl Pts',(-181.196440449825,-3.78043496869995,
127.658332246758));
#120112=CARTESIAN_POINT('Ctrl Pts',(-181.203930785587,-3.86474854698411,
127.759647925484));
#120113=CARTESIAN_POINT('Ctrl Pts',(-181.21142112135,-3.94487863715625,
127.864225857211));
#120114=CARTESIAN_POINT('Ctrl Pts',(-181.218911457112,-4.02058271306412,
127.971676782418));
#120115=CARTESIAN_POINT('Ctrl Pts',(-181.226774298583,-4.10005166699623,
128.084471404409));
#120116=CARTESIAN_POINT('Ctrl Pts',(-181.234637140055,-4.174892552443,128.200785850527));
#120117=CARTESIAN_POINT('Ctrl Pts',(-181.242499981526,-4.24478179121977,
128.320208728605));
#120118=CARTESIAN_POINT('Ctrl Pts',(-181.250349252588,-4.31455040877096,
128.439425495782));
#120119=CARTESIAN_POINT('Ctrl Pts',(-181.25819852365,-4.37938421453783,
128.56173968249));
#120120=CARTESIAN_POINT('Ctrl Pts',(-181.266047794713,-4.43900175716958,
128.686709451216));
#120121=CARTESIAN_POINT('Ctrl Pts',(-181.273889191536,-4.49855949261664,
128.811553852646));
#120122=CARTESIAN_POINT('Ctrl Pts',(-181.281730588359,-4.55291121398804,
128.939048195462));
#120123=CARTESIAN_POINT('Ctrl Pts',(-181.289571985181,-4.60182013260226,
129.0687239823));
#120124=CARTESIAN_POINT('Ctrl Pts',(-181.297405522347,-4.65068002839995,
129.198269791365));
#120125=CARTESIAN_POINT('Ctrl Pts',(-181.305239059512,-4.69410785428418,
129.329992335658));
#120126=CARTESIAN_POINT('Ctrl Pts',(-181.313072596677,-4.73191416286347,
129.463401476581));
#120127=CARTESIAN_POINT('Ctrl Pts',(-181.315395044115,-4.74312278581986,
129.502953943239));
#120128=CARTESIAN_POINT('Ctrl Pts',(-181.317717491553,-4.75383761304045,
129.542654522032));
#120129=CARTESIAN_POINT('Ctrl Pts',(-181.320039938991,-4.76405452823418,
129.582490119309));
#120130=CARTESIAN_POINT('Origin',(213.235140564004,0.,130.804360617566));
#120131=CARTESIAN_POINT('',(-183.415149158805,-4.76405452823414,129.582490119309));
#120132=CARTESIAN_POINT('',(-183.069718605797,-4.76405452823406,129.582490119308));
#120133=CARTESIAN_POINT('',(213.235140564004,-4.76405452823405,129.582490119308));
#120134=CARTESIAN_POINT('',(-181.735140563977,-4.91824950327072,130.806571064885));
#120135=CARTESIAN_POINT('Ctrl Pts',(-181.735140564012,-4.91824950327044,
130.806571065507));
#120136=CARTESIAN_POINT('Ctrl Pts',(-181.742166278867,-4.91819404319526,
130.929969803894));
#120137=CARTESIAN_POINT('Ctrl Pts',(-181.749191993722,-4.91349490493225,
131.053259845395));
#120138=CARTESIAN_POINT('Ctrl Pts',(-181.756217708576,-4.90417395891944,
131.176195047328));
#120139=CARTESIAN_POINT('Ctrl Pts',(-181.763992042696,-4.89385982717492,
131.312229508533));
#120140=CARTESIAN_POINT('Ctrl Pts',(-181.771766376815,-4.87786497991832,
131.448049965438));
#120141=CARTESIAN_POINT('Ctrl Pts',(-181.779540710934,-4.85620016088216,
131.583143681036));
#120142=CARTESIAN_POINT('Ctrl Pts',(-181.787305463881,-4.83456204179922,
131.718070905703));
#120143=CARTESIAN_POINT('Ctrl Pts',(-181.795070216828,-4.80726791575691,
131.852272788801));
#120144=CARTESIAN_POINT('Ctrl Pts',(-181.802834969775,-4.77438044942487,
131.98523926783));
#120145=CARTESIAN_POINT('Ctrl Pts',(-181.81059201066,-4.74152564738802,
132.118073682678));
#120146=CARTESIAN_POINT('Ctrl Pts',(-181.818349051545,-4.70308865379099,
132.249674758213));
#120147=CARTESIAN_POINT('Ctrl Pts',(-181.82610609243,-4.6591835323683,132.379540567352));
#120148=CARTESIAN_POINT('Ctrl Pts',(-181.833857283671,-4.61531152013915,
132.509308443675));
#120149=CARTESIAN_POINT('Ctrl Pts',(-181.841608474911,-4.56597971248463,
132.637343289375));
#120150=CARTESIAN_POINT('Ctrl Pts',(-181.849359666151,-4.51135246061705,
132.763156686223));
#120151=CARTESIAN_POINT('Ctrl Pts',(-181.857107562928,-4.45674842678867,
132.888916609021));
#120152=CARTESIAN_POINT('Ctrl Pts',(-181.864855459705,-4.39685358061205,
133.012456602989));
#120153=CARTESIAN_POINT('Ctrl Pts',(-181.872603356482,-4.33188094023251,
133.133306856136));
#120154=CARTESIAN_POINT('Ctrl Pts',(-181.880349632566,-4.26692189072869,
133.254131830015));
#120155=CARTESIAN_POINT('Ctrl Pts',(-181.888095908651,-4.19688734474357,
133.372267838051));
#120156=CARTESIAN_POINT('Ctrl Pts',(-181.895842184735,-4.12203676652123,
133.487268733389));
#120157=CARTESIAN_POINT('Ctrl Pts',(-181.903588518,-4.04718563576903,133.602270477636));
#120158=CARTESIAN_POINT('Ctrl Pts',(-181.911334851265,-3.9675186151122,
133.714136735334));
#120159=CARTESIAN_POINT('Ctrl Pts',(-181.919081184531,-3.88333885679162,
133.822449812045));
#120160=CARTESIAN_POINT('Ctrl Pts',(-181.926829252534,-3.79914024699795,
133.930787144718));
#120161=CARTESIAN_POINT('Ctrl Pts',(-181.934577320537,-3.71042712844116,
134.035569404395));
#120162=CARTESIAN_POINT('Ctrl Pts',(-181.94232538854,-3.61754307876341,
134.136411808018));
#120163=CARTESIAN_POINT('Ctrl Pts',(-181.950081691281,-3.52456031081195,
134.237361388148));
#120164=CARTESIAN_POINT('Ctrl Pts',(-181.957837994024,-3.42739802181008,
134.334362459562));
#120165=CARTESIAN_POINT('Ctrl Pts',(-181.965594296765,-3.32643720759424,
134.427066590514));
#120166=CARTESIAN_POINT('Ctrl Pts',(-181.97335473928,-3.22542250755198,
134.519820200452));
#120167=CARTESIAN_POINT('Ctrl Pts',(-181.981115181794,-3.12060554120253,
134.608272048101));
#120168=CARTESIAN_POINT('Ctrl Pts',(-181.988875624308,-3.01239977711739,
134.692114550793));
#120169=CARTESIAN_POINT('Ctrl Pts',(-181.996648524573,-2.90402031153368,
134.776091644914));
#120170=CARTESIAN_POINT('Ctrl Pts',(-182.004421424839,-2.79224149634652,
134.85544438141));
#120171=CARTESIAN_POINT('Ctrl Pts',(-182.012194325104,-2.67750585984077,
134.929908512454));
#120172=CARTESIAN_POINT('Ctrl Pts',(-182.019684660866,-2.5669411527255,
135.001665684771));
#120173=CARTESIAN_POINT('Ctrl Pts',(-182.027174996628,-2.4536311327147,
135.068883350007));
#120174=CARTESIAN_POINT('Ctrl Pts',(-182.03466533239,-2.33799097923109,
135.131366654485));
#120175=CARTESIAN_POINT('Ctrl Pts',(-182.042439666509,-2.21796629417824,
135.196219032444));
#120176=CARTESIAN_POINT('Ctrl Pts',(-182.050214000628,-2.09505109151086,
135.256176389005));
#120177=CARTESIAN_POINT('Ctrl Pts',(-182.057988334747,-1.96968255864387,
135.310970616298));
#120178=CARTESIAN_POINT('Ctrl Pts',(-182.065753087694,-1.84446853128913,
135.365697314603));
#120179=CARTESIAN_POINT('Ctrl Pts',(-182.073517840642,-1.71680754442264,
135.415273389231));
#120180=CARTESIAN_POINT('Ctrl Pts',(-182.081282593589,-1.5871626009352,
135.459475862186));
#120181=CARTESIAN_POINT('Ctrl Pts',(-182.089039634474,-1.45764642263331,
135.503634432622));
#120182=CARTESIAN_POINT('Ctrl Pts',(-182.096796675359,-1.32615057673516,
135.542429897177));
#120183=CARTESIAN_POINT('Ctrl Pts',(-182.104553716244,-1.19315900294414,
135.575686917055));
#120184=CARTESIAN_POINT('Ctrl Pts',(-182.112304907484,-1.06026771913327,
135.608918857555));
#120185=CARTESIAN_POINT('Ctrl Pts',(-182.120056098724,-0.925883330276927,
135.636620572151));
#120186=CARTESIAN_POINT('Ctrl Pts',(-182.127807289964,-0.790505592309228,
135.65866633219));
#120187=CARTESIAN_POINT('Ctrl Pts',(-182.135555186741,-0.655185393491669,
135.680702722192));
#120188=CARTESIAN_POINT('Ctrl Pts',(-182.143303083518,-0.518873070360332,
135.697087876165));
#120189=CARTESIAN_POINT('Ctrl Pts',(-182.151050980295,-0.382079030561141,
135.70774706745));
#120190=CARTESIAN_POINT('Ctrl Pts',(-182.15879725638,-0.245313605126137,
135.718404029062));
#120191=CARTESIAN_POINT('Ctrl Pts',(-182.166543532464,-0.108067052986587,
135.723337380018));
#120192=CARTESIAN_POINT('Ctrl Pts',(-182.174289808548,0.0291450231112156,
135.722524261664));
#120193=CARTESIAN_POINT('Ctrl Pts',(-182.182036141813,0.16635811207758,
135.721711137307));
#120194=CARTESIAN_POINT('Ctrl Pts',(-182.189782475079,0.303536333536031,
135.715151461312));
#120195=CARTESIAN_POINT('Ctrl Pts',(-182.197528808344,0.440164408135673,
135.702874510198));
#120196=CARTESIAN_POINT('Ctrl Pts',(-182.205276876347,0.576823079645122,
135.690594809746));
#120197=CARTESIAN_POINT('Ctrl Pts',(-182.21302494435,0.712930969817092,
135.672595321422));
#120198=CARTESIAN_POINT('Ctrl Pts',(-182.220773012353,0.847978637660013,
135.648957122186));
#120199=CARTESIAN_POINT('Ctrl Pts',(-182.228529315095,0.983169835771588,
135.62529379999));
#120200=CARTESIAN_POINT('Ctrl Pts',(-182.236285617837,1.1172981748916,135.595979862955));
#120201=CARTESIAN_POINT('Ctrl Pts',(-182.244041920579,1.24986457196712,
135.5611475178));
#120202=CARTESIAN_POINT('Ctrl Pts',(-182.251802363093,1.38250172372027,
135.526296581574));
#120203=CARTESIAN_POINT('Ctrl Pts',(-182.259562805607,1.51357489884223,
135.485921483424));
#120204=CARTESIAN_POINT('Ctrl Pts',(-182.267323248121,1.64260182946052,
135.440203830225));
#120205=CARTESIAN_POINT('Ctrl Pts',(-182.275096148387,1.77183588556232,
135.39441278699));
#120206=CARTESIAN_POINT('Ctrl Pts',(-182.282869048652,1.89901677012015,
135.343262196406));
#120207=CARTESIAN_POINT('Ctrl Pts',(-182.290641948918,2.02368296660664,
135.286981537649));
#120208=CARTESIAN_POINT('Ctrl Pts',(-182.298132284679,2.14381723283161,
135.232746822602));
#120209=CARTESIAN_POINT('Ctrl Pts',(-182.305622620441,2.26161619186303,
135.173748683604));
#120210=CARTESIAN_POINT('Ctrl Pts',(-182.313112956203,2.37669149316271,
135.11023109969));
#120211=CARTESIAN_POINT('Ctrl Pts',(-182.320887290322,2.49612990949109,
135.044305227274));
#120212=CARTESIAN_POINT('Ctrl Pts',(-182.328661624441,2.61301240105838,
134.973301601892));
#120213=CARTESIAN_POINT('Ctrl Pts',(-182.33643595856,2.72687709064381,134.897443122845));
#120214=CARTESIAN_POINT('Ctrl Pts',(-182.344200711507,2.84060145217569,
134.821678132594));
#120215=CARTESIAN_POINT('Ctrl Pts',(-182.351965464454,2.9513150895211,134.741070408096));
#120216=CARTESIAN_POINT('Ctrl Pts',(-182.359730217402,3.05858014060573,
134.655888961742));
#120217=CARTESIAN_POINT('Ctrl Pts',(-182.367487258287,3.16573865452946,
134.570792118802));
#120218=CARTESIAN_POINT('Ctrl Pts',(-182.375244299171,3.26945509427675,
134.481130835716));
#120219=CARTESIAN_POINT('Ctrl Pts',(-182.383001340056,3.369320361121,134.387217489761));
#120220=CARTESIAN_POINT('Ctrl Pts',(-182.390752531297,3.46911031879082,
134.29337496459));
#120221=CARTESIAN_POINT('Ctrl Pts',(-182.398503722537,3.56505460053173,
134.195287025673));
#120222=CARTESIAN_POINT('Ctrl Pts',(-182.406254913777,3.6567772969768,134.093306172423));
#120223=CARTESIAN_POINT('Ctrl Pts',(-182.414002810554,3.74846100882897,
133.991368663756));
#120224=CARTESIAN_POINT('Ctrl Pts',(-182.421750707331,3.83592644318413,
133.885541821693));
#120225=CARTESIAN_POINT('Ctrl Pts',(-182.429498604108,3.91883484258758,
133.776214675056));
#120226=CARTESIAN_POINT('Ctrl Pts',(-182.437244880192,4.00172589934117,
133.666910397302));
#120227=CARTESIAN_POINT('Ctrl Pts',(-182.444991156276,4.08006158108549,
133.554107582659));
#120228=CARTESIAN_POINT('Ctrl Pts',(-182.45273743236,4.15354396030729,133.438227666658));
#120229=CARTESIAN_POINT('Ctrl Pts',(-182.460483765626,4.22702688195942,
133.322346895258));
#120230=CARTESIAN_POINT('Ctrl Pts',(-182.468230098891,4.29565622022754,
133.203389307352));
#120231=CARTESIAN_POINT('Ctrl Pts',(-182.475976432157,4.35917808520141,
133.081804246726));
#120232=CARTESIAN_POINT('Ctrl Pts',(-182.48372450016,4.42271417545642,132.960191957968));
#120233=CARTESIAN_POINT('Ctrl Pts',(-182.491472568163,4.48114033541539,
132.83595137209));
#120234=CARTESIAN_POINT('Ctrl Pts',(-182.499220636166,4.53424941212098,
132.709554920303));
#120235=CARTESIAN_POINT('Ctrl Pts',(-182.506976938907,4.58741493378524,
132.583024132863));
#120236=CARTESIAN_POINT('Ctrl Pts',(-182.514733241649,4.63525193190573,
132.45433326345));
#120237=CARTESIAN_POINT('Ctrl Pts',(-182.522489544391,4.67760186915715,
132.323973665732));
#120238=CARTESIAN_POINT('Ctrl Pts',(-182.530249986905,4.71997440984532,
132.193544491172));
#120239=CARTESIAN_POINT('Ctrl Pts',(-182.53801042942,4.75685394908354,132.06144518999));
#120240=CARTESIAN_POINT('Ctrl Pts',(-182.545770871934,4.78813260031306,
131.928179670759));
#120241=CARTESIAN_POINT('Ctrl Pts',(-182.553543772199,4.81946146281031,
131.794700221885));
#120242=CARTESIAN_POINT('Ctrl Pts',(-182.561316672464,4.84517139696213,
131.660051198124));
#120243=CARTESIAN_POINT('Ctrl Pts',(-182.56908957273,4.86520600914096,131.524744925501));
#120244=CARTESIAN_POINT('Ctrl Pts',(-182.576579908492,4.88451231270299,
131.394357376703));
#120245=CARTESIAN_POINT('Ctrl Pts',(-182.584070244254,4.89854872220694,
131.263359840987));
#120246=CARTESIAN_POINT('Ctrl Pts',(-182.591560580016,4.90731059117172,
131.132210925289));
#120247=CARTESIAN_POINT('Ctrl Pts',(-182.599334914135,4.91640466906136,
130.99608945859));
#120248=CARTESIAN_POINT('Ctrl Pts',(-182.607109248254,4.91984514980589,
130.859373714271));
#120249=CARTESIAN_POINT('Ctrl Pts',(-182.614883582373,4.91756990898058,
130.722572765236));
#120250=CARTESIAN_POINT('Ctrl Pts',(-182.62264833532,4.91529747218625,130.585940411145));
#120251=CARTESIAN_POINT('Ctrl Pts',(-182.630413088267,4.90732333595251,
130.449223448429));
#120252=CARTESIAN_POINT('Ctrl Pts',(-182.638177841215,4.89363715287714,
130.31293567062));
#120253=CARTESIAN_POINT('Ctrl Pts',(-182.6459348821,4.87996456311174,130.176783255754));
#120254=CARTESIAN_POINT('Ctrl Pts',(-182.653691922985,4.86059125541069,
130.041059563987));
#120255=CARTESIAN_POINT('Ctrl Pts',(-182.66144896387,4.83555891376832,129.906277629209));
#120256=CARTESIAN_POINT('Ctrl Pts',(-182.66920015511,4.81054544920946,129.771597334537));
#120257=CARTESIAN_POINT('Ctrl Pts',(-182.67695134635,4.77988151605426,129.63785776611));
#120258=CARTESIAN_POINT('Ctrl Pts',(-182.68470253759,4.74366049384699,129.505565721666));
#120259=CARTESIAN_POINT('Ctrl Pts',(-182.692450434367,4.70745486654033,
129.37332990487));
#120260=CARTESIAN_POINT('Ctrl Pts',(-182.700198331144,4.66569695087129,
129.242540764698));
#120261=CARTESIAN_POINT('Ctrl Pts',(-182.707946227921,4.618530941128,129.11369358697));
#120262=CARTESIAN_POINT('Ctrl Pts',(-182.715692504005,4.57137479749729,
128.984873361295));
#120263=CARTESIAN_POINT('Ctrl Pts',(-182.72343878009,4.51881294423457,128.857994656986));
#120264=CARTESIAN_POINT('Ctrl Pts',(-182.731185056174,4.46103890988972,
128.733535925094));
#120265=CARTESIAN_POINT('Ctrl Pts',(-182.738931389439,4.40326444907,128.609076274477));
#120266=CARTESIAN_POINT('Ctrl Pts',(-182.746677722704,4.34027789500933,
128.487036986544));
#120267=CARTESIAN_POINT('Ctrl Pts',(-182.75442405597,4.27232005966242,128.36787454736));
#120268=CARTESIAN_POINT('Ctrl Pts',(-182.762172123973,4.20434700562956,
128.248685422574));
#120269=CARTESIAN_POINT('Ctrl Pts',(-182.769920191976,4.13140064865017,
128.132374768074));
#120270=CARTESIAN_POINT('Ctrl Pts',(-182.777668259979,4.05376648724896,
128.019372228119));
#120271=CARTESIAN_POINT('Ctrl Pts',(-182.78542456272,3.97604981533704,127.906249587719));
#120272=CARTESIAN_POINT('Ctrl Pts',(-182.793180865462,3.89363560815299,
127.796442408019));
#120273=CARTESIAN_POINT('Ctrl Pts',(-182.800937168204,3.80685156215607,
127.69034965962));
#120274=CARTESIAN_POINT('Ctrl Pts',(-182.808697610718,3.72002119690079,
127.584200286326));
#120275=CARTESIAN_POINT('Ctrl Pts',(-182.816458053233,3.62881660536122,
127.481769586489));
#120276=CARTESIAN_POINT('Ctrl Pts',(-182.824218495747,3.5336034247693,127.383420703016));
#120277=CARTESIAN_POINT('Ctrl Pts',(-182.831991396012,3.43823739952725,
127.284913941185));
#120278=CARTESIAN_POINT('Ctrl Pts',(-182.839764296278,3.33885020978783,
127.190502359112));
#120279=CARTESIAN_POINT('Ctrl Pts',(-182.847537196543,3.23584240781202,
127.100510327084));
#120280=CARTESIAN_POINT('Ctrl Pts',(-182.855027532305,3.1365791988993,127.013789732096));
#120281=CARTESIAN_POINT('Ctrl Pts',(-182.862517868067,3.03395428425488,
126.931173135403));
#120282=CARTESIAN_POINT('Ctrl Pts',(-182.870008203829,2.92835099134394,
126.852912334468));
#120283=CARTESIAN_POINT('Ctrl Pts',(-182.877782537948,2.818743717485,126.77168425148));
#120284=CARTESIAN_POINT('Ctrl Pts',(-182.885556872067,2.70558055367971,
126.694891478318));
#120285=CARTESIAN_POINT('Ctrl Pts',(-182.893331206186,2.58925621761079,
126.622861448361));
#120286=CARTESIAN_POINT('Ctrl Pts',(-182.901095959133,2.47307524088987,
126.550920188978));
#120287=CARTESIAN_POINT('Ctrl Pts',(-182.90886071208,2.35374117271796,126.483730197785));
#120288=CARTESIAN_POINT('Ctrl Pts',(-182.916625465027,2.23168068912202,
126.4215778983));
#120289=CARTESIAN_POINT('Ctrl Pts',(-182.924382505912,2.10974143771914,
126.359487329355));
#120290=CARTESIAN_POINT('Ctrl Pts',(-182.932139546797,1.98508150590871,
126.302424671168));
#120291=CARTESIAN_POINT('Ctrl Pts',(-182.939896587682,1.85815505485159,
126.250632161166));
#120292=CARTESIAN_POINT('Ctrl Pts',(-182.947647778922,1.73132432001839,
126.198878708298));
#120293=CARTESIAN_POINT('Ctrl Pts',(-182.955398970163,1.60223082852072,
126.152387640204));
#120294=CARTESIAN_POINT('Ctrl Pts',(-182.963150161403,1.47135143757472,
126.111354330585));
#120295=CARTESIAN_POINT('Ctrl Pts',(-182.97089805818,1.34052767386137,126.070338461217));
#120296=CARTESIAN_POINT('Ctrl Pts',(-182.978645954957,1.20791989268096,
126.034775853349));
#120297=CARTESIAN_POINT('Ctrl Pts',(-182.986393851734,1.07402273255796,
126.004812906328));
#120298=CARTESIAN_POINT('Ctrl Pts',(-182.994140127818,0.940153580834378,
125.97485622691));
#120299=CARTESIAN_POINT('Ctrl Pts',(-183.001886403902,0.804995967924261,
125.950496963824));
#120300=CARTESIAN_POINT('Ctrl Pts',(-183.009632679986,0.669057035157692,
125.931830910504));
#120301=CARTESIAN_POINT('Ctrl Pts',(-183.017379013251,0.533117098920988,
125.913164719394));
#120302=CARTESIAN_POINT('Ctrl Pts',(-183.025125346517,0.39639621864993,
125.900191875094));
#120303=CARTESIAN_POINT('Ctrl Pts',(-183.032871679782,0.259408613742112,
125.892956517554));
#120304=CARTESIAN_POINT('Ctrl Pts',(-183.040619747785,0.122390331409793,
125.885719539705));
#120305=CARTESIAN_POINT('Ctrl Pts',(-183.048367815788,-0.0148944040710403,
125.884222625977));
#120306=CARTESIAN_POINT('Ctrl Pts',(-183.056115883791,-0.151929801890471,
125.888457811591));
#120307=CARTESIAN_POINT('Ctrl Pts',(-183.063872186533,-0.289110842561633,
125.89269749841));
#120308=CARTESIAN_POINT('Ctrl Pts',(-183.071628489275,-0.426041624805545,
125.902681442188));
#120309=CARTESIAN_POINT('Ctrl Pts',(-183.079384792016,-0.562209355415556,
125.918349595967));
#120310=CARTESIAN_POINT('Ctrl Pts',(-183.08714523453,-0.698449762843326,
125.934026112312));
#120311=CARTESIAN_POINT('Ctrl Pts',(-183.094905677045,-0.833925921127289,
125.955392822951));
#120312=CARTESIAN_POINT('Ctrl Pts',(-183.102666119559,-0.968134671998613,
125.982338394538));
#120313=CARTESIAN_POINT('Ctrl Pts',(-183.110439019824,-1.10255886667133,
126.009327221549));
#120314=CARTESIAN_POINT('Ctrl Pts',(-183.11821192009,-1.2357112082651,126.041912712826));
#120315=CARTESIAN_POINT('Ctrl Pts',(-183.125984820355,-1.36710228659016,
126.079933202471));
#120316=CARTESIAN_POINT('Ctrl Pts',(-183.133475156117,-1.49371696826858,
126.116571551551));
#120317=CARTESIAN_POINT('Ctrl Pts',(-183.14096549188,-1.61869592401328,
126.158256510196));
#120318=CARTESIAN_POINT('Ctrl Pts',(-183.148455827642,-1.74162011162668,
126.204801676833));
#120319=CARTESIAN_POINT('Ctrl Pts',(-183.15623038486,-1.86920866845707,
126.253113003952));
#120320=CARTESIAN_POINT('Ctrl Pts',(-183.164004942078,-1.99498761497027,
126.306813704835));
#120321=CARTESIAN_POINT('Ctrl Pts',(-183.171779499296,-2.11846807574788,
126.365748663978));
#120322=CARTESIAN_POINT('Ctrl Pts',(-183.179544423664,-2.24179554147299,
126.424610601388));
#120323=CARTESIAN_POINT('Ctrl Pts',(-183.187309348032,-2.36282983852742,
126.488693725991));
#120324=CARTESIAN_POINT('Ctrl Pts',(-183.195074272399,-2.48109933137568,
126.557793866607));
#120325=CARTESIAN_POINT('Ctrl Pts',(-183.202831433245,-2.59925057609296,
126.626824919564));
#120326=CARTESIAN_POINT('Ctrl Pts',(-183.210588594091,-2.71464218244685,
126.700862809964));
#120327=CARTESIAN_POINT('Ctrl Pts',(-183.218345754937,-2.82682484457249,
126.779656360033));
#120328=CARTESIAN_POINT('Ctrl Pts',(-183.226097014844,-2.93892216838622,
126.858389971173));
#120329=CARTESIAN_POINT('Ctrl Pts',(-183.233848274751,-3.04781508831774,
126.941871817109));
#120330=CARTESIAN_POINT('Ctrl Pts',(-183.241599534659,-3.15308146877894,
127.029806297684));
#120331=CARTESIAN_POINT('Ctrl Pts',(-183.249347240883,-3.25829958826959,
127.11770046336));
#120332=CARTESIAN_POINT('Ctrl Pts',(-183.257094947108,-3.35989417716957,
127.210042951671));
#120333=CARTESIAN_POINT('Ctrl Pts',(-183.264842653332,-3.45747473226868,
127.30649676398));
#120334=CARTESIAN_POINT('Ctrl Pts',(-183.272588665805,-3.55503395496101,
127.402929490203));
#120335=CARTESIAN_POINT('Ctrl Pts',(-183.280334678278,-3.6485806119105,
127.503471477585));
#120336=CARTESIAN_POINT('Ctrl Pts',(-183.28808069075,-3.73776002458828,
127.607747869501));
#120337=CARTESIAN_POINT('Ctrl Pts',(-183.295826687299,-3.82693925393412,
127.71202404705));
#120338=CARTESIAN_POINT('Ctrl Pts',(-183.303572683848,-3.91175100311841,
127.820034316536));
#120339=CARTESIAN_POINT('Ctrl Pts',(-183.311318680397,-3.9918802286738,
127.931369962791));
#120340=CARTESIAN_POINT('Ctrl Pts',(-183.319066338468,-4.07202664200908,
128.042729490627));
#120341=CARTESIAN_POINT('Ctrl Pts',(-183.326813996539,-4.14748830531724,
128.157415497046));
#120342=CARTESIAN_POINT('Ctrl Pts',(-183.33456165461,-4.21799316285316,
128.274989798444));
#120343=CARTESIAN_POINT('Ctrl Pts',(-183.342316556619,-4.28856394132185,
128.392674029965));
#120344=CARTESIAN_POINT('Ctrl Pts',(-183.350071458629,-4.35416845854172,
128.5132516133));
#120345=CARTESIAN_POINT('Ctrl Pts',(-183.357826360638,-4.4145801711371,
128.636258919051));
#120346=CARTESIAN_POINT('Ctrl Pts',(-183.365585372232,-4.47502389793923,
128.759331410527));
#120347=CARTESIAN_POINT('Ctrl Pts',(-183.373344383826,-4.53026917973013,
128.884835832641));
#120348=CARTESIAN_POINT('Ctrl Pts',(-183.38110339542,-4.58013779618434,
129.012288958713));
#120349=CARTESIAN_POINT('Ctrl Pts',(-183.388872575828,-4.63007176950502,
129.139909122444));
#120350=CARTESIAN_POINT('Ctrl Pts',(-183.396641756236,-4.67461487900791,
129.269482721212));
#120351=CARTESIAN_POINT('Ctrl Pts',(-183.404410936644,-4.71363875007996,
129.400511339244));
#120352=CARTESIAN_POINT('Ctrl Pts',(-183.407990344031,-4.73161778069228,
129.460878685434));
#120353=CARTESIAN_POINT('Ctrl Pts',(-183.411569751418,-4.74842600050534,
129.52155472689));
#120354=CARTESIAN_POINT('Ctrl Pts',(-183.415149158805,-4.76405452823414,
129.582490119309));
#120355=CARTESIAN_POINT('Ctrl Pts',(-181.664999290689,-4.76405452823418,
129.582490119309));
#120356=CARTESIAN_POINT('Ctrl Pts',(-181.672675880478,-4.79779503273996,
129.714043834293));
#120357=CARTESIAN_POINT('Ctrl Pts',(-181.680352470268,-4.82605765331497,
129.846900063432));
#120358=CARTESIAN_POINT('Ctrl Pts',(-181.688029060058,-4.84876606521478,
129.980558027547));
#120359=CARTESIAN_POINT('Ctrl Pts',(-181.695880977377,-4.87199312014276,
130.117268638917));
#120360=CARTESIAN_POINT('Ctrl Pts',(-181.703732894697,-4.88940914158996,
130.254817604855));
#120361=CARTESIAN_POINT('Ctrl Pts',(-181.711584812017,-4.90098872141958,
130.392665809464));
#120362=CARTESIAN_POINT('Ctrl Pts',(-181.719436729337,-4.9125683012492,
130.530514014073));
#120363=CARTESIAN_POINT('Ctrl Pts',(-181.727288646657,-4.91831148526274,
130.668661014282));
#120364=CARTESIAN_POINT('Ctrl Pts',(-181.735140563977,-4.91824950327072,
130.806571064884));
#120365=CARTESIAN_POINT('',(-181.389859436049,-4.91824915695527,130.807240306567));
#120366=CARTESIAN_POINT('Ctrl Pts',(-181.320039938991,-4.76405452823418,
129.582490119309));
#120367=CARTESIAN_POINT('Ctrl Pts',(-181.327866674491,-4.79848591795568,
129.716737585264));
#120368=CARTESIAN_POINT('Ctrl Pts',(-181.33569340999,-4.82725862397902,
129.852519526693));
#120369=CARTESIAN_POINT('Ctrl Pts',(-181.34352014549,-4.8502474171004,129.989325001528));
#120370=CARTESIAN_POINT('Ctrl Pts',(-181.351344753954,-4.8732299626622,
130.126093297362));
#120371=CARTESIAN_POINT('Ctrl Pts',(-181.359169362417,-4.89043165683097,
130.263884199659));
#120372=CARTESIAN_POINT('Ctrl Pts',(-181.366993970881,-4.90177834412933,
130.40217642155));
#120373=CARTESIAN_POINT('Ctrl Pts',(-181.374615792586,-4.91283096458077,
130.536884587887));
#120374=CARTESIAN_POINT('Ctrl Pts',(-181.38223761429,-4.91832830176703,
130.672068059881));
#120375=CARTESIAN_POINT('Ctrl Pts',(-181.389859435995,-4.91824915695583,
130.807240305618));
#120376=CARTESIAN_POINT('Ctrl Pts',(-181.389859436049,-4.91824915695527,
130.807240306567));
#120377=CARTESIAN_POINT('Ctrl Pts',(-181.398817739788,-4.91815613411647,
130.966114927541));
#120378=CARTESIAN_POINT('Ctrl Pts',(-181.407776043528,-4.91036021059812,
131.124708256897));
#120379=CARTESIAN_POINT('Ctrl Pts',(-181.416734347267,-4.89497108865333,
131.282315744903));
#120380=CARTESIAN_POINT('Ctrl Pts',(-181.425417497863,-4.88005464160356,
131.43508233925));
#120381=CARTESIAN_POINT('Ctrl Pts',(-181.434100648459,-4.8580046953391,
131.58692260436));
#120382=CARTESIAN_POINT('Ctrl Pts',(-181.442783799056,-4.82897206538774,
131.737212081736));
#120383=CARTESIAN_POINT('Ctrl Pts',(-181.451879679367,-4.79855944910979,
131.89464515665));
#120384=CARTESIAN_POINT('Ctrl Pts',(-181.460975559678,-4.76048430540328,
132.050376121223));
#120385=CARTESIAN_POINT('Ctrl Pts',(-181.47007143999,-4.71497645596076,
132.203710495987));
#120386=CARTESIAN_POINT('Ctrl Pts',(-181.479167320301,-4.66946860651813,
132.35704487075));
#120387=CARTESIAN_POINT('Ctrl Pts',(-181.488263200613,-4.61652822818693,
132.507982437687));
#120388=CARTESIAN_POINT('Ctrl Pts',(-181.497359080924,-4.5564403008889,
132.65585591784));
#120389=CARTESIAN_POINT('Ctrl Pts',(-181.505133415044,-4.50508258647963,
132.782244766713));
#120390=CARTESIAN_POINT('Ctrl Pts',(-181.512907749162,-4.44838078293223,
132.906695307599));
#120391=CARTESIAN_POINT('Ctrl Pts',(-181.520682083282,-4.386501677665,133.028722569754));
#120392=CARTESIAN_POINT('Ctrl Pts',(-181.528446836229,-4.32469883286472,
133.150599444214));
#120393=CARTESIAN_POINT('Ctrl Pts',(-181.536211589176,-4.25773155688373,
133.27005863679));
#120394=CARTESIAN_POINT('Ctrl Pts',(-181.543976342123,-4.18581526386889,
133.386633577433));
#120395=CARTESIAN_POINT('Ctrl Pts',(-181.551733383008,-4.11397039913011,
133.503092734203));
#120396=CARTESIAN_POINT('Ctrl Pts',(-181.559490423893,-4.0371865032356,
133.616673009293));
#120397=CARTESIAN_POINT('Ctrl Pts',(-181.567247464778,-3.95572544889312,
133.72693127291));
#120398=CARTESIAN_POINT('Ctrl Pts',(-181.574998656018,-3.87432582496551,
133.837106389913));
#120399=CARTESIAN_POINT('Ctrl Pts',(-181.582749847258,-3.78825629441504,
133.943964168621));
#120400=CARTESIAN_POINT('Ctrl Pts',(-181.590501038498,-3.69782249121197,
134.047089697521));
#120401=CARTESIAN_POINT('Ctrl Pts',(-181.598248935275,-3.60742712478753,
134.150171395321));
#120402=CARTESIAN_POINT('Ctrl Pts',(-181.605996832053,-3.51267143226317,
134.249523705019));
#120403=CARTESIAN_POINT('Ctrl Pts',(-181.61374472883,-3.41390170930395,
134.344764292532));
#120404=CARTESIAN_POINT('Ctrl Pts',(-181.621491004914,-3.31515264684154,
134.439984957767));
#120405=CARTESIAN_POINT('Ctrl Pts',(-181.629237280998,-3.21239150530955,
134.531095340363));
#120406=CARTESIAN_POINT('Ctrl Pts',(-181.636983557082,-3.10600158262843,
134.617749822881));
#120407=CARTESIAN_POINT('Ctrl Pts',(-181.644729890347,-2.99961087460092,
134.704404945062));
#120408=CARTESIAN_POINT('Ctrl Pts',(-181.652476223613,-2.88959163510988,
134.786603854625));
#120409=CARTESIAN_POINT('Ctrl Pts',(-181.660222556878,-2.77636007621668,
134.864041367291));
#120410=CARTESIAN_POINT('Ctrl Pts',(-181.667970624881,-2.66310315990082,
134.941496221552));
#120411=CARTESIAN_POINT('Ctrl Pts',(-181.675718692884,-2.54663281535994,
135.01418733648));
#120412=CARTESIAN_POINT('Ctrl Pts',(-181.683466760887,-2.4273937005275,
135.081853210796));
#120413=CARTESIAN_POINT('Ctrl Pts',(-181.691223063629,-2.30802785694534,
135.149591001208));
#120414=CARTESIAN_POINT('Ctrl Pts',(-181.698979366371,-2.18588770531916,
135.212292688746));
#120415=CARTESIAN_POINT('Ctrl Pts',(-181.706735669113,-2.06144243552465,
135.269742812577));
#120416=CARTESIAN_POINT('Ctrl Pts',(-181.714496111627,-1.93693074554234,
135.327223599268));
#120417=CARTESIAN_POINT('Ctrl Pts',(-181.722256554141,-1.81011184722903,
135.379447088406));
#120418=CARTESIAN_POINT('Ctrl Pts',(-181.730016996655,-1.68147337978646,
135.426246632557));
#120419=CARTESIAN_POINT('Ctrl Pts',(-181.737789896921,-1.55262841045597,
135.473121303491));
#120420=CARTESIAN_POINT('Ctrl Pts',(-181.745562797186,-1.42195840793301,
135.514554511845));
#120421=CARTESIAN_POINT('Ctrl Pts',(-181.753335697452,-1.28996545172147,
135.550429748527));
#120422=CARTESIAN_POINT('Ctrl Pts',(-181.760826033214,-1.16277077193805,
135.585000829992));
#120423=CARTESIAN_POINT('Ctrl Pts',(-181.768316368976,-1.03434795419006,
135.614410947926));
#120424=CARTESIAN_POINT('Ctrl Pts',(-181.775806704738,-0.905151846678698,
135.638601322884));
#120425=CARTESIAN_POINT('Ctrl Pts',(-181.783581038857,-0.771057229483291,
135.663708883261));
#120426=CARTESIAN_POINT('Ctrl Pts',(-181.791355372976,-0.635704754977355,
135.68327260728));
#120427=CARTESIAN_POINT('Ctrl Pts',(-181.799129707095,-0.499592595456683,
135.697170679388));
#120428=CARTESIAN_POINT('Ctrl Pts',(-181.806894460042,-0.363648182007928,
135.711051623364));
#120429=CARTESIAN_POINT('Ctrl Pts',(-181.814659212989,-0.226946331599816,
135.719280769009));
#120430=CARTESIAN_POINT('Ctrl Pts',(-181.822423965936,-0.08999601943478,
135.721787157839));
#120431=CARTESIAN_POINT('Ctrl Pts',(-181.830181006821,0.0468182717495528,
135.724291057289));
#120432=CARTESIAN_POINT('Ctrl Pts',(-181.837938047706,0.18388014522574,
135.721083504079));
#120433=CARTESIAN_POINT('Ctrl Pts',(-181.845695088591,0.320675234751949,
135.712145296657));
#120434=CARTESIAN_POINT('Ctrl Pts',(-181.853446279831,0.457367166036849,
135.703213829606));
#120435=CARTESIAN_POINT('Ctrl Pts',(-181.861197471071,0.593792325261312,
135.688560335476));
#120436=CARTESIAN_POINT('Ctrl Pts',(-181.868948662312,0.7294364329914,135.668217682975));
#120437=CARTESIAN_POINT('Ctrl Pts',(-181.876696559089,0.865022888357463,
135.647883676643));
#120438=CARTESIAN_POINT('Ctrl Pts',(-181.884444455866,0.999828566655742,
135.621865379108));
#120439=CARTESIAN_POINT('Ctrl Pts',(-181.892192352643,1.13334461812831,
135.59024747781));
#120440=CARTESIAN_POINT('Ctrl Pts',(-181.899938628727,1.26683274092118,
135.558636190296));
#120441=CARTESIAN_POINT('Ctrl Pts',(-181.907684904811,1.39903139325775,
135.521427718866));
#120442=CARTESIAN_POINT('Ctrl Pts',(-181.915431180895,1.5294426155094,135.478757728249));
#120443=CARTESIAN_POINT('Ctrl Pts',(-181.92317751416,1.65985480042725,135.436087422652));
#120444=CARTESIAN_POINT('Ctrl Pts',(-181.930923847426,1.78847915735103,
135.387955639));
#120445=CARTESIAN_POINT('Ctrl Pts',(-181.938670180691,1.91483395331802,
135.334547588732));
#120446=CARTESIAN_POINT('Ctrl Pts',(-181.946418248694,2.0412170455653,135.281127578101));
#120447=CARTESIAN_POINT('Ctrl Pts',(-181.954166316697,2.16532920544419,
135.222429101825));
#120448=CARTESIAN_POINT('Ctrl Pts',(-181.9619143847,2.2867100760472,135.158684915388));
#120449=CARTESIAN_POINT('Ctrl Pts',(-181.969670687442,2.40821995168409,
135.094872980871));
#120450=CARTESIAN_POINT('Ctrl Pts',(-181.977426990184,2.52699239260691,
135.026004805807));
#120451=CARTESIAN_POINT('Ctrl Pts',(-181.985183292925,2.64259251692664,
134.952358671083));
#120452=CARTESIAN_POINT('Ctrl Pts',(-181.99294373544,2.75825434051338,134.8786732292));
#120453=CARTESIAN_POINT('Ctrl Pts',(-182.000704177954,2.87074015323274,
134.80020496986));
#120454=CARTESIAN_POINT('Ctrl Pts',(-182.008464620468,2.97964616898119,
134.717274080726));
#120455=CARTESIAN_POINT('Ctrl Pts',(-182.016237520733,3.08872701033434,
134.634210063566));
#120456=CARTESIAN_POINT('Ctrl Pts',(-182.024010420999,3.19421627012777,
134.546669350855));
#120457=CARTESIAN_POINT('Ctrl Pts',(-182.031783321264,3.29574453972754,
134.455011380287));
#120458=CARTESIAN_POINT('Ctrl Pts',(-182.039273657026,3.39358200099335,
134.366685407822));
#120459=CARTESIAN_POINT('Ctrl Pts',(-182.046763992788,3.48774123604373,
134.274536541253));
#120460=CARTESIAN_POINT('Ctrl Pts',(-182.05425432855,3.57792693550293,134.178915685527));
#120461=CARTESIAN_POINT('Ctrl Pts',(-182.062028662669,3.67153205316809,
134.079669335994));
#120462=CARTESIAN_POINT('Ctrl Pts',(-182.069802996788,3.76115288689754,
133.976368136514));
#120463=CARTESIAN_POINT('Ctrl Pts',(-182.077577330907,3.84641767552078,
133.869365369266));
#120464=CARTESIAN_POINT('Ctrl Pts',(-182.085342083855,3.93157738291237,
133.762494473365));
#120465=CARTESIAN_POINT('Ctrl Pts',(-182.093106836802,4.01239148547918,
133.651931389249));
#120466=CARTESIAN_POINT('Ctrl Pts',(-182.100871589749,4.0885251703094,133.538065977375));
#120467=CARTESIAN_POINT('Ctrl Pts',(-182.108628630634,4.16458323809056,
133.424313658233));
#120468=CARTESIAN_POINT('Ctrl Pts',(-182.116385671519,4.23596992326855,
133.307265861425));
#120469=CARTESIAN_POINT('Ctrl Pts',(-182.124142712404,4.30239104351552,
133.187344958928));
#120470=CARTESIAN_POINT('Ctrl Pts',(-182.131893903644,4.36876207507913,
133.067514489717));
#120471=CARTESIAN_POINT('Ctrl Pts',(-182.139645094884,4.43017480638999,
132.944815567991));
#120472=CARTESIAN_POINT('Ctrl Pts',(-182.147396286124,4.48637891022631,
132.819698637943));
#120473=CARTESIAN_POINT('Ctrl Pts',(-182.155144182901,4.54255912581914,
132.694634885927));
#120474=CARTESIAN_POINT('Ctrl Pts',(-182.162892079678,4.59353495715868,
132.56715552553));
#120475=CARTESIAN_POINT('Ctrl Pts',(-182.170639976455,4.639102608463,132.437734442094));
#120476=CARTESIAN_POINT('Ctrl Pts',(-182.178386252539,4.68466072799699,
132.308340430758));
#120477=CARTESIAN_POINT('Ctrl Pts',(-182.186132528623,4.724812787904,132.177005872811));
#120478=CARTESIAN_POINT('Ctrl Pts',(-182.193878804708,4.75940376741928,
132.044223045892));
#120479=CARTESIAN_POINT('Ctrl Pts',(-182.201625137973,4.79399500227735,
131.911439238801));
#120480=CARTESIAN_POINT('Ctrl Pts',(-182.209371471238,4.82302497627006,
131.777207519742));
#120481=CARTESIAN_POINT('Ctrl Pts',(-182.217117804504,4.8463891245921,131.642033295606));
#120482=CARTESIAN_POINT('Ctrl Pts',(-182.224865872507,4.86975850515314,
131.506828800141));
#120483=CARTESIAN_POINT('Ctrl Pts',(-182.23261394051,4.88745946865773,131.370681764779));
#120484=CARTESIAN_POINT('Ctrl Pts',(-182.240362008513,4.89943900473265,
131.234105310848));
#120485=CARTESIAN_POINT('Ctrl Pts',(-182.248118311254,4.91143127280104,
131.097383701837));
#120486=CARTESIAN_POINT('Ctrl Pts',(-182.255874613996,4.91768993216839,
130.960232152658));
#120487=CARTESIAN_POINT('Ctrl Pts',(-182.263630916738,4.91821404414322,
130.823166959378));
#120488=CARTESIAN_POINT('Ctrl Pts',(-182.271391359252,4.9187384358524,130.686028610276));
#120489=CARTESIAN_POINT('Ctrl Pts',(-182.279151801766,4.91352219632619,
130.548977099404));
#120490=CARTESIAN_POINT('Ctrl Pts',(-182.28691224428,4.90261645226236,130.4125252127));
#120491=CARTESIAN_POINT('Ctrl Pts',(-182.294685144546,4.89169320132999,
130.275854281314));
#120492=CARTESIAN_POINT('Ctrl Pts',(-182.302458044811,4.8750622420806,130.139785285917));
#120493=CARTESIAN_POINT('Ctrl Pts',(-182.310230945077,4.85282630523814,
130.004823305311));
#120494=CARTESIAN_POINT('Ctrl Pts',(-182.317721280839,4.83139870070879,
129.874767532648));
#120495=CARTESIAN_POINT('Ctrl Pts',(-182.325211616601,4.80476661598463,
129.74573998823));
#120496=CARTESIAN_POINT('Ctrl Pts',(-182.332701952363,4.77306565540504,
129.618178796894));
#120497=CARTESIAN_POINT('Ctrl Pts',(-182.340476286482,4.74016274326992,
129.485781084218));
#120498=CARTESIAN_POINT('Ctrl Pts',(-182.348250620601,4.70169476824667,
129.354543717016));
#120499=CARTESIAN_POINT('Ctrl Pts',(-182.35602495472,4.65775801064424,129.224970426138));
#120500=CARTESIAN_POINT('Ctrl Pts',(-182.363789707667,4.61387540116881,
129.09555682276));
#120501=CARTESIAN_POINT('Ctrl Pts',(-182.371554460614,4.56453754362383,
128.967803581878));
#120502=CARTESIAN_POINT('Ctrl Pts',(-182.379319213561,4.50989146409757,
128.842203120177));
#120503=CARTESIAN_POINT('Ctrl Pts',(-182.387076254446,4.45529965982786,
128.716727406625));
#120504=CARTESIAN_POINT('Ctrl Pts',(-182.394833295331,4.39541028046255,
128.593400573383));
#120505=CARTESIAN_POINT('Ctrl Pts',(-182.402590336216,4.33041966677546,
128.472698426745));
#120506=CARTESIAN_POINT('Ctrl Pts',(-182.410341527457,4.26547806301561,
128.352087302535));
#120507=CARTESIAN_POINT('Ctrl Pts',(-182.418092718697,4.19544306651655,
128.234097268103));
#120508=CARTESIAN_POINT('Ctrl Pts',(-182.425843909937,4.1205583407563,128.119182406921));
#120509=CARTESIAN_POINT('Ctrl Pts',(-182.433591806714,4.04570544300221,
128.00431638762));
#120510=CARTESIAN_POINT('Ctrl Pts',(-182.441339703491,3.96600712868981,
127.892523268852));
#120511=CARTESIAN_POINT('Ctrl Pts',(-182.449087600268,3.88175193438076,
127.784230656384));
#120512=CARTESIAN_POINT('Ctrl Pts',(-182.456833876352,3.79751436444203,
127.675960696395));
#120513=CARTESIAN_POINT('Ctrl Pts',(-182.464580152436,3.70872205040214,
127.571190094635));
#120514=CARTESIAN_POINT('Ctrl Pts',(-182.47232642852,3.61570536686982,127.470315362551));
#120515=CARTESIAN_POINT('Ctrl Pts',(-182.480072761786,3.52268799670936,
127.369439885832));
#120516=CARTESIAN_POINT('Ctrl Pts',(-182.487819095051,3.42544645986479,
127.272460623597));
#120517=CARTESIAN_POINT('Ctrl Pts',(-182.495565428317,3.32434944963606,
127.179738733948));
#120518=CARTESIAN_POINT('Ctrl Pts',(-182.50331349632,3.22322979943299,127.086996079874));
#120519=CARTESIAN_POINT('Ctrl Pts',(-182.511061564323,3.11825324584275,
126.998512959771));
#120520=CARTESIAN_POINT('Ctrl Pts',(-182.518809632326,3.00982283896963,
126.914611327378));
#120521=CARTESIAN_POINT('Ctrl Pts',(-182.526565935067,2.9012771909699,126.830620523332));
#120522=CARTESIAN_POINT('Ctrl Pts',(-182.534322237809,2.78927066657606,
126.751221173508));
#120523=CARTESIAN_POINT('Ctrl Pts',(-182.542078540551,2.67423713290575,
126.676693138288));
#120524=CARTESIAN_POINT('Ctrl Pts',(-182.549838983065,2.55914220237462,
126.602125325212));
#120525=CARTESIAN_POINT('Ctrl Pts',(-182.557599425579,2.44101737989998,
126.532434205961));
#120526=CARTESIAN_POINT('Ctrl Pts',(-182.565359868094,2.32032172204335,
126.467853939523));
#120527=CARTESIAN_POINT('Ctrl Pts',(-182.573132768359,2.19943231280187,
126.403170003107));
#120528=CARTESIAN_POINT('Ctrl Pts',(-182.580905668624,2.07596417359235,
126.343613484455));
#120529=CARTESIAN_POINT('Ctrl Pts',(-182.58867856889,1.95039776998001,126.289370960728));
#120530=CARTESIAN_POINT('Ctrl Pts',(-182.596168904652,1.82939602142133,
126.237100289366));
#120531=CARTESIAN_POINT('Ctrl Pts',(-182.603659240414,1.70644620173451,
126.189764077074));
#120532=CARTESIAN_POINT('Ctrl Pts',(-182.611149576176,1.5819902152108,126.147485053255));
#120533=CARTESIAN_POINT('Ctrl Pts',(-182.618923910295,1.45281544213099,
126.103603007398));
#120534=CARTESIAN_POINT('Ctrl Pts',(-182.626698244414,1.3216088481364,126.065030201631));
#120535=CARTESIAN_POINT('Ctrl Pts',(-182.634472578533,1.18884627811505,
126.031957911432));
#120536=CARTESIAN_POINT('Ctrl Pts',(-182.64223733148,1.05624732609592,125.998926379875));
#120537=CARTESIAN_POINT('Ctrl Pts',(-182.650002084427,0.922096589234707,
125.971381969506));
#120538=CARTESIAN_POINT('Ctrl Pts',(-182.657766837375,0.786887822827249,
125.949467146357));
#120539=CARTESIAN_POINT('Ctrl Pts',(-182.66552387826,0.651813347672695,
125.92757408932));
#120540=CARTESIAN_POINT('Ctrl Pts',(-182.673280919145,0.515683317642029,
125.911299554543));
#120541=CARTESIAN_POINT('Ctrl Pts',(-182.68103796003,0.379004169031384,
125.900735539896));
#120542=CARTESIAN_POINT('Ctrl Pts',(-182.68878915127,0.242428091229729,
125.890179491655));
#120543=CARTESIAN_POINT('Ctrl Pts',(-182.69654034251,0.105304107303662,
125.885325422026));
#120544=CARTESIAN_POINT('Ctrl Pts',(-182.70429153375,-0.0318540434016616,
125.886213773233));
#120545=CARTESIAN_POINT('Ctrl Pts',(-182.712039430527,-0.168953898234309,
125.887101746867));
#120546=CARTESIAN_POINT('Ctrl Pts',(-182.719787327304,-0.306087500824971,
125.893727284479));
#120547=CARTESIAN_POINT('Ctrl Pts',(-182.727535224081,-0.442739133272749,
125.906078763449));
#120548=CARTESIAN_POINT('Ctrl Pts',(-182.735281500165,-0.579362181144514,
125.918427658756));
#120549=CARTESIAN_POINT('Ctrl Pts',(-182.743027776249,-0.715503070274265,
125.936500077871));
#120550=CARTESIAN_POINT('Ctrl Pts',(-182.750774052334,-0.85064962880552,
125.960232391403));
#120551=CARTESIAN_POINT('Ctrl Pts',(-182.758520385599,-0.985797184958153,
125.98396488012));
#120552=CARTESIAN_POINT('Ctrl Pts',(-182.766266718864,-1.11995001079294,
126.013357279003));
#120553=CARTESIAN_POINT('Ctrl Pts',(-182.77401305213,-1.25260496603569,
126.048294610711));
#120554=CARTESIAN_POINT('Ctrl Pts',(-182.781761120133,-1.38528962843572,
126.083239766392));
#120555=CARTESIAN_POINT('Ctrl Pts',(-182.789509188136,-1.51647537476105,
126.123732226282));
#120556=CARTESIAN_POINT('Ctrl Pts',(-182.797257256139,-1.6456734777856,
126.169606916773));
#120557=CARTESIAN_POINT('Ctrl Pts',(-182.80501355888,-1.7750088940917,126.215530363432));
#120558=CARTESIAN_POINT('Ctrl Pts',(-182.812769861622,-1.902352078152,126.266847336577));
#120559=CARTESIAN_POINT('Ctrl Pts',(-182.820526164364,-2.02723305972525,
126.323344082888));
#120560=CARTESIAN_POINT('Ctrl Pts',(-182.828286606878,-2.15218069403846,
126.379870983214));
#120561=CARTESIAN_POINT('Ctrl Pts',(-182.836047049393,-2.27466315832567,
126.441582989575));
#120562=CARTESIAN_POINT('Ctrl Pts',(-182.843807491907,-2.39423531671549,
126.508220453338));
#120563=CARTESIAN_POINT('Ctrl Pts',(-182.851580392172,-2.51399942294907,
126.574964889473));
#120564=CARTESIAN_POINT('Ctrl Pts',(-182.859353292438,-2.63084355393906,
126.646650378709));
#120565=CARTESIAN_POINT('Ctrl Pts',(-182.867126192703,-2.74435103366134,
126.722973541272));
#120566=CARTESIAN_POINT('Ctrl Pts',(-182.874616528465,-2.85373223058731,
126.796522164628));
#120567=CARTESIAN_POINT('Ctrl Pts',(-182.882106864227,-2.9600149073766,
126.874376951055));
#120568=CARTESIAN_POINT('Ctrl Pts',(-182.889597199989,-3.06285694824154,
126.956232452197));
#120569=CARTESIAN_POINT('Ctrl Pts',(-182.897271718051,-3.16822780545898,
127.040100724848));
#120570=CARTESIAN_POINT('Ctrl Pts',(-182.904946236112,-3.27033860869109,
127.128449457481));
#120571=CARTESIAN_POINT('Ctrl Pts',(-182.912620754173,-3.36877703830128,
127.220992881942));
#120572=CARTESIAN_POINT('Ctrl Pts',(-182.920286491824,-3.46710284456976,
127.313430427532));
#120573=CARTESIAN_POINT('Ctrl Pts',(-182.927952229474,-3.56176434009002,
127.410052852803));
#120574=CARTESIAN_POINT('Ctrl Pts',(-182.935617967125,-3.65237997082311,
127.510532508628));
#120575=CARTESIAN_POINT('Ctrl Pts',(-182.943276696308,-3.74291275542632,
127.610920300052));
#120576=CARTESIAN_POINT('Ctrl Pts',(-182.95093542549,-3.82940676294885,
127.715158013987));
#120577=CARTESIAN_POINT('Ctrl Pts',(-182.958594154673,-3.9115156180739,
127.822879671448));
#120578=CARTESIAN_POINT('Ctrl Pts',(-182.966247640976,-3.99356826453599,
127.930527586676));
#120579=CARTESIAN_POINT('Ctrl Pts',(-182.973901127278,-4.07124148666013,
128.041654383705));
#120580=CARTESIAN_POINT('Ctrl Pts',(-182.98155461358,-4.14422807866773,
128.15585977851));
#120581=CARTESIAN_POINT('Ctrl Pts',(-182.989205542012,-4.2171902778377,
128.270027004747));
#120582=CARTESIAN_POINT('Ctrl Pts',(-182.996856470444,-4.28546874152419,
128.387270447522));
#120583=CARTESIAN_POINT('Ctrl Pts',(-183.004507398876,-4.34879885726115,
128.50715980754));
#120584=CARTESIAN_POINT('Ctrl Pts',(-183.012156622058,-4.41211485788887,
128.627022446441));
#120585=CARTESIAN_POINT('Ctrl Pts',(-183.019805845239,-4.47048452011149,
128.749529472692));
#120586=CARTESIAN_POINT('Ctrl Pts',(-183.027455068421,-4.52368893671273,
128.874225527381));
#120587=CARTESIAN_POINT('Ctrl Pts',(-183.035106947243,-4.57691182470863,
128.998964873778));
#120588=CARTESIAN_POINT('Ctrl Pts',(-183.042758826066,-4.62496572459593,
129.125894397969));
#120589=CARTESIAN_POINT('Ctrl Pts',(-183.050410704888,-4.66767971122647,
129.254538312944));
#120590=CARTESIAN_POINT('Ctrl Pts',(-183.056846671858,-4.7036062873606,
129.362740233909));
#120591=CARTESIAN_POINT('Ctrl Pts',(-183.063282638827,-4.73575598385233,
129.472154524254));
#120592=CARTESIAN_POINT('Ctrl Pts',(-183.069718605797,-4.76405452823406,
129.582490119308));
#120593=CARTESIAN_POINT('Origin',(213.235140564004,0.,130.804360617566));
#120594=CARTESIAN_POINT('',(-185.165421073984,-4.76405452823401,129.582490119308));
#120595=CARTESIAN_POINT('',(-184.819837330039,-4.76405452823405,129.582490119308));
#120596=CARTESIAN_POINT('',(213.235140564004,-4.76405452823405,129.582490119308));
#120597=CARTESIAN_POINT('',(-183.485140564052,-4.91824798071509,130.799903859564));
#120598=CARTESIAN_POINT('Ctrl Pts',(-183.485140564052,-4.91824798071509,
130.799903859564));
#120599=CARTESIAN_POINT('Ctrl Pts',(-183.492790120517,-4.91837024179223,
130.934824870645));
#120600=CARTESIAN_POINT('Ctrl Pts',(-183.500439676982,-4.91293645195532,
131.069920615074));
#120601=CARTESIAN_POINT('Ctrl Pts',(-183.508089233447,-4.90193026440357,
131.204688914623));
#120602=CARTESIAN_POINT('Ctrl Pts',(-183.515732635828,-4.89093293135145,
131.339348792808));
#120603=CARTESIAN_POINT('Ctrl Pts',(-183.52337603821,-4.8743721510898,131.473681350422));
#120604=CARTESIAN_POINT('Ctrl Pts',(-183.531019440591,-4.85228364227142,
131.607184706296));
#120605=CARTESIAN_POINT('Ctrl Pts',(-183.538659228572,-4.83020557863537,
131.740624931294));
#120606=CARTESIAN_POINT('Ctrl Pts',(-183.546299016552,-4.80260504893871,
131.873236337474));
#120607=CARTESIAN_POINT('Ctrl Pts',(-183.553938804532,-4.76956954354201,
132.004522869854));
#120608=CARTESIAN_POINT('Ctrl Pts',(-183.561576868312,-4.73654149382951,
132.135779772569));
#120609=CARTESIAN_POINT('Ctrl Pts',(-183.569214932091,-4.69808100518792,
132.265712005344));
#120610=CARTESIAN_POINT('Ctrl Pts',(-183.576852995871,-4.65432642489983,
132.393834930973));
#120611=CARTESIAN_POINT('Ctrl Pts',(-183.584491098882,-4.6105716198721,
132.521958514688));
#120612=CARTESIAN_POINT('Ctrl Pts',(-183.592129201894,-4.56152279959267,
132.648272391449));
#120613=CARTESIAN_POINT('Ctrl Pts',(-183.599767304905,-4.50736762758277,
132.772308821234));
#120614=CARTESIAN_POINT('Ctrl Pts',(-183.607407210404,-4.45319967569707,
132.89637452191));
#120615=CARTESIAN_POINT('Ctrl Pts',(-183.615047115903,-4.39392313754426,
133.018161337874));
#120616=CARTESIAN_POINT('Ctrl Pts',(-183.622687021401,-4.32977284733201,
133.137223698205));
#120617=CARTESIAN_POINT('Ctrl Pts',(-183.63033486744,-4.26555588247997,
133.256409806066));
#120618=CARTESIAN_POINT('Ctrl Pts',(-183.637982713479,-4.19645524369809,
133.372865449847));
#120619=CARTESIAN_POINT('Ctrl Pts',(-183.645630559517,-4.12275070500498,
133.486171514494));
#120620=CARTESIAN_POINT('Ctrl Pts',(-183.653282768779,-4.04900411665295,
133.599542222126));
#120621=CARTESIAN_POINT('Ctrl Pts',(-183.66093497804,-3.97064863261913,
133.709759445809));
#120622=CARTESIAN_POINT('Ctrl Pts',(-183.668587187302,-3.8880051776028,
133.816436114866));
#120623=CARTESIAN_POINT('Ctrl Pts',(-183.676250761655,-3.80523898019318,
133.923271220542));
#120624=CARTESIAN_POINT('Ctrl Pts',(-183.683914336009,-3.71817235596996,
134.026554965782));
#120625=CARTESIAN_POINT('Ctrl Pts',(-183.691577910362,-3.62716431972376,
134.125935855344));
#120626=CARTESIAN_POINT('Ctrl Pts',(-183.696168965331,-3.5726436903536,
134.1854724509));
#120627=CARTESIAN_POINT('Ctrl Pts',(-183.700760020299,-3.51670920889025,
134.243609084722));
#120628=CARTESIAN_POINT('Ctrl Pts',(-183.705351075268,-3.45944366050394,
134.300277181544));
#120629=CARTESIAN_POINT('Ctrl Pts',(-183.713125409387,-3.36247215619332,
134.396236981985));
#120630=CARTESIAN_POINT('Ctrl Pts',(-183.720899743506,-3.26135135780418,
134.488310951084));
#120631=CARTESIAN_POINT('Ctrl Pts',(-183.728674077625,-3.15642552453558,
134.57611895693));
#120632=CARTESIAN_POINT('Ctrl Pts',(-183.736438830572,-3.05162900297956,
134.663818747256));
#120633=CARTESIAN_POINT('Ctrl Pts',(-183.744203583519,-2.94303707393275,
134.74726278652));
#120634=CARTESIAN_POINT('Ctrl Pts',(-183.751968336466,-2.83103145099696,
134.826107002654));
#120635=CARTESIAN_POINT('Ctrl Pts',(-183.759725377351,-2.71913707362488,
134.9048729096));
#120636=CARTESIAN_POINT('Ctrl Pts',(-183.767482418236,-2.60383606730024,
134.979047861564));
#120637=CARTESIAN_POINT('Ctrl Pts',(-183.775239459121,-2.48554362280428,
135.048327625171));
#120638=CARTESIAN_POINT('Ctrl Pts',(-183.782990650361,-2.36734038356073,
135.117555144369));
#120639=CARTESIAN_POINT('Ctrl Pts',(-183.790741841601,-2.24615053231144,
135.181894626134));
#120640=CARTESIAN_POINT('Ctrl Pts',(-183.798493032841,-2.12241837636851,
135.241085005913));
#120641=CARTESIAN_POINT('Ctrl Pts',(-183.806240929618,-1.99873880989235,
135.300250228202));
#120642=CARTESIAN_POINT('Ctrl Pts',(-183.813988826396,-1.87251943979781,
135.354270532912));
#120643=CARTESIAN_POINT('Ctrl Pts',(-183.821736723173,-1.7442291244233,
135.402930811008));
#120644=CARTESIAN_POINT('Ctrl Pts',(-183.829482999257,-1.61596564461714,
135.451580910423));
#120645=CARTESIAN_POINT('Ctrl Pts',(-183.837229275341,-1.48563244650519,
135.494873074791));
#120646=CARTESIAN_POINT('Ctrl Pts',(-183.844975551425,-1.35371794589048,
135.532640514682));
#120647=CARTESIAN_POINT('Ctrl Pts',(-183.85272188469,-1.22180247151308,
135.570408233365));
#120648=CARTESIAN_POINT('Ctrl Pts',(-183.860468217956,-1.08830604720463,
135.602651038582));
#120649=CARTESIAN_POINT('Ctrl Pts',(-183.868214551221,-0.953731425044513,
135.62925226727));
#120650=CARTESIAN_POINT('Ctrl Pts',(-183.875962619224,-0.81912666583066,
135.655859453118));
#120651=CARTESIAN_POINT('Ctrl Pts',(-183.883710687227,-0.683443611768262,
135.676822472633));
#120652=CARTESIAN_POINT('Ctrl Pts',(-183.89145875523,-0.547193964316623,
135.69207601721));
#120653=CARTESIAN_POINT('Ctrl Pts',(-183.899215057972,-0.410799509118467,
135.707345773435));
#120654=CARTESIAN_POINT('Ctrl Pts',(-183.906971360713,-0.273837646764738,
135.716893889475));
#120655=CARTESIAN_POINT('Ctrl Pts',(-183.914727663455,-0.136824502115776,
135.720707037228));
#120656=CARTESIAN_POINT('Ctrl Pts',(-183.922488105969,0.000261770573871722,
135.724522220172));
#120657=CARTESIAN_POINT('Ctrl Pts',(-183.930248548483,0.137398989362215,
135.722596341163));
#120658=CARTESIAN_POINT('Ctrl Pts',(-183.938008990998,0.274073289081115,
135.714968206726));
#120659=CARTESIAN_POINT('Ctrl Pts',(-183.945781891263,0.410966990519299,
135.70732782693));
#120660=CARTESIAN_POINT('Ctrl Pts',(-183.953554791528,0.547395898572235,
135.693966937693));
#120661=CARTESIAN_POINT('Ctrl Pts',(-183.961327691794,0.682852614635353,
135.674976119655));
#120662=CARTESIAN_POINT('Ctrl Pts',(-183.968818027556,0.813385137877262,
135.656675665687));
#120663=CARTESIAN_POINT('Ctrl Pts',(-183.976308363318,0.943014622152609,
135.633147555643));
#120664=CARTESIAN_POINT('Ctrl Pts',(-183.98379869908,1.07129981466353,135.604516841024));
#120665=CARTESIAN_POINT('Ctrl Pts',(-183.991573033199,1.20444897923751,
135.574800584158));
#120666=CARTESIAN_POINT('Ctrl Pts',(-183.999347367318,1.3365716786525,135.539493021914));
#120667=CARTESIAN_POINT('Ctrl Pts',(-184.007121701437,1.46716201666007,
135.49867831872));
#120668=CARTESIAN_POINT('Ctrl Pts',(-184.014886454385,1.5975914137469,135.457913916001));
#120669=CARTESIAN_POINT('Ctrl Pts',(-184.022651207332,1.72649183739355,
135.411655992067));
#120670=CARTESIAN_POINT('Ctrl Pts',(-184.030415960279,1.85336748449725,
135.360039714024));
#120671=CARTESIAN_POINT('Ctrl Pts',(-184.038173001164,1.98011711691926,
135.308474701997));
#120672=CARTESIAN_POINT('Ctrl Pts',(-184.045930042049,2.10484561505189,
135.251562073242));
#120673=CARTESIAN_POINT('Ctrl Pts',(-184.053687082934,2.22707259798284,
135.189486693954));
#120674=CARTESIAN_POINT('Ctrl Pts',(-184.061438274174,2.34920740859568,
135.127458126191));
#120675=CARTESIAN_POINT('Ctrl Pts',(-184.069189465414,2.46884411162038,
135.060274733533));
#120676=CARTESIAN_POINT('Ctrl Pts',(-184.076940656654,2.58552290710035,
134.988169212538));
#120677=CARTESIAN_POINT('Ctrl Pts',(-184.084688553431,2.70215211097956,
134.916094338312));
#120678=CARTESIAN_POINT('Ctrl Pts',(-184.092436450208,2.81582557588218,
134.839101701749));
#120679=CARTESIAN_POINT('Ctrl Pts',(-184.100184346985,2.92610889510012,
134.757469494958));
#120680=CARTESIAN_POINT('Ctrl Pts',(-184.107930623069,3.03636914542542,
134.675854363865));
#120681=CARTESIAN_POINT('Ctrl Pts',(-184.115676899153,3.14324034655068,
134.589601825376));
#120682=CARTESIAN_POINT('Ctrl Pts',(-184.123423175237,3.24631817313421,
134.499032643779));
#120683=CARTESIAN_POINT('Ctrl Pts',(-184.131169508503,3.34939676061442,
134.40846279362));
#120684=CARTESIAN_POINT('Ctrl Pts',(-184.138915841768,3.44868162397767,
134.313576494829));
#120685=CARTESIAN_POINT('Ctrl Pts',(-184.146662175034,3.54380286150397,
134.214733667732));
#120686=CARTESIAN_POINT('Ctrl Pts',(-184.154410243036,3.63894540077176,
134.115868705469));
#120687=CARTESIAN_POINT('Ctrl Pts',(-184.162158311039,3.72992218775639,
134.013045733441));
#120688=CARTESIAN_POINT('Ctrl Pts',(-184.169906379042,3.81640168934142,
133.906659959682));
#120689=CARTESIAN_POINT('Ctrl Pts',(-184.177662681784,3.90297310236997,
133.800161117856));
#120690=CARTESIAN_POINT('Ctrl Pts',(-184.185418984526,3.98503743489305,
133.690092214043));
#120691=CARTESIAN_POINT('Ctrl Pts',(-184.193175287268,4.06230449550591,
133.576880274537));
#120692=CARTESIAN_POINT('Ctrl Pts',(-184.200935729782,4.13961279587571,
133.463607910411));
#120693=CARTESIAN_POINT('Ctrl Pts',(-184.208696172296,4.21211851583949,
133.34718949967));
#120694=CARTESIAN_POINT('Ctrl Pts',(-184.21645661481,4.27957654775137,133.228078347508));
#120695=CARTESIAN_POINT('Ctrl Pts',(-184.224229515076,4.34714286928472,
133.108775987551));
#120696=CARTESIAN_POINT('Ctrl Pts',(-184.232002415341,4.40964513203329,
132.986772596348));
#120697=CARTESIAN_POINT('Ctrl Pts',(-184.239775315607,4.46688528271646,
132.862544023765));
#120698=CARTESIAN_POINT('Ctrl Pts',(-184.247265651369,4.52204460974522,
132.742831472703));
#120699=CARTESIAN_POINT('Ctrl Pts',(-184.254755987131,4.57231764704277,
132.621052998097));
#120700=CARTESIAN_POINT('Ctrl Pts',(-184.262246322894,4.61757109606277,
132.497647431814));
#120701=CARTESIAN_POINT('Ctrl Pts',(-184.270020657013,4.66454034335519,
132.369562905981));
#120702=CARTESIAN_POINT('Ctrl Pts',(-184.277794991132,4.70625063758659,
132.239319737225));
#120703=CARTESIAN_POINT('Ctrl Pts',(-184.285569325251,4.74249933939709,
132.107389043318));
#120704=CARTESIAN_POINT('Ctrl Pts',(-184.293334078198,4.77870336792206,
131.975620942201));
#120705=CARTESIAN_POINT('Ctrl Pts',(-184.301098831145,4.80945909397288,
131.842169827338));
#120706=CARTESIAN_POINT('Ctrl Pts',(-184.308863584092,4.83461224377596,
131.707525893045));
#120707=CARTESIAN_POINT('Ctrl Pts',(-184.316620624977,4.85974041111613,
131.573015689005));
#120708=CARTESIAN_POINT('Ctrl Pts',(-184.324377665862,4.87927700459897,
131.437315405021));
#120709=CARTESIAN_POINT('Ctrl Pts',(-184.332134706747,4.89311789977162,
131.300929123851));
#120710=CARTESIAN_POINT('Ctrl Pts',(-184.339885897987,4.9069483574176,131.164645692637));
#120711=CARTESIAN_POINT('Ctrl Pts',(-184.347637089227,4.91509162671567,
131.027677681317));
#120712=CARTESIAN_POINT('Ctrl Pts',(-184.355388280468,4.91749494876237,
130.89053771079));
#120713=CARTESIAN_POINT('Ctrl Pts',(-184.363136177245,4.91989724933307,
130.75345602841));
#120714=CARTESIAN_POINT('Ctrl Pts',(-184.370884074022,4.9165644480558,130.616202922275));
#120715=CARTESIAN_POINT('Ctrl Pts',(-184.378631970799,4.90749578839558,
130.479294240683));
#120716=CARTESIAN_POINT('Ctrl Pts',(-184.386378246883,4.89842902570346,
130.342414197436));
#120717=CARTESIAN_POINT('Ctrl Pts',(-184.394124522967,4.88362881695607,
130.205878825291));
#120718=CARTESIAN_POINT('Ctrl Pts',(-184.401870799051,4.86314648250967,
130.070201675542));
#120719=CARTESIAN_POINT('Ctrl Pts',(-184.409617132316,4.84266399686724,
129.934523524254));
#120720=CARTESIAN_POINT('Ctrl Pts',(-184.417363465582,4.81649936018953,
129.799703994589));
#120721=CARTESIAN_POINT('Ctrl Pts',(-184.425109798847,4.78475544272591,
129.666248841067));
#120722=CARTESIAN_POINT('Ctrl Pts',(-184.43285786685,4.75300441643203,129.532763801189));
#120723=CARTESIAN_POINT('Ctrl Pts',(-184.440605934853,4.7156717135631,129.400644125729));
#120724=CARTESIAN_POINT('Ctrl Pts',(-184.448354002856,4.67291063208325,
129.270382362484));
#120725=CARTESIAN_POINT('Ctrl Pts',(-184.456110305598,4.6301041036172,129.139982155487));
#120726=CARTESIAN_POINT('Ctrl Pts',(-184.46386660834,4.58185779378596,129.011444177258));
#120727=CARTESIAN_POINT('Ctrl Pts',(-184.471622911082,4.52837411636472,
128.885243392189));
#120728=CARTESIAN_POINT('Ctrl Pts',(-184.479383353596,4.47486189309462,
128.758975249962));
#120729=CARTESIAN_POINT('Ctrl Pts',(-184.48714379611,4.41610689968782,128.635047139604));
#120730=CARTESIAN_POINT('Ctrl Pts',(-184.494904238624,4.35235802797307,
128.513910299651));
#120731=CARTESIAN_POINT('Ctrl Pts',(-184.50267713889,4.28850682091009,128.392579000088));
#120732=CARTESIAN_POINT('Ctrl Pts',(-184.510450039155,4.21964591229296,
128.274048263238));
#120733=CARTESIAN_POINT('Ctrl Pts',(-184.518222939421,4.14606859545448,
128.15874192541));
#120734=CARTESIAN_POINT('Ctrl Pts',(-184.525713275183,4.07516599941415,
128.047627263403));
#120735=CARTESIAN_POINT('Ctrl Pts',(-184.533203610945,3.99988412443292,
127.939506893194));
#120736=CARTESIAN_POINT('Ctrl Pts',(-184.540693946706,3.92052012106803,
127.83473016197));
#120737=CARTESIAN_POINT('Ctrl Pts',(-184.548468280826,3.83814700739212,
127.725980789134));
#120738=CARTESIAN_POINT('Ctrl Pts',(-184.556242614945,3.75111517370212,
127.620489123221));
#120739=CARTESIAN_POINT('Ctrl Pts',(-184.564016949064,3.65971145319893,
127.518680301129));
#120740=CARTESIAN_POINT('Ctrl Pts',(-184.571781702011,3.56842037961253,
127.41699694931));
#120741=CARTESIAN_POINT('Ctrl Pts',(-184.579546454958,3.47276839832737,
127.318987698628));
#120742=CARTESIAN_POINT('Ctrl Pts',(-184.587311207905,3.37308453496028,
127.225047305978));
#120743=CARTESIAN_POINT('Ctrl Pts',(-184.59506824879,3.27349967901132,127.13120021625));
#120744=CARTESIAN_POINT('Ctrl Pts',(-184.602825289675,3.16989119284842,
127.04141420869));
#120745=CARTESIAN_POINT('Ctrl Pts',(-184.61058233056,3.06262689376355,126.956049355194));
#120746=CARTESIAN_POINT('Ctrl Pts',(-184.6183335218,2.95544348352117,126.870748875999));
#120747=CARTESIAN_POINT('Ctrl Pts',(-184.62608471304,2.84461005242828,126.789863157161));
#120748=CARTESIAN_POINT('Ctrl Pts',(-184.63383590428,2.73052936548945,126.713713670358));
#120749=CARTESIAN_POINT('Ctrl Pts',(-184.641583801057,2.61649716588561,
126.637596549119));
#120750=CARTESIAN_POINT('Ctrl Pts',(-184.649331697835,2.49922077998541,
126.566211872763));
#120751=CARTESIAN_POINT('Ctrl Pts',(-184.657079594612,2.37913379664567,
126.499839106392));
#120752=CARTESIAN_POINT('Ctrl Pts',(-184.664825870696,2.25907193291407,
126.433480223773));
#120753=CARTESIAN_POINT('Ctrl Pts',(-184.67257214678,2.13620098310233,126.372131354849));
#120754=CARTESIAN_POINT('Ctrl Pts',(-184.680318422864,2.01098075236442,
126.316026909371));
#120755=CARTESIAN_POINT('Ctrl Pts',(-184.688064756129,1.88575959727938,
126.259922049742));
#120756=CARTESIAN_POINT('Ctrl Pts',(-184.695811089395,1.75818948345372,
126.209061850666));
#120757=CARTESIAN_POINT('Ctrl Pts',(-184.70355742266,1.62875152037251,126.163633137161));
#120758=CARTESIAN_POINT('Ctrl Pts',(-184.711305490663,1.49928457055711,
126.118194250211));
#120759=CARTESIAN_POINT('Ctrl Pts',(-184.719053558666,1.36794930796729,
126.078189398663));
#120760=CARTESIAN_POINT('Ctrl Pts',(-184.726801626669,1.23524298830775,
126.043755842715));
#120761=CARTESIAN_POINT('Ctrl Pts',(-184.734557929411,1.10239562679191,
126.009285690373));
#120762=CARTESIAN_POINT('Ctrl Pts',(-184.742314232153,0.968174676377767,
125.980398760293));
#120763=CARTESIAN_POINT('Ctrl Pts',(-184.750070534895,0.833089147649478,
125.957181485889));
#120764=CARTESIAN_POINT('Ctrl Pts',(-184.757830977409,0.697931519707528,
125.933951819726));
#120765=CARTESIAN_POINT('Ctrl Pts',(-184.765591419923,0.561908781530276,
125.916397888946));
#120766=CARTESIAN_POINT('Ctrl Pts',(-184.773351862437,0.425535104989546,
125.904554199255));
#120767=CARTESIAN_POINT('Ctrl Pts',(-184.781124762703,0.288942509316547,
125.892691497022));
#120768=CARTESIAN_POINT('Ctrl Pts',(-184.788897662968,0.1519982403108,125.886557371142));
#120769=CARTESIAN_POINT('Ctrl Pts',(-184.796670563234,0.0152174156738462,
125.886134159506));
#120770=CARTESIAN_POINT('Ctrl Pts',(-184.804160898996,-0.116591081455591,
125.885726332679));
#120771=CARTESIAN_POINT('Ctrl Pts',(-184.811651234757,-0.248247503329108,
125.89062140511));
#120772=CARTESIAN_POINT('Ctrl Pts',(-184.819141570519,-0.379297317131378,
125.900758206306));
#120773=CARTESIAN_POINT('Ctrl Pts',(-184.826915904638,-0.515315924457791,
125.9112793474));
#120774=CARTESIAN_POINT('Ctrl Pts',(-184.834690238758,-0.651111882649554,
125.92748087175));
#120775=CARTESIAN_POINT('Ctrl Pts',(-184.842464572877,-0.786172471644022,
125.949351255337));
#120776=CARTESIAN_POINT('Ctrl Pts',(-184.850229325824,-0.921066610532533,
125.971194685631));
#120777=CARTESIAN_POINT('Ctrl Pts',(-184.857994078771,-1.05522680121144,
125.998693012488));
#120778=CARTESIAN_POINT('Ctrl Pts',(-184.865758831718,-1.18814307714153,
126.031782793084));
#120779=CARTESIAN_POINT('Ctrl Pts',(-184.873515872603,-1.3209273387533,
126.064839708443));
#120780=CARTESIAN_POINT('Ctrl Pts',(-184.881272913488,-1.45246976733426,
126.103476931965));
#120781=CARTESIAN_POINT('Ctrl Pts',(-184.889029954373,-1.58226860997003,
126.147579636201));
#120782=CARTESIAN_POINT('Ctrl Pts',(-184.896781145613,-1.71196957028905,
126.191649082245));
#120783=CARTESIAN_POINT('Ctrl Pts',(-184.904532336853,-1.83992919311302,
126.241175680014));
#120784=CARTESIAN_POINT('Ctrl Pts',(-184.912283528093,-1.96565931089237,
126.295994335197));
#120785=CARTESIAN_POINT('Ctrl Pts',(-184.92003142487,-2.09133599001719,
126.350789690989));
#120786=CARTESIAN_POINT('Ctrl Pts',(-184.927779321648,-2.21478469116771,
126.410872474649));
#120787=CARTESIAN_POINT('Ctrl Pts',(-184.935527218425,-2.33553592707272,
126.476028953304));
#120788=CARTESIAN_POINT('Ctrl Pts',(-184.943273494509,-2.45626190442228,
126.541171802628));
#120789=CARTESIAN_POINT('Ctrl Pts',(-184.951019770593,-2.57429119500066,
126.611386050408));
#120790=CARTESIAN_POINT('Ctrl Pts',(-184.958766046677,-2.68917804732998,
126.686411553741));
#120791=CARTESIAN_POINT('Ctrl Pts',(-184.966512379942,-2.8040657477281,
126.761437610895));
#120792=CARTESIAN_POINT('Ctrl Pts',(-184.974258713208,-2.9158106362426,
126.8412747807));
#120793=CARTESIAN_POINT('Ctrl Pts',(-184.982005046473,-3.02399548026597,
126.925619275606));
#120794=CARTESIAN_POINT('Ctrl Pts',(-184.989753114476,-3.1322045515355,
127.009982658877));
#120795=CARTESIAN_POINT('Ctrl Pts',(-184.997501182479,-3.2368516836113,
127.098855135468));
#120796=CARTESIAN_POINT('Ctrl Pts',(-185.005249250482,-3.33755261674843,
127.19189254256));
#120797=CARTESIAN_POINT('Ctrl Pts',(-185.013005553224,-3.43836057603525,
127.285028830915));
#120798=CARTESIAN_POINT('Ctrl Pts',(-185.020761855966,-3.53521367065951,
127.382338626523));
#120799=CARTESIAN_POINT('Ctrl Pts',(-185.028518158708,-3.62776404908838,
127.483440403733));
#120800=CARTESIAN_POINT('Ctrl Pts',(-185.036278601222,-3.72036382444085,
127.584596142007));
#120801=CARTESIAN_POINT('Ctrl Pts',(-185.044039043736,-3.80865605608395,
127.689547595635));
#120802=CARTESIAN_POINT('Ctrl Pts',(-185.05179948625,-3.89233379093432,
127.797880828435));
#120803=CARTESIAN_POINT('Ctrl Pts',(-185.059572386516,-3.976145852713,127.906387967359));
#120804=CARTESIAN_POINT('Ctrl Pts',(-185.067345286781,-4.05532838899046,
128.018287414464));
#120805=CARTESIAN_POINT('Ctrl Pts',(-185.075118187046,-4.12961782569921,
128.133136239838));
#120806=CARTESIAN_POINT('Ctrl Pts',(-185.082608522808,-4.20120665425939,
128.243810021123));
#120807=CARTESIAN_POINT('Ctrl Pts',(-185.09009885857,-4.26825180309765,
128.357222203767));
#120808=CARTESIAN_POINT('Ctrl Pts',(-185.097589194332,-4.33055905059273,
128.472957312295));
#120809=CARTESIAN_POINT('Ctrl Pts',(-185.10578677954,-4.39874944774409,
128.599620314307));
#120810=CARTESIAN_POINT('Ctrl Pts',(-185.113984364748,-4.46146195184884,
128.729431206875));
#120811=CARTESIAN_POINT('Ctrl Pts',(-185.122181949956,-4.51841101832934,
128.86190214132));
#120812=CARTESIAN_POINT('Ctrl Pts',(-185.130360998453,-4.57523130928227,
128.994073527142));
#120813=CARTESIAN_POINT('Ctrl Pts',(-185.13854004695,-4.62631401768098,
129.128892662092));
#120814=CARTESIAN_POINT('Ctrl Pts',(-185.146719095448,-4.6714196002999,
129.265847705552));
#120815=CARTESIAN_POINT('Ctrl Pts',(-185.152953088293,-4.70579864566502,
129.370233534949));
#120816=CARTESIAN_POINT('Ctrl Pts',(-185.159187081138,-4.73670625024354,
129.475859598491));
#120817=CARTESIAN_POINT('Ctrl Pts',(-185.165421073984,-4.76405452823401,
129.582490119308));
#120818=CARTESIAN_POINT('Ctrl Pts',(-183.415149158805,-4.76405452823414,
129.582490119309));
#120819=CARTESIAN_POINT('Ctrl Pts',(-183.419067256354,-4.78116185622988,
129.649191331524));
#120820=CARTESIAN_POINT('Ctrl Pts',(-183.422985353904,-4.79685563415493,
129.716203290357));
#120821=CARTESIAN_POINT('Ctrl Pts',(-183.426903451454,-4.81112741488386,
129.783460984765));
#120822=CARTESIAN_POINT('Ctrl Pts',(-183.437819003722,-4.85088762159933,
129.970836329416));
#120823=CARTESIAN_POINT('Ctrl Pts',(-183.448734555991,-4.87971282541858,
130.160606736013));
#120824=CARTESIAN_POINT('Ctrl Pts',(-183.459650108259,-4.89737607248764,
130.351712114724));
#120825=CARTESIAN_POINT('Ctrl Pts',(-183.468146926843,-4.91112539109944,
130.500471214907));
#120826=CARTESIAN_POINT('Ctrl Pts',(-183.476643745428,-4.91811217802289,
130.650039045172));
#120827=CARTESIAN_POINT('Ctrl Pts',(-183.485140564012,-4.91824798071445,
130.799903858857));
#120828=CARTESIAN_POINT('',(-183.139859435957,-4.91824917715616,130.807205596086));
#120829=CARTESIAN_POINT('Ctrl Pts',(-183.069718605797,-4.76405452823406,
129.582490119308));
#120830=CARTESIAN_POINT('Ctrl Pts',(-183.077377441043,-4.79772994797449,
129.71379006978));
#120831=CARTESIAN_POINT('Ctrl Pts',(-183.085036276289,-4.825950394775,129.846394602858));
#120832=CARTESIAN_POINT('Ctrl Pts',(-183.092695111536,-4.84863804824104,
129.97980489498));
#120833=CARTESIAN_POINT('Ctrl Pts',(-183.100555832273,-4.87192374408618,
130.116731857903));
#120834=CARTESIAN_POINT('Ctrl Pts',(-183.10841655301,-4.88938085774212,
130.254507194701));
#120835=CARTESIAN_POINT('Ctrl Pts',(-183.116277273746,-4.90098218359303,
130.392587987825));
#120836=CARTESIAN_POINT('Ctrl Pts',(-183.124137994483,-4.91258350944392,
130.530668780949));
#120837=CARTESIAN_POINT('Ctrl Pts',(-183.13199871522,-4.91832909109846,
130.669054577283));
#120838=CARTESIAN_POINT('Ctrl Pts',(-183.139859435957,-4.91824917715616,
130.807205596086));
#120839=CARTESIAN_POINT('Ctrl Pts',(-183.139859435995,-4.91824917715577,
130.807205596751));
#120840=CARTESIAN_POINT('Ctrl Pts',(-183.149254565264,-4.91815366403183,
130.972323621388));
#120841=CARTESIAN_POINT('Ctrl Pts',(-183.158649694533,-4.90974370090652,
131.137198293807));
#120842=CARTESIAN_POINT('Ctrl Pts',(-183.168044823802,-4.89308820514277,
131.301221643601));
#120843=CARTESIAN_POINT('Ctrl Pts',(-183.175819157921,-4.87930602234573,
131.436948602553));
#120844=CARTESIAN_POINT('Ctrl Pts',(-183.18359349204,-4.85985043506831,
131.572316662951));
#120845=CARTESIAN_POINT('Ctrl Pts',(-183.191367826159,-4.83474526787819,
131.70681352893));
#120846=CARTESIAN_POINT('Ctrl Pts',(-183.199132579106,-4.80967104056291,
131.841144639542));
#120847=CARTESIAN_POINT('Ctrl Pts',(-183.206897332053,-4.77896115788808,
131.974606311377));
#120848=CARTESIAN_POINT('Ctrl Pts',(-183.214662085,-4.74269128219991,132.106690247209));
#120849=CARTESIAN_POINT('Ctrl Pts',(-183.222419125885,-4.70645743026349,
132.238642995413));
#120850=CARTESIAN_POINT('Ctrl Pts',(-183.23017616677,-4.664674677723,132.369220356194));
#120851=CARTESIAN_POINT('Ctrl Pts',(-183.237933207655,-4.61746985964742,
132.497923476673));
#120852=CARTESIAN_POINT('Ctrl Pts',(-183.245684398895,-4.57030063909242,
132.626529541128));
#120853=CARTESIAN_POINT('Ctrl Pts',(-183.253435590136,-4.5177176256354,
132.753263812955));
#120854=CARTESIAN_POINT('Ctrl Pts',(-183.261186781376,-4.45989758071983,
132.877642226993));
#120855=CARTESIAN_POINT('Ctrl Pts',(-183.268934678153,-4.40210211086567,
133.001967776888));
#120856=CARTESIAN_POINT('Ctrl Pts',(-183.27668257493,-4.33907420112053,
133.123939106722));
#120857=CARTESIAN_POINT('Ctrl Pts',(-183.284430471707,-4.27103878920714,
133.243091993423));
#120858=CARTESIAN_POINT('Ctrl Pts',(-183.292176747791,-4.20301760883524,
133.362219955909));
#120859=CARTESIAN_POINT('Ctrl Pts',(-183.299923023875,-4.12999120349208,
133.478530308623));
#120860=CARTESIAN_POINT('Ctrl Pts',(-183.307669299959,-4.05223033797251,
133.591583671165));
#120861=CARTESIAN_POINT('Ctrl Pts',(-183.315415633224,-3.97446889844,133.704637868242));
#120862=CARTESIAN_POINT('Ctrl Pts',(-183.32316196649,-3.89197315055749,
133.814434705049));
#120863=CARTESIAN_POINT('Ctrl Pts',(-183.330908299755,-3.80505680682347,
133.920564359196));
#120864=CARTESIAN_POINT('Ctrl Pts',(-183.338656367758,-3.7181209987768,
134.026717780342));
#120865=CARTESIAN_POINT('Ctrl Pts',(-183.346404435761,-3.62676287263744,
134.129202082239));
#120866=CARTESIAN_POINT('Ctrl Pts',(-183.354152503764,-3.53133571328797,
134.227641374757));
#120867=CARTESIAN_POINT('Ctrl Pts',(-183.361908806506,-3.43580713281808,
134.326185289727));
#120868=CARTESIAN_POINT('Ctrl Pts',(-183.369665109248,-3.33620115280986,
134.420675326271));
#120869=CARTESIAN_POINT('Ctrl Pts',(-183.37742141199,-3.23290753652007,
134.510772888592));
#120870=CARTESIAN_POINT('Ctrl Pts',(-183.385181854504,-3.12955878931717,
134.600918538695));
#120871=CARTESIAN_POINT('Ctrl Pts',(-183.392942297018,-3.02251878900405,
134.686666798853));
#120872=CARTESIAN_POINT('Ctrl Pts',(-183.400702739532,-2.91220871858613,
134.767720737703));
#120873=CARTESIAN_POINT('Ctrl Pts',(-183.408475639798,-2.80172156865031,
134.848904791531));
#120874=CARTESIAN_POINT('Ctrl Pts',(-183.416248540063,-2.68795418328053,
134.925379247005));
#120875=CARTESIAN_POINT('Ctrl Pts',(-183.424021440328,-2.57135568988743,
134.996891235055));
#120876=CARTESIAN_POINT('Ctrl Pts',(-183.43151177609,-2.45899584542431,
135.065803582211));
#120877=CARTESIAN_POINT('Ctrl Pts',(-183.439002111852,-2.34400742397867,
135.130107844031));
#120878=CARTESIAN_POINT('Ctrl Pts',(-183.446492447614,-2.22681044216329,
135.18961982509));
#120879=CARTESIAN_POINT('Ctrl Pts',(-183.454266781733,-2.1051699011596,
135.251388221));
#120880=CARTESIAN_POINT('Ctrl Pts',(-183.462041115852,-1.98076469797066,
135.308189427607));
#120881=CARTESIAN_POINT('Ctrl Pts',(-183.469815449971,-1.85403871937935,
135.359766580764));
#120882=CARTESIAN_POINT('Ctrl Pts',(-183.477580202919,-1.72746891923083,
135.41128016969));
#120883=CARTESIAN_POINT('Ctrl Pts',(-183.485344955866,-1.59858439316792,
135.457582369257));
#120884=CARTESIAN_POINT('Ctrl Pts',(-183.493109708813,-1.467853683391,135.49846208927));
#120885=CARTESIAN_POINT('Ctrl Pts',(-183.500866749698,-1.33725281719802,
135.539301206969));
#120886=CARTESIAN_POINT('Ctrl Pts',(-183.508623790583,-1.204809787081,135.57472844694));
#120887=CARTESIAN_POINT('Ctrl Pts',(-183.516380831468,-1.07101284954884,
135.60458087695));
#120888=CARTESIAN_POINT('Ctrl Pts',(-183.524132022708,-0.937316809328249,
135.634410795011));
#120889=CARTESIAN_POINT('Ctrl Pts',(-183.531883213948,-0.802269273954129,
135.65867418614));
#120890=CARTESIAN_POINT('Ctrl Pts',(-183.539634405188,-0.66637304503378,
135.677258115703));
#120891=CARTESIAN_POINT('Ctrl Pts',(-183.547382301965,-0.530534575635689,
135.695834146601));
#120892=CARTESIAN_POINT('Ctrl Pts',(-183.555130198743,-0.393848516679804,
135.708735464179));
#120893=CARTESIAN_POINT('Ctrl Pts',(-183.56287809552,-0.256827016516643,
135.715900391006));
#120894=CARTESIAN_POINT('Ctrl Pts',(-183.570624371604,-0.119834178297475,
135.723063819085));
#120895=CARTESIAN_POINT('Ctrl Pts',(-183.578370647688,0.01749357137839,
135.724493222735));
#120896=CARTESIAN_POINT('Ctrl Pts',(-183.586116923772,0.15464021435102,
135.720178908207));
#120897=CARTESIAN_POINT('Ctrl Pts',(-183.593863257037,0.291787869708826,
135.715864561833));
#120898=CARTESIAN_POINT('Ctrl Pts',(-183.601609590303,0.42875402492383,
135.705806424969));
#120899=CARTESIAN_POINT('Ctrl Pts',(-183.609355923568,0.565024315543222,
135.690046913814));
#120900=CARTESIAN_POINT('Ctrl Pts',(-183.617103991571,0.701325122949181,
135.674283873426));
#120901=CARTESIAN_POINT('Ctrl Pts',(-183.624852059574,0.836929367365514,
135.652816963002));
#120902=CARTESIAN_POINT('Ctrl Pts',(-183.632600127577,0.971329842672489,
135.625740233323));
#120903=CARTESIAN_POINT('Ctrl Pts',(-183.640356430319,1.10587316040419,
135.598634726173));
#120904=CARTESIAN_POINT('Ctrl Pts',(-183.648112733061,1.23920976945106,
135.565907567004));
#120905=CARTESIAN_POINT('Ctrl Pts',(-183.655869035803,1.37084412301909,
135.527703655382));
#120906=CARTESIAN_POINT('Ctrl Pts',(-183.663629478317,1.50254873380541,
135.489479353182));
#120907=CARTESIAN_POINT('Ctrl Pts',(-183.671389920831,1.63254890835973,
135.445772598521));
#120908=CARTESIAN_POINT('Ctrl Pts',(-183.679150363345,1.76036717021572,
135.396777245936));
#120909=CARTESIAN_POINT('Ctrl Pts',(-183.686923263611,1.88839061729247,
135.347703241661));
#120910=CARTESIAN_POINT('Ctrl Pts',(-183.694696163876,2.01422479326663,
135.293323829465));
#120911=CARTESIAN_POINT('Ctrl Pts',(-183.702469064142,2.13741418789364,
135.233880191051));
#120912=CARTESIAN_POINT('Ctrl Pts',(-183.709959399904,2.25612533772893,
135.176597478624));
#120913=CARTESIAN_POINT('Ctrl Pts',(-183.717449735665,2.37238038492857,
135.114612487253));
#120914=CARTESIAN_POINT('Ctrl Pts',(-183.724940071427,2.48579733142663,
135.048179026684));
#120915=CARTESIAN_POINT('Ctrl Pts',(-183.732714405547,2.60351451592501,
134.979226721265));
#120916=CARTESIAN_POINT('Ctrl Pts',(-183.740488739666,2.71854703082651,
134.905263540102));
#120917=CARTESIAN_POINT('Ctrl Pts',(-183.748263073785,2.83043883740145,
134.826524096371));
#120918=CARTESIAN_POINT('Ctrl Pts',(-183.756027826732,2.94219274732453,
134.747881691967));
#120919=CARTESIAN_POINT('Ctrl Pts',(-183.763792579679,3.05081333368219,
134.664474959851));
#120920=CARTESIAN_POINT('Ctrl Pts',(-183.771557332626,3.15586974181246,
134.57658399844));
#120921=CARTESIAN_POINT('Ctrl Pts',(-183.779314373511,3.26082180643742,
134.488780331571));
#120922=CARTESIAN_POINT('Ctrl Pts',(-183.787071414396,3.36221643965492,
134.396501547914));
#120923=CARTESIAN_POINT('Ctrl Pts',(-183.794828455281,3.45965264739519,
134.300070362649));
#120924=CARTESIAN_POINT('Ctrl Pts',(-183.802579646521,3.55701537773313,
134.203711896892));
#120925=CARTESIAN_POINT('Ctrl Pts',(-183.810330837761,3.65042534745426,
134.103207536208));
#120926=CARTESIAN_POINT('Ctrl Pts',(-183.818082029001,3.73951576490132,
133.998919257903));
#120927=CARTESIAN_POINT('Ctrl Pts',(-183.825829925778,3.82856831654428,
133.894675304899));
#120928=CARTESIAN_POINT('Ctrl Pts',(-183.833577822555,3.91330471401534,
133.786650929633));
#120929=CARTESIAN_POINT('Ctrl Pts',(-183.841325719332,3.99339623765048,
133.675243678859));
#120930=CARTESIAN_POINT('Ctrl Pts',(-183.849071995416,4.07347100786544,
133.56385973208));
#120931=CARTESIAN_POINT('Ctrl Pts',(-183.8568182715,4.14890260875522,133.449094634542));
#120932=CARTESIAN_POINT('Ctrl Pts',(-183.864564547585,4.21940396427489,
133.33137728723));
#120933=CARTESIAN_POINT('Ctrl Pts',(-183.87231088085,4.28990584021965,133.213659070955));
#120934=CARTESIAN_POINT('Ctrl Pts',(-183.880057214115,4.35547719729329,
133.092988896832));
#120935=CARTESIAN_POINT('Ctrl Pts',(-183.887803547381,4.41587569489273,
132.969822441232));
#120936=CARTESIAN_POINT('Ctrl Pts',(-183.895551615384,4.47628771831701,
132.846628403359));
#120937=CARTESIAN_POINT('Ctrl Pts',(-183.903299683387,4.53152440502785,
132.720937322577));
#120938=CARTESIAN_POINT('Ctrl Pts',(-183.911047751389,4.58139072531399,
132.593226762504));
#120939=CARTESIAN_POINT('Ctrl Pts',(-183.918804054131,4.63131004411868,
132.465380470129));
#120940=CARTESIAN_POINT('Ctrl Pts',(-183.926560356873,4.67584745234577,
132.335510775713));
#120941=CARTESIAN_POINT('Ctrl Pts',(-183.934316659615,4.71485700295889,
132.204112918564));
#120942=CARTESIAN_POINT('Ctrl Pts',(-183.942077102129,4.75388737414372,
132.072644930422));
#120943=CARTESIAN_POINT('Ctrl Pts',(-183.949837544643,4.78738391338526,
131.939647533283));
#120944=CARTESIAN_POINT('Ctrl Pts',(-183.957597987157,4.81525162830277,
131.805627224733));
#120945=CARTESIAN_POINT('Ctrl Pts',(-183.965370887423,4.84316407895025,
131.671391774886));
#120946=CARTESIAN_POINT('Ctrl Pts',(-183.973143787688,4.86542958515006,
131.536130518247));
#120947=CARTESIAN_POINT('Ctrl Pts',(-183.980916687954,4.88200484548556,
131.400357053089));
#120948=CARTESIAN_POINT('Ctrl Pts',(-183.988407023716,4.8979775533577,131.269519295378));
#120949=CARTESIAN_POINT('Ctrl Pts',(-183.995897359478,4.90866651731051,
131.138206229746));
#120950=CARTESIAN_POINT('Ctrl Pts',(-184.00338769524,4.91407879538588,131.006876432353));
#120951=CARTESIAN_POINT('Ctrl Pts',(-184.011162029359,4.91969628162939,
130.870567225777));
#120952=CARTESIAN_POINT('Ctrl Pts',(-184.018936363479,4.91964684670001,
130.73380820703));
#120953=CARTESIAN_POINT('Ctrl Pts',(-184.026710697598,4.91388137723509,
130.597109868563));
#120954=CARTESIAN_POINT('Ctrl Pts',(-184.034475450545,4.90812301319603,
130.460579998582));
#120955=CARTESIAN_POINT('Ctrl Pts',(-184.042240203492,4.89666264739697,
130.324111046953));
#120956=CARTESIAN_POINT('Ctrl Pts',(-184.050004956439,4.87950304710029,
130.188216903941));
#120957=CARTESIAN_POINT('Ctrl Pts',(-184.057761997324,4.86236048996048,
130.052457732909));
#120958=CARTESIAN_POINT('Ctrl Pts',(-184.065519038209,4.83953001175498,
129.917272619736));
#120959=CARTESIAN_POINT('Ctrl Pts',(-184.073276079094,4.81106637481358,
129.783173367529));
#120960=CARTESIAN_POINT('Ctrl Pts',(-184.081027270334,4.78262420252226,
129.649175240611));
#120961=CARTESIAN_POINT('Ctrl Pts',(-184.088778461574,4.74855740774753,
129.516261725672));
#120962=CARTESIAN_POINT('Ctrl Pts',(-184.096529652814,4.70897227239641,
129.384937072495));
#120963=CARTESIAN_POINT('Ctrl Pts',(-184.104277549591,4.66940396178373,
129.253668235799));
#120964=CARTESIAN_POINT('Ctrl Pts',(-184.112025446369,4.62432208809752,
129.123987291273));
#120965=CARTESIAN_POINT('Ctrl Pts',(-184.119773343146,4.57388343767266,
128.996385683812));
#120966=CARTESIAN_POINT('Ctrl Pts',(-184.12751961923,4.52345533792613,128.868810767856));
#120967=CARTESIAN_POINT('Ctrl Pts',(-184.135265895314,4.46767283385089,
128.74331468718));
#120968=CARTESIAN_POINT('Ctrl Pts',(-184.143012171398,4.40674160037786,
128.620370798451));
#120969=CARTESIAN_POINT('Ctrl Pts',(-184.150758504663,4.3458099171244,128.497426002177));
#120970=CARTESIAN_POINT('Ctrl Pts',(-184.158504837929,4.2797296022448,128.377033785747));
#120971=CARTESIAN_POINT('Ctrl Pts',(-184.166251171194,4.20875303816093,
128.259644341383));
#120972=CARTESIAN_POINT('Ctrl Pts',(-184.173999239197,4.13776057936755,
128.142228608466));
#120973=CARTESIAN_POINT('Ctrl Pts',(-184.1817473072,4.06186989174729,128.027817320214));
#120974=CARTESIAN_POINT('Ctrl Pts',(-184.189495375203,3.98137734477428,
127.916832695447));
#120975=CARTESIAN_POINT('Ctrl Pts',(-184.197251677945,3.90079924936458,
127.8057301149));
#120976=CARTESIAN_POINT('Ctrl Pts',(-184.205007980687,3.81560975438436,
127.698061789918));
#120977=CARTESIAN_POINT('Ctrl Pts',(-184.212764283429,3.72614663075139,
127.594218198819));
#120978=CARTESIAN_POINT('Ctrl Pts',(-184.220524725943,3.63663575795566,
127.490319183269));
#120979=CARTESIAN_POINT('Ctrl Pts',(-184.228285168457,3.54284697871845,
127.390249254338));
#120980=CARTESIAN_POINT('Ctrl Pts',(-184.236045610971,3.44515507810191,
127.294362106124));
#120981=CARTESIAN_POINT('Ctrl Pts',(-184.243818511237,3.34730635377383,
127.198321031346));
#120982=CARTESIAN_POINT('Ctrl Pts',(-184.251591411502,3.2455422777318,127.106476417236));
#120983=CARTESIAN_POINT('Ctrl Pts',(-184.259364311768,3.14027154927359,
127.01914230691));
#120984=CARTESIAN_POINT('Ctrl Pts',(-184.26685464753,3.03882767695724,126.934983011478));
#120985=CARTESIAN_POINT('Ctrl Pts',(-184.274344983291,2.93412792197492,
126.855012163906));
#120986=CARTESIAN_POINT('Ctrl Pts',(-184.281835319053,2.82656191248064,
126.779471697681));
#120987=CARTESIAN_POINT('Ctrl Pts',(-184.289609653172,2.71491750504099,
126.701067091717));
#120988=CARTESIAN_POINT('Ctrl Pts',(-184.297383987292,2.59983154856586,
126.627187092566));
#120989=CARTESIAN_POINT('Ctrl Pts',(-184.305158321411,2.4817069878406,126.55814895433));
#120990=CARTESIAN_POINT('Ctrl Pts',(-184.312923074358,2.36372800507934,
126.489195899429));
#120991=CARTESIAN_POINT('Ctrl Pts',(-184.320687827305,2.2427182034227,126.425073027955));
#120992=CARTESIAN_POINT('Ctrl Pts',(-184.328452580252,2.11911142907846,
126.366055781973));
#120993=CARTESIAN_POINT('Ctrl Pts',(-184.336209621137,1.99562742272505,
126.307097152752));
#120994=CARTESIAN_POINT('Ctrl Pts',(-184.343966662022,1.8695519272367,126.253234224909));
#120995=CARTESIAN_POINT('Ctrl Pts',(-184.351723702907,1.74134513743703,
126.204697567426));
#120996=CARTESIAN_POINT('Ctrl Pts',(-184.359474894147,1.61323502937467,
126.156197511813));
#120997=CARTESIAN_POINT('Ctrl Pts',(-184.367226085387,1.48299719024648,
126.113015869661));
#120998=CARTESIAN_POINT('Ctrl Pts',(-184.374977276627,1.35111330764339,
126.075335782316));
#120999=CARTESIAN_POINT('Ctrl Pts',(-184.382725173404,1.2192854792087,126.037671710014));
#121000=CARTESIAN_POINT('Ctrl Pts',(-184.390473070181,1.08581337391095,
126.005504648981));
#121001=CARTESIAN_POINT('Ctrl Pts',(-184.398220966959,0.951195205101593,
125.978968328405));
#121002=CARTESIAN_POINT('Ctrl Pts',(-184.405967243043,0.816605195511116,
125.952437558655));
#121003=CARTESIAN_POINT('Ctrl Pts',(-184.413713519127,0.680869982589351,
125.931535262159));
#121004=CARTESIAN_POINT('Ctrl Pts',(-184.421459795211,0.544498987029324,
125.916344259612));
#121005=CARTESIAN_POINT('Ctrl Pts',(-184.429206128476,0.408126984809772,
125.901153144929));
#121006=CARTESIAN_POINT('Ctrl Pts',(-184.436952461741,0.271119579148865,
125.891673451605));
#121007=CARTESIAN_POINT('Ctrl Pts',(-184.444698795007,0.133991948377302,
125.887936183054));
#121008=CARTESIAN_POINT('Ctrl Pts',(-184.45244686301,-0.00316639117658285,
125.884198077567));
#121009=CARTESIAN_POINT('Ctrl Pts',(-184.460194931013,-0.140444618670646,
125.886204966446));
#121010=CARTESIAN_POINT('Ctrl Pts',(-184.467942999016,-0.277327314513638,
125.893935725245));
#121011=CARTESIAN_POINT('Ctrl Pts',(-184.475699301758,-0.41435549091451,
125.901674700386));
#121012=CARTESIAN_POINT('Ctrl Pts',(-184.4834556045,-0.550986904952897,
125.915149675607));
#121013=CARTESIAN_POINT('Ctrl Pts',(-184.491211907241,-0.686710462729283,
125.934287537737));
#121014=CARTESIAN_POINT('Ctrl Pts',(-184.498972349756,-0.822506460255012,
125.95343561432));
#121015=CARTESIAN_POINT('Ctrl Pts',(-184.50673279227,-0.957393251687999,
125.978252529597));
#121016=CARTESIAN_POINT('Ctrl Pts',(-184.514493234784,-1.09087068368609,
126.00861414658));
#121017=CARTESIAN_POINT('Ctrl Pts',(-184.522266135049,-1.22456238550795,
126.039024502726));
#121018=CARTESIAN_POINT('Ctrl Pts',(-184.530039035315,-1.35683982936047,
126.074997244652));
#121019=CARTESIAN_POINT('Ctrl Pts',(-184.53781193558,-1.48721788992002,
126.116358270041));
#121020=CARTESIAN_POINT('Ctrl Pts',(-184.545302271342,-1.61285637957678,
126.156215717975));
#121021=CARTESIAN_POINT('Ctrl Pts',(-184.552792607104,-1.73673089353513,
126.201076390584));
#121022=CARTESIAN_POINT('Ctrl Pts',(-184.560282942866,-1.85842728276808,
126.250743253627));
#121023=CARTESIAN_POINT('Ctrl Pts',(-184.568057639186,-1.98474371230457,
126.302295652556));
#121024=CARTESIAN_POINT('Ctrl Pts',(-184.575832335506,-2.10911352182145,
126.359189682738));
#121025=CARTESIAN_POINT('Ctrl Pts',(-184.583607031826,-2.23105192754482,
126.421257794326));
#121026=CARTESIAN_POINT('Ctrl Pts',(-184.591372063905,-2.35283875923919,
126.483248752913));
#121027=CARTESIAN_POINT('Ctrl Pts',(-184.599137095985,-2.4721998557502,
126.550400819786));
#121028=CARTESIAN_POINT('Ctrl Pts',(-184.606902128064,-2.5886689263795,
126.622497844579));
#121029=CARTESIAN_POINT('Ctrl Pts',(-184.614659365366,-2.70502108178013,
126.694522496164));
#121030=CARTESIAN_POINT('Ctrl Pts',(-184.622416602668,-2.81848665856598,
126.771482022306));
#121031=CARTESIAN_POINT('Ctrl Pts',(-184.63017383997,-2.92862289471845,
126.85311385192));
#121032=CARTESIAN_POINT('Ctrl Pts',(-184.63807648539,-3.0408236162226,126.936275856545));
#121033=CARTESIAN_POINT('Ctrl Pts',(-184.645979130809,-3.1495685597896,
127.02428690553));
#121034=CARTESIAN_POINT('Ctrl Pts',(-184.653881776229,-3.25441882467343,
127.116821983719));
#121035=CARTESIAN_POINT('Ctrl Pts',(-184.66162933114,-3.35721138861581,
127.207541048209));
#121036=CARTESIAN_POINT('Ctrl Pts',(-184.669376886051,-3.45626042849622,
127.30260793449));
#121037=CARTESIAN_POINT('Ctrl Pts',(-184.677124440961,-3.55118486455092,
127.401675042864));
#121038=CARTESIAN_POINT('Ctrl Pts',(-184.684870290526,-3.64608840639422,
127.500720345166));
#121039=CARTESIAN_POINT('Ctrl Pts',(-184.69261614009,-3.73686888073763,
127.603763835403));
#121040=CARTESIAN_POINT('Ctrl Pts',(-184.700361989654,-3.82318206752826,
127.710421067247));
#121041=CARTESIAN_POINT('Ctrl Pts',(-184.708107811659,-3.90949494721215,
127.817077919599));
#121042=CARTESIAN_POINT('Ctrl Pts',(-184.715853633663,-3.99134032571703,
127.927348183657));
#121043=CARTESIAN_POINT('Ctrl Pts',(-184.723599455667,-4.06841453913728,
128.040814670737));
#121044=CARTESIAN_POINT('Ctrl Pts',(-184.731619278531,-4.1482151773007,
128.158294923565));
#121045=CARTESIAN_POINT('Ctrl Pts',(-184.739639101396,-4.22290061394825,
128.279201330047));
#121046=CARTESIAN_POINT('Ctrl Pts',(-184.74765892426,-4.29218348010272,
128.403039307197));
#121047=CARTESIAN_POINT('Ctrl Pts',(-184.755413217867,-4.35917245170187,
128.522777118212));
#121048=CARTESIAN_POINT('Ctrl Pts',(-184.763167511474,-4.42111077918117,
128.645255083161));
#121049=CARTESIAN_POINT('Ctrl Pts',(-184.770921805081,-4.4777865008787,
128.770002951115));
#121050=CARTESIAN_POINT('Ctrl Pts',(-184.779074392574,-4.53737333151672,
128.901158406353));
#121051=CARTESIAN_POINT('Ctrl Pts',(-184.787226980067,-4.59114243408741,
129.034822659559));
#121052=CARTESIAN_POINT('Ctrl Pts',(-184.79537956756,-4.63890608312226,
129.170428729612));
#121053=CARTESIAN_POINT('Ctrl Pts',(-184.803532155053,-4.68666973215712,
129.306034799666));
#121054=CARTESIAN_POINT('Ctrl Pts',(-184.811684742546,-4.72842783798587,
129.443582194741));
#121055=CARTESIAN_POINT('Ctrl Pts',(-184.819837330039,-4.76405452823405,
129.582490119308));
#121056=CARTESIAN_POINT('Origin',(213.235140564004,0.,130.804360617566));
#121057=CARTESIAN_POINT('',(-186.915092859931,-4.76405452823404,129.582490119308));
#121058=CARTESIAN_POINT('',(-186.570144995258,-4.76405452823391,129.582490119308));
#121059=CARTESIAN_POINT('',(213.235140564004,-4.76405452823405,129.582490119308));
#121060=CARTESIAN_POINT('',(-185.235140563977,-4.91824999726717,130.804196661748));
#121061=CARTESIAN_POINT('Ctrl Pts',(-185.235140564012,-4.91824999726719,
130.804196662373));
#121062=CARTESIAN_POINT('Ctrl Pts',(-185.243235275636,-4.91825478877005,
130.947929889419));
#121063=CARTESIAN_POINT('Ctrl Pts',(-185.251329987261,-4.91195447570265,
131.09154808551));
#121064=CARTESIAN_POINT('Ctrl Pts',(-185.259424698885,-4.89940510202952,
131.234491654236));
#121065=CARTESIAN_POINT('Ctrl Pts',(-185.267529366981,-4.88684029266407,
131.377611043127));
#121066=CARTESIAN_POINT('Ctrl Pts',(-185.275634035077,-4.86801111637512,
131.520053813894));
#121067=CARTESIAN_POINT('Ctrl Pts',(-185.283738703172,-4.84302506459005,
131.661268597604));
#121068=CARTESIAN_POINT('Ctrl Pts',(-185.291861849205,-4.8179820467862,
131.802805338704));
#121069=CARTESIAN_POINT('Ctrl Pts',(-185.299984995237,-4.78675414792536,
131.9431081626));
#121070=CARTESIAN_POINT('Ctrl Pts',(-185.308108141269,-4.74949972502816,
132.081637182942));
#121071=CARTESIAN_POINT('Ctrl Pts',(-185.316240943695,-4.71220101591753,
132.220330879723));
#121072=CARTESIAN_POINT('Ctrl Pts',(-185.324373746121,-4.66886158835768,
132.357246244439));
#121073=CARTESIAN_POINT('Ctrl Pts',(-185.332506548547,-4.61968871556572,
132.491861501647));
#121074=CARTESIAN_POINT('Ctrl Pts',(-185.340657905423,-4.57040365811858,
132.626783874656));
#121075=CARTESIAN_POINT('Ctrl Pts',(-185.3488092623,-4.51525867281962,132.759395335421));
#121076=CARTESIAN_POINT('Ctrl Pts',(-185.356960619176,-4.45450870042069,
132.889195215412));
#121077=CARTESIAN_POINT('Ctrl Pts',(-185.363319352166,-4.40711869413288,
132.990449864361));
#121078=CARTESIAN_POINT('Ctrl Pts',(-185.369678085156,-4.35631884409728,
133.08999403756));
#121079=CARTESIAN_POINT('Ctrl Pts',(-185.376036818146,-4.3022485761293,
133.187602160443));
#121080=CARTESIAN_POINT('Ctrl Pts',(-185.383811152265,-4.23614101511718,
133.306940110507));
#121081=CARTESIAN_POINT('Ctrl Pts',(-185.391585486384,-4.16495959670137,
133.423714411295));
#121082=CARTESIAN_POINT('Ctrl Pts',(-185.399359820503,-4.08892792282361,
133.537463525335));
#121083=CARTESIAN_POINT('Ctrl Pts',(-185.40712457345,-4.01298995118897,
133.651072453757));
#121084=CARTESIAN_POINT('Ctrl Pts',(-185.414889326397,-3.93221383272465,
133.761663291662));
#121085=CARTESIAN_POINT('Ctrl Pts',(-185.422654079344,-3.84686924586274,
133.868798586874));
#121086=CARTESIAN_POINT('Ctrl Pts',(-185.430411120229,-3.76160942444742,
133.9758274738));
#121087=CARTESIAN_POINT('Ctrl Pts',(-185.438168161114,-3.67179040642328,
134.079407344235));
#121088=CARTESIAN_POINT('Ctrl Pts',(-185.445925201999,-3.57772519128268,
134.179129575311));
#121089=CARTESIAN_POINT('Ctrl Pts',(-185.453676393239,-3.48373091145266,
134.278776605077));
#121090=CARTESIAN_POINT('Ctrl Pts',(-185.461427584479,-3.38549707525688,
134.37457150257));
#121091=CARTESIAN_POINT('Ctrl Pts',(-185.469178775719,-3.28337675376989,
134.466138895303));
#121092=CARTESIAN_POINT('Ctrl Pts',(-185.476926672496,-3.18129983614355,
134.557667369451));
#121093=CARTESIAN_POINT('Ctrl Pts',(-185.484674569273,-3.07534000912483,
134.644971652084));
#121094=CARTESIAN_POINT('Ctrl Pts',(-185.49242246605,-2.96588681661787,
134.727713578174));
#121095=CARTESIAN_POINT('Ctrl Pts',(-185.500168742134,-2.85645651935925,
134.810438196437));
#121096=CARTESIAN_POINT('Ctrl Pts',(-185.507915018218,-2.74353462176835,
134.888602120789));
#121097=CARTESIAN_POINT('Ctrl Pts',(-185.515661294302,-2.62754301228335,
134.961908065413));
#121098=CARTESIAN_POINT('Ctrl Pts',(-185.523407627568,-2.51155054657478,
135.035214551166));
#121099=CARTESIAN_POINT('Ctrl Pts',(-185.531153960833,-2.39248865425077,
135.103662776763));
#121100=CARTESIAN_POINT('Ctrl Pts',(-185.538900294098,-2.27080706495366,
135.166999536415));
#121101=CARTESIAN_POINT('Ctrl Pts',(-185.546648362101,-2.14909822590848,
135.230350479895));
#121102=CARTESIAN_POINT('Ctrl Pts',(-185.554396430104,-2.02476886923059,
135.288587499175));
#121103=CARTESIAN_POINT('Ctrl Pts',(-185.562144498107,-1.89829174083592,
135.341504160499));
#121104=CARTESIAN_POINT('Ctrl Pts',(-185.569900800848,-1.77168019104392,
135.394477062279));
#121105=CARTESIAN_POINT('Ctrl Pts',(-185.57765710359,-1.64291667088637,
135.442118159409));
#121106=CARTESIAN_POINT('Ctrl Pts',(-185.585413406332,-1.51249277472832,
135.484269662504));
#121107=CARTESIAN_POINT('Ctrl Pts',(-185.593173848846,-1.38199926740991,
135.526443663125));
#121108=CARTESIAN_POINT('Ctrl Pts',(-185.60093429136,-1.24984399481776,
135.563122127009));
#121109=CARTESIAN_POINT('Ctrl Pts',(-185.608694733874,-1.11653102912432,
135.594197934584));
#121110=CARTESIAN_POINT('Ctrl Pts',(-185.61646763414,-0.983004057623368,
135.625323627805));
#121111=CARTESIAN_POINT('Ctrl Pts',(-185.624240534405,-0.848316063641948,
135.650828619293));
#121112=CARTESIAN_POINT('Ctrl Pts',(-185.63201343467,-0.712979458432716,
135.670657295159));
#121113=CARTESIAN_POINT('Ctrl Pts',(-185.639503770433,-0.582562679703454,
135.689765148714));
#121114=CARTESIAN_POINT('Ctrl Pts',(-185.646994106196,-0.451543934645043,
135.703602186016));
#121115=CARTESIAN_POINT('Ctrl Pts',(-185.654484441958,-0.320381836731385,
135.712164458511));
#121116=CARTESIAN_POINT('Ctrl Pts',(-185.662258776077,-0.184246688020785,
135.721051372169));
#121117=CARTESIAN_POINT('Ctrl Pts',(-185.670033110196,-0.047525866190644,
135.72428379084));
#121118=CARTESIAN_POINT('Ctrl Pts',(-185.677807444315,0.0892714619018228,
135.721800364893));
#121119=CARTESIAN_POINT('Ctrl Pts',(-185.685572197262,0.225900199513344,
135.719319999546));
#121120=CARTESIAN_POINT('Ctrl Pts',(-185.69333695021,0.362604868635719,
135.711137812602));
#121121=CARTESIAN_POINT('Ctrl Pts',(-185.701101703157,0.498871660584027,
135.697244238578));
#121122=CARTESIAN_POINT('Ctrl Pts',(-185.708858744042,0.635003110433547,
135.683364463847));
#121123=CARTESIAN_POINT('Ctrl Pts',(-185.716615784927,0.770697162159242,
135.663784630225));
#121124=CARTESIAN_POINT('Ctrl Pts',(-185.724372825812,0.905440845898517,
135.638547202409));
#121125=CARTESIAN_POINT('Ctrl Pts',(-185.732124017052,1.04008291837792,
135.613328806334));
#121126=CARTESIAN_POINT('Ctrl Pts',(-185.739875208292,1.17377566665088,
135.58246137983));
#121127=CARTESIAN_POINT('Ctrl Pts',(-185.747626399532,1.3060124356725,135.546039073595));
#121128=CARTESIAN_POINT('Ctrl Pts',(-185.755374296309,1.43819300053959,
135.509632247811));
#121129=CARTESIAN_POINT('Ctrl Pts',(-185.763122193086,1.56891844082116,
135.46767534169));
#121130=CARTESIAN_POINT('Ctrl Pts',(-185.770870089863,1.69769369070752,
135.420313303094));
#121131=CARTESIAN_POINT('Ctrl Pts',(-185.778616365947,1.82644200358802,
135.372961171615));
#121132=CARTESIAN_POINT('Ctrl Pts',(-185.786362642032,1.95324057078163,
135.320206291428));
#121133=CARTESIAN_POINT('Ctrl Pts',(-185.794108918116,2.07761123630648,
135.262242918981));
#121134=CARTESIAN_POINT('Ctrl Pts',(-185.801855251381,2.20198281990683,
135.204279118662));
#121135=CARTESIAN_POINT('Ctrl Pts',(-185.809601584646,2.32392611170664,
135.141106914518));
#121136=CARTESIAN_POINT('Ctrl Pts',(-185.817347917912,2.44298499264541,
135.072967812918));
#121137=CARTESIAN_POINT('Ctrl Pts',(-185.825095985915,2.56207053599523,
135.004813452038));
#121138=CARTESIAN_POINT('Ctrl Pts',(-185.832844053918,2.67827004387223,
134.931690174513));
#121139=CARTESIAN_POINT('Ctrl Pts',(-185.840592121921,2.79115430699464,
134.853884132382));
#121140=CARTESIAN_POINT('Ctrl Pts',(-185.848348424663,2.9041585448554,134.775995397063));
#121141=CARTESIAN_POINT('Ctrl Pts',(-185.856104727404,3.01384017700653,
134.693414177478));
#121142=CARTESIAN_POINT('Ctrl Pts',(-185.863861030146,3.11980073200734,
134.606468776873));
#121143=CARTESIAN_POINT('Ctrl Pts',(-185.871621472661,3.22581784134676,
134.519476970889));
#121144=CARTESIAN_POINT('Ctrl Pts',(-185.879381915175,3.32810962470852,
134.428116602875));
#121145=CARTESIAN_POINT('Ctrl Pts',(-185.887142357689,3.42631349604209,
134.33275386228));
#121146=CARTESIAN_POINT('Ctrl Pts',(-185.894915257954,3.52467501294806,
134.237238036947));
#121147=CARTESIAN_POINT('Ctrl Pts',(-185.90268815822,3.61893523531003,134.13770728394));
#121148=CARTESIAN_POINT('Ctrl Pts',(-185.910461058485,3.70877040278946,
134.034562648692));
#121149=CARTESIAN_POINT('Ctrl Pts',(-185.917951394247,3.79533983565013,
133.935167580741));
#121150=CARTESIAN_POINT('Ctrl Pts',(-185.925441730009,3.8778001590255,133.832417056538));
#121151=CARTESIAN_POINT('Ctrl Pts',(-185.932932065771,3.9559001591004,133.726694786296));
#121152=CARTESIAN_POINT('Ctrl Pts',(-185.94070639989,4.03696134441601,133.616964024045));
#121153=CARTESIAN_POINT('Ctrl Pts',(-185.948480734009,4.11358181358176,
133.503684125752));
#121154=CARTESIAN_POINT('Ctrl Pts',(-185.956255068128,4.18543473429262,
133.38725030694));
#121155=CARTESIAN_POINT('Ctrl Pts',(-185.964019821076,4.25719910270018,
133.270959982405));
#121156=CARTESIAN_POINT('Ctrl Pts',(-185.971784574023,4.32420740995068,
133.15152380069));
#121157=CARTESIAN_POINT('Ctrl Pts',(-185.97954932697,4.38617388218686,133.029368873219));
#121158=CARTESIAN_POINT('Ctrl Pts',(-185.987306367855,4.44807880844942,
132.907335271742));
#121159=CARTESIAN_POINT('Ctrl Pts',(-185.99506340874,4.50495168936313,132.782588644633));
#121160=CARTESIAN_POINT('Ctrl Pts',(-186.002820449625,4.55655097893896,
132.655583521171));
#121161=CARTESIAN_POINT('Ctrl Pts',(-186.010571640865,4.60811135708892,
132.52867417326));
#121162=CARTESIAN_POINT('Ctrl Pts',(-186.018322832105,4.65440591302887,
132.399510079759));
#121163=CARTESIAN_POINT('Ctrl Pts',(-186.026074023345,4.69523999897835,
132.268568394657));
#121164=CARTESIAN_POINT('Ctrl Pts',(-186.033821920122,4.73605672935219,
132.137682363264));
#121165=CARTESIAN_POINT('Ctrl Pts',(-186.041569816899,4.77141748956988,
132.005020615405));
#121166=CARTESIAN_POINT('Ctrl Pts',(-186.049317713676,4.80117663320995,
131.871078011827));
#121167=CARTESIAN_POINT('Ctrl Pts',(-186.05706398976,4.83092955187871,131.737163426154));
#121168=CARTESIAN_POINT('Ctrl Pts',(-186.064810265844,4.85508309987727,
131.601968899102));
#121169=CARTESIAN_POINT('Ctrl Pts',(-186.072556541928,4.87354225566816,
131.466001717194));
#121170=CARTESIAN_POINT('Ctrl Pts',(-186.080302875194,4.89200154772027,
131.330033531608));
#121171=CARTESIAN_POINT('Ctrl Pts',(-186.088049208459,4.90476631109189,
131.193293067196));
#121172=CARTESIAN_POINT('Ctrl Pts',(-186.095795541724,4.91179318843833,
131.056294609935));
#121173=CARTESIAN_POINT('Ctrl Pts',(-186.103543609727,4.91882163940525,
130.919265472818));
#121174=CARTESIAN_POINT('Ctrl Pts',(-186.11129167773,4.92010962740263,130.781978618262));
#121175=CARTESIAN_POINT('Ctrl Pts',(-186.119039745733,4.91566590214478,
130.644949824358));
#121176=CARTESIAN_POINT('Ctrl Pts',(-186.126796048475,4.91121745404283,
130.507775394621));
#121177=CARTESIAN_POINT('Ctrl Pts',(-186.134552351217,4.90102513648487,
130.370859964803));
#121178=CARTESIAN_POINT('Ctrl Pts',(-186.142308653959,4.88514977674217,
130.234716236135));
#121179=CARTESIAN_POINT('Ctrl Pts',(-186.150069096473,4.86926594384197,
130.09849984346));
#121180=CARTESIAN_POINT('Ctrl Pts',(-186.157829538987,4.84769308629387,
129.963056358551));
#121181=CARTESIAN_POINT('Ctrl Pts',(-186.165589981501,4.82054330303636,
129.828888769663));
#121182=CARTESIAN_POINT('Ctrl Pts',(-186.173362881767,4.79334993653653,
129.694505803051));
#121183=CARTESIAN_POINT('Ctrl Pts',(-186.181135782032,4.76056184779475,
129.561403205215));
#121184=CARTESIAN_POINT('Ctrl Pts',(-186.188908682298,4.72234144732119,
129.430070139751));
#121185=CARTESIAN_POINT('Ctrl Pts',(-186.19639901806,4.68551045467694,129.303511362027));
#121186=CARTESIAN_POINT('Ctrl Pts',(-186.203889353822,4.6436353476091,129.178595988423));
#121187=CARTESIAN_POINT('Ctrl Pts',(-186.211379689583,4.59690316518476,
129.05574277698));
#121188=CARTESIAN_POINT('Ctrl Pts',(-186.219154023703,4.54839911785924,
128.928231548683));
#121189=CARTESIAN_POINT('Ctrl Pts',(-186.226928357822,4.49450876631522,
128.802538025928));
#121190=CARTESIAN_POINT('Ctrl Pts',(-186.234702691941,4.43538795572149,
128.679150805632));
#121191=CARTESIAN_POINT('Ctrl Pts',(-186.242467444888,4.37634000624273,
128.555915649057));
#121192=CARTESIAN_POINT('Ctrl Pts',(-186.250232197835,4.31207459079579,
128.434981488786));
#121193=CARTESIAN_POINT('Ctrl Pts',(-186.257996950782,4.2427965825651,128.316819618613));
#121194=CARTESIAN_POINT('Ctrl Pts',(-186.265753991667,4.17358738222901,
128.198775108475));
#121195=CARTESIAN_POINT('Ctrl Pts',(-186.273511032552,4.09937569316561,
128.083497743981));
#121196=CARTESIAN_POINT('Ctrl Pts',(-186.281268073437,4.02041336222315,
127.971436428789));
#121197=CARTESIAN_POINT('Ctrl Pts',(-186.289019264677,3.94151057738879,
127.859459619907));
#121198=CARTESIAN_POINT('Ctrl Pts',(-186.296770455917,3.85786450570213,
127.750694351319));
#121199=CARTESIAN_POINT('Ctrl Pts',(-186.304521647158,3.76977137844832,
127.645562299102));
#121200=CARTESIAN_POINT('Ctrl Pts',(-186.312269543935,3.68171569312366,
127.540474930812));
#121201=CARTESIAN_POINT('Ctrl Pts',(-186.320017440712,3.58921696210682,
127.439018006611));
#121202=CARTESIAN_POINT('Ctrl Pts',(-186.327765337489,3.49261280031067,
127.341581547281));
#121203=CARTESIAN_POINT('Ctrl Pts',(-186.335511613573,3.39602884602262,
127.244165469557));
#121204=CARTESIAN_POINT('Ctrl Pts',(-186.343257889657,3.29534144418254,
127.15076846138));
#121205=CARTESIAN_POINT('Ctrl Pts',(-186.351004165741,3.19092602784825,
127.061744667819));
#121206=CARTESIAN_POINT('Ctrl Pts',(-186.358750499007,3.08650984074266,
126.972720217104));
#121207=CARTESIAN_POINT('Ctrl Pts',(-186.366496832272,2.97836588174077,
126.888069299076));
#121208=CARTESIAN_POINT('Ctrl Pts',(-186.374243165537,2.86690339849536,
126.808106375629));
#121209=CARTESIAN_POINT('Ctrl Pts',(-186.38199123354,2.75541595399981,126.728125545041));
#121210=CARTESIAN_POINT('Ctrl Pts',(-186.389739301543,2.64060882406983,
126.652835025955));
#121211=CARTESIAN_POINT('Ctrl Pts',(-186.397487369546,2.52292067685579,
126.582506247648));
#121212=CARTESIAN_POINT('Ctrl Pts',(-186.405243672288,2.40510744927854,
126.512102723079));
#121213=CARTESIAN_POINT('Ctrl Pts',(-186.41299997503,2.2844074239254,126.44667167434));
#121214=CARTESIAN_POINT('Ctrl Pts',(-186.420756277772,2.16128482948886,
126.386439053264));
#121215=CARTESIAN_POINT('Ctrl Pts',(-186.428516720286,2.03809652081653,
126.326174284226));
#121216=CARTESIAN_POINT('Ctrl Pts',(-186.4362771628,1.9124834245532,126.271113628271));
#121217=CARTESIAN_POINT('Ctrl Pts',(-186.444037605315,1.78492931117828,
126.221434650829));
#121218=CARTESIAN_POINT('Ctrl Pts',(-186.45181050558,1.65717043661684,126.171675924281));
#121219=CARTESIAN_POINT('Ctrl Pts',(-186.459583405845,1.52746468853852,
126.127316266604));
#121220=CARTESIAN_POINT('Ctrl Pts',(-186.467356306111,1.39631140097754,
126.088483442109));
#121221=CARTESIAN_POINT('Ctrl Pts',(-186.474846641873,1.26992586577211,
126.051062288597));
#121222=CARTESIAN_POINT('Ctrl Pts',(-186.482336977635,1.14219650594113,
126.018773191476));
#121223=CARTESIAN_POINT('Ctrl Pts',(-186.489827313397,1.0135767336687,125.991685138431));
#121224=CARTESIAN_POINT('Ctrl Pts',(-186.497601647516,0.880080303639861,
125.963570033623));
#121225=CARTESIAN_POINT('Ctrl Pts',(-186.505375981635,0.745201731765015,
125.940969093346));
#121226=CARTESIAN_POINT('Ctrl Pts',(-186.513150315754,0.609436326590159,
125.924015299217));
#121227=CARTESIAN_POINT('Ctrl Pts',(-186.520915068702,0.47383824014311,
125.907082399123));
#121228=CARTESIAN_POINT('Ctrl Pts',(-186.528679821649,0.337355879254183,
125.895782845622));
#121229=CARTESIAN_POINT('Ctrl Pts',(-186.536444574596,0.200496495701578,
125.890199018909));
#121230=CARTESIAN_POINT('Ctrl Pts',(-186.544201615481,0.0637730428177244,
125.884620738132));
#121231=CARTESIAN_POINT('Ctrl Pts',(-186.551958656366,-0.0733262994167068,
125.88474690261));
#121232=CARTESIAN_POINT('Ctrl Pts',(-186.559715697251,-0.2102877262663,
125.89060826985));
#121233=CARTESIAN_POINT('Ctrl Pts',(-186.567466888491,-0.34714586943757,
125.896465216988));
#121234=CARTESIAN_POINT('Ctrl Pts',(-186.575218079731,-0.483865915208605,
125.908048741667));
#121235=CARTESIAN_POINT('Ctrl Pts',(-186.582969270971,-0.619932975308011,
125.925337542336));
#121236=CARTESIAN_POINT('Ctrl Pts',(-186.590717167748,-0.755942203277722,
125.942618994804));
#121237=CARTESIAN_POINT('Ctrl Pts',(-186.598465064525,-0.891298610539438,
125.965600851155));
#121238=CARTESIAN_POINT('Ctrl Pts',(-186.606212961302,-1.02549157245746,
125.994209882161));
#121239=CARTESIAN_POINT('Ctrl Pts',(-186.613959237386,-1.15965646410071,
126.022812928774));
#121240=CARTESIAN_POINT('Ctrl Pts',(-186.62170551347,-1.29265801234209,
126.057040727289));
#121241=CARTESIAN_POINT('Ctrl Pts',(-186.629451789554,-1.42399533416772,
126.096768839303));
#121242=CARTESIAN_POINT('Ctrl Pts',(-186.63719812282,-1.55533362549545,
126.136497244581));
#121243=CARTESIAN_POINT('Ctrl Pts',(-186.644944456085,-1.68500729167432,
126.181725931178));
#121244=CARTESIAN_POINT('Ctrl Pts',(-186.65269078935,-1.81253055865413,
126.232280561788));
#121245=CARTESIAN_POINT('Ctrl Pts',(-186.660438857353,-1.94008238358522,
126.282846513757));
#121246=CARTESIAN_POINT('Ctrl Pts',(-186.668186925356,-2.06548248767706,
126.338740639035));
#121247=CARTESIAN_POINT('Ctrl Pts',(-186.675934993359,-2.18826539894326,
126.399740587837));
#121248=CARTESIAN_POINT('Ctrl Pts',(-186.683691296101,-2.31117880534887,
126.460805368111));
#121249=CARTESIAN_POINT('Ctrl Pts',(-186.691447598843,-2.43146911172216,
126.526986637757));
#121250=CARTESIAN_POINT('Ctrl Pts',(-186.699203901585,-2.54869529143897,
126.598015960516));
#121251=CARTESIAN_POINT('Ctrl Pts',(-186.706964344099,-2.66598403829782,
126.669083193762));
#121252=CARTESIAN_POINT('Ctrl Pts',(-186.714724786613,-2.7802050743521,
126.745003419722));
#121253=CARTESIAN_POINT('Ctrl Pts',(-186.722485229127,-2.89094751901861,
126.825465607041));
#121254=CARTESIAN_POINT('Ctrl Pts',(-186.730258129393,-3.00186773728824,
126.906056959406));
#121255=CARTESIAN_POINT('Ctrl Pts',(-186.738031029658,-3.10929789869776,
126.991204600203));
#121256=CARTESIAN_POINT('Ctrl Pts',(-186.745803929924,-3.21286060927254,
127.080557485299));
#121257=CARTESIAN_POINT('Ctrl Pts',(-186.753294265686,-3.31265855445779,
127.166662167953));
#121258=CARTESIAN_POINT('Ctrl Pts',(-186.760784601447,-3.40886512528903,
127.256671450161));
#121259=CARTESIAN_POINT('Ctrl Pts',(-186.768274937209,-3.50117720011197,
127.350241152939));
#121260=CARTESIAN_POINT('Ctrl Pts',(-186.775943029108,-3.5956799694917,
127.446031395543));
#121261=CARTESIAN_POINT('Ctrl Pts',(-186.783611121006,-3.68641809312052,
127.545874838496));
#121262=CARTESIAN_POINT('Ctrl Pts',(-186.791279212905,-3.77301654595831,
127.649439191219));
#121263=CARTESIAN_POINT('Ctrl Pts',(-186.798938310547,-3.85951342349731,
127.75288206856));
#121264=CARTESIAN_POINT('Ctrl Pts',(-186.806597408188,-3.94188002817934,
127.860036873487));
#121265=CARTESIAN_POINT('Ctrl Pts',(-186.81425650583,-4.0197769009932,127.970533394756));
#121266=CARTESIAN_POINT('Ctrl Pts',(-186.821908387342,-4.09760038214203,
128.080925810129));
#121267=CARTESIAN_POINT('Ctrl Pts',(-186.829560268854,-4.17096227552672,
128.194653354138));
#121268=CARTESIAN_POINT('Ctrl Pts',(-186.837212150366,-4.23956264999936,
128.311311961958));
#121269=CARTESIAN_POINT('Ctrl Pts',(-186.844858218946,-4.30811091057845,
128.427881947313));
#121270=CARTESIAN_POINT('Ctrl Pts',(-186.852504287526,-4.37190464719919,
128.547378219883));
#121271=CARTESIAN_POINT('Ctrl Pts',(-186.860150356106,-4.43068697554932,
128.669367412144));
#121272=CARTESIAN_POINT('Ctrl Pts',(-186.867793074609,-4.48944354879428,
128.791303155613));
#121273=CARTESIAN_POINT('Ctrl Pts',(-186.875435793112,-4.54319290765865,
128.915729283918));
#121274=CARTESIAN_POINT('Ctrl Pts',(-186.883078511615,-4.59172410237677,
129.04218785925));
#121275=CARTESIAN_POINT('Ctrl Pts',(-186.890720376631,-4.64024987745937,
129.168632312543));
#121276=CARTESIAN_POINT('Ctrl Pts',(-186.898362241647,-4.68355850002953,
129.297108387139));
#121277=CARTESIAN_POINT('Ctrl Pts',(-186.906004106664,-4.72148732126051,
129.427138581119));
#121278=CARTESIAN_POINT('Ctrl Pts',(-186.909033691086,-4.73652403883128,
129.478688490636));
#121279=CARTESIAN_POINT('Ctrl Pts',(-186.912063275508,-4.75071576216139,
129.530482472835));
#121280=CARTESIAN_POINT('Ctrl Pts',(-186.915092859931,-4.76405452823404,
129.582490119308));
#121281=CARTESIAN_POINT('Ctrl Pts',(-185.165421073984,-4.76405452823401,
129.582490119308));
#121282=CARTESIAN_POINT('Ctrl Pts',(-185.17357585509,-4.79982922771808,
129.72197512964));
#121283=CARTESIAN_POINT('Ctrl Pts',(-185.181730636195,-4.82951156155369,
129.863179394967));
#121284=CARTESIAN_POINT('Ctrl Pts',(-185.189885417301,-4.85294732447109,
130.005558183663));
#121285=CARTESIAN_POINT('Ctrl Pts',(-185.198024167137,-4.87633701563996,
130.147657073652));
#121286=CARTESIAN_POINT('Ctrl Pts',(-185.206162916974,-4.89350457056318,
130.29092555989));
#121287=CARTESIAN_POINT('Ctrl Pts',(-185.21430166681,-4.90434637358492,
130.434807224395));
#121288=CARTESIAN_POINT('Ctrl Pts',(-185.221247965866,-4.9135996873744,
130.557608034144));
#121289=CARTESIAN_POINT('Ctrl Pts',(-185.228194264921,-4.91824588552851,
130.680855148721));
#121290=CARTESIAN_POINT('Ctrl Pts',(-185.235140563977,-4.91824999726717,
130.804196661748));
#121291=CARTESIAN_POINT('',(-184.889859436036,-4.91824816211532,130.800108753356));
#121292=CARTESIAN_POINT('Ctrl Pts',(-184.819837330039,-4.76405452823405,
129.582490119308));
#121293=CARTESIAN_POINT('Ctrl Pts',(-184.826135075586,-4.79157558581711,
129.689794305134));
#121294=CARTESIAN_POINT('Ctrl Pts',(-184.832432821132,-4.8154390765796,
129.797910017712));
#121295=CARTESIAN_POINT('Ctrl Pts',(-184.838730566679,-4.83561259437176,
129.906566710451));
#121296=CARTESIAN_POINT('Ctrl Pts',(-184.850410110173,-4.87302558235891,
130.108077006377));
#121297=CARTESIAN_POINT('Ctrl Pts',(-184.862089653666,-4.89785094753426,
130.311991589822));
#121298=CARTESIAN_POINT('Ctrl Pts',(-184.87376919716,-4.90985019127264,
130.517038217186));
#121299=CARTESIAN_POINT('Ctrl Pts',(-184.879132610105,-4.91536041512924,
130.611198552825));
#121300=CARTESIAN_POINT('Ctrl Pts',(-184.88449602305,-4.9181664561817,130.705597270812));
#121301=CARTESIAN_POINT('Ctrl Pts',(-184.889859435995,-4.9182481621147,
130.800108752638));
#121302=CARTESIAN_POINT('Ctrl Pts',(-184.889859436036,-4.91824816211532,
130.800108753357));
#121303=CARTESIAN_POINT('Ctrl Pts',(-184.897506058226,-4.91836465031066,
130.934853849735));
#121304=CARTESIAN_POINT('Ctrl Pts',(-184.905152680416,-4.91293956817794,
131.069789576618));
#121305=CARTESIAN_POINT('Ctrl Pts',(-184.912799302606,-4.90195264080868,
131.204414826104));
#121306=CARTESIAN_POINT('Ctrl Pts',(-184.920439094191,-4.89097552788502,
131.338919817018));
#121307=CARTESIAN_POINT('Ctrl Pts',(-184.928078885776,-4.87444648449873,
131.473114482282));
#121308=CARTESIAN_POINT('Ctrl Pts',(-184.935718677362,-4.85239729067965,
131.60649751106));
#121309=CARTESIAN_POINT('Ctrl Pts',(-184.943353957593,-4.83036111707372,
131.739801776167));
#121310=CARTESIAN_POINT('Ctrl Pts',(-184.950989237825,-4.80281134123516,
131.872294960994));
#121311=CARTESIAN_POINT('Ctrl Pts',(-184.958624518056,-4.76983155314398,
132.003481135751));
#121312=CARTESIAN_POINT('Ctrl Pts',(-184.96625747086,-4.73686181813173,
132.134627321622));
#121313=CARTESIAN_POINT('Ctrl Pts',(-184.973890423664,-4.69846545941638,
132.264466898419));
#121314=CARTESIAN_POINT('Ctrl Pts',(-184.981523376467,-4.65477702326063,
132.392514868961));
#121315=CARTESIAN_POINT('Ctrl Pts',(-184.989155769078,-4.61109179346305,
132.520553441876));
#121316=CARTESIAN_POINT('Ctrl Pts',(-184.996788161688,-4.56211538887205,
132.646800288048));
#121317=CARTESIAN_POINT('Ctrl Pts',(-185.004420554298,-4.50803182670943,
132.770786846));
#121318=CARTESIAN_POINT('Ctrl Pts',(-185.012054153287,-4.45393971608056,
132.89479300131));
#121319=CARTESIAN_POINT('Ctrl Pts',(-185.019687752276,-4.39473900456917,
133.016537788303));
#121320=CARTESIAN_POINT('Ctrl Pts',(-185.027321351264,-4.33066108607502,
133.13557438298));
#121321=CARTESIAN_POINT('Ctrl Pts',(-185.034962554895,-4.26651933273594,
133.254729562698));
#121322=CARTESIAN_POINT('Ctrl Pts',(-185.042603758525,-4.19749086029851,
133.371170805936));
#121323=CARTESIAN_POINT('Ctrl Pts',(-185.050244962156,-4.12385227870567,
133.484477302696));
#121324=CARTESIAN_POINT('Ctrl Pts',(-185.057889999776,-4.05017674879779,
133.597840651233));
#121325=CARTESIAN_POINT('Ctrl Pts',(-185.065535037397,-3.9718867376698,
133.708065792888));
#121326=CARTESIAN_POINT('Ctrl Pts',(-185.073180075017,-3.88930031472982,
133.814763601278));
#121327=CARTESIAN_POINT('Ctrl Pts',(-185.080837121003,-3.80658417000405,
133.921629004168));
#121328=CARTESIAN_POINT('Ctrl Pts',(-185.088494166989,-3.7195583925844,
134.024955697636));
#121329=CARTESIAN_POINT('Ctrl Pts',(-185.096151212975,-3.62857964916102,
134.124389652408));
#121330=CARTESIAN_POINT('Ctrl Pts',(-185.103160205481,-3.54530088447839,
134.215408022297));
#121331=CARTESIAN_POINT('Ctrl Pts',(-185.110169197986,-3.45871056569238,
134.303164978857));
#121332=CARTESIAN_POINT('Ctrl Pts',(-185.117178190492,-3.36910616455944,
134.387418908248));
#121333=CARTESIAN_POINT('Ctrl Pts',(-185.124952524611,-3.26971747889623,
134.480872881472));
#121334=CARTESIAN_POINT('Ctrl Pts',(-185.13272685873,-3.1662800113838,134.570336404582));
#121335=CARTESIAN_POINT('Ctrl Pts',(-185.140501192849,-3.05914760954894,
134.655438254474));
#121336=CARTESIAN_POINT('Ctrl Pts',(-185.148265945796,-2.95214723882493,
134.740435223941));
#121337=CARTESIAN_POINT('Ctrl Pts',(-185.156030698744,-2.84146129743104,
134.821080974734));
#121338=CARTESIAN_POINT('Ctrl Pts',(-185.163795451691,-2.7274801549028,
134.897041287629));
#121339=CARTESIAN_POINT('Ctrl Pts',(-185.171552492576,-2.61361222005217,
134.972926155671));
#121340=CARTESIAN_POINT('Ctrl Pts',(-185.179309533461,-2.4964559204001,
135.044134631363));
#121341=CARTESIAN_POINT('Ctrl Pts',(-185.187066574346,-2.37643407513157,
135.110373175496));
#121342=CARTESIAN_POINT('Ctrl Pts',(-185.194817765586,-2.25650273927002,
135.176561768628));
#121343=CARTESIAN_POINT('Ctrl Pts',(-185.202568956826,-2.13371049990436,
135.237787701952));
#121344=CARTESIAN_POINT('Ctrl Pts',(-185.210320148066,-2.00850818166039,
135.293801334037));
#121345=CARTESIAN_POINT('Ctrl Pts',(-185.218068044844,-1.88335907774139,
135.349791158833));
#121346=CARTESIAN_POINT('Ctrl Pts',(-185.225815941621,-1.75580228842462,
135.400572929258));
#121347=CARTESIAN_POINT('Ctrl Pts',(-185.233563838398,-1.62631200864633,
135.445943570938));
#121348=CARTESIAN_POINT('Ctrl Pts',(-185.241310114482,-1.49684881544309,
135.491304722058));
#121349=CARTESIAN_POINT('Ctrl Pts',(-185.249056390566,-1.36545330497909,
135.531256866629));
#121350=CARTESIAN_POINT('Ctrl Pts',(-185.25680266665,-1.23261799023726,
135.56564573323));
#121351=CARTESIAN_POINT('Ctrl Pts',(-185.264548999916,-1.09978169493548,
135.600034853681));
#121352=CARTESIAN_POINT('Ctrl Pts',(-185.272295333181,-0.965505952635501,
135.628860516231));
#121353=CARTESIAN_POINT('Ctrl Pts',(-185.280041666446,-0.830296328772982,
135.65201892534));
#121354=CARTESIAN_POINT('Ctrl Pts',(-185.287789734449,-0.695056425652861,
135.675182520613));
#121355=CARTESIAN_POINT('Ctrl Pts',(-185.295537802453,-0.558882610093101,
135.692676271008));
#121356=CARTESIAN_POINT('Ctrl Pts',(-185.303285870456,-0.42228808350065,
135.704447947097));
#121357=CARTESIAN_POINT('Ctrl Pts',(-185.311042173197,-0.285548382619655,
135.716232134264));
#121358=CARTESIAN_POINT('Ctrl Pts',(-185.318798475939,-0.148387467644769,
135.722282065073));
#121359=CARTESIAN_POINT('Ctrl Pts',(-185.326554778681,-0.0113216354735307,
135.722597586549));
#121360=CARTESIAN_POINT('Ctrl Pts',(-185.334315221195,0.125817352859683,
135.722913276428));
#121361=CARTESIAN_POINT('Ctrl Pts',(-185.34207566371,0.262860766800342,
135.717488473873));
#121362=CARTESIAN_POINT('Ctrl Pts',(-185.349836106224,0.399295898810333,
135.706375085894));
#121363=CARTESIAN_POINT('Ctrl Pts',(-185.357609006489,0.535950048605996,
135.695243857718));
#121364=CARTESIAN_POINT('Ctrl Pts',(-185.365381906755,0.671993576948554,
135.678405843878));
#121365=CARTESIAN_POINT('Ctrl Pts',(-185.37315480702,0.806921561960867,
135.655964543624));
#121366=CARTESIAN_POINT('Ctrl Pts',(-185.380645142782,0.936944574849048,
135.634339041161));
#121367=CARTESIAN_POINT('Ctrl Pts',(-185.388135478544,1.06593144034985,
135.60751062932));
#121368=CARTESIAN_POINT('Ctrl Pts',(-185.395625814305,1.19344424050067,
135.575615579032));
#121369=CARTESIAN_POINT('Ctrl Pts',(-185.403400148425,1.32579172723165,
135.542511218217));
#121370=CARTESIAN_POINT('Ctrl Pts',(-185.411174482543,1.45697040075332,
135.503843566807));
#121371=CARTESIAN_POINT('Ctrl Pts',(-185.418948816663,1.5864766773227,135.459709671591));
#121372=CARTESIAN_POINT('Ctrl Pts',(-185.42671356961,1.71582334898017,135.415630167457));
#121373=CARTESIAN_POINT('Ctrl Pts',(-185.434478322557,1.84350135810591,
135.366097948359));
#121374=CARTESIAN_POINT('Ctrl Pts',(-185.442243075504,1.9690185123329,135.31126078959));
#121375=CARTESIAN_POINT('Ctrl Pts',(-185.450000116389,2.09441100115318,
135.25647809586));
#121376=CARTESIAN_POINT('Ctrl Pts',(-185.457757157274,2.21764655014518,
135.196401103399));
#121377=CARTESIAN_POINT('Ctrl Pts',(-185.465514198159,2.33824965236156,
135.13122687685));
#121378=CARTESIAN_POINT('Ctrl Pts',(-185.473265389399,2.45876180684023,
135.066101798692));
#121379=CARTESIAN_POINT('Ctrl Pts',(-185.481016580639,2.5766451232984,134.995887322545));
#121380=CARTESIAN_POINT('Ctrl Pts',(-185.488767771879,2.69144588960641,
134.920827802644));
#121381=CARTESIAN_POINT('Ctrl Pts',(-185.496515668657,2.80619786252648,
134.84580018504));
#121382=CARTESIAN_POINT('Ctrl Pts',(-185.504263565434,2.91786956457255,
134.76593183292));
#121383=CARTESIAN_POINT('Ctrl Pts',(-185.512011462211,3.02603382957723,
134.681511933256));
#121384=CARTESIAN_POINT('Ctrl Pts',(-185.519757738295,3.13417546894943,
134.597109692414));
#121385=CARTESIAN_POINT('Ctrl Pts',(-185.527504014379,3.23881082260025,
134.508158038173));
#121386=CARTESIAN_POINT('Ctrl Pts',(-185.535250290463,3.33954388231524,
134.414987948182));
#121387=CARTESIAN_POINT('Ctrl Pts',(-185.542996623729,3.44027768561866,
134.32181717043));
#121388=CARTESIAN_POINT('Ctrl Pts',(-185.550742956994,3.53710885048758,
134.224428160262));
#121389=CARTESIAN_POINT('Ctrl Pts',(-185.558489290259,3.62967678032664,
134.123190160169));
#121390=CARTESIAN_POINT('Ctrl Pts',(-185.566237358262,3.72226544011165,
134.021929488529));
#121391=CARTESIAN_POINT('Ctrl Pts',(-185.573985426265,3.81058870130834,
133.916818400254));
#121392=CARTESIAN_POINT('Ctrl Pts',(-185.581733494268,3.89432522392317,
133.808260434939));
#121393=CARTESIAN_POINT('Ctrl Pts',(-185.58948979701,3.97815074271105,133.699587092927));
#121394=CARTESIAN_POINT('Ctrl Pts',(-185.597246099752,4.05737954572931,
133.58745986594));
#121395=CARTESIAN_POINT('Ctrl Pts',(-185.605002402494,4.13173243319085,
133.472313046493));
#121396=CARTESIAN_POINT('Ctrl Pts',(-185.612762845008,4.20612500502695,
133.357104769722));
#121397=CARTESIAN_POINT('Ctrl Pts',(-185.620523287522,4.27563627770473,
133.238874026014));
#121398=CARTESIAN_POINT('Ctrl Pts',(-185.628283730036,4.3400327911151,133.118080227749));
#121399=CARTESIAN_POINT('Ctrl Pts',(-185.636056630302,4.40453267952583,
132.997092520555));
#121400=CARTESIAN_POINT('Ctrl Pts',(-185.643829530567,4.46390123172262,
132.873533889436));
#121401=CARTESIAN_POINT('Ctrl Pts',(-185.651602430833,4.51795260194687,
132.74788508334));
#121402=CARTESIAN_POINT('Ctrl Pts',(-185.659092766595,4.57003906871526,
132.626803927838));
#121403=CARTESIAN_POINT('Ctrl Pts',(-185.666583102356,4.61718811749639,
132.50378221287));
#121404=CARTESIAN_POINT('Ctrl Pts',(-185.674073438118,4.65927769153067,
132.37926202899));
#121405=CARTESIAN_POINT('Ctrl Pts',(-185.681847772237,4.70296310455798,
132.250020624489));
#121406=CARTESIAN_POINT('Ctrl Pts',(-185.689622106357,4.74133619155718,
132.118755481185));
#121407=CARTESIAN_POINT('Ctrl Pts',(-185.697396440476,4.77420640142745,
131.985942734505));
#121408=CARTESIAN_POINT('Ctrl Pts',(-185.705161193423,4.80703610170175,
131.853293667665));
#121409=CARTESIAN_POINT('Ctrl Pts',(-185.71292594637,4.83437632559071,131.719101168244));
#121410=CARTESIAN_POINT('Ctrl Pts',(-185.720690699317,4.85608535863617,
131.583859207776));
#121411=CARTESIAN_POINT('Ctrl Pts',(-185.728447740202,4.87777282996403,
131.448751571529));
#121412=CARTESIAN_POINT('Ctrl Pts',(-185.736204781087,4.89384017916371,
131.312596932063));
#121413=CARTESIAN_POINT('Ctrl Pts',(-185.743961821972,4.90419617918031,
131.175901865092));
#121414=CARTESIAN_POINT('Ctrl Pts',(-185.751713013212,4.9145443696567,131.039309880935));
#121415=CARTESIAN_POINT('Ctrl Pts',(-185.759464204452,4.91918975430297,
130.902178668729));
#121416=CARTESIAN_POINT('Ctrl Pts',(-185.767215395692,4.91809267276772,
130.76502202877));
#121417=CARTESIAN_POINT('Ctrl Pts',(-185.774963292469,4.91699605752139,
130.627923684042));
#121418=CARTESIAN_POINT('Ctrl Pts',(-185.782711189246,4.91016183358293,
130.490800323191));
#121419=CARTESIAN_POINT('Ctrl Pts',(-185.790459086024,4.89760240839343,
130.354167645832));
#121420=CARTESIAN_POINT('Ctrl Pts',(-185.798205362108,4.88504561036494,
130.217563549084));
#121421=CARTESIAN_POINT('Ctrl Pts',(-185.805951638192,4.86676602891934,
130.081450320748));
#121422=CARTESIAN_POINT('Ctrl Pts',(-185.813697914276,4.84282807281364,
129.946340035256));
#121423=CARTESIAN_POINT('Ctrl Pts',(-185.821444247541,4.81888994000336,
129.81122875241));
#121424=CARTESIAN_POINT('Ctrl Pts',(-185.829190580807,4.78929341739268,
129.677120812149));
#121425=CARTESIAN_POINT('Ctrl Pts',(-185.836936914072,4.75415424788159,
129.54451917919));
#121426=CARTESIAN_POINT('Ctrl Pts',(-185.844684982075,4.71900720919718,
129.411887851015));
#121427=CARTESIAN_POINT('Ctrl Pts',(-185.852433050078,4.67831515382283,
129.280763879231));
#121428=CARTESIAN_POINT('Ctrl Pts',(-185.860181118081,4.63224389893416,
129.151635739286));
#121429=CARTESIAN_POINT('Ctrl Pts',(-185.867937420823,4.5861236789676,129.022370360416));
#121430=CARTESIAN_POINT('Ctrl Pts',(-185.875693723564,4.5346129705982,128.895105419515));
#121431=CARTESIAN_POINT('Ctrl Pts',(-185.883450026306,4.47792624211395,
128.770310560983));
#121432=CARTESIAN_POINT('Ctrl Pts',(-185.89121046882,4.42120925821574,128.645449095676));
#121433=CARTESIAN_POINT('Ctrl Pts',(-185.898970911335,4.35931092585522,
128.52306068839));
#121434=CARTESIAN_POINT('Ctrl Pts',(-185.906731353849,4.29249157078739,
128.403590079339));
#121435=CARTESIAN_POINT('Ctrl Pts',(-185.914504254114,4.22556495135886,
128.28392768546));
#121436=CARTESIAN_POINT('Ctrl Pts',(-185.922277154379,4.15370172825647,
128.167192782885));
#121437=CARTESIAN_POINT('Ctrl Pts',(-185.930050054645,4.07720591501325,
128.053801585463));
#121438=CARTESIAN_POINT('Ctrl Pts',(-185.937540390407,4.00349091726232,
127.944532443683));
#121439=CARTESIAN_POINT('Ctrl Pts',(-185.945030726169,3.92547447684811,
127.838368371698));
#121440=CARTESIAN_POINT('Ctrl Pts',(-185.952521061931,3.84346256241335,
127.73565102006));
#121441=CARTESIAN_POINT('Ctrl Pts',(-185.96029539605,3.75834114131641,127.629039108815));
#121442=CARTESIAN_POINT('Ctrl Pts',(-185.968069730169,3.66864564947082,
127.525802727655));
#121443=CARTESIAN_POINT('Ctrl Pts',(-185.975844064288,3.57467367557063,
127.426359555446));
#121444=CARTESIAN_POINT('Ctrl Pts',(-185.983608817235,3.48081751372976,
127.32703893806));
#121445=CARTESIAN_POINT('Ctrl Pts',(-185.991373570182,3.38269562227221,
127.231502509616));
#121446=CARTESIAN_POINT('Ctrl Pts',(-185.99913832313,3.28064699331261,127.140136502181));
#121447=CARTESIAN_POINT('Ctrl Pts',(-186.006895364015,3.17869972048965,
127.048861240753));
#121448=CARTESIAN_POINT('Ctrl Pts',(-186.0146524049,3.07283376091616,126.961748416427));
#121449=CARTESIAN_POINT('Ctrl Pts',(-186.022409445785,2.96342600063647,
126.879148597655));
#121450=CARTESIAN_POINT('Ctrl Pts',(-186.030160637025,2.85410074559971,
126.79661106805));
#121451=CARTESIAN_POINT('Ctrl Pts',(-186.037911828265,2.74123931688351,
126.718580004569));
#121452=CARTESIAN_POINT('Ctrl Pts',(-186.045663019505,2.6252525518401,126.6453664962));
#121453=CARTESIAN_POINT('Ctrl Pts',(-186.053410916282,2.50931508426635,
126.572184105526));
#121454=CARTESIAN_POINT('Ctrl Pts',(-186.061158813059,2.39025525227261,
126.503815405716));
#121455=CARTESIAN_POINT('Ctrl Pts',(-186.068906709836,2.26851363507625,
126.440528706278));
#121456=CARTESIAN_POINT('Ctrl Pts',(-186.07665298592,2.14679748360143,126.377255245054));
#121457=CARTESIAN_POINT('Ctrl Pts',(-186.084399262004,2.02240100940056,
126.319061849963));
#121458=CARTESIAN_POINT('Ctrl Pts',(-186.092145538088,1.89578984970093,
126.266171120832));
#121459=CARTESIAN_POINT('Ctrl Pts',(-186.099891871354,1.769177755387,126.213280001273));
#121460=CARTESIAN_POINT('Ctrl Pts',(-186.107638204619,1.64035130370563,
126.165691776484));
#121461=CARTESIAN_POINT('Ctrl Pts',(-186.115384537884,1.50979621498143,
126.123580933397));
#121462=CARTESIAN_POINT('Ctrl Pts',(-186.123132605887,1.37921188934978,
126.081460659879));
#121463=CARTESIAN_POINT('Ctrl Pts',(-186.13088067389,1.24689852837551,126.044820328894));
#121464=CARTESIAN_POINT('Ctrl Pts',(-186.138628741893,1.11335672851959,
126.013784466667));
#121465=CARTESIAN_POINT('Ctrl Pts',(-186.146385044635,0.979672998849801,
125.982715619156));
#121466=CARTESIAN_POINT('Ctrl Pts',(-186.154141347377,0.844758603646081,
125.957263227791));
#121467=CARTESIAN_POINT('Ctrl Pts',(-186.161897650119,0.709124593392249,
125.937500708595));
#121468=CARTESIAN_POINT('Ctrl Pts',(-186.169658092633,0.573418191182914,
125.917727641549));
#121469=CARTESIAN_POINT('Ctrl Pts',(-186.177418535147,0.436991797321192,
125.903650537974));
#121470=CARTESIAN_POINT('Ctrl Pts',(-186.185178977661,0.300360296774949,
125.895290771391));
#121471=CARTESIAN_POINT('Ctrl Pts',(-186.192951877927,0.163509463214826,
125.886917584969));
#121472=CARTESIAN_POINT('Ctrl Pts',(-186.200724778192,0.0264532561306669,
125.884280083587));
#121473=CARTESIAN_POINT('Ctrl Pts',(-186.208497678457,-0.110293825237829,
125.887347465803));
#121474=CARTESIAN_POINT('Ctrl Pts',(-186.215988014219,-0.242069805751984,
125.890303340948));
#121475=CARTESIAN_POINT('Ctrl Pts',(-186.223478349981,-0.37355843793483,
125.898556507699));
#121476=CARTESIAN_POINT('Ctrl Pts',(-186.230968685743,-0.504306897976589,
125.91203421644));
#121477=CARTESIAN_POINT('Ctrl Pts',(-186.238743019862,-0.640012725620837,
125.926022936604));
#121478=CARTESIAN_POINT('Ctrl Pts',(-186.246517353981,-0.775351021172049,
125.945684508496));
#121479=CARTESIAN_POINT('Ctrl Pts',(-186.2542916881,-0.909809525613153,
125.970994327949));
#121480=CARTESIAN_POINT('Ctrl Pts',(-186.262056441047,-1.0441023219648,
125.996272955312));
#121481=CARTESIAN_POINT('Ctrl Pts',(-186.269821193994,-1.17751710403923,
126.02718590837));
#121482=CARTESIAN_POINT('Ctrl Pts',(-186.277585946941,-1.3095456903417,
126.063656751323));
#121483=CARTESIAN_POINT('Ctrl Pts',(-186.285342987826,-1.44144314399063,
126.100091370921));
#121484=CARTESIAN_POINT('Ctrl Pts',(-186.293100028711,-1.57195676732722,
126.142072791592));
#121485=CARTESIAN_POINT('Ctrl Pts',(-186.300857069596,-1.7005879010708,
126.189473419245));
#121486=CARTESIAN_POINT('Ctrl Pts',(-186.308608260836,-1.8291220330753,
126.236838301715));
#121487=CARTESIAN_POINT('Ctrl Pts',(-186.316359452076,-1.95577613574888,
126.289614122268));
#121488=CARTESIAN_POINT('Ctrl Pts',(-186.324110643316,-2.08006641349185,
126.347623383));
#121489=CARTESIAN_POINT('Ctrl Pts',(-186.331858540093,-2.20430386455207,
126.40560798825));
#121490=CARTESIAN_POINT('Ctrl Pts',(-186.33960643687,-2.32617913539421,
126.46882144461));
#121491=CARTESIAN_POINT('Ctrl Pts',(-186.347354333647,-2.4452283458019,
126.537038108148));
#121492=CARTESIAN_POINT('Ctrl Pts',(-186.355100609731,-2.56425265368117,
126.605240502231));
#121493=CARTESIAN_POINT('Ctrl Pts',(-186.362846885815,-2.68045173795131,
126.678443827566));
#121494=CARTESIAN_POINT('Ctrl Pts',(-186.370593161899,-2.79338663077894,
126.756376651011));
#121495=CARTESIAN_POINT('Ctrl Pts',(-186.378339495165,-2.90632235726645,
126.834310049738));
#121496=CARTESIAN_POINT('Ctrl Pts',(-186.38608582843,-3.01599352244523,
126.916972794186));
#121497=CARTESIAN_POINT('Ctrl Pts',(-186.393832161695,-3.12199078181559,
127.004050548538));
#121498=CARTESIAN_POINT('Ctrl Pts',(-186.401580229698,-3.2280117785374,
127.091147803349));
#121499=CARTESIAN_POINT('Ctrl Pts',(-186.409328297701,-3.33035693024278,
127.182661787357));
#121500=CARTESIAN_POINT('Ctrl Pts',(-186.417076365704,-3.42865088487751,
127.278238644048));
#121501=CARTESIAN_POINT('Ctrl Pts',(-186.424832668446,-3.52704930749682,
127.373917080959));
#121502=CARTESIAN_POINT('Ctrl Pts',(-186.432588971188,-3.62138765127686,
127.473666743374));
#121503=CARTESIAN_POINT('Ctrl Pts',(-186.440345273929,-3.71132791396644,
127.577097353202));
#121504=CARTESIAN_POINT('Ctrl Pts',(-186.448105716444,-3.8013161804825,
127.680583167061));
#121505=CARTESIAN_POINT('Ctrl Pts',(-186.455866158958,-3.8869014446861,
127.787753537677));
#121506=CARTESIAN_POINT('Ctrl Pts',(-186.463626601472,-3.96778741652845,
127.898186830653));
#121507=CARTESIAN_POINT('Ctrl Pts',(-186.471399501737,-4.04880323371331,
128.008797400955));
#121508=CARTESIAN_POINT('Ctrl Pts',(-186.479172402003,-4.12510446603694,
128.122681035685));
#121509=CARTESIAN_POINT('Ctrl Pts',(-186.486945302268,-4.19643892821958,
128.239388223129));
#121510=CARTESIAN_POINT('Ctrl Pts',(-186.494435638031,-4.26518020302876,
128.351852810354));
#121511=CARTESIAN_POINT('Ctrl Pts',(-186.501925973793,-4.32930939758988,
128.466938958798));
#121512=CARTESIAN_POINT('Ctrl Pts',(-186.509416309556,-4.38864295588559,
128.584226372018));
#121513=CARTESIAN_POINT('Ctrl Pts',(-186.517717331537,-4.45439824205773,
128.714207914373));
#121514=CARTESIAN_POINT('Ctrl Pts',(-186.526018353518,-4.51445011624346,
128.847261066043));
#121515=CARTESIAN_POINT('Ctrl Pts',(-186.534319375498,-4.56852078633726,
128.982877461645));
#121516=CARTESIAN_POINT('Ctrl Pts',(-186.542600349557,-4.62246086954897,
129.118166328066));
#121517=CARTESIAN_POINT('Ctrl Pts',(-186.550881323616,-4.670448438029,129.256005807444));
#121518=CARTESIAN_POINT('Ctrl Pts',(-186.559162297674,-4.71225244919594,
129.39586499544));
#121519=CARTESIAN_POINT('Ctrl Pts',(-186.562823196869,-4.73073339959214,
129.45769472526));
#121520=CARTESIAN_POINT('Ctrl Pts',(-186.566484096064,-4.74800643982495,
129.519918866165));
#121521=CARTESIAN_POINT('Ctrl Pts',(-186.570144995258,-4.76405452823391,
129.582490119308));
#121522=CARTESIAN_POINT('Origin',(213.235140564004,0.,130.804360617566));
#121523=CARTESIAN_POINT('',(-188.665047832579,-4.76405452823406,129.582490119308));
#121524=CARTESIAN_POINT('',(-188.319844903182,-4.76405452823404,129.582490119308));
#121525=CARTESIAN_POINT('',(213.235140564004,-4.76405452823405,129.582490119308));
#121526=CARTESIAN_POINT('',(-186.985140563973,-4.91824792938353,130.808873666935));
#121527=CARTESIAN_POINT('Ctrl Pts',(-186.985140564012,-4.9182479293829,
130.808873667626));
#121528=CARTESIAN_POINT('Ctrl Pts',(-186.995772027482,-4.91807578782115,
130.996470718023));
#121529=CARTESIAN_POINT('Ctrl Pts',(-187.006403490951,-4.90716688700063,
131.183595083917));
#121530=CARTESIAN_POINT('Ctrl Pts',(-187.017034954421,-4.88570371797789,
131.369234269489));
#121531=CARTESIAN_POINT('Ctrl Pts',(-187.026930823288,-4.86572559297847,
131.542029016165));
#121532=CARTESIAN_POINT('Ctrl Pts',(-187.036826692156,-4.83660372490796,
131.71353778882));
#121533=CARTESIAN_POINT('Ctrl Pts',(-187.046722561023,-4.79852032900577,
131.882964212321));
#121534=CARTESIAN_POINT('Ctrl Pts',(-187.054496895142,-4.76860147618899,
132.016067999625));
#121535=CARTESIAN_POINT('Ctrl Pts',(-187.062271229261,-4.73309288657269,
132.148136813944));
#121536=CARTESIAN_POINT('Ctrl Pts',(-187.07004556338,-4.69207949437852,
132.278664887699));
#121537=CARTESIAN_POINT('Ctrl Pts',(-187.077810316327,-4.65111664752476,
132.409032097269));
#121538=CARTESIAN_POINT('Ctrl Pts',(-187.085575069274,-4.60466261265512,
132.537861974965));
#121539=CARTESIAN_POINT('Ctrl Pts',(-187.093339822221,-4.55285331124662,
132.66465892396));
#121540=CARTESIAN_POINT('Ctrl Pts',(-187.101096863106,-4.50109546756681,
132.791329936437));
#121541=CARTESIAN_POINT('Ctrl Pts',(-187.108853903991,-4.44399308917469,
132.915971678803));
#121542=CARTESIAN_POINT('Ctrl Pts',(-187.116610944876,-4.38173177310754,
133.038104052036));
#121543=CARTESIAN_POINT('Ctrl Pts',(-187.124362136116,-4.31951740878307,
133.160144324298));
#121544=CARTESIAN_POINT('Ctrl Pts',(-187.132113327356,-4.25215202722686,
133.279678647097));
#121545=CARTESIAN_POINT('Ctrl Pts',(-187.139864518596,-4.17986902446443,
133.396247575136));
#121546=CARTESIAN_POINT('Ctrl Pts',(-187.147612415373,-4.1076167439063,
133.512766958271));
#121547=CARTESIAN_POINT('Ctrl Pts',(-187.15536031215,-4.03045120483651,
133.626323121855));
#121548=CARTESIAN_POINT('Ctrl Pts',(-187.163108208927,-3.9486512601369,
133.736482083044));
#121549=CARTESIAN_POINT('Ctrl Pts',(-187.170854485011,-3.86686842622231,
133.846618001354));
#121550=CARTESIAN_POINT('Ctrl Pts',(-187.178600761095,-3.78045334783767,
133.953357817043));
#121551=CARTESIAN_POINT('Ctrl Pts',(-187.186347037179,-3.68972740421345,
134.056297693387));
#121552=CARTESIAN_POINT('Ctrl Pts',(-187.194093370445,-3.59900079087104,
134.159238329609));
#121553=CARTESIAN_POINT('Ctrl Pts',(-187.20183970371,-3.50396350729632,
134.258378677208));
#121554=CARTESIAN_POINT('Ctrl Pts',(-187.209586036975,-3.40497603632671,
134.353349382629));
#121555=CARTESIAN_POINT('Ctrl Pts',(-187.217334104978,-3.30596639779917,
134.44834135608));
#121556=CARTESIAN_POINT('Ctrl Pts',(-187.225082172981,-3.20300509365603,
134.539161558656));
#121557=CARTESIAN_POINT('Ctrl Pts',(-187.232830240984,-3.09648783601041,
134.625479059062));
#121558=CARTESIAN_POINT('Ctrl Pts',(-187.240586543725,-2.98985737055593,
134.711888298734));
#121559=CARTESIAN_POINT('Ctrl Pts',(-187.248342846467,-2.8796637062563,
134.793785030094));
#121560=CARTESIAN_POINT('Ctrl Pts',(-187.256099149209,-2.76633431053606,
134.870879711933));
#121561=CARTESIAN_POINT('Ctrl Pts',(-187.263859591723,-2.65294442750473,
134.948015541525));
#121562=CARTESIAN_POINT('Ctrl Pts',(-187.271620034237,-2.53641581021152,
135.020344008526));
#121563=CARTESIAN_POINT('Ctrl Pts',(-187.279380476751,-2.41720213633815,
135.087620695425));
#121564=CARTESIAN_POINT('Ctrl Pts',(-187.287153377017,-2.2977970900922,
135.155005380835));
#121565=CARTESIAN_POINT('Ctrl Pts',(-187.294926277282,-2.1756987223634,
135.217321902815));
#121566=CARTESIAN_POINT('Ctrl Pts',(-187.302699177547,-2.05138318386969,
135.274372932475));
#121567=CARTESIAN_POINT('Ctrl Pts',(-187.31018951331,-1.93158682832274,
135.329350013508));
#121568=CARTESIAN_POINT('Ctrl Pts',(-187.317679849073,-1.80973198772532,
135.379437666485));
#121569=CARTESIAN_POINT('Ctrl Pts',(-187.325170184835,-1.68625769629345,
135.424503260839));
#121570=CARTESIAN_POINT('Ctrl Pts',(-187.332944518954,-1.5581018395823,
135.471277530897));
#121571=CARTESIAN_POINT('Ctrl Pts',(-187.340718853073,-1.42779534567859,
135.512789568897));
#121572=CARTESIAN_POINT('Ctrl Pts',(-187.348493187192,-1.29580964019177,
135.548837452675));
#121573=CARTESIAN_POINT('Ctrl Pts',(-187.356257940139,-1.16398659529106,
135.584840910658));
#121574=CARTESIAN_POINT('Ctrl Pts',(-187.364022693087,-1.03048882998293,
135.615393511214));
#121575=CARTESIAN_POINT('Ctrl Pts',(-187.371787446034,-0.895806772792648,
135.640341726743));
#121576=CARTESIAN_POINT('Ctrl Pts',(-187.379544486919,-0.761258483720252,
135.665265163353));
#121577=CARTESIAN_POINT('Ctrl Pts',(-187.387301527804,-0.625528625504841,
135.68459522148));
#121578=CARTESIAN_POINT('Ctrl Pts',(-187.395058568689,-0.48912143878214,
135.698228543923));
#121579=CARTESIAN_POINT('Ctrl Pts',(-187.402809759929,-0.352817117779854,
135.711851585371));
#121580=CARTESIAN_POINT('Ctrl Pts',(-187.410560951169,-0.215836872397206,
135.719786403242));
#121581=CARTESIAN_POINT('Ctrl Pts',(-187.418312142409,-0.0786934032297544,
135.721981018816));
#121582=CARTESIAN_POINT('Ctrl Pts',(-187.426060039186,0.0583917763046921,
135.72417470162));
#121583=CARTESIAN_POINT('Ctrl Pts',(-187.433807935963,0.195639651546684,
135.720633028339));
#121584=CARTESIAN_POINT('Ctrl Pts',(-187.44155583274,0.33253437364453,135.711356027473));
#121585=CARTESIAN_POINT('Ctrl Pts',(-187.449302108824,0.469400460317623,
135.702080967155));
#121586=CARTESIAN_POINT('Ctrl Pts',(-187.457048384909,0.605913150958659,
135.687072991952));
#121587=CARTESIAN_POINT('Ctrl Pts',(-187.464794660993,0.741558972969566,
135.666384203698));
#121588=CARTESIAN_POINT('Ctrl Pts',(-187.472540994258,0.877205796287302,
135.645695262725));
#121589=CARTESIAN_POINT('Ctrl Pts',(-187.480287327523,1.01198535171049,
135.619325483972));
#121590=CARTESIAN_POINT('Ctrl Pts',(-187.488033660789,1.14539204185446,
135.587378507242));
#121591=CARTESIAN_POINT('Ctrl Pts',(-187.495781728792,1.27882860750151,
135.555424376208));
#121592=CARTESIAN_POINT('Ctrl Pts',(-187.503529796795,1.41089131594959,
135.517890652914));
#121593=CARTESIAN_POINT('Ctrl Pts',(-187.511277864798,1.54108785326631,
135.474931384722));
#121594=CARTESIAN_POINT('Ctrl Pts',(-187.51903416754,1.67142276501208,135.431926458909));
#121595=CARTESIAN_POINT('Ctrl Pts',(-187.526790470281,1.79988717172503,
135.383484592025));
#121596=CARTESIAN_POINT('Ctrl Pts',(-187.534546773023,1.92600641760273,
135.329808920425));
#121597=CARTESIAN_POINT('Ctrl Pts',(-187.542307215538,2.05219297711968,
135.276104600504));
#121598=CARTESIAN_POINT('Ctrl Pts',(-187.550067658052,2.17603152887269,
135.217161077647));
#121599=CARTESIAN_POINT('Ctrl Pts',(-187.557828100566,2.29707121362073,
135.153227930103));
#121600=CARTESIAN_POINT('Ctrl Pts',(-187.565601000831,2.41830520201613,
135.089192151395));
#121601=CARTESIAN_POINT('Ctrl Pts',(-187.573373901097,2.53673100702913,
135.020150938914));
#121602=CARTESIAN_POINT('Ctrl Pts',(-187.581146801362,2.65192523918329,
134.94639823066));
#121603=CARTESIAN_POINT('Ctrl Pts',(-187.588637137124,2.7629318708422,134.875326619122));
#121604=CARTESIAN_POINT('Ctrl Pts',(-187.596127472886,2.87093754965219,
134.799880290516));
#121605=CARTESIAN_POINT('Ctrl Pts',(-187.603617808648,2.9755933810453,134.720356926704));
#121606=CARTESIAN_POINT('Ctrl Pts',(-187.611392142768,3.08421727009468,
134.637818410382));
#121607=CARTESIAN_POINT('Ctrl Pts',(-187.619166476887,3.18957636621408,
134.550626137116));
#121608=CARTESIAN_POINT('Ctrl Pts',(-187.626940811006,3.29124596951094,
134.45906758676));
#121609=CARTESIAN_POINT('Ctrl Pts',(-187.634705563953,3.3927902741082,134.367621874136));
#121610=CARTESIAN_POINT('Ctrl Pts',(-187.6424703169,3.49065384526458,134.271820850219));
#121611=CARTESIAN_POINT('Ctrl Pts',(-187.650235069847,3.58444242726253,
134.171994140998));
#121612=CARTESIAN_POINT('Ctrl Pts',(-187.657992110732,3.67813785711891,
134.072266581071));
#121613=CARTESIAN_POINT('Ctrl Pts',(-187.665749151617,3.76776608622933,
133.968521575866));
#121614=CARTESIAN_POINT('Ctrl Pts',(-187.673506192502,3.85296760287033,
133.861127490216));
#121615=CARTESIAN_POINT('Ctrl Pts',(-187.681257383742,3.93810486838475,
133.753814391282));
#121616=CARTESIAN_POINT('Ctrl Pts',(-187.689008574982,4.01882182394327,
133.642857994237));
#121617=CARTESIAN_POINT('Ctrl Pts',(-187.696759766223,4.0947976111808,133.528661552846));
#121618=CARTESIAN_POINT('Ctrl Pts',(-187.704507663,4.17074110668214,133.414513647989));
#121619=CARTESIAN_POINT('Ctrl Pts',(-187.712255559777,4.24194722567974,
133.297128762567));
#121620=CARTESIAN_POINT('Ctrl Pts',(-187.720003456554,4.30813716324615,
133.176940910234));
#121621=CARTESIAN_POINT('Ctrl Pts',(-187.727749732638,4.37431325530452,
133.056778198609));
#121622=CARTESIAN_POINT('Ctrl Pts',(-187.735496008722,4.43547506451776,
132.933814028545));
#121623=CARTESIAN_POINT('Ctrl Pts',(-187.743242284806,4.4913888811533,132.808508561395));
#121624=CARTESIAN_POINT('Ctrl Pts',(-187.750988618071,4.54730311053187,
132.683202169268));
#121625=CARTESIAN_POINT('Ctrl Pts',(-187.758734951337,4.59796911071568,
132.555554802601));
#121626=CARTESIAN_POINT('Ctrl Pts',(-187.766481284602,4.64320078906951,
132.426047854639));
#121627=CARTESIAN_POINT('Ctrl Pts',(-187.774229352605,4.68844259674417,
132.296511904493));
#121628=CARTESIAN_POINT('Ctrl Pts',(-187.781977420608,4.72824753205442,
132.165115913412));
#121629=CARTESIAN_POINT('Ctrl Pts',(-187.789725488611,4.76247909170162,
132.032357345414));
#121630=CARTESIAN_POINT('Ctrl Pts',(-187.797481791353,4.79674703305773,
131.899457680029));
#121631=CARTESIAN_POINT('Ctrl Pts',(-187.805238094095,4.82542966824893,
131.765192924051));
#121632=CARTESIAN_POINT('Ctrl Pts',(-187.812994396837,4.8484413385891,131.630072219011));
#121633=CARTESIAN_POINT('Ctrl Pts',(-187.820754839351,4.87146529095061,
131.494879395982));
#121634=CARTESIAN_POINT('Ctrl Pts',(-187.828515281865,4.88881219795085,
131.358830101222));
#121635=CARTESIAN_POINT('Ctrl Pts',(-187.836275724379,4.90044833640633,
131.22243855852));
#121636=CARTESIAN_POINT('Ctrl Pts',(-187.844048624645,4.91210315422426,
131.085828068006));
#121637=CARTESIAN_POINT('Ctrl Pts',(-187.85182152491,4.9180288671356,130.948874622484));
#121638=CARTESIAN_POINT('Ctrl Pts',(-187.859594425176,4.91824392115051,
130.812093312181));
#121639=CARTESIAN_POINT('Ctrl Pts',(-187.867084760937,4.9184511574103,130.68028434704));
#121640=CARTESIAN_POINT('Ctrl Pts',(-187.874575096699,4.91335573198571,
130.548635527089));
#121641=CARTESIAN_POINT('Ctrl Pts',(-187.882065432461,4.90301950702024,
130.417601291526));
#121642=CARTESIAN_POINT('Ctrl Pts',(-187.88983976658,4.89229138094348,130.281598853093));
#121643=CARTESIAN_POINT('Ctrl Pts',(-187.897614100699,4.87588321702286,
130.145827708113));
#121644=CARTESIAN_POINT('Ctrl Pts',(-187.905388434818,4.85380731953623,
130.010800558518));
#121645=CARTESIAN_POINT('Ctrl Pts',(-187.913153187766,4.83175862862026,
129.875939817817));
#121646=CARTESIAN_POINT('Ctrl Pts',(-187.920917940713,4.80405616463346,
129.741821630265));
#121647=CARTESIAN_POINT('Ctrl Pts',(-187.92868269366,4.77076414640998,129.608955865263));
#121648=CARTESIAN_POINT('Ctrl Pts',(-187.936439734545,4.73750519428833,
129.476222064411));
#121649=CARTESIAN_POINT('Ctrl Pts',(-187.94419677543,4.69866783032351,129.344738587432));
#121650=CARTESIAN_POINT('Ctrl Pts',(-187.951953816315,4.65436764541508,
129.21500701191));
#121651=CARTESIAN_POINT('Ctrl Pts',(-187.959705007555,4.61010086762063,
129.085373267977));
#121652=CARTESIAN_POINT('Ctrl Pts',(-187.967456198795,4.56037959443934,
128.95748916438));
#121653=CARTESIAN_POINT('Ctrl Pts',(-187.975207390035,4.50536966289933,
128.831842616856));
#121654=CARTESIAN_POINT('Ctrl Pts',(-187.982955286812,4.45038311204773,
128.706249472466));
#121655=CARTESIAN_POINT('Ctrl Pts',(-187.990703183589,4.39011253005438,
128.582892350036));
#121656=CARTESIAN_POINT('Ctrl Pts',(-187.998451080366,4.32477236402399,
128.462240411028));
#121657=CARTESIAN_POINT('Ctrl Pts',(-188.006197356451,4.25944586574759,
128.341613709804));
#121658=CARTESIAN_POINT('Ctrl Pts',(-188.013943632535,4.18905207878634,
128.223691410034));
#121659=CARTESIAN_POINT('Ctrl Pts',(-188.021689908619,4.11385182410005,
128.108918866786));
#121660=CARTESIAN_POINT('Ctrl Pts',(-188.029436241884,4.03865101430267,
127.994145476313));
#121661=CARTESIAN_POINT('Ctrl Pts',(-188.03718257515,3.95864388025005,127.882522215779));
#121662=CARTESIAN_POINT('Ctrl Pts',(-188.044928908415,3.87413484409709,
127.774465854995));
#121663=CARTESIAN_POINT('Ctrl Pts',(-188.052676976418,3.78960688273153,
127.666385295739));
#121664=CARTESIAN_POINT('Ctrl Pts',(-188.060425044421,3.70057525393309,
127.561873533624));
#121665=CARTESIAN_POINT('Ctrl Pts',(-188.068173112424,3.60738470489975,
127.461314304193));
#121666=CARTESIAN_POINT('Ctrl Pts',(-188.075929415166,3.51409511184179,
127.360648199217));
#121667=CARTESIAN_POINT('Ctrl Pts',(-188.083685717908,3.416638034995,127.26394330569));
#121668=CARTESIAN_POINT('Ctrl Pts',(-188.091442020649,3.31539552893747,
127.171546894128));
#121669=CARTESIAN_POINT('Ctrl Pts',(-188.099202463164,3.21409898670611,
127.079101167818));
#121670=CARTESIAN_POINT('Ctrl Pts',(-188.106962905678,3.10901328886408,
126.990968756662));
#121671=CARTESIAN_POINT('Ctrl Pts',(-188.114723348192,3.00055283824357,
126.907455983448));
#121672=CARTESIAN_POINT('Ctrl Pts',(-188.122496248457,2.89191827727905,
126.823809148117));
#121673=CARTESIAN_POINT('Ctrl Pts',(-188.130269148723,2.77989845741056,
126.744796995441));
#121674=CARTESIAN_POINT('Ctrl Pts',(-188.138042048988,2.66493670915268,
126.670682425119));
#121675=CARTESIAN_POINT('Ctrl Pts',(-188.14553238475,2.55415411001514,126.599262106112));
#121676=CARTESIAN_POINT('Ctrl Pts',(-188.153022720512,2.44064002739613,
126.532389628946));
#121677=CARTESIAN_POINT('Ctrl Pts',(-188.160513056274,2.32481023186287,
126.470258582735));
#121678=CARTESIAN_POINT('Ctrl Pts',(-188.168287390393,2.2045887144261,126.405771819022));
#121679=CARTESIAN_POINT('Ctrl Pts',(-188.176061724512,2.0814915915248,126.346188851776));
#121680=CARTESIAN_POINT('Ctrl Pts',(-188.183836058631,1.95595686457699,
126.291776456975));
#121681=CARTESIAN_POINT('Ctrl Pts',(-188.191600811579,1.83057684796112,
126.237431120589));
#121682=CARTESIAN_POINT('Ctrl Pts',(-188.199365564526,1.70276555989438,
126.188243831725));
#121683=CARTESIAN_POINT('Ctrl Pts',(-188.207130317473,1.5729866797913,126.144436158125));
#121684=CARTESIAN_POINT('Ctrl Pts',(-188.214887358358,1.4433366979015,126.100671994924));
#121685=CARTESIAN_POINT('Ctrl Pts',(-188.222644399243,1.3117233810346,126.062276938189));
#121686=CARTESIAN_POINT('Ctrl Pts',(-188.230401440128,1.17863120032339,
126.029424852959));
#121687=CARTESIAN_POINT('Ctrl Pts',(-188.238152631368,1.04563938546079,
125.996597541742));
#121688=CARTESIAN_POINT('Ctrl Pts',(-188.245903822608,0.911171304574001,
125.969304975312));
#121689=CARTESIAN_POINT('Ctrl Pts',(-188.253655013848,0.775727093957084,
125.947671360654));
#121690=CARTESIAN_POINT('Ctrl Pts',(-188.261402910625,0.640340450742956,
125.92604694086));
#121691=CARTESIAN_POINT('Ctrl Pts',(-188.269150807402,0.503978888229026,
125.910076750604));
#121692=CARTESIAN_POINT('Ctrl Pts',(-188.276898704179,0.36715303913928,
125.899833962694));
#121693=CARTESIAN_POINT('Ctrl Pts',(-188.284644980264,0.230355811067541,
125.889593317354));
#121694=CARTESIAN_POINT('Ctrl Pts',(-188.292391256348,0.0930948792217825,
125.885077720542));
#121695=CARTESIAN_POINT('Ctrl Pts',(-188.300137532432,-0.0441140864660505,
125.886308461491));
#121696=CARTESIAN_POINT('Ctrl Pts',(-188.307883865697,-0.181324064999486,
125.887539211525));
#121697=CARTESIAN_POINT('Ctrl Pts',(-188.315630198963,-0.318481685660068,
125.894516380455));
#121698=CARTESIAN_POINT('Ctrl Pts',(-188.323376532228,-0.455071760591299,
125.907209123563));
#121699=CARTESIAN_POINT('Ctrl Pts',(-188.331124600231,-0.591692423922576,
125.919904709124));
#121700=CARTESIAN_POINT('Ctrl Pts',(-188.338872668234,-0.727744899400813,
125.938318379674));
#121701=CARTESIAN_POINT('Ctrl Pts',(-188.346620736237,-0.862719995164512,
125.962367508066));
#121702=CARTESIAN_POINT('Ctrl Pts',(-188.354377038979,-0.997838544066398,
125.986442196158));
#121703=CARTESIAN_POINT('Ctrl Pts',(-188.362133341721,-1.13187704037199,
126.016164237938));
#121704=CARTESIAN_POINT('Ctrl Pts',(-188.369889644462,-1.26433680573185,
126.051399908264));
#121705=CARTESIAN_POINT('Ctrl Pts',(-188.377650086977,-1.39686726885678,
126.086654384927));
#121706=CARTESIAN_POINT('Ctrl Pts',(-188.385410529491,-1.52781694894612,
126.12742823772));
#121707=CARTESIAN_POINT('Ctrl Pts',(-188.393170972005,-1.65670413311006,
126.173538392751));
#121708=CARTESIAN_POINT('Ctrl Pts',(-188.40094387227,-1.78579821842409,
126.219722567897));
#121709=CARTESIAN_POINT('Ctrl Pts',(-188.408716772536,-1.91282282908581,
126.271260016418));
#121710=CARTESIAN_POINT('Ctrl Pts',(-188.416489672801,-2.03731714916122,
126.327919855506));
#121711=CARTESIAN_POINT('Ctrl Pts',(-188.423980008563,-2.15728578711929,
126.382519966725));
#121712=CARTESIAN_POINT('Ctrl Pts',(-188.431470344325,-2.27490463047672,
126.441876371959));
#121713=CARTESIAN_POINT('Ctrl Pts',(-188.438960680087,-2.38978607308234,
126.505743911299));
#121714=CARTESIAN_POINT('Ctrl Pts',(-188.446736064809,-2.50903939390405,
126.572041965939));
#121715=CARTESIAN_POINT('Ctrl Pts',(-188.454511449531,-2.62572065138844,
126.643411342122));
#121716=CARTESIAN_POINT('Ctrl Pts',(-188.462286834253,-2.73936846326012,
126.719627641594));
#121717=CARTESIAN_POINT('Ctrl Pts',(-188.470052407546,-2.85287286776605,
126.795747766942));
#121718=CARTESIAN_POINT('Ctrl Pts',(-188.477817980839,-2.96335112181759,
126.876702429187));
#121719=CARTESIAN_POINT('Ctrl Pts',(-188.485583554132,-3.07036605036914,
126.96222119021));
#121720=CARTESIAN_POINT('Ctrl Pts',(-188.493339764738,-3.177251954663,127.047636844174));
#121721=CARTESIAN_POINT('Ctrl Pts',(-188.501095975344,-3.28068254643464,
127.137605394597));
#121722=CARTESIAN_POINT('Ctrl Pts',(-188.508852185949,-3.38024981628517,
127.23181331319));
#121723=CARTESIAN_POINT('Ctrl Pts',(-188.516603088238,-3.47974894273336,
127.325956756297));
#121724=CARTESIAN_POINT('Ctrl Pts',(-188.524353990527,-3.57538972474253,
127.424333527832));
#121725=CARTESIAN_POINT('Ctrl Pts',(-188.532104892816,-3.66679737349336,
127.526590020919));
#121726=CARTESIAN_POINT('Ctrl Pts',(-188.539852169042,-3.75816225948245,
127.628798675886));
#121727=CARTESIAN_POINT('Ctrl Pts',(-188.547599445267,-3.84529769319432,
127.734883149714));
#121728=CARTESIAN_POINT('Ctrl Pts',(-188.555346721492,-3.92786618611514,
127.844453476037));
#121729=CARTESIAN_POINT('Ctrl Pts',(-188.563092051104,-4.01041393253067,
127.953996271261));
#121730=CARTESIAN_POINT('Ctrl Pts',(-188.570837380716,-4.08839678790403,
128.067022863189));
#121731=CARTESIAN_POINT('Ctrl Pts',(-188.578582710328,-4.1615182156311,
128.183111067548));
#121732=CARTESIAN_POINT('Ctrl Pts',(-188.586330187877,-4.23465992141677,
128.299231465526));
#121733=CARTESIAN_POINT('Ctrl Pts',(-188.594077665427,-4.302937292578,128.41841484449));
#121734=CARTESIAN_POINT('Ctrl Pts',(-188.601825142976,-4.36609769469263,
128.540210891311));
#121735=CARTESIAN_POINT('Ctrl Pts',(-188.609573616128,-4.42926621333887,
128.662022589734));
#121736=CARTESIAN_POINT('Ctrl Pts',(-188.617322089279,-4.48731628029937,
128.78644727399));
#121737=CARTESIAN_POINT('Ctrl Pts',(-188.625070562431,-4.54004215253343,
128.913011808985));
#121738=CARTESIAN_POINT('Ctrl Pts',(-188.632825393423,-4.59281128782829,
129.03968019374));
#121739=CARTESIAN_POINT('Ctrl Pts',(-188.640580224415,-4.64024735853174,
129.168491572479));
#121740=CARTESIAN_POINT('Ctrl Pts',(-188.648335055407,-4.68219341291706,
129.298954391149));
#121741=CARTESIAN_POINT('Ctrl Pts',(-188.653905981131,-4.7123266748338,
129.392676443031));
#121742=CARTESIAN_POINT('Ctrl Pts',(-188.659476906855,-4.73962772385923,
129.487250379779));
#121743=CARTESIAN_POINT('Ctrl Pts',(-188.665047832579,-4.76405452823406,
129.582490119308));
#121744=CARTESIAN_POINT('Ctrl Pts',(-186.915092859931,-4.76405452823404,
129.582490119308));
#121745=CARTESIAN_POINT('Ctrl Pts',(-186.922737472684,-4.79771251131355,
129.713722084504));
#121746=CARTESIAN_POINT('Ctrl Pts',(-186.930382085436,-4.82593597496495,
129.846315094707));
#121747=CARTESIAN_POINT('Ctrl Pts',(-186.938026698189,-4.84863265225042,
129.979773165545));
#121748=CARTESIAN_POINT('Ctrl Pts',(-186.945879009153,-4.87194598068921,
130.116857188863));
#121749=CARTESIAN_POINT('Ctrl Pts',(-186.953731320117,-4.88942783458341,
130.2548535049));
#121750=CARTESIAN_POINT('Ctrl Pts',(-186.961583631081,-4.90103510324496,
130.393218331659));
#121751=CARTESIAN_POINT('Ctrl Pts',(-186.969435942045,-4.91264237190651,
130.531583158419));
#121752=CARTESIAN_POINT('Ctrl Pts',(-186.977288253009,-4.91837507169744,
130.670316037513));
#121753=CARTESIAN_POINT('Ctrl Pts',(-186.985140563973,-4.91824792938353,
130.808873666936));
#121754=CARTESIAN_POINT('',(-186.639859435958,-4.91824992550734,130.803504611091));
#121755=CARTESIAN_POINT('Ctrl Pts',(-186.570144995258,-4.76405452823391,
129.582490119308));
#121756=CARTESIAN_POINT('Ctrl Pts',(-186.57840025716,-4.80024267923322,
129.723587170822));
#121757=CARTESIAN_POINT('Ctrl Pts',(-186.586655519063,-4.83019874442568,
129.866450467451));
#121758=CARTESIAN_POINT('Ctrl Pts',(-186.594910780965,-4.8537620318651,
130.010523606257));
#121759=CARTESIAN_POINT('Ctrl Pts',(-186.603145195941,-4.87726581518243,
130.154232918679));
#121760=CARTESIAN_POINT('Ctrl Pts',(-186.611379610917,-4.89440896454415,
130.299145675755));
#121761=CARTESIAN_POINT('Ctrl Pts',(-186.619614025893,-4.90508133671532,
130.444693906975));
#121762=CARTESIAN_POINT('Ctrl Pts',(-186.626362495915,-4.9138278213004,
130.563977168498));
#121763=CARTESIAN_POINT('Ctrl Pts',(-186.633110965936,-4.91822907159551,
130.683686883876));
#121764=CARTESIAN_POINT('Ctrl Pts',(-186.639859435957,-4.91824992550734,
130.803504611091));
#121765=CARTESIAN_POINT('Ctrl Pts',(-186.639859435995,-4.91824992550745,
130.803504611754));
#121766=CARTESIAN_POINT('Ctrl Pts',(-186.647875869329,-4.91827469762084,
130.945834772432));
#121767=CARTESIAN_POINT('Ctrl Pts',(-186.655892302664,-4.91211675181942,
131.08808080582));
#121768=CARTESIAN_POINT('Ctrl Pts',(-186.663908735998,-4.89982403781472,
131.229692794756));
#121769=CARTESIAN_POINT('Ctrl Pts',(-186.671932409808,-4.88752022097909,
131.371432688235));
#121770=CARTESIAN_POINT('Ctrl Pts',(-186.679956083619,-4.86907061660121,
131.512537046391));
#121771=CARTESIAN_POINT('Ctrl Pts',(-186.68797975743,-4.84457475465937,
131.652463505792));
#121772=CARTESIAN_POINT('Ctrl Pts',(-186.696303438758,-4.81916298525302,
131.797621856561));
#121773=CARTESIAN_POINT('Ctrl Pts',(-186.704627120086,-4.78724414801483,
131.941512102986));
#121774=CARTESIAN_POINT('Ctrl Pts',(-186.712950801415,-4.74898628261018,
132.083544869377));
#121775=CARTESIAN_POINT('Ctrl Pts',(-186.720998349268,-4.71199760050266,
132.220865778145));
#121776=CARTESIAN_POINT('Ctrl Pts',(-186.729045897121,-4.6690839408078,
132.356450179057));
#121777=CARTESIAN_POINT('Ctrl Pts',(-186.737093444975,-4.62044665828881,
132.489785116144));
#121778=CARTESIAN_POINT('Ctrl Pts',(-186.745555193041,-4.56930605760306,
132.629982685208));
#121779=CARTESIAN_POINT('Ctrl Pts',(-186.754016941106,-4.51183726098221,
132.767692681952));
#121780=CARTESIAN_POINT('Ctrl Pts',(-186.762478689172,-4.44832931978521,
132.902347587316));
#121781=CARTESIAN_POINT('Ctrl Pts',(-186.770940437238,-4.38482137858837,
133.037002492679));
#121782=CARTESIAN_POINT('Ctrl Pts',(-186.779402185303,-4.31527456651344,
133.168601951196));
#121783=CARTESIAN_POINT('Ctrl Pts',(-186.787863933369,-4.2400305344674,
133.29661343967));
#121784=CARTESIAN_POINT('Ctrl Pts',(-186.795638267488,-4.17089916337693,
133.414225554185));
#121785=CARTESIAN_POINT('Ctrl Pts',(-186.803412601607,-4.09676100795466,
133.529145376511));
#121786=CARTESIAN_POINT('Ctrl Pts',(-186.811186935727,-4.0178513751189,
133.64091722549));
#121787=CARTESIAN_POINT('Ctrl Pts',(-186.818951688674,-3.93903899135325,
133.752551325653));
#121788=CARTESIAN_POINT('Ctrl Pts',(-186.826716441621,-3.85546705377721,
133.861044855384));
#121789=CARTESIAN_POINT('Ctrl Pts',(-186.834481194568,-3.76741631617132,
133.965967386781));
#121790=CARTESIAN_POINT('Ctrl Pts',(-186.842238235453,-3.67945303179932,
134.070785707641));
#121791=CARTESIAN_POINT('Ctrl Pts',(-186.849995276338,-3.5870200496273,
134.172039790846));
#121792=CARTESIAN_POINT('Ctrl Pts',(-186.857752317224,-3.49044069470467,
134.269329133909));
#121793=CARTESIAN_POINT('Ctrl Pts',(-186.865503508464,-3.39393417102474,
134.366545110322));
#121794=CARTESIAN_POINT('Ctrl Pts',(-186.873254699704,-3.29328777264913,
134.459802021349));
#121795=CARTESIAN_POINT('Ctrl Pts',(-186.881005890944,-3.18886403465664,
134.548733626626));
#121796=CARTESIAN_POINT('Ctrl Pts',(-186.888753787722,-3.08448467953826,
134.637627433597));
#121797=CARTESIAN_POINT('Ctrl Pts',(-186.896501684499,-2.97633147498796,
134.722199338236));
#121798=CARTESIAN_POINT('Ctrl Pts',(-186.904249581276,-2.86480246755412,
134.802121226256));
#121799=CARTESIAN_POINT('Ctrl Pts',(-186.91199585736,-2.75329678958435,
134.882026396341));
#121800=CARTESIAN_POINT('Ctrl Pts',(-186.919742133444,-2.63841703088417,
134.957283256941));
#121801=CARTESIAN_POINT('Ctrl Pts',(-186.927488409529,-2.52059252882238,
135.027605385058));
#121802=CARTESIAN_POINT('Ctrl Pts',(-186.935234742794,-2.40276715700672,
135.097928032277));
#121803=CARTESIAN_POINT('Ctrl Pts',(-186.94298107606,-2.2819973341713,135.163315673957));
#121804=CARTESIAN_POINT('Ctrl Pts',(-186.950727409325,-2.15873910496181,
135.223526663237));
#121805=CARTESIAN_POINT('Ctrl Pts',(-186.958475477328,-2.03545327292633,
135.28375113635));
#121806=CARTESIAN_POINT('Ctrl Pts',(-186.966223545331,-1.90967827685561,
135.338796478669));
#121807=CARTESIAN_POINT('Ctrl Pts',(-186.973971613335,-1.78189197661644,
135.388468387478));
#121808=CARTESIAN_POINT('Ctrl Pts',(-186.981727916077,-1.65396986357687,
135.438193088183));
#121809=CARTESIAN_POINT('Ctrl Pts',(-186.989484218819,-1.52403254119107,
135.482532805269));
#121810=CARTESIAN_POINT('Ctrl Pts',(-186.997240521561,-1.3925754703003,
135.521342345538));
#121811=CARTESIAN_POINT('Ctrl Pts',(-187.005000964075,-1.2610482368127,
135.560172599627));
#121812=CARTESIAN_POINT('Ctrl Pts',(-187.012761406589,-1.12800001764879,
135.59346670068));
#121813=CARTESIAN_POINT('Ctrl Pts',(-187.020521849103,-0.993937454370752,
135.621130427231));
#121814=CARTESIAN_POINT('Ctrl Pts',(-187.028294749369,-0.85965968196463,
135.648838562051));
#121815=CARTESIAN_POINT('Ctrl Pts',(-187.036067649635,-0.724364697643503,
135.670898197859));
#121816=CARTESIAN_POINT('Ctrl Pts',(-187.0438405499,-0.588566164980932,
135.687266814898));
#121817=CARTESIAN_POINT('Ctrl Pts',(-187.051330885661,-0.457704251061874,
135.703040391474));
#121818=CARTESIAN_POINT('Ctrl Pts',(-187.058821221422,-0.326375070731452,
135.713529506913));
#121819=CARTESIAN_POINT('Ctrl Pts',(-187.066311557182,-0.19503718887608,
135.718741917125));
#121820=CARTESIAN_POINT('Ctrl Pts',(-187.074085891301,-0.0587195912883398,
135.724151957455));
#121821=CARTESIAN_POINT('Ctrl Pts',(-187.08186022542,0.0780391938607504,
135.723894398637));
#121822=CARTESIAN_POINT('Ctrl Pts',(-187.089634559539,0.214728599968461,
135.717920904248));
#121823=CARTESIAN_POINT('Ctrl Pts',(-187.097399312486,0.351249548599797,
135.711954771656));
#121824=CARTESIAN_POINT('Ctrl Pts',(-187.105164065433,0.48770090147341,
135.700286736615));
#121825=CARTESIAN_POINT('Ctrl Pts',(-187.11292881838,0.62356877312973,135.682920348437));
#121826=CARTESIAN_POINT('Ctrl Pts',(-187.120685859265,0.759301698900149,
135.665571208801));
#121827=CARTESIAN_POINT('Ctrl Pts',(-187.12844290015,0.894451911427142,
135.642535028303));
#121828=CARTESIAN_POINT('Ctrl Pts',(-187.136199941035,1.028507691538,135.613867348089));
#121829=CARTESIAN_POINT('Ctrl Pts',(-187.143951132275,1.16246237914208,
135.585221286396));
#121830=CARTESIAN_POINT('Ctrl Pts',(-187.151702323515,1.2953238963055,135.550952259327));
#121831=CARTESIAN_POINT('Ctrl Pts',(-187.159453514755,1.42658815557148,
135.511167316049));
#121832=CARTESIAN_POINT('Ctrl Pts',(-187.167201411532,1.55779662402658,
135.471399282433));
#121833=CARTESIAN_POINT('Ctrl Pts',(-187.174949308309,1.68740881144558,
135.42612010863));
#121834=CARTESIAN_POINT('Ctrl Pts',(-187.182697205086,1.81493351210572,
135.375487328688));
#121835=CARTESIAN_POINT('Ctrl Pts',(-187.19044348117,1.94243153734725,135.324865140033));
#121836=CARTESIAN_POINT('Ctrl Pts',(-187.198189757255,2.0678425812239,135.268891716883));
#121837=CARTESIAN_POINT('Ctrl Pts',(-187.205936033339,2.19069360062039,
135.207773454299));
#121838=CARTESIAN_POINT('Ctrl Pts',(-187.213682366604,2.31354552687536,
135.146654740553));
#121839=CARTESIAN_POINT('Ctrl Pts',(-187.221428699869,2.43383704090215,
135.080391285736));
#121840=CARTESIAN_POINT('Ctrl Pts',(-187.229175033134,2.55111833508265,
135.009236157092));
#121841=CARTESIAN_POINT('Ctrl Pts',(-187.236923101137,2.66842589359566,
134.938065093751));
#121842=CARTESIAN_POINT('Ctrl Pts',(-187.24467116914,2.78272155665276,134.862000379508));
#121843=CARTESIAN_POINT('Ctrl Pts',(-187.252419237143,2.89358355694662,
134.78133902604));
#121844=CARTESIAN_POINT('Ctrl Pts',(-187.260175539885,3.00456338269382,
134.700591944726));
#121845=CARTESIAN_POINT('Ctrl Pts',(-187.267931842627,3.11210193908768,
134.615238695533));
#121846=CARTESIAN_POINT('Ctrl Pts',(-187.275688145368,3.21580926229213,
134.52561764323));
#121847=CARTESIAN_POINT('Ctrl Pts',(-187.283448587883,3.31957193721782,
134.435948757473));
#121848=CARTESIAN_POINT('Ctrl Pts',(-187.291209030397,3.41949901971309,
134.342007797447));
#121849=CARTESIAN_POINT('Ctrl Pts',(-187.298969472911,3.51523738644899,
134.244170086041));
#121850=CARTESIAN_POINT('Ctrl Pts',(-187.306742373176,3.61112944091017,
134.146175316856));
#121851=CARTESIAN_POINT('Ctrl Pts',(-187.314515273441,3.70281908106574,
134.044271586789));
#121852=CARTESIAN_POINT('Ctrl Pts',(-187.322288173707,3.7899928861312,133.938868072586));
#121853=CARTESIAN_POINT('Ctrl Pts',(-187.329778509469,3.87399770381394,
133.837296241609));
#121854=CARTESIAN_POINT('Ctrl Pts',(-187.337268845232,3.95380912358556,
133.732474905839));
#121855=CARTESIAN_POINT('Ctrl Pts',(-187.344759180995,4.02918580518921,
133.624794061163));
#121856=CARTESIAN_POINT('Ctrl Pts',(-187.352533515114,4.10742041657999,
133.513030464541));
#121857=CARTESIAN_POINT('Ctrl Pts',(-187.360307849233,4.181125188946,133.39783220855));
#121858=CARTESIAN_POINT('Ctrl Pts',(-187.368082183353,4.24998348176541,
133.279602720315));
#121859=CARTESIAN_POINT('Ctrl Pts',(-187.3758469363,4.31875691289296,133.161518939358));
#121860=CARTESIAN_POINT('Ctrl Pts',(-187.383611689247,4.38269555379604,
133.040411693732));
#121861=CARTESIAN_POINT('Ctrl Pts',(-187.391376442194,4.44152462296868,
132.916715248319));
#121862=CARTESIAN_POINT('Ctrl Pts',(-187.399133483079,4.50029526228031,
132.793141659959));
#121863=CARTESIAN_POINT('Ctrl Pts',(-187.406890523964,4.55396626230861,
132.666984340256));
#121864=CARTESIAN_POINT('Ctrl Pts',(-187.414647564849,4.60230775467839,
132.538703834385));
#121865=CARTESIAN_POINT('Ctrl Pts',(-187.42239875609,4.6506127923528,132.410520065842));
#121866=CARTESIAN_POINT('Ctrl Pts',(-187.43014994733,4.69359618468073,132.280216662417));
#121867=CARTESIAN_POINT('Ctrl Pts',(-187.43790113857,4.73107552357416,132.148275589853));
#121868=CARTESIAN_POINT('Ctrl Pts',(-187.445649035347,4.76853893274882,
132.016390595764));
#121869=CARTESIAN_POINT('Ctrl Pts',(-187.453396932125,4.80050283470879,
131.882869692232));
#121870=CARTESIAN_POINT('Ctrl Pts',(-187.461144828902,4.82683425861936,
131.748211295543));
#121871=CARTESIAN_POINT('Ctrl Pts',(-187.468891104986,4.85316017456368,
131.613581066489));
#121872=CARTESIAN_POINT('Ctrl Pts',(-187.47663738107,4.87385588096731,131.477814201007));
#121873=CARTESIAN_POINT('Ctrl Pts',(-187.484383657154,4.88883933248194,
131.34142024524));
#121874=CARTESIAN_POINT('Ctrl Pts',(-187.49212999042,4.90382289460099,131.205025282644));
#121875=CARTESIAN_POINT('Ctrl Pts',(-187.499876323685,4.91309407499838,
131.068003609154));
#121876=CARTESIAN_POINT('Ctrl Pts',(-187.507622656951,4.91662265431028,
130.930870449686));
#121877=CARTESIAN_POINT('Ctrl Pts',(-187.515370724954,4.92015202382305,
130.793706580197));
#121878=CARTESIAN_POINT('Ctrl Pts',(-187.523118792957,4.91793622317329,
130.65643156581));
#121879=CARTESIAN_POINT('Ctrl Pts',(-187.53086686096,4.90999716116407,130.519560793372));
#121880=CARTESIAN_POINT('Ctrl Pts',(-187.538623163702,4.90204966142525,
130.382544553048));
#121881=CARTESIAN_POINT('Ctrl Pts',(-187.546379466444,4.88836677205368,
130.245933803843));
#121882=CARTESIAN_POINT('Ctrl Pts',(-187.554135769186,4.86902238393298,
130.110239527799));
#121883=CARTESIAN_POINT('Ctrl Pts',(-187.5618962117,4.8496676711299,129.974472827634));
#121884=CARTESIAN_POINT('Ctrl Pts',(-187.569656654214,4.82464550985388,
129.839623959516));
#121885=CARTESIAN_POINT('Ctrl Pts',(-187.577417096728,4.79408079809747,
129.706192887293));
#121886=CARTESIAN_POINT('Ctrl Pts',(-187.585189996994,4.76346702115233,
129.572547619668));
#121887=CARTESIAN_POINT('Ctrl Pts',(-187.59296289726,4.72729301712821,129.440325073378));
#121888=CARTESIAN_POINT('Ctrl Pts',(-187.600735797525,4.6857336264191,129.310010108232));
#121889=CARTESIAN_POINT('Ctrl Pts',(-187.608226133286,4.64568502424898,
129.184432420329));
#121890=CARTESIAN_POINT('Ctrl Pts',(-187.615716469048,4.60063588766843,
129.060626320137));
#121891=CARTESIAN_POINT('Ctrl Pts',(-187.623206804809,4.55078388095632,
128.939005656351));
#121892=CARTESIAN_POINT('Ctrl Pts',(-187.630981138928,4.49904172025193,
128.812773708119));
#121893=CARTESIAN_POINT('Ctrl Pts',(-187.638755473047,4.4419613947056,128.688496324464));
#121894=CARTESIAN_POINT('Ctrl Pts',(-187.646529807166,4.37971116704724,
128.566657966242));
#121895=CARTESIAN_POINT('Ctrl Pts',(-187.654294560113,4.31753765723083,
128.444969762907));
#121896=CARTESIAN_POINT('Ctrl Pts',(-187.66205931306,4.25020709874698,128.325714949011));
#121897=CARTESIAN_POINT('Ctrl Pts',(-187.669824066007,4.17793632482349,
128.209359436792));
#121898=CARTESIAN_POINT('Ctrl Pts',(-187.677581106892,4.1057373312515,128.093119490508));
#121899=CARTESIAN_POINT('Ctrl Pts',(-187.685338147778,4.02860809172652,
127.979773445279));
#121900=CARTESIAN_POINT('Ctrl Pts',(-187.693095188663,3.94681182647804,
127.869763631799));
#121901=CARTESIAN_POINT('Ctrl Pts',(-187.700846379903,3.86507724442891,
127.759836777574));
#121902=CARTESIAN_POINT('Ctrl Pts',(-187.708597571143,3.77868287422416,
127.653241459867));
#121903=CARTESIAN_POINT('Ctrl Pts',(-187.716348762383,3.68793561126631,
127.550391658025));
#121904=CARTESIAN_POINT('Ctrl Pts',(-187.72409665916,3.59722691831658,127.447585570094));
#121905=CARTESIAN_POINT('Ctrl Pts',(-187.731844555937,3.50216927043818,
127.348522124323));
#121906=CARTESIAN_POINT('Ctrl Pts',(-187.739592452715,3.40311012538557,
127.253582599019));
#121907=CARTESIAN_POINT('Ctrl Pts',(-187.747338728799,3.30407170137063,
127.158662933017));
#121908=CARTESIAN_POINT('Ctrl Pts',(-187.755085004883,3.20103372715624,
127.067865742005));
#121909=CARTESIAN_POINT('Ctrl Pts',(-187.762831280967,3.09438055082806,
126.981535475193));
#121910=CARTESIAN_POINT('Ctrl Pts',(-187.770577614232,2.9877265872108,126.895204571112));
#121911=CARTESIAN_POINT('Ctrl Pts',(-187.778323947498,2.87745767211547,
126.813340903009));
#121912=CARTESIAN_POINT('Ctrl Pts',(-187.786070280763,2.76399094455158,
126.736248386944));
#121913=CARTESIAN_POINT('Ctrl Pts',(-187.793818348766,2.6504988069003,126.659138606544));
#121914=CARTESIAN_POINT('Ctrl Pts',(-187.801566416769,2.53380775509228,
126.586802323981));
#121915=CARTESIAN_POINT('Ctrl Pts',(-187.809314484772,2.41436324092127,
126.519499685938));
#121916=CARTESIAN_POINT('Ctrl Pts',(-187.817070787514,2.29479177969936,
126.452125517851));
#121917=CARTESIAN_POINT('Ctrl Pts',(-187.824827090256,2.17246135144864,
126.389795873351));
#121918=CARTESIAN_POINT('Ctrl Pts',(-187.832583392998,2.0478417996602,126.33272478422));
#121919=CARTESIAN_POINT('Ctrl Pts',(-187.840343835512,1.92315573466474,
126.27562323453));
#121920=CARTESIAN_POINT('Ctrl Pts',(-187.848104278026,1.79617847343045,
126.223785980392));
#121921=CARTESIAN_POINT('Ctrl Pts',(-187.855864720541,1.66739816011783,
126.177378184259));
#121922=CARTESIAN_POINT('Ctrl Pts',(-187.863637620806,1.53841111721335,
126.130895890211));
#121923=CARTESIAN_POINT('Ctrl Pts',(-187.871410521072,1.40761561151015,
126.089860588313));
#121924=CARTESIAN_POINT('Ctrl Pts',(-187.879183421337,1.27551407480012,
126.054387258958));
#121925=CARTESIAN_POINT('Ctrl Pts',(-187.886673757098,1.14821476170498,
126.02020347448));
#121926=CARTESIAN_POINT('Ctrl Pts',(-187.89416409286,1.01970302453186,125.991184367656));
#121927=CARTESIAN_POINT('Ctrl Pts',(-187.901654428621,0.890433888279403,
125.967387333259));
#121928=CARTESIAN_POINT('Ctrl Pts',(-187.90942876274,0.756263473425365,
125.942688027067));
#121929=CARTESIAN_POINT('Ctrl Pts',(-187.917203096859,0.620852080617946,
125.923536360038));
#121930=CARTESIAN_POINT('Ctrl Pts',(-187.924977430978,0.484698250610068,
125.910052630899));
#121931=CARTESIAN_POINT('Ctrl Pts',(-187.932742183925,0.34871221802889,
125.89658551925));
#121932=CARTESIAN_POINT('Ctrl Pts',(-187.940506936872,0.211985954126687,
125.888772485131));
#121933=CARTESIAN_POINT('Ctrl Pts',(-187.948271689819,0.0750286477215531,
125.886682937551));
#121934=CARTESIAN_POINT('Ctrl Pts',(-187.956028730704,-0.0617926307557264,
125.884595465339));
#121935=CARTESIAN_POINT('Ctrl Pts',(-187.963785771589,-0.198844106680892,
125.888220172887));
#121936=CARTESIAN_POINT('Ctrl Pts',(-187.971542812474,-0.33561135775171,
125.897574696105));
#121937=CARTESIAN_POINT('Ctrl Pts',(-187.979294003714,-0.472275471574414,
125.906922165004));
#121938=CARTESIAN_POINT('Ctrl Pts',(-187.987045194954,-0.608655398690284,
125.921990822516));
#121939=CARTESIAN_POINT('Ctrl Pts',(-187.994796386194,-0.744236962088531,
125.942746234795));
#121940=CARTESIAN_POINT('Ctrl Pts',(-188.002544282971,-0.879760899705762,
125.963492825471));
#121941=CARTESIAN_POINT('Ctrl Pts',(-188.010292179749,-1.01448676284468,
125.989921304604));
#121942=CARTESIAN_POINT('Ctrl Pts',(-188.018040076526,-1.14790596186375,
126.021945436382));
#121943=CARTESIAN_POINT('Ctrl Pts',(-188.02578635261,-1.28129725246294,
126.053962869403));
#121944=CARTESIAN_POINT('Ctrl Pts',(-188.033532628694,-1.41338204267613,
126.091573535708));
#121945=CARTESIAN_POINT('Ctrl Pts',(-188.041278904778,-1.54366278809802,
126.134640255581));
#121946=CARTESIAN_POINT('Ctrl Pts',(-188.049025238043,-1.67394449522224,
126.177707293362));
#121947=CARTESIAN_POINT('Ctrl Pts',(-188.056771571308,-1.80242175977307,
126.226230342367));
#121948=CARTESIAN_POINT('Ctrl Pts',(-188.064517904574,-1.928613414739,126.280022725787));
#121949=CARTESIAN_POINT('Ctrl Pts',(-188.072265972577,-2.05483332945198,
126.333827155638));
#121950=CARTESIAN_POINT('Ctrl Pts',(-188.080014040579,-2.17876625648171,
126.392903114748));
#121951=CARTESIAN_POINT('Ctrl Pts',(-188.087762108582,-2.29995254948067,
126.457016447543));
#121952=CARTESIAN_POINT('Ctrl Pts',(-188.095518411324,-2.42126764071347,
126.52119792075));
#121953=CARTESIAN_POINT('Ctrl Pts',(-188.103274714066,-2.53982992045492,
126.590427279275));
#121954=CARTESIAN_POINT('Ctrl Pts',(-188.111031016808,-2.65520535582168,
126.664424919887));
#121955=CARTESIAN_POINT('Ctrl Pts',(-188.118791459322,-2.77064237053186,
126.738462055268));
#121956=CARTESIAN_POINT('Ctrl Pts',(-188.126551901836,-2.88288883183471,
126.817272319268));
#121957=CARTESIAN_POINT('Ctrl Pts',(-188.13431234435,-2.99154193003811,
126.900534296721));
#121958=CARTESIAN_POINT('Ctrl Pts',(-188.142085244616,-3.1003694478408,
126.983929933691));
#121959=CARTESIAN_POINT('Ctrl Pts',(-188.149858144881,-3.20559177519847,
127.071791313939));
#121960=CARTESIAN_POINT('Ctrl Pts',(-188.157631045146,-3.30684059919295,
127.163757877081));
#121961=CARTESIAN_POINT('Ctrl Pts',(-188.165121380909,-3.4044087734147,
127.252381224011));
#121962=CARTESIAN_POINT('Ctrl Pts',(-188.172611716672,-3.49828710288302,
127.344816252083));
#121963=CARTESIAN_POINT('Ctrl Pts',(-188.180102052434,-3.58818134762388,
127.440711159156));
#121964=CARTESIAN_POINT('Ctrl Pts',(-188.187783968033,-3.6803748116775,
127.539058764095));
#121965=CARTESIAN_POINT('Ctrl Pts',(-188.195465883631,-3.76868519027518,
127.641374004402));
#121966=CARTESIAN_POINT('Ctrl Pts',(-188.20314779923,-3.85274535651832,
127.747313630631));
#121967=CARTESIAN_POINT('Ctrl Pts',(-188.210820609535,-3.93670588713396,
127.85312768774));
#121968=CARTESIAN_POINT('Ctrl Pts',(-188.21849341984,-4.01642597523958,
127.962557278402));
#121969=CARTESIAN_POINT('Ctrl Pts',(-188.226166230145,-4.09157506968238,
128.075222198274));
#121970=CARTESIAN_POINT('Ctrl Pts',(-188.233972786232,-4.16803409802803,
128.189850995414));
#121971=CARTESIAN_POINT('Ctrl Pts',(-188.241779342318,-4.23976097868823,
128.307828684763));
#121972=CARTESIAN_POINT('Ctrl Pts',(-188.249585898404,-4.3064496647105,
128.428718736344));
#121973=CARTESIAN_POINT('Ctrl Pts',(-188.257245164482,-4.37188010355881,
128.547327897795));
#121974=CARTESIAN_POINT('Ctrl Pts',(-188.26490443056,-4.43246057085316,
128.668740130964));
#121975=CARTESIAN_POINT('Ctrl Pts',(-188.272563696638,-4.4879455798733,
128.792513820567));
#121976=CARTESIAN_POINT('Ctrl Pts',(-188.280443897728,-4.54503107920871,
128.919857818529));
#121977=CARTESIAN_POINT('Ctrl Pts',(-188.288324098819,-4.59672247009533,
129.049701204745));
#121978=CARTESIAN_POINT('Ctrl Pts',(-188.29620429991,-4.64280362102202,
129.181536659422));
#121979=CARTESIAN_POINT('Ctrl Pts',(-188.304084501,-4.68888477194858,129.3133721141));
#121980=CARTESIAN_POINT('Ctrl Pts',(-188.311964702091,-4.72935551781386,
129.447199204311));
#121981=CARTESIAN_POINT('Ctrl Pts',(-188.319844903182,-4.76405452823404,
129.582490119308));
#121982=CARTESIAN_POINT('Origin',(213.235140564004,0.,130.804360617566));
#121983=CARTESIAN_POINT('',(-190.415359814329,-4.76405452823405,129.582490119308));
#121984=CARTESIAN_POINT('',(-190.06976504276,-4.76405452823418,129.582490119309));
#121985=CARTESIAN_POINT('',(213.235140564004,-4.76405452823405,129.582490119308));
#121986=CARTESIAN_POINT('',(-188.735140564044,-4.9182496381179,130.802473913264));
#121987=CARTESIAN_POINT('Ctrl Pts',(-188.735140564045,-4.9182496381179,
130.802473913264));
#121988=CARTESIAN_POINT('Ctrl Pts',(-188.742840932869,-4.91830150830916,
130.937688821655));
#121989=CARTESIAN_POINT('Ctrl Pts',(-188.750541301692,-4.91277307334292,
131.073131498441));
#121990=CARTESIAN_POINT('Ctrl Pts',(-188.758241670516,-4.90163420131192,
131.208297764941));
#121991=CARTESIAN_POINT('Ctrl Pts',(-188.76593290635,-4.89050854049381,
131.343303718052));
#121992=CARTESIAN_POINT('Ctrl Pts',(-188.773624142184,-4.87378571052704,
131.478033519156));
#121993=CARTESIAN_POINT('Ctrl Pts',(-188.781315378017,-4.85148756347388,
131.611981496418));
#121994=CARTESIAN_POINT('Ctrl Pts',(-188.788999416841,-4.82921028172503,
131.745804132983));
#121995=CARTESIAN_POINT('Ctrl Pts',(-188.796683455665,-4.80136812688925,
131.87884601002));
#121996=CARTESIAN_POINT('Ctrl Pts',(-188.804367494489,-4.76803483755962,
132.010605555511));
#121997=CARTESIAN_POINT('Ctrl Pts',(-188.812346179207,-4.73342337706943,
132.147417445207));
#121998=CARTESIAN_POINT('Ctrl Pts',(-188.820324863925,-4.69289129475855,
132.282846262811));
#121999=CARTESIAN_POINT('Ctrl Pts',(-188.828303548642,-4.64657983212241,
132.416340433263));
#122000=CARTESIAN_POINT('Ctrl Pts',(-188.835979763627,-4.6020240242359,
132.544773876606));
#122001=CARTESIAN_POINT('Ctrl Pts',(-188.843655978612,-4.55211916674477,
132.671416266738));
#122002=CARTESIAN_POINT('Ctrl Pts',(-188.851332193597,-4.49704201443896,
132.795791305004));
#122003=CARTESIAN_POINT('Ctrl Pts',(-188.859007503027,-4.44197135952829,
132.920151670875));
#122004=CARTESIAN_POINT('Ctrl Pts',(-188.866682812457,-4.3817297846288,
133.042244852048));
#122005=CARTESIAN_POINT('Ctrl Pts',(-188.874358121887,-4.31654198168248,
133.161615033804));
#122006=CARTESIAN_POINT('Ctrl Pts',(-188.882034263867,-4.25134710773214,
133.280998163795));
#122007=CARTESIAN_POINT('Ctrl Pts',(-188.889710405848,-4.18120513001891,
133.397657356846));
#122008=CARTESIAN_POINT('Ctrl Pts',(-188.897386547828,-4.10638618677583,
133.511162336857));
#122009=CARTESIAN_POINT('Ctrl Pts',(-188.905065260793,-4.03154218428859,
133.624705333297));
#122010=CARTESIAN_POINT('Ctrl Pts',(-188.912743973757,-3.95201832019808,
133.735091682711));
#122011=CARTESIAN_POINT('Ctrl Pts',(-188.920422686722,-3.86812714267184,
133.841921394016));
#122012=CARTESIAN_POINT('Ctrl Pts',(-188.928109823954,-3.78414392866631,
133.94886830752));
#122013=CARTESIAN_POINT('Ctrl Pts',(-188.935796961185,-3.69578408429893,
134.052250480927));
#122014=CARTESIAN_POINT('Ctrl Pts',(-188.943484098417,-3.60339959857195,
134.151702009703));
#122015=CARTESIAN_POINT('Ctrl Pts',(-188.951176241949,-3.5109549468263,
134.251218306957));
#122016=CARTESIAN_POINT('Ctrl Pts',(-188.958868385481,-3.41448071785227,
134.346798583313));
#122017=CARTESIAN_POINT('Ctrl Pts',(-188.966560529013,-3.31436367286446,
134.438115769815));
#122018=CARTESIAN_POINT('Ctrl Pts',(-188.974263479165,-3.21410597437231,
134.529561246983));
#122019=CARTESIAN_POINT('Ctrl Pts',(-188.981966429318,-3.11019555105514,
134.616731427316));
#122020=CARTESIAN_POINT('Ctrl Pts',(-188.98966937947,-3.00305014572403,
134.699341090529));
#122021=CARTESIAN_POINT('Ctrl Pts',(-188.991731562218,-2.97436588814104,
134.721456801895));
#122022=CARTESIAN_POINT('Ctrl Pts',(-188.993793744965,-2.94544992466852,
134.743245908247));
#122023=CARTESIAN_POINT('Ctrl Pts',(-188.995855927712,-2.91631057808861,
134.764703490933));
#122024=CARTESIAN_POINT('Ctrl Pts',(-189.003630261831,-2.80645658157905,
134.84559759084));
#122025=CARTESIAN_POINT('Ctrl Pts',(-189.01140459595,-2.69306021115118,
134.92204557856));
#122026=CARTESIAN_POINT('Ctrl Pts',(-189.01917893007,-2.57651717925398,
134.993721223614));
#122027=CARTESIAN_POINT('Ctrl Pts',(-189.026943683017,-2.46011777622816,
135.065308534842));
#122028=CARTESIAN_POINT('Ctrl Pts',(-189.034708435964,-2.34057975758224,
135.132135002961));
#122029=CARTESIAN_POINT('Ctrl Pts',(-189.042473188911,-2.21833066914151,
135.193915504436));
#122030=CARTESIAN_POINT('Ctrl Pts',(-189.050230229796,-2.09620300021883,
135.255634644646));
#122031=CARTESIAN_POINT('Ctrl Pts',(-189.057987270681,-1.97136996672141,
135.312317616571));
#122032=CARTESIAN_POINT('Ctrl Pts',(-189.065744311566,-1.84428646499388,
135.363723566218));
#122033=CARTESIAN_POINT('Ctrl Pts',(-189.073495502806,-1.71729879792339,
135.415090750238));
#122034=CARTESIAN_POINT('Ctrl Pts',(-189.081246694046,-1.58806440155843,
135.461188686808));
#122035=CARTESIAN_POINT('Ctrl Pts',(-189.088997885286,-1.4570607255567,
135.501823454517));
#122036=CARTESIAN_POINT('Ctrl Pts',(-189.096745782063,-1.32611272961209,
135.542440951367));
#122037=CARTESIAN_POINT('Ctrl Pts',(-189.10449367884,-1.19339732231602,
135.57759978204));
#122038=CARTESIAN_POINT('Ctrl Pts',(-189.112241575618,-1.05940958549109,
135.607155053378));
#122039=CARTESIAN_POINT('Ctrl Pts',(-189.119987851702,-0.925449876012263,
135.636704142391));
#122040=CARTESIAN_POINT('Ctrl Pts',(-189.127734127786,-0.790218747924846,
135.660651919364));
#122041=CARTESIAN_POINT('Ctrl Pts',(-189.13548040387,-0.65422363177214,
135.678904134874));
#122042=CARTESIAN_POINT('Ctrl Pts',(-189.143226737135,-0.518227511734195,
135.697156485118));
#122043=CARTESIAN_POINT('Ctrl Pts',(-189.150973070401,-0.381467779868424,
135.709713137999));
#122044=CARTESIAN_POINT('Ctrl Pts',(-189.158719403666,-0.244458787537432,
135.716531518878));
#122045=CARTESIAN_POINT('Ctrl Pts',(-189.166467471669,-0.107419112992374,
135.723351426686));
#122046=CARTESIAN_POINT('Ctrl Pts',(-189.174215539672,0.0298695426863131,
135.72443048597));
#122047=CARTESIAN_POINT('Ctrl Pts',(-189.181963607675,0.166891415319874,
135.71977823136));
#122048=CARTESIAN_POINT('Ctrl Pts',(-189.189719910417,0.304058916429691,
135.715121032278));
#122049=CARTESIAN_POINT('Ctrl Pts',(-189.197476213158,0.440958676729197,
135.704720364546));
#122050=CARTESIAN_POINT('Ctrl Pts',(-189.2052325159,0.577078088149238,135.688637835607));
#122051=CARTESIAN_POINT('Ctrl Pts',(-189.212992958415,0.713270150598,135.672546722939));
#122052=CARTESIAN_POINT('Ctrl Pts',(-189.220753400929,0.848680648448811,
135.650767768445));
#122053=CARTESIAN_POINT('Ctrl Pts',(-189.228513843443,0.982806764623835,
135.623413836395));
#122054=CARTESIAN_POINT('Ctrl Pts',(-189.236286743708,1.1171481919477,135.596015993386));
#122055=CARTESIAN_POINT('Ctrl Pts',(-189.244059643974,1.25020073776289,
135.563025383117));
#122056=CARTESIAN_POINT('Ctrl Pts',(-189.251832544239,1.38147548620193,
135.524605160333));
#122057=CARTESIAN_POINT('Ctrl Pts',(-189.259322880001,1.50797806687371,
135.487581609423));
#122058=CARTESIAN_POINT('Ctrl Pts',(-189.266813215763,1.63282956904491,
135.445516450911));
#122059=CARTESIAN_POINT('Ctrl Pts',(-189.274303551525,1.75561151980122,
135.398597360926));
#122060=CARTESIAN_POINT('Ctrl Pts',(-189.282077885644,1.88304878554009,
135.349899319384));
#122061=CARTESIAN_POINT('Ctrl Pts',(-189.289852219764,2.0086601508045,135.295817746099));
#122062=CARTESIAN_POINT('Ctrl Pts',(-189.297626553883,2.1319572564113,135.23650922962));
#122063=CARTESIAN_POINT('Ctrl Pts',(-189.30539130683,2.25510240935448,135.177273805588));
#122064=CARTESIAN_POINT('Ctrl Pts',(-189.313156059777,2.37593862856379,
135.112824423354));
#122065=CARTESIAN_POINT('Ctrl Pts',(-189.320920812724,2.49399493257179,
135.043366673094));
#122066=CARTESIAN_POINT('Ctrl Pts',(-189.328677853609,2.61193398139434,
134.973977909251));
#122067=CARTESIAN_POINT('Ctrl Pts',(-189.336434894494,2.72709827484188,
134.899590873599));
#122068=CARTESIAN_POINT('Ctrl Pts',(-189.344191935379,2.8390392930429,134.820458095847));
#122069=CARTESIAN_POINT('Ctrl Pts',(-189.351943126619,2.95089589565147,
134.741384992739));
#122070=CARTESIAN_POINT('Ctrl Pts',(-189.359694317859,3.0595337432095,134.657573495689));
#122071=CARTESIAN_POINT('Ctrl Pts',(-189.3674455091,3.16453161094203,134.569320477358));
#122072=CARTESIAN_POINT('Ctrl Pts',(-189.375193405877,3.26948485177972,
134.481104968915));
#122073=CARTESIAN_POINT('Ctrl Pts',(-189.382941302654,3.37080089117263,
134.388451944842));
#122074=CARTESIAN_POINT('Ctrl Pts',(-189.390689199431,3.46809022258434,
134.291699613207));
#122075=CARTESIAN_POINT('Ctrl Pts',(-189.398435475515,3.5653592031655,134.194967520073));
#122076=CARTESIAN_POINT('Ctrl Pts',(-189.406181751599,3.65860287410479,
134.094138100479));
#122077=CARTESIAN_POINT('Ctrl Pts',(-189.413928027683,3.74746766208944,
133.989587325996));
#122078=CARTESIAN_POINT('Ctrl Pts',(-189.421674360949,3.83633310605366,
133.885035779743));
#122079=CARTESIAN_POINT('Ctrl Pts',(-189.429420694214,3.92081934936079,
133.776763121682));
#122080=CARTESIAN_POINT('Ctrl Pts',(-189.437167027479,4.00061255328625,
133.665179077551));
#122081=CARTESIAN_POINT('Ctrl Pts',(-189.444915095482,4.08042362634638,
133.553570044946));
#122082=CARTESIAN_POINT('Ctrl Pts',(-189.452663163485,4.15553934133821,
133.438648468607));
#122083=CARTESIAN_POINT('Ctrl Pts',(-189.460411231488,4.22568893687965,
133.320853429245));
#122084=CARTESIAN_POINT('Ctrl Pts',(-189.46816753423,4.29591308824612,133.202933195913));
#122085=CARTESIAN_POINT('Ctrl Pts',(-189.475923836972,4.36116037632517,
133.08213373541));
#122086=CARTESIAN_POINT('Ctrl Pts',(-189.483680139714,4.42120555602244,
132.958919619751));
#122087=CARTESIAN_POINT('Ctrl Pts',(-189.491440582228,4.4812827836402,132.835639741008));
#122088=CARTESIAN_POINT('Ctrl Pts',(-189.499201024743,4.53615221408563,
132.709942997256));
#122089=CARTESIAN_POINT('Ctrl Pts',(-189.506961467257,4.58563701835403,
132.582313428639));
#122090=CARTESIAN_POINT('Ctrl Pts',(-189.514734367522,4.63520126002316,
132.454478977708));
#122091=CARTESIAN_POINT('Ctrl Pts',(-189.522507267788,4.67936347626291,
132.324705871978));
#122092=CARTESIAN_POINT('Ctrl Pts',(-189.530280168053,4.7179966628129,132.193493639341));
#122093=CARTESIAN_POINT('Ctrl Pts',(-189.537770503815,4.7552254357191,132.06705130187));
#122094=CARTESIAN_POINT('Ctrl Pts',(-189.545260839577,4.78732011310547,
131.939272951445));
#122095=CARTESIAN_POINT('Ctrl Pts',(-189.552751175338,4.81421239738261,
131.810612104714));
#122096=CARTESIAN_POINT('Ctrl Pts',(-189.560525509457,4.84212431079291,
131.677073042868));
#122097=CARTESIAN_POINT('Ctrl Pts',(-189.568299843577,4.86451996267185,
131.542160232397));
#122098=CARTESIAN_POINT('Ctrl Pts',(-189.576074177696,4.88126712533379,
131.406369183648));
#122099=CARTESIAN_POINT('Ctrl Pts',(-189.583838930643,4.89799364861444,
131.27074548523));
#122100=CARTESIAN_POINT('Ctrl Pts',(-189.59160368359,4.90908548611105,131.134246086389));
#122101=CARTESIAN_POINT('Ctrl Pts',(-189.599368436537,4.91446102967388,
130.997378363685));
#122102=CARTESIAN_POINT('Ctrl Pts',(-189.607125477422,4.91983123417105,
130.860646579932));
#122103=CARTESIAN_POINT('Ctrl Pts',(-189.614882518307,4.91949642797885,
130.723547588459));
#122104=CARTESIAN_POINT('Ctrl Pts',(-189.622639559192,4.91342663554939,
130.586595240213));
#122105=CARTESIAN_POINT('Ctrl Pts',(-189.630390750432,4.90736142039758,
130.449746168797));
#122106=CARTESIAN_POINT('Ctrl Pts',(-189.638141941672,4.8955698444968,130.313043909499));
#122107=CARTESIAN_POINT('Ctrl Pts',(-189.645893132912,4.87807399294504,
130.177003317574));
#122108=CARTESIAN_POINT('Ctrl Pts',(-189.653641029689,4.86058557759692,
130.04102054653));
#122109=CARTESIAN_POINT('Ctrl Pts',(-189.661388926466,4.83739775844842,
129.905699270483));
#122110=CARTESIAN_POINT('Ctrl Pts',(-189.669136823243,4.80858454172782,
129.771550002034));
#122111=CARTESIAN_POINT('Ctrl Pts',(-189.676883099327,4.77977735211094,
129.637428794719));
#122112=CARTESIAN_POINT('Ctrl Pts',(-189.684629375411,4.74534718751536,
129.504479489374));
#122113=CARTESIAN_POINT('Ctrl Pts',(-189.692375651495,4.70541924846024,
129.373202779059));
#122114=CARTESIAN_POINT('Ctrl Pts',(-189.700121984761,4.66549101466631,
129.241925099689));
#122115=CARTESIAN_POINT('Ctrl Pts',(-189.707868318026,4.62006503919849,
129.112320414033));
#122116=CARTESIAN_POINT('Ctrl Pts',(-189.715614651291,4.56931639842622,
128.984874230265));
#122117=CARTESIAN_POINT('Ctrl Pts',(-189.723362719294,4.51855639284751,
128.857399505808));
#122118=CARTESIAN_POINT('Ctrl Pts',(-189.731110787297,4.46247149468235,
128.732084608271));
#122119=CARTESIAN_POINT('Ctrl Pts',(-189.7388588553,4.40128476182806,128.609394670723));
#122120=CARTESIAN_POINT('Ctrl Pts',(-189.746615158042,4.34003299898604,
128.48657433685));
#122121=CARTESIAN_POINT('Ctrl Pts',(-189.754371460784,4.2736687446074,128.366384886397));
#122122=CARTESIAN_POINT('Ctrl Pts',(-189.762127763526,4.20246110581043,
128.249266936964));
#122123=CARTESIAN_POINT('Ctrl Pts',(-189.76988820604,4.13121546135242,128.132086478155));
#122124=CARTESIAN_POINT('Ctrl Pts',(-189.777648648554,4.0551214983341,128.017981112027));
#122125=CARTESIAN_POINT('Ctrl Pts',(-189.785409091068,3.97449087304063,
127.907361245351));
#122126=CARTESIAN_POINT('Ctrl Pts',(-189.793181991334,3.89373081230961,
127.796563801844));
#122127=CARTESIAN_POINT('Ctrl Pts',(-189.800954891599,3.80841977969454,
127.689263345051));
#122128=CARTESIAN_POINT('Ctrl Pts',(-189.808727791865,3.71890939325291,
127.585836734281));
#122129=CARTESIAN_POINT('Ctrl Pts',(-189.816218127627,3.63265293481907,
127.486169941325));
#122130=CARTESIAN_POINT('Ctrl Pts',(-189.823708463389,3.54249734681371,
127.390100460701));
#122131=CARTESIAN_POINT('Ctrl Pts',(-189.831198799151,3.44878726912054,
127.29793088993));
#122132=CARTESIAN_POINT('Ctrl Pts',(-189.83897313327,3.3515241453514,127.20226668187));
#122133=CARTESIAN_POINT('Ctrl Pts',(-189.846747467389,3.25012357385693,
127.110500916178));
#122134=CARTESIAN_POINT('Ctrl Pts',(-189.854521801508,3.14493096923238,
127.023012675196));
#122135=CARTESIAN_POINT('Ctrl Pts',(-189.862286554456,3.03986800509226,
126.935632255653));
#122136=CARTESIAN_POINT('Ctrl Pts',(-189.870051307403,2.93102260408373,
126.852519119373));
#122137=CARTESIAN_POINT('Ctrl Pts',(-189.87781606035,2.81877752527758,126.774016175029));
#122138=CARTESIAN_POINT('Ctrl Pts',(-189.885573101235,2.70664392986547,
126.695591200915));
#122139=CARTESIAN_POINT('Ctrl Pts',(-189.89333014212,2.59111769456779,126.621767529126));
#122140=CARTESIAN_POINT('Ctrl Pts',(-189.901087183005,2.47261493422438,
126.552848127928));
#122141=CARTESIAN_POINT('Ctrl Pts',(-189.908838374245,2.35420153773453,
126.483980699386));
#122142=CARTESIAN_POINT('Ctrl Pts',(-189.916589565485,2.23281642057723,
126.420010375857));
#122143=CARTESIAN_POINT('Ctrl Pts',(-189.924340756725,2.10890468259733,
126.361196868364));
#122144=CARTESIAN_POINT('Ctrl Pts',(-189.932088653502,1.98504561041135,
126.302408358181));
#122145=CARTESIAN_POINT('Ctrl Pts',(-189.93983655028,1.8586624057305,126.248772472034));
#122146=CARTESIAN_POINT('Ctrl Pts',(-189.947584447057,1.73022457943941,
126.200502890919));
#122147=CARTESIAN_POINT('Ctrl Pts',(-189.955330723141,1.60181361957279,
126.15224340676));
#122148=CARTESIAN_POINT('Ctrl Pts',(-189.963076999225,1.47134925869841,
126.109348132341));
#122149=CARTESIAN_POINT('Ctrl Pts',(-189.970823275309,1.33932041800663,
126.071982369749));
#122150=CARTESIAN_POINT('Ctrl Pts',(-189.978569608574,1.20729060270813,
126.034616331331));
#122151=CARTESIAN_POINT('Ctrl Pts',(-189.98631594184,1.07369666073754,126.002779992655));
#122152=CARTESIAN_POINT('Ctrl Pts',(-189.994062275105,0.939041696927769,
125.976588486041));
#122153=CARTESIAN_POINT('Ctrl Pts',(-190.001810343108,0.804356578073038,
125.95039111402));
#122154=CARTESIAN_POINT('Ctrl Pts',(-190.009558411111,0.668610348265179,
125.929841164149));
#122155=CARTESIAN_POINT('Ctrl Pts',(-190.017306479114,0.532314905370259,
125.915002387285));
#122156=CARTESIAN_POINT('Ctrl Pts',(-190.025062781856,0.395874606056136,
125.900147839592));
#122157=CARTESIAN_POINT('Ctrl Pts',(-190.032819084598,0.258884316919199,
125.891016632574));
#122158=CARTESIAN_POINT('Ctrl Pts',(-190.040575387339,0.12186020099531,
125.887620523366));
#122159=CARTESIAN_POINT('Ctrl Pts',(-190.048335829854,-0.0152370488249634,
125.884222601552));
#122160=CARTESIAN_POINT('Ctrl Pts',(-190.056096272368,-0.152367770690179,
125.886565870162));
#122161=CARTESIAN_POINT('Ctrl Pts',(-190.063856714882,-0.28901821992613,
125.894609958821));
#122162=CARTESIAN_POINT('Ctrl Pts',(-190.071629615147,-0.42588803259445,
125.902666960564));
#122163=CARTESIAN_POINT('Ctrl Pts',(-190.079402515413,-0.562275642767436,
125.916443030582));
#122164=CARTESIAN_POINT('Ctrl Pts',(-190.087175415678,-0.697673929887046,
125.935846044305));
#122165=CARTESIAN_POINT('Ctrl Pts',(-190.09466575144,-0.82815014822142,
125.954543709606));
#122166=CARTESIAN_POINT('Ctrl Pts',(-190.102156087202,-0.957707420585213,
125.978466258228));
#122167=CARTESIAN_POINT('Ctrl Pts',(-190.109646422964,-1.0859048768382,
126.007487296229));
#122168=CARTESIAN_POINT('Ctrl Pts',(-190.117420757083,-1.21896297860964,
126.037608675706));
#122169=CARTESIAN_POINT('Ctrl Pts',(-190.125195091202,-1.35097760196638,
126.073318210457));
#122170=CARTESIAN_POINT('Ctrl Pts',(-190.132969425321,-1.48144310917082,
126.114530196667));
#122171=CARTESIAN_POINT('Ctrl Pts',(-190.140734178268,-1.61174782929803,
126.155691392787));
#122172=CARTESIAN_POINT('Ctrl Pts',(-190.148498931215,-1.74050686267825,
126.202341431007));
#122173=CARTESIAN_POINT('Ctrl Pts',(-190.156263684163,-1.86722481990743,
126.254343635793));
#122174=CARTESIAN_POINT('Ctrl Pts',(-190.164020725047,-1.9938169190744,
126.306294191256));
#122175=CARTESIAN_POINT('Ctrl Pts',(-190.171777765932,-2.11837161700793,
126.363586187039));
#122176=CARTESIAN_POINT('Ctrl Pts',(-190.179534806817,-2.24040909768993,
126.42603329569));
#122177=CARTESIAN_POINT('Ctrl Pts',(-190.187285998058,-2.36235454895925,
126.488433312491));
#122178=CARTESIAN_POINT('Ctrl Pts',(-190.195037189298,-2.48178621469771,
126.55598052693));
#122179=CARTESIAN_POINT('Ctrl Pts',(-190.202788380538,-2.59824500532673,
126.628440844056));
#122180=CARTESIAN_POINT('Ctrl Pts',(-190.210536277315,-2.71465429786326,
126.700870363613));
#122181=CARTESIAN_POINT('Ctrl Pts',(-190.218284174092,-2.82809289713704,
126.778208626477));
#122182=CARTESIAN_POINT('Ctrl Pts',(-190.226032070869,-2.93812724517321,
126.860176119641));
#122183=CARTESIAN_POINT('Ctrl Pts',(-190.233778346953,-3.04813857639583,
126.942126466972));
#122184=CARTESIAN_POINT('Ctrl Pts',(-190.241524623037,-3.15474675944337,
127.028703885119));
#122185=CARTESIAN_POINT('Ctrl Pts',(-190.249270899121,-3.25754844714305,
127.119586380653));
#122186=CARTESIAN_POINT('Ctrl Pts',(-190.257017232387,-3.36035089370159,
127.210469547061));
#122187=CARTESIAN_POINT('Ctrl Pts',(-190.264763565652,-3.45934649593055,
127.305657595318));
#122188=CARTESIAN_POINT('Ctrl Pts',(-190.272509898917,-3.55416644929697,
127.404789480909));
#122189=CARTESIAN_POINT('Ctrl Pts',(-190.28025796692,-3.64900763693438,
127.503943566399));
#122190=CARTESIAN_POINT('Ctrl Pts',(-190.288006034923,-3.73967104476384,
127.607042964203));
#122191=CARTESIAN_POINT('Ctrl Pts',(-190.295754102926,-3.82582634408186,
127.713691459046));
#122192=CARTESIAN_POINT('Ctrl Pts',(-190.303510405668,-3.91207321027691,
127.820453301177));
#122193=CARTESIAN_POINT('Ctrl Pts',(-190.31126670841,-3.99380215080234,
127.930771470759));
#122194=CARTESIAN_POINT('Ctrl Pts',(-190.319023011152,-4.07072427531871,
128.044218060228));
#122195=CARTESIAN_POINT('Ctrl Pts',(-190.326783453666,-4.14768745548943,
128.157725199558));
#122196=CARTESIAN_POINT('Ctrl Pts',(-190.33454389618,-4.21983850201565,
128.274363753527));
#122197=CARTESIAN_POINT('Ctrl Pts',(-190.342304338694,-4.28693368809188,
128.393679673019));
#122198=CARTESIAN_POINT('Ctrl Pts',(-190.35007723896,-4.35413658131705,
128.513187129016));
#122199=CARTESIAN_POINT('Ctrl Pts',(-190.357850139225,-4.41626721820383,
128.635380190496));
#122200=CARTESIAN_POINT('Ctrl Pts',(-190.36562303949,-4.47312899471228,
128.759782406989));
#122201=CARTESIAN_POINT('Ctrl Pts',(-190.373113375253,-4.52792370242032,
128.879662289568));
#122202=CARTESIAN_POINT('Ctrl Pts',(-190.380603711015,-4.57782585506955,
129.001593213935));
#122203=CARTESIAN_POINT('Ctrl Pts',(-190.388094046777,-4.62270349038433,
129.125135944543));
#122204=CARTESIAN_POINT('Ctrl Pts',(-190.397182635961,-4.67715690927988,
129.275039655247));
#122205=CARTESIAN_POINT('Ctrl Pts',(-190.406271225145,-4.72435719403422,
129.427710815754));
#122206=CARTESIAN_POINT('Ctrl Pts',(-190.415359814329,-4.76405452823405,
129.582490119308));
#122207=CARTESIAN_POINT('Ctrl Pts',(-188.665047832579,-4.76405452823406,
129.582490119308));
#122208=CARTESIAN_POINT('Ctrl Pts',(-188.672812177752,-4.7980988056188,
129.715228240137));
#122209=CARTESIAN_POINT('Ctrl Pts',(-188.680576522925,-4.82655782458609,
129.849259699109));
#122210=CARTESIAN_POINT('Ctrl Pts',(-188.688340868098,-4.84936224031761,
129.984074737716));
#122211=CARTESIAN_POINT('Ctrl Pts',(-188.696116115444,-4.87219867648161,
130.119079074566));
#122212=CARTESIAN_POINT('Ctrl Pts',(-188.703891362791,-4.88936461210996,
130.254868801069));
#122213=CARTESIAN_POINT('Ctrl Pts',(-188.711666610137,-4.90084263355078,
130.390930401361));
#122214=CARTESIAN_POINT('Ctrl Pts',(-188.713580508058,-4.90366797921412,
130.424422328024));
#122215=CARTESIAN_POINT('Ctrl Pts',(-188.715494405978,-4.90614893497245,
130.457930736052));
#122216=CARTESIAN_POINT('Ctrl Pts',(-188.717408303899,-4.90828572440508,
130.491447993817));
#122217=CARTESIAN_POINT('Ctrl Pts',(-188.72331905727,-4.91488484090139,
130.594960434142));
#122218=CARTESIAN_POINT('Ctrl Pts',(-188.729229810641,-4.9182098228819,
130.6986838224));
#122219=CARTESIAN_POINT('Ctrl Pts',(-188.735140564012,-4.91824963811768,
130.802473912695));
#122220=CARTESIAN_POINT('',(-188.389859436034,-4.91824789781227,130.808907942626));
#122221=CARTESIAN_POINT('Ctrl Pts',(-188.319844903182,-4.76405452823404,
129.582490119308));
#122222=CARTESIAN_POINT('Ctrl Pts',(-188.327501512409,-4.79776899317125,
129.71394230641));
#122223=CARTESIAN_POINT('Ctrl Pts',(-188.335158121637,-4.82603476089132,
129.846775959306));
#122224=CARTESIAN_POINT('Ctrl Pts',(-188.342814730864,-4.84875524607537,
129.980494350411));
#122225=CARTESIAN_POINT('Ctrl Pts',(-188.350655515053,-4.87202225836387,
130.117429254037));
#122226=CARTESIAN_POINT('Ctrl Pts',(-188.358496299241,-4.88947373540814,
130.255291565461));
#122227=CARTESIAN_POINT('Ctrl Pts',(-188.36633708343,-4.90106215269356,
130.393540902929));
#122228=CARTESIAN_POINT('Ctrl Pts',(-188.374177867618,-4.91265056997894,
130.531790240396));
#122229=CARTESIAN_POINT('Ctrl Pts',(-188.382018651807,-4.91837593560674,
130.670426153596));
#122230=CARTESIAN_POINT('Ctrl Pts',(-188.389859435995,-4.91824789781291,
130.808907941932));
#122231=CARTESIAN_POINT('Ctrl Pts',(-188.389859436034,-4.91824789781227,
130.808907942627));
#122232=CARTESIAN_POINT('Ctrl Pts',(-188.399867117337,-4.9180844751749,
130.985660875825));
#122233=CARTESIAN_POINT('Ctrl Pts',(-188.409874798639,-4.90838934841572,
131.161987856138));
#122234=CARTESIAN_POINT('Ctrl Pts',(-188.419882479942,-4.88932061848566,
131.33702087716));
#122235=CARTESIAN_POINT('Ctrl Pts',(-188.430125673914,-4.86980314050388,
131.516172983589));
#122236=CARTESIAN_POINT('Ctrl Pts',(-188.440368867886,-4.84046566695456,
131.693969810191));
#122237=CARTESIAN_POINT('Ctrl Pts',(-188.450612061858,-4.80152560262522,
131.86950612398));
#122238=CARTESIAN_POINT('Ctrl Pts',(-188.453257933321,-4.79146717697613,
131.914848087107));
#122239=CARTESIAN_POINT('Ctrl Pts',(-188.455903804784,-4.78076829602226,
131.960039341272));
#122240=CARTESIAN_POINT('Ctrl Pts',(-188.458549676247,-4.76943321745608,
132.005064513923));
#122241=CARTESIAN_POINT('Ctrl Pts',(-188.466324010366,-4.73612748463049,
132.137361468194));
#122242=CARTESIAN_POINT('Ctrl Pts',(-188.474098344485,-4.69726024638632,
132.268481144229));
#122243=CARTESIAN_POINT('Ctrl Pts',(-188.481872678604,-4.65292931576995,
132.397920106556));
#122244=CARTESIAN_POINT('Ctrl Pts',(-188.489637431551,-4.60865301906372,
132.527199546929));
#122245=CARTESIAN_POINT('Ctrl Pts',(-188.497402184498,-4.55892655312866,
132.654802028599));
#122246=CARTESIAN_POINT('Ctrl Pts',(-188.505166937445,-4.503898442119,132.780235584657));
#122247=CARTESIAN_POINT('Ctrl Pts',(-188.51292397833,-4.44892498580481,
132.90554455834));
#122248=CARTESIAN_POINT('Ctrl Pts',(-188.520681019215,-4.38866051938554,
133.028688537671));
#122249=CARTESIAN_POINT('Ctrl Pts',(-188.5284380601,-4.32330283091627,133.149192316152));
#122250=CARTESIAN_POINT('Ctrl Pts',(-188.53618925134,-4.25799442918837,
133.269605221796));
#122251=CARTESIAN_POINT('Ctrl Pts',(-188.54394044258,-4.18760063600923,
133.387381547266));
#122252=CARTESIAN_POINT('Ctrl Pts',(-188.551691633821,-4.11236649580212,
133.502067952824));
#122253=CARTESIAN_POINT('Ctrl Pts',(-188.559439530598,-4.03716433211143,
133.6167056136));
#122254=CARTESIAN_POINT('Ctrl Pts',(-188.567187427375,-3.95712612715828,
133.728255640296));
#122255=CARTESIAN_POINT('Ctrl Pts',(-188.574935324152,-3.87254171765271,
133.836291307331));
#122256=CARTESIAN_POINT('Ctrl Pts',(-188.582681600236,-3.78797500138217,
133.944304375634));
#122257=CARTESIAN_POINT('Ctrl Pts',(-188.59042787632,-3.69886421295048,
134.048804238843));
#122258=CARTESIAN_POINT('Ctrl Pts',(-188.598174152404,-3.60554093228053,
134.149395392893));
#122259=CARTESIAN_POINT('Ctrl Pts',(-188.605920485669,-3.51221696271946,
134.249987289485));
#122260=CARTESIAN_POINT('Ctrl Pts',(-188.613666818935,-3.41468070477701,
134.34667013273));
#122261=CARTESIAN_POINT('Ctrl Pts',(-188.6214131522,-3.31330194928639,134.439083888374));
#122262=CARTESIAN_POINT('Ctrl Pts',(-188.629161220203,-3.21190049072653,
134.531518339438));
#122263=CARTESIAN_POINT('Ctrl Pts',(-188.636909288206,-3.10665511120062,
134.619681537175));
#122264=CARTESIAN_POINT('Ctrl Pts',(-188.644657356209,-2.99796983886249,
134.703252756081));
#122265=CARTESIAN_POINT('Ctrl Pts',(-188.652413658951,-2.88916905452341,
134.786912795473));
#122266=CARTESIAN_POINT('Ctrl Pts',(-188.660169961693,-2.77692138462799,
134.865970868193));
#122267=CARTESIAN_POINT('Ctrl Pts',(-188.667926264434,-2.661661546083,134.940148435697));
#122268=CARTESIAN_POINT('Ctrl Pts',(-188.675686706949,-2.54634018989178,
135.014365594003));
#122269=CARTESIAN_POINT('Ctrl Pts',(-188.683447149463,-2.4280037987698,
135.083696859122));
#122270=CARTESIAN_POINT('Ctrl Pts',(-188.691207591977,-2.30711213985166,
135.147909470365));
#122271=CARTESIAN_POINT('Ctrl Pts',(-188.698980492242,-2.18602641491037,
135.212225161391));
#122272=CARTESIAN_POINT('Ctrl Pts',(-188.706753392507,-2.06237757804144,
135.271405609637));
#122273=CARTESIAN_POINT('Ctrl Pts',(-188.714526292773,-1.93664666046133,
135.325265701177));
#122274=CARTESIAN_POINT('Ctrl Pts',(-188.722016628535,-1.81548637842552,
135.377167842728));
#122275=CARTESIAN_POINT('Ctrl Pts',(-188.729506964298,-1.69239305308073,
135.424129618806));
#122276=CARTESIAN_POINT('Ctrl Pts',(-188.73699730006,-1.56780896021745,
135.466029645582));
#122277=CARTESIAN_POINT('Ctrl Pts',(-188.744771634179,-1.43850122361313,
135.509518324605));
#122278=CARTESIAN_POINT('Ctrl Pts',(-188.752545968298,-1.30717783500581,
135.547691603967));
#122279=CARTESIAN_POINT('Ctrl Pts',(-188.760320302418,-1.17431521925618,
135.580359657382));
#122280=CARTESIAN_POINT('Ctrl Pts',(-188.768085055365,-1.04161634480655,
135.612987450341));
#122281=CARTESIAN_POINT('Ctrl Pts',(-188.775849808312,-0.907382393612003,
135.64012342443));
#122282=CARTESIAN_POINT('Ctrl Pts',(-188.783614561259,-0.772107552298939,
135.661626617095));
#122283=CARTESIAN_POINT('Ctrl Pts',(-188.791371602144,-0.636967067865308,
135.683108452486));
#122284=CARTESIAN_POINT('Ctrl Pts',(-188.799128643029,-0.500788134293892,
135.698968578897));
#122285=CARTESIAN_POINT('Ctrl Pts',(-188.806885683914,-0.36407746554492,
135.709116540299));
#122286=CARTESIAN_POINT('Ctrl Pts',(-188.814636875154,-0.227469891374892,
135.719256849044));
#122287=CARTESIAN_POINT('Ctrl Pts',(-188.822388066394,-0.0903317684798211,
135.72369353795));
#122288=CARTESIAN_POINT('Ctrl Pts',(-188.830139257634,0.0468230430825336,
135.722387728628));
#122289=CARTESIAN_POINT('Ctrl Pts',(-188.837887154411,0.183919560191437,
135.721082474309));
#122290=CARTESIAN_POINT('Ctrl Pts',(-188.845635051188,0.321032361730929,
135.714039579871));
#122291=CARTESIAN_POINT('Ctrl Pts',(-188.853382947965,0.457645767564134,
135.70127223755));
#122292=CARTESIAN_POINT('Ctrl Pts',(-188.861129224049,0.594230596817883,
135.688507565881));
#122293=CARTESIAN_POINT('Ctrl Pts',(-188.868875500133,0.730315849125278,
135.670020864439));
#122294=CARTESIAN_POINT('Ctrl Pts',(-188.876621776217,0.865389548668166,
135.645877321199));
#122295=CARTESIAN_POINT('Ctrl Pts',(-188.884368109483,1.0004642452946,135.621733599736));
#122296=CARTESIAN_POINT('Ctrl Pts',(-188.892114442748,1.1345269893911,135.591933021942));
#122297=CARTESIAN_POINT('Ctrl Pts',(-188.899860776013,1.26707499296545,
135.556592096009));
#122298=CARTESIAN_POINT('Ctrl Pts',(-188.907608844016,1.39965267974599,
135.52124325572));
#122299=CARTESIAN_POINT('Ctrl Pts',(-188.915356912019,1.53071457330889,
135.480351699103));
#122300=CARTESIAN_POINT('Ctrl Pts',(-188.923104980022,1.65977245111908,
135.434083986516));
#122301=CARTESIAN_POINT('Ctrl Pts',(-188.930861282764,1.7889674931778,135.387767100054));
#122302=CARTESIAN_POINT('Ctrl Pts',(-188.938617585506,1.91615389617927,
135.336062775758));
#122303=CARTESIAN_POINT('Ctrl Pts',(-188.946373888248,2.04086234265069,
135.279186196385));
#122304=CARTESIAN_POINT('Ctrl Pts',(-188.954134330762,2.16563734977488,
135.222279260269));
#122305=CARTESIAN_POINT('Ctrl Pts',(-188.961894773276,2.2879314166124,135.160194745264));
#122306=CARTESIAN_POINT('Ctrl Pts',(-188.96965521579,2.40730019963481,135.093193653642));
#122307=CARTESIAN_POINT('Ctrl Pts',(-188.977428116055,2.5268606040248,135.02608500592));
#122308=CARTESIAN_POINT('Ctrl Pts',(-188.985201016321,2.64348600783031,
134.954044215384));
#122309=CARTESIAN_POINT('Ctrl Pts',(-188.992973916586,2.75676066034094,
134.877375928622));
#122310=CARTESIAN_POINT('Ctrl Pts',(-189.000464252348,2.86591749391118,
134.803494727199));
#122311=CARTESIAN_POINT('Ctrl Pts',(-189.00795458811,2.97196271521771,134.725316813482));
#122312=CARTESIAN_POINT('Ctrl Pts',(-189.015444923872,3.07455513973725,
134.643148675693));
#122313=CARTESIAN_POINT('Ctrl Pts',(-189.023219257991,3.18103738721459,
134.557865107985));
#122314=CARTESIAN_POINT('Ctrl Pts',(-189.03099359211,3.2841371475586,134.468012611807));
#122315=CARTESIAN_POINT('Ctrl Pts',(-189.038767926229,3.38343719526661,
134.373889411145));
#122316=CARTESIAN_POINT('Ctrl Pts',(-189.046532679176,3.48261486454052,
134.279882208915));
#122317=CARTESIAN_POINT('Ctrl Pts',(-189.054297432124,3.57800185753944,
134.1816150409));
#122318=CARTESIAN_POINT('Ctrl Pts',(-189.062062185071,3.66921245853213,
134.079427486601));
#122319=CARTESIAN_POINT('Ctrl Pts',(-189.069819225956,3.76033246787007,
133.977341426422));
#122320=CARTESIAN_POINT('Ctrl Pts',(-189.077576266841,3.84728408135189,
133.87134301855));
#122321=CARTESIAN_POINT('Ctrl Pts',(-189.085333307726,3.92971730448732,
133.7618096821));
#122322=CARTESIAN_POINT('Ctrl Pts',(-189.093084498966,4.01208836408783,
133.652358945591));
#122323=CARTESIAN_POINT('Ctrl Pts',(-189.100835690206,4.0899475813276,133.539378897572));
#122324=CARTESIAN_POINT('Ctrl Pts',(-189.108586881446,4.16298449280398,
133.423280848343));
#122325=CARTESIAN_POINT('Ctrl Pts',(-189.116334778223,4.23599036164477,
133.307232143882));
#122326=CARTESIAN_POINT('Ctrl Pts',(-189.124082675,4.30417779348807,133.188068404235));
#122327=CARTESIAN_POINT('Ctrl Pts',(-189.131830571777,4.36727914962361,
133.06623061643));
#122328=CARTESIAN_POINT('Ctrl Pts',(-189.139576847861,4.43036730631575,
132.944418314464));
#122329=CARTESIAN_POINT('Ctrl Pts',(-189.147323123945,4.48837132376201,
132.819933423872));
#122330=CARTESIAN_POINT('Ctrl Pts',(-189.15506940003,4.54106931101448,132.6932419201));
#122331=CARTESIAN_POINT('Ctrl Pts',(-189.162815733295,4.59376768727144,
132.56654948112));
#122332=CARTESIAN_POINT('Ctrl Pts',(-189.17056206656,4.64115980502555,132.437650757441));
#122333=CARTESIAN_POINT('Ctrl Pts',(-189.178308399826,4.68307191672785,
132.307031734363));
#122334=CARTESIAN_POINT('Ctrl Pts',(-189.186056467829,4.72499341435691,
132.17638346006));
#122335=CARTESIAN_POINT('Ctrl Pts',(-189.193804535832,4.76143234450105,
132.044014491957));
#122336=CARTESIAN_POINT('Ctrl Pts',(-189.201552603835,4.7922649429027,131.910425615442));
#122337=CARTESIAN_POINT('Ctrl Pts',(-189.209308906576,4.82313031055689,
131.776694759079));
#122338=CARTESIAN_POINT('Ctrl Pts',(-189.217065209318,4.84837735570641,
131.641741785897));
#122339=CARTESIAN_POINT('Ctrl Pts',(-189.22482151206,4.86793344014249,131.506077857516));
#122340=CARTESIAN_POINT('Ctrl Pts',(-189.232581954574,4.8874999622497,131.37034152121));
#122341=CARTESIAN_POINT('Ctrl Pts',(-189.240342397089,4.90136943177558,
131.233893862373));
#122342=CARTESIAN_POINT('Ctrl Pts',(-189.248102839603,4.90952125879313,
131.097249797903));
#122343=CARTESIAN_POINT('Ctrl Pts',(-189.255875739868,4.91768617184709,
130.960386380249));
#122344=CARTESIAN_POINT('Ctrl Pts',(-189.263648640134,4.92011509395886,
130.823326318046));
#122345=CARTESIAN_POINT('Ctrl Pts',(-189.271421540399,4.91683960951637,
130.686584063062));
#122346=CARTESIAN_POINT('Ctrl Pts',(-189.278911876161,4.91368319718378,
130.554812733478));
#122347=CARTESIAN_POINT('Ctrl Pts',(-189.286402211923,4.90522993667453,
130.423336813468));
#122348=CARTESIAN_POINT('Ctrl Pts',(-189.293892547685,4.8915532666416,130.292609015607));
#122349=CARTESIAN_POINT('Ctrl Pts',(-189.301666881805,4.87735804150758,
130.156924633557));
#122350=CARTESIAN_POINT('Ctrl Pts',(-189.309441215924,4.85749053053571,
130.021616416288));
#122351=CARTESIAN_POINT('Ctrl Pts',(-189.317215550043,4.83197611743572,
129.887196584783));
#122352=CARTESIAN_POINT('Ctrl Pts',(-189.32498030299,4.80649314856966,129.752942413707));
#122353=CARTESIAN_POINT('Ctrl Pts',(-189.332745055937,4.77537719672058,
129.619574830376));
#122354=CARTESIAN_POINT('Ctrl Pts',(-189.340509808884,4.73870547096616,
129.487601899374));
#122355=CARTESIAN_POINT('Ctrl Pts',(-189.348266849769,4.70207016808673,
129.355760045747));
#122356=CARTESIAN_POINT('Ctrl Pts',(-189.356023890654,4.6598901765116,129.225310462118));
#122357=CARTESIAN_POINT('Ctrl Pts',(-189.363780931539,4.61229384905882,
129.096751613012));
#122358=CARTESIAN_POINT('Ctrl Pts',(-189.371532122779,4.56473341436676,
128.968289711134));
#122359=CARTESIAN_POINT('Ctrl Pts',(-189.379283314019,4.5117649089419,128.841716070937));
#122360=CARTESIAN_POINT('Ctrl Pts',(-189.387034505259,4.45356656673678,
128.717514217338));
#122361=CARTESIAN_POINT('Ctrl Pts',(-189.394782402037,4.39539296037968,
128.59336515284));
#122362=CARTESIAN_POINT('Ctrl Pts',(-189.402530298814,4.33199410380397,
128.471586223247));
#122363=CARTESIAN_POINT('Ctrl Pts',(-189.410278195591,4.26359634662585,
128.352640964845));
#122364=CARTESIAN_POINT('Ctrl Pts',(-189.418024471675,4.19521289678404,
128.233720587227));
#122365=CARTESIAN_POINT('Ctrl Pts',(-189.425770747759,4.12183282098978,
128.117633040512));
#122366=CARTESIAN_POINT('Ctrl Pts',(-189.433517023843,4.04372822010655,
128.004816878952));
#122367=CARTESIAN_POINT('Ctrl Pts',(-189.441263357108,3.9656230426728,127.891999884608));
#122368=CARTESIAN_POINT('Ctrl Pts',(-189.449009690374,3.88279349310222,
127.782454645051));
#122369=CARTESIAN_POINT('Ctrl Pts',(-189.456756023639,3.7955545297986,127.676590025942));
#122370=CARTESIAN_POINT('Ctrl Pts',(-189.464504091642,3.70829602993413,
127.570701699186));
#122371=CARTESIAN_POINT('Ctrl Pts',(-189.472252159645,3.61662639999776,
127.4684959347));
#122372=CARTESIAN_POINT('Ctrl Pts',(-189.480000227648,3.5209000673159,127.370347545594));
#122373=CARTESIAN_POINT('Ctrl Pts',(-189.48775653039,3.42507199554838,127.272094843212));
#122374=CARTESIAN_POINT('Ctrl Pts',(-189.495512833132,3.32517888174022,
127.17790841068));
#122375=CARTESIAN_POINT('Ctrl Pts',(-189.503269135873,3.22161151791196,
127.08812565592));
#122376=CARTESIAN_POINT('Ctrl Pts',(-189.511029578388,3.11798887706327,
126.998294981402));
#122377=CARTESIAN_POINT('Ctrl Pts',(-189.518790020902,3.01068838434436,
126.912872911365));
#122378=CARTESIAN_POINT('Ctrl Pts',(-189.526550463416,2.90013212456667,
126.832155093861));
#122379=CARTESIAN_POINT('Ctrl Pts',(-189.534323363681,2.78939839006606,
126.751307700949));
#122380=CARTESIAN_POINT('Ctrl Pts',(-189.542096263947,2.67539876972268,
126.675179868487));
#122381=CARTESIAN_POINT('Ctrl Pts',(-189.549869164212,2.55858315851329,
126.604023097381));
#122382=CARTESIAN_POINT('Ctrl Pts',(-189.557359499974,2.44601408901245,
126.535453054138));
#122383=CARTESIAN_POINT('Ctrl Pts',(-189.564849835736,2.33083048013107,
126.471499075371));
#122384=CARTESIAN_POINT('Ctrl Pts',(-189.572340171498,2.21345290716398,
126.412344077266));
#122385=CARTESIAN_POINT('Ctrl Pts',(-189.580114505617,2.0916249278412,126.350946199428));
#122386=CARTESIAN_POINT('Ctrl Pts',(-189.587888839736,1.96704741755451,
126.294523902565));
#122387=CARTESIAN_POINT('Ctrl Pts',(-189.595663173855,1.84016504283681,
126.243332698596));
#122388=CARTESIAN_POINT('Ctrl Pts',(-189.603427926802,1.7134390393065,126.192204583211));
#122389=CARTESIAN_POINT('Ctrl Pts',(-189.61119267975,1.58441418226004,126.146294878277));
#122390=CARTESIAN_POINT('Ctrl Pts',(-189.618957432697,1.45355965421348,
126.105813246927));
#122391=CARTESIAN_POINT('Ctrl Pts',(-189.626714473582,1.3228350927289,126.065371822503));
#122392=CARTESIAN_POINT('Ctrl Pts',(-189.634471514467,1.19028484774728,
126.030347857655));
#122393=CARTESIAN_POINT('Ctrl Pts',(-189.642228555352,1.0563976694256,126.000902797773));
#122394=CARTESIAN_POINT('Ctrl Pts',(-189.649979746592,0.922611456466401,
125.971479942639));
#122395=CARTESIAN_POINT('Ctrl Pts',(-189.657730937832,0.787490697206884,
125.94762770214));
#122396=CARTESIAN_POINT('Ctrl Pts',(-189.665482129072,0.651538534659585,
125.92945748003));
#122397=CARTESIAN_POINT('Ctrl Pts',(-189.673230025849,0.515644155408197,
125.91129498075));
#122398=CARTESIAN_POINT('Ctrl Pts',(-189.680977922626,0.378919462400322,
125.898809748275));
#122399=CARTESIAN_POINT('Ctrl Pts',(-189.688725819403,0.241876789339127,
125.892061900949));
#122400=CARTESIAN_POINT('Ctrl Pts',(-189.696472095488,0.104862782650838,
125.885315465126));
#122401=CARTESIAN_POINT('Ctrl Pts',(-189.704218371572,-0.0324686815449168,
125.884304046529));
#122402=CARTESIAN_POINT('Ctrl Pts',(-189.711964647656,-0.169601557973934,
125.889035768278));
#122403=CARTESIAN_POINT('Ctrl Pts',(-189.719710980921,-0.30673544668688,
125.893767524955));
#122404=CARTESIAN_POINT('Ctrl Pts',(-189.727457314187,-0.443670353975256,
125.904242493092));
#122405=CARTESIAN_POINT('Ctrl Pts',(-189.735203647452,-0.57989204686906,
125.92041669114));
#122406=CARTESIAN_POINT('Ctrl Pts',(-189.742951715455,-0.716144245666308,
125.936594511287));
#122407=CARTESIAN_POINT('Ctrl Pts',(-189.750699783458,-0.851682524082018,
125.958474054952));
#122408=CARTESIAN_POINT('Ctrl Pts',(-189.758447851461,-0.985999964604032,
125.985959728028));
#122409=CARTESIAN_POINT('Ctrl Pts',(-189.766204154203,-1.12046015930041,
126.013474613205));
#122410=CARTESIAN_POINT('Ctrl Pts',(-189.773960456944,-1.25369654052637,
126.046607451556));
#122411=CARTESIAN_POINT('Ctrl Pts',(-189.781716759686,-1.38521400480768,
126.085211835912));
#122412=CARTESIAN_POINT('Ctrl Pts',(-189.7894772022,-1.51680166391959,126.12383682459));
#122413=CARTESIAN_POINT('Ctrl Pts',(-189.797237644715,-1.64666820799493,
126.167939052618));
#122414=CARTESIAN_POINT('Ctrl Pts',(-189.804998087229,-1.77433675280554,
126.217323213081));
#122415=CARTESIAN_POINT('Ctrl Pts',(-189.812770987494,-1.90221024249816,
126.266786649383));
#122416=CARTESIAN_POINT('Ctrl Pts',(-189.82054388776,-2.02787832339203,
126.321548805643));
#122417=CARTESIAN_POINT('Ctrl Pts',(-189.828316788025,-2.1508862214266,
126.38136711486));
#122418=CARTESIAN_POINT('Ctrl Pts',(-189.835807123787,-2.26942247252908,
126.439010877864));
#122419=CARTESIAN_POINT('Ctrl Pts',(-189.843297459549,-2.38548832025277,
126.501349422499));
#122420=CARTESIAN_POINT('Ctrl Pts',(-189.850787795311,-2.49870254081068,
126.568127777524));
#122421=CARTESIAN_POINT('Ctrl Pts',(-189.858563333984,-2.61622751943143,
126.637448793101));
#122422=CARTESIAN_POINT('Ctrl Pts',(-189.866338872658,-2.73105175223908,
126.711774041575));
#122423=CARTESIAN_POINT('Ctrl Pts',(-189.874114411331,-2.84271970669593,
126.790867409441));
#122424=CARTESIAN_POINT('Ctrl Pts',(-189.882266520974,-2.95979576362285,
126.873791285713));
#122425=CARTESIAN_POINT('Ctrl Pts',(-189.890418630616,-3.07340178179484,
126.961956537243));
#122426=CARTESIAN_POINT('Ctrl Pts',(-189.898570740259,-3.18304092391845,
127.055036206534));
#122427=CARTESIAN_POINT('Ctrl Pts',(-189.906326693971,-3.28735209593799,
127.14359262176));
#122428=CARTESIAN_POINT('Ctrl Pts',(-189.914082647682,-3.38807246231964,
127.236596825632));
#122429=CARTESIAN_POINT('Ctrl Pts',(-189.921838601394,-3.48480374559348,
127.333722935929));
#122430=CARTESIAN_POINT('Ctrl Pts',(-189.929589286311,-3.58146931712576,
127.43078306627));
#122431=CARTESIAN_POINT('Ctrl Pts',(-189.937339971229,-3.67415092233515,
127.531959256202));
#122432=CARTESIAN_POINT('Ctrl Pts',(-189.945090656146,-3.7624847314623,
127.636886591151));
#122433=CARTESIAN_POINT('Ctrl Pts',(-189.952837754435,-3.8507776641283,
127.741765370987));
#122434=CARTESIAN_POINT('Ctrl Pts',(-189.960584852723,-3.93472655359425,
127.850391542837));
#122435=CARTESIAN_POINT('Ctrl Pts',(-189.968331951012,-4.01400597908118,
127.962365004902));
#122436=CARTESIAN_POINT('Ctrl Pts',(-189.976077142051,-4.09326588685833,
128.07431090035));
#122437=CARTESIAN_POINT('Ctrl Pts',(-189.983822333091,-4.1678583942436,
128.189602126264));
#122438=CARTESIAN_POINT('Ctrl Pts',(-189.99156752413,-4.23750000942929,
128.307807647452));
#122439=CARTESIAN_POINT('Ctrl Pts',(-189.999314507378,-4.30715773942337,
128.426040520954));
#122440=CARTESIAN_POINT('Ctrl Pts',(-190.007061490626,-4.37186208637682,
128.54718870223));
#122441=CARTESIAN_POINT('Ctrl Pts',(-190.014808473873,-4.43137434301563,
128.67079447269));
#122442=CARTESIAN_POINT('Ctrl Pts',(-190.022556509817,-4.49089468645619,
128.794417039275));
#122443=CARTESIAN_POINT('Ctrl Pts',(-190.030304545761,-4.54522137225773,
128.920497504471));
#122444=CARTESIAN_POINT('Ctrl Pts',(-190.038052581704,-4.59416325289056,
129.04855679359));
#122445=CARTESIAN_POINT('Ctrl Pts',(-190.045805933935,-4.64313871481742,
129.176703950126));
#122446=CARTESIAN_POINT('Ctrl Pts',(-190.053559286166,-4.68672186348919,
129.30683227332));
#122447=CARTESIAN_POINT('Ctrl Pts',(-190.061312638396,-4.72477092847605,
129.438446002399));
#122448=CARTESIAN_POINT('Ctrl Pts',(-190.064130106518,-4.73859746756062,
129.486272732696));
#122449=CARTESIAN_POINT('Ctrl Pts',(-190.066947574639,-4.75169371319282,
129.534295489064));
#122450=CARTESIAN_POINT('Ctrl Pts',(-190.06976504276,-4.76405452823418,
129.582490119309));
#122451=CARTESIAN_POINT('Origin',(213.235140564004,0.,130.804360617566));
#122452=CARTESIAN_POINT('',(-192.165295998532,-4.76405452823416,129.582490119309));
#122453=CARTESIAN_POINT('',(-191.820046567589,-4.76405452823394,129.582490119308));
#122454=CARTESIAN_POINT('',(213.235140564004,-4.76405452823405,129.582490119308));
#122455=CARTESIAN_POINT('',(-190.485140563957,-4.91824868249715,130.800760671037));
#122456=CARTESIAN_POINT('Ctrl Pts',(-190.485140564012,-4.91824868249786,
130.800760672006));
#122457=CARTESIAN_POINT('Ctrl Pts',(-190.492903044254,-4.9183493592558,
130.938305344235));
#122458=CARTESIAN_POINT('Ctrl Pts',(-190.500665524497,-4.91267582439302,
131.075902460375));
#122459=CARTESIAN_POINT('Ctrl Pts',(-190.508428004739,-4.90124163143306,
131.213033509752));
#122460=CARTESIAN_POINT('Ctrl Pts',(-190.516189892968,-4.88980831051287,
131.350154100696));
#122461=CARTESIAN_POINT('Ctrl Pts',(-190.523951781197,-4.87261523719499,
131.486808308646));
#122462=CARTESIAN_POINT('Ctrl Pts',(-190.531713669427,-4.8497279622425,
131.622481485619));
#122463=CARTESIAN_POINT('Ctrl Pts',(-190.539476617656,-4.8268375616964,
131.758173190757));
#122464=CARTESIAN_POINT('Ctrl Pts',(-190.547239565885,-4.7982514760145,
131.892883215297));
#122465=CARTESIAN_POINT('Ctrl Pts',(-190.555002514114,-4.76408655954542,
132.026106219424));
#122466=CARTESIAN_POINT('Ctrl Pts',(-190.562768174686,-4.72990970599202,
132.159375771132));
#122467=CARTESIAN_POINT('Ctrl Pts',(-190.570533835258,-4.69015023823709,
132.291156892345));
#122468=CARTESIAN_POINT('Ctrl Pts',(-190.57829949583,-4.64497503635937,
132.420958889895));
#122469=CARTESIAN_POINT('Ctrl Pts',(-190.586074494797,-4.59974551020291,
132.550916977504));
#122470=CARTESIAN_POINT('Ctrl Pts',(-190.593849493765,-4.54908737022984,
132.678890820855));
#122471=CARTESIAN_POINT('Ctrl Pts',(-190.601624492733,-4.49321610342936,
132.804408644585));
#122472=CARTESIAN_POINT('Ctrl Pts',(-190.609404441072,-4.4373092703673,
132.930006369846));
#122473=CARTESIAN_POINT('Ctrl Pts',(-190.617184389411,-4.37618287100597,
133.053144613246));
#122474=CARTESIAN_POINT('Ctrl Pts',(-190.62496433775,-4.31009818111834,
133.173376601391));
#122475=CARTESIAN_POINT('Ctrl Pts',(-190.632757105409,-4.24390460094357,
133.293806700412));
#122476=CARTESIAN_POINT('Ctrl Pts',(-190.640549873068,-4.17273660894555,
133.411320645231));
#122477=CARTESIAN_POINT('Ctrl Pts',(-190.648342640727,-4.09689905135302,
133.52550030996));
#122478=CARTESIAN_POINT('Ctrl Pts',(-190.654408984015,-4.0378626885938,
133.614384397484));
#122479=CARTESIAN_POINT('Ctrl Pts',(-190.660475327302,-3.97599746982579,
133.701248499452));
#122480=CARTESIAN_POINT('Ctrl Pts',(-190.66654167059,-3.91146342789147,
133.78591003268));
#122481=CARTESIAN_POINT('Ctrl Pts',(-190.674316004709,-3.82875970007991,
133.894408186373));
#122482=CARTESIAN_POINT('Ctrl Pts',(-190.682090338828,-3.74140718917245,
133.999634468692));
#122483=CARTESIAN_POINT('Ctrl Pts',(-190.689864672947,-3.64969402101185,
134.101164617729));
#122484=CARTESIAN_POINT('Ctrl Pts',(-190.697629425894,-3.55809388113412,
134.202569639932));
#122485=CARTESIAN_POINT('Ctrl Pts',(-190.705394178841,-3.46214403645708,
134.300287304914));
#122486=CARTESIAN_POINT('Ctrl Pts',(-190.713158931788,-3.36217471257771,
134.393923859049));
#122487=CARTESIAN_POINT('Ctrl Pts',(-190.720915972673,-3.26230467964042,
134.487467412037));
#122488=CARTESIAN_POINT('Ctrl Pts',(-190.728673013558,-3.15842339566355,
134.576937655122));
#122489=CARTESIAN_POINT('Ctrl Pts',(-190.736430054443,-3.05089977217039,
134.661975637584));
#122490=CARTESIAN_POINT('Ctrl Pts',(-190.744181245683,-2.94345723307797,
134.746949492243));
#122491=CARTESIAN_POINT('Ctrl Pts',(-190.751932436923,-2.83237812705361,
134.827497497584));
#122492=CARTESIAN_POINT('Ctrl Pts',(-190.759683628163,-2.7180661956855,
134.903299409299));
#122493=CARTESIAN_POINT('Ctrl Pts',(-190.76743152494,-2.60380284993743,
134.979069103179));
#122494=CARTESIAN_POINT('Ctrl Pts',(-190.775179421717,-2.48630973685419,
135.050096499908));
#122495=CARTESIAN_POINT('Ctrl Pts',(-190.782927318495,-2.36602129387989,
135.116103455376));
#122496=CARTESIAN_POINT('Ctrl Pts',(-190.790673594579,-2.24575801265473,
135.182096603612));
#122497=CARTESIAN_POINT('Ctrl Pts',(-190.798419870663,-2.12270090711924,
135.243071211466));
#122498=CARTESIAN_POINT('Ctrl Pts',(-190.806166146747,-1.99731049376025,
135.298794269765));
#122499=CARTESIAN_POINT('Ctrl Pts',(-190.813912480012,-1.87191915479789,
135.354517739398));
#122500=CARTESIAN_POINT('Ctrl Pts',(-190.821658813278,-1.74419483091776,
135.404989423349));
#122501=CARTESIAN_POINT('Ctrl Pts',(-190.829405146543,-1.61461919800756,
135.450023961796));
#122502=CARTESIAN_POINT('Ctrl Pts',(-190.837153214546,-1.4850145475326,
135.495068585417));
#122503=CARTESIAN_POINT('Ctrl Pts',(-190.844901282549,-1.35355813227166,
135.534673512303));
#122504=CARTESIAN_POINT('Ctrl Pts',(-190.852649350552,-1.22074762339899,
135.56870299637));
#122505=CARTESIAN_POINT('Ctrl Pts',(-190.860405653294,-1.0877959619372,
135.602768647377));
#122506=CARTESIAN_POINT('Ctrl Pts',(-190.868161956036,-0.953487711347482,
135.631246921252));
#122507=CARTESIAN_POINT('Ctrl Pts',(-190.875918258778,-0.818332142929902,
135.654052934234));
#122508=CARTESIAN_POINT('Ctrl Pts',(-190.883678701292,-0.683104437916002,
135.676871119472));
#122509=CARTESIAN_POINT('Ctrl Pts',(-190.891439143806,-0.54702890166007,
135.694010962518));
#122510=CARTESIAN_POINT('Ctrl Pts',(-190.89919958632,-0.410619808675805,
135.705439522789));
#122511=CARTESIAN_POINT('Ctrl Pts',(-190.906972486586,-0.273991739705651,
135.7168864292));
#122512=CARTESIAN_POINT('Ctrl Pts',(-190.914745386851,-0.137029434847546,
135.722603715419));
#122513=CARTESIAN_POINT('Ctrl Pts',(-190.922518287116,-0.00024795565964834,
135.722610611316));
#122514=CARTESIAN_POINT('Ctrl Pts',(-190.930008622879,0.131561172230973,
135.722617256529));
#122515=CARTESIAN_POINT('Ctrl Pts',(-190.937498958641,0.263202085368852,
135.717321489911));
#122516=CARTESIAN_POINT('Ctrl Pts',(-190.944989294403,0.394220439225914,
135.706785865114));
#122517=CARTESIAN_POINT('Ctrl Pts',(-190.952763628522,0.530206393788766,
135.695850778901));
#122518=CARTESIAN_POINT('Ctrl Pts',(-190.960537962641,0.665952411115588,
135.67923601341));
#122519=CARTESIAN_POINT('Ctrl Pts',(-190.96831229676,0.800945808593782,
135.656954653151));
#122520=CARTESIAN_POINT('Ctrl Pts',(-190.976077049707,0.935772838774291,
135.634700752677));
#122521=CARTESIAN_POINT('Ctrl Pts',(-190.983841802654,1.06984871258484,
135.606794215719));
#122522=CARTESIAN_POINT('Ctrl Pts',(-190.991606555601,1.20266365894648,
135.57330003697));
#122523=CARTESIAN_POINT('Ctrl Pts',(-190.999363596486,1.33534669163104,
135.539839125113));
#122524=CARTESIAN_POINT('Ctrl Pts',(-191.007120637371,1.46677091249836,
135.500801710651));
#122525=CARTESIAN_POINT('Ctrl Pts',(-191.014877678256,1.59643492045341,
135.456304147668));
#122526=CARTESIAN_POINT('Ctrl Pts',(-191.022628869497,1.7260011477716,135.411840140643));
#122527=CARTESIAN_POINT('Ctrl Pts',(-191.030380060737,1.85380943596783,
135.361924307202));
#122528=CARTESIAN_POINT('Ctrl Pts',(-191.038131251977,1.97937212224398,
135.306723226706));
#122529=CARTESIAN_POINT('Ctrl Pts',(-191.045879148754,2.10488144102913,
135.251545608142));
#122530=CARTESIAN_POINT('Ctrl Pts',(-191.053627045531,2.22814669904816,
135.191087367399));
#122531=CARTESIAN_POINT('Ctrl Pts',(-191.061374942308,2.34869906173386,
135.125563665319));
#122532=CARTESIAN_POINT('Ctrl Pts',(-191.069121218392,2.46922620746376,
135.060053669385));
#122533=CARTESIAN_POINT('Ctrl Pts',(-191.076867494477,2.58704124332095,
134.989480506272));
#122534=CARTESIAN_POINT('Ctrl Pts',(-191.084613770561,2.70169921167772,
134.914105674394));
#122535=CARTESIAN_POINT('Ctrl Pts',(-191.092360103826,2.81635802641402,
134.838730286115));
#122536=CARTESIAN_POINT('Ctrl Pts',(-191.100106437091,2.927859400452,134.758553373108));
#122537=CARTESIAN_POINT('Ctrl Pts',(-191.107852770357,3.03578702774157,
134.673879991428));
#122538=CARTESIAN_POINT('Ctrl Pts',(-191.11560083836,3.14373882467452,134.589187647732));
#122539=CARTESIAN_POINT('Ctrl Pts',(-191.123348906363,3.24811497478342,
134.49999707292));
#122540=CARTESIAN_POINT('Ctrl Pts',(-191.131096974365,3.34853226761644,
134.406653597771));
#122541=CARTESIAN_POINT('Ctrl Pts',(-191.138853277107,3.44905628514341,
134.313210916065));
#122542=CARTESIAN_POINT('Ctrl Pts',(-191.146609579849,3.54561275360605,
134.215606783686));
#122543=CARTESIAN_POINT('Ctrl Pts',(-191.154365882591,3.63785498431555,
134.114223783256));
#122544=CARTESIAN_POINT('Ctrl Pts',(-191.162126325105,3.73014644748118,
134.012786671666));
#122545=CARTESIAN_POINT('Ctrl Pts',(-191.16988676762,3.81811883403782,133.907566972984));
#122546=CARTESIAN_POINT('Ctrl Pts',(-191.177647210134,3.9014664522032,133.798979555734));
#122547=CARTESIAN_POINT('Ctrl Pts',(-191.185420110399,3.98494786736428,
133.690217824322));
#122548=CARTESIAN_POINT('Ctrl Pts',(-191.193193010664,4.06378945344856,
133.578077891125));
#122549=CARTESIAN_POINT('Ctrl Pts',(-191.20096591093,4.1377289857357,133.463003486231));
#122550=CARTESIAN_POINT('Ctrl Pts',(-191.208456246692,4.20898062978117,
133.352112325811));
#122551=CARTESIAN_POINT('Ctrl Pts',(-191.215946582454,4.27568028039896,
133.238496606114));
#122552=CARTESIAN_POINT('Ctrl Pts',(-191.223436918216,4.33763498143187,
133.122572391835));
#122553=CARTESIAN_POINT('Ctrl Pts',(-191.231211252335,4.40193871378563,
133.002252875736));
#122554=CARTESIAN_POINT('Ctrl Pts',(-191.238985586454,4.46133427916974,
132.879065220246));
#122555=CARTESIAN_POINT('Ctrl Pts',(-191.246759920573,4.51555556847681,
132.753447832264));
#122556=CARTESIAN_POINT('Ctrl Pts',(-191.25452467352,4.56971003489071,132.627985256485));
#122557=CARTESIAN_POINT('Ctrl Pts',(-191.262289426467,4.61870275977333,
132.500099261741));
#122558=CARTESIAN_POINT('Ctrl Pts',(-191.270054179414,4.66231288128167,
132.370253864098));
#122559=CARTESIAN_POINT('Ctrl Pts',(-191.277811220299,4.70587968860265,
132.240537430734));
#122560=CARTESIAN_POINT('Ctrl Pts',(-191.285568261184,4.74407440781323,
132.108865835533));
#122561=CARTESIAN_POINT('Ctrl Pts',(-191.293325302069,4.77672391135812,
131.975723813658));
#122562=CARTESIAN_POINT('Ctrl Pts',(-191.301076493309,4.80934879365846,
131.842682195218));
#122563=CARTESIAN_POINT('Ctrl Pts',(-191.30882768455,4.83643669095588,131.708172735403));
#122564=CARTESIAN_POINT('Ctrl Pts',(-191.31657887579,4.85786415753015,131.572695758949));
#122565=CARTESIAN_POINT('Ctrl Pts',(-191.324326772567,4.87928251685945,
131.437276363824));
#122566=CARTESIAN_POINT('Ctrl Pts',(-191.332074669344,4.89504516953697,
131.300890655304));
#122567=CARTESIAN_POINT('Ctrl Pts',(-191.339822566121,4.9050797199358,131.164049376877));
#122568=CARTESIAN_POINT('Ctrl Pts',(-191.347568842205,4.91511217132304,
131.027236722695));
#122569=CARTESIAN_POINT('Ctrl Pts',(-191.355315118289,4.91941887513359,
130.889969077825));
#122570=CARTESIAN_POINT('Ctrl Pts',(-191.363061394373,4.91797932692134,
130.752762144001));
#122571=CARTESIAN_POINT('Ctrl Pts',(-191.370807727638,4.91653976808269,
130.615554197346));
#122572=CARTESIAN_POINT('Ctrl Pts',(-191.378554060904,4.90935387668189,
130.478407353576));
#122573=CARTESIAN_POINT('Ctrl Pts',(-191.386300394169,4.89645328142879,
130.341836753008));
#122574=CARTESIAN_POINT('Ctrl Pts',(-191.394048462172,4.88354979717682,
130.205235568402));
#122575=CARTESIAN_POINT('Ctrl Pts',(-191.401796530175,4.86492909924203,
130.069211272942));
#122576=CARTESIAN_POINT('Ctrl Pts',(-191.409544598178,4.84067458957936,
129.934272932157));
#122577=CARTESIAN_POINT('Ctrl Pts',(-191.41730090092,4.81639430193517,129.799191177297));
#122578=CARTESIAN_POINT('Ctrl Pts',(-191.425057203662,4.78646831079896,
129.665198068094));
#122579=CARTESIAN_POINT('Ctrl Pts',(-191.432813506404,4.75103110006152,
129.532792078812));
#122580=CARTESIAN_POINT('Ctrl Pts',(-191.440573948918,4.71557497541762,
129.400315420467));
#122581=CARTESIAN_POINT('Ctrl Pts',(-191.448334391432,4.67460188671874,
129.269427942878));
#122582=CARTESIAN_POINT('Ctrl Pts',(-191.456094833946,4.6282956407281,129.14061107977));
#122583=CARTESIAN_POINT('Ctrl Pts',(-191.463867734212,4.58191505984064,
129.011587428397));
#122584=CARTESIAN_POINT('Ctrl Pts',(-191.471640634477,4.53018436116495,
128.884641396051));
#122585=CARTESIAN_POINT('Ctrl Pts',(-191.479413534742,4.47333512852615,
128.760233446768));
#122586=CARTESIAN_POINT('Ctrl Pts',(-191.486903870504,4.41855250868881,
128.640348039807));
#122587=CARTESIAN_POINT('Ctrl Pts',(-191.494394206266,4.35901717633166,
128.522819662996));
#122588=CARTESIAN_POINT('Ctrl Pts',(-191.501884542028,4.29497488095036,
128.408035548944));
#122589=CARTESIAN_POINT('Ctrl Pts',(-191.509658876147,4.22850440247415,
128.28889936032));
#122590=CARTESIAN_POINT('Ctrl Pts',(-191.517433210267,4.15696789296251,
128.172342252175));
#122591=CARTESIAN_POINT('Ctrl Pts',(-191.525207544386,4.08059035808282,
128.058825079275));
#122592=CARTESIAN_POINT('Ctrl Pts',(-191.532972297333,4.0043069516886,127.945447806144));
#122593=CARTESIAN_POINT('Ctrl Pts',(-191.54073705028,3.92319460690395,127.835103335206));
#122594=CARTESIAN_POINT('Ctrl Pts',(-191.548501803227,3.83752433236579,
127.728228295802));
#122595=CARTESIAN_POINT('Ctrl Pts',(-191.556258844112,3.75193914675227,
127.621459406194));
#122596=CARTESIAN_POINT('Ctrl Pts',(-191.564015884997,3.6618052832676,127.518153393728));
#122597=CARTESIAN_POINT('Ctrl Pts',(-191.571772925882,3.5674369836618,127.418717926717));
#122598=CARTESIAN_POINT('Ctrl Pts',(-191.579524117122,3.47313984792494,
127.319357444764));
#122599=CARTESIAN_POINT('Ctrl Pts',(-191.587275308362,3.37461490002521,
127.223861980993));
#122600=CARTESIAN_POINT('Ctrl Pts',(-191.595026499602,3.27221635190649,
127.132605831525));
#122601=CARTESIAN_POINT('Ctrl Pts',(-191.602774396379,3.16986132590188,
127.041388468354));
#122602=CARTESIAN_POINT('Ctrl Pts',(-191.610522293156,3.06363626547616,
126.954407095373));
#122603=CARTESIAN_POINT('Ctrl Pts',(-191.618270189933,2.95393174198714,
126.871998690406));
#122604=CARTESIAN_POINT('Ctrl Pts',(-191.626016466018,2.84425016631949,
126.789607523499));
#122605=CARTESIAN_POINT('Ctrl Pts',(-191.633762742102,2.73109088767587,
126.711787656611));
#122606=CARTESIAN_POINT('Ctrl Pts',(-191.641509018186,2.61487669737603,
126.638835090094));
#122607=CARTESIAN_POINT('Ctrl Pts',(-191.649255351451,2.49866164920991,
126.565881985059));
#122608=CARTESIAN_POINT('Ctrl Pts',(-191.657001684716,2.37939197551846,
126.497796459953));
#122609=CARTESIAN_POINT('Ctrl Pts',(-191.664748017982,2.25751817453226,
126.434830350574));
#122610=CARTESIAN_POINT('Ctrl Pts',(-191.672496085985,2.1356170807535,126.371850140372));
#122611=CARTESIAN_POINT('Ctrl Pts',(-191.680244153988,2.01111104650626,
126.313991806636));
#122612=CARTESIAN_POINT('Ctrl Pts',(-191.687992221991,1.88447344383008,
126.261460343292));
#122613=CARTESIAN_POINT('Ctrl Pts',(-191.695748524732,1.75770124920225,
126.208873048883));
#122614=CARTESIAN_POINT('Ctrl Pts',(-191.703504827474,1.62879332235594,
126.161624084286));
#122615=CARTESIAN_POINT('Ctrl Pts',(-191.711261130216,1.49824173563579,
126.119869741911));
#122616=CARTESIAN_POINT('Ctrl Pts',(-191.71902157273,1.36762046960263,126.078093113985));
#122617=CARTESIAN_POINT('Ctrl Pts',(-191.726782015244,1.23535417251634,
126.041817055184));
#122618=CARTESIAN_POINT('Ctrl Pts',(-191.734542457759,1.10194724024969,
126.01114715036));
#122619=CARTESIAN_POINT('Ctrl Pts',(-191.742315358024,0.968326151332061,
125.980428011482));
#122620=CARTESIAN_POINT('Ctrl Pts',(-191.750088258289,0.833561152794384,
125.955333082055));
#122621=CARTESIAN_POINT('Ctrl Pts',(-191.757861158555,0.698164822785404,
125.935916416106));
#122622=CARTESIAN_POINT('Ctrl Pts',(-191.765351494317,0.567690490411714,
125.917205594873));
#122623=CARTESIAN_POINT('Ctrl Pts',(-191.772841830079,0.436630237048816,
125.903767397656));
#122624=CARTESIAN_POINT('Ctrl Pts',(-191.780332165842,0.305442686064309,
125.895604377129));
#122625=CARTESIAN_POINT('Ctrl Pts',(-191.788106499961,0.169281119213901,
125.887131853198));
#122626=CARTESIAN_POINT('Ctrl Pts',(-191.79588083408,0.0325510922944527,
125.884315580651));
#122627=CARTESIAN_POINT('Ctrl Pts',(-191.803655168199,-0.104238043468105,
125.887215359106));
#122628=CARTESIAN_POINT('Ctrl Pts',(-191.811419921146,-0.240858598845289,
125.890111563843));
#122629=CARTESIAN_POINT('Ctrl Pts',(-191.819184674093,-0.377537730998018,
125.898709794876));
#122630=CARTESIAN_POINT('Ctrl Pts',(-191.82694942704,-0.513761604507242,
125.913018053787));
#122631=CARTESIAN_POINT('Ctrl Pts',(-191.834706467925,-0.649850178545986,
125.927312101534));
#122632=CARTESIAN_POINT('Ctrl Pts',(-191.84246350881,-0.785484007468369,
125.94730485048));
#122633=CARTESIAN_POINT('Ctrl Pts',(-191.850220549695,-0.920150253035749,
125.972952274822));
#122634=CARTESIAN_POINT('Ctrl Pts',(-191.857971740935,-1.05471494573815,
125.998580358241));
#122635=CARTESIAN_POINT('Ctrl Pts',(-191.865722932175,-1.18831312492588,
126.029854556506));
#122636=CARTESIAN_POINT('Ctrl Pts',(-191.873474123415,-1.32043842446319,
126.066679177273));
#122637=CARTESIAN_POINT('Ctrl Pts',(-191.881222020193,-1.4525075672249,
126.103488146594));
#122638=CARTESIAN_POINT('Ctrl Pts',(-191.88896991697,-1.58310469960573,
126.145842741646));
#122639=CARTESIAN_POINT('Ctrl Pts',(-191.896717813747,-1.71173519926051,
126.193596508428));
#122640=CARTESIAN_POINT('Ctrl Pts',(-191.904464089831,-1.84033879218771,
126.241340286152));
#122641=CARTESIAN_POINT('Ctrl Pts',(-191.912210365915,-1.96697620435051,
126.294480853203));
#122642=CARTESIAN_POINT('Ctrl Pts',(-191.919956641999,-2.09116987323163,
126.352822498692));
#122643=CARTESIAN_POINT('Ctrl Pts',(-191.927702975264,-2.21536445888204,
126.411164574845));
#122644=CARTESIAN_POINT('Ctrl Pts',(-191.93544930853,-2.33711491138994,
126.474707639814));
#122645=CARTESIAN_POINT('Ctrl Pts',(-191.943195641795,-2.45596584886988,
126.543208800078));
#122646=CARTESIAN_POINT('Ctrl Pts',(-191.950943709798,-2.57484340219369,
126.611725300701));
#122647=CARTESIAN_POINT('Ctrl Pts',(-191.958691777801,-2.69081980973953,
126.685201910856));
#122648=CARTESIAN_POINT('Ctrl Pts',(-191.966439845804,-2.80346673516209,
126.763351173462));
#122649=CARTESIAN_POINT('Ctrl Pts',(-191.974196148546,-2.91623338307735,
126.841583494034));
#122650=CARTESIAN_POINT('Ctrl Pts',(-191.981952451288,-3.02566315836508,
126.924498164268));
#122651=CARTESIAN_POINT('Ctrl Pts',(-191.98970875403,-3.13135859067244,
127.011765669628));
#122652=CARTESIAN_POINT('Ctrl Pts',(-191.997469196544,-3.23711043581445,
127.099079752284));
#122653=CARTESIAN_POINT('Ctrl Pts',(-192.005229639058,-3.33912367583414,
127.190751038126));
#122654=CARTESIAN_POINT('Ctrl Pts',(-192.012990081572,-3.43703684091518,
127.286412235811));
#122655=CARTESIAN_POINT('Ctrl Pts',(-192.020762981838,-3.53510718490086,
127.382226997343));
#122656=CARTESIAN_POINT('Ctrl Pts',(-192.028535882103,-3.62906403328069,
127.482044185023));
#122657=CARTESIAN_POINT('Ctrl Pts',(-192.036308782368,-3.71858484786014,
127.58546176986));
#122658=CARTESIAN_POINT('Ctrl Pts',(-192.04379911813,-3.80485135533908,
127.685119864993));
#122659=CARTESIAN_POINT('Ctrl Pts',(-192.051289453892,-3.88699855951138,
127.78812089412));
#122660=CARTESIAN_POINT('Ctrl Pts',(-192.058779789654,-3.9647764156074,
127.894080384196));
#122661=CARTESIAN_POINT('Ctrl Pts',(-192.066605571333,-4.04603746191827,
128.004785145967));
#122662=CARTESIAN_POINT('Ctrl Pts',(-192.074431353011,-4.12278666815336,
128.119070688909));
#122663=CARTESIAN_POINT('Ctrl Pts',(-192.08225713469,-4.19469433982913,
128.236536157463));
#122664=CARTESIAN_POINT('Ctrl Pts',(-192.090069792819,-4.26648142497111,
128.353804640724));
#122665=CARTESIAN_POINT('Ctrl Pts',(-192.097882450948,-4.33344294894402,
128.474242102797));
#122666=CARTESIAN_POINT('Ctrl Pts',(-192.105695109077,-4.3952906467389,
128.597416306264));
#122667=CARTESIAN_POINT('Ctrl Pts',(-192.113500201717,-4.4570784535094,
128.720471232385));
#122668=CARTESIAN_POINT('Ctrl Pts',(-192.121305294356,-4.51376211373051,
128.846257287088));
#122669=CARTESIAN_POINT('Ctrl Pts',(-192.129110386996,-4.5650974649776,
128.974314662472));
#122670=CARTESIAN_POINT('Ctrl Pts',(-192.136908171869,-4.61638475186583,
129.102252140057));
#122671=CARTESIAN_POINT('Ctrl Pts',(-192.144705956742,-4.66233355954381,
129.232456348203));
#122672=CARTESIAN_POINT('Ctrl Pts',(-192.152503741615,-4.70274661817135,
129.364444888164));
#122673=CARTESIAN_POINT('Ctrl Pts',(-192.156767827254,-4.72484580989491,
129.436620569713));
#122674=CARTESIAN_POINT('Ctrl Pts',(-192.161031912893,-4.7452904916293,
129.50932942537));
#122675=CARTESIAN_POINT('Ctrl Pts',(-192.165295998532,-4.76405452823416,
129.582490119309));
#122676=CARTESIAN_POINT('Ctrl Pts',(-190.415359814329,-4.76405452823405,
129.582490119308));
#122677=CARTESIAN_POINT('Ctrl Pts',(-190.424329050674,-4.80323055054687,
129.735236835727));
#122678=CARTESIAN_POINT('Ctrl Pts',(-190.433298287018,-4.83509936457335,
129.890036533855));
#122679=CARTESIAN_POINT('Ctrl Pts',(-190.442267523362,-4.85946771299443,
130.04623357751));
#122680=CARTESIAN_POINT('Ctrl Pts',(-190.451168803988,-4.88365143381179,
130.201247189058));
#122681=CARTESIAN_POINT('Ctrl Pts',(-190.460070084614,-4.9004478339706,
130.357636916376));
#122682=CARTESIAN_POINT('Ctrl Pts',(-190.46897136524,-4.90971529438901,
130.51474226431));
#122683=CARTESIAN_POINT('Ctrl Pts',(-190.474361098146,-4.9153267494672,
130.609869684625));
#122684=CARTESIAN_POINT('Ctrl Pts',(-190.479750831051,-4.9181787794553,
130.705259101589));
#122685=CARTESIAN_POINT('Ctrl Pts',(-190.485140563957,-4.91824868249715,
130.800760671037));
#122686=CARTESIAN_POINT('',(-190.13985943604,-4.91824986400714,130.803204030469));
#122687=CARTESIAN_POINT('Ctrl Pts',(-190.06976504276,-4.76405452823418,
129.582490119309));
#122688=CARTESIAN_POINT('Ctrl Pts',(-190.077527632497,-4.79811061399697,
129.715274280825));
#122689=CARTESIAN_POINT('Ctrl Pts',(-190.085290222234,-4.82658033576797,
129.849363494492));
#122690=CARTESIAN_POINT('Ctrl Pts',(-190.093052811971,-4.84939154448578,
129.984247996782));
#122691=CARTESIAN_POINT('Ctrl Pts',(-190.100826943755,-4.87223667075837,
130.119333056286));
#122692=CARTESIAN_POINT('Ctrl Pts',(-190.10860107554,-4.88940643253583,
130.255215378942));
#122693=CARTESIAN_POINT('Ctrl Pts',(-190.116375207325,-4.90088061235472,
130.391380852994));
#122694=CARTESIAN_POINT('Ctrl Pts',(-190.120661944591,-4.90720759465933,
130.466463914131));
#122695=CARTESIAN_POINT('Ctrl Pts',(-190.124948681858,-4.91180373898945,
130.541633066273));
#122696=CARTESIAN_POINT('Ctrl Pts',(-190.129235419125,-4.91467242218679,
130.616802506313));
#122697=CARTESIAN_POINT('Ctrl Pts',(-190.132776758081,-4.91704228507516,
130.678901125798));
#122698=CARTESIAN_POINT('Ctrl Pts',(-190.136318097038,-4.91823524652186,
130.741044945587));
#122699=CARTESIAN_POINT('Ctrl Pts',(-190.139859435995,-4.91824986400696,
130.803204029673));
#122700=CARTESIAN_POINT('Ctrl Pts',(-190.13985943604,-4.91824986400714,
130.803204030469));
#122701=CARTESIAN_POINT('Ctrl Pts',(-190.147585601233,-4.91828175505972,
130.938816960416));
#122702=CARTESIAN_POINT('Ctrl Pts',(-190.155311766426,-4.91270043226599,
131.074655996844));
#122703=CARTESIAN_POINT('Ctrl Pts',(-190.163037931618,-4.90147587807679,
131.210214383264));
#122704=CARTESIAN_POINT('Ctrl Pts',(-190.170754697744,-4.89026497882958,
131.345607859624));
#122705=CARTESIAN_POINT('Ctrl Pts',(-190.178471463869,-4.87342453696202,
131.48072097409));
#122706=CARTESIAN_POINT('Ctrl Pts',(-190.186188229995,-4.85097651155595,
131.615045480403));
#122707=CARTESIAN_POINT('Ctrl Pts',(-190.193897512807,-4.82855025506256,
131.749239725884));
#122708=CARTESIAN_POINT('Ctrl Pts',(-190.201606795619,-4.80052729930736,
131.882646496431));
#122709=CARTESIAN_POINT('Ctrl Pts',(-190.209316078432,-4.76698148662643,
132.014761612551));
#122710=CARTESIAN_POINT('Ctrl Pts',(-190.217019786611,-4.73345993114099,
132.14678119537));
#122711=CARTESIAN_POINT('Ctrl Pts',(-190.224723494791,-4.69442356335619,
132.277510599873));
#122712=CARTESIAN_POINT('Ctrl Pts',(-190.232427202971,-4.6499974110266,
132.406455227739));
#122713=CARTESIAN_POINT('Ctrl Pts',(-190.240128016859,-4.60558794964859,
132.535351410974));
#122714=CARTESIAN_POINT('Ctrl Pts',(-190.247828830748,-4.55579285811654,
132.662463776619));
#122715=CARTESIAN_POINT('Ctrl Pts',(-190.255529644636,-4.50078711110052,
132.787312569342));
#122716=CARTESIAN_POINT('Ctrl Pts',(-190.263229171694,-4.44579055572119,
132.912140499431));
#122717=CARTESIAN_POINT('Ctrl Pts',(-190.270928698752,-4.38558523610426,
133.034705246309));
#122718=CARTESIAN_POINT('Ctrl Pts',(-190.27862822581,-4.32039420672799,
133.1545471976));
#122719=CARTESIAN_POINT('Ctrl Pts',(-190.286328185659,-4.25519951295482,
133.274395885223));
#122720=CARTESIAN_POINT('Ctrl Pts',(-190.294028145508,-4.18501874133744,
133.391521124698));
#122721=CARTESIAN_POINT('Ctrl Pts',(-190.301728105358,-4.1101205931154,
133.505488488021));
#122722=CARTESIAN_POINT('Ctrl Pts',(-190.309430217604,-4.03520150834462,
133.619487709051));
#122723=CARTESIAN_POINT('Ctrl Pts',(-190.317132329851,-3.95556264143853,
133.73032696698));
#122724=CARTESIAN_POINT('Ctrl Pts',(-190.324834442098,-3.87151536636673,
133.837601760384));
#122725=CARTESIAN_POINT('Ctrl Pts',(-190.332544856977,-3.78737749100206,
133.944992192609));
#122726=CARTESIAN_POINT('Ctrl Pts',(-190.340255271856,-3.69882196354237,
134.048810176041));
#122727=CARTESIAN_POINT('Ctrl Pts',(-190.347965686736,-3.60619996799212,
134.148684892117));
#122728=CARTESIAN_POINT('Ctrl Pts',(-190.3556806963,-3.51352277841163,134.248619124166));
#122729=CARTESIAN_POINT('Ctrl Pts',(-190.363395705863,-3.41677457553636,
134.344605130585));
#122730=CARTESIAN_POINT('Ctrl Pts',(-190.371110715427,-3.31634172458628,
134.43631059358));
#122731=CARTESIAN_POINT('Ctrl Pts',(-190.378837231148,-3.21575908819369,
134.528152826001));
#122732=CARTESIAN_POINT('Ctrl Pts',(-190.386563746869,-3.11148113317161,
134.615701512883));
#122733=CARTESIAN_POINT('Ctrl Pts',(-190.394290262589,-3.00392586603647,
134.698665748633));
#122734=CARTESIAN_POINT('Ctrl Pts',(-190.398754522705,-2.94178211240861,
134.746601188372));
#122735=CARTESIAN_POINT('Ctrl Pts',(-190.403218782821,-2.87854480706385,
134.793006993218));
#122736=CARTESIAN_POINT('Ctrl Pts',(-190.407683042937,-2.81429844266184,
134.837833976612));
#122737=CARTESIAN_POINT('Ctrl Pts',(-190.415457377056,-2.70241591570069,
134.915898412238));
#122738=CARTESIAN_POINT('Ctrl Pts',(-190.423231711176,-2.58710562699183,
134.989427787118));
#122739=CARTESIAN_POINT('Ctrl Pts',(-190.431006045295,-2.46877148506654,
135.058106075045));
#122740=CARTESIAN_POINT('Ctrl Pts',(-190.438770798242,-2.35058317939566,
135.126699723119));
#122741=CARTESIAN_POINT('Ctrl Pts',(-190.446535551189,-2.2293787702848,
135.19045398537));
#122742=CARTESIAN_POINT('Ctrl Pts',(-190.454300304136,-2.1055929402831,
135.249094741485));
#122743=CARTESIAN_POINT('Ctrl Pts',(-190.462057345021,-1.98193005611249,
135.307677254775));
#122744=CARTESIAN_POINT('Ctrl Pts',(-190.469814385906,-1.85569120437271,
135.361156202688));
#122745=CARTESIAN_POINT('Ctrl Pts',(-190.477571426791,-1.72733727952841,
135.409302417986));
#122746=CARTESIAN_POINT('Ctrl Pts',(-190.485322618031,-1.59908014737782,
135.457412325848));
#122747=CARTESIAN_POINT('Ctrl Pts',(-190.493073809271,-1.46871148143803,
135.500197368803));
#122748=CARTESIAN_POINT('Ctrl Pts',(-190.500825000511,-1.3367135244881,
135.537475872443));
#122749=CARTESIAN_POINT('Ctrl Pts',(-190.508572897288,-1.2047716701905,
135.574738531725));
#122750=CARTESIAN_POINT('Ctrl Pts',(-190.516320794066,-1.07120227765744,
135.606499200586));
#122751=CARTESIAN_POINT('Ctrl Pts',(-190.524068690843,-0.9365039649583,
135.632625666848));
#122752=CARTESIAN_POINT('Ctrl Pts',(-190.531814966927,-0.80183382824242,
135.658746668017));
#122753=CARTESIAN_POINT('Ctrl Pts',(-190.539561243011,-0.666035624636225,
135.679235736398));
#122754=CARTESIAN_POINT('Ctrl Pts',(-190.547307519095,-0.529619024550856,
135.69401160218));
#122755=CARTESIAN_POINT('Ctrl Pts',(-190.55505385236,-0.39320141746932,
135.708787577034));
#122756=CARTESIAN_POINT('Ctrl Pts',(-190.562800185626,-0.25616579349155,
135.717850223034));
#122757=CARTESIAN_POINT('Ctrl Pts',(-190.570546518891,-0.119027422925699,
135.721170104936));
#122758=CARTESIAN_POINT('Ctrl Pts',(-190.578294586894,0.0181416588272017,
135.724490730303));
#122759=CARTESIAN_POINT('Ctrl Pts',(-190.586042654897,0.155413142178313,
135.722066023016));
#122760=CARTESIAN_POINT('Ctrl Pts',(-190.5937907229,0.292271674219316,135.713918676185));
#122761=CARTESIAN_POINT('Ctrl Pts',(-190.601547025642,0.429275661136996,
135.705762670257));
#122762=CARTESIAN_POINT('Ctrl Pts',(-190.609303328384,0.565865429118824,
135.691871898426));
#122763=CARTESIAN_POINT('Ctrl Pts',(-190.617059631125,0.70153010916397,
135.672321029118));
#122764=CARTESIAN_POINT('Ctrl Pts',(-190.62482007364,0.837267197534009,
135.652759724922));
#122765=CARTESIAN_POINT('Ctrl Pts',(-190.632580516154,0.972077830027677,
135.627532375601));
#122766=CARTESIAN_POINT('Ctrl Pts',(-190.640340958668,1.1054622334498,135.596764639862));
#122767=CARTESIAN_POINT('Ctrl Pts',(-190.648113858933,1.23906075735725,
135.565947513022));
#122768=CARTESIAN_POINT('Ctrl Pts',(-190.655886759199,1.37122809985715,
135.529572330681));
#122769=CARTESIAN_POINT('Ctrl Pts',(-190.663659659464,1.50147966778053,
135.487814670905));
#122770=CARTESIAN_POINT('Ctrl Pts',(-190.671149995226,1.62699626312459,
135.447575007244));
#122771=CARTESIAN_POINT('Ctrl Pts',(-190.678640330988,1.75073366284605,
135.402337511017));
#122772=CARTESIAN_POINT('Ctrl Pts',(-190.68613066675,1.8722783195407,135.352300476082));
#122773=CARTESIAN_POINT('Ctrl Pts',(-190.693905000869,1.99843137883754,
135.300366271758));
#122774=CARTESIAN_POINT('Ctrl Pts',(-190.701679334988,2.12262175204157,
135.243096883288));
#122775=CARTESIAN_POINT('Ctrl Pts',(-190.709453669107,2.24436523492668,
135.180661310475));
#122776=CARTESIAN_POINT('Ctrl Pts',(-190.717218422054,2.36595867984999,
135.118302683924));
#122777=CARTESIAN_POINT('Ctrl Pts',(-190.724983175001,2.48511089000259,
135.050790717883));
#122778=CARTESIAN_POINT('Ctrl Pts',(-190.732747927949,2.6013562836682,134.978342954366));
#122779=CARTESIAN_POINT('Ctrl Pts',(-190.740504968834,2.71748622077004,
134.90596714699));
#122780=CARTESIAN_POINT('Ctrl Pts',(-190.748262009719,2.83071475717223,
134.828665503394));
#122781=CARTESIAN_POINT('Ctrl Pts',(-190.756019050603,2.94059996327127,
134.746701916656));
#122782=CARTESIAN_POINT('Ctrl Pts',(-190.763770241844,3.05040230408146,
134.664800139296));
#122783=CARTESIAN_POINT('Ctrl Pts',(-190.771521433084,3.15686602082719,
134.578243649209));
#122784=CARTESIAN_POINT('Ctrl Pts',(-190.779272624324,3.25957760168308,
134.487339971446));
#122785=CARTESIAN_POINT('Ctrl Pts',(-190.787020521101,3.36224552737705,
134.396474930171));
#122786=CARTESIAN_POINT('Ctrl Pts',(-190.794768417878,3.46116419687574,
134.301266634669));
#122787=CARTESIAN_POINT('Ctrl Pts',(-190.802516314655,3.55595286108516,
134.20206312253));
#122788=CARTESIAN_POINT('Ctrl Pts',(-190.810262590739,3.65072169754968,
134.102880361628));
#122789=CARTESIAN_POINT('Ctrl Pts',(-190.818008866823,3.74136197716383,
133.999704328862));
#122790=CARTESIAN_POINT('Ctrl Pts',(-190.825755142907,3.82752983602749,
133.892919896068));
#122791=CARTESIAN_POINT('Ctrl Pts',(-190.833501476173,3.91369833096282,
133.786134675015));
#122792=CARTESIAN_POINT('Ctrl Pts',(-190.841247809438,3.99539409375177,
133.675741305042));
#122793=CARTESIAN_POINT('Ctrl Pts',(-190.848994142703,4.07231384350195,
133.562157387185));
#122794=CARTESIAN_POINT('Ctrl Pts',(-190.856742210706,4.14925081889687,
133.448548032997));
#122795=CARTESIAN_POINT('Ctrl Pts',(-190.864490278709,4.2214094337795,133.331747032808));
#122796=CARTESIAN_POINT('Ctrl Pts',(-190.872238346712,4.28853021966979,
133.212200233794));
#122797=CARTESIAN_POINT('Ctrl Pts',(-190.879994649454,4.3557223423298,133.092526379021));
#122798=CARTESIAN_POINT('Ctrl Pts',(-190.887750952196,4.41786574856622,
132.970101237319));
#122799=CARTESIAN_POINT('Ctrl Pts',(-190.895507254938,4.47474712186675,
132.845394977356));
#122800=CARTESIAN_POINT('Ctrl Pts',(-190.903267697452,4.53165885446903,
132.720622157908));
#122801=CARTESIAN_POINT('Ctrl Pts',(-190.911028139966,4.5833028108051,132.593566156235));
#122802=CARTESIAN_POINT('Ctrl Pts',(-190.91878858248,4.62951457148501,132.464715367283));
#122803=CARTESIAN_POINT('Ctrl Pts',(-190.926561482746,4.67580051538552,
132.335657735606));
#122804=CARTESIAN_POINT('Ctrl Pts',(-190.934334383011,4.71663672127184,
132.204799932619));
#122805=CARTESIAN_POINT('Ctrl Pts',(-190.942107283277,4.75190897349856,
132.072644564513));
#122806=CARTESIAN_POINT('Ctrl Pts',(-190.949597619039,4.78589899051188,
131.945293376915));
#122807=CARTESIAN_POINT('Ctrl Pts',(-190.957087954801,4.81472249074796,
131.816737626403));
#122808=CARTESIAN_POINT('Ctrl Pts',(-190.964578290563,4.83832277197152,
131.687432424795));
#122809=CARTESIAN_POINT('Ctrl Pts',(-190.972352624682,4.86281786503052,
131.553224577167));
#122810=CARTESIAN_POINT('Ctrl Pts',(-190.980126958801,4.88176343679289,
131.417784195585));
#122811=CARTESIAN_POINT('Ctrl Pts',(-190.98790129292,4.89503994736683,131.281610003299));
#122812=CARTESIAN_POINT('Ctrl Pts',(-190.995666045867,4.90830009582805,
131.145603633535));
#122813=CARTESIAN_POINT('Ctrl Pts',(-191.003430798814,4.91590504680117,
131.008865637851));
#122814=CARTESIAN_POINT('Ctrl Pts',(-191.011195551762,4.91778616625509,
130.871905310104));
#122815=CARTESIAN_POINT('Ctrl Pts',(-191.018952592647,4.91966541735466,
130.735081013285));
#122816=CARTESIAN_POINT('Ctrl Pts',(-191.026709633532,4.9158321449874,130.59803521225));
#122817=CARTESIAN_POINT('Ctrl Pts',(-191.034466674417,4.90626949612716,
130.461282355544));
#122818=CARTESIAN_POINT('Ctrl Pts',(-191.042217865657,4.89671405853478,
130.324632625231));
#122819=CARTESIAN_POINT('Ctrl Pts',(-191.049969056897,4.88143787143859,
130.18827578797));
#122820=CARTESIAN_POINT('Ctrl Pts',(-191.057720248137,4.86047615113323,
130.052725967776));
#122821=CARTESIAN_POINT('Ctrl Pts',(-191.065468144914,4.83952334011826,
129.917233759872));
#122822=CARTESIAN_POINT('Ctrl Pts',(-191.073216041691,4.81288986175936,
129.782548272388));
#122823=CARTESIAN_POINT('Ctrl Pts',(-191.080963938468,4.78066272575466,
129.649177963143));
#122824=CARTESIAN_POINT('Ctrl Pts',(-191.088710214552,4.74844233097209,
129.515835552091));
#122825=CARTESIAN_POINT('Ctrl Pts',(-191.096456490636,4.71063069765271,
129.383808151861));
#122826=CARTESIAN_POINT('Ctrl Pts',(-191.104202766721,4.66736576253298,
129.253593097518));
#122827=CARTESIAN_POINT('Ctrl Pts',(-191.111949099986,4.62410050804126,
129.123377081957));
#122828=CARTESIAN_POINT('Ctrl Pts',(-191.119695433251,4.57538199469793,
128.994973810001));
#122829=CARTESIAN_POINT('Ctrl Pts',(-191.127441766517,4.52139763135042,
128.868864164012));
#122830=CARTESIAN_POINT('Ctrl Pts',(-191.13518983452,4.46740117857896,128.742726276643));
#122831=CARTESIAN_POINT('Ctrl Pts',(-191.142937902523,4.40813668305963,
128.618883396679));
#122832=CARTESIAN_POINT('Ctrl Pts',(-191.150685970526,4.34383899959804,
128.49779481359));
#122833=CARTESIAN_POINT('Ctrl Pts',(-191.158442273267,4.2794729797934,128.376577536114));
#122834=CARTESIAN_POINT('Ctrl Pts',(-191.166198576009,4.21006326982718,
128.258120748965));
#122835=CARTESIAN_POINT('Ctrl Pts',(-191.173954878751,4.13589013312932,
128.142858059013));
#122836=CARTESIAN_POINT('Ctrl Pts',(-191.181715321265,4.0616774079951,128.027533849893));
#122837=CARTESIAN_POINT('Ctrl Pts',(-191.18947576378,3.98269641524828,127.915407454376));
#122838=CARTESIAN_POINT('Ctrl Pts',(-191.197236206294,3.89926918269119,
127.806881192547));
#122839=CARTESIAN_POINT('Ctrl Pts',(-191.205009106559,3.81570802533407,
127.698180714727));
#122840=CARTESIAN_POINT('Ctrl Pts',(-191.212782006825,3.72768661635664,
127.59309221928));
#122841=CARTESIAN_POINT('Ctrl Pts',(-191.22055490709,3.63556607623541,127.491983469984));
#122842=CARTESIAN_POINT('Ctrl Pts',(-191.228045242852,3.54679434978573,
127.394550278402));
#122843=CARTESIAN_POINT('Ctrl Pts',(-191.235535578614,3.4542165619243,127.300812728031));
#122844=CARTESIAN_POINT('Ctrl Pts',(-191.243025914376,3.35818496216893,
127.21106452312));
#122845=CARTESIAN_POINT('Ctrl Pts',(-191.250800248495,3.25851229511997,
127.11791348774));
#122846=CARTESIAN_POINT('Ctrl Pts',(-191.258574582614,3.15480301053301,
127.02876520709));
#122847=CARTESIAN_POINT('Ctrl Pts',(-191.266348916733,3.04741208417123,
126.943989825563));
#122848=CARTESIAN_POINT('Ctrl Pts',(-191.27411366968,2.94015350752896,126.859318922119));
#122849=CARTESIAN_POINT('Ctrl Pts',(-191.281878422628,2.82922262090105,
126.779010434803));
#122850=CARTESIAN_POINT('Ctrl Pts',(-191.289643175575,2.71501080926322,
126.703397393141));
#122851=CARTESIAN_POINT('Ctrl Pts',(-191.29740021646,2.60091243440618,126.627859451418));
#122852=CARTESIAN_POINT('Ctrl Pts',(-191.305157257345,2.48353994330888,
126.557007889035));
#122853=CARTESIAN_POINT('Ctrl Pts',(-191.31291429823,2.3633170466302,126.491134956926));
#122854=CARTESIAN_POINT('Ctrl Pts',(-191.32066548947,2.24318481097262,126.425311700106));
#122855=CARTESIAN_POINT('Ctrl Pts',(-191.32841668071,2.12020678969177,126.364459787714));
#122856=CARTESIAN_POINT('Ctrl Pts',(-191.33616787195,1.99483456514794,126.30882748787));
#122857=CARTESIAN_POINT('Ctrl Pts',(-191.343915768727,1.86951562714447,
126.253218833238));
#122858=CARTESIAN_POINT('Ctrl Pts',(-191.351663665504,1.74180486642149,
126.20282553702));
#122859=CARTESIAN_POINT('Ctrl Pts',(-191.359411562281,1.61217709380733,
126.157849229363));
#122860=CARTESIAN_POINT('Ctrl Pts',(-191.367157838366,1.48257643652876,
126.112882329779));
#122861=CARTESIAN_POINT('Ctrl Pts',(-191.37490411445,1.35105993409509,126.073330292999));
#122862=CARTESIAN_POINT('Ctrl Pts',(-191.382650390534,1.21812056675712,
126.03934589069));
#122863=CARTESIAN_POINT('Ctrl Pts',(-191.390396723799,1.08518021809113,
126.005361237516));
#122864=CARTESIAN_POINT('Ctrl Pts',(-191.398143057064,0.950817362346455,
125.976944397655));
#122865=CARTESIAN_POINT('Ctrl Pts',(-191.40588939033,0.815537878534929,
125.9541976274));
#122866=CARTESIAN_POINT('Ctrl Pts',(-191.413637458333,0.68022809982115,
125.931445763164));
#122867=CARTESIAN_POINT('Ctrl Pts',(-191.421385526336,0.544001670051006,
125.914366560051));
#122868=CARTESIAN_POINT('Ctrl Pts',(-191.429133594339,0.407371947222745,
125.90301068524));
#122869=CARTESIAN_POINT('Ctrl Pts',(-191.436889897081,0.270597012698589,
125.89164274127));
#122870=CARTESIAN_POINT('Ctrl Pts',(-191.444646199823,0.133418319135421,
125.886010309127));
#122871=CARTESIAN_POINT('Ctrl Pts',(-191.452402502564,-0.00364783849507481,
125.886111970357));
#122872=CARTESIAN_POINT('Ctrl Pts',(-191.460162945079,-0.14078715246088,
125.886213685846));
#122873=CARTESIAN_POINT('Ctrl Pts',(-191.467923387593,-0.277813420392517,
125.892055576286));
#122874=CARTESIAN_POINT('Ctrl Pts',(-191.475683830107,-0.414214095113777,
125.903584174398));
#122875=CARTESIAN_POINT('Ctrl Pts',(-191.483456730372,-0.550833732307181,
125.91513127924));
#122876=CARTESIAN_POINT('Ctrl Pts',(-191.491229630638,-0.686825381383332,
125.93238328479));
#122877=CARTESIAN_POINT('Ctrl Pts',(-191.499002530903,-0.821684437819978,
125.95523515547));
#122878=CARTESIAN_POINT('Ctrl Pts',(-191.506492866665,-0.951641027862406,
125.977256303091));
#122879=CARTESIAN_POINT('Ctrl Pts',(-191.513983202427,-1.08054563945036,
126.004477182315));
#122880=CARTESIAN_POINT('Ctrl Pts',(-191.521473538189,-1.20796077141146,
126.036760189968));
#122881=CARTESIAN_POINT('Ctrl Pts',(-191.529247872308,-1.3402068868303,
126.07026721767));
#122882=CARTESIAN_POINT('Ctrl Pts',(-191.537022206427,-1.47126726171084,
126.109333952733));
#122883=CARTESIAN_POINT('Ctrl Pts',(-191.544796540546,-1.6006386100197,
126.153861816081));
#122884=CARTESIAN_POINT('Ctrl Pts',(-191.552561293493,-1.72985051970473,
126.198334802817));
#122885=CARTESIAN_POINT('Ctrl Pts',(-191.560326046441,-1.85737717839847,
126.248255400426));
#122886=CARTESIAN_POINT('Ctrl Pts',(-191.568090799388,-1.98272684579087,
126.303474336234));
#122887=CARTESIAN_POINT('Ctrl Pts',(-191.575847840273,-2.10795201412615,
126.358638427817));
#122888=CARTESIAN_POINT('Ctrl Pts',(-191.583604881158,-2.2310041385998,
126.419090228625));
#122889=CARTESIAN_POINT('Ctrl Pts',(-191.591361922043,-2.35140831426397,
126.484631227649));
#122890=CARTESIAN_POINT('Ctrl Pts',(-191.599113113283,-2.47172169220282,
126.550122801696));
#122891=CARTESIAN_POINT('Ctrl Pts',(-191.606864304523,-2.58939075392098,
126.62069574888));
#122892=CARTESIAN_POINT('Ctrl Pts',(-191.614615495763,-2.70396253312058,
126.696104335154));
#122893=CARTESIAN_POINT('Ctrl Pts',(-191.62236339254,-2.81848561625756,
126.771480870767));
#122894=CARTESIAN_POINT('Ctrl Pts',(-191.630111289317,-2.92991370925743,
126.851688743189));
#122895=CARTESIAN_POINT('Ctrl Pts',(-191.637859186094,-3.03782052811709,
126.936437466642));
#122896=CARTESIAN_POINT('Ctrl Pts',(-191.645605462178,-3.14570477519644,
127.02116846249));
#122897=CARTESIAN_POINT('Ctrl Pts',(-191.653351738262,-3.25006890594588,
127.110438178736));
#122898=CARTESIAN_POINT('Ctrl Pts',(-191.661098014347,-3.35051792136731,
127.203914433953));
#122899=CARTESIAN_POINT('Ctrl Pts',(-191.668844347612,-3.45096767828041,
127.29739137919));
#122900=CARTESIAN_POINT('Ctrl Pts',(-191.676590680877,-3.54750197598732,
127.395074659016));
#122901=CARTESIAN_POINT('Ctrl Pts',(-191.684337014142,-3.63976134341008,
127.496593935117));
#122902=CARTESIAN_POINT('Ctrl Pts',(-191.692085082145,-3.73204137167862,
127.598135945756));
#122903=CARTESIAN_POINT('Ctrl Pts',(-191.699833150149,-3.82004430177213,
127.70351537279));
#122904=CARTESIAN_POINT('Ctrl Pts',(-191.707581218151,-3.90345002342118,
127.812327700442));
#122905=CARTESIAN_POINT('Ctrl Pts',(-191.715337520893,-3.98694438966386,
127.921255675131));
#122906=CARTESIAN_POINT('Ctrl Pts',(-191.723093823635,-4.06583154899084,
128.033623527975));
#122907=CARTESIAN_POINT('Ctrl Pts',(-191.730850126377,-4.13983362474526,
128.148996118683));
#122908=CARTESIAN_POINT('Ctrl Pts',(-191.738610568891,-4.21387519763547,
128.264430287216));
#122909=CARTESIAN_POINT('Ctrl Pts',(-191.746371011405,-4.28302629462755,
128.38287205169));
#122910=CARTESIAN_POINT('Ctrl Pts',(-191.754131453919,-4.34705485498703,
128.503861291282));
#122911=CARTESIAN_POINT('Ctrl Pts',(-191.761904354185,-4.41118619967579,
128.625044753542));
#122912=CARTESIAN_POINT('Ctrl Pts',(-191.76967725445,-4.47017840691058,
128.748783509796));
#122913=CARTESIAN_POINT('Ctrl Pts',(-191.777450154716,-4.52384709502806,
128.874596247674));
#122914=CARTESIAN_POINT('Ctrl Pts',(-191.784940490478,-4.57556479114977,
128.995835375627));
#122915=CARTESIAN_POINT('Ctrl Pts',(-191.79243082624,-4.62233918575824,
129.119000026256));
#122916=CARTESIAN_POINT('Ctrl Pts',(-191.799921162002,-4.6640495682308,
129.243647739556));
#122917=CARTESIAN_POINT('Ctrl Pts',(-191.806629630531,-4.70140607627558,
129.355284292103));
#122918=CARTESIAN_POINT('Ctrl Pts',(-191.81333809906,-4.73477224984779,
129.468318960301));
#122919=CARTESIAN_POINT('Ctrl Pts',(-191.820046567589,-4.76405452823394,
129.582490119308));
#122920=CARTESIAN_POINT('Origin',(213.235140564004,0.,130.804360617566));
#122921=CARTESIAN_POINT('',(-193.914998640423,-4.76405452823412,129.582490119309));
#122922=CARTESIAN_POINT('',(-193.570047426085,-4.7640545282341,129.582490119308));
#122923=CARTESIAN_POINT('',(213.235140564004,-4.76405452823405,129.582490119308));
#122924=CARTESIAN_POINT('',(-192.235140564068,-4.9182489107902,130.807633843951));
#122925=CARTESIAN_POINT('Ctrl Pts',(-192.235140564068,-4.9182489107902,
130.80763384395));
#122926=CARTESIAN_POINT('Ctrl Pts',(-192.243918515748,-4.9181453490622,
130.963242499187));
#122927=CARTESIAN_POINT('Ctrl Pts',(-192.252696467428,-4.91065281771742,
131.118565439462));
#122928=CARTESIAN_POINT('Ctrl Pts',(-192.261474419109,-4.89587660554873,
131.272949270588));
#122929=CARTESIAN_POINT('Ctrl Pts',(-192.270289110367,-4.88103854845119,
131.42797926576));
#122930=CARTESIAN_POINT('Ctrl Pts',(-192.279103801625,-4.85885582307568,
131.582062100835));
#122931=CARTESIAN_POINT('Ctrl Pts',(-192.287918492883,-4.8294847853578,
131.734554022454));
#122932=CARTESIAN_POINT('Ctrl Pts',(-192.296783739358,-4.79994529486645,
131.887920536499));
#122933=CARTESIAN_POINT('Ctrl Pts',(-192.305648985834,-4.76313489578936,
132.039677664175));
#122934=CARTESIAN_POINT('Ctrl Pts',(-192.314514232309,-4.71926132012198,
132.189191168536));
#122935=CARTESIAN_POINT('Ctrl Pts',(-192.322085292695,-4.68179259416399,
132.316878060629));
#122936=CARTESIAN_POINT('Ctrl Pts',(-192.329656353081,-4.63917323850466,
132.442928873986));
#122937=CARTESIAN_POINT('Ctrl Pts',(-192.337227413468,-4.59155968143751,
132.566961750635));
#122938=CARTESIAN_POINT('Ctrl Pts',(-192.345001747587,-4.54266775846242,
132.694324758674));
#122939=CARTESIAN_POINT('Ctrl Pts',(-192.352776081706,-4.48839508868817,
132.819853675534));
#122940=CARTESIAN_POINT('Ctrl Pts',(-192.360550415825,-4.42889900368266,
132.943060380899));
#122941=CARTESIAN_POINT('Ctrl Pts',(-192.368315168772,-4.3694762422846,
133.06611524501));
#122942=CARTESIAN_POINT('Ctrl Pts',(-192.376079921719,-4.30484304252658,
133.186853243304));
#122943=CARTESIAN_POINT('Ctrl Pts',(-192.383844674666,-4.23520571110023,
133.304803707733));
#122944=CARTESIAN_POINT('Ctrl Pts',(-192.391601715551,-4.16563754445317,
133.422637022098));
#122945=CARTESIAN_POINT('Ctrl Pts',(-192.399358756436,-4.09107533448945,
133.537687977781));
#122946=CARTESIAN_POINT('Ctrl Pts',(-192.407115797321,-4.01177229319911,
133.64950843974));
#122947=CARTESIAN_POINT('Ctrl Pts',(-192.414866988561,-3.9325290549492,
133.761244577018));
#122948=CARTESIAN_POINT('Ctrl Pts',(-192.422618179801,-3.84855232664149,
133.869754751943));
#122949=CARTESIAN_POINT('Ctrl Pts',(-192.430369371041,-3.76013962162594,
133.974618192019));
#122950=CARTESIAN_POINT('Ctrl Pts',(-192.438117267819,-3.67176449436839,
134.079437062336));
#122951=CARTESIAN_POINT('Ctrl Pts',(-192.445865164596,-3.57895739182149,
134.180611982277));
#122952=CARTESIAN_POINT('Ctrl Pts',(-192.453613061373,-3.4820571144234,
134.27775396045));
#122953=CARTESIAN_POINT('Ctrl Pts',(-192.461359337457,-3.38517710647442,
134.374875618616));
#122954=CARTESIAN_POINT('Ctrl Pts',(-192.469105613541,-3.28420590264548,
134.467965736369));
#122955=CARTESIAN_POINT('Ctrl Pts',(-192.476851889625,-3.17952001215119,
134.556671312968));
#122956=CARTESIAN_POINT('Ctrl Pts',(-192.48459822289,-3.07483334888957,
134.645377544372));
#122957=CARTESIAN_POINT('Ctrl Pts',(-192.492344556156,-2.96643224252753,
134.729698917291));
#122958=CARTESIAN_POINT('Ctrl Pts',(-192.500090889421,-2.85472689593607,
134.809322216897));
#122959=CARTESIAN_POINT('Ctrl Pts',(-192.507838957424,-2.7429965337069,
134.888963347589));
#122960=CARTESIAN_POINT('Ctrl Pts',(-192.515587025427,-2.62796077711468,
134.963904084522));
#122961=CARTESIAN_POINT('Ctrl Pts',(-192.52333509343,-2.51005911841526,
135.033874334834));
#122962=CARTESIAN_POINT('Ctrl Pts',(-192.531091396171,-2.39203215242945,
135.103918950361));
#122963=CARTESIAN_POINT('Ctrl Pts',(-192.538847698913,-2.27113353654513,
135.16898232667));
#122964=CARTESIAN_POINT('Ctrl Pts',(-192.546604001655,-2.14782818502421,
135.228839925927));
#122965=CARTESIAN_POINT('Ctrl Pts',(-192.554364444169,-2.02445702172452,
135.288729472987));
#122966=CARTESIAN_POINT('Ctrl Pts',(-192.562124886684,-1.89867692159537,
135.343407550848));
#122967=CARTESIAN_POINT('Ctrl Pts',(-192.569885329198,-1.77097219332344,
135.392698067337));
#122968=CARTESIAN_POINT('Ctrl Pts',(-192.577658229463,-1.64306246208459,
135.442067709339));
#122969=CARTESIAN_POINT('Ctrl Pts',(-192.585431129729,-1.51322229925508,
135.486032381865));
#122970=CARTESIAN_POINT('Ctrl Pts',(-192.593204029994,-1.38195142542684,
135.524465840997));
#122971=CARTESIAN_POINT('Ctrl Pts',(-192.600694365756,-1.25545257851221,
135.561502147082));
#122972=CARTESIAN_POINT('Ctrl Pts',(-192.608184701518,-1.12762553341084,
135.593402330408));
#122973=CARTESIAN_POINT('Ctrl Pts',(-192.61567503728,-0.998923910181445,
135.620098783639));
#122974=CARTESIAN_POINT('Ctrl Pts',(-192.623449371399,-0.865342525790616,
135.647807441008));
#122975=CARTESIAN_POINT('Ctrl Pts',(-192.631223705518,-0.730395789175812,
135.669997752622));
#122976=CARTESIAN_POINT('Ctrl Pts',(-192.638998039637,-0.594579411339083,
135.68653824503));
#122977=CARTESIAN_POINT('Ctrl Pts',(-192.646762792585,-0.45893041504978,
135.70305835276));
#122978=CARTESIAN_POINT('Ctrl Pts',(-192.654527545532,-0.32241429438374,
135.713942448564));
#122979=CARTESIAN_POINT('Ctrl Pts',(-192.662292298479,-0.185538549506594,
135.719109696527));
#122980=CARTESIAN_POINT('Ctrl Pts',(-192.670049339364,-0.0487987515492415,
135.724271812306));
#122981=CARTESIAN_POINT('Ctrl Pts',(-192.677806380249,0.0882995716484737,
135.723728365175));
#122982=CARTESIAN_POINT('Ctrl Pts',(-192.685563421134,0.225242524115774,
135.717450161614));
#122983=CARTESIAN_POINT('Ctrl Pts',(-192.693314612374,0.362082206837544,
135.711176692494));
#122984=CARTESIAN_POINT('Ctrl Pts',(-192.701065803614,0.498766363066561,
135.69917709268));
#122985=CARTESIAN_POINT('Ctrl Pts',(-192.708816994854,0.63478017175093,
135.681474230765));
#122986=CARTESIAN_POINT('Ctrl Pts',(-192.716564891631,0.770736170938507,
135.663778893039));
#122987=CARTESIAN_POINT('Ctrl Pts',(-192.724312788408,0.906022002373333,
135.640385164795));
#122988=CARTESIAN_POINT('Ctrl Pts',(-192.732060685185,1.04012726666948,
135.611367829089));
#122989=CARTESIAN_POINT('Ctrl Pts',(-192.73980696127,1.17420447903531,135.582356563184));
#122990=CARTESIAN_POINT('Ctrl Pts',(-192.747553237354,1.30710123357782,
135.547724112247));
#122991=CARTESIAN_POINT('Ctrl Pts',(-192.755299513438,1.4383170283509,135.507596438621));
#122992=CARTESIAN_POINT('Ctrl Pts',(-192.763045846703,1.56953379172899,
135.467468468782));
#122993=CARTESIAN_POINT('Ctrl Pts',(-192.770792179969,1.69906919670432,
135.421845309648));
#122994=CARTESIAN_POINT('Ctrl Pts',(-192.778538513234,1.82643800209956,
135.370902776244));
#122995=CARTESIAN_POINT('Ctrl Pts',(-192.786286581237,1.95383533085548,
135.319948834614));
#122996=CARTESIAN_POINT('Ctrl Pts',(-192.79403464924,2.07906473161203,135.263673293452));
#122997=CARTESIAN_POINT('Ctrl Pts',(-192.801782717243,2.20166141129512,
135.202299918251));
#122998=CARTESIAN_POINT('Ctrl Pts',(-192.809539019985,2.32438838818846,
135.140861314697));
#122999=CARTESIAN_POINT('Ctrl Pts',(-192.817295322727,2.44447670436585,
135.074314229283));
#123000=CARTESIAN_POINT('Ctrl Pts',(-192.825051625468,2.56148615227356,
135.002928439361));
#123001=CARTESIAN_POINT('Ctrl Pts',(-192.832812067983,2.67855805164703,
134.931504548693));
#123002=CARTESIAN_POINT('Ctrl Pts',(-192.840572510497,2.79254748358488,
134.855237024847));
#123003=CARTESIAN_POINT('Ctrl Pts',(-192.848332953011,2.90304451607954,
134.774438148315));
#123004=CARTESIAN_POINT('Ctrl Pts',(-192.856105853276,3.01371892821992,
134.693509566255));
#123005=CARTESIAN_POINT('Ctrl Pts',(-192.863878753542,3.12088943189119,
134.608035339398));
#123006=CARTESIAN_POINT('Ctrl Pts',(-192.871651653807,3.22417970332439,
134.518367658912));
#123007=CARTESIAN_POINT('Ctrl Pts',(-192.879141989569,3.32371511321709,
134.431959624473));
#123008=CARTESIAN_POINT('Ctrl Pts',(-192.886632325331,3.41964728113286,
134.341657939474));
#123009=CARTESIAN_POINT('Ctrl Pts',(-192.894122661093,3.51167413438388,
134.247807703902));
#123010=CARTESIAN_POINT('Ctrl Pts',(-192.901896995212,3.60719021374836,
134.150399108123));
#123011=CARTESIAN_POINT('Ctrl Pts',(-192.909671329331,3.69880155876895,
134.048859002174));
#123012=CARTESIAN_POINT('Ctrl Pts',(-192.91744566345,3.78612961320351,133.943533377151));
#123013=CARTESIAN_POINT('Ctrl Pts',(-192.925210416397,3.87335004361548,
133.838337556548));
#123014=CARTESIAN_POINT('Ctrl Pts',(-192.932975169344,3.95629743948013,
133.729365797536));
#123015=CARTESIAN_POINT('Ctrl Pts',(-192.940739922292,4.0346294750173,133.61700138059));
#123016=CARTESIAN_POINT('Ctrl Pts',(-192.948496963177,4.11288371007249,
133.504748565566));
#123017=CARTESIAN_POINT('Ctrl Pts',(-192.956254004062,4.18653148511081,
133.389110116985));
#123018=CARTESIAN_POINT('Ctrl Pts',(-192.964011044947,4.25527046547266,
133.27050261027));
#123019=CARTESIAN_POINT('Ctrl Pts',(-192.971762236187,4.32395760923461,
133.151984546398));
#123020=CARTESIAN_POINT('Ctrl Pts',(-192.979513427427,4.38774313120223,
133.03050221786));
#123021=CARTESIAN_POINT('Ctrl Pts',(-192.987264618667,4.44636799801797,
132.906501119222));
#123022=CARTESIAN_POINT('Ctrl Pts',(-192.995012515444,4.50496794770152,
132.782552724358));
#123023=CARTESIAN_POINT('Ctrl Pts',(-193.002760412221,4.55841143801551,
132.656088041339));
#123024=CARTESIAN_POINT('Ctrl Pts',(-193.010508308998,4.60648550272751,
132.527576905692));
#123025=CARTESIAN_POINT('Ctrl Pts',(-193.018254585082,4.65454951138154,
132.399092651803));
#123026=CARTESIAN_POINT('Ctrl Pts',(-193.026000861166,4.69724619158006,
132.268563162699));
#123027=CARTESIAN_POINT('Ctrl Pts',(-193.03374713725,4.73441098548304,132.136477610565));
#123028=CARTESIAN_POINT('Ctrl Pts',(-193.041493470516,4.77157605372813,
132.004391083406));
#123029=CARTESIAN_POINT('Ctrl Pts',(-193.049239803781,4.80320904830049,
131.870748846647));
#123030=CARTESIAN_POINT('Ctrl Pts',(-193.056986137046,4.82919560265308,
131.736054179751));
#123031=CARTESIAN_POINT('Ctrl Pts',(-193.064734205049,4.8551879765143,131.601329348918));
#123032=CARTESIAN_POINT('Ctrl Pts',(-193.072482273053,4.87553131993598,
131.465552002776));
#123033=CARTESIAN_POINT('Ctrl Pts',(-193.080230341056,4.89016266115448,
131.329234135616));
#123034=CARTESIAN_POINT('Ctrl Pts',(-193.087986643797,4.90480955273655,
131.192771388205));
#123035=CARTESIAN_POINT('Ctrl Pts',(-193.095742946539,4.91373227328045,
131.055767361558));
#123036=CARTESIAN_POINT('Ctrl Pts',(-193.103499249281,4.91691985117717,
130.918738236006));
#123037=CARTESIAN_POINT('Ctrl Pts',(-193.111259691795,4.92010913038018,
130.781635973883));
#123038=CARTESIAN_POINT('Ctrl Pts',(-193.119020134309,4.91755717486896,
130.644508976869));
#123039=CARTESIAN_POINT('Ctrl Pts',(-193.126780576824,4.90930513680369,
130.507870927605));
#123040=CARTESIAN_POINT('Ctrl Pts',(-193.134553477089,4.90103985183434,
130.371013534815));
#123041=CARTESIAN_POINT('Ctrl Pts',(-193.142326377354,4.88705623904379,
130.23464704741));
#123042=CARTESIAN_POINT('Ctrl Pts',(-193.15009927762,4.86744719464528,130.099278445164));
#123043=CARTESIAN_POINT('Ctrl Pts',(-193.157589613382,4.84855098840286,
129.968830832581));
#123044=CARTESIAN_POINT('Ctrl Pts',(-193.165079949144,4.82443130336841,
129.839310116289));
#123045=CARTESIAN_POINT('Ctrl Pts',(-193.172570284906,4.79521520426802,
129.711156973565));
#123046=CARTESIAN_POINT('Ctrl Pts',(-193.180344619025,4.76489136789024,
129.578144865484));
#123047=CARTESIAN_POINT('Ctrl Pts',(-193.188118953144,4.7289809707059,129.44618473883));
#123048=CARTESIAN_POINT('Ctrl Pts',(-193.195893287263,4.68757048592578,
129.31578210033));
#123049=CARTESIAN_POINT('Ctrl Pts',(-193.20365804021,4.64621103586719,129.185540171426));
#123050=CARTESIAN_POINT('Ctrl Pts',(-193.211422793157,4.59936510233688,
129.056852280564));
#123051=CARTESIAN_POINT('Ctrl Pts',(-193.219187546105,4.54717011460856,
128.930213608575));
#123052=CARTESIAN_POINT('Ctrl Pts',(-193.22694458699,4.49502696767788,128.8037007159));
#123053=CARTESIAN_POINT('Ctrl Pts',(-193.234701627874,4.43754548719051,
128.679233350863));
#123054=CARTESIAN_POINT('Ctrl Pts',(-193.242458668759,4.37491273058033,
128.557291045366));
#123055=CARTESIAN_POINT('Ctrl Pts',(-193.25020986,4.31232720581922,128.435440697511));
#123056=CARTESIAN_POINT('Ctrl Pts',(-193.25796105124,4.24459831493363,128.316111965434));
#123057=CARTESIAN_POINT('Ctrl Pts',(-193.26571224248,4.17196085126148,128.19976358193));
#123058=CARTESIAN_POINT('Ctrl Pts',(-193.273460139257,4.09935426044897,
128.083464649593));
#123059=CARTESIAN_POINT('Ctrl Pts',(-193.281208036034,4.02184345290365,
127.97014387735));
#123060=CARTESIAN_POINT('Ctrl Pts',(-193.288955932811,3.93970860111024,
127.860234397303));
#123061=CARTESIAN_POINT('Ctrl Pts',(-193.296702208895,3.8575909301572,127.75034790795));
#123062=CARTESIAN_POINT('Ctrl Pts',(-193.304448484979,3.77085137275848,
127.643871604446));
#123063=CARTESIAN_POINT('Ctrl Pts',(-193.312194761063,3.67981253579604,
127.541208343476));
#123064=CARTESIAN_POINT('Ctrl Pts',(-193.319941094329,3.58877302680572,
127.43854432467));
#123065=CARTESIAN_POINT('Ctrl Pts',(-193.327687427594,3.49343443432112,
127.339693697082));
#123066=CARTESIAN_POINT('Ctrl Pts',(-193.335433760859,3.39415836369511,
127.24502471537));
#123067=CARTESIAN_POINT('Ctrl Pts',(-193.343181828862,3.29486006088155,
127.150334533197));
#123068=CARTESIAN_POINT('Ctrl Pts',(-193.350929896865,3.19162280819176,
127.059828130087));
#123069=CARTESIAN_POINT('Ctrl Pts',(-193.358677964868,3.08484332314698,
126.97383523139));
#123070=CARTESIAN_POINT('Ctrl Pts',(-193.36643426761,2.97795035159466,126.887750938417));
#123071=CARTESIAN_POINT('Ctrl Pts',(-193.374190570352,2.86750793222474,
126.806189978007));
#123072=CARTESIAN_POINT('Ctrl Pts',(-193.381946873094,2.7539444117456,126.729440588962));
#123073=CARTESIAN_POINT('Ctrl Pts',(-193.389707315608,2.64032027899594,
126.652650236458));
#123074=CARTESIAN_POINT('Ctrl Pts',(-193.397467758122,2.52357205848088,
126.580676777505));
#123075=CARTESIAN_POINT('Ctrl Pts',(-193.405228200636,2.40415416970356,
126.513763247642));
#123076=CARTESIAN_POINT('Ctrl Pts',(-193.413001100902,2.28454458072975,
126.446742302241));
#123077=CARTESIAN_POINT('Ctrl Pts',(-193.420774001167,2.16225710849449,
126.384797694339));
#123078=CARTESIAN_POINT('Ctrl Pts',(-193.428546901433,2.03776850211148,
126.328125302672));
#123079=CARTESIAN_POINT('Ctrl Pts',(-193.436037237195,1.91780537013702,
126.273513095191));
#123080=CARTESIAN_POINT('Ctrl Pts',(-193.443527572957,1.79579864438425,
126.223796558439));
#123081=CARTESIAN_POINT('Ctrl Pts',(-193.451017908719,1.67218776071735,
126.179106986098));
#123082=CARTESIAN_POINT('Ctrl Pts',(-193.458792242838,1.54389013282677,
126.132722995039));
#123083=CARTESIAN_POINT('Ctrl Pts',(-193.466566576957,1.41345789412949,
126.091607757464));
#123084=CARTESIAN_POINT('Ctrl Pts',(-193.474340911076,1.28136308263296,
126.055961759744));
#123085=CARTESIAN_POINT('Ctrl Pts',(-193.482105664023,1.1494310661863,126.020359692531));
#123086=CARTESIAN_POINT('Ctrl Pts',(-193.48987041697,1.01584092762441,125.990213554768));
#123087=CARTESIAN_POINT('Ctrl Pts',(-193.497635169917,0.88108356048614,
125.965675380651));
#123088=CARTESIAN_POINT('Ctrl Pts',(-193.505392210802,0.746460036264656,
125.941161578194));
#123089=CARTESIAN_POINT('Ctrl Pts',(-193.513149251688,0.610671972693172,
125.922244724601));
#123090=CARTESIAN_POINT('Ctrl Pts',(-193.520906292573,0.47422392265558,
125.909026641862));
#123091=CARTESIAN_POINT('Ctrl Pts',(-193.528657483813,0.337878769153747,
125.895818526982));
#123092=CARTESIAN_POINT('Ctrl Pts',(-193.536408675053,0.200875007398296,
125.888300666612));
#123093=CARTESIAN_POINT('Ctrl Pts',(-193.544159866293,0.0637254938153366,
125.886523478748));
#123094=CARTESIAN_POINT('Ctrl Pts',(-193.55190776307,-0.0733657275659535,
125.884747046236));
#123095=CARTESIAN_POINT('Ctrl Pts',(-193.559655659847,-0.210602187450144,
125.888706438433));
#123096=CARTESIAN_POINT('Ctrl Pts',(-193.567403556624,-0.347468039461664,
125.898400056773));
#123097=CARTESIAN_POINT('Ctrl Pts',(-193.575149832708,-0.48430526208743,
125.908091647417));
#123098=CARTESIAN_POINT('Ctrl Pts',(-193.582896108792,-0.620771641297166,
125.923515050776));
#123099=CARTESIAN_POINT('Ctrl Pts',(-193.590642384876,-0.756353865451232,
125.944616602423));
#123100=CARTESIAN_POINT('Ctrl Pts',(-193.598388718142,-0.891937090442292,
125.965718309837));
#123101=CARTESIAN_POINT('Ctrl Pts',(-193.606135051407,-1.02663576103986,
125.992498189051));
#123102=CARTESIAN_POINT('Ctrl Pts',(-193.613881384672,-1.15994459764504,
126.02485106188));
#123103=CARTESIAN_POINT('Ctrl Pts',(-193.621629452675,-1.29328328784007,
126.05721117991));
#123104=CARTESIAN_POINT('Ctrl Pts',(-193.629377520678,-1.42523114484017,
126.095146682807));
#123105=CARTESIAN_POINT('Ctrl Pts',(-193.637125588681,-1.55529632586053,
126.138502025488));
#123106=CARTESIAN_POINT('Ctrl Pts',(-193.644881891423,-1.68549974170325,
126.181903446744));
#123107=CARTESIAN_POINT('Ctrl Pts',(-193.652638194165,-1.81381611299879,
126.230736090713));
#123108=CARTESIAN_POINT('Ctrl Pts',(-193.660394496907,-1.93977140442049,
126.284795377292));
#123109=CARTESIAN_POINT('Ctrl Pts',(-193.668154939421,-2.06579392197332,
126.33888351694));
#123110=CARTESIAN_POINT('Ctrl Pts',(-193.675915381935,-2.1894524963065,
126.398203688727));
#123111=CARTESIAN_POINT('Ctrl Pts',(-193.683675824449,-2.31029702989768,
126.462504943301));
#123112=CARTESIAN_POINT('Ctrl Pts',(-193.691448724715,-2.43133555386226,
126.526909419958));
#123113=CARTESIAN_POINT('Ctrl Pts',(-193.69922162498,-2.54955067263316,
126.596310760058));
#123114=CARTESIAN_POINT('Ctrl Pts',(-193.706994525246,-2.6645198933412,
126.670413738313));
#123115=CARTESIAN_POINT('Ctrl Pts',(-193.714484861008,-2.77530969328494,
126.741822886652));
#123116=CARTESIAN_POINT('Ctrl Pts',(-193.72197519677,-2.88308523914618,
126.817597597928));
#123117=CARTESIAN_POINT('Ctrl Pts',(-193.729465532532,-2.98749854401419,
126.897439129743));
#123118=CARTESIAN_POINT('Ctrl Pts',(-193.737196078694,-3.0952603185036,
126.97984112973));
#123119=CARTESIAN_POINT('Ctrl Pts',(-193.744926624856,-3.19980039402153,
127.066850545295));
#123120=CARTESIAN_POINT('Ctrl Pts',(-193.752657171018,-3.30069311752396,
127.158183440517));
#123121=CARTESIAN_POINT('Ctrl Pts',(-193.760334883215,-3.40089629561768,
127.248892126417));
#123122=CARTESIAN_POINT('Ctrl Pts',(-193.768012595413,-3.49750149279864,
127.343865140785));
#123123=CARTESIAN_POINT('Ctrl Pts',(-193.77569030761,-3.5901203904032,127.44278083346));
#123124=CARTESIAN_POINT('Ctrl Pts',(-193.783361016429,-3.68265480383977,
127.54160629822));
#123125=CARTESIAN_POINT('Ctrl Pts',(-193.791031725249,-3.77120987628044,
127.644366999939));
#123126=CARTESIAN_POINT('Ctrl Pts',(-193.798702434068,-3.855431774176,127.750702336557));
#123127=CARTESIAN_POINT('Ctrl Pts',(-193.80636789687,-3.93959607249805,
127.856964950164));
#123128=CARTESIAN_POINT('Ctrl Pts',(-193.814033359672,-4.01943284300044,
127.966797023577));
#123129=CARTESIAN_POINT('Ctrl Pts',(-193.821698822474,-4.09462678788818,
128.079802941464));
#123130=CARTESIAN_POINT('Ctrl Pts',(-193.829473807303,-4.17089508320833,
128.194423456868));
#123131=CARTESIAN_POINT('Ctrl Pts',(-193.837248792132,-4.24238657353508,
128.312308902551));
#123132=CARTESIAN_POINT('Ctrl Pts',(-193.845023776961,-4.30881615492087,
128.433013657378));
#123133=CARTESIAN_POINT('Ctrl Pts',(-193.852685093457,-4.37427455244702,
128.551953738889));
#123134=CARTESIAN_POINT('Ctrl Pts',(-193.860346409954,-4.43481787122632,
128.673630879259));
#123135=CARTESIAN_POINT('Ctrl Pts',(-193.86800772645,-4.49021873156322,
128.79759236856));
#123136=CARTESIAN_POINT('Ctrl Pts',(-193.875839545445,-4.54685253732966,
128.924312619201));
#123137=CARTESIAN_POINT('Ctrl Pts',(-193.883671364441,-4.5981120887347,
129.053419710477));
#123138=CARTESIAN_POINT('Ctrl Pts',(-193.891503183436,-4.64380612801652,
129.184407621984));
#123139=CARTESIAN_POINT('Ctrl Pts',(-193.899335002432,-4.68950016729845,
129.315395533491));
#123140=CARTESIAN_POINT('Ctrl Pts',(-193.907166821427,-4.72962857139135,
129.448263836065));
#123141=CARTESIAN_POINT('Ctrl Pts',(-193.914998640423,-4.76405452823412,
129.582490119309));
#123142=CARTESIAN_POINT('Ctrl Pts',(-192.165295998532,-4.76405452823416,
129.582490119309));
#123143=CARTESIAN_POINT('Ctrl Pts',(-192.173087299489,-4.79834001608084,
129.716168716068));
#123144=CARTESIAN_POINT('Ctrl Pts',(-192.180878600447,-4.82701148740486,
129.851356535398));
#123145=CARTESIAN_POINT('Ctrl Pts',(-192.188669901404,-4.84994811259561,
129.987545848092));
#123146=CARTESIAN_POINT('Ctrl Pts',(-192.196460544,-4.87288279965338,130.12372365286));
#123147=CARTESIAN_POINT('Ctrl Pts',(-192.204251186596,-4.89008353206788,
130.260902405253));
#123148=CARTESIAN_POINT('Ctrl Pts',(-192.212041829192,-4.90148064217082,
130.398564391703));
#123149=CARTESIAN_POINT('Ctrl Pts',(-192.219741407466,-4.9127445321833,
130.534617256005));
#123150=CARTESIAN_POINT('Ctrl Pts',(-192.227440985739,-4.91833974990952,
130.671141747254));
#123151=CARTESIAN_POINT('Ctrl Pts',(-192.235140564013,-4.91824891079085,
130.807633842979));
#123152=CARTESIAN_POINT('',(-191.889859435946,-4.91824838362704,130.800373206121));
#123153=CARTESIAN_POINT('Ctrl Pts',(-191.820046567589,-4.76405452823394,
129.582490119308));
#123154=CARTESIAN_POINT('Ctrl Pts',(-191.82924828616,-4.80421977364591,
129.739093801576));
#123155=CARTESIAN_POINT('Ctrl Pts',(-191.83845000473,-4.83669951198726,
129.897836547039));
#123156=CARTESIAN_POINT('Ctrl Pts',(-191.847651723301,-4.86129257036642,
130.058024495031));
#123157=CARTESIAN_POINT('Ctrl Pts',(-191.856764218548,-4.88564716520422,
130.216659200447));
#123158=CARTESIAN_POINT('Ctrl Pts',(-191.865876713795,-4.90226722063982,
130.376711144536));
#123159=CARTESIAN_POINT('Ctrl Pts',(-191.874989209043,-4.91100407682167,
130.537486077864));
#123160=CARTESIAN_POINT('Ctrl Pts',(-191.879945951344,-4.91575649023196,
130.624939611869));
#123161=CARTESIAN_POINT('Ctrl Pts',(-191.884902693645,-4.9181772279881,
130.712606716241));
#123162=CARTESIAN_POINT('Ctrl Pts',(-191.889859435946,-4.91824838362704,
130.800373206121));
#123163=CARTESIAN_POINT('Ctrl Pts',(-191.889859435995,-4.91824838362774,
130.800373206994));
#123164=CARTESIAN_POINT('Ctrl Pts',(-191.897713992238,-4.91836113829842,
130.939449799867));
#123165=CARTESIAN_POINT('Ctrl Pts',(-191.90556854848,-4.91257017733928,
131.078607516704));
#123166=CARTESIAN_POINT('Ctrl Pts',(-191.913423104722,-4.90088344947465,
131.217306712311));
#123167=CARTESIAN_POINT('Ctrl Pts',(-191.921150059273,-4.88938657908931,
131.353752661333));
#123168=CARTESIAN_POINT('Ctrl Pts',(-191.928877013823,-4.87218410818176,
131.489754471933));
#123169=CARTESIAN_POINT('Ctrl Pts',(-191.936603968374,-4.84933606598093,
131.624801219728));
#123170=CARTESIAN_POINT('Ctrl Pts',(-191.944330975815,-4.82648786738739,
131.759848891906));
#123171=CARTESIAN_POINT('Ctrl Pts',(-191.952057983256,-4.7979940857108,
131.893941100987));
#123172=CARTESIAN_POINT('Ctrl Pts',(-191.959784990697,-4.76396615906066,
132.02657561413));
#123173=CARTESIAN_POINT('Ctrl Pts',(-191.967513741978,-4.72993055294498,
132.159240060396));
#123174=CARTESIAN_POINT('Ctrl Pts',(-191.97524249326,-4.69035841421798,
132.290445775788));
#123175=CARTESIAN_POINT('Ctrl Pts',(-191.982971244541,-4.64541136803275,
132.419704631778));
#123176=CARTESIAN_POINT('Ctrl Pts',(-191.990921039647,-4.59917882738299,
132.552660316771));
#123177=CARTESIAN_POINT('Ctrl Pts',(-191.998870834754,-4.54725946423311,
132.6835556899));
#123178=CARTESIAN_POINT('Ctrl Pts',(-192.00682062986,-4.48988223286208,
132.811881625558));
#123179=CARTESIAN_POINT('Ctrl Pts',(-192.01456223062,-4.43400763331795,
132.936846879103));
#123180=CARTESIAN_POINT('Ctrl Pts',(-192.022303831381,-4.37295770825076,
133.059375276236));
#123181=CARTESIAN_POINT('Ctrl Pts',(-192.030045432141,-4.30699015546567,
133.179022459434));
#123182=CARTESIAN_POINT('Ctrl Pts',(-192.03809932442,-4.23836151127706,
133.30349613804));
#123183=CARTESIAN_POINT('Ctrl Pts',(-192.046153216699,-4.16441045295695,
133.424850879837));
#123184=CARTESIAN_POINT('Ctrl Pts',(-192.054207108978,-4.08547567197879,
133.542621305698));
#123185=CARTESIAN_POINT('Ctrl Pts',(-192.062261001257,-4.00654089100041,
133.660391731559));
#123186=CARTESIAN_POINT('Ctrl Pts',(-192.070314893536,-3.9226227251379,
133.77457750615));
#123187=CARTESIAN_POINT('Ctrl Pts',(-192.078368785815,-3.83410466332919,
133.88475417897));
#123188=CARTESIAN_POINT('Ctrl Pts',(-192.086143119934,-3.74865914652369,
133.99110651607));
#123189=CARTESIAN_POINT('Ctrl Pts',(-192.093917454053,-3.65864985410877,
134.094069416823));
#123190=CARTESIAN_POINT('Ctrl Pts',(-192.101691788172,-3.56437564467085,
134.193226110054));
#123191=CARTESIAN_POINT('Ctrl Pts',(-192.109456541119,-3.47021761977078,
134.292260601523));
#123192=CARTESIAN_POINT('Ctrl Pts',(-192.117221294066,-3.37180540278206,
134.387497938163));
#123193=CARTESIAN_POINT('Ctrl Pts',(-192.124986047013,-3.26947915980666,
134.478552921473));
#123194=CARTESIAN_POINT('Ctrl Pts',(-192.132743087898,-3.16725454869806,
134.56951746769));
#123195=CARTESIAN_POINT('Ctrl Pts',(-192.140500128783,-3.06112393801676,
134.656307668951));
#123196=CARTESIAN_POINT('Ctrl Pts',(-192.148257169668,-2.95146527907113,
134.738574105538));
#123197=CARTESIAN_POINT('Ctrl Pts',(-192.156008360908,-2.84188931457368,
134.820778504364));
#123198=CARTESIAN_POINT('Ctrl Pts',(-192.163759552148,-2.72879090890884,
134.898465695044));
#123199=CARTESIAN_POINT('Ctrl Pts',(-192.171510743389,-2.6125818443738,
134.971325840477));
#123200=CARTESIAN_POINT('Ctrl Pts',(-192.179258640166,-2.49642217179069,
135.044155018405));
#123201=CARTESIAN_POINT('Ctrl Pts',(-192.187006536943,-2.37715480046932,
135.112161024362));
#123202=CARTESIAN_POINT('Ctrl Pts',(-192.19475443372,-2.25522112422815,
135.175076891054));
#123203=CARTESIAN_POINT('Ctrl Pts',(-192.202500709804,-2.13331295388346,
135.237979597104));
#123204=CARTESIAN_POINT('Ctrl Pts',(-192.210246985888,-2.00873993520163,
135.29579410257));
#123205=CARTESIAN_POINT('Ctrl Pts',(-192.217993261972,-1.88196838077047,
135.348299225897));
#123206=CARTESIAN_POINT('Ctrl Pts',(-192.225739595237,-1.75519589054102,
135.400804736805));
#123207=CARTESIAN_POINT('Ctrl Pts',(-192.233485928503,-1.62622519338845,
135.448000637764));
#123208=CARTESIAN_POINT('Ctrl Pts',(-192.241232261768,-1.49554253846573,
135.489713921015));
#123209=CARTESIAN_POINT('Ctrl Pts',(-192.248980329771,-1.36483061806836,
135.531436545666));
#123210=CARTESIAN_POINT('Ctrl Pts',(-192.256728397774,-1.2324063493972,
135.567673990578));
#123211=CARTESIAN_POINT('Ctrl Pts',(-192.264476465777,-1.09877070560949,
135.598303253747));
#123212=CARTESIAN_POINT('Ctrl Pts',(-192.272232768519,-0.964993032269096,
135.628965070061));
#123213=CARTESIAN_POINT('Ctrl Pts',(-192.279989071261,-0.830001793655666,
135.654006710523));
#123214=CARTESIAN_POINT('Ctrl Pts',(-192.287745374002,-0.694308261338982,
135.673356314908));
#123215=CARTESIAN_POINT('Ctrl Pts',(-192.295505816517,-0.558542305298078,
135.69271624676));
#123216=CARTESIAN_POINT('Ctrl Pts',(-192.303266259031,-0.422073697493207,
135.706378050116));
#123217=CARTESIAN_POINT('Ctrl Pts',(-192.311026701545,-0.28541738556099,
135.714321918688));
#123218=CARTESIAN_POINT('Ctrl Pts',(-192.31879960181,-0.148541700785455,
135.722278539464));
#123219=CARTESIAN_POINT('Ctrl Pts',(-192.326572502076,-0.0114781008894383,
135.72449887668));
#123220=CARTESIAN_POINT('Ctrl Pts',(-192.334345402341,0.125259011019499,
135.721015297596));
#123221=CARTESIAN_POINT('Ctrl Pts',(-192.341835738103,0.257025384489433,
135.717658355386));
#123222=CARTESIAN_POINT('Ctrl Pts',(-192.349326073865,0.388488287825575,
135.709005020696));
#123223=CARTESIAN_POINT('Ctrl Pts',(-192.356816409627,0.519195120740406,
135.695129421047));
#123224=CARTESIAN_POINT('Ctrl Pts',(-192.364590743746,0.654857742953279,
135.680727723819));
#123225=CARTESIAN_POINT('Ctrl Pts',(-192.372365077865,0.790135568566218,
135.66065431978));
#123226=CARTESIAN_POINT('Ctrl Pts',(-192.380139411984,0.924516415821493,
135.634935372124));
#123227=CARTESIAN_POINT('Ctrl Pts',(-192.387904164931,1.05873165069249,
135.609248120773));
#123228=CARTESIAN_POINT('Ctrl Pts',(-192.395668917878,1.19205172640386,
135.577929242197));
#123229=CARTESIAN_POINT('Ctrl Pts',(-192.403433670826,1.32396869645902,
135.541056718573));
#123230=CARTESIAN_POINT('Ctrl Pts',(-192.411190711711,1.45575464472018,
135.504220817259));
#123231=CARTESIAN_POINT('Ctrl Pts',(-192.418947752595,1.58613988652435,
135.461842352468));
#123232=CARTESIAN_POINT('Ctrl Pts',(-192.42670479348,1.71462615325309,135.414050435448));
#123233=CARTESIAN_POINT('Ctrl Pts',(-192.43445598472,1.84301552748845,135.366294558683));
#123234=CARTESIAN_POINT('Ctrl Pts',(-192.442207175961,1.96950841206677,
135.313133491062));
#123235=CARTESIAN_POINT('Ctrl Pts',(-192.449958367201,2.0936215538718,135.254746202171));
#123236=CARTESIAN_POINT('Ctrl Pts',(-192.457706263978,2.21768194428091,
135.196383729436));
#123237=CARTESIAN_POINT('Ctrl Pts',(-192.465454160755,2.33936425058921,
135.132799619475));
#123238=CARTESIAN_POINT('Ctrl Pts',(-192.473202057532,2.45820528151151,
135.064220927065));
#123239=CARTESIAN_POINT('Ctrl Pts',(-192.480948333616,2.57702145345207,
134.99565657984));
#123240=CARTESIAN_POINT('Ctrl Pts',(-192.4886946097,2.6929971937552,134.922099923534));
#123241=CARTESIAN_POINT('Ctrl Pts',(-192.496440885784,2.80569436276991,
134.843823726102));
#123242=CARTESIAN_POINT('Ctrl Pts',(-192.50418721905,2.91839236368936,134.765546950852));
#123243=CARTESIAN_POINT('Ctrl Pts',(-192.511933552315,3.0278114239197,134.682550787991));
#123244=CARTESIAN_POINT('Ctrl Pts',(-192.51967988558,3.13354315758743,134.59515081778));
#123245=CARTESIAN_POINT('Ctrl Pts',(-192.527427953583,3.23929856914339,
134.507731274952));
#123246=CARTESIAN_POINT('Ctrl Pts',(-192.535176021586,3.34136470970479,
134.415906211393));
#123247=CARTESIAN_POINT('Ctrl Pts',(-192.542924089589,3.43936730597353,
134.320030624421));
#123248=CARTESIAN_POINT('Ctrl Pts',(-192.550680392331,3.53747406056822,
134.224053139734));
#123249=CARTESIAN_POINT('Ctrl Pts',(-192.558436695073,3.63150836371962,
134.124016805884));
#123250=CARTESIAN_POINT('Ctrl Pts',(-192.566192997815,3.72113340261438,
134.020312927916));
#123251=CARTESIAN_POINT('Ctrl Pts',(-192.573953440329,3.81080627709143,
133.916553700066));
#123252=CARTESIAN_POINT('Ctrl Pts',(-192.581713882843,3.896064955127,133.80912333375));
#123253=CARTESIAN_POINT('Ctrl Pts',(-192.589474325357,3.97661443135476,
133.698444363217));
#123254=CARTESIAN_POINT('Ctrl Pts',(-192.597247225623,4.05729321275217,
133.587587720975));
#123255=CARTESIAN_POINT('Ctrl Pts',(-192.605020125888,4.13324746904369,
133.47347237904));
#123256=CARTESIAN_POINT('Ctrl Pts',(-192.612793026153,4.20422638427667,
133.356548614609));
#123257=CARTESIAN_POINT('Ctrl Pts',(-192.620283361916,4.27262503715757,
133.243875323526));
#123258=CARTESIAN_POINT('Ctrl Pts',(-192.627773697678,4.3364036520234,133.128594520953));
#123259=CARTESIAN_POINT('Ctrl Pts',(-192.63526403344,4.39537995294483,133.011127060068));
#123260=CARTESIAN_POINT('Ctrl Pts',(-192.643038367559,4.45659235823986,
132.889205784701));
#123261=CARTESIAN_POINT('Ctrl Pts',(-192.650812701678,4.51282500400254,
132.764542553542));
#123262=CARTESIAN_POINT('Ctrl Pts',(-192.658587035797,4.56382305531772,
132.637582421454));
#123263=CARTESIAN_POINT('Ctrl Pts',(-192.666351788744,4.6147582560922,132.510778756383));
#123264=CARTESIAN_POINT('Ctrl Pts',(-192.674116541692,4.66047155399552,
132.381684181989));
#123265=CARTESIAN_POINT('Ctrl Pts',(-192.681881294639,4.70075400015228,
132.250768199319));
#123266=CARTESIAN_POINT('Ctrl Pts',(-192.689638335524,4.74099643721574,
132.119982244248));
#123267=CARTESIAN_POINT('Ctrl Pts',(-192.697395376409,4.77581864259817,
131.987378852245));
#123268=CARTESIAN_POINT('Ctrl Pts',(-192.705152417294,4.80505991488965,
131.853447018593));
#123269=CARTESIAN_POINT('Ctrl Pts',(-192.712903608534,4.83427913611028,
131.71961618398));
#123270=CARTESIAN_POINT('Ctrl Pts',(-192.720654799774,4.85792571819555,
131.584459282138));
#123271=CARTESIAN_POINT('Ctrl Pts',(-192.728405991014,4.87588902321573,
131.448479625036));
#123272=CARTESIAN_POINT('Ctrl Pts',(-192.736153887791,4.89384469335207,
131.312557762916));
#123273=CARTESIAN_POINT('Ctrl Pts',(-192.743901784568,4.90612183966131,
131.175814227835));
#123274=CARTESIAN_POINT('Ctrl Pts',(-192.751649681345,4.91266112355447,
131.038761444392));
#123275=CARTESIAN_POINT('Ctrl Pts',(-192.759395957429,4.9191990395704,130.901737329437));
#123276=CARTESIAN_POINT('Ctrl Pts',(-192.767142233513,4.92000146188634,
130.764404485061));
#123277=CARTESIAN_POINT('Ctrl Pts',(-192.774888509598,4.91506105272305,
130.627278968305));
#123278=CARTESIAN_POINT('Ctrl Pts',(-192.782634842863,4.91012060709078,
130.490152439319));
#123279=CARTESIAN_POINT('Ctrl Pts',(-192.790381176128,4.89943725946526,
130.353233631717));
#123280=CARTESIAN_POINT('Ctrl Pts',(-192.798127509394,4.88305577391945,
130.217036710942));
#123281=CARTESIAN_POINT('Ctrl Pts',(-192.805875577397,4.86667061985355,
130.080809289811));
#123282=CARTESIAN_POINT('Ctrl Pts',(-192.8136236454,4.84458483533778,129.945304465287));
#123283=CARTESIAN_POINT('Ctrl Pts',(-192.821371713403,4.81689478580987,
129.811029008818));
#123284=CARTESIAN_POINT('Ctrl Pts',(-192.829128016144,4.78917530696777,
129.676610842796));
#123285=CARTESIAN_POINT('Ctrl Pts',(-192.836884318886,4.75583974389208,
129.543425038395));
#123286=CARTESIAN_POINT('Ctrl Pts',(-192.844640621628,4.71703525704713,
129.41196647571));
#123287=CARTESIAN_POINT('Ctrl Pts',(-192.852401064142,4.67821005907918,
129.280437749632));
#123288=CARTESIAN_POINT('Ctrl Pts',(-192.860161506656,4.63391024734856,
129.150638472024));
#123289=CARTESIAN_POINT('Ctrl Pts',(-192.867921949171,4.58433185427907,
129.023045229337));
#123290=CARTESIAN_POINT('Ctrl Pts',(-192.875694849436,4.53467387357166,
128.895247162649));
#123291=CARTESIAN_POINT('Ctrl Pts',(-192.883467749701,4.47972053529839,
128.769662565957));
#123292=CARTESIAN_POINT('Ctrl Pts',(-192.891240649967,4.41971509826897,
128.646745843647));
#123293=CARTESIAN_POINT('Ctrl Pts',(-192.898730985729,4.36189101002015,
128.528297453802));
#123294=CARTESIAN_POINT('Ctrl Pts',(-192.906221321491,4.29937590510965,
128.412326609133));
#123295=CARTESIAN_POINT('Ctrl Pts',(-192.913711657253,4.23242533464076,
128.299214144964));
#123296=CARTESIAN_POINT('Ctrl Pts',(-192.921485991372,4.16293631294325,
128.181812987336));
#123297=CARTESIAN_POINT('Ctrl Pts',(-192.929260325491,4.08844872451645,
128.067119348354));
#123298=CARTESIAN_POINT('Ctrl Pts',(-192.93703465961,4.00919926212544,127.955588190875));
#123299=CARTESIAN_POINT('Ctrl Pts',(-192.944799412557,3.93004746761452,
127.844194485581));
#123300=CARTESIAN_POINT('Ctrl Pts',(-192.952564165504,3.84614570015536,
127.735955822617));
#123301=CARTESIAN_POINT('Ctrl Pts',(-192.960328918452,3.75777602230254,
127.631301773374));
#123302=CARTESIAN_POINT('Ctrl Pts',(-192.968085959337,3.66949411445908,
127.526751668006));
#123303=CARTESIAN_POINT('Ctrl Pts',(-192.975843000222,3.57675337783237,
127.425779388006));
#123304=CARTESIAN_POINT('Ctrl Pts',(-192.983600041107,3.47987835496601,
127.328784449916));
#123305=CARTESIAN_POINT('Ctrl Pts',(-192.991351232347,3.38307638630784,
127.231862656463));
#123306=CARTESIAN_POINT('Ctrl Pts',(-192.999102423587,3.28214661216284,
127.138912510412));
#123307=CARTESIAN_POINT('Ctrl Pts',(-193.006853614827,3.17745268064025,
127.050299146999));
#123308=CARTESIAN_POINT('Ctrl Pts',(-193.014601511604,3.07280324683178,
126.961723446631));
#123309=CARTESIAN_POINT('Ctrl Pts',(-193.022349408381,2.96439313545571,
126.877481114876));
#123310=CARTESIAN_POINT('Ctrl Pts',(-193.030097305158,2.85262138988372,
126.797899052983));
#123311=CARTESIAN_POINT('Ctrl Pts',(-193.037843581242,2.74087302455107,
126.718333637942));
#123312=CARTESIAN_POINT('Ctrl Pts',(-193.045589857326,2.62576474197169,
126.643426780396));
#123313=CARTESIAN_POINT('Ctrl Pts',(-193.053336133411,2.50772674929877,
126.573463595261));
#123314=CARTESIAN_POINT('Ctrl Pts',(-193.061082466676,2.38968788529636,
126.503499893673));
#123315=CARTESIAN_POINT('Ctrl Pts',(-193.068828799941,2.26871960437203,
126.438480136662));
#123316=CARTESIAN_POINT('Ctrl Pts',(-193.076575133207,2.145278684549,126.378644581926));
#123317=CARTESIAN_POINT('Ctrl Pts',(-193.08432320121,2.02181012098801,126.318795627432));
#123318=CARTESIAN_POINT('Ctrl Pts',(-193.092071269213,1.89586816841405,
126.264133355903));
#123319=CARTESIAN_POINT('Ctrl Pts',(-193.099819337216,1.7679312758711,126.214850614712));
#123320=CARTESIAN_POINT('Ctrl Pts',(-193.107575639958,1.63985841047612,
126.165515495237));
#123321=CARTESIAN_POINT('Ctrl Pts',(-193.115331942699,1.50978673510698,
126.121571468042));
#123322=CARTESIAN_POINT('Ctrl Pts',(-193.123088245441,1.37821215022817,
126.08316221764));
#123323=CARTESIAN_POINT('Ctrl Pts',(-193.130848687956,1.24656734003178,
126.044732467064));
#123324=CARTESIAN_POINT('Ctrl Pts',(-193.13860913047,1.11341840134966,126.011843473238));
#123325=CARTESIAN_POINT('Ctrl Pts',(-193.146369572984,0.979272260174981,
125.98458791515));
#123326=CARTESIAN_POINT('Ctrl Pts',(-193.154142473249,0.844910775705553,
125.957288604021));
#123327=CARTESIAN_POINT('Ctrl Pts',(-193.161915373515,0.70954927612074,
125.935640861783));
#123328=CARTESIAN_POINT('Ctrl Pts',(-193.16968827378,0.573701552030352,
125.919685644582));
#123329=CARTESIAN_POINT('Ctrl Pts',(-193.177178609542,0.442792234891523,
125.904310439715));
#123330=CARTESIAN_POINT('Ctrl Pts',(-193.184668945304,0.311431737587399,
125.894221093707));
#123331=CARTESIAN_POINT('Ctrl Pts',(-193.192159281066,0.180078599274265,
125.889408454972));
#123332=CARTESIAN_POINT('Ctrl Pts',(-193.199933615185,0.0437451667967284,
125.884413343577));
#123333=CARTESIAN_POINT('Ctrl Pts',(-193.207707949304,-0.0930122009763956,
125.885087147901));
#123334=CARTESIAN_POINT('Ctrl Pts',(-193.215482283423,-0.229682792687816,
125.891476650155));
#123335=CARTESIAN_POINT('Ctrl Pts',(-193.22324703637,-0.366184950108441,
125.897858277918));
#123336=CARTESIAN_POINT('Ctrl Pts',(-193.231011789318,-0.502600157464022,
125.909941569895));
#123337=CARTESIAN_POINT('Ctrl Pts',(-193.238776542265,-0.638414542478167,
125.927721412698));
#123338=CARTESIAN_POINT('Ctrl Pts',(-193.24653358315,-0.774094034730837,
125.945483596311));
#123339=CARTESIAN_POINT('Ctrl Pts',(-193.254290624035,-0.909173507043042,
125.968931020864));
#123340=CARTESIAN_POINT('Ctrl Pts',(-193.26204766492,-1.04314141166046,
125.998006587974));
#123341=CARTESIAN_POINT('Ctrl Pts',(-193.26979885616,-1.17700829003943,
126.027060228972));
#123342=CARTESIAN_POINT('Ctrl Pts',(-193.2775500474,-1.30976488866881,126.061733482066));
#123343=CARTESIAN_POINT('Ctrl Pts',(-193.28530123864,-1.44090744824757,
126.101917764316));
#123344=CARTESIAN_POINT('Ctrl Pts',(-193.293049135417,-1.57199426873999,
126.142084967174));
#123345=CARTESIAN_POINT('Ctrl Pts',(-193.300797032194,-1.70146804157518,
126.187758426161));
#123346=CARTESIAN_POINT('Ctrl Pts',(-193.308544928971,-1.82883804278507,
126.238779112898));
#123347=CARTESIAN_POINT('Ctrl Pts',(-193.316291205055,-1.95618140093683,
126.289789127208));
#123348=CARTESIAN_POINT('Ctrl Pts',(-193.324037481139,-2.08142150007336,
126.346143999172));
#123349=CARTESIAN_POINT('Ctrl Pts',(-193.331783757224,-2.20408592746605,
126.407635894906));
#123350=CARTESIAN_POINT('Ctrl Pts',(-193.339530090489,-2.32675126033885,
126.469128244559));
#123351=CARTESIAN_POINT('Ctrl Pts',(-193.347276423754,-2.44684053402099,
126.53575751844));
#123352=CARTESIAN_POINT('Ctrl Pts',(-193.35502275702,-2.5639047132275,126.607269281415));
#123353=CARTESIAN_POINT('Ctrl Pts',(-193.362770825023,-2.68099510814607,
126.678797058955));
#123354=CARTESIAN_POINT('Ctrl Pts',(-193.370518893026,-2.79505872696956,
126.755209297555));
#123355=CARTESIAN_POINT('Ctrl Pts',(-193.378266961029,-2.90567470834559,
126.836207703201));
#123356=CARTESIAN_POINT('Ctrl Pts',(-193.38602326377,-3.01640825370252,
126.917292194916));
#123357=CARTESIAN_POINT('Ctrl Pts',(-193.393779566512,-3.12368652605522,
127.002972359134));
#123358=CARTESIAN_POINT('Ctrl Pts',(-193.401535869254,-3.22712059323985,
127.092908645738));
#123359=CARTESIAN_POINT('Ctrl Pts',(-193.409296311768,-3.33060986630048,
127.182892934046));
#123360=CARTESIAN_POINT('Ctrl Pts',(-193.417056754283,-3.4302505619723,
127.277137602611));
#123361=CARTESIAN_POINT('Ctrl Pts',(-193.424817196797,-3.52569070091577,
127.375266255497));
#123362=CARTESIAN_POINT('Ctrl Pts',(-193.432590097062,-3.62128404884331,
127.473552433207));
#123363=CARTESIAN_POINT('Ctrl Pts',(-193.440362997328,-3.71266310439815,
127.57573476299));
#123364=CARTESIAN_POINT('Ctrl Pts',(-193.448135897593,-3.79951569364077,
127.68140311605));
#123365=CARTESIAN_POINT('Ctrl Pts',(-193.455626233355,-3.88321097249688,
127.783230158314));
#123366=CARTESIAN_POINT('Ctrl Pts',(-193.463116569117,-3.9627029824913,
127.888293927058));
#123367=CARTESIAN_POINT('Ctrl Pts',(-193.470606904879,-4.03775157149843,
127.996203693646));
#123368=CARTESIAN_POINT('Ctrl Pts',(-193.47889361498,-4.12077934492612,
128.115586453127));
#123369=CARTESIAN_POINT('Ctrl Pts',(-193.48718032508,-4.19864109136327,
128.238845638589));
#123370=CARTESIAN_POINT('Ctrl Pts',(-193.495467035181,-4.27096326554449,
128.365496979133));
#123371=CARTESIAN_POINT('Ctrl Pts',(-193.503328207986,-4.33957156751243,
128.485644548189));
#123372=CARTESIAN_POINT('Ctrl Pts',(-193.511189380792,-4.40319473039249,
128.608844226595));
#123373=CARTESIAN_POINT('Ctrl Pts',(-193.519050553597,-4.46155570869261,
128.734649594082));
#123374=CARTESIAN_POINT('Ctrl Pts',(-193.526903815789,-4.51985795897289,
128.86032836499));
#123375=CARTESIAN_POINT('Ctrl Pts',(-193.534757077982,-4.57290840298805,
128.988607267093));
#123376=CARTESIAN_POINT('Ctrl Pts',(-193.542610340174,-4.62047497514472,
129.119013749244));
#123377=CARTESIAN_POINT('Ctrl Pts',(-193.550455704939,-4.66799371322391,
129.249289091533));
#123378=CARTESIAN_POINT('Ctrl Pts',(-193.558301069704,-4.71003943508657,
129.381687398499));
#123379=CARTESIAN_POINT('Ctrl Pts',(-193.566146434469,-4.74642766497959,
129.515715017094));
#123380=CARTESIAN_POINT('Ctrl Pts',(-193.567446765008,-4.75245883472166,
129.537929434235));
#123381=CARTESIAN_POINT('Ctrl Pts',(-193.568747095547,-4.75833469270917,
129.560188567407));
#123382=CARTESIAN_POINT('Ctrl Pts',(-193.570047426085,-4.76405452823409,
129.582490119308));
#123383=CARTESIAN_POINT('Origin',(213.235140564004,0.,130.804360617566));
#123384=CARTESIAN_POINT('',(-195.665141276266,-4.76405452823396,129.582490119308));
#123385=CARTESIAN_POINT('',(-195.319719904489,-4.76405452823413,129.582490119309));
#123386=CARTESIAN_POINT('',(213.235140564004,-4.76405452823405,129.582490119308));
#123387=CARTESIAN_POINT('',(-193.985140563976,-4.91824942956879,130.80672938227));
#123388=CARTESIAN_POINT('Ctrl Pts',(-193.985140564012,-4.91824942956849,
130.806729382913));
#123389=CARTESIAN_POINT('Ctrl Pts',(-193.992731428123,-4.91818520775937,
130.940072635538));
#123390=CARTESIAN_POINT('Ctrl Pts',(-194.000322292233,-4.91269870967798,
131.073280898492));
#123391=CARTESIAN_POINT('Ctrl Pts',(-194.007913156344,-4.90181963422078,
131.206041256965));
#123392=CARTESIAN_POINT('Ctrl Pts',(-194.015687490463,-4.89067761319646,
131.342010412719));
#123393=CARTESIAN_POINT('Ctrl Pts',(-194.023461824582,-4.87385628461547,
131.47773098801));
#123394=CARTESIAN_POINT('Ctrl Pts',(-194.031236158701,-4.85136951318697,
131.612690320732));
#123395=CARTESIAN_POINT('Ctrl Pts',(-194.039000911648,-4.82891045469462,
131.747483328137));
#123396=CARTESIAN_POINT('Ctrl Pts',(-194.046765664595,-4.80079990939565,
131.881516577692));
#123397=CARTESIAN_POINT('Ctrl Pts',(-194.054530417543,-4.76710364769382,
132.014280397818));
#123398=CARTESIAN_POINT('Ctrl Pts',(-194.062287458428,-4.73344085359424,
132.146912355046));
#123399=CARTESIAN_POINT('Ctrl Pts',(-194.070044499313,-4.69420347904607,
132.278277015427));
#123400=CARTESIAN_POINT('Ctrl Pts',(-194.077801540198,-4.64950864104312,
132.407873155517));
#123401=CARTESIAN_POINT('Ctrl Pts',(-194.085552731438,-4.604847507765,132.53737156615));
#123402=CARTESIAN_POINT('Ctrl Pts',(-194.093303922678,-4.55473722966819,
132.665103742946));
#123403=CARTESIAN_POINT('Ctrl Pts',(-194.101055113918,-4.49934512806033,
132.790582277175));
#123404=CARTESIAN_POINT('Ctrl Pts',(-194.108803010695,-4.44397656957337,
132.91600747968));
#123405=CARTESIAN_POINT('Ctrl Pts',(-194.116550907472,-4.38333081010158,
133.039180587809));
#123406=CARTESIAN_POINT('Ctrl Pts',(-194.124298804249,-4.3176237237225,
133.159633094977));
#123407=CARTESIAN_POINT('Ctrl Pts',(-194.132045080334,-4.25193038184923,
133.280060406077));
#123408=CARTESIAN_POINT('Ctrl Pts',(-194.139791356418,-4.18117800603018,
133.397767905166));
#123409=CARTESIAN_POINT('Ctrl Pts',(-194.147537632502,-4.10562877152469,
133.512311033089));
#123410=CARTESIAN_POINT('Ctrl Pts',(-194.155283965767,-4.03007897933201,
133.626855006542));
#123411=CARTESIAN_POINT('Ctrl Pts',(-194.163030299033,-3.94973247305859,
133.73823423585));
#123412=CARTESIAN_POINT('Ctrl Pts',(-194.170776632298,-3.86489494195318,
133.846032879688));
#123413=CARTESIAN_POINT('Ctrl Pts',(-194.178524700301,-3.78003841207102,
133.953855664285));
#123414=CARTESIAN_POINT('Ctrl Pts',(-194.186272768304,-3.69068909780753,
134.058095960657));
#123415=CARTESIAN_POINT('Ctrl Pts',(-194.194020836307,-3.59719291272284,
134.158371084329));
#123416=CARTESIAN_POINT('Ctrl Pts',(-194.201777139049,-3.50359735877989,
134.258752781596));
#123417=CARTESIAN_POINT('Ctrl Pts',(-194.209533441791,-3.40584639691667,
134.355160601374));
#123418=CARTESIAN_POINT('Ctrl Pts',(-194.217289744533,-3.30432313691359,
134.447248437601));
#123419=CARTESIAN_POINT('Ctrl Pts',(-194.225050187047,-3.20274569088985,
134.539385423878));
#123420=CARTESIAN_POINT('Ctrl Pts',(-194.232810629561,-3.09739223505416,
134.627197582094));
#123421=CARTESIAN_POINT('Ctrl Pts',(-194.240571072075,-2.9886781026604,
134.71037985218));
#123422=CARTESIAN_POINT('Ctrl Pts',(-194.248343972341,-2.87978945269014,
134.793695653831));
#123423=CARTESIAN_POINT('Ctrl Pts',(-194.256116872606,-2.76752966587593,
134.87236649073));
#123424=CARTESIAN_POINT('Ctrl Pts',(-194.263889772872,-2.65234287085514,
134.946130813741));
#123425=CARTESIAN_POINT('Ctrl Pts',(-194.271380108634,-2.54134340597169,
135.01721361781));
#123426=CARTESIAN_POINT('Ctrl Pts',(-194.278870444396,-2.427626312325,135.083740287406));
#123427=CARTESIAN_POINT('Ctrl Pts',(-194.286360780158,-2.31160794777514,
135.145518499777));
#123428=CARTESIAN_POINT('Ctrl Pts',(-194.294135114277,-2.19119071166986,
135.209639051847));
#123429=CARTESIAN_POINT('Ctrl Pts',(-194.301909448396,-2.06791280888925,
135.268847077811));
#123430=CARTESIAN_POINT('Ctrl Pts',(-194.309683782515,-1.94221305079689,
135.32287713605));
#123431=CARTESIAN_POINT('Ctrl Pts',(-194.317448535462,-1.81666820642226,
135.376840607072));
#123432=CARTESIAN_POINT('Ctrl Pts',(-194.325213288409,-1.68870780118061,
135.425638654508));
#123433=CARTESIAN_POINT('Ctrl Pts',(-194.332978041356,-1.55879618671472,
135.469051122925));
#123434=CARTESIAN_POINT('Ctrl Pts',(-194.340735082241,-1.42901360229611,
135.512420473466));
#123435=CARTESIAN_POINT('Ctrl Pts',(-194.348492123126,-1.29728403370762,
135.550414766694));
#123436=CARTESIAN_POINT('Ctrl Pts',(-194.356249164011,-1.1640924790234,
135.582861612939));
#123437=CARTESIAN_POINT('Ctrl Pts',(-194.364000355251,-1.03100136512646,
135.615283990765));
#123438=CARTESIAN_POINT('Ctrl Pts',(-194.371751546491,-0.896450837902563,
135.642167156194));
#123439=CARTESIAN_POINT('Ctrl Pts',(-194.379502737732,-0.760941409372517,
135.66338842506));
#123440=CARTESIAN_POINT('Ctrl Pts',(-194.387250634509,-0.625489575964244,
135.684600674321));
#123441=CARTESIAN_POINT('Ctrl Pts',(-194.394998531286,-0.489080037301672,
135.700155752914));
#123442=CARTESIAN_POINT('Ctrl Pts',(-194.402746428063,-0.352223646456436,
135.709982042562));
#123443=CARTESIAN_POINT('Ctrl Pts',(-194.410492704147,-0.215395883017882,
135.719806276762));
#123444=CARTESIAN_POINT('Ctrl Pts',(-194.418238980231,-0.0781218430315514,
135.723904077597));
#123445=CARTESIAN_POINT('Ctrl Pts',(-194.425985256315,0.0590827411620631,
135.722255725455));
#123446=CARTESIAN_POINT('Ctrl Pts',(-194.433731589581,0.196288338168563,
135.720607361145));
#123447=CARTESIAN_POINT('Ctrl Pts',(-194.441477922846,0.333424087422282,
135.713212763916));
#123448=CARTESIAN_POINT('Ctrl Pts',(-194.449224256111,0.469974897333745,
135.700104346396));
#123449=CARTESIAN_POINT('Ctrl Pts',(-194.456972324114,0.606556286852497,
135.686992993336));
#123450=CARTESIAN_POINT('Ctrl Pts',(-194.464720392117,0.742552087266234,
135.668165311142));
#123451=CARTESIAN_POINT('Ctrl Pts',(-194.47246846012,0.877453360560609,
135.643705476381));
#123452=CARTESIAN_POINT('Ctrl Pts',(-194.480224762862,1.0124980085334,135.619219645417));
#123453=CARTESIAN_POINT('Ctrl Pts',(-194.487981065604,1.1464454203106,135.589089774232));
#123454=CARTESIAN_POINT('Ctrl Pts',(-194.495737368346,1.27879732686596,
135.553451105154));
#123455=CARTESIAN_POINT('Ctrl Pts',(-194.50349781086,1.41121987361924,135.517793414645));
#123456=CARTESIAN_POINT('Ctrl Pts',(-194.511258253374,1.54204484557664,
135.476621184933));
#123457=CARTESIAN_POINT('Ctrl Pts',(-194.519018695888,1.67079108929357,
135.430118955227));
#123458=CARTESIAN_POINT('Ctrl Pts',(-194.526791596154,1.79974400791011,
135.383542076013));
#123459=CARTESIAN_POINT('Ctrl Pts',(-194.534564496419,1.92661116793729,
135.33161824699));
#123460=CARTESIAN_POINT('Ctrl Pts',(-194.542337396684,2.05093245830343,
135.274579752461));
#123461=CARTESIAN_POINT('Ctrl Pts',(-194.549827732446,2.17073435661631,
135.21961475088));
#123462=CARTESIAN_POINT('Ctrl Pts',(-194.557318068208,2.28817199468981,
135.159900629281));
#123463=CARTESIAN_POINT('Ctrl Pts',(-194.56480840397,2.40285851435058,135.095683726179));
#123464=CARTESIAN_POINT('Ctrl Pts',(-194.572582738089,2.52189340826435,
135.029032019675));
#123465=CARTESIAN_POINT('Ctrl Pts',(-194.580357072209,2.63834151504885,
134.957318212925));
#123466=CARTESIAN_POINT('Ctrl Pts',(-194.588131406328,2.75174232289214,
134.880768012676));
#123467=CARTESIAN_POINT('Ctrl Pts',(-194.595896159275,2.86500337437468,
134.804312153707));
#123468=CARTESIAN_POINT('Ctrl Pts',(-194.603660912222,2.97522427835457,
134.723031977348));
#123469=CARTESIAN_POINT('Ctrl Pts',(-194.611425665169,3.08196881842492,
134.637199156398));
#123470=CARTESIAN_POINT('Ctrl Pts',(-194.619182706054,3.18860733831322,
134.551451585816));
#123471=CARTESIAN_POINT('Ctrl Pts',(-194.626939746939,3.29177606275606,
134.461160612539));
#123472=CARTESIAN_POINT('Ctrl Pts',(-194.634696787824,3.39106780213559,
134.366641098356));
#123473=CARTESIAN_POINT('Ctrl Pts',(-194.642447979064,3.49028466484221,
134.272192862074));
#123474=CARTESIAN_POINT('Ctrl Pts',(-194.650199170304,3.58563007983292,
134.173522700424));
#123475=CARTESIAN_POINT('Ctrl Pts',(-194.657950361544,3.6767302904695,134.070985394556));
#123476=CARTESIAN_POINT('Ctrl Pts',(-194.665698258321,3.76779178108626,
133.968491669778));
#123477=CARTESIAN_POINT('Ctrl Pts',(-194.673446155098,3.85461139688462,
133.862134361516));
#123478=CARTESIAN_POINT('Ctrl Pts',(-194.681194051876,3.93685275481512,
133.752304553499));
#123479=CARTESIAN_POINT('Ctrl Pts',(-194.68894032796,4.01907690962669,133.64249771951));
#123480=CARTESIAN_POINT('Ctrl Pts',(-194.696686604044,4.09672447724247,
133.529220143312));
#123481=CARTESIAN_POINT('Ctrl Pts',(-194.704432880128,4.1695001010668,133.412895066199));
#123482=CARTESIAN_POINT('Ctrl Pts',(-194.712179213393,4.24227626210415,
133.2965691304));
#123483=CARTESIAN_POINT('Ctrl Pts',(-194.719925546659,4.31018020022778,
133.177195980241));
#123484=CARTESIAN_POINT('Ctrl Pts',(-194.727671879924,4.3729607655146,133.055226496682));
#123485=CARTESIAN_POINT('Ctrl Pts',(-194.735419947927,4.43575539007363,
132.933229698903));
#123486=CARTESIAN_POINT('Ctrl Pts',(-194.74316801593,4.49342417982122,132.808635758297));
#123487=CARTESIAN_POINT('Ctrl Pts',(-194.750916083933,4.54576286146099,
132.681918358319));
#123488=CARTESIAN_POINT('Ctrl Pts',(-194.758672386675,4.59815716927451,
132.555066281581));
#123489=CARTESIAN_POINT('Ctrl Pts',(-194.766428689417,4.64520990323737,
132.426086599126));
#123490=CARTESIAN_POINT('Ctrl Pts',(-194.774184992159,4.68676551997081,
132.295471620581));
#123491=CARTESIAN_POINT('Ctrl Pts',(-194.781945434673,4.72834331618813,
132.164786928889));
#123492=CARTESIAN_POINT('Ctrl Pts',(-194.789705877187,4.76441804619331,
132.032465578979));
#123493=CARTESIAN_POINT('Ctrl Pts',(-194.797466319701,4.79488489286097,
131.899012126821));
#123494=CARTESIAN_POINT('Ctrl Pts',(-194.805239219967,4.82540064761563,
131.765344443334));
#123495=CARTESIAN_POINT('Ctrl Pts',(-194.813012120232,4.85029045859629,
131.630541410641));
#123496=CARTESIAN_POINT('Ctrl Pts',(-194.820785020498,4.86950105189414,
131.495115688559));
#123497=CARTESIAN_POINT('Ctrl Pts',(-194.82827535626,4.88801329173705,131.36461303259));
#123498=CARTESIAN_POINT('Ctrl Pts',(-194.835765692022,4.90125202199734,
131.233532480348));
#123499=CARTESIAN_POINT('Ctrl Pts',(-194.843256027784,4.90921538795057,
131.102332658552));
#123500=CARTESIAN_POINT('Ctrl Pts',(-194.851030361903,4.91748068734433,
130.966158355635));
#123501=CARTESIAN_POINT('Ctrl Pts',(-194.858804696022,4.92008887680447,
130.82942420116));
#123502=CARTESIAN_POINT('Ctrl Pts',(-194.866579030141,4.91698093192857,
130.692639636767));
#123503=CARTESIAN_POINT('Ctrl Pts',(-194.874343783088,4.91387681731697,
130.556023647124));
#123504=CARTESIAN_POINT('Ctrl Pts',(-194.882108536035,4.90507059386854,
130.419357758287));
#123505=CARTESIAN_POINT('Ctrl Pts',(-194.889873288982,4.89055504197982,
130.283155817256));
#123506=CARTESIAN_POINT('Ctrl Pts',(-194.897630329867,4.87605390714187,
130.147089153914));
#123507=CARTESIAN_POINT('Ctrl Pts',(-194.905387370752,4.85585476974856,
130.011485907615));
#123508=CARTESIAN_POINT('Ctrl Pts',(-194.913144411637,4.83000243600482,
129.876858849003));
#123509=CARTESIAN_POINT('Ctrl Pts',(-194.920895602877,4.80416959770702,
129.742333313703));
#123510=CARTESIAN_POINT('Ctrl Pts',(-194.928646794117,4.77269212197063,
129.608782883225));
#123511=CARTESIAN_POINT('Ctrl Pts',(-194.936397985358,4.73566647163151,
129.476713777489));
#123512=CARTESIAN_POINT('Ctrl Pts',(-194.944145882135,4.69865655818142,
129.344700804647));
#123513=CARTESIAN_POINT('Ctrl Pts',(-194.951893778912,4.6561032655712,129.214168279979));
#123514=CARTESIAN_POINT('Ctrl Pts',(-194.959641675689,4.6081538003628,129.08561060238));
#123515=CARTESIAN_POINT('Ctrl Pts',(-194.967387951773,4.56021436514899,
128.957079816276));
#123516=CARTESIAN_POINT('Ctrl Pts',(-194.975134227857,4.50688113905005,
128.830523421655));
#123517=CARTESIAN_POINT('Ctrl Pts',(-194.982880503941,4.44835055949762,
128.706418682641));
#123518=CARTESIAN_POINT('Ctrl Pts',(-194.990626837206,4.38981954788566,
128.582313027514));
#123519=CARTESIAN_POINT('Ctrl Pts',(-194.998373170472,4.32609127303541,
128.460659417719));
#123520=CARTESIAN_POINT('Ctrl Pts',(-195.006119503737,4.25740932120014,
128.341912864971));
#123521=CARTESIAN_POINT('Ctrl Pts',(-195.01386757174,4.18871198851806,128.223139719757));
#123522=CARTESIAN_POINT('Ctrl Pts',(-195.021615639743,4.11505896709885,
128.107275265403));
#123523=CARTESIAN_POINT('Ctrl Pts',(-195.029363707746,4.03673836554418,
127.994747400299));
#123524=CARTESIAN_POINT('Ctrl Pts',(-195.037120010488,3.95833452392204,
127.88209993924));
#123525=CARTESIAN_POINT('Ctrl Pts',(-195.04487631323,3.87525341621253,127.772796472684));
#123526=CARTESIAN_POINT('Ctrl Pts',(-195.052632615971,3.78782516145076,
127.667233969058));
#123527=CARTESIAN_POINT('Ctrl Pts',(-195.060393058486,3.70035024359701,
127.561615123545));
#123528=CARTESIAN_POINT('Ctrl Pts',(-195.068153501,3.60852381712407,127.459741509747));
#123529=CARTESIAN_POINT('Ctrl Pts',(-195.075913943514,3.51271372304341,
127.361974038107));
#123530=CARTESIAN_POINT('Ctrl Pts',(-195.083686843779,3.41674982609412,
127.264049621441));
#123531=CARTESIAN_POINT('Ctrl Pts',(-195.091459744045,3.31678976767184,
127.170244786629));
#123532=CARTESIAN_POINT('Ctrl Pts',(-195.09923264431,3.21323606715028,127.080881459673));
#123533=CARTESIAN_POINT('Ctrl Pts',(-195.106722980072,3.11344680447899,
126.994766714744));
#123534=CARTESIAN_POINT('Ctrl Pts',(-195.114213315834,3.01032088056308,
126.912776355728));
#123535=CARTESIAN_POINT('Ctrl Pts',(-195.121703651596,2.90424314852822,
126.835159842003));
#123536=CARTESIAN_POINT('Ctrl Pts',(-195.129477985715,2.79414344704178,
126.75460047457));
#123537=CARTESIAN_POINT('Ctrl Pts',(-195.137252319834,2.68051492048119,
126.678497980498));
#123538=CARTESIAN_POINT('Ctrl Pts',(-195.145026653953,2.56375427239589,
126.60717738434));
#123539=CARTESIAN_POINT('Ctrl Pts',(-195.1527914069,2.44713752137415,126.535944684443));
#123540=CARTESIAN_POINT('Ctrl Pts',(-195.160556159847,2.32739665963895,
126.469482358469));
#123541=CARTESIAN_POINT('Ctrl Pts',(-195.168320912794,2.20496009885318,
126.408074227331));
#123542=CARTESIAN_POINT('Ctrl Pts',(-195.176077953679,2.0826451437853,126.346727087614));
#123543=CARTESIAN_POINT('Ctrl Pts',(-195.183834994564,1.95764016503764,
126.290424327054));
#123544=CARTESIAN_POINT('Ctrl Pts',(-195.191592035449,1.83040078992447,
126.23940541398));
#123545=CARTESIAN_POINT('Ctrl Pts',(-195.19934322669,1.70325736701403,126.188424974666));
#123546=CARTESIAN_POINT('Ctrl Pts',(-195.20709441793,1.57388326299252,126.142720596667));
#123547=CARTESIAN_POINT('Ctrl Pts',(-195.21484560917,1.44275651553619,126.102484747301));
#123548=CARTESIAN_POINT('Ctrl Pts',(-195.222593505947,1.31168550044528,
126.062265999245));
#123549=CARTESIAN_POINT('Ctrl Pts',(-195.230341402724,1.17886369649157,
126.027511271472));
#123550=CARTESIAN_POINT('Ctrl Pts',(-195.238089299501,1.04478662420943,
125.998363949613));
#123551=CARTESIAN_POINT('Ctrl Pts',(-195.245835575585,0.910737597960802,
125.969222724746));
#123552=CARTESIAN_POINT('Ctrl Pts',(-195.253581851669,0.775434207459803,
125.945686655733));
#123553=CARTESIAN_POINT('Ctrl Pts',(-195.261328127753,0.63938416776216,
125.927848447119));
#123554=CARTESIAN_POINT('Ctrl Pts',(-195.269074461019,0.503333123773844,
125.910010106827));
#123555=CARTESIAN_POINT('Ctrl Pts',(-195.276820794284,0.366535807238244,
125.897869761689));
#123556=CARTESIAN_POINT('Ctrl Pts',(-195.284567127549,0.229506696718071,
125.891468420635));
#123557=CARTESIAN_POINT('Ctrl Pts',(-195.292315195552,0.0924468994788774,
125.885065646046));
#123558=CARTESIAN_POINT('Ctrl Pts',(-195.300063263555,-0.0448444045725537,
125.884404451203));
#123559=CARTESIAN_POINT('Ctrl Pts',(-195.307811331558,-0.181851482666569,
125.889473731711));
#123560=CARTESIAN_POINT('Ctrl Pts',(-195.3155676343,-0.319004173513774,
125.89454839991));
#123561=CARTESIAN_POINT('Ctrl Pts',(-195.323323937042,-0.455871643647917,
125.905365695246));
#123562=CARTESIAN_POINT('Ctrl Pts',(-195.331080239784,-0.591941474886092,
125.921862450356));
#123563=CARTESIAN_POINT('Ctrl Pts',(-195.338840682298,-0.728083930690183,
125.938368010281));
#123564=CARTESIAN_POINT('Ctrl Pts',(-195.346601124812,-0.863427513682498,
125.960559006873));
#123565=CARTESIAN_POINT('Ctrl Pts',(-195.354361567326,-0.997469752634241,
125.98832104598));
#123566=CARTESIAN_POINT('Ctrl Pts',(-195.362134467592,-1.13172716808766,
126.016127651178));
#123567=CARTESIAN_POINT('Ctrl Pts',(-195.369907367857,-1.26467868554271,
126.049523074818));
#123568=CARTESIAN_POINT('Ctrl Pts',(-195.377680268122,-1.39583588798348,
126.088342674818));
#123569=CARTESIAN_POINT('Ctrl Pts',(-195.385170603885,-1.52222519575403,
126.12575108458));
#123570=CARTESIAN_POINT('Ctrl Pts',(-195.392660939647,-1.64694808775228,
126.168196053275));
#123571=CARTESIAN_POINT('Ctrl Pts',(-195.400151275409,-1.76958666422382,
126.215488631958));
#123572=CARTESIAN_POINT('Ctrl Pts',(-195.407925865569,-1.89687931172836,
126.264575939728));
#123573=CARTESIAN_POINT('Ctrl Pts',(-195.415700455729,-2.02232956017334,
126.319041551411));
#123574=CARTESIAN_POINT('Ctrl Pts',(-195.423475045889,-2.1454494812566,
126.378727376336));
#123575=CARTESIAN_POINT('Ctrl Pts',(-195.431239995709,-2.26841673604816,
126.438339192008));
#123576=CARTESIAN_POINT('Ctrl Pts',(-195.43900494553,-2.38905906452119,
126.503158172355));
#123577=CARTESIAN_POINT('Ctrl Pts',(-195.44676989535,-2.50690607821073,
126.57297727668));
#123578=CARTESIAN_POINT('Ctrl Pts',(-195.454527074191,-2.62463515337862,
126.642726507686));
#123579=CARTESIAN_POINT('Ctrl Pts',(-195.462284253032,-2.73957414685786,
126.717465706102));
#123580=CARTESIAN_POINT('Ctrl Pts',(-195.470041431874,-2.85127528719056,
126.796940961583));
#123581=CARTESIAN_POINT('Ctrl Pts',(-195.478170592057,-2.96833285167254,
126.880227307771));
#123582=CARTESIAN_POINT('Ctrl Pts',(-195.48629975224,-3.08183394409786,
126.968714999343));
#123583=CARTESIAN_POINT('Ctrl Pts',(-195.494428912423,-3.19129454302132,
127.0620588924));
#123584=CARTESIAN_POINT('Ctrl Pts',(-195.50217647144,-3.29561681384803,
127.151021011987));
#123585=CARTESIAN_POINT('Ctrl Pts',(-195.509924030457,-3.39626895266872,
127.244393515566));
#123586=CARTESIAN_POINT('Ctrl Pts',(-195.517671589474,-3.49286418306127,
127.341835114239));
#123587=CARTESIAN_POINT('Ctrl Pts',(-195.525417525999,-3.58943918449754,
127.43925630671));
#123588=CARTESIAN_POINT('Ctrl Pts',(-195.533163462523,-3.68195869289281,
127.540744621327));
#123589=CARTESIAN_POINT('Ctrl Pts',(-195.540909399048,-3.77007218189079,
127.645921318508));
#123590=CARTESIAN_POINT('Ctrl Pts',(-195.548655390858,-3.85818629978034,
127.751098766365));
#123591=CARTESIAN_POINT('Ctrl Pts',(-195.556401382667,-3.94189408507239,
127.859964349216));
#123592=CARTESIAN_POINT('Ctrl Pts',(-195.564147374477,-4.02088502556128,
127.972105919677));
#123593=CARTESIAN_POINT('Ctrl Pts',(-195.571895099012,-4.09989363577994,
128.084272575435));
#123594=CARTESIAN_POINT('Ctrl Pts',(-195.579642823547,-4.17418307720177,
128.199716357132));
#123595=CARTESIAN_POINT('Ctrl Pts',(-195.587390548081,-4.24348615363837,
128.317996137772));
#123596=CARTESIAN_POINT('Ctrl Pts',(-195.595145422041,-4.31285318138828,
128.436385064323));
#123597=CARTESIAN_POINT('Ctrl Pts',(-195.602900296001,-4.37722445952681,
128.557614877344));
#123598=CARTESIAN_POINT('Ctrl Pts',(-195.610655169961,-4.43637859937377,
128.681219551711));
#123599=CARTESIAN_POINT('Ctrl Pts',(-195.61841422265,-4.49556461454609,
128.804890830702));
#123600=CARTESIAN_POINT('Ctrl Pts',(-195.626173275339,-4.54952773652002,
128.930939161969));
#123601=CARTESIAN_POINT('Ctrl Pts',(-195.633932328028,-4.59809510986851,
129.05887947384));
#123602=CARTESIAN_POINT('Ctrl Pts',(-195.64170116025,-4.64672369767602,
129.186981042053));
#123603=CARTESIAN_POINT('Ctrl Pts',(-195.649469992472,-4.68994283555458,
129.316978981968));
#123604=CARTESIAN_POINT('Ctrl Pts',(-195.657238824693,-4.72762969271982,
129.448373688789));
#123605=CARTESIAN_POINT('Ctrl Pts',(-195.659872975218,-4.74040804237829,
129.492925228326));
#123606=CARTESIAN_POINT('Ctrl Pts',(-195.662507125742,-4.7525508024199,
129.537637266952));
#123607=CARTESIAN_POINT('Ctrl Pts',(-195.665141276266,-4.76405452823396,
129.582490119308));
#123608=CARTESIAN_POINT('Ctrl Pts',(-193.914998640423,-4.76405452823412,
129.582490119309));
#123609=CARTESIAN_POINT('Ctrl Pts',(-193.92267052425,-4.79777746561117,
129.713975340325));
#123610=CARTESIAN_POINT('Ctrl Pts',(-193.930342408077,-4.82602859703584,
129.84676320345));
#123611=CARTESIAN_POINT('Ctrl Pts',(-193.938014291904,-4.84873130167584,
129.980353441233));
#123612=CARTESIAN_POINT('Ctrl Pts',(-193.945868670583,-4.87197404665051,
130.117121455314));
#123613=CARTESIAN_POINT('Ctrl Pts',(-193.953723049261,-4.88940102937192,
130.254730049252));
#123614=CARTESIAN_POINT('Ctrl Pts',(-193.96157742794,-4.90098647655538,
130.392639086527));
#123615=CARTESIAN_POINT('Ctrl Pts',(-193.969431806619,-4.91257192373883,
130.530548123802));
#123616=CARTESIAN_POINT('Ctrl Pts',(-193.977286185297,-4.91831588080072,
130.668757158678));
#123617=CARTESIAN_POINT('Ctrl Pts',(-193.985140563975,-4.91824942956879,
130.806729382271));
#123618=CARTESIAN_POINT('',(-193.639859436047,-4.91824923219391,130.807108803159));
#123619=CARTESIAN_POINT('Ctrl Pts',(-193.570047426085,-4.76405452823409,
129.582490119308));
#123620=CARTESIAN_POINT('Ctrl Pts',(-193.577886143416,-4.79853512568151,
129.71692944544));
#123621=CARTESIAN_POINT('Ctrl Pts',(-193.585724860747,-4.82734183515294,
129.852911410386));
#123622=CARTESIAN_POINT('Ctrl Pts',(-193.593563578078,-4.85034802871446,
129.989923963893));
#123623=CARTESIAN_POINT('Ctrl Pts',(-193.601399678027,-4.87334654040656,
130.126890768305));
#123624=CARTESIAN_POINT('Ctrl Pts',(-193.609235777976,-4.8905483261116,
130.264887104432));
#123625=CARTESIAN_POINT('Ctrl Pts',(-193.617071877925,-4.90187780366035,
130.40339046845));
#123626=CARTESIAN_POINT('Ctrl Pts',(-193.624667730615,-4.91285993036604,
130.537647453052));
#123627=CARTESIAN_POINT('Ctrl Pts',(-193.632263583305,-4.91832451473222,
130.672380489236));
#123628=CARTESIAN_POINT('Ctrl Pts',(-193.639859435995,-4.91824923219442,
130.807108802231));
#123629=CARTESIAN_POINT('Ctrl Pts',(-193.639859436047,-4.91824923219391,
130.80710880316));
#123630=CARTESIAN_POINT('Ctrl Pts',(-193.648453682647,-4.91816405453979,
130.959545717499));
#123631=CARTESIAN_POINT('Ctrl Pts',(-193.657047929247,-4.91098784782448,
131.11172896582));
#123632=CARTESIAN_POINT('Ctrl Pts',(-193.665642175847,-4.89681553245056,
131.263033380711));
#123633=CARTESIAN_POINT('Ctrl Pts',(-193.674285738832,-4.88256189204551,
131.415206026086));
#123634=CARTESIAN_POINT('Ctrl Pts',(-193.682929301818,-4.86123170846623,
131.566489499949));
#123635=CARTESIAN_POINT('Ctrl Pts',(-193.691572864804,-4.83297164334981,
131.716264207359));
#123636=CARTESIAN_POINT('Ctrl Pts',(-193.700242045639,-4.8046278208643,
131.866482818043));
#123637=CARTESIAN_POINT('Ctrl Pts',(-193.708911226474,-4.76931309557723,
132.015183498403));
#123638=CARTESIAN_POINT('Ctrl Pts',(-193.717580407309,-4.7272241103825,
132.161760806426));
#123639=CARTESIAN_POINT('Ctrl Pts',(-193.726281692355,-4.6849792588291,
132.308880927995));
#123640=CARTESIAN_POINT('Ctrl Pts',(-193.734982977401,-4.63590999828547,
132.453861718932));
#123641=CARTESIAN_POINT('Ctrl Pts',(-193.743684262447,-4.5802623667498,
132.596113869059));
#123642=CARTESIAN_POINT('Ctrl Pts',(-193.745474351195,-4.56881414978355,
132.625378968644));
#123643=CARTESIAN_POINT('Ctrl Pts',(-193.747264439944,-4.55708766805062,
132.654528665305));
#123644=CARTESIAN_POINT('Ctrl Pts',(-193.749054528692,-4.5450853031912,
132.683557959309));
#123645=CARTESIAN_POINT('Ctrl Pts',(-193.756828862811,-4.49295917552469,
132.809631837505));
#123646=CARTESIAN_POINT('Ctrl Pts',(-193.76460319693,-4.4355008567645,132.933734912639));
#123647=CARTESIAN_POINT('Ctrl Pts',(-193.772377531049,-4.37288008339332,
133.055383238235));
#123648=CARTESIAN_POINT('Ctrl Pts',(-193.780142283997,-4.31033648452892,
133.17688164314));
#123649=CARTESIAN_POINT('Ctrl Pts',(-193.787907036944,-4.24264326728463,
133.295930973597));
#123650=CARTESIAN_POINT('Ctrl Pts',(-193.795671789891,-4.17001868196047,
133.412065979489));
#123651=CARTESIAN_POINT('Ctrl Pts',(-193.803428830776,-4.09746622839829,
133.528085638456));
#123652=CARTESIAN_POINT('Ctrl Pts',(-193.811185871661,-4.01999235975909,
133.641196403798));
#123653=CARTESIAN_POINT('Ctrl Pts',(-193.818942912546,-3.93786164135559,
133.750956748026));
#123654=CARTESIAN_POINT('Ctrl Pts',(-193.826694103786,-3.8557928583656,
133.860634321124));
#123655=CARTESIAN_POINT('Ctrl Pts',(-193.834445295026,-3.76907444885508,
133.966966190343));
#123656=CARTESIAN_POINT('Ctrl Pts',(-193.842196486266,-3.67801456681571,
134.069539312338));
#123657=CARTESIAN_POINT('Ctrl Pts',(-193.849944383043,-3.58699338765545,
134.172068838019));
#123658=CARTESIAN_POINT('Ctrl Pts',(-193.85769227982,-3.4916346650259,134.270842502153));
#123659=CARTESIAN_POINT('Ctrl Pts',(-193.865440176597,-3.39228701555218,
134.365480085741));
#123660=CARTESIAN_POINT('Ctrl Pts',(-193.873186452681,-3.29296014746504,
134.460097873187));
#123661=CARTESIAN_POINT('Ctrl Pts',(-193.880932728766,-3.18964629509992,
134.550581031482));
#123662=CARTESIAN_POINT('Ctrl Pts',(-193.88867900485,-3.0827308531471,134.636586282836));
#123663=CARTESIAN_POINT('Ctrl Pts',(-193.896425338115,-2.97581462196864,
134.722592169061));
#123664=CARTESIAN_POINT('Ctrl Pts',(-193.90417167138,-2.86529705278595,
134.804119837331));
#123665=CARTESIAN_POINT('Ctrl Pts',(-193.911918004646,-2.75159620769232,
134.880866642621));
#123666=CARTESIAN_POINT('Ctrl Pts',(-193.919666072649,-2.63786990008324,
134.957630634827));
#123667=CARTESIAN_POINT('Ctrl Pts',(-193.927414140652,-2.52095922202,135.029611414911));
#123668=CARTESIAN_POINT('Ctrl Pts',(-193.935162208655,-2.40131041503007,
135.096550193198));
#123669=CARTESIAN_POINT('Ctrl Pts',(-193.942918511396,-2.28153444386374,
135.163560114816));
#123670=CARTESIAN_POINT('Ctrl Pts',(-193.950674814138,-2.15901487224249,
135.225517138867));
#123671=CARTESIAN_POINT('Ctrl Pts',(-193.95843111688,-2.03422219292027,
135.2822086646));
#123672=CARTESIAN_POINT('Ctrl Pts',(-193.966191559394,-1.90936290798765,
135.338930448309));
#123673=CARTESIAN_POINT('Ctrl Pts',(-193.973952001908,-1.78222846013368,
135.390380987236));
#123674=CARTESIAN_POINT('Ctrl Pts',(-193.981712444423,-1.65330749395548,
135.436396605437));
#123675=CARTESIAN_POINT('Ctrl Pts',(-193.989485344688,-1.52417957239731,
135.482486091993));
#123676=CARTESIAN_POINT('Ctrl Pts',(-193.997258244953,-1.39325977518751,
135.523123107292));
#123677=CARTESIAN_POINT('Ctrl Pts',(-194.005031145219,-1.26105088175151,
135.5581942007));
#123678=CARTESIAN_POINT('Ctrl Pts',(-194.012521480981,-1.133648114606,135.591990371525));
#123679=CARTESIAN_POINT('Ctrl Pts',(-194.020011816743,-1.00504864850035,
135.620618198415));
#123680=CARTESIAN_POINT('Ctrl Pts',(-194.027502152505,-0.875707681015639,
135.644021671804));
#123681=CARTESIAN_POINT('Ctrl Pts',(-194.035276486624,-0.741462711436587,
135.668312495));
#123682=CARTESIAN_POINT('Ctrl Pts',(-194.043050820743,-0.605993654757619,
135.687051927619));
#123683=CARTESIAN_POINT('Ctrl Pts',(-194.050825154862,-0.469799415570403,
135.70012118888));
#123684=CARTESIAN_POINT('Ctrl Pts',(-194.058589907809,-0.333773023610957,
135.713174343443));
#123685=CARTESIAN_POINT('Ctrl Pts',(-194.066354660756,-0.197023612826312,
135.720571193658));
#123686=CARTESIAN_POINT('Ctrl Pts',(-194.074119413703,-0.0600605809332014,
135.722243880629));
#123687=CARTESIAN_POINT('Ctrl Pts',(-194.081876454588,0.0767664173457922,
135.723914906265));
#123688=CARTESIAN_POINT('Ctrl Pts',(-194.089633495473,0.213806226096077,
135.719873077956));
#123689=CARTESIAN_POINT('Ctrl Pts',(-194.097390536358,0.35054437172053,
135.710102325601));
#123690=CARTESIAN_POINT('Ctrl Pts',(-194.105141727599,0.487179402045514,
135.700338941446));
#123691=CARTESIAN_POINT('Ctrl Pts',(-194.112892918839,0.6235128336498,135.684855260145));
#123692=CARTESIAN_POINT('Ctrl Pts',(-194.120644110079,0.759030596709005,
135.663687280362));
#123693=CARTESIAN_POINT('Ctrl Pts',(-194.128392006856,0.894490761104039,
135.642528297535));
#123694=CARTESIAN_POINT('Ctrl Pts',(-194.136139903633,1.02913556100334,
135.615689881632));
#123695=CARTESIAN_POINT('Ctrl Pts',(-194.14388780041,1.16245667159326,135.583259816039));
#123696=CARTESIAN_POINT('Ctrl Pts',(-194.151634076494,1.29574989428092,
135.550836534117));
#123697=CARTESIAN_POINT('Ctrl Pts',(-194.159380352578,1.42771959875601,
135.512824021355));
#123698=CARTESIAN_POINT('Ctrl Pts',(-194.167126628662,1.55786866044568,
135.469360971189));
#123699=CARTESIAN_POINT('Ctrl Pts',(-194.174872961928,1.68801868286598,
135.425897600189));
#123700=CARTESIAN_POINT('Ctrl Pts',(-194.182619295193,1.81634766484947,
135.376983735339));
#123701=CARTESIAN_POINT('Ctrl Pts',(-194.190365628458,1.9423750097934,135.322807517091));
#123702=CARTESIAN_POINT('Ctrl Pts',(-194.198113696461,2.06843057768725,
135.268619166455));
#123703=CARTESIAN_POINT('Ctrl Pts',(-194.205861764464,2.19218312376924,
135.209166271782));
#123704=CARTESIAN_POINT('Ctrl Pts',(-194.213609832467,2.31317371650994,
135.144684386566));
#123705=CARTESIAN_POINT('Ctrl Pts',(-194.221366135209,2.43429289949258,
135.080133969235));
#123706=CARTESIAN_POINT('Ctrl Pts',(-194.229122437951,2.55264391970813,
135.010544068579));
#123707=CARTESIAN_POINT('Ctrl Pts',(-194.236878740693,2.66779359729971,
134.93619560758));
#123708=CARTESIAN_POINT('Ctrl Pts',(-194.244639183207,2.78300473374162,
134.861807464569));
#123709=CARTESIAN_POINT('Ctrl Pts',(-194.252399625721,2.8950108037929,134.782655925994));
#123710=CARTESIAN_POINT('Ctrl Pts',(-194.260160068235,3.00340997790441,
134.699063631548));
#123711=CARTESIAN_POINT('Ctrl Pts',(-194.2679329685,3.11198316399314,134.615337147331));
#123712=CARTESIAN_POINT('Ctrl Pts',(-194.275705868766,3.2169375841494,134.527155913481));
#123713=CARTESIAN_POINT('Ctrl Pts',(-194.283478769031,3.3179060245828,134.434881609729));
#123714=CARTESIAN_POINT('Ctrl Pts',(-194.290969104794,3.41520400788394,
134.345961709343));
#123715=CARTESIAN_POINT('Ctrl Pts',(-194.298459440556,3.50880056207708,
134.253241376088));
#123716=CARTESIAN_POINT('Ctrl Pts',(-194.305949776318,3.59840251931591,
134.157073306044));
#123717=CARTESIAN_POINT('Ctrl Pts',(-194.313724110437,3.69140176199619,
134.057258994396));
#123718=CARTESIAN_POINT('Ctrl Pts',(-194.321498444556,3.78039211153777,
133.953414161395));
#123719=CARTESIAN_POINT('Ctrl Pts',(-194.329272778675,3.8650039641869,133.845894345691));
#123720=CARTESIAN_POINT('Ctrl Pts',(-194.337037531622,3.94951154028939,
133.73850703855));
#123721=CARTESIAN_POINT('Ctrl Pts',(-194.344802284569,4.02965111668345,
133.627454064531));
#123722=CARTESIAN_POINT('Ctrl Pts',(-194.352567037516,4.10509025985185,
133.513127314971));
#123723=CARTESIAN_POINT('Ctrl Pts',(-194.360324078401,4.18045447579975,
133.39891411635));
#123724=CARTESIAN_POINT('Ctrl Pts',(-194.368081119286,4.25112733518645,
133.281433937151));
#123725=CARTESIAN_POINT('Ctrl Pts',(-194.375838160171,4.31681723223276,
133.1611109323));
#123726=CARTESIAN_POINT('Ctrl Pts',(-194.383589351411,4.38245759201679,
133.040878663962));
#123727=CARTESIAN_POINT('Ctrl Pts',(-194.391340542651,4.44312228232928,
132.917808178837));
#123728=CARTESIAN_POINT('Ctrl Pts',(-194.399091733892,4.49856372256806,
132.792351436583));
#123729=CARTESIAN_POINT('Ctrl Pts',(-194.406839630669,4.55398159871571,
132.666948016791));
#123730=CARTESIAN_POINT('Ctrl Pts',(-194.414587527446,4.60418048254142,
132.539160713937));
#123731=CARTESIAN_POINT('Ctrl Pts',(-194.422335424223,4.64895946671369,
132.409464645146));
#123732=CARTESIAN_POINT('Ctrl Pts',(-194.430081700307,4.69372908408779,
132.279795705977));
#123733=CARTESIAN_POINT('Ctrl Pts',(-194.437827976391,4.73308092933866,
132.14821916437));
#123734=CARTESIAN_POINT('Ctrl Pts',(-194.445574252475,4.76686298120744,
132.015228232499));
#123735=CARTESIAN_POINT('Ctrl Pts',(-194.45332058574,4.80064528244769,131.882236318919));
#123736=CARTESIAN_POINT('Ctrl Pts',(-194.461066919006,4.82885761200875,
131.747830373172));
#123737=CARTESIAN_POINT('Ctrl Pts',(-194.468813252271,4.85139848357786,
131.612516429299));
#123738=CARTESIAN_POINT('Ctrl Pts',(-194.476561320274,4.87394440301884,
131.477172182808));
#123739=CARTESIAN_POINT('Ctrl Pts',(-194.484309388277,4.89081627291814,
131.340919919146));
#123740=CARTESIAN_POINT('Ctrl Pts',(-194.49205745628,4.90196420739985,131.204273072824));
#123741=CARTESIAN_POINT('Ctrl Pts',(-194.499813759022,4.913123990039,131.067480996608));
#123742=CARTESIAN_POINT('Ctrl Pts',(-194.507570061764,4.91854765303973,
130.930293890293));
#123743=CARTESIAN_POINT('Ctrl Pts',(-194.515326364506,4.91823740056867,
130.793228046095));
#123744=CARTESIAN_POINT('Ctrl Pts',(-194.52308680702,4.91792698250651,130.656089045728));
#123745=CARTESIAN_POINT('Ctrl Pts',(-194.530847249534,4.91187656817852,
130.519071826834));
#123746=CARTESIAN_POINT('Ctrl Pts',(-194.538607692048,4.90014040480876,
130.382688854626));
#123747=CARTESIAN_POINT('Ctrl Pts',(-194.546380592313,4.88838540150768,
130.246086948365));
#123748=CARTESIAN_POINT('Ctrl Pts',(-194.554153492579,4.8709264597954,130.110121711381));
#123749=CARTESIAN_POINT('Ctrl Pts',(-194.561926392844,4.84786938305054,
129.975297587766));
#123750=CARTESIAN_POINT('Ctrl Pts',(-194.569416728606,4.8256504891227,129.845374660647));
#123751=CARTESIAN_POINT('Ctrl Pts',(-194.576907064368,4.79823347054425,
129.71651162387));
#123752=CARTESIAN_POINT('Ctrl Pts',(-194.58439740013,4.76575659613236,129.589145768693));
#123753=CARTESIAN_POINT('Ctrl Pts',(-194.592171734249,4.73204835115597,
129.456950798405));
#123754=CARTESIAN_POINT('Ctrl Pts',(-194.599946068368,4.69278220975143,
129.325950028211));
#123755=CARTESIAN_POINT('Ctrl Pts',(-194.607720402487,4.64805751679649,
129.196646593539));
#123756=CARTESIAN_POINT('Ctrl Pts',(-194.615485155434,4.60338794302845,
129.067502513795));
#123757=CARTESIAN_POINT('Ctrl Pts',(-194.623249908382,4.55327332936175,
128.940051973427));
#123758=CARTESIAN_POINT('Ctrl Pts',(-194.631014661329,4.49786369664073,
128.814786485009));
#123759=CARTESIAN_POINT('Ctrl Pts',(-194.638771702214,4.44250909754792,
128.689645412039));
#123760=CARTESIAN_POINT('Ctrl Pts',(-194.646528743099,4.38187010235564,
128.566685427407));
#123761=CARTESIAN_POINT('Ctrl Pts',(-194.654285783984,4.31614594456795,
128.446381133412));
#123762=CARTESIAN_POINT('Ctrl Pts',(-194.662036975224,4.250471349879,128.326167561822));
#123763=CARTESIAN_POINT('Ctrl Pts',(-194.669788166464,4.17971941213704,
128.208606036374));
#123764=CARTESIAN_POINT('Ctrl Pts',(-194.677539357704,4.10413655444054,
128.094149148879));
#123765=CARTESIAN_POINT('Ctrl Pts',(-194.685287254481,4.0285858214747,127.979740908613));
#123766=CARTESIAN_POINT('Ctrl Pts',(-194.693035151258,3.94820846734261,
127.868435007373));
#123767=CARTESIAN_POINT('Ctrl Pts',(-194.700783048035,3.86329562621768,
127.760657286598));
#123768=CARTESIAN_POINT('Ctrl Pts',(-194.708529324119,3.77840054702884,
127.652902110599));
#123769=CARTESIAN_POINT('Ctrl Pts',(-194.716275600204,3.68897210971447,
127.548673954013));
#123770=CARTESIAN_POINT('Ctrl Pts',(-194.724021876288,3.59534309643996,
127.448367309858));
#123771=CARTESIAN_POINT('Ctrl Pts',(-194.731768209553,3.50171339201721,
127.348059925262));
#123772=CARTESIAN_POINT('Ctrl Pts',(-194.739514542818,3.40388331653783,
127.251674396663));
#123773=CARTESIAN_POINT('Ctrl Pts',(-194.747260876084,3.3022237549426,127.159569631132));
#123774=CARTESIAN_POINT('Ctrl Pts',(-194.755008944087,3.20054142739355,
127.067444239377));
#123775=CARTESIAN_POINT('Ctrl Pts',(-194.76275701209,3.09502819690908,126.979601780738));
#123776=CARTESIAN_POINT('Ctrl Pts',(-194.770505080093,2.98608906594972,
126.896361749511));
#123777=CARTESIAN_POINT('Ctrl Pts',(-194.778261382835,2.87703415318544,
126.813033249789));
#123778=CARTESIAN_POINT('Ctrl Pts',(-194.786017685576,2.76454637763411,
126.734317186555));
#123779=CARTESIAN_POINT('Ctrl Pts',(-194.793773988318,2.6490613019644,126.660490773937));
#123780=CARTESIAN_POINT('Ctrl Pts',(-194.801534430832,2.53351458843263,
126.58662495794));
#123781=CARTESIAN_POINT('Ctrl Pts',(-194.809294873347,2.41496772491371,
126.517654189227));
#123782=CARTESIAN_POINT('Ctrl Pts',(-194.817055315861,2.29388118485612,
126.453809828038));
#123783=CARTESIAN_POINT('Ctrl Pts',(-194.824828216126,2.17260026593488,
126.389862978213));
#123784=CARTESIAN_POINT('Ctrl Pts',(-194.832601116392,2.04877187687075,
126.331059148613));
#123785=CARTESIAN_POINT('Ctrl Pts',(-194.840374016657,1.92287761007517,
126.277581988213));
#123786=CARTESIAN_POINT('Ctrl Pts',(-194.847864352419,1.80155991698648,
126.226048857294));
#123787=CARTESIAN_POINT('Ctrl Pts',(-194.855354688181,1.67832422631585,
126.179461952482));
#123788=CARTESIAN_POINT('Ctrl Pts',(-194.862845023943,1.55361318125574,
126.13794131091));
#123789=CARTESIAN_POINT('Ctrl Pts',(-194.870619358062,1.42417367901689,
126.094846401594));
#123790=CARTESIAN_POINT('Ctrl Pts',(-194.878393692181,1.29273471235955,
126.05707300227));
#123791=CARTESIAN_POINT('Ctrl Pts',(-194.886168026301,1.15977328170358,
126.024809488271));
#123792=CARTESIAN_POINT('Ctrl Pts',(-194.893932779248,1.02697571412778,
125.992585736169));
#123793=CARTESIAN_POINT('Ctrl Pts',(-194.901697532195,0.892659792124973,
125.965858449745));
#123794=CARTESIAN_POINT('Ctrl Pts',(-194.909462285142,0.757320129074038,
125.944767086765));
#123795=CARTESIAN_POINT('Ctrl Pts',(-194.917219326027,0.6221148872844,125.923696672025));
#123796=CARTESIAN_POINT('Ctrl Pts',(-194.924976366912,0.485888311715355,
125.908251100908));
#123797=CARTESIAN_POINT('Ctrl Pts',(-194.932733407797,0.349147389297095,
125.89851928676));
#123798=CARTESIAN_POINT('Ctrl Pts',(-194.940484599037,0.212509584271935,
125.888794811448));
#123799=CARTESIAN_POINT('Ctrl Pts',(-194.948235790277,0.0753585928360218,
125.884775544365));
#123800=CARTESIAN_POINT('Ctrl Pts',(-194.955986981517,-0.0617916090006001,
125.886498799707));
#123801=CARTESIAN_POINT('Ctrl Pts',(-194.963734878294,-0.198883518342653,
125.888221322619));
#123802=CARTESIAN_POINT('Ctrl Pts',(-194.971482775071,-0.335974248637008,
125.895681508637));
#123803=CARTESIAN_POINT('Ctrl Pts',(-194.979230671849,-0.472548162288011,
125.908864596036));
#123804=CARTESIAN_POINT('Ctrl Pts',(-194.986976947933,-0.60909350762047,
125.922044925817));
#123805=CARTESIAN_POINT('Ctrl Pts',(-194.994723224017,-0.745121862430249,
125.940945738326));
#123806=CARTESIAN_POINT('Ctrl Pts',(-195.002469500101,-0.880121451680396,
125.965500287613));
#123807=CARTESIAN_POINT('Ctrl Pts',(-195.010215833366,-1.01512203746703,
125.990055018157));
#123808=CARTESIAN_POINT('Ctrl Pts',(-195.017962166632,-1.14909345788622,
126.020263498794));
#123809=CARTESIAN_POINT('Ctrl Pts',(-195.025708499897,-1.28153328188549,
126.056007691559));
#123810=CARTESIAN_POINT('Ctrl Pts',(-195.0334565679,-1.41400276486489,126.091759888988));
#123811=CARTESIAN_POINT('Ctrl Pts',(-195.041204635903,-1.54493959152582,
126.133050163519));
#123812=CARTESIAN_POINT('Ctrl Pts',(-195.048952703906,-1.67385604854705,
126.179710469583));
#123813=CARTESIAN_POINT('Ctrl Pts',(-195.056709006648,-1.80290951951275,
126.226420366775));
#123814=CARTESIAN_POINT('Ctrl Pts',(-195.06446530939,-1.92993796321751,
126.278511563241));
#123815=CARTESIAN_POINT('Ctrl Pts',(-195.072221612131,-2.0544727193047,
126.335767448779));
#123816=CARTESIAN_POINT('Ctrl Pts',(-195.079982054646,-2.17907394334121,
126.393053893507));
#123817=CARTESIAN_POINT('Ctrl Pts',(-195.08774249716,-2.30117847981346,
126.455510342012));
#123818=CARTESIAN_POINT('Ctrl Pts',(-195.095502939674,-2.42034278165234,
126.522874440804));
#123819=CARTESIAN_POINT('Ctrl Pts',(-195.10327583994,-2.53969837660744,
126.590346678427));
#123820=CARTESIAN_POINT('Ctrl Pts',(-195.111048740205,-2.65610397282664,
126.662742102887));
#123821=CARTESIAN_POINT('Ctrl Pts',(-195.11882164047,-2.76914474876468,
126.739754803605));
#123822=CARTESIAN_POINT('Ctrl Pts',(-195.126311976232,-2.87807620776515,
126.813967898668));
#123823=CARTESIAN_POINT('Ctrl Pts',(-195.133802311994,-2.98388299120046,
126.892468215446));
#123824=CARTESIAN_POINT('Ctrl Pts',(-195.141292647756,-3.08622484897237,
126.974948228689));
#123825=CARTESIAN_POINT('Ctrl Pts',(-195.148964038384,-3.19104049321887,
127.059421931958));
#123826=CARTESIAN_POINT('Ctrl Pts',(-195.156635429012,-3.29257225117811,
127.148353103153));
#123827=CARTESIAN_POINT('Ctrl Pts',(-195.164306819639,-3.39040972582631,
127.241453805211));
#123828=CARTESIAN_POINT('Ctrl Pts',(-195.171969427545,-3.48813518957756,
127.334447919347));
#123829=CARTESIAN_POINT('Ctrl Pts',(-195.17963203545,-3.58217448966821,
127.431601801204));
#123830=CARTESIAN_POINT('Ctrl Pts',(-195.187294643356,-3.67214823682183,
127.532585810324));
#123831=CARTESIAN_POINT('Ctrl Pts',(-195.194950242633,-3.76203968920446,
127.633477454101));
#123832=CARTESIAN_POINT('Ctrl Pts',(-195.20260584191,-3.84787271682651,
127.738191961579));
#123833=CARTESIAN_POINT('Ctrl Pts',(-195.210261441187,-3.92930333398827,
127.846361568883));
#123834=CARTESIAN_POINT('Ctrl Pts',(-195.217911799506,-4.01067820443681,
127.954457124187));
#123835=CARTESIAN_POINT('Ctrl Pts',(-195.225562157824,-4.0876564179061,
128.066002754977));
#123836=CARTESIAN_POINT('Ctrl Pts',(-195.233212516142,-4.15993336229173,
128.180596625933));
#123837=CARTESIAN_POINT('Ctrl Pts',(-195.24086026656,-4.23218566846759,
128.295151433424));
#123838=CARTESIAN_POINT('Ctrl Pts',(-195.248508016977,-4.29973967457936,
128.412752077692));
#123839=CARTESIAN_POINT('Ctrl Pts',(-195.256155767394,-4.36233354812221,
128.532966975454));
#123840=CARTESIAN_POINT('Ctrl Pts',(-195.263801822143,-4.42491354327928,
128.65315521903));
#123841=CARTESIAN_POINT('Ctrl Pts',(-195.271447876892,-4.48253541118757,
128.775956204889));
#123842=CARTESIAN_POINT('Ctrl Pts',(-195.279093931642,-4.53498317575593,
128.900913571255));
#123843=CARTESIAN_POINT('Ctrl Pts',(-195.286742468474,-4.58744796606283,
129.025911501627));
#123844=CARTESIAN_POINT('Ctrl Pts',(-195.294391005307,-4.63473514030973,
129.153066840563));
#123845=CARTESIAN_POINT('Ctrl Pts',(-195.30203954214,-4.67667684027603,
129.281903132404));
#123846=CARTESIAN_POINT('Ctrl Pts',(-195.307932996256,-4.70899432657831,
129.38117581568));
#123847=CARTESIAN_POINT('Ctrl Pts',(-195.313826450373,-4.73813905169708,
129.481446069613));
#123848=CARTESIAN_POINT('Ctrl Pts',(-195.319719904489,-4.76405452823413,
129.582490119309));
#123849=CARTESIAN_POINT('Origin',(213.235140564004,0.,130.804360617566));
#123850=CARTESIAN_POINT('',(-197.415422870675,-4.76405452823413,129.582490119309));
#123851=CARTESIAN_POINT('',(-197.069830899744,-4.76405452823391,129.582490119308));
#123852=CARTESIAN_POINT('',(213.235140564004,-4.76405452823405,129.582490119308));
#123853=CARTESIAN_POINT('',(-195.735140564062,-4.91824801533315,130.799942227414));
#123854=CARTESIAN_POINT('Ctrl Pts',(-195.735140564062,-4.91824801533315,
130.799942227414));
#123855=CARTESIAN_POINT('Ctrl Pts',(-195.742788954033,-4.91836917860973,
130.934812853151));
#123856=CARTESIAN_POINT('Ctrl Pts',(-195.750437344004,-4.91293844047973,
131.069862221547));
#123857=CARTESIAN_POINT('Ctrl Pts',(-195.758085733975,-4.90193846711678,
131.204588461551));
#123858=CARTESIAN_POINT('Ctrl Pts',(-195.765727802631,-4.89094758511626,
131.339203351733));
#123859=CARTESIAN_POINT('Ctrl Pts',(-195.773369871288,-4.87439665663672,
131.473495244947));
#123860=CARTESIAN_POINT('Ctrl Pts',(-195.781011939945,-4.85232041130353,
131.606962441977));
#123861=CARTESIAN_POINT('Ctrl Pts',(-195.788650174382,-4.83025524218319,
131.740362675125));
#123862=CARTESIAN_POINT('Ctrl Pts',(-195.796288408819,-4.80267033378295,
131.872938638019));
#123863=CARTESIAN_POINT('Ctrl Pts',(-195.803926643255,-4.7696521975637,
132.00419434637));
#123864=CARTESIAN_POINT('Ctrl Pts',(-195.811563004816,-4.73664215730885,
132.13541787115));
#123865=CARTESIAN_POINT('Ctrl Pts',(-195.819199366377,-4.69820163590381,
132.265321394214));
#123866=CARTESIAN_POINT('Ctrl Pts',(-195.826835727938,-4.65446802695667,
132.393420228952));
#123867=CARTESIAN_POINT('Ctrl Pts',(-195.834471981253,-4.6107350379391,
132.521517247872));
#123868=CARTESIAN_POINT('Ctrl Pts',(-195.842108234567,-4.56170924103285,
132.647809247807));
#123869=CARTESIAN_POINT('Ctrl Pts',(-195.849744487881,-4.50757738476626,
132.771828325775));
#123870=CARTESIAN_POINT('Ctrl Pts',(-195.857382397285,-4.4534337888199,
132.895874299998));
#123871=CARTESIAN_POINT('Ctrl Pts',(-195.865020306688,-4.39418209327545,
133.01764600283));
#123872=CARTESIAN_POINT('Ctrl Pts',(-195.872658216092,-4.33005626833118,
133.136697594846));
#123873=CARTESIAN_POINT('Ctrl Pts',(-195.880303983217,-4.26586447207508,
133.255871664657));
#123874=CARTESIAN_POINT('Ctrl Pts',(-195.887949750342,-4.19678872589688,
133.37231968092));
#123875=CARTESIAN_POINT('Ctrl Pts',(-195.895595517468,-4.12310800759558,
133.485622152777));
#123876=CARTESIAN_POINT('Ctrl Pts',(-195.903245518399,-4.04938648895914,
133.59898736532));
#123877=CARTESIAN_POINT('Ctrl Pts',(-195.91089551933,-3.9710551549251,133.709203237835));
#123878=CARTESIAN_POINT('Ctrl Pts',(-195.918545520261,-3.88843420921999,
133.815882236792));
#123879=CARTESIAN_POINT('Ctrl Pts',(-195.926207035089,-3.8056889120232,
133.922721796641));
#123880=CARTESIAN_POINT('Ctrl Pts',(-195.933868549917,-3.71864137075232,
134.026013545911));
#123881=CARTESIAN_POINT('Ctrl Pts',(-195.941530064745,-3.62765000128713,
134.125405412606));
#123882=CARTESIAN_POINT('Ctrl Pts',(-195.946702217508,-3.56622334173219,
134.192503098836));
#123883=CARTESIAN_POINT('Ctrl Pts',(-195.951874370271,-3.50300009789946,
134.257824245905));
#123884=CARTESIAN_POINT('Ctrl Pts',(-195.957046523035,-3.43809892864949,
134.321271025768));
#123885=CARTESIAN_POINT('Ctrl Pts',(-195.964820857154,-3.34054508645473,
134.416638755225));
#123886=CARTESIAN_POINT('Ctrl Pts',(-195.972595191273,-3.23886568121659,
134.508095467405));
#123887=CARTESIAN_POINT('Ctrl Pts',(-195.980369525392,-3.13340727972664,
134.595263133044));
#123888=CARTESIAN_POINT('Ctrl Pts',(-195.988134278339,-3.02807884629143,
134.682323372325));
#123889=CARTESIAN_POINT('Ctrl Pts',(-195.995899031286,-2.91898098165016,
134.765104835671));
#123890=CARTESIAN_POINT('Ctrl Pts',(-196.003663784233,-2.80649748679672,
134.843265780986));
#123891=CARTESIAN_POINT('Ctrl Pts',(-196.011420825118,-2.69412571213581,
134.921349095749));
#123892=CARTESIAN_POINT('Ctrl Pts',(-196.019177866003,-2.5783753180853,
134.994820803471));
#123893=CARTESIAN_POINT('Ctrl Pts',(-196.026934906888,-2.45966333968881,
135.063379203801));
#123894=CARTESIAN_POINT('Ctrl Pts',(-196.034686098128,-2.34104088291883,
135.131885903706));
#123895=CARTESIAN_POINT('Ctrl Pts',(-196.042437289368,-2.21946162434935,
135.195486476388));
#123896=CARTESIAN_POINT('Ctrl Pts',(-196.050188480608,-2.09537145223453,
135.253922566754));
#123897=CARTESIAN_POINT('Ctrl Pts',(-196.057936377386,-1.9713340217529,
135.312333820223));
#123898=CARTESIAN_POINT('Ctrl Pts',(-196.065684274163,-1.84478815328316,
135.365584790931));
#123899=CARTESIAN_POINT('Ctrl Pts',(-196.07343217094,-1.71620400590661,
135.413463227902));
#123900=CARTESIAN_POINT('Ctrl Pts',(-196.081178447024,-1.58764675556175,
135.461331649737));
#123901=CARTESIAN_POINT('Ctrl Pts',(-196.088924723108,-1.45705244052956,
135.503829636831));
#123902=CARTESIAN_POINT('Ctrl Pts',(-196.096670999192,-1.32491048285849,
135.540793375973));
#123903=CARTESIAN_POINT('Ctrl Pts',(-196.104417332458,-1.19276754974533,
135.577757387973));
#123904=CARTESIAN_POINT('Ctrl Pts',(-196.112163665723,-1.05907732770887,
135.60918696518));
#123905=CARTESIAN_POINT('Ctrl Pts',(-196.119909998988,-0.92434326967486,
135.634968507087));
#123906=CARTESIAN_POINT('Ctrl Pts',(-196.127658066991,-0.789579038882551,
135.660755822592));
#123907=CARTESIAN_POINT('Ctrl Pts',(-196.135406134994,-0.653770890862492,
135.680892512449));
#123908=CARTESIAN_POINT('Ctrl Pts',(-196.143154202997,-0.517430915145343,
135.695316384137));
#123909=CARTESIAN_POINT('Ctrl Pts',(-196.150910505739,-0.380946035680092,
135.709755585687));
#123910=CARTESIAN_POINT('Ctrl Pts',(-196.158666808481,-0.243928588819814,
135.718469799092));
#123911=CARTESIAN_POINT('Ctrl Pts',(-196.166423111223,-0.106894770994205,
135.721448838295));
#123912=CARTESIAN_POINT('Ctrl Pts',(-196.174183553737,0.0302121859059867,
135.724429467501));
#123913=CARTESIAN_POINT('Ctrl Pts',(-196.181943996251,0.167335140487332,
135.721668830999));
#123914=CARTESIAN_POINT('Ctrl Pts',(-196.189704438765,0.303960473328762,
135.713208862639));
#123915=CARTESIAN_POINT('Ctrl Pts',(-196.197477339031,0.440805129283496,
135.704735313586));
#123916=CARTESIAN_POINT('Ctrl Pts',(-196.205250239296,0.577150178099871,
135.690544190408));
#123917=CARTESIAN_POINT('Ctrl Pts',(-196.213023139562,0.712488781964307,
135.670729160748));
#123918=CARTESIAN_POINT('Ctrl Pts',(-196.220513475324,0.842907486683093,
135.651634457327));
#123919=CARTESIAN_POINT('Ctrl Pts',(-196.228003811086,0.972391346940213,
135.627317691741));
#123920=CARTESIAN_POINT('Ctrl Pts',(-196.235494146848,1.10049987933717,
135.597906599204));
#123921=CARTESIAN_POINT('Ctrl Pts',(-196.243268480967,1.23346568567565,
135.567380376155));
#123922=CARTESIAN_POINT('Ctrl Pts',(-196.251042815086,1.3653710100103,135.531269199705));
#123923=CARTESIAN_POINT('Ctrl Pts',(-196.258817149205,1.49571047779856,
135.48966031226));
#123924=CARTESIAN_POINT('Ctrl Pts',(-196.266581902152,1.62588931384153,
135.448102704051));
#123925=CARTESIAN_POINT('Ctrl Pts',(-196.274346655099,1.75450576414976,
135.401060983704));
#123926=CARTESIAN_POINT('Ctrl Pts',(-196.282111408047,1.88106485760708,
135.348673333915));
#123927=CARTESIAN_POINT('Ctrl Pts',(-196.289868448932,2.00749825078861,
135.296337716279));
#123928=CARTESIAN_POINT('Ctrl Pts',(-196.297625489817,2.1318779946668,135.238666884213));
#123929=CARTESIAN_POINT('Ctrl Pts',(-196.305382530702,2.25372484256268,
135.1758486247));
#123930=CARTESIAN_POINT('Ctrl Pts',(-196.313133721942,2.37547980480323,
135.113077736925));
#123931=CARTESIAN_POINT('Ctrl Pts',(-196.320884913182,2.49470532685751,
135.045167326451));
#123932=CARTESIAN_POINT('Ctrl Pts',(-196.328636104422,2.61094303377791,
134.972352884457));
#123933=CARTESIAN_POINT('Ctrl Pts',(-196.336384001199,2.72713133657197,
134.899569390544));
#123934=CARTESIAN_POINT('Ctrl Pts',(-196.344131897976,2.8403340193372,134.82188621783));
#123935=CARTESIAN_POINT('Ctrl Pts',(-196.351879794753,2.95011837684841,
134.739584197629));
#123936=CARTESIAN_POINT('Ctrl Pts',(-196.359626070838,3.05987976983901,
134.657299393235));
#123937=CARTESIAN_POINT('Ctrl Pts',(-196.367372346922,3.16622394720568,
134.57039789747));
#123938=CARTESIAN_POINT('Ctrl Pts',(-196.375118623006,3.26874854368119,
134.479202929922));
#123939=CARTESIAN_POINT('Ctrl Pts',(-196.382864956271,3.37127389696957,
134.388007289193));
#123940=CARTESIAN_POINT('Ctrl Pts',(-196.390611289537,3.46997932098188,
134.292518373281));
#123941=CARTESIAN_POINT('Ctrl Pts',(-196.398357622802,3.56449711178872,
134.19309834754));
#123942=CARTESIAN_POINT('Ctrl Pts',(-196.406105690805,3.6590360691996,134.093656057373));
#123943=CARTESIAN_POINT('Ctrl Pts',(-196.413853758808,3.74938525798013,
133.990281188891));
#123944=CARTESIAN_POINT('Ctrl Pts',(-196.421601826811,3.83521555689988,
133.883370960941));
#123945=CARTESIAN_POINT('Ctrl Pts',(-196.429358129553,3.92113707728282,
133.776347107529));
#123946=CARTESIAN_POINT('Ctrl Pts',(-196.437114432295,4.00252986868535,
133.665780694151));
#123947=CARTESIAN_POINT('Ctrl Pts',(-196.444870735037,4.07910634450957,
133.552100505671));
#123948=CARTESIAN_POINT('Ctrl Pts',(-196.452631177551,4.1557236915046,133.438359642651));
#123949=CARTESIAN_POINT('Ctrl Pts',(-196.460391620065,4.22751939619557,
133.321502025975));
#123950=CARTESIAN_POINT('Ctrl Pts',(-196.468152062579,4.29425111487522,
133.20198244448));
#123951=CARTESIAN_POINT('Ctrl Pts',(-196.475924962845,4.36108995723385,
133.082270999541));
#123952=CARTESIAN_POINT('Ctrl Pts',(-196.48369786311,4.42284839268908,132.959889399764));
#123953=CARTESIAN_POINT('Ctrl Pts',(-196.491470763375,4.47933126826296,
132.835314691803));
#123954=CARTESIAN_POINT('Ctrl Pts',(-196.498961099137,4.53376084903658,
132.715268588265));
#123955=CARTESIAN_POINT('Ctrl Pts',(-196.506451434899,4.58329165474819,
132.593186343692));
#123956=CARTESIAN_POINT('Ctrl Pts',(-196.513941770661,4.62779306061534,
132.469507593247));
#123957=CARTESIAN_POINT('Ctrl Pts',(-196.52171610478,4.67398175081282,132.341139525385));
#123958=CARTESIAN_POINT('Ctrl Pts',(-196.529490438899,4.71489844511337,
132.210644867334));
#123959=CARTESIAN_POINT('Ctrl Pts',(-196.537264773018,4.75034337573913,
132.078495961661));
#123960=CARTESIAN_POINT('Ctrl Pts',(-196.545029525966,4.7857446236558,131.946509917703));
#123961=CARTESIAN_POINT('Ctrl Pts',(-196.552794278913,4.81568742506033,
131.812874056546));
#123962=CARTESIAN_POINT('Ctrl Pts',(-196.56055903186,4.84002049298939,131.67807950253));
#123963=CARTESIAN_POINT('Ctrl Pts',(-196.568316072745,4.86432939297227,
131.543418828366));
#123964=CARTESIAN_POINT('Ctrl Pts',(-196.57607311363,4.88303957834233,131.407602133804));
#123965=CARTESIAN_POINT('Ctrl Pts',(-196.583830154515,4.89604999507073,
131.271134126099));
#123966=CARTESIAN_POINT('Ctrl Pts',(-196.591581345755,4.90905060054271,
131.134769029979));
#123967=CARTESIAN_POINT('Ctrl Pts',(-196.599332536995,4.91635995580379,
130.997753985968));
#123968=CARTESIAN_POINT('Ctrl Pts',(-196.607083728235,4.91792842339693,
130.860601926624));
#123969=CARTESIAN_POINT('Ctrl Pts',(-196.614831625012,4.91949622434951,
130.723508160564));
#123970=CARTESIAN_POINT('Ctrl Pts',(-196.622579521789,4.91532798620717,
130.586277885118));
#123971=CARTESIAN_POINT('Ctrl Pts',(-196.630327418567,4.90542609256398,
130.449426943632));
#123972=CARTESIAN_POINT('Ctrl Pts',(-196.638073694651,4.89552627018349,
130.312604628412));
#123973=CARTESIAN_POINT('Ctrl Pts',(-196.645819970735,4.87989520608599,
130.176161879023));
#123974=CARTESIAN_POINT('Ctrl Pts',(-196.653566246819,4.85858734580939,
130.04061192484));
#123975=CARTESIAN_POINT('Ctrl Pts',(-196.661312580084,4.83727932824304,
129.905060970058));
#123976=CARTESIAN_POINT('Ctrl Pts',(-196.669058913349,4.81029449159206,
129.770403209857));
#123977=CARTESIAN_POINT('Ctrl Pts',(-196.676805246615,4.77773878287119,
129.637143763186));
#123978=CARTESIAN_POINT('Ctrl Pts',(-196.684553314618,4.74517578352494,
129.503854473986));
#123979=CARTESIAN_POINT('Ctrl Pts',(-196.692301382621,4.70703952237994,
129.371964501156));
#123980=CARTESIAN_POINT('Ctrl Pts',(-196.700049450624,4.6634862928383,129.2419654502));
#123981=CARTESIAN_POINT('Ctrl Pts',(-196.707805753366,4.61988677440618,
129.111828234706));
#123982=CARTESIAN_POINT('Ctrl Pts',(-196.715562056108,4.57085891131053,
128.98358632697));
#123983=CARTESIAN_POINT('Ctrl Pts',(-196.723318358849,4.51660800481933,
128.857713450434));
#123984=CARTESIAN_POINT('Ctrl Pts',(-196.731078801364,4.46232814298588,
128.731773391754));
#123985=CARTESIAN_POINT('Ctrl Pts',(-196.738839243878,4.40281985259029,
128.608205235819));
#123986=CARTESIAN_POINT('Ctrl Pts',(-196.746599686392,4.33833476766696,
128.487458697727));
#123987=CARTESIAN_POINT('Ctrl Pts',(-196.754372586657,4.27374616556059,
128.366518326573));
#123988=CARTESIAN_POINT('Ctrl Pts',(-196.762145486923,4.20416500253837,
128.248408961719));
#123989=CARTESIAN_POINT('Ctrl Pts',(-196.769918387188,4.12988714651096,
128.133552646262));
#123990=CARTESIAN_POINT('Ctrl Pts',(-196.77740872295,4.05830947764578,128.022871647178));
#123991=CARTESIAN_POINT('Ctrl Pts',(-196.784899058712,3.98237083808165,
127.915211542331));
#123992=CARTESIAN_POINT('Ctrl Pts',(-196.792389394474,3.90237049944579,
127.810919863592));
#123993=CARTESIAN_POINT('Ctrl Pts',(-196.800163728593,3.81933692365392,
127.702673934153));
#123994=CARTESIAN_POINT('Ctrl Pts',(-196.807938062712,3.73166454474996,
127.597714010231));
#123995=CARTESIAN_POINT('Ctrl Pts',(-196.815712396831,3.63964277854941,
127.49646347481));
#123996=CARTESIAN_POINT('Ctrl Pts',(-196.823477149778,3.54773442095174,
127.395337721625));
#123997=CARTESIAN_POINT('Ctrl Pts',(-196.831241902725,3.4514876017493,127.297912547587));
#123998=CARTESIAN_POINT('Ctrl Pts',(-196.839006655673,3.35123374346011,
127.204580699405));
#123999=CARTESIAN_POINT('Ctrl Pts',(-196.846763696558,3.25107945871658,
127.111341549731));
#124000=CARTESIAN_POINT('Ctrl Pts',(-196.854520737442,3.14692633926754,
127.022187899961));
#124001=CARTESIAN_POINT('Ctrl Pts',(-196.862277778327,3.03914438745001,
126.937477576313));
#124002=CARTESIAN_POINT('Ctrl Pts',(-196.870028969567,2.93144371484062,
126.852831133378));
#124003=CARTESIAN_POINT('Ctrl Pts',(-196.877780160808,2.82011996290654,
126.772621587719));
#124004=CARTESIAN_POINT('Ctrl Pts',(-196.885531352048,2.70557784607938,
126.697167953312));
#124005=CARTESIAN_POINT('Ctrl Pts',(-196.893279248825,2.59108441270722,
126.621746388711));
#124006=CARTESIAN_POINT('Ctrl Pts',(-196.901027145602,2.47337566088124,
126.551076929597));
#124007=CARTESIAN_POINT('Ctrl Pts',(-196.908775042379,2.35288687260822,
126.485436396512));
#124008=CARTESIAN_POINT('Ctrl Pts',(-196.916521318463,2.23242328799227,
126.419809594011));
#124009=CARTESIAN_POINT('Ctrl Pts',(-196.924267594547,2.10918116671744,
126.359209812087));
#124010=CARTESIAN_POINT('Ctrl Pts',(-196.932013870631,1.98362173233724,
126.30386865718));
#124011=CARTESIAN_POINT('Ctrl Pts',(-196.939760203896,1.85806137110565,
126.248527093757));
#124012=CARTESIAN_POINT('Ctrl Pts',(-196.947506537162,1.73018402039162,
126.198444392494));
#124013=CARTESIAN_POINT('Ctrl Pts',(-196.955252870427,1.60047191802326,
126.153804446298));
#124014=CARTESIAN_POINT('Ctrl Pts',(-196.96300093843,1.47073076752877,126.109154503295));
#124015=CARTESIAN_POINT('Ctrl Pts',(-196.970749006433,1.33915441739122,
126.069949867965));
#124016=CARTESIAN_POINT('Ctrl Pts',(-196.978497074436,1.2062409496441,126.036324771025));
#124017=CARTESIAN_POINT('Ctrl Pts',(-196.986253377178,1.07318621988194,
126.002663936931));
#124018=CARTESIAN_POINT('Ctrl Pts',(-196.99400967992,0.938791913329507,
125.974594583081));
#124019=CARTESIAN_POINT('Ctrl Pts',(-197.001765982662,0.803567557284923,
125.952200042793));
#124020=CARTESIAN_POINT('Ctrl Pts',(-197.009526425176,0.668271027929991,
125.929793549866));
#124021=CARTESIAN_POINT('Ctrl Pts',(-197.01728686769,0.532143954180493,
125.913067953334));
#124022=CARTESIAN_POINT('Ctrl Pts',(-197.025047310204,0.395700708427855,
125.902054628355));
#124023=CARTESIAN_POINT('Ctrl Pts',(-197.032820210469,0.259038431864272,
125.89102362381));
#124024=CARTESIAN_POINT('Ctrl Pts',(-197.040593110735,0.122059359953858,
125.885723230215));
#124025=CARTESIAN_POINT('Ctrl Pts',(-197.048366011,-0.0147215066600589,
125.886132650123));
#124026=CARTESIAN_POINT('Ctrl Pts',(-197.055856346762,-0.146530044246793,
125.886527186585));
#124027=CARTESIAN_POINT('Ctrl Pts',(-197.063346682525,-0.27815422914227,
125.89222359833));
#124028=CARTESIAN_POINT('Ctrl Pts',(-197.070837018287,-0.409139909314695,
125.903157949128));
#124029=CARTESIAN_POINT('Ctrl Pts',(-197.078611352406,-0.545091951359064,
125.914506879159));
#124030=CARTESIAN_POINT('Ctrl Pts',(-197.086385686525,-0.680786770288788,
125.931534731873));
#124031=CARTESIAN_POINT('Ctrl Pts',(-197.094160020644,-0.815711725690703,
125.954226862393));
#124032=CARTESIAN_POINT('Ctrl Pts',(-197.101924773591,-0.950470398142942,
125.976891026889));
#124033=CARTESIAN_POINT('Ctrl Pts',(-197.109689526538,-1.08446071302349,
126.005205515426));
#124034=CARTESIAN_POINT('Ctrl Pts',(-197.117454279485,-1.21717309943613,
126.039103782042));
#124035=CARTESIAN_POINT('Ctrl Pts',(-197.12521132037,-1.3497536740364,126.072968380422));
#124036=CARTESIAN_POINT('Ctrl Pts',(-197.132968361255,-1.48105846969448,
126.112405624185));
#124037=CARTESIAN_POINT('Ctrl Pts',(-197.14072540214,-1.61058644177957,
126.157297633696));
#124038=CARTESIAN_POINT('Ctrl Pts',(-197.148476593381,-1.74001673581351,
126.202155789794));
#124039=CARTESIAN_POINT('Ctrl Pts',(-197.156227784621,-1.86767250538385,
126.252460396493));
#124040=CARTESIAN_POINT('Ctrl Pts',(-197.163978975861,-1.99306659696161,
126.308043390926));
#124041=CARTESIAN_POINT('Ctrl Pts',(-197.171726872638,-2.11840739270528,
126.363602761105));
#124042=CARTESIAN_POINT('Ctrl Pts',(-197.179474769415,-2.24148806567971,
126.424435898852));
#124043=CARTESIAN_POINT('Ctrl Pts',(-197.187222666192,-2.3618404383649,
126.490326217355));
#124044=CARTESIAN_POINT('Ctrl Pts',(-197.194968942276,-2.48216763592822,
126.556202753023));
#124045=CARTESIAN_POINT('Ctrl Pts',(-197.20271521836,-2.59976732564188,
126.627134177688));
#124046=CARTESIAN_POINT('Ctrl Pts',(-197.210461494444,-2.71419534785042,
126.702857639851));
#124047=CARTESIAN_POINT('Ctrl Pts',(-197.21820782771,-2.82862421474047,
126.778581660986));
#124048=CARTESIAN_POINT('Ctrl Pts',(-197.225954160975,-2.93988104136766,
126.859097574447));
#124049=CARTESIAN_POINT('Ctrl Pts',(-197.23370049424,-3.0475504520959,126.944099058496));
#124050=CARTESIAN_POINT('Ctrl Pts',(-197.241448562243,-3.15524397464228,
127.029119578039));
#124051=CARTESIAN_POINT('Ctrl Pts',(-197.249196630246,-3.25934817585858,
127.118627424824));
#124052=CARTESIAN_POINT('Ctrl Pts',(-197.256944698249,-3.35948089813607,
127.21227610331));
#124053=CARTESIAN_POINT('Ctrl Pts',(-197.264701000991,-3.45972004266226,
127.306024312726));
#124054=CARTESIAN_POINT('Ctrl Pts',(-197.272457303733,-3.55597899047717,
127.403921877684));
#124055=CARTESIAN_POINT('Ctrl Pts',(-197.280213606475,-3.64791221894775,
127.505585162135));
#124056=CARTESIAN_POINT('Ctrl Pts',(-197.287974048989,-3.73989451495042,
127.607302707342));
#124057=CARTESIAN_POINT('Ctrl Pts',(-197.295734491503,-3.82754624145586,
127.712789676336));
#124058=CARTESIAN_POINT('Ctrl Pts',(-197.303494934017,-3.91056297081482,
127.821630272095));
#124059=CARTESIAN_POINT('Ctrl Pts',(-197.311267834283,-3.99371296599786,
127.930645588441));
#124060=CARTESIAN_POINT('Ctrl Pts',(-197.319040734548,-4.07221287151127,
128.043024968882));
#124061=CARTESIAN_POINT('Ctrl Pts',(-197.326813634813,-4.14580181441111,
128.158323887261));
#124062=CARTESIAN_POINT('Ctrl Pts',(-197.334303970575,-4.21671561387579,
128.269431399534));
#124063=CARTESIAN_POINT('Ctrl Pts',(-197.341794306337,-4.2830691483762,
128.383249603762));
#124064=CARTESIAN_POINT('Ctrl Pts',(-197.349284642099,-4.3446707290067,
128.499361849885));
#124065=CARTESIAN_POINT('Ctrl Pts',(-197.357505688457,-4.41228177691909,
128.626801284969));
#124066=CARTESIAN_POINT('Ctrl Pts',(-197.365726734815,-4.47436294437082,
128.757370335874));
#124067=CARTESIAN_POINT('Ctrl Pts',(-197.373947781172,-4.5306305492326,
128.890576437242));
#124068=CARTESIAN_POINT('Ctrl Pts',(-197.382149938232,-4.58676886939006,
129.023476474196));
#124069=CARTESIAN_POINT('Ctrl Pts',(-197.390352095292,-4.63712013449305,
129.159001183372));
#124070=CARTESIAN_POINT('Ctrl Pts',(-197.398554252352,-4.68144684635498,
129.296634353534));
#124071=CARTESIAN_POINT('Ctrl Pts',(-197.404177125126,-4.71183439678685,
129.390986826878));
#124072=CARTESIAN_POINT('Ctrl Pts',(-197.409799997901,-4.73939157229638,
129.48632962842));
#124073=CARTESIAN_POINT('Ctrl Pts',(-197.415422870675,-4.76405452823413,
129.582490119309));
#124074=CARTESIAN_POINT('Ctrl Pts',(-195.665141276266,-4.76405452823396,
129.582490119308));
#124075=CARTESIAN_POINT('Ctrl Pts',(-195.669627150585,-4.78364500634694,
129.658873096143));
#124076=CARTESIAN_POINT('Ctrl Pts',(-195.674113024903,-4.80138190659694,
129.735664461695));
#124077=CARTESIAN_POINT('Ctrl Pts',(-195.678598899222,-4.81725278166829,
129.812766597813));
#124078=CARTESIAN_POINT('Ctrl Pts',(-195.689674595893,-4.85643823041579,
130.00313302623));
#124079=CARTESIAN_POINT('Ctrl Pts',(-195.700750292564,-4.88435001913631,
130.195892860283));
#124080=CARTESIAN_POINT('Ctrl Pts',(-195.711825989234,-4.90075931060626,
130.38994386838));
#124081=CARTESIAN_POINT('Ctrl Pts',(-195.71959751416,-4.91227327866349,
130.526104354821));
#124082=CARTESIAN_POINT('Ctrl Pts',(-195.727369039086,-4.91812490136763,
130.662900256424));
#124083=CARTESIAN_POINT('Ctrl Pts',(-195.735140564012,-4.91824801533235,
130.799942226527));
#124084=CARTESIAN_POINT('',(-195.389859435957,-4.9182490946383,130.807344841003));
#124085=CARTESIAN_POINT('Ctrl Pts',(-195.319719904489,-4.76405452823413,
129.582490119309));
#124086=CARTESIAN_POINT('Ctrl Pts',(-195.327375268945,-4.79771771013328,
129.713742354623));
#124087=CARTESIAN_POINT('Ctrl Pts',(-195.335030633401,-4.82593039702568,
129.846300244023));
#124088=CARTESIAN_POINT('Ctrl Pts',(-195.342685997857,-4.84861431659377,
129.979665357836));
#124089=CARTESIAN_POINT('Ctrl Pts',(-195.35054823754,-4.87191123650242,
130.116634472268));
#124090=CARTESIAN_POINT('Ctrl Pts',(-195.358410477224,-4.88937627244404,
130.25445460389));
#124091=CARTESIAN_POINT('Ctrl Pts',(-195.366272716907,-4.90098169012487,
130.392582114532));
#124092=CARTESIAN_POINT('Ctrl Pts',(-195.37413495659,-4.91258710780571,
130.530709625174));
#124093=CARTESIAN_POINT('Ctrl Pts',(-195.381997196274,-4.91833295009223,
130.669144059767));
#124094=CARTESIAN_POINT('Ctrl Pts',(-195.389859435957,-4.9182490946383,
130.807344841003));
#124095=CARTESIAN_POINT('Ctrl Pts',(-195.389859435995,-4.9182490946379,
130.807344841668));
#124096=CARTESIAN_POINT('Ctrl Pts',(-195.39981971452,-4.91814286233046,
130.982424504574));
#124097=CARTESIAN_POINT('Ctrl Pts',(-195.409779993045,-4.90868858456078,
131.157218844946));
#124098=CARTESIAN_POINT('Ctrl Pts',(-195.41974027157,-4.88997301345931,
131.330998054651));
#124099=CARTESIAN_POINT('Ctrl Pts',(-195.427514605689,-4.87536487749105,
131.466638602838));
#124100=CARTESIAN_POINT('Ctrl Pts',(-195.435288939808,-4.85508562687483,
131.601885723498));
#124101=CARTESIAN_POINT('Ctrl Pts',(-195.443063273927,-4.82916220422726,
131.736227275282));
#124102=CARTESIAN_POINT('Ctrl Pts',(-195.450828026874,-4.80327072988126,
131.87040326311));
#124103=CARTESIAN_POINT('Ctrl Pts',(-195.458592779821,-4.77174899711198,
132.003675522438));
#124104=CARTESIAN_POINT('Ctrl Pts',(-195.466357532768,-4.73467576101327,
132.135536226031));
#124105=CARTESIAN_POINT('Ctrl Pts',(-195.474114573653,-4.69763934657529,
132.267265963715));
#124106=CARTESIAN_POINT('Ctrl Pts',(-195.481871614538,-4.65506250671518,
132.397586561726));
#124107=CARTESIAN_POINT('Ctrl Pts',(-195.489628655423,-4.60707511081103,
132.525999948508));
#124108=CARTESIAN_POINT('Ctrl Pts',(-195.497379846663,-4.55912390257549,
132.654316497755));
#124109=CARTESIAN_POINT('Ctrl Pts',(-195.505131037903,-4.50577039587603,
132.780728333762));
#124110=CARTESIAN_POINT('Ctrl Pts',(-195.512882229143,-4.44719429552313,
132.904752476331));
#124111=CARTESIAN_POINT('Ctrl Pts',(-195.52063012592,-4.38864309157538,
133.028723905332));
#124112=CARTESIAN_POINT('Ctrl Pts',(-195.528378022698,-4.32487387548738,
133.150309306542));
#124113=CARTESIAN_POINT('Ctrl Pts',(-195.536125919475,-4.2561144066719,
133.269045834753));
#124114=CARTESIAN_POINT('Ctrl Pts',(-195.543872195559,-4.18736932085501,
133.387757525841));
#124115=CARTESIAN_POINT('Ctrl Pts',(-195.551618471643,-4.11363625439252,
133.503621191137));
#124116=CARTESIAN_POINT('Ctrl Pts',(-195.559364747727,-4.03518864169585,
133.616199106603));
#124117=CARTESIAN_POINT('Ctrl Pts',(-195.567111080992,-3.95674044991661,
133.728777853093));
#124118=CARTESIAN_POINT('Ctrl Pts',(-195.574857414257,-3.87357786597965,
133.838070480587));
#124119=CARTESIAN_POINT('Ctrl Pts',(-195.582603747523,-3.78601709127631,
133.943669083943));
#124120=CARTESIAN_POINT('Ctrl Pts',(-195.590351815526,-3.69843670794469,
134.049291335373));
#124121=CARTESIAN_POINT('Ctrl Pts',(-195.598099883529,-3.60645642342602,
134.151217615629));
#124122=CARTESIAN_POINT('Ctrl Pts',(-195.605847951532,-3.51043180420721,
134.24907419209));
#124123=CARTESIAN_POINT('Ctrl Pts',(-195.613604254274,-3.41430512888052,
134.347034771685));
#124124=CARTESIAN_POINT('Ctrl Pts',(-195.621360557015,-3.3141258066689,
134.440916727675));
#124125=CARTESIAN_POINT('Ctrl Pts',(-195.629116859757,-3.21028565473641,
134.530383843137));
#124126=CARTESIAN_POINT('Ctrl Pts',(-195.636877302271,-3.10639008018798,
134.619898709892));
#124127=CARTESIAN_POINT('Ctrl Pts',(-195.644637744786,-2.99883008908042,
134.704993798469));
#124128=CARTESIAN_POINT('Ctrl Pts',(-195.6523981873,-2.88802866412109,134.78537474687));
#124129=CARTESIAN_POINT('Ctrl Pts',(-195.660171087565,-2.77704937087823,
134.865884729904));
#124130=CARTESIAN_POINT('Ctrl Pts',(-195.667943987831,-2.66281857163852,
134.941665234117));
#124131=CARTESIAN_POINT('Ctrl Pts',(-195.675716888096,-2.54578692477708,
135.012466129092));
#124132=CARTESIAN_POINT('Ctrl Pts',(-195.683207223858,-2.43300967306273,
135.080693233198));
#124133=CARTESIAN_POINT('Ctrl Pts',(-195.69069755962,-2.31763194379055,
135.144296336452));
#124134=CARTESIAN_POINT('Ctrl Pts',(-195.698187895382,-2.20007486704126,
135.2030938036));
#124135=CARTESIAN_POINT('Ctrl Pts',(-195.705962229501,-2.07806057799752,
135.264120594585));
#124136=CARTESIAN_POINT('Ctrl Pts',(-195.71373656362,-1.95331191468248,
135.320163459015));
#124137=CARTESIAN_POINT('Ctrl Pts',(-195.721510897739,-1.82627431925977,
135.370968239566));
#124138=CARTESIAN_POINT('Ctrl Pts',(-195.729275650686,-1.69939328631975,
135.421710407767));
#124139=CARTESIAN_POINT('Ctrl Pts',(-195.737040403634,-1.57022929355805,
135.467227192768));
#124140=CARTESIAN_POINT('Ctrl Pts',(-195.744805156581,-1.43925215945998,
135.507310360439));
#124141=CARTESIAN_POINT('Ctrl Pts',(-195.752562197466,-1.30840511369795,
135.547353716943));
#124142=CARTESIAN_POINT('Ctrl Pts',(-195.760319238351,-1.17574888177873,
135.581974082212));
#124143=CARTESIAN_POINT('Ctrl Pts',(-195.768076279236,-1.04177270297969,
135.611011499191));
#124144=CARTESIAN_POINT('Ctrl Pts',(-195.775827470476,-0.907897556659447,
135.640027018828));
#124145=CARTESIAN_POINT('Ctrl Pts',(-195.783578661716,-0.772704825255148,
135.663467887734));
#124146=CARTESIAN_POINT('Ctrl Pts',(-195.791329852956,-0.63669798852352,
135.681224234063));
#124147=CARTESIAN_POINT('Ctrl Pts',(-195.799077749733,-0.500748958325419,
135.698973033471));
#124148=CARTESIAN_POINT('Ctrl Pts',(-195.80682564651,-0.363986897864043,
135.711042065181));
#124149=CARTESIAN_POINT('Ctrl Pts',(-195.814573543287,-0.226924321449017,
135.717372770496));
#124150=CARTESIAN_POINT('Ctrl Pts',(-195.822319819371,-0.0898904155702491,
135.723702151564));
#124151=CARTESIAN_POINT('Ctrl Pts',(-195.830066095455,0.0474434909258787,
135.724295575739));
#124152=CARTESIAN_POINT('Ctrl Pts',(-195.837812371539,0.184561330431458,
135.719146490604));
#124153=CARTESIAN_POINT('Ctrl Pts',(-195.845558704805,0.321680182109967,
135.713997367458));
#124154=CARTESIAN_POINT('Ctrl Pts',(-195.85330503807,0.458582572925475,
135.703105665086));
#124155=CARTESIAN_POINT('Ctrl Pts',(-195.861051371335,0.594754406154578,
135.686516929982));
#124156=CARTESIAN_POINT('Ctrl Pts',(-195.868799439338,0.730956734121398,
135.669924479945));
#124157=CARTESIAN_POINT('Ctrl Pts',(-195.876547507341,0.866427790928436,
135.647632505728));
#124158=CARTESIAN_POINT('Ctrl Pts',(-195.884295575344,1.00066095236712,
135.619738143878));
#124159=CARTESIAN_POINT('Ctrl Pts',(-195.892051878086,1.13503677840698,
135.591814135568));
#124160=CARTESIAN_POINT('Ctrl Pts',(-195.899808180828,1.26817169752809,
135.558275924972));
#124161=CARTESIAN_POINT('Ctrl Pts',(-195.90756448357,1.39957105416255,135.519271425508));
#124162=CARTESIAN_POINT('Ctrl Pts',(-195.915324926084,1.53104054259037,
135.480246108168));
#124163=CARTESIAN_POINT('Ctrl Pts',(-195.923085368598,1.66077225312122,
135.435748815331));
#124164=CARTESIAN_POINT('Ctrl Pts',(-195.930845811113,1.78828989818289,
135.385976304478));
#124165=CARTESIAN_POINT('Ctrl Pts',(-195.938618711378,1.91601224588891,
135.336123894371));
#124166=CARTESIAN_POINT('Ctrl Pts',(-195.946391611643,2.04151306753059,
135.280979501355));
#124167=CARTESIAN_POINT('Ctrl Pts',(-195.954164511909,2.16433832944441,
135.220787075484));
#124168=CARTESIAN_POINT('Ctrl Pts',(-195.961654847671,2.28269858371017,
135.162782795908));
#124169=CARTESIAN_POINT('Ctrl Pts',(-195.969145183433,2.39857415673948,
135.100091275505));
#124170=CARTESIAN_POINT('Ctrl Pts',(-195.976635519195,2.5115846025559,135.032968644648));
#124171=CARTESIAN_POINT('Ctrl Pts',(-195.984409853314,2.6288798737734,134.963301038841));
#124172=CARTESIAN_POINT('Ctrl Pts',(-195.992184187433,2.74346002251183,
134.888638992476));
#124173=CARTESIAN_POINT('Ctrl Pts',(-195.999958521552,2.85487044664782,
134.809219890419));
#124174=CARTESIAN_POINT('Ctrl Pts',(-196.007723274499,2.9661435673931,134.729898665308));
#124175=CARTESIAN_POINT('Ctrl Pts',(-196.015488027446,3.07425442081109,
134.645832274185));
#124176=CARTESIAN_POINT('Ctrl Pts',(-196.023252780394,3.17877386526114,
134.557303433015));
#124177=CARTESIAN_POINT('Ctrl Pts',(-196.031009821279,3.2831894995255,134.468862519938));
#124178=CARTESIAN_POINT('Ctrl Pts',(-196.038766862164,3.38402052698728,
134.375968228082));
#124179=CARTESIAN_POINT('Ctrl Pts',(-196.046523903049,3.48086792546511,
134.278945707612));
#124180=CARTESIAN_POINT('Ctrl Pts',(-196.054275094289,3.57764229056651,
134.181996352578));
#124181=CARTESIAN_POINT('Ctrl Pts',(-196.062026285529,3.67043873104742,
134.080925241009));
#124182=CARTESIAN_POINT('Ctrl Pts',(-196.069777476769,3.75889266550496,
133.976096576266));
#124183=CARTESIAN_POINT('Ctrl Pts',(-196.077525373546,3.84730900468066,
133.871312466503));
#124184=CARTESIAN_POINT('Ctrl Pts',(-196.085273270323,3.93138625714945,
133.762774278175));
#124185=CARTESIAN_POINT('Ctrl Pts',(-196.0930211671,4.01079812931765,133.650881551682));
#124186=CARTESIAN_POINT('Ctrl Pts',(-196.100767443184,4.09019339023412,
133.539012230735));
#124187=CARTESIAN_POINT('Ctrl Pts',(-196.108513719268,4.16492498582819,
133.423790085964));
#124188=CARTESIAN_POINT('Ctrl Pts',(-196.116259995352,4.23470845621583,
133.30564575792));
#124189=CARTESIAN_POINT('Ctrl Pts',(-196.124006328618,4.30449244172929,
133.187500557761));
#124190=CARTESIAN_POINT('Ctrl Pts',(-196.131752661883,4.36932803031741,
133.066433467914));
#124191=CARTESIAN_POINT('Ctrl Pts',(-196.139498995149,4.42897565969853,
132.942901631505));
#124192=CARTESIAN_POINT('Ctrl Pts',(-196.147247063151,4.48863664675259,
132.819342130998));
#124193=CARTESIAN_POINT('Ctrl Pts',(-196.154995131154,4.54310719277129,
132.69331713759));
#124194=CARTESIAN_POINT('Ctrl Pts',(-196.162743199157,4.59219517872211,
132.565305393254));
#124195=CARTESIAN_POINT('Ctrl Pts',(-196.170499501899,4.64133533596847,
132.437157596512));
#124196=CARTESIAN_POINT('Ctrl Pts',(-196.178255804641,4.68508136532905,
132.307019196435));
#124197=CARTESIAN_POINT('Ctrl Pts',(-196.186012107383,4.72329033713375,
132.175386311577));
#124198=CARTESIAN_POINT('Ctrl Pts',(-196.193772549897,4.76151970221726,
132.043683170285));
#124199=CARTESIAN_POINT('Ctrl Pts',(-196.201532992411,4.79420602793986,
131.910484334337));
#124200=CARTESIAN_POINT('Ctrl Pts',(-196.209293434926,4.8212574068754,131.776296870182));
#124201=CARTESIAN_POINT('Ctrl Pts',(-196.217066335191,4.84835221108591,
131.641893996397));
#124202=CARTESIAN_POINT('Ctrl Pts',(-196.224839235456,4.86979393109643,
131.50649970938));
#124203=CARTESIAN_POINT('Ctrl Pts',(-196.232612135722,4.88554239271103,
131.370627861474));
#124204=CARTESIAN_POINT('Ctrl Pts',(-196.240102471484,4.900718358078,131.23969529748));
#124205=CARTESIAN_POINT('Ctrl Pts',(-196.247592807246,4.91060778408717,
131.108319598021));
#124206=CARTESIAN_POINT('Ctrl Pts',(-196.255083143008,4.91522052013289,
130.976959287794));
#124207=CARTESIAN_POINT('Ctrl Pts',(-196.262857477127,4.92000814946778,
130.84061841148));
#124208=CARTESIAN_POINT('Ctrl Pts',(-196.270631811246,4.91912622449037,
130.703862227485));
#124209=CARTESIAN_POINT('Ctrl Pts',(-196.278406145365,4.91252874026042,
130.567201517771));
#124210=CARTESIAN_POINT('Ctrl Pts',(-196.286170898312,4.90593938684015,
130.430709230169));
#124211=CARTESIAN_POINT('Ctrl Pts',(-196.293935651259,4.89364850813207,
130.294312569492));
#124212=CARTESIAN_POINT('Ctrl Pts',(-196.301700404207,4.87566199954319,
130.158525399642));
#124213=CARTESIAN_POINT('Ctrl Pts',(-196.309457445092,4.85769335540821,
130.022873095524));
#124214=CARTESIAN_POINT('Ctrl Pts',(-196.317214485976,4.8340403900447,129.88782946262));
#124215=CARTESIAN_POINT('Ctrl Pts',(-196.324971526861,4.8047609802586,129.753905961198));
#124216=CARTESIAN_POINT('Ctrl Pts',(-196.332722718102,4.77550365030315,
129.620083452531));
#124217=CARTESIAN_POINT('Ctrl Pts',(-196.340473909342,4.74062840441648,
129.48737977442));
#124218=CARTESIAN_POINT('Ctrl Pts',(-196.348225100582,4.70024459204801,
129.35629852034));
#124219=CARTESIAN_POINT('Ctrl Pts',(-196.355972997359,4.65987794387701,
129.225272979288));
#124220=CARTESIAN_POINT('Ctrl Pts',(-196.363720894136,4.61400750073638,
129.095868863611));
#124221=CARTESIAN_POINT('Ctrl Pts',(-196.371468790913,4.56279303762065,
128.968576654693));
#124222=CARTESIAN_POINT('Ctrl Pts',(-196.379215066997,4.51158928746668,
128.841311072562));
#124223=CARTESIAN_POINT('Ctrl Pts',(-196.386961343081,4.45504388664914,
128.716156880974));
#124224=CARTESIAN_POINT('Ctrl Pts',(-196.394707619166,4.39336538774464,
128.593586175822));
#124225=CARTESIAN_POINT('Ctrl Pts',(-196.402453952431,4.33168643354339,
128.471014565882));
#124226=CARTESIAN_POINT('Ctrl Pts',(-196.410200285696,4.26487448138624,
128.351026829673));
#124227=CARTESIAN_POINT('Ctrl Pts',(-196.417946618962,4.19318464946682,
128.234071614754));
#124228=CARTESIAN_POINT('Ctrl Pts',(-196.425694686965,4.1214787631067,128.117090208526));
#124229=CARTESIAN_POINT('Ctrl Pts',(-196.433442754968,4.04489302757999,
128.003143008206));
#124230=CARTESIAN_POINT('Ctrl Pts',(-196.441190822971,3.96372637703559,
127.892650420707));
#124231=CARTESIAN_POINT('Ctrl Pts',(-196.448947125713,3.88247346160899,
127.782040400371));
#124232=CARTESIAN_POINT('Ctrl Pts',(-196.456703428454,3.79663013733879,
127.674892642869));
#124233=CARTESIAN_POINT('Ctrl Pts',(-196.464459731196,3.70653654583702,
127.571595563178));
#124234=CARTESIAN_POINT('Ctrl Pts',(-196.47222017371,3.6163948686728,127.468243350725));
#124235=CARTESIAN_POINT('Ctrl Pts',(-196.479980616225,3.52199867306387,
127.368746194777));
#124236=CARTESIAN_POINT('Ctrl Pts',(-196.487741058739,3.42372489016486,
127.273455501457));
#124237=CARTESIAN_POINT('Ctrl Pts',(-196.495513959004,3.32529334946519,
127.178011839056));
#124238=CARTESIAN_POINT('Ctrl Pts',(-196.50328685927,3.22297207464116,127.086788393428));
#124239=CARTESIAN_POINT('Ctrl Pts',(-196.511059759535,3.11717166908787,
127.000096714005));
#124240=CARTESIAN_POINT('Ctrl Pts',(-196.518550095297,3.01521737477187,
126.916556495492));
#124241=CARTESIAN_POINT('Ctrl Pts',(-196.526040431059,2.91003275438475,
126.837224466721));
#124242=CARTESIAN_POINT('Ctrl Pts',(-196.533530766821,2.80200890157942,
126.762340184915));
#124243=CARTESIAN_POINT('Ctrl Pts',(-196.54130510094,2.68988929156167,126.684616642804));
#124244=CARTESIAN_POINT('Ctrl Pts',(-196.549079435059,2.57435573883828,
126.61143857336));
#124245=CARTESIAN_POINT('Ctrl Pts',(-196.556853769178,2.45581311194474,
126.543120771969));
#124246=CARTESIAN_POINT('Ctrl Pts',(-196.564618522125,2.33741657824439,
126.474887166163));
#124247=CARTESIAN_POINT('Ctrl Pts',(-196.572383275073,2.2160186845002,126.411502103747));
#124248=CARTESIAN_POINT('Ctrl Pts',(-196.58014802802,2.09205494557583,126.353238380737));
#124249=CARTESIAN_POINT('Ctrl Pts',(-196.587905068905,1.96821432918454,
126.295032526079));
#124250=CARTESIAN_POINT('Ctrl Pts',(-196.59566210979,1.84181329065324,126.241938053517));
#124251=CARTESIAN_POINT('Ctrl Pts',(-196.603419150675,1.71331341981801,
126.194182726424));
#124252=CARTESIAN_POINT('Ctrl Pts',(-196.611170341915,1.58491045173478,
126.146463411995));
#124253=CARTESIAN_POINT('Ctrl Pts',(-196.618921533155,1.45441216669993,
126.104075364592));
#124254=CARTESIAN_POINT('Ctrl Pts',(-196.626672724395,1.32230135821319,
126.067198789998));
#124255=CARTESIAN_POINT('Ctrl Pts',(-196.634420621172,1.19024670034405,
126.030337888932));
#124256=CARTESIAN_POINT('Ctrl Pts',(-196.642168517949,1.05658125794433,
125.99898390647));
#124257=CARTESIAN_POINT('Ctrl Pts',(-196.649916414726,0.921804049182246,
125.973267536553));
#124258=CARTESIAN_POINT('Ctrl Pts',(-196.65766269081,0.78705503290714,125.947556545946));
#124259=CARTESIAN_POINT('Ctrl Pts',(-196.665408966895,0.651195096632955,
125.927480895489));
#124260=CARTESIAN_POINT('Ctrl Pts',(-196.673155242979,0.514734155767422,
125.913120303353));
#124261=CARTESIAN_POINT('Ctrl Pts',(-196.680901576244,0.378272207578036,
125.89875960521));
#124262=CARTESIAN_POINT('Ctrl Pts',(-196.688647909509,0.241209634762758,
125.890114090488));
#124263=CARTESIAN_POINT('Ctrl Pts',(-196.696394242775,0.104061794833803,
125.88721162599));
#124264=CARTESIAN_POINT('Ctrl Pts',(-196.704142310778,-0.0331167584028003,
125.884308511505));
#124265=CARTESIAN_POINT('Ctrl Pts',(-196.711890378781,-0.170380225947006,
125.887151014736));
#124266=CARTESIAN_POINT('Ctrl Pts',(-196.719638446784,-0.307213326347598,
125.895714874124));
#124267=CARTESIAN_POINT('Ctrl Pts',(-196.727394749525,-0.444191854595816,
125.904287835283));
#124268=CARTESIAN_POINT('Ctrl Pts',(-196.735151052267,-0.580738711172077,
125.918594275041));
#124269=CARTESIAN_POINT('Ctrl Pts',(-196.742907355009,-0.716343256706872,
125.93855797041));
#124270=CARTESIAN_POINT('Ctrl Pts',(-196.750667797523,-0.852020178470593,
125.958532321004));
#124271=CARTESIAN_POINT('Ctrl Pts',(-196.758428240037,-0.986753403156911,
125.984169870666));
#124272=CARTESIAN_POINT('Ctrl Pts',(-196.766188682552,-1.12004354234743,
126.015343440133));
#124273=CARTESIAN_POINT('Ctrl Pts',(-196.773961582817,-1.25354765070231,
126.046567052181));
#124274=CARTESIAN_POINT('Ctrl Pts',(-196.781734483082,-1.38560366746973,
126.083344337961));
#124275=CARTESIAN_POINT('Ctrl Pts',(-196.789507383348,-1.51572753612455,
126.125498245286));
#124276=CARTESIAN_POINT('Ctrl Pts',(-196.79699771911,-1.64112107439117,
126.166119751901));
#124277=CARTESIAN_POINT('Ctrl Pts',(-196.804488054872,-1.76472021359313,
126.211733652672));
#124278=CARTESIAN_POINT('Ctrl Pts',(-196.811978390634,-1.88611201178001,
126.262140395965));
#124279=CARTESIAN_POINT('Ctrl Pts',(-196.819753120516,-2.01211283081602,
126.31446098957));
#124280=CARTESIAN_POINT('Ctrl Pts',(-196.827527850399,-2.13613453277524,
126.372111311885));
#124281=CARTESIAN_POINT('Ctrl Pts',(-196.835302580282,-2.25769335655606,
126.434920862831));
#124282=CARTESIAN_POINT('Ctrl Pts',(-196.84306763844,-2.37910096178886,
126.49765227902));
#124283=CARTESIAN_POINT('Ctrl Pts',(-196.850832696599,-2.49805144108238,
126.565529975486));
#124284=CARTESIAN_POINT('Ctrl Pts',(-196.858597754758,-2.61407982358089,
126.638334964927));
#124285=CARTESIAN_POINT('Ctrl Pts',(-196.866355010688,-2.72999162227744,
126.711066800866));
#124286=CARTESIAN_POINT('Ctrl Pts',(-196.874112266618,-2.84298683835341,
126.788715870278));
#124287=CARTESIAN_POINT('Ctrl Pts',(-196.881869522548,-2.95262431338359,
126.871016909407));
#124288=CARTESIAN_POINT('Ctrl Pts',(-196.889701246598,-3.06331428645066,
126.954108022204));
#124289=CARTESIAN_POINT('Ctrl Pts',(-196.897532970648,-3.17058134690447,
127.041940717171));
#124290=CARTESIAN_POINT('Ctrl Pts',(-196.905364694697,-3.27400009449339,
127.134196255612));
#124291=CARTESIAN_POINT('Ctrl Pts',(-196.913112250324,-3.37630738911646,
127.225460313357));
#124292=CARTESIAN_POINT('Ctrl Pts',(-196.92085980595,-3.47484838652523,
127.321052344723));
#124293=CARTESIAN_POINT('Ctrl Pts',(-196.928607361577,-3.56924381249012,
127.420622792394));
#124294=CARTESIAN_POINT('Ctrl Pts',(-196.936353185915,-3.66361814461469,
127.520170989801));
#124295=CARTESIAN_POINT('Ctrl Pts',(-196.944099010253,-3.75384847999537,
127.623695550915));
#124296=CARTESIAN_POINT('Ctrl Pts',(-196.951844834592,-3.83959259305698,
127.730810263034));
#124297=CARTESIAN_POINT('Ctrl Pts',(-196.959590605432,-3.92533611390858,
127.837924235343));
#124298=CARTESIAN_POINT('Ctrl Pts',(-196.967336376272,-4.00659323053975,
127.948628003653));
#124299=CARTESIAN_POINT('Ctrl Pts',(-196.975082147112,-4.08306244107213,
128.062502823149));
#124300=CARTESIAN_POINT('Ctrl Pts',(-196.982977876498,-4.16101209969199,
128.178582265363));
#124301=CARTESIAN_POINT('Ctrl Pts',(-196.990873605884,-4.23398630132602,
128.297956468713));
#124302=CARTESIAN_POINT('Ctrl Pts',(-196.99876933527,-4.30171285759348,
128.420152247202));
#124303=CARTESIAN_POINT('Ctrl Pts',(-197.006523360613,-4.36822393061056,
128.540154987535));
#124304=CARTESIAN_POINT('Ctrl Pts',(-197.014277385956,-4.42967400356862,
128.662878498698));
#124305=CARTESIAN_POINT('Ctrl Pts',(-197.0220314113,-4.48585278789196,128.787851795899));
#124306=CARTESIAN_POINT('Ctrl Pts',(-197.029997992707,-4.54357156476701,
128.916250904981));
#124307=CARTESIAN_POINT('Ctrl Pts',(-197.037964574115,-4.59572572575124,
129.047024507953));
#124308=CARTESIAN_POINT('Ctrl Pts',(-197.045931155522,-4.64214130697621,
129.179643057938));
#124309=CARTESIAN_POINT('Ctrl Pts',(-197.053897736929,-4.68855688820118,
129.312261607922));
#124310=CARTESIAN_POINT('Ctrl Pts',(-197.061864318336,-4.72923380978975,
129.446724666572));
#124311=CARTESIAN_POINT('Ctrl Pts',(-197.069830899744,-4.76405452823391,
129.582490119308));
#124312=CARTESIAN_POINT('Origin',(213.235140564004,0.,130.804360617566));
#124313=CARTESIAN_POINT('',(-199.165100499421,-4.76405452823391,129.582490119308));
#124314=CARTESIAN_POINT('',(-198.820145221536,-4.76405452823399,129.582490119308));
#124315=CARTESIAN_POINT('',(213.235140564004,-4.76405452823405,129.582490119308));
#124316=CARTESIAN_POINT('',(-197.485140563979,-4.91824998893204,130.804030662974));
#124317=CARTESIAN_POINT('Ctrl Pts',(-197.485140564012,-4.91824998893207,
130.804030663556));
#124318=CARTESIAN_POINT('Ctrl Pts',(-197.493215691151,-4.91825960822969,
130.947414616808));
#124319=CARTESIAN_POINT('Ctrl Pts',(-197.501290818289,-4.91199470079414,
131.0906909398));
#124320=CARTESIAN_POINT('Ctrl Pts',(-197.509365945428,-4.8995093582954,
131.233302467326));
#124321=CARTESIAN_POINT('Ctrl Pts',(-197.517450328902,-4.88700970413012,
131.37607746723));
#124322=CARTESIAN_POINT('Ctrl Pts',(-197.525534712377,-4.86827541990526,
131.518185812766));
#124323=CARTESIAN_POINT('Ctrl Pts',(-197.533619095851,-4.84341207736157,
131.659078413899));
#124324=CARTESIAN_POINT('Ctrl Pts',(-197.541721259799,-4.81849405136742,
131.800280888636));
#124325=CARTESIAN_POINT('Ctrl Pts',(-197.549823423746,-4.78742007700962,
131.940261937201));
#124326=CARTESIAN_POINT('Ctrl Pts',(-197.557925587693,-4.75034662328381,
132.078483853818));
#124327=CARTESIAN_POINT('Ctrl Pts',(-197.566036944332,-4.71323110612685,
132.216862596612));
#124328=CARTESIAN_POINT('Ctrl Pts',(-197.57414830097,-4.67010262962301,
132.353477900727));
#124329=CARTESIAN_POINT('Ctrl Pts',(-197.582259657609,-4.62116662589813,
132.487810075728));
#124330=CARTESIAN_POINT('Ctrl Pts',(-197.590389437885,-4.57211947193716,
132.622447364588));
#124331=CARTESIAN_POINT('Ctrl Pts',(-197.598519218162,-4.51723854412096,
132.754790839472));
#124332=CARTESIAN_POINT('Ctrl Pts',(-197.606648998438,-4.45677700646237,
132.884341813916));
#124333=CARTESIAN_POINT('Ctrl Pts',(-197.613676754263,-4.40451127368774,
132.996331632124));
#124334=CARTESIAN_POINT('Ctrl Pts',(-197.620704510087,-4.34807614872925,
133.106234993745));
#124335=CARTESIAN_POINT('Ctrl Pts',(-197.627732265912,-4.28766139771813,
133.213747012692));
#124336=CARTESIAN_POINT('Ctrl Pts',(-197.635506600031,-4.22082861755148,
133.332680336215));
#124337=CARTESIAN_POINT('Ctrl Pts',(-197.64328093415,-4.14893767964865,
133.449019171949));
#124338=CARTESIAN_POINT('Ctrl Pts',(-197.651055268269,-4.0722149913182,
133.562303352103));
#124339=CARTESIAN_POINT('Ctrl Pts',(-197.658820021216,-3.99558685684443,
133.675447919629));
#124340=CARTESIAN_POINT('Ctrl Pts',(-197.666584774163,-3.91413903715416,
133.785545001383));
#124341=CARTESIAN_POINT('Ctrl Pts',(-197.67434952711,-3.82814386857856,
133.892158794903));
#124342=CARTESIAN_POINT('Ctrl Pts',(-197.682106567995,-3.74223411161671,
133.9986666981));
#124343=CARTESIAN_POINT('Ctrl Pts',(-197.68986360888,-3.65178623765968,
134.101697895584));
#124344=CARTESIAN_POINT('Ctrl Pts',(-197.697620649765,-3.55711572780408,
134.200845677375));
#124345=CARTESIAN_POINT('Ctrl Pts',(-197.705371841005,-3.46251660971625,
134.299918691053));
#124346=CARTESIAN_POINT('Ctrl Pts',(-197.713123032246,-3.36370146283428,
134.395113836446));
#124347=CARTESIAN_POINT('Ctrl Pts',(-197.720874223486,-3.26102563669002,
134.486057897266));
#124348=CARTESIAN_POINT('Ctrl Pts',(-197.728622120263,-3.15839345051069,
134.576963304434));
#124349=CARTESIAN_POINT('Ctrl Pts',(-197.73637001704,-3.05190414073299,
134.663620961979));
#124350=CARTESIAN_POINT('Ctrl Pts',(-197.744117913817,-2.94194930255022,
134.745695082405));
#124351=CARTESIAN_POINT('Ctrl Pts',(-197.751864189901,-2.83201746454923,
134.827752034693));
#124352=CARTESIAN_POINT('Ctrl Pts',(-197.759610465985,-2.71862185314553,
134.905227123207));
#124353=CARTESIAN_POINT('Ctrl Pts',(-197.767356742069,-2.6021861586238,
134.977825635793));
#124354=CARTESIAN_POINT('Ctrl Pts',(-197.775103075335,-2.48574960460007,
135.050424684285));
#124355=CARTESIAN_POINT('Ctrl Pts',(-197.7828494086,-2.3662732544387,135.118146878164));
#124356=CARTESIAN_POINT('Ctrl Pts',(-197.790595741865,-2.24420837078515,
135.180741753961));
#124357=CARTESIAN_POINT('Ctrl Pts',(-197.798343809868,-2.12211615154708,
135.243350647447));
#124358=CARTESIAN_POINT('Ctrl Pts',(-197.806091877871,-1.9974345931365,
135.300829759648));
#124359=CARTESIAN_POINT('Ctrl Pts',(-197.813839945874,-1.87063768933132,
135.352975538369));
#124360=CARTESIAN_POINT('Ctrl Pts',(-197.821596248616,-1.74370602426839,
135.405176738244));
#124361=CARTESIAN_POINT('Ctrl Pts',(-197.829352551358,-1.61465488491918,
135.452033132601));
#124362=CARTESIAN_POINT('Ctrl Pts',(-197.8371088541,-1.48397681704943,135.493389927451));
#124363=CARTESIAN_POINT('Ctrl Pts',(-197.844869296614,-1.35322900236022,
135.534768795668));
#124364=CARTESIAN_POINT('Ctrl Pts',(-197.852629739128,-1.22085290607787,
135.57064211333));
#124365=CARTESIAN_POINT('Ctrl Pts',(-197.860390181642,-1.08735324310278,
135.600905831281));
#124366=CARTESIAN_POINT('Ctrl Pts',(-197.868163081908,-0.953639274617129,
135.631218131239));
#124367=CARTESIAN_POINT('Ctrl Pts',(-197.875935982173,-0.818798519968866,
135.65590276613));
#124368=CARTESIAN_POINT('Ctrl Pts',(-197.883708882439,-0.683343719454388,
135.674907242287));
#124369=CARTESIAN_POINT('Ctrl Pts',(-197.891199218201,-0.55281304212647,
135.693220857867));
#124370=CARTESIAN_POINT('Ctrl Pts',(-197.898689553963,-0.421712494577103,
135.706260090511));
#124371=CARTESIAN_POINT('Ctrl Pts',(-197.906179889725,-0.290500705819022,
135.714023783448));
#124372=CARTESIAN_POINT('Ctrl Pts',(-197.913954223844,-0.154313982210954,
135.722081839163));
#124373=CARTESIAN_POINT('Ctrl Pts',(-197.921728557963,-0.0175760168504587,
135.724481939496));
#124374=CARTESIAN_POINT('Ctrl Pts',(-197.929502892082,0.119203659386324,
135.721165835397));
#124375=CARTESIAN_POINT('Ctrl Pts',(-197.937267645029,0.255814766896124,
135.7178538181));
#124376=CARTESIAN_POINT('Ctrl Pts',(-197.945032397976,0.392467095903496,
135.708839622631));
#124377=CARTESIAN_POINT('Ctrl Pts',(-197.952797150924,0.528646789015383,
135.694116811382));
#124378=CARTESIAN_POINT('Ctrl Pts',(-197.960554191809,0.664691226536644,
135.679408623037));
#124379=CARTESIAN_POINT('Ctrl Pts',(-197.968311232694,0.800263576161697,
135.659003143977));
#124380=CARTESIAN_POINT('Ctrl Pts',(-197.976068273579,0.93485113602674,
135.632945960704));
#124381=CARTESIAN_POINT('Ctrl Pts',(-197.983819464819,1.0693372023654,135.606908427356));
#124382=CARTESIAN_POINT('Ctrl Pts',(-197.991570656059,1.20283957483479,
135.575227747049));
#124383=CARTESIAN_POINT('Ctrl Pts',(-197.999321847299,1.33485218089917,
135.538001152889));
#124384=CARTESIAN_POINT('Ctrl Pts',(-198.007069744076,1.46680867808496,
135.500790381023));
#124385=CARTESIAN_POINT('Ctrl Pts',(-198.014817640853,1.59727629273097,
135.458038489407));
#124386=CARTESIAN_POINT('Ctrl Pts',(-198.02256553763,1.72576085053872,135.409893436822));
#124387=CARTESIAN_POINT('Ctrl Pts',(-198.030311813714,1.85421853214679,
135.361758455145));
#124388=CARTESIAN_POINT('Ctrl Pts',(-198.038058089798,1.98069361612735,
135.308232693516));
#124389=CARTESIAN_POINT('Ctrl Pts',(-198.045804365883,2.1047091378518,135.249513315454));
#124390=CARTESIAN_POINT('Ctrl Pts',(-198.053550699148,2.22872557503048,
135.19079350394));
#124391=CARTESIAN_POINT('Ctrl Pts',(-198.061297032413,2.35028206036682,
135.126880166801));
#124392=CARTESIAN_POINT('Ctrl Pts',(-198.069043365679,2.46892395336895,
135.058017582459));
#124393=CARTESIAN_POINT('Ctrl Pts',(-198.076791433682,2.58759241540058,
134.989139576819));
#124394=CARTESIAN_POINT('Ctrl Pts',(-198.084539501685,2.70334464822494,
134.915310314712));
#124395=CARTESIAN_POINT('Ctrl Pts',(-198.092287569688,2.8157531924012,134.836818555596));
#124396=CARTESIAN_POINT('Ctrl Pts',(-198.10004387243,2.92828120571605,134.758243374504));
#124397=CARTESIAN_POINT('Ctrl Pts',(-198.107800175171,3.03745811039781,
134.674996021732));
#124398=CARTESIAN_POINT('Ctrl Pts',(-198.115556477913,3.14288744086359,
134.587407220049));
#124399=CARTESIAN_POINT('Ctrl Pts',(-198.123316920427,3.24837304213745,
134.499771669587));
#124400=CARTESIAN_POINT('Ctrl Pts',(-198.131077362942,3.35010679377825,
134.407790315149));
#124401=CARTESIAN_POINT('Ctrl Pts',(-198.138837805456,3.44772834555247,
134.311831546565));
#124402=CARTESIAN_POINT('Ctrl Pts',(-198.146610705722,3.54550660810803,
134.215718736448));
#124403=CARTESIAN_POINT('Ctrl Pts',(-198.154383605987,3.6391592121027,134.115616038787));
#124404=CARTESIAN_POINT('Ctrl Pts',(-198.162156506252,3.7283648444739,134.011926462407));
#124405=CARTESIAN_POINT('Ctrl Pts',(-198.169646842014,3.81432762741104,
133.912006263309));
#124406=CARTESIAN_POINT('Ctrl Pts',(-198.177137177776,3.89616095138074,
133.808755683444));
#124407=CARTESIAN_POINT('Ctrl Pts',(-198.184627513538,3.97361594297526,
133.702559955126));
#124408=CARTESIAN_POINT('Ctrl Pts',(-198.192401847657,4.05400766411971,
133.592337783489));
#124409=CARTESIAN_POINT('Ctrl Pts',(-198.200176181776,4.12993714679204,
133.478593573467));
#124410=CARTESIAN_POINT('Ctrl Pts',(-198.207950515895,4.20107997053173,
133.361724522781));
#124411=CARTESIAN_POINT('Ctrl Pts',(-198.215715268842,4.27213511709918,
133.244999502756));
#124412=CARTESIAN_POINT('Ctrl Pts',(-198.22348002179,4.33841514090281,133.125157635332));
#124413=CARTESIAN_POINT('Ctrl Pts',(-198.231244774737,4.39963687332856,
133.002627763603));
#124414=CARTESIAN_POINT('Ctrl Pts',(-198.239001815622,4.46079779946676,
132.88021959027));
#124415=CARTESIAN_POINT('Ctrl Pts',(-198.246758856507,4.5169102585312,132.755129073059));
#124416=CARTESIAN_POINT('Ctrl Pts',(-198.254515897392,4.56773547585683,
132.627812203186));
#124417=CARTESIAN_POINT('Ctrl Pts',(-198.262267088632,4.61852236549037,
132.500591343955));
#124418=CARTESIAN_POINT('Ctrl Pts',(-198.270018279872,4.66402980520103,
132.371147835464));
#124419=CARTESIAN_POINT('Ctrl Pts',(-198.277769471112,4.70406605538651,
132.239960007737));
#124420=CARTESIAN_POINT('Ctrl Pts',(-198.285517367889,4.74408528909782,
132.108827938336));
#124421=CARTESIAN_POINT('Ctrl Pts',(-198.293265264666,4.77863784444936,
131.975953397409));
#124422=CARTESIAN_POINT('Ctrl Pts',(-198.301013161443,4.80758109007599,
131.841832123124));
#124423=CARTESIAN_POINT('Ctrl Pts',(-198.308759437527,4.83651828139958,
131.707738904118));
#124424=CARTESIAN_POINT('Ctrl Pts',(-198.316505713611,4.8598484144299,131.572399852405));
#124425=CARTESIAN_POINT('Ctrl Pts',(-198.324251989695,4.87747955738707,
131.436322823533));
#124426=CARTESIAN_POINT('Ctrl Pts',(-198.331998322961,4.89511083049331,
131.300244790173));
#124427=CARTESIAN_POINT('Ctrl Pts',(-198.339744656226,4.90704297934507,
131.163429156507));
#124428=CARTESIAN_POINT('Ctrl Pts',(-198.347490989491,4.91323577800568,
131.026390462913));
#124429=CARTESIAN_POINT('Ctrl Pts',(-198.355239057494,4.91942996350062,
130.889321080454));
#124430=CARTESIAN_POINT('Ctrl Pts',(-198.362987125497,4.91988222358433,
130.752028929157));
#124431=CARTESIAN_POINT('Ctrl Pts',(-198.3707351935,4.91460444749664,130.615029724296));
#124432=CARTESIAN_POINT('Ctrl Pts',(-198.378491496242,4.9093210621257,130.47788491505));
#124433=CARTESIAN_POINT('Ctrl Pts',(-198.386247798984,4.8982954903254,130.341034065488));
#124434=CARTESIAN_POINT('Ctrl Pts',(-198.394004101726,4.88159167919793,
130.204989497069));
#124435=CARTESIAN_POINT('Ctrl Pts',(-198.40176454424,4.86487895274352,130.068872317568));
#124436=CARTESIAN_POINT('Ctrl Pts',(-198.409524986754,4.84248201195462,
129.93356266222));
#124437=CARTESIAN_POINT('Ctrl Pts',(-198.417285429268,4.8145160155251,129.799562827584));
#124438=CARTESIAN_POINT('Ctrl Pts',(-198.425058329534,4.78650512559541,
129.665347884518));
#124439=CARTESIAN_POINT('Ctrl Pts',(-198.432831229799,4.7529074110492,129.532447343168));
#124440=CARTESIAN_POINT('Ctrl Pts',(-198.440604130065,4.71388825706518,
129.401349369428));
#124441=CARTESIAN_POINT('Ctrl Pts',(-198.448094465827,4.67628754761169,
129.275017137248));
#124442=CARTESIAN_POINT('Ctrl Pts',(-198.455584801589,4.6336528210575,129.150358983697));
#124443=CARTESIAN_POINT('Ctrl Pts',(-198.463075137351,4.58617366210336,
129.027792520495));
#124444=CARTESIAN_POINT('Ctrl Pts',(-198.47084947147,4.53689431640671,128.900578912589));
#124445=CARTESIAN_POINT('Ctrl Pts',(-198.478623805589,4.48223983117683,
128.775215764509));
#124446=CARTESIAN_POINT('Ctrl Pts',(-198.486398139708,4.42236902292319,
128.652190715446));
#124447=CARTESIAN_POINT('Ctrl Pts',(-198.494162892655,4.36257200009024,
128.529317283763));
#124448=CARTESIAN_POINT('Ctrl Pts',(-198.501927645602,4.29757161477436,
128.408776565947));
#124449=CARTESIAN_POINT('Ctrl Pts',(-198.509692398549,4.22757560526325,
128.29103859994));
#124450=CARTESIAN_POINT('Ctrl Pts',(-198.517449439434,4.15764911677518,
128.173417572941));
#124451=CARTESIAN_POINT('Ctrl Pts',(-198.525206480319,4.08273707664526,
128.058594091884));
#124452=CARTESIAN_POINT('Ctrl Pts',(-198.532963521204,4.0030940596596,127.947015519049));
#124453=CARTESIAN_POINT('Ctrl Pts',(-198.540714712445,3.92351110209268,
127.835521088484));
#124454=CARTESIAN_POINT('Ctrl Pts',(-198.548465903685,3.8392044951129,127.727267012445));
#124455=CARTESIAN_POINT('Ctrl Pts',(-198.556217094925,3.7504730313789,127.622673155951));
#124456=CARTESIAN_POINT('Ctrl Pts',(-198.563964991702,3.66177928088409,
127.518123754636));
#124457=CARTESIAN_POINT('Ctrl Pts',(-198.571712888479,3.56866466656006,
127.417231776227));
#124458=CARTESIAN_POINT('Ctrl Pts',(-198.579460785256,3.47146917123165,
127.320385179121));
#124459=CARTESIAN_POINT('Ctrl Pts',(-198.58720706134,3.37429400710557,127.223558840235));
#124460=CARTESIAN_POINT('Ctrl Pts',(-198.594953337424,3.27303993667195,
127.130776475282));
#124461=CARTESIAN_POINT('Ctrl Pts',(-198.602699613508,3.16808454181421,
127.042389937401));
#124462=CARTESIAN_POINT('Ctrl Pts',(-198.610445946774,3.06312837219946,
126.954002747071));
#124463=CARTESIAN_POINT('Ctrl Pts',(-198.618192280039,2.95447112269024,
126.870011700402));
#124464=CARTESIAN_POINT('Ctrl Pts',(-198.625938613304,2.84252394757572,
126.790728762256));
#124465=CARTESIAN_POINT('Ctrl Pts',(-198.633686681307,2.73055170266768,
126.711428069246));
#124466=CARTESIAN_POINT('Ctrl Pts',(-198.64143474931,2.61528838508869,126.636837808705));
#124467=CARTESIAN_POINT('Ctrl Pts',(-198.649182817313,2.49717430712868,
126.567226734584));
#124468=CARTESIAN_POINT('Ctrl Pts',(-198.656939120055,2.37893469612088,
126.497541676984));
#124469=CARTESIAN_POINT('Ctrl Pts',(-198.664695422797,2.2578386096946,126.432846575844));
#124470=CARTESIAN_POINT('Ctrl Pts',(-198.672451725539,2.13435164337421,
126.373364552918));
#124471=CARTESIAN_POINT('Ctrl Pts',(-198.680212168053,2.01079876834144,
126.313850782646));
#124472=CARTESIAN_POINT('Ctrl Pts',(-198.687972610567,1.88485282955681,
126.259555789408));
#124473=CARTESIAN_POINT('Ctrl Pts',(-198.695733053081,1.75699866942774,
126.210654190493));
#124474=CARTESIAN_POINT('Ctrl Pts',(-198.703505953346,1.62893926645082,
126.161674090391));
#124475=CARTESIAN_POINT('Ctrl Pts',(-198.711278853612,1.49896589169275,
126.1181048103));
#124476=CARTESIAN_POINT('Ctrl Pts',(-198.719051753877,1.36757864767384,
126.080071072573));
#124477=CARTESIAN_POINT('Ctrl Pts',(-198.726542089639,1.24096766091596,
126.043419957014));
#124478=CARTESIAN_POINT('Ctrl Pts',(-198.734032425402,1.11304411471436,
126.011908983002));
#124479=CARTESIAN_POINT('Ctrl Pts',(-198.741522761164,0.984261832800122,
125.985604376896));
#124480=CARTESIAN_POINT('Ctrl Pts',(-198.749297095283,0.850596731528147,
125.958302423656));
#124481=CARTESIAN_POINT('Ctrl Pts',(-198.757071429402,0.715583080302673,
125.936522946273));
#124482=CARTESIAN_POINT('Ctrl Pts',(-198.764845763521,0.579716987989611,
125.920395908814));
#124483=CARTESIAN_POINT('Ctrl Pts',(-198.772610516468,0.444018338491886,
125.904288746487));
#124484=CARTESIAN_POINT('Ctrl Pts',(-198.780375269415,0.307469722715481,
125.89382020921));
#124485=CARTESIAN_POINT('Ctrl Pts',(-198.788140022362,0.170578884512039,
125.889069587865));
#124486=CARTESIAN_POINT('Ctrl Pts',(-198.795897063247,0.0338240082189226,
125.884323684905));
#124487=CARTESIAN_POINT('Ctrl Pts',(-198.803654104132,-0.103272025883022,
125.885284409655));
#124488=CARTESIAN_POINT('Ctrl Pts',(-198.811411145017,-0.240195235348314,
125.891979391377));
#124489=CARTESIAN_POINT('Ctrl Pts',(-198.819162336258,-0.377015189955682,
125.898669324361));
#124490=CARTESIAN_POINT('Ctrl Pts',(-198.826913527498,-0.513662190418549,
125.911084888148));
#124491=CARTESIAN_POINT('Ctrl Pts',(-198.834664718738,-0.649621487673782,
125.929201647312));
#124492=CARTESIAN_POINT('Ctrl Pts',(-198.842412615515,-0.785522998601034,
125.947310706369));
#124493=CARTESIAN_POINT('Ctrl Pts',(-198.850160512292,-0.920737000939123,
125.971116089789));
#124494=CARTESIAN_POINT('Ctrl Pts',(-198.857908409069,-1.05475332528018,
126.000541461383));
#124495=CARTESIAN_POINT('Ctrl Pts',(-198.865654685153,-1.18874161629487,
126.029960677823));
#124496=CARTESIAN_POINT('Ctrl Pts',(-198.873400961237,-1.32153234600044,
126.064997460351));
#124497=CARTESIAN_POINT('Ctrl Pts',(-198.881147237321,-1.45262539815508,
126.105524323851));
#124498=CARTESIAN_POINT('Ctrl Pts',(-198.888893570586,-1.58371941800903,
126.14605148651));
#124499=CARTESIAN_POINT('Ctrl Pts',(-198.896639903852,-1.71311536178222,
126.192068695536));
#124500=CARTESIAN_POINT('Ctrl Pts',(-198.904386237117,-1.84032852566538,
126.243398659807));
#124501=CARTESIAN_POINT('Ctrl Pts',(-198.91213430512,-1.96757017805508,
126.294740119068));
#124502=CARTESIAN_POINT('Ctrl Pts',(-198.919882373123,-2.09262771536865,
126.351396554784));
#124503=CARTESIAN_POINT('Ctrl Pts',(-198.927630441126,-2.2150370277501,
126.413142787829));
#124504=CARTESIAN_POINT('Ctrl Pts',(-198.935386743868,-2.33757643820495,
126.474954645506));
#124505=CARTESIAN_POINT('Ctrl Pts',(-198.94314304661,-2.4574616517044,126.541866930204));
#124506=CARTESIAN_POINT('Ctrl Pts',(-198.950899349351,-2.57425328384323,
126.613608525981));
#124507=CARTESIAN_POINT('Ctrl Pts',(-198.958659791866,-2.69110725119298,
126.685388412409));
#124508=CARTESIAN_POINT('Ctrl Pts',(-198.96642023438,-2.80486402303167,
126.762002527609));
#124509=CARTESIAN_POINT('Ctrl Pts',(-198.974180676894,-2.91511461972486,
126.843137344842));
#124510=CARTESIAN_POINT('Ctrl Pts',(-198.981953577159,-3.02554220046346,
126.924402406887));
#124511=CARTESIAN_POINT('Ctrl Pts',(-198.989726477425,-3.13245205358369,
127.010202427981));
#124512=CARTESIAN_POINT('Ctrl Pts',(-198.99749937769,-3.23546892900845,
127.100184073188));
#124513=CARTESIAN_POINT('Ctrl Pts',(-199.004989713452,-3.33474088152516,
127.186894658939));
#124514=CARTESIAN_POINT('Ctrl Pts',(-199.012480049214,-3.43039775782205,
127.277487910186));
#124515=CARTESIAN_POINT('Ctrl Pts',(-199.019970384976,-3.52213853697615,
127.371617809133));
#124516=CARTESIAN_POINT('Ctrl Pts',(-199.027641276347,-3.6160907406696,
127.468016722693));
#124517=CARTESIAN_POINT('Ctrl Pts',(-199.035312167719,-3.70625045185473,
127.568448295507));
#124518=CARTESIAN_POINT('Ctrl Pts',(-199.04298305909,-3.79224452810265,
127.672577658679));
#124519=CARTESIAN_POINT('Ctrl Pts',(-199.0506449325,-3.87813750901698,127.776584606526));
#124520=CARTESIAN_POINT('Ctrl Pts',(-199.058306805909,-3.9598743377894,
127.884280395336));
#124521=CARTESIAN_POINT('Ctrl Pts',(-199.065968679319,-4.03711767976908,
127.995292462075));
#124522=CARTESIAN_POINT('Ctrl Pts',(-199.073623311162,-4.11428801574521,
128.106199606536));
#124523=CARTESIAN_POINT('Ctrl Pts',(-199.081277943005,-4.1869730825278,
128.220416467907));
#124524=CARTESIAN_POINT('Ctrl Pts',(-199.088932574849,-4.25487528640376,
128.337536878494));
#124525=CARTESIAN_POINT('Ctrl Pts',(-199.096581319393,-4.32272526561704,
128.454567209913));
#124526=CARTESIAN_POINT('Ctrl Pts',(-199.104230063938,-4.38579950174855,
128.574496299718));
#124527=CARTESIAN_POINT('Ctrl Pts',(-199.111878808483,-4.44384363448245,
128.696888953517));
#124528=CARTESIAN_POINT('Ctrl Pts',(-199.119524183703,-4.50186219837772,
128.819227692512));
#124529=CARTESIAN_POINT('Ctrl Pts',(-199.127169558923,-4.55485489515574,
128.944027473816));
#124530=CARTESIAN_POINT('Ctrl Pts',(-199.134814934143,-4.60261344758878,
129.070828813827));
#124531=CARTESIAN_POINT('Ctrl Pts',(-199.142459303634,-4.65036571750983,
129.197613473455));
#124532=CARTESIAN_POINT('Ctrl Pts',(-199.150103673125,-4.69288506876711,
129.32639879276));
#124533=CARTESIAN_POINT('Ctrl Pts',(-199.157748042617,-4.73001164933185,
129.456706040278));
#124534=CARTESIAN_POINT('Ctrl Pts',(-199.160198861551,-4.74191459655825,
129.498483124697));
#124535=CARTESIAN_POINT('Ctrl Pts',(-199.162649680486,-4.75326361641396,
129.540416517897));
#124536=CARTESIAN_POINT('Ctrl Pts',(-199.165100499421,-4.76405452823391,
129.582490119308));
#124537=CARTESIAN_POINT('Ctrl Pts',(-197.415422870675,-4.76405452823413,
129.582490119309));
#124538=CARTESIAN_POINT('Ctrl Pts',(-197.423600431488,-4.79992281658223,
129.722340031201));
#124539=CARTESIAN_POINT('Ctrl Pts',(-197.431777992302,-4.82966733555782,
129.863920110019));
#124540=CARTESIAN_POINT('Ctrl Pts',(-197.439955553115,-4.85313234200592,
130.006683030144));
#124541=CARTESIAN_POINT('Ctrl Pts',(-197.448116021641,-4.87654830318953,
130.149147555073));
#124542=CARTESIAN_POINT('Ctrl Pts',(-197.456276490167,-4.89371087298272,
130.292789672346));
#124543=CARTESIAN_POINT('Ctrl Pts',(-197.464436958693,-4.90451488430555,
130.437050377952));
#124544=CARTESIAN_POINT('Ctrl Pts',(-197.471338160455,-4.91365169572061,
130.559049774504));
#124545=CARTESIAN_POINT('Ctrl Pts',(-197.478239362217,-4.91824176802981,
130.681491218841));
#124546=CARTESIAN_POINT('Ctrl Pts',(-197.485140563979,-4.91824998893204,
130.804030662974));
#124547=CARTESIAN_POINT('',(-197.13985943604,-4.91824821858491,130.800174582878));
#124548=CARTESIAN_POINT('Ctrl Pts',(-197.069830899744,-4.76405452823391,
129.582490119308));
#124549=CARTESIAN_POINT('Ctrl Pts',(-197.076695937978,-4.79406056862158,
129.699483215374));
#124550=CARTESIAN_POINT('Ctrl Pts',(-197.083560976212,-4.81971881788819,
129.817443076));
#124551=CARTESIAN_POINT('Ctrl Pts',(-197.090426014446,-4.84098812800867,
129.936019090873));
#124552=CARTESIAN_POINT('Ctrl Pts',(-197.102330337474,-4.87787018599897,
130.14163588954));
#124553=CARTESIAN_POINT('Ctrl Pts',(-197.114234660503,-4.90165998726396,
130.349666738386));
#124554=CARTESIAN_POINT('Ctrl Pts',(-197.126138983531,-4.91211451822462,
130.558771484364));
#124555=CARTESIAN_POINT('Ctrl Pts',(-197.130712467685,-4.91613101135752,
130.639106774339));
#124556=CARTESIAN_POINT('Ctrl Pts',(-197.13528595184,-4.91817963992249,
130.719600281634));
#124557=CARTESIAN_POINT('Ctrl Pts',(-197.139859435995,-4.91824821858423,
130.80017458208));
#124558=CARTESIAN_POINT('Ctrl Pts',(-197.13985943604,-4.91824821858491,
130.800174582878));
#124559=CARTESIAN_POINT('Ctrl Pts',(-197.147506112978,-4.91836287925791,
130.93489149106));
#124560=CARTESIAN_POINT('Ctrl Pts',(-197.155152789915,-4.91293828803124,
131.069802457209));
#124561=CARTESIAN_POINT('Ctrl Pts',(-197.162799466852,-4.9019533167259,
131.204406543854));
#124562=CARTESIAN_POINT('Ctrl Pts',(-197.170439161222,-4.89097837635308,
131.338887716705));
#124563=CARTESIAN_POINT('Ctrl Pts',(-197.178078855592,-4.87445318757935,
131.473062167562));
#124564=CARTESIAN_POINT('Ctrl Pts',(-197.185718549962,-4.85240867394315,
131.606428646814));
#124565=CARTESIAN_POINT('Ctrl Pts',(-197.193353528545,-4.83037776781788,
131.73971280237));
#124566=CARTESIAN_POINT('Ctrl Pts',(-197.200988507129,-4.80283437820965,
131.872189581299));
#124567=CARTESIAN_POINT('Ctrl Pts',(-197.208623485712,-4.76986124614636,
132.003363017485));
#124568=CARTESIAN_POINT('Ctrl Pts',(-197.216256000669,-4.73689875372977,
132.134494127118));
#124569=CARTESIAN_POINT('Ctrl Pts',(-197.223888515626,-4.69851009985092,
132.264322339006));
#124570=CARTESIAN_POINT('Ctrl Pts',(-197.231521030583,-4.6548290030468,
132.392362511423));
#124571=CARTESIAN_POINT('Ctrl Pts',(-197.239152849597,-4.61115188914653,
132.520391008958));
#124572=CARTESIAN_POINT('Ctrl Pts',(-197.24678466861,-4.56218342217936,
132.646631409198));
#124573=CARTESIAN_POINT('Ctrl Pts',(-197.254416487624,-4.50810682560393,
132.770614902099));
#124574=CARTESIAN_POINT('Ctrl Pts',(-197.262049377602,-4.45402264051946,
132.894615793466));
#124575=CARTESIAN_POINT('Ctrl Pts',(-197.26968226758,-4.39482906232151,
133.016358777953));
#124576=CARTESIAN_POINT('Ctrl Pts',(-197.277315157558,-4.33075673716147,
133.135396684647));
#124577=CARTESIAN_POINT('Ctrl Pts',(-197.284955576458,-4.26662121241328,
133.254552007817));
#124578=CARTESIAN_POINT('Ctrl Pts',(-197.292595995358,-4.19759752046628,
133.37099656774));
#124579=CARTESIAN_POINT('Ctrl Pts',(-197.300236414258,-4.1239615861599,
133.484309105574));
#124580=CARTESIAN_POINT('Ctrl Pts',(-197.307880546064,-4.05028986803414,
133.597676708309));
#124581=CARTESIAN_POINT('Ctrl Pts',(-197.315524677871,-3.97200167824627,
133.707908929455));
#124582=CARTESIAN_POINT('Ctrl Pts',(-197.323168809677,-3.88941447193958,
133.814616109707));
#124583=CARTESIAN_POINT('Ctrl Pts',(-197.330825110679,-3.8066957896451,
133.921493164115));
#124584=CARTESIAN_POINT('Ctrl Pts',(-197.33848141168,-3.71966467800465,
134.024833657621));
#124585=CARTESIAN_POINT('Ctrl Pts',(-197.346137712681,-3.62867730838004,
134.124282913968));
#124586=CARTESIAN_POINT('Ctrl Pts',(-197.35371635454,-3.53861283886426,
134.222723439874));
#124587=CARTESIAN_POINT('Ctrl Pts',(-197.3612949964,-3.44467233174058,134.317351104802));
#124588=CARTESIAN_POINT('Ctrl Pts',(-197.368873638259,-3.34723265001436,
134.407861227969));
#124589=CARTESIAN_POINT('Ctrl Pts',(-197.376647972378,-3.24727692493325,
134.500708462567));
#124590=CARTESIAN_POINT('Ctrl Pts',(-197.384422306497,-3.14329678401998,
134.589540674901));
#124591=CARTESIAN_POINT('Ctrl Pts',(-197.392196640617,-3.03564832798573,
134.673988802715));
#124592=CARTESIAN_POINT('Ctrl Pts',(-197.399961393564,-2.92813253905301,
134.758332855758));
#124593=CARTESIAN_POINT('Ctrl Pts',(-197.407726146511,-2.81695773483861,
134.83830333563));
#124594=CARTESIAN_POINT('Ctrl Pts',(-197.415490899458,-2.70251631213269,
134.91356840559));
#124595=CARTESIAN_POINT('Ctrl Pts',(-197.423247940343,-2.58818855426113,
134.988758721222));
#124596=CARTESIAN_POINT('Ctrl Pts',(-197.431004981228,-2.47060095904148,
135.059252713936));
#124597=CARTESIAN_POINT('Ctrl Pts',(-197.438762022113,-2.35017812468133,
135.124759423784));
#124598=CARTESIAN_POINT('Ctrl Pts',(-197.446513213353,-2.22984610211716,
135.190216734512));
#124599=CARTESIAN_POINT('Ctrl Pts',(-197.454264404593,-2.1066834381736,
135.250694062248));
#124600=CARTESIAN_POINT('Ctrl Pts',(-197.462015595833,-1.98114246876202,
135.305944514481));
#124601=CARTESIAN_POINT('Ctrl Pts',(-197.46976349261,-1.85565485761151,
135.361171483799));
#124602=CARTESIAN_POINT('Ctrl Pts',(-197.477511389387,-1.72779130857727,
135.411175838973));
#124603=CARTESIAN_POINT('Ctrl Pts',(-197.485259286164,-1.59802724398115,
135.455757395954));
#124604=CARTESIAN_POINT('Ctrl Pts',(-197.493005562248,-1.46829032322996,
135.500329627433));
#124605=CARTESIAN_POINT('Ctrl Pts',(-197.500751838333,-1.33665404717749,
135.539481190017));
#124606=CARTESIAN_POINT('Ctrl Pts',(-197.508498114417,-1.20361185877549,
135.573060813208));
#124607=CARTESIAN_POINT('Ctrl Pts',(-197.516244447682,-1.0705686882861,
135.606640684276));
#124608=CARTESIAN_POINT('Ctrl Pts',(-197.523990780947,-0.936119963815441,
135.634648438198));
#124609=CARTESIAN_POINT('Ctrl Pts',(-197.531737114213,-0.800771873265166,
135.656983358877));
#124610=CARTESIAN_POINT('Ctrl Pts',(-197.539485182216,-0.665393472448266,
135.679323281307));
#124611=CARTESIAN_POINT('Ctrl Pts',(-197.547233250219,-0.52911569045003,
135.695987778918));
#124612=CARTESIAN_POINT('Ctrl Pts',(-197.554981318222,-0.392452037104296,
135.706927747252));
#124613=CARTESIAN_POINT('Ctrl Pts',(-197.562737620963,-0.255643136002026,
135.717879342714));
#124614=CARTESIAN_POINT('Ctrl Pts',(-197.570493923705,-0.118447934655994,
135.723094224012));
#124615=CARTESIAN_POINT('Ctrl Pts',(-197.578250226447,0.0186172786708312,
135.722575381018));
#124616=CARTESIAN_POINT('Ctrl Pts',(-197.586010668961,0.155755647829336,
135.722056261102));
#124617=CARTESIAN_POINT('Ctrl Pts',(-197.593771111476,0.292763500359275,
135.715797336897));
#124618=CARTESIAN_POINT('Ctrl Pts',(-197.60153155399,0.429128454194537,
135.703853635451));
#124619=CARTESIAN_POINT('Ctrl Pts',(-197.609304454255,0.565712313159607,
135.691890760914));
#124620=CARTESIAN_POINT('Ctrl Pts',(-197.617077354521,0.701650823160877,
135.674224923474));
#124621=CARTESIAN_POINT('Ctrl Pts',(-197.624850254786,0.836439701705548,
135.650962694064));
#124622=CARTESIAN_POINT('Ctrl Pts',(-197.632340590548,0.966328665002057,
135.628546105287));
#124623=CARTESIAN_POINT('Ctrl Pts',(-197.63983092631,1.09514982852237,135.600933010851));
#124624=CARTESIAN_POINT('Ctrl Pts',(-197.647321262072,1.2224661119373,135.568262344897));
#124625=CARTESIAN_POINT('Ctrl Pts',(-197.655095596191,1.35460963093539,
135.534352960713));
#124626=CARTESIAN_POINT('Ctrl Pts',(-197.66286993031,1.48555049305068,135.494887503906));
#124627=CARTESIAN_POINT('Ctrl Pts',(-197.670644264429,1.61478571462178,
135.449966084925));
#124628=CARTESIAN_POINT('Ctrl Pts',(-197.678409017376,1.74386166533168,
135.405100027578));
#124629=CARTESIAN_POINT('Ctrl Pts',(-197.686173770323,1.87123579220267,
135.354791513917));
#124630=CARTESIAN_POINT('Ctrl Pts',(-197.693938523271,1.99641681153709,
135.29919131261));
#124631=CARTESIAN_POINT('Ctrl Pts',(-197.701695564156,2.1214734993187,135.243646334207));
#124632=CARTESIAN_POINT('Ctrl Pts',(-197.70945260504,2.24434105933608,135.182820285069));
#124633=CARTESIAN_POINT('Ctrl Pts',(-197.717209645925,2.36454519304033,
135.116913120733));
#124634=CARTESIAN_POINT('Ctrl Pts',(-197.724960837166,2.4846586798728,135.051055657502));
#124635=CARTESIAN_POINT('Ctrl Pts',(-197.732712028406,2.60211239678094,
134.98012489306));
#124636=CARTESIAN_POINT('Ctrl Pts',(-197.740463219646,2.7164541274949,134.904367938988));
#124637=CARTESIAN_POINT('Ctrl Pts',(-197.748211116423,2.83074725992267,
134.828643183643));
#124638=CARTESIAN_POINT('Ctrl Pts',(-197.7559590132,2.94193071162179,134.748096533953));
#124639=CARTESIAN_POINT('Ctrl Pts',(-197.763706909977,3.04957908470244,
134.663019771812));
#124640=CARTESIAN_POINT('Ctrl Pts',(-197.771453186061,3.15720494006407,
134.577960805895));
#124641=CARTESIAN_POINT('Ctrl Pts',(-197.779199462145,3.26129688109708,
134.488373854626));
#124642=CARTESIAN_POINT('Ctrl Pts',(-197.786945738229,3.361460921679,134.394592300135));
#124643=CARTESIAN_POINT('Ctrl Pts',(-197.794692071495,3.46162570164924,
134.30081005337));
#124644=CARTESIAN_POINT('Ctrl Pts',(-197.80243840476,3.55786223791384,134.20283340881));
#124645=CARTESIAN_POINT('Ctrl Pts',(-197.810184738026,3.64981218824234,
134.101033797161));
#124646=CARTESIAN_POINT('Ctrl Pts',(-197.817932806029,3.74178273012479,
133.999211388194));
#124647=CARTESIAN_POINT('Ctrl Pts',(-197.825680874032,3.82946451386792,
133.893564598623));
#124648=CARTESIAN_POINT('Ctrl Pts',(-197.833428942035,3.91253866189194,
133.784498916656));
#124649=CARTESIAN_POINT('Ctrl Pts',(-197.841185244776,3.99570110210896,
133.675317318384));
#124650=CARTESIAN_POINT('Ctrl Pts',(-197.848941547518,4.07424588694472,
133.562709880643));
#124651=CARTESIAN_POINT('Ctrl Pts',(-197.85669785026,4.14789646544683,133.44711258747));
#124652=CARTESIAN_POINT('Ctrl Pts',(-197.864458292774,4.22158635348026,
133.331453596542));
#124653=CARTESIAN_POINT('Ctrl Pts',(-197.872218735289,4.29037663418042,
133.212801908529));
#124654=CARTESIAN_POINT('Ctrl Pts',(-197.879979177803,4.35403664833725,
133.091618348439));
#124655=CARTESIAN_POINT('Ctrl Pts',(-197.887752078068,4.41779885520026,
132.970240253739));
#124656=CARTESIAN_POINT('Ctrl Pts',(-197.895524978334,4.4764141709775,132.846322518647));
#124657=CARTESIAN_POINT('Ctrl Pts',(-197.903297878599,4.52969967980894,
132.720347014501));
#124658=CARTESIAN_POINT('Ctrl Pts',(-197.910788214361,4.58104812617597,
132.598951037243));
#124659=CARTESIAN_POINT('Ctrl Pts',(-197.918278550123,4.62744743329827,
132.475644591939));
#124660=CARTESIAN_POINT('Ctrl Pts',(-197.925768885885,4.66877823780837,
132.350870503945));
#124661=CARTESIAN_POINT('Ctrl Pts',(-197.933543220004,4.71167611233399,
132.221365568478));
#124662=CARTESIAN_POINT('Ctrl Pts',(-197.941317554123,4.74924944018407,
132.089869269341));
#124663=CARTESIAN_POINT('Ctrl Pts',(-197.949091888242,4.78131057215974,
131.956858893076));
#124664=CARTESIAN_POINT('Ctrl Pts',(-197.956856641189,4.81333219165545,
131.824012440213));
#124665=CARTESIAN_POINT('Ctrl Pts',(-197.964621394136,4.83985504116094,
131.689655999366));
#124666=CARTESIAN_POINT('Ctrl Pts',(-197.972386147084,4.86074041578861,
131.554284395572));
#124667=CARTESIAN_POINT('Ctrl Pts',(-197.980143187969,4.88160504676788,
131.419047244763));
#124668=CARTESIAN_POINT('Ctrl Pts',(-197.987900228854,4.89684328634105,
131.282797321412));
#124669=CARTESIAN_POINT('Ctrl Pts',(-197.995657269739,4.90636699281359,
131.146041747173));
#124670=CARTESIAN_POINT('Ctrl Pts',(-198.003408460979,4.91588351738501,
131.009389301376));
#124671=CARTESIAN_POINT('Ctrl Pts',(-198.011159652219,4.91969405935185,
130.872232352118));
#124672=CARTESIAN_POINT('Ctrl Pts',(-198.018910843459,4.91776208674575,
130.7350849316));
#124673=CARTESIAN_POINT('Ctrl Pts',(-198.026658740236,4.91583093527955,
130.597995802394));
#124674=CARTESIAN_POINT('Ctrl Pts',(-198.034406637013,4.90816212914558,
130.460916583982));
#124675=CARTESIAN_POINT('Ctrl Pts',(-198.04215453379,4.89477121476498,130.324362890896));
#124676=CARTESIAN_POINT('Ctrl Pts',(-198.049900809875,4.881383101475,130.187837761899));
#124677=CARTESIAN_POINT('Ctrl Pts',(-198.057647085959,4.86227529885319,
130.051838328427));
#124678=CARTESIAN_POINT('Ctrl Pts',(-198.065393362043,4.83751533160561,
129.916876263349));
#124679=CARTESIAN_POINT('Ctrl Pts',(-198.073139695308,4.81275518158554,
129.78191320201));
#124680=CARTESIAN_POINT('Ctrl Pts',(-198.080886028573,4.78234285423304,
129.647987908893));
#124681=CARTESIAN_POINT('Ctrl Pts',(-198.088632361839,4.74639715199262,
129.515602634834));
#124682=CARTESIAN_POINT('Ctrl Pts',(-198.096380429842,4.71044339996136,
129.38318771401));
#124683=CARTESIAN_POINT('Ctrl Pts',(-198.104128497845,4.66895390968266,
129.25231387574));
#124684=CARTESIAN_POINT('Ctrl Pts',(-198.111876565848,4.62209746874859,
129.123468577045));
#124685=CARTESIAN_POINT('Ctrl Pts',(-198.11963286859,4.57519122823157,128.994486340033));
#124686=CARTESIAN_POINT('Ctrl Pts',(-198.127389171331,4.52290677641864,
128.867537317358));
#124687=CARTESIAN_POINT('Ctrl Pts',(-198.135145474073,4.46546143648297,
128.743089839191));
#124688=CARTESIAN_POINT('Ctrl Pts',(-198.142905916588,4.40798543623973,
128.618575939658));
#124689=CARTESIAN_POINT('Ctrl Pts',(-198.150666359102,4.34534323773866,
128.496566592663));
#124690=CARTESIAN_POINT('Ctrl Pts',(-198.158426801616,4.27779786917148,
128.377504945506));
#124691=CARTESIAN_POINT('Ctrl Pts',(-198.166199701881,4.21014407078227,
128.258252170022));
#124692=CARTESIAN_POINT('Ctrl Pts',(-198.173972602147,4.13757158065354,
128.141956882111));
#124693=CARTESIAN_POINT('Ctrl Pts',(-198.181745502412,4.06038694029745,
128.029033437293));
#124694=CARTESIAN_POINT('Ctrl Pts',(-198.189235838174,3.98600815603532,
127.920215044132));
#124695=CARTESIAN_POINT('Ctrl Pts',(-198.196726173936,3.90734691024696,
127.81452784734));
#124696=CARTESIAN_POINT('Ctrl Pts',(-198.204216509698,3.8247112456301,127.712311628619));
#124697=CARTESIAN_POINT('Ctrl Pts',(-198.211990843817,3.73894242467187,
127.606219850896));
#124698=CARTESIAN_POINT('Ctrl Pts',(-198.219765177936,3.64862016552164,
127.503531384384));
#124699=CARTESIAN_POINT('Ctrl Pts',(-198.227539512055,3.55404459388961,
127.404662088704));
#124700=CARTESIAN_POINT('Ctrl Pts',(-198.235304265002,3.45958557819766,
127.305914640596));
#124701=CARTESIAN_POINT('Ctrl Pts',(-198.24306901795,3.36088394735533,127.210977278024));
#124702=CARTESIAN_POINT('Ctrl Pts',(-198.250833770897,3.25828103830071,
127.12023416236));
#124703=CARTESIAN_POINT('Ctrl Pts',(-198.258590811782,3.15578003590126,
127.029581174037));
#124704=CARTESIAN_POINT('Ctrl Pts',(-198.266347852667,3.04938575729155,
126.943114399854));
#124705=CARTESIAN_POINT('Ctrl Pts',(-198.274104893552,2.93947721554274,
126.861182107556));
#124706=CARTESIAN_POINT('Ctrl Pts',(-198.281856084792,2.82965155668068,
126.779311601038));
#124707=CARTESIAN_POINT('Ctrl Pts',(-198.289607276032,2.71631722179468,
126.701969002842));
#124708=CARTESIAN_POINT('Ctrl Pts',(-198.297358467272,2.59988693431213,
126.629462895311));
#124709=CARTESIAN_POINT('Ctrl Pts',(-198.305106364049,2.48350613280748,
126.556987604809));
#124710=CARTESIAN_POINT('Ctrl Pts',(-198.312854260826,2.36403232703562,
126.489344922703));
#124711=CARTESIAN_POINT('Ctrl Pts',(-198.320602157603,2.24190772132709,
126.4268004716));
#124712=CARTESIAN_POINT('Ctrl Pts',(-198.328348433687,2.11980866145337,
126.364269103447));
#124713=CARTESIAN_POINT('Ctrl Pts',(-198.336094709771,1.99506025231821,
126.306834023191));
#124714=CARTESIAN_POINT('Ctrl Pts',(-198.343840985855,1.8681294775501,126.254714992069));
#124715=CARTESIAN_POINT('Ctrl Pts',(-198.351587319121,1.74119776580766,
126.202595576215));
#124716=CARTESIAN_POINT('Ctrl Pts',(-198.359333652386,1.61208401795031,
126.155792436301));
#124717=CARTESIAN_POINT('Ctrl Pts',(-198.367079985652,1.48127500745482,
126.114477099312));
#124718=CARTESIAN_POINT('Ctrl Pts',(-198.374828053655,1.35043670318858,
126.07315251004));
#124719=CARTESIAN_POINT('Ctrl Pts',(-198.382576121657,1.21790275358034,
126.037318286899));
#124720=CARTESIAN_POINT('Ctrl Pts',(-198.39032418966,1.08417450384265,126.007095906534));
#124721=CARTESIAN_POINT('Ctrl Pts',(-198.398080492402,0.950304126129575,
125.976841405463));
#124722=CARTESIAN_POINT('Ctrl Pts',(-198.405836795144,0.81523729464666,
125.952210747888));
#124723=CARTESIAN_POINT('Ctrl Pts',(-198.413593097886,0.679485497313303,
125.933274237564));
#124724=CARTESIAN_POINT('Ctrl Pts',(-198.4213535404,0.543661245157932,125.914327620255));
#124725=CARTESIAN_POINT('Ctrl Pts',(-198.429113982914,0.407151687636302,
125.901081243678));
#124726=CARTESIAN_POINT('Ctrl Pts',(-198.436874425429,0.270471830283358,
125.893553346707));
#124727=CARTESIAN_POINT('Ctrl Pts',(-198.444647325694,0.133572562289896,
125.886013365287));
#124728=CARTESIAN_POINT('Ctrl Pts',(-198.45242022596,-0.00349716067967948,
125.884210212806));
#124729=CARTESIAN_POINT('Ctrl Pts',(-198.460193126225,-0.140223036415281,
125.888109956487));
#124730=CARTESIAN_POINT('Ctrl Pts',(-198.467683461987,-0.271978582175825,
125.891867934663));
#124731=CARTESIAN_POINT('Ctrl Pts',(-198.475173797749,-0.403414538811383,
125.900921357127));
#124732=CARTESIAN_POINT('Ctrl Pts',(-198.482664133511,-0.534078533749533,
125.915194719144));
#124733=CARTESIAN_POINT('Ctrl Pts',(-198.49043846763,-0.669696693770792,
125.930009260021));
#124734=CARTESIAN_POINT('Ctrl Pts',(-198.498212801749,-0.804912796249909,
125.950494310249));
#124735=CARTESIAN_POINT('Ctrl Pts',(-198.505987135868,-0.939214741433294,
125.97662214785));
#124736=CARTESIAN_POINT('Ctrl Pts',(-198.513751888815,-1.07335117147142,
126.002717785227));
#124737=CARTESIAN_POINT('Ctrl Pts',(-198.521516641762,-1.20657530576016,
126.034442299186));
#124738=CARTESIAN_POINT('Ctrl Pts',(-198.529281394709,-1.33837943750662,
126.071716161899));
#124739=CARTESIAN_POINT('Ctrl Pts',(-198.537038435594,-1.47005265953166,
126.108953003685));
#124740=CARTESIAN_POINT('Ctrl Pts',(-198.544795476479,-1.60030831193102,
126.151728120008));
#124741=CARTESIAN_POINT('Ctrl Pts',(-198.552552517364,-1.72864852136443,
126.199910883658));
#124742=CARTESIAN_POINT('Ctrl Pts',(-198.560303708605,-1.85689194844843,
126.248057312312));
#124743=CARTESIAN_POINT('Ctrl Pts',(-198.568054899845,-1.9832224431181,
126.301603134525));
#124744=CARTESIAN_POINT('Ctrl Pts',(-198.575806091085,-2.10715729921745,
126.36036791068));
#124745=CARTESIAN_POINT('Ctrl Pts',(-198.583553987862,-2.23103947969604,
126.419107710238));
#124746=CARTESIAN_POINT('Ctrl Pts',(-198.591301884639,-2.3525276942214,
126.483061884765));
#124747=CARTESIAN_POINT('Ctrl Pts',(-198.599049781416,-2.47115944473042,
126.552001970742));
#124748=CARTESIAN_POINT('Ctrl Pts',(-198.6067960575,-2.58976638003497,126.620927635939));
#124749=CARTESIAN_POINT('Ctrl Pts',(-198.614542333584,-2.70551770198718,
126.694836941795));
#124750=CARTESIAN_POINT('Ctrl Pts',(-198.622288609669,-2.81797610317734,
126.773455788074));
#124751=CARTESIAN_POINT('Ctrl Pts',(-198.630034942934,-2.93043533450971,
126.852075214699));
#124752=CARTESIAN_POINT('Ctrl Pts',(-198.637781276199,-3.03960127614829,
126.93540402711));
#124753=CARTESIAN_POINT('Ctrl Pts',(-198.645527609465,-3.14506650462893,
127.023125403517));
#124754=CARTESIAN_POINT('Ctrl Pts',(-198.653275677468,-3.25055535131611,
127.110866424519));
#124755=CARTESIAN_POINT('Ctrl Pts',(-198.661023745471,-3.35234153520745,
127.203001716974));
#124756=CARTESIAN_POINT('Ctrl Pts',(-198.668771813474,-3.4500518652282,
127.299175146049));
#124757=CARTESIAN_POINT('Ctrl Pts',(-198.676528116215,-3.54786604295059,
127.395450789389));
#124758=CARTESIAN_POINT('Ctrl Pts',(-198.684284418957,-3.64159543435231,
127.49577286795));
#124759=CARTESIAN_POINT('Ctrl Pts',(-198.692040721699,-3.73090441917804,
127.599749053358));
#124760=CARTESIAN_POINT('Ctrl Pts',(-198.699801164213,-3.82026107089802,
127.703780733986));
#124761=CARTESIAN_POINT('Ctrl Pts',(-198.707561606727,-3.90519237294011,
127.81147010078));
#124762=CARTESIAN_POINT('Ctrl Pts',(-198.715322049242,-3.98540460735336,
127.922393723553));
#124763=CARTESIAN_POINT('Ctrl Pts',(-198.723094949507,-4.06574560556619,
128.033495410773));
#124764=CARTESIAN_POINT('Ctrl Pts',(-198.730867849773,-4.14135218219585,
128.147841402763));
#124765=CARTESIAN_POINT('Ctrl Pts',(-198.738640750038,-4.21197489294038,
128.264980661014));
#124766=CARTESIAN_POINT('Ctrl Pts',(-198.7461310858,-4.28003029026089,128.37786161217));
#124767=CARTESIAN_POINT('Ctrl Pts',(-198.753621421562,-4.34345773459829,
128.493336000931));
#124768=CARTESIAN_POINT('Ctrl Pts',(-198.761111757324,-4.40207623179987,
128.610982421285));
#124769=CARTESIAN_POINT('Ctrl Pts',(-198.769439516326,-4.46724830596083,
128.741781769581));
#124770=CARTESIAN_POINT('Ctrl Pts',(-198.777767275329,-4.52666005472299,
128.87563467257));
#124771=CARTESIAN_POINT('Ctrl Pts',(-198.786095034331,-4.58003551060785,
129.012027561443));
#124772=CARTESIAN_POINT('Ctrl Pts',(-198.794402369264,-4.63328006164643,
129.148085942819));
#124773=CARTESIAN_POINT('Ctrl Pts',(-198.802709704197,-4.6805177289175,
129.2866716051));
#124774=CARTESIAN_POINT('Ctrl Pts',(-198.811017039129,-4.72151946632294,
129.427248787817));
#124775=CARTESIAN_POINT('Ctrl Pts',(-198.814059766598,-4.73653717220337,
129.478737990889));
#124776=CARTESIAN_POINT('Ctrl Pts',(-198.817102494067,-4.75071875239664,
129.530494131717));
#124777=CARTESIAN_POINT('Ctrl Pts',(-198.820145221536,-4.76405452823399,
129.582490119308));
#124778=CARTESIAN_POINT('Origin',(213.235140564004,0.,130.804360617566));
#124779=CARTESIAN_POINT('',(-200.91504706349,-4.76405452823395,129.582490119308));
#124780=CARTESIAN_POINT('',(-200.569853205643,-4.76405452823395,129.582490119308));
#124781=CARTESIAN_POINT('',(213.235140564004,-4.76405452823405,129.582490119308));
#124782=CARTESIAN_POINT('',(-199.235140563976,-4.91824791219353,130.808892361601));
#124783=CARTESIAN_POINT('Ctrl Pts',(-199.235140564013,-4.91824791219293,
130.80889236225));
#124784=CARTESIAN_POINT('Ctrl Pts',(-199.245686804809,-4.91807640527225,
130.995026757141));
#124785=CARTESIAN_POINT('Ctrl Pts',(-199.256233045605,-4.90733475277425,
131.180693350563));
#124786=CARTESIAN_POINT('Ctrl Pts',(-199.266779286401,-4.88620319730163,
131.364897304304));
#124787=CARTESIAN_POINT('Ctrl Pts',(-199.277325527197,-4.86507164182904,
131.549101258045));
#124788=CARTESIAN_POINT('Ctrl Pts',(-199.287871767993,-4.83355032983892,
131.731843197017));
#124789=CARTESIAN_POINT('Ctrl Pts',(-199.298418008789,-4.79186565731639,
131.912154183503));
#124790=CARTESIAN_POINT('Ctrl Pts',(-199.306192342908,-4.76113711829408,
132.045073380155));
#124791=CARTESIAN_POINT('Ctrl Pts',(-199.313966677027,-4.72482524621133,
132.176923596683));
#124792=CARTESIAN_POINT('Ctrl Pts',(-199.321741011146,-4.68301805246697,
132.307199591897));
#124793=CARTESIAN_POINT('Ctrl Pts',(-199.329505764093,-4.64126238235248,
132.43731503359));
#124794=CARTESIAN_POINT('Ctrl Pts',(-199.337270517041,-4.59402498413645,
132.565859745473));
#124795=CARTESIAN_POINT('Ctrl Pts',(-199.345035269988,-4.54144479361619,
132.692338967293));
#124796=CARTESIAN_POINT('Ctrl Pts',(-199.352792310873,-4.48891682648241,
132.818692568166));
#124797=CARTESIAN_POINT('Ctrl Pts',(-199.360549351758,-4.43105677640118,
132.942984402826));
#124798=CARTESIAN_POINT('Ctrl Pts',(-199.368306392643,-4.36805315947013,
133.064735510928));
#124799=CARTESIAN_POINT('Ctrl Pts',(-199.376057583883,-4.3050970540568,
133.186394805573));
#124800=CARTESIAN_POINT('Ctrl Pts',(-199.383808775123,-4.2370052812737,
133.305516841482));
#124801=CARTESIAN_POINT('Ctrl Pts',(-199.391559966363,-4.16401402959605,
133.421643602615));
#124802=CARTESIAN_POINT('Ctrl Pts',(-199.39930786314,-4.09105380114736,
133.537721006777));
#124803=CARTESIAN_POINT('Ctrl Pts',(-199.407055759917,-4.01319844317672,
133.650805337891));
#124804=CARTESIAN_POINT('Ctrl Pts',(-199.414803656695,-3.93072944517622,
133.76046431861));
#124805=CARTESIAN_POINT('Ctrl Pts',(-199.422549932779,-3.84827769791228,
133.870100361034));
#124806=CARTESIAN_POINT('Ctrl Pts',(-199.430296208863,-3.76121446504357,
133.976312165972));
#124807=CARTESIAN_POINT('Ctrl Pts',(-199.438042484947,-3.66986357811492,
134.078697860509));
#124808=CARTESIAN_POINT('Ctrl Pts',(-199.445788818212,-3.57851201685465,
134.181084310835));
#124809=CARTESIAN_POINT('Ctrl Pts',(-199.453535151478,-3.48287299866424,
134.279644302673));
#124810=CARTESIAN_POINT('Ctrl Pts',(-199.461281484743,-3.38330924806213,
134.374010683676));
#124811=CARTESIAN_POINT('Ctrl Pts',(-199.469029552746,-3.28372320084826,
134.468398197375));
#124812=CARTESIAN_POINT('Ctrl Pts',(-199.476777620749,-3.18021095598737,
134.558589962581));
#124813=CARTESIAN_POINT('Ctrl Pts',(-199.484525688752,-3.07317023273365,
134.644257462943));
#124814=CARTESIAN_POINT('Ctrl Pts',(-199.492281991494,-2.9660157453259,
134.730016011745));
#124815=CARTESIAN_POINT('Ctrl Pts',(-199.500038294236,-2.85532559400969,
134.811240445636));
#124816=CARTESIAN_POINT('Ctrl Pts',(-199.507794596978,-2.74152900080911,
134.887643830891));
#124817=CARTESIAN_POINT('Ctrl Pts',(-199.515555039492,-2.62767167094008,
134.964087994933));
#124818=CARTESIAN_POINT('Ctrl Pts',(-199.523315482006,-2.51070492874323,
135.035705779087));
#124819=CARTESIAN_POINT('Ctrl Pts',(-199.53107592452,-2.39108393133343,
135.102255532035));
#124820=CARTESIAN_POINT('Ctrl Pts',(-199.538848824786,-2.27127090767914,
135.168912116555));
#124821=CARTESIAN_POINT('Ctrl Pts',(-199.546621725051,-2.14879546379233,
135.230484236534));
#124822=CARTESIAN_POINT('Ctrl Pts',(-199.554394625317,-2.02413494276591,
135.286777465202));
#124823=CARTESIAN_POINT('Ctrl Pts',(-199.561884961079,-1.90400614567938,
135.341024293215));
#124824=CARTESIAN_POINT('Ctrl Pts',(-199.569375296841,-1.781848665018,135.390369253178));
#124825=CARTESIAN_POINT('Ctrl Pts',(-199.576865632603,-1.65810233422333,
135.43468238951));
#124826=CARTESIAN_POINT('Ctrl Pts',(-199.584639966722,-1.52966412368488,
135.480675671875));
#124827=CARTESIAN_POINT('Ctrl Pts',(-199.592414300841,-1.39910734850033,
135.52139372814));
#124828=CARTESIAN_POINT('Ctrl Pts',(-199.60018863496,-1.26690465470224,
135.556637509582));
#124829=CARTESIAN_POINT('Ctrl Pts',(-199.607953387907,-1.13486488890897,
135.591837856214));
#124830=CARTESIAN_POINT('Ctrl Pts',(-199.615718140854,-1.00118361465327,
135.621577251914));
#124831=CARTESIAN_POINT('Ctrl Pts',(-199.623482893801,-0.866352185939986,
135.645705157301));
#124832=CARTESIAN_POINT('Ctrl Pts',(-199.631239934686,-0.731654673702493,
135.669809098511));
#124833=CARTESIAN_POINT('Ctrl Pts',(-199.638996975571,-0.595809662696144,
135.688312572326));
#124834=CARTESIAN_POINT('Ctrl Pts',(-199.646754016456,-0.459322013378897,
135.701115292912));
#124835=CARTESIAN_POINT('Ctrl Pts',(-199.654505207696,-0.322937290459533,
135.713908358867));
#124836=CARTESIAN_POINT('Ctrl Pts',(-199.662256398937,-0.185911281514558,
135.721009192091));
#124837=CARTESIAN_POINT('Ctrl Pts',(-199.670007590177,-0.0487569940496048,
135.722368935781));
#124838=CARTESIAN_POINT('Ctrl Pts',(-199.677755486954,0.0883389991842788,
135.723728101544));
#124839=CARTESIAN_POINT('Ctrl Pts',(-199.685503383731,0.225562772370937,
135.719351027109));
#124840=CARTESIAN_POINT('Ctrl Pts',(-199.693251280508,0.362398486389647,
135.709240881096));
#124841=CARTESIAN_POINT('Ctrl Pts',(-199.700997556592,0.499205577326821,
135.699132849906));
#124842=CARTESIAN_POINT('Ctrl Pts',(-199.708743832676,0.635624380899426,
135.683294161272));
#124843=CARTESIAN_POINT('Ctrl Pts',(-199.71649010876,0.771141751181498,
135.661780041713));
#124844=CARTESIAN_POINT('Ctrl Pts',(-199.724236442026,0.906660121822196,
135.640265763343));
#124845=CARTESIAN_POINT('Ctrl Pts',(-199.731982775291,1.04127665976482,
135.613076031752));
#124846=CARTESIAN_POINT('Ctrl Pts',(-199.739729108556,1.17448640787711,
135.580317562536));
#124847=CARTESIAN_POINT('Ctrl Pts',(-199.747477176559,1.3077259873887,135.547551757289));
#124848=CARTESIAN_POINT('Ctrl Pts',(-199.755225244562,1.43955777059391,
135.509214826219));
#124849=CARTESIAN_POINT('Ctrl Pts',(-199.762973312565,1.56949039041183,
135.465463810685));
#124850=CARTESIAN_POINT('Ctrl Pts',(-199.770729615307,1.69956110416447,
135.421666296052));
#124851=CARTESIAN_POINT('Ctrl Pts',(-199.778485918049,1.82772825133692,
135.372443327376));
#124852=CARTESIAN_POINT('Ctrl Pts',(-199.786242220791,1.95351842146964,
135.318000926616));
#124853=CARTESIAN_POINT('Ctrl Pts',(-199.794002663305,2.07937572960363,
135.263529468307));
#124854=CARTESIAN_POINT('Ctrl Pts',(-199.801763105819,2.20285318096146,
135.203833197122));
#124855=CARTESIAN_POINT('Ctrl Pts',(-199.809523548333,2.32350144390913,
135.139164431195));
#124856=CARTESIAN_POINT('Ctrl Pts',(-199.817296448599,2.44434338215913,
135.074391853224));
#124857=CARTESIAN_POINT('Ctrl Pts',(-199.825069348864,2.56234671955976,
135.004631028427));
#124858=CARTESIAN_POINT('Ctrl Pts',(-199.83284224913,2.67708986376302,134.930178466652));
#124859=CARTESIAN_POINT('Ctrl Pts',(-199.840332584892,2.78766180565022,
134.858432443034));
#124860=CARTESIAN_POINT('Ctrl Pts',(-199.847822920653,2.89520622014493,
134.782330051055));
#124861=CARTESIAN_POINT('Ctrl Pts',(-199.855313256415,2.99937603121739,
134.702171090878));
#124862=CARTESIAN_POINT('Ctrl Pts',(-199.863087590534,3.1074954723416,134.618972879359));
#124863=CARTESIAN_POINT('Ctrl Pts',(-199.870861924653,3.21232185228549,
134.531140870842));
#124864=CARTESIAN_POINT('Ctrl Pts',(-199.878636258772,3.31343222899665,
134.438965125122));
#124865=CARTESIAN_POINT('Ctrl Pts',(-199.886401011719,3.414417996205,134.346902977771));
#124866=CARTESIAN_POINT('Ctrl Pts',(-199.894165764666,3.51169658615192,
134.25050800549));
#124867=CARTESIAN_POINT('Ctrl Pts',(-199.901930517614,3.60487575695146,
134.150112228108));
#124868=CARTESIAN_POINT('Ctrl Pts',(-199.909687558499,3.69796238088497,
134.049816165227));
#124869=CARTESIAN_POINT('Ctrl Pts',(-199.917444599384,3.78695742409865,
133.945527489707));
#124870=CARTESIAN_POINT('Ctrl Pts',(-199.925201640269,3.87150362387128,
133.837616748006));
#124871=CARTESIAN_POINT('Ctrl Pts',(-199.932952831509,3.95598606669709,
133.729787382635));
#124872=CARTESIAN_POINT('Ctrl Pts',(-199.940704022749,4.03602610367543,
133.618341694337));
#124873=CARTESIAN_POINT('Ctrl Pts',(-199.948455213989,4.11130533710608,
133.50368488256));
#124874=CARTESIAN_POINT('Ctrl Pts',(-199.956203110766,4.18655257485428,
133.389076802986));
#124875=CARTESIAN_POINT('Ctrl Pts',(-199.963951007543,4.25704281945193,
133.271260640578));
#124876=CARTESIAN_POINT('Ctrl Pts',(-199.97169890432,4.32249991310147,133.150672098111));
#124877=CARTESIAN_POINT('Ctrl Pts',(-199.979445180404,4.38794331453812,
133.030108780168));
#124878=CARTESIAN_POINT('Ctrl Pts',(-199.987191456488,4.44835547276005,
132.906774579053));
#124879=CARTESIAN_POINT('Ctrl Pts',(-199.994937732572,4.50350548349756,
132.781131070251));
#124880=CARTESIAN_POINT('Ctrl Pts',(-200.002684065838,4.55865590134,132.655486633977));
#124881=CARTESIAN_POINT('Ctrl Pts',(-200.010430399103,4.60854393704874,
132.527533213996));
#124882=CARTESIAN_POINT('Ctrl Pts',(-200.018176732369,4.65298643181374,
132.397753327433));
#124883=CARTESIAN_POINT('Ctrl Pts',(-200.025924800372,4.69743887916725,
132.267944377564));
#124884=CARTESIAN_POINT('Ctrl Pts',(-200.033672868375,4.73644323229192,
132.136308517008));
#124885=CARTESIAN_POINT('Ctrl Pts',(-200.041420936378,4.76986601862287,
132.003344031499));
#124886=CARTESIAN_POINT('Ctrl Pts',(-200.04917723912,4.80332432708882,131.870238229753));
#124887=CARTESIAN_POINT('Ctrl Pts',(-200.056933541861,4.83118912317878,
131.735801362048));
#124888=CARTESIAN_POINT('Ctrl Pts',(-200.064689844603,4.85337784908269,
131.600543081913));
#124889=CARTESIAN_POINT('Ctrl Pts',(-200.072450287117,4.87557841777776,
131.465212610361));
#124890=CARTESIAN_POINT('Ctrl Pts',(-200.080210729631,4.89209683270756,
131.329060240733));
#124891=CARTESIAN_POINT('Ctrl Pts',(-200.087971172146,4.90290250153954,
131.192600392573));
#124892=CARTESIAN_POINT('Ctrl Pts',(-200.095744072411,4.9137255165904,131.05592148695));
#124893=CARTESIAN_POINT('Ctrl Pts',(-200.103516972676,4.91881744521724,
130.918934507362));
#124894=CARTESIAN_POINT('Ctrl Pts',(-200.111289872942,4.91819986858887,
130.782154422205));
#124895=CARTESIAN_POINT('Ctrl Pts',(-200.118780208704,4.91760474242652,
130.650346637671));
#124896=CARTESIAN_POINT('Ctrl Pts',(-200.126270544466,4.91170802767491,
130.518731274167));
#124897=CARTESIAN_POINT('Ctrl Pts',(-200.133760880228,4.90057435163176,
130.387762385898));
#124898=CARTESIAN_POINT('Ctrl Pts',(-200.141535214347,4.88901853887747,
130.251827772423));
#124899=CARTESIAN_POINT('Ctrl Pts',(-200.149309548466,4.87178420146617,
130.116159024119));
#124900=CARTESIAN_POINT('Ctrl Pts',(-200.157083882586,4.8488867644099,129.981268758518));
#124901=CARTESIAN_POINT('Ctrl Pts',(-200.164848635533,4.8260175463984,129.846544733114));
#124902=CARTESIAN_POINT('Ctrl Pts',(-200.17261338848,4.79749918019917,129.712597663223));
#124903=CARTESIAN_POINT('Ctrl Pts',(-200.180378141427,4.76339898717628,
129.57993701788));
#124904=CARTESIAN_POINT('Ctrl Pts',(-200.188135182312,4.72933266294583,
129.44740813296));
#124905=CARTESIAN_POINT('Ctrl Pts',(-200.195892223197,4.68969564130355,
129.316163506122));
#124906=CARTESIAN_POINT('Ctrl Pts',(-200.203649264082,4.64460656425249,
129.186704002025));
#124907=CARTESIAN_POINT('Ctrl Pts',(-200.211400455322,4.59955148922512,
129.057342124347));
#124908=CARTESIAN_POINT('Ctrl Pts',(-200.219151646562,4.5490526704274,128.929763057648));
#124909=CARTESIAN_POINT('Ctrl Pts',(-200.226902837802,4.49327891189645,
128.80445369913));
#124910=CARTESIAN_POINT('Ctrl Pts',(-200.23465073458,4.43752885870062,128.679197600433));
#124911=CARTESIAN_POINT('Ctrl Pts',(-200.242398631357,4.37650848356419,
128.556209647663));
#124912=CARTESIAN_POINT('Ctrl Pts',(-200.250146528134,4.31043508553766,
128.435957688192));
#124913=CARTESIAN_POINT('Ctrl Pts',(-200.257892804218,4.2443755086418,128.315730882839));
#124914=CARTESIAN_POINT('Ctrl Pts',(-200.265639080302,4.17326519940549,
128.198239274858));
#124915=CARTESIAN_POINT('Ctrl Pts',(-200.273385356386,4.09736768495884,
128.083926623374));
#124916=CARTESIAN_POINT('Ctrl Pts',(-200.281131689651,4.02146961025387,
127.96961312806));
#124917=CARTESIAN_POINT('Ctrl Pts',(-200.288878022917,3.94078447607879,
127.85847896178));
#124918=CARTESIAN_POINT('Ctrl Pts',(-200.296624356182,3.85561923594436,
127.75093903352));
#124919=CARTESIAN_POINT('Ctrl Pts',(-200.304372424185,3.770434923645,127.643375022439));
#124920=CARTESIAN_POINT('Ctrl Pts',(-200.312120492188,3.68076875163644,
127.53940715748));
#124921=CARTESIAN_POINT('Ctrl Pts',(-200.319868560191,3.58696779663645,
127.439417068501));
#124922=CARTESIAN_POINT('Ctrl Pts',(-200.327624862933,3.49306714886511,
127.339320708866));
#124923=CARTESIAN_POINT('Ctrl Pts',(-200.335381165675,3.39502320753719,
127.243210855946));
#124924=CARTESIAN_POINT('Ctrl Pts',(-200.343137468417,3.29322013408638,
127.151432448145));
#124925=CARTESIAN_POINT('Ctrl Pts',(-200.350897910931,3.19136272527004,
127.059605055445));
#124926=CARTESIAN_POINT('Ctrl Pts',(-200.358658353445,3.08574248742091,
126.972113963648));
#124927=CARTESIAN_POINT('Ctrl Pts',(-200.366418795959,2.97677568036702,
126.88926296728));
#124928=CARTESIAN_POINT('Ctrl Pts',(-200.374191696225,2.86763395012082,
126.806278971137));
#124929=CARTESIAN_POINT('Ctrl Pts',(-200.38196459649,2.75513523632046,126.727950178812));
#124930=CARTESIAN_POINT('Ctrl Pts',(-200.389737496756,2.63972446161173,
126.654536786454));
#124931=CARTESIAN_POINT('Ctrl Pts',(-200.397227832518,2.52850915926618,
126.583792155825));
#124932=CARTESIAN_POINT('Ctrl Pts',(-200.40471816828,2.41459010805134,126.517611910091));
#124933=CARTESIAN_POINT('Ctrl Pts',(-200.412208504042,2.29838424926308,
126.456187103866));
#124934=CARTESIAN_POINT('Ctrl Pts',(-200.419982838161,2.17777241001932,
126.392433357444));
#124935=CARTESIAN_POINT('Ctrl Pts',(-200.42775717228,2.05431486939034,126.333600821259));
#124936=CARTESIAN_POINT('Ctrl Pts',(-200.435531506399,1.92845124462011,
126.279953600108));
#124937=CARTESIAN_POINT('Ctrl Pts',(-200.443296259346,1.8027427355183,126.226372494363));
#124938=CARTESIAN_POINT('Ctrl Pts',(-200.451061012293,1.67463439851077,
126.177964140413));
#124939=CARTESIAN_POINT('Ctrl Pts',(-200.45882576524,1.54459125316685,126.134947279347));
#124940=CARTESIAN_POINT('Ctrl Pts',(-200.466582806125,1.41467726850817,
126.091973143233));
#124941=CARTESIAN_POINT('Ctrl Pts',(-200.47433984701,1.28283266852345,126.054379965485));
#124942=CARTESIAN_POINT('Ctrl Pts',(-200.482096887895,1.14954297373518,
126.022338658809));
#124943=CARTESIAN_POINT('Ctrl Pts',(-200.489848079135,1.01635379374277,
125.990321514731));
#124944=CARTESIAN_POINT('Ctrl Pts',(-200.497599270375,0.881722066640452,
125.963847999343));
#124945=CARTESIAN_POINT('Ctrl Pts',(-200.505350461615,0.746148675539075,
125.94303927286));
#124946=CARTESIAN_POINT('Ctrl Pts',(-200.513098358392,0.61063290674527,
125.922239390641));
#124947=CARTESIAN_POINT('Ctrl Pts',(-200.520846255169,0.474176655614721,
125.90709956781));
#124948=CARTESIAN_POINT('Ctrl Pts',(-200.528594151946,0.337290990834222,
125.897689867454));
#124949=CARTESIAN_POINT('Ctrl Pts',(-200.53634042803,0.200433959583882,
125.888282135405));
#124950=CARTESIAN_POINT('Ctrl Pts',(-200.544086704114,0.0631480831462334,
125.884602168507));
#124951=CARTESIAN_POINT('Ctrl Pts',(-200.551832980198,-0.0740508485073515,
125.886668116572));
#124952=CARTESIAN_POINT('Ctrl Pts',(-200.559579313464,-0.211250792932096,
125.888734079886));
#124953=CARTESIAN_POINT('Ctrl Pts',(-200.567325646729,-0.348363400371211,
125.896546036912));
#124954=CARTESIAN_POINT('Ctrl Pts',(-200.575071979994,-0.484873680273991,
125.910070007408));
#124955=CARTESIAN_POINT('Ctrl Pts',(-200.582820047997,-0.621414530707646,
125.923597006504));
#124956=CARTESIAN_POINT('Ctrl Pts',(-200.590568116,-0.757352396209157,125.942838525925));
#124957=CARTESIAN_POINT('Ctrl Pts',(-200.598316184003,-0.892178597326069,
125.967708840461));
#124958=CARTESIAN_POINT('Ctrl Pts',(-200.606072486745,-1.0271480933338,
125.992605587463));
#124959=CARTESIAN_POINT('Ctrl Pts',(-200.613828789487,-1.16100317971131,
126.023143008933));
#124960=CARTESIAN_POINT('Ctrl Pts',(-200.621585092229,-1.29324600137144,
126.059184346611));
#124961=CARTESIAN_POINT('Ctrl Pts',(-200.629345534743,-1.42555940500761,
126.095244920636));
#124962=CARTESIAN_POINT('Ctrl Pts',(-200.637105977257,-1.55625845688736,
126.136815145853));
#124963=CARTESIAN_POINT('Ctrl Pts',(-200.644866419771,-1.68486256746866,
126.183709019442));
#124964=CARTESIAN_POINT('Ctrl Pts',(-200.652639320036,-1.8136731247852,
126.23067817124));
#124965=CARTESIAN_POINT('Ctrl Pts',(-200.660412220302,-1.94038165889755,
126.28298789975));
#124966=CARTESIAN_POINT('Ctrl Pts',(-200.668185120567,-2.06452876785875,
126.340404521323));
#124967=CARTESIAN_POINT('Ctrl Pts',(-200.675675456329,-2.18416281670689,
126.395733904081));
#124968=CARTESIAN_POINT('Ctrl Pts',(-200.683165792092,-2.30141816157879,
126.455805188864));
#124969=CARTESIAN_POINT('Ctrl Pts',(-200.690656127854,-2.41590869586259,
126.520370860837));
#124970=CARTESIAN_POINT('Ctrl Pts',(-200.698431549059,-2.53475678976688,
126.587393930419));
#124971=CARTESIAN_POINT('Ctrl Pts',(-200.706206970264,-2.65100197297227,
126.659472618184));
#124972=CARTESIAN_POINT('Ctrl Pts',(-200.713982391469,-2.7641842313008,
126.736379718161));
#124973=CARTESIAN_POINT('Ctrl Pts',(-200.721747993784,-2.87722356178429,
126.813189698976));
#124974=CARTESIAN_POINT('Ctrl Pts',(-200.729513596099,-2.98720734372281,
126.894815740927));
#124975=CARTESIAN_POINT('Ctrl Pts',(-200.737279198413,-3.09370005168907,
126.980984746339));
#124976=CARTESIAN_POINT('Ctrl Pts',(-200.745035419852,-3.20006411607945,
127.067049659281));
#124977=CARTESIAN_POINT('Ctrl Pts',(-200.752791641291,-3.30294520389971,
127.15764636104));
#124978=CARTESIAN_POINT('Ctrl Pts',(-200.76054786273,-3.40193722042223,
127.252458843754));
#124979=CARTESIAN_POINT('Ctrl Pts',(-200.768298765275,-3.50086135232833,
127.347206308003));
#124980=CARTESIAN_POINT('Ctrl Pts',(-200.776049667819,-3.5959014377128,
127.446163532372));
#124981=CARTESIAN_POINT('Ctrl Pts',(-200.783800570363,-3.68668484751337,
127.548974634673));
#124982=CARTESIAN_POINT('Ctrl Pts',(-200.791547836284,-3.77742566291104,
127.651737499334));
#124983=CARTESIAN_POINT('Ctrl Pts',(-200.799295102205,-3.86391351900049,
127.758350351215));
#124984=CARTESIAN_POINT('Ctrl Pts',(-200.807042368126,-3.94581330905367,
127.868421178035));
#124985=CARTESIAN_POINT('Ctrl Pts',(-200.814787676884,-4.0276924090674,
127.97846419807));
#124986=CARTESIAN_POINT('Ctrl Pts',(-200.822532985642,-4.10498551777313,
128.091963140353));
#124987=CARTESIAN_POINT('Ctrl Pts',(-200.8302782944,-4.17739867669816,128.208494026537));
#124988=CARTESIAN_POINT('Ctrl Pts',(-200.838025646966,-4.24983094378865,
128.325055662539));
#124989=CARTESIAN_POINT('Ctrl Pts',(-200.845772999533,-4.31738047721026,
128.444650511683));
#124990=CARTESIAN_POINT('Ctrl Pts',(-200.8535203521,-4.37979740039574,128.566826753244));
#124991=CARTESIAN_POINT('Ctrl Pts',(-200.861268696023,-4.4422223104952,
128.689018628564));
#124992=CARTESIAN_POINT('Ctrl Pts',(-200.869017039946,-4.49951313147677,
128.813792202435));
#124993=CARTESIAN_POINT('Ctrl Pts',(-200.87676538387,-4.55146701346846,
128.940673120208));
#124994=CARTESIAN_POINT('Ctrl Pts',(-200.884519834436,-4.60346184147747,
129.067654035672));
#124995=CARTESIAN_POINT('Ctrl Pts',(-200.892274285003,-4.65011118842505,
129.19674524743));
#124996=CARTESIAN_POINT('Ctrl Pts',(-200.90002873557,-4.69126111778874,
129.327454328317));
#124997=CARTESIAN_POINT('Ctrl Pts',(-200.905034844876,-4.71782664201108,
129.411837346905));
#124998=CARTESIAN_POINT('Ctrl Pts',(-200.910040954183,-4.74210117247926,
129.496894318409));
#124999=CARTESIAN_POINT('Ctrl Pts',(-200.91504706349,-4.76405452823395,
129.582490119308));
#125000=CARTESIAN_POINT('Ctrl Pts',(-199.165100499421,-4.76405452823391,
129.582490119308));
#125001=CARTESIAN_POINT('Ctrl Pts',(-199.172747479307,-4.79772404353953,
129.713767048478));
#125002=CARTESIAN_POINT('Ctrl Pts',(-199.180394459193,-4.8259562660387,
129.846409655637));
#125003=CARTESIAN_POINT('Ctrl Pts',(-199.188041439078,-4.84865793162383,
129.979921823839));
#125004=CARTESIAN_POINT('Ctrl Pts',(-199.195891293228,-4.87196187206307,
130.116976067901));
#125005=CARTESIAN_POINT('Ctrl Pts',(-199.203741147378,-4.8894376250516,
130.254946212889));
#125006=CARTESIAN_POINT('Ctrl Pts',(-199.211591001527,-4.90104104578751,
130.393289176079));
#125007=CARTESIAN_POINT('Ctrl Pts',(-199.219440855677,-4.91264446652345,
130.53163213927));
#125008=CARTESIAN_POINT('Ctrl Pts',(-199.227290709826,-4.91837556944563,
130.67034746391));
#125009=CARTESIAN_POINT('Ctrl Pts',(-199.235140563976,-4.91824791219353,
130.808892361601));
#125010=CARTESIAN_POINT('',(-198.889859435951,-4.91824989448309,130.8033418354));
#125011=CARTESIAN_POINT('Ctrl Pts',(-198.820145221536,-4.76405452823399,
129.582490119308));
#125012=CARTESIAN_POINT('Ctrl Pts',(-198.828426476198,-4.80034991023985,
129.72400526289));
#125013=CARTESIAN_POINT('Ctrl Pts',(-198.836707730859,-4.83037656394087,
129.867298369273));
#125014=CARTESIAN_POINT('Ctrl Pts',(-198.844988985521,-4.85397223469977,
130.011809920598));
#125015=CARTESIAN_POINT('Ctrl Pts',(-198.853248087719,-4.87750478673457,
130.155934901657));
#125016=CARTESIAN_POINT('Ctrl Pts',(-198.861507189918,-4.89464061291577,
130.301271527841));
#125017=CARTESIAN_POINT('Ctrl Pts',(-198.869766292116,-4.90526800462946,
130.44724877898));
#125018=CARTESIAN_POINT('Ctrl Pts',(-198.876464006728,-4.91388628238558,
130.5656289545));
#125019=CARTESIAN_POINT('Ctrl Pts',(-198.883161721339,-4.91822526271462,
130.684430063471));
#125020=CARTESIAN_POINT('Ctrl Pts',(-198.889859435951,-4.91824989448309,
130.803341835399));
#125021=CARTESIAN_POINT('Ctrl Pts',(-198.889859435995,-4.91824989448325,
130.803341836187));
#125022=CARTESIAN_POINT('Ctrl Pts',(-198.897858632837,-4.91827931260921,
130.945360229872));
#125023=CARTESIAN_POINT('Ctrl Pts',(-198.905857829679,-4.91215304597155,
131.087301810736));
#125024=CARTESIAN_POINT('Ctrl Pts',(-198.913857026521,-4.89991714960293,
131.228618781338));
#125025=CARTESIAN_POINT('Ctrl Pts',(-198.921862893465,-4.88767105037535,
131.370053588597));
#125026=CARTESIAN_POINT('Ctrl Pts',(-198.929868760409,-4.86930519372858,
131.510862395327));
#125027=CARTESIAN_POINT('Ctrl Pts',(-198.937874627353,-4.84491724488214,
131.650504785391));
#125028=CARTESIAN_POINT('Ctrl Pts',(-198.945888336214,-4.82050540752001,
131.790283958152));
#125029=CARTESIAN_POINT('Ctrl Pts',(-198.953902045075,-4.79005977639878,
131.928894088689));
#125030=CARTESIAN_POINT('Ctrl Pts',(-198.961915753937,-4.75372862315488,
132.065807104698));
#125031=CARTESIAN_POINT('Ctrl Pts',(-198.969944216913,-4.71733058028216,
132.202972192552));
#125032=CARTESIAN_POINT('Ctrl Pts',(-198.977972679889,-4.67502545496002,
132.338433581101));
#125033=CARTESIAN_POINT('Ctrl Pts',(-198.986001142865,-4.62701107698537,
132.471679290152));
#125034=CARTESIAN_POINT('Ctrl Pts',(-198.994038134277,-4.57894569453759,
132.605066542788));
#125035=CARTESIAN_POINT('Ctrl Pts',(-199.002075125689,-4.52515909597119,
132.736233095487));
#125036=CARTESIAN_POINT('Ctrl Pts',(-199.0101121171,-4.46589624387441,132.864689183948));
#125037=CARTESIAN_POINT('Ctrl Pts',(-199.018163714144,-4.40652569334159,
132.993378715777));
#125038=CARTESIAN_POINT('Ctrl Pts',(-199.026215311188,-4.34165916726409,
133.119347629071));
#125039=CARTESIAN_POINT('Ctrl Pts',(-199.034266908231,-4.27158681882194,
133.242131958723));
#125040=CARTESIAN_POINT('Ctrl Pts',(-199.036031065866,-4.25623350843576,
133.269034809357));
#125041=CARTESIAN_POINT('Ctrl Pts',(-199.037795223501,-4.2406304385508,
133.295784893293));
#125042=CARTESIAN_POINT('Ctrl Pts',(-199.039559381137,-4.2247809262074,
133.322377533326));
#125043=CARTESIAN_POINT('Ctrl Pts',(-199.047333715256,-4.15493489763892,
133.439566646481));
#125044=CARTESIAN_POINT('Ctrl Pts',(-199.055108049375,-4.08009856624961,
133.554033039613));
#125045=CARTESIAN_POINT('Ctrl Pts',(-199.062882383494,-4.00051000845862,
133.665322472384));
#125046=CARTESIAN_POINT('Ctrl Pts',(-199.070647136441,-3.92101953645207,
133.776474750875));
#125047=CARTESIAN_POINT('Ctrl Pts',(-199.078411889388,-3.83678871636238,
133.884457544366));
#125048=CARTESIAN_POINT('Ctrl Pts',(-199.086176642335,-3.74810091690515,
133.988842141958));
#125049=CARTESIAN_POINT('Ctrl Pts',(-199.09393368322,-3.65950120342062,
134.093123063297));
#125050=CARTESIAN_POINT('Ctrl Pts',(-199.101690724105,-3.56645357147556,
134.193812604699));
#125051=CARTESIAN_POINT('Ctrl Pts',(-199.10944776499,-3.46928377810122,
134.290512239269));
#125052=CARTESIAN_POINT('Ctrl Pts',(-199.11719895623,-3.37218726122407,
134.387138951893));
#125053=CARTESIAN_POINT('Ctrl Pts',(-199.12495014747,-3.27097504630834,
134.47978147189));
#125054=CARTESIAN_POINT('Ctrl Pts',(-199.132701338711,-3.16601189112494,
134.568075772537));
#125055=CARTESIAN_POINT('Ctrl Pts',(-199.140449235488,-3.06109334808233,
134.65633254575));
#125056=CARTESIAN_POINT('Ctrl Pts',(-199.148197132265,-2.95242733417478,
134.740244524213));
#125057=CARTESIAN_POINT('Ctrl Pts',(-199.155945029042,-2.84041388590054,
134.819486022741));
#125058=CARTESIAN_POINT('Ctrl Pts',(-199.163691305126,-2.72842386842495,
134.898710945656));
#125059=CARTESIAN_POINT('Ctrl Pts',(-199.17143758121,-2.61308812831208,
134.973267106223));
#125060=CARTESIAN_POINT('Ctrl Pts',(-199.179183857294,-2.49483773851418,
135.042870700247));
#125061=CARTESIAN_POINT('Ctrl Pts',(-199.186930190559,-2.3765864758186,
135.112474808069));
#125062=CARTESIAN_POINT('Ctrl Pts',(-199.194676523825,-2.25542085743659,
135.177126078077));
#125063=CARTESIAN_POINT('Ctrl Pts',(-199.20242285709,-2.13179839053741,
135.236585643961));
#125064=CARTESIAN_POINT('Ctrl Pts',(-199.210170925093,-2.0081482392444,
135.296058525402));
#125065=CARTESIAN_POINT('Ctrl Pts',(-199.217918993096,-1.88204049687381,
135.350337219758));
#125066=CARTESIAN_POINT('Ctrl Pts',(-199.225667061099,-1.75395419721453,
135.399230336783));
#125067=CARTESIAN_POINT('Ctrl Pts',(-199.233423363841,-1.6257317659112,
135.448175417994));
#125068=CARTESIAN_POINT('Ctrl Pts',(-199.241179666583,-1.49552694252251,
135.491723348206));
#125069=CARTESIAN_POINT('Ctrl Pts',(-199.248935969325,-1.3638360625422,
135.529731952923));
#125070=CARTESIAN_POINT('Ctrl Pts',(-199.256696411839,-1.23207489517375,
135.567760843976));
#125071=CARTESIAN_POINT('Ctrl Pts',(-199.264456854353,-1.0988264704442,
135.600244425895));
#125072=CARTESIAN_POINT('Ctrl Pts',(-199.272217296867,-0.96459799408161,
135.627091563028));
#125073=CARTESIAN_POINT('Ctrl Pts',(-199.279990197133,-0.830154042252889,
135.653981797568));
#125074=CARTESIAN_POINT('Ctrl Pts',(-199.287763097398,-0.694727281372439,
135.675217445693));
#125075=CARTESIAN_POINT('Ctrl Pts',(-199.295535997664,-0.558831624326638,
135.690759115248));
#125076=CARTESIAN_POINT('Ctrl Pts',(-199.303026333426,-0.427876116714585,
135.705735805968));
#125077=CARTESIAN_POINT('Ctrl Pts',(-199.310516669188,-0.296485519363162,
135.715425289075));
#125078=CARTESIAN_POINT('Ctrl Pts',(-199.31800700495,-0.16511834145049,
135.719838111749));
#125079=CARTESIAN_POINT('Ctrl Pts',(-199.325781339069,-0.0287703370596385,
135.724418247935));
#125080=CARTESIAN_POINT('Ctrl Pts',(-199.333555673188,0.10798434643372,
135.723328204347));
#125081=CARTESIAN_POINT('Ctrl Pts',(-199.341330007307,0.244634857648935,
135.716522753421));
#125082=CARTESIAN_POINT('Ctrl Pts',(-199.349094760254,0.381116959321885,
135.709725689604));
#125083=CARTESIAN_POINT('Ctrl Pts',(-199.356859513201,0.517494757427955,
135.69722725263));
#125084=CARTESIAN_POINT('Ctrl Pts',(-199.364624266149,0.653254397634356,
135.679034119912));
#125085=CARTESIAN_POINT('Ctrl Pts',(-199.372381307034,0.788879199452228,
135.660859056869));
#125086=CARTESIAN_POINT('Ctrl Pts',(-199.380138347918,0.923886680191096,
135.637000605475));
#125087=CARTESIAN_POINT('Ctrl Pts',(-199.387895388803,1.05776546825392,
135.607517420823));
#125088=CARTESIAN_POINT('Ctrl Pts',(-199.395646580044,1.19154329728142,
135.578056469669));
#125089=CARTESIAN_POINT('Ctrl Pts',(-199.403397771284,1.32419374753591,
135.542979311759));
#125090=CARTESIAN_POINT('Ctrl Pts',(-199.411148962524,1.45521339253885,
135.5023960628));
#125091=CARTESIAN_POINT('Ctrl Pts',(-199.418896859301,1.58617735069778,
135.461830062804));
#125092=CARTESIAN_POINT('Ctrl Pts',(-199.426644756078,1.71551150952141,
135.415762741745));
#125093=CARTESIAN_POINT('Ctrl Pts',(-199.434392652855,1.84272563134234,
135.364354620862));
#125094=CARTESIAN_POINT('Ctrl Pts',(-199.442138928939,1.96991314271106,
135.312957253449));
#125095=CARTESIAN_POINT('Ctrl Pts',(-199.449885205023,2.09498113689857,
135.256221454736));
#125096=CARTESIAN_POINT('Ctrl Pts',(-199.457631481108,2.21745783593928,
135.194356495506));
#125097=CARTESIAN_POINT('Ctrl Pts',(-199.465377814373,2.33993543907532,
135.132491079603));
#125098=CARTESIAN_POINT('Ctrl Pts',(-199.473124147638,2.45982135992249,
135.065496603904));
#125099=CARTESIAN_POINT('Ctrl Pts',(-199.480870480904,2.57666733968873,
134.993628869073));
#125100=CARTESIAN_POINT('Ctrl Pts',(-199.488618548907,2.69353948630213,
134.92174503996));
#125101=CARTESIAN_POINT('Ctrl Pts',(-199.49636661691,2.80737000422098,134.844985984877));
#125102=CARTESIAN_POINT('Ctrl Pts',(-199.504114684913,2.91773894194668,
134.763651277413));
#125103=CARTESIAN_POINT('Ctrl Pts',(-199.511870987655,3.02822518109265,
134.682230126454));
#125104=CARTESIAN_POINT('Ctrl Pts',(-199.519627290396,3.13524217559271,
134.596223840941));
#125105=CARTESIAN_POINT('Ctrl Pts',(-199.527383593138,3.23840202855827,
134.505973153196));
#125106=CARTESIAN_POINT('Ctrl Pts',(-199.535144035652,3.34161694104344,
134.41567429594));
#125107=CARTESIAN_POINT('Ctrl Pts',(-199.542904478166,3.44097032683412,
134.321126791907));
#125108=CARTESIAN_POINT('Ctrl Pts',(-199.550664920681,3.5361113538409,134.222708106593));
#125109=CARTESIAN_POINT('Ctrl Pts',(-199.558437820946,3.63140510967045,
134.124131430869));
#125110=CARTESIAN_POINT('Ctrl Pts',(-199.566210721212,3.72247273410093,
134.021671447976));
#125111=CARTESIAN_POINT('Ctrl Pts',(-199.573983621477,3.80900330292975,
133.915739234959));
#125112=CARTESIAN_POINT('Ctrl Pts',(-199.581473957239,3.89238826762382,
133.813657924713));
#125113=CARTESIAN_POINT('Ctrl Pts',(-199.588964293001,3.97156013144357,
133.708352696285));
#125114=CARTESIAN_POINT('Ctrl Pts',(-199.596454628763,4.04627993261936,
133.600215007441));
#125115=CARTESIAN_POINT('Ctrl Pts',(-199.604228962882,4.12383275776765,
133.487977245255));
#125116=CARTESIAN_POINT('Ctrl Pts',(-199.612003297001,4.1968349200723,133.372332461753));
#125117=CARTESIAN_POINT('Ctrl Pts',(-199.61977763112,4.26497224065351,133.253686004066));
#125118=CARTESIAN_POINT('Ctrl Pts',(-199.627542384067,4.33302558807671,
133.135185767535));
#125119=CARTESIAN_POINT('Ctrl Pts',(-199.635307137014,4.39622583016546,
133.013691553092));
#125120=CARTESIAN_POINT('Ctrl Pts',(-199.643071889961,4.45430083399845,
132.889639290248));
#125121=CARTESIAN_POINT('Ctrl Pts',(-199.650828930846,4.51231815691907,
132.765710237859));
#125122=CARTESIAN_POINT('Ctrl Pts',(-199.658585971731,4.56522020713492,
132.639228544949));
#125123=CARTESIAN_POINT('Ctrl Pts',(-199.666343012616,4.61277992399897,
132.510656147435));
#125124=CARTESIAN_POINT('Ctrl Pts',(-199.674094203857,4.66030377571063,
132.382180707367));
#125125=CARTESIAN_POINT('Ctrl Pts',(-199.681845395097,4.70249317785453,
132.251618066054));
#125126=CARTESIAN_POINT('Ctrl Pts',(-199.689596586337,4.73916865958453,
132.11945129068));
#125127=CARTESIAN_POINT('Ctrl Pts',(-199.697344483114,4.77582855325628,
131.987340689712));
#125128=CARTESIAN_POINT('Ctrl Pts',(-199.705092379891,4.80697908336153,
131.853627686671));
#125129=CARTESIAN_POINT('Ctrl Pts',(-199.712840276668,4.83249031553063,
131.718811498042));
#125130=CARTESIAN_POINT('Ctrl Pts',(-199.720586552752,4.85799621129998,
131.584023510052));
#125131=CARTESIAN_POINT('Ctrl Pts',(-199.728332828836,4.87786508281496,
131.448133179379));
#125132=CARTESIAN_POINT('Ctrl Pts',(-199.73607910492,4.89201798799939,131.311650542156));
#125133=CARTESIAN_POINT('Ctrl Pts',(-199.743825438185,4.9061709976573,131.17516689745));
#125134=CARTESIAN_POINT('Ctrl Pts',(-199.751571771451,4.91460791646383,
131.038091326349));
#125135=CARTESIAN_POINT('Ctrl Pts',(-199.759318104716,4.91730166193535,
130.900939228179));
#125136=CARTESIAN_POINT('Ctrl Pts',(-199.767066172719,4.91999601065249,
130.763756415746));
#125137=CARTESIAN_POINT('Ctrl Pts',(-199.774814240722,4.91694461908141,
130.626497432957));
#125138=CARTESIAN_POINT('Ctrl Pts',(-199.782562308725,4.90817253292527,
130.489677523743));
#125139=CARTESIAN_POINT('Ctrl Pts',(-199.790318611467,4.89939112369156,
130.352712200701));
#125140=CARTESIAN_POINT('Ctrl Pts',(-199.798074914209,4.88487689942825,
130.21618727421));
#125141=CARTESIAN_POINT('Ctrl Pts',(-199.805831216951,4.8647068601427,130.080613267049));
#125142=CARTESIAN_POINT('Ctrl Pts',(-199.813591659465,4.84452605549987,
129.944966899958));
#125143=CARTESIAN_POINT('Ctrl Pts',(-199.821352101979,4.81868349449313,
129.810272847277));
#125144=CARTESIAN_POINT('Ctrl Pts',(-199.829112544493,4.78730711622281,
129.6770303033));
#125145=CARTESIAN_POINT('Ctrl Pts',(-199.836885444758,4.75588036980463,
129.543573866563));
#125146=CARTESIAN_POINT('Ctrl Pts',(-199.844658345024,4.71890215983434,
129.411573971483));
#125147=CARTESIAN_POINT('Ctrl Pts',(-199.852431245289,4.67655027494581,
129.281514404581));
#125148=CARTESIAN_POINT('Ctrl Pts',(-199.859921581051,4.63573798775117,
129.156182830536));
#125149=CARTESIAN_POINT('Ctrl Pts',(-199.867411916813,4.58993604295062,
129.032653251052));
#125150=CARTESIAN_POINT('Ctrl Pts',(-199.874902252575,4.53934462037534,
128.911338303918));
#125151=CARTESIAN_POINT('Ctrl Pts',(-199.882676586694,4.48683500863597,
128.78542366369));
#125152=CARTESIAN_POINT('Ctrl Pts',(-199.890450920813,4.42899922894786,
128.66149604675));
#125153=CARTESIAN_POINT('Ctrl Pts',(-199.898225254932,4.36600848997413,
128.540038880715));
#125154=CARTESIAN_POINT('Ctrl Pts',(-199.905990007879,4.30309538145654,
128.418731399783));
#125155=CARTESIAN_POINT('Ctrl Pts',(-199.913754760827,4.23504013255191,
128.299888655622));
#125156=CARTESIAN_POINT('Ctrl Pts',(-199.921519513774,4.16206240861067,
128.183975231916));
#125157=CARTESIAN_POINT('Ctrl Pts',(-199.929276554659,4.08915716717364,
128.068176935055));
#125158=CARTESIAN_POINT('Ctrl Pts',(-199.937033595544,4.01133938712683,
127.95530249744));
#125159=CARTESIAN_POINT('Ctrl Pts',(-199.944790636429,3.9288749764153,127.84579263927));
#125160=CARTESIAN_POINT('Ctrl Pts',(-199.952541827669,3.84647275275725,
127.736365363336));
#125161=CARTESIAN_POINT('Ctrl Pts',(-199.960293018909,3.75943110728714,
127.630297927647));
#125162=CARTESIAN_POINT('Ctrl Pts',(-199.968044210149,3.6680594497312,127.528002435722));
#125163=CARTESIAN_POINT('Ctrl Pts',(-199.975792106926,3.57672662756702,
127.425750422109));
#125164=CARTESIAN_POINT('Ctrl Pts',(-199.983540003703,3.48106771357534,
127.327267454637));
#125165=CARTESIAN_POINT('Ctrl Pts',(-199.99128790048,3.38143248002231,127.232932689475));
#125166=CARTESIAN_POINT('Ctrl Pts',(-199.999034176564,3.2818180880128,127.138617657112));
#125167=CARTESIAN_POINT('Ctrl Pts',(-200.006780452648,3.17822931458165,
127.048449369756));
#125168=CARTESIAN_POINT('Ctrl Pts',(-200.014526728732,3.07105259745354,
126.962769930601));
#125169=CARTESIAN_POINT('Ctrl Pts',(-200.022273061998,2.9638750891711,126.87708985898));
#125170=CARTESIAN_POINT('Ctrl Pts',(-200.030019395263,2.85310988972064,
126.795898945805));
#125171=CARTESIAN_POINT('Ctrl Pts',(-200.037765728529,2.73917598040633,
126.719498562262));
#125172=CARTESIAN_POINT('Ctrl Pts',(-200.045513796531,2.62521655638345,
126.643081069382));
#125173=CARTESIAN_POINT('Ctrl Pts',(-200.053261864534,2.50808733510855,
126.571456458597));
#125174=CARTESIAN_POINT('Ctrl Pts',(-200.061009932537,2.38823534370891,
126.504882160176));
#125175=CARTESIAN_POINT('Ctrl Pts',(-200.068766235279,2.26825597218606,
126.438237105799));
#125176=CARTESIAN_POINT('Ctrl Pts',(-200.076522538021,2.14554839219856,
126.37665327616));
#125177=CARTESIAN_POINT('Ctrl Pts',(-200.084278840763,2.02058374140458,
126.320341839007));
#125178=CARTESIAN_POINT('Ctrl Pts',(-200.092039283277,1.89555239321386,
126.264000346744));
#125179=CARTESIAN_POINT('Ctrl Pts',(-200.099799725791,1.76826193649607,
126.212936999659));
#125180=CARTESIAN_POINT('Ctrl Pts',(-200.107560168305,1.63920151175827,
126.167313985673));
#125181=CARTESIAN_POINT('Ctrl Pts',(-200.115333068571,1.50993390776888,
126.121617733575));
#125182=CARTESIAN_POINT('Ctrl Pts',(-200.123105968836,1.37889103187466,
126.081379381333));
#125183=CARTESIAN_POINT('Ctrl Pts',(-200.130878869102,1.24657600647687,
126.046710848765));
#125184=CARTESIAN_POINT('Ctrl Pts',(-200.138369204864,1.11907096553192,
126.01330260468));
#125185=CARTESIAN_POINT('Ctrl Pts',(-200.145859540626,0.99038496183093,
125.985066322929));
#125186=CARTESIAN_POINT('Ctrl Pts',(-200.153349876388,0.860973361320397,
125.962056627357));
#125187=CARTESIAN_POINT('Ctrl Pts',(-200.161124210507,0.726655080644413,
125.938174512183));
#125188=CARTESIAN_POINT('Ctrl Pts',(-200.168898544626,0.591129615061729,
125.919847487573));
#125189=CARTESIAN_POINT('Ctrl Pts',(-200.176672878745,0.454896228380958,
125.907192815264));
#125190=CARTESIAN_POINT('Ctrl Pts',(-200.184437631692,0.318830737174114,
125.894553738707));
#125191=CARTESIAN_POINT('Ctrl Pts',(-200.19220238464,0.182059446335804,
125.887573140922));
#125192=CARTESIAN_POINT('Ctrl Pts',(-200.199967137587,0.0450919577624086,
125.886317330054));
#125193=CARTESIAN_POINT('Ctrl Pts',(-200.207724178472,-0.0917394927708051,
125.885062766475));
#125194=CARTESIAN_POINT('Ctrl Pts',(-200.215481219357,-0.228766364827308,
125.8895216781));
#125195=CARTESIAN_POINT('Ctrl Pts',(-200.223238260242,-0.365474138281122,
125.899708569077));
#125196=CARTESIAN_POINT('Ctrl Pts',(-200.230989451482,-0.502078819338985,
125.90988777804));
#125197=CARTESIAN_POINT('Ctrl Pts',(-200.238740642722,-0.638364492456307,
125.925786339691));
#125198=CARTESIAN_POINT('Ctrl Pts',(-200.246491833962,-0.773817199757398,
125.947366690881));
#125199=CARTESIAN_POINT('Ctrl Pts',(-200.254239730739,-0.909212336044752,
125.968937869845));
#125200=CARTESIAN_POINT('Ctrl Pts',(-200.261987627516,-1.04377482537243,
125.996185973889));
#125201=CARTESIAN_POINT('Ctrl Pts',(-200.269735524293,-1.17699661246376,
126.029021672868));
#125202=CARTESIAN_POINT('Ctrl Pts',(-200.277481800377,-1.31019053242917,
126.061850503327));
#125203=CARTESIAN_POINT('Ctrl Pts',(-200.285228076462,-1.44204392861639,
126.100264510403));
#125204=CARTESIAN_POINT('Ctrl Pts',(-200.292974352546,-1.57206010089031,
126.144123488225));
#125205=CARTESIAN_POINT('Ctrl Pts',(-200.300720685811,-1.70207723291426,
126.187982789804));
#125206=CARTESIAN_POINT('Ctrl Pts',(-200.308467019076,-1.83025674350794,
126.237287017366));
#125207=CARTESIAN_POINT('Ctrl Pts',(-200.316213352342,-1.9561186109295,
126.29184656856));
#125208=CARTESIAN_POINT('Ctrl Pts',(-200.323961420345,-2.08200866424412,
126.346418337987));
#125209=CARTESIAN_POINT('Ctrl Pts',(-200.331709488348,-2.20557968295316,
126.40624761746));
#125210=CARTESIAN_POINT('Ctrl Pts',(-200.339457556351,-2.32637345459673,
126.471097457747));
#125211=CARTESIAN_POINT('Ctrl Pts',(-200.347213859093,-2.44729560729777,
126.536016221215));
#125212=CARTESIAN_POINT('Ctrl Pts',(-200.354970161835,-2.56543427159992,
126.605966019329));
#125213=CARTESIAN_POINT('Ctrl Pts',(-200.362726464576,-2.68035712468567,
126.68066461196));
#125214=CARTESIAN_POINT('Ctrl Pts',(-200.370486907091,-2.79534131555868,
126.75540307348));
#125215=CARTESIAN_POINT('Ctrl Pts',(-200.378247349605,-2.90710595674912,
126.834895153379));
#125216=CARTESIAN_POINT('Ctrl Pts',(-200.386007792119,-3.01525020257337,
126.918816990429));
#125217=CARTESIAN_POINT('Ctrl Pts',(-200.393780692384,-3.12356805114131,
127.002873546263));
#125218=CARTESIAN_POINT('Ctrl Pts',(-200.40155359265,-3.22825359181314,
127.091373816816));
#125219=CARTESIAN_POINT('Ctrl Pts',(-200.409326492915,-3.32894071332805,
127.183955006361));
#125220=CARTESIAN_POINT('Ctrl Pts',(-200.416816828677,-3.42596760435925,
127.273170636466));
#125221=CARTESIAN_POINT('Ctrl Pts',(-200.424307164439,-3.51928151621706,
127.366175415959));
#125222=CARTESIAN_POINT('Ctrl Pts',(-200.431797500201,-3.60859035589865,
127.462615758093));
#125223=CARTESIAN_POINT('Ctrl Pts',(-200.439483530572,-3.70023250333136,
127.561575727608));
#125224=CARTESIAN_POINT('Ctrl Pts',(-200.447169560944,-3.78796263802236,
127.664483128439));
#125225=CARTESIAN_POINT('Ctrl Pts',(-200.454855591315,-3.87141551944836,
127.770992038202));
#125226=CARTESIAN_POINT('Ctrl Pts',(-200.462532485089,-3.95476919812291,
127.877374337873));
#125227=CARTESIAN_POINT('Ctrl Pts',(-200.470209378863,-4.03385548881044,
127.987349321958));
#125228=CARTESIAN_POINT('Ctrl Pts',(-200.477886272637,-4.10834596593192,
128.100534349717));
#125229=CARTESIAN_POINT('Ctrl Pts',(-200.48555463187,-4.18275363065011,
128.213593547645));
#125230=CARTESIAN_POINT('Ctrl Pts',(-200.493222991104,-4.25257543216279,
128.329855354119));
#125231=CARTESIAN_POINT('Ctrl Pts',(-200.500891350337,-4.3175236951057,
128.44890477958));
#125232=CARTESIAN_POINT('Ctrl Pts',(-200.508554665913,-4.38242924007743,
128.567875903488));
#125233=CARTESIAN_POINT('Ctrl Pts',(-200.516217981489,-4.44246742915597,
128.689630650553));
#125234=CARTESIAN_POINT('Ctrl Pts',(-200.523881297066,-4.49739444895502,
128.813725986849));
#125235=CARTESIAN_POINT('Ctrl Pts',(-200.531543281829,-4.55231193011296,
128.937799772716));
#125236=CARTESIAN_POINT('Ctrl Pts',(-200.539205266592,-4.60211982992361,
129.064212980692));
#125237=CARTESIAN_POINT('Ctrl Pts',(-200.546867251355,-4.64662086241272,
129.192499077765));
#125238=CARTESIAN_POINT('Ctrl Pts',(-200.554529236118,-4.69112189490171,
129.320785174837));
#125239=CARTESIAN_POINT('Ctrl Pts',(-200.56219122088,-4.73031591701161,
129.450943786207));
#125240=CARTESIAN_POINT('Ctrl Pts',(-200.569853205643,-4.76405452823395,
129.582490119308));
#125241=CARTESIAN_POINT('Origin',(213.235140564004,0.,130.804360617566));
#125242=CARTESIAN_POINT('',(-202.665364488388,-4.77027151308326,129.580941132323));
#125243=CARTESIAN_POINT('',(-202.319765235154,-4.76405452823411,129.582490119309));
#125244=CARTESIAN_POINT('',(213.235140564004,-4.76405452823405,129.582490119308));
#125245=CARTESIAN_POINT('',(-200.985142080239,-4.92392244591489,130.802667972596));
#125246=CARTESIAN_POINT('Ctrl Pts',(-200.985142543985,-4.92565748492521,
130.802675521279));
#125247=CARTESIAN_POINT('Ctrl Pts',(-201.072612154484,-4.9187069394712,
132.340745200837));
#125248=CARTESIAN_POINT('Ctrl Pts',(-201.252897639586,-3.31467917127183,
135.523358464972));
#125249=CARTESIAN_POINT('Ctrl Pts',(-201.525998999293,2.10959714028603,
136.225733113176));
#125250=CARTESIAN_POINT('Ctrl Pts',(-201.804446623106,5.70144300590434,
131.959881054809));
#125251=CARTESIAN_POINT('Ctrl Pts',(-202.082894246919,4.05394128007133,
126.632162164928));
#125252=CARTESIAN_POINT('Ctrl Pts',(-202.361341870732,-1.31893443610527,
125.138489829794));
#125253=CARTESIAN_POINT('Ctrl Pts',(-202.555498617888,-4.22021631041374,
127.727491303473));
#125254=CARTESIAN_POINT('Ctrl Pts',(-202.65683949044,-4.73402528963851,
129.435398865923));
#125255=CARTESIAN_POINT('Ctrl Pts',(-202.665364488388,-4.77027151308407,
129.580941132326));
#125256=CARTESIAN_POINT('Ctrl Pts',(-200.91504706349,-4.76405452823395,
129.582490119308));
#125257=CARTESIAN_POINT('Ctrl Pts',(-200.922810977094,-4.79810171876979,
129.715239598469));
#125258=CARTESIAN_POINT('Ctrl Pts',(-200.930574890699,-4.82656335624725,
129.849285219688));
#125259=CARTESIAN_POINT('Ctrl Pts',(-200.938338804304,-4.84936942606639,
129.984117219523));
#125260=CARTESIAN_POINT('Ctrl Pts',(-200.946113769782,-4.87220796015882,
130.119141151722));
#125261=CARTESIAN_POINT('Ctrl Pts',(-200.953888735261,-4.88937480602331,
130.254953310856));
#125262=CARTESIAN_POINT('Ctrl Pts',(-200.96166370074,-4.90085188096385,
130.39104003575));
#125263=CARTESIAN_POINT('Ctrl Pts',(-200.964143717715,-4.90451277704879,
130.434448252648));
#125264=CARTESIAN_POINT('Ctrl Pts',(-200.966623734691,-4.90759516567256,
130.477884416332));
#125265=CARTESIAN_POINT('Ctrl Pts',(-200.969103751666,-4.91009957319356,
130.521331919685));
#125266=CARTESIAN_POINT('Ctrl Pts',(-200.974449355782,-4.91549775041753,
130.614981743472));
#125267=CARTESIAN_POINT('Ctrl Pts',(-200.979794959898,-4.91821692815383,
130.708787473997));
#125268=CARTESIAN_POINT('Ctrl Pts',(-200.985140564013,-4.91824970017718,
130.802643292019));
#125269=CARTESIAN_POINT('',(-200.639859436051,-4.91824790596759,130.808899113513));
#125270=CARTESIAN_POINT('Ctrl Pts',(-200.569853205643,-4.76405452823395,
129.582490119308));
#125271=CARTESIAN_POINT('Ctrl Pts',(-200.577513488277,-4.79778564433713,
129.714007229053));
#125272=CARTESIAN_POINT('Ctrl Pts',(-200.58517377091,-4.82606367990543,
129.846911054034));
#125273=CARTESIAN_POINT('Ctrl Pts',(-200.592834053543,-4.84879096813837,
129.980704615463));
#125274=CARTESIAN_POINT('Ctrl Pts',(-200.600671617285,-4.87204423159276,
130.117594547097));
#125275=CARTESIAN_POINT('Ctrl Pts',(-200.608509181027,-4.88948659380923,
130.255415469519));
#125276=CARTESIAN_POINT('Ctrl Pts',(-200.616346744769,-4.90106945198536,
130.393627992473));
#125277=CARTESIAN_POINT('Ctrl Pts',(-200.624184308511,-4.9126523101615,
130.531840515427));
#125278=CARTESIAN_POINT('Ctrl Pts',(-200.632021872253,-4.91837567036258,
130.670444191001));
#125279=CARTESIAN_POINT('Ctrl Pts',(-200.639859435995,-4.91824790596849,
130.808899112527));
#125280=CARTESIAN_POINT('Ctrl Pts',(-200.639859436051,-4.91824790596758,
130.808899113514));
#125281=CARTESIAN_POINT('Ctrl Pts',(-200.649775499558,-4.91808625878195,
130.984071889128));
#125282=CARTESIAN_POINT('Ctrl Pts',(-200.659691563065,-4.9085624689396,
131.15882584626));
#125283=CARTESIAN_POINT('Ctrl Pts',(-200.669607626572,-4.8898314044626,
131.332311276654));
#125284=CARTESIAN_POINT('Ctrl Pts',(-200.679740109887,-4.87069153125199,
131.50958305668));
#125285=CARTESIAN_POINT('Ctrl Pts',(-200.689872593201,-4.84193809215862,
131.685530583323));
#125286=CARTESIAN_POINT('Ctrl Pts',(-200.700005076516,-4.80378435667934,
131.859272422895));
#125287=CARTESIAN_POINT('Ctrl Pts',(-200.703418425682,-4.7909314343376,
131.917801170958));
#125288=CARTESIAN_POINT('Ctrl Pts',(-200.706831774848,-4.77701213815199,
131.976079801564));
#125289=CARTESIAN_POINT('Ctrl Pts',(-200.710245124013,-4.76203582549044,
132.034075161371));
#125290=CARTESIAN_POINT('Ctrl Pts',(-200.718019458133,-4.72792538063196,
132.166166923039));
#125291=CARTESIAN_POINT('Ctrl Pts',(-200.725793792252,-4.68826069982342,
132.297047573819));
#125292=CARTESIAN_POINT('Ctrl Pts',(-200.733568126371,-4.64314265885356,
132.426214282985));
#125293=CARTESIAN_POINT('Ctrl Pts',(-200.741332879318,-4.59808022183689,
132.555221805726));
#125294=CARTESIAN_POINT('Ctrl Pts',(-200.749097632265,-4.5475779246939,
132.682519224107));
#125295=CARTESIAN_POINT('Ctrl Pts',(-200.756862385212,-4.49178728356926,
132.807615484443));
#125296=CARTESIAN_POINT('Ctrl Pts',(-200.764619426097,-4.43605205449589,
132.932587497409));
#125297=CARTESIAN_POINT('Ctrl Pts',(-200.772376466982,-4.37503909228266,
133.055362348256));
#125298=CARTESIAN_POINT('Ctrl Pts',(-200.780133507867,-4.30894907403695,
133.175466043281));
#125299=CARTESIAN_POINT('Ctrl Pts',(-200.787884699107,-4.2429088947882,
133.295479167176));
#125300=CARTESIAN_POINT('Ctrl Pts',(-200.795635890348,-4.17179946792055,
133.412824803525));
#125301=CARTESIAN_POINT('Ctrl Pts',(-200.803387081588,-4.09586859292485,
133.527051112645));
#125302=CARTESIAN_POINT('Ctrl Pts',(-200.811134978365,-4.01996999057645,
133.641228872536));
#125303=CARTESIAN_POINT('Ctrl Pts',(-200.818882875142,-3.93925423187122,
133.752289617197));
#125304=CARTESIAN_POINT('Ctrl Pts',(-200.826630771919,-3.85401374574893,
133.859808393274));
#125305=CARTESIAN_POINT('Ctrl Pts',(-200.834377048003,-3.76879109009876,
133.96730467874));
#125306=CARTESIAN_POINT('Ctrl Pts',(-200.842123324087,-3.67904583235511,
134.071260163147));
#125307=CARTESIAN_POINT('Ctrl Pts',(-200.849869600171,-3.58511195384299,
134.17128136818));
#125308=CARTESIAN_POINT('Ctrl Pts',(-200.857615933436,-3.49117738193219,
134.271303311546));
#125309=CARTESIAN_POINT('Ctrl Pts',(-200.865362266702,-3.39305439520117,
134.367390632596));
#125310=CARTESIAN_POINT('Ctrl Pts',(-200.873108599967,-3.29111496926247,
134.459185554768));
#125311=CARTESIAN_POINT('Ctrl Pts',(-200.88085666797,-3.18915271469628,
134.551001033777));
#125312=CARTESIAN_POINT('Ctrl Pts',(-200.888604735973,-3.08337261071428,
134.638521939557));
#125313=CARTESIAN_POINT('Ctrl Pts',(-200.896352803976,-2.9741806303318,
134.721430011981));
#125314=CARTESIAN_POINT('Ctrl Pts',(-200.904109106718,-2.86487259941302,
134.80442620009));
#125315=CARTESIAN_POINT('Ctrl Pts',(-200.91186540946,-2.75214576027803,
134.882799524622));
#125316=CARTESIAN_POINT('Ctrl Pts',(-200.919621712202,-2.63643651732246,
134.956274098436));
#125317=CARTESIAN_POINT('Ctrl Pts',(-200.927382154716,-2.52066551685999,
135.029787887842));
#125318=CARTESIAN_POINT('Ctrl Pts',(-200.93514259723,-2.40190927914698,
135.098397521213));
#125319=CARTESIAN_POINT('Ctrl Pts',(-200.942903039744,-2.28062897968,135.161873040904));
#125320=CARTESIAN_POINT('Ctrl Pts',(-200.95067594001,-2.15915399030956,
135.225450457134));
#125321=CARTESIAN_POINT('Ctrl Pts',(-200.958448840275,-2.03514719618037,
135.283877123337));
#125322=CARTESIAN_POINT('Ctrl Pts',(-200.966221740541,-1.90909074643751,
135.336970857192));
#125323=CARTESIAN_POINT('Ctrl Pts',(-200.973712076303,-1.78761676615949,
135.388134500087));
#125324=CARTESIAN_POINT('Ctrl Pts',(-200.981202412065,-1.66423985179437,
135.434346102061));
#125325=CARTESIAN_POINT('Ctrl Pts',(-200.988692747827,-1.5394030098361,
135.47548697379));
#125326=CARTESIAN_POINT('Ctrl Pts',(-200.996467081946,-1.40983294107218,
135.518187714174));
#125327=CARTESIAN_POINT('Ctrl Pts',(-201.004241416065,-1.27827961399708,
135.555560883532));
#125328=CARTESIAN_POINT('Ctrl Pts',(-201.012015750184,-1.14522060017088,
135.587419559231));
#125329=CARTESIAN_POINT('Ctrl Pts',(-201.019780503131,-1.01232556968741,
135.61923897196));
#125330=CARTESIAN_POINT('Ctrl Pts',(-201.027545256078,-0.877928921160667,
135.645557323121));
#125331=CARTESIAN_POINT('Ctrl Pts',(-201.035310009025,-0.742525690139992,
135.666236661027));
#125332=CARTESIAN_POINT('Ctrl Pts',(-201.04306704991,-0.607256943517217,
135.686895459924));
#125333=CARTESIAN_POINT('Ctrl Pts',(-201.050824090795,-0.470983987934914,
135.701926332662));
#125334=CARTESIAN_POINT('Ctrl Pts',(-201.05858113168,-0.33421407859659,
135.711241909402));
#125335=CARTESIAN_POINT('Ctrl Pts',(-201.066332322921,-0.197547308510626,
135.720550461193));
#125336=CARTESIAN_POINT('Ctrl Pts',(-201.074083514161,-0.0603847190823009,
135.724152269219));
#125337=CARTESIAN_POINT('Ctrl Pts',(-201.081834705401,0.076759602487468,
135.722011583823));
#125338=CARTESIAN_POINT('Ctrl Pts',(-201.089582602178,0.213845634062312,
135.719871808275));
#125339=CARTESIAN_POINT('Ctrl Pts',(-201.097330498955,0.350913023122092,
135.711994399786));
#125340=CARTESIAN_POINT('Ctrl Pts',(-201.105078395732,0.487446179389158,
135.698395689437));
#125341=CARTESIAN_POINT('Ctrl Pts',(-201.112824671816,0.623950775863247,
135.684799823644));
#125342=CARTESIAN_POINT('Ctrl Pts',(-201.1205709479,0.759920973027649,135.665485075162));
#125343=CARTESIAN_POINT('Ctrl Pts',(-201.128317223985,0.894845201367628,
135.640519747298));
#125344=CARTESIAN_POINT('Ctrl Pts',(-201.13606355725,1.02977042568743,135.615554235145));
#125345=CARTESIAN_POINT('Ctrl Pts',(-201.143809890515,1.16364928133632,
135.584938131512));
#125346=CARTESIAN_POINT('Ctrl Pts',(-201.151556223781,1.29597969885603,
135.548791003045));
#125347=CARTESIAN_POINT('Ctrl Pts',(-201.159304291784,1.42833975085505,
135.512635779679));
#125348=CARTESIAN_POINT('Ctrl Pts',(-201.167052359787,1.55915029763305,
135.470947169741));
#125349=CARTESIAN_POINT('Ctrl Pts',(-201.17480042779,1.68792413960081,135.423894702455));
#125350=CARTESIAN_POINT('Ctrl Pts',(-201.182556730532,1.81683484394041,
135.376792227247));
#125351=CARTESIAN_POINT('Ctrl Pts',(-201.190313033273,1.94370415157494,
135.324314641176));
#125352=CARTESIAN_POINT('Ctrl Pts',(-201.198069336015,2.06806406360551,
135.266679979885));
#125353=CARTESIAN_POINT('Ctrl Pts',(-201.205829778529,2.19249035026554,
135.209014557239));
#125354=CARTESIAN_POINT('Ctrl Pts',(-201.213590221043,2.31440422521268,
135.14618675382));
#125355=CARTESIAN_POINT('Ctrl Pts',(-201.221350663558,2.4333629419461,135.07846027191));
#125356=CARTESIAN_POINT('Ctrl Pts',(-201.229123563823,2.55251262177229,
135.010625069439));
#125357=CARTESIAN_POINT('Ctrl Pts',(-201.236896464089,2.66869733203954,
134.937875681717));
#125358=CARTESIAN_POINT('Ctrl Pts',(-201.244669364354,2.7815031842106,134.860519280479));
#125359=CARTESIAN_POINT('Ctrl Pts',(-201.252159700116,2.89020825951414,
134.785974979276));
#125360=CARTESIAN_POINT('Ctrl Pts',(-201.259650035878,2.99577562489767,
134.707152986653));
#125361=CARTESIAN_POINT('Ctrl Pts',(-201.26714037164,3.09786596784007,134.624361862042));
#125362=CARTESIAN_POINT('Ctrl Pts',(-201.274914705759,3.20382709716525,
134.538431686777));
#125363=CARTESIAN_POINT('Ctrl Pts',(-201.282689039878,3.30637798966232,
134.447953257853));
#125364=CARTESIAN_POINT('Ctrl Pts',(-201.290463373997,3.40510324293289,
134.353227333501));
#125365=CARTESIAN_POINT('Ctrl Pts',(-201.298228126944,3.50370682615185,
134.258618150384));
#125366=CARTESIAN_POINT('Ctrl Pts',(-201.305992879892,3.59849387170741,
134.159772155332));
#125367=CARTESIAN_POINT('Ctrl Pts',(-201.313757632839,3.68908073813156,
134.057031269514));
#125368=CARTESIAN_POINT('Ctrl Pts',(-201.321514673724,3.77957763240292,
133.954392427393));
#125369=CARTESIAN_POINT('Ctrl Pts',(-201.329271714609,3.86588239247803,
133.847866684276));
#125370=CARTESIAN_POINT('Ctrl Pts',(-201.337028755494,3.94764732780846,
133.737833582798));
#125371=CARTESIAN_POINT('Ctrl Pts',(-201.344779946734,4.02935060356523,
133.627883458138));
#125372=CARTESIAN_POINT('Ctrl Pts',(-201.352531137974,4.10652063663432,
133.514431552222));
#125373=CARTESIAN_POINT('Ctrl Pts',(-201.360282329214,4.1788494731278,133.397891057611));
#125374=CARTESIAN_POINT('Ctrl Pts',(-201.368030225991,4.25114756793644,
133.281400095818));
#125375=CARTESIAN_POINT('Ctrl Pts',(-201.375778122768,4.31860835291871,
133.161823487747));
#125376=CARTESIAN_POINT('Ctrl Pts',(-201.383526019545,4.38096687873627,
133.039603841449));
#125377=CARTESIAN_POINT('Ctrl Pts',(-201.39127229563,4.44331236049435,132.917409760867));
#125378=CARTESIAN_POINT('Ctrl Pts',(-201.399018571714,4.50055752839833,
132.792574089773));
#125379=CARTESIAN_POINT('Ctrl Pts',(-201.406764847798,4.55248333213625,
132.665564145695));
#125380=CARTESIAN_POINT('Ctrl Pts',(-201.414511181063,4.60440951917872,
132.538553264059));
#125381=CARTESIAN_POINT('Ctrl Pts',(-201.422257514328,4.65101611574979,
132.409368439302));
#125382=CARTESIAN_POINT('Ctrl Pts',(-201.430003847594,4.69213233585013,
132.278496705371));
#125383=CARTESIAN_POINT('Ctrl Pts',(-201.437751915597,4.73325776364294,
132.147595663623));
#125384=CARTESIAN_POINT('Ctrl Pts',(-201.4454999836,4.76889025117849,132.015007333899));
#125385=CARTESIAN_POINT('Ctrl Pts',(-201.453248051603,4.79890908491508,
131.881233245698));
#125386=CARTESIAN_POINT('Ctrl Pts',(-201.461004354345,4.82895982302535,
131.747316980804));
#125387=CARTESIAN_POINT('Ctrl Pts',(-201.468760657086,4.85338490335348,
131.612212822058));
#125388=CARTESIAN_POINT('Ctrl Pts',(-201.476516959828,4.87211480062235,
131.476432363778));
#125389=CARTESIAN_POINT('Ctrl Pts',(-201.484277402342,4.89085469460135,
131.340579435379));
#125390=CARTESIAN_POINT('Ctrl Pts',(-201.492037844857,4.90389331153006,
131.204049877203));
#125391=CARTESIAN_POINT('Ctrl Pts',(-201.499798287371,4.91121319630827,
131.067358721946));
#125392=CARTESIAN_POINT('Ctrl Pts',(-201.507571187636,4.91854483161535,
130.930448137912));
#125393=CARTESIAN_POINT('Ctrl Pts',(-201.515344087902,4.92013938522368,
130.793375829575));
#125394=CARTESIAN_POINT('Ctrl Pts',(-201.523116988167,4.91603157254995,
130.656656046912));
#125395=CARTESIAN_POINT('Ctrl Pts',(-201.530607323929,4.9120730892139,130.524906372726));
#125396=CARTESIAN_POINT('Ctrl Pts',(-201.538097659691,4.90281965408166,
130.39348434606));
#125397=CARTESIAN_POINT('Ctrl Pts',(-201.545587995453,4.88834746023548,
130.262842224056));
#125398=CARTESIAN_POINT('Ctrl Pts',(-201.553362329572,4.87332654876078,
130.127246766288));
#125399=CARTESIAN_POINT('Ctrl Pts',(-201.561136663691,4.8526357463644,129.992061995147));
#125400=CARTESIAN_POINT('Ctrl Pts',(-201.56891099781,4.82630355432022,129.857799967604));
#125401=CARTESIAN_POINT('Ctrl Pts',(-201.576675750757,4.80000381434937,
129.723703406011));
#125402=CARTESIAN_POINT('Ctrl Pts',(-201.584440503704,4.76807659267288,
129.590527705303));
#125403=CARTESIAN_POINT('Ctrl Pts',(-201.592205256651,4.73060218967124,
129.458780450657));
#125404=CARTESIAN_POINT('Ctrl Pts',(-201.599962297536,4.69316500677496,
129.327164049242));
#125405=CARTESIAN_POINT('Ctrl Pts',(-201.607719338421,4.65019171305585,
129.196973644122));
#125406=CARTESIAN_POINT('Ctrl Pts',(-201.615476379306,4.60181369324896,
129.068706909269));
#125407=CARTESIAN_POINT('Ctrl Pts',(-201.623227570546,4.5534721556832,128.940536901358));
#125408=CARTESIAN_POINT('Ctrl Pts',(-201.630978761786,4.49973414196849,
128.814288040604));
#125409=CARTESIAN_POINT('Ctrl Pts',(-201.638729953027,4.44078082610854,
128.690442758006));
#125410=CARTESIAN_POINT('Ctrl Pts',(-201.646477849804,4.38185256698038,
128.566650112956));
#125411=CARTESIAN_POINT('Ctrl Pts',(-201.654225746581,4.31771358212929,
128.445259366479));
#125412=CARTESIAN_POINT('Ctrl Pts',(-201.661973643358,4.24859303865466,
128.326732668419));
#125413=CARTESIAN_POINT('Ctrl Pts',(-201.669719919442,4.17948695370766,
128.208230763589));
#125414=CARTESIAN_POINT('Ctrl Pts',(-201.677466195526,4.10540157962988,
128.092592053057));
#125415=CARTESIAN_POINT('Ctrl Pts',(-201.68521247161,4.0266116818476,127.980253426592));
#125416=CARTESIAN_POINT('Ctrl Pts',(-201.692958804875,3.9478212024563,127.86791397087));
#125417=CARTESIAN_POINT('Ctrl Pts',(-201.700705138141,3.86432635455989,
127.758874967912));
#125418=CARTESIAN_POINT('Ctrl Pts',(-201.708451471406,3.77644457960803,
127.65354335856));
#125419=CARTESIAN_POINT('Ctrl Pts',(-201.716199539409,3.68854312414213,
127.548188160925));
#125420=CARTESIAN_POINT('Ctrl Pts',(-201.723947607412,3.59625303713412,
127.446542309132));
#125421=CARTESIAN_POINT('Ctrl Pts',(-201.731695675415,3.49993102093752,
127.348978451846));
#125422=CARTESIAN_POINT('Ctrl Pts',(-201.739451978156,3.40350663255572,
127.251310902531));
#125423=CARTESIAN_POINT('Ctrl Pts',(-201.747208280898,3.30304202998784,
127.157734292792));
#125424=CARTESIAN_POINT('Ctrl Pts',(-201.75496458364,3.19893005191173,127.068583645439));
#125425=CARTESIAN_POINT('Ctrl Pts',(-201.762725026154,3.09476250613789,
126.979385415701));
#125426=CARTESIAN_POINT('Ctrl Pts',(-201.770485468669,2.98694401306269,
126.894618096892));
#125427=CARTESIAN_POINT('Ctrl Pts',(-201.778245911183,2.87589844937092,
126.814574762234));
#125428=CARTESIAN_POINT('Ctrl Pts',(-201.786018811448,2.76467462548215,
126.73440293491));
#125429=CARTESIAN_POINT('Ctrl Pts',(-201.793791711714,2.65021370556392,
126.658970460966));
#125430=CARTESIAN_POINT('Ctrl Pts',(-201.801564611979,2.5329671072149,126.588526098011));
#125431=CARTESIAN_POINT('Ctrl Pts',(-201.809054947741,2.41998271804094,
126.520642565088));
#125432=CARTESIAN_POINT('Ctrl Pts',(-201.816545283503,2.3044119372224,126.45739092656));
#125433=CARTESIAN_POINT('Ctrl Pts',(-201.824035619265,2.18667644572457,
126.398951535061));
#125434=CARTESIAN_POINT('Ctrl Pts',(-201.831809953384,2.06447697728321,
126.338296396273));
#125435=CARTESIAN_POINT('Ctrl Pts',(-201.839584287503,1.93955831659402,
126.282633483449));
#125436=CARTESIAN_POINT('Ctrl Pts',(-201.847358621622,1.81236667732486,
126.232215596963));
#125437=CARTESIAN_POINT('Ctrl Pts',(-201.85512337457,1.68533179038399,126.181859846017));
#125438=CARTESIAN_POINT('Ctrl Pts',(-201.862888127517,1.55602985846499,
126.136736402609));
#125439=CARTESIAN_POINT('Ctrl Pts',(-201.870652880464,1.42493133167005,
126.097052069943));
#125440=CARTESIAN_POINT('Ctrl Pts',(-201.878409921349,1.29396301378008,
126.057407152316));
#125441=CARTESIAN_POINT('Ctrl Pts',(-201.886166962234,1.16120202383286,
126.023190707344));
#125442=CARTESIAN_POINT('Ctrl Pts',(-201.893924003119,1.02713808569387,
125.994561202266));
#125443=CARTESIAN_POINT('Ctrl Pts',(-201.901675194359,0.893175246212959,
125.965953286921));
#125444=CARTESIAN_POINT('Ctrl Pts',(-201.909426385599,0.757911795070179,
125.942924006762));
#125445=CARTESIAN_POINT('Ctrl Pts',(-201.917177576839,0.621851544102284,
125.925581700706));
#125446=CARTESIAN_POINT('Ctrl Pts',(-201.924925473616,0.485849122370762,
125.908246765593));
#125447=CARTESIAN_POINT('Ctrl Pts',(-201.932673370393,0.349050961400987,
125.896594046454));
#125448=CARTESIAN_POINT('Ctrl Pts',(-201.940421267171,0.211969751361186,
125.890680541797));
#125449=CARTESIAN_POINT('Ctrl Pts',(-201.948167543255,0.0749172157553973,
125.884768274118));
#125450=CARTESIAN_POINT('Ctrl Pts',(-201.955913819339,-0.0624178607984672,
125.884592849862));
#125451=CARTESIAN_POINT('Ctrl Pts',(-201.963660095423,-0.199519393139578,
125.890159250684));
#125452=CARTESIAN_POINT('Ctrl Pts',(-201.971406428688,-0.336621937532869,
125.895725692597));
#125453=CARTESIAN_POINT('Ctrl Pts',(-201.979152761954,-0.473490543629981,
125.907034028304));
#125454=CARTESIAN_POINT('Ctrl Pts',(-201.986899095219,-0.609611255716637,
125.92403714679));
#125455=CARTESIAN_POINT('Ctrl Pts',(-201.994647163222,-0.745762451093156,
125.941044073007));
#125456=CARTESIAN_POINT('Ctrl Pts',(-202.002395231225,-0.881165031306035,
125.963748271266));
#125457=CARTESIAN_POINT('Ctrl Pts',(-202.010143299228,-1.01531267014358,
125.99205106348));
#125458=CARTESIAN_POINT('Ctrl Pts',(-202.01789960197,-1.14960288268788,
126.020383936239));
#125459=CARTESIAN_POINT('Ctrl Pts',(-202.025655904712,-1.28263510636064,
126.054327208385));
#125460=CARTESIAN_POINT('Ctrl Pts',(-202.033412207453,-1.41391513808278,
126.093731461625));
#125461=CARTESIAN_POINT('Ctrl Pts',(-202.041172649968,-1.54526523791097,
126.133156746102));
#125462=CARTESIAN_POINT('Ctrl Pts',(-202.048933092482,-1.67486091308033,
126.178048691531));
#125463=CARTESIAN_POINT('Ctrl Pts',(-202.056693534996,-1.80222647708686,
126.228209091689));
#125464=CARTESIAN_POINT('Ctrl Pts',(-202.064466435261,-1.92979649960372,
126.278450013774));
#125465=CARTESIAN_POINT('Ctrl Pts',(-202.072239335527,-2.0551288993706,
126.333976132696));
#125466=CARTESIAN_POINT('Ctrl Pts',(-202.080012235792,-2.17777038732706,
126.394542117607));
#125467=CARTESIAN_POINT('Ctrl Pts',(-202.087502571554,-2.29595354828237,
126.452906376411));
#125468=CARTESIAN_POINT('Ctrl Pts',(-202.094992907316,-2.41163777316133,
126.515950291816));
#125469=CARTESIAN_POINT('Ctrl Pts',(-202.102483243079,-2.52444339732246,
126.583416576689));
#125470=CARTESIAN_POINT('Ctrl Pts',(-202.110258818857,-2.64154478059957,
126.653452050026));
#125471=CARTESIAN_POINT('Ctrl Pts',(-202.118034394636,-2.7559149798318,
126.728475270979));
#125472=CARTESIAN_POINT('Ctrl Pts',(-202.125809970415,-2.86709990176267,
126.808247353929));
#125473=CARTESIAN_POINT('Ctrl Pts',(-202.133891439779,-2.98265887332797,
126.891157695595));
#125474=CARTESIAN_POINT('Ctrl Pts',(-202.141972909144,-3.09477643568045,
126.979198038385));
#125475=CARTESIAN_POINT('Ctrl Pts',(-202.150054378508,-3.20297036422735,
127.072047138183));
#125476=CARTESIAN_POINT('Ctrl Pts',(-202.157810400925,-3.30680724058814,
127.161157133776));
#125477=CARTESIAN_POINT('Ctrl Pts',(-202.165566423341,-3.40702999075184,
127.254695853762));
#125478=CARTESIAN_POINT('Ctrl Pts',(-202.173322445758,-3.50324203012239,
127.352335365503));
#125479=CARTESIAN_POINT('Ctrl Pts',(-202.181073173471,-3.59938838965428,
127.44990822293));
#125480=CARTESIAN_POINT('Ctrl Pts',(-202.188823901183,-3.69152921254174,
127.551576025106));
#125481=CARTESIAN_POINT('Ctrl Pts',(-202.196574628896,-3.77930256283194,
127.65697198553));
#125482=CARTESIAN_POINT('Ctrl Pts',(-202.20432174412,-3.86703500338546,
127.762318822604));
#125483=CARTESIAN_POINT('Ctrl Pts',(-202.212068859344,-3.95040377296826,
127.871390059986));
#125484=CARTESIAN_POINT('Ctrl Pts',(-202.219815974568,-4.02908552554411,
127.983783922925));
#125485=CARTESIAN_POINT('Ctrl Pts',(-202.227561156713,-4.10774764526049,
128.096149741079));
#125486=CARTESIAN_POINT('Ctrl Pts',(-202.235306338858,-4.18172485302055,
128.211836213856));
#125487=CARTESIAN_POINT('Ctrl Pts',(-202.243051521003,-4.25073589056795,
128.330410850263));
#125488=CARTESIAN_POINT('Ctrl Pts',(-202.250798386813,-4.31976192988371,
128.449011262681));
#125489=CARTESIAN_POINT('Ctrl Pts',(-202.258545252622,-4.38381944209067,
128.570500757135));
#125490=CARTESIAN_POINT('Ctrl Pts',(-202.266292118432,-4.44267209747922,
128.694420405906));
#125491=CARTESIAN_POINT('Ctrl Pts',(-202.274040018994,-4.50153261384766,
128.818356606689));
#125492=CARTESIAN_POINT('Ctrl Pts',(-202.281787919557,-4.55518672851136,
128.944723251757));
#125493=CARTESIAN_POINT('Ctrl Pts',(-202.289535820119,-4.60344577788972,
129.07304030274));
#125494=CARTESIAN_POINT('Ctrl Pts',(-202.297288826251,-4.6517366281298,
129.201441909736));
#125495=CARTESIAN_POINT('Ctrl Pts',(-202.305041832382,-4.6946251865411,
129.331796119675));
#125496=CARTESIAN_POINT('Ctrl Pts',(-202.312794838514,-4.73197225875476,
129.463606499588));
#125497=CARTESIAN_POINT('Ctrl Pts',(-202.315118304061,-4.74316464453239,
129.503108193671));
#125498=CARTESIAN_POINT('Ctrl Pts',(-202.317441769608,-4.75385968611253,
129.542740584605));
#125499=CARTESIAN_POINT('Ctrl Pts',(-202.319765235154,-4.76405452823412,
129.582490119309));
#125500=CARTESIAN_POINT('Origin',(213.235140564004,0.,130.804360617566));
#125501=CARTESIAN_POINT('',(-204.415385129731,-4.7580624943176,129.583982083009));
#125502=CARTESIAN_POINT('',(-204.070038127516,-4.76405452823409,129.582490119308));
#125503=CARTESIAN_POINT('',(213.235140564004,-4.76405452823405,129.582490119308));
#125504=CARTESIAN_POINT('',(-202.735140564013,-4.91326211273809,130.800663901985));
#125505=CARTESIAN_POINT('Ctrl Pts',(-202.735140564013,-4.91326211273809,
130.800663901985));
#125506=CARTESIAN_POINT('Ctrl Pts',(-202.796172748794,-4.90575607440281,
131.880836901629));
#125507=CARTESIAN_POINT('Ctrl Pts',(-202.950020808181,-4.02207680521533,
134.614867738963));
#125508=CARTESIAN_POINT('Ctrl Pts',(-203.19668474217,0.501577616433585,
136.600057273287));
#125509=CARTESIAN_POINT('Ctrl Pts',(-203.475132365984,5.14719869251641,
133.515084773622));
#125510=CARTESIAN_POINT('Ctrl Pts',(-203.753579989796,5.06279562480976,
127.939089200777));
#125511=CARTESIAN_POINT('Ctrl Pts',(-204.032027613609,0.325930709221482,
124.996138083671));
#125512=CARTESIAN_POINT('Ctrl Pts',(-204.25262932692,-3.66416944143293,
126.893211472255));
#125513=CARTESIAN_POINT('Ctrl Pts',(-204.380415165628,-4.60798580335201,
128.983142737816));
#125514=CARTESIAN_POINT('Ctrl Pts',(-204.415385129731,-4.7580624943176,
129.583982083009));
#125515=CARTESIAN_POINT('Ctrl Pts',(-202.665364488388,-4.77027151308407,
129.580941132326));
#125516=CARTESIAN_POINT('Ctrl Pts',(-202.688623180263,-4.86916182929373,
129.978023072962));
#125517=CARTESIAN_POINT('Ctrl Pts',(-202.711881872138,-4.91612258108715,
130.389021896046));
#125518=CARTESIAN_POINT('Ctrl Pts',(-202.735140564013,-4.91326211273809,
130.800663901985));
#125519=CARTESIAN_POINT('',(-202.389859436034,-4.91824990320504,130.803384849354));
#125520=CARTESIAN_POINT('Ctrl Pts',(-202.319765235154,-4.76405452823412,
129.582490119309));
#125521=CARTESIAN_POINT('Ctrl Pts',(-202.327527427096,-4.79811327357253,
129.715284650469));
#125522=CARTESIAN_POINT('Ctrl Pts',(-202.335289619037,-4.82658544150759,
129.849387011775));
#125523=CARTESIAN_POINT('Ctrl Pts',(-202.343051810979,-4.84939821559733,
129.984287444574));
#125524=CARTESIAN_POINT('Ctrl Pts',(-202.350825702342,-4.87224537382299,
130.11939120358));
#125525=CARTESIAN_POINT('Ctrl Pts',(-202.358599593705,-4.88941605217232,
130.255295049384));
#125526=CARTESIAN_POINT('Ctrl Pts',(-202.366373485068,-4.90088936486764,
130.391484733277));
#125527=CARTESIAN_POINT('Ctrl Pts',(-202.371225945676,-4.90805100313769,
130.476494292247));
#125528=CARTESIAN_POINT('Ctrl Pts',(-202.376078406283,-4.91299384376543,
130.561615199731));
#125529=CARTESIAN_POINT('Ctrl Pts',(-202.380930866891,-4.91572308414765,
130.646722987294));
#125530=CARTESIAN_POINT('Ctrl Pts',(-202.383907056592,-4.91739702604547,
130.698922673462));
#125531=CARTESIAN_POINT('Ctrl Pts',(-202.386883246294,-4.9182395397714,
130.751149164821));
#125532=CARTESIAN_POINT('Ctrl Pts',(-202.389859435995,-4.9182499032049,
130.803384848665));
#125533=CARTESIAN_POINT('Ctrl Pts',(-202.389859436034,-4.91824990320504,
130.803384849353));
#125534=CARTESIAN_POINT('Ctrl Pts',(-202.397592511015,-4.91827683063906,
130.939109551199));
#125535=CARTESIAN_POINT('Ctrl Pts',(-202.405325585996,-4.91268128621269,
131.075059385912));
#125536=CARTESIAN_POINT('Ctrl Pts',(-202.413058660977,-4.90143341606133,
131.210726869139));
#125537=CARTESIAN_POINT('Ctrl Pts',(-202.42078228894,-4.89019928673439,
131.346228615827));
#125538=CARTESIAN_POINT('Ctrl Pts',(-202.428505916903,-4.87332660037077,
131.481448306892));
#125539=CARTESIAN_POINT('Ctrl Pts',(-202.436229544867,-4.8508374788153,
131.615876986237));
#125540=CARTESIAN_POINT('Ctrl Pts',(-202.443945635588,-4.82837030367676,
131.750174480918));
#125541=CARTESIAN_POINT('Ctrl Pts',(-202.451661726309,-4.80029766335863,
131.883682112162));
#125542=CARTESIAN_POINT('Ctrl Pts',(-202.45937781703,-4.76669356115084,
132.015894998664));
#125543=CARTESIAN_POINT('Ctrl Pts',(-202.467088273264,-4.73311399751808,
132.148011339935));
#125544=CARTESIAN_POINT('Ctrl Pts',(-202.474798729498,-4.69401110747945,
132.278834436168));
#125545=CARTESIAN_POINT('Ctrl Pts',(-202.482509185732,-4.64951007925511,
132.407868985304));
#125546=CARTESIAN_POINT('Ctrl Pts',(-202.490216665053,-4.6050262323335,
132.536853715778));
#125547=CARTESIAN_POINT('Ctrl Pts',(-202.497924144375,-4.55514851955673,
132.664050898828));
#125548=CARTESIAN_POINT('Ctrl Pts',(-202.505631623696,-4.50005207787166,
132.788980066968));
#125549=CARTESIAN_POINT('Ctrl Pts',(-202.513337751278,-4.44496529901407,
132.913887324999));
#125550=CARTESIAN_POINT('Ctrl Pts',(-202.521043878859,-4.38466177095691,
133.036526997411));
#125551=CARTESIAN_POINT('Ctrl Pts',(-202.528750006441,-4.31936471923195,
133.156438738028));
#125552=CARTESIAN_POINT('Ctrl Pts',(-202.536456496514,-4.25406459597308,
133.27635611922));
#125553=CARTESIAN_POINT('Ctrl Pts',(-202.544162986588,-4.18377067092648,
133.39354496595));
#125554=CARTESIAN_POINT('Ctrl Pts',(-202.551869476661,-4.10875183304938,
133.507570087236));
#125555=CARTESIAN_POINT('Ctrl Pts',(-202.559578043381,-4.03371278004685,
133.621625934566));
#125556=CARTESIAN_POINT('Ctrl Pts',(-202.567286610102,-3.95394649875435,
133.732516030231));
#125557=CARTESIAN_POINT('Ctrl Pts',(-202.574995176822,-3.86976457714697,
133.839835074708));
#125558=CARTESIAN_POINT('Ctrl Pts',(-202.582712029366,-3.78549216965473,
133.947269474815));
#125559=CARTESIAN_POINT('Ctrl Pts',(-202.590428881909,-3.69679488857133,
134.051124847371));
#125560=CARTESIAN_POINT('Ctrl Pts',(-202.598145734452,-3.60402417816858,
134.151029526448));
#125561=CARTESIAN_POINT('Ctrl Pts',(-202.605867103336,-3.51119917307237,
134.250992675422));
#125562=CARTESIAN_POINT('Ctrl Pts',(-202.61358847222,-3.41429627095629,
134.347000247896));
#125563=CARTESIAN_POINT('Ctrl Pts',(-202.621309841104,-3.31370214936235,
134.438719037949));
#125564=CARTESIAN_POINT('Ctrl Pts',(-202.629042866836,-3.21295616217193,
134.530576294631));
#125565=CARTESIAN_POINT('Ctrl Pts',(-202.636775892567,-3.10850812896895,
134.618131584567));
#125566=CARTESIAN_POINT('Ctrl Pts',(-202.644508918298,-3.00077647222385,
134.701093046954));
#125567=CARTESIAN_POINT('Ctrl Pts',(-202.649465442433,-2.93172529156538,
134.754267639271));
#125568=CARTESIAN_POINT('Ctrl Pts',(-202.654421966569,-2.86132571321719,
134.80555585624));
#125569=CARTESIAN_POINT('Ctrl Pts',(-202.659378490704,-2.7896934030652,
134.8548906791));
#125570=CARTESIAN_POINT('Ctrl Pts',(-202.667152824823,-2.67733774865093,
134.932272607676));
#125571=CARTESIAN_POINT('Ctrl Pts',(-202.674927158942,-2.56158200219939,
135.005098693772));
#125572=CARTESIAN_POINT('Ctrl Pts',(-202.682701493061,-2.4428319884996,
135.07305537574));
#125573=CARTESIAN_POINT('Ctrl Pts',(-202.690466246008,-2.32422832357901,
135.140928307171));
#125574=CARTESIAN_POINT('Ctrl Pts',(-202.698230998955,-2.20263806981494,
135.203943582563));
#125575=CARTESIAN_POINT('Ctrl Pts',(-202.705995751903,-2.078497570351,135.261829732719));
#125576=CARTESIAN_POINT('Ctrl Pts',(-202.713752792788,-1.95448036898086,
135.319658389536));
#125577=CARTESIAN_POINT('Ctrl Pts',(-202.721509833673,-1.82791831461926,
135.372367894886));
#125578=CARTESIAN_POINT('Ctrl Pts',(-202.729266874558,-1.69927368819759,
135.419731891375));
#125579=CARTESIAN_POINT('Ctrl Pts',(-202.737018065798,-1.57072607368995,
135.467060170305));
#125580=CARTESIAN_POINT('Ctrl Pts',(-202.744769257038,-1.44009937847901,
135.50905082948));
#125581=CARTESIAN_POINT('Ctrl Pts',(-202.752520448278,-1.30787694231266,
135.545525133407));
#125582=CARTESIAN_POINT('Ctrl Pts',(-202.760268345055,-1.17571070420829,
135.581983934782));
#125583=CARTESIAN_POINT('Ctrl Pts',(-202.768016241832,-1.04195045020032,
135.612930940387));
#125584=CARTESIAN_POINT('Ctrl Pts',(-202.77576413861,-0.907095593932953,
135.638236975725));
#125585=CARTESIAN_POINT('Ctrl Pts',(-202.783510414694,-0.772268946394382,
135.663537717586));
#125586=CARTESIAN_POINT('Ctrl Pts',(-202.791256690778,-0.636348536039387,
135.683199764143));
#125587=CARTESIAN_POINT('Ctrl Pts',(-202.799002966862,-0.49984451854849,
135.697144949598));
#125588=CARTESIAN_POINT('Ctrl Pts',(-202.806749300127,-0.363339493416131,
135.711090237993));
#125589=CARTESIAN_POINT('Ctrl Pts',(-202.814495633393,-0.226251241492333,
135.719318541345));
#125590=CARTESIAN_POINT('Ctrl Pts',(-202.822241966658,-0.0890952027191759,
135.721803561551));
#125591=CARTESIAN_POINT('Ctrl Pts',(-202.829990034661,0.0480915511977042,
135.724289138261));
#125592=CARTESIAN_POINT('Ctrl Pts',(-202.837738102664,0.18534573134494,
135.721028865417));
#125593=CARTESIAN_POINT('Ctrl Pts',(-202.845486170667,0.322152132501905,
135.712048572808));
#125594=CARTESIAN_POINT('Ctrl Pts',(-202.853242473409,0.459103933130223,
135.703058735837));
#125595=CARTESIAN_POINT('Ctrl Pts',(-202.860998776151,0.595606613349426,
135.688336760683));
#125596=CARTESIAN_POINT('Ctrl Pts',(-202.868755078893,0.731149768151804,
135.667960424194));
#125597=CARTESIAN_POINT('Ctrl Pts',(-202.876515521407,0.866765266417027,
135.647573212241));
#125598=CARTESIAN_POINT('Ctrl Pts',(-202.884275963921,1.00141983514607,
135.62152569974));
#125599=CARTESIAN_POINT('Ctrl Pts',(-202.892036406435,1.1346144753236,135.589946585333));
#125600=CARTESIAN_POINT('Ctrl Pts',(-202.899809306701,1.268022931362,135.558316777328));
#125601=CARTESIAN_POINT('Ctrl Pts',(-202.907582206966,1.39996639904794,
135.521137728808));
#125602=CARTESIAN_POINT('Ctrl Pts',(-202.915355107232,1.52996136298433,
135.478587964441));
#125603=CARTESIAN_POINT('Ctrl Pts',(-202.922845442994,1.65523068254303,
135.437584991186));
#125604=CARTESIAN_POINT('Ctrl Pts',(-202.930335778755,1.77869041621811,
135.391595108432));
#125605=CARTESIAN_POINT('Ctrl Pts',(-202.937826114517,1.89992823133841,
135.340819123743));
#125606=CARTESIAN_POINT('Ctrl Pts',(-202.945600448637,2.02576281507001,
135.28811795216));
#125607=CARTESIAN_POINT('Ctrl Pts',(-202.953374782756,2.14960227229255,
135.230093642708));
#125608=CARTESIAN_POINT('Ctrl Pts',(-202.961149116875,2.27096343650089,
135.166918139545));
#125609=CARTESIAN_POINT('Ctrl Pts',(-202.968913869822,2.39217503392037,
135.103820494544));
#125610=CARTESIAN_POINT('Ctrl Pts',(-202.976678622769,2.51091407195934,
135.03558446602));
#125611=CARTESIAN_POINT('Ctrl Pts',(-202.984443375716,2.62671630176767,
134.962430426086));
#125612=CARTESIAN_POINT('Ctrl Pts',(-202.992200416601,2.74240351516851,
134.889349043777));
#125613=CARTESIAN_POINT('Ctrl Pts',(-202.999957457486,2.85515939666273,
134.811359578162));
#125614=CARTESIAN_POINT('Ctrl Pts',(-203.007714498371,2.96454363122682,
134.728728607581));
#125615=CARTESIAN_POINT('Ctrl Pts',(-203.015465689611,3.07384537828889,
134.646159949657));
#125616=CARTESIAN_POINT('Ctrl Pts',(-203.023216880851,3.1797802285859,134.558956988398));
#125617=CARTESIAN_POINT('Ctrl Pts',(-203.030968072092,3.28193654994615,
134.467429760324));
#125618=CARTESIAN_POINT('Ctrl Pts',(-203.038715968869,3.38404945214513,
134.375941433763));
#125619=CARTESIAN_POINT('Ctrl Pts',(-203.046463865646,3.48238672899254,
134.280132756231));
#125620=CARTESIAN_POINT('Ctrl Pts',(-203.054211762423,3.57656975705238,
134.1803540766));
#125621=CARTESIAN_POINT('Ctrl Pts',(-203.061958038507,3.67073308405285,
134.080596268517));
#125622=CARTESIAN_POINT('Ctrl Pts',(-203.069704314591,3.76074362251624,
133.976870394256));
#125623=CARTESIAN_POINT('Ctrl Pts',(-203.077450590675,3.84625985773754,
133.869563411715));
#125624=CARTESIAN_POINT('Ctrl Pts',(-203.085196923941,3.93177672422038,
133.762255637058));
#125625=CARTESIAN_POINT('Ctrl Pts',(-203.092943257206,4.01279897759957,
133.651367007122));
#125626=CARTESIAN_POINT('Ctrl Pts',(-203.100689590471,4.08902588465788,
133.537316961363));
#125627=CARTESIAN_POINT('Ctrl Pts',(-203.108437658474,4.1652698622036,133.423241374886));
#125628=CARTESIAN_POINT('Ctrl Pts',(-203.116185726477,4.23671613931385,
133.306003288778));
#125629=CARTESIAN_POINT('Ctrl Pts',(-203.12393379448,4.30310796631424,133.186050121415));
#125630=CARTESIAN_POINT('Ctrl Pts',(-203.131690097222,4.36957035533834,
133.065969466397));
#125631=CARTESIAN_POINT('Ctrl Pts',(-203.139446399964,4.43096737361537,
132.943168308397));
#125632=CARTESIAN_POINT('Ctrl Pts',(-203.147202702706,4.48708857063544,
132.818118105888));
#125633=CARTESIAN_POINT('Ctrl Pts',(-203.15496314522,4.54323972122798,132.693001160321));
#125634=CARTESIAN_POINT('Ctrl Pts',(-203.162723587734,4.59410929477576,
132.565633141281));
#125635=CARTESIAN_POINT('Ctrl Pts',(-203.170484030249,4.63953584793378,
132.436503435532));
#125636=CARTESIAN_POINT('Ctrl Pts',(-203.178256930514,4.68503532382784,
132.307166439315));
#125637=CARTESIAN_POINT('Ctrl Pts',(-203.18602983078,4.72507420452498,132.176062479243));
#125638=CARTESIAN_POINT('Ctrl Pts',(-203.193802731045,4.75954133600245,
132.043694847459));
#125639=CARTESIAN_POINT('Ctrl Pts',(-203.201293066807,4.79275550043213,
131.916139112508));
#125640=CARTESIAN_POINT('Ctrl Pts',(-203.208783402569,4.82079591129226,
131.787410287015));
#125641=CARTESIAN_POINT('Ctrl Pts',(-203.21627373833,4.84360863779292,131.657963819527));
#125642=CARTESIAN_POINT('Ctrl Pts',(-203.224048072449,4.86728631575333,
131.523609349876));
#125643=CARTESIAN_POINT('Ctrl Pts',(-203.231822406569,4.8854070724529,131.388056150618));
#125644=CARTESIAN_POINT('Ctrl Pts',(-203.239596740688,4.89785440608457,
131.251803663437));
#125645=CARTESIAN_POINT('Ctrl Pts',(-203.247361493635,4.91028639949003,
131.115719095268));
#125646=CARTESIAN_POINT('Ctrl Pts',(-203.255126246582,4.91705884657044,
130.978937339527));
#125647=CARTESIAN_POINT('Ctrl Pts',(-203.262890999529,4.91810621478259,
130.841968098429));
#125648=CARTESIAN_POINT('Ctrl Pts',(-203.270648040414,4.91915254273387,
130.705134897112));
#125649=CARTESIAN_POINT('Ctrl Pts',(-203.278405081299,4.91448510469911,
130.568114969434));
#125650=CARTESIAN_POINT('Ctrl Pts',(-203.286162122184,4.90409017955869,
130.431422857));
#125651=CARTESIAN_POINT('Ctrl Pts',(-203.293913313424,4.89370309331222,
130.294833825151));
#125652=CARTESIAN_POINT('Ctrl Pts',(-203.301664504664,4.8775971464774,130.158572504755));
#125653=CARTESIAN_POINT('Ctrl Pts',(-203.309415695904,4.85581068431517,
130.023152795927));
#125654=CARTESIAN_POINT('Ctrl Pts',(-203.317163592681,4.8340334819805,129.887790644087));
#125655=CARTESIAN_POINT('Ctrl Pts',(-203.324911489458,4.8065806282877,129.753269777556));
#125656=CARTESIAN_POINT('Ctrl Pts',(-203.332659386236,4.77354222644985,
129.620098115078));
#125657=CARTESIAN_POINT('Ctrl Pts',(-203.34040566232,4.74051073553344,129.48695430924));
#125658=CARTESIAN_POINT('Ctrl Pts',(-203.348151938404,4.70189611451706,
129.355159525316));
#125659=CARTESIAN_POINT('Ctrl Pts',(-203.355898214488,4.65783932500118,
129.225210249497));
#125660=CARTESIAN_POINT('Ctrl Pts',(-203.363644547753,4.61378221026816,
129.095260014422));
#125661=CARTESIAN_POINT('Ctrl Pts',(-203.371390881019,4.56428297240465,
128.967155684899));
#125662=CARTESIAN_POINT('Ctrl Pts',(-203.379137214284,4.50953194405326,
128.841376993573));
#125663=CARTESIAN_POINT('Ctrl Pts',(-203.386885282287,4.45476865458861,
128.715570134981));
#125664=CARTESIAN_POINT('Ctrl Pts',(-203.39463335029,4.39475139034221,128.592090309345));
#125665=CARTESIAN_POINT('Ctrl Pts',(-203.402381418293,4.32971779759376,
128.471395367996));
#125666=CARTESIAN_POINT('Ctrl Pts',(-203.410137721035,4.26461508636893,
128.350572150628));
#125667=CARTESIAN_POINT('Ctrl Pts',(-203.417894023777,4.19448558231854,
128.232540074813));
#125668=CARTESIAN_POINT('Ctrl Pts',(-203.425650326518,4.11961218316801,
128.117731033348));
#125669=CARTESIAN_POINT('Ctrl Pts',(-203.433410769033,4.04469882182997,
128.002860714841));
#125670=CARTESIAN_POINT('Ctrl Pts',(-203.441171211547,3.96503674722332,
127.891217176486));
#125671=CARTESIAN_POINT('Ctrl Pts',(-203.448931654061,3.88095043022052,
127.783200770641));
#125672=CARTESIAN_POINT('Ctrl Pts',(-203.456704554326,3.79672913039707,
127.675010967273));
#125673=CARTESIAN_POINT('Ctrl Pts',(-203.464477454592,3.70806964875335,
127.570460230171));
#125674=CARTESIAN_POINT('Ctrl Pts',(-203.472250354857,3.61533533775766,
127.469914118061));
#125675=CARTESIAN_POINT('Ctrl Pts',(-203.479740690619,3.52597215254956,
127.373023110385));
#125676=CARTESIAN_POINT('Ctrl Pts',(-203.487231026381,3.4328254728641,127.279850844024));
#125677=CARTESIAN_POINT('Ctrl Pts',(-203.494721362143,3.3362493295539,127.190688873543));
#125678=CARTESIAN_POINT('Ctrl Pts',(-203.502495696262,3.23601147241738,
127.098146299852));
#125679=CARTESIAN_POINT('Ctrl Pts',(-203.510270030382,3.13176143843621,
127.009630978764));
#125680=CARTESIAN_POINT('Ctrl Pts',(-203.518044364501,3.0238564499707,126.92551088698));
#125681=CARTESIAN_POINT('Ctrl Pts',(-203.525809117448,2.91608444475944,
126.84149446569));
#125682=CARTESIAN_POINT('Ctrl Pts',(-203.533573870395,2.80466675286709,
126.761862734097));
#125683=CARTESIAN_POINT('Ctrl Pts',(-203.541338623342,2.68999677926315,
126.686946333084));
#125684=CARTESIAN_POINT('Ctrl Pts',(-203.549095664227,2.57544069749386,
126.612104340097));
#125685=CARTESIAN_POINT('Ctrl Pts',(-203.556852705112,2.45763908746732,
126.541968570097));
#125686=CARTESIAN_POINT('Ctrl Pts',(-203.564609745997,2.33701743100642,
126.476828689357));
#125687=CARTESIAN_POINT('Ctrl Pts',(-203.572360937237,2.2164867362748,126.411737931106));
#125688=CARTESIAN_POINT('Ctrl Pts',(-203.580112128477,2.09314057063032,
126.35163574828));
#125689=CARTESIAN_POINT('Ctrl Pts',(-203.587863319717,1.96743201934503,
126.29676765549));
#125690=CARTESIAN_POINT('Ctrl Pts',(-203.595611216494,1.84177689754726,
126.241922883103));
#125691=CARTESIAN_POINT('Ctrl Pts',(-203.603359113271,1.71376174471187,
126.192307932205));
#125692=CARTESIAN_POINT('Ctrl Pts',(-203.611107010048,1.58386259025,126.148121538899));
#125693=CARTESIAN_POINT('Ctrl Pts',(-203.618853286132,1.45399060789093,
126.103944388434));
#125694=CARTESIAN_POINT('Ctrl Pts',(-203.626599562217,1.32223577767975,
126.06519366274));
#125695=CARTESIAN_POINT('Ctrl Pts',(-203.634345838301,1.18909200069798,
126.032019129745));
#125696=CARTESIAN_POINT('Ctrl Pts',(-203.642092171566,1.05594724087891,
125.998844351863));
#125697=CARTESIAN_POINT('Ctrl Pts',(-203.649838504831,0.921413893196879,
125.97124594334));
#125698=CARTESIAN_POINT('Ctrl Pts',(-203.657584838097,0.785998449754042,
125.949323079144));
#125699=CARTESIAN_POINT('Ctrl Pts',(-203.6653329061,0.650552680961736,125.927395305475));
#125700=CARTESIAN_POINT('Ctrl Pts',(-203.673080974103,0.514224809194846,
125.911145667744));
#125701=CARTESIAN_POINT('Ctrl Pts',(-203.680829042106,0.377528491365758,
125.900621707234));
#125702=CARTESIAN_POINT('Ctrl Pts',(-203.688585344847,0.240686891063561,
125.890086561733));
#125703=CARTESIAN_POINT('Ctrl Pts',(-203.696341647589,0.103476452891485,
125.88528927959));
#125704=CARTESIAN_POINT('Ctrl Pts',(-203.704097950331,-0.0335865463790532,
125.886225299541));
#125705=CARTESIAN_POINT('Ctrl Pts',(-203.711858392845,-0.17072270029919,
125.887161819075));
#125706=CARTESIAN_POINT('Ctrl Pts',(-203.719618835359,-0.307710868205461,
125.893837719063));
#125707=CARTESIAN_POINT('Ctrl Pts',(-203.727379277873,-0.44403883788848,
125.906196413199));
#125708=CARTESIAN_POINT('Ctrl Pts',(-203.735152178139,-0.580585653331063,
125.918574946608));
#125709=CARTESIAN_POINT('Ctrl Pts',(-203.742925078404,-0.716469764941721,
125.936654452284));
#125710=CARTESIAN_POINT('Ctrl Pts',(-203.75069797867,-0.851187216928724,
125.960326824926));
#125711=CARTESIAN_POINT('Ctrl Pts',(-203.758188314432,-0.981007350205763,
125.983138647196));
#125712=CARTESIAN_POINT('Ctrl Pts',(-203.765678650194,-1.10974387227684,
126.011143701039));
#125713=CARTESIAN_POINT('Ctrl Pts',(-203.773168985956,-1.23696012770498,
126.044201722637));
#125714=CARTESIAN_POINT('Ctrl Pts',(-203.780943320075,-1.36899982612075,
126.078513149172));
#125715=CARTESIAN_POINT('Ctrl Pts',(-203.788717654194,-1.4998199624505,
126.118376962119));
#125716=CARTESIAN_POINT('Ctrl Pts',(-203.796491988313,-1.62891786006441,
126.163691520586));
#125717=CARTESIAN_POINT('Ctrl Pts',(-203.80425674126,-1.75785665605768,
126.20895023291));
#125718=CARTESIAN_POINT('Ctrl Pts',(-203.812021494207,-1.88507707112989,
126.259646196572));
#125719=CARTESIAN_POINT('Ctrl Pts',(-203.819786247154,-2.01008828274693,
126.315627148305));
#125720=CARTESIAN_POINT('Ctrl Pts',(-203.827543288039,-2.13497533146623,
126.371552498967));
#125721=CARTESIAN_POINT('Ctrl Pts',(-203.835300328924,-2.25765718879851,
126.432752232951));
#125722=CARTESIAN_POINT('Ctrl Pts',(-203.843057369809,-2.37766016698767,
126.499024952043));
#125723=CARTESIAN_POINT('Ctrl Pts',(-203.850808561049,-2.49757264999765,
126.565247694363));
#125724=CARTESIAN_POINT('Ctrl Pts',(-203.858559752289,-2.61480993401946,
126.63653561897));
#125725=CARTESIAN_POINT('Ctrl Pts',(-203.866310943529,-2.72892055700057,
126.712640239036));
#125726=CARTESIAN_POINT('Ctrl Pts',(-203.874058840306,-2.84298267992244,
126.788712512608));
#125727=CARTESIAN_POINT('Ctrl Pts',(-203.881806737083,-2.95392046033182,
126.869597193392));
#125728=CARTESIAN_POINT('Ctrl Pts',(-203.88955463386,-3.06130939039301,
126.955001206081));
#125729=CARTESIAN_POINT('Ctrl Pts',(-203.897300909944,-3.16867585700537,
127.040387354091));
#125730=CARTESIAN_POINT('Ctrl Pts',(-203.905047186028,-3.27249464402813,
127.130290710461));
#125731=CARTESIAN_POINT('Ctrl Pts',(-203.912793462112,-3.3723727818643,
127.224376695446));
#125732=CARTESIAN_POINT('Ctrl Pts',(-203.920539795377,-3.47225165697833,
127.318463374952));
#125733=CARTESIAN_POINT('Ctrl Pts',(-203.928286128643,-3.56818954027803,
127.416732476603));
#125734=CARTESIAN_POINT('Ctrl Pts',(-203.936032461908,-3.65982922170008,
127.518811480741));
#125735=CARTESIAN_POINT('Ctrl Pts',(-203.943780529911,-3.75148942519278,
127.620913344764));
#125736=CARTESIAN_POINT('Ctrl Pts',(-203.951528597914,-3.83884925031249,
127.726826518173));
#125737=CARTESIAN_POINT('Ctrl Pts',(-203.959276665916,-3.92159105512307,
127.836144544084));
#125738=CARTESIAN_POINT('Ctrl Pts',(-203.967032968658,-4.00442079890878,
127.945578754494));
#125739=CARTESIAN_POINT('Ctrl Pts',(-203.9747892714,-4.08262248162509,128.05842473395));
#125740=CARTESIAN_POINT('Ctrl Pts',(-203.982545574142,-4.15592088058601,
128.174245658708));
#125741=CARTESIAN_POINT('Ctrl Pts',(-203.990306016656,-4.22925840110944,
128.290128400581));
#125742=CARTESIAN_POINT('Ctrl Pts',(-203.99806645917,-4.29768722825386,
128.408988912957));
#125743=CARTESIAN_POINT('Ctrl Pts',(-204.005826901684,-4.36097810647042,
128.530365670917));
#125744=CARTESIAN_POINT('Ctrl Pts',(-204.013599801949,-4.42437058482357,
128.651937273624));
#125745=CARTESIAN_POINT('Ctrl Pts',(-204.021372702215,-4.48260846613932,
128.776032839594));
#125746=CARTESIAN_POINT('Ctrl Pts',(-204.02914560248,-4.53551030205551,
128.902169942989));
#125747=CARTESIAN_POINT('Ctrl Pts',(-204.036635938243,-4.58648902298876,
129.023721644965));
#125748=CARTESIAN_POINT('Ctrl Pts',(-204.044126274005,-4.63251281279301,
129.147168742662));
#125749=CARTESIAN_POINT('Ctrl Pts',(-204.051616609768,-4.67346365646167,
129.272068049473));
#125750=CARTESIAN_POINT('Ctrl Pts',(-204.057757115684,-4.70703476806217,
129.374459311585));
#125751=CARTESIAN_POINT('Ctrl Pts',(-204.0638976216,-4.73725521212647,129.477999992541));
#125752=CARTESIAN_POINT('Ctrl Pts',(-204.070038127516,-4.76405452823409,
129.582490119308));
#125753=CARTESIAN_POINT('Origin',(213.235140564004,0.,130.804360617566));
#125754=CARTESIAN_POINT('',(-206.164998470905,-4.76405452823394,129.582490119308));
#125755=CARTESIAN_POINT('',(-205.820054717884,-4.76405452823395,129.582490119308));
#125756=CARTESIAN_POINT('',(213.235140564004,-4.76405452823405,129.582490119308));
#125757=CARTESIAN_POINT('',(-204.485140564013,-4.91519744545431,130.807513129082));
#125758=CARTESIAN_POINT('Ctrl Pts',(-204.485140564013,-4.91824898839283,
130.807515086282));
#125759=CARTESIAN_POINT('Ctrl Pts',(-204.49387773296,-4.91814963363141,
130.962422774028));
#125760=CARTESIAN_POINT('Ctrl Pts',(-204.502614901907,-4.91072767197462,
131.117052050995));
#125761=CARTESIAN_POINT('Ctrl Pts',(-204.511352070854,-4.8960860736549,
131.27075553806));
#125762=CARTESIAN_POINT('Ctrl Pts',(-204.520123591854,-4.88138690875277,
131.425063343332));
#125763=CARTESIAN_POINT('Ctrl Pts',(-204.528895112854,-4.85941133515114,
131.578437879815));
#125764=CARTESIAN_POINT('Ctrl Pts',(-204.537666633853,-4.83031338638245,
131.73024163143));
#125765=CARTESIAN_POINT('Ctrl Pts',(-204.546486847053,-4.8010539099665,
131.882888071409));
#125766=CARTESIAN_POINT('Ctrl Pts',(-204.555307060253,-4.76459286084652,
132.033946055602));
#125767=CARTESIAN_POINT('Ctrl Pts',(-204.564127273453,-4.72113560423765,
132.182787862255));
#125768=CARTESIAN_POINT('Ctrl Pts',(-204.572392469381,-4.68041292189577,
132.322263707821));
#125769=CARTESIAN_POINT('Ctrl Pts',(-204.580657665308,-4.63354733828304,
132.459793589481));
#125770=CARTESIAN_POINT('Ctrl Pts',(-204.588922861235,-4.58074515708572,
132.594879220747));
#125771=CARTESIAN_POINT('Ctrl Pts',(-204.596697195354,-4.53107884518496,
132.721942250031));
#125772=CARTESIAN_POINT('Ctrl Pts',(-204.604471529473,-4.47604305081149,
132.847138467984));
#125773=CARTESIAN_POINT('Ctrl Pts',(-204.612245863592,-4.41579807394511,
132.969980721057));
#125774=CARTESIAN_POINT('Ctrl Pts',(-204.620010616539,-4.35562734362847,
133.092671582031));
#125775=CARTESIAN_POINT('Ctrl Pts',(-204.627775369486,-4.29026037490912,
133.213013902697));
#125776=CARTESIAN_POINT('Ctrl Pts',(-204.635540122433,-4.21990633574634,
133.330538279574));
#125777=CARTESIAN_POINT('Ctrl Pts',(-204.643297163318,-4.14962217320707,
133.447945929583));
#125778=CARTESIAN_POINT('Ctrl Pts',(-204.651054204203,-4.07436099688629,
133.562540872303));
#125779=CARTESIAN_POINT('Ctrl Pts',(-204.658811245088,-3.99437874200781,
133.673876522365));
#125780=CARTESIAN_POINT('Ctrl Pts',(-204.666562436328,-3.91445680236981,
133.785128213348));
#125781=CARTESIAN_POINT('Ctrl Pts',(-204.674313627568,-3.82982109772313,
133.89312518765));
#125782=CARTESIAN_POINT('Ctrl Pts',(-204.682064818808,-3.74077169726714,
133.997448491619));
#125783=CARTESIAN_POINT('Ctrl Pts',(-204.689812715585,-3.65176014518169,
134.101727455401));
#125784=CARTESIAN_POINT('Ctrl Pts',(-204.697560612362,-3.55833888168141,
134.202335557629));
#125785=CARTESIAN_POINT('Ctrl Pts',(-204.705308509139,-3.46084906882826,
134.298885876495));
#125786=CARTESIAN_POINT('Ctrl Pts',(-204.713054785223,-3.36337964874233,
134.395415999115));
#125787=CARTESIAN_POINT('Ctrl Pts',(-204.720801061307,-3.26184364970766,
134.487889751746));
#125788=CARTESIAN_POINT('Ctrl Pts',(-204.728547337392,-3.15661972277871,
134.575956432107));
#125789=CARTESIAN_POINT('Ctrl Pts',(-204.736293670657,-3.05139501911078,
134.664023762557));
#125790=CARTESIAN_POINT('Ctrl Pts',(-204.744040003922,-2.94248263304068,
134.747683704894));
#125791=CARTESIAN_POINT('Ctrl Pts',(-204.751786337187,-2.83029466646686,
134.826625547114));
#125792=CARTESIAN_POINT('Ctrl Pts',(-204.75953440519,-2.71808157617563,
134.905585067812));
#125793=CARTESIAN_POINT('Ctrl Pts',(-204.767282473193,-2.60259176539364,
134.979824160965));
#125794=CARTESIAN_POINT('Ctrl Pts',(-204.775030541196,-2.48426636236587,
135.04907541403));
#125795=CARTESIAN_POINT('Ctrl Pts',(-204.782786843938,-2.36581520169152,
135.11840026815));
#125796=CARTESIAN_POINT('Ctrl Pts',(-204.79054314668,-2.24452276654071,
135.182726494795));
#125797=CARTESIAN_POINT('Ctrl Pts',(-204.798299449421,-2.12085532938707,
135.241832390356));
#125798=CARTESIAN_POINT('Ctrl Pts',(-204.806059891935,-1.99712188719867,
135.300969832514));
#125799=CARTESIAN_POINT('Ctrl Pts',(-204.81382033445,-1.87101127650509,
135.354881238147));
#125800=CARTESIAN_POINT('Ctrl Pts',(-204.821580776964,-1.74300886894293,
135.403393466469));
#125801=CARTESIAN_POINT('Ctrl Pts',(-204.829353677229,-1.61480098055263,
135.451983570926));
#125802=CARTESIAN_POINT('Ctrl Pts',(-204.837126577494,-1.48469559792147,
135.495157054964));
#125803=CARTESIAN_POINT('Ctrl Pts',(-204.84489947776,-1.35319320086527,
135.532790718946));
#125804=CARTESIAN_POINT('Ctrl Pts',(-204.852389813522,-1.22647124717054,
135.569056304449));
#125805=CARTESIAN_POINT('Ctrl Pts',(-204.859880149284,-1.09845238493452,
135.600177777234));
#125806=CARTESIAN_POINT('Ctrl Pts',(-204.867370485047,-0.969590637356454,
135.626090292532));
#125807=CARTESIAN_POINT('Ctrl Pts',(-204.875144819166,-0.835843057454864,
135.652985288723));
#125808=CARTESIAN_POINT('Ctrl Pts',(-204.882919153285,-0.700763742363002,
135.674353730114));
#125809=CARTESIAN_POINT('Ctrl Pts',(-204.890693487405,-0.564849194214768,
135.690067163225));
#125810=CARTESIAN_POINT('Ctrl Pts',(-204.898458240352,-0.42910214860009,
135.705761230934));
#125811=CARTESIAN_POINT('Ctrl Pts',(-204.906222993299,-0.292522302678767,
135.715814112706));
#125812=CARTESIAN_POINT('Ctrl Pts',(-204.913987746246,-0.155617639284803,
135.720148063423));
#125813=CARTESIAN_POINT('Ctrl Pts',(-204.921744787131,-0.0188489515325352,
135.724477709599));
#125814=CARTESIAN_POINT('Ctrl Pts',(-204.929501828017,0.118243523436565,
135.723099716129));
#125815=CARTESIAN_POINT('Ctrl Pts',(-204.937258868902,0.255145721463766,
135.715988018267));
#125816=CARTESIAN_POINT('Ctrl Pts',(-204.945010060142,0.391944680478308,
135.708881683392));
#125817=CARTESIAN_POINT('Ctrl Pts',(-204.952761251382,0.528553259298798,
135.696050270647));
#125818=CARTESIAN_POINT('Ctrl Pts',(-204.960512442623,0.664456785619391,
135.677519782065));
#125819=CARTESIAN_POINT('Ctrl Pts',(-204.9682603394,0.80030254931577,135.658997169436));
#125820=CARTESIAN_POINT('Ctrl Pts',(-204.976008236177,0.935443469955528,
135.634780351368));
#125821=CARTESIAN_POINT('Ctrl Pts',(-204.983756132954,1.06936961283493,
135.604947216477));
#125822=CARTESIAN_POINT('Ctrl Pts',(-204.991502409038,1.20326774125236,
135.575120322035));
#125823=CARTESIAN_POINT('Ctrl Pts',(-204.999248685123,1.33595121596879,
135.53967953249));
#125824=CARTESIAN_POINT('Ctrl Pts',(-205.006994961207,1.46692031107978,
135.49875385455));
#125825=CARTESIAN_POINT('Ctrl Pts',(-205.014741294472,1.59789037297505,
135.457827874506));
#125826=CARTESIAN_POINT('Ctrl Pts',(-205.022487627738,1.72714565684219,
135.411417041884));
#125827=CARTESIAN_POINT('Ctrl Pts',(-205.030233961003,1.85420200073023,
135.359700122256));
#125828=CARTESIAN_POINT('Ctrl Pts',(-205.037982029006,1.98128679800571,
135.307971620982));
#125829=CARTESIAN_POINT('Ctrl Pts',(-205.04573009701,2.10617131336159,135.250934815567));
#125830=CARTESIAN_POINT('Ctrl Pts',(-205.053478165013,2.22839212445938,
135.188816296684));
#125831=CARTESIAN_POINT('Ctrl Pts',(-205.061234467755,2.35074283328949,
135.1266317575));
#125832=CARTESIAN_POINT('Ctrl Pts',(-205.068990770497,2.47042383351275,
135.059354893381));
#125833=CARTESIAN_POINT('Ctrl Pts',(-205.076747073239,2.58699656794278,
134.987258156348));
#125834=CARTESIAN_POINT('Ctrl Pts',(-205.084507515753,2.70363152075111,
134.915122939117));
#125835=CARTESIAN_POINT('Ctrl Pts',(-205.092267958267,2.81715457866475,
134.838162942302));
#125836=CARTESIAN_POINT('Ctrl Pts',(-205.100028400782,2.9271577182112,134.756692935985));
#125837=CARTESIAN_POINT('Ctrl Pts',(-205.107801301047,3.03733744456286,
134.67509214678));
#125838=CARTESIAN_POINT('Ctrl Pts',(-205.115574201313,3.1439856567345,134.588967126286));
#125839=CARTESIAN_POINT('Ctrl Pts',(-205.123347101578,3.24672818181712,
134.498672349932));
#125840=CARTESIAN_POINT('Ctrl Pts',(-205.130837437339,3.3457357573013,134.411660016153));
#125841=CARTESIAN_POINT('Ctrl Pts',(-205.1383277731,3.4411164558133,134.320776037914));
#125842=CARTESIAN_POINT('Ctrl Pts',(-205.145818108861,3.53257031098373,
134.226367347609));
#125843=CARTESIAN_POINT('Ctrl Pts',(-205.15359244298,3.62749166688566,134.128379123099));
#125844=CARTESIAN_POINT('Ctrl Pts',(-205.161366777099,3.71848321111434,
134.026283234194));
#125845=CARTESIAN_POINT('Ctrl Pts',(-205.169141111218,3.80516850058741,
133.920427969957));
#125846=CARTESIAN_POINT('Ctrl Pts',(-205.176905864165,3.89174695818848,
133.814703162873));
#125847=CARTESIAN_POINT('Ctrl Pts',(-205.184670617112,3.97402947520282,
133.705228498512));
#125848=CARTESIAN_POINT('Ctrl Pts',(-205.192435370059,4.05167606532983,
133.592389334085));
#125849=CARTESIAN_POINT('Ctrl Pts',(-205.200192410944,4.1292455357689,133.479662243106));
#125850=CARTESIAN_POINT('Ctrl Pts',(-205.207949451829,4.2021880222257,133.363577622127));
#125851=CARTESIAN_POINT('Ctrl Pts',(-205.215706492714,4.27020373145505,
133.24455387925));
#125852=CARTESIAN_POINT('Ctrl Pts',(-205.223457683954,4.33816814950907,
133.125619893103));
#125853=CARTESIAN_POINT('Ctrl Pts',(-205.231208875195,4.40121299226405,
133.003751534774));
#125854=CARTESIAN_POINT('Ctrl Pts',(-205.238960066435,4.45908194301358,
132.879395867385));
#125855=CARTESIAN_POINT('Ctrl Pts',(-205.246707963212,4.51692629791526,
132.755093054471));
#125856=CARTESIAN_POINT('Ctrl Pts',(-205.254455859989,4.56959897162442,
132.628305388855));
#125857=CARTESIAN_POINT('Ctrl Pts',(-205.262203756766,4.61688986187661,
132.499503993744));
#125858=CARTESIAN_POINT('Ctrl Pts',(-205.26995003285,4.66417085989403,132.370729541109));
#125859=CARTESIAN_POINT('Ctrl Pts',(-205.277696308934,4.70607217897284,
132.239942563603));
#125860=CARTESIAN_POINT('Ctrl Pts',(-205.285442585018,4.74243224205182,
132.107633226059));
#125861=CARTESIAN_POINT('Ctrl Pts',(-205.293188918284,4.77879257353258,
131.975322911837));
#125862=CARTESIAN_POINT('Ctrl Pts',(-205.300935251549,4.80961146379121,
131.841490592143));
#125863=CARTESIAN_POINT('Ctrl Pts',(-205.308681584814,4.83477761200457,
131.706640233295));
#125864=CARTESIAN_POINT('Ctrl Pts',(-205.316429652817,4.8599493960023,131.571759675644));
#125865=CARTESIAN_POINT('Ctrl Pts',(-205.32417772082,4.8794658472645,131.435861009436));
#125866=CARTESIAN_POINT('Ctrl Pts',(-205.331925788823,4.89326711184883,
131.299456602804));
#125867=CARTESIAN_POINT('Ctrl Pts',(-205.339682091565,4.90708304458142,
131.162907223945));
#125868=CARTESIAN_POINT('Ctrl Pts',(-205.347438394307,4.91517161741112,
131.025851420532));
#125869=CARTESIAN_POINT('Ctrl Pts',(-205.355194697049,4.91752500106838,
130.888805430121));
#125870=CARTESIAN_POINT('Ctrl Pts',(-205.362955139563,4.91987964079736,
130.751686294138));
#125871=CARTESIAN_POINT('Ctrl Pts',(-205.370715582077,4.91649300161557,
130.614577372247));
#125872=CARTESIAN_POINT('Ctrl Pts',(-205.378476024592,4.9074093618528,130.477992087068));
#125873=CARTESIAN_POINT('Ctrl Pts',(-205.386248924857,4.89831114022507,
130.341187543064));
#125874=CARTESIAN_POINT('Ctrl Pts',(-205.394021825122,4.88349768500393,
130.204908704434));
#125875=CARTESIAN_POINT('Ctrl Pts',(-205.401794725388,4.86306497681123,
130.069661976073));
#125876=CARTESIAN_POINT('Ctrl Pts',(-205.40928506115,4.84337504902889,129.939331806958));
#125877=CARTESIAN_POINT('Ctrl Pts',(-205.416775396912,4.81846738151463,
129.809960313757));
#125878=CARTESIAN_POINT('Ctrl Pts',(-205.424265732673,4.78847171916799,
129.681987392107));
#125879=CARTESIAN_POINT('Ctrl Pts',(-205.432040066792,4.75733876216599,
129.549162338233));
#125880=CARTESIAN_POINT('Ctrl Pts',(-205.439814400911,4.72062575157316,
129.417423253277));
#125881=CARTESIAN_POINT('Ctrl Pts',(-205.44758873503,4.67842223616104,129.287275108211));
#125882=CARTESIAN_POINT('Ctrl Pts',(-205.455353487977,4.63627073280972,
129.157287359103));
#125883=CARTESIAN_POINT('Ctrl Pts',(-205.463118240924,4.58864230750925,
129.028887017024));
#125884=CARTESIAN_POINT('Ctrl Pts',(-205.470882993871,4.53567740129338,
128.902568417062));
#125885=CARTESIAN_POINT('Ctrl Pts',(-205.478640034756,4.48276510056905,
128.776375278515));
#125886=CARTESIAN_POINT('Ctrl Pts',(-205.486397075641,4.4245270169024,128.652260125658));
#125887=CARTESIAN_POINT('Ctrl Pts',(-205.494154116526,4.36115312330836,
128.530701342838));
#125888=CARTESIAN_POINT('Ctrl Pts',(-205.501905307766,4.29782702046055,
128.409234228441));
#125889=CARTESIAN_POINT('Ctrl Pts',(-205.509656499006,4.22937299657398,
128.290319992233));
#125890=CARTESIAN_POINT('Ctrl Pts',(-205.517407690246,4.15602863307309,
128.174415929255));
#125891=CARTESIAN_POINT('Ctrl Pts',(-205.525155587023,4.08271544288332,
128.058561128595));
#125892=CARTESIAN_POINT('Ctrl Pts',(-205.5329034838,4.00451625573041,127.94571428621));
#125893=CARTESIAN_POINT('Ctrl Pts',(-205.540651380577,3.92171387550616,
127.836306820688));
#125894=CARTESIAN_POINT('Ctrl Pts',(-205.548397656661,3.83892881575483,
127.726922240849));
#125895=CARTESIAN_POINT('Ctrl Pts',(-205.556143932745,3.75154271395995,
127.62097591841));
#125896=CARTESIAN_POINT('Ctrl Pts',(-205.563890208829,3.65988062332928,
127.518868738794));
#125897=CARTESIAN_POINT('Ctrl Pts',(-205.571636542094,3.56821785606976,
127.416760805445));
#125898=CARTESIAN_POINT('Ctrl Pts',(-205.579382875359,3.47227929816279,
127.318492362404));
#125899=CARTESIAN_POINT('Ctrl Pts',(-205.587129208625,3.37242878993213,
127.224429456309));
#125900=CARTESIAN_POINT('Ctrl Pts',(-205.594877276628,3.27255592087287,
127.130345485479));
#125901=CARTESIAN_POINT('Ctrl Pts',(-205.60262534463,3.16876964276772,127.040469193703));
#125902=CARTESIAN_POINT('Ctrl Pts',(-205.610373412633,3.06146867291942,
126.955127885289));
#125903=CARTESIAN_POINT('Ctrl Pts',(-205.618129715375,2.95405366232302,
126.869695875116));
#125904=CARTESIAN_POINT('Ctrl Pts',(-205.625886018117,2.84311680448129,
126.788808720195));
#125905=CARTESIAN_POINT('Ctrl Pts',(-205.633642320859,2.72908819275771,
126.712752046521));
#125906=CARTESIAN_POINT('Ctrl Pts',(-205.641402763373,2.61499872053071,
126.63665477911));
#125907=CARTESIAN_POINT('Ctrl Pts',(-205.649163205887,2.4978145402187,126.565393333214));
#125908=CARTESIAN_POINT('Ctrl Pts',(-205.656923648401,2.37799154233177,
126.499207973687));
#125909=CARTESIAN_POINT('Ctrl Pts',(-205.664696548666,2.25797619393123,
126.432916367546));
#125910=CARTESIAN_POINT('Ctrl Pts',(-205.672469448932,2.13531391299143,
126.371717305886));
#125911=CARTESIAN_POINT('Ctrl Pts',(-205.680242349197,2.01048263216247,
126.315803761708));
#125912=CARTESIAN_POINT('Ctrl Pts',(-205.68773268496,1.89018928280237,126.261922815689));
#125913=CARTESIAN_POINT('Ctrl Pts',(-205.695223020723,1.76788217886368,
126.212949889631));
#125914=CARTESIAN_POINT('Ctrl Pts',(-205.702713356486,1.64400154729095,
126.169013599812));
#125915=CARTESIAN_POINT('Ctrl Pts',(-205.710487690606,1.5154239439371,126.123411452216));
#125916=CARTESIAN_POINT('Ctrl Pts',(-205.718262024725,1.38474384172379,
126.083090954468));
#125917=CARTESIAN_POINT('Ctrl Pts',(-205.726036358844,1.25243449033019,
126.048249715796));
#125918=CARTESIAN_POINT('Ctrl Pts',(-205.733801111791,1.12028819838735,
126.013451415837));
#125919=CARTESIAN_POINT('Ctrl Pts',(-205.741565864738,0.986517026841535,
125.984119037703));
#125920=CARTESIAN_POINT('Ctrl Pts',(-205.749330617686,0.85161278561181,
125.960401624564));
#125921=CARTESIAN_POINT('Ctrl Pts',(-205.757087658571,0.716842533176288,
125.936707767895));
#125922=CARTESIAN_POINT('Ctrl Pts',(-205.764844699456,0.5809418331833,125.918617845271));
#125923=CARTESIAN_POINT('Ctrl Pts',(-205.772601740341,0.444415848987914,
125.906230605442));
#125924=CARTESIAN_POINT('Ctrl Pts',(-205.780352931581,0.307992820099411,
125.893852706927));
#125925=CARTESIAN_POINT('Ctrl Pts',(-205.788104122822,0.170945833354071,
125.88716896663));
#125926=CARTESIAN_POINT('Ctrl Pts',(-205.795855314062,0.0337880425846281,
125.886226679711));
#125927=CARTESIAN_POINT('Ctrl Pts',(-205.803603210839,-0.103311452464748,
125.885284793289));
#125928=CARTESIAN_POINT('Ctrl Pts',(-205.811351107616,-0.240521267733049,
125.890079509413));
#125929=CARTESIAN_POINT('Ctrl Pts',(-205.819099004394,-0.377325576133052,
125.900606089442));
#125930=CARTESIAN_POINT('Ctrl Pts',(-205.826845280478,-0.514101268020897,
125.911130467538));
#125931=CARTESIAN_POINT('Ctrl Pts',(-205.834591556562,-0.650471232192675,
125.927384294722));
#125932=CARTESIAN_POINT('Ctrl Pts',(-205.842337832646,-0.785922493189801,
125.949310782889));
#125933=CARTESIAN_POINT('Ctrl Pts',(-205.850084165912,-0.921374754057551,
125.971237432912));
#125934=CARTESIAN_POINT('Ctrl Pts',(-205.857830499177,-1.05590791227709,
125.998836764999));
#125935=CARTESIAN_POINT('Ctrl Pts',(-205.865576832443,-1.18901733786065,
126.032000527132));
#125936=CARTESIAN_POINT('Ctrl Pts',(-205.873324900446,-1.32215657237697,
126.065171716059));
#125937=CARTESIAN_POINT('Ctrl Pts',(-205.881072968449,-1.45387106051707,
126.103909720158));
#125938=CARTESIAN_POINT('Ctrl Pts',(-205.888821036452,-1.58366991545586,
126.148056003241));
#125939=CARTESIAN_POINT('Ctrl Pts',(-205.896577339194,-1.71360672216248,
126.19224920552));
#125940=CARTESIAN_POINT('Ctrl Pts',(-205.904333641936,-1.8416234578902,
126.241862042909));
#125941=CARTESIAN_POINT('Ctrl Pts',(-205.912089944678,-1.96724734143226,
126.296687053506));
#125942=CARTESIAN_POINT('Ctrl Pts',(-205.919850387192,-2.09293827422343,
126.351541325862));
#125943=CARTESIAN_POINT('Ctrl Pts',(-205.927610829707,-2.21623345872856,
126.411613143427));
#125944=CARTESIAN_POINT('Ctrl Pts',(-205.935371272221,-2.33668433336452,
126.476648821627));
#125945=CARTESIAN_POINT('Ctrl Pts',(-205.943144172487,-2.45732856643756,
126.541788900871));
#125946=CARTESIAN_POINT('Ctrl Pts',(-205.950917072752,-2.57511902930189,
126.61190856411));
#125947=CARTESIAN_POINT('Ctrl Pts',(-205.958689973018,-2.68963503403625,
126.68671001969));
#125948=CARTESIAN_POINT('Ctrl Pts',(-205.966180308779,-2.79998809352685,
126.758792253932));
#125949=CARTESIAN_POINT('Ctrl Pts',(-205.973670644539,-2.90730038036246,
126.835221621603));
#125950=CARTESIAN_POINT('Ctrl Pts',(-205.9811609803,-3.0112257326097,126.915697267549));
#125951=CARTESIAN_POINT('Ctrl Pts',(-205.988843416406,-3.11781639876974,
126.998236826237));
#125952=CARTESIAN_POINT('Ctrl Pts',(-205.996525852513,-3.22119867281582,
127.085307874707));
#125953=CARTESIAN_POINT('Ctrl Pts',(-206.004208288619,-3.32095599792357,
127.1766293262));
#125954=CARTESIAN_POINT('Ctrl Pts',(-206.01188194727,-3.42059934675241,
127.267846439699));
#125955=CARTESIAN_POINT('Ctrl Pts',(-206.019555605921,-3.5166256876976,
127.363304034671));
#125956=CARTESIAN_POINT('Ctrl Pts',(-206.027229264572,-3.60864870074115,
127.462678762999));
#125957=CARTESIAN_POINT('Ctrl Pts',(-206.034895912193,-3.70058763704767,
127.561962697703));
#125958=CARTESIAN_POINT('Ctrl Pts',(-206.042562559813,-3.78853024788272,
127.665156357538));
#125959=CARTESIAN_POINT('Ctrl Pts',(-206.050229207433,-3.87212489877666,
127.771897620137));
#125960=CARTESIAN_POINT('Ctrl Pts',(-206.057890604246,-3.95566229656263,
127.878565776755));
#125961=CARTESIAN_POINT('Ctrl Pts',(-206.065552001059,-4.03485741114901,
127.988776389217));
#125962=CARTESIAN_POINT('Ctrl Pts',(-206.073213397872,-4.10939732791692,
128.102132525082));
#125963=CARTESIAN_POINT('Ctrl Pts',(-206.080872341447,-4.18391337642932,
128.215452363439));
#125964=CARTESIAN_POINT('Ctrl Pts',(-206.088531285021,-4.25377696648902,
128.331915391257));
#125965=CARTESIAN_POINT('Ctrl Pts',(-206.096190228596,-4.31871736387104,
128.451094080707));
#125966=CARTESIAN_POINT('Ctrl Pts',(-206.103847441602,-4.38364308771443,
128.570245841263));
#125967=CARTESIAN_POINT('Ctrl Pts',(-206.111504654608,-4.44364764309317,
128.692111689209));
#125968=CARTESIAN_POINT('Ctrl Pts',(-206.119161867614,-4.49850566380742,
128.816238424341));
#125969=CARTESIAN_POINT('Ctrl Pts',(-206.1268221242,-4.55338548942266,128.940414497221));
#125970=CARTESIAN_POINT('Ctrl Pts',(-206.134482380787,-4.60311452764392,
129.066852887145));
#125971=CARTESIAN_POINT('Ctrl Pts',(-206.142142637373,-4.64751508729958,
129.195079232654));
#125972=CARTESIAN_POINT('Ctrl Pts',(-206.14976124855,-4.69167426085744,
129.322608468546));
#125973=CARTESIAN_POINT('Ctrl Pts',(-206.157379859728,-4.73056267205465,
129.451905880375));
#125974=CARTESIAN_POINT('Ctrl Pts',(-206.164998470905,-4.76405452823394,
129.582490119308));
#125975=CARTESIAN_POINT('Ctrl Pts',(-204.415385129731,-4.7580624943176,
129.583982083009));
#125976=CARTESIAN_POINT('Ctrl Pts',(-204.438636941158,-4.85784969763347,
129.983485013898));
#125977=CARTESIAN_POINT('Ctrl Pts',(-204.461888752586,-4.90979750657223,
130.395767923279));
#125978=CARTESIAN_POINT('Ctrl Pts',(-204.485140564013,-4.91220180825584,
130.807511207739));
#125979=CARTESIAN_POINT('',(-204.139859435948,-4.91824831916273,130.80029447038));
#125980=CARTESIAN_POINT('Ctrl Pts',(-204.070038127516,-4.76405452823409,
129.582490119308));
#125981=CARTESIAN_POINT('Ctrl Pts',(-204.079301788646,-4.80448438634937,
129.740125522491));
#125982=CARTESIAN_POINT('Ctrl Pts',(-204.088565449776,-4.837125792116,129.899922785572));
#125983=CARTESIAN_POINT('Ctrl Pts',(-204.097829110906,-4.86177557562907,
130.061177386649));
#125984=CARTESIAN_POINT('Ctrl Pts',(-204.106997320508,-4.88617137106238,
130.220770441836));
#125985=CARTESIAN_POINT('Ctrl Pts',(-204.11616553011,-4.9027393278596,130.381790901728));
#125986=CARTESIAN_POINT('Ctrl Pts',(-204.125333739712,-4.91132906577983,
130.543535254293));
#125987=CARTESIAN_POINT('Ctrl Pts',(-204.130175638457,-4.91586546307692,
130.628955397563));
#125988=CARTESIAN_POINT('Ctrl Pts',(-204.135017537202,-4.91817745258136,
130.71457709991));
#125989=CARTESIAN_POINT('Ctrl Pts',(-204.139859435948,-4.91824831916273,
130.80029447038));
#125990=CARTESIAN_POINT('Ctrl Pts',(-204.139859435995,-4.91824831916343,
130.800294471219));
#125991=CARTESIAN_POINT('Ctrl Pts',(-204.147784635894,-4.91836431326766,
130.94059630973));
#125992=CARTESIAN_POINT('Ctrl Pts',(-204.155709835794,-4.91247201397862,
131.080987232013));
#125993=CARTESIAN_POINT('Ctrl Pts',(-204.163635035693,-4.900578301156,131.220912387145));
#125994=CARTESIAN_POINT('Ctrl Pts',(-204.171354581511,-4.88899322289429,
131.357206570228));
#125995=CARTESIAN_POINT('Ctrl Pts',(-204.179074127329,-4.87171440627009,
131.493058448163));
#125996=CARTESIAN_POINT('Ctrl Pts',(-204.186793673146,-4.84880093828704,
131.627957924122));
#125997=CARTESIAN_POINT('Ctrl Pts',(-204.194513059106,-4.8258879448005,
131.762854606557));
#125998=CARTESIAN_POINT('Ctrl Pts',(-204.202232445066,-4.79734059760185,
131.896798538118));
#125999=CARTESIAN_POINT('Ctrl Pts',(-204.209951831025,-4.76326941003805,
132.029288203138));
#126000=CARTESIAN_POINT('Ctrl Pts',(-204.217672755543,-4.72919143171145,
132.161804274807));
#126001=CARTESIAN_POINT('Ctrl Pts',(-204.225393680062,-4.68958752045796,
132.29286512203));
#126002=CARTESIAN_POINT('Ctrl Pts',(-204.23311460458,-4.6446184041067,132.421983238183));
#126003=CARTESIAN_POINT('Ctrl Pts',(-204.24119374033,-4.59756295178294,
132.55709177159));
#126004=CARTESIAN_POINT('Ctrl Pts',(-204.24927287608,-4.54463267751754,
132.69007253139));
#126005=CARTESIAN_POINT('Ctrl Pts',(-204.25735201183,-4.48606813212016,
132.820390323814));
#126006=CARTESIAN_POINT('Ctrl Pts',(-204.265085528802,-4.43000892977471,
132.945133228333));
#126007=CARTESIAN_POINT('Ctrl Pts',(-204.272819045774,-4.36878776769414,
133.067435961724));
#126008=CARTESIAN_POINT('Ctrl Pts',(-204.280552562746,-4.30266231755848,
133.186855117783));
#126009=CARTESIAN_POINT('Ctrl Pts',(-204.288291669847,-4.23648906901836,
133.306360595297));
#126010=CARTESIAN_POINT('Ctrl Pts',(-204.296030776948,-4.16540467691822,
133.422978009958));
#126011=CARTESIAN_POINT('Ctrl Pts',(-204.303769884048,-4.08970977527734,
133.53629345285));
#126012=CARTESIAN_POINT('Ctrl Pts',(-204.311519964139,-4.01390754867324,
133.649769561459));
#126013=CARTESIAN_POINT('Ctrl Pts',(-204.319270044229,-3.93348199885383,
133.759934040129));
#126014=CARTESIAN_POINT('Ctrl Pts',(-204.32702012432,-3.84877374515481,
133.866406293435));
#126015=CARTESIAN_POINT('Ctrl Pts',(-204.328034827407,-3.83768305634567,
133.880346500872));
#126016=CARTESIAN_POINT('Ctrl Pts',(-204.329049530494,-3.82651900354742,
133.894223468265));
#126017=CARTESIAN_POINT('Ctrl Pts',(-204.330064233581,-3.81528239632779,
133.908036389739));
#126018=CARTESIAN_POINT('Ctrl Pts',(-204.3378385677,-3.72919106576708,134.013866625264));
#126019=CARTESIAN_POINT('Ctrl Pts',(-204.345612901819,-3.63855667661419,
134.116279706243));
#126020=CARTESIAN_POINT('Ctrl Pts',(-204.353387235938,-3.54368061892281,
134.21486068846));
#126021=CARTESIAN_POINT('Ctrl Pts',(-204.361151988886,-3.44892148749296,
134.313320178428));
#126022=CARTESIAN_POINT('Ctrl Pts',(-204.368916741833,-3.3499313571539,
134.407956687445));
#126023=CARTESIAN_POINT('Ctrl Pts',(-204.37668149478,-3.24705273251776,
134.498387094833));
#126024=CARTESIAN_POINT('Ctrl Pts',(-204.384438535665,-3.14427628838194,
134.588727685466));
#126025=CARTESIAN_POINT('Ctrl Pts',(-204.39219557655,-3.03761932746507,
134.674870231555));
#126026=CARTESIAN_POINT('Ctrl Pts',(-204.399952617435,-2.92746192108998,
134.756467620554));
#126027=CARTESIAN_POINT('Ctrl Pts',(-204.407703808675,-2.81738758527178,
134.838003476328));
#126028=CARTESIAN_POINT('Ctrl Pts',(-204.415454999916,-2.70381837107695,
134.915000765548));
#126029=CARTESIAN_POINT('Ctrl Pts',(-204.423206191156,-2.58716793923965,
134.987152163492));
#126030=CARTESIAN_POINT('Ctrl Pts',(-204.430954087933,-2.47056708694779,
135.059272895167));
#126031=CARTESIAN_POINT('Ctrl Pts',(-204.43870198471,-2.35088795351289,
135.126551626789));
#126032=CARTESIAN_POINT('Ctrl Pts',(-204.446449881487,-2.22857354968108,
135.188724082901));
#126033=CARTESIAN_POINT('Ctrl Pts',(-204.454196157571,-2.1062847313861,
135.250883533874));
#126034=CARTESIAN_POINT('Ctrl Pts',(-204.461942433656,-1.98136208744859,
135.307938656849));
#126035=CARTESIAN_POINT('Ctrl Pts',(-204.46968870974,-1.85427326821161,
135.359671112943));
#126036=CARTESIAN_POINT('Ctrl Pts',(-204.477435043005,-1.72718351083332,
135.411403950916));
#126037=CARTESIAN_POINT('Ctrl Pts',(-204.485181376271,-1.59792790836239,
135.457813896205));
#126038=CARTESIAN_POINT('Ctrl Pts',(-204.492927709536,-1.46699375409005,
135.498730904192));
#126039=CARTESIAN_POINT('Ctrl Pts',(-204.500675777539,-1.33603027802187,
135.53965707526));
#126040=CARTESIAN_POINT('Ctrl Pts',(-204.508423845542,-1.20338787525171,
135.575087744666));
#126041=CARTESIAN_POINT('Ctrl Pts',(-204.516171913545,-1.06956825840305,
135.604902962251));
#126042=CARTESIAN_POINT('Ctrl Pts',(-204.523928216287,-0.935606416472946,
135.634749867804));
#126043=CARTESIAN_POINT('Ctrl Pts',(-204.531684519029,-0.800465243359993,
135.658969314318));
#126044=CARTESIAN_POINT('Ctrl Pts',(-204.539440821771,-0.664656438594865,
135.677492555153));
#126045=CARTESIAN_POINT('Ctrl Pts',(-204.547201264285,-0.528775148581879,
135.696025682401));
#126046=CARTESIAN_POINT('Ctrl Pts',(-204.5549617068,-0.392225905948943,
135.708856509484));
#126047=CARTESIAN_POINT('Ctrl Pts',(-204.562722149314,-0.255523769358385,
135.715968365116));
#126048=CARTESIAN_POINT('Ctrl Pts',(-204.570495049579,-0.118602186361955,
135.72309163733));
#126049=CARTESIAN_POINT('Ctrl Pts',(-204.578267949845,0.0184723898871198,
135.724477588372));
#126050=CARTESIAN_POINT('Ctrl Pts',(-204.58604085011,0.155185762840657,
135.720161716218));
#126051=CARTESIAN_POINT('Ctrl Pts',(-204.593531185872,0.286929260314916,
135.716002736889));
#126052=CARTESIAN_POINT('Ctrl Pts',(-204.601021521633,0.418337052633677,
135.70654931052));
#126053=CARTESIAN_POINT('Ctrl Pts',(-204.608511857394,0.548956999130425,
135.691878318363));
#126054=CARTESIAN_POINT('Ctrl Pts',(-204.616286191514,0.684529440611316,
135.676651071078));
#126055=CARTESIAN_POINT('Ctrl Pts',(-204.624060525633,0.819682567332442,
135.655754564432));
#126056=CARTESIAN_POINT('Ctrl Pts',(-204.631834859752,0.953904366288411,
135.62921807893));
#126057=CARTESIAN_POINT('Ctrl Pts',(-204.639599612699,1.08796074887291,
135.602714297274));
#126058=CARTESIAN_POINT('Ctrl Pts',(-204.647364365646,1.22108770756962,
135.570584441822));
#126059=CARTESIAN_POINT('Ctrl Pts',(-204.655129118593,1.35277777999265,
135.532909585321));
#126060=CARTESIAN_POINT('Ctrl Pts',(-204.662886159478,1.48433705597924,
135.495272148018));
#126061=CARTESIAN_POINT('Ctrl Pts',(-204.670643200363,1.6144619123036,135.452100776427));
#126062=CARTESIAN_POINT('Ctrl Pts',(-204.678400241248,1.74265487551586,
135.403527612506));
#126063=CARTESIAN_POINT('Ctrl Pts',(-204.686151432488,1.8707511674172,135.354991077985));
#126064=CARTESIAN_POINT('Ctrl Pts',(-204.693902623728,1.99691810186812,
135.301060997223));
#126065=CARTESIAN_POINT('Ctrl Pts',(-204.701653814969,2.12067352414457,
135.241919278191));
#126066=CARTESIAN_POINT('Ctrl Pts',(-204.709401711746,2.24437634706579,
135.182802695968));
#126067=CARTESIAN_POINT('Ctrl Pts',(-204.717149608523,2.36566934435866,
135.118479049337));
#126068=CARTESIAN_POINT('Ctrl Pts',(-204.7248975053,2.48409071546674,135.049178208445));
#126069=CARTESIAN_POINT('Ctrl Pts',(-204.732643781384,2.60248731537686,
134.979891863794));
#126070=CARTESIAN_POINT('Ctrl Pts',(-204.740390057468,2.71801314667377,
134.905630593073));
#126071=CARTESIAN_POINT('Ctrl Pts',(-204.748136333552,2.83023173824012,
134.826669826262));
#126072=CARTESIAN_POINT('Ctrl Pts',(-204.755882666818,2.94245115817848,
134.74770847658));
#126073=CARTESIAN_POINT('Ctrl Pts',(-204.763629000083,3.05136296992693,
134.664047786568));
#126074=CARTESIAN_POINT('Ctrl Pts',(-204.771375333349,3.15656071620505,
134.576005816602));
#126075=CARTESIAN_POINT('Ctrl Pts',(-204.779123401352,3.26178202078891,
134.487944130248));
#126076=CARTESIAN_POINT('Ctrl Pts',(-204.786871469354,3.36328730507665,
134.395499462426));
#126077=CARTESIAN_POINT('Ctrl Pts',(-204.794619537357,3.46070446367402,
134.299029082186));
#126078=CARTESIAN_POINT('Ctrl Pts',(-204.802375840099,3.55822515838696,
134.202456172077));
#126079=CARTESIAN_POINT('Ctrl Pts',(-204.810132142841,3.65164876974275,
134.101849278174));
#126080=CARTESIAN_POINT('Ctrl Pts',(-204.817888445583,3.74064087315327,
133.997601748548));
#126081=CARTESIAN_POINT('Ctrl Pts',(-204.825648888097,3.82968047432912,
133.893298578876));
#126082=CARTESIAN_POINT('Ctrl Pts',(-204.833409330612,3.91428361358645,
133.785351209223));
#126083=CARTESIAN_POINT('Ctrl Pts',(-204.841169773126,3.99415786311061,
133.67418396179));
#126084=CARTESIAN_POINT('Ctrl Pts',(-204.848942673391,4.07416033387079,
133.562838258822));
#126085=CARTESIAN_POINT('Ctrl Pts',(-204.856715573657,4.14941853042956,
133.448262676063));
#126086=CARTESIAN_POINT('Ctrl Pts',(-204.864488473922,4.21968438244643,
133.330909009154));
#126087=CARTESIAN_POINT('Ctrl Pts',(-204.871978809684,4.28739589375082,
133.217821443638));
#126088=CARTESIAN_POINT('Ctrl Pts',(-204.879469145446,4.35047157997676,
133.102154538428));
#126089=CARTESIAN_POINT('Ctrl Pts',(-204.886959481207,4.40873173042483,
132.984330248466));
#126090=CARTESIAN_POINT('Ctrl Pts',(-204.894733815326,4.4692008321869,132.862038614734));
#126091=CARTESIAN_POINT('Ctrl Pts',(-204.902508149446,4.52467357561692,
132.737035389221));
#126092=CARTESIAN_POINT('Ctrl Pts',(-204.910282483565,4.57489783969652,
132.609767169797));
#126093=CARTESIAN_POINT('Ctrl Pts',(-204.918047236512,4.62506020685945,
132.48265579708));
#126094=CARTESIAN_POINT('Ctrl Pts',(-204.925811989459,4.66998682248568,
132.35328534469));
#126095=CARTESIAN_POINT('Ctrl Pts',(-204.933576742406,4.70947159955726,
132.222126576906));
#126096=CARTESIAN_POINT('Ctrl Pts',(-204.941333783291,4.74891715979151,
132.091098077859));
#126097=CARTESIAN_POINT('Ctrl Pts',(-204.949090824176,4.78293152551465,
131.958285170043));
#126098=CARTESIAN_POINT('Ctrl Pts',(-204.956847865061,4.81135697494726,
131.824177817914));
#126099=CARTESIAN_POINT('Ctrl Pts',(-204.964599056301,4.8397609885273,131.690171597184));
#126100=CARTESIAN_POINT('Ctrl Pts',(-204.972350247541,4.86258439407255,
131.55487325603));
#126101=CARTESIAN_POINT('Ctrl Pts',(-204.980101438781,4.87971961950594,
131.418786770581));
#126102=CARTESIAN_POINT('Ctrl Pts',(-204.987849335558,4.89684756201144,
131.282758125518));
#126103=CARTESIAN_POINT('Ctrl Pts',(-204.995597232335,4.90829208414323,
131.145942389504));
#126104=CARTESIAN_POINT('Ctrl Pts',(-205.003345129112,4.91399696768572,
131.008852338855));
#126105=CARTESIAN_POINT('Ctrl Pts',(-205.011091405196,4.91970065788955,
130.871790964489));
#126106=CARTESIAN_POINT('Ctrl Pts',(-205.01883768128,4.91966708133521,130.734455780001));
#126107=CARTESIAN_POINT('Ctrl Pts',(-205.026583957365,4.91389204176511,
130.597362877536));
#126108=CARTESIAN_POINT('Ctrl Pts',(-205.03433029063,4.90811695956499,130.460268963083));
#126109=CARTESIAN_POINT('Ctrl Pts',(-205.042076623895,4.89660034623337,
130.323417724839));
#126110=CARTESIAN_POINT('Ctrl Pts',(-205.04982295716,4.87939009488483,130.18732304623));
#126111=CARTESIAN_POINT('Ctrl Pts',(-205.057571025163,4.86217598941975,
130.051197890161));
#126112=CARTESIAN_POINT('Ctrl Pts',(-205.065319093166,4.83926575777492,
129.915830018667));
#126113=CARTESIAN_POINT('Ctrl Pts',(-205.073067161169,4.81075884846427,
129.781725607202));
#126114=CARTESIAN_POINT('Ctrl Pts',(-205.080823463911,4.78222164167122,
129.647478667972));
#126115=CARTESIAN_POINT('Ctrl Pts',(-205.088579766653,4.74807595643261,
129.514498254231));
#126116=CARTESIAN_POINT('Ctrl Pts',(-205.096336069395,4.70847196296183,
129.383278341094));
#126117=CARTESIAN_POINT('Ctrl Pts',(-205.104096511909,4.66884683164728,
129.251988391939));
#126118=CARTESIAN_POINT('Ctrl Pts',(-205.111856954423,4.62375771564571,
129.122461184739));
#126119=CARTESIAN_POINT('Ctrl Pts',(-205.119617396937,4.5734035448659,128.99517210381));
#126120=CARTESIAN_POINT('Ctrl Pts',(-205.127390297203,4.52296854110091,
128.867678687148));
#126121=CARTESIAN_POINT('Ctrl Pts',(-205.135163197468,4.46725175190091,
128.742430933815));
#126122=CARTESIAN_POINT('Ctrl Pts',(-205.142936097734,4.40649919765708,
128.619881758994));
#126123=CARTESIAN_POINT('Ctrl Pts',(-205.150426433496,4.34795515178448,
128.501787555357));
#126124=CARTESIAN_POINT('Ctrl Pts',(-205.157916769258,4.28473525768429,
128.386199406543));
#126125=CARTESIAN_POINT('Ctrl Pts',(-205.16540710502,4.21709737997774,128.273496585208));
#126126=CARTESIAN_POINT('Ctrl Pts',(-205.17318143914,4.14689499158213,128.15652060215));
#126127=CARTESIAN_POINT('Ctrl Pts',(-205.180955773259,4.0717106105036,128.042282515269));
#126128=CARTESIAN_POINT('Ctrl Pts',(-205.188730107378,3.9917836946099,127.931235838176));
#126129=CARTESIAN_POINT('Ctrl Pts',(-205.196494860325,3.91195528149677,
127.820326016188));
#126130=CARTESIAN_POINT('Ctrl Pts',(-205.204259613272,3.82739618907955,
127.712600092508));
#126131=CARTESIAN_POINT('Ctrl Pts',(-205.212024366219,3.73839108960982,
127.608485913572));
#126132=CARTESIAN_POINT('Ctrl Pts',(-205.219781407104,3.64947439125963,
127.504475142307));
#126133=CARTESIAN_POINT('Ctrl Pts',(-205.227538447989,3.55612072597651,
127.404069272277));
#126134=CARTESIAN_POINT('Ctrl Pts',(-205.235295488874,3.45865706226162,
127.307665837039));
#126135=CARTESIAN_POINT('Ctrl Pts',(-205.243046680114,3.36126689665303,
127.21133510038));
#126136=CARTESIAN_POINT('Ctrl Pts',(-205.250797871354,3.2597731785813,127.119001064663));
#126137=CARTESIAN_POINT('Ctrl Pts',(-205.258549062594,3.15454177209991,
127.031026644728));
#126138=CARTESIAN_POINT('Ctrl Pts',(-205.266296959371,3.04935509177414,
126.943089616268));
#126139=CARTESIAN_POINT('Ctrl Pts',(-205.274044856149,2.94043418200212,
126.859508768447));
#126140=CARTESIAN_POINT('Ctrl Pts',(-205.281792752926,2.82818006870287,
126.780608567366));
#126141=CARTESIAN_POINT('Ctrl Pts',(-205.28953902901,2.71594943654389,126.701724870505));
#126142=CARTESIAN_POINT('Ctrl Pts',(-205.297285305094,2.60038730735141,
126.627520097597));
#126143=CARTESIAN_POINT('Ctrl Pts',(-205.305031581178,2.48192561588327,
126.558276739482));
#126144=CARTESIAN_POINT('Ctrl Pts',(-205.312777914443,2.36346304995832,
126.489032870229));
#126145=CARTESIAN_POINT('Ctrl Pts',(-205.320524247709,2.24210121658067,
126.424750686145));
#126146=CARTESIAN_POINT('Ctrl Pts',(-205.328270580974,2.11829834782731,
126.365667659938));
#126147=CARTESIAN_POINT('Ctrl Pts',(-205.336018648977,1.99446775428004,
126.306571402498));
#126148=CARTESIAN_POINT('Ctrl Pts',(-205.34376671698,1.86819539035735,126.252676788146));
#126149=CARTESIAN_POINT('Ctrl Pts',(-205.351514784983,1.73996087015536,
126.204173748228));
#126150=CARTESIAN_POINT('Ctrl Pts',(-205.359271087725,1.61159006077877,
126.155619158702));
#126151=CARTESIAN_POINT('Ctrl Pts',(-205.367027390467,1.48125329557024,
126.112467728895));
#126152=CARTESIAN_POINT('Ctrl Pts',(-205.374783693208,1.34944734045477,
126.07486012197));
#126153=CARTESIAN_POINT('Ctrl Pts',(-205.382544135723,1.21757103653245,
126.037232442734));
#126154=CARTESIAN_POINT('Ctrl Pts',(-205.390304578237,1.0842243601514,126.005154573647));
#126155=CARTESIAN_POINT('Ctrl Pts',(-205.398065020751,0.94991479207595,
125.978716106177));
#126156=CARTESIAN_POINT('Ctrl Pts',(-205.405837921016,0.815389618358384,
125.952235197333));
#126157=CARTESIAN_POINT('Ctrl Pts',(-205.413610821282,0.679898850757354,
125.931411840046));
#126158=CARTESIAN_POINT('Ctrl Pts',(-205.421383721547,0.543956519674996,
125.916283862113));
#126159=CARTESIAN_POINT('Ctrl Pts',(-205.428874057309,0.412956034745918,
125.901705824283));
#126160=CARTESIAN_POINT('Ctrl Pts',(-205.436364393071,0.281536554534047,
125.892416293839));
#126161=CARTESIAN_POINT('Ctrl Pts',(-205.443854728833,0.150156553991709,
125.888403328106));
#126162=CARTESIAN_POINT('Ctrl Pts',(-205.451629062952,0.0137952407976317,
125.884238209558));
#126163=CARTESIAN_POINT('Ctrl Pts',(-205.459403397071,-0.122955491538462,
125.885744482312));
#126164=CARTESIAN_POINT('Ctrl Pts',(-205.46717773119,-0.259584656345014,
125.892965818867));
#126165=CARTESIAN_POINT('Ctrl Pts',(-205.474942484137,-0.396045437916839,
125.900178255769));
#126166=CARTESIAN_POINT('Ctrl Pts',(-205.482707237084,-0.532384563386209,
125.913091721957));
#126167=CARTESIAN_POINT('Ctrl Pts',(-205.490471990031,-0.668088201124236,
125.931697976051));
#126168=CARTESIAN_POINT('Ctrl Pts',(-205.498229030916,-0.803657056095805,
125.950285750151));
#126169=CARTESIAN_POINT('Ctrl Pts',(-205.505986071801,-0.938591294568638,
125.974555007365));
#126170=CARTESIAN_POINT('Ctrl Pts',(-205.513743112686,-1.07237972584027,
126.004445536431));
#126171=CARTESIAN_POINT('Ctrl Pts',(-205.521494303926,-1.20606726621606,
126.034313524817));
#126172=CARTESIAN_POINT('Ctrl Pts',(-205.529245495166,-1.33861033923932,
126.069794262592));
#126173=CARTESIAN_POINT('Ctrl Pts',(-205.536996686406,-1.4695058559177,
126.110776102302));
#126174=CARTESIAN_POINT('Ctrl Pts',(-205.544744583183,-1.60034573850956,
126.151740523638));
#126175=CARTESIAN_POINT('Ctrl Pts',(-205.55249247996,-1.72953908518632,
126.198201280005));
#126176=CARTESIAN_POINT('Ctrl Pts',(-205.560240376737,-1.85659614912279,
126.249996358796));
#126177=CARTESIAN_POINT('Ctrl Pts',(-205.567986652821,-1.98362663546017,
126.301780603172));
#126178=CARTESIAN_POINT('Ctrl Pts',(-205.575732928906,-2.10852136608529,
126.358896803041));
#126179=CARTESIAN_POINT('Ctrl Pts',(-205.58347920499,-2.23080920216611,
126.421134252657));
#126180=CARTESIAN_POINT('Ctrl Pts',(-205.591225538255,-2.35309794094813,
126.483372161696));
#126181=CARTESIAN_POINT('Ctrl Pts',(-205.59897187152,-2.47277939835213,
126.550731218584));
#126182=CARTESIAN_POINT('Ctrl Pts',(-205.606718204785,-2.58940609623158,
126.622954259497));
#126183=CARTESIAN_POINT('Ctrl Pts',(-205.614466272788,-2.70605891185186,
126.69519347426));
#126184=CARTESIAN_POINT('Ctrl Pts',(-205.622214340791,-2.81965527435539,
126.77229863474));
#126185=CARTESIAN_POINT('Ctrl Pts',(-205.629962408794,-2.92977614598774,
126.853968890547));
#126186=CARTESIAN_POINT('Ctrl Pts',(-205.637718711536,-3.04001405539247,
126.935725946473));
#126187=CARTESIAN_POINT('Ctrl Pts',(-205.645475014278,-3.14676878064829,
127.022057556528));
#126188=CARTESIAN_POINT('Ctrl Pts',(-205.65323131702,-3.24965346373534,
127.112621809344));
#126189=CARTESIAN_POINT('Ctrl Pts',(-205.660991759534,-3.35259305947554,
127.203234399029));
#126190=CARTESIAN_POINT('Ctrl Pts',(-205.668752202048,-3.45165821498836,
127.298083862653));
#126191=CARTESIAN_POINT('Ctrl Pts',(-205.676512644562,-3.54649924868453,
127.396791668655));
#126192=CARTESIAN_POINT('Ctrl Pts',(-205.684285544827,-3.64149252962784,
127.495657929191));
#126193=CARTESIAN_POINT('Ctrl Pts',(-205.692058445093,-3.73224787929608,
127.598394616017));
#126194=CARTESIAN_POINT('Ctrl Pts',(-205.699831345358,-3.81845562610398,
127.704589707648));
#126195=CARTESIAN_POINT('Ctrl Pts',(-205.707321681121,-3.90152950417868,
127.806924340218));
#126196=CARTESIAN_POINT('Ctrl Pts',(-205.714812016883,-3.98038048839516,
127.912470052807));
#126197=CARTESIAN_POINT('Ctrl Pts',(-205.722302352646,-4.05477080955335,
128.020834662146));
#126198=CARTESIAN_POINT('Ctrl Pts',(-205.730448383082,-4.13567316687673,
128.138685374571));
#126199=CARTESIAN_POINT('Ctrl Pts',(-205.738594413519,-4.21155944536966,
128.260249366182));
#126200=CARTESIAN_POINT('Ctrl Pts',(-205.746740443956,-4.28207823747369,
128.385065465946));
#126201=CARTESIAN_POINT('Ctrl Pts',(-205.754614573043,-4.35024322610434,
128.505715405734));
#126202=CARTESIAN_POINT('Ctrl Pts',(-205.76248870213,-4.41339304358188,
128.629403491818));
#126203=CARTESIAN_POINT('Ctrl Pts',(-205.770362831217,-4.47125192901984,
128.755680737805));
#126204=CARTESIAN_POINT('Ctrl Pts',(-205.778228904709,-4.52905162216871,
128.881828796388));
#126205=CARTESIAN_POINT('Ctrl Pts',(-205.786094978202,-4.58157099847426,
129.010560404246));
#126206=CARTESIAN_POINT('Ctrl Pts',(-205.793961051694,-4.62857939142672,
129.141400642173));
#126207=CARTESIAN_POINT('Ctrl Pts',(-205.801819026306,-4.67553938470417,
129.272106167454));
#126208=CARTESIAN_POINT('Ctrl Pts',(-205.809677000917,-4.7169995704176,
129.404915645517));
#126209=CARTESIAN_POINT('Ctrl Pts',(-205.817534975528,-4.75277695961418,
129.539333252383));
#126210=CARTESIAN_POINT('Ctrl Pts',(-205.818374889647,-4.75660109188932,
129.553700726375));
#126211=CARTESIAN_POINT('Ctrl Pts',(-205.819214803765,-4.76036034493871,
129.568086554707));
#126212=CARTESIAN_POINT('Ctrl Pts',(-205.820054717884,-4.76405452823395,
129.582490119308));
#126213=CARTESIAN_POINT('Origin',(213.235140564004,0.,130.804360617566));
#126214=CARTESIAN_POINT('',(-207.915133748109,-4.76405452823406,129.582490119308));
#126215=CARTESIAN_POINT('',(-207.569721641055,-4.76405452823393,129.582490119308));
#126216=CARTESIAN_POINT('',(213.235140564004,-4.76405452823405,129.582490119308));
#126217=CARTESIAN_POINT('',(-206.235140563976,-4.91824935292959,130.806883494435));
#126218=CARTESIAN_POINT('Ctrl Pts',(-206.235140564013,-4.91824935292925,
130.806883495092));
#126219=CARTESIAN_POINT('Ctrl Pts',(-206.243296577379,-4.91817584971133,
130.950175093808));
#126220=CARTESIAN_POINT('Ctrl Pts',(-206.251452590746,-4.9118408081057,
131.09330184757));
#126221=CARTESIAN_POINT('Ctrl Pts',(-206.259608604113,-4.89928367079141,
131.235872582194));
#126222=CARTESIAN_POINT('Ctrl Pts',(-206.267382938232,-4.88731417335877,
131.371771394107));
#126223=CARTESIAN_POINT('Ctrl Pts',(-206.275157272351,-4.86966698677397,
131.507387058606));
#126224=CARTESIAN_POINT('Ctrl Pts',(-206.28293160647,-4.846359096209,131.64220700748));
#126225=CARTESIAN_POINT('Ctrl Pts',(-206.290696359417,-4.82307993053606,
131.776860802817));
#126226=CARTESIAN_POINT('Ctrl Pts',(-206.298461112364,-4.79415400762733,
131.910720452176));
#126227=CARTESIAN_POINT('Ctrl Pts',(-206.306225865311,-4.75965019918353,
132.043276693784));
#126228=CARTESIAN_POINT('Ctrl Pts',(-206.313982906196,-4.72518066040869,
132.175701278665));
#126229=CARTESIAN_POINT('Ctrl Pts',(-206.321739947081,-4.68514435886508,
132.306824656126));
#126230=CARTESIAN_POINT('Ctrl Pts',(-206.329496987965,-4.63966146046592,
132.436146324933));
#126231=CARTESIAN_POINT('Ctrl Pts',(-206.337248179205,-4.59421286107431,
132.565370471264));
#126232=CARTESIAN_POINT('Ctrl Pts',(-206.344999370445,-4.5433259693909,
132.69279524599));
#126233=CARTESIAN_POINT('Ctrl Pts',(-206.352750561685,-4.48717107061851,
132.817934267946));
#126234=CARTESIAN_POINT('Ctrl Pts',(-206.360498458462,-4.43104003917615,
132.943020102479));
#126235=CARTESIAN_POINT('Ctrl Pts',(-206.368246355239,-4.36964561366111,
133.065821760543));
#126236=CARTESIAN_POINT('Ctrl Pts',(-206.375994252016,-4.30320651608381,
133.185872058318));
#126237=CARTESIAN_POINT('Ctrl Pts',(-206.3837405281,-4.23678131613346,133.305897244159));
#126238=CARTESIAN_POINT('Ctrl Pts',(-206.391486804184,-4.16531373223735,
133.423171872606));
#126239=CARTESIAN_POINT('Ctrl Pts',(-206.399233080268,-4.08906864095504,
133.537252988674));
#126240=CARTESIAN_POINT('Ctrl Pts',(-206.406979413534,-4.01282298684869,
133.651334946862));
#126241=CARTESIAN_POINT('Ctrl Pts',(-206.414725746799,-3.93179997222957,
133.762223020581));
#126242=CARTESIAN_POINT('Ctrl Pts',(-206.422472080064,-3.84630781202687,
133.869503237028));
#126243=CARTESIAN_POINT('Ctrl Pts',(-206.430220148067,-3.76079650644777,
133.976807478135));
#126244=CARTESIAN_POINT('Ctrl Pts',(-206.43796821607,-3.67081430735097,
134.080501948538));
#126245=CARTESIAN_POINT('Ctrl Pts',(-206.445716284073,-3.5767094513966,
134.180206076527));
#126246=CARTESIAN_POINT('Ctrl Pts',(-206.453472586815,-3.48250457968159,
134.280016171251));
#126247=CARTESIAN_POINT('Ctrl Pts',(-206.461228889557,-3.38416856715666,
134.375827166964));
#126248=CARTESIAN_POINT('Ctrl Pts',(-206.468985192298,-3.28208662334993,
134.467295296116));
#126249=CARTESIAN_POINT('Ctrl Pts',(-206.476745634812,-3.17995019533615,
134.558812244563));
#126250=CARTESIAN_POINT('Ctrl Pts',(-206.484506077326,-3.07406415392714,
134.645981459434));
#126251=CARTESIAN_POINT('Ctrl Pts',(-206.49226651984,-2.96484568166884,
134.728500414565));
#126252=CARTESIAN_POINT('Ctrl Pts',(-206.500039420106,-2.8554518822229,
134.811151836448));
#126253=CARTESIAN_POINT('Ctrl Pts',(-206.507812320371,-2.74271528361125,
134.889137858572));
#126254=CARTESIAN_POINT('Ctrl Pts',(-206.515585220636,-2.62708159836639,
134.962199640186));
#126255=CARTESIAN_POINT('Ctrl Pts',(-206.523075556399,-2.51565148882853,
135.032605442017));
#126256=CARTESIAN_POINT('Ctrl Pts',(-206.530565892162,-2.40153153536177,
135.098438650812));
#126257=CARTESIAN_POINT('Ctrl Pts',(-206.538056227925,-2.2851392588354,
135.159509481868));
#126258=CARTESIAN_POINT('Ctrl Pts',(-206.545830562044,-2.16433393378268,
135.222895832038));
#126259=CARTESIAN_POINT('Ctrl Pts',(-206.553604896163,-2.04069789899693,
135.281352333429));
#126260=CARTESIAN_POINT('Ctrl Pts',(-206.561379230282,-1.91467157352999,
135.334616220511));
#126261=CARTESIAN_POINT('Ctrl Pts',(-206.56914398323,-1.78880056424624,
135.387814464613));
#126262=CARTESIAN_POINT('Ctrl Pts',(-206.576908736177,-1.66054548224971,
135.435832676627));
#126263=CARTESIAN_POINT('Ctrl Pts',(-206.584673489124,-1.53037201072842,
135.478453531841));
#126264=CARTESIAN_POINT('Ctrl Pts',(-206.592430530009,-1.40032782933418,
135.521032055421));
#126265=CARTESIAN_POINT('Ctrl Pts',(-206.600187570894,-1.26836941934266,
135.55822376943));
#126266=CARTESIAN_POINT('Ctrl Pts',(-206.607944611779,-1.13498281922694,
135.589859239712));
#126267=CARTESIAN_POINT('Ctrl Pts',(-206.615695803019,-1.00169680698415,
135.62147085344));
#126268=CARTESIAN_POINT('Ctrl Pts',(-206.623446994259,-0.866985127212026,
135.647534473537));
#126269=CARTESIAN_POINT('Ctrl Pts',(-206.631198185499,-0.731349029471388,
135.667930464869));
#126270=CARTESIAN_POINT('Ctrl Pts',(-206.638946082276,-0.595770580690315,
135.688317787359));
#126271=CARTESIAN_POINT('Ctrl Pts',(-206.646693979053,-0.459268881202547,
135.703042214174));
#126272=CARTESIAN_POINT('Ctrl Pts',(-206.65444187583,-0.322355210575576,
135.712035238068));
#126273=CARTESIAN_POINT('Ctrl Pts',(-206.662188151914,-0.185470179336983,
135.721026380815));
#126274=CARTESIAN_POINT('Ctrl Pts',(-206.669934427998,-0.0481737382443191,
135.724288479683));
#126275=CARTESIAN_POINT('Ctrl Pts',(-206.677680704082,0.0890182698783709,
135.721804954834));
#126276=CARTESIAN_POINT('Ctrl Pts',(-206.685427037348,0.226211290721486,
135.719321411652));
#126277=CARTESIAN_POINT('Ctrl Pts',(-206.693173370613,0.36329948615519,
135.711092167198));
#126278=CARTESIAN_POINT('Ctrl Pts',(-206.700919703878,0.499767971438338,
135.697152769009));
#126279=CARTESIAN_POINT('Ctrl Pts',(-206.708667771881,0.636267017892372,
135.683210249189));
#126280=CARTESIAN_POINT('Ctrl Pts',(-206.716415839884,0.772145689173082,
135.66355507079));
#126281=CARTESIAN_POINT('Ctrl Pts',(-206.724163907887,0.906895569102237,
135.638274506874));
#126282=CARTESIAN_POINT('Ctrl Pts',(-206.731920210629,1.04178866280751,
135.612967074473));
#126283=CARTESIAN_POINT('Ctrl Pts',(-206.739676513371,1.17555018377165,
135.582022385611));
#126284=CARTESIAN_POINT('Ctrl Pts',(-206.747432816113,1.30768269545861,
135.545578713214));
#126285=CARTESIAN_POINT('Ctrl Pts',(-206.755193258627,1.4398857302455,135.509115589732));
#126286=CARTESIAN_POINT('Ctrl Pts',(-206.762953701141,1.57045765127054,
135.467147754108));
#126287=CARTESIAN_POINT('Ctrl Pts',(-206.770714143655,1.69891843734635,
135.419862671053));
#126288=CARTESIAN_POINT('Ctrl Pts',(-206.77848704392,1.82758544008018,135.372501681785));
#126289=CARTESIAN_POINT('Ctrl Pts',(-206.786259944186,1.9541341744678,135.319806538378));
#126290=CARTESIAN_POINT('Ctrl Pts',(-206.794032844451,2.07810595194281,
135.262012321659));
#126291=CARTESIAN_POINT('Ctrl Pts',(-206.801523180213,2.19757104304053,
135.206319070292));
#126292=CARTESIAN_POINT('Ctrl Pts',(-206.809013515975,2.31464300846158,
135.145891178822));
#126293=CARTESIAN_POINT('Ctrl Pts',(-206.816503851737,2.42893649673259,
135.080977336111));
#126294=CARTESIAN_POINT('Ctrl Pts',(-206.824278185856,2.5475634573503,135.013602265324));
#126295=CARTESIAN_POINT('Ctrl Pts',(-206.832052519975,2.66357286432491,
134.941180934586));
#126296=CARTESIAN_POINT('Ctrl Pts',(-206.839826854094,2.77650558831772,
134.86394184973));
#126297=CARTESIAN_POINT('Ctrl Pts',(-206.847591607042,2.88929913282099,
134.786797955144));
#126298=CARTESIAN_POINT('Ctrl Pts',(-206.855356359989,2.99902321915925,
134.704848338791));
#126299=CARTESIAN_POINT('Ctrl Pts',(-206.863121112936,3.1052432927571,134.618367323812));
#126300=CARTESIAN_POINT('Ctrl Pts',(-206.870878153821,3.21135786708041,
134.531972202995));
#126301=CARTESIAN_POINT('Ctrl Pts',(-206.878635194706,3.31397505326374,
134.441054885293));
#126302=CARTESIAN_POINT('Ctrl Pts',(-206.886392235591,3.41268958588663,
134.345932705337));
#126303=CARTESIAN_POINT('Ctrl Pts',(-206.894143426831,3.51132967711271,
134.250882257758));
#126304=CARTESIAN_POINT('Ctrl Pts',(-206.901894618071,3.6060726922938,134.151633529634));
#126305=CARTESIAN_POINT('Ctrl Pts',(-206.909645809311,3.69654704137007,
134.048543570705));
#126306=CARTESIAN_POINT('Ctrl Pts',(-206.917393706088,3.78698293643439,
133.945497427759));
#126307=CARTESIAN_POINT('Ctrl Pts',(-206.925141602865,3.87315351654314,
133.838613594408));
#126308=CARTESIAN_POINT('Ctrl Pts',(-206.932889499642,3.95472478551692,
133.728285194794));
#126309=CARTESIAN_POINT('Ctrl Pts',(-206.940635775726,4.0362789915397,133.617979873503));
#126310=CARTESIAN_POINT('Ctrl Pts',(-206.948382051811,4.11323556776735,
133.504231733294));
#126311=CARTESIAN_POINT('Ctrl Pts',(-206.956128327895,4.18530173946635,
133.387465805536));
#126312=CARTESIAN_POINT('Ctrl Pts',(-206.96387466116,4.25736844314155,133.270699015839));
#126313=CARTESIAN_POINT('Ctrl Pts',(-206.971620994426,4.32454446491532,
133.150914726844));
#126314=CARTESIAN_POINT('Ctrl Pts',(-206.979367327691,4.38658140415818,
133.028565339977));
#126315=CARTESIAN_POINT('Ctrl Pts',(-206.987115395694,4.44863223614336,
132.906188553813));
#126316=CARTESIAN_POINT('Ctrl Pts',(-206.994863463697,4.50554151874139,
132.781245875352));
#126317=CARTESIAN_POINT('Ctrl Pts',(-207.0026115317,4.55710786588625,132.654212222743));
#126318=CARTESIAN_POINT('Ctrl Pts',(-207.010367834442,4.60872901835857,
132.527043557257));
#126319=CARTESIAN_POINT('Ctrl Pts',(-207.018124137184,4.65499574460735,
132.397779841151));
#126320=CARTESIAN_POINT('Ctrl Pts',(-207.025880439925,4.69575550096411,
132.266914321765));
#126321=CARTESIAN_POINT('Ctrl Pts',(-207.03364088244,4.73653701203008,132.13597895551));
#126322=CARTESIAN_POINT('Ctrl Pts',(-207.041401324954,4.77180559603988,
132.003440460087));
#126323=CARTESIAN_POINT('Ctrl Pts',(-207.049161767468,4.80145950918554,
131.86980402017));
#126324=CARTESIAN_POINT('Ctrl Pts',(-207.056934667734,4.83116102542514,
131.735953055175));
#126325=CARTESIAN_POINT('Ctrl Pts',(-207.064707567999,4.85522979093357,
131.601001008726));
#126326=CARTESIAN_POINT('Ctrl Pts',(-207.072480468265,4.87361565349489,
131.465460855434));
#126327=CARTESIAN_POINT('Ctrl Pts',(-207.079970804027,4.89133314364086,
131.33484792812));
#126328=CARTESIAN_POINT('Ctrl Pts',(-207.087461139788,4.90377370409151,
131.203689216588));
#126329=CARTESIAN_POINT('Ctrl Pts',(-207.09495147555,4.91093827194779,131.072443350353));
#126330=CARTESIAN_POINT('Ctrl Pts',(-207.102725809669,4.91837448657198,
130.936221257207));
#126331=CARTESIAN_POINT('Ctrl Pts',(-207.110500143789,4.92015028810036,
130.79947375931));
#126332=CARTESIAN_POINT('Ctrl Pts',(-207.118274477908,4.91620975433994,
130.66271064816));
#126333=CARTESIAN_POINT('Ctrl Pts',(-207.126039230855,4.91227407693521,
130.526116085322));
#126334=CARTESIAN_POINT('Ctrl Pts',(-207.133803983802,4.90263609258996,
130.389506334569));
#126335=CARTESIAN_POINT('Ctrl Pts',(-207.141568736749,4.88729170976703,
130.253395277329));
#126336=CARTESIAN_POINT('Ctrl Pts',(-207.149325777634,4.87196256720145,
130.11741940751));
#126337=CARTESIAN_POINT('Ctrl Pts',(-207.157082818519,4.85093834860235,
129.981941631508));
#126338=CARTESIAN_POINT('Ctrl Pts',(-207.164839859404,4.824266980725,129.847474437717));
#126339=CARTESIAN_POINT('Ctrl Pts',(-207.172591050644,4.79761572593367,
129.713108646683));
#126340=CARTESIAN_POINT('Ctrl Pts',(-207.180342241884,4.76532587402565,
129.579752302914));
#126341=CARTESIAN_POINT('Ctrl Pts',(-207.188093433124,4.72749696755391,
129.447911029756));
#126342=CARTESIAN_POINT('Ctrl Pts',(-207.195841329901,4.68968413937648,
129.316125792657));
#126343=CARTESIAN_POINT('Ctrl Pts',(-207.203589226679,4.64633704665318,
129.185854720425));
#126344=CARTESIAN_POINT('Ctrl Pts',(-207.211337123456,4.59760590276493,
129.057591306706));
#126345=CARTESIAN_POINT('Ctrl Pts',(-207.21908339954,4.54888495238146,128.929354722929));
#126346=CARTESIAN_POINT('Ctrl Pts',(-207.226829675624,4.49478232972868,
128.80312532759));
#126347=CARTESIAN_POINT('Ctrl Pts',(-207.234575951708,4.43549737384086,
128.6793791802));
#126348=CARTESIAN_POINT('Ctrl Pts',(-207.242322284973,4.37621198032504,
128.555632119344));
#126349=CARTESIAN_POINT('Ctrl Pts',(-207.250068618239,4.31174434616013,
128.434368695606));
#126350=CARTESIAN_POINT('Ctrl Pts',(-207.257814951504,4.24234082287173,
128.316042429493));
#126351=CARTESIAN_POINT('Ctrl Pts',(-207.265563019507,4.17292175714561,
128.197689665032));
#126352=CARTESIAN_POINT('Ctrl Pts',(-207.27331108751,4.09856480052667,128.082275704225));
#126353=CARTESIAN_POINT('Ctrl Pts',(-207.281059155513,4.01956066101754,
127.970226683734));
#126354=CARTESIAN_POINT('Ctrl Pts',(-207.288815458255,3.94047255496867,
127.858058576209));
#126355=CARTESIAN_POINT('Ctrl Pts',(-207.296571760996,3.85672762533503,
127.749262873077));
#126356=CARTESIAN_POINT('Ctrl Pts',(-207.304328063738,3.76865840149489,
127.644234525882));
#126357=CARTESIAN_POINT('Ctrl Pts',(-207.312088506252,3.68054217245802,
127.539150121895));
#126358=CARTESIAN_POINT('Ctrl Pts',(-207.319848948767,3.58809731371382,
127.437837369101));
#126359=CARTESIAN_POINT('Ctrl Pts',(-207.327609391281,3.4916938564228,127.340654932101));
#126360=CARTESIAN_POINT('Ctrl Pts',(-207.335382291546,3.3951356437441,127.243316489227));
#126361=CARTESIAN_POINT('Ctrl Pts',(-207.343155191811,3.29460642069608,
127.15012187765));
#126362=CARTESIAN_POINT('Ctrl Pts',(-207.350928092077,3.19051065884962,
127.061390567156));
#126363=CARTESIAN_POINT('Ctrl Pts',(-207.358418427839,3.090199040146,126.975884863298));
#126364=CARTESIAN_POINT('Ctrl Pts',(-207.365908763601,2.98657592832593,
126.894523780142));
#126365=CARTESIAN_POINT('Ctrl Pts',(-207.373399099363,2.88002768791472,
126.817554429733));
#126366=CARTESIAN_POINT('Ctrl Pts',(-207.381173433482,2.7694396385851,126.73766676301));
#126367=CARTESIAN_POINT('Ctrl Pts',(-207.388947767602,2.65534995981542,
126.662257368034));
#126368=CARTESIAN_POINT('Ctrl Pts',(-207.396722101721,2.53815732632183,
126.591648848487));
#126369=CARTESIAN_POINT('Ctrl Pts',(-207.404486854668,2.42110912227552,
126.52112734763));
#126370=CARTESIAN_POINT('Ctrl Pts',(-207.412251607615,2.30096590401835,
126.455395149661));
#126371=CARTESIAN_POINT('Ctrl Pts',(-207.420016360562,2.17815780297416,
126.39473346237));
#126372=CARTESIAN_POINT('Ctrl Pts',(-207.427773401447,2.05547167666722,
126.334132025122));
#126373=CARTESIAN_POINT('Ctrl Pts',(-207.435530442332,1.93012628308811,
126.278591248508));
#126374=CARTESIAN_POINT('Ctrl Pts',(-207.443287483217,1.80257869882107,
126.228347822888));
#126375=CARTESIAN_POINT('Ctrl Pts',(-207.451038674457,1.67512729917933,
126.178142286226));
#126376=CARTESIAN_POINT('Ctrl Pts',(-207.458789865697,1.54547737663862,
126.133226291915));
#126377=CARTESIAN_POINT('Ctrl Pts',(-207.466541056937,1.41410813162145,
126.093789393757));
#126378=CARTESIAN_POINT('Ctrl Pts',(-207.474288953714,1.28279472203762,
126.054369257331));
#126379=CARTESIAN_POINT('Ctrl Pts',(-207.482036850492,1.1497638170714,126.020423697504));
#126380=CARTESIAN_POINT('Ctrl Pts',(-207.489784747269,1.01551180090532,
125.992093080872));
#126381=CARTESIAN_POINT('Ctrl Pts',(-207.497531023353,0.881287867367254,
125.963768390394));
#126382=CARTESIAN_POINT('Ctrl Pts',(-207.505277299437,0.745843712991892,
125.941056387592));
#126383=CARTESIAN_POINT('Ctrl Pts',(-207.513023575521,0.609687607747052,
125.924046684686));
#126384=CARTESIAN_POINT('Ctrl Pts',(-207.520769908786,0.473530497428588,
125.907036856218));
#126385=CARTESIAN_POINT('Ctrl Pts',(-207.528516242052,0.33666181370332,
125.895729460106));
#126386=CARTESIAN_POINT('Ctrl Pts',(-207.536262575317,0.199596275234876,
125.890162372744));
#126387=CARTESIAN_POINT('Ctrl Pts',(-207.54401064332,0.0625000418892514,
125.884594038672));
#126388=CARTESIAN_POINT('Ctrl Pts',(-207.551758711323,-0.0747927433537585,
125.884768587215));
#126389=CARTESIAN_POINT('Ctrl Pts',(-207.559506779326,-0.211766424875434,
125.890671774772));
#126390=CARTESIAN_POINT('Ctrl Pts',(-207.567263082068,-0.348885683655652,
125.896581236308));
#126391=CARTESIAN_POINT('Ctrl Pts',(-207.57501938481,-0.485684770005954,
125.908231482363));
#126392=CARTESIAN_POINT('Ctrl Pts',(-207.582775687552,-0.621651659755012,
125.925556227511));
#126393=CARTESIAN_POINT('Ctrl Pts',(-207.590536130066,-0.757691119127012,
125.942890219397));
#126394=CARTESIAN_POINT('Ctrl Pts',(-207.59829657258,-0.892897111621781,
125.965904679646));
#126395=CARTESIAN_POINT('Ctrl Pts',(-207.606057015094,-1.02676787166982,
125.994482157542));
#126396=CARTESIAN_POINT('Ctrl Pts',(-207.61382991536,-1.16085353294637,
126.023105510542));
#126397=CARTESIAN_POINT('Ctrl Pts',(-207.621602815625,-1.29359929969567,
126.057309629066));
#126398=CARTESIAN_POINT('Ctrl Pts',(-207.629375715891,-1.42451776617409,
126.096926900948));
#126399=CARTESIAN_POINT('Ctrl Pts',(-207.636866051653,-1.55067701663124,
126.135103985207));
#126400=CARTESIAN_POINT('Ctrl Pts',(-207.644356387415,-1.67513922322726,
126.178307391138));
#126401=CARTESIAN_POINT('Ctrl Pts',(-207.651846723176,-1.79748764413635,
126.226345629421));
#126402=CARTESIAN_POINT('Ctrl Pts',(-207.659621346427,-1.92447966532862,
126.276207106413));
#126403=CARTESIAN_POINT('Ctrl Pts',(-207.667395969677,-2.0495965663628,
126.331435618184));
#126404=CARTESIAN_POINT('Ctrl Pts',(-207.675170592927,-2.17235138413133,
126.391870104674));
#126405=CARTESIAN_POINT('Ctrl Pts',(-207.68293556835,-2.29495387074919,
126.452229595697));
#126406=CARTESIAN_POINT('Ctrl Pts',(-207.690700543772,-2.41519975904507,
126.517782035912));
#126407=CARTESIAN_POINT('Ctrl Pts',(-207.698465519195,-2.53261992505663,
126.588317522707));
#126408=CARTESIAN_POINT('Ctrl Pts',(-207.706222716183,-2.64992246736666,
126.65878235175));
#126409=CARTESIAN_POINT('Ctrl Pts',(-207.71397991317,-2.7644045876617,126.734220093246));
#126410=CARTESIAN_POINT('Ctrl Pts',(-207.721737110158,-2.87562006548463,
126.814374113644));
#126411=CARTESIAN_POINT('Ctrl Pts',(-207.729795303405,-2.99115094782568,
126.89763828587));
#126412=CARTESIAN_POINT('Ctrl Pts',(-207.737853496653,-3.10315618232721,
126.985991940956));
#126413=CARTESIAN_POINT('Ctrl Pts',(-207.745911689901,-3.2111662156833,
127.07909625141));
#126414=CARTESIAN_POINT('Ctrl Pts',(-207.753659246585,-3.31501255320105,
127.168611469092));
#126415=CARTESIAN_POINT('Ctrl Pts',(-207.761406803268,-3.41516565824468,
127.262517606759));
#126416=CARTESIAN_POINT('Ctrl Pts',(-207.769154359952,-3.51124052762793,
127.360471388853));
#126417=CARTESIAN_POINT('Ctrl Pts',(-207.776900268185,-3.60729495512799,
127.458404329287));
#126418=CARTESIAN_POINT('Ctrl Pts',(-207.784646176418,-3.69927259997578,
127.560382921643));
#126419=CARTESIAN_POINT('Ctrl Pts',(-207.792392084651,-3.78682490105777,
127.666026627815));
#126420=CARTESIAN_POINT('Ctrl Pts',(-207.800138022213,-3.87437753365062,
127.771670733999));
#126421=CARTESIAN_POINT('Ctrl Pts',(-207.807883959776,-3.95750454018412,
127.880979680284));
#126422=CARTESIAN_POINT('Ctrl Pts',(-207.815629897339,-4.0358975446204,
127.993539728248));
#126423=CARTESIAN_POINT('Ctrl Pts',(-207.823377541653,-4.114307822298,128.106124577875));
#126424=CARTESIAN_POINT('Ctrl Pts',(-207.831125185968,-4.18798179960877,
128.221961633515));
#126425=CARTESIAN_POINT('Ctrl Pts',(-207.838872830283,-4.25665456438336,
128.340608401532));
#126426=CARTESIAN_POINT('Ctrl Pts',(-207.846627482129,-4.3253894417789,
128.459362482276));
#126427=CARTESIAN_POINT('Ctrl Pts',(-207.854382133974,-4.38911387975285,
128.580931010513));
#126428=CARTESIAN_POINT('Ctrl Pts',(-207.86213678582,-4.44760890967717,
128.704846852653));
#126429=CARTESIAN_POINT('Ctrl Pts',(-207.869895598211,-4.50613532350585,
128.82882917844));
#126430=CARTESIAN_POINT('Ctrl Pts',(-207.877654410602,-4.55942658739599,
128.955160967813));
#126431=CARTESIAN_POINT('Ctrl Pts',(-207.885413222994,-4.60731235870681,
129.083356291073));
#126432=CARTESIAN_POINT('Ctrl Pts',(-207.893181538738,-4.65525678273092,
129.21170863391));
#126433=CARTESIAN_POINT('Ctrl Pts',(-207.900949854483,-4.6977823753859,
129.34192869686));
#126434=CARTESIAN_POINT('Ctrl Pts',(-207.908718170227,-4.73476889932119,
129.473516324449));
#126435=CARTESIAN_POINT('Ctrl Pts',(-207.910856696188,-4.74495085435851,
129.50974085071));
#126436=CARTESIAN_POINT('Ctrl Pts',(-207.912995222148,-4.7547133384679,
129.546068962182));
#126437=CARTESIAN_POINT('Ctrl Pts',(-207.915133748109,-4.76405452823406,
129.582490119308));
#126438=CARTESIAN_POINT('Ctrl Pts',(-206.164998470905,-4.76405452823394,
129.582490119308));
#126439=CARTESIAN_POINT('Ctrl Pts',(-206.172665944474,-4.79776118631657,
129.713911867602));
#126440=CARTESIAN_POINT('Ctrl Pts',(-206.180333418043,-4.82600172992664,
129.846636618208));
#126441=CARTESIAN_POINT('Ctrl Pts',(-206.188000891612,-4.84869920343357,
129.980164586805));
#126442=CARTESIAN_POINT('Ctrl Pts',(-206.195857503673,-4.87195657008729,
130.116986375504));
#126443=CARTESIAN_POINT('Ctrl Pts',(-206.203714115733,-4.88939378574457,
130.254651075192));
#126444=CARTESIAN_POINT('Ctrl Pts',(-206.211570727794,-4.90098467145666,
130.392617599839));
#126445=CARTESIAN_POINT('Ctrl Pts',(-206.219427339854,-4.91257555716875,
130.530584124486));
#126446=CARTESIAN_POINT('Ctrl Pts',(-206.227283951915,-4.91832015787954,
130.668852025862));
#126447=CARTESIAN_POINT('Ctrl Pts',(-206.235140563975,-4.91824935292959,
130.806883494435));
#126448=CARTESIAN_POINT('',(-205.889859436046,-4.91824930584068,130.806973680448));
#126449=CARTESIAN_POINT('Ctrl Pts',(-205.820054717884,-4.76405452823395,
129.582490119308));
#126450=CARTESIAN_POINT('Ctrl Pts',(-205.827905852165,-4.79858606955834,
129.717128074842));
#126451=CARTESIAN_POINT('Ctrl Pts',(-205.835756986446,-4.82742791349959,
129.853316954026));
#126452=CARTESIAN_POINT('Ctrl Pts',(-205.843608120727,-4.85045202410955,
129.99054354702));
#126453=CARTESIAN_POINT('Ctrl Pts',(-205.851456131429,-4.87346697456125,
130.12771554432));
#126454=CARTESIAN_POINT('Ctrl Pts',(-205.859304142131,-4.8906687356244,
130.265924063211));
#126455=CARTESIAN_POINT('Ctrl Pts',(-205.867152152832,-4.9019802890764,
130.404645333887));
#126456=CARTESIAN_POINT('Ctrl Pts',(-205.87472124722,-4.91288983278145,
130.538436485711));
#126457=CARTESIAN_POINT('Ctrl Pts',(-205.882290341607,-4.91832064309359,
130.672704230441));
#126458=CARTESIAN_POINT('Ctrl Pts',(-205.889859435995,-4.91824930584116,
130.806973679544));
#126459=CARTESIAN_POINT('Ctrl Pts',(-205.889859436046,-4.91824930584068,
130.806973680447));
#126460=CARTESIAN_POINT('Ctrl Pts',(-205.898419073697,-4.91816863288146,
130.958814544507));
#126461=CARTESIAN_POINT('Ctrl Pts',(-205.906978711349,-4.91105222461682,
131.11040905316));
#126462=CARTESIAN_POINT('Ctrl Pts',(-205.915538349,-4.89699280558849,131.261136847809));
#126463=CARTESIAN_POINT('Ctrl Pts',(-205.924144711242,-4.88285664025042,
131.412687421976));
#126464=CARTESIAN_POINT('Ctrl Pts',(-205.932751073485,-4.86170154469193,
131.563361562213));
#126465=CARTESIAN_POINT('Ctrl Pts',(-205.941357435727,-4.8336719627189,
131.712544750507));
#126466=CARTESIAN_POINT('Ctrl Pts',(-205.949987994199,-4.80556357739427,
131.862147357658));
#126467=CARTESIAN_POINT('Ctrl Pts',(-205.95861855267,-4.77054211518795,
132.010250401408));
#126468=CARTESIAN_POINT('Ctrl Pts',(-205.967249111142,-4.72880199806623,
132.15625363315));
#126469=CARTESIAN_POINT('Ctrl Pts',(-205.975911032462,-4.68691020026427,
132.302787430473));
#126470=CARTESIAN_POINT('Ctrl Pts',(-205.984572953782,-4.63825094856085,
132.447205915682));
#126471=CARTESIAN_POINT('Ctrl Pts',(-205.993234875102,-4.58306805029199,
132.588925076725));
#126472=CARTESIAN_POINT('Ctrl Pts',(-205.995739908888,-4.5671091169981,
132.629910358551));
#126473=CARTESIAN_POINT('Ctrl Pts',(-205.998244942673,-4.55060485959071,
132.67067003316));
#126474=CARTESIAN_POINT('Ctrl Pts',(-206.000749976459,-4.53356188569129,
132.711190366418));
#126475=CARTESIAN_POINT('Ctrl Pts',(-206.008524310578,-4.48066927631869,
132.836944602228));
#126476=CARTESIAN_POINT('Ctrl Pts',(-206.016298644698,-4.42245657148283,
132.960695612929));
#126477=CARTESIAN_POINT('Ctrl Pts',(-206.024072978817,-4.35909645044119,
133.081960494246));
#126478=CARTESIAN_POINT('Ctrl Pts',(-206.031837731764,-4.29581441508608,
133.203075927434));
#126479=CARTESIAN_POINT('Ctrl Pts',(-206.039602484712,-4.22739776497256,
133.321710984359));
#126480=CARTESIAN_POINT('Ctrl Pts',(-206.047367237659,-4.15406757846652,
133.437401752078));
#126481=CARTESIAN_POINT('Ctrl Pts',(-206.055124278544,-4.0808102245355,
133.552977614096));
#126482=CARTESIAN_POINT('Ctrl Pts',(-206.06288131943,-4.00264925397073,
133.665614678334));
#126483=CARTESIAN_POINT('Ctrl Pts',(-206.070638360315,-3.91985191488636,
133.774873035965));
#126484=CARTESIAN_POINT('Ctrl Pts',(-206.078389551555,-3.83711701391935,
133.884049001019));
#126485=CARTESIAN_POINT('Ctrl Pts',(-206.086140742796,-3.7497529388275,
133.989851020585));
#126486=CARTESIAN_POINT('Ctrl Pts',(-206.093891934036,-3.65807035220528,
134.091867934792));
#126487=CARTESIAN_POINT('Ctrl Pts',(-206.101639830814,-3.5664267331282,
134.193841489089));
#126488=CARTESIAN_POINT('Ctrl Pts',(-206.109387727591,-3.47046851394157,
134.292032847568));
#126489=CARTESIAN_POINT('Ctrl Pts',(-206.117135624368,-3.37054661931243,
134.386063920401));
#126490=CARTESIAN_POINT('Ctrl Pts',(-206.124881900453,-3.2706456261893,
134.480075323962));
#126491=CARTESIAN_POINT('Ctrl Pts',(-206.132628176537,-3.16678289131879,
134.569927905073));
#126492=CARTESIAN_POINT('Ctrl Pts',(-206.140374452621,-3.0593458918801,
134.655280738308));
#126493=CARTESIAN_POINT('Ctrl Pts',(-206.148120785887,-2.95190809936603,
134.740634201599));
#126494=CARTESIAN_POINT('Ctrl Pts',(-206.155867119153,-2.84089629575584,
134.821487607538));
#126495=CARTESIAN_POINT('Ctrl Pts',(-206.163613452418,-2.72673037768329,
134.897540861572));
#126496=CARTESIAN_POINT('Ctrl Pts',(-206.171361520422,-2.61253889294479,
134.973611147205));
#126497=CARTESIAN_POINT('Ctrl Pts',(-206.179109588425,-2.49519221352086,
135.044878925172));
#126498=CARTESIAN_POINT('Ctrl Pts',(-206.186857656428,-2.37513814799737,
135.11108812699));
#126499=CARTESIAN_POINT('Ctrl Pts',(-206.19461395917,-2.25495648758455,
135.177367696735));
#126500=CARTESIAN_POINT('Ctrl Pts',(-206.202370261912,-2.13206203597101,
135.238577761457));
#126501=CARTESIAN_POINT('Ctrl Pts',(-206.210126564654,-2.00692657135467,
135.294508588367));
#126502=CARTESIAN_POINT('Ctrl Pts',(-206.217887007169,-1.88172431817278,
135.350469267244));
#126503=CARTESIAN_POINT('Ctrl Pts',(-206.225647449683,-1.75427903178613,
135.401144949441));
#126504=CARTESIAN_POINT('Ctrl Pts',(-206.233407892198,-1.6250803440804,
135.446374936564));
#126505=CARTESIAN_POINT('Ctrl Pts',(-206.241180792463,-1.49567425517145,
135.491677530877));
#126506=CARTESIAN_POINT('Ctrl Pts',(-206.248953692729,-1.36450951455032,
135.531516847299));
#126507=CARTESIAN_POINT('Ctrl Pts',(-206.256726592995,-1.23208958293334,
135.565782497858));
#126508=CARTESIAN_POINT('Ctrl Pts',(-206.264216928754,-1.10448344942972,
135.598802505697));
#126509=CARTESIAN_POINT('Ctrl Pts',(-206.271707264513,-0.975712100315515,
135.626646980716));
#126510=CARTESIAN_POINT('Ctrl Pts',(-206.279197600272,-0.846231065683617,
135.649262685304));
#126511=CARTESIAN_POINT('Ctrl Pts',(-206.286971934391,-0.711840718217051,
135.672735871215));
#126512=CARTESIAN_POINT('Ctrl Pts',(-206.29474626851,-0.576260099220195,
135.690650318037));
#126513=CARTESIAN_POINT('Ctrl Pts',(-206.302520602629,-0.439988827093508,
135.702890284163));
#126514=CARTESIAN_POINT('Ctrl Pts',(-206.310285355577,-0.303885497130804,
135.715115165626));
#126515=CARTESIAN_POINT('Ctrl Pts',(-206.318050108524,-0.16709359326881,
135.721679446316));
#126516=CARTESIAN_POINT('Ctrl Pts',(-206.325814861471,-0.030122916862644,
135.722518369446));
#126517=CARTESIAN_POINT('Ctrl Pts',(-206.333571902356,0.106711718336767,
135.723356459347));
#126518=CARTESIAN_POINT('Ctrl Pts',(-206.341328943241,0.243724384301109,
135.718480505712));
#126519=CARTESIAN_POINT('Ctrl Pts',(-206.349085984126,0.380400519141976,
135.707877570482));
#126520=CARTESIAN_POINT('Ctrl Pts',(-206.356837175366,0.516973585446189,
135.697282631009));
#126521=CARTESIAN_POINT('Ctrl Pts',(-206.364588366606,0.653210237545264,
135.68096933629));
#126522=CARTESIAN_POINT('Ctrl Pts',(-206.372339557846,0.78859663427342,
135.658976813612));
#126523=CARTESIAN_POINT('Ctrl Pts',(-206.380087454624,0.9239254881716,135.636993638342));
#126524=CARTESIAN_POINT('Ctrl Pts',(-206.387835351401,1.0584044203597,135.60933609858));
#126525=CARTESIAN_POINT('Ctrl Pts',(-206.395583248178,1.19152564980452,
135.576095070399));
#126526=CARTESIAN_POINT('Ctrl Pts',(-206.403329524262,1.3246190331579,135.542860995525));
#126527=CARTESIAN_POINT('Ctrl Pts',(-206.411075800346,1.45635489958587,
135.504045849998));
#126528=CARTESIAN_POINT('Ctrl Pts',(-206.41882207643,1.58623697799247,135.459791350823));
#126529=CARTESIAN_POINT('Ctrl Pts',(-206.426568409696,1.71612001515889,
135.41553652497));
#126530=CARTESIAN_POINT('Ctrl Pts',(-206.434314742961,1.84414886692504,
135.365842391443));
#126531=CARTESIAN_POINT('Ctrl Pts',(-206.442061076226,1.96984409085683,
135.310900012736));
#126532=CARTESIAN_POINT('Ctrl Pts',(-206.449809144229,2.09556746336268,
135.255945330063));
#126533=CARTESIAN_POINT('Ctrl Pts',(-206.457557212232,2.21895580995249,
135.195740220041));
#126534=CARTESIAN_POINT('Ctrl Pts',(-206.465305280235,2.33955164148073,
135.130523025445));
#126535=CARTESIAN_POINT('Ctrl Pts',(-206.473061582977,2.46027564369365,
135.065236517239));
#126536=CARTESIAN_POINT('Ctrl Pts',(-206.480817885719,2.57820085766173,
134.99492746967));
#126537=CARTESIAN_POINT('Ctrl Pts',(-206.488574188461,2.69289582161183,
134.919879437405));
#126538=CARTESIAN_POINT('Ctrl Pts',(-206.496334630975,2.80765200171758,
134.844791349744));
#126539=CARTESIAN_POINT('Ctrl Pts',(-206.504095073489,2.91917417867433,
134.764959464925));
#126540=CARTESIAN_POINT('Ctrl Pts',(-206.511855516003,3.02706249437732,
134.68070886271));
#126541=CARTESIAN_POINT('Ctrl Pts',(-206.519628416269,3.13512400198284,
134.59632301395));
#126542=CARTESIAN_POINT('Ctrl Pts',(-206.527401316534,3.23953969337777,
134.507504526547));
#126543=CARTESIAN_POINT('Ctrl Pts',(-206.5351742168,3.33994456322253,134.414617308869));
#126544=CARTESIAN_POINT('Ctrl Pts',(-206.542664552561,3.43669946314165,
134.325106775525));
#126545=CARTESIAN_POINT('Ctrl Pts',(-206.550154888323,3.52972986821838,
134.231818411375));
#126546=CARTESIAN_POINT('Ctrl Pts',(-206.557645224085,3.61874476299928,
134.13510669056));
#126547=CARTESIAN_POINT('Ctrl Pts',(-206.565419558204,3.71113468457249,
134.034728115454));
#126548=CARTESIAN_POINT('Ctrl Pts',(-206.573193892323,3.79949125235512,
133.930343496942));
#126549=CARTESIAN_POINT('Ctrl Pts',(-206.580968226442,3.88344703370601,
133.82231061697));
#126550=CARTESIAN_POINT('Ctrl Pts',(-206.588732979389,3.9672993470595,133.714410877866));
#126551=CARTESIAN_POINT('Ctrl Pts',(-206.596497732336,4.04676142767885,
133.602872129055));
#126552=CARTESIAN_POINT('Ctrl Pts',(-206.604262485283,4.12150323375985,
133.488088278229));
#126553=CARTESIAN_POINT('Ctrl Pts',(-206.612019526168,4.19617080522537,
133.373418432341));
#126554=CARTESIAN_POINT('Ctrl Pts',(-206.619776567053,4.2661272200117,133.255510224025));
#126555=CARTESIAN_POINT('Ctrl Pts',(-206.627533607938,4.33108345969385,
133.134789575433));
#126556=CARTESIAN_POINT('Ctrl Pts',(-206.635284799178,4.39599071537045,
133.014159963221));
#126557=CARTESIAN_POINT('Ctrl Pts',(-206.643035990418,4.45590511673205,
132.890722475119));
#126558=CARTESIAN_POINT('Ctrl Pts',(-206.650787181658,4.51058183897033,
132.764930569506));
#126559=CARTESIAN_POINT('Ctrl Pts',(-206.658535078435,4.56523532214318,
132.639192128808));
#126560=CARTESIAN_POINT('Ctrl Pts',(-206.666282975212,4.61465539831717,
132.511101618704));
#126561=CARTESIAN_POINT('Ctrl Pts',(-206.674030871989,4.65864405605593,
132.381135370495));
#126562=CARTESIAN_POINT('Ctrl Pts',(-206.681777148073,4.70262351231578,
132.251196308424));
#126563=CARTESIAN_POINT('Ctrl Pts',(-206.689523424157,4.74117368471374,
132.119382658775));
#126564=CARTESIAN_POINT('Ctrl Pts',(-206.697269700241,4.77414555713005,
131.986188549981));
#126565=CARTESIAN_POINT('Ctrl Pts',(-206.705016033506,4.80711767293719,
131.852993457978));
#126566=CARTESIAN_POINT('Ctrl Pts',(-206.712762366772,4.83451131264874,
131.718418266004));
#126567=CARTESIAN_POINT('Ctrl Pts',(-206.720508700037,4.8562280722051,131.582969616504));
#126568=CARTESIAN_POINT('Ctrl Pts',(-206.72825676804,4.87794969507915,131.447490634218));
#126569=CARTESIAN_POINT('Ctrl Pts',(-206.736004836043,4.89399184618037,
131.311138191135));
#126570=CARTESIAN_POINT('Ctrl Pts',(-206.743752904046,4.90430776597871,
131.174426015923));
#126571=CARTESIAN_POINT('Ctrl Pts',(-206.751509206787,4.91463464965938,
131.037568541384));
#126572=CARTESIAN_POINT('Ctrl Pts',(-206.759265509529,4.91922311531838,
130.900350961453));
#126573=CARTESIAN_POINT('Ctrl Pts',(-206.767021812271,4.91807850989876,
130.763289545363));
#126574=CARTESIAN_POINT('Ctrl Pts',(-206.774782254785,4.91693329356877,
130.626154975468));
#126575=CARTESIAN_POINT('Ctrl Pts',(-206.782542697299,4.91004892864024,
130.489177125775));
#126576=CARTESIAN_POINT('Ctrl Pts',(-206.790303139813,4.89748278085339,
130.352868121787));
#126577=CARTESIAN_POINT('Ctrl Pts',(-206.798076040079,4.88489646077053,
130.216340302485));
#126578=CARTESIAN_POINT('Ctrl Pts',(-206.805848940344,4.86661018354394,
130.080483862156));
#126579=CARTESIAN_POINT('Ctrl Pts',(-206.813621840609,4.84273282128629,
129.945802591492));
#126580=CARTESIAN_POINT('Ctrl Pts',(-206.821112176372,4.81972346128801,
129.816017324245));
#126581=CARTESIAN_POINT('Ctrl Pts',(-206.828602512135,4.79152252480077,
129.687323570165));
#126582=CARTESIAN_POINT('Ctrl Pts',(-206.836092847897,4.75827093999596,
129.560157770724));
#126583=CARTESIAN_POINT('Ctrl Pts',(-206.843867182016,4.72375861124946,
129.428170441356));
#126584=CARTESIAN_POINT('Ctrl Pts',(-206.851641516135,4.68369575848463,
129.29741112245));
#126585=CARTESIAN_POINT('Ctrl Pts',(-206.859415850255,4.63818478746673,
129.168382335371));
#126586=CARTESIAN_POINT('Ctrl Pts',(-206.867180603202,4.59272990465331,
129.039512564742));
#126587=CARTESIAN_POINT('Ctrl Pts',(-206.874945356149,4.54184039188006,
128.912369447615));
#126588=CARTESIAN_POINT('Ctrl Pts',(-206.882710109096,4.4856692591883,128.787443574236));
#126589=CARTESIAN_POINT('Ctrl Pts',(-206.890467149981,4.42955391645741,
128.662641778997));
#126590=CARTESIAN_POINT('Ctrl Pts',(-206.898224190866,4.36816755243845,
128.540053199304));
#126591=CARTESIAN_POINT('Ctrl Pts',(-206.905981231751,4.30171228598306,
128.420151215873));
#126592=CARTESIAN_POINT('Ctrl Pts',(-206.913732422991,4.23530713396096,
128.300339651459));
#126593=CARTESIAN_POINT('Ctrl Pts',(-206.921483614231,4.16384087671486,
128.183210991282));
#126594=CARTESIAN_POINT('Ctrl Pts',(-206.929234805471,4.08756268783238,
128.069216318714));
#126595=CARTESIAN_POINT('Ctrl Pts',(-206.936982702249,4.01131691921485,
127.955270096924));
#126596=CARTESIAN_POINT('Ctrl Pts',(-206.944730599026,3.93026350367536,
127.844455537692));
#126597=CARTESIAN_POINT('Ctrl Pts',(-206.952478495803,3.844696162211,127.737196702354));
#126598=CARTESIAN_POINT('Ctrl Pts',(-206.960224771887,3.75914671958986,
127.629960303251));
#126599=CARTESIAN_POINT('Ctrl Pts',(-206.967971047971,3.66908547280403,
127.526278454052));
#126600=CARTESIAN_POINT('Ctrl Pts',(-206.975717324055,3.5748475992442,127.426543614726));
#126601=CARTESIAN_POINT('Ctrl Pts',(-206.983463657321,3.48060903004192,
127.326808039179));
#126602=CARTESIAN_POINT('Ctrl Pts',(-206.991209990586,3.38219404105675,
127.231019815818));
#126603=CARTESIAN_POINT('Ctrl Pts',(-206.998956323851,3.27997569512705,
127.13953558738));
#126604=CARTESIAN_POINT('Ctrl Pts',(-207.006704391854,3.17773445810738,
127.048030871684));
#126605=CARTESIAN_POINT('Ctrl Pts',(-207.014452459857,3.07168846055954,
126.960832329545));
#126606=CARTESIAN_POINT('Ctrl Pts',(-207.022200527861,2.96224464229277,
126.878256983974));
#126607=CARTESIAN_POINT('Ctrl Pts',(-207.029956830602,2.85268450583369,
126.795593876342));
#126608=CARTESIAN_POINT('Ctrl Pts',(-207.037713133344,2.73971964740064,
126.717564016553));
#126609=CARTESIAN_POINT('Ctrl Pts',(-207.045469436086,2.62378730907338,
126.644441962202));
#126610=CARTESIAN_POINT('Ctrl Pts',(-207.0532298786,2.50779309416619,126.571280880408));
#126611=CARTESIAN_POINT('Ctrl Pts',(-207.060990321115,2.38882858239987,
126.50303301797));
#126612=CARTESIAN_POINT('Ctrl Pts',(-207.068750763629,2.26735564704684,
126.439926927807));
#126613=CARTESIAN_POINT('Ctrl Pts',(-207.076523663894,2.14568771255446,
126.376719534146));
#126614=CARTESIAN_POINT('Ctrl Pts',(-207.08429656416,2.02150366214178,126.318670572596));
#126615=CARTESIAN_POINT('Ctrl Pts',(-207.092069464425,1.89528619722091,
126.265960757139));
#126616=CARTESIAN_POINT('Ctrl Pts',(-207.099559800187,1.77365705507833,
126.215167076244));
#126617=CARTESIAN_POINT('Ctrl Pts',(-207.107050135949,1.65014005997225,
126.16933120521));
#126618=CARTESIAN_POINT('Ctrl Pts',(-207.11454047171,1.52517857759403,126.12857048445));
#126619=CARTESIAN_POINT('Ctrl Pts',(-207.122314805829,1.39547914262526,
126.086264308572));
#126620=CARTESIAN_POINT('Ctrl Pts',(-207.130089139948,1.26381267382523,
126.049291715399));
#126621=CARTESIAN_POINT('Ctrl Pts',(-207.137863474068,1.13065730947015,
126.017838173135));
#126622=CARTESIAN_POINT('Ctrl Pts',(-207.145628227015,0.997666047201566,
125.986423394551));
#126623=CARTESIAN_POINT('Ctrl Pts',(-207.153392979962,0.863189917184256,
125.960514222462));
#126624=CARTESIAN_POINT('Ctrl Pts',(-207.161157732909,0.727724372552056,
125.9402471012));
#126625=CARTESIAN_POINT('Ctrl Pts',(-207.168914773794,0.592393374208515,
125.920000109528));
#126626=CARTESIAN_POINT('Ctrl Pts',(-207.176671814678,0.45607530102819,
125.905384074413));
#126627=CARTESIAN_POINT('Ctrl Pts',(-207.184428855563,0.319277671788742,
125.896484821379));
#126628=CARTESIAN_POINT('Ctrl Pts',(-207.192180046803,0.182583202705448,
125.887592279341));
#126629=CARTESIAN_POINT('Ctrl Pts',(-207.199931238044,0.0454102859413843,
125.884407963739));
#126630=CARTESIAN_POINT('Ctrl Pts',(-207.207682429284,-0.0917268848740953,
125.886966059358));
#126631=CARTESIAN_POINT('Ctrl Pts',(-207.215430326061,-0.228805768733537,
125.889523067719));
#126632=CARTESIAN_POINT('Ctrl Pts',(-207.223178222838,-0.365848546783255,
125.897817625703));
#126633=CARTESIAN_POINT('Ctrl Pts',(-207.230926119615,-0.502339680839985,
125.911831833026));
#126634=CARTESIAN_POINT('Ctrl Pts',(-207.238672395699,-0.638802263893879,
125.925843108879));
#126635=CARTESIAN_POINT('Ctrl Pts',(-207.246418671783,-0.774713043801706,
125.945571614404));
#126636=CARTESIAN_POINT('Ctrl Pts',(-207.254164947867,-0.909560661310067,
125.970947489569));
#126637=CARTESIAN_POINT('Ctrl Pts',(-207.261911281132,-1.04440927423309,
125.996323552053));
#126638=CARTESIAN_POINT('Ctrl Pts',(-207.269657614397,-1.17819432487519,
126.027346995058));
#126639=CARTESIAN_POINT('Ctrl Pts',(-207.277403947663,-1.3104141100234,
126.063896724364));
#126640=CARTESIAN_POINT('Ctrl Pts',(-207.285152015665,-1.44266350487555,
126.100454638729));
#126641=CARTESIAN_POINT('Ctrl Pts',(-207.292900083668,-1.57334655995862,
126.142541197874));
#126642=CARTESIAN_POINT('Ctrl Pts',(-207.300648151671,-1.70197659392866,
126.189985390494));
#126643=CARTESIAN_POINT('Ctrl Pts',(-207.308404454413,-1.8307433374297,
126.237480007366));
#126644=CARTESIAN_POINT('Ctrl Pts',(-207.316160757155,-1.95745233369282,
126.290343496894));
#126645=CARTESIAN_POINT('Ctrl Pts',(-207.323917059897,-2.08163624961235,
126.348356400019));
#126646=CARTESIAN_POINT('Ctrl Pts',(-207.331677502411,-2.20588644622692,
126.406400266377));
#126647=CARTESIAN_POINT('Ctrl Pts',(-207.339437944925,-2.32760853025468,
126.469598842679));
#126648=CARTESIAN_POINT('Ctrl Pts',(-207.347198387439,-2.44636055986463,
126.537687080296));
#126649=CARTESIAN_POINT('Ctrl Pts',(-207.354971287704,-2.56530322077482,
126.605884619197));
#126650=CARTESIAN_POINT('Ctrl Pts',(-207.36274418797,-2.68126596877018,
126.67898729624));
#126651=CARTESIAN_POINT('Ctrl Pts',(-207.370517088235,-2.79383585215566,
126.756686681376));
#126652=CARTESIAN_POINT('Ctrl Pts',(-207.378007423998,-2.90231353674432,
126.831561498158));
#126653=CARTESIAN_POINT('Ctrl Pts',(-207.38549775976,-3.00764050612485,
126.910704436435));
#126654=CARTESIAN_POINT('Ctrl Pts',(-207.392988095523,-3.10947838849646,
126.993805905457));
#126655=CARTESIAN_POINT('Ctrl Pts',(-207.400656660266,-3.21373945489434,
127.078884734452));
#126656=CARTESIAN_POINT('Ctrl Pts',(-207.40832522501,-3.31469263021925,
127.168398207827));
#126657=CARTESIAN_POINT('Ctrl Pts',(-207.415993789753,-3.41192943455653,
127.262056198673));
#126658=CARTESIAN_POINT('Ctrl Pts',(-207.423653568804,-3.50905483699829,
127.355606887786));
#126659=CARTESIAN_POINT('Ctrl Pts',(-207.431313347855,-3.60247204570966,
127.453292379642));
#126660=CARTESIAN_POINT('Ctrl Pts',(-207.438973126906,-3.69180383118984,
127.554781024063));
#126661=CARTESIAN_POINT('Ctrl Pts',(-207.446625896291,-3.78105386678786,
127.656176793538));
#126662=CARTESIAN_POINT('Ctrl Pts',(-207.454278665675,-3.86622564885268,
127.761368495727));
#126663=CARTESIAN_POINT('Ctrl Pts',(-207.461931435059,-3.946977576186,127.869986565816));
#126664=CARTESIAN_POINT('Ctrl Pts',(-207.469578964315,-4.02767420974882,
127.978530261176));
#126665=CARTESIAN_POINT('Ctrl Pts',(-207.477226493571,-4.10395676880122,
128.090495336564));
#126666=CARTESIAN_POINT('Ctrl Pts',(-207.484874022827,-4.17552322907947,
128.205478391316));
#126667=CARTESIAN_POINT('Ctrl Pts',(-207.49251889284,-4.24706480385526,
128.320421463497));
#126668=CARTESIAN_POINT('Ctrl Pts',(-207.500163762853,-4.31389332535797,
128.438380089298));
#126669=CARTESIAN_POINT('Ctrl Pts',(-207.507808632866,-4.37574973386624,
128.558921389025));
#126670=CARTESIAN_POINT('Ctrl Pts',(-207.515451815557,-4.4375924898678,
128.679436083734));
#126671=CARTESIAN_POINT('Ctrl Pts',(-207.523094998249,-4.49446513553793,
128.802531958918));
#126672=CARTESIAN_POINT('Ctrl Pts',(-207.53073818094,-4.54615461705261,
128.927751638489));
#126673=CARTESIAN_POINT('Ctrl Pts',(-207.538383674744,-4.59785972820617,
129.053009181439));
#126674=CARTESIAN_POINT('Ctrl Pts',(-207.546029168548,-4.64437838974133,
129.180391439886));
#126675=CARTESIAN_POINT('Ctrl Pts',(-207.553674662351,-4.68554579883754,
129.309421277828));
#126676=CARTESIAN_POINT('Ctrl Pts',(-207.559023655253,-4.71434762441938,
129.399694019515));
#126677=CARTESIAN_POINT('Ctrl Pts',(-207.564372648154,-4.74053114460319,
129.490772803549));
#126678=CARTESIAN_POINT('Ctrl Pts',(-207.569721641055,-4.76405452823393,
129.582490119308));
#126679=CARTESIAN_POINT('Origin',(213.235140564004,0.,130.804360617566));
#126680=CARTESIAN_POINT('',(-209.665424299527,-4.76405452823394,129.582490119308));
#126681=CARTESIAN_POINT('',(-209.319824802869,-4.76405452823399,129.582490119308));
#126682=CARTESIAN_POINT('',(213.235140564004,-4.76405452823405,129.582490119308));
#126683=CARTESIAN_POINT('',(-207.985140564043,-4.91824805552431,130.799987194266));
#126684=CARTESIAN_POINT('Ctrl Pts',(-207.985140564043,-4.91824805552431,
130.799987194267));
#126685=CARTESIAN_POINT('Ctrl Pts',(-207.992788080768,-4.91836794557653,
130.93481270186));
#126686=CARTESIAN_POINT('Ctrl Pts',(-208.000435597493,-4.91293964861326,
131.069820827236));
#126687=CARTESIAN_POINT('Ctrl Pts',(-208.008083114218,-4.90194487473793,
131.204509974095));
#126688=CARTESIAN_POINT('Ctrl Pts',(-208.015724146108,-4.89095942405694,
131.339084909138));
#126689=CARTESIAN_POINT('Ctrl Pts',(-208.023365177999,-4.87441691822112,
131.473341003815));
#126690=CARTESIAN_POINT('Ctrl Pts',(-208.03100620989,-4.85235112844437,
131.606776712111));
#126691=CARTESIAN_POINT('Ctrl Pts',(-208.038643191443,-4.83029703524341,
131.740141689157));
#126692=CARTESIAN_POINT('Ctrl Pts',(-208.046280172995,-4.8027255454322,
131.872686747673));
#126693=CARTESIAN_POINT('Ctrl Pts',(-208.053917154548,-4.76972222154673,
132.003915948421));
#126694=CARTESIAN_POINT('Ctrl Pts',(-208.06155211758,-4.73672762072607,
132.135110464153));
#126695=CARTESIAN_POINT('Ctrl Pts',(-208.069187080612,-4.69830413812791,
132.264989422662));
#126696=CARTESIAN_POINT('Ctrl Pts',(-208.076822043645,-4.6545882427032,
132.393068064955));
#126697=CARTESIAN_POINT('Ctrl Pts',(-208.084456753798,-4.61087379520155,
132.52114246513));
#126698=CARTESIAN_POINT('Ctrl Pts',(-208.092091463951,-4.56186741386925,
132.647416285964));
#126699=CARTESIAN_POINT('Ctrl Pts',(-208.099726174104,-4.50775496015573,
132.771421440645));
#126700=CARTESIAN_POINT('Ctrl Pts',(-208.107362396608,-4.45363178736365,
132.895451159376));
#126701=CARTESIAN_POINT('Ctrl Pts',(-208.114998619113,-4.39440069272263,
133.017210948925));
#126702=CARTESIAN_POINT('Ctrl Pts',(-208.122634841618,-4.33029480919843,
133.13625468204));
#126703=CARTESIAN_POINT('Ctrl Pts',(-208.130278840718,-4.26612364136049,
133.255419647217));
#126704=CARTESIAN_POINT('Ctrl Pts',(-208.137922839819,-4.19706796319404,
133.371862677257));
#126705=CARTESIAN_POINT('Ctrl Pts',(-208.145566838919,-4.12340598189315,
133.485163887295));
#126706=CARTESIAN_POINT('Ctrl Pts',(-208.153214944412,-4.04970442903014,
133.598525963275));
#126707=CARTESIAN_POINT('Ctrl Pts',(-208.160863049905,-3.97139187990211,
133.708742530803));
#126708=CARTESIAN_POINT('Ctrl Pts',(-208.168511155397,-3.88878784192218,
133.815425575852));
#126709=CARTESIAN_POINT('Ctrl Pts',(-208.176170926514,-3.80605780834674,
133.922271344106));
#126710=CARTESIAN_POINT('Ctrl Pts',(-208.18383069763,-3.71902347321935,
134.025572518618));
#126711=CARTESIAN_POINT('Ctrl Pts',(-208.191490468746,-3.62804267754195,
134.124976432808));
#126712=CARTESIAN_POINT('Ctrl Pts',(-208.197240969432,-3.55973970608588,
134.199602980784));
#126713=CARTESIAN_POINT('Ctrl Pts',(-208.202991470117,-3.48921325557276,
134.272033733371));
#126714=CARTESIAN_POINT('Ctrl Pts',(-208.208741970803,-3.4166267967544,
134.342134549603));
#126715=CARTESIAN_POINT('Ctrl Pts',(-208.216516304922,-3.31849423156944,
134.436906674189));
#126716=CARTESIAN_POINT('Ctrl Pts',(-208.224290639041,-3.21625998725054,
134.527742740487));
#126717=CARTESIAN_POINT('Ctrl Pts',(-208.23206497316,-3.1102729253396,134.614266835887));
#126718=CARTESIAN_POINT('Ctrl Pts',(-208.239829726106,-3.00441648301042,
134.700684298072));
#126719=CARTESIAN_POINT('Ctrl Pts',(-208.247594479054,-2.89481672543764,
134.782800118));
#126720=CARTESIAN_POINT('Ctrl Pts',(-208.255359232,-2.78185952678535,134.860274896213));
#126721=CARTESIAN_POINT('Ctrl Pts',(-208.263116272885,-2.66901451881519,
134.937672725384));
#126722=CARTESIAN_POINT('Ctrl Pts',(-208.27087331377,-2.55281902621447,
135.010438466342));
#126723=CARTESIAN_POINT('Ctrl Pts',(-208.278630354655,-2.43369191283578,
135.078272962935));
#126724=CARTESIAN_POINT('Ctrl Pts',(-208.286381545895,-2.31465463414012,
135.146056305006));
#126725=CARTESIAN_POINT('Ctrl Pts',(-208.294132737135,-2.19269047341665,
135.20891561186));
#126726=CARTESIAN_POINT('Ctrl Pts',(-208.301883928375,-2.06824688333898,
135.266595247441));
#126727=CARTESIAN_POINT('Ctrl Pts',(-208.309631825152,-1.94385618510623,
135.324250367639));
#126728=CARTESIAN_POINT('Ctrl Pts',(-208.317379721929,-1.81698850746676,
135.37673003111));
#126729=CARTESIAN_POINT('Ctrl Pts',(-208.325127618706,-1.68811529282284,
135.423824852803));
#126730=CARTESIAN_POINT('Ctrl Pts',(-208.33287389479,-1.55926903567759,
135.470909823275));
#126731=CARTESIAN_POINT('Ctrl Pts',(-208.340620170874,-1.4284184429477,
135.512612058317));
#126732=CARTESIAN_POINT('Ctrl Pts',(-208.348366446958,-1.29605392479125,
135.548770727004));
#126733=CARTESIAN_POINT('Ctrl Pts',(-208.356112780224,-1.16368842954982,
135.584929662605));
#126734=CARTESIAN_POINT('Ctrl Pts',(-208.363859113489,-1.0298093637282,
135.615544847168));
#126735=CARTESIAN_POINT('Ctrl Pts',(-208.371605446754,-0.894920862442862,
135.64050574695));
#126736=CARTESIAN_POINT('Ctrl Pts',(-208.379353514757,-0.760002153813462,
135.665472236552));
#126737=CARTESIAN_POINT('Ctrl Pts',(-208.38710158276,-0.624073944259812,
135.684781850579));
#126738=CARTESIAN_POINT('Ctrl Pts',(-208.394849650763,-0.487648692408282,
135.698375514896));
#126739=CARTESIAN_POINT('Ctrl Pts',(-208.402605953505,-0.351078446175044,
135.711983626722));
#126740=CARTESIAN_POINT('Ctrl Pts',(-208.410362256246,-0.214010492041764,
135.719863614585));
#126741=CARTESIAN_POINT('Ctrl Pts',(-208.418118558988,-0.0769610788796258,
135.72200843485));
#126742=CARTESIAN_POINT('Ctrl Pts',(-208.425879001502,0.0601614816807967,
135.724154399871));
#126743=CARTESIAN_POINT('Ctrl Pts',(-208.433639444016,0.197265090912087,
135.720559108173));
#126744=CARTESIAN_POINT('Ctrl Pts',(-208.44139988653,0.333836394172614,
135.711267619377));
#126745=CARTESIAN_POINT('Ctrl Pts',(-208.449172786796,0.470626933813368,
135.701961215059));
#126746=CARTESIAN_POINT('Ctrl Pts',(-208.456945687061,0.606883071075844,
135.6869403838));
#126747=CARTESIAN_POINT('Ctrl Pts',(-208.464718587327,0.742098547718523,
135.666301876772));
#126748=CARTESIAN_POINT('Ctrl Pts',(-208.47220892309,0.872398601215581,
135.646413631458));
#126749=CARTESIAN_POINT('Ctrl Pts',(-208.479699258852,1.00173203939671,
135.621309111393));
#126750=CARTESIAN_POINT('Ctrl Pts',(-208.487189594615,1.12965916458491,
135.591118730775));
#126751=CARTESIAN_POINT('Ctrl Pts',(-208.494963928734,1.26243668558986,
135.559783672703));
#126752=CARTESIAN_POINT('Ctrl Pts',(-208.502738262854,1.39411974704277,
135.522870220161));
#126753=CARTESIAN_POINT('Ctrl Pts',(-208.510512596973,1.52420351483378,
135.480468690298));
#126754=CARTESIAN_POINT('Ctrl Pts',(-208.51827734992,1.65412696600691,135.438119416531));
#126755=CARTESIAN_POINT('Ctrl Pts',(-208.526042102867,1.78245467704559,
135.39029564292));
#126756=CARTESIAN_POINT('Ctrl Pts',(-208.533806855814,1.90869252716161,
135.33713856263));
#126757=CARTESIAN_POINT('Ctrl Pts',(-208.541563896699,2.03480499606526,
135.284034278702));
#126758=CARTESIAN_POINT('Ctrl Pts',(-208.549320937584,2.15883137675045,
135.225607380339));
#126759=CARTESIAN_POINT('Ctrl Pts',(-208.557077978469,2.28029357453021,
135.162048568356));
#126760=CARTESIAN_POINT('Ctrl Pts',(-208.564829169709,2.40166417672196,
135.098537686567));
#126761=CARTESIAN_POINT('Ctrl Pts',(-208.572580360949,2.52047409985873,
135.029902774723));
#126762=CARTESIAN_POINT('Ctrl Pts',(-208.580331552189,2.63626641098722,
134.9563821099));
#126763=CARTESIAN_POINT('Ctrl Pts',(-208.588079448966,2.75200950729446,
134.88289269332));
#126764=CARTESIAN_POINT('Ctrl Pts',(-208.595827345743,2.86473721315403,
134.804521863035));
#126765=CARTESIAN_POINT('Ctrl Pts',(-208.60357524252,2.97401854085767,134.721553079156));
#126766=CARTESIAN_POINT('Ctrl Pts',(-208.611321518604,3.08327700926309,
134.638601650557));
#126767=CARTESIAN_POINT('Ctrl Pts',(-208.619067794688,3.18909022224706,
134.551054417686));
#126768=CARTESIAN_POINT('Ctrl Pts',(-208.626814070772,3.2910577895266,134.459237043452));
#126769=CARTESIAN_POINT('Ctrl Pts',(-208.634560404037,3.3930261095077,134.367418991443));
#126770=CARTESIAN_POINT('Ctrl Pts',(-208.642306737303,3.49114843660265,
134.271330996788));
#126771=CARTESIAN_POINT('Ctrl Pts',(-208.650053070568,3.58505927829805,
134.171337456451));
#126772=CARTESIAN_POINT('Ctrl Pts',(-208.657801138571,3.67899115067519,
134.071321523254));
#126773=CARTESIAN_POINT('Ctrl Pts',(-208.665549206574,3.7687093933284,133.967398588914));
#126774=CARTESIAN_POINT('Ctrl Pts',(-208.673297274577,3.85388730910897,
133.859967868374));
#126775=CARTESIAN_POINT('Ctrl Pts',(-208.681053577318,3.93915575299218,
133.752422969185));
#126776=CARTESIAN_POINT('Ctrl Pts',(-208.68880988006,4.01987398723393,133.641363143325));
#126777=CARTESIAN_POINT('Ctrl Pts',(-208.696566182802,4.09575704069982,
133.527218918333));
#126778=CARTESIAN_POINT('Ctrl Pts',(-208.704326625316,4.17168059523614,
133.413013771132));
#126779=CARTESIAN_POINT('Ctrl Pts',(-208.71208706783,4.24276362423822,133.295721278727));
#126780=CARTESIAN_POINT('Ctrl Pts',(-208.719847510344,4.30876655691763,
133.175797696741));
#126781=CARTESIAN_POINT('Ctrl Pts',(-208.72762041061,4.37487544336421,133.055681602776));
#126782=CARTESIAN_POINT('Ctrl Pts',(-208.735393310875,4.43588776304528,
132.932926329322));
#126783=CARTESIAN_POINT('Ctrl Pts',(-208.743166211141,4.49161127051699,
132.808010102148));
#126784=CARTESIAN_POINT('Ctrl Pts',(-208.750656546903,4.54530908813745,
132.687634894467));
#126785=CARTESIAN_POINT('Ctrl Pts',(-208.758146882666,4.59409582688949,
132.56525340371));
#126786=CARTESIAN_POINT('Ctrl Pts',(-208.765637218428,4.6378435405948,132.441306052045));
#126787=CARTESIAN_POINT('Ctrl Pts',(-208.773411552547,4.68324996215869,
132.312659198879));
#126788=CARTESIAN_POINT('Ctrl Pts',(-208.781185886666,4.72337154034538,
132.181917887059));
#126789=CARTESIAN_POINT('Ctrl Pts',(-208.788960220785,4.75801138636156,
132.049555666445));
#126790=CARTESIAN_POINT('Ctrl Pts',(-208.796724973733,4.79260854186337,
131.917356570439));
#126791=CARTESIAN_POINT('Ctrl Pts',(-208.80448972668,4.82173730907985,131.783540914914));
#126792=CARTESIAN_POINT('Ctrl Pts',(-208.812254479627,4.8452493934639,131.648600736038));
#126793=CARTESIAN_POINT('Ctrl Pts',(-208.820011520512,4.86873812531435,
131.51379458165));
#126794=CARTESIAN_POINT('Ctrl Pts',(-208.827768561397,4.88662120925884,
131.377866509247));
#126795=CARTESIAN_POINT('Ctrl Pts',(-208.835525602282,4.89880066543715,
131.241321831877));
#126796=CARTESIAN_POINT('Ctrl Pts',(-208.843276793522,4.91097093699282,
131.104880123912));
#126797=CARTESIAN_POINT('Ctrl Pts',(-208.851027984762,4.91744610736595,
130.967823124351));
#126798=CARTESIAN_POINT('Ctrl Pts',(-208.858779176003,4.91817966238524,
130.830664058409));
#126799=CARTESIAN_POINT('Ctrl Pts',(-208.86652707278,4.91891290562408,130.693563288729));
#126800=CARTESIAN_POINT('Ctrl Pts',(-208.874274969557,4.91390938507212,
130.556360929091));
#126801=CARTESIAN_POINT('Ctrl Pts',(-208.882022866334,4.90317462436412,
130.419572798773));
#126802=CARTESIAN_POINT('Ctrl Pts',(-208.889769142418,4.89244210913667,
130.282813281582));
#126803=CARTESIAN_POINT('Ctrl Pts',(-208.897515418502,4.87598076890379,
130.146468210885));
#126804=CARTESIAN_POINT('Ctrl Pts',(-208.905261694586,4.85384817236754,
130.011050475122));
#126805=CARTESIAN_POINT('Ctrl Pts',(-208.913008027852,4.83171541245352,
129.875631739737));
#126806=CARTESIAN_POINT('Ctrl Pts',(-208.920754361117,4.80391137576211,
129.741140738792));
#126807=CARTESIAN_POINT('Ctrl Pts',(-208.928500694382,4.77054508214752,
129.608081936949));
#126808=CARTESIAN_POINT('Ctrl Pts',(-208.936248762385,4.73717131638278,
129.474993337511));
#126809=CARTESIAN_POINT('Ctrl Pts',(-208.943996830388,4.69823291011487,
129.343337954543));
#126810=CARTESIAN_POINT('Ctrl Pts',(-208.951744898391,4.65388914639238,
129.213606433039));
#126811=CARTESIAN_POINT('Ctrl Pts',(-208.959501201133,4.60949825359005,
129.083737031329));
#126812=CARTESIAN_POINT('Ctrl Pts',(-208.967257503875,4.55969065397508,
128.955795946137));
#126813=CARTESIAN_POINT('Ctrl Pts',(-208.975013806617,4.50467452870077,
128.8302556424));
#126814=CARTESIAN_POINT('Ctrl Pts',(-208.982774249131,4.44962903966375,
128.704648334023));
#126815=CARTESIAN_POINT('Ctrl Pts',(-208.990534691645,4.38936965738045,
128.581444711373));
#126816=CARTESIAN_POINT('Ctrl Pts',(-208.99829513416,4.32415074876651,128.461092949449));
#126817=CARTESIAN_POINT('Ctrl Pts',(-209.006068034425,4.25882714497078,
128.340547988193));
#126818=CARTESIAN_POINT('Ctrl Pts',(-209.013840934691,4.18852830589864,
128.22286437192));
#126819=CARTESIAN_POINT('Ctrl Pts',(-209.021613834956,4.11355266307514,
128.108462334877));
#126820=CARTESIAN_POINT('Ctrl Pts',(-209.029104170718,4.04130257372357,
127.998219100045));
#126821=CARTESIAN_POINT('Ctrl Pts',(-209.036594506479,3.96470998351261,
127.891023249946));
#126822=CARTESIAN_POINT('Ctrl Pts',(-209.044084842241,3.88407627404977,
127.787220488261));
#126823=CARTESIAN_POINT('Ctrl Pts',(-209.05185917636,3.80038531298161,127.679482013312));
#126824=CARTESIAN_POINT('Ctrl Pts',(-209.059633510479,3.71207563759592,
127.57505772071));
#126825=CARTESIAN_POINT('Ctrl Pts',(-209.067407844598,3.6194392355984,127.474369223837));
#126826=CARTESIAN_POINT('Ctrl Pts',(-209.075172597545,3.52691699968669,
127.373804816537));
#126827=CARTESIAN_POINT('Ctrl Pts',(-209.082937350492,3.43007890902742,
127.276967329268));
#126828=CARTESIAN_POINT('Ctrl Pts',(-209.090702103439,3.32925877075882,
127.184247483999));
#126829=CARTESIAN_POINT('Ctrl Pts',(-209.098459144324,3.22853876847313,
127.091619729388));
#126830=CARTESIAN_POINT('Ctrl Pts',(-209.106216185209,3.12384487516857,
127.003101741029));
#126831=CARTESIAN_POINT('Ctrl Pts',(-209.113973226094,3.0155492645166,126.919049086199));
#126832=CARTESIAN_POINT('Ctrl Pts',(-209.121724417335,2.9073353204266,126.83505981613));
#126833=CARTESIAN_POINT('Ctrl Pts',(-209.129475608575,2.79552537279217,
126.755529415843));
#126834=CARTESIAN_POINT('Ctrl Pts',(-209.137226799815,2.68052607047514,
126.680774429792));
#126835=CARTESIAN_POINT('Ctrl Pts',(-209.144974696592,2.56557564592976,
126.606051216604));
#126836=CARTESIAN_POINT('Ctrl Pts',(-209.152722593369,2.44743888991785,
126.536099593413));
#126837=CARTESIAN_POINT('Ctrl Pts',(-209.160470490146,2.32655276146665,
126.471193725948));
#126838=CARTESIAN_POINT('Ctrl Pts',(-209.16821676623,2.20569191978752,126.406301435392));
#126839=CARTESIAN_POINT('Ctrl Pts',(-209.175963042314,2.08208319383041,
126.346452986013));
#126840=CARTESIAN_POINT('Ctrl Pts',(-209.183709318398,1.95618920845762,
126.291877172365));
#126841=CARTESIAN_POINT('Ctrl Pts',(-209.191455651664,1.83029429376386,
126.23730095585));
#126842=CARTESIAN_POINT('Ctrl Pts',(-209.199201984929,1.7021144447027,126.187997608234));
#126843=CARTESIAN_POINT('Ctrl Pts',(-209.206948318194,1.57213300957585,
126.144148083496));
#126844=CARTESIAN_POINT('Ctrl Pts',(-209.214696386197,1.44212246600765,
126.100288738961));
#126845=CARTESIAN_POINT('Ctrl Pts',(-209.2224444542,1.31030990393177,126.061885772592));
#126846=CARTESIAN_POINT('Ctrl Pts',(-209.230192522203,1.17719421325383,
126.02907038065));
#126847=CARTESIAN_POINT('Ctrl Pts',(-209.237948824945,1.04393704563628,
125.99622011212));
#126848=CARTESIAN_POINT('Ctrl Pts',(-209.245705127687,0.90937436297501,
125.968969374619));
#126849=CARTESIAN_POINT('Ctrl Pts',(-209.253461430428,0.774016190401353,
125.947398398288));
#126850=CARTESIAN_POINT('Ctrl Pts',(-209.261221872943,0.63858577309507,
125.925815908877));
#126851=CARTESIAN_POINT('Ctrl Pts',(-209.268982315457,0.502359408011086,
125.909919266368));
#126852=CARTESIAN_POINT('Ctrl Pts',(-209.276742757971,0.365851649000174,
125.899736714205));
#126853=CARTESIAN_POINT('Ctrl Pts',(-209.284515658236,0.229124755615908,
125.889537816105));
#126854=CARTESIAN_POINT('Ctrl Pts',(-209.292288558502,0.092115956609699,
125.885071351205));
#126855=CARTESIAN_POINT('Ctrl Pts',(-209.300061458767,-0.0446598835168608,
125.886313387485));
#126856=CARTESIAN_POINT('Ctrl Pts',(-209.307551794529,-0.176463577336899,
125.887510272618));
#126857=CARTESIAN_POINT('Ctrl Pts',(-209.315042130291,-0.308050647861612,
125.894007812595));
#126858=CARTESIAN_POINT('Ctrl Pts',(-209.322532466053,-0.438967340671629,
125.905739307817));
#126859=CARTESIAN_POINT('Ctrl Pts',(-209.330306800172,-0.57484777968248,
125.917915606247));
#126860=CARTESIAN_POINT('Ctrl Pts',(-209.338081134292,-0.710436431130188,
125.935769156352));
#126861=CARTESIAN_POINT('Ctrl Pts',(-209.345855468411,-0.845220753247153,
125.95928219294));
#126862=CARTESIAN_POINT('Ctrl Pts',(-209.353620221358,-0.979838965733497,
125.982766251811));
#126863=CARTESIAN_POINT('Ctrl Pts',(-209.361384974305,-1.11365443975783,
126.011895852824));
#126864=CARTESIAN_POINT('Ctrl Pts',(-209.369149727252,-1.24615801894924,
126.046601349349));
#126865=CARTESIAN_POINT('Ctrl Pts',(-209.376906768137,-1.37852999371783,
126.081272375885));
#126866=CARTESIAN_POINT('Ctrl Pts',(-209.384663809022,-1.50959229090726,
126.121508178528));
#126867=CARTESIAN_POINT('Ctrl Pts',(-209.392420849908,-1.63884459273675,
126.167187829826));
#126868=CARTESIAN_POINT('Ctrl Pts',(-209.400172041148,-1.76799942440017,
126.212833033743));
#126869=CARTESIAN_POINT('Ctrl Pts',(-209.407923232388,-1.8953466103871,
126.263913785318));
#126870=CARTESIAN_POINT('Ctrl Pts',(-209.415674423628,-2.02040002924071,
126.320259059356));
#126871=CARTESIAN_POINT('Ctrl Pts',(-209.423422320405,-2.14540029705488,
126.376580385148));
#126872=CARTESIAN_POINT('Ctrl Pts',(-209.431170217183,-2.26810838105454,
126.438161622791));
#126873=CARTESIAN_POINT('Ctrl Pts',(-209.43891811396,-2.38805743081934,
126.504783339553));
#126874=CARTESIAN_POINT('Ctrl Pts',(-209.446664390044,-2.50798138982873,
126.571391120487));
#126875=CARTESIAN_POINT('Ctrl Pts',(-209.454410666128,-2.62514712097876,
126.643037093649));
#126876=CARTESIAN_POINT('Ctrl Pts',(-209.462156942213,-2.73911207289486,
126.719455708682));
#126877=CARTESIAN_POINT('Ctrl Pts',(-209.469903275478,-2.85307786607418,
126.795874887821));
#126878=CARTESIAN_POINT('Ctrl Pts',(-209.477649608743,-2.96384250815246,
126.877066561391));
#126879=CARTESIAN_POINT('Ctrl Pts',(-209.485395942009,-3.07099249585687,
126.962721884826));
#126880=CARTESIAN_POINT('Ctrl Pts',(-209.493144010012,-3.17816647905854,
127.048396390176));
#126881=CARTESIAN_POINT('Ctrl Pts',(-209.500892078015,-3.28172389179726,
127.138536290411));
#126882=CARTESIAN_POINT('Ctrl Pts',(-209.508640146018,-3.38128469276149,
127.232792770108));
#126883=CARTESIAN_POINT('Ctrl Pts',(-209.51639644876,-3.48095130812937,
127.327149426712));
#126884=CARTESIAN_POINT('Ctrl Pts',(-209.524152751502,-3.57661254222479,
127.425631133395));
#126885=CARTESIAN_POINT('Ctrl Pts',(-209.531909054244,-3.66792521411793,
127.527852157919));
#126886=CARTESIAN_POINT('Ctrl Pts',(-209.539669496758,-3.75928662233343,
127.630127740881));
#126887=CARTESIAN_POINT('Ctrl Pts',(-209.547429939272,-3.84629459573451,
127.736146316386));
#126888=CARTESIAN_POINT('Ctrl Pts',(-209.555190381787,-3.92864724338677,
127.845490241978));
#126889=CARTESIAN_POINT('Ctrl Pts',(-209.562963282052,-4.01113209081997,
127.955009696147));
#126890=CARTESIAN_POINT('Ctrl Pts',(-209.570736182318,-4.08894645672586,
128.067864845666));
#126891=CARTESIAN_POINT('Ctrl Pts',(-209.578509082584,-4.1618321789507,
128.183609584608));
#126892=CARTESIAN_POINT('Ctrl Pts',(-209.585999418345,-4.23206832157534,
128.295146710731));
#126893=CARTESIAN_POINT('Ctrl Pts',(-209.593489754106,-4.29772778297644,
128.409366718959));
#126894=CARTESIAN_POINT('Ctrl Pts',(-209.600980089867,-4.35862141406717,
128.525851800086));
#126895=CARTESIAN_POINT('Ctrl Pts',(-209.609225337078,-4.42565219318398,
128.654076798391));
#126896=CARTESIAN_POINT('Ctrl Pts',(-209.617470584289,-4.48710001139767,
128.785413186329));
#126897=CARTESIAN_POINT('Ctrl Pts',(-209.6257158315,-4.5426830412027,128.919363575216));
#126898=CARTESIAN_POINT('Ctrl Pts',(-209.633941832449,-4.59813632770947,
129.053001293755));
#126899=CARTESIAN_POINT('Ctrl Pts',(-209.642167833397,-4.64775199956008,
129.189240552761));
#126900=CARTESIAN_POINT('Ctrl Pts',(-209.650393834346,-4.69129459316533,
129.327560664073));
#126901=CARTESIAN_POINT('Ctrl Pts',(-209.655403989406,-4.71781478773465,
129.411806363769));
#126902=CARTESIAN_POINT('Ctrl Pts',(-209.660414144467,-4.74208300097035,
129.496823467972));
#126903=CARTESIAN_POINT('Ctrl Pts',(-209.665424299527,-4.76405452823394,
129.582490119308));
#126904=CARTESIAN_POINT('Ctrl Pts',(-207.915133748109,-4.76405452823406,
129.582490119308));
#126905=CARTESIAN_POINT('Ctrl Pts',(-207.920187281069,-4.78612861629524,
129.668556653638));
#126906=CARTESIAN_POINT('Ctrl Pts',(-207.92524081403,-4.8058494769431,129.755142810851));
#126907=CARTESIAN_POINT('Ctrl Pts',(-207.930294346991,-4.82319964338405,
129.842108954767));
#126908=CARTESIAN_POINT('Ctrl Pts',(-207.94154281492,-4.86181872280981,
130.035683606093));
#126909=CARTESIAN_POINT('Ctrl Pts',(-207.95279128285,-4.88879425702603,
130.231652183515));
#126910=CARTESIAN_POINT('Ctrl Pts',(-207.96403975078,-4.90389504104624,
130.428865625719));
#126911=CARTESIAN_POINT('Ctrl Pts',(-207.971073355191,-4.91333747727461,
130.552182093851));
#126912=CARTESIAN_POINT('Ctrl Pts',(-207.978106959602,-4.91813778975611,
130.675984943192));
#126913=CARTESIAN_POINT('Ctrl Pts',(-207.985140564013,-4.91824805552383,
130.799987193734));
#126914=CARTESIAN_POINT('',(-207.639859435957,-4.91824901139309,130.80747901955));
#126915=CARTESIAN_POINT('Ctrl Pts',(-207.569721641055,-4.76405452823393,
129.582490119308));
#126916=CARTESIAN_POINT('Ctrl Pts',(-207.577373827926,-4.79770671860123,
129.713699498807));
#126917=CARTESIAN_POINT('Ctrl Pts',(-207.585026014798,-4.8259125172616,
129.846215817631));
#126918=CARTESIAN_POINT('Ctrl Pts',(-207.592678201669,-4.84859316521369,
129.979541012596));
#126919=CARTESIAN_POINT('Ctrl Pts',(-207.600541740717,-4.87190024903275,
130.11654862811));
#126920=CARTESIAN_POINT('Ctrl Pts',(-207.608405279765,-4.88937248762533,
130.254409993629));
#126921=CARTESIAN_POINT('Ctrl Pts',(-207.616268818813,-4.90098158156969,
130.392580822512));
#126922=CARTESIAN_POINT('Ctrl Pts',(-207.624132357861,-4.91259067551404,
130.530751651395));
#126923=CARTESIAN_POINT('Ctrl Pts',(-207.631995896909,-4.91833666685329,
130.669231486794));
#126924=CARTESIAN_POINT('Ctrl Pts',(-207.639859435957,-4.91824901139309,
130.80747901955));
#126925=CARTESIAN_POINT('Ctrl Pts',(-207.639859435995,-4.91824901139267,
130.807479020212));
#126926=CARTESIAN_POINT('Ctrl Pts',(-207.650384863776,-4.91813168363402,
130.992524762711));
#126927=CARTESIAN_POINT('Ctrl Pts',(-207.660910291556,-4.90757161966847,
131.177239249296));
#126928=CARTESIAN_POINT('Ctrl Pts',(-207.671435719336,-4.88667662202955,
131.360754950939));
#126929=CARTESIAN_POINT('Ctrl Pts',(-207.679210053455,-4.87124307420014,
131.496304062153));
#126930=CARTESIAN_POINT('Ctrl Pts',(-207.686984387574,-4.85014091170025,
131.631425231444));
#126931=CARTESIAN_POINT('Ctrl Pts',(-207.694758721693,-4.82340019419708,
131.765606490961));
#126932=CARTESIAN_POINT('Ctrl Pts',(-207.702523474641,-4.79669243223834,
131.899622384068));
#126933=CARTESIAN_POINT('Ctrl Pts',(-207.710288227588,-4.76436001742371,
132.032700292437));
#126934=CARTESIAN_POINT('Ctrl Pts',(-207.718052980535,-4.72648479467642,
132.164332877648));
#126935=CARTESIAN_POINT('Ctrl Pts',(-207.72581002142,-4.68864719013421,
132.29583472352));
#126936=CARTESIAN_POINT('Ctrl Pts',(-207.733567062305,-4.64527784065412,
132.425893729685));
#126937=CARTESIAN_POINT('Ctrl Pts',(-207.74132410319,-4.59650964511101,
132.554012624367));
#126938=CARTESIAN_POINT('Ctrl Pts',(-207.749075294431,-4.54777822604359,
132.682034903593));
#126939=CARTESIAN_POINT('Ctrl Pts',(-207.756826485671,-4.49365620313431,
132.808119619543));
#126940=CARTESIAN_POINT('Ctrl Pts',(-207.764577676911,-4.4343262179017,
132.931784894886));
#126941=CARTESIAN_POINT('Ctrl Pts',(-207.772325573688,-4.37502144949558,
133.055397609187));
#126942=CARTESIAN_POINT('Ctrl Pts',(-207.780073470465,-4.3105132900552,
133.176592576385));
#126943=CARTESIAN_POINT('Ctrl Pts',(-207.787821367242,-4.24103231224365,
133.294908346281));
#126944=CARTESIAN_POINT('Ctrl Pts',(-207.795567643327,-4.17156586835463,
133.413199367068));
#126945=CARTESIAN_POINT('Ctrl Pts',(-207.803313919411,-4.09712887297701,
133.528612051576));
#126946=CARTESIAN_POINT('Ctrl Pts',(-207.811060195495,-4.01799742000656,
133.64071034835));
#126947=CARTESIAN_POINT('Ctrl Pts',(-207.818806528761,-3.93886538290582,
133.752809472609));
#126948=CARTESIAN_POINT('Ctrl Pts',(-207.826552862026,-3.85503904453311,
133.861593840911));
#126949=CARTESIAN_POINT('Ctrl Pts',(-207.834299195291,-3.76683708345568,
133.966657480481));
#126950=CARTESIAN_POINT('Ctrl Pts',(-207.842047263294,-3.6786153701605,
134.071744648325));
#126951=CARTESIAN_POINT('Ctrl Pts',(-207.849795331298,-3.58601633562376,
134.173109130025));
#126952=CARTESIAN_POINT('Ctrl Pts',(-207.857543399301,-3.4893978147611,
134.270379364319));
#126953=CARTESIAN_POINT('Ctrl Pts',(-207.865299702043,-3.39267660658457,
134.367752978575));
#126954=CARTESIAN_POINT('Ctrl Pts',(-207.873056004784,-3.29192765434873,
134.461023375182));
#126955=CARTESIAN_POINT('Ctrl Pts',(-207.880812307526,-3.18754481460604,
134.549856728548));
#126956=CARTESIAN_POINT('Ctrl Pts',(-207.888572750041,-3.08310626259888,
134.638737494948));
#126957=CARTESIAN_POINT('Ctrl Pts',(-207.896333192555,-2.97503026636996,
134.723176258716));
#126958=CARTESIAN_POINT('Ctrl Pts',(-207.904093635069,-2.86374159265479,
134.80288123812));
#126959=CARTESIAN_POINT('Ctrl Pts',(-207.911866535335,-2.75227426848084,
134.882714167034));
#126960=CARTESIAN_POINT('Ctrl Pts',(-207.9196394356,-2.63758428823285,134.957797911912));
#126961=CARTESIAN_POINT('Ctrl Pts',(-207.927412335866,-2.52012382455114,
135.027885090258));
#126962=CARTESIAN_POINT('Ctrl Pts',(-207.934902671627,-2.40693334460267,
135.095424423125));
#126963=CARTESIAN_POINT('Ctrl Pts',(-207.942393007388,-2.29117058288348,
135.158324010965));
#126964=CARTESIAN_POINT('Ctrl Pts',(-207.949883343149,-2.17325776733692,
135.216404785433));
#126965=CARTESIAN_POINT('Ctrl Pts',(-207.957657677268,-2.05087425153848,
135.276687710124));
#126966=CARTESIAN_POINT('Ctrl Pts',(-207.965432011387,-1.92578675070595,
135.331970155687));
#126967=CARTESIAN_POINT('Ctrl Pts',(-207.973206345506,-1.79844224587773,
135.382000681042));
#126968=CARTESIAN_POINT('Ctrl Pts',(-207.980971098453,-1.67125468177061,
135.431969548246));
#126969=CARTESIAN_POINT('Ctrl Pts',(-207.9887358514,-1.54181600853049,135.476699232042));
#126970=CARTESIAN_POINT('Ctrl Pts',(-207.996500604347,-1.41059730351827,
135.515984362074));
#126971=CARTESIAN_POINT('Ctrl Pts',(-208.004257645232,-1.27950892677373,
135.55523047356));
#126972=CARTESIAN_POINT('Ctrl Pts',(-208.012014686117,-1.14664440867894,
135.589042681258));
#126973=CARTESIAN_POINT('Ctrl Pts',(-208.019771727002,-1.01249395315079,
135.617264009214));
#126974=CARTESIAN_POINT('Ctrl Pts',(-208.027522918242,-0.878444661524504,
135.645464055246));
#126975=CARTESIAN_POINT('Ctrl Pts',(-208.035274109482,-0.743111743707259,
135.668081533319));
#126976=CARTESIAN_POINT('Ctrl Pts',(-208.043025300722,-0.60699933894857,
135.685009638446));
#126977=CARTESIAN_POINT('Ctrl Pts',(-208.050773197499,-0.470944785593006,
135.701930548676));
#126978=CARTESIAN_POINT('Ctrl Pts',(-208.058521094276,-0.334111791395838,
135.713166847296));
#126979=CARTESIAN_POINT('Ctrl Pts',(-208.066268991053,-0.197013217634391,
135.718663096512));
#126980=CARTESIAN_POINT('Ctrl Pts',(-208.074015267137,-0.0599433219390715,
135.724158196032));
#126981=CARTESIAN_POINT('Ctrl Pts',(-208.081761543221,0.0773916524176224,
135.723915618745));
#126982=CARTESIAN_POINT('Ctrl Pts',(-208.089507819305,0.214475607502896,
135.717931953803));
#126983=CARTESIAN_POINT('Ctrl Pts',(-208.09725415257,0.351560574510971,
135.71194824469));
#126984=CARTESIAN_POINT('Ctrl Pts',(-208.105000485836,0.488394127956879,
135.700223380407));
#126985=CARTESIAN_POINT('Ctrl Pts',(-208.112746819101,0.624462457896682,
135.682806036055));
#126986=CARTESIAN_POINT('Ctrl Pts',(-208.120494887104,0.760561259395359,
135.66538479121));
#126987=CARTESIAN_POINT('Ctrl Pts',(-208.128242955107,0.895894108661634,
135.642268579239));
#126988=CARTESIAN_POINT('Ctrl Pts',(-208.13599102311,1.02995498217124,135.613557618854));
#126989=CARTESIAN_POINT('Ctrl Pts',(-208.143747325851,1.16415833717274,
135.584816144119));
#126990=CARTESIAN_POINT('Ctrl Pts',(-208.151503628593,1.29708663300382,
135.55046812487));
#126991=CARTESIAN_POINT('Ctrl Pts',(-208.159259931335,1.42824612365238,
135.510664482891));
#126992=CARTESIAN_POINT('Ctrl Pts',(-208.167020373849,1.55947561807024,
135.47083959651));
#126993=CARTESIAN_POINT('Ctrl Pts',(-208.174780816363,1.6889340573202,135.425553414362));
#126994=CARTESIAN_POINT('Ctrl Pts',(-208.182541258877,1.8161463603732,135.375005589581));
#126995=CARTESIAN_POINT('Ctrl Pts',(-208.190314159142,1.94356287590843,
135.324376620943));
#126996=CARTESIAN_POINT('Ctrl Pts',(-208.198087059408,2.06872569273712,
135.268469290505));
#126997=CARTESIAN_POINT('Ctrl Pts',(-208.205859959673,2.19118227060116,
135.207530307631));
#126998=CARTESIAN_POINT('Ctrl Pts',(-208.213350295436,2.30918724342625,
135.148806610272));
#126999=CARTESIAN_POINT('Ctrl Pts',(-208.220840631199,2.42467904848438,
135.085410883889));
#127000=CARTESIAN_POINT('Ctrl Pts',(-208.228330966962,2.53727880598606,
135.017601569991));
#127001=CARTESIAN_POINT('Ctrl Pts',(-208.236105301081,2.65414781750716,
134.947221245354));
#127002=CARTESIAN_POINT('Ctrl Pts',(-208.243879635201,2.76827135427662,
134.871863100413));
#127003=CARTESIAN_POINT('Ctrl Pts',(-208.25165396932,2.87919626762285,134.791767282932));
#127004=CARTESIAN_POINT('Ctrl Pts',(-208.259418722267,2.98998447592703,
134.711770176388));
#127005=CARTESIAN_POINT('Ctrl Pts',(-208.267183475215,3.09758159032083,
134.627047241368));
#127006=CARTESIAN_POINT('Ctrl Pts',(-208.274948228162,3.20156019808689,
134.537883800904));
#127007=CARTESIAN_POINT('Ctrl Pts',(-208.282705269047,3.30543553283387,
134.448808918827));
#127008=CARTESIAN_POINT('Ctrl Pts',(-208.290462309932,3.40569921821184,
134.355302561001));
#127009=CARTESIAN_POINT('Ctrl Pts',(-208.298219350818,3.50195421871368,
134.257692300526));
#127010=CARTESIAN_POINT('Ctrl Pts',(-208.305970542058,3.59813663257102,
134.160155648707));
#127011=CARTESIAN_POINT('Ctrl Pts',(-208.313721733299,3.6903161052074,134.058521531476));
#127012=CARTESIAN_POINT('Ctrl Pts',(-208.321472924539,3.778130278984,133.953156364756));
#127013=CARTESIAN_POINT('Ctrl Pts',(-208.329220821316,3.86590712939388,
133.847835981044));
#127014=CARTESIAN_POINT('Ctrl Pts',(-208.336968718093,3.94932212134805,
133.738788001574));
#127015=CARTESIAN_POINT('Ctrl Pts',(-208.344716614871,4.02805139941409,
133.626413945584));
#127016=CARTESIAN_POINT('Ctrl Pts',(-208.352462890955,4.10676420901237,
133.514063395824));
#127017=CARTESIAN_POINT('Ctrl Pts',(-208.360209167039,4.18079303010462,
133.398388473415));
#127018=CARTESIAN_POINT('Ctrl Pts',(-208.367955443124,4.24985602950842,
133.279821542515));
#127019=CARTESIAN_POINT('Ctrl Pts',(-208.375701776389,4.3189195387197,133.161253736382));
#127020=CARTESIAN_POINT('Ctrl Pts',(-208.383448109655,4.38301695631581,
133.039794216993));
#127021=CARTESIAN_POINT('Ctrl Pts',(-208.39119444292,4.44191150721355,132.915901577288));
#127022=CARTESIAN_POINT('Ctrl Pts',(-208.398942510924,4.50081924713754,
132.791981192686));
#127023=CARTESIAN_POINT('Ctrl Pts',(-208.406690578927,4.55452163403762,
132.665626956551));
#127024=CARTESIAN_POINT('Ctrl Pts',(-208.41443864693,4.60282946667902,132.537318771467));
#127025=CARTESIAN_POINT('Ctrl Pts',(-208.422194949672,4.65118864145976,
132.408874218917));
#127026=CARTESIAN_POINT('Ctrl Pts',(-208.429951252414,4.69414167092756,
132.278471935501));
#127027=CARTESIAN_POINT('Ctrl Pts',(-208.437707555156,4.73154864807493,
132.146608900635));
#127028=CARTESIAN_POINT('Ctrl Pts',(-208.445467997671,4.76897559045231,
132.014675486496));
#127029=CARTESIAN_POINT('Ctrl Pts',(-208.453228440185,4.80085049145022,
131.881280147467));
#127030=CARTESIAN_POINT('Ctrl Pts',(-208.460988882699,4.82708453200273,
131.746930500068));
#127031=CARTESIAN_POINT('Ctrl Pts',(-208.468761782965,4.85336068576608,
131.612365182688));
#127032=CARTESIAN_POINT('Ctrl Pts',(-208.476534683231,4.87397782505391,
131.476842882373));
#127033=CARTESIAN_POINT('Ctrl Pts',(-208.484307583496,4.88889890437966,
131.340877686498));
#127034=CARTESIAN_POINT('Ctrl Pts',(-208.491797919256,4.90327756488348,
131.209855168009));
#127035=CARTESIAN_POINT('Ctrl Pts',(-208.499288255016,4.91236708648847,
131.078421702932));
#127036=CARTESIAN_POINT('Ctrl Pts',(-208.506778590776,4.91618010957647,
130.947035747511));
#127037=CARTESIAN_POINT('Ctrl Pts',(-208.514552924895,4.92013770459477,
130.810668253622));
#127038=CARTESIAN_POINT('Ctrl Pts',(-208.522327259014,4.9184233222491,130.673919971935));
#127039=CARTESIAN_POINT('Ctrl Pts',(-208.530101593133,4.91099406772633,
130.53730195499));
#127040=CARTESIAN_POINT('Ctrl Pts',(-208.53786634608,4.90357396909578,130.400852307542));
#127041=CARTESIAN_POINT('Ctrl Pts',(-208.545631099026,4.89045303292205,
130.264532992051));
#127042=CARTESIAN_POINT('Ctrl Pts',(-208.553395851973,4.87164028253833,
130.128857827009));
#127043=CARTESIAN_POINT('Ctrl Pts',(-208.561152892858,4.8528462172435,129.993317416455));
#127044=CARTESIAN_POINT('Ctrl Pts',(-208.568909933743,4.82837164119221,
129.858420267914));
#127045=CARTESIAN_POINT('Ctrl Pts',(-208.576666974628,4.7982775435219,129.724677479866));
#127046=CARTESIAN_POINT('Ctrl Pts',(-208.584418165868,4.76820614004469,
129.591035548295));
#127047=CARTESIAN_POINT('Ctrl Pts',(-208.592169357107,4.73252373536271,
129.4585466244));
#127048=CARTESIAN_POINT('Ctrl Pts',(-208.599920548347,4.69134274241578,
129.327713626683));
#127049=CARTESIAN_POINT('Ctrl Pts',(-208.607668445124,4.65017925248945,
129.196936236481));
#127050=CARTESIAN_POINT('Ctrl Pts',(-208.615416341901,4.60352193964285,
129.067813744772));
#127051=CARTESIAN_POINT('Ctrl Pts',(-208.623164238678,4.55153356160966,
128.940835651261));
#127052=CARTESIAN_POINT('Ctrl Pts',(-208.630910514762,4.49955605842443,
128.81388411883));
#127053=CARTESIAN_POINT('Ctrl Pts',(-208.638656790846,4.44224985617784,
128.689076453966));
#127054=CARTESIAN_POINT('Ctrl Pts',(-208.64640306693,4.37982637736422,128.566883474298));
#127055=CARTESIAN_POINT('Ctrl Pts',(-208.654149400195,4.31740243775458,
128.44468959263));
#127056=CARTESIAN_POINT('Ctrl Pts',(-208.66189573346,4.24986132406468,128.325110782835));
#127057=CARTESIAN_POINT('Ctrl Pts',(-208.669642066725,4.17746088080643,
128.208594131182));
#127058=CARTESIAN_POINT('Ctrl Pts',(-208.677390134728,4.105044223971,128.092051386434));
#127059=CARTESIAN_POINT('Ctrl Pts',(-208.685138202731,4.02776627845415,
127.978572496404));
#127060=CARTESIAN_POINT('Ctrl Pts',(-208.692886270733,3.94592853200238,
127.868576040519));
#127061=CARTESIAN_POINT('Ctrl Pts',(-208.700642573475,3.86400380741969,
127.758462679091));
#127062=CARTESIAN_POINT('Ctrl Pts',(-208.708398876217,3.7775098348199,127.65183945947));
#127063=CARTESIAN_POINT('Ctrl Pts',(-208.716155178958,3.68678911390519,
127.549092718899));
#127064=CARTESIAN_POINT('Ctrl Pts',(-208.723915621472,3.59601997261018,
127.446291139299));
#127065=CARTESIAN_POINT('Ctrl Pts',(-208.731676063986,3.50101985852024,
127.34737044324));
#127066=CARTESIAN_POINT('Ctrl Pts',(-208.7394365065,3.40216783491512,127.252679735847));
#127067=CARTESIAN_POINT('Ctrl Pts',(-208.747209406765,3.30315712526576,
127.157837022523));
#127068=CARTESIAN_POINT('Ctrl Pts',(-208.754982307031,3.20028244321735,
127.067238125697));
#127069=CARTESIAN_POINT('Ctrl Pts',(-208.762755207296,3.0939562810473,126.981192089569));
#127070=CARTESIAN_POINT('Ctrl Pts',(-208.77024554306,2.99149534266338,126.898274043568));
#127071=CARTESIAN_POINT('Ctrl Pts',(-208.777735878824,2.8858297545026,126.819583773253));
#127072=CARTESIAN_POINT('Ctrl Pts',(-208.785226214587,2.77735206122495,
126.745358450714));
#127073=CARTESIAN_POINT('Ctrl Pts',(-208.793000548707,2.66476140326243,
126.668318852529));
#127074=CARTESIAN_POINT('Ctrl Pts',(-208.800774882826,2.54878453542897,
126.595845424432));
#127075=CARTESIAN_POINT('Ctrl Pts',(-208.808549216945,2.42982823500761,
126.528250491428));
#127076=CARTESIAN_POINT('Ctrl Pts',(-208.816313969892,2.31101853759509,
126.460738863137));
#127077=CARTESIAN_POINT('Ctrl Pts',(-208.824078722839,2.18923705020673,
126.398093958535));
#127078=CARTESIAN_POINT('Ctrl Pts',(-208.831843475786,2.06492094022386,
126.34058591748));
#127079=CARTESIAN_POINT('Ctrl Pts',(-208.839600516671,1.94072830275398,
126.283134994223));
#127080=CARTESIAN_POINT('Ctrl Pts',(-208.847357557556,1.81400640501634,
126.230810944377));
#127081=CARTESIAN_POINT('Ctrl Pts',(-208.855114598441,1.68521821475511,
126.183838717265));
#127082=CARTESIAN_POINT('Ctrl Pts',(-208.862865789681,1.55652714467016,
126.136901912276));
#127083=CARTESIAN_POINT('Ctrl Pts',(-208.870616980922,1.42577324939049,
126.095309030325));
#127084=CARTESIAN_POINT('Ctrl Pts',(-208.878368172162,1.29344041043454,
126.059237334957));
#127085=CARTESIAN_POINT('Ctrl Pts',(-208.886116068939,1.16116381646543,
126.023180971022));
#127086=CARTESIAN_POINT('Ctrl Pts',(-208.893863965716,1.02730998998639,
125.992641228963));
#127087=CARTESIAN_POINT('Ctrl Pts',(-208.901611862493,0.892378735491116,
125.967745762635));
#127088=CARTESIAN_POINT('Ctrl Pts',(-208.909358138577,0.7574757057055,125.942855503901));
#127089=CARTESIAN_POINT('Ctrl Pts',(-208.917104414661,0.621496080418521,
125.923607243392));
#127090=CARTESIAN_POINT('Ctrl Pts',(-208.924850690745,0.484950250857501,
125.910077593803));
#127091=CARTESIAN_POINT('Ctrl Pts',(-208.932597024011,0.348403413345999,
125.896547844342));
#127092=CARTESIAN_POINT('Ctrl Pts',(-208.940343357276,0.211290752280387,
125.888736828585));
#127093=CARTESIAN_POINT('Ctrl Pts',(-208.948089690541,0.0741277852576398,
125.886669275691));
#127094=CARTESIAN_POINT('Ctrl Pts',(-208.955837758544,-0.0630658984603644,
125.884601259783));
#127095=CARTESIAN_POINT('Ctrl Pts',(-208.963585826547,-0.200309519706907,
125.888279272036));
#127096=CARTESIAN_POINT('Ctrl Pts',(-208.97133389455,-0.337087954264749,
125.897675914674));
#127097=CARTESIAN_POINT('Ctrl Pts',(-208.979090197292,-0.474011758570708,
125.907082544177));
#127098=CARTESIAN_POINT('Ctrl Pts',(-208.986846500034,-0.610468997891036,
125.922219918342));
#127099=CARTESIAN_POINT('Ctrl Pts',(-208.994602802776,-0.745949506308154,
125.943008707188));
#127100=CARTESIAN_POINT('Ctrl Pts',(-209.00236324529,-0.881502324751852,
125.963808591636));
#127101=CARTESIAN_POINT('Ctrl Pts',(-209.010123687804,-1.01607699010257,
125.990265825674));
#127102=CARTESIAN_POINT('Ctrl Pts',(-209.017884130318,-1.14917489737068,
126.022250192476));
#127103=CARTESIAN_POINT('Ctrl Pts',(-209.025657030584,-1.28248646521542,
126.054285903423));
#127104=CARTESIAN_POINT('Ctrl Pts',(-209.033429930849,-1.41431616151418,
126.091866370262));
#127105=CARTESIAN_POINT('Ctrl Pts',(-209.041202831114,-1.54418101647718,
126.134811597494));
#127106=CARTESIAN_POINT('Ctrl Pts',(-209.048693166877,-1.66932495685847,
126.176195657547));
#127107=CARTESIAN_POINT('Ctrl Pts',(-209.056183502639,-1.79264414130074,
126.222561096243));
#127108=CARTESIAN_POINT('Ctrl Pts',(-209.063673838402,-1.91372685023181,
126.27370585195));
#127109=CARTESIAN_POINT('Ctrl Pts',(-209.071448601995,-2.03940738940923,
126.326792709108));
#127110=CARTESIAN_POINT('Ctrl Pts',(-209.079223365589,-2.1630763871519,
126.385197194931));
#127111=CARTESIAN_POINT('Ctrl Pts',(-209.086998129183,-2.28425112295715,
126.448745865345));
#127112=CARTESIAN_POINT('Ctrl Pts',(-209.094763213571,-2.4052750020561,
126.512215420726));
#127113=CARTESIAN_POINT('Ctrl Pts',(-209.102528297959,-2.52381045499339,
126.580816237645));
#127114=CARTESIAN_POINT('Ctrl Pts',(-209.110293382346,-2.63939384798977,
126.654326499912));
#127115=CARTESIAN_POINT('Ctrl Pts',(-209.118050657055,-2.75486099380381,
126.727762829751));
#127116=CARTESIAN_POINT('Ctrl Pts',(-209.125807931764,-2.86738166066909,
126.806098569736));
#127117=CARTESIAN_POINT('Ctrl Pts',(-209.133565206473,-2.97651631010486,
126.889065773218));
#127118=CARTESIAN_POINT('Ctrl Pts',(-209.14132602299,-3.08570078811257,
126.97207085777));
#127119=CARTESIAN_POINT('Ctrl Pts',(-209.149086839506,-3.19149581646136,
127.059711439138));
#127120=CARTESIAN_POINT('Ctrl Pts',(-209.156847656023,-3.29348919977197,
127.151675036588));
#127121=CARTESIAN_POINT('Ctrl Pts',(-209.164595213319,-3.39530832916146,
127.243481515832));
#127122=CARTESIAN_POINT('Ctrl Pts',(-209.172342770616,-3.49333849204953,
127.339596001324));
#127123=CARTESIAN_POINT('Ctrl Pts',(-209.180090327912,-3.58720222976018,
127.439666987337));
#127124=CARTESIAN_POINT('Ctrl Pts',(-209.187836127983,-3.68104467821264,
127.539715276224));
#127125=CARTESIAN_POINT('Ctrl Pts',(-209.195581928054,-3.77072231479238,
127.643717994952));
#127126=CARTESIAN_POINT('Ctrl Pts',(-209.203327728125,-3.85589491745125,
127.751287174612));
#127127=CARTESIAN_POINT('Ctrl Pts',(-209.211073448765,-3.94106664669009,
127.858855251181));
#127128=CARTESIAN_POINT('Ctrl Pts',(-209.218819169406,-4.0217331920826,
127.969989408906));
#127129=CARTESIAN_POINT('Ctrl Pts',(-209.226564890046,-4.09759522176032,
128.084269357864));
#127130=CARTESIAN_POINT('Ctrl Pts',(-209.234336549448,-4.17371129715035,
128.19893200593));
#127131=CARTESIAN_POINT('Ctrl Pts',(-209.24210820885,-4.24499039396231,
128.316761227611));
#127132=CARTESIAN_POINT('Ctrl Pts',(-209.249879868252,-4.31117491106617,
128.437304651034));
#127133=CARTESIAN_POINT('Ctrl Pts',(-209.257633629026,-4.37720700100607,
128.557570455265));
#127134=CARTESIAN_POINT('Ctrl Pts',(-209.265387389801,-4.43816780660334,
128.680537606677));
#127135=CARTESIAN_POINT('Ctrl Pts',(-209.273141150576,-4.49384871502306,
128.805734392134));
#127136=CARTESIAN_POINT('Ctrl Pts',(-209.280921759291,-4.5497224224962,
128.931364680247));
#127137=CARTESIAN_POINT('Ctrl Pts',(-209.288702368007,-4.60027945897932,
129.059239701905));
#127138=CARTESIAN_POINT('Ctrl Pts',(-209.296482976722,-4.64535888444512,
129.188865678791));
#127139=CARTESIAN_POINT('Ctrl Pts',(-209.304263585438,-4.69043830991079,
129.318491655677));
#127140=CARTESIAN_POINT('Ctrl Pts',(-209.312044194154,-4.73004005339845,
129.449868198166));
#127141=CARTESIAN_POINT('Ctrl Pts',(-209.319824802869,-4.76405452823398,
129.582490119308));
#127142=CARTESIAN_POINT('Origin',(213.235140564004,0.,130.804360617566));
#127143=CARTESIAN_POINT('',(-211.415108320184,-4.76405452823408,129.582490119308));
#127144=CARTESIAN_POINT('',(-211.070145064099,-4.76405452823395,129.582490119308));
#127145=CARTESIAN_POINT('',(213.235140564004,-4.76405452823405,129.582490119308));
#127146=CARTESIAN_POINT('',(-209.735140563965,-4.91824997503721,130.803865091055));
#127147=CARTESIAN_POINT('Ctrl Pts',(-209.735140564013,-4.91824997503729,
130.803865091902));
#127148=CARTESIAN_POINT('Ctrl Pts',(-209.743196689866,-4.91826438707087,
130.946909113438));
#127149=CARTESIAN_POINT('Ctrl Pts',(-209.751252815718,-4.91203396140685,
131.089852888571));
#127150=CARTESIAN_POINT('Ctrl Pts',(-209.759308941571,-4.89961085085684,
131.232141604364));
#127151=CARTESIAN_POINT('Ctrl Pts',(-209.767373658041,-4.88717449297359,
131.374582049149));
#127152=CARTESIAN_POINT('Ctrl Pts',(-209.77543837451,-4.86853230799063,
131.516365699231));
#127153=CARTESIAN_POINT('Ctrl Pts',(-209.78350309098,-4.84378796086789,
131.656945658868));
#127154=CARTESIAN_POINT('Ctrl Pts',(-209.791584921351,-4.81899110448103,
131.797823939175));
#127155=CARTESIAN_POINT('Ctrl Pts',(-209.799666751723,-4.78806625848942,
131.937493083153));
#127156=CARTESIAN_POINT('Ctrl Pts',(-209.807748582094,-4.75116801749538,
132.075417473898));
#127157=CARTESIAN_POINT('Ctrl Pts',(-209.815839159132,-4.71422984289908,
132.213491135113));
#127158=CARTESIAN_POINT('Ctrl Pts',(-209.82392973617,-4.67130547793691,
132.349815948105));
#127159=CARTESIAN_POINT('Ctrl Pts',(-209.832020313208,-4.62259852859672,
132.483874209626));
#127160=CARTESIAN_POINT('Ctrl Pts',(-209.840129193615,-4.57378138918253,
132.618235752095));
#127161=CARTESIAN_POINT('Ctrl Pts',(-209.848238074022,-4.5191556368364,
132.750320170896));
#127162=CARTESIAN_POINT('Ctrl Pts',(-209.856346954429,-4.45897267597615,
132.879630657199));
#127163=CARTESIAN_POINT('Ctrl Pts',(-209.864040540846,-4.40187196823782,
133.002318543942));
#127164=CARTESIAN_POINT('Ctrl Pts',(-209.871734127263,-4.3397691994306,
133.122509340562));
#127165=CARTESIAN_POINT('Ctrl Pts',(-209.87942771368,-4.27291533841665,
133.239802584278));
#127166=CARTESIAN_POINT('Ctrl Pts',(-209.887202047799,-4.20535981560865,
133.358326874139));
#127167=CARTESIAN_POINT('Ctrl Pts',(-209.894976381918,-4.13276202216405,
133.474225933839));
#127168=CARTESIAN_POINT('Ctrl Pts',(-209.902750716037,-4.05535116236854,
133.587040982318));
#127169=CARTESIAN_POINT('Ctrl Pts',(-209.910515468984,-3.97803570453932,
133.699716996333));
#127170=CARTESIAN_POINT('Ctrl Pts',(-209.918280221931,-3.8959192017021,
133.809316242246));
#127171=CARTESIAN_POINT('Ctrl Pts',(-209.926044974879,-3.80927663799556,
133.915404583459));
#127172=CARTESIAN_POINT('Ctrl Pts',(-209.933802015764,-3.72272012890474,
134.021387556237));
#127173=CARTESIAN_POINT('Ctrl Pts',(-209.941559056648,-3.63164675059403,
134.12386626291));
#127174=CARTESIAN_POINT('Ctrl Pts',(-209.949316097533,-3.53637445407398,
134.222435921458));
#127175=CARTESIAN_POINT('Ctrl Pts',(-209.957067288774,-3.44117400313397,
134.320931247859));
#127176=CARTESIAN_POINT('Ctrl Pts',(-209.964818480014,-3.34178120719801,
134.415523113659));
#127177=CARTESIAN_POINT('Ctrl Pts',(-209.972569671254,-3.23855368108763,
134.505840472599));
#127178=CARTESIAN_POINT('Ctrl Pts',(-209.980317568031,-3.13537002942939,
134.596119444252));
#127179=CARTESIAN_POINT('Ctrl Pts',(-209.988065464808,-3.02835518289397,
134.682127265576));
#127180=CARTESIAN_POINT('Ctrl Pts',(-209.995813361585,-2.91790277345313,
134.763530539049));
#127181=CARTESIAN_POINT('Ctrl Pts',(-210.003559637669,-2.80747346827526,
134.844916784711));
#127182=CARTESIAN_POINT('Ctrl Pts',(-210.011305913753,-2.69360834497568,
134.921700166518));
#127183=CARTESIAN_POINT('Ctrl Pts',(-210.019052189837,-2.5767328799856,
134.993588556901));
#127184=CARTESIAN_POINT('Ctrl Pts',(-210.026798523103,-2.45985655224754,
135.065477477947));
#127185=CARTESIAN_POINT('Ctrl Pts',(-210.034544856368,-2.33997017149051,
135.132471130634));
#127186=CARTESIAN_POINT('Ctrl Pts',(-210.042291189633,-2.21752651664132,
135.1943218031));
#127187=CARTESIAN_POINT('Ctrl Pts',(-210.050039257636,-2.09505544138409,
135.256186326595));
#127188=CARTESIAN_POINT('Ctrl Pts',(-210.057787325639,-1.97002630136351,
135.312905401805));
#127189=CARTESIAN_POINT('Ctrl Pts',(-210.065535393642,-1.84291432065546,
135.364278365642));
#127190=CARTESIAN_POINT('Ctrl Pts',(-210.073291696384,-1.71566724382218,
135.415705929277));
#127191=CARTESIAN_POINT('Ctrl Pts',(-210.081047999126,-1.58633326731982,
135.461775884578));
#127192=CARTESIAN_POINT('Ctrl Pts',(-210.088804301868,-1.4554058700633,
135.502336438692));
#127193=CARTESIAN_POINT('Ctrl Pts',(-210.096564744382,-1.32440859291271,
135.542918641195));
#127194=CARTESIAN_POINT('Ctrl Pts',(-210.104325186896,-1.19181657818618,
135.577985483336));
#127195=CARTESIAN_POINT('Ctrl Pts',(-210.11208562941,-1.05813516480963,
135.60743599023));
#127196=CARTESIAN_POINT('Ctrl Pts',(-210.119858529675,-0.924239154160643,
135.636933773692));
#127197=CARTESIAN_POINT('Ctrl Pts',(-210.127631429941,-0.789250635420359,
135.660797137288));
#127198=CARTESIAN_POINT('Ctrl Pts',(-210.135404330206,-0.653682658929158,
135.678976709518));
#127199=CARTESIAN_POINT('Ctrl Pts',(-210.142894665968,-0.523042919860747,
135.696495408506));
#127200=CARTESIAN_POINT('Ctrl Pts',(-210.15038500173,-0.391865427795292,
135.708736353318));
#127201=CARTESIAN_POINT('Ctrl Pts',(-210.157875337492,-0.26060881028972,
135.715701179011));
#127202=CARTESIAN_POINT('Ctrl Pts',(-210.165649671611,-0.12437555823472,
135.722930078188));
#127203=CARTESIAN_POINT('Ctrl Pts',(-210.17342400573,0.0123744837791795,
135.724497771247));
#127204=CARTESIAN_POINT('Ctrl Pts',(-210.181198339849,0.149131439737756,
135.720349111875));
#127205=CARTESIAN_POINT('Ctrl Pts',(-210.188963092796,0.285719854970061,
135.716205565356));
#127206=CARTESIAN_POINT('Ctrl Pts',(-210.196727845743,0.422314780159226,
135.706359695386));
#127207=CARTESIAN_POINT('Ctrl Pts',(-210.20449259869,0.558402328245245,
135.690808192473));
#127208=CARTESIAN_POINT('Ctrl Pts',(-210.212249639575,0.694354712260006,
135.675272135531));
#127209=CARTESIAN_POINT('Ctrl Pts',(-210.22000668046,0.82980033609962,135.654041767165));
#127210=CARTESIAN_POINT('Ctrl Pts',(-210.227763721345,0.96422678489746,
135.627165793995));
#127211=CARTESIAN_POINT('Ctrl Pts',(-210.235514912586,1.09855186166439,
135.600310088204));
#127212=CARTESIAN_POINT('Ctrl Pts',(-210.243266103826,1.23185891135041,
135.567817328034));
#127213=CARTESIAN_POINT('Ctrl Pts',(-210.251017295066,1.36364246268163,
135.529787825393));
#127214=CARTESIAN_POINT('Ctrl Pts',(-210.258765191843,1.49537000248827,
135.491774486305));
#127215=CARTESIAN_POINT('Ctrl Pts',(-210.26651308862,1.62557495697206,135.448229193382));
#127216=CARTESIAN_POINT('Ctrl Pts',(-210.274260985397,1.7537640616575,135.399302910842));
#127217=CARTESIAN_POINT('Ctrl Pts',(-210.282007261481,1.88192635194604,
135.350386862626));
#127218=CARTESIAN_POINT('Ctrl Pts',(-210.289753537565,2.0080732661324,135.296092202972));
#127219=CARTESIAN_POINT('Ctrl Pts',(-210.297499813649,2.13172904861533,
135.236618995164));
#127220=CARTESIAN_POINT('Ctrl Pts',(-210.305246146914,2.255385743897,135.177145348339));
#127221=CARTESIAN_POINT('Ctrl Pts',(-210.31299248018,2.37655091844898,135.112493246538));
#127222=CARTESIAN_POINT('Ctrl Pts',(-210.320738813445,2.49477142719497,
135.042909731184));
#127223=CARTESIAN_POINT('Ctrl Pts',(-210.328486881448,2.61301841060405,
134.973310633084));
#127224=CARTESIAN_POINT('Ctrl Pts',(-210.336234949451,2.72831907913344,
134.898778122168));
#127225=CARTESIAN_POINT('Ctrl Pts',(-210.343983017454,2.84024773902294,
134.819603554609));
#127226=CARTESIAN_POINT('Ctrl Pts',(-210.351739320196,2.95229535802428,
134.740344839378));
#127227=CARTESIAN_POINT('Ctrl Pts',(-210.359495622938,3.06096348964574,
134.65643443818));
#127228=CARTESIAN_POINT('Ctrl Pts',(-210.36725192568,3.16585768885339,134.568205481057));
#127229=CARTESIAN_POINT('Ctrl Pts',(-210.375012368194,3.27080787325346,
134.479929433483));
#127230=CARTESIAN_POINT('Ctrl Pts',(-210.382772810708,3.37197982339132,
134.387330501026));
#127231=CARTESIAN_POINT('Ctrl Pts',(-210.390533253222,3.46901543820338,
134.290779260243));
#127232=CARTESIAN_POINT('Ctrl Pts',(-210.398306153487,3.56620682319875,
134.194073026837));
#127233=CARTESIAN_POINT('Ctrl Pts',(-210.406079053753,3.65924833849426,
134.093402093866));
#127234=CARTESIAN_POINT('Ctrl Pts',(-210.413851954018,3.74782113020959,
133.989171418611));
#127235=CARTESIAN_POINT('Ctrl Pts',(-210.421342289781,3.83317407784731,
133.88872979094));
#127236=CARTESIAN_POINT('Ctrl Pts',(-210.428832625543,3.91437737005352,
133.784982981394));
#127237=CARTESIAN_POINT('Ctrl Pts',(-210.436322961305,3.9911844830499,133.678317730113));
#127238=CARTESIAN_POINT('Ctrl Pts',(-210.444097295424,4.07090376107842,
133.567608233413));
#127239=CARTESIAN_POINT('Ctrl Pts',(-210.451871629543,4.14613944366244,
133.453403926496));
#127240=CARTESIAN_POINT('Ctrl Pts',(-210.459645963662,4.21656953420747,
133.336103974562));
#127241=CARTESIAN_POINT('Ctrl Pts',(-210.467410716609,4.28691282596003,
133.218948584336));
#127242=CARTESIAN_POINT('Ctrl Pts',(-210.475175469556,4.352462110286,133.098705471988));
#127243=CARTESIAN_POINT('Ctrl Pts',(-210.482940222504,4.41293683430738,
132.975805196392));
#127244=CARTESIAN_POINT('Ctrl Pts',(-210.490697263389,4.47335149398065,
132.853026987082));
#127245=CARTESIAN_POINT('Ctrl Pts',(-210.498454304274,4.52870145192803,
132.727597215043));
#127246=CARTESIAN_POINT('Ctrl Pts',(-210.506211345159,4.57875071365639,
132.599973316533));
#127247=CARTESIAN_POINT('Ctrl Pts',(-210.513962536399,4.62876223284708,
132.472445660197));
#127248=CARTESIAN_POINT('Ctrl Pts',(-210.521713727639,4.6734808700339,132.342727533292));
#127249=CARTESIAN_POINT('Ctrl Pts',(-210.529464918879,4.71271780089766,
132.211298424152));
#127250=CARTESIAN_POINT('Ctrl Pts',(-210.537212815656,4.75193805501908,
132.079925175891));
#127251=CARTESIAN_POINT('Ctrl Pts',(-210.544960712433,4.78568112514685,
131.946842765609));
#127252=CARTESIAN_POINT('Ctrl Pts',(-210.55270860921,4.81380740025742,131.812547790529));
#127253=CARTESIAN_POINT('Ctrl Pts',(-210.560454885294,4.84192779195757,
131.678280907063));
#127254=CARTESIAN_POINT('Ctrl Pts',(-210.568201161378,4.86443364551295,
131.542802345727));
#127255=CARTESIAN_POINT('Ctrl Pts',(-210.575947437463,4.88123612230785,
131.406620512277));
#127256=CARTESIAN_POINT('Ctrl Pts',(-210.583693770728,4.89803872313483,
131.270437673563));
#127257=CARTESIAN_POINT('Ctrl Pts',(-210.591440103993,4.90913781531647,
131.133551940397));
#127258=CARTESIAN_POINT('Ctrl Pts',(-210.599186437259,4.91449630581469,
130.996478088489));
#127259=CARTESIAN_POINT('Ctrl Pts',(-210.606934505262,4.91985599630972,
130.859373539841));
#127260=CARTESIAN_POINT('Ctrl Pts',(-210.614682573265,4.9194725117209,130.722081179214));
#127261=CARTESIAN_POINT('Ctrl Pts',(-210.622430641268,4.91336088037301,
130.585116639952));
#127262=CARTESIAN_POINT('Ctrl Pts',(-210.630186944009,4.90724275351062,
130.448006533148));
#127263=CARTESIAN_POINT('Ctrl Pts',(-210.637943246751,4.89538433602431,
130.3112253349));
#127264=CARTESIAN_POINT('Ctrl Pts',(-210.645699549493,4.87785269247762,
130.175284967911));
#127265=CARTESIAN_POINT('Ctrl Pts',(-210.653459992007,4.8603116917649,130.039272045455));
#127266=CARTESIAN_POINT('Ctrl Pts',(-210.661220434522,4.83709149766175,
129.904101233618));
#127267=CARTESIAN_POINT('Ctrl Pts',(-210.668980877036,4.80831032435012,
129.770274118646));
#127268=CARTESIAN_POINT('Ctrl Pts',(-210.676753777301,4.77948294894402,
129.636232172509));
#127269=CARTESIAN_POINT('Ctrl Pts',(-210.684526677567,4.74507685356864,
129.503538612323));
#127270=CARTESIAN_POINT('Ctrl Pts',(-210.692299577832,4.70526039194284,
129.37268058819));
#127271=CARTESIAN_POINT('Ctrl Pts',(-210.699789913594,4.66689135898908,
129.246579582847));
#127272=CARTESIAN_POINT('Ctrl Pts',(-210.707280249356,4.62349859279517,
129.122183268605));
#127273=CARTESIAN_POINT('Ctrl Pts',(-210.714770585118,4.5752742166704,128.999908095395));
#127274=CARTESIAN_POINT('Ctrl Pts',(-210.722544919237,4.52522139866675,
128.872996821825));
#127275=CARTESIAN_POINT('Ctrl Pts',(-210.730319253356,4.46980480499287,
128.747968693797));
#127276=CARTESIAN_POINT('Ctrl Pts',(-210.738093587475,4.40918621761393,
128.625310374707));
#127277=CARTESIAN_POINT('Ctrl Pts',(-210.745858340422,4.34864233722662,
128.502803221033));
#127278=CARTESIAN_POINT('Ctrl Pts',(-210.75362309337,4.282909390654,128.382660412352));
#127279=CARTESIAN_POINT('Ctrl Pts',(-210.761387846317,4.21219797358922,
128.265350713333));
#127280=CARTESIAN_POINT('Ctrl Pts',(-210.769144887202,4.14155678810053,
128.148157527962));
#127281=CARTESIAN_POINT('Ctrl Pts',(-210.776901928087,4.06594717279689,
128.033792185169));
#127282=CARTESIAN_POINT('Ctrl Pts',(-210.784658968972,3.98562642096889,
127.922700489276));
#127283=CARTESIAN_POINT('Ctrl Pts',(-210.792410160212,3.90536623964476,
127.811692568496));
#127284=CARTESIAN_POINT('Ctrl Pts',(-210.800161351452,3.82040222138373,
127.703953696399));
#127285=CARTESIAN_POINT('Ctrl Pts',(-210.807912542692,3.73103570914607,
127.599901911392));
#127286=CARTESIAN_POINT('Ctrl Pts',(-210.815660439469,3.64170718005991,
127.495894351168));
#127287=CARTESIAN_POINT('Ctrl Pts',(-210.823408336246,3.54798013282419,
127.39557105714));
#127288=CARTESIAN_POINT('Ctrl Pts',(-210.831156233023,3.45019690557752,
127.299317910944));
#127289=CARTESIAN_POINT('Ctrl Pts',(-210.838902509108,3.35243413247403,
127.203084898831));
#127290=CARTESIAN_POINT('Ctrl Pts',(-210.846648785192,3.25061714545276,
127.110920615187));
#127291=CARTESIAN_POINT('Ctrl Pts',(-210.854395061276,3.1451256612314,127.023174608182));
#127292=CARTESIAN_POINT('Ctrl Pts',(-210.862141394541,3.03963339829572,
126.935427953456));
#127293=CARTESIAN_POINT('Ctrl Pts',(-210.869887727807,2.93046688461224,
126.852099890465));
#127294=CARTESIAN_POINT('Ctrl Pts',(-210.877634061072,2.81803916587099,
126.773499875477));
#127295=CARTESIAN_POINT('Ctrl Pts',(-210.885382129075,2.70558626972242,
126.694882258561));
#127296=CARTESIAN_POINT('Ctrl Pts',(-210.893130197078,2.58987103561829,
126.620995020536));
#127297=CARTESIAN_POINT('Ctrl Pts',(-210.900878265081,2.4713354036721,126.552104230063));
#127298=CARTESIAN_POINT('Ctrl Pts',(-210.908634567823,2.35267379064488,
126.483140221639));
#127299=CARTESIAN_POINT('Ctrl Pts',(-210.916390870565,2.23118613040431,
126.419183465398));
#127300=CARTESIAN_POINT('Ctrl Pts',(-210.924147173307,2.1073393680538,126.36045424475));
#127301=CARTESIAN_POINT('Ctrl Pts',(-210.931907615821,1.9834265049576,126.301693678549));
#127302=CARTESIAN_POINT('Ctrl Pts',(-210.939668058335,1.85715239062455,
126.24816635995));
#127303=CARTESIAN_POINT('Ctrl Pts',(-210.947428500849,1.72900292142403,
126.200043951631));
#127304=CARTESIAN_POINT('Ctrl Pts',(-210.955201401115,1.60064773531863,
126.15184429295));
#127305=CARTESIAN_POINT('Ctrl Pts',(-210.96297430138,1.4704115500907,126.10906700492));
#127306=CARTESIAN_POINT('Ctrl Pts',(-210.970747201646,1.33879521821518,
126.071833763317));
#127307=CARTESIAN_POINT('Ctrl Pts',(-210.978237537407,1.2119634715277,126.035954043833));
#127308=CARTESIAN_POINT('Ctrl Pts',(-210.985727873169,1.08385047921586,
126.005222360583));
#127309=CARTESIAN_POINT('Ctrl Pts',(-210.993218208931,0.954910459740987,
125.979702176145));
#127310=CARTESIAN_POINT('Ctrl Pts',(-211.00099254305,0.821081640234792,
125.953214386157));
#127311=CARTESIAN_POINT('Ctrl Pts',(-211.008766877169,0.685937912638592,
125.932257178713));
#127312=CARTESIAN_POINT('Ctrl Pts',(-211.016541211288,0.549976167754722,
125.916957495518));
#127313=CARTESIAN_POINT('Ctrl Pts',(-211.024305964236,0.414181983569803,
125.901676667816));
#127314=CARTESIAN_POINT('Ctrl Pts',(-211.032070717183,0.277572172765213,
125.892039534677));
#127315=CARTESIAN_POINT('Ctrl Pts',(-211.03983547013,0.140654952451376,
125.888122294737));
#127316=CARTESIAN_POINT('Ctrl Pts',(-211.047592511015,0.00387372025132052,
125.884208945455));
#127317=CARTESIAN_POINT('Ctrl Pts',(-211.0553495519,-0.13321392557411,125.886004194877));
#127318=CARTESIAN_POINT('Ctrl Pts',(-211.063106592785,-0.270093843915168,
125.893532542997));
#127319=CARTESIAN_POINT('Ctrl Pts',(-211.070857784025,-0.40687054004522,
125.90105521393));
#127320=CARTESIAN_POINT('Ctrl Pts',(-211.078608975265,-0.543439431695396,
125.914302356763));
#127321=CARTESIAN_POINT('Ctrl Pts',(-211.086360166505,-0.67928592808505,
125.933246403097));
#127322=CARTESIAN_POINT('Ctrl Pts',(-211.094108063282,-0.815074686089728,
125.952182397706));
#127323=CARTESIAN_POINT('Ctrl Pts',(-211.101855960059,-0.950141273099997,
125.976810426078));
#127324=CARTESIAN_POINT('Ctrl Pts',(-211.109603856837,-1.08397599384027,
126.007051047893));
#127325=CARTESIAN_POINT('Ctrl Pts',(-211.117350132921,-1.21778271924211,
126.037285344021));
#127326=CARTESIAN_POINT('Ctrl Pts',(-211.125096409005,-1.35035770980363,
126.073129812261));
#127327=CARTESIAN_POINT('Ctrl Pts',(-211.132842685089,-1.48120163458712,
126.114453925509));
#127328=CARTESIAN_POINT('Ctrl Pts',(-211.140589018354,-1.61204652523055,
126.155778343803));
#127329=CARTESIAN_POINT('Ctrl Pts',(-211.14833535162,-1.74115995178414,
126.202582370073));
#127330=CARTESIAN_POINT('Ctrl Pts',(-211.156081684885,-1.86805829864045,
126.254685765955));
#127331=CARTESIAN_POINT('Ctrl Pts',(-211.163829752888,-1.99498506350151,
126.306800830031));
#127332=CARTESIAN_POINT('Ctrl Pts',(-211.171577820891,-2.11969539998282,
126.36421747676));
#127333=CARTESIAN_POINT('Ctrl Pts',(-211.179325888894,-2.24172657755652,
126.426707706019));
#127334=CARTESIAN_POINT('Ctrl Pts',(-211.187082191636,-2.3638874513181,
126.489264350637));
#127335=CARTESIAN_POINT('Ctrl Pts',(-211.194838494378,-2.48336312955346,
126.556905170928));
#127336=CARTESIAN_POINT('Ctrl Pts',(-211.20259479712,-2.59971588635782,
126.629356381314));
#127337=CARTESIAN_POINT('Ctrl Pts',(-211.210355239634,-2.71613074413179,
126.701846261094));
#127338=CARTESIAN_POINT('Ctrl Pts',(-211.218115682148,-2.82941903645592,
126.77915142657));
#127339=CARTESIAN_POINT('Ctrl Pts',(-211.225876124662,-2.93917369979947,
126.860955867238));
#127340=CARTESIAN_POINT('Ctrl Pts',(-211.233649024928,-3.04910455107218,
126.942891627657));
#127341=CARTESIAN_POINT('Ctrl Pts',(-211.241421925193,-3.15549013431897,
127.029340849696));
#127342=CARTESIAN_POINT('Ctrl Pts',(-211.249194825458,-3.2579573572653,
127.119947920712));
#127343=CARTESIAN_POINT('Ctrl Pts',(-211.256685161221,-3.35669963855956,
127.207261196472));
#127344=CARTESIAN_POINT('Ctrl Pts',(-211.264175496983,-3.45180327572581,
127.298435059796));
#127345=CARTESIAN_POINT('Ctrl Pts',(-211.271665832745,-3.54296935972677,
127.393121666901));
#127346=CARTESIAN_POINT('Ctrl Pts',(-211.279339833884,-3.63637086463484,
127.49013001924));
#127347=CARTESIAN_POINT('Ctrl Pts',(-211.287013835023,-3.72595178177155,
127.591150574736));
#127348=CARTESIAN_POINT('Ctrl Pts',(-211.294687836162,-3.81134085198831,
127.695845864108));
#127349=CARTESIAN_POINT('Ctrl Pts',(-211.30235279395,-3.89662929630337,
127.800417776356));
#127350=CARTESIAN_POINT('Ctrl Pts',(-211.310017751738,-3.97773546367402,
127.908655504759));
#127351=CARTESIAN_POINT('Ctrl Pts',(-211.317682709527,-4.05432414393831,
128.020184114832));
#127352=CARTESIAN_POINT('Ctrl Pts',(-211.3253403984,-4.13084019279955,128.131606958891));
#127353=CARTESIAN_POINT('Ctrl Pts',(-211.332998087273,-4.20284704831621,
128.246314149174));
#127354=CARTESIAN_POINT('Ctrl Pts',(-211.340655776146,-4.27004945328258,
128.363897397392));
#127355=CARTESIAN_POINT('Ctrl Pts',(-211.348307502504,-4.33719953236235,
128.48138909163));
#127356=CARTESIAN_POINT('Ctrl Pts',(-211.355959228862,-4.39955240749439,
128.601752039367));
#127357=CARTESIAN_POINT('Ctrl Pts',(-211.36361095522,-4.45685623973759,
128.724549202843));
#127358=CARTESIAN_POINT('Ctrl Pts',(-211.371259291001,-4.5141346799327,
128.847291953353));
#127359=CARTESIAN_POINT('Ctrl Pts',(-211.378907626783,-4.56636835876335,
128.972466410226));
#127360=CARTESIAN_POINT('Ctrl Pts',(-211.386555962565,-4.61335166716167,
129.099611528229));
#127361=CARTESIAN_POINT('Ctrl Pts',(-211.394203146325,-4.66032789875526,
129.226737495149));
#127362=CARTESIAN_POINT('Ctrl Pts',(-211.401850330086,-4.70205519260479,
129.35583315652));
#127363=CARTESIAN_POINT('Ctrl Pts',(-211.409497513846,-4.73837648641222,
129.486418534045));
#127364=CARTESIAN_POINT('Ctrl Pts',(-211.411367782625,-4.74725957121321,
129.518355749401));
#127365=CARTESIAN_POINT('Ctrl Pts',(-211.413238051405,-4.75581953262355,
129.550381996406));
#127366=CARTESIAN_POINT('Ctrl Pts',(-211.415108320184,-4.76405452823408,
129.582490119308));
#127367=CARTESIAN_POINT('Ctrl Pts',(-209.665424299527,-4.76405452823394,
129.582490119308));
#127368=CARTESIAN_POINT('Ctrl Pts',(-209.673625365142,-4.80001947035231,
129.722716882783));
#127369=CARTESIAN_POINT('Ctrl Pts',(-209.681826430757,-4.82982807170211,
129.86468490532));
#127370=CARTESIAN_POINT('Ctrl Pts',(-209.690027496371,-4.85332304546196,
130.007844152647));
#127371=CARTESIAN_POINT('Ctrl Pts',(-209.698210356522,-4.87676586296161,
130.150685602174));
#127372=CARTESIAN_POINT('Ctrl Pts',(-209.706393216672,-4.89392295084962,
130.294712688466));
#127373=CARTESIAN_POINT('Ctrl Pts',(-209.714576076822,-4.90468758703764,
130.439363718868));
#127374=CARTESIAN_POINT('Ctrl Pts',(-209.72143090587,-4.91370518473249,
130.560538719633));
#127375=CARTESIAN_POINT('Ctrl Pts',(-209.728285734918,-4.91823771204663,
130.68215121371));
#127376=CARTESIAN_POINT('Ctrl Pts',(-209.735140563965,-4.91824997503721,
130.803865091054));
#127377=CARTESIAN_POINT('',(-209.389859436045,-4.91824827956038,130.80024684784));
#127378=CARTESIAN_POINT('Ctrl Pts',(-209.319824802869,-4.76405452823398,
129.582490119308));
#127379=CARTESIAN_POINT('Ctrl Pts',(-209.327257022651,-4.79654595171651,
129.70917368634));
#127380=CARTESIAN_POINT('Ctrl Pts',(-209.334689242432,-4.82393958829447,
129.836993228704));
#127381=CARTESIAN_POINT('Ctrl Pts',(-209.342121462214,-4.84618427704989,
129.965503648009));
#127382=CARTESIAN_POINT('Ctrl Pts',(-209.354271274709,-4.8825487556775,
130.17558590394));
#127383=CARTESIAN_POINT('Ctrl Pts',(-209.366421087205,-4.90525992748157,
130.388095669113));
#127384=CARTESIAN_POINT('Ctrl Pts',(-209.378570899701,-4.91406934757996,
130.601615680083));
#127385=CARTESIAN_POINT('Ctrl Pts',(-209.382333745132,-4.91679766015132,
130.667743679844));
#127386=CARTESIAN_POINT('Ctrl Pts',(-209.386096590564,-4.91819284223868,
130.7339683558));
#127387=CARTESIAN_POINT('Ctrl Pts',(-209.389859435995,-4.91824827955965,
130.800246846965));
#127388=CARTESIAN_POINT('Ctrl Pts',(-209.389859436045,-4.91824827956038,
130.80024684784));
#127389=CARTESIAN_POINT('Ctrl Pts',(-209.397506456235,-4.91836094170136,
130.934940916295));
#127390=CARTESIAN_POINT('Ctrl Pts',(-209.405153476426,-4.91293622999767,
131.069832323817));
#127391=CARTESIAN_POINT('Ctrl Pts',(-209.412800496617,-4.90195219649436,
131.204420270348));
#127392=CARTESIAN_POINT('Ctrl Pts',(-209.420440385843,-4.89097840577219,
131.338882711537));
#127393=CARTESIAN_POINT('Ctrl Pts',(-209.428080275069,-4.87445563693796,
131.473041854784));
#127394=CARTESIAN_POINT('Ctrl Pts',(-209.435720164295,-4.85241399032164,
131.606396482743));
#127395=CARTESIAN_POINT('Ctrl Pts',(-209.4434222027,-4.83019303871642,131.740835927572));
#127396=CARTESIAN_POINT('Ctrl Pts',(-209.451124241106,-4.80236300573932,
131.874457293552));
#127397=CARTESIAN_POINT('Ctrl Pts',(-209.458826279512,-4.7690082265291,
132.006751401711));
#127398=CARTESIAN_POINT('Ctrl Pts',(-209.466458640287,-4.73595519626658,
132.137848691638));
#127399=CARTESIAN_POINT('Ctrl Pts',(-209.474091001061,-4.69747708121146,
132.267642243255));
#127400=CARTESIAN_POINT('Ctrl Pts',(-209.481723361836,-4.65370724643205,
132.395646866801));
#127401=CARTESIAN_POINT('Ctrl Pts',(-209.489354909185,-4.60994207646628,
132.523637848128));
#127402=CARTESIAN_POINT('Ctrl Pts',(-209.496986456533,-4.56088643870788,
132.649839898546));
#127403=CARTESIAN_POINT('Ctrl Pts',(-209.504618003882,-4.50672322038455,
132.77378410614));
#127404=CARTESIAN_POINT('Ctrl Pts',(-209.512250504877,-4.45255323376128,
132.897743801949));
#127405=CARTESIAN_POINT('Ctrl Pts',(-209.519883005873,-4.39327455956056,
133.0194447242));
#127406=CARTESIAN_POINT('Ctrl Pts',(-209.527515506869,-4.32911753163796,
133.138439549343));
#127407=CARTESIAN_POINT('Ctrl Pts',(-209.535269971799,-4.26393530325576,
133.259335858289));
#127408=CARTESIAN_POINT('Ctrl Pts',(-209.543024436729,-4.19371767192674,
133.377438459046));
#127409=CARTESIAN_POINT('Ctrl Pts',(-209.550778901658,-4.1187531996581,
133.492306886152));
#127410=CARTESIAN_POINT('Ctrl Pts',(-209.558422540026,-4.04486011720237,
133.605533617413));
#127411=CARTESIAN_POINT('Ctrl Pts',(-209.566066178394,-3.96635527115312,
133.715617718784));
#127412=CARTESIAN_POINT('Ctrl Pts',(-209.573709816762,-3.88355647376137,
133.822169786086));
#127413=CARTESIAN_POINT('Ctrl Pts',(-209.581519694973,-3.79895690317604,
133.931039231329));
#127414=CARTESIAN_POINT('Ctrl Pts',(-209.589329573184,-3.70987474966135,
134.036220898821));
#127415=CARTESIAN_POINT('Ctrl Pts',(-209.597139451395,-3.61668886684718,
134.13733897077));
#127416=CARTESIAN_POINT('Ctrl Pts',(-209.604949329605,-3.52350298403301,
134.238457042718));
#127417=CARTESIAN_POINT('Ctrl Pts',(-209.612759207816,-3.42621373416068,
134.335511257294));
#127418=CARTESIAN_POINT('Ctrl Pts',(-209.620569086027,-3.32523510253084,
134.428170018652));
#127419=CARTESIAN_POINT('Ctrl Pts',(-209.628343420146,-3.22471604192765,
134.520407074136));
#127420=CARTESIAN_POINT('Ctrl Pts',(-209.636117754265,-3.12019708063552,
134.608604683983));
#127421=CARTESIAN_POINT('Ctrl Pts',(-209.643892088384,-3.01203655935464,
134.692395960462));
#127422=CARTESIAN_POINT('Ctrl Pts',(-209.651656841331,-2.90400933624994,
134.776083971682));
#127423=CARTESIAN_POINT('Ctrl Pts',(-209.659421594278,-2.7923497888379,
134.855376217297));
#127424=CARTESIAN_POINT('Ctrl Pts',(-209.667186347225,-2.67745232662292,
134.929943255347));
#127425=CARTESIAN_POINT('Ctrl Pts',(-209.67494338811,-2.56266898218686,
135.004436232364));
#127426=CARTESIAN_POINT('Ctrl Pts',(-209.682700428995,-2.44465444865051,
135.074213129921));
#127427=CARTESIAN_POINT('Ctrl Pts',(-209.69045746988,-2.32383508751043,
135.138985578108));
#127428=CARTESIAN_POINT('Ctrl Pts',(-209.698208661121,-2.20310683719059,
135.203709180888));
#127429=CARTESIAN_POINT('Ctrl Pts',(-209.705959852361,-2.07957831250657,
135.263435662026));
#127430=CARTESIAN_POINT('Ctrl Pts',(-209.713711043601,-1.95370334389376,
135.317920887083));
#127431=CARTESIAN_POINT('Ctrl Pts',(-209.721458940378,-1.82788187550026,
135.372382954465));
#127432=CARTESIAN_POINT('Ctrl Pts',(-209.729206837155,-1.69971630477828,
135.42160804146));
#127433=CARTESIAN_POINT('Ctrl Pts',(-209.736954733932,-1.56968326381835,
135.465398861755));
#127434=CARTESIAN_POINT('Ctrl Pts',(-209.744701010016,-1.43967742296741,
135.509180521954));
#127435=CARTESIAN_POINT('Ctrl Pts',(-209.7524472861,-1.30780525915599,135.547530051775));
#127436=CARTESIAN_POINT('Ctrl Pts',(-209.760193562184,-1.17456112701993,
135.58029918725));
#127437=CARTESIAN_POINT('Ctrl Pts',(-209.76793989545,-1.04131601130613,
135.613068564619));
#127438=CARTESIAN_POINT('Ctrl Pts',(-209.775686228715,-0.906699286711348,
135.640257372075));
#127439=CARTESIAN_POINT('Ctrl Pts',(-209.78343256198,-0.771217744846221,
135.661767976696));
#127440=CARTESIAN_POINT('Ctrl Pts',(-209.791180629983,-0.635705862828972,
135.683283398468));
#127441=CARTESIAN_POINT('Ctrl Pts',(-209.798928697986,-0.499329164215588,
135.699118025785));
#127442=CARTESIAN_POINT('Ctrl Pts',(-209.806676765989,-0.362601448238541,
135.709225880979));
#127443=CARTESIAN_POINT('Ctrl Pts',(-209.814433068731,-0.22572841641806,
135.719344478922));
#127444=CARTESIAN_POINT('Ctrl Pts',(-209.822189371473,-0.0885040125184699,
135.723724117468));
#127445=CARTESIAN_POINT('Ctrl Pts',(-209.829945674215,0.0485555029631042,
135.72237092923));
#127446=CARTESIAN_POINT('Ctrl Pts',(-209.837706116729,0.185688171234873,
135.721017018754));
#127447=CARTESIAN_POINT('Ctrl Pts',(-209.845466559243,0.322655385478393,
135.713924204827));
#127448=CARTESIAN_POINT('Ctrl Pts',(-209.853227001757,0.458945108086046,
135.70115063249));
#127449=CARTESIAN_POINT('Ctrl Pts',(-209.860999902023,0.595453615055662,
135.688356554881));
#127450=CARTESIAN_POINT('Ctrl Pts',(-209.868772802288,0.731282069464407,
135.669863548454));
#127451=CARTESIAN_POINT('Ctrl Pts',(-209.876545702554,0.865926846890192,
135.645781251877));
#127452=CARTESIAN_POINT('Ctrl Pts',(-209.884036038315,0.995676947504995,
135.622574407441));
#127453=CARTESIAN_POINT('Ctrl Pts',(-209.891526374077,1.12432763552259,
135.594177653627));
#127454=CARTESIAN_POINT('Ctrl Pts',(-209.899016709839,1.25144268444344,
135.560732582631));
#127455=CARTESIAN_POINT('Ctrl Pts',(-209.906791043958,1.38337733908158,
135.526019431602));
#127456=CARTESIAN_POINT('Ctrl Pts',(-209.914565378078,1.51407553772831,
135.485757631805));
#127457=CARTESIAN_POINT('Ctrl Pts',(-209.922339712197,1.64303491544211,
135.44005035364));
#127458=CARTESIAN_POINT('Ctrl Pts',(-209.930104465144,1.7718353622483,135.394399405609));
#127459=CARTESIAN_POINT('Ctrl Pts',(-209.937869218091,1.8989008869701,135.343316461585));
#127460=CARTESIAN_POINT('Ctrl Pts',(-209.945633971038,2.02374113278387,
135.286955278025));
#127461=CARTESIAN_POINT('Ctrl Pts',(-209.953391011923,2.14845738550555,
135.230650073188));
#127462=CARTESIAN_POINT('Ctrl Pts',(-209.961148052808,2.27095240364596,
135.169077221304));
#127463=CARTESIAN_POINT('Ctrl Pts',(-209.968905093693,2.39075311462998,
135.102439561395));
#127464=CARTESIAN_POINT('Ctrl Pts',(-209.976656284933,2.51046348296641,
135.035852153464));
#127465=CARTESIAN_POINT('Ctrl Pts',(-209.984407476173,2.62748324803347,
134.964207729093));
#127466=CARTESIAN_POINT('Ctrl Pts',(-209.992158667413,2.74136170617812,
134.887756148053));
#127467=CARTESIAN_POINT('Ctrl Pts',(-209.99990656419,2.8551917629398,134.811337060975));
#127468=CARTESIAN_POINT('Ctrl Pts',(-210.007654460968,2.9658828443485,134.730115098399));
#127469=CARTESIAN_POINT('Ctrl Pts',(-210.015402357745,3.07301133655527,
134.644384626332));
#127470=CARTESIAN_POINT('Ctrl Pts',(-210.023148633829,3.1801174197909,134.558672087232));
#127471=CARTESIAN_POINT('Ctrl Pts',(-210.030894909913,3.28366209104112,
134.468453158612));
#127472=CARTESIAN_POINT('Ctrl Pts',(-210.038641185997,3.38325340087477,
134.374063614731));
#127473=CARTESIAN_POINT('Ctrl Pts',(-210.046387519262,3.48284544586898,
134.279673374088));
#127474=CARTESIAN_POINT('Ctrl Pts',(-210.054133852528,3.57848378744892,
134.181112725696));
#127475=CARTESIAN_POINT('Ctrl Pts',(-210.061880185793,3.6698123510275,134.078755274712));
#127476=CARTESIAN_POINT('Ctrl Pts',(-210.069628253796,3.76116136700454,
133.976374901486));
#127477=CARTESIAN_POINT('Ctrl Pts',(-210.077376321799,3.84819842421281,
133.870196325401));
#127478=CARTESIAN_POINT('Ctrl Pts',(-210.085124389802,3.93060711930239,
133.76062696825));
#127479=CARTESIAN_POINT('Ctrl Pts',(-210.092880692544,4.01310339933368,
133.650941159483));
#127480=CARTESIAN_POINT('Ctrl Pts',(-210.100636995286,4.090961255481,133.537857683699));
#127481=CARTESIAN_POINT('Ctrl Pts',(-210.108393298028,4.16390679587436,
133.421814200301));
#127482=CARTESIAN_POINT('Ctrl Pts',(-210.116153740542,4.23689126949917,
133.305708781002));
#127483=CARTESIAN_POINT('Ctrl Pts',(-210.123914183056,4.30495800917251,
133.186640545366));
#127484=CARTESIAN_POINT('Ctrl Pts',(-210.13167462557,4.3678791651305,133.065071713951));
#127485=CARTESIAN_POINT('Ctrl Pts',(-210.139447525836,4.43090132771374,
132.943307729456));
#127486=CARTESIAN_POINT('Ctrl Pts',(-210.147220426101,4.4887612350593,132.819035482209));
#127487=CARTESIAN_POINT('Ctrl Pts',(-210.154993326366,4.54127890798377,
132.692737948081));
#127488=CARTESIAN_POINT('Ctrl Pts',(-210.162483662128,4.59188743121382,
132.571031647441));
#127489=CARTESIAN_POINT('Ctrl Pts',(-210.169973997891,4.63753527733388,
132.447445040966));
#127490=CARTESIAN_POINT('Ctrl Pts',(-210.177464333653,4.67810578079159,
132.322421672407));
#127491=CARTESIAN_POINT('Ctrl Pts',(-210.185238667772,4.72021452721886,
132.192658004829));
#127492=CARTESIAN_POINT('Ctrl Pts',(-210.193013001891,4.75698670362623,
132.060935422502));
#127493=CARTESIAN_POINT('Ctrl Pts',(-210.20078733601,4.78823756967018,131.927732345401));
#127494=CARTESIAN_POINT('Ctrl Pts',(-210.208552088957,4.81944992181453,
131.794693429188));
#127495=CARTESIAN_POINT('Ctrl Pts',(-210.216316841904,4.84515441412268,
131.660178025542));
#127496=CARTESIAN_POINT('Ctrl Pts',(-210.224081594851,4.86521535641737,
131.524681794667));
#127497=CARTESIAN_POINT('Ctrl Pts',(-210.231838635736,4.88525637390142,
131.389320140559));
#127498=CARTESIAN_POINT('Ctrl Pts',(-210.239595676621,4.89966493918948,
131.252979982114));
#127499=CARTESIAN_POINT('Ctrl Pts',(-210.247352717506,4.90835599921353,
131.116168968135));
#127500=CARTESIAN_POINT('Ctrl Pts',(-210.255103908746,4.91704050524162,
130.979461124405));
#127501=CARTESIAN_POINT('Ctrl Pts',(-210.262855099986,4.92001606332805,
130.842283520498));
#127502=CARTESIAN_POINT('Ctrl Pts',(-210.270606291227,4.9172492712412,130.70515040147));
#127503=CARTESIAN_POINT('Ctrl Pts',(-210.278354188004,4.91448365511481,
130.568075567676));
#127504=CARTESIAN_POINT('Ctrl Pts',(-210.286102084781,4.9059805509559,130.431045571223));
#127505=CARTESIAN_POINT('Ctrl Pts',(-210.293849981558,4.8917586435896,130.294575922458));
#127506=CARTESIAN_POINT('Ctrl Pts',(-210.301596257642,4.87753971113974,
130.158134820201));
#127507=CARTESIAN_POINT('Ctrl Pts',(-210.309342533726,4.85760439538852,
130.022254221102));
#127508=CARTESIAN_POINT('Ctrl Pts',(-210.31708880981,4.83202333448889,129.887445377506));
#127509=CARTESIAN_POINT('Ctrl Pts',(-210.324835143075,4.80644208475572,
129.752635538782));
#127510=CARTESIAN_POINT('Ctrl Pts',(-210.332581476341,4.77521507960163,
129.618897855459));
#127511=CARTESIAN_POINT('Ctrl Pts',(-210.340327809606,4.73846417661337,
129.486733845885));
#127512=CARTESIAN_POINT('Ctrl Pts',(-210.348075877609,4.70170504351525,
129.354540239097));
#127513=CARTESIAN_POINT('Ctrl Pts',(-210.355823945612,4.65941965574108,
129.22392138392));
#127514=CARTESIAN_POINT('Ctrl Pts',(-210.363572013615,4.61177976504491,
129.095363700886));
#127515=CARTESIAN_POINT('Ctrl Pts',(-210.371328316357,4.56408924210593,
128.966669385216));
#127516=CARTESIAN_POINT('Ctrl Pts',(-210.379084619098,4.51103298426964,
128.840040984911));
#127517=CARTESIAN_POINT('Ctrl Pts',(-210.38684092184,4.45283116154137,128.715945498557));
#127518=CARTESIAN_POINT('Ctrl Pts',(-210.394601364354,4.39459827474774,
128.591783778705));
#127519=CARTESIAN_POINT('Ctrl Pts',(-210.402361806869,4.33121453133613,
128.470158013103));
#127520=CARTESIAN_POINT('Ctrl Pts',(-210.410122249383,4.26294565218836,
128.351509739712));
#127521=CARTESIAN_POINT('Ctrl Pts',(-210.417895149648,4.19456718177516,
128.23267100158));
#127522=CARTESIAN_POINT('Ctrl Pts',(-210.425668049914,4.12128811382067,
128.116819637697));
#127523=CARTESIAN_POINT('Ctrl Pts',(-210.433440950179,4.04341750645725,
128.004368129902));
#127524=CARTESIAN_POINT('Ctrl Pts',(-210.440931285941,3.96837769181507,
127.896004517663));
#127525=CARTESIAN_POINT('Ctrl Pts',(-210.448421621703,3.88907455547164,
127.790798112337));
#127526=CARTESIAN_POINT('Ctrl Pts',(-210.455911957465,3.80581820276506,
127.68908681419));
#127527=CARTESIAN_POINT('Ctrl Pts',(-210.463686291584,3.71940516014076,
127.583519101259));
#127528=CARTESIAN_POINT('Ctrl Pts',(-210.471460625704,3.6284594806104,127.481382354555));
#127529=CARTESIAN_POINT('Ctrl Pts',(-210.479234959823,3.53328381577912,
127.383090599042));
#127530=CARTESIAN_POINT('Ctrl Pts',(-210.48699971277,3.43822544644917,127.284919979333));
#127531=CARTESIAN_POINT('Ctrl Pts',(-210.494764465717,3.33894773364673,
127.190585200573));
#127532=CARTESIAN_POINT('Ctrl Pts',(-210.502529218664,3.23579434648503,
127.100468339198));
#127533=CARTESIAN_POINT('Ctrl Pts',(-210.510286259549,3.13274341272166,
127.01044098316));
#127534=CARTESIAN_POINT('Ctrl Pts',(-210.518043300434,3.02582475755512,
126.924623463178));
#127535=CARTESIAN_POINT('Ctrl Pts',(-210.525800341319,2.91541950703893,
126.843361733386));
#127536=CARTESIAN_POINT('Ctrl Pts',(-210.533551532559,2.80509751398143,
126.762161283696));
#127537=CARTESIAN_POINT('Ctrl Pts',(-210.541302723799,2.6912944725708,126.685510016745));
#127538=CARTESIAN_POINT('Ctrl Pts',(-210.549053915039,2.57442497701588,
126.613713996791));
#127539=CARTESIAN_POINT('Ctrl Pts',(-210.556801811817,2.45760515411368,
126.541948492059));
#127540=CARTESIAN_POINT('Ctrl Pts',(-210.564549708594,2.33772180170944,
126.475034334182));
#127541=CARTESIAN_POINT('Ctrl Pts',(-210.572297605371,2.21521873286088,
126.413234449021));
#127542=CARTESIAN_POINT('Ctrl Pts',(-210.580043881455,2.09274128901346,
126.351447491063));
#127543=CARTESIAN_POINT('Ctrl Pts',(-210.587790157539,1.96764556754184,
126.29477285392));
#127544=CARTESIAN_POINT('Ctrl Pts',(-210.595536433623,1.84039988117138,
126.243427452096));
#127545=CARTESIAN_POINT('Ctrl Pts',(-210.603282766888,1.71315325550235,
126.192081671251));
#127546=CARTESIAN_POINT('Ctrl Pts',(-210.611029100154,1.58375699582705,
126.146065350522));
#127547=CARTESIAN_POINT('Ctrl Pts',(-210.618775433419,1.45269891073695,
126.105547050585));
#127548=CARTESIAN_POINT('Ctrl Pts',(-210.626523501422,1.32161147609756,
126.065019676856));
#127549=CARTESIAN_POINT('Ctrl Pts',(-210.634271569425,1.18886184894955,
126.029992889409));
#127550=CARTESIAN_POINT('Ctrl Pts',(-210.642019637428,1.05495210467951,
126.000585110808));
#127551=CARTESIAN_POINT('Ctrl Pts',(-210.64977594017,0.920900039539174,
125.971146077269));
#127552=CARTESIAN_POINT('Ctrl Pts',(-210.657532242912,0.785685776728094,
125.947338066182));
#127553=CARTESIAN_POINT('Ctrl Pts',(-210.665288545654,0.649821222647911,
125.92922826643));
#127554=CARTESIAN_POINT('Ctrl Pts',(-210.673048988168,0.513884153564413,
125.911108800932));
#127555=CARTESIAN_POINT('Ctrl Pts',(-210.680809430682,0.377296490795038,
125.898693642202));
#127556=CARTESIAN_POINT('Ctrl Pts',(-210.688569873196,0.240573341358052,
125.891997893792));
#127557=CARTESIAN_POINT('Ctrl Pts',(-210.696342773462,0.103630711783879,
125.885291396771));
#127558=CARTESIAN_POINT('Ctrl Pts',(-210.704115673727,-0.033447447902223,
125.884322660007));
#127559=CARTESIAN_POINT('Ctrl Pts',(-210.711888573992,-0.17014705157744,
125.889054620648));
#127560=CARTESIAN_POINT('Ctrl Pts',(-210.719378909755,-0.301877280334283,
125.893614562601));
#127561=CARTESIAN_POINT('Ctrl Pts',(-210.726869245517,-0.433255691014989,
125.9034679053));
#127562=CARTESIAN_POINT('Ctrl Pts',(-210.734359581279,-0.563830379047278,
125.918536391689));
#127563=CARTESIAN_POINT('Ctrl Pts',(-210.742133915398,-0.699355846063048,
125.93417620432));
#127564=CARTESIAN_POINT('Ctrl Pts',(-210.749908249517,-0.834444744985957,
125.955483973802));
#127565=CARTESIAN_POINT('Ctrl Pts',(-210.757682583636,-0.968585154302004,
125.982428861375));
#127566=CARTESIAN_POINT('Ctrl Pts',(-210.765447336583,-1.10256024755131,
126.009340541782));
#127567=CARTESIAN_POINT('Ctrl Pts',(-210.77321208953,-1.23558879738455,
126.041875441078));
#127568=CARTESIAN_POINT('Ctrl Pts',(-210.780976842477,-1.36716359052389,
126.079950942353));
#127569=CARTESIAN_POINT('Ctrl Pts',(-210.788733883362,-1.49860770172451,
126.117988626503));
#127570=CARTESIAN_POINT('Ctrl Pts',(-210.796490924247,-1.62860055651468,
126.161555853429));
#127571=CARTESIAN_POINT('Ctrl Pts',(-210.804247965132,-1.75664508594344,
126.210518967647));
#127572=CARTESIAN_POINT('Ctrl Pts',(-210.811999156372,-1.88459305599669,
126.259445158399));
#127573=CARTESIAN_POINT('Ctrl Pts',(-210.819750347612,-2.01059526143671,
126.31375899811));
#127574=CARTESIAN_POINT('Ctrl Pts',(-210.827501538852,-2.13417010343808,
126.373277112136));
#127575=CARTESIAN_POINT('Ctrl Pts',(-210.835249435629,-2.25769242283462,
126.432769929376));
#127576=CARTESIAN_POINT('Ctrl Pts',(-210.842997332407,-2.3787890792521,
126.497462452225));
#127577=CARTESIAN_POINT('Ctrl Pts',(-210.850745229184,-2.49699897391876,
126.567123406039));
#127578=CARTESIAN_POINT('Ctrl Pts',(-210.858491505268,-2.61518414162376,
126.636769788283));
#127579=CARTESIAN_POINT('Ctrl Pts',(-210.866237781352,-2.73048341204913,
126.711382335922));
#127580=CARTESIAN_POINT('Ctrl Pts',(-210.873984057436,-2.84246115441336,
126.790684291783));
#127581=CARTESIAN_POINT('Ctrl Pts',(-210.881730390701,-2.9544397233717,
126.869986833033));
#127582=CARTESIAN_POINT('Ctrl Pts',(-210.889476723967,-3.06309639628533,
126.953978625625));
#127583=CARTESIAN_POINT('Ctrl Pts',(-210.897223057232,-3.16802568582288,
127.042340373539));
#127584=CARTESIAN_POINT('Ctrl Pts',(-210.904971125235,-3.272978473548,127.130721909455));
#127585=CARTESIAN_POINT('Ctrl Pts',(-210.912719193238,-3.37420191790143,
127.223475096248));
#127586=CARTESIAN_POINT('Ctrl Pts',(-210.920467261241,-3.47132500261658,
127.320241533966));
#127587=CARTESIAN_POINT('Ctrl Pts',(-210.928223563983,-3.56855131090154,
127.417110816204));
#127588=CARTESIAN_POINT('Ctrl Pts',(-210.935979866725,-3.66166827674774,
127.518001593439));
#127589=CARTESIAN_POINT('Ctrl Pts',(-210.943736169466,-3.75034267433231,
127.622519501548));
#127590=CARTESIAN_POINT('Ctrl Pts',(-210.951496611981,-3.8390644001128,
127.727093194012));
#127591=CARTESIAN_POINT('Ctrl Pts',(-210.959257054495,-3.92333859283302,
127.835297566513));
#127592=CARTESIAN_POINT('Ctrl Pts',(-210.967017497009,-4.00287411752363,
127.946707408767));
#127593=CARTESIAN_POINT('Ctrl Pts',(-210.974790397274,-4.08253731969931,
128.05829609599));
#127594=CARTESIAN_POINT('Ctrl Pts',(-210.98256329754,-4.15744643900569,
128.173100208105));
#127595=CARTESIAN_POINT('Ctrl Pts',(-210.990336197805,-4.22735478136186,
128.290667196523));
#127596=CARTESIAN_POINT('Ctrl Pts',(-210.997826533567,-4.29472177938432,
128.403960328777));
#127597=CARTESIAN_POINT('Ctrl Pts',(-211.005316869329,-4.3574451231781,
128.519818678921));
#127598=CARTESIAN_POINT('Ctrl Pts',(-211.012807205091,-4.41534638716189,
128.63781974699));
#127599=CARTESIAN_POINT('Ctrl Pts',(-211.021162556032,-4.47993433033233,
128.769448070002));
#127600=CARTESIAN_POINT('Ctrl Pts',(-211.029517906973,-4.53870371440234,
128.904111953051));
#127601=CARTESIAN_POINT('Ctrl Pts',(-211.037873257915,-4.59138038536787,
129.041292490873));
#127602=CARTESIAN_POINT('Ctrl Pts',(-211.046207800767,-4.64392587083518,
129.178131395543));
#127603=CARTESIAN_POINT('Ctrl Pts',(-211.054542343618,-4.69040879233743,
129.317474177873));
#127604=CARTESIAN_POINT('Ctrl Pts',(-211.06287688647,-4.73060208665202,
129.458780088477));
#127605=CARTESIAN_POINT('Ctrl Pts',(-211.065299612346,-4.74228567097247,
129.499855585016));
#127606=CARTESIAN_POINT('Ctrl Pts',(-211.067722338222,-4.75343809550135,
129.54109680921));
#127607=CARTESIAN_POINT('Ctrl Pts',(-211.070145064099,-4.76405452823395,
129.582490119308));
#127608=CARTESIAN_POINT('Origin',(213.235140564004,0.,130.804360617566));
#127609=CARTESIAN_POINT('',(-213.165046531412,-4.76405452823396,129.582490119308));
#127610=CARTESIAN_POINT('',(-212.819861628446,-4.76405452823406,129.582490119308));
#127611=CARTESIAN_POINT('',(213.235140564004,-4.76405452823405,129.582490119308));
#127612=CARTESIAN_POINT('',(-211.485140564044,-4.91824790103933,130.808904450997));
#127613=CARTESIAN_POINT('Ctrl Pts',(-211.485140564044,-4.91824790103933,
130.808904450997));
#127614=CARTESIAN_POINT('Ctrl Pts',(-211.495366712974,-4.91808111918583,
130.98942922449));
#127615=CARTESIAN_POINT('Ctrl Pts',(-211.505592861904,-4.90797173471146,
131.169512207673));
#127616=CARTESIAN_POINT('Ctrl Pts',(-211.515819010834,-4.88808531502141,
131.348240214142));
#127617=CARTESIAN_POINT('Ctrl Pts',(-211.526332245936,-4.86764060929875,
131.531985782908));
#127618=CARTESIAN_POINT('Ctrl Pts',(-211.536845481038,-4.8368621460543,
131.714299654373));
#127619=CARTESIAN_POINT('Ctrl Pts',(-211.547358716141,-4.79597733691819,
131.894215858535));
#127620=CARTESIAN_POINT('Ctrl Pts',(-211.548276962946,-4.79240637659797,
131.909930096649));
#127621=CARTESIAN_POINT('Ctrl Pts',(-211.549195209752,-4.78875834852051,
131.925626057538));
#127622=CARTESIAN_POINT('Ctrl Pts',(-211.550113456558,-4.7850334212715,
131.941303105036));
#127623=CARTESIAN_POINT('Ctrl Pts',(-211.557887790677,-4.75349633470017,
132.074032785663));
#127624=CARTESIAN_POINT('Ctrl Pts',(-211.565662124796,-4.71638252570012,
132.205659518639));
#127625=CARTESIAN_POINT('Ctrl Pts',(-211.573436458915,-4.67378307958606,
132.335678607885));
#127626=CARTESIAN_POINT('Ctrl Pts',(-211.581201211862,-4.63123613348211,
132.465537460224));
#127627=CARTESIAN_POINT('Ctrl Pts',(-211.588965964809,-4.58321712231859,
132.593792243019));
#127628=CARTESIAN_POINT('Ctrl Pts',(-211.596730717756,-4.52986799106473,
132.719949050927));
#127629=CARTESIAN_POINT('Ctrl Pts',(-211.604487758641,-4.47657184692026,
132.845980558115));
#127630=CARTESIAN_POINT('Ctrl Pts',(-211.612244799526,-4.4179562691757,
132.969917879386));
#127631=CARTESIAN_POINT('Ctrl Pts',(-211.620001840411,-4.35421268600348,
133.091283210822));
#127632=CARTESIAN_POINT('Ctrl Pts',(-211.627753031651,-4.2905171723631,
133.212557019718));
#127633=CARTESIAN_POINT('Ctrl Pts',(-211.635504222891,-4.2217015315191,
133.331262354623));
#127634=CARTESIAN_POINT('Ctrl Pts',(-211.643255414131,-4.14800473564428,
133.446942645729));
#127635=CARTESIAN_POINT('Ctrl Pts',(-211.651003310908,-4.07433926287374,
133.562573769626));
#127636=CARTESIAN_POINT('Ctrl Pts',(-211.658751207686,-3.9957969709619,
133.675182077886));
#127637=CARTESIAN_POINT('Ctrl Pts',(-211.666499104463,-3.9126619755804,
133.784337014678));
#127638=CARTESIAN_POINT('Ctrl Pts',(-211.674245380547,-3.82954437024774,
133.893469118611));
#127639=CARTESIAN_POINT('Ctrl Pts',(-211.681991656631,-3.741836209056,133.99914897708));
#127640=CARTESIAN_POINT('Ctrl Pts',(-211.689737932715,-3.64986376386465,
134.100976695869));
#127641=CARTESIAN_POINT('Ctrl Pts',(-211.69748426598,-3.55789063975373,
134.202805166328));
#127642=CARTESIAN_POINT('Ctrl Pts',(-211.705230599245,-3.46165343088827,
134.300781150227));
#127643=CARTESIAN_POINT('Ctrl Pts',(-211.712976932511,-3.36151709002681,
134.394539710029));
#127644=CARTESIAN_POINT('Ctrl Pts',(-211.720725000514,-3.26135832432624,
134.48831926641));
#127645=CARTESIAN_POINT('Ctrl Pts',(-211.728473068517,-3.15729897443404,
134.577879252155));
#127646=CARTESIAN_POINT('Ctrl Pts',(-211.73622113652,-3.04973875200786,
134.662893578032));
#127647=CARTESIAN_POINT('Ctrl Pts',(-211.743977439262,-2.94206421329685,
134.747998258146));
#127648=CARTESIAN_POINT('Ctrl Pts',(-211.751733742003,-2.83088167662946,
134.828547384768));
#127649=CARTESIAN_POINT('Ctrl Pts',(-211.759490044745,-2.71662210272428,
134.904256642283));
#127650=CARTESIAN_POINT('Ctrl Pts',(-211.767250487259,-2.60230154504422,
134.980006308108));
#127651=CARTESIAN_POINT('Ctrl Pts',(-211.775010929774,-2.48490101219084,
135.05091075559));
#127652=CARTESIAN_POINT('Ctrl Pts',(-211.782771372288,-2.36487712384615,
135.116731108562));
#127653=CARTESIAN_POINT('Ctrl Pts',(-211.790544272553,-2.24466056250067,
135.182657122207));
#127654=CARTESIAN_POINT('Ctrl Pts',(-211.798317172819,-2.12181258082996,
135.243482558607));
#127655=CARTESIAN_POINT('Ctrl Pts',(-211.806090073084,-1.99681169661381,
135.299015900318));
#127656=CARTESIAN_POINT('Ctrl Pts',(-211.813580408846,-1.87635490939715,
135.352530465177));
#127657=CARTESIAN_POINT('Ctrl Pts',(-211.821070744608,-1.7538993152546,
135.401130903635));
#127658=CARTESIAN_POINT('Ctrl Pts',(-211.82856108037,-1.62988553055513,
135.444689939908));
#127659=CARTESIAN_POINT('Ctrl Pts',(-211.836335414489,-1.50116972551577,
135.489900530281));
#127660=CARTESIAN_POINT('Ctrl Pts',(-211.844109748608,-1.37036750688096,
135.529823095987));
#127661=CARTESIAN_POINT('Ctrl Pts',(-211.851884082727,-1.23795272359228,
135.564261469123));
#127662=CARTESIAN_POINT('Ctrl Pts',(-211.859648835674,-1.10570112969012,
135.598657400042));
#127663=CARTESIAN_POINT('Ctrl Pts',(-211.867413588621,-0.971841300097183,
135.627582488879));
#127664=CARTESIAN_POINT('Ctrl Pts',(-211.875178341568,-0.836865496090621,
135.650889190055));
#127665=CARTESIAN_POINT('Ctrl Pts',(-211.882935382453,-0.702023751955058,
135.674172742687));
#127666=CARTESIAN_POINT('Ctrl Pts',(-211.890692423338,-0.566068621945752,
135.691848946536));
#127667=CARTESIAN_POINT('Ctrl Pts',(-211.898449464223,-0.429505567635087,
135.703820590856));
#127668=CARTESIAN_POINT('Ctrl Pts',(-211.906200655464,-0.29304549658617,
135.715783207266));
#127669=CARTESIAN_POINT('Ctrl Pts',(-211.913951846704,-0.155978801629436,
135.722049792719));
#127670=CARTESIAN_POINT('Ctrl Pts',(-211.921703037944,-0.0188187781709079,
135.722574614139));
#127671=CARTESIAN_POINT('Ctrl Pts',(-211.929450934721,0.1182829486186,135.723099212496));
#127672=CARTESIAN_POINT('Ctrl Pts',(-211.937198831498,0.25547753487123,
135.717886899103));
#127673=CARTESIAN_POINT('Ctrl Pts',(-211.944946728275,0.392249170311845,
135.706943982578));
#127674=CARTESIAN_POINT('Ctrl Pts',(-211.952693004359,0.528992196074782,
135.696003355074));
#127675=CARTESIAN_POINT('Ctrl Pts',(-211.960439280443,0.665312057528826,
135.679334539916));
#127676=CARTESIAN_POINT('Ctrl Pts',(-211.968185556527,0.800695954434944,
135.656995886268));
#127677=CARTESIAN_POINT('Ctrl Pts',(-211.975931889793,0.936080850714418,
135.634657067721));
#127678=CARTESIAN_POINT('Ctrl Pts',(-211.983678223058,1.07052938291009,
135.606648390818));
#127679=CARTESIAN_POINT('Ctrl Pts',(-211.991424556323,1.20353725285352,
135.573079642996));
#127680=CARTESIAN_POINT('Ctrl Pts',(-211.999172624326,1.3365749089874,135.539503377685));
#127681=CARTESIAN_POINT('Ctrl Pts',(-212.006920692329,1.46817088187399,
135.500364659427));
#127682=CARTESIAN_POINT('Ctrl Pts',(-212.014668760332,1.59783476949158,
135.455823517762));
#127683=CARTESIAN_POINT('Ctrl Pts',(-212.022425063074,1.72763646543178,
135.411235037243));
#127684=CARTESIAN_POINT('Ctrl Pts',(-212.030181365816,1.85550160378182,
135.361232790753));
#127685=CARTESIAN_POINT('Ctrl Pts',(-212.037937668558,1.98095803696752,
135.306025678216));
#127686=CARTESIAN_POINT('Ctrl Pts',(-212.045698111072,2.10648143002903,
135.25078909998));
#127687=CARTESIAN_POINT('Ctrl Pts',(-212.053458553586,2.22959320548871,
135.190342292537));
#127688=CARTESIAN_POINT('Ctrl Pts',(-212.0612189961,2.34984557596974,135.124940304552));
#127689=CARTESIAN_POINT('Ctrl Pts',(-212.068991896365,2.47029098623136,
135.05943332749));
#127690=CARTESIAN_POINT('Ctrl Pts',(-212.076764796631,2.58786748336211,
134.988955475393));
#127691=CARTESIAN_POINT('Ctrl Pts',(-212.084537696896,2.70215528776471,
134.913805818965));
#127692=CARTESIAN_POINT('Ctrl Pts',(-212.092028032659,2.81228844260644,
134.841388041838));
#127693=CARTESIAN_POINT('Ctrl Pts',(-212.099518368421,2.91936760769774,
134.764632406479));
#127694=CARTESIAN_POINT('Ctrl Pts',(-212.107008704183,3.02304753840801,
134.683840820251));
#127695=CARTESIAN_POINT('Ctrl Pts',(-212.114783038302,3.13065852520142,
134.599985996477));
#127696=CARTESIAN_POINT('Ctrl Pts',(-212.122557372421,3.23494830458973,
134.511517507355));
#127697=CARTESIAN_POINT('Ctrl Pts',(-212.13033170654,3.335495708033,134.418727981877));
#127698=CARTESIAN_POINT('Ctrl Pts',(-212.138096459487,3.4359191957877,134.326052811196));
#127699=CARTESIAN_POINT('Ctrl Pts',(-212.145861212434,3.53260919983123,
134.229067462502));
#127700=CARTESIAN_POINT('Ctrl Pts',(-212.153625965381,3.62517550664391,
134.128106337161));
#127701=CARTESIAN_POINT('Ctrl Pts',(-212.161383006266,3.7176498752957,134.027245487833));
#127702=CARTESIAN_POINT('Ctrl Pts',(-212.169140047151,3.8060084348688,133.922417006453));
#127703=CARTESIAN_POINT('Ctrl Pts',(-212.176897088036,3.88989618488271,
133.813993607373));
#127704=CARTESIAN_POINT('Ctrl Pts',(-212.184648279277,3.97372067449189,
133.705651971222));
#127705=CARTESIAN_POINT('Ctrl Pts',(-212.192399470517,4.053080826977,133.593721121331));
#127706=CARTESIAN_POINT('Ctrl Pts',(-212.200150661757,4.12766071710104,
133.478608187818));
#127707=CARTESIAN_POINT('Ctrl Pts',(-212.207898558534,4.20220890878219,
133.363544180373));
#127708=CARTESIAN_POINT('Ctrl Pts',(-212.215646455311,4.27198066693807,
133.245301106699));
#127709=CARTESIAN_POINT('Ctrl Pts',(-212.223394352088,4.33670249113417,
133.124316342551));
#127710=CARTESIAN_POINT('Ctrl Pts',(-212.231140628172,4.40141077691988,
133.003356885807));
#127711=CARTESIAN_POINT('Ctrl Pts',(-212.238886904256,4.46107104555584,
132.879657223835));
#127712=CARTESIAN_POINT('Ctrl Pts',(-212.246633180341,4.51545520679142,
132.753680329148));
#127713=CARTESIAN_POINT('Ctrl Pts',(-212.254379513606,4.56983976947861,
132.627702504527));
#127714=CARTESIAN_POINT('Ctrl Pts',(-212.262125846871,4.61894799209267,
132.499447772594));
#127715=CARTESIAN_POINT('Ctrl Pts',(-212.269872180137,4.66259965643574,
132.369399756471));
#127716=CARTESIAN_POINT('Ctrl Pts',(-212.277620248139,4.70626109626633,
132.239322616997));
#127717=CARTESIAN_POINT('Ctrl Pts',(-212.285368316143,4.74446342188477,
132.107451764781));
#127718=CARTESIAN_POINT('Ctrl Pts',(-212.293116384146,4.77707619640578,
131.974286288809));
#127719=CARTESIAN_POINT('Ctrl Pts',(-212.300872686887,4.8097236321717,131.840979282984));
#127720=CARTESIAN_POINT('Ctrl Pts',(-212.308628989629,4.83676955662014,
131.70637528516));
#127721=CARTESIAN_POINT('Ctrl Pts',(-212.316385292371,4.85813451587632,
131.570984441975));
#127722=CARTESIAN_POINT('Ctrl Pts',(-212.324145734885,4.87951087825454,
131.43552133662));
#127723=CARTESIAN_POINT('Ctrl Pts',(-212.331906177399,4.89520018901777,
131.2992709373));
#127724=CARTESIAN_POINT('Ctrl Pts',(-212.339666619914,4.90517498781803,
131.162747840252));
#127725=CARTESIAN_POINT('Ctrl Pts',(-212.347439520179,4.91516579905085,
131.026005584208));
#127726=CARTESIAN_POINT('Ctrl Pts',(-212.355212420445,4.91942375470973,
130.888990146657));
#127727=CARTESIAN_POINT('Ctrl Pts',(-212.36298532071,4.91797357032243,130.752216355082));
#127728=CARTESIAN_POINT('Ctrl Pts',(-212.370475656472,4.91657610379041,
130.620414635343));
#127729=CARTESIAN_POINT('Ctrl Pts',(-212.377965992234,4.9098783182167,130.488837605343));
#127730=CARTESIAN_POINT('Ctrl Pts',(-212.385456327996,4.89794760365846,
130.35793891747));
#127731=CARTESIAN_POINT('Ctrl Pts',(-212.393230662115,4.88556453243154,
130.222077166062));
#127732=CARTESIAN_POINT('Ctrl Pts',(-212.401004996234,4.86750466015426,
130.086515841689));
#127733=CARTESIAN_POINT('Ctrl Pts',(-212.408779330353,4.84378653200132,
129.95176745849));
#127734=CARTESIAN_POINT('Ctrl Pts',(-212.4165440833,4.82009763432157,129.817185140631));
#127735=CARTESIAN_POINT('Ctrl Pts',(-212.424308836247,4.79076442266846,
129.683414151859));
#127736=CARTESIAN_POINT('Ctrl Pts',(-212.432073589195,4.75585731844136,
129.550963541964));
#127737=CARTESIAN_POINT('Ctrl Pts',(-212.43983063008,4.72098488444229,129.418644483882));
#127738=CARTESIAN_POINT('Ctrl Pts',(-212.447587670965,4.68054967388698,
129.287643570505));
#127739=CARTESIAN_POINT('Ctrl Pts',(-212.45534471185,4.63467337548564,129.158460935002));
#127740=CARTESIAN_POINT('Ctrl Pts',(-212.46309590309,4.58883167275773,129.029375717129));
#127741=CARTESIAN_POINT('Ctrl Pts',(-212.47084709433,4.5375571795959,128.902106414819));
#127742=CARTESIAN_POINT('Ctrl Pts',(-212.47859828557,4.48102166079118,128.777138888692));
#127743=CARTESIAN_POINT('Ctrl Pts',(-212.486346182347,4.42451017109,128.652224477097));
#127744=CARTESIAN_POINT('Ctrl Pts',(-212.494094079124,4.36274226394313,
128.529610251353));
#127745=CARTESIAN_POINT('Ctrl Pts',(-212.501841975901,4.29593808229475,
128.4097627274));
#127746=CARTESIAN_POINT('Ctrl Pts',(-212.509588251985,4.22914787464121,
128.289940272965));
#127747=CARTESIAN_POINT('Ctrl Pts',(-212.517334528069,4.15732367814835,
128.172883710467));
#127748=CARTESIAN_POINT('Ctrl Pts',(-212.525080804154,4.08073171635147,
128.059035186645));
#127749=CARTESIAN_POINT('Ctrl Pts',(-212.532827137419,4.00413918917002,
127.945185822418));
#127750=CARTESIAN_POINT('Ctrl Pts',(-212.540573470684,3.9227790446898,127.83454486851));
#127751=CARTESIAN_POINT('Ctrl Pts',(-212.54831980395,3.83696075640322,127.727525357705));
#127752=CARTESIAN_POINT('Ctrl Pts',(-212.556067871953,3.75112324970611,
127.620481880623));
#127753=CARTESIAN_POINT('Ctrl Pts',(-212.563815939956,3.66082585710043,
127.517061765387));
#127754=CARTESIAN_POINT('Ctrl Pts',(-212.571564007959,3.56641797196269,
127.41764452203));
#127755=CARTESIAN_POINT('Ctrl Pts',(-212.5793203107,3.47190974900103,127.318121616844));
#127756=CARTESIAN_POINT('Ctrl Pts',(-212.587076613442,3.37328257624632,
127.222610365916));
#127757=CARTESIAN_POINT('Ctrl Pts',(-212.594832916184,3.27092270775256,
127.13145336276));
#127758=CARTESIAN_POINT('Ctrl Pts',(-212.602593358698,3.168508206715,127.040247706366));
#127759=CARTESIAN_POINT('Ctrl Pts',(-212.610353801213,3.06235734265556,
126.953401175943));
#127760=CARTESIAN_POINT('Ctrl Pts',(-212.618114243727,2.95288821697341,
126.871215026495));
#127761=CARTESIAN_POINT('Ctrl Pts',(-212.625887143992,2.8432433617325,126.788896944544));
#127762=CARTESIAN_POINT('Ctrl Pts',(-212.633660044258,2.73026992268151,
126.711254415072));
#127763=CARTESIAN_POINT('Ctrl Pts',(-212.641432944523,2.61441439811064,
126.638544921036));
#127764=CARTESIAN_POINT('Ctrl Pts',(-212.648923280285,2.50277051368069,
126.568478600254));
#127765=CARTESIAN_POINT('Ctrl Pts',(-212.656413616047,2.38845071518206,
126.502993038286));
#127766=CARTESIAN_POINT('Ctrl Pts',(-212.663903951809,2.27187309918929,
126.442276748166));
#127767=CARTESIAN_POINT('Ctrl Pts',(-212.671678285928,2.15087540745265,
126.379258381452));
#127768=CARTESIAN_POINT('Ctrl Pts',(-212.679452620047,2.02706202385851,
126.321178456388));
#127769=CARTESIAN_POINT('Ctrl Pts',(-212.687226954166,1.90087416518663,
126.268298396804));
#127770=CARTESIAN_POINT('Ctrl Pts',(-212.694991707113,1.77484182177283,
126.215483507167));
#127771=CARTESIAN_POINT('Ctrl Pts',(-212.70275646006,1.64644118292491,126.167855881921));
#127772=CARTESIAN_POINT('Ctrl Pts',(-212.710521213007,1.51613859113558,
126.125631427394));
#127773=CARTESIAN_POINT('Ctrl Pts',(-212.718278253892,1.38596541771736,
126.08344891079));
#127774=CARTESIAN_POINT('Ctrl Pts',(-212.726035294777,1.25389442016377,
126.046659005059));
#127775=CARTESIAN_POINT('Ctrl Pts',(-212.733792335662,1.12041215039591,
126.015429664238));
#127776=CARTESIAN_POINT('Ctrl Pts',(-212.741543526903,0.987030540646194,
125.984223873706));
#127777=CARTESIAN_POINT('Ctrl Pts',(-212.749294718143,0.852240156154917,
125.958570390347));
#127778=CARTESIAN_POINT('Ctrl Pts',(-212.757045909383,0.716542608289347,
125.938587323114));
#127779=CARTESIAN_POINT('Ctrl Pts',(-212.76479380616,0.580902735501286,
125.918612749217));
#127780=CARTESIAN_POINT('Ctrl Pts',(-212.772541702937,0.444356852189445,
125.904303854824));
#127781=CARTESIAN_POINT('Ctrl Pts',(-212.780289599714,0.307416444065595,
125.895727590702));
#127782=CARTESIAN_POINT('Ctrl Pts',(-212.788035875798,0.17050468092303,
125.88715312055));
#127783=CARTESIAN_POINT('Ctrl Pts',(-212.795782151882,0.0331989470708777,
125.884308919931));
#127784=CARTESIAN_POINT('Ctrl Pts',(-212.803528427967,-0.103984866592843,
125.887209998557));
#127785=CARTESIAN_POINT('Ctrl Pts',(-212.811274761232,-0.241169692916126,
125.890111098598));
#127786=CARTESIAN_POINT('Ctrl Pts',(-212.819021094497,-0.378232206377305,
125.898757554246));
#127787=CARTESIAN_POINT('Ctrl Pts',(-212.826767427762,-0.514657632814622,
125.913112250995));
#127788=CARTESIAN_POINT('Ctrl Pts',(-212.834515495765,-0.651113610780467,
125.927470162379));
#127789=CARTESIAN_POINT('Ctrl Pts',(-212.842263563768,-0.786931829078878,
125.947538817671));
#127790=CARTESIAN_POINT('Ctrl Pts',(-212.850011631771,-0.921604139515747,
125.973229396772));
#127791=CARTESIAN_POINT('Ctrl Pts',(-212.857767934513,-1.05641958128695,
125.998947280127));
#127792=CARTESIAN_POINT('Ctrl Pts',(-212.865524237255,-1.19008629768885,
126.030298949714));
#127793=CARTESIAN_POINT('Ctrl Pts',(-212.873280539997,-1.32210727534472,
126.06714461922));
#127794=CARTESIAN_POINT('Ctrl Pts',(-212.881040982511,-1.45419871657143,
126.10400995437));
#127795=CARTESIAN_POINT('Ctrl Pts',(-212.888801425025,-1.58464229714127,
126.146375011615));
#127796=CARTESIAN_POINT('Ctrl Pts',(-212.89656186754,-1.71295856866838,
126.194050866093));
#127797=CARTESIAN_POINT('Ctrl Pts',(-212.904334767805,-1.84148082486593,
126.241803254086));
#127798=CARTESIAN_POINT('Ctrl Pts',(-212.912107668071,-1.96786858719859,
126.29488332423));
#127799=CARTESIAN_POINT('Ctrl Pts',(-212.919880568336,-2.09166388472976,
126.353054600697));
#127800=CARTESIAN_POINT('Ctrl Pts',(-212.927370904098,-2.21095891137079,
126.409111204738));
#127801=CARTESIAN_POINT('Ctrl Pts',(-212.93486123986,-2.32784641280421,
126.469895143101));
#127802=CARTESIAN_POINT('Ctrl Pts',(-212.942351575622,-2.44194179626499,
126.535156555196));
#127803=CARTESIAN_POINT('Ctrl Pts',(-212.950127033458,-2.56038025772637,
126.602902164238));
#127804=CARTESIAN_POINT('Ctrl Pts',(-212.957902491295,-2.6761850569002,
126.675687500662));
#127805=CARTESIAN_POINT('Ctrl Pts',(-212.965677949132,-2.78889756476613,
126.753282559105));
#127806=CARTESIAN_POINT('Ctrl Pts',(-212.973443580617,-2.90146763051654,
126.830779555635));
#127807=CARTESIAN_POINT('Ctrl Pts',(-212.981209212103,-3.01095286230411,
126.913073958956));
#127808=CARTESIAN_POINT('Ctrl Pts',(-212.988974843589,-3.11691940047498,
126.99989002188));
#127809=CARTESIAN_POINT('Ctrl Pts',(-212.996731076475,-3.22275768931839,
127.086601012939));
#127810=CARTESIAN_POINT('Ctrl Pts',(-213.004487309362,-3.32508546591033,
127.177822517787));
#127811=CARTESIAN_POINT('Ctrl Pts',(-213.012243542249,-3.42349856516967,
127.273236060604));
#127812=CARTESIAN_POINT('Ctrl Pts',(-213.019994445663,-3.52184404270403,
127.368584042755));
#127813=CARTESIAN_POINT('Ctrl Pts',(-213.027745349078,-3.61627991492908,
127.468118061299));
#127814=CARTESIAN_POINT('Ctrl Pts',(-213.035496252493,-3.70643572626988,
127.571479971837));
#127815=CARTESIAN_POINT('Ctrl Pts',(-213.043243508726,-3.7965491148681,
127.674793245513));
#127816=CARTESIAN_POINT('Ctrl Pts',(-213.05099076496,-3.88238619414116,
127.781930532739));
#127817=CARTESIAN_POINT('Ctrl Pts',(-213.058738021193,-3.96361425147899,
127.892497789758));
#127818=CARTESIAN_POINT('Ctrl Pts',(-213.066483309715,-4.04482167785262,
128.003036964002));
#127819=CARTESIAN_POINT('Ctrl Pts',(-213.074228598237,-4.12142218203461,
128.117004058679));
#127820=CARTESIAN_POINT('Ctrl Pts',(-213.08197388676,-4.19312439448118,
128.233973317001));
#127821=CARTESIAN_POINT('Ctrl Pts',(-213.089721116824,-4.26484458080633,
128.350971896472));
#127822=CARTESIAN_POINT('Ctrl Pts',(-213.097468346889,-4.33166381333356,
128.470973812513));
#127823=CARTESIAN_POINT('Ctrl Pts',(-213.105215576953,-4.39333498212897,
128.593525753244));
#127824=CARTESIAN_POINT('Ctrl Pts',(-213.112963794129,-4.45501400874135,
128.7160933089));
#127825=CARTESIAN_POINT('Ctrl Pts',(-213.120712011305,-4.5115434965853,
128.841211183594));
#127826=CARTESIAN_POINT('Ctrl Pts',(-213.128460228481,-4.56272349602907,
128.968403820339));
#127827=CARTESIAN_POINT('Ctrl Pts',(-213.13621430851,-4.61394222190882,
129.0956927001));
#127828=CARTESIAN_POINT('Ctrl Pts',(-213.143968388539,-4.65980323682197,
129.225059111539));
#127829=CARTESIAN_POINT('Ctrl Pts',(-213.151722468569,-4.70015562376695,
129.356009770957));
#127830=CARTESIAN_POINT('Ctrl Pts',(-213.15616382285,-4.72326851992387,
129.431015222232));
#127831=CARTESIAN_POINT('Ctrl Pts',(-213.160605177131,-4.74457510560391,
129.506540146115));
#127832=CARTESIAN_POINT('Ctrl Pts',(-213.165046531412,-4.76405452823396,
129.582490119308));
#127833=CARTESIAN_POINT('Ctrl Pts',(-211.415108320184,-4.76405452823408,
129.582490119308));
#127834=CARTESIAN_POINT('Ctrl Pts',(-211.422757975275,-4.79773678652557,
129.713816733187));
#127835=CARTESIAN_POINT('Ctrl Pts',(-211.430407630367,-4.8259785998609,
129.846513808639));
#127836=CARTESIAN_POINT('Ctrl Pts',(-211.438057285458,-4.84868568598776,
129.980085068373));
#127837=CARTESIAN_POINT('Ctrl Pts',(-211.44590449855,-4.87197919941048,
130.117105904694));
#127838=CARTESIAN_POINT('Ctrl Pts',(-211.453751711643,-4.88944813592392,
130.255046251775));
#127839=CARTESIAN_POINT('Ctrl Pts',(-211.461598924736,-4.90104730394483,
130.393363796416));
#127840=CARTESIAN_POINT('Ctrl Pts',(-211.469446137828,-4.91264647196571,
130.531681341057));
#127841=CARTESIAN_POINT('Ctrl Pts',(-211.477293350921,-4.91837588397801,
130.670375628325));
#127842=CARTESIAN_POINT('Ctrl Pts',(-211.485140564013,-4.91824790103983,
130.808904450448));
#127843=CARTESIAN_POINT('',(-211.139859435944,-4.91824985838884,130.803180381106));
#127844=CARTESIAN_POINT('Ctrl Pts',(-211.070145064099,-4.76405452823395,
129.582490119308));
#127845=CARTESIAN_POINT('Ctrl Pts',(-211.078453150991,-4.80046072940634,
129.724437345138));
#127846=CARTESIAN_POINT('Ctrl Pts',(-211.086761237883,-4.83056016471545,
129.868174465631));
#127847=CARTESIAN_POINT('Ctrl Pts',(-211.095069324776,-4.85418901054387,
130.013138706586));
#127848=CARTESIAN_POINT('Ctrl Pts',(-211.103353884107,-4.87775094215576,
130.157692425221));
#127849=CARTESIAN_POINT('Ctrl Pts',(-211.111638443438,-4.89487877747,130.30346603943));
#127850=CARTESIAN_POINT('Ctrl Pts',(-211.119923002769,-4.90545923950509,
130.449885354601));
#127851=CARTESIAN_POINT('Ctrl Pts',(-211.126568480494,-4.91394638069955,
130.567335934484));
#127852=CARTESIAN_POINT('Ctrl Pts',(-211.133213958219,-4.91822154692877,
130.685201620831));
#127853=CARTESIAN_POINT('Ctrl Pts',(-211.139859435944,-4.91824985838884,
130.803180381105));
#127854=CARTESIAN_POINT('Ctrl Pts',(-211.139859435995,-4.91824985838906,
130.803180382015));
#127855=CARTESIAN_POINT('Ctrl Pts',(-211.147841921195,-4.91828386582182,
130.944895356739));
#127856=CARTESIAN_POINT('Ctrl Pts',(-211.155824406396,-4.91218844142533,
131.086540806449));
#127857=CARTESIAN_POINT('Ctrl Pts',(-211.163806891596,-4.90000775983892,
131.227570986081));
#127858=CARTESIAN_POINT('Ctrl Pts',(-211.171795502414,-4.88781773101396,
131.368709389765));
#127859=CARTESIAN_POINT('Ctrl Pts',(-211.179784113232,-4.86953316549332,
131.509231227511));
#127860=CARTESIAN_POINT('Ctrl Pts',(-211.187772724049,-4.84524987723052,
131.648597959608));
#127861=CARTESIAN_POINT('Ctrl Pts',(-211.195768680695,-4.82094425957045,
131.788092844658));
#127862=CARTESIAN_POINT('Ctrl Pts',(-211.203764637341,-4.79062898235596,
131.926430156233));
#127863=CARTESIAN_POINT('Ctrl Pts',(-211.211760593987,-4.75445050736873,
132.063083555897));
#127864=CARTESIAN_POINT('Ctrl Pts',(-211.219770864681,-4.71820726709368,
132.199981587122));
#127865=CARTESIAN_POINT('Ctrl Pts',(-211.227781135375,-4.6760799487421,
132.335189339058));
#127866=CARTESIAN_POINT('Ctrl Pts',(-211.235791406069,-4.62826461706551,
132.468196455898));
#127867=CARTESIAN_POINT('Ctrl Pts',(-211.243809861851,-4.58040042652914,
132.60133948262));
#127868=CARTESIAN_POINT('Ctrl Pts',(-211.251828317633,-4.5268367648255,
132.732277060875));
#127869=CARTESIAN_POINT('Ctrl Pts',(-211.259846773415,-4.46781688210603,
132.860520964054));
#127870=CARTESIAN_POINT('Ctrl Pts',(-211.267879825772,-4.40868956121954,
132.988998318897));
#127871=CARTESIAN_POINT('Ctrl Pts',(-211.27591287813,-4.34408633677997,
133.114771885697));
#127872=CARTESIAN_POINT('Ctrl Pts',(-211.283945930488,-4.27429572649051,
133.237379134759));
#127873=CARTESIAN_POINT('Ctrl Pts',(-211.28638222996,-4.25312932305676,
133.274564000843));
#127874=CARTESIAN_POINT('Ctrl Pts',(-211.288818529432,-4.23148607004176,
133.311457838392));
#127875=CARTESIAN_POINT('Ctrl Pts',(-211.291254828904,-4.20937476713397,
133.348048320944));
#127876=CARTESIAN_POINT('Ctrl Pts',(-211.299029163023,-4.13881666925639,
133.464810090256));
#127877=CARTESIAN_POINT('Ctrl Pts',(-211.306803497142,-4.0632849349863,
133.5788188126));
#127878=CARTESIAN_POINT('Ctrl Pts',(-211.314577831261,-3.98302040142171,
133.689621705294));
#127879=CARTESIAN_POINT('Ctrl Pts',(-211.322342584209,-3.90285478672151,
133.800288043326));
#127880=CARTESIAN_POINT('Ctrl Pts',(-211.330107337156,-3.81796820532065,
133.907756099236));
#127881=CARTESIAN_POINT('Ctrl Pts',(-211.337872090103,-3.72864663036949,
134.011598895015));
#127882=CARTESIAN_POINT('Ctrl Pts',(-211.345629130988,-3.63941377086579,
134.115338552666));
#127883=CARTESIAN_POINT('Ctrl Pts',(-211.353386171873,-3.54575493706022,
134.215459821178));
#127884=CARTESIAN_POINT('Ctrl Pts',(-211.361143212758,-3.44799830589485,
134.311566164016));
#127885=CARTESIAN_POINT('Ctrl Pts',(-211.368894403998,-3.35031539376534,
134.407600032312));
#127886=CARTESIAN_POINT('Ctrl Pts',(-211.376645595238,-3.24854111276296,
134.499624728379));
#127887=CARTESIAN_POINT('Ctrl Pts',(-211.384396786478,-3.14304242983449,
134.587278452619));
#127888=CARTESIAN_POINT('Ctrl Pts',(-211.392144683255,-3.03758858666068,
134.674894921687));
#127889=CARTESIAN_POINT('Ctrl Pts',(-211.399892580032,-2.92841379005274,
134.758143864586));
#127890=CARTESIAN_POINT('Ctrl Pts',(-211.407640476809,-2.81592005163532,
134.836702037299));
#127891=CARTESIAN_POINT('Ctrl Pts',(-211.415386752893,-2.7034498444829,
134.915243777337));
#127892=CARTESIAN_POINT('Ctrl Pts',(-211.423133028978,-2.58766239676326,
134.989096475164));
#127893=CARTESIAN_POINT('Ctrl Pts',(-211.430879305062,-2.46899050103855,
135.057978955908));
#127894=CARTESIAN_POINT('Ctrl Pts',(-211.438625638327,-2.3503177293047,
135.126861945128));
#127895=CARTESIAN_POINT('Ctrl Pts',(-211.446371971592,-2.22876080521027,
135.190774447787));
#127896=CARTESIAN_POINT('Ctrl Pts',(-211.454118304858,-2.10477868149494,
135.249480386979));
#127897=CARTESIAN_POINT('Ctrl Pts',(-211.461866372861,-1.98076879284282,
135.308199472958));
#127898=CARTESIAN_POINT('Ctrl Pts',(-211.469614440864,-1.85433297713764,
135.361709508034));
#127899=CARTESIAN_POINT('Ctrl Pts',(-211.477362508867,-1.72595142433968,
135.409822021521));
#127900=CARTESIAN_POINT('Ctrl Pts',(-211.485118811609,-1.59743342609947,
135.45798566956));
#127901=CARTESIAN_POINT('Ctrl Pts',(-211.49287511435,-1.46696592649307,
135.500740199213));
#127902=CARTESIAN_POINT('Ctrl Pts',(-211.500631417092,-1.33504611727477,
135.537946459953));
#127903=CARTESIAN_POINT('Ctrl Pts',(-211.508391859606,-1.20305589848227,
135.575172578795));
#127904=CARTESIAN_POINT('Ctrl Pts',(-211.516152302121,-1.06961220575475,
135.606844437886));
#127905=CARTESIAN_POINT('Ctrl Pts',(-211.523912744635,-0.935222790191522,
135.63287399077));
#127906=CARTESIAN_POINT('Ctrl Pts',(-211.5316856449,-0.800617640807904,
135.658945328602));
#127907=CARTESIAN_POINT('Ctrl Pts',(-211.539458545166,-0.665064121654209,
135.679356202147));
#127908=CARTESIAN_POINT('Ctrl Pts',(-211.547231445431,-0.529076375886424,
135.694070348315));
#127909=CARTESIAN_POINT('Ctrl Pts',(-211.554721781193,-0.398032127210128,
135.708249598206));
#127910=CARTESIAN_POINT('Ctrl Pts',(-211.562212116955,-0.266584981589111,
135.71713908993));
#127911=CARTESIAN_POINT('Ctrl Pts',(-211.569702452717,-0.135193375502677,
135.720752161546));
#127912=CARTESIAN_POINT('Ctrl Pts',(-211.577476786836,0.00117998326470839,
135.72450222387));
#127913=CARTESIAN_POINT('Ctrl Pts',(-211.585251120955,0.137925497606106,
135.722579735904));
#127914=CARTESIAN_POINT('Ctrl Pts',(-211.593025455074,0.274532050292743,
135.714942580619));
#127915=CARTESIAN_POINT('Ctrl Pts',(-211.600790208021,0.410970247611329,
135.707314837445));
#127916=CARTESIAN_POINT('Ctrl Pts',(-211.608554960968,0.547269437418897,
135.693986461672));
#127917=CARTESIAN_POINT('Ctrl Pts',(-211.616319713915,0.682915815550491,
135.674967258568));
#127918=CARTESIAN_POINT('Ctrl Pts',(-211.6240767548,0.818427467787413,135.655966945604));
#127919=CARTESIAN_POINT('Ctrl Pts',(-211.631833795686,0.953287213984832,
135.631287107396));
#127920=CARTESIAN_POINT('Ctrl Pts',(-211.639590836571,1.08698404907044,
135.600989510817));
#127921=CARTESIAN_POINT('Ctrl Pts',(-211.647342027811,1.22058006233288,
135.57071476189));
#127922=CARTESIAN_POINT('Ctrl Pts',(-211.655093219051,1.35301453026544,
135.534830772938));
#127923=CARTESIAN_POINT('Ctrl Pts',(-211.662844410291,1.48378470602246,
135.493450722125));
#127924=CARTESIAN_POINT('Ctrl Pts',(-211.670592307068,1.61449930096619,
135.452088258938));
#127925=CARTESIAN_POINT('Ctrl Pts',(-211.678340203845,1.74355063866827,
135.405234497666));
#127926=CARTESIAN_POINT('Ctrl Pts',(-211.686088100622,1.87044946768263,
135.353052940789));
#127927=CARTESIAN_POINT('Ctrl Pts',(-211.693834376706,1.99732175219757,
135.300882299169));
#127928=CARTESIAN_POINT('Ctrl Pts',(-211.70158065279,2.12204206225449,135.243386227259));
#127929=CARTESIAN_POINT('Ctrl Pts',(-211.709326928874,2.24413990251942,
135.180776863814));
#127930=CARTESIAN_POINT('Ctrl Pts',(-211.71707326214,2.36623864408271,135.1181670382));
#127931=CARTESIAN_POINT('Ctrl Pts',(-211.724819595405,2.48571452933222,
135.050444024126));
#127932=CARTESIAN_POINT('Ctrl Pts',(-211.73256592867,2.60212086491236,134.977866346194));
#127933=CARTESIAN_POINT('Ctrl Pts',(-211.740313996673,2.71855326888377,
134.905272414994));
#127934=CARTESIAN_POINT('Ctrl Pts',(-211.748062064676,2.83191442363078,
134.827821863407));
#127935=CARTESIAN_POINT('Ctrl Pts',(-211.755810132679,2.94178620902499,
134.745816815837));
#127936=CARTESIAN_POINT('Ctrl Pts',(-211.763566435421,3.05177476746066,
134.663724612327));
#127937=CARTESIAN_POINT('Ctrl Pts',(-211.771322738163,3.15826623451207,
134.577068477491));
#127938=CARTESIAN_POINT('Ctrl Pts',(-211.779079040905,3.26087479461181,
134.486191498577));
#127939=CARTESIAN_POINT('Ctrl Pts',(-211.786839483419,3.36353811998983,
134.395266015882));
#127940=CARTESIAN_POINT('Ctrl Pts',(-211.794599925933,3.46231412749967,
134.300115471336));
#127941=CARTESIAN_POINT('Ctrl Pts',(-211.802360368447,3.55685428929164,
134.201119459057));
#127942=CARTESIAN_POINT('Ctrl Pts',(-211.810133268713,3.6515462153442,134.101964529591));
#127943=CARTESIAN_POINT('Ctrl Pts',(-211.817906168978,3.74198844950517,
133.998952090566));
#127944=CARTESIAN_POINT('Ctrl Pts',(-211.825679069244,3.82787257567532,
133.892495104096));
#127945=CARTESIAN_POINT('Ctrl Pts',(-211.833169405006,3.91063459753106,
133.789908097231));
#127946=CARTESIAN_POINT('Ctrl Pts',(-211.840659740768,3.98916397166631,
133.684122878256));
#127947=CARTESIAN_POINT('Ctrl Pts',(-211.84815007653,4.06322412365334,133.575532352313));
#127948=CARTESIAN_POINT('Ctrl Pts',(-211.855924410649,4.1400922888123,133.462824583575));
#127949=CARTESIAN_POINT('Ctrl Pts',(-211.863698744768,4.21238913593506,
133.34673755782));
#127950=CARTESIAN_POINT('Ctrl Pts',(-211.871473078887,4.27980295942585,
133.227678527166));
#127951=CARTESIAN_POINT('Ctrl Pts',(-211.879237831834,4.34713370140377,
133.108766226128));
#127952=CARTESIAN_POINT('Ctrl Pts',(-211.887002584781,4.40959320277074,
132.986889544881));
#127953=CARTESIAN_POINT('Ctrl Pts',(-211.894767337728,4.46691198927408,
132.862486061405));
#127954=CARTESIAN_POINT('Ctrl Pts',(-211.902524378613,4.52417384595077,
132.738206137224));
#127955=CARTESIAN_POINT('Ctrl Pts',(-211.910281419498,4.57630498604949,
132.611404757931));
#127956=CARTESIAN_POINT('Ctrl Pts',(-211.918038460383,4.62308116506517,
132.482545233072));
#127957=CARTESIAN_POINT('Ctrl Pts',(-211.925789651624,4.66982206980045,
132.353782882182));
#127958=CARTESIAN_POINT('Ctrl Pts',(-211.933540842864,4.71121591841661,
132.222965841027));
#127959=CARTESIAN_POINT('Ctrl Pts',(-211.941292034104,4.74708618395972,
132.090578260331));
#127960=CARTESIAN_POINT('Ctrl Pts',(-211.949039930881,4.78294120368305,
131.958246947888));
#127961=CARTESIAN_POINT('Ctrl Pts',(-211.956787827658,4.81327720763939,
131.824346800121));
#127962=CARTESIAN_POINT('Ctrl Pts',(-211.964535724435,4.83796730273891,
131.689377815212));
#127963=CARTESIAN_POINT('Ctrl Pts',(-211.972282000519,4.8626522332028,131.554437062905));
#127964=CARTESIAN_POINT('Ctrl Pts',(-211.980028276603,4.88169353358055,
131.418428302505));
#127965=CARTESIAN_POINT('Ctrl Pts',(-211.987774552687,4.89501536799332,
131.281862041238));
#127966=CARTESIAN_POINT('Ctrl Pts',(-211.995520885953,4.90833730074482,
131.145294771871));
#127967=CARTESIAN_POINT('Ctrl Pts',(-212.003267219218,4.9159396453269,131.008170382544));
#127968=CARTESIAN_POINT('Ctrl Pts',(-212.011013552483,4.91779845713967,
130.871004427891));
#127969=CARTESIAN_POINT('Ctrl Pts',(-212.018761620486,4.91965768522046,
130.733807755874));
#127970=CARTESIAN_POINT('Ctrl Pts',(-212.026509688489,4.91577081579773,
130.596569890862));
#127971=CARTESIAN_POINT('Ctrl Pts',(-212.034257756492,4.90616603054668,
130.459805914783));
#127972=CARTESIAN_POINT('Ctrl Pts',(-212.042014059234,4.89655103721554,
130.322896584322));
#127973=CARTESIAN_POINT('Ctrl Pts',(-212.049770361976,4.88120601588943,
130.186462539525));
#127974=CARTESIAN_POINT('Ctrl Pts',(-212.057526664718,4.86021107284611,
130.05101382499));
#127975=CARTESIAN_POINT('Ctrl Pts',(-212.065287107232,4.83920492416949,
129.915492817398));
#127976=CARTESIAN_POINT('Ctrl Pts',(-212.073047549746,4.81254292103631,
129.78095857129));
#127977=CARTESIAN_POINT('Ctrl Pts',(-212.08080799226,4.78035603891383,129.647909492909));
#127978=CARTESIAN_POINT('Ctrl Pts',(-212.088580892526,4.74811748755075,
129.514646832336));
#127979=CARTESIAN_POINT('Ctrl Pts',(-212.096353792791,4.7103364418738,129.382874479768));
#127980=CARTESIAN_POINT('Ctrl Pts',(-212.104126693057,4.66719363216871,
129.253075130512));
#127981=CARTESIAN_POINT('Ctrl Pts',(-212.111617028819,4.62561917226623,
129.127994314546));
#127982=CARTESIAN_POINT('Ctrl Pts',(-212.119107364581,4.57906611645686,
129.004745833215));
#127983=CARTESIAN_POINT('Ctrl Pts',(-212.126597700343,4.52773715270625,
128.883741098113));
#127984=CARTESIAN_POINT('Ctrl Pts',(-212.134372034462,4.47446203569445,
128.758148431702));
#127985=CARTESIAN_POINT('Ctrl Pts',(-212.142146368581,4.41587294499023,
128.634575173661));
#127986=CARTESIAN_POINT('Ctrl Pts',(-212.1499207027,4.35214402884569,128.513503700453));
#127987=CARTESIAN_POINT('Ctrl Pts',(-212.157685455647,4.28849365289468,
128.392581437016));
#127988=CARTESIAN_POINT('Ctrl Pts',(-212.165450208594,4.2197162353809,128.274155166353));
#127989=CARTESIAN_POINT('Ctrl Pts',(-212.173214961542,4.14603426563759,
128.158688126372));
#127990=CARTESIAN_POINT('Ctrl Pts',(-212.180972002427,4.07242547786517,
128.043335769884));
#127991=CARTESIAN_POINT('Ctrl Pts',(-212.188729043312,3.99392204086201,
127.930937122484));
#127992=CARTESIAN_POINT('Ctrl Pts',(-212.196486084197,3.91079254043548,
127.821931277552));
#127993=CARTESIAN_POINT('Ctrl Pts',(-212.204237275437,3.82772572861176,
127.713007634776));
#127994=CARTESIAN_POINT('Ctrl Pts',(-212.211988466677,3.74004003323491,
127.607472011472));
#127995=CARTESIAN_POINT('Ctrl Pts',(-212.219739657917,3.64804736688959,
127.505734620059));
#127996=CARTESIAN_POINT('Ctrl Pts',(-212.227487554694,3.55609379988157,
127.404040469751));
#127997=CARTESIAN_POINT('Ctrl Pts',(-212.235235451471,3.45983716445215,
127.306141629901));
#127998=CARTESIAN_POINT('Ctrl Pts',(-212.242983348248,3.35962953441825,
127.21241512049));
#127999=CARTESIAN_POINT('Ctrl Pts',(-212.250729624333,3.25944286566032,
127.118708216644));
#128000=CARTESIAN_POINT('Ctrl Pts',(-212.258475900417,3.15530713153065,
127.029172174163));
#128001=CARTESIAN_POINT('Ctrl Pts',(-212.266222176501,3.04761084507334,
126.944146737547));
#128002=CARTESIAN_POINT('Ctrl Pts',(-212.273968509766,2.93991376362695,
126.859120673292));
#128003=CARTESIAN_POINT('Ctrl Pts',(-212.281714843031,2.82865638426578,
126.778605523605));
#128004=CARTESIAN_POINT('Ctrl Pts',(-212.289461176297,2.71425951506319,
126.702900103628));
#128005=CARTESIAN_POINT('Ctrl Pts',(-212.2972092443,2.59983702747476,126.627177729947));
#128006=CARTESIAN_POINT('Ctrl Pts',(-212.304957312303,2.48227397699698,
126.556267445015));
#128007=CARTESIAN_POINT('Ctrl Pts',(-212.312705380306,2.36201894952585,
126.490423953151));
#128008=CARTESIAN_POINT('Ctrl Pts',(-212.320461683048,2.24163611358032,
126.424510482041));
#128009=CARTESIAN_POINT('Ctrl Pts',(-212.328217985789,2.11855592882903,
126.363674749277));
#128010=CARTESIAN_POINT('Ctrl Pts',(-212.335974288531,1.99325080963909,
126.308125050742));
#128011=CARTESIAN_POINT('Ctrl Pts',(-212.343734731046,1.86787881133419,
126.252545703661));
#128012=CARTESIAN_POINT('Ctrl Pts',(-212.35149517356,1.74027987592607,126.202258155801));
#128013=CARTESIAN_POINT('Ctrl Pts',(-212.359255616074,1.61094412214307,
126.157421614541));
#128014=CARTESIAN_POINT('Ctrl Pts',(-212.367028516339,1.4814007471262,126.112513097685));
#128015=CARTESIAN_POINT('Ctrl Pts',(-212.374801416605,1.35011535688172,
126.073073186146));
#128016=CARTESIAN_POINT('Ctrl Pts',(-212.38257431687,1.21759174577694,126.039210735021));
#128017=CARTESIAN_POINT('Ctrl Pts',(-212.390064652632,1.08988570174336,
126.006579269289));
#128018=CARTESIAN_POINT('Ctrl Pts',(-212.397554988394,0.961030200037002,
125.979126858922));
#128019=CARTESIAN_POINT('Ctrl Pts',(-212.405045324156,0.831480930678297,
125.95690535481));
#128020=CARTESIAN_POINT('Ctrl Pts',(-212.412819658275,0.697019761395268,
125.933841315615));
#128021=CARTESIAN_POINT('Ctrl Pts',(-212.420593992394,0.561385244984867,
125.916339612538));
#128022=CARTESIAN_POINT('Ctrl Pts',(-212.428368326513,0.425077349810972,
125.904514465984));
#128023=CARTESIAN_POINT('Ctrl Pts',(-212.43613307946,0.288937441936431,
125.892703892865));
#128024=CARTESIAN_POINT('Ctrl Pts',(-212.443897832408,0.152126192273598,
125.886555990081));
#128025=CARTESIAN_POINT('Ctrl Pts',(-212.451662585355,0.0151535969136297,
125.886133962459));
#128026=CARTESIAN_POINT('Ctrl Pts',(-212.45941962624,-0.121682955334768,
125.885712354002));
#128027=CARTESIAN_POINT('Ctrl Pts',(-212.467176667125,-0.258680145940508,
125.891005304476));
#128028=CARTESIAN_POINT('Ctrl Pts',(-212.47493370801,-0.395323376019601,
125.902024185733));
#128029=CARTESIAN_POINT('Ctrl Pts',(-212.48268489925,-0.531863562375405,
125.913034757567));
#128030=CARTESIAN_POINT('Ctrl Pts',(-212.49043609049,-0.668049931377992,
125.929762634228));
#128031=CARTESIAN_POINT('Ctrl Pts',(-212.49818728173,-0.803368763331662,
125.95216712466));
#128032=CARTESIAN_POINT('Ctrl Pts',(-212.505935178507,-0.93863008117182,
125.974562092585));
#128033=CARTESIAN_POINT('Ctrl Pts',(-212.513683075284,-1.07302421042508,
126.00262881185));
#128034=CARTESIAN_POINT('Ctrl Pts',(-212.521430972061,-1.20604364900575,
126.036274861291));
#128035=CARTESIAN_POINT('Ctrl Pts',(-212.529177248145,-1.3390352627878,
126.069913872704));
#128036=CARTESIAN_POINT('Ctrl Pts',(-212.536923524229,-1.47065237907312,
126.109129797104));
#128037=CARTESIAN_POINT('Ctrl Pts',(-212.544669800314,-1.60039916040225,
126.153779407665));
#128038=CARTESIAN_POINT('Ctrl Pts',(-212.552416133579,-1.73014689949246,
126.198429347819));
#128039=CARTESIAN_POINT('Ctrl Pts',(-212.560162466844,-1.85802390638936,
126.248512926951));
#128040=CARTESIAN_POINT('Ctrl Pts',(-212.56790880011,-1.9835513224081,126.303837624194));
#128041=CARTESIAN_POINT('Ctrl Pts',(-212.575656868113,-2.10910684942115,
126.359174711019));
#128042=CARTESIAN_POINT('Ctrl Pts',(-212.583404936116,-2.23231138083907,
126.419755093858));
#128043=CARTESIAN_POINT('Ctrl Pts',(-212.591153004119,-2.35270815506882,
126.4853390386));
#128044=CARTESIAN_POINT('Ctrl Pts',(-212.59890930686,-2.47323288842312,
126.550992686739));
#128045=CARTESIAN_POINT('Ctrl Pts',(-212.606665609602,-2.59094355961426,
126.621660332428));
#128046=CARTESIAN_POINT('Ctrl Pts',(-212.614421912344,-2.70540957191042,
126.697057109093));
#128047=CARTESIAN_POINT('Ctrl Pts',(-212.622182354858,-2.81993667816385,
126.772494127288));
#128048=CARTESIAN_POINT('Ctrl Pts',(-212.629942797372,-2.9312153577612,
126.852665077476));
#128049=CARTESIAN_POINT('Ctrl Pts',(-212.637703239887,-3.03884674388082,
126.937243664369));
#128050=CARTESIAN_POINT('Ctrl Pts',(-212.645476140152,-3.14665090945651,
127.021958024317));
#128051=CARTESIAN_POINT('Ctrl Pts',(-212.653249040417,-3.25079578428155,
127.111093905765));
#128052=CARTESIAN_POINT('Ctrl Pts',(-212.661021940683,-3.3509174723189,
127.204286291082));
#128053=CARTESIAN_POINT('Ctrl Pts',(-212.668512276445,-3.44739948480396,
127.294090898454));
#128054=CARTESIAN_POINT('Ctrl Pts',(-212.676002612207,-3.54014552128071,
127.387661983052));
#128055=CARTESIAN_POINT('Ctrl Pts',(-212.683492947969,-3.62886564654099,
127.484644186626));
#128056=CARTESIAN_POINT('Ctrl Pts',(-212.691183413032,-3.71995622584122,
127.584217593217));
#128057=CARTESIAN_POINT('Ctrl Pts',(-212.698873878095,-3.80710559154992,
127.687718300335));
#128058=CARTESIAN_POINT('Ctrl Pts',(-212.706564343158,-3.88995039074112,
127.794797689154));
#128059=CARTESIAN_POINT('Ctrl Pts',(-212.714245638282,-3.97269640763924,
127.901749398894));
#128060=CARTESIAN_POINT('Ctrl Pts',(-212.721926933406,-4.05114782160935,
128.012270992388));
#128061=CARTESIAN_POINT('Ctrl Pts',(-212.72960822853,-4.12497833315283,
128.125977371367));
#128062=CARTESIAN_POINT('Ctrl Pts',(-212.737280901644,-4.19872597229643,
128.239556118553));
#128063=CARTESIAN_POINT('Ctrl Pts',(-212.744953574759,-4.26786281658607,
128.356312202527));
#128064=CARTESIAN_POINT('Ctrl Pts',(-212.752626247873,-4.33210352833311,
128.475828444221));
#128065=CARTESIAN_POINT('Ctrl Pts',(-212.760293849226,-4.39630177591927,
128.595265683725));
#128066=CARTESIAN_POINT('Ctrl Pts',(-212.767961450578,-4.45561013783136,
128.717459102105));
#128067=CARTESIAN_POINT('Ctrl Pts',(-212.77562905193,-4.50978731104797,
128.841963748528));
#128068=CARTESIAN_POINT('Ctrl Pts',(-212.783293992805,-4.56394568606493,
128.966425194779));
#128069=CARTESIAN_POINT('Ctrl Pts',(-212.790958933681,-4.61297624916482,
129.093195910092));
#128070=CARTESIAN_POINT('Ctrl Pts',(-212.798623874557,-4.65668446113259,
129.221807966958));
#128071=CARTESIAN_POINT('Ctrl Pts',(-212.805703125853,-4.69705286334965,
129.340592584489));
#128072=CARTESIAN_POINT('Ctrl Pts',(-212.812782377149,-4.7328816197208,
129.46094742213));
#128073=CARTESIAN_POINT('Ctrl Pts',(-212.819861628446,-4.76405452823406,
129.582490119308));
#128074=CARTESIAN_POINT('Origin',(213.235140564004,0.,130.804360617566));
#128075=CARTESIAN_POINT('',(-214.915345176019,-4.76405452823394,129.582490119308));
#128076=CARTESIAN_POINT('',(-214.569765644412,-4.76405452823405,129.582490119308));
#128077=CARTESIAN_POINT('',(213.235140564004,-4.76405452823405,129.582490119308));
#128078=CARTESIAN_POINT('',(-213.235140564069,-4.91824975740887,130.80281586917));
#128079=CARTESIAN_POINT('Ctrl Pts',(-213.23514056407,-4.91824975740887,
130.802815869171));
#128080=CARTESIAN_POINT('Ctrl Pts',(-213.242852601799,-4.9182922816069,
130.93820660807));
#128081=CARTESIAN_POINT('Ctrl Pts',(-213.250564639529,-4.91273997424585,
131.073824800331));
#128082=CARTESIAN_POINT('Ctrl Pts',(-213.258276677259,-4.90156264554618,
131.209165131234));
#128083=CARTESIAN_POINT('Ctrl Pts',(-213.265979442628,-4.89039875560677,
131.344342739335));
#128084=CARTESIAN_POINT('Ctrl Pts',(-213.273682207996,-4.87362332935581,
131.479242758052));
#128085=CARTESIAN_POINT('Ctrl Pts',(-213.281384973365,-4.85125815681078,
131.613358366931));
#128086=CARTESIAN_POINT('Ctrl Pts',(-213.289080393618,-4.82891431099335,
131.747346087368));
#128087=CARTESIAN_POINT('Ctrl Pts',(-213.296775813871,-4.80099138833436,
131.88055049623));
#128088=CARTESIAN_POINT('Ctrl Pts',(-213.304471234125,-4.76756306468317,
132.012468843996));
#128089=CARTESIAN_POINT('Ctrl Pts',(-213.312161229336,-4.73415830700125,
132.14429419327));
#128090=CARTESIAN_POINT('Ctrl Pts',(-213.319851224548,-4.69525596895756,
132.274834901479));
#128091=CARTESIAN_POINT('Ctrl Pts',(-213.32754121976,-4.65098090936588,
132.403597824241));
#128092=CARTESIAN_POINT('Ctrl Pts',(-213.335228522826,-4.60672134977473,
132.532315669134));
#128093=CARTESIAN_POINT('Ctrl Pts',(-213.342915825891,-4.55709293612188,
132.659256590072));
#128094=CARTESIAN_POINT('Ctrl Pts',(-213.350603128957,-4.50227046527684,
132.783942320855));
#128095=CARTESIAN_POINT('Ctrl Pts',(-213.358289301112,-4.44745605959028,
132.908609708609));
#128096=CARTESIAN_POINT('Ctrl Pts',(-213.365975473267,-4.38744927623874,
133.031022201947));
#128097=CARTESIAN_POINT('Ctrl Pts',(-213.373661645422,-4.32247296612338,
133.150721740589));
#128098=CARTESIAN_POINT('Ctrl Pts',(-213.38134841673,-4.25749159096851,
133.27043061006));
#128099=CARTESIAN_POINT('Ctrl Pts',(-213.389035188039,-4.18754010838411,
133.387425754647));
#128100=CARTESIAN_POINT('Ctrl Pts',(-213.396721959347,-4.11288697205642,
133.501274375473));
#128101=CARTESIAN_POINT('Ctrl Pts',(-213.404411060001,-4.03821121336109,
133.615157496194));
#128102=CARTESIAN_POINT('Ctrl Pts',(-213.412100160655,-3.95883118507137,
133.725891864193));
#128103=CARTESIAN_POINT('Ctrl Pts',(-213.419789261309,-3.87505794807738,
133.833074694785));
#128104=CARTESIAN_POINT('Ctrl Pts',(-213.427486708261,-3.79119377763857,
133.940373869263));
#128105=CARTESIAN_POINT('Ctrl Pts',(-213.435184155213,-3.70292712355384,
134.044113496638));
#128106=CARTESIAN_POINT('Ctrl Pts',(-213.442881602165,-3.61060874719674,
134.143924591675));
#128107=CARTESIAN_POINT('Ctrl Pts',(-213.450583822761,-3.51823311873419,
134.243797585497));
#128108=CARTESIAN_POINT('Ctrl Pts',(-213.458286043357,-3.42180104588926,
134.339736915968));
#128109=CARTESIAN_POINT('Ctrl Pts',(-213.465988263953,-3.32169834938428,
134.431412194012));
#128110=CARTESIAN_POINT('Ctrl Pts',(-213.473701663331,-3.22145036669574,
134.523220526926));
#128111=CARTESIAN_POINT('Ctrl Pts',(-213.481415062709,-3.1175214283961,
134.610752197681));
#128112=CARTESIAN_POINT('Ctrl Pts',(-213.489128462087,-3.01032876205514,
134.693718380339));
#128113=CARTESIAN_POINT('Ctrl Pts',(-213.492501249141,-2.9634573348724,
134.729996453474));
#128114=CARTESIAN_POINT('Ctrl Pts',(-213.495874036194,-2.91596223817887,
134.76540218225));
#128115=CARTESIAN_POINT('Ctrl Pts',(-213.499246823248,-2.86787988118274,
134.799914152385));
#128116=CARTESIAN_POINT('Ctrl Pts',(-213.507021157367,-2.75704919351243,
134.879464857092));
#128117=CARTESIAN_POINT('Ctrl Pts',(-213.514795491486,-2.64273052294015,
134.95452665304));
#128118=CARTESIAN_POINT('Ctrl Pts',(-213.522569825605,-2.52532352423003,
135.024778151468));
#128119=CARTESIAN_POINT('Ctrl Pts',(-213.530334578552,-2.40806121915254,
135.094943071204));
#128120=CARTESIAN_POINT('Ctrl Pts',(-213.538099331499,-2.28771849119061,
135.160309290077));
#128121=CARTESIAN_POINT('Ctrl Pts',(-213.545864084446,-2.16472632567553,
135.220596910772));
#128122=CARTESIAN_POINT('Ctrl Pts',(-213.553621125331,-2.04185631771346,
135.280824652951));
#128123=CARTESIAN_POINT('Ctrl Pts',(-213.561378166216,-1.91634245770695,
135.335983664043));
#128124=CARTESIAN_POINT('Ctrl Pts',(-213.569135207101,-1.78864254052713,
135.385838645967));
#128125=CARTESIAN_POINT('Ctrl Pts',(-213.576886398341,-1.6610389228477,
135.435656031861));
#128126=CARTESIAN_POINT('Ctrl Pts',(-213.584637589582,-1.53125289200009,
135.480177208357));
#128127=CARTESIAN_POINT('Ctrl Pts',(-213.592388780822,-1.39976422312377,
135.519214081054));
#128128=CARTESIAN_POINT('Ctrl Pts',(-213.600136677599,-1.26833144043982,
135.558234362038));
#128129=CARTESIAN_POINT('Ctrl Pts',(-213.607884574376,-1.13519783305681,
135.591774864318));
#128130=CARTESIAN_POINT('Ctrl Pts',(-213.615632471153,-1.00086021008568,
135.619696732768));
#128131=CARTESIAN_POINT('Ctrl Pts',(-213.623378747237,-0.866550687648937,
135.647612760565));
#128132=CARTESIAN_POINT('Ctrl Pts',(-213.631125023321,-0.731038033117482,
135.669912412751));
#128133=CARTESIAN_POINT('Ctrl Pts',(-213.638871299405,-0.594830786853627,
135.68650762452));
#128134=CARTESIAN_POINT('Ctrl Pts',(-213.64661763267,-0.458622535139378,
135.703102958792));
#128135=CARTESIAN_POINT('Ctrl Pts',(-213.654363965936,-0.321720069556817,
135.713993721337));
#128136=CARTESIAN_POINT('Ctrl Pts',(-213.662110299201,-0.184638221668168,
135.719143602561));
#128137=CARTESIAN_POINT('Ctrl Pts',(-213.669858367204,-0.0475256752495831,
135.724294637066));
#128138=CARTESIAN_POINT('Ctrl Pts',(-213.677606435207,0.0897659427967536,
135.72370221732));
#128139=CARTESIAN_POINT('Ctrl Pts',(-213.68535450321,0.226721022593234,
135.717382156336));
#128140=CARTESIAN_POINT('Ctrl Pts',(-213.693110805952,0.363821659878121,
135.711055378316));
#128141=CARTESIAN_POINT('Ctrl Pts',(-213.700867108694,0.500584653242775,
135.698988816862));
#128142=CARTESIAN_POINT('Ctrl Pts',(-213.708623411436,0.636498182637569,
135.681250315519));
#128143=CARTESIAN_POINT('Ctrl Pts',(-213.71638385395,0.772484253175279,
135.663502346604));
#128144=CARTESIAN_POINT('Ctrl Pts',(-213.724144296464,0.90761957130462,
135.640076472424));
#128145=CARTESIAN_POINT('Ctrl Pts',(-213.731904738978,1.04140273125982,
135.611091670353));
#128146=CARTESIAN_POINT('Ctrl Pts',(-213.739677639243,1.17540065182008,
135.582060339304));
#128147=CARTESIAN_POINT('Ctrl Pts',(-213.747450539509,1.30804169812883,
135.54745234676));
#128148=CARTESIAN_POINT('Ctrl Pts',(-213.755223439774,1.43883897685387,
135.507436787605));
#128149=CARTESIAN_POINT('Ctrl Pts',(-213.762713775536,1.56488144503772,
135.468875894818));
#128150=CARTESIAN_POINT('Ctrl Pts',(-213.770204111298,1.68921157882685,
135.425293868858));
#128151=CARTESIAN_POINT('Ctrl Pts',(-213.77769444706,1.81141322115339,135.376883466577));
#128152=CARTESIAN_POINT('Ctrl Pts',(-213.785468781179,1.93824817589203,
135.32663756918));
#128153=CARTESIAN_POINT('Ctrl Pts',(-213.793243115298,2.06319182451666,
135.271030768151));
#128154=CARTESIAN_POINT('Ctrl Pts',(-213.801017449417,2.18575775039907,
135.210225585886));
#128155=CARTESIAN_POINT('Ctrl Pts',(-213.808782202364,2.30817262473185,
135.149495340574));
#128156=CARTESIAN_POINT('Ctrl Pts',(-213.816546955312,2.42821525993514,
135.083579633217));
#128157=CARTESIAN_POINT('Ctrl Pts',(-213.824311708259,2.5454172123711,135.012689772642));
#128158=CARTESIAN_POINT('Ctrl Pts',(-213.832068749144,2.66250275817564,
134.941870320877));
#128159=CARTESIAN_POINT('Ctrl Pts',(-213.839825790029,2.77675290357153,
134.866086748545));
#128160=CARTESIAN_POINT('Ctrl Pts',(-213.847582830914,2.8877222363102,134.785597027077));
#128161=CARTESIAN_POINT('Ctrl Pts',(-213.855334022154,2.99860788621168,
134.705168003535));
#128162=CARTESIAN_POINT('Ctrl Pts',(-213.863085213394,3.10621733277591,
134.620040123438));
#128163=CARTESIAN_POINT('Ctrl Pts',(-213.870836404634,3.21013299667426,
134.530515365582));
#128164=CARTESIAN_POINT('Ctrl Pts',(-213.878584301411,3.31400449364355,
134.441028658136));
#128165=CARTESIAN_POINT('Ctrl Pts',(-213.886332198188,3.41418503488793,
134.34714904446));
#128166=CARTESIAN_POINT('Ctrl Pts',(-213.894080094965,3.51028926019803,
134.249219449541));
#128167=CARTESIAN_POINT('Ctrl Pts',(-213.901826371049,3.60637338257596,
134.151310339383));
#128168=CARTESIAN_POINT('Ctrl Pts',(-213.909572647133,3.69838261137393,
134.049353211914));
#128169=CARTESIAN_POINT('Ctrl Pts',(-213.917318923217,3.78596797668907,
133.943728315365));
#128170=CARTESIAN_POINT('Ctrl Pts',(-213.925065256483,3.87355398853936,
133.838102639117));
#128171=CARTESIAN_POINT('Ctrl Pts',(-213.932811589748,3.95671582218726,
133.728809440721));
#128172=CARTESIAN_POINT('Ctrl Pts',(-213.940557923013,4.03514465030808,
133.616262236327));
#128173=CARTESIAN_POINT('Ctrl Pts',(-213.948305991016,4.11359104202148,
133.503689827767));
#128174=CARTESIAN_POINT('Ctrl Pts',(-213.956054059019,4.18730209559916,
133.38786228386));
#128175=CARTESIAN_POINT('Ctrl Pts',(-213.963802127022,4.25601241524396,
133.26922194912));
#128176=CARTESIAN_POINT('Ctrl Pts',(-213.971558429764,4.32479576103385,
133.150455522021));
#128177=CARTESIAN_POINT('Ctrl Pts',(-213.979314732506,4.3885675596754,133.028870671166));
#128178=CARTESIAN_POINT('Ctrl Pts',(-213.987071035248,4.4471082386258,132.904934676352));
#128179=CARTESIAN_POINT('Ctrl Pts',(-213.994831477762,4.50568016249934,
132.780932533167));
#128180=CARTESIAN_POINT('Ctrl Pts',(-214.002591920276,4.55901525140929,
132.65457710559));
#128181=CARTESIAN_POINT('Ctrl Pts',(-214.01035236279,4.60694258232605,132.526354550671));
#128182=CARTESIAN_POINT('Ctrl Pts',(-214.018125263056,4.65494685044905,
132.397926161524));
#128183=CARTESIAN_POINT('Ctrl Pts',(-214.025898163321,4.69752589164035,
132.267625027358));
#128184=CARTESIAN_POINT('Ctrl Pts',(-214.033671063587,4.73455879247533,
132.135952185238));
#128185=CARTESIAN_POINT('Ctrl Pts',(-214.041161399349,4.7702454540851,132.009065982591));
#128186=CARTESIAN_POINT('Ctrl Pts',(-214.048651735111,4.80078213558388,
131.880906370238));
#128187=CARTESIAN_POINT('Ctrl Pts',(-214.056142070873,4.82610606571059,
131.751927662693));
#128188=CARTESIAN_POINT('Ctrl Pts',(-214.063916404992,4.85239016034483,
131.618058688252));
#128189=CARTESIAN_POINT('Ctrl Pts',(-214.071690739111,4.87314167777241,
131.482883223848));
#128190=CARTESIAN_POINT('Ctrl Pts',(-214.07946507323,4.88823443261954,131.346898352892));
#128191=CARTESIAN_POINT('Ctrl Pts',(-214.087229826177,4.90330858699525,
131.211081071136));
#128192=CARTESIAN_POINT('Ctrl Pts',(-214.094994579124,4.91273781209716,
131.074456752448));
#128193=CARTESIAN_POINT('Ctrl Pts',(-214.102759332071,4.91644668279933,
130.93753372931));
#128194=CARTESIAN_POINT('Ctrl Pts',(-214.110516372956,4.92015186979883,
130.800746700049));
#128195=CARTESIAN_POINT('Ctrl Pts',(-214.118273413842,4.9181479983951,130.663661945033));
#128196=CARTESIAN_POINT('Ctrl Pts',(-214.126030454727,4.91041135105898,
130.526793642061));
#128197=CARTESIAN_POINT('Ctrl Pts',(-214.133781645967,4.90268053798878,
130.390028552541));
#128198=CARTESIAN_POINT('Ctrl Pts',(-214.141532837207,4.88922557589138,
130.253479978932));
#128199=CARTESIAN_POINT('Ctrl Pts',(-214.149284028447,4.8700748162521,130.117662469464));
#128200=CARTESIAN_POINT('Ctrl Pts',(-214.157031925224,4.85093219619655,
129.981902686061));
#128201=CARTESIAN_POINT('Ctrl Pts',(-214.164779822001,4.82609864799007,
129.846873735122));
#128202=CARTESIAN_POINT('Ctrl Pts',(-214.172527718778,4.7956543875314,129.713085190439));
#128203=CARTESIAN_POINT('Ctrl Pts',(-214.180273994862,4.76521649535572,
129.579324631435));
#128204=CARTESIAN_POINT('Ctrl Pts',(-214.188020270946,4.72917031205577,
129.446804343573));
#128205=CARTESIAN_POINT('Ctrl Pts',(-214.195766547031,4.68764712448072,
129.31602345857));
#128206=CARTESIAN_POINT('Ctrl Pts',(-214.203512880296,4.64612363039088,
129.185241608173));
#128207=CARTESIAN_POINT('Ctrl Pts',(-214.211259213561,4.59912316966279,
129.056199558891));
#128208=CARTESIAN_POINT('Ctrl Pts',(-214.219005546827,4.54682671643361,
128.92938065148));
#128209=CARTESIAN_POINT('Ctrl Pts',(-214.22675361483,4.4945185517764,128.802533343853));
#128210=CARTESIAN_POINT('Ctrl Pts',(-214.234501682833,4.43691218363262,
128.677910530147));
#128211=CARTESIAN_POINT('Ctrl Pts',(-214.242249750835,4.37423631605783,
128.555974593374));
#128212=CARTESIAN_POINT('Ctrl Pts',(-214.250006053577,4.31149383582504,
128.433909061637));
#128213=CARTESIAN_POINT('Ctrl Pts',(-214.257762356319,4.24367127221741,
128.314536459566));
#128214=CARTESIAN_POINT('Ctrl Pts',(-214.265518659061,4.17104307663906,
128.198294095905));
#128215=CARTESIAN_POINT('Ctrl Pts',(-214.273279101575,4.09837611720594,
128.081989690195));
#128216=CARTESIAN_POINT('Ctrl Pts',(-214.281039544089,4.02089863575193,
127.968819174359));
#128217=CARTESIAN_POINT('Ctrl Pts',(-214.288799986604,3.93892726189776,
127.859189130542));
#128218=CARTESIAN_POINT('Ctrl Pts',(-214.296572886869,3.8568243003172,127.749383098847));
#128219=CARTESIAN_POINT('Ctrl Pts',(-214.304345787134,3.7702132776379,127.643129199792));
#128220=CARTESIAN_POINT('Ctrl Pts',(-214.3121186874,3.67945037387307,127.540799984039));
#128221=CARTESIAN_POINT('Ctrl Pts',(-214.319609023162,3.59198693027806,
127.442190693031));
#128222=CARTESIAN_POINT('Ctrl Pts',(-214.327099358924,3.50066844098738,
127.347225917093));
#128223=CARTESIAN_POINT('Ctrl Pts',(-214.334589694686,3.40584320426917,
127.25620403556));
#128224=CARTESIAN_POINT('Ctrl Pts',(-214.342364028805,3.30742263987888,
127.161731031722));
#128225=CARTESIAN_POINT('Ctrl Pts',(-214.350138362924,3.20491239536073,
127.071206552042));
#128226=CARTESIAN_POINT('Ctrl Pts',(-214.357912697043,3.09866247478941,
126.985005445573));
#128227=CARTESIAN_POINT('Ctrl Pts',(-214.365677449991,2.99254349774966,
126.898910574264));
#128228=CARTESIAN_POINT('Ctrl Pts',(-214.373442202938,2.88269431552433,
126.81712871865));
#128229=CARTESIAN_POINT('Ctrl Pts',(-214.381206955885,2.7695018335054,126.739998102151));
#128230=CARTESIAN_POINT('Ctrl Pts',(-214.38896399677,2.65642177585566,126.662944092868));
#128231=CARTESIAN_POINT('Ctrl Pts',(-214.396721037655,2.54000534757768,
126.590532348065));
#128232=CARTESIAN_POINT('Ctrl Pts',(-214.40447807854,2.42067232111235,126.523060747632));
#128233=CARTESIAN_POINT('Ctrl Pts',(-214.41222926978,2.30142928461039,126.455640028057));
#128234=CARTESIAN_POINT('Ctrl Pts',(-214.41998046102,2.17927436670708,126.393152229314));
#128235=CARTESIAN_POINT('Ctrl Pts',(-214.42773165226,2.05465579607173,126.335851624382));
#128236=CARTESIAN_POINT('Ctrl Pts',(-214.435479549037,1.93009019165303,
126.278575373735));
#128237=CARTESIAN_POINT('Ctrl Pts',(-214.443227445814,1.80306337161081,
126.226482094916));
#128238=CARTESIAN_POINT('Ctrl Pts',(-214.450975342591,1.6740474134597,126.179779737098));
#128239=CARTESIAN_POINT('Ctrl Pts',(-214.458721618676,1.54505844266578,
126.133087148407));
#128240=CARTESIAN_POINT('Ctrl Pts',(-214.46646789476,1.41408152876622,126.09178337072));
#128241=CARTESIAN_POINT('Ctrl Pts',(-214.474214170844,1.28160756916159,
126.05602774158));
#128242=CARTESIAN_POINT('Ctrl Pts',(-214.481960504109,1.14913263166411,
126.0202718485));
#128243=CARTESIAN_POINT('Ctrl Pts',(-214.489706837375,1.0151610038684,125.990064287569));
#128244=CARTESIAN_POINT('Ctrl Pts',(-214.49745317064,0.880197154982506,
125.965514057604));
#128245=CARTESIAN_POINT('Ctrl Pts',(-214.505201238643,0.745203081878611,
125.940958329784));
#128246=CARTESIAN_POINT('Ctrl Pts',(-214.512949306646,0.609216730109788,
125.922062523911));
#128247=CARTESIAN_POINT('Ctrl Pts',(-214.520697374649,0.472750735730102,
125.908884154098));
#128248=CARTESIAN_POINT('Ctrl Pts',(-214.528453677391,0.336139703667811,
125.895691778157));
#128249=CARTESIAN_POINT('Ctrl Pts',(-214.536209980133,0.19904840044981,
125.888229014498));
#128250=CARTESIAN_POINT('Ctrl Pts',(-214.543966282875,0.0619930939944813,
125.88650133544));
#128251=CARTESIAN_POINT('Ctrl Pts',(-214.551726725389,-0.0751353630049309,
125.884772734267));
#128252=CARTESIAN_POINT('Ctrl Pts',(-214.559487167903,-0.212227394352379,
125.888785305537));
#128253=CARTESIAN_POINT('Ctrl Pts',(-214.567247610417,-0.348769784930064,
125.898492427366));
#128254=CARTESIAN_POINT('Ctrl Pts',(-214.575020510683,-0.485531365474397,
125.908215131928));
#128255=CARTESIAN_POINT('Ctrl Pts',(-214.582793410948,-0.621741153365783,
125.923650610425));
#128256=CARTESIAN_POINT('Ctrl Pts',(-214.590566311214,-0.756893187184922,
125.944700571257));
#128257=CARTESIAN_POINT('Ctrl Pts',(-214.598056646975,-0.88713210414437,
125.964985312991));
#128258=CARTESIAN_POINT('Ctrl Pts',(-214.605546982737,-1.01638853371941,
125.990483363267));
#128259=CARTESIAN_POINT('Ctrl Pts',(-214.613037318499,-1.14422317720585,
126.021062970205));
#128260=CARTESIAN_POINT('Ctrl Pts',(-214.620811652618,-1.27690471005774,
126.052802012236));
#128261=CARTESIAN_POINT('Ctrl Pts',(-214.628585986737,-1.40847480971311,
126.09011609174));
#128262=CARTESIAN_POINT('Ctrl Pts',(-214.636360320856,-1.5384289192948,
126.132913355445));
#128263=CARTESIAN_POINT('Ctrl Pts',(-214.644125073803,-1.66822287204971,
126.175657875347));
#128264=CARTESIAN_POINT('Ctrl Pts',(-214.651889826751,-1.79640442956711,
126.223872012852));
#128265=CARTESIAN_POINT('Ctrl Pts',(-214.659654579698,-1.92247990309097,
126.277413071513));
#128266=CARTESIAN_POINT('Ctrl Pts',(-214.667411620583,-2.04843015667717,
126.330900952441));
#128267=CARTESIAN_POINT('Ctrl Pts',(-214.675168661468,-2.17227813150008,
126.389705073814));
#128268=CARTESIAN_POINT('Ctrl Pts',(-214.682925702353,-2.29354631551489,
126.453633280547));
#128269=CARTESIAN_POINT('Ctrl Pts',(-214.690676893593,-2.41472305024863,
126.517513278521));
#128270=CARTESIAN_POINT('Ctrl Pts',(-214.698428084833,-2.53332352200339,
126.586509488989));
#128271=CARTESIAN_POINT('Ctrl Pts',(-214.706179276073,-2.64889152517579,
126.660382245234));
#128272=CARTESIAN_POINT('Ctrl Pts',(-214.71392717285,-2.76441040886476,
126.734223603588));
#128273=CARTESIAN_POINT('Ctrl Pts',(-214.721675069627,-2.8768990587289,
126.812937175225));
#128274=CARTESIAN_POINT('Ctrl Pts',(-214.729422966404,-2.98592735181132,
126.89623818957));
#128275=CARTESIAN_POINT('Ctrl Pts',(-214.737169242488,-3.09493283852521,
126.979521779139));
#128276=CARTESIAN_POINT('Ctrl Pts',(-214.744915518572,-3.20047909772844,
127.06739066552));
#128277=CARTESIAN_POINT('Ctrl Pts',(-214.752661794656,-3.3021667321985,
127.159517968663));
#128278=CARTESIAN_POINT('Ctrl Pts',(-214.760408127922,-3.40385511730371,
127.251645951869));
#128279=CARTESIAN_POINT('Ctrl Pts',(-214.768154461187,-3.50168453110043,
127.348032152063));
#128280=CARTESIAN_POINT('Ctrl Pts',(-214.775900794452,-3.59529059186724,
127.448311061536));
#128281=CARTESIAN_POINT('Ctrl Pts',(-214.783648862455,-3.68891761506246,
127.548612427776));
#128282=CARTESIAN_POINT('Ctrl Pts',(-214.791396930458,-3.77831913648335,
127.652807952222));
#128283=CARTESIAN_POINT('Ctrl Pts',(-214.799144998461,-3.86316967556741,
127.760497427428));
#128284=CARTESIAN_POINT('Ctrl Pts',(-214.806901301203,-3.94811039481379,
127.86830135629));
#128285=CARTESIAN_POINT('Ctrl Pts',(-214.814657603945,-4.0284902272672,
127.979606346268));
#128286=CARTESIAN_POINT('Ctrl Pts',(-214.822413906687,-4.10402551349094,
128.093981004465));
#128287=CARTESIAN_POINT('Ctrl Pts',(-214.830174349201,-4.17960111517126,
128.20841670786));
#128288=CARTESIAN_POINT('Ctrl Pts',(-214.837934791715,-4.25032681692145,
128.325925009264));
#128289=CARTESIAN_POINT('Ctrl Pts',(-214.84569523423,-4.31596443774793,
128.446048925996));
#128290=CARTESIAN_POINT('Ctrl Pts',(-214.853468134495,-4.38170742591057,
128.566365676303));
#128291=CARTESIAN_POINT('Ctrl Pts',(-214.86124103476,-4.44234583816004,
128.689306081678));
#128292=CARTESIAN_POINT('Ctrl Pts',(-214.869013935026,-4.49768888549772,
128.814391333439));
#128293=CARTESIAN_POINT('Ctrl Pts',(-214.876504270788,-4.55102007366499,
128.934929421229));
#128294=CARTESIAN_POINT('Ctrl Pts',(-214.88399460655,-4.59943409927662,
129.057458835167));
#128295=CARTESIAN_POINT('Ctrl Pts',(-214.891484942312,-4.64280435724053,
129.181538765702));
#128296=CARTESIAN_POINT('Ctrl Pts',(-214.899438353548,-4.68885589724191,
129.313289697161));
#128297=CARTESIAN_POINT('Ctrl Pts',(-214.907391764783,-4.72932661485808,
129.447086512125));
#128298=CARTESIAN_POINT('Ctrl Pts',(-214.915345176019,-4.76405452823394,
129.582490119308));
#128299=CARTESIAN_POINT('Ctrl Pts',(-213.165046531412,-4.76405452823396,
129.582490119308));
#128300=CARTESIAN_POINT('Ctrl Pts',(-213.17281002151,-4.79810457133673,
129.715250720584));
#128301=CARTESIAN_POINT('Ctrl Pts',(-213.180573511608,-4.82656878613077,
129.849310261608));
#128302=CARTESIAN_POINT('Ctrl Pts',(-213.188337001706,-4.84937648881122,
129.984158976343));
#128303=CARTESIAN_POINT('Ctrl Pts',(-213.196111695209,-4.87221710502965,
130.119202289734));
#128304=CARTESIAN_POINT('Ctrl Pts',(-213.203886388712,-4.88938486259401,
130.255036664043));
#128305=CARTESIAN_POINT('Ctrl Pts',(-213.211661082215,-4.90086100994425,
130.391148294773));
#128306=CARTESIAN_POINT('Ctrl Pts',(-213.214707121288,-4.90535723776683,
130.444475328871));
#128307=CARTESIAN_POINT('Ctrl Pts',(-213.217753160361,-4.90898037685139,
130.497844933484));
#128308=CARTESIAN_POINT('Ctrl Pts',(-213.220799199435,-4.91173147644005,
130.551226333345));
#128309=CARTESIAN_POINT('Ctrl Pts',(-213.225579654294,-4.91604905316183,
130.635003122221));
#128310=CARTESIAN_POINT('Ctrl Pts',(-213.230360109153,-4.91822339794989,
130.718891315629));
#128311=CARTESIAN_POINT('Ctrl Pts',(-213.235140564013,-4.91824975740856,
130.802815868178));
#128312=CARTESIAN_POINT('',(-212.889859436032,-4.91824792006025,130.808883815883));
#128313=CARTESIAN_POINT('Ctrl Pts',(-212.819861628446,-4.76405452823406,
129.582490119308));
#128314=CARTESIAN_POINT('Ctrl Pts',(-212.827525902297,-4.79780353608479,
129.714076988706));
#128315=CARTESIAN_POINT('Ctrl Pts',(-212.835190176148,-4.82609468643265,
129.847055964322));
#128316=CARTESIAN_POINT('Ctrl Pts',(-212.842854449999,-4.84882921225431,
129.980929786901));
#128317=CARTESIAN_POINT('Ctrl Pts',(-212.850688614332,-4.87206768399697,
130.117771129778));
#128318=CARTESIAN_POINT('Ctrl Pts',(-212.858522778665,-4.88950020618528,
130.255547027938));
#128319=CARTESIAN_POINT('Ctrl Pts',(-212.866356942997,-4.90107709067464,
130.393719151364));
#128320=CARTESIAN_POINT('Ctrl Pts',(-212.87419110733,-4.91265397516397,
130.531891274791));
#128321=CARTESIAN_POINT('Ctrl Pts',(-212.882025271663,-4.91837522596484,
130.670459178147));
#128322=CARTESIAN_POINT('Ctrl Pts',(-212.889859435996,-4.91824792006084,
130.808883815247));
#128323=CARTESIAN_POINT('Ctrl Pts',(-212.889859436032,-4.91824792006025,
130.808883815883));
#128324=CARTESIAN_POINT('Ctrl Pts',(-212.899688380504,-4.91808819876975,
130.982554933039));
#128325=CARTESIAN_POINT('Ctrl Pts',(-212.909517324976,-4.90872606161266,
131.155814327766));
#128326=CARTESIAN_POINT('Ctrl Pts',(-212.919346269448,-4.89031323752669,
131.327829338094));
#128327=CARTESIAN_POINT('Ctrl Pts',(-212.929374726559,-4.87152666108868,
131.503335991767));
#128328=CARTESIAN_POINT('Ctrl Pts',(-212.93940318367,-4.84331824636661,
131.677547435274));
#128329=CARTESIAN_POINT('Ctrl Pts',(-212.949431640781,-4.80589734544945,
131.849604018646));
#128330=CARTESIAN_POINT('Ctrl Pts',(-212.953601284448,-4.7903384393498,
131.921141906802));
#128331=CARTESIAN_POINT('Ctrl Pts',(-212.957770928114,-4.77318750011992,
131.992307548351));
#128332=CARTESIAN_POINT('Ctrl Pts',(-212.961940571781,-4.75446197453151,
132.063040241312));
#128333=CARTESIAN_POINT('Ctrl Pts',(-212.9697149059,-4.71954808161507,132.194921915666));
#128334=CARTESIAN_POINT('Ctrl Pts',(-212.977489240019,-4.67908742803143,
132.32555869136));
#128335=CARTESIAN_POINT('Ctrl Pts',(-212.985263574138,-4.63318394857371,
132.454448361045));
#128336=CARTESIAN_POINT('Ctrl Pts',(-212.993028327086,-4.58733704105191,
132.58317918573));
#128337=CARTESIAN_POINT('Ctrl Pts',(-213.000793080033,-4.53606078408245,
132.710166823768));
#128338=CARTESIAN_POINT('Ctrl Pts',(-213.00855783298,-4.4795096801859,132.834921152891));
#128339=CARTESIAN_POINT('Ctrl Pts',(-213.016314873865,-4.42301474364282,
132.959551574257));
#128340=CARTESIAN_POINT('Ctrl Pts',(-213.02407191475,-4.36125554649349,
133.081952747152));
#128341=CARTESIAN_POINT('Ctrl Pts',(-213.031828955635,-4.2944356474614,
133.201651908234));
#128342=CARTESIAN_POINT('Ctrl Pts',(-213.039580146875,-4.22766613783504,
133.321260803248));
#128343=CARTESIAN_POINT('Ctrl Pts',(-213.047331338115,-4.15584371226501,
133.43817140219));
#128344=CARTESIAN_POINT('Ctrl Pts',(-213.055082529355,-4.0792189161274,
133.551933382173));
#128345=CARTESIAN_POINT('Ctrl Pts',(-213.062830426133,-4.00262668757228,
133.665647010279));
#128346=CARTESIAN_POINT('Ctrl Pts',(-213.070578322909,-3.92123636606752,
133.776214357509));
#128347=CARTESIAN_POINT('Ctrl Pts',(-213.078326219686,-3.83534296194653,
133.883212258478));
#128348=CARTESIAN_POINT('Ctrl Pts',(-213.086072495771,-3.74946752487404,
133.990187777793));
#128349=CARTESIAN_POINT('Ctrl Pts',(-213.093818771855,-3.65909112336248,
134.093595031289));
#128350=CARTESIAN_POINT('Ctrl Pts',(-213.101565047939,-3.56455012776312,
134.193042580979));
#128351=CARTESIAN_POINT('Ctrl Pts',(-213.109311381204,-3.47000843428349,
134.29249086477));
#128352=CARTESIAN_POINT('Ctrl Pts',(-213.11705771447,-3.37130235474808,
134.387979103073));
#128353=CARTESIAN_POINT('Ctrl Pts',(-213.124804047735,-3.26880603576509,
134.479151790279));
#128354=CARTESIAN_POINT('Ctrl Pts',(-213.132552115738,-3.16628676344253,
134.570344894975));
#128355=CARTESIAN_POINT('Ctrl Pts',(-213.140300183741,-3.0599758547263,
134.657220265677));
#128356=CARTESIAN_POINT('Ctrl Pts',(-213.148048251744,-2.95028121244969,
134.739462119429));
#128357=CARTESIAN_POINT('Ctrl Pts',(-213.155804554486,-2.84046998540144,
134.821791380802));
#128358=CARTESIAN_POINT('Ctrl Pts',(-213.163560857228,-2.72726815416231,
134.899477052992));
#128359=CARTESIAN_POINT('Ctrl Pts',(-213.171317159969,-2.61111379444569,
134.972245910488));
#128360=CARTESIAN_POINT('Ctrl Pts',(-213.179077602484,-2.49489743964994,
135.045053606914));
#128361=CARTESIAN_POINT('Ctrl Pts',(-213.186838044998,-2.37572575590294,
135.112939066182));
#128362=CARTESIAN_POINT('Ctrl Pts',(-213.194598487512,-2.25406130997421,
135.175675142212));
#128363=CARTESIAN_POINT('Ctrl Pts',(-213.202371387777,-2.132201557476,135.23851192776));
#128364=CARTESIAN_POINT('Ctrl Pts',(-213.210144288043,-2.0078414012049,
135.296182646899));
#128365=CARTESIAN_POINT('Ctrl Pts',(-213.217917188308,-1.88146409036836,
135.348508055662));
#128366=CARTESIAN_POINT('Ctrl Pts',(-213.22540752407,-1.75968091310596,
135.398931304016));
#128367=CARTESIAN_POINT('Ctrl Pts',(-213.232897859832,-1.63602498149208,
135.4443910195));
#128368=CARTESIAN_POINT('Ctrl Pts',(-213.240388195594,-1.51094001630837,
135.484771211693));
#128369=CARTESIAN_POINT('Ctrl Pts',(-213.248162529713,-1.38111241665115,
135.526682431147));
#128370=CARTESIAN_POINT('Ctrl Pts',(-213.255936863832,-1.2493340258649,
135.563254105625));
#128371=CARTESIAN_POINT('Ctrl Pts',(-213.263711197951,-1.11608354451254,
135.594302223073));
#128372=CARTESIAN_POINT('Ctrl Pts',(-213.271475950898,-0.982997282469519,
135.625312076491));
#128373=CARTESIAN_POINT('Ctrl Pts',(-213.279240703846,-0.848442916727878,
135.650811829488));
#128374=CARTESIAN_POINT('Ctrl Pts',(-213.287005456793,-0.712916313416165,
135.670666546355));
#128375=CARTESIAN_POINT('Ctrl Pts',(-213.294762497678,-0.577524317037452,
135.690501543237));
#128376=CARTESIAN_POINT('Ctrl Pts',(-213.302519538563,-0.441162389088791,
135.704702605328));
#128377=CARTESIAN_POINT('Ctrl Pts',(-213.310276579448,-0.30433830722044,
135.713185452214));
#128378=CARTESIAN_POINT('Ctrl Pts',(-213.318027770688,-0.167617405456748,
135.721661902119));
#128379=CARTESIAN_POINT('Ctrl Pts',(-213.325778961928,-0.0304354321061462,
135.724428695799));
#128380=CARTESIAN_POINT('Ctrl Pts',(-213.333530153168,0.106693317536995,
135.721453213653));
#128381=CARTESIAN_POINT('Ctrl Pts',(-213.341278049945,0.243763783803695,
135.718478996166));
#128382=CARTESIAN_POINT('Ctrl Pts',(-213.349025946722,0.38078068130049,
135.709767365526));
#128383=CARTESIAN_POINT('Ctrl Pts',(-213.356773843499,0.517228528714356,
135.695337791054));
#128384=CARTESIAN_POINT('Ctrl Pts',(-213.364520119583,0.653647834180018,
135.680911234939));
#128385=CARTESIAN_POINT('Ctrl Pts',(-213.372266395667,0.789497937775043,
135.660769155131));
#128386=CARTESIAN_POINT('Ctrl Pts',(-213.380012671751,0.924267695244507,
135.634982967743));
#128387=CARTESIAN_POINT('Ctrl Pts',(-213.387759005017,1.05903844755389,
135.609196590006));
#128388=CARTESIAN_POINT('Ctrl Pts',(-213.395505338282,1.19272845382499,
135.577766095025));
#128389=CARTESIAN_POINT('Ctrl Pts',(-213.403251671548,1.32483638173783,
135.540814103469));
#128390=CARTESIAN_POINT('Ctrl Pts',(-213.41099973955,1.45697389430497,135.503853836771));
#128391=CARTESIAN_POINT('Ctrl Pts',(-213.418747807553,1.58752824706523,
135.4613697183));
#128392=CARTESIAN_POINT('Ctrl Pts',(-213.426495875556,1.71601328142853,
135.413534239861));
#128393=CARTESIAN_POINT('Ctrl Pts',(-213.434252178298,1.84463487121552,
135.365647921306));
#128394=CARTESIAN_POINT('Ctrl Pts',(-213.44200848104,1.97118238229435,135.312399018039));
#128395=CARTESIAN_POINT('Ctrl Pts',(-213.449764783782,2.09518915168188,
135.254008410501));
#128396=CARTESIAN_POINT('Ctrl Pts',(-213.457525226296,2.219262107216,135.195586638139));
#128397=CARTESIAN_POINT('Ctrl Pts',(-213.46528566881,2.34079127270939,135.132017874414));
#128398=CARTESIAN_POINT('Ctrl Pts',(-213.473046111324,2.45933551509492,
135.063568511846));
#128399=CARTESIAN_POINT('Ctrl Pts',(-213.48081901159,2.57807005522219,134.995009268284));
#128400=CARTESIAN_POINT('Ctrl Pts',(-213.488591911855,2.69380976668411,
134.921553979131));
#128401=CARTESIAN_POINT('Ctrl Pts',(-213.496364812121,2.80614263845336,
134.843512329888));
#128402=CARTESIAN_POINT('Ctrl Pts',(-213.503855147883,2.91439192738467,
134.76830769117));
#128403=CARTESIAN_POINT('Ctrl Pts',(-213.511345483645,3.01947752500861,
134.688844540419));
#128404=CARTESIAN_POINT('Ctrl Pts',(-213.518835819407,3.12106200337956,
134.605433496841));
#128405=CARTESIAN_POINT('Ctrl Pts',(-213.526610153526,3.22649808812344,
134.518859898194));
#128406=CARTESIAN_POINT('Ctrl Pts',(-213.534384487645,3.32849631271204,
134.427758889236));
#128407=CARTESIAN_POINT('Ctrl Pts',(-213.542158821764,3.42664311324413,
134.332433751297));
#128408=CARTESIAN_POINT('Ctrl Pts',(-213.549923574711,3.5246689566162,134.237226093072));
#128409=CARTESIAN_POINT('Ctrl Pts',(-213.557688327658,3.61885254235966,
134.137804933757));
#128410=CARTESIAN_POINT('Ctrl Pts',(-213.565453080606,3.70881231748571,
134.034514523523));
#128411=CARTESIAN_POINT('Ctrl Pts',(-213.573210121491,3.79868274329489,
133.93132670278));
#128412=CARTESIAN_POINT('Ctrl Pts',(-213.580967162376,3.88433745190876,
133.824277571767));
#128413=CARTESIAN_POINT('Ctrl Pts',(-213.588724203261,3.96543106960454,
133.713748782579));
#128414=CARTESIAN_POINT('Ctrl Pts',(-213.596475394501,4.04646353397251,
133.60330334401));
#128415=CARTESIAN_POINT('Ctrl Pts',(-213.604226585741,4.12294152330685,
133.489383784201));
#128416=CARTESIAN_POINT('Ctrl Pts',(-213.611977776981,4.19455960464572,
133.372405162658));
#128417=CARTESIAN_POINT('Ctrl Pts',(-213.619725673758,4.26614724638944,
133.255476260149));
#128418=CARTESIAN_POINT('Ctrl Pts',(-213.627473570535,4.33287888472626,
133.13549121461));
#128419=CARTESIAN_POINT('Ctrl Pts',(-213.635221467312,4.39449226950757,
133.012894238713));
#128420=CARTESIAN_POINT('Ctrl Pts',(-213.642967743396,4.45609276609701,
132.890322907461));
#128421=CARTESIAN_POINT('Ctrl Pts',(-213.65071401948,4.51257696321814,132.765141081698));
#128422=CARTESIAN_POINT('Ctrl Pts',(-213.658460295564,4.56372865931191,
132.637817403715));
#128423=CARTESIAN_POINT('Ctrl Pts',(-213.66620662883,4.61488073299595,132.510492785857));
#128424=CARTESIAN_POINT('Ctrl Pts',(-213.673952962095,4.66070008135946,
132.381026647013));
#128425=CARTESIAN_POINT('Ctrl Pts',(-213.681699295361,4.70101888628126,
132.249907051731));
#128426=CARTESIAN_POINT('Ctrl Pts',(-213.689447363364,4.74134672031982,
132.118758093124));
#128427=CARTESIAN_POINT('Ctrl Pts',(-213.697195431367,4.77617144487178,
131.98595531489));
#128428=CARTESIAN_POINT('Ctrl Pts',(-213.70494349937,4.80537540158441,131.852000972052));
#128429=CARTESIAN_POINT('Ctrl Pts',(-213.712699802111,4.83461039660973,
131.717904260944));
#128430=CARTESIAN_POINT('Ctrl Pts',(-213.720456104853,4.85821260703629,
131.58265392297));
#128431=CARTESIAN_POINT('Ctrl Pts',(-213.728212407595,4.87611562309497,
131.446761966186));
#128432=CARTESIAN_POINT('Ctrl Pts',(-213.735972850109,4.89402819453241,
131.310797479774));
#128433=CARTESIAN_POINT('Ctrl Pts',(-213.743733292623,4.90623547571352,
131.174191081412));
#128434=CARTESIAN_POINT('Ctrl Pts',(-213.751493735138,4.91272314701169,
131.037457900509));
#128435=CARTESIAN_POINT('Ctrl Pts',(-213.759266635403,4.91922123289577,
130.900505223366));
#128436=CARTESIAN_POINT('Ctrl Pts',(-213.767039535668,4.91998135891421,
130.763425748162));
#128437=CARTESIAN_POINT('Ctrl Pts',(-213.774812435934,4.91504137022605,
130.626733504021));
#128438=CARTESIAN_POINT('Ctrl Pts',(-213.782302771696,4.91028096256978,
130.495010367261));
#128439=CARTESIAN_POINT('Ctrl Pts',(-213.789793107458,4.90022769570384,
130.363647103825));
#128440=CARTESIAN_POINT('Ctrl Pts',(-213.79728344322,4.8849605143164,130.233095498668));
#128441=CARTESIAN_POINT('Ctrl Pts',(-213.805057777339,4.86911447310636,
130.097593989721));
#128442=CARTESIAN_POINT('Ctrl Pts',(-213.812832111458,4.84760114599064,
129.962537674027));
#128443=CARTESIAN_POINT('Ctrl Pts',(-213.820606445577,4.82045215075121,
129.828438425576));
#128444=CARTESIAN_POINT('Ctrl Pts',(-213.828371198524,4.79333661422204,
129.694504442464));
#128445=CARTESIAN_POINT('Ctrl Pts',(-213.836135951471,4.76059930579301,
129.561525559254));
#128446=CARTESIAN_POINT('Ctrl Pts',(-213.843900704418,4.72232361417188,
129.430008862907));
#128447=CARTESIAN_POINT('Ctrl Pts',(-213.851657745303,4.68408593850726,
129.298622790797));
#128448=CARTESIAN_POINT('Ctrl Pts',(-213.859414786189,4.64032093503532,
129.16869638844));
#128449=CARTESIAN_POINT('Ctrl Pts',(-213.867171827074,4.59116301553957,
129.04072652081));
#128450=CARTESIAN_POINT('Ctrl Pts',(-213.874923018314,4.54204216641324,
128.912853156252));
#128451=CARTESIAN_POINT('Ctrl Pts',(-213.882674209554,4.48753663569018,
128.786933753139));
#128452=CARTESIAN_POINT('Ctrl Pts',(-213.890425400794,4.42783053071177,
128.663449630674));
#128453=CARTESIAN_POINT('Ctrl Pts',(-213.898173297571,4.3681498024206,128.540017992254));
#128454=CARTESIAN_POINT('Ctrl Pts',(-213.905921194348,4.30327306598751,
128.419019927071));
#128455=CARTESIAN_POINT('Ctrl Pts',(-213.913669091125,4.23343229750322,
128.300916181403));
#128456=CARTESIAN_POINT('Ctrl Pts',(-213.921415367209,4.1636061382023,128.182837140492));
#128457=CARTESIAN_POINT('Ctrl Pts',(-213.929161643293,4.08881821110166,
128.067651551178));
#128458=CARTESIAN_POINT('Ctrl Pts',(-213.936907919378,4.00934593600885,
127.955794622559));
#128459=CARTESIAN_POINT('Ctrl Pts',(-213.944654252643,3.92987307426966,
127.843936868238));
#128460=CARTESIAN_POINT('Ctrl Pts',(-213.952400585908,3.84571602197914,
127.735408142357));
#128461=CARTESIAN_POINT('Ctrl Pts',(-213.960146919174,3.75719469186991,
127.630613445864));
#128462=CARTESIAN_POINT('Ctrl Pts',(-213.967894987177,3.6686535380227,127.525795281326));
#128463=CARTESIAN_POINT('Ctrl Pts',(-213.97564305518,3.57574641378552,127.424713108749));
#128464=CARTESIAN_POINT('Ctrl Pts',(-213.983391123182,3.47883228332121,
127.327737398547));
#128465=CARTESIAN_POINT('Ctrl Pts',(-213.991147425924,3.38181515136562,
127.230658621406));
#128466=CARTESIAN_POINT('Ctrl Pts',(-213.998903728666,3.28078278279008,
127.137695301976));
#128467=CARTESIAN_POINT('Ctrl Pts',(-214.006660031408,3.17613004837301,
127.049180065539));
#128468=CARTESIAN_POINT('Ctrl Pts',(-214.014420473922,3.07142145764054,
126.960617585855));
#128469=CARTESIAN_POINT('Ctrl Pts',(-214.022180916436,2.96308895946279,
126.876508159358));
#128470=CARTESIAN_POINT('Ctrl Pts',(-214.029941358951,2.85155820669096,
126.797142273583));
#128471=CARTESIAN_POINT('Ctrl Pts',(-214.037714259216,2.73984841485356,
126.717648982642));
#128472=CARTESIAN_POINT('Ctrl Pts',(-214.045487159481,2.62493043675181,
126.642914662395));
#128473=CARTESIAN_POINT('Ctrl Pts',(-214.053260059747,2.50725719587883,
126.573185317934));
#128474=CARTESIAN_POINT('Ctrl Pts',(-214.060750395509,2.39386167371291,
126.505990810783));
#128475=CARTESIAN_POINT('Ctrl Pts',(-214.068240731271,2.27790800347818,
126.443443856307));
#128476=CARTESIAN_POINT('Ctrl Pts',(-214.075731067033,2.15981895618485,
126.38572223691));
#128477=CARTESIAN_POINT('Ctrl Pts',(-214.083505401152,2.03725252677082,
126.325812084769));
#128478=CARTESIAN_POINT('Ctrl Pts',(-214.091279735271,1.91199734458572,
126.270910618594));
#128479=CARTESIAN_POINT('Ctrl Pts',(-214.09905406939,1.7845011538977,126.221267917845));
#128480=CARTESIAN_POINT('Ctrl Pts',(-214.106818822337,1.65716209087004,
126.171686397287));
#128481=CARTESIAN_POINT('Ctrl Pts',(-214.114583575284,1.52758787540842,
126.127350887472));
#128482=CARTESIAN_POINT('Ctrl Pts',(-214.122348328231,1.39625020776847,
126.088465324008));
#128483=CARTESIAN_POINT('Ctrl Pts',(-214.130105369116,1.26504298655157,
126.049618382233));
#128484=CARTESIAN_POINT('Ctrl Pts',(-214.137862410001,1.13207617114529,
126.01621072504));
#128485=CARTESIAN_POINT('Ctrl Pts',(-214.145619450886,0.997840440976765,
125.988397835645));
#128486=CARTESIAN_POINT('Ctrl Pts',(-214.153370642126,0.863705939016377,
125.960605920165));
#128487=CARTESIAN_POINT('Ctrl Pts',(-214.161121833366,0.728304808227223,
125.938400453705));
#128488=CARTESIAN_POINT('Ctrl Pts',(-214.168873024607,0.592141510601337,
125.921886706328));
#128489=CARTESIAN_POINT('Ctrl Pts',(-214.176620921384,0.456036086009031,
125.905379977734));
#128490=CARTESIAN_POINT('Ctrl Pts',(-214.184368818161,0.319169526183115,
125.894560203726));
#128491=CARTESIAN_POINT('Ctrl Pts',(-214.192116714938,0.182054858758954,
125.889481260867));
#128492=CARTESIAN_POINT('Ctrl Pts',(-214.199862991022,0.0449688727677412,
125.884403380414));
#128493=CARTESIAN_POINT('Ctrl Pts',(-214.207609267106,-0.0923647271424954,
125.885063956999));
#128494=CARTESIAN_POINT('Ctrl Pts',(-214.21535554319,-0.229429835048029,
125.89146483063));
#128495=CARTESIAN_POINT('Ctrl Pts',(-214.223101876455,-0.36649595473724,
125.897865751512));
#128496=CARTESIAN_POINT('Ctrl Pts',(-214.230848209721,-0.503293187927333,
125.910007035755));
#128497=CARTESIAN_POINT('Ctrl Pts',(-214.238594542986,-0.639307875204561,
125.927838444623));
#128498=CARTESIAN_POINT('Ctrl Pts',(-214.246342610989,-0.775353022027759,
125.945673846712));
#128499=CARTESIAN_POINT('Ctrl Pts',(-214.254090678992,-0.910614886645424,
125.969201858252));
#128500=CARTESIAN_POINT('Ctrl Pts',(-214.261838746995,-1.04458775290843,
125.998320720835));
#128501=CARTESIAN_POINT('Ctrl Pts',(-214.269595049737,-1.17870300712818,
126.027470531291));
#128502=CARTESIAN_POINT('Ctrl Pts',(-214.277351352479,-1.31152614369052,
126.062222979452));
#128503=CARTESIAN_POINT('Ctrl Pts',(-214.285107655221,-1.44256387822435,
126.102425641437));
#128504=CARTESIAN_POINT('Ctrl Pts',(-214.292868097735,-1.57367155154257,
126.142649760794));
#128505=CARTESIAN_POINT('Ctrl Pts',(-214.300628540249,-1.70299155559054,
126.188329760138));
#128506=CARTESIAN_POINT('Ctrl Pts',(-214.308388982763,-1.83004941921517,
126.239264541279));
#128507=CARTESIAN_POINT('Ctrl Pts',(-214.316161883029,-1.95731124740217,
126.290281087452));
#128508=CARTESIAN_POINT('Ctrl Pts',(-214.323934783294,-2.08230332180388,
126.346569111495));
#128509=CARTESIAN_POINT('Ctrl Pts',(-214.331707683559,-2.20457385515677,
126.407880527806));
#128510=CARTESIAN_POINT('Ctrl Pts',(-214.339198019321,-2.32239954664107,
126.466963119699));
#128511=CARTESIAN_POINT('Ctrl Pts',(-214.346688355083,-2.43769786195061,
126.530710069758));
#128512=CARTESIAN_POINT('Ctrl Pts',(-214.354178690845,-2.55009070965804,
126.598861784489));
#128513=CARTESIAN_POINT('Ctrl Pts',(-214.361954303879,-2.66676415652064,
126.669609128553));
#128514=CARTESIAN_POINT('Ctrl Pts',(-214.369729916912,-2.78067608162571,
126.745327550003));
#128515=CARTESIAN_POINT('Ctrl Pts',(-214.377505529946,-2.89137384784176,
126.825775399864));
#128516=CARTESIAN_POINT('Ctrl Pts',(-214.385516368049,-3.00542040335608,
126.908656929354));
#128517=CARTESIAN_POINT('Ctrl Pts',(-214.393527206152,-3.11605486394476,
126.996558427291));
#128518=CARTESIAN_POINT('Ctrl Pts',(-214.401538044254,-3.22280931507134,
127.089164366869));
#128519=CARTESIAN_POINT('Ctrl Pts',(-214.409294136315,-3.32616895612055,
127.178825421494));
#128520=CARTESIAN_POINT('Ctrl Pts',(-214.417050228375,-3.42589125052493,
127.272896014297));
#128521=CARTESIAN_POINT('Ctrl Pts',(-214.424806320435,-3.52158131705236,
127.371046170871));
#128522=CARTESIAN_POINT('Ctrl Pts',(-214.432557091884,-3.61720574102127,
127.469128997285));
#128523=CARTESIAN_POINT('Ctrl Pts',(-214.440307863332,-3.7088031687662,
127.571285540742));
#128524=CARTESIAN_POINT('Ctrl Pts',(-214.448058634781,-3.79601356772482,
127.677147152491));
#128525=CARTESIAN_POINT('Ctrl Pts',(-214.455805767883,-3.88318302861947,
127.782959070974));
#128526=CARTESIAN_POINT('Ctrl Pts',(-214.463552900986,-3.96596931125054,
127.892472295287));
#128527=CARTESIAN_POINT('Ctrl Pts',(-214.471300034089,-4.04405115289793,
128.005283388327));
#128528=CARTESIAN_POINT('Ctrl Pts',(-214.479045208286,-4.12211325112459,
128.118065956465));
#128529=CARTESIAN_POINT('Ctrl Pts',(-214.486790382484,-4.19547305505162,
128.234144411599));
#128530=CARTESIAN_POINT('Ctrl Pts',(-214.494535556682,-4.26385154744425,
128.353084818343));
#128531=CARTESIAN_POINT('Ctrl Pts',(-214.50228230773,-4.33224396110775,
128.472049440327));
#128532=CARTESIAN_POINT('Ctrl Pts',(-214.510029058778,-4.39565283897423,
128.593876840954));
#128533=CARTESIAN_POINT('Ctrl Pts',(-214.517775809827,-4.45384423488585,
128.718106895251));
#128534=CARTESIAN_POINT('Ctrl Pts',(-214.525523577688,-4.51204326880627,
128.842353255571));
#128535=CARTESIAN_POINT('Ctrl Pts',(-214.533271345549,-4.56502329847948,
128.969002540315));
#128536=CARTESIAN_POINT('Ctrl Pts',(-214.54101911341,-4.6125981490606,129.097573759818));
#128537=CARTESIAN_POINT('Ctrl Pts',(-214.548771782394,-4.66020309478569,
129.226226311565));
#128538=CARTESIAN_POINT('Ctrl Pts',(-214.556524451378,-4.70239590896414,
129.356802855539));
#128539=CARTESIAN_POINT('Ctrl Pts',(-214.564277120362,-4.73903997613716,
129.488806298249));
#128540=CARTESIAN_POINT('Ctrl Pts',(-214.566106628378,-4.74768739998518,
129.519957035778));
#128541=CARTESIAN_POINT('Ctrl Pts',(-214.567936136395,-4.75602604445474,
129.551187182902));
#128542=CARTESIAN_POINT('Ctrl Pts',(-214.569765644412,-4.76405452823405,
129.582490119308));
#128543=CARTESIAN_POINT('Origin',(213.235140564004,0.,130.804360617566));
#128544=CARTESIAN_POINT('',(-216.665311899804,-4.76405452823409,129.582490119308));
#128545=CARTESIAN_POINT('',(-216.320029411505,-4.76405452823406,129.582490119308));
#128546=CARTESIAN_POINT('',(213.235140564004,-4.76405452823405,129.582490119308));
#128547=CARTESIAN_POINT('',(-214.98514056396,-4.91824853507356,130.800564600342));
#128548=CARTESIAN_POINT('Ctrl Pts',(-214.985140564013,-4.91824853507428,
130.800564601278));
#128549=CARTESIAN_POINT('Ctrl Pts',(-214.99288611369,-4.91835442857352,
130.937763840683));
#128550=CARTESIAN_POINT('Ctrl Pts',(-215.000631663367,-4.9127150672855,
131.075028143919));
#128551=CARTESIAN_POINT('Ctrl Pts',(-215.008377213043,-4.90134090327774,
131.211841184411));
#128552=CARTESIAN_POINT('Ctrl Pts',(-215.016121641906,-4.88996838516001,
131.348634427474));
#128553=CARTESIAN_POINT('Ctrl Pts',(-215.023866070769,-4.87286274698048,
131.484976148621));
#128554=CARTESIAN_POINT('Ctrl Pts',(-215.031610499632,-4.85008645906864,
131.620353510954));
#128555=CARTESIAN_POINT('Ctrl Pts',(-215.039355480027,-4.82730854910443,
131.755740514417));
#128556=CARTESIAN_POINT('Ctrl Pts',(-215.047100460423,-4.79885925015112,
131.890162637197));
#128557=CARTESIAN_POINT('Ctrl Pts',(-215.054845440818,-4.76485239545887,
132.023116012217));
#128558=CARTESIAN_POINT('Ctrl Pts',(-215.062592645102,-4.73083577606034,
132.156107563383));
#128559=CARTESIAN_POINT('Ctrl Pts',(-215.070339849386,-4.69125852180174,
132.287629149257));
#128560=CARTESIAN_POINT('Ctrl Pts',(-215.078087053671,-4.64628458195234,
132.417191249099));
#128561=CARTESIAN_POINT('Ctrl Pts',(-215.085843204596,-4.6012587052108,
132.546902970096));
#128562=CARTESIAN_POINT('Ctrl Pts',(-215.093599355522,-4.55082382223927,
132.674650315509));
#128563=CARTESIAN_POINT('Ctrl Pts',(-215.101355506447,-4.49519260513584,
132.799962407812));
#128564=CARTESIAN_POINT('Ctrl Pts',(-215.10911621037,-4.43952873153182,
132.925348060511));
#128565=CARTESIAN_POINT('Ctrl Pts',(-215.116876914292,-4.3786626195065,
133.048295262303));
#128566=CARTESIAN_POINT('Ctrl Pts',(-215.124637618214,-4.31285286816823,
133.168357910296));
#128567=CARTESIAN_POINT('Ctrl Pts',(-215.132411345463,-4.24693268073255,
133.288622036793));
#128568=CARTESIAN_POINT('Ctrl Pts',(-215.140185072711,-4.17605247877902,
133.405991602627));
#128569=CARTESIAN_POINT('Ctrl Pts',(-215.14795879996,-4.10051464529449,
133.520048874017));
#128570=CARTESIAN_POINT('Ctrl Pts',(-215.155283388682,-4.02934112125313,
133.627516318778));
#128571=CARTESIAN_POINT('Ctrl Pts',(-215.162607977403,-3.95403316724271,
133.732043222698));
#128572=CARTESIAN_POINT('Ctrl Pts',(-215.169932566125,-3.87487514656703,
133.833308563804));
#128573=CARTESIAN_POINT('Ctrl Pts',(-215.177706900244,-3.79085665429191,
133.940791813218));
#128574=CARTESIAN_POINT('Ctrl Pts',(-215.185481234363,-3.70222955632382,
134.04494683786));
#128575=CARTESIAN_POINT('Ctrl Pts',(-215.193255568482,-3.60928712226211,
134.145352915009));
#128576=CARTESIAN_POINT('Ctrl Pts',(-215.201020321429,-3.51645923144414,
134.245635250641));
#128577=CARTESIAN_POINT('Ctrl Pts',(-215.208785074376,-3.41932684933196,
134.342177547528));
#128578=CARTESIAN_POINT('Ctrl Pts',(-215.216549827323,-3.3182249707409,
134.434590101504));
#128579=CARTESIAN_POINT('Ctrl Pts',(-215.224306868208,-3.2172235079604,
134.526910870029));
#128580=CARTESIAN_POINT('Ctrl Pts',(-215.232063909093,-3.11226068128255,
134.615109796181));
#128581=CARTESIAN_POINT('Ctrl Pts',(-215.239820949979,-3.00370974487943,
134.698832447098));
#128582=CARTESIAN_POINT('Ctrl Pts',(-215.247572141219,-2.8952406675823,
134.782491962112));
#128583=CARTESIAN_POINT('Ctrl Pts',(-215.255323332459,-2.78318917466306,
134.861681683));
#128584=CARTESIAN_POINT('Ctrl Pts',(-215.263074523699,-2.66796287655237,
134.936086304472));
#128585=CARTESIAN_POINT('Ctrl Pts',(-215.270822420476,-2.55278555269229,
135.010459301995));
#128586=CARTESIAN_POINT('Ctrl Pts',(-215.278570317253,-2.43443643520314,
135.080051033527));
#128587=CARTESIAN_POINT('Ctrl Pts',(-215.28631821403,-2.31335331555439,
135.14458866456));
#128588=CARTESIAN_POINT('Ctrl Pts',(-215.294064490114,-2.19229552388369,
135.209112795712));
#128589=CARTESIAN_POINT('Ctrl Pts',(-215.301810766198,-2.06850521238057,
135.268584745434));
#128590=CARTESIAN_POINT('Ctrl Pts',(-215.309557042282,-1.94244570013637,
135.322777128305));
#128591=CARTESIAN_POINT('Ctrl Pts',(-215.317303375548,-1.81638525734966,
135.376969911212));
#128592=CARTESIAN_POINT('Ctrl Pts',(-215.325049708813,-1.68805593957835,
135.42588289509));
#128593=CARTESIAN_POINT('Ctrl Pts',(-215.332796042078,-1.55794164364699,
135.469336597943));
#128594=CARTESIAN_POINT('Ctrl Pts',(-215.340544110081,-1.42779820952138,
135.51280003195));
#128595=CARTESIAN_POINT('Ctrl Pts',(-215.348292178084,-1.29586937257314,
135.550801628342));
#128596=CARTESIAN_POINT('Ctrl Pts',(-215.356040246087,-1.16265441971338,
135.583211709912));
#128597=CARTESIAN_POINT('Ctrl Pts',(-215.363796548829,-1.02929788441625,
135.615656237303));
#128598=CARTESIAN_POINT('Ctrl Pts',(-215.371552851571,-0.894652883168756,
135.642497286061));
#128599=CARTESIAN_POINT('Ctrl Pts',(-215.379309154313,-0.759229682932765,
135.663656178761));
#128600=CARTESIAN_POINT('Ctrl Pts',(-215.387069596827,-0.623734203257294,
135.6848263646));
#128601=CARTESIAN_POINT('Ctrl Pts',(-215.394830039341,-0.487460085253025,
135.700308307281));
#128602=CARTESIAN_POINT('Ctrl Pts',(-215.402590481855,-0.350921966350669,
135.710075329617));
#128603=CARTESIAN_POINT('Ctrl Pts',(-215.410363382121,-0.214164664338566,
135.719858030844));
#128604=CARTESIAN_POINT('Ctrl Pts',(-215.418136282386,-0.0771429055650763,
135.723907467401));
#128605=CARTESIAN_POINT('Ctrl Pts',(-215.425909182652,0.059628520693869,
135.722249138265));
#128606=CARTESIAN_POINT('Ctrl Pts',(-215.433399518413,0.191427961100384,
135.72065109357));
#128607=CARTESIAN_POINT('Ctrl Pts',(-215.440889854175,0.32299464584498,
135.713753077911));
#128608=CARTESIAN_POINT('Ctrl Pts',(-215.448380189937,0.453875025620668,
135.701623171648));
#128609=CARTESIAN_POINT('Ctrl Pts',(-215.456154524056,0.589717774777498,
135.689033356303));
#128610=CARTESIAN_POINT('Ctrl Pts',(-215.463928858176,0.725251458121523,
135.67076720368));
#128611=CARTESIAN_POINT('Ctrl Pts',(-215.471703192295,0.859963590330364,
135.646844038891));
#128612=CARTESIAN_POINT('Ctrl Pts',(-215.479467945242,0.994509701875095,
135.622950357265));
#128613=CARTESIAN_POINT('Ctrl Pts',(-215.487232698189,1.12823589558778,
135.593413602906));
#128614=CARTESIAN_POINT('Ctrl Pts',(-215.494997451136,1.26063322943629,
135.55830497182));
#128615=CARTESIAN_POINT('Ctrl Pts',(-215.502754492021,1.39289906438635,
135.523231211121));
#128616=CARTESIAN_POINT('Ctrl Pts',(-215.510511532906,1.52383829055938,
135.482596686299));
#128617=CARTESIAN_POINT('Ctrl Pts',(-215.518268573791,1.6529509605536,135.436523847042));
#128618=CARTESIAN_POINT('Ctrl Pts',(-215.526019765031,1.78196626567921,
135.39048575167));
#128619=CARTESIAN_POINT('Ctrl Pts',(-215.533770956271,1.90915738956395,
135.339017635671));
#128620=CARTESIAN_POINT('Ctrl Pts',(-215.541522147511,2.03403873354458,
135.282292003032));
#128621=CARTESIAN_POINT('Ctrl Pts',(-215.549270044288,2.15886699962287,
135.2255904803));
#128622=CARTESIAN_POINT('Ctrl Pts',(-215.557017941065,2.28138708314162,
135.163636046701));
#128623=CARTESIAN_POINT('Ctrl Pts',(-215.564765837842,2.40113280372063,
135.096649554881));
#128624=CARTESIAN_POINT('Ctrl Pts',(-215.572512113927,2.52085347607631,
135.029677075191));
#128625=CARTESIAN_POINT('Ctrl Pts',(-215.580258390011,2.63780059882454,
134.957674821708));
#128626=CARTESIAN_POINT('Ctrl Pts',(-215.588004666095,2.75153243088458,
134.880909690531));
#128627=CARTESIAN_POINT('Ctrl Pts',(-215.59575099936,2.86526510248701,134.804143992691));
#128628=CARTESIAN_POINT('Ctrl Pts',(-215.603497332626,2.9757821119846,134.722615565727));
#128629=CARTESIAN_POINT('Ctrl Pts',(-215.611243665891,3.0826708980365,134.63663451134));
#128630=CARTESIAN_POINT('Ctrl Pts',(-215.618991733894,3.18958362109106,
134.550634202091));
#128631=CARTESIAN_POINT('Ctrl Pts',(-215.626739801897,3.29286619930851,
134.460179526238));
#128632=CARTESIAN_POINT('Ctrl Pts',(-215.6344878699,3.39213965481177,134.365620454303));
#128633=CARTESIAN_POINT('Ctrl Pts',(-215.642244172642,3.49151861932478,
134.27096088386));
#128634=CARTESIAN_POINT('Ctrl Pts',(-215.650000475384,3.58687966588461,
134.17218847345));
#128635=CARTESIAN_POINT('Ctrl Pts',(-215.657756778126,3.67788078918729,
134.069689998046));
#128636=CARTESIAN_POINT('Ctrl Pts',(-215.66551722064,3.76893048252947,133.96713681612));
#128637=CARTESIAN_POINT('Ctrl Pts',(-215.673277663154,3.85561536884039,
133.860853909347));
#128638=CARTESIAN_POINT('Ctrl Pts',(-215.681038105668,3.93763482974399,
133.751259837099));
#128639=CARTESIAN_POINT('Ctrl Pts',(-215.688811005933,4.01978595556757,
133.641489834718));
#128640=CARTESIAN_POINT('Ctrl Pts',(-215.696583906199,4.09725646878812,
133.528398367776));
#128641=CARTESIAN_POINT('Ctrl Pts',(-215.704356806464,4.16978956624069,
133.412432325892));
#128642=CARTESIAN_POINT('Ctrl Pts',(-215.711847142226,4.23968590290239,
133.300681941729));
#128643=CARTESIAN_POINT('Ctrl Pts',(-215.719337477989,4.30499741376793,
133.186262617731));
#128644=CARTESIAN_POINT('Ctrl Pts',(-215.726827813751,4.36553622229401,
133.069592736873));
#128645=CARTESIAN_POINT('Ctrl Pts',(-215.73460214787,4.42837037814476,132.948499282023));
#128646=CARTESIAN_POINT('Ctrl Pts',(-215.742376481989,4.48626181306018,
132.824597654044));
#128647=CARTESIAN_POINT('Ctrl Pts',(-215.750150816108,4.53894977496981,
132.698329467046));
#128648=CARTESIAN_POINT('Ctrl Pts',(-215.757915569055,4.59157280367481,
132.572216894305));
#128649=CARTESIAN_POINT('Ctrl Pts',(-215.765680322002,4.63900496985399,
132.443743923006));
#128650=CARTESIAN_POINT('Ctrl Pts',(-215.773445074949,4.68103107712272,
132.313377223675));
#128651=CARTESIAN_POINT('Ctrl Pts',(-215.781202115834,4.72301544346936,
132.183140006386));
#128652=CARTESIAN_POINT('Ctrl Pts',(-215.788959156719,4.7596043170223,132.051013173795));
#128653=CARTESIAN_POINT('Ctrl Pts',(-215.796716197604,4.79063048438847,
131.917483532858));
#128654=CARTESIAN_POINT('Ctrl Pts',(-215.804467388844,4.82163325468052,
131.784054587661));
#128655=CARTESIAN_POINT('Ctrl Pts',(-215.812218580084,4.84708158031289,
131.649225319021));
#128656=CARTESIAN_POINT('Ctrl Pts',(-215.819969771324,4.86685811583843,
131.513497517464));
#128657=CARTESIAN_POINT('Ctrl Pts',(-215.827717668101,4.88662624580884,
131.377827403844));
#128658=CARTESIAN_POINT('Ctrl Pts',(-215.835465564878,4.90072732404231,
131.241259902949));
#128659=CARTESIAN_POINT('Ctrl Pts',(-215.843213461656,4.90909517824313,
131.104306601787));
#128660=CARTESIAN_POINT('Ctrl Pts',(-215.85095973774,4.91746128206925,130.967381948302));
#128661=CARTESIAN_POINT('Ctrl Pts',(-215.858706013824,4.92009652344186,
130.830072045059));
#128662=CARTESIAN_POINT('Ctrl Pts',(-215.866452289908,4.91698667776376,
130.6928928052));
#128663=CARTESIAN_POINT('Ctrl Pts',(-215.874198623173,4.91387680912948,
130.555712552715));
#128664=CARTESIAN_POINT('Ctrl Pts',(-215.881944956439,4.90502177768142,
130.418663356403));
#128665=CARTESIAN_POINT('Ctrl Pts',(-215.889691289704,4.89045948127991,
130.282259933349));
#128666=CARTESIAN_POINT('Ctrl Pts',(-215.897439357707,4.87589392375314,
130.145825963695));
#128667=CARTESIAN_POINT('Ctrl Pts',(-215.90518742571,4.8556185994924,130.01003844375));
#128668=CARTESIAN_POINT('Ctrl Pts',(-215.912935493713,4.82972310180959,
129.87540538595));
#128669=CARTESIAN_POINT('Ctrl Pts',(-215.920691796455,4.80380008208358,
129.740629238534));
#128670=CARTESIAN_POINT('Ctrl Pts',(-215.928448099196,4.77224503081357,
129.60701038882));
#128671=CARTESIAN_POINT('Ctrl Pts',(-215.936204401938,4.73519849051996,
129.47504563688));
#128672=CARTESIAN_POINT('Ctrl Pts',(-215.943964844452,4.69813217737235,
129.343010451377));
#128673=CARTESIAN_POINT('Ctrl Pts',(-215.951725286967,4.65556865626244,
129.212631494265));
#128674=CARTESIAN_POINT('Ctrl Pts',(-215.959485729481,4.60769758147039,
129.084387925861));
#128675=CARTESIAN_POINT('Ctrl Pts',(-215.967258629746,4.55974965977929,
128.955938489496));
#128676=CARTESIAN_POINT('Ctrl Pts',(-215.975031530012,4.50647731044224,
128.829631652349));
#128677=CARTESIAN_POINT('Ctrl Pts',(-215.982804430277,4.44811770596836,
128.705925024952));
#128678=CARTESIAN_POINT('Ctrl Pts',(-215.990294766039,4.39187962011544,
128.586715445057));
#128679=CARTESIAN_POINT('Ctrl Pts',(-215.997785101801,4.33091786925767,
128.46992058178));
#128680=CARTESIAN_POINT('Ctrl Pts',(-216.005275437563,4.26548289898048,
128.355924647195));
#128681=CARTESIAN_POINT('Ctrl Pts',(-216.013049771683,4.1975669419172,128.237606522104));
#128682=CARTESIAN_POINT('Ctrl Pts',(-216.020824105802,4.12461672787026,
128.12192896195));
#128683=CARTESIAN_POINT('Ctrl Pts',(-216.028598439921,4.04686285643546,
128.009350048051));
#128684=CARTESIAN_POINT('Ctrl Pts',(-216.036363192868,3.96920480969835,
127.896909877601));
#128685=CARTESIAN_POINT('Ctrl Pts',(-216.044127945815,3.88675510481507,
127.787561073731));
#128686=CARTESIAN_POINT('Ctrl Pts',(-216.051892698762,3.79979004601305,
127.681736934072));
#128687=CARTESIAN_POINT('Ctrl Pts',(-216.059649739647,3.71291136213365,
127.57601790044));
#128688=CARTESIAN_POINT('Ctrl Pts',(-216.067406780532,3.6215264957368,127.473816864476));
#128689=CARTESIAN_POINT('Ctrl Pts',(-216.075163821417,3.52595462837755,
127.375537638595));
#128690=CARTESIAN_POINT('Ctrl Pts',(-216.082915012657,3.4304548325068,127.277332525842));
#128691=CARTESIAN_POINT('Ctrl Pts',(-216.090666203897,3.33077459185006,
127.183043615665));
#128692=CARTESIAN_POINT('Ctrl Pts',(-216.098417395138,3.2272726489096,127.093040864149));
#128693=CARTESIAN_POINT('Ctrl Pts',(-216.106165291915,3.12381469705575,
127.003076366204));
#128694=CARTESIAN_POINT('Ctrl Pts',(-216.113913188692,3.01653856798293,
126.917394659643));
#128695=CARTESIAN_POINT('Ctrl Pts',(-216.121661085469,2.90583890658699,
126.836327942365));
#128696=CARTESIAN_POINT('Ctrl Pts',(-216.129407361553,2.79516240117381,
126.755278182496));
#128697=CARTESIAN_POINT('Ctrl Pts',(-216.137153637637,2.68106410308762,
126.678841722612));
#128698=CARTESIAN_POINT('Ctrl Pts',(-216.144899913721,2.56397037592471,
126.607309393923));
#128699=CARTESIAN_POINT('Ctrl Pts',(-216.152646246987,2.44687578440235,
126.535776537199));
#128700=CARTESIAN_POINT('Ctrl Pts',(-216.160392580252,2.32678605331634,
126.469148087725));
#128701=CARTESIAN_POINT('Ctrl Pts',(-216.168138913517,2.20415471344594,
126.407670378114));
#128702=CARTESIAN_POINT('Ctrl Pts',(-216.17588698152,2.08149591113775,126.346178900996));
#128703=CARTESIAN_POINT('Ctrl Pts',(-216.183635049523,1.95629471688963,
126.289840634199));
#128704=CARTESIAN_POINT('Ctrl Pts',(-216.191383117526,1.82902696332566,
126.238854793462));
#128705=CARTESIAN_POINT('Ctrl Pts',(-216.199139420268,1.70162394807853,
126.187814764367));
#128706=CARTESIAN_POINT('Ctrl Pts',(-216.20689572301,1.5721503495455,126.142138670594));
#128707=CARTESIAN_POINT('Ctrl Pts',(-216.214652025752,1.44110010636099,
126.101976802314));
#128708=CARTESIAN_POINT('Ctrl Pts',(-216.222412468266,1.30997991771584,
126.061793498435));
#128709=CARTESIAN_POINT('Ctrl Pts',(-216.23017291078,1.17728178574119,126.027130383204));
#128710=CARTESIAN_POINT('Ctrl Pts',(-216.237933353295,1.04351135435509,
125.998086892961));
#128711=CARTESIAN_POINT('Ctrl Pts',(-216.24570625356,0.909526182796591,
125.968996779528));
#128712=CARTESIAN_POINT('Ctrl Pts',(-216.253479153825,0.774465657443131,
125.945544385083));
#128713=CARTESIAN_POINT('Ctrl Pts',(-216.261252054091,0.638842976528521,
125.927777519346));
#128714=CARTESIAN_POINT('Ctrl Pts',(-216.268742389853,0.508150521681008,
125.910656523932));
#128715=CARTESIAN_POINT('Ctrl Pts',(-216.276232725615,0.376936379995533,
125.898814894981));
#128716=CARTESIAN_POINT('Ctrl Pts',(-216.283723061377,0.245659171928131,
125.892249601542));
#128717=CARTESIAN_POINT('Ctrl Pts',(-216.291497395496,0.109404548613506,
125.885435383006));
#128718=CARTESIAN_POINT('Ctrl Pts',(-216.299271729615,-0.0273496315022193,
125.884283917297));
#128719=CARTESIAN_POINT('Ctrl Pts',(-216.307046063734,-0.164093326920127,
125.888848798583));
#128720=CARTESIAN_POINT('Ctrl Pts',(-216.314810816681,-0.300668497954566,
125.893408054062));
#128721=CARTESIAN_POINT('Ctrl Pts',(-216.322575569628,-0.437232823004622,
125.903669626392));
#128722=CARTESIAN_POINT('Ctrl Pts',(-216.330340322575,-0.57327240731763,
125.919635260956));
#128723=CARTESIAN_POINT('Ctrl Pts',(-216.33809736346,-0.709176875197306,
125.935585038227));
#128724=CARTESIAN_POINT('Ctrl Pts',(-216.345854404345,-0.844557253723871,
125.957227558143));
#128725=CARTESIAN_POINT('Ctrl Pts',(-216.35361144523,-0.978901278650385,
125.984512554695));
#128726=CARTESIAN_POINT('Ctrl Pts',(-216.36136263647,-1.11314399370211,
126.01177697542));
#128727=CARTESIAN_POINT('Ctrl Pts',(-216.36911382771,-1.24635152913388,
126.04467532589));
#128728=CARTESIAN_POINT('Ctrl Pts',(-216.37686501895,-1.37801872132805,
126.083105756179));
#128729=CARTESIAN_POINT('Ctrl Pts',(-216.384612915727,-1.5096299514541,
126.121519852511));
#128730=CARTESIAN_POINT('Ctrl Pts',(-216.392360812504,-1.63970176594521,
126.165461242829));
#128731=CARTESIAN_POINT('Ctrl Pts',(-216.400108709281,-1.76774136209383,
126.214777462285));
#128732=CARTESIAN_POINT('Ctrl Pts',(-216.407854985365,-1.89575417511915,
126.264083365851));
#128733=CARTESIAN_POINT('Ctrl Pts',(-216.41560126145,-2.02173525073432,
126.31876172183));
#128734=CARTESIAN_POINT('Ctrl Pts',(-216.423347537534,-2.14520944446556,
126.378611019828));
#128735=CARTESIAN_POINT('Ctrl Pts',(-216.431093870799,-2.26868454965508,
126.43846075962));
#128736=CARTESIAN_POINT('Ctrl Pts',(-216.438840204064,-2.38965238421982,
126.503481347069));
#128737=CARTESIAN_POINT('Ctrl Pts',(-216.446586537329,-2.50766055709152,
126.57342436268));
#128738=CARTESIAN_POINT('Ctrl Pts',(-216.454334605332,-2.62569515707485,
126.643383041544));
#128739=CARTESIAN_POINT('Ctrl Pts',(-216.462082673335,-2.74076844021403,
126.718266142804));
#128740=CARTESIAN_POINT('Ctrl Pts',(-216.469830741338,-2.85245560150862,
126.79778101597));
#128741=CARTESIAN_POINT('Ctrl Pts',(-216.47758704408,-2.96426146524777,
126.87738039849));
#128742=CARTESIAN_POINT('Ctrl Pts',(-216.485343346822,-3.07267369912862,
126.961621159434));
#128743=CARTESIAN_POINT('Ctrl Pts',(-216.493099649564,-3.17729887387752,
127.050168969747));
#128744=CARTESIAN_POINT('Ctrl Pts',(-216.500860092078,-3.28197989023268,
127.138764040692));
#128745=CARTESIAN_POINT('Ctrl Pts',(-216.508620534592,-3.38286953245154,
127.231670476853));
#128746=CARTESIAN_POINT('Ctrl Pts',(-216.516380977106,-3.47961082903677,
127.32851661345));
#128747=CARTESIAN_POINT('Ctrl Pts',(-216.524153877372,-3.57650742333931,
127.425518216063));
#128748=CARTESIAN_POINT('Ctrl Pts',(-216.531926777637,-3.66924209998222,
127.526471869101));
#128749=CARTESIAN_POINT('Ctrl Pts',(-216.539699677902,-3.75749723911274,
127.630971646677));
#128750=CARTESIAN_POINT('Ctrl Pts',(-216.547190013665,-3.84254408163722,
127.731672594122));
#128751=CARTESIAN_POINT('Ctrl Pts',(-216.554680349427,-3.9234312281144,
127.835666078009));
#128752=CARTESIAN_POINT('Ctrl Pts',(-216.562170685189,-3.99991333301181,
127.942564609655));
#128753=CARTESIAN_POINT('Ctrl Pts',(-216.570019181474,-4.08005253306471,
128.054574638987));
#128754=CARTESIAN_POINT('Ctrl Pts',(-216.577867677758,-4.15560765333159,
128.170127216817));
#128755=CARTESIAN_POINT('Ctrl Pts',(-216.585716174042,-4.22625283006534,
128.28881493544));
#128756=CARTESIAN_POINT('Ctrl Pts',(-216.59355127153,-4.29677740275395,
128.407300032742));
#128757=CARTESIAN_POINT('Ctrl Pts',(-216.601386369017,-4.3624085362298,
128.5289092839));
#128758=CARTESIAN_POINT('Ctrl Pts',(-216.609221466504,-4.42286223498663,
128.65320448357));
#128759=CARTESIAN_POINT('Ctrl Pts',(-216.617048812269,-4.48325612334443,
128.77737671069));
#128760=CARTESIAN_POINT('Ctrl Pts',(-216.624876158033,-4.53848260209349,
128.904229258941));
#128761=CARTESIAN_POINT('Ctrl Pts',(-216.632703503798,-4.58830213122882,
129.03329692163));
#128762=CARTESIAN_POINT('Ctrl Pts',(-216.640523190109,-4.6380729094399,
129.162238285096));
#128763=CARTESIAN_POINT('Ctrl Pts',(-216.648342876421,-4.68244713921057,
129.293390091506));
#128764=CARTESIAN_POINT('Ctrl Pts',(-216.656162562732,-4.72123245764585,
129.426265140695));
#128765=CARTESIAN_POINT('Ctrl Pts',(-216.659212341756,-4.73635923458945,
129.478088132269));
#128766=CARTESIAN_POINT('Ctrl Pts',(-216.66226212078,-4.75063639532078,
129.530173022728));
#128767=CARTESIAN_POINT('Ctrl Pts',(-216.665311899804,-4.76405452823409,
129.582490119308));
#128768=CARTESIAN_POINT('Ctrl Pts',(-214.915345176019,-4.76405452823394,
129.582490119308));
#128769=CARTESIAN_POINT('Ctrl Pts',(-214.924420213177,-4.80367992857624,
129.736988953843));
#128770=CARTESIAN_POINT('Ctrl Pts',(-214.933495250334,-4.83582756235508,
129.893580088636));
#128771=CARTESIAN_POINT('Ctrl Pts',(-214.942570287492,-4.86030047730767,
130.051590843476));
#128772=CARTESIAN_POINT('Ctrl Pts',(-214.951568093968,-4.88456512205087,
130.208256889971));
#128773=CARTESIAN_POINT('Ctrl Pts',(-214.960565900445,-4.90128504720006,
130.366318388601));
#128774=CARTESIAN_POINT('Ctrl Pts',(-214.969563706922,-4.91031530497346,
130.525099685384));
#128775=CARTESIAN_POINT('Ctrl Pts',(-214.974755992601,-4.91552631703969,
130.616726222985));
#128776=CARTESIAN_POINT('Ctrl Pts',(-214.979948278281,-4.91817754857704,
130.708592090226));
#128777=CARTESIAN_POINT('Ctrl Pts',(-214.98514056396,-4.91824853507356,
130.800564600342));
#128778=CARTESIAN_POINT('',(-214.639859436029,-4.91824993606532,130.803567589537));
#128779=CARTESIAN_POINT('Ctrl Pts',(-214.569765644412,-4.76405452823405,
129.582490119308));
#128780=CARTESIAN_POINT('Ctrl Pts',(-214.577527446603,-4.79811587282819,
129.715294784928));
#128781=CARTESIAN_POINT('Ctrl Pts',(-214.585289248795,-4.82659044595685,
129.849410052572));
#128782=CARTESIAN_POINT('Ctrl Pts',(-214.593051050987,-4.84940476436363,
129.984326170809));
#128783=CARTESIAN_POINT('Ctrl Pts',(-214.600824711805,-4.87225393891184,
130.11944841641));
#128784=CARTESIAN_POINT('Ctrl Pts',(-214.608598372623,-4.88942553542031,
130.255373569285));
#128785=CARTESIAN_POINT('Ctrl Pts',(-214.616372033441,-4.9008979999614,
130.391587245757));
#128786=CARTESIAN_POINT('Ctrl Pts',(-214.62179012718,-4.9088940895464,130.486525587547));
#128787=CARTESIAN_POINT('Ctrl Pts',(-214.627208220919,-4.91412273629671,
130.581604036906));
#128788=CARTESIAN_POINT('Ctrl Pts',(-214.632626314659,-4.91659159218293,
130.676649309624));
#128789=CARTESIAN_POINT('Ctrl Pts',(-214.635037355104,-4.91769022791769,
130.718944258313));
#128790=CARTESIAN_POINT('Ctrl Pts',(-214.63744839555,-4.91824311324674,
130.761253444763));
#128791=CARTESIAN_POINT('Ctrl Pts',(-214.639859435996,-4.91824993606523,
130.803567588965));
#128792=CARTESIAN_POINT('Ctrl Pts',(-214.639859436029,-4.91824993606532,
130.803567589537));
#128793=CARTESIAN_POINT('Ctrl Pts',(-214.647599714426,-4.91827183966986,
130.939410709401));
#128794=CARTESIAN_POINT('Ctrl Pts',(-214.655339992823,-4.91266145491847,
131.075477757422));
#128795=CARTESIAN_POINT('Ctrl Pts',(-214.66308027122,-4.90138914671146,
131.211260476253));
#128796=CARTESIAN_POINT('Ctrl Pts',(-214.670811061266,-4.89013065656297,
131.346876747048));
#128797=CARTESIAN_POINT('Ctrl Pts',(-214.678541851312,-4.87322408275251,
131.48220899249));
#128798=CARTESIAN_POINT('Ctrl Pts',(-214.686272641357,-4.85069176530766,
131.616747508448));
#128799=CARTESIAN_POINT('Ctrl Pts',(-214.693995846345,-4.82818155542907,
131.751154022042));
#128800=CARTESIAN_POINT('Ctrl Pts',(-214.701719051331,-4.80005664939924,
131.884767968886));
#128801=CARTESIAN_POINT('Ctrl Pts',(-214.709442256318,-4.76639126647814,
132.017083734086));
#128802=CARTESIAN_POINT('Ctrl Pts',(-214.717159772577,-4.73275068067482,
132.14930203865));
#128803=CARTESIAN_POINT('Ctrl Pts',(-214.724877288835,-4.69357783671161,
132.280223683519));
#128804=CARTESIAN_POINT('Ctrl Pts',(-214.732594805094,-4.64899813726028,
132.409352636939));
#128805=CARTESIAN_POINT('Ctrl Pts',(-214.740309268324,-4.60443607341942,
132.538430507288));
#128806=CARTESIAN_POINT('Ctrl Pts',(-214.748023731553,-4.55447153555235,
132.665716723847));
#128807=CARTESIAN_POINT('Ctrl Pts',(-214.755738194783,-4.49927987544658,
132.790730085943));
#128808=CARTESIAN_POINT('Ctrl Pts',(-214.763451245489,-4.44409832097267,
132.915720558004));
#128809=CARTESIAN_POINT('Ctrl Pts',(-214.771164296195,-4.38369170702797,
133.038438642288));
#128810=CARTESIAN_POINT('Ctrl Pts',(-214.778877346901,-4.31828348084661,
133.15842324238));
#128811=CARTESIAN_POINT('Ctrl Pts',(-214.78659069349,-4.25287274551902,
133.278412445241));
#128812=CARTESIAN_POINT('Ctrl Pts',(-214.794304040078,-4.1824602051556,
133.395667608655));
#128813=CARTESIAN_POINT('Ctrl Pts',(-214.802017386667,-4.10731498489418,
133.509752766103));
#128814=CARTESIAN_POINT('Ctrl Pts',(-214.809732737415,-4.03215023965263,
133.623867566293));
#128815=CARTESIAN_POINT('Ctrl Pts',(-214.817448088162,-3.95225058525506,
133.734810392369));
#128816=CARTESIAN_POINT('Ctrl Pts',(-214.82516343891,-3.86792786982101,
133.842175137309));
#128817=CARTESIAN_POINT('Ctrl Pts',(-214.832887060762,-3.78351475771584,
133.949654980719));
#128818=CARTESIAN_POINT('Ctrl Pts',(-214.840610682614,-3.69466935959324,
134.053548772069));
#128819=CARTESIAN_POINT('Ctrl Pts',(-214.848334304467,-3.60174342374308,
134.15348399123));
#128820=CARTESIAN_POINT('Ctrl Pts',(-214.856062366428,-3.50876406718808,
134.25347666055));
#128821=CARTESIAN_POINT('Ctrl Pts',(-214.86379042839,-3.41169978064607,
134.349505947649));
#128822=CARTESIAN_POINT('Ctrl Pts',(-214.871518490352,-3.31093759543724,
134.441237753464));
#128823=CARTESIAN_POINT('Ctrl Pts',(-214.87925836052,-3.21002144915805,
134.533109722249));
#128824=CARTESIAN_POINT('Ctrl Pts',(-214.886998230688,-3.10539642093301,
134.620670841333));
#128825=CARTESIAN_POINT('Ctrl Pts',(-214.894738100857,-2.99748138846424,
134.7036282909));
#128826=CARTESIAN_POINT('Ctrl Pts',(-214.900183380062,-2.92155925160314,
134.761991863571));
#128827=CARTESIAN_POINT('Ctrl Pts',(-214.905628659266,-2.84400932084468,
134.818077683594));
#128828=CARTESIAN_POINT('Ctrl Pts',(-214.911073938471,-2.7649849903439,
134.871797287715));
#128829=CARTESIAN_POINT('Ctrl Pts',(-214.91884827259,-2.65216037185725,
134.948493841824));
#128830=CARTESIAN_POINT('Ctrl Pts',(-214.92662260671,-2.53596345703543,
135.020613940536));
#128831=CARTESIAN_POINT('Ctrl Pts',(-214.934396940829,-2.41680197188725,
135.087846498386));
#128832=CARTESIAN_POINT('Ctrl Pts',(-214.942161693776,-2.29778734261974,
135.154996198116));
#128833=CARTESIAN_POINT('Ctrl Pts',(-214.949926446723,-2.17581574977439,
135.217270151595));
#128834=CARTESIAN_POINT('Ctrl Pts',(-214.95769119967,-2.05132518092044,
135.274399550799));
#128835=CARTESIAN_POINT('Ctrl Pts',(-214.965448240555,-1.92695825785448,
135.331472208279));
#128836=CARTESIAN_POINT('Ctrl Pts',(-214.97320528144,-1.80007769067526,
135.383410317897));
#128837=CARTESIAN_POINT('Ctrl Pts',(-214.980962322325,-1.67114712965089,
135.429990340486));
#128838=CARTESIAN_POINT('Ctrl Pts',(-214.988713513565,-1.54231379616465,
135.476535236717));
#128839=CARTESIAN_POINT('Ctrl Pts',(-214.996464704805,-1.41143391210209,
135.517729956133));
#128840=CARTESIAN_POINT('Ctrl Pts',(-215.004215896046,-1.27899189626959,
135.553398708777));
#128841=CARTESIAN_POINT('Ctrl Pts',(-215.011963792823,-1.14660617182772,
135.58905230125));
#128842=CARTESIAN_POINT('Ctrl Pts',(-215.0197116896,-1.01266001288096,135.619184496847));
#128843=CARTESIAN_POINT('Ctrl Pts',(-215.027459586377,-0.877653610142368,
135.643669163537));
#128844=CARTESIAN_POINT('Ctrl Pts',(-215.035205862461,-0.742675447832825,
135.668148708562));
#128845=CARTESIAN_POINT('Ctrl Pts',(-215.042952138545,-0.606637867310519,
135.686983004709));
#128846=CARTESIAN_POINT('Ctrl Pts',(-215.050698414629,-0.470051490621363,
135.700096993094));
#128847=CARTESIAN_POINT('Ctrl Pts',(-215.058444747895,-0.333464105682415,
135.713211078282));
#128848=CARTESIAN_POINT('Ctrl Pts',(-215.06619108116,-0.196328305668506,
135.720604734083));
#128849=CARTESIAN_POINT('Ctrl Pts',(-215.073937414425,-0.0591596810558063,
135.72225480051));
#128850=CARTESIAN_POINT('Ctrl Pts',(-215.081685482428,0.0780396615191281,
135.723905236458));
#128851=CARTESIAN_POINT('Ctrl Pts',(-215.089433550431,0.215271452458073,
135.719809518868));
#128852=CARTESIAN_POINT('Ctrl Pts',(-215.097181618434,0.352020653319216,
135.709996613249));
#128853=CARTESIAN_POINT('Ctrl Pts',(-215.104937921176,0.488915192858183,
135.700173278356));
#128854=CARTESIAN_POINT('Ctrl Pts',(-215.112694223918,0.625325727157111,
135.684620645409));
#128855=CARTESIAN_POINT('Ctrl Pts',(-215.12045052666,0.760742334114661,
135.663419596791));
#128856=CARTESIAN_POINT('Ctrl Pts',(-215.128210969174,0.896231216993028,
135.642207232535));
#128857=CARTESIAN_POINT('Ctrl Pts',(-215.135971411688,1.03072473228301,
135.615340522055));
#128858=CARTESIAN_POINT('Ctrl Pts',(-215.143731854202,1.16372467363971,
135.582951199156));
#128859=CARTESIAN_POINT('Ctrl Pts',(-215.151504754468,1.29693811830946,
135.550509882041));
#128860=CARTESIAN_POINT('Ctrl Pts',(-215.159277654733,1.4286528219675,135.512528345024));
#128861=CARTESIAN_POINT('Ctrl Pts',(-215.167050554999,1.55838636490553,
135.469188052764));
#128862=CARTESIAN_POINT('Ctrl Pts',(-215.174540890761,1.68340376677833,
135.427423289295));
#128863=CARTESIAN_POINT('Ctrl Pts',(-215.182031226523,1.80658125956134,
135.380682724186));
#128864=CARTESIAN_POINT('Ctrl Pts',(-215.189521562285,1.92750774059563,
135.329169671266));
#128865=CARTESIAN_POINT('Ctrl Pts',(-215.197295896404,2.05301918591367,
135.275703485287));
#128866=CARTESIAN_POINT('Ctrl Pts',(-215.205070230523,2.17650313823665,
135.216926404965));
#128867=CARTESIAN_POINT('Ctrl Pts',(-215.212844564642,2.29747748668428,
135.153013312445));
#128868=CARTESIAN_POINT('Ctrl Pts',(-215.220609317589,2.41830274505891,
135.0891789871));
#128869=CARTESIAN_POINT('Ctrl Pts',(-215.228374070536,2.53662421106492,
135.020221424605));
#128870=CARTESIAN_POINT('Ctrl Pts',(-215.236138823483,2.65197898592121,
134.946363819005));
#128871=CARTESIAN_POINT('Ctrl Pts',(-215.243895864368,2.76721918878921,
134.87257956982));
#128872=CARTESIAN_POINT('Ctrl Pts',(-215.251652905253,2.87949823716522,
134.793905172115));
#128873=CARTESIAN_POINT('Ctrl Pts',(-215.259409946138,2.98837744692175,
134.710609879611));
#128874=CARTESIAN_POINT('Ctrl Pts',(-215.267161137378,3.0971745500188,134.627377400736));
#128875=CARTESIAN_POINT('Ctrl Pts',(-215.274912328618,3.20257660841183,
134.539531199645));
#128876=CARTESIAN_POINT('Ctrl Pts',(-215.282663519859,3.30417388483606,
134.447383812835));
#128877=CARTESIAN_POINT('Ctrl Pts',(-215.290411416636,3.40572797970774,
134.355275591123));
#128878=CARTESIAN_POINT('Ctrl Pts',(-215.298159313413,3.50348021997888,
134.258870081788));
#128879=CARTESIAN_POINT('Ctrl Pts',(-215.30590721019,3.5970541219015,134.158519932001));
#128880=CARTESIAN_POINT('Ctrl Pts',(-215.313653486274,3.69060845018106,
134.058190773302));
#128881=CARTESIAN_POINT('Ctrl Pts',(-215.321399762358,3.77998591212003,
133.953918901145));
#128882=CARTESIAN_POINT('Ctrl Pts',(-215.329146038442,3.86484735486342,
133.846093345158));
#128883=CARTESIAN_POINT('Ctrl Pts',(-215.336892371707,3.94970942403482,
133.738266993227));
#128884=CARTESIAN_POINT('Ctrl Pts',(-215.344638704973,4.03005516569492,
133.626887212348));
#128885=CARTESIAN_POINT('Ctrl Pts',(-215.352385038238,4.10558640544539,
133.512375264853));
#128886=CARTESIAN_POINT('Ctrl Pts',(-215.360133106241,4.18113455989361,
133.397837673201));
#128887=CARTESIAN_POINT('Ctrl Pts',(-215.367881174244,4.25186585176375,
133.280166845476));
#128888=CARTESIAN_POINT('Ctrl Pts',(-215.375629242247,4.31752625970104,
133.159811754672));
#128889=CARTESIAN_POINT('Ctrl Pts',(-215.383385544989,4.38325645230099,
133.039328749045));
#128890=CARTESIAN_POINT('Ctrl Pts',(-215.391141847731,4.44390480752966,
132.916156125189));
#128891=CARTESIAN_POINT('Ctrl Pts',(-215.398898150473,4.49926374867785,
132.790766613916));
#128892=CARTESIAN_POINT('Ctrl Pts',(-215.406658592987,4.55465223655975,
132.665310178484));
#128893=CARTESIAN_POINT('Ctrl Pts',(-215.414419035501,4.60474554232912,
132.537634861746));
#128894=CARTESIAN_POINT('Ctrl Pts',(-215.422179478015,4.64938520466827,
132.408231024149));
#128895=CARTESIAN_POINT('Ctrl Pts',(-215.42995237828,4.69409652655633,132.278619456023));
#128896=CARTESIAN_POINT('Ctrl Pts',(-215.437725278546,4.73333659840917,
132.147274196973));
#128897=CARTESIAN_POINT('Ctrl Pts',(-215.445498178811,4.76699733194558,
132.014699206443));
#128898=CARTESIAN_POINT('Ctrl Pts',(-215.452988514573,4.7994344130314,131.886943650755));
#128899=CARTESIAN_POINT('Ctrl Pts',(-215.460478850335,4.82669069547001,
131.758046520366));
#128900=CARTESIAN_POINT('Ctrl Pts',(-215.467969186097,4.84871502191527,
131.628463583677));
#128901=CARTESIAN_POINT('Ctrl Pts',(-215.475743520216,4.87157440739208,
131.493967470556));
#128902=CARTESIAN_POINT('Ctrl Pts',(-215.483517854335,4.88886967755753,
131.358306476596));
#128903=CARTESIAN_POINT('Ctrl Pts',(-215.491292188454,4.90048737300637,
131.221980743404));
#128904=CARTESIAN_POINT('Ctrl Pts',(-215.499056941401,4.91209075068382,
131.085823019496));
#128905=CARTESIAN_POINT('Ctrl Pts',(-215.506821694349,4.91803044291591,
130.949002572196));
#128906=CARTESIAN_POINT('Ctrl Pts',(-215.514586447296,4.91824402107567,
130.812029493194));
#128907=CARTESIAN_POINT('Ctrl Pts',(-215.522343488181,4.9184573871066,130.675192457785));
#128908=CARTESIAN_POINT('Ctrl Pts',(-215.530100529066,4.912955956358,130.53820348079));
#128909=CARTESIAN_POINT('Ctrl Pts',(-215.537857569951,4.90172914012527,
130.401577177804));
#128910=CARTESIAN_POINT('Ctrl Pts',(-215.545608761191,4.89051079012195,
130.265053905775));
#128911=CARTESIAN_POINT('Ctrl Pts',(-215.553359952431,4.87357568036007,
130.128893151454));
#128912=CARTESIAN_POINT('Ctrl Pts',(-215.561111143671,4.85096528364601,
129.993608572017));
#128913=CARTESIAN_POINT('Ctrl Pts',(-215.568859040448,4.8283644969538,129.858381492137));
#128914=CARTESIAN_POINT('Ctrl Pts',(-215.576606937225,4.80009328520259,
129.724030231278));
#128915=CARTESIAN_POINT('Ctrl Pts',(-215.584354834002,4.76624484178161,
129.591062150292));
#128916=CARTESIAN_POINT('Ctrl Pts',(-215.592101110086,4.73240347872531,
129.458121883361));
#128917=CARTESIAN_POINT('Ctrl Pts',(-215.599847386171,4.69298730089078,
129.326564599448));
#128918=CARTESIAN_POINT('Ctrl Pts',(-215.607593662255,4.64814028951919,
129.19688591747));
#128919=CARTESIAN_POINT('Ctrl Pts',(-215.61533999552,4.6032929470971,129.067206278234));
#128920=CARTESIAN_POINT('Ctrl Pts',(-215.623086328785,4.55301481892545,
128.939405638098));
#128921=CARTESIAN_POINT('Ctrl Pts',(-215.630832662051,4.49749915438921,
128.813962562209));
#128922=CARTESIAN_POINT('Ctrl Pts',(-215.638580730054,4.44197105750459,
128.688491394213));
#128923=CARTESIAN_POINT('Ctrl Pts',(-215.646328798057,4.38120324849224,
128.565379198493));
#128924=CARTESIAN_POINT('Ctrl Pts',(-215.65407686606,4.31543615629982,128.44508237128));
#128925=CARTESIAN_POINT('Ctrl Pts',(-215.661833168802,4.24959916605946,
128.324657691167));
#128926=CARTESIAN_POINT('Ctrl Pts',(-215.669589471544,4.17875246659923,
128.20705470041));
#128927=CARTESIAN_POINT('Ctrl Pts',(-215.677345774285,4.10318157945714,
128.092703561723));
#128928=CARTESIAN_POINT('Ctrl Pts',(-215.6851062168,4.02757035785719,127.97829139039));
#128929=CARTESIAN_POINT('Ctrl Pts',(-215.692866659314,3.94723015329797,
127.86713484619));
#128930=CARTESIAN_POINT('Ctrl Pts',(-215.700627101828,3.86248786769865,
127.759632298917));
#128931=CARTESIAN_POINT('Ctrl Pts',(-215.708400002093,3.77760954625942,
127.651957179012));
#128932=CARTESIAN_POINT('Ctrl Pts',(-215.716172902359,3.68831527725839,
127.547948074423));
#128933=CARTESIAN_POINT('Ctrl Pts',(-215.723945802624,3.59497063169151,
127.447968325271));
#128934=CARTESIAN_POINT('Ctrl Pts',(-215.731436138386,3.50501929911271,
127.351623091836));
#128935=CARTESIAN_POINT('Ctrl Pts',(-215.738926474148,3.41130717918996,
127.25901956202));
#128936=CARTESIAN_POINT('Ctrl Pts',(-215.74641680991,3.31419007099185,127.1704471299));
#128937=CARTESIAN_POINT('Ctrl Pts',(-215.754191144029,3.21339073811732,
127.078516447095));
#128938=CARTESIAN_POINT('Ctrl Pts',(-215.761965478148,3.10860381776411,
126.990637365538));
#128939=CARTESIAN_POINT('Ctrl Pts',(-215.769739812267,3.00018876565265,
126.907175680595));
#128940=CARTESIAN_POINT('Ctrl Pts',(-215.777504565214,2.89190732540418,
126.823816854721));
#128941=CARTESIAN_POINT('Ctrl Pts',(-215.785269318162,2.78000695687148,
126.744864829635));
#128942=CARTESIAN_POINT('Ctrl Pts',(-215.793034071109,2.66488307044007,
126.670647845326));
#128943=CARTESIAN_POINT('Ctrl Pts',(-215.800791111994,2.54987352667468,
126.596504574371));
#128944=CARTESIAN_POINT('Ctrl Pts',(-215.808548152879,2.43164716289924,
126.527087195661));
#128945=CARTESIAN_POINT('Ctrl Pts',(-215.816305193764,2.31063121633424,
126.46268278007));
#128946=CARTESIAN_POINT('Ctrl Pts',(-215.824056385004,2.18970652883707,
126.398326932351));
#128947=CARTESIAN_POINT('Ctrl Pts',(-215.831807576244,2.06599678946577,
126.3389767062));
#128948=CARTESIAN_POINT('Ctrl Pts',(-215.839558767484,1.93995656961486,
126.28487485362));
#128949=CARTESIAN_POINT('Ctrl Pts',(-215.847306664261,1.81396992021911,
126.230795995771));
#128950=CARTESIAN_POINT('Ctrl Pts',(-215.855054561038,1.68565511891946,
126.181961228694));
#128951=CARTESIAN_POINT('Ctrl Pts',(-215.862802457815,1.55548939607039,
126.138566387083));
#128952=CARTESIAN_POINT('Ctrl Pts',(-215.870548733899,1.4253509010845,126.095180622736));
#128953=CARTESIAN_POINT('Ctrl Pts',(-215.878295009983,1.29336262531912,
126.057232644052));
#128954=CARTESIAN_POINT('Ctrl Pts',(-215.886041286067,1.16001937238477,
126.024869209666));
#128955=CARTESIAN_POINT('Ctrl Pts',(-215.893787619333,1.026675135141,125.99250553638));
#128956=CARTESIAN_POINT('Ctrl Pts',(-215.901533952598,0.89197628070464,
125.965726581864));
#128957=CARTESIAN_POINT('Ctrl Pts',(-215.909280285863,0.756429895499917,
125.944628436088));
#128958=CARTESIAN_POINT('Ctrl Pts',(-215.917028353866,0.620853155622594,
125.923525565529));
#128959=CARTESIAN_POINT('Ctrl Pts',(-215.924776421869,0.484428893539116,
125.908106095316));
#128960=CARTESIAN_POINT('Ctrl Pts',(-215.932524489872,0.347671046042293,
125.898414439076));
#128961=CARTESIAN_POINT('Ctrl Pts',(-215.940280792614,0.210767850677151,
125.888712482428));
#128962=CARTESIAN_POINT('Ctrl Pts',(-215.948037095356,0.0735307522787072,
125.88475052805));
#128963=CARTESIAN_POINT('Ctrl Pts',(-215.955793398098,-0.0635240097127495,
125.886520872039));
#128964=CARTESIAN_POINT('Ctrl Pts',(-215.963553840612,-0.200651921957693,
125.888292160913));
#128965=CARTESIAN_POINT('Ctrl Pts',(-215.971314283126,-0.337596913692748,
125.895801823072));
#128966=CARTESIAN_POINT('Ctrl Pts',(-215.97907472564,-0.473847126655544,
125.908990155276));
#128967=CARTESIAN_POINT('Ctrl Pts',(-215.986847625906,-0.610316060555913,
125.922199658562));
#128968=CARTESIAN_POINT('Ctrl Pts',(-215.994620526171,-0.746087599466408,
125.941105994423));
#128969=CARTESIAN_POINT('Ctrl Pts',(-216.002393426437,-0.880658455000069,
125.965597991839));
#128970=CARTESIAN_POINT('Ctrl Pts',(-216.009883762199,-1.01033732097301,
125.989199643456));
#128971=CARTESIAN_POINT('Ctrl Pts',(-216.017374097961,-1.13890098314221,
126.01798783418));
#128972=CARTESIAN_POINT('Ctrl Pts',(-216.024864433723,-1.26591364798658,
126.051819644745));
#128973=CARTESIAN_POINT('Ctrl Pts',(-216.032638767842,-1.39774203662189,
126.08693419869));
#128974=CARTESIAN_POINT('Ctrl Pts',(-216.040413101961,-1.52831708681475,
126.127593612355));
#128975=CARTESIAN_POINT('Ctrl Pts',(-216.04818743608,-1.65713674996577,
126.173693186794));
#128976=CARTESIAN_POINT('Ctrl Pts',(-216.055952189027,-1.78579765439419,
126.219735947627));
#128977=CARTESIAN_POINT('Ctrl Pts',(-216.063716941974,-1.91270711164699,
126.271205398787));
#128978=CARTESIAN_POINT('Ctrl Pts',(-216.071481694922,-2.03737523515358,
126.32794629205));
#128979=CARTESIAN_POINT('Ctrl Pts',(-216.079238735807,-2.16191953652273,
126.384630829458));
#128980=CARTESIAN_POINT('Ctrl Pts',(-216.086995776692,-2.28422658069359,
126.44657622884));
#128981=CARTESIAN_POINT('Ctrl Pts',(-216.094752817577,-2.40382391465449,
126.513578212242));
#128982=CARTESIAN_POINT('Ctrl Pts',(-216.102504008817,-2.52333105933633,
126.580529668928));
#128983=CARTESIAN_POINT('Ctrl Pts',(-216.110255200057,-2.64013222139294,
126.652529929359));
#128984=CARTESIAN_POINT('Ctrl Pts',(-216.118006391297,-2.75377745974615,
126.729327763135));
#128985=CARTESIAN_POINT('Ctrl Pts',(-216.125754288074,-2.86737439584101,
126.806092955782));
#128986=CARTESIAN_POINT('Ctrl Pts',(-216.133502184851,-2.97781775282151,
126.887651447719));
#128987=CARTESIAN_POINT('Ctrl Pts',(-216.141250081628,-3.08468481474969,
126.973707584968));
#128988=CARTESIAN_POINT('Ctrl Pts',(-216.148996357712,-3.1915295223923,
127.059745721128));
#128989=CARTESIAN_POINT('Ctrl Pts',(-216.156742633797,-3.29479911864613,
127.150279386222));
#128990=CARTESIAN_POINT('Ctrl Pts',(-216.164488909881,-3.39410267787684,
127.244971614587));
#128991=CARTESIAN_POINT('Ctrl Pts',(-216.172235243146,-3.49340697014373,
127.339664541948));
#128992=CARTESIAN_POINT('Ctrl Pts',(-216.179981576411,-3.588744884023,127.438515824027));
#128993=CARTESIAN_POINT('Ctrl Pts',(-216.187727909677,-3.67976148370246,
127.54115077363));
#128994=CARTESIAN_POINT('Ctrl Pts',(-216.19547597768,-3.77079846591823,
127.643808707619));
#128995=CARTESIAN_POINT('Ctrl Pts',(-216.203224045683,-3.85751194891496,
127.750251702754));
#128996=CARTESIAN_POINT('Ctrl Pts',(-216.210972113686,-3.93958677086006,
127.860071376108));
#128997=CARTESIAN_POINT('Ctrl Pts',(-216.218728416428,-4.02174882290297,
127.970007767118));
#128998=CARTESIAN_POINT('Ctrl Pts',(-216.226484719169,-4.09926213121704,
128.08332769164));
#128999=CARTESIAN_POINT('Ctrl Pts',(-216.234241021911,-4.17185413728566,
128.199592658666));
#129000=CARTESIAN_POINT('Ctrl Pts',(-216.242001464426,-4.24448488789342,
128.315919679805));
#129001=CARTESIAN_POINT('Ctrl Pts',(-216.24976190694,-4.31218890953456,
128.435194535666));
#129002=CARTESIAN_POINT('Ctrl Pts',(-216.257522349454,-4.37473976034095,
128.556954314337));
#129003=CARTESIAN_POINT('Ctrl Pts',(-216.265295249719,-4.43739102332606,
128.678909552615));
#129004=CARTESIAN_POINT('Ctrl Pts',(-216.273068149985,-4.49487242069567,
128.803357329896));
#129005=CARTESIAN_POINT('Ctrl Pts',(-216.28084105025,-4.54700544411243,
128.929814124755));
#129006=CARTESIAN_POINT('Ctrl Pts',(-216.288331386012,-4.59724330081212,
129.051673896593));
#129007=CARTESIAN_POINT('Ctrl Pts',(-216.295821721774,-4.64251478037536,
129.175398866962));
#129008=CARTESIAN_POINT('Ctrl Pts',(-216.303312057536,-4.68270456778482,
129.300545139076));
#129009=CARTESIAN_POINT('Ctrl Pts',(-216.308884508859,-4.71260384615303,
129.393647976086));
#129010=CARTESIAN_POINT('Ctrl Pts',(-216.314456960182,-4.73973772792483,
129.487679283962));
#129011=CARTESIAN_POINT('Ctrl Pts',(-216.320029411505,-4.76405452823406,
129.582490119308));
#129012=CARTESIAN_POINT('Origin',(213.235140564004,0.,130.804360617566));
#129013=CARTESIAN_POINT('',(-218.414998772423,-4.76405452823415,129.582490119309));
#129014=CARTESIAN_POINT('',(-218.070061802556,-4.76405452823401,129.582490119308));
#129015=CARTESIAN_POINT('',(213.235140564004,-4.76405452823405,129.582490119308));
#129016=CARTESIAN_POINT('',(-216.735140564067,-4.91824906570699,130.807392147263));
#129017=CARTESIAN_POINT('Ctrl Pts',(-216.735140564067,-4.91824906570699,
130.807392147263));
#129018=CARTESIAN_POINT('Ctrl Pts',(-216.743930376145,-4.91815299469981,
130.963254430834));
#129019=CARTESIAN_POINT('Ctrl Pts',(-216.752720188223,-4.91064364192366,
131.11883983252));
#129020=CARTESIAN_POINT('Ctrl Pts',(-216.761510000301,-4.89582518385855,
131.273486220786));
#129021=CARTESIAN_POINT('Ctrl Pts',(-216.770240213936,-4.88110720086741,
131.427084044672));
#129022=CARTESIAN_POINT('Ctrl Pts',(-216.778970427572,-4.85917909410244,
131.579755377644));
#129023=CARTESIAN_POINT('Ctrl Pts',(-216.787700641208,-4.8301931353919,
131.730868759631));
#129024=CARTESIAN_POINT('Ctrl Pts',(-216.796520252507,-4.80091035954813,
131.883529547426));
#129025=CARTESIAN_POINT('Ctrl Pts',(-216.805339863806,-4.76442450715711,
132.034600100351));
#129026=CARTESIAN_POINT('Ctrl Pts',(-216.814159475105,-4.72094222459015,
132.18345001807));
#129027=CARTESIAN_POINT('Ctrl Pts',(-216.822979086404,-4.67745994202318,
132.332299935789));
#129028=CARTESIAN_POINT('Ctrl Pts',(-216.831798697704,-4.62698137325245,
132.478929048469));
#129029=CARTESIAN_POINT('Ctrl Pts',(-216.840618309003,-4.56976089153752,
132.622730342532));
#129030=CARTESIAN_POINT('Ctrl Pts',(-216.848392643122,-4.51932203111415,
132.749488684696));
#129031=CARTESIAN_POINT('Ctrl Pts',(-216.856166977241,-4.46352515151253,
132.874347564552));
#129032=CARTESIAN_POINT('Ctrl Pts',(-216.86394131136,-4.40253351518442,
132.996820813368));
#129033=CARTESIAN_POINT('Ctrl Pts',(-216.871706064307,-4.3416170455971,
133.119143124851));
#129034=CARTESIAN_POINT('Ctrl Pts',(-216.879470817254,-4.27551873011275,
133.239085308561));
#129035=CARTESIAN_POINT('Ctrl Pts',(-216.887235570201,-4.20445059020745,
133.356179242979));
#129036=CARTESIAN_POINT('Ctrl Pts',(-216.894992611086,-4.13345303618059,
133.47315687805));
#129037=CARTESIAN_POINT('Ctrl Pts',(-216.902749651971,-4.05749568233232,
133.58729156145));
#129038=CARTESIAN_POINT('Ctrl Pts',(-216.910506692856,-3.97683717763647,
133.698138274033));
#129039=CARTESIAN_POINT('Ctrl Pts',(-216.918257884096,-3.89623949814654,
133.808901396248));
#129040=CARTESIAN_POINT('Ctrl Pts',(-216.926009075336,-3.81094795336731,
133.91638116806));
#129041=CARTESIAN_POINT('Ctrl Pts',(-216.933760266576,-3.72126515722831,
134.020160470184));
#129042=CARTESIAN_POINT('Ctrl Pts',(-216.941508163353,-3.63162047866992,
134.123895663336));
#129043=CARTESIAN_POINT('Ctrl Pts',(-216.949256060131,-3.53758851597458,
134.223933219782));
#129044=CARTESIAN_POINT('Ctrl Pts',(-216.957003956908,-3.43951278018621,
134.319888301632));
#129045=CARTESIAN_POINT('Ctrl Pts',(-216.964750232992,-3.3414575597275,
134.415823311748));
#129046=CARTESIAN_POINT('Ctrl Pts',(-216.972496509076,-3.23936052793977,
134.507677272608));
#129047=CARTESIAN_POINT('Ctrl Pts',(-216.98024278516,-3.13360246368624,
134.595101793389));
#129048=CARTESIAN_POINT('Ctrl Pts',(-216.987989118425,-3.02784361875057,
134.682526959518));
#129049=CARTESIAN_POINT('Ctrl Pts',(-216.99573545169,-2.91842398875929,
134.765522371223));
#129050=CARTESIAN_POINT('Ctrl Pts',(-217.003481784956,-2.80575755936771,
134.843779830838));
#129051=CARTESIAN_POINT('Ctrl Pts',(-217.011229852959,-2.69306589911059,
134.922054815669));
#129052=CARTESIAN_POINT('Ctrl Pts',(-217.018977920962,-2.57712631365499,
134.995589514085));
#129053=CARTESIAN_POINT('Ctrl Pts',(-217.026725988965,-2.45838155088886,
135.064119203771));
#129054=CARTESIAN_POINT('Ctrl Pts',(-217.034482291707,-2.33951058477595,
135.132721727627));
#129055=CARTESIAN_POINT('Ctrl Pts',(-217.042238594448,-2.217828824893,135.196308420976));
#129056=CARTESIAN_POINT('Ctrl Pts',(-217.04999489719,-2.09380388464748,
135.25466042265));
#129057=CARTESIAN_POINT('Ctrl Pts',(-217.057755339704,-1.9697127485567,
135.313043568546));
#129058=CARTESIAN_POINT('Ctrl Pts',(-217.065515782218,-1.84327630037177,
135.366186304243));
#129059=CARTESIAN_POINT('Ctrl Pts',(-217.073276224733,-1.71498095669357,
135.413918446759));
#129060=CARTESIAN_POINT('Ctrl Pts',(-217.081049124998,-1.58647966194018,
135.461727213148));
#129061=CARTESIAN_POINT('Ctrl Pts',(-217.088822025264,-1.45611388060796,
135.504107908889));
#129062=CARTESIAN_POINT('Ctrl Pts',(-217.096594925529,-1.32438483319117,
135.540940383189));
#129063=CARTESIAN_POINT('Ctrl Pts',(-217.104085261291,-1.1974444684527,
135.576433904274));
#129064=CARTESIAN_POINT('Ctrl Pts',(-217.111575597053,-1.06923853287591,
135.606775513298));
#129065=CARTESIAN_POINT('Ctrl Pts',(-217.119065932815,-0.940221435976484,
135.631903130463));
#129066=CARTESIAN_POINT('Ctrl Pts',(-217.126840266934,-0.806312616635522,
135.65798346887));
#129067=CARTESIAN_POINT('Ctrl Pts',(-217.134614601053,-0.671105728485961,
135.678529248222));
#129068=CARTESIAN_POINT('Ctrl Pts',(-217.142388935172,-0.535098046395437,
135.693415039767));
#129069=CARTESIAN_POINT('Ctrl Pts',(-217.150153688119,-0.399257981617734,
135.708282485904));
#129070=CARTESIAN_POINT('Ctrl Pts',(-217.157918441066,-0.262619471463193,
135.717503781132));
#129071=CARTESIAN_POINT('Ctrl Pts',(-217.165683194014,-0.125690962610648,
135.721004274007));
#129072=CARTESIAN_POINT('Ctrl Pts',(-217.173440234899,0.0111015469165498,
135.724501290142));
#129073=CARTESIAN_POINT('Ctrl Pts',(-217.181197275784,0.14818309363905,
135.722288801398));
#129074=CARTESIAN_POINT('Ctrl Pts',(-217.188954316669,0.285039464259041,
135.714343872763));
#129075=CARTESIAN_POINT('Ctrl Pts',(-217.196705507909,0.421792630425546,
135.70640493546));
#129076=CARTESIAN_POINT('Ctrl Pts',(-217.204456699149,0.5583205697514,135.692742185259));
#129077=CARTESIAN_POINT('Ctrl Pts',(-217.212207890389,0.694108777748216,
135.673384756667));
#129078=CARTESIAN_POINT('Ctrl Pts',(-217.219955787166,0.829839272134179,
135.654035555499));
#129079=CARTESIAN_POINT('Ctrl Pts',(-217.227703683943,0.964830274277994,
135.628996544972));
#129080=CARTESIAN_POINT('Ctrl Pts',(-217.23545158072,1.09857233305397,135.598348716378));
#129081=CARTESIAN_POINT('Ctrl Pts',(-217.243197856804,1.23228641587475,
135.567707298648));
#129082=CARTESIAN_POINT('Ctrl Pts',(-217.250944132888,1.36475169412645,
135.53145948377));
#129083=CARTESIAN_POINT('Ctrl Pts',(-217.258690408972,1.49546923646382,
135.489737318034));
#129084=CARTESIAN_POINT('Ctrl Pts',(-217.266436742238,1.62618774372821,
135.448014844315));
#129085=CARTESIAN_POINT('Ctrl Pts',(-217.274183075503,1.75515811688103,
135.400818057981));
#129086=CARTESIAN_POINT('Ctrl Pts',(-217.281929408768,1.88189729113848,
135.348328668522));
#129087=CARTESIAN_POINT('Ctrl Pts',(-217.289677476771,2.00866484775509,
135.295827524428));
#129088=CARTESIAN_POINT('Ctrl Pts',(-217.297425544774,2.13319985006438,
135.238031568284));
#129089=CARTESIAN_POINT('Ctrl Pts',(-217.305173612777,2.25504026363577,
135.175170207548));
#129090=CARTESIAN_POINT('Ctrl Pts',(-217.312929915519,2.37701017064879,
135.112242037011));
#129091=CARTESIAN_POINT('Ctrl Pts',(-217.320686218261,2.49627942009138,
135.044237887161));
#129092=CARTESIAN_POINT('Ctrl Pts',(-217.328442521003,2.6124111213954,134.971432874596));
#129093=CARTESIAN_POINT('Ctrl Pts',(-217.336202963517,2.72860480568506,
134.898589003804));
#129094=CARTESIAN_POINT('Ctrl Pts',(-217.343963406031,2.84165728293365,
134.820939385808));
#129095=CARTESIAN_POINT('Ctrl Pts',(-217.351723848545,2.95116245332322,
134.738801268611));
#129096=CARTESIAN_POINT('Ctrl Pts',(-217.359496748811,3.06084341113371,
134.656531296017));
#129097=CARTESIAN_POINT('Ctrl Pts',(-217.367269649076,3.16696537991514,
134.569758673285));
#129098=CARTESIAN_POINT('Ctrl Pts',(-217.375042549341,3.26915635148366,
134.478840146976));
#129099=CARTESIAN_POINT('Ctrl Pts',(-217.382532885104,3.36763242383518,
134.391226738105));
#129100=CARTESIAN_POINT('Ctrl Pts',(-217.390023220866,3.46245811861199,
134.299763834334));
#129101=CARTESIAN_POINT('Ctrl Pts',(-217.397513556628,3.55333558687814,
134.204800187611));
#129102=CARTESIAN_POINT('Ctrl Pts',(-217.405287890747,3.64765870197242,
134.106235965361));
#129103=CARTESIAN_POINT('Ctrl Pts',(-217.413062224866,3.73802707368471,
134.0035880767));
#129104=CARTESIAN_POINT('Ctrl Pts',(-217.420836558985,3.82406638604163,
133.897207095755));
#129105=CARTESIAN_POINT('Ctrl Pts',(-217.428601311932,3.90999966263562,
133.790957219861));
#129106=CARTESIAN_POINT('Ctrl Pts',(-217.436366064879,3.99161425179114,
133.680983706778));
#129107=CARTESIAN_POINT('Ctrl Pts',(-217.444130817827,4.06857251928545,
133.567673976166));
#129108=CARTESIAN_POINT('Ctrl Pts',(-217.451887858712,4.14545435074356,
133.454476786376));
#129109=CARTESIAN_POINT('Ctrl Pts',(-217.459644899597,4.21768884570861,
133.337950294557));
#129110=CARTESIAN_POINT('Ctrl Pts',(-217.467401940482,4.28497876345877,
133.218514725987));
#129111=CARTESIAN_POINT('Ctrl Pts',(-217.475153131722,4.35221793735861,
133.099169224709));
#129112=CARTESIAN_POINT('Ctrl Pts',(-217.482904322962,4.41451976475138,
132.976919352466));
#129113=CARTESIAN_POINT('Ctrl Pts',(-217.490655514202,4.47163065507978,
132.852213724371));
#129114=CARTESIAN_POINT('Ctrl Pts',(-217.498403410979,4.52871727175639,
132.727561099494));
#129115=CARTESIAN_POINT('Ctrl Pts',(-217.506151307756,4.58061717705603,
132.600455149444));
#129116=CARTESIAN_POINT('Ctrl Pts',(-217.513899204533,4.62712314046767,
132.471368267653));
#129117=CARTESIAN_POINT('Ctrl Pts',(-217.521645480617,4.67361937583419,
132.342308388055));
#129118=CARTESIAN_POINT('Ctrl Pts',(-217.529391756702,4.71472378112498,
132.211268768507));
#129119=CARTESIAN_POINT('Ctrl Pts',(-217.537138032786,4.75027776604493,
132.078740548324));
#129120=CARTESIAN_POINT('Ctrl Pts',(-217.544884366051,4.78583201341638,
131.946211349848));
#129121=CARTESIAN_POINT('Ctrl Pts',(-217.552630699316,4.81583565735647,
131.812193906424));
#129122=CARTESIAN_POINT('Ctrl Pts',(-217.560377032582,4.84018046689022,
131.677192852554));
#129123=CARTESIAN_POINT('Ctrl Pts',(-217.568125100585,4.86453072827524,
131.542161566134));
#129124=CARTESIAN_POINT('Ctrl Pts',(-217.575873168588,4.8832195641892,131.406146615636));
#129125=CARTESIAN_POINT('Ctrl Pts',(-217.583621236591,4.89619024072895,
131.269660724046));
#129126=CARTESIAN_POINT('Ctrl Pts',(-217.591377539332,4.9091747026581,131.133029773627));
#129127=CARTESIAN_POINT('Ctrl Pts',(-217.599133842074,4.91642882804909,
130.995927272103));
#129128=CARTESIAN_POINT('Ctrl Pts',(-217.606890144816,4.91794793026193,
130.858869495122));
#129129=CARTESIAN_POINT('Ctrl Pts',(-217.61465058733,4.91946784326536,130.721738566278));
#129130=CARTESIAN_POINT('Ctrl Pts',(-217.622411029845,4.91524664590671,
130.584652800132));
#129131=CARTESIAN_POINT('Ctrl Pts',(-217.630171472359,4.9053317410446,130.448125340256));
#129132=CARTESIAN_POINT('Ctrl Pts',(-217.637944372624,4.895400919897,130.31137871438));
#129133=CARTESIAN_POINT('Ctrl Pts',(-217.64571727289,4.87975817116386,130.175192574388));
#129134=CARTESIAN_POINT('Ctrl Pts',(-217.653490173155,4.85850255631906,
130.04007273153));
#129135=CARTESIAN_POINT('Ctrl Pts',(-217.660980508917,4.83801963661359,
129.909864835307));
#129136=CARTESIAN_POINT('Ctrl Pts',(-217.668470844679,4.81232490958092,
129.780647359098));
#129137=CARTESIAN_POINT('Ctrl Pts',(-217.675961180441,4.7815507954863,129.652859400596));
#129138=CARTESIAN_POINT('Ctrl Pts',(-217.68373551456,4.74960987150215,129.520226322806));
#129139=CARTESIAN_POINT('Ctrl Pts',(-217.691509848679,4.71209560791352,
129.388713161184));
#129140=CARTESIAN_POINT('Ctrl Pts',(-217.699284182798,4.66910062573446,
129.258824332238));
#129141=CARTESIAN_POINT('Ctrl Pts',(-217.707048935745,4.62615863102837,
129.129095579664));
#129142=CARTESIAN_POINT('Ctrl Pts',(-217.714813688693,4.57774947884485,
129.000987544288));
#129143=CARTESIAN_POINT('Ctrl Pts',(-217.72257844164,4.52401661677361,128.874993697134));
#129144=CARTESIAN_POINT('Ctrl Pts',(-217.730335482525,4.47033712293848,
128.749124988845));
#129145=CARTESIAN_POINT('Ctrl Pts',(-217.73809252341,4.41134459412404,128.625366647298));
#129146=CARTESIAN_POINT('Ctrl Pts',(-217.745849564295,4.34723191188681,
128.504195891558));
#129147=CARTESIAN_POINT('Ctrl Pts',(-217.753600755535,4.28316757752189,
128.383116511626));
#129148=CARTESIAN_POINT('Ctrl Pts',(-217.761351946775,4.21399095722072,
128.264621177695));
#129149=CARTESIAN_POINT('Ctrl Pts',(-217.769103138015,4.13994241169063,
128.149165730108));
#129150=CARTESIAN_POINT('Ctrl Pts',(-217.776851034792,4.06592533876761,
128.033759354165));
#129151=CARTESIAN_POINT('Ctrl Pts',(-217.784598931569,3.98704066970332,
127.921390623217));
#129152=CARTESIAN_POINT('Ctrl Pts',(-217.792346828346,3.90357382931725,
127.812489226351));
#129153=CARTESIAN_POINT('Ctrl Pts',(-217.80009310443,3.82012444839508,127.70361060931));
#129154=CARTESIAN_POINT('Ctrl Pts',(-217.807839380515,3.7320950403246,127.598198193815));
#129155=CARTESIAN_POINT('Ctrl Pts',(-217.815585656599,3.63981309259449,
127.49665087917));
#129156=CARTESIAN_POINT('Ctrl Pts',(-217.823331989864,3.54753046365987,
127.395102814926));
#129157=CARTESIAN_POINT('Ctrl Pts',(-217.831078323129,3.45099549536551,
127.297420197803));
#129158=CARTESIAN_POINT('Ctrl Pts',(-217.838824656395,3.35057424952384,
127.203966852861));
#129159=CARTESIAN_POINT('Ctrl Pts',(-217.846572724398,3.25013051504058,
127.11049257969));
#129160=CARTESIAN_POINT('Ctrl Pts',(-217.854320792401,3.14579905735444,
127.021249729646));
#129161=CARTESIAN_POINT('Ctrl Pts',(-217.862068860403,3.03798057877508,
126.936563173867));
#129162=CARTESIAN_POINT('Ctrl Pts',(-217.869825163145,2.93004750943348,
126.851786612209));
#129163=CARTESIAN_POINT('Ctrl Pts',(-217.877581465887,2.81862032392208,
126.771576260081));
#129164=CARTESIAN_POINT('Ctrl Pts',(-217.885337768629,2.70413084632223,
126.696215120086));
#129165=CARTESIAN_POINT('Ctrl Pts',(-217.893098211143,2.58958026224098,
126.620813757581));
#129166=CARTESIAN_POINT('Ctrl Pts',(-217.900858653657,2.47196446443058,
126.550266965361));
#129167=CARTESIAN_POINT('Ctrl Pts',(-217.908619096172,2.35174079751491,
126.484812228694));
#129168=CARTESIAN_POINT('Ctrl Pts',(-217.916391996437,2.23132413689615,
126.419252418274));
#129169=CARTESIAN_POINT('Ctrl Pts',(-217.924164896703,2.10829159254333,
126.358801170611));
#129170=CARTESIAN_POINT('Ctrl Pts',(-217.931937796968,1.98312226293299,
126.30364854582));
#129171=CARTESIAN_POINT('Ctrl Pts',(-217.93942813273,1.86250315373684,126.250500857861));
#129172=CARTESIAN_POINT('Ctrl Pts',(-217.946918468492,1.73990020378354,
126.202273357223));
#129173=CARTESIAN_POINT('Ctrl Pts',(-217.954408804254,1.61575441478483,
126.159091978014));
#129174=CARTESIAN_POINT('Ctrl Pts',(-217.962183138373,1.48690160046274,
126.114273363688));
#129175=CARTESIAN_POINT('Ctrl Pts',(-217.969957472492,1.35597847713742,
126.07474909986));
#129176=CARTESIAN_POINT('Ctrl Pts',(-217.977731806611,1.22345948862323,
126.040713911292));
#129177=CARTESIAN_POINT('Ctrl Pts',(-217.985496559558,1.09110381791882,
126.006720668052));
#129178=CARTESIAN_POINT('Ctrl Pts',(-217.993261312505,0.957156570334292,
125.978203136469));
#129179=CARTESIAN_POINT('Ctrl Pts',(-218.001026065452,0.822110453944658,
125.955307363165));
#129180=CARTESIAN_POINT('Ctrl Pts',(-218.008783106337,0.687198467261639,
125.932434330267));
#129181=CARTESIAN_POINT('Ctrl Pts',(-218.016540147222,0.551190166702867,
125.915172008942));
#129182=CARTESIAN_POINT('Ctrl Pts',(-218.024297188107,0.414591307375536,
125.903616071035));
#129183=CARTESIAN_POINT('Ctrl Pts',(-218.032048379347,0.278095458310422,
125.892068847552));
#129184=CARTESIAN_POINT('Ctrl Pts',(-218.039799570588,0.141010324906225,
125.886219474996));
#129185=CARTESIAN_POINT('Ctrl Pts',(-218.047550761828,0.00384933938717165,
125.886112123937));
#129186=CARTESIAN_POINT('Ctrl Pts',(-218.055298658605,-0.133253349054334,
125.886004818505));
#129187=CARTESIAN_POINT('Ctrl Pts',(-218.063046555382,-0.270431435342874,
125.891634680883));
#129188=CARTESIAN_POINT('Ctrl Pts',(-218.070794452159,-0.407169130793765,
125.902993832533));
#129189=CARTESIAN_POINT('Ctrl Pts',(-218.078540728243,-0.543878223666119,
125.914350608093));
#129190=CARTESIAN_POINT('Ctrl Pts',(-218.086287004327,-0.680146719556824,
125.931434256809));
#129191=CARTESIAN_POINT('Ctrl Pts',(-218.094033280411,-0.815461998196878,
125.954184868998));
#129192=CARTESIAN_POINT('Ctrl Pts',(-218.101779613677,-0.950778275703764,
125.976935649127));
#129193=CARTESIAN_POINT('Ctrl Pts',(-218.109525946942,-1.08514093636551,
126.00535341138));
#129194=CARTESIAN_POINT('Ctrl Pts',(-218.117272280207,-1.21804601850475,
126.039326833918));
#129195=CARTESIAN_POINT('Ctrl Pts',(-218.12502034821,-1.35098086381546,
126.073307864568));
#129196=CARTESIAN_POINT('Ctrl Pts',(-218.132768416213,-1.48245710236326,
126.112846934414));
#129197=CARTESIAN_POINT('Ctrl Pts',(-218.140516484216,-1.61198482147285,
126.157782522038));
#129198=CARTESIAN_POINT('Ctrl Pts',(-218.148272786958,-1.74165020418388,
126.20276586774));
#129199=CARTESIAN_POINT('Ctrl Pts',(-218.1560290897,-1.86936256063338,126.253157060121));
#129200=CARTESIAN_POINT('Ctrl Pts',(-218.163785392442,-1.99465038125361,
126.30874576317));
#129201=CARTESIAN_POINT('Ctrl Pts',(-218.171545834956,-2.12000507175605,
126.364364135584));
#129202=CARTESIAN_POINT('Ctrl Pts',(-218.17930627747,-2.24293229768162,
126.425185372939));
#129203=CARTESIAN_POINT('Ctrl Pts',(-218.187066719984,-2.362985050008,126.490953064837));
#129204=CARTESIAN_POINT('Ctrl Pts',(-218.19483962025,-2.48323052167021,
126.556826332873));
#129205=CARTESIAN_POINT('Ctrl Pts',(-218.202612520515,-2.60059196385641,
126.627661720935));
#129206=CARTESIAN_POINT('Ctrl Pts',(-218.210385420781,-2.71465050918209,
126.703158882038));
#129207=CARTESIAN_POINT('Ctrl Pts',(-218.217875756543,-2.82456273908872,
126.775911531169));
#129208=CARTESIAN_POINT('Ctrl Pts',(-218.225366092304,-2.93140779044264,
126.852992723144));
#129209=CARTESIAN_POINT('Ctrl Pts',(-218.232856428066,-3.03484133911457,
126.934099501194));
#129210=CARTESIAN_POINT('Ctrl Pts',(-218.240535071511,-3.14087521606131,
127.017245310593));
#129211=CARTESIAN_POINT('Ctrl Pts',(-218.248213714956,-3.24367723813166,
127.104899227514));
#129212=CARTESIAN_POINT('Ctrl Pts',(-218.255892358401,-3.34283278498365,
127.196778042747));
#129213=CARTESIAN_POINT('Ctrl Pts',(-218.263562223384,-3.44187497416621,
127.288551819294));
#129214=CARTESIAN_POINT('Ctrl Pts',(-218.271232088368,-3.53727868431221,
127.384540622821));
#129215=CARTESIAN_POINT('Ctrl Pts',(-218.278901953351,-3.62865977266997,
127.484419154723));
#129216=CARTESIAN_POINT('Ctrl Pts',(-218.286564808957,-3.71995734917867,
127.584206409085));
#129217=CARTESIAN_POINT('Ctrl Pts',(-218.294227664562,-3.80723934465359,
127.687876029734));
#129218=CARTESIAN_POINT('Ctrl Pts',(-218.301890520167,-3.89015652682691,
127.795064145085));
#129219=CARTESIAN_POINT('Ctrl Pts',(-218.309548129204,-3.97301693764679,
127.902178871372));
#129220=CARTESIAN_POINT('Ctrl Pts',(-218.317205738241,-4.05151823457572,
128.012806984851));
#129221=CARTESIAN_POINT('Ctrl Pts',(-218.324863347278,-4.12535011066304,
128.126550032974));
#129222=CARTESIAN_POINT('Ctrl Pts',(-218.332518456262,-4.1991578821534,
128.240255946319));
#129223=CARTESIAN_POINT('Ctrl Pts',(-218.340173565246,-4.26829904160328,
128.357074439064));
#129224=CARTESIAN_POINT('Ctrl Pts',(-218.34782867423,-4.33250565152588,
128.476576726824));
#129225=CARTESIAN_POINT('Ctrl Pts',(-218.355482064927,-4.39669784945617,
128.596052190772));
#129226=CARTESIAN_POINT('Ctrl Pts',(-218.363135455624,-4.45595751446596,
128.718209896309));
#129227=CARTESIAN_POINT('Ctrl Pts',(-218.370788846322,-4.51006223187696,
128.842595665515));
#129228=CARTESIAN_POINT('Ctrl Pts',(-218.378445102554,-4.56418720684235,
128.967028006472));
#129229=CARTESIAN_POINT('Ctrl Pts',(-218.386101358787,-4.61315321508459,
129.093689710612));
#129230=CARTESIAN_POINT('Ctrl Pts',(-218.39375761502,-4.65678565856786,
129.222105773157));
#129231=CARTESIAN_POINT('Ctrl Pts',(-218.400838000821,-4.69713625864268,
129.3408629357));
#129232=CARTESIAN_POINT('Ctrl Pts',(-218.407918386622,-4.73292588820427,
129.461120024275));
#129233=CARTESIAN_POINT('Ctrl Pts',(-218.414998772423,-4.76405452823415,
129.582490119309));
#129234=CARTESIAN_POINT('Ctrl Pts',(-216.665311899804,-4.76405452823409,
129.582490119308));
#129235=CARTESIAN_POINT('Ctrl Pts',(-216.673124903711,-4.79842945311828,
129.71651742972));
#129236=CARTESIAN_POINT('Ctrl Pts',(-216.680937907617,-4.82716305674291,
129.852069638674));
#129237=CARTESIAN_POINT('Ctrl Pts',(-216.688750911523,-4.85013176536874,
129.988637060801));
#129238=CARTESIAN_POINT('Ctrl Pts',(-216.696562353585,-4.87309588247662,
130.125177182666));
#129239=CARTESIAN_POINT('Ctrl Pts',(-216.704373795646,-4.8902973289301,
130.262731738906));
#129240=CARTESIAN_POINT('Ctrl Pts',(-216.712185237708,-4.90166363789405,
130.400780831839));
#129241=CARTESIAN_POINT('Ctrl Pts',(-216.719837013143,-4.91279761840987,
130.536008188039));
#129242=CARTESIAN_POINT('Ctrl Pts',(-216.727488788578,-4.91833269816011,
130.67170970144));
#129243=CARTESIAN_POINT('Ctrl Pts',(-216.735140564013,-4.91824906570758,
130.807392146309));
#129244=CARTESIAN_POINT('',(-216.389859435951,-4.91824825810323,130.800221274069));
#129245=CARTESIAN_POINT('Ctrl Pts',(-216.320029411505,-4.76405452823406,
129.582490119308));
#129246=CARTESIAN_POINT('Ctrl Pts',(-216.329357889193,-4.80476169927653,
129.741206761385));
#129247=CARTESIAN_POINT('Ctrl Pts',(-216.338686366881,-4.83757175068434,
129.90210909891));
#129248=CARTESIAN_POINT('Ctrl Pts',(-216.348014844569,-4.86227946236605,
130.064481240672));
#129249=CARTESIAN_POINT('Ctrl Pts',(-216.357241090068,-4.88671639852329,
130.225073921737));
#129250=CARTESIAN_POINT('Ctrl Pts',(-216.366467335568,-4.90322755997727,
130.387104331365));
#129251=CARTESIAN_POINT('Ctrl Pts',(-216.375693581067,-4.91166082555106,
130.549859149501));
#129252=CARTESIAN_POINT('Ctrl Pts',(-216.380415532695,-4.91597693356135,
130.633156345365));
#129253=CARTESIAN_POINT('Ctrl Pts',(-216.385137484323,-4.91817791611439,
130.716642956803));
#129254=CARTESIAN_POINT('Ctrl Pts',(-216.389859435951,-4.91824825810323,
130.800221274069));
#129255=CARTESIAN_POINT('Ctrl Pts',(-216.389859435996,-4.9182482581039,
130.800221274869));
#129256=CARTESIAN_POINT('Ctrl Pts',(-216.397855279552,-4.91836737059673,
130.941747322197));
#129257=CARTESIAN_POINT('Ctrl Pts',(-216.405851123109,-4.91237278108348,
131.083370584201));
#129258=CARTESIAN_POINT('Ctrl Pts',(-216.413846966665,-4.90027025063863,
131.22452074562));
#129259=CARTESIAN_POINT('Ctrl Pts',(-216.421559449529,-4.88859661570527,
131.360668757202));
#129260=CARTESIAN_POINT('Ctrl Pts',(-216.429271932392,-4.87124062050356,
131.496376205221));
#129261=CARTESIAN_POINT('Ctrl Pts',(-216.436984415256,-4.8482604298453,
131.631133782888));
#129262=CARTESIAN_POINT('Ctrl Pts',(-216.444696531458,-4.82528133169602,
131.765884953999));
#129263=CARTESIAN_POINT('Ctrl Pts',(-216.452408647659,-4.79667863591924,
131.899685955664));
#129264=CARTESIAN_POINT('Ctrl Pts',(-216.460120763861,-4.76256195054892,
132.032035953184));
#129265=CARTESIAN_POINT('Ctrl Pts',(-216.467834218713,-4.72843934328693,
132.164408923695));
#129266=CARTESIAN_POINT('Ctrl Pts',(-216.475547673566,-4.68880094066914,
132.295330006971));
#129267=CARTESIAN_POINT('Ctrl Pts',(-216.483261128418,-4.6438065921186,
132.424312282739));
#129268=CARTESIAN_POINT('Ctrl Pts',(-216.490977627811,-4.59879448406275,
132.553345468487));
#129269=CARTESIAN_POINT('Ctrl Pts',(-216.498694127205,-4.54842235383041,
132.68043795203));
#129270=CARTESIAN_POINT('Ctrl Pts',(-216.506410626598,-4.49289850045566,
132.805122004414));
#129271=CARTESIAN_POINT('Ctrl Pts',(-216.51413612443,-4.43730989906964,
132.929951454568));
#129272=CARTESIAN_POINT('Ctrl Pts',(-216.521861622262,-4.37655774306682,
133.052366506946));
#129273=CARTESIAN_POINT('Ctrl Pts',(-216.529587120094,-4.31089685359044,
133.17192294625));
#129274=CARTESIAN_POINT('Ctrl Pts',(-216.537317978554,-4.24519040282833,
133.291562344301));
#129275=CARTESIAN_POINT('Ctrl Pts',(-216.545048837014,-4.17456863917805,
133.408338842937));
#129276=CARTESIAN_POINT('Ctrl Pts',(-216.552779695475,-4.09932953803423,
133.521837462196));
#129277=CARTESIAN_POINT('Ctrl Pts',(-216.560521712347,-4.0239818397777,
133.635499900828));
#129278=CARTESIAN_POINT('Ctrl Pts',(-216.568263729219,-3.94400373330105,
133.745874699803));
#129279=CARTESIAN_POINT('Ctrl Pts',(-216.576005746092,-3.85973344391655,
133.85257990174));
#129280=CARTESIAN_POINT('Ctrl Pts',(-216.577923724511,-3.83885663635282,
133.879014650964));
#129281=CARTESIAN_POINT('Ctrl Pts',(-216.57984170293,-3.8177165790828,133.905224363624));
#129282=CARTESIAN_POINT('Ctrl Pts',(-216.581759681349,-3.79631875262702,
133.931203592669));
#129283=CARTESIAN_POINT('Ctrl Pts',(-216.589534015468,-3.70958479845807,
134.03650780504));
#129284=CARTESIAN_POINT('Ctrl Pts',(-216.597308349587,-3.61832867105896,
134.138367271289));
#129285=CARTESIAN_POINT('Ctrl Pts',(-216.605082683706,-3.52285428078253,
134.236368889536));
#129286=CARTESIAN_POINT('Ctrl Pts',(-216.612847436653,-3.42749755415933,
134.334249729547));
#129287=CARTESIAN_POINT('Ctrl Pts',(-216.6206121896,-3.32793317858773,134.428281904148));
#129288=CARTESIAN_POINT('Ctrl Pts',(-216.628376942547,-3.22450598449832,
134.518084384681));
#129289=CARTESIAN_POINT('Ctrl Pts',(-216.636133983432,-3.12118151575588,
134.607797672124));
#129290=CARTESIAN_POINT('Ctrl Pts',(-216.643891024317,-3.01400215681808,
134.693289370998));
#129291=CARTESIAN_POINT('Ctrl Pts',(-216.651648065202,-2.9033500849385,
134.774214688787));
#129292=CARTESIAN_POINT('Ctrl Pts',(-216.659399256443,-2.79278145664752,
134.855078980164));
#129293=CARTESIAN_POINT('Ctrl Pts',(-216.667150447682,-2.67874564227477,
134.93138351476));
#129294=CARTESIAN_POINT('Ctrl Pts',(-216.674901638923,-2.56165816566304,
135.002823491618));
#129295=CARTESIAN_POINT('Ctrl Pts',(-216.6826495357,-2.44462045435212,135.07423310458));
#129296=CARTESIAN_POINT('Ctrl Pts',(-216.690397432477,-2.32453399356024,
135.140782068828));
#129297=CARTESIAN_POINT('Ctrl Pts',(-216.698145329254,-2.20184339454529,
135.202208810535));
#129298=CARTESIAN_POINT('Ctrl Pts',(-216.705891605338,-2.07917845975876,
135.263622703091));
#129299=CARTESIAN_POINT('Ctrl Pts',(-216.713637881422,-1.95391081962171,
135.319916329375));
#129300=CARTESIAN_POINT('Ctrl Pts',(-216.721384157506,-1.82650944490343,
135.370874201273));
#129301=CARTESIAN_POINT('Ctrl Pts',(-216.729130490772,-1.69910712973698,
135.42183244933));
#129302=CARTESIAN_POINT('Ctrl Pts',(-216.736876824037,-1.56957141156456,
135.467454719211));
#129303=CARTESIAN_POINT('Ctrl Pts',(-216.744623157302,-1.43839060975884,
135.507573935741));
#129304=CARTESIAN_POINT('Ctrl Pts',(-216.752371225305,-1.30718043092263,
135.547702136691));
#129305=CARTESIAN_POINT('Ctrl Pts',(-216.760119293308,-1.17432480916949,
135.582324717695));
#129306=CARTESIAN_POINT('Ctrl Pts',(-216.767867361311,-1.04032617799798,
135.611324784883));
#129307=CARTESIAN_POINT('Ctrl Pts',(-216.775623664053,-0.906185131486111,
135.640355673688));
#129308=CARTESIAN_POINT('Ctrl Pts',(-216.783379966795,-0.770899031582092,
135.663752028793));
#129309=CARTESIAN_POINT('Ctrl Pts',(-216.791136269537,-0.634979986816272,
135.681448219695));
#129310=CARTESIAN_POINT('Ctrl Pts',(-216.798896712051,-0.498988397963817,
135.699153855587));
#129311=CARTESIAN_POINT('Ctrl Pts',(-216.806657154565,-0.362363580386605,
135.711153230949));
#129312=CARTESIAN_POINT('Ctrl Pts',(-216.814417597079,-0.225620684686972,
135.717432810109));
#129313=CARTESIAN_POINT('Ctrl Pts',(-216.822190497345,-0.0886582771516972,
135.723722469808));
#129314=CARTESIAN_POINT('Ctrl Pts',(-216.82996339761,0.0484221960992154,
135.72427398332));
#129315=CARTESIAN_POINT('Ctrl Pts',(-216.837736297876,0.185106764130735,
135.719125978026));
#129316=CARTESIAN_POINT('Ctrl Pts',(-216.845226633638,0.316822503827401,
135.714165115691));
#129317=CARTESIAN_POINT('Ctrl Pts',(-216.8527169694,0.448170315786501,135.703911947942));
#129318=CARTESIAN_POINT('Ctrl Pts',(-216.860207305162,0.578698535716503,
135.688446106914));
#129319=CARTESIAN_POINT('Ctrl Pts',(-216.867981639281,0.714175772777397,
135.672393873823));
#129320=CARTESIAN_POINT('Ctrl Pts',(-216.8757559734,0.849199192456625,135.650675038898));
#129321=CARTESIAN_POINT('Ctrl Pts',(-216.883530307519,0.983256969473938,
135.623321998868));
#129322=CARTESIAN_POINT('Ctrl Pts',(-216.891295060466,1.11714953226253,
135.596002669015));
#129323=CARTESIAN_POINT('Ctrl Pts',(-216.899059813413,1.25007844087534,
135.563063027272));
#129324=CARTESIAN_POINT('Ctrl Pts',(-216.906824566361,1.38153673584142,
135.52458723395));
#129325=CARTESIAN_POINT('Ctrl Pts',(-216.914581607246,1.51286446457534,
135.486149655328));
#129326=CARTESIAN_POINT('Ctrl Pts',(-216.922338648131,1.6427241135948,135.442186976668));
#129327=CARTESIAN_POINT('Ctrl Pts',(-216.930095689016,1.77061902305256,
135.392834365742));
#129328=CARTESIAN_POINT('Ctrl Pts',(-216.937846880256,1.89841748596474,
135.343518972004));
#129329=CARTESIAN_POINT('Ctrl Pts',(-216.945598071496,2.02425379512616,
135.288821876501));
#129330=CARTESIAN_POINT('Ctrl Pts',(-216.953349262736,2.14764691207149,
135.228927918848));
#129331=CARTESIAN_POINT('Ctrl Pts',(-216.961097159513,2.27098758365,135.169059417724));
#129332=CARTESIAN_POINT('Ctrl Pts',(-216.96884505629,2.3918867773697,135.103998617959));
#129333=CARTESIAN_POINT('Ctrl Pts',(-216.976592953067,2.50988410051506,
135.033978196554));
#129334=CARTESIAN_POINT('Ctrl Pts',(-216.984339229152,2.62785674116447,
134.96397242191));
#129335=CARTESIAN_POINT('Ctrl Pts',(-216.992085505236,2.74292838260234,
134.889009288554));
#129336=CARTESIAN_POINT('Ctrl Pts',(-216.99983178132,2.8546642384186,134.809366878284));
#129337=CARTESIAN_POINT('Ctrl Pts',(-217.007578114585,2.9664009190431,134.729723880113));
#129338=CARTESIAN_POINT('Ctrl Pts',(-217.01532444785,3.07480144654163,134.645401763029));
#129339=CARTESIAN_POINT('Ctrl Pts',(-217.023070781116,3.17946130728828,
134.556721055738));
#129340=CARTESIAN_POINT('Ctrl Pts',(-217.030818849119,3.28414460588493,
134.468020489017));
#129341=CARTESIAN_POINT('Ctrl Pts',(-217.038566917121,3.38508527258254,
134.374959642505));
#129342=CARTESIAN_POINT('Ctrl Pts',(-217.046314985124,3.4819133836792,134.277898043743));
#129343=CARTESIAN_POINT('Ctrl Pts',(-217.054071287866,3.57884440484499,
134.180733286759));
#129344=CARTESIAN_POINT('Ctrl Pts',(-217.061827590608,3.67165386255878,
134.07955956083));
#129345=CARTESIAN_POINT('Ctrl Pts',(-217.06958389335,3.76000973284992,133.974772242477));
#129346=CARTESIAN_POINT('Ctrl Pts',(-217.077344335864,3.84841276132963,
133.869928995977));
#129347=CARTESIAN_POINT('Ctrl Pts',(-217.085104778378,3.93235722680857,
133.761468623017));
#129348=CARTESIAN_POINT('Ctrl Pts',(-217.092865220893,4.01155328985978,
133.649817218028));
#129349=CARTESIAN_POINT('Ctrl Pts',(-217.100638121158,4.09087648546188,
133.537986580292));
#129350=CARTESIAN_POINT('Ctrl Pts',(-217.108411021424,4.16543583356797,
133.42295500235));
#129351=CARTESIAN_POINT('Ctrl Pts',(-217.116183921689,4.23498601864203,
133.305175781549));
#129352=CARTESIAN_POINT('Ctrl Pts',(-217.123674257451,4.30200787930193,
133.191678132092));
#129353=CARTESIAN_POINT('Ctrl Pts',(-217.131164593213,4.36437829960137,
133.075629410313));
#129354=CARTESIAN_POINT('Ctrl Pts',(-217.138654928975,4.42192014073003,
132.957452657286));
#129355=CARTESIAN_POINT('Ctrl Pts',(-217.146429263094,4.48164369825481,
132.834795196749));
#129356=CARTESIAN_POINT('Ctrl Pts',(-217.154203597213,4.53635448378965,
132.709456608922));
#129357=CARTESIAN_POINT('Ctrl Pts',(-217.161977931332,4.58580309955537,
132.581885018132));
#129358=CARTESIAN_POINT('Ctrl Pts',(-217.169742684279,4.63519077432152,
132.454470647927));
#129359=CARTESIAN_POINT('Ctrl Pts',(-217.177507437226,4.67932904289815,
132.324829111412));
#129360=CARTESIAN_POINT('Ctrl Pts',(-217.185272190173,4.7180146877614,132.19343241865));
#129361=CARTESIAN_POINT('Ctrl Pts',(-217.193029231058,4.75666190949679,
132.062166230937));
#129362=CARTESIAN_POINT('Ctrl Pts',(-217.200786271943,4.78986717514584,
131.929148728737));
#129363=CARTESIAN_POINT('Ctrl Pts',(-217.208543312828,4.81747574840408,
131.794870827528));
#129364=CARTESIAN_POINT('Ctrl Pts',(-217.216294504068,4.8450635018225,131.660694186329));
#129365=CARTESIAN_POINT('Ctrl Pts',(-217.224045695308,4.86706288509805,
131.525259419392));
#129366=CARTESIAN_POINT('Ctrl Pts',(-217.231796886549,4.88336939599244,
131.389071148328));
#129367=CARTESIAN_POINT('Ctrl Pts',(-217.239544783326,4.89966897618474,
131.252940760913));
#129368=CARTESIAN_POINT('Ctrl Pts',(-217.247292680103,4.91028045005785,
131.116057893722));
#129369=CARTESIAN_POINT('Ctrl Pts',(-217.25504057688,4.91515072185277,130.978935655788));
#129370=CARTESIAN_POINT('Ctrl Pts',(-217.262786852964,4.92001997489181,
130.84184210087));
#129371=CARTESIAN_POINT('Ctrl Pts',(-217.270533129048,4.91915040071098,
130.704509665275));
#129372=CARTESIAN_POINT('Ctrl Pts',(-217.278279405132,4.91254094472982,
130.567454457129));
#129373=CARTESIAN_POINT('Ctrl Pts',(-217.286025738397,4.90593143995914,
130.430398237272));
#129374=CARTESIAN_POINT('Ctrl Pts',(-217.293772071663,4.89358198767317,
130.293619639459));
#129375=CARTESIAN_POINT('Ctrl Pts',(-217.301518404928,4.87554360825335,
130.157632246053));
#129376=CARTESIAN_POINT('Ctrl Pts',(-217.309266472931,4.85750118926352,
130.021614399213));
#129377=CARTESIAN_POINT('Ctrl Pts',(-217.317014540934,4.83376735943609,
129.886388496855));
#129378=CARTESIAN_POINT('Ctrl Pts',(-217.324762608937,4.8044446466761,129.752460099682));
#129379=CARTESIAN_POINT('Ctrl Pts',(-217.332518911679,4.77509076938816,
129.618389361815));
#129380=CARTESIAN_POINT('Ctrl Pts',(-217.340275214421,4.74013622726691,
129.48561926637));
#129381=CARTESIAN_POINT('Ctrl Pts',(-217.348031517162,4.69973419471019,
129.354642865184));
#129382=CARTESIAN_POINT('Ctrl Pts',(-217.355791959677,4.6593105983721,129.223596557949));
#129383=CARTESIAN_POINT('Ctrl Pts',(-217.363552402191,4.61343384889255,
129.094346220834));
#129384=CARTESIAN_POINT('Ctrl Pts',(-217.371312844705,4.56230576629388,
128.967366018406));
#129385=CARTESIAN_POINT('Ctrl Pts',(-217.37908574497,4.51109560835809,128.840181976085));
#129386=CARTESIAN_POINT('Ctrl Pts',(-217.386858645236,4.45461743283658,
128.715275707213));
#129387=CARTESIAN_POINT('Ctrl Pts',(-217.394631545501,4.39312001258564,
128.593098620986));
#129388=CARTESIAN_POINT('Ctrl Pts',(-217.402121881263,4.33385817846364,
128.475362979589));
#129389=CARTESIAN_POINT('Ctrl Pts',(-217.409612217025,4.26993583781402,
128.360161809799));
#129390=CARTESIAN_POINT('Ctrl Pts',(-217.417102552787,4.20161315922065,
128.247872807549));
#129391=CARTESIAN_POINT('Ctrl Pts',(-217.424876886906,4.13070000550227,
128.13132633365));
#129392=CARTESIAN_POINT('Ctrl Pts',(-217.432651221026,4.05482161775692,
128.017548032004));
#129393=CARTESIAN_POINT('Ctrl Pts',(-217.440425555145,3.97422021008183,
127.906989950172));
#129394=CARTESIAN_POINT('Ctrl Pts',(-217.448190308092,3.8937181364377,127.796568121294));
#129395=CARTESIAN_POINT('Ctrl Pts',(-217.455955061039,3.80850485243069,
127.689358928722));
#129396=CARTESIAN_POINT('Ctrl Pts',(-217.463719813986,3.71886762946074,
127.585788478084));
#129397=CARTESIAN_POINT('Ctrl Pts',(-217.471476854871,3.62931943544432,
127.482320895078));
#129398=CARTESIAN_POINT('Ctrl Pts',(-217.479233895756,3.53535630075866,
127.382485155592));
#129399=CARTESIAN_POINT('Ctrl Pts',(-217.486990936641,3.43730760774658,
127.286676795471));
#129400=CARTESIAN_POINT('Ctrl Pts',(-217.494742127881,3.33933285401701,
127.19094068518));
#129401=CARTESIAN_POINT('Ctrl Pts',(-217.502493319121,3.23727895290669,
127.099226181268));
#129402=CARTESIAN_POINT('Ctrl Pts',(-217.510244510361,3.13151397085618,
127.011893964735));
#129403=CARTESIAN_POINT('Ctrl Pts',(-217.517992407138,3.02579394174426,
126.924598866724));
#129404=CARTESIAN_POINT('Ctrl Pts',(-217.525740303916,2.91636626968072,
126.841682599956));
#129405=CARTESIAN_POINT('Ctrl Pts',(-217.533488200693,2.80363394827169,
126.763467183361));
#129406=CARTESIAN_POINT('Ctrl Pts',(-217.541234476777,2.69092520803408,
126.685268127746));
#129407=CARTESIAN_POINT('Ctrl Pts',(-217.548980752861,2.57491351442602,
126.611768189162));
#129408=CARTESIAN_POINT('Ctrl Pts',(-217.556727028945,2.45603251380457,
126.543247223905));
#129409=CARTESIAN_POINT('Ctrl Pts',(-217.56447336221,2.33715063563075,126.474725752843));
#129410=CARTESIAN_POINT('Ctrl Pts',(-217.572219695476,2.21539974690685,
126.411183523685));
#129411=CARTESIAN_POINT('Ctrl Pts',(-217.579966028741,2.09123951678367,
126.352855215352));
#129412=CARTESIAN_POINT('Ctrl Pts',(-217.587714096744,1.96705148183798,
126.294513844799));
#129413=CARTESIAN_POINT('Ctrl Pts',(-217.595462164747,1.8404533856351,126.241388884708));
#129414=CARTESIAN_POINT('Ctrl Pts',(-217.60321023275,1.71192598955102,126.193667343361));
#129415=CARTESIAN_POINT('Ctrl Pts',(-217.610966535492,1.58326199302071,
126.145895082991));
#129416=CARTESIAN_POINT('Ctrl Pts',(-217.618722838234,1.45266496764989,
126.103537849564));
#129417=CARTESIAN_POINT('Ctrl Pts',(-217.626479140976,1.32063252641623,
126.066733279681));
#129418=CARTESIAN_POINT('Ctrl Pts',(-217.63423958349,1.18852961549327,126.029909066092));
#129419=CARTESIAN_POINT('Ctrl Pts',(-217.642000026004,1.05499014262379,
125.9986435104));
#129420=CARTESIAN_POINT('Ctrl Pts',(-217.649760468518,0.920522124538358,
125.973023113237));
#129421=CARTESIAN_POINT('Ctrl Pts',(-217.657533368783,0.785838246452424,
125.947361587938));
#129422=CARTESIAN_POINT('Ctrl Pts',(-217.665306269049,0.650223231495372,
125.927363387218));
#129423=CARTESIAN_POINT('Ctrl Pts',(-217.673079169314,0.514191330814086,
125.913063209126));
#129424=CARTESIAN_POINT('Ctrl Pts',(-217.680569505077,0.383104532364767,
125.899282878527));
#129425=CARTESIAN_POINT('Ctrl Pts',(-217.688059840839,0.251630939041171,
125.890793507873));
#129426=CARTESIAN_POINT('Ctrl Pts',(-217.695550176601,0.120228944602715,
125.887580363845));
#129427=CARTESIAN_POINT('Ctrl Pts',(-217.70332451072,-0.0161551963919251,
125.884245392485));
#129428=CARTESIAN_POINT('Ctrl Pts',(-217.711098844839,-0.15289422594497,
125.886584077853));
#129429=CARTESIAN_POINT('Ctrl Pts',(-217.718873178958,-0.28947690100534,
125.894636981119));
#129430=CARTESIAN_POINT('Ctrl Pts',(-217.726637931905,-0.425891250125812,
125.902679959902));
#129431=CARTESIAN_POINT('Ctrl Pts',(-217.734402684852,-0.562149241614417,
125.916423121787));
#129432=CARTESIAN_POINT('Ctrl Pts',(-217.742167437799,-0.697737103529993,
125.935855097711));
#129433=CARTESIAN_POINT('Ctrl Pts',(-217.749924478684,-0.833190297669292,
125.955267773522));
#129434=CARTESIAN_POINT('Ctrl Pts',(-217.757681519569,-0.967974302267498,
125.980357964092));
#129435=CARTESIAN_POINT('Ctrl Pts',(-217.765438560454,-1.10157830261635,
126.011062347512));
#129436=CARTESIAN_POINT('Ctrl Pts',(-217.773189751695,-1.23508155114943,
126.041743576517));
#129437=CARTESIAN_POINT('Ctrl Pts',(-217.780940942935,-1.3674061871357,
126.078030484222));
#129438=CARTESIAN_POINT('Ctrl Pts',(-217.788692134175,-1.49804981053356,
126.119808362797));
#129439=CARTESIAN_POINT('Ctrl Pts',(-217.796440030952,-1.62863790690626,
126.161568484659));
#129440=CARTESIAN_POINT('Ctrl Pts',(-217.804187927729,-1.75754604011895,
126.208814816788));
#129441=CARTESIAN_POINT('Ctrl Pts',(-217.811935824506,-1.88428545863704,
126.261382368348));
#129442=CARTESIAN_POINT('Ctrl Pts',(-217.81968210059,-2.01099836600097,
126.313938923909));
#129443=CARTESIAN_POINT('Ctrl Pts',(-217.827428376674,-2.13554310009676,
126.371814335222));
#129444=CARTESIAN_POINT('Ctrl Pts',(-217.835174652758,-2.2574498134471,
126.434795032491));
#129445=CARTESIAN_POINT('Ctrl Pts',(-217.842920986024,-2.37935742668561,
126.49777619467));
#129446=CARTESIAN_POINT('Ctrl Pts',(-217.850667319289,-2.49862663297239,
126.565862538553));
#129447=CARTESIAN_POINT('Ctrl Pts',(-217.858413652554,-2.61481152788086,
126.638794181154));
#129448=CARTESIAN_POINT('Ctrl Pts',(-217.866161720557,-2.73102244159018,
126.711742156291));
#129449=CARTESIAN_POINT('Ctrl Pts',(-217.87390978856,-2.84414733841905,
126.789537381492));
#129450=CARTESIAN_POINT('Ctrl Pts',(-217.881657856563,-2.95376901973853,
126.871876461141));
#129451=CARTESIAN_POINT('Ctrl Pts',(-217.889414159305,-3.06350720828588,
126.954303051744));
#129452=CARTESIAN_POINT('Ctrl Pts',(-217.897170462047,-3.16973443061021,
127.041282908588));
#129453=CARTESIAN_POINT('Ctrl Pts',(-217.904926764788,-3.27206591717074,
127.132471771728));
#129454=CARTESIAN_POINT('Ctrl Pts',(-217.912687207303,-3.37445202112679,
127.22370930511));
#129455=CARTESIAN_POINT('Ctrl Pts',(-217.920447649817,-3.47293796558554,
127.319160049115));
#129456=CARTESIAN_POINT('Ctrl Pts',(-217.928208092331,-3.56717637966557,
127.418443350583));
#129457=CARTESIAN_POINT('Ctrl Pts',(-217.935980992596,-3.66156607361398,
127.51788603042));
#129458=CARTESIAN_POINT('Ctrl Pts',(-217.943753892862,-3.75169435442291,
127.621173267348));
#129459=CARTESIAN_POINT('Ctrl Pts',(-217.951526793127,-3.83725406433632,
127.727891162454));
#129460=CARTESIAN_POINT('Ctrl Pts',(-217.959017128889,-3.91970346328225,
127.830729593267));
#129461=CARTESIAN_POINT('Ctrl Pts',(-217.966507464651,-3.99791049985563,
127.936753338652));
#129462=CARTESIAN_POINT('Ctrl Pts',(-217.973997800413,-4.07163979659263,
128.045568775237));
#129463=CARTESIAN_POINT('Ctrl Pts',(-217.982003133925,-4.15043834831716,
128.161865813017));
#129464=CARTESIAN_POINT('Ctrl Pts',(-217.990008467437,-4.2243696337197,
128.281717260381));
#129465=CARTESIAN_POINT('Ctrl Pts',(-217.998013800949,-4.29310342630013,
128.404684382406));
#129466=CARTESIAN_POINT('Ctrl Pts',(-218.005901336472,-4.3608258053641,
128.525842050819));
#129467=CARTESIAN_POINT('Ctrl Pts',(-218.013788871995,-4.42350238015926,
128.650024005891));
#129468=CARTESIAN_POINT('Ctrl Pts',(-218.021676407519,-4.48085866676351,
128.776778641174));
#129469=CARTESIAN_POINT('Ctrl Pts',(-218.029740640025,-4.53949985189756,
128.90637284042));
#129470=CARTESIAN_POINT('Ctrl Pts',(-218.037804872531,-4.59257930400782,
129.038656048285));
#129471=CARTESIAN_POINT('Ctrl Pts',(-218.045869105037,-4.63985180547736,
129.173116219657));
#129472=CARTESIAN_POINT('Ctrl Pts',(-218.053933337543,-4.68712430694703,
129.30757639103));
#129473=CARTESIAN_POINT('Ctrl Pts',(-218.06199757005,-4.72858966366545,
129.44421315061));
#129474=CARTESIAN_POINT('Ctrl Pts',(-218.070061802556,-4.76405452823401,
129.582490119308));
#129475=CARTESIAN_POINT('Origin',(213.235140564004,0.,130.804360617566));
#129476=CARTESIAN_POINT('',(-220.165126569317,-4.76405452823396,129.582490119308));
#129477=CARTESIAN_POINT('',(-219.819723804473,-4.76405452823394,129.582490119308));
#129478=CARTESIAN_POINT('',(213.235140564004,-4.76405452823405,129.582490119308));
#129479=CARTESIAN_POINT('',(-218.485140563976,-4.91824927387013,130.807033177378));
#129480=CARTESIAN_POINT('Ctrl Pts',(-218.485140564013,-4.91824927386977,
130.807033178037));
#129481=CARTESIAN_POINT('Ctrl Pts',(-218.493861726635,-4.91816600161387,
130.960277123876));
#129482=CARTESIAN_POINT('Ctrl Pts',(-218.502582889257,-4.91092116974832,
131.113322683078));
#129483=CARTESIAN_POINT('Ctrl Pts',(-218.511304051879,-4.89656616260664,
131.265687917556));
#129484=CARTESIAN_POINT('Ctrl Pts',(-218.519078385998,-4.88376963230029,
131.401511349852));
#129485=CARTESIAN_POINT('Ctrl Pts',(-218.526852720118,-4.86529724163473,
131.537017078275));
#129486=CARTESIAN_POINT('Ctrl Pts',(-218.534627054237,-4.84116909561546,
131.671692647505));
#129487=CARTESIAN_POINT('Ctrl Pts',(-218.542391807184,-4.81707068537976,
131.806202241132));
#129488=CARTESIAN_POINT('Ctrl Pts',(-218.550156560131,-4.78733045672144,
131.93988333008));
#129489=CARTESIAN_POINT('Ctrl Pts',(-218.557921313078,-4.75202038008617,
132.072227081254));
#129490=CARTESIAN_POINT('Ctrl Pts',(-218.565678353963,-4.71674537391679,
132.20443938675));
#129491=CARTESIAN_POINT('Ctrl Pts',(-218.573435394848,-4.67591162893664,
132.335316622468));
#129492=CARTESIAN_POINT('Ctrl Pts',(-218.581192435733,-4.62964235552562,
132.464359027934));
#129493=CARTESIAN_POINT('Ctrl Pts',(-218.588943626973,-4.58340797413354,
132.593304121518));
#129494=CARTESIAN_POINT('Ctrl Pts',(-218.596694818213,-4.53174635449418,
132.720416772406));
#129495=CARTESIAN_POINT('Ctrl Pts',(-218.604446009453,-4.47483073939558,
132.84521164502));
#129496=CARTESIAN_POINT('Ctrl Pts',(-218.612193906231,-4.41793931495175,
132.969953476484));
#129497=CARTESIAN_POINT('Ctrl Pts',(-218.619941803008,-4.35579849838412,
133.092379134025));
#129498=CARTESIAN_POINT('Ctrl Pts',(-218.627689699785,-4.28862985153125,
133.212022773903));
#129499=CARTESIAN_POINT('Ctrl Pts',(-218.635435975869,-4.22147525491131,
133.33164138691));
#129500=CARTESIAN_POINT('Ctrl Pts',(-218.643182251953,-4.14929511119276,
133.448478799062));
#129501=CARTESIAN_POINT('Ctrl Pts',(-218.650928528037,-4.07235698842037,
133.562093675961));
#129502=CARTESIAN_POINT('Ctrl Pts',(-218.658674861302,-3.99541829770834,
133.675709391538));
#129503=CARTESIAN_POINT('Ctrl Pts',(-218.666421194567,-3.91372177707821,
133.786102200672));
#129504=CARTESIAN_POINT('Ctrl Pts',(-218.674167527833,-3.82757815571865,
133.89286001442));
#129505=CARTESIAN_POINT('Ctrl Pts',(-218.681915595836,-3.74141524309224,
133.99964173584));
#129506=CARTESIAN_POINT('Ctrl Pts',(-218.689663663839,-3.65080349348223,
134.102786537839));
#129507=CARTESIAN_POINT('Ctrl Pts',(-218.697411731842,-3.55609345374474,
134.201915975575));
#129508=CARTESIAN_POINT('Ctrl Pts',(-218.705168034584,-3.46128275505009,
134.301150769256));
#129509=CARTESIAN_POINT('Ctrl Pts',(-218.712924337325,-3.3623653357367,
134.396361390595));
#129510=CARTESIAN_POINT('Ctrl Pts',(-218.720680640067,-3.25972849080631,
134.487206423288));
#129511=CARTESIAN_POINT('Ctrl Pts',(-218.728441082581,-3.15703686550117,
134.578099942711));
#129512=CARTESIAN_POINT('Ctrl Pts',(-218.736201525096,-3.0506221621607,
134.664622984151));
#129513=CARTESIAN_POINT('Ctrl Pts',(-218.74396196761,-2.94090339716407,
134.746475566556));
#129514=CARTESIAN_POINT('Ctrl Pts',(-218.751734867875,-2.83100850186549,
134.828459545992));
#129515=CARTESIAN_POINT('Ctrl Pts',(-218.759507768141,-2.71779926894801,
134.905757863542));
#129516=CARTESIAN_POINT('Ctrl Pts',(-218.767280668406,-2.60172297832326,
134.978114396428));
#129517=CARTESIAN_POINT('Ctrl Pts',(-218.774771004168,-2.4898663532403,
135.047840587089));
#129518=CARTESIAN_POINT('Ctrl Pts',(-218.78226133993,-2.37534776873736,
135.112977895591));
#129519=CARTESIAN_POINT('Ctrl Pts',(-218.789751675692,-2.25858589322123,
135.173339082315));
#129520=CARTESIAN_POINT('Ctrl Pts',(-218.797526009811,-2.13739695570709,
135.23598888178));
#129521=CARTESIAN_POINT('Ctrl Pts',(-218.80530034393,-2.01340737029519,
135.293691692472));
#129522=CARTESIAN_POINT('Ctrl Pts',(-218.813074678049,-1.88705914740581,
135.346187434684));
#129523=CARTESIAN_POINT('Ctrl Pts',(-218.820839430997,-1.76086663740907,
135.398618480585));
#129524=CARTESIAN_POINT('Ctrl Pts',(-218.828604183944,-1.63232163119647,
135.445855077847));
#129525=CARTESIAN_POINT('Ctrl Pts',(-218.836368936891,-1.50189112624523,
135.487682740526));
#129526=CARTESIAN_POINT('Ctrl Pts',(-218.844125977776,-1.37159016671026,
135.529468859381));
#129527=CARTESIAN_POINT('Ctrl Pts',(-218.851883018661,-1.23940780508304,
135.565856616018));
#129528=CARTESIAN_POINT('Ctrl Pts',(-218.859640059546,-1.10583110222529,
135.596679538073));
#129529=CARTESIAN_POINT('Ctrl Pts',(-218.867391250786,-0.972355130598418,
135.627479216324));
#129530=CARTESIAN_POINT('Ctrl Pts',(-218.875142442026,-0.837487290068465,
135.652722325292));
#129531=CARTESIAN_POINT('Ctrl Pts',(-218.882893633266,-0.701729549162282,
135.672292283308));
#129532=CARTESIAN_POINT('Ctrl Pts',(-218.890641530043,-0.566029508917255,
135.691853923569));
#129533=CARTESIAN_POINT('Ctrl Pts',(-218.89838942682,-0.42944070672453,
135.705747152985));
#129534=CARTESIAN_POINT('Ctrl Pts',(-218.906137323597,-0.29247482970181,
135.713906577886));
#129535=CARTESIAN_POINT('Ctrl Pts',(-218.913883599681,-0.155537602987922,
135.72206429601));
#129536=CARTESIAN_POINT('Ctrl Pts',(-218.921629875765,-0.0182238483586181,
135.724490572033));
#129537=CARTESIAN_POINT('Ctrl Pts',(-218.929376151849,0.118950499993249,
135.721171966505));
#129538=CARTESIAN_POINT('Ctrl Pts',(-218.937122485115,0.256125860934807,
135.717853336479));
#129539=CARTESIAN_POINT('Ctrl Pts',(-218.94486881838,0.393161422694661,
135.708789749738));
#129540=CARTESIAN_POINT('Ctrl Pts',(-218.952615151645,0.529542526459238,
135.69401988741));
#129541=CARTESIAN_POINT('Ctrl Pts',(-218.960363219648,0.665954171826218,
135.679246717473));
#129542=CARTESIAN_POINT('Ctrl Pts',(-218.968111287651,0.801710678939786,
135.658764771201));
#129543=CARTESIAN_POINT('Ctrl Pts',(-218.975859355654,0.936304172297377,
135.632664414909));
#129544=CARTESIAN_POINT('Ctrl Pts',(-218.983615658396,1.07104071322157,
135.606536318848));
#129545=CARTESIAN_POINT('Ctrl Pts',(-218.991371961138,1.20461138678995,
135.574777958975));
#129546=CARTESIAN_POINT('Ctrl Pts',(-218.99912826388,1.33651960738935,135.537530633693));
#129547=CARTESIAN_POINT('Ctrl Pts',(-219.006888706394,1.46849823137813,
135.500263428392));
#129548=CARTESIAN_POINT('Ctrl Pts',(-219.014649148908,1.5988122630806,135.457501541991));
#129549=CARTESIAN_POINT('Ctrl Pts',(-219.022409591422,1.72698283135395,
135.409435357753));
#129550=CARTESIAN_POINT('Ctrl Pts',(-219.030182491688,1.8553591504016,135.361292013409));
#129551=CARTESIAN_POINT('Ctrl Pts',(-219.037955391953,1.98158476983939,
135.307827508256));
#129552=CARTESIAN_POINT('Ctrl Pts',(-219.045728292219,2.10520244060309,
135.249279710933));
#129553=CARTESIAN_POINT('Ctrl Pts',(-219.053218627981,2.22432629766242,
135.192860273515));
#129554=CARTESIAN_POINT('Ctrl Pts',(-219.060708963743,2.34102825228591,
135.13172085135));
#129555=CARTESIAN_POINT('Ctrl Pts',(-219.068199299505,2.45492447397956,
135.066112474439));
#129556=CARTESIAN_POINT('Ctrl Pts',(-219.075973633624,2.57313910553523,
134.998016535976));
#129557=CARTESIAN_POINT('Ctrl Pts',(-219.083747967743,2.68870551392837,
134.92489036485));
#129558=CARTESIAN_POINT('Ctrl Pts',(-219.091522301862,2.80116596930678,
134.84696525751));
#129559=CARTESIAN_POINT('Ctrl Pts',(-219.099287054809,2.9134878272245,134.769136185901));
#129560=CARTESIAN_POINT('Ctrl Pts',(-219.107051807757,3.02271103005475,
134.686520166229));
#129561=CARTESIAN_POINT('Ctrl Pts',(-219.114816560704,3.12840270115622,
134.599394161805));
#129562=CARTESIAN_POINT('Ctrl Pts',(-219.122573601589,3.23398939779997,
134.512354692157));
#129563=CARTESIAN_POINT('Ctrl Pts',(-219.130330642474,3.33605124320624,
134.420814399003));
#129564=CARTESIAN_POINT('Ctrl Pts',(-219.138087683359,3.43418491116918,
134.325093078063));
#129565=CARTESIAN_POINT('Ctrl Pts',(-219.145838874599,3.53224457576961,
134.229443941316));
#129566=CARTESIAN_POINT('Ctrl Pts',(-219.153590065839,3.62638168040358,
134.129620324417));
#129567=CARTESIAN_POINT('Ctrl Pts',(-219.161341257079,3.71622681535907,
134.025981532464));
#129568=CARTESIAN_POINT('Ctrl Pts',(-219.169089153856,3.80603376373563,
133.922386789762));
#129569=CARTESIAN_POINT('Ctrl Pts',(-219.176837050633,3.89155211507228,
133.814980391941));
#129570=CARTESIAN_POINT('Ctrl Pts',(-219.18458494741,3.97245027243601,133.70415748899));
#129571=CARTESIAN_POINT('Ctrl Pts',(-219.192331223494,4.05333150764919,
133.593357767802));
#129572=CARTESIAN_POINT('Ctrl Pts',(-219.200077499578,4.12959424083472,
133.47914327856));
#129573=CARTESIAN_POINT('Ctrl Pts',(-219.207823775662,4.20094828997011,
133.361940826963));
#129574=CARTESIAN_POINT('Ctrl Pts',(-219.215570108928,4.27230286582498,
133.244737510203));
#129575=CARTESIAN_POINT('Ctrl Pts',(-219.223316442193,4.33874848201673,
133.124546521022));
#129576=CARTESIAN_POINT('Ctrl Pts',(-219.231062775459,4.40003949641406,
133.001821764548));
#129577=CARTESIAN_POINT('Ctrl Pts',(-219.238810843462,4.46134423650901,
132.879069524716));
#129578=CARTESIAN_POINT('Ctrl Pts',(-219.246558911465,4.51749190316311,
132.753782738198));
#129579=CARTESIAN_POINT('Ctrl Pts',(-219.254306979468,4.56828400500315,
132.626437540238));
#129580=CARTESIAN_POINT('Ctrl Pts',(-219.262063282209,4.61913008929352,
132.498956998285));
#129581=CARTESIAN_POINT('Ctrl Pts',(-219.269819584951,4.66460909339769,
132.369414038441));
#129582=CARTESIAN_POINT('Ctrl Pts',(-219.277575887693,4.70457147901002,
132.238302827484));
#129583=CARTESIAN_POINT('Ctrl Pts',(-219.285336330207,4.7445551937508,132.107121638526));
#129584=CARTESIAN_POINT('Ctrl Pts',(-219.293096772721,4.7790163248749,131.974370908853));
#129585=CARTESIAN_POINT('Ctrl Pts',(-219.300857215236,4.80785620566194,
131.840556433123));
#129586=CARTESIAN_POINT('Ctrl Pts',(-219.308630115501,4.8367423827859,131.706527146517));
#129587=CARTESIAN_POINT('Ctrl Pts',(-219.316403015766,4.85998921094519,
131.57143108701));
#129588=CARTESIAN_POINT('Ctrl Pts',(-219.324175916032,4.87754966147512,
131.435781524999));
#129589=CARTESIAN_POINT('Ctrl Pts',(-219.331666251794,4.89447174539619,
131.305063166248));
#129590=CARTESIAN_POINT('Ctrl Pts',(-219.339156587556,4.90611367504773,
131.173831155561));
#129591=CARTESIAN_POINT('Ctrl Pts',(-219.346646923318,4.91247917932139,
131.042544108249));
#129592=CARTESIAN_POINT('Ctrl Pts',(-219.354421257437,4.91908603362435,
130.906279272634));
#129593=CARTESIAN_POINT('Ctrl Pts',(-219.362195591556,4.92002938141795,
130.769523498542));
#129594=CARTESIAN_POINT('Ctrl Pts',(-219.369969925675,4.91525640479089,
130.632786908443));
#129595=CARTESIAN_POINT('Ctrl Pts',(-219.377734678622,4.91048931043095,
130.496218833971));
#129596=CARTESIAN_POINT('Ctrl Pts',(-219.38549943157,4.9000199223279,130.359670283427));
#129597=CARTESIAN_POINT('Ctrl Pts',(-219.393264184517,4.88384727716248,
130.223655153624));
#129598=CARTESIAN_POINT('Ctrl Pts',(-219.401021225402,4.86769069489623,
130.087775115965));
#129599=CARTESIAN_POINT('Ctrl Pts',(-219.408778266287,4.84584217415149,
129.952427830437));
#129600=CARTESIAN_POINT('Ctrl Pts',(-219.416535307172,4.81835276045784,
129.818125484199));
#129601=CARTESIAN_POINT('Ctrl Pts',(-219.424286498412,4.79088407674486,
129.683924416404));
#129602=CARTESIAN_POINT('Ctrl Pts',(-219.432037689652,4.75778304517731,
129.550767100912));
#129603=CARTESIAN_POINT('Ctrl Pts',(-219.439788880892,4.71915228433671,
129.419158545759));
#129604=CARTESIAN_POINT('Ctrl Pts',(-219.447536777669,4.68053794260003,
129.287605927752));
#129605=CARTESIAN_POINT('Ctrl Pts',(-219.455284674446,4.63639865600589,
129.157601135198));
#129606=CARTESIAN_POINT('Ctrl Pts',(-219.463032571223,4.58688763918803,
129.029636738208));
#129607=CARTESIAN_POINT('Ctrl Pts',(-219.470778847307,4.53738697900755,
128.901699108611));
#129608=CARTESIAN_POINT('Ctrl Pts',(-219.478525123392,4.48251696459341,
128.77580139003));
#129609=CARTESIAN_POINT('Ctrl Pts',(-219.486271399476,4.42247982919597,
128.652418419724));
#129610=CARTESIAN_POINT('Ctrl Pts',(-219.494017732741,4.36244225061795,
128.529034538632));
#129611=CARTESIAN_POINT('Ctrl Pts',(-219.501764066006,4.2972376460098,128.408165794411));
#129612=CARTESIAN_POINT('Ctrl Pts',(-219.509510399272,4.22711512304086,
128.290264199554));
#129613=CARTESIAN_POINT('Ctrl Pts',(-219.517258467275,4.15697689661919,
128.172336201453));
#129614=CARTESIAN_POINT('Ctrl Pts',(-219.525006535278,4.08191876012435,
128.057377010899));
#129615=CARTESIAN_POINT('Ctrl Pts',(-219.53275460328,4.0022340101876,127.945810987037));
#129616=CARTESIAN_POINT('Ctrl Pts',(-219.540510906022,3.92246457035024,
127.834126389477));
#129617=CARTESIAN_POINT('Ctrl Pts',(-219.548267208764,3.838058921991,127.725842481234));
#129618=CARTESIAN_POINT('Ctrl Pts',(-219.556023511506,3.74935199250927,
127.621352182333));
#129619=CARTESIAN_POINT('Ctrl Pts',(-219.56378395402,3.66059771746836,127.516806113813));
#129620=CARTESIAN_POINT('Ctrl Pts',(-219.571544396534,3.56753785203093,
127.416057976203));
#129621=CARTESIAN_POINT('Ctrl Pts',(-219.579304839049,3.47054460379491,
127.319464174977));
#129622=CARTESIAN_POINT('Ctrl Pts',(-219.587077739314,3.37339565338617,
127.222715312806));
#129623=CARTESIAN_POINT('Ctrl Pts',(-219.59485063958,3.27230099085897,127.130134377822));
#129624=CARTESIAN_POINT('Ctrl Pts',(-219.602623539845,3.16766702499355,
127.042038371762));
#129625=CARTESIAN_POINT('Ctrl Pts',(-219.610113875607,3.06683676734468,
126.957144877423));
#129626=CARTESIAN_POINT('Ctrl Pts',(-219.617604211369,2.96272030741638,
126.876416084994));
#129627=CARTESIAN_POINT('Ctrl Pts',(-219.625094547131,2.85570550681664,
126.800096750032));
#129628=CARTESIAN_POINT('Ctrl Pts',(-219.63286888125,2.74463320752525,126.720883744288));
#129629=CARTESIAN_POINT('Ctrl Pts',(-219.640643215369,2.6300866041821,126.64617024273));
#129630=CARTESIAN_POINT('Ctrl Pts',(-219.648417549488,2.51246632789698,
126.576276416219));
#129631=CARTESIAN_POINT('Ctrl Pts',(-219.656182302435,2.39499100809067,
126.506468727602));
#129632=CARTESIAN_POINT('Ctrl Pts',(-219.663947055382,2.27444988526298,
126.441469093369));
#129633=CARTESIAN_POINT('Ctrl Pts',(-219.67171180833,2.15127479466006,126.381556097766));
#129634=CARTESIAN_POINT('Ctrl Pts',(-219.679468849215,2.02822204329359,
126.321702608596));
#129635=CARTESIAN_POINT('Ctrl Pts',(-219.6872258901,1.90254087960268,126.266925874012));
#129636=CARTESIAN_POINT('Ctrl Pts',(-219.694982930985,1.7746898125044,126.217459797634));
#129637=CARTESIAN_POINT('Ctrl Pts',(-219.702734122225,1.64693515889017,
126.168031024009));
#129638=CARTESIAN_POINT('Ctrl Pts',(-219.710485313465,1.51701422205617,
126.123905077765));
#129639=CARTESIAN_POINT('Ctrl Pts',(-219.718236504705,1.38540734741418,
126.085268592162));
#129640=CARTESIAN_POINT('Ctrl Pts',(-219.725984401482,1.25385640920447,
126.046648528096));
#129641=CARTESIAN_POINT('Ctrl Pts',(-219.733732298259,1.1206213327352,126.013513394078));
#129642=CARTESIAN_POINT('Ctrl Pts',(-219.741480195036,0.986199347443375,
125.986000532475));
#129643=CARTESIAN_POINT('Ctrl Pts',(-219.74922647112,0.851805480333436,
125.958493425969));
#129644=CARTESIAN_POINT('Ctrl Pts',(-219.756972747204,0.716225581017021,
125.936606330979));
#129645=CARTESIAN_POINT('Ctrl Pts',(-219.764719023289,0.579968455539898,
125.920425764082));
#129646=CARTESIAN_POINT('Ctrl Pts',(-219.772465356554,0.443710324243442,
125.904245077743));
#129647=CARTESIAN_POINT('Ctrl Pts',(-219.780211689819,0.306775345048278,
125.893771049656));
#129648=CARTESIAN_POINT('Ctrl Pts',(-219.787958023085,0.169678457645862,
125.889038422276));
#129649=CARTESIAN_POINT('Ctrl Pts',(-219.795706091088,0.0325508683458896,
125.884304735057));
#129650=CARTESIAN_POINT('Ctrl Pts',(-219.803454159091,-0.104738310653312,
125.885315020518));
#129651=CARTESIAN_POINT('Ctrl Pts',(-219.811202227094,-0.241673519991771,
125.892051896381));
#129652=CARTESIAN_POINT('Ctrl Pts',(-219.818958529836,-0.378754265700079,
125.898795932275));
#129653=CARTESIAN_POINT('Ctrl Pts',(-219.826714832577,-0.515479899125724,
125.911278697344));
#129654=CARTESIAN_POINT('Ctrl Pts',(-219.834471135319,-0.651338809082206,
125.929430790555));
#129655=CARTESIAN_POINT('Ctrl Pts',(-219.842231577834,-0.787270231029564,
125.947592572084));
#129656=CARTESIAN_POINT('Ctrl Pts',(-219.849992020348,-0.922333622918667,
125.971429643181));
#129657=CARTESIAN_POINT('Ctrl Pts',(-219.857752462862,-1.05602794343241,
126.000821500916));
#129658=CARTESIAN_POINT('Ctrl Pts',(-219.865525363127,-1.18993688193827,
126.03026054107));
#129659=CARTESIAN_POINT('Ctrl Pts',(-219.873298263393,-1.32247197903826,
126.06527208703));
#129660=CARTESIAN_POINT('Ctrl Pts',(-219.881071163658,-1.45314685832208,
126.105685562761));
#129661=CARTESIAN_POINT('Ctrl Pts',(-219.88856149942,-1.57907137659272,
126.144629906853));
#129662=CARTESIAN_POINT('Ctrl Pts',(-219.896051835182,-1.70326828579786,
126.188590149103));
#129663=CARTESIAN_POINT('Ctrl Pts',(-219.903542170944,-1.8253220174828,
126.237372266914));
#129664=CARTESIAN_POINT('Ctrl Pts',(-219.911316827432,-1.95200870645148,
126.288006073033));
#129665=CARTESIAN_POINT('Ctrl Pts',(-219.91909148392,-2.07678762301751,
126.343995445933));
#129666=CARTESIAN_POINT('Ctrl Pts',(-219.926866140409,-2.19917278731122,
126.405176362042));
#129667=CARTESIAN_POINT('Ctrl Pts',(-219.934631141583,-2.32140596197137,
126.466281297822));
#129668=CARTESIAN_POINT('Ctrl Pts',(-219.942396142757,-2.44125095312209,
126.532564774866));
#129669=CARTESIAN_POINT('Ctrl Pts',(-219.950161143931,-2.55823991868953,
126.603814036355));
#129670=CARTESIAN_POINT('Ctrl Pts',(-219.957918359215,-2.67511158058155,
126.674991856916));
#129671=CARTESIAN_POINT('Ctrl Pts',(-219.9656755745,-2.78913258425368,126.751125350685));
#129672=CARTESIAN_POINT('Ctrl Pts',(-219.973432789784,-2.89985827678652,
126.831955170352));
#129673=CARTESIAN_POINT('Ctrl Pts',(-219.981420030598,-3.01386733004928,
126.915181845254));
#129674=CARTESIAN_POINT('Ctrl Pts',(-219.989407271412,-3.1243822208978,
127.003387519341));
#129675=CARTESIAN_POINT('Ctrl Pts',(-219.997394512226,-3.2309475571713,
127.096239672221));
#129676=CARTESIAN_POINT('Ctrl Pts',(-220.005142067531,-3.33431502231414,
127.186305466707));
#129677=CARTESIAN_POINT('Ctrl Pts',(-220.012889622837,-3.43396625633552,
127.280742596255));
#129678=CARTESIAN_POINT('Ctrl Pts',(-220.020637178142,-3.52951803945245,
127.379205807681));
#129679=CARTESIAN_POINT('Ctrl Pts',(-220.028383059044,-3.62504917190008,
127.477647739219));
#129680=CARTESIAN_POINT('Ctrl Pts',(-220.036128939946,-3.71648234431109,
127.580113740925));
#129681=CARTESIAN_POINT('Ctrl Pts',(-220.043874820849,-3.80347097002815,
127.686221486184));
#129682=CARTESIAN_POINT('Ctrl Pts',(-220.05162070513,-3.89045963369587,
127.792329277736));
#129683=CARTESIAN_POINT('Ctrl Pts',(-220.059366589412,-3.97300349954177,
127.902078513306));
#129684=CARTESIAN_POINT('Ctrl Pts',(-220.067112473693,-4.05079633585681,
128.015053874322));
#129685=CARTESIAN_POINT('Ctrl Pts',(-220.074860038761,-4.12860605250429,
128.128053749955));
#129686=CARTESIAN_POINT('Ctrl Pts',(-220.082607603828,-4.20166246736009,
128.244280821682));
#129687=CARTESIAN_POINT('Ctrl Pts',(-220.090355168896,-4.26970295929672,
128.363291240864));
#129688=CARTESIAN_POINT('Ctrl Pts',(-220.098109601356,-4.33780376189924,
128.482407150136));
#129689=CARTESIAN_POINT('Ctrl Pts',(-220.105864033817,-4.40087957149622,
128.604310992629));
#129690=CARTESIAN_POINT('Ctrl Pts',(-220.113618466278,-4.45871384497264,
128.728534538351));
#129691=CARTESIAN_POINT('Ctrl Pts',(-220.121377041106,-4.51657901314775,
128.852824443496));
#129692=CARTESIAN_POINT('Ctrl Pts',(-220.129135615935,-4.56919691659541,
128.979436160509));
#129693=CARTESIAN_POINT('Ctrl Pts',(-220.136894190764,-4.616399729699,129.107882914166));
#129694=CARTESIAN_POINT('Ctrl Pts',(-220.144661999102,-4.66365871904769,
129.236482532786));
#129695=CARTESIAN_POINT('Ctrl Pts',(-220.15242980744,-4.70548963466743,
129.366921176344));
#129696=CARTESIAN_POINT('Ctrl Pts',(-220.160197615777,-4.74177483484259,
129.498698150405));
#129697=CARTESIAN_POINT('Ctrl Pts',(-220.161840600291,-4.74944958933631,
129.526570558962));
#129698=CARTESIAN_POINT('Ctrl Pts',(-220.163483584804,-4.75687642643801,
129.554502809348));
#129699=CARTESIAN_POINT('Ctrl Pts',(-220.165126569317,-4.76405452823397,
129.582490119308));
#129700=CARTESIAN_POINT('Ctrl Pts',(-218.414998772423,-4.76405452823415,
129.582490119309));
#129701=CARTESIAN_POINT('Ctrl Pts',(-218.422662130679,-4.79774618392612,
129.713853373509));
#129702=CARTESIAN_POINT('Ctrl Pts',(-218.430325488935,-4.82597703335009,
129.846520217875));
#129703=CARTESIAN_POINT('Ctrl Pts',(-218.437988847192,-4.84866974835229,
129.979991322945));
#129704=CARTESIAN_POINT('Ctrl Pts',(-218.445847466656,-4.87194067029563,
130.116863251557));
#129705=CARTESIAN_POINT('Ctrl Pts',(-218.45370608612,-4.88938739281945,
130.254580524333));
#129706=CARTESIAN_POINT('Ctrl Pts',(-218.461564705584,-4.90098329172141,
130.392601177155));
#129707=CARTESIAN_POINT('Ctrl Pts',(-218.469423325048,-4.91257919062336,
130.530621829977));
#129708=CARTESIAN_POINT('Ctrl Pts',(-218.477281944512,-4.91832431028879,
130.668945412283));
#129709=CARTESIAN_POINT('Ctrl Pts',(-218.485140563975,-4.91824927387013,
130.807033177379));
#129710=CARTESIAN_POINT('',(-218.139859436045,-4.91824937750444,130.80683512301));
#129711=CARTESIAN_POINT('Ctrl Pts',(-218.070061802556,-4.76405452823401,
129.582490119308));
#129712=CARTESIAN_POINT('Ctrl Pts',(-218.077925797649,-4.79863878913083,
129.717333627655));
#129713=CARTESIAN_POINT('Ctrl Pts',(-218.085789792741,-4.82751692160361,
129.853736466587));
#129714=CARTESIAN_POINT('Ctrl Pts',(-218.093653787834,-4.85055947271794,
129.991184213502));
#129715=CARTESIAN_POINT('Ctrl Pts',(-218.101514136411,-4.87359133905553,
130.12856822622));
#129716=CARTESIAN_POINT('Ctrl Pts',(-218.109374484987,-4.89079294912702,
130.266995813564));
#129717=CARTESIAN_POINT('Ctrl Pts',(-218.117234833564,-4.90208583965905,
130.405941889198));
#129718=CARTESIAN_POINT('Ctrl Pts',(-218.124776367708,-4.91292069242709,
130.539252335087));
#129719=CARTESIAN_POINT('Ctrl Pts',(-218.132317901852,-4.91831669360595,
130.673039704548));
#129720=CARTESIAN_POINT('Ctrl Pts',(-218.139859435996,-4.91824937750488,
130.806835122136));
#129721=CARTESIAN_POINT('Ctrl Pts',(-218.139859436045,-4.91824937750444,
130.806835123011));
#129722=CARTESIAN_POINT('Ctrl Pts',(-218.148385548635,-4.91817327298129,
130.958098085236));
#129723=CARTESIAN_POINT('Ctrl Pts',(-218.156911661225,-4.91111483647233,
131.109122025211));
#129724=CARTESIAN_POINT('Ctrl Pts',(-218.165437773815,-4.89716461096416,
131.259291200864));
#129725=CARTESIAN_POINT('Ctrl Pts',(-218.174008185907,-4.88314190364959,
131.410240617175));
#129726=CARTESIAN_POINT('Ctrl Pts',(-218.182578597998,-4.86215569217589,
131.56032612373));
#129727=CARTESIAN_POINT('Ctrl Pts',(-218.19114901009,-4.83434822261198,
131.708938046551));
#129728=CARTESIAN_POINT('Ctrl Pts',(-218.199742282965,-4.80646657919078,
131.857946377952));
#129729=CARTESIAN_POINT('Ctrl Pts',(-218.208335555839,-4.77172735794309,
132.00547302904));
#129730=CARTESIAN_POINT('Ctrl Pts',(-218.216928828714,-4.73032278608913,
132.150922685169));
#129731=CARTESIAN_POINT('Ctrl Pts',(-218.225552752069,-4.68877053243292,
132.296891131044));
#129732=CARTESIAN_POINT('Ctrl Pts',(-218.234176675425,-4.6405054176299,
132.440767519449));
#129733=CARTESIAN_POINT('Ctrl Pts',(-218.24280059878,-4.58576905108392,
132.581972856672));
#129734=CARTESIAN_POINT('Ctrl Pts',(-218.246015540595,-4.56536369422066,
132.634613276175));
#129735=CARTESIAN_POINT('Ctrl Pts',(-218.24923048241,-4.54405945670397,
132.686882729135));
#129736=CARTESIAN_POINT('Ctrl Pts',(-218.252445424226,-4.52187047538647,
132.738752115254));
#129737=CARTESIAN_POINT('Ctrl Pts',(-218.260219758345,-4.46821334426689,
132.864182048798));
#129738=CARTESIAN_POINT('Ctrl Pts',(-218.267994092464,-4.40924841045326,
132.987576409418));
#129739=CARTESIAN_POINT('Ctrl Pts',(-218.275768426583,-4.34515128957907,
133.108453352933));
#129740=CARTESIAN_POINT('Ctrl Pts',(-218.28353317953,-4.28113316267801,
133.229181326417));
#129741=CARTESIAN_POINT('Ctrl Pts',(-218.291297932477,-4.21199561490571,
133.347397713737));
#129742=CARTESIAN_POINT('Ctrl Pts',(-218.299062685424,-4.13796254450172,
133.462639956311));
#129743=CARTESIAN_POINT('Ctrl Pts',(-218.306819726309,-4.06400300478674,
133.577767738666));
#129744=CARTESIAN_POINT('Ctrl Pts',(-218.314576767194,-3.98515782858715,
133.689926927984));
#129745=CARTESIAN_POINT('Ctrl Pts',(-218.322333808079,-3.90169693691545,
133.798679250405));
#129746=CARTESIAN_POINT('Ctrl Pts',(-218.330084999319,-3.81829898375128,
133.907349561853));
#129747=CARTESIAN_POINT('Ctrl Pts',(-218.33783619056,-3.73029248039418,
134.012617811229));
#129748=CARTESIAN_POINT('Ctrl Pts',(-218.3455873818,-3.63799058652956,134.114074737369));
#129749=CARTESIAN_POINT('Ctrl Pts',(-218.353335278577,-3.54572792343219,
134.215488541609));
#129750=CARTESIAN_POINT('Ctrl Pts',(-218.361083175354,-3.44917376346446,
134.313093955911));
#129751=CARTESIAN_POINT('Ctrl Pts',(-218.368831072131,-3.34868132633162,
134.406515033631));
#129752=CARTESIAN_POINT('Ctrl Pts',(-218.376577348215,-3.24820991005026,
134.499916569676));
#129753=CARTESIAN_POINT('Ctrl Pts',(-218.384323624299,-3.14380214135624,
134.589135244078));
#129754=CARTESIAN_POINT('Ctrl Pts',(-218.392069900383,-3.0358475655595,
134.673832496413));
#129755=CARTESIAN_POINT('Ctrl Pts',(-218.399816233649,-2.92789219286647,
134.758530373963));
#129756=CARTESIAN_POINT('Ctrl Pts',(-218.407562566914,-2.81639026842193,
134.838706521518));
#129757=CARTESIAN_POINT('Ctrl Pts',(-218.415308900179,-2.70176350784062,
134.914063406114));
#129758=CARTESIAN_POINT('Ctrl Pts',(-218.423056968182,-2.5871110773912,
134.989437166362));
#129759=CARTESIAN_POINT('Ctrl Pts',(-218.430805036185,-2.46933274494215,
135.059989301358));
#129760=CARTESIAN_POINT('Ctrl Pts',(-218.438553104188,-2.34887786954401,
135.125466473301));
#129761=CARTESIAN_POINT('Ctrl Pts',(-218.44630940693,-2.2282949732707,135.191013235162));
#129762=CARTESIAN_POINT('Ctrl Pts',(-218.454065709672,-2.10503019557442,
135.251474072395));
#129763=CARTESIAN_POINT('Ctrl Pts',(-218.461822012414,-1.97955658261512,
135.306642127948));
#129764=CARTESIAN_POINT('Ctrl Pts',(-218.469582454928,-1.85401600061064,
135.361839628353));
#129765=CARTESIAN_POINT('Ctrl Pts',(-218.477342897442,-1.72626459823451,
135.411738576017));
#129766=CARTESIAN_POINT('Ctrl Pts',(-218.485103339957,-1.59679297651733,
135.456181256052));
#129767=CARTESIAN_POINT('Ctrl Pts',(-218.492876240222,-1.46711351545902,
135.500695279422));
#129768=CARTESIAN_POINT('Ctrl Pts',(-218.500649140487,-1.33570869179546,
135.539735420711));
#129769=CARTESIAN_POINT('Ctrl Pts',(-218.508422040753,-1.20308262887788,
135.573194358701));
#129770=CARTESIAN_POINT('Ctrl Pts',(-218.515912376515,-1.07527785741188,
135.605436980018));
#129771=CARTESIAN_POINT('Ctrl Pts',(-218.523402712277,-0.946339396860306,
135.632497071405));
#129772=CARTESIAN_POINT('Ctrl Pts',(-218.530893048039,-0.816723092949144,
135.654324169176));
#129773=CARTESIAN_POINT('Ctrl Pts',(-218.538667382158,-0.682192347479364,
135.676978847993));
#129774=CARTESIAN_POINT('Ctrl Pts',(-218.546441716277,-0.546505190154853,
135.694067645192));
#129775=CARTESIAN_POINT('Ctrl Pts',(-218.554216050396,-0.410161934671308,
135.705477862628));
#129776=CARTESIAN_POINT('Ctrl Pts',(-218.561980803344,-0.27398671006517,
135.716874017992));
#129777=CARTESIAN_POINT('Ctrl Pts',(-218.569745556291,-0.137157382000985,
135.722605485916));
#129778=CARTESIAN_POINT('Ctrl Pts',(-218.577510309238,-0.000184136581379461,
135.722610614119));
#129779=CARTESIAN_POINT('Ctrl Pts',(-218.585267350123,0.136653065079891,
135.722615737229));
#129780=CARTESIAN_POINT('Ctrl Pts',(-218.593024391008,0.273633511202761,
135.716905838947));
#129781=CARTESIAN_POINT('Ctrl Pts',(-218.600781431893,0.410242570674838,
135.70547111374));
#129782=CARTESIAN_POINT('Ctrl Pts',(-218.608532623133,0.54674861219269,
135.694045011548));
#129783=CARTESIAN_POINT('Ctrl Pts',(-218.616283814373,0.682883436486953,
135.676902707907));
#129784=CARTESIAN_POINT('Ctrl Pts',(-218.624035005613,0.818133450091018,
135.654086457275));
#129785=CARTESIAN_POINT('Ctrl Pts',(-218.63178290239,0.953325978831206,
135.631279904158));
#129786=CARTESIAN_POINT('Ctrl Pts',(-218.639530799167,1.08763406014116,
135.602804265396));
#129787=CARTESIAN_POINT('Ctrl Pts',(-218.647278695945,1.22055047558416,
135.568753506387));
#129788=CARTESIAN_POINT('Ctrl Pts',(-218.655024972029,1.35343908777875,
135.534709870063));
#129789=CARTESIAN_POINT('Ctrl Pts',(-218.662771248113,1.48493623463844,
135.49509353008));
#129790=CARTESIAN_POINT('Ctrl Pts',(-218.670517524197,1.61454651693362,
135.450049221762));
#129791=CARTESIAN_POINT('Ctrl Pts',(-218.678263857462,1.74415775598228,
135.405004580937));
#129792=CARTESIAN_POINT('Ctrl Pts',(-218.686010190728,1.87188173337477,
135.354532020168));
#129793=CARTESIAN_POINT('Ctrl Pts',(-218.693756523993,1.99724017861159,
135.29882551691));
#129794=CARTESIAN_POINT('Ctrl Pts',(-218.701504591996,2.12262669700287,
135.243106538568));
#129795=CARTESIAN_POINT('Ctrl Pts',(-218.709252659999,2.24564627189922,
135.18215144412));
#129796=CARTESIAN_POINT('Ctrl Pts',(-218.717000728002,2.36584287349146,
135.116201356792));
#129797=CARTESIAN_POINT('Ctrl Pts',(-218.724757030744,2.4861672214624,135.050181176927));
#129798=CARTESIAN_POINT('Ctrl Pts',(-218.732513333486,2.60366225942089,
134.979155587774));
#129799=CARTESIAN_POINT('Ctrl Pts',(-218.740269636228,2.71789825966552,
134.903410765174));
#129800=CARTESIAN_POINT('Ctrl Pts',(-218.748030078742,2.83219523110306,
134.827625515283));
#129801=CARTESIAN_POINT('Ctrl Pts',(-218.755790521256,2.94322938247043,
134.747116242418));
#129802=CARTESIAN_POINT('Ctrl Pts',(-218.76355096377,3.05060284192411,134.662210454372));
#129803=CARTESIAN_POINT('Ctrl Pts',(-218.771323864036,3.15814866678707,
134.577168368018));
#129804=CARTESIAN_POINT('Ctrl Pts',(-218.779096764301,3.26202176025846,
134.487715918266));
#129805=CARTESIAN_POINT('Ctrl Pts',(-218.786869664567,3.36185933897489,
134.394219228632));
#129806=CARTESIAN_POINT('Ctrl Pts',(-218.794360000329,3.45806757022903,
134.304121379171));
#129807=CARTESIAN_POINT('Ctrl Pts',(-218.801850336091,3.55052837891852,
134.210268440956));
#129808=CARTESIAN_POINT('Ctrl Pts',(-218.809340671853,3.63895291276647,
134.113016653054));
#129809=CARTESIAN_POINT('Ctrl Pts',(-218.817115005972,3.73073008969169,
134.012077534053));
#129810=CARTESIAN_POINT('Ctrl Pts',(-218.824889340091,3.81844960163169,
133.907156998039));
#129811=CARTESIAN_POINT('Ctrl Pts',(-218.83266367421,3.90174620067321,133.798615056994));
#129812=CARTESIAN_POINT('Ctrl Pts',(-218.840428427157,3.98494014410062,
133.69020688419));
#129813=CARTESIAN_POINT('Ctrl Pts',(-218.848193180104,4.06372178444967,
133.578186493694));
#129814=CARTESIAN_POINT('Ctrl Pts',(-218.855957933051,4.13776348385898,
133.462949794957));
#129815=CARTESIAN_POINT('Ctrl Pts',(-218.863714973936,4.21173164400863,
133.347827550935));
#129816=CARTESIAN_POINT('Ctrl Pts',(-218.871472014821,4.28096902193457,
133.229495682631));
#129817=CARTESIAN_POINT('Ctrl Pts',(-218.879229055706,4.34518919727565,
133.108381863644));
#129818=CARTESIAN_POINT('Ctrl Pts',(-218.886980246946,4.40936094368304,
132.98735937753));
#129819=CARTESIAN_POINT('Ctrl Pts',(-218.894731438186,4.46852283594386,
132.863559460471));
#129820=CARTESIAN_POINT('Ctrl Pts',(-218.902482629427,4.52243281411565,
132.737437052762));
#129821=CARTESIAN_POINT('Ctrl Pts',(-218.910230526204,4.57631987910856,
132.611368250441));
#129822=CARTESIAN_POINT('Ctrl Pts',(-218.917978422981,4.62495931635136,
132.482979279525));
#129823=CARTESIAN_POINT('Ctrl Pts',(-218.925726319758,4.66815601764025,
132.352747667844));
#129824=CARTESIAN_POINT('Ctrl Pts',(-218.933472595842,4.71134368311044,
132.222543297809));
#129825=CARTESIAN_POINT('Ctrl Pts',(-218.941218871926,4.74909075416409,
132.09049742452));
#129826=CARTESIAN_POINT('Ctrl Pts',(-218.94896514801,4.78125122534236,131.957105074357));
#129827=CARTESIAN_POINT('Ctrl Pts',(-218.956711481275,4.81341193392196,
131.823711739522));
#129828=CARTESIAN_POINT('Ctrl Pts',(-218.964457814541,4.83998586870189,
131.688972288054));
#129829=CARTESIAN_POINT('Ctrl Pts',(-218.972204147806,4.8608777115221,131.553393952023));
#129830=CARTESIAN_POINT('Ctrl Pts',(-218.979952215809,4.88177423292563,
131.417785254164));
#129831=CARTESIAN_POINT('Ctrl Pts',(-218.987700283812,4.89698607077991,
131.281337684248));
#129832=CARTESIAN_POINT('Ctrl Pts',(-218.995448351815,4.90646959363344,
131.144565246063));
#129833=CARTESIAN_POINT('Ctrl Pts',(-219.003204654557,4.91596319568793,
131.007647444502));
#129834=CARTESIAN_POINT('Ctrl Pts',(-219.010960957299,4.91971629397654,
130.870404475602));
#129835=CARTESIAN_POINT('Ctrl Pts',(-219.01871726004,4.91773737802059,130.733352566479));
#129836=CARTESIAN_POINT('Ctrl Pts',(-219.026477702555,4.91575740585761,
130.596227508626));
#129837=CARTESIAN_POINT('Ctrl Pts',(-219.034238145069,4.90803934542951,
130.459294103899));
#129838=CARTESIAN_POINT('Ctrl Pts',(-219.041998587583,4.89464367886692,
130.323064119108));
#129839=CARTESIAN_POINT('Ctrl Pts',(-219.049771487848,4.88122650839115,
130.186615445852));
#129840=CARTESIAN_POINT('Ctrl Pts',(-219.057544388114,4.86211357325294,
130.050872836387));
#129841=CARTESIAN_POINT('Ctrl Pts',(-219.065317288379,4.83741681026475,
129.916339409335));
#129842=CARTESIAN_POINT('Ctrl Pts',(-219.072807624141,4.81361783681864,
129.786696611226));
#129843=CARTESIAN_POINT('Ctrl Pts',(-219.080297959903,4.78463402742281,
129.658176908659));
#129844=CARTESIAN_POINT('Ctrl Pts',(-219.087788295665,4.7506089643807,129.531215877151));
#129845=CARTESIAN_POINT('Ctrl Pts',(-219.095562629784,4.7152938307316,129.399441079545));
#129846=CARTESIAN_POINT('Ctrl Pts',(-219.103336963903,4.67443575115081,
129.268928057262));
#129847=CARTESIAN_POINT('Ctrl Pts',(-219.111111298022,4.62814018849646,
129.140178698987));
#129848=CARTESIAN_POINT('Ctrl Pts',(-219.118876050969,4.58190168098552,
129.01158801279));
#129849=CARTESIAN_POINT('Ctrl Pts',(-219.126640803917,4.53023915483583,
128.884757030239));
#129850=CARTESIAN_POINT('Ctrl Pts',(-219.134405556864,4.47330860361587,
128.760175401076));
#129851=CARTESIAN_POINT('Ctrl Pts',(-219.142162597749,4.41643459662197,
128.635717508144));
#129852=CARTESIAN_POINT('Ctrl Pts',(-219.149919638634,4.35430313847106,
128.513504875955));
#129853=CARTESIAN_POINT('Ctrl Pts',(-219.157676679519,4.28711922587275,
128.394009646099));
#129854=CARTESIAN_POINT('Ctrl Pts',(-219.165427870759,4.21998597718546,
128.274604528525));
#129855=CARTESIAN_POINT('Ctrl Pts',(-219.173179061999,4.14780804864432,
128.157913073863));
#129856=CARTESIAN_POINT('Ctrl Pts',(-219.180930253239,4.07083735509288,
128.044384840339));
#129857=CARTESIAN_POINT('Ctrl Pts',(-219.188678150016,3.99389937613956,
127.930904859343));
#129858=CARTESIAN_POINT('Ctrl Pts',(-219.196426046793,3.91217290265776,
127.820585748395));
#129859=CARTESIAN_POINT('Ctrl Pts',(-219.20417394357,3.82595423158429,127.713849773009));
#129860=CARTESIAN_POINT('Ctrl Pts',(-219.211920219654,3.73975359559815,
127.607136124488));
#129861=CARTESIAN_POINT('Ctrl Pts',(-219.219666495738,3.64906287659481,
127.504004424646));
#129862=CARTESIAN_POINT('Ctrl Pts',(-219.227412771822,3.55421963477011,
127.404845085859));
#129863=CARTESIAN_POINT('Ctrl Pts',(-219.235159105088,3.45937569283428,
127.305685015101));
#129864=CARTESIAN_POINT('Ctrl Pts',(-219.242905438353,3.36037943714812,
127.210497646446));
#129865=CARTESIAN_POINT('Ctrl Pts',(-219.250651771618,3.25760609462358,
127.119637345084));
#129866=CARTESIAN_POINT('Ctrl Pts',(-219.258399839621,3.15480973672142,
127.028756696187));
#129867=CARTESIAN_POINT('Ctrl Pts',(-219.266147907624,3.04823490168521,
126.942205301722));
#129868=CARTESIAN_POINT('Ctrl Pts',(-219.273895975627,2.93829045159357,
126.860297701666));
#129869=CARTESIAN_POINT('Ctrl Pts',(-219.281652278369,2.82822915123217,
126.778303049239));
#129870=CARTESIAN_POINT('Ctrl Pts',(-219.289408581111,2.71479139587311,
126.700962284319));
#129871=CARTESIAN_POINT('Ctrl Pts',(-219.297164883853,2.59841609080511,
126.628547297799));
#129872=CARTESIAN_POINT('Ctrl Pts',(-219.304925326367,2.4819786727328,126.55609366122));
#129873=CARTESIAN_POINT('Ctrl Pts',(-219.312685768881,2.36260092099488,
126.488571234006));
#129874=CARTESIAN_POINT('Ctrl Pts',(-219.320446211395,2.24074609157281,
126.426205753288));
#129875=CARTESIAN_POINT('Ctrl Pts',(-219.328219111661,2.11869564996046,
126.363740157964));
#129876=CARTESIAN_POINT('Ctrl Pts',(-219.335992011926,1.99416053988601,
126.306448215489));
#129877=CARTESIAN_POINT('Ctrl Pts',(-219.343764912191,1.86762455387554,
126.254507698156));
#129878=CARTESIAN_POINT('Ctrl Pts',(-219.351255247953,1.74568846968043,
126.204455349458));
#129879=CARTESIAN_POINT('Ctrl Pts',(-219.358745583716,1.62189474709496,
126.159372210661));
#129880=CARTESIAN_POINT('Ctrl Pts',(-219.366235919478,1.49668745788046,
126.119372921112));
#129881=CARTESIAN_POINT('Ctrl Pts',(-219.374010253597,1.36673289624037,
126.077857046343));
#129882=CARTESIAN_POINT('Ctrl Pts',(-219.381784587716,1.23484380424537,
126.041686629354));
#129883=CARTESIAN_POINT('Ctrl Pts',(-219.389558921835,1.10149944031048,
126.011044224348));
#129884=CARTESIAN_POINT('Ctrl Pts',(-219.397323674782,0.968319411387163,
125.980439583367));
#129885=CARTESIAN_POINT('Ctrl Pts',(-219.405088427729,0.833688056415686,
125.955349485688));
#129886=CARTESIAN_POINT('Ctrl Pts',(-219.412853180676,0.698101649925656,
125.935907357148));
#129887=CARTESIAN_POINT('Ctrl Pts',(-219.420610221561,0.562649909765617,
125.916484538805));
#129888=CARTESIAN_POINT('Ctrl Pts',(-219.428367262446,0.426245390287803,
125.902698581294));
#129889=CARTESIAN_POINT('Ctrl Pts',(-219.436124303331,0.289396123311074,
125.89463221914));
#129890=CARTESIAN_POINT('Ctrl Pts',(-219.443875494571,0.152650055431291,
125.886571939892));
#129891=CARTESIAN_POINT('Ctrl Pts',(-219.451626685811,0.0154602963297696,
125.884222693766));
#129892=CARTESIAN_POINT('Ctrl Pts',(-219.459377877051,-0.121658761798457,
125.887615534874));
#129893=CARTESIAN_POINT('Ctrl Pts',(-219.467125773828,-0.258719540669395,
125.891006933933));
#129894=CARTESIAN_POINT('Ctrl Pts',(-219.474873670606,-0.395709288306496,
125.900135556526));
#129895=CARTESIAN_POINT('Ctrl Pts',(-219.482621567383,-0.53211258504232,
125.914980364473));
#129896=CARTESIAN_POINT('Ctrl Pts',(-219.490367843467,-0.668487349148981,
125.929822067205));
#129897=CARTESIAN_POINT('Ctrl Pts',(-219.498114119551,-0.804275517933435,
125.950377534701));
#129898=CARTESIAN_POINT('Ctrl Pts',(-219.505860395635,-0.938966166874421,
125.976573795433));
#129899=CARTESIAN_POINT('Ctrl Pts',(-219.5136067289,-1.073657810071,126.002770249539));
#129900=CARTESIAN_POINT('Ctrl Pts',(-219.521353062166,-1.20725153348383,
126.034607505329));
#129901=CARTESIAN_POINT('Ctrl Pts',(-219.529099395431,-1.33924638033021,
126.071961416815));
#129902=CARTESIAN_POINT('Ctrl Pts',(-219.536847463434,-1.47127078650754,
126.10932369345));
#129903=CARTESIAN_POINT('Ctrl Pts',(-219.544595531437,-1.60169522750637,
126.152204977679));
#129904=CARTESIAN_POINT('Ctrl Pts',(-219.55234359944,-1.73003407199424,
126.200431298795));
#129905=CARTESIAN_POINT('Ctrl Pts',(-219.560099902182,-1.8585093165331,
126.248708875419));
#129906=CARTESIAN_POINT('Ctrl Pts',(-219.567856204924,-1.98489417010757,
126.302342699135));
#129907=CARTESIAN_POINT('Ctrl Pts',(-219.575612507665,-2.10872264418015,
126.36111047016));
#129908=CARTESIAN_POINT('Ctrl Pts',(-219.58337295018,-2.23261720923775,
126.419909607314));
#129909=CARTESIAN_POINT('Ctrl Pts',(-219.591133392694,-2.35395233036607,
126.483847969569));
#129910=CARTESIAN_POINT('Ctrl Pts',(-219.598893835208,-2.47228768734846,
126.552657822981));
#129911=CARTESIAN_POINT('Ctrl Pts',(-219.606666735473,-2.59081300675119,
126.621578136078));
#129912=CARTESIAN_POINT('Ctrl Pts',(-219.614439635739,-2.70632860948182,
126.69538535686));
#129913=CARTESIAN_POINT('Ctrl Pts',(-219.622212536004,-2.81842342899755,
126.77376854724));
#129914=CARTESIAN_POINT('Ctrl Pts',(-219.629702871766,-2.92644331947255,
126.849302311213));
#129915=CARTESIAN_POINT('Ctrl Pts',(-219.637193207528,-3.03128657184853,
126.929084938306));
#129916=CARTESIAN_POINT('Ctrl Pts',(-219.64468354329,-3.13261670516085,
127.012804783736));
#129917=CARTESIAN_POINT('Ctrl Pts',(-219.652349582752,-3.23632377855823,
127.098488477926));
#129918=CARTESIAN_POINT('Ctrl Pts',(-219.660015622214,-3.33669878099961,
127.188584155804));
#129919=CARTESIAN_POINT('Ctrl Pts',(-219.667681661675,-3.43333514465959,
127.282799479811));
#129920=CARTESIAN_POINT('Ctrl Pts',(-219.675338911775,-3.52986071160705,
127.376906782906));
#129921=CARTESIAN_POINT('Ctrl Pts',(-219.682996161875,-3.62265587551738,
127.475124065198));
#129922=CARTESIAN_POINT('Ctrl Pts',(-219.690653411975,-3.71134556209773,
127.577117648529));
#129923=CARTESIAN_POINT('Ctrl Pts',(-219.69830365046,-3.79995403703036,
127.67901783806));
#129924=CARTESIAN_POINT('Ctrl Pts',(-219.705953888946,-3.88446424695242,
127.784687151707));
#129925=CARTESIAN_POINT('Ctrl Pts',(-219.713604127431,-3.96453697041456,
127.893754207775));
#129926=CARTESIAN_POINT('Ctrl Pts',(-219.721249125501,-4.04455484404159,
128.002746552883));
#129927=CARTESIAN_POINT('Ctrl Pts',(-219.728894123571,-4.12014103953239,
128.115131688097));
#129928=CARTESIAN_POINT('Ctrl Pts',(-219.736539121641,-4.19099611494774,
128.230504633445));
#129929=CARTESIAN_POINT('Ctrl Pts',(-219.744181407903,-4.26182605688949,
128.345836654091));
#129930=CARTESIAN_POINT('Ctrl Pts',(-219.751823694165,-4.32792800274121,
128.464154036666));
#129931=CARTESIAN_POINT('Ctrl Pts',(-219.759465980427,-4.3890456586599,
128.585022592681));
#129932=CARTESIAN_POINT('Ctrl Pts',(-219.767106586471,-4.45014987736727,
128.705864574766));
#129933=CARTESIAN_POINT('Ctrl Pts',(-219.774747192515,-4.50627180773774,
128.829256253692));
#129934=CARTESIAN_POINT('Ctrl Pts',(-219.782387798558,-4.55720130961135,
128.954739227612));
#129935=CARTESIAN_POINT('Ctrl Pts',(-219.790030547643,-4.60814509621734,
129.080257397059));
#129936=CARTESIAN_POINT('Ctrl Pts',(-219.797673296727,-4.6538933931612,
129.207867660123));
#129937=CARTESIAN_POINT('Ctrl Pts',(-219.805316045812,-4.69428444174175,
129.337092188641));
#129938=CARTESIAN_POINT('Ctrl Pts',(-219.810118632032,-4.71966555672841,
129.418294898961));
#129939=CARTESIAN_POINT('Ctrl Pts',(-219.814921218252,-4.74293224799498,
129.500134669231));
#129940=CARTESIAN_POINT('Ctrl Pts',(-219.819723804473,-4.76405452823394,
129.582490119308));
#129941=CARTESIAN_POINT('Origin',(213.235140564004,0.,130.804360617566));
#129942=CARTESIAN_POINT('',(-221.915425355964,-4.76405452823393,129.582490119308));
#129943=CARTESIAN_POINT('',(-221.569819034442,-4.76405452823418,129.582490119309));
#129944=CARTESIAN_POINT('',(213.235140564004,-4.76405452823405,129.582490119308));
#129945=CARTESIAN_POINT('',(-220.235140564048,-4.91824810108724,130.800038736987));
#129946=CARTESIAN_POINT('Ctrl Pts',(-220.235140564048,-4.91824810108724,
130.800038736987));
#129947=CARTESIAN_POINT('Ctrl Pts',(-220.242787499465,-4.91836654317577,
130.934824408715));
#129948=CARTESIAN_POINT('Ctrl Pts',(-220.250434434882,-4.91294007670036,
131.069796436303));
#129949=CARTESIAN_POINT('Ctrl Pts',(-220.258081370299,-4.90194948723364,
131.204453465677));
#129950=CARTESIAN_POINT('Ctrl Pts',(-220.265721661022,-4.89096844788083,
131.338993486772));
#129951=CARTESIAN_POINT('Ctrl Pts',(-220.273361951745,-4.87443293515955,
131.473218654188));
#129952=CARTESIAN_POINT('Ctrl Pts',(-220.281002242468,-4.85237579310271,
131.606627546344));
#129953=CARTESIAN_POINT('Ctrl Pts',(-220.288638270407,-4.83033095749057,
131.739962005051));
#129954=CARTESIAN_POINT('Ctrl Pts',(-220.296274298347,-4.80277068438332,
131.872480697236));
#129955=CARTESIAN_POINT('Ctrl Pts',(-220.303910326287,-4.76977961799604,
132.003687703164));
#129956=CARTESIAN_POINT('Ctrl Pts',(-220.311544193053,-4.73679788884799,
132.134857574458));
#129957=CARTESIAN_POINT('Ctrl Pts',(-220.319178059819,-4.6983885201489,
132.264716106547));
#129958=CARTESIAN_POINT('Ctrl Pts',(-220.326811926585,-4.65468708584121,
132.392778445281));
#129959=CARTESIAN_POINT('Ctrl Pts',(-220.33444539865,-4.6109879110682,132.520834162693));
#129960=CARTESIAN_POINT('Ctrl Pts',(-220.342078870716,-4.56199734517058,
132.647093489588));
#129961=CARTESIAN_POINT('Ctrl Pts',(-220.349712342781,-4.50790039104962,
132.771088134757));
#129962=CARTESIAN_POINT('Ctrl Pts',(-220.357347186093,-4.45379371916913,
132.895105053825));
#129963=CARTESIAN_POINT('Ctrl Pts',(-220.364982029405,-4.39457899688891,
133.01685611266));
#129964=CARTESIAN_POINT('Ctrl Pts',(-220.372616872716,-4.33048854730502,
133.135894877267));
#129965=CARTESIAN_POINT('Ctrl Pts',(-220.380259413188,-4.26633348415524,
133.255053652252));
#129966=CARTESIAN_POINT('Ctrl Pts',(-220.38790195366,-4.19729306907339,
133.371494316662));
#129967=CARTESIAN_POINT('Ctrl Pts',(-220.395544494132,-4.12364476480766,
133.484796573931));
#129968=CARTESIAN_POINT('Ctrl Pts',(-220.403191015574,-4.04995809742099,
133.598157849914));
#129969=CARTESIAN_POINT('Ctrl Pts',(-220.410837537016,-3.97165899553329,
133.708377135488));
#129970=CARTESIAN_POINT('Ctrl Pts',(-220.418484058458,-3.88906629538656,
133.815065919084));
#129971=CARTESIAN_POINT('Ctrl Pts',(-220.426142400143,-3.80634592074331,
133.92191962569));
#129972=CARTESIAN_POINT('Ctrl Pts',(-220.433800741827,-3.71931895115071,
134.025231621794));
#129973=CARTESIAN_POINT('Ctrl Pts',(-220.441459083512,-3.62834267717324,
134.124648629095));
#129974=CARTESIAN_POINT('Ctrl Pts',(-220.447785195198,-3.55319245619403,
134.206771250094));
#129975=CARTESIAN_POINT('Ctrl Pts',(-220.454111306884,-3.47534820372095,
134.286236755806));
#129976=CARTESIAN_POINT('Ctrl Pts',(-220.46043741857,-3.39502806051355,
134.362866979908));
#129977=CARTESIAN_POINT('Ctrl Pts',(-220.468211752689,-3.29632040867479,
134.45703998781));
#129978=CARTESIAN_POINT('Ctrl Pts',(-220.475986086808,-3.19353511360062,
134.547252042264));
#129979=CARTESIAN_POINT('Ctrl Pts',(-220.483760420927,-3.08702331865612,
134.633129361245));
#129980=CARTESIAN_POINT('Ctrl Pts',(-220.491525173874,-2.98064278997966,
134.718900844105));
#129981=CARTESIAN_POINT('Ctrl Pts',(-220.499289926821,-2.87054520073186,
134.800347977787));
#129982=CARTESIAN_POINT('Ctrl Pts',(-220.507054679768,-2.75711848394831,
134.877133718043));
#129983=CARTESIAN_POINT('Ctrl Pts',(-220.514811720653,-2.6438044241789,
134.95384319362));
#129984=CARTESIAN_POINT('Ctrl Pts',(-220.522568761538,-2.52716813869132,
135.025900271455));
#129985=CARTESIAN_POINT('Ctrl Pts',(-220.530325802423,-2.40763030462598,
135.09300835068));
#129986=CARTESIAN_POINT('Ctrl Pts',(-220.538076993663,-2.28818261497133,
135.160065823181));
#129987=CARTESIAN_POINT('Ctrl Pts',(-220.545828184903,-2.16583807151714,
135.222181534935));
#129988=CARTESIAN_POINT('Ctrl Pts',(-220.553579376144,-2.04104567477602,
135.279102578392));
#129989=CARTESIAN_POINT('Ctrl Pts',(-220.561327272921,-1.91630631813264,
135.335999428888));
#129990=CARTESIAN_POINT('Ctrl Pts',(-220.569075169698,-1.7891215324493,
135.387705840469));
#129991=CARTESIAN_POINT('Ctrl Pts',(-220.576823066475,-1.65996402597979,
135.434015301768));
#129992=CARTESIAN_POINT('Ctrl Pts',(-220.584569342559,-1.53083353647596,
135.480315076126));
#129993=CARTESIAN_POINT('Ctrl Pts',(-220.592315618643,-1.39973151476155,
135.521220013824));
#129994=CARTESIAN_POINT('Ctrl Pts',(-220.600061894727,-1.26714934093197,
135.556572272183));
#129995=CARTESIAN_POINT('Ctrl Pts',(-220.607808227992,-1.13456618841109,
135.591924791503));
#129996=CARTESIAN_POINT('Ctrl Pts',(-220.615554561258,-1.00050323973906,
135.621724448965));
#129997=CARTESIAN_POINT('Ctrl Pts',(-220.623300894523,-0.865465293542188,
135.645863781685));
#129998=CARTESIAN_POINT('Ctrl Pts',(-220.631048962526,-0.730397106533365,
135.670008520241));
#129999=CARTESIAN_POINT('Ctrl Pts',(-220.638797030529,-0.594353872311261,
135.688490342913));
#130000=CARTESIAN_POINT('Ctrl Pts',(-220.646545098532,-0.457848399608611,
135.70125329614));
#130001=CARTESIAN_POINT('Ctrl Pts',(-220.654301401274,-0.321197847265323,
135.714029813986));
#130002=CARTESIAN_POINT('Ctrl Pts',(-220.662057704015,-0.18408446495979,
135.721075284309));
#130003=CARTESIAN_POINT('Ctrl Pts',(-220.669814006757,-0.0470245348749268,
135.722385806157));
#130004=CARTESIAN_POINT('Ctrl Pts',(-220.677574449271,0.0901085482214175,
135.723697027471));
#130005=CARTESIAN_POINT('Ctrl Pts',(-220.685334891786,0.227187731680498,
135.719267213801));
#130006=CARTESIAN_POINT('Ctrl Pts',(-220.6930953343,0.363699944662658,135.709144548867));
#130007=CARTESIAN_POINT('Ctrl Pts',(-220.700868234565,0.500431299168082,
135.699005634134));
#130008=CARTESIAN_POINT('Ctrl Pts',(-220.70864113483,0.636593475857676,
135.683155651393));
#130009=CARTESIAN_POINT('Ctrl Pts',(-220.716414035096,0.77168081482156,
135.661694431762));
#130010=CARTESIAN_POINT('Ctrl Pts',(-220.723904370858,0.90185738875219,
135.641013381523));
#130011=CARTESIAN_POINT('Ctrl Pts',(-220.73139470662,1.03103561233125,135.615122037242));
#130012=CARTESIAN_POINT('Ctrl Pts',(-220.738885042382,1.1587765898967,135.584153487263));
#130013=CARTESIAN_POINT('Ctrl Pts',(-220.746659376501,1.29136090545014,
135.5520107553));
#130014=CARTESIAN_POINT('Ctrl Pts',(-220.75443371062,1.42281682445883,135.514296394508));
#130015=CARTESIAN_POINT('Ctrl Pts',(-220.762208044739,1.55264007195242,
135.471103793429));
#130016=CARTESIAN_POINT('Ctrl Pts',(-220.769972797687,1.68230332389576,
135.427964423372));
#130017=CARTESIAN_POINT('Ctrl Pts',(-220.777737550634,1.81033754043559,
135.379360368624));
#130018=CARTESIAN_POINT('Ctrl Pts',(-220.785502303581,1.93624946942148,
135.325435827587));
#130019=CARTESIAN_POINT('Ctrl Pts',(-220.793259344466,2.06203634090445,
135.271564845165));
#130020=CARTESIAN_POINT('Ctrl Pts',(-220.801016385351,2.1857047625545,135.212384045534));
#130021=CARTESIAN_POINT('Ctrl Pts',(-220.808773426236,2.30677780939265,
135.148087036275));
#130022=CARTESIAN_POINT('Ctrl Pts',(-220.816524617476,2.42775955410453,
135.083838513891));
#130023=CARTESIAN_POINT('Ctrl Pts',(-220.824275808716,2.54614947577954,
135.014481643969));
#130024=CARTESIAN_POINT('Ctrl Pts',(-220.832026999956,2.66149210039046,
134.940257480649));
#130025=CARTESIAN_POINT('Ctrl Pts',(-220.839774896733,2.77678570130921,
134.866064864578));
#130026=CARTESIAN_POINT('Ctrl Pts',(-220.84752279351,2.8890342530977,134.787009280781));
#130027=CARTESIAN_POINT('Ctrl Pts',(-220.855270690287,2.99780850153503,
134.703376807661));
#130028=CARTESIAN_POINT('Ctrl Pts',(-220.863016966371,3.10655999674449,
134.619761828651));
#130029=CARTESIAN_POINT('Ctrl Pts',(-220.870763242455,3.21183832439996,
134.531572102766));
#130030=CARTESIAN_POINT('Ctrl Pts',(-220.87850951854,3.31324508403936,134.43913572417));
#130031=CARTESIAN_POINT('Ctrl Pts',(-220.886255851805,3.41465259224029,
134.34669866323));
#130032=CARTESIAN_POINT('Ctrl Pts',(-220.89400218507,3.5121881864595,134.250015150408));
#130033=CARTESIAN_POINT('Ctrl Pts',(-220.901748518335,3.60548859914309,
134.14945180077));
#130034=CARTESIAN_POINT('Ctrl Pts',(-220.909496586338,3.69880990580707,
134.048865930668));
#130035=CARTESIAN_POINT('Ctrl Pts',(-220.917244654342,3.78789387779097,
133.94439878137));
#130036=CARTESIAN_POINT('Ctrl Pts',(-220.924992722345,3.87241625413368,
133.836451549122));
#130037=CARTESIAN_POINT('Ctrl Pts',(-220.932749025086,3.95702846186391,
133.72838958927));
#130038=CARTESIAN_POINT('Ctrl Pts',(-220.940505327828,4.03706914790117,
133.616840466288));
#130039=CARTESIAN_POINT('Ctrl Pts',(-220.94826163057,4.11225596713424,133.502236434439));
#130040=CARTESIAN_POINT('Ctrl Pts',(-220.956022073084,4.18748291583656,
133.387571234968));
#130041=CARTESIAN_POINT('Ctrl Pts',(-220.963782515598,4.25785063514177,
133.269848213147));
#130042=CARTESIAN_POINT('Ctrl Pts',(-220.971542958113,4.3231223360576,133.149525074482));
#130043=CARTESIAN_POINT('Ctrl Pts',(-220.979315858378,4.38849881690228,
133.029008782433));
#130044=CARTESIAN_POINT('Ctrl Pts',(-220.987088758643,4.44876275997436,
132.905884384042));
#130045=CARTESIAN_POINT('Ctrl Pts',(-220.994861658909,4.50372483448786,
132.780631266469));
#130046=CARTESIAN_POINT('Ctrl Pts',(-221.002351994671,4.55668889915317,
132.659931415211));
#130047=CARTESIAN_POINT('Ctrl Pts',(-221.009842330433,4.60472976312694,
132.537255213181));
#130048=CARTESIAN_POINT('Ctrl Pts',(-221.017332666195,4.64772216357618,
132.413043853229));
#130049=CARTESIAN_POINT('Ctrl Pts',(-221.025107000315,4.69234463395464,
132.284122981814));
#130050=CARTESIAN_POINT('Ctrl Pts',(-221.032881334434,4.73166960930753,
132.153139860894));
#130051=CARTESIAN_POINT('Ctrl Pts',(-221.040655668553,4.76550308712181,
132.020569230071));
#130052=CARTESIAN_POINT('Ctrl Pts',(-221.0484204215,4.79929486819829,131.888161980704));
#130053=CARTESIAN_POINT('Ctrl Pts',(-221.056185174447,4.82760852184945,
131.7541714894));
#130054=CARTESIAN_POINT('Ctrl Pts',(-221.063949927394,4.85029875143955,
131.619090685922));
#130055=CARTESIAN_POINT('Ctrl Pts',(-221.071706968279,4.87296644477388,
131.484144046603));
#130056=CARTESIAN_POINT('Ctrl Pts',(-221.079464009164,4.89002176462856,
131.348109633224));
#130057=CARTESIAN_POINT('Ctrl Pts',(-221.087221050049,4.90136980894267,
131.211493345906));
#130058=CARTESIAN_POINT('Ctrl Pts',(-221.094972241289,4.9127092956083,131.074980081992));
#130059=CARTESIAN_POINT('Ctrl Pts',(-221.102723432529,4.91835004115387,
130.93788620558));
#130060=CARTESIAN_POINT('Ctrl Pts',(-221.11047462377,4.91824865641744,130.800725215521));
#130061=CARTESIAN_POINT('Ctrl Pts',(-221.118222520547,4.91814731477223,
130.663622522542));
#130062=CARTESIAN_POINT('Ctrl Pts',(-221.125970417324,4.91230869721828,
130.526453162796));
#130063=CARTESIAN_POINT('Ctrl Pts',(-221.133718314101,4.90074146722637,
130.38973291238));
#130064=CARTESIAN_POINT('Ctrl Pts',(-221.141464590185,4.88917665684962,
130.253041260893));
#130065=CARTESIAN_POINT('Ctrl Pts',(-221.149210866269,4.87188565046273,
130.116798921204));
#130066=CARTESIAN_POINT('Ctrl Pts',(-221.156957142353,4.84892913779867,
129.981518421816));
#130067=CARTESIAN_POINT('Ctrl Pts',(-221.164703475618,4.82597245567487,
129.846236923818));
#130068=CARTESIAN_POINT('Ctrl Pts',(-221.172449808884,4.79735024923217,
129.711917665742));
#130069=CARTESIAN_POINT('Ctrl Pts',(-221.180196142149,4.76317460712446,
129.579064439271));
#130070=CARTESIAN_POINT('Ctrl Pts',(-221.187944210152,4.72899131161871,
129.446181461241));
#130071=CARTESIAN_POINT('Ctrl Pts',(-221.195692278155,4.68925220310519,
129.314765546674));
#130072=CARTESIAN_POINT('Ctrl Pts',(-221.203440346158,4.64411954837663,
129.18530636187));
#130073=CARTESIAN_POINT('Ctrl Pts',(-221.2111966489,4.59893892612549,129.055709586305));
#130074=CARTESIAN_POINT('Ctrl Pts',(-221.218952951642,4.54835343563073,
128.928074064561));
#130075=CARTESIAN_POINT('Ctrl Pts',(-221.226709254384,4.49257413021671,
128.802870985565));
#130076=CARTESIAN_POINT('Ctrl Pts',(-221.234469696898,4.43676505370791,
128.677601081916));
#130077=CARTESIAN_POINT('Ctrl Pts',(-221.242230139412,4.37575681247151,
128.554766557908));
#130078=CARTESIAN_POINT('Ctrl Pts',(-221.249990581926,4.30980649687876,
128.434814031832));
#130079=CARTESIAN_POINT('Ctrl Pts',(-221.257763482192,4.24375031198462,
128.314668947313));
#130080=CARTESIAN_POINT('Ctrl Pts',(-221.265536382457,4.17273640181274,
128.197415440432));
#130081=CARTESIAN_POINT('Ctrl Pts',(-221.273309282723,4.09706575044405,
128.083471921011));
#130082=CARTESIAN_POINT('Ctrl Pts',(-221.280799618485,4.02414591785631,
127.97367053553));
#130083=CARTESIAN_POINT('Ctrl Pts',(-221.288289954246,3.9469022151612,127.866942912354));
#130084=CARTESIAN_POINT('Ctrl Pts',(-221.295780290008,3.86563812277885,
127.763632914167));
#130085=CARTESIAN_POINT('Ctrl Pts',(-221.303554624127,3.7812928776333,127.656405885997));
#130086=CARTESIAN_POINT('Ctrl Pts',(-221.311328958247,3.69234917811289,
127.552521094194));
#130087=CARTESIAN_POINT('Ctrl Pts',(-221.319103292366,3.5991015729938,127.452398366917));
#130088=CARTESIAN_POINT('Ctrl Pts',(-221.326868045313,3.50596888721424,
127.352399031954));
#130089=CARTESIAN_POINT('Ctrl Pts',(-221.33463279826,3.40854311347,127.256152819803));
#130090=CARTESIAN_POINT('Ctrl Pts',(-221.342397551207,3.30716043115016,
127.164048413217));
#130091=CARTESIAN_POINT('Ctrl Pts',(-221.350154592092,3.20587844353936,
127.072035486025));
#130092=CARTESIAN_POINT('Ctrl Pts',(-221.357911632977,3.10064765585033,
126.984156439143));
#130093=CARTESIAN_POINT('Ctrl Pts',(-221.365668673862,2.99184239929796,
126.900764567734));
#130094=CARTESIAN_POINT('Ctrl Pts',(-221.373419865102,2.88311919363638,
126.817435582784));
#130095=CARTESIAN_POINT('Ctrl Pts',(-221.381171056342,2.77082719346199,
126.738587274899));
#130096=CARTESIAN_POINT('Ctrl Pts',(-221.388922247582,2.65537496699824,
126.664533707279));
#130097=CARTESIAN_POINT('Ctrl Pts',(-221.396670144359,2.53997181081038,
126.5905116144));
#130098=CARTESIAN_POINT('Ctrl Pts',(-221.404418041136,2.42141142821396,
126.521280419216));
#130099=CARTESIAN_POINT('Ctrl Pts',(-221.412165937914,2.30013243906503,
126.457111622482));
#130100=CARTESIAN_POINT('Ctrl Pts',(-221.419912213998,2.17887881886615,
126.392956248477));
#130101=CARTESIAN_POINT('Ctrl Pts',(-221.427658490082,2.0549080685941,126.333861349351));
#130102=CARTESIAN_POINT('Ctrl Pts',(-221.435404766166,1.92868419727716,
126.280052899288));
#130103=CARTESIAN_POINT('Ctrl Pts',(-221.443151099431,1.80245939420445,
126.226244052023));
#130104=CARTESIAN_POINT('Ctrl Pts',(-221.450897432696,1.67398179654851,
126.177721885006));
#130105=CARTESIAN_POINT('Ctrl Pts',(-221.458643765962,1.54373584517392,
126.134664406588));
#130106=CARTESIAN_POINT('Ctrl Pts',(-221.466391833965,1.41346072612213,
126.091597285746));
#130107=CARTESIAN_POINT('Ctrl Pts',(-221.474139901968,1.28141683647249,
126.053997411372));
#130108=CARTESIAN_POINT('Ctrl Pts',(-221.481887969971,1.14810385551625,
126.021992940416));
#130109=CARTESIAN_POINT('Ctrl Pts',(-221.489644272712,1.0146491879365,125.989954454727));
#130110=CARTESIAN_POINT('Ctrl Pts',(-221.497400575454,0.8799231154359,125.963523343362));
#130111=CARTESIAN_POINT('Ctrl Pts',(-221.505156878196,0.744436142079828,
125.942776730306));
#130112=CARTESIAN_POINT('Ctrl Pts',(-221.51291732071,0.608876855246642,
125.922019044158));
#130113=CARTESIAN_POINT('Ctrl Pts',(-221.520677763225,0.472556246746744,
125.906951944727));
#130114=CARTESIAN_POINT('Ctrl Pts',(-221.528438205739,0.335989032823276,
125.897600542698));
#130115=CARTESIAN_POINT('Ctrl Pts',(-221.536211106004,0.199202589084151,
125.888234128968));
#130116=CARTESIAN_POINT('Ctrl Pts',(-221.54398400627,0.062169139894083,
125.884601758268));
#130117=CARTESIAN_POINT('Ctrl Pts',(-221.551756906535,-0.07459660546559,
125.886676364897));
#130118=CARTESIAN_POINT('Ctrl Pts',(-221.559247242297,-0.20639057149043,
125.888675554349));
#130119=CARTESIAN_POINT('Ctrl Pts',(-221.566737578059,-0.337935651642949,
125.895973981788));
#130120=CARTESIAN_POINT('Ctrl Pts',(-221.574227913821,-0.46877850593014,
125.908502186721));
#130121=CARTESIAN_POINT('Ctrl Pts',(-221.58200224794,-0.604582306805123,
125.921505402352));
#130122=CARTESIAN_POINT('Ctrl Pts',(-221.58977658206,-0.740059766480778,
125.940183988278));
#130123=CARTESIAN_POINT('Ctrl Pts',(-221.597550916179,-0.874698460827502,
125.964517059647));
#130124=CARTESIAN_POINT('Ctrl Pts',(-221.605315669126,-1.00917122501645,
125.988820142681));
#130125=CARTESIAN_POINT('Ctrl Pts',(-221.613080422073,-1.14280689959888,
126.018763776762));
#130126=CARTESIAN_POINT('Ctrl Pts',(-221.62084517502,-1.27509676159619,
126.054275217169));
#130127=CARTESIAN_POINT('Ctrl Pts',(-221.628602215905,-1.40725523143761,
126.089751387113));
#130128=CARTESIAN_POINT('Ctrl Pts',(-221.63635925679,-1.53807017359358,
126.130784257681));
#130129=CARTESIAN_POINT('Ctrl Pts',(-221.644116297675,-1.66704201567277,
126.177249858088));
#130130=CARTESIAN_POINT('Ctrl Pts',(-221.651867488915,-1.79591659908276,
126.223680418423));
#130131=CARTESIAN_POINT('Ctrl Pts',(-221.659618680155,-1.92295048258643,
126.275535422055));
#130132=CARTESIAN_POINT('Ctrl Pts',(-221.667369871395,-2.04765859481255,
126.332640887799));
#130133=CARTESIAN_POINT('Ctrl Pts',(-221.675117768172,-2.17231370276445,
126.389722082196));
#130134=CARTESIAN_POINT('Ctrl Pts',(-221.682865664949,-2.29464465079435,
126.452049137816));
#130135=CARTESIAN_POINT('Ctrl Pts',(-221.690613561726,-2.41418593288091,
126.519399784142));
#130136=CARTESIAN_POINT('Ctrl Pts',(-221.698359837811,-2.53370220950794,
126.586736342164));
#130137=CARTESIAN_POINT('Ctrl Pts',(-221.706106113895,-2.65042964047315,
126.659094208951));
#130138=CARTESIAN_POINT('Ctrl Pts',(-221.713852389979,-2.76392729908182,
126.736205145133));
#130139=CARTESIAN_POINT('Ctrl Pts',(-221.721598723244,-2.87742579550457,
126.813316650529));
#130140=CARTESIAN_POINT('Ctrl Pts',(-221.72934505651,-2.98769414860806,
126.89518107562));
#130141=CARTESIAN_POINT('Ctrl Pts',(-221.737091389775,-3.09432074280527,
126.981487064446));
#130142=CARTESIAN_POINT('Ctrl Pts',(-221.744839457778,-3.20097121528938,
127.0678123809));
#130143=CARTESIAN_POINT('Ctrl Pts',(-221.752587525781,-3.3039780021912,
127.158580994414));
#130144=CARTESIAN_POINT('Ctrl Pts',(-221.760335593784,-3.40296319257896,
127.253441782609));
#130145=CARTESIAN_POINT('Ctrl Pts',(-221.768091896526,-3.50205358560459,
127.348403389978));
#130146=CARTESIAN_POINT('Ctrl Pts',(-221.775848199268,-3.59711356121764,
127.447465589105));
#130147=CARTESIAN_POINT('Ctrl Pts',(-221.78360450201,-3.68780229290825,
127.550240565859));
#130148=CARTESIAN_POINT('Ctrl Pts',(-221.791364944524,-3.77853942790554,
127.653070396713));
#130149=CARTESIAN_POINT('Ctrl Pts',(-221.799125387038,-3.86490042408959,
127.759616650167));
#130150=CARTESIAN_POINT('Ctrl Pts',(-221.806885829552,-3.94658593842749,
127.869459853808));
#130151=CARTESIAN_POINT('Ctrl Pts',(-221.814658729818,-4.02840258160471,
127.979479387511));
#130152=CARTESIAN_POINT('Ctrl Pts',(-221.822431630083,-4.10552852446355,
128.092806124215));
#130153=CARTESIAN_POINT('Ctrl Pts',(-221.830204530348,-4.17770832520685,
128.208992394751));
#130154=CARTESIAN_POINT('Ctrl Pts',(-221.83769486611,-4.2472642083826,128.320955001697));
#130155=CARTESIAN_POINT('Ctrl Pts',(-221.845185201872,-4.31222716366422,
128.435572581482));
#130156=CARTESIAN_POINT('Ctrl Pts',(-221.852675537634,-4.37241058879256,
128.552426181239));
#130157=CARTESIAN_POINT('Ctrl Pts',(-221.860945750391,-4.43886017744144,
128.681446316258));
#130158=CARTESIAN_POINT('Ctrl Pts',(-221.869215963147,-4.49967258269311,
128.813559665546));
#130159=CARTESIAN_POINT('Ctrl Pts',(-221.877486175903,-4.55456782312679,
128.948263904828));
#130160=CARTESIAN_POINT('Ctrl Pts',(-221.885736780321,-4.60933290917299,
129.082648765824));
#130161=CARTESIAN_POINT('Ctrl Pts',(-221.893987384739,-4.65820868546935,
129.219611977023));
#130162=CARTESIAN_POINT('Ctrl Pts',(-221.902237989156,-4.70096171190115,
129.358628261374));
#130163=CARTESIAN_POINT('Ctrl Pts',(-221.906633778092,-4.72373983469675,
129.432693895081));
#130164=CARTESIAN_POINT('Ctrl Pts',(-221.911029567028,-4.74478073337568,
129.507341885676));
#130165=CARTESIAN_POINT('Ctrl Pts',(-221.915425355964,-4.76405452823393,
129.582490119308));
#130166=CARTESIAN_POINT('Ctrl Pts',(-220.165126569317,-4.76405452823397,
129.582490119308));
#130167=CARTESIAN_POINT('Ctrl Pts',(-220.170747644464,-4.7886126718321,
129.678241948475));
#130168=CARTESIAN_POINT('Ctrl Pts',(-220.17636871961,-4.81025828360901,
129.774638318243));
#130169=CARTESIAN_POINT('Ctrl Pts',(-220.181989794757,-4.82896777965386,
129.871486968262));
#130170=CARTESIAN_POINT('Ctrl Pts',(-220.19342524438,-4.86703015987755,
130.068514730655));
#130171=CARTESIAN_POINT('Ctrl Pts',(-220.204860694004,-4.89304326287675,
130.267939432194));
#130172=CARTESIAN_POINT('Ctrl Pts',(-220.216296143627,-4.90677295268619,
130.468559704394));
#130173=CARTESIAN_POINT('Ctrl Pts',(-220.222577617089,-4.91431464846764,
130.578760086305));
#130174=CARTESIAN_POINT('Ctrl Pts',(-220.228859090551,-4.91815080839338,
130.689320837773));
#130175=CARTESIAN_POINT('Ctrl Pts',(-220.235140564013,-4.9182481010867,
130.800038736369));
#130176=CARTESIAN_POINT('',(-219.889859435959,-4.9182489279511,130.807607956143));
#130177=CARTESIAN_POINT('Ctrl Pts',(-219.819723804473,-4.76405452823394,
129.582490119308));
#130178=CARTESIAN_POINT('Ctrl Pts',(-219.827373106639,-4.79769696515867,
129.713661470282));
#130179=CARTESIAN_POINT('Ctrl Pts',(-219.835022408805,-4.82589674123163,
129.84614125547));
#130180=CARTESIAN_POINT('Ctrl Pts',(-219.842671710971,-4.84857457688245,
129.979431750991));
#130181=CARTESIAN_POINT('Ctrl Pts',(-219.850536331803,-4.87189076635859,
130.116474213807));
#130182=CARTESIAN_POINT('Ctrl Pts',(-219.858400952634,-4.88936948971227,
130.254373244885));
#130183=CARTESIAN_POINT('Ctrl Pts',(-219.866265573465,-4.90098184698049,
130.39258398143));
#130184=CARTESIAN_POINT('Ctrl Pts',(-219.874130194296,-4.91259420424872,
130.530794717974));
#130185=CARTESIAN_POINT('Ctrl Pts',(-219.881994815128,-4.91834023657183,
130.669316701531));
#130186=CARTESIAN_POINT('Ctrl Pts',(-219.889859435959,-4.9182489279511,
130.807607956143));
#130187=CARTESIAN_POINT('Ctrl Pts',(-219.889859435996,-4.91824892795067,
130.807607956796));
#130188=CARTESIAN_POINT('Ctrl Pts',(-219.900950013032,-4.91812016579959,
131.00262432765));
#130189=CARTESIAN_POINT('Ctrl Pts',(-219.912040590068,-4.90639276669605,
131.197259495506));
#130190=CARTESIAN_POINT('Ctrl Pts',(-219.923131167104,-4.88319915299843,
131.390491229849));
#130191=CARTESIAN_POINT('Ctrl Pts',(-219.930905501223,-4.86694076520351,
131.525943881264));
#130192=CARTESIAN_POINT('Ctrl Pts',(-219.938679835342,-4.84501647276845,
131.66093409222));
#130193=CARTESIAN_POINT('Ctrl Pts',(-219.946454169461,-4.81745945129712,
131.79495008733));
#130194=CARTESIAN_POINT('Ctrl Pts',(-219.954218922408,-4.78993639139199,
131.928800919704));
#130195=CARTESIAN_POINT('Ctrl Pts',(-219.961983675355,-4.75679449262221,
132.06167954586));
#130196=CARTESIAN_POINT('Ctrl Pts',(-219.969748428302,-4.71811868670756,
132.193079134992));
#130197=CARTESIAN_POINT('Ctrl Pts',(-219.977505469187,-4.67948129414857,
132.324348216199));
#130198=CARTESIAN_POINT('Ctrl Pts',(-219.985262510072,-4.63532104211707,
132.45414081113));
#130199=CARTESIAN_POINT('Ctrl Pts',(-219.993019550957,-4.58577385406006,
132.581960466216));
#130200=CARTESIAN_POINT('Ctrl Pts',(-220.000770742197,-4.53626402992305,
132.709683731505));
#130201=CARTESIAN_POINT('Ctrl Pts',(-220.008521933437,-4.4813754963173,
132.835436655281));
#130202=CARTESIAN_POINT('Ctrl Pts',(-220.016273124677,-4.42129382470151,
132.958738480931));
#130203=CARTESIAN_POINT('Ctrl Pts',(-220.024021021455,-4.36123768939881,
133.081987900016));
#130204=CARTESIAN_POINT('Ctrl Pts',(-220.031768918232,-4.29599297698157,
133.202787942275));
#130205=CARTESIAN_POINT('Ctrl Pts',(-220.039516815009,-4.22579306481921,
133.320678569619));
#130206=CARTESIAN_POINT('Ctrl Pts',(-220.047263091093,-4.15560783696496,
133.438544536787));
#130207=CARTESIAN_POINT('Ctrl Pts',(-220.055009367177,-4.08046967096488,
133.553501963846));
#130208=CARTESIAN_POINT('Ctrl Pts',(-220.062755643261,-4.00065730996832,
133.665116488083));
#130209=CARTESIAN_POINT('Ctrl Pts',(-220.070501976526,-3.92084435981515,
133.776731836233));
#130210=CARTESIAN_POINT('Ctrl Pts',(-220.078248309792,-3.83635737322495,
133.885003914298));
#130211=CARTESIAN_POINT('Ctrl Pts',(-220.085994643057,-3.74751749413209,
133.98952869691));
#130212=CARTESIAN_POINT('Ctrl Pts',(-220.09374271106,-3.65865771996439,
134.094076887123));
#130213=CARTESIAN_POINT('Ctrl Pts',(-220.101490779063,-3.56544336670402,
134.194875814167));
#130214=CARTESIAN_POINT('Ctrl Pts',(-220.109238847066,-3.4682345244356,
134.291556101908));
#130215=CARTESIAN_POINT('Ctrl Pts',(-220.116995149808,-3.37092236745269,
134.388339142609));
#130216=CARTESIAN_POINT('Ctrl Pts',(-220.12475145255,-3.26960751848575,
134.480994523663));
#130217=CARTESIAN_POINT('Ctrl Pts',(-220.132507755291,-3.16468585888112,
134.569190823179));
#130218=CARTESIAN_POINT('Ctrl Pts',(-220.140268197806,-3.05970819942764,
134.657434195716));
#130219=CARTESIAN_POINT('Ctrl Pts',(-220.14802864032,-2.95112020287667,
134.741213505764));
#130220=CARTESIAN_POINT('Ctrl Pts',(-220.155789082834,-2.839348404252,134.820239562675));
#130221=CARTESIAN_POINT('Ctrl Pts',(-220.163561983099,-2.72739717961353,
134.899392479229));
#130222=CARTESIAN_POINT('Ctrl Pts',(-220.171334883365,-2.61225226824061,
134.973776682517));
#130223=CARTESIAN_POINT('Ctrl Pts',(-220.17910778363,-2.49436734028331,
135.043147547128));
#130224=CARTESIAN_POINT('Ctrl Pts',(-220.186598119392,-2.38076782639178,
135.109996606076));
#130225=CARTESIAN_POINT('Ctrl Pts',(-220.194088455154,-2.2646243218323,
135.172190347753));
#130226=CARTESIAN_POINT('Ctrl Pts',(-220.201578790916,-2.14636013676526,
135.229552277348));
#130227=CARTESIAN_POINT('Ctrl Pts',(-220.209353125035,-2.02361192917527,
135.289089101939));
#130228=CARTESIAN_POINT('Ctrl Pts',(-220.217127459154,-1.89819022598548,
135.343609080126));
#130229=CARTESIAN_POINT('Ctrl Pts',(-220.224901793273,-1.77054353054598,
135.392863496386));
#130230=CARTESIAN_POINT('Ctrl Pts',(-220.23266654622,-1.64305414825084,
135.442057210981));
#130231=CARTESIAN_POINT('Ctrl Pts',(-220.240431299168,-1.51334559092697,
135.485998136096));
#130232=CARTESIAN_POINT('Ctrl Pts',(-220.248196052115,-1.38189017735495,
135.524483772763));
#130233=CARTESIAN_POINT('Ctrl Pts',(-220.255953093,-1.2505653271529,135.562931184954));
#130234=CARTESIAN_POINT('Ctrl Pts',(-220.263710133885,-1.11749744622303,
135.595933982157));
#130235=CARTESIAN_POINT('Ctrl Pts',(-220.27146717477,-0.983177684957099,
135.623338175337));
#130236=CARTESIAN_POINT('Ctrl Pts',(-220.27921836601,-0.848959215267808,
135.650721702802));
#130237=CARTESIAN_POINT('Ctrl Pts',(-220.28696955725,-0.71349112584585,
135.672514951943));
#130238=CARTESIAN_POINT('Ctrl Pts',(-220.29472074849,-0.57727819675249,
135.688614188589));
#130239=CARTESIAN_POINT('Ctrl Pts',(-220.302468645267,-0.441123161787408,
135.704706582631));
#130240=CARTESIAN_POINT('Ctrl Pts',(-220.310216542045,-0.304224304247776,
135.715109731794));
#130241=CARTESIAN_POINT('Ctrl Pts',(-220.317964438822,-0.167094813374376,
135.719771321245));
#130242=CARTESIAN_POINT('Ctrl Pts',(-220.325710714906,-0.0299940070346701,
135.724431935593));
#130243=CARTESIAN_POINT('Ctrl Pts',(-220.33345699099,0.107336946187845,
135.72335336583));
#130244=CARTESIAN_POINT('Ctrl Pts',(-220.341203267074,0.244381937159659,
135.716535342806));
#130245=CARTESIAN_POINT('Ctrl Pts',(-220.348949600339,0.381427939766652,
135.709717269454));
#130246=CARTESIAN_POINT('Ctrl Pts',(-220.356695933605,0.518187585428513,
135.697159677726));
#130247=CARTESIAN_POINT('Ctrl Pts',(-220.36444226687,0.654147370020168,
135.678914369531));
#130248=CARTESIAN_POINT('Ctrl Pts',(-220.372190334873,0.790137601862718,
135.660664975425));
#130249=CARTESIAN_POINT('Ctrl Pts',(-220.379938402876,0.925327228782847,
135.636725382278));
#130250=CARTESIAN_POINT('Ctrl Pts',(-220.387686470879,1.05921084669146,
135.607198887251));
#130251=CARTESIAN_POINT('Ctrl Pts',(-220.395442773621,1.1932367577026,135.577641011114));
#130252=CARTESIAN_POINT('Ctrl Pts',(-220.403199076363,1.32595350453939,
135.542484455986));
#130253=CARTESIAN_POINT('Ctrl Pts',(-220.410955379105,1.45686826904143,
135.501883146427));
#130254=CARTESIAN_POINT('Ctrl Pts',(-220.418715821619,1.58785290669506,
135.461260166728));
#130255=CARTESIAN_POINT('Ctrl Pts',(-220.426476264133,1.71703327753685,
135.415186773362));
#130256=CARTESIAN_POINT('Ctrl Pts',(-220.434236706647,1.84393552468517,
135.363865507716));
#130257=CARTESIAN_POINT('Ctrl Pts',(-220.442009606913,1.97104148658646,
135.312461856619));
#130258=CARTESIAN_POINT('Ctrl Pts',(-220.449782507178,2.09586166065049,
135.25579366042));
#130259=CARTESIAN_POINT('Ctrl Pts',(-220.457555407443,2.2179450167936,135.194110378655));
#130260=CARTESIAN_POINT('Ctrl Pts',(-220.465045743205,2.33559033543083,
135.134669439553));
#130261=CARTESIAN_POINT('Ctrl Pts',(-220.472536078967,2.45069409289816,
135.070571856355));
#130262=CARTESIAN_POINT('Ctrl Pts',(-220.480026414729,2.56287898963283,
135.002078372132));
#130263=CARTESIAN_POINT('Ctrl Pts',(-220.487800748849,2.67931741082588,
134.930987936636));
#130264=CARTESIAN_POINT('Ctrl Pts',(-220.495575082967,2.79298010672972,
134.854936485549));
#130265=CARTESIAN_POINT('Ctrl Pts',(-220.503349417087,2.90341539891617,
134.774166920629));
#130266=CARTESIAN_POINT('Ctrl Pts',(-220.511114170034,3.01371458947458,
134.693496896978));
#130267=CARTESIAN_POINT('Ctrl Pts',(-220.518878922981,3.12079397778714,
134.608120557506));
#130268=CARTESIAN_POINT('Ctrl Pts',(-220.526643675928,3.22422789589776,
134.51832582174));
#130269=CARTESIAN_POINT('Ctrl Pts',(-220.534400716813,3.32755908198275,
134.428620271371));
#130270=CARTESIAN_POINT('Ctrl Pts',(-220.542157757698,3.4272517099638,134.334505312493));
#130271=CARTESIAN_POINT('Ctrl Pts',(-220.549914798583,3.52291074572038,
134.236310929005));
#130272=CARTESIAN_POINT('Ctrl Pts',(-220.557665989823,3.61849764425412,
134.138190594666));
#130273=CARTESIAN_POINT('Ctrl Pts',(-220.565417181063,3.71005673329742,
134.03599723787));
#130274=CARTESIAN_POINT('Ctrl Pts',(-220.573168372303,3.7972278924029,133.930099473526));
#130275=CARTESIAN_POINT('Ctrl Pts',(-220.58091626908,3.8843620014405,133.824246718557));
#130276=CARTESIAN_POINT('Ctrl Pts',(-220.588664165858,3.9671116419044,133.714692988765));
#130277=CARTESIAN_POINT('Ctrl Pts',(-220.596412062635,4.04515540852403,
133.601841767349));
#130278=CARTESIAN_POINT('Ctrl Pts',(-220.604158338719,4.12318285006989,
133.489014151975));
#130279=CARTESIAN_POINT('Ctrl Pts',(-220.611904614803,4.19650615349358,
133.372890738312));
#130280=CARTESIAN_POINT('Ctrl Pts',(-220.619650890887,4.26484612275778,
133.253905598108));
#130281=CARTESIAN_POINT('Ctrl Pts',(-220.627397224152,4.33318659649221,
133.134919579582));
#130282=CARTESIAN_POINT('Ctrl Pts',(-220.635143557418,4.3965434679426,133.013072131388));
#130283=CARTESIAN_POINT('Ctrl Pts',(-220.642889890683,4.45468275799805,
132.888823279284));
#130284=CARTESIAN_POINT('Ctrl Pts',(-220.650637958686,4.51283506794448,
132.76454660251));
#130285=CARTESIAN_POINT('Ctrl Pts',(-220.658386026689,4.56576730576534,
132.637867805759));
#130286=CARTESIAN_POINT('Ctrl Pts',(-220.666134094692,4.61329319503459,
132.509267934445));
#130287=CARTESIAN_POINT('Ctrl Pts',(-220.673890397434,4.66086959538445,
132.380531385657));
#130288=CARTESIAN_POINT('Ctrl Pts',(-220.681646700176,4.70302803332159,
132.249870051016));
#130289=CARTESIAN_POINT('Ctrl Pts',(-220.689403002918,4.73963162968545,
132.117781752383));
#130290=CARTESIAN_POINT('Ctrl Pts',(-220.697163445432,4.7762547624908,131.985622954249));
#130291=CARTESIAN_POINT('Ctrl Pts',(-220.704923887946,4.80731705763174,
131.852036055162));
#130292=CARTESIAN_POINT('Ctrl Pts',(-220.71268433046,4.83273278769379,131.717529202905));
#130293=CARTESIAN_POINT('Ctrl Pts',(-220.720457230726,4.85818931734204,
131.582806428307));
#130294=CARTESIAN_POINT('Ctrl Pts',(-220.728230130991,4.87798111193681,
131.447161136533));
#130295=CARTESIAN_POINT('Ctrl Pts',(-220.736003031256,4.89207425607369,
131.311107630938));
#130296=CARTESIAN_POINT('Ctrl Pts',(-220.743493367018,4.9056550789226,131.18000001297));
#130297=CARTESIAN_POINT('Ctrl Pts',(-220.75098370278,4.91394435931675,131.048513652516));
#130298=CARTESIAN_POINT('Ctrl Pts',(-220.758474038542,4.91695752815712,
130.917106920383));
#130299=CARTESIAN_POINT('Ctrl Pts',(-220.766248372661,4.92008494220994,
130.78071786206));
#130300=CARTESIAN_POINT('Ctrl Pts',(-220.774022706781,4.91753816602361,
130.643982549929));
#130301=CARTESIAN_POINT('Ctrl Pts',(-220.7817970409,4.90927741650165,130.507412288177));
#130302=CARTESIAN_POINT('Ctrl Pts',(-220.789561793847,4.90102684761518,
130.371010337067));
#130303=CARTESIAN_POINT('Ctrl Pts',(-220.797326546794,4.88707634017612,
130.234773418115));
#130304=CARTESIAN_POINT('Ctrl Pts',(-220.805091299741,4.86743804510946,
130.099215285368));
#130305=CARTESIAN_POINT('Ctrl Pts',(-220.812848340626,4.84781925507433,
129.963791790869));
#130306=CARTESIAN_POINT('Ctrl Pts',(-220.820605381511,4.82252397524754,
129.829046125347));
#130307=CARTESIAN_POINT('Ctrl Pts',(-220.828362422396,4.7916163048381,129.695489006553));
#130308=CARTESIAN_POINT('Ctrl Pts',(-220.836113613636,4.76073194214338,
129.562032604223));
#130309=CARTESIAN_POINT('Ctrl Pts',(-220.843864804876,4.72424370088741,
129.429763343962));
#130310=CARTESIAN_POINT('Ctrl Pts',(-220.851615996116,4.68226705333496,
129.299183450667));
#130311=CARTESIAN_POINT('Ctrl Pts',(-220.859363892894,4.64030824697743,
129.168659057309));
#130312=CARTESIAN_POINT('Ctrl Pts',(-220.867111789671,4.59286579332397,
129.039822974245));
#130313=CARTESIAN_POINT('Ctrl Pts',(-220.874859686448,4.54010542681638,
128.913163701353));
#130314=CARTESIAN_POINT('Ctrl Pts',(-220.882605962532,4.48735609664008,
128.786530922851));
#130315=CARTESIAN_POINT('Ctrl Pts',(-220.890352238616,4.42929121646095,
128.6620744095));
#130316=CARTESIAN_POINT('Ctrl Pts',(-220.8980985147,4.36612507085669,128.540263683215));
#130317=CARTESIAN_POINT('Ctrl Pts',(-220.905844847965,4.30295845897437,
128.418452057752));
#130318=CARTESIAN_POINT('Ctrl Pts',(-220.913591181231,4.23469068650564,
128.299286605402));
#130319=CARTESIAN_POINT('Ctrl Pts',(-220.921337514496,4.16158231472618,
128.183212834579));
#130320=CARTESIAN_POINT('Ctrl Pts',(-220.929085582499,4.08845757083364,
128.067113069839));
#130321=CARTESIAN_POINT('Ctrl Pts',(-220.936833650502,4.0104902788811,127.954106695096));
#130322=CARTESIAN_POINT('Ctrl Pts',(-220.944581718505,3.92798446904098,
127.844610446779));
#130323=CARTESIAN_POINT('Ctrl Pts',(-220.952338021247,3.84539097104444,
127.734997824546));
#130324=CARTESIAN_POINT('Ctrl Pts',(-220.960094323989,3.75824955517193,
127.628903093767));
#130325=CARTESIAN_POINT('Ctrl Pts',(-220.967850626731,3.66690506652434,
127.526710499631));
#130326=CARTESIAN_POINT('Ctrl Pts',(-220.975611069245,3.57551182457258,
127.424463362231));
#130327=CARTESIAN_POINT('Ctrl Pts',(-220.983371511759,3.47991131225539,
127.326122791601));
#130328=CARTESIAN_POINT('Ctrl Pts',(-220.991131954273,3.38048471093133,
127.232035578931));
#130329=CARTESIAN_POINT('Ctrl Pts',(-220.998904854539,3.28089850120042,
127.137797329115));
#130330=CARTESIAN_POINT('Ctrl Pts',(-221.006677754804,3.17747422397626,
127.047826338265));
#130331=CARTESIAN_POINT('Ctrl Pts',(-221.01445065507,3.07062624513349,126.962429133898));
#130332=CARTESIAN_POINT('Ctrl Pts',(-221.021940990832,2.96766245945721,
126.880136333014));
#130333=CARTESIAN_POINT('Ctrl Pts',(-221.029431326594,2.86151981905106,
126.802090737096));
#130334=CARTESIAN_POINT('Ctrl Pts',(-221.036921662355,2.75259230503557,
126.728527124309));
#130335=CARTESIAN_POINT('Ctrl Pts',(-221.044695996474,2.63953477121693,
126.652174324782));
#130336=CARTESIAN_POINT('Ctrl Pts',(-221.052470330594,2.52311888583939,
126.580408223564));
#130337=CARTESIAN_POINT('Ctrl Pts',(-221.060244664713,2.40375331986032,
126.513538663702));
#130338=CARTESIAN_POINT('Ctrl Pts',(-221.06800941766,2.28453486127299,126.446751514597));
#130339=CARTESIAN_POINT('Ctrl Pts',(-221.075774170607,2.16237429289868,
126.384849089139));
#130340=CARTESIAN_POINT('Ctrl Pts',(-221.083538923554,2.03771041843704,
126.328098861023));
#130341=CARTESIAN_POINT('Ctrl Pts',(-221.091295964439,1.91317036189297,
126.271404998033));
#130342=CARTESIAN_POINT('Ctrl Pts',(-221.099053005324,1.78613230067616,
126.21985330979));
#130343=CARTESIAN_POINT('Ctrl Pts',(-221.106810046209,1.65706056328343,
126.173665923234));
#130344=CARTESIAN_POINT('Ctrl Pts',(-221.114561237449,1.52808615989209,
126.127513366946));
#130345=CARTESIAN_POINT('Ctrl Pts',(-221.122312428689,1.39708149950177,
126.086717191689));
#130346=CARTESIAN_POINT('Ctrl Pts',(-221.130063619929,1.26453153371922,
126.051451712198));
#130347=CARTESIAN_POINT('Ctrl Pts',(-221.137811516706,1.13203790520784,
126.016201221476));
#130348=CARTESIAN_POINT('Ctrl Pts',(-221.145559413483,0.998000654652205,
125.986476851482));
#130349=CARTESIAN_POINT('Ctrl Pts',(-221.15330731026,0.862920354351025,
125.962403211253));
#130350=CARTESIAN_POINT('Ctrl Pts',(-221.161053586345,0.727868309937043,
125.938334606711));
#130351=CARTESIAN_POINT('Ctrl Pts',(-221.168799862429,0.59177403441315,
125.919914449403));
#130352=CARTESIAN_POINT('Ctrl Pts',(-221.176546138513,0.455148375913521,
125.907216243709));
#130353=CARTESIAN_POINT('Ctrl Pts',(-221.184292471778,0.318521708874132,
125.894517944279));
#130354=CARTESIAN_POINT('Ctrl Pts',(-221.192038805043,0.181364040319306,
125.887541716927));
#130355=CARTESIAN_POINT('Ctrl Pts',(-221.199785138309,0.0441910288280734,
125.886309152253));
#130356=CARTESIAN_POINT('Ctrl Pts',(-221.207533206312,-0.0930127016078046,
125.885076311553));
#130357=CARTESIAN_POINT('Ctrl Pts',(-221.215281274314,-0.23023139094262,
125.889589696539));
#130358=CARTESIAN_POINT('Ctrl Pts',(-221.223029342317,-0.366950091281238,
125.899818774233));
#130359=CARTESIAN_POINT('Ctrl Pts',(-221.230785645059,-0.503814097881735,
125.910058723512));
#130360=CARTESIAN_POINT('Ctrl Pts',(-221.238541947801,-0.64017666347159,
125.926026471164));
#130361=CARTESIAN_POINT('Ctrl Pts',(-221.246298250543,-0.775528114489551,
125.94763958315));
#130362=CARTESIAN_POINT('Ctrl Pts',(-221.254058693057,-0.910951806652642,
125.969264230705));
#130363=CARTESIAN_POINT('Ctrl Pts',(-221.261819135571,-1.04536292595293,
125.996540168737));
#130364=CARTESIAN_POINT('Ctrl Pts',(-221.269579578086,-1.17826366930557,
126.029334147682));
#130365=CARTESIAN_POINT('Ctrl Pts',(-221.277352478351,-1.31137775672946,
126.062180770433));
#130366=CARTESIAN_POINT('Ctrl Pts',(-221.285125378616,-1.44297624756009,
126.100563025771));
#130367=CARTESIAN_POINT('Ctrl Pts',(-221.292898278882,-1.57257727663969,
126.14429798156));
#130368=CARTESIAN_POINT('Ctrl Pts',(-221.300388614644,-1.69746698186977,
126.186443061546));
#130369=CARTESIAN_POINT('Ctrl Pts',(-221.307878950406,-1.82050164190373,
126.233558320073));
#130370=CARTESIAN_POINT('Ctrl Pts',(-221.315369286168,-1.94127077480415,
126.285439193001));
#130371=CARTESIAN_POINT('Ctrl Pts',(-221.323144083621,-2.06662637656044,
126.339290354215));
#130372=CARTESIAN_POINT('Ctrl Pts',(-221.330918881074,-2.1899380864231,
126.398446846992));
#130373=CARTESIAN_POINT('Ctrl Pts',(-221.338693678526,-2.3107242423772,
126.462732289601));
#130374=CARTESIAN_POINT('Ctrl Pts',(-221.346458789292,-2.4313599098228,
126.526937638425));
#130375=CARTESIAN_POINT('Ctrl Pts',(-221.354223900058,-2.54947594257647,
126.59625903987));
#130376=CARTESIAN_POINT('Ctrl Pts',(-221.361989010823,-2.66461006112031,
126.670471857007));
#130377=CARTESIAN_POINT('Ctrl Pts',(-221.369746304462,-2.77962827428892,
126.744609964192));
#130378=CARTESIAN_POINT('Ctrl Pts',(-221.3775035981,-2.89167022096498,126.823629476611));
#130379=CARTESIAN_POINT('Ctrl Pts',(-221.385260891738,-3.0002979989038,
126.907259774596));
#130380=CARTESIAN_POINT('Ctrl Pts',(-221.393011880304,-3.10883748497579,
126.990822098484));
#130381=CARTESIAN_POINT('Ctrl Pts',(-221.400762868871,-3.21396801915762,
127.078987508418));
#130382=CARTESIAN_POINT('Ctrl Pts',(-221.408513857437,-3.31528085322855,
127.171442241561));
#130383=CARTESIAN_POINT('Ctrl Pts',(-221.416261396742,-3.41654860215193,
127.263855831492));
#130384=CARTESIAN_POINT('Ctrl Pts',(-221.424008936047,-3.5140017427338,
127.360554684248));
#130385=CARTESIAN_POINT('Ctrl Pts',(-221.431756475352,-3.6072649213944,
127.461185053917));
#130386=CARTESIAN_POINT('Ctrl Pts',(-221.439502244726,-3.70050679401147,
127.561792434503));
#130387=CARTESIAN_POINT('Ctrl Pts',(-221.4472480141,-3.78956034409026,127.666329258117));
#130388=CARTESIAN_POINT('Ctrl Pts',(-221.454993783473,-3.87408767204341,
127.774405540041));
#130389=CARTESIAN_POINT('Ctrl Pts',(-221.462739460707,-3.95861399450273,
127.882480536344));
#130390=CARTESIAN_POINT('Ctrl Pts',(-221.470485137941,-4.03861396203924,
127.994094598687));
#130391=CARTESIAN_POINT('Ctrl Pts',(-221.478230815175,-4.11379075744866,
128.108825667611));
#130392=CARTESIAN_POINT('Ctrl Pts',(-221.485981813398,-4.18901919648106,
128.223635552452));
#130393=CARTESIAN_POINT('Ctrl Pts',(-221.49373281162,-4.25941762770265,
128.341566395407));
#130394=CARTESIAN_POINT('Ctrl Pts',(-221.501483809842,-4.32473311558681,
128.462167939444));
#130395=CARTESIAN_POINT('Ctrl Pts',(-221.50923737993,-4.39007027586261,
128.58280950039));
#130396=CARTESIAN_POINT('Ctrl Pts',(-221.516990950017,-4.45032095711604,
128.706123178454));
#130397=CARTESIAN_POINT('Ctrl Pts',(-221.524744520105,-4.5052792459048,
128.831636110971));
#130398=CARTESIAN_POINT('Ctrl Pts',(-221.532507821331,-4.56030651023185,
128.957306568809));
#130399=CARTESIAN_POINT('Ctrl Pts',(-221.540271122556,-4.61002796411655,
129.085181433099));
#130400=CARTESIAN_POINT('Ctrl Pts',(-221.548034423782,-4.65428647230588,
129.214769319084));
#130401=CARTESIAN_POINT('Ctrl Pts',(-221.555295960669,-4.69568442666006,
129.335981569752));
#130402=CARTESIAN_POINT('Ctrl Pts',(-221.562557497555,-4.73230319573831,
129.458692155801));
#130403=CARTESIAN_POINT('Ctrl Pts',(-221.569819034442,-4.76405452823418,
129.582490119309));
#130404=CARTESIAN_POINT('Origin',(213.235140564004,0.,130.804360617566));
#130405=CARTESIAN_POINT('',(-223.665116307759,-4.76405452823394,129.582490119308));
#130406=CARTESIAN_POINT('',(-223.320144520485,-4.76405452823402,129.582490119308));
#130407=CARTESIAN_POINT('',(213.235140564004,-4.76405452823405,129.582490119308));
#130408=CARTESIAN_POINT('',(-221.985140563982,-4.91824995565472,130.803700161376));
#130409=CARTESIAN_POINT('Ctrl Pts',(-221.985140564013,-4.91824995565479,
130.803700161931));
#130410=CARTESIAN_POINT('Ctrl Pts',(-221.993178256749,-4.91826912013828,
130.946413336073));
#130411=CARTESIAN_POINT('Ctrl Pts',(-222.001215949486,-4.91207227540122,
131.089033628501));
#130412=CARTESIAN_POINT('Ctrl Pts',(-222.009253642222,-4.89970964901554,
131.231008502647));
#130413=CARTESIAN_POINT('Ctrl Pts',(-222.017299291977,-4.88733478408705,
131.373123926667));
#130414=CARTESIAN_POINT('Ctrl Pts',(-222.025344941732,-4.86878199361895,
131.514592312837));
#130415=CARTESIAN_POINT('Ctrl Pts',(-222.033390591486,-4.84415304880318,
131.654868878708));
#130416=CARTESIAN_POINT('Ctrl Pts',(-222.041534972316,-4.81922187330652,
131.796866829005));
#130417=CARTESIAN_POINT('Ctrl Pts',(-222.049679353146,-4.78806451638956,
131.937643156266));
#130418=CARTESIAN_POINT('Ctrl Pts',(-222.057823733976,-4.75083869372908,
132.076647836973));
#130419=CARTESIAN_POINT('Ctrl Pts',(-222.06589426754,-4.71395040750041,
132.214392125281));
#130420=CARTESIAN_POINT('Ctrl Pts',(-222.073964801103,-4.6711034313127,
132.350396457847));
#130421=CARTESIAN_POINT('Ctrl Pts',(-222.082035334667,-4.62250005030999,
132.484145230957));
#130422=CARTESIAN_POINT('Ctrl Pts',(-222.09021663913,-4.57322957088086,
132.61972975282));
#130423=CARTESIAN_POINT('Ctrl Pts',(-222.098397943593,-4.51804366592107,
132.752996004699));
#130424=CARTESIAN_POINT('Ctrl Pts',(-222.106579248056,-4.45720141736564,
132.883432186208));
#130425=CARTESIAN_POINT('Ctrl Pts',(-222.11476055252,-4.39635916881021,
133.013868367716));
#130426=CARTESIAN_POINT('Ctrl Pts',(-222.122941856983,-4.32986080206274,
133.141474185439));
#130427=CARTESIAN_POINT('Ctrl Pts',(-222.131123161446,-4.25801094468777,
133.265767909629));
#130428=CARTESIAN_POINT('Ctrl Pts',(-222.138897495565,-4.18973518253385,
133.383878773867));
#130429=CARTESIAN_POINT('Ctrl Pts',(-222.146671829684,-4.11643322368602,
133.499333762852));
#130430=CARTESIAN_POINT('Ctrl Pts',(-222.154446163803,-4.03833706091389,
133.611675499254));
#130431=CARTESIAN_POINT('Ctrl Pts',(-222.16221091675,-3.96033714468272,
133.723878784507));
#130432=CARTESIAN_POINT('Ctrl Pts',(-222.169975669698,-3.87755500155651,
133.832976133341));
#130433=CARTESIAN_POINT('Ctrl Pts',(-222.177740422645,-3.79026825329181,
133.938535091106));
#130434=CARTESIAN_POINT('Ctrl Pts',(-222.18549746353,-3.70306819945601,
134.043989206226));
#130435=CARTESIAN_POINT('Ctrl Pts',(-222.193254504415,-3.61137269154984,
134.145911624703));
#130436=CARTESIAN_POINT('Ctrl Pts',(-222.2010115453,-3.51550213871602,134.243899507473));
#130437=CARTESIAN_POINT('Ctrl Pts',(-222.20876273654,-3.41970388261198,
134.341813496818));
#130438=CARTESIAN_POINT('Ctrl Pts',(-222.21651392778,-3.31973712065904,
134.435798577891));
#130439=CARTESIAN_POINT('Ctrl Pts',(-222.22426511902,-3.21596171971684,
134.525485888209));
#130440=CARTESIAN_POINT('Ctrl Pts',(-222.232013015797,-3.1122304260882,
134.615135079027));
#130441=CARTESIAN_POINT('Ctrl Pts',(-222.239760912574,-3.0046940082699,
134.700489877081));
#130442=CARTESIAN_POINT('Ctrl Pts',(-222.247508809351,-2.89374812042594,
134.781219287173));
#130443=CARTESIAN_POINT('Ctrl Pts',(-222.255255085435,-2.78282544007,134.861931810413));
#130444=CARTESIAN_POINT('Ctrl Pts',(-222.26300136152,-2.66849502418884,
134.938020640278));
#130445=CARTESIAN_POINT('Ctrl Pts',(-222.270747637604,-2.55118411959399,
135.009196244607));
#130446=CARTESIAN_POINT('Ctrl Pts',(-222.278493970869,-2.43387234903685,
135.080372374338));
#130447=CARTESIAN_POINT('Ctrl Pts',(-222.286240304134,-2.31358038011799,
135.146635003361));
#130448=CARTESIAN_POINT('Ctrl Pts',(-222.2939866374,-2.19076249126769,135.207739180596));
#130449=CARTESIAN_POINT('Ctrl Pts',(-222.301734705403,-2.06791709820258,
135.268857041689));
#130450=CARTESIAN_POINT('Ctrl Pts',(-222.309482773406,-1.9425450095733,
135.324813978163));
#130451=CARTESIAN_POINT('Ctrl Pts',(-222.317230841409,-1.8151226621441,
135.375412223474));
#130452=CARTESIAN_POINT('Ctrl Pts',(-222.32498714415,-1.68756488872789,
135.426064245201));
#130453=CARTESIAN_POINT('Ctrl Pts',(-222.332743446892,-1.5579528675906,
135.471346054309));
#130454=CARTESIAN_POINT('Ctrl Pts',(-222.340499749634,-1.42678099251033,
135.511108864701));
#130455=CARTESIAN_POINT('Ctrl Pts',(-222.348260192148,-1.29553910705082,
135.550892897703));
#130456=CARTESIAN_POINT('Ctrl Pts',(-222.356020634663,-1.16273608712611,
135.585151964909));
#130457=CARTESIAN_POINT('Ctrl Pts',(-222.363781077177,-1.02887787696217,
135.613788169448));
#130458=CARTESIAN_POINT('Ctrl Pts',(-222.371553977442,-0.894804785715897,
135.642470343364));
#130459=CARTESIAN_POINT('Ctrl Pts',(-222.379326877708,-0.759673504932953,
135.665511551398));
#130460=CARTESIAN_POINT('Ctrl Pts',(-222.387099777973,-0.623997375986374,
135.682865546052));
#130461=CARTESIAN_POINT('Ctrl Pts',(-222.394590113735,-0.49325341607235,
135.699588679288));
#130462=CARTESIAN_POINT('Ctrl Pts',(-222.402080449497,-0.362003840312219,
135.711030882678));
#130463=CARTESIAN_POINT('Ctrl Pts',(-222.409570785259,-0.23070725781262,
135.717196583044));
#130464=CARTESIAN_POINT('Ctrl Pts',(-222.417345119379,-0.0944325254829208,
135.723596057813));
#130465=CARTESIAN_POINT('Ctrl Pts',(-222.425119453498,0.0423245258622504,
135.724331285506));
#130466=CARTESIAN_POINT('Ctrl Pts',(-222.432893787617,0.179053693964256,
135.719350224592));
#130467=CARTESIAN_POINT('Ctrl Pts',(-222.440658540564,0.315614355586413,
135.714375302391));
#130468=CARTESIAN_POINT('Ctrl Pts',(-222.448423293511,0.452146815383447,
135.703698122763));
#130469=CARTESIAN_POINT('Ctrl Pts',(-222.456188046458,0.588137175670653,
135.687318504451));
#130470=CARTESIAN_POINT('Ctrl Pts',(-222.463945087343,0.723992468414893,
135.670955154608));
#130471=CARTESIAN_POINT('Ctrl Pts',(-222.471702128228,0.859306347483183,
135.648900683635));
#130472=CARTESIAN_POINT('Ctrl Pts',(-222.479459169113,0.993566703993762,
135.621206916465));
#130473=CARTESIAN_POINT('Ctrl Pts',(-222.487210360353,1.12772581372565,
135.59353403338));
#130474=CARTESIAN_POINT('Ctrl Pts',(-222.494961551593,1.26083260088827,
135.560230397376));
#130475=CARTESIAN_POINT('Ctrl Pts',(-222.502712742833,1.39238221420001,
135.521399395452));
#130476=CARTESIAN_POINT('Ctrl Pts',(-222.510460639611,1.52387591541635,
135.48258489774));
#130477=CARTESIAN_POINT('Ctrl Pts',(-222.518208536388,1.65381338494664,
135.438247817095));
#130478=CARTESIAN_POINT('Ctrl Pts',(-222.525956433165,1.78170228641648,
135.388542117581));
#130479=CARTESIAN_POINT('Ctrl Pts',(-222.533702709249,1.90956443628511,
135.338846815428));
#130480=CARTESIAN_POINT('Ctrl Pts',(-222.541448985333,2.03537850625734,
135.283785269656));
#130481=CARTESIAN_POINT('Ctrl Pts',(-222.549195261417,2.15866996738857,
135.223560435904));
#130482=CARTESIAN_POINT('Ctrl Pts',(-222.556941594682,2.28196233862919,
135.163335157585));
#130483=CARTESIAN_POINT('Ctrl Pts',(-222.564687927948,2.40273171257697,
135.09794668683));
#130484=CARTESIAN_POINT('Ctrl Pts',(-222.572434261213,2.52052645636256,
135.027644818905));
#130485=CARTESIAN_POINT('Ctrl Pts',(-222.580182329216,2.63834757946446,
134.957327207364));
#130486=CARTESIAN_POINT('Ctrl Pts',(-222.587930397219,2.75319241119095,
134.882094209466));
#130487=CARTESIAN_POINT('Ctrl Pts',(-222.595678465222,2.86463703923666,
134.802239767307));
#130488=CARTESIAN_POINT('Ctrl Pts',(-222.603434767964,2.97620011195942,
134.722300454896));
#130489=CARTESIAN_POINT('Ctrl Pts',(-222.611191070706,3.08435544378355,
134.637730114602));
#130490=CARTESIAN_POINT('Ctrl Pts',(-222.618947373447,3.1887106248404,134.548864271394));
#130491=CARTESIAN_POINT('Ctrl Pts',(-222.626707815962,3.29312150339945,
134.45995099781));
#130492=CARTESIAN_POINT('Ctrl Pts',(-222.634468258476,3.39372790307092,
134.366737918619));
#130493=CARTESIAN_POINT('Ctrl Pts',(-222.64222870099,3.4901739852307,134.269597783377));
#130494=CARTESIAN_POINT('Ctrl Pts',(-222.650001601255,3.58677489120363,
134.172301710167));
#130495=CARTESIAN_POINT('Ctrl Pts',(-222.657774501521,3.67920187011259,
134.071066272282));
#130496=CARTESIAN_POINT('Ctrl Pts',(-222.665547401786,3.76713853907477,
133.966298360457));
#130497=CARTESIAN_POINT('Ctrl Pts',(-222.673037737548,3.85187848862107,
133.865339026121));
#130498=CARTESIAN_POINT('Ctrl Pts',(-222.68052807331,3.93244874003939,133.761099831278));
#130499=CARTESIAN_POINT('Ctrl Pts',(-222.688018409072,4.00860512831597,
133.653969009563));
#130500=CARTESIAN_POINT('Ctrl Pts',(-222.695792743191,4.08764900920118,
133.542776290181));
#130501=CARTESIAN_POINT('Ctrl Pts',(-222.70356707731,4.16218810381081,133.428116118251));
#130502=CARTESIAN_POINT('Ctrl Pts',(-222.711341411429,4.23190285134811,
133.310389611662));
#130503=CARTESIAN_POINT('Ctrl Pts',(-222.719106164377,4.30153168168965,
133.192808192472));
#130504=CARTESIAN_POINT('Ctrl Pts',(-222.726870917324,4.36634779758546,
133.07216829085));
#130505=CARTESIAN_POINT('Ctrl Pts',(-222.734635670271,4.42607327228962,
132.948902165502));
#130506=CARTESIAN_POINT('Ctrl Pts',(-222.742392711156,4.48573942681049,
132.825758469807));
#130507=CARTESIAN_POINT('Ctrl Pts',(-222.750149752041,4.54032483262773,
132.699994090787));
#130508=CARTESIAN_POINT('Ctrl Pts',(-222.757906792926,4.58959628416496,
132.57206789279));
#130509=CARTESIAN_POINT('Ctrl Pts',(-222.765657984166,4.63883057971725,
132.444238164934));
#130510=CARTESIAN_POINT('Ctrl Pts',(-222.773409175406,4.68275875731443,
132.314250226368));
#130511=CARTESIAN_POINT('Ctrl Pts',(-222.781160366646,4.72119491491737,
132.18258470597));
#130512=CARTESIAN_POINT('Ctrl Pts',(-222.788908263423,4.75961473612796,
132.050975146932));
#130513=CARTESIAN_POINT('Ctrl Pts',(-222.7966561602,4.79254707067012,131.917689798713));
#130514=CARTESIAN_POINT('Ctrl Pts',(-222.804404056977,4.81985533303518,
131.783226099189));
#130515=CARTESIAN_POINT('Ctrl Pts',(-222.812150333062,4.84715788310045,
131.648790526571));
#130516=CARTESIAN_POINT('Ctrl Pts',(-222.819896609146,4.86883862321824,
131.513177475821));
#130517=CARTESIAN_POINT('Ctrl Pts',(-222.82764288523,4.88481181122892,131.376895884059));
#130518=CARTESIAN_POINT('Ctrl Pts',(-222.835389218495,4.90078511715007,
131.240613286297));
#130519=CARTESIAN_POINT('Ctrl Pts',(-222.843135551761,4.91105074138065,
131.103662525983));
#130520=CARTESIAN_POINT('Ctrl Pts',(-222.850881885026,4.91557472515568,
130.966558595083));
#130521=CARTESIAN_POINT('Ctrl Pts',(-222.858629953029,4.92009972204552,
130.829423960709));
#130522=CARTESIAN_POINT('Ctrl Pts',(-222.866378021032,4.91888050699444,
130.69213647817));
#130523=CARTESIAN_POINT('Ctrl Pts',(-222.874126089035,4.91193524685531,
130.555211679779));
#130524=CARTESIAN_POINT('Ctrl Pts',(-222.881882391777,4.90498260521107,
130.418141356082));
#130525=CARTESIAN_POINT('Ctrl Pts',(-222.889638694519,4.89229178145694,
130.281434877626));
#130526=CARTESIAN_POINT('Ctrl Pts',(-222.89739499726,4.87393295513269,130.145603749388));
#130527=CARTESIAN_POINT('Ctrl Pts',(-222.905155439775,4.85556433015007,
130.009700123987));
#130528=CARTESIAN_POINT('Ctrl Pts',(-222.912915882289,4.83152174316566,
129.874673164464));
#130529=CARTESIAN_POINT('Ctrl Pts',(-222.920676324803,4.80192645946905,
129.74102372817));
#130530=CARTESIAN_POINT('Ctrl Pts',(-222.928449225068,4.77228366679571,
129.607159745936));
#130531=CARTESIAN_POINT('Ctrl Pts',(-222.936222125334,4.73707046552185,
129.474678083922));
#130532=CARTESIAN_POINT('Ctrl Pts',(-222.943995025599,4.69645817166808,
129.344064858388));
#130533=CARTESIAN_POINT('Ctrl Pts',(-222.951485361361,4.6573222369923,129.218199752598));
#130534=CARTESIAN_POINT('Ctrl Pts',(-222.958975697123,4.61317303909308,
129.094069887216));
#130535=CARTESIAN_POINT('Ctrl Pts',(-222.966466032885,4.56420523276902,
128.972090534946));
#130536=CARTESIAN_POINT('Ctrl Pts',(-222.974240367004,4.51338079718451,
128.845486298459));
#130537=CARTESIAN_POINT('Ctrl Pts',(-222.982014701123,4.4572041485496,128.720797823449));
#130538=CARTESIAN_POINT('Ctrl Pts',(-222.989789035243,4.3958400282902,128.598510779481));
#130539=CARTESIAN_POINT('Ctrl Pts',(-222.99755378819,4.33455153382442,128.476374443364));
#130540=CARTESIAN_POINT('Ctrl Pts',(-223.005318541137,4.26808846175371,
128.356633995753));
#130541=CARTESIAN_POINT('Ctrl Pts',(-223.013083294084,4.19666425737296,
128.239756910677));
#130542=CARTESIAN_POINT('Ctrl Pts',(-223.020840334969,4.12531099251929,
128.12299590957));
#130543=CARTESIAN_POINT('Ctrl Pts',(-223.028597375854,4.04900660378461,
128.009092942892));
#130544=CARTESIAN_POINT('Ctrl Pts',(-223.036354416739,3.9680110934299,127.898492240485));
#130545=CARTESIAN_POINT('Ctrl Pts',(-223.044105607979,3.88707666241971,
127.787974942929));
#130546=CARTESIAN_POINT('Ctrl Pts',(-223.051856799219,3.80145838125106,
127.680755267079));
#130547=CARTESIAN_POINT('Ctrl Pts',(-223.059607990459,3.71146013201945,
127.577249409236));
#130548=CARTESIAN_POINT('Ctrl Pts',(-223.067355887236,3.62150013444443,
127.473787544143));
#130549=CARTESIAN_POINT('Ctrl Pts',(-223.075103784013,3.52716412738826,
127.374036652013));
#130550=CARTESIAN_POINT('Ctrl Pts',(-223.08285168079,3.42879679161789,127.278380523423));
#130551=CARTESIAN_POINT('Ctrl Pts',(-223.090597956875,3.33045003217361,
127.182744404034));
#130552=CARTESIAN_POINT('Ctrl Pts',(-223.098344232959,3.2280739014318,127.091201616879));
#130553=CARTESIAN_POINT('Ctrl Pts',(-223.106090509043,3.1220502368738,127.004099392211));
#130554=CARTESIAN_POINT('Ctrl Pts',(-223.113836842308,3.01602578967334,
126.916996524574));
#130555=CARTESIAN_POINT('Ctrl Pts',(-223.121583175573,2.90635405702249,
126.834334533014));
#130556=CARTESIAN_POINT('Ctrl Pts',(-223.129329508839,2.79344996070668,
126.756420353737));
#130557=CARTESIAN_POINT('Ctrl Pts',(-223.137077576842,2.68052058030087,
126.67848872612));
#130558=CARTESIAN_POINT('Ctrl Pts',(-223.144825644845,2.56435771754198,
126.605307248527));
#130559=CARTESIAN_POINT('Ctrl Pts',(-223.152573712848,2.44540492399086,
126.537139294477));
#130560=CARTESIAN_POINT('Ctrl Pts',(-223.16033001559,2.32632570599536,126.468898890715));
#130561=CARTESIAN_POINT('Ctrl Pts',(-223.168086318332,2.2044509737119,126.405682849315));
#130562=CARTESIAN_POINT('Ctrl Pts',(-223.175842621073,2.08024900452012,
126.347708607178));
#130563=CARTESIAN_POINT('Ctrl Pts',(-223.183603063588,1.95598074499774,
126.289703422443));
#130564=CARTESIAN_POINT('Ctrl Pts',(-223.191363506102,1.82938313425054,
126.236945761955));
#130565=CARTESIAN_POINT('Ctrl Pts',(-223.199123948616,1.70094310460485,
126.189604327425));
#130566=CARTESIAN_POINT('Ctrl Pts',(-223.206896848881,1.57229689162119,
126.142186896221));
#130567=CARTESIAN_POINT('Ctrl Pts',(-223.214669749147,1.44180272187478,
126.10020318538));
#130568=CARTESIAN_POINT('Ctrl Pts',(-223.222442649412,1.30996217923589,
126.063771819593));
#130569=CARTESIAN_POINT('Ctrl Pts',(-223.229932985174,1.18291437240822,
126.028664825717));
#130570=CARTESIAN_POINT('Ctrl Pts',(-223.237423320936,1.05461668125239,
125.998713572));
#130571=CARTESIAN_POINT('Ctrl Pts',(-223.244913656698,0.925523702128874,
125.973978754887));
#130572=CARTESIAN_POINT('Ctrl Pts',(-223.252687990817,0.791536123465112,
125.948306109666));
#130573=CARTESIAN_POINT('Ctrl Pts',(-223.260462324936,0.656267327299282,
125.928171948739));
#130574=CARTESIAN_POINT('Ctrl Pts',(-223.268236659056,0.520214967957649,
125.913700186744));
#130575=CARTESIAN_POINT('Ctrl Pts',(-223.276001412003,0.384330280989925,
125.899246259901));
#130576=CARTESIAN_POINT('Ctrl Pts',(-223.28376616495,0.247664337284899,
125.89044088801));
#130577=CARTESIAN_POINT('Ctrl Pts',(-223.291530917897,0.110725808379627,
125.887357174629));
#130578=CARTESIAN_POINT('Ctrl Pts',(-223.299287958782,-0.0260767112482416,
125.884276524035));
#130579=CARTESIAN_POINT('Ctrl Pts',(-223.307044999667,-0.163150888963735,
125.886906231606));
#130580=CARTESIAN_POINT('Ctrl Pts',(-223.314802040552,-0.299982444044545,
125.895267667156));
#130581=CARTESIAN_POINT('Ctrl Pts',(-223.322553231792,-0.436710813385089,
125.903622797283));
#130582=CARTESIAN_POINT('Ctrl Pts',(-223.330304423032,-0.573196535610651,
125.917701028282));
#130583=CARTESIAN_POINT('Ctrl Pts',(-223.338055614272,-0.708925197291414,
125.937471659808));
#130584=CARTESIAN_POINT('Ctrl Pts',(-223.345803511049,-0.844596170670836,
125.957233888288));
#130585=CARTESIAN_POINT('Ctrl Pts',(-223.353551407826,-0.979510337410891,
125.982683649012));
#130586=CARTESIAN_POINT('Ctrl Pts',(-223.361299304603,-1.11315849525526,
126.013738400469));
#130587=CARTESIAN_POINT('Ctrl Pts',(-223.369045580687,-1.24677869678613,
126.044786655942));
#130588=CARTESIAN_POINT('Ctrl Pts',(-223.376791856771,-1.37913303558788,
126.081437481664));
#130589=CARTESIAN_POINT('Ctrl Pts',(-223.384538132856,-1.50972298452976,
126.12355731338));
#130590=CARTESIAN_POINT('Ctrl Pts',(-223.392284466121,-1.64031389745681,
126.165677456014));
#130591=CARTESIAN_POINT('Ctrl Pts',(-223.400030799386,-1.76914002244498,
126.213266565188));
#130592=CARTESIAN_POINT('Ctrl Pts',(-223.407777132651,-1.89571885000921,
126.26614146197));
#130593=CARTESIAN_POINT('Ctrl Pts',(-223.415525200654,-2.02232602402372,
126.319028199718));
#130594=CARTESIAN_POINT('Ctrl Pts',(-223.423273268657,-2.14668453848543,
126.377202929864));
#130595=CARTESIAN_POINT('Ctrl Pts',(-223.43102133666,-2.26833305934123,
126.440434839737));
#130596=CARTESIAN_POINT('Ctrl Pts',(-223.438777639402,-2.39011086969346,
126.503733953237));
#130597=CARTESIAN_POINT('Ctrl Pts',(-223.446533942144,-2.50917258544954,
126.572100802664));
#130598=CARTESIAN_POINT('Ctrl Pts',(-223.454290244886,-2.62508215542526,
126.645258942953));
#130599=CARTESIAN_POINT('Ctrl Pts',(-223.4620506874,-2.74105358982813,126.718456129944));
#130600=CARTESIAN_POINT('Ctrl Pts',(-223.469811129914,-2.85386920469839,
126.796449481124));
#130601=CARTESIAN_POINT('Ctrl Pts',(-223.477571572429,-2.96312386769293,
126.878920513933));
#130602=CARTESIAN_POINT('Ctrl Pts',(-223.485344472694,-3.07255391597198,
126.961523936566));
#130603=CARTESIAN_POINT('Ctrl Pts',(-223.493117372959,-3.17841128718878,
127.048619156141));
#130604=CARTESIAN_POINT('Ctrl Pts',(-223.500890273225,-3.28032506069638,
127.139848295487));
#130605=CARTESIAN_POINT('Ctrl Pts',(-223.508380608987,-3.3785340118339,
127.227761025828));
#130606=CARTESIAN_POINT('Ctrl Pts',(-223.515870944749,-3.47308088576673,
127.319512122745));
#130607=CARTESIAN_POINT('Ctrl Pts',(-223.523361280511,-3.56366889641953,
127.414751929356));
#130608=CARTESIAN_POINT('Ctrl Pts',(-223.531038703737,-3.65651954011178,
127.51237055775));
#130609=CARTESIAN_POINT('Ctrl Pts',(-223.538716126964,-3.74552124665173,
127.61398101524));
#130610=CARTESIAN_POINT('Ctrl Pts',(-223.54639355019,-3.83030464099324,
127.719243209802));
#130611=CARTESIAN_POINT('Ctrl Pts',(-223.554061902916,-3.91498786790322,
127.824381042234));
#130612=CARTESIAN_POINT('Ctrl Pts',(-223.561730255642,-3.99546244221144,
127.933161724535));
#130613=CARTESIAN_POINT('Ctrl Pts',(-223.569398608368,-4.07139527848321,
128.045207930808));
#130614=CARTESIAN_POINT('Ctrl Pts',(-223.577375083318,-4.15037917345655,
128.161756267772));
#130615=CARTESIAN_POINT('Ctrl Pts',(-223.585351558267,-4.22444840748029,
128.281837740302));
#130616=CARTESIAN_POINT('Ctrl Pts',(-223.593328033216,-4.29327333591575,
128.404988381831));
#130617=CARTESIAN_POINT('Ctrl Pts',(-223.600982877338,-4.35932307621505,
128.523173290637));
#130618=CARTESIAN_POINT('Ctrl Pts',(-223.608637721461,-4.42054296849811,
128.644184290527));
#130619=CARTESIAN_POINT('Ctrl Pts',(-223.616292565583,-4.47668554955064,
128.767581406914));
#130620=CARTESIAN_POINT('Ctrl Pts',(-223.623944060619,-4.53280356755143,
128.890924535585));
#130621=CARTESIAN_POINT('Ctrl Pts',(-223.631595555656,-4.5838485280795,
129.016651338951));
#130622=CARTESIAN_POINT('Ctrl Pts',(-223.639247050692,-4.6296194500434,
129.144298326482));
#130623=CARTESIAN_POINT('Ctrl Pts',(-223.646897290597,-4.67538286386451,
129.271924375133));
#130624=CARTESIAN_POINT('Ctrl Pts',(-223.654547530502,-4.71587382474148,
129.401469603691));
#130625=CARTESIAN_POINT('Ctrl Pts',(-223.662197770407,-4.75094010211205,
129.532452126894));
#130626=CARTESIAN_POINT('Ctrl Pts',(-223.663170616191,-4.75539931914727,
129.549108571278));
#130627=CARTESIAN_POINT('Ctrl Pts',(-223.664143461975,-4.7597708795161,
129.56578823797));
#130628=CARTESIAN_POINT('Ctrl Pts',(-223.665116307759,-4.76405452823394,
129.582490119308));
#130629=CARTESIAN_POINT('Ctrl Pts',(-221.915425355964,-4.76405452823393,
129.582490119308));
#130630=CARTESIAN_POINT('Ctrl Pts',(-221.923650676202,-4.80011930232353,
129.723106126124));
#130631=CARTESIAN_POINT('Ctrl Pts',(-221.93187599644,-4.82999394762387,
129.865474671377));
#130632=CARTESIAN_POINT('Ctrl Pts',(-221.940101316678,-4.85351962780969,
130.00904289177));
#130633=CARTESIAN_POINT('Ctrl Pts',(-221.948307262482,-4.87698989413297,
130.152272942572));
#130634=CARTESIAN_POINT('Ctrl Pts',(-221.956513208285,-4.89414096725091,
130.296696723046));
#130635=CARTESIAN_POINT('Ctrl Pts',(-221.964719154088,-4.90486456665709,
130.441749744519));
#130636=CARTESIAN_POINT('Ctrl Pts',(-221.971526290719,-4.91376019040219,
130.562076609897));
#130637=CARTESIAN_POINT('Ctrl Pts',(-221.97833342735,-4.91823372520509,
130.682836114026));
#130638=CARTESIAN_POINT('Ctrl Pts',(-221.985140563982,-4.91824995565472,
130.803700161377));
#130639=CARTESIAN_POINT('',(-221.63985943605,-4.91824834470546,130.800325484114));
#130640=CARTESIAN_POINT('Ctrl Pts',(-221.569819034442,-4.76405452823418,
129.582490119309));
#130641=CARTESIAN_POINT('Ctrl Pts',(-221.577818326288,-4.79903172095484,
129.718865662874));
#130642=CARTESIAN_POINT('Ctrl Pts',(-221.585817618134,-4.82810131954953,
129.856560455278));
#130643=CARTESIAN_POINT('Ctrl Pts',(-221.59381690998,-4.85120084894627,
129.995019289273));
#130644=CARTESIAN_POINT('Ctrl Pts',(-221.60623517544,-4.88706103426808,
130.209965635635));
#130645=CARTESIAN_POINT('Ctrl Pts',(-221.6186534409,-4.90864232357969,130.427356960295));
#130646=CARTESIAN_POINT('Ctrl Pts',(-221.631071706359,-4.91568978847973,
130.64568810597));
#130647=CARTESIAN_POINT('Ctrl Pts',(-221.634000949572,-4.9173521574143,
130.697188456688));
#130648=CARTESIAN_POINT('Ctrl Pts',(-221.636930192784,-4.91820602261817,
130.748740948094));
#130649=CARTESIAN_POINT('Ctrl Pts',(-221.639859435996,-4.91824834470469,
130.800325483166));
#130650=CARTESIAN_POINT('Ctrl Pts',(-221.63985943605,-4.91824834470546,
130.800325484114));
#130651=CARTESIAN_POINT('Ctrl Pts',(-221.647507087154,-4.9183588389363,
130.935002087601));
#130652=CARTESIAN_POINT('Ctrl Pts',(-221.655154738257,-4.9129333950563,
131.069879161911));
#130653=CARTESIAN_POINT('Ctrl Pts',(-221.662802389361,-4.90194927947247,
131.204456011165));
#130654=CARTESIAN_POINT('Ctrl Pts',(-221.670442764659,-4.89097561393384,
131.338904826975));
#130655=CARTESIAN_POINT('Ctrl Pts',(-221.678083139956,-4.87445382754039,
131.473053586129));
#130656=CARTESIAN_POINT('Ctrl Pts',(-221.685723515254,-4.85241323137012,
131.606401074478));
#130657=CARTESIAN_POINT('Ctrl Pts',(-221.693496057693,-4.8299913656306,
131.742055276269));
#130658=CARTESIAN_POINT('Ctrl Pts',(-221.701268600132,-4.80185797109265,
131.876879804697));
#130659=CARTESIAN_POINT('Ctrl Pts',(-221.709041142571,-4.76809913468922,
132.010351373864));
#130660=CARTESIAN_POINT('Ctrl Pts',(-221.716673644061,-4.7349485444982,
132.141418133355));
#130661=CARTESIAN_POINT('Ctrl Pts',(-221.724306145551,-4.69637363020573,
132.271179871615));
#130662=CARTESIAN_POINT('Ctrl Pts',(-221.73193864704,-4.65250745695608,
132.399151332822));
#130663=CARTESIAN_POINT('Ctrl Pts',(-221.73957022108,-4.60864661403101,
132.527107243792));
#130664=CARTESIAN_POINT('Ctrl Pts',(-221.747201795119,-4.55949592136922,
132.653272928435));
#130665=CARTESIAN_POINT('Ctrl Pts',(-221.754833369158,-4.50523798177773,
132.777179359886));
#130666=CARTESIAN_POINT('Ctrl Pts',(-221.762465782816,-4.45097407278124,
132.9010994234));
#130667=CARTESIAN_POINT('Ctrl Pts',(-221.770098196473,-4.39160196193224,
133.022759369872));
#130668=CARTESIAN_POINT('Ctrl Pts',(-221.77773061013,-4.32735172049636,
133.141711714346));
#130669=CARTESIAN_POINT('Ctrl Pts',(-221.785608437102,-4.26103557102442,
133.264488863191));
#130670=CARTESIAN_POINT('Ctrl Pts',(-221.793486264074,-4.1895225256721,
133.384380951238));
#130671=CARTESIAN_POINT('Ctrl Pts',(-221.801364091046,-4.11311528286112,
133.500926161437));
#130672=CARTESIAN_POINT('Ctrl Pts',(-221.809007544998,-4.03898122989655,
133.614004038191));
#130673=CARTESIAN_POINT('Ctrl Pts',(-221.816650998949,-3.96024034488612,
133.723931060195));
#130674=CARTESIAN_POINT('Ctrl Pts',(-221.824294452901,-3.87721088908293,
133.830318116289));
#130675=CARTESIAN_POINT('Ctrl Pts',(-221.832289466383,-3.79036250577627,
133.941598429247));
#130676=CARTESIAN_POINT('Ctrl Pts',(-221.840284479865,-3.6988220030243,
134.049005008741));
#130677=CARTESIAN_POINT('Ctrl Pts',(-221.848279493347,-3.60299682209848,
134.152135544655));
#130678=CARTESIAN_POINT('Ctrl Pts',(-221.856274506829,-3.50717164117241,
134.25526608057));
#130679=CARTESIAN_POINT('Ctrl Pts',(-221.864269520312,-3.40706219025543,
134.354120279752));
#130680=CARTESIAN_POINT('Ctrl Pts',(-221.872264533794,-3.30311433724849,
134.448344527734));
#130681=CARTESIAN_POINT('Ctrl Pts',(-221.880038867913,-3.20203566589346,
134.539967986227));
#130682=CARTESIAN_POINT('Ctrl Pts',(-221.887813202032,-3.09698175721047,
134.627527725395));
#130683=CARTESIAN_POINT('Ctrl Pts',(-221.895587536151,-2.98831317861025,
134.710659045623));
#130684=CARTESIAN_POINT('Ctrl Pts',(-221.903352289099,-2.87977852432117,
134.79368791393));
#130685=CARTESIAN_POINT('Ctrl Pts',(-221.911117042046,-2.76763837129617,
134.872298987086));
#130686=CARTESIAN_POINT('Ctrl Pts',(-221.918881794993,-2.65228912713886,
134.946165230118));
#130687=CARTESIAN_POINT('Ctrl Pts',(-221.926638835878,-2.53705444947731,
135.019958108156));
#130688=CARTESIAN_POINT('Ctrl Pts',(-221.934395876763,-2.41861735069616,
135.089015324947));
#130689=CARTESIAN_POINT('Ctrl Pts',(-221.942152917648,-2.297405939782,135.153051111307));
#130690=CARTESIAN_POINT('Ctrl Pts',(-221.949904108888,-2.17628593533553,
135.217038607783));
#130691=CARTESIAN_POINT('Ctrl Pts',(-221.957655300128,-2.05239612730527,
135.276012029136));
#130692=CARTESIAN_POINT('Ctrl Pts',(-221.965406491369,-1.92619182383379,
135.329730008046));
#130693=CARTESIAN_POINT('Ctrl Pts',(-221.973154388146,-1.80004116055772,
135.383425155383));
#130694=CARTESIAN_POINT('Ctrl Pts',(-221.980902284923,-1.67157831737001,
135.431869150144));
#130695=CARTESIAN_POINT('Ctrl Pts',(-221.9886501817,-1.54128111846809,135.474867611068));
#130696=CARTESIAN_POINT('Ctrl Pts',(-221.996396457784,-1.4110111749313,
135.517857077642));
#130697=CARTESIAN_POINT('Ctrl Pts',(-222.004142733868,-1.2789080099321,
135.555403153644));
#130698=CARTESIAN_POINT('Ctrl Pts',(-222.011889009952,-1.14546687147195,
135.587360587131));
#130699=CARTESIAN_POINT('Ctrl Pts',(-222.019635343218,-1.01202474797981,
135.619318256521));
#130700=CARTESIAN_POINT('Ctrl Pts',(-222.027381676483,-0.877245011532458,
135.64568711002));
#130701=CARTESIAN_POINT('Ctrl Pts',(-222.035128009748,-0.741635038670149,
135.6663726015));
#130702=CARTESIAN_POINT('Ctrl Pts',(-222.042876077751,-0.605994696894486,
135.687062725352));
#130703=CARTESIAN_POINT('Ctrl Pts',(-222.050624145754,-0.469524135153988,
135.702066895617));
#130704=CARTESIAN_POINT('Ctrl Pts',(-222.058372213758,-0.332737423040753,
135.71134226312));
#130705=CARTESIAN_POINT('Ctrl Pts',(-222.066128516499,-0.195805332382288,
135.720627488595));
#130706=CARTESIAN_POINT('Ctrl Pts',(-222.073884819241,-0.0585568108295851,
135.724171722101));
#130707=CARTESIAN_POINT('Ctrl Pts',(-222.081641121983,0.0784919280162668,
135.721984238761));
#130708=CARTESIAN_POINT('Ctrl Pts',(-222.089401564497,0.215613813900871,
135.719795587895));
#130709=CARTESIAN_POINT('Ctrl Pts',(-222.097162007012,0.352535314488479,
135.711869147072));
#130710=CARTESIAN_POINT('Ctrl Pts',(-222.104922449526,0.48874475560372,
135.698266177175));
#130711=CARTESIAN_POINT('Ctrl Pts',(-222.112695349791,0.625172852205945,
135.684641370582));
#130712=CARTESIAN_POINT('Ctrl Pts',(-222.120468250057,0.760886217849805,
135.665321880432));
#130713=CARTESIAN_POINT('Ctrl Pts',(-222.128241150322,0.895381904845901,
135.640420409067));
#130714=CARTESIAN_POINT('Ctrl Pts',(-222.135731486084,1.02498833483822,
135.616424168911));
#130715=CARTESIAN_POINT('Ctrl Pts',(-222.143221821846,1.15346378015151,
135.58724480797));
#130716=CARTESIAN_POINT('Ctrl Pts',(-222.150712157607,1.28037288428042,
135.553026571252));
#130717=CARTESIAN_POINT('Ctrl Pts',(-222.158486491726,1.41209378567244,
135.517510939688));
#130718=CARTESIAN_POINT('Ctrl Pts',(-222.166260825845,1.54254447778172,
135.476454288817));
#130719=CARTESIAN_POINT('Ctrl Pts',(-222.174035159964,1.67122323300192,
135.429962845166));
#130720=CARTESIAN_POINT('Ctrl Pts',(-222.181799912911,1.79974340315665,
135.383528698064));
#130721=CARTESIAN_POINT('Ctrl Pts',(-222.189564665859,1.92649561726965,
135.331673216573));
#130722=CARTESIAN_POINT('Ctrl Pts',(-222.197329418806,2.05099046356164,
135.274553139245));
#130723=CARTESIAN_POINT('Ctrl Pts',(-222.205086459691,2.17536165981756,
135.217489794384));
#130724=CARTESIAN_POINT('Ctrl Pts',(-222.212843500576,2.29747959698378,
135.155172421358));
#130725=CARTESIAN_POINT('Ctrl Pts',(-222.220600541461,2.41687244598882,
135.087806735159));
#130726=CARTESIAN_POINT('Ctrl Pts',(-222.228351732701,2.53617525991816,
135.020491849947));
#130727=CARTESIAN_POINT('Ctrl Pts',(-222.236102923941,2.65275673693429,
134.948136420457));
#130728=CARTESIAN_POINT('Ctrl Pts',(-222.243854115181,2.76616770270203,
134.87099304539));
#130729=CARTESIAN_POINT('Ctrl Pts',(-222.251602011958,2.87953046578353,
134.793882458315));
#130730=CARTESIAN_POINT('Ctrl Pts',(-222.259349908735,2.98972507520356,
134.711988192564));
#130731=CARTESIAN_POINT('Ctrl Pts',(-222.267097805512,3.0963297168512,134.625607187345));
#130732=CARTESIAN_POINT('Ctrl Pts',(-222.274844081597,3.20291205910594,
134.539244251169));
#130733=CARTESIAN_POINT('Ctrl Pts',(-222.282590357681,3.30590562368785,
134.448396688293));
#130734=CARTESIAN_POINT('Ctrl Pts',(-222.290336633765,3.40492051238091,
134.353402652661));
#130735=CARTESIAN_POINT('Ctrl Pts',(-222.29808296703,3.50393613197952,134.258407915804));
#130736=CARTESIAN_POINT('Ctrl Pts',(-222.305829300296,3.59897273496108,
134.159266915781));
#130737=CARTESIAN_POINT('Ctrl Pts',(-222.313575633561,3.6896765275764,134.056355418354));
#130738=CARTESIAN_POINT('Ctrl Pts',(-222.321323701564,3.78040063267682,
133.953420874611));
#130739=CARTESIAN_POINT('Ctrl Pts',(-222.329071769567,3.86678973816017,
133.846714446497));
#130740=CARTESIAN_POINT('Ctrl Pts',(-222.33681983757,3.94852992663087,133.736645474295));
#130741=CARTESIAN_POINT('Ctrl Pts',(-222.344576140312,4.03035698954692,
133.626459519478));
#130742=CARTESIAN_POINT('Ctrl Pts',(-222.352332443053,4.10752503195465,
133.512904195999));
#130743=CARTESIAN_POINT('Ctrl Pts',(-222.360088745795,4.17976283121569,
133.396418822408));
#130744=CARTESIAN_POINT('Ctrl Pts',(-222.36784918831,4.25203918596504,133.279871277066));
#130745=CARTESIAN_POINT('Ctrl Pts',(-222.375609630824,4.31937986237311,
133.160390905925));
#130746=CARTESIAN_POINT('Ctrl Pts',(-222.383370073338,4.38155982856529,
133.038441307963));
#130747=CARTESIAN_POINT('Ctrl Pts',(-222.391142973604,4.44383961155944,
132.916295945679));
#130748=CARTESIAN_POINT('Ctrl Pts',(-222.398915873869,4.50094196645316,
132.79167379123));
#130749=CARTESIAN_POINT('Ctrl Pts',(-222.406688774134,4.55268985740884,
132.665058907119));
#130750=CARTESIAN_POINT('Ctrl Pts',(-222.414179109896,4.60255658218026,
132.543046792977));
#130751=CARTESIAN_POINT('Ctrl Pts',(-222.421669445658,4.64745127579681,
132.419184604888));
#130752=CARTESIAN_POINT('Ctrl Pts',(-222.429159781419,4.68725997484442,
132.293916588559));
#130753=CARTESIAN_POINT('Ctrl Pts',(-222.436934115538,4.72857803281806,
132.163898997311));
#130754=CARTESIAN_POINT('Ctrl Pts',(-222.444708449657,4.76454769517606,
132.031955012825));
#130755=CARTESIAN_POINT('Ctrl Pts',(-222.452482783776,4.79498713727588,
131.898564170777));
#130756=CARTESIAN_POINT('Ctrl Pts',(-222.460247536723,4.82538906548385,
131.76533772102));
#130757=CARTESIAN_POINT('Ctrl Pts',(-222.46801228967,4.85027424810539,131.630668339092));
#130758=CARTESIAN_POINT('Ctrl Pts',(-222.475777042618,4.86951001470163,
131.495052501998));
#130759=CARTESIAN_POINT('Ctrl Pts',(-222.483534083502,4.88872667606326,
131.359571360467));
#130760=CARTESIAN_POINT('Ctrl Pts',(-222.491291124388,4.90230503315158,
131.223146019063));
#130761=CARTESIAN_POINT('Ctrl Pts',(-222.499048165273,4.91016312467678,
131.086284634926));
#130762=CARTESIAN_POINT('Ctrl Pts',(-222.506799356513,4.91801529035404,
130.949526459023));
#130763=CARTESIAN_POINT('Ctrl Pts',(-222.514550547753,4.9201557542997,130.812333283633));
#130764=CARTESIAN_POINT('Ctrl Pts',(-222.522301738993,4.91655424525667,
130.675219547613));
#130765=CARTESIAN_POINT('Ctrl Pts',(-222.53004963577,4.91295426695105,130.538164088589));
#130766=CARTESIAN_POINT('Ctrl Pts',(-222.537797532547,4.90361717985295,
130.401188391794));
#130767=CARTESIAN_POINT('Ctrl Pts',(-222.545545429324,4.88856480649907,
130.264807844282));
#130768=CARTESIAN_POINT('Ctrl Pts',(-222.553291705408,4.87351558177722,
130.12845582464));
#130769=CARTESIAN_POINT('Ctrl Pts',(-222.561037981492,4.85275349160718,
129.992699095019));
#130770=CARTESIAN_POINT('Ctrl Pts',(-222.568784257576,4.82635228497129,
129.858048468298));
#130771=CARTESIAN_POINT('Ctrl Pts',(-222.576530590842,4.79995088344766,
129.723396847616));
#130772=CARTESIAN_POINT('Ctrl Pts',(-222.584276924107,4.76791035762011,
129.589851729786));
#130773=CARTESIAN_POINT('Ctrl Pts',(-222.592023257372,4.7303556157022,129.457913882082));
#130774=CARTESIAN_POINT('Ctrl Pts',(-222.599771325375,4.69279246366037,
129.325946487813));
#130775=CARTESIAN_POINT('Ctrl Pts',(-222.607519393378,4.64971274529124,
129.195587455859));
#130776=CARTESIAN_POINT('Ctrl Pts',(-222.615267461381,4.60129117014654,
129.067322152237));
#130777=CARTESIAN_POINT('Ctrl Pts',(-222.623023764123,4.55281813197549,
128.938920526724));
#130778=CARTESIAN_POINT('Ctrl Pts',(-222.630780066865,4.498992034135,128.812617441051));
#130779=CARTESIAN_POINT('Ctrl Pts',(-222.638536369607,4.4400358853041,128.688878544914));
#130780=CARTESIAN_POINT('Ctrl Pts',(-222.646296812121,4.38104826980127,
128.565073605602));
#130781=CARTESIAN_POINT('Ctrl Pts',(-222.654057254635,4.31692533018726,
128.443835928281));
#130782=CARTESIAN_POINT('Ctrl Pts',(-222.661817697149,4.24793547018755,
128.325605425212));
#130783=CARTESIAN_POINT('Ctrl Pts',(-222.669590597415,4.17883486153994,
128.207185128044));
#130784=CARTESIAN_POINT('Ctrl Pts',(-222.67736349768,4.10485193114276,128.091781981104));
#130785=CARTESIAN_POINT('Ctrl Pts',(-222.685136397945,4.02629824229625,
127.979806577265));
#130786=CARTESIAN_POINT('Ctrl Pts',(-222.692626733708,3.95060017790136,
127.8719017614));
#130787=CARTESIAN_POINT('Ctrl Pts',(-222.70011706947,3.87065808960908,127.767180046003));
#130788=CARTESIAN_POINT('Ctrl Pts',(-222.707607405232,3.78678413390681,
127.665977437377));
#130789=CARTESIAN_POINT('Ctrl Pts',(-222.715381739351,3.69973007168445,
127.56093770109));
#130790=CARTESIAN_POINT('Ctrl Pts',(-222.723156073471,3.60816434180061,
127.459356458908));
#130791=CARTESIAN_POINT('Ctrl Pts',(-222.73093040759,3.51239211054046,127.361645885801));
#130792=CARTESIAN_POINT('Ctrl Pts',(-222.738695160537,3.41673790999567,
127.264055732242));
#130793=CARTESIAN_POINT('Ctrl Pts',(-222.746459913484,3.31688779400566,
127.170327032902));
#130794=CARTESIAN_POINT('Ctrl Pts',(-222.754224666431,3.21318775112395,
127.08083976513));
#130795=CARTESIAN_POINT('Ctrl Pts',(-222.761981707316,3.10959070458702,
126.991441377373));
#130796=CARTESIAN_POINT('Ctrl Pts',(-222.769738748201,3.00215163477383,
126.906276291593));
#130797=CARTESIAN_POINT('Ctrl Pts',(-222.777495789086,2.8912537665975,126.825688135489));
#130798=CARTESIAN_POINT('Ctrl Pts',(-222.785246980326,2.78043952736638,
126.745160751541));
#130799=CARTESIAN_POINT('Ctrl Pts',(-222.792998171566,2.66617199644442,
126.669203656174));
#130800=CARTESIAN_POINT('Ctrl Pts',(-222.800749362806,2.54886762345901,
126.598120384224));
#130801=CARTESIAN_POINT('Ctrl Pts',(-222.808497259583,2.43161310796084,
126.527067324561));
#130802=CARTESIAN_POINT('Ctrl Pts',(-222.81624515636,2.31132465124602,126.460884170441));
#130803=CARTESIAN_POINT('Ctrl Pts',(-222.823993053137,2.18844765865376,
126.399831141239));
#130804=CARTESIAN_POINT('Ctrl Pts',(-222.831739329221,2.06559636927942,
126.338790883014));
#130805=CARTESIAN_POINT('Ctrl Pts',(-222.839485605305,1.94015797093936,
126.282878789084));
#130806=CARTESIAN_POINT('Ctrl Pts',(-222.84723188139,1.81260208810232,126.232308919181));
#130807=CARTESIAN_POINT('Ctrl Pts',(-222.854978214655,1.68504526367691,
126.181738675982));
#130808=CARTESIAN_POINT('Ctrl Pts',(-222.86272454792,1.55537128700937,126.136510879588));
#130809=CARTESIAN_POINT('Ctrl Pts',(-222.870470881186,1.42406898372989,
126.096791118124));
#130810=CARTESIAN_POINT('Ctrl Pts',(-222.878218949189,1.29273727621052,
126.057062461695));
#130811=CARTESIAN_POINT('Ctrl Pts',(-222.885967017192,1.15977689060906,
126.022844407872));
#130812=CARTESIAN_POINT('Ctrl Pts',(-222.893715085194,1.02569061388157,
125.99425232075));
#130813=CARTESIAN_POINT('Ctrl Pts',(-222.901471387936,0.891461828662974,
125.965629845618));
#130814=CARTESIAN_POINT('Ctrl Pts',(-222.909227690678,0.756105144938412,
125.942645363234));
#130815=CARTESIAN_POINT('Ctrl Pts',(-222.91698399342,0.620132868622877,
125.925362945118));
#130816=CARTESIAN_POINT('Ctrl Pts',(-222.924744435934,0.484088019809057,
125.908071302854));
#130817=CARTESIAN_POINT('Ctrl Pts',(-222.932504878448,0.347427313097739,
125.896487822021));
#130818=CARTESIAN_POINT('Ctrl Pts',(-222.940265320962,0.210665937903024,
125.890624470284));
#130819=CARTESIAN_POINT('Ctrl Pts',(-222.948038221228,0.0736850212077413,
125.884751706174));
#130820=CARTESIAN_POINT('Ctrl Pts',(-222.955811121493,-0.0633964957131659,
125.884617421023));
#130821=CARTESIAN_POINT('Ctrl Pts',(-222.963584021759,-0.200064761873793,
125.89018142328));
#130822=CARTESIAN_POINT('Ctrl Pts',(-222.971074357521,-0.331764792315863,
125.895543160039));
#130823=CARTESIAN_POINT('Ctrl Pts',(-222.978564693283,-0.463080788767365,
125.906196057855));
#130824=CARTESIAN_POINT('Ctrl Pts',(-222.986055029045,-0.593561331401663,
125.922059110247));
#130825=CARTESIAN_POINT('Ctrl Pts',(-222.993829363164,-0.728989083464304,
125.938523615093));
#130826=CARTESIAN_POINT('Ctrl Pts',(-223.001603697283,-0.86394577306058,
125.960653314261));
#130827=CARTESIAN_POINT('Ctrl Pts',(-223.009378031402,-0.997919675885488,
125.988414253353));
#130828=CARTESIAN_POINT('Ctrl Pts',(-223.017142784349,-1.13172846784912,
126.016140979568));
#130829=CARTESIAN_POINT('Ctrl Pts',(-223.024907537296,-1.26455650380447,
126.049485058608));
#130830=CARTESIAN_POINT('Ctrl Pts',(-223.032672290243,-1.39589708278385,
126.088360787543));
#130831=CARTESIAN_POINT('Ctrl Pts',(-223.040429331128,-1.52710721244824,
126.127197904556));
#130832=CARTESIAN_POINT('Ctrl Pts',(-223.048186372013,-1.65683245269427,
126.171555627685));
#130833=CARTESIAN_POINT('Ctrl Pts',(-223.055943412898,-1.78457655737942,
126.221297278122));
#130834=CARTESIAN_POINT('Ctrl Pts',(-223.063694604138,-1.91222432924239,
126.271001417995));
#130835=CARTESIAN_POINT('Ctrl Pts',(-223.071445795379,-2.03789357639425,
126.326081262583));
#130836=CARTESIAN_POINT('Ctrl Pts',(-223.079196986619,-2.16110382518599,
126.386350509014));
#130837=CARTESIAN_POINT('Ctrl Pts',(-223.086944883396,-2.28426170633475,
126.446594139407));
#130838=CARTESIAN_POINT('Ctrl Pts',(-223.094692780173,-2.40496231736249,
126.512022613372));
#130839=CARTESIAN_POINT('Ctrl Pts',(-223.10244067695,-2.52274597587496,
126.582401853709));
#130840=CARTESIAN_POINT('Ctrl Pts',(-223.110186953034,-2.64050499658552,
126.652766372227));
#130841=CARTESIAN_POINT('Ctrl Pts',(-223.117933229118,-2.75534794302714,
126.728079396852));
#130842=CARTESIAN_POINT('Ctrl Pts',(-223.125679505202,-2.866840877189,126.808061523732));
#130843=CARTESIAN_POINT('Ctrl Pts',(-223.133425838467,-2.97833463436652,
126.888044241022));
#130844=CARTESIAN_POINT('Ctrl Pts',(-223.141172171733,-3.08647801224248,
126.972695901448));
#130845=CARTESIAN_POINT('Ctrl Pts',(-223.148918504998,-3.19086747464377,
127.061694746591));
#130846=CARTESIAN_POINT('Ctrl Pts',(-223.156666573001,-3.29528031434096,
127.150713522408));
#130847=CARTESIAN_POINT('Ctrl Pts',(-223.164414641004,-3.39593726828292,
127.244081166534));
#130848=CARTESIAN_POINT('Ctrl Pts',(-223.172162709007,-3.4924695087594,
127.341437027175));
#130849=CARTESIAN_POINT('Ctrl Pts',(-223.179919011748,-3.58910434484994,
127.438896358783));
#130850=CARTESIAN_POINT('Ctrl Pts',(-223.18767531449,-3.68160543465689,
127.540352096145));
#130851=CARTESIAN_POINT('Ctrl Pts',(-223.195431617232,-3.76964195913766,
127.645407854005));
#130852=CARTESIAN_POINT('Ctrl Pts',(-223.203192059746,-3.85772547136227,
127.750519683286));
#130853=CARTESIAN_POINT('Ctrl Pts',(-223.21095250226,-3.94133943194928,
127.859235051941));
#130854=CARTESIAN_POINT('Ctrl Pts',(-223.218712944774,-4.0201952996991,
127.97112698534));
#130855=CARTESIAN_POINT('Ctrl Pts',(-223.22648584504,-4.09917775388832,
128.083198537604));
#130856=CARTESIAN_POINT('Ctrl Pts',(-223.234258745305,-4.17338664008651,
128.198456515734));
#130857=CARTESIAN_POINT('Ctrl Pts',(-223.242031645571,-4.24257802357517,
128.316446877828));
#130858=CARTESIAN_POINT('Ctrl Pts',(-223.249521981333,-4.30925412599592,
128.430147993068));
#130859=CARTESIAN_POINT('Ctrl Pts',(-223.257012317096,-4.37127104501416,
128.546386011429));
#130860=CARTESIAN_POINT('Ctrl Pts',(-223.264502652858,-4.42845293023154,
128.664737354647));
#130861=CARTESIAN_POINT('Ctrl Pts',(-223.27288648263,-4.4924558276875,128.797206384917));
#130862=CARTESIAN_POINT('Ctrl Pts',(-223.281270312402,-4.5505805484293,
128.932693044058));
#130863=CARTESIAN_POINT('Ctrl Pts',(-223.289654142175,-4.60255473983701,
129.070672949817));
#130864=CARTESIAN_POINT('Ctrl Pts',(-223.298016770948,-4.65439749909419,
129.208303932482));
#130865=CARTESIAN_POINT('Ctrl Pts',(-223.306379399721,-4.70012064041638,
129.348415314029));
#130866=CARTESIAN_POINT('Ctrl Pts',(-223.314742028494,-4.73949906895975,
129.49046121585));
#130867=CARTESIAN_POINT('Ctrl Pts',(-223.316542859158,-4.7479789242218,
129.521049757155));
#130868=CARTESIAN_POINT('Ctrl Pts',(-223.318343689822,-4.75616473135832,
129.551727921034));
#130869=CARTESIAN_POINT('Ctrl Pts',(-223.320144520485,-4.76405452823402,
129.582490119308));
#130870=CARTESIAN_POINT('Origin',(213.235140564004,0.,130.804360617566));
#130871=CARTESIAN_POINT('',(-225.41504623153,-4.76405452823393,129.582490119308));
#130872=CARTESIAN_POINT('',(-225.069870156977,-4.76405452823402,129.582490119308));
#130873=CARTESIAN_POINT('',(213.235140564004,-4.76405452823405,129.582490119308));
#130874=CARTESIAN_POINT('',(-223.735140564051,-4.91824789595331,130.808909952771));
#130875=CARTESIAN_POINT('Ctrl Pts',(-223.735140564051,-4.91824789595331,
130.808909952771));
#130876=CARTESIAN_POINT('Ctrl Pts',(-223.745263896723,-4.91808255474622,
130.987658936367));
#130877=CARTESIAN_POINT('Ctrl Pts',(-223.755387229394,-4.90816914338085,
131.165973392137));
#130878=CARTESIAN_POINT('Ctrl Pts',(-223.765510562065,-4.88866975464819,
131.342961668891));
#130879=CARTESIAN_POINT('Ctrl Pts',(-223.775895587255,-4.86866629829984,
131.524525168995));
#130880=CARTESIAN_POINT('Ctrl Pts',(-223.786280612445,-4.83857481507823,
131.704693402866));
#130881=CARTESIAN_POINT('Ctrl Pts',(-223.796665637636,-4.79861797404513,
131.882529714541));
#130882=CARTESIAN_POINT('Ctrl Pts',(-223.798380059865,-4.7920216591378,
131.911887999216));
#130883=CARTESIAN_POINT('Ctrl Pts',(-223.800094482094,-4.78515658405584,
131.941182779772));
#130884=CARTESIAN_POINT('Ctrl Pts',(-223.801808904323,-4.7780238740645,
131.9704098967));
#130885=CARTESIAN_POINT('Ctrl Pts',(-223.809583238442,-4.7456794085625,
132.102945142961));
#130886=CARTESIAN_POINT('Ctrl Pts',(-223.817357572562,-4.70776503791059,
132.234343514913));
#130887=CARTESIAN_POINT('Ctrl Pts',(-223.825131906681,-4.6643749179642,
132.364100880291));
#130888=CARTESIAN_POINT('Ctrl Pts',(-223.832896659628,-4.62103827246275,
132.493698331313));
#130889=CARTESIAN_POINT('Ctrl Pts',(-223.840661412576,-4.57223942771272,
132.621658432498));
#130890=CARTESIAN_POINT('Ctrl Pts',(-223.848426165523,-4.51812333259547,
132.747488151712));
#130891=CARTESIAN_POINT('Ctrl Pts',(-223.856183206408,-4.46406098634694,
132.873192895074));
#130892=CARTESIAN_POINT('Ctrl Pts',(-223.863940247293,-4.40469205295891,
132.996771110419));
#130893=CARTESIAN_POINT('Ctrl Pts',(-223.871697288178,-4.34021086558519,
133.117746167957));
#130894=CARTESIAN_POINT('Ctrl Pts',(-223.879448479419,-4.27577830397654,
133.238629997262));
#130895=CARTESIAN_POINT('Ctrl Pts',(-223.887199670659,-4.20624134505839,
133.356914232497));
#130896=CARTESIAN_POINT('Ctrl Pts',(-223.894950861899,-4.13184173584594,
133.472143767003));
#130897=CARTESIAN_POINT('Ctrl Pts',(-223.902698758677,-4.05747374845178,
133.587324325885));
#130898=CARTESIAN_POINT('Ctrl Pts',(-223.910446655454,-3.97824743300902,
133.699452438552));
#130899=CARTESIAN_POINT('Ctrl Pts',(-223.918194552231,-3.89444952084087,
133.808099286645));
#130900=CARTESIAN_POINT('Ctrl Pts',(-223.925940828316,-3.81066913738947,
133.91672340816));
#130901=CARTESIAN_POINT('Ctrl Pts',(-223.9336871044,-3.72231929792916,134.021867404156));
#130902=CARTESIAN_POINT('Ctrl Pts',(-223.941433380485,-3.62972870254399,
134.123133373937));
#130903=CARTESIAN_POINT('Ctrl Pts',(-223.94917971375,-3.53713742367594,
134.22440009124));
#130904=CARTESIAN_POINT('Ctrl Pts',(-223.956926047016,-3.44030559023594,
134.321788436668));
#130905=CARTESIAN_POINT('Ctrl Pts',(-223.964672380282,-3.3396003696992,
134.414935701013));
#130906=CARTESIAN_POINT('Ctrl Pts',(-223.972420448285,-3.2388725969267,
134.508103825041));
#130907=CARTESIAN_POINT('Ctrl Pts',(-223.980168516288,-3.13426999795533,
134.59702871265));
#130908=CARTESIAN_POINT('Ctrl Pts',(-223.987916584291,-3.02619426203474,
134.681386713806));
#130909=CARTESIAN_POINT('Ctrl Pts',(-223.995672887034,-2.91800366193575,
134.76583437165));
#130910=CARTESIAN_POINT('Ctrl Pts',(-224.003429189776,-2.80633285982248,
134.845705206225));
#130911=CARTESIAN_POINT('Ctrl Pts',(-224.011185492518,-2.6916145391387,
134.920717530565));
#130912=CARTESIAN_POINT('Ctrl Pts',(-224.018945935032,-2.57683498983308,
134.995769891242));
#130913=CARTESIAN_POINT('Ctrl Pts',(-224.026706377547,-2.45900501663815,
135.065958374662));
#130914=CARTESIAN_POINT('Ctrl Pts',(-224.034466820061,-2.3385826848829,
135.131046888659));
#130915=CARTESIAN_POINT('Ctrl Pts',(-224.042239720327,-2.21796704051013,
135.196239888517));
#130916=CARTESIAN_POINT('Ctrl Pts',(-224.050012620593,-2.09475107322762,
135.256316387428));
#130917=CARTESIAN_POINT('Ctrl Pts',(-224.057785520858,-1.96941445777039,
135.311087784372));
#130918=CARTESIAN_POINT('Ctrl Pts',(-224.065275856618,-1.84863414402862,
135.363868103058));
#130919=CARTESIAN_POINT('Ctrl Pts',(-224.072766192378,-1.72588497407771,
135.411722219088));
#130920=CARTESIAN_POINT('Ctrl Pts',(-224.080256528138,-1.60160833088641,
135.454525541193));
#130921=CARTESIAN_POINT('Ctrl Pts',(-224.088030862257,-1.47261970095671,
135.49895176428));
#130922=CARTESIAN_POINT('Ctrl Pts',(-224.095805196376,-1.34157688579506,
135.538077360082));
#130923=CARTESIAN_POINT('Ctrl Pts',(-224.103579530495,-1.2089549196934,
135.571709048785));
#130924=CARTESIAN_POINT('Ctrl Pts',(-224.111344283442,-1.07649639831256,
135.605299289438));
#130925=CARTESIAN_POINT('Ctrl Pts',(-224.119109036389,-0.94246297360639,
135.633408999584));
#130926=CARTESIAN_POINT('Ctrl Pts',(-224.126873789336,-0.807347795883414,
135.655893632911));
#130927=CARTESIAN_POINT('Ctrl Pts',(-224.134630830222,-0.672366816459376,
135.678355934183));
#130928=CARTESIAN_POINT('Ctrl Pts',(-224.142387871107,-0.536306605313661,
135.695204213068));
#130929=CARTESIAN_POINT('Ctrl Pts',(-224.150144911992,-0.399673206403032,
135.706344337509));
#130930=CARTESIAN_POINT('Ctrl Pts',(-224.157896103232,-0.26314284380156,
135.717476061094));
#130931=CARTESIAN_POINT('Ctrl Pts',(-224.165647294472,-0.126040541888781,
135.722908166566));
#130932=CARTESIAN_POINT('Ctrl Pts',(-224.173398485712,0.0111201350492467,
135.722598046269));
#130933=CARTESIAN_POINT('Ctrl Pts',(-224.181146382489,0.148222515040508,
135.722288057782));
#130934=CARTESIAN_POINT('Ctrl Pts',(-224.188894279266,0.285382830564257,
135.716240698574));
#130935=CARTESIAN_POINT('Ctrl Pts',(-224.196642176043,0.422085319304466,
135.70446541703));
#130936=CARTESIAN_POINT('Ctrl Pts',(-224.204388452127,0.558759212830996,
135.692692598621));
#130937=CARTESIAN_POINT('Ctrl Pts',(-224.212134728211,0.69497508078477,
135.675194274608));
#130938=CARTESIAN_POINT('Ctrl Pts',(-224.219881004295,0.830220487615677,
135.652031914637));
#130939=CARTESIAN_POINT('Ctrl Pts',(-224.22762733756,0.965466892797638,
135.628869383686));
#130940=CARTESIAN_POINT('Ctrl Pts',(-224.235373670826,1.09974243720733,
135.600042799342));
#130941=CARTESIAN_POINT('Ctrl Pts',(-224.243120004091,1.23254350032708,
135.565665016814));
#130942=CARTESIAN_POINT('Ctrl Pts',(-224.250868072094,1.36537430332433,
135.531279535621));
#130943=CARTESIAN_POINT('Ctrl Pts',(-224.258616140097,1.49672958955542,
135.491340480474));
#130944=CARTESIAN_POINT('Ctrl Pts',(-224.2663642081,1.62611994022991,135.446010863167));
#130945=CARTESIAN_POINT('Ctrl Pts',(-224.274120510841,1.75564780850868,
135.400633069003));
#130946=CARTESIAN_POINT('Ctrl Pts',(-224.281876813583,1.88320619994714,
135.34985339755));
#130947=CARTESIAN_POINT('Ctrl Pts',(-224.289633116325,2.00832424735202,
135.293883618955));
#130948=CARTESIAN_POINT('Ctrl Pts',(-224.297393558839,2.13350907402604,
135.237883967604));
#130949=CARTESIAN_POINT('Ctrl Pts',(-224.305154001353,2.25625061163589,
135.176688863779));
#130950=CARTESIAN_POINT('Ctrl Pts',(-224.312914443867,2.37610263365482,
135.110556077231));
#130951=CARTESIAN_POINT('Ctrl Pts',(-224.320687344133,2.49614705277945,
135.044317128463));
#130952=CARTESIAN_POINT('Ctrl Pts',(-224.328460244398,2.61329235280028,
134.973124860647));
#130953=CARTESIAN_POINT('Ctrl Pts',(-224.336233144664,2.72712058242583,
134.897280894264));
#130954=CARTESIAN_POINT('Ctrl Pts',(-224.343723480426,2.83681086919125,
134.824194047097));
#130955=CARTESIAN_POINT('Ctrl Pts',(-224.351213816188,2.94342081701531,
134.746788012573));
#130956=CARTESIAN_POINT('Ctrl Pts',(-224.35870415195,3.04660702545978,134.665366794059));
#130957=CARTESIAN_POINT('Ctrl Pts',(-224.366478486069,3.15370557035735,
134.580858465301));
#130958=CARTESIAN_POINT('Ctrl Pts',(-224.374252820188,3.25745488469366,
134.491756773807));
#130959=CARTESIAN_POINT('Ctrl Pts',(-224.382027154307,3.35743558904776,
134.398356906921));
#130960=CARTESIAN_POINT('Ctrl Pts',(-224.389791907254,3.45729307611901,
134.305072147023));
#130961=CARTESIAN_POINT('Ctrl Pts',(-224.397556660201,3.55339091137502,
134.207500015746));
#130962=CARTESIAN_POINT('Ctrl Pts',(-224.405321413148,3.64534092412187,
134.105977283598));
#130963=CARTESIAN_POINT('Ctrl Pts',(-224.413078454033,3.73719961082005,
134.004555385259));
#130964=CARTESIAN_POINT('Ctrl Pts',(-224.420835494918,3.82491841259353,
133.899190982477));
#130965=CARTESIAN_POINT('Ctrl Pts',(-224.428592535803,3.90814460435721,
133.790258943687));
#130966=CARTESIAN_POINT('Ctrl Pts',(-224.436343727043,3.99130803460216,
133.681409051396));
#130967=CARTESIAN_POINT('Ctrl Pts',(-224.444094918283,4.06998536187414,
133.568997187552));
#130968=CARTESIAN_POINT('Ctrl Pts',(-224.451846109524,4.14386314510612,
133.453432397856));
#130969=CARTESIAN_POINT('Ctrl Pts',(-224.459594006301,4.21770952830937,
133.33791672628));
#130970=CARTESIAN_POINT('Ctrl Pts',(-224.467341903078,4.2867602146052,133.219251122881));
#130971=CARTESIAN_POINT('Ctrl Pts',(-224.475089799855,4.35074437105678,
133.097874620187));
#130972=CARTESIAN_POINT('Ctrl Pts',(-224.482836075939,4.41471514340217,
132.97652350684));
#130973=CARTESIAN_POINT('Ctrl Pts',(-224.490582352023,4.47362131171893,
132.852462967748));
#130974=CARTESIAN_POINT('Ctrl Pts',(-224.498328628107,4.52723760822754,
132.726157355296));
#130975=CARTESIAN_POINT('Ctrl Pts',(-224.506074961372,4.58085430051955,
132.599850810484));
#130976=CARTESIAN_POINT('Ctrl Pts',(-224.513821294638,4.62918089031577,
132.471299519126));
#130977=CARTESIAN_POINT('Ctrl Pts',(-224.521567627903,4.6720401067086,132.340988192421));
#130978=CARTESIAN_POINT('Ctrl Pts',(-224.529315695906,4.71490892112572,
132.2106476834));
#130979=CARTESIAN_POINT('Ctrl Pts',(-224.537063763909,4.75230780363691,
132.078546726046));
#130980=CARTESIAN_POINT('Ctrl Pts',(-224.544811831912,4.78410935786991,
131.945185194108));
#130981=CARTESIAN_POINT('Ctrl Pts',(-224.552568134654,4.81594471117315,
131.811681923946));
#130982=CARTESIAN_POINT('Ctrl Pts',(-224.560324437395,4.8421707617836,131.676915783805));
#130983=CARTESIAN_POINT('Ctrl Pts',(-224.568080740137,4.86271116270596,
131.541397394528));
#130984=CARTESIAN_POINT('Ctrl Pts',(-224.575841182651,4.88326252665881,
131.405806675006));
#130985=CARTESIAN_POINT('Ctrl Pts',(-224.583601625165,4.89812215188278,
131.269463294804));
#130986=CARTESIAN_POINT('Ctrl Pts',(-224.59136206768,4.90726571103205,131.132882007782));
#130987=CARTESIAN_POINT('Ctrl Pts',(-224.599134967945,4.91642394823418,
130.996081468352));
#130988=CARTESIAN_POINT('Ctrl Pts',(-224.60690786821,4.91984777314559,130.859042649995));
#130989=CARTESIAN_POINT('Ctrl Pts',(-224.614680768476,4.91756503473715,
130.722280220207));
#130990=CARTESIAN_POINT('Ctrl Pts',(-224.622171104238,4.91536527961958,
130.590489449217));
#130991=CARTESIAN_POINT('Ctrl Pts',(-224.629661440001,4.90786667141257,
130.458955628349));
#130992=CARTESIAN_POINT('Ctrl Pts',(-224.637151775763,4.89513936043556,
130.328131991364));
#130993=CARTESIAN_POINT('Ctrl Pts',(-224.644926109882,4.88192948959521,
130.192348136427));
#130994=CARTESIAN_POINT('Ctrl Pts',(-224.652700444001,4.86304475166706,
130.05689925926));
#130995=CARTESIAN_POINT('Ctrl Pts',(-224.660474778121,4.83850681130121,
129.922297751614));
#130996=CARTESIAN_POINT('Ctrl Pts',(-224.668239531068,4.81399911175392,
129.787862128297));
#130997=CARTESIAN_POINT('Ctrl Pts',(-224.676004284015,4.78385214159972,
129.654272177576));
#130998=CARTESIAN_POINT('Ctrl Pts',(-224.683769036962,4.74813941966383,
129.522036511135));
#130999=CARTESIAN_POINT('Ctrl Pts',(-224.691526077847,4.71246216810684,
129.389932183022));
#131000=CARTESIAN_POINT('Ctrl Pts',(-224.699283118732,4.67123026697988,
129.259179837391));
#131001=CARTESIAN_POINT('Ctrl Pts',(-224.707040159617,4.62456844719116,
129.130278857393));
#131002=CARTESIAN_POINT('Ctrl Pts',(-224.714791350857,4.57794181544364,
129.001475082626));
#131003=CARTESIAN_POINT('Ctrl Pts',(-224.722542542097,4.52589354791264,
128.874520260714));
#131004=CARTESIAN_POINT('Ctrl Pts',(-224.730293733337,4.46859836377831,
128.749899197695));
#131005=CARTESIAN_POINT('Ctrl Pts',(-224.738041630114,4.41132753162555,
128.625331101952));
#131006=CARTESIAN_POINT('Ctrl Pts',(-224.745789526891,4.34881438130046,
128.503095146748));
#131007=CARTESIAN_POINT('Ctrl Pts',(-224.753537423668,4.28128189148343,
128.383656499307));
#131008=CARTESIAN_POINT('Ctrl Pts',(-224.761283699753,4.21376352800743,
128.264242835856));
#131009=CARTESIAN_POINT('Ctrl Pts',(-224.769029975837,4.14122810572948,
128.147625656414));
#131010=CARTESIAN_POINT('Ctrl Pts',(-224.776776251921,4.06394453472509,
128.034245478952));
#131011=CARTESIAN_POINT('Ctrl Pts',(-224.784522585186,3.98666039323103,
127.920864464543));
#131012=CARTESIAN_POINT('Ctrl Pts',(-224.792268918451,3.90462825327537,
127.810720822848));
#131013=CARTESIAN_POINT('Ctrl Pts',(-224.800015251717,3.81816009686446,
127.704225695145));
#131014=CARTESIAN_POINT('Ctrl Pts',(-224.80776331972,3.73167257650934,127.597706718597));
#131015=CARTESIAN_POINT('Ctrl Pts',(-224.815511387723,3.64074730930894,
127.494838185354));
#131016=CARTESIAN_POINT('Ctrl Pts',(-224.823259455726,3.54573599235164,
127.395997471561));
#131017=CARTESIAN_POINT('Ctrl Pts',(-224.831015758468,3.45062369623616,
127.297051708682));
#131018=CARTESIAN_POINT('Ctrl Pts',(-224.838772061209,3.35141694672032,
127.20214259895));
#131019=CARTESIAN_POINT('Ctrl Pts',(-224.846528363951,3.24850407616572,
127.111610378295));
#131020=CARTESIAN_POINT('Ctrl Pts',(-224.854288806465,3.14553627791346,
127.021029837868));
#131021=CARTESIAN_POINT('Ctrl Pts',(-224.86204924898,3.03885872110251,126.934831086949));
#131022=CARTESIAN_POINT('Ctrl Pts',(-224.869809691494,2.92889133321031,
126.853312829859));
#131023=CARTESIAN_POINT('Ctrl Pts',(-224.877582591759,2.81874741590463,
126.771663712426));
#131024=CARTESIAN_POINT('Ctrl Pts',(-224.885355492025,2.70530343787483,
126.694710322879));
#131025=CARTESIAN_POINT('Ctrl Pts',(-224.89312839229,2.58900745651038,126.622707421444));
#131026=CARTESIAN_POINT('Ctrl Pts',(-224.900618728052,2.47693912700546,
126.553322006844));
#131027=CARTESIAN_POINT('Ctrl Pts',(-224.908109063813,2.36222281738965,
126.488533555236));
#131028=CARTESIAN_POINT('Ctrl Pts',(-224.915599399575,2.24527776402342,
126.428528031088));
#131029=CARTESIAN_POINT('Ctrl Pts',(-224.923373733694,2.12389870340883,
126.366247379251));
#131030=CARTESIAN_POINT('Ctrl Pts',(-224.931148067813,1.99973406480101,
126.308922217482));
#131031=CARTESIAN_POINT('Ctrl Pts',(-224.938922401932,1.87322664816605,
126.256811278955));
#131032=CARTESIAN_POINT('Ctrl Pts',(-224.946687154879,1.74687514061615,
126.204764562503));
#131033=CARTESIAN_POINT('Ctrl Pts',(-224.954451907826,1.61818695786183,
126.15791943082));
#131034=CARTESIAN_POINT('Ctrl Pts',(-224.962216660774,1.48762974803866,
126.116488947474));
#131035=CARTESIAN_POINT('Ctrl Pts',(-224.969973701659,1.35720220947681,
126.075099613469));
#131036=CARTESIAN_POINT('Ctrl Pts',(-224.977730742544,1.22490970829489,
126.039114343018));
#131037=CARTESIAN_POINT('Ctrl Pts',(-224.985487783429,1.09123980978319,
126.008698125267));
#131038=CARTESIAN_POINT('Ctrl Pts',(-224.993238974669,0.957670712781931,
125.978304844622));
#131039=CARTESIAN_POINT('Ctrl Pts',(-225.000990165909,0.822726665610151,
125.953472343892));
#131040=CARTESIAN_POINT('Ctrl Pts',(-225.008741357149,0.686909989304128,
125.934315676388));
#131041=CARTESIAN_POINT('Ctrl Pts',(-225.016489253926,0.551151038708379,
125.915167150978));
#131042=CARTESIAN_POINT('Ctrl Pts',(-225.024237150703,0.414520582974383,
125.901689715244));
#131043=CARTESIAN_POINT('Ctrl Pts',(-225.03198504748,0.277530505885588,
125.893947205153));
#131044=CARTESIAN_POINT('Ctrl Pts',(-225.039731323564,0.140569084167755,
125.886206314629));
#131045=CARTESIAN_POINT('Ctrl Pts',(-225.047477599648,0.00324858081679325,
125.88419798568));
#131046=CARTESIAN_POINT('Ctrl Pts',(-225.055223875733,-0.133915031459165,
125.887934087367));
#131047=CARTESIAN_POINT('Ctrl Pts',(-225.062970208998,-0.271079656245937,
125.891670216632));
#131048=CARTESIAN_POINT('Ctrl Pts',(-225.070716542263,-0.408086996826478,
125.901150850503));
#131049=CARTESIAN_POINT('Ctrl Pts',(-225.078462875529,-0.544422514503125,
125.916335741586));
#131050=CARTESIAN_POINT('Ctrl Pts',(-225.086210943532,-0.680788563573486,
125.931524033219));
#131051=CARTESIAN_POINT('Ctrl Pts',(-225.093959011535,-0.816482101873551,
125.95241908073));
#131052=CARTESIAN_POINT('Ctrl Pts',(-225.101707079538,-0.950995531297179,
125.978928972422));
#131053=CARTESIAN_POINT('Ctrl Pts',(-225.10946338228,-1.08565192319451,
126.005467039143));
#131054=CARTESIAN_POINT('Ctrl Pts',(-225.117219685022,-1.21912531654991,
126.037631795098));
#131055=CARTESIAN_POINT('Ctrl Pts',(-225.124975987764,-1.35091955811411,
126.075280431102));
#131056=CARTESIAN_POINT('Ctrl Pts',(-225.132736430278,-1.48278414223329,
126.112949161317));
#131057=CARTESIAN_POINT('Ctrl Pts',(-225.140496872792,-1.61296741785725,
126.156107480734));
#131058=CARTESIAN_POINT('Ctrl Pts',(-225.148257315306,-1.74099109552245,
126.204563549454));
#131059=CARTESIAN_POINT('Ctrl Pts',(-225.156030215571,-1.86922028816044,
126.253097404157));
#131060=CARTESIAN_POINT('Ctrl Pts',(-225.163803115837,-1.99528259536736,
126.306945849033));
#131061=CARTESIAN_POINT('Ctrl Pts',(-225.171576016102,-2.11872149418723,
126.365869624833));
#131062=CARTESIAN_POINT('Ctrl Pts',(-225.179066351864,-2.23767307811118,
126.422651372963));
#131063=CARTESIAN_POINT('Ctrl Pts',(-225.186556687627,-2.35418840480747,
126.48414571254));
#131064=CARTESIAN_POINT('Ctrl Pts',(-225.194047023389,-2.46788440960898,
126.550100446478));
#131065=CARTESIAN_POINT('Ctrl Pts',(-225.201822518005,-2.58590884821408,
126.618566092741));
#131066=CARTESIAN_POINT('Ctrl Pts',(-225.209598012622,-2.70126896985381,
126.692055388726));
#131067=CARTESIAN_POINT('Ctrl Pts',(-225.217373507239,-2.813507547675,126.770335538111));
#131068=CARTESIAN_POINT('Ctrl Pts',(-225.225139168045,-2.92560417530918,
126.848516685155));
#131069=CARTESIAN_POINT('Ctrl Pts',(-225.232904828851,-3.03458679731917,
126.931476406748));
#131070=CARTESIAN_POINT('Ctrl Pts',(-225.240670489657,-3.14002323591865,
127.01893631633));
#131071=CARTESIAN_POINT('Ctrl Pts',(-225.248426734605,-3.24533183291024,
127.106290180832));
#131072=CARTESIAN_POINT('Ctrl Pts',(-225.256182979553,-3.34710251134443,
127.198133117486));
#131073=CARTESIAN_POINT('Ctrl Pts',(-225.263939224501,-3.44493305069194,
127.294144194217));
#131074=CARTESIAN_POINT('Ctrl Pts',(-225.271690129401,-3.54269623531167,
127.39008916889));
#131075=CARTESIAN_POINT('Ctrl Pts',(-225.279441034301,-3.63652440006573,
127.490196301678));
#131076=CARTESIAN_POINT('Ctrl Pts',(-225.2871919392,-3.72604927651803,127.594105199152));
#131077=CARTESIAN_POINT('Ctrl Pts',(-225.294939186363,-3.81553190519101,
127.697965060867));
#131078=CARTESIAN_POINT('Ctrl Pts',(-225.302686433525,-3.90071503239147,
127.805622821377));
#131079=CARTESIAN_POINT('Ctrl Pts',(-225.310433680687,-3.98126835187258,
127.916682419969));
#131080=CARTESIAN_POINT('Ctrl Pts',(-225.318178949591,-4.06180110207999,
128.027713659515));
#131081=CARTESIAN_POINT('Ctrl Pts',(-225.325924218495,-4.13770616936105,
128.142144691342));
#131082=CARTESIAN_POINT('Ctrl Pts',(-225.3336694874,-4.20869478380431,128.259547995922));
#131083=CARTESIAN_POINT('Ctrl Pts',(-225.341416597441,-4.27970027303588,
128.376979208581));
#131084=CARTESIAN_POINT('Ctrl Pts',(-225.349163707482,-4.34578676788941,
128.497383773566));
#131085=CARTESIAN_POINT('Ctrl Pts',(-225.356910817524,-4.40670993374779,
128.620306904328));
#131086=CARTESIAN_POINT('Ctrl Pts',(-225.364658910431,-4.46764082885362,
128.743245630197));
#131087=CARTESIAN_POINT('Ctrl Pts',(-225.372407003339,-4.52340692386009,
128.868703204464));
#131088=CARTESIAN_POINT('Ctrl Pts',(-225.380155096247,-4.57381117634789,
128.996202885062));
#131089=CARTESIAN_POINT('Ctrl Pts',(-225.387908815622,-4.62425203111784,
129.123795152674));
#131090=CARTESIAN_POINT('Ctrl Pts',(-225.395662534997,-4.66932313191583,
129.253432121399));
#131091=CARTESIAN_POINT('Ctrl Pts',(-225.403416254372,-4.70887658549987,
129.384619667593));
#131092=CARTESIAN_POINT('Ctrl Pts',(-225.407292913424,-4.72865228880864,
129.450210046087));
#131093=CARTESIAN_POINT('Ctrl Pts',(-225.411169572477,-4.74704950926761,
129.516187808445));
#131094=CARTESIAN_POINT('Ctrl Pts',(-225.41504623153,-4.76405452823393,
129.582490119308));
#131095=CARTESIAN_POINT('Ctrl Pts',(-223.665116307759,-4.76405452823394,
129.582490119308));
#131096=CARTESIAN_POINT('Ctrl Pts',(-223.672768948211,-4.79775074606203,
129.713871161208));
#131097=CARTESIAN_POINT('Ctrl Pts',(-223.680421588662,-4.82600298496374,
129.846627596572));
#131098=CARTESIAN_POINT('Ctrl Pts',(-223.688074229114,-4.84871592411686,
129.980262959691));
#131099=CARTESIAN_POINT('Ctrl Pts',(-223.695918618263,-4.87199797095897,
130.117246762752));
#131100=CARTESIAN_POINT('Ctrl Pts',(-223.703763007413,-4.88945937353219,
130.255153683256));
#131101=CARTESIAN_POINT('Ctrl Pts',(-223.711607396563,-4.90105388213603,
130.393442247449));
#131102=CARTESIAN_POINT('Ctrl Pts',(-223.719451785713,-4.91264839073989,
130.531730811643));
#131103=CARTESIAN_POINT('Ctrl Pts',(-223.727296174863,-4.91837601587455,
130.670400566594));
#131104=CARTESIAN_POINT('Ctrl Pts',(-223.735140564013,-4.91824789595394,
130.808909952094));
#131105=CARTESIAN_POINT('',(-223.389859435967,-4.91824981741226,130.803020459256));
#131106=CARTESIAN_POINT('Ctrl Pts',(-223.320144520485,-4.76405452823402,
129.582490119308));
#131107=CARTESIAN_POINT('Ctrl Pts',(-223.328480310977,-4.80057528230012,
129.724883985132));
#131108=CARTESIAN_POINT('Ctrl Pts',(-223.33681610147,-4.83074977404695,
129.869079901701));
#131109=CARTESIAN_POINT('Ctrl Pts',(-223.345151891962,-4.85441260434725,
130.014511689445));
#131110=CARTESIAN_POINT('Ctrl Pts',(-223.353462705121,-4.87800453142564,
130.159507705889));
#131111=CARTESIAN_POINT('Ctrl Pts',(-223.361773518279,-4.89512365879074,
130.305731919146));
#131112=CARTESIAN_POINT('Ctrl Pts',(-223.370084331438,-4.90565513818706,
130.45260682913));
#131113=CARTESIAN_POINT('Ctrl Pts',(-223.376676032948,-4.91400815579326,
130.569100311465));
#131114=CARTESIAN_POINT('Ctrl Pts',(-223.383267734457,-4.91821793163162,
130.68600276536));
#131115=CARTESIAN_POINT('Ctrl Pts',(-223.389859435967,-4.91824981741226,
130.803020459257));
#131116=CARTESIAN_POINT('Ctrl Pts',(-223.389859435996,-4.9182498174124,
130.803020459769));
#131117=CARTESIAN_POINT('Ctrl Pts',(-223.397825722162,-4.91828835240305,
130.94444015766));
#131118=CARTESIAN_POINT('Ctrl Pts',(-223.405792008328,-4.91222295066778,
131.085797589312));
#131119=CARTESIAN_POINT('Ctrl Pts',(-223.413758294494,-4.90009592097111,
131.226548997063));
#131120=CARTESIAN_POINT('Ctrl Pts',(-223.421730186026,-4.88796035826073,
131.36739944256));
#131121=CARTESIAN_POINT('Ctrl Pts',(-223.429702077557,-4.86975469569824,
131.50764265691));
#131122=CARTESIAN_POINT('Ctrl Pts',(-223.437673969088,-4.84557290965292,
131.646741908751));
#131123=CARTESIAN_POINT('Ctrl Pts',(-223.445652730692,-4.82137028405894,
131.785961034517));
#131124=CARTESIAN_POINT('Ctrl Pts',(-223.453631492296,-4.79118132918627,
131.924033879671));
#131125=CARTESIAN_POINT('Ctrl Pts',(-223.461610253899,-4.75515071053607,
132.060435767622));
#131126=CARTESIAN_POINT('Ctrl Pts',(-223.469602905369,-4.71905736780639,
132.197075111469));
#131127=CARTESIAN_POINT('Ctrl Pts',(-223.477595556839,-4.67710213439243,
132.33203733918));
#131128=CARTESIAN_POINT('Ctrl Pts',(-223.485588208309,-4.62947932429489,
132.464813642625));
#131129=CARTESIAN_POINT('Ctrl Pts',(-223.493588711762,-4.58180972953302,
132.597720385554));
#131130=CARTESIAN_POINT('Ctrl Pts',(-223.501589215216,-4.52846158909981,
132.728436590422));
#131131=CARTESIAN_POINT('Ctrl Pts',(-223.509589718669,-4.46967645655695,
132.856475486719));
#131132=CARTESIAN_POINT('Ctrl Pts',(-223.517604814205,-4.41078410607477,
132.984747912585));
#131133=CARTESIAN_POINT('Ctrl Pts',(-223.525619909741,-4.34643511271477,
133.110332954569));
#131134=CARTESIAN_POINT('Ctrl Pts',(-223.533635005277,-4.27691637680558,
133.232769431648));
#131135=CARTESIAN_POINT('Ctrl Pts',(-223.536740095741,-4.2499844502882,
133.280201971389));
#131136=CARTESIAN_POINT('Ctrl Pts',(-223.539845186206,-4.22227708499426,
133.327162289319));
#131137=CARTESIAN_POINT('Ctrl Pts',(-223.542950276671,-4.19381262813753,
133.373624851267));
#131138=CARTESIAN_POINT('Ctrl Pts',(-223.55072461079,-4.12254507550592,
133.489954950088));
#131139=CARTESIAN_POINT('Ctrl Pts',(-223.558498944909,-4.04632073720989,
133.603501777012));
#131140=CARTESIAN_POINT('Ctrl Pts',(-223.566273279029,-3.96538320210203,
133.71381402379));
#131141=CARTESIAN_POINT('Ctrl Pts',(-223.574038031976,-3.88454541527281,
133.823990320582));
#131142=CARTESIAN_POINT('Ctrl Pts',(-223.581802784923,-3.79900621806242,
133.930939656645));
#131143=CARTESIAN_POINT('Ctrl Pts',(-223.589567537871,-3.70905417745916,
134.034236802681));
#131144=CARTESIAN_POINT('Ctrl Pts',(-223.597324578756,-3.61919147849049,
134.137431352535));
#131145=CARTESIAN_POINT('Ctrl Pts',(-223.605081619641,-3.52492491338456,
134.236980638129));
#131146=CARTESIAN_POINT('Ctrl Pts',(-223.612838660526,-3.42658506683357,
134.33249012798));
#131147=CARTESIAN_POINT('Ctrl Pts',(-223.620589851766,-3.32831937912596,
134.427927593381));
#131148=CARTESIAN_POINT('Ctrl Pts',(-223.628341043007,-3.22598680331828,
134.519331055509));
#131149=CARTESIAN_POINT('Ctrl Pts',(-223.636092234247,-3.11995650193513,
134.606340955302));
#131150=CARTESIAN_POINT('Ctrl Pts',(-223.643840131024,-3.01397126625837,
134.693313873567));
#131151=CARTESIAN_POINT('Ctrl Pts',(-223.651588027801,-2.90429173245949,
134.775896696082));
#131152=CARTESIAN_POINT('Ctrl Pts',(-223.659335924579,-2.79132187239289,
134.85376863198));
#131153=CARTESIAN_POINT('Ctrl Pts',(-223.667082200663,-2.67837564318566,
134.931624278748));
#131154=CARTESIAN_POINT('Ctrl Pts',(-223.674828476747,-2.5621407784028,
135.004770777197));
#131155=CARTESIAN_POINT('Ctrl Pts',(-223.682574752831,-2.44305177417905,
135.072929592197));
#131156=CARTESIAN_POINT('Ctrl Pts',(-223.690321086097,-2.32396189086749,
135.141088910329));
#131157=CARTESIAN_POINT('Ctrl Pts',(-223.698067419362,-2.20201816539445,
135.204260277339));
#131158=CARTESIAN_POINT('Ctrl Pts',(-223.705813752628,-2.07768097906349,
135.262210414468));
#131159=CARTESIAN_POINT('Ctrl Pts',(-223.713561820631,-1.95331594828191,
135.320173529128));
#131160=CARTESIAN_POINT('Ctrl Pts',(-223.721309888634,-1.82655674436542,
135.372912922089));
#131161=CARTESIAN_POINT('Ctrl Pts',(-223.729057956637,-1.69788469565208,
135.420243049211));
#131162=CARTESIAN_POINT('Ctrl Pts',(-223.736814259379,-1.56907589275363,
135.467623479355));
#131163=CARTESIAN_POINT('Ctrl Pts',(-223.744570562121,-1.43835055144765,
135.509583024164));
#131164=CARTESIAN_POINT('Ctrl Pts',(-223.752326864863,-1.30620670132538,
135.545985562236));
#131165=CARTESIAN_POINT('Ctrl Pts',(-223.760087307378,-1.17399232205152,
135.582407529438));
#131166=CARTESIAN_POINT('Ctrl Pts',(-223.767847749892,-1.04035830612776,
135.613266492088));
#131167=CARTESIAN_POINT('Ctrl Pts',(-223.775608192406,-0.905812931209745,
135.638477496185));
#131168=CARTESIAN_POINT('Ctrl Pts',(-223.783381092672,-0.771051572111542,
135.663728971225));
#131169=CARTESIAN_POINT('Ctrl Pts',(-223.791153992937,-0.635376317667153,
135.683314313856));
#131170=CARTESIAN_POINT('Ctrl Pts',(-223.798926893203,-0.499301522250402,
135.697200391397));
#131171=CARTESIAN_POINT('Ctrl Pts',(-223.806417228963,-0.368173388428244,
135.710581675038));
#131172=CARTESIAN_POINT('Ctrl Pts',(-223.813907564724,-0.236674565385695,
135.718670845973));
#131173=CARTESIAN_POINT('Ctrl Pts',(-223.821397900484,-0.105263399915473,
135.721484032647));
#131174=CARTESIAN_POINT('Ctrl Pts',(-223.829172234604,0.0311302598637276,
135.724403882149));
#131175=CARTESIAN_POINT('Ctrl Pts',(-223.836946568723,0.167861537898053,
135.721649021043));
#131176=CARTESIAN_POINT('Ctrl Pts',(-223.844720902842,0.304419070050243,
135.713180444397));
#131177=CARTESIAN_POINT('Ctrl Pts',(-223.852485655789,0.440808307248184,
135.704722304515));
#131178=CARTESIAN_POINT('Ctrl Pts',(-223.860250408736,0.577023838141903,
135.690564483831));
#131179=CARTESIAN_POINT('Ctrl Pts',(-223.868015161683,0.712551927773481,
135.670719915103));
#131180=CARTESIAN_POINT('Ctrl Pts',(-223.875772202568,0.847945408995826,
135.650895056281));
#131181=CARTESIAN_POINT('Ctrl Pts',(-223.883529243453,0.982652423374748,
135.62539474578));
#131182=CARTESIAN_POINT('Ctrl Pts',(-223.891286284338,1.11616235129815,
135.594283859962));
#131183=CARTESIAN_POINT('Ctrl Pts',(-223.899037475578,1.24957159834654,
135.563196435105));
#131184=CARTESIAN_POINT('Ctrl Pts',(-223.906788666818,1.38178517654963,
135.526506944803));
#131185=CARTESIAN_POINT('Ctrl Pts',(-223.914539858059,1.51230103732411,
135.48433162549));
#131186=CARTESIAN_POINT('Ctrl Pts',(-223.922287754836,1.64276142537632,
135.442174231812));
#131187=CARTESIAN_POINT('Ctrl Pts',(-223.930035651613,1.77152515991307,
135.39453576651));
#131188=CARTESIAN_POINT('Ctrl Pts',(-223.93778354839,1.898103993839,135.341582707245));
#131189=CARTESIAN_POINT('Ctrl Pts',(-223.945529824474,2.0246563502016,135.288640724619));
#131190=CARTESIAN_POINT('Ctrl Pts',(-223.953276100558,2.14902435457151,
135.230386510051));
#131191=CARTESIAN_POINT('Ctrl Pts',(-223.961022376642,2.27073881168078,
135.167035062402));
#131192=CARTESIAN_POINT('Ctrl Pts',(-223.968768709908,2.39245416725835,
135.103683147107));
#131193=CARTESIAN_POINT('Ctrl Pts',(-223.976515043173,2.51151558968812,
135.035234104158));
#131194=CARTESIAN_POINT('Ctrl Pts',(-223.984261376438,2.62747796760326,
134.961949172517));
#131195=CARTESIAN_POINT('Ctrl Pts',(-223.992009444441,2.74346631448908,
134.888647829223));
#131196=CARTESIAN_POINT('Ctrl Pts',(-223.999757512445,2.85635390542677,
134.81050865109));
#131197=CARTESIAN_POINT('Ctrl Pts',(-224.007505580448,2.96572446715174,
134.727836302139));
#131198=CARTESIAN_POINT('Ctrl Pts',(-224.015261883189,3.07521126921138,
134.645076088032));
#131199=CARTESIAN_POINT('Ctrl Pts',(-224.023018185931,3.18117326273432,
134.557773314948));
#131200=CARTESIAN_POINT('Ctrl Pts',(-224.030774488673,3.28322672777085,
134.466273412343));
#131201=CARTESIAN_POINT('Ctrl Pts',(-224.038534931187,3.38533466181416,
134.374724673485));
#131202=CARTESIAN_POINT('Ctrl Pts',(-224.046295373702,3.48352963086155,
134.278974614264));
#131203=CARTESIAN_POINT('Ctrl Pts',(-224.054055816216,3.57746542421788,
134.179404943353));
#131204=CARTESIAN_POINT('Ctrl Pts',(-224.061828716481,3.67155201164893,
134.079675434367));
#131205=CARTESIAN_POINT('Ctrl Pts',(-224.069601616747,3.76136550416974,
133.976114356373));
#131206=CARTESIAN_POINT('Ctrl Pts',(-224.077374517012,3.84660000521288,
133.869136541251));
#131207=CARTESIAN_POINT('Ctrl Pts',(-224.084864852774,3.92873601744643,
133.766047639173));
#131208=CARTESIAN_POINT('Ctrl Pts',(-224.092355188536,4.00661999195626,
133.65978634957));
#131209=CARTESIAN_POINT('Ctrl Pts',(-224.099845524297,4.08001775042296,
133.550747010398));
#131210=CARTESIAN_POINT('Ctrl Pts',(-224.107619858416,4.15619840721381,
133.437573411535));
#131211=CARTESIAN_POINT('Ctrl Pts',(-224.115394192535,4.22778726016786,
133.321048445176));
#131212=CARTESIAN_POINT('Ctrl Pts',(-224.123168526655,4.29447508852375,
133.201581253333));
#131213=CARTESIAN_POINT('Ctrl Pts',(-224.130933279602,4.36108073009126,
133.082261294128));
#131214=CARTESIAN_POINT('Ctrl Pts',(-224.138698032549,4.42279717627691,
132.96000666226));
#131215=CARTESIAN_POINT('Ctrl Pts',(-224.146462785496,4.47935762148213,
132.835256567971));
#131216=CARTESIAN_POINT('Ctrl Pts',(-224.154219826381,4.53586189005581,
132.710630377234));
#131217=CARTESIAN_POINT('Ctrl Pts',(-224.161976867266,4.58722018829892,
132.583514010232));
#131218=CARTESIAN_POINT('Ctrl Pts',(-224.169733908151,4.6332110961578,132.454372132962));
#131219=CARTESIAN_POINT('Ctrl Pts',(-224.177485099391,4.67916732191513,
132.325327642588));
#131220=CARTESIAN_POINT('Ctrl Pts',(-224.185236290631,4.71976408313914,
132.194261049065));
#131221=CARTESIAN_POINT('Ctrl Pts',(-224.192987481871,4.75482780330945,
132.061657568718));
#131222=CARTESIAN_POINT('Ctrl Pts',(-224.200735378648,4.78987662046337,
131.929110448386));
#131223=CARTESIAN_POINT('Ctrl Pts',(-224.208483275425,4.81939697415904,
131.795028117613));
#131224=CARTESIAN_POINT('Ctrl Pts',(-224.216231172202,4.8432650172885,131.659911337751));
#131225=CARTESIAN_POINT('Ctrl Pts',(-224.223977448286,4.86712806773788,
131.524822821407));
#131226=CARTESIAN_POINT('Ctrl Pts',(-224.23172372437,4.88534109139618,131.388700671134));
#131227=CARTESIAN_POINT('Ctrl Pts',(-224.239470000454,4.89783136139199,
131.252055846338));
#131228=CARTESIAN_POINT('Ctrl Pts',(-224.247216333719,4.91032172358816,
131.11541001286));
#131229=CARTESIAN_POINT('Ctrl Pts',(-224.254962666985,4.91708921223833,
130.978241886502));
#131230=CARTESIAN_POINT('Ctrl Pts',(-224.26270900025,4.91811302151363,130.841067158101));
#131231=CARTESIAN_POINT('Ctrl Pts',(-224.270457068253,4.91913706006392,
130.703861710372));
#131232=CARTESIAN_POINT('Ctrl Pts',(-224.278205136256,4.91441485681918,
130.566650048538));
#131233=CARTESIAN_POINT('Ctrl Pts',(-224.285953204259,4.90397772838234,
130.429947073433));
#131234=CARTESIAN_POINT('Ctrl Pts',(-224.293709507001,4.89352950724115,
130.293098808779));
#131235=CARTESIAN_POINT('Ctrl Pts',(-224.301465809742,4.87735425746788,
130.156760701289));
#131236=CARTESIAN_POINT('Ctrl Pts',(-224.309222112484,4.85553518864238,
130.021442298483));
#131237=CARTESIAN_POINT('Ctrl Pts',(-224.316982554998,4.83370447432288,
129.886051672171));
#131238=CARTESIAN_POINT('Ctrl Pts',(-224.324742997512,4.80622401703399,
129.751682217852));
#131239=CARTESIAN_POINT('Ctrl Pts',(-224.332503440026,4.77322782375656,
129.61883153525));
#131240=CARTESIAN_POINT('Ctrl Pts',(-224.340276340292,4.74017866206041,
129.485767588939));
#131241=CARTESIAN_POINT('Ctrl Pts',(-224.348049240557,4.70159618066785,
129.354227661756));
#131242=CARTESIAN_POINT('Ctrl Pts',(-224.355822140823,4.65766404481944,
129.22469333991));
#131243=CARTESIAN_POINT('Ctrl Pts',(-224.363312476585,4.61532895276476,
129.099867916933));
#131244=CARTESIAN_POINT('Ctrl Pts',(-224.370802812348,4.56802651098553,
128.976905100769));
#131245=CARTESIAN_POINT('Ctrl Pts',(-224.37829314811,4.51596190807124,128.856215061569));
#131246=CARTESIAN_POINT('Ctrl Pts',(-224.386067482229,4.46192325991574,
128.730949022857));
#131247=CARTESIAN_POINT('Ctrl Pts',(-224.393841816348,4.40258302923531,
128.607734702767));
#131248=CARTESIAN_POINT('Ctrl Pts',(-224.401616150467,4.33811829741793,
128.487053408733));
#131249=CARTESIAN_POINT('Ctrl Pts',(-224.409380903414,4.2737330126215,128.36652084361));
#131250=CARTESIAN_POINT('Ctrl Pts',(-224.417145656361,4.20423597507095,
128.248515434773));
#131251=CARTESIAN_POINT('Ctrl Pts',(-224.424910409309,4.12985248983799,
128.133499057193));
#131252=CARTESIAN_POINT('Ctrl Pts',(-224.432667450194,4.05554288333078,
128.0185969155));
#131253=CARTESIAN_POINT('Ctrl Pts',(-224.440424491079,3.97635669834492,
127.90667822329));
#131254=CARTESIAN_POINT('Ctrl Pts',(-224.448181531964,3.89256518859751,
127.798180430848));
#131255=CARTESIAN_POINT('Ctrl Pts',(-224.455932723204,3.8088368666793,127.689764457434));
#131256=CARTESIAN_POINT('Ctrl Pts',(-224.463683914444,3.72051037062131,
127.584764557177));
#131257=CARTESIAN_POINT('Ctrl Pts',(-224.471435105684,3.62790010430862,
127.483589036193));
#131258=CARTESIAN_POINT('Ctrl Pts',(-224.479183002461,3.53532919982994,
127.382456517504));
#131259=CARTESIAN_POINT('Ctrl Pts',(-224.486930899238,3.43847840978776,
127.285145432954));
#131260=CARTESIAN_POINT('Ctrl Pts',(-224.494678796015,3.33770209650352,
127.192030652364));
#131261=CARTESIAN_POINT('Ctrl Pts',(-224.502425072099,3.23694686345152,
127.098935349379));
#131262=CARTESIAN_POINT('Ctrl Pts',(-224.510171348183,3.13226802741177,
127.010034869565));
#131263=CARTESIAN_POINT('Ctrl Pts',(-224.517917624268,3.02405616235136,
126.925666586137));
#131264=CARTESIAN_POINT('Ctrl Pts',(-224.525663957533,2.91584349849538,
126.841297679921));
#131265=CARTESIAN_POINT('Ctrl Pts',(-224.533410290798,2.804098061906,126.76146127724));
#131266=CARTESIAN_POINT('Ctrl Pts',(-224.541156624064,2.68924247183255,
126.686453626121));
#131267=CARTESIAN_POINT('Ctrl Pts',(-224.548904692067,2.57436116064653,
126.611429177559));
#131268=CARTESIAN_POINT('Ctrl Pts',(-224.55665276007,2.45636863730857,126.541235846087));
#131269=CARTESIAN_POINT('Ctrl Pts',(-224.564400828072,2.33571502986092,
126.476125600636));
#131270=CARTESIAN_POINT('Ctrl Pts',(-224.572157130814,2.21493319032331,
126.410946155241));
#131271=CARTESIAN_POINT('Ctrl Pts',(-224.579913433556,2.09148496159011,
126.35086077364));
#131272=CARTESIAN_POINT('Ctrl Pts',(-224.587669736298,1.96584401723188,
126.29607487214));
#131273=CARTESIAN_POINT('Ctrl Pts',(-224.595430178812,1.84013601451799,
126.241259729754));
#131274=CARTESIAN_POINT('Ctrl Pts',(-224.603190621326,1.71223332864473,
126.191749844542));
#131275=CARTESIAN_POINT('Ctrl Pts',(-224.610951063841,1.58262703840013,
126.147701437443));
#131276=CARTESIAN_POINT('Ctrl Pts',(-224.618723964106,1.45281269263288,
126.10358231993));
#131277=CARTESIAN_POINT('Ctrl Pts',(-224.626496864372,1.32128965286626,
126.064942310556));
#131278=CARTESIAN_POINT('Ctrl Pts',(-224.634269764637,1.18856236676532,
126.031887195659));
#131279=CARTESIAN_POINT('Ctrl Pts',(-224.641760100399,1.06066005183867,
126.000033717451));
#131280=CARTESIAN_POINT('Ctrl Pts',(-224.649250436161,0.93163982691611,
125.973366195727));
#131281=CARTESIAN_POINT('Ctrl Pts',(-224.656740771922,0.801957689206216,
125.951933706501));
#131282=CARTESIAN_POINT('Ctrl Pts',(-224.664515106041,0.66735861382538,
125.929688597932));
#131283=CARTESIAN_POINT('Ctrl Pts',(-224.67228944016,0.531620072575311,
125.91301286492));
#131284=CARTESIAN_POINT('Ctrl Pts',(-224.680063774279,0.395242719848658,
125.902017682305));
#131285=CARTESIAN_POINT('Ctrl Pts',(-224.687828527226,0.259033440021218,
125.891036050269));
#131286=CARTESIAN_POINT('Ctrl Pts',(-224.695593280173,0.122187301125484,
125.8857210703));
#131287=CARTESIAN_POINT('Ctrl Pts',(-224.70335803312,-0.0147853254507163,
125.886132841563));
#131288=CARTESIAN_POINT('Ctrl Pts',(-224.711115074005,-0.151621908883225,
125.886544203848));
#131289=CARTESIAN_POINT('Ctrl Pts',(-224.71887211489,-0.288584341554595,
125.89267099704));
#131290=CARTESIAN_POINT('Ctrl Pts',(-224.726629155775,-0.425157964891527,
125.904521460268));
#131291=CARTESIAN_POINT('Ctrl Pts',(-224.734380347015,-0.561628596996526,
125.916362986969));
#131292=CARTESIAN_POINT('Ctrl Pts',(-224.742131538255,-0.697710615446485,
125.933919558784));
#131293=CARTESIAN_POINT('Ctrl Pts',(-224.749882729495,-0.832890557761763,
125.95714735825));
#131294=CARTESIAN_POINT('Ctrl Pts',(-224.757630626272,-0.968013044996067,
125.980365285281));
#131295=CARTESIAN_POINT('Ctrl Pts',(-224.765378523049,-1.10223383415023,
126.009249579745));
#131296=CARTESIAN_POINT('Ctrl Pts',(-224.773126419827,-1.23504599513528,
126.043704732879));
#131297=CARTESIAN_POINT('Ctrl Pts',(-224.780872695911,-1.36783037467863,
126.078152678739));
#131298=CARTESIAN_POINT('Ctrl Pts',(-224.788618971995,-1.49920633393927,
126.118169067302));
#131299=CARTESIAN_POINT('Ctrl Pts',(-224.796365248079,-1.62867891650682,
126.163607656092));
#131300=CARTESIAN_POINT('Ctrl Pts',(-224.804111581344,-1.7581524548121,
126.2090465803));
#131301=CARTESIAN_POINT('Ctrl Pts',(-224.811857914609,-1.88572221948171,
126.259907655135));
#131302=CARTESIAN_POINT('Ctrl Pts',(-224.819604247875,-2.01091053263215,
126.315995448348));
#131303=CARTESIAN_POINT('Ctrl Pts',(-224.827352315878,-2.13612688083783,
126.372095802034));
#131304=CARTESIAN_POINT('Ctrl Pts',(-224.83510038388,-2.25896035957585,
126.433425043411));
#131305=CARTESIAN_POINT('Ctrl Pts',(-224.842848451883,-2.37895567504547,
126.49974066237));
#131306=CARTESIAN_POINT('Ctrl Pts',(-224.850604754625,-2.49907852296384,
126.566126762359));
#131307=CARTESIAN_POINT('Ctrl Pts',(-224.858361057367,-2.61635683923091,
126.637509637004));
#131308=CARTESIAN_POINT('Ctrl Pts',(-224.866117360109,-2.73036176915656,
126.713601803846));
#131309=CARTESIAN_POINT('Ctrl Pts',(-224.873877802623,-2.84442754694593,
126.789734583369));
#131310=CARTESIAN_POINT('Ctrl Pts',(-224.881638245137,-2.95521614147743,
126.870581433081));
#131311=CARTESIAN_POINT('Ctrl Pts',(-224.889398687651,-3.06233067957151,
126.955813635723));
#131312=CARTESIAN_POINT('Ctrl Pts',(-224.897171587916,-3.16961716743133,
127.041182660663));
#131313=CARTESIAN_POINT('Ctrl Pts',(-224.904944488182,-3.27321751728239,
127.130950850041));
#131314=CARTESIAN_POINT('Ctrl Pts',(-224.912717388447,-3.37277006179579,
127.224750977849));
#131315=CARTESIAN_POINT('Ctrl Pts',(-224.92020772421,-3.46870362056756,
127.315141234752));
#131316=CARTESIAN_POINT('Ctrl Pts',(-224.927698059972,-3.56087834493337,
127.409275157151));
#131317=CARTESIAN_POINT('Ctrl Pts',(-224.935188395735,-3.64900646822336,
127.506795628462));
#131318=CARTESIAN_POINT('Ctrl Pts',(-224.942883618158,-3.73954520131624,
127.606983622868));
#131319=CARTESIAN_POINT('Ctrl Pts',(-224.95057884058,-3.82611323979784,
127.711078857721));
#131320=CARTESIAN_POINT('Ctrl Pts',(-224.958274063002,-3.90834911965968,
127.818729993836));
#131321=CARTESIAN_POINT('Ctrl Pts',(-224.965960080009,-3.99048662478202,
127.926252352189));
#131322=CARTESIAN_POINT('Ctrl Pts',(-224.973646097015,-4.06830203621734,
128.037321839102));
#131323=CARTESIAN_POINT('Ctrl Pts',(-224.981332114021,-4.14147118111289,
128.151550877213));
#131324=CARTESIAN_POINT('Ctrl Pts',(-224.989009420355,-4.21455740237118,
128.265650457923));
#131325=CARTESIAN_POINT('Ctrl Pts',(-224.996686726688,-4.28300762449184,
128.382902128035));
#131326=CARTESIAN_POINT('Ctrl Pts',(-225.004364033021,-4.34653884654452,
128.502886499098));
#131327=CARTESIAN_POINT('Ctrl Pts',(-225.012036237156,-4.41002784689328,
128.622791130712));
#131328=CARTESIAN_POINT('Ctrl Pts',(-225.01970844129,-4.46860416159031,
128.745424500333));
#131329=CARTESIAN_POINT('Ctrl Pts',(-225.027380645424,-4.52202899545416,
128.870339721409));
#131330=CARTESIAN_POINT('Ctrl Pts',(-225.035049996425,-4.57543396173566,
128.995208489118));
#131331=CARTESIAN_POINT('Ctrl Pts',(-225.042719347426,-4.62369109700592,
129.122357055415));
#131332=CARTESIAN_POINT('Ctrl Pts',(-225.050388698427,-4.66660851965282,
129.251315870367));
#131333=CARTESIAN_POINT('Ctrl Pts',(-225.056882517944,-4.70294770881461,
129.360508326054));
#131334=CARTESIAN_POINT('Ctrl Pts',(-225.063376337461,-4.73545938964632,
129.470998107947));
#131335=CARTESIAN_POINT('Ctrl Pts',(-225.069870156977,-4.76405452823403,
129.582490119308));
#131336=CARTESIAN_POINT('Origin',(213.235140564004,0.,130.804360617566));
#131337=CARTESIAN_POINT('',(-227.165337382971,-4.76405452823413,129.582490119309));
#131338=CARTESIAN_POINT('',(-226.819766265743,-4.76405452823404,129.582490119308));
#131339=CARTESIAN_POINT('',(213.235140564004,-4.76405452823405,129.582490119308));
#131340=CARTESIAN_POINT('',(-225.485140564065,-4.91824980939642,130.802991357867));
#131341=CARTESIAN_POINT('Ctrl Pts',(-225.485140564065,-4.91824980939641,
130.802991357866));
#131342=CARTESIAN_POINT('Ctrl Pts',(-225.492858871425,-4.91828752983759,
130.938479572856));
#131343=CARTESIAN_POINT('Ctrl Pts',(-225.500577178786,-4.9127223578869,
131.074194759287));
#131344=CARTESIAN_POINT('Ctrl Pts',(-225.508295486146,-4.90152415104786,
131.20963097078));
#131345=CARTESIAN_POINT('Ctrl Pts',(-225.516004459813,-4.89033948612087,
131.344903400225));
#131346=CARTESIAN_POINT('Ctrl Pts',(-225.523713433479,-4.87353536893283,
131.479897133919));
#131347=CARTESIAN_POINT('Ctrl Pts',(-225.531422407145,-4.85113363514974,
131.614104723083));
#131348=CARTESIAN_POINT('Ctrl Pts',(-225.539123969384,-4.82875343845062,
131.748183284728));
#131349=CARTESIAN_POINT('Ctrl Pts',(-225.546825531624,-4.8007863969902,
131.88147681636));
#131350=CARTESIAN_POINT('Ctrl Pts',(-225.554527093863,-4.76730623132601,
132.013481934581));
#131351=CARTESIAN_POINT('Ctrl Pts',(-225.562223159812,-4.73384995908458,
132.145392846157));
#131352=CARTESIAN_POINT('Ctrl Pts',(-225.569919225762,-4.69488848950265,
132.276016790645));
#131353=CARTESIAN_POINT('Ctrl Pts',(-225.577615291712,-4.65054672781533,
132.40485997555));
#131354=CARTESIAN_POINT('Ctrl Pts',(-225.58530856989,-4.60622102819074,
132.533656489162));
#131355=CARTESIAN_POINT('Ctrl Pts',(-225.593001848068,-4.55651903941725,
132.660673150561));
#131356=CARTESIAN_POINT('Ctrl Pts',(-225.600695126247,-4.50161560965181,
132.785431026572));
#131357=CARTESIAN_POINT('Ctrl Pts',(-225.608387200152,-4.4467207742352,
132.910169373517));
#131358=CARTESIAN_POINT('Ctrl Pts',(-225.616079274058,-4.38662627684785,
133.032649274864));
#131359=CARTESIAN_POINT('Ctrl Pts',(-225.623771347963,-4.32155503253321,
133.152411972048));
#131360=CARTESIAN_POINT('Ctrl Pts',(-225.63146394312,-4.2564793786793,133.272182784927));
#131361=CARTESIAN_POINT('Ctrl Pts',(-225.639156538277,-4.1864264967233,
133.389235678472));
#131362=CARTESIAN_POINT('Ctrl Pts',(-225.646849133434,-4.11166492579988,
133.503137118213));
#131363=CARTESIAN_POINT('Ctrl Pts',(-225.654543975428,-4.036881518678,133.617071826042));
#131364=CARTESIAN_POINT('Ctrl Pts',(-225.662238817422,-3.95738690479067,
133.727852917352));
#131365=CARTESIAN_POINT('Ctrl Pts',(-225.669933659416,-3.87349226168471,
133.835076830142));
#131366=CARTESIAN_POINT('Ctrl Pts',(-225.677636826674,-3.78950685061555,
133.942416751485));
#131367=CARTESIAN_POINT('Ctrl Pts',(-225.685339993933,-3.70111215078513,
134.046191497544));
#131368=CARTESIAN_POINT('Ctrl Pts',(-225.693043161192,-3.60865909155127,
134.146031251166));
#131369=CARTESIAN_POINT('Ctrl Pts',(-225.700751019266,-3.51614973336657,
134.24593180184));
#131370=CARTESIAN_POINT('Ctrl Pts',(-225.70845887734,-3.41957737552138,
134.341892309152));
#131371=CARTESIAN_POINT('Ctrl Pts',(-225.716166735414,-3.31932806359591,
134.433581507609));
#131372=CARTESIAN_POINT('Ctrl Pts',(-225.723885921011,-3.21893142457809,
134.525405453155));
#131373=CARTESIAN_POINT('Ctrl Pts',(-225.731605106607,-3.11484734573308,
134.61294530241));
#131374=CARTESIAN_POINT('Ctrl Pts',(-225.739324292203,-3.00749338761577,
134.695911283553));
#131375=CARTESIAN_POINT('Ctrl Pts',(-225.743196951807,-2.95363468300403,
134.737534716444));
#131376=CARTESIAN_POINT('Ctrl Pts',(-225.747069611411,-2.89895340086588,
134.7780076219));
#131377=CARTESIAN_POINT('Ctrl Pts',(-225.750942271014,-2.84350467758067,
134.817297722864));
#131378=CARTESIAN_POINT('Ctrl Pts',(-225.758716605133,-2.73219179562714,
134.896172295827));
#131379=CARTESIAN_POINT('Ctrl Pts',(-225.766490939252,-2.61741832065757,
134.970536810859));
#131380=CARTESIAN_POINT('Ctrl Pts',(-225.774265273371,-2.49958585641601,
135.040072317966));
#131381=CARTESIAN_POINT('Ctrl Pts',(-225.782030026319,-2.38189861015628,
135.109522128774));
#131382=CARTESIAN_POINT('Ctrl Pts',(-225.789794779266,-2.2611602091394,
135.17415457622));
#131383=CARTESIAN_POINT('Ctrl Pts',(-225.797559532213,-2.13780333452593,
135.233692391704));
#131384=CARTESIAN_POINT('Ctrl Pts',(-225.805316573098,-2.01456897969869,
135.293171073391));
#131385=CARTESIAN_POINT('Ctrl Pts',(-225.813073613983,-1.88872167661626,
135.347565024023));
#131386=CARTESIAN_POINT('Ctrl Pts',(-225.820830654868,-1.76072064399407,
135.396641736608));
#131387=CARTESIAN_POINT('Ctrl Pts',(-225.828581846108,-1.63281613794611,
135.445681440063));
#131388=CARTESIAN_POINT('Ctrl Pts',(-225.836333037348,-1.50276149869489,
135.489411747278));
#131389=CARTESIAN_POINT('Ctrl Pts',(-225.844084228588,-1.37103763747473,
135.527647487864));
#131390=CARTESIAN_POINT('Ctrl Pts',(-225.851832125365,-1.23936976240962,
135.56586697724));
#131391=CARTESIAN_POINT('Ctrl Pts',(-225.859580022142,-1.10603445112609,
135.598596436037));
#131392=CARTESIAN_POINT('Ctrl Pts',(-225.86732791892,-0.971529348780938,
135.625700035918));
#131393=CARTESIAN_POINT('Ctrl Pts',(-225.875074195004,-0.837052382003607,
135.652797966311));
#131394=CARTESIAN_POINT('Ctrl Pts',(-225.882820471088,-0.701406493895269,
135.674272301345));
#131395=CARTESIAN_POINT('Ctrl Pts',(-225.890566747172,-0.565100751471642,
135.690038073476));
#131396=CARTESIAN_POINT('Ctrl Pts',(-225.898313080437,-0.428794002870174,
135.705803961986));
#131397=CARTESIAN_POINT('Ctrl Pts',(-225.906059413703,-0.291827778609822,
135.715861158585));
#131398=CARTESIAN_POINT('Ctrl Pts',(-225.913805746968,-0.15471712174097,
135.720176488278));
#131399=CARTESIAN_POINT('Ctrl Pts',(-225.921553814971,-0.0175757598913571,
135.724492784358));
#131400=CARTESIAN_POINT('Ctrl Pts',(-225.929301882974,0.11970970823201,
135.723064642541));
#131401=CARTESIAN_POINT('Ctrl Pts',(-225.937049950977,0.256623778562881,
135.71591101421));
#131402=CARTESIAN_POINT('Ctrl Pts',(-225.944806253719,0.393683362797184,
135.708749782918));
#131403=CARTESIAN_POINT('Ctrl Pts',(-225.952562556461,0.530370369676102,
135.695850929871));
#131404=CARTESIAN_POINT('Ctrl Pts',(-225.960318859203,0.666173401615767,
135.677285412951));
#131405=CARTESIAN_POINT('Ctrl Pts',(-225.968079301717,0.802048915722529,
135.658709987056));
#131406=CARTESIAN_POINT('Ctrl Pts',(-225.975839744231,0.937039130162459,
135.634461939866));
#131407=CARTESIAN_POINT('Ctrl Pts',(-225.983600186745,1.07064337270872,
135.604663298749));
#131408=CARTESIAN_POINT('Ctrl Pts',(-225.991373087011,1.20446208864594,
135.574816822208));
#131409=CARTESIAN_POINT('Ctrl Pts',(-225.999145987276,1.33689000875,135.539402047174));
#131410=CARTESIAN_POINT('Ctrl Pts',(-226.006918887542,1.46744127803828,
135.498591029253));
#131411=CARTESIAN_POINT('Ctrl Pts',(-226.014409223304,1.5932466798477,135.459263594631));
#131412=CARTESIAN_POINT('Ctrl Pts',(-226.021899559065,1.71730921392521,
135.414925543332));
#131413=CARTESIAN_POINT('Ctrl Pts',(-226.029389894827,1.83921390427903,
135.365772161903));
#131414=CARTESIAN_POINT('Ctrl Pts',(-226.037164228946,1.96574064801962,
135.314755115076));
#131415=CARTESIAN_POINT('Ctrl Pts',(-226.044938563065,2.09034348734575,
135.258388776861));
#131416=CARTESIAN_POINT('Ctrl Pts',(-226.052712897184,2.21253700396133,
135.196838627597));
#131417=CARTESIAN_POINT('Ctrl Pts',(-226.060477650131,2.33457992798875,
135.13536433339));
#131418=CARTESIAN_POINT('Ctrl Pts',(-226.068242403078,2.45421909145953,
135.068719113706));
#131419=CARTESIAN_POINT('Ctrl Pts',(-226.076007156025,2.57098734571181,
134.997117125007));
#131420=CARTESIAN_POINT('Ctrl Pts',(-226.08376419691,2.68763962408718,134.925586252413));
#131421=CARTESIAN_POINT('Ctrl Pts',(-226.091521237795,2.8014263365765,134.849108611113));
#131422=CARTESIAN_POINT('Ctrl Pts',(-226.09927827868,2.91190364952899,134.76794487911));
#131423=CARTESIAN_POINT('Ctrl Pts',(-226.10702946992,3.02229765068023,134.686842353309));
#131424=CARTESIAN_POINT('Ctrl Pts',(-226.11478066116,3.12938690592123,134.601061001191));
#131425=CARTESIAN_POINT('Ctrl Pts',(-226.1225318524,3.23275568189076,134.510905337882));
#131426=CARTESIAN_POINT('Ctrl Pts',(-226.130279749177,3.33608052337347,
134.420787993134));
#131427=CARTESIAN_POINT('Ctrl Pts',(-226.138027645954,3.43568773664912,
134.326300291442));
#131428=CARTESIAN_POINT('Ctrl Pts',(-226.145775542731,3.53119405612993,
134.227787497237));
#131429=CARTESIAN_POINT('Ctrl Pts',(-226.153521818815,3.62668039774784,
134.129295309784));
#131430=CARTESIAN_POINT('Ctrl Pts',(-226.161268094899,3.71806727985388,
134.026779985055));
#131431=CARTESIAN_POINT('Ctrl Pts',(-226.169014370983,3.80500805368966,
133.920623888514));
#131432=CARTESIAN_POINT('Ctrl Pts',(-226.176760704248,3.89194946930259,
133.814467008352));
#131433=CARTESIAN_POINT('Ctrl Pts',(-226.184507037514,3.97444446343468,
133.704669605221));
#131434=CARTESIAN_POINT('Ctrl Pts',(-226.192253370779,4.05218673167326,
133.59164706753));
#131435=CARTESIAN_POINT('Ctrl Pts',(-226.200001438782,4.12994640975347,
133.478599219226));
#131436=CARTESIAN_POINT('Ctrl Pts',(-226.207749506785,4.20295102250017,
133.362325121232));
#131437=CARTESIAN_POINT('Ctrl Pts',(-226.215497574788,4.27093787170999,
133.243268725407));
#131438=CARTESIAN_POINT('Ctrl Pts',(-226.223253877529,4.33899697815228,
133.124085795028));
#131439=CARTESIAN_POINT('Ctrl Pts',(-226.231010180271,4.40202747375333,
133.002114999821));
#131440=CARTESIAN_POINT('Ctrl Pts',(-226.238766483013,4.45981263450326,
132.877824947528));
#131441=CARTESIAN_POINT('Ctrl Pts',(-226.246526925527,4.51762863693335,
132.753468557892));
#131442=CARTESIAN_POINT('Ctrl Pts',(-226.254287368041,4.57019357631639,
132.626790805566));
#131443=CARTESIAN_POINT('Ctrl Pts',(-226.262047810555,4.61733949216553,
132.49827887905));
#131444=CARTESIAN_POINT('Ctrl Pts',(-226.26982071082,4.66456109082433,132.36956065378));
#131445=CARTESIAN_POINT('Ctrl Pts',(-226.277593611086,4.70634616313795,
132.239002743085));
#131446=CARTESIAN_POINT('Ctrl Pts',(-226.285366511351,4.74257684787682,
132.10710691078));
#131447=CARTESIAN_POINT('Ctrl Pts',(-226.292856847114,4.77749045597035,
131.980005824189));
#131448=CARTESIAN_POINT('Ctrl Pts',(-226.300347182877,4.80724642776265,
131.851662700875));
#131449=CARTESIAN_POINT('Ctrl Pts',(-226.30783751864,4.83178475869705,131.722532229043));
#131450=CARTESIAN_POINT('Ctrl Pts',(-226.315611852759,4.85725346790459,
131.588505736137));
#131451=CARTESIAN_POINT('Ctrl Pts',(-226.323386186878,4.87718174943586,
131.453206455842));
#131452=CARTESIAN_POINT('Ctrl Pts',(-226.331160520997,4.89144644614283,
131.317132230486));
#131453=CARTESIAN_POINT('Ctrl Pts',(-226.338925273945,4.90569356288602,
131.181225704451));
#131454=CARTESIAN_POINT('Ctrl Pts',(-226.346690026892,4.9142909422798,131.044546518723));
#131455=CARTESIAN_POINT('Ctrl Pts',(-226.354454779839,4.91716625495979,
130.9076034555));
#131456=CARTESIAN_POINT('Ctrl Pts',(-226.362211820724,4.92003871183869,
130.770796406058));
#131457=CARTESIAN_POINT('Ctrl Pts',(-226.36996886161,4.91720040374859,130.633726389037));
#131458=CARTESIAN_POINT('Ctrl Pts',(-226.377725902495,4.90863074354596,
130.496907717083));
#131459=CARTESIAN_POINT('Ctrl Pts',(-226.385477093735,4.90006754579078,
130.360192221155));
#131460=CARTESIAN_POINT('Ctrl Pts',(-226.393228284975,4.88578162305726,
130.223728081646));
#131461=CARTESIAN_POINT('Ctrl Pts',(-226.400979476215,4.86580445850655,
130.088029664669));
#131462=CARTESIAN_POINT('Ctrl Pts',(-226.408727372993,4.84583578478367,
129.95238892314));
#131463=CARTESIAN_POINT('Ctrl Pts',(-226.41647526977,4.82018073713402,129.81751364283));
#131464=CARTESIAN_POINT('Ctrl Pts',(-226.424223166547,4.78892263189044,
129.683912899791));
#131465=CARTESIAN_POINT('Ctrl Pts',(-226.431969442631,4.75767106516864,
129.550340103147));
#131466=CARTESIAN_POINT('Ctrl Pts',(-226.439715718716,4.72081886111349,
129.418041693925));
#131467=CARTESIAN_POINT('Ctrl Pts',(-226.4474619948,4.67850034249818,129.287515995416));
#131468=CARTESIAN_POINT('Ctrl Pts',(-226.455208328065,4.63618151149724,
129.156989333396));
#131469=CARTESIAN_POINT('Ctrl Pts',(-226.462954661331,4.5883964059966,129.028235780108));
#131470=CARTESIAN_POINT('Ctrl Pts',(-226.470700994596,4.53532893901277,
128.90173756571));
#131471=CARTESIAN_POINT('Ctrl Pts',(-226.478449062599,4.48224958793759,
128.775211022914));
#131472=CARTESIAN_POINT('Ctrl Pts',(-226.486197130603,4.42388567266496,
128.650941184491));
#131473=CARTESIAN_POINT('Ctrl Pts',(-226.493945198606,4.36046870766976,
128.529389032703));
#131474=CARTESIAN_POINT('Ctrl Pts',(-226.501701501348,4.29698434236941,
128.407707693842));
#131475=CARTESIAN_POINT('Ctrl Pts',(-226.50945780409,4.22843638044344,128.288750158662));
#131476=CARTESIAN_POINT('Ctrl Pts',(-226.517214106832,4.15510193023349,
128.172952057143));
#131477=CARTESIAN_POINT('Ctrl Pts',(-226.524974549346,4.08172833921941,
128.057092150689));
#131478=CARTESIAN_POINT('Ctrl Pts',(-226.53273499186,4.00356339218927,127.94439535906));
#131479=CARTESIAN_POINT('Ctrl Pts',(-226.540495434375,3.92092618787832,
127.835266329452));
#131480=CARTESIAN_POINT('Ctrl Pts',(-226.54826833464,3.83815632699083,127.725962116238));
#131481=CARTESIAN_POINT('Ctrl Pts',(-226.556041234906,3.75090011136795,
127.6202374117));
#131482=CARTESIAN_POINT('Ctrl Pts',(-226.563814135171,3.65951598224535,
127.518462591426));
#131483=CARTESIAN_POINT('Ctrl Pts',(-226.571304470932,3.57145389641489,
127.420387542242));
#131484=CARTESIAN_POINT('Ctrl Pts',(-226.578794806693,3.47955902151275,
127.325980407362));
#131485=CARTESIAN_POINT('Ctrl Pts',(-226.586285142454,3.3841814656734,127.235537440398));
#131486=CARTESIAN_POINT('Ctrl Pts',(-226.594059476573,3.28518764079927,
127.141665300837));
#131487=CARTESIAN_POINT('Ctrl Pts',(-226.601833810692,3.18212824735688,
127.05176650732));
#131488=CARTESIAN_POINT('Ctrl Pts',(-226.609608144811,3.07535556474875,
126.966213771382));
#131489=CARTESIAN_POINT('Ctrl Pts',(-226.617372897758,2.96871446992938,
126.880766471546));
#131490=CARTESIAN_POINT('Ctrl Pts',(-226.625137650705,2.85836949358723,
126.799654814312));
#131491=CARTESIAN_POINT('Ctrl Pts',(-226.632902403652,2.74470959280777,
126.72321466163));
#131492=CARTESIAN_POINT('Ctrl Pts',(-226.640659444537,2.6311625806444,126.646850430386));
#131493=CARTESIAN_POINT('Ctrl Pts',(-226.648416485422,2.51430751844954,
126.575148687048));
#131494=CARTESIAN_POINT('Ctrl Pts',(-226.656173526307,2.39456598416612,
126.50840475071));
#131495=CARTESIAN_POINT('Ctrl Pts',(-226.663924717547,2.27491474790499,
126.441711146494));
#131496=CARTESIAN_POINT('Ctrl Pts',(-226.671675908788,2.15238171228218,
126.379968097162));
#131497=CARTESIAN_POINT('Ctrl Pts',(-226.679427100028,2.02741664549414,
126.323427142488));
#131498=CARTESIAN_POINT('Ctrl Pts',(-226.687174996805,1.90250469219253,
126.266910219228));
#131499=CARTESIAN_POINT('Ctrl Pts',(-226.694922893582,1.77516311908862,
126.215591153885));
#131500=CARTESIAN_POINT('Ctrl Pts',(-226.702670790359,1.64586526079623,
126.16967501811));
#131501=CARTESIAN_POINT('Ctrl Pts',(-226.710417066443,1.51659444882881,
126.123768487001));
#131502=CARTESIAN_POINT('Ctrl Pts',(-226.718163342527,1.38536853380987,
126.083262768229));
#131503=CARTESIAN_POINT('Ctrl Pts',(-226.725909618612,1.25267937397761,
126.048314208151));
#131504=CARTESIAN_POINT('Ctrl Pts',(-226.733655951877,1.11998923466429,
126.013365390091));
#131505=CARTESIAN_POINT('Ctrl Pts',(-226.741402285142,0.98583620705556,
125.98397391216));
#131506=CARTESIAN_POINT('Ctrl Pts',(-226.749148618408,0.850725414519564,
125.960245700309));
#131507=CARTESIAN_POINT('Ctrl Pts',(-226.756896686411,0.71558436485782,
125.93651217469));
#131508=CARTESIAN_POINT('Ctrl Pts',(-226.764644754414,0.579485508467145,
125.918444506433));
#131509=CARTESIAN_POINT('Ctrl Pts',(-226.772392822417,0.442941822008387,
125.906097088027));
#131510=CARTESIAN_POINT('Ctrl Pts',(-226.780149125159,0.306253015294957,
125.893736546637));
#131511=CARTESIAN_POINT('Ctrl Pts',(-226.787905427901,0.169118824100376,
125.88710843492));
#131512=CARTESIAN_POINT('Ctrl Pts',(-226.795661730643,0.0320555400893031,
125.886215082423));
#131513=CARTESIAN_POINT('Ctrl Pts',(-226.803422173157,-0.105080898722969,
125.885321253116));
#131514=CARTESIAN_POINT('Ctrl Pts',(-226.811182615671,-0.242145964411954,
125.89016826815));
#131515=CARTESIAN_POINT('Ctrl Pts',(-226.818943058185,-0.378626735169176,
125.900706382415));
#131516=CARTESIAN_POINT('Ctrl Pts',(-226.82671595845,-0.515326596976182,
125.911261413396));
#131517=CARTESIAN_POINT('Ctrl Pts',(-226.834488858716,-0.65143990107724,
125.92752575355));
#131518=CARTESIAN_POINT('Ctrl Pts',(-226.842261758982,-0.786461293756218,
125.949398033166));
#131519=CARTESIAN_POINT('Ctrl Pts',(-226.849752094743,-0.916574318704911,
125.970475200324));
#131520=CARTESIAN_POINT('Ctrl Pts',(-226.857242430505,-1.04567313958366,
125.996759598753));
#131521=CARTESIAN_POINT('Ctrl Pts',(-226.864732766266,-1.1733192678386,
126.02811680488));
#131522=CARTESIAN_POINT('Ctrl Pts',(-226.872507100385,-1.30580513785045,
126.06066292901));
#131523=CARTESIAN_POINT('Ctrl Pts',(-226.880281434504,-1.43714565842267,
126.09877722171));
#131524=CARTESIAN_POINT('Ctrl Pts',(-226.888055768624,-1.56683684116329,
126.142364760031));
#131525=CARTESIAN_POINT('Ctrl Pts',(-226.895820521571,-1.69636819111237,
126.185898580607));
#131526=CARTESIAN_POINT('Ctrl Pts',(-226.903585274518,-1.82425388058314,
126.234892102338));
#131527=CARTESIAN_POINT('Ctrl Pts',(-226.911350027465,-1.95000109860021,
126.289199626199));
#131528=CARTESIAN_POINT('Ctrl Pts',(-226.91910706835,-2.07562342270729,
126.343453211063));
#131529=CARTESIAN_POINT('Ctrl Pts',(-226.926864109235,-2.19911114553693,
126.403010140707));
#131530=CARTESIAN_POINT('Ctrl Pts',(-226.93462115012,-2.31998793359411,
126.467675356854));
#131531=CARTESIAN_POINT('Ctrl Pts',(-226.94237234136,-2.44077356752529,
126.532291808458));
#131532=CARTESIAN_POINT('Ctrl Pts',(-226.9501235326,-2.55895184237208,126.602008695321));
#131533=CARTESIAN_POINT('Ctrl Pts',(-226.95787472384,-2.67406801990288,
126.676583578113));
#131534=CARTESIAN_POINT('Ctrl Pts',(-226.965622620617,-2.78913526998725,
126.751126764591));
#131535=CARTESIAN_POINT('Ctrl Pts',(-226.973370517394,-2.90114268384491,
126.830523628187));
#131536=CARTESIAN_POINT('Ctrl Pts',(-226.981118414171,-3.00966187996747,
126.914486785323));
#131537=CARTESIAN_POINT('Ctrl Pts',(-226.988864690255,-3.1181583762136,
126.998432379176));
#131538=CARTESIAN_POINT('Ctrl Pts',(-226.996610966339,-3.22316779703744,
127.086942127588));
#131539=CARTESIAN_POINT('Ctrl Pts',(-227.004357242424,-3.32429274242802,
127.179686725319));
#131540=CARTESIAN_POINT('Ctrl Pts',(-227.012103575689,-3.42541843429956,
127.272432007668));
#131541=CARTESIAN_POINT('Ctrl Pts',(-227.019849908954,-3.52265930538509,
127.369411937457));
#131542=CARTESIAN_POINT('Ctrl Pts',(-227.027596242219,-3.61565320566346,
127.470258795654));
#131543=CARTESIAN_POINT('Ctrl Pts',(-227.035344310222,-3.7086679312814,
127.571128237806));
#131544=CARTESIAN_POINT('Ctrl Pts',(-227.043092378225,-3.79743352856755,
127.675866044187));
#131545=CARTESIAN_POINT('Ctrl Pts',(-227.050840446228,-3.88162695916609,
127.784070033471));
#131546=CARTESIAN_POINT('Ctrl Pts',(-227.05859674897,-3.96590987154448,
127.892389023242));
#131547=CARTESIAN_POINT('Ctrl Pts',(-227.066353051712,-4.04561066967987,
128.004181245852));
#131548=CARTESIAN_POINT('Ctrl Pts',(-227.074109354454,-4.1204483254021,
128.119013589677));
#131549=CARTESIAN_POINT('Ctrl Pts',(-227.081869796968,-4.1953259242345,
128.233907222982));
#131550=CARTESIAN_POINT('Ctrl Pts',(-227.089630239482,-4.26533500921803,
128.351843874651));
#131551=CARTESIAN_POINT('Ctrl Pts',(-227.097390681996,-4.3302401855553,
128.472365120593));
#131552=CARTESIAN_POINT('Ctrl Pts',(-227.105163582262,-4.39524955344365,
128.593079837938));
#131553=CARTESIAN_POINT('Ctrl Pts',(-227.112936482527,-4.45513846906175,
128.716387088739));
#131554=CARTESIAN_POINT('Ctrl Pts',(-227.120709382793,-4.5097190615902,
128.841806911796));
#131555=CARTESIAN_POINT('Ctrl Pts',(-227.128199718555,-4.56231551210254,
128.962667408378));
#131556=CARTESIAN_POINT('Ctrl Pts',(-227.135690054317,-4.60998276939513,
129.085489262049));
#131557=CARTESIAN_POINT('Ctrl Pts',(-227.14318039008,-4.65259691405446,
129.209830900743));
#131558=CARTESIAN_POINT('Ctrl Pts',(-227.150566054377,-4.69461556004669,
129.332434964257));
#131559=CARTESIAN_POINT('Ctrl Pts',(-227.157951718674,-4.73181060005727,
129.456771532717));
#131560=CARTESIAN_POINT('Ctrl Pts',(-227.165337382971,-4.76405452823413,
129.582490119309));
#131561=CARTESIAN_POINT('Ctrl Pts',(-225.41504623153,-4.76405452823393,
129.582490119308));
#131562=CARTESIAN_POINT('Ctrl Pts',(-225.422809306179,-4.79810736338305,
129.71526160673));
#131563=CARTESIAN_POINT('Ctrl Pts',(-225.430572380828,-4.82657411435382,
129.84933482539));
#131564=CARTESIAN_POINT('Ctrl Pts',(-225.438335455478,-4.84938342871073,
129.984200008999));
#131565=CARTESIAN_POINT('Ctrl Pts',(-225.446109886893,-4.87222611129406,
130.119262489725));
#131566=CARTESIAN_POINT('Ctrl Pts',(-225.453884318307,-4.88939478205187,
130.25511886208));
#131567=CARTESIAN_POINT('Ctrl Pts',(-225.461658749722,-4.90087002073647,
130.391255180242));
#131568=CARTESIAN_POINT('Ctrl Pts',(-225.465270715548,-4.90620136495505,
130.454503500623));
#131569=CARTESIAN_POINT('Ctrl Pts',(-225.468882681374,-4.91030452498705,
130.517812256196));
#131570=CARTESIAN_POINT('Ctrl Pts',(-225.472494647201,-4.9131813736671,
130.581130126928));
#131571=CARTESIAN_POINT('Ctrl Pts',(-225.476709952805,-4.91653876876631,
130.655024562308));
#131572=CARTESIAN_POINT('Ctrl Pts',(-225.480925258409,-4.91822920859789,
130.728995310251));
#131573=CARTESIAN_POINT('Ctrl Pts',(-225.485140564013,-4.91824980939616,
130.802991356954));
#131574=CARTESIAN_POINT('',(-225.13985943604,-4.91824793997955,130.80886210475));
#131575=CARTESIAN_POINT('Ctrl Pts',(-225.069870156977,-4.76405452823403,
129.582490119308));
#131576=CARTESIAN_POINT('Ctrl Pts',(-225.077538742587,-4.79782267774008,
129.714151621729));
#131577=CARTESIAN_POINT('Ctrl Pts',(-225.085207328198,-4.82612779473598,
129.847210760949));
#131578=CARTESIAN_POINT('Ctrl Pts',(-225.092875913808,-4.84886999374076,
129.981169967534));
#131579=CARTESIAN_POINT('Ctrl Pts',(-225.100706500839,-4.87209262926181,
130.117959106902));
#131580=CARTESIAN_POINT('Ctrl Pts',(-225.108537087871,-4.88951458321308,
130.255686342715));
#131581=CARTESIAN_POINT('Ctrl Pts',(-225.116367674902,-4.90108507640122,
130.393814473537));
#131582=CARTESIAN_POINT('Ctrl Pts',(-225.124198261933,-4.91265556958939,
130.531942604359));
#131583=CARTESIAN_POINT('Ctrl Pts',(-225.132028848965,-4.9183746039543,
130.670471187608));
#131584=CARTESIAN_POINT('Ctrl Pts',(-225.139859435996,-4.91824793998026,
130.808862103977));
#131585=CARTESIAN_POINT('Ctrl Pts',(-225.13985943604,-4.91824793997955,
130.80886210475));
#131586=CARTESIAN_POINT('Ctrl Pts',(-225.149605429622,-4.91809029324308,
130.981104233894));
#131587=CARTESIAN_POINT('Ctrl Pts',(-225.159351423203,-4.90888095054794,
131.15294170875));
#131588=CARTESIAN_POINT('Ctrl Pts',(-225.169097416785,-4.89076858680166,
131.323557779398));
#131589=CARTESIAN_POINT('Ctrl Pts',(-225.179027880941,-4.8723133951939,
131.497403243152));
#131590=CARTESIAN_POINT('Ctrl Pts',(-225.188958345097,-4.84461498244356,
131.669980793286));
#131591=CARTESIAN_POINT('Ctrl Pts',(-225.198888809253,-4.80787897277174,
131.840450790128));
#131592=CARTESIAN_POINT('Ctrl Pts',(-225.203804546018,-4.7896940671611,
131.92483613382));
#131593=CARTESIAN_POINT('Ctrl Pts',(-225.208720282783,-4.76929531813874,
132.008705397411));
#131594=CARTESIAN_POINT('Ctrl Pts',(-225.213636019548,-4.74671194523966,
132.091958680402));
#131595=CARTESIAN_POINT('Ctrl Pts',(-225.221410353667,-4.71099589801225,
132.223625380519));
#131596=CARTESIAN_POINT('Ctrl Pts',(-225.229184687787,-4.66974077093761,
132.354013440337));
#131597=CARTESIAN_POINT('Ctrl Pts',(-225.236959021906,-4.62305355396191,
132.482621294487));
#131598=CARTESIAN_POINT('Ctrl Pts',(-225.244723774853,-4.57642387480845,
132.611070650952));
#131599=CARTESIAN_POINT('Ctrl Pts',(-225.2524885278,-4.52437555807236,132.737743803074));
#131600=CARTESIAN_POINT('Ctrl Pts',(-225.260253280747,-4.46706608692499,
132.86215157817));
#131601=CARTESIAN_POINT('Ctrl Pts',(-225.268010321632,-4.40981353635229,
132.98643578971));
#131602=CARTESIAN_POINT('Ctrl Pts',(-225.275767362517,-4.34731039277597,
133.108458749034));
#131603=CARTESIAN_POINT('Ctrl Pts',(-225.283524403403,-4.27976308899272,
133.227748940678));
#131604=CARTESIAN_POINT('Ctrl Pts',(-225.291275594643,-4.21226672315697,
133.34694917466));
#131605=CARTESIAN_POINT('Ctrl Pts',(-225.299026785883,-4.13973396029038,
133.46342040403));
#131606=CARTESIAN_POINT('Ctrl Pts',(-225.306777977123,-4.06241808237026,
133.576713839385));
#131607=CARTESIAN_POINT('Ctrl Pts',(-225.3145258739,-3.98513506576062,133.689959122008));
#131608=CARTESIAN_POINT('Ctrl Pts',(-225.322273770677,-3.90307319740353,
133.800028974693));
#131609=CARTESIAN_POINT('Ctrl Pts',(-225.330021667455,-3.81653005809438,
133.90650203571));
#131610=CARTESIAN_POINT('Ctrl Pts',(-225.337767943539,-3.73000502174408,
134.012952824857));
#131611=CARTESIAN_POINT('Ctrl Pts',(-225.345514219623,-3.63900082539391,
134.115808015649));
#131612=CARTESIAN_POINT('Ctrl Pts',(-225.353260495707,-3.54385621595714,
134.214678224934));
#131613=CARTESIAN_POINT('Ctrl Pts',(-225.361006828973,-3.44871090418461,
134.313549164056));
#131614=CARTESIAN_POINT('Ctrl Pts',(-225.368753162238,-3.34942538943357,
134.408434781261));
#131615=CARTESIAN_POINT('Ctrl Pts',(-225.376499495504,-3.2463759754437,
134.498981855063));
#131616=CARTESIAN_POINT('Ctrl Pts',(-225.384247563507,-3.14330348425193,
134.589549206254));
#131617=CARTESIAN_POINT('Ctrl Pts',(-225.39199563151,-3.036465710189,134.675775822682));
#131618=CARTESIAN_POINT('Ctrl Pts',(-225.399743699513,-2.92627247079122,
134.75734841026));
#131619=CARTESIAN_POINT('Ctrl Pts',(-225.407500002255,-2.81596211670714,
134.839007694156));
#131620=CARTESIAN_POINT('Ctrl Pts',(-225.415256304996,-2.70228948809756,
134.916002835333));
#131621=CARTESIAN_POINT('Ctrl Pts',(-225.423012607738,-2.58569431576058,
134.988063280034));
#131622=CARTESIAN_POINT('Ctrl Pts',(-225.430773050253,-2.46903691306952,
135.060162185565));
#131623=CARTESIAN_POINT('Ctrl Pts',(-225.438533492767,-2.34945419923728,
135.127320955208));
#131624=CARTESIAN_POINT('Ctrl Pts',(-225.446293935281,-2.22741011516574,
135.189315262868));
#131625=CARTESIAN_POINT('Ctrl Pts',(-225.454066835547,-2.10517011509589,
135.251409089295));
#131626=CARTESIAN_POINT('Ctrl Pts',(-225.461839735812,-1.98046120489236,
135.30832172436));
#131627=CARTESIAN_POINT('Ctrl Pts',(-225.469612636078,-1.85376771591805,
135.359876869092));
#131628=CARTESIAN_POINT('Ctrl Pts',(-225.477102971839,-1.731679854404,135.409557854448));
#131629=CARTESIAN_POINT('Ctrl Pts',(-225.4845933076,-1.60774948767011,135.454263998909));
#131630=CARTESIAN_POINT('Ctrl Pts',(-225.492083643361,-1.48242103434339,
135.493882015261));
#131631=CARTESIAN_POINT('Ctrl Pts',(-225.49985797748,-1.35234071460227,
135.535002160748));
#131632=CARTESIAN_POINT('Ctrl Pts',(-225.507632311599,-1.22034214320157,
135.57077098517));
#131633=CARTESIAN_POINT('Ctrl Pts',(-225.515406645719,-1.08690513196861,
135.601007393867));
#131634=CARTESIAN_POINT('Ctrl Pts',(-225.523171398666,-0.953632569926398,
135.631206538893));
#131635=CARTESIAN_POINT('Ctrl Pts',(-225.530936151613,-0.818925472931342,
135.655886748823));
#131636=CARTESIAN_POINT('Ctrl Pts',(-225.53870090456,-0.683280519316704,
135.674916108927));
#131637=CARTESIAN_POINT('Ctrl Pts',(-225.546457945445,-0.547770290182254,
135.693926568801));
#131638=CARTESIAN_POINT('Ctrl Pts',(-225.55421498633,-0.411324442808616,
135.70729729402));
#131639=CARTESIAN_POINT('Ctrl Pts',(-225.561972027215,-0.274451258476907,
135.714947096717));
#131640=CARTESIAN_POINT('Ctrl Pts',(-225.569723218455,-0.137681291278408,
135.722591130638));
#131641=CARTESIAN_POINT('Ctrl Pts',(-225.577474409695,-0.000485017333626381,
135.724522807447));
#131642=CARTESIAN_POINT('Ctrl Pts',(-225.585225600935,0.136623079027003,
135.720712638809));
#131643=CARTESIAN_POINT('Ctrl Pts',(-225.592973497712,0.273672900789388,
135.716904089594));
#131644=CARTESIAN_POINT('Ctrl Pts',(-225.600721394489,0.410634229512033,
135.707358559615));
#131645=CARTESIAN_POINT('Ctrl Pts',(-225.608469291266,0.546991711947881,
135.692098655714));
#131646=CARTESIAN_POINT('Ctrl Pts',(-225.616215567351,0.683320671337931,
135.676841943856));
#131647=CARTESIAN_POINT('Ctrl Pts',(-225.623961843435,0.819045647388365,
135.655873279096));
#131648=CARTESIAN_POINT('Ctrl Pts',(-225.631708119519,0.953655940044716,
135.629267187699));
#131649=CARTESIAN_POINT('Ctrl Pts',(-225.639454452784,1.08826722636385,
135.602660899903));
#131650=CARTESIAN_POINT('Ctrl Pts',(-225.647200786049,1.22176342932477,
135.570417178242));
#131651=CARTESIAN_POINT('Ctrl Pts',(-225.654947119315,1.35364397232283,
135.532661692867));
#131652=CARTESIAN_POINT('Ctrl Pts',(-225.662695187318,1.48555404905392,
135.494897752413));
#131653=CARTESIAN_POINT('Ctrl Pts',(-225.670443255321,1.61584737005681,
135.451619699674));
#131654=CARTESIAN_POINT('Ctrl Pts',(-225.678191323324,1.7440388357554,135.403002982643));
#131655=CARTESIAN_POINT('Ctrl Pts',(-225.685947626066,1.87236654486941,
135.354334595186));
#131656=CARTESIAN_POINT('Ctrl Pts',(-225.693703928808,1.99858757012791,
135.300316347879));
#131657=CARTESIAN_POINT('Ctrl Pts',(-225.701460231549,2.12223660175588,
135.241171957782));
#131658=CARTESIAN_POINT('Ctrl Pts',(-225.709220674064,2.24595162859504,
135.181996000543));
#131659=CARTESIAN_POINT('Ctrl Pts',(-225.716981116578,2.36709158132668,
135.117688632075));
#131660=CARTESIAN_POINT('Ctrl Pts',(-225.724741559092,2.48521695666374,
135.048518925265));
#131661=CARTESIAN_POINT('Ctrl Pts',(-225.732514459357,2.60353195733997,
134.979238181101));
#131662=CARTESIAN_POINT('Ctrl Pts',(-225.740287359623,2.71882238121892,
134.90507971243));
#131663=CARTESIAN_POINT('Ctrl Pts',(-225.748060259888,2.83067811005041,
134.826355707044));
#131664=CARTESIAN_POINT('Ctrl Pts',(-225.75555059565,2.9384676013916,134.750493517547));
#131665=CARTESIAN_POINT('Ctrl Pts',(-225.763040931412,3.04306753726984,
134.670392153204));
#131666=CARTESIAN_POINT('Ctrl Pts',(-225.770531267175,3.14414238681853,
134.586364281487));
#131667=CARTESIAN_POINT('Ctrl Pts',(-225.778305601294,3.24904952000846,
134.499150467474));
#131668=CARTESIAN_POINT('Ctrl Pts',(-225.786079935412,3.35049129710711,
134.407430254263));
#131669=CARTESIAN_POINT('Ctrl Pts',(-225.793854269532,3.44805600803517,
134.311509435046));
#131670=CARTESIAN_POINT('Ctrl Pts',(-225.801619022479,3.54550047917662,
134.215706829666));
#131671=CARTESIAN_POINT('Ctrl Pts',(-225.809383775426,3.63907711510054,
134.115714190176));
#131672=CARTESIAN_POINT('Ctrl Pts',(-225.817148528373,3.7284064654359,134.011878082989));
#131673=CARTESIAN_POINT('Ctrl Pts',(-225.824905569258,3.81764709260095,
133.908145107288));
#131674=CARTESIAN_POINT('Ctrl Pts',(-225.832662610143,3.90264857578659,
133.800576555125));
#131675=CARTESIAN_POINT('Ctrl Pts',(-225.840419651028,3.98306787089368,
133.689556173911));
#131676=CARTESIAN_POINT('Ctrl Pts',(-225.848170842268,4.06342652118486,
133.578619514031));
#131677=CARTESIAN_POINT('Ctrl Pts',(-225.855922033508,4.13920963286425,
133.464236521659));
#131678=CARTESIAN_POINT('Ctrl Pts',(-225.863673224748,4.21011430521399,
133.346824107871));
#131679=CARTESIAN_POINT('Ctrl Pts',(-225.871421121525,4.28098884118663,
133.22946159749));
#131680=CARTESIAN_POINT('Ctrl Pts',(-225.879169018302,4.34698886011281,
133.109072560573));
#131681=CARTESIAN_POINT('Ctrl Pts',(-225.88691691508,4.40785482075141,132.986102797953));
#131682=CARTESIAN_POINT('Ctrl Pts',(-225.894663191164,4.46870804954317,
132.863158757956));
#131683=CARTESIAN_POINT('Ctrl Pts',(-225.902409467248,4.52442918283877,
132.737635416182));
#131684=CARTESIAN_POINT('Ctrl Pts',(-225.910155743332,4.5748048758435,132.610002722319));
#131685=CARTESIAN_POINT('Ctrl Pts',(-225.917902076597,4.62518094071009,
132.482369086301));
#131686=CARTESIAN_POINT('Ctrl Pts',(-225.925648409863,4.67021134301315,
132.352626430787));
#131687=CARTESIAN_POINT('Ctrl Pts',(-225.933394743128,4.70973123872821,
132.221263832838));
#131688=CARTESIAN_POINT('Ctrl Pts',(-225.941142811131,4.74925998464985,
132.089871817146));
#131689=CARTESIAN_POINT('Ctrl Pts',(-225.948890879134,4.78327565577531,
131.956859511457));
#131690=CARTESIAN_POINT('Ctrl Pts',(-225.956638947137,4.81166365330068,
131.822729877709));
#131691=CARTESIAN_POINT('Ctrl Pts',(-225.964395249878,4.84008182192769,
131.688457689391));
#131692=CARTESIAN_POINT('Ctrl Pts',(-225.97215155262,4.86286028786421,131.553066183937));
#131693=CARTESIAN_POINT('Ctrl Pts',(-225.979907855362,4.87993575930992,
131.417067764177));
#131694=CARTESIAN_POINT('Ctrl Pts',(-225.987668297876,4.89702034444886,
131.280996757965));
#131695=CARTESIAN_POINT('Ctrl Pts',(-225.99542874039,4.90839583753709,131.144318581419));
#131696=CARTESIAN_POINT('Ctrl Pts',(-226.003189182905,4.91405105495221,
131.007548441569));
#131697=CARTESIAN_POINT('Ctrl Pts',(-226.01096208317,4.91971535062437,130.870558746149));
#131698=CARTESIAN_POINT('Ctrl Pts',(-226.018734983435,4.91964102088623,
130.733477183607));
#131699=CARTESIAN_POINT('Ctrl Pts',(-226.026507883701,4.91386903923685,
130.596817543171));
#131700=CARTESIAN_POINT('Ctrl Pts',(-226.033998219463,4.90830688365904,
130.465125824886));
#131701=CARTESIAN_POINT('Ctrl Pts',(-226.041488555225,4.89745415758686,
130.333826192394));
#131702=CARTESIAN_POINT('Ctrl Pts',(-226.048978890987,4.88139255438909,
130.203369941719));
#131703=CARTESIAN_POINT('Ctrl Pts',(-226.056753225106,4.8647219706246,130.067967402652));
#131704=CARTESIAN_POINT('Ctrl Pts',(-226.064527559225,4.8423869159738,129.933044546967));
#131705=CARTESIAN_POINT('Ctrl Pts',(-226.072301893345,4.81442212355511,
129.799113046704));
#131706=CARTESIAN_POINT('Ctrl Pts',(-226.080066646292,4.7864917952438,129.665346605046));
#131707=CARTESIAN_POINT('Ctrl Pts',(-226.087831399239,4.75294561315524,
129.532569466915));
#131708=CARTESIAN_POINT('Ctrl Pts',(-226.095596152186,4.71387005123443,
129.401288202266));
#131709=CARTESIAN_POINT('Ctrl Pts',(-226.103353193071,4.67483329971259,
129.270137328021));
#131710=CARTESIAN_POINT('Ctrl Pts',(-226.111110233956,4.63027820821611,
129.140479742897));
#131711=CARTESIAN_POINT('Ctrl Pts',(-226.118867274841,4.58034221059627,
129.012811484461));
#131712=CARTESIAN_POINT('Ctrl Pts',(-226.126618466081,4.53044387010061,
128.885239501651));
#131713=CARTESIAN_POINT('Ctrl Pts',(-226.134369657321,4.47517284209181,
128.759654222169));
#131714=CARTESIAN_POINT('Ctrl Pts',(-226.142120848561,4.41471616042677,
128.636535835586));
#131715=CARTESIAN_POINT('Ctrl Pts',(-226.149868745338,4.35428517446425,
128.513469777602));
#131716=CARTESIAN_POINT('Ctrl Pts',(-226.157616642115,4.28867309048085,
128.392868877342));
#131717=CARTESIAN_POINT('Ctrl Pts',(-226.165364538892,4.21811468496269,
128.275192460444));
#131718=CARTESIAN_POINT('Ctrl Pts',(-226.173110814977,4.1475710387419,128.157540658915));
#131719=CARTESIAN_POINT('Ctrl Pts',(-226.180857091061,4.07208332991259,
128.042812459062));
#131720=CARTESIAN_POINT('Ctrl Pts',(-226.188603367145,3.99193162238366,
127.931441373189));
#131721=CARTESIAN_POINT('Ctrl Pts',(-226.19634970041,3.91177932319293,127.820069465199));
#131722=CARTESIAN_POINT('Ctrl Pts',(-226.204096033676,3.82696318497908,
127.712055037968));
#131723=CARTESIAN_POINT('Ctrl Pts',(-226.211842366941,3.73780557990322,
127.60780113754));
#131724=CARTESIAN_POINT('Ctrl Pts',(-226.219590434944,3.6486280086,127.503523890174));
#131725=CARTESIAN_POINT('Ctrl Pts',(-226.227338502947,3.55510728984161,
127.403009142451));
#131726=CARTESIAN_POINT('Ctrl Pts',(-226.23508657095,3.45760463629866,127.306625172804));
#131727=CARTESIAN_POINT('Ctrl Pts',(-226.242842873692,3.35999835577536,
127.210138765127));
#131728=CARTESIAN_POINT('Ctrl Pts',(-226.250599176433,3.25840196498437,
127.117792180796));
#131729=CARTESIAN_POINT('Ctrl Pts',(-226.258355479175,3.15321235217255,
127.02991563524));
#131730=CARTESIAN_POINT('Ctrl Pts',(-226.266115921689,3.04796659649689,
126.941992187325));
#131731=CARTESIAN_POINT('Ctrl Pts',(-226.273876364204,2.93912410751723,
126.858543769846));
#131732=CARTESIAN_POINT('Ctrl Pts',(-226.281636806718,2.8271122984785,126.779858273885));
#131733=CARTESIAN_POINT('Ctrl Pts',(-226.289409706983,2.71492067813996,
126.701046464981));
#131734=CARTESIAN_POINT('Ctrl Pts',(-226.297182607249,2.59954990018272,
126.627013067738));
#131735=CARTESIAN_POINT('Ctrl Pts',(-226.304955507514,2.48145437721108,
126.558001325617));
#131736=CARTESIAN_POINT('Ctrl Pts',(-226.312445843276,2.3676519239638,126.491498334153));
#131737=CARTESIAN_POINT('Ctrl Pts',(-226.319936179038,2.25131966101654,
126.42965838143));
#131738=CARTESIAN_POINT('Ctrl Pts',(-226.3274265148,2.13288143375845,126.372656673029));
#131739=CARTESIAN_POINT('Ctrl Pts',(-226.335200848919,2.00995258511587,
126.313493727529));
#131740=CARTESIAN_POINT('Ctrl Pts',(-226.342975183039,1.88436552281168,
126.259355742396));
#131741=CARTESIAN_POINT('Ctrl Pts',(-226.350749517158,1.75656950512303,
126.210490066911));
#131742=CARTESIAN_POINT('Ctrl Pts',(-226.358514270105,1.62893098460473,
126.161684614004));
#131743=CARTESIAN_POINT('Ctrl Pts',(-226.366279023052,1.49908928702106,
126.118138680651));
#131744=CARTESIAN_POINT('Ctrl Pts',(-226.374043775999,1.36751734530206,
126.080053327307));
#131745=CARTESIAN_POINT('Ctrl Pts',(-226.381800816884,1.23607608269007,
126.042005800872));
#131746=CARTESIAN_POINT('Ctrl Pts',(-226.389557857769,1.102908368959,126.009408169392));
#131747=CARTESIAN_POINT('Ctrl Pts',(-226.397314898654,0.968505820915303,
125.982412926295));
#131748=CARTESIAN_POINT('Ctrl Pts',(-226.405066089894,0.834204626878764,
125.955438040521));
#131749=CARTESIAN_POINT('Ctrl Pts',(-226.412817281134,0.69867083378196,
125.934057210591));
#131750=CARTESIAN_POINT('Ctrl Pts',(-226.420568472374,0.562409535079179,
125.918372633816));
#131751=CARTESIAN_POINT('Ctrl Pts',(-226.428316369152,0.42620615106305,
125.902694723404));
#131752=CARTESIAN_POINT('Ctrl Pts',(-226.436064265929,0.2892762640221,125.892708295459));
#131753=CARTESIAN_POINT('Ctrl Pts',(-226.443812162706,0.152133220048413,
125.8884641026));
#131754=CARTESIAN_POINT('Ctrl Pts',(-226.45155843879,0.0150188634430627,
125.884220797534));
#131755=CARTESIAN_POINT('Ctrl Pts',(-226.459304714874,-0.122308170876832,
125.885717350483));
#131756=CARTESIAN_POINT('Ctrl Pts',(-226.467050990958,-0.259331775349145,
125.892952459736));
#131757=CARTESIAN_POINT('Ctrl Pts',(-226.474797324223,-0.396356391298392,
125.900187622398));
#131758=CARTESIAN_POINT('Ctrl Pts',(-226.482543657489,-0.533077182509269,
125.913161405278));
#131759=CARTESIAN_POINT('Ctrl Pts',(-226.490289990754,-0.668980804902403,
125.931820443779));
#131760=CARTESIAN_POINT('Ctrl Pts',(-226.498038058757,-0.804914861969297,
125.950483660841));
#131761=CARTESIAN_POINT('Ctrl Pts',(-226.50578612676,-0.940030998813575,
125.974834613824));
#131762=CARTESIAN_POINT('Ctrl Pts',(-226.513534194763,-1.07382412808817,
126.004768467765));
#131763=CARTESIAN_POINT('Ctrl Pts',(-226.521290497505,-1.20775945429291,
126.034734135762));
#131764=CARTESIAN_POINT('Ctrl Pts',(-226.529046800247,-1.34036858193426,
126.070294472172));
#131765=CARTESIAN_POINT('Ctrl Pts',(-226.536803102989,-1.47115916362795,
126.111294053178));
#131766=CARTESIAN_POINT('Ctrl Pts',(-226.544563545503,-1.60201955219313,
126.152315516896));
#131767=CARTESIAN_POINT('Ctrl Pts',(-226.552323988017,-1.73105909311937,
126.198781877465));
#131768=CARTESIAN_POINT('Ctrl Pts',(-226.560084430531,-1.85780454818622,
126.250489152182));
#131769=CARTESIAN_POINT('Ctrl Pts',(-226.567857330797,-1.98475346630948,
126.302279432006));
#131770=CARTESIAN_POINT('Ctrl Pts',(-226.575630231062,-2.10940058371873,
126.359327275396));
#131771=CARTESIAN_POINT('Ctrl Pts',(-226.583403131327,-2.23129563168847,
126.421381851189));
#131772=CARTESIAN_POINT('Ctrl Pts',(-226.590893467089,-2.34875948762841,
126.481180586846));
#131773=CARTESIAN_POINT('Ctrl Pts',(-226.598383802851,-2.463667620948,126.545628209392));
#131774=CARTESIAN_POINT('Ctrl Pts',(-226.605874138613,-2.57564352744432,
126.614462828594));
#131775=CARTESIAN_POINT('Ctrl Pts',(-226.61364978905,-2.69188471260912,
126.685919429989));
#131776=CARTESIAN_POINT('Ctrl Pts',(-226.621425439487,-2.80533413994567,
126.7623302542));
#131777=CARTESIAN_POINT('Ctrl Pts',(-226.629201089924,-2.91554064523804,
126.843450897759));
#131778=CARTESIAN_POINT('Ctrl Pts',(-226.637141305583,-3.0280795802354,
126.92628839277));
#131779=CARTESIAN_POINT('Ctrl Pts',(-226.645081521242,-3.13723639965859,
127.014037165253));
#131780=CARTESIAN_POINT('Ctrl Pts',(-226.653021736901,-3.24255719969909,
127.106387406579));
#131781=CARTESIAN_POINT('Ctrl Pts',(-226.660777899543,-3.34543667926793,
127.196596983053));
#131782=CARTESIAN_POINT('Ctrl Pts',(-226.668534062185,-3.4446556925028,
127.291196790052));
#131783=CARTESIAN_POINT('Ctrl Pts',(-226.676290224826,-3.53982107198123,
127.38985482011));
#131784=CARTESIAN_POINT('Ctrl Pts',(-226.684041040951,-3.63492085157508,
127.488444842713));
#131785=CARTESIAN_POINT('Ctrl Pts',(-226.691791857075,-3.72597228670709,
127.59108724237));
#131786=CARTESIAN_POINT('Ctrl Pts',(-226.699542673199,-3.8126172577398,
127.697411517808));
#131787=CARTESIAN_POINT('Ctrl Pts',(-226.707289825123,-3.89922126734433,
127.803685528423));
#131788=CARTESIAN_POINT('Ctrl Pts',(-226.715036977048,-3.9814227124175,
127.913637648249));
#131789=CARTESIAN_POINT('Ctrl Pts',(-226.722784128972,-4.05890242207442,
128.02686278848));
#131790=CARTESIAN_POINT('Ctrl Pts',(-226.730865973703,-4.13972941364076,
128.144979486323));
#131791=CARTESIAN_POINT('Ctrl Pts',(-226.738947818434,-4.21541727253825,
128.266657995164));
#131792=CARTESIAN_POINT('Ctrl Pts',(-226.747029663165,-4.28565263699557,
128.391402984802));
#131793=CARTESIAN_POINT('Ctrl Pts',(-226.754776314275,-4.35297499744343,
128.510974189727));
#131794=CARTESIAN_POINT('Ctrl Pts',(-226.762522965385,-4.41528789834733,
128.633362234604));
#131795=CARTESIAN_POINT('Ctrl Pts',(-226.770269616496,-4.47236181691145,
128.758104807279));
#131796=CARTESIAN_POINT('Ctrl Pts',(-226.778017331852,-4.52944357637199,
128.882864517268));
#131797=CARTESIAN_POINT('Ctrl Pts',(-226.785765047208,-4.5812847650445,
129.009979040522));
#131798=CARTESIAN_POINT('Ctrl Pts',(-226.793512762565,-4.62770382906203,
129.138965669518));
#131799=CARTESIAN_POINT('Ctrl Pts',(-226.801265156259,-4.67415092251131,
129.268030185089));
#131800=CARTESIAN_POINT('Ctrl Pts',(-226.809017549953,-4.71516923349835,
129.398968691975));
#131801=CARTESIAN_POINT('Ctrl Pts',(-226.816769943647,-4.7506269304247,
129.531282917493));
#131802=CARTESIAN_POINT('Ctrl Pts',(-226.817768717679,-4.75519509715136,
129.548329524996));
#131803=CARTESIAN_POINT('Ctrl Pts',(-226.818767491711,-4.7596710365228,
129.565398951655));
#131804=CARTESIAN_POINT('Ctrl Pts',(-226.819766265743,-4.76405452823404,
129.582490119308));
#131805=CARTESIAN_POINT('Origin',(213.235140564004,0.,130.804360617566));
#131806=CARTESIAN_POINT('',(-228.915319603984,-4.76405452823406,129.582490119308));
#131807=CARTESIAN_POINT('',(-228.570020432611,-4.76405452823418,129.582490119309));
#131808=CARTESIAN_POINT('',(213.235140564004,-4.76405452823405,129.582490119308));
#131809=CARTESIAN_POINT('',(-227.235140563962,-4.91824846444471,130.800474168388));
#131810=CARTESIAN_POINT('Ctrl Pts',(-227.235140564014,-4.91824846444543,
130.800474169299));
#131811=CARTESIAN_POINT('Ctrl Pts',(-227.242910874425,-4.91835720842715,
130.938088228303));
#131812=CARTESIAN_POINT('Ctrl Pts',(-227.250681184837,-4.9126858626062,
131.075774149936));
#131813=CARTESIAN_POINT('Ctrl Pts',(-227.258451495249,-4.9012435845361,
131.213010085379));
#131814=CARTESIAN_POINT('Ctrl Pts',(-227.266187743251,-4.88985146553826,
131.349644424954));
#131815=CARTESIAN_POINT('Ctrl Pts',(-227.273923991253,-4.87273895711793,
131.485832323658));
#131816=CARTESIAN_POINT('Ctrl Pts',(-227.281660239255,-4.84996723784876,
131.621061820145));
#131817=CARTESIAN_POINT('Ctrl Pts',(-227.289396802041,-4.82719459200822,
131.756296819061));
#131818=CARTESIAN_POINT('Ctrl Pts',(-227.297133364828,-4.79876234172717,
131.890572951961));
#131819=CARTESIAN_POINT('Ctrl Pts',(-227.304869927615,-4.76478305287311,
132.023387082231));
#131820=CARTESIAN_POINT('Ctrl Pts',(-227.312608486423,-4.73079499741358,
132.156235478347));
#131821=CARTESIAN_POINT('Ctrl Pts',(-227.320347045231,-4.69125715245796,
132.287620741974));
#131822=CARTESIAN_POINT('Ctrl Pts',(-227.328085604039,-4.64633223752828,
132.417053955124));
#131823=CARTESIAN_POINT('Ctrl Pts',(-227.33588080486,-4.60107849682236,
132.547434548517));
#131824=CARTESIAN_POINT('Ctrl Pts',(-227.343676005681,-4.55035863971752,
132.675834019239));
#131825=CARTESIAN_POINT('Ctrl Pts',(-227.351471206502,-4.4943882496115,
132.801773275044));
#131826=CARTESIAN_POINT('Ctrl Pts',(-227.359222925504,-4.43873006370029,
132.927010038623));
#131827=CARTESIAN_POINT('Ctrl Pts',(-227.366974644506,-4.37788000325017,
133.049813640815));
#131828=CARTESIAN_POINT('Ctrl Pts',(-227.374726363507,-4.31209581913861,
133.169738538548));
#131829=CARTESIAN_POINT('Ctrl Pts',(-227.382543305238,-4.24575812889225,
133.290672480741));
#131830=CARTESIAN_POINT('Ctrl Pts',(-227.390360246969,-4.17440312209688,
133.408678710674));
#131831=CARTESIAN_POINT('Ctrl Pts',(-227.3981771887,-4.0983386554529,133.523331622877));
#131832=CARTESIAN_POINT('Ctrl Pts',(-227.405994130431,-4.02227418880913,
133.637984535079));
#131833=CARTESIAN_POINT('Ctrl Pts',(-227.413811072162,-3.94150054956011,
133.749283842464));
#131834=CARTESIAN_POINT('Ctrl Pts',(-227.421628013892,-3.85636528823487,
133.856839909256));
#131835=CARTESIAN_POINT('Ctrl Pts',(-227.429402348011,-3.77169407158126,
133.963809722845));
#131836=CARTESIAN_POINT('Ctrl Pts',(-227.43717668213,-3.68243459447034,
134.067423319435));
#131837=CARTESIAN_POINT('Ctrl Pts',(-227.44495101625,-3.58888268212647,
134.167261769315));
#131838=CARTESIAN_POINT('Ctrl Pts',(-227.452715769197,-3.4954460641536,
134.266977177228));
#131839=CARTESIAN_POINT('Ctrl Pts',(-227.460480522144,-3.39772780131615,
134.362926413031));
#131840=CARTESIAN_POINT('Ctrl Pts',(-227.468245275091,-3.29606525446265,
134.454721818985));
#131841=CARTESIAN_POINT('Ctrl Pts',(-227.476002315976,-3.19450368028387,
134.546426052448));
#131842=CARTESIAN_POINT('Ctrl Pts',(-227.483759356861,-3.08900590642713,
134.633984405959));
#131843=CARTESIAN_POINT('Ctrl Pts',(-227.491516397746,-2.97994733768238,
134.717044725329));
#131844=CARTESIAN_POINT('Ctrl Pts',(-227.499267588986,-2.87097101085252,
134.800042408265));
#131845=CARTESIAN_POINT('Ctrl Pts',(-227.507018780226,-2.75843954367994,
134.878548572709));
#131846=CARTESIAN_POINT('Ctrl Pts',(-227.514769971466,-2.64276245839599,
134.952250400455));
#131847=CARTESIAN_POINT('Ctrl Pts',(-227.522517868243,-2.52713453895924,
135.025920902957));
#131848=CARTESIAN_POINT('Ctrl Pts',(-227.53026576502,-2.40836398958257,
135.094790920445));
#131849=CARTESIAN_POINT('Ctrl Pts',(-227.538013661797,-2.28689025444527,
135.158590288429));
#131850=CARTESIAN_POINT('Ctrl Pts',(-227.545759937882,-2.1654419289947,
135.22237631096));
#131851=CARTESIAN_POINT('Ctrl Pts',(-227.553506213966,-2.04129188840132,
135.281093612043));
#131852=CARTESIAN_POINT('Ctrl Pts',(-227.56125249005,-1.91490482733184,
135.334517630823));
#131853=CARTESIAN_POINT('Ctrl Pts',(-227.568998823315,-1.78851683330196,
135.387942043967));
#131854=CARTESIAN_POINT('Ctrl Pts',(-227.576745156581,-1.65989214595977,
135.436072944619));
#131855=CARTESIAN_POINT('Ctrl Pts',(-227.584491489846,-1.52951574572216,
135.478733799725));
#131856=CARTESIAN_POINT('Ctrl Pts',(-227.592239557849,-1.39911014859386,
135.521404208433));
#131857=CARTESIAN_POINT('Ctrl Pts',(-227.599987625852,-1.26695242947814,
135.558602012467));
#131858=CARTESIAN_POINT('Ctrl Pts',(-227.607735693855,-1.13354265541742,
135.590200576324));
#131859=CARTESIAN_POINT('Ctrl Pts',(-227.615491996597,-0.999991091861054,
135.621832723511));
#131860=CARTESIAN_POINT('Ctrl Pts',(-227.623248299339,-0.865185196191498,
135.647853652628));
#131861=CARTESIAN_POINT('Ctrl Pts',(-227.63100460208,-0.729635704848385,
135.668187793845));
#131862=CARTESIAN_POINT('Ctrl Pts',(-227.638765044595,-0.594013866660427,
135.688532788006));
#131863=CARTESIAN_POINT('Ctrl Pts',(-227.646525487109,-0.457648030520637,
135.703184904607));
#131864=CARTESIAN_POINT('Ctrl Pts',(-227.654285929623,-0.321052986716322,
135.712120599698));
#131865=CARTESIAN_POINT('Ctrl Pts',(-227.662058829889,-0.184238668420982,
135.721070639161));
#131866=CARTESIAN_POINT('Ctrl Pts',(-227.669831730154,-0.0471947982733746,
135.724285910354));
#131867=CARTESIAN_POINT('Ctrl Pts',(-227.677604630419,0.0895639992079477,
135.721795045451));
#131868=CARTESIAN_POINT('Ctrl Pts',(-227.685094966181,0.221351269923615,
135.719394729761));
#131869=CARTESIAN_POINT('Ctrl Pts',(-227.692585301943,0.352873526862216,
135.711695958153));
#131870=CARTESIAN_POINT('Ctrl Pts',(-227.700075637705,0.483677643544477,
135.69876957061));
#131871=CARTESIAN_POINT('Ctrl Pts',(-227.707849971824,0.619441238069909,
135.685353075154));
#131872=CARTESIAN_POINT('Ctrl Pts',(-227.715624305943,0.75486121903268,
135.66626222896));
#131873=CARTESIAN_POINT('Ctrl Pts',(-227.723398640062,0.889425228243008,
135.641519476428));
#131874=CARTESIAN_POINT('Ctrl Pts',(-227.731163393009,1.02382339933795,
135.616807217127));
#131875=CARTESIAN_POINT('Ctrl Pts',(-227.738928145956,1.15736731680661,
135.586456980718));
#131876=CARTESIAN_POINT('Ctrl Pts',(-227.746692898903,1.28954848143668,
135.550543059964));
#131877=CARTESIAN_POINT('Ctrl Pts',(-227.754449939788,1.4215983618706,135.514664809422));
#131878=CARTESIAN_POINT('Ctrl Pts',(-227.762206980673,1.55228780815694,
135.473233973229));
#131879=CARTESIAN_POINT('Ctrl Pts',(-227.769964021558,1.68111762754279,
135.426376042125));
#131880=CARTESIAN_POINT('Ctrl Pts',(-227.777715212799,1.80985029535952,
135.379553446952));
#131881=CARTESIAN_POINT('Ctrl Pts',(-227.785466404039,1.93672576165647,
135.327312036066));
#131882=CARTESIAN_POINT('Ctrl Pts',(-227.793217595279,2.06125948684816,
135.269827266235));
#131883=CARTESIAN_POINT('Ctrl Pts',(-227.800965492056,2.18574028188509,
135.212366928965));
#131884=CARTESIAN_POINT('Ctrl Pts',(-227.808713388833,2.30788096116836,
135.149667828715));
#131885=CARTESIAN_POINT('Ctrl Pts',(-227.81646128561,2.42721669734777,135.08195365181));
#131886=CARTESIAN_POINT('Ctrl Pts',(-227.824207561694,2.54652747106343,
135.014253639252));
#131887=CARTESIAN_POINT('Ctrl Pts',(-227.831953837778,2.6630341288984,134.941540829475));
#131888=CARTESIAN_POINT('Ctrl Pts',(-227.839700113862,2.7762965626287,134.864084802635));
#131889=CARTESIAN_POINT('Ctrl Pts',(-227.847446447127,2.88955983243672,
134.786628204033));
#131890=CARTESIAN_POINT('Ctrl Pts',(-227.855192780393,2.99957850763467,
134.704428539197));
#131891=CARTESIAN_POINT('Ctrl Pts',(-227.862939113658,3.10594192220258,
134.61779841546));
#131892=CARTESIAN_POINT('Ctrl Pts',(-227.870687181661,3.21232915611956,
134.531148891507));
#131893=CARTESIAN_POINT('Ctrl Pts',(-227.878435249664,3.31505919746381,
134.440067181202));
#131894=CARTESIAN_POINT('Ctrl Pts',(-227.886183317667,3.41375520574974,
134.344905555526));
#131895=CARTESIAN_POINT('Ctrl Pts',(-227.893939620409,3.51255610932791,
134.249642790943));
#131896=CARTESIAN_POINT('Ctrl Pts',(-227.901695923151,3.60731413337136,
134.150291720799));
#131897=CARTESIAN_POINT('Ctrl Pts',(-227.909452225892,3.69768963332176,
134.047241194788));
#131898=CARTESIAN_POINT('Ctrl Pts',(-227.917212668407,3.78811336939789,
133.944135667609));
#131899=CARTESIAN_POINT('Ctrl Pts',(-227.924973110921,3.87414967541873,
133.837327054504));
#131900=CARTESIAN_POINT('Ctrl Pts',(-227.932733553435,3.95550048646769,
133.727235737042));
#131901=CARTESIAN_POINT('Ctrl Pts',(-227.9405064537,4.03698188906032,133.616967691225));
#131902=CARTESIAN_POINT('Ctrl Pts',(-227.948279353966,4.11376254707328,
133.503406734603));
#131903=CARTESIAN_POINT('Ctrl Pts',(-227.956052254231,4.18558838244359,
133.38700131175));
#131904=CARTESIAN_POINT('Ctrl Pts',(-227.963542589993,4.25480316778177,
133.274827519221));
#131905=CARTESIAN_POINT('Ctrl Pts',(-227.971032925756,4.31941696567561,
133.160012745443));
#131906=CARTESIAN_POINT('Ctrl Pts',(-227.978523261518,4.37924444987864,
133.042976509296));
#131907=CARTESIAN_POINT('Ctrl Pts',(-227.986297595637,4.44134031132791,
132.921502808687));
#131908=CARTESIAN_POINT('Ctrl Pts',(-227.994071929756,4.49847644927214,
132.797251074722));
#131909=CARTESIAN_POINT('Ctrl Pts',(-228.001846263875,4.55039480470242,
132.670664500603));
#131910=CARTESIAN_POINT('Ctrl Pts',(-228.009611016822,4.60224917539944,
132.544233933123));
#131911=CARTESIAN_POINT('Ctrl Pts',(-228.017375769769,4.64889841132926,
132.415474609072));
#131912=CARTESIAN_POINT('Ctrl Pts',(-228.025140522716,4.69013016085034,
132.28485450029));
#131913=CARTESIAN_POINT('Ctrl Pts',(-228.032897563601,4.73132095841674,
132.15436412524));
#131914=CARTESIAN_POINT('Ctrl Pts',(-228.040654604486,4.76710486053068,
132.022017013794));
#131915=CARTESIAN_POINT('Ctrl Pts',(-228.048411645371,4.7973176202293,131.888300981764));
#131916=CARTESIAN_POINT('Ctrl Pts',(-228.056162836611,4.82750759625084,
131.754685786033));
#131917=CARTESIAN_POINT('Ctrl Pts',(-228.063914027851,4.85213470635737,
131.619704104285));
#131918=CARTESIAN_POINT('Ctrl Pts',(-228.071665219092,4.87108466181725,
131.483858432065));
#131919=CARTESIAN_POINT('Ctrl Pts',(-228.079413115869,4.89002656304048,
131.34807049788));
#131920=CARTESIAN_POINT('Ctrl Pts',(-228.087161012646,4.90329605487305,
131.211419689999));
#131921=CARTESIAN_POINT('Ctrl Pts',(-228.094908909423,4.91083008042062,
131.07441798876));
#131922=CARTESIAN_POINT('Ctrl Pts',(-228.102655185507,4.91836253001247,
130.937444945323));
#131923=CARTESIAN_POINT('Ctrl Pts',(-228.110401461591,4.92016187820577,
130.800121544652));
#131924=CARTESIAN_POINT('Ctrl Pts',(-228.118147737675,4.91621704117659,
130.662963776919));
#131925=CARTESIAN_POINT('Ctrl Pts',(-228.125894070941,4.91227217502753,
130.52580499672));
#131926=CARTESIAN_POINT('Ctrl Pts',(-228.133640404206,4.90258305028537,
130.388812242702));
#131927=CARTESIAN_POINT('Ctrl Pts',(-228.141386737471,4.88719069733727,
130.252499991719));
#131928=CARTESIAN_POINT('Ctrl Pts',(-228.149134805474,4.87179489737851,
130.116157214553));
#131929=CARTESIAN_POINT('Ctrl Pts',(-228.156882873477,4.8506933715974,129.98049563209));
#131930=CARTESIAN_POINT('Ctrl Pts',(-228.16463094148,4.82397880406177,129.846022701973));
#131931=CARTESIAN_POINT('Ctrl Pts',(-228.172387244222,4.79723584396575,
129.711406852426));
#131932=CARTESIAN_POINT('Ctrl Pts',(-228.180143546964,4.76486800147383,
129.577982562913));
#131933=CARTESIAN_POINT('Ctrl Pts',(-228.187899849706,4.72701884066552,
129.44624576878));
#131934=CARTESIAN_POINT('Ctrl Pts',(-228.19566029222,4.68914947862057,129.314438662753));
#131935=CARTESIAN_POINT('Ctrl Pts',(-228.203420734734,4.64579309239619,
129.184321217495));
#131936=CARTESIAN_POINT('Ctrl Pts',(-228.211181177248,4.59714224954354,
129.056371429967));
#131937=CARTESIAN_POINT('Ctrl Pts',(-228.218954077513,4.54841330803879,
128.928216246082));
#131938=CARTESIAN_POINT('Ctrl Pts',(-228.226726977779,4.49437308014699,
128.802236033019));
#131939=CARTESIAN_POINT('Ctrl Pts',(-228.234499878044,4.43526151958818,
128.678886949096));
#131940=CARTESIAN_POINT('Ctrl Pts',(-228.241990213806,4.37829881314889,
128.560021915071));
#131941=CARTESIAN_POINT('Ctrl Pts',(-228.249480549568,4.31662722828887,
128.443600307214));
#131942=CARTESIAN_POINT('Ctrl Pts',(-228.25697088533,4.25049954476134,128.330004805949));
#131943=CARTESIAN_POINT('Ctrl Pts',(-228.264745219449,4.18186461001331,
128.212102296725));
#131944=CARTESIAN_POINT('Ctrl Pts',(-228.272519553568,4.10821158542302,
128.096870948468));
#131945=CARTESIAN_POINT('Ctrl Pts',(-228.280293887688,4.02977385478476,
127.984767430279));
#131946=CARTESIAN_POINT('Ctrl Pts',(-228.288058640635,3.95143279163954,
127.872802069659));
#131947=CARTESIAN_POINT('Ctrl Pts',(-228.295823393582,3.86831897715227,
127.763957186524));
#131948=CARTESIAN_POINT('Ctrl Pts',(-228.303588146529,3.78071134803678,
127.658664388537));
#131949=CARTESIAN_POINT('Ctrl Pts',(-228.311345187414,3.69319073205381,
127.553476168842));
#131950=CARTESIAN_POINT('Ctrl Pts',(-228.319102228299,3.60118543209285,
127.451833312047));
#131951=CARTESIAN_POINT('Ctrl Pts',(-228.326859269184,3.50501708191603,
127.354137680135));
#131952=CARTESIAN_POINT('Ctrl Pts',(-228.334610460424,3.40892125304029,
127.256515721259));
#131953=CARTESIAN_POINT('Ctrl Pts',(-228.342361651664,3.30866889586918,
127.162835339955));
#131954=CARTESIAN_POINT('Ctrl Pts',(-228.350112842904,3.20462099828599,
127.073464301686));
#131955=CARTESIAN_POINT('Ctrl Pts',(-228.357860739681,3.10061732383441,
126.984131248493));
#131956=CARTESIAN_POINT('Ctrl Pts',(-228.365608636458,2.99282161347258,
126.899104149661));
#131957=CARTESIAN_POINT('Ctrl Pts',(-228.373356533235,2.88163052696741,
126.818712794621));
#131958=CARTESIAN_POINT('Ctrl Pts',(-228.38110280932,2.77046269924055,126.738338255719));
#131959=CARTESIAN_POINT('Ctrl Pts',(-228.388849085404,2.65590122470499,
126.66259776075));
#131960=CARTESIAN_POINT('Ctrl Pts',(-228.396595361488,2.5383742294296,126.591779540142));
#131961=CARTESIAN_POINT('Ctrl Pts',(-228.404341694753,2.42084636659648,
126.52096079677));
#131962=CARTESIAN_POINT('Ctrl Pts',(-228.412088028019,2.30035327421165,
126.455064602046));
#131963=CARTESIAN_POINT('Ctrl Pts',(-228.419834361284,2.17734997414808,
126.394334523247));
#131964=CARTESIAN_POINT('Ctrl Pts',(-228.427582429287,2.0543191283488,126.333590844368));
#131965=CARTESIAN_POINT('Ctrl Pts',(-228.43533049729,1.92877730676809,126.278015756594));
#131966=CARTESIAN_POINT('Ctrl Pts',(-228.443078565293,1.80120154589672,
126.227805575445));
#131967=CARTESIAN_POINT('Ctrl Pts',(-228.450834868035,1.67349019598835,
126.177542030319));
#131968=CARTESIAN_POINT('Ctrl Pts',(-228.458591170777,1.54374095295396,
126.132654925362));
#131969=CARTESIAN_POINT('Ctrl Pts',(-228.466347473518,1.41244866113536,
126.093291541214));
#131970=CARTESIAN_POINT('Ctrl Pts',(-228.474107916033,1.28108629466748,
126.053907147644));
#131971=CARTESIAN_POINT('Ctrl Pts',(-228.481868358547,1.14817961706084,
126.020052445834));
#131972=CARTESIAN_POINT('Ctrl Pts',(-228.489628801061,1.01423486816231,
125.991823792283));
#131973=CARTESIAN_POINT('Ctrl Pts',(-228.497401701326,0.880075099261423,
125.963549823592));
#131974=CARTESIAN_POINT('Ctrl Pts',(-228.505174601592,0.744874314885049,
125.940920015418));
#131975=CARTESIAN_POINT('Ctrl Pts',(-228.512947501857,0.609145994789944,
125.923979052613));
#131976=CARTESIAN_POINT('Ctrl Pts',(-228.520437837619,0.47835174101187,
125.907653936478));
#131977=CARTESIAN_POINT('Ctrl Pts',(-228.527928173381,0.347067947063592,
125.896611264649));
#131978=CARTESIAN_POINT('Ctrl Pts',(-228.535418509143,0.215753206453727,
125.890845214476));
#131979=CARTESIAN_POINT('Ctrl Pts',(-228.543192843262,0.0794596275388981,
125.884860542758));
#131980=CARTESIAN_POINT('Ctrl Pts',(-228.550967177381,-0.0572990281376561,
125.884541559892));
#131981=CARTESIAN_POINT('Ctrl Pts',(-228.5587415115,-0.194012402284007,
125.889938754288));
#131982=CARTESIAN_POINT('Ctrl Pts',(-228.566506264448,-0.330557289414035,
125.895329297125));
#131983=CARTESIAN_POINT('Ctrl Pts',(-228.574271017395,-0.467056619139458,
125.906421985141));
#131984=CARTESIAN_POINT('Ctrl Pts',(-228.582035770342,-0.602996495604233,
125.923215435461));
#131985=CARTESIAN_POINT('Ctrl Pts',(-228.589792811227,-0.738801354667286,
125.939992206289));
#131986=CARTESIAN_POINT('Ctrl Pts',(-228.597549852112,-0.874047480747141,
125.962458424009));
#131987=CARTESIAN_POINT('Ctrl Pts',(-228.605306892997,-1.00822292507135,
125.990560705245));
#131988=CARTESIAN_POINT('Ctrl Pts',(-228.613058084237,-1.14229718664944,
126.018641794332));
#131989=CARTESIAN_POINT('Ctrl Pts',(-228.620809275477,-1.27530199245758,
126.052350407349));
#131990=CARTESIAN_POINT('Ctrl Pts',(-228.628560466717,-1.40673280822708,
126.091581621182));
#131991=CARTESIAN_POINT('Ctrl Pts',(-228.636308363494,-1.53810776239401,
126.130796160703));
#131992=CARTESIAN_POINT('Ctrl Pts',(-228.644056260271,-1.6679096832405,
126.175528520942));
#131993=CARTESIAN_POINT('Ctrl Pts',(-228.651804157048,-1.79564670528629,
126.225623240046));
#131994=CARTESIAN_POINT('Ctrl Pts',(-228.659550433132,-1.92335700750075,
126.275707480416));
#131995=CARTESIAN_POINT('Ctrl Pts',(-228.667296709216,-2.04900290630574,
126.331151705897));
#131996=CARTESIAN_POINT('Ctrl Pts',(-228.675042985301,-2.17211049268177,
126.391751517489));
#131997=CARTESIAN_POINT('Ctrl Pts',(-228.682789318566,-2.29521898781021,
126.452351776416));
#131998=CARTESIAN_POINT('Ctrl Pts',(-228.690535651831,-2.41578878235045,
126.518107524728));
#131999=CARTESIAN_POINT('Ctrl Pts',(-228.698281985097,-2.53336900581594,
126.5887675937));
#132000=CARTESIAN_POINT('Ctrl Pts',(-228.7060300531,-2.65097556055739,126.659443486504));
#132001=CARTESIAN_POINT('Ctrl Pts',(-228.713778121103,-2.76559087696416,
126.73502568409));
#132002=CARTESIAN_POINT('Ctrl Pts',(-228.721526189106,-2.87679193935304,
126.815218955482));
#132003=CARTESIAN_POINT('Ctrl Pts',(-228.729282491847,-2.98811118755449,
126.895497457237));
#132004=CARTESIAN_POINT('Ctrl Pts',(-228.737038794589,-3.09600861538586,
126.980396593434));
#132005=CARTESIAN_POINT('Ctrl Pts',(-228.744795097331,-3.2000928360187,
127.069579646296));
#132006=CARTESIAN_POINT('Ctrl Pts',(-228.752555539845,-3.30423260953428,
127.158810298839));
#132007=CARTESIAN_POINT('Ctrl Pts',(-228.76031598236,-3.40455483465514,
127.252329157547));
#132008=CARTESIAN_POINT('Ctrl Pts',(-228.768076424874,-3.5007048089268,
127.349762391541));
#132009=CARTESIAN_POINT('Ctrl Pts',(-228.775849325139,-3.59700913167244,
127.447352034011));
#132010=CARTESIAN_POINT('Ctrl Pts',(-228.783622225405,-3.68912755661647,
127.54886831891));
#132011=CARTESIAN_POINT('Ctrl Pts',(-228.79139512567,-3.77674494077698,
127.653903394429));
#132012=CARTESIAN_POINT('Ctrl Pts',(-228.798885461432,-3.86117721233052,
127.755120180388));
#132013=CARTESIAN_POINT('Ctrl Pts',(-228.806375797194,-3.94142982230247,
127.859604120536));
#132014=CARTESIAN_POINT('Ctrl Pts',(-228.813866132957,-4.01725978845964,
127.96696623988));
#132015=CARTESIAN_POINT('Ctrl Pts',(-228.821726616999,-4.09683702743094,
128.07963384954));
#132016=CARTESIAN_POINT('Ctrl Pts',(-228.829587101042,-4.17179334796039,
128.195824948763));
#132017=CARTESIAN_POINT('Ctrl Pts',(-228.837447585084,-4.24180480278559,
128.315128792772));
#132018=CARTESIAN_POINT('Ctrl Pts',(-228.845294526829,-4.31169563959784,
128.434227096236));
#132019=CARTESIAN_POINT('Ctrl Pts',(-228.853141468574,-4.37665839146968,
128.556427136261));
#132020=CARTESIAN_POINT('Ctrl Pts',(-228.860988410319,-4.43641119637584,
128.681287665647));
#132021=CARTESIAN_POINT('Ctrl Pts',(-228.868827498221,-4.49610419592812,
128.806023224696));
#132022=CARTESIAN_POINT('Ctrl Pts',(-228.876666586123,-4.55059746044838,
128.933413634851));
#132023=CARTESIAN_POINT('Ctrl Pts',(-228.884505674025,-4.59965375729813,
129.062990933819));
#132024=CARTESIAN_POINT('Ctrl Pts',(-228.892336934124,-4.64866106846908,
129.192438842018));
#132025=CARTESIAN_POINT('Ctrl Pts',(-228.900168194223,-4.69224209171157,
129.324068935704));
#132026=CARTESIAN_POINT('Ctrl Pts',(-228.907999454322,-4.73020690944459,
129.457391554691));
#132027=CARTESIAN_POINT('Ctrl Pts',(-228.910439504209,-4.74203591883365,
129.49893197569));
#132028=CARTESIAN_POINT('Ctrl Pts',(-228.912879554097,-4.75332005219438,
129.540636560148));
#132029=CARTESIAN_POINT('Ctrl Pts',(-228.915319603984,-4.76405452823406,
129.582490119308));
#132030=CARTESIAN_POINT('Ctrl Pts',(-227.165337382971,-4.76405452823413,
129.582490119309));
#132031=CARTESIAN_POINT('Ctrl Pts',(-227.174468718987,-4.80391961427429,
129.737923484742));
#132032=CARTESIAN_POINT('Ctrl Pts',(-227.183600055004,-4.83621507933807,
129.895469963794));
#132033=CARTESIAN_POINT('Ctrl Pts',(-227.19273139102,-4.86074207082464,
130.054447566996));
#132034=CARTESIAN_POINT('Ctrl Pts',(-227.20178028834,-4.88504762996015,
130.211989903077));
#132035=CARTESIAN_POINT('Ctrl Pts',(-227.21082918566,-4.90172428360133,
130.370937546404));
#132036=CARTESIAN_POINT('Ctrl Pts',(-227.219878082981,-4.91062540018657,
130.530606637609));
#132037=CARTESIAN_POINT('Ctrl Pts',(-227.224965576641,-4.91562980819314,
130.620376193009));
#132038=CARTESIAN_POINT('Ctrl Pts',(-227.230053070302,-4.91817726594451,
130.710373436795));
#132039=CARTESIAN_POINT('Ctrl Pts',(-227.235140563963,-4.91824846444471,
130.800474168387));
#132040=CARTESIAN_POINT('',(-226.889859436047,-4.91824996233216,130.803751914262));
#132041=CARTESIAN_POINT('Ctrl Pts',(-226.819766265743,-4.76405452823404,
129.582490119308));
#132042=CARTESIAN_POINT('Ctrl Pts',(-226.827527686226,-4.79811841182178,
129.715304684425));
#132043=CARTESIAN_POINT('Ctrl Pts',(-226.83528910671,-4.82659534922294,
129.849432617361));
#132044=CARTESIAN_POINT('Ctrl Pts',(-226.843050527193,-4.84941119093025,
129.984364176244));
#132045=CARTESIAN_POINT('Ctrl Pts',(-226.850823967339,-4.87226236620946,
130.119504695813));
#132046=CARTESIAN_POINT('Ctrl Pts',(-226.858597407484,-4.88943488249307,
130.255450939986));
#132047=CARTESIAN_POINT('Ctrl Pts',(-226.86637084763,-4.90090651786403,
130.391688392116));
#132048=CARTESIAN_POINT('Ctrl Pts',(-226.872354485895,-4.90973685746664,
130.496557744218));
#132049=CARTESIAN_POINT('Ctrl Pts',(-226.87833812416,-4.91519036663282,
130.601599545051));
#132050=CARTESIAN_POINT('Ctrl Pts',(-226.884321762425,-4.91727791410797,
130.706580364314));
#132051=CARTESIAN_POINT('Ctrl Pts',(-226.886167653615,-4.91792190114796,
130.738965873079));
#132052=CARTESIAN_POINT('Ctrl Pts',(-226.888013544806,-4.91824595309002,
130.771357764929));
#132053=CARTESIAN_POINT('Ctrl Pts',(-226.889859435996,-4.91824996233205,
130.803751913359));
#132054=CARTESIAN_POINT('Ctrl Pts',(-226.889859436047,-4.91824996233216,
130.803751914262));
#132055=CARTESIAN_POINT('Ctrl Pts',(-226.897607212581,-4.91826679033664,
130.939720179568));
#132056=CARTESIAN_POINT('Ctrl Pts',(-226.905354989115,-4.91264094686343,
131.075910932816));
#132057=CARTESIAN_POINT('Ctrl Pts',(-226.913102765649,-4.90134307196643,
131.211815097707));
#132058=CARTESIAN_POINT('Ctrl Pts',(-226.920841019478,-4.89005908316085,
131.347552224311));
#132059=CARTESIAN_POINT('Ctrl Pts',(-226.928579273306,-4.87311696449167,
131.483003074584));
#132060=CARTESIAN_POINT('Ctrl Pts',(-226.936317527135,-4.85053933090291,
131.617657157497));
#132061=CARTESIAN_POINT('Ctrl Pts',(-226.94404815453,-4.82798394869374,
131.752178532122));
#132062=CARTESIAN_POINT('Ctrl Pts',(-226.951778781925,-4.7998041677737,
131.885904315899));
#132063=CARTESIAN_POINT('Ctrl Pts',(-226.95950940932,-4.76607447969522,
132.018328128045));
#132064=CARTESIAN_POINT('Ctrl Pts',(-226.967234299652,-4.73236982313674,
132.150653665659));
#132065=CARTESIAN_POINT('Ctrl Pts',(-226.974959189984,-4.69312355336305,
132.281678774401));
#132066=CARTESIAN_POINT('Ctrl Pts',(-226.982684080315,-4.64846134277032,
132.410906666477));
#132067=CARTESIAN_POINT('Ctrl Pts',(-226.990405848413,-4.60381718368202,
132.540082327419));
#132068=CARTESIAN_POINT('Ctrl Pts',(-226.99812761651,-4.55376156498401,
132.667461844523));
#132069=CARTESIAN_POINT('Ctrl Pts',(-227.005849384607,-4.49847010713594,
132.792563262596));
#132070=CARTESIAN_POINT('Ctrl Pts',(-227.013569683712,-4.44318916795728,
132.917640881324));
#132071=CARTESIAN_POINT('Ctrl Pts',(-227.021289982817,-4.38267452978856,
133.040440902818));
#132072=CARTESIAN_POINT('Ctrl Pts',(-227.029010281922,-4.31714991344633,
133.160501463808));
#132073=CARTESIAN_POINT('Ctrl Pts',(-227.036730814151,-4.25162331850994,
133.28056565017));
#132074=CARTESIAN_POINT('Ctrl Pts',(-227.04445134638,-4.1810866330653,133.397889865601));
#132075=CARTESIAN_POINT('Ctrl Pts',(-227.052171878608,-4.10580926808051,
133.512037355407));
#132076=CARTESIAN_POINT('Ctrl Pts',(-227.059894345895,-4.03051303573446,
133.626213454901));
#132077=CARTESIAN_POINT('Ctrl Pts',(-227.067616813182,-3.95047397675962,
133.737210915949));
#132078=CARTESIAN_POINT('Ctrl Pts',(-227.075339280468,-3.86600424669483,
133.844622814653));
#132079=CARTESIAN_POINT('Ctrl Pts',(-227.08307000635,-3.78144418264038,
133.952149582262));
#132080=CARTESIAN_POINT('Ctrl Pts',(-227.090800732232,-3.69244422831664,
134.056082819457));
#132081=CARTESIAN_POINT('Ctrl Pts',(-227.098531458113,-3.59935648086937,
134.156049145178));
#132082=CARTESIAN_POINT('Ctrl Pts',(-227.106266550032,-3.50621616079846,
134.256071928296));
#132083=CARTESIAN_POINT('Ctrl Pts',(-227.11400164195,-3.4089837286687,134.352123060586));
#132084=CARTESIAN_POINT('Ctrl Pts',(-227.121736733869,-3.30804661206096,
134.443867545013));
#132085=CARTESIAN_POINT('Ctrl Pts',(-227.129483785872,-3.2069534253635,
134.535753885779));
#132086=CARTESIAN_POINT('Ctrl Pts',(-227.137230837876,-3.10214441355839,
134.623320024407));
#132087=CARTESIAN_POINT('Ctrl Pts',(-227.144977889879,-2.99403894980162,
134.706272178528));
#132088=CARTESIAN_POINT('Ctrl Pts',(-227.150908388666,-2.91128239655924,
134.769773449607));
#132089=CARTESIAN_POINT('Ctrl Pts',(-227.156838887452,-2.82659472533501,
134.830571701648));
#132090=CARTESIAN_POINT('Ctrl Pts',(-227.162769386238,-2.74017412009895,
134.88855317596));
#132091=CARTESIAN_POINT('Ctrl Pts',(-227.170543720357,-2.62688471829739,
134.964561513583));
#132092=CARTESIAN_POINT('Ctrl Pts',(-227.178318054476,-2.51025094082447,
135.035972952477));
#132093=CARTESIAN_POINT('Ctrl Pts',(-227.186092388595,-2.39068239980026,
135.102478894881));
#132094=CARTESIAN_POINT('Ctrl Pts',(-227.193857141543,-2.2712612163164,
135.168902874654));
#132095=CARTESIAN_POINT('Ctrl Pts',(-227.20162189449,-2.1489128040917,135.230433198636));
#132096=CARTESIAN_POINT('Ctrl Pts',(-227.209386647437,-2.02407677889124,
135.286803729938));
#132097=CARTESIAN_POINT('Ctrl Pts',(-227.217143688322,-1.89936474259122,
135.343118273234));
#132098=CARTESIAN_POINT('Ctrl Pts',(-227.224900729207,-1.77217036420014,
135.394283062534));
#132099=CARTESIAN_POINT('Ctrl Pts',(-227.232657770092,-1.6429586461421,
135.440077385183));
#132100=CARTESIAN_POINT('Ctrl Pts',(-227.240408961332,-1.51384436764594,
135.485837173977));
#132101=CARTESIAN_POINT('Ctrl Pts',(-227.248160152572,-1.38271614453616,
135.526234427148));
#132102=CARTESIAN_POINT('Ctrl Pts',(-227.255911343812,-1.25005945672734,
135.561096306791));
#132103=CARTESIAN_POINT('Ctrl Pts',(-227.263659240589,-1.1174591515494,
135.595943369206));
#132104=CARTESIAN_POINT('Ctrl Pts',(-227.271407137366,-0.983332051087742,
135.625259638235));
#132105=CARTESIAN_POINT('Ctrl Pts',(-227.279155034143,-0.848179104589514,
135.648922028988));
#132106=CARTESIAN_POINT('Ctrl Pts',(-227.286901310227,-0.713054429174133,
135.672579470079));
#132107=CARTESIAN_POINT('Ctrl Pts',(-227.294647586311,-0.576904719406775,
135.690585317906));
#132108=CARTESIAN_POINT('Ctrl Pts',(-227.302393862396,-0.440241044777452,
135.702867623276));
#132109=CARTESIAN_POINT('Ctrl Pts',(-227.310140195661,-0.303576361327743,
135.715150019312));
#132110=CARTESIAN_POINT('Ctrl Pts',(-227.317886528926,-0.166398094841255,
135.721708753587));
#132111=CARTESIAN_POINT('Ctrl Pts',(-227.325632862192,-0.0292219672228785,
135.722523805092));
#132112=CARTESIAN_POINT('Ctrl Pts',(-227.333380930195,0.107984880038353,
135.723339039121));
#132113=CARTESIAN_POINT('Ctrl Pts',(-227.341128998198,0.245189196594871,
135.718408028553));
#132114=CARTESIAN_POINT('Ctrl Pts',(-227.348877066201,0.381876129868607,
135.707762873545));
#132115=CARTESIAN_POINT('Ctrl Pts',(-227.356633368943,0.518708335641436,
135.697106404739));
#132116=CARTESIAN_POINT('Ctrl Pts',(-227.364389671685,0.655021669278292,
135.680723690306));
#132117=CARTESIAN_POINT('Ctrl Pts',(-227.372145974426,0.790306710479554,
135.658698715172));
#132118=CARTESIAN_POINT('Ctrl Pts',(-227.379906416941,0.92566395738066,
135.636661984646));
#132119=CARTESIAN_POINT('Ctrl Pts',(-227.387666859455,1.05999143552488,
135.608977071743));
#132120=CARTESIAN_POINT('Ctrl Pts',(-227.395427301969,1.192791749699,135.575778740551));
#132121=CARTESIAN_POINT('Ctrl Pts',(-227.403200202234,1.32580524672689,
135.54252711645));
#132122=CARTESIAN_POINT('Ctrl Pts',(-227.4109731025,1.45728630562025,135.503744498358));
#132123=CARTESIAN_POINT('Ctrl Pts',(-227.418746002765,1.58675362023576,
135.459615284195));
#132124=CARTESIAN_POINT('Ctrl Pts',(-227.426236338527,1.71151447186036,
135.41709027812));
#132125=CARTESIAN_POINT('Ctrl Pts',(-227.43372667429,1.83440515936743,135.369600762643));
#132126=CARTESIAN_POINT('Ctrl Pts',(-227.441217010052,1.95501582534376,
135.317352550326));
#132127=CARTESIAN_POINT('Ctrl Pts',(-227.448991344171,2.0801994813757,135.26312333116));
#132128=CARTESIAN_POINT('Ctrl Pts',(-227.45676567829,2.20332335305605,135.203595657974));
#132129=CARTESIAN_POINT('Ctrl Pts',(-227.464540012409,2.32390640299417,
135.13894734442));
#132130=CARTESIAN_POINT('Ctrl Pts',(-227.472304765356,2.44434084510039,
135.074378704135));
#132131=CARTESIAN_POINT('Ctrl Pts',(-227.480069518303,2.56224035462873,
135.004702162917));
#132132=CARTESIAN_POINT('Ctrl Pts',(-227.48783427125,2.67714340002008,134.930143728471));
#132133=CARTESIAN_POINT('Ctrl Pts',(-227.495591312135,2.7919323220872,134.855659346513));
#132134=CARTESIAN_POINT('Ctrl Pts',(-227.50334835302,2.9037303768036,134.776302932026));
#132135=CARTESIAN_POINT('Ctrl Pts',(-227.511105393906,3.01210052719341,
134.692346404137));
#132136=CARTESIAN_POINT('Ctrl Pts',(-227.518856585146,3.12038895480938,
134.60845318852));
#132137=CARTESIAN_POINT('Ctrl Pts',(-227.526607776386,3.22525431558695,
134.519967002769));
#132138=CARTESIAN_POINT('Ctrl Pts',(-227.534358967626,3.32628878235119,
134.427202871778));
#132139=CARTESIAN_POINT('Ctrl Pts',(-227.542106864403,3.427280306772,134.334478168017));
#132140=CARTESIAN_POINT('Ctrl Pts',(-227.54985476118,3.52444388822232,134.237479399222));
#132141=CARTESIAN_POINT('Ctrl Pts',(-227.557602657957,3.61740519659297,
134.13656149779));
#132142=CARTESIAN_POINT('Ctrl Pts',(-227.565348934041,3.71034705946217,
134.035664706207));
#132143=CARTESIAN_POINT('Ctrl Pts',(-227.573095210126,3.79908813296247,
133.930850699986));
#132144=CARTESIAN_POINT('Ctrl Pts',(-227.58084148621,3.8832916386564,133.822510566068));
#132145=CARTESIAN_POINT('Ctrl Pts',(-227.588587819475,3.96749576592113,
133.714169632407));
#132146=CARTESIAN_POINT('Ctrl Pts',(-227.59633415274,4.04716201862105,133.602302827803));
#132147=CARTESIAN_POINT('Ctrl Pts',(-227.604080486006,4.12199479222569,
133.487333221855));
#132148=CARTESIAN_POINT('Ctrl Pts',(-227.611828554009,4.19684432411102,
133.37233786926));
#132149=CARTESIAN_POINT('Ctrl Pts',(-227.619576622012,4.26685800976634,
133.254238660254));
#132150=CARTESIAN_POINT('Ctrl Pts',(-227.627324690015,4.33178456556933,
133.133486105812));
#132151=CARTESIAN_POINT('Ctrl Pts',(-227.635080992757,4.39678012608874,
133.012605214117));
#132152=CARTESIAN_POINT('Ctrl Pts',(-227.642837295498,4.45667757092194,
132.889065688612));
#132153=CARTESIAN_POINT('Ctrl Pts',(-227.65059359824,4.51127220485229,132.763341514927));
#132154=CARTESIAN_POINT('Ctrl Pts',(-227.658354040754,4.56589597758258,
132.637550238466));
#132155=CARTESIAN_POINT('Ctrl Pts',(-227.666114483269,4.61521115934745,
132.509572355085));
#132156=CARTESIAN_POINT('Ctrl Pts',(-227.673874925783,4.65906227672837,
132.379899180746));
#132157=CARTESIAN_POINT('Ctrl Pts',(-227.681647826048,4.70298378781583,
132.250017843515));
#132158=CARTESIAN_POINT('Ctrl Pts',(-227.689420726314,4.74142359676889,
132.118436152533));
#132159=CARTESIAN_POINT('Ctrl Pts',(-227.697193626579,4.77427668505314,
131.985658715871));
#132160=CARTESIAN_POINT('Ctrl Pts',(-227.704683962341,4.80593548082553,
131.85770807348));
#132161=CARTESIAN_POINT('Ctrl Pts',(-227.712174298103,4.83240662484983,
131.728647414531));
#132162=CARTESIAN_POINT('Ctrl Pts',(-227.719664633865,4.85364173511936,
131.598932810389));
#132163=CARTESIAN_POINT('Ctrl Pts',(-227.727438967984,4.87568198104955,
131.464300037602));
#132164=CARTESIAN_POINT('Ctrl Pts',(-227.735213302103,4.89215112379825,
131.328536275907));
#132165=CARTESIAN_POINT('Ctrl Pts',(-227.742987636222,4.90293875056628,
131.192142348306));
#132166=CARTESIAN_POINT('Ctrl Pts',(-227.750752389169,4.91371308254838,
131.055916514031));
#132167=CARTESIAN_POINT('Ctrl Pts',(-227.758517142116,4.91881979983472,
130.919062445106));
#132168=CARTESIAN_POINT('Ctrl Pts',(-227.766281895063,4.91819958002786,
130.782090603786));
#132169=CARTESIAN_POINT('Ctrl Pts',(-227.774038935948,4.91757997623206,
130.64525480483));
#132170=CARTESIAN_POINT('Ctrl Pts',(-227.781795976833,4.9112447566271,130.508301854694));
#132171=CARTESIAN_POINT('Ctrl Pts',(-227.789553017718,4.89918646531574,
130.371746423893));
#132172=CARTESIAN_POINT('Ctrl Pts',(-227.797304208959,4.8871372672556,130.235293970605));
#132173=CARTESIAN_POINT('Ctrl Pts',(-227.805055400199,4.86937362210339,
130.099238827847));
#132174=CARTESIAN_POINT('Ctrl Pts',(-227.812806591439,4.8459401286741,129.964094390822));
#132175=CARTESIAN_POINT('Ctrl Pts',(-227.820554488216,4.82251659510478,
129.829007393789));
#132176=CARTESIAN_POINT('Ctrl Pts',(-227.828302384993,4.79342807289527,
129.694830717039));
#132177=CARTESIAN_POINT('Ctrl Pts',(-227.83605028177,4.75877084215767,129.562071144726));
#132178=CARTESIAN_POINT('Ctrl Pts',(-227.843796557854,4.72412086096552,
129.429339342852));
#132179=CARTESIAN_POINT('Ctrl Pts',(-227.851542833938,4.68390458689369,
129.298024433852));
#132180=CARTESIAN_POINT('Ctrl Pts',(-227.859289110022,4.63826901548873,
129.168621151007));
#132181=CARTESIAN_POINT('Ctrl Pts',(-227.867035443288,4.59263310721242,
129.039216912937));
#132182=CARTESIAN_POINT('Ctrl Pts',(-227.874781776553,4.54157795180728,
128.911724697888));
#132183=CARTESIAN_POINT('Ctrl Pts',(-227.882528109818,4.48529970823971,
128.786621885776));
#132184=CARTESIAN_POINT('Ctrl Pts',(-227.890276177821,4.42900886154946,
128.661491057756));
#132185=CARTESIAN_POINT('Ctrl Pts',(-227.898024245824,4.36749275954502,
128.538751053922));
#132186=CARTESIAN_POINT('Ctrl Pts',(-227.905772313827,4.30099460493286,
128.418856798487));
#132187=CARTESIAN_POINT('Ctrl Pts',(-227.913528616569,4.23442577529109,
128.298835118012));
#132188=CARTESIAN_POINT('Ctrl Pts',(-227.921284919311,4.16286450567179,
128.181665570135));
#132189=CARTESIAN_POINT('Ctrl Pts',(-227.929041222053,4.08659893084545,
128.067776571549));
#132190=CARTESIAN_POINT('Ctrl Pts',(-227.936801664567,4.01029265078531,
127.953826786976));
#132191=CARTESIAN_POINT('Ctrl Pts',(-227.944562107081,3.92927729330941,
127.843161355878));
#132192=CARTESIAN_POINT('Ctrl Pts',(-227.952322549595,3.84388217927022,
127.736176650724));
#132193=CARTESIAN_POINT('Ctrl Pts',(-227.960095449861,3.75834998141294,
127.629020204223));
#132194=CARTESIAN_POINT('Ctrl Pts',(-227.967868350126,3.66842423388693,
127.525556586242));
#132195=CARTESIAN_POINT('Ctrl Pts',(-227.975641250391,3.57447271266937,
127.426146904835));
#132196=CARTESIAN_POINT('Ctrl Pts',(-227.983131586153,3.48393656589894,
127.330351015747));
#132197=CARTESIAN_POINT('Ctrl Pts',(-227.990621921915,3.38966247827523,
127.238319653933));
#132198=CARTESIAN_POINT('Ctrl Pts',(-227.998112257677,3.29200800389859,
127.150340042259));
#132199=CARTESIAN_POINT('Ctrl Pts',(-228.005886591796,3.19065093044351,
127.059024656867));
#132200=CARTESIAN_POINT('Ctrl Pts',(-228.013660925915,3.08533100663732,
126.971785071232));
#132201=CARTESIAN_POINT('Ctrl Pts',(-228.021435260034,2.97640990824081,
126.888984885835));
#132202=CARTESIAN_POINT('Ctrl Pts',(-228.029200012981,2.86762304536323,
126.806286744267));
#132203=CARTESIAN_POINT('Ctrl Pts',(-228.036964765929,2.75524414669896,
126.728017351283));
#132204=CARTESIAN_POINT('Ctrl Pts',(-228.044729518876,2.63967061339744,
126.654502533816));
#132205=CARTESIAN_POINT('Ctrl Pts',(-228.052486559761,2.52421186935945,
126.581060732302));
#132206=CARTESIAN_POINT('Ctrl Pts',(-228.060243600645,2.40556513275915,
126.512364317169));
#132207=CARTESIAN_POINT('Ctrl Pts',(-228.06800064153,2.28415938038325,126.448697753259));
#132208=CARTESIAN_POINT('Ctrl Pts',(-228.07575183277,2.16284518102912,126.385079200799));
#132209=CARTESIAN_POINT('Ctrl Pts',(-228.08350302401,2.03877645204067,126.326483130566));
#132210=CARTESIAN_POINT('Ctrl Pts',(-228.091254215251,1.91240923409061,
126.273149522962));
#132211=CARTESIAN_POINT('Ctrl Pts',(-228.099002112028,1.78609572557931,
126.219838583563));
#132212=CARTESIAN_POINT('Ctrl Pts',(-228.106750008805,1.65748603056837,
126.171785809897));
#132213=CARTESIAN_POINT('Ctrl Pts',(-228.114497905582,1.52705856267167,
126.129184127991));
#132214=CARTESIAN_POINT('Ctrl Pts',(-228.122244181666,1.39665837738921,
126.08659135744));
#132215=CARTESIAN_POINT('Ctrl Pts',(-228.12999045775,1.26444154694417,126.049447531941));
#132216=CARTESIAN_POINT('Ctrl Pts',(-228.137736733834,1.13090375914098,
126.017896395402));
#132217=CARTESIAN_POINT('Ctrl Pts',(-228.145483067099,0.997364985591997,
125.986345025959));
#132218=CARTESIAN_POINT('Ctrl Pts',(-228.153229400365,0.862505615716626,
125.960386517753));
#132219=CARTESIAN_POINT('Ctrl Pts',(-228.16097573363,0.726833311470884,
125.940113872197));
#132220=CARTESIAN_POINT('Ctrl Pts',(-228.168723801633,0.591130624353477,
125.919836686721));
#132221=CARTESIAN_POINT('Ctrl Pts',(-228.176471869636,0.454615027203587,
125.9052479554));
#132222=CARTESIAN_POINT('Ctrl Pts',(-228.184219937639,0.317800717650317,
125.896388962558));
#132223=CARTESIAN_POINT('Ctrl Pts',(-228.191976240381,0.180841000220929,
125.887520554273));
#132224=CARTESIAN_POINT('Ctrl Pts',(-228.199732543123,0.0435823269677124,
125.884394074471));
#132225=CARTESIAN_POINT('Ctrl Pts',(-228.207488845864,-0.0934591191296018,
125.886998676896));
#132226=CARTESIAN_POINT('Ctrl Pts',(-228.215249288379,-0.23057370837331,
125.889604669476));
#132227=CARTESIAN_POINT('Ctrl Pts',(-228.223009730893,-0.367470449389297,
125.897947815532));
#132228=CARTESIAN_POINT('Ctrl Pts',(-228.230770173407,-0.503637856829301,
125.911965297105));
#132229=CARTESIAN_POINT('Ctrl Pts',(-228.238543073672,-0.640023852280102,
125.926005280784));
#132230=CARTESIAN_POINT('Ctrl Pts',(-228.246315973938,-0.775677787425283,
125.945737746248));
#132231=CARTESIAN_POINT('Ctrl Pts',(-228.254088874203,-0.910097059932253,
125.971048460876));
#132232=CARTESIAN_POINT('Ctrl Pts',(-228.261579209965,-1.03962985330771,
125.995439067275));
#132233=CARTESIAN_POINT('Ctrl Pts',(-228.269069545728,-1.16801589160583,
126.025009328124));
#132234=CARTESIAN_POINT('Ctrl Pts',(-228.27655988149,-1.29482025936989,
126.059613674006));
#132235=CARTESIAN_POINT('Ctrl Pts',(-228.284334215609,-1.42643245327404,
126.095530054178));
#132236=CARTESIAN_POINT('Ctrl Pts',(-228.292108549728,-1.55675757882226,
126.136983561911));
#132237=CARTESIAN_POINT('Ctrl Pts',(-228.299882883847,-1.68529423404915,
126.183866444084));
#132238=CARTESIAN_POINT('Ctrl Pts',(-228.307647636794,-1.81367247933542,
126.230691547295));
#132239=CARTESIAN_POINT('Ctrl Pts',(-228.315412389742,-1.94026627609201,
126.282932578733));
#132240=CARTESIAN_POINT('Ctrl Pts',(-228.323177142689,-2.06458669186481,
126.340431310971));
#132241=CARTESIAN_POINT('Ctrl Pts',(-228.330934183574,-2.18878363084839,
126.397872934659));
#132242=CARTESIAN_POINT('Ctrl Pts',(-228.338691224459,-2.31071132972482,
126.460561704028));
#132243=CARTESIAN_POINT('Ctrl Pts',(-228.346448265344,-2.42989858773376,
126.528290468956));
#132244=CARTESIAN_POINT('Ctrl Pts',(-228.354199456584,-2.54899596570382,
126.595968159096));
#132245=CARTESIAN_POINT('Ctrl Pts',(-228.361950647824,-2.66535667768285,
126.668678087354));
#132246=CARTESIAN_POINT('Ctrl Pts',(-228.369701839064,-2.77853232023985,
126.746166289064));
#132247=CARTESIAN_POINT('Ctrl Pts',(-228.377449735841,-2.89165986013017,
126.823621556223));
#132248=CARTESIAN_POINT('Ctrl Pts',(-228.385197632618,-3.00160470116137,
126.905850837131));
#132249=CARTESIAN_POINT('Ctrl Pts',(-228.392945529395,-3.10794593495714,
126.992555910097));
#132250=CARTESIAN_POINT('Ctrl Pts',(-228.400691805479,-3.21426492445924,
127.079242846231));
#132251=CARTESIAN_POINT('Ctrl Pts',(-228.408438081563,-3.31698150325051,
127.170403465289));
#132252=CARTESIAN_POINT('Ctrl Pts',(-228.416184357647,-3.4157068041452,
127.265698428176));
#132253=CARTESIAN_POINT('Ctrl Pts',(-228.423930690913,-3.51443283380775,
127.360994094509));
#132254=CARTESIAN_POINT('Ctrl Pts',(-228.431677024178,-3.60916724548504,
127.460423894045));
#132255=CARTESIAN_POINT('Ctrl Pts',(-228.439423357444,-3.69955739076832,
127.563610985936));
#132256=CARTESIAN_POINT('Ctrl Pts',(-228.447171425446,-3.78996777829778,
127.666821185861));
#132257=CARTESIAN_POINT('Ctrl Pts',(-228.454919493449,-3.8760317059711,
127.773790058437));
#132258=CARTESIAN_POINT('Ctrl Pts',(-228.462667561452,-3.95743650373772,
127.884107309823));
#132259=CARTESIAN_POINT('Ctrl Pts',(-228.470423864194,-4.03892781949202,
127.994541807696));
#132260=CARTESIAN_POINT('Ctrl Pts',(-228.478180166936,-4.11574988111916,
128.10833147817));
#132261=CARTESIAN_POINT('Ctrl Pts',(-228.485936469678,-4.18763280437161,
128.22503617922));
#132262=CARTESIAN_POINT('Ctrl Pts',(-228.493696912192,-4.25955409370456,
128.341803169082));
#132263=CARTESIAN_POINT('Ctrl Pts',(-228.501457354706,-4.32653080104514,
128.461487948652));
#132264=CARTESIAN_POINT('Ctrl Pts',(-228.50921779722,-4.3883393065969,128.583626236178));
#132265=CARTESIAN_POINT('Ctrl Pts',(-228.516990697486,-4.45024703264903,
128.705960590928));
#132266=CARTESIAN_POINT('Ctrl Pts',(-228.524763597751,-4.50696981607893,
128.83075596806));
#132267=CARTESIAN_POINT('Ctrl Pts',(-228.532536498017,-4.55833209518877,
128.957527768478));
#132268=CARTESIAN_POINT('Ctrl Pts',(-228.540026833778,-4.60782722607807,
129.079691094628));
#132269=CARTESIAN_POINT('Ctrl Pts',(-228.54751716954,-4.65234471785363,
129.203689353004));
#132270=CARTESIAN_POINT('Ctrl Pts',(-228.555007505302,-4.69177195976037,
129.329077953089));
#132271=CARTESIAN_POINT('Ctrl Pts',(-228.560011814405,-4.71811338314223,
129.41285034097));
#132272=CARTESIAN_POINT('Ctrl Pts',(-228.565016123508,-4.74221981315879,
129.497356896618));
#132273=CARTESIAN_POINT('Ctrl Pts',(-228.570020432611,-4.76405452823418,
129.582490119309));
#132274=CARTESIAN_POINT('Origin',(213.235140564004,0.,130.804360617566));
#132275=CARTESIAN_POINT('',(-230.664999534934,-4.76405452823393,129.582490119308));
#132276=CARTESIAN_POINT('',(-230.320068668528,-4.76405452823411,129.582490119308));
#132277=CARTESIAN_POINT('',(213.235140564004,-4.76405452823405,129.582490119308));
#132278=CARTESIAN_POINT('',(-228.985140564067,-4.91824914231909,130.807265196277));
#132279=CARTESIAN_POINT('Ctrl Pts',(-228.985140564067,-4.91824914231909,
130.807265196277));
#132280=CARTESIAN_POINT('Ctrl Pts',(-228.994071663459,-4.9181556026837,
130.965653478122));
#132281=CARTESIAN_POINT('Ctrl Pts',(-229.003002762851,-4.91040629817827,
131.123761141962));
#132282=CARTESIAN_POINT('Ctrl Pts',(-229.011933862243,-4.89511003228873,
131.280890610626));
#132283=CARTESIAN_POINT('Ctrl Pts',(-229.020624482857,-4.8802256336469,
131.433789211296));
#132284=CARTESIAN_POINT('Ctrl Pts',(-229.029315103471,-4.85819560038952,
131.585761459511));
#132285=CARTESIAN_POINT('Ctrl Pts',(-229.038005724085,-4.82917098077785,
131.736181791887));
#132286=CARTESIAN_POINT('Ctrl Pts',(-229.047057062866,-4.79894164771243,
131.892845561751));
#132287=CARTESIAN_POINT('Ctrl Pts',(-229.056108401646,-4.7611248288635,
132.047825549675));
#132288=CARTESIAN_POINT('Ctrl Pts',(-229.065159740427,-4.71594648954949,
132.200437897019));
#132289=CARTESIAN_POINT('Ctrl Pts',(-229.074211079208,-4.67076815023558,
132.353050244363));
#132290=CARTESIAN_POINT('Ctrl Pts',(-229.083262417989,-4.61822846161815,
132.503294741504));
#132291=CARTESIAN_POINT('Ctrl Pts',(-229.09231375677,-4.55860729181921,
132.650514083958));
#132292=CARTESIAN_POINT('Ctrl Pts',(-229.100088090889,-4.50739775190382,
132.776963041924));
#132293=CARTESIAN_POINT('Ctrl Pts',(-229.107862425008,-4.45084185464803,
132.901479956991));
#132294=CARTESIAN_POINT('Ctrl Pts',(-229.115636759127,-4.38910581892583,
133.02357966326));
#132295=CARTESIAN_POINT('Ctrl Pts',(-229.123401512074,-4.32744586735014,
133.145528892553));
#132296=CARTESIAN_POINT('Ctrl Pts',(-229.131166265021,-4.26061865439832,
133.265066494805));
#132297=CARTESIAN_POINT('Ctrl Pts',(-229.138931017968,-4.18883904720675,
133.381725647804));
#132298=CARTESIAN_POINT('Ctrl Pts',(-229.146688058853,-4.11713073253315,
133.498268933288));
#132299=CARTESIAN_POINT('Ctrl Pts',(-229.154445099738,-4.04048001578551,
133.611939128064));
#132300=CARTESIAN_POINT('Ctrl Pts',(-229.162202140623,-3.95914825010333,
133.722292795702));
#132301=CARTESIAN_POINT('Ctrl Pts',(-229.169953331863,-3.87787781733799,
133.832563244782));
#132302=CARTESIAN_POINT('Ctrl Pts',(-229.177704523104,-3.79193359293558,
133.939521831402));
#132303=CARTESIAN_POINT('Ctrl Pts',(-229.185455714344,-3.70162072434241,
134.042753286101));
#132304=CARTESIAN_POINT('Ctrl Pts',(-229.193203611121,-3.61134624112769,
134.145940864677));
#132305=CARTESIAN_POINT('Ctrl Pts',(-229.200951507898,-3.51670706362638,
134.245404168413));
#132306=CARTESIAN_POINT('Ctrl Pts',(-229.208699404675,-3.41804903913538,
134.340760457596));
#132307=CARTESIAN_POINT('Ctrl Pts',(-229.216445680759,-3.31941165177628,
134.4360968003));
#132308=CARTESIAN_POINT('Ctrl Pts',(-229.224191956843,-3.21675737047872,
134.527327565708));
#132309=CARTESIAN_POINT('Ctrl Pts',(-229.231938232927,-3.1104690878048,
134.61410668736));
#132310=CARTESIAN_POINT('Ctrl Pts',(-229.239684566193,-3.00418002053507,
134.700886449595));
#132311=CARTESIAN_POINT('Ctrl Pts',(-229.247430899458,-2.8942572012081,
134.783214255243));
#132312=CARTESIAN_POINT('Ctrl Pts',(-229.255177232723,-2.78111648389569,
134.860784432394));
#132313=CARTESIAN_POINT('Ctrl Pts',(-229.262925300726,-2.66795042950424,
134.938371980849));
#132314=CARTESIAN_POINT('Ctrl Pts',(-229.270673368729,-2.55156536555972,
135.011199559673));
#132315=CARTESIAN_POINT('Ctrl Pts',(-229.278421436732,-2.43240564318684,
135.079005146587));
#132316=CARTESIAN_POINT('Ctrl Pts',(-229.286177739474,-2.31311927644285,
135.146882798086));
#132317=CARTESIAN_POINT('Ctrl Pts',(-229.293934042216,-2.19105270079028,
135.209727601912));
#132318=CARTESIAN_POINT('Ctrl Pts',(-229.301690344958,-2.06667485324285,
135.267323547445));
#132319=CARTESIAN_POINT('Ctrl Pts',(-229.309450787472,-1.94223062149324,
135.324950233669));
#132320=CARTESIAN_POINT('Ctrl Pts',(-229.317211229986,-1.81547302096695,
135.377322330207));
#132321=CARTESIAN_POINT('Ctrl Pts',(-229.3249716725,-1.68688949520486,135.424272618185));
#132322=CARTESIAN_POINT('Ctrl Pts',(-229.332744572765,-1.55809955575209,
135.471298274934));
#132323=CARTESIAN_POINT('Ctrl Pts',(-229.340517473031,-1.42747820647184,
135.512884611945));
#132324=CARTESIAN_POINT('Ctrl Pts',(-229.348290373296,-1.29552738996386,
135.548914531724));
#132325=CARTESIAN_POINT('Ctrl Pts',(-229.355780709058,-1.16837331800179,
135.583634673165));
#132326=CARTESIAN_POINT('Ctrl Pts',(-229.36327104482,-1.03998505980053,
135.61319529411));
#132327=CARTESIAN_POINT('Ctrl Pts',(-229.370761380582,-0.910817394353961,
135.637537082029));
#132328=CARTESIAN_POINT('Ctrl Pts',(-229.378535714701,-0.776752297610621,
135.662801796237));
#132329=CARTESIAN_POINT('Ctrl Pts',(-229.38631004882,-0.641422846540744,
135.682524152218));
#132330=CARTESIAN_POINT('Ctrl Pts',(-229.394084382939,-0.505327070319028,
135.6965817506));
#132331=CARTESIAN_POINT('Ctrl Pts',(-229.401849135886,-0.369399019978647,
135.710622024247));
#132332=CARTESIAN_POINT('Ctrl Pts',(-229.409613888834,-0.232706908777922,
135.719011391232));
#132333=CARTESIAN_POINT('Ctrl Pts',(-229.417378641781,-0.0957596283998767,
135.721678296552));
#132334=CARTESIAN_POINT('Ctrl Pts',(-229.425135682666,0.0410516340090508,
135.724342553064));
#132335=CARTESIAN_POINT('Ctrl Pts',(-229.43289272355,0.17811717288134,135.721295651029));
#132336=CARTESIAN_POINT('Ctrl Pts',(-229.440649764435,0.314922644834436,
135.712517786022));
#132337=CARTESIAN_POINT('Ctrl Pts',(-229.448400955676,0.451624950716754,
135.703746540472));
#132338=CARTESIAN_POINT('Ctrl Pts',(-229.456152146916,0.588067191457631,
135.689252959092));
#132339=CARTESIAN_POINT('Ctrl Pts',(-229.463903338156,0.723735049451271,
135.669069307785));
#132340=CARTESIAN_POINT('Ctrl Pts',(-229.471651234933,0.85934524498602,
135.648894235069));
#132341=CARTESIAN_POINT('Ctrl Pts',(-229.47939913171,0.994181326495175,
135.623033959912));
#132342=CARTESIAN_POINT('Ctrl Pts',(-229.487147028487,1.12773434530897,
135.591572573278));
#132343=CARTESIAN_POINT('Ctrl Pts',(-229.494893304571,1.26125942771029,
135.560117767688));
#132344=CARTESIAN_POINT('Ctrl Pts',(-229.502639580655,1.39350160094927,
135.523064270651));
#132345=CARTESIAN_POINT('Ctrl Pts',(-229.510385856739,1.52396274672794,
135.480547163148));
#132346=CARTESIAN_POINT('Ctrl Pts',(-229.518132190005,1.65442485554134,
135.438029741794));
#132347=CARTESIAN_POINT('Ctrl Pts',(-229.52587852327,1.78310553893736,135.390048750639));
#132348=CARTESIAN_POINT('Ctrl Pts',(-229.533624856535,1.90952284719952,
135.33678883636));
#132349=CARTESIAN_POINT('Ctrl Pts',(-229.541372924538,2.03596846574152,
135.283516994893));
#132350=CARTESIAN_POINT('Ctrl Pts',(-229.549120992541,2.16014934031646,
135.224964029667));
#132351=CARTESIAN_POINT('Ctrl Pts',(-229.556869060544,2.28160484152249,
135.161362156427));
#132352=CARTESIAN_POINT('Ctrl Pts',(-229.564625363286,2.40318942708037,
135.09769268636));
#132353=CARTESIAN_POINT('Ctrl Pts',(-229.572381666028,2.52204250617795,
135.028963770696));
#132354=CARTESIAN_POINT('Ctrl Pts',(-229.58013796877,2.63772887105447,134.955453180411));
#132355=CARTESIAN_POINT('Ctrl Pts',(-229.587898411284,2.75347698122716,
134.88190335531));
#132356=CARTESIAN_POINT('Ctrl Pts',(-229.595658853798,2.86605468861081,
134.803566993465));
#132357=CARTESIAN_POINT('Ctrl Pts',(-229.603419296312,2.9750578320902,134.720763809044));
#132358=CARTESIAN_POINT('Ctrl Pts',(-229.611192196578,3.08423595709235,
134.6378277016));
#132359=CARTESIAN_POINT('Ctrl Pts',(-229.618965096843,3.18982775009587,
134.55041069202));
#132360=CARTESIAN_POINT('Ctrl Pts',(-229.626737997109,3.29146338142692,
134.458871784771));
#132361=CARTESIAN_POINT('Ctrl Pts',(-229.634228332871,3.38940430155686,
134.370660547371));
#132362=CARTESIAN_POINT('Ctrl Pts',(-229.641718668633,3.48367147877708,
134.278622107277));
#132363=CARTESIAN_POINT('Ctrl Pts',(-229.649209004395,3.57396919262221,
134.183107023067));
#132364=CARTESIAN_POINT('Ctrl Pts',(-229.656983338514,3.66769057173093,
134.08397045541));
#132365=CARTESIAN_POINT('Ctrl Pts',(-229.664757672633,3.75743242229338,
133.980774370649));
#132366=CARTESIAN_POINT('Ctrl Pts',(-229.672532006752,3.84282256931558,
133.873871614982));
#132367=CARTESIAN_POINT('Ctrl Pts',(-229.680296759699,3.92810748061311,
133.767100607407));
#132368=CARTESIAN_POINT('Ctrl Pts',(-229.688061512647,4.00905111765098,
133.656632320709));
#132369=CARTESIAN_POINT('Ctrl Pts',(-229.695826265594,4.08531821079547,
133.542856222646));
#132370=CARTESIAN_POINT('Ctrl Pts',(-229.703583306479,4.16150955438787,
133.429193128608));
#132371=CARTESIAN_POINT('Ctrl Pts',(-229.711340347364,4.23303338118517,
133.312229083882));
#132372=CARTESIAN_POINT('Ctrl Pts',(-229.719097388249,4.29959501400327,
133.192386115348));
#132373=CARTESIAN_POINT('Ctrl Pts',(-229.726848579489,4.36610645217638,
133.072633521329));
#132374=CARTESIAN_POINT('Ctrl Pts',(-229.734599770729,4.42766295558962,
132.950006665187));
#132375=CARTESIAN_POINT('Ctrl Pts',(-229.742350961969,4.48401366923161,
132.824955697399));
#132376=CARTESIAN_POINT('Ctrl Pts',(-229.750098858746,4.54034043231702,
132.699957879608));
#132377=CARTESIAN_POINT('Ctrl Pts',(-229.757846755523,4.59146564603659,
132.572538355083));
#132378=CARTESIAN_POINT('Ctrl Pts',(-229.7655946523,4.63718495931166,132.443170769973));
#132379=CARTESIAN_POINT('Ctrl Pts',(-229.773340928384,4.68289470909199,
132.313830245774));
#132380=CARTESIAN_POINT('Ctrl Pts',(-229.781087204469,4.72320067745572,
132.182542839905));
#132381=CARTESIAN_POINT('Ctrl Pts',(-229.788833480553,4.75794726675048,
132.049800647966));
#132382=CARTESIAN_POINT('Ctrl Pts',(-229.796579813818,4.79269411253672,
131.917057476154));
#132383=CARTESIAN_POINT('Ctrl Pts',(-229.804326147083,4.82188139836201,
131.782859875066));
#132384=CARTESIAN_POINT('Ctrl Pts',(-229.812072480349,4.84540396711009,
131.647713128687));
#132385=CARTESIAN_POINT('Ctrl Pts',(-229.819820548351,4.86893180357431,
131.512536117131));
#132386=CARTESIAN_POINT('Ctrl Pts',(-229.827568616355,4.88679233161814,
131.376409922426));
#132387=CARTESIAN_POINT('Ctrl Pts',(-229.835316684358,4.89893193947992,
131.239847603415));
#132388=CARTESIAN_POINT('Ctrl Pts',(-229.843072987099,4.91108444946142,
131.103140144345));
#132389=CARTESIAN_POINT('Ctrl Pts',(-229.850829289841,4.91750385860919,
130.965996025092));
#132390=CARTESIAN_POINT('Ctrl Pts',(-229.858585592583,4.91818862308651,
130.828931540268));
#132391=CARTESIAN_POINT('Ctrl Pts',(-229.866346035097,4.91887375304324,
130.691793900002));
#132392=CARTESIAN_POINT('Ctrl Pts',(-229.874106477611,4.91381815392553,
130.554736369364));
#132393=CARTESIAN_POINT('Ctrl Pts',(-229.881866920126,4.9030723513643,130.418271793865));
#132394=CARTESIAN_POINT('Ctrl Pts',(-229.889639820391,4.89230929868683,
130.281588153315));
#132395=CARTESIAN_POINT('Ctrl Pts',(-229.897412720656,4.87583783608927,
130.145499758388));
#132396=CARTESIAN_POINT('Ctrl Pts',(-229.905185620922,4.85376010222676,
130.010511807948));
#132397=CARTESIAN_POINT('Ctrl Pts',(-229.912675956684,4.83248494960055,
129.880431009521));
#132398=CARTESIAN_POINT('Ctrl Pts',(-229.920166292446,4.80600411517754,
129.751372338508));
#132399=CARTESIAN_POINT('Ctrl Pts',(-229.927656628208,4.77445268968183,
129.623774078387));
#132400=CARTESIAN_POINT('Ctrl Pts',(-229.935430962327,4.74170498229866,
129.491337891452));
#132401=CARTESIAN_POINT('Ctrl Pts',(-229.943205296446,4.70339085581963,
129.360055526434));
#132402=CARTESIAN_POINT('Ctrl Pts',(-229.950979630565,4.6596060000692,129.230430826686));
#132403=CARTESIAN_POINT('Ctrl Pts',(-229.958744383512,4.61587510524033,
129.100965877796));
#132404=CARTESIAN_POINT('Ctrl Pts',(-229.96650913646,4.56668701999335,128.973154896214));
#132405=CARTESIAN_POINT('Ctrl Pts',(-229.974273889407,4.51218819315842,
128.847490470617));
#132406=CARTESIAN_POINT('Ctrl Pts',(-229.982030930292,4.45774349532661,
128.721950856698));
#132407=CARTESIAN_POINT('Ctrl Pts',(-229.989787971177,4.39799870735506,
128.598553912373));
#132408=CARTESIAN_POINT('Ctrl Pts',(-229.997545012062,4.33314961219451,
128.47777567374));
#132409=CARTESIAN_POINT('Ctrl Pts',(-230.005296203302,4.26834942024117,
128.357088514916));
#132410=CARTESIAN_POINT('Ctrl Pts',(-230.013047394542,4.19845276689184,
128.239016474151));
#132411=CARTESIAN_POINT('Ctrl Pts',(-230.020798585782,4.12370278323008,
128.1240139202));
#132412=CARTESIAN_POINT('Ctrl Pts',(-230.028546482559,4.0489845703053,128.009060245402));
#132413=CARTESIAN_POINT('Ctrl Pts',(-230.036294379336,3.96941734243181,
127.897173789757));
#132414=CARTESIAN_POINT('Ctrl Pts',(-230.044042276113,3.88528913478027,
127.78878249693));
#132415=CARTESIAN_POINT('Ctrl Pts',(-230.051788552198,3.80117852493617,
127.680413877225));
#132416=CARTESIAN_POINT('Ctrl Pts',(-230.059534828282,3.71250907255368,
127.57553927477));
#132417=CARTESIAN_POINT('Ctrl Pts',(-230.067281104366,3.61961068726716,
127.47455558797));
#132418=CARTESIAN_POINT('Ctrl Pts',(-230.075027437631,3.52671161622599,
127.373571155732));
#132419=CARTESIAN_POINT('Ctrl Pts',(-230.082773770897,3.42958381468484,
127.276477984194));
#132420=CARTESIAN_POINT('Ctrl Pts',(-230.090520104162,3.32859555238029,
127.183637663352));
#132421=CARTESIAN_POINT('Ctrl Pts',(-230.098268172165,3.22758467445474,
127.090776551564));
#132422=CARTESIAN_POINT('Ctrl Pts',(-230.106016240168,3.12271190323041,
127.002170450179));
#132423=CARTESIAN_POINT('Ctrl Pts',(-230.113764308171,3.01437991117571,
126.918141785127));
#132424=CARTESIAN_POINT('Ctrl Pts',(-230.121520610913,2.90593278259053,
126.834023813411));
#132425=CARTESIAN_POINT('Ctrl Pts',(-230.129276913654,2.79401939838689,
126.7544932363));
#132426=CARTESIAN_POINT('Ctrl Pts',(-230.137033216396,2.67907329736261,
126.679830422518));
#132427=CARTESIAN_POINT('Ctrl Pts',(-230.14479365891,2.56406584614293,126.605127758945));
#132428=CARTESIAN_POINT('Ctrl Pts',(-230.152554101425,2.44602278913262,
126.535298234538));
#132429=CARTESIAN_POINT('Ctrl Pts',(-230.160314543939,2.32540290812225,
126.47057654618));
#132430=CARTESIAN_POINT('Ctrl Pts',(-230.168087444205,2.20458939737075,
126.405750960822));
#132431=CARTESIAN_POINT('Ctrl Pts',(-230.17586034447,2.08119114862293,126.3460497672));
#132432=CARTESIAN_POINT('Ctrl Pts',(-230.183633244735,1.95568840842861,
126.291660105496));
#132433=CARTESIAN_POINT('Ctrl Pts',(-230.191123580497,1.8347480089654,126.239247644995));
#132434=CARTESIAN_POINT('Ctrl Pts',(-230.198613916259,1.71185375607781,
126.191767356857));
#132435=CARTESIAN_POINT('Ctrl Pts',(-230.206104252021,1.58744740990348,
126.149342488354));
#132436=CARTESIAN_POINT('Ctrl Pts',(-230.21387858614,1.45832415929943,126.105309068067));
#132437=CARTESIAN_POINT('Ctrl Pts',(-230.221652920259,1.32716286626439,
126.066582502744));
#132438=CARTESIAN_POINT('Ctrl Pts',(-230.229427254378,1.19443915116726,
126.033354625466));
#132439=CARTESIAN_POINT('Ctrl Pts',(-230.237192007325,1.06187900618678,
126.000167698576));
#132440=CARTESIAN_POINT('Ctrl Pts',(-230.244956760272,0.927760646025438,
125.972466070272));
#132441=CARTESIAN_POINT('Ctrl Pts',(-230.252721513219,0.792577658656779,
125.950392785215));
#132442=CARTESIAN_POINT('Ctrl Pts',(-230.260478554104,0.657528936937288,
125.928341423656));
#132443=CARTESIAN_POINT('Ctrl Pts',(-230.26823559499,0.521418075648059,
125.911907343292));
#132444=CARTESIAN_POINT('Ctrl Pts',(-230.275992635875,0.38475140290749,
125.901183135518));
#132445=CARTESIAN_POINT('Ctrl Pts',(-230.283743827115,0.248187791567389,
125.890467014953));
#132446=CARTESIAN_POINT('Ctrl Pts',(-230.291495018355,0.111069591242116,
125.885452226889));
#132447=CARTESIAN_POINT('Ctrl Pts',(-230.299246209595,-0.0260895064780241,
125.886179815669));
#132448=CARTESIAN_POINT('Ctrl Pts',(-230.306994106372,-0.163190307922608,
125.886907095204));
#132449=CARTESIAN_POINT('Ctrl Pts',(-230.314742003149,-0.300331582048426,
125.89337189522));
#132450=CARTESIAN_POINT('Ctrl Pts',(-230.322489899926,-0.436997597686054,
125.905563197574));
#132451=CARTESIAN_POINT('Ctrl Pts',(-230.33023617601,-0.573635025739016,
125.917751949771));
#132452=CARTESIAN_POINT('Ctrl Pts',(-230.337982452094,-0.709797003871202,
125.935664786978));
#132453=CARTESIAN_POINT('Ctrl Pts',(-230.345728728178,-0.844971285998511,
125.959238680159));
#132454=CARTESIAN_POINT('Ctrl Pts',(-230.353475061444,-0.980146565951848,
125.982812747358));
#132455=CARTESIAN_POINT('Ctrl Pts',(-230.361221394709,-1.11433375019969,
126.012047886748));
#132456=CARTESIAN_POINT('Ctrl Pts',(-230.368967727974,-1.24702956404957,
126.046829710794));
#132457=CARTESIAN_POINT('Ctrl Pts',(-230.376715795977,-1.37975509420672,
126.08161932399));
#132458=CARTESIAN_POINT('Ctrl Pts',(-230.38446386398,-1.51098821126345,
126.121957994449));
#132459=CARTESIAN_POINT('Ctrl Pts',(-230.392211931983,-1.64023999484809,
126.167681221511));
#132460=CARTESIAN_POINT('Ctrl Pts',(-230.399968234725,-1.76962914876662,
126.213453043763));
#132461=CARTESIAN_POINT('Ctrl Pts',(-230.407724537467,-1.89703239351101,
126.264620723875));
#132462=CARTESIAN_POINT('Ctrl Pts',(-230.415480840209,-2.02197950862451,
126.320971059519));
#132463=CARTESIAN_POINT('Ctrl Pts',(-230.423241282723,-2.14699331177578,
126.377351471035));
#132464=CARTESIAN_POINT('Ctrl Pts',(-230.431001725237,-2.26954802400983,
126.438919874428));
#132465=CARTESIAN_POINT('Ctrl Pts',(-230.438762167751,-2.38919820542926,
126.505417142981));
#132466=CARTESIAN_POINT('Ctrl Pts',(-230.446535068017,-2.50904045994162,
126.572021158854));
#132467=CARTESIAN_POINT('Ctrl Pts',(-230.454307968282,-2.62596853257937,
126.643569646909));
#132468=CARTESIAN_POINT('Ctrl Pts',(-230.462080868548,-2.73956539201596,
126.719759715964));
#132469=CARTESIAN_POINT('Ctrl Pts',(-230.46957120431,-2.84903271948127,
126.793180084099));
#132470=CARTESIAN_POINT('Ctrl Pts',(-230.477061540072,-2.95540657615255,
126.870910244093));
#132471=CARTESIAN_POINT('Ctrl Pts',(-230.484551875834,-3.0583444884639,
126.952645148793));
#132472=CARTESIAN_POINT('Ctrl Pts',(-230.492227030782,-3.16382232711922,
127.036396809351));
#132473=CARTESIAN_POINT('Ctrl Pts',(-230.49990218573,-3.2660446810198,127.12463337676));
#132474=CARTESIAN_POINT('Ctrl Pts',(-230.507577340678,-3.36459885966315,
127.217069498065));
#132475=CARTESIAN_POINT('Ctrl Pts',(-230.515243715587,-3.46304029667819,
127.309399876529));
#132476=CARTESIAN_POINT('Ctrl Pts',(-230.522910090497,-3.55782161046869,
127.405919987239));
#132477=CARTESIAN_POINT('Ctrl Pts',(-230.530576465406,-3.64856082956961,
127.506302562372));
#132478=CARTESIAN_POINT('Ctrl Pts',(-230.538235831781,-3.73921709565125,
127.606593368612));
#132479=CARTESIAN_POINT('Ctrl Pts',(-230.545895198156,-3.82583834707426,
127.710739322577));
#132480=CARTESIAN_POINT('Ctrl Pts',(-230.553554564531,-3.90807774779082,
127.818374787104));
#132481=CARTESIAN_POINT('Ctrl Pts',(-230.561208687532,-3.99026084986255,
127.925936567596));
#132482=CARTESIAN_POINT('Ctrl Pts',(-230.568862810533,-4.06806782454047,
128.036982789623));
#132483=CARTESIAN_POINT('Ctrl Pts',(-230.576516933534,-4.14119096594603,
128.151113466231));
#132484=CARTESIAN_POINT('Ctrl Pts',(-230.58416850814,-4.21428976142867,
128.265206143697));
#132485=CARTESIAN_POINT('Ctrl Pts',(-230.591820082745,-4.28270760419785,
128.38238089874));
#132486=CARTESIAN_POINT('Ctrl Pts',(-230.59947165735,-4.34617934566822,
128.502207677862));
#132487=CARTESIAN_POINT('Ctrl Pts',(-230.607121524719,-4.40963692518023,
128.622007720963));
#132488=CARTESIAN_POINT('Ctrl Pts',(-230.614771392088,-4.46815041392961,
128.744458254543));
#132489=CARTESIAN_POINT('Ctrl Pts',(-230.622421259457,-4.52150033928332,
128.869104111477));
#132490=CARTESIAN_POINT('Ctrl Pts',(-230.630073816153,-4.57486901992336,
128.993793787942));
#132491=CARTESIAN_POINT('Ctrl Pts',(-230.63772637285,-4.62307035019042,
129.12067996096));
#132492=CARTESIAN_POINT('Ctrl Pts',(-230.645378929547,-4.6659328130657,
129.249286970932));
#132493=CARTESIAN_POINT('Ctrl Pts',(-230.651919131343,-4.70256490450463,
129.359200014488));
#132494=CARTESIAN_POINT('Ctrl Pts',(-230.658459333138,-4.73529817055404,
129.470369517153));
#132495=CARTESIAN_POINT('Ctrl Pts',(-230.664999534934,-4.76405452823392,
129.582490119308));
#132496=CARTESIAN_POINT('Ctrl Pts',(-228.915319603984,-4.76405452823406,
129.582490119308));
#132497=CARTESIAN_POINT('Ctrl Pts',(-228.923144081678,-4.79847663933562,
129.716701408065));
#132498=CARTESIAN_POINT('Ctrl Pts',(-228.930968559371,-4.82724292611982,
129.852445614384));
#132499=CARTESIAN_POINT('Ctrl Pts',(-228.938793037064,-4.85022842761036,
129.989212003815));
#132500=CARTESIAN_POINT('Ctrl Pts',(-228.946615480386,-4.87320795285048,
130.125942833865));
#132501=CARTESIAN_POINT('Ctrl Pts',(-228.954437923709,-4.89040961687128,
130.263694944493));
#132502=CARTESIAN_POINT('Ctrl Pts',(-228.962260367031,-4.90175953779381,
130.401947277644));
#132503=CARTESIAN_POINT('Ctrl Pts',(-228.969887099359,-4.91282549318019,
130.536740652959));
#132504=CARTESIAN_POINT('Ctrl Pts',(-228.977513831686,-4.91832902067497,
130.672009167332));
#132505=CARTESIAN_POINT('Ctrl Pts',(-228.985140564014,-4.91824914231965,
130.807265195338));
#132506=CARTESIAN_POINT('',(-228.639859435953,-4.91824820079851,130.800153737225));
#132507=CARTESIAN_POINT('Ctrl Pts',(-228.570020432611,-4.76405452823418,
129.582490119309));
#132508=CARTESIAN_POINT('Ctrl Pts',(-228.579416817742,-4.80505267360792,
129.742341265887));
#132509=CARTESIAN_POINT('Ctrl Pts',(-228.588813202874,-4.83803882552062,
129.904403081114));
#132510=CARTESIAN_POINT('Ctrl Pts',(-228.598209588006,-4.86280565366006,
130.06794752885));
#132511=CARTESIAN_POINT('Ctrl Pts',(-228.607496341774,-4.88728351736155,
130.229583838445));
#132512=CARTESIAN_POINT('Ctrl Pts',(-228.616783095542,-4.90373268959774,
130.392668369278));
#132513=CARTESIAN_POINT('Ctrl Pts',(-228.62606984931,-4.91199928481153,
130.556477402098));
#132514=CARTESIAN_POINT('Ctrl Pts',(-228.630666378191,-4.91609088071229,
130.637555566669));
#132515=CARTESIAN_POINT('Ctrl Pts',(-228.635262907072,-4.91817862326256,
130.718810898069));
#132516=CARTESIAN_POINT('Ctrl Pts',(-228.639859435953,-4.91824820079851,
130.800153737224));
#132517=CARTESIAN_POINT('Ctrl Pts',(-228.639859435996,-4.91824820079916,
130.800153737983));
#132518=CARTESIAN_POINT('Ctrl Pts',(-228.647925923209,-4.91837030298047,
130.942902970921));
#132519=CARTESIAN_POINT('Ctrl Pts',(-228.655992410423,-4.91227246476482,
131.085757714811));
#132520=CARTESIAN_POINT('Ctrl Pts',(-228.664058897636,-4.89995927907239,
131.228131930815));
#132521=CARTESIAN_POINT('Ctrl Pts',(-228.671764659131,-4.88819672745851,
131.36413930584));
#132522=CARTESIAN_POINT('Ctrl Pts',(-228.679470420626,-4.87076271627191,
131.499707764516));
#132523=CARTESIAN_POINT('Ctrl Pts',(-228.687176182121,-4.84771450852914,
131.634328753277));
#132524=CARTESIAN_POINT('Ctrl Pts',(-228.69488137582,-4.82466799908442,
131.768939822545));
#132525=CARTESIAN_POINT('Ctrl Pts',(-228.702586569519,-4.79600818229881,
131.902603171099));
#132526=CARTESIAN_POINT('Ctrl Pts',(-228.710291763218,-4.76184378070591,
132.0348186098));
#132527=CARTESIAN_POINT('Ctrl Pts',(-228.717998100802,-4.7276743071932,
132.167053676713));
#132528=CARTESIAN_POINT('Ctrl Pts',(-228.725704438385,-4.68799872201766,
132.297840023391));
#132529=CARTESIAN_POINT('Ctrl Pts',(-228.733410775968,-4.64297601545842,
132.426691281265));
#132530=CARTESIAN_POINT('Ctrl Pts',(-228.741119969578,-4.59793662314605,
132.555590292383));
#132531=CARTESIAN_POINT('Ctrl Pts',(-228.748829163188,-4.54754629724368,
132.682552415039));
#132532=CARTESIAN_POINT('Ctrl Pts',(-228.756538356798,-4.49201251122566,
132.807110392623));
#132533=CARTESIAN_POINT('Ctrl Pts',(-228.76425641601,-4.43641486114215,
132.931811612356));
#132534=CARTESIAN_POINT('Ctrl Pts',(-228.771974475222,-4.37566210427146,
133.054102806771));
#132535=CARTESIAN_POINT('Ctrl Pts',(-228.779692534434,-4.31000827834484,
133.173540159749));
#132536=CARTESIAN_POINT('Ctrl Pts',(-228.787415798043,-4.24431018110684,
133.293058051038));
#132537=CARTESIAN_POINT('Ctrl Pts',(-228.795139061652,-4.17370463775003,
133.40971793172));
#132538=CARTESIAN_POINT('Ctrl Pts',(-228.802862325262,-4.09848888371967,
133.52310516837));
#132539=CARTESIAN_POINT('Ctrl Pts',(-228.810596840686,-4.02316354988221,
133.636657595833));
#132540=CARTESIAN_POINT('Ctrl Pts',(-228.81833135611,-3.94321483021496,
133.746927544111));
#132541=CARTESIAN_POINT('Ctrl Pts',(-228.826065871534,-3.85898028499445,
133.853533328733));
#132542=CARTESIAN_POINT('Ctrl Pts',(-228.828528957395,-3.83215547362489,
133.887482346394));
#132543=CARTESIAN_POINT('Ctrl Pts',(-228.830992043255,-3.80489630373702,
133.921060052229));
#132544=CARTESIAN_POINT('Ctrl Pts',(-228.833455129115,-3.7772144349493,
133.954254929271));
#132545=CARTESIAN_POINT('Ctrl Pts',(-228.841229463234,-3.68984107112999,
134.059029216402));
#132546=CARTESIAN_POINT('Ctrl Pts',(-228.849003797354,-3.59796658701326,
134.160331293483));
#132547=CARTESIAN_POINT('Ctrl Pts',(-228.856778131473,-3.5018974019896,
134.257749916275));
#132548=CARTESIAN_POINT('Ctrl Pts',(-228.86454288442,-3.40594661365079,
134.355048479321));
#132549=CARTESIAN_POINT('Ctrl Pts',(-228.872307637367,-3.30581168224031,
134.44847283511));
#132550=CARTESIAN_POINT('Ctrl Pts',(-228.880072390314,-3.20183975122941,
134.537644061124));
#132551=CARTESIAN_POINT('Ctrl Pts',(-228.887829431199,-3.09797108660615,
134.62672672102));
#132552=CARTESIAN_POINT('Ctrl Pts',(-228.895586472084,-2.99027330121759,
134.711564404751));
#132553=CARTESIAN_POINT('Ctrl Pts',(-228.903343512969,-2.87913066408634,
134.791814652614));
#132554=CARTESIAN_POINT('Ctrl Pts',(-228.911094704209,-2.76807184048247,
134.87200438314));
#132555=CARTESIAN_POINT('Ctrl Pts',(-228.918845895449,-2.65357365156948,
134.947613335621));
#132556=CARTESIAN_POINT('Ctrl Pts',(-228.926597086689,-2.53605346890143,
135.018339244158));
#132557=CARTESIAN_POINT('Ctrl Pts',(-228.934344983466,-2.41858323544549,
135.089035092297));
#132558=CARTESIAN_POINT('Ctrl Pts',(-228.942092880244,-2.29809389714317,
135.154851823177));
#132559=CARTESIAN_POINT('Ctrl Pts',(-228.949840777021,-2.1750316492889,
135.215530574289));
#132560=CARTESIAN_POINT('Ctrl Pts',(-228.957587053105,-2.0519951434043,
135.276196632713));
#132561=CARTESIAN_POINT('Ctrl Pts',(-228.965333329189,-1.92638714890538,
135.331726676327));
#132562=CARTESIAN_POINT('Ctrl Pts',(-228.973079605273,-1.79867793960982,
135.381908075765));
#132563=CARTESIAN_POINT('Ctrl Pts',(-228.980825938538,-1.67096778759372,
135.43208984563));
#132564=CARTESIAN_POINT('Ctrl Pts',(-228.988572271804,-1.54115675371234,
135.476922749554));
#132565=CARTESIAN_POINT('Ctrl Pts',(-228.996318605069,-1.40973416532496,
135.516242687993));
#132566=CARTESIAN_POINT('Ctrl Pts',(-229.004066673072,-1.27828214576031,
135.555571431861));
#132567=CARTESIAN_POINT('Ctrl Pts',(-229.011814741075,-1.14521822803625,
135.589384641511));
#132568=CARTESIAN_POINT('Ctrl Pts',(-229.019562809078,-1.0110455479086,
135.617568483694));
#132569=CARTESIAN_POINT('Ctrl Pts',(-229.02731911182,-0.876730267459646,
135.64578228));
#132570=CARTESIAN_POINT('Ctrl Pts',(-229.035075414562,-0.741304253839631,
135.668354676736));
#132571=CARTESIAN_POINT('Ctrl Pts',(-229.042831717303,-0.605280005602222,
135.685223161965));
#132572=CARTESIAN_POINT('Ctrl Pts',(-229.050592159818,-0.469183157127547,
135.702100650413));
#132573=CARTESIAN_POINT('Ctrl Pts',(-229.058352602332,-0.332487827287851,
135.713268129411));
#132574=CARTESIAN_POINT('Ctrl Pts',(-229.066113044846,-0.195709239536393,
135.718715199407));
#132575=CARTESIAN_POINT('Ctrl Pts',(-229.073885945111,-0.0587110826536159,
135.724171013523));
#132576=CARTESIAN_POINT('Ctrl Pts',(-229.081658845377,0.0783702080327963,
135.723888069069));
#132577=CARTESIAN_POINT('Ctrl Pts',(-229.089431745642,0.215020906246339,
135.717908121394));
#132578=CARTESIAN_POINT('Ctrl Pts',(-229.096922081404,0.346704007381179,
135.71214555988));
#132579=CARTESIAN_POINT('Ctrl Pts',(-229.104412417167,0.477986971830102,
135.701093030686));
#132580=CARTESIAN_POINT('Ctrl Pts',(-229.111902752929,0.608418628413239,
135.684832913881));
#132581=CARTESIAN_POINT('Ctrl Pts',(-229.119677087048,0.743795640896688,
135.667956289806));
#132582=CARTESIAN_POINT('Ctrl Pts',(-229.127451421167,0.878684350192887,
135.6454159314));
#132583=CARTESIAN_POINT('Ctrl Pts',(-229.135225755286,1.01257313771261,
135.61724735042));
#132584=CARTESIAN_POINT('Ctrl Pts',(-229.142990508233,1.14629691926734,
135.589113484698));
#132585=CARTESIAN_POINT('Ctrl Pts',(-229.15075526118,1.27902285206684,135.555365277254));
#132586=CARTESIAN_POINT('Ctrl Pts',(-229.158520014128,1.41024449834063,
135.516089972845));
#132587=CARTESIAN_POINT('Ctrl Pts',(-229.166277055013,1.54133581342509,
135.476853677222));
#132588=CARTESIAN_POINT('Ctrl Pts',(-229.174034095898,1.67092544314303,
135.432101320547));
#132589=CARTESIAN_POINT('Ctrl Pts',(-229.181791136783,1.79851755965378,
135.381971091396));
#132590=CARTESIAN_POINT('Ctrl Pts',(-229.189542328023,1.92601345795746,
135.33187866584));
#132591=CARTESIAN_POINT('Ctrl Pts',(-229.197293519263,2.0515144789184,135.276416582417));
#132592=CARTESIAN_POINT('Ctrl Pts',(-229.205044710503,2.17454071815496,
135.215772605534));
#132593=CARTESIAN_POINT('Ctrl Pts',(-229.21279260728,2.29751466795817,135.155154403958));
#132594=CARTESIAN_POINT('Ctrl Pts',(-229.220540504057,2.41801557814188,
135.089358861912));
#132595=CARTESIAN_POINT('Ctrl Pts',(-229.228288400835,2.53558448089151,
135.018621454624));
#132596=CARTESIAN_POINT('Ctrl Pts',(-229.236034676919,2.65312879076117,
134.947898844077));
#132597=CARTESIAN_POINT('Ctrl Pts',(-229.243780953003,2.76774197831851,
134.872236625871));
#132598=CARTESIAN_POINT('Ctrl Pts',(-229.251527229087,2.87899095797187,
134.791915523322));
#132599=CARTESIAN_POINT('Ctrl Pts',(-229.259273562352,2.99024075883978,
134.71159382786));
#132600=CARTESIAN_POINT('Ctrl Pts',(-229.267019895618,3.09812598526795,
134.626613408291));
#132601=CARTESIAN_POINT('Ctrl Pts',(-229.274766228883,3.20224408227435,
134.537297249768));
#132602=CARTESIAN_POINT('Ctrl Pts',(-229.282514296886,3.30638549580652,
134.447961089512));
#132603=CARTESIAN_POINT('Ctrl Pts',(-229.290262364889,3.40675780452122,
134.354287512713));
#132604=CARTESIAN_POINT('Ctrl Pts',(-229.298010432892,3.50299328011654,
134.256638292082));
#132605=CARTESIAN_POINT('Ctrl Pts',(-229.305766735634,3.59933103592067,
134.158885288696));
#132606=CARTESIAN_POINT('Ctrl Pts',(-229.313523038376,3.69152290090394,
134.05714847977));
#132607=CARTESIAN_POINT('Ctrl Pts',(-229.321279341118,3.77923926401644,
133.951825255623));
#132608=CARTESIAN_POINT('Ctrl Pts',(-229.329039783632,3.86700244399303,
133.846445817299));
#132609=CARTESIAN_POINT('Ctrl Pts',(-229.336800226146,3.95028512510027,
133.73747646007));
#132610=CARTESIAN_POINT('Ctrl Pts',(-229.34456066866,4.02880006703898,133.625345034809));
#132611=CARTESIAN_POINT('Ctrl Pts',(-229.352333568926,4.10744104813272,
133.513033606229));
#132612=CARTESIAN_POINT('Ctrl Pts',(-229.360106469191,4.18129878496189,
133.397550295641));
#132613=CARTESIAN_POINT('Ctrl Pts',(-229.367879369457,4.25013072588525,
133.279349885298));
#132614=CARTESIAN_POINT('Ctrl Pts',(-229.375369705218,4.31646045237624,
133.165446357604));
#132615=CARTESIAN_POINT('Ctrl Pts',(-229.38286004098,4.37812329558615,133.049020119491));
#132616=CARTESIAN_POINT('Ctrl Pts',(-229.390350376742,4.43494469515777,
132.93049528249));
#132617=CARTESIAN_POINT('Ctrl Pts',(-229.398124710861,4.49392049536689,
132.807476540265));
#132618=CARTESIAN_POINT('Ctrl Pts',(-229.40589904498,4.54786729567827,132.681807234591));
#132619=CARTESIAN_POINT('Ctrl Pts',(-229.413673379099,4.59653843079351,
132.553936999648));
#132620=CARTESIAN_POINT('Ctrl Pts',(-229.421438132046,4.64514958308432,
132.426224353342));
#132621=CARTESIAN_POINT('Ctrl Pts',(-229.429202884993,4.6884978690515,132.296316536615));
#132622=CARTESIAN_POINT('Ctrl Pts',(-229.436967637941,4.72638294819557,
132.16468678783));
#132623=CARTESIAN_POINT('Ctrl Pts',(-229.444724678826,4.76423039934506,
132.033187775567));
#132624=CARTESIAN_POINT('Ctrl Pts',(-229.45248171971,4.79662533448668,131.899970607996));
#132625=CARTESIAN_POINT('Ctrl Pts',(-229.460238760595,4.82341600852472,
131.765527133424));
#132626=CARTESIAN_POINT('Ctrl Pts',(-229.467989951836,4.85018647950719,
131.631185043722));
#132627=CARTESIAN_POINT('Ctrl Pts',(-229.475741143076,4.87136102531784,
131.495618869587));
#132628=CARTESIAN_POINT('Ctrl Pts',(-229.483492334316,4.88683821742956,
131.359333859416));
#132629=CARTESIAN_POINT('Ctrl Pts',(-229.491240231093,4.9023088313217,131.223106774011));
#132630=CARTESIAN_POINT('Ctrl Pts',(-229.49898812787,4.91208686372415,131.08616184789));
#132631=CARTESIAN_POINT('Ctrl Pts',(-229.506736024647,4.91612234330196,
130.949012503787));
#132632=CARTESIAN_POINT('Ctrl Pts',(-229.514482300731,4.92015697874445,
130.81189184837));
#132633=CARTESIAN_POINT('Ctrl Pts',(-229.522228576816,4.91845143915975,
130.674567250572));
#132634=CARTESIAN_POINT('Ctrl Pts',(-229.5299748529,4.9110078116836,130.537554815375));
#132635=CARTESIAN_POINT('Ctrl Pts',(-229.537721186165,4.90356412926028,
130.400541368784));
#132636=CARTESIAN_POINT('Ctrl Pts',(-229.54546751943,4.89038229563376,130.263840479783));
#132637=CARTESIAN_POINT('Ctrl Pts',(-229.553213852696,4.87151645656185,
130.127965410644));
#132638=CARTESIAN_POINT('Ctrl Pts',(-229.560961920699,4.85264639261607,
129.992059913225));
#132639=CARTESIAN_POINT('Ctrl Pts',(-229.568709988702,4.82808984407219,
129.856980990848));
#132640=CARTESIAN_POINT('Ctrl Pts',(-229.576458056705,4.79795241442714,
129.723233570733));
#132641=CARTESIAN_POINT('Ctrl Pts',(-229.584214359446,4.76778295436327,
129.589344002269));
#132642=CARTESIAN_POINT('Ctrl Pts',(-229.591970662188,4.732020850613,129.456789144966));
#132643=CARTESIAN_POINT('Ctrl Pts',(-229.59972696493,4.69082227608267,129.326061109108));
#132644=CARTESIAN_POINT('Ctrl Pts',(-229.607487407444,4.64960171263276,
129.195263299762));
#132645=CARTESIAN_POINT('Ctrl Pts',(-229.615247849959,4.6029390296556,129.066294622153));
#132646=CARTESIAN_POINT('Ctrl Pts',(-229.623008292473,4.55103892980856,
128.939628003525));
#132647=CARTESIAN_POINT('Ctrl Pts',(-229.630781192738,4.49905551531364,
128.812758048396));
#132648=CARTESIAN_POINT('Ctrl Pts',(-229.638554093004,4.44181804629066,
128.688197892433));
#132649=CARTESIAN_POINT('Ctrl Pts',(-229.646326993269,4.37957803884262,
128.566397422116));
#132650=CARTESIAN_POINT('Ctrl Pts',(-229.653817329031,4.3196006124386,128.449024705693));
#132651=CARTESIAN_POINT('Ctrl Pts',(-229.661307664793,4.2549781939034,128.334214783745));
#132652=CARTESIAN_POINT('Ctrl Pts',(-229.668798000555,4.1859732461429,128.222343761487));
#132653=CARTESIAN_POINT('Ctrl Pts',(-229.676572334674,4.11435195481475,
128.106231115418));
#132654=CARTESIAN_POINT('Ctrl Pts',(-229.684346668793,4.03778237210415,
127.992916815104));
#132655=CARTESIAN_POINT('Ctrl Pts',(-229.692121002912,3.95650945936246,
127.882851425303));
#132656=CARTESIAN_POINT('Ctrl Pts',(-229.699885755859,3.87533670822194,
127.772921681259));
#132657=CARTESIAN_POINT('Ctrl Pts',(-229.707650508806,3.78947239023545,
127.666233192472));
#132658=CARTESIAN_POINT('Ctrl Pts',(-229.715415261753,3.69920636530636,
127.563210307973));
#132659=CARTESIAN_POINT('Ctrl Pts',(-229.723172302638,3.60902999386576,
127.460289747255));
#132660=CARTESIAN_POINT('Ctrl Pts',(-229.730929343523,3.51446087161696,
127.361027837766));
#132661=CARTESIAN_POINT('Ctrl Pts',(-229.738686384408,3.415830782539,127.265818102976));
#132662=CARTESIAN_POINT('Ctrl Pts',(-229.746437575648,3.31727507117885,
127.170680166588));
#132663=CARTESIAN_POINT('Ctrl Pts',(-229.754188766888,3.21466476867465,
127.079588592997));
#132664=CARTESIAN_POINT('Ctrl Pts',(-229.761939958128,3.10837013021514,
126.992901815993));
#132665=CARTESIAN_POINT('Ctrl Pts',(-229.769687854906,3.00212066981205,
126.906251883182));
#132666=CARTESIAN_POINT('Ctrl Pts',(-229.777435751683,2.89219029034001,
126.824003269959));
#132667=CARTESIAN_POINT('Ctrl Pts',(-229.78518364846,2.77898393815928,126.746475536153));
#132668=CARTESIAN_POINT('Ctrl Pts',(-229.792929924544,2.66580126630697,
126.668964019478));
#132669=CARTESIAN_POINT('Ctrl Pts',(-229.800676200628,2.54934430713946,
126.596171638784));
#132670=CARTESIAN_POINT('Ctrl Pts',(-229.808422476712,2.43004840254403,
126.528375605456));
#132671=CARTESIAN_POINT('Ctrl Pts',(-229.816168809977,2.31075161733382,
126.460579071673));
#132672=CARTESIAN_POINT('Ctrl Pts',(-229.823915143242,2.18861618478844,
126.397779152022));
#132673=CARTESIAN_POINT('Ctrl Pts',(-229.831661476508,2.06410319409927,
126.340207722939));
#132674=CARTESIAN_POINT('Ctrl Pts',(-229.839409544511,1.93956231958897,
126.282623401133));
#132675=CARTESIAN_POINT('Ctrl Pts',(-229.847157612514,1.81264318224541,
126.23027006387));
#132676=CARTESIAN_POINT('Ctrl Pts',(-229.854905680517,1.68382767290969,
126.183331789432));
#132677=CARTESIAN_POINT('Ctrl Pts',(-229.862661983258,1.55487525691755,
126.136343628438));
#132678=CARTESIAN_POINT('Ctrl Pts',(-229.870418286,1.42402281070542,126.094782160953));
#132679=CARTESIAN_POINT('Ctrl Pts',(-229.878174588742,1.29176877586443,
126.058781991919));
#132680=CARTESIAN_POINT('Ctrl Pts',(-229.885935031256,1.15944415306258,
126.02276260851));
#132681=CARTESIAN_POINT('Ctrl Pts',(-229.89369547377,1.02571683205874,125.992310524771));
#132682=CARTESIAN_POINT('Ctrl Pts',(-229.901455916284,0.891095346725003,
125.967509147286));
#132683=CARTESIAN_POINT('Ctrl Pts',(-229.90922881655,0.756257755031871,
125.942667956429));
#132684=CARTESIAN_POINT('Ctrl Pts',(-229.917001716815,0.620523517983609,
125.923495653318));
#132685=CARTESIAN_POINT('Ctrl Pts',(-229.924774617081,0.484407088416055,
125.910023804964));
#132686=CARTESIAN_POINT('Ctrl Pts',(-229.932264952843,0.353238833912496,
125.89704169223));
#132687=CARTESIAN_POINT('Ctrl Pts',(-229.939755288605,0.221715999275977,
125.889352795944));
#132688=CARTESIAN_POINT('Ctrl Pts',(-229.947245624368,0.0902968800871135,
125.886939592685));
#132689=CARTESIAN_POINT('Ctrl Pts',(-229.955019958487,-0.0461050349422831,
125.88443489209));
#132690=CARTESIAN_POINT('Ctrl Pts',(-229.962794292606,-0.182827294795918,
125.887605903412));
#132691=CARTESIAN_POINT('Ctrl Pts',(-229.970568626725,-0.319358418987533,
125.896490074986));
#132692=CARTESIAN_POINT('Ctrl Pts',(-229.978333379672,-0.45572128077146,
125.905363297613));
#132693=CARTESIAN_POINT('Ctrl Pts',(-229.986098132619,-0.591893089188019,
125.919935645938));
#132694=CARTESIAN_POINT('Ctrl Pts',(-229.993862885566,-0.727360151021741,
125.940192623633));
#132695=CARTESIAN_POINT('Ctrl Pts',(-230.001619926451,-0.862692665059899,
125.960429481811));
#132696=CARTESIAN_POINT('Ctrl Pts',(-230.009376967337,-0.997321441311664,
125.98633967601));
#132697=CARTESIAN_POINT('Ctrl Pts',(-230.017134008222,-1.13073605999144,
126.01785677602));
#132698=CARTESIAN_POINT('Ctrl Pts',(-230.024885199462,-1.26405006966928,
126.049350108739));
#132699=CARTESIAN_POINT('Ctrl Pts',(-230.032636390702,-1.3961513652799,
126.08644184175));
#132700=CARTESIAN_POINT('Ctrl Pts',(-230.040387581942,-1.52653825434919,
126.129014211094));
#132701=CARTESIAN_POINT('Ctrl Pts',(-230.048135478719,-1.65686972551225,
126.171568486046));
#132702=CARTESIAN_POINT('Ctrl Pts',(-230.055883375496,-1.78548786852207,
126.219598643205));
#132703=CARTESIAN_POINT('Ctrl Pts',(-230.063631272273,-1.91190494524551,
126.272936719623));
#132704=CARTESIAN_POINT('Ctrl Pts',(-230.071377548357,-2.03829557824208,
126.326263638866));
#132705=CARTESIAN_POINT('Ctrl Pts',(-230.079123824441,-2.16248570075706,
126.384896117029));
#132706=CARTESIAN_POINT('Ctrl Pts',(-230.086870100526,-2.28400677407834,
126.448617728177));
#132707=CARTESIAN_POINT('Ctrl Pts',(-230.094616433791,-2.40552874444075,
126.512339809704));
#132708=CARTESIAN_POINT('Ctrl Pts',(-230.102362767056,-2.52438128004492,
126.581150917615));
#132709=CARTESIAN_POINT('Ctrl Pts',(-230.110109100322,-2.64012006670736,
126.654788459395));
#132710=CARTESIAN_POINT('Ctrl Pts',(-230.117857168324,-2.75588477226749,
126.72844249179));
#132711=CARTESIAN_POINT('Ctrl Pts',(-230.125605236327,-2.86853401153698,
126.806924898982));
#132712=CARTESIAN_POINT('Ctrl Pts',(-230.13335330433,-2.97765244047183,
126.889929751367));
#132713=CARTESIAN_POINT('Ctrl Pts',(-230.141109607072,-3.08688684177222,
126.973022822297));
#132714=CARTESIAN_POINT('Ctrl Pts',(-230.148865909814,-3.19258262487569,
127.060647702859));
#132715=CARTESIAN_POINT('Ctrl Pts',(-230.156622212556,-3.29435712297832,
127.152457797284));
#132716=CARTESIAN_POINT('Ctrl Pts',(-230.16438265507,-3.39618594119524,
127.244316893521));
#132717=CARTESIAN_POINT('Ctrl Pts',(-230.172143097584,-3.49408902516683,
127.340365380943));
#132718=CARTESIAN_POINT('Ctrl Pts',(-230.179903540098,-3.5877213275915,
127.440220498896));
#132719=CARTESIAN_POINT('Ctrl Pts',(-230.187676440364,-3.68150393690005,
127.540235913149));
#132720=CARTESIAN_POINT('Ctrl Pts',(-230.195449340629,-3.77100180911301,
127.64406987283));
#132721=CARTESIAN_POINT('Ctrl Pts',(-230.203222240895,-3.85591031168543,
127.75130661694));
#132722=CARTESIAN_POINT('Ctrl Pts',(-230.210712576656,-3.9377321763145,
127.854645035284));
#132723=CARTESIAN_POINT('Ctrl Pts',(-230.218202912418,-4.01529236725859,
127.96114288472));
#132724=CARTESIAN_POINT('Ctrl Pts',(-230.22569324818,-4.08835790751209,
128.070405116358));
#132725=CARTESIAN_POINT('Ctrl Pts',(-230.233604311068,-4.16552749006171,
128.185804534124));
#132726=CARTESIAN_POINT('Ctrl Pts',(-230.241515373956,-4.23792147660652,
128.304644037511));
#132727=CARTESIAN_POINT('Ctrl Pts',(-230.249426436844,-4.30522448242884,
128.426499137497));
#132728=CARTESIAN_POINT('Ctrl Pts',(-230.257327785396,-4.37244484398277,
128.548204606342));
#132729=CARTESIAN_POINT('Ctrl Pts',(-230.265229133948,-4.43458648535344,
128.672917980837));
#132730=CARTESIAN_POINT('Ctrl Pts',(-230.2731304825,-4.49137645005342,128.800184815296));
#132731=CARTESIAN_POINT('Ctrl Pts',(-230.281020837594,-4.54808740063468,
128.927274578386));
#132732=CARTESIAN_POINT('Ctrl Pts',(-230.288911192688,-4.59946135799188,
129.056910385611));
#132733=CARTESIAN_POINT('Ctrl Pts',(-230.296801547782,-4.64527092374599,
129.188612769819));
#132734=CARTESIAN_POINT('Ctrl Pts',(-230.304557254697,-4.69029875350489,
129.318067665043));
#132735=CARTESIAN_POINT('Ctrl Pts',(-230.312312961613,-4.72995044961027,
129.449518834356));
#132736=CARTESIAN_POINT('Ctrl Pts',(-230.320068668528,-4.76405452823411,
129.582490119308));
#132737=CARTESIAN_POINT('Origin',(213.235140564004,0.,130.804360617566));
#132738=CARTESIAN_POINT('',(-232.415119734886,-4.76405452823408,129.582490119308));
#132739=CARTESIAN_POINT('',(-232.069726383436,-4.76405452823406,129.582490119308));
#132740=CARTESIAN_POINT('',(213.235140564004,-4.76405452823405,129.582490119308));
#132741=CARTESIAN_POINT('',(-230.735140563976,-4.91824919291643,130.807178218822));
#132742=CARTESIAN_POINT('Ctrl Pts',(-230.735140564014,-4.91824919291605,
130.807178219487));
#132743=CARTESIAN_POINT('Ctrl Pts',(-230.744426875891,-4.91815569747121,
130.970378667585));
#132744=CARTESIAN_POINT('Ctrl Pts',(-230.753713187769,-4.90993976197208,
131.133343395079));
#132745=CARTESIAN_POINT('Ctrl Pts',(-230.762999499647,-4.89366721036058,
131.29548615828));
#132746=CARTESIAN_POINT('Ctrl Pts',(-230.770773833766,-4.8800441213604,
131.431229177971));
#132747=CARTESIAN_POINT('Ctrl Pts',(-230.778548167885,-4.86074721111518,
131.566619949102));
#132748=CARTESIAN_POINT('Ctrl Pts',(-230.786322502004,-4.83579970371893,
131.701146148232));
#132749=CARTESIAN_POINT('Ctrl Pts',(-230.794087254951,-4.81088294189593,
131.835506555845));
#132750=CARTESIAN_POINT('Ctrl Pts',(-230.801852007898,-4.78032950952325,
131.969004130779));
#132751=CARTESIAN_POINT('Ctrl Pts',(-230.809616760845,-4.74421447312459,
132.101130487472));
#132752=CARTESIAN_POINT('Ctrl Pts',(-230.81737380173,-4.70813530668931,
132.233125614404));
#132753=CARTESIAN_POINT('Ctrl Pts',(-230.825130842615,-4.66650563138251,
132.363751858674));
#132754=CARTESIAN_POINT('Ctrl Pts',(-230.8328878835,-4.61945169748514,132.492510219083));
#132755=CARTESIAN_POINT('Ctrl Pts',(-230.84063907474,-4.57243324732528,
132.62117148181));
#132756=CARTESIAN_POINT('Ctrl Pts',(-230.848390265981,-4.51999881407111,
132.747967298654));
#132757=CARTESIAN_POINT('Ctrl Pts',(-230.856141457221,-4.46232459167631,
132.872413397604));
#132758=CARTESIAN_POINT('Ctrl Pts',(-230.863889353998,-4.40467488236445,
132.996806603642));
#132759=CARTESIAN_POINT('Ctrl Pts',(-230.871637250775,-4.34178997739594,
133.118851724131));
#132760=CARTESIAN_POINT('Ctrl Pts',(-230.879385147552,-4.27389427022736,
133.238084272671));
#132761=CARTESIAN_POINT('Ctrl Pts',(-230.887131423636,-4.20601276537707,
133.357291880332));
#132762=CARTESIAN_POINT('Ctrl Pts',(-230.89487769972,-4.1331227364989,133.473687746736));
#132763=CARTESIAN_POINT('Ctrl Pts',(-230.902623975804,-4.05549443320797,
133.586832174423));
#132764=CARTESIAN_POINT('Ctrl Pts',(-230.91037030907,-3.97786555688265,
133.699977437316));
#132765=CARTESIAN_POINT('Ctrl Pts',(-230.918116642335,-3.89549855753708,
133.809870891217));
#132766=CARTESIAN_POINT('Ctrl Pts',(-230.9258629756,-3.80870666710518,133.916102346317));
#132767=CARTESIAN_POINT('Ctrl Pts',(-230.933611043603,-3.72189534023132,
134.022357591214));
#132768=CARTESIAN_POINT('Ctrl Pts',(-230.941359111606,-3.63065739776129,
134.12494890274));
#132769=CARTESIAN_POINT('Ctrl Pts',(-230.949107179609,-3.53534568375761,
134.223499976942));
#132770=CARTESIAN_POINT('Ctrl Pts',(-230.956863482351,-3.43993267133019,
134.322155792399));
#132771=CARTESIAN_POINT('Ctrl Pts',(-230.964619785093,-3.34043751065132,
134.416762511298));
#132772=CARTESIAN_POINT('Ctrl Pts',(-230.972376087835,-3.23724956784499,
134.506981081236));
#132773=CARTESIAN_POINT('Ctrl Pts',(-230.980136530349,-3.13400655052636,
134.597247803542));
#132774=CARTESIAN_POINT('Ctrl Pts',(-230.987896972863,-3.02706712849241,
134.683121465406));
#132775=CARTESIAN_POINT('Ctrl Pts',(-230.995657415377,-2.9168521364287,
134.764304642008));
#132776=CARTESIAN_POINT('Ctrl Pts',(-231.003430315642,-2.8064602174753,
134.845618141051));
#132777=CARTESIAN_POINT('Ctrl Pts',(-231.011203215908,-2.69278254526388,
134.922225889709));
#132778=CARTESIAN_POINT('Ctrl Pts',(-231.018976116173,-2.57626795051102,
134.993874492668));
#132779=CARTESIAN_POINT('Ctrl Pts',(-231.026466451935,-2.46398895476093,
135.062918488437));
#132780=CARTESIAN_POINT('Ctrl Pts',(-231.033956787697,-2.34907598273907,
135.127357482966));
#132781=CARTESIAN_POINT('Ctrl Pts',(-231.041447123459,-2.23194883487598,
135.187006788659));
#132782=CARTESIAN_POINT('Ctrl Pts',(-231.049221457578,-2.1103807756011,
135.248917715908));
#132783=CARTESIAN_POINT('Ctrl Pts',(-231.056995791697,-1.98604223404277,
135.305864697701));
#132784=CARTESIAN_POINT('Ctrl Pts',(-231.064770125816,-1.85937679561084,
135.357590349794));
#132785=CARTESIAN_POINT('Ctrl Pts',(-231.072534878763,-1.73286746101136,
135.409252254643));
#132786=CARTESIAN_POINT('Ctrl Pts',(-231.08029963171,-1.60403729386557,
135.455705486781));
#132787=CARTESIAN_POINT('Ctrl Pts',(-231.088064384657,-1.4733545886351,
135.496738406987));
#132788=CARTESIAN_POINT('Ctrl Pts',(-231.095821425542,-1.34280167930977,
135.537730572717));
#132789=CARTESIAN_POINT('Ctrl Pts',(-231.103578466427,-1.21040026411328,
135.57331302362));
#132790=CARTESIAN_POINT('Ctrl Pts',(-231.111335507312,-1.07663840824776,
135.603322255294));
#132791=CARTESIAN_POINT('Ctrl Pts',(-231.119086698553,-0.942977423238074,
135.633308856774));
#132792=CARTESIAN_POINT('Ctrl Pts',(-231.126837889793,-0.807958419527763,
135.657730519221));
#132793=CARTESIAN_POINT('Ctrl Pts',(-231.134589081033,-0.672084066009092,
135.676473718749));
#132794=CARTESIAN_POINT('Ctrl Pts',(-231.14233697781,-0.536267462715418,
135.695208951917));
#132795=CARTESIAN_POINT('Ctrl Pts',(-231.150084874587,-0.399596619166442,
135.708270469117));
#132796=CARTESIAN_POINT('Ctrl Pts',(-231.157832771364,-0.262583611069324,
135.715595992673));
#132797=CARTESIAN_POINT('Ctrl Pts',(-231.165579047448,-0.125599263139469,
135.722919983887));
#132798=CARTESIAN_POINT('Ctrl Pts',(-231.173325323532,0.0117267168147697,
135.724510347158));
#132799=CARTESIAN_POINT('Ctrl Pts',(-231.181071599616,0.148878322349868,
135.720356783923));
#132800=CARTESIAN_POINT('Ctrl Pts',(-231.188817932882,0.286030940306776,
135.716203190027));
#132801=CARTESIAN_POINT('Ctrl Pts',(-231.196564266147,0.423008790490003,
135.706305596854));
#132802=CARTESIAN_POINT('Ctrl Pts',(-231.204310599412,0.559297459084418,
135.690705817689));
#132803=CARTESIAN_POINT('Ctrl Pts',(-231.212058667415,0.69561664858102,
135.675102545061));
#132804=CARTESIAN_POINT('Ctrl Pts',(-231.219806735418,0.831245961020516,
135.653794589881));
#132805=CARTESIAN_POINT('Ctrl Pts',(-231.227554803421,0.965678080395513,
135.626875408372));
#132806=CARTESIAN_POINT('Ctrl Pts',(-231.235311106163,1.10025307582693,
135.599927616837));
#132807=CARTESIAN_POINT('Ctrl Pts',(-231.243067408905,1.23362795248946,
135.567356762771));
#132808=CARTESIAN_POINT('Ctrl Pts',(-231.250823711647,1.36530699409404,
135.529307164817));
#132809=CARTESIAN_POINT('Ctrl Pts',(-231.258584154161,1.49705631676791,
135.491237258647));
#132810=CARTESIAN_POINT('Ctrl Pts',(-231.266344596675,1.6271076303131,135.447682906027));
#132811=CARTESIAN_POINT('Ctrl Pts',(-231.274105039189,1.75498323137612,
135.398837401715));
#132812=CARTESIAN_POINT('Ctrl Pts',(-231.281877939454,1.88306410970624,
135.349913486265));
#132813=CARTESIAN_POINT('Ctrl Pts',(-231.28965083972,2.00896193685782,135.295681600512));
#132814=CARTESIAN_POINT('Ctrl Pts',(-231.297423739985,2.13222092021232,
135.236382392096));
#132815=CARTESIAN_POINT('Ctrl Pts',(-231.304914075748,2.25099912905492,
135.17923885927));
#132816=CARTESIAN_POINT('Ctrl Pts',(-231.31240441151,2.36732674844701,135.117390171954));
#132817=CARTESIAN_POINT('Ctrl Pts',(-231.319894747272,2.48082148309694,
135.051089691984));
#132818=CARTESIAN_POINT('Ctrl Pts',(-231.327669081391,2.59861940510362,
134.982275409166));
#132819=CARTESIAN_POINT('Ctrl Pts',(-231.33544341551,2.71373853255926,134.908447107369));
#132820=CARTESIAN_POINT('Ctrl Pts',(-231.343217749629,2.82572255205946,
134.829838865089));
#132821=CARTESIAN_POINT('Ctrl Pts',(-231.350982502576,2.93756856126392,
134.751327500443));
#132822=CARTESIAN_POINT('Ctrl Pts',(-231.358747255523,3.04628683328025,
134.668048138817));
#132823=CARTESIAN_POINT('Ctrl Pts',(-231.36651200847,3.15144618544165,134.580280373435));
#132824=CARTESIAN_POINT('Ctrl Pts',(-231.374269049355,3.25650109185199,
134.492599780236));
#132825=CARTESIAN_POINT('Ctrl Pts',(-231.382026090241,3.35800381454203,
134.40043990369));
#132826=CARTESIAN_POINT('Ctrl Pts',(-231.389783131126,3.45555298146591,
134.304122988754));
#132827=CARTESIAN_POINT('Ctrl Pts',(-231.397534322366,3.55302858580432,
134.207878707152));
#132828=CARTESIAN_POINT('Ctrl Pts',(-231.405285513606,3.64655629160666,
134.107483900478));
#132829=CARTESIAN_POINT('Ctrl Pts',(-231.413036704846,3.73576888319733,
134.003300115874));
#132830=CARTESIAN_POINT('Ctrl Pts',(-231.420784601623,3.82494355705663,
133.899160612157));
#132831=CARTESIAN_POINT('Ctrl Pts',(-231.4285324984,3.9098065107072,133.791235629851));
#132832=CARTESIAN_POINT('Ctrl Pts',(-231.436280395177,3.99002855874991,
133.679922330147));
#132833=CARTESIAN_POINT('Ctrl Pts',(-231.444026671261,4.07023382606955,
133.568632314785));
#132834=CARTESIAN_POINT('Ctrl Pts',(-231.451772947345,4.14579989026932,
133.45395570877));
#132835=CARTESIAN_POINT('Ctrl Pts',(-231.45951922343,4.21643917279056,133.336321076313));
#132836=CARTESIAN_POINT('Ctrl Pts',(-231.467265556695,4.28707897675503,
133.218685575503));
#132837=CARTESIAN_POINT('Ctrl Pts',(-231.47501188996,4.352791725198,133.098092339857));
#132838=CARTESIAN_POINT('Ctrl Pts',(-231.482758223226,4.41333454358869,
132.974996761388));
#132839=CARTESIAN_POINT('Ctrl Pts',(-231.490506291229,4.47389092012371,
132.851873616518));
#132840=CARTESIAN_POINT('Ctrl Pts',(-231.498254359232,4.52927489026144,
132.726247364489));
#132841=CARTESIAN_POINT('Ctrl Pts',(-231.506002427235,4.57929086467661,
132.59859534));
#132842=CARTESIAN_POINT('Ctrl Pts',(-231.513758729976,4.62935999666452,
132.470807645421));
#132843=CARTESIAN_POINT('Ctrl Pts',(-231.521515032718,4.67404959338273,
132.340990242102));
#132844=CARTESIAN_POINT('Ctrl Pts',(-231.52927133546,4.71321312742965,132.209638197948));
#132845=CARTESIAN_POINT('Ctrl Pts',(-231.537031777974,4.75239756423399,
132.078216047253));
#132846=CARTESIAN_POINT('Ctrl Pts',(-231.544792220488,4.78604996550251,
131.945258002457));
#132847=CARTESIAN_POINT('Ctrl Pts',(-231.552552663003,4.81407474525854,
131.81127044946));
#132848=CARTESIAN_POINT('Ctrl Pts',(-231.560325563268,4.84214451287896,
131.677067807747));
#132849=CARTESIAN_POINT('Ctrl Pts',(-231.568098463533,4.86456854226935,
131.541832741215));
#132850=CARTESIAN_POINT('Ctrl Pts',(-231.575871363799,4.88130293005894,
131.40607879703));
#132851=CARTESIAN_POINT('Ctrl Pts',(-231.583361699561,4.89742898070105,
131.27525985066));
#132852=CARTESIAN_POINT('Ctrl Pts',(-231.590852035323,4.90827184815751,
131.143959403667));
#132853=CARTESIAN_POINT('Ctrl Pts',(-231.598342371085,4.91383805297244,
131.012636040168));
#132854=CARTESIAN_POINT('Ctrl Pts',(-231.606116705204,4.91961530213471,
130.876333511428));
#132855=CARTESIAN_POINT('Ctrl Pts',(-231.613891039323,4.91972616123747,
130.739574528679));
#132856=CARTESIAN_POINT('Ctrl Pts',(-231.621665373442,4.91412091860825,
130.602869526456));
#132857=CARTESIAN_POINT('Ctrl Pts',(-231.629430126389,4.90852258393961,
130.46633300093));
#132858=CARTESIAN_POINT('Ctrl Pts',(-231.637194879336,4.89722218002583,
130.329850710451));
#132859=CARTESIAN_POINT('Ctrl Pts',(-231.644959632284,4.88022187180129,
130.193936548175));
#132860=CARTESIAN_POINT('Ctrl Pts',(-231.652716673169,4.86323844852254,
130.05815737776));
#132861=CARTESIAN_POINT('Ctrl Pts',(-231.660473714054,4.84056643523716,
129.922945598052));
#132862=CARTESIAN_POINT('Ctrl Pts',(-231.668230754939,4.81225999435761,
129.788813075988));
#132863=CARTESIAN_POINT('Ctrl Pts',(-231.675981946179,4.78397489958527,
129.654781704302));
#132864=CARTESIAN_POINT('Ctrl Pts',(-231.683733137419,4.75006391492926,
129.521828351282));
#132865=CARTESIAN_POINT('Ctrl Pts',(-231.691484328659,4.71063273119703,
129.390457390936));
#132866=CARTESIAN_POINT('Ctrl Pts',(-231.699232225436,4.67121830676979,
129.259142266752));
#132867=CARTESIAN_POINT('Ctrl Pts',(-231.706980122213,4.6262884619024,129.129408571252));
#132868=CARTESIAN_POINT('Ctrl Pts',(-231.71472801899,4.57599940680393,129.001747932758));
#132869=CARTESIAN_POINT('Ctrl Pts',(-231.722474295074,4.52572087109168,
128.874113998118));
#132870=CARTESIAN_POINT('Ctrl Pts',(-231.730220571158,4.47008549814481,
128.748552621482));
#132871=CARTESIAN_POINT('Ctrl Pts',(-231.737966847243,4.40929840793594,
128.62553740026));
#132872=CARTESIAN_POINT('Ctrl Pts',(-231.745713180508,4.3485108690105,128.502521270967));
#132873=CARTESIAN_POINT('Ctrl Pts',(-231.753459513773,4.28257171013996,
128.3820516851));
#132874=CARTESIAN_POINT('Ctrl Pts',(-231.761205847039,4.21173278590663,
128.264579130387));
#132875=CARTESIAN_POINT('Ctrl Pts',(-231.768953915042,4.14087799778748,
128.14708026851));
#132876=CARTESIAN_POINT('Ctrl Pts',(-231.776701983045,4.06512146272388,
128.032580108064));
#132877=CARTESIAN_POINT('Ctrl Pts',(-231.784450051048,3.98475905510755,
127.921501214952));
#132878=CARTESIAN_POINT('Ctrl Pts',(-231.792206353789,3.9043112373682,127.810304265871));
#132879=CARTESIAN_POINT('Ctrl Pts',(-231.799962656531,3.81924799796628,
127.702536165017));
#132880=CARTESIAN_POINT('Ctrl Pts',(-231.807718959273,3.7299066499115,127.598587786337));
#132881=CARTESIAN_POINT('Ctrl Pts',(-231.815479401787,3.64051761768901,
127.494583927278));
#132882=CARTESIAN_POINT('Ctrl Pts',(-231.823239844301,3.54684619392603,
127.394404138112));
#132883=CARTESIAN_POINT('Ctrl Pts',(-231.831000286816,3.44926674886565,
127.298402551977));
#132884=CARTESIAN_POINT('Ctrl Pts',(-231.838773187081,3.35153066061737,
127.202246855573));
#132885=CARTESIAN_POINT('Ctrl Pts',(-231.846546087346,3.24987430471133,
127.110283027805));
#132886=CARTESIAN_POINT('Ctrl Pts',(-231.854318987612,3.1447060120775,127.022825590609));
#132887=CARTESIAN_POINT('Ctrl Pts',(-231.861809323374,3.04336085178356,
126.938547451546));
#132888=CARTESIAN_POINT('Ctrl Pts',(-231.869299659136,2.93875490181847,
126.858453941278));
#132889=CARTESIAN_POINT('Ctrl Pts',(-231.876789994898,2.83127750650062,
126.782787449801));
#132890=CARTESIAN_POINT('Ctrl Pts',(-231.884564329017,2.7197250730724,126.704252040302));
#132891=CARTESIAN_POINT('Ctrl Pts',(-231.892338663136,2.60472578972233,
126.6302372007));
#132892=CARTESIAN_POINT('Ctrl Pts',(-231.900112997255,2.48668222910833,
126.561060657165));
#132893=CARTESIAN_POINT('Ctrl Pts',(-231.907877750202,2.36878414663293,
126.491969367538));
#132894=CARTESIAN_POINT('Ctrl Pts',(-231.91564250315,2.24784958593007,126.427704705626));
#132895=CARTESIAN_POINT('Ctrl Pts',(-231.923407256097,2.1243120700664,126.36854262181));
#132896=CARTESIAN_POINT('Ctrl Pts',(-231.931164296982,2.00089725340506,
126.30943929861));
#132897=CARTESIAN_POINT('Ctrl Pts',(-231.938921337867,1.87488497676378,
126.255428635828));
#132898=CARTESIAN_POINT('Ctrl Pts',(-231.946678378752,1.74673516440225,
126.206741741676));
#132899=CARTESIAN_POINT('Ctrl Pts',(-231.954429569992,1.61868199081126,
126.158091562689));
#132900=CARTESIAN_POINT('Ctrl Pts',(-231.962180761232,1.48849485395208,
126.114757299616));
#132901=CARTESIAN_POINT('Ctrl Pts',(-231.969931952472,1.35665522642646,
126.076922658258));
#132902=CARTESIAN_POINT('Ctrl Pts',(-231.977679849249,1.2248716342593,126.039104097631));
#132903=CARTESIAN_POINT('Ctrl Pts',(-231.985427746026,1.09143732336178,
126.006780617258));
#132904=CARTESIAN_POINT('Ctrl Pts',(-231.993175642803,0.956850350000342,
125.980086530182));
#132905=CARTESIAN_POINT('Ctrl Pts',(-232.000921918888,0.822291529332377,
125.953398026934));
#132906=CARTESIAN_POINT('Ctrl Pts',(-232.008668194972,0.686580909037609,
125.932336650791));
#132907=CARTESIAN_POINT('Ctrl Pts',(-232.016414471056,0.550227812385761,
125.916985819479));
#132908=CARTESIAN_POINT('Ctrl Pts',(-232.024160804321,0.413873709206515,
125.901634874851));
#132909=CARTESIAN_POINT('Ctrl Pts',(-232.031907137587,0.276877508717496,
125.891994602908));
#132910=CARTESIAN_POINT('Ctrl Pts',(-232.039653470852,0.139754352556722,
125.888096610879));
#132911=CARTESIAN_POINT('Ctrl Pts',(-232.047401538855,0.00260048861568343,
125.884197745922));
#132912=CARTESIAN_POINT('Ctrl Pts',(-232.055149606858,-0.134679996838661,
125.886043730865));
#132913=CARTESIAN_POINT('Ctrl Pts',(-232.062897674861,-0.271571659809338,
125.893614045395));
#132914=CARTESIAN_POINT('Ctrl Pts',(-232.070653977603,-0.408608812868637,
125.901192405745));
#132915=CARTESIAN_POINT('Ctrl Pts',(-232.078410280345,-0.545255926951344,
125.914507227276));
#132916=CARTESIAN_POINT('Ctrl Pts',(-232.086166583086,-0.681001822813728,
125.933485995917));
#132917=CARTESIAN_POINT('Ctrl Pts',(-232.093927025601,-0.816820170347593,
125.952474894098));
#132918=CARTESIAN_POINT('Ctrl Pts',(-232.101687468115,-0.951735956807356,
125.977133692751));
#132919=CARTESIAN_POINT('Ctrl Pts',(-232.109447910629,-1.08524888369458,
126.007338841199));
#132920=CARTESIAN_POINT('Ctrl Pts',(-232.117220810894,-1.21897613738514,
126.037592477633));
#132921=CARTESIAN_POINT('Ctrl Pts',(-232.12499371116,-1.3512956536994,126.073410153665));
#132922=CARTESIAN_POINT('Ctrl Pts',(-232.132766611425,-1.48172210358327,
126.114618335707));
#132923=CARTESIAN_POINT('Ctrl Pts',(-232.140256947187,-1.60740722348663,
126.154328496535));
#132924=CARTESIAN_POINT('Ctrl Pts',(-232.147747282949,-1.73133423313736,
126.199043946141));
#132925=CARTESIAN_POINT('Ctrl Pts',(-232.155237618711,-1.85308875285092,
126.248568135839));
#132926=CARTESIAN_POINT('Ctrl Pts',(-232.163012308585,-1.97946541494861,
126.299972402407));
#132927=CARTESIAN_POINT('Ctrl Pts',(-232.17078699846,-2.10390172246025,
126.356720569307));
#132928=CARTESIAN_POINT('Ctrl Pts',(-232.178561688334,-2.22591269676149,
126.418645655454));
#132929=CARTESIAN_POINT('Ctrl Pts',(-232.186326715409,-2.34777202931791,
126.480493777801));
#132930=CARTESIAN_POINT('Ctrl Pts',(-232.194091742484,-2.46721168116132,
126.547505841568));
#132931=CARTESIAN_POINT('Ctrl Pts',(-232.20185676956,-2.58376510944525,
126.619466243545));
#132932=CARTESIAN_POINT('Ctrl Pts',(-232.209614003292,-2.70020155928215,
126.691354422712));
#132933=CARTESIAN_POINT('Ctrl Pts',(-232.217371237025,-2.81375721993365,
126.768180852184));
#132934=CARTESIAN_POINT('Ctrl Pts',(-232.225128470757,-2.92398902249743,
126.849683480452));
#132935=CARTESIAN_POINT('Ctrl Pts',(-232.233044773429,-3.03648122567941,
126.932857392206));
#132936=CARTESIAN_POINT('Ctrl Pts',(-232.240961076101,-3.14551139310726,
127.020901197916));
#132937=CARTESIAN_POINT('Ctrl Pts',(-232.248877378773,-3.25063799032476,
127.113488672028));
#132938=CARTESIAN_POINT('Ctrl Pts',(-232.256624933656,-3.35352365744953,
127.204102506144));
#132939=CARTESIAN_POINT('Ctrl Pts',(-232.264372488539,-3.45267019726962,
127.299067970012));
#132940=CARTESIAN_POINT('Ctrl Pts',(-232.272120043421,-3.54769618352665,
127.398037841919));
#132941=CARTESIAN_POINT('Ctrl Pts',(-232.279865897953,-3.64270131449172,
127.496985992972));
#132942=CARTESIAN_POINT('Ctrl Pts',(-232.287611752485,-3.73358742085743,
127.599936521495));
#132943=CARTESIAN_POINT('Ctrl Pts',(-232.295357607017,-3.82000989958489,
127.706505322435));
#132944=CARTESIAN_POINT('Ctrl Pts',(-232.303103438983,-3.9064321265463,
127.813073812918));
#132945=CARTESIAN_POINT('Ctrl Pts',(-232.31084927095,-3.98839050616377,
127.923260250786));
#132946=CARTESIAN_POINT('Ctrl Pts',(-232.318595102916,-4.06558095916253,
128.036647748247));
#132947=CARTESIAN_POINT('Ctrl Pts',(-232.326638822247,-4.1457399842507,
128.154395875127));
#132948=CARTESIAN_POINT('Ctrl Pts',(-232.334682541578,-4.22075675822784,
128.275595825386));
#132949=CARTESIAN_POINT('Ctrl Pts',(-232.342726260909,-4.29034091977056,
128.399748828806));
#132950=CARTESIAN_POINT('Ctrl Pts',(-232.350480606593,-4.35742178380676,
128.519435414913));
#132951=CARTESIAN_POINT('Ctrl Pts',(-232.358234952278,-4.41945400593222,
128.64186588242));
#132952=CARTESIAN_POINT('Ctrl Pts',(-232.365989297962,-4.47622530264491,
128.766570122333));
#132953=CARTESIAN_POINT('Ctrl Pts',(-232.373747825468,-4.53302721540442,
128.891341613675));
#132954=CARTESIAN_POINT('Ctrl Pts',(-232.381506352974,-4.58456240334656,
129.018388959012));
#132955=CARTESIAN_POINT('Ctrl Pts',(-232.389264880479,-4.63066746230612,
129.147223955718));
#132956=CARTESIAN_POINT('Ctrl Pts',(-232.397032317361,-4.67682546524075,
129.276206897944));
#132957=CARTESIAN_POINT('Ctrl Pts',(-232.404799754242,-4.71754077822091,
129.406981216686));
#132958=CARTESIAN_POINT('Ctrl Pts',(-232.412567191124,-4.75270031384212,
129.539045325117));
#132959=CARTESIAN_POINT('Ctrl Pts',(-232.413418039044,-4.75655170243177,
129.553511676601));
#132960=CARTESIAN_POINT('Ctrl Pts',(-232.414268886965,-4.76033647757936,
129.567993496235));
#132961=CARTESIAN_POINT('Ctrl Pts',(-232.415119734886,-4.76405452823408,
129.582490119308));
#132962=CARTESIAN_POINT('Ctrl Pts',(-230.664999534934,-4.76405452823392,
129.582490119308));
#132963=CARTESIAN_POINT('Ctrl Pts',(-230.672659072166,-4.7977324481482,
129.71379981792));
#132964=CARTESIAN_POINT('Ctrl Pts',(-230.680318609397,-4.82595448970105,
129.846413917723));
#132965=CARTESIAN_POINT('Ctrl Pts',(-230.687978146629,-4.84864291544807,
129.979833516146));
#132966=CARTESIAN_POINT('Ctrl Pts',(-230.69583854952,-4.8719263282634,130.116751944177));
#132967=CARTESIAN_POINT('Ctrl Pts',(-230.703698952411,-4.88938183373582,
130.254518247733));
#132968=CARTESIAN_POINT('Ctrl Pts',(-230.711559355303,-4.90098232377429,
130.392589656288));
#132969=CARTESIAN_POINT('Ctrl Pts',(-230.719419758194,-4.91258281381275,
130.530661064843));
#132970=CARTESIAN_POINT('Ctrl Pts',(-230.727280161085,-4.91832833215937,
130.669037125676));
#132971=CARTESIAN_POINT('Ctrl Pts',(-230.735140563976,-4.91824919291643,
130.807178218823));
#132972=CARTESIAN_POINT('',(-230.389859436043,-4.91824944680572,130.806693318839));
#132973=CARTESIAN_POINT('Ctrl Pts',(-230.320068668528,-4.76405452823411,
129.582490119308));
#132974=CARTESIAN_POINT('Ctrl Pts',(-230.327945977475,-4.79869332603803,
129.717546266229));
#132975=CARTESIAN_POINT('Ctrl Pts',(-230.335823286422,-4.82760892536237,
129.854170273547));
#132976=CARTESIAN_POINT('Ctrl Pts',(-230.343700595369,-4.85067044761666,
129.991846450847));
#132977=CARTESIAN_POINT('Ctrl Pts',(-230.351573717171,-4.87371971163376,
130.129449447062));
#132978=CARTESIAN_POINT('Ctrl Pts',(-230.359446838974,-4.89092103358712,
130.268103132679));
#132979=CARTESIAN_POINT('Ctrl Pts',(-230.367319960776,-4.90219449651391,
130.407281052682));
#132980=CARTESIAN_POINT('Ctrl Pts',(-230.374833119183,-4.91295253060557,
130.540095682749));
#132981=CARTESIAN_POINT('Ctrl Pts',(-230.382346277589,-4.91831267314133,
130.673387350445));
#132982=CARTESIAN_POINT('Ctrl Pts',(-230.389859435996,-4.91824944680612,
130.806693317998));
#132983=CARTESIAN_POINT('Ctrl Pts',(-230.389859436043,-4.91824944680572,
130.806693318839));
#132984=CARTESIAN_POINT('Ctrl Pts',(-230.398353064532,-4.91817796938352,
130.957395766794));
#132985=CARTESIAN_POINT('Ctrl Pts',(-230.406846693021,-4.91117576199927,
131.107866546464));
#132986=CARTESIAN_POINT('Ctrl Pts',(-230.41534032151,-4.89733120001217,
131.257494350461));
#132987=CARTESIAN_POINT('Ctrl Pts',(-230.423875977821,-4.88341813293515,
131.407862536579));
#132988=CARTESIAN_POINT('Ctrl Pts',(-230.432411634131,-4.86259491593276,
131.557379136073));
#132989=CARTESIAN_POINT('Ctrl Pts',(-230.440947290442,-4.83500161639621,
131.705439100244));
#132990=CARTESIAN_POINT('Ctrl Pts',(-230.449504551637,-4.80733847453758,
131.853873823936));
#132991=CARTESIAN_POINT('Ctrl Pts',(-230.458061812833,-4.77287105429389,
132.000844296161));
#132992=CARTESIAN_POINT('Ctrl Pts',(-230.466619074028,-4.73178941265174,
132.145759893254));
#132993=CARTESIAN_POINT('Ctrl Pts',(-230.475206302526,-4.69056390418703,
132.291182980936));
#132994=CARTESIAN_POINT('Ctrl Pts',(-230.483793531024,-4.64267789167879,
132.434536548416));
#132995=CARTESIAN_POINT('Ctrl Pts',(-230.492380759522,-4.58837081720295,
132.575246358189));
#132996=CARTESIAN_POINT('Ctrl Pts',(-230.496300797012,-4.56357984209304,
132.639479856779));
#132997=CARTESIAN_POINT('Ctrl Pts',(-230.500220834503,-4.53745142796362,
132.703162757044));
#132998=CARTESIAN_POINT('Ctrl Pts',(-230.504140871994,-4.51001150550466,
132.76624218451));
#132999=CARTESIAN_POINT('Ctrl Pts',(-230.511915206113,-4.4555918409206,
132.891343167941));
#133000=CARTESIAN_POINT('Ctrl Pts',(-230.519689540232,-4.39587686309395,
133.014376306061));
#133001=CARTESIAN_POINT('Ctrl Pts',(-230.527463874351,-4.33104511752674,
133.134860832637));
#133002=CARTESIAN_POINT('Ctrl Pts',(-230.535228627298,-4.26629327129177,
133.255196872803));
#133003=CARTESIAN_POINT('Ctrl Pts',(-230.542993380245,-4.19643738777442,
133.37299020997));
#133004=CARTESIAN_POINT('Ctrl Pts',(-230.550758133192,-4.12170417679129,
133.48777965706));
#133005=CARTESIAN_POINT('Ctrl Pts',(-230.558515174077,-4.04704519188666,
133.602455093654));
#133006=CARTESIAN_POINT('Ctrl Pts',(-230.566272214962,-3.96751873168534,
133.714132251955));
#133007=CARTESIAN_POINT('Ctrl Pts',(-230.574029255847,-3.88339738009621,
133.82237450931));
#133008=CARTESIAN_POINT('Ctrl Pts',(-230.581780447088,-3.79933946507302,
133.930535140337));
#133009=CARTESIAN_POINT('Ctrl Pts',(-230.589531638328,-3.71069379456016,
134.03526571877));
#133010=CARTESIAN_POINT('Ctrl Pts',(-230.597282829568,-3.61777601372976,
134.136158897321));
#133011=CARTESIAN_POINT('Ctrl Pts',(-230.605030726345,-3.52489772543451,
134.237009193581));
#133012=CARTESIAN_POINT('Ctrl Pts',(-230.612778623122,-3.42775120253087,
134.334025046904));
#133013=CARTESIAN_POINT('Ctrl Pts',(-230.620526519899,-3.32669194667371,
134.42683266776));
#133014=CARTESIAN_POINT('Ctrl Pts',(-230.628272795983,-3.22565383023456,
134.519620875262));
#133015=CARTESIAN_POINT('Ctrl Pts',(-230.636019072067,-3.12070489658031,
134.608202336927));
#133016=CARTESIAN_POINT('Ctrl Pts',(-230.643765348152,-3.01223674471693,
134.692240869873));
#133017=CARTESIAN_POINT('Ctrl Pts',(-230.651511681417,-2.90376779216615,
134.776280023172));
#133018=CARTESIAN_POINT('Ctrl Pts',(-230.659258014682,-2.79177987862718,
134.855775941387));
#133019=CARTESIAN_POINT('Ctrl Pts',(-230.667004347948,-2.67669652306891,
134.930433664167));
#133020=CARTESIAN_POINT('Ctrl Pts',(-230.674752415951,-2.56158739539156,
135.005108106027));
#133021=CARTESIAN_POINT('Ctrl Pts',(-230.682500483953,-2.44338177423179,
135.074941983716));
#133022=CARTESIAN_POINT('Ctrl Pts',(-230.690248551956,-2.32253055245363,
135.139684699503));
#133023=CARTESIAN_POINT('Ctrl Pts',(-230.698004854698,-2.20155088855865,
135.204496224618));
#133024=CARTESIAN_POINT('Ctrl Pts',(-230.70576115744,-2.07792035239654,
135.264205593964));
#133025=CARTESIAN_POINT('Ctrl Pts',(-230.713517460182,-1.95211324056038,
135.318608833884));
#133026=CARTESIAN_POINT('Ctrl Pts',(-230.721277902696,-1.82623898168032,
135.373041110451));
#133027=CARTESIAN_POINT('Ctrl Pts',(-230.72903834521,-1.69818619718442,
135.422161474557));
#133028=CARTESIAN_POINT('Ctrl Pts',(-230.736798787724,-1.56844643906889,
135.465815200663));
#133029=CARTESIAN_POINT('Ctrl Pts',(-230.74457168799,-1.43849841117587,
135.509539003604));
#133030=CARTESIAN_POINT('Ctrl Pts',(-230.752344588255,-1.3068583737185,
135.54777852311));
#133031=CARTESIAN_POINT('Ctrl Pts',(-230.760117488521,-1.17403109400243,
135.580429508696));
#133032=CARTESIAN_POINT('Ctrl Pts',(-230.767607824283,-1.04603242047541,
135.611893548712));
#133033=CARTESIAN_POINT('Ctrl Pts',(-230.775098160045,-0.916931626398108,
135.638168253731));
#133034=CARTESIAN_POINT('Ctrl Pts',(-230.782588495807,-0.787184856237522,
135.659205935865));
#133035=CARTESIAN_POINT('Ctrl Pts',(-230.790362829926,-0.652518697851182,
135.681041268111));
#133036=CARTESIAN_POINT('Ctrl Pts',(-230.798137164045,-0.516730030136942,
135.697303782455));
#133037=CARTESIAN_POINT('Ctrl Pts',(-230.805911498164,-0.380319843546427,
135.707883828392));
#133038=CARTESIAN_POINT('Ctrl Pts',(-230.813676251111,-0.244077770319558,
135.718450835367));
#133039=CARTESIAN_POINT('Ctrl Pts',(-230.821441004058,-0.107216088313928,
135.723349278144));
#133040=CARTESIAN_POINT('Ctrl Pts',(-230.829205757005,0.0297546505254653,
135.722520611229));
#133041=CARTESIAN_POINT('Ctrl Pts',(-230.83696279789,0.166589348096094,
135.721692767359));
#133042=CARTESIAN_POINT('Ctrl Pts',(-230.844719838775,0.303532498517019,
135.715149136013));
#133043=CARTESIAN_POINT('Ctrl Pts',(-230.85247687966,0.440069420521692,
135.702883044546));
#133044=CARTESIAN_POINT('Ctrl Pts',(-230.8602280709,0.576503378971193,135.690626203033));
#133045=CARTESIAN_POINT('Ctrl Pts',(-230.86797926214,0.712531330934243,
135.672655525684));
#133046=CARTESIAN_POINT('Ctrl Pts',(-230.87573045338,0.847639949674806,
135.649016392563));
#133047=CARTESIAN_POINT('Ctrl Pts',(-230.883478350158,0.982691143648449,
135.625387306705));
#133048=CARTESIAN_POINT('Ctrl Pts',(-230.891226246935,1.11682339724522,
135.596094624118));
#133049=CARTESIAN_POINT('Ctrl Pts',(-230.898974143712,1.24953007342004,
135.561235396044));
#133050=CARTESIAN_POINT('Ctrl Pts',(-230.906720419796,1.38220899021903,
135.526383459769));
#133051=CARTESIAN_POINT('Ctrl Pts',(-230.91446669588,1.51346254483487,135.485967393329));
#133052=CARTESIAN_POINT('Ctrl Pts',(-230.922212971964,1.64279622826155,
135.440134945001));
#133053=CARTESIAN_POINT('Ctrl Pts',(-230.929959305229,1.77213086640027,
135.394302158349));
#133054=CARTESIAN_POINT('Ctrl Pts',(-230.937705638495,1.89954523656009,
135.343053040617));
#133055=CARTESIAN_POINT('Ctrl Pts',(-230.94545197176,2.02456225789857,135.286584477035));
#133056=CARTESIAN_POINT('Ctrl Pts',(-230.953200039763,2.14960727593201,
135.23010326771));
#133057=CARTESIAN_POINT('Ctrl Pts',(-230.960948107766,2.27225352059958,
135.168400447549));
#133058=CARTESIAN_POINT('Ctrl Pts',(-230.968696175769,2.39204643832679,
135.101719911294));
#133059=CARTESIAN_POINT('Ctrl Pts',(-230.976452478511,2.51196667339268,
135.034968506171));
#133060=CARTESIAN_POINT('Ctrl Pts',(-230.984208781252,2.62902718151966,
134.963229007313));
#133061=CARTESIAN_POINT('Ctrl Pts',(-230.991965083994,2.74279998500172,
134.886790201132));
#133062=CARTESIAN_POINT('Ctrl Pts',(-230.999725526508,2.85663351245464,
134.810310597259));
#133063=CARTESIAN_POINT('Ctrl Pts',(-231.007485969023,2.96717552382122,
134.72912691965));
#133064=CARTESIAN_POINT('Ctrl Pts',(-231.015246411537,3.07403014826247,
134.643569091988));
#133065=CARTESIAN_POINT('Ctrl Pts',(-231.023019311802,3.18105630523297,
134.557873919305));
#133066=CARTESIAN_POINT('Ctrl Pts',(-231.030792212067,3.2843829517253,134.467790821898));
#133067=CARTESIAN_POINT('Ctrl Pts',(-231.038565112333,3.38364953979536,
134.373688124862));
#133068=CARTESIAN_POINT('Ctrl Pts',(-231.046055448095,3.4793075373519,134.283006297894));
#133069=CARTESIAN_POINT('Ctrl Pts',(-231.053545783857,3.57119532348375,
134.18859226337));
#133070=CARTESIAN_POINT('Ctrl Pts',(-231.061036119619,3.65902621979407,
134.090804012082));
#133071=CARTESIAN_POINT('Ctrl Pts',(-231.068810453738,3.75018725123324,
133.989308089525));
#133072=CARTESIAN_POINT('Ctrl Pts',(-231.076584787857,3.83726645685091,
133.883855523879));
#133073=CARTESIAN_POINT('Ctrl Pts',(-231.084359121976,3.91990078699615,
133.774808543823));
#133074=CARTESIAN_POINT('Ctrl Pts',(-231.092123874923,4.00243327771474,
133.665895954425));
#133075=CARTESIAN_POINT('Ctrl Pts',(-231.09988862787,4.08053155851035,133.553398073202));
#133076=CARTESIAN_POINT('Ctrl Pts',(-231.107653380818,4.1538704076052,133.437712796695));
#133077=CARTESIAN_POINT('Ctrl Pts',(-231.115410421703,4.22713641552123,
133.322142420435));
#133078=CARTESIAN_POINT('Ctrl Pts',(-231.123167462588,4.29565219096999,
133.203391276975));
#133079=CARTESIAN_POINT('Ctrl Pts',(-231.130924503473,4.35913392226761,
133.081888775512));
#133080=CARTESIAN_POINT('Ctrl Pts',(-231.138675694713,4.42256778149777,
132.96047790003));
#133081=CARTESIAN_POINT('Ctrl Pts',(-231.146426885953,4.48097497239187,
132.836320141467));
#133082=CARTESIAN_POINT('Ctrl Pts',(-231.154178077193,4.534116208843,132.709871905175));
#133083=CARTESIAN_POINT('Ctrl Pts',(-231.16192597397,4.58723485885113,132.583477412758));
#133084=CARTESIAN_POINT('Ctrl Pts',(-231.169673870747,4.63509185481077,
132.454794738532));
#133085=CARTESIAN_POINT('Ctrl Pts',(-231.177421767524,4.67749499898044,
132.32430258916));
#133086=CARTESIAN_POINT('Ctrl Pts',(-231.185168043608,4.71988927332645,
132.193837735932));
#133087=CARTESIAN_POINT('Ctrl Pts',(-231.192914319692,4.75683184430455,
132.061564532012));
#133088=CARTESIAN_POINT('Ctrl Pts',(-231.200660595776,4.78817972252712,
131.927978883384));
#133089=CARTESIAN_POINT('Ctrl Pts',(-231.208406929042,4.81952783215265,
131.794392248657));
#133090=CARTESIAN_POINT('Ctrl Pts',(-231.216153262307,4.84528107729446,
131.659493530516));
#133091=CARTESIAN_POINT('Ctrl Pts',(-231.223899595572,4.86534722922412,
131.52379053186));
#133092=CARTESIAN_POINT('Ctrl Pts',(-231.231647663575,4.88541787482935,
131.388057143459));
#133093=CARTESIAN_POINT('Ctrl Pts',(-231.239395731579,4.89979883575703,
131.251519502826));
#133094=CARTESIAN_POINT('Ctrl Pts',(-231.247143799581,4.90844961025101,
131.114691869822));
#133095=CARTESIAN_POINT('Ctrl Pts',(-231.254900102323,4.91710957889109,
130.977718814781));
#133096=CARTESIAN_POINT('Ctrl Pts',(-231.262656405065,4.92002717073763,
130.8404555425));
#133097=CARTESIAN_POINT('Ctrl Pts',(-231.270412707807,4.91721401757565,
130.703418218855));
#133098=CARTESIAN_POINT('Ctrl Pts',(-231.278173150321,4.91439936294913,
130.566307754264));
#133099=CARTESIAN_POINT('Ctrl Pts',(-231.285933592835,4.90584789301795,
130.42942386862));
#133100=CARTESIAN_POINT('Ctrl Pts',(-231.29369403535,4.89162320406197,130.29327795108));
#133101=CARTESIAN_POINT('Ctrl Pts',(-231.301466935615,4.87737568037248,
130.156913480027));
#133102=CARTESIAN_POINT('Ctrl Pts',(-231.30923983588,4.85743679556057,130.021289731419));
#133103=CARTESIAN_POINT('Ctrl Pts',(-231.317012736146,4.83192154699064,
129.886909133166));
#133104=CARTESIAN_POINT('Ctrl Pts',(-231.324503071908,4.80733384197518,
129.757413608143));
#133105=CARTESIAN_POINT('Ctrl Pts',(-231.33199340767,4.77756823367429,129.629072719422));
#133106=CARTESIAN_POINT('Ctrl Pts',(-231.339483743432,4.74277095320295,
129.502321160424));
#133107=CARTESIAN_POINT('Ctrl Pts',(-231.347258077551,4.70665432326629,
129.370763777542));
#133108=CARTESIAN_POINT('Ctrl Pts',(-231.35503241167,4.66500253088041,129.24050188809));
#133109=CARTESIAN_POINT('Ctrl Pts',(-231.362806745789,4.61792409208834,
129.112036729473));
#133110=CARTESIAN_POINT('Ctrl Pts',(-231.370571498736,4.57090367326456,
128.983729892682));
#133111=CARTESIAN_POINT('Ctrl Pts',(-231.378336251684,4.51847004811209,
128.857215744476));
#133112=CARTESIAN_POINT('Ctrl Pts',(-231.386101004631,4.46078218794617,
128.732982975946));
#133113=CARTESIAN_POINT('Ctrl Pts',(-231.393858045516,4.40315162417623,
128.608873597154));
#133114=CARTESIAN_POINT('Ctrl Pts',(-231.401615086401,4.34027737419711,
128.487041441103));
#133115=CARTESIAN_POINT('Ctrl Pts',(-231.409372127286,4.27236730498015,
128.367957392762));
#133116=CARTESIAN_POINT('Ctrl Pts',(-231.417123318526,4.20450844727456,
128.248963146627));
#133117=CARTESIAN_POINT('Ctrl Pts',(-231.424874509766,4.13162152201772,
128.132713221525));
#133118=CARTESIAN_POINT('Ctrl Pts',(-231.432625701006,4.05396117597433,
128.019655633875));
#133119=CARTESIAN_POINT('Ctrl Pts',(-231.440373597783,3.97633383764977,
127.906646098716));
#133120=CARTESIAN_POINT('Ctrl Pts',(-231.44812149456,3.89393733462957,127.796826523967));
#133121=CARTESIAN_POINT('Ctrl Pts',(-231.455869391337,3.80707052881091,
127.690617363674));
#133122=CARTESIAN_POINT('Ctrl Pts',(-231.463615667421,3.72022189365538,
127.584430420047));
#133123=CARTESIAN_POINT('Ctrl Pts',(-231.471361943505,3.62890506301179,
127.481852691144));
#133124=CARTESIAN_POINT('Ctrl Pts',(-231.47910821959,3.5334599673727,127.383272527283));
#133125=CARTESIAN_POINT('Ctrl Pts',(-231.486854552855,3.43801416717946,
127.284691635726));
#133126=CARTESIAN_POINT('Ctrl Pts',(-231.49460088612,3.33844031313392,127.190108648978));
#133127=CARTESIAN_POINT('Ctrl Pts',(-231.502347219386,3.23511578231743,
127.099875641554));
#133128=CARTESIAN_POINT('Ctrl Pts',(-231.510095287389,3.1317681126888,127.009622427073));
#133129=CARTESIAN_POINT('Ctrl Pts',(-231.517843355392,3.02466838933307,
126.923721387475));
#133130=CARTESIAN_POINT('Ctrl Pts',(-231.525591423395,2.9142273814477,126.842484568051));
#133131=CARTESIAN_POINT('Ctrl Pts',(-231.533347726136,2.80366899554474,
126.761161409169));
#133132=CARTESIAN_POINT('Ctrl Pts',(-231.541104028878,2.68976254673618,
126.684512605008));
#133133=CARTESIAN_POINT('Ctrl Pts',(-231.54886033162,2.57294858725588,126.612807369683));
#133134=CARTESIAN_POINT('Ctrl Pts',(-231.556620774134,2.4560722806482,126.541063863115));
#133135=CARTESIAN_POINT('Ctrl Pts',(-231.564381216648,2.33628571252351,
126.474269373193));
#133136=CARTESIAN_POINT('Ctrl Pts',(-231.572141659163,2.2140535044062,126.412646812896));
#133137=CARTESIAN_POINT('Ctrl Pts',(-231.579914559428,2.09162507829717,
126.350925330595));
#133138=CARTESIAN_POINT('Ctrl Pts',(-231.587687459693,1.96674352325454,
126.29439253017));
#133139=CARTESIAN_POINT('Ctrl Pts',(-231.595460359959,1.83989370499123,
126.243223235637));
#133140=CARTESIAN_POINT('Ctrl Pts',(-231.602950695721,1.7176551971372,126.193914073847));
#133141=CARTESIAN_POINT('Ctrl Pts',(-231.610441031483,1.59358933430168,
126.149585337863));
#133142=CARTESIAN_POINT('Ctrl Pts',(-231.617931367245,1.4681408778606,126.110348961716));
#133143=CARTESIAN_POINT('Ctrl Pts',(-231.625705701364,1.3379360050645,126.069624926442));
#133144=CARTESIAN_POINT('Ctrl Pts',(-231.633480035483,1.20582917707458,
126.034258025945));
#133145=CARTESIAN_POINT('Ctrl Pts',(-231.641254369602,1.07230075468556,
126.004427893662));
#133146=CARTESIAN_POINT('Ctrl Pts',(-231.649019122549,0.938936894143365,
125.974634524352));
#133147=CARTESIAN_POINT('Ctrl Pts',(-231.656783875496,0.804155303032998,
125.950364430805));
#133148=CARTESIAN_POINT('Ctrl Pts',(-231.664548628443,0.668453058890205,
125.931748015423));
#133149=CARTESIAN_POINT('Ctrl Pts',(-231.672305669328,0.532885596129361,
125.913150090128));
#133150=CARTESIAN_POINT('Ctrl Pts',(-231.680062710214,0.396399684875361,
125.900194721065));
#133151=CARTESIAN_POINT('Ctrl Pts',(-231.687819751098,0.259503851162931,
125.892961548692));
#133152=CARTESIAN_POINT('Ctrl Pts',(-231.695570942339,0.122711251663413,
125.885733830911));
#133153=CARTESIAN_POINT('Ctrl Pts',(-231.703322133579,-0.0144902661576784,
125.884219741315));
#133154=CARTESIAN_POINT('Ctrl Pts',(-231.711073324819,-0.151586130600617,
125.888447202186));
#133155=CARTESIAN_POINT('Ctrl Pts',(-231.718821221596,-0.288623725644202,
125.892672866274));
#133156=CARTESIAN_POINT('Ctrl Pts',(-231.726569118373,-0.425555366661926,
125.902635215211));
#133157=CARTESIAN_POINT('Ctrl Pts',(-231.73431701515,-0.561865771601263,
125.918310073701));
#133158=CARTESIAN_POINT('Ctrl Pts',(-231.742063291234,-0.698147663342027,
125.933981653348));
#133159=CARTESIAN_POINT('Ctrl Pts',(-231.749809567318,-0.833808189320973,
125.955363321123));
#133160=CARTESIAN_POINT('Ctrl Pts',(-231.757555843402,-0.968336878681481,
125.982378996709));
#133161=CARTESIAN_POINT('Ctrl Pts',(-231.765302176668,-1.1028665611024,
126.009394871718));
#133162=CARTESIAN_POINT('Ctrl Pts',(-231.773048509933,-1.23626400692059,
126.04204476055));
#133163=CARTESIAN_POINT('Ctrl Pts',(-231.780794843198,-1.36802902434677,
126.080201470052));
#133164=CARTESIAN_POINT('Ctrl Pts',(-231.788542911201,-1.49982354963519,
126.118366724484));
#133165=CARTESIAN_POINT('Ctrl Pts',(-231.796290979204,-1.62998454362307,
126.162041144813));
#133166=CARTESIAN_POINT('Ctrl Pts',(-231.804039047207,-1.75802744298462,
126.211047807381));
#133167=CARTESIAN_POINT('Ctrl Pts',(-231.811795349949,-1.88620642786315,
126.260106554812));
#133168=CARTESIAN_POINT('Ctrl Pts',(-231.819551652691,-2.01226245551108,
126.314508725294));
#133169=CARTESIAN_POINT('Ctrl Pts',(-231.827307955433,-2.13573089922645,
126.374029186557));
#133170=CARTESIAN_POINT('Ctrl Pts',(-231.835068397947,-2.25926524176812,
126.433581415682));
#133171=CARTESIAN_POINT('Ctrl Pts',(-231.842828840461,-2.38020890387919,
126.498257194629));
#133172=CARTESIAN_POINT('Ctrl Pts',(-231.850589282975,-2.49812320327363,
126.567786114059));
#133173=CARTESIAN_POINT('Ctrl Pts',(-231.858362183241,-2.61622678916907,
126.637426647483));
#133174=CARTESIAN_POINT('Ctrl Pts',(-231.866135083506,-2.73129096616132,
126.711935677049));
#133175=CARTESIAN_POINT('Ctrl Pts',(-231.873907983772,-2.84290656809211,
126.790999768153));
#133176=CARTESIAN_POINT('Ctrl Pts',(-231.881398319534,-2.95046466174907,
126.867189680394));
#133177=CARTESIAN_POINT('Ctrl Pts',(-231.888888655296,-3.05482031212694,
126.947609039936));
#133178=CARTESIAN_POINT('Ctrl Pts',(-231.896378991058,-3.15563894156551,
127.031944159515));
#133179=CARTESIAN_POINT('Ctrl Pts',(-231.904042805045,-3.25879255804118,
127.118232503533));
#133180=CARTESIAN_POINT('Ctrl Pts',(-231.911706619032,-3.35858974585892,
127.208910327928));
#133181=CARTESIAN_POINT('Ctrl Pts',(-231.919370433019,-3.45462584472503,
127.303683063798));
#133182=CARTESIAN_POINT('Ctrl Pts',(-231.927025453236,-3.55055174788039,
127.398347053591));
#133183=CARTESIAN_POINT('Ctrl Pts',(-231.934680473452,-3.64272485724723,
127.497096335079));
#133184=CARTESIAN_POINT('Ctrl Pts',(-231.942335493669,-3.73077224957203,
127.599595183978));
#133185=CARTESIAN_POINT('Ctrl Pts',(-231.949983499379,-3.81873896164382,
127.702000110355));
#133186=CARTESIAN_POINT('Ctrl Pts',(-231.95763150509,-3.9025872127649,127.808147469355));
#133187=CARTESIAN_POINT('Ctrl Pts',(-231.9652795108,-3.98198015682655,127.917664046546));
#133188=CARTESIAN_POINT('Ctrl Pts',(-231.972922274665,-4.06131868597262,
128.027105562465));
#133189=CARTESIAN_POINT('Ctrl Pts',(-231.980565038529,-4.13620774589511,
128.139911378913));
#133190=CARTESIAN_POINT('Ctrl Pts',(-231.988207802394,-4.20635047176246,
128.255674922702));
#133191=CARTESIAN_POINT('Ctrl Pts',(-231.995847800743,-4.27646781665669,
128.371396577737));
#133192=CARTESIAN_POINT('Ctrl Pts',(-232.003487799092,-4.34184203188347,
128.49007348944));
#133193=CARTESIAN_POINT('Ctrl Pts',(-232.011127797441,-4.40221958282907,
128.611270148147));
#133194=CARTESIAN_POINT('Ctrl Pts',(-232.018766121419,-4.46258390151233,
128.732440245558));
#133195=CARTESIAN_POINT('Ctrl Pts',(-232.026404445396,-4.51795355806227,
128.856128629348));
#133196=CARTESIAN_POINT('Ctrl Pts',(-232.034042769374,-4.56812131761873,
128.981875860423));
#133197=CARTESIAN_POINT('Ctrl Pts',(-232.04168307152,-4.61830206959523,
129.10765565745));
#133198=CARTESIAN_POINT('Ctrl Pts',(-232.049323373667,-4.66327808431924,
129.235494992454));
#133199=CARTESIAN_POINT('Ctrl Pts',(-232.056963675813,-4.70289063616154,
129.364915333158));
#133200=CARTESIAN_POINT('Ctrl Pts',(-232.061217911688,-4.72494750457854,
129.436978537689));
#133201=CARTESIAN_POINT('Ctrl Pts',(-232.065472147562,-4.74534234988716,
129.509531619931));
#133202=CARTESIAN_POINT('Ctrl Pts',(-232.069726383436,-4.76405452823406,
129.582490119308));
#133203=CARTESIAN_POINT('Origin',(213.235140564004,0.,130.804360617566));
#133204=CARTESIAN_POINT('',(-234.165426035895,-4.76405452823417,129.582490119309));
#133205=CARTESIAN_POINT('',(-233.819813589496,-4.76405452823394,129.582490119308));
#133206=CARTESIAN_POINT('',(213.235140564004,-4.76405452823405,129.582490119308));
#133207=CARTESIAN_POINT('',(-232.485140564054,-4.91824815178585,130.800096821715));
#133208=CARTESIAN_POINT('Ctrl Pts',(-232.485140564054,-4.91824815178585,
130.800096821715));
#133209=CARTESIAN_POINT('Ctrl Pts',(-232.492787208904,-4.91836497210817,
130.934847957654));
#133210=CARTESIAN_POINT('Ctrl Pts',(-232.500433853755,-4.91293972528396,
131.069789047598));
#133211=CARTESIAN_POINT('Ctrl Pts',(-232.508080498605,-4.90195230449137,
131.204418947053));
#133212=CARTESIAN_POINT('Ctrl Pts',(-232.515720342521,-4.89097465592257,
131.338929106531));
#133213=CARTESIAN_POINT('Ctrl Pts',(-232.523360186437,-4.87444470582854,
131.473128226128));
#133214=CARTESIAN_POINT('Ctrl Pts',(-232.531000030354,-4.85239440291908,
131.606514979905));
#133215=CARTESIAN_POINT('Ctrl Pts',(-232.538635402698,-4.83035700596813,
131.739823662922));
#133216=CARTESIAN_POINT('Ctrl Pts',(-232.546270775043,-4.80280574736142,
131.872320528752));
#133217=CARTESIAN_POINT('Ctrl Pts',(-232.553906147388,-4.76982438423958,
132.003509651679));
#133218=CARTESIAN_POINT('Ctrl Pts',(-232.561539218865,-4.73685295982771,
132.134659241654));
#133219=CARTESIAN_POINT('Ctrl Pts',(-232.569172290342,-4.69845478193037,
132.26450148112));
#133220=CARTESIAN_POINT('Ctrl Pts',(-232.576805361819,-4.65476455977488,
132.39255139816));
#133221=CARTESIAN_POINT('Ctrl Pts',(-232.584437899556,-4.61107739264138,
132.520592361358));
#133222=CARTESIAN_POINT('Ctrl Pts',(-232.592070437294,-4.56209904742062,
132.646840869405));
#133223=CARTESIAN_POINT('Ctrl Pts',(-232.599702975031,-4.5080136976276,
132.770828406395));
#133224=CARTESIAN_POINT('Ctrl Pts',(-232.607336745517,-4.45391961238895,
132.894835968889));
#133225=CARTESIAN_POINT('Ctrl Pts',(-232.614970516002,-4.39471704425763,
133.016581464515));
#133226=CARTESIAN_POINT('Ctrl Pts',(-232.622604286488,-4.33063753442429,
133.135618134001));
#133227=CARTESIAN_POINT('Ctrl Pts',(-232.63024567639,-4.26649406557284,
133.254773616327));
#133228=CARTESIAN_POINT('Ctrl Pts',(-232.637887066292,-4.19746412495438,
133.371214516855));
#133229=CARTESIAN_POINT('Ctrl Pts',(-232.645528456194,-4.12382445759133,
133.48452011011));
#133230=CARTESIAN_POINT('Ctrl Pts',(-232.653173703627,-4.05014761540808,
133.597882902361));
#133231=CARTESIAN_POINT('Ctrl Pts',(-232.66081895106,-3.97185664666404,
133.708106907284));
#133232=CARTESIAN_POINT('Ctrl Pts',(-232.668464198493,-3.88926974207377,
133.81480309931));
#133233=CARTESIAN_POINT('Ctrl Pts',(-232.676121423645,-3.80655344955241,
133.921666451004));
#133234=CARTESIAN_POINT('Ctrl Pts',(-232.683778648797,-3.71952803684931,
134.024990640997));
#133235=CARTESIAN_POINT('Ctrl Pts',(-232.691435873949,-3.62855026895896,
134.124421762807));
#133236=CARTESIAN_POINT('Ctrl Pts',(-232.698334871412,-3.5465812296047,
134.214007094758));
#133237=CARTESIAN_POINT('Ctrl Pts',(-232.705233868875,-3.46140445807237,
134.300432531783));
#133238=CARTESIAN_POINT('Ctrl Pts',(-232.712132866337,-3.37330352024979,
134.38346754846));
#133239=CARTESIAN_POINT('Ctrl Pts',(-232.719907200456,-3.27402443940633,
134.477037950061));
#133240=CARTESIAN_POINT('Ctrl Pts',(-232.727681534575,-3.17069190232462,
134.566622649829));
#133241=CARTESIAN_POINT('Ctrl Pts',(-232.735455868695,-3.06365932118117,
134.651850010175));
#133242=CARTESIAN_POINT('Ctrl Pts',(-232.743220621642,-2.9567586481285,
134.736972335416));
#133243=CARTESIAN_POINT('Ctrl Pts',(-232.750985374589,-2.84616730691387,
134.817747764795));
#133244=CARTESIAN_POINT('Ctrl Pts',(-232.758750127536,-2.73227527506937,
134.89384162177));
#133245=CARTESIAN_POINT('Ctrl Pts',(-232.766507168421,-2.6184963623965,
134.969859901253));
#133246=CARTESIAN_POINT('Ctrl Pts',(-232.774264209306,-2.50142360602416,
135.041205645862));
#133247=CARTESIAN_POINT('Ctrl Pts',(-232.782021250191,-2.38147948079228,
135.107584821005));
#133248=CARTESIAN_POINT('Ctrl Pts',(-232.789772441431,-2.26162580635811,
135.173913939096));
#133249=CARTESIAN_POINT('Ctrl Pts',(-232.797523632671,-2.1389054136967,
135.235283754028));
#133250=CARTESIAN_POINT('Ctrl Pts',(-232.805274823911,-2.01376883452175,
135.291444096131));
#133251=CARTESIAN_POINT('Ctrl Pts',(-232.813022720688,-1.88868544173091,
135.34758056859));
#133252=CARTESIAN_POINT('Ctrl Pts',(-232.820770617465,-1.76118826088311,
135.398511812282));
#133253=CARTESIAN_POINT('Ctrl Pts',(-232.828518514242,-1.6317512485673,
135.444034197173));
#133254=CARTESIAN_POINT('Ctrl Pts',(-232.836264790326,-1.50234131168448,
135.489547059761));
#133255=CARTESIAN_POINT('Ctrl Pts',(-232.84401106641,-1.37099271902099,
135.529653184369));
#133256=CARTESIAN_POINT('Ctrl Pts',(-232.851757342494,-1.23819780240132,
135.564197722408));
#133257=CARTESIAN_POINT('Ctrl Pts',(-232.85950367576,-1.10540190551956,
135.598742515447));
#133258=CARTESIAN_POINT('Ctrl Pts',(-232.867250009025,-0.971160041750084,
135.627725541569));
#133259=CARTESIAN_POINT('Ctrl Pts',(-232.87499634229,-0.8359776545235,135.651042412737));
#133260=CARTESIAN_POINT('Ctrl Pts',(-232.882744410293,-0.700764994138032,
135.674364505556));
#133261=CARTESIAN_POINT('Ctrl Pts',(-232.890492478296,-0.564611776380961,
135.692017852022));
#133262=CARTESIAN_POINT('Ctrl Pts',(-232.898240546299,-0.42803114108908,
135.703949621223));
#133263=CARTESIAN_POINT('Ctrl Pts',(-232.905996849041,-0.291305346272868,
135.715894071651));
#133264=CARTESIAN_POINT('Ctrl Pts',(-232.913753151783,-0.154151616582536,
135.722104763362));
#133265=CARTESIAN_POINT('Ctrl Pts',(-232.921509454525,-0.0170862483816585,
135.722580938232));
#133266=CARTESIAN_POINT('Ctrl Pts',(-232.929269897039,0.120052275732813,
135.723057367252));
#133267=CARTESIAN_POINT('Ctrl Pts',(-232.937030339553,0.25710195389921,
135.717793195758));
#133268=CARTESIAN_POINT('Ctrl Pts',(-232.944790782067,0.393550018091851,
135.706839729787));
#133269=CARTESIAN_POINT('Ctrl Pts',(-232.952563682333,0.530217120830424,
135.695868680339));
#133270=CARTESIAN_POINT('Ctrl Pts',(-232.960336582598,0.666280291406744,
135.679190133444));
#133271=CARTESIAN_POINT('Ctrl Pts',(-232.968109482864,0.801234486979995,
135.656906996466));
#133272=CARTESIAN_POINT('Ctrl Pts',(-232.975599818625,0.931282757613221,
135.635433907645));
#133273=CARTESIAN_POINT('Ctrl Pts',(-232.983090154387,1.06030097985337,
135.608756698559));
#133274=CARTESIAN_POINT('Ctrl Pts',(-232.990580490149,1.18785107631667,
135.577011126769));
#133275=CARTESIAN_POINT('Ctrl Pts',(-232.998354824268,1.32023727345744,
135.544061911975));
#133276=CARTESIAN_POINT('Ctrl Pts',(-233.006129158388,1.45146117887392,
135.505548040452));
#133277=CARTESIAN_POINT('Ctrl Pts',(-233.013903492507,1.58101909542139,
135.461565968677));
#133278=CARTESIAN_POINT('Ctrl Pts',(-233.021668245454,1.71041734341494,
135.417638100874));
#133279=CARTESIAN_POINT('Ctrl Pts',(-233.029432998401,1.83815332110045,
135.36825556603));
#133280=CARTESIAN_POINT('Ctrl Pts',(-233.037197751348,1.96373466324294,
135.31356556244));
#133281=CARTESIAN_POINT('Ctrl Pts',(-233.044954792233,2.08919127622636,
135.258929877733));
#133282=CARTESIAN_POINT('Ctrl Pts',(-233.052711833118,2.21249715626237,
135.198997369802));
#133283=CARTESIAN_POINT('Ctrl Pts',(-233.060468874003,2.33317656575259,
135.133964545817));
#133284=CARTESIAN_POINT('Ctrl Pts',(-233.068220065243,2.45376496996152,
135.06898076359));
#133285=CARTESIAN_POINT('Ctrl Pts',(-233.075971256483,2.57173050319267,
134.998904505633));
#133286=CARTESIAN_POINT('Ctrl Pts',(-233.083722447723,2.68661916722265,
134.92397959422));
#133287=CARTESIAN_POINT('Ctrl Pts',(-233.0914703445,2.80145900050519,134.849086527894));
#133288=CARTESIAN_POINT('Ctrl Pts',(-233.099218241277,2.91322423881038,
134.76934912002));
#133289=CARTESIAN_POINT('Ctrl Pts',(-233.106966138054,3.02148737731084,
134.685056056692));
#133290=CARTESIAN_POINT('Ctrl Pts',(-233.114712414138,3.12972786949719,
134.600780625655));
#133291=CARTESIAN_POINT('Ctrl Pts',(-233.122458690222,3.23446741069658,
134.511951674658));
#133292=CARTESIAN_POINT('Ctrl Pts',(-233.130204966307,3.3353096050307,134.418899716966));
#133293=CARTESIAN_POINT('Ctrl Pts',(-233.137951299572,3.43615254375856,
134.325847072385));
#133294=CARTESIAN_POINT('Ctrl Pts',(-233.145697632837,3.53309779088441,
134.228571624038));
#133295=CARTESIAN_POINT('Ctrl Pts',(-233.153443966103,3.62578431727483,
134.127442191513));
#133296=CARTESIAN_POINT('Ctrl Pts',(-233.161192034106,3.71849160016981,
134.026290111752));
#133297=CARTESIAN_POINT('Ctrl Pts',(-233.168940102108,3.80693800044464,
133.921282618567));
#133298=CARTESIAN_POINT('Ctrl Pts',(-233.176688170111,3.89080170534141,
133.812822874636));
#133299=CARTESIAN_POINT('Ctrl Pts',(-233.184444472853,3.97475454158207,
133.704247858397));
#133300=CARTESIAN_POINT('Ctrl Pts',(-233.192200775595,4.05411471347774,
133.592213571788));
#133301=CARTESIAN_POINT('Ctrl Pts',(-233.199957078337,4.12860251240276,
133.477153979777));
#133302=CARTESIAN_POINT('Ctrl Pts',(-233.207717520851,4.20313006770885,
133.362032976998));
#133303=CARTESIAN_POINT('Ctrl Pts',(-233.215477963365,4.27277986981554,
133.243883788031));
#133304=CARTESIAN_POINT('Ctrl Pts',(-233.223238405879,4.33731792030103,
133.123165551306));
#133305=CARTESIAN_POINT('Ctrl Pts',(-233.231011306145,4.40195957299458,
133.002253526949));
#133306=CARTESIAN_POINT('Ctrl Pts',(-233.23878420641,4.46147290635544,132.878764566042));
#133307=CARTESIAN_POINT('Ctrl Pts',(-233.246557106676,4.5156715112712,132.753179199372));
#133308=CARTESIAN_POINT('Ctrl Pts',(-233.254047442438,4.56789986038125,
132.632159177109));
#133309=CARTESIAN_POINT('Ctrl Pts',(-233.2615377782,4.61519306940726,132.509192809611));
#133310=CARTESIAN_POINT('Ctrl Pts',(-233.269028113962,4.65742856350315,
132.384722044065));
#133311=CARTESIAN_POINT('Ctrl Pts',(-233.276802448081,4.70126542919421,
132.255531931613));
#133312=CARTESIAN_POINT('Ctrl Pts',(-233.2845767822,4.73979234451194,132.12431185522));
#133313=CARTESIAN_POINT('Ctrl Pts',(-233.292351116319,4.77281820041242,
131.991537726641));
#133314=CARTESIAN_POINT('Ctrl Pts',(-233.300115869266,4.80580335489693,
131.85892723031));
#133315=CARTESIAN_POINT('Ctrl Pts',(-233.307880622214,4.83330084581008,
131.724766868294));
#133316=CARTESIAN_POINT('Ctrl Pts',(-233.315645375161,4.85516837981154,
131.589550445683));
#133317=CARTESIAN_POINT('Ctrl Pts',(-233.323402416046,4.87701419467007,
131.454468321929));
#133318=CARTESIAN_POINT('Ctrl Pts',(-233.331159456931,4.8932411184438,131.31833260838));
#133319=CARTESIAN_POINT('Ctrl Pts',(-233.338916497816,4.90375733038771,
131.181649773478));
#133320=CARTESIAN_POINT('Ctrl Pts',(-233.346667689056,4.9142656119744,131.045070012165));
#133321=CARTESIAN_POINT('Ctrl Pts',(-233.354418880296,4.91907172367244,
130.907944338966));
#133322=CARTESIAN_POINT('Ctrl Pts',(-233.362170071536,4.91813540293703,
130.77078650734));
#133323=CARTESIAN_POINT('Ctrl Pts',(-233.369917968313,4.9171994801629,130.633686971452));
#133324=CARTESIAN_POINT('Ctrl Pts',(-233.37766586509,4.91052598195897,130.496555694459));
#133325=CARTESIAN_POINT('Ctrl Pts',(-233.385413761867,4.898126711311,130.359908390165));
#133326=CARTESIAN_POINT('Ctrl Pts',(-233.393160037952,4.88573003432314,
130.223289669542));
#133327=CARTESIAN_POINT('Ctrl Pts',(-233.400906314035,4.86761000250677,
130.087155109372));
#133328=CARTESIAN_POINT('Ctrl Pts',(-233.40865259012,4.84383042437688,129.952016859226));
#133329=CARTESIAN_POINT('Ctrl Pts',(-233.416398923385,4.82005067071157,
129.816877611521));
#133330=CARTESIAN_POINT('Ctrl Pts',(-233.42414525665,4.79061135512395,129.682735073565));
#133331=CARTESIAN_POINT('Ctrl Pts',(-233.431891589916,4.75562763091414,
129.550092345391));
#133332=CARTESIAN_POINT('Ctrl Pts',(-233.439639657919,4.72063607234171,
129.417419912796));
#133333=CARTESIAN_POINT('Ctrl Pts',(-233.447387725922,4.68009773412952,
129.286248336294));
#133334=CARTESIAN_POINT('Ctrl Pts',(-233.455135793925,4.63417786080164,
129.157066285348));
#133335=CARTESIAN_POINT('Ctrl Pts',(-233.462892096666,4.58820918328613,
129.027746938182));
#133336=CARTESIAN_POINT('Ctrl Pts',(-233.470648399408,4.53684767637541,
128.900421709468));
#133337=CARTESIAN_POINT('Ctrl Pts',(-233.47840470215,4.48030725774423,128.77556049466));
#133338=CARTESIAN_POINT('Ctrl Pts',(-233.486165144664,4.42373666178922,
128.650632637662));
#133339=CARTESIAN_POINT('Ctrl Pts',(-233.493925587178,4.36198182228225,
128.528171763974));
#133340=CARTESIAN_POINT('Ctrl Pts',(-233.501686029693,4.29530254352355,
128.408622918631));
#133341=CARTESIAN_POINT('Ctrl Pts',(-233.509458929958,4.22851622526691,
128.288882162868));
#133342=CARTESIAN_POINT('Ctrl Pts',(-233.517231830224,4.1567898754415,128.17206311025));
#133343=CARTESIAN_POINT('Ctrl Pts',(-233.525004730489,4.08042701953107,
128.058582330672));
#133344=CARTESIAN_POINT('Ctrl Pts',(-233.532495066251,4.00684014577942,
127.949226863272));
#133345=CARTESIAN_POINT('Ctrl Pts',(-233.539985402013,3.9289481928952,127.842971421854));
#133346=CARTESIAN_POINT('Ctrl Pts',(-233.547475737775,3.8470567288655,127.740158015356));
#133347=CARTESIAN_POINT('Ctrl Pts',(-233.555250071894,3.76206032508663,
127.633446407301));
#133348=CARTESIAN_POINT('Ctrl Pts',(-233.563024406013,3.67248589727299,
127.530104965787));
#133349=CARTESIAN_POINT('Ctrl Pts',(-233.570798740132,3.57863054435664,
127.430551718192));
#133350=CARTESIAN_POINT('Ctrl Pts',(-233.578563493079,3.48489085977491,
127.331121161077));
#133351=CARTESIAN_POINT('Ctrl Pts',(-233.586328246026,3.3868810130933,127.235469790483));
#133352=CARTESIAN_POINT('Ctrl Pts',(-233.594092998974,3.28493954349448,
127.143984235541));
#133353=CARTESIAN_POINT('Ctrl Pts',(-233.601850039859,3.18309932360012,
127.052589545341));
#133354=CARTESIAN_POINT('Ctrl Pts',(-233.609607080744,3.07733554089243,
126.965352696328));
#133355=CARTESIAN_POINT('Ctrl Pts',(-233.617364121629,2.96802467025874,
126.882624698456));
#133356=CARTESIAN_POINT('Ctrl Pts',(-233.625115312869,2.85879623180336,
126.799959086412));
#133357=CARTESIAN_POINT('Ctrl Pts',(-233.632866504109,2.74602634010971,
126.72179579268));
#133358=CARTESIAN_POINT('Ctrl Pts',(-233.640617695349,2.6301254676233,126.648446387573));
#133359=CARTESIAN_POINT('Ctrl Pts',(-233.648365592126,2.51427385609897,
126.575128157919));
#133360=CARTESIAN_POINT('Ctrl Pts',(-233.656113488903,2.39529424021625,
126.506619956129));
#133361=CARTESIAN_POINT('Ctrl Pts',(-233.66386138568,2.27362688440672,126.443190607924));
#133362=CARTESIAN_POINT('Ctrl Pts',(-233.671607661765,2.15198497878518,
126.379774527771));
#133363=CARTESIAN_POINT('Ctrl Pts',(-233.679353937848,2.02765679797953,
126.32143536868));
#133364=CARTESIAN_POINT('Ctrl Pts',(-233.687100213933,1.90110771798999,
126.268396276095));
#133365=CARTESIAN_POINT('Ctrl Pts',(-233.694846547198,1.77455770384406,
126.215356791987));
#133366=CARTESIAN_POINT('Ctrl Pts',(-233.702592880463,1.64578711837715,
126.167617603576));
#133367=CARTESIAN_POINT('Ctrl Pts',(-233.710339213729,1.51528147706566,
126.125353766987));
#133368=CARTESIAN_POINT('Ctrl Pts',(-233.718087281732,1.38474660992119,
126.083080465705));
#133369=CARTESIAN_POINT('Ctrl Pts',(-233.725835349735,1.25247628563114,
126.046285076606));
#133370=CARTESIAN_POINT('Ctrl Pts',(-233.733583417738,1.11897095435657,
126.015092712572));
#133371=CARTESIAN_POINT('Ctrl Pts',(-233.741339720479,0.985323732026644,
125.983867196922));
#133372=CARTESIAN_POINT('Ctrl Pts',(-233.749096023221,0.850439262011116,
125.958256691108));
#133373=CARTESIAN_POINT('Ctrl Pts',(-233.756852325963,0.714828508392514,
125.938335210102));
#133374=CARTESIAN_POINT('Ctrl Pts',(-233.764612768478,0.579145375231176,
125.918403096401));
#133375=CARTESIAN_POINT('Ctrl Pts',(-233.772373210992,0.442735574725181,
125.904166098365));
#133376=CARTESIAN_POINT('Ctrl Pts',(-233.780133653506,0.306113966437026,
125.895646192989));
#133377=CARTESIAN_POINT('Ctrl Pts',(-233.787906553771,0.169273041014923,
125.887112610705));
#133378=CARTESIAN_POINT('Ctrl Pts',(-233.795679454037,0.0322200194657413,
125.884314468805));
#133379=CARTESIAN_POINT('Ctrl Pts',(-233.803452354302,-0.104530563222136,
125.887221568906));
#133380=CARTESIAN_POINT('Ctrl Pts',(-233.810942690064,-0.236309917774265,
125.890022988597));
#133381=CARTESIAN_POINT('Ctrl Pts',(-233.818433025826,-0.367808133099621,
125.898122033053));
#133382=CARTESIAN_POINT('Ctrl Pts',(-233.825923361588,-0.49857230043032,
125.911446483459));
#133383=CARTESIAN_POINT('Ctrl Pts',(-233.833697695707,-0.634294430911234,
125.925276134452));
#133384=CARTESIAN_POINT('Ctrl Pts',(-233.841472029826,-0.769655678649314,
125.944779064057));
#133385=CARTESIAN_POINT('Ctrl Pts',(-233.849246363946,-0.904143756141013,
125.969931268539));
#133386=CARTESIAN_POINT('Ctrl Pts',(-233.857011116893,-1.03846608909711,
125.995052475177));
#133387=CARTESIAN_POINT('Ctrl Pts',(-233.86477586984,-1.17191701232081,
126.025809032753));
#133388=CARTESIAN_POINT('Ctrl Pts',(-233.872540622787,-1.30398825507674,
126.062125101154));
#133389=CARTESIAN_POINT('Ctrl Pts',(-233.880297663672,-1.43592832281212,
126.098405099923));
#133390=CARTESIAN_POINT('Ctrl Pts',(-233.888054704557,-1.56649106254064,
126.140233517931));
#133391=CARTESIAN_POINT('Ctrl Pts',(-233.895811745442,-1.69517766577222,
126.187483345646));
#133392=CARTESIAN_POINT('Ctrl Pts',(-233.903562936682,-1.82376722543543,
126.2346975419));
#133393=CARTESIAN_POINT('Ctrl Pts',(-233.911314127922,-1.95048309917022,
126.287324876084));
#133394=CARTESIAN_POINT('Ctrl Pts',(-233.919065319162,-2.0748412836655,
126.345188417471));
#133395=CARTESIAN_POINT('Ctrl Pts',(-233.926813215939,-2.19914661261483,
126.40302736531));
#133396=CARTESIAN_POINT('Ctrl Pts',(-233.934561112717,-2.32109589165727,
126.466097929356));
#133397=CARTESIAN_POINT('Ctrl Pts',(-233.942309009494,-2.44022497641992,
126.534175009544));
#133398=CARTESIAN_POINT('Ctrl Pts',(-233.950055285578,-2.55932914194616,
126.602237849475));
#133399=CARTESIAN_POINT('Ctrl Pts',(-233.957801561662,-2.67561394734977,
126.675304928642));
#133400=CARTESIAN_POINT('Ctrl Pts',(-233.965547837746,-2.78864010695454,
126.753105328599));
#133401=CARTESIAN_POINT('Ctrl Pts',(-233.973294171011,-2.90166710089289,
126.830906302861));
#133402=CARTESIAN_POINT('Ctrl Pts',(-233.981040504277,-3.01143507898782,
126.913440445956));
#133403=CARTESIAN_POINT('Ctrl Pts',(-233.988786837542,-3.11753432859071,
127.000393902076));
#133404=CARTESIAN_POINT('Ctrl Pts',(-233.996534905545,-3.22365733838504,
127.087366830819));
#133405=CARTESIAN_POINT('Ctrl Pts',(-234.004282973548,-3.32610968249579,
127.178760794149));
#133406=CARTESIAN_POINT('Ctrl Pts',(-234.012031041551,-3.42451559437457,
127.274222375742));
#133407=CARTESIAN_POINT('Ctrl Pts',(-234.019787344293,-3.52302609322741,
127.369785415041));
#133408=CARTESIAN_POINT('Ctrl Pts',(-234.027543647035,-3.61748128787602,
127.469424435827));
#133409=CARTESIAN_POINT('Ctrl Pts',(-234.035299949777,-3.70754271885999,
127.57274955645));
#133410=CARTESIAN_POINT('Ctrl Pts',(-234.043060392291,-3.79765221834138,
127.6761298248));
#133411=CARTESIAN_POINT('Ctrl Pts',(-234.050820834805,-3.88336303717,127.783199808095));
#133412=CARTESIAN_POINT('Ctrl Pts',(-234.058581277319,-3.96437839130675,
127.893538219507));
#133413=CARTESIAN_POINT('Ctrl Pts',(-234.066354177585,-4.04552379848216,
128.004053755933));
#133414=CARTESIAN_POINT('Ctrl Pts',(-234.07412707785,-4.12195846036362,
128.11784788046));
#133415=CARTESIAN_POINT('Ctrl Pts',(-234.081899978116,-4.19342966497602,
128.234471377268));
#133416=CARTESIAN_POINT('Ctrl Pts',(-234.089390313878,-4.26230271127547,
128.34685531621));
#133417=CARTESIAN_POINT('Ctrl Pts',(-234.09688064964,-4.32656675320381,
128.461866220346));
#133418=CARTESIAN_POINT('Ctrl Pts',(-234.104370985402,-4.38603774224419,
128.579084008668));
#133419=CARTESIAN_POINT('Ctrl Pts',(-234.112666954865,-4.45190521797911,
128.7089093227));
#133420=CARTESIAN_POINT('Ctrl Pts',(-234.120962924329,-4.51208009368256,
128.841809729011));
#133421=CARTESIAN_POINT('Ctrl Pts',(-234.129258893793,-4.56628422471798,
128.977277849438));
#133422=CARTESIAN_POINT('Ctrl Pts',(-234.137534886936,-4.62035783465243,
129.112419768744));
#133423=CARTESIAN_POINT('Ctrl Pts',(-234.14581088008,-4.66848925287003,
129.250116785686));
#133424=CARTESIAN_POINT('Ctrl Pts',(-234.154086873223,-4.71044705088237,
129.389838916307));
#133425=CARTESIAN_POINT('Ctrl Pts',(-234.157866594114,-4.72960955656794,
129.453651276565));
#133426=CARTESIAN_POINT('Ctrl Pts',(-234.161646315004,-4.7474849804627,
129.517885704026));
#133427=CARTESIAN_POINT('Ctrl Pts',(-234.165426035895,-4.76405452823417,
129.582490119309));
#133428=CARTESIAN_POINT('Ctrl Pts',(-232.415119734886,-4.76405452823408,
129.582490119308));
#133429=CARTESIAN_POINT('Ctrl Pts',(-232.421308237432,-4.79109715874973,
129.68792892526));
#133430=CARTESIAN_POINT('Ctrl Pts',(-232.427496739978,-4.81460826343985,
129.794150964176));
#133431=CARTESIAN_POINT('Ctrl Pts',(-232.433685242524,-4.8345569767513,
129.900899549758));
#133432=CARTESIAN_POINT('Ctrl Pts',(-232.445323692852,-4.87207366309676,
130.101657019204));
#133433=CARTESIAN_POINT('Ctrl Pts',(-232.45696214318,-4.89709405481899,
130.304817288689));
#133434=CARTESIAN_POINT('Ctrl Pts',(-232.468600593508,-4.90938042835421,
130.509120254146));
#133435=CARTESIAN_POINT('Ctrl Pts',(-232.47411391701,-4.91520068363373,
130.605901896826));
#133436=CARTESIAN_POINT('Ctrl Pts',(-232.479627240512,-4.91816392290484,
130.702939620798));
#133437=CARTESIAN_POINT('Ctrl Pts',(-232.485140564014,-4.91824815178524,
130.800096821013));
#133438=CARTESIAN_POINT('',(-232.13985943596,-4.91824884483728,130.807731486412));
#133439=CARTESIAN_POINT('Ctrl Pts',(-232.069726383436,-4.76405452823406,
129.582490119308));
#133440=CARTESIAN_POINT('Ctrl Pts',(-232.077373093558,-4.79768844224308,
129.713628239564));
#133441=CARTESIAN_POINT('Ctrl Pts',(-232.085019803679,-4.82588305575135,
129.846076494561));
#133442=CARTESIAN_POINT('Ctrl Pts',(-232.092666513801,-4.84855853558596,
129.979337472741));
#133443=CARTESIAN_POINT('Ctrl Pts',(-232.100532000827,-4.8718827743262,
130.116411126419));
#133444=CARTESIAN_POINT('Ctrl Pts',(-232.108397487854,-4.88936726615883,
130.254344247945));
#133445=CARTESIAN_POINT('Ctrl Pts',(-232.11626297488,-4.90098247622702,
130.392591470815));
#133446=CARTESIAN_POINT('Ctrl Pts',(-232.124128461907,-4.91259768629521,
130.530838693686));
#133447=CARTESIAN_POINT('Ctrl Pts',(-232.131993948933,-4.91834365475898,
130.669399558018));
#133448=CARTESIAN_POINT('Ctrl Pts',(-232.139859435959,-4.91824884483728,
130.807731486412));
#133449=CARTESIAN_POINT('Ctrl Pts',(-232.139859435996,-4.91824884483684,
130.807731487053));
#133450=CARTESIAN_POINT('Ctrl Pts',(-232.151515162288,-4.91810834766186,
131.012723128297));
#133451=CARTESIAN_POINT('Ctrl Pts',(-232.16317088858,-4.90515198395722,
131.217279571715));
#133452=CARTESIAN_POINT('Ctrl Pts',(-232.174826614871,-4.87954073522697,
131.420205789473));
#133453=CARTESIAN_POINT('Ctrl Pts',(-232.18260094899,-4.86245810992703,
131.555556961842));
#133454=CARTESIAN_POINT('Ctrl Pts',(-232.190375283109,-4.83971249996939,
131.69041121235));
#133455=CARTESIAN_POINT('Ctrl Pts',(-232.198149617228,-4.81134019566529,
131.824256977044));
#133456=CARTESIAN_POINT('Ctrl Pts',(-232.205914370175,-4.78300285769054,
131.957937788794));
#133457=CARTESIAN_POINT('Ctrl Pts',(-232.213679123123,-4.74905270305039,
132.090612208872));
#133458=CARTESIAN_POINT('Ctrl Pts',(-232.22144387607,-4.709577747114,132.221773932866));
#133459=CARTESIAN_POINT('Ctrl Pts',(-232.229200916955,-4.67014199826045,
132.352805385186));
#133460=CARTESIAN_POINT('Ctrl Pts',(-232.23695795784,-4.62519248005125,
132.482326759372));
#133461=CARTESIAN_POINT('Ctrl Pts',(-232.244714998725,-4.57486813546882,
132.609842438458));
#133462=CARTESIAN_POINT('Ctrl Pts',(-232.252466189965,-4.52458174086604,
132.737261956979));
#133463=CARTESIAN_POINT('Ctrl Pts',(-232.260217381205,-4.46892873047756,
132.862678428762));
#133464=CARTESIAN_POINT('Ctrl Pts',(-232.267968572445,-4.40809759882585,
132.985612235726));
#133465=CARTESIAN_POINT('Ctrl Pts',(-232.275716469222,-4.34729232202789,
133.108493792543));
#133466=CARTESIAN_POINT('Ctrl Pts',(-232.283464365999,-4.28131347429969,
133.228894433573));
#133467=CARTESIAN_POINT('Ctrl Pts',(-232.291212262776,-4.21039722906912,
133.346355549887));
#133468=CARTESIAN_POINT('Ctrl Pts',(-232.298958538861,-4.13949581798827,
133.463792095868));
#133469=CARTESIAN_POINT('Ctrl Pts',(-232.306704814945,-4.06365926563728,
133.578290005688));
#133470=CARTESIAN_POINT('Ctrl Pts',(-232.314451091029,-3.98316895409016,
133.689416621472));
#133471=CARTESIAN_POINT('Ctrl Pts',(-232.322197424294,-3.90267804838196,
133.800544057566));
#133472=CARTESIAN_POINT('Ctrl Pts',(-232.329943757559,-3.81753354426975,
133.908299833332));
#133473=CARTESIAN_POINT('Ctrl Pts',(-232.337690090825,-3.72805903915496,
134.012281885782));
#133474=CARTESIAN_POINT('Ctrl Pts',(-232.345438158828,-3.63856449684499,
134.116287224292));
#133475=CARTESIAN_POINT('Ctrl Pts',(-232.353186226831,-3.54473827895168,
134.21651686154));
#133476=CARTESIAN_POINT('Ctrl Pts',(-232.360934294834,-3.44694271738539,
134.312603620205));
#133477=CARTESIAN_POINT('Ctrl Pts',(-232.368690597575,-3.34904321753236,
134.408792501021));
#133478=CARTESIAN_POINT('Ctrl Pts',(-232.376446900317,-3.24716622609176,
134.500829433143));
#133479=CARTESIAN_POINT('Ctrl Pts',(-232.384203203059,-3.14170963453427,
134.588385410663));
#133480=CARTESIAN_POINT('Ctrl Pts',(-232.391963645573,-3.03619675761863,
134.675988119445));
#133481=CARTESIAN_POINT('Ctrl Pts',(-232.399724088088,-2.92710078451211,
134.759104871301));
#133482=CARTESIAN_POINT('Ctrl Pts',(-232.407484530602,-2.81485000272133,
134.837449077379));
#133483=CARTESIAN_POINT('Ctrl Pts',(-232.415257430867,-2.70241902601045,
134.915919048533));
#133484=CARTESIAN_POINT('Ctrl Pts',(-232.423030331133,-2.58682345024791,
134.989600953896));
#133485=CARTESIAN_POINT('Ctrl Pts',(-232.430803231398,-2.46851842628261,
135.05825293421));
#133486=CARTESIAN_POINT('Ctrl Pts',(-232.43829356716,-2.35451408793114,
135.124409242116));
#133487=CARTESIAN_POINT('Ctrl Pts',(-232.445783902922,-2.23799414428353,
135.185894833008));
#133488=CARTESIAN_POINT('Ctrl Pts',(-232.453274238684,-2.11938297203123,
135.242535792158));
#133489=CARTESIAN_POINT('Ctrl Pts',(-232.461048572803,-1.99627462113138,
135.30132431049));
#133490=CARTESIAN_POINT('Ctrl Pts',(-232.468822906922,-1.87052336313341,
135.355079801041));
#133491=CARTESIAN_POINT('Ctrl Pts',(-232.476597241041,-1.74257920707969,
135.403556283066));
#133492=CARTESIAN_POINT('Ctrl Pts',(-232.484361993988,-1.61479273076394,
135.451973022159));
#133493=CARTESIAN_POINT('Ctrl Pts',(-232.492126746935,-1.48481909575611,
135.495123560347));
#133494=CARTESIAN_POINT('Ctrl Pts',(-232.499891499883,-1.35313184475452,
135.53280827755));
#133495=CARTESIAN_POINT('Ctrl Pts',(-232.507648540768,-1.22157538738709,
135.570455565762));
#133496=CARTESIAN_POINT('Ctrl Pts',(-232.515405581653,-1.08830907450297,
135.602647729539));
#133497=CARTESIAN_POINT('Ctrl Pts',(-232.523162622538,-0.953824984768978,
135.629233772472));
#133498=CARTESIAN_POINT('Ctrl Pts',(-232.530913813778,-0.819442310533371,
135.655799766663));
#133499=CARTESIAN_POINT('Ctrl Pts',(-232.538665005018,-0.683844069328535,
135.676767979314));
#133500=CARTESIAN_POINT('Ctrl Pts',(-232.546416196258,-0.547535663322658,
135.692037750918));
#133501=CARTESIAN_POINT('Ctrl Pts',(-232.554164093035,-0.411285192025293,
135.707301032461));
#133502=CARTESIAN_POINT('Ctrl Pts',(-232.561911989812,-0.274325543983062,
135.716870646676));
#133503=CARTESIAN_POINT('Ctrl Pts',(-232.569659886589,-0.137170217383779,
135.720697403626));
#133504=CARTESIAN_POINT('Ctrl Pts',(-232.577406162673,-4.35807220934559E-5,
135.724523360101));
#133505=CARTESIAN_POINT('Ctrl Pts',(-232.585152438757,0.13727826251566,
135.72260883783));
#133506=CARTESIAN_POINT('Ctrl Pts',(-232.592898714841,0.274279211119887,
135.714956709371));
#133507=CARTESIAN_POINT('Ctrl Pts',(-232.600645048107,0.411281171034182,
135.707304524425));
#133508=CARTESIAN_POINT('Ctrl Pts',(-232.608391381372,0.547961841231461,
135.693914670581));
#133509=CARTESIAN_POINT('Ctrl Pts',(-232.616137714638,0.683808042433603,
135.67484207463));
#133510=CARTESIAN_POINT('Ctrl Pts',(-232.623885782641,0.819684665450428,
135.655765207504));
#133511=CARTESIAN_POINT('Ctrl Pts',(-232.631633850644,0.954726060521546,
135.631003120271));
#133512=CARTESIAN_POINT('Ctrl Pts',(-232.639381918647,1.08842746172099,
135.600662184719));
#133513=CARTESIAN_POINT('Ctrl Pts',(-232.647138221388,1.22227096236087,
135.57028900246));
#133514=CARTESIAN_POINT('Ctrl Pts',(-232.65489452413,1.35477124233406,135.534325214193));
#133515=CARTESIAN_POINT('Ctrl Pts',(-232.662650826872,1.48543642959345,
135.492927741554));
#133516=CARTESIAN_POINT('Ctrl Pts',(-232.670411269386,1.61617135679754,
135.451508173836));
#133517=CARTESIAN_POINT('Ctrl Pts',(-232.6781717119,1.74506887240367,135.404649276521));
#133518=CARTESIAN_POINT('Ctrl Pts',(-232.685932154415,1.87165636123661,
135.352556471742));
#133519=CARTESIAN_POINT('Ctrl Pts',(-232.69370505468,1.99844705954452,135.300380042968));
#133520=CARTESIAN_POINT('Ctrl Pts',(-232.701477954945,2.12291996558523,
135.242953080872));
#133521=CARTESIAN_POINT('Ctrl Pts',(-232.709250855211,2.24462557616264,
135.180527785915));
#133522=CARTESIAN_POINT('Ctrl Pts',(-232.716741190973,2.36190688123762,
135.12037180767));
#133523=CARTESIAN_POINT('Ctrl Pts',(-232.724231526735,2.47661832591759,
135.055574742809));
#133524=CARTESIAN_POINT('Ctrl Pts',(-232.731721862497,2.58838420484736,
134.986399626303));
#133525=CARTESIAN_POINT('Ctrl Pts',(-232.739496196616,2.70438772104741,
134.914601714229));
#133526=CARTESIAN_POINT('Ctrl Pts',(-232.747270530735,2.81758536427601,
134.837859775108));
#133527=CARTESIAN_POINT('Ctrl Pts',(-232.755044864854,2.92752694308547,
134.756419455692));
#133528=CARTESIAN_POINT('Ctrl Pts',(-232.762809617801,3.03733302872451,
134.675079504191));
#133529=CARTESIAN_POINT('Ctrl Pts',(-232.770574370748,3.14389072309296,
134.589052923915));
#133530=CARTESIAN_POINT('Ctrl Pts',(-232.778339123695,3.24677611876926,
134.498630220219));
#133531=CARTESIAN_POINT('Ctrl Pts',(-232.78609616458,3.34955932722015,134.408297325628));
#133532=CARTESIAN_POINT('Ctrl Pts',(-232.793853205465,3.44867720366,134.31357725316));
#133533=CARTESIAN_POINT('Ctrl Pts',(-232.80161024635,3.54373672999305,134.214802385284));
#133534=CARTESIAN_POINT('Ctrl Pts',(-232.809361437591,3.63872457119796,
134.116102004305));
#133535=CARTESIAN_POINT('Ctrl Pts',(-232.817112628831,3.72965988389467,
134.013353194753));
#133536=CARTESIAN_POINT('Ctrl Pts',(-232.824863820071,3.81618479817155,
133.906926756862));
#133537=CARTESIAN_POINT('Ctrl Pts',(-232.832611716848,3.90267293705162,
133.800545553046));
#133538=CARTESIAN_POINT('Ctrl Pts',(-232.840359613625,3.98475415970784,
133.690490132483));
#133539=CARTESIAN_POINT('Ctrl Pts',(-232.848107510402,4.0621095229413,133.577165927379));
#133540=CARTESIAN_POINT('Ctrl Pts',(-232.855853786486,4.13944870510036,
133.463865427257));
#133541=CARTESIAN_POINT('Ctrl Pts',(-232.86360006257,4.21206377383438,133.347297825332));
#133542=CARTESIAN_POINT('Ctrl Pts',(-232.871346338654,4.27967818059685,
133.227898884857));
#133543=CARTESIAN_POINT('Ctrl Pts',(-232.87909267192,4.3472930864736,133.108499063006));
#133544=CARTESIAN_POINT('Ctrl Pts',(-232.886839005185,4.40990706406635,
132.986268201103));
#133545=CARTESIAN_POINT('Ctrl Pts',(-232.89458533845,4.46728893890667,132.861667740682));
#133546=CARTESIAN_POINT('Ctrl Pts',(-232.902333406453,4.52468366401992,
132.737039376851));
#133547=CARTESIAN_POINT('Ctrl Pts',(-232.910081474456,4.57684379133737,
132.61004071361));
#133548=CARTESIAN_POINT('Ctrl Pts',(-232.917829542459,4.62358597614422,
132.481153921376));
#133549=CARTESIAN_POINT('Ctrl Pts',(-232.925585845201,4.67037783910138,
132.352130146726));
#133550=CARTESIAN_POINT('Ctrl Pts',(-232.933342147943,4.7117401233103,132.221214602559));
#133551=CARTESIAN_POINT('Ctrl Pts',(-232.941098450685,4.74753898252945,
132.088905934736));
#133552=CARTESIAN_POINT('Ctrl Pts',(-232.948858893199,4.78335694867765,
131.956526649793));
#133553=CARTESIAN_POINT('Ctrl Pts',(-232.956619335713,4.81360548693504,
131.822753140755));
#133554=CARTESIAN_POINT('Ctrl Pts',(-232.964379778227,4.83820196471525,
131.688094067836));
#133555=CARTESIAN_POINT('Ctrl Pts',(-232.972152678493,4.86283792694517,
131.553218828218));
#133556=CARTESIAN_POINT('Ctrl Pts',(-232.979925578758,4.88180364345212,
131.417455571365));
#133557=CARTESIAN_POINT('Ctrl Pts',(-232.987698479024,4.89506833017058,
131.281318797558));
#133558=CARTESIAN_POINT('Ctrl Pts',(-232.995188814786,4.90785081211506,
131.150130938386));
#133559=CARTESIAN_POINT('Ctrl Pts',(-233.002679150547,4.91533954413174,
131.018596554867));
#133560=CARTESIAN_POINT('Ctrl Pts',(-233.010169486309,4.9175527470689,130.887173915382));
#133561=CARTESIAN_POINT('Ctrl Pts',(-233.017943820429,4.91984986426811,
130.750768346575));
#133562=CARTESIAN_POINT('Ctrl Pts',(-233.025718154548,4.91647078861257,
130.614051070782));
#133563=CARTESIAN_POINT('Ctrl Pts',(-233.033492488667,4.90737885019658,
130.477533624887));
#133564=CARTESIAN_POINT('Ctrl Pts',(-233.041257241614,4.89829811678214,
130.341184424544));
#133565=CARTESIAN_POINT('Ctrl Pts',(-233.049021994561,4.88351855501939,
130.205034950446));
#133566=CARTESIAN_POINT('Ctrl Pts',(-233.056786747508,4.86305544297488,
130.069598873153));
#133567=CARTESIAN_POINT('Ctrl Pts',(-233.064543788393,4.84261265518175,
129.934297312882));
#133568=CARTESIAN_POINT('Ctrl Pts',(-233.072300829278,4.81649760890657,
129.799708123433));
#133569=CARTESIAN_POINT('Ctrl Pts',(-233.080057870163,4.78477751105465,
129.666341622907));
#133570=CARTESIAN_POINT('Ctrl Pts',(-233.087809061403,4.75308133357522,
129.533075695095));
#133571=CARTESIAN_POINT('Ctrl Pts',(-233.095560252643,4.71578860783217,
129.401030999759));
#133572=CARTESIAN_POINT('Ctrl Pts',(-233.103311443884,4.6730178611363,129.270709049575));
#133573=CARTESIAN_POINT('Ctrl Pts',(-233.111059340661,4.63026529314866,
129.140442489696));
#133574=CARTESIAN_POINT('Ctrl Pts',(-233.118807237438,4.58203945668833,
129.011897589346));
#133575=CARTESIAN_POINT('Ctrl Pts',(-233.126555134215,4.52850905676385,
128.885561830484));
#133576=CARTESIAN_POINT('Ctrl Pts',(-233.134301410299,4.47498985424519,
128.759252498339));
#133577=CARTESIAN_POINT('Ctrl Pts',(-233.142047686383,4.41616844775224,
128.635151748285));
#133578=CARTESIAN_POINT('Ctrl Pts',(-233.149793962467,4.35226197600564,
128.513727789129));
#133579=CARTESIAN_POINT('Ctrl Pts',(-233.157540295733,4.2883550325159,128.392302933647));
#133580=CARTESIAN_POINT('Ctrl Pts',(-233.165286628998,4.21936313095926,
128.273555254465));
#133581=CARTESIAN_POINT('Ctrl Pts',(-233.173032962263,4.14554953971994,
128.15792866563));
#133582=CARTESIAN_POINT('Ctrl Pts',(-233.180781030266,4.07171941843855,
128.042276183022));
#133583=CARTESIAN_POINT('Ctrl Pts',(-233.188529098269,3.99306566916125,
127.929746511061));
#133584=CARTESIAN_POINT('Ctrl Pts',(-233.196277166272,3.90989485322046,
127.820754527738));
#133585=CARTESIAN_POINT('Ctrl Pts',(-233.204033469014,3.82663564234684,
127.711646706438));
#133586=CARTESIAN_POINT('Ctrl Pts',(-233.211789771756,3.73885001226341,
127.60608439588));
#133587=CARTESIAN_POINT('Ctrl Pts',(-233.219546074498,3.64688514069141,
127.504449734966));
#133588=CARTESIAN_POINT('Ctrl Pts',(-233.227306517012,3.55487118469845,
127.402760828572));
#133589=CARTESIAN_POINT('Ctrl Pts',(-233.235066959526,3.4586738166718,127.305004027419));
#133590=CARTESIAN_POINT('Ctrl Pts',(-233.24282740204,3.35867632192402,127.21152379591));
#133591=CARTESIAN_POINT('Ctrl Pts',(-233.250600302306,3.25851830232031,
127.117893501635));
#133592=CARTESIAN_POINT('Ctrl Pts',(-233.258373202571,3.15454826235037,
127.02855375067));
#133593=CARTESIAN_POINT('Ctrl Pts',(-233.266146102837,3.0471824261316,126.94380854249));
#133594=CARTESIAN_POINT('Ctrl Pts',(-233.273636438599,2.94371960849848,
126.862144036088));
#133595=CARTESIAN_POINT('Ctrl Pts',(-233.281126774361,2.83710384897438,
126.784746006553));
#133596=CARTESIAN_POINT('Ctrl Pts',(-233.288617110123,2.7277305505416,126.711846829423));
#133597=CARTESIAN_POINT('Ctrl Pts',(-233.296391444242,2.61421033025465,
126.636183657834));
#133598=CARTESIAN_POINT('Ctrl Pts',(-233.304165778361,2.49735974116572,
126.565127542813));
#133599=CARTESIAN_POINT('Ctrl Pts',(-233.31194011248,2.37758933276305,126.498985833969));
#133600=CARTESIAN_POINT('Ctrl Pts',(-233.319704865427,2.25796653068454,
126.432925638871));
#133601=CARTESIAN_POINT('Ctrl Pts',(-233.327469618374,2.13543140802883,
126.371767986375));
#133602=CARTESIAN_POINT('Ctrl Pts',(-233.335234371321,2.01042438855384,
126.315777674096));
#133603=CARTESIAN_POINT('Ctrl Pts',(-233.342991412206,1.88554152781289,
126.259842972185));
#133604=CARTESIAN_POINT('Ctrl Pts',(-233.350748453091,1.75819201055864,
126.209065555812));
#133605=CARTESIAN_POINT('Ctrl Pts',(-233.358505493976,1.62884150883475,
126.163664721302));
#133606=CARTESIAN_POINT('Ctrl Pts',(-233.366256685216,1.49958855133058,
126.118298123915));
#133607=CARTESIAN_POINT('Ctrl Pts',(-233.374007876456,1.36833798025505,
126.078300167068));
#133608=CARTESIAN_POINT('Ctrl Pts',(-233.381759067696,1.23557579933317,
126.043842210228));
#133609=CARTESIAN_POINT('Ctrl Pts',(-233.389506964473,1.10287004587954,
126.009398898939));
#133610=CARTESIAN_POINT('Ctrl Pts',(-233.397254861251,0.968654338046777,
125.980491002458));
#133611=CARTESIAN_POINT('Ctrl Pts',(-233.405002758028,0.833429997389721,
125.957240080386));
#133612=CARTESIAN_POINT('Ctrl Pts',(-233.412749034112,0.698233942749631,
125.933994021906));
#133613=CARTESIAN_POINT('Ctrl Pts',(-233.420495310196,0.562030060011294,
125.916402650364));
#133614=CARTESIAN_POINT('Ctrl Pts',(-233.42824158628,0.425329635286075,
125.9045363591));
#133615=CARTESIAN_POINT('Ctrl Pts',(-233.435987919545,0.288628201469933,
125.892669980243));
#133616=CARTESIAN_POINT('Ctrl Pts',(-233.443734252811,0.151430607853447,
125.886528799803));
#133617=CARTESIAN_POINT('Ctrl Pts',(-233.451480586076,0.0142526348897896,
125.88613126902));
#133618=CARTESIAN_POINT('Ctrl Pts',(-233.459228654079,-0.122956058129974,
125.885733649213));
#133619=CARTESIAN_POINT('Ctrl Pts',(-233.466976722082,-0.260144730864806,
125.891082239685));
#133620=CARTESIAN_POINT('Ctrl Pts',(-233.474724790085,-0.396798630823245,
125.902143373392));
#133621=CARTESIAN_POINT('Ctrl Pts',(-233.482481092827,-0.533597768172948,
125.913216263004));
#133622=CARTESIAN_POINT('Ctrl Pts',(-233.490237395568,-0.669860607068107,
125.930013792452));
#133623=CARTESIAN_POINT('Ctrl Pts',(-233.49799369831,-0.805077985189934,
125.952450426697));
#133624=CARTESIAN_POINT('Ctrl Pts',(-233.505754140824,-0.940367532897782,
125.974899036049));
#133625=CARTESIAN_POINT('Ctrl Pts',(-233.513514583338,-1.07461012549429,
126.002992667354));
#133626=CARTESIAN_POINT('Ctrl Pts',(-233.521275025852,-1.20730878024569,
126.036595043249));
#133627=CARTESIAN_POINT('Ctrl Pts',(-233.529047926118,-1.34022045465813,
126.070251360661));
#133628=CARTESIAN_POINT('Ctrl Pts',(-233.536820826383,-1.47158286359105,
126.109433982231));
#133629=CARTESIAN_POINT('Ctrl Pts',(-233.544593726649,-1.60091526437436,
126.153957045961));
#133630=CARTESIAN_POINT('Ctrl Pts',(-233.552084062411,-1.72554610662334,
126.19686158418));
#133631=CARTESIAN_POINT('Ctrl Pts',(-233.559574398173,-1.8482916831584,
126.244724916668));
#133632=CARTESIAN_POINT('Ctrl Pts',(-233.567064733935,-1.96874276488739,
126.297339984353));
#133633=CARTESIAN_POINT('Ctrl Pts',(-233.574839565395,-2.093768783658,126.351953461839));
#133634=CARTESIAN_POINT('Ctrl Pts',(-233.582614396855,-2.21671863517069,
126.411859777179));
#133635=CARTESIAN_POINT('Ctrl Pts',(-233.590389228315,-2.33711173374839,
126.476879617437));
#133636=CARTESIAN_POINT('Ctrl Pts',(-233.598154365608,-2.45735471836534,
126.541818386721));
#133637=CARTESIAN_POINT('Ctrl Pts',(-233.605919502901,-2.57504695260555,
126.611857810093));
#133638=CARTESIAN_POINT('Ctrl Pts',(-233.613684640195,-2.68972752834779,
126.686770438135));
#133639=CARTESIAN_POINT('Ctrl Pts',(-233.621441952913,-2.80429254570409,
126.761607580138));
#133640=CARTESIAN_POINT('Ctrl Pts',(-233.629199265632,-2.91585161890929,
126.841307941542));
#133641=CARTESIAN_POINT('Ctrl Pts',(-233.636956578351,-3.02396849818628,
126.925598239632));
#133642=CARTESIAN_POINT('Ctrl Pts',(-233.644707556841,-3.13199709470004,
127.009819710537));
#133643=CARTESIAN_POINT('Ctrl Pts',(-233.652458535331,-3.2365887867988,
127.098623415991));
#133644=CARTESIAN_POINT('Ctrl Pts',(-233.660209513821,-3.3373367456812,
127.191693111633));
#133645=CARTESIAN_POINT('Ctrl Pts',(-233.667957032468,-3.43803973317778,
127.284721263274));
#133646=CARTESIAN_POINT('Ctrl Pts',(-233.675704551114,-3.534902114388,127.382011351971));
#133647=CARTESIAN_POINT('Ctrl Pts',(-233.68345206976,-3.62755069929318,
127.483207356038));
#133648=CARTESIAN_POINT('Ctrl Pts',(-233.691197807897,-3.72017799201285,
127.584380103581));
#133649=CARTESIAN_POINT('Ctrl Pts',(-233.698943546035,-3.80859315191726,
127.689456691966));
#133650=CARTESIAN_POINT('Ctrl Pts',(-233.706689284172,-3.89246066385488,
127.798045091404));
#133651=CARTESIAN_POINT('Ctrl Pts',(-233.714434919588,-3.97632706357252,
127.906632050783));
#133652=CARTESIAN_POINT('Ctrl Pts',(-233.722180555005,-4.05564569735638,
128.018730418551));
#133653=CARTESIAN_POINT('Ctrl Pts',(-233.729926190421,-4.13012232744392,
128.133916343134));
#133654=CARTESIAN_POINT('Ctrl Pts',(-233.737677017795,-4.20464887977663,
128.249179477708));
#133655=CARTESIAN_POINT('Ctrl Pts',(-233.745427845169,-4.27432673041007,
128.367533975942));
#133656=CARTESIAN_POINT('Ctrl Pts',(-233.753178672543,-4.33890570523499,
128.48852807967));
#133657=CARTESIAN_POINT('Ctrl Pts',(-233.76093206748,-4.40350607269246,
128.609562264281));
#133658=CARTESIAN_POINT('Ctrl Pts',(-233.768685462417,-4.46300402586445,
128.733237445952));
#133659=CARTESIAN_POINT('Ctrl Pts',(-233.776438857354,-4.51719654556064,
128.859079550143));
#133660=CARTESIAN_POINT('Ctrl Pts',(-233.784201671387,-4.57145490022168,
128.985074531715));
#133661=CARTESIAN_POINT('Ctrl Pts',(-233.791964485419,-4.62039480057076,
129.113241331318));
#133662=CARTESIAN_POINT('Ctrl Pts',(-233.799727299451,-4.66386213048879,
129.243087710515));
#133663=CARTESIAN_POINT('Ctrl Pts',(-233.806422729466,-4.70135271885186,
129.355080261289));
#133664=CARTESIAN_POINT('Ctrl Pts',(-233.813118159481,-4.73477299282818,
129.46832185717));
#133665=CARTESIAN_POINT('Ctrl Pts',(-233.819813589496,-4.76405452823394,
129.582490119308));
#133666=CARTESIAN_POINT('Origin',(213.235140564004,0.,130.804360617566));
#133667=CARTESIAN_POINT('',(-235.915124447633,-4.76405452823405,129.582490119308));
#133668=CARTESIAN_POINT('',(-235.570143588767,-4.76405452823401,129.582490119308));
#133669=CARTESIAN_POINT('',(213.235140564004,-4.76405452823405,129.582490119308));
#133670=CARTESIAN_POINT('',(-234.235140563976,-4.91824993088488,130.803536086871));
#133671=CARTESIAN_POINT('Ctrl Pts',(-234.235140564014,-4.91824993088499,
130.803536087554));
#133672=CARTESIAN_POINT('Ctrl Pts',(-234.243160377497,-4.91827380234173,
130.945927254282));
#133673=CARTESIAN_POINT('Ctrl Pts',(-234.25118019098,-4.91210965921112,
131.088232882481));
#133674=CARTESIAN_POINT('Ctrl Pts',(-234.259200004463,-4.89980581763934,
131.229902638908));
#133675=CARTESIAN_POINT('Ctrl Pts',(-234.267227171366,-4.88749069459418,
131.371702293267));
#133676=CARTESIAN_POINT('Ctrl Pts',(-234.275254338268,-4.86902467683493,
131.512864564863));
#133677=CARTESIAN_POINT('Ctrl Pts',(-234.283281505171,-4.84450765492664,
131.652846706938));
#133678=CARTESIAN_POINT('Ctrl Pts',(-234.291576263841,-4.81917333928226,
131.79749526112));
#133679=CARTESIAN_POINT('Ctrl Pts',(-234.299871022512,-4.78737768946012,
131.94088323545));
#133680=CARTESIAN_POINT('Ctrl Pts',(-234.308165781182,-4.74928705413213,
132.082427728462));
#133681=CARTESIAN_POINT('Ctrl Pts',(-234.31621698266,-4.71231486583196,
132.219816081358));
#133682=CARTESIAN_POINT('Ctrl Pts',(-234.324268184138,-4.66941234589774,
132.355467387));
#133683=CARTESIAN_POINT('Ctrl Pts',(-234.332319385617,-4.6207809978444,
132.488868270401));
#133684=CARTESIAN_POINT('Ctrl Pts',(-234.340735922883,-4.56994292674358,
132.628322426347));
#133685=CARTESIAN_POINT('Ctrl Pts',(-234.349152460149,-4.51284414580398,
132.765316738622));
#133686=CARTESIAN_POINT('Ctrl Pts',(-234.357568997416,-4.44976871876674,
132.899292934369));
#133687=CARTESIAN_POINT('Ctrl Pts',(-234.365985534682,-4.38669329172966,
133.033269130116));
#133688=CARTESIAN_POINT('Ctrl Pts',(-234.374402071948,-4.31764148397627,
133.164226864535));
#133689=CARTESIAN_POINT('Ctrl Pts',(-234.382818609214,-4.24294876878563,
133.291642026647));
#133690=CARTESIAN_POINT('Ctrl Pts',(-234.390592943333,-4.17395529726889,
133.409335088621));
#133691=CARTESIAN_POINT('Ctrl Pts',(-234.398367277452,-4.09995188924855,
133.524341728663));
#133692=CARTESIAN_POINT('Ctrl Pts',(-234.406141611571,-4.02117331738154,
133.636205990124));
#133693=CARTESIAN_POINT('Ctrl Pts',(-234.413906364519,-3.94249183306371,
133.74793238888));
#133694=CARTESIAN_POINT('Ctrl Pts',(-234.421671117466,-3.859047117171,133.856523797991));
#133695=CARTESIAN_POINT('Ctrl Pts',(-234.429435870413,-3.77111941879046,
133.961549460781));
#133696=CARTESIAN_POINT('Ctrl Pts',(-234.437192911298,-3.68327905143929,
134.066470810603));
#133697=CARTESIAN_POINT('Ctrl Pts',(-234.444949952183,-3.59096481174796,
134.167833164111));
#133698=CARTESIAN_POINT('Ctrl Pts',(-234.452706993068,-3.49449955511849,
134.265235640126));
#133699=CARTESIAN_POINT('Ctrl Pts',(-234.460458184308,-3.39810704368956,
134.362564664176));
#133700=CARTESIAN_POINT('Ctrl Pts',(-234.468209375548,-3.29757002002429,
134.455939477869));
#133701=CARTESIAN_POINT('Ctrl Pts',(-234.475960566788,-3.19325058968546,
134.544993416168));
#133702=CARTESIAN_POINT('Ctrl Pts',(-234.483708463565,-3.0889754978872,
134.634009504167));
#133703=CARTESIAN_POINT('Ctrl Pts',(-234.491456360342,-2.98092149358705,
134.718708116097));
#133704=CARTESIAN_POINT('Ctrl Pts',(-234.499204257119,-2.86948623848019,
134.79876067135));
#133705=CARTESIAN_POINT('Ctrl Pts',(-234.506950533203,-2.75807429322643,
134.878796481335));
#133706=CARTESIAN_POINT('Ctrl Pts',(-234.514696809287,-2.64328282131883,
134.954187939758));
#133707=CARTESIAN_POINT('Ctrl Pts',(-234.522443085372,-2.52554082411746,
135.024648120594));
#133708=CARTESIAN_POINT('Ctrl Pts',(-234.530189418637,-2.40779795777158,
135.095108821552));
#133709=CARTESIAN_POINT('Ctrl Pts',(-234.537935751902,-2.28710485815356,
135.160637971524));
#133710=CARTESIAN_POINT('Ctrl Pts',(-234.545682085168,-2.16391728636374,
135.220993389291));
#133711=CARTESIAN_POINT('Ctrl Pts',(-234.553430153171,-2.0407021275715,
135.281362323235));
#133712=CARTESIAN_POINT('Ctrl Pts',(-234.561178221174,-1.9149917360419,
135.336555047469));
#133713=CARTESIAN_POINT('Ctrl Pts',(-234.568926289177,-1.78726374357305,
135.386376699315));
#133714=CARTESIAN_POINT('Ctrl Pts',(-234.576682591918,-1.65940000027365,
135.436251302206));
#133715=CARTESIAN_POINT('Ctrl Pts',(-234.58443889466,-1.52951473732209,
135.480743287185));
#133716=CARTESIAN_POINT('Ctrl Pts',(-234.592195197402,-1.39810324503968,
135.51970688043));
#133717=CARTESIAN_POINT('Ctrl Pts',(-234.599955639917,-1.26662161448711,
135.558691269718));
#133718=CARTESIAN_POINT('Ctrl Pts',(-234.607716082431,-1.13361251042853,
135.592141292507));
#133719=CARTESIAN_POINT('Ctrl Pts',(-234.615476524945,-0.999582463641959,
135.619962133564));
#133720=CARTESIAN_POINT('Ctrl Pts',(-234.62324942521,-0.86533725992566,
135.647827635104));
#133721=CARTESIAN_POINT('Ctrl Pts',(-234.631022325476,-0.730068224438899,
135.670045833778));
#133722=CARTESIAN_POINT('Ctrl Pts',(-234.638795225741,-0.594288970565359,
135.686573607795));
#133723=CARTESIAN_POINT('Ctrl Pts',(-234.646285561503,-0.463445634578529,
135.702500555596));
#133724=CARTESIAN_POINT('Ctrl Pts',(-234.653775897265,-0.332128838632401,
135.713143593568));
#133725=CARTESIAN_POINT('Ctrl Pts',(-234.661266233027,-0.200797156389273,
135.718509940133));
#133726=CARTESIAN_POINT('Ctrl Pts',(-234.669040567146,-0.0644859934955289,
135.724079753359));
#133727=CARTESIAN_POINT('Ctrl Pts',(-234.676814901265,0.0722729995977941,
135.723982488443));
#133728=CARTESIAN_POINT('Ctrl Pts',(-234.684589235384,0.208969313293336,
135.718169210562));
#133729=CARTESIAN_POINT('Ctrl Pts',(-234.692353988331,0.345497160998777,
135.712363097027));
#133730=CARTESIAN_POINT('Ctrl Pts',(-234.700118741278,0.48196209614215,
135.700855003386));
#133731=CARTESIAN_POINT('Ctrl Pts',(-234.707883494225,0.61785022945676,
135.68364787663));
#133732=CARTESIAN_POINT('Ctrl Pts',(-234.71564053511,0.753603396761675,
135.666457840234));
#133733=CARTESIAN_POINT('Ctrl Pts',(-234.723397575995,0.888780516952143,
135.643580083891));
#133734=CARTESIAN_POINT('Ctrl Pts',(-234.73115461688,1.02286980610768,135.615069548925));
#133735=CARTESIAN_POINT('Ctrl Pts',(-234.738905808121,1.15685797748738,
135.586580513975));
#133736=CARTESIAN_POINT('Ctrl Pts',(-234.746656999361,1.28975956980372,
135.552467236216));
#133737=CARTESIAN_POINT('Ctrl Pts',(-234.754408190601,1.42107037047482,
135.512836173907));
#133738=CARTESIAN_POINT('Ctrl Pts',(-234.762156087378,1.55232536055298,
135.473221955856));
#133739=CARTESIAN_POINT('Ctrl Pts',(-234.769903984155,1.68199053024865,
135.428094730416));
#133740=CARTESIAN_POINT('Ctrl Pts',(-234.777651880932,1.80957448953227,
135.377611455792));
#133741=CARTESIAN_POINT('Ctrl Pts',(-234.785398157016,1.93713176100199,
135.32713874118));
#133742=CARTESIAN_POINT('Ctrl Pts',(-234.7931444331,2.0626083246735,135.271312349617));
#133743=CARTESIAN_POINT('Ctrl Pts',(-234.800890709184,2.18553089584264,
135.210338121573));
#133744=CARTESIAN_POINT('Ctrl Pts',(-234.80863704245,2.30845437439844,135.149363443431));
#133745=CARTESIAN_POINT('Ctrl Pts',(-234.816383375715,2.42882347258885,
135.083241026715));
#133746=CARTESIAN_POINT('Ctrl Pts',(-234.824129708981,2.54618808648691,
135.012223411281));
#133747=CARTESIAN_POINT('Ctrl Pts',(-234.831877776983,2.66357898337634,
134.941189891945));
#133748=CARTESIAN_POINT('Ctrl Pts',(-234.839625844986,2.77796372268226,
134.865259194853));
#133749=CARTESIAN_POINT('Ctrl Pts',(-234.847373912989,2.88892018926236,
134.784727837129));
#133750=CARTESIAN_POINT('Ctrl Pts',(-234.855130215731,2.99999458169539,
134.70411088972));
#133751=CARTESIAN_POINT('Ctrl Pts',(-234.862886518473,3.10763310598619,
134.618883744115));
#133752=CARTESIAN_POINT('Ctrl Pts',(-234.870642821215,3.21144540197229,
134.529384307779));
#133753=CARTESIAN_POINT('Ctrl Pts',(-234.878403263729,3.31531310570647,
134.439837102899));
#133754=CARTESIAN_POINT('Ctrl Pts',(-234.886163706243,3.41535022690414,
134.346013331021));
#133755=CARTESIAN_POINT('Ctrl Pts',(-234.893924148757,3.51120320256636,
134.248287900885));
#133756=CARTESIAN_POINT('Ctrl Pts',(-234.901697049023,3.60721004993455,
134.150405593212));
#133757=CARTESIAN_POINT('Ctrl Pts',(-234.909469949288,3.69901906754108,
134.048609401732));
#133758=CARTESIAN_POINT('Ctrl Pts',(-234.917242849554,3.7863163552244,133.94330813555));
#133759=CARTESIAN_POINT('Ctrl Pts',(-234.924733185316,3.87044016661349,
133.84183483563));
#133760=CARTESIAN_POINT('Ctrl Pts',(-234.932223521078,3.95037439168747,
133.737107118107));
#133761=CARTESIAN_POINT('Ctrl Pts',(-234.93971385684,4.0258772332447,133.629514695726));
#133762=CARTESIAN_POINT('Ctrl Pts',(-234.947488190959,4.10424278798674,
133.517842873949));
#133763=CARTESIAN_POINT('Ctrl Pts',(-234.955262525078,4.17808253254862,
133.402731085781));
#133764=CARTESIAN_POINT('Ctrl Pts',(-234.963036859197,4.24707935377274,
133.284582386936));
#133765=CARTESIAN_POINT('Ctrl Pts',(-234.970801612144,4.31599114258113,
133.166579295804));
#133766=CARTESIAN_POINT('Ctrl Pts',(-234.978566365092,4.38007168826157,
133.045547075266));
#133767=CARTESIAN_POINT('Ctrl Pts',(-234.986331118039,4.43904570049892,
132.921919667836));
#133768=CARTESIAN_POINT('Ctrl Pts',(-234.994088158924,4.49796113891594,
132.798415048891));
#133769=CARTESIAN_POINT('Ctrl Pts',(-235.001845199809,4.55177996992062,
132.672320723136));
#133770=CARTESIAN_POINT('Ctrl Pts',(-235.009602240694,4.60027178549489,
132.544096966005));
#133771=CARTESIAN_POINT('Ctrl Pts',(-235.017353431934,4.64872703301389,
132.415969903407));
#133772=CARTESIAN_POINT('Ctrl Pts',(-235.025104623174,4.69186312324668,
132.28571696993));
#133773=CARTESIAN_POINT('Ctrl Pts',(-235.032855814414,4.7294970833229,132.153819917189));
#133774=CARTESIAN_POINT('Ctrl Pts',(-235.040603711191,4.76711504796221,
132.021978924214));
#133775=CARTESIAN_POINT('Ctrl Pts',(-235.048351607968,4.79923542659909,
131.888495576997));
#133776=CARTESIAN_POINT('Ctrl Pts',(-235.056099504745,4.82572466430102,
131.753868135628));
#133777=CARTESIAN_POINT('Ctrl Pts',(-235.063845780829,4.85220836102539,
131.619268855419));
#133778=CARTESIAN_POINT('Ctrl Pts',(-235.071592056914,4.87306318431779,
131.483526340446));
#133779=CARTESIAN_POINT('Ctrl Pts',(-235.079338332998,4.88820649165192,
131.347150040337));
#133780=CARTESIAN_POINT('Ctrl Pts',(-235.087084666263,4.90334991077052,
131.210772733529));
#133781=CARTESIAN_POINT('Ctrl Pts',(-235.094830999528,4.91278168665356,
131.073762020827));
#133782=CARTESIAN_POINT('Ctrl Pts',(-235.102577332794,4.91647099606753,
130.936633091372));
#133783=CARTESIAN_POINT('Ctrl Pts',(-235.110325400797,4.92016113167677,
130.799473452844));
#133784=CARTESIAN_POINT('Ctrl Pts',(-235.1180734688,4.91810623134189,130.662195935634));
#133785=CARTESIAN_POINT('Ctrl Pts',(-235.125821536802,4.9103275997707,130.525315951912));
#133786=CARTESIAN_POINT('Ctrl Pts',(-235.133577839544,4.90254070097732,
130.388290490514));
#133787=CARTESIAN_POINT('Ctrl Pts',(-235.141334142286,4.88901794121855,
130.251663797559));
#133788=CARTESIAN_POINT('Ctrl Pts',(-235.149090445028,4.86983261240989,
130.115946941344));
#133789=CARTESIAN_POINT('Ctrl Pts',(-235.156850887542,4.85063704381353,
129.980157648956));
#133790=CARTESIAN_POINT('Ctrl Pts',(-235.164611330056,4.82577295485478,
129.845279545221));
#133791=CARTESIAN_POINT('Ctrl Pts',(-235.172371772571,4.79536465743734,
129.711812740033));
#133792=CARTESIAN_POINT('Ctrl Pts',(-235.180144672836,4.76490754592135,
129.578131682082));
#133793=CARTESIAN_POINT('Ctrl Pts',(-235.187917573101,4.72888854358715,
129.445866827397));
#133794=CARTESIAN_POINT('Ctrl Pts',(-235.195690473367,4.68748192240888,
129.315503240384));
#133795=CARTESIAN_POINT('Ctrl Pts',(-235.203180809129,4.64758053620742,
129.189878698124));
#133796=CARTESIAN_POINT('Ctrl Pts',(-235.210671144891,4.60267654256751,
129.066019881279));
#133797=CARTESIAN_POINT('Ctrl Pts',(-235.218161480653,4.55296712056405,
128.944340869939));
#133798=CARTESIAN_POINT('Ctrl Pts',(-235.225935814772,4.50137295071654,
128.818048361901));
#133799=CARTESIAN_POINT('Ctrl Pts',(-235.233710148891,4.4444383287666,128.693704160284));
#133800=CARTESIAN_POINT('Ctrl Pts',(-235.24148448301,4.38233094949637,128.571792922828));
#133801=CARTESIAN_POINT('Ctrl Pts',(-235.249249235957,4.32030011202039,
128.450031930078));
#133802=CARTESIAN_POINT('Ctrl Pts',(-235.257013988904,4.25310937726583,
128.330698280564));
#133803=CARTESIAN_POINT('Ctrl Pts',(-235.264778741851,4.18097503222005,
128.214258140355));
#133804=CARTESIAN_POINT('Ctrl Pts',(-235.272535782736,4.1089123320225,128.097933650135));
#133805=CARTESIAN_POINT('Ctrl Pts',(-235.280292823621,4.03191599734352,
127.984497280286));
#133806=CARTESIAN_POINT('Ctrl Pts',(-235.288049864506,3.95024872978003,
127.874391669715));
#133807=CARTESIAN_POINT('Ctrl Pts',(-235.295801055747,3.86864304813795,
127.764369090641));
#133808=CARTESIAN_POINT('Ctrl Pts',(-235.303552246987,3.78237367667754,
127.657672584101));
#133809=CARTESIAN_POINT('Ctrl Pts',(-235.311303438227,3.69174702536906,
127.554716488868));
#133810=CARTESIAN_POINT('Ctrl Pts',(-235.319051335004,3.60115889280556,
127.451804152723));
#133811=CARTESIAN_POINT('Ctrl Pts',(-235.326799231781,3.50621742158396,
127.352629358797));
#133812=CARTESIAN_POINT('Ctrl Pts',(-235.334547128558,3.40726962232724,
127.257573792387));
#133813=CARTESIAN_POINT('Ctrl Pts',(-235.342293404642,3.3083425208168,127.162538109552));
#133814=CARTESIAN_POINT('Ctrl Pts',(-235.350039680726,3.20541103993886,
127.071620211038));
#133815=CARTESIAN_POINT('Ctrl Pts',(-235.35778595681,3.09885912378931,126.985164996312));
#133816=CARTESIAN_POINT('Ctrl Pts',(-235.365532290076,2.99230642109786,
126.898709143393));
#133817=CARTESIAN_POINT('Ctrl Pts',(-235.373278623341,2.88213353340489,
126.816716286332));
#133818=CARTESIAN_POINT('Ctrl Pts',(-235.381024956606,2.76875724321614,
126.739490829905));
#133819=CARTESIAN_POINT('Ctrl Pts',(-235.388773024609,2.65535556319314,
126.662248079372));
#133820=CARTESIAN_POINT('Ctrl Pts',(-235.396521092612,2.53874937623747,
126.58977507398));
#133821=CARTESIAN_POINT('Ctrl Pts',(-235.404269160615,2.41938382892133,
126.522332482342));
#133822=CARTESIAN_POINT('Ctrl Pts',(-235.412025463357,2.2998914184812,126.454818211915));
#133823=CARTESIAN_POINT('Ctrl Pts',(-235.419781766099,2.17763413026731,
126.392345227849));
#133824=CARTESIAN_POINT('Ctrl Pts',(-235.427538068841,2.05308155658333,
126.33512811248));
#133825=CARTESIAN_POINT('Ctrl Pts',(-235.435298511355,1.92846250544056,
126.277880458613));
#133826=CARTESIAN_POINT('Ctrl Pts',(-235.443058953869,1.80154608939999,
126.225894411192));
#133827=CARTESIAN_POINT('Ctrl Pts',(-235.450819396383,1.67282025870139,
126.179335704706));
#133828=CARTESIAN_POINT('Ctrl Pts',(-235.458592296649,1.54388778587162,
126.13270225805));
#133829=CARTESIAN_POINT('Ctrl Pts',(-235.466365196914,1.41314046711555,
126.09151368012));
#133830=CARTESIAN_POINT('Ctrl Pts',(-235.47413809718,1.28108059911248,126.055885540125));
#133831=CARTESIAN_POINT('Ctrl Pts',(-235.481628432942,1.15382143995185,
126.021552572762));
#133832=CARTESIAN_POINT('Ctrl Pts',(-235.489118768703,1.0253438040743,125.992382858434));
#133833=CARTESIAN_POINT('Ctrl Pts',(-235.496609104465,0.896102648894132,
125.968434325205));
#133834=CARTESIAN_POINT('Ctrl Pts',(-235.504383438584,0.761961276031598,
125.94357777606));
#133835=CARTESIAN_POINT('Ctrl Pts',(-235.512157772703,0.626572423730888,
125.924267407729));
#133836=CARTESIAN_POINT('Ctrl Pts',(-235.519932106822,0.490434491401467,
125.910624103189));
#133837=CARTESIAN_POINT('Ctrl Pts',(-235.52769685977,0.354464336906645,
125.896997612803));
#133838=CARTESIAN_POINT('Ctrl Pts',(-235.535461612717,0.217747324506621,
125.889024328444));
#133839=CARTESIAN_POINT('Ctrl Pts',(-235.543226365664,0.0807925613160798,
125.886774255891));
#133840=CARTESIAN_POINT('Ctrl Pts',(-235.550983406549,-0.0560261764729365,
125.884526418141));
#133841=CARTESIAN_POINT('Ctrl Pts',(-235.558740447434,-0.193081806745442,
125.887990486415));
#133842=CARTESIAN_POINT('Ctrl Pts',(-235.566497488319,-0.329859928223438,
125.897184699561));
#133843=CARTESIAN_POINT('Ctrl Pts',(-235.574248679559,-0.466534904256606,
125.906371979279));
#133844=CARTESIAN_POINT('Ctrl Pts',(-235.581999870799,-0.60293239953105,
125.921280776772));
#133845=CARTESIAN_POINT('Ctrl Pts',(-235.589751062039,-0.738538197029567,
125.941877260882));
#133846=CARTESIAN_POINT('Ctrl Pts',(-235.597498958816,-0.87408635844619,
125.962464990937));
#133847=CARTESIAN_POINT('Ctrl Pts',(-235.605246855593,-1.00884310562224,
125.988735540962));
#133848=CARTESIAN_POINT('Ctrl Pts',(-235.61299475237,-1.14229974818933,
126.020603271317));
#133849=CARTESIAN_POINT('Ctrl Pts',(-235.620741028455,-1.27572847450378,
126.052464335631));
#133850=CARTESIAN_POINT('Ctrl Pts',(-235.628487304539,-1.40785725710731,
126.089920160725));
#133851=CARTESIAN_POINT('Ctrl Pts',(-235.636233580623,-1.53818839114926,
126.132834150143));
#133852=CARTESIAN_POINT('Ctrl Pts',(-235.643979913888,-1.66852048726621,
126.175748456342));
#133853=CARTESIAN_POINT('Ctrl Pts',(-235.651726247154,-1.79705453699011,
126.224120884989));
#133854=CARTESIAN_POINT('Ctrl Pts',(-235.659472580419,-1.92330915483781,
126.277765323372));
#133855=CARTESIAN_POINT('Ctrl Pts',(-235.667220648422,-2.04959204653161,
126.331421775056));
#133856=CARTESIAN_POINT('Ctrl Pts',(-235.674968716425,-2.17359413082439,
126.390352432934));
#133857=CARTESIAN_POINT('Ctrl Pts',(-235.682716784428,-2.29485548723273,
126.454323680341));
#133858=CARTESIAN_POINT('Ctrl Pts',(-235.69047308717,-2.41624572165387,
126.518362917152));
#133859=CARTESIAN_POINT('Ctrl Pts',(-235.698229389912,-2.53488906305481,
126.587453262358));
#133860=CARTESIAN_POINT('Ctrl Pts',(-235.705985692653,-2.65035115112993,
126.661315621648));
#133861=CARTESIAN_POINT('Ctrl Pts',(-235.713746135168,-2.76587486479795,
126.735217403502));
#133862=CARTESIAN_POINT('Ctrl Pts',(-235.721506577682,-2.87821362179063,
126.813896050316));
#133863=CARTESIAN_POINT('Ctrl Pts',(-235.729267020196,-2.98696423596475,
126.897030619272));
#133864=CARTESIAN_POINT('Ctrl Pts',(-235.737039920461,-3.09588942627917,
126.980298643219));
#133865=CARTESIAN_POINT('Ctrl Pts',(-235.744812820727,-3.20121466288184,
127.068036632986));
#133866=CARTESIAN_POINT('Ctrl Pts',(-235.752585720993,-3.30257121049804,
127.159884460134));
#133867=CARTESIAN_POINT('Ctrl Pts',(-235.760076056755,-3.40024319230638,
127.248393387414));
#133868=CARTESIAN_POINT('Ctrl Pts',(-235.767566392516,-3.49422979953322,
127.340718318051));
#133869=CARTESIAN_POINT('Ctrl Pts',(-235.775056728278,-3.58423638006266,
127.436507795019));
#133870=CARTESIAN_POINT('Ctrl Pts',(-235.782737888104,-3.67653597147935,
127.534737608153));
#133871=CARTESIAN_POINT('Ctrl Pts',(-235.79041904793,-3.76495801641091,
127.636938955501));
#133872=CARTESIAN_POINT('Ctrl Pts',(-235.798100207756,-3.84913502487534,
127.742769099617));
#133873=CARTESIAN_POINT('Ctrl Pts',(-235.805772268089,-3.9332123129778,
127.848473871966));
#133874=CARTESIAN_POINT('Ctrl Pts',(-235.813444328422,-4.01305431640041,
127.957798583208));
#133875=CARTESIAN_POINT('Ctrl Pts',(-235.821116388756,-4.08833007477147,
128.070363495728));
#133876=CARTESIAN_POINT('Ctrl Pts',(-235.828950393662,-4.16519478057272,
128.185304468381));
#133877=CARTESIAN_POINT('Ctrl Pts',(-235.836784398569,-4.23729799436331,
128.303623684976));
#133878=CARTESIAN_POINT('Ctrl Pts',(-235.844618403475,-4.30432994138626,
128.424880250304));
#133879=CARTESIAN_POINT('Ctrl Pts',(-235.852276925475,-4.36986036255376,
128.543420650041));
#133880=CARTESIAN_POINT('Ctrl Pts',(-235.859935447474,-4.43054409252308,
128.664767828783));
#133881=CARTESIAN_POINT('Ctrl Pts',(-235.867593969474,-4.48613532636867,
128.788480438585));
#133882=CARTESIAN_POINT('Ctrl Pts',(-235.875515715834,-4.54363723788437,
128.916445066282));
#133883=CARTESIAN_POINT('Ctrl Pts',(-235.883437462194,-4.59569007538285,
129.046940270349));
#133884=CARTESIAN_POINT('Ctrl Pts',(-235.891359208554,-4.64207398189659,
129.179450709571));
#133885=CARTESIAN_POINT('Ctrl Pts',(-235.899280954914,-4.68845788841033,
129.311961148794));
#133886=CARTESIAN_POINT('Ctrl Pts',(-235.907202701273,-4.72917269435152,
129.446486378406));
#133887=CARTESIAN_POINT('Ctrl Pts',(-235.915124447633,-4.76405452823405,
129.582490119308));
#133888=CARTESIAN_POINT('Ctrl Pts',(-234.165426035895,-4.76405452823417,
129.582490119309));
#133889=CARTESIAN_POINT('Ctrl Pts',(-234.173676386822,-4.80022243263185,
129.723508229631));
#133890=CARTESIAN_POINT('Ctrl Pts',(-234.181926737749,-4.83016515151601,
129.866290352672));
#133891=CARTESIAN_POINT('Ctrl Pts',(-234.190177088676,-4.8537222931255,
130.010280669628));
#133892=CARTESIAN_POINT('Ctrl Pts',(-234.198406836468,-4.87722060681593,
130.1539114077));
#133893=CARTESIAN_POINT('Ctrl Pts',(-234.20663658426,-4.89436509346828,
130.298744017136));
#133894=CARTESIAN_POINT('Ctrl Pts',(-234.214866332052,-4.90504591090372,
130.4442111008));
#133895=CARTESIAN_POINT('Ctrl Pts',(-234.22162440936,-4.91381674954474,
130.563665283601));
#133896=CARTESIAN_POINT('Ctrl Pts',(-234.228382486668,-4.91822981504504,
130.683546948129));
#133897=CARTESIAN_POINT('Ctrl Pts',(-234.235140563976,-4.91824993088488,
130.803536086871));
#133898=CARTESIAN_POINT('',(-233.889859436025,-4.91824841365468,130.800410417158));
#133899=CARTESIAN_POINT('Ctrl Pts',(-233.819813589496,-4.76405452823394,
129.582490119308));
#133900=CARTESIAN_POINT('Ctrl Pts',(-233.827589425366,-4.79806106893753,
129.71508110539));
#133901=CARTESIAN_POINT('Ctrl Pts',(-233.835365261237,-4.82648427381513,
129.848921751465));
#133902=CARTESIAN_POINT('Ctrl Pts',(-233.843141097107,-4.84926531900179,
129.983501964431));
#133903=CARTESIAN_POINT('Ctrl Pts',(-233.84393151732,-4.85158103128089,
129.997182155535));
#133904=CARTESIAN_POINT('Ctrl Pts',(-233.844721937534,-4.85383848810793,
130.010869986596));
#133905=CARTESIAN_POINT('Ctrl Pts',(-233.845512357748,-4.85603765781549,
130.024564921003));
#133906=CARTESIAN_POINT('Ctrl Pts',(-233.858223934682,-4.89140481372163,
130.244807532866));
#133907=CARTESIAN_POINT('Ctrl Pts',(-233.870935511616,-4.91179492626046,
130.467516694233));
#133908=CARTESIAN_POINT('Ctrl Pts',(-233.88364708855,-4.91694540615843,
130.691086898824));
#133909=CARTESIAN_POINT('Ctrl Pts',(-233.885717871032,-4.91778444631852,
130.727507656495));
#133910=CARTESIAN_POINT('Ctrl Pts',(-233.887788653514,-4.91821913060618,
130.763951181314));
#133911=CARTESIAN_POINT('Ctrl Pts',(-233.889859435996,-4.91824841365427,
130.800410416651));
#133912=CARTESIAN_POINT('Ctrl Pts',(-233.889859436025,-4.91824841365468,
130.800410417158));
#133913=CARTESIAN_POINT('Ctrl Pts',(-233.897508004962,-4.91835657247153,
130.935074959338));
#133914=CARTESIAN_POINT('Ctrl Pts',(-233.9051565739,-4.91292978437815,131.069942951738));
#133915=CARTESIAN_POINT('Ctrl Pts',(-233.912805142837,-4.90194456494051,
131.204513769185));
#133916=CARTESIAN_POINT('Ctrl Pts',(-233.920446294681,-4.89096999826641,
131.338954088455));
#133917=CARTESIAN_POINT('Ctrl Pts',(-233.928087446525,-4.87444775344177,
131.473097406374));
#133918=CARTESIAN_POINT('Ctrl Pts',(-233.935728598369,-4.85240638693835,
131.606442482777));
#133919=CARTESIAN_POINT('Ctrl Pts',(-233.943571572669,-4.82978285130596,
131.743309545304));
#133920=CARTESIAN_POINT('Ctrl Pts',(-233.951414546968,-4.80134457381579,
131.879335180831));
#133921=CARTESIAN_POINT('Ctrl Pts',(-233.959257521268,-4.76717942709186,
132.013981786533));
#133922=CARTESIAN_POINT('Ctrl Pts',(-233.966890458481,-4.73392923273431,
132.145022517759));
#133923=CARTESIAN_POINT('Ctrl Pts',(-233.974523395693,-4.69525510859911,
132.274756725189));
#133924=CARTESIAN_POINT('Ctrl Pts',(-233.982156332906,-4.6512898508898,
132.402699062799));
#133925=CARTESIAN_POINT('Ctrl Pts',(-233.989788231278,-4.60733057684236,
132.530623987485));
#133926=CARTESIAN_POINT('Ctrl Pts',(-233.997420129649,-4.55808173209536,
132.656757145564));
#133927=CARTESIAN_POINT('Ctrl Pts',(-234.005052028021,-4.5037256650884,
132.780629373612));
#133928=CARTESIAN_POINT('Ctrl Pts',(-234.012684654446,-4.44936441272463,
132.904513418587));
#133929=CARTESIAN_POINT('Ctrl Pts',(-234.020317280871,-4.38989513193338,
133.026135735191));
#133930=CARTESIAN_POINT('Ctrl Pts',(-234.027949907296,-4.32554766040755,
133.145048657447));
#133931=CARTESIAN_POINT('Ctrl Pts',(-234.035950746818,-4.25809593872375,
133.269698175857));
#133932=CARTESIAN_POINT('Ctrl Pts',(-234.04395158634,-4.18528385613835,
133.391369933456));
#133933=CARTESIAN_POINT('Ctrl Pts',(-234.051952425862,-4.10742865771344,
133.509580180613));
#133934=CARTESIAN_POINT('Ctrl Pts',(-234.059595996102,-4.033050003314,133.622511870438));
#133935=CARTESIAN_POINT('Ctrl Pts',(-234.067239566342,-3.9540691714229,
133.732284209412));
#133936=CARTESIAN_POINT('Ctrl Pts',(-234.074883136582,-3.87080489606674,
133.838508359369));
#133937=CARTESIAN_POINT('Ctrl Pts',(-234.082531777,-3.7874853893612,133.944802970554));
#133938=CARTESIAN_POINT('Ctrl Pts',(-234.090180417419,-3.6998770452929,
134.047544402806));
#133939=CARTESIAN_POINT('Ctrl Pts',(-234.097829057837,-3.60833627717124,
134.146379823578));
#133940=CARTESIAN_POINT('Ctrl Pts',(-234.105488112923,-3.51667086380252,
134.245349822261));
#133941=CARTESIAN_POINT('Ctrl Pts',(-234.113147168008,-3.42106263007849,
134.34040291786));
#133942=CARTESIAN_POINT('Ctrl Pts',(-234.120806223094,-3.32190199557209,
134.431225681821));
#133943=CARTESIAN_POINT('Ctrl Pts',(-234.121857475916,-3.30829158335825,
134.44369166958));
#133944=CARTESIAN_POINT('Ctrl Pts',(-234.122908728739,-3.29461429213465,
134.45607802709));
#133945=CARTESIAN_POINT('Ctrl Pts',(-234.123959981561,-3.28087117384239,
134.468384007659));
#133946=CARTESIAN_POINT('Ctrl Pts',(-234.13173431568,-3.17923663724405,
134.559390474019));
#133947=CARTESIAN_POINT('Ctrl Pts',(-234.139508649799,-3.07365167398268,
134.646309097947));
#133948=CARTESIAN_POINT('Ctrl Pts',(-234.147282983918,-2.9644790648186,
134.728777381463));
#133949=CARTESIAN_POINT('Ctrl Pts',(-234.155047736865,-2.85544100113827,
134.811144030189));
#133950=CARTESIAN_POINT('Ctrl Pts',(-234.162812489812,-2.74282439789659,
134.889071017924));
#133951=CARTESIAN_POINT('Ctrl Pts',(-234.170577242759,-2.62702764610736,
134.962233728796));
#133952=CARTESIAN_POINT('Ctrl Pts',(-234.178334283644,-2.51134590528445,
135.035323773432));
#133953=CARTESIAN_POINT('Ctrl Pts',(-234.186091324529,-2.39249062998956,
135.103658750515));
#133954=CARTESIAN_POINT('Ctrl Pts',(-234.193848365414,-2.27089166083551,
135.166955502179));
#133955=CARTESIAN_POINT('Ctrl Pts',(-234.201599556655,-2.14938439040983,
135.230204521269));
#133956=CARTESIAN_POINT('Ctrl Pts',(-234.209350747895,-2.02513788981683,
135.288422697556));
#133957=CARTESIAN_POINT('Ctrl Pts',(-234.217101939135,-1.89860892803468,
135.34137143978));
#133958=CARTESIAN_POINT('Ctrl Pts',(-234.224849835912,-1.77213374443672,
135.394297677376));
#133959=CARTESIAN_POINT('Ctrl Pts',(-234.232597732689,-1.64337838902263,
135.441958784794));
#133960=CARTESIAN_POINT('Ctrl Pts',(-234.240345629466,-1.51282186039079,
135.484163293024));
#133961=CARTESIAN_POINT('Ctrl Pts',(-234.24809190555,-1.38229264136992,
135.526358972981));
#133962=CARTESIAN_POINT('Ctrl Pts',(-234.255838181634,-1.24996337031541,
135.563100203881));
#133963=CARTESIAN_POINT('Ctrl Pts',(-234.263584457719,-1.11633017024271,
135.594244751186));
#133964=CARTESIAN_POINT('Ctrl Pts',(-234.271330790984,-0.982695983720628,
135.625389528393));
#133965=CARTESIAN_POINT('Ctrl Pts',(-234.279077124249,-0.847758229734812,
135.650937450828));
#133966=CARTESIAN_POINT('Ctrl Pts',(-234.286823457515,-0.712024850954133,
135.670797062658));
#133967=CARTESIAN_POINT('Ctrl Pts',(-234.294571525518,-0.576261075624201,
135.690661121911));
#133968=CARTESIAN_POINT('Ctrl Pts',(-234.30231959352,-0.439701707724825,
135.70483427914));
#133969=CARTESIAN_POINT('Ctrl Pts',(-234.310067661523,-0.302861068158666,
135.713276815251));
#133970=CARTESIAN_POINT('Ctrl Pts',(-234.317823964265,-0.165874992732165,
135.72172832419));
#133971=CARTESIAN_POINT('Ctrl Pts',(-234.325580267007,-0.0286074393217352,
135.724437021324));
#133972=CARTESIAN_POINT('Ctrl Pts',(-234.333336569749,0.108425444496076,
135.721415323941));
#133973=CARTESIAN_POINT('Ctrl Pts',(-234.341097012263,0.24553146688996,
135.718392013787));
#133974=CARTESIAN_POINT('Ctrl Pts',(-234.348857454777,0.382402180143489,
135.709632239786));
#133975=CARTESIAN_POINT('Ctrl Pts',(-234.356617897292,0.518526292473832,
135.695200376392));
#133976=CARTESIAN_POINT('Ctrl Pts',(-234.364390797557,0.654868923313818,
135.680745345689));
#133977=CARTESIAN_POINT('Ctrl Pts',(-234.372163697823,0.790462171282616,
135.660600087708));
#133978=CARTESIAN_POINT('Ctrl Pts',(-234.379936598088,0.924803784060439,
135.63488036429));
#133979=CARTESIAN_POINT('Ctrl Pts',(-234.38742693385,1.05426174082805,135.610095617601));
#133980=CARTESIAN_POINT('Ctrl Pts',(-234.394917269612,1.18255718274369,
135.580134730783));
#133981=CARTESIAN_POINT('Ctrl Pts',(-234.402407605374,1.3092556394284,135.545144596311));
#133982=CARTESIAN_POINT('Ctrl Pts',(-234.410181939493,1.44075790660692,
135.508827800255));
#133983=CARTESIAN_POINT('Ctrl Pts',(-234.417956273612,1.57095625827954,
135.46697781968));
#133984=CARTESIAN_POINT('Ctrl Pts',(-234.425730607731,1.69934962276673,
135.419703933301));
#133985=CARTESIAN_POINT('Ctrl Pts',(-234.433495360678,1.82758475390704,
135.372488307763));
#133986=CARTESIAN_POINT('Ctrl Pts',(-234.441260113626,1.95401896056059,
135.31986221033));
#133987=CARTESIAN_POINT('Ctrl Pts',(-234.449024866573,2.07816379412782,
135.26198535584));
#133988=CARTESIAN_POINT('Ctrl Pts',(-234.456781907458,2.20218532529621,
135.204165985458));
#133989=CARTESIAN_POINT('Ctrl Pts',(-234.464538948342,2.32392165636191,
135.141106400485));
#133990=CARTESIAN_POINT('Ctrl Pts',(-234.472295989227,2.44290221924087,
135.073015184257));
#133991=CARTESIAN_POINT('Ctrl Pts',(-234.480047180468,2.56179305795231,
135.004975316144));
#133992=CARTESIAN_POINT('Ctrl Pts',(-234.487798371708,2.67793192694694,
134.931911562692));
#133993=CARTESIAN_POINT('Ctrl Pts',(-234.495549562948,2.79087119785176,
134.854079252175));
#133994=CARTESIAN_POINT('Ctrl Pts',(-234.503297459725,2.90376246655354,
134.776280022467));
#133995=CARTESIAN_POINT('Ctrl Pts',(-234.511045356502,3.01345652068257,
134.693716488162));
#133996=CARTESIAN_POINT('Ctrl Pts',(-234.518793253279,3.11953336149638,
134.606688150671));
#133997=CARTESIAN_POINT('Ctrl Pts',(-234.526539529364,3.22558801332185,
134.519678017633));
#133998=CARTESIAN_POINT('Ctrl Pts',(-234.534285805448,3.32802665477062,
134.428205186891));
#133999=CARTESIAN_POINT('Ctrl Pts',(-234.542032081532,3.42646145328966,
134.332610179547));
#134000=CARTESIAN_POINT('Ctrl Pts',(-234.549778414797,3.52489697843161,
134.237014466543));
#134001=CARTESIAN_POINT('Ctrl Pts',(-234.557524748062,3.61932832119783,
134.137296788598));
#134002=CARTESIAN_POINT('Ctrl Pts',(-234.565271081328,3.70940398178691,
134.033835058153));
#134003=CARTESIAN_POINT('Ctrl Pts',(-234.573019149331,3.79949981419577,
133.93035015817));
#134004=CARTESIAN_POINT('Ctrl Pts',(-234.580767217334,3.88523776677434,
133.823119832075));
#134005=CARTESIAN_POINT('Ctrl Pts',(-234.588515285337,3.96630641971367,
133.712555323468));
#134006=CARTESIAN_POINT('Ctrl Pts',(-234.596271588078,4.04746123338219,
133.601873305586));
#134007=CARTESIAN_POINT('Ctrl Pts',(-234.60402789082,4.12393660255991,133.487850342247));
#134008=CARTESIAN_POINT('Ctrl Pts',(-234.611784193562,4.19546398389031,
133.370927394874));
#134009=CARTESIAN_POINT('Ctrl Pts',(-234.619544636077,4.26702954153776,
133.253942042203));
#134010=CARTESIAN_POINT('Ctrl Pts',(-234.62730507859,4.33364165934758,133.134053962946));
#134011=CARTESIAN_POINT('Ctrl Pts',(-234.635065521105,4.39507813167303,
133.011728117324));
#134012=CARTESIAN_POINT('Ctrl Pts',(-234.64283842137,4.45661322727793,132.889205903396));
#134013=CARTESIAN_POINT('Ctrl Pts',(-234.650611321635,4.5129559137713,132.764238459666));
#134014=CARTESIAN_POINT('Ctrl Pts',(-234.658384221901,4.56393210522144,
132.637310917337));
#134015=CARTESIAN_POINT('Ctrl Pts',(-234.665874557663,4.61305518371081,
132.514997510883));
#134016=CARTESIAN_POINT('Ctrl Pts',(-234.673364893425,4.65719506123983,
132.390864330924));
#134017=CARTESIAN_POINT('Ctrl Pts',(-234.680855229187,4.6962404807556,132.265356308666));
#134018=CARTESIAN_POINT('Ctrl Pts',(-234.688629563306,4.73676631922008,
132.135089611596));
#134019=CARTESIAN_POINT('Ctrl Pts',(-234.696403897425,4.77193213465986,
132.002929114181));
#134020=CARTESIAN_POINT('Ctrl Pts',(-234.704178231544,4.80155902487095,
131.869355450032));
#134021=CARTESIAN_POINT('Ctrl Pts',(-234.711942984491,4.8311494025877,131.735946403487));
#134022=CARTESIAN_POINT('Ctrl Pts',(-234.719707737438,4.85521435339285,
131.601128033501));
#134023=CARTESIAN_POINT('Ctrl Pts',(-234.727472490386,4.87362423150206,
131.465397615484));
#134024=CARTESIAN_POINT('Ctrl Pts',(-234.735229531271,4.8920158246608,131.329802006831));
#134025=CARTESIAN_POINT('Ctrl Pts',(-234.742986572156,4.90476347039832,
131.193296537759));
#134026=CARTESIAN_POINT('Ctrl Pts',(-234.75074361304,4.91178830224006,131.056389854913));
#134027=CARTESIAN_POINT('Ctrl Pts',(-234.758494804281,4.9188078366015,130.919586414461));
#134028=CARTESIAN_POINT('Ctrl Pts',(-234.766245995521,4.92011312709053,
130.78238275133));
#134029=CARTESIAN_POINT('Ctrl Pts',(-234.773997186761,4.91567703454626,
130.645293479117));
#134030=CARTESIAN_POINT('Ctrl Pts',(-234.781745083538,4.91124282745968,
130.508262473502));
#134031=CARTESIAN_POINT('Ctrl Pts',(-234.789492980315,4.90107210341125,
130.371346152049));
#134032=CARTESIAN_POINT('Ctrl Pts',(-234.797240877092,4.88518982184064,
130.235059759421));
#134033=CARTESIAN_POINT('Ctrl Pts',(-234.804987153176,4.86931086250096,
130.098801874969));
#134034=CARTESIAN_POINT('Ctrl Pts',(-234.812733429261,4.84772276725855,
129.963174045341));
#134035=CARTESIAN_POINT('Ctrl Pts',(-234.820479705345,4.82050239319234,
129.828686625022));
#134036=CARTESIAN_POINT('Ctrl Pts',(-234.82822603861,4.79328181819148,129.694198211947));
#134037=CARTESIAN_POINT('Ctrl Pts',(-234.835972371875,4.7604289589635,129.560850608174));
#134038=CARTESIAN_POINT('Ctrl Pts',(-234.843718705141,4.72207176972025,
129.429143811346));
#134039=CARTESIAN_POINT('Ctrl Pts',(-234.851466773144,4.68370599065036,
129.297407519693));
#134040=CARTESIAN_POINT('Ctrl Pts',(-234.859214841147,4.63983353802021,
129.167313141463));
#134041=CARTESIAN_POINT('Ctrl Pts',(-234.86696290915,4.59063207270527,129.039344970171));
#134042=CARTESIAN_POINT('Ctrl Pts',(-234.874719211891,4.54137831548755,
128.911240792784));
#134043=CARTESIAN_POINT('Ctrl Pts',(-234.882475514633,4.48678437218778,
128.785267701949));
#134044=CARTESIAN_POINT('Ctrl Pts',(-234.890231817375,4.42707608189503,
128.661889981218));
#134045=CARTESIAN_POINT('Ctrl Pts',(-234.897992259889,4.3673359234898,128.538446410082));
#134046=CARTESIAN_POINT('Ctrl Pts',(-234.905752702404,4.30247616377143,
128.417601313548));
#134047=CARTESIAN_POINT('Ctrl Pts',(-234.913513144918,4.23276787936328,
128.299792961876));
#134048=CARTESIAN_POINT('Ctrl Pts',(-234.921286045183,4.16294769302879,
128.181795493779));
#134049=CARTESIAN_POINT('Ctrl Pts',(-234.929058945449,4.08826364165262,
128.066844840089));
#134050=CARTESIAN_POINT('Ctrl Pts',(-234.936831845714,4.00902978215786,
127.955349689494));
#134051=CARTESIAN_POINT('Ctrl Pts',(-234.944322181476,3.93267627303442,
127.847907668465));
#134052=CARTESIAN_POINT('Ctrl Pts',(-234.951812517238,3.85209819508192,
127.743674523504));
#134053=CARTESIAN_POINT('Ctrl Pts',(-234.959302853,3.76760974436991,127.642984354508));
#134054=CARTESIAN_POINT('Ctrl Pts',(-234.967077187119,3.67991788836859,
127.538476487148));
#134055=CARTESIAN_POINT('Ctrl Pts',(-234.974851521238,3.58773550113176,
127.437454513619));
#134056=CARTESIAN_POINT('Ctrl Pts',(-234.982625855357,3.49137025231658,
127.340328743616));
#134057=CARTESIAN_POINT('Ctrl Pts',(-234.990390608304,3.39512376505842,
127.243322672445));
#134058=CARTESIAN_POINT('Ctrl Pts',(-234.998155361251,3.29470494586347,
127.150203525679));
#134059=CARTESIAN_POINT('Ctrl Pts',(-235.005920114198,3.19046208990488,
127.061349167493));
#134060=CARTESIAN_POINT('Ctrl Pts',(-235.013677155083,3.08632276941954,
126.972583060707));
#134061=CARTESIAN_POINT('Ctrl Pts',(-235.021434195969,2.97836726615232,
126.888073564951));
#134062=CARTESIAN_POINT('Ctrl Pts',(-235.029191236854,2.86698088967546,
126.808161968758));
#134063=CARTESIAN_POINT('Ctrl Pts',(-235.036942428094,2.75567851053171,
126.728310634522));
#134064=CARTESIAN_POINT('Ctrl Pts',(-235.044693619334,2.64095072432235,
126.653050525357));
#134065=CARTESIAN_POINT('Ctrl Pts',(-235.052444810574,2.52321582066163,
126.582682635429));
#134066=CARTESIAN_POINT('Ctrl Pts',(-235.060192707351,2.40553095747613,
126.512344653731));
#134067=CARTESIAN_POINT('Ctrl Pts',(-235.067940604128,2.28484185378314,
126.44689495581));
#134068=CARTESIAN_POINT('Ctrl Pts',(-235.075688500905,2.16159549069878,
126.386591044909));
#134069=CARTESIAN_POINT('Ctrl Pts',(-235.083434776989,2.03837490809635,
126.326299748287));
#134070=CARTESIAN_POINT('Ctrl Pts',(-235.091181053074,1.91259848105292,
126.271152269413));
#134071=CARTESIAN_POINT('Ctrl Pts',(-235.098927329158,1.78473712837853,
126.221359805316));
#134072=CARTESIAN_POINT('Ctrl Pts',(-235.106673662423,1.6568748318612,126.171566973662));
#134073=CARTESIAN_POINT('Ctrl Pts',(-235.114419995688,1.52692794331774,
126.127129377536));
#134074=CARTESIAN_POINT('Ctrl Pts',(-235.122166328954,1.39538628730345,
126.088209626376));
#134075=CARTESIAN_POINT('Ctrl Pts',(-235.129914396957,1.26381517344716,
126.049281159407));
#134076=CARTESIAN_POINT('Ctrl Pts',(-235.13766246496,1.13064895628658,126.015873107172));
#134077=CARTESIAN_POINT('Ctrl Pts',(-235.145410532963,0.996391115716242,
125.98809777102));
#134078=CARTESIAN_POINT('Ctrl Pts',(-235.153166835705,0.861990584315074,
125.96029291491));
#134079=CARTESIAN_POINT('Ctrl Pts',(-235.160923138446,0.726496495367408,
125.938132812929));
#134080=CARTESIAN_POINT('Ctrl Pts',(-235.168679441188,0.590421535317904,
125.921678416856));
#134081=CARTESIAN_POINT('Ctrl Pts',(-235.176439883703,0.454273947965083,
125.905215238576));
#134082=CARTESIAN_POINT('Ctrl Pts',(-235.184200326217,0.317545261323974,
125.894463864868));
#134083=CARTESIAN_POINT('Ctrl Pts',(-235.191960768731,0.180750728114019,
125.889433127075));
#134084=CARTESIAN_POINT('Ctrl Pts',(-235.199733668996,0.0437366001753084,
125.884394313494));
#134085=CARTESIAN_POINT('Ctrl Pts',(-235.207506569262,-0.0933431943749275,
125.885094484934));
#134086=CARTESIAN_POINT('Ctrl Pts',(-235.215279469527,-0.229975058728639,
125.89149032263));
#134087=CARTESIAN_POINT('Ctrl Pts',(-235.222769805289,-0.361640010653015,
125.897653655516));
#134088=CARTESIAN_POINT('Ctrl Pts',(-235.230260141051,-0.492888726902967,
125.9091057137));
#134089=CARTESIAN_POINT('Ctrl Pts',(-235.237750476813,-0.623270289125128,
125.925762744284));
#134090=CARTESIAN_POINT('Ctrl Pts',(-235.245524810932,-0.758595307911966,
125.943051331246));
#134091=CARTESIAN_POINT('Ctrl Pts',(-235.253299145051,-0.893414787314326,
125.966002140077));
#134092=CARTESIAN_POINT('Ctrl Pts',(-235.26107347917,-1.02721721919833,
125.994578101996));
#134093=CARTESIAN_POINT('Ctrl Pts',(-235.268838232117,-1.16085475154366,
126.023118846596));
#134094=CARTESIAN_POINT('Ctrl Pts',(-235.276602985064,-1.29347735163081,
126.057270869804));
#134095=CARTESIAN_POINT('Ctrl Pts',(-235.284367738011,-1.42457884957813,
126.096945385845));
#134096=CARTESIAN_POINT('Ctrl Pts',(-235.292124778896,-1.55555013566913,
126.136580496598));
#134097=CARTESIAN_POINT('Ctrl Pts',(-235.299881819781,-1.68500295435694,
126.181727072239));
#134098=CARTESIAN_POINT('Ctrl Pts',(-235.307638860666,-1.81244190069604,
126.232245415704));
#134099=CARTESIAN_POINT('Ctrl Pts',(-235.315390051906,-1.9397847443342,
126.282725662892));
#134100=CARTESIAN_POINT('Ctrl Pts',(-235.323141243146,-2.06511637647834,
126.338569471355));
#134101=CARTESIAN_POINT('Ctrl Pts',(-235.330892434386,-2.18795746645997,
126.399587616893));
#134102=CARTESIAN_POINT('Ctrl Pts',(-235.338640331164,-2.31074634570197,
126.46057982809));
#134103=CARTESIAN_POINT('Ctrl Pts',(-235.346388227941,-2.43104643873598,
126.526741828696));
#134104=CARTESIAN_POINT('Ctrl Pts',(-235.354136124718,-2.54839949657897,
126.597836747631));
#134105=CARTESIAN_POINT('Ctrl Pts',(-235.361882400802,-2.66572800669178,
126.668916795041));
#134106=CARTESIAN_POINT('Ctrl Pts',(-235.369628676886,-2.78011037360252,
126.744927505902));
#134107=CARTESIAN_POINT('Ctrl Pts',(-235.37737495297,-2.89111436815078,
126.825586840035));
#134108=CARTESIAN_POINT('Ctrl Pts',(-235.385121286235,-3.00211918210516,
126.906246769576));
#134109=CARTESIAN_POINT('Ctrl Pts',(-235.392867619501,-3.1097452576507,
126.99155516104));
#134110=CARTESIAN_POINT('Ctrl Pts',(-235.400613952766,-3.21359102472567,
127.081187805528));
#134111=CARTESIAN_POINT('Ctrl Pts',(-235.408362020769,-3.31746004734059,
127.170840522625));
#134112=CARTESIAN_POINT('Ctrl Pts',(-235.416110088772,-3.41754678099235,
127.264819164315));
#134113=CARTESIAN_POINT('Ctrl Pts',(-235.423858156775,-3.51348460019401,
127.362760840326));
#134114=CARTESIAN_POINT('Ctrl Pts',(-235.431614459517,-3.60952438325146,
127.460806609915));
#134115=CARTESIAN_POINT('Ctrl Pts',(-235.439370762259,-3.70140616935787,
127.562823547927));
#134116=CARTESIAN_POINT('Ctrl Pts',(-235.447127065001,-3.78880155850952,
127.668413262661));
#134117=CARTESIAN_POINT('Ctrl Pts',(-235.454887507515,-3.87624359321179,
127.774059333805));
#134118=CARTESIAN_POINT('Ctrl Pts',(-235.462647950029,-3.95919422331985,
127.883281670127));
#134119=CARTESIAN_POINT('Ctrl Pts',(-235.470408392543,-4.03736751209587,
127.995651548479));
#134120=CARTESIAN_POINT('Ctrl Pts',(-235.478181292809,-4.11566629157493,
128.108201812935));
#134121=CARTESIAN_POINT('Ctrl Pts',(-235.485954193074,-4.18917219482737,
128.223909386157));
#134122=CARTESIAN_POINT('Ctrl Pts',(-235.49372709334,-4.25764405553614,
128.342318749754));
#134123=CARTESIAN_POINT('Ctrl Pts',(-235.501217429102,-4.32362679163999,
128.456423634733));
#134124=CARTESIAN_POINT('Ctrl Pts',(-235.508707764864,-4.38493498781607,
128.57303701406));
#134125=CARTESIAN_POINT('Ctrl Pts',(-235.516198100627,-4.4413953753653,
128.691734246864));
#134126=CARTESIAN_POINT('Ctrl Pts',(-235.524611330118,-4.50481231856901,
128.825056315627));
#134127=CARTESIAN_POINT('Ctrl Pts',(-235.533024559609,-4.56229001563584,
128.961378149476));
#134128=CARTESIAN_POINT('Ctrl Pts',(-235.5414377891,-4.61355790223604,129.100169740576));
#134129=CARTESIAN_POINT('Ctrl Pts',(-235.549829414691,-4.66469414065789,
129.238604935863));
#134130=CARTESIAN_POINT('Ctrl Pts',(-235.558221040281,-4.70965226663767,
129.379496971179));
#134131=CARTESIAN_POINT('Ctrl Pts',(-235.566612665872,-4.74820913826364,
129.522294690318));
#134132=CARTESIAN_POINT('Ctrl Pts',(-235.56778964017,-4.75361696377262,
129.542322901001));
#134133=CARTESIAN_POINT('Ctrl Pts',(-235.568966614468,-4.75889894093515,
129.562388562677));
#134134=CARTESIAN_POINT('Ctrl Pts',(-235.570143588767,-4.76405452823401,
129.582490119308));
#134135=CARTESIAN_POINT('Origin',(213.235140564004,0.,130.804360617566));
#134136=CARTESIAN_POINT('',(-237.665046159034,-4.76405452823396,129.582490119308));
#134137=CARTESIAN_POINT('',(-237.319878776621,-4.76405452823405,129.582490119308));
#134138=CARTESIAN_POINT('',(213.235140564004,-4.76405452823405,129.582490119308));
#134139=CARTESIAN_POINT('',(-235.98514056405,-4.91824789693063,130.808908896076));
#134140=CARTESIAN_POINT('Ctrl Pts',(-235.98514056405,-4.91824789693063,
130.808908896075));
#134141=CARTESIAN_POINT('Ctrl Pts',(-235.995166432559,-4.91808414983754,
130.985975624643));
#134142=CARTESIAN_POINT('Ctrl Pts',(-236.005192301068,-4.90835484506816,
131.162615021248));
#134143=CARTESIAN_POINT('Ctrl Pts',(-236.015218169578,-4.8892187176409,
131.33795540162));
#134144=CARTESIAN_POINT('Ctrl Pts',(-236.025483509521,-4.86962551700637,
131.517483849318));
#134145=CARTESIAN_POINT('Ctrl Pts',(-236.035748849464,-4.84017073368366,
131.695650792814));
#134146=CARTESIAN_POINT('Ctrl Pts',(-236.046014189407,-4.8010725964576,
131.871546161904));
#134147=CARTESIAN_POINT('Ctrl Pts',(-236.048510910302,-4.7915632049812,
131.914327175073));
#134148=CARTESIAN_POINT('Ctrl Pts',(-236.051007631197,-4.7814835776014,
131.956973916247));
#134149=CARTESIAN_POINT('Ctrl Pts',(-236.053504352091,-4.77083727542129,
131.999473479998));
#134150=CARTESIAN_POINT('Ctrl Pts',(-236.061278686211,-4.73768662952635,
132.131809380741));
#134151=CARTESIAN_POINT('Ctrl Pts',(-236.06905302033,-4.69897310215588,
132.262974522646));
#134152=CARTESIAN_POINT('Ctrl Pts',(-236.076827354449,-4.65479391621698,
132.392465355941));
#134153=CARTESIAN_POINT('Ctrl Pts',(-236.084592107396,-4.61066917717633,
132.521796603357));
#134154=CARTESIAN_POINT('Ctrl Pts',(-236.092356860343,-4.56109230710251,
132.649457281315));
#134155=CARTESIAN_POINT('Ctrl Pts',(-236.10012161329,-4.5062112534178,132.774955249161));
#134156=CARTESIAN_POINT('Ctrl Pts',(-236.107878654175,-4.4513847083693,
132.900328570656));
#134157=CARTESIAN_POINT('Ctrl Pts',(-236.11563569506,-4.39126461927995,
133.023543100831));
#134158=CARTESIAN_POINT('Ctrl Pts',(-236.123392735945,-4.32604821708376,
133.144123401689));
#134159=CARTESIAN_POINT('Ctrl Pts',(-236.131143927185,-4.26088099508388,
133.264612772004));
#134160=CARTESIAN_POINT('Ctrl Pts',(-236.138895118425,-4.19062529481431,
133.382471524497));
#134161=CARTESIAN_POINT('Ctrl Pts',(-236.146646309665,-4.11552562917464,
133.497246032526));
#134162=CARTESIAN_POINT('Ctrl Pts',(-236.154394206442,-4.04045788289612,
133.611971758329));
#134163=CARTESIAN_POINT('Ctrl Pts',(-236.162142103219,-3.96055047968925,
133.723615520451));
#134164=CARTESIAN_POINT('Ctrl Pts',(-236.169889999996,-3.87609275590384,
133.831750253891));
#134165=CARTESIAN_POINT('Ctrl Pts',(-236.17763627608,-3.79165269885331,
133.939862367877));
#134166=CARTESIAN_POINT('Ctrl Pts',(-236.185382552165,-3.70266445496727,
134.044466605248));
#134167=CARTESIAN_POINT('Ctrl Pts',(-236.193128828249,-3.60945914037416,
134.145167073569));
#134168=CARTESIAN_POINT('Ctrl Pts',(-236.200875161514,-3.51625313776097,
134.245868285237));
#134169=CARTESIAN_POINT('Ctrl Pts',(-236.208621494779,-3.41883026789406,
134.342665383429));
#134170=CARTESIAN_POINT('Ctrl Pts',(-236.216367828044,-3.31755989935976,
134.435197900709));
#134171=CARTESIAN_POINT('Ctrl Pts',(-236.224115896047,-3.21626685202845,
134.527751140004));
#134172=CARTESIAN_POINT('Ctrl Pts',(-236.231863964051,-3.1111248800744,
134.616037634331));
#134173=CARTESIAN_POINT('Ctrl Pts',(-236.239612032054,-3.00253763545448,
134.699736184848));
#134174=CARTESIAN_POINT('Ctrl Pts',(-236.247368334795,-2.89383498301892,
134.783523691181));
#134175=CARTESIAN_POINT('Ctrl Pts',(-236.255124637537,-2.78168005347156,
134.862713274066));
#134176=CARTESIAN_POINT('Ctrl Pts',(-236.262880940279,-2.66650723694804,
134.937025885623));
#134177=CARTESIAN_POINT('Ctrl Pts',(-236.270641382793,-2.55127294922425,
135.011378160058));
#134178=CARTESIAN_POINT('Ctrl Pts',(-236.278401825307,-2.43301790192989,
135.080848078559));
#134179=CARTESIAN_POINT('Ctrl Pts',(-236.286162267822,-2.31220158906708,
135.145202341704));
#134180=CARTESIAN_POINT('Ctrl Pts',(-236.293935168087,-2.19119133113328,
135.209659912025));
#134181=CARTESIAN_POINT('Ctrl Pts',(-236.301708068352,-2.06761194406125,
135.268985247294));
#134182=CARTESIAN_POINT('Ctrl Pts',(-236.309480968618,-1.94194424176665,
135.322992669899));
#134183=CARTESIAN_POINT('Ctrl Pts',(-236.31697130438,-1.82084487698727,
135.375036786656));
#134184=CARTESIAN_POINT('Ctrl Pts',(-236.324461640142,-1.69780667966961,
135.422142807038));
#134185=CARTESIAN_POINT('Ctrl Pts',(-236.331951975904,-1.57327178302742,
135.464188828909));
#134186=CARTESIAN_POINT('Ctrl Pts',(-236.339726310023,-1.44401510792876,
135.507829038479));
#134187=CARTESIAN_POINT('Ctrl Pts',(-236.347500644142,-1.31273655208019,
135.546156214564));
#134188=CARTESIAN_POINT('Ctrl Pts',(-236.355274978261,-1.17991231752151,
135.5789799726));
#134189=CARTESIAN_POINT('Ctrl Pts',(-236.363039731208,-1.04725177696108,
135.611763278287));
#134190=CARTESIAN_POINT('Ctrl Pts',(-236.370804484156,-0.913049723799389,
135.639056568126));
#134191=CARTESIAN_POINT('Ctrl Pts',(-236.378569237103,-0.777800179102438,
135.660718300428));
#134192=CARTESIAN_POINT('Ctrl Pts',(-236.386326277988,-0.642684966159964,
135.682358517992));
#134193=CARTESIAN_POINT('Ctrl Pts',(-236.394083318873,-0.506524715639203,
135.698378247593));
#134194=CARTESIAN_POINT('Ctrl Pts',(-236.401840359758,-0.369826035129639,
135.708686439352));
#134195=CARTESIAN_POINT('Ctrl Pts',(-236.409591550998,-0.233230440158594,
135.718986857624));
#134196=CARTESIAN_POINT('Ctrl Pts',(-236.417342742238,-0.0960976116661581,
135.723584281825));
#134197=CARTESIAN_POINT('Ctrl Pts',(-236.425093933478,0.0410586362118856,
135.722439231303));
#134198=CARTESIAN_POINT('Ctrl Pts',(-236.432841830255,0.178156589026005,
135.721294667457));
#134199=CARTESIAN_POINT('Ctrl Pts',(-236.440589727032,0.315277551295167,
135.714412486521));
#134200=CARTESIAN_POINT('Ctrl Pts',(-236.448337623809,0.451905827774221,
135.701805276296));
#134201=CARTESIAN_POINT('Ctrl Pts',(-236.456083899893,0.5885055245632,135.689200703227));
#134202=CARTESIAN_POINT('Ctrl Pts',(-236.463830175977,0.72461235148788,
135.670873518767));
#134203=CARTESIAN_POINT('Ctrl Pts',(-236.471576452061,0.859714256675553,
135.646888310762));
#134204=CARTESIAN_POINT('Ctrl Pts',(-236.479322785327,0.994817159154617,
135.622902925703));
#134205=CARTESIAN_POINT('Ctrl Pts',(-236.487069118592,1.12891474014856,
135.593259502098));
#134206=CARTESIAN_POINT('Ctrl Pts',(-236.494815451857,1.26150407545233,
135.558073958746));
#134207=CARTESIAN_POINT('Ctrl Pts',(-236.50256351986,1.39412310321826,135.522880535836));
#134208=CARTESIAN_POINT('Ctrl Pts',(-236.510311587863,1.525232835375,135.482142623757));
#134209=CARTESIAN_POINT('Ctrl Pts',(-236.518059655866,1.65434485449897,
135.436026210513));
#134210=CARTESIAN_POINT('Ctrl Pts',(-236.525815958608,1.78359409541349,
135.389860784197));
#134211=CARTESIAN_POINT('Ctrl Pts',(-236.53357226135,1.91084101321725,135.338305569438));
#134212=CARTESIAN_POINT('Ctrl Pts',(-236.541328564092,2.03561603854606,
135.281575198766));
#134213=CARTESIAN_POINT('Ctrl Pts',(-236.549089006606,2.16045766006314,
135.224814549387));
#134214=CARTESIAN_POINT('Ctrl Pts',(-236.55684944912,2.28282441159067,135.162873416788));
#134215=CARTESIAN_POINT('Ctrl Pts',(-236.564609891634,2.40227164398708,
135.096012282251));
#134216=CARTESIAN_POINT('Ctrl Pts',(-236.5723827919,2.52191062368496,135.029043816285));
#134217=CARTESIAN_POINT('Ctrl Pts',(-236.580155692165,2.63862038573402,
134.957139770806));
#134218=CARTESIAN_POINT('Ctrl Pts',(-236.587928592431,2.75198482263593,
134.880604304894));
#134219=CARTESIAN_POINT('Ctrl Pts',(-236.595418928193,2.8612281767099,134.806851095948));
#134220=CARTESIAN_POINT('Ctrl Pts',(-236.602909263955,2.96736495679474,
134.728797530567));
#134221=CARTESIAN_POINT('Ctrl Pts',(-236.610399599717,3.07005361936947,
134.646749696862));
#134222=CARTESIAN_POINT('Ctrl Pts',(-236.618173933836,3.17663575379591,
134.561590994606));
#134223=CARTESIAN_POINT('Ctrl Pts',(-236.625948267955,3.27984075861181,
134.471859402436));
#134224=CARTESIAN_POINT('Ctrl Pts',(-236.633722602074,3.37925105905551,
134.377852655107));
#134225=CARTESIAN_POINT('Ctrl Pts',(-236.641487355021,3.47853884518846,
134.283961762693));
#134226=CARTESIAN_POINT('Ctrl Pts',(-236.649252107968,3.57404095071726,
134.185806464402));
#134227=CARTESIAN_POINT('Ctrl Pts',(-236.657016860916,3.66537126215758,
134.083725887409));
#134228=CARTESIAN_POINT('Ctrl Pts',(-236.664773901801,3.75661086304505,
133.981746698283));
#134229=CARTESIAN_POINT('Ctrl Pts',(-236.672530942686,3.8436866565667,133.875850278415));
#134230=CARTESIAN_POINT('Ctrl Pts',(-236.680287983571,3.92624820610317,
133.766413636432));
#134231=CARTESIAN_POINT('Ctrl Pts',(-236.688039174811,4.00874749533279,
133.657059521472));
#134232=CARTESIAN_POINT('Ctrl Pts',(-236.695790366051,4.08673908197466,
133.544170809137));
#134233=CARTESIAN_POINT('Ctrl Pts',(-236.703541557291,4.15991202074636,
133.428158445553));
#134234=CARTESIAN_POINT('Ctrl Pts',(-236.711289454068,4.23305385906723,
133.312195390319));
#134235=CARTESIAN_POINT('Ctrl Pts',(-236.719037350845,4.30138091480472,
133.193111654392));
#134236=CARTESIAN_POINT('Ctrl Pts',(-236.726785247622,4.36462503255551,
133.071347910801));
#134237=CARTESIAN_POINT('Ctrl Pts',(-236.734531523706,4.42785592100025,
132.949609637561));
#134238=CARTESIAN_POINT('Ctrl Pts',(-236.74227779979,4.48600580620815,132.825192818456));
#134239=CARTESIAN_POINT('Ctrl Pts',(-236.750024075874,4.53885225121814,
132.698563168539));
#134240=CARTESIAN_POINT('Ctrl Pts',(-236.75777040914,4.59169908632851,132.57193258387));
#134241=CARTESIAN_POINT('Ctrl Pts',(-236.765516742405,4.63924225254704,
132.4430894966));
#134242=CARTESIAN_POINT('Ctrl Pts',(-236.77326307567,4.68130743282521,132.312519688047));
#134243=CARTESIAN_POINT('Ctrl Pts',(-236.781011143673,4.72338203330879,
132.181920639292));
#134244=CARTESIAN_POINT('Ctrl Pts',(-236.788759211676,4.75997608688292,
132.04959447185));
#134245=CARTESIAN_POINT('Ctrl Pts',(-236.796507279679,4.79096524240906,
131.916041825704));
#134246=CARTESIAN_POINT('Ctrl Pts',(-236.804263582421,4.82198733357852,
131.782347238217));
#134247=CARTESIAN_POINT('Ctrl Pts',(-236.812019885163,4.8473925385345,131.647423949566));
#134248=CARTESIAN_POINT('Ctrl Pts',(-236.819776187905,4.86710761999026,
131.51178303588));
#134249=CARTESIAN_POINT('Ctrl Pts',(-236.827536630419,4.88683322397865,
131.376069726554));
#134250=CARTESIAN_POINT('Ctrl Pts',(-236.835297072933,4.90086261303366,
131.239638417721));
#134251=CARTESIAN_POINT('Ctrl Pts',(-236.843057515447,4.90917459371302,
131.103004001793));
#134252=CARTESIAN_POINT('Ctrl Pts',(-236.850830415713,4.91749991752167,
130.966150248171));
#134253=CARTESIAN_POINT('Ctrl Pts',(-236.858603315978,4.92008948481346,
130.829093127031));
#134254=CARTESIAN_POINT('Ctrl Pts',(-236.866376216244,4.91697427697041,
130.69234712681));
#134255=CARTESIAN_POINT('Ctrl Pts',(-236.873866552006,4.91397231477915,
130.560572188138));
#134256=CARTESIAN_POINT('Ctrl Pts',(-236.881356887768,4.90567316180276,
130.429086450449));
#134257=CARTESIAN_POINT('Ctrl Pts',(-236.88884722353,4.8921497260235,130.298342712084));
#134258=CARTESIAN_POINT('Ctrl Pts',(-236.896621557649,4.87811354506645,
130.162641785142));
#134259=CARTESIAN_POINT('Ctrl Pts',(-236.904395891768,4.85840464126854,
130.027310374288));
#134260=CARTESIAN_POINT('Ctrl Pts',(-236.912170225887,4.83304779795251,
129.892860729905));
#134261=CARTESIAN_POINT('Ctrl Pts',(-236.919934978834,4.80772220467972,
129.758576782692));
#134262=CARTESIAN_POINT('Ctrl Pts',(-236.927699731781,4.77676259313181,
129.625172820248));
#134263=CARTESIAN_POINT('Ctrl Pts',(-236.935464484729,4.74024557683553,
129.493156997303));
#134264=CARTESIAN_POINT('Ctrl Pts',(-236.943221525614,4.70376482975463,
129.361272294334));
#134265=CARTESIAN_POINT('Ctrl Pts',(-236.950978566499,4.66173776591971,
129.230773361527));
#134266=CARTESIAN_POINT('Ctrl Pts',(-236.958735607384,4.61429215381493,
129.102158813507));
#134267=CARTESIAN_POINT('Ctrl Pts',(-236.966486798624,4.56688232081526,
128.973641254718));
#134268=CARTESIAN_POINT('Ctrl Pts',(-236.974237989864,4.51406220758329,
128.847005617562));
#134269=CARTESIAN_POINT('Ctrl Pts',(-236.981989181104,4.45600948121401,
128.722735635531));
#134270=CARTESIAN_POINT('Ctrl Pts',(-236.989737077881,4.39798142880212,
128.598518471558));
#134271=CARTESIAN_POINT('Ctrl Pts',(-236.997484974658,4.33472535174735,
128.476665316393));
#134272=CARTESIAN_POINT('Ctrl Pts',(-237.005232871435,4.26646705620375,
128.357639971307));
#134273=CARTESIAN_POINT('Ctrl Pts',(-237.012979147519,4.1982230388241,128.238639523758));
#134274=CARTESIAN_POINT('Ctrl Pts',(-237.020725423603,4.12497907858892,
128.122466048667));
#134275=CARTESIAN_POINT('Ctrl Pts',(-237.028471699688,4.04700676214935,
128.009558418909));
#134276=CARTESIAN_POINT('Ctrl Pts',(-237.036218032953,3.96903387013575,
127.896649955693));
#134277=CARTESIAN_POINT('Ctrl Pts',(-237.043964366218,3.88633277443656,
127.787007707624));
#134278=CARTESIAN_POINT('Ctrl Pts',(-237.051710699484,3.79921795401148,
127.68104090924));
#134279=CARTESIAN_POINT('Ctrl Pts',(-237.059458767487,3.71208362482651,
127.575050380327));
#134280=CARTESIAN_POINT('Ctrl Pts',(-237.06720683549,3.62053385230199,127.472737240909));
#134281=CARTESIAN_POINT('Ctrl Pts',(-237.074954903493,3.52492262420586,
127.37447671926));
#134282=CARTESIAN_POINT('Ctrl Pts',(-237.082711206234,3.42920977935859,
127.276111765158));
#134283=CARTESIAN_POINT('Ctrl Pts',(-237.090467508976,3.32942712922516,
127.181808313515));
#134284=CARTESIAN_POINT('Ctrl Pts',(-237.098223811718,3.22596507008493,
127.091904230066));
#134285=CARTESIAN_POINT('Ctrl Pts',(-237.105984254232,3.12244779012856,
127.0019521621));
#134286=CARTESIAN_POINT('Ctrl Pts',(-237.113744696746,3.01524749354317,
126.916404384811));
#134287=CARTESIAN_POINT('Ctrl Pts',(-237.121505139261,2.90478591832392,
126.835557040768));
#134288=CARTESIAN_POINT('Ctrl Pts',(-237.129278039526,2.79414702037781,
126.754579913391));
#134289=CARTESIAN_POINT('Ctrl Pts',(-237.137050939792,2.68023670707852,
126.678318515306));
#134290=CARTESIAN_POINT('Ctrl Pts',(-237.144823840057,2.56350457831185,
126.607024874565));
#134291=CARTESIAN_POINT('Ctrl Pts',(-237.152314175819,2.45101595645665,
126.538322937243));
#134292=CARTESIAN_POINT('Ctrl Pts',(-237.159804511581,2.33590738656979,
126.474233996749));
#134293=CARTESIAN_POINT('Ctrl Pts',(-237.167294847343,2.2185992292628,126.414941462095));
#134294=CARTESIAN_POINT('Ctrl Pts',(-237.175069181462,2.09684329751596,
126.353400832968));
#134295=CARTESIAN_POINT('Ctrl Pts',(-237.182843515581,1.97233200486079,
126.296832558698));
#134296=CARTESIAN_POINT('Ctrl Pts',(-237.1906178497,1.84550971804157,126.245492672219));
#134297=CARTESIAN_POINT('Ctrl Pts',(-237.198382602647,1.71884372835678,
126.194216057561));
#134298=CARTESIAN_POINT('Ctrl Pts',(-237.206147355594,1.58987277028362,
126.148155155304));
#134299=CARTESIAN_POINT('Ctrl Pts',(-237.213912108542,1.45906578027165,
126.107520178362));
#134300=CARTESIAN_POINT('Ctrl Pts',(-237.221669149427,1.32838870960621,
126.066925560652));
#134301=CARTESIAN_POINT('Ctrl Pts',(-237.229426190312,1.19587960694285,
126.031746258929));
#134302=CARTESIAN_POINT('Ctrl Pts',(-237.237183231197,1.06202703287415,
126.002144291332));
#134303=CARTESIAN_POINT('Ctrl Pts',(-237.244934422437,0.928275398072595,
125.97256464681));
#134304=CARTESIAN_POINT('Ctrl Pts',(-237.252685613677,0.793182688620832,
125.948554048885));
#134305=CARTESIAN_POINT('Ctrl Pts',(-237.260436804917,0.657251916610459,
125.930224490968));
#134306=CARTESIAN_POINT('Ctrl Pts',(-237.268184701694,0.521378918804447,
125.911902723601));
#134307=CARTESIAN_POINT('Ctrl Pts',(-237.275932598471,0.384668953539662,
125.899257245937));
#134308=CARTESIAN_POINT('Ctrl Pts',(-237.283680495248,0.247634283703189,
125.892348776779));
#134309=CARTESIAN_POINT('Ctrl Pts',(-237.291426771332,0.11062827856552,
125.885441752723));
#134310=CARTESIAN_POINT('Ctrl Pts',(-237.299173047416,-0.0267019058229216,
125.884269369864));
#134311=CARTESIAN_POINT('Ctrl Pts',(-237.306919323501,-0.16384023406344,
125.888840356169));
#134312=CARTESIAN_POINT('Ctrl Pts',(-237.314665656766,-0.30097957462813,
125.893411376216));
#134313=CARTESIAN_POINT('Ctrl Pts',(-237.322411990031,-0.437926665470685,
125.903725837003));
#134314=CARTESIAN_POINT('Ctrl Pts',(-237.330158323297,-0.574167222423959,
125.919740359737));
#134315=CARTESIAN_POINT('Ctrl Pts',(-237.3379063913,-0.710438289505151,
125.935758468813));
#134316=CARTESIAN_POINT('Ctrl Pts',(-237.345654459303,-0.846002119633315,
125.957479134269));
#134317=CARTESIAN_POINT('Ctrl Pts',(-237.353402527306,-0.980351683599512,
125.984807356219));
#134318=CARTESIAN_POINT('Ctrl Pts',(-237.361158830047,-1.11484403588126,
126.012164622928));
#134319=CARTESIAN_POINT('Ctrl Pts',(-237.368915132789,-1.24811916028487,
126.045141273374));
#134320=CARTESIAN_POINT('Ctrl Pts',(-237.376671435531,-1.37968178207371,
126.083591480792));
#134321=CARTESIAN_POINT('Ctrl Pts',(-237.384431878045,-1.51131462279508,
126.122062210244));
#134322=CARTESIAN_POINT('Ctrl Pts',(-237.39219232056,-1.64123276948438,
126.166012192587));
#134323=CARTESIAN_POINT('Ctrl Pts',(-237.399952763074,-1.76895910932358,
126.215246679991));
#134324=CARTESIAN_POINT('Ctrl Pts',(-237.407725663339,-1.89689048682249,
126.264560202966));
#134325=CARTESIAN_POINT('Ctrl Pts',(-237.415498563605,-2.02262266761886,
126.3191750272));
#134326=CARTESIAN_POINT('Ctrl Pts',(-237.42327146387,-2.14570059365397,
126.378849118892));
#134327=CARTESIAN_POINT('Ctrl Pts',(-237.430761799632,-2.26430432706278,
126.436353907042));
#134328=CARTESIAN_POINT('Ctrl Pts',(-237.438252135394,-2.38044316150043,
126.498556369135));
#134329=CARTESIAN_POINT('Ctrl Pts',(-237.445742471156,-2.49373557459233,
126.565201980936));
#134330=CARTESIAN_POINT('Ctrl Pts',(-237.453518002701,-2.61134161520883,
126.634385135522));
#134331=CARTESIAN_POINT('Ctrl Pts',(-237.461293534247,-2.72625278222702,
126.708575675901));
#134332=CARTESIAN_POINT('Ctrl Pts',(-237.469069065792,-2.83801326791923,
126.787538023324));
#134333=CARTESIAN_POINT('Ctrl Pts',(-237.477234778011,-2.9553819594637,
126.870462747039));
#134334=CARTESIAN_POINT('Ctrl Pts',(-237.485400490229,-3.06927518001104,
126.958650444667));
#134335=CARTESIAN_POINT('Ctrl Pts',(-237.493566202448,-3.17919324362247,
127.051773059333));
#134336=CARTESIAN_POINT('Ctrl Pts',(-237.501322143038,-3.28359540088084,
127.140222596572));
#134337=CARTESIAN_POINT('Ctrl Pts',(-237.509078083628,-3.38441125422789,
127.233123579161));
#134338=CARTESIAN_POINT('Ctrl Pts',(-237.516834024218,-3.48124220144521,
127.33015052067));
#134339=CARTESIAN_POINT('Ctrl Pts',(-237.524584701003,-3.5780074313946,
127.427111611892));
#134340=CARTESIAN_POINT('Ctrl Pts',(-237.532335377788,-3.67079286097035,
127.528192815284));
#134341=CARTESIAN_POINT('Ctrl Pts',(-237.540086054573,-3.75923429687218,
127.63302957781));
#134342=CARTESIAN_POINT('Ctrl Pts',(-237.54783314971,-3.84763486328633,
127.737817894438));
#134343=CARTESIAN_POINT('Ctrl Pts',(-237.555580244846,-3.93169517954091,
127.846358018197));
#134344=CARTESIAN_POINT('Ctrl Pts',(-237.563327339982,-4.01108942636183,
127.958250170618));
#134345=CARTESIAN_POINT('Ctrl Pts',(-237.571072532842,-4.09046417817019,
128.070114848266));
#134346=CARTESIAN_POINT('Ctrl Pts',(-237.578817725703,-4.16517491616811,
128.185329597026));
#134347=CARTESIAN_POINT('Ctrl Pts',(-237.586562918564,-4.23493771934843,
128.303463663323));
#134348=CARTESIAN_POINT('Ctrl Pts',(-237.594309924731,-4.30471685541391,
128.421625387199));
#134349=CARTESIAN_POINT('Ctrl Pts',(-237.602056930898,-4.36954553988217,
128.542707459543));
#134350=CARTESIAN_POINT('Ctrl Pts',(-237.609803937065,-4.42918460838025,
128.666252395939));
#134351=CARTESIAN_POINT('Ctrl Pts',(-237.617551999384,-4.48883180748766,
128.789814175248));
#134352=CARTESIAN_POINT('Ctrl Pts',(-237.625300061702,-4.54328781899816,
128.915839131811));
#134353=CARTESIAN_POINT('Ctrl Pts',(-237.633048124021,-4.59236101766155,
129.043848377915));
#134354=CARTESIAN_POINT('Ctrl Pts',(-237.640801543919,-4.6414681491421,
129.171946139021));
#134355=CARTESIAN_POINT('Ctrl Pts',(-237.648554963818,-4.68518490462915,
129.302030561176));
#134356=CARTESIAN_POINT('Ctrl Pts',(-237.656308383716,-4.72336901801277,
129.433606014372));
#134357=CARTESIAN_POINT('Ctrl Pts',(-237.659220975489,-4.73771297667216,
129.483032665772));
#134358=CARTESIAN_POINT('Ctrl Pts',(-237.662133567262,-4.75127670841368,
129.532669593759));
#134359=CARTESIAN_POINT('Ctrl Pts',(-237.665046159034,-4.76405452823396,
129.582490119308));
#134360=CARTESIAN_POINT('Ctrl Pts',(-235.915124447633,-4.76405452823405,
129.582490119308));
#134361=CARTESIAN_POINT('Ctrl Pts',(-235.92278038583,-4.79776592875833,
129.713930358311));
#134362=CARTESIAN_POINT('Ctrl Pts',(-235.930436324027,-4.82602943120796,
129.846751068765));
#134363=CARTESIAN_POINT('Ctrl Pts',(-235.938092262223,-4.84874865630454,
129.980455568131));
#134364=CARTESIAN_POINT('Ctrl Pts',(-235.945933645855,-4.87201819626461,
130.117398715514));
#134365=CARTESIAN_POINT('Ctrl Pts',(-235.953775029487,-4.8894713453082,
130.255268579083));
#134366=CARTESIAN_POINT('Ctrl Pts',(-235.961616413119,-4.90106078561815,
130.393524594102));
#134367=CARTESIAN_POINT('Ctrl Pts',(-235.969457796751,-4.91265022592809,
130.53178060912));
#134368=CARTESIAN_POINT('Ctrl Pts',(-235.977299180382,-4.9183759659952,
130.670422324837));
#134369=CARTESIAN_POINT('Ctrl Pts',(-235.985140564014,-4.91824789693122,
130.808908895438));
#134370=CARTESIAN_POINT('',(-235.639859435964,-4.9182497717662,130.802862277926));
#134371=CARTESIAN_POINT('Ctrl Pts',(-235.570143588767,-4.76405452823401,
129.582490119308));
#134372=CARTESIAN_POINT('Ctrl Pts',(-235.578507988208,-4.80069372382362,
129.725345786835));
#134373=CARTESIAN_POINT('Ctrl Pts',(-235.586872387649,-4.83094563354471,
129.870015896342));
#134374=CARTESIAN_POINT('Ctrl Pts',(-235.59523678709,-4.85464327593405,
130.015930705698));
#134375=CARTESIAN_POINT('Ctrl Pts',(-235.60357467919,-4.87826581890725,
130.161383101249));
#134376=CARTESIAN_POINT('Ctrl Pts',(-235.611912571289,-4.89537546784984,
130.308072046637));
#134377=CARTESIAN_POINT('Ctrl Pts',(-235.620250463388,-4.9058558003801,
130.455416598593));
#134378=CARTESIAN_POINT('Ctrl Pts',(-235.62678678758,-4.91407164801207,
130.570924420962));
#134379=CARTESIAN_POINT('Ctrl Pts',(-235.633323111772,-4.91821442410782,
130.686834771104));
#134380=CARTESIAN_POINT('Ctrl Pts',(-235.639859435964,-4.9182497717662,
130.802862277926));
#134381=CARTESIAN_POINT('Ctrl Pts',(-235.639859435996,-4.91824977176638,
130.802862278495));
#134382=CARTESIAN_POINT('Ctrl Pts',(-235.647810024064,-4.91829276757809,
130.943994646501));
#134383=CARTESIAN_POINT('Ctrl Pts',(-235.655760612132,-4.91225658512499,
131.085071975645));
#134384=CARTESIAN_POINT('Ctrl Pts',(-235.6637112002,-4.90018168205869,131.225552432914));
#134385=CARTESIAN_POINT('Ctrl Pts',(-235.671666896077,-4.88809902154042,
131.366123141045));
#134386=CARTESIAN_POINT('Ctrl Pts',(-235.679622591955,-4.86996993824622,
131.506095853258));
#134387=CARTESIAN_POINT('Ctrl Pts',(-235.687578287832,-4.84588658484825,
131.644935581081));
#134388=CARTESIAN_POINT('Ctrl Pts',(-235.695540397151,-4.82178381678535,
131.783887233799));
#134389=CARTESIAN_POINT('Ctrl Pts',(-235.70350250647,-4.79171727221365,
131.921703726235));
#134390=CARTESIAN_POINT('Ctrl Pts',(-235.711464615788,-4.75582983404403,
132.057861974612));
#134391=CARTESIAN_POINT('Ctrl Pts',(-235.719440205943,-4.71988163400236,
132.194250755747));
#134392=CARTESIAN_POINT('Ctrl Pts',(-235.727415796098,-4.67809294156459,
132.328975333825));
#134393=CARTESIAN_POINT('Ctrl Pts',(-235.735391386252,-4.63065633426484,
132.461528375046));
#134394=CARTESIAN_POINT('Ctrl Pts',(-235.743374505099,-4.58317494838628,
132.594206541928));
#134395=CARTESIAN_POINT('Ctrl Pts',(-235.751357623945,-4.53003515153502,
132.724708750582));
#134396=CARTESIAN_POINT('Ctrl Pts',(-235.759340742791,-4.47147681634625,
132.852549608694));
#134397=CARTESIAN_POINT('Ctrl Pts',(-235.767338454143,-4.41281144118253,
132.980624149717));
#134398=CARTESIAN_POINT('Ctrl Pts',(-235.775336165496,-4.3487079005738,
133.10602729868));
#134399=CARTESIAN_POINT('Ctrl Pts',(-235.783333876848,-4.27945149522177,
133.228299140414));
#134400=CARTESIAN_POINT('Ctrl Pts',(-235.787104492712,-4.24679974158869,
133.285945650253));
#134401=CARTESIAN_POINT('Ctrl Pts',(-235.790875108575,-4.21300324443521,
133.342896578187));
#134402=CARTESIAN_POINT('Ctrl Pts',(-235.794645724439,-4.17809508585806,
133.399106176581));
#134403=CARTESIAN_POINT('Ctrl Pts',(-235.802420058558,-4.10612071932053,
133.51500029425));
#134404=CARTESIAN_POINT('Ctrl Pts',(-235.810194392677,-4.02920660152256,
133.62808101823));
#134405=CARTESIAN_POINT('Ctrl Pts',(-235.817968726796,-3.94759906404498,
133.737898531426));
#134406=CARTESIAN_POINT('Ctrl Pts',(-235.825733479744,-3.8660921005641,
133.847580704351));
#134407=CARTESIAN_POINT('Ctrl Pts',(-235.833498232691,-3.77990345723433,
133.954007357516));
#134408=CARTESIAN_POINT('Ctrl Pts',(-235.841262985638,-3.68932428418892,
134.056755026089));
#134409=CARTESIAN_POINT('Ctrl Pts',(-235.849020026523,-3.59883507565487,
134.15940064423));
#134410=CARTESIAN_POINT('Ctrl Pts',(-235.856777067408,-3.50396427233535,
134.258374258067));
#134411=CARTESIAN_POINT('Ctrl Pts',(-235.864534108293,-3.40504485442267,
134.353283355788));
#134412=CARTESIAN_POINT('Ctrl Pts',(-235.872285299533,-3.30620003241265,
134.44812088182));
#134413=CARTESIAN_POINT('Ctrl Pts',(-235.880036490773,-3.2033129537756,
134.538899723017));
#134414=CARTESIAN_POINT('Ctrl Pts',(-235.887787682013,-3.09675496293443,
134.625262574178));
#134415=CARTESIAN_POINT('Ctrl Pts',(-235.89553557879,-2.99024226208174,
134.711588718823));
#134416=CARTESIAN_POINT('Ctrl Pts',(-235.903283475567,-2.8800620553127,
134.793502360815));
#134417=CARTESIAN_POINT('Ctrl Pts',(-235.911031372344,-2.76662025974206,
134.870685174323));
#134418=CARTESIAN_POINT('Ctrl Pts',(-235.918777648428,-2.65320219374954,
134.94785184285));
#134419=CARTESIAN_POINT('Ctrl Pts',(-235.926523924512,-2.53652421903467,
135.02028943145));
#134420=CARTESIAN_POINT('Ctrl Pts',(-235.934270200596,-2.41702251920439,
135.087722055054));
#134421=CARTESIAN_POINT('Ctrl Pts',(-235.942016533862,-2.29751993723986,
135.15515517643));
#134422=CARTESIAN_POINT('Ctrl Pts',(-235.949762867127,-2.17519392906321,
135.217583066952));
#134423=CARTESIAN_POINT('Ctrl Pts',(-235.957509200392,-2.05050628748219,
135.274775254655));
#134424=CARTESIAN_POINT('Ctrl Pts',(-235.965257268395,-1.92579072296819,
135.331980250151));
#134425=CARTESIAN_POINT('Ctrl Pts',(-235.973005336398,-1.79871282795443,
135.383947046721));
#134426=CARTESIAN_POINT('Ctrl Pts',(-235.980753404401,-1.66975505132088,
135.430493033644));
#134427=CARTESIAN_POINT('Ctrl Pts',(-235.988509707143,-1.54066021682789,
135.477088490195));
#134428=CARTESIAN_POINT('Ctrl Pts',(-235.996266009885,-1.40968187790405,
135.518251495335));
#134429=CARTESIAN_POINT('Ctrl Pts',(-236.004022312627,-1.27731888352287,
135.55384896183));
#134430=CARTESIAN_POINT('Ctrl Pts',(-236.011782755141,-1.14488524302586,
135.589465427764));
#134431=CARTESIAN_POINT('Ctrl Pts',(-236.019543197655,-1.01106585576917,
135.619510350486));
#134432=CARTESIAN_POINT('Ctrl Pts',(-236.027303640169,-0.876369507130365,
135.643901871597));
#134433=CARTESIAN_POINT('Ctrl Pts',(-236.035076540435,-0.741456931954944,
135.668332548144));
#134434=CARTESIAN_POINT('Ctrl Pts',(-236.0428494407,-0.605664969721866,
135.687091634123));
#134435=CARTESIAN_POINT('Ctrl Pts',(-236.050622340966,-0.469508166963199,
135.700149128486));
#134436=CARTESIAN_POINT('Ctrl Pts',(-236.058112676728,-0.338301006946043,
135.712731950038));
#134437=CARTESIAN_POINT('Ctrl Pts',(-236.065603012489,-0.206755379168454,
135.720020500442));
#134438=CARTESIAN_POINT('Ctrl Pts',(-236.073093348251,-0.0753295237528726,
135.722033697931));
#134439=CARTESIAN_POINT('Ctrl Pts',(-236.08086768237,0.0610793829189508,
135.724123226415));
#134440=CARTESIAN_POINT('Ctrl Pts',(-236.088642016489,0.197791358016512,
135.720536094252));
#134441=CARTESIAN_POINT('Ctrl Pts',(-236.096416350609,0.334294809442846,
135.711236410051));
#134442=CARTESIAN_POINT('Ctrl Pts',(-236.104181103556,0.47063003256496,
135.70194818688));
#134443=CARTESIAN_POINT('Ctrl Pts',(-236.111945856503,0.606756857026472,
135.686961445909));
#134444=CARTESIAN_POINT('Ctrl Pts',(-236.11971060945,0.742161636113154,
135.666292246907));
#134445=CARTESIAN_POINT('Ctrl Pts',(-236.127467650335,0.877431929264741,
135.645643576844));
#134446=CARTESIAN_POINT('Ctrl Pts',(-236.13522469122,1.01198122020633,135.619323738974));
#134447=CARTESIAN_POINT('Ctrl Pts',(-236.142981732105,1.14529929370727,
135.587400716743));
#134448=CARTESIAN_POINT('Ctrl Pts',(-236.150732923345,1.27851683101101,
135.555501767911));
#134449=CARTESIAN_POINT('Ctrl Pts',(-236.158484114585,1.41050462026009,
135.518008135805));
#134450=CARTESIAN_POINT('Ctrl Pts',(-236.166235305825,1.54076132973715,
135.475039110814));
#134451=CARTESIAN_POINT('Ctrl Pts',(-236.173983202602,1.6709626766385,135.432088348804));
#134452=CARTESIAN_POINT('Ctrl Pts',(-236.181731099379,1.79943403662083,
135.383666944733));
#134453=CARTESIAN_POINT('Ctrl Pts',(-236.189478996156,1.92568818503164,
135.329944345278));
#134454=CARTESIAN_POINT('Ctrl Pts',(-236.19722527224,2.05191592379634,135.276232983432));
#134455=CARTESIAN_POINT('Ctrl Pts',(-236.204971548324,2.17592701397578,
135.217222784838));
#134456=CARTESIAN_POINT('Ctrl Pts',(-236.212717824408,2.29725357775422,
135.153131600498));
#134457=CARTESIAN_POINT('Ctrl Pts',(-236.220464157673,2.41858103713762,
135.089039943053));
#134458=CARTESIAN_POINT('Ctrl Pts',(-236.228210490939,2.53722358488175,
135.019867407635));
#134459=CARTESIAN_POINT('Ctrl Pts',(-236.235956824204,2.6527377081024,134.945877937886));
#134460=CARTESIAN_POINT('Ctrl Pts',(-236.243704892207,2.76827769991019,
134.871871898709));
#134461=CARTESIAN_POINT('Ctrl Pts',(-236.25145296021,2.88068754394595,134.793046989507));
#134462=CARTESIAN_POINT('Ctrl Pts',(-236.259201028213,2.98955282923405,
134.709710402632));
#134463=CARTESIAN_POINT('Ctrl Pts',(-236.266957330955,3.09853381784301,
134.626285244642));
#134464=CARTESIAN_POINT('Ctrl Pts',(-236.274713633697,3.20396241137607,
134.538339068346));
#134465=CARTESIAN_POINT('Ctrl Pts',(-236.282469936439,3.3054569997201,134.446219632616));
#134466=CARTESIAN_POINT('Ctrl Pts',(-236.290230378953,3.40700575878188,
134.354051029969));
#134467=CARTESIAN_POINT('Ctrl Pts',(-236.297990821467,3.50461605071644,
134.257705004128));
#134468=CARTESIAN_POINT('Ctrl Pts',(-236.305751263981,3.59794399481218,
134.157565364177));
#134469=CARTESIAN_POINT('Ctrl Pts',(-236.313524164246,3.69142175720905,
134.057264971186));
#134470=CARTESIAN_POINT('Ctrl Pts',(-236.321297064512,3.78060318001821,
133.95315909172));
#134471=CARTESIAN_POINT('Ctrl Pts',(-236.329069964777,3.86518489753918,
133.845664412049));
#134472=CARTESIAN_POINT('Ctrl Pts',(-236.336560300539,3.94669185658299,
133.742077434742));
#134473=CARTESIAN_POINT('Ctrl Pts',(-236.344050636302,4.0239275454595,133.635344012048));
#134474=CARTESIAN_POINT('Ctrl Pts',(-236.351540972064,4.09666019063509,
133.525859900124));
#134475=CARTESIAN_POINT('Ctrl Pts',(-236.359315306183,4.17215051615626,
133.412224664825));
#134476=CARTESIAN_POINT('Ctrl Pts',(-236.367089640302,4.24302872219089,
133.295266075736));
#134477=CARTESIAN_POINT('Ctrl Pts',(-236.374863974421,4.30898808427034,
133.175395149604));
#134478=CARTESIAN_POINT('Ctrl Pts',(-236.382628727368,4.37486615733117,
133.055671953675));
#134479=CARTESIAN_POINT('Ctrl Pts',(-236.390393480315,4.43583726141008,
132.933043901376));
#134480=CARTESIAN_POINT('Ctrl Pts',(-236.398158233263,4.49163726944919,
132.807951818933));
#134481=CARTESIAN_POINT('Ctrl Pts',(-236.405915274148,4.54738185613368,
132.682983979709));
#134482=CARTESIAN_POINT('Ctrl Pts',(-236.413672315033,4.59796540942072,
132.55555733534));
#134483=CARTESIAN_POINT('Ctrl Pts',(-236.421429355918,4.64316934191289,
132.42613789106));
#134484=CARTESIAN_POINT('Ctrl Pts',(-236.429180547158,4.68833918576774,
132.29681604299));
#134485=CARTESIAN_POINT('Ctrl Pts',(-236.436931738398,4.72813735527188,
132.165504753819));
#134486=CARTESIAN_POINT('Ctrl Pts',(-236.444682929638,4.76239323077036,
132.032690287489));
#134487=CARTESIAN_POINT('Ctrl Pts',(-236.452430826415,4.796634546608,131.89993227085));
#134488=CARTESIAN_POINT('Ctrl Pts',(-236.460178723192,4.82533815615523,
131.765672725539));
#134489=CARTESIAN_POINT('Ctrl Pts',(-236.467926619969,4.84838326287521,
131.630413157524));
#134490=CARTESIAN_POINT('Ctrl Pts',(-236.475672896053,4.87142354905567,
131.495181882895));
#134491=CARTESIAN_POINT('Ctrl Pts',(-236.483419172137,4.88880762110378,
131.358951386806));
#134492=CARTESIAN_POINT('Ctrl Pts',(-236.491165448221,4.90046586385056,
131.222233061902));
#134493=CARTESIAN_POINT('Ctrl Pts',(-236.498911781487,4.91212419265584,
131.085513727775));
#134494=CARTESIAN_POINT('Ctrl Pts',(-236.506658114752,4.91805657460166,
130.948306947199));
#134495=CARTESIAN_POINT('Ctrl Pts',(-236.514404448018,4.91824534340113,
130.81112852811));
#134496=CARTESIAN_POINT('Ctrl Pts',(-236.522152516021,4.91843415447406,
130.673919388866));
#134497=CARTESIAN_POINT('Ctrl Pts',(-236.529900584023,4.91287679238941,
130.536739014637));
#134498=CARTESIAN_POINT('Ctrl Pts',(-236.537648652026,4.9016077075174,130.400102106084));
#134499=CARTESIAN_POINT('Ctrl Pts',(-236.545404954768,4.89032664572788,
130.263319978198));
#134500=CARTESIAN_POINT('Ctrl Pts',(-236.55316125751,4.87332176688625,130.127082860073));
#134501=CARTESIAN_POINT('Ctrl Pts',(-236.560917560252,4.85067938079108,
129.991899783268));
#134502=CARTESIAN_POINT('Ctrl Pts',(-236.568678002766,4.8280249097727,129.856644555185));
#134503=CARTESIAN_POINT('Ctrl Pts',(-236.57643844528,4.79972701662529,129.722444871763));
#134504=CARTESIAN_POINT('Ctrl Pts',(-236.584198887795,4.76592273487762,
129.58979750777));
#134505=CARTESIAN_POINT('Ctrl Pts',(-236.59197178806,4.73206418749589,129.456937206453));
#134506=CARTESIAN_POINT('Ctrl Pts',(-236.599744688325,4.6926817000743,129.325634578915));
#134507=CARTESIAN_POINT('Ctrl Pts',(-236.607517588591,4.64796186600247,
129.19637008442));
#134508=CARTESIAN_POINT('Ctrl Pts',(-236.615007924353,4.60486771054161,
129.071804679898));
#134509=CARTESIAN_POINT('Ctrl Pts',(-236.622498260115,4.55681763560663,
128.949132085347));
#134510=CARTESIAN_POINT('Ctrl Pts',(-236.629988595877,4.50401932280744,
128.828761214277));
#134511=CARTESIAN_POINT('Ctrl Pts',(-236.637762929996,4.44921914593055,
128.703826445044));
#134512=CARTESIAN_POINT('Ctrl Pts',(-236.645537264115,4.38912997414836,
128.580975628656));
#134513=CARTESIAN_POINT('Ctrl Pts',(-236.653311598234,4.32393181542294,
128.460688985687));
#134514=CARTESIAN_POINT('Ctrl Pts',(-236.661076351181,4.2588140076014,128.340550585256));
#134515=CARTESIAN_POINT('Ctrl Pts',(-236.668841104129,4.18859992525228,
128.222970410979));
#134516=CARTESIAN_POINT('Ctrl Pts',(-236.676605857076,4.11351768083691,
128.108408957773));
#134517=CARTESIAN_POINT('Ctrl Pts',(-236.684362897961,4.03851000916537,
127.993961288617));
#134518=CARTESIAN_POINT('Ctrl Pts',(-236.692119938846,3.95864401047074,
127.882526698786));
#134519=CARTESIAN_POINT('Ctrl Pts',(-236.699876979731,3.87419359632847,
127.77454097926));
#134520=CARTESIAN_POINT('Ctrl Pts',(-236.707628170971,3.78980686690009,
127.666636692604));
#134521=CARTESIAN_POINT('Ctrl Pts',(-236.715379362211,3.70084284313236,
127.562176406203));
#134522=CARTESIAN_POINT('Ctrl Pts',(-236.723130553451,3.60761840856041,
127.461566504744));
#134523=CARTESIAN_POINT('Ctrl Pts',(-236.730878450228,3.51443359685987,
127.360999365177));
#134524=CARTESIAN_POINT('Ctrl Pts',(-236.738626347005,3.41699224104641,
127.264279641824));
#134525=CARTESIAN_POINT('Ctrl Pts',(-236.746374243783,3.31565097881498,
127.171780040458));
#134526=CARTESIAN_POINT('Ctrl Pts',(-236.754120519867,3.21433091499121,
127.079299788015));
#134527=CARTESIAN_POINT('Ctrl Pts',(-236.761866795951,3.10911285595423,
126.991038165107));
#134528=CARTESIAN_POINT('Ctrl Pts',(-236.769613072035,3.0003894221212,126.907330161164));
#134529=CARTESIAN_POINT('Ctrl Pts',(-236.7773594053,2.89166518571693,126.823621539308));
#134530=CARTESIAN_POINT('Ctrl Pts',(-236.785105738566,2.77943583266885,
126.744466842001));
#134531=CARTESIAN_POINT('Ctrl Pts',(-236.792852071831,2.66412577774201,
126.670159739177));
#134532=CARTESIAN_POINT('Ctrl Pts',(-236.800600139834,2.54878989992771,
126.595835995793));
#134533=CARTESIAN_POINT('Ctrl Pts',(-236.808348207837,2.43037227598597,
126.52636221882));
#134534=CARTESIAN_POINT('Ctrl Pts',(-236.81609627584,2.30932455942561,126.461987632465));
#134535=CARTESIAN_POINT('Ctrl Pts',(-236.823852578582,2.18814819191144,
126.397544628034));
#134536=CARTESIAN_POINT('Ctrl Pts',(-236.831608881324,2.06433649361586,
126.338211824083));
#134537=CARTESIAN_POINT('Ctrl Pts',(-236.839365184066,1.93836437976073,
126.284191749728));
#134538=CARTESIAN_POINT('Ctrl Pts',(-236.84712562658,1.81232503079513,126.230142843232));
#134539=CARTESIAN_POINT('Ctrl Pts',(-236.854886069094,1.68412333393879,
126.181412455276));
#134540=CARTESIAN_POINT('Ctrl Pts',(-236.862646511608,1.55425130984237,
126.138153814567));
#134541=CARTESIAN_POINT('Ctrl Pts',(-236.870419411874,1.42417080364338,
126.094825731248));
#134542=CARTESIAN_POINT('Ctrl Pts',(-236.878192312139,1.29241498798955,
126.056987055857));
#134543=CARTESIAN_POINT('Ctrl Pts',(-236.885965212404,1.15948894515113,
126.024740502058));
#134544=CARTESIAN_POINT('Ctrl Pts',(-236.893455548166,1.03139509879362,
125.993666191714));
#134545=CARTESIAN_POINT('Ctrl Pts',(-236.900945883928,0.902214931541491,
125.967784546807));
#134546=CARTESIAN_POINT('Ctrl Pts',(-236.90843621969,0.772404730894424,
125.947141866656));
#134547=CARTESIAN_POINT('Ctrl Pts',(-236.916210553809,0.637672737032011,
125.925716513012));
#134548=CARTESIAN_POINT('Ctrl Pts',(-236.923984887928,0.501835200781801,
125.909867367991));
#134549=CARTESIAN_POINT('Ctrl Pts',(-236.931759222047,0.365393444013297,
125.899702556745));
#134550=CARTESIAN_POINT('Ctrl Pts',(-236.939523974995,0.229119839515861,
125.889550272721));
#134551=CARTESIAN_POINT('Ctrl Pts',(-236.947288727942,0.0922438822691649,
125.885068412515));
#134552=CARTESIAN_POINT('Ctrl Pts',(-236.955053480889,-0.0447236999542945,
125.886313967405));
#134553=CARTESIAN_POINT('Ctrl Pts',(-236.962810521774,-0.181555244044185,
125.887558285191));
#134554=CARTESIAN_POINT('Ctrl Pts',(-236.970567562659,-0.318477843591094,
125.894518694071));
#134555=CARTESIAN_POINT('Ctrl Pts',(-236.978324603544,-0.454976799403212,
125.907200300147));
#134556=CARTESIAN_POINT('Ctrl Pts',(-236.986075794784,-0.591372820290759,
125.919872342925));
#134557=CARTESIAN_POINT('Ctrl Pts',(-236.993826986024,-0.727345445621648,
125.938256959329));
#134558=CARTESIAN_POINT('Ctrl Pts',(-237.001578177264,-0.862381489158824,
125.962307207115));
#134559=CARTESIAN_POINT('Ctrl Pts',(-237.009326074041,-0.997360138775109,
125.986347232905));
#134560=CARTESIAN_POINT('Ctrl Pts',(-237.017073970818,-1.13140261423075,
126.01604803225));
#134561=CARTESIAN_POINT('Ctrl Pts',(-237.024821867595,-1.26400257621797,
126.051311012332));
#134562=CARTESIAN_POINT('Ctrl Pts',(-237.032568143679,-1.39657480115202,
126.086566616159));
#134563=CARTESIAN_POINT('Ctrl Pts',(-237.040314419764,-1.52770473520686,
126.127381986065));
#134564=CARTESIAN_POINT('Ctrl Pts',(-237.048060695848,-1.65689832136193,
126.173607869344));
#134565=CARTESIAN_POINT('Ctrl Pts',(-237.055807029113,-1.78609286119453,
126.219834093851));
#134566=CARTESIAN_POINT('Ctrl Pts',(-237.063553362379,-1.91335065649412,
126.271470779715));
#134567=CARTESIAN_POINT('Ctrl Pts',(-237.071299695644,-2.03819522787897,
126.328319590548));
#134568=CARTESIAN_POINT('Ctrl Pts',(-237.079047763647,-2.16306775734049,
126.385181132277));
#134569=CARTESIAN_POINT('Ctrl Pts',(-237.08679583165,-2.28552563175982,
126.447256959616));
#134570=CARTESIAN_POINT('Ctrl Pts',(-237.094543899653,-2.40511504199968,
126.514301795446));
#134571=CARTESIAN_POINT('Ctrl Pts',(-237.102300202395,-2.52483155328705,
126.581417887326));
#134572=CARTESIAN_POINT('Ctrl Pts',(-237.110056505137,-2.64167316884011,
126.653513345811));
#134573=CARTESIAN_POINT('Ctrl Pts',(-237.117812807878,-2.75521279190169,
126.73029808321));
#134574=CARTESIAN_POINT('Ctrl Pts',(-237.125573250393,-2.86881301447933,
126.807123802936));
#134575=CARTESIAN_POINT('Ctrl Pts',(-237.133333692907,-2.97910741863439,
126.888643556366));
#134576=CARTESIAN_POINT('Ctrl Pts',(-237.141094135421,-3.08570113953568,
126.97452621645));
#134577=CARTESIAN_POINT('Ctrl Pts',(-237.148867035686,-3.19246597414043,
127.060546743005));
#134578=CARTESIAN_POINT('Ctrl Pts',(-237.156639935952,-3.29551796006939,
127.150943913923));
#134579=CARTESIAN_POINT('Ctrl Pts',(-237.164412836217,-3.39449767210342,
127.24534830843));
#134580=CARTESIAN_POINT('Ctrl Pts',(-237.171903171979,-3.48987922229177,
127.336320865407));
#134581=CARTESIAN_POINT('Ctrl Pts',(-237.179393507741,-3.58147921896272,
127.431014137426));
#134582=CARTESIAN_POINT('Ctrl Pts',(-237.186883843504,-3.6690120746481,
127.529069262803));
#134583=CARTESIAN_POINT('Ctrl Pts',(-237.194584148885,-3.75899865749865,
127.629873076349));
#134584=CARTESIAN_POINT('Ctrl Pts',(-237.202284454265,-3.8449847776776,
127.734564138519));
#134585=CARTESIAN_POINT('Ctrl Pts',(-237.209984759646,-3.92661086149957,
127.842788365391));
#134586=CARTESIAN_POINT('Ctrl Pts',(-237.217675821897,-4.00813896472519,
127.950882684349));
#134587=CARTESIAN_POINT('Ctrl Pts',(-237.225366884148,-4.08531720106446,
128.06250141918));
#134588=CARTESIAN_POINT('Ctrl Pts',(-237.233057946399,-4.15782352492297,
128.177254491408));
#134589=CARTESIAN_POINT('Ctrl Pts',(-237.240740208052,-4.23024688248011,
128.291876255944));
#134590=CARTESIAN_POINT('Ctrl Pts',(-237.248422469705,-4.2980087575144,
128.409624883436));
#134591=CARTESIAN_POINT('Ctrl Pts',(-237.256104731358,-4.36082848494722,
128.530078755665));
#134592=CARTESIAN_POINT('Ctrl Pts',(-237.263781857921,-4.42360622149408,
128.650452112345));
#134593=CARTESIAN_POINT('Ctrl Pts',(-237.271458984483,-4.48144819595658,
128.77352676561));
#134594=CARTESIAN_POINT('Ctrl Pts',(-237.279136111046,-4.53411811845468,
128.898853873836));
#134595=CARTESIAN_POINT('Ctrl Pts',(-237.286810197679,-4.58676718512242,
129.024131355998));
#134596=CARTESIAN_POINT('Ctrl Pts',(-237.294484284313,-4.63424811655263,
129.151659153016));
#134597=CARTESIAN_POINT('Ctrl Pts',(-237.302158370946,-4.67637168339331,
129.280966072067));
#134598=CARTESIAN_POINT('Ctrl Pts',(-237.308065172838,-4.70879450791701,
129.380494575005));
#134599=CARTESIAN_POINT('Ctrl Pts',(-237.313971974729,-4.73804429293833,
129.481076606651));
#134600=CARTESIAN_POINT('Ctrl Pts',(-237.319878776621,-4.76405452823405,
129.582490119308));
#134601=CARTESIAN_POINT('Origin',(213.235140564004,0.,130.804360617566));
#134602=CARTESIAN_POINT('',(-239.415329287988,-4.76405452823416,129.582490119309));
#134603=CARTESIAN_POINT('',(-239.069767094363,-4.76405452823403,129.582490119308));
#134604=CARTESIAN_POINT('',(213.235140564004,-4.76405452823405,129.582490119308));
#134605=CARTESIAN_POINT('',(-237.73514056406,-4.91824985575658,130.803169462491));
#134606=CARTESIAN_POINT('Ctrl Pts',(-237.735140564061,-4.91824985575658,
130.803169462492));
#134607=CARTESIAN_POINT('Ctrl Pts',(-237.742865432421,-4.91828269493721,
130.938761627506));
#134608=CARTESIAN_POINT('Ctrl Pts',(-237.750590300782,-4.91270403941569,
131.074580060301));
#134609=CARTESIAN_POINT('Ctrl Pts',(-237.758315169143,-4.90148384634299,
131.210118139417));
#134610=CARTESIAN_POINT('Ctrl Pts',(-237.766030648401,-4.89027729072596,
131.345491480321));
#134611=CARTESIAN_POINT('Ctrl Pts',(-237.773746127658,-4.87344286997585,
131.480584754197));
#134612=CARTESIAN_POINT('Ctrl Pts',(-237.781461606916,-4.85100251809047,
131.614889847131));
#134613=CARTESIAN_POINT('Ctrl Pts',(-237.78916961392,-4.82858389913852,
131.749064868859));
#134614=CARTESIAN_POINT('Ctrl Pts',(-237.796877620924,-4.80057021590841,
131.882452839898));
#134615=CARTESIAN_POINT('Ctrl Pts',(-237.804585627929,-4.76703528595467,
132.014549712279));
#134616=CARTESIAN_POINT('Ctrl Pts',(-237.812288072446,-4.73352455649721,
132.146551256897));
#134617=CARTESIAN_POINT('Ctrl Pts',(-237.819990516964,-4.6945006066077,
132.277263174278));
#134618=CARTESIAN_POINT('Ctrl Pts',(-237.827692961482,-4.65008843923634,
132.406190998655));
#134619=CARTESIAN_POINT('Ctrl Pts',(-237.835392528332,-4.60569286444811,
132.535070655024));
#134620=CARTESIAN_POINT('Ctrl Pts',(-237.843092095182,-4.55591320289364,
132.662167169325));
#134621=CARTESIAN_POINT('Ctrl Pts',(-237.850791662032,-4.50092440392816,
132.787000920955));
#134622=CARTESIAN_POINT('Ctrl Pts',(-237.858489955009,-4.44594470272169,
132.911814019155));
#134623=CARTESIAN_POINT('Ctrl Pts',(-237.866188247985,-4.38575773771776,
133.034364736533));
#134624=CARTESIAN_POINT('Ctrl Pts',(-237.873886540961,-4.32058653617298,
133.154193600129));
#134625=CARTESIAN_POINT('Ctrl Pts',(-237.881585280676,-4.2554115526847,
133.274029417502));
#134626=CARTESIAN_POINT('Ctrl Pts',(-237.889284020391,-4.18525194673164,
133.391142718648));
#134627=CARTESIAN_POINT('Ctrl Pts',(-237.896982760106,-4.1103763888758,
133.505099221036));
#134628=CARTESIAN_POINT('Ctrl Pts',(-237.904683667168,-4.03547975206986,
133.619087804432));
#134629=CARTESIAN_POINT('Ctrl Pts',(-237.912384574231,-3.955864740056,133.729917490131));
#134630=CARTESIAN_POINT('Ctrl Pts',(-237.920085481293,-3.87184269080206,
133.837183929298));
#134631=CARTESIAN_POINT('Ctrl Pts',(-237.927794694456,-3.78773001643866,
133.944566064676));
#134632=CARTESIAN_POINT('Ctrl Pts',(-237.935503907619,-3.69920105859463,
134.048376967458));
#134633=CARTESIAN_POINT('Ctrl Pts',(-237.943213120781,-3.606606956095,134.148245981442));
#134634=CARTESIAN_POINT('Ctrl Pts',(-237.950926943952,-3.51395748353554,
134.248174715789));
#134635=CARTESIAN_POINT('Ctrl Pts',(-237.958640767123,-3.41723830596076,
134.344156588317));
#134636=CARTESIAN_POINT('Ctrl Pts',(-237.966354590294,-3.3168357331299,
134.435859451647));
#134637=CARTESIAN_POINT('Ctrl Pts',(-237.974079890696,-3.21628377348235,
134.527698757684));
#134638=CARTESIAN_POINT('Ctrl Pts',(-237.981805191097,-3.11203777795702,
134.615246087266));
#134639=CARTESIAN_POINT('Ctrl Pts',(-237.989530491499,-3.00451567741233,
134.698210718261));
#134640=CARTESIAN_POINT('Ctrl Pts',(-237.99389956726,-2.94370610641383,
134.745131710255));
#134641=CARTESIAN_POINT('Ctrl Pts',(-237.998268643021,-2.88184918344584,
134.790587717055));
#134642=CARTESIAN_POINT('Ctrl Pts',(-238.002637718782,-2.81902410685448,
134.834532592491));
#134643=CARTESIAN_POINT('Ctrl Pts',(-238.010412052901,-2.70723315535801,
134.912728110985));
#134644=CARTESIAN_POINT('Ctrl Pts',(-238.01818638702,-2.592009128965,134.986392589495));
#134645=CARTESIAN_POINT('Ctrl Pts',(-238.025960721139,-2.47375556551788,
135.055209528615));
#134646=CARTESIAN_POINT('Ctrl Pts',(-238.033725474086,-2.35564773901972,
135.123941657008));
#134647=CARTESIAN_POINT('Ctrl Pts',(-238.041490227033,-2.23451813895336,
135.187837938047));
#134648=CARTESIAN_POINT('Ctrl Pts',(-238.04925497998,-2.11080112627545,
135.246623742125));
#134649=CARTESIAN_POINT('Ctrl Pts',(-238.057012020865,-1.9872069910783,
135.305351159313));
#134650=CARTESIAN_POINT('Ctrl Pts',(-238.06476906175,-1.86103090823899,
135.358978033897));
#134651=CARTESIAN_POINT('Ctrl Pts',(-238.072526102635,-1.73273350330077,
135.407274658588));
#134652=CARTESIAN_POINT('Ctrl Pts',(-238.080277293875,-1.60453284843345,
135.455534862419));
#134653=CARTESIAN_POINT('Ctrl Pts',(-238.088028485115,-1.47421442000175,
135.498472679909));
#134654=CARTESIAN_POINT('Ctrl Pts',(-238.095779676355,-1.34226024751455,
135.535905871544));
#134655=CARTESIAN_POINT('Ctrl Pts',(-238.103527573132,-1.21036215907084,
135.573323153074));
#134656=CARTESIAN_POINT('Ctrl Pts',(-238.11127546991,-1.07683008467684,
135.605240355585));
#134657=CARTESIAN_POINT('Ctrl Pts',(-238.119023366687,-0.94216248709477,
135.631524682564));
#134658=CARTESIAN_POINT('Ctrl Pts',(-238.126769642771,-0.807523059071014,
135.657803511429));
#134659=CARTESIAN_POINT('Ctrl Pts',(-238.134515918855,-0.671748963794779,
135.678451733572));
#134660=CARTESIAN_POINT('Ctrl Pts',(-238.142262194939,-0.535349776071497,
135.693387481857));
#134661=CARTESIAN_POINT('Ctrl Pts',(-238.150008528204,-0.398949581480582,
135.708323340394));
#134662=CARTESIAN_POINT('Ctrl Pts',(-238.157754861469,-0.26192467387732,
135.717546598374));
#134663=CARTESIAN_POINT('Ctrl Pts',(-238.165501194735,-0.124790288715148,
135.721027216629));
#134664=CARTESIAN_POINT('Ctrl Pts',(-238.173249262738,0.0123748067419455,
135.724508614344));
#134665=CARTESIAN_POINT('Ctrl Pts',(-238.180997330741,0.149649037778895,
135.722244803376));
#134666=CARTESIAN_POINT('Ctrl Pts',(-238.188745398744,0.286517025242996,
135.714257872779));
#134667=CARTESIAN_POINT('Ctrl Pts',(-238.196501701486,0.423530477633109,
135.706262453576));
#134668=CARTESIAN_POINT('Ctrl Pts',(-238.204258004227,0.560136433038687,
135.692531786908));
#134669=CARTESIAN_POINT('Ctrl Pts',(-238.212014306969,0.695823935291642,
135.673139942363));
#134670=CARTESIAN_POINT('Ctrl Pts',(-238.219774749484,0.83158385805002,
135.653737747808));
#134671=CARTESIAN_POINT('Ctrl Pts',(-238.227535191998,0.966423966688222,
135.628668426128));
#134672=CARTESIAN_POINT('Ctrl Pts',(-238.235295634512,1.09984434107092,
135.598057050165));
#134673=CARTESIAN_POINT('Ctrl Pts',(-238.243068534777,1.23347889368309,
135.567396534104));
#134674=CARTESIAN_POINT('Ctrl Pts',(-238.250841435043,1.36568878041693,
135.531176288886));
#134675=CARTESIAN_POINT('Ctrl Pts',(-238.258614335308,1.49598920264289,
135.489571324469));
#134676=CARTESIAN_POINT('Ctrl Pts',(-238.26610467107,1.62155287631434,135.449478805304));
#134677=CARTESIAN_POINT('Ctrl Pts',(-238.273595006832,1.74534321349922,
135.404386371627));
#134678=CARTESIAN_POINT('Ctrl Pts',(-238.281085342594,1.86694643465895,
135.354491832445));
#134679=CARTESIAN_POINT('Ctrl Pts',(-238.288859676713,1.99316027890892,
135.302705526644));
#134680=CARTESIAN_POINT('Ctrl Pts',(-238.296634010832,2.11741769173488,
135.245581739916));
#134681=CARTESIAN_POINT('Ctrl Pts',(-238.304408344952,2.2392342711602,135.183288904414));
#134682=CARTESIAN_POINT('Ctrl Pts',(-238.312173097899,2.36090072253878,
135.121072839265));
#134683=CARTESIAN_POINT('Ctrl Pts',(-238.319937850846,2.48013198100569,
135.053700576816));
#134684=CARTESIAN_POINT('Ctrl Pts',(-238.327702603793,2.59646221018546,
134.981389113229));
#134685=CARTESIAN_POINT('Ctrl Pts',(-238.335459644678,2.71267689854133,
134.909149470407));
#134686=CARTESIAN_POINT('Ctrl Pts',(-238.343216685563,2.8259959617182,134.831980594044));
#134687=CARTESIAN_POINT('Ctrl Pts',(-238.350973726448,2.93597716110945,
134.750145859054));
#134688=CARTESIAN_POINT('Ctrl Pts',(-238.358724917688,3.04587542282287,
134.668372836274));
#134689=CARTESIAN_POINT('Ctrl Pts',(-238.366476108928,3.15244051851142,
134.581941190793));
#134690=CARTESIAN_POINT('Ctrl Pts',(-238.374227300168,3.25525857618644,
134.491157962778));
#134691=CARTESIAN_POINT('Ctrl Pts',(-238.381975196946,3.35803293344406,
134.400413320058));
#134692=CARTESIAN_POINT('Ctrl Pts',(-238.389723093723,3.45706312777038,
134.305321031623));
#134693=CARTESIAN_POINT('Ctrl Pts',(-238.3974709905,3.55196800240126,134.206228688555));
#134694=CARTESIAN_POINT('Ctrl Pts',(-238.405217266584,3.64685302497828,
134.10715707347));
#134695=CARTESIAN_POINT('Ctrl Pts',(-238.412963542668,3.73761417401833,
134.004087350221));
#134696=CARTESIAN_POINT('Ctrl Pts',(-238.420709818752,3.82390713475273,
133.897403987337));
#134697=CARTESIAN_POINT('Ctrl Pts',(-238.428456152017,3.91020073248229,
133.790719836942));
#134698=CARTESIAN_POINT('Ctrl Pts',(-238.436202485283,3.99202583021619,
133.680422297656));
#134699=CARTESIAN_POINT('Ctrl Pts',(-238.443948818548,4.06907865780404,
133.566928614757));
#134700=CARTESIAN_POINT('Ctrl Pts',(-238.451696886551,4.14614874083827,
133.453409515734));
#134701=CARTESIAN_POINT('Ctrl Pts',(-238.459444954554,4.21844420754164,
133.33669317223));
#134702=CARTESIAN_POINT('Ctrl Pts',(-238.467193022557,4.28570506703893,
133.217225126994));
#134703=CARTESIAN_POINT('Ctrl Pts',(-238.474949325299,4.35303741217801,
133.097630109698));
#134704=CARTESIAN_POINT('Ctrl Pts',(-238.482705628041,4.41532426911977,
132.975277889809));
#134705=CARTESIAN_POINT('Ctrl Pts',(-238.490461930783,4.47235177041802,
132.850638385646));
#134706=CARTESIAN_POINT('Ctrl Pts',(-238.498222373297,4.52940970901094,
132.725932357626));
#134707=CARTESIAN_POINT('Ctrl Pts',(-238.505982815811,4.58120255105312,
132.598936974638));
#134708=CARTESIAN_POINT('Ctrl Pts',(-238.513743258325,4.6275653048243,132.470140438577));
#134709=CARTESIAN_POINT('Ctrl Pts',(-238.521516158591,4.67400248420373,
132.341137146881));
#134710=CARTESIAN_POINT('Ctrl Pts',(-238.529289058856,4.71499203927674,
132.210327297524));
#134711=CARTESIAN_POINT('Ctrl Pts',(-238.537061959122,4.75041916537622,
132.078213362481));
#134712=CARTESIAN_POINT('Ctrl Pts',(-238.544552294884,4.78455842620654,
131.95090210175));
#134713=CARTESIAN_POINT('Ctrl Pts',(-238.552042630646,4.81353258566578,
131.822380223306));
#134714=CARTESIAN_POINT('Ctrl Pts',(-238.559532966408,4.83728440812522,
131.693102772192));
#134715=CARTESIAN_POINT('Ctrl Pts',(-238.567307300527,4.86193678815231,
131.558923727226));
#134716=CARTESIAN_POINT('Ctrl Pts',(-238.575081634646,4.88104109533654,
131.42350564461));
#134717=CARTESIAN_POINT('Ctrl Pts',(-238.582855968765,4.89447720531924,
131.287347107139));
#134718=CARTESIAN_POINT('Ctrl Pts',(-238.590620721712,4.90789675649721,
131.151356372897));
#134719=CARTESIAN_POINT('Ctrl Pts',(-238.598385474659,4.9156619716037,131.014627384832));
#134720=CARTESIAN_POINT('Ctrl Pts',(-238.606150227606,4.91770361971606,
130.877669356005));
#134721=CARTESIAN_POINT('Ctrl Pts',(-238.613907268491,4.91974324003474,
130.740847355824));
#134722=CARTESIAN_POINT('Ctrl Pts',(-238.621664309376,4.9160706004336,130.603797155981));
#134723=CARTESIAN_POINT('Ctrl Pts',(-238.629421350261,4.90666824491761,
130.467033184918));
#134724=CARTESIAN_POINT('Ctrl Pts',(-238.637172541501,4.89727297979103,
130.330372348628));
#134725=CARTESIAN_POINT('Ctrl Pts',(-238.644923732741,4.88215662579298,
130.193997699952));
#134726=CARTESIAN_POINT('Ctrl Pts',(-238.652674923982,4.86135379659384,
130.058423403826));
#134727=CARTESIAN_POINT('Ctrl Pts',(-238.660422820759,4.84055980915201,
129.922906730392));
#134728=CARTESIAN_POINT('Ctrl Pts',(-238.668170717536,4.81408421271863,
129.788190118567));
#134729=CARTESIAN_POINT('Ctrl Pts',(-238.675918614313,4.78201342097328,
129.654782127801));
#134730=CARTESIAN_POINT('Ctrl Pts',(-238.683664890397,4.74994933774629,
129.521402043111));
#134731=CARTESIAN_POINT('Ctrl Pts',(-238.691411166481,4.71229247851094,
129.3893304149));
#134732=CARTESIAN_POINT('Ctrl Pts',(-238.699157442565,4.66918019698701,
129.259064739566));
#134733=CARTESIAN_POINT('Ctrl Pts',(-238.70690377583,4.62606759721795,129.12879810264));
#134734=CARTESIAN_POINT('Ctrl Pts',(-238.714650109096,4.57749961764288,
129.000337816358));
#134735=CARTESIAN_POINT('Ctrl Pts',(-238.722396442361,4.52366310334266,
128.874164982415));
#134736=CARTESIAN_POINT('Ctrl Pts',(-238.730144510364,4.46981453272827,
128.74796389294));
#134737=CARTESIAN_POINT('Ctrl Pts',(-238.737892578367,4.41069523302737,
128.624051634669));
#134738=CARTESIAN_POINT('Ctrl Pts',(-238.74564064637,4.34653952055527,128.502887772027));
#134739=CARTESIAN_POINT('Ctrl Pts',(-238.753396949112,4.28231562262857,
128.381595134991));
#134740=CARTESIAN_POINT('Ctrl Pts',(-238.761153251854,4.21304480245928,
128.263057074722));
#134741=CARTESIAN_POINT('Ctrl Pts',(-238.768909554596,4.13900681505815,
128.147707526287));
#134742=CARTESIAN_POINT('Ctrl Pts',(-238.77666999711,4.06492931135391,128.032296412325));
#134743=CARTESIAN_POINT('Ctrl Pts',(-238.784430439624,3.98607979518424,
127.920077520926));
#134744=CARTESIAN_POINT('Ctrl Pts',(-238.792190882138,3.90277982257457,
127.811453549345));
#134745=CARTESIAN_POINT('Ctrl Pts',(-238.799963782403,3.81934612945383,
127.702655204922));
#134746=CARTESIAN_POINT('Ctrl Pts',(-238.807736682669,3.73144795420495,
127.597463612569));
#134747=CARTESIAN_POINT('Ctrl Pts',(-238.815509582934,3.63944598600381,
127.49624695908));
#134748=CARTESIAN_POINT('Ctrl Pts',(-238.822999918696,3.55078852108624,
127.398709785895));
#134749=CARTESIAN_POINT('Ctrl Pts',(-238.830490254458,3.45832066574396,
127.304863790331));
#134750=CARTESIAN_POINT('Ctrl Pts',(-238.83798059022,3.36239432500475,127.215003089306));
#134751=CARTESIAN_POINT('Ctrl Pts',(-238.845754924339,3.26283090789981,
127.121735292488));
#134752=CARTESIAN_POINT('Ctrl Pts',(-238.853529258458,3.15922618443732,
127.032465516368));
#134753=CARTESIAN_POINT('Ctrl Pts',(-238.861303592577,3.05193469629379,
126.947564321149));
#134754=CARTESIAN_POINT('Ctrl Pts',(-238.869068345525,2.94477543532019,
126.862767759065));
#134755=CARTESIAN_POINT('Ctrl Pts',(-238.876833098471,2.83393875373527,
126.782329305833));
#134756=CARTESIAN_POINT('Ctrl Pts',(-238.884597851419,2.71981564590503,
126.706582449486));
#134757=CARTESIAN_POINT('Ctrl Pts',(-238.892354892304,2.60580588675465,
126.630910825986));
#134758=CARTESIAN_POINT('Ctrl Pts',(-238.900111933189,2.48851652075054,
126.559921741045));
#134759=CARTESIAN_POINT('Ctrl Pts',(-238.907868974074,2.36837091571589,
126.493907942024));
#134760=CARTESIAN_POINT('Ctrl Pts',(-238.915620165314,2.2483159134161,126.427943924521));
#134761=CARTESIAN_POINT('Ctrl Pts',(-238.923371356554,2.12540930058039,
126.366947912511));
#134762=CARTESIAN_POINT('Ctrl Pts',(-238.931122547794,2.00010236826604,
126.311168703241));
#134763=CARTESIAN_POINT('Ctrl Pts',(-238.938870444571,1.87484869474111,
126.255413201622));
#134764=CARTESIAN_POINT('Ctrl Pts',(-238.946618341348,1.74719708726558,
126.204870251402));
#134765=CARTESIAN_POINT('Ctrl Pts',(-238.954366238125,1.61762212001283,
126.159742039109));
#134766=CARTESIAN_POINT('Ctrl Pts',(-238.962112514209,1.48807425704957,
126.114623266665));
#134767=CARTESIAN_POINT('Ctrl Pts',(-238.969858790294,1.35660420353594,
126.074917107761));
#134768=CARTESIAN_POINT('Ctrl Pts',(-238.977605066378,1.22370476032179,
126.040776911776));
#134769=CARTESIAN_POINT('Ctrl Pts',(-238.985351399643,1.09080433607469,
126.006636463776));
#134770=CARTESIAN_POINT('Ctrl Pts',(-238.993097732908,0.956474879742828,
125.978062157958));
#134771=CARTESIAN_POINT('Ctrl Pts',(-239.000844066174,0.821222150136914,
125.955156843479));
#134772=CARTESIAN_POINT('Ctrl Pts',(-239.008592134177,0.685939131619796,
125.932246399513));
#134773=CARTESIAN_POINT('Ctrl Pts',(-239.01634020218,0.549732813801621,
125.915007538376));
#134774=CARTESIAN_POINT('Ctrl Pts',(-239.024088270183,0.413116494941459,
125.903491528914));
#134775=CARTESIAN_POINT('Ctrl Pts',(-239.031844572924,0.276354978631671,
125.891963280099));
#134776=CARTESIAN_POINT('Ctrl Pts',(-239.039600875666,0.139182981019117,
125.88617006593));
#134777=CARTESIAN_POINT('Ctrl Pts',(-239.047357178408,0.00211679838342098,
125.886111073098));
#134778=CARTESIAN_POINT('Ctrl Pts',(-239.055117620922,-0.135022540601304,
125.886052048778));
#134779=CARTESIAN_POINT('Ctrl Pts',(-239.062878063437,-0.27205556163619,
125.891733327966));
#134780=CARTESIAN_POINT('Ctrl Pts',(-239.070638505951,-0.408469655228604,
125.903102044173));
#134781=CARTESIAN_POINT('Ctrl Pts',(-239.078411406216,-0.545102732833955,
125.914489010453));
#134782=CARTESIAN_POINT('Ctrl Pts',(-239.086184306482,-0.681114509415501,
125.931581609581));
#134783=CARTESIAN_POINT('Ctrl Pts',(-239.093957206747,-0.816000257686342,
125.954275397495));
#134784=CARTESIAN_POINT('Ctrl Pts',(-239.101447542509,-0.945982569249743,
125.976144209055));
#134785=CARTESIAN_POINT('Ctrl Pts',(-239.108937878271,-1.07491899763921,
126.003213981662));
#134786=CARTESIAN_POINT('Ctrl Pts',(-239.116428214033,-1.20237188069945,
126.035347625027));
#134787=CARTESIAN_POINT('Ctrl Pts',(-239.124202548152,-1.33465717856032,
126.068699625248));
#134788=CARTESIAN_POINT('Ctrl Pts',(-239.131976882271,-1.46576325317964,
126.107612718806));
#134789=CARTESIAN_POINT('Ctrl Pts',(-239.13975121639,-1.5951867033261,126.151988916591));
#134790=CARTESIAN_POINT('Ctrl Pts',(-239.147515969337,-1.72445065063717,
126.196310424679));
#134791=CARTESIAN_POINT('Ctrl Pts',(-239.155280722284,-1.85203573320956,
126.246081515163));
#134792=CARTESIAN_POINT('Ctrl Pts',(-239.163045475232,-1.97745003610985,
126.30115349184));
#134793=CARTESIAN_POINT('Ctrl Pts',(-239.170802516117,-2.10273977575715,
126.356170770254));
#134794=CARTESIAN_POINT('Ctrl Pts',(-239.178559557002,-2.22586267071119,
126.416478301265));
#134795=CARTESIAN_POINT('Ctrl Pts',(-239.186316597887,-2.3463435836774,
126.481878130634));
#134796=CARTESIAN_POINT('Ctrl Pts',(-239.194067789127,-2.46673364104879,
126.547228641482));
#134797=CARTESIAN_POINT('Ctrl Pts',(-239.201818980367,-2.58448533984699,
126.617663621354));
#134798=CARTESIAN_POINT('Ctrl Pts',(-239.209570171607,-2.69914542606264,
126.692937867293));
#134799=CARTESIAN_POINT('Ctrl Pts',(-239.217318068384,-2.81375677868376,
126.768180119669));
#134800=CARTESIAN_POINT('Ctrl Pts',(-239.225065965161,-2.9252788060595,
126.848257333146));
#134801=CARTESIAN_POINT('Ctrl Pts',(-239.232813861938,-3.03328488400385,
126.932879521787));
#134802=CARTESIAN_POINT('Ctrl Pts',(-239.240560138022,-3.14126836940444,
127.017484009291));
#134803=CARTESIAN_POINT('Ctrl Pts',(-239.248306414107,-3.24573706068587,
127.106631339972));
#134804=CARTESIAN_POINT('Ctrl Pts',(-239.256052690191,-3.34629556977457,
127.199989795605));
#134805=CARTESIAN_POINT('Ctrl Pts',(-239.263799023456,-3.44685482116347,
127.293348940388));
#134806=CARTESIAN_POINT('Ctrl Pts',(-239.271545356721,-3.54350354624211,
127.390919006147));
#134807=CARTESIAN_POINT('Ctrl Pts',(-239.279291689987,-3.63588184010929,
127.492330076151));
#134808=CARTESIAN_POINT('Ctrl Pts',(-239.28703975799,-3.72828082145476,
127.593763856462));
#134809=CARTESIAN_POINT('Ctrl Pts',(-239.294787825993,-3.81640720536389,
127.699040063678));
#134810=CARTESIAN_POINT('Ctrl Pts',(-239.302535893995,-3.89994040765793,
127.807754557501));
#134811=CARTESIAN_POINT('Ctrl Pts',(-239.310292196737,-3.98356239003378,
127.916584594383));
#134812=CARTESIAN_POINT('Ctrl Pts',(-239.318048499479,-4.06258120050844,
128.028859907122));
#134813=CARTESIAN_POINT('Ctrl Pts',(-239.325804802221,-4.13671845259193,
128.144145681422));
#134814=CARTESIAN_POINT('Ctrl Pts',(-239.333565244735,-4.2108952739593,
128.259492987211));
#134815=CARTESIAN_POINT('Ctrl Pts',(-239.34132568725,-4.28018514796353,
128.377853618958));
#134816=CARTESIAN_POINT('Ctrl Pts',(-239.349086129764,-4.34435547472612,
128.498767728152));
#134817=CARTESIAN_POINT('Ctrl Pts',(-239.356859030029,-4.40862881339384,
128.619875939407));
#134818=CARTESIAN_POINT('Ctrl Pts',(-239.364631930295,-4.46776601317441,
128.743545466438));
#134819=CARTESIAN_POINT('Ctrl Pts',(-239.37240483056,-4.52158212838933,
128.869295213315));
#134820=CARTESIAN_POINT('Ctrl Pts',(-239.379895166322,-4.57344189226171,
128.990473640149));
#134821=CARTESIAN_POINT('Ctrl Pts',(-239.387385502084,-4.62036061490404,
129.113583382334));
#134822=CARTESIAN_POINT('Ctrl Pts',(-239.394875837846,-4.66221706717321,
129.238182121653));
#134823=CARTESIAN_POINT('Ctrl Pts',(-239.40169365456,-4.70031544205587,
129.351593775608));
#134824=CARTESIAN_POINT('Ctrl Pts',(-239.408511471274,-4.73429411224294,
129.466454709036));
#134825=CARTESIAN_POINT('Ctrl Pts',(-239.415329287988,-4.76405452823416,
129.582490119309));
#134826=CARTESIAN_POINT('Ctrl Pts',(-237.665046159034,-4.76405452823396,
129.582490119308));
#134827=CARTESIAN_POINT('Ctrl Pts',(-237.672808826289,-4.7981100949745,
129.715272257164));
#134828=CARTESIAN_POINT('Ctrl Pts',(-237.680571493544,-4.82657934103726,
129.849358911575));
#134829=CARTESIAN_POINT('Ctrl Pts',(-237.688334160799,-4.84939024592774,
129.984240318341));
#134830=CARTESIAN_POINT('Ctrl Pts',(-237.696108340009,-4.87223497915706,
130.119321752855));
#134831=CARTESIAN_POINT('Ctrl Pts',(-237.70388251922,-4.88940456463171,
130.25519990647));
#134832=CARTESIAN_POINT('Ctrl Pts',(-237.711656698431,-4.90087891358886,
130.391360694031));
#134833=CARTESIAN_POINT('Ctrl Pts',(-237.715834497277,-4.90704516220861,
130.464532712025));
#134834=CARTESIAN_POINT('Ctrl Pts',(-237.720012296123,-4.91156756503128,
130.537786353004));
#134835=CARTESIAN_POINT('Ctrl Pts',(-237.724190094969,-4.91444921115301,
130.611042192429));
#134836=CARTESIAN_POINT('Ctrl Pts',(-237.727840251317,-4.91696691467898,
130.675046055994));
#134837=CARTESIAN_POINT('Ctrl Pts',(-237.731490407665,-4.91823433856953,
130.739099424647));
#134838=CARTESIAN_POINT('Ctrl Pts',(-237.735140564014,-4.91824985575638,
130.803169461676));
#134839=CARTESIAN_POINT('',(-237.389859436047,-4.91824796558502,130.80883404118));
#134840=CARTESIAN_POINT('Ctrl Pts',(-237.319878776621,-4.76405452823405,
129.582490119308));
#134841=CARTESIAN_POINT('Ctrl Pts',(-237.327551997428,-4.79784307952382,
129.714231167974));
#134842=CARTESIAN_POINT('Ctrl Pts',(-237.335225218235,-4.82616302052628,
129.847375521758));
#134843=CARTESIAN_POINT('Ctrl Pts',(-237.342898439042,-4.84891332956483,
129.981425270854));
#134844=CARTESIAN_POINT('Ctrl Pts',(-237.350725271868,-4.87211908240996,
130.118158593517));
#134845=CARTESIAN_POINT('Ctrl Pts',(-237.358552104693,-4.88952973660893,
130.255833525603));
#134846=CARTESIAN_POINT('Ctrl Pts',(-237.366378937519,-4.90109341756267,
130.393914062185));
#134847=CARTESIAN_POINT('Ctrl Pts',(-237.374205770345,-4.91265709851642,
130.531994598767));
#134848=CARTESIAN_POINT('Ctrl Pts',(-237.38203260317,-4.91837380608168,
130.670480300192));
#134849=CARTESIAN_POINT('Ctrl Pts',(-237.389859435996,-4.91824796558584,
130.808834040274));
#134850=CARTESIAN_POINT('Ctrl Pts',(-237.389859436047,-4.91824796558502,
130.80883404118));
#134851=CARTESIAN_POINT('Ctrl Pts',(-237.399526347849,-4.91809254010862,
130.979714579011));
#134852=CARTESIAN_POINT('Ctrl Pts',(-237.40919325965,-4.9090278711784,131.150197511862));
#134853=CARTESIAN_POINT('Ctrl Pts',(-237.418860171452,-4.89119965687045,
131.319480971591));
#134854=CARTESIAN_POINT('Ctrl Pts',(-237.428698113485,-4.87305601984195,
131.491759450814));
#134855=CARTESIAN_POINT('Ctrl Pts',(-237.438536055518,-4.84583602828776,
131.662795767414));
#134856=CARTESIAN_POINT('Ctrl Pts',(-237.448373997551,-4.80974174435836,
131.831768722983));
#134857=CARTESIAN_POINT('Ctrl Pts',(-237.454026487473,-4.78900340543954,
131.928853857781));
#134858=CARTESIAN_POINT('Ctrl Pts',(-237.459678977395,-4.76533637393173,
132.025258266715));
#134859=CARTESIAN_POINT('Ctrl Pts',(-237.465331467317,-4.73878602478449,
132.120829407096));
#134860=CARTESIAN_POINT('Ctrl Pts',(-237.473105801436,-4.70226914671795,
132.252276254015));
#134861=CARTESIAN_POINT('Ctrl Pts',(-237.480880135554,-4.66022107487715,
132.382410766373));
#134862=CARTESIAN_POINT('Ctrl Pts',(-237.488654469673,-4.61275185039667,
132.510732039374));
#134863=CARTESIAN_POINT('Ctrl Pts',(-237.49641922262,-4.56534112749304,
132.638895167874));
#134864=CARTESIAN_POINT('Ctrl Pts',(-237.504183975567,-4.5125226796618,
132.765249140156));
#134865=CARTESIAN_POINT('Ctrl Pts',(-237.511948728514,-4.45445696488943,
132.889305751244));
#134866=CARTESIAN_POINT('Ctrl Pts',(-237.519705769399,-4.39644892180355,
133.013239147557));
#134867=CARTESIAN_POINT('Ctrl Pts',(-237.527462810284,-4.33320414787966,
133.1348793717));
#134868=CARTESIAN_POINT('Ctrl Pts',(-237.535219851169,-4.26493194233811,
133.25375617356));
#134869=CARTESIAN_POINT('Ctrl Pts',(-237.542971042409,-4.19671122139775,
133.3725433295));
#134870=CARTESIAN_POINT('Ctrl Pts',(-237.550722233649,-4.1234708089651,
133.488570873411));
#134871=CARTESIAN_POINT('Ctrl Pts',(-237.558473424889,-4.04546671423317,
133.601391566006));
#134872=CARTESIAN_POINT('Ctrl Pts',(-237.566221321666,-3.96749577332244,
133.714164306797));
#134873=CARTESIAN_POINT('Ctrl Pts',(-237.573969218443,-3.88476539894875,
133.823732586256));
#134874=CARTESIAN_POINT('Ctrl Pts',(-237.58171711522,-3.79757573134244,
133.929676861919));
#134875=CARTESIAN_POINT('Ctrl Pts',(-237.589463391304,-3.710404301935,134.035598976324));
#134876=CARTESIAN_POINT('Ctrl Pts',(-237.597209667388,-3.618775682944,134.137898293073));
#134877=CARTESIAN_POINT('Ctrl Pts',(-237.604955943472,-3.52303098529225,
134.236187498277));
#134878=CARTESIAN_POINT('Ctrl Pts',(-237.612702276738,-3.42728558087503,
134.33447742903));
#134879=CARTESIAN_POINT('Ctrl Pts',(-237.620448610003,-3.32742430997343,
134.428756909115));
#134880=CARTESIAN_POINT('Ctrl Pts',(-237.628194943268,-3.22382561951452,
134.518675014256));
#134881=CARTESIAN_POINT('Ctrl Pts',(-237.635943011271,-3.12020372884704,
134.608613255934));
#134882=CARTESIAN_POINT('Ctrl Pts',(-237.643691079274,-3.01284304835499,
134.694187922927));
#134883=CARTESIAN_POINT('Ctrl Pts',(-237.651439147277,-2.9021552950917,
134.775088221629));
#134884=CARTESIAN_POINT('Ctrl Pts',(-237.659195450019,-2.79134990156718,
134.856074502132));
#134885=CARTESIAN_POINT('Ctrl Pts',(-237.66695175276,-2.67721068777296,
134.932376259212));
#134886=CARTESIAN_POINT('Ctrl Pts',(-237.674708055502,-2.56017902329741,
135.003725620893));
#134887=CARTESIAN_POINT('Ctrl Pts',(-237.682468498016,-2.44308489549878,
135.075113063876));
#134888=CARTESIAN_POINT('Ctrl Pts',(-237.69022894053,-2.32309558276755,
135.141542655303));
#134889=CARTESIAN_POINT('Ctrl Pts',(-237.697989383044,-2.20067638294647,
135.202792897372));
#134890=CARTESIAN_POINT('Ctrl Pts',(-237.70576228331,-2.07806066495797,
135.264141463768));
#134891=CARTESIAN_POINT('Ctrl Pts',(-237.713535183575,-1.9530076219614,
135.320293905842));
#134892=CARTESIAN_POINT('Ctrl Pts',(-237.721308083841,-1.82600264952798,
135.37107687615));
#134893=CARTESIAN_POINT('Ctrl Pts',(-237.728798419603,-1.7036146277391,
135.420013757577));
#134894=CARTESIAN_POINT('Ctrl Pts',(-237.736288755366,-1.57941441813558,
135.463964674428));
#134895=CARTESIAN_POINT('Ctrl Pts',(-237.743779091128,-1.45384712072204,
135.502819046888));
#134896=CARTESIAN_POINT('Ctrl Pts',(-237.751553425247,-1.32351890107106,
135.543146594687));
#134897=CARTESIAN_POINT('Ctrl Pts',(-237.759327759367,-1.19130504031147,
135.578111243626));
#134898=CARTESIAN_POINT('Ctrl Pts',(-237.767102093486,-1.0576864437554,
135.607534823151));
#134899=CARTESIAN_POINT('Ctrl Pts',(-237.774866846433,-0.924232520177739,
135.636922140744));
#134900=CARTESIAN_POINT('Ctrl Pts',(-237.78263159938,-0.789377683550235,
135.660781893073));
#134901=CARTESIAN_POINT('Ctrl Pts',(-237.790396352327,-0.653619406006261,
135.678985191273));
#134902=CARTESIAN_POINT('Ctrl Pts',(-237.798153393212,-0.517995965497401,
135.697170409701));
#134903=CARTESIAN_POINT('Ctrl Pts',(-237.805910434097,-0.381471254749789,
135.709710302591));
#134904=CARTESIAN_POINT('Ctrl Pts',(-237.813667474982,-0.244554039840854,
135.716526777632));
#134905=CARTESIAN_POINT('Ctrl Pts',(-237.821418666222,-0.107740075268928,
135.723338112317));
#134906=CARTESIAN_POINT('Ctrl Pts',(-237.829169857462,0.0294654154116941,
135.724434600675));
#134907=CARTESIAN_POINT('Ctrl Pts',(-237.836921048702,0.16654777789893,
135.719789886732));
#134908=CARTESIAN_POINT('Ctrl Pts',(-237.844668945479,0.303571876725503,
135.715147146917));
#134909=CARTESIAN_POINT('Ctrl Pts',(-237.852416842256,0.440472561521645,
135.704768071312));
#134910=CARTESIAN_POINT('Ctrl Pts',(-237.860164739033,0.576734626202866,
135.688678403443));
#134911=CARTESIAN_POINT('Ctrl Pts',(-237.867911015118,0.712968187797626,
135.672592101186));
#134912=CARTESIAN_POINT('Ctrl Pts',(-237.875657291202,0.848563006964617,
135.650797628474));
#134913=CARTESIAN_POINT('Ctrl Pts',(-237.883403567286,0.983008846773999,
135.623372618969));
#134914=CARTESIAN_POINT('Ctrl Pts',(-237.891149900551,1.11745567903185,
135.595947407018));
#134915=CARTESIAN_POINT('Ctrl Pts',(-237.898896233816,1.25075313193135,
135.56289165348));
#134916=CARTESIAN_POINT('Ctrl Pts',(-237.906642567082,1.38240140313231,
135.52433407333));
#134917=CARTESIAN_POINT('Ctrl Pts',(-237.914390635085,1.51407915605063,
135.485767858477));
#134918=CARTESIAN_POINT('Ctrl Pts',(-237.922138703088,1.64410661722893,
135.441697475153));
#134919=CARTESIAN_POINT('Ctrl Pts',(-237.929886771091,1.77199976408061,
135.392301321041));
#134920=CARTESIAN_POINT('Ctrl Pts',(-237.937643073832,1.90002883729089,
135.342852668107));
#134921=CARTESIAN_POINT('Ctrl Pts',(-237.945399376574,2.02591869956226,
135.288067078427));
#134922=CARTESIAN_POINT('Ctrl Pts',(-237.953155679316,2.14920541157007,
135.228171097387));
#134923=CARTESIAN_POINT('Ctrl Pts',(-237.96091612183,2.2725579254085,135.168243148059));
#134924=CARTESIAN_POINT('Ctrl Pts',(-237.968676564344,2.39330417649297,
135.103199557782));
#134925=CARTESIAN_POINT('Ctrl Pts',(-237.976437006859,2.5110063076024,135.033312069839));
#134926=CARTESIAN_POINT('Ctrl Pts',(-237.984209907124,2.6288973846218,134.963312392296));
#134927=CARTESIAN_POINT('Ctrl Pts',(-237.99198280739,2.74373424878877,134.888453492076));
#134928=CARTESIAN_POINT('Ctrl Pts',(-237.999755707655,2.85510868982739,
134.809050047693));
#134929=CARTESIAN_POINT('Ctrl Pts',(-238.007246043417,2.96243438940019,
134.732533118518));
#134930=CARTESIAN_POINT('Ctrl Pts',(-238.014736379179,3.06654478754454,
134.651796508769));
#134931=CARTESIAN_POINT('Ctrl Pts',(-238.022226714941,3.16710626290611,
134.567154922595));
#134932=CARTESIAN_POINT('Ctrl Pts',(-238.030001049061,3.27148055716997,
134.479304124956));
#134933=CARTESIAN_POINT('Ctrl Pts',(-238.03777538318,3.37236212781656,134.386968106218));
#134934=CARTESIAN_POINT('Ctrl Pts',(-238.045549717299,3.46934113384456,
134.290455160104));
#134935=CARTESIAN_POINT('Ctrl Pts',(-238.053314470246,3.56620062191489,
134.194061157571));
#134936=CARTESIAN_POINT('Ctrl Pts',(-238.061079223193,3.65916684050278,
134.093500743169));
#134937=CARTESIAN_POINT('Ctrl Pts',(-238.06884397614,3.74786245591568,133.989122786714));
#134938=CARTESIAN_POINT('Ctrl Pts',(-238.076601017025,3.83646997759296,
133.884848499917));
#134939=CARTESIAN_POINT('Ctrl Pts',(-238.08435805791,3.92081508558972,133.776764512595));
#134940=CARTESIAN_POINT('Ctrl Pts',(-238.092115098795,4.00055707814202,
133.665256653256));
#134941=CARTESIAN_POINT('Ctrl Pts',(-238.099866290035,4.08023893663733,
133.553832882862));
#134942=CARTESIAN_POINT('Ctrl Pts',(-238.107617481275,4.15532436249089,
133.438990696431));
#134943=CARTESIAN_POINT('Ctrl Pts',(-238.115368672515,4.22551299845294,
133.321148841157));
#134944=CARTESIAN_POINT('Ctrl Pts',(-238.123116569293,4.29567180237245,
133.203357071814));
#134945=CARTESIAN_POINT('Ctrl Pts',(-238.13086446607,4.36093775623293,133.082568504578));
#134946=CARTESIAN_POINT('Ctrl Pts',(-238.138612362847,4.42105403731816,
132.959230511925));
#134947=CARTESIAN_POINT('Ctrl Pts',(-238.146358638931,4.48115774337334,
132.83591831892));
#134948=CARTESIAN_POINT('Ctrl Pts',(-238.154104915015,4.53611374807617,
132.710058112449));
#134949=CARTESIAN_POINT('Ctrl Pts',(-238.161851191099,4.58571157130187,
132.582121132182));
#134950=CARTESIAN_POINT('Ctrl Pts',(-238.169597524365,4.63530976064736,
132.454183207514));
#134951=CARTESIAN_POINT('Ctrl Pts',(-238.17734385763,4.67954954827176,132.32416884299));
#134952=CARTESIAN_POINT('Ctrl Pts',(-238.185090190895,4.71826907035566,
132.192568110063));
#134953=CARTESIAN_POINT('Ctrl Pts',(-238.192838258898,4.75699726340812,
132.060937906064));
#134954=CARTESIAN_POINT('Ctrl Pts',(-238.200586326901,4.79020262064375,
131.92772100174));
#134955=CARTESIAN_POINT('Ctrl Pts',(-238.208334394904,4.81777360705397,
131.793421047304));
#134956=CARTESIAN_POINT('Ctrl Pts',(-238.216090697646,4.8453738962366,131.65897835728));
#134957=CARTESIAN_POINT('Ctrl Pts',(-238.223847000388,4.86732777361825,
131.523450701329));
#134958=CARTESIAN_POINT('Ctrl Pts',(-238.23160330313,4.88357506771269,131.387350858063));
#134959=CARTESIAN_POINT('Ctrl Pts',(-238.239363745644,4.89983103347718,
131.251178374213));
#134960=CARTESIAN_POINT('Ctrl Pts',(-238.247124188158,4.91037431694902,
131.114433484141));
#134961=CARTESIAN_POINT('Ctrl Pts',(-238.254884630672,4.91519687092446,
130.977631453411));
#134962=CARTESIAN_POINT('Ctrl Pts',(-238.262657530938,4.92002716649167,
130.840609815916));
#134963=CARTESIAN_POINT('Ctrl Pts',(-238.270430431203,4.91911838375073,
130.703531245644));
#134964=CARTESIAN_POINT('Ctrl Pts',(-238.278203331469,4.91251462302238,
130.566909272884));
#134965=CARTESIAN_POINT('Ctrl Pts',(-238.285693667231,4.90615092563052,
130.435253852967));
#134966=CARTESIAN_POINT('Ctrl Pts',(-238.293184002992,4.89449914250425,
130.304022716782));
#134967=CARTESIAN_POINT('Ctrl Pts',(-238.300674338754,4.87764371266572,
130.173666654702));
#134968=CARTESIAN_POINT('Ctrl Pts',(-238.308448672873,4.86014920408149,
130.038368102906));
#134969=CARTESIAN_POINT('Ctrl Pts',(-238.316223006992,4.8369932495294,129.903583706847));
#134970=CARTESIAN_POINT('Ctrl Pts',(-238.323997341111,4.8082136961773,129.769824917654));
#134971=CARTESIAN_POINT('Ctrl Pts',(-238.331762094059,4.77946961105252,
129.636230974213));
#134972=CARTESIAN_POINT('Ctrl Pts',(-238.339526847006,4.74511579837063,
129.503660501267));
#134973=CARTESIAN_POINT('Ctrl Pts',(-238.347291599953,4.70524181410956,
129.372619532993));
#134974=CARTESIAN_POINT('Ctrl Pts',(-238.355048640838,4.66540743325179,
129.241708716456));
#134975=CARTESIAN_POINT('Ctrl Pts',(-238.362805681723,4.62006390473615,
129.112324753075));
#134976=CARTESIAN_POINT('Ctrl Pts',(-238.370562722608,4.56935167938908,
128.984962834627));
#134977=CARTESIAN_POINT('Ctrl Pts',(-238.378313913848,4.51867769652569,
128.857696960792));
#134978=CARTESIAN_POINT('Ctrl Pts',(-238.386065105088,4.46264321931968,
128.73245045855));
#134979=CARTESIAN_POINT('Ctrl Pts',(-238.393816296328,4.40143820121287,
128.609702370047));
#134980=CARTESIAN_POINT('Ctrl Pts',(-238.401564193105,4.34025919687138,
128.487006452755));
#134981=CARTESIAN_POINT('Ctrl Pts',(-238.409312089882,4.27391419661751,
128.366807186329));
#134982=CARTESIAN_POINT('Ctrl Pts',(-238.417059986659,4.20264076863304,
128.249562458743));
#134983=CARTESIAN_POINT('Ctrl Pts',(-238.424806262743,4.13138224951323,
128.132342256227));
#134984=CARTESIAN_POINT('Ctrl Pts',(-238.432552538828,4.05519755618014,
128.018075697132));
#134985=CARTESIAN_POINT('Ctrl Pts',(-238.440298814912,3.97436938626618,
127.9071945809));
#134986=CARTESIAN_POINT('Ctrl Pts',(-238.448045148177,3.89354061969715,
127.796312646169));
#134987=CARTESIAN_POINT('Ctrl Pts',(-238.455791481442,3.80806853845349,
127.688816520103));
#134988=CARTESIAN_POINT('Ctrl Pts',(-238.463537814708,3.71827796217919,
127.585107278906));
#134989=CARTESIAN_POINT('Ctrl Pts',(-238.471285882711,3.62846727792776,
127.481374812744));
#134990=CARTESIAN_POINT('Ctrl Pts',(-238.479033950713,3.53433643009288,
127.381431214486));
#134991=CARTESIAN_POINT('Ctrl Pts',(-238.486782018716,3.43624886646806,
127.285642556937));
#134992=CARTESIAN_POINT('Ctrl Pts',(-238.494538321458,3.3380570542135,127.189752094063));
#134993=CARTESIAN_POINT('Ctrl Pts',(-238.5022946242,3.23590040589847,127.098025666768));
#134994=CARTESIAN_POINT('Ctrl Pts',(-238.510050926942,3.13017781253146,
127.01079106839));
#134995=CARTESIAN_POINT('Ctrl Pts',(-238.517811369456,3.02439879183313,
126.92350991028));
#134996=CARTESIAN_POINT('Ctrl Pts',(-238.52557181197,2.91505034525037,126.840725594031));
#134997=CARTESIAN_POINT('Ctrl Pts',(-238.533332254485,2.80256163058388,
126.762723403604));
#134998=CARTESIAN_POINT('Ctrl Pts',(-238.54110515475,2.68989233904632,126.684595997137));
#134999=CARTESIAN_POINT('Ctrl Pts',(-238.548878055015,2.57407303634056,
126.611266266233));
#135000=CARTESIAN_POINT('Ctrl Pts',(-238.556650955281,2.45555960734366,
126.542974683708));
#135001=CARTESIAN_POINT('Ctrl Pts',(-238.564141291043,2.34135444000556,
126.477165672223));
#135002=CARTESIAN_POINT('Ctrl Pts',(-238.571631626805,2.22464789507923,
126.416035012753));
#135003=CARTESIAN_POINT('Ctrl Pts',(-238.579121962567,2.10586487662709,
126.359755327567));
#135004=CARTESIAN_POINT('Ctrl Pts',(-238.586896296686,1.98257816392963,
126.301341781012));
#135005=CARTESIAN_POINT('Ctrl Pts',(-238.594670630806,1.85666387518112,
126.247969283026));
#135006=CARTESIAN_POINT('Ctrl Pts',(-238.602444964925,1.72857276602027,
126.199882443541));
#135007=CARTESIAN_POINT('Ctrl Pts',(-238.610209717872,1.60063951770362,
126.151854866788));
#135008=CARTESIAN_POINT('Ctrl Pts',(-238.617974470819,1.47053514932972,
126.109100123507));
#135009=CARTESIAN_POINT('Ctrl Pts',(-238.625739223766,1.33873380897834,
126.07181639155));
#135010=CARTESIAN_POINT('Ctrl Pts',(-238.633496264651,1.2070633755759,126.034569690321));
#135011=CARTESIAN_POINT('Ctrl Pts',(-238.641253305536,1.07369969809899,
126.00278329247));
#135012=CARTESIAN_POINT('Ctrl Pts',(-238.649010346421,0.939135312516304,
125.976606695991));
#135013=CARTESIAN_POINT('Ctrl Pts',(-238.656761537661,0.804672402983724,
125.950449839486));
#135014=CARTESIAN_POINT('Ctrl Pts',(-238.664512728901,0.669010969833791,
125.929894438361));
#135015=CARTESIAN_POINT('Ctrl Pts',(-238.672263920141,0.53265671926662,
125.915039613386));
#135016=CARTESIAN_POINT('Ctrl Pts',(-238.680011816918,0.396360422893123,
125.900191102107));
#135017=CARTESIAN_POINT('Ctrl Pts',(-238.687759713696,0.259372282624431,
125.891038390275));
#135018=CARTESIAN_POINT('Ctrl Pts',(-238.695507610473,0.122205943987116,
125.887629104685));
#135019=CARTESIAN_POINT('Ctrl Pts',(-238.703253886557,-0.0149317024091209,
125.884220532244));
#135020=CARTESIAN_POINT('Ctrl Pts',(-238.711000162641,-0.152247082434574,
125.886553006101));
#135021=CARTESIAN_POINT('Ctrl Pts',(-238.718746438725,-0.289224106013271,
125.894622082878));
#135022=CARTESIAN_POINT('Ctrl Pts',(-238.72649277199,-0.426202140725053,
125.902691219219));
#135023=CARTESIAN_POINT('Ctrl Pts',(-238.734239105256,-0.562841423717549,
125.916497019986));
#135024=CARTESIAN_POINT('Ctrl Pts',(-238.741985438521,-0.698628945267916,
125.935982996702));
#135025=CARTESIAN_POINT('Ctrl Pts',(-238.749733506524,-0.834446875492065,
125.955473337166));
#135026=CARTESIAN_POINT('Ctrl Pts',(-238.757481574527,-0.969412277784851,
125.980646329257));
#135027=CARTESIAN_POINT('Ctrl Pts',(-238.76522964253,-1.10302071231747,
126.011394065346));
#135028=CARTESIAN_POINT('Ctrl Pts',(-238.772985945272,-1.23677114748446,
126.042174480495));
#135029=CARTESIAN_POINT('Ctrl Pts',(-238.780742248014,-1.36916135232485,
126.078541387453));
#135030=CARTESIAN_POINT('Ctrl Pts',(-238.788498550756,-1.49969993468534,
126.120336368226));
#135031=CARTESIAN_POINT('Ctrl Pts',(-238.79625899327,-1.63030818941768,
126.162153656238));
#135032=CARTESIAN_POINT('Ctrl Pts',(-238.804019435784,-1.75906248561458,
126.209404656206));
#135033=CARTESIAN_POINT('Ctrl Pts',(-238.811779878298,-1.88549083552424,
126.261882508466));
#135034=CARTESIAN_POINT('Ctrl Pts',(-238.819552778564,-2.01212213944494,
126.314444602833));
#135035=CARTESIAN_POINT('Ctrl Pts',(-238.827325678829,-2.13641968101698,
126.372250151641));
#135036=CARTESIAN_POINT('Ctrl Pts',(-238.835098579094,-2.25793472673775,
126.435045587462));
#135037=CARTESIAN_POINT('Ctrl Pts',(-238.842588914856,-2.37503239446765,
126.495558251018));
#135038=CARTESIAN_POINT('Ctrl Pts',(-238.850079250618,-2.48954608783481,
126.560704157921));
#135039=CARTESIAN_POINT('Ctrl Pts',(-238.85756958638,-2.60110090381225,
126.630219130902));
#135040=CARTESIAN_POINT('Ctrl Pts',(-238.86534527437,-2.71690551795641,
126.702382349969));
#135041=CARTESIAN_POINT('Ctrl Pts',(-238.873120962359,-2.829888240962,126.779482753564));
#135042=CARTESIAN_POINT('Ctrl Pts',(-238.880896650348,-2.93959939826533,
126.86127319269));
#135043=CARTESIAN_POINT('Ctrl Pts',(-238.888766252182,-3.05063563402061,
126.944051487118));
#135044=CARTESIAN_POINT('Ctrl Pts',(-238.896635854016,-3.15832037898057,
127.031633709791));
#135045=CARTESIAN_POINT('Ctrl Pts',(-238.90450545585,-3.26221344406456,
127.123715768105));
#135046=CARTESIAN_POINT('Ctrl Pts',(-238.912261690011,-3.3646098495665,
127.214471313482));
#135047=CARTESIAN_POINT('Ctrl Pts',(-238.920017924172,-3.4633227704474,
127.309597660825));
#135048=CARTESIAN_POINT('Ctrl Pts',(-238.927774158334,-3.55796076349559,
127.408760778373));
#135049=CARTESIAN_POINT('Ctrl Pts',(-238.935525020074,-3.65253320474194,
127.507855209754));
#135050=CARTESIAN_POINT('Ctrl Pts',(-238.943275881815,-3.74303606522609,
127.610980566509));
#135051=CARTESIAN_POINT('Ctrl Pts',(-238.951026743555,-3.82911314771992,
127.717764504619));
#135052=CARTESIAN_POINT('Ctrl Pts',(-238.958773915244,-3.91514925040071,
127.824497604739));
#135053=CARTESIAN_POINT('Ctrl Pts',(-238.966521086933,-3.99676352385031,
127.934885515953));
#135054=CARTESIAN_POINT('Ctrl Pts',(-238.974268258622,-4.0736388974835,
128.048521508436));
#135055=CARTESIAN_POINT('Ctrl Pts',(-238.982226494934,-4.15260867051577,
128.165253409832));
#135056=CARTESIAN_POINT('Ctrl Pts',(-238.990184731246,-4.22657735310258,
128.285412585883));
#135057=CARTESIAN_POINT('Ctrl Pts',(-238.998142967557,-4.29524780853793,
128.408524787266));
#135058=CARTESIAN_POINT('Ctrl Pts',(-239.005889503974,-4.36209153658539,
128.528362036872));
#135059=CARTESIAN_POINT('Ctrl Pts',(-239.01363604039,-4.42391518069558,
128.650996819491));
#135060=CARTESIAN_POINT('Ctrl Pts',(-239.021382576807,-4.48049086939839,
128.775966022883));
#135061=CARTESIAN_POINT('Ctrl Pts',(-239.029446663066,-4.53938573664773,
128.906058025523));
#135062=CARTESIAN_POINT('Ctrl Pts',(-239.037510749325,-4.5925930445791,
129.038679492564));
#135063=CARTESIAN_POINT('Ctrl Pts',(-239.045574835585,-4.63991114167916,
129.173285003187));
#135064=CARTESIAN_POINT('Ctrl Pts',(-239.053638921844,-4.68722923877922,
129.30789051381));
#135065=CARTESIAN_POINT('Ctrl Pts',(-239.061703008104,-4.72865800359389,
129.444479606954));
#135066=CARTESIAN_POINT('Ctrl Pts',(-239.069767094363,-4.76405452823403,
129.582490119308));
#135067=CARTESIAN_POINT('Origin',(213.235140564004,0.,130.804360617566));
#135068=CARTESIAN_POINT('',(-241.165327127303,-4.76405452823409,129.582490119308));
#135069=CARTESIAN_POINT('',(-240.820011204651,-4.76405452823406,129.582490119308));
#135070=CARTESIAN_POINT('',(213.235140564004,-4.76405452823405,129.582490119308));
#135071=CARTESIAN_POINT('',(-239.485140563964,-4.91824839639984,130.800388991906));
#135072=CARTESIAN_POINT('Ctrl Pts',(-239.485140564014,-4.91824839640055,
130.800388992789));
#135073=CARTESIAN_POINT('Ctrl Pts',(-239.492981518083,-4.91836051407927,
130.939229549107));
#135074=CARTESIAN_POINT('Ctrl Pts',(-239.500822472151,-4.91258895669507,
131.078149716857));
#135075=CARTESIAN_POINT('Ctrl Pts',(-239.50866342622,-4.90094187300933,
131.216612749014));
#135076=CARTESIAN_POINT('Ctrl Pts',(-239.516391847359,-4.88946194760979,
131.353088567567));
#135077=CARTESIAN_POINT('Ctrl Pts',(-239.524120268498,-4.8722740815105,
131.489119884404));
#135078=CARTESIAN_POINT('Ctrl Pts',(-239.531848689638,-4.84943848763251,
131.624195611433));
#135079=CARTESIAN_POINT('Ctrl Pts',(-239.539577205338,-4.82660261435007,
131.759272991178));
#135080=CARTESIAN_POINT('Ctrl Pts',(-239.547305721038,-4.79811894081519,
131.893394370734));
#135081=CARTESIAN_POINT('Ctrl Pts',(-239.555034236738,-4.76409908540016,
132.026057374945));
#135082=CARTESIAN_POINT('Ctrl Pts',(-239.562764536443,-4.73007137704356,
132.158751002296));
#135083=CARTESIAN_POINT('Ctrl Pts',(-239.570494836148,-4.690505041369,132.289985204269));
#135084=CARTESIAN_POINT('Ctrl Pts',(-239.578225135853,-4.64556187844975,
132.419271728431));
#135085=CARTESIAN_POINT('Ctrl Pts',(-239.586149996337,-4.59948755928598,
132.551812212698));
#135086=CARTESIAN_POINT('Ctrl Pts',(-239.594074856821,-4.54776231027495,
132.682305263779));
#135087=CARTESIAN_POINT('Ctrl Pts',(-239.601999717305,-4.49061289323881,
132.81024668252));
#135088=CARTESIAN_POINT('Ctrl Pts',(-239.609742916342,-4.4347735113534,
132.935255302215));
#135089=CARTESIAN_POINT('Ctrl Pts',(-239.617486115378,-4.37375617727099,
133.057827681082));
#135090=CARTESIAN_POINT('Ctrl Pts',(-239.625229314415,-4.30781859575813,
133.177519273986));
#135091=CARTESIAN_POINT('Ctrl Pts',(-239.633245005623,-4.23956059414176,
133.301422953109));
#135092=CARTESIAN_POINT('Ctrl Pts',(-239.64126069683,-4.16602995590322,
133.422238978381));
#135093=CARTESIAN_POINT('Ctrl Pts',(-239.649276388037,-4.08756026267536,
133.539508540713));
#135094=CARTESIAN_POINT('Ctrl Pts',(-239.657292079245,-4.00909056944729,
133.656778103046));
#135095=CARTESIAN_POINT('Ctrl Pts',(-239.665307770452,-3.92568215040277,
133.77050087529));
#135096=CARTESIAN_POINT('Ctrl Pts',(-239.67332346166,-3.83771253088084,
133.880258143951));
#135097=CARTESIAN_POINT('Ctrl Pts',(-239.681097795779,-3.752391727372,133.986710557909));
#135098=CARTESIAN_POINT('Ctrl Pts',(-239.688872129898,-3.66250317866118,
134.089778887007));
#135099=CARTESIAN_POINT('Ctrl Pts',(-239.696646464017,-3.56834525463581,
134.189046010068));
#135100=CARTESIAN_POINT('Ctrl Pts',(-239.704411216964,-3.47430337183668,
134.288190795272));
#135101=CARTESIAN_POINT('Ctrl Pts',(-239.712175969911,-3.37600284926054,
134.383543414556));
#135102=CARTESIAN_POINT('Ctrl Pts',(-239.719940722858,-3.27378340128807,
134.474718270977));
#135103=CARTESIAN_POINT('Ctrl Pts',(-239.727697763743,-3.17166547911209,
134.565802571245));
#135104=CARTESIAN_POINT('Ctrl Pts',(-239.735454804628,-3.06563666733478,
134.65271710761));
#135105=CARTESIAN_POINT('Ctrl Pts',(-239.743211845513,-2.95607450745325,
134.735112017602));
#135106=CARTESIAN_POINT('Ctrl Pts',(-239.750963036753,-2.84659496924861,
134.817444792952));
#135107=CARTESIAN_POINT('Ctrl Pts',(-239.758714227994,-2.73358769771764,
134.895264491878));
#135108=CARTESIAN_POINT('Ctrl Pts',(-239.766465419234,-2.61746411171743,
134.968260794848));
#135109=CARTESIAN_POINT('Ctrl Pts',(-239.774213316011,-2.50138988133944,
135.041226072442));
#135110=CARTESIAN_POINT('Ctrl Pts',(-239.781961212788,-2.38220230116201,
135.109371823884));
#135111=CARTESIAN_POINT('Ctrl Pts',(-239.789709109565,-2.26034245179049,
135.172430564709));
#135112=CARTESIAN_POINT('Ctrl Pts',(-239.797455385649,-2.13850809287213,
135.235476115005));
#135113=CARTESIAN_POINT('Ctrl Pts',(-239.805201661733,-2.01400292361361,
135.293436591657));
#135114=CARTESIAN_POINT('Ctrl Pts',(-239.812947937817,-1.88729299703757,
135.346090266701));
#135115=CARTESIAN_POINT('Ctrl Pts',(-239.820694271083,-1.76058213511816,
135.398744330422));
#135116=CARTESIAN_POINT('Ctrl Pts',(-239.828440604348,-1.6316668444402,
135.446091364341));
#135117=CARTESIAN_POINT('Ctrl Pts',(-239.836186937613,-1.50103317104183,
135.487957790886));
#135118=CARTESIAN_POINT('Ctrl Pts',(-239.843935005616,-1.37037024313823,
135.529833593128));
#135119=CARTESIAN_POINT('Ctrl Pts',(-239.851683073619,-1.23798853900794,
135.566226226425));
#135120=CARTESIAN_POINT('Ctrl Pts',(-239.859431141622,-1.10438888729454,
135.597012101674));
#135121=CARTESIAN_POINT('Ctrl Pts',(-239.867187444364,-0.970647244280896,
135.627830696517));
#135122=CARTESIAN_POINT('Ctrl Pts',(-239.874943747106,-0.835685449470971,
135.653030541777));
#135123=CARTESIAN_POINT('Ctrl Pts',(-239.882700049847,-0.700014689856641,
135.672539178022));
#135124=CARTESIAN_POINT('Ctrl Pts',(-239.890460492361,-0.564271518672938,
135.692058226614));
#135125=CARTESIAN_POINT('Ctrl Pts',(-239.898220934876,-0.4278190174835,
135.705879974196));
#135126=CARTESIAN_POINT('Ctrl Pts',(-239.90598137739,-0.291172110356458,
135.713984010928));
#135127=CARTESIAN_POINT('Ctrl Pts',(-239.913754277655,-0.154305845483154,
135.72210105698));
#135128=CARTESIAN_POINT('Ctrl Pts',(-239.921527177921,-0.0172449421728213,
135.724482043666));
#135129=CARTESIAN_POINT('Ctrl Pts',(-239.929300078186,0.119496158882949,
135.721158735296));
#135130=CARTESIAN_POINT('Ctrl Pts',(-239.936790413948,0.251266376484923,
135.717956237556));
#135131=CARTESIAN_POINT('Ctrl Pts',(-239.94428074971,0.382739332014857,
135.70945699528));
#135132=CARTESIAN_POINT('Ctrl Pts',(-239.951771085472,0.513462338611925,
135.695734605448));
#135133=CARTESIAN_POINT('Ctrl Pts',(-239.959545419591,0.649141747736717,
135.681491927034));
#135134=CARTESIAN_POINT('Ctrl Pts',(-239.96731975371,0.784443008281681,
135.661577094689));
#135135=CARTESIAN_POINT('Ctrl Pts',(-239.975094087829,0.918853908175262,
135.636015671265));
#135136=CARTESIAN_POINT('Ctrl Pts',(-239.982858840776,1.05309915864737,
135.61048575001));
#135137=CARTESIAN_POINT('Ctrl Pts',(-239.990623593723,1.18645585135361,
135.579323156191));
#135138=CARTESIAN_POINT('Ctrl Pts',(-239.99838834667,1.3184159487441,135.542605276572));
#135139=CARTESIAN_POINT('Ctrl Pts',(-240.006145387555,1.45024498150556,
135.505923865668));
#135140=CARTESIAN_POINT('Ctrl Pts',(-240.01390242844,1.58067980516023,135.463698253339));
#135141=CARTESIAN_POINT('Ctrl Pts',(-240.021659469325,1.70922200010184,
135.416056966727));
#135142=CARTESIAN_POINT('Ctrl Pts',(-240.029410660565,1.83766726037521,
135.36845160678));
#135143=CARTESIAN_POINT('Ctrl Pts',(-240.037161851805,1.96422236766908,
135.31543883683));
#135144=CARTESIAN_POINT('Ctrl Pts',(-240.044913043046,2.08840385943053,
135.257197059927));
#135145=CARTESIAN_POINT('Ctrl Pts',(-240.052660939823,2.21253257074448,
135.198980037332));
#135146=CARTESIAN_POINT('Ctrl Pts',(-240.0604088366,2.33428931982447,135.135538593768));
#135147=CARTESIAN_POINT('Ctrl Pts',(-240.068156733377,2.45321064957463,
135.067099240953));
#135148=CARTESIAN_POINT('Ctrl Pts',(-240.075903009461,2.57210710354691,
134.998674204175));
#135149=CARTESIAN_POINT('Ctrl Pts',(-240.083649285545,2.68816897927273,
134.925253532501));
#135150=CARTESIAN_POINT('Ctrl Pts',(-240.091395561629,2.80095781769323,
134.84710948016));
#135151=CARTESIAN_POINT('Ctrl Pts',(-240.099141894895,2.91374748869485,
134.768964850977));
#135152=CARTESIAN_POINT('Ctrl Pts',(-240.10688822816,3.02326375281079,134.686096994207));
#135153=CARTESIAN_POINT('Ctrl Pts',(-240.114634561425,3.12909785455932,
134.598821011231));
#135154=CARTESIAN_POINT('Ctrl Pts',(-240.122382629428,3.23495565712099,
134.511525483404));
#135155=CARTESIAN_POINT('Ctrl Pts',(-240.130130697431,3.33712935489285,
134.419820113711));
#135156=CARTESIAN_POINT('Ctrl Pts',(-240.137878765434,3.43524425874479,
134.324059460544));
#135157=CARTESIAN_POINT('Ctrl Pts',(-240.145635068176,3.53346344028425,
134.228197031815));
#135158=CARTESIAN_POINT('Ctrl Pts',(-240.153391370918,3.62761493051781,
134.128270983428));
#135159=CARTESIAN_POINT('Ctrl Pts',(-240.16114767366,3.71736145821841,134.024672225385));
#135160=CARTESIAN_POINT('Ctrl Pts',(-240.168908116174,3.80715588634307,
133.921018173565));
#135161=CARTESIAN_POINT('Ctrl Pts',(-240.176668558688,3.89254042396627,
133.813687811961));
#135162=CARTESIAN_POINT('Ctrl Pts',(-240.184429001202,3.97321957067578,
133.70310332876));
#135163=CARTESIAN_POINT('Ctrl Pts',(-240.192201901467,4.05402823071395,
133.592341325529));
#135164=CARTESIAN_POINT('Ctrl Pts',(-240.199974801733,4.13011618838364,
133.47831508727));
#135165=CARTESIAN_POINT('Ctrl Pts',(-240.207747701998,4.20123210013872,
133.361474596892));
#135166=CARTESIAN_POINT('Ctrl Pts',(-240.21523803776,4.26976276937055,133.248881552644));
#135167=CARTESIAN_POINT('Ctrl Pts',(-240.222728373522,4.33367646000155,
133.133675583595));
#135168=CARTESIAN_POINT('Ctrl Pts',(-240.230218709284,4.39279040294944,
133.016277328985));
#135169=CARTESIAN_POINT('Ctrl Pts',(-240.237993043403,4.45414566901211,
132.894427883869));
#135170=CARTESIAN_POINT('Ctrl Pts',(-240.245767377522,4.51052439278442,
132.769830648112));
#135171=CARTESIAN_POINT('Ctrl Pts',(-240.253541711642,4.56167121788152,
132.642930377584));
#135172=CARTESIAN_POINT('Ctrl Pts',(-240.261306464589,4.61275500908781,
132.516186500297));
#135173=CARTESIAN_POINT('Ctrl Pts',(-240.269071217536,4.65861958616375,
132.387145594718));
#135174=CARTESIAN_POINT('Ctrl Pts',(-240.276835970483,4.69905545007956,
132.256276916661));
#135175=CARTESIAN_POINT('Ctrl Pts',(-240.284593011368,4.73945115252529,
132.12553821922));
#135176=CARTESIAN_POINT('Ctrl Pts',(-240.292350052253,4.77442875721439,
131.992975733091));
#135177=CARTESIAN_POINT('Ctrl Pts',(-240.300107093138,4.80382698970042,
131.859078264866));
#135178=CARTESIAN_POINT('Ctrl Pts',(-240.307858284378,4.83320305275076,
131.725281769763));
#135179=CARTESIAN_POINT('Ctrl Pts',(-240.315609475618,4.85700803476486,
131.590152676703));
#135180=CARTESIAN_POINT('Ctrl Pts',(-240.323360666858,4.8751307079616,131.454194167631));
#135181=CARTESIAN_POINT('Ctrl Pts',(-240.331108563635,4.89324567853873,
131.318293444552));
#135182=CARTESIAN_POINT('Ctrl Pts',(-240.338856460412,4.90568309226471,
131.181564393331));
#135183=CARTESIAN_POINT('Ctrl Pts',(-240.346604357189,4.91238300998312,
131.044519368665));
#135184=CARTESIAN_POINT('Ctrl Pts',(-240.354350633274,4.91908152622316,
130.907503010863));
#135185=CARTESIAN_POINT('Ctrl Pts',(-240.362096909358,4.92004491456186,
130.770171201334));
#135186=CARTESIAN_POINT('Ctrl Pts',(-240.369843185442,4.91526523235931,
130.633039988161));
#135187=CARTESIAN_POINT('Ctrl Pts',(-240.377589518707,4.91048551487422,
130.495907762716));
#135188=CARTESIAN_POINT('Ctrl Pts',(-240.385335851972,4.89996265587237,
130.35897652731));
#135189=CARTESIAN_POINT('Ctrl Pts',(-240.393082185238,4.88374081674733,
130.222760499498));
#135190=CARTESIAN_POINT('Ctrl Pts',(-240.400830253241,4.86751534485396,
130.086513967053));
#135191=CARTESIAN_POINT('Ctrl Pts',(-240.408578321244,4.84558839947765,
129.950983349061));
#135192=CARTESIAN_POINT('Ctrl Pts',(-240.416326389247,4.81805575200773,
129.816675529572));
#135193=CARTESIAN_POINT('Ctrl Pts',(-240.424082691988,4.79049384251232,
129.682224966134));
#135194=CARTESIAN_POINT('Ctrl Pts',(-240.43183899473,4.75731440820122,129.549000180909));
#135195=CARTESIAN_POINT('Ctrl Pts',(-240.439595297472,4.71866402939323,
129.417496226138));
#135196=CARTESIAN_POINT('Ctrl Pts',(-240.447355739986,4.67999302171433,
129.285922083747));
#135197=CARTESIAN_POINT('Ctrl Pts',(-240.455116182501,4.63584537696253,
129.156070971893));
#135198=CARTESIAN_POINT('Ctrl Pts',(-240.462876625015,4.58641656882432,
129.028419706467));
#135199=CARTESIAN_POINT('Ctrl Pts',(-240.47064952528,4.53690841317508,128.900563523898));
#135200=CARTESIAN_POINT('Ctrl Pts',(-240.478422425545,4.48210230920935,
128.774914603163));
#135201=CARTESIAN_POINT('Ctrl Pts',(-240.486195325811,4.42224098296653,
128.651927633459));
#135202=CARTESIAN_POINT('Ctrl Pts',(-240.493685661573,4.36455576671341,
128.533411549888));
#135203=CARTESIAN_POINT('Ctrl Pts',(-240.501175997335,4.30217663311262,
128.417367511494));
#135204=CARTESIAN_POINT('Ctrl Pts',(-240.508666333097,4.23535868671833,
128.304176652867));
#135205=CARTESIAN_POINT('Ctrl Pts',(-240.516440667216,4.16600731757869,
128.186694128433));
#135206=CARTESIAN_POINT('Ctrl Pts',(-240.524215001336,4.09165421168538,
128.071913262012));
#135207=CARTESIAN_POINT('Ctrl Pts',(-240.531989335455,4.0125355283831,127.960289293572));
#135208=CARTESIAN_POINT('Ctrl Pts',(-240.539754088402,3.93351435178673,
127.848802891697));
#135209=CARTESIAN_POINT('Ctrl Pts',(-240.547518841349,3.8497395075085,127.740465962586));
#135210=CARTESIAN_POINT('Ctrl Pts',(-240.555283594296,3.76149255441252,
127.635708407935));
#135211=CARTESIAN_POINT('Ctrl Pts',(-240.563040635181,3.67333324943442,
127.531054899964));
#135212=CARTESIAN_POINT('Ctrl Pts',(-240.570797676066,3.58071092519937,
127.429973988751));
#135213=CARTESIAN_POINT('Ctrl Pts',(-240.578554716951,3.48394965575835,
127.332865570955));
#135214=CARTESIAN_POINT('Ctrl Pts',(-240.586305908191,3.38726135474396,
127.235830383374));
#135215=CARTESIAN_POINT('Ctrl Pts',(-240.594057099431,3.28644059594651,
127.142762002304));
#135216=CARTESIAN_POINT('Ctrl Pts',(-240.601808290671,3.18185059925376,
127.054025988959));
#135217=CARTESIAN_POINT('Ctrl Pts',(-240.609556187448,3.07730505609921,
126.965327690786));
#135218=CARTESIAN_POINT('Ctrl Pts',(-240.617304084225,2.96899375885845,
126.880958350395));
#135219=CARTESIAN_POINT('Ctrl Pts',(-240.625051981003,2.85731536747108,
126.801245336524));
#135220=CARTESIAN_POINT('Ctrl Pts',(-240.632798257087,2.74566033679537,
126.721548996897));
#135221=CARTESIAN_POINT('Ctrl Pts',(-240.640544533171,2.63063993092811,
126.646507273436));
#135222=CARTESIAN_POINT('Ctrl Pts',(-240.648290809255,2.5126840225464,126.576405785104));
#135223=CARTESIAN_POINT('Ctrl Pts',(-240.65603714252,2.39472724344113,126.506303779299));
#135224=CARTESIAN_POINT('Ctrl Pts',(-240.663783475786,2.27383525467382,
126.441142281131));
#135225=CARTESIAN_POINT('Ctrl Pts',(-240.671529809051,2.15046455235006,
126.38116208352));
#135226=CARTESIAN_POINT('Ctrl Pts',(-240.679277877054,2.02706622201242,
126.321168453759));
#135227=CARTESIAN_POINT('Ctrl Pts',(-240.687025945057,1.90118842509697,
126.266358604363));
#135228=CARTESIAN_POINT('Ctrl Pts',(-240.69477401306,1.77330938428439,126.21692594336));
#135229=CARTESIAN_POINT('Ctrl Pts',(-240.702530315802,1.64529443210598,
126.167440744736));
#135230=CARTESIAN_POINT('Ctrl Pts',(-240.710286618544,1.51527435247633,
126.123344291902));
#135231=CARTESIAN_POINT('Ctrl Pts',(-240.718042921286,1.38374487710798,
126.084780850513));
#135232=CARTESIAN_POINT('Ctrl Pts',(-240.7258033638,1.25214520049835,126.046196826654));
#135233=CARTESIAN_POINT('Ctrl Pts',(-240.733563806314,1.11903490216574,
126.013151792763));
#135234=CARTESIAN_POINT('Ctrl Pts',(-240.741324248828,0.984920799126915,
125.985739021928));
#135235=CARTESIAN_POINT('Ctrl Pts',(-240.749097149094,0.850591404223804,
125.95828224568));
#135236=CARTESIAN_POINT('Ctrl Pts',(-240.756870049359,0.71525537073989,
125.936475862334));
#135237=CARTESIAN_POINT('Ctrl Pts',(-240.764642949624,0.579426440927723,
125.920361430214));
#135238=CARTESIAN_POINT('Ctrl Pts',(-240.772133285386,0.448535234847394,
125.904832798292));
#135239=CARTESIAN_POINT('Ctrl Pts',(-240.779623621148,0.31718665340473,
125.894589492774));
#135240=CARTESIAN_POINT('Ctrl Pts',(-240.78711395691,0.18583924616756,125.88962289953));
#135241=CARTESIAN_POINT('Ctrl Pts',(-240.794888291029,0.0495117620622287,
125.884467996394));
#135242=CARTESIAN_POINT('Ctrl Pts',(-240.802662625149,-0.087246301531893,
125.884981508192));
#135243=CARTESIAN_POINT('Ctrl Pts',(-240.810436959268,-0.223924288441308,
125.891210815703));
#135244=CARTESIAN_POINT('Ctrl Pts',(-240.818201712215,-0.360433831946748,
125.897432446149));
#135245=CARTESIAN_POINT('Ctrl Pts',(-240.825966465162,-0.496863108315479,
125.909355838806));
#135246=CARTESIAN_POINT('Ctrl Pts',(-240.833731218109,-0.632698239630725,
125.926976482595));
#135247=CARTESIAN_POINT('Ctrl Pts',(-240.841488258994,-0.768398457578609,
125.944579625312));
#135248=CARTESIAN_POINT('Ctrl Pts',(-240.849245299879,-0.903505319617219,
125.967868708342));
#135249=CARTESIAN_POINT('Ctrl Pts',(-240.857002340764,-1.03750721141912,
125.99678723292));
#135250=CARTESIAN_POINT('Ctrl Pts',(-240.864753532004,-1.17140805135184,
126.025683949815));
#135251=CARTESIAN_POINT('Ctrl Pts',(-240.872504723244,-1.30420519899371,
126.060201576293));
#135252=CARTESIAN_POINT('Ctrl Pts',(-240.880255914484,-1.43539476812064,
126.100232119943));
#135253=CARTESIAN_POINT('Ctrl Pts',(-240.888003811261,-1.56652857818128,
126.140245649543));
#135254=CARTESIAN_POINT('Ctrl Pts',(-240.895751708038,-1.69605579552528,
126.18576732213));
#135255=CARTESIAN_POINT('Ctrl Pts',(-240.903499604815,-1.82348551012593,
126.236638684604));
#135256=CARTESIAN_POINT('Ctrl Pts',(-240.911245880899,-1.9508885691777,
126.287499405886));
#135257=CARTESIAN_POINT('Ctrl Pts',(-240.918992156983,-2.07619463531786,
126.343707446363));
#135258=CARTESIAN_POINT('Ctrl Pts',(-240.926738433067,-2.19893105254213,
126.405055526001));
#135259=CARTESIAN_POINT('Ctrl Pts',(-240.934484766333,-2.32166837577857,
126.466404058498));
#135260=CARTESIAN_POINT('Ctrl Pts',(-240.942231099598,-2.44183566253587,
126.532892531069));
#135261=CARTESIAN_POINT('Ctrl Pts',(-240.949977432863,-2.55898357961639,
126.604267035066));
#135262=CARTESIAN_POINT('Ctrl Pts',(-240.957725500866,-2.67615773116052,
126.675657522889));
#135263=CARTESIAN_POINT('Ctrl Pts',(-240.965473568869,-2.79031083372095,
126.751936016075));
#135264=CARTESIAN_POINT('Ctrl Pts',(-240.973221636872,-2.90102167660669,
126.8328047141));
#135265=CARTESIAN_POINT('Ctrl Pts',(-240.980977939614,-3.01185018429387,
126.913759360339));
#135266=CARTESIAN_POINT('Ctrl Pts',(-240.988734242356,-3.11922880789606,
126.999313725819));
#135267=CARTESIAN_POINT('Ctrl Pts',(-240.996490545098,-3.22276821753299,
127.089128716519));
#135268=CARTESIAN_POINT('Ctrl Pts',(-241.004250987612,-3.32636288927064,
127.178991644184));
#135269=CARTESIAN_POINT('Ctrl Pts',(-241.012011430126,-3.42611397981587,
127.273119460062));
#135270=CARTESIAN_POINT('Ctrl Pts',(-241.01977187264,-3.52166906890069,
127.371136181027));
#135271=CARTESIAN_POINT('Ctrl Pts',(-241.027544772906,-3.61737755149723,
127.469310247134));
#135272=CARTESIAN_POINT('Ctrl Pts',(-241.035317673171,-3.7088763112602,
127.571385402169));
#135273=CARTESIAN_POINT('Ctrl Pts',(-241.043090573436,-3.79585269375627,
127.676951883517));
#135274=CARTESIAN_POINT('Ctrl Pts',(-241.050580909199,-3.87966726567068,
127.778680757365));
#135275=CARTESIAN_POINT('Ctrl Pts',(-241.058071244961,-3.95928236534808,
127.883651282082));
#135276=CARTESIAN_POINT('Ctrl Pts',(-241.065561580723,-4.03445738285836,
127.991473010782));
#135277=CARTESIAN_POINT('Ctrl Pts',(-241.07343448358,-4.11347194628202,
128.104801708306));
#135278=CARTESIAN_POINT('Ctrl Pts',(-241.081307386438,-4.18782825269689,
128.221634873634));
#135279=CARTESIAN_POINT('Ctrl Pts',(-241.089180289295,-4.25720427185024,
128.341558382258));
#135280=CARTESIAN_POINT('Ctrl Pts',(-241.09703950209,-4.32645965418085,
128.461273357857));
#135281=CARTESIAN_POINT('Ctrl Pts',(-241.104898714886,-4.39075181436689,
128.584067646285));
#135282=CARTESIAN_POINT('Ctrl Pts',(-241.112757927681,-4.44980102277204,
128.709496917886));
#135283=CARTESIAN_POINT('Ctrl Pts',(-241.120609178014,-4.50879040621353,
128.834799112397));
#135284=CARTESIAN_POINT('Ctrl Pts',(-241.128460428347,-4.56254724686084,
128.96273063843));
#135285=CARTESIAN_POINT('Ctrl Pts',(-241.136311678679,-4.61083661661783,
129.092820738581));
#135286=CARTESIAN_POINT('Ctrl Pts',(-241.144154937712,-4.65907683562503,
129.2227784281));
#135287=CARTESIAN_POINT('Ctrl Pts',(-241.151998196745,-4.70186053741541,
129.354889962274));
#135288=CARTESIAN_POINT('Ctrl Pts',(-241.159841455778,-4.73900024403813,
129.48866317913));
#135289=CARTESIAN_POINT('Ctrl Pts',(-241.161670012953,-4.74765889941888,
129.51985072177));
#135290=CARTESIAN_POINT('Ctrl Pts',(-241.163498570128,-4.7560109927566,
129.551128496559));
#135291=CARTESIAN_POINT('Ctrl Pts',(-241.165327127303,-4.76405452823409,
129.582490119308));
#135292=CARTESIAN_POINT('Ctrl Pts',(-239.415329287988,-4.76405452823416,
129.582490119309));
#135293=CARTESIAN_POINT('Ctrl Pts',(-239.424519392981,-4.80417020735727,
129.738900543369));
#135294=CARTESIAN_POINT('Ctrl Pts',(-239.433709497975,-4.83661958135147,
129.89744575293));
#135295=CARTESIAN_POINT('Ctrl Pts',(-239.442899602968,-4.86120185625379,
130.057433863958));
#135296=CARTESIAN_POINT('Ctrl Pts',(-239.452001625382,-4.88554852229458,
130.215888568626));
#135297=CARTESIAN_POINT('Ctrl Pts',(-239.461103647797,-4.90217810768683,
130.375758571777));
#135298=CARTESIAN_POINT('Ctrl Pts',(-239.470205670211,-4.91094228169329,
130.536351348366));
#135299=CARTESIAN_POINT('Ctrl Pts',(-239.475183968129,-4.91573579540056,
130.624186628143));
#135300=CARTESIAN_POINT('Ctrl Pts',(-239.480162266046,-4.9181772117805,
130.71223777378));
#135301=CARTESIAN_POINT('Ctrl Pts',(-239.485140563964,-4.91824839639984,
130.800388991905));
#135302=CARTESIAN_POINT('',(-239.139859436032,-4.9182499817972,130.803937472346));
#135303=CARTESIAN_POINT('Ctrl Pts',(-239.069767094363,-4.76405452823403,
129.582490119308));
#135304=CARTESIAN_POINT('Ctrl Pts',(-239.077528141177,-4.79812089061503,
129.715314349202));
#135305=CARTESIAN_POINT('Ctrl Pts',(-239.085289187991,-4.82660015141963,
129.849454706652));
#135306=CARTESIAN_POINT('Ctrl Pts',(-239.093050234805,-4.84941749545066,
129.984401461683));
#135307=CARTESIAN_POINT('Ctrl Pts',(-239.100823464149,-4.87227065590867,
130.119560042883));
#135308=CARTESIAN_POINT('Ctrl Pts',(-239.108596693492,-4.88944409361158,
130.255527162905));
#135309=CARTESIAN_POINT('Ctrl Pts',(-239.116369922836,-4.90091491880955,
130.391788174121));
#135310=CARTESIAN_POINT('Ctrl Pts',(-239.122919018622,-4.91057931048617,
130.506590706626));
#135311=CARTESIAN_POINT('Ctrl Pts',(-239.129468114408,-4.91619668330171,
130.621601691157));
#135312=CARTESIAN_POINT('Ctrl Pts',(-239.136017210194,-4.9177820244927,
130.736515042349));
#135313=CARTESIAN_POINT('Ctrl Pts',(-239.137297952128,-4.91809205400046,
130.758987510679));
#135314=CARTESIAN_POINT('Ctrl Pts',(-239.138578694062,-4.91824804811001,
130.781462108982));
#135315=CARTESIAN_POINT('Ctrl Pts',(-239.139859435996,-4.91824998179714,
130.803937471706));
#135316=CARTESIAN_POINT('Ctrl Pts',(-239.139859436033,-4.9182499817972,
130.803937472346));
#135317=CARTESIAN_POINT('Ctrl Pts',(-239.147615006544,-4.91826169127885,
130.940037693392));
#135318=CARTESIAN_POINT('Ctrl Pts',(-239.155370577054,-4.91261977115477,
131.076358722153));
#135319=CARTESIAN_POINT('Ctrl Pts',(-239.163126147566,-4.90129519437534,
131.212390616577));
#135320=CARTESIAN_POINT('Ctrl Pts',(-239.170872168394,-4.88998456191076,
131.348255010564));
#135321=CARTESIAN_POINT('Ctrl Pts',(-239.178618189222,-4.87300522619465,
131.48383059062));
#135322=CARTESIAN_POINT('Ctrl Pts',(-239.18636421005,-4.8503801351783,131.618606039271));
#135323=CARTESIAN_POINT('Ctrl Pts',(-239.194102569871,-4.82777742093952,
131.753248191652));
#135324=CARTESIAN_POINT('Ctrl Pts',(-239.201840929692,-4.79954012706133,
131.887091402182));
#135325=CARTESIAN_POINT('Ctrl Pts',(-239.209579289513,-4.76574307505788,
132.019628491344));
#135326=CARTESIAN_POINT('Ctrl Pts',(-239.217311870164,-4.73197126340409,
132.152066599019));
#135327=CARTESIAN_POINT('Ctrl Pts',(-239.225044450815,-4.69264805427752,
132.283200147361));
#135328=CARTESIAN_POINT('Ctrl Pts',(-239.232777031466,-4.64789944639699,
132.412531565781));
#135329=CARTESIAN_POINT('Ctrl Pts',(-239.240506428028,-4.60316926490614,
132.541809728665));
#135330=CARTESIAN_POINT('Ctrl Pts',(-239.24823582459,-4.55301825560546,
132.669286866611));
#135331=CARTESIAN_POINT('Ctrl Pts',(-239.255965221152,-4.49762236276382,
132.794480248258));
#135332=CARTESIAN_POINT('Ctrl Pts',(-239.263693096776,-4.44223737034809,
132.919648995206));
#135333=CARTESIAN_POINT('Ctrl Pts',(-239.271420972401,-4.38160970598779,
133.042534520364));
#135334=CARTESIAN_POINT('Ctrl Pts',(-239.279148848025,-4.31596341722965,
133.162674176793));
#135335=CARTESIAN_POINT('Ctrl Pts',(-239.286876898036,-4.25031564710143,
133.282816544286));
#135336=CARTESIAN_POINT('Ctrl Pts',(-239.294604948047,-4.17964921561703,
133.400212574749));
#135337=CARTESIAN_POINT('Ctrl Pts',(-239.302332998058,-4.10423387044656,
133.514424712598));
#135338=CARTESIAN_POINT('Ctrl Pts',(-239.310062917552,-4.02880028164126,
133.628664479366));
#135339=CARTESIAN_POINT('Ctrl Pts',(-239.317792837046,-3.94861571002192,
133.739718493164));
#135340=CARTESIAN_POINT('Ctrl Pts',(-239.32552275654,-3.86399266699195,
133.847179003854));
#135341=CARTESIAN_POINT('Ctrl Pts',(-239.333260924453,-3.77927932466312,
133.954754183178));
#135342=CARTESIAN_POINT('Ctrl Pts',(-239.340999092366,-3.69011829490393,
134.058727891459));
#135343=CARTESIAN_POINT('Ctrl Pts',(-239.34873726028,-3.59686206967548,
134.158725880061));
#135344=CARTESIAN_POINT('Ctrl Pts',(-239.356479722365,-3.50355409339292,
134.25877936095));
#135345=CARTESIAN_POINT('Ctrl Pts',(-239.364222184451,-3.40614667385498,
134.354852451133));
#135346=CARTESIAN_POINT('Ctrl Pts',(-239.371964646537,-3.30502767844634,
134.446609250925));
#135347=CARTESIAN_POINT('Ctrl Pts',(-239.379719220947,-3.20375049227857,
134.538509595238));
#135348=CARTESIAN_POINT('Ctrl Pts',(-239.387473795356,-3.09875043182109,
134.626079907394));
#135349=CARTESIAN_POINT('Ctrl Pts',(-239.395228369765,-2.99044740688375,
134.709025439182));
#135350=CARTESIAN_POINT('Ctrl Pts',(-239.401640524512,-2.90089307174618,
134.777611999494));
#135351=CARTESIAN_POINT('Ctrl Pts',(-239.408052679259,-2.80908100330681,
134.843037134247));
#135352=CARTESIAN_POINT('Ctrl Pts',(-239.414464834006,-2.71526171166901,
134.905157722964));
#135353=CARTESIAN_POINT('Ctrl Pts',(-239.422239168125,-2.60151172453313,
134.980475027585));
#135354=CARTESIAN_POINT('Ctrl Pts',(-239.430013502245,-2.48444540631676,
135.05117516048));
#135355=CARTESIAN_POINT('Ctrl Pts',(-239.437787836364,-2.36447424007298,
135.116952023036));
#135356=CARTESIAN_POINT('Ctrl Pts',(-239.445552589311,-2.24465092756914,
135.182647821487));
#135357=CARTESIAN_POINT('Ctrl Pts',(-239.453317342258,-2.12193022963106,
135.243432235941));
#135358=CARTESIAN_POINT('Ctrl Pts',(-239.461082095205,-1.99675337392947,
135.29904181051));
#135359=CARTESIAN_POINT('Ctrl Pts',(-239.46883913609,-1.871700845646,135.354596152864));
#135360=CARTESIAN_POINT('Ctrl Pts',(-239.476596176975,-1.74419736927777,
135.404985725915));
#135361=CARTESIAN_POINT('Ctrl Pts',(-239.48435321786,-1.61470928217404,
135.449992651699));
#135362=CARTESIAN_POINT('Ctrl Pts',(-239.4921044091,-1.4853188430439,135.494965637409));
#135363=CARTESIAN_POINT('Ctrl Pts',(-239.49985560034,-1.35394713989028,
135.534563927399));
#135364=CARTESIAN_POINT('Ctrl Pts',(-239.50760679158,-1.2210806957463,135.568617642221));
#135365=CARTESIAN_POINT('Ctrl Pts',(-239.515354688357,-1.08827072338559,
135.602656883306));
#135366=CARTESIAN_POINT('Ctrl Pts',(-239.523102585134,-0.95396765153832,
135.631156139442));
#135367=CARTESIAN_POINT('Ctrl Pts',(-239.530850481911,-0.81867316942286,
135.653995377439));
#135368=CARTESIAN_POINT('Ctrl Pts',(-239.538596757995,-0.683406987996448,
135.67682983796));
#135369=CARTESIAN_POINT('Ctrl Pts',(-239.546343034079,-0.54715019406188,
135.694006570253));
#135370=CARTESIAN_POINT('Ctrl Pts',(-239.554089310164,-0.410414285615395,
135.705456737483));
#135371=CARTESIAN_POINT('Ctrl Pts',(-239.561835643429,-0.273677367815681,
135.716906989235));
#135372=CARTESIAN_POINT('Ctrl Pts',(-239.569581976694,-0.136461718048383,
135.722630558948));
#135373=CARTESIAN_POINT('Ctrl Pts',(-239.57732830996,0.000716829463151165,
135.722610565327));
#135374=CARTESIAN_POINT('Ctrl Pts',(-239.585076377963,0.137926097159832,
135.722590567229));
#135375=CARTESIAN_POINT('Ctrl Pts',(-239.592824445965,0.275097855176846,
135.716824446403));
#135376=CARTESIAN_POINT('Ctrl Pts',(-239.600572513968,0.411717455877931,
135.705347436465));
#135377=CARTESIAN_POINT('Ctrl Pts',(-239.60832881671,0.54848225751625,135.693858228625));
#135378=CARTESIAN_POINT('Ctrl Pts',(-239.616085119452,0.68469333934966,
135.676646039773));
#135379=CARTESIAN_POINT('Ctrl Pts',(-239.623841422194,0.819841801757023,
135.653797954267));
#135380=CARTESIAN_POINT('Ctrl Pts',(-239.631601864708,0.955062396968015,
135.63093767405));
#135381=CARTESIAN_POINT('Ctrl Pts',(-239.639362307222,1.08921886041209,
135.602435584598));
#135382=CARTESIAN_POINT('Ctrl Pts',(-239.647122749736,1.22181462643886,
135.568429475288));
#135383=CARTESIAN_POINT('Ctrl Pts',(-239.654895650002,1.35462324696057,
135.534368776353));
#135384=CARTESIAN_POINT('Ctrl Pts',(-239.662668550267,1.48586578900997,
135.494786514289));
#135385=CARTESIAN_POINT('Ctrl Pts',(-239.670441450533,1.61506207784371,
135.449870013446));
#135386=CARTESIAN_POINT('Ctrl Pts',(-239.677931786295,1.73956175615639,
135.406586340546));
#135387=CARTESIAN_POINT('Ctrl Pts',(-239.685422122057,1.86216108462354,
135.358349634445));
#135388=CARTESIAN_POINT('Ctrl Pts',(-239.692912457819,1.98245146626512,
135.305368198809));
#135389=CARTESIAN_POINT('Ctrl Pts',(-239.700686791938,2.10730269428409,
135.250377955939));
#135390=CARTESIAN_POINT('Ctrl Pts',(-239.708461126058,2.23006192292105,
135.19010189571));
#135391=CARTESIAN_POINT('Ctrl Pts',(-239.716235460177,2.35024920610005,
135.124720756689));
#135392=CARTESIAN_POINT('Ctrl Pts',(-239.724000213124,2.47028836919398,
135.059420194079));
#135393=CARTESIAN_POINT('Ctrl Pts',(-239.731764966071,2.58776155343375,
134.989027256028));
#135394=CARTESIAN_POINT('Ctrl Pts',(-239.739529719018,2.70220861158442,
134.913770755527));
#135395=CARTESIAN_POINT('Ctrl Pts',(-239.747286759903,2.8165419993032,134.838589000844));
#135396=CARTESIAN_POINT('Ctrl Pts',(-239.755043800788,2.92785491764034,
134.758553510157));
#135397=CARTESIAN_POINT('Ctrl Pts',(-239.762800841673,3.03571199296619,
134.673938857925));
#135398=CARTESIAN_POINT('Ctrl Pts',(-239.770552032913,3.14348773243238,
134.589388014261));
#135399=CARTESIAN_POINT('Ctrl Pts',(-239.778303224153,3.24781250976893,
134.500265122739));
#135400=CARTESIAN_POINT('Ctrl Pts',(-239.786054415393,3.34828042300292,
134.406887684978));
#135401=CARTESIAN_POINT('Ctrl Pts',(-239.79380231217,3.44870563469413,134.313549935118));
#135402=CARTESIAN_POINT('Ctrl Pts',(-239.801550208947,3.54527695689084,
134.215961501187));
#135403=CARTESIAN_POINT('Ctrl Pts',(-239.809298105724,3.63762222699359,
134.114479587661));
#135404=CARTESIAN_POINT('Ctrl Pts',(-239.817044381808,3.72994818045657,
134.013018901964));
#135405=CARTESIAN_POINT('Ctrl Pts',(-239.824790657892,3.81804957718431,
133.907666645603));
#135406=CARTESIAN_POINT('Ctrl Pts',(-239.832536933976,3.90159202563624,
133.798815948338));
#135407=CARTESIAN_POINT('Ctrl Pts',(-239.840283267242,3.98513509077967,
133.689964447563));
#135408=CARTESIAN_POINT('Ctrl Pts',(-239.848029600507,4.06411890245744,
133.5776147645));
#135409=CARTESIAN_POINT('Ctrl Pts',(-239.855775933772,4.13825043696067,
133.462191760339));
#135410=CARTESIAN_POINT('Ctrl Pts',(-239.863524001775,4.21239857270696,
133.346742907997));
#135411=CARTESIAN_POINT('Ctrl Pts',(-239.871272069778,4.28169205776535,
133.22821969392));
#135412=CARTESIAN_POINT('Ctrl Pts',(-239.879020137781,4.3458823555574,133.107074150369));
#135413=CARTESIAN_POINT('Ctrl Pts',(-239.886776440523,4.41014087556173,
132.985799851894));
#135414=CARTESIAN_POINT('Ctrl Pts',(-239.894532743265,4.46928519047763,
132.861898002543));
#135415=CARTESIAN_POINT('Ctrl Pts',(-239.902289046006,4.52311349416601,
132.735843825206));
#135416=CARTESIAN_POINT('Ctrl Pts',(-239.910049488521,4.57697052764095,
132.609722368957));
#135417=CARTESIAN_POINT('Ctrl Pts',(-239.917809931035,4.62550575800948,
132.481446661202));
#135418=CARTESIAN_POINT('Ctrl Pts',(-239.925570373549,4.66856670551333,
132.351508955209));
#135419=CARTESIAN_POINT('Ctrl Pts',(-239.933343273814,4.71169677827276,
132.221362661676));
#135420=CARTESIAN_POINT('Ctrl Pts',(-239.94111617408,4.74933489992523,132.089549414572));
#135421=CARTESIAN_POINT('Ctrl Pts',(-239.948889074345,4.78137912557462,
131.956574451895));
#135422=CARTESIAN_POINT('Ctrl Pts',(-239.956379410107,4.81225846290869,
131.828433464049));
#135423=CARTESIAN_POINT('Ctrl Pts',(-239.96386974587,4.83794348762328,131.699214058919));
#135424=CARTESIAN_POINT('Ctrl Pts',(-239.971360081632,4.85838859484396,
131.569372593936));
#135425=CARTESIAN_POINT('Ctrl Pts',(-239.979134415751,4.87960888451809,
131.434608150351));
#135426=CARTESIAN_POINT('Ctrl Pts',(-239.98690874987,4.89525128957989,131.298746651697));
#135427=CARTESIAN_POINT('Ctrl Pts',(-239.994683083989,4.90520844792763,
131.162289583814));
#135428=CARTESIAN_POINT('Ctrl Pts',(-240.002447836936,4.91515333496764,
131.026000687071));
#135429=CARTESIAN_POINT('Ctrl Pts',(-240.010212589883,4.91942688807697,
130.889118067696));
#135430=CARTESIAN_POINT('Ctrl Pts',(-240.01797734283,4.91797289328593,130.752152539601));
#135431=CARTESIAN_POINT('Ctrl Pts',(-240.025734383715,4.91652034262302,
130.6153230476));
#135432=CARTESIAN_POINT('Ctrl Pts',(-240.033491424601,4.90935156891561,
130.478411199165));
#135433=CARTESIAN_POINT('Ctrl Pts',(-240.041248465485,4.89646224935012,
130.341931700662));
#135434=CARTESIAN_POINT('Ctrl Pts',(-240.048999656726,4.88358264972073,
130.20555512241));
#135435=CARTESIAN_POINT('Ctrl Pts',(-240.056750847966,4.86499112741673,
130.069610632789));
#135436=CARTESIAN_POINT('Ctrl Pts',(-240.064502039206,4.84073540560912,
129.934611346004));
#135437=CARTESIAN_POINT('Ctrl Pts',(-240.072249935983,4.81648999313036,
129.799669437517));
#135438=CARTESIAN_POINT('Ctrl Pts',(-240.07999783276,4.78658523834844,129.665672316841));
#135439=CARTESIAN_POINT('Ctrl Pts',(-240.087745729537,4.75112050453059,
129.533126172655));
#135440=CARTESIAN_POINT('Ctrl Pts',(-240.095492005621,4.71566318917052,
129.400607754264));
#135441=CARTESIAN_POINT('Ctrl Pts',(-240.103238281705,4.67464830909037,
129.269540086101));
#135442=CARTESIAN_POINT('Ctrl Pts',(-240.110984557789,4.62822586869511,
129.140416997475));
#135443=CARTESIAN_POINT('Ctrl Pts',(-240.118730891055,4.58180308562001,
129.011292955692));
#135444=CARTESIAN_POINT('Ctrl Pts',(-240.12647722432,4.52997279484901,128.884113890001));
#135445=CARTESIAN_POINT('Ctrl Pts',(-240.134223557585,4.47293405766117,
128.759355977397));
#135446=CARTESIAN_POINT('Ctrl Pts',(-240.141971625588,4.41588254704354,
128.634570126123));
#135447=CARTESIAN_POINT('Ctrl Pts',(-240.149719693591,4.35362043154904,
128.51220686235));
#135448=CARTESIAN_POINT('Ctrl Pts',(-240.157467761594,4.28639367863097,
128.39271962142));
#135449=CARTESIAN_POINT('Ctrl Pts',(-240.165224064336,4.21909547631998,
128.273105388029));
#135450=CARTESIAN_POINT('Ctrl Pts',(-240.172980367078,4.14682228827045,
128.156373624791));
#135451=CARTESIAN_POINT('Ctrl Pts',(-240.18073666982,4.0698648518084,128.042950986505));
#135452=CARTESIAN_POINT('Ctrl Pts',(-240.188497112334,3.99286634084558,
127.929467811143));
#135453=CARTESIAN_POINT('Ctrl Pts',(-240.196257554848,3.91117883250713,
127.819297593895));
#135454=CARTESIAN_POINT('Ctrl Pts',(-240.204017997362,3.82513405437569,
127.712834695217));
#135455=CARTESIAN_POINT('Ctrl Pts',(-240.211790897628,3.73895114952747,
127.606200892842));
#135456=CARTESIAN_POINT('Ctrl Pts',(-240.219563797893,3.64839725570815,
127.503286595352));
#135457=CARTESIAN_POINT('Ctrl Pts',(-240.227336698158,3.55384234024813,
127.404450665353));
#135458=CARTESIAN_POINT('Ctrl Pts',(-240.23482703392,3.46272473413556,127.309207670363));
#135459=CARTESIAN_POINT('Ctrl Pts',(-240.242317369682,3.36789217217108,
127.217751886806));
#135460=CARTESIAN_POINT('Ctrl Pts',(-240.249807705444,3.26970395023753,
127.130368355693));
#135461=CARTESIAN_POINT('Ctrl Pts',(-240.257582039563,3.16779289202469,
127.039671651438));
#135462=CARTESIAN_POINT('Ctrl Pts',(-240.265356373682,3.06194386743316,
126.95307479442));
#135463=CARTESIAN_POINT('Ctrl Pts',(-240.273130707801,2.952520758862,126.87093917676));
#135464=CARTESIAN_POINT('Ctrl Pts',(-240.280895460749,2.84323250449244,
126.788904783909));
#135465=CARTESIAN_POINT('Ctrl Pts',(-240.288660213696,2.73037923993795,
126.711320923329));
#135466=CARTESIAN_POINT('Ctrl Pts',(-240.296424966643,2.61436034238606,
126.638510996821));
#135467=CARTESIAN_POINT('Ctrl Pts',(-240.304182007528,2.4984566764388,126.565773386159));
#135468=CARTESIAN_POINT('Ctrl Pts',(-240.311939048413,2.37939396350909,
126.497800480172));
#135469=CARTESIAN_POINT('Ctrl Pts',(-240.319696089298,2.25760290405394,
126.434874127129));
#135470=CARTESIAN_POINT('Ctrl Pts',(-240.327447280538,2.13590368818494,
126.371995227339));
#135471=CARTESIAN_POINT('Ctrl Pts',(-240.335198471778,2.01148056699154,
126.314155484325));
#135472=CARTESIAN_POINT('Ctrl Pts',(-240.342949663018,1.88479103352591,
126.261592097991));
#135473=CARTESIAN_POINT('Ctrl Pts',(-240.350697559795,1.75815534649068,
126.209051052499));
#135474=CARTESIAN_POINT('Ctrl Pts',(-240.358445456572,1.62925552344608,
126.161782052856));
#135475=CARTESIAN_POINT('Ctrl Pts',(-240.366193353349,1.49857114353756,
126.119975109278));
#135476=CARTESIAN_POINT('Ctrl Pts',(-240.373939629434,1.36791409998444,
126.078176910812));
#135477=CARTESIAN_POINT('Ctrl Pts',(-240.381685905518,1.23547361420208,
126.041838614877));
#135478=CARTESIAN_POINT('Ctrl Pts',(-240.389432181602,1.10174623982095,
126.011100945324));
#135479=CARTESIAN_POINT('Ctrl Pts',(-240.397178514867,0.968017878294181,
125.980363048873));
#135480=CARTESIAN_POINT('Ctrl Pts',(-240.404924848133,0.833002990242403,
125.955225948881));
#135481=CARTESIAN_POINT('Ctrl Pts',(-240.412671181398,0.697209794341811,
125.935779554754));
#135482=CARTESIAN_POINT('Ctrl Pts',(-240.420419249401,0.561386188497077,
125.916328805742));
#135483=CARTESIAN_POINT('Ctrl Pts',(-240.428167317404,0.424784314916213,
125.902571353904));
#135484=CARTESIAN_POINT('Ctrl Pts',(-240.435915385407,0.287918613010828,
125.894545352734));
#135485=CARTESIAN_POINT('Ctrl Pts',(-240.443671688149,0.150907448608548,
125.886510821434));
#135486=CARTESIAN_POINT('Ctrl Pts',(-240.451427990891,0.0136322866698129,
125.884219932061));
#135487=CARTESIAN_POINT('Ctrl Pts',(-240.459184293633,-0.123390765413529,
125.887658696409));
#135488=CARTESIAN_POINT('Ctrl Pts',(-240.466944736147,-0.260486950825825,
125.891099296129));
#135489=CARTESIAN_POINT('Ctrl Pts',(-240.474705178661,-0.397330368365009,
125.900275616925));
#135490=CARTESIAN_POINT('Ctrl Pts',(-240.482465621175,-0.533409924550205,
125.915121728445));
#135491=CARTESIAN_POINT('Ctrl Pts',(-240.490238521441,-0.669707927719194,
125.929991672262));
#135492=CARTESIAN_POINT('Ctrl Pts',(-240.498011421706,-0.805239232393605,
125.950549536136));
#135493=CARTESIAN_POINT('Ctrl Pts',(-240.505784321971,-0.93950194091927,
125.976678030081));
#135494=CARTESIAN_POINT('Ctrl Pts',(-240.513274657733,-1.06888386180158,
126.001856687456));
#135495=CARTESIAN_POINT('Ctrl Pts',(-240.520764993495,-1.19708751882659,
126.032207922691));
#135496=CARTESIAN_POINT('Ctrl Pts',(-240.528255329257,-1.32367889071797,
126.067583521611));
#135497=CARTESIAN_POINT('Ctrl Pts',(-240.536029663376,-1.45507001295323,
126.104300397116));
#135498=CARTESIAN_POINT('Ctrl Pts',(-240.543803997496,-1.58514038461186,
126.146546462842));
#135499=CARTESIAN_POINT('Ctrl Pts',(-240.551578331615,-1.71338926894211,
126.194210915488));
#135500=CARTESIAN_POINT('Ctrl Pts',(-240.559343084562,-1.84148009798436,
126.241816625955));
#135501=CARTESIAN_POINT('Ctrl Pts',(-240.567107837509,-1.96775354326625,
126.294827301861));
#135502=CARTESIAN_POINT('Ctrl Pts',(-240.574872590456,-2.09172164456772,
126.35308174244));
#135503=CARTESIAN_POINT('Ctrl Pts',(-240.582629631341,-2.21556661900333,
126.411278323886));
#135504=CARTESIAN_POINT('Ctrl Pts',(-240.590386672226,-2.33711045451045,
126.474708140289));
#135505=CARTESIAN_POINT('Ctrl Pts',(-240.598143713111,-2.45588322004057,
126.54316117703));
#135506=CARTESIAN_POINT('Ctrl Pts',(-240.605894904352,-2.57456641810446,
126.611562592804));
#135507=CARTESIAN_POINT('Ctrl Pts',(-240.613646095592,-2.69048236821961,
126.684979494597));
#135508=CARTESIAN_POINT('Ctrl Pts',(-240.621397286832,-2.80318422121785,
126.763155192892));
#135509=CARTESIAN_POINT('Ctrl Pts',(-240.629145183609,-2.91583817292199,
126.841297664429));
#135510=CARTESIAN_POINT('Ctrl Pts',(-240.636893080386,-3.02528042395828,
126.924194687274));
#135511=CARTESIAN_POINT('Ctrl Pts',(-240.644640977164,-3.13109188910893,
127.011545483071));
#135512=CARTESIAN_POINT('Ctrl Pts',(-240.652387253248,-3.23688122078211,
127.098878006964));
#135513=CARTESIAN_POINT('Ctrl Pts',(-240.660133529332,-3.33904097591098,
127.190662201998));
#135514=CARTESIAN_POINT('Ctrl Pts',(-240.667879805416,-3.43718436016796,
127.28655636822));
#135515=CARTESIAN_POINT('Ctrl Pts',(-240.675626138681,-3.53532846889725,
127.382451242311));
#135516=CARTESIAN_POINT('Ctrl Pts',(-240.683372471947,-3.62945586795442,
127.482455874897));
#135517=CARTESIAN_POINT('Ctrl Pts',(-240.691118805212,-3.71921620940167,
127.586191285442));
#135518=CARTESIAN_POINT('Ctrl Pts',(-240.698866873215,-3.80899665205466,
127.689949926813));
#135519=CARTESIAN_POINT('Ctrl Pts',(-240.706614941218,-3.89440783527399,
127.797440713061));
#135520=CARTESIAN_POINT('Ctrl Pts',(-240.714363009221,-3.97513959237725,
127.908251454635));
#135521=CARTESIAN_POINT('Ctrl Pts',(-240.722119311963,-4.05595715215256,
128.019179967183));
#135522=CARTESIAN_POINT('Ctrl Pts',(-240.729875614705,-4.13208512042318,
128.133435167094));
#135523=CARTESIAN_POINT('Ctrl Pts',(-240.737631917447,-4.20325629721131,
128.250575277634));
#135524=CARTESIAN_POINT('Ctrl Pts',(-240.745392359961,-4.2744654601996,
128.367777909378));
#135525=CARTESIAN_POINT('Ctrl Pts',(-240.753152802475,-4.34071237139295,
128.487868177696));
#135526=CARTESIAN_POINT('Ctrl Pts',(-240.76091324499,-4.40177624135282,
128.610380448202));
#135527=CARTESIAN_POINT('Ctrl Pts',(-240.768686145255,-4.46293813645775,
128.733089386281));
#135528=CARTESIAN_POINT('Ctrl Pts',(-240.776459045521,-4.51890020406355,
128.858227738929));
#135529=CARTESIAN_POINT('Ctrl Pts',(-240.784231945786,-4.56948983561737,
128.985309847332));
#135530=CARTESIAN_POINT('Ctrl Pts',(-240.791722281548,-4.61824040663265,
129.107772200984));
#135531=CARTESIAN_POINT('Ctrl Pts',(-240.799212617309,-4.6620022610055,
129.232039152562));
#135532=CARTESIAN_POINT('Ctrl Pts',(-240.806702953071,-4.70066549641594,
129.357665434293));
#135533=CARTESIAN_POINT('Ctrl Pts',(-240.811139036931,-4.72356344919756,
129.432066467644));
#135534=CARTESIAN_POINT('Ctrl Pts',(-240.815575120791,-4.74470148622331,
129.507032902232));
#135535=CARTESIAN_POINT('Ctrl Pts',(-240.820011204651,-4.76405452823406,
129.582490119308));
#135536=CARTESIAN_POINT('Origin',(213.235140564004,0.,130.804360617566));
#135537=CARTESIAN_POINT('',(-242.915000748075,-4.76405452823401,129.582490119308));
#135538=CARTESIAN_POINT('',(-242.570075304501,-4.76405452823394,129.582490119308));
#135539=CARTESIAN_POINT('',(213.235140564004,-4.76405452823405,129.582490119308));
#135540=CARTESIAN_POINT('',(-241.235140564066,-4.91824921781847,130.807134410642));
#135541=CARTESIAN_POINT('Ctrl Pts',(-241.235140564066,-4.91824921781847,
130.807134410642));
#135542=CARTESIAN_POINT('Ctrl Pts',(-241.243741602721,-4.91816318054272,
130.959688243065));
#135543=CARTESIAN_POINT('Ctrl Pts',(-241.252342641376,-4.91097524265387,
131.111987004567));
#135544=CARTESIAN_POINT('Ctrl Pts',(-241.260943680032,-4.89678074903758,
131.26340457881));
#135545=CARTESIAN_POINT('Ctrl Pts',(-241.269594554463,-4.88250401028414,
131.415699490386));
#135546=CARTESIAN_POINT('Ctrl Pts',(-241.278245428894,-4.8611393738467,
131.567102752248));
#135547=CARTESIAN_POINT('Ctrl Pts',(-241.286896303325,-4.83283393080042,
131.716993763909));
#135548=CARTESIAN_POINT('Ctrl Pts',(-241.295573079827,-4.80444373683379,
131.867333572685));
#135549=CARTESIAN_POINT('Ctrl Pts',(-241.304249856328,-4.76907122737263,
132.016151856431));
#135550=CARTESIAN_POINT('Ctrl Pts',(-241.312926632829,-4.7269134761016,
132.162842141897));
#135551=CARTESIAN_POINT('Ctrl Pts',(-241.321635659586,-4.68459903089536,
132.310077652794));
#135552=CARTESIAN_POINT('Ctrl Pts',(-241.330344686343,-4.63544892768495,
132.455169116496));
#135553=CARTESIAN_POINT('Ctrl Pts',(-241.3390537131,-4.57970963792587,132.597526168983));
#135554=CARTESIAN_POINT('Ctrl Pts',(-241.340705543579,-4.56913763484539,
132.624526857437));
#135555=CARTESIAN_POINT('Ctrl Pts',(-241.342357374058,-4.55832872367434,
132.651429248468));
#135556=CARTESIAN_POINT('Ctrl Pts',(-241.344009204537,-4.54728477123908,
132.67822941547));
#135557=CARTESIAN_POINT('Ctrl Pts',(-241.351783538656,-4.49530644941974,
132.804364303626));
#135558=CARTESIAN_POINT('Ctrl Pts',(-241.359557872775,-4.43799363020899,
132.928534639887));
#135559=CARTESIAN_POINT('Ctrl Pts',(-241.367332206894,-4.37551548274368,
133.050256279161));
#135560=CARTESIAN_POINT('Ctrl Pts',(-241.375096959842,-4.31311433401129,
133.171827907393));
#135561=CARTESIAN_POINT('Ctrl Pts',(-241.382861712789,-4.24556069989832,
133.290956498679));
#135562=CARTESIAN_POINT('Ctrl Pts',(-241.390626465736,-4.17307228523948,
133.407176547413));
#135563=CARTESIAN_POINT('Ctrl Pts',(-241.398383506621,-4.10065586709599,
133.523281164757));
#135564=CARTESIAN_POINT('Ctrl Pts',(-241.406140547506,-4.0233146277682,
133.63648265882));
#135565=CARTESIAN_POINT('Ctrl Pts',(-241.413897588391,-3.94131261487676,
133.74633919232));
#135566=CARTESIAN_POINT('Ctrl Pts',(-241.421648779632,-3.85937244034102,
133.856112882154));
#135567=CARTESIAN_POINT('Ctrl Pts',(-241.429399970872,-3.77277872100946,
133.962546320192));
#135568=CARTESIAN_POINT('Ctrl Pts',(-241.437151162112,-3.6818391265378,
134.065226102187));
#135569=CARTESIAN_POINT('Ctrl Pts',(-241.444899058889,-3.5909381838198,
134.167862242536));
#135570=CARTESIAN_POINT('Ctrl Pts',(-241.452646955666,-3.49569529840085,
134.266747607913));
#135571=CARTESIAN_POINT('Ctrl Pts',(-241.460394852444,-3.39645864101536,
134.361501570968));
#135572=CARTESIAN_POINT('Ctrl Pts',(-241.468141128528,-3.29724274179929,
134.456235713538));
#135573=CARTESIAN_POINT('Ctrl Pts',(-241.475887404612,-3.19403501488272,
134.546839902905));
#135574=CARTESIAN_POINT('Ctrl Pts',(-241.483633680696,-3.08722045233845,
134.632970409796));
#135575=CARTESIAN_POINT('Ctrl Pts',(-241.491380013962,-2.9804051013135,
134.719101552484));
#135576=CARTESIAN_POINT('Ctrl Pts',(-241.499126347227,-2.86998316587963,
134.800758701387));
#135577=CARTESIAN_POINT('Ctrl Pts',(-241.506872680492,-2.7563723531155,
134.877638721683));
#135578=CARTESIAN_POINT('Ctrl Pts',(-241.514620748495,-2.64273609799741,
134.954535958727));
#135579=CARTESIAN_POINT('Ctrl Pts',(-241.522368816498,-2.52590986825316,
135.026653719308));
#135580=CARTESIAN_POINT('Ctrl Pts',(-241.530116884501,-2.40633960177869,
135.09373269089));
#135581=CARTESIAN_POINT('Ctrl Pts',(-241.537873187243,-2.28664225460227,
135.160882954802));
#135582=CARTESIAN_POINT('Ctrl Pts',(-241.545629489985,-2.16419538640035,
135.222983540365));
#135583=CARTESIAN_POINT('Ctrl Pts',(-241.553385792727,-2.03946924041631,
135.279821295518));
#135584=CARTESIAN_POINT('Ctrl Pts',(-241.561146235242,-1.91467652433272,
135.336689386692));
#135585=CARTESIAN_POINT('Ctrl Pts',(-241.568906677756,-1.78760246851266,
135.388288903404));
#135586=CARTESIAN_POINT('Ctrl Pts',(-241.57666712027,-1.65873552537455,
135.434455597084));
#135587=CARTESIAN_POINT('Ctrl Pts',(-241.584440020535,-1.52966171357904,
135.48069640164));
#135588=CARTESIAN_POINT('Ctrl Pts',(-241.592212920801,-1.39878963657093,
135.521486838924));
#135589=CARTESIAN_POINT('Ctrl Pts',(-241.599985821066,-1.26662194045584,
135.556712869078));
#135590=CARTESIAN_POINT('Ctrl Pts',(-241.607476156827,-1.13925887302456,
135.590658344303));
#135591=CARTESIAN_POINT('Ctrl Pts',(-241.614966492588,-1.01069304968676,
135.619436881785));
#135592=CARTESIAN_POINT('Ctrl Pts',(-241.622456828349,-0.881379602062333,
135.642991938463));
#135593=CARTESIAN_POINT('Ctrl Pts',(-241.630231162468,-0.747163195748146,
135.667440092278));
#135594=CARTESIAN_POINT('Ctrl Pts',(-241.638005496587,-0.611716196440621,
135.686338294071));
#135595=CARTESIAN_POINT('Ctrl Pts',(-241.645779830706,-0.475537369166859,
135.699567178379));
#135596=CARTESIAN_POINT('Ctrl Pts',(-241.653544583653,-0.339526370127431,
135.71277975927));
#135597=CARTESIAN_POINT('Ctrl Pts',(-241.6613093366,-0.202785723056727,
135.72033688714));
#135598=CARTESIAN_POINT('Ctrl Pts',(-241.669074089547,-0.0658247457847857,
135.722170106082));
#135599=CARTESIAN_POINT('Ctrl Pts',(-241.676831130432,0.0710001999140895,
135.724001504246));
#135600=CARTESIAN_POINT('Ctrl Pts',(-241.684588171317,0.20804465192206,
135.720120301824));
#135601=CARTESIAN_POINT('Ctrl Pts',(-241.692345212202,0.344794155831017,
135.710509825713));
#135602=CARTESIAN_POINT('Ctrl Pts',(-241.700096403443,0.481440535875133,
135.700906596937));
#135603=CARTESIAN_POINT('Ctrl Pts',(-241.707847594683,0.617792022113812,
135.685582721444));
#135604=CARTESIAN_POINT('Ctrl Pts',(-241.715598785923,0.753334502882079,
135.664573595334));
#135605=CARTESIAN_POINT('Ctrl Pts',(-241.7233466827,0.888819374480489,135.643573398664));
#135606=CARTESIAN_POINT('Ctrl Pts',(-241.731094579477,1.02349553895492,
135.616892817139));
#135607=CARTESIAN_POINT('Ctrl Pts',(-241.738842476254,1.15685456895081,
135.584619038279));
#135608=CARTESIAN_POINT('Ctrl Pts',(-241.746588752338,1.2901857031125,135.552352010398));
#135609=CARTESIAN_POINT('Ctrl Pts',(-241.754335028422,1.42219987105723,
135.514494204234));
#135610=CARTESIAN_POINT('Ctrl Pts',(-241.762081304506,1.55239978599228,
135.47118373045));
#135611=CARTESIAN_POINT('Ctrl Pts',(-241.769827637772,1.68260066203335,
135.427872936959));
#135612=CARTESIAN_POINT('Ctrl Pts',(-241.777573971037,1.8109868873626,135.379109518937));
#135613=CARTESIAN_POINT('Ctrl Pts',(-241.785320304303,1.93707764518968,
135.325081053404));
#135614=CARTESIAN_POINT('Ctrl Pts',(-241.793068372306,2.06319664016754,
135.271040488571));
#135615=CARTESIAN_POINT('Ctrl Pts',(-241.800816440309,2.18701878543954,
135.211732683966));
#135616=CARTESIAN_POINT('Ctrl Pts',(-241.808564508312,2.30808487370135,
135.147392655013));
#135617=CARTESIAN_POINT('Ctrl Pts',(-241.816320811053,2.42927963244263,
135.082984244711));
#135618=CARTESIAN_POINT('Ctrl Pts',(-241.824077113795,2.5477121370507,135.013533110008));
#135619=CARTESIAN_POINT('Ctrl Pts',(-241.831833416537,2.66294887869895,
134.939319665965));
#135620=CARTESIAN_POINT('Ctrl Pts',(-241.839593859051,2.77824712566594,
134.865066611973));
#135621=CARTESIAN_POINT('Ctrl Pts',(-241.847354301566,2.89034589157634,
134.78604640906));
#135622=CARTESIAN_POINT('Ctrl Pts',(-241.85511474408,2.998842968994,134.702581225717));
#135623=CARTESIAN_POINT('Ctrl Pts',(-241.862887644345,3.10751421555226,
134.618982056652));
#135624=CARTESIAN_POINT('Ctrl Pts',(-241.87066054461,3.21257192003518,134.530923899492));
#135625=CARTESIAN_POINT('Ctrl Pts',(-241.878433444876,3.31364844498309,
134.438768003311));
#135626=CARTESIAN_POINT('Ctrl Pts',(-241.885923780638,3.41105058365493,
134.349962206082));
#135627=CARTESIAN_POINT('Ctrl Pts',(-241.8934141164,3.50475575021393,134.257351640184));
#135628=CARTESIAN_POINT('Ctrl Pts',(-241.900904452163,3.5944703636233,134.161288657833));
#135629=CARTESIAN_POINT('Ctrl Pts',(-241.908678786282,3.68758653386628,
134.061583418312));
#135630=CARTESIAN_POINT('Ctrl Pts',(-241.916453120401,3.7766985378616,133.957842961419));
#135631=CARTESIAN_POINT('Ctrl Pts',(-241.92422745452,3.86143635538579,133.850422392351));
#135632=CARTESIAN_POINT('Ctrl Pts',(-241.931992207467,3.94606974112289,
133.743134209534));
#135633=CARTESIAN_POINT('Ctrl Pts',(-241.939756960414,4.02633942664666,
133.632175242664));
#135634=CARTESIAN_POINT('Ctrl Pts',(-241.947521713361,4.10191251933598,
133.517936993166));
#135635=CARTESIAN_POINT('Ctrl Pts',(-241.955278754246,4.17741055176445,
133.403812206708));
#135636=CARTESIAN_POINT('Ctrl Pts',(-241.963035795131,4.24822106005234,
133.28641494322));
#135637=CARTESIAN_POINT('Ctrl Pts',(-241.970792836016,4.31405194147264,
133.166169015548));
#135638=CARTESIAN_POINT('Ctrl Pts',(-241.978544027256,4.37983317931309,
133.046013766265));
#135639=CARTESIAN_POINT('Ctrl Pts',(-241.986295218496,4.4406420777478,132.923014470207));
#135640=CARTESIAN_POINT('Ctrl Pts',(-241.994046409736,4.49623052660688,
132.797622796535));
#135641=CARTESIAN_POINT('Ctrl Pts',(-242.001794306513,4.55179534889241,
132.67228441767));
#135642=CARTESIAN_POINT('Ctrl Pts',(-242.00954220329,4.6021439765685,132.544556040246));
#135643=CARTESIAN_POINT('Ctrl Pts',(-242.017290100067,4.64707494556122,
132.414912545582));
#135644=CARTESIAN_POINT('Ctrl Pts',(-242.025036376152,4.69199651596382,
132.285296169543));
#135645=CARTESIAN_POINT('Ctrl Pts',(-242.032782652236,4.73150255384806,
132.153765842255));
#135646=CARTESIAN_POINT('Ctrl Pts',(-242.04052892832,4.76544045997002,132.02081459737));
#135647=CARTESIAN_POINT('Ctrl Pts',(-242.048275261585,4.79937861661385,
131.887862371069));
#135648=CARTESIAN_POINT('Ctrl Pts',(-242.056021594851,4.82774846277871,
131.753489585059));
#135649=CARTESIAN_POINT('Ctrl Pts',(-242.063767928116,4.85044791910369,
131.618202154084));
#135650=CARTESIAN_POINT('Ctrl Pts',(-242.071515996119,4.8731524588145,131.482884426428));
#135651=CARTESIAN_POINT('Ctrl Pts',(-242.079264064122,4.8901840171598,131.346652031722));
#135652=CARTESIAN_POINT('Ctrl Pts',(-242.087012132125,4.90149210650604,
131.210018345656));
#135653=CARTESIAN_POINT('Ctrl Pts',(-242.094768434866,4.91281221422421,
131.073239443682));
#135654=CARTESIAN_POINT('Ctrl Pts',(-242.102524737608,4.9183966692553,130.936058788627));
#135655=CARTESIAN_POINT('Ctrl Pts',(-242.11028104035,4.91824707062302,130.798992674935));
#135656=CARTESIAN_POINT('Ctrl Pts',(-242.118041482864,4.91809739214544,
130.661853404931));
#135657=CARTESIAN_POINT('Ctrl Pts',(-242.125801925378,4.9122075786059,130.524829188518));
#135658=CARTESIAN_POINT('Ctrl Pts',(-242.133562367893,4.90063127653539,
130.388432554143));
#135659=CARTESIAN_POINT('Ctrl Pts',(-242.141335268158,4.8890363911571,130.251816963781));
#135660=CARTESIAN_POINT('Ctrl Pts',(-242.149108168423,4.87173682505142,
130.115831356725));
#135661=CARTESIAN_POINT('Ctrl Pts',(-242.156881068689,4.84883779026997,
129.980980300732));
#135662=CARTESIAN_POINT('Ctrl Pts',(-242.164371404451,4.82677119308153,
129.851031420291));
#135663=CARTESIAN_POINT('Ctrl Pts',(-242.171861740213,4.79950523252502,
129.72213633679));
#135664=CARTESIAN_POINT('Ctrl Pts',(-242.179352075975,4.76717766477755,
129.594732503249));
#135665=CARTESIAN_POINT('Ctrl Pts',(-242.187126410094,4.73362438747381,
129.462498114639));
#135666=CARTESIAN_POINT('Ctrl Pts',(-242.194900744213,4.69451181784857,
129.331451410942));
#135667=CARTESIAN_POINT('Ctrl Pts',(-242.202675078333,4.64993871099088,
129.202095643684));
#135668=CARTESIAN_POINT('Ctrl Pts',(-242.21043983128,4.6054205365039,129.072899295849));
#135669=CARTESIAN_POINT('Ctrl Pts',(-242.218204584227,4.55545534087641,
128.945390104145));
#135670=CARTESIAN_POINT('Ctrl Pts',(-242.225969337174,4.50019256875227,
128.820059756646));
#135671=CARTESIAN_POINT('Ctrl Pts',(-242.233726378059,4.44498468439248,
128.694853889015));
#135672=CARTESIAN_POINT('Ctrl Pts',(-242.241483418944,4.38448985112935,
128.571822914432));
#135673=CARTESIAN_POINT('Ctrl Pts',(-242.249240459829,4.31890674605306,
128.451441668389));
#135674=CARTESIAN_POINT('Ctrl Pts',(-242.256991651069,4.25337309770639,
128.331151202779));
#135675=CARTESIAN_POINT('Ctrl Pts',(-242.264742842309,4.18275900135524,
128.213506830384));
#135676=CARTESIAN_POINT('Ctrl Pts',(-242.272494033549,4.10731034945009,
128.098961431531));
#135677=CARTESIAN_POINT('Ctrl Pts',(-242.280241930326,4.03189376523455,
127.984464717527));
#135678=CARTESIAN_POINT('Ctrl Pts',(-242.287989827104,3.95164692694489,
127.87306468318));
#135679=CARTESIAN_POINT('Ctrl Pts',(-242.295737723881,3.86686046942969,
127.76518751087));
#135680=CARTESIAN_POINT('Ctrl Pts',(-242.303483999965,3.78209174741384,
127.65733290414));
#135681=CARTESIAN_POINT('Ctrl Pts',(-242.311230276049,3.69278553639915,
127.553000000893));
#135682=CARTESIAN_POINT('Ctrl Pts',(-242.318976552133,3.59927415594075,
127.452583683927));
#135683=CARTESIAN_POINT('Ctrl Pts',(-242.326722885398,3.50576208520245,
127.352166625709));
#135684=CARTESIAN_POINT('Ctrl Pts',(-242.334469218664,3.40804504952111,
127.255666497579));
#135685=CARTESIAN_POINT('Ctrl Pts',(-242.342215551929,3.30649351291106,
127.163442641069));
#135686=CARTESIAN_POINT('Ctrl Pts',(-242.349963619932,3.20491923453835,
127.071198131666));
#135687=CARTESIAN_POINT('Ctrl Pts',(-242.357711687935,3.09950903587483,
126.983232062272));
#135688=CARTESIAN_POINT('Ctrl Pts',(-242.365459755938,2.99066754462646,
126.899864401661));
#135689=CARTESIAN_POINT('Ctrl Pts',(-242.37321605868,2.88171037534611,126.816408136908));
#135690=CARTESIAN_POINT('Ctrl Pts',(-242.380972361422,2.76931493944201,
126.737560281849));
#135691=CARTESIAN_POINT('Ctrl Pts',(-242.388728664163,2.65391647436352,
126.663598560939));
#135692=CARTESIAN_POINT('Ctrl Pts',(-242.396489106678,2.53845641764963,
126.589597364431));
#135693=CARTESIAN_POINT('Ctrl Pts',(-242.404249549192,2.41999047556914,
126.520487695397));
#135694=CARTESIAN_POINT('Ctrl Pts',(-242.412009991706,2.298978850079,126.456501453634));
#135695=CARTESIAN_POINT('Ctrl Pts',(-242.419782891971,2.17777296598471,
126.392412495475));
#135696=CARTESIAN_POINT('Ctrl Pts',(-242.427555792237,2.05401358541031,
126.333463568142));
#135697=CARTESIAN_POINT('Ctrl Pts',(-242.435328692502,1.92818208518315,
126.279838884954));
#135698=CARTESIAN_POINT('Ctrl Pts',(-242.442819028264,1.80692487694069,
126.228163594072));
#135699=CARTESIAN_POINT('Ctrl Pts',(-242.450309364026,1.68374387500729,
126.181432277832));
#135700=CARTESIAN_POINT('Ctrl Pts',(-242.457799699788,1.55908158157693,
126.139765492104));
#135701=CARTESIAN_POINT('Ctrl Pts',(-242.465574033907,1.42969267939995,
126.096518897529));
#135702=CARTESIAN_POINT('Ctrl Pts',(-242.473348368026,1.29829807688462,
126.058591465739));
#135703=CARTESIAN_POINT('Ctrl Pts',(-242.481122702145,1.1653745533301,126.026172131021));
#135704=CARTESIAN_POINT('Ctrl Pts',(-242.488887455092,1.03261484613901,
125.993792750236));
#135705=CARTESIAN_POINT('Ctrl Pts',(-242.496652208039,0.8983303432066,125.966908051704));
#135706=CARTESIAN_POINT('Ctrl Pts',(-242.504416960986,0.763015494114828,
125.945658072828));
#135707=CARTESIAN_POINT('Ctrl Pts',(-242.512174001871,0.627835041638779,
125.924429199731));
#135708=CARTESIAN_POINT('Ctrl Pts',(-242.519931042756,0.491626663256989,
125.908823969297));
#135709=CARTESIAN_POINT('Ctrl Pts',(-242.527688083641,0.354897241336885,
125.898931889046));
#135710=CARTESIAN_POINT('Ctrl Pts',(-242.535439274881,0.218270928137265,
125.889047268489));
#135711=CARTESIAN_POINT('Ctrl Pts',(-242.543190466121,0.0811247418568937,
125.884867250741));
#135712=CARTESIAN_POINT('Ctrl Pts',(-242.550941657362,-0.0560273855828691,
125.886429752399));
#135713=CARTESIAN_POINT('Ctrl Pts',(-242.558689554139,-0.19312121970963,
125.887991589951));
#135714=CARTESIAN_POINT('Ctrl Pts',(-242.566437450916,-0.330220599852082,
125.895291088051));
#135715=CARTESIAN_POINT('Ctrl Pts',(-242.574185347693,-0.466809871466674,
125.908314089356));
#135716=CARTESIAN_POINT('Ctrl Pts',(-242.581931623777,-0.603370571550168,
125.921334366529));
#135717=CARTESIAN_POINT('Ctrl Pts',(-242.589677899861,-0.739420986391715,
125.940075728461));
#135718=CARTESIAN_POINT('Ctrl Pts',(-242.597424175945,-0.87444926307359,
125.964472029095));
#135719=CARTESIAN_POINT('Ctrl Pts',(-242.60517050921,-1.00947853650371,
125.988868509817));
#135720=CARTESIAN_POINT('Ctrl Pts',(-242.612916842475,-1.14348527198223,
126.018919943024));
#135721=CARTESIAN_POINT('Ctrl Pts',(-242.620663175741,-1.27596690045057,
126.054508879727));
#135722=CARTESIAN_POINT('Ctrl Pts',(-242.628411243744,-1.40847819726086,
126.090105786325));
#135723=CARTESIAN_POINT('Ctrl Pts',(-242.636159311747,-1.53946332993511,
126.131242562633));
#135724=CARTESIAN_POINT('Ctrl Pts',(-242.64390737975,-1.66843438852243,
126.177751734843));
#135725=CARTESIAN_POINT('Ctrl Pts',(-242.651663682491,-1.79754251908576,
126.224310337553));
#135726=CARTESIAN_POINT('Ctrl Pts',(-242.659419985233,-1.92463193115093,
126.276252609358));
#135727=CARTESIAN_POINT('Ctrl Pts',(-242.667176287975,-2.04923371079638,
126.333362489515));
#135728=CARTESIAN_POINT('Ctrl Pts',(-242.674936730489,-2.17390199416364,
126.390502850935));
#135729=CARTESIAN_POINT('Ctrl Pts',(-242.682697173003,-2.29607965139587,
126.452816138926));
#135730=CARTESIAN_POINT('Ctrl Pts',(-242.690457615517,-2.4153228282265,
126.520040520054));
#135731=CARTESIAN_POINT('Ctrl Pts',(-242.698230515783,-2.53475742479017,
126.587372815726));
#135732=CARTESIAN_POINT('Ctrl Pts',(-242.706003416048,-2.65124779506669,
126.659631752519));
#135733=CARTESIAN_POINT('Ctrl Pts',(-242.713776316314,-2.76437875924074,
126.736511906274));
#135734=CARTESIAN_POINT('Ctrl Pts',(-242.721266652076,-2.87339712791043,
126.810597272793));
#135735=CARTESIAN_POINT('Ctrl Pts',(-242.728756987838,-2.9792958481746,
126.888973520485));
#135736=CARTESIAN_POINT('Ctrl Pts',(-242.7362473236,-3.0817343097212,126.971333523116));
#135737=CARTESIAN_POINT('Ctrl Pts',(-242.743919292931,-3.18665680721284,
127.055690678026));
#135738=CARTESIAN_POINT('Ctrl Pts',(-242.751591262261,-3.28830002056774,
127.14450971462));
#135739=CARTESIAN_POINT('Ctrl Pts',(-242.759263231591,-3.3862531830133,
127.237503115081));
#135740=CARTESIAN_POINT('Ctrl Pts',(-242.766926418694,-3.48409421689378,
127.330390064497));
#135741=CARTESIAN_POINT('Ctrl Pts',(-242.774589605797,-3.57825330852022,
127.427441605249));
#135742=CARTESIAN_POINT('Ctrl Pts',(-242.7822527929,-3.66835065220018,127.528328481734));
#135743=CARTESIAN_POINT('Ctrl Pts',(-242.789908971473,-3.75836559544404,
127.629123089988));
#135744=CARTESIAN_POINT('Ctrl Pts',(-242.797565150046,-3.84432591104526,
127.733745761908));
#135745=CARTESIAN_POINT('Ctrl Pts',(-242.805221328619,-3.92588715360147,
127.841829078546));
#135746=CARTESIAN_POINT('Ctrl Pts',(-242.812872265948,-4.00739256119842,
127.949838403821));
#135747=CARTESIAN_POINT('Ctrl Pts',(-242.820523203276,-4.08450464423534,
128.061303342346));
#135748=CARTESIAN_POINT('Ctrl Pts',(-242.828174140605,-4.15691829166909,
128.175822358593));
#135749=CARTESIAN_POINT('Ctrl Pts',(-242.83582247977,-4.22930734832785,
128.290302485604));
#135750=CARTESIAN_POINT('Ctrl Pts',(-242.843470818935,-4.29700092391433,
128.407834291233));
#135751=CARTESIAN_POINT('Ctrl Pts',(-242.8511191581,-4.35973665121918,128.527986440389));
#135752=CARTESIAN_POINT('Ctrl Pts',(-242.858765799848,-4.42245845540937,
128.648111923845));
#135753=CARTESIAN_POINT('Ctrl Pts',(-242.866412441596,-4.48022441733024,
128.770856236093));
#135754=CARTESIAN_POINT('Ctrl Pts',(-242.874059083344,-4.53281799721013,
128.895763209345));
#135755=CARTESIAN_POINT('Ctrl Pts',(-242.881708240402,-4.58542887738673,
129.020711269887));
#135756=CARTESIAN_POINT('Ctrl Pts',(-242.88935739746,-4.63286381874236,
129.147823042512));
#135757=CARTESIAN_POINT('Ctrl Pts',(-242.897006554518,-4.6749543734349,
129.276622201213));
#135758=CARTESIAN_POINT('Ctrl Pts',(-242.903004619037,-4.70795956090417,
129.377619691263));
#135759=CARTESIAN_POINT('Ctrl Pts',(-242.909002683556,-4.73767949876136,
129.479654279691));
#135760=CARTESIAN_POINT('Ctrl Pts',(-242.915000748075,-4.76405452823401,
129.582490119308));
#135761=CARTESIAN_POINT('Ctrl Pts',(-241.165327127303,-4.76405452823409,
129.582490119308));
#135762=CARTESIAN_POINT('Ctrl Pts',(-241.173163504015,-4.79852551714263,
129.716891981893));
#135763=CARTESIAN_POINT('Ctrl Pts',(-241.180999880728,-4.82732559214713,
129.852834902042));
#135764=CARTESIAN_POINT('Ctrl Pts',(-241.18883625744,-4.85032839536548,
129.989807046822));
#135765=CARTESIAN_POINT('Ctrl Pts',(-241.196670112391,-4.87332379623385,
130.126735113681));
#135766=CARTESIAN_POINT('Ctrl Pts',(-241.204503967341,-4.89052557304048,
130.264691373754));
#135767=CARTESIAN_POINT('Ctrl Pts',(-241.212337822291,-4.90185841905944,
130.403153561302));
#135768=CARTESIAN_POINT('Ctrl Pts',(-241.219938736198,-4.91285428092652,
130.537498551567));
#135769=CARTESIAN_POINT('Ctrl Pts',(-241.227539650106,-4.91832525069541,
130.672319465504));
#135770=CARTESIAN_POINT('Ctrl Pts',(-241.235140564014,-4.91824921781899,
130.807134409724));
#135771=CARTESIAN_POINT('',(-240.889859435956,-4.91824814758057,130.800091973715));
#135772=CARTESIAN_POINT('Ctrl Pts',(-240.820011204651,-4.76405452823406,
129.582490119308));
#135773=CARTESIAN_POINT('Ctrl Pts',(-240.829478829728,-4.80535837902586,
129.743533206672));
#135774=CARTESIAN_POINT('Ctrl Pts',(-240.838946454805,-4.83852861212123,
129.906813185049));
#135775=CARTESIAN_POINT('Ctrl Pts',(-240.848414079882,-4.86335571906152,
130.071589021247));
#135776=CARTESIAN_POINT('Ctrl Pts',(-240.857763979629,-4.8878741129549,
130.234315949751));
#135777=CARTESIAN_POINT('Ctrl Pts',(-240.867113879375,-4.90425553807115,
130.398501772666));
#135778=CARTESIAN_POINT('Ctrl Pts',(-240.876463779121,-4.91234431771532,
130.563411729397));
#135779=CARTESIAN_POINT('Ctrl Pts',(-240.880928998066,-4.91620726524315,
130.642167553846));
#135780=CARTESIAN_POINT('Ctrl Pts',(-240.885394217011,-4.91817957867735,
130.721088221468));
#135781=CARTESIAN_POINT('Ctrl Pts',(-240.889859435956,-4.91824814758057,
130.800091973715));
#135782=CARTESIAN_POINT('Ctrl Pts',(-240.889859435996,-4.91824814758118,
130.800091974427));
#135783=CARTESIAN_POINT('Ctrl Pts',(-240.897561156383,-4.91836641690644,
130.936359605821));
#135784=CARTESIAN_POINT('Ctrl Pts',(-240.90526287677,-4.91281717295408,
131.072729329552));
#135785=CARTESIAN_POINT('Ctrl Pts',(-240.912964597156,-4.90160180444283,
131.208690697059));
#135786=CARTESIAN_POINT('Ctrl Pts',(-240.920664069363,-4.89038970976659,
131.344612376607));
#135787=CARTESIAN_POINT('Ctrl Pts',(-240.928363541571,-4.87351480886842,
131.480125542569));
#135788=CARTESIAN_POINT('Ctrl Pts',(-240.936063013778,-4.85103055027703,
131.614722057159));
#135789=CARTESIAN_POINT('Ctrl Pts',(-240.943761625337,-4.82854880497805,
131.749303526538));
#135790=CARTESIAN_POINT('Ctrl Pts',(-240.951460236897,-4.80045901402057,
131.882968157685));
#135791=CARTESIAN_POINT('Ctrl Pts',(-240.959158848456,-4.76686614985544,
132.015215758308));
#135792=CARTESIAN_POINT('Ctrl Pts',(-240.966858316943,-4.73326954648901,
132.147478079332));
#135793=CARTESIAN_POINT('Ctrl Pts',(-240.97455778543,-4.69416874887371,
132.27832267213));
#135794=CARTESIAN_POINT('Ctrl Pts',(-240.982257253918,-4.6497191058681,
132.40726276649));
#135795=CARTESIAN_POINT('Ctrl Pts',(-240.989959297187,-4.60525459843776,
132.536245979764));
#135796=CARTESIAN_POINT('Ctrl Pts',(-240.997661340457,-4.55543781628651,
132.663323053388));
#135797=CARTESIAN_POINT('Ctrl Pts',(-241.005363383727,-4.50047274065077,
132.78802595556));
#135798=CARTESIAN_POINT('Ctrl Pts',(-241.013074120844,-4.44544562200206,
132.912869618819));
#135799=CARTESIAN_POINT('Ctrl Pts',(-241.020784857961,-4.38525876797335,
133.03533339777));
#135800=CARTESIAN_POINT('Ctrl Pts',(-241.028495595079,-4.32016291498794,
133.15497233592));
#135801=CARTESIAN_POINT('Ctrl Pts',(-241.036211295946,-4.25502515685459,
133.274688291071));
#135802=CARTESIAN_POINT('Ctrl Pts',(-241.043926996814,-4.1849723098661,
133.391575445388));
#135803=CARTESIAN_POINT('Ctrl Pts',(-241.051642697681,-4.1102985330867,
133.505217709566));
#135804=CARTESIAN_POINT('Ctrl Pts',(-241.05936986681,-4.03551376465894,
133.61902888635));
#135805=CARTESIAN_POINT('Ctrl Pts',(-241.067097035939,-3.95609458477475,
133.72958522377));
#135806=CARTESIAN_POINT('Ctrl Pts',(-241.074824205067,-3.87237578563073,
133.83650323251));
#135807=CARTESIAN_POINT('Ctrl Pts',(-241.078266329006,-3.83508263495013,
133.884130640586));
#135808=CARTESIAN_POINT('Ctrl Pts',(-241.081708452945,-3.79693679776537,
133.931036570226));
#135809=CARTESIAN_POINT('Ctrl Pts',(-241.085150576883,-3.75797015117827,
133.977189545408));
#135810=CARTESIAN_POINT('Ctrl Pts',(-241.092924911002,-3.6699606153614,
134.081430024848));
#135811=CARTESIAN_POINT('Ctrl Pts',(-241.100699245122,-3.57747117897063,
134.182170958972));
#135812=CARTESIAN_POINT('Ctrl Pts',(-241.108473579241,-3.48081075907961,
134.279002976425));
#135813=CARTESIAN_POINT('Ctrl Pts',(-241.116238332188,-3.38426946451757,
134.37571565707));
#135814=CARTESIAN_POINT('Ctrl Pts',(-241.124003085134,-3.28356768780561,
134.468528732171));
#135815=CARTESIAN_POINT('Ctrl Pts',(-241.131767838081,-3.17905487259213,
134.557065399393));
#135816=CARTESIAN_POINT('Ctrl Pts',(-241.139524878966,-3.07464586097981,
134.64551413075));
#135817=CARTESIAN_POINT('Ctrl Pts',(-241.147281919851,-2.96643363992176,
134.729694655646));
#135818=CARTESIAN_POINT('Ctrl Pts',(-241.155038960736,-2.85480455597037,
134.809266859878));
#135819=CARTESIAN_POINT('Ctrl Pts',(-241.162790151976,-2.74325965237968,
134.888779058092));
#135820=CARTESIAN_POINT('Ctrl Pts',(-241.170541343216,-2.62830333169952,
134.963689626739));
#135821=CARTESIAN_POINT('Ctrl Pts',(-241.178292534457,-2.51035479772931,
135.03369884618));
#135822=CARTESIAN_POINT('Ctrl Pts',(-241.186040431234,-2.39245639503258,
135.103678309835));
#135823=CARTESIAN_POINT('Ctrl Pts',(-241.193788328011,-2.27156864399816,
135.168760368481));
#135824=CARTESIAN_POINT('Ctrl Pts',(-241.201536224788,-2.14813930742305,
135.228688880523));
#135825=CARTESIAN_POINT('Ctrl Pts',(-241.209282500872,-2.02473578960399,
135.288604856813));
#135826=CARTESIAN_POINT('Ctrl Pts',(-241.217028776956,-1.89879209519428,
135.343369260069));
#135827=CARTESIAN_POINT('Ctrl Pts',(-241.22477505304,-1.7707797836338,135.392772327556));
#135828=CARTESIAN_POINT('Ctrl Pts',(-241.232521386305,-1.64276652711604,
135.442175759725));
#135829=CARTESIAN_POINT('Ctrl Pts',(-241.24026771957,-1.51268498772267,
135.48621763639));
#135830=CARTESIAN_POINT('Ctrl Pts',(-241.248014052836,-1.38102548266735,
135.524736839725));
#135831=CARTESIAN_POINT('Ctrl Pts',(-241.255762120838,-1.24933649337855,
135.563264669168));
#135832=CARTESIAN_POINT('Ctrl Pts',(-241.263510188841,-1.11606921041738,
135.596267254502));
#135833=CARTESIAN_POINT('Ctrl Pts',(-241.271258256844,-0.98172745315296,
135.623633827317));
#135834=CARTESIAN_POINT('Ctrl Pts',(-241.279014559586,-0.847242915870052,
135.651029485652));
#135835=CARTESIAN_POINT('Ctrl Pts',(-241.286770862328,-0.711682006795786,
135.67277708759));
#135836=CARTESIAN_POINT('Ctrl Pts',(-241.29452716507,-0.575557595516321,
135.688817242078));
#135837=CARTESIAN_POINT('Ctrl Pts',(-241.302287607584,-0.43936053053993,
135.70486595768));
#135838=CARTESIAN_POINT('Ctrl Pts',(-241.310048050098,-0.302599753735192,
135.715201126499));
#135839=CARTESIAN_POINT('Ctrl Pts',(-241.317808492612,-0.165790542314485,
135.719815485488));
#135840=CARTESIAN_POINT('Ctrl Pts',(-241.325581392878,-0.0287617126022537,
135.724437251856));
#135841=CARTESIAN_POINT('Ctrl Pts',(-241.333354293143,0.108315315921087,
135.723319859919));
#135842=CARTESIAN_POINT('Ctrl Pts',(-241.341127193408,0.244927080673861,
135.716508191454));
#135843=CARTESIAN_POINT('Ctrl Pts',(-241.348617529171,0.376572663686177,
135.709944144294));
#135844=CARTESIAN_POINT('Ctrl Pts',(-241.356107864934,0.507785915891403,
135.69809266321));
#135845=CARTESIAN_POINT('Ctrl Pts',(-241.363598200696,0.638116175939619,
135.681038873152));
#135846=CARTESIAN_POINT('Ctrl Pts',(-241.371372534816,0.773387947398587,
135.663338483462));
#135847=CARTESIAN_POINT('Ctrl Pts',(-241.379146868935,0.908136947959049,
135.639977436818));
#135848=CARTESIAN_POINT('Ctrl Pts',(-241.386921203054,1.04185178468103,
135.610994358684));
#135849=CARTESIAN_POINT('Ctrl Pts',(-241.394685956001,1.17540182981682,
135.582046999605));
#135850=CARTESIAN_POINT('Ctrl Pts',(-241.402450708948,1.30791986859366,
135.547491477012));
#135851=CARTESIAN_POINT('Ctrl Pts',(-241.410215461895,1.43890000370779,
135.507418116877));
#135852=CARTESIAN_POINT('Ctrl Pts',(-241.41797250278,1.56975004750523,135.46738455817));
#135853=CARTESIAN_POINT('Ctrl Pts',(-241.425729543665,1.69906485592968,
135.421844181794));
#135854=CARTESIAN_POINT('Ctrl Pts',(-241.43348658455,1.8263494515201,135.370938192012));
#135855=CARTESIAN_POINT('Ctrl Pts',(-241.44123777579,1.95353806080668,135.320070590833));
#135856=CARTESIAN_POINT('Ctrl Pts',(-241.44898896703,2.07869914307951,135.263845574658));
#135857=CARTESIAN_POINT('Ctrl Pts',(-241.45674015827,2.20135394582371,135.202453825731));
#135858=CARTESIAN_POINT('Ctrl Pts',(-241.464488055047,2.32395661700498,
135.141088169934));
#135859=CARTESIAN_POINT('Ctrl Pts',(-241.472235951824,2.44405477844558,
135.074560323685));
#135860=CARTESIAN_POINT('Ctrl Pts',(-241.479983848601,2.56119090423909,
135.003108551718));
#135861=CARTESIAN_POINT('Ctrl Pts',(-241.487730124685,2.67830252768056,
134.93167172592));
#135862=CARTESIAN_POINT('Ctrl Pts',(-241.495476400769,2.79245301432282,
134.855313226557));
#135863=CARTESIAN_POINT('Ctrl Pts',(-241.503222676854,2.90321099544081,
134.774316408057));
#135864=CARTESIAN_POINT('Ctrl Pts',(-241.510969010119,3.01396979414861,
134.693318991657));
#135865=CARTESIAN_POINT('Ctrl Pts',(-241.518715343384,3.12133572177857,
134.607683418584));
#135866=CARTESIAN_POINT('Ctrl Pts',(-241.52646167665,3.2249081969094,134.517735118476));
#135867=CARTESIAN_POINT('Ctrl Pts',(-241.534209744653,3.32850386637805,
134.427766675069));
#135868=CARTESIAN_POINT('Ctrl Pts',(-241.541957812655,3.42830409777646,
134.333483839093));
#135869=CARTESIAN_POINT('Ctrl Pts',(-241.549705880658,3.52394337182907,
134.235250615022));
#135870=CARTESIAN_POINT('Ctrl Pts',(-241.5574621834,3.6196842924404,134.136912987511));
#135871=CARTESIAN_POINT('Ctrl Pts',(-241.565218486142,3.71125514848963,
134.034616865484));
#135872=CARTESIAN_POINT('Ctrl Pts',(-241.572974788884,3.79832875406143,
133.928761638333));
#135873=CARTESIAN_POINT('Ctrl Pts',(-241.580735231398,3.8854488334385,133.82284991306));
#135874=CARTESIAN_POINT('Ctrl Pts',(-241.588495673912,3.96806664410421,
133.713375609464));
#135875=CARTESIAN_POINT('Ctrl Pts',(-241.596256116426,4.04589755553098,
133.600768319002));
#135876=CARTESIAN_POINT('Ctrl Pts',(-241.604029016692,4.12385340804606,
133.48798026132));
#135877=CARTESIAN_POINT('Ctrl Pts',(-241.611801916957,4.19700679677301,
133.372049497364));
#135878=CARTESIAN_POINT('Ctrl Pts',(-241.619574817223,4.26511794295314,
133.25343227744));
#135879=CARTESIAN_POINT('Ctrl Pts',(-241.627065152985,4.33075307741003,
133.139127092236));
#135880=CARTESIAN_POINT('Ctrl Pts',(-241.634555488747,4.39170605859743,
133.022327651996));
#135881=CARTESIAN_POINT('Ctrl Pts',(-241.642045824509,4.44780491107956,
132.903459122991));
#135882=CARTESIAN_POINT('Ctrl Pts',(-241.649820158629,4.50603076860302,
132.780083657582));
#135883=CARTESIAN_POINT('Ctrl Pts',(-241.657594492748,4.55921158467241,
132.654088290784));
#135884=CARTESIAN_POINT('Ctrl Pts',(-241.665368826867,4.6071034356103,132.525924149965));
#135885=CARTESIAN_POINT('Ctrl Pts',(-241.673133579814,4.65493626412201,
132.397917959997));
#135886=CARTESIAN_POINT('Ctrl Pts',(-241.680898332761,4.69749296119333,
132.26774867684));
#135887=CARTESIAN_POINT('Ctrl Pts',(-241.688663085708,4.73457607077286,
132.135890749619));
#135888=CARTESIAN_POINT('Ctrl Pts',(-241.696420126593,4.77162234888519,
132.00416378555));
#135889=CARTESIAN_POINT('Ctrl Pts',(-241.704177167478,4.80320575311308,
131.870751889019));
#135890=CARTESIAN_POINT('Ctrl Pts',(-241.711934208363,4.82917753519255,
131.736147822936));
#135891=CARTESIAN_POINT('Ctrl Pts',(-241.719685399603,4.85512973174916,
131.601645262826));
#135892=CARTESIAN_POINT('Ctrl Pts',(-241.727436590843,4.87547865546412,
131.465952704948));
#135893=CARTESIAN_POINT('Ctrl Pts',(-241.735187782084,4.89012595527993,
131.329576005762));
#135894=CARTESIAN_POINT('Ctrl Pts',(-241.742935678861,4.90476702960261,
131.19325727031));
#135895=CARTESIAN_POINT('Ctrl Pts',(-241.750683575638,4.9137112582057,131.056255359802));
#135896=CARTESIAN_POINT('Ctrl Pts',(-241.758431472415,4.91691179603002,
130.919083991648));
#135897=CARTESIAN_POINT('Ctrl Pts',(-241.766177748499,4.92011166437083,
130.781941316788));
#135898=CARTESIAN_POINT('Ctrl Pts',(-241.773924024583,4.91757022258139,
130.644629645399));
#135899=CARTESIAN_POINT('Ctrl Pts',(-241.781670300667,4.90929269943627,
130.507665060198));
#135900=CARTESIAN_POINT('Ctrl Pts',(-241.789416633933,4.90101511518837,
130.370699463956));
#135901=CARTESIAN_POINT('Ctrl Pts',(-241.797162967198,4.88700138867867,
130.234081349268));
#135902=CARTESIAN_POINT('Ctrl Pts',(-241.804909300463,4.8673087890349,130.098323639297));
#135903=CARTESIAN_POINT('Ctrl Pts',(-241.812657368466,4.84761177937007,
129.962535527328));
#135904=CARTESIAN_POINT('Ctrl Pts',(-241.820405436469,4.82223342206145,
129.827608590332));
#135905=CARTESIAN_POINT('Ctrl Pts',(-241.828153504472,4.7912823922847,129.694047103336));
#135906=CARTESIAN_POINT('Ctrl Pts',(-241.835909807214,4.76029846738506,
129.560343665601));
#135907=CARTESIAN_POINT('Ctrl Pts',(-241.843666109956,4.7237301271834,129.428008958308));
#135908=CARTESIAN_POINT('Ctrl Pts',(-241.851422412698,4.68173653730752,
129.297534131955));
#135909=CARTESIAN_POINT('Ctrl Pts',(-241.859182855212,4.63972053418833,
129.166989667258));
#135910=CARTESIAN_POINT('Ctrl Pts',(-241.866943297726,4.59227364681575,
129.038307428135));
#135911=CARTESIAN_POINT('Ctrl Pts',(-241.874703740241,4.53960345289688,
128.911959086985));
#135912=CARTESIAN_POINT('Ctrl Pts',(-241.882476640506,4.4868487081069,128.785407920261));
#135913=CARTESIAN_POINT('Ctrl Pts',(-241.890249540772,4.42885406653741,
128.661198492828));
#135914=CARTESIAN_POINT('Ctrl Pts',(-241.898022441037,4.36587377821813,
128.539779151783));
#135915=CARTESIAN_POINT('Ctrl Pts',(-241.905512776799,4.30518298201941,
128.422773709627));
#135916=CARTESIAN_POINT('Ctrl Pts',(-241.913003112561,4.23986288020815,
128.308359289848));
#135917=CARTESIAN_POINT('Ctrl Pts',(-241.920493448322,4.17017822028657,
128.196910393008));
#135918=CARTESIAN_POINT('Ctrl Pts',(-241.928267782441,4.09785144530113,
128.081235877365));
#135919=CARTESIAN_POINT('Ctrl Pts',(-241.936042116561,4.02059350493841,
127.968389777285));
#135920=CARTESIAN_POINT('Ctrl Pts',(-241.94381645068,3.93865209872679,127.858821158028));
#135921=CARTESIAN_POINT('Ctrl Pts',(-241.951581203627,3.85681167797545,
127.749387572303));
#135922=CARTESIAN_POINT('Ctrl Pts',(-241.959345956574,3.77029950774274,
127.643223740681));
#135923=CARTESIAN_POINT('Ctrl Pts',(-241.967110709521,3.6794080256946,127.540752239872));
#135924=CARTESIAN_POINT('Ctrl Pts',(-241.974867750406,3.58860681834752,
127.438382515202));
#135925=CARTESIAN_POINT('Ctrl Pts',(-241.982624791291,3.49343521282821,
127.339698113895));
#135926=CARTESIAN_POINT('Ctrl Pts',(-241.990381832176,3.39422738245755,
127.245090532468));
#135927=CARTESIAN_POINT('Ctrl Pts',(-241.998133023416,3.2950943654831,127.150554295353));
#135928=CARTESIAN_POINT('Ctrl Pts',(-242.005884214656,3.19193146384553,
127.060089027512));
#135929=CARTESIAN_POINT('Ctrl Pts',(-242.013635405896,3.08511110776185,
126.974050902247));
#135930=CARTESIAN_POINT('Ctrl Pts',(-242.021383302673,2.97833615317946,
126.888049345481));
#135931=CARTESIAN_POINT('Ctrl Pts',(-242.02913119945,2.8679071398086,126.806471433557));
#135932=CARTESIAN_POINT('Ctrl Pts',(-242.036879096228,2.75423095175817,
126.729634255357));
#135933=CARTESIAN_POINT('Ctrl Pts',(-242.044625372312,2.64057854231601,
126.65281314984));
#135934=CARTESIAN_POINT('Ctrl Pts',(-242.052371648396,2.52368063294376,
126.580731024385));
#135935=CARTESIAN_POINT('Ctrl Pts',(-242.06011792448,2.40397424492724,126.513662435192));
#135936=CARTESIAN_POINT('Ctrl Pts',(-242.067864257745,2.28426697326519,
126.446593350914));
#135937=CARTESIAN_POINT('Ctrl Pts',(-242.07561059101,2.16175152266993,126.384538067844));
#135938=CARTESIAN_POINT('Ctrl Pts',(-242.083356924276,2.0368903852876,126.327725651342));
#135939=CARTESIAN_POINT('Ctrl Pts',(-242.091104992279,1.91200128611978,
126.270900512093));
#135940=CARTESIAN_POINT('Ctrl Pts',(-242.098853060282,1.78476581067006,
126.219320737629));
#135941=CARTESIAN_POINT('Ctrl Pts',(-242.106601128285,1.65566696138794,
126.173167469416));
#135942=CARTESIAN_POINT('Ctrl Pts',(-242.114357431026,1.52643090431199,
126.126965148961));
#135943=CARTESIAN_POINT('Ctrl Pts',(-242.122113733768,1.39532788604286,
126.086200987495));
#135944=CARTESIAN_POINT('Ctrl Pts',(-242.12987003651,1.2628571583152,126.051006553309));
#135945=CARTESIAN_POINT('Ctrl Pts',(-242.137630479024,1.13031572697117,
126.015793334793));
#135946=CARTESIAN_POINT('Ctrl Pts',(-242.145390921539,0.996405513147183,
125.98615585142));
#135947=CARTESIAN_POINT('Ctrl Pts',(-242.153151364053,0.861635549012902,
125.96217441264));
#135948=CARTESIAN_POINT('Ctrl Pts',(-242.160924264318,0.726649240168245,
125.938154476725));
#135949=CARTESIAN_POINT('Ctrl Pts',(-242.168697164583,0.590800810709943,
125.919808781659));
#135950=CARTESIAN_POINT('Ctrl Pts',(-242.176470064849,0.454604896099585,
125.907165762249));
#135951=CARTESIAN_POINT('Ctrl Pts',(-242.183960400611,0.323360046039914,
125.89498234844));
#135952=CARTESIAN_POINT('Ctrl Pts',(-242.191450736373,0.191792843727768,
125.888094211437));
#135953=CARTESIAN_POINT('Ctrl Pts',(-242.198941072135,0.0603614695825091,
125.886481038368));
#135954=CARTESIAN_POINT('Ctrl Pts',(-242.206715406254,-0.076053165060172,
125.884806701352));
#135955=CARTESIAN_POINT('Ctrl Pts',(-242.214489740374,-0.212753588922461,
125.888809921125));
#135956=CARTESIAN_POINT('Ctrl Pts',(-242.222264074493,-0.349228103035995,
125.898525031802));
#135957=CARTESIAN_POINT('Ctrl Pts',(-242.23002882744,-0.485534424507592,
125.908228169473));
#135958=CARTESIAN_POINT('Ctrl Pts',(-242.237793580387,-0.621615003955867,
125.923629164255));
#135959=CARTESIAN_POINT('Ctrl Pts',(-242.245558333334,-0.75695624592618,
125.94471039309));
#135960=CARTESIAN_POINT('Ctrl Pts',(-242.253315374219,-0.892163065066992,
125.965770683751));
#135961=CARTESIAN_POINT('Ctrl Pts',(-242.261072415104,-1.02663162425341,
125.992499921468));
#135962=CARTESIAN_POINT('Ctrl Pts',(-242.268829455989,-1.15985191753626,
126.024828570191));
#135963=CARTESIAN_POINT('Ctrl Pts',(-242.276580647229,-1.29297174835875,
126.057132839628));
#135964=CARTESIAN_POINT('Ctrl Pts',(-242.284331838469,-1.42484480853124,
126.095028023496));
#135965=CARTESIAN_POINT('Ctrl Pts',(-242.29208302971,-1.55497013173743,
126.138393306075));
#135966=CARTESIAN_POINT('Ctrl Pts',(-242.299830926487,-1.68504014821093,
126.181740157252));
#135967=CARTESIAN_POINT('Ctrl Pts',(-242.307578823264,-1.81336353502592,
126.230552359667));
#135968=CARTESIAN_POINT('Ctrl Pts',(-242.315326720041,-1.93945358552411,
126.284658984483));
#135969=CARTESIAN_POINT('Ctrl Pts',(-242.323072996125,-2.06551726070193,
126.338754291358));
#135970=CARTESIAN_POINT('Ctrl Pts',(-242.330819272209,-2.18934816972546,
126.398141663723));
#135971=CARTESIAN_POINT('Ctrl Pts',(-242.338565548293,-2.31047910000963,
126.462601827523));
#135972=CARTESIAN_POINT('Ctrl Pts',(-242.346311881559,-2.43161092445432,
126.527062467153));
#135973=CARTESIAN_POINT('Ctrl Pts',(-242.354058214824,-2.55004238525122,
126.596595789273));
#135974=CARTESIAN_POINT('Ctrl Pts',(-242.361804548089,-2.66533077492409,
126.670936501565));
#135975=CARTESIAN_POINT('Ctrl Pts',(-242.369552616092,-2.78064498263262,
126.745293861943));
#135976=CARTESIAN_POINT('Ctrl Pts',(-242.377300684096,-2.89281439008498,
126.824460542932));
#135977=CARTESIAN_POINT('Ctrl Pts',(-242.385048752099,-3.00142552321289,
126.908128092279));
#135978=CARTESIAN_POINT('Ctrl Pts',(-242.39280505484,-3.11015208954572,
126.991884564493));
#135979=CARTESIAN_POINT('Ctrl Pts',(-242.400561357582,-3.21531251683247,
127.080151221801));
#135980=CARTESIAN_POINT('Ctrl Pts',(-242.408317660324,-3.31652625518601,
127.172579145456));
#135981=CARTESIAN_POINT('Ctrl Pts',(-242.416078102838,-3.41779401435919,
127.265056400677));
#135982=CARTESIAN_POINT('Ctrl Pts',(-242.423838545352,-3.51511061000858,
127.361699072403));
#135983=CARTESIAN_POINT('Ctrl Pts',(-242.431598987867,-3.60813333119822,
127.462122306674));
#135984=CARTESIAN_POINT('Ctrl Pts',(-242.439371888132,-3.70130538071808,
127.562706749235));
#135985=CARTESIAN_POINT('Ctrl Pts',(-242.447144788398,-3.79016952795871,
127.667083584065));
#135986=CARTESIAN_POINT('Ctrl Pts',(-242.454917688663,-3.87442367687448,
127.774835203483));
#135987=CARTESIAN_POINT('Ctrl Pts',(-242.462408024425,-3.95561497525035,
127.878669780121));
#135988=CARTESIAN_POINT('Ctrl Pts',(-242.469898360187,-4.03252544654635,
127.985637787295));
#135989=CARTESIAN_POINT('Ctrl Pts',(-242.477388695948,-4.10492452284809,
128.09534276524));
#135990=CARTESIAN_POINT('Ctrl Pts',(-242.485314034205,-4.18152818754758,
128.211418878026));
#135991=CARTESIAN_POINT('Ctrl Pts',(-242.493239372462,-4.25331672785682,
128.330916190021));
#135992=CARTESIAN_POINT('Ctrl Pts',(-242.501164710719,-4.31997667751242,
128.453406647738));
#135993=CARTESIAN_POINT('Ctrl Pts',(-242.509080214655,-4.38655391078081,
128.575745110619));
#135994=CARTESIAN_POINT('Ctrl Pts',(-242.516995718591,-4.44801504155588,
128.701069006151));
#135995=CARTESIAN_POINT('Ctrl Pts',(-242.524911222527,-4.50408923847976,
128.828920617386));
#135996=CARTESIAN_POINT('Ctrl Pts',(-242.532815485652,-4.56008380441048,
128.956590666489));
#135997=CARTESIAN_POINT('Ctrl Pts',(-242.540719748777,-4.61070653017702,
129.086780942342));
#135998=CARTESIAN_POINT('Ctrl Pts',(-242.548624011902,-4.65573231343456,
129.219009019926));
#135999=CARTESIAN_POINT('Ctrl Pts',(-242.555774442768,-4.69646397245246,
129.338626460846));
#136000=CARTESIAN_POINT('Ctrl Pts',(-242.562924873635,-4.73261581172073,
129.459911040772));
#136001=CARTESIAN_POINT('Ctrl Pts',(-242.570075304501,-4.76405452823394,
129.582490119308));
#136002=CARTESIAN_POINT('Origin',(213.235140564004,0.,130.804360617566));
#136003=CARTESIAN_POINT('',(-244.66511323982,-4.76405452823407,129.582490119308));
#136004=CARTESIAN_POINT('',(-244.319729366371,-4.76405452823391,129.582490119308));
#136005=CARTESIAN_POINT('',(213.235140564004,-4.76405452823405,129.582490119308));
#136006=CARTESIAN_POINT('',(-242.985140563976,-4.9182491105998,130.807318418142));
#136007=CARTESIAN_POINT('Ctrl Pts',(-242.985140564014,-4.9182491105994,
130.807318418808));
#136008=CARTESIAN_POINT('Ctrl Pts',(-242.994992025147,-4.91814497261588,
130.98047966355));
#136009=CARTESIAN_POINT('Ctrl Pts',(-243.00484348628,-4.9088965499763,131.15336397321));
#136010=CARTESIAN_POINT('Ctrl Pts',(-243.014694947413,-4.89058692147893,
131.325266200142));
#136011=CARTESIAN_POINT('Ctrl Pts',(-243.022469281532,-4.87613777859409,
131.460923777221));
#136012=CARTESIAN_POINT('Ctrl Pts',(-243.030243615651,-4.85601706382389,
131.596194574106));
#136013=CARTESIAN_POINT('Ctrl Pts',(-243.03801794977,-4.83025111949025,
131.730566418219));
#136014=CARTESIAN_POINT('Ctrl Pts',(-243.045782702718,-4.80451692938022,
131.864772661044));
#136015=CARTESIAN_POINT('Ctrl Pts',(-243.053547455665,-4.77315142546234,
131.998081775163));
#136016=CARTESIAN_POINT('Ctrl Pts',(-243.061312208612,-4.7362327675567,
132.129985841384));
#136017=CARTESIAN_POINT('Ctrl Pts',(-243.069069249497,-4.69935077778265,
132.261758898627));
#136018=CARTESIAN_POINT('Ctrl Pts',(-243.076826290382,-4.6569267147524,
132.392129311046));
#136019=CARTESIAN_POINT('Ctrl Pts',(-243.084583331267,-4.60908986396974,
132.52059885521));
#136020=CARTESIAN_POINT('Ctrl Pts',(-243.092334522507,-4.5612890873283,
132.648971519491));
#136021=CARTESIAN_POINT('Ctrl Pts',(-243.100085713747,-4.5080837834367,
132.775445803825));
#136022=CARTESIAN_POINT('Ctrl Pts',(-243.107836904987,-4.44965309088534,
132.899538517715));
#136023=CARTESIAN_POINT('Ctrl Pts',(-243.115584801765,-4.39124723293692,
133.023578488893));
#136024=CARTESIAN_POINT('Ctrl Pts',(-243.123332698542,-4.32762056979108,
133.145238549903));
#136025=CARTESIAN_POINT('Ctrl Pts',(-243.131080595319,-4.25900031820745,
133.264055588901));
#136026=CARTESIAN_POINT('Ctrl Pts',(-243.138826871403,-4.19039442050118,
133.382847773935));
#136027=CARTESIAN_POINT('Ctrl Pts',(-243.146573147487,-4.11679720743047,
133.498797781499));
#136028=CARTESIAN_POINT('Ctrl Pts',(-243.154319423571,-4.03848160016657,
133.611467567366));
#136029=CARTESIAN_POINT('Ctrl Pts',(-243.162065756837,-3.96016541479474,
133.724138184936));
#136030=CARTESIAN_POINT('Ctrl Pts',(-243.169812090102,-3.87713098887342,
133.833528211463));
#136031=CARTESIAN_POINT('Ctrl Pts',(-243.177558423367,-3.78969404547483,
133.939229371468));
#136032=CARTESIAN_POINT('Ctrl Pts',(-243.18530649137,-3.7022375211789,134.044954202516));
#136033=CARTESIAN_POINT('Ctrl Pts',(-243.193054559373,-3.61037676670409,
134.146988222011));
#136034=CARTESIAN_POINT('Ctrl Pts',(-243.200802627376,-3.51446691024449,
134.244957280835));
#136035=CARTESIAN_POINT('Ctrl Pts',(-243.208558930118,-3.41845511964823,
134.34303046234));
#136036=CARTESIAN_POINT('Ctrl Pts',(-243.21631523286,-3.31838590443326,
134.437029773113));
#136037=CARTESIAN_POINT('Ctrl Pts',(-243.224071535602,-3.21465068741773,
134.526618537214));
#136038=CARTESIAN_POINT('Ctrl Pts',(-243.231831978116,-3.11086010379319,
134.616255117537));
#136039=CARTESIAN_POINT('Ctrl Pts',(-243.23959242063,-3.00339992574493,
134.701476217747));
#136040=CARTESIAN_POINT('Ctrl Pts',(-243.247352863144,-2.89269279067072,
134.781986980273));
#136041=CARTESIAN_POINT('Ctrl Pts',(-243.25512576341,-2.78180793867518,
134.862626985822));
#136042=CARTESIAN_POINT('Ctrl Pts',(-243.262898663675,-2.66766603953724,
134.93854132686));
#136043=CARTESIAN_POINT('Ctrl Pts',(-243.270671563941,-2.5507174581469,
135.009479344927));
#136044=CARTESIAN_POINT('Ctrl Pts',(-243.278161899702,-2.43802025226833,
135.077838587354));
#136045=CARTESIAN_POINT('Ctrl Pts',(-243.285652235464,-2.32271715086915,
135.141576880101));
#136046=CARTESIAN_POINT('Ctrl Pts',(-243.293142571226,-2.20522907084774,
135.200512094436));
#136047=CARTESIAN_POINT('Ctrl Pts',(-243.300916905345,-2.08328639456036,
135.261681855337));
#136048=CARTESIAN_POINT('Ctrl Pts',(-243.308691239464,-1.95860350426506,
135.317870898042));
#136049=CARTESIAN_POINT('Ctrl Pts',(-243.316465573584,-1.83162554392404,
135.368824543302));
#136050=CARTESIAN_POINT('Ctrl Pts',(-243.324230326531,-1.7048040725708,
135.419715392748));
#136051=CARTESIAN_POINT('Ctrl Pts',(-243.331995079478,-1.57569351834008,
135.465383538422));
#136052=CARTESIAN_POINT('Ctrl Pts',(-243.339759832425,-1.44476345532513,
135.505620195664));
#136053=CARTESIAN_POINT('Ctrl Pts',(-243.34751687331,-1.31396343389456,
135.54581688929));
#136054=CARTESIAN_POINT('Ctrl Pts',(-243.355273914195,-1.18134787131098,
135.580592715938));
#136055=CARTESIAN_POINT('Ctrl Pts',(-243.36303095508,-1.0474058190315,135.609787145228));
#136056=CARTESIAN_POINT('Ctrl Pts',(-243.37078214632,-0.913564773495737,
135.638959558772));
#136057=CARTESIAN_POINT('Ctrl Pts',(-243.37853333756,-0.778399609783712,
135.662558869744));
#136058=CARTESIAN_POINT('Ctrl Pts',(-243.3862845288,-0.64241367852652,135.680474616248));
#136059=CARTESIAN_POINT('Ctrl Pts',(-243.394032425577,-0.50648554491747,
135.698382748082));
#136060=CARTESIAN_POINT('Ctrl Pts',(-243.401780322354,-0.369737724399718,
135.710612069065));
#136061=CARTESIAN_POINT('Ctrl Pts',(-243.409528219131,-0.232682662294731,
135.717103419827));
#136062=CARTESIAN_POINT('Ctrl Pts',(-243.417274495216,-0.0956562691541705,
135.723593412738));
#136063=CARTESIAN_POINT('Ctrl Pts',(-243.4250207713,0.0416768474604148,
135.724347804325));
#136064=CARTESIAN_POINT('Ctrl Pts',(-243.432767047384,0.178800627975639,
135.719359437295));
#136065=CARTESIAN_POINT('Ctrl Pts',(-243.440513380649,0.315925420707648,
135.714371033441));
#136066=CARTESIAN_POINT('Ctrl Pts',(-243.448259713914,0.452840483550059,
135.703639800594));
#136067=CARTESIAN_POINT('Ctrl Pts',(-243.45600604718,0.589031666747969,
135.687210682648));
#136068=CARTESIAN_POINT('Ctrl Pts',(-243.463754115183,0.725253349016888,
135.670777885514));
#136069=CARTESIAN_POINT('Ctrl Pts',(-243.471502183186,0.860750440988623,
135.648644710999));
#136070=CARTESIAN_POINT('Ctrl Pts',(-243.479250251189,0.995016204949736,
135.620907701773));
#136071=CARTESIAN_POINT('Ctrl Pts',(-243.487006553931,1.12942466816275,
135.593141213324));
#136072=CARTESIAN_POINT('Ctrl Pts',(-243.494762856672,1.26259880566465,
135.55975907199));
#136073=CARTESIAN_POINT('Ctrl Pts',(-243.502519159414,1.39404378885936,
135.520908611305));
#136074=CARTESIAN_POINT('Ctrl Pts',(-243.510279601928,1.52555892819933,
135.482037414959));
#136075=CARTESIAN_POINT('Ctrl Pts',(-243.518040044443,1.65534270448857,
135.437692210042));
#136076=CARTESIAN_POINT('Ctrl Pts',(-243.525800486957,1.78291859986438,
135.388069195645));
#136077=CARTESIAN_POINT('Ctrl Pts',(-243.533573387222,1.9106992913931,135.338366521981));
#136078=CARTESIAN_POINT('Ctrl Pts',(-243.541346287488,2.03626466106833,
135.283369265211));
#136079=CARTESIAN_POINT('Ctrl Pts',(-243.549119187753,2.1591603896068,135.223320843055));
#136080=CARTESIAN_POINT('Ctrl Pts',(-243.556609523515,2.27758854885757,
135.165455332297));
#136081=CARTESIAN_POINT('Ctrl Pts',(-243.564099859277,2.39353752245083,
135.102899671658));
#136082=CARTESIAN_POINT('Ctrl Pts',(-243.571590195039,2.5066265644634,135.03590954542));
#136083=CARTESIAN_POINT('Ctrl Pts',(-243.579364529158,2.62400341187606,
134.966379468185));
#136084=CARTESIAN_POINT('Ctrl Pts',(-243.587138863278,2.73867099261287,
134.891851771452));
#136085=CARTESIAN_POINT('Ctrl Pts',(-243.594913197397,2.85017442662608,
134.81256330709));
#136086=CARTESIAN_POINT('Ctrl Pts',(-243.602677950344,2.96154044262223,
134.733372558674));
#136087=CARTESIAN_POINT('Ctrl Pts',(-243.610442703291,3.06974975522903,
134.649432941042));
#136088=CARTESIAN_POINT('Ctrl Pts',(-243.618207456238,3.17437289173182,
134.561026666969));
#136089=CARTESIAN_POINT('Ctrl Pts',(-243.625964497123,3.27889211506078,
134.472708199254));
#136090=CARTESIAN_POINT('Ctrl Pts',(-243.633721538008,3.37983195381406,
134.379932154334));
#136091=CARTESIAN_POINT('Ctrl Pts',(-243.641478578893,3.47679300497879,
134.28302321446));
#136092=CARTESIAN_POINT('Ctrl Pts',(-243.649229770133,3.57368093706045,
134.186187354372));
#136093=CARTESIAN_POINT('Ctrl Pts',(-243.656980961373,3.6665957783273,134.085225078089));
#136094=CARTESIAN_POINT('Ctrl Pts',(-243.664732152613,3.75517252074743,
133.980500161403));
#136095=CARTESIAN_POINT('Ctrl Pts',(-243.67248004939,3.84371161568929,133.875819755599));
#136096=CARTESIAN_POINT('Ctrl Pts',(-243.680227946168,3.92791602702597,
133.767380188007));
#136097=CARTESIAN_POINT('Ctrl Pts',(-243.687975842945,4.00745899309027,
133.655580616303));
#136098=CARTESIAN_POINT('Ctrl Pts',(-243.695722119029,4.08698532048081,
133.54380443066));
#136099=CARTESIAN_POINT('Ctrl Pts',(-243.703468395113,4.16185191556661,
133.428669957256));
#136100=CARTESIAN_POINT('Ctrl Pts',(-243.711214671197,4.23177381390916,
133.310607502933));
#136101=CARTESIAN_POINT('Ctrl Pts',(-243.718961004462,4.30169622839919,
133.192544177101));
#136102=CARTESIAN_POINT('Ctrl Pts',(-243.726707337728,4.36667367408318,
133.071553163616));
#136103=CARTESIAN_POINT('Ctrl Pts',(-243.734453670993,4.42646605303072,
132.948091324503));
#136104=CARTESIAN_POINT('Ctrl Pts',(-243.742201738996,4.48627182206704,
132.824601836968));
#136105=CARTESIAN_POINT('Ctrl Pts',(-243.749949806999,4.54089004341501,
132.698640774556));
#136106=CARTESIAN_POINT('Ctrl Pts',(-243.757697875002,4.59012803704497,
132.570686653731));
#136107=CARTESIAN_POINT('Ctrl Pts',(-243.765454177744,4.63941836140043,
132.442596541743));
#136108=CARTESIAN_POINT('Ctrl Pts',(-243.773210480486,4.6833168947433,132.31250950538));
#136109=CARTESIAN_POINT('Ctrl Pts',(-243.780966783228,4.72168012600565,
132.180921495327));
#136110=CARTESIAN_POINT('Ctrl Pts',(-243.788727225742,4.76006383287962,
132.049263252792));
#136111=CARTESIAN_POINT('Ctrl Pts',(-243.796487668256,4.79290625729025,
131.916102819682));
#136112=CARTESIAN_POINT('Ctrl Pts',(-243.80424811077,4.82011489754655,131.781947154375));
#136113=CARTESIAN_POINT('Ctrl Pts',(-243.812021011035,4.84736721552766,
131.647576130483));
#136114=CARTESIAN_POINT('Ctrl Pts',(-243.819793911301,4.86896761521828,
131.512207068113));
#136115=CARTESIAN_POINT('Ctrl Pts',(-243.827566811566,4.88487532016844,
131.376353772166));
#136116=CARTESIAN_POINT('Ctrl Pts',(-243.835057147328,4.9002047399744,131.245439085722));
#136117=CARTESIAN_POINT('Ctrl Pts',(-243.84254748309,4.91024814344905,131.114075067812));
#136118=CARTESIAN_POINT('Ctrl Pts',(-243.850037818852,4.91501484254739,
130.982720254365));
#136119=CARTESIAN_POINT('Ctrl Pts',(-243.857812152971,4.91996227249089,
130.846385083239));
#136120=CARTESIAN_POINT('Ctrl Pts',(-243.86558648709,4.91924063879485,130.709627959486));
#136121=CARTESIAN_POINT('Ctrl Pts',(-243.87336082121,4.91280333786775,130.572959610793));
#136122=CARTESIAN_POINT('Ctrl Pts',(-243.881125574157,4.90637397033873,
130.436459693626));
#136123=CARTESIAN_POINT('Ctrl Pts',(-243.888890327104,4.89424296935481,
130.300048720613));
#136124=CARTESIAN_POINT('Ctrl Pts',(-243.896655080051,4.87641562802379,
130.164240562213));
#136125=CARTESIAN_POINT('Ctrl Pts',(-243.904412120936,4.8586059930595,130.02856729039));
#136126=CARTESIAN_POINT('Ctrl Pts',(-243.912169161821,4.83511132735324,
129.893496026822));
#136127=CARTESIAN_POINT('Ctrl Pts',(-243.919926202706,4.80598890819332,
129.759538299264));
#136128=CARTESIAN_POINT('Ctrl Pts',(-243.927677393946,4.77688845047619,
129.625681590269));
#136129=CARTESIAN_POINT('Ctrl Pts',(-243.935428585186,4.74216876931568,
129.492937126355));
#136130=CARTESIAN_POINT('Ctrl Pts',(-243.943179776426,4.7019386238288,129.361808628816));
#136131=CARTESIAN_POINT('Ctrl Pts',(-243.950927673203,4.66172557722698,
129.230735864386));
#136132=CARTESIAN_POINT('Ctrl Pts',(-243.95867556998,4.61600683897823,129.101278073269));
#136133=CARTESIAN_POINT('Ctrl Pts',(-243.966423466757,4.56494160907855,
128.973925923783));
#136134=CARTESIAN_POINT('Ctrl Pts',(-243.974169742842,4.51388706092413,
128.846600413622));
#136135=CARTESIAN_POINT('Ctrl Pts',(-243.981916018926,4.45748839103371,
128.721380031654));
#136136=CARTESIAN_POINT('Ctrl Pts',(-243.98966229501,4.39595359850137,128.59873711789));
#136137=CARTESIAN_POINT('Ctrl Pts',(-243.997408628275,4.33441835173309,
128.476093298804));
#136138=CARTESIAN_POINT('Ctrl Pts',(-244.005154961541,4.26774708199992,
128.356027335335));
#136139=CARTESIAN_POINT('Ctrl Pts',(-244.012901294806,4.19619438146456,
128.238988173755));
#136140=CARTESIAN_POINT('Ctrl Pts',(-244.020649362809,4.12462565719812,
128.121922802066));
#136141=CARTESIAN_POINT('Ctrl Pts',(-244.028397430812,4.048173530752,128.007885914574));
#136142=CARTESIAN_POINT('Ctrl Pts',(-244.036145498815,3.96713644331463,
127.897298268282));
#136143=CARTESIAN_POINT('Ctrl Pts',(-244.043901801557,3.88601322869649,
127.786593088123));
#136144=CARTESIAN_POINT('Ctrl Pts',(-244.051658104299,3.80029555030125,
127.679344788044));
#136145=CARTESIAN_POINT('Ctrl Pts',(-244.05941440704,3.71032309424963,127.575942181431));
#136146=CARTESIAN_POINT('Ctrl Pts',(-244.067174849555,3.62030261718895,
127.472484385733));
#136147=CARTESIAN_POINT('Ctrl Pts',(-244.074935292069,3.52602310612943,
127.37287665721));
#136148=CARTESIAN_POINT('Ctrl Pts',(-244.082695734583,3.42786108008685,
127.27747084354));
#136149=CARTESIAN_POINT('Ctrl Pts',(-244.090468634848,3.32954147564566,
127.181911875989));
#136150=CARTESIAN_POINT('Ctrl Pts',(-244.098241535114,3.22732719327437,
127.09056856319));
#136151=CARTESIAN_POINT('Ctrl Pts',(-244.106014435379,3.12162847092181,
127.003752935625));
#136152=CARTESIAN_POINT('Ctrl Pts',(-244.113504771141,3.01977216336549,
126.920093274797));
#136153=CARTESIAN_POINT('Ctrl Pts',(-244.120995106903,2.91468059957612,
126.840638014584));
#136154=CARTESIAN_POINT('Ctrl Pts',(-244.128485442665,2.80674459215513,
126.765627170443));
#136155=CARTESIAN_POINT('Ctrl Pts',(-244.136259776785,2.6947161582068,126.687772267348));
#136156=CARTESIAN_POINT('Ctrl Pts',(-244.144034110904,2.57926845619083,
126.614458832348));
#136157=CARTESIAN_POINT('Ctrl Pts',(-244.151808445023,2.46080598539578,
126.546002135153));
#136158=CARTESIAN_POINT('Ctrl Pts',(-244.15957319797,2.34248950900869,126.477629804719));
#136159=CARTESIAN_POINT('Ctrl Pts',(-244.167337950917,2.22116599170592,
126.414102496478));
#136160=CARTESIAN_POINT('Ctrl Pts',(-244.175102703864,2.09727062831025,
126.355693516723));
#136161=CARTESIAN_POINT('Ctrl Pts',(-244.182859744749,1.97349831953612,
126.297342549589));
#136162=CARTESIAN_POINT('Ctrl Pts',(-244.190616785634,1.84715959937641,
126.244099959994));
#136163=CARTESIAN_POINT('Ctrl Pts',(-244.198373826519,1.71871579039075,
126.196194052178));
#136164=CARTESIAN_POINT('Ctrl Pts',(-244.206125017759,1.59036884188042,
126.14832427058));
#136165=CARTESIAN_POINT('Ctrl Pts',(-244.213876208999,1.4599203291283,126.105783296443));
#136166=CARTESIAN_POINT('Ctrl Pts',(-244.221627400239,1.32785283408493,
126.068751901307));
#136167=CARTESIAN_POINT('Ctrl Pts',(-244.229375297016,1.19584147125015,
126.031736245501));
#136168=CARTESIAN_POINT('Ctrl Pts',(-244.237123193793,1.06221287038219,
126.00022561653));
#136169=CARTESIAN_POINT('Ctrl Pts',(-244.244871090571,0.927465896121306,
125.974351293141));
#136170=CARTESIAN_POINT('Ctrl Pts',(-244.252617366655,0.792747108022631,
125.948482382103));
#136171=CARTESIAN_POINT('Ctrl Pts',(-244.260363642739,0.656910795557193,
125.928247505243));
#136172=CARTESIAN_POINT('Ctrl Pts',(-244.268109918823,0.520466780345514,
125.913726978347));
#136173=CARTESIAN_POINT('Ctrl Pts',(-244.275856252088,0.384021757934924,
125.899206344265));
#136174=CARTESIAN_POINT('Ctrl Pts',(-244.283602585354,0.246969412596659,
125.89040018569));
#136175=CARTESIAN_POINT('Ctrl Pts',(-244.291348918619,0.109825068826519,
125.887336973454));
#136176=CARTESIAN_POINT('Ctrl Pts',(-244.299096986622,-0.0273499874683305,
125.884273075232));
#136177=CARTESIAN_POINT('Ctrl Pts',(-244.306845054625,-0.16461669239856,
125.886954691253));
#136178=CARTESIAN_POINT('Ctrl Pts',(-244.314593122628,-0.301459736430147,
125.895358163929));
#136179=CARTESIAN_POINT('Ctrl Pts',(-244.32234942537,-0.438448218877197,
125.903770567916));
#136180=CARTESIAN_POINT('Ctrl Pts',(-244.330105728112,-0.575011750106765,
125.917916952523));
#136181=CARTESIAN_POINT('Ctrl Pts',(-244.337862030853,-0.710639601759831,
125.937721693328));
#136182=CARTESIAN_POINT('Ctrl Pts',(-244.345622473368,-0.846339842081371,
125.957537004519));
#136183=CARTESIAN_POINT('Ctrl Pts',(-244.353382915882,-0.981103023757691,
125.983016616988));
#136184=CARTESIAN_POINT('Ctrl Pts',(-244.361143358396,-1.11442960964777,
126.014033936885));
#136185=CARTESIAN_POINT('Ctrl Pts',(-244.368916258661,-1.2479702232097,
126.045101048539));
#136186=CARTESIAN_POINT('Ctrl Pts',(-244.376689158927,-1.38006925558917,
126.081723527404));
#136187=CARTESIAN_POINT('Ctrl Pts',(-244.384462059192,-1.51024244307228,
126.123724888774));
#136188=CARTESIAN_POINT('Ctrl Pts',(-244.391952394954,-1.63568350730427,
126.164199394864));
#136189=CARTESIAN_POINT('Ctrl Pts',(-244.399442730716,-1.75933602524378,
126.209668394879));
#136190=CARTESIAN_POINT('Ctrl Pts',(-244.406933066479,-1.88078682133141,
126.25993282133));
#136191=CARTESIAN_POINT('Ctrl Pts',(-244.414707789887,-2.00684877333719,
126.312105651141));
#136192=CARTESIAN_POINT('Ctrl Pts',(-244.422482513296,-2.13093785983965,
126.36961051682));
#136193=CARTESIAN_POINT('Ctrl Pts',(-244.430257236704,-2.25257012143072,
126.432277485861));
#136194=CARTESIAN_POINT('Ctrl Pts',(-244.43802228983,-2.37405109553231,
126.494866509066));
#136195=CARTESIAN_POINT('Ctrl Pts',(-244.445787342956,-2.49308098086626,
126.562604682468));
#136196=CARTESIAN_POINT('Ctrl Pts',(-244.453552396082,-2.60919455110486,
126.635273564387));
#136197=CARTESIAN_POINT('Ctrl Pts',(-244.461309648413,-2.72519147332305,
126.707869442942));
#136198=CARTESIAN_POINT('Ctrl Pts',(-244.469066900744,-2.83827758174439,
126.785385965881));
#136199=CARTESIAN_POINT('Ctrl Pts',(-244.476824153076,-2.94801140790485,
126.867558387156));
#136200=CARTESIAN_POINT('Ctrl Pts',(-244.48466953169,-3.05899186544952,
126.950664328412));
#136201=CARTESIAN_POINT('Ctrl Pts',(-244.492514910304,-3.16654303521455,
127.038532436224));
#136202=CARTESIAN_POINT('Ctrl Pts',(-244.500360288919,-3.27023694056918,
127.130842764739));
#136203=CARTESIAN_POINT('Ctrl Pts',(-244.508107844333,-3.37263789753697,
127.222002085489));
#136204=CARTESIAN_POINT('Ctrl Pts',(-244.515855399748,-3.47127693412199,
127.317493210834));
#136205=CARTESIAN_POINT('Ctrl Pts',(-244.523602955162,-3.56577442766546,
127.416966959677));
#136206=CARTESIAN_POINT('Ctrl Pts',(-244.531348784283,-3.66025086547981,
127.516418543992));
#136207=CARTESIAN_POINT('Ctrl Pts',(-244.539094613404,-3.75058732754578,
127.619850702729));
#136208=CARTESIAN_POINT('Ctrl Pts',(-244.546840442525,-3.83644120355387,
127.726877562507));
#136209=CARTESIAN_POINT('Ctrl Pts',(-244.554586223141,-3.9222945419454,
127.833903752083));
#136210=CARTESIAN_POINT('Ctrl Pts',(-244.562332003758,-4.0036651062496,
127.944524292504));
#136211=CARTESIAN_POINT('Ctrl Pts',(-244.570077784374,-4.0802509776755,
128.058320737725));
#136212=CARTESIAN_POINT('Ctrl Pts',(-244.577997405661,-4.15855568673843,
128.174671147657));
#136213=CARTESIAN_POINT('Ctrl Pts',(-244.585917026949,-4.23185812882442,
128.294341367758));
#136214=CARTESIAN_POINT('Ctrl Pts',(-244.593836648236,-4.29988323917117,
128.416854137576));
#136215=CARTESIAN_POINT('Ctrl Pts',(-244.601590724945,-4.36648641433009,
128.536806011609));
#136216=CARTESIAN_POINT('Ctrl Pts',(-244.609344801654,-4.42803057786307,
128.659482391777));
#136217=CARTESIAN_POINT('Ctrl Pts',(-244.617098878363,-4.48430511884091,
128.784412434162));
#136218=CARTESIAN_POINT('Ctrl Pts',(-244.625101271939,-4.54238179800055,
128.913343241289));
#136219=CARTESIAN_POINT('Ctrl Pts',(-244.633103665515,-4.59484552599068,
129.044674046821));
#136220=CARTESIAN_POINT('Ctrl Pts',(-244.641106059091,-4.64151974732242,
129.177868226647));
#136221=CARTESIAN_POINT('Ctrl Pts',(-244.649108452668,-4.68819396865428,
129.311062406474));
#136222=CARTESIAN_POINT('Ctrl Pts',(-244.657110846244,-4.729078601635,129.446119512332));
#136223=CARTESIAN_POINT('Ctrl Pts',(-244.66511323982,-4.76405452823407,
129.582490119308));
#136224=CARTESIAN_POINT('Ctrl Pts',(-242.915000748075,-4.76405452823401,
129.582490119308));
#136225=CARTESIAN_POINT('Ctrl Pts',(-242.922656758014,-4.79771996933577,
129.713751163219));
#136226=CARTESIAN_POINT('Ctrl Pts',(-242.930312767954,-4.82593408241573,
129.846317638161));
#136227=CARTESIAN_POINT('Ctrl Pts',(-242.937968777893,-4.84861868490206,
129.979691040754));
#136228=CARTESIAN_POINT('Ctrl Pts',(-242.94583074224,-4.8719135261307,130.116652322726));
#136229=CARTESIAN_POINT('Ctrl Pts',(-242.953692706587,-4.88937709266357,
130.254464105846));
#136230=CARTESIAN_POINT('Ctrl Pts',(-242.961554670935,-4.90098175486698,
130.392582885093));
#136231=CARTESIAN_POINT('Ctrl Pts',(-242.969416635282,-4.91258641707036,
130.530701664339));
#136232=CARTESIAN_POINT('Ctrl Pts',(-242.977278599629,-4.91833221796005,
130.669126985006));
#136233=CARTESIAN_POINT('Ctrl Pts',(-242.985140563976,-4.9182491105998,
130.807318418143));
#136234=CARTESIAN_POINT('',(-242.639859436042,-4.91824951337863,130.806548459172));
#136235=CARTESIAN_POINT('Ctrl Pts',(-242.570075304501,-4.76405452823394,
129.582490119308));
#136236=CARTESIAN_POINT('Ctrl Pts',(-242.577966389988,-4.79874972412332,
129.717766161507));
#136237=CARTESIAN_POINT('Ctrl Pts',(-242.585857475476,-4.82770399415613,
129.854618717759));
#136238=CARTESIAN_POINT('Ctrl Pts',(-242.593748560963,-4.85078502570779,
129.99253077279));
#136239=CARTESIAN_POINT('Ctrl Pts',(-242.601634899969,-4.8738521740395,
130.130359873843));
#136240=CARTESIAN_POINT('Ctrl Pts',(-242.609521238975,-4.89105305932652,
130.269246839461));
#136241=CARTESIAN_POINT('Ctrl Pts',(-242.617407577981,-4.90230630263031,
130.408663792091));
#136242=CARTESIAN_POINT('Ctrl Pts',(-242.624891530653,-4.91298536933349,
130.540967244216));
#136243=CARTESIAN_POINT('Ctrl Pts',(-242.632375483325,-4.91830858868205,
130.673747625574));
#136244=CARTESIAN_POINT('Ctrl Pts',(-242.639859435997,-4.91824951337898,
130.806548458368));
#136245=CARTESIAN_POINT('Ctrl Pts',(-242.639859436043,-4.91824951337863,
130.806548459173));
#136246=CARTESIAN_POINT('Ctrl Pts',(-242.648321581103,-4.91818271659492,
130.956707066607));
#136247=CARTESIAN_POINT('Ctrl Pts',(-242.656783726164,-4.91123507379679,
131.106641378728));
#136248=CARTESIAN_POINT('Ctrl Pts',(-242.665245871225,-4.89749280632251,
131.255744350679));
#136249=CARTESIAN_POINT('Ctrl Pts',(-242.673747913812,-4.88368574647396,
131.405550316921));
#136250=CARTESIAN_POINT('Ctrl Pts',(-242.682249956398,-4.86301992565743,
131.55451682982));
#136251=CARTESIAN_POINT('Ctrl Pts',(-242.690751998985,-4.83563325073444,
131.702043260203));
#136252=CARTESIAN_POINT('Ctrl Pts',(-242.699274464072,-4.80818079110469,
131.849924059379));
#136253=CARTESIAN_POINT('Ctrl Pts',(-242.707796929159,-4.77397527050883,
131.996357608693));
#136254=CARTESIAN_POINT('Ctrl Pts',(-242.716319394246,-4.73320459872661,
132.140757747574));
#136255=CARTESIAN_POINT('Ctrl Pts',(-242.724871172668,-4.6922936947056,
132.285654556092));
#136256=CARTESIAN_POINT('Ctrl Pts',(-242.73342295109,-4.64477252547405,
132.428503706896));
#136257=CARTESIAN_POINT('Ctrl Pts',(-242.741974729512,-4.5908783944708,
132.568735472771));
#136258=CARTESIAN_POINT('Ctrl Pts',(-242.746595259595,-4.56175936901203,
132.644502764769));
#136259=CARTESIAN_POINT('Ctrl Pts',(-242.751215789678,-4.53078072435257,
132.719506386205));
#136260=CARTESIAN_POINT('Ctrl Pts',(-242.755836319761,-4.49798541549023,
132.793659555518));
#136261=CARTESIAN_POINT('Ctrl Pts',(-242.76361065388,-4.44280523398341,
132.918426953171));
#136262=CARTESIAN_POINT('Ctrl Pts',(-242.771384987999,-4.38234242490538,
133.04109430975));
#136263=CARTESIAN_POINT('Ctrl Pts',(-242.779159322118,-4.31677845701063,
133.161181954789));
#136264=CARTESIAN_POINT('Ctrl Pts',(-242.786924075065,-4.2512952908467,
133.281121602538));
#136265=CARTESIAN_POINT('Ctrl Pts',(-242.794688828012,-4.18072366012136,
133.398487524675));
#136266=CARTESIAN_POINT('Ctrl Pts',(-242.802453580959,-4.10529307782744,
133.512819922714));
#136267=CARTESIAN_POINT('Ctrl Pts',(-242.810210621844,-4.02993741425145,
133.627038764203));
#136268=CARTESIAN_POINT('Ctrl Pts',(-242.817967662728,-3.94973261693294,
133.738229753248));
#136269=CARTESIAN_POINT('Ctrl Pts',(-242.825724703613,-3.86495392257645,
133.845957934579));
#136270=CARTESIAN_POINT('Ctrl Pts',(-242.833475894853,-3.78023916049298,
133.953604877251));
#136271=CARTESIAN_POINT('Ctrl Pts',(-242.841227086093,-3.69095760762414,
134.05779390391));
#136272=CARTESIAN_POINT('Ctrl Pts',(-242.848978277333,-3.59742738293242,
134.158119596239));
#136273=CARTESIAN_POINT('Ctrl Pts',(-242.85672617411,-3.50393691108082,
134.258402647472));
#136274=CARTESIAN_POINT('Ctrl Pts',(-242.864474070887,-3.40620162504394,
134.354825344856));
#136275=CARTESIAN_POINT('Ctrl Pts',(-242.872221967664,-3.30457929525294,
134.447016069827));
#136276=CARTESIAN_POINT('Ctrl Pts',(-242.879968243748,-3.20297822266261,
134.539187510485));
#136277=CARTESIAN_POINT('Ctrl Pts',(-242.887714519832,-3.09749201297154,
134.627128476993));
#136278=CARTESIAN_POINT('Ctrl Pts',(-242.895460795916,-2.98851430437089,
134.710505176472));
#136279=CARTESIAN_POINT('Ctrl Pts',(-242.903207129181,-2.8795357913217,
134.793882491419));
#136280=CARTESIAN_POINT('Ctrl Pts',(-242.910953462446,-2.76706603844406,
134.872695234542));
#136281=CARTESIAN_POINT('Ctrl Pts',(-242.918699795712,-2.65153035236737,
134.946651029038));
#136282=CARTESIAN_POINT('Ctrl Pts',(-242.926447863714,-2.53596879287502,
135.020623385422));
#136283=CARTESIAN_POINT('Ctrl Pts',(-242.934195931717,-2.41734026315914,
135.089736418084));
#136284=CARTESIAN_POINT('Ctrl Pts',(-242.94194399972,-2.29609717318926,
135.15374227865));
#136285=CARTESIAN_POINT('Ctrl Pts',(-242.949700302462,-2.17472522462039,
135.217816165406));
#136286=CARTESIAN_POINT('Ctrl Pts',(-242.957456605203,-2.05073351116927,
135.276771854312));
#136287=CARTESIAN_POINT('Ctrl Pts',(-242.965212907945,-1.92459756228686,
135.330408262669));
#136288=CARTESIAN_POINT('Ctrl Pts',(-242.972973350459,-1.798394290851,135.384073298392));
#136289=CARTESIAN_POINT('Ctrl Pts',(-242.980733792973,-1.6700448692812,
135.432413258767));
#136290=CARTESIAN_POINT('Ctrl Pts',(-242.988494235487,-1.54004178232462,
135.475276413338));
#136291=CARTESIAN_POINT('Ctrl Pts',(-242.996267135752,-1.40983000287137,
135.518208375651));
#136292=CARTESIAN_POINT('Ctrl Pts',(-243.004040036018,-1.27795962959266,
135.555645856396));
#136293=CARTESIAN_POINT('Ctrl Pts',(-243.011812936283,-1.14493605504428,
135.587487679683));
#136294=CARTESIAN_POINT('Ctrl Pts',(-243.019303272046,-1.01674822247133,
135.618171972495));
#136295=CARTESIAN_POINT('Ctrl Pts',(-243.02679360781,-0.887489878722426,
135.643660317534));
#136296=CARTESIAN_POINT('Ctrl Pts',(-243.034283943573,-0.757617450103246,
135.663907804475));
#136297=CARTESIAN_POINT('Ctrl Pts',(-243.042058277692,-0.622820868903974,
135.684922981035));
#136298=CARTESIAN_POINT('Ctrl Pts',(-243.049832611811,-0.486935722498623,
135.70035860991));
#136299=CARTESIAN_POINT('Ctrl Pts',(-243.05760694593,-0.350463659530369,
135.710108092299));
#136300=CARTESIAN_POINT('Ctrl Pts',(-243.065371698877,-0.214159786182866,
135.719845559323));
#136301=CARTESIAN_POINT('Ctrl Pts',(-243.073136451825,-0.0772708216957249,
135.723910795438));
#136302=CARTESIAN_POINT('Ctrl Pts',(-243.080901204772,0.0596923350623777,
135.722248364113));
#136303=CARTESIAN_POINT('Ctrl Pts',(-243.088658245657,0.196519458082346,
135.720587583938));
#136304=CARTESIAN_POINT('Ctrl Pts',(-243.096415286542,0.333420238322542,
135.713210462005));
#136305=CARTESIAN_POINT('Ctrl Pts',(-243.104172327427,0.469879963433971,
135.700113458801));
#136306=CARTESIAN_POINT('Ctrl Pts',(-243.111923518667,0.606236783205005,
135.68702633215));
#136307=CARTESIAN_POINT('Ctrl Pts',(-243.119674709907,0.742152822271439,
135.668227947003));
#136308=CARTESIAN_POINT('Ctrl Pts',(-243.127425901147,0.877115039649322,
135.64376680735));
#136309=CARTESIAN_POINT('Ctrl Pts',(-243.135173797924,1.01201989448477,
135.619316064334));
#136310=CARTESIAN_POINT('Ctrl Pts',(-243.142921694701,1.14597135004838,
135.589207423374));
#136311=CARTESIAN_POINT('Ctrl Pts',(-243.150669591478,1.27846336946034,
135.553541017956));
#136312=CARTESIAN_POINT('Ctrl Pts',(-243.158415867562,1.41092767439804,
135.517882073181));
#136313=CARTESIAN_POINT('Ctrl Pts',(-243.166162143647,1.54193277312165,
135.476667777916));
#136314=CARTESIAN_POINT('Ctrl Pts',(-243.173908419731,1.67098506517296,
135.430048887918));
#136315=CARTESIAN_POINT('Ctrl Pts',(-243.181654752996,1.80003830985915,
135.383429653789));
#136316=CARTESIAN_POINT('Ctrl Pts',(-243.189401086261,1.92713835139993,
135.331405878148));
#136317=CARTESIAN_POINT('Ctrl Pts',(-243.197147419527,2.05180931628837,
135.274177346705));
#136318=CARTESIAN_POINT('Ctrl Pts',(-243.20489548753,2.17650820037481,135.216935999329));
#136319=CARTESIAN_POINT('Ctrl Pts',(-243.212643555533,2.29877657011188,
135.154487739876));
#136320=CARTESIAN_POINT('Ctrl Pts',(-243.220391623536,2.41816136500342,
135.087079225565));
#136321=CARTESIAN_POINT('Ctrl Pts',(-243.228147926278,2.53767304347551,
135.019599068684));
#136322=CARTESIAN_POINT('Ctrl Pts',(-243.235904229019,2.65429468405046,
134.947148318453));
#136323=CARTESIAN_POINT('Ctrl Pts',(-243.243660531761,2.76760007487659,
134.87001836116));
#136324=CARTESIAN_POINT('Ctrl Pts',(-243.251420974275,2.88096594020166,
134.792847237285));
#136325=CARTESIAN_POINT('Ctrl Pts',(-243.25918141679,2.99101171539257,134.710992163223));
#136326=CARTESIAN_POINT('Ctrl Pts',(-243.266941859304,3.09734354528397,
134.624785466321));
#136327=CARTESIAN_POINT('Ctrl Pts',(-243.274714759569,3.20384606846841,
134.538440382777));
#136328=CARTESIAN_POINT('Ctrl Pts',(-243.282487659835,3.3066224391748,134.447729975776));
#136329=CARTESIAN_POINT('Ctrl Pts',(-243.2902605601,3.40531435823856,134.353024758348));
#136330=CARTESIAN_POINT('Ctrl Pts',(-243.297750895862,3.50041857745495,
134.261762314122));
#136331=CARTESIAN_POINT('Ctrl Pts',(-243.305241231624,3.5917299360932,134.166790681836));
#136332=CARTESIAN_POINT('Ctrl Pts',(-243.312731567386,3.67896394025951,
134.068469590742));
#136333=CARTESIAN_POINT('Ctrl Pts',(-243.320505901506,3.76950544820759,
133.966420625596));
#136334=CARTESIAN_POINT('Ctrl Pts',(-243.328280235625,3.85594112075141,
133.860439937901));
#136335=CARTESIAN_POINT('Ctrl Pts',(-243.336054569744,3.9379101199553,133.750891959611));
#136336=CARTESIAN_POINT('Ctrl Pts',(-243.343819322691,4.01977809969345,
133.641478989414));
#136337=CARTESIAN_POINT('Ctrl Pts',(-243.351584075638,4.09719012697526,
133.528507786113));
#136338=CARTESIAN_POINT('Ctrl Pts',(-243.359348828585,4.16982340815775,
133.412378218596));
#136339=CARTESIAN_POINT('Ctrl Pts',(-243.36710586947,4.24238454894141,133.296363992601));
#136340=CARTESIAN_POINT('Ctrl Pts',(-243.374862910355,4.31017618303581,
133.177197974352));
#136341=CARTESIAN_POINT('Ctrl Pts',(-243.38261995124,4.37291711795113,133.055311292732));
#136342=CARTESIAN_POINT('Ctrl Pts',(-243.39037114248,4.4356107394393,132.933516526806));
#136343=CARTESIAN_POINT('Ctrl Pts',(-243.39812233372,4.49326106466692,132.809005527449));
#136344=CARTESIAN_POINT('Ctrl Pts',(-243.405873524961,4.54563159022945,
132.682236148161));
#136345=CARTESIAN_POINT('Ctrl Pts',(-243.413621421738,4.59797985692164,
132.555520649241));
#136346=CARTESIAN_POINT('Ctrl Pts',(-243.421369318515,4.64505263823946,
132.426549040089));
#136347=CARTESIAN_POINT('Ctrl Pts',(-243.429117215292,4.6866606540257,132.29580118846));
#136348=CARTESIAN_POINT('Ctrl Pts',(-243.436863491376,4.72825996631201,
132.165080686462));
#136349=CARTESIAN_POINT('Ctrl Pts',(-243.44460976746,4.76439666829387,132.032585053343));
#136350=CARTESIAN_POINT('Ctrl Pts',(-243.452356043544,4.79493079195341,
131.898811056315));
#136351=CARTESIAN_POINT('Ctrl Pts',(-243.46010237681,4.82546514100888,131.765036071798));
#136352=CARTESIAN_POINT('Ctrl Pts',(-243.467848710075,4.85039674221636,
131.629983085704));
#136353=CARTESIAN_POINT('Ctrl Pts',(-243.47559504334,4.86963645969658,131.494160452949));
#136354=CARTESIAN_POINT('Ctrl Pts',(-243.483343111343,4.88888048577816,
131.358307403656));
#136355=CARTESIAN_POINT('Ctrl Pts',(-243.491091179346,4.90243003688723,
131.221684751758));
#136356=CARTESIAN_POINT('Ctrl Pts',(-243.498839247349,4.91024774246378,
131.084806994133));
#136357=CARTESIAN_POINT('Ctrl Pts',(-243.506595550091,4.91807375679086,
130.947783761198));
#136358=CARTESIAN_POINT('Ctrl Pts',(-243.514351852833,4.92015573408261,
130.810505271877));
#136359=CARTESIAN_POINT('Ctrl Pts',(-243.522108155575,4.91650844795673,
130.673487611678));
#136360=CARTESIAN_POINT('Ctrl Pts',(-243.529868598089,4.91285921516442,
130.536396821028));
#136361=CARTESIAN_POINT('Ctrl Pts',(-243.537629040603,4.90347465260768,
130.399567526749));
#136362=CARTESIAN_POINT('Ctrl Pts',(-243.545389483117,4.88842146835904,
130.263510721397));
#136363=CARTESIAN_POINT('Ctrl Pts',(-243.553162383383,4.87334411940269,
130.127235505581));
#136364=CARTESIAN_POINT('Ctrl Pts',(-243.560935283648,4.85258002375941,
129.991735643419));
#136365=CARTESIAN_POINT('Ctrl Pts',(-243.568708183914,4.82624723508423,
129.857512853487));
#136366=CARTESIAN_POINT('Ctrl Pts',(-243.576198519676,4.8008717096064,129.728169400059));
#136367=CARTESIAN_POINT('Ctrl Pts',(-243.583688855438,4.77032540537688,
129.600012080907));
#136368=CARTESIAN_POINT('Ctrl Pts',(-243.591179191199,4.73475719690355,
129.473474691248));
#136369=CARTESIAN_POINT('Ctrl Pts',(-243.598953525318,4.69784040899436,
129.342139597997));
#136370=CARTESIAN_POINT('Ctrl Pts',(-243.606727859438,4.6553964472259,129.21213366828));
#136371=CARTESIAN_POINT('Ctrl Pts',(-243.614502193557,4.607536876805,129.083957469643));
#136372=CARTESIAN_POINT('Ctrl Pts',(-243.622266946504,4.55973628902731,
128.955939236717));
#136373=CARTESIAN_POINT('Ctrl Pts',(-243.630031699451,4.50653350781934,
128.829746610883));
#136374=CARTESIAN_POINT('Ctrl Pts',(-243.637796452398,4.44809047635236,
128.705867306477));
#136375=CARTESIAN_POINT('Ctrl Pts',(-243.645553493283,4.38970549132814,
128.582111040743));
#136376=CARTESIAN_POINT('Ctrl Pts',(-243.653310534168,4.32609077934927,
128.460663875366));
#136377=CARTESIAN_POINT('Ctrl Pts',(-243.661067575053,4.25745706994627,
128.341995421243));
#136378=CARTESIAN_POINT('Ctrl Pts',(-243.668818766293,4.18887511775732,
128.223416455924));
#136379=CARTESIAN_POINT('Ctrl Pts',(-243.676569957533,4.11528189663663,
128.107612368065));
#136380=CARTESIAN_POINT('Ctrl Pts',(-243.684321148773,4.03693477583397,
127.995029615679));
#136381=CARTESIAN_POINT('Ctrl Pts',(-243.69206904555,3.95862095464774,127.882494713967));
#136382=CARTESIAN_POINT('Ctrl Pts',(-243.699816942327,3.87555747532189,
127.773178744821));
#136383=CARTESIAN_POINT('Ctrl Pts',(-243.707564839105,3.78804575363947,
127.66750033524));
#136384=CARTESIAN_POINT('Ctrl Pts',(-243.715311115189,3.70055233752269,
127.561844031305));
#136385=CARTESIAN_POINT('Ctrl Pts',(-243.723057391273,3.60861277901759,
127.459824074396));
#136386=CARTESIAN_POINT('Ctrl Pts',(-243.730803667357,3.51256936631723,
127.361826738385));
#136387=CARTESIAN_POINT('Ctrl Pts',(-243.738550000622,3.41652524464635,
127.26382867898));
#136388=CARTESIAN_POINT('Ctrl Pts',(-243.746296333887,3.31637748198778,
127.169853578948));
#136389=CARTESIAN_POINT('Ctrl Pts',(-243.754042667153,3.21250559160844,
127.080251209079));
#136390=CARTESIAN_POINT('Ctrl Pts',(-243.761790735156,3.1086104398393,126.990628773379));
#136391=CARTESIAN_POINT('Ctrl Pts',(-243.769538803159,3.00098979678373,
126.905381271743));
#136392=CARTESIAN_POINT('Ctrl Pts',(-243.777286871162,2.89005632353684,
126.824818243211));
#136393=CARTESIAN_POINT('Ctrl Pts',(-243.785043173904,2.77900494887462,
126.744169591334));
#136394=CARTESIAN_POINT('Ctrl Pts',(-243.792799476646,2.66463402746259,
126.668215588183));
#136395=CARTESIAN_POINT('Ctrl Pts',(-243.800555779387,2.54738574215493,
126.597222761117));
#136396=CARTESIAN_POINT('Ctrl Pts',(-243.808316221902,2.4300748779068,126.526192043042));
#136397=CARTESIAN_POINT('Ctrl Pts',(-243.816076664416,2.30988393213108,
126.460127965506));
#136398=CARTESIAN_POINT('Ctrl Pts',(-243.82383710693,2.1872788746784,126.399250609077));
#136399=CARTESIAN_POINT('Ctrl Pts',(-243.831610007195,2.06447700070312,
126.338275526912));
#136400=CARTESIAN_POINT('Ctrl Pts',(-243.839382907461,1.93925362822435,
126.282503963379));
#136401=CARTESIAN_POINT('Ctrl Pts',(-243.847155807726,1.81209467817496,
126.232107787742));
#136402=CARTESIAN_POINT('Ctrl Pts',(-243.854646143488,1.68955827625325,
126.18354364003));
#136403=CARTESIAN_POINT('Ctrl Pts',(-243.86213647925,1.56522487047215,126.139970949475));
#136404=CARTESIAN_POINT('Ctrl Pts',(-243.869626815012,1.43953989534146,
126.101498940648));
#136405=CARTESIAN_POINT('Ctrl Pts',(-243.877401149132,1.30908953617813,
126.061568253914));
#136406=CARTESIAN_POINT('Ctrl Pts',(-243.88517548325,1.17676986745971,126.027006180441));
#136407=CARTESIAN_POINT('Ctrl Pts',(-243.89294981737,1.04306233456069,125.997989426249));
#136408=CARTESIAN_POINT('Ctrl Pts',(-243.900714570317,0.909519584246181,
125.969008432613));
#136409=CARTESIAN_POINT('Ctrl Pts',(-243.908479323264,0.77459275137802,
125.945559242535));
#136410=CARTESIAN_POINT('Ctrl Pts',(-243.916244076211,0.638779698078696,
125.92776923015));
#136411=CARTESIAN_POINT('Ctrl Pts',(-243.924001117096,0.503101536218538,
125.909996887055));
#136412=CARTESIAN_POINT('Ctrl Pts',(-243.931758157981,0.366539290723279,
125.897872586507));
#136413=CARTESIAN_POINT('Ctrl Pts',(-243.939515198866,0.229601962999908,
125.891472871944));
#136414=CARTESIAN_POINT('Ctrl Pts',(-243.947266390106,0.0927679007807761,
125.885077983455));
#136415=CARTESIAN_POINT('Ctrl Pts',(-243.955017581346,-0.0444402917071382,
125.884399106492));
#136416=CARTESIAN_POINT('Ctrl Pts',(-243.962768772587,-0.181507882327065,
125.889461030478));
#136417=CARTESIAN_POINT('Ctrl Pts',(-243.970516669364,-0.318517215564767,
125.894520803012));
#136418=CARTESIAN_POINT('Ctrl Pts',(-243.978264566141,-0.455385675910752,
125.905316509134));
#136419=CARTESIAN_POINT('Ctrl Pts',(-243.986012462918,-0.591598138021364,
125.92182083733));
#136420=CARTESIAN_POINT('Ctrl Pts',(-243.993758739002,-0.727782107421303,
125.938321713175));
#136421=CARTESIAN_POINT('Ctrl Pts',(-244.001505015086,-0.863309963644738,
125.960528788925));
#136422=CARTESIAN_POINT('Ctrl Pts',(-244.00925129117,-0.997671708415375,
125.988362878288));
#136423=CARTESIAN_POINT('Ctrl Pts',(-244.016997624436,-1.13203444501371,
126.016197173117));
#136424=CARTESIAN_POINT('Ctrl Pts',(-244.024743957701,-1.26523067014577,
126.049658485138));
#136425=CARTESIAN_POINT('Ctrl Pts',(-244.032490290966,-1.39676097555051,
126.088616578745));
#136426=CARTESIAN_POINT('Ctrl Pts',(-244.040238358969,-1.52832073625535,
126.127583396747));
#136427=CARTESIAN_POINT('Ctrl Pts',(-244.047986426972,-1.65821346006871,
126.172049334804));
#136428=CARTESIAN_POINT('Ctrl Pts',(-244.055734494975,-1.78595566962713,
126.221834522864));
#136429=CARTESIAN_POINT('Ctrl Pts',(-244.063490797717,-1.9138336451262,
126.271672623214));
#136430=CARTESIAN_POINT('Ctrl Pts',(-244.071247100459,-2.03955617579538,
126.326841124568));
#136431=CARTESIAN_POINT('Ctrl Pts',(-244.079003403201,-2.16266001398518,
126.387112070517));
#136432=CARTESIAN_POINT('Ctrl Pts',(-244.086763845715,-2.28582955640001,
126.447415184884));
#136433=CARTESIAN_POINT('Ctrl Pts',(-244.094524288229,-2.40637727788154,
126.512825983937));
#136434=CARTESIAN_POINT('Ctrl Pts',(-244.102284730743,-2.52386615032989,
126.583071392967));
#136435=CARTESIAN_POINT('Ctrl Pts',(-244.110057631009,-2.64154362634616,
126.653429566162));
#136436=CARTESIAN_POINT('Ctrl Pts',(-244.117830531274,-2.75615211385458,
126.728637643554));
#136437=CARTESIAN_POINT('Ctrl Pts',(-244.12560343154,-2.86728436224317,
126.808379705633));
#136438=CARTESIAN_POINT('Ctrl Pts',(-244.133093767302,-2.97437667347519,
126.885222942895));
#136439=CARTESIAN_POINT('Ctrl Pts',(-244.140584103063,-3.07824085491587,
126.966276054915));
#136440=CARTESIAN_POINT('Ctrl Pts',(-244.148074438825,-3.17854424460739,
127.051223323571));
#136441=CARTESIAN_POINT('Ctrl Pts',(-244.1557363265,-3.28114489291352,127.138116148059));
#136442=CARTESIAN_POINT('Ctrl Pts',(-244.163398214174,-3.38036457420796,
127.229376101691));
#136443=CARTESIAN_POINT('Ctrl Pts',(-244.171060101849,-3.47580053161289,
127.324706363629));
#136444=CARTESIAN_POINT('Ctrl Pts',(-244.178713190564,-3.57112688977339,
127.419927147705));
#136445=CARTESIAN_POINT('Ctrl Pts',(-244.18636627928,-3.6626778796112,127.519208666794));
#136446=CARTESIAN_POINT('Ctrl Pts',(-244.194019367995,-3.75008272512324,
127.622213132418));
#136447=CARTESIAN_POINT('Ctrl Pts',(-244.201665438334,-3.83740741475088,
127.7251231363));
#136448=CARTESIAN_POINT('Ctrl Pts',(-244.209311508673,-3.9205932611194,
127.831748993263));
#136449=CARTESIAN_POINT('Ctrl Pts',(-244.216957579012,-3.99930578937825,
127.941715640356));
#136450=CARTESIAN_POINT('Ctrl Pts',(-244.224598404901,-4.077964328606,128.051606861175));
#136451=CARTESIAN_POINT('Ctrl Pts',(-244.23223923079,-4.15215541853202,
128.164833988209));
#136452=CARTESIAN_POINT('Ctrl Pts',(-244.239880056679,-4.22158476649726,
128.280988841196));
#136453=CARTESIAN_POINT('Ctrl Pts',(-244.247518062277,-4.29098848752677,
128.397100820486));
#136454=CARTESIAN_POINT('Ctrl Pts',(-244.255156067875,-4.35563375322521,
128.516138032661));
#136455=CARTESIAN_POINT('Ctrl Pts',(-244.262794073473,-4.41526978179896,
128.637663634499));
#136456=CARTESIAN_POINT('Ctrl Pts',(-244.270430409274,-4.47489277292685,
128.759162668782));
#136457=CARTESIAN_POINT('Ctrl Pts',(-244.278066745075,-4.52950853128234,
128.883148647215));
#136458=CARTESIAN_POINT('Ctrl Pts',(-244.285703080875,-4.57891271916398,
129.009161081921));
#136459=CARTESIAN_POINT('Ctrl Pts',(-244.293341233457,-4.62832866092438,
129.135203496574));
#136460=CARTESIAN_POINT('Ctrl Pts',(-244.300979386038,-4.67253040905139,
129.263272954891));
#136461=CARTESIAN_POINT('Ctrl Pts',(-244.308617538619,-4.71136226016039,
129.39289020837));
#136462=CARTESIAN_POINT('Ctrl Pts',(-244.312321481203,-4.7301928537381,
129.455745049208));
#136463=CARTESIAN_POINT('Ctrl Pts',(-244.316025423787,-4.74776144086651,
129.518963618944));
#136464=CARTESIAN_POINT('Ctrl Pts',(-244.319729366371,-4.76405452823392,
129.582490119308));
#136465=CARTESIAN_POINT('Origin',(213.235140564004,0.,130.804360617566));
#136466=CARTESIAN_POINT('',(-246.415426335729,-4.76405452823406,129.582490119308));
#136467=CARTESIAN_POINT('',(-246.069808463078,-4.7640545282341,129.582490119308));
#136468=CARTESIAN_POINT('',(213.235140564004,-4.76405452823405,129.582490119308));
#136469=CARTESIAN_POINT('',(-244.735140564058,-4.91824820735174,130.800161405576));
#136470=CARTESIAN_POINT('Ctrl Pts',(-244.735140564058,-4.91824820735175,
130.800161405576));
#136471=CARTESIAN_POINT('Ctrl Pts',(-244.742787207999,-4.91836323324733,
130.934883326289));
#136472=CARTESIAN_POINT('Ctrl Pts',(-244.750433851939,-4.91293859501576,
131.069798656309));
#136473=CARTESIAN_POINT('Ctrl Pts',(-244.75808049588,-4.90195332618797,
131.204406427911));
#136474=CARTESIAN_POINT('Ctrl Pts',(-244.765720186235,-4.89097804697146,
131.338891792012));
#136475=CARTESIAN_POINT('Ctrl Pts',(-244.773359876591,-4.87445222745457,
131.473069754113));
#136476=CARTESIAN_POINT('Ctrl Pts',(-244.780999566946,-4.85240695352329,
131.606439055064));
#136477=CARTESIAN_POINT('Ctrl Pts',(-244.788634580594,-4.83037517481314,
131.739726712746));
#136478=CARTESIAN_POINT('Ctrl Pts',(-244.796269594241,-4.80283072701636,
131.87220629686));
#136479=CARTESIAN_POINT('Ctrl Pts',(-244.803904607888,-4.7698565121021,
132.003381850263));
#136480=CARTESIAN_POINT('Ctrl Pts',(-244.811537183907,-4.73689282485557,
132.134515523285));
#136481=CARTESIAN_POINT('Ctrl Pts',(-244.819169759926,-4.69850291474428,
132.264345602206));
#136482=CARTESIAN_POINT('Ctrl Pts',(-244.826802335945,-4.65482065723309,
132.392386974871));
#136483=CARTESIAN_POINT('Ctrl Pts',(-244.834434241945,-4.61114223432908,
132.520417107541));
#136484=CARTESIAN_POINT('Ctrl Pts',(-244.842066147945,-4.56217251812639,
132.646658464179));
#136485=CARTESIAN_POINT('Ctrl Pts',(-244.849698053946,-4.50809488256194,
132.770642284144));
#136486=CARTESIAN_POINT('Ctrl Pts',(-244.857331056784,-4.45400947509808,
132.894643922746));
#136487=CARTESIAN_POINT('Ctrl Pts',(-244.864964059622,-4.39481485040865,
133.016387009761));
#136488=CARTESIAN_POINT('Ctrl Pts',(-244.87259706246,-4.33074179636042,
133.135424442466));
#136489=CARTESIAN_POINT('Ctrl Pts',(-244.880237608667,-4.26660542166536,
133.254579514752));
#136490=CARTESIAN_POINT('Ctrl Pts',(-244.887878154874,-4.19758117985893,
133.371023236098));
#136491=CARTESIAN_POINT('Ctrl Pts',(-244.895518701081,-4.12394512553602,
133.484334435361));
#136492=CARTESIAN_POINT('Ctrl Pts',(-244.903162983355,-4.05027306471865,
133.597701041437));
#136493=CARTESIAN_POINT('Ctrl Pts',(-244.91080726563,-3.97198493477172,
133.707931746652));
#136494=CARTESIAN_POINT('Ctrl Pts',(-244.918451547904,-3.88939830704602,
133.814636995517));
#136495=CARTESIAN_POINT('Ctrl Pts',(-244.92610796819,-3.8066805437355,133.921511676838));
#136496=CARTESIAN_POINT('Ctrl Pts',(-244.933764388476,-3.71965090705499,
134.024849409731));
#136497=CARTESIAN_POINT('Ctrl Pts',(-244.941420808762,-3.62866566174346,
134.124295643705));
#136498=CARTESIAN_POINT('Ctrl Pts',(-244.948889977209,-3.5399056279364,
134.221309737136));
#136499=CARTESIAN_POINT('Ctrl Pts',(-244.956359145657,-3.44738152776796,
134.314620289459));
#136500=CARTESIAN_POINT('Ctrl Pts',(-244.963828314104,-3.35145398099632,
134.403935491876));
#136501=CARTESIAN_POINT('Ctrl Pts',(-244.971602648223,-3.25160714997087,
134.496899819891));
#136502=CARTESIAN_POINT('Ctrl Pts',(-244.979376982342,-3.14773119990663,
134.585853845381));
#136503=CARTESIAN_POINT('Ctrl Pts',(-244.987151316461,-3.04018179869569,
134.670428088961));
#136504=CARTESIAN_POINT('Ctrl Pts',(-244.994916069408,-2.93276494250978,
134.754898102344));
#136505=CARTESIAN_POINT('Ctrl Pts',(-245.002680822355,-2.82168394733032,
134.834998834259));
#136506=CARTESIAN_POINT('Ctrl Pts',(-245.010445575302,-2.70733082073511,
134.910397988268));
#136507=CARTESIAN_POINT('Ctrl Pts',(-245.018202616187,-2.59309127127702,
134.985722254774));
#136508=CARTESIAN_POINT('Ctrl Pts',(-245.025959657072,-2.47558638219273,
135.056354022414));
#136509=CARTESIAN_POINT('Ctrl Pts',(-245.033716697957,-2.35524041036667,
135.122001833771));
#136510=CARTESIAN_POINT('Ctrl Pts',(-245.041467889198,-2.23498519237462,
135.187600139603));
#136511=CARTESIAN_POINT('Ctrl Pts',(-245.049219080438,-2.11189349795492,
135.248221783632));
#136512=CARTESIAN_POINT('Ctrl Pts',(-245.056970271678,-1.98641737332774,
135.303619343339));
#136513=CARTESIAN_POINT('Ctrl Pts',(-245.064718168455,-1.8609945794009,
135.358993357605));
#136514=CARTESIAN_POINT('Ctrl Pts',(-245.072466065232,-1.73318972784394,
135.409147546131));
#136515=CARTESIAN_POINT('Ctrl Pts',(-245.080213962009,-1.6034780060183,
135.453881167764));
#136516=CARTESIAN_POINT('Ctrl Pts',(-245.087960238093,-1.47379341708825,
135.498605432089));
#136517=CARTESIAN_POINT('Ctrl Pts',(-245.095706514178,-1.34220312064503,
135.537911257458));
#136518=CARTESIAN_POINT('Ctrl Pts',(-245.103452790262,-1.20920038199867,
135.571646795118));
#136519=CARTESIAN_POINT('Ctrl Pts',(-245.111199123527,-1.07619666155649,
135.605382581805));
#136520=CARTESIAN_POINT('Ctrl Pts',(-245.118945456792,-0.941780857070866,
135.633547902612));
#136521=CARTESIAN_POINT('Ctrl Pts',(-245.126691790058,-0.806459038047317,
135.656041448211));
#136522=CARTESIAN_POINT('Ctrl Pts',(-245.134439858061,-0.671106914640469,
135.678540031084));
#136523=CARTESIAN_POINT('Ctrl Pts',(-245.142187926064,-0.534848758556416,
135.695364247193));
#136524=CARTESIAN_POINT('Ctrl Pts',(-245.149935994067,-0.39819802172141,
135.706464390233));
#136525=CARTESIAN_POINT('Ctrl Pts',(-245.157692296809,-0.261402050856946,
135.717576330637));
#136526=CARTESIAN_POINT('Ctrl Pts',(-245.16544859955,-0.124213056063751,
135.722952013597));
#136527=CARTESIAN_POINT('Ctrl Pts',(-245.173204902292,0.0128526712454422,
135.722593823845));
#136528=CARTESIAN_POINT('Ctrl Pts',(-245.180965344807,0.149991554660269,
135.722235442916));
#136529=CARTESIAN_POINT('Ctrl Pts',(-245.188725787321,0.2870066491084,135.716137108664));
#136530=CARTESIAN_POINT('Ctrl Pts',(-245.196486229835,0.423385508378977,
135.70435324754));
#136531=CARTESIAN_POINT('Ctrl Pts',(-245.2042591301,0.559983295101601,135.692550469915));
#136532=CARTESIAN_POINT('Ctrl Pts',(-245.212032030366,0.695942417694476,
135.675043976896));
#136533=CARTESIAN_POINT('Ctrl Pts',(-245.219804930631,0.830758469100371,
135.651939748278));
#136534=CARTESIAN_POINT('Ctrl Pts',(-245.227295266393,0.96067361744886,
135.629675416569));
#136535=CARTESIAN_POINT('Ctrl Pts',(-245.234785602155,1.08952705753159,
135.602213331212));
#136536=CARTESIAN_POINT('Ctrl Pts',(-245.242275937916,1.21688154647621,
135.569691913955));
#136537=CARTESIAN_POINT('Ctrl Pts',(-245.250050272035,1.34906471958535,
135.535937437276));
#136538=CARTESIAN_POINT('Ctrl Pts',(-245.257824606155,1.48005174885979,
135.496625482168));
#136539=CARTESIAN_POINT('Ctrl Pts',(-245.265598940274,1.60933953364511,
135.451855569467));
#136540=CARTESIAN_POINT('Ctrl Pts',(-245.273363693221,1.7384679827901,135.407140831683));
#136541=CARTESIAN_POINT('Ctrl Pts',(-245.281128446168,1.86590098831853,
135.35698164663));
#136542=CARTESIAN_POINT('Ctrl Pts',(-245.288893199115,1.9911470901556,135.301528207046));
#136543=CARTESIAN_POINT('Ctrl Pts',(-245.29665024,2.11626879579832,135.246129844599));
#136544=CARTESIAN_POINT('Ctrl Pts',(-245.304407280885,2.23920756507533,
135.185447849188));
#136545=CARTESIAN_POINT('Ctrl Pts',(-245.31216432177,2.35948886539747,135.119681620292));
#136546=CARTESIAN_POINT('Ctrl Pts',(-245.31991551301,2.47967946065555,135.05396498622));
#136547=CARTESIAN_POINT('Ctrl Pts',(-245.32766670425,2.59721623418635,134.983171936931));
#136548=CARTESIAN_POINT('Ctrl Pts',(-245.33541789549,2.71164668039344,134.907549053796));
#136549=CARTESIAN_POINT('Ctrl Pts',(-245.343165792268,2.82602849060851,
134.831958312404));
#136550=CARTESIAN_POINT('Ctrl Pts',(-245.350913689045,2.9373062739293,134.75154203515));
#136551=CARTESIAN_POINT('Ctrl Pts',(-245.358661585822,3.04505429076332,
134.666591505124));
#136552=CARTESIAN_POINT('Ctrl Pts',(-245.366407861906,3.15277976903499,
134.581658744917));
#136553=CARTESIAN_POINT('Ctrl Pts',(-245.37415413799,3.25697664261577,134.492193860399));
#136554=CARTESIAN_POINT('Ctrl Pts',(-245.381900414074,3.35725053489967,
134.398529771684));
#136555=CARTESIAN_POINT('Ctrl Pts',(-245.389646747339,3.45752516738281,
134.304864991563));
#136556=CARTESIAN_POINT('Ctrl Pts',(-245.397393080605,3.55387647507396,
134.207001212268));
#136557=CARTESIAN_POINT('Ctrl Pts',(-245.40513941387,3.64594568063828,134.105309444242));
#136558=CARTESIAN_POINT('Ctrl Pts',(-245.412887481873,3.73803550446295,
134.00359490305));
#136559=CARTESIAN_POINT('Ctrl Pts',(-245.420635549876,3.82584105561582,
133.898050957066));
#136560=CARTESIAN_POINT('Ctrl Pts',(-245.428383617879,3.90904298146711,
133.789082720466));
#136561=CARTESIAN_POINT('Ctrl Pts',(-245.436139920621,3.99233333531543,
133.679998671128));
#136562=CARTESIAN_POINT('Ctrl Pts',(-245.443896223363,4.07101005234948,
133.567483372362));
#136563=CARTESIAN_POINT('Ctrl Pts',(-245.451652526105,4.14479607079393,
133.451972483764));
#136564=CARTESIAN_POINT('Ctrl Pts',(-245.459412968619,4.21862147105788,
133.336399943527));
#136565=CARTESIAN_POINT('Ctrl Pts',(-245.467173411133,4.28755077506701,
133.217828965476));
#136566=CARTESIAN_POINT('Ctrl Pts',(-245.474933853648,4.35135278364091,
133.096720103947));
#136567=CARTESIAN_POINT('Ctrl Pts',(-245.482706753913,4.41525721286305,
132.975416827722));
#136568=CARTESIAN_POINT('Ctrl Pts',(-245.490479654179,4.47401773122411,
132.851567880226));
#136569=CARTESIAN_POINT('Ctrl Pts',(-245.498252554444,4.52745085819272,
132.72565491807));
#136570=CARTESIAN_POINT('Ctrl Pts',(-245.505742890206,4.57894155640422,
132.604319209249));
#136571=CARTESIAN_POINT('Ctrl Pts',(-245.513233225968,4.62548535801299,
132.481067232852));
#136572=CARTESIAN_POINT('Ctrl Pts',(-245.520723561729,4.66696238070201,
132.356341674027));
#136573=CARTESIAN_POINT('Ctrl Pts',(-245.528497895849,4.71001201731434,
132.226887107725));
#136574=CARTESIAN_POINT('Ctrl Pts',(-245.536272229967,4.74773944496779,
132.095434938267));
#136575=CARTESIAN_POINT('Ctrl Pts',(-245.544046564087,4.77995645516916,
131.962462231928));
#136576=CARTESIAN_POINT('Ctrl Pts',(-245.551811317034,4.81213376078468,
131.829653402564));
#136577=CARTESIAN_POINT('Ctrl Pts',(-245.559576069981,4.83881407003022,
131.695328141197));
#136578=CARTESIAN_POINT('Ctrl Pts',(-245.567340822928,4.85985809813354,
131.559981109947));
#136579=CARTESIAN_POINT('Ctrl Pts',(-245.575097863813,4.88088122501143,
131.424768507277));
#136580=CARTESIAN_POINT('Ctrl Pts',(-245.582854904698,4.89627915140953,
131.288536538118));
#136581=CARTESIAN_POINT('Ctrl Pts',(-245.590611945583,4.90596314130119,
131.151792220467));
#136582=CARTESIAN_POINT('Ctrl Pts',(-245.598363136823,4.91563982842079,
131.015151022768));
#136583=CARTESIAN_POINT('Ctrl Pts',(-245.606114328063,4.9196111281792,130.877998634025));
#136584=CARTESIAN_POINT('Ctrl Pts',(-245.613865519303,4.91783990614071,
130.740849043267));
#136585=CARTESIAN_POINT('Ctrl Pts',(-245.62161341608,4.91606943691884,130.603757744744));
#136586=CARTESIAN_POINT('Ctrl Pts',(-245.629361312857,4.90856130535406,
130.466669631953));
#136587=CARTESIAN_POINT('Ctrl Pts',(-245.637109209634,4.89533045350976,
130.330100337298));
#136588=CARTESIAN_POINT('Ctrl Pts',(-245.644855485718,4.88210236927443,
130.193559609995));
#136589=CARTESIAN_POINT('Ctrl Pts',(-245.652601761802,4.86315398347323,
130.05753787386));
#136590=CARTESIAN_POINT('Ctrl Pts',(-245.660348037887,4.83855222103871,
129.922546880555));
#136591=CARTESIAN_POINT('Ctrl Pts',(-245.668094371152,4.81395027699961,
129.787554890777));
#136592=CARTESIAN_POINT('Ctrl Pts',(-245.675840704417,4.78369494315194,
129.653594043642));
#136593=CARTESIAN_POINT('Ctrl Pts',(-245.683587037682,4.74790443317498,
129.521166728889));
#136594=CARTESIAN_POINT('Ctrl Pts',(-245.691335105685,4.71210590816133,
129.388709757957));
#136595=CARTESIAN_POINT('Ctrl Pts',(-245.699083173688,4.67076984241394,
129.257787380131));
#136596=CARTESIAN_POINT('Ctrl Pts',(-245.706831241691,4.62406445206503,
129.128887249933));
#136597=CARTESIAN_POINT('Ctrl Pts',(-245.714587544433,4.57730942267152,
128.999850123142));
#136598=CARTESIAN_POINT('Ctrl Pts',(-245.722343847175,4.52517380256445,
128.87283990554));
#136599=CARTESIAN_POINT('Ctrl Pts',(-245.730100149917,4.46787436584216,
128.748325181697));
#136600=CARTESIAN_POINT('Ctrl Pts',(-245.737860592431,4.41054434668524,
128.623744000596));
#136601=CARTESIAN_POINT('Ctrl Pts',(-245.745621034945,4.34804519725599,
128.501661315061));
#136602=CARTESIAN_POINT('Ctrl Pts',(-245.753381477459,4.28063942615653,
128.382520580376));
#136603=CARTESIAN_POINT('Ctrl Pts',(-245.761154377725,4.2131254493293,128.263188590408));
#136604=CARTESIAN_POINT('Ctrl Pts',(-245.76892727799,4.140689317697,128.146808320826));
#136605=CARTESIAN_POINT('Ctrl Pts',(-245.776700178256,4.06363708689892,
128.033794486163));
#136606=CARTESIAN_POINT('Ctrl Pts',(-245.784190514018,3.9893858987707,127.92488898905));
#136607=CARTESIAN_POINT('Ctrl Pts',(-245.79168084978,3.91084858201084,127.819109666721));
#136608=CARTESIAN_POINT('Ctrl Pts',(-245.799171185542,3.82833278085045,
127.7167966617));
#136609=CARTESIAN_POINT('Ctrl Pts',(-245.806945519661,3.74268836801147,
127.610604427999));
#136610=CARTESIAN_POINT('Ctrl Pts',(-245.81471985378,3.65248653111821,127.507810166128));
#136611=CARTESIAN_POINT('Ctrl Pts',(-245.8224941879,3.55802690824946,127.408830087196));
#136612=CARTESIAN_POINT('Ctrl Pts',(-245.830258940847,3.46368369842405,
127.309971992366));
#136613=CARTESIAN_POINT('Ctrl Pts',(-245.838023693794,3.36509341059598,
127.214919007726));
#136614=CARTESIAN_POINT('Ctrl Pts',(-245.845788446741,3.26259693119686,
127.124055694459));
#136615=CARTESIAN_POINT('Ctrl Pts',(-245.853545487626,3.16020225274574,
127.033282627916));
#136616=CARTESIAN_POINT('Ctrl Pts',(-245.861302528511,3.05390939413526,
126.946691209363));
#136617=CARTESIAN_POINT('Ctrl Pts',(-245.869059569396,2.94409695997478,
126.864630150546));
#136618=CARTESIAN_POINT('Ctrl Pts',(-245.876810760636,2.83436733622586,
126.782630974612));
#136619=CARTESIAN_POINT('Ctrl Pts',(-245.884561951876,2.7211237317431,126.705155591403));
#136620=CARTESIAN_POINT('Ctrl Pts',(-245.892313143116,2.60477850798382,
126.632513066798));
#136621=CARTESIAN_POINT('Ctrl Pts',(-245.900061039893,2.48848273404778,
126.559901417204));
#136622=CARTESIAN_POINT('Ctrl Pts',(-245.90780893667,2.36908829371289,126.492118747404));
#136623=CARTESIAN_POINT('Ctrl Pts',(-245.915556833448,2.24703707967212,
126.429431198126));
#136624=CARTESIAN_POINT('Ctrl Pts',(-245.923303109532,2.12501139611388,
126.366756761732));
#136625=CARTESIAN_POINT('Ctrl Pts',(-245.931049385616,2.00033039180147,
126.309175504456));
#136626=CARTESIAN_POINT('Ctrl Pts',(-245.9387956617,1.87346079246246,126.256907734731));
#136627=CARTESIAN_POINT('Ctrl Pts',(-245.946541994965,1.74659025660072,
126.204639579177));
#136628=CARTESIAN_POINT('Ctrl Pts',(-245.954288328231,1.61753145496436,
126.157685138366));
#136629=CARTESIAN_POINT('Ctrl Pts',(-245.962034661496,1.4867709596506,126.116216509708));
#136630=CARTESIAN_POINT('Ctrl Pts',(-245.969782729499,1.35598118143071,
126.074738594439));
#136631=CARTESIAN_POINT('Ctrl Pts',(-245.977530797502,1.2234893238255,126.038749054079));
#136632=CARTESIAN_POINT('Ctrl Pts',(-245.985278865505,1.08979658932149,
126.008369952812));
#136633=CARTESIAN_POINT('Ctrl Pts',(-245.993035168247,0.955961764588458,
125.977958564275));
#136634=CARTESIAN_POINT('Ctrl Pts',(-246.000791470989,0.820923895251775,
125.953169613018));
#136635=CARTESIAN_POINT('Ctrl Pts',(-246.008547773731,0.685194386477115,
125.934074002259));
#136636=CARTESIAN_POINT('Ctrl Pts',(-246.016308216245,0.549392434776516,
125.914968199597));
#136637=CARTESIAN_POINT('Ctrl Pts',(-246.024068658759,0.412898496980256,
125.901561830513));
#136638=CARTESIAN_POINT('Ctrl Pts',(-246.031829101273,0.27622755689187,
125.893873737499));
#136639=CARTESIAN_POINT('Ctrl Pts',(-246.039602001539,0.13933722047775,
125.886173302875));
#136640=CARTESIAN_POINT('Ctrl Pts',(-246.047374901804,0.00226970511973851,
125.884209493461));
#136641=CARTESIAN_POINT('Ctrl Pts',(-246.05514780207,-0.134460647553049,
125.887948979312));
#136642=CARTESIAN_POINT('Ctrl Pts',(-246.062638137831,-0.266220507501721,
125.891552525433));
#136643=CARTESIAN_POINT('Ctrl Pts',(-246.070128473593,-0.397666985286885,
125.900451886793));
#136644=CARTESIAN_POINT('Ctrl Pts',(-246.077618809355,-0.528347620148437,
125.91457208893));
#136645=CARTESIAN_POINT('Ctrl Pts',(-246.085393143474,-0.663983051000893,
125.929227662822));
#136646=CARTESIAN_POINT('Ctrl Pts',(-246.093167477593,-0.799223070939665,
125.949554213418));
#136647=CARTESIAN_POINT('Ctrl Pts',(-246.100941811712,-0.933555548070249,
125.975524618988));
#136648=CARTESIAN_POINT('Ctrl Pts',(-246.10870656466,-1.06772247242841,
126.001463018353));
#136649=CARTESIAN_POINT('Ctrl Pts',(-246.116471317607,-1.20098369921872,
126.033031359728));
#136650=CARTESIAN_POINT('Ctrl Pts',(-246.124236070554,-1.33283142878319,
126.070150710417));
#136651=CARTESIAN_POINT('Ctrl Pts',(-246.131993111439,-1.46454820532394,
126.107233193643));
#136652=CARTESIAN_POINT('Ctrl Pts',(-246.139750152324,-1.59485390457379,
126.149855609121));
#136653=CARTESIAN_POINT('Ctrl Pts',(-246.147507193208,-1.72325050042752,
126.197887913286));
#136654=CARTESIAN_POINT('Ctrl Pts',(-246.155258384449,-1.85155027140936,
126.245883995916));
#136655=CARTESIAN_POINT('Ctrl Pts',(-246.163009575689,-1.97794343987086,
126.299281710527));
#136656=CARTESIAN_POINT('Ctrl Pts',(-246.170760766929,-2.10194708849594,
126.357901183402));
#136657=CARTESIAN_POINT('Ctrl Pts',(-246.178508663706,-2.22589803226261,
126.416495741438));
#136658=CARTESIAN_POINT('Ctrl Pts',(-246.186256560483,-2.3474611234418,
126.480307476806));
#136659=CARTESIAN_POINT('Ctrl Pts',(-246.19400445726,-2.46617359650813,
126.549108468235));
#136660=CARTESIAN_POINT('Ctrl Pts',(-246.201750733344,-2.58486123748424,
126.617895067979));
#136661=CARTESIAN_POINT('Ctrl Pts',(-246.209497009428,-2.70069910834935,
126.691668651998));
#136662=CARTESIAN_POINT('Ctrl Pts',(-246.217243285512,-2.8132495807237,
126.770155632807));
#136663=CARTESIAN_POINT('Ctrl Pts',(-246.224989618777,-2.92580088392023,
126.848643192988));
#136664=CARTESIAN_POINT('Ctrl Pts',(-246.232735952043,-3.03506441951327,
126.931843995755));
#136665=CARTESIAN_POINT('Ctrl Pts',(-246.240482285308,-3.14063239297462,
127.019441697074));
#136666=CARTESIAN_POINT('Ctrl Pts',(-246.248230353311,-3.24622400765125,
127.10705901529));
#136667=CARTESIAN_POINT('Ctrl Pts',(-246.255978421314,-3.34811811256095,
127.199074941799));
#136668=CARTESIAN_POINT('Ctrl Pts',(-246.263726489317,-3.44594109946291,
127.295133779425));
#136669=CARTESIAN_POINT('Ctrl Pts',(-246.271482792058,-3.54386805379986,
127.391294709527));
#136670=CARTESIAN_POINT('Ctrl Pts',(-246.2792390948,-3.63771496741181,127.491506859811));
#136671=CARTESIAN_POINT('Ctrl Pts',(-246.286995397542,-3.72714576042953,
127.59537829555));
#136672=CARTESIAN_POINT('Ctrl Pts',(-246.294755840056,-3.81662428535419,
127.699305170601));
#136673=CARTESIAN_POINT('Ctrl Pts',(-246.30251628257,-3.90168175078138,
127.806894916218));
#136674=CARTESIAN_POINT('Ctrl Pts',(-246.310276725084,-3.98202394266324,
127.917724446768));
#136675=CARTESIAN_POINT('Ctrl Pts',(-246.31804962535,-4.06249510696395,
128.02873189072));
#136676=CARTESIAN_POINT('Ctrl Pts',(-246.325822525615,-4.13823565555365,
128.142989186386));
#136677=CARTESIAN_POINT('Ctrl Pts',(-246.33359542588,-4.20899561564361,
128.260045587938));
#136678=CARTESIAN_POINT('Ctrl Pts',(-246.341085761643,-4.2771832729557,
128.372846694454));
#136679=CARTESIAN_POINT('Ctrl Pts',(-246.348576097405,-4.34074602020749,
128.488246661174));
#136680=CARTESIAN_POINT('Ctrl Pts',(-246.356066433168,-4.39950236944441,
128.60582429452));
#136681=CARTESIAN_POINT('Ctrl Pts',(-246.364388978553,-4.46478681045179,
128.736465325959));
#136682=CARTESIAN_POINT('Ctrl Pts',(-246.372711523939,-4.52432198526346,
128.870163383883));
#136683=CARTESIAN_POINT('Ctrl Pts',(-246.381034069324,-4.57783157591476,
129.006405911502));
#136684=CARTESIAN_POINT('Ctrl Pts',(-246.389336263648,-4.63121031994061,
129.142315286227));
#136685=CARTESIAN_POINT('Ctrl Pts',(-246.397638457972,-4.67859274881165,
129.280756439759));
#136686=CARTESIAN_POINT('Ctrl Pts',(-246.405940652296,-4.71974943304564,
129.42119455676));
#136687=CARTESIAN_POINT('Ctrl Pts',(-246.409102546774,-4.7354239749219,
129.474680477381));
#136688=CARTESIAN_POINT('Ctrl Pts',(-246.412264441251,-4.75019596795281,
129.528455803105));
#136689=CARTESIAN_POINT('Ctrl Pts',(-246.415426335729,-4.76405452823406,
129.582490119308));
#136690=CARTESIAN_POINT('Ctrl Pts',(-244.66511323982,-4.76405452823407,
129.582490119308));
#136691=CARTESIAN_POINT('Ctrl Pts',(-244.671869056643,-4.79358206285183,
129.69761752864));
#136692=CARTESIAN_POINT('Ctrl Pts',(-244.678624873467,-4.81889935167107,
129.813680728645));
#136693=CARTESIAN_POINT('Ctrl Pts',(-244.685380690291,-4.83996702755722,
129.930345609309));
#136694=CARTESIAN_POINT('Ctrl Pts',(-244.697240193739,-4.87695029417567,
130.135145057045));
#136695=CARTESIAN_POINT('Ctrl Pts',(-244.709099697187,-4.90094261302808,
130.342356399354));
#136696=CARTESIAN_POINT('Ctrl Pts',(-244.720959200635,-4.91170190698836,
130.550653228263));
#136697=CARTESIAN_POINT('Ctrl Pts',(-244.725686321761,-4.91599049175143,
130.633678992774));
#136698=CARTESIAN_POINT('Ctrl Pts',(-244.730413442888,-4.91817709884299,
130.716876915213));
#136699=CARTESIAN_POINT('Ctrl Pts',(-244.735140564014,-4.91824820735108,
130.800161404793));
#136700=CARTESIAN_POINT('',(-244.389859435961,-4.91824876256771,130.807849457083));
#136701=CARTESIAN_POINT('Ctrl Pts',(-244.319729366371,-4.76405452823392,
129.582490119308));
#136702=CARTESIAN_POINT('Ctrl Pts',(-244.327373776998,-4.79768114295139,
129.713599779736));
#136703=CARTESIAN_POINT('Ctrl Pts',(-244.335018187624,-4.82587144870702,
129.846021477176));
#136704=CARTESIAN_POINT('Ctrl Pts',(-244.342662598251,-4.84854502652125,
129.979258085576));
#136705=CARTESIAN_POINT('Ctrl Pts',(-244.350528737869,-4.87187625994725,
130.116359271677));
#136706=CARTESIAN_POINT('Ctrl Pts',(-244.358394877488,-4.88936580544387,
130.254322902373));
#136707=CARTESIAN_POINT('Ctrl Pts',(-244.366261017106,-4.90098345999153,
130.392603180002));
#136708=CARTESIAN_POINT('Ctrl Pts',(-244.374127156724,-4.91260111453918,
130.53088345763));
#136709=CARTESIAN_POINT('Ctrl Pts',(-244.381993296342,-4.91834691724198,
130.669479921059));
#136710=CARTESIAN_POINT('Ctrl Pts',(-244.389859435961,-4.91824876256771,
130.807849457083));
#136711=CARTESIAN_POINT('Ctrl Pts',(-244.389859435997,-4.91824876256727,
130.807849457707));
#136712=CARTESIAN_POINT('Ctrl Pts',(-244.402080311544,-4.91809626892601,
131.022821090721));
#136713=CARTESIAN_POINT('Ctrl Pts',(-244.414301187091,-4.90384922761825,
131.237299465543));
#136714=CARTESIAN_POINT('Ctrl Pts',(-244.426522062639,-4.8757015042787,
131.449897528729));
#136715=CARTESIAN_POINT('Ctrl Pts',(-244.434296396758,-4.85779527447666,
131.585142206566));
#136716=CARTESIAN_POINT('Ctrl Pts',(-244.442070730877,-4.83422918984339,
131.719855499553));
#136717=CARTESIAN_POINT('Ctrl Pts',(-244.449845064996,-4.80504265405272,
131.853526074124));
#136718=CARTESIAN_POINT('Ctrl Pts',(-244.457609817943,-4.77589208805894,
131.987031911658));
#136719=CARTESIAN_POINT('Ctrl Pts',(-244.46537457089,-4.74113493558406,
132.119497209358));
#136720=CARTESIAN_POINT('Ctrl Pts',(-244.473139323837,-4.70086229238518,
132.250416207967));
#136721=CARTESIAN_POINT('Ctrl Pts',(-244.480896364722,-4.66062964854326,
132.381205175981));
#136722=CARTESIAN_POINT('Ctrl Pts',(-244.488653405607,-4.61489252977729,
132.510450529961));
#136723=CARTESIAN_POINT('Ctrl Pts',(-244.496410446492,-4.56379289345655,
132.637657507907));
#136724=CARTESIAN_POINT('Ctrl Pts',(-244.504161637732,-4.51273179176927,
132.764768558082));
#136725=CARTESIAN_POINT('Ctrl Pts',(-244.511912828972,-4.45631636684135,
132.889843930516));
#136726=CARTESIAN_POINT('Ctrl Pts',(-244.519664020212,-4.39473802927427,
133.012405163437));
#136727=CARTESIAN_POINT('Ctrl Pts',(-244.527411916989,-4.33318586414306,
133.134914304565));
#136728=CARTESIAN_POINT('Ctrl Pts',(-244.535159813766,-4.26647532597446,
133.254911082877));
#136729=CARTESIAN_POINT('Ctrl Pts',(-244.542907710543,-4.19484537550331,
133.371938335595));
#136730=CARTESIAN_POINT('Ctrl Pts',(-244.550653986627,-4.12323040847365,
133.488941108735));
#136731=CARTESIAN_POINT('Ctrl Pts',(-244.558400262711,-4.04669827992298,
133.602975258555));
#136732=CARTESIAN_POINT('Ctrl Pts',(-244.566146538795,-3.96553300042325,
133.713609848047));
#136733=CARTESIAN_POINT('Ctrl Pts',(-244.573892872061,-3.88436712177997,
133.824245254218));
#136734=CARTESIAN_POINT('Ctrl Pts',(-244.581639205326,-3.79856825520651,
133.931480734756));
#136735=CARTESIAN_POINT('Ctrl Pts',(-244.589385538591,-3.70846243958028,
134.034916203951));
#136736=CARTESIAN_POINT('Ctrl Pts',(-244.597133606594,-3.61833644538152,
134.138374836802));
#136737=CARTESIAN_POINT('Ctrl Pts',(-244.604881674597,-3.52390183962061,
134.238031470206));
#136738=CARTESIAN_POINT('Ctrl Pts',(-244.6126297426,-3.42552318260732,134.333521139265));
#136739=CARTESIAN_POINT('Ctrl Pts',(-244.620386045342,-3.32703996758649,
134.429112295881));
#136740=CARTESIAN_POINT('Ctrl Pts',(-244.628142348084,-3.22460460876199,
134.520527368608));
#136741=CARTESIAN_POINT('Ctrl Pts',(-244.635898650826,-3.11861699298481,
134.607439779714));
#136742=CARTESIAN_POINT('Ctrl Pts',(-244.64365909334,-3.01257280842588,
134.694398578591));
#136743=CARTESIAN_POINT('Ctrl Pts',(-244.651419535854,-2.90297290135563,
134.776849692332));
#136744=CARTESIAN_POINT('Ctrl Pts',(-244.659179978368,-2.79024729589318,
134.854509144504));
#136745=CARTESIAN_POINT('Ctrl Pts',(-244.666952878634,-2.67734073328153,
134.932293262524));
#136746=CARTESIAN_POINT('Ctrl Pts',(-244.674725778899,-2.56129877656639,
135.005270139652));
#136747=CARTESIAN_POINT('Ctrl Pts',(-244.682498679164,-2.44257804042975,
135.073200691744));
#136748=CARTESIAN_POINT('Ctrl Pts',(-244.689989014927,-2.3281731020886,
135.138661797162));
#136749=CARTESIAN_POINT('Ctrl Pts',(-244.697479350689,-2.21128103703968,
135.199436958901));
#136750=CARTESIAN_POINT('Ctrl Pts',(-244.704969686451,-2.0923272727801,
135.255354848755));
#136751=CARTESIAN_POINT('Ctrl Pts',(-244.71274402057,-1.968863340396,135.313392882398));
#136752=CARTESIAN_POINT('Ctrl Pts',(-244.720518354689,-1.8427871873494,
135.366381893384));
#136753=CARTESIAN_POINT('Ctrl Pts',(-244.728292688808,-1.71455031169962,
135.414078644859));
#136754=CARTESIAN_POINT('Ctrl Pts',(-244.736057441755,-1.58647147653822,
135.46171661435));
#136755=CARTESIAN_POINT('Ctrl Pts',(-244.743822194702,-1.45623758006734,
135.504075166652));
#136756=CARTESIAN_POINT('Ctrl Pts',(-244.75158694765,-1.32432337135576,
135.54095756797));
#136757=CARTESIAN_POINT('Ctrl Pts',(-244.759343988535,-1.19254018169593,
135.577803337168));
#136758=CARTESIAN_POINT('Ctrl Pts',(-244.767101029419,-1.05908037508984,
135.609183674628));
#136759=CARTESIAN_POINT('Ctrl Pts',(-244.774858070304,-0.924436940245247,
135.634950582157));
#136760=CARTESIAN_POINT('Ctrl Pts',(-244.782609261545,-0.78989504106243,
135.660698058662));
#136761=CARTESIAN_POINT('Ctrl Pts',(-244.790360452785,-0.654171672717092,
135.680840457839));
#136762=CARTESIAN_POINT('Ctrl Pts',(-244.798111644025,-0.517772840756482,
135.695280198573));
#136763=CARTESIAN_POINT('Ctrl Pts',(-244.805859540802,-0.381431981937829,
135.709713802032));
#136764=CARTESIAN_POINT('Ctrl Pts',(-244.813607437579,-0.244416618482797,
135.718449526692));
#136765=CARTESIAN_POINT('Ctrl Pts',(-244.821355334356,-0.107240538498359,
135.721441309339));
#136766=CARTESIAN_POINT('Ctrl Pts',(-244.82910161044,0.0299068472073198,
135.724432466169));
#136767=CARTESIAN_POINT('Ctrl Pts',(-244.836847886524,0.167214491948882,
135.721682062334));
#136768=CARTESIAN_POINT('Ctrl Pts',(-244.844594162608,0.304166321564958,
135.713196111991));
#136769=CARTESIAN_POINT('Ctrl Pts',(-244.852340495874,0.441119162128515,
135.704710099007));
#136770=CARTESIAN_POINT('Ctrl Pts',(-244.860086829139,0.577715792108683,
135.690488479211));
#136771=CARTESIAN_POINT('Ctrl Pts',(-244.867833162404,0.713443376090342,
135.670589302247));
#136772=CARTESIAN_POINT('Ctrl Pts',(-244.875581230407,0.849201355323179,
135.650685669));
#136773=CARTESIAN_POINT('Ctrl Pts',(-244.88332929841,0.984089514536704,
135.62510200525));
#136774=CARTESIAN_POINT('Ctrl Pts',(-244.891077366413,1.11760374467236,
135.593947753468));
#136775=CARTESIAN_POINT('Ctrl Pts',(-244.898833669155,1.25125987532045,
135.562760390576));
#136776=CARTESIAN_POINT('Ctrl Pts',(-244.906589971897,1.38353877858307,
135.525990701823));
#136777=CARTESIAN_POINT('Ctrl Pts',(-244.914346274639,1.51394954675287,
135.483798600101));
#136778=CARTESIAN_POINT('Ctrl Pts',(-244.922106717153,1.64442991907659,
135.441583979183));
#136779=CARTESIAN_POINT('Ctrl Pts',(-244.929867159667,1.77303980310222,
135.393941314291));
#136780=CARTESIAN_POINT('Ctrl Pts',(-244.937627602181,1.89930784287381,
135.341078900697));
#136781=CARTESIAN_POINT('Ctrl Pts',(-244.945400502447,2.02577857931204,
135.288131627664));
#136782=CARTESIAN_POINT('Ctrl Pts',(-244.953173402712,2.14989960493979,
135.229948027648));
#136783=CARTESIAN_POINT('Ctrl Pts',(-244.960946302978,2.27122296010501,
135.166783032692));
#136784=CARTESIAN_POINT('Ctrl Pts',(-244.96843663874,2.38813590571619,135.105914244405));
#136785=CARTESIAN_POINT('Ctrl Pts',(-244.975926974502,2.50245078693436,
135.04042009896));
#136786=CARTESIAN_POINT('Ctrl Pts',(-244.983417310264,2.61379350653377,
134.97056591348));
#136787=CARTESIAN_POINT('Ctrl Pts',(-244.991191644383,2.72935781918755,
134.898063185326));
#136788=CARTESIAN_POINT('Ctrl Pts',(-244.998965978502,2.84208621516031,
134.820633601873));
#136789=CARTESIAN_POINT('Ctrl Pts',(-245.006740312621,2.95153000666685,
134.738525545762));
#136790=CARTESIAN_POINT('Ctrl Pts',(-245.014505065568,3.06083891848163,
134.656518680491));
#136791=CARTESIAN_POINT('Ctrl Pts',(-245.022269818515,3.16687097037143,
134.569845047159));
#136792=CARTESIAN_POINT('Ctrl Pts',(-245.030034571462,3.26920403115723,
134.478797726181));
#136793=CARTESIAN_POINT('Ctrl Pts',(-245.037791612347,3.37143545330441,
134.387840834685));
#136794=CARTESIAN_POINT('Ctrl Pts',(-245.045548653233,3.46997490535372,
134.292519158514));
#136795=CARTESIAN_POINT('Ctrl Pts',(-245.053305694118,3.56443139979751,
134.19316746639));
#136796=CARTESIAN_POINT('Ctrl Pts',(-245.061056885358,3.65881666386421,
134.09389069615));
#136797=CARTESIAN_POINT('Ctrl Pts',(-245.068808076598,3.74912483057287,
133.990590241236));
#136798=CARTESIAN_POINT('Ctrl Pts',(-245.076559267838,3.83500029380863,
133.883639073469));
#136799=CARTESIAN_POINT('Ctrl Pts',(-245.084307164615,3.9208392576816,133.776733362801));
#136800=CARTESIAN_POINT('Ctrl Pts',(-245.092055061392,4.00224902098047,
133.66618032961));
#136801=CARTESIAN_POINT('Ctrl Pts',(-245.099802958169,4.07891311439651,
133.55238734009));
#136802=CARTESIAN_POINT('Ctrl Pts',(-245.107549234253,4.15556117133711,
133.438618153609));
#136803=CARTESIAN_POINT('Ctrl Pts',(-245.115295510337,4.22746531460354,
133.321610682878));
#136804=CARTESIAN_POINT('Ctrl Pts',(-245.123041786421,4.29435165338769,
133.201802366503));
#136805=CARTESIAN_POINT('Ctrl Pts',(-245.130788119687,4.36123848591151,
133.081993165731));
#136806=CARTESIAN_POINT('Ctrl Pts',(-245.138534452952,4.42310724946262,
132.959383419429));
#136807=CARTESIAN_POINT('Ctrl Pts',(-245.146280786218,4.47972958278128,
132.834435967807));
#136808=CARTESIAN_POINT('Ctrl Pts',(-245.154028854221,4.53636459627882,
132.709460535069));
#136809=CARTESIAN_POINT('Ctrl Pts',(-245.161776922224,4.58775068028024,
132.582146711319));
#136810=CARTESIAN_POINT('Ctrl Pts',(-245.169524990227,4.63370742857589,
132.452977774113));
#136811=CARTESIAN_POINT('Ctrl Pts',(-245.177281292968,4.67971302025059,
132.323671554623));
#136812=CARTESIAN_POINT('Ctrl Pts',(-245.18503759571,4.72027761803658,132.192506652054));
#136813=CARTESIAN_POINT('Ctrl Pts',(-245.192793898452,4.75527041357106,
132.059982517787));
#136814=CARTESIAN_POINT('Ctrl Pts',(-245.200554340966,4.79028188581423,
131.9273876514));
#136815=CARTESIAN_POINT('Ctrl Pts',(-245.208314783481,4.81971554631737,
131.793432489437));
#136816=CARTESIAN_POINT('Ctrl Pts',(-245.216075225995,4.84349186038418,
131.658626185696));
#136817=CARTESIAN_POINT('Ctrl Pts',(-245.22384812626,4.86730634230103,131.523603478909));
#136818=CARTESIAN_POINT('Ctrl Pts',(-245.231621026526,4.88544527793848,
131.387727287736));
#136819=CARTESIAN_POINT('Ctrl Pts',(-245.239393926791,4.8978810157106,131.251512290314));
#136820=CARTESIAN_POINT('Ctrl Pts',(-245.246884262553,4.90986468309093,
131.120249051155));
#136821=CARTESIAN_POINT('Ctrl Pts',(-245.254374598315,4.91655258923234,
130.988671518625));
#136822=CARTESIAN_POINT('Ctrl Pts',(-245.261864934077,4.9179657442552,130.857237841703));
#136823=CARTESIAN_POINT('Ctrl Pts',(-245.269639268196,4.91943247948028,
130.720820816971));
#136824=CARTESIAN_POINT('Ctrl Pts',(-245.277413602315,4.91522122956841,
130.584126643625));
#136825=CARTESIAN_POINT('Ctrl Pts',(-245.285187936434,4.90529843916352,
130.447667072292));
#136826=CARTESIAN_POINT('Ctrl Pts',(-245.292952689381,4.895387877711,130.311375675186));
#136827=CARTESIAN_POINT('Ctrl Pts',(-245.300717442328,4.87977980928659,
130.175318691009));
#136828=CARTESIAN_POINT('Ctrl Pts',(-245.308482195276,4.85849263853231,
130.040009687804));
#136829=CARTESIAN_POINT('Ctrl Pts',(-245.31623923616,4.83722661049611,129.904835075409));
#136830=CARTESIAN_POINT('Ctrl Pts',(-245.323996277046,4.81029276547509,
129.770407349285));
#136831=CARTESIAN_POINT('Ctrl Pts',(-245.331753317931,4.77776141558045,
129.63723640897));
#136832=CARTESIAN_POINT('Ctrl Pts',(-245.339504509171,4.74525459782977,
129.504165893897));
#136833=CARTESIAN_POINT('Ctrl Pts',(-245.347255700411,4.70715876949526,
129.37235065645));
#136834=CARTESIAN_POINT('Ctrl Pts',(-245.355006891651,4.66359550854168,
129.242291478504));
#136835=CARTESIAN_POINT('Ctrl Pts',(-245.362754788428,4.62005076313615,
129.112287579179));
#136836=CARTESIAN_POINT('Ctrl Pts',(-245.370502685205,4.57104333089517,
128.984038624823));
#136837=CARTESIAN_POINT('Ctrl Pts',(-245.378250581982,4.5167448811426,128.858031061409));
#136838=CARTESIAN_POINT('Ctrl Pts',(-245.385996858066,4.46245778945517,
128.732049856059));
#136839=CARTESIAN_POINT('Ctrl Pts',(-245.39374313415,4.40288203629706,128.608309467902));
#136840=CARTESIAN_POINT('Ctrl Pts',(-245.401489410235,4.33823760648576,
128.487276775282));
#136841=CARTESIAN_POINT('Ctrl Pts',(-245.4092357435,4.27359269948386,128.366243189226));
#136842=CARTESIAN_POINT('Ctrl Pts',(-245.416982076765,4.20387922535956,
128.247917683451));
#136843=CARTESIAN_POINT('Ctrl Pts',(-245.424728410031,4.12936314985014,
128.132742561189));
#136844=CARTESIAN_POINT('Ctrl Pts',(-245.432476478034,4.05483038698237,
128.017541646257));
#136845=CARTESIAN_POINT('Ctrl Pts',(-245.440224546036,3.97549309492416,
127.905492846907));
#136846=CARTESIAN_POINT('Ctrl Pts',(-245.447972614039,3.89166035480809,
127.797009167317));
#136847=CARTESIAN_POINT('Ctrl Pts',(-245.455728916781,3.8077385162581,127.688410189981));
#136848=CARTESIAN_POINT('Ctrl Pts',(-245.463485219523,3.71931192489257,
127.583384211295));
#136849=CARTESIAN_POINT('Ctrl Pts',(-245.471241522265,3.62673007818832,
127.482311249711));
#136850=CARTESIAN_POINT('Ctrl Pts',(-245.479001964779,3.5340988177649,127.381184342445));
#136851=CARTESIAN_POINT('Ctrl Pts',(-245.486762407293,3.43730815865739,
127.284014933181));
#136852=CARTESIAN_POINT('Ctrl Pts',(-245.494522849808,3.33674347592955,
127.191145146778));
#136853=CARTESIAN_POINT('Ctrl Pts',(-245.502295750073,3.23601735784529,
127.098126277549));
#136854=CARTESIAN_POINT('Ctrl Pts',(-245.510068650338,3.13150540777764,
127.009421076986));
#136855=CARTESIAN_POINT('Ctrl Pts',(-245.517841550604,3.02362569266342,
126.925331005258));
#136856=CARTESIAN_POINT('Ctrl Pts',(-245.525331886366,2.9196676769265,126.844297819447));
#136857=CARTESIAN_POINT('Ctrl Pts',(-245.532822222128,2.81258274897094,
126.767550224307));
#136858=CARTESIAN_POINT('Ctrl Pts',(-245.54031255789,2.702767718989,126.695318184141));
#136859=CARTESIAN_POINT('Ctrl Pts',(-245.548086892009,2.58878901876726,
126.620347444217));
#136860=CARTESIAN_POINT('Ctrl Pts',(-245.555861226128,2.47150805590852,
126.550003948402));
#136861=CARTESIAN_POINT('Ctrl Pts',(-245.563635560247,2.35133724321879,
126.484592541482));
#136862=CARTESIAN_POINT('Ctrl Pts',(-245.571400313194,2.23131453031604,
126.419261748275));
#136863=CARTESIAN_POINT('Ctrl Pts',(-245.579165066141,2.10840939396299,
126.35885113496));
#136864=CARTESIAN_POINT('Ctrl Pts',(-245.586929819088,1.98306386165576,
126.303622813262));
#136865=CARTESIAN_POINT('Ctrl Pts',(-245.594686859973,1.85784282429827,
126.24844934511));
#136866=CARTESIAN_POINT('Ctrl Pts',(-245.602443900858,1.73018656998981,
126.198448082183));
#136867=CARTESIAN_POINT('Ctrl Pts',(-245.610200941743,1.60056209706517,
126.153835482064));
#136868=CARTESIAN_POINT('Ctrl Pts',(-245.617952132983,1.47103537496371,
126.109256524653));
#136869=CARTESIAN_POINT('Ctrl Pts',(-245.625703324224,1.33954375674082,
126.070058268355));
#136870=CARTESIAN_POINT('Ctrl Pts',(-245.633454515464,1.20657428023067,
126.036409111019));
#136871=CARTESIAN_POINT('Ctrl Pts',(-245.641202412241,1.07366131929493,
126.002774255473));
#136872=CARTESIAN_POINT('Ctrl Pts',(-245.648950309018,0.939272127597074,
125.974683903696));
#136873=CARTESIAN_POINT('Ctrl Pts',(-245.656698205795,0.803908757371429,
125.952256561353));
#136874=CARTESIAN_POINT('Ctrl Pts',(-245.664444481879,0.668573702245107,
125.929833910326));
#136875=CARTESIAN_POINT('Ctrl Pts',(-245.672190757963,0.532265259377637,
125.913071976405));
#136876=CARTESIAN_POINT('Ctrl Pts',(-245.679937034047,0.395495133911688,
125.902038039282));
#136877=CARTESIAN_POINT('Ctrl Pts',(-245.687683367313,0.258723998839555,
125.891004020709));
#136878=CARTESIAN_POINT('Ctrl Pts',(-245.695429700578,0.121491564067545,
125.885698114745));
#136879=CARTESIAN_POINT('Ctrl Pts',(-245.703176033843,-0.0156862871894603,
125.886135632585));
#136880=CARTESIAN_POINT('Ctrl Pts',(-245.710924101846,-0.152894858475317,
125.886573248404));
#136881=CARTESIAN_POINT('Ctrl Pts',(-245.718672169849,-0.290048431034229,
125.892756846168));
#136882=CARTESIAN_POINT('Ctrl Pts',(-245.726420237852,-0.426632466852755,
125.904649626015));
#136883=CARTESIAN_POINT('Ctrl Pts',(-245.734176540594,-0.563361665809733,
125.916555045649));
#136884=CARTESIAN_POINT('Ctrl Pts',(-245.741932843336,-0.699519728741003,
125.934181734455));
#136885=CARTESIAN_POINT('Ctrl Pts',(-245.749689146078,-0.834598023437429,
125.957441059561));
#136886=CARTESIAN_POINT('Ctrl Pts',(-245.757449588592,-0.969748413486863,
125.980712798869));
#136887=CARTESIAN_POINT('Ctrl Pts',(-245.765210031106,-1.10381750497173,
126.009623082428));
#136888=CARTESIAN_POINT('Ctrl Pts',(-245.77297047362,-1.23630915392517,
126.044032610126));
#136889=CARTESIAN_POINT('Ctrl Pts',(-245.780743373886,-1.36901349023557,
126.078497375051));
#136890=CARTESIAN_POINT('Ctrl Pts',(-245.788516274151,-1.50013494958879,
126.118478910927));
#136891=CARTESIAN_POINT('Ctrl Pts',(-245.796289174417,-1.62919392961649,
126.163788432781));
#136892=CARTESIAN_POINT('Ctrl Pts',(-245.803779510179,-1.75356129063918,
126.207450839388));
#136893=CARTESIAN_POINT('Ctrl Pts',(-245.81126984594,-1.87601323528946,
126.256060472242));
#136894=CARTESIAN_POINT('Ctrl Pts',(-245.818760181702,-1.99614180248465,
126.309407785013));
#136895=CARTESIAN_POINT('Ctrl Pts',(-245.826535047318,-2.12083360485025,
126.364781562759));
#136896=CARTESIAN_POINT('Ctrl Pts',(-245.834309912933,-2.24341704088224,
126.425435488505));
#136897=CARTESIAN_POINT('Ctrl Pts',(-245.842084778548,-2.36341261905234,
126.491187324664));
#136898=CARTESIAN_POINT('Ctrl Pts',(-245.849849942518,-2.48325846415421,
126.556857114264));
#136899=CARTESIAN_POINT('Ctrl Pts',(-245.857615106489,-2.60052253719137,
126.627611970366));
#136900=CARTESIAN_POINT('Ctrl Pts',(-245.865380270459,-2.71474531852435,
126.703221639422));
#136901=CARTESIAN_POINT('Ctrl Pts',(-245.873137602409,-2.82885289363855,
126.778755047824));
#136902=CARTESIAN_POINT('Ctrl Pts',(-245.880894934358,-2.93992495792657,
126.859133309541));
#136903=CARTESIAN_POINT('Ctrl Pts',(-245.888652266308,-3.0475269302497,
126.944080488883));
#136904=CARTESIAN_POINT('Ctrl Pts',(-245.896403235343,-3.15504064256633,
127.028957990705));
#136905=CARTESIAN_POINT('Ctrl Pts',(-245.904154204378,-3.25908962490112,
127.118396706554));
#136906=CARTESIAN_POINT('Ctrl Pts',(-245.911905173413,-3.35926898284293,
127.212077922202));
#136907=CARTESIAN_POINT('Ctrl Pts',(-245.919652672023,-3.45940348639811,
127.305717192948));
#136908=CARTESIAN_POINT('Ctrl Pts',(-245.927400170633,-3.55567152767521,
127.403594917894));
#136909=CARTESIAN_POINT('Ctrl Pts',(-245.935147669243,-3.64770209393112,
127.505352812721));
#136910=CARTESIAN_POINT('Ctrl Pts',(-245.942893376769,-3.7397113843556,
127.60708718293));
#136911=CARTESIAN_POINT('Ctrl Pts',(-245.950639084294,-3.82748488742137,
127.712699648068));
#136912=CARTESIAN_POINT('Ctrl Pts',(-245.95838479182,-3.91068948471904,
127.82179614775));
#136913=CARTESIAN_POINT('Ctrl Pts',(-245.966130386046,-3.99389286494193,
127.930891051624));
#136914=CARTESIAN_POINT('Ctrl Pts',(-245.973875980271,-4.07252723637829,
128.043469577149));
#136915=CARTESIAN_POINT('Ctrl Pts',(-245.981621574497,-4.14630095147046,
128.159106096289));
#136916=CARTESIAN_POINT('Ctrl Pts',(-245.98937223353,-4.22012290684803,
128.274818229606));
#136917=CARTESIAN_POINT('Ctrl Pts',(-245.997122892564,-4.28907764469264,
128.393592022008));
#136918=CARTESIAN_POINT('Ctrl Pts',(-246.004873551597,-4.35291776099921,
128.514974230676));
#136919=CARTESIAN_POINT('Ctrl Pts',(-246.012626773891,-4.41677899020802,
128.636396582296));
#136920=CARTESIAN_POINT('Ctrl Pts',(-246.020379996186,-4.47552205677387,
128.760428717293));
#136921=CARTESIAN_POINT('Ctrl Pts',(-246.028133218481,-4.52894684272933,
128.886595366491));
#136922=CARTESIAN_POINT('Ctrl Pts',(-246.035895555285,-4.582434433631,129.012910334292));
#136923=CARTESIAN_POINT('Ctrl Pts',(-246.043657892089,-4.63059111254368,
129.141364464471));
#136924=CARTESIAN_POINT('Ctrl Pts',(-246.051420228893,-4.67326578655212,
129.271464681522));
#136925=CARTESIAN_POINT('Ctrl Pts',(-246.057549640288,-4.7069631949169,
129.374196342493));
#136926=CARTESIAN_POINT('Ctrl Pts',(-246.063679051683,-4.7372434144468,
129.477953993567));
#136927=CARTESIAN_POINT('Ctrl Pts',(-246.069808463078,-4.7640545282341,
129.582490119308));
#136928=CARTESIAN_POINT('Origin',(213.235140564004,0.,130.804360617566));
#136929=CARTESIAN_POINT('',(-248.165132725248,-4.76405452823402,129.582490119308));
#136930=CARTESIAN_POINT('',(-247.820142267558,-4.76405452823396,129.582490119308));
#136931=CARTESIAN_POINT('',(213.235140564004,-4.76405452823405,129.582490119308));
#136932=CARTESIAN_POINT('',(-246.485140563968,-4.91824990085616,130.803373081029));
#136933=CARTESIAN_POINT('Ctrl Pts',(-246.485140564014,-4.91824990085632,
130.803373081837));
#136934=CARTESIAN_POINT('Ctrl Pts',(-246.493143038491,-4.91827842866088,
130.94545084961));
#136935=CARTESIAN_POINT('Ctrl Pts',(-246.501145512967,-4.91214612793223,
131.087450398188));
#136936=CARTESIAN_POINT('Ctrl Pts',(-246.509147987444,-4.89989941741298,
131.228823527295));
#136937=CARTESIAN_POINT('Ctrl Pts',(-246.51715723978,-4.88764233429156,
131.370316395269));
#136938=CARTESIAN_POINT('Ctrl Pts',(-246.525166492117,-4.86926054547988,
131.511181434629));
#136939=CARTESIAN_POINT('Ctrl Pts',(-246.533175744453,-4.84485207420658,
131.650877859893));
#136940=CARTESIAN_POINT('Ctrl Pts',(-246.541192936668,-4.8204194058791,
131.790712771583));
#136941=CARTESIAN_POINT('Ctrl Pts',(-246.549210128884,-4.78994820222126,
131.929376412285));
#136942=CARTESIAN_POINT('Ctrl Pts',(-246.557227321099,-4.75358708490067,
132.066340367311));
#136943=CARTESIAN_POINT('Ctrl Pts',(-246.56525935405,-4.71715865901031,
132.203557858218));
#136944=CARTESIAN_POINT('Ctrl Pts',(-246.573291387001,-4.67481862502022,
132.339069035744));
#136945=CARTESIAN_POINT('Ctrl Pts',(-246.581323419953,-4.6267651542245,
132.472361597828));
#136946=CARTESIAN_POINT('Ctrl Pts',(-246.589364048663,-4.57866025733882,
132.605796807574));
#136947=CARTESIAN_POINT('Ctrl Pts',(-246.597404677373,-4.52482986083124,
132.737008340676));
#136948=CARTESIAN_POINT('Ctrl Pts',(-246.605445306083,-4.46551925885111,
132.865506127065));
#136949=CARTESIAN_POINT('Ctrl Pts',(-246.61350054266,-4.40610090393464,
132.994237362675));
#136950=CARTESIAN_POINT('Ctrl Pts',(-246.621555779237,-4.34118261308319,
133.120244688913));
#136951=CARTESIAN_POINT('Ctrl Pts',(-246.629611015813,-4.27105485649333,
133.243063853986));
#136952=CARTESIAN_POINT('Ctrl Pts',(-246.631245362869,-4.25682646091178,
133.267982940958));
#136953=CARTESIAN_POINT('Ctrl Pts',(-246.632879709925,-4.24238375381644,
133.292770887925));
#136954=CARTESIAN_POINT('Ctrl Pts',(-246.634514056981,-4.22772936886875,
133.317423976518));
#136955=CARTESIAN_POINT('Ctrl Pts',(-246.6422883911,-4.15802074456785,133.434694875069));
#136956=CARTESIAN_POINT('Ctrl Pts',(-246.650062725219,-4.08331862959862,
133.549248904555));
#136957=CARTESIAN_POINT('Ctrl Pts',(-246.657837059338,-4.00386056780575,
133.660631545904));
#136958=CARTESIAN_POINT('Ctrl Pts',(-246.665601812285,-3.92450043097288,
133.771876918102));
#136959=CARTESIAN_POINT('Ctrl Pts',(-246.673366565232,-3.84039623438855,
133.879958363595));
#136960=CARTESIAN_POINT('Ctrl Pts',(-246.681131318179,-3.75183084408561,
133.984446839647));
#136961=CARTESIAN_POINT('Ctrl Pts',(-246.688888359064,-3.66335341817663,
134.088831536271));
#136962=CARTESIAN_POINT('Ctrl Pts',(-246.696645399949,-3.57042386743871,
134.189630068791));
#136963=CARTESIAN_POINT('Ctrl Pts',(-246.704402440834,-3.47336748156961,
134.286443528767));
#136964=CARTESIAN_POINT('Ctrl Pts',(-246.712153632074,-3.37638428667622,
134.383183980959));
#136965=CARTESIAN_POINT('Ctrl Pts',(-246.719904823314,-3.27528072673547,
134.475945067235));
#136966=CARTESIAN_POINT('Ctrl Pts',(-246.727656014554,-3.17042113259532,
134.564362333589));
#136967=CARTESIAN_POINT('Ctrl Pts',(-246.735403911332,-3.06560610657977,
134.652742020246));
#136968=CARTESIAN_POINT('Ctrl Pts',(-246.743151808109,-2.9570385197791,
134.736781307513));
#136969=CARTESIAN_POINT('Ctrl Pts',(-246.750899704886,-2.84511802668416,
134.816154041552));
#136970=CARTESIAN_POINT('Ctrl Pts',(-246.75864598097,-2.73322094494365,
134.895510172526));
#136971=CARTESIAN_POINT('Ctrl Pts',(-246.766392257054,-2.61797267065027,
134.970201465848));
#136972=CARTESIAN_POINT('Ctrl Pts',(-246.774138533138,-2.49980394381585,
135.039943612265));
#136973=CARTESIAN_POINT('Ctrl Pts',(-246.781884866404,-2.3816343446869,
135.109686273502));
#136974=CARTESIAN_POINT('Ctrl Pts',(-246.789631199669,-2.26054458669738,
135.174479516217));
#136975=CARTESIAN_POINT('Ctrl Pts',(-246.797377532934,-2.13699189672926,
135.234083938024));
#136976=CARTESIAN_POINT('Ctrl Pts',(-246.805125600937,-2.01341153799237,
135.293701707829));
#136977=CARTESIAN_POINT('Ctrl Pts',(-246.81287366894,-1.88736750180669,
135.348128174635));
#136978=CARTESIAN_POINT('Ctrl Pts',(-246.820621736943,-1.7593385973053,
135.397171386859));
#136979=CARTESIAN_POINT('Ctrl Pts',(-246.828378039685,-1.63117362216117,
135.446266722791));
#136980=CARTESIAN_POINT('Ctrl Pts',(-246.836134342427,-1.50101993034195,
135.489967234976));
#136981=CARTESIAN_POINT('Ctrl Pts',(-246.843890645169,-1.369373690359,135.528130167264));
#136982=CARTESIAN_POINT('Ctrl Pts',(-246.851651087683,-1.23765718681399,
135.566313468257));
#136983=CARTESIAN_POINT('Ctrl Pts',(-246.859411530197,-1.10444692732322,
135.598953207126));
#136984=CARTESIAN_POINT('Ctrl Pts',(-246.867171972711,-0.970250010447131,
135.62595765379));
#136985=CARTESIAN_POINT('Ctrl Pts',(-246.874944872977,-0.835837668766627,
135.65300545039));
#136986=CARTESIAN_POINT('Ctrl Pts',(-246.882717773242,-0.700435891020341,
135.674399816399));
#136987=CARTESIAN_POINT('Ctrl Pts',(-246.890490673508,-0.564558543570453,
135.690100757338));
#136988=CARTESIAN_POINT('Ctrl Pts',(-246.89798100927,-0.433620679952551,
135.705230929527));
#136989=CARTESIAN_POINT('Ctrl Pts',(-246.905471345032,-0.302241529806322,
135.715074407698));
#136990=CARTESIAN_POINT('Ctrl Pts',(-246.912961680794,-0.170879614357212,
135.719641201612));
#136991=CARTESIAN_POINT('Ctrl Pts',(-246.920736014913,-0.0345370719589941,
135.724381146904));
#136992=CARTESIAN_POINT('Ctrl Pts',(-246.928510349032,0.102218795228362,
135.723451392982));
#136993=CARTESIAN_POINT('Ctrl Pts',(-246.936284683151,0.238877189185913,
135.716806113547));
#136994=CARTESIAN_POINT('Ctrl Pts',(-246.944049436098,0.375367163886053,
135.710169023826));
#136995=CARTESIAN_POINT('Ctrl Pts',(-246.951814189045,0.511759517618411,
135.69783044261));
#136996=CARTESIAN_POINT('Ctrl Pts',(-246.959578941993,0.647540388576628,
135.679796445024));
#136997=CARTESIAN_POINT('Ctrl Pts',(-246.967335982878,0.783186400060004,
135.661780359059));
#136998=CARTESIAN_POINT('Ctrl Pts',(-246.975093023763,0.918221752336038,
135.638080165089));
#136999=CARTESIAN_POINT('Ctrl Pts',(-246.982850064648,1.05213500540984,
135.608753918795));
#137000=CARTESIAN_POINT('Ctrl Pts',(-246.990601255888,1.18594727345799,
135.579449787651));
#137001=CARTESIAN_POINT('Ctrl Pts',(-246.998352447128,1.31863874621221,
135.544528132218));
#137002=CARTESIAN_POINT('Ctrl Pts',(-247.006103638368,1.44970586847414,
135.504098478065));
#137003=CARTESIAN_POINT('Ctrl Pts',(-247.013851535145,1.5807172837126,135.463686007595));
#137004=CARTESIAN_POINT('Ctrl Pts',(-247.021599431922,1.71010534878347,
135.417770309567));
#137005=CARTESIAN_POINT('Ctrl Pts',(-247.029347328699,1.83737963821065,
135.366511330507));
#137006=CARTESIAN_POINT('Ctrl Pts',(-247.037093604784,1.96462730460019,
135.315263073721));
#137007=CARTESIAN_POINT('Ctrl Pts',(-247.044839880868,2.08976171239102,
135.258673905034));
#137008=CARTESIAN_POINT('Ctrl Pts',(-247.052586156952,2.21231083865722,
135.19695254212));
#137009=CARTESIAN_POINT('Ctrl Pts',(-247.060332490217,2.33486086955307,
135.135230723594));
#137010=CARTESIAN_POINT('Ctrl Pts',(-247.068078823482,2.45482523166445,
135.068376811107));
#137011=CARTESIAN_POINT('Ctrl Pts',(-247.075825156748,2.57175536668559,
134.996646079748));
#137012=CARTESIAN_POINT('Ctrl Pts',(-247.083573224751,2.68871168739957,
134.924899284789));
#137013=CARTESIAN_POINT('Ctrl Pts',(-247.091321292754,2.80263209571617,
134.848273702143));
#137014=CARTESIAN_POINT('Ctrl Pts',(-247.099069360757,2.9130962892978,134.767068412973));
#137015=CARTESIAN_POINT('Ctrl Pts',(-247.106825663499,3.02367788553906,
134.685776817855));
#137016=CARTESIAN_POINT('Ctrl Pts',(-247.11458196624,3.1307956137118,134.599896025063));
#137017=CARTESIAN_POINT('Ctrl Pts',(-247.122338268982,3.23406117782463,
134.509766312033));
#137018=CARTESIAN_POINT('Ctrl Pts',(-247.130098711496,3.3373818578783,134.419588494061));
#137019=CARTESIAN_POINT('Ctrl Pts',(-247.137859154011,3.43684599369009,
134.325157506169));
#137020=CARTESIAN_POINT('Ctrl Pts',(-247.145619596525,3.53210231098769,
134.226850402389));
#137021=CARTESIAN_POINT('Ctrl Pts',(-247.15339249679,3.62751154218227,134.128385487318));
#137022=CARTESIAN_POINT('Ctrl Pts',(-247.161165397056,3.71869919646961,
134.026032314337));
#137023=CARTESIAN_POINT('Ctrl Pts',(-247.168938297321,3.80535386804103,
133.920201595775));
#137024=CARTESIAN_POINT('Ctrl Pts',(-247.176428633083,3.88885842402971,
133.818218090406));
#137025=CARTESIAN_POINT('Ctrl Pts',(-247.183918968845,3.9681536607632,133.713005730932));
#137026=CARTESIAN_POINT('Ctrl Pts',(-247.191409304607,4.04300015781193,
133.604955694765));
#137027=CARTESIAN_POINT('Ctrl Pts',(-247.199183638726,4.12068448254636,
133.492808908635));
#137028=CARTESIAN_POINT('Ctrl Pts',(-247.206957972845,4.19382214090159,
133.377249769737));
#137029=CARTESIAN_POINT('Ctrl Pts',(-247.214732306964,4.26209847910996,
133.25868325668));
#137030=CARTESIAN_POINT('Ctrl Pts',(-247.222497059911,4.3302906728337,133.140262866253));
#137031=CARTESIAN_POINT('Ctrl Pts',(-247.230261812858,4.39363327377075,
133.018842811692));
#137032=CARTESIAN_POINT('Ctrl Pts',(-247.238026565806,4.45185363823772,
132.894858703241));
#137033=CARTESIAN_POINT('Ctrl Pts',(-247.245783606691,4.51001617741795,
132.770997737554));
#137034=CARTESIAN_POINT('Ctrl Pts',(-247.253540647576,4.56306643933374,
132.644578137534));
#137035=CARTESIAN_POINT('Ctrl Pts',(-247.261297688461,4.61077682206316,
132.516061572647));
#137036=CARTESIAN_POINT('Ctrl Pts',(-247.269048879701,4.65845122602164,
132.387641923102));
#137037=CARTESIAN_POINT('Ctrl Pts',(-247.276800070941,4.70079363046617,
132.257128821287));
#137038=CARTESIAN_POINT('Ctrl Pts',(-247.284551262181,4.73762399847527,
132.125005123696));
#137039=CARTESIAN_POINT('Ctrl Pts',(-247.292299158958,4.77443871259552,
131.992937582201));
#137040=CARTESIAN_POINT('Ctrl Pts',(-247.300047055735,4.80574594509449,
131.85926118226));
#137041=CARTESIAN_POINT('Ctrl Pts',(-247.307794952512,4.8314151765647,131.724474987718));
#137042=CARTESIAN_POINT('Ctrl Pts',(-247.315541228596,4.85707903858505,
131.589716987543));
#137043=CARTESIAN_POINT('Ctrl Pts',(-247.32328750468,4.87710717226894,131.453850038335));
#137044=CARTESIAN_POINT('Ctrl Pts',(-247.331033780764,4.89142003778569,
131.317384083354));
#137045=CARTESIAN_POINT('Ctrl Pts',(-247.33878011403,4.90573300895675,131.180917121011));
#137046=CARTESIAN_POINT('Ctrl Pts',(-247.346526447295,4.91433058699434,
131.043851532903));
#137047=CARTESIAN_POINT('Ctrl Pts',(-247.35427278056,4.91718508533857,130.906702686257));
#137048=CARTESIAN_POINT('Ctrl Pts',(-247.362020848563,4.92004022292792,
130.769523126077));
#137049=CARTESIAN_POINT('Ctrl Pts',(-247.369768916566,4.91714971345435,
130.632260661062));
#137050=CARTESIAN_POINT('Ctrl Pts',(-247.377516984569,4.90853799869109,
130.495430564147));
#137051=CARTESIAN_POINT('Ctrl Pts',(-247.385273287311,4.89991713129493,
130.358455042577));
#137052=CARTESIAN_POINT('Ctrl Pts',(-247.393029590053,4.8855629366223,130.221913197875));
#137053=CARTESIAN_POINT('Ctrl Pts',(-247.400785892795,4.86555181624854,
130.086315642721));
#137054=CARTESIAN_POINT('Ctrl Pts',(-247.408546335309,4.84553001533726,
129.950645715068));
#137055=CARTESIAN_POINT('Ctrl Pts',(-247.416306777823,4.81984534575211,
129.815921465078));
#137056=CARTESIAN_POINT('Ctrl Pts',(-247.424067220337,4.78862516140443,
129.682642236659));
#137057=CARTESIAN_POINT('Ctrl Pts',(-247.431840120603,4.75735485964524,
129.54914905659));
#137058=CARTESIAN_POINT('Ctrl Pts',(-247.439613020868,4.72053139094803,
129.417105910358));
#137059=CARTESIAN_POINT('Ctrl Pts',(-247.447385921134,4.67833197678282,
129.286996792535));
#137060=CARTESIAN_POINT('Ctrl Pts',(-247.454876256896,4.6376666176163,129.16161746887));
#137061=CARTESIAN_POINT('Ctrl Pts',(-247.462366592658,4.5920094921698,129.038034290196));
#137062=CARTESIAN_POINT('Ctrl Pts',(-247.46985692842,4.54156029648799,128.916660128647));
#137063=CARTESIAN_POINT('Ctrl Pts',(-247.477631262539,4.48919830421857,
128.790684028873));
#137064=CARTESIAN_POINT('Ctrl Pts',(-247.485405596658,4.43150781868713,
128.66668870827));
#137065=CARTESIAN_POINT('Ctrl Pts',(-247.493179930777,4.36865948181805,
128.545157794794));
#137066=CARTESIAN_POINT('Ctrl Pts',(-247.500944683724,4.30588859990707,
128.423776657307));
#137067=CARTESIAN_POINT('Ctrl Pts',(-247.508709436671,4.23797269224571,
128.304854227843));
#137068=CARTESIAN_POINT('Ctrl Pts',(-247.516474189618,4.16513087949918,
128.188855347233));
#137069=CARTESIAN_POINT('Ctrl Pts',(-247.524231230503,4.09236141426837,
128.072971678346));
#137070=CARTESIAN_POINT('Ctrl Pts',(-247.531988271388,4.01467598677348,
127.960006108755));
#137071=CARTESIAN_POINT('Ctrl Pts',(-247.539745312273,3.93233998821283,
127.850399670024));
#137072=CARTESIAN_POINT('Ctrl Pts',(-247.547496503513,3.85006607986883,
127.740875886361));
#137073=CARTESIAN_POINT('Ctrl Pts',(-247.555247694753,3.76314881486151,
127.634706502812));
#137074=CARTESIAN_POINT('Ctrl Pts',(-247.562998885993,3.67189711968179,
127.532303985267));
#137075=CARTESIAN_POINT('Ctrl Pts',(-247.57074678277,3.58068420890661,127.429944991524));
#137076=CARTESIAN_POINT('Ctrl Pts',(-247.578494679548,3.48514079161095,
127.331349970759));
#137077=CARTESIAN_POINT('Ctrl Pts',(-247.586242576325,3.38561619541522,
127.236898488847));
#137078=CARTESIAN_POINT('Ctrl Pts',(-247.593988852409,3.28611241761951,
127.142466764149));
#137079=CARTESIAN_POINT('Ctrl Pts',(-247.601735128493,3.18262940077015,
127.052177123273));
#137080=CARTESIAN_POINT('Ctrl Pts',(-247.609481404577,3.07555318135034,
126.966372122119));
#137081=CARTESIAN_POINT('Ctrl Pts',(-247.617227737842,2.96847617151864,
126.880566487571));
#137082=CARTESIAN_POINT('Ctrl Pts',(-247.624974071107,2.85780621128164,
126.799245803287));
#137083=CARTESIAN_POINT('Ctrl Pts',(-247.632720404373,2.74396192842133,
126.722711931327));
#137084=CARTESIAN_POINT('Ctrl Pts',(-247.640468472376,2.63009215092305,
126.646160920137));
#137085=CARTESIAN_POINT('Ctrl Pts',(-247.648216540379,2.5130469606567,126.574399072459));
#137086=CARTESIAN_POINT('Ctrl Pts',(-247.655964608381,2.39327308271081,
126.507684342342));
#137087=CARTESIAN_POINT('Ctrl Pts',(-247.663720911123,2.27337190766194,
126.440898707016));
#137088=CARTESIAN_POINT('Ctrl Pts',(-247.671477213865,2.15073659380708,
126.379171095245));
#137089=CARTESIAN_POINT('Ctrl Pts',(-247.679233516607,2.025838030973,126.322713226844));
#137090=CARTESIAN_POINT('Ctrl Pts',(-247.686993959121,1.90087280601532,
126.266225225179));
#137091=CARTESIAN_POINT('Ctrl Pts',(-247.694754401635,1.77364228761655,
126.215012717187));
#137092=CARTESIAN_POINT('Ctrl Pts',(-247.702514844149,1.64463542584875,
126.169238463993));
#137093=CARTESIAN_POINT('Ctrl Pts',(-247.710287744415,1.51542147081341,
126.123390729904));
#137094=CARTESIAN_POINT('Ctrl Pts',(-247.71806064468,1.38442584793804,126.082998811142));
#137095=CARTESIAN_POINT('Ctrl Pts',(-247.725833544946,1.25215154809811,
126.048175217154));
#137096=CARTESIAN_POINT('Ctrl Pts',(-247.733323880708,1.12468575223299,
126.014617548521));
#137097=CARTESIAN_POINT('Ctrl Pts',(-247.74081421647,0.996032932413138,
125.986230454475));
#137098=CARTESIAN_POINT('Ctrl Pts',(-247.748304552232,0.866648390248171,
125.963069092551));
#137099=CARTESIAN_POINT('Ctrl Pts',(-247.756078886351,0.732358193845027,
125.939029560551));
#137100=CARTESIAN_POINT('Ctrl Pts',(-247.76385322047,0.596854302293437,
125.920543700368));
#137101=CARTESIAN_POINT('Ctrl Pts',(-247.77162755459,0.460635841617658,
125.907729358842));
#137102=CARTESIAN_POINT('Ctrl Pts',(-247.779392307537,0.324585258020469,
125.894930809846));
#137103=CARTESIAN_POINT('Ctrl Pts',(-247.787157060484,0.187822243025281,
125.887789908473));
#137104=CARTESIAN_POINT('Ctrl Pts',(-247.794921813431,0.0508563204592624,
125.886373560124));
#137105=CARTESIAN_POINT('Ctrl Pts',(-247.802678854316,-0.0859735656223271,
125.884958618512));
#137106=CARTESIAN_POINT('Ctrl Pts',(-247.810435895201,-0.223005569805123,
125.889256919127));
#137107=CARTESIAN_POINT('Ctrl Pts',(-247.818192936086,-0.359725189316763,
125.899283569173));
#137108=CARTESIAN_POINT('Ctrl Pts',(-247.825944127326,-0.496341707498876,
125.909302658044));
#137109=CARTESIAN_POINT('Ctrl Pts',(-247.833695318566,-0.632645921560685,
125.92504146958));
#137110=CARTESIAN_POINT('Ctrl Pts',(-247.841446509806,-0.768123829952101,
125.946463043063));
#137111=CARTESIAN_POINT('Ctrl Pts',(-247.849194406583,-0.903544156619012,
125.967875511807));
#137112=CARTESIAN_POINT('Ctrl Pts',(-247.85694230336,-1.03813849077029,
125.994965877667));
#137113=CARTESIAN_POINT('Ctrl Pts',(-247.864690200137,-1.17139867277518,
126.027645406051));
#137114=CARTESIAN_POINT('Ctrl Pts',(-247.872436476222,-1.30463097962311,
126.060318098582));
#137115=CARTESIAN_POINT('Ctrl Pts',(-247.880182752306,-1.4365293099482,
126.098577535108));
#137116=CARTESIAN_POINT('Ctrl Pts',(-247.88792902839,-1.5665967996225,126.142284092034));
#137117=CARTESIAN_POINT('Ctrl Pts',(-247.895675361655,-1.69666524942494,
126.185990971593));
#137118=CARTESIAN_POINT('Ctrl Pts',(-247.903421694921,-1.82490246100744,
126.235144927253));
#137119=CARTESIAN_POINT('Ctrl Pts',(-247.911168028186,-1.95082819072668,
126.289556919423));
#137120=CARTESIAN_POINT('Ctrl Pts',(-247.918916096189,-2.0767821206405,
126.343981096782));
#137121=CARTESIAN_POINT('Ctrl Pts',(-247.926664164192,-2.20042317982122,
126.403665498695));
#137122=CARTESIAN_POINT('Ctrl Pts',(-247.934412232195,-2.32129287839771,
126.468373713158));
#137123=CARTESIAN_POINT('Ctrl Pts',(-247.942168534937,-2.44229103872771,
126.533150700281));
#137124=CARTESIAN_POINT('Ctrl Pts',(-247.949924837679,-2.56051160940061,
126.602961981097));
#137125=CARTESIAN_POINT('Ctrl Pts',(-247.957681140421,-2.67552193708478,
126.67752582239));
#137126=CARTESIAN_POINT('Ctrl Pts',(-247.965441582935,-2.79059364924404,
126.75212946065));
#137127=CARTESIAN_POINT('Ctrl Pts',(-247.973202025449,-2.90245138560497,
126.83149048763));
#137128=CARTESIAN_POINT('Ctrl Pts',(-247.980962467963,-3.0106939211645,
126.91528551215));
#137129=CARTESIAN_POINT('Ctrl Pts',(-247.988735368229,-3.11911021725144,
126.999215051883));
#137130=CARTESIAN_POINT('Ctrl Pts',(-247.996508268494,-3.22389941637474,
127.087592560679));
#137131=CARTESIAN_POINT('Ctrl Pts',(-248.00428116876,-3.32469498229554,
127.180055672173));
#137132=CARTESIAN_POINT('Ctrl Pts',(-248.011771504521,-3.42182637550397,
127.269157516662));
#137133=CARTESIAN_POINT('Ctrl Pts',(-248.019261840283,-3.51524923331697,
127.362052859884));
#137134=CARTESIAN_POINT('Ctrl Pts',(-248.026752176045,-3.60467104849656,
127.458388457695));
#137135=CARTESIAN_POINT('Ctrl Pts',(-248.034437389345,-3.69641936861804,
127.55723043769));
#137136=CARTESIAN_POINT('Ctrl Pts',(-248.042122602644,-3.78426126690538,
127.660023733442));
#137137=CARTESIAN_POINT('Ctrl Pts',(-248.049807815944,-3.86783113952899,
127.766422939043));
#137138=CARTESIAN_POINT('Ctrl Pts',(-248.057483898829,-3.95130172700292,
127.872695737115));
#137139=CARTESIAN_POINT('Ctrl Pts',(-248.065159981715,-4.03051013549663,
127.982565615255));
#137140=CARTESIAN_POINT('Ctrl Pts',(-248.0728360646,-4.10512753012237,128.095650403473));
#137141=CARTESIAN_POINT('Ctrl Pts',(-248.080527452988,-4.17989370592884,
128.208960673811));
#137142=CARTESIAN_POINT('Ctrl Pts',(-248.088218841375,-4.25005025496661,
128.325498400309));
#137143=CARTESIAN_POINT('Ctrl Pts',(-248.095910229762,-4.3153064234439,
128.444845087996));
#137144=CARTESIAN_POINT('Ctrl Pts',(-248.103572743103,-4.38031760690732,
128.563743723787));
#137145=CARTESIAN_POINT('Ctrl Pts',(-248.111235256444,-4.44046492976471,
128.685429923047));
#137146=CARTESIAN_POINT('Ctrl Pts',(-248.118897769785,-4.49550423590677,
128.809460939025));
#137147=CARTESIAN_POINT('Ctrl Pts',(-248.126603595696,-4.55085465325594,
128.934193043766));
#137148=CARTESIAN_POINT('Ctrl Pts',(-248.134309421606,-4.60103890736235,
129.061296210318));
#137149=CARTESIAN_POINT('Ctrl Pts',(-248.142015247517,-4.64585601780006,
129.19029589632));
#137150=CARTESIAN_POINT('Ctrl Pts',(-248.149721073427,-4.69067312823778,
129.319295582322));
#137151=CARTESIAN_POINT('Ctrl Pts',(-248.157426899337,-4.73012294771376,
129.450191401843));
#137152=CARTESIAN_POINT('Ctrl Pts',(-248.165132725248,-4.76405452823402,
129.582490119308));
#137153=CARTESIAN_POINT('Ctrl Pts',(-246.415426335729,-4.76405452823406,
129.582490119308));
#137154=CARTESIAN_POINT('Ctrl Pts',(-246.423702521276,-4.80032898872548,
129.723923690223));
#137155=CARTESIAN_POINT('Ctrl Pts',(-246.431978706823,-4.83034188283307,
129.867132951389));
#137156=CARTESIAN_POINT('Ctrl Pts',(-246.44025489237,-4.85393125729227,
130.011558995481));
#137157=CARTESIAN_POINT('Ctrl Pts',(-246.448509182087,-4.87745822269407,
130.155602939857));
#137158=CARTESIAN_POINT('Ctrl Pts',(-246.456763471804,-4.89459550936722,
130.300856946525));
#137159=CARTESIAN_POINT('Ctrl Pts',(-246.465017761521,-4.90523171034105,
130.446750592029));
#137160=CARTESIAN_POINT('Ctrl Pts',(-246.471725362337,-4.91387489985538,
130.565306684578));
#137161=CARTESIAN_POINT('Ctrl Pts',(-246.478432963153,-4.91822598909207,
130.684284797298));
#137162=CARTESIAN_POINT('Ctrl Pts',(-246.485140563968,-4.91824990085616,
130.803373081029));
#137163=CARTESIAN_POINT('',(-246.139859436028,-4.91824848601657,130.800501563838));
#137164=CARTESIAN_POINT('Ctrl Pts',(-246.069808463078,-4.7640545282341,
129.582490119308));
#137165=CARTESIAN_POINT('Ctrl Pts',(-246.077583997001,-4.79806606887736,
129.715100600079));
#137166=CARTESIAN_POINT('Ctrl Pts',(-246.085359530925,-4.8264933030139,
129.84896373178));
#137167=CARTESIAN_POINT('Ctrl Pts',(-246.093135064848,-4.8492767216106,
129.983569328781));
#137168=CARTESIAN_POINT('Ctrl Pts',(-246.094492645071,-4.85325462445185,
130.007070981287));
#137169=CARTESIAN_POINT('Ctrl Pts',(-246.095850225293,-4.85706061005185,
130.030595261098));
#137170=CARTESIAN_POINT('Ctrl Pts',(-246.097207805516,-4.86069452442358,
130.054139448351));
#137171=CARTESIAN_POINT('Ctrl Pts',(-246.110238294451,-4.89557399617043,
130.280124083671));
#137172=CARTESIAN_POINT('Ctrl Pts',(-246.123268783386,-4.91469973543392,
130.508600512009));
#137173=CARTESIAN_POINT('Ctrl Pts',(-246.136299272322,-4.91780024632565,
130.737848966411));
#137174=CARTESIAN_POINT('Ctrl Pts',(-246.137485993547,-4.91808261808478,
130.758727231835));
#137175=CARTESIAN_POINT('Ctrl Pts',(-246.138672714772,-4.91823209512877,
130.779611870769));
#137176=CARTESIAN_POINT('Ctrl Pts',(-246.139859435997,-4.91824848601615,
130.8005015633));
#137177=CARTESIAN_POINT('Ctrl Pts',(-246.139859436027,-4.91824848601657,
130.800501563838));
#137178=CARTESIAN_POINT('Ctrl Pts',(-246.147509209082,-4.91835414398288,
130.935159479865));
#137179=CARTESIAN_POINT('Ctrl Pts',(-246.155158982137,-4.91292539923117,
131.07002367009));
#137180=CARTESIAN_POINT('Ctrl Pts',(-246.162808755192,-4.90193805195921,
131.204593546314));
#137181=CARTESIAN_POINT('Ctrl Pts',(-246.170450973431,-4.8909615556474,
131.339030523093));
#137182=CARTESIAN_POINT('Ctrl Pts',(-246.17809319167,-4.87443740755454,
131.473173364555));
#137183=CARTESIAN_POINT('Ctrl Pts',(-246.185735409909,-4.8523934448977,
131.606520775149));
#137184=CARTESIAN_POINT('Ctrl Pts',(-246.193648744052,-4.82956744898002,
131.744598828412));
#137185=CARTESIAN_POINT('Ctrl Pts',(-246.201562078194,-4.80082273554776,
131.881823530467));
#137186=CARTESIAN_POINT('Ctrl Pts',(-246.209475412337,-4.76624899930714,
132.017642752563));
#137187=CARTESIAN_POINT('Ctrl Pts',(-246.217109079795,-4.73289714021657,
132.148661961064));
#137188=CARTESIAN_POINT('Ctrl Pts',(-246.224742747254,-4.69412137968988,
132.27837291988));
#137189=CARTESIAN_POINT('Ctrl Pts',(-246.232376414712,-4.65005427662074,
132.406290168758));
#137190=CARTESIAN_POINT('Ctrl Pts',(-246.240008934568,-4.60599379835271,
132.534188187274));
#137191=CARTESIAN_POINT('Ctrl Pts',(-246.247641454423,-4.55664369045626,
132.6602926505));
#137192=CARTESIAN_POINT('Ctrl Pts',(-246.255273974279,-4.50218607768833,
132.784134237041));
#137193=CARTESIAN_POINT('Ctrl Pts',(-246.262907113082,-4.44772404876844,
132.907985866315));
#137194=CARTESIAN_POINT('Ctrl Pts',(-246.270540251884,-4.38815385424924,
133.029573884721));
#137195=CARTESIAN_POINT('Ctrl Pts',(-246.278173390687,-4.32370512787218,
133.148450425938));
#137196=CARTESIAN_POINT('Ctrl Pts',(-246.285808915305,-4.25923625738789,
133.267364123231));
#137197=CARTESIAN_POINT('Ctrl Pts',(-246.293444439923,-4.18988601568527,
133.383564303824));
#137198=CARTESIAN_POINT('Ctrl Pts',(-246.301079964541,-4.11592890471563,
133.496629607438));
#137199=CARTESIAN_POINT('Ctrl Pts',(-246.308723686376,-4.0418923961166,
133.609816293796));
#137200=CARTESIAN_POINT('Ctrl Pts',(-246.316367408212,-3.96323936901022,
133.719861048954));
#137201=CARTESIAN_POINT('Ctrl Pts',(-246.324011130048,-3.88028651580862,
133.826373128747));
#137202=CARTESIAN_POINT('Ctrl Pts',(-246.331659746566,-3.79728054347419,
133.932953413901));
#137203=CARTESIAN_POINT('Ctrl Pts',(-246.339308363085,-3.70996952495838,
134.035996214606));
#137204=CARTESIAN_POINT('Ctrl Pts',(-246.346956979603,-3.61870806410886,
134.135146562242));
#137205=CARTESIAN_POINT('Ctrl Pts',(-246.354616228249,-3.52731974325678,
134.234434736002));
#137206=CARTESIAN_POINT('Ctrl Pts',(-246.362275476895,-3.43197030759929,
134.329819377562));
#137207=CARTESIAN_POINT('Ctrl Pts',(-246.369934725541,-3.3330486836757,
134.420984669738));
#137208=CARTESIAN_POINT('Ctrl Pts',(-246.371841626804,-3.30842044946405,
134.443681832184));
#137209=CARTESIAN_POINT('Ctrl Pts',(-246.373748528066,-3.28357094003826,
134.466117666397));
#137210=CARTESIAN_POINT('Ctrl Pts',(-246.375655429329,-3.2585064365443,
134.488287715854));
#137211=CARTESIAN_POINT('Ctrl Pts',(-246.383429763448,-3.15631980080681,
134.578673817803));
#137212=CARTESIAN_POINT('Ctrl Pts',(-246.391204097567,-3.05020769545569,
134.66494810569));
#137213=CARTESIAN_POINT('Ctrl Pts',(-246.398978431686,-2.94053510115786,
134.746750296601));
#137214=CARTESIAN_POINT('Ctrl Pts',(-246.406743184633,-2.83099766853138,
134.828451673621));
#137215=CARTESIAN_POINT('Ctrl Pts',(-246.41450793758,-2.7179087881222,134.90569168832));
#137216=CARTESIAN_POINT('Ctrl Pts',(-246.422272690527,-2.60166881959181,
134.978148155961));
#137217=CARTESIAN_POINT('Ctrl Pts',(-246.430029731412,-2.48554430223623,
135.050532658818));
#137218=CARTESIAN_POINT('Ctrl Pts',(-246.437786772297,-2.36627525465273,
135.118142864016));
#137219=CARTESIAN_POINT('Ctrl Pts',(-246.445543813182,-2.24429323315252,
135.180698235498));
#137220=CARTESIAN_POINT('Ctrl Pts',(-246.453295004422,-2.12240319924411,
135.243206433487));
#137221=CARTESIAN_POINT('Ctrl Pts',(-246.461046195662,-1.99780461008804,
135.300667207411));
#137222=CARTESIAN_POINT('Ctrl Pts',(-246.468797386903,-1.87095567857234,
135.352844750914));
#137223=CARTESIAN_POINT('Ctrl Pts',(-246.47654528368,-1.74416066123617,
135.405000117569));
#137224=CARTESIAN_POINT('Ctrl Pts',(-246.484293180457,-1.61511756467201,
135.451876571543));
#137225=CARTESIAN_POINT('Ctrl Pts',(-246.492041077234,-1.48430654412968,
135.493285563175));
#137226=CARTESIAN_POINT('Ctrl Pts',(-246.499787353318,-1.35352288643289,
135.534685892938));
#137227=CARTESIAN_POINT('Ctrl Pts',(-246.507533629402,-1.22097241283283,
135.570620917276));
#137228=CARTESIAN_POINT('Ctrl Pts',(-246.515279905486,-1.08715210297495,
135.600951424326));
#137229=CARTESIAN_POINT('Ctrl Pts',(-246.523026238751,-0.953330805285754,
135.63128215527));
#137230=CARTESIAN_POINT('Ctrl Pts',(-246.530772572017,-0.81824003392849,
135.656008199952));
#137231=CARTESIAN_POINT('Ctrl Pts',(-246.538518905282,-0.682388278878623,
135.675041196227));
#137232=CARTESIAN_POINT('Ctrl Pts',(-246.546266973285,-0.546506100770328,
135.69407845481));
#137233=CARTESIAN_POINT('Ctrl Pts',(-246.554015041288,-0.409862986968956,
135.70742007381));
#137234=CARTESIAN_POINT('Ctrl Pts',(-246.561763109291,-0.272973490629409,
135.715029465688));
#137235=CARTESIAN_POINT('Ctrl Pts',(-246.569519412033,-0.13593850650396,
135.722646944918));
#137236=CARTESIAN_POINT('Ctrl Pts',(-246.577275714774,0.0013429922648055,
135.724520005307));
#137237=CARTESIAN_POINT('Ctrl Pts',(-246.585032017516,0.138354943250946,
135.72066420585));
#137238=CARTESIAN_POINT('Ctrl Pts',(-246.59279246003,0.275440021640677,
135.716806348438));
#137239=CARTESIAN_POINT('Ctrl Pts',(-246.600552902545,0.412254875766161,
135.707213565855));
#137240=CARTESIAN_POINT('Ctrl Pts',(-246.608313345059,0.548288615183166,
135.691953343741));
#137241=CARTESIAN_POINT('Ctrl Pts',(-246.616086245324,0.68454072803519,
135.676668624564));
#137242=CARTESIAN_POINT('Ctrl Pts',(-246.62385914559,0.820008833871837,
135.655698345242));
#137243=CARTESIAN_POINT('Ctrl Pts',(-246.631632045855,0.95419139435407,
135.629161322822));
#137244=CARTESIAN_POINT('Ctrl Pts',(-246.639122381617,1.0834960807773,135.60358898801));
#137245=CARTESIAN_POINT('Ctrl Pts',(-246.646612717379,1.21160676525314,
135.572847685529));
#137246=CARTESIAN_POINT('Ctrl Pts',(-246.654103053141,1.33808987962855,
135.537086949875));
#137247=CARTESIAN_POINT('Ctrl Pts',(-246.66187738726,1.46936863972905,135.499970335061));
#137248=CARTESIAN_POINT('Ctrl Pts',(-246.669651721379,1.59930982641751,
135.457328575547));
#137249=CARTESIAN_POINT('Ctrl Pts',(-246.677426055498,1.72741304250867,
135.409273998192));
#137250=CARTESIAN_POINT('Ctrl Pts',(-246.685190808445,1.85535838283491,
135.361278643809));
#137251=CARTESIAN_POINT('Ctrl Pts',(-246.692955561393,1.98146989696326,
135.307883880514));
#137252=CARTESIAN_POINT('Ctrl Pts',(-246.70072031434,2.10526011757353,135.24925239351));
#137253=CARTESIAN_POINT('Ctrl Pts',(-246.708477355225,2.22892738799189,
135.190679140125));
#137254=CARTESIAN_POINT('Ctrl Pts',(-246.71623439611,2.35027760197344,135.126879679899));
#137255=CARTESIAN_POINT('Ctrl Pts',(-246.723991436995,2.46884146985864,
135.058065456786));
#137256=CARTESIAN_POINT('Ctrl Pts',(-246.731742628235,2.58731592780863,
134.989303127015));
#137257=CARTESIAN_POINT('Ctrl Pts',(-246.739493819475,2.70300788521343,
134.915533757005));
#137258=CARTESIAN_POINT('Ctrl Pts',(-246.747245010715,2.81547127624926,
134.837015395143));
#137259=CARTESIAN_POINT('Ctrl Pts',(-246.754992907492,2.92788686734368,
134.758530405679));
#137260=CARTESIAN_POINT('Ctrl Pts',(-246.762740804269,3.037076301428,134.675300662244));
#137261=CARTESIAN_POINT('Ctrl Pts',(-246.770488701046,3.14262141069146,
134.587628217348));
#137262=CARTESIAN_POINT('Ctrl Pts',(-246.77823497713,3.24814444219306,134.499974111639));
#137263=CARTESIAN_POINT('Ctrl Pts',(-246.785981253214,3.35002436460675,
134.407879402591));
#137264=CARTESIAN_POINT('Ctrl Pts',(-246.793727529298,3.44787542541367,
134.311686965844));
#137265=CARTESIAN_POINT('Ctrl Pts',(-246.801473862564,3.54572720853504,
134.215493819027));
#137266=CARTESIAN_POINT('Ctrl Pts',(-246.809220195829,3.63954979189833,
134.115203158233));
#137267=CARTESIAN_POINT('Ctrl Pts',(-246.816966529095,3.72899398267495,
134.011195028582));
#137268=CARTESIAN_POINT('Ctrl Pts',(-246.824714597097,3.81845820385781,
133.907163607031));
#137269=CARTESIAN_POINT('Ctrl Pts',(-246.8324626651,3.90354182648,133.799413356413));
#137270=CARTESIAN_POINT('Ctrl Pts',(-246.840210733103,3.983935939859,133.68835740841));
#137271=CARTESIAN_POINT('Ctrl Pts',(-246.847967035845,4.0644154970585,133.577183428824));
#137272=CARTESIAN_POINT('Ctrl Pts',(-246.855723338587,4.14019535918323,
133.462697050789));
#137273=CARTESIAN_POINT('Ctrl Pts',(-246.863479641329,4.21100967210949,
133.345340862255));
#137274=CARTESIAN_POINT('Ctrl Pts',(-246.871240083843,4.28186178076673,
133.22792203719));
#137275=CARTESIAN_POINT('Ctrl Pts',(-246.879000526357,4.34774287164151,
133.107630692314));
#137276=CARTESIAN_POINT('Ctrl Pts',(-246.886760968871,4.40843357354889,
132.984933131863));
#137277=CARTESIAN_POINT('Ctrl Pts',(-246.894533869137,4.46922170155901,
132.862038606395));
#137278=CARTESIAN_POINT('Ctrl Pts',(-246.902306769402,4.52480263185307,
132.736730504097));
#137279=CARTESIAN_POINT('Ctrl Pts',(-246.910079669668,4.57500523485611,
132.609495006895));
#137280=CARTESIAN_POINT('Ctrl Pts',(-246.91757000543,4.62338284678781,132.486884840502));
#137281=CARTESIAN_POINT('Ctrl Pts',(-246.925060341192,4.66676627260832,
132.362485268479));
#137282=CARTESIAN_POINT('Ctrl Pts',(-246.932550676954,4.70504696574861,
132.23674189104));
#137283=CARTESIAN_POINT('Ctrl Pts',(-246.940325011073,4.74477908300408,
132.106230915229));
#137284=CARTESIAN_POINT('Ctrl Pts',(-246.948099345192,4.77913974844341,
131.973858802142));
#137285=CARTESIAN_POINT('Ctrl Pts',(-246.955873679311,4.80795298893047,
131.840107265514));
#137286=CARTESIAN_POINT('Ctrl Pts',(-246.963638432258,4.83673071967359,
131.706520565701));
#137287=CARTESIAN_POINT('Ctrl Pts',(-246.971403185205,4.85997454692671,
131.571558203401));
#137288=CARTESIAN_POINT('Ctrl Pts',(-246.979167938152,4.87755785436409,
131.435718234002));
#137289=CARTESIAN_POINT('Ctrl Pts',(-246.986924979037,4.89512369781274,
131.300013182774));
#137290=CARTESIAN_POINT('Ctrl Pts',(-246.994682019923,4.90704015983078,
131.163432644294));
#137291=CARTESIAN_POINT('Ctrl Pts',(-247.002439060808,4.91323147168139,
131.026485735865));
#137292=CARTESIAN_POINT('Ctrl Pts',(-247.010190252048,4.91941811461557,
130.889642100166));
#137293=CARTESIAN_POINT('Ctrl Pts',(-247.017941443288,4.91988818328002,
130.752433033427));
#137294=CARTESIAN_POINT('Ctrl Pts',(-247.025692634528,4.91461767161569,
130.615373304916));
#137295=CARTESIAN_POINT('Ctrl Pts',(-247.033440531305,4.90934940005942,
130.478371830445));
#137296=CARTESIAN_POINT('Ctrl Pts',(-247.041188428082,4.89834541594072,
130.341519957818));
#137297=CARTESIAN_POINT('Ctrl Pts',(-247.048936324859,4.88163381467735,
130.205332770218));
#137298=CARTESIAN_POINT('Ctrl Pts',(-247.056682600943,4.86492570912065,
130.069174070041));
#137299=CARTESIAN_POINT('Ctrl Pts',(-247.064428877027,4.84251240876081,
129.933680166145));
#137300=CARTESIAN_POINT('Ctrl Pts',(-247.072175153112,4.81447387592537,
129.799360935709));
#137301=CARTESIAN_POINT('Ctrl Pts',(-247.079921486377,4.78643513611589,
129.665040713759));
#137302=CARTESIAN_POINT('Ctrl Pts',(-247.087667819642,4.75277116086249,
129.531895565287));
#137303=CARTESIAN_POINT('Ctrl Pts',(-247.095414152908,4.71361294563391,
129.400424699779));
#137304=CARTESIAN_POINT('Ctrl Pts',(-247.103162220911,4.67444596119468,
129.268924392283));
#137305=CARTESIAN_POINT('Ctrl Pts',(-247.110910288914,4.62978240001419,
129.139099488472));
#137306=CARTESIAN_POINT('Ctrl Pts',(-247.118658356916,4.57980286770836,
129.011433191419));
#137307=CARTESIAN_POINT('Ctrl Pts',(-247.126414659658,4.52977021656062,
128.883631209106));
#137308=CARTESIAN_POINT('Ctrl Pts',(-247.1341709624,4.47441045080083,128.757992781089));
#137309=CARTESIAN_POINT('Ctrl Pts',(-247.141927265142,4.41395223155954,
128.634980807572));
#137310=CARTESIAN_POINT('Ctrl Pts',(-247.149687707656,4.35346174394628,
128.51190317886));
#137311=CARTESIAN_POINT('Ctrl Pts',(-247.15744815017,4.28786756752669,128.391455141073));
#137312=CARTESIAN_POINT('Ctrl Pts',(-247.165208592685,4.2174434417772,128.274073306229));
#137313=CARTESIAN_POINT('Ctrl Pts',(-247.17298149295,4.14690626496909,128.156503039644));
#137314=CARTESIAN_POINT('Ctrl Pts',(-247.180754393216,4.07152386005955,
128.042009138742));
#137315=CARTESIAN_POINT('Ctrl Pts',(-247.188527293481,3.99161276595695,
127.930998372887));
#137316=CARTESIAN_POINT('Ctrl Pts',(-247.196017629243,3.91460664140931,
127.82402312799));
#137317=CARTESIAN_POINT('Ctrl Pts',(-247.203507965005,3.83339555964348,
127.720282415859));
#137318=CARTESIAN_POINT('Ctrl Pts',(-247.210998300767,3.74829574466858,
127.620108417598));
#137319=CARTESIAN_POINT('Ctrl Pts',(-247.218772634886,3.659969344343,127.516136291745));
#137320=CARTESIAN_POINT('Ctrl Pts',(-247.226546969005,3.56717371560623,
127.415677330275));
#137321=CARTESIAN_POINT('Ctrl Pts',(-247.234321303124,3.47021902008662,
127.31913996241));
#137322=CARTESIAN_POINT('Ctrl Pts',(-247.242086056071,3.37338381256389,
127.222721568222));
#137323=CARTESIAN_POINT('Ctrl Pts',(-247.249850809018,3.2724000112201,127.130215424592));
#137324=CARTESIAN_POINT('Ctrl Pts',(-247.257615561966,3.16761820494175,
127.041997268523));
#137325=CARTESIAN_POINT('Ctrl Pts',(-247.265372602851,3.06294046943085,
126.953866731971));
#137326=CARTESIAN_POINT('Ctrl Pts',(-247.273129643736,2.95447253304266,
126.87001595777));
#137327=CARTESIAN_POINT('Ctrl Pts',(-247.280886684621,2.84260177573071,
126.790783882643));
#137328=CARTESIAN_POINT('Ctrl Pts',(-247.288637875861,2.73081538102692,
126.711611557041));
#137329=CARTESIAN_POINT('Ctrl Pts',(-247.296389067101,2.61563159081257,
126.637051222871));
#137330=CARTESIAN_POINT('Ctrl Pts',(-247.304140258341,2.49747051918889,
126.567401322472));
#137331=CARTESIAN_POINT('Ctrl Pts',(-247.311888155118,2.37935966917286,
126.497781025139));
#137332=CARTESIAN_POINT('Ctrl Pts',(-247.319636051895,2.2582743906818,126.43306720868));
#137333=CARTESIAN_POINT('Ctrl Pts',(-247.327383948672,2.13466322404559,
126.373514650665));
#137334=CARTESIAN_POINT('Ctrl Pts',(-247.335130224756,2.01107791420071,
126.313974549761));
#137335=CARTESIAN_POINT('Ctrl Pts',(-247.34287650084,1.88496811914733,126.259593729453));
#137336=CARTESIAN_POINT('Ctrl Pts',(-247.350622776924,1.75680603458676,
126.21058051624));
#137337=CARTESIAN_POINT('Ctrl Pts',(-247.35836911019,1.62864300396261,126.161566941222));
#137338=CARTESIAN_POINT('Ctrl Pts',(-247.366115443455,1.49842801877366,
126.117921192016));
#137339=CARTESIAN_POINT('Ctrl Pts',(-247.373861776721,1.36665188434967,
126.079802893344));
#137340=CARTESIAN_POINT('Ctrl Pts',(-247.381609844724,1.23484623957424,
126.041676058344));
#137341=CARTESIAN_POINT('Ctrl Pts',(-247.389357912726,1.10147912537945,
126.009079245644));
#137342=CARTESIAN_POINT('Ctrl Pts',(-247.397105980729,0.967054695941718,
125.982121689686));
#137343=CARTESIAN_POINT('Ctrl Pts',(-247.404862283471,0.832487398620895,
125.955135482918));
#137344=CARTESIAN_POINT('Ctrl Pts',(-247.412618586213,0.696860925235222,
125.93380058249));
#137345=CARTESIAN_POINT('Ctrl Pts',(-247.420374888955,0.560688323761253,
125.918174818182));
#137346=CARTESIAN_POINT('Ctrl Pts',(-247.428135331469,0.424443042869429,
125.902540713934));
#137347=CARTESIAN_POINT('Ctrl Pts',(-247.435895773983,0.287651442831393,
125.892621845748));
#137348=CARTESIAN_POINT('Ctrl Pts',(-247.443656216497,0.150828820579001,
125.888423908313));
#137349=CARTESIAN_POINT('Ctrl Pts',(-247.451429116763,0.0137865585068277,
125.884219231975));
#137350=CARTESIAN_POINT('Ctrl Pts',(-247.459202017028,-0.123286434129482,
125.885753834059));
#137351=CARTESIAN_POINT('Ctrl Pts',(-247.466974917294,-0.259876833731254,
125.892981270194));
#137352=CARTESIAN_POINT('Ctrl Pts',(-247.474465253056,-0.391501828257419,
125.899945970821));
#137353=CARTESIAN_POINT('Ctrl Pts',(-247.481955588818,-0.522678400849008,
125.912196765013));
#137354=CARTESIAN_POINT('Ctrl Pts',(-247.48944592458,-0.652956151334717,
125.929647156558));
#137355=CARTESIAN_POINT('Ctrl Pts',(-247.497220258699,-0.788173422326592,
125.947759185002));
#137356=CARTESIAN_POINT('Ctrl Pts',(-247.504994592818,-0.9228506957488,
125.971530253045));
#137357=CARTESIAN_POINT('Ctrl Pts',(-247.512768926937,-1.05647669859273,
126.000920178898));
#137358=CARTESIAN_POINT('Ctrl Pts',(-247.520533679884,-1.18993801933101,
126.030273884294));
#137359=CARTESIAN_POINT('Ctrl Pts',(-247.528298432831,-1.32235026916988,
126.065232586154));
#137360=CARTESIAN_POINT('Ctrl Pts',(-247.536063185778,-1.45320782807006,
126.105704419148));
#137361=CARTESIAN_POINT('Ctrl Pts',(-247.543820226663,-1.58393541739797,
126.146136054946));
#137362=CARTESIAN_POINT('Ctrl Pts',(-247.551577267548,-1.71311101760524,
126.192069810176));
#137363=CARTESIAN_POINT('Ctrl Pts',(-247.559334308433,-1.84024008330074,
126.243362974691));
#137364=CARTESIAN_POINT('Ctrl Pts',(-247.567085499674,-1.96727327997871,
126.294617458631));
#137365=CARTESIAN_POINT('Ctrl Pts',(-247.574836690914,-2.09226265290587,
126.351223161656));
#137366=CARTESIAN_POINT('Ctrl Pts',(-247.582587882154,-2.21473003215606,
126.41298794525));
#137367=CARTESIAN_POINT('Ctrl Pts',(-247.590335778931,-2.33714535950298,
126.474726477163));
#137368=CARTESIAN_POINT('Ctrl Pts',(-247.598083675708,-2.45704047677789,
126.541619552751));
#137369=CARTESIAN_POINT('Ctrl Pts',(-247.605831572485,-2.5739585853895,
126.613427515833));
#137370=CARTESIAN_POINT('Ctrl Pts',(-247.613577848569,-2.69085223725357,
126.685220458238));
#137371=CARTESIAN_POINT('Ctrl Pts',(-247.621324124653,-2.80476978615282,
126.76192603873));
#137372=CARTESIAN_POINT('Ctrl Pts',(-247.629070400737,-2.9152807277937,
126.843259591253));
#137373=CARTESIAN_POINT('Ctrl Pts',(-247.636816734003,-3.02579248520049,
126.924593744163));
#137374=CARTESIAN_POINT('Ctrl Pts',(-247.644563067268,-3.13289727029155,
127.010555705529));
#137375=CARTESIAN_POINT('Ctrl Pts',(-247.652309400533,-3.23619549399687,
127.10081882799));
#137376=CARTESIAN_POINT('Ctrl Pts',(-247.660057468536,-3.33951685062416,
127.191102164253));
#137377=CARTESIAN_POINT('Ctrl Pts',(-247.667805536539,-3.43902965523445,
127.285688321092));
#137378=CARTESIAN_POINT('Ctrl Pts',(-247.675553604542,-3.53436949814966,
127.384212183207));
#137379=CARTESIAN_POINT('Ctrl Pts',(-247.683309907284,-3.62981066938408,
127.482840757654));
#137380=CARTESIAN_POINT('Ctrl Pts',(-247.691066210026,-3.72106974707619,
127.58541511604));
#137381=CARTESIAN_POINT('Ctrl Pts',(-247.698822512768,-3.80782076243008,
127.69153487498));
#137382=CARTESIAN_POINT('Ctrl Pts',(-247.706582955282,-3.89461807941312,
127.797711273231));
#137383=CARTESIAN_POINT('Ctrl Pts',(-247.714343397796,-3.97690230527603,
127.907436529947));
#137384=CARTESIAN_POINT('Ctrl Pts',(-247.72210384031,-4.05439011833824,
128.020280189342));
#137385=CARTESIAN_POINT('Ctrl Pts',(-247.729876740576,-4.13200232171682,
128.133304995396));
#137386=CARTESIAN_POINT('Ctrl Pts',(-247.737649640841,-4.20480251823506,
128.249457876122));
#137387=CARTESIAN_POINT('Ctrl Pts',(-247.745422541107,-4.27255231891392,
128.368281853518));
#137388=CARTESIAN_POINT('Ctrl Pts',(-247.752912876869,-4.33783924368592,
128.482786280036));
#137389=CARTESIAN_POINT('Ctrl Pts',(-247.760403212631,-4.39843644522186,
128.599770699173));
#137390=CARTESIAN_POINT('Ctrl Pts',(-247.767893548393,-4.45417324294245,
128.718809423192));
#137391=CARTESIAN_POINT('Ctrl Pts',(-247.776601668254,-4.51897176875433,
128.857201547361));
#137392=CARTESIAN_POINT('Ctrl Pts',(-247.785309788114,-4.5773862407022,
128.998765569001));
#137393=CARTESIAN_POINT('Ctrl Pts',(-247.794017907975,-4.62912257715997,
129.142913288239));
#137394=CARTESIAN_POINT('Ctrl Pts',(-247.802726027836,-4.68085891361773,
129.287061007477));
#137395=CARTESIAN_POINT('Ctrl Pts',(-247.811434147697,-4.72591691600598,
129.43379214805));
#137396=CARTESIAN_POINT('Ctrl Pts',(-247.820142267558,-4.76405452823397,
129.582490119308));
#137397=CARTESIAN_POINT('Origin',(213.235140564004,0.,130.804360617566));
#137398=CARTESIAN_POINT('',(-249.915046309122,-4.76405452823416,129.582490119309));
#137399=CARTESIAN_POINT('',(-249.569887472766,-4.76405452823394,129.582490119308));
#137400=CARTESIAN_POINT('',(213.235140564004,-4.76405452823405,129.582490119308));
#137401=CARTESIAN_POINT('',(-248.235140564067,-4.91824790393295,130.808901317858));
#137402=CARTESIAN_POINT('Ctrl Pts',(-248.235140564067,-4.91824790393295,
130.808901317859));
#137403=CARTESIAN_POINT('Ctrl Pts',(-248.245073907718,-4.91808590314736,
130.984372054252));
#137404=CARTESIAN_POINT('Ctrl Pts',(-248.255007251369,-4.90852990301773,
131.159422601792));
#137405=CARTESIAN_POINT('Ctrl Pts',(-248.26494059502,-4.88973538646957,
131.333199830189));
#137406=CARTESIAN_POINT('Ctrl Pts',(-248.275093853796,-4.87052477655029,
131.510824327155));
#137407=CARTESIAN_POINT('Ctrl Pts',(-248.285247112572,-4.84166205004334,
131.687118758878));
#137408=CARTESIAN_POINT('Ctrl Pts',(-248.295400371347,-4.80336125477624,
131.86119727411));
#137409=CARTESIAN_POINT('Ctrl Pts',(-248.298666847518,-4.79103923700606,
131.917201295518));
#137410=CARTESIAN_POINT('Ctrl Pts',(-248.301933323689,-4.77774072783249,
131.972976140221));
#137411=CARTESIAN_POINT('Ctrl Pts',(-248.30519979986,-4.7634738916458,132.028492777959));
#137412=CARTESIAN_POINT('Ctrl Pts',(-248.312974133979,-4.72951829376561,
132.160624429435));
#137413=CARTESIAN_POINT('Ctrl Pts',(-248.320748468098,-4.69000704421847,
132.291551480925));
#137414=CARTESIAN_POINT('Ctrl Pts',(-248.328522802217,-4.64504042936055,
132.420770983812));
#137415=CARTESIAN_POINT('Ctrl Pts',(-248.336287555164,-4.60012923183666,
132.549831235209));
#137416=CARTESIAN_POINT('Ctrl Pts',(-248.344052308111,-4.54977617352532,
132.677187759432));
#137417=CARTESIAN_POINT('Ctrl Pts',(-248.351817061059,-4.49413219490759,
132.802349325541));
#137418=CARTESIAN_POINT('Ctrl Pts',(-248.359574101944,-4.43854348267371,
132.927386579419));
#137419=CARTESIAN_POINT('Ctrl Pts',(-248.367331142829,-4.3776744656515,
133.050232858668));
#137420=CARTESIAN_POINT('Ctrl Pts',(-248.375088183714,-4.31172526524681,
133.170413934702));
#137421=CARTESIAN_POINT('Ctrl Pts',(-248.382839374954,-4.24582579764725,
133.290504381252));
#137422=CARTESIAN_POINT('Ctrl Pts',(-248.390590566194,-4.17485395937299,
133.407933283708));
#137423=CARTESIAN_POINT('Ctrl Pts',(-248.398341757434,-4.0990570201475,
133.522248512252));
#137424=CARTESIAN_POINT('Ctrl Pts',(-248.406089654211,-4.02329229664303,
133.636515153774));
#137425=CARTESIAN_POINT('Ctrl Pts',(-248.413837550989,-3.94270676666548,
133.747670428353));
#137426=CARTESIAN_POINT('Ctrl Pts',(-248.421585447766,-3.85759236086982,
133.855289040171));
#137427=CARTESIAN_POINT('Ctrl Pts',(-248.42933172385,-3.77249575917322,
133.962885140495));
#137428=CARTESIAN_POINT('Ctrl Pts',(-248.437077999934,-3.6828724083491,
134.066945743093));
#137429=CARTESIAN_POINT('Ctrl Pts',(-248.444824276018,-3.58905582830071,
134.167076978462));
#137430=CARTESIAN_POINT('Ctrl Pts',(-248.452570609284,-3.49523855571951,
134.267208952978));
#137431=CARTESIAN_POINT('Ctrl Pts',(-248.460316942549,-3.3972282594602,
134.363411217083));
#137432=CARTESIAN_POINT('Ctrl Pts',(-248.468063275814,-3.29539649553318,
134.455325558472));
#137433=CARTESIAN_POINT('Ctrl Pts',(-248.475811343817,-3.19354192708882,
134.547260483441));
#137434=CARTESIAN_POINT('Ctrl Pts',(-248.483559411821,-3.08786447822106,
134.634905312997));
#137435=CARTESIAN_POINT('Ctrl Pts',(-248.491307479824,-2.97876974863656,
134.717941311395));
#137436=CARTESIAN_POINT('Ctrl Pts',(-248.499063782565,-2.86955907187506,
134.80106556144));
#137437=CARTESIAN_POINT('Ctrl Pts',(-248.506820085307,-2.75692417082953,
134.879570958235));
#137438=CARTESIAN_POINT('Ctrl Pts',(-248.514576388049,-2.64130112623105,
134.953181103327));
#137439=CARTESIAN_POINT('Ctrl Pts',(-248.522336830563,-2.52561637013232,
135.02683053637));
#137440=CARTESIAN_POINT('Ctrl Pts',(-248.530097273078,-2.4069406307171,
135.095579315715));
#137441=CARTESIAN_POINT('Ctrl Pts',(-248.537857715592,-2.28573481363392,
135.159196943336));
#137442=CARTESIAN_POINT('Ctrl Pts',(-248.545630615857,-2.16433442621301,
135.22291669562));
#137443=CARTESIAN_POINT('Ctrl Pts',(-248.553403516123,-2.04039619862537,
135.281488668921));
#137444=CARTESIAN_POINT('Ctrl Pts',(-248.561176416388,-1.91440206615066,
135.33473011592));
#137445=CARTESIAN_POINT('Ctrl Pts',(-248.568666752149,-1.79298813777539,
135.386036102204));
#137446=CARTESIAN_POINT('Ctrl Pts',(-248.576157087909,-1.66966547237897,
135.432392281381));
#137447=CARTESIAN_POINT('Ctrl Pts',(-248.58364742367,-1.5448769370361,135.473679444966));
#137448=CARTESIAN_POINT('Ctrl Pts',(-248.591421757789,-1.4153570064224,
135.516532023916));
#137449=CARTESIAN_POINT('Ctrl Pts',(-248.599196091908,-1.28384757446238,
135.554059360057));
#137450=CARTESIAN_POINT('Ctrl Pts',(-248.606970426027,-1.15082599329778,
135.58607397113));
#137451=CARTESIAN_POINT('Ctrl Pts',(-248.614735178974,-1.01796834934349,
135.618049127055));
#137452=CARTESIAN_POINT('Ctrl Pts',(-248.622499931921,-0.883602640633271,
135.644524985225));
#137453=CARTESIAN_POINT('Ctrl Pts',(-248.630264684868,-0.748223740684508,
135.665363013819));
#137454=CARTESIAN_POINT('Ctrl Pts',(-248.638021725753,-0.612979300967315,
135.686180345789));
#137455=CARTESIAN_POINT('Ctrl Pts',(-248.645778766639,-0.47672405653943,
135.701370932492));
#137456=CARTESIAN_POINT('Ctrl Pts',(-248.653535807524,-0.339965159850539,
135.710846809597));
#137457=CARTESIAN_POINT('Ctrl Pts',(-248.661286998764,-0.203309394110027,
135.720315540869));
#137458=CARTESIAN_POINT('Ctrl Pts',(-248.669038190004,-0.0661511205453898,
135.724078113441));
#137459=CARTESIAN_POINT('Ctrl Pts',(-248.676789381244,0.0709956158974349,
135.722098175125));
#137460=CARTESIAN_POINT('Ctrl Pts',(-248.684537278021,0.208084061318949,
135.720119078335));
#137461=CARTESIAN_POINT('Ctrl Pts',(-248.692285174798,0.345160589265472,
135.712402330694));
#137462=CARTESIAN_POINT('Ctrl Pts',(-248.700033071575,0.48170959067201,
135.698963658953));
#137463=CARTESIAN_POINT('Ctrl Pts',(-248.707779347659,0.618230028971109,
135.685527798293));
#137464=CARTESIAN_POINT('Ctrl Pts',(-248.715525623743,0.754222771377872,
135.666372432507));
#137465=CARTESIAN_POINT('Ctrl Pts',(-248.723271899827,0.889176168671283,
135.641565265249));
#137466=CARTESIAN_POINT('Ctrl Pts',(-248.731018233092,1.0241305621602,135.616757914871));
#137467=CARTESIAN_POINT('Ctrl Pts',(-248.738764566358,1.15804521070374,
135.586298750453));
#137468=CARTESIAN_POINT('Ctrl Pts',(-248.746510899623,1.29041790504549,
135.550306750092));
#137469=CARTESIAN_POINT('Ctrl Pts',(-248.754258967626,1.42282024333416,
135.514306689572));
#137470=CARTESIAN_POINT('Ctrl Pts',(-248.762007035629,1.55367956309814,
135.472771430119));
#137471=CARTESIAN_POINT('Ctrl Pts',(-248.769755103632,1.68250846637917,
135.4258699298));
#137472=CARTESIAN_POINT('Ctrl Pts',(-248.777511406374,1.81147429055153,
135.378918582007));
#137473=CARTESIAN_POINT('Ctrl Pts',(-248.785267709116,1.93840501953951,
135.326589734343));
#137474=CARTESIAN_POINT('Ctrl Pts',(-248.793024011857,2.0628323992081,135.26910087376));
#137475=CARTESIAN_POINT('Ctrl Pts',(-248.800784454372,2.18732618951599,
135.21158132964));
#137476=CARTESIAN_POINT('Ctrl Pts',(-248.808544896886,2.30931362061622,
135.14889646352));
#137477=CARTESIAN_POINT('Ctrl Pts',(-248.8163053394,2.42835163722904,135.081309458559));
#137478=CARTESIAN_POINT('Ctrl Pts',(-248.824078239665,2.54758074423383,
135.013613956937));
#137479=CARTESIAN_POINT('Ctrl Pts',(-248.831851139931,2.66385064358805,
134.941000798226));
#137480=CARTESIAN_POINT('Ctrl Pts',(-248.839624040196,2.77674708700557,
134.863776668836));
#137481=CARTESIAN_POINT('Ctrl Pts',(-248.847114375959,2.88553946034968,
134.789359831055));
#137482=CARTESIAN_POINT('Ctrl Pts',(-248.854604711722,2.99119913977137,
134.710661627111));
#137483=CARTESIAN_POINT('Ctrl Pts',(-248.862095047485,3.09338645132278,
134.627990218518));
#137484=CARTESIAN_POINT('Ctrl Pts',(-248.869869381604,3.19944822583808,
134.54218429835));
#137485=CARTESIAN_POINT('Ctrl Pts',(-248.877643715723,3.30210509683432,
134.451826130541));
#137486=CARTESIAN_POINT('Ctrl Pts',(-248.885418049842,3.40094130968244,
134.357215986223));
#137487=CARTESIAN_POINT('Ctrl Pts',(-248.893182802789,3.49965571573175,
134.262722440453));
#137488=CARTESIAN_POINT('Ctrl Pts',(-248.900947555737,3.59455855266774,
134.163987612328));
#137489=CARTESIAN_POINT('Ctrl Pts',(-248.908712308684,3.68526577852324,
134.061352973121));
#137490=CARTESIAN_POINT('Ctrl Pts',(-248.916469349569,3.77588291268327,
133.958820272086));
#137491=CARTESIAN_POINT('Ctrl Pts',(-248.924226390454,3.86231247132771,
133.852395759161));
#137492=CARTESIAN_POINT('Ctrl Pts',(-248.931983431339,3.94420631928851,
133.742458569198));
#137493=CARTESIAN_POINT('Ctrl Pts',(-248.939734622579,4.0260384104614,133.632604283726));
#137494=CARTESIAN_POINT('Ctrl Pts',(-248.947485813819,4.10334136646626,
133.519242906031));
#137495=CARTESIAN_POINT('Ctrl Pts',(-248.955237005059,4.17580674932749,
133.402787267439));
#137496=CARTESIAN_POINT('Ctrl Pts',(-248.962984901836,4.24824133246802,
133.2863811256));
#137497=CARTESIAN_POINT('Ctrl Pts',(-248.970732798614,4.3158422257627,133.166883669836));
#137498=CARTESIAN_POINT('Ctrl Pts',(-248.978480695391,4.37834396127831,
133.044737197348));
#137499=CARTESIAN_POINT('Ctrl Pts',(-248.986226971475,4.44083262277824,
132.92261627527));
#137500=CARTESIAN_POINT('Ctrl Pts',(-248.993973247559,4.4982240701115,132.797847786463));
#137501=CARTESIAN_POINT('Ctrl Pts',(-249.001719523643,4.55029870537798,
132.670898791388));
#137502=CARTESIAN_POINT('Ctrl Pts',(-249.009465856909,4.60237372504752,
132.543948859205));
#137503=CARTESIAN_POINT('Ctrl Pts',(-249.017212190174,4.64913170595849,
132.41481875035));
#137504=CARTESIAN_POINT('Ctrl Pts',(-249.024958523439,4.69040129138085,
132.28399529826));
#137505=CARTESIAN_POINT('Ctrl Pts',(-249.032706591443,4.73168011884067,
132.153142549166));
#137506=CARTESIAN_POINT('Ctrl Pts',(-249.040454659446,4.76746798747111,
132.020596075029));
#137507=CARTESIAN_POINT('Ctrl Pts',(-249.048202727449,4.79764359597526,
131.886857263518));
#137508=CARTESIAN_POINT('Ctrl Pts',(-249.05595903019,4.82785127547527,131.752976312806));
#137509=CARTESIAN_POINT('Ctrl Pts',(-249.063715332932,4.85243469337686,
131.617900875276));
#137510=CARTESIAN_POINT('Ctrl Pts',(-249.071471635674,4.87132372481567,
131.482142463404));
#137511=CARTESIAN_POINT('Ctrl Pts',(-249.079232078188,4.89022283789929,
131.34631159318));
#137512=CARTESIAN_POINT('Ctrl Pts',(-249.086992520703,4.90342147092034,
131.20979741123));
#137513=CARTESIAN_POINT('Ctrl Pts',(-249.094752963217,4.91090156512548,
131.073114929435));
#137514=CARTESIAN_POINT('Ctrl Pts',(-249.102525863482,4.9183936670419,130.936213032786));
#137515=CARTESIAN_POINT('Ctrl Pts',(-249.110298763748,4.92014888075586,
130.799142687565));
#137516=CARTESIAN_POINT('Ctrl Pts',(-249.118071664013,4.91620131891253,
130.662418184084));
#137517=CARTESIAN_POINT('Ctrl Pts',(-249.125561999775,4.91239726088594,
130.530663960708));
#137518=CARTESIAN_POINT('Ctrl Pts',(-249.133052335536,4.90329787066862,
130.399231178461));
#137519=CARTESIAN_POINT('Ctrl Pts',(-249.140542671297,4.88897881120401,
130.268572183482));
#137520=CARTESIAN_POINT('Ctrl Pts',(-249.148317005416,4.87411684024612,
130.132959212982));
#137521=CARTESIAN_POINT('Ctrl Pts',(-249.156091339535,4.85358450089919,
129.997750283198));
#137522=CARTESIAN_POINT('Ctrl Pts',(-249.163865673654,4.82740969424021,
129.863457484159));
#137523=CARTESIAN_POINT('Ctrl Pts',(-249.171630426601,4.80126714569114,
129.729330188992));
#137524=CARTESIAN_POINT('Ctrl Pts',(-249.179395179549,4.76949603996935,
129.596117158157));
#137525=CARTESIAN_POINT('Ctrl Pts',(-249.187159932496,4.73217608246419,
129.464326070603));
#137526=CARTESIAN_POINT('Ctrl Pts',(-249.194916973381,4.69489319166695,
129.332665879815));
#137527=CARTESIAN_POINT('Ctrl Pts',(-249.202674014265,4.65207252245242,
129.202425195518));
#137528=CARTESIAN_POINT('Ctrl Pts',(-249.21043105515,4.60384487614628,129.074101845335));
#137529=CARTESIAN_POINT('Ctrl Pts',(-249.218182246391,4.5556535986833,128.945875264789));
#137530=CARTESIAN_POINT('Ctrl Pts',(-249.225933437631,4.50206359701916,
128.81956350492));
#137531=CARTESIAN_POINT('Ctrl Pts',(-249.233684628871,4.44325547958013,
128.695649208748));
#137532=CARTESIAN_POINT('Ctrl Pts',(-249.241432525648,4.38447235715986,
128.571787579457));
#137533=CARTESIAN_POINT('Ctrl Pts',(-249.249180422425,4.32047569735252,
128.450321739644));
#137534=CARTESIAN_POINT('Ctrl Pts',(-249.256928319202,4.25149412541846,
128.331714107441));
#137535=CARTESIAN_POINT('Ctrl Pts',(-249.264674595286,4.18252698294219,
128.213131285398));
#137536=CARTESIAN_POINT('Ctrl Pts',(-249.27242087137,4.10857719883152,128.097405819508));
#137537=CARTESIAN_POINT('Ctrl Pts',(-249.280167147454,4.02991902624946,
127.984974921289));
#137538=CARTESIAN_POINT('Ctrl Pts',(-249.287913480719,3.95126027303076,
127.872543193131));
#137539=CARTESIAN_POINT('Ctrl Pts',(-249.295659813985,3.86789328610782,
127.763406401521));
#137540=CARTESIAN_POINT('Ctrl Pts',(-249.30340614725,3.78013502974059,127.657971859096));
#137541=CARTESIAN_POINT('Ctrl Pts',(-249.311154215253,3.69235712052021,
127.552513705335));
#137542=CARTESIAN_POINT('Ctrl Pts',(-249.318902283256,3.60018623508184,
127.450759750993));
#137543=CARTESIAN_POINT('Ctrl Pts',(-249.326650351259,3.50397863875588,
127.353083062567));
#137544=CARTESIAN_POINT('Ctrl Pts',(-249.334406654001,3.40766879185178,
127.255302562194));
#137545=CARTESIAN_POINT('Ctrl Pts',(-249.342162956743,3.30731393858388,
127.161608263089));
#137546=CARTESIAN_POINT('Ctrl Pts',(-249.349919259484,3.20330652468301,
127.072335648273));
#137547=CARTESIAN_POINT('Ctrl Pts',(-249.357679701999,3.09924359889373,
126.983015385976));
#137548=CARTESIAN_POINT('Ctrl Pts',(-249.365440144513,2.99152453488068,
126.898121752322));
#137549=CARTESIAN_POINT('Ctrl Pts',(-249.373200587027,2.88057286552903,
126.817948317154));
#137550=CARTESIAN_POINT('Ctrl Pts',(-249.380973487292,2.76944308670791,
126.73764618047));
#137551=CARTESIAN_POINT('Ctrl Pts',(-249.388746387558,2.65507065912805,
126.662079599741));
#137552=CARTESIAN_POINT('Ctrl Pts',(-249.396519287823,2.53790670851151,
126.591497861507));
#137553=CARTESIAN_POINT('Ctrl Pts',(-249.404009623585,2.42500196261268,
126.523481947239));
#137554=CARTESIAN_POINT('Ctrl Pts',(-249.411499959348,2.30950539784452,
126.460094892698));
#137555=CARTESIAN_POINT('Ctrl Pts',(-249.41899029511,2.19183848349302,126.401517544644));
#137556=CARTESIAN_POINT('Ctrl Pts',(-249.426764629229,2.06971019232514,
126.340719218637));
#137557=CARTESIAN_POINT('Ctrl Pts',(-249.434538963348,1.94485685943472,
126.284909928026));
#137558=CARTESIAN_POINT('Ctrl Pts',(-249.442313297467,1.81772440187811,
126.234342996012));
#137559=CARTESIAN_POINT('Ctrl Pts',(-249.450078050414,1.69074862371295,
126.183838383222));
#137560=CARTESIAN_POINT('Ctrl Pts',(-249.457842803361,1.56149966938691,
126.138563417195));
#137561=CARTESIAN_POINT('Ctrl Pts',(-249.465607556308,1.43044774628691,
126.0987254524));
#137562=CARTESIAN_POINT('Ctrl Pts',(-249.473364597193,1.29952598580481,
126.058927055234));
#137563=CARTESIAN_POINT('Ctrl Pts',(-249.481121638079,1.16680519183354,
126.024555025821));
#137564=CARTESIAN_POINT('Ctrl Pts',(-249.488878678964,1.03277490216421,
125.99576840529));
#137565=CARTESIAN_POINT('Ctrl Pts',(-249.496629870204,0.898845685778742,
125.967003492974));
#137566=CARTESIAN_POINT('Ctrl Pts',(-249.504381061444,0.763609319957393,
125.943815687576));
#137567=CARTESIAN_POINT('Ctrl Pts',(-249.512132252684,0.627569489207782,
125.926313918454));
#137568=CARTESIAN_POINT('Ctrl Pts',(-249.519880149461,0.491587479015407,
125.908819588051));
#137569=CARTESIAN_POINT('Ctrl Pts',(-249.527628046238,0.354803070057864,
125.897006537039));
#137570=CARTESIAN_POINT('Ctrl Pts',(-249.535375943015,0.217728885343782,
125.890932364809));
#137571=CARTESIAN_POINT('Ctrl Pts',(-249.543122219099,0.0806833735941654,
125.884859463165));
#137572=CARTESIAN_POINT('Ctrl Pts',(-249.550868495183,-0.0566514030112906,
125.884523069839));
#137573=CARTESIAN_POINT('Ctrl Pts',(-249.558614771267,-0.193759365505211,
125.889928771383));
#137574=CARTESIAN_POINT('Ctrl Pts',(-249.566361104533,-0.330868340099152,
125.89533451283));
#137575=CARTESIAN_POINT('Ctrl Pts',(-249.574107437798,-0.467750106578944,
125.906482418326));
#137576=CARTESIAN_POINT('Ctrl Pts',(-249.581853771064,-0.603890654364946,
125.923325979288));
#137577=CARTESIAN_POINT('Ctrl Pts',(-249.589601839067,-0.740061689882508,
125.940173312249));
#137578=CARTESIAN_POINT('Ctrl Pts',(-249.597349907069,-0.875490788471238,
125.962718790783));
#137579=CARTESIAN_POINT('Ctrl Pts',(-249.605097975072,-1.00967150860756,
125.990864330333));
#137580=CARTESIAN_POINT('Ctrl Pts',(-249.612854277814,-1.14399483761019,
126.019039783297));
#137581=CARTESIAN_POINT('Ctrl Pts',(-249.620610580556,-1.27706675450334,
126.052827106273));
#137582=CARTESIAN_POINT('Ctrl Pts',(-249.628366883298,-1.40839288141555,
126.092077460319));
#137583=CARTESIAN_POINT('Ctrl Pts',(-249.636127325812,-1.53978910103584,
126.13134876346));
#137584=CARTESIAN_POINT('Ctrl Pts',(-249.643887768326,-1.66943730462585,
126.176088780145));
#137585=CARTESIAN_POINT('Ctrl Pts',(-249.65164821084,-1.79686157369262,
126.226099861833));
#137586=CARTESIAN_POINT('Ctrl Pts',(-249.659421111106,-1.92449039550829,
126.276191225748));
#137587=CARTESIAN_POINT('Ctrl Pts',(-249.667194011371,-2.04988779084198,
126.331570405567));
#137588=CARTESIAN_POINT('Ctrl Pts',(-249.674966911637,-2.17260018339459,
126.391992601907));
#137589=CARTESIAN_POINT('Ctrl Pts',(-249.682457247399,-2.29085167138406,
126.450218299215));
#137590=CARTESIAN_POINT('Ctrl Pts',(-249.689947583161,-2.40660970999656,
126.513126578891));
#137591=CARTESIAN_POINT('Ctrl Pts',(-249.697437918923,-2.5194943332875,
126.580460598977));
#137592=CARTESIAN_POINT('Ctrl Pts',(-249.705213487546,-2.63667761621944,
126.650358706415));
#137593=CARTESIAN_POINT('Ctrl Pts',(-249.712989056169,-2.75113556809579,
126.725247750044));
#137594=CARTESIAN_POINT('Ctrl Pts',(-249.720764624791,-2.86241381722082,
126.804889377329));
#137595=CARTESIAN_POINT('Ctrl Pts',(-249.728859694972,-2.97826453887508,
126.887803514343));
#137596=CARTESIAN_POINT('Ctrl Pts',(-249.736954765152,-3.09066828496617,
126.97586899289));
#137597=CARTESIAN_POINT('Ctrl Pts',(-249.745049835333,-3.19914004090874,
127.06876346836));
#137598=CARTESIAN_POINT('Ctrl Pts',(-249.752805844448,-3.30306847007098,
127.157767069616));
#137599=CARTESIAN_POINT('Ctrl Pts',(-249.760561853563,-3.40338725556096,
127.251203075515));
#137600=CARTESIAN_POINT('Ctrl Pts',(-249.768317862678,-3.49969948600923,
127.348743947545));
#137601=CARTESIAN_POINT('Ctrl Pts',(-249.776068582077,-3.59594603005828,
127.446218295224));
#137602=CARTESIAN_POINT('Ctrl Pts',(-249.783819301476,-3.68819118215815,
127.547791662028));
#137603=CARTESIAN_POINT('Ctrl Pts',(-249.791570020876,-3.77607264096405,
127.653097621137));
#137604=CARTESIAN_POINT('Ctrl Pts',(-249.799317132766,-3.86391319605633,
127.75835456644));
#137605=CARTESIAN_POINT('Ctrl Pts',(-249.807064244655,-3.94739385008372,
127.867340347028));
#137606=CARTESIAN_POINT('Ctrl Pts',(-249.814811356545,-4.02619085685783,
127.979653509448));
#137607=CARTESIAN_POINT('Ctrl Pts',(-249.822556540329,-4.10496825258799,
128.091938719303));
#137608=CARTESIAN_POINT('Ctrl Pts',(-249.830301724113,-4.17906409811855,
128.207549342181));
#137609=CARTESIAN_POINT('Ctrl Pts',(-249.838046907898,-4.24819670454866,
128.32605316651));
#137610=CARTESIAN_POINT('Ctrl Pts',(-249.845793796111,-4.31734452451827,
128.444583069164));
#137611=CARTESIAN_POINT('Ctrl Pts',(-249.853540684325,-4.38152672280169,
128.566007109581));
#137612=CARTESIAN_POINT('Ctrl Pts',(-249.861287572539,-4.44050651143091,
128.689866591933));
#137613=CARTESIAN_POINT('Ctrl Pts',(-249.86903549896,-4.4994942043001,128.813742673446));
#137614=CARTESIAN_POINT('Ctrl Pts',(-249.876783425381,-4.55327793829618,
128.940054490589));
#137615=CARTESIAN_POINT('Ctrl Pts',(-249.884531351803,-4.60166857118941,
129.068322189585));
#137616=CARTESIAN_POINT('Ctrl Pts',(-249.892284423878,-4.65009134190414,
129.196675075406));
#137617=CARTESIAN_POINT('Ctrl Pts',(-249.900037495954,-4.69311373133983,
129.32698606768));
#137618=CARTESIAN_POINT('Ctrl Pts',(-249.90779056803,-4.73059604889384,
129.45875886196));
#137619=CARTESIAN_POINT('Ctrl Pts',(-249.910209148394,-4.74228870392702,
129.499865547107));
#137620=CARTESIAN_POINT('Ctrl Pts',(-249.912627728758,-4.75344260573139,
129.541114394529));
#137621=CARTESIAN_POINT('Ctrl Pts',(-249.915046309122,-4.76405452823416,
129.582490119309));
#137622=CARTESIAN_POINT('Ctrl Pts',(-248.165132725248,-4.76405452823402,
129.582490119308));
#137623=CARTESIAN_POINT('Ctrl Pts',(-248.172792275957,-4.79778234205211,
129.713994353494));
#137624=CARTESIAN_POINT('Ctrl Pts',(-248.180451826665,-4.82605794979784,
129.84688428109));
#137625=CARTESIAN_POINT('Ctrl Pts',(-248.188111377374,-4.84878389437866,
129.980662973941));
#137626=CARTESIAN_POINT('Ctrl Pts',(-248.195949575147,-4.87203988614429,
130.117561845989));
#137627=CARTESIAN_POINT('Ctrl Pts',(-248.203787772921,-4.88948405967343,
130.255391020222));
#137628=CARTESIAN_POINT('Ctrl Pts',(-248.211625970694,-4.90106802037398,
130.393610910119));
#137629=CARTESIAN_POINT('Ctrl Pts',(-248.219464168467,-4.91265198107455,
130.531830800017));
#137630=CARTESIAN_POINT('Ctrl Pts',(-248.227302366241,-4.91837573540535,
130.670440957191));
#137631=CARTESIAN_POINT('Ctrl Pts',(-248.235140564014,-4.91824790393381,
130.808901316927));
#137632=CARTESIAN_POINT('',(-247.889859435962,-4.91824972168853,130.802706044916));
#137633=CARTESIAN_POINT('Ctrl Pts',(-247.820142267558,-4.76405452823397,
129.582490119308));
#137634=CARTESIAN_POINT('Ctrl Pts',(-247.828536217527,-4.80081621894209,
129.725823393442));
#137635=CARTESIAN_POINT('Ctrl Pts',(-247.836930167496,-4.83114800021644,
129.870983747846));
#137636=CARTESIAN_POINT('Ctrl Pts',(-247.845324117465,-4.85488130107452,
130.017397711847));
#137637=CARTESIAN_POINT('Ctrl Pts',(-247.853689943783,-4.87853508429589,
130.163321120723));
#137638=CARTESIAN_POINT('Ctrl Pts',(-247.862055770101,-4.89563442656382,
130.310489485434));
#137639=CARTESIAN_POINT('Ctrl Pts',(-247.870421596419,-4.90606132854246,
130.458318274665));
#137640=CARTESIAN_POINT('Ctrl Pts',(-247.876900876267,-4.91413689852136,
130.572810741822));
#137641=CARTESIAN_POINT('Ctrl Pts',(-247.883380156114,-4.9182110315957,
130.687698983515));
#137642=CARTESIAN_POINT('Ctrl Pts',(-247.889859435962,-4.91824972168853,
130.802706044916));
#137643=CARTESIAN_POINT('Ctrl Pts',(-247.889859435997,-4.91824972168874,
130.802706045539));
#137644=CARTESIAN_POINT('Ctrl Pts',(-247.897794815772,-4.91829710665618,
130.94355884562));
#137645=CARTESIAN_POINT('Ctrl Pts',(-247.905730195547,-4.91228935523591,
131.084363800434));
#137646=CARTESIAN_POINT('Ctrl Pts',(-247.913665575322,-4.90026508898193,
131.224580940974));
#137647=CARTESIAN_POINT('Ctrl Pts',(-247.921605586623,-4.88823380470223,
131.364879919979));
#137648=CARTESIAN_POINT('Ctrl Pts',(-247.929545597924,-4.8701790377454,
131.504590038808));
#137649=CARTESIAN_POINT('Ctrl Pts',(-247.937485609225,-4.84619113119443,
131.643177988889));
#137650=CARTESIAN_POINT('Ctrl Pts',(-247.945431595334,-4.82218517389707,
131.781870225516));
#137651=CARTESIAN_POINT('Ctrl Pts',(-247.953377581442,-4.79223724032085,
131.919438252654));
#137652=CARTESIAN_POINT('Ctrl Pts',(-247.961323567551,-4.75648844461589,
132.055360513144));
#137653=CARTESIAN_POINT('Ctrl Pts',(-247.969282639919,-4.72068077415252,
132.191506624258));
#137654=CARTESIAN_POINT('Ctrl Pts',(-247.977241712287,-4.67905324684613,
132.326001201571));
#137655=CARTESIAN_POINT('Ctrl Pts',(-247.985200784655,-4.63179671806932,
132.458338315415));
#137656=CARTESIAN_POINT('Ctrl Pts',(-247.993167071821,-4.58449735185158,
132.590795391166));
#137657=CARTESIAN_POINT('Ctrl Pts',(-248.001133358986,-4.53155894570825,
132.721090767681));
#137658=CARTESIAN_POINT('Ctrl Pts',(-248.009099646152,-4.47321970686905,
132.848740356406));
#137659=CARTESIAN_POINT('Ctrl Pts',(-248.017080531472,-4.41477356186177,
132.976623861936));
#137660=CARTESIAN_POINT('Ctrl Pts',(-248.025061416793,-4.35090697226165,
133.10185156794));
#137661=CARTESIAN_POINT('Ctrl Pts',(-248.033042302113,-4.28190365658586,
133.223964745976));
#137662=CARTESIAN_POINT('Ctrl Pts',(-248.037475258811,-4.24357599015597,
133.291792112076));
#137663=CARTESIAN_POINT('Ctrl Pts',(-248.041908215508,-4.20366430447484,
133.358659105839));
#137664=CARTESIAN_POINT('Ctrl Pts',(-248.046341172206,-4.16222272274684,
133.424491352615));
#137665=CARTESIAN_POINT('Ctrl Pts',(-248.054115506325,-4.08954420933897,
133.539945194637));
#137666=CARTESIAN_POINT('Ctrl Pts',(-248.061889840444,-4.01194316211871,
133.652555625427));
#137667=CARTESIAN_POINT('Ctrl Pts',(-248.069664174563,-3.92966864626729,
133.761874335716));
#137668=CARTESIAN_POINT('Ctrl Pts',(-248.07742892751,-3.84749552640357,
133.871058320464));
#137669=CARTESIAN_POINT('Ctrl Pts',(-248.085193680457,-3.76066063070443,
133.976958347055));
#137670=CARTESIAN_POINT('Ctrl Pts',(-248.092958433404,-3.66945768165939,
134.079152730817));
#137671=CARTESIAN_POINT('Ctrl Pts',(-248.100715474289,-3.57834531666907,
134.181245613677));
#137672=CARTESIAN_POINT('Ctrl Pts',(-248.108472515174,-3.48287379060651,
134.279639888254));
#137673=CARTESIAN_POINT('Ctrl Pts',(-248.116229556059,-3.38337846682548,
134.373945076956));
#137674=CARTESIAN_POINT('Ctrl Pts',(-248.1239807473,-3.28395817324195,134.468179149382));
#137675=CARTESIAN_POINT('Ctrl Pts',(-248.13173193854,-3.18052040429157,
134.558330005808));
#137676=CARTESIAN_POINT('Ctrl Pts',(-248.13948312978,-3.07343867253532,
134.64404260813));
#137677=CARTESIAN_POINT('Ctrl Pts',(-248.147231026557,-2.96640245337171,
134.72971878031));
#137678=CARTESIAN_POINT('Ctrl Pts',(-248.154978923334,-2.8557256563982,
134.810960206441));
#137679=CARTESIAN_POINT('Ctrl Pts',(-248.162726820111,-2.74181612894852,
134.887451037522));
#137680=CARTESIAN_POINT('Ctrl Pts',(-248.170473096195,-2.62793042891638,
134.963925868371));
#137681=CARTESIAN_POINT('Ctrl Pts',(-248.178219372279,-2.51081366781225,
135.035651862921));
#137682=CARTESIAN_POINT('Ctrl Pts',(-248.185965648363,-2.39090370055229,
135.102355796389));
#137683=CARTESIAN_POINT('Ctrl Pts',(-248.193711981629,-2.27099284814436,
135.16906022225));
#137684=CARTESIAN_POINT('Ctrl Pts',(-248.201458314894,-2.14828909009672,
135.230742322996));
#137685=CARTESIAN_POINT('Ctrl Pts',(-248.209204648159,-2.02325561360943,
135.287174441996));
#137686=CARTESIAN_POINT('Ctrl Pts',(-248.216952716162,-1.89819413674217,
135.343619198577));
#137687=CARTESIAN_POINT('Ctrl Pts',(-248.224700784165,-1.77080225954732,
135.394811473107));
#137688=CARTESIAN_POINT('Ctrl Pts',(-248.232448852168,-1.64156353356948,
135.440571595051));
#137689=CARTESIAN_POINT('Ctrl Pts',(-248.24020515491,-1.51218745113518,
135.486380351398));
#137690=CARTESIAN_POINT('Ctrl Pts',(-248.247961457652,-1.38096096804064,
135.526745291558));
#137691=CARTESIAN_POINT('Ctrl Pts',(-248.255717760394,-1.24838373415665,
135.561536367398));
#137692=CARTESIAN_POINT('Ctrl Pts',(-248.263478202908,-1.1157357398111,
135.596346012284));
#137693=CARTESIAN_POINT('Ctrl Pts',(-248.271238645422,-0.981735939945509,
135.62557578175));
#137694=CARTESIAN_POINT('Ctrl Pts',(-248.278999087936,-0.846893608806071,
135.649146916038));
#137695=CARTESIAN_POINT('Ctrl Pts',(-248.286771988202,-0.711834816785949,
135.672755888804));
#137696=CARTESIAN_POINT('Ctrl Pts',(-248.294544888467,-0.575931178582748,
135.690688023004));
#137697=CARTESIAN_POINT('Ctrl Pts',(-248.302317788733,-0.439697413820081,
135.702916450338));
#137698=CARTESIAN_POINT('Ctrl Pts',(-248.309808124495,-0.308416089557942,
135.714700343536));
#137699=CARTESIAN_POINT('Ctrl Pts',(-248.317298460257,-0.176828531537549,
135.721188003327));
#137700=CARTESIAN_POINT('Ctrl Pts',(-248.324788796019,-0.0453928562305962,
135.722401137031));
#137701=CARTESIAN_POINT('Ctrl Pts',(-248.332563130138,0.0910262426536748,
135.723660267069));
#137702=CARTESIAN_POINT('Ctrl Pts',(-248.340337464257,0.227713848903923,
135.719240996771));
#137703=CARTESIAN_POINT('Ctrl Pts',(-248.348111798376,0.364158161420716,
135.709110549619));
#137704=CARTESIAN_POINT('Ctrl Pts',(-248.355876551323,0.500434318516711,
135.698992587337));
#137705=CARTESIAN_POINT('Ctrl Pts',(-248.36364130427,0.636467392317943,
135.683177481418));
#137706=CARTESIAN_POINT('Ctrl Pts',(-248.371406057217,0.77174384338724,
135.661684418044));
#137707=CARTESIAN_POINT('Ctrl Pts',(-248.379163098102,0.906885935978272,
135.640212701885));
#137708=CARTESIAN_POINT('Ctrl Pts',(-248.386920138987,1.04127251770969,
135.613074311937));
#137709=CARTESIAN_POINT('Ctrl Pts',(-248.394677179872,1.17439379663845,
135.580340336212));
#137710=CARTESIAN_POINT('Ctrl Pts',(-248.402428371112,1.30741468777542,
135.547631045432));
#137711=CARTESIAN_POINT('Ctrl Pts',(-248.410179562353,1.43917179721702,
135.50933466086));
#137712=CARTESIAN_POINT('Ctrl Pts',(-248.417930753593,1.56916452868885,
135.465573522423));
#137713=CARTESIAN_POINT('Ctrl Pts',(-248.42567865037,1.69910200978197,135.421830983637));
#137714=CARTESIAN_POINT('Ctrl Pts',(-248.433426547147,1.8272762346577,135.37262843507));
#137715=CARTESIAN_POINT('Ctrl Pts',(-248.441174443924,1.95320101916071,
135.318138286132));
#137716=CARTESIAN_POINT('Ctrl Pts',(-248.448920720008,2.07909946291343,
135.26365953536));
#137717=CARTESIAN_POINT('Ctrl Pts',(-248.456666996092,2.20274904362696,
135.203895539383));
#137718=CARTESIAN_POINT('Ctrl Pts',(-248.464413272176,2.32368321827512,
135.139066993274));
#137719=CARTESIAN_POINT('Ctrl Pts',(-248.472159605441,2.44461828563171,
135.074237968616));
#137720=CARTESIAN_POINT('Ctrl Pts',(-248.479905938707,2.56283756234785,
135.004344503942));
#137721=CARTESIAN_POINT('Ctrl Pts',(-248.487652271972,2.67789915045646,
134.929653237791));
#137722=CARTESIAN_POINT('Ctrl Pts',(-248.495400339975,2.79298650580979,
134.85494524505));
#137723=CARTESIAN_POINT('Ctrl Pts',(-248.503148407978,2.90491443755587,
134.775437525664));
#137724=CARTESIAN_POINT('Ctrl Pts',(-248.510896475981,3.01327041236418,
134.691439788932));
#137725=CARTESIAN_POINT('Ctrl Pts',(-248.518652778723,3.12174154919241,
134.607352778406));
#137726=CARTESIAN_POINT('Ctrl Pts',(-248.526409081465,3.22663283604072,
134.518766457776));
#137727=CARTESIAN_POINT('Ctrl Pts',(-248.534165384206,3.32756478677328,
134.426030902438));
#137728=CARTESIAN_POINT('Ctrl Pts',(-248.541925826721,3.42855060792695,
134.333245851342));
#137729=CARTESIAN_POINT('Ctrl Pts',(-248.549686269235,3.52557260576337,
134.236307429017));
#137730=CARTESIAN_POINT('Ctrl Pts',(-248.557446711749,3.61828924229707,
134.135601530736));
#137731=CARTESIAN_POINT('Ctrl Pts',(-248.565219612014,3.71115471580673,
134.034733970407));
#137732=CARTESIAN_POINT('Ctrl Pts',(-248.57299251228,3.79970076425357,133.930087147147));
#137733=CARTESIAN_POINT('Ctrl Pts',(-248.580765412545,3.88362656404538,
133.822079586181));
#137734=CARTESIAN_POINT('Ctrl Pts',(-248.588255748307,3.96450144961888,
133.717998372111));
#137735=CARTESIAN_POINT('Ctrl Pts',(-248.595746084069,4.04108599085593,
133.610796771382));
#137736=CARTESIAN_POINT('Ctrl Pts',(-248.603236419831,4.11315082759725,
133.500871943694));
#137737=CARTESIAN_POINT('Ctrl Pts',(-248.61101075395,4.18794802452673,133.386779282754));
#137738=CARTESIAN_POINT('Ctrl Pts',(-248.618785088069,4.25811295722376,
133.269391404879));
#137739=CARTESIAN_POINT('Ctrl Pts',(-248.626559422189,4.32334140887819,
133.149121186319));
#137740=CARTESIAN_POINT('Ctrl Pts',(-248.634324175136,4.3884894722956,133.028999190055));
#137741=CARTESIAN_POINT('Ctrl Pts',(-248.642088928083,4.44871297496066,
132.906002261354));
#137742=CARTESIAN_POINT('Ctrl Pts',(-248.64985368103,4.50375047814352,132.780572826091));
#137743=CARTESIAN_POINT('Ctrl Pts',(-248.657610721915,4.55873331730233,
132.655267969111));
#137744=CARTESIAN_POINT('Ctrl Pts',(-248.6653677628,4.6085402512409,132.527535769216));
#137745=CARTESIAN_POINT('Ctrl Pts',(-248.673124803685,4.65295553331785,
132.397843553611));
#137746=CARTESIAN_POINT('Ctrl Pts',(-248.680875994925,4.69733732148527,
132.268249139915));
#137747=CARTESIAN_POINT('Ctrl Pts',(-248.688627186165,4.73633542453395,
132.136698020883));
#137748=CARTESIAN_POINT('Ctrl Pts',(-248.696378377405,4.76978218599676,
132.00367749006));
#137749=CARTESIAN_POINT('Ctrl Pts',(-248.704126274182,4.80321473169359,
131.870713496511));
#137750=CARTESIAN_POINT('Ctrl Pts',(-248.711874170959,4.83110053346967,
131.7362817117));
#137751=CARTESIAN_POINT('Ctrl Pts',(-248.719622067737,4.85332184983542,
131.600884367626));
#137752=CARTESIAN_POINT('Ctrl Pts',(-248.727368343821,4.87553851798082,
131.465515345758));
#137753=CARTESIAN_POINT('Ctrl Pts',(-248.735114619905,4.89209299424579,
131.329181551923));
#137754=CARTESIAN_POINT('Ctrl Pts',(-248.742860895989,4.90291877774331,
131.192394793061));
#137755=CARTESIAN_POINT('Ctrl Pts',(-248.750607229255,4.91374464115433,
131.05560702447));
#137756=CARTESIAN_POINT('Ctrl Pts',(-248.75835356252,4.91884169656952,130.918366673925));
#137757=CARTESIAN_POINT('Ctrl Pts',(-248.766099895785,4.91819541789862,
130.781189647345));
#137758=CARTESIAN_POINT('Ctrl Pts',(-248.773847963788,4.9175489944981,130.643981900921));
#137759=CARTESIAN_POINT('Ctrl Pts',(-248.781596031791,4.91115667950407,
130.506837897567));
#137760=CARTESIAN_POINT('Ctrl Pts',(-248.789344099794,4.89905605577746,
130.370272118697));
#137761=CARTESIAN_POINT('Ctrl Pts',(-248.797100402536,4.88694257136397,
130.233561196092));
#137762=CARTESIAN_POINT('Ctrl Pts',(-248.804856705278,4.86910869357656,
130.09743011565));
#137763=CARTESIAN_POINT('Ctrl Pts',(-248.81261300802,4.84564382923425,129.962387374105));
#137764=CARTESIAN_POINT('Ctrl Pts',(-248.820373450534,4.82216644098725,
129.827272556183));
#137765=CARTESIAN_POINT('Ctrl Pts',(-248.828133893048,4.79305216057069,
129.693247616478));
#137766=CARTESIAN_POINT('Ctrl Pts',(-248.835894335562,4.75844104298344,
129.560808486391));
#137767=CARTESIAN_POINT('Ctrl Pts',(-248.843667235828,4.7237743645577,129.428156753255));
#137768=CARTESIAN_POINT('Ctrl Pts',(-248.851440136093,4.68359333044033,
129.29709629083));
#137769=CARTESIAN_POINT('Ctrl Pts',(-248.859213036359,4.63808745525572,
129.16810641363));
#137770=CARTESIAN_POINT('Ctrl Pts',(-248.866703372121,4.59423583325682,
129.043805643373));
#137771=CARTESIAN_POINT('Ctrl Pts',(-248.874193707883,4.54543990567714,
128.921427816106));
#137772=CARTESIAN_POINT('Ctrl Pts',(-248.881684043645,4.49190983945131,
128.801380573546));
#137773=CARTESIAN_POINT('Ctrl Pts',(-248.889458377764,4.43635016449402,
128.676781703297));
#137774=CARTESIAN_POINT('Ctrl Pts',(-248.897232711883,4.37551427823678,
128.554298942895));
#137775=CARTESIAN_POINT('Ctrl Pts',(-248.905007046002,4.30958510854546,
128.434411408257));
#137776=CARTESIAN_POINT('Ctrl Pts',(-248.912771798949,4.24373719066353,
128.314671624291));
#137777=CARTESIAN_POINT('Ctrl Pts',(-248.920536551896,4.17280866532491,
128.197521041551));
#137778=CARTESIAN_POINT('Ctrl Pts',(-248.928301304843,4.09703044392781,
128.083418757836));
#137779=CARTESIAN_POINT('Ctrl Pts',(-248.936058345728,4.0213274865287,127.969429802119));
#137780=CARTESIAN_POINT('Ctrl Pts',(-248.943815386613,3.94078463358913,
127.858483443915));
#137781=CARTESIAN_POINT('Ctrl Pts',(-248.951572427498,3.85567844439299,
127.751013798755));
#137782=CARTESIAN_POINT('Ctrl Pts',(-248.959323618738,3.77063643443604,
127.64362519729));
#137783=CARTESIAN_POINT('Ctrl Pts',(-248.967074809978,3.68103817955354,
127.539708395561));
#137784=CARTESIAN_POINT('Ctrl Pts',(-248.974826001218,3.5872030311884,127.439667841764));
#137785=CARTESIAN_POINT('Ctrl Pts',(-248.982573897995,3.49340776526433,
127.339669807871));
#137786=CARTESIAN_POINT('Ctrl Pts',(-248.990321794772,3.39537945440582,
127.243545029701));
#137787=CARTESIAN_POINT('Ctrl Pts',(-248.99806969155,3.29347699846595,127.151664035166));
#137788=CARTESIAN_POINT('Ctrl Pts',(-249.005815967634,3.1915958583231,127.059802260155));
#137789=CARTESIAN_POINT('Ctrl Pts',(-249.013562243718,3.08584247518324,
126.97218276472));
#137790=CARTESIAN_POINT('Ctrl Pts',(-249.021308519802,2.97661150136495,
126.889138142094));
#137791=CARTESIAN_POINT('Ctrl Pts',(-249.029054853067,2.86737972122827,
126.806092906451));
#137792=CARTESIAN_POINT('Ctrl Pts',(-249.036801186332,2.75467061042075,
126.727622847623));
#137793=CARTESIAN_POINT('Ctrl Pts',(-249.044547519598,2.63891036349626,
126.654019046571));
#137794=CARTESIAN_POINT('Ctrl Pts',(-249.052295587601,2.52312419286693,
126.580398762458));
#137795=CARTESIAN_POINT('Ctrl Pts',(-249.060043655604,2.40428585632989,
126.51164711436));
#137796=CARTESIAN_POINT('Ctrl Pts',(-249.067791723607,2.28284851612436,
126.448010572525));
#137797=CARTESIAN_POINT('Ctrl Pts',(-249.075548026349,2.16128211086871,
126.384306397016));
#137798=CARTESIAN_POINT('Ctrl Pts',(-249.083304329091,2.03711153089903,
126.325728369314));
#137799=CARTESIAN_POINT('Ctrl Pts',(-249.091060631832,1.91081291549025,
126.272476123838));
#137800=CARTESIAN_POINT('Ctrl Pts',(-249.098821074346,1.78444689070799,
126.219195456034));
#137801=CARTESIAN_POINT('Ctrl Pts',(-249.106581516861,1.65595093343024,
126.171246371056));
#137802=CARTESIAN_POINT('Ctrl Pts',(-249.114341959375,1.52581798793829,
126.128779099703));
#137803=CARTESIAN_POINT('Ctrl Pts',(-249.12211485964,1.39547614148924,126.086243656115));
#137804=CARTESIAN_POINT('Ctrl Pts',(-249.129887759906,1.2634924322091,126.049207716833));
#137805=CARTESIAN_POINT('Ctrl Pts',(-249.137660660171,1.13037255825735,
126.01777091904));
#137806=CARTESIAN_POINT('Ctrl Pts',(-249.145150995933,1.00209192703174,
125.98747692803));
#137807=CARTESIAN_POINT('Ctrl Pts',(-249.152641331695,0.87275660426685,
125.962382118993));
#137808=CARTESIAN_POINT('Ctrl Pts',(-249.160131667457,0.74282315084553,
125.942530012838));
#137809=CARTESIAN_POINT('Ctrl Pts',(-249.167906001576,0.607963231046265,
125.921925208045));
#137810=CARTESIAN_POINT('Ctrl Pts',(-249.175680335695,0.472031733306959,
125.90690323831));
#137811=CARTESIAN_POINT('Ctrl Pts',(-249.183454669814,0.335530628397265,
125.897569175095));
#137812=CARTESIAN_POINT('Ctrl Pts',(-249.191219422762,0.199197748899919,
125.888246615279));
#137813=CARTESIAN_POINT('Ctrl Pts',(-249.198984175709,0.0622970452927646,
125.884598040913));
#137814=CARTESIAN_POINT('Ctrl Pts',(-249.206748928656,-0.074660417192231,
125.886677333274));
#137815=CARTESIAN_POINT('Ctrl Pts',(-249.214505969541,-0.211481851594725,
125.888754560453));
#137816=CARTESIAN_POINT('Ctrl Pts',(-249.222263010426,-0.348359544298285,
125.896548327098));
#137817=CARTESIAN_POINT('Ctrl Pts',(-249.230020051311,-0.484778774564979,
125.910060606101));
#137818=CARTESIAN_POINT('Ctrl Pts',(-249.237771242551,-0.621095130028756,
125.923562695388));
#137819=CARTESIAN_POINT('Ctrl Pts',(-249.245522433791,-0.756953323723316,
125.942774675131));
#137820=CARTESIAN_POINT('Ctrl Pts',(-249.253273625031,-0.891840464670545,
125.967646480047));
#137821=CARTESIAN_POINT('Ctrl Pts',(-249.261021521808,-1.02667027498482,
125.992507713782));
#137822=CARTESIAN_POINT('Ctrl Pts',(-249.268769418585,-1.16052946974826,
126.023023917434));
#137823=CARTESIAN_POINT('Ctrl Pts',(-249.276517315362,-1.29291231919679,
126.05909341778));
#137824=CARTESIAN_POINT('Ctrl Pts',(-249.284263591447,-1.42526747700707,
126.095155373163));
#137825=CARTESIAN_POINT('Ctrl Pts',(-249.292009867531,-1.55614652678626,
126.136768211983));
#137826=CARTESIAN_POINT('Ctrl Pts',(-249.299756143615,-1.68505632921115,
126.183779676831));
#137827=CARTESIAN_POINT('Ctrl Pts',(-249.30750247688,-1.81396708321909,
126.230791488707));
#137828=CARTESIAN_POINT('Ctrl Pts',(-249.315248810145,-1.94090819356345,
126.283201872183));
#137829=CARTESIAN_POINT('Ctrl Pts',(-249.322995143411,-2.06540439702046,
126.340809594079));
#137830=CARTESIAN_POINT('Ctrl Pts',(-249.330743211414,-2.18992848053819,
126.398430216826));
#137831=CARTESIAN_POINT('Ctrl Pts',(-249.338491279417,-2.3120062129153,
126.461250329881));
#137832=CARTESIAN_POINT('Ctrl Pts',(-249.34623934742,-2.4311852864939,126.529021898209));
#137833=CARTESIAN_POINT('Ctrl Pts',(-249.353995650161,-2.55049102501095,
126.596865494966));
#137834=CARTESIAN_POINT('Ctrl Pts',(-249.361751952903,-2.66689161024097,
126.669670865767));
#137835=CARTESIAN_POINT('Ctrl Pts',(-249.369508255645,-2.77996171918606,
126.747145328435));
#137836=CARTESIAN_POINT('Ctrl Pts',(-249.377268698159,-2.89309217705247,
126.824661141555));
#137837=CARTESIAN_POINT('Ctrl Pts',(-249.385029140673,-3.00288830383,126.906850777956));
#137838=CARTESIAN_POINT('Ctrl Pts',(-249.392789583188,-3.10895725766776,
126.993380713067));
#137839=CARTESIAN_POINT('Ctrl Pts',(-249.400562483453,-3.21519648280686,
127.080049553712));
#137840=CARTESIAN_POINT('Ctrl Pts',(-249.408335383719,-3.3176962861842,
127.171072356468));
#137841=CARTESIAN_POINT('Ctrl Pts',(-249.416108283984,-3.41609949800904,
127.26607751948));
#137842=CARTESIAN_POINT('Ctrl Pts',(-249.423598619746,-3.51092550522239,
127.357629005514));
#137843=CARTESIAN_POINT('Ctrl Pts',(-249.431088955508,-3.6019473799333,
127.452878118264));
#137844=CARTESIAN_POINT('Ctrl Pts',(-249.43857929127,-3.68888172445778,
127.551464264243));
#137845=CARTESIAN_POINT('Ctrl Pts',(-249.446285008328,-3.77831582765243,
127.652885211296));
#137846=CARTESIAN_POINT('Ctrl Pts',(-249.453990725386,-3.86371940592775,
127.758173481036));
#137847=CARTESIAN_POINT('Ctrl Pts',(-249.461696442444,-3.9447347773999,
127.866972219946));
#137848=CARTESIAN_POINT('Ctrl Pts',(-249.469392876313,-4.02565254848667,
127.975639887448));
#137849=CARTESIAN_POINT('Ctrl Pts',(-249.477089310182,-4.1021923901458,
128.087809297744));
#137850=CARTESIAN_POINT('Ctrl Pts',(-249.484785744052,-4.17403438468894,
128.203087848721));
#137851=CARTESIAN_POINT('Ctrl Pts',(-249.492473286064,-4.24579337861153,
128.318233215878));
#137852=CARTESIAN_POINT('Ctrl Pts',(-249.500160828075,-4.31286512077841,
128.436480237057));
#137853=CARTESIAN_POINT('Ctrl Pts',(-249.507848370087,-4.37497128105645,
128.557405043365));
#137854=CARTESIAN_POINT('Ctrl Pts',(-249.515530741533,-4.43703566933476,
128.678248516824));
#137855=CARTESIAN_POINT('Ctrl Pts',(-249.523213112979,-4.49414093610544,
128.801765840908));
#137856=CARTESIAN_POINT('Ctrl Pts',(-249.530895484424,-4.54605329422833,
128.927506198988));
#137857=CARTESIAN_POINT('Ctrl Pts',(-249.538574635081,-4.59794388839659,
129.053193841153));
#137858=CARTESIAN_POINT('Ctrl Pts',(-249.546253785737,-4.64464575123465,
129.181102296535));
#137859=CARTESIAN_POINT('Ctrl Pts',(-249.553932936393,-4.68597230028519,
129.310758708268));
#137860=CARTESIAN_POINT('Ctrl Pts',(-249.559251115184,-4.71459291036385,
129.40055196925));
#137861=CARTESIAN_POINT('Ctrl Pts',(-249.564569293975,-4.74063637976063,
129.49118311383));
#137862=CARTESIAN_POINT('Ctrl Pts',(-249.569887472766,-4.76405452823394,
129.582490119308));
#137863=CARTESIAN_POINT('Origin',(213.235140564004,0.,130.804360617566));
#137864=CARTESIAN_POINT('',(-251.665320902482,-4.76405452823412,129.582490119309));
#137865=CARTESIAN_POINT('',(-251.319768125496,-4.76405452823393,129.582490119308));
#137866=CARTESIAN_POINT('',(213.235140564004,-4.76405452823405,129.582490119308));
#137867=CARTESIAN_POINT('',(-249.985140564054,-4.91824989614162,130.803349873801));
#137868=CARTESIAN_POINT('Ctrl Pts',(-249.985140564054,-4.91824989614162,
130.803349873801));
#137869=CARTESIAN_POINT('Ctrl Pts',(-249.992872285789,-4.91827778423735,
130.939052540223));
#137870=CARTESIAN_POINT('Ctrl Pts',(-250.000604007523,-4.91268502623554,
131.074980544808));
#137871=CARTESIAN_POINT('Ctrl Pts',(-250.008335729258,-4.90144173251262,
131.210626546834));
#137872=CARTESIAN_POINT('Ctrl Pts',(-250.016058012704,-4.8902121637339,
131.346106962701));
#137873=CARTESIAN_POINT('Ctrl Pts',(-250.02378029615,-4.87334581320459,
131.481305670362));
#137874=CARTESIAN_POINT('Ctrl Pts',(-250.031502579596,-4.85086476716184,
131.615713853344));
#137875=CARTESIAN_POINT('Ctrl Pts',(-250.039217335718,-4.82840563460076,
131.74999102146));
#137876=CARTESIAN_POINT('Ctrl Pts',(-250.04693209184,-4.80034276065878,
131.883478810325));
#137877=CARTESIAN_POINT('Ctrl Pts',(-250.054646847962,-4.76675011339768,
132.015672476223));
#137878=CARTESIAN_POINT('Ctrl Pts',(-250.062355980694,-4.7331819522699,
132.147769784376));
#137879=CARTESIAN_POINT('Ctrl Pts',(-250.070065113426,-4.69409213639154,
132.278574464824));
#137880=CARTESIAN_POINT('Ctrl Pts',(-250.077774246158,-4.64960581892818,
132.407591353015));
#137881=CARTESIAN_POINT('Ctrl Pts',(-250.085480417393,-4.60513659108468,
132.536558678786));
#137882=CARTESIAN_POINT('Ctrl Pts',(-250.093186588627,-4.55527511194571,
132.66373920435));
#137883=CARTESIAN_POINT('Ctrl Pts',(-250.100892759861,-4.50019648316473,
132.788652600973));
#137884=CARTESIAN_POINT('Ctrl Pts',(-250.108597591538,-4.44512742865141,
132.913544284013));
#137885=CARTESIAN_POINT('Ctrl Pts',(-250.116302423215,-4.384843187584,133.036169259948));
#137886=CARTESIAN_POINT('Ctrl Pts',(-250.124007254893,-4.31956694865875,
133.156067325163));
#137887=CARTESIAN_POINT('Ctrl Pts',(-250.131712462316,-4.25428752637525,
133.275971237505));
#137888=CARTESIAN_POINT('Ctrl Pts',(-250.139417669738,-4.18401581114635,
133.393147627045));
#137889=CARTESIAN_POINT('Ctrl Pts',(-250.147122877161,-4.10902065205373,
133.507161450683));
#137890=CARTESIAN_POINT('Ctrl Pts',(-250.154830175567,-4.03400514132315,
133.621206214559));
#137891=CARTESIAN_POINT('Ctrl Pts',(-250.162537473972,-3.95426385422254,
133.732086374822));
#137892=CARTESIAN_POINT('Ctrl Pts',(-250.170244772378,-3.87010833396887,
133.839396786353));
#137893=CARTESIAN_POINT('Ctrl Pts',(-250.177960359683,-3.78586230772042,
133.946822606065));
#137894=CARTESIAN_POINT('Ctrl Pts',(-250.185675946989,-3.69719281317067,
134.050670699348));
#137895=CARTESIAN_POINT('Ctrl Pts',(-250.193391534295,-3.60445124110995,
134.150569563965));
#137896=CARTESIAN_POINT('Ctrl Pts',(-250.201111652863,-3.51165520314561,
134.250527097869));
#137897=CARTESIAN_POINT('Ctrl Pts',(-250.208831771432,-3.41478260520544,
134.346530505772));
#137898=CARTESIAN_POINT('Ctrl Pts',(-250.21655189,-3.31422006150349,134.438246753155));
#137899=CARTESIAN_POINT('Ctrl Pts',(-250.224283636345,-3.21350605397486,
134.530101140379));
#137900=CARTESIAN_POINT('Ctrl Pts',(-250.232015382689,-3.10909130424726,
134.617655217992));
#137901=CARTESIAN_POINT('Ctrl Pts',(-250.239747129033,-3.00139415167609,
134.700617309416));
#137902=CARTESIAN_POINT('Ctrl Pts',(-250.244609141538,-2.93367013703912,
134.752786988555));
#137903=CARTESIAN_POINT('Ctrl Pts',(-250.249471154044,-2.86464872179104,
134.803141697023));
#137904=CARTESIAN_POINT('Ctrl Pts',(-250.254333166549,-2.79443907615148,
134.851618122615));
#137905=CARTESIAN_POINT('Ctrl Pts',(-250.262107500668,-2.6821741975678,
134.929131689074));
#137906=CARTESIAN_POINT('Ctrl Pts',(-250.269881834787,-2.566503889421,135.002093401399));
#137907=CARTESIAN_POINT('Ctrl Pts',(-250.277656168906,-2.44783360869859,
135.070189222494));
#137908=CARTESIAN_POINT('Ctrl Pts',(-250.285420921853,-2.3293095784913,
135.138201121577));
#137909=CARTESIAN_POINT('Ctrl Pts',(-250.2931856748,-2.20779326787769,135.20135886851));
#137910=CARTESIAN_POINT('Ctrl Pts',(-250.300950427747,-2.08372070151509,
135.259390482851));
#137911=CARTESIAN_POINT('Ctrl Pts',(-250.308707468632,-1.95977136577452,
135.317364459374));
#137912=CARTESIAN_POINT('Ctrl Pts',(-250.316464509517,-1.83327117867985,
135.370222270747));
#137913=CARTESIAN_POINT('Ctrl Pts',(-250.324221550402,-1.70468215553347,
135.417737017894));
#137914=CARTESIAN_POINT('Ctrl Pts',(-250.331972741642,-1.57619010237024,
135.465215933801));
#137915=CARTESIAN_POINT('Ctrl Pts',(-250.339723932882,-1.44561271375644,
135.507359670489));
#137916=CARTESIAN_POINT('Ctrl Pts',(-250.347475124122,-1.31343311961368,
135.543988926073));
#137917=CARTESIAN_POINT('Ctrl Pts',(-250.355223020899,-1.18130970532426,
135.580602613246));
#137918=CARTESIAN_POINT('Ctrl Pts',(-250.362970917676,-1.04758581590064,
135.611706376767));
#137919=CARTESIAN_POINT('Ctrl Pts',(-250.370718814453,-0.912760713239713,
135.637170456869));
#137920=CARTESIAN_POINT('Ctrl Pts',(-250.378465090537,-0.777963813083406,
135.662629210435));
#137921=CARTESIAN_POINT('Ctrl Pts',(-250.386211366621,-0.642066541798643,
135.682450554559));
#137922=CARTESIAN_POINT('Ctrl Pts',(-250.393957642705,-0.505578963098105,
135.696555725549));
#137923=CARTESIAN_POINT('Ctrl Pts',(-250.401703975971,-0.369090376877453,
135.71066100066));
#137924=CARTESIAN_POINT('Ctrl Pts',(-250.409450309236,-0.23201186343995,
135.71904997825));
#137925=CARTESIAN_POINT('Ctrl Pts',(-250.417196642501,-0.0948588315498516,
135.721695756091));
#137926=CARTESIAN_POINT('Ctrl Pts',(-250.424944710504,0.0423249148105995,
135.724342126437));
#137927=CARTESIAN_POINT('Ctrl Pts',(-250.432692778507,0.179582822012945,
135.721242730205));
#137928=CARTESIAN_POINT('Ctrl Pts',(-250.44044084651,0.316399654915623,
135.7124227933));
#137929=CARTESIAN_POINT('Ctrl Pts',(-250.448197149252,0.453361898376639,
135.703593482461));
#137930=CARTESIAN_POINT('Ctrl Pts',(-250.455953451994,0.589881740323937,
135.689031510967));
#137931=CARTESIAN_POINT('Ctrl Pts',(-250.463709754735,0.725448684938885,
135.66881405737));
#137932=CARTESIAN_POINT('Ctrl Pts',(-250.47147019725,0.861087985714016,
135.64858581311));
#137933=CARTESIAN_POINT('Ctrl Pts',(-250.479230639764,0.995772991999703,
135.622696145893));
#137934=CARTESIAN_POINT('Ctrl Pts',(-250.486991082278,1.12900455427687,
135.591273169402));
#137935=CARTESIAN_POINT('Ctrl Pts',(-250.494763982543,1.26244999168555,
135.559799749958));
#137936=CARTESIAN_POINT('Ctrl Pts',(-250.502536882808,1.39443694596228,
135.522775376713));
#137937=CARTESIAN_POINT('Ctrl Pts',(-250.510309783074,1.524481692795,135.480378007486));
#137938=CARTESIAN_POINT('Ctrl Pts',(-250.517800118837,1.64979898552902,
135.439521889419));
#137939=CARTESIAN_POINT('Ctrl Pts',(-250.525290454599,1.77331253873323,
135.393676744279));
#137940=CARTESIAN_POINT('Ctrl Pts',(-250.532780790362,1.89460978465488,
135.3430428962));
#137941=CARTESIAN_POINT('Ctrl Pts',(-250.540555124481,2.02050605251541,
135.290489250385));
#137942=CARTESIAN_POINT('Ctrl Pts',(-250.5483294586,2.14441343443857,135.232610131886));
#137943=CARTESIAN_POINT('Ctrl Pts',(-250.55610379272,2.2658485627169,135.169576918431));
#137944=CARTESIAN_POINT('Ctrl Pts',(-250.563868545667,2.38713403305226,
135.106621387777));
#137945=CARTESIAN_POINT('Ctrl Pts',(-250.571633298614,2.50595296835785,
135.038524579066));
#137946=CARTESIAN_POINT('Ctrl Pts',(-250.579398051561,2.62184086180627,
134.965506320118));
#137947=CARTESIAN_POINT('Ctrl Pts',(-250.587155092447,2.73761365376549,
134.892560583933));
#137948=CARTESIAN_POINT('Ctrl Pts',(-250.594912133332,2.85046086855112,
134.814703332027));
#137949=CARTESIAN_POINT('Ctrl Pts',(-250.602669174217,2.95994187898805,
134.732200626466));
#137950=CARTESIAN_POINT('Ctrl Pts',(-250.610420365457,3.06934032894264,
134.649760136837));
#137951=CARTESIAN_POINT('Ctrl Pts',(-250.618171556697,3.17537731626941,
134.562681400748));
#137952=CARTESIAN_POINT('Ctrl Pts',(-250.625922747938,3.27764084568845,
134.471273972034));
#137953=CARTESIAN_POINT('Ctrl Pts',(-250.633670644715,3.37986091037994,
134.379905393915));
#137954=CARTESIAN_POINT('Ctrl Pts',(-250.641418541492,3.47831041615716,
134.284212042417));
#137955=CARTESIAN_POINT('Ctrl Pts',(-250.649166438269,3.57261032920346,
134.184543822389));
#137956=CARTESIAN_POINT('Ctrl Pts',(-250.656912714353,3.66689051674082,
134.084896450805));
#137957=CARTESIAN_POINT('Ctrl Pts',(-250.664658990438,3.75702256952765,
133.98127614832));
#137958=CARTESIAN_POINT('Ctrl Pts',(-250.672405266522,3.84266451954371,
133.874069472285));
#137959=CARTESIAN_POINT('Ctrl Pts',(-250.680151599788,3.92830710174906,
133.766862004874));
#137960=CARTESIAN_POINT('Ctrl Pts',(-250.687897933053,4.00945927102577,
133.65606841655));
#137961=CARTESIAN_POINT('Ctrl Pts',(-250.695644266319,4.085819802742,133.542107793991));
#137962=CARTESIAN_POINT('Ctrl Pts',(-250.703392334322,4.16219743486997,
133.42812165074));
#137963=CARTESIAN_POINT('Ctrl Pts',(-250.711140402325,4.2337810765948,133.310967386691));
#137964=CARTESIAN_POINT('Ctrl Pts',(-250.718888470328,4.30031345400347,
133.191092118975));
#137965=CARTESIAN_POINT('Ctrl Pts',(-250.72664477307,4.3669165428145,133.071089446398));
#137966=CARTESIAN_POINT('Ctrl Pts',(-250.734401075812,4.42845745303442,
132.948360335632));
#137967=CARTESIAN_POINT('Ctrl Pts',(-250.742157378554,4.4847251817057,132.82337599816));
#137968=CARTESIAN_POINT('Ctrl Pts',(-250.749917821068,4.54102294215796,
132.698324952784));
#137969=CARTESIAN_POINT('Ctrl Pts',(-250.757678263583,4.59204176765584,
132.571016644993));
#137970=CARTESIAN_POINT('Ctrl Pts',(-250.765438706097,4.63761964135948,
132.441940271988));
#137971=CARTESIAN_POINT('Ctrl Pts',(-250.773211606363,4.68327068071221,
132.31265669413));
#137972=CARTESIAN_POINT('Ctrl Pts',(-250.780984506628,4.72346319966091,
132.181599753318));
#137973=CARTESIAN_POINT('Ctrl Pts',(-250.788757406894,4.75808545435506,
132.049272611064));
#137974=CARTESIAN_POINT('Ctrl Pts',(-250.796247742654,4.79144910287435,
131.921755893775));
#137975=CARTESIAN_POINT('Ctrl Pts',(-250.803738078414,4.81964037634877,
131.793060022642));
#137976=CARTESIAN_POINT('Ctrl Pts',(-250.811228414174,4.84260481019838,
131.663640382685));
#137977=CARTESIAN_POINT('Ctrl Pts',(-250.819002748293,4.86643994754257,
131.529313757714));
#137978=CARTESIAN_POINT('Ctrl Pts',(-250.826777082412,4.88471957246311,
131.393781890743));
#137979=CARTESIAN_POINT('Ctrl Pts',(-250.834551416531,4.89732659784195,
131.25754408656));
#137980=CARTESIAN_POINT('Ctrl Pts',(-250.842316169478,4.90991808618873,
131.121474183296));
#137981=CARTESIAN_POINT('Ctrl Pts',(-250.850080922425,4.91685084926534,
130.984700459435));
#137982=CARTESIAN_POINT('Ctrl Pts',(-250.857845675372,4.91805875715627,
130.847732540034));
#137983=CARTESIAN_POINT('Ctrl Pts',(-250.865602716257,4.91926546533605,
130.710900659101));
#137984=CARTESIAN_POINT('Ctrl Pts',(-250.873359757142,4.91475863031501,
130.573875354883));
#137985=CARTESIAN_POINT('Ctrl Pts',(-250.881116798027,4.90452392789344,
130.437171152547));
#137986=CARTESIAN_POINT('Ctrl Pts',(-250.888867989267,4.8942969435406,130.300570039914));
#137987=CARTESIAN_POINT('Ctrl Pts',(-250.896619180507,4.87835071842023,
130.164289935484));
#137988=CARTESIAN_POINT('Ctrl Pts',(-250.904370371747,4.85672299542931,
130.028844783964));
#137989=CARTESIAN_POINT('Ctrl Pts',(-250.912118268524,4.83510446479751,
129.893457200245));
#137990=CARTESIAN_POINT('Ctrl Pts',(-250.919866165301,4.80780930064345,
129.758904248879));
#137991=CARTESIAN_POINT('Ctrl Pts',(-250.927614062078,4.77492701079141,
129.625693953867));
#137992=CARTESIAN_POINT('Ctrl Pts',(-250.935360338162,4.74205159920555,
129.492511523578));
#137993=CARTESIAN_POINT('Ctrl Pts',(-250.943106614246,4.70359148017861,
129.36067157034));
#137994=CARTESIAN_POINT('Ctrl Pts',(-250.95085289033,4.6596870332873,129.230670745223));
#137995=CARTESIAN_POINT('Ctrl Pts',(-250.958599223595,4.61578226230341,
129.10066896047));
#137996=CARTESIAN_POINT('Ctrl Pts',(-250.96634555686,4.56643320835827,128.972506701338));
#137997=CARTESIAN_POINT('Ctrl Pts',(-250.974091890126,4.51182964167352,
128.846663923229));
#137998=CARTESIAN_POINT('Ctrl Pts',(-250.981839958129,4.45721384689853,
128.720792963503));
#137999=CARTESIAN_POINT('Ctrl Pts',(-250.989588026131,4.39734135345676,
128.597242876998));
#138000=CARTESIAN_POINT('Ctrl Pts',(-250.997336094134,4.3324492708213,128.476471793275));
#138001=CARTESIAN_POINT('Ctrl Pts',(-251.005092396876,4.26748822010809,
128.355572352607));
#138002=CARTESIAN_POINT('Ctrl Pts',(-251.012848699618,4.19749710855081,
128.237458159717));
#138003=CARTESIAN_POINT('Ctrl Pts',(-251.02060500236,4.12275832746292,128.122561438687));
#138004=CARTESIAN_POINT('Ctrl Pts',(-251.028365444874,4.04797965603722,
128.007603393818));
#138005=CARTESIAN_POINT('Ctrl Pts',(-251.036125887388,3.96844849252535,
127.89586656096));
#138006=CARTESIAN_POINT('Ctrl Pts',(-251.043886329902,3.88448883832754,
127.787751672507));
#138007=CARTESIAN_POINT('Ctrl Pts',(-251.051659230167,3.80039440463922,
127.679463228437));
#138008=CARTESIAN_POINT('Ctrl Pts',(-251.059432130433,3.71185752686294,
127.574808646183));
#138009=CARTESIAN_POINT('Ctrl Pts',(-251.067205030698,3.61924112874938,
127.474153910097));
#138010=CARTESIAN_POINT('Ctrl Pts',(-251.074695366461,3.52999156997782,
127.377158227185));
#138011=CARTESIAN_POINT('Ctrl Pts',(-251.082185702224,3.43695416062381,
127.283876848435));
#138012=CARTESIAN_POINT('Ctrl Pts',(-251.089676037988,3.34048258956851,
127.194601743169));
#138013=CARTESIAN_POINT('Ctrl Pts',(-251.097450372106,3.24035326959588,
127.101941745171));
#138014=CARTESIAN_POINT('Ctrl Pts',(-251.105224706225,3.13620705522876,
127.013304294375));
#138015=CARTESIAN_POINT('Ctrl Pts',(-251.112999040344,3.0284007372799,126.929057785923));
#138016=CARTESIAN_POINT('Ctrl Pts',(-251.120763793291,2.92072728098357,
126.844915103764));
#138017=CARTESIAN_POINT('Ctrl Pts',(-251.128528546237,2.80940300125583,
126.765152835213));
#138018=CARTESIAN_POINT('Ctrl Pts',(-251.136293299184,2.69482091525471,
126.690102082033));
#138019=CARTESIAN_POINT('Ctrl Pts',(-251.144050340069,2.58035263379673,
126.615125870319));
#138020=CARTESIAN_POINT('Ctrl Pts',(-251.151807380953,2.46263331018998,
126.544852074305));
#138021=CARTESIAN_POINT('Ctrl Pts',(-251.159564421838,2.34208808644987,
126.479570858767));
#138022=CARTESIAN_POINT('Ctrl Pts',(-251.167315613078,2.22163376680053,
126.414338872302));
#138023=CARTESIAN_POINT('Ctrl Pts',(-251.175066804317,2.09835813110865,
126.354092157846));
#138024=CARTESIAN_POINT('Ctrl Pts',(-251.182817995557,1.97271397656958,
126.299076760899));
#138025=CARTESIAN_POINT('Ctrl Pts',(-251.190565892334,1.84712322414803,
126.244084746963));
#138026=CARTESIAN_POINT('Ctrl Pts',(-251.19831378911,1.71916631248399,126.194319784753));
#138027=CARTESIAN_POINT('Ctrl Pts',(-251.206061685887,1.58931903772481,
126.149981168184));
#138028=CARTESIAN_POINT('Ctrl Pts',(-251.213807961971,1.45949892421632,
126.105651826298));
#138029=CARTESIAN_POINT('Ctrl Pts',(-251.221554238055,1.32778960388612,
126.066746698588));
#138030=CARTESIAN_POINT('Ctrl Pts',(-251.229300514138,1.1946848019348,126.033416131772));
#138031=CARTESIAN_POINT('Ctrl Pts',(-251.237046847403,1.06157901743389,
126.000085318918));
#138032=CARTESIAN_POINT('Ctrl Pts',(-251.244793180668,0.927078110012168,
125.972329244041));
#138033=CARTESIAN_POINT('Ctrl Pts',(-251.252539513933,0.791688455181783,
125.950247675696));
#138034=CARTESIAN_POINT('Ctrl Pts',(-251.260287581936,0.656268480777476,
125.928161162337));
#138035=CARTESIAN_POINT('Ctrl Pts',(-251.268035649938,0.519959748713128,
125.91175174711));
#138036=CARTESIAN_POINT('Ctrl Pts',(-251.275783717941,0.383275859825544,
125.901067573318));
#138037=CARTESIAN_POINT('Ctrl Pts',(-251.283540020682,0.246446701673726,
125.890372044259));
#138038=CARTESIAN_POINT('Ctrl Pts',(-251.291296323424,0.109241980607997,
125.885413942304));
#138039=CARTESIAN_POINT('Ctrl Pts',(-251.299052626165,-0.0278220216086831,
125.886189311317));
#138040=CARTESIAN_POINT('Ctrl Pts',(-251.306813068679,-0.164959179010641,
125.886965094168));
#138041=CARTESIAN_POINT('Ctrl Pts',(-251.314573511193,-0.301955077575977,
125.893480426983));
#138042=CARTESIAN_POINT('Ctrl Pts',(-251.322333953706,-0.438297439122899,
125.905679323855));
#138043=CARTESIAN_POINT('Ctrl Pts',(-251.330106853972,-0.574858669532121,
125.917897803479));
#138044=CARTESIAN_POINT('Ctrl Pts',(-251.337879754237,-0.710763878622392,
125.935818028203));
#138045=CARTESIAN_POINT('Ctrl Pts',(-251.345652654502,-0.845508984238931,
125.959332483481));
#138046=CARTESIAN_POINT('Ctrl Pts',(-251.353142990268,-0.975355765941941,
125.981992129095));
#138047=CARTESIAN_POINT('Ctrl Pts',(-251.360633326034,-1.10412502412161,
126.009846272811));
#138048=CARTESIAN_POINT('Ctrl Pts',(-251.3681236618,-1.23137993923824,126.042755162707));
#138049=CARTESIAN_POINT('Ctrl Pts',(-251.37589799592,-1.36345976308712,
126.076911803153));
#138050=CARTESIAN_POINT('Ctrl Pts',(-251.383672330041,-1.49432653358835,
126.116622255637));
#138051=CARTESIAN_POINT('Ctrl Pts',(-251.391446664161,-1.62347745532496,
126.161785468519));
#138052=CARTESIAN_POINT('Ctrl Pts',(-251.399211417109,-1.75246921009344,
126.206893021777));
#138053=CARTESIAN_POINT('Ctrl Pts',(-251.406976170058,-1.879748958073,126.257439836739));
#138054=CARTESIAN_POINT('Ctrl Pts',(-251.414740923006,-2.00482569860016,
126.31327422553));
#138055=CARTESIAN_POINT('Ctrl Pts',(-251.422497963892,-2.12977821114571,
126.369053158819));
#138056=CARTESIAN_POINT('Ctrl Pts',(-251.430255004778,-2.2525317158745,
126.430109056492));
#138057=CARTESIAN_POINT('Ctrl Pts',(-251.438012045665,-2.37261228929872,
126.496241075681));
#138058=CARTESIAN_POINT('Ctrl Pts',(-251.445763236906,-2.49260230902894,
126.5623232242));
#138059=CARTESIAN_POINT('Ctrl Pts',(-251.453514428148,-2.60992306846137,
126.633473687105));
#138060=CARTESIAN_POINT('Ctrl Pts',(-251.461265619389,-2.72412281460433,
126.709444506893));
#138061=CARTESIAN_POINT('Ctrl Pts',(-251.469013516167,-2.83827402280803,
126.785383037055));
#138062=CARTESIAN_POINT('Ctrl Pts',(-251.476761412945,-2.94930653122269,
126.866137633138));
#138063=CARTESIAN_POINT('Ctrl Pts',(-251.484509309724,-3.05679548879321,
126.951415717597));
#138064=CARTESIAN_POINT('Ctrl Pts',(-251.492255585809,-3.16426196199071,
127.03667596372));
#138065=CARTESIAN_POINT('Ctrl Pts',(-251.500001861894,-3.26818605261292,
127.126457573303));
#138066=CARTESIAN_POINT('Ctrl Pts',(-251.50774813798,-3.3681743991748,127.220426427428));
#138067=CARTESIAN_POINT('Ctrl Pts',(-251.515494471246,-3.46816348382808,
127.314395975209));
#138068=CARTESIAN_POINT('Ctrl Pts',(-251.523240804513,-3.56421648155155,
127.412552561464));
#138069=CARTESIAN_POINT('Ctrl Pts',(-251.530987137779,-3.65597574590025,
127.514524085474));
#138070=CARTESIAN_POINT('Ctrl Pts',(-251.538735205783,-3.74775555909936,
127.616518445299));
#138071=CARTESIAN_POINT('Ctrl Pts',(-251.546483273788,-3.83523946407887,
127.722329152326));
#138072=CARTESIAN_POINT('Ctrl Pts',(-251.554231341792,-3.91810934271634,
127.831550122257));
#138073=CARTESIAN_POINT('Ctrl Pts',(-251.561987644535,-4.00106729644708,
127.940887173535));
#138074=CARTESIAN_POINT('Ctrl Pts',(-251.569743947278,-4.07940119118924,
128.053641416024));
#138075=CARTESIAN_POINT('Ctrl Pts',(-251.577500250021,-4.15283529244867,
128.169376348867));
#138076=CARTESIAN_POINT('Ctrl Pts',(-251.585260692536,-4.2263085876992,
128.285173052928));
#138077=CARTESIAN_POINT('Ctrl Pts',(-251.593021135052,-4.29487668315844,
128.403953278882));
#138078=CARTESIAN_POINT('Ctrl Pts',(-251.600781577567,-4.3583097824858,
128.525255770836));
#138079=CARTESIAN_POINT('Ctrl Pts',(-251.608554477834,-4.42184471025516,
128.646752988318));
#138080=CARTESIAN_POINT('Ctrl Pts',(-251.6163273781,-4.48022800284043,128.770780208984));
#138081=CARTESIAN_POINT('Ctrl Pts',(-251.624100278367,-4.53327764655705,
128.896855220005));
#138082=CARTESIAN_POINT('Ctrl Pts',(-251.631590614116,-4.58439880200303,
129.018347086578));
#138083=CARTESIAN_POINT('Ctrl Pts',(-251.639080949865,-4.63056725131765,
129.141740155193));
#138084=CARTESIAN_POINT('Ctrl Pts',(-251.646571285614,-4.67166446012101,
129.266591377874));
#138085=CARTESIAN_POINT('Ctrl Pts',(-251.652821157903,-4.70595562076918,
129.370766173651));
#138086=CARTESIAN_POINT('Ctrl Pts',(-251.659071030192,-4.7367771621133,
129.476136082795));
#138087=CARTESIAN_POINT('Ctrl Pts',(-251.665320902482,-4.76405452823413,
129.582490119309));
#138088=CARTESIAN_POINT('Ctrl Pts',(-249.915046309122,-4.76405452823416,
129.582490119309));
#138089=CARTESIAN_POINT('Ctrl Pts',(-249.922808577032,-4.79811276617232,
129.715282672124));
#138090=CARTESIAN_POINT('Ctrl Pts',(-249.930570844942,-4.82658446629422,
129.849382520667));
#138091=CARTESIAN_POINT('Ctrl Pts',(-249.938333112852,-4.84939694061544,
129.984279905167));
#138092=CARTESIAN_POINT('Ctrl Pts',(-249.946107049739,-4.87224370881249,
130.119380080213));
#138093=CARTESIAN_POINT('Ctrl Pts',(-249.953880986627,-4.88941421055682,
130.255279798624));
#138094=CARTESIAN_POINT('Ctrl Pts',(-249.961654923514,-4.90088768873931,
130.391464837903));
#138095=CARTESIAN_POINT('Ctrl Pts',(-249.966398463255,-4.90788863311393,
130.474562907162));
#138096=CARTESIAN_POINT('Ctrl Pts',(-249.971142002996,-4.91276945039334,
130.557767191997));
#138097=CARTESIAN_POINT('Ctrl Pts',(-249.975885542736,-4.91553494191603,
130.640961421416));
#138098=CARTESIAN_POINT('Ctrl Pts',(-249.978970549829,-4.9173335061588,
130.695067595674));
#138099=CARTESIAN_POINT('Ctrl Pts',(-249.982055556921,-4.91823876860267,
130.749203629498));
#138100=CARTESIAN_POINT('Ctrl Pts',(-249.985140564014,-4.91824989614147,
130.803349873091));
#138101=CARTESIAN_POINT('',(-249.639859436026,-4.91824799670603,130.808799693728));
#138102=CARTESIAN_POINT('Ctrl Pts',(-249.569887472766,-4.76405452823394,
129.582490119308));
#138103=CARTESIAN_POINT('Ctrl Pts',(-249.577565655275,-4.79786475257207,
129.71431567086));
#138104=CARTESIAN_POINT('Ctrl Pts',(-249.585243837783,-4.82620038099429,
129.847550331812));
#138105=CARTESIAN_POINT('Ctrl Pts',(-249.592922020292,-4.848959238378,129.98169582128));
#138106=CARTESIAN_POINT('Ctrl Pts',(-249.600744922909,-4.87214705981838,
130.118369715068));
#138107=CARTESIAN_POINT('Ctrl Pts',(-249.608567825527,-4.88954567913427,
130.25598869821));
#138108=CARTESIAN_POINT('Ctrl Pts',(-249.616390728144,-4.90110212331456,
130.394018029791));
#138109=CARTESIAN_POINT('Ctrl Pts',(-249.624213630762,-4.91265856749487,
130.532047361373));
#138110=CARTESIAN_POINT('Ctrl Pts',(-249.63203653338,-4.91837283430366,
130.670486604846));
#138111=CARTESIAN_POINT('Ctrl Pts',(-249.639859435997,-4.91824799670649,
130.808799693213));
#138112=CARTESIAN_POINT('Ctrl Pts',(-249.639859436026,-4.91824799670602,
130.808799693728));
#138113=CARTESIAN_POINT('Ctrl Pts',(-249.649450864241,-4.91809493702354,
130.978381257395));
#138114=CARTESIAN_POINT('Ctrl Pts',(-249.659042292456,-4.90916748110856,
131.147572254414));
#138115=CARTESIAN_POINT('Ctrl Pts',(-249.668633720671,-4.89160842038733,
131.315584760282));
#138116=CARTESIAN_POINT('Ctrl Pts',(-249.678384122473,-4.87375832617249,
131.486381997482));
#138117=CARTESIAN_POINT('Ctrl Pts',(-249.688134524275,-4.84698816366428,
131.655961449596));
#138118=CARTESIAN_POINT('Ctrl Pts',(-249.697884926077,-4.81149657870729,
131.823518964236));
#138119=CARTESIAN_POINT('Ctrl Pts',(-249.704265589079,-4.78827088528351,
131.933168602893));
#138120=CARTESIAN_POINT('Ctrl Pts',(-249.710646252081,-4.76131132158729,
132.041952848757));
#138121=CARTESIAN_POINT('Ctrl Pts',(-249.717026915082,-4.7306845068774,
132.14965135153));
#138122=CARTESIAN_POINT('Ctrl Pts',(-249.724801249201,-4.69336815111763,
132.280873474443));
#138123=CARTESIAN_POINT('Ctrl Pts',(-249.732575583321,-4.65052869261664,
132.410749617163));
#138124=CARTESIAN_POINT('Ctrl Pts',(-249.74034991744,-4.60227921961991,
132.538779554027));
#138125=CARTESIAN_POINT('Ctrl Pts',(-249.748114670387,-4.55408920978661,
132.666651705436));
#138126=CARTESIAN_POINT('Ctrl Pts',(-249.755879423334,-4.50050258806562,
132.792681815789));
#138127=CARTESIAN_POINT('Ctrl Pts',(-249.763644176281,-4.44168278131277,
132.91638266591));
#138128=CARTESIAN_POINT('Ctrl Pts',(-249.771401217166,-4.38292139522121,
133.039960654602));
#138129=CARTESIAN_POINT('Ctrl Pts',(-249.779158258051,-4.31893733450593,
133.161213636144));
#138130=CARTESIAN_POINT('Ctrl Pts',(-249.786915298936,-4.24994275705539,
133.279672643201));
#138131=CARTESIAN_POINT('Ctrl Pts',(-249.794666490176,-4.18100020895249,
133.398042319399));
#138132=CARTESIAN_POINT('Ctrl Pts',(-249.802417681416,-4.1070548609022,
133.51362187841));
#138133=CARTESIAN_POINT('Ctrl Pts',(-249.810168872656,-4.0283654398268,
133.625965647635));
#138134=CARTESIAN_POINT('Ctrl Pts',(-249.817916769434,-3.94970946385435,
133.73826166776));
#138135=CARTESIAN_POINT('Ctrl Pts',(-249.825664666211,-3.86631364906585,
133.847324313904));
#138136=CARTESIAN_POINT('Ctrl Pts',(-249.833412562988,-3.77848068400477,
133.952735878411));
#138137=CARTESIAN_POINT('Ctrl Pts',(-249.841158839072,-3.69066609170653,
134.058125393092));
#138138=CARTESIAN_POINT('Ctrl Pts',(-249.848905115156,-3.59841644540369,
134.159865045061));
#138139=CARTESIAN_POINT('Ctrl Pts',(-249.85665139124,-3.50207520738866,
134.257569604044));
#138140=CARTESIAN_POINT('Ctrl Pts',(-249.864397724505,-3.40573325820436,
134.355274884261));
#138141=CARTESIAN_POINT('Ctrl Pts',(-249.872144057771,-3.30529993154463,
134.448944733666));
#138142=CARTESIAN_POINT('Ctrl Pts',(-249.879890391036,-3.20115580350047,
134.5382305382));
#138143=CARTESIAN_POINT('Ctrl Pts',(-249.887638459039,-3.09698835310106,
134.627536337671));
#138144=CARTESIAN_POINT('Ctrl Pts',(-249.895386527042,-2.98910874446581,
134.712455884229));
#138145=CARTESIAN_POINT('Ctrl Pts',(-249.903134595045,-2.8779305789088,
134.792680896265));
#138146=CARTESIAN_POINT('Ctrl Pts',(-249.910890897787,-2.76663425187424,
134.872991172399));
#138147=CARTESIAN_POINT('Ctrl Pts',(-249.918647200529,-2.6520326823616,
134.948596717994));
#138148=CARTESIAN_POINT('Ctrl Pts',(-249.926403503271,-2.5345688623945,
135.019232352777));
#138149=CARTESIAN_POINT('Ctrl Pts',(-249.934163945785,-2.4170423484496,
135.089905687925));
#138150=CARTESIAN_POINT('Ctrl Pts',(-249.941924388299,-2.29665088306278,
135.155603639562));
#138151=CARTESIAN_POINT('Ctrl Pts',(-249.949684830813,-2.17386110377588,
135.21610754639));
#138152=CARTESIAN_POINT('Ctrl Pts',(-249.957457731079,-2.05087421143483,
135.276708579461));
#138153=CARTESIAN_POINT('Ctrl Pts',(-249.965230631344,-1.9254816695273,
135.332098747793));
#138154=CARTESIAN_POINT('Ctrl Pts',(-249.97300353161,-1.79816991984631,
135.382107661895));
#138155=CARTESIAN_POINT('Ctrl Pts',(-249.980493867372,-1.67548627294552,
135.430298626004));
#138156=CARTESIAN_POINT('Ctrl Pts',(-249.987984203134,-1.55102082278758,
135.473492686614));
#138157=CARTESIAN_POINT('Ctrl Pts',(-249.995474538896,-1.42521933426106,
135.511581975411));
#138158=CARTESIAN_POINT('Ctrl Pts',(-250.003248873015,-1.29464804406033,
135.551115431169));
#138159=CARTESIAN_POINT('Ctrl Pts',(-250.011023207134,-1.16222379317508,
135.585274608996));
#138160=CARTESIAN_POINT('Ctrl Pts',(-250.018797541253,-1.02842856258211,
135.613884269048));
#138161=CARTESIAN_POINT('Ctrl Pts',(-250.0265622942,-0.894798222653221,
135.642458670251));
#138162=CARTESIAN_POINT('Ctrl Pts',(-250.034327047147,-0.759800643488834,
135.665497080847));
#138163=CARTESIAN_POINT('Ctrl Pts',(-250.042091800095,-0.623934072588422,
135.682873642614));
#138164=CARTESIAN_POINT('Ctrl Pts',(-250.04984884098,-0.488202446281613,
135.700232945735));
#138165=CARTESIAN_POINT('Ctrl Pts',(-250.057605881864,-0.351603931133389,
135.711941541624));
#138166=CARTESIAN_POINT('Ctrl Pts',(-250.065362922749,-0.214647759164977,
135.717924436423));
#138167=CARTESIAN_POINT('Ctrl Pts',(-250.07311411399,-0.0777948669113959,
135.723902819475));
#138168=CARTESIAN_POINT('Ctrl Pts',(-250.08086530523,0.0594147563051551,
135.724164078753));
#138169=CARTESIAN_POINT('Ctrl Pts',(-250.08861649647,0.196466305281641,
135.718684991617));
#138170=CARTESIAN_POINT('Ctrl Pts',(-250.096364393247,0.333459603694028,
135.713208233239));
#138171=CARTESIAN_POINT('Ctrl Pts',(-250.104112290024,0.470294571658441,
135.701995996609));
#138172=CARTESIAN_POINT('Ctrl Pts',(-250.111860186801,0.606456169344113,
135.685077160981));
#138173=CARTESIAN_POINT('Ctrl Pts',(-250.119606462885,0.742589284958854,
135.668161864409));
#138174=CARTESIAN_POINT('Ctrl Pts',(-250.127352738969,0.878048922726506,
135.645542391347));
#138175=CARTESIAN_POINT('Ctrl Pts',(-250.135099015053,1.01232532774888,
135.617299479976));
#138176=CARTESIAN_POINT('Ctrl Pts',(-250.142845348319,1.14660272396899,
135.589056360123));
#138177=CARTESIAN_POINT('Ctrl Pts',(-250.150591681584,1.27969648742131,
135.555189799601));
#138178=CARTESIAN_POINT('Ctrl Pts',(-250.158338014849,1.4111076085504,135.515831553441));
#138179=CARTESIAN_POINT('Ctrl Pts',(-250.166086082852,1.54254815828874,
135.476464493274));
#138180=CARTESIAN_POINT('Ctrl Pts',(-250.173834150855,1.67230494142739,
135.431603412409));
#138181=CARTESIAN_POINT('Ctrl Pts',(-250.181582218858,1.7998950303049,135.381429651608));
#138182=CARTESIAN_POINT('Ctrl Pts',(-250.1893385216,1.92762072344738,135.331202565536));
#138183=CARTESIAN_POINT('Ctrl Pts',(-250.197094824342,2.05317475783678,
135.275651663582));
#138184=CARTESIAN_POINT('Ctrl Pts',(-250.204851127084,2.17609458179027,
135.215006311067));
#138185=CARTESIAN_POINT('Ctrl Pts',(-250.212611569598,2.29908001175517,
135.154328590302));
#138186=CARTESIAN_POINT('Ctrl Pts',(-250.220372012112,2.41942808689568,
135.08855118843));
#138187=CARTESIAN_POINT('Ctrl Pts',(-250.228132454626,2.53670261228168,
135.01794850906));
#138188=CARTESIAN_POINT('Ctrl Pts',(-250.235905354892,2.65416539714665,
134.947232492001));
#138189=CARTESIAN_POINT('Ctrl Pts',(-250.243678255157,2.76854444627906,
134.871675934157));
#138190=CARTESIAN_POINT('Ctrl Pts',(-250.251451155423,2.87943347250361,
134.791595993102));
#138191=CARTESIAN_POINT('Ctrl Pts',(-250.258941491185,2.98629140331409,
134.714427159613));
#138192=CARTESIAN_POINT('Ctrl Pts',(-250.266431826947,3.08990840587486,
134.633058296182));
#138193=CARTESIAN_POINT('Ctrl Pts',(-250.273922162709,3.18995278070627,
134.547806131977));
#138194=CARTESIAN_POINT('Ctrl Pts',(-250.281696496828,3.29379036841621,
134.459321606055));
#138195=CARTESIAN_POINT('Ctrl Pts',(-250.289470830947,3.39410799440705,
134.366373203335));
#138196=CARTESIAN_POINT('Ctrl Pts',(-250.297245165066,3.49049770194225,
134.269271706647));
#138197=CARTESIAN_POINT('Ctrl Pts',(-250.305009918014,3.58676861777726,
134.172289878875));
#138198=CARTESIAN_POINT('Ctrl Pts',(-250.312774670961,3.67912097413148,
134.071165415866));
#138199=CARTESIAN_POINT('Ctrl Pts',(-250.320539423908,3.76717956797308,
133.966249477907));
#138200=CARTESIAN_POINT('Ctrl Pts',(-250.328296464793,3.85515070077786,
133.861437743936));
#138201=CARTESIAN_POINT('Ctrl Pts',(-250.336053505678,3.93883630814634,
133.752842326548));
#138202=CARTESIAN_POINT('Ctrl Pts',(-250.343810546563,4.01789804327467,
133.640851121049));
#138203=CARTESIAN_POINT('Ctrl Pts',(-250.351561737803,4.09690015733341,
133.52894436899));
#138204=CARTESIAN_POINT('Ctrl Pts',(-250.359312929043,4.17128511504299,
133.41364724402));
#138205=CARTESIAN_POINT('Ctrl Pts',(-250.367064120283,4.24075511375156,
133.295380313933));
#138206=CARTESIAN_POINT('Ctrl Pts',(-250.37481201706,4.31019558585761,133.177163650446));
#138207=CARTESIAN_POINT('Ctrl Pts',(-250.382559913837,4.37472505619843,
133.055980028757));
#138208=CARTESIAN_POINT('Ctrl Pts',(-250.390307810615,4.43408943009937,
132.932278376405));
#138209=CARTESIAN_POINT('Ctrl Pts',(-250.398054086699,4.49344138625305,
132.808602599771));
#138210=CARTESIAN_POINT('Ctrl Pts',(-250.405800362783,4.54763022594817,
132.682410192399));
#138211=CARTESIAN_POINT('Ctrl Pts',(-250.413546638867,4.5964483415293,132.554173666481));
#138212=CARTESIAN_POINT('Ctrl Pts',(-250.421292972132,4.6452668174746,132.42593619395));
#138213=CARTESIAN_POINT('Ctrl Pts',(-250.429039305398,4.68871435109881,
132.295654938147));
#138214=CARTESIAN_POINT('Ctrl Pts',(-250.436785638663,4.72663206478553,
132.163820946756));
#138215=CARTESIAN_POINT('Ctrl Pts',(-250.444533706666,4.76455826988137,
132.031957432056));
#138216=CARTESIAN_POINT('Ctrl Pts',(-250.452281774669,4.7969520827905,131.898540865498));
#138217=CARTESIAN_POINT('Ctrl Pts',(-250.460029842672,4.82370503643262,
131.76407556691));
#138218=CARTESIAN_POINT('Ctrl Pts',(-250.467786145414,4.85048642343228,
131.629467357002));
#138219=CARTESIAN_POINT('Ctrl Pts',(-250.475542448156,4.87161489875032,
131.493808572583));
#138220=CARTESIAN_POINT('Ctrl Pts',(-250.483298750898,4.88703341344428,
131.35761234904));
#138221=CARTESIAN_POINT('Ctrl Pts',(-250.491059193412,4.90246015746378,
131.221343433472));
#138222=CARTESIAN_POINT('Ctrl Pts',(-250.498819635926,4.91217084063423,
131.084536897008));
#138223=CARTESIAN_POINT('Ctrl Pts',(-250.50658007844,4.91616055246869,130.947708044647));
#138224=CARTESIAN_POINT('Ctrl Pts',(-250.514352978706,4.92015666894279,
130.810659542465));
#138225=CARTESIAN_POINT('Ctrl Pts',(-250.522125878971,4.91841346687458,
130.67358904396));
#138226=CARTESIAN_POINT('Ctrl Pts',(-250.529898779237,4.91097817177237,
130.537009801455));
#138227=CARTESIAN_POINT('Ctrl Pts',(-250.537389114998,4.90381316837573,
130.405395558441));
#138228=CARTESIAN_POINT('Ctrl Pts',(-250.54487945076,4.89136275995624,130.274237781377));
#138229=CARTESIAN_POINT('Ctrl Pts',(-250.552369786522,4.87371412806055,
130.14398673828));
#138230=CARTESIAN_POINT('Ctrl Pts',(-250.560144120641,4.85539634292187,
130.008797187292));
#138231=CARTESIAN_POINT('Ctrl Pts',(-250.56791845476,4.83142034652068,129.874156245343));
#138232=CARTESIAN_POINT('Ctrl Pts',(-250.575692788879,4.8018270986718,129.740575123699));
#138233=CARTESIAN_POINT('Ctrl Pts',(-250.583457541826,4.77227032185607,
129.60715862885));
#138234=CARTESIAN_POINT('Ctrl Pts',(-250.591222294773,4.73711015157387,
129.474799733536));
#138235=CARTESIAN_POINT('Ctrl Pts',(-250.598987047721,4.69643922251756,
129.344003917407));
#138236=CARTESIAN_POINT('Ctrl Pts',(-250.606744088606,4.65580868840135,
129.213338009527));
#138237=CARTESIAN_POINT('Ctrl Pts',(-250.614501129491,4.60967840308756,
129.084232462259));
#138238=CARTESIAN_POINT('Ctrl Pts',(-250.622258170376,4.55819182917327,
128.957181603242));
#138239=CARTESIAN_POINT('Ctrl Pts',(-250.630009361616,4.50674408168482,
128.830226554266));
#138240=CARTESIAN_POINT('Ctrl Pts',(-250.637760552856,4.44994823165931,
128.705323470318));
#138241=CARTESIAN_POINT('Ctrl Pts',(-250.645511744096,4.38799714508469,
128.58295022837));
#138242=CARTESIAN_POINT('Ctrl Pts',(-250.653259640873,4.32607238937454,
128.460628998314));
#138243=CARTESIAN_POINT('Ctrl Pts',(-250.66100753765,4.25899693128842,128.340835819749));
#138244=CARTESIAN_POINT('Ctrl Pts',(-250.668755434427,4.18701112190058,
128.224027126023));
#138245=CARTESIAN_POINT('Ctrl Pts',(-250.676501710511,4.11504037039223,
128.107242866157));
#138246=CARTESIAN_POINT('Ctrl Pts',(-250.684247986595,4.03816151560704,
127.993442182008));
#138247=CARTESIAN_POINT('Ctrl Pts',(-250.69199426268,3.95665987842547,127.883055144159));
#138248=CARTESIAN_POINT('Ctrl Pts',(-250.699740595945,3.87515763961723,
127.772667291457));
#138249=CARTESIAN_POINT('Ctrl Pts',(-250.70748692921,3.78903278254256,127.665693449863));
#138250=CARTESIAN_POINT('Ctrl Pts',(-250.715233262476,3.69861256229198,
127.562532710882));
#138251=CARTESIAN_POINT('Ctrl Pts',(-250.722981330479,3.60817209306012,
127.459348869768));
#138252=CARTESIAN_POINT('Ctrl Pts',(-250.730729398481,3.51343460420178,
127.359980124422));
#138253=CARTESIAN_POINT('Ctrl Pts',(-250.738477466484,3.41476576516571,
127.264790328456));
#138254=CARTESIAN_POINT('Ctrl Pts',(-250.746233769226,3.31599205971319,
127.169499363641));
#138255=CARTESIAN_POINT('Ctrl Pts',(-250.753990071968,3.21327893932589,
127.078396492338));
#138256=CARTESIAN_POINT('Ctrl Pts',(-250.76174637471,3.10702728299285,126.991807073648));
#138257=CARTESIAN_POINT('Ctrl Pts',(-250.769506817224,3.00071891695165,
126.905171439579));
#138258=CARTESIAN_POINT('Ctrl Pts',(-250.777267259738,2.89086856471197,
126.823054292162));
#138259=CARTESIAN_POINT('Ctrl Pts',(-250.785027702253,2.77790711272766,
126.74573829767));
#138260=CARTESIAN_POINT('Ctrl Pts',(-250.792800602518,2.66476432499238,
126.66829818868));
#138261=CARTESIAN_POINT('Ctrl Pts',(-250.800573502783,2.54850078926418,
126.595674841375));
#138262=CARTESIAN_POINT('Ctrl Pts',(-250.808346403049,2.42957384579995,
126.528105949015));
#138263=CARTESIAN_POINT('Ctrl Pts',(-250.815836738811,2.31497019628955,
126.462993356088));
#138264=CARTESIAN_POINT('Ctrl Pts',(-250.823327074573,2.19789369399235,
126.402574255094));
#138265=CARTESIAN_POINT('Ctrl Pts',(-250.830817410335,2.07877028589902,
126.347018678589));
#138266=CARTESIAN_POINT('Ctrl Pts',(-250.838591744454,1.95513027758222,
126.289356695516));
#138267=CARTESIAN_POINT('Ctrl Pts',(-250.846366078573,1.82889342819074,
126.236751662413));
#138268=CARTESIAN_POINT('Ctrl Pts',(-250.854140412692,1.70051197402192,
126.189445440804));
#138269=CARTESIAN_POINT('Ctrl Pts',(-250.861905165639,1.57228873852158,
126.142197519886));
#138270=CARTESIAN_POINT('Ctrl Pts',(-250.869669918586,1.44192652042377,
126.100235550969));
#138271=CARTESIAN_POINT('Ctrl Pts',(-250.877434671533,1.30990066538821,
126.063754821962));
#138272=CARTESIAN_POINT('Ctrl Pts',(-250.885191712418,1.17800594029348,
126.027310326129));
#138273=CARTESIAN_POINT('Ctrl Pts',(-250.892948753303,1.04445124091266,
125.996336339765));
#138274=CARTESIAN_POINT('Ctrl Pts',(-250.900705794188,0.909730004125608,
125.970979359886));
#138275=CARTESIAN_POINT('Ctrl Pts',(-250.908456985428,0.775110361671008,
125.945641501903));
#138276=CARTESIAN_POINT('Ctrl Pts',(-250.916208176668,0.639326315453693,
125.92591229127));
#138277=CARTESIAN_POINT('Ctrl Pts',(-250.923959367908,0.50288416568047,
125.911887768545));
#138278=CARTESIAN_POINT('Ctrl Pts',(-250.931707264685,0.366500007460429,
125.897869206616));
#138279=CARTESIAN_POINT('Ctrl Pts',(-250.939455161462,0.229458690111338,
125.889550550054));
#138280=CARTESIAN_POINT('Ctrl Pts',(-250.947203058239,0.0922741395609136,
125.886976298066));
#138281=CARTESIAN_POINT('Ctrl Pts',(-250.954949334323,-0.0448817149388916,
125.884402584555));
#138282=CARTESIAN_POINT('Ctrl Pts',(-250.962695610407,-0.182180352396627,
125.887570892889));
#138283=CARTESIAN_POINT('Ctrl Pts',(-250.970441886491,-0.319105719346386,
125.896473638185));
#138284=CARTESIAN_POINT('Ctrl Pts',(-250.978188219756,-0.456032097047913,
125.905376449198));
#138285=CARTESIAN_POINT('Ctrl Pts',(-250.985934553022,-0.592584808601845,
125.920013756274));
#138286=CARTESIAN_POINT('Ctrl Pts',(-250.993680886287,-0.728251197651638,
125.940325949143));
#138287=CARTESIAN_POINT('Ctrl Pts',(-251.00142895429,-0.863947968248428,
125.960642690787));
#138288=CARTESIAN_POINT('Ctrl Pts',(-251.009177022293,-0.998757634795884,
125.986636789191));
#138289=CARTESIAN_POINT('Ctrl Pts',(-251.016925090296,-1.13217642367568,
126.018197268058));
#138290=CARTESIAN_POINT('Ctrl Pts',(-251.024681393037,-1.26573701163219,
126.049791289777));
#138291=CARTESIAN_POINT('Ctrl Pts',(-251.032437695779,-1.3979033879028,
126.086963419694));
#138292=CARTESIAN_POINT('Ctrl Pts',(-251.040193998521,-1.52818513377386,
126.129552251503));
#138293=CARTESIAN_POINT('Ctrl Pts',(-251.047954441035,-1.65853641493575,
126.172163814254));
#138294=CARTESIAN_POINT('Ctrl Pts',(-251.055714883549,-1.78700069536488,
126.220197702714));
#138295=CARTESIAN_POINT('Ctrl Pts',(-251.063475326063,-1.91310725526774,
126.27344418793));
#138296=CARTESIAN_POINT('Ctrl Pts',(-251.071248226329,-2.03941625261544,
126.326776149132));
#138297=CARTESIAN_POINT('Ctrl Pts',(-251.079021126594,-2.16335961245829,
126.38533726135));
#138298=CARTESIAN_POINT('Ctrl Pts',(-251.086794026859,-2.28449015314461,
126.448871230289));
#138299=CARTESIAN_POINT('Ctrl Pts',(-251.094284362622,-2.40121729358167,
126.510095579431));
#138300=CARTESIAN_POINT('Ctrl Pts',(-251.101774698385,-2.51533230366311,
126.575937356693));
#138301=CARTESIAN_POINT('Ctrl Pts',(-251.109265034148,-2.62646189542995,
126.646130107559));
#138302=CARTESIAN_POINT('Ctrl Pts',(-251.117040759838,-2.74182564533264,
126.718997278463));
#138303=CARTESIAN_POINT('Ctrl Pts',(-251.124816485528,-2.85433747466235,
126.796784412517));
#138304=CARTESIAN_POINT('Ctrl Pts',(-251.132592211218,-2.96354921518992,
126.879241624255));
#138305=CARTESIAN_POINT('Ctrl Pts',(-251.140391207646,-3.07308779824208,
126.961945609126));
#138306=CARTESIAN_POINT('Ctrl Pts',(-251.148190204075,-3.1793061411131,
127.049347514605));
#138307=CARTESIAN_POINT('Ctrl Pts',(-251.155989200503,-3.28177747678981,
127.141148959016));
#138308=CARTESIAN_POINT('Ctrl Pts',(-251.163745507121,-3.38368790929289,
127.232447904644));
#138309=CARTESIAN_POINT('Ctrl Pts',(-251.171501813739,-3.48189194093155,
127.328098103309));
#138310=CARTESIAN_POINT('Ctrl Pts',(-251.179258120358,-3.57599986306124,
127.42776350777));
#138311=CARTESIAN_POINT('Ctrl Pts',(-251.187009028654,-3.67004228689541,
127.527359545975));
#138312=CARTESIAN_POINT('Ctrl Pts',(-251.19475993695,-3.75999400619828,
127.63096494677));
#138313=CARTESIAN_POINT('Ctrl Pts',(-251.202510845247,-3.84550075558553,
127.738205533215));
#138314=CARTESIAN_POINT('Ctrl Pts',(-251.210258037643,-3.93096651176949,
127.845394706933));
#138315=CARTESIAN_POINT('Ctrl Pts',(-251.218005230038,-4.01199129613124,
127.956215292766));
#138316=CARTESIAN_POINT('Ctrl Pts',(-251.225752422434,-4.08826014679485,
128.070258930608));
#138317=CARTESIAN_POINT('Ctrl Pts',(-251.233587064356,-4.16538991254661,
128.185589881522));
#138318=CARTESIAN_POINT('Ctrl Pts',(-251.241421706278,-4.23765544892985,
128.30421678704));
#138319=CARTESIAN_POINT('Ctrl Pts',(-251.2492563482,-4.30477522581095,128.42568591981));
#138320=CARTESIAN_POINT('Ctrl Pts',(-251.257002773549,-4.37113924681997,
128.545787333339));
#138321=CARTESIAN_POINT('Ctrl Pts',(-251.264749198899,-4.43247263153778,
128.668666932258));
#138322=CARTESIAN_POINT('Ctrl Pts',(-251.272495624249,-4.48854916261805,
128.793860809742));
#138323=CARTESIAN_POINT('Ctrl Pts',(-251.280374374456,-4.54558359604531,
128.921193255835));
#138324=CARTESIAN_POINT('Ctrl Pts',(-251.288253124664,-4.59717974895373,
129.05091939507));
#138325=CARTESIAN_POINT('Ctrl Pts',(-251.296131874872,-4.64315073532577,
129.182530074154));
#138326=CARTESIAN_POINT('Ctrl Pts',(-251.30401062508,-4.68912172169794,
129.314140753238));
#138327=CARTESIAN_POINT('Ctrl Pts',(-251.311889375288,-4.72946743343979,
129.447635561638));
#138328=CARTESIAN_POINT('Ctrl Pts',(-251.319768125496,-4.76405452823393,
129.582490119308));
#138329=CARTESIAN_POINT('Origin',(213.235140564004,0.,130.804360617566));
#138330=CARTESIAN_POINT('',(-253.415334457588,-4.76405452823403,129.582490119308));
#138331=CARTESIAN_POINT('',(-253.070001742224,-4.7640545282341,129.582490119308));
#138332=CARTESIAN_POINT('',(213.235140564004,-4.76405452823405,129.582490119308));
#138333=CARTESIAN_POINT('',(-251.735140563966,-4.91824833132154,130.800309203871));
#138334=CARTESIAN_POINT('Ctrl Pts',(-251.735140564014,-4.91824833132224,
130.800309204721));
#138335=CARTESIAN_POINT('Ctrl Pts',(-251.74305216174,-4.91836371085688,
130.940375207723));
#138336=CARTESIAN_POINT('Ctrl Pts',(-251.750963759465,-4.91249099768164,
131.080528748395));
#138337=CARTESIAN_POINT('Ctrl Pts',(-251.75887535719,-4.90063728135767,
131.220217923703));
#138338=CARTESIAN_POINT('Ctrl Pts',(-251.766596302519,-4.8890692139637,
131.35654089196));
#138339=CARTESIAN_POINT('Ctrl Pts',(-251.774317247848,-4.8718051620345,
131.492421209125));
#138340=CARTESIAN_POINT('Ctrl Pts',(-251.782038193177,-4.84890439244957,
131.627348621964));
#138341=CARTESIAN_POINT('Ctrl Pts',(-251.789759019141,-4.82600397690774,
131.762273948842));
#138342=CARTESIAN_POINT('Ctrl Pts',(-251.797479845106,-4.79746708251017,
131.896246012727));
#138343=CARTESIAN_POINT('Ctrl Pts',(-251.80520067107,-4.76340439916263,
132.028763162703));
#138344=CARTESIAN_POINT('Ctrl Pts',(-251.812923074694,-4.72933475550731,
132.161307390996));
#138345=CARTESIAN_POINT('Ctrl Pts',(-251.820645478317,-4.68973717418013,
132.292395732819));
#138346=CARTESIAN_POINT('Ctrl Pts',(-251.828367881941,-4.6447725543266,
132.421540564595));
#138347=CARTESIAN_POINT('Ctrl Pts',(-251.836422134232,-4.59787570587356,
132.556235033804));
#138348=CARTESIAN_POINT('Ctrl Pts',(-251.844476386522,-4.54514044073534,
132.688814793964));
#138349=CARTESIAN_POINT('Ctrl Pts',(-251.852530638813,-4.48680504939182,
132.818749733713));
#138350=CARTESIAN_POINT('Ctrl Pts',(-251.860265684137,-4.43078161235955,
132.943535078385));
#138351=CARTESIAN_POINT('Ctrl Pts',(-251.86800072946,-4.36959367777433,
133.065880905503));
#138352=CARTESIAN_POINT('Ctrl Pts',(-251.875735774784,-4.30349892103463,
133.185343628667));
#138353=CARTESIAN_POINT('Ctrl Pts',(-251.883476435969,-4.23735617763905,
133.304893085136));
#138354=CARTESIAN_POINT('Ctrl Pts',(-251.891217097154,-4.16629972156714,
133.421554934597));
#138355=CARTESIAN_POINT('Ctrl Pts',(-251.898957758339,-4.0906301933765,
133.534915082054));
#138356=CARTESIAN_POINT('Ctrl Pts',(-251.906709382642,-4.01485349424142,
133.648435781776));
#138357=CARTESIAN_POINT('Ctrl Pts',(-251.914461006945,-3.93445091636207,
133.758645132567));
#138358=CARTESIAN_POINT('Ctrl Pts',(-251.922212631247,-3.8497630856514,
133.865162350259));
#138359=CARTESIAN_POINT('Ctrl Pts',(-251.923148057307,-3.83954339482556,
133.87801629897));
#138360=CARTESIAN_POINT('Ctrl Pts',(-251.924083483367,-3.82926134363088,
133.890816526164));
#138361=CARTESIAN_POINT('Ctrl Pts',(-251.925018909426,-3.81891756565244,
133.903562400163));
#138362=CARTESIAN_POINT('Ctrl Pts',(-251.932793243543,-3.73295033690651,
134.009493469825));
#138363=CARTESIAN_POINT('Ctrl Pts',(-251.94056757766,-3.64243604747541,
134.112012712167));
#138364=CARTESIAN_POINT('Ctrl Pts',(-251.948341911777,-3.54767560085317,
134.210704830004));
#138365=CARTESIAN_POINT('Ctrl Pts',(-251.956106664722,-3.45303193801269,
134.309275318626));
#138366=CARTESIAN_POINT('Ctrl Pts',(-251.963871417667,-3.35415279828997,
134.404027788042));
#138367=CARTESIAN_POINT('Ctrl Pts',(-251.971636170612,-3.25138023700927,
134.49457871639));
#138368=CARTESIAN_POINT('Ctrl Pts',(-251.979393211495,-3.14870975088558,
134.585039708279));
#138369=CARTESIAN_POINT('Ctrl Pts',(-251.987150252378,-3.04215383015814,
134.671307206829));
#138370=CARTESIAN_POINT('Ctrl Pts',(-251.994907293261,-2.93209213904093,
134.753033654255));
#138371=CARTESIAN_POINT('Ctrl Pts',(-252.002658484498,-2.82211344630132,
134.834698471131));
#138372=CARTESIAN_POINT('Ctrl Pts',(-252.010409675736,-2.70863455797444,
134.911828820889));
#138373=CARTESIAN_POINT('Ctrl Pts',(-252.018160866974,-2.5920687742975,
134.98411689417));
#138374=CARTESIAN_POINT('Ctrl Pts',(-252.025908763749,-2.47555253418798,
135.056374243092));
#138375=CARTESIAN_POINT('Ctrl Pts',(-252.033656660524,-2.35595233978666,
135.123793203315));
#138376=CARTESIAN_POINT('Ctrl Pts',(-252.041404557299,-2.23371089178026,
135.186108980314));
#138377=CARTESIAN_POINT('Ctrl Pts',(-252.049150833381,-2.1114950140499,
135.248411722195));
#138378=CARTESIAN_POINT('Ctrl Pts',(-252.056897109463,-1.9866393297505,
135.30561322667));
#138379=CARTESIAN_POINT('Ctrl Pts',(-252.064643385545,-1.85961123299061,
135.357494606879));
#138380=CARTESIAN_POINT('Ctrl Pts',(-252.072389718808,-1.73258219853835,
135.409376370064));
#138381=CARTESIAN_POINT('Ctrl Pts',(-252.080136052071,-1.60338108156755,
135.455937782793));
#138382=CARTESIAN_POINT('Ctrl Pts',(-252.087882385335,-1.47249497572673,
135.497008229412));
#138383=CARTESIAN_POINT('Ctrl Pts',(-252.095630453335,-1.34157955884983,
135.538087873472));
#138384=CARTESIAN_POINT('Ctrl Pts',(-252.103378521336,-1.20897877519691,
135.573673987504));
#138385=CARTESIAN_POINT('Ctrl Pts',(-252.111126589337,-1.0751941964541,
135.603646033377));
#138386=CARTESIAN_POINT('Ctrl Pts',(-252.118882892077,-0.941267429868731,
135.633649933896));
#138387=CARTESIAN_POINT('Ctrl Pts',(-252.126639194817,-0.806154737017025,
135.658027761528));
#138388=CARTESIAN_POINT('Ctrl Pts',(-252.134395497556,-0.670367736500607,
135.676710169924));
#138389=CARTESIAN_POINT('Ctrl Pts',(-252.142155940068,-0.534508262373896,
135.695402549683));
#138390=CARTESIAN_POINT('Ctrl Pts',(-252.14991638258,-0.397974152471628,
135.7083934161));
#138391=CARTESIAN_POINT('Ctrl Pts',(-252.157676825092,-0.261280445561837,
135.715665494202));
#138392=CARTESIAN_POINT('Ctrl Pts',(-252.165449725356,-0.124367305777813,
135.72294924609));
#138393=CARTESIAN_POINT('Ctrl Pts',(-252.173222625619,0.0127055518162359,
135.724495860071));
#138394=CARTESIAN_POINT('Ctrl Pts',(-252.180995525882,0.14942388941872,
135.720340231414));
#138395=CARTESIAN_POINT('Ctrl Pts',(-252.188485861668,0.281172171527148,
135.716335670313));
#138396=CARTESIAN_POINT('Ctrl Pts',(-252.195976197453,0.412590954282281,
135.707036272297));
#138397=CARTESIAN_POINT('Ctrl Pts',(-252.203466533239,0.543228007211834,
135.692518388616));
#138398=CARTESIAN_POINT('Ctrl Pts',(-252.211240867366,0.678818203424962,
135.677450054995));
#138399=CARTESIAN_POINT('Ctrl Pts',(-252.219015201493,0.813995730049785,
135.656711974421));
#138400=CARTESIAN_POINT('Ctrl Pts',(-252.226789535621,0.948248540112327,
135.630332827253));
#138401=CARTESIAN_POINT('Ctrl Pts',(-252.234554288576,1.08233589558552,
135.603986190027));
#138402=CARTESIAN_POINT('Ctrl Pts',(-252.242319041531,1.21550042207451,
135.572012393489));
#138403=CARTESIAN_POINT('Ctrl Pts',(-252.250083794487,1.34723456251655,
135.534491915539));
#138404=CARTESIAN_POINT('Ctrl Pts',(-252.25784083538,1.47883786275332,135.497008703456));
#138405=CARTESIAN_POINT('Ctrl Pts',(-252.265597876273,1.60901323058164,
135.453989879606));
#138406=CARTESIAN_POINT('Ctrl Pts',(-252.273354917166,1.73726303801028,
135.405567002772));
#138407=CARTESIAN_POINT('Ctrl Pts',(-252.281106108414,1.86541613126107,
135.357180642007));
#138408=CARTESIAN_POINT('Ctrl Pts',(-252.288857299663,1.99164619010694,
135.303398477313));
#138409=CARTESIAN_POINT('Ctrl Pts',(-252.296608490911,2.11547084694168,
135.244401851411));
#138410=CARTESIAN_POINT('Ctrl Pts',(-252.304356387696,2.23924287499403,
135.185430300648));
#138411=CARTESIAN_POINT('Ctrl Pts',(-252.312104284481,2.36061118221925,
135.12124886451));
#138412=CARTESIAN_POINT('Ctrl Pts',(-252.319852181266,2.47911369894876,
135.052086871715));
#138413=CARTESIAN_POINT('Ctrl Pts',(-252.327598457359,2.59759142750609,
134.982939346118));
#138414=CARTESIAN_POINT('Ctrl Pts',(-252.335344733451,2.71320422048017,
134.908813533058));
#138415=CARTESIAN_POINT('Ctrl Pts',(-252.343091009543,2.8255152842239,134.829984350743));
#138416=CARTESIAN_POINT('Ctrl Pts',(-252.350837342816,2.93782717702192,
134.751154586529));
#138417=CARTESIAN_POINT('Ctrl Pts',(-252.35858367609,3.04683697194792,134.667621608388));
#138418=CARTESIAN_POINT('Ctrl Pts',(-252.366330009363,3.15213783920438,
134.579703000073));
#138419=CARTESIAN_POINT('Ctrl Pts',(-252.374078077374,3.2574622878592,134.491764702997));
#138420=CARTESIAN_POINT('Ctrl Pts',(-252.381826145385,3.35907585601441,
134.399439071944));
#138421=CARTESIAN_POINT('Ctrl Pts',(-252.389574213396,3.45660601977891,
134.303082939576));
#138422=CARTESIAN_POINT('Ctrl Pts',(-252.397330516146,3.55423983976079,
134.206624398765));
#138423=CARTESIAN_POINT('Ctrl Pts',(-252.405086818896,3.64778130738623,
134.106127074771));
#138424=CARTESIAN_POINT('Ctrl Pts',(-252.412843121646,3.73689553725653,
134.001983923419));
#138425=CARTESIAN_POINT('Ctrl Pts',(-252.420603564168,3.82605733007419,
133.897785187731));
#138426=CARTESIAN_POINT('Ctrl Pts',(-252.42836400669,3.91078693534454,133.789937054624));
#138427=CARTESIAN_POINT('Ctrl Pts',(-252.436124449212,3.99079142810894,
133.678863503255));
#138428=CARTESIAN_POINT('Ctrl Pts',(-252.443897349485,4.07092435118573,
133.567611646763));
#138429=CARTESIAN_POINT('Ctrl Pts',(-252.451670249758,4.14631678902233,
133.453124351972));
#138430=CARTESIAN_POINT('Ctrl Pts',(-252.459443150031,4.21672014190244,
133.335853123455));
#138431=CARTESIAN_POINT('Ctrl Pts',(-252.466933485705,4.28456415470126,
133.222845000931));
#138432=CARTESIAN_POINT('Ctrl Pts',(-252.474423821378,4.34777536893473,
133.107252106937));
#138433=CARTESIAN_POINT('Ctrl Pts',(-252.481914157052,4.40617357946336,
132.989496185475));
#138434=CARTESIAN_POINT('Ctrl Pts',(-252.489688491162,4.46678597653833,
132.867275511159));
#138435=CARTESIAN_POINT('Ctrl Pts',(-252.497462825272,4.52240519695692,
132.742337390744));
#138436=CARTESIAN_POINT('Ctrl Pts',(-252.505237159382,4.57277859642071,
132.615128126281));
#138437=CARTESIAN_POINT('Ctrl Pts',(-252.51300191232,4.62308991517185,132.488075635867));
#138438=CARTESIAN_POINT('Ctrl Pts',(-252.520766665258,4.66816813384111,
132.358757930559));
#138439=CARTESIAN_POINT('Ctrl Pts',(-252.528531418196,4.70780661377364,
132.227645532757));
#138440=CARTESIAN_POINT('Ctrl Pts',(-252.536288459072,4.74740572420926,
132.096663357636));
#138441=CARTESIAN_POINT('Ctrl Pts',(-252.544045499948,4.78157573536534,
131.963890409119));
#138442=CARTESIAN_POINT('Ctrl Pts',(-252.551802540823,4.81015835128799,
131.829816466462));
#138443=CARTESIAN_POINT('Ctrl Pts',(-252.559553732055,4.83871941283779,
131.695843630007));
#138444=CARTESIAN_POINT('Ctrl Pts',(-252.567304923286,4.86170138468028,
131.560572133038));
#138445=CARTESIAN_POINT('Ctrl Pts',(-252.575056114517,4.87899610410646,
131.42450582525));
#138446=CARTESIAN_POINT('Ctrl Pts',(-252.582804011285,4.89628347281573,
131.288497349272));
#138447=CARTESIAN_POINT('Ctrl Pts',(-252.590551908053,4.90788834760884,
131.151695121396));
#138448=CARTESIAN_POINT('Ctrl Pts',(-252.598299804821,4.9137539092884,131.014611851695));
#138449=CARTESIAN_POINT('Ctrl Pts',(-252.606046080896,4.91961824401895,
130.877557256858));
#138450=CARTESIAN_POINT('Ctrl Pts',(-252.613792356972,4.91974563687403,
130.740222127488));
#138451=CARTESIAN_POINT('Ctrl Pts',(-252.621538633047,4.91413128669204,
130.603122550455));
#138452=CARTESIAN_POINT('Ctrl Pts',(-252.629284966303,4.90851689506614,
130.466021961383));
#138453=CARTESIAN_POINT('Ctrl Pts',(-252.63703129956,4.89716069182535,130.329157318756));
#138454=CARTESIAN_POINT('Ctrl Pts',(-252.644777632817,4.88010996773329,
130.19304256178));
#138455=CARTESIAN_POINT('Ctrl Pts',(-252.652525700811,4.86305542524957,
130.056897322845));
#138456=CARTESIAN_POINT('Ctrl Pts',(-252.660273768805,4.8403038729037,129.921502691585));
#138457=CARTESIAN_POINT('Ctrl Pts',(-252.668021836799,4.81195416585766,
129.787364959667));
#138458=CARTESIAN_POINT('Ctrl Pts',(-252.675778139533,4.783574328405,129.653084664569));
#138459=CARTESIAN_POINT('Ctrl Pts',(-252.683534442266,4.74958453188733,
129.520064320437));
#138460=CARTESIAN_POINT('Ctrl Pts',(-252.691290744999,4.71013436743116,
129.388798078063));
#138461=CARTESIAN_POINT('Ctrl Pts',(-252.699051187505,4.67066314723384,
129.257461774941));
#138462=CARTESIAN_POINT('Ctrl Pts',(-252.706811630011,4.62572588001987,
129.127881808272));
#138463=CARTESIAN_POINT('Ctrl Pts',(-252.714572072516,4.57552093836776,
129.000533795208));
#138464=CARTESIAN_POINT('Ctrl Pts',(-252.722344972774,4.52523540328487,
128.872981351804));
#138465=CARTESIAN_POINT('Ctrl Pts',(-252.730117873031,4.46966545428416,
128.747668379448));
#138466=CARTESIAN_POINT('Ctrl Pts',(-252.737890773288,4.40905658073008,
128.62504808137));
#138467=CARTESIAN_POINT('Ctrl Pts',(-252.745381109147,4.35065099157668,
128.506885338335));
#138468=CARTESIAN_POINT('Ctrl Pts',(-252.752871445006,4.28756661996266,
128.391223167946));
#138469=CARTESIAN_POINT('Ctrl Pts',(-252.760361780865,4.22006088580106,
128.278441144853));
#138470=CARTESIAN_POINT('Ctrl Pts',(-252.768136114974,4.14999565221084,
128.161382958746));
#138471=CARTESIAN_POINT('Ctrl Pts',(-252.775910449082,4.07494522030888,
128.047056827574));
#138472=CARTESIAN_POINT('Ctrl Pts',(-252.783684783191,3.99514851623755,
127.935916545302));
#138473=CARTESIAN_POINT('Ctrl Pts',(-252.791449536127,3.91545015447357,
127.824913233498));
#138474=CARTESIAN_POINT('Ctrl Pts',(-252.799214289064,3.83101738484741,
127.717088273015));
#138475=CARTESIAN_POINT('Ctrl Pts',(-252.806979042001,3.74213437793858,
127.612869843656));
#138476=CARTESIAN_POINT('Ctrl Pts',(-252.814736082875,3.65333965088656,
127.508754925513));
#138477=CARTESIAN_POINT('Ctrl Pts',(-252.822493123749,3.56010373468657,
127.408239705586));
#138478=CARTESIAN_POINT('Ctrl Pts',(-252.830250164624,3.46275313166815,
127.311722100396));
#138479=CARTESIAN_POINT('Ctrl Pts',(-252.838001355853,3.36547594149777,
127.215277279883));
#138480=CARTESIAN_POINT('Ctrl Pts',(-252.845752547083,3.26409051719386,
127.122824347816));
#138481=CARTESIAN_POINT('Ctrl Pts',(-252.853503738312,3.15896229718796,
127.03472664761));
#138482=CARTESIAN_POINT('Ctrl Pts',(-252.861251635079,3.05387875948159,
126.946666391279));
#138483=CARTESIAN_POINT('Ctrl Pts',(-252.868999531845,2.94505588906063,
126.862957935722));
#138484=CARTESIAN_POINT('Ctrl Pts',(-252.876747428611,2.83289433126341,
126.783926216858));
#138485=CARTESIAN_POINT('Ctrl Pts',(-252.884493704684,2.72075623524711,
126.704911029726));
#138486=CARTESIAN_POINT('Ctrl Pts',(-252.892239980758,2.60528116036644,
126.630570858501));
#138487=CARTESIAN_POINT('Ctrl Pts',(-252.899986256831,2.48690070997629,
126.561188700094));
#138488=CARTESIAN_POINT('Ctrl Pts',(-252.907732590086,2.36851938572904,
126.491806029525));
#138489=CARTESIAN_POINT('Ctrl Pts',(-252.91547892334,2.24723298047813,126.427381642497));
#138490=CARTESIAN_POINT('Ctrl Pts',(-252.923225256594,2.12349944764491,
126.368153548644));
#138491=CARTESIAN_POINT('Ctrl Pts',(-252.930973324587,1.99973820554539,
126.308912191071));
#138492=CARTESIAN_POINT('Ctrl Pts',(-252.938721392579,1.87352909795146,
126.254869611021));
#138493=CARTESIAN_POINT('Ctrl Pts',(-252.946469460571,1.74535151601177,
126.20621630186));
#138494=CARTESIAN_POINT('Ctrl Pts',(-252.954225763302,1.61703770541265,
126.157511283384));
#138495=CARTESIAN_POINT('Ctrl Pts',(-252.961982066033,1.48675160733874,
126.114207116621));
#138496=CARTESIAN_POINT('Ctrl Pts',(-252.969738368763,1.35498982250258,
126.076445046893));
#138497=CARTESIAN_POINT('Ctrl Pts',(-252.977498811267,1.22315771243448,
126.038662822411));
#138498=CARTESIAN_POINT('Ctrl Pts',(-252.98525925377,1.08984872603554,126.006428680841));
#138499=CARTESIAN_POINT('Ctrl Pts',(-252.993019696273,0.955570238710946,
125.979832808403));
#138500=CARTESIAN_POINT('Ctrl Pts',(-253.000792596528,0.821076195636046,
125.953194241909));
#138501=CARTESIAN_POINT('Ctrl Pts',(-253.008565496782,0.685609928174875,
125.932212091306));
#138502=CARTESIAN_POINT('Ctrl Pts',(-253.016338397037,0.549685422037678,
125.916924786857));
#138503=CARTESIAN_POINT('Ctrl Pts',(-253.023828732917,0.41870211182428,
125.902193214178));
#138504=CARTESIAN_POINT('Ctrl Pts',(-253.031319068797,0.287293607987546,
125.892749654319));
#138505=CARTESIAN_POINT('Ctrl Pts',(-253.038809404677,0.155918399185276,
125.888582701987));
#138506=CARTESIAN_POINT('Ctrl Pts',(-253.04658373885,0.0195620606171169,
125.884257758429));
#138507=CARTESIAN_POINT('Ctrl Pts',(-253.054358073023,-0.11719034419708,
125.885603745921));
#138508=CARTESIAN_POINT('Ctrl Pts',(-253.062132407196,-0.253827880118555,
125.892664935851));
#138509=CARTESIAN_POINT('Ctrl Pts',(-253.069897160197,-0.390297022492045,
125.899717423496));
#138510=CARTESIAN_POINT('Ctrl Pts',(-253.077661913198,-0.526651190950291,
125.912471079177));
#138511=CARTESIAN_POINT('Ctrl Pts',(-253.085426666199,-0.662376544551844,
125.930918263775));
#138512=CARTESIAN_POINT('Ctrl Pts',(-253.093183707138,-0.797967093821589,
125.949347126369));
#138513=CARTESIAN_POINT('Ctrl Pts',(-253.100940748077,-0.932929686216431,
125.973458212074));
#138514=CARTESIAN_POINT('Ctrl Pts',(-253.108697789016,-1.06675306080651,
126.003191908829));
#138515=CARTESIAN_POINT('Ctrl Pts',(-253.11644898031,-1.20047551814897,
126.032903183171));
#138516=CARTESIAN_POINT('Ctrl Pts',(-253.124200171604,-1.33306008754539,
126.068228544534));
#138517=CARTESIAN_POINT('Ctrl Pts',(-253.131951362898,-1.46400354948286,
126.109056935204));
#138518=CARTESIAN_POINT('Ctrl Pts',(-253.139699259729,-1.59489135695368,
126.149867972718));
#138519=CARTESIAN_POINT('Ctrl Pts',(-253.14744715656,-1.72413907180751,
126.196177271443));
#138520=CARTESIAN_POINT('Ctrl Pts',(-253.155195053391,-1.85125675765714,
126.247823392904));
#138521=CARTESIAN_POINT('Ctrl Pts',(-253.162941329529,-1.97834785322533,
126.299458711109));
#138522=CARTESIAN_POINT('Ctrl Pts',(-253.170687605667,-2.10330944404284,
126.356428484504));
#138523=CARTESIAN_POINT('Ctrl Pts',(-253.178433881805,-2.22567014463019,
126.418522559703));
#138524=CARTESIAN_POINT('Ctrl Pts',(-253.186180215124,-2.3480317484546,
126.480617093265));
#138525=CARTESIAN_POINT('Ctrl Pts',(-253.193926548443,-2.46779207509605,
126.547835827185));
#138526=CARTESIAN_POINT('Ctrl Pts',(-253.201672881761,-2.58450334529135,
126.619922122298));
#138527=CARTESIAN_POINT('Ctrl Pts',(-253.209420949818,-2.70124075216193,
126.692024560635));
#138528=CARTESIAN_POINT('Ctrl Pts',(-253.217169017874,-2.81492741129484,
126.76899652384));
#138529=CARTESIAN_POINT('Ctrl Pts',(-253.22491708593,-2.92514393259481,
126.850537652877));
#138530=CARTESIAN_POINT('Ctrl Pts',(-253.232673388725,-3.03547759331555,
126.932165444789));
#138531=CARTESIAN_POINT('Ctrl Pts',(-253.24042969152,-3.14233343401797,
127.018371870343));
#138532=CARTESIAN_POINT('Ctrl Pts',(-253.248185994314,-3.24532419619202,
127.108815471838));
#138533=CARTESIAN_POINT('Ctrl Pts',(-253.255946436881,-3.34836992763311,
127.199307345804));
#138534=CARTESIAN_POINT('Ctrl Pts',(-253.263706879447,-3.44754618744979,
127.294040632039));
#138535=CARTESIAN_POINT('Ctrl Pts',(-253.271467322014,-3.54250285061481,
127.392637209098));
#138536=CARTESIAN_POINT('Ctrl Pts',(-253.279240222331,-3.63761194663223,
127.491392062122));
#138537=CARTESIAN_POINT('Ctrl Pts',(-253.287013122648,-3.72848765071348,
127.594022306059));
#138538=CARTESIAN_POINT('Ctrl Pts',(-253.294786022964,-3.81481980855446,
127.700116282666));
#138539=CARTESIAN_POINT('Ctrl Pts',(-253.30227635814,-3.8980135679346,127.802353467305));
#138540=CARTESIAN_POINT('Ctrl Pts',(-253.309766693315,-3.97698820068931,
127.90780667886));
#138541=CARTESIAN_POINT('Ctrl Pts',(-253.317257028491,-4.0515054781619,
128.016084013116));
#138542=CARTESIAN_POINT('Ctrl Pts',(-253.325430147582,-4.13281540206915,
128.134231402659));
#138543=CARTESIAN_POINT('Ctrl Pts',(-253.333603266674,-4.20908046165086,
128.256123151092));
#138544=CARTESIAN_POINT('Ctrl Pts',(-253.341776385765,-4.27994506192049,
128.381293691243));
#138545=CARTESIAN_POINT('Ctrl Pts',(-253.349647985341,-4.34819535304647,
128.501846488735));
#138546=CARTESIAN_POINT('Ctrl Pts',(-253.357519584916,-4.41143630189487,
128.625440112942));
#138547=CARTESIAN_POINT('Ctrl Pts',(-253.365391184492,-4.46939190082812,
128.751626075714));
#138548=CARTESIAN_POINT('Ctrl Pts',(-253.373254756906,-4.52728839882145,
128.877683358788));
#138549=CARTESIAN_POINT('Ctrl Pts',(-253.381118329321,-4.57991011563706,
129.006327380166));
#138550=CARTESIAN_POINT('Ctrl Pts',(-253.388981901735,-4.62702611600136,
129.137083680659));
#138551=CARTESIAN_POINT('Ctrl Pts',(-253.396837413988,-4.67409382246811,
129.267705955952));
#138552=CARTESIAN_POINT('Ctrl Pts',(-253.404692926241,-4.71566692654559,
129.400435844763));
#138553=CARTESIAN_POINT('Ctrl Pts',(-253.412548438494,-4.75156215372704,
129.53477794528));
#138554=CARTESIAN_POINT('Ctrl Pts',(-253.413477111525,-4.75580566177188,
129.550659772171));
#138555=CARTESIAN_POINT('Ctrl Pts',(-253.414405784557,-4.75996987254124,
129.566564108755));
#138556=CARTESIAN_POINT('Ctrl Pts',(-253.415334457588,-4.76405452823403,
129.582490119308));
#138557=CARTESIAN_POINT('Ctrl Pts',(-251.665320902482,-4.76405452823413,
129.582490119309));
#138558=CARTESIAN_POINT('Ctrl Pts',(-251.674572419706,-4.80443247690585,
129.739923128359));
#138559=CARTESIAN_POINT('Ctrl Pts',(-251.683823936931,-4.83704222570981,
129.899513529989));
#138560=CARTESIAN_POINT('Ctrl Pts',(-251.693075454155,-4.86168099319561,
130.06055890817));
#138561=CARTESIAN_POINT('Ctrl Pts',(-251.702232760127,-4.88606885598187,
130.219964308124));
#138562=CARTESIAN_POINT('Ctrl Pts',(-251.711390066099,-4.9026471949439,
130.380795143411));
#138563=CARTESIAN_POINT('Ctrl Pts',(-251.720547372071,-4.91126596260942,
130.542349726544));
#138564=CARTESIAN_POINT('Ctrl Pts',(-251.725411769369,-4.91584428622076,
130.62816816268));
#138565=CARTESIAN_POINT('Ctrl Pts',(-251.730276166667,-4.918177390908,130.714190481682));
#138566=CARTESIAN_POINT('Ctrl Pts',(-251.735140563966,-4.91824833132153,
130.800309203871));
#138567=CARTESIAN_POINT('',(-251.389859436039,-4.91824999430341,130.804123901556));
#138568=CARTESIAN_POINT('Ctrl Pts',(-251.319768125496,-4.76405452823393,
129.582490119308));
#138569=CARTESIAN_POINT('Ctrl Pts',(-251.327528806674,-4.79812330926081,
129.715323779466));
#138570=CARTESIAN_POINT('Ctrl Pts',(-251.335289487853,-4.82660485264554,
129.849476320883));
#138571=CARTESIAN_POINT('Ctrl Pts',(-251.343050169032,-4.84942367805967,
129.984438027821));
#138572=CARTESIAN_POINT('Ctrl Pts',(-251.350823197439,-4.87227880818138,
130.119614458576));
#138573=CARTESIAN_POINT('Ctrl Pts',(-251.358596225847,-4.88945316897587,
130.255602239287));
#138574=CARTESIAN_POINT('Ctrl Pts',(-251.366369254255,-4.90092320301354,
130.391886593337));
#138575=CARTESIAN_POINT('Ctrl Pts',(-251.373483722157,-4.91142145217891,
130.516624419002));
#138576=CARTESIAN_POINT('Ctrl Pts',(-251.380598190058,-4.9171416332976,
130.6416104416));
#138577=CARTESIAN_POINT('Ctrl Pts',(-251.38771265796,-4.91810390465499,
130.766452234359));
#138578=CARTESIAN_POINT('Ctrl Pts',(-251.388428250639,-4.91820069254526,
130.779009164009));
#138579=CARTESIAN_POINT('Ctrl Pts',(-251.389143843318,-4.91824938991048,
130.791566464814));
#138580=CARTESIAN_POINT('Ctrl Pts',(-251.389859435997,-4.91824999430338,
130.804123900822));
#138581=CARTESIAN_POINT('Ctrl Pts',(-251.389859436039,-4.91824999430341,
130.804123901557));
#138582=CARTESIAN_POINT('Ctrl Pts',(-251.397623097505,-4.91825655150756,
130.940362972942));
#138583=CARTESIAN_POINT('Ctrl Pts',(-251.405386758971,-4.9125979373634,
131.076820927194));
#138584=CARTESIAN_POINT('Ctrl Pts',(-251.413150420438,-4.90124551686362,
131.212986908845));
#138585=CARTESIAN_POINT('Ctrl Pts',(-251.420904513053,-4.88990708842368,
131.348985063505));
#138586=CARTESIAN_POINT('Ctrl Pts',(-251.428658605669,-4.87288884830977,
131.484691574514));
#138587=CARTESIAN_POINT('Ctrl Pts',(-251.436412698285,-4.85021413697419,
131.619594257694));
#138588=CARTESIAN_POINT('Ctrl Pts',(-251.444159102514,-4.82756190821258,
131.754363181307));
#138589=CARTESIAN_POINT('Ctrl Pts',(-251.451905506742,-4.79926443348876,
131.888329478876));
#138590=CARTESIAN_POINT('Ctrl Pts',(-251.459651910971,-4.76539692333789,
132.020985138748));
#138591=CARTESIAN_POINT('Ctrl Pts',(-251.467392500501,-4.73155483522072,
132.15354122305));
#138592=CARTESIAN_POINT('Ctrl Pts',(-251.475133090031,-4.69215113002352,
132.284788249317));
#138593=CARTESIAN_POINT('Ctrl Pts',(-251.482873679562,-4.64731219075221,
132.414227836993));
#138594=CARTESIAN_POINT('Ctrl Pts',(-251.490611030979,-4.60249200890738,
132.543613276342));
#138595=CARTESIAN_POINT('Ctrl Pts',(-251.498348382397,-4.55224124296833,
132.671192411002));
#138596=CARTESIAN_POINT('Ctrl Pts',(-251.506085733815,-4.49673621749552,
132.796481711467));
#138597=CARTESIAN_POINT('Ctrl Pts',(-251.513821517098,-4.44124244126378,
132.921745619465));
#138598=CARTESIAN_POINT('Ctrl Pts',(-251.521557300381,-4.38049668226015,
133.044720257957));
#138599=CARTESIAN_POINT('Ctrl Pts',(-251.529293083665,-4.31472336921529,
133.16494217931));
#138600=CARTESIAN_POINT('Ctrl Pts',(-251.537028986808,-4.2489490370617,
133.285165963414));
#138601=CARTESIAN_POINT('Ctrl Pts',(-251.544764889952,-4.1781471839442,
133.402636601372));
#138602=CARTESIAN_POINT('Ctrl Pts',(-251.552500793096,-4.10258794636578,
133.516915723888));
#138603=CARTESIAN_POINT('Ctrl Pts',(-251.560238503824,-4.02701105348838,
133.631221549056));
#138604=CARTESIAN_POINT('Ctrl Pts',(-251.567976214551,-3.94667478058135,
133.742334047912));
#138605=CARTESIAN_POINT('Ctrl Pts',(-251.575713925279,-3.86189204456478,
133.849844634701));
#138606=CARTESIAN_POINT('Ctrl Pts',(-251.583459876721,-3.77701901436072,
133.957469720993));
#138607=CARTESIAN_POINT('Ctrl Pts',(-251.591205828163,-3.68769030538339,
134.061484924554));
#138608=CARTESIAN_POINT('Ctrl Pts',(-251.598951779605,-3.59425885152675,
134.161515122608));
#138609=CARTESIAN_POINT('Ctrl Pts',(-251.606701955618,-3.50077644102186,
134.261599876203));
#138610=CARTESIAN_POINT('Ctrl Pts',(-251.61445213163,-3.40318710676369,
134.35769501918));
#138611=CARTESIAN_POINT('Ctrl Pts',(-251.622202307642,-3.3018792005806,
134.449463744677));
#138612=CARTESIAN_POINT('Ctrl Pts',(-251.629964748407,-3.20041097334431,
134.541377695352));
#138613=CARTESIAN_POINT('Ctrl Pts',(-251.637727189171,-3.09521271771393,
134.628951297797));
#138614=CARTESIAN_POINT('Ctrl Pts',(-251.645489629936,-2.98670492236545,
134.711888834894));
#138615=CARTESIAN_POINT('Ctrl Pts',(-251.652379847215,-2.89038956111025,
134.78550712952));
#138616=CARTESIAN_POINT('Ctrl Pts',(-251.659270064494,-2.79146721128591,
134.855473202726));
#138617=CARTESIAN_POINT('Ctrl Pts',(-251.666160281774,-2.6902486882225,
134.921610313421));
#138618=CARTESIAN_POINT('Ctrl Pts',(-251.673934615893,-2.57604233080481,
134.996233794124));
#138619=CARTESIAN_POINT('Ctrl Pts',(-251.681708950011,-2.45854780978557,
135.066220001201));
#138620=CARTESIAN_POINT('Ctrl Pts',(-251.68948328413,-2.33817846390311,
135.131265346519));
#138621=CARTESIAN_POINT('Ctrl Pts',(-251.697248037077,-2.21795746248174,
135.196230529263));
#138622=CARTESIAN_POINT('Ctrl Pts',(-251.705012790023,-2.09486902629651,
135.2562667818));
#138623=CARTESIAN_POINT('Ctrl Pts',(-251.71277754297,-1.96935597857399,
135.311113339));
#138624=CARTESIAN_POINT('Ctrl Pts',(-251.720534583855,-1.84396759218024,
135.365905421826));
#138625=CARTESIAN_POINT('Ctrl Pts',(-251.728291624739,-1.71615974252891,
135.415517911423));
#138626=CARTESIAN_POINT('Ctrl Pts',(-251.736048665624,-1.58640008461407,
135.459735772592));
#138627=CARTESIAN_POINT('Ctrl Pts',(-251.743799856864,-1.45673827946648,
135.503920288729));
#138628=CARTESIAN_POINT('Ctrl Pts',(-251.751551048103,-1.32512796430206,
135.542718148208));
#138629=CARTESIAN_POINT('Ctrl Pts',(-251.759302239343,-1.19205668724417,
135.575962436337));
#138630=CARTESIAN_POINT('Ctrl Pts',(-251.76705013612,-1.05904196902864,
135.609192594756));
#138631=CARTESIAN_POINT('Ctrl Pts',(-251.774798032897,-0.924567902451036,
135.636873781949));
#138632=CARTESIAN_POINT('Ctrl Pts',(-251.782545929673,-0.789136898110652,
135.658889020876));
#138633=CARTESIAN_POINT('Ctrl Pts',(-251.790292205757,-0.653734223016822,
135.680899654689));
#138634=CARTESIAN_POINT('Ctrl Pts',(-251.798038481841,-0.517375393966117,
135.69724663496));
#138635=CARTESIAN_POINT('Ctrl Pts',(-251.805784757924,-0.380572318507233,
135.707864239762));
#138636=CARTESIAN_POINT('Ctrl Pts',(-251.813531091189,-0.243768233198938,
135.718481922941));
#138637=CARTESIAN_POINT('Ctrl Pts',(-251.821277424454,-0.106520284731784,
135.723370116005));
#138638=CARTESIAN_POINT('Ctrl Pts',(-251.829023757719,0.030655599466925,
135.722515078004));
#138639=CARTESIAN_POINT('Ctrl Pts',(-251.836771825722,0.167862203253604,
135.721659848522));
#138640=CARTESIAN_POINT('Ctrl Pts',(-251.844519893725,0.304996319775712,
135.715058831107));
#138641=CARTESIAN_POINT('Ctrl Pts',(-251.852267961727,0.441543525409281,
135.702750391529));
#138642=CARTESIAN_POINT('Ctrl Pts',(-251.860024264469,0.578235855037751,
135.690428870396));
#138643=CARTESIAN_POINT('Ctrl Pts',(-251.86778056721,0.714339637710827,
135.672387844934));
#138644=CARTESIAN_POINT('Ctrl Pts',(-251.875536869952,0.849346513343336,
135.648717495705));
#138645=CARTESIAN_POINT('Ctrl Pts',(-251.883297312465,0.98442544621072,
135.625034512898));
#138646=CARTESIAN_POINT('Ctrl Pts',(-251.891057754979,1.11840592373312,
135.595716303058));
#138647=CARTESIAN_POINT('Ctrl Pts',(-251.898818197493,1.25079222822346,
135.560903675746));
#138648=CARTESIAN_POINT('Ctrl Pts',(-251.906591097758,1.38339105096212,
135.526035164113));
#138649=CARTESIAN_POINT('Ctrl Pts',(-251.914363998023,1.51439021292255,
135.485654724819));
#138650=CARTESIAN_POINT('Ctrl Pts',(-251.922136898288,1.64331068855447,
135.439952601702));
#138651=CARTESIAN_POINT('Ctrl Pts',(-251.929627234054,1.76754458023938,
135.395911865851));
#138652=CARTESIAN_POINT('Ctrl Pts',(-251.93711756982,1.88984800676703,135.346929756531));
#138653=CARTESIAN_POINT('Ctrl Pts',(-251.944607905586,2.0098136467306,135.293217060795));
#138654=CARTESIAN_POINT('Ctrl Pts',(-251.952382239706,2.13432782034755,
135.237467831896));
#138655=CARTESIAN_POINT('Ctrl Pts',(-251.960156573827,2.25671785707082,
135.176445618165));
#138656=CARTESIAN_POINT('Ctrl Pts',(-251.967930907947,2.37650491992359,
135.110334076388));
#138657=CARTESIAN_POINT('Ctrl Pts',(-251.975695660895,2.49614435592709,
135.044304011178));
#138658=CARTESIAN_POINT('Ctrl Pts',(-251.983460413844,2.61318686188228,
134.973197284716));
#138659=CARTESIAN_POINT('Ctrl Pts',(-251.991225166792,2.72717369192919,
134.897245506804));
#138660=CARTESIAN_POINT('Ctrl Pts',(-251.998982207678,2.84104730864958,
134.821369165267));
#138661=CARTESIAN_POINT('Ctrl Pts',(-252.006739248564,2.95187096588072,
134.740657564109));
#138662=CARTESIAN_POINT('Ctrl Pts',(-252.01449628945,3.059210969472,134.655387922943));
#138663=CARTESIAN_POINT('Ctrl Pts',(-252.022247480692,3.16647002713174,
134.570182584277));
#138664=CARTESIAN_POINT('Ctrl Pts',(-252.029998671933,3.27025035524586,
134.480426289448));
#138665=CARTESIAN_POINT('Ctrl Pts',(-252.037749863174,3.37014799208426,
134.386439005032));
#138666=CARTESIAN_POINT('Ctrl Pts',(-252.045497759952,3.47000316976201,
134.292491667719));
#138667=CARTESIAN_POINT('Ctrl Pts',(-252.053245656731,3.56597865422714,
134.194317184808));
#138668=CARTESIAN_POINT('Ctrl Pts',(-252.060993553509,3.65770446418048,
134.092275019617));
#138669=CARTESIAN_POINT('Ctrl Pts',(-252.068739829594,3.74941108707175,
133.990254199447));
#138670=CARTESIAN_POINT('Ctrl Pts',(-252.076486105679,3.83686954240243,
133.884367596792));
#138671=CARTESIAN_POINT('Ctrl Pts',(-252.084232381765,3.91974783791985,
133.775010369661));
#138672=CARTESIAN_POINT('Ctrl Pts',(-252.091978715031,4.0026267452259,133.665652335281));
#138673=CARTESIAN_POINT('Ctrl Pts',(-252.099725048298,4.08092518910878,
133.552823936896));
#138674=CARTESIAN_POINT('Ctrl Pts',(-252.107471381564,4.15435273753924,
133.436951811542));
#138675=CARTESIAN_POINT('Ctrl Pts',(-252.115219449568,4.22779672955995,
133.32105373743));
#138676=CARTESIAN_POINT('Ctrl Pts',(-252.122967517572,4.2963674463242,133.202110910179));
#138677=CARTESIAN_POINT('Ctrl Pts',(-252.130715585577,4.35981910750697,
133.080576866589));
#138678=CARTESIAN_POINT('Ctrl Pts',(-252.13847188832,4.42333820587024,132.958913655172));
#138679=CARTESIAN_POINT('Ctrl Pts',(-252.146228191063,4.48172719924991,
132.834654073181));
#138680=CARTESIAN_POINT('Ctrl Pts',(-252.153984493806,4.53478717806245,
132.708274563148));
#138681=CARTESIAN_POINT('Ctrl Pts',(-252.161744936321,4.58787547658327,
132.581827600565));
#138682=CARTESIAN_POINT('Ctrl Pts',(-252.169505378836,4.63562895705639,
132.453258821715));
#138683=CARTESIAN_POINT('Ctrl Pts',(-252.177265821352,4.67789813903392,
132.323061398932));
#138684=CARTESIAN_POINT('Ctrl Pts',(-252.185038721618,4.72023517525472,
132.192654971689));
#138685=CARTESIAN_POINT('Ctrl Pts',(-252.192811621885,4.75707021490048,
132.060615052825));
#138686=CARTESIAN_POINT('Ctrl Pts',(-252.200584522151,4.78830439049094,
131.927447491546));
#138687=CARTESIAN_POINT('Ctrl Pts',(-252.208074857901,4.81840312506873,
131.799120906785));
#138688=CARTESIAN_POINT('Ctrl Pts',(-252.21556519365,4.84330107865172,131.66974754398));
#138689=CARTESIAN_POINT('Ctrl Pts',(-252.223055529399,4.86295542518781,
131.539784029715));
#138690=CARTESIAN_POINT('Ctrl Pts',(-252.230829863517,4.88335497227861,
131.404892909092));
#138691=CARTESIAN_POINT('Ctrl Pts',(-252.238604197635,4.89817006001821,
131.268938707896));
#138692=CARTESIAN_POINT('Ctrl Pts',(-252.246378531753,4.90729638098068,
131.132423556213));
#138693=CARTESIAN_POINT('Ctrl Pts',(-252.254143284699,4.91641145456825,
130.996076647254));
#138694=CARTESIAN_POINT('Ctrl Pts',(-252.261908037645,4.919851685145,130.859170549683));
#138695=CARTESIAN_POINT('Ctrl Pts',(-252.269672790591,4.91756396925203,
130.722216410137));
#138696=CARTESIAN_POINT('Ctrl Pts',(-252.277429831475,4.91527852555074,
130.585398295373));
#138697=CARTESIAN_POINT('Ctrl Pts',(-252.285186872359,4.90727646338769,
130.448532621974));
#138698=CARTESIAN_POINT('Ctrl Pts',(-252.292943913243,4.8935565931931,130.312134113082));
#138699=CARTESIAN_POINT('Ctrl Pts',(-252.300695104482,4.87984706925933,
130.175838463367));
#138700=CARTESIAN_POINT('Ctrl Pts',(-252.308446295721,4.86042835872714,
130.040009664371));
#138701=CARTESIAN_POINT('Ctrl Pts',(-252.31619748696,4.83535130735511,129.905160530289));
#138702=CARTESIAN_POINT('Ctrl Pts',(-252.323945383736,4.81028491439884,
129.770368710685));
#138703=CARTESIAN_POINT('Ctrl Pts',(-252.331693280512,4.77956503518677,
129.63655611141));
#138704=CARTESIAN_POINT('Ctrl Pts',(-252.339441177288,4.74329411245932,
129.504228306911));
#138705=CARTESIAN_POINT('Ctrl Pts',(-252.347187453371,4.70703077682679,
129.371928182536));
#138706=CARTESIAN_POINT('Ctrl Pts',(-252.354933729454,4.6652188105726,129.241112611982));
#138707=CARTESIAN_POINT('Ctrl Pts',(-252.362680005537,4.61801122140165,
129.11227450229));
#138708=CARTESIAN_POINT('Ctrl Pts',(-252.370426338802,4.57080328375507,
128.983435441546));
#138709=CARTESIAN_POINT('Ctrl Pts',(-252.378172672066,4.5181997782239,128.85657423789));
#138710=CARTESIAN_POINT('Ctrl Pts',(-252.38591900533,4.46040266102354,128.732165847755));
#138711=CARTESIAN_POINT('Ctrl Pts',(-252.393667073332,4.40259260055961,
128.607729597223));
#138712=CARTESIAN_POINT('Ctrl Pts',(-252.401415141334,4.33958677873817,
128.485747607737));
#138713=CARTESIAN_POINT('Ctrl Pts',(-252.409163209336,4.27163391864493,
128.366671808964));
#138714=CARTESIAN_POINT('Ctrl Pts',(-252.416919512077,4.20360883744303,
128.247469455015));
#138715=CARTESIAN_POINT('Ctrl Pts',(-252.424675814818,4.13062640909264,
128.131179801964));
#138716=CARTESIAN_POINT('Ctrl Pts',(-252.432432117559,4.05297996270192,
128.018227726903));
#138717=CARTESIAN_POINT('Ctrl Pts',(-252.440192560072,3.97529207406466,
127.905215365918));
#138718=CARTESIAN_POINT('Ctrl Pts',(-252.447953002585,3.89293544184546,
127.795544444923));
#138719=CARTESIAN_POINT('Ctrl Pts',(-252.455713445098,3.80624418806478,
127.689607297747));
#138720=CARTESIAN_POINT('Ctrl Pts',(-252.463486345363,3.71941376978695,
127.583500090857));
#138721=CARTESIAN_POINT('Ctrl Pts',(-252.471259245627,3.62823508520527,
127.481138927387));
#138722=CARTESIAN_POINT('Ctrl Pts',(-252.479032145892,3.533080279294,127.382880411199));
#138723=CARTESIAN_POINT('Ctrl Pts',(-252.486522481665,3.44138459010734,
127.288193839416));
#138724=CARTESIAN_POINT('Ctrl Pts',(-252.494012817439,3.34599706771789,
127.197317022901));
#138725=CARTESIAN_POINT('Ctrl Pts',(-252.501503153212,3.24727873647887,
127.110532810248));
#138726=CARTESIAN_POINT('Ctrl Pts',(-252.509277487329,3.14481746988947,
127.020458147957));
#138727=CARTESIAN_POINT('Ctrl Pts',(-252.517051821446,3.03844326681808,
126.934507228457));
#138728=CARTESIAN_POINT('Ctrl Pts',(-252.524826155563,2.92852220281797,
126.853039222121));
#138729=CARTESIAN_POINT('Ctrl Pts',(-252.532590908508,2.81873660670535,
126.771671617821));
#138730=CARTESIAN_POINT('Ctrl Pts',(-252.540355661453,2.70541315811351,
126.694776164561));
#138731=CARTESIAN_POINT('Ctrl Pts',(-252.548120414398,2.58895319546871,
126.622673827027));
#138732=CARTESIAN_POINT('Ctrl Pts',(-252.555877455281,2.47260890250127,
126.550643102551));
#138733=CARTESIAN_POINT('Ctrl Pts',(-252.563634496164,2.35313462519186,
126.483396224484));
#138734=CARTESIAN_POINT('Ctrl Pts',(-252.571391537047,2.2309627717077,126.421212414076));
#138735=CARTESIAN_POINT('Ctrl Pts',(-252.579142728285,2.10888304896848,
126.359075496964));
#138736=CARTESIAN_POINT('Ctrl Pts',(-252.586893919523,1.98411014615064,
126.301994224445));
#138737=CARTESIAN_POINT('Ctrl Pts',(-252.594645110761,1.85710299173296,
126.250203007141));
#138738=CARTESIAN_POINT('Ctrl Pts',(-252.602393007536,1.73014981874447,
126.198433802485));
#138739=CARTESIAN_POINT('Ctrl Pts',(-252.610140904311,1.6009646441356,126.151950328436));
#138740=CARTESIAN_POINT('Ctrl Pts',(-252.617888801086,1.47002819481218,
126.110939672354));
#138741=CARTESIAN_POINT('Ctrl Pts',(-252.625635077168,1.33911913457094,
126.069937594816));
#138742=CARTESIAN_POINT('Ctrl Pts',(-252.63338135325,1.20645990112001,126.034406174967));
#138743=CARTESIAN_POINT('Ctrl Pts',(-252.641127629332,1.0725478955156,126.004483111387));
#138744=CARTESIAN_POINT('Ctrl Pts',(-252.648873962595,0.938634901403728,
125.974559826921));
#138745=CARTESIAN_POINT('Ctrl Pts',(-252.656620295858,0.803469498240778,
125.950245066594));
#138746=CARTESIAN_POINT('Ctrl Pts',(-252.664366629121,0.667560442590652,
125.931625644475));
#138747=CARTESIAN_POINT('Ctrl Pts',(-252.672114697122,0.531620951049647,
125.913002052664));
#138748=CARTESIAN_POINT('Ctrl Pts',(-252.679862765123,0.394937862907427,
125.900076390078));
#138749=CARTESIAN_POINT('Ctrl Pts',(-252.687610833124,0.258025840295146,
125.892883677964));
#138750=CARTESIAN_POINT('Ctrl Pts',(-252.695367135864,0.120968305955731,
125.88568332135));
#138751=CARTESIAN_POINT('Ctrl Pts',(-252.703123438603,-0.0163182578508794,
125.884228107272));
#138752=CARTESIAN_POINT('Ctrl Pts',(-252.710879741343,-0.153317838445549,
125.88850090609));
#138753=CARTESIAN_POINT('Ctrl Pts',(-252.718640183855,-0.290390539841379,
125.892775985429));
#138754=CARTESIAN_POINT('Ctrl Pts',(-252.726400626367,-0.427175563086022,
125.902785140902));
#138755=CARTESIAN_POINT('Ctrl Pts',(-252.734161068879,-0.563162225504971,
125.918459332208));
#138756=CARTESIAN_POINT('Ctrl Pts',(-252.741933969142,-0.699367185787194,
125.934158685117));
#138757=CARTESIAN_POINT('Ctrl Pts',(-252.749706869406,-0.8347708377973,
125.955541185586));
#138758=CARTESIAN_POINT('Ctrl Pts',(-252.757479769669,-0.968872007157794,
125.982486490606));
#138759=CARTESIAN_POINT('Ctrl Pts',(-252.764970105454,-1.098098261668,126.008452266005));
#138760=CARTESIAN_POINT('Ctrl Pts',(-252.77246044124,-1.2261147871949,126.039583351033));
#138761=CARTESIAN_POINT('Ctrl Pts',(-252.779950777025,-1.35248847272114,
126.075728892251));
#138762=CARTESIAN_POINT('Ctrl Pts',(-252.787725111152,-1.48365365467449,
126.113244902573));
#138763=CARTESIAN_POINT('Ctrl Pts',(-252.79549944528,-1.61346445276583,
126.156281960898));
#138764=CARTESIAN_POINT('Ctrl Pts',(-252.803273779407,-1.74142081401129,
126.204726217852));
#138765=CARTESIAN_POINT('Ctrl Pts',(-252.811038532362,-1.86921948047746,
126.25311077159));
#138766=CARTESIAN_POINT('Ctrl Pts',(-252.818803285317,-1.99516789529014,
126.306889127703));
#138767=CARTESIAN_POINT('Ctrl Pts',(-252.826568038273,-2.11877908854417,
126.36589711806));
#138768=CARTESIAN_POINT('Ctrl Pts',(-252.834325079166,-2.2422675094189,
126.424846500849));
#138769=CARTESIAN_POINT('Ctrl Pts',(-252.842082120059,-2.36342297780638,
126.489015013957));
#138770=CARTESIAN_POINT('Ctrl Pts',(-252.849839160952,-2.48177684978281,
126.558189786054));
#138771=CARTESIAN_POINT('Ctrl Pts',(-252.8575903522,-2.60004147018366,126.627312392917));
#138772=CARTESIAN_POINT('Ctrl Pts',(-252.865341543449,-2.71550836321191,
126.701433547859));
#138773=CARTESIAN_POINT('Ctrl Pts',(-252.873092734697,-2.82773225051986,
126.780293846019));
#138774=CARTESIAN_POINT('Ctrl Pts',(-252.880840631482,-2.93990843968162,
126.859120626448));
#138775=CARTESIAN_POINT('Ctrl Pts',(-252.888588528267,-3.04884404536948,
126.942682319567));
#138776=CARTESIAN_POINT('Ctrl Pts',(-252.896336425053,-3.15412182105297,
127.030675601503));
#138777=CARTESIAN_POINT('Ctrl Pts',(-252.904082701145,-3.25937757489534,
127.118650477141));
#138778=CARTESIAN_POINT('Ctrl Pts',(-252.911828977237,-3.36097672084659,
127.211054847185));
#138779=CARTESIAN_POINT('Ctrl Pts',(-252.919575253329,-3.45853455176965,
127.307544663485));
#138780=CARTESIAN_POINT('Ctrl Pts',(-252.927321586603,-3.55609310284179,
127.40403519205));
#138781=CARTESIAN_POINT('Ctrl Pts',(-252.935067919876,-3.64961000138655,
127.50461095212));
#138782=CARTESIAN_POINT('Ctrl Pts',(-252.94281425315,-3.73873721291884,
127.608890837512));
#138783=CARTESIAN_POINT('Ctrl Pts',(-252.950562321161,-3.8278843838718,
127.713194075662));
#138784=CARTESIAN_POINT('Ctrl Pts',(-252.958310389172,-3.91263965770853,
127.821202792624));
#138785=CARTESIAN_POINT('Ctrl Pts',(-252.966058457183,-3.99269538260755,
127.93250291841));
#138786=CARTESIAN_POINT('Ctrl Pts',(-252.973814759933,-4.07283619168238,
128.043921335292));
#138787=CARTESIAN_POINT('Ctrl Pts',(-252.981571062683,-4.1482672456395,
128.15863783103));
#138788=CARTESIAN_POINT('Ctrl Pts',(-252.989327365432,-4.21872403867159,
128.276209010555));
#138789=CARTESIAN_POINT('Ctrl Pts',(-252.997087807955,-4.28921843661511,
128.393842941357));
#138790=CARTESIAN_POINT('Ctrl Pts',(-253.004848250477,-4.35473309682876,
128.5143342486));
#138791=CARTESIAN_POINT('Ctrl Pts',(-253.012608692999,-4.41505006841288,
128.637215962517));
#138792=CARTESIAN_POINT('Ctrl Pts',(-253.020381593272,-4.47546386615323,
128.760294937068));
#138793=CARTESIAN_POINT('Ctrl Pts',(-253.028154493545,-4.5306631441883,
128.885771628353));
#138794=CARTESIAN_POINT('Ctrl Pts',(-253.035927393818,-4.5804782535058,
129.013159335839));
#138795=CARTESIAN_POINT('Ctrl Pts',(-253.043417729492,-4.62848245750808,
129.135916177715));
#138796=CARTESIAN_POINT('Ctrl Pts',(-253.050908065165,-4.67148705231427,
129.260447216305));
#138797=CARTESIAN_POINT('Ctrl Pts',(-253.058398400839,-4.70938484811523,
129.386306523096));
#138798=CARTESIAN_POINT('Ctrl Pts',(-253.062266181301,-4.72895411183443,
129.451296423275));
#138799=CARTESIAN_POINT('Ctrl Pts',(-253.066133961763,-4.74718276800677,
129.516707382247));
#138800=CARTESIAN_POINT('Ctrl Pts',(-253.070001742224,-4.7640545282341,
129.582490119308));
#138801=CARTESIAN_POINT('Origin',(213.235140564004,0.,130.804360617566));
#138802=CARTESIAN_POINT('',(-255.165002394563,-4.76405452823405,129.582490119308));
#138803=CARTESIAN_POINT('',(-254.820081699213,-4.76405452823396,129.582490119308));
#138804=CARTESIAN_POINT('',(213.235140564004,-4.76405452823405,129.582490119308));
#138805=CARTESIAN_POINT('',(-253.485140564065,-4.91824929180127,130.806999972842));
#138806=CARTESIAN_POINT('Ctrl Pts',(-253.485140564065,-4.91824929180127,
130.806999972842));
#138807=CARTESIAN_POINT('Ctrl Pts',(-253.493706779917,-4.91816774629876,
130.958954169261));
#138808=CARTESIAN_POINT('Ctrl Pts',(-253.50227299577,-4.91103996867778,
131.110660600794));
#138809=CARTESIAN_POINT('Ctrl Pts',(-253.510839211622,-4.8969591051712,
131.261497998209));
#138810=CARTESIAN_POINT('Ctrl Pts',(-253.519452637721,-4.88280063901485,
131.413166692775));
#138811=CARTESIAN_POINT('Ctrl Pts',(-253.528066063821,-4.86161232316216,
131.563956517786));
#138812=CARTESIAN_POINT('Ctrl Pts',(-253.53667948992,-4.83353902686892,
131.713251996244));
#138813=CARTESIAN_POINT('Ctrl Pts',(-253.545317379068,-4.80538599942276,
131.86297148977));
#138814=CARTESIAN_POINT('Ctrl Pts',(-253.553955268215,-4.770308945894,132.011187921938));
#138815=CARTESIAN_POINT('Ctrl Pts',(-253.562593157362,-4.72850271380084,
132.157300064873));
#138816=CARTESIAN_POINT('Ctrl Pts',(-253.571262549868,-4.6865440096535,
132.303945095308));
#138817=CARTESIAN_POINT('Ctrl Pts',(-253.579931942374,-4.63780707281119,
132.448470249791));
#138818=CARTESIAN_POINT('Ctrl Pts',(-253.588601334879,-4.58253613751236,
132.590290518456));
#138819=CARTESIAN_POINT('Ctrl Pts',(-253.590969107354,-4.56744061620894,
132.629024273825));
#138820=CARTESIAN_POINT('Ctrl Pts',(-253.593336879829,-4.55185796435086,
132.667556402421));
#138821=CARTESIAN_POINT('Ctrl Pts',(-253.595704652304,-4.53579374871089,
132.705875311607));
#138822=CARTESIAN_POINT('Ctrl Pts',(-253.60347898638,-4.48304857138345,
132.831691455099));
#138823=CARTESIAN_POINT('Ctrl Pts',(-253.611253320455,-4.4249809543474,
132.955510610546));
#138824=CARTESIAN_POINT('Ctrl Pts',(-253.619027654531,-4.36176301072568,
133.076849671613));
#138825=CARTESIAN_POINT('Ctrl Pts',(-253.626792407435,-4.29862297757613,
133.198039193119));
#138826=CARTESIAN_POINT('Ctrl Pts',(-253.634557160338,-4.23034542602361,
133.316754358359));
#138827=CARTESIAN_POINT('Ctrl Pts',(-253.642321913241,-4.15715089052608,
133.432530995585));
#138828=CARTESIAN_POINT('Ctrl Pts',(-253.650078954082,-4.08402905288004,
133.548192641812));
#138829=CARTESIAN_POINT('Ctrl Pts',(-253.657835994922,-4.00600015747823,
133.660921239823));
#138830=CARTESIAN_POINT('Ctrl Pts',(-253.665593035762,-3.92333093663046,
133.770276567855));
#138831=CARTESIAN_POINT('Ctrl Pts',(-253.673344226957,-3.84072405729242,
133.879549430174));
#138832=CARTESIAN_POINT('Ctrl Pts',(-253.681095418152,-3.75348405247946,
133.985453775198));
#138833=CARTESIAN_POINT('Ctrl Pts',(-253.688846609347,-3.66192110264863,
134.087578079215));
#138834=CARTESIAN_POINT('Ctrl Pts',(-253.696594506078,-3.57039706952383,
134.189658977667));
#138835=CARTESIAN_POINT('Ctrl Pts',(-253.704342402809,-3.47455400621042,
134.287962740067));
#138836=CARTESIAN_POINT('Ctrl Pts',(-253.71209029954,-3.3747423939718,134.382110865533));
#138837=CARTESIAN_POINT('Ctrl Pts',(-253.719836575578,-3.27495166017714,
134.476239297235));
#138838=CARTESIAN_POINT('Ctrl Pts',(-253.727582851616,-3.17119431286658,
134.566213552931));
#138839=CARTESIAN_POINT('Ctrl Pts',(-253.735329127653,-3.06385742935098,
134.651692253273));
#138840=CARTESIAN_POINT('Ctrl Pts',(-253.743075460872,-2.95651975350517,
134.737171584594));
#138841=CARTESIAN_POINT('Ctrl Pts',(-253.75082179409,-2.84560279456388,
134.818155050787));
#138842=CARTESIAN_POINT('Ctrl Pts',(-253.758568127308,-2.73152609712807,
134.894342065349));
#138843=CARTESIAN_POINT('Ctrl Pts',(-253.766316195264,-2.61742385301241,
134.970546141461));
#138844=CARTESIAN_POINT('Ctrl Pts',(-253.77406426322,-2.50016078741905,
135.041951411448));
#138845=CARTESIAN_POINT('Ctrl Pts',(-253.781812331175,-2.38018440848479,
135.108301282132));
#138846=CARTESIAN_POINT('Ctrl Pts',(-253.789568633869,-2.26008051723188,
135.174721670246));
#138847=CARTESIAN_POINT('Ctrl Pts',(-253.797324936564,-2.13725789473119,
135.236075736524));
#138848=CARTESIAN_POINT('Ctrl Pts',(-253.805081239258,-2.01218807302497,
135.292153195357));
#138849=CARTESIAN_POINT('Ctrl Pts',(-253.812841681724,-1.88705149779281,
135.348260584417));
#138850=CARTESIAN_POINT('Ctrl Pts',(-253.82060212419,-1.75966569640479,
135.399085609535));
#138851=CARTESIAN_POINT('Ctrl Pts',(-253.828362566656,-1.63052011205161,
135.444466998533));
#138852=CARTESIAN_POINT('Ctrl Pts',(-253.836135466874,-1.50116721173979,
135.489921237767));
#138853=CARTESIAN_POINT('Ctrl Pts',(-253.843908367092,-1.37004925746463,
135.52991426423));
#138854=CARTESIAN_POINT('Ctrl Pts',(-253.851681267309,-1.23766958020655,
135.564335099927));
#138855=CARTESIAN_POINT('Ctrl Pts',(-253.859171603578,-1.11010222824022,
135.597504653996));
#138856=CARTESIAN_POINT('Ctrl Pts',(-253.866661939847,-0.981363595088982,
135.625500043834));
#138857=CARTESIAN_POINT('Ctrl Pts',(-253.874152276116,-0.851909148230417,
135.648267497932));
#138858=CARTESIAN_POINT('Ctrl Pts',(-253.881926610583,-0.717546399757441,
135.671898186431));
#138859=CARTESIAN_POINT('Ctrl Pts',(-253.88970094505,-0.581986865247745,
135.689971534245));
#138860=CARTESIAN_POINT('Ctrl Pts',(-253.897475279516,-0.445730027143223,
135.702371214268));
#138861=CARTESIAN_POINT('Ctrl Pts',(-253.905240032812,-0.309641113389513,
135.714755612795));
#138862=CARTESIAN_POINT('Ctrl Pts',(-253.913004786108,-0.172856991538168,
135.721480221007));
#138863=CARTESIAN_POINT('Ctrl Pts',(-253.920769539404,-0.0358873867344748,
135.722479684646));
#138864=CARTESIAN_POINT('Ctrl Pts',(-253.928526580638,0.10094617794333,
135.723478155603));
#138865=CARTESIAN_POINT('Ctrl Pts',(-253.936283621872,0.237964470533983,
135.718762795134));
#138866=CARTESIAN_POINT('Ctrl Pts',(-253.944040663107,0.374652944628602,
135.708320062095));
#138867=CARTESIAN_POINT('Ctrl Pts',(-253.951791854696,0.511238340890916,
135.697885204));
#138868=CARTESIAN_POINT('Ctrl Pts',(-253.959543046286,0.647494025464798,
135.681731599816));
#138869=CARTESIAN_POINT('Ctrl Pts',(-253.967294237876,0.782906111640338,
135.65989777455));
#138870=CARTESIAN_POINT('Ctrl Pts',(-253.975042135001,0.918260644054309,
135.638073229245));
#138871=CARTESIAN_POINT('Ctrl Pts',(-253.982790032127,1.05277190603047,
135.610573326714));
#138872=CARTESIAN_POINT('Ctrl Pts',(-253.990537929253,1.18593201033485,
135.577488347825));
#138873=CARTESIAN_POINT('Ctrl Pts',(-253.998284205685,1.31906426040746,
135.544410289601));
#138874=CARTESIAN_POINT('Ctrl Pts',(-254.006030482117,1.4508455357925,135.505749573001));
#138875=CARTESIAN_POINT('Ctrl Pts',(-254.013776758549,1.58077939959622,
135.461647333274));
#138876=CARTESIAN_POINT('Ctrl Pts',(-254.021523092162,1.71071422252711,
135.417544768));
#138877=CARTESIAN_POINT('Ctrl Pts',(-254.029269425775,1.83880123644463,
135.36800072511));
#138878=CARTESIAN_POINT('Ctrl Pts',(-254.037015759387,1.96456077526858,
135.313205705033));
#138879=CARTESIAN_POINT('Ctrl Pts',(-254.044763827736,2.09034847704797,
135.258398414001));
#138880=CARTESIAN_POINT('Ctrl Pts',(-254.052511896085,2.21380730821146,
135.198337961979));
#138881=CARTESIAN_POINT('Ctrl Pts',(-254.060259964434,2.33447950053559,
135.133262155379));
#138882=CARTESIAN_POINT('Ctrl Pts',(-254.068016267518,2.45527994463568,
135.068117185473));
#138883=CARTESIAN_POINT('Ctrl Pts',(-254.075772570602,2.57328748897384,
134.997946398859));
#138884=CARTESIAN_POINT('Ctrl Pts',(-254.083528873686,2.68807033968866,
134.923032844314));
#138885=CARTESIAN_POINT('Ctrl Pts',(-254.09128931654,2.80291445344082,134.848079306166));
#138886=CARTESIAN_POINT('Ctrl Pts',(-254.099049759395,2.91453012608298,
134.768378183231));
#138887=CARTESIAN_POINT('Ctrl Pts',(-254.10681020225,3.02251711872841,134.684254086399));
#138888=CARTESIAN_POINT('Ctrl Pts',(-254.114583102849,3.13067746158827,
134.599994946171));
#138889=CARTESIAN_POINT('Ctrl Pts',(-254.122356003449,3.23519718582483,
134.511298896802));
#138890=CARTESIAN_POINT('Ctrl Pts',(-254.130128904049,3.33571085978134,
134.41852941861));
#138891=CARTESIAN_POINT('Ctrl Pts',(-254.137619236009,3.43257055517851,
134.329132393845));
#138892=CARTESIAN_POINT('Ctrl Pts',(-254.145109567969,3.52571018997497,
134.235953179316));
#138893=CARTESIAN_POINT('Ctrl Pts',(-254.152599899929,3.61483833388053,
134.13934590725));
#138894=CARTESIAN_POINT('Ctrl Pts',(-254.160374233492,3.70734583879135,
134.039075697376));
#138895=CARTESIAN_POINT('Ctrl Pts',(-254.168148567055,3.79582468878446,
133.934794719803));
#138896=CARTESIAN_POINT('Ctrl Pts',(-254.175922900618,3.8799070321371,133.826860325502));
#138897=CARTESIAN_POINT('Ctrl Pts',(-254.18368765301,3.96388575151609,133.719058950695));
#138898=CARTESIAN_POINT('Ctrl Pts',(-254.191452405401,4.04347850709934,
133.607613423275));
#138899=CARTESIAN_POINT('Ctrl Pts',(-254.199217157793,4.11835479563008,
133.492917263763));
#138900=CARTESIAN_POINT('Ctrl Pts',(-254.206974198124,4.19315671598237,
133.378335022083));
#138901=CARTESIAN_POINT('Ctrl Pts',(-254.214731238455,4.26325127923338,
133.260508898578));
#138902=CARTESIAN_POINT('Ctrl Pts',(-254.222488278785,4.3283489679517,133.139864476294));
#138903=CARTESIAN_POINT('Ctrl Pts',(-254.230239469473,4.39339756600839,
133.019311032884));
#138904=CARTESIAN_POINT('Ctrl Pts',(-254.237990660161,4.4534566049638,132.895943863657));
#138905=CARTESIAN_POINT('Ctrl Pts',(-254.245741850849,4.50828072869673,
132.770216139664));
#138906=CARTESIAN_POINT('Ctrl Pts',(-254.253489747078,4.563081550746,132.644541853235));
#138907=CARTESIAN_POINT('Ctrl Pts',(-254.261237643308,4.61265172693553,
132.516509365148));
#138908=CARTESIAN_POINT('Ctrl Pts',(-254.268985539537,4.65679268767404,
132.386594774234));
#138909=CARTESIAN_POINT('Ctrl Pts',(-254.276731815076,4.70092441509108,
132.256707358604));
#138910=CARTESIAN_POINT('Ctrl Pts',(-254.284478090616,4.73962906027621,
132.124938993175));
#138911=CARTESIAN_POINT('Ctrl Pts',(-254.292224366155,4.77275702806113,
131.99178363132));
#138912=CARTESIAN_POINT('Ctrl Pts',(-254.299970698879,4.80588524040378,
131.858627286484));
#138913=CARTESIAN_POINT('Ctrl Pts',(-254.307717031603,4.83343659880648,
131.724084304192));
#138914=CARTESIAN_POINT('Ctrl Pts',(-254.315463364327,4.85531210545887,
131.588661211143));
#138915=CARTESIAN_POINT('Ctrl Pts',(-254.323211431793,4.87719251099064,
131.453207790961));
#138916=CARTESIAN_POINT('Ctrl Pts',(-254.330959499258,4.8933944731545,131.316874253714));
#138917=CARTESIAN_POINT('Ctrl Pts',(-254.338707566724,4.90387063032863,
131.180174272853));
#138918=CARTESIAN_POINT('Ctrl Pts',(-254.346463868937,4.91435792170045,
131.043329005454));
#138919=CARTESIAN_POINT('Ctrl Pts',(-254.354220171151,4.91910722179682,
130.906116906895));
#138920=CARTESIAN_POINT('Ctrl Pts',(-254.361976473364,4.91812327245555,
130.769054252261));
#138921=CARTESIAN_POINT('Ctrl Pts',(-254.369736915355,4.91713879795033,
130.631918443083));
#138922=CARTESIAN_POINT('Ctrl Pts',(-254.377497357344,4.9104149958339,130.494932627069));
#138923=CARTESIAN_POINT('Ctrl Pts',(-254.385257799334,4.89800863156218,
130.358608996546));
#138924=CARTESIAN_POINT('Ctrl Pts',(-254.393030699088,4.88558235147199,
130.222066526996));
#138925=CARTESIAN_POINT('Ctrl Pts',(-254.400803598842,4.8674553319674,130.086188754904));
#138926=CARTESIAN_POINT('Ctrl Pts',(-254.408576498596,4.84373585461035,
129.95147959816));
#138927=CARTESIAN_POINT('Ctrl Pts',(-254.416066840311,4.82087862032894,
129.821667346853));
#138928=CARTESIAN_POINT('Ctrl Pts',(-254.423557182027,4.79282852551927,
129.692940524602));
#138929=CARTESIAN_POINT('Ctrl Pts',(-254.431047523742,4.75972598709712,
129.565735738818));
#138930=CARTESIAN_POINT('Ctrl Pts',(-254.438821857757,4.72536838363919,
129.433708051632));
#138931=CARTESIAN_POINT('Ctrl Pts',(-254.446596191771,4.68545882085699,
129.302901868167));
#138932=CARTESIAN_POINT('Ctrl Pts',(-254.454370525786,4.64009911541028,
129.173819829463));
#138933=CARTESIAN_POINT('Ctrl Pts',(-254.462135278623,4.59479531177607,
129.044896872919));
#138934=CARTESIAN_POINT('Ctrl Pts',(-254.469900031461,4.54405485831362,
128.91769419862));
#138935=CARTESIAN_POINT('Ctrl Pts',(-254.477664784299,4.48803018990912,
128.792702575809));
#138936=CARTESIAN_POINT('Ctrl Pts',(-254.48542182507,4.43206116602998,128.667835096519));
#138937=CARTESIAN_POINT('Ctrl Pts',(-254.49317886584,4.3708185305596,128.545174652937));
#138938=CARTESIAN_POINT('Ctrl Pts',(-254.500935906611,4.30450384733297,
128.425194862349));
#138939=CARTESIAN_POINT('Ctrl Pts',(-254.508687097733,4.23823917256443,
128.305305549527));
#138940=CARTESIAN_POINT('Ctrl Pts',(-254.516438288854,4.16691025157994,
128.188093206812));
#138941=CARTESIAN_POINT('Ctrl Pts',(-254.524189479975,4.09076572905404,
128.074009209323));
#138942=CARTESIAN_POINT('Ctrl Pts',(-254.531937376627,4.01465357004527,
127.959973700671));
#138943=CARTESIAN_POINT('Ctrl Pts',(-254.539685273279,3.93373009693972,
127.849064217211));
#138944=CARTESIAN_POINT('Ctrl Pts',(-254.547433169931,3.84828853346442,
127.741705164253));
#138945=CARTESIAN_POINT('Ctrl Pts',(-254.555179445886,3.76286484256564,
127.63436856855));
#138946=CARTESIAN_POINT('Ctrl Pts',(-254.562925721841,3.6729251844364,127.530581231843));
#138947=CARTESIAN_POINT('Ctrl Pts',(-254.570671997796,3.57880427621025,
127.430736006694));
#138948=CARTESIAN_POINT('Ctrl Pts',(-254.578418330929,3.48468267325045,
127.330890044559));
#138949=CARTESIAN_POINT('Ctrl Pts',(-254.586164664061,3.38638002678753,
127.234986536532));
#138950=CARTESIAN_POINT('Ctrl Pts',(-254.593910997194,3.2842689813596,127.143382562377));
#138951=CARTESIAN_POINT('Ctrl Pts',(-254.60165906506,3.18213506891837,127.051758074188));
#138952=CARTESIAN_POINT('Ctrl Pts',(-254.609407132927,3.07619135137947,
126.964435296853));
#138953=CARTESIAN_POINT('Ctrl Pts',(-254.617155200794,2.96684439666846,
126.881731730142));
#138954=CARTESIAN_POINT('Ctrl Pts',(-254.624911503394,2.85738122677966,
126.798940265145));
#138955=CARTESIAN_POINT('Ctrl Pts',(-254.632667805995,2.74450790669163,
126.720778053945));
#138956=CARTESIAN_POINT('Ctrl Pts',(-254.640424108595,2.62866135635465,
126.647520166441));
#138957=CARTESIAN_POINT('Ctrl Pts',(-254.648184550965,2.51275297526742,
126.574223179024));
#138958=CARTESIAN_POINT('Ctrl Pts',(-254.655944993335,2.39386854062481,
126.505835925912));
#138959=CARTESIAN_POINT('Ctrl Pts',(-254.663705435705,2.27246965747638,
126.442587501235));
#138960=CARTESIAN_POINT('Ctrl Pts',(-254.671478335823,2.15087589411364,
126.379237544598));
#138961=CARTESIAN_POINT('Ctrl Pts',(-254.679251235941,2.02675997039196,
126.321043067199));
#138962=CARTESIAN_POINT('Ctrl Pts',(-254.687024136058,1.90060437555955,
126.268185348674));
#138963=CARTESIAN_POINT('Ctrl Pts',(-254.694514473224,1.7790348292785,126.217249130848));
#138964=CARTESIAN_POINT('Ctrl Pts',(-254.70200481039,1.65557161951262,126.171268508598));
#138965=CARTESIAN_POINT('Ctrl Pts',(-254.709495147555,1.53065797437531,
126.130361342001));
#138966=CARTESIAN_POINT('Ctrl Pts',(-254.71726948387,1.40100817808425,126.087903163711));
#138967=CARTESIAN_POINT('Ctrl Pts',(-254.725043820186,1.26938509756202,
126.050776262233));
#138968=CARTESIAN_POINT('Ctrl Pts',(-254.732818156501,1.13626665366864,
126.019166665984));
#138969=CARTESIAN_POINT('Ctrl Pts',(-254.740582911652,1.00331226618556,
125.987596025695));
#138970=CARTESIAN_POINT('Ctrl Pts',(-254.748347666802,0.868866558888896,
125.961529250959));
#138971=CARTESIAN_POINT('Ctrl Pts',(-254.756112421953,0.73342482492517,
125.94110336664));
#138972=CARTESIAN_POINT('Ctrl Pts',(-254.763869465047,0.598117613473356,
125.920697769578));
#138973=CARTESIAN_POINT('Ctrl Pts',(-254.771626508141,0.461816728131874,
125.905921971419));
#138974=CARTESIAN_POINT('Ctrl Pts',(-254.779383551234,0.32502958699541,
125.896862392393));
#138975=CARTESIAN_POINT('Ctrl Pts',(-254.787134744686,0.188345598026315,
125.887809645261));
#138976=CARTESIAN_POINT('Ctrl Pts',(-254.794885938138,0.0511764716662484,
125.884464562924));
#138977=CARTESIAN_POINT('Ctrl Pts',(-254.80263713159,-0.0859636386297147,
125.886861932733));
#138978=CARTESIAN_POINT('Ctrl Pts',(-254.810385030575,-0.223045460675289,
125.889258283595));
#138979=CARTESIAN_POINT('Ctrl Pts',(-254.81813292956,-0.360097901098543,
125.897392225423));
#138980=CARTESIAN_POINT('Ctrl Pts',(-254.825880828545,-0.49660540085496,
125.911246462108));
#138981=CARTESIAN_POINT('Ctrl Pts',(-254.833627106835,-0.633084346150557,
125.925097800782));
#138982=CARTESIAN_POINT('Ctrl Pts',(-254.841373385125,-0.769018188791224,
125.94466701483));
#138983=CARTESIAN_POINT('Ctrl Pts',(-254.849119663415,-0.903895487765914,
125.969884843535));
#138984=CARTESIAN_POINT('Ctrl Pts',(-254.856865998881,-1.03877378229616,
125.995102858377));
#138985=CARTESIAN_POINT('Ctrl Pts',(-254.864612334348,-1.17259513329347,
126.025969499218));
#138986=CARTESIAN_POINT('Ctrl Pts',(-254.872358669815,-1.30485769573404,
126.062364259872));
#138987=CARTESIAN_POINT('Ctrl Pts',(-254.880106740012,-1.43714987733809,
126.098767170847));
#138988=CARTESIAN_POINT('Ctrl Pts',(-254.88785481021,-1.56788219887774,
126.140700561361));
#138989=CARTESIAN_POINT('Ctrl Pts',(-254.895602880408,-1.69656777868186,
126.18799399057));
#138990=CARTESIAN_POINT('Ctrl Pts',(-254.903359185322,-1.82539012663506,
126.235337683646));
#138991=CARTESIAN_POINT('Ctrl Pts',(-254.911115490235,-1.95216101991438,
126.288052660099));
#138992=CARTESIAN_POINT('Ctrl Pts',(-254.918871795149,-2.07641286828906,
126.345920008687));
#138993=CARTESIAN_POINT('Ctrl Pts',(-254.926632239826,-2.20073103345476,
126.403818242746));
#138994=CARTESIAN_POINT('Ctrl Pts',(-254.934392684504,-2.32252712768721,
126.466874148827));
#138995=CARTESIAN_POINT('Ctrl Pts',(-254.942153129181,-2.44135889857268,
126.534823196386));
#138996=CARTESIAN_POINT('Ctrl Pts',(-254.949926031572,-2.56038142814344,
126.602881321431));
#138997=CARTESIAN_POINT('Ctrl Pts',(-254.957698933963,-2.67642979404177,
126.675848076281));
#138998=CARTESIAN_POINT('Ctrl Pts',(-254.965471836354,-2.7890906831194,
126.753415515021));
#138999=CARTESIAN_POINT('Ctrl Pts',(-254.972962148026,-2.89765568624046,
126.828162921133));
#139000=CARTESIAN_POINT('Ctrl Pts',(-254.980452459697,-3.00307499878199,
126.90718211095));
#139001=CARTESIAN_POINT('Ctrl Pts',(-254.987942771368,-3.10500988958206,
126.990163893733));
#139002=CARTESIAN_POINT('Ctrl Pts',(-254.995611852538,-3.2093776363245,
127.075126183109));
#139003=CARTESIAN_POINT('Ctrl Pts',(-255.003280933707,-3.31044213216741,
127.164527494784));
#139004=CARTESIAN_POINT('Ctrl Pts',(-255.010950014877,-3.40779452867065,
127.258078125595));
#139005=CARTESIAN_POINT('Ctrl Pts',(-255.018610310982,-3.50503540633297,
127.351521592552));
#139006=CARTESIAN_POINT('Ctrl Pts',(-255.026270607087,-3.59857235074418,
127.449104654649));
#139007=CARTESIAN_POINT('Ctrl Pts',(-255.033930903193,-3.68802771709246,
127.550496050554));
#139008=CARTESIAN_POINT('Ctrl Pts',(-255.041584189907,-3.77740122920827,
127.651794670416));
#139009=CARTESIAN_POINT('Ctrl Pts',(-255.049237476621,-3.8627003248688,
127.756894395887));
#139010=CARTESIAN_POINT('Ctrl Pts',(-255.056890763335,-3.9435829442897,
127.865426010603));
#139011=CARTESIAN_POINT('Ctrl Pts',(-255.064538809855,-4.02441018350123,
127.973883313883));
#139012=CARTESIAN_POINT('Ctrl Pts',(-255.072186856375,-4.10082672142748,
128.085767511594));
#139013=CARTESIAN_POINT('Ctrl Pts',(-255.079834902895,-4.17253003611261,
128.200675505991));
#139014=CARTESIAN_POINT('Ctrl Pts',(-255.087480300179,-4.24420851321359,
128.31554369697));
#139015=CARTESIAN_POINT('Ctrl Pts',(-255.095125697463,-4.31117679765856,
128.433433263226));
#139016=CARTESIAN_POINT('Ctrl Pts',(-255.102771094747,-4.37317529652245,
128.553911576067));
#139017=CARTESIAN_POINT('Ctrl Pts',(-255.11041480321,-4.43516010029642,
128.674363275983));
#139018=CARTESIAN_POINT('Ctrl Pts',(-255.118058511672,-4.49217712152607,
128.79740222569));
#139019=CARTESIAN_POINT('Ctrl Pts',(-255.125702220135,-4.54401274453013,
128.922571245705));
#139020=CARTESIAN_POINT('Ctrl Pts',(-255.133348272447,-4.59586426229855,
129.047778647281));
#139021=CARTESIAN_POINT('Ctrl Pts',(-255.14099432476,-4.64253105279218,
129.175117052467));
#139022=CARTESIAN_POINT('Ctrl Pts',(-255.148640377073,-4.68384772590579,
129.304109457584));
#139023=CARTESIAN_POINT('Ctrl Pts',(-255.154094382903,-4.71331932338101,
129.396121034376));
#139024=CARTESIAN_POINT('Ctrl Pts',(-255.159548388733,-4.74006973265035,
129.488973765347));
#139025=CARTESIAN_POINT('Ctrl Pts',(-255.165002394563,-4.76405452823405,
129.582490119308));
#139026=CARTESIAN_POINT('Ctrl Pts',(-253.415334457588,-4.76405452823403,
129.582490119308));
#139027=CARTESIAN_POINT('Ctrl Pts',(-253.423183166685,-4.79857612324911,
129.717089294334));
#139028=CARTESIAN_POINT('Ctrl Pts',(-253.431031875783,-4.82741111287845,
129.853237788276));
#139029=CARTESIAN_POINT('Ctrl Pts',(-253.43888058488,-4.85043173299432,
129.990422618661));
#139030=CARTESIAN_POINT('Ctrl Pts',(-253.446726269139,-4.87344348112395,
130.12755457897));
#139031=CARTESIAN_POINT('Ctrl Pts',(-253.454571953398,-4.89064525643546,
130.265721710007));
#139032=CARTESIAN_POINT('Ctrl Pts',(-253.462417637657,-4.90196031792918,
130.404400489619));
#139033=CARTESIAN_POINT('Ctrl Pts',(-253.469991946443,-4.91288400117358,
130.538282489468));
#139034=CARTESIAN_POINT('Ctrl Pts',(-253.477566255229,-4.91832139488876,
130.672640994209));
#139035=CARTESIAN_POINT('Ctrl Pts',(-253.485140564015,-4.91824929180175,
130.806999971948));
#139036=CARTESIAN_POINT('',(-253.13985943596,-4.91824809876146,130.800036091088));
#139037=CARTESIAN_POINT('Ctrl Pts',(-253.070001742224,-4.7640545282341,
129.582490119308));
#139038=CARTESIAN_POINT('Ctrl Pts',(-253.07954420969,-4.80568000947843,
129.744787238925));
#139039=CARTESIAN_POINT('Ctrl Pts',(-253.089086677157,-4.83904288583247,
129.909348847311));
#139040=CARTESIAN_POINT('Ctrl Pts',(-253.098629144623,-4.86393139366922,
130.075419975141));
#139041=CARTESIAN_POINT('Ctrl Pts',(-253.108045009558,-4.88848969885077,
130.2392877918));
#139042=CARTESIAN_POINT('Ctrl Pts',(-253.117460874493,-4.90479697694862,
130.404625368815));
#139043=CARTESIAN_POINT('Ctrl Pts',(-253.126876739428,-4.9126957295879,
130.570686205212));
#139044=CARTESIAN_POINT('Ctrl Pts',(-253.131204304938,-4.91632602481152,
130.647008365018));
#139045=CARTESIAN_POINT('Ctrl Pts',(-253.135531870449,-4.91818078701807,
130.723483003563));
#139046=CARTESIAN_POINT('Ctrl Pts',(-253.13985943596,-4.91824809876146,
130.800036091088));
#139047=CARTESIAN_POINT('Ctrl Pts',(-253.139859435997,-4.91824809876204,
130.800036091749));
#139048=CARTESIAN_POINT('Ctrl Pts',(-253.147555448689,-4.91836780392906,
130.936175806272));
#139049=CARTESIAN_POINT('Ctrl Pts',(-253.155251461381,-4.91283062992671,
131.072423279795));
#139050=CARTESIAN_POINT('Ctrl Pts',(-253.162947474073,-4.90163658373028,
131.208268854096));
#139051=CARTESIAN_POINT('Ctrl Pts',(-253.170640926388,-4.8904462616678,
131.344069234094));
#139052=CARTESIAN_POINT('Ctrl Pts',(-253.178334378702,-4.87360283988483,
131.479467585744));
#139053=CARTESIAN_POINT('Ctrl Pts',(-253.186027831017,-4.85115838920778,
131.613956408883));
#139054=CARTESIAN_POINT('Ctrl Pts',(-253.193720214653,-4.82871705623311,
131.748426550518));
#139055=CARTESIAN_POINT('Ctrl Pts',(-253.20141259829,-4.80067630673908,
131.881987023561));
#139056=CARTESIAN_POINT('Ctrl Pts',(-253.209104981926,-4.76713975822367,
132.014138112837));
#139057=CARTESIAN_POINT('Ctrl Pts',(-253.216798019897,-4.73360035700124,
132.146300443232));
#139058=CARTESIAN_POINT('Ctrl Pts',(-253.224491057868,-4.69456432442808,
132.277052766712));
#139059=CARTESIAN_POINT('Ctrl Pts',(-253.232184095839,-4.65018569343382,
132.40590864341));
#139060=CARTESIAN_POINT('Ctrl Pts',(-253.239879511309,-4.60579334742024,
132.534804342445));
#139061=CARTESIAN_POINT('Ctrl Pts',(-253.247574926779,-4.55605524774839,
132.661802053837));
#139062=CARTESIAN_POINT('Ctrl Pts',(-253.25527034225,-4.50117411226919,
132.786433944549));
#139063=CARTESIAN_POINT('Ctrl Pts',(-253.262974316368,-4.44623193936449,
132.911204447731));
#139064=CARTESIAN_POINT('Ctrl Pts',(-253.270678290487,-4.38613547050944,
133.033603513458));
#139065=CARTESIAN_POINT('Ctrl Pts',(-253.278382264606,-4.32113424600608,
133.153186258284));
#139066=CARTESIAN_POINT('Ctrl Pts',(-253.286091036346,-4.25609254222782,
133.272843472827));
#139067=CARTESIAN_POINT('Ctrl Pts',(-253.293799808087,-4.18614020375855,
133.389680534304));
#139068=CARTESIAN_POINT('Ctrl Pts',(-253.301508579827,-4.11157026886499,
133.503281325309));
#139069=CARTESIAN_POINT('Ctrl Pts',(-253.309228941747,-4.03688821767641,
133.61705291571));
#139070=CARTESIAN_POINT('Ctrl Pts',(-253.316949303667,-3.95757493897604,
133.727578199157));
#139071=CARTESIAN_POINT('Ctrl Pts',(-253.324669665587,-3.87396422101779,
133.834473532421));
#139072=CARTESIAN_POINT('Ctrl Pts',(-253.328728451942,-3.83000798623275,
133.890671068828));
#139073=CARTESIAN_POINT('Ctrl Pts',(-253.332787238297,-3.78486462953533,
133.945865935702));
#139074=CARTESIAN_POINT('Ctrl Pts',(-253.336846024651,-3.73858661432107,
134.000006591343));
#139075=CARTESIAN_POINT('Ctrl Pts',(-253.34462035876,-3.64994416786029,
134.103709400265));
#139076=CARTESIAN_POINT('Ctrl Pts',(-253.352394692869,-3.55684320656323,
134.203885458297));
#139077=CARTESIAN_POINT('Ctrl Pts',(-253.360169026978,-3.45959513373787,
134.300127282136));
#139078=CARTESIAN_POINT('Ctrl Pts',(-253.367933779914,-3.36246691047244,
134.396250496526));
#139079=CARTESIAN_POINT('Ctrl Pts',(-253.375698532851,-3.26120202015508,
134.488448851603));
#139080=CARTESIAN_POINT('Ctrl Pts',(-253.383463285787,-3.15615219366089,
134.576347679176));
#139081=CARTESIAN_POINT('Ctrl Pts',(-253.391220326662,-3.0512067041369,
134.664159204392));
#139082=CARTESIAN_POINT('Ctrl Pts',(-253.398977367536,-2.94248405742258,
134.747679451028));
#139083=CARTESIAN_POINT('Ctrl Pts',(-253.406734408411,-2.83037266328232,
134.826570662982));
#139084=CARTESIAN_POINT('Ctrl Pts',(-253.41448559964,-2.71834581321827,
134.905402382458));
#139085=CARTESIAN_POINT('Ctrl Pts',(-253.422236790869,-2.60293562070072,
134.979611791377));
#139086=CARTESIAN_POINT('Ctrl Pts',(-253.429987982099,-2.48456310623925,
135.048901727464));
#139087=CARTESIAN_POINT('Ctrl Pts',(-253.437735878865,-2.36624090325532,
135.118162213479));
#139088=CARTESIAN_POINT('Ctrl Pts',(-253.445483775631,-2.24495921921734,
135.182507188226));
#139089=CARTESIAN_POINT('Ctrl Pts',(-253.453231672398,-2.12116736783148,
135.241683240516));
#139090=CARTESIAN_POINT('Ctrl Pts',(-253.460977948471,-1.99740141103332,
135.300846914451));
#139091=CARTESIAN_POINT('Ctrl Pts',(-253.468724224544,-1.87112668379759,
135.354843648039));
#139092=CARTESIAN_POINT('Ctrl Pts',(-253.476470500617,-1.7428160137112,
135.403466552946));
#139093=CARTESIAN_POINT('Ctrl Pts',(-253.484216833872,-1.61450439646546,
135.452089816777));
#139094=CARTESIAN_POINT('Ctrl Pts',(-253.491963167126,-1.48415717197565,
135.495339034232));
#139095=CARTESIAN_POINT('Ctrl Pts',(-253.499709500381,-1.35226562913962,
135.533056075168));
#139096=CARTESIAN_POINT('Ctrl Pts',(-253.507457568373,-1.22034455010754,
135.570781562575));
#139097=CARTESIAN_POINT('Ctrl Pts',(-253.515205636365,-1.08687884037397,
135.602972300736));
#139098=CARTESIAN_POINT('Ctrl Pts',(-253.522953704357,-0.952372984250942,
135.629520590185));
#139099=CARTESIAN_POINT('Ctrl Pts',(-253.530710007088,-0.817724173703003,
135.656097095473));
#139100=CARTESIAN_POINT('Ctrl Pts',(-253.538466309819,-0.682033392627136,
135.677019096846));
#139101=CARTESIAN_POINT('Ctrl Pts',(-253.54622261255,-0.545813862636227,
135.69223032633));
#139102=CARTESIAN_POINT('Ctrl Pts',(-253.553983055053,-0.409521628180569,
135.707449674506));
#139103=CARTESIAN_POINT('Ctrl Pts',(-253.561743497556,-0.272700472318955,
135.7169521503));
#139104=CARTESIAN_POINT('Ctrl Pts',(-253.56950394006,-0.135865706927921,
135.720733627436));
#139105=CARTESIAN_POINT('Ctrl Pts',(-253.577276840314,0.00118871777756249,
135.724521174936));
#139106=CARTESIAN_POINT('Ctrl Pts',(-253.585049740569,0.13825640451962,
135.72256937708));
#139107=CARTESIAN_POINT('Ctrl Pts',(-253.592822640824,0.274824173439137,
135.714926240404));
#139108=CARTESIAN_POINT('Ctrl Pts',(-253.600312976704,0.406427362220847,
135.707560950871));
#139109=CARTESIAN_POINT('Ctrl Pts',(-253.607803312583,0.537566042083476,
135.694910956932));
#139110=CARTESIAN_POINT('Ctrl Pts',(-253.615293648463,0.667790078184718,
135.677064125269));
#139111=CARTESIAN_POINT('Ctrl Pts',(-253.623067982636,0.802951597001489,
135.658540625722));
#139112=CARTESIAN_POINT('Ctrl Pts',(-253.630842316809,0.937555896552514,
135.634359756279));
#139113=CARTESIAN_POINT('Ctrl Pts',(-253.638616650982,1.07109182849129,
135.604563254689));
#139114=CARTESIAN_POINT('Ctrl Pts',(-253.646381403983,1.20446318933245,
135.574803474623));
#139115=CARTESIAN_POINT('Ctrl Pts',(-253.654146156984,1.33676842441923,
135.539441916995));
#139116=CARTESIAN_POINT('Ctrl Pts',(-253.661910909985,1.46750219565566,
135.49857198565));
#139117=CARTESIAN_POINT('Ctrl Pts',(-253.669667950924,1.59810612026909,
135.457742646895));
#139118=CARTESIAN_POINT('Ctrl Pts',(-253.677424991863,1.7271413163536,135.41141593785));
#139119=CARTESIAN_POINT('Ctrl Pts',(-253.685182032802,1.85411367516457,
135.35973607323));
#139120=CARTESIAN_POINT('Ctrl Pts',(-253.692933224096,1.98099028313289,
135.308095180798));
#139121=CARTESIAN_POINT('Ctrl Pts',(-253.70068441539,2.10580678950429,135.251109314703));
#139122=CARTESIAN_POINT('Ctrl Pts',(-253.708435606684,2.22808561136653,
135.188972067959));
#139123=CARTESIAN_POINT('Ctrl Pts',(-253.716183503515,2.35031246146511,
135.126861231205));
#139124=CARTESIAN_POINT('Ctrl Pts',(-253.723931400346,2.47000342446012,
135.059603545246));
#139125=CARTESIAN_POINT('Ctrl Pts',(-253.731679297177,2.58670243330287,
134.987440055497));
#139126=CARTESIAN_POINT('Ctrl Pts',(-253.739425573315,2.70337703122698,
134.915291660796));
#139127=CARTESIAN_POINT('Ctrl Pts',(-253.747171849453,2.81706058753968,
134.838239708944));
#139128=CARTESIAN_POINT('Ctrl Pts',(-253.75491812559,2.92732346636293,134.756570174988));
#139129=CARTESIAN_POINT('Ctrl Pts',(-253.762664458909,3.03758715911975,
134.674900038169));
#139130=CARTESIAN_POINT('Ctrl Pts',(-253.770410792228,3.14442980982937,
134.588612483931));
#139131=CARTESIAN_POINT('Ctrl Pts',(-253.778157125547,3.24745282547091,
134.498035374342));
#139132=CARTESIAN_POINT('Ctrl Pts',(-253.785905193603,3.35049891239881,
134.407437980639));
#139133=CARTESIAN_POINT('Ctrl Pts',(-253.79365326166,3.449723368586,134.312549378169));
#139134=CARTESIAN_POINT('Ctrl Pts',(-253.801401329716,3.54476289732365,
134.213735789684));
#139135=CARTESIAN_POINT('Ctrl Pts',(-253.80915763251,3.63990343519483,134.114817180951));
#139136=CARTESIAN_POINT('Ctrl Pts',(-253.816913935305,3.73084988922346,
134.011965535371));
#139137=CARTESIAN_POINT('Ctrl Pts',(-253.824670238099,3.81727751074879,
133.905582226615));
#139138=CARTESIAN_POINT('Ctrl Pts',(-253.832430680666,3.9037512612951,133.799142137887));
#139139=CARTESIAN_POINT('Ctrl Pts',(-253.840191123233,3.98570114005506,
133.689166943396));
#139140=CARTESIAN_POINT('Ctrl Pts',(-253.847951565799,4.06284513681559,
133.576087959271));
#139141=CARTESIAN_POINT('Ctrl Pts',(-253.855724466116,4.14011297195755,
133.462827450737));
#139142=CARTESIAN_POINT('Ctrl Pts',(-253.863497366433,4.21255930167557,
133.346453528086));
#139143=CARTESIAN_POINT('Ctrl Pts',(-253.87127026675,4.27994712897441,133.227423892779));
#139144=CARTESIAN_POINT('Ctrl Pts',(-253.878760601925,4.34488523349815,
133.11272129427));
#139145=CARTESIAN_POINT('Ctrl Pts',(-253.886250937101,4.40512608899376,
132.99555298893));
#139146=CARTESIAN_POINT('Ctrl Pts',(-253.893741272277,4.46050031135695,
132.876345181911));
#139147=CARTESIAN_POINT('Ctrl Pts',(-253.901515606323,4.51797406815235,
132.752617566131));
#139148=CARTESIAN_POINT('Ctrl Pts',(-253.909289940369,4.57038692897968,
132.626300808125));
#139149=CARTESIAN_POINT('Ctrl Pts',(-253.917064274415,4.61749772082124,
132.497847511732));
#139150=CARTESIAN_POINT('Ctrl Pts',(-253.92482902729,4.66455045282275,132.369552522545));
#139151=CARTESIAN_POINT('Ctrl Pts',(-253.932593780164,4.70631398387226,
132.239126597573));
#139152=CARTESIAN_POINT('Ctrl Pts',(-253.940358533039,4.74259374968307,
132.107045379113));
#139153=CARTESIAN_POINT('Ctrl Pts',(-253.948115573851,4.77883748191978,
131.975095345579));
#139154=CARTESIAN_POINT('Ctrl Pts',(-253.955872614664,4.80960818491979,
131.841493664873));
#139155=CARTESIAN_POINT('Ctrl Pts',(-253.963629655476,4.83476011276247,
131.706733996241));
#139156=CARTESIAN_POINT('Ctrl Pts',(-253.971380846644,4.8598930733414,131.572075950919));
#139157=CARTESIAN_POINT('Ctrl Pts',(-253.979132037812,4.8794156211349,131.43626203859));
#139158=CARTESIAN_POINT('Ctrl Pts',(-253.98688322898,4.89323248619918,131.299798705025));
#139159=CARTESIAN_POINT('Ctrl Pts',(-253.994631125686,4.90704347872852,
131.163393372004));
#139160=CARTESIAN_POINT('Ctrl Pts',(-254.002379022391,4.9151535725004,131.026339554893));
#139161=CARTESIAN_POINT('Ctrl Pts',(-254.010126919097,4.91751905046686,
130.889151246739));
#139162=CARTESIAN_POINT('Ctrl Pts',(-254.01787319511,4.91988403362645,130.751991635413));
#139163=CARTESIAN_POINT('Ctrl Pts',(-254.025619471123,4.91650678439137,
130.614697979661));
#139164=CARTESIAN_POINT('Ctrl Pts',(-254.033365747136,4.90739567298088,
130.477786320799));
#139165=CARTESIAN_POINT('Ctrl Pts',(-254.041112080331,4.89828449431365,
130.340873651278));
#139166=CARTESIAN_POINT('Ctrl Pts',(-254.048858413526,4.88343939497198,
130.204343374377));
#139167=CARTESIAN_POINT('Ctrl Pts',(-254.056604746721,4.86292076533104,
130.068708055134));
#139168=CARTESIAN_POINT('Ctrl Pts',(-254.064352814654,4.84239754068363,
129.933042361292));
#139169=CARTESIAN_POINT('Ctrl Pts',(-254.072100882587,4.81619831596094,
129.798272410412));
#139170=CARTESIAN_POINT('Ctrl Pts',(-254.07984895052,4.78443483398994,129.664901806637));
#139171=CARTESIAN_POINT('Ctrl Pts',(-254.087605253193,4.75263759340677,
129.531389454973));
#139172=CARTESIAN_POINT('Ctrl Pts',(-254.095361555866,4.71526437292624,
129.399279802276));
#139173=CARTESIAN_POINT('Ctrl Pts',(-254.103117858539,4.67247732499925,
129.26906302105));
#139174=CARTESIAN_POINT('Ctrl Pts',(-254.110878300986,4.6296674403329,129.138776739196));
#139175=CARTESIAN_POINT('Ctrl Pts',(-254.118638743432,4.58143810801695,
129.010385707703));
#139176=CARTESIAN_POINT('Ctrl Pts',(-254.126399185878,4.52799977311575,
128.884360326638));
#139177=CARTESIAN_POINT('Ctrl Pts',(-254.134172086077,4.47447565424295,
128.758132638414));
#139178=CARTESIAN_POINT('Ctrl Pts',(-254.141944986276,4.41572599058927,
128.634278542783));
#139179=CARTESIAN_POINT('Ctrl Pts',(-254.149717886475,4.35200775668906,
128.513244830833));
#139180=CARTESIAN_POINT('Ctrl Pts',(-254.157208223013,4.29060583420141,
128.396610986097));
#139181=CARTESIAN_POINT('Ctrl Pts',(-254.164698559551,4.22459046320145,
128.282596296163));
#139182=CARTESIAN_POINT('Ctrl Pts',(-254.172188896089,4.15422866606825,
128.171573643176));
#139183=CARTESIAN_POINT('Ctrl Pts',(-254.179963230165,4.08119908798231,
128.056341545135));
#139184=CARTESIAN_POINT('Ctrl Pts',(-254.187737564241,4.00325565330251,
127.943967827592));
#139185=CARTESIAN_POINT('Ctrl Pts',(-254.195511898317,3.92064879054702,
127.834900039669));
#139186=CARTESIAN_POINT('Ctrl Pts',(-254.203276651221,3.83814373337573,
127.72596666806));
#139187=CARTESIAN_POINT('Ctrl Pts',(-254.211041404124,3.75098691724529,
127.620331428173));
#139188=CARTESIAN_POINT('Ctrl Pts',(-254.218806157027,3.65947334673958,
127.518415108736));
#139189=CARTESIAN_POINT('Ctrl Pts',(-254.226563197868,3.56805066881094,
127.416600014034));
#139190=CARTESIAN_POINT('Ctrl Pts',(-254.234320238708,3.47228010732953,
127.318496778202));
#139191=CARTESIAN_POINT('Ctrl Pts',(-254.242077279549,3.37249821256741,
127.224494856294));
#139192=CARTESIAN_POINT('Ctrl Pts',(-254.249828470744,3.27279156411731,
127.130563821975));
#139193=CARTESIAN_POINT('Ctrl Pts',(-254.257579661939,3.16907988684366,
127.040728212488));
#139194=CARTESIAN_POINT('Ctrl Pts',(-254.265330853134,3.06173777218382,
126.955341927447));
#139195=CARTESIAN_POINT('Ctrl Pts',(-254.273078749865,2.95444128079738,
126.869991933865));
#139196=CARTESIAN_POINT('Ctrl Pts',(-254.280826646596,2.84351772632847,
126.789087746387));
#139197=CARTESIAN_POINT('Ctrl Pts',(-254.288574543327,2.72937591555043,
126.712943971206));
#139198=CARTESIAN_POINT('Ctrl Pts',(-254.296320819365,2.61525798078589,
126.636816123665));
#139199=CARTESIAN_POINT('Ctrl Pts',(-254.304067095402,2.49792345375603,
126.565446924596));
#139200=CARTESIAN_POINT('Ctrl Pts',(-254.31181337144,2.37781101894459,126.499108264836));
#139201=CARTESIAN_POINT('Ctrl Pts',(-254.319559704658,2.25769769749779,
126.432769115384));
#139202=CARTESIAN_POINT('Ctrl Pts',(-254.327306037877,2.13480676958809,
126.371460768358));
#139203=CARTESIAN_POINT('Ctrl Pts',(-254.335052371095,2.00960211317238,
126.315409469555));
#139204=CARTESIAN_POINT('Ctrl Pts',(-254.342800439051,1.88436941804778,
126.259345618454));
#139205=CARTESIAN_POINT('Ctrl Pts',(-254.350548507006,1.75682232014265,
126.208541317943));
#139206=CARTESIAN_POINT('Ctrl Pts',(-254.358296574962,1.62744491561126,
126.16317476596));
#139207=CARTESIAN_POINT('Ctrl Pts',(-254.366052877656,1.49793000724005,
126.117759997867));
#139208=CARTESIAN_POINT('Ctrl Pts',(-254.373809180351,1.36658127588195,
126.077794652661));
#139209=CARTESIAN_POINT('Ctrl Pts',(-254.381565483045,1.23389876490954,
126.043407257108));
#139210=CARTESIAN_POINT('Ctrl Pts',(-254.389325925511,1.10114543728956,
126.009001507968));
#139211=CARTESIAN_POINT('Ctrl Pts',(-254.397086367977,0.967057293625354,
125.980179722764));
#139212=CARTESIAN_POINT('Ctrl Pts',(-254.404846810444,0.832143845516441,
125.957019110836));
#139213=CARTESIAN_POINT('Ctrl Pts',(-254.412619710661,0.697013822361867,
125.933821319437));
#139214=CARTESIAN_POINT('Ctrl Pts',(-254.420392610879,0.561056235268857,
125.916302911662));
#139215=CARTESIAN_POINT('Ctrl Pts',(-254.428165511096,0.424785883249542,
125.90448918906));
#139216=CARTESIAN_POINT('Ctrl Pts',(-254.435655847365,0.293469292076369,
125.893104924191));
#139217=CARTESIAN_POINT('Ctrl Pts',(-254.443146183634,0.161862588416898,
125.887017800988));
#139218=CARTESIAN_POINT('Ctrl Pts',(-254.450636519903,0.0304238206479022,
125.886204717878));
#139219=CARTESIAN_POINT('Ctrl Pts',(-254.458410854369,-0.105998484822487,
125.885360806493));
#139220=CARTESIAN_POINT('Ctrl Pts',(-254.466185188836,-0.242672013207798,
125.890196086895));
#139221=CARTESIAN_POINT('Ctrl Pts',(-254.473959523303,-0.379084865978152,
125.90074177768));
#139222=CARTESIAN_POINT('Ctrl Pts',(-254.481724276599,-0.515329602123221,
125.911274471845));
#139223=CARTESIAN_POINT('Ctrl Pts',(-254.489489029895,-0.651313915803659,
125.927503543881));
#139224=CARTESIAN_POINT('Ctrl Pts',(-254.497253783191,-0.786524328319661,
125.949408244632));
#139225=CARTESIAN_POINT('Ctrl Pts',(-254.505010824425,-0.921600447964142,
125.971291189327));
#139226=CARTESIAN_POINT('Ctrl Pts',(-254.512767865659,-1.05590381265517,
125.998838482507));
#139227=CARTESIAN_POINT('Ctrl Pts',(-254.520524906893,-1.18892484914377,
126.031977484834));
#139228=CARTESIAN_POINT('Ctrl Pts',(-254.528276098483,-1.32184557344231,
126.065091496783));
#139229=CARTESIAN_POINT('Ctrl Pts',(-254.536027290072,-1.45348551648552,
126.103788730564));
#139230=CARTESIAN_POINT('Ctrl Pts',(-254.543778481662,-1.5833444566458,
126.147945323146));
#139231=CARTESIAN_POINT('Ctrl Pts',(-254.551526378788,-1.71314820328092,
126.192083147994));
#139232=CARTESIAN_POINT('Ctrl Pts',(-254.559274275913,-1.84117208322022,
126.241675590997));
#139233=CARTESIAN_POINT('Ctrl Pts',(-254.567022173039,-1.96693043928436,
126.296548763738));
#139234=CARTESIAN_POINT('Ctrl Pts',(-254.574768449471,-2.09266248940304,
126.35141045819));
#139235=CARTESIAN_POINT('Ctrl Pts',(-254.582514725904,-2.21612960014617,
126.411550528982));
#139236=CARTESIAN_POINT('Ctrl Pts',(-254.590261002336,-2.33686590233866,
126.476746862044));
#139237=CARTESIAN_POINT('Ctrl Pts',(-254.598007335948,-2.45760309576507,
126.541943676362));
#139238=CARTESIAN_POINT('Ctrl Pts',(-254.605753669561,-2.57560909640333,
126.612196641663));
#139239=CARTESIAN_POINT('Ctrl Pts',(-254.613500003173,-2.6904428198599,
126.687237775633));
#139240=CARTESIAN_POINT('Ctrl Pts',(-254.621248071522,-2.8053022595138,
126.762295714532));
#139241=CARTESIAN_POINT('Ctrl Pts',(-254.628996139871,-2.9169876811357,
126.842143741976));
#139242=CARTESIAN_POINT('Ctrl Pts',(-254.63674420822,-3.02508749592522,
126.92647089447));
#139243=CARTESIAN_POINT('Ctrl Pts',(-254.644500511304,-3.13330220042483,
127.010887670818));
#139244=CARTESIAN_POINT('Ctrl Pts',(-254.652256814388,-3.23792337680575,
127.099792840901));
#139245=CARTESIAN_POINT('Ctrl Pts',(-254.660013117472,-3.33857260616974,
127.192835175896));
#139246=CARTESIAN_POINT('Ctrl Pts',(-254.667773560327,-3.43927555503557,
127.285927170365));
#139247=CARTESIAN_POINT('Ctrl Pts',(-254.675534003181,-3.53600205711497,
127.383160452591));
#139248=CARTESIAN_POINT('Ctrl Pts',(-254.683294446036,-3.62841175050696,
127.484148089537));
#139249=CARTESIAN_POINT('Ctrl Pts',(-254.691067346636,-3.72096978806263,
127.585297840715));
#139250=CARTESIAN_POINT('Ctrl Pts',(-254.698840247236,-3.80919691736656,
127.690213690724));
#139251=CARTESIAN_POINT('Ctrl Pts',(-254.706613147835,-3.89279359003628,
127.798476200648));
#139252=CARTESIAN_POINT('Ctrl Pts',(-254.714103479795,-3.97335126873092,
127.902803038195));
#139253=CARTESIAN_POINT('Ctrl Pts',(-254.721593811756,-4.04960912989874,
128.0102371864));
#139254=CARTESIAN_POINT('Ctrl Pts',(-254.729084143716,-4.12133902359766,
128.120380789946));
#139255=CARTESIAN_POINT('Ctrl Pts',(-254.737024238098,-4.19737599085458,
128.237138046155));
#139256=CARTESIAN_POINT('Ctrl Pts',(-254.74496433248,-4.26855771158485,
128.357297650974));
#139257=CARTESIAN_POINT('Ctrl Pts',(-254.752904426862,-4.33457263714298,
128.480427934412));
#139258=CARTESIAN_POINT('Ctrl Pts',(-254.760834559692,-4.40050474112921,
128.603403740002));
#139259=CARTESIAN_POINT('Ctrl Pts',(-254.768764692523,-4.46128277734,128.729342485631));
#139260=CARTESIAN_POINT('Ctrl Pts',(-254.776694825353,-4.5166380372809,
128.857783133188));
#139261=CARTESIAN_POINT('Ctrl Pts',(-254.784613472957,-4.57191312609647,
128.986037759917));
#139262=CARTESIAN_POINT('Ctrl Pts',(-254.792532120561,-4.62178094224067,
129.116786732569));
#139263=CARTESIAN_POINT('Ctrl Pts',(-254.800450768166,-4.66601867417977,
129.249544617293));
#139264=CARTESIAN_POINT('Ctrl Pts',(-254.806994411848,-4.70257491074876,
129.359250256068));
#139265=CARTESIAN_POINT('Ctrl Pts',(-254.813538055531,-4.73528730506565,
129.470327152778));
#139266=CARTESIAN_POINT('Ctrl Pts',(-254.820081699213,-4.76405452823395,
129.582490119308));
#139267=CARTESIAN_POINT('Origin',(213.235140564004,0.,130.804360617566));
#139268=CARTESIAN_POINT('',(-256.915106732785,-4.76405452823404,129.582490119308));
#139269=CARTESIAN_POINT('',(-256.569732696692,-4.76405452823406,129.582490119308));
#139270=CARTESIAN_POINT('',(213.235140564004,-4.76405452823405,129.582490119308));
#139271=CARTESIAN_POINT('',(-255.235140563976,-4.91824902737425,130.807453711842));
#139272=CARTESIAN_POINT('Ctrl Pts',(-255.235140564014,-4.91824902737384,
130.807453712504));
#139273=CARTESIAN_POINT('Ctrl Pts',(-255.245557174403,-4.91813385884421,
130.990580166781));
#139274=CARTESIAN_POINT('Ctrl Pts',(-255.255973784792,-4.90779148807459,
131.173384516713));
#139275=CARTESIAN_POINT('Ctrl Pts',(-255.266390395181,-4.88732539910615,
131.355027037236));
#139276=CARTESIAN_POINT('Ctrl Pts',(-255.27416472986,-4.87205073496179,
131.490594145323));
#139277=CARTESIAN_POINT('Ctrl Pts',(-255.281939064539,-4.85110695834174,
131.6257399563));
#139278=CARTESIAN_POINT('Ctrl Pts',(-255.289713399218,-4.82452352870267,
131.759952467413));
#139279=CARTESIAN_POINT('Ctrl Pts',(-255.297478152694,-4.79797286086927,
131.893999573074));
#139280=CARTESIAN_POINT('Ctrl Pts',(-255.30524290617,-4.76579644445566,
132.027115287618));
#139281=CARTESIAN_POINT('Ctrl Pts',(-255.313007659645,-4.72807552956579,
132.158792177011));
#139282=CARTESIAN_POINT('Ctrl Pts',(-255.320764701028,-4.69039207976998,
132.290338282539));
#139283=CARTESIAN_POINT('Ctrl Pts',(-255.32852174241,-4.64717519744029,
132.420448033409));
#139284=CARTESIAN_POINT('Ctrl Pts',(-255.336278783793,-4.59855719839869,
132.548624002366));
#139285=CARTESIAN_POINT('Ctrl Pts',(-255.344029975499,-4.54997586276346,
132.676703312315));
#139286=CARTESIAN_POINT('Ctrl Pts',(-255.351781167205,-4.49600165566221,
132.802851378912));
#139287=CARTESIAN_POINT('Ctrl Pts',(-255.359532358911,-4.43681665357432,
132.92658611102));
#139288=CARTESIAN_POINT('Ctrl Pts',(-255.367280256105,-4.3776568070638,
133.050268251787));
#139289=CARTESIAN_POINT('Ctrl Pts',(-255.375028153299,-4.3132907389033,
133.171538746241));
#139290=CARTESIAN_POINT('Ctrl Pts',(-255.382776050493,-4.2439484806307,
133.289935874172));
#139291=CARTESIAN_POINT('Ctrl Pts',(-255.390522326964,-4.17462072752967,
133.408308235522));
#139292=CARTESIAN_POINT('Ctrl Pts',(-255.398268603435,-4.10031905224497,
133.523808088737));
#139293=CARTESIAN_POINT('Ctrl Pts',(-255.406014879907,-4.02131903729324,
133.635999058964));
#139294=CARTESIAN_POINT('Ctrl Pts',(-255.413761213529,-3.94231843948762,
133.748190856924));
#139295=CARTESIAN_POINT('Ctrl Pts',(-255.421507547151,-3.85861965794036,
133.857073403517));
#139296=CARTESIAN_POINT('Ctrl Pts',(-255.429253880774,-3.77054089507489,
133.962240352621));
#139297=CARTESIAN_POINT('Ctrl Pts',(-255.437001949104,-3.68244240792615,
134.067430852721));
#139298=CARTESIAN_POINT('Ctrl Pts',(-255.444750017433,-3.58996223866315,
134.168903799941));
#139299=CARTESIAN_POINT('Ctrl Pts',(-255.452498085763,-3.49345778637573,
134.266287213742));
#139300=CARTESIAN_POINT('Ctrl Pts',(-255.460254388783,-3.39685076862586,
134.36377412717));
#139301=CARTESIAN_POINT('Ctrl Pts',(-255.468010691802,-3.29621119965999,
134.457162546673));
#139302=CARTESIAN_POINT('Ctrl Pts',(-255.475766994821,-3.19193254441991,
134.546118185123));
#139303=CARTESIAN_POINT('Ctrl Pts',(-255.483527437587,-3.08759823287794,
134.635121301573));
#139304=CARTESIAN_POINT('Ctrl Pts',(-255.491287880352,-2.97962127256047,
134.719686681781));
#139305=CARTESIAN_POINT('Ctrl Pts',(-255.499048323118,-2.86842608786575,
134.799522046213));
#139306=CARTESIAN_POINT('Ctrl Pts',(-255.506821223587,-2.75705240347212,
134.87948556897));
#139307=CARTESIAN_POINT('Ctrl Pts',(-255.514594124056,-2.6424504981078,
134.954703688043));
#139308=CARTESIAN_POINT('Ctrl Pts',(-255.522367024526,-2.52507225411039,
135.024928490971));
#139309=CARTESIAN_POINT('Ctrl Pts',(-255.529857356015,-2.41196107242921,
135.09260040505));
#139310=CARTESIAN_POINT('Ctrl Pts',(-255.537347687505,-2.29627217499392,
135.155635597492));
#139311=CARTESIAN_POINT('Ctrl Pts',(-255.544838018994,-2.17842757880106,
135.213854505352));
#139312=CARTESIAN_POINT('Ctrl Pts',(-255.552612366624,-2.05611458658772,
135.274280940281));
#139313=CARTESIAN_POINT('Ctrl Pts',(-255.560386714254,-1.93109174547298,
135.329710048654));
#139314=CARTESIAN_POINT('Ctrl Pts',(-255.568161061884,-1.80380574339727,
135.379889865925));
#139315=CARTESIAN_POINT('Ctrl Pts',(-255.575925828398,-1.67667660875542,
135.430007841523));
#139316=CARTESIAN_POINT('Ctrl Pts',(-255.583690594912,-1.5472902229039,
135.474889255854));
#139317=CARTESIAN_POINT('Ctrl Pts',(-255.591455361427,-1.41611742396956,
135.514328186884));
#139318=CARTESIAN_POINT('Ctrl Pts',(-255.59921241592,-1.28507490678246,
135.553727946891));
#139319=CARTESIAN_POINT('Ctrl Pts',(-255.606969470413,-1.15224987939031,
135.58769586897));
#139320=CARTESIAN_POINT('Ctrl Pts',(-255.614726524906,-1.01813236307906,
135.616074403085));
#139321=CARTESIAN_POINT('Ctrl Pts',(-255.622477729782,-0.884115985187912,
135.644431536862));
#139322=CARTESIAN_POINT('Ctrl Pts',(-255.630228934657,-0.748809439346092,
135.667207591719));
#139323=CARTESIAN_POINT('Ctrl Pts',(-255.637980139532,-0.612716740876425,
135.684295172245));
#139324=CARTESIAN_POINT('Ctrl Pts',(-255.645728049937,-0.476681885459189,
135.70137549009));
#139325=CARTESIAN_POINT('Ctrl Pts',(-255.653475960342,-0.339861929090951,
135.712772093729));
#139326=CARTESIAN_POINT('Ctrl Pts',(-255.661223870747,-0.202769669246156,
135.718428944699));
#139327=CARTESIAN_POINT('Ctrl Pts',(-255.668970160453,-0.0657060862072468,
135.724084612376));
#139328=CARTESIAN_POINT('Ctrl Pts',(-255.676716450159,0.0716292966275856,
135.724002899405));
#139329=CARTESIAN_POINT('Ctrl Pts',(-255.684462739865,0.208720384205294,
135.718179790441));
#139330=CARTESIAN_POINT('Ctrl Pts',(-255.692209086732,0.345812483418953,
135.712356638507));
#139331=CARTESIAN_POINT('Ctrl Pts',(-255.6999554336,0.482659893166817,135.700792022632));
#139332=CARTESIAN_POINT('Ctrl Pts',(-255.707701780468,0.618748745367988,
135.683534016064));
#139333=CARTESIAN_POINT('Ctrl Pts',(-255.715449862042,0.754868073110716,
135.666272144762));
#139334=CARTESIAN_POINT('Ctrl Pts',(-255.723197943616,0.890228117501376,
135.643314394903));
#139335=CARTESIAN_POINT('Ctrl Pts',(-255.730946025189,1.02432273647311,
135.614760392433));
#139336=CARTESIAN_POINT('Ctrl Pts',(-255.738702341375,1.1585598703514,135.586176042952));
#139337=CARTESIAN_POINT('Ctrl Pts',(-255.74645865756,1.2915285092558,135.551983641321));
#139338=CARTESIAN_POINT('Ctrl Pts',(-255.754214973746,1.42273472920243,
135.512333530914));
#139339=CARTESIAN_POINT('Ctrl Pts',(-255.761975429655,1.55401097692936,
135.472662258331));
#139340=CARTESIAN_POINT('Ctrl Pts',(-255.769735885565,1.68352256238016,
135.42752760136));
#139341=CARTESIAN_POINT('Ctrl Pts',(-255.777496341475,1.81079416939543,
135.377128656575));
#139342=CARTESIAN_POINT('Ctrl Pts',(-255.785269254919,1.93827008016889,
135.326648808484));
#139343=CARTESIAN_POINT('Ctrl Pts',(-255.793042168362,2.06349846970333,
135.27088794483));
#139344=CARTESIAN_POINT('Ctrl Pts',(-255.800815081806,2.18602650742093,
135.210092244816));
#139345=CARTESIAN_POINT('Ctrl Pts',(-255.808305268806,2.30409779716003,
135.151507884494));
#139346=CARTESIAN_POINT('Ctrl Pts',(-255.815795455806,2.41966149372262,
135.088248740042));
#139347=CARTESIAN_POINT('Ctrl Pts',(-255.823285642807,2.53233843750942,
135.020572792067));
#139348=CARTESIAN_POINT('Ctrl Pts',(-255.831059947351,2.64928943966847,
134.950329762112));
#139349=CARTESIAN_POINT('Ctrl Pts',(-255.838834251894,2.76350083179706,
134.875105728614));
#139350=CARTESIAN_POINT('Ctrl Pts',(-255.846608556438,2.87451918596033,
134.795140304801));
#139351=CARTESIAN_POINT('Ctrl Pts',(-255.854373279807,2.98540071936351,
134.715273431629));
#139352=CARTESIAN_POINT('Ctrl Pts',(-255.862138003176,3.09309673038082,
134.630677021003));
#139353=CARTESIAN_POINT('Ctrl Pts',(-255.869902726545,3.19717947386991,
134.541635891661));
#139354=CARTESIAN_POINT('Ctrl Pts',(-255.877659737879,3.30115884088379,
134.452683199247));
#139355=CARTESIAN_POINT('Ctrl Pts',(-255.885416749213,3.40153178697501,
134.359294825797));
#139356=CARTESIAN_POINT('Ctrl Pts',(-255.893173760547,3.49790089452245,
134.261797875796));
#139357=CARTESIAN_POINT('Ctrl Pts',(-255.900924922294,3.59419732981155,
134.164374448564));
#139358=CARTESIAN_POINT('Ctrl Pts',(-255.908676084041,3.68649566257353,
134.062848888677));
#139359=CARTESIAN_POINT('Ctrl Pts',(-255.916427245787,3.77443310740116,
133.957587184157));
#139360=CARTESIAN_POINT('Ctrl Pts',(-255.92417511326,3.86233317847696,133.852370216265));
#139361=CARTESIAN_POINT('Ctrl Pts',(-255.931922980733,3.94587579774067,
133.743420561318));
#139362=CARTESIAN_POINT('Ctrl Pts',(-255.939670848206,4.02473664074394,
133.631139355839));
#139363=CARTESIAN_POINT('Ctrl Pts',(-255.947417095106,4.10358098890874,
133.518881635531));
#139364=CARTESIAN_POINT('Ctrl Pts',(-255.955163342005,4.17774528404333,
133.403294070481));
#139365=CARTESIAN_POINT('Ctrl Pts',(-255.962909588904,4.24694718773835,
133.284808691415));
#139366=CARTESIAN_POINT('Ctrl Pts',(-255.970655893131,4.31614960357181,
133.166322435481));
#139367=CARTESIAN_POINT('Ctrl Pts',(-255.978402197357,4.380389357505,133.044938660342));
#139368=CARTESIAN_POINT('Ctrl Pts',(-255.986148501584,4.43942913845158,
132.921115678306));
#139369=CARTESIAN_POINT('Ctrl Pts',(-255.993896540721,4.4984821423154,132.797264964102));
#139370=CARTESIAN_POINT('Ctrl Pts',(-256.001644579858,4.55233268750128,
132.670974308765));
#139371=CARTESIAN_POINT('Ctrl Pts',(-256.009392618995,4.60079101177705,
132.542723389962));
#139372=CARTESIAN_POINT('Ctrl Pts',(-256.017148893306,4.64930084105,132.414336156845));
#139373=CARTESIAN_POINT('Ctrl Pts',(-256.024905167617,4.6924068622338,132.283984864543));
#139374=CARTESIAN_POINT('Ctrl Pts',(-256.032661441928,4.72996858728783,
132.152166325289));
#139375=CARTESIAN_POINT('Ctrl Pts',(-256.040421856202,4.76755036116648,
132.020277426999));
#139376=CARTESIAN_POINT('Ctrl Pts',(-256.048182270477,4.79958185098399,
131.886920101229));
#139377=CARTESIAN_POINT('Ctrl Pts',(-256.055942684752,4.82597364416927,
131.752601857063));
#139378=CARTESIAN_POINT('Ctrl Pts',(-256.063715557391,4.85240780604265,
131.618067981934));
#139379=CARTESIAN_POINT('Ctrl Pts',(-256.071488430031,4.87318411957688,
131.482570492412));
#139380=CARTESIAN_POINT('Ctrl Pts',(-256.07926130267,4.88826493817758,131.346623429018));
#139381=CARTESIAN_POINT('Ctrl Pts',(-256.086751957319,4.90279820138934,
131.215612340861));
#139382=CARTESIAN_POINT('Ctrl Pts',(-256.094242611969,4.91204236174855,
131.084184066446));
#139383=CARTESIAN_POINT('Ctrl Pts',(-256.101733266619,4.91600952625544,
130.952797136879));
#139384=CARTESIAN_POINT('Ctrl Pts',(-256.109507612938,4.92012693818049,
130.816434223354));
#139385=CARTESIAN_POINT('Ctrl Pts',(-256.117281959258,4.91857281033011,
130.679683873794));
#139386=CARTESIAN_POINT('Ctrl Pts',(-256.125056305577,4.91130364868276,
130.543057091116));
#139387=CARTESIAN_POINT('Ctrl Pts',(-256.132821070531,4.90404344579439,
130.406598691873));
#139388=CARTESIAN_POINT('Ctrl Pts',(-256.140585835484,4.89108224394783,
130.270263943168));
#139389=CARTESIAN_POINT('Ctrl Pts',(-256.148350600438,4.87242846398543,
130.134566674741));
#139390=CARTESIAN_POINT('Ctrl Pts',(-256.156107653126,4.85379321167978,
129.999004186098));
#139391=CARTESIAN_POINT('Ctrl Pts',(-256.163864705815,4.8294766860502,129.864078302512));
#139392=CARTESIAN_POINT('Ctrl Pts',(-256.171621758503,4.79953927689507,
129.730300194665));
#139393=CARTESIAN_POINT('Ctrl Pts',(-256.179372961334,4.76962444456061,
129.59662297345));
#139394=CARTESIAN_POINT('Ctrl Pts',(-256.187124164164,4.7340972510083,129.464092185079));
#139395=CARTESIAN_POINT('Ctrl Pts',(-256.194875366995,4.69306951939789,
129.333210880592));
#139396=CARTESIAN_POINT('Ctrl Pts',(-256.202623275001,4.65205922755306,
129.202385210165));
#139397=CARTESIAN_POINT('Ctrl Pts',(-256.210371183007,4.60555316471098,
129.073208001369));
#139398=CARTESIAN_POINT('Ctrl Pts',(-256.218119091014,4.55371351452655,
128.946168945505));
#139399=CARTESIAN_POINT('Ctrl Pts',(-256.225865378107,4.50188470954078,
128.819156467054));
#139400=CARTESIAN_POINT('Ctrl Pts',(-256.233611665199,4.44472468426253,
128.694281613556));
#139401=CARTESIAN_POINT('Ctrl Pts',(-256.241357952292,4.38244430899901,
128.572015451374));
#139402=CARTESIAN_POINT('Ctrl Pts',(-256.249104296336,4.32016347584558,
128.449748390282));
#139403=CARTESIAN_POINT('Ctrl Pts',(-256.25685064038,4.25276239504261,128.330090407149));
#139404=CARTESIAN_POINT('Ctrl Pts',(-256.264596984424,4.18049838674326,
128.213488891498));
#139405=CARTESIAN_POINT('Ctrl Pts',(-256.272345062966,4.10821819767546,
128.096861267386));
#139406=CARTESIAN_POINT('Ctrl Pts',(-256.280093141508,4.03107312030725,
127.983291804847));
#139407=CARTESIAN_POINT('Ctrl Pts',(-256.287841220051,3.94936415147337,
127.873199437836));
#139408=CARTESIAN_POINT('Ctrl Pts',(-256.295597532897,3.86756834608115,
127.762990069688));
#139409=CARTESIAN_POINT('Ctrl Pts',(-256.303353845743,3.78119919361253,
127.656265493271));
#139410=CARTESIAN_POINT('Ctrl Pts',(-256.311110158589,3.69059874068027,
127.553412448525));
#139411=CARTESIAN_POINT('Ctrl Pts',(-256.318870610986,3.59994993419757,
127.450504511009));
#139412=CARTESIAN_POINT('Ctrl Pts',(-256.326631063385,3.50506559784399,
127.351472504486));
#139413=CARTESIAN_POINT('Ctrl Pts',(-256.334391515782,3.40632438553531,
127.256665979776));
#139414=CARTESIAN_POINT('Ctrl Pts',(-256.342164425457,3.30742467131085,
127.16170726921));
#139415=CARTESIAN_POINT('Ctrl Pts',(-256.349937335131,3.20465600249904,
127.07098785364));
#139416=CARTESIAN_POINT('Ctrl Pts',(-256.357710244805,3.0984305090419,126.98481726225));
#139417=CARTESIAN_POINT('Ctrl Pts',(-256.365200460014,2.99606835123671,
126.901780625875));
#139418=CARTESIAN_POINT('Ctrl Pts',(-256.372690675223,2.89049669188504,
126.822967871032));
#139419=CARTESIAN_POINT('Ctrl Pts',(-256.380180890432,2.78210777718279,
126.748616619403));
#139420=CARTESIAN_POINT('Ctrl Pts',(-256.387955305096,2.6696062876589,126.671444275909));
#139421=CARTESIAN_POINT('Ctrl Pts',(-256.39572971976,2.55371319387958,126.598834247598));
#139422=CARTESIAN_POINT('Ctrl Pts',(-256.403504134424,2.43483491863965,
126.53109933589));
#139423=CARTESIAN_POINT('Ctrl Pts',(-256.411268968321,2.3161031425358,126.463447897011));
#139424=CARTESIAN_POINT('Ctrl Pts',(-256.419033802218,2.19439384106692,
126.400659812629));
#139425=CARTESIAN_POINT('Ctrl Pts',(-256.426798636115,2.07014387587007,
126.343005734159));
#139426=CARTESIAN_POINT('Ctrl Pts',(-256.434555758268,1.94601731112681,
126.28540891558));
#139427=CARTESIAN_POINT('Ctrl Pts',(-256.44231288042,1.81935545646732,126.232936119353));
#139428=CARTESIAN_POINT('Ctrl Pts',(-256.450070002572,1.69062102621373,
126.185812836258));
#139429=CARTESIAN_POINT('Ctrl Pts',(-256.45782127531,1.56198367075648,126.138725087427));
#139430=CARTESIAN_POINT('Ctrl Pts',(-256.465572548048,1.43127721614667,
126.09697895632));
#139431=CARTESIAN_POINT('Ctrl Pts',(-256.473323820785,1.29898534580503,
126.060752272236));
#139432=CARTESIAN_POINT('Ctrl Pts',(-256.481071799121,1.1667497013993,126.024540985011));
#139433=CARTESIAN_POINT('Ctrl Pts',(-256.488819777457,1.03293035773216,
125.993844582143));
#139434=CARTESIAN_POINT('Ctrl Pts',(-256.496567755794,0.898026978859469,
125.968791301783));
#139435=CARTESIAN_POINT('Ctrl Pts',(-256.504314113463,0.763151818115598,
125.94374326189));
#139436=CARTESIAN_POINT('Ctrl Pts',(-256.512060471132,0.627193457326346,
125.924336067988));
#139437=CARTESIAN_POINT('Ctrl Pts',(-256.519806828801,0.490662206737524,
125.910646929437));
#139438=CARTESIAN_POINT('Ctrl Pts',(-256.5275532436,0.354129949215721,125.896957689928));
#139439=CARTESIAN_POINT('Ctrl Pts',(-256.535299658399,0.217025182469028,
125.888986628924));
#139440=CARTESIAN_POINT('Ctrl Pts',(-256.543046073199,0.0798634036778129,
125.886759078273));
#139441=CARTESIAN_POINT('Ctrl Pts',(-256.550794222607,-0.0573290889515717,
125.88453102882));
#139442=CARTESIAN_POINT('Ctrl Pts',(-256.558542372016,-0.194578228199409,
125.88804905528));
#139443=CARTESIAN_POINT('Ctrl Pts',(-256.566290521425,-0.331368849287899,
125.897286362144));
#139444=CARTESIAN_POINT('Ctrl Pts',(-256.574046904909,-0.468304839833111,
125.906533485634));
#139445=CARTESIAN_POINT('Ctrl Pts',(-256.581803288393,-0.604780948146652,
125.921512004537));
#139446=CARTESIAN_POINT('Ctrl Pts',(-256.589559671878,-0.740286906957838,
125.942143185377));
#139447=CARTESIAN_POINT('Ctrl Pts',(-256.597320194901,-0.875865184559755,
125.962785376964));
#139448=CARTESIAN_POINT('Ctrl Pts',(-256.605080717925,-1.01047189745824,
125.989086166776));
#139449=CARTESIAN_POINT('Ctrl Pts',(-256.612841240949,-1.14360827952286,
126.020915920958));
#139450=CARTESIAN_POINT('Ctrl Pts',(-256.620614220507,-1.27695836084543,
126.052796765569));
#139451=CARTESIAN_POINT('Ctrl Pts',(-256.628387200066,-1.40883301888172,
126.090224202077));
#139452=CARTESIAN_POINT('Ctrl Pts',(-256.636160179625,-1.53874906425391,
126.133018799656));
#139453=CARTESIAN_POINT('Ctrl Pts',(-256.643649624498,-1.66392616688881,
126.174252380296));
#139454=CARTESIAN_POINT('Ctrl Pts',(-256.651139069372,-1.78728476738983,
126.220468281193));
#139455=CARTESIAN_POINT('Ctrl Pts',(-256.658628514245,-1.90841305938302,
126.271465002479));
#139456=CARTESIAN_POINT('Ctrl Pts',(-256.666403063451,-2.03415240084404,
126.3244030407));
#139457=CARTESIAN_POINT('Ctrl Pts',(-256.674177612657,-2.15788660754819,
126.382660805064));
#139458=CARTESIAN_POINT('Ctrl Pts',(-256.681952161862,-2.27913277366472,
126.446065439115));
#139459=CARTESIAN_POINT('Ctrl Pts',(-256.68971703315,-2.40022801007117,
126.50939114578));
#139460=CARTESIAN_POINT('Ctrl Pts',(-256.697481904438,-2.51884102536472,
126.577850794189));
#139461=CARTESIAN_POINT('Ctrl Pts',(-256.705246775725,-2.63450794188062,
126.651223132884));
#139462=CARTESIAN_POINT('Ctrl Pts',(-256.71300383883,-2.75005854629814,
126.724521689975));
#139463=CARTESIAN_POINT('Ctrl Pts',(-256.720760901934,-2.86266861975698,
126.802722897663));
#139464=CARTESIAN_POINT('Ctrl Pts',(-256.728517965039,-2.97189832430596,
126.885559345176));
#139465=CARTESIAN_POINT('Ctrl Pts',(-256.736292497028,-3.08137401385148,
126.968582340142));
#139466=CARTESIAN_POINT('Ctrl Pts',(-256.744067029018,-3.18745374186974,
127.056261291037));
#139467=CARTESIAN_POINT('Ctrl Pts',(-256.751841561007,-3.28972276324023,
127.148282499757));
#139468=CARTESIAN_POINT('Ctrl Pts',(-256.759588911131,-3.39163422447051,
127.23998197746));
#139469=CARTESIAN_POINT('Ctrl Pts',(-256.767336261256,-3.48976128720013,
127.335993139251));
#139470=CARTESIAN_POINT('Ctrl Pts',(-256.77508361138,-3.58372615583562,
127.435964871446));
#139471=CARTESIAN_POINT('Ctrl Pts',(-256.782829210042,-3.67766978161093,
127.535914002795));
#139472=CARTESIAN_POINT('Ctrl Pts',(-256.790574808705,-3.76745281825126,
127.639821638118));
#139473=CARTESIAN_POINT('Ctrl Pts',(-256.798320407367,-3.85273467051478,
127.747300163288));
#139474=CARTESIAN_POINT('Ctrl Pts',(-256.806065932552,-3.93801571375518,
127.854777668866));
#139475=CARTESIAN_POINT('Ctrl Pts',(-256.813811457736,-4.01879541538737,
127.965825690128));
#139476=CARTESIAN_POINT('Ctrl Pts',(-256.82155698292,-4.09477403842602,
128.080024251268));
#139477=CARTESIAN_POINT('Ctrl Pts',(-256.829352795409,-4.17124594759677,
128.194964238935));
#139478=CARTESIAN_POINT('Ctrl Pts',(-256.837148607897,-4.24285397776989,
128.313095497808));
#139479=CARTESIAN_POINT('Ctrl Pts',(-256.844944420386,-4.309337732552,128.433961628091));
#139480=CARTESIAN_POINT('Ctrl Pts',(-256.852698030591,-4.37546158048252,
128.55417345495));
#139481=CARTESIAN_POINT('Ctrl Pts',(-256.860451640795,-4.43651636272949,
128.677090242758));
#139482=CARTESIAN_POINT('Ctrl Pts',(-256.868205250999,-4.49229316026251,
128.80224043517));
#139483=CARTESIAN_POINT('Ctrl Pts',(-256.87602216463,-4.54852534081278,
128.928412401415));
#139484=CARTESIAN_POINT('Ctrl Pts',(-256.883839078261,-4.59939281359841,
129.056854029583));
#139485=CARTESIAN_POINT('Ctrl Pts',(-256.891655991892,-4.64473216300896,
129.187064665549));
#139486=CARTESIAN_POINT('Ctrl Pts',(-256.899472905523,-4.69007151241964,
129.317275301515));
#139487=CARTESIAN_POINT('Ctrl Pts',(-256.907289819154,-4.72988266582926,
129.449254546422));
#139488=CARTESIAN_POINT('Ctrl Pts',(-256.915106732785,-4.76405452823404,
129.582490119308));
#139489=CARTESIAN_POINT('Ctrl Pts',(-255.165002394563,-4.76405452823405,
129.582490119308));
#139490=CARTESIAN_POINT('Ctrl Pts',(-255.172655166336,-4.79770872156121,
129.713707308317));
#139491=CARTESIAN_POINT('Ctrl Pts',(-255.180307938108,-4.82591576732456,
129.846231170376));
#139492=CARTESIAN_POINT('Ctrl Pts',(-255.187960709881,-4.84859700324015,
129.979563574245));
#139493=CARTESIAN_POINT('Ctrl Pts',(-255.195824018897,-4.87190222808818,
130.116564117922));
#139494=CARTESIAN_POINT('Ctrl Pts',(-255.203687327913,-4.88937314622007,
130.254417878155));
#139495=CARTESIAN_POINT('Ctrl Pts',(-255.211550636929,-4.90098157013989,
130.392580686475));
#139496=CARTESIAN_POINT('Ctrl Pts',(-255.219413945945,-4.91258999405968,
130.530743494795));
#139497=CARTESIAN_POINT('Ctrl Pts',(-255.22727725496,-4.91833596597612,
130.669214894679));
#139498=CARTESIAN_POINT('Ctrl Pts',(-255.235140563976,-4.91824902737425,
130.807453711842));
#139499=CARTESIAN_POINT('',(-254.88985943604,-4.91824957686614,130.806400753838));
#139500=CARTESIAN_POINT('Ctrl Pts',(-254.820081699213,-4.76405452823395,
129.582490119308));
#139501=CARTESIAN_POINT('Ctrl Pts',(-254.827987033215,-4.79880802620788,
129.71799348045));
#139502=CARTESIAN_POINT('Ctrl Pts',(-254.835892367217,-4.8278021954462,
129.855082133978));
#139503=CARTESIAN_POINT('Ctrl Pts',(-254.843797701219,-4.85090328122655,
129.993237680715));
#139504=CARTESIAN_POINT('Ctrl Pts',(-254.851697709623,-4.87398880446313,
130.131300155994));
#139505=CARTESIAN_POINT('Ctrl Pts',(-254.859597718027,-4.89118909248049,
130.270427729865));
#139506=CARTESIAN_POINT('Ctrl Pts',(-254.867497726431,-4.90242129645858,
130.410091046676));
#139507=CARTESIAN_POINT('Ctrl Pts',(-254.874951629619,-4.91301922962145,
130.541867722008));
#139508=CARTESIAN_POINT('Ctrl Pts',(-254.882405532808,-4.91830444773814,
130.674120990215));
#139509=CARTESIAN_POINT('Ctrl Pts',(-254.889859435997,-4.91824957686646,
130.806400753076));
#139510=CARTESIAN_POINT('Ctrl Pts',(-254.88985943604,-4.91824957686614,
130.806400753838));
#139511=CARTESIAN_POINT('Ctrl Pts',(-254.898291060281,-4.91818750861372,
130.956031521351));
#139512=CARTESIAN_POINT('Ctrl Pts',(-254.906722684522,-4.91129283825743,
131.105445383408));
#139513=CARTESIAN_POINT('Ctrl Pts',(-254.915154308762,-4.8976496465132,
131.254039394594));
#139514=CARTESIAN_POINT('Ctrl Pts',(-254.923623830761,-4.88394513249381,
131.403301293691));
#139515=CARTESIAN_POINT('Ctrl Pts',(-254.932093352761,-4.86343138027049,
131.551735692772));
#139516=CARTESIAN_POINT('Ctrl Pts',(-254.94056287476,-4.8362441535837,131.698746188462));
#139517=CARTESIAN_POINT('Ctrl Pts',(-254.949051704908,-4.80899494759928,
131.8460918271));
#139518=CARTESIAN_POINT('Ctrl Pts',(-254.957540535056,-4.77504192517439,
131.992006814685));
#139519=CARTESIAN_POINT('Ctrl Pts',(-254.966029365204,-4.73457087064609,
132.135909239784));
#139520=CARTESIAN_POINT('Ctrl Pts',(-254.97454688385,-4.69396304182292,
132.280297991541));
#139521=CARTESIAN_POINT('Ctrl Pts',(-254.983064402496,-4.64679317755957,
132.422660312185));
#139522=CARTESIAN_POINT('Ctrl Pts',(-254.991581921142,-4.59329646968355,
132.56243075385));
#139523=CARTESIAN_POINT('Ctrl Pts',(-254.996898536605,-4.55990394821213,
132.649675140648));
#139524=CARTESIAN_POINT('Ctrl Pts',(-255.002215152067,-4.52404728017144,
132.7359101305));
#139525=CARTESIAN_POINT('Ctrl Pts',(-255.007531767529,-4.48579264567317,
132.821003224109));
#139526=CARTESIAN_POINT('Ctrl Pts',(-255.015306101543,-4.42985399291509,
132.945432409695));
#139527=CARTESIAN_POINT('Ctrl Pts',(-255.023080435558,-4.3686455941954,
133.067729436475));
#139528=CARTESIAN_POINT('Ctrl Pts',(-255.030854769572,-4.30235183476065,
133.187415747527));
#139529=CARTESIAN_POINT('Ctrl Pts',(-255.038619522409,-4.23613977650277,
133.306954555818));
#139530=CARTESIAN_POINT('Ctrl Pts',(-255.046384275247,-4.16485501511812,
133.423888711477));
#139531=CARTESIAN_POINT('Ctrl Pts',(-255.054149028084,-4.08872985823644,
133.537759821646));
#139532=CARTESIAN_POINT('Ctrl Pts',(-255.061906068855,-4.01268030998117,
133.651517833353));
#139533=CARTESIAN_POINT('Ctrl Pts',(-255.069663109626,-3.93180014935378,
133.762218530888));
#139534=CARTESIAN_POINT('Ctrl Pts',(-255.077420150396,-3.84636725562247,
133.869428642484));
#139535=CARTESIAN_POINT('Ctrl Pts',(-255.085171341517,-3.76099878755241,
133.976557906036));
#139536=CARTESIAN_POINT('Ctrl Pts',(-255.092922532638,-3.67108466272751,
134.080201518523));
#139537=CARTESIAN_POINT('Ctrl Pts',(-255.10067372376,-3.57694546208149,
134.179956005612));
#139538=CARTESIAN_POINT('Ctrl Pts',(-255.108421620411,-3.48284627318568,
134.279668094299));
#139539=CARTESIAN_POINT('Ctrl Pts',(-255.116169517063,-3.38452584789885,
134.375494061506));
#139540=CARTESIAN_POINT('Ctrl Pts',(-255.123917413715,-3.28234421214176,
134.467064473397));
#139541=CARTESIAN_POINT('Ctrl Pts',(-255.131663689669,-3.18018395063194,
134.558615730686));
#139542=CARTESIAN_POINT('Ctrl Pts',(-255.139409965624,-3.07416437615344,
134.645912942504));
#139543=CARTESIAN_POINT('Ctrl Pts',(-255.147156241579,-2.9646811514689,
134.72862471834));
#139544=CARTESIAN_POINT('Ctrl Pts',(-255.154902574711,-2.85519711865731,
134.811337104695));
#139545=CARTESIAN_POINT('Ctrl Pts',(-255.162648907844,-2.74224969657472,
134.889463751859));
#139546=CARTESIAN_POINT('Ctrl Pts',(-255.170395240976,-2.62626596372606,
134.962714877399));
#139547=CARTESIAN_POINT('Ctrl Pts',(-255.178143308842,-2.51025625717804,
135.035982406987));
#139548=CARTESIAN_POINT('Ctrl Pts',(-255.185891376708,-2.39120921731934,
135.104372033592));
#139549=CARTESIAN_POINT('Ctrl Pts',(-255.193639444575,-2.2695787544378,
135.16763866737));
#139550=CARTESIAN_POINT('Ctrl Pts',(-255.201395747175,-2.14781902132732,
135.230972541641));
#139551=CARTESIAN_POINT('Ctrl Pts',(-255.209152049775,-2.0234707277822,
135.289172365858));
#139552=CARTESIAN_POINT('Ctrl Pts',(-255.216908352375,-1.89701061846926,
135.342039955721));
#139553=CARTESIAN_POINT('Ctrl Pts',(-255.224668794745,-1.77048301363391,
135.394935762589));
#139554=CARTESIAN_POINT('Ctrl Pts',(-255.232429237115,-1.64184171363962,
135.442493528761));
#139555=CARTESIAN_POINT('Ctrl Pts',(-255.240189679485,-1.5115801177162,
135.484564524473));
#139556=CARTESIAN_POINT('Ctrl Pts',(-255.247962579602,-1.38110941436878,
135.526703056265));
#139557=CARTESIAN_POINT('Ctrl Pts',(-255.255735479719,-1.24901359434345,
135.563337112166));
#139558=CARTESIAN_POINT('Ctrl Pts',(-255.263508379837,-1.11579865670131,
135.594368594616));
#139559=CARTESIAN_POINT('Ctrl Pts',(-255.270998717005,-0.987426391052345,
135.624272010697));
#139560=CARTESIAN_POINT('Ctrl Pts',(-255.278489054173,-0.858015262777696,
135.648973056799));
#139561=CARTESIAN_POINT('Ctrl Pts',(-255.285979391341,-0.728021963377957,
135.668429601795));
#139562=CARTESIAN_POINT('Ctrl Pts',(-255.293753727656,-0.593099915733337,
135.688623849522));
#139563=CARTESIAN_POINT('Ctrl Pts',(-255.301528063971,-0.457123287592099,
135.703232023219));
#139564=CARTESIAN_POINT('Ctrl Pts',(-255.309302400287,-0.320594367480395,
135.712150579865));
#139565=CARTESIAN_POINT('Ctrl Pts',(-255.317067155437,-0.184233706881655,
135.721058145199));
#139566=CARTESIAN_POINT('Ctrl Pts',(-255.324831910588,-0.0473224949908735,
135.724290019907));
#139567=CARTESIAN_POINT('Ctrl Pts',(-255.332596665739,0.0896280410715395,
135.721793878603));
#139568=CARTESIAN_POINT('Ctrl Pts',(-255.340353708832,0.226442556060319,
135.7193002165));
#139569=CARTESIAN_POINT('Ctrl Pts',(-255.348110751926,0.363295929124422,
135.71108986711));
#139570=CARTESIAN_POINT('Ctrl Pts',(-255.35586779502,0.499673435663358,
135.697162424322));
#139571=CARTESIAN_POINT('Ctrl Pts',(-255.363618988471,0.63594809894258,
135.683245484318));
#139572=CARTESIAN_POINT('Ctrl Pts',(-255.371370181923,0.771747222606243,
135.663620071859));
#139573=CARTESIAN_POINT('Ctrl Pts',(-255.379121375375,0.906558070205984,
135.638337813193));
#139574=CARTESIAN_POINT('Ctrl Pts',(-255.38686927436,1.04131161955525,135.61306630017));
#139575=CARTESIAN_POINT('Ctrl Pts',(-255.394617173345,1.17507734481474,
135.582142794849));
#139576=CARTESIAN_POINT('Ctrl Pts',(-255.40236507233,1.3073498278057,135.545670509382));
#139577=CARTESIAN_POINT('Ctrl Pts',(-255.41011135062,1.43959464221113,135.509205853141));
#139578=CARTESIAN_POINT('Ctrl Pts',(-255.41785762891,1.57034645897749,135.467194829281));
#139579=CARTESIAN_POINT('Ctrl Pts',(-255.4256039072,1.69911260427714,135.419791195582));
#139580=CARTESIAN_POINT('Ctrl Pts',(-255.433350242666,1.82787970002439,
135.372387211988));
#139581=CARTESIAN_POINT('Ctrl Pts',(-255.441096578133,1.95466072816569,
135.319590674196));
#139582=CARTESIAN_POINT('Ctrl Pts',(-255.448842913599,2.07898103995985,
135.261604261118));
#139583=CARTESIAN_POINT('Ctrl Pts',(-255.456590983797,2.2033291923131,135.203604862438));
#139584=CARTESIAN_POINT('Ctrl Pts',(-255.464339053995,2.32521517752682,
135.140413440998));
#139585=CARTESIAN_POINT('Ctrl Pts',(-255.472087124192,2.44418744476934,
135.072279407484));
#139586=CARTESIAN_POINT('Ctrl Pts',(-255.479843429106,2.56328615676787,
135.004072960528));
#139587=CARTESIAN_POINT('Ctrl Pts',(-255.48759973402,2.67946462494469,134.930913602568));
#139588=CARTESIAN_POINT('Ctrl Pts',(-255.495356038933,2.79229841889414,
134.853095309089));
#139589=CARTESIAN_POINT('Ctrl Pts',(-255.503116483611,2.90519243549031,
134.775235481745));
#139590=CARTESIAN_POINT('Ctrl Pts',(-255.510876928288,3.01473790867863,
134.692711999233));
#139591=CARTESIAN_POINT('Ctrl Pts',(-255.518637372965,3.12054301335554,
134.605859580383));
#139592=CARTESIAN_POINT('Ctrl Pts',(-255.526410275356,3.22651796522496,
134.518867738775));
#139593=CARTESIAN_POINT('Ctrl Pts',(-255.534183177747,3.32874025826255,
134.427533334813));
#139594=CARTESIAN_POINT('Ctrl Pts',(-255.541956080138,3.42685385515063,
134.332229055864));
#139595=CARTESIAN_POINT('Ctrl Pts',(-255.54944639181,3.52140044571991,134.240389648003));
#139596=CARTESIAN_POINT('Ctrl Pts',(-255.556936703482,3.61213169130486,
134.144864233102));
#139597=CARTESIAN_POINT('Ctrl Pts',(-255.564427015153,3.69876529575126,
134.046014261842));
#139598=CARTESIAN_POINT('Ctrl Pts',(-255.572201345162,3.78868388130008,
133.943416088142));
#139599=CARTESIAN_POINT('Ctrl Pts',(-255.579975675171,3.87447277901351,
133.836911261055));
#139600=CARTESIAN_POINT('Ctrl Pts',(-255.58775000518,3.95577337616257,133.726866401811));
#139601=CARTESIAN_POINT('Ctrl Pts',(-255.59551475402,4.03697377756145,133.616957163061));
#139602=CARTESIAN_POINT('Ctrl Pts',(-255.603279502859,4.11369665420668,
133.503516884211));
#139603=CARTESIAN_POINT('Ctrl Pts',(-255.611044251698,4.18562165265169,
133.386947391201));
#139604=CARTESIAN_POINT('Ctrl Pts',(-255.618801288481,4.25747521419536,
133.27049367662));
#139605=CARTESIAN_POINT('Ctrl Pts',(-255.626558325265,4.32454017676951,
133.15091726347));
#139606=CARTESIAN_POINT('Ctrl Pts',(-255.634315362048,4.3865379775844,133.028650983887));
#139607=CARTESIAN_POINT('Ctrl Pts',(-255.642066549197,4.44848902543446,
132.906476906141));
#139608=CARTESIAN_POINT('Ctrl Pts',(-255.649817736346,4.50538034125497,
132.78161734675));
#139609=CARTESIAN_POINT('Ctrl Pts',(-255.657568923495,4.55697821318472,
132.654531589952));
#139610=CARTESIAN_POINT('Ctrl Pts',(-255.665316816211,4.60855415483123,
132.527499847526));
#139611=CARTESIAN_POINT('Ctrl Pts',(-255.673064708927,4.65484098057059,
132.398244151073));
#139612=CARTESIAN_POINT('Ctrl Pts',(-255.680812601643,4.6956523349151,132.267245511229));
#139613=CARTESIAN_POINT('Ctrl Pts',(-255.688558873685,4.73645515249877,
132.136274273172));
#139614=CARTESIAN_POINT('Ctrl Pts',(-255.696305145727,4.77178466061213,
132.003561189931));
#139615=CARTESIAN_POINT('Ctrl Pts',(-255.704051417769,4.80150391786348,
131.86960387112));
#139616=CARTESIAN_POINT('Ctrl Pts',(-255.711797747015,4.83122339458221,
131.735645563075));
#139617=CARTESIAN_POINT('Ctrl Pts',(-255.719544076261,4.85533245308934,
131.60044338281));
#139618=CARTESIAN_POINT('Ctrl Pts',(-255.727290405506,4.87374505372797,
131.464506217992));
#139619=CARTESIAN_POINT('Ctrl Pts',(-255.735038469516,4.89216177780544,
131.328538610512));
#139620=CARTESIAN_POINT('Ctrl Pts',(-255.742786533526,4.90487945304789,
131.191836078304));
#139621=CARTESIAN_POINT('Ctrl Pts',(-255.750534597535,4.91186384154735,
131.054913335771));
#139622=CARTESIAN_POINT('Ctrl Pts',(-255.758290896348,4.91885565319941,
130.917845068914));
#139623=CARTESIAN_POINT('Ctrl Pts',(-255.76604719516,4.92010198582534,130.780556515283));
#139624=CARTESIAN_POINT('Ctrl Pts',(-255.773803493972,4.91562075439972,
130.643563660459));
#139625=CARTESIAN_POINT('Ctrl Pts',(-255.781563932585,4.91113713118828,
130.506497687884));
#139626=CARTESIAN_POINT('Ctrl Pts',(-255.789324371199,4.90091988171353,
130.369728118281));
#139627=CARTESIAN_POINT('Ctrl Pts',(-255.797084809812,4.88503882343902,
130.233765528213));
#139628=CARTESIAN_POINT('Ctrl Pts',(-255.804857706264,4.86913227128675,
130.097584677272));
#139629=CARTESIAN_POINT('Ctrl Pts',(-255.812630602717,4.84754380299392,
129.962213780887));
#139630=CARTESIAN_POINT('Ctrl Pts',(-255.82040349917,4.82039452419987,129.828153829245));
#139631=CARTESIAN_POINT('Ctrl Pts',(-255.827893879102,4.79423202296297,
129.698966469343));
#139632=CARTESIAN_POINT('Ctrl Pts',(-255.835384259034,4.76290599817105,
129.570996711417));
#139633=CARTESIAN_POINT('Ctrl Pts',(-255.842874638966,4.72656796529398,
129.444677444192));
#139634=CARTESIAN_POINT('Ctrl Pts',(-255.850648973645,4.68885238454662,
129.313569507252));
#139635=CARTESIAN_POINT('Ctrl Pts',(-255.858423308324,4.64561782316634,
129.183824354334));
#139636=CARTESIAN_POINT('Ctrl Pts',(-255.866197643003,4.59697889127745,
129.055941864621));
#139637=CARTESIAN_POINT('Ctrl Pts',(-255.873962396479,4.54839990271601,
128.928216979149));
#139638=CARTESIAN_POINT('Ctrl Pts',(-255.881727149955,4.49442993355858,
128.802350551294));
#139639=CARTESIAN_POINT('Ctrl Pts',(-255.889491903431,4.43523389272254,
128.678829300614));
#139640=CARTESIAN_POINT('Ctrl Pts',(-255.897248944813,4.37609664646376,
128.555430733471));
#139641=CARTESIAN_POINT('Ctrl Pts',(-255.905005986196,4.31174382598289,
128.434373058433));
#139642=CARTESIAN_POINT('Ctrl Pts',(-255.912763027578,4.24238901545678,
128.316124594993));
#139643=CARTESIAN_POINT('Ctrl Pts',(-255.920514219284,4.17308650621095,
128.197965304113));
#139644=CARTESIAN_POINT('Ctrl Pts',(-255.92826541099,4.09878971197225,128.082611344041));
#139645=CARTESIAN_POINT('Ctrl Pts',(-255.936016602696,4.0197587148412,127.97050759792));
#139646=CARTESIAN_POINT('Ctrl Pts',(-255.94376449989,3.94076130849002,127.858451499587));
#139647=CARTESIAN_POINT('Ctrl Pts',(-255.951512397084,3.85703392614292,
127.749643186482));
#139648=CARTESIAN_POINT('Ctrl Pts',(-255.959260294278,3.76888052620867,
127.644499443137));
#139649=CARTESIAN_POINT('Ctrl Pts',(-255.967006570749,3.68074556640345,
127.539377693999));
#139650=CARTESIAN_POINT('Ctrl Pts',(-255.974752847221,3.58818668159333,
127.437919289294));
#139651=CARTESIAN_POINT('Ctrl Pts',(-255.982499123692,3.49154850490718,
127.340508412234));
#139652=CARTESIAN_POINT('Ctrl Pts',(-255.990245457314,3.39490961523462,
127.243096816488));
#139653=CARTESIAN_POINT('Ctrl Pts',(-255.997991790937,3.2941916489815,127.149733085528));
#139654=CARTESIAN_POINT('Ctrl Pts',(-256.005738124559,3.18977624146807,
127.060764673575));
#139655=CARTESIAN_POINT('Ctrl Pts',(-256.013486192889,3.08533745125707,
126.971776338112));
#139656=CARTESIAN_POINT('Ctrl Pts',(-256.021234261218,2.9771998696897,126.887185533782));
#139657=CARTESIAN_POINT('Ctrl Pts',(-256.028982329548,2.86577803441173,
126.807299282037));
#139658=CARTESIAN_POINT('Ctrl Pts',(-256.036738632568,2.75423777939466,
126.727328126743));
#139659=CARTESIAN_POINT('Ctrl Pts',(-256.044494935587,2.6394066162155,126.652071740293));
#139660=CARTESIAN_POINT('Ctrl Pts',(-256.052251238606,2.52172834191952,
126.58179395355));
#139661=CARTESIAN_POINT('Ctrl Pts',(-256.060011681372,2.40398725958728,
126.511478657677));
#139662=CARTESIAN_POINT('Ctrl Pts',(-256.067772124137,2.283396381839,126.446147442374));
#139663=CARTESIAN_POINT('Ctrl Pts',(-256.075532566902,2.16042300955805,
126.386017547786));
#139664=CARTESIAN_POINT('Ctrl Pts',(-256.083305467372,2.03725223025821,
126.325791127723));
#139665=CARTESIAN_POINT('Ctrl Pts',(-256.091078367841,1.91169167201454,
126.270782870492));
#139666=CARTESIAN_POINT('Ctrl Pts',(-256.098851268311,1.78422829296174,
126.221161684387));
#139667=CARTESIAN_POINT('Ctrl Pts',(-256.1063415998,1.66139860208187,126.173344381913));
#139668=CARTESIAN_POINT('Ctrl Pts',(-256.11383193129,1.53680232659375,126.130529377399));
#139669=CARTESIAN_POINT('Ctrl Pts',(-256.121322262779,1.41088555684552,
126.092823181868));
#139670=CARTESIAN_POINT('Ctrl Pts',(-256.12909661041,1.28019431282663,126.053687254135));
#139671=CARTESIAN_POINT('Ctrl Pts',(-256.13687095804,1.14766647288937,126.019931239898));
#139672=CARTESIAN_POINT('Ctrl Pts',(-256.14464530567,1.01378455099754,125.991728910625));
#139673=CARTESIAN_POINT('Ctrl Pts',(-256.152410072184,0.880067625359694,
125.963561337938));
#139674=CARTESIAN_POINT('Ctrl Pts',(-256.160174838698,0.745000317022461,
125.940933911775));
#139675=CARTESIAN_POINT('Ctrl Pts',(-256.167939605212,0.609081255968552,
125.923970972658));
#139676=CARTESIAN_POINT('Ctrl Pts',(-256.175696659705,0.473297190682827,
125.907024881251));
#139677=CARTESIAN_POINT('Ctrl Pts',(-256.183453714199,0.336663441636364,
125.895732128981));
#139678=CARTESIAN_POINT('Ctrl Pts',(-256.191210768692,0.199689468356939,
125.890166158784));
#139679=CARTESIAN_POINT('Ctrl Pts',(-256.198961973567,0.0628187875599876,
125.884604385901));
#139680=CARTESIAN_POINT('Ctrl Pts',(-256.206713178443,-0.0743912177338724,
125.88476081502));
#139681=CARTESIAN_POINT('Ctrl Pts',(-256.214464383318,-0.211425672508862,
125.890657101123));
#139682=CARTESIAN_POINT('Ctrl Pts',(-256.222212293723,-0.348401883959695,
125.896550881146));
#139683=CARTESIAN_POINT('Ctrl Pts',(-256.229960204128,-0.485202303508083,
125.908179649215));
#139684=CARTESIAN_POINT('Ctrl Pts',(-256.237708114533,-0.621311980170193,
125.925512957944));
#139685=CARTESIAN_POINT('Ctrl Pts',(-256.245454404239,-0.75739318556207,
125.942842640911));
#139686=CARTESIAN_POINT('Ctrl Pts',(-256.253200693945,-0.892783547878109,
125.965874441702));
#139687=CARTESIAN_POINT('Ctrl Pts',(-256.260946983651,-1.02697355893801,
125.994526070334));
#139688=CARTESIAN_POINT('Ctrl Pts',(-256.268693330519,-1.16116456022594,
126.023177910396));
#139689=CARTESIAN_POINT('Ctrl Pts',(-256.276439677387,-1.29415481023727,
126.057449579415));
#139690=CARTESIAN_POINT('Ctrl Pts',(-256.284186024255,-1.42544570139586,
126.09720780351));
#139691=CARTESIAN_POINT('Ctrl Pts',(-256.291934105829,-1.55676599364681,
126.136974931005));
#139692=CARTESIAN_POINT('Ctrl Pts',(-256.299682187402,-1.6863857956792,
126.182230945161));
#139693=CARTESIAN_POINT('Ctrl Pts',(-256.307430268976,-1.81382273267125,
126.232793035549));
#139694=CARTESIAN_POINT('Ctrl Pts',(-256.315186585161,-1.94139510882823,
126.283408863005));
#139695=CARTESIAN_POINT('Ctrl Pts',(-256.322942901347,-2.06677962164013,
126.339341887316));
#139696=CARTESIAN_POINT('Ctrl Pts',(-256.330699217532,-2.18951441834683,
126.400361335737));
#139697=CARTESIAN_POINT('Ctrl Pts',(-256.338459673442,-2.31231472144022,
126.461413351642));
#139698=CARTESIAN_POINT('Ctrl Pts',(-256.346220129352,-2.43246214816031,
126.527557012553));
#139699=CARTESIAN_POINT('Ctrl Pts',(-256.353980585262,-2.54952133943239,
126.598516587852));
#139700=CARTESIAN_POINT('Ctrl Pts',(-256.361753498706,-2.66676844090148,
126.669590071574));
#139701=CARTESIAN_POINT('Ctrl Pts',(-256.369526412149,-2.78091707468402,
126.745494701648));
#139702=CARTESIAN_POINT('Ctrl Pts',(-256.377299325593,-2.89156191943161,
126.825912084709));
#139703=CARTESIAN_POINT('Ctrl Pts',(-256.384789512593,-2.99818224702861,
126.903404422883));
#139704=CARTESIAN_POINT('Ctrl Pts',(-256.392279699593,-3.10154900471017,
126.985086738741));
#139705=CARTESIAN_POINT('Ctrl Pts',(-256.399769886592,-3.2013314782914,
127.070641315235));
#139706=CARTESIAN_POINT('Ctrl Pts',(-256.407430116474,-3.3033792223307,
127.15813815922));
#139707=CARTESIAN_POINT('Ctrl Pts',(-256.415090346355,-3.40202131093705,
127.249979901927));
#139708=CARTESIAN_POINT('Ctrl Pts',(-256.422750576237,-3.49685688824348,
127.345867453536));
#139709=CARTESIAN_POINT('Ctrl Pts',(-256.430402001156,-3.59158345789778,
127.441644788313));
#139710=CARTESIAN_POINT('Ctrl Pts',(-256.438053426075,-3.6825119332072,
127.541458404519));
#139711=CARTESIAN_POINT('Ctrl Pts',(-256.445704850994,-3.76927368310696,
127.644968434829));
#139712=CARTESIAN_POINT('Ctrl Pts',(-256.453349252676,-3.85595579445533,
127.748383453353));
#139713=CARTESIAN_POINT('Ctrl Pts',(-256.460993654357,-3.93847852763003,
127.855487833074));
#139714=CARTESIAN_POINT('Ctrl Pts',(-256.468638056039,-4.01650977625177,
127.965904650007));
#139715=CARTESIAN_POINT('Ctrl Pts',(-256.476277209502,-4.09448745298127,
128.076245660927));
#139716=CARTESIAN_POINT('Ctrl Pts',(-256.483916362964,-4.1679795463751,
128.189894258021));
#139717=CARTESIAN_POINT('Ctrl Pts',(-256.491555516427,-4.23669433217617,
128.306440643226));
#139718=CARTESIAN_POINT('Ctrl Pts',(-256.499191793952,-4.30538324868746,
128.422943151816));
#139719=CARTESIAN_POINT('Ctrl Pts',(-256.506828071476,-4.36929822806934,
128.542340933306));
#139720=CARTESIAN_POINT('Ctrl Pts',(-256.514464349001,-4.42819123600362,
128.664195801511));
#139721=CARTESIAN_POINT('Ctrl Pts',(-256.522098960068,-4.48707139177239,
128.786024077443));
#139722=CARTESIAN_POINT('Ctrl Pts',(-256.529733571135,-4.54093158425627,
128.910308008879));
#139723=CARTESIAN_POINT('Ctrl Pts',(-256.537368182202,-4.58957036579766,
129.036586050521));
#139724=CARTESIAN_POINT('Ctrl Pts',(-256.545004452601,-4.63821971865693,
129.162891537861));
#139725=CARTESIAN_POINT('Ctrl Pts',(-256.552640723,-4.68164525005835,129.291191624277));
#139726=CARTESIAN_POINT('Ctrl Pts',(-256.560276993399,-4.71969426905031,
129.421006335687));
#139727=CARTESIAN_POINT('Ctrl Pts',(-256.563428894497,-4.73539915356272,
129.47458787615));
#139728=CARTESIAN_POINT('Ctrl Pts',(-256.566580795594,-4.75018865139969,
129.528427275975));
#139729=CARTESIAN_POINT('Ctrl Pts',(-256.569732696692,-4.76405452823407,
129.582490119308));
#139730=CARTESIAN_POINT('Origin',(213.235140564004,0.,130.804360617566));
#139731=CARTESIAN_POINT('',(-258.665423831404,-4.76405452823398,129.582490119308));
#139732=CARTESIAN_POINT('',(-258.319801180437,-4.76405452823418,129.582490119309));
#139733=CARTESIAN_POINT('',(213.235140564004,-4.76405452823405,129.582490119308));
#139734=CARTESIAN_POINT('',(-256.985140564063,-4.91824826888146,130.800234100334));
#139735=CARTESIAN_POINT('Ctrl Pts',(-256.985140564063,-4.91824826888146,
130.800234100334));
#139736=CARTESIAN_POINT('Ctrl Pts',(-256.992787534705,-4.91836128350308,
130.934932184893));
#139737=CARTESIAN_POINT('Ctrl Pts',(-257.000434505347,-4.91293659407798,
131.069827034711));
#139738=CARTESIAN_POINT('Ctrl Pts',(-257.00808147599,-4.90195239602637,
131.204417825464));
#139739=CARTESIAN_POINT('Ctrl Pts',(-257.015721341468,-4.8909784039146,
131.338883561525));
#139740=CARTESIAN_POINT('Ctrl Pts',(-257.023361206947,-4.8744552100032,
131.47304540063));
#139741=CARTESIAN_POINT('Ctrl Pts',(-257.031001072426,-4.8524130586271,
131.606402119588));
#139742=CARTESIAN_POINT('Ctrl Pts',(-257.038689517819,-4.83023074695118,
131.740606819189));
#139743=CARTESIAN_POINT('Ctrl Pts',(-257.046377963213,-4.80245903531062,
131.873995709716));
#139744=CARTESIAN_POINT('Ctrl Pts',(-257.054066408607,-4.76918191165742,
132.006062309343));
#139745=CARTESIAN_POINT('Ctrl Pts',(-257.061698806436,-4.73614737302964,
132.13716616412));
#139746=CARTESIAN_POINT('Ctrl Pts',(-257.069331204265,-4.69768753437786,
132.26696654803));
#139747=CARTESIAN_POINT('Ctrl Pts',(-257.076963602095,-4.65393581023225,
132.394978276445));
#139748=CARTESIAN_POINT('Ctrl Pts',(-257.084595206406,-4.61018863482752,
132.522976695849));
#139749=CARTESIAN_POINT('Ctrl Pts',(-257.092226810717,-4.56115079839951,
132.64918644757));
#139750=CARTESIAN_POINT('Ctrl Pts',(-257.099858415028,-4.50700523503668,
132.773138632948));
#139751=CARTESIAN_POINT('Ctrl Pts',(-257.107490992867,-4.45285276457458,
132.897106630333));
#139752=CARTESIAN_POINT('Ctrl Pts',(-257.115123570707,-4.39359143362793,
133.018816119003));
#139753=CARTESIAN_POINT('Ctrl Pts',(-257.122756148546,-4.32945161927853,
133.137819796302));
#139754=CARTESIAN_POINT('Ctrl Pts',(-257.13048678299,-4.26448779336661,
133.258352327512));
#139755=CARTESIAN_POINT('Ctrl Pts',(-257.138217417433,-4.19451945678236,
133.376108660477));
#139756=CARTESIAN_POINT('Ctrl Pts',(-257.145948051877,-4.11983247940448,
133.490652374644));
#139757=CARTESIAN_POINT('Ctrl Pts',(-257.153591779927,-4.04598511951259,
133.603908409101));
#139758=CARTESIAN_POINT('Ctrl Pts',(-257.161235507977,-3.96752495530406,
133.71402339357));
#139759=CARTESIAN_POINT('Ctrl Pts',(-257.168879236027,-3.88476970613984,
133.820607854242));
#139760=CARTESIAN_POINT('Ctrl Pts',(-257.176653323668,-3.80060311157986,
133.929010054447));
#139761=CARTESIAN_POINT('Ctrl Pts',(-257.184427411309,-3.71199388470393,
134.03375987988));
#139762=CARTESIAN_POINT('Ctrl Pts',(-257.192201498949,-3.61931550348488,
134.134486493375));
#139763=CARTESIAN_POINT('Ctrl Pts',(-257.19997558659,-3.52663712226583,
134.235213106871));
#139764=CARTESIAN_POINT('Ctrl Pts',(-257.20774967423,-3.42988994053418,
134.331916252334));
#139765=CARTESIAN_POINT('Ctrl Pts',(-257.215523761871,-3.3294819563702,
134.424268484447));
#139766=CARTESIAN_POINT('Ctrl Pts',(-257.223298557193,-3.22906483198696,
134.516629123457));
#139767=CARTESIAN_POINT('Ctrl Pts',(-257.231073352515,-3.12464272484351,
134.604954364295));
#139768=CARTESIAN_POINT('Ctrl Pts',(-257.238848147837,-3.01657361527509,
134.688876891972));
#139769=CARTESIAN_POINT('Ctrl Pts',(-257.246613364855,-2.90863764345205,
134.772696029733));
#139770=CARTESIAN_POINT('Ctrl Pts',(-257.254378581874,-2.79706391473311,
134.852123009051));
#139771=CARTESIAN_POINT('Ctrl Pts',(-257.262143798892,-2.68224651844936,
134.926827922078));
#139772=CARTESIAN_POINT('Ctrl Pts',(-257.269901306206,-2.56754311875833,
135.00145866424));
#139773=CARTESIAN_POINT('Ctrl Pts',(-257.277658813519,-2.44960278596319,
135.071376458272));
#139774=CARTESIAN_POINT('Ctrl Pts',(-257.285416320832,-2.32885160599809,
135.136292433712));
#139775=CARTESIAN_POINT('Ctrl Pts',(-257.293167980352,-2.2081914511474,
135.201159473945));
#139776=CARTESIAN_POINT('Ctrl Pts',(-257.300919639872,-2.08472500956599,
135.261032016185));
#139777=CARTESIAN_POINT('Ctrl Pts',(-257.308671299391,-1.95890588475593,
135.315665395252));
#139778=CARTESIAN_POINT('Ctrl Pts',(-257.316419665594,-1.833140214598,135.370275563155));
#139779=CARTESIAN_POINT('Ctrl Pts',(-257.324168031796,-1.70502420705359,
135.419650839623));
#139780=CARTESIAN_POINT('Ctrl Pts',(-257.331916397999,-1.57503431937467,
135.463593382227));
#139781=CARTESIAN_POINT('Ctrl Pts',(-257.339663144139,-1.44507161054926,
135.507526737133));
#139782=CARTESIAN_POINT('Ctrl Pts',(-257.34740989028,-1.31323617099235,
135.546029492443));
#139783=CARTESIAN_POINT('Ctrl Pts',(-257.35515663642,-1.18002223567149,
135.578952808091));
#139784=CARTESIAN_POINT('Ctrl Pts',(-257.362903439926,-1.04680731388757,
135.61187636754));
#139785=CARTESIAN_POINT('Ctrl Pts',(-257.370650243432,-0.912214255464911,
135.639220311094));
#139786=CARTESIAN_POINT('Ctrl Pts',(-257.378397046938,-0.7767497900252,
135.66088641552));
#139787=CARTESIAN_POINT('Ctrl Pts',(-257.386145584919,-0.641254994689473,
135.682557370892));
#139788=CARTESIAN_POINT('Ctrl Pts',(-257.3938941229,-0.504888790033397,
135.698547895776));
#139789=CARTESIAN_POINT('Ctrl Pts',(-257.401642660881,-0.368164972862441,
135.708811414063));
#139790=CARTESIAN_POINT('Ctrl Pts',(-257.409399430516,-0.231295907226831,
135.719085835792));
#139791=CARTESIAN_POINT('Ctrl Pts',(-257.417156200152,-0.0940688606027882,
135.723621068002));
#139792=CARTESIAN_POINT('Ctrl Pts',(-257.424912969787,0.0429998485669047,
135.722422641933));
#139793=CARTESIAN_POINT('Ctrl Pts',(-257.432673878259,0.180141694477021,
135.721223576412));
#139794=CARTESIAN_POINT('Ctrl Pts',(-257.44043478673,0.317124644366466,
135.714284776344));
#139795=CARTESIAN_POINT('Ctrl Pts',(-257.448195695201,0.45343654122407,
135.701663790291));
#139796=CARTESIAN_POINT('Ctrl Pts',(-257.455969055081,0.589967133498706,
135.689022555442));
#139797=CARTESIAN_POINT('Ctrl Pts',(-257.46374241496,0.725824133687792,
135.670680969544));
#139798=CARTESIAN_POINT('Ctrl Pts',(-257.47151577484,0.860503737315126,
135.646748084567));
#139799=CARTESIAN_POINT('Ctrl Pts',(-257.479000978455,0.990190805907493,
135.623702384906));
#139800=CARTESIAN_POINT('Ctrl Pts',(-257.48648618207,1.11878592285715,135.595472640323));
#139801=CARTESIAN_POINT('Ctrl Pts',(-257.493971385684,1.24585361515672,
135.562199605184));
#139802=CARTESIAN_POINT('Ctrl Pts',(-257.501744289864,1.37780526903188,
135.527647690873));
#139803=CARTESIAN_POINT('Ctrl Pts',(-257.509517194043,1.50852789871494,
135.487547546984));
#139804=CARTESIAN_POINT('Ctrl Pts',(-257.517290098223,1.63751915163922,
135.442001622486));
#139805=CARTESIAN_POINT('Ctrl Pts',(-257.525053419543,1.76635137712096,
135.396511849485));
#139806=CARTESIAN_POINT('Ctrl Pts',(-257.532816740863,1.89345610764402,
135.345589783312));
#139807=CARTESIAN_POINT('Ctrl Pts',(-257.540580062182,2.01834292803111,
135.289388475603));
#139808=CARTESIAN_POINT('Ctrl Pts',(-257.54833567123,2.14310568281374,135.23324299964));
#139809=CARTESIAN_POINT('Ctrl Pts',(-257.556091280278,2.26565455778836,
135.171828878374));
#139810=CARTESIAN_POINT('Ctrl Pts',(-257.563846889326,2.38551635535023,
135.105348269357));
#139811=CARTESIAN_POINT('Ctrl Pts',(-257.571596649984,2.50528776691088,
135.03891779238));
#139812=CARTESIAN_POINT('Ctrl Pts',(-257.579346410642,2.62237579357889,
134.967428621133));
#139813=CARTESIAN_POINT('Ctrl Pts',(-257.5870961713,2.73632954467773,134.891129963324));
#139814=CARTESIAN_POINT('Ctrl Pts',(-257.594842644384,2.8502349547566,134.814863672636));
#139815=CARTESIAN_POINT('Ctrl Pts',(-257.602589117469,2.96100840939698,
134.733792170391));
#139816=CARTESIAN_POINT('Ctrl Pts',(-257.610335590554,3.06822605017053,
134.648209205577));
#139817=CARTESIAN_POINT('Ctrl Pts',(-257.618080447319,3.17542131973774,
134.562644097844));
#139818=CARTESIAN_POINT('Ctrl Pts',(-257.625825304084,3.27906194566963,
134.472569643717));
#139819=CARTESIAN_POINT('Ctrl Pts',(-257.633570160849,3.37875568273299,
134.378321039689));
#139820=CARTESIAN_POINT('Ctrl Pts',(-257.641315080479,3.47845022900745,
134.284071670648));
#139821=CARTESIAN_POINT('Ctrl Pts',(-257.649060000109,3.57419753827989,
134.185648352807));
#139822=CARTESIAN_POINT('Ctrl Pts',(-257.656804919739,3.66564119490863,
134.083424156549));
#139823=CARTESIAN_POINT('Ctrl Pts',(-257.664551581105,3.75710541607468,
133.981176971345));
#139824=CARTESIAN_POINT('Ctrl Pts',(-257.672298242471,3.84426379800583,
133.875127498292));
#139825=CARTESIAN_POINT('Ctrl Pts',(-257.680044903836,3.92679955720989,
133.765682670298));
#139826=CARTESIAN_POINT('Ctrl Pts',(-257.687799818904,4.00942325436452,
133.656121234012));
#139827=CARTESIAN_POINT('Ctrl Pts',(-257.695554733971,4.08741425434609,
133.543157529048));
#139828=CARTESIAN_POINT('Ctrl Pts',(-257.703309649038,4.16049825033351,
133.427228775036));
#139829=CARTESIAN_POINT('Ctrl Pts',(-257.711068711982,4.23362133680738,
133.311238014133));
#139830=CARTESIAN_POINT('Ctrl Pts',(-257.718827774927,4.30183199513327,
133.192279383277));
#139831=CARTESIAN_POINT('Ctrl Pts',(-257.726586837871,4.36490193450261,
133.070814712551));
#139832=CARTESIAN_POINT('Ctrl Pts',(-257.734358386394,4.42807336354529,
132.94915458564));
#139833=CARTESIAN_POINT('Ctrl Pts',(-257.742129934918,4.48608737743533,
132.82498071497));
#139834=CARTESIAN_POINT('Ctrl Pts',(-257.749901483442,4.53876353342889,
132.698775738419));
#139835=CARTESIAN_POINT('Ctrl Pts',(-257.75740732546,4.58963871020913,132.576885665549));
#139836=CARTESIAN_POINT('Ctrl Pts',(-257.764913167478,4.63553498217158,
132.453101406161));
#139837=CARTESIAN_POINT('Ctrl Pts',(-257.772419009496,4.67633451815619,
132.327869244651));
#139838=CARTESIAN_POINT('Ctrl Pts',(-257.780194620124,4.71860043647074,
132.198136094971));
#139839=CARTESIAN_POINT('Ctrl Pts',(-257.787970230752,4.75553046150047,
132.066437493625));
#139840=CARTESIAN_POINT('Ctrl Pts',(-257.79574584138,4.78693929394865,131.933251780854));
#139841=CARTESIAN_POINT('Ctrl Pts',(-257.803511864073,4.8183093968543,131.800230296465));
#139842=CARTESIAN_POINT('Ctrl Pts',(-257.811277886767,4.84417176442526,
131.665725725988));
#139843=CARTESIAN_POINT('Ctrl Pts',(-257.81904390946,4.86439012903196,131.530233702255));
#139844=CARTESIAN_POINT('Ctrl Pts',(-257.826802212121,4.88458839500891,
131.394876368151));
#139845=CARTESIAN_POINT('Ctrl Pts',(-257.834560514782,4.89915376608289,
131.258533918293));
#139846=CARTESIAN_POINT('Ctrl Pts',(-257.842318817444,4.90800059843263,
131.121714029845));
#139847=CARTESIAN_POINT('Ctrl Pts',(-257.850071261287,4.91684074994213,
130.984997463329));
#139848=CARTESIAN_POINT('Ctrl Pts',(-257.85782370513,4.91997093328085,130.847804564311));
#139849=CARTESIAN_POINT('Ctrl Pts',(-257.865576148974,4.91735714788234,
130.710649664788));
#139850=CARTESIAN_POINT('Ctrl Pts',(-257.873325280157,4.91474447936821,
130.573553372283));
#139851=CARTESIAN_POINT('Ctrl Pts',(-257.88107441134,4.90639273133353,130.436495436918));
#139852=CARTESIAN_POINT('Ctrl Pts',(-257.888823542523,4.89231998862875,
130.299991515257));
#139853=CARTESIAN_POINT('Ctrl Pts',(-257.896571041791,4.87825020954869,
130.163516340402));
#139854=CARTESIAN_POINT('Ctrl Pts',(-257.90431854106,4.85846187230104,130.027595335706));
#139855=CARTESIAN_POINT('Ctrl Pts',(-257.912066040328,4.83302501993536,
129.892739962261));
#139856=CARTESIAN_POINT('Ctrl Pts',(-257.91981358446,4.80758802027207,129.757883807906));
#139857=CARTESIAN_POINT('Ctrl Pts',(-257.927561128591,4.77650251262282,
129.624093681182));
#139858=CARTESIAN_POINT('Ctrl Pts',(-257.935308672723,4.7398897713283,129.491871372598));
#139859=CARTESIAN_POINT('Ctrl Pts',(-257.94305793817,4.70326889557698,129.359619687446));
#139860=CARTESIAN_POINT('Ctrl Pts',(-257.950807203617,4.66111844684277,
129.228936890161));
#139861=CARTESIAN_POINT('Ctrl Pts',(-257.958556469064,4.6136096127303,129.100309736922));
#139862=CARTESIAN_POINT('Ctrl Pts',(-257.966313941403,4.56605046418237,
128.971546360543));
#139863=CARTESIAN_POINT('Ctrl Pts',(-257.974071413743,4.51312172979363,
128.844843344298));
#139864=CARTESIAN_POINT('Ctrl Pts',(-257.981828886083,4.45504303968147,
128.720668083365));
#139865=CARTESIAN_POINT('Ctrl Pts',(-257.989590484902,4.39693345542028,
128.596426769134));
#139866=CARTESIAN_POINT('Ctrl Pts',(-257.997352083721,4.33366863695595,
128.474716236107));
#139867=CARTESIAN_POINT('Ctrl Pts',(-258.00511368254,4.26551379943042,128.355978480446));
#139868=CARTESIAN_POINT('Ctrl Pts',(-258.01288770478,4.19724987146726,128.237050669989));
#139869=CARTESIAN_POINT('Ctrl Pts',(-258.020661727019,4.12408049208502,
128.121105476245));
#139870=CARTESIAN_POINT('Ctrl Pts',(-258.028435749259,4.04631425159911,
128.008555896237));
#139871=CARTESIAN_POINT('Ctrl Pts',(-258.035912710609,3.9715196142071,127.900307060074));
#139872=CARTESIAN_POINT('Ctrl Pts',(-258.04338967196,3.89247317935221,127.795199323993));
#139873=CARTESIAN_POINT('Ctrl Pts',(-258.05086663331,3.80948286040464,127.693569175058));
#139874=CARTESIAN_POINT('Ctrl Pts',(-258.058643465866,3.72316412958299,
127.587863044745));
#139875=CARTESIAN_POINT('Ctrl Pts',(-258.066420298421,3.6323063418413,127.485585869392));
#139876=CARTESIAN_POINT('Ctrl Pts',(-258.074197130977,3.53721205379093,
127.387152115145));
#139877=CARTESIAN_POINT('Ctrl Pts',(-258.081964402288,3.44223467962177,
127.288839380493));
#139878=CARTESIAN_POINT('Ctrl Pts',(-258.0897316736,3.34303143766935,127.194360943156));
#139879=CARTESIAN_POINT('Ctrl Pts',(-258.097498944911,3.23994592104352,
127.104099344194));
#139880=CARTESIAN_POINT('Ctrl Pts',(-258.105258521243,3.13696253050272,
127.013927166754));
#139881=CARTESIAN_POINT('Ctrl Pts',(-258.113018097574,3.03010481143685,
126.927963769676));
#139882=CARTESIAN_POINT('Ctrl Pts',(-258.120777673905,2.91975383782572,
126.846555595966));
#139883=CARTESIAN_POINT('Ctrl Pts',(-258.128531414864,2.80948585058243,
126.765208642999));
#139884=CARTESIAN_POINT('Ctrl Pts',(-258.136285155823,2.69573015088393,
126.688410325789));
#139885=CARTESIAN_POINT('Ctrl Pts',(-258.144038896781,2.57890131011219,
126.616467221692));
#139886=CARTESIAN_POINT('Ctrl Pts',(-258.151789355802,2.46212191966585,
126.544554569065));
#139887=CARTESIAN_POINT('Ctrl Pts',(-258.159539814823,2.34227230728373,
126.477493246544));
#139888=CARTESIAN_POINT('Ctrl Pts',(-258.167290273843,2.21979629815279,
126.415546716612));
#139889=CARTESIAN_POINT('Ctrl Pts',(-258.175039119409,2.09734578551536,
126.353613082424));
#139890=CARTESIAN_POINT('Ctrl Pts',(-258.182787964974,1.97227031206583,
126.296792299111));
#139891=CARTESIAN_POINT('Ctrl Pts',(-258.19053681054,1.84503824287365,126.245301839174));
#139892=CARTESIAN_POINT('Ctrl Pts',(-258.198285718053,1.71780515653942,
126.193810967602));
#139893=CARTESIAN_POINT('Ctrl Pts',(-258.206034625566,1.58841580221056,
126.147650650974));
#139894=CARTESIAN_POINT('Ctrl Pts',(-258.213783533079,1.4573580867132,126.106990026523));
#139895=CARTESIAN_POINT('Ctrl Pts',(-258.221534177625,1.32627099267363,
126.066320287388));
#139896=CARTESIAN_POINT('Ctrl Pts',(-258.229284822171,1.19351516631886,
126.031152809411));
#139897=CARTESIAN_POINT('Ctrl Pts',(-258.237035466717,1.05959283264569,
126.001606606428));
#139898=CARTESIAN_POINT('Ctrl Pts',(-258.24479433493,0.925528403350393,
125.972029054035));
#139899=CARTESIAN_POINT('Ctrl Pts',(-258.252553203143,0.790295376400809,
125.948084775374));
#139900=CARTESIAN_POINT('Ctrl Pts',(-258.260312071356,0.654405862237226,
125.929841561293));
#139901=CARTESIAN_POINT('Ctrl Pts',(-258.268075077377,0.518443878131305,
125.911588618097));
#139902=CARTESIAN_POINT('Ctrl Pts',(-258.275838083398,0.381825098035721,
125.899042833517));
#139903=CARTESIAN_POINT('Ctrl Pts',(-258.283601089419,0.245064894361125,
125.892219917214));
#139904=CARTESIAN_POINT('Ctrl Pts',(-258.291376523712,0.108085742901093,
125.885386077687));
#139905=CARTESIAN_POINT('Ctrl Pts',(-258.299151958005,-0.0290348936966784,
125.884293418368));
#139906=CARTESIAN_POINT('Ctrl Pts',(-258.306927392298,-0.165782603154849,
125.888905481875));
#139907=CARTESIAN_POINT('Ctrl Pts',(-258.314389680573,-0.297022967417457,
125.893331800217));
#139908=CARTESIAN_POINT('Ctrl Pts',(-258.321851968847,-0.42791956262217,
125.903012206386));
#139909=CARTESIAN_POINT('Ctrl Pts',(-258.329314257122,-0.558025608205252,
125.917870007416));
#139910=CARTESIAN_POINT('Ctrl Pts',(-258.337078965247,-0.693404386406557,
125.933329941972));
#139911=CARTESIAN_POINT('Ctrl Pts',(-258.344843673372,-0.828357737740643,
125.95444493456));
#139912=CARTESIAN_POINT('Ctrl Pts',(-258.352608381497,-0.962374722353744,
125.981185526791));
#139913=CARTESIAN_POINT('Ctrl Pts',(-258.36036349259,-1.09622606452778,
126.007893068159));
#139914=CARTESIAN_POINT('Ctrl Pts',(-258.368118603684,-1.22914296192161,
126.040212299277));
#139915=CARTESIAN_POINT('Ctrl Pts',(-258.375873714777,-1.36061904066752,
126.078061971831));
#139916=CARTESIAN_POINT('Ctrl Pts',(-258.383621107811,-1.49196427147542,
126.115873975544));
#139917=CARTESIAN_POINT('Ctrl Pts',(-258.391368500844,-1.62187116284061,
126.159205360274));
#139918=CARTESIAN_POINT('Ctrl Pts',(-258.399115893877,-1.74984335866182,
126.20792381471));
#139919=CARTESIAN_POINT('Ctrl Pts',(-258.406857441036,-1.87771899175559,
126.25660550814));
#139920=CARTESIAN_POINT('Ctrl Pts',(-258.414598988195,-2.00366247002254,
126.310666041904));
#139921=CARTESIAN_POINT('Ctrl Pts',(-258.422340535354,-2.12719279761935,
126.369923351773));
#139922=CARTESIAN_POINT('Ctrl Pts',(-258.430078827125,-2.25067117965424,
126.429155743434));
#139923=CARTESIAN_POINT('Ctrl Pts',(-258.437817118897,-2.37173807634447,
126.493580396106));
#139924=CARTESIAN_POINT('Ctrl Pts',(-258.445555410669,-2.48993289461645,
126.562967303712));
#139925=CARTESIAN_POINT('Ctrl Pts',(-258.453292106575,-2.60810333760513,
126.632339901676));
#139926=CARTESIAN_POINT('Ctrl Pts',(-258.461028802482,-2.72340254235218,
126.706672520862));
#139927=CARTESIAN_POINT('Ctrl Pts',(-258.468765498388,-2.83539530810336,
126.785689629629));
#139928=CARTESIAN_POINT('Ctrl Pts',(-258.476502285018,-2.94738938713674,
126.86470766499));
#139929=CARTESIAN_POINT('Ctrl Pts',(-258.484239071649,-3.05607662954166,
126.948410073452));
#139930=CARTESIAN_POINT('Ctrl Pts',(-258.491975858279,-3.16105191900665,
127.03647874205));
#139931=CARTESIAN_POINT('Ctrl Pts',(-258.499714421935,-3.2660513197487,
127.124567638723));
#139932=CARTESIAN_POINT('Ctrl Pts',(-258.507452985592,-3.36733677080673,
127.217024539132));
#139933=CARTESIAN_POINT('Ctrl Pts',(-258.515191549248,-3.46453758341159,
127.313492187558));
#139934=CARTESIAN_POINT('Ctrl Pts',(-258.522938467807,-3.56184333840171,
127.410063986812));
#139935=CARTESIAN_POINT('Ctrl Pts',(-258.530685386366,-3.65505536697492,
127.510654907398));
#139936=CARTESIAN_POINT('Ctrl Pts',(-258.538432304925,-3.74384073218759,
127.614871687578));
#139937=CARTESIAN_POINT('Ctrl Pts',(-258.546183413452,-3.83267411749838,
127.719144834031));
#139938=CARTESIAN_POINT('Ctrl Pts',(-258.553934521978,-3.91707582783379,
127.827047438742));
#139939=CARTESIAN_POINT('Ctrl Pts',(-258.561685630505,-3.99675500185125,
127.93815537061));
#139940=CARTESIAN_POINT('Ctrl Pts',(-258.56944937751,-4.07656409580551,
128.049444468205));
#139941=CARTESIAN_POINT('Ctrl Pts',(-258.577213124515,-4.15163505097128,
128.163949008845));
#139942=CARTESIAN_POINT('Ctrl Pts',(-258.58497687152,-4.22172142935844,
128.281217491345));
#139943=CARTESIAN_POINT('Ctrl Pts',(-258.592571874658,-4.29028449091672,
128.395937161123));
#139944=CARTESIAN_POINT('Ctrl Pts',(-258.600166877797,-4.35407734153579,
128.513301519617));
#139945=CARTESIAN_POINT('Ctrl Pts',(-258.607761880935,-4.41291389643242,
128.632869423669));
#139946=CARTESIAN_POINT('Ctrl Pts',(-258.616142080685,-4.47783316948833,
128.764798654153));
#139947=CARTESIAN_POINT('Ctrl Pts',(-258.624522280435,-4.53690193565634,
128.899782543912));
#139948=CARTESIAN_POINT('Ctrl Pts',(-258.632902480184,-4.58984492952747,
129.037299049484));
#139949=CARTESIAN_POINT('Ctrl Pts',(-258.641261557762,-4.64265448135215,
129.174468946703));
#139950=CARTESIAN_POINT('Ctrl Pts',(-258.64962063534,-4.68936894459055,
129.314158454846));
#139951=CARTESIAN_POINT('Ctrl Pts',(-258.657979712918,-4.72976019490264,
129.455823795223));
#139952=CARTESIAN_POINT('Ctrl Pts',(-258.660461085747,-4.74175024405593,
129.497876823573));
#139953=CARTESIAN_POINT('Ctrl Pts',(-258.662942458575,-4.75318341178602,
129.54010380127));
#139954=CARTESIAN_POINT('Ctrl Pts',(-258.665423831404,-4.76405452823398,
129.582490119308));
#139955=CARTESIAN_POINT('Ctrl Pts',(-256.915106732785,-4.76405452823404,
129.582490119308));
#139956=CARTESIAN_POINT('Ctrl Pts',(-256.922429867876,-4.79606782357288,
129.707309471965));
#139957=CARTESIAN_POINT('Ctrl Pts',(-256.929753002967,-4.8231322264902,
129.833231074052));
#139958=CARTESIAN_POINT('Ctrl Pts',(-256.937076138058,-4.84519862184994,
129.959829163253));
#139959=CARTESIAN_POINT('Ctrl Pts',(-256.949180993161,-4.88167350796509,
130.169090839695));
#139960=CARTESIAN_POINT('Ctrl Pts',(-256.961285848263,-4.90459890573453,
130.380778486436));
#139961=CARTESIAN_POINT('Ctrl Pts',(-256.973390703365,-4.91372733444181,
130.593489222495));
#139962=CARTESIAN_POINT('Ctrl Pts',(-256.977307323581,-4.91668090869941,
130.66231343907));
#139963=CARTESIAN_POINT('Ctrl Pts',(-256.981223943798,-4.91819038511672,
130.731244526239));
#139964=CARTESIAN_POINT('Ctrl Pts',(-256.985140564014,-4.91824826888074,
130.800234099472));
#139965=CARTESIAN_POINT('',(-256.639859435963,-4.9182486809668,130.807962654264));
#139966=CARTESIAN_POINT('Ctrl Pts',(-256.569732696692,-4.76405452823407,
129.582490119308));
#139967=CARTESIAN_POINT('Ctrl Pts',(-256.577375070971,-4.79767494244943,
129.713575604073));
#139968=CARTESIAN_POINT('Ctrl Pts',(-256.585017445249,-4.82586170849428,
129.84597521023));
#139969=CARTESIAN_POINT('Ctrl Pts',(-256.592659819528,-4.84853379240785,
129.979192073341));
#139970=CARTESIAN_POINT('Ctrl Pts',(-256.600526422267,-4.87187107882093,
130.116317540118));
#139971=CARTESIAN_POINT('Ctrl Pts',(-256.608393025006,-4.88936503882379,
130.254308498874));
#139972=CARTESIAN_POINT('Ctrl Pts',(-256.616259627745,-4.90098477109259,
130.392618785809));
#139973=CARTESIAN_POINT('Ctrl Pts',(-256.624126230484,-4.91260450336143,
130.530929072745));
#139974=CARTESIAN_POINT('Ctrl Pts',(-256.631992833224,-4.91835004587602,
130.66955822564));
#139975=CARTESIAN_POINT('Ctrl Pts',(-256.639859435963,-4.9182486809668,
130.807962654264));
#139976=CARTESIAN_POINT('Ctrl Pts',(-256.639859435997,-4.91824868096635,
130.807962654868));
#139977=CARTESIAN_POINT('Ctrl Pts',(-256.6526454608,-4.91808392694182,131.032919032592));
#139978=CARTESIAN_POINT('Ctrl Pts',(-256.665431485602,-4.90248437098539,
131.257319986635));
#139979=CARTESIAN_POINT('Ctrl Pts',(-256.678217510405,-4.87168150318488,
131.479566063357));
#139980=CARTESIAN_POINT('Ctrl Pts',(-256.685991856725,-4.85295229175362,
131.614699382361));
#139981=CARTESIAN_POINT('Ctrl Pts',(-256.693766203044,-4.82856655252723,
131.749266871525));
#139982=CARTESIAN_POINT('Ctrl Pts',(-256.701540549363,-4.7985668010147,
131.882757445593));
#139983=CARTESIAN_POINT('Ctrl Pts',(-256.709305314317,-4.76860402220363,
132.016083501394));
#139984=CARTESIAN_POINT('Ctrl Pts',(-256.71707007927,-4.73304108255198,
132.148334905095));
#139985=CARTESIAN_POINT('Ctrl Pts',(-256.724834844224,-4.69197215476163,
132.279006460283));
#139986=CARTESIAN_POINT('Ctrl Pts',(-256.732591896912,-4.65094401822101,
132.40954822742));
#139987=CARTESIAN_POINT('Ctrl Pts',(-256.740348949601,-4.60442089308742,
132.538512898194));
#139988=CARTESIAN_POINT('Ctrl Pts',(-256.748106002289,-4.55254774579543,
132.665406582811));
#139989=CARTESIAN_POINT('Ctrl Pts',(-256.75585720512,-4.5007137178118,132.792204572575));
#139990=CARTESIAN_POINT('Ctrl Pts',(-256.76360840795,-4.4435378457051,132.916934324425));
#139991=CARTESIAN_POINT('Ctrl Pts',(-256.771359610781,-4.38121444901763,
133.039118549473));
#139992=CARTESIAN_POINT('Ctrl Pts',(-256.779107518787,-4.31891754429999,
133.161250837351));
#139993=CARTESIAN_POINT('Ctrl Pts',(-256.786855426793,-4.25147764418569,
133.280839402966));
#139994=CARTESIAN_POINT('Ctrl Pts',(-256.7946033348,-4.17913648783132,133.397428545442));
#139995=CARTESIAN_POINT('Ctrl Pts',(-256.802349621893,-4.10681046572665,
133.513993296696));
#139996=CARTESIAN_POINT('Ctrl Pts',(-256.810095908985,-4.02958543290878,
133.627559540941));
#139997=CARTESIAN_POINT('Ctrl Pts',(-256.817842196078,-3.94774801793461,
133.73769807674));
#139998=CARTESIAN_POINT('Ctrl Pts',(-256.825588540122,-3.86591000128596,
133.847837422285));
#139999=CARTESIAN_POINT('Ctrl Pts',(-256.833334884166,-3.77945976799264,
133.95454869528));
#140000=CARTESIAN_POINT('Ctrl Pts',(-256.84108122821,-3.6887257863977,134.057433800767));
#140001=CARTESIAN_POINT('Ctrl Pts',(-256.848829306752,-3.59797148838824,
134.16034194345));
#140002=CARTESIAN_POINT('Ctrl Pts',(-256.856577385294,-3.50293179196144,
134.259421920673));
#140003=CARTESIAN_POINT('Ctrl Pts',(-256.864325463836,-3.40397347246881,
134.35431099204));
#140004=CARTESIAN_POINT('Ctrl Pts',(-256.872081776682,-3.30490998459592,
134.449300907176));
#140005=CARTESIAN_POINT('Ctrl Pts',(-256.879838089528,-3.20191983719705,
134.540090748283));
#140006=CARTESIAN_POINT('Ctrl Pts',(-256.887594402374,-3.09540489790895,
134.626356376394));
#140007=CARTESIAN_POINT('Ctrl Pts',(-256.895354854772,-2.98883311149377,
134.712668044555));
#140008=CARTESIAN_POINT('Ctrl Pts',(-256.90311530717,-2.87873309846759,
134.794450455455));
#140009=CARTESIAN_POINT('Ctrl Pts',(-256.910875759568,-2.76553660397908,
134.871422254));
#140010=CARTESIAN_POINT('Ctrl Pts',(-256.918648669242,-2.65215840358668,
134.948517609642));
#140011=CARTESIAN_POINT('Ctrl Pts',(-256.926421578916,-2.53567412139693,
135.020786715443));
#140012=CARTESIAN_POINT('Ctrl Pts',(-256.93419448859,-2.41654181946556,
135.087993269565));
#140013=CARTESIAN_POINT('Ctrl Pts',(-256.9416847038,-2.30174226340984,135.15275557544));
#140014=CARTESIAN_POINT('Ctrl Pts',(-256.949174919009,-2.1844842287566,
135.212817034756));
#140015=CARTESIAN_POINT('Ctrl Pts',(-256.956665134218,-2.06519415639283,
135.268008919001));
#140016=CARTESIAN_POINT('Ctrl Pts',(-256.964439548882,-1.9413778891806,
135.325294935785));
#140017=CARTESIAN_POINT('Ctrl Pts',(-256.972213963546,-1.81498016000566,
135.377515999124));
#140018=CARTESIAN_POINT('Ctrl Pts',(-256.97998837821,-1.68645395088644,
135.424431627198));
#140019=CARTESIAN_POINT('Ctrl Pts',(-256.987753212107,-1.55808613049318,
135.471289438997));
#140020=CARTESIAN_POINT('Ctrl Pts',(-256.995518046004,-1.4275954129211,
135.512854691697));
#140021=CARTESIAN_POINT('Ctrl Pts',(-257.003282879901,-1.2954577469346,
135.5489335476));
#140022=CARTESIAN_POINT('Ctrl Pts',(-257.011040002054,-1.1634513151737,
135.584976571322));
#140023=CARTESIAN_POINT('Ctrl Pts',(-257.018797124206,-1.02980156480316,
135.61554393947));
#140024=CARTESIAN_POINT('Ctrl Pts',(-257.026554246358,-0.895002386540549,
135.640490660336));
#140025=CARTESIAN_POINT('Ctrl Pts',(-257.034305519096,-0.760304856319965,
135.665418569624));
#140026=CARTESIAN_POINT('Ctrl Pts',(-257.042056791834,-0.624460006293084,
135.68473419698));
#140027=CARTESIAN_POINT('Ctrl Pts',(-257.049808064571,-0.487974436285498,
135.698343046226));
#140028=CARTESIAN_POINT('Ctrl Pts',(-257.057556042907,-0.351546874596144,
135.711946111517));
#140029=CARTESIAN_POINT('Ctrl Pts',(-257.065304021244,-0.214479522753159,
135.719847184052));
#140030=CARTESIAN_POINT('Ctrl Pts',(-257.07305199958,-0.0772864488981899,
135.72200333205));
#140031=CARTESIAN_POINT('Ctrl Pts',(-257.080798357249,0.0598779278858586,
135.72415902904));
#140032=CARTESIAN_POINT('Ctrl Pts',(-257.088544714918,0.197167583714288,
135.720572185566));
#140033=CARTESIAN_POINT('Ctrl Pts',(-257.096291072587,0.334066481811716,
135.711251960181));
#140034=CARTESIAN_POINT('Ctrl Pts',(-257.104037487386,0.470966389553566,
135.701931666059));
#140035=CARTESIAN_POINT('Ctrl Pts',(-257.111783902185,0.607475143760713,
135.686877932206));
#140036=CARTESIAN_POINT('Ctrl Pts',(-257.119530316984,0.743080263342752,
135.666151931961));
#140037=CARTESIAN_POINT('Ctrl Pts',(-257.127278466393,0.878715748189702,
135.645421290665));
#140038=CARTESIAN_POINT('Ctrl Pts',(-257.135026615802,1.01344680937286,
135.619015914566));
#140039=CARTESIAN_POINT('Ctrl Pts',(-257.142774765211,1.14677000495776,
135.587048315736));
#140040=CARTESIAN_POINT('Ctrl Pts',(-257.150531148695,1.28023488511363,
135.555046744457));
#140041=CARTESIAN_POINT('Ctrl Pts',(-257.158287532179,1.41228853014399,
135.517471233775));
#140042=CARTESIAN_POINT('Ctrl Pts',(-257.166043915663,1.54244100652532,
135.474484684857));
#140043=CARTESIAN_POINT('Ctrl Pts',(-257.173804438687,1.67266294457373,
135.431475194252));
#140044=CARTESIAN_POINT('Ctrl Pts',(-257.181564961711,1.80098132661255,
135.383049049112));
#140045=CARTESIAN_POINT('Ctrl Pts',(-257.189325484734,1.92692606489398,
135.329417413114));
#140046=CARTESIAN_POINT('Ctrl Pts',(-257.197098464293,2.05307295901443,
135.27569969215));
#140047=CARTESIAN_POINT('Ctrl Pts',(-257.204871443852,2.1768382426607,135.21675995174));
#140048=CARTESIAN_POINT('Ctrl Pts',(-257.21264442341,2.29777550775867,135.152855849074));
#140049=CARTESIAN_POINT('Ctrl Pts',(-257.220133868284,2.41430134875486,
135.091282773974));
#140050=CARTESIAN_POINT('Ctrl Pts',(-257.227623313158,2.52820162523055,
135.02510135035));
#140051=CARTESIAN_POINT('Ctrl Pts',(-257.235112758031,2.63910399638473,
134.95457906468));
#140052=CARTESIAN_POINT('Ctrl Pts',(-257.242886884259,2.75422187852779,
134.881376155799));
#140053=CARTESIAN_POINT('Ctrl Pts',(-257.250661010486,2.86647411356299,
134.803263961844));
#140054=CARTESIAN_POINT('Ctrl Pts',(-257.258435136714,2.97541354663934,
134.720493568447));
#140055=CARTESIAN_POINT('Ctrl Pts',(-257.266199681633,3.08421871609441,
134.637825186346));
#140056=CARTESIAN_POINT('Ctrl Pts',(-257.273964226551,3.18971889900276,
134.550510262036));
#140057=CARTESIAN_POINT('Ctrl Pts',(-257.28172877147,3.29149376730582,134.458844417268));
#140058=CARTESIAN_POINT('Ctrl Pts',(-257.289485604404,3.39316754967603,
134.367269617841));
#140059=CARTESIAN_POINT('Ctrl Pts',(-257.297242437338,3.49112309215199,
134.271352757835));
#140060=CARTESIAN_POINT('Ctrl Pts',(-257.304999270271,3.58497146246548,
134.171430957759));
#140061=CARTESIAN_POINT('Ctrl Pts',(-257.312750253849,3.6787490625934,134.071584507786));
#140062=CARTESIAN_POINT('Ctrl Pts',(-257.320501237427,3.76842538871227,
133.967739412882));
#140063=CARTESIAN_POINT('Ctrl Pts',(-257.328252221005,3.85364712108406,
133.860270781275));
#140064=CARTESIAN_POINT('Ctrl Pts',(-257.335999911282,3.93883264375147,
133.752847811816));
#140065=CARTESIAN_POINT('Ctrl Pts',(-257.343747601559,4.01956709467813,
133.641804673502));
#140066=CARTESIAN_POINT('Ctrl Pts',(-257.351495291836,4.09553649901408,
133.52755063072));
#140067=CARTESIAN_POINT('Ctrl Pts',(-257.359241362153,4.17149001895948,
133.413320477238));
#140068=CARTESIAN_POINT('Ctrl Pts',(-257.366987432471,4.24268025769708,
133.295881080046));
#140069=CARTESIAN_POINT('Ctrl Pts',(-257.374733502789,4.30883600091209,
133.175671516572));
#140070=CARTESIAN_POINT('Ctrl Pts',(-257.382479631211,4.37499224037473,
133.055461051381));
#140071=CARTESIAN_POINT('Ctrl Pts',(-257.390225759633,4.43611372044746,
132.932480720985));
#140072=CARTESIAN_POINT('Ctrl Pts',(-257.397971888056,4.49197491009745,
132.807194726911));
#140073=CARTESIAN_POINT('Ctrl Pts',(-257.40571975233,4.54784861783948,132.681880657143));
#140074=CARTESIAN_POINT('Ctrl Pts',(-257.413467616605,4.59845953030864,
132.55426025259));
#140075=CARTESIAN_POINT('Ctrl Pts',(-257.421215480879,4.64363019511848,
132.424817859669));
#140076=CARTESIAN_POINT('Ctrl Pts',(-257.428971582797,4.68884888604488,
132.295237841688));
#140077=CARTESIAN_POINT('Ctrl Pts',(-257.436727684715,4.72861564582192,
132.163832335389));
#140078=CARTESIAN_POINT('Ctrl Pts',(-257.444483786632,4.7628027175212,132.031101558626));
#140079=CARTESIAN_POINT('Ctrl Pts',(-257.452244029583,4.79700804191968,
131.898299916041));
#140080=CARTESIAN_POINT('Ctrl Pts',(-257.460004272534,4.82562766072816,
131.764171975294));
#140081=CARTESIAN_POINT('Ctrl Pts',(-257.467764515485,4.84858514897815,
131.629227343534));
#140082=CARTESIAN_POINT('Ctrl Pts',(-257.475537220362,4.87157950392382,
131.494066008508));
#140083=CARTESIAN_POINT('Ctrl Pts',(-257.483309925238,4.88889350892239,
131.358085749759));
#140084=CARTESIAN_POINT('Ctrl Pts',(-257.491082630115,4.90050265488211,
131.221801382218));
#140085=CARTESIAN_POINT('Ctrl Pts',(-257.498575214025,4.91169341814975,
131.090428574991));
#140086=CARTESIAN_POINT('Ctrl Pts',(-257.506067797935,4.9175834303487,130.958773509831));
#140087=CARTESIAN_POINT('Ctrl Pts',(-257.513560381844,4.91819652859018,
130.827294624271));
#140088=CARTESIAN_POINT('Ctrl Pts',(-257.521334853192,4.91883269293202,
130.690869214703));
#140089=CARTESIAN_POINT('Ctrl Pts',(-257.52910932454,4.91378912490896,130.554201241754));
#140090=CARTESIAN_POINT('Ctrl Pts',(-257.536883795887,4.90303538749604,
130.417802664005));
#140091=CARTESIAN_POINT('Ctrl Pts',(-257.544648684898,4.89229490448109,
130.281572202787));
#140092=CARTESIAN_POINT('Ctrl Pts',(-257.552413573909,4.87585828604941,
130.145610862108));
#140093=CARTESIAN_POINT('Ctrl Pts',(-257.560178462919,4.85374706526777,
130.010432101323));
#140094=CARTESIAN_POINT('Ctrl Pts',(-257.567935638579,4.83165780894596,
129.875387622062));
#140095=CARTESIAN_POINT('Ctrl Pts',(-257.57569281424,4.8039052307422,129.741124558989));
#140096=CARTESIAN_POINT('Ctrl Pts',(-257.5834499899,4.7705627478743,129.608152386908));
#140097=CARTESIAN_POINT('Ctrl Pts',(-257.591201314504,4.73724541446206,
129.475280512629));
#140098=CARTESIAN_POINT('Ctrl Pts',(-257.598952639107,4.69834666345011,
129.343697968952));
#140099=CARTESIAN_POINT('Ctrl Pts',(-257.606703963711,4.65399112145413,
129.213904801164));
#140100=CARTESIAN_POINT('Ctrl Pts',(-257.614451991261,4.60965444625133,
129.084166841379));
#140101=CARTESIAN_POINT('Ctrl Pts',(-257.62220001881,4.55986572266236,128.956217112845));
#140102=CARTESIAN_POINT('Ctrl Pts',(-257.62994804636,4.50479958044842,128.830541020315));
#140103=CARTESIAN_POINT('Ctrl Pts',(-257.637694451625,4.44974496799959,
128.704891241882));
#140104=CARTESIAN_POINT('Ctrl Pts',(-257.64544085689,4.38941529160877,128.581514510411));
#140105=CARTESIAN_POINT('Ctrl Pts',(-257.653187262155,4.32403337665568,
128.460876369685));
#140106=CARTESIAN_POINT('Ctrl Pts',(-257.660933722896,4.25865099346387,
128.340237364997));
#140107=CARTESIAN_POINT('Ctrl Pts',(-257.668680183638,4.18821648578911,
128.222337333908));
#140108=CARTESIAN_POINT('Ctrl Pts',(-257.67642664438,4.11299850975596,128.107616966188));
#140109=CARTESIAN_POINT('Ctrl Pts',(-257.68417483804,4.03776370712001,127.992870935002));
#140110=CARTESIAN_POINT('Ctrl Pts',(-257.6919230317,3.95774352110598,127.881306309479));
#140111=CARTESIAN_POINT('Ctrl Pts',(-257.69967122536,3.87324954452746,127.77333421908));
#140112=CARTESIAN_POINT('Ctrl Pts',(-257.707427650194,3.7886658070849,127.665247426208));
#140113=CARTESIAN_POINT('Ctrl Pts',(-257.715184075027,3.69959902644132,
127.560761100655));
#140114=CARTESIAN_POINT('Ctrl Pts',(-257.72294049986,3.60640101062734,127.460253141266));
#140115=CARTESIAN_POINT('Ctrl Pts',(-257.730701062721,3.51315327398186,
127.359691561215));
#140116=CARTESIAN_POINT('Ctrl Pts',(-257.738461625581,3.41577018795562,
127.263112851648));
#140117=CARTESIAN_POINT('Ctrl Pts',(-257.746222188441,3.31463920771752,
127.170856800978));
#140118=CARTESIAN_POINT('Ctrl Pts',(-257.753995204865,3.21334594014211,
127.078452704785));
#140119=CARTESIAN_POINT('Ctrl Pts',(-257.761768221289,3.10829305956532,
126.990385380488));
#140120=CARTESIAN_POINT('Ctrl Pts',(-257.769541237712,2.99990046564037,
126.906953754182));
#140121=CARTESIAN_POINT('Ctrl Pts',(-257.777030160361,2.89546948192646,
126.826571446753));
#140122=CARTESIAN_POINT('Ctrl Pts',(-257.784519083009,2.78793889786747,
126.750492074074));
#140123=CARTESIAN_POINT('Ctrl Pts',(-257.792008005657,2.67770667734081,
126.678943061412));
#140124=CARTESIAN_POINT('Ctrl Pts',(-257.799782800979,2.56326659126626,
126.604662827117));
#140125=CARTESIAN_POINT('Ctrl Pts',(-257.807557596301,2.44555223334035,
126.535030546044));
#140126=CARTESIAN_POINT('Ctrl Pts',(-257.815332391623,2.32497793458195,
126.47034854257));
#140127=CARTESIAN_POINT('Ctrl Pts',(-257.823097608641,2.20455217956887,
126.405746225291));
#140128=CARTESIAN_POINT('Ctrl Pts',(-257.83086282566,2.08127383534646,126.34608223423));
#140129=CARTESIAN_POINT('Ctrl Pts',(-257.838628042678,1.95558658271125,
126.291615978212));
#140130=CARTESIAN_POINT('Ctrl Pts',(-257.846385549992,1.83002411881898,
126.237203799083));
#140131=CARTESIAN_POINT('Ctrl Pts',(-257.854143057305,1.70205786245693,
126.187979239617));
#140132=CARTESIAN_POINT('Ctrl Pts',(-257.861900564618,1.57215618295987,
126.144155901153));
#140133=CARTESIAN_POINT('Ctrl Pts',(-257.869652224138,1.44235242644127,
126.100365597765));
#140134=CARTESIAN_POINT('Ctrl Pts',(-257.877403883657,1.31061651968804,
126.0619685356));
#140135=CARTESIAN_POINT('Ctrl Pts',(-257.885155543177,1.17743657511444,
126.029130133696));
#140136=CARTESIAN_POINT('Ctrl Pts',(-257.89290390938,1.04431321246085,125.996305683291));
#140137=CARTESIAN_POINT('Ctrl Pts',(-257.900652275582,0.909747410954359,
125.969035289451));
#140138=CARTESIAN_POINT('Ctrl Pts',(-257.908400641785,0.774241990431667,
125.94743438766));
#140139=CARTESIAN_POINT('Ctrl Pts',(-257.916147387925,0.638764901973453,
125.925838002279));
#140140=CARTESIAN_POINT('Ctrl Pts',(-257.923894134065,0.502348971063077,
125.909908812609));
#140141=CARTESIAN_POINT('Ctrl Pts',(-257.931640880206,0.365506356057829,
125.899710969917));
#140142=CARTESIAN_POINT('Ctrl Pts',(-257.939387683711,0.228662727719137,
125.88951305171));
#140143=CARTESIAN_POINT('Ctrl Pts',(-257.947134487217,0.0913927988120277,
125.885046594219));
#140144=CARTESIAN_POINT('Ctrl Pts',(-257.954881290723,-0.0457874123577805,
125.886323755629));
#140145=CARTESIAN_POINT('Ctrl Pts',(-257.962629828704,-0.182998337571502,
125.887601202991));
#140146=CARTESIAN_POINT('Ctrl Pts',(-257.970378366685,-0.320119114255745,
125.894624824555));
#140147=CARTESIAN_POINT('Ctrl Pts',(-257.978126904666,-0.456635387480373,
125.907354676647));
#140148=CARTESIAN_POINT('Ctrl Pts',(-257.985883674301,-0.593296688685096,
125.920098052289));
#140149=CARTESIAN_POINT('Ctrl Pts',(-257.993640443937,-0.729351813734129,
125.938559731631));
#140150=CARTESIAN_POINT('Ctrl Pts',(-258.001397213572,-0.864292629606964,
125.962647975029));
#140151=CARTESIAN_POINT('Ctrl Pts',(-258.009158122043,-0.999305446825205,
125.986749071364));
#140152=CARTESIAN_POINT('Ctrl Pts',(-258.016919030515,-1.13320238870135,
126.016482629223));
#140153=CARTESIAN_POINT('Ctrl Pts',(-258.024679938986,-1.26548811816278,
126.05170631862));
#140154=CARTESIAN_POINT('Ctrl Pts',(-258.032453298865,-1.39798608355804,
126.086986520028));
#140155=CARTESIAN_POINT('Ctrl Pts',(-258.040226658745,-1.52886729747962,
126.127774338258));
#140156=CARTESIAN_POINT('Ctrl Pts',(-258.048000018625,-1.65765326508232,
126.173878060071));
#140157=CARTESIAN_POINT('Ctrl Pts',(-258.05548522224,-1.78166517308229,
126.218272729882));
#140158=CARTESIAN_POINT('Ctrl Pts',(-258.062970425854,-1.90373413762637,
126.267596055785));
#140159=CARTESIAN_POINT('Ctrl Pts',(-258.070455629469,-2.02345433243006,
126.321636487411));
#140160=CARTESIAN_POINT('Ctrl Pts',(-258.078229099559,-2.14778513240421,
126.377758097521));
#140161=CARTESIAN_POINT('Ctrl Pts',(-258.086002569648,-2.2699766705071,
126.439145286734));
#140162=CARTESIAN_POINT('Ctrl Pts',(-258.093776039737,-2.38955067604954,
126.505613052392));
#140163=CARTESIAN_POINT('Ctrl Pts',(-258.101539798875,-2.50897530461983,
126.571997783668));
#140164=CARTESIAN_POINT('Ctrl Pts',(-258.109303558012,-2.62578856848527,
126.643450274066));
#140165=CARTESIAN_POINT('Ctrl Pts',(-258.11706731715,-2.73953245162599,
126.719737622847));
#140166=CARTESIAN_POINT('Ctrl Pts',(-258.124823236471,-2.85316147660633,
126.79594793694));
#140167=CARTESIAN_POINT('Ctrl Pts',(-258.132579155793,-2.96372696652871,
126.876983176398));
#140168=CARTESIAN_POINT('Ctrl Pts',(-258.140335075115,-3.07079611464425,
126.962564906601));
#140169=CARTESIAN_POINT('Ctrl Pts',(-258.148084607211,-3.17777708819573,
127.048076157755));
#140170=CARTESIAN_POINT('Ctrl Pts',(-258.155834139307,-3.28126714906281,
127.138126200936));
#140171=CARTESIAN_POINT('Ctrl Pts',(-258.163583671403,-3.38086343512353,
127.232394003004));
#140172=CARTESIAN_POINT('Ctrl Pts',(-258.171329725354,-3.48041502037351,
127.326619495792));
#140173=CARTESIAN_POINT('Ctrl Pts',(-258.179075779304,-3.57607602433451,
127.425058713004));
#140174=CARTESIAN_POINT('Ctrl Pts',(-258.186821833255,-3.66747770404219,
127.527351256448));
#140175=CARTESIAN_POINT('Ctrl Pts',(-258.194566089714,-3.75885817376112,
127.629620062652));
#140176=CARTESIAN_POINT('Ctrl Pts',(-258.202310346174,-3.84598102601229,
127.735740124088));
#140177=CARTESIAN_POINT('Ctrl Pts',(-258.210054602633,-3.9285156279429,
127.845315497344));
#140178=CARTESIAN_POINT('Ctrl Pts',(-258.217798740691,-4.01104896800664,
127.954889195309));
#140179=CARTESIAN_POINT('Ctrl Pts',(-258.225542878749,-4.08899396318763,
128.067917786909));
#140180=CARTESIAN_POINT('Ctrl Pts',(-258.233287016807,-4.16206164266541,
128.183974015335));
#140181=CARTESIAN_POINT('Ctrl Pts',(-258.241036109274,-4.23517606810922,
128.300104492191));
#140182=CARTESIAN_POINT('Ctrl Pts',(-258.248785201742,-4.30340673492681,
128.419266144586));
#140183=CARTESIAN_POINT('Ctrl Pts',(-258.256534294209,-4.36650909341112,
128.541004392917));
#140184=CARTESIAN_POINT('Ctrl Pts',(-258.264285952437,-4.42963234537518,
128.662782949339));
#140185=CARTESIAN_POINT('Ctrl Pts',(-258.272037610665,-4.48762373703312,
128.787139448687));
#140186=CARTESIAN_POINT('Ctrl Pts',(-258.279789268892,-4.54028613560329,
128.913597578645));
#140187=CARTESIAN_POINT('Ctrl Pts',(-258.287549765891,-4.59300858208599,
129.040199901556));
#140188=CARTESIAN_POINT('Ctrl Pts',(-258.29531026289,-4.64038975854418,
129.168908276302));
#140189=CARTESIAN_POINT('Ctrl Pts',(-258.303070759888,-4.68228167746306,
129.299228943793));
#140190=CARTESIAN_POINT('Ctrl Pts',(-258.308647566738,-4.71238582419431,
129.392879284897));
#140191=CARTESIAN_POINT('Ctrl Pts',(-258.314224373587,-4.73965632075143,
129.487361878628));
#140192=CARTESIAN_POINT('Ctrl Pts',(-258.319801180436,-4.76405452823419,
129.582490119309));
#140193=CARTESIAN_POINT('Origin',(210.,0.,130.804360617566));
#140194=CARTESIAN_POINT('',(209.436623794218,-5.91986778237144,130.801550299888));
#140195=CARTESIAN_POINT('',(209.999781618288,2.5839291206855,125.481650700449));
#140196=CARTESIAN_POINT('Ctrl Pts',(209.436624807795,-5.91674932306679,
130.801530336897));
#140197=CARTESIAN_POINT('Ctrl Pts',(209.445314454709,-5.91666144223196,
130.617813974195));
#140198=CARTESIAN_POINT('Ctrl Pts',(209.454004101622,-5.90801760417395,
130.434327549234));
#140199=CARTESIAN_POINT('Ctrl Pts',(209.462693748535,-5.89087755369375,
130.251647120456));
#140200=CARTESIAN_POINT('Ctrl Pts',(209.470129292751,-5.87621118065508,
130.095331401409));
#140201=CARTESIAN_POINT('Ctrl Pts',(209.477564836966,-5.85529721592649,
129.939370695698));
#140202=CARTESIAN_POINT('Ctrl Pts',(209.485000381182,-5.82815696752497,
129.784303303299));
#140203=CARTESIAN_POINT('Ctrl Pts',(209.492427278008,-5.80104828268818,
129.629416251167));
#140204=CARTESIAN_POINT('Ctrl Pts',(209.499854174835,-5.76772779211504,
129.475420807086));
#140205=CARTESIAN_POINT('Ctrl Pts',(209.507281071662,-5.72826867527633,
129.322851742686));
#140206=CARTESIAN_POINT('Ctrl Pts',(209.51470093492,-5.68884692779981,129.170427167293));
#140207=CARTESIAN_POINT('Ctrl Pts',(209.522120798179,-5.64329822100986,
129.0194266398));
#140208=CARTESIAN_POINT('Ctrl Pts',(209.529540661437,-5.59174703436072,
128.870376215815));
#140209=CARTESIAN_POINT('Ctrl Pts',(209.536955099496,-5.54023354052269,
128.721434773403));
#140210=CARTESIAN_POINT('Ctrl Pts',(209.544369537554,-5.48272642729368,
128.574440945163));
#140211=CARTESIAN_POINT('Ctrl Pts',(209.551783975613,-5.41940037535893,
128.429906967974));
#140212=CARTESIAN_POINT('Ctrl Pts',(209.559194592598,-5.35610695887099,
128.285447477206));
#140213=CARTESIAN_POINT('Ctrl Pts',(209.566605209583,-5.28700072526885,
128.143445652368));
#140214=CARTESIAN_POINT('Ctrl Pts',(209.574015826567,-5.21230494212194,
128.004394947628));
#140215=CARTESIAN_POINT('Ctrl Pts',(209.581425300872,-5.13762067669639,
127.865365683821));
#140216=CARTESIAN_POINT('Ctrl Pts',(209.588834775176,-5.05734874775978,
127.729286964407));
#140217=CARTESIAN_POINT('Ctrl Pts',(209.596244249481,-4.97175901792443,
127.596628890911));
#140218=CARTESIAN_POINT('Ctrl Pts',(209.603653447896,-4.88617247499418,
127.463975756894));
#140219=CARTESIAN_POINT('Ctrl Pts',(209.611062646311,-4.79526872641441,
127.334743328014));
#140220=CARTESIAN_POINT('Ctrl Pts',(209.618471844726,-4.69936158985239,
127.209373662051));
#140221=CARTESIAN_POINT('Ctrl Pts',(209.625882215991,-4.60343927153547,
127.083984150522));
#140222=CARTESIAN_POINT('Ctrl Pts',(209.633292587255,-4.5025122140518,126.962458914826));
#140223=CARTESIAN_POINT('Ctrl Pts',(209.64070295852,-4.39693514121467,126.845207687146));
#140224=CARTESIAN_POINT('Ctrl Pts',(209.648115951785,-4.2913207121981,126.727914972638));
#140225=CARTESIAN_POINT('Ctrl Pts',(209.655528945051,-4.18105324043719,
126.61489955342));
#140226=CARTESIAN_POINT('Ctrl Pts',(209.662941938316,-4.06652488048987,
126.506534892987));
#140227=CARTESIAN_POINT('Ctrl Pts',(209.670363046154,-3.95187115301046,
126.398051612064));
#140228=CARTESIAN_POINT('Ctrl Pts',(209.677784153991,-3.83294749285477,
126.294229512671));
#140229=CARTESIAN_POINT('Ctrl Pts',(209.685205261829,-3.71018032603156,
126.195402762386));
#140230=CARTESIAN_POINT('Ctrl Pts',(209.692630935426,-3.58733762799181,
126.096515209975));
#140231=CARTESIAN_POINT('Ctrl Pts',(209.700056609023,-3.4606470090426,126.002629352074));
#140232=CARTESIAN_POINT('Ctrl Pts',(209.70748228262,-3.33056413386467,125.914036179176));
#140233=CARTESIAN_POINT('Ctrl Pts',(209.71491844568,-3.20029750436431,125.825317860071));
#140234=CARTESIAN_POINT('Ctrl Pts',(209.722354608741,-3.06662936267343,
125.741907354593));
#140235=CARTESIAN_POINT('Ctrl Pts',(209.729790771801,-2.93004094085217,
125.664050252673));
#140236=CARTESIAN_POINT('Ctrl Pts',(209.733574305317,-2.86054449925481,
125.624436415245));
#140237=CARTESIAN_POINT('Ctrl Pts',(209.737357838833,-2.79029240399966,
125.586259478074));
#140238=CARTESIAN_POINT('Ctrl Pts',(209.741141372349,-2.71934995185403,
125.549546976546));
#140239=CARTESIAN_POINT('Ctrl Pts',(209.748429935947,-2.58268707519309,
125.478824356781));
#140240=CARTESIAN_POINT('Ctrl Pts',(209.755718499544,-2.44301584246147,
125.413308818321));
#140241=CARTESIAN_POINT('Ctrl Pts',(209.763007063142,-2.30077949620412,
125.353274095381));
#140242=CARTESIAN_POINT('Ctrl Pts',(209.770286840669,-2.15871461013878,
125.293311741883));
#140243=CARTESIAN_POINT('Ctrl Pts',(209.777566618197,-2.01409111408332,
125.238817210897));
#140244=CARTESIAN_POINT('Ctrl Pts',(209.784846395724,-1.86737837579021,
125.190019288066));
#140245=CARTESIAN_POINT('Ctrl Pts',(209.792119116272,-1.72080786008898,
125.141268669697));
#140246=CARTESIAN_POINT('Ctrl Pts',(209.799391836819,-1.5721524963476,125.098203794501));
#140247=CARTESIAN_POINT('Ctrl Pts',(209.806664557367,-1.42190296680508,
125.061005978029));
#140248=CARTESIAN_POINT('Ctrl Pts',(209.813931941926,-1.27176367521208,
125.023835453562));
#140249=CARTESIAN_POINT('Ctrl Pts',(209.821199326485,-1.1200329197269,124.992523514836));
#140250=CARTESIAN_POINT('Ctrl Pts',(209.828466711043,-0.967217642662254,
124.967202011341));
#140251=CARTESIAN_POINT('Ctrl Pts',(209.835731111368,-0.814465116728247,
124.941890905714));
#140252=CARTESIAN_POINT('Ctrl Pts',(209.842995511692,-0.660629336190675,
124.922565407679));
#140253=CARTESIAN_POINT('Ctrl Pts',(209.850259912017,-0.506228400192777,
124.909306472833));
#140254=CARTESIAN_POINT('Ctrl Pts',(209.857522871346,-0.351858091776005,
124.896050168081));
#140255=CARTESIAN_POINT('Ctrl Pts',(209.864785830675,-0.196923236786615,
124.88885806683));
#140256=CARTESIAN_POINT('Ctrl Pts',(209.872048790004,-0.041947692904324,
124.887759316687));
#140257=CARTESIAN_POINT('Ctrl Pts',(209.879311856424,0.113030136058688,
124.886660550344));
#140258=CARTESIAN_POINT('Ctrl Pts',(209.886574922844,0.268048267459926,
124.891655316722));
#140259=CARTESIAN_POINT('Ctrl Pts',(209.893837989264,0.422582550641461,
124.90272062936));
#140260=CARTESIAN_POINT('Ctrl Pts',(209.901102710863,0.577152050615399,
124.913788463671));
#140261=CARTESIAN_POINT('Ctrl Pts',(209.908367432462,0.731237096509864,
124.930929568337));
#140262=CARTESIAN_POINT('Ctrl Pts',(209.915632154061,0.884318713515213,
124.954069088469));
#140263=CARTESIAN_POINT('Ctrl Pts',(209.922904372259,1.03755829824375,124.977232486695));
#140264=CARTESIAN_POINT('Ctrl Pts',(209.930176590457,1.18979200252811,125.006406603914));
#140265=CARTESIAN_POINT('Ctrl Pts',(209.937448808656,1.34051053729742,125.041465332911));
#140266=CARTESIAN_POINT('Ctrl Pts',(209.944724904051,1.491309427951,125.076542753539));
#140267=CARTESIAN_POINT('Ctrl Pts',(209.952000999447,1.64059116756246,125.117510930441));
#140268=CARTESIAN_POINT('Ctrl Pts',(209.959277094843,1.78786254938573,125.164194124722));
#140269=CARTESIAN_POINT('Ctrl Pts',(209.966564295703,1.93535871072363,125.210948571309));
#140270=CARTESIAN_POINT('Ctrl Pts',(209.973851496564,2.08083802164559,125.263435326559));
#140271=CARTESIAN_POINT('Ctrl Pts',(209.981138697425,2.22382735036804,125.321430517861));
#140272=CARTESIAN_POINT('Ctrl Pts',(209.987353004379,2.34576437349178,125.370887082528));
#140273=CARTESIAN_POINT('Ctrl Pts',(209.993567311334,2.46589090244907,125.42434861294));
#140274=CARTESIAN_POINT('Ctrl Pts',(209.999781618288,2.5839291206855,125.481650700449));
#140275=CARTESIAN_POINT('',(210.,-2.58391981636517,125.481646183642));
#140276=CARTESIAN_POINT('Origin',(210.,0.,130.804360617566));
#140277=CARTESIAN_POINT('',(209.688375192173,-5.9167497157184,130.802526483902));
#140278=CARTESIAN_POINT('Ctrl Pts',(209.999999999999,-2.58391981636503,
125.481646183643));
#140279=CARTESIAN_POINT('Ctrl Pts',(209.99131183034,-2.74995620526197,125.562248801129));
#140280=CARTESIAN_POINT('Ctrl Pts',(209.982623660682,-2.91209254072039,
125.650562775723));
#140281=CARTESIAN_POINT('Ctrl Pts',(209.973935491023,-3.06969027976343,
125.746205603252));
#140282=CARTESIAN_POINT('Ctrl Pts',(209.965231695902,-3.22757145453489,
125.842020442098));
#140283=CARTESIAN_POINT('Ctrl Pts',(209.95652790078,-3.38089761558052,125.94519044461));
#140284=CARTESIAN_POINT('Ctrl Pts',(209.947824105658,-3.52905730190805,
126.05528859007));
#140285=CARTESIAN_POINT('Ctrl Pts',(209.939119990154,-3.67722244191973,
126.165390788187));
#140286=CARTESIAN_POINT('Ctrl Pts',(209.93041587465,-3.82022064776757,126.282421571801));
#140287=CARTESIAN_POINT('Ctrl Pts',(209.921711759146,-3.9574720567728,126.405912540987));
#140288=CARTESIAN_POINT('Ctrl Pts',(209.913018683697,-4.09454937995234,
126.529246877702));
#140289=CARTESIAN_POINT('Ctrl Pts',(209.904325608248,-4.22589438898566,
126.659024962998));
#140290=CARTESIAN_POINT('Ctrl Pts',(209.895632532799,-4.35096223417733,
126.794739912404));
#140291=CARTESIAN_POINT('Ctrl Pts',(209.886971363206,-4.47557104773246,
126.929956752522));
#140292=CARTESIAN_POINT('Ctrl Pts',(209.878310193613,-4.59394860132631,
127.071066895327));
#140293=CARTESIAN_POINT('Ctrl Pts',(209.86964902402,-4.70558990066976,127.217529948408));
#140294=CARTESIAN_POINT('Ctrl Pts',(209.866691412045,-4.74371311720728,
127.267544080455));
#140295=CARTESIAN_POINT('Ctrl Pts',(209.863733800069,-4.78105112881579,
127.318182073746));
#140296=CARTESIAN_POINT('Ctrl Pts',(209.860776188094,-4.81758476774297,
127.369421379659));
#140297=CARTESIAN_POINT('Ctrl Pts',(209.853352615767,-4.90928378479419,
127.498031453132));
#140298=CARTESIAN_POINT('Ctrl Pts',(209.84592904344,-4.99586157637515,127.63036143513));
#140299=CARTESIAN_POINT('Ctrl Pts',(209.838505471113,-5.07701336223303,
127.765962045586));
#140300=CARTESIAN_POINT('Ctrl Pts',(209.831082830258,-5.15815496558327,
127.901545641577));
#140301=CARTESIAN_POINT('Ctrl Pts',(209.823660189402,-5.23387172917773,
128.040398730499));
#140302=CARTESIAN_POINT('Ctrl Pts',(209.816237548547,-5.30390330506813,
128.182044791242));
#140303=CARTESIAN_POINT('Ctrl Pts',(209.808814397566,-5.37393969391849,
128.323700586692));
#140304=CARTESIAN_POINT('Ctrl Pts',(209.801391246585,-5.43828995410957,
128.468149403269));
#140305=CARTESIAN_POINT('Ctrl Pts',(209.793968095605,-5.4967406783166,128.614892079806));
#140306=CARTESIAN_POINT('Ctrl Pts',(209.786540360911,-5.55522749519685,
128.761725368317));
#140307=CARTESIAN_POINT('Ctrl Pts',(209.779112626217,-5.60780736360233,
128.910855000888));
#140308=CARTESIAN_POINT('Ctrl Pts',(209.771684891523,-5.65431567064078,
129.061763458368));
#140309=CARTESIAN_POINT('Ctrl Pts',(209.764254403954,-5.70084121463515,
129.212727845693));
#140310=CARTESIAN_POINT('Ctrl Pts',(209.756823916385,-5.74129061476954,
129.365472014495));
#140311=CARTESIAN_POINT('Ctrl Pts',(209.749393428817,-5.77554982777,129.519465777727));
#140312=CARTESIAN_POINT('Ctrl Pts',(209.74195603147,-5.80984089918891,129.673602743248));
#140313=CARTESIAN_POINT('Ctrl Pts',(209.734518634122,-5.8379302216951,129.828991259508));
#140314=CARTESIAN_POINT('Ctrl Pts',(209.727081236775,-5.85975521629992,
129.985093037623));
#140315=CARTESIAN_POINT('Ctrl Pts',(209.725238283246,-5.86516335155979,
130.023774354418));
#140316=CARTESIAN_POINT('Ctrl Pts',(209.723395329716,-5.87018709070327,
130.062499450682));
#140317=CARTESIAN_POINT('Ctrl Pts',(209.721552376187,-5.87482597569107,
130.101260114192));
#140318=CARTESIAN_POINT('Ctrl Pts',(209.71049331486,-5.90266265890184,130.333852281056));
#140319=CARTESIAN_POINT('Ctrl Pts',(209.699434253533,-5.91667702418257,
130.568030238081));
#140320=CARTESIAN_POINT('Ctrl Pts',(209.688375192206,-5.91674971571818,
130.802526483197));
#140321=CARTESIAN_POINT('',(207.938375235231,-5.91423241434992,130.80143089854));
#140322=CARTESIAN_POINT('Ctrl Pts',(209.688375192173,-5.9167497157184,130.802526483902));
#140323=CARTESIAN_POINT('Ctrl Pts',(209.680943409138,-5.91679856502823,
130.960109950051));
#140324=CARTESIAN_POINT('Ctrl Pts',(209.673511626102,-5.9105476477549,131.117854987543));
#140325=CARTESIAN_POINT('Ctrl Pts',(209.666079843067,-5.8979845522807,131.27522023949));
#140326=CARTESIAN_POINT('Ctrl Pts',(209.658653719117,-5.88543102323509,
131.432465662415));
#140327=CARTESIAN_POINT('Ctrl Pts',(209.651227595166,-5.8665749164667,131.589331507636));
#140328=CARTESIAN_POINT('Ctrl Pts',(209.643801471216,-5.8414558785676,131.745277075732));
#140329=CARTESIAN_POINT('Ctrl Pts',(209.636379410181,-5.81635058357617,
131.901137324257));
#140330=CARTESIAN_POINT('Ctrl Pts',(209.628957349147,-5.78498924065305,
132.056077933289));
#140331=CARTESIAN_POINT('Ctrl Pts',(209.621535288112,-5.74746325356225,
132.20956405887));
#140332=CARTESIAN_POINT('Ctrl Pts',(209.614100682456,-5.70987384078865,
132.36330960367));
#140333=CARTESIAN_POINT('Ctrl Pts',(209.606666076801,-5.66609898337391,
132.515595374754));
#140334=CARTESIAN_POINT('Ctrl Pts',(209.599231471145,-5.61628193033324,
132.665894351215));
#140335=CARTESIAN_POINT('Ctrl Pts',(209.59181124687,-5.56656124259613,132.815902591761));
#140336=CARTESIAN_POINT('Ctrl Pts',(209.584391022596,-5.51082184033433,
132.963931367112));
#140337=CARTESIAN_POINT('Ctrl Pts',(209.576970798321,-5.4492558567059,133.109472582451));
#140338=CARTESIAN_POINT('Ctrl Pts',(209.569549627897,-5.38768202282445,
133.25503235569));
#140339=CARTESIAN_POINT('Ctrl Pts',(209.562128457473,-5.32028027222218,
133.398103595494));
#140340=CARTESIAN_POINT('Ctrl Pts',(209.554707287049,-5.24729052265184,
133.538199079032));
#140341=CARTESIAN_POINT('Ctrl Pts',(209.547283729025,-5.17427729022698,
133.678339635224));
#140342=CARTESIAN_POINT('Ctrl Pts',(209.539860171002,-5.09567264996152,
133.815502199823));
#140343=CARTESIAN_POINT('Ctrl Pts',(209.532436612979,-5.01176195446012,
133.94922510977));
#140344=CARTESIAN_POINT('Ctrl Pts',(209.524992291262,-4.92761656072304,
134.083322042729));
#140345=CARTESIAN_POINT('Ctrl Pts',(209.517547969545,-4.83813559558281,
134.213959741109));
#140346=CARTESIAN_POINT('Ctrl Pts',(209.510103647828,-4.74364932018439,
134.340703600029));
#140347=CARTESIAN_POINT('Ctrl Pts',(209.50266720501,-4.64926304689699,134.467313316149));
#140348=CARTESIAN_POINT('Ctrl Pts',(209.495230762193,-4.54988231892117,
134.590037168706));
#140349=CARTESIAN_POINT('Ctrl Pts',(209.487794319376,-4.44587511023585,
134.708477043428));
#140350=CARTESIAN_POINT('Ctrl Pts',(209.480345730974,-4.3416980315738,134.827110360307));
#140351=CARTESIAN_POINT('Ctrl Pts',(209.472897142572,-4.23287962656979,
134.941445447219));
#140352=CARTESIAN_POINT('Ctrl Pts',(209.46544855417,-4.11982451206075,135.05112133043));
#140353=CARTESIAN_POINT('Ctrl Pts',(209.458000620238,-4.00677933114232,
135.160787576966));
#140354=CARTESIAN_POINT('Ctrl Pts',(209.450552686306,-3.88949849868325,
135.265795238245));
#140355=CARTESIAN_POINT('Ctrl Pts',(209.443104752375,-3.76841686049243,
135.365825834802));
#140356=CARTESIAN_POINT('Ctrl Pts',(209.435742893708,-3.64873455454395,
135.464700384571));
#140357=CARTESIAN_POINT('Ctrl Pts',(209.428381035041,-3.52494699684348,
135.559035800125));
#140358=CARTESIAN_POINT('Ctrl Pts',(209.421019176375,-3.39743599074722,
135.648466236901));
#140359=CARTESIAN_POINT('Ctrl Pts',(209.413666779922,-3.27008887484194,
135.73778172853));
#140360=CARTESIAN_POINT('Ctrl Pts',(209.406314383469,-3.13902814043842,
135.822204569766));
#140361=CARTESIAN_POINT('Ctrl Pts',(209.398961987017,-3.00467057976207,
135.901407337934));
#140362=CARTESIAN_POINT('Ctrl Pts',(209.391617367729,-2.87045513886034,
135.980526327567));
#140363=CARTESIAN_POINT('Ctrl Pts',(209.384272748441,-2.73295013636556,
136.054436040991));
#140364=CARTESIAN_POINT('Ctrl Pts',(209.376928129154,-2.59260326520279,
136.122850898817));
#140365=CARTESIAN_POINT('Ctrl Pts',(209.369589609032,-2.45237294179964,
136.191208943132));
#140366=CARTESIAN_POINT('Ctrl Pts',(209.362251088911,-2.309305786928,136.254081048402));
#140367=CARTESIAN_POINT('Ctrl Pts',(209.35491256879,-2.16387596942645,136.311226454995));
#140368=CARTESIAN_POINT('Ctrl Pts',(209.34757847529,-2.01853387570421,136.368337391276));
#140369=CARTESIAN_POINT('Ctrl Pts',(209.34024438179,-1.87083230938491,136.419728367192));
#140370=CARTESIAN_POINT('Ctrl Pts',(209.33291028829,-1.7212672027132,136.465205941311));
#140371=CARTESIAN_POINT('Ctrl Pts',(209.325578014926,-1.57173921429979,
136.510672229051));
#140372=CARTESIAN_POINT('Ctrl Pts',(209.318245741561,-1.42034896766245,
136.550227919959));
#140373=CARTESIAN_POINT('Ctrl Pts',(209.310913468197,-1.26760940802185,
136.58372883141));
#140374=CARTESIAN_POINT('Ctrl Pts',(209.303581889688,-1.11488432301136,
136.61722656809));
#140375=CARTESIAN_POINT('Ctrl Pts',(209.296250311179,-0.960810550721905,
136.644670584959));
#140376=CARTESIAN_POINT('Ctrl Pts',(209.288918732671,-0.805912813346689,
136.665967487681));
#140377=CARTESIAN_POINT('Ctrl Pts',(209.281586340522,-0.650997885813834,
136.68726675388));
#140378=CARTESIAN_POINT('Ctrl Pts',(209.274253948373,-0.495259187985151,
136.702417496254));
#140379=CARTESIAN_POINT('Ctrl Pts',(209.266921556224,-0.339227930045618,
136.711378052277));
#140380=CARTESIAN_POINT('Ctrl Pts',(209.259586841621,-0.183147250917642,
136.720341446458));
#140381=CARTESIAN_POINT('Ctrl Pts',(209.252252127018,-0.0267742067296978,
136.723110730372));
#140382=CARTESIAN_POINT('Ctrl Pts',(209.244917412414,0.129358863151292,
136.719696351658));
#140383=CARTESIAN_POINT('Ctrl Pts',(209.237574655162,0.285663135787447,
136.716278229015));
#140384=CARTESIAN_POINT('Ctrl Pts',(209.230231897911,0.441726528171486,
136.706662911789));
#140385=CARTESIAN_POINT('Ctrl Pts',(209.222889140659,0.597020032079499,
136.690912888955));
#140386=CARTESIAN_POINT('Ctrl Pts',(209.215541982281,0.752406616329664,
136.67515342582));
#140387=CARTESIAN_POINT('Ctrl Pts',(209.208194823903,0.907022017350668,
136.653251986223));
#140388=CARTESIAN_POINT('Ctrl Pts',(209.200847665525,1.06034700512894,136.625322289937));
#140389=CARTESIAN_POINT('Ctrl Pts',(209.193489593897,1.21389973726609,136.597351107714));
#140390=CARTESIAN_POINT('Ctrl Pts',(209.186131522269,1.36615785808255,136.563333868863));
#140391=CARTESIAN_POINT('Ctrl Pts',(209.178773450641,1.51661609478376,136.523434509687));
#140392=CARTESIAN_POINT('Ctrl Pts',(209.174068009948,1.61283319423839,136.497919119542));
#140393=CARTESIAN_POINT('Ctrl Pts',(209.169362569255,1.70831457266076,136.469999222647));
#140394=CARTESIAN_POINT('Ctrl Pts',(209.164657128562,1.80293258570797,136.439727921823));
#140395=CARTESIAN_POINT('Ctrl Pts',(209.157221130164,1.95245724009132,136.391890246442));
#140396=CARTESIAN_POINT('Ctrl Pts',(209.149785131767,2.10029751050973,136.338026748851));
#140397=CARTESIAN_POINT('Ctrl Pts',(209.14234913337,2.24593212653075,136.278273244336));
#140398=CARTESIAN_POINT('Ctrl Pts',(209.134921860703,2.39139584842722,136.218589857237));
#140399=CARTESIAN_POINT('Ctrl Pts',(209.127494588036,2.53465872740355,136.15303036157));
#140400=CARTESIAN_POINT('Ctrl Pts',(209.12006731537,2.67521401390798,136.081780493063));
#140401=CARTESIAN_POINT('Ctrl Pts',(209.112647154316,2.81563471872803,136.010598846304));
#140402=CARTESIAN_POINT('Ctrl Pts',(209.105226993263,2.95335266314768,135.93373784144));
#140403=CARTESIAN_POINT('Ctrl Pts',(209.09780683221,3.08788056468555,135.851431469133));
#140404=CARTESIAN_POINT('Ctrl Pts',(209.090392174166,3.22230869637828,135.769186137651));
#140405=CARTESIAN_POINT('Ctrl Pts',(209.082977516123,3.35355118035611,135.681503673601));
#140406=CARTESIAN_POINT('Ctrl Pts',(209.075562858079,3.48114495184259,135.588664160064));
#140407=CARTESIAN_POINT('Ctrl Pts',(209.06815209874,3.60867163319029,135.495873462514));
#140408=CARTESIAN_POINT('Ctrl Pts',(209.060741339401,3.73255312323486,135.397931334398));
#140409=CARTESIAN_POINT('Ctrl Pts',(209.053330580062,3.85235507996995,135.295161314583));
#140410=CARTESIAN_POINT('Ctrl Pts',(209.045921079812,3.97213668232604,135.192408755417));
#140411=CARTESIAN_POINT('Ctrl Pts',(209.038511579563,4.08783984546415,135.084830174857));
#140412=CARTESIAN_POINT('Ctrl Pts',(209.031102079314,4.19906299594078,134.972789640426));
#140413=CARTESIAN_POINT('Ctrl Pts',(209.023692927238,4.31028092002014,134.860754370801));
#140414=CARTESIAN_POINT('Ctrl Pts',(209.016283775163,4.41701898816564,134.744257828168));
#140415=CARTESIAN_POINT('Ctrl Pts',(209.008874623087,4.51891240724618,134.6237010342));
#140416=CARTESIAN_POINT('Ctrl Pts',(209.001464370453,4.62082096162604,134.503126332667));
#140417=CARTESIAN_POINT('Ctrl Pts',(208.994054117818,4.71788319396834,134.378490462857));
#140418=CARTESIAN_POINT('Ctrl Pts',(208.986643865183,4.80977462402228,134.250227508293));
#140419=CARTESIAN_POINT('Ctrl Pts',(208.979231062888,4.90169767134631,134.121920422035));
#140420=CARTESIAN_POINT('Ctrl Pts',(208.971818260593,4.98844615751906,133.989984068232));
#140421=CARTESIAN_POINT('Ctrl Pts',(208.964405458297,5.0697390257851,133.85488135556));
#140422=CARTESIAN_POINT('Ctrl Pts',(208.956984650393,5.15111968796501,133.71963273592));
#140423=CARTESIAN_POINT('Ctrl Pts',(208.949563842489,5.22703277370046,133.58121124698));
#140424=CARTESIAN_POINT('Ctrl Pts',(208.942143034584,5.29724293660821,133.440104883054));
#140425=CARTESIAN_POINT('Ctrl Pts',(208.93471772318,5.36749570828399,133.298912885253));
#140426=CARTESIAN_POINT('Ctrl Pts',(208.927292411775,5.43203850821355,133.155033103922));
#140427=CARTESIAN_POINT('Ctrl Pts',(208.919867100371,5.49068441292632,133.008972882829));
#140428=CARTESIAN_POINT('Ctrl Pts',(208.912431393417,5.54941242279996,132.862708175199));
#140429=CARTESIAN_POINT('Ctrl Pts',(208.904995686463,5.60222692426299,132.714257280312));
#140430=CARTESIAN_POINT('Ctrl Pts',(208.897559979509,5.64899080795368,132.564142824021));
#140431=CARTESIAN_POINT('Ctrl Pts',(208.893776487922,5.67278555425194,132.487760472487));
#140432=CARTESIAN_POINT('Ctrl Pts',(208.889992996336,5.69501458077322,132.410947592297));
#140433=CARTESIAN_POINT('Ctrl Pts',(208.886209504749,5.71566493562994,132.33377387307));
#140434=CARTESIAN_POINT('Ctrl Pts',(208.878777025297,5.75623152197345,132.182169972497));
#140435=CARTESIAN_POINT('Ctrl Pts',(208.871344545846,5.79082171676416,132.028728443607));
#140436=CARTESIAN_POINT('Ctrl Pts',(208.863912066394,5.81926846734694,131.873961041763));
#140437=CARTESIAN_POINT('Ctrl Pts',(208.856488197357,5.84768226280323,131.719372935591));
#140438=CARTESIAN_POINT('Ctrl Pts',(208.849064328319,5.86996671485046,131.56346237674));
#140439=CARTESIAN_POINT('Ctrl Pts',(208.841640459282,5.88600463401675,131.406755845662));
#140440=CARTESIAN_POINT('Ctrl Pts',(208.834223583446,5.90202744564246,131.250196930385));
#140441=CARTESIAN_POINT('Ctrl Pts',(208.82680670761,5.91181540164507,131.092843903578));
#140442=CARTESIAN_POINT('Ctrl Pts',(208.819389831774,5.91530244428613,130.935232903106));
#140443=CARTESIAN_POINT('Ctrl Pts',(208.811978337368,5.91878695684913,130.777736259749));
#140444=CARTESIAN_POINT('Ctrl Pts',(208.804566842962,5.91597965131232,130.619982386042));
#140445=CARTESIAN_POINT('Ctrl Pts',(208.797155348556,5.90686634525875,130.46251190578));
#140446=CARTESIAN_POINT('Ctrl Pts',(208.78974762803,5.89775767963602,130.30512160837));
#140447=CARTESIAN_POINT('Ctrl Pts',(208.782339907505,5.88234943013702,130.148014787699));
#140448=CARTESIAN_POINT('Ctrl Pts',(208.774932186979,5.86067950054184,129.991731332819));
#140449=CARTESIAN_POINT('Ctrl Pts',(208.767525527194,5.8390126739486,129.835470256778));
#140450=CARTESIAN_POINT('Ctrl Pts',(208.760118867408,5.81108599671315,129.680032681036));
#140451=CARTESIAN_POINT('Ctrl Pts',(208.752712207623,5.77698917900472,129.525952784297));
#140452=CARTESIAN_POINT('Ctrl Pts',(208.745305772146,5.74289339390685,129.371877553816));
#140453=CARTESIAN_POINT('Ctrl Pts',(208.737899336669,5.70262792010967,129.219160284054));
#140454=CARTESIAN_POINT('Ctrl Pts',(208.730492901192,5.65633342585285,129.068324115047));
#140455=CARTESIAN_POINT('Ctrl Pts',(208.723085238113,5.61003125837413,128.917462945239));
#140456=CARTESIAN_POINT('Ctrl Pts',(208.715677575033,5.55769818979722,128.768483852881));
#140457=CARTESIAN_POINT('Ctrl Pts',(208.708269911954,5.49952447183615,128.621893860391));
#140458=CARTESIAN_POINT('Ctrl Pts',(208.700859568914,5.44132970765705,128.475250834244));
#140459=CARTESIAN_POINT('Ctrl Pts',(208.693449225874,5.37729022396487,128.330998974698));
#140460=CARTESIAN_POINT('Ctrl Pts',(208.686038882833,5.30764396275474,128.189624277678));
#140461=CARTESIAN_POINT('Ctrl Pts',(208.678620321859,5.23792046511928,128.048092798713));
#140462=CARTESIAN_POINT('Ctrl Pts',(208.671201760884,5.16257793705867,127.909445188496));
#140463=CARTESIAN_POINT('Ctrl Pts',(208.66378319991,5.08190010003917,127.77414248421));
#140464=CARTESIAN_POINT('Ctrl Pts',(208.656360018143,5.0011720112898,127.638755504053));
#140465=CARTESIAN_POINT('Ctrl Pts',(208.648936836376,4.91510219414187,127.506717892626));
#140466=CARTESIAN_POINT('Ctrl Pts',(208.641513654609,4.82401676740594,127.378460328549));
#140467=CARTESIAN_POINT('Ctrl Pts',(208.634079874691,4.73280129709001,127.250019649858));
#140468=CARTESIAN_POINT('Ctrl Pts',(208.626646094773,4.63655614217903,127.125370091038));
#140469=CARTESIAN_POINT('Ctrl Pts',(208.619212314855,4.53564714939468,127.004908617779));
#140470=CARTESIAN_POINT('Ctrl Pts',(208.615395503548,4.4838362821366,126.943058695106));
#140471=CARTESIAN_POINT('Ctrl Pts',(208.611578692242,4.43079651974987,126.882312244135));
#140472=CARTESIAN_POINT('Ctrl Pts',(208.607761880936,4.37658094580437,126.822719023032));
#140473=CARTESIAN_POINT('Ctrl Pts',(208.600347300224,4.27126116010103,126.706952559281));
#140474=CARTESIAN_POINT('Ctrl Pts',(208.592932719512,4.16118202673538,126.59518870569));
#140475=CARTESIAN_POINT('Ctrl Pts',(208.585518138801,4.04668003584927,126.487844516593));
#140476=CARTESIAN_POINT('Ctrl Pts',(208.578112433415,3.93231510497043,126.380628819544));
#140477=CARTESIAN_POINT('Ctrl Pts',(208.570706728029,3.81353812445766,126.277822510432));
#140478=CARTESIAN_POINT('Ctrl Pts',(208.563301022643,3.69072512918956,126.179808900559));
#140479=CARTESIAN_POINT('Ctrl Pts',(208.555902556337,3.56803218366444,126.081891099022));
#140480=CARTESIAN_POINT('Ctrl Pts',(208.548504090031,3.44131136762011,125.988756902431));
#140481=CARTESIAN_POINT('Ctrl Pts',(208.541105623725,3.31097468788467,125.900752030139));
#140482=CARTESIAN_POINT('Ctrl Pts',(208.53371276603,3.18073681346501,125.812813872368));
#140483=CARTESIAN_POINT('Ctrl Pts',(208.526319908335,3.04688884180788,125.729997505443));
#140484=CARTESIAN_POINT('Ctrl Pts',(208.51892705064,2.90987480129162,125.652607595214));
#140485=CARTESIAN_POINT('Ctrl Pts',(208.511538175579,2.77293457211052,125.575259375987));
#140486=CARTESIAN_POINT('Ctrl Pts',(208.504149300517,2.63283199574196,125.503331975456));
#140487=CARTESIAN_POINT('Ctrl Pts',(208.496760425456,2.49003883636241,125.437085968742));
#140488=CARTESIAN_POINT('Ctrl Pts',(208.489372864132,2.34727106551612,125.370851740526));
#140489=CARTESIAN_POINT('Ctrl Pts',(208.481985302808,2.20181400050144,125.310297058228));
#140490=CARTESIAN_POINT('Ctrl Pts',(208.474597741484,2.05416277777801,125.255635913196));
#140491=CARTESIAN_POINT('Ctrl Pts',(208.467210559759,1.90651914189565,125.200977576845));
#140492=CARTESIAN_POINT('Ctrl Pts',(208.459823378033,1.75668192351523,125.152212305522));
#140493=CARTESIAN_POINT('Ctrl Pts',(208.452436196308,1.60516468869492,125.109505317853));
#140494=CARTESIAN_POINT('Ctrl Pts',(208.445047926206,1.45362513034552,125.066792038024));
#140495=CARTESIAN_POINT('Ctrl Pts',(208.437659656103,1.30040542302256,125.030138920576));
#140496=CARTESIAN_POINT('Ctrl Pts',(208.430271386,1.14603252496013,124.999660796366));
#140497=CARTESIAN_POINT('Ctrl Pts',(208.42288055916,0.991606205605298,124.969172125093));
#140498=CARTESIAN_POINT('Ctrl Pts',(208.41548973232,0.836026268007994,124.94486277379));
#140499=CARTESIAN_POINT('Ctrl Pts',(208.40809890548,0.679827884668699,124.926796104119));
#140500=CARTESIAN_POINT('Ctrl Pts',(208.400699950783,0.523457726470988,
124.908709566127));
#140501=CARTESIAN_POINT('Ctrl Pts',(208.393300996085,0.366468136359524,
124.896879462965));
#140502=CARTESIAN_POINT('Ctrl Pts',(208.385902041387,0.209398135492758,
124.891317155579));
#140503=CARTESIAN_POINT('Ctrl Pts',(208.378498546358,0.0522317494068543,
124.88575143491));
#140504=CARTESIAN_POINT('Ctrl Pts',(208.371095051329,-0.105014772330601,
124.886461171952));
#140505=CARTESIAN_POINT('Ctrl Pts',(208.3636915563,-0.261804959028031,124.893405641767));
#140506=CARTESIAN_POINT('Ctrl Pts',(208.356277419713,-0.418820511142279,
124.900360093349));
#140507=CARTESIAN_POINT('Ctrl Pts',(208.348863283127,-0.575378046221946,
124.91356714454));
#140508=CARTESIAN_POINT('Ctrl Pts',(208.341449146541,-0.730947916145645,
124.932934410384));
#140509=CARTESIAN_POINT('Ctrl Pts',(208.337404183401,-0.81582285500014,
124.943500694878));
#140510=CARTESIAN_POINT('Ctrl Pts',(208.333359220262,-0.900404006088913,
124.955899684651));
#140511=CARTESIAN_POINT('Ctrl Pts',(208.329314257123,-0.984607096318311,
124.970110072005));
#140512=CARTESIAN_POINT('Ctrl Pts',(208.321888582056,-1.13918570830919,
124.996197261288));
#140513=CARTESIAN_POINT('Ctrl Pts',(208.31446290699,-1.2929594256917,125.028471290496));
#140514=CARTESIAN_POINT('Ctrl Pts',(208.307037231924,-1.44539418231598,
125.066872820609));
#140515=CARTESIAN_POINT('Ctrl Pts',(208.299620316285,-1.59764912481468,
125.105229051752));
#140516=CARTESIAN_POINT('Ctrl Pts',(208.292203400647,-1.74856789230455,
125.149698305817));
#140517=CARTESIAN_POINT('Ctrl Pts',(208.284786485008,-1.89762360100986,
125.200169754347));
#140518=CARTESIAN_POINT('Ctrl Pts',(208.277376703944,-2.04653592813962,
125.250592652735));
#140519=CARTESIAN_POINT('Ctrl Pts',(208.26996692288,-2.19358841336712,125.307006132278));
#140520=CARTESIAN_POINT('Ctrl Pts',(208.262557141816,-2.3382665050408,125.369248814309));
#140521=CARTESIAN_POINT('Ctrl Pts',(208.255152876074,-2.48283690848986,
125.431445167253));
#140522=CARTESIAN_POINT('Ctrl Pts',(208.247748610331,-2.62503609623895,
125.49946193655));
#140523=CARTESIAN_POINT('Ctrl Pts',(208.240344344589,-2.76436687577973,
125.57308865574));
#140524=CARTESIAN_POINT('Ctrl Pts',(208.232943979269,-2.90362425857356,
125.646676589805));
#140525=CARTESIAN_POINT('Ctrl Pts',(208.22554361395,-3.04001591349676,125.725868414398));
#140526=CARTESIAN_POINT('Ctrl Pts',(208.218143248631,-3.17306685816016,
125.810406545276));
#140527=CARTESIAN_POINT('Ctrl Pts',(208.210744110281,-3.30609574317275,
125.894930659855));
#140528=CARTESIAN_POINT('Ctrl Pts',(208.203344971931,-3.43578470271374,
125.984799121566));
#140529=CARTESIAN_POINT('Ctrl Pts',(208.195945833582,-3.56168539721341,
126.079709551744));
#140530=CARTESIAN_POINT('Ctrl Pts',(208.188547021966,-3.68758053213906,
126.174615790828));
#140531=CARTESIAN_POINT('Ctrl Pts',(208.181148210351,-3.80968743678457,
126.274563331131));
#140532=CARTESIAN_POINT('Ctrl Pts',(208.173749398735,-3.92758891228548,
126.37920797629));
#140533=CARTESIAN_POINT('Ctrl Pts',(208.166349455627,-4.04550841834104,
126.48386862465));
#140534=CARTESIAN_POINT('Ctrl Pts',(208.158949512519,-4.15922093567722,
126.593227560529));
#140535=CARTESIAN_POINT('Ctrl Pts',(208.15154956941,-4.26834446912122,126.706902130232));
#140536=CARTESIAN_POINT('Ctrl Pts',(208.144147036186,-4.37750619780807,
126.820616488125));
#140537=CARTESIAN_POINT('Ctrl Pts',(208.136744502961,-4.48207548641057,
126.938649218448));
#140538=CARTESIAN_POINT('Ctrl Pts',(208.129341969737,-4.5817092353704,127.060582973926));
#140539=CARTESIAN_POINT('Ctrl Pts',(208.121931316487,-4.68145227509573,
127.182650481607));
#140540=CARTESIAN_POINT('Ctrl Pts',(208.114520663238,-4.77624872702756,
127.308627271148));
#140541=CARTESIAN_POINT('Ctrl Pts',(208.107110009989,-4.86579718354771,
127.438064681217));
#140542=CARTESIAN_POINT('Ctrl Pts',(208.099694803174,-4.95540066419993,
127.567581625668));
#140543=CARTESIAN_POINT('Ctrl Pts',(208.092279596359,-5.03974952437945,
127.700563113604));
#140544=CARTESIAN_POINT('Ctrl Pts',(208.084864389544,-5.1185875629994,127.836534490178));
#140545=CARTESIAN_POINT('Ctrl Pts',(208.077438621532,-5.1975378876451,127.972699525621));
#140546=CARTESIAN_POINT('Ctrl Pts',(208.070012853519,-5.27096154115178,
128.111862625628));
#140547=CARTESIAN_POINT('Ctrl Pts',(208.062587085507,-5.33864947802633,
128.25352696692));
#140548=CARTESIAN_POINT('Ctrl Pts',(208.058680268108,-5.37426120317554,
128.328058882332));
#140549=CARTESIAN_POINT('Ctrl Pts',(208.054773450709,-5.40828610965599,
128.403282833115));
#140550=CARTESIAN_POINT('Ctrl Pts',(208.05086663331,-5.44069928145357,128.479124738931));
#140551=CARTESIAN_POINT('Ctrl Pts',(208.042629123207,-5.50904233485686,
128.639037118127));
#140552=CARTESIAN_POINT('Ctrl Pts',(208.034391613105,-5.57039277901538,
128.802108281298));
#140553=CARTESIAN_POINT('Ctrl Pts',(208.026154103002,-5.62447863771873,
128.967741273133));
#140554=CARTESIAN_POINT('Ctrl Pts',(208.01794965263,-5.67834743278805,129.132709527456));
#140555=CARTESIAN_POINT('Ctrl Pts',(208.009745202257,-5.72500972152271,
129.300218882322));
#140556=CARTESIAN_POINT('Ctrl Pts',(208.001540751885,-5.76424268442704,
129.469655842146));
#140557=CARTESIAN_POINT('Ctrl Pts',(207.993357644752,-5.80337358582728,
129.638652024886));
#140558=CARTESIAN_POINT('Ctrl Pts',(207.98517453762,-5.83511364888881,129.80956558809));
#140559=CARTESIAN_POINT('Ctrl Pts',(207.976991430487,-5.85928927127411,
129.981767280593));
#140560=CARTESIAN_POINT('Ctrl Pts',(207.968843187868,-5.88336189228223,
130.153235299679));
#140561=CARTESIAN_POINT('Ctrl Pts',(207.960694945248,-5.8999343002241,130.325980274811));
#140562=CARTESIAN_POINT('Ctrl Pts',(207.952546702629,-5.90888377768745,
130.49936379089));
#140563=CARTESIAN_POINT('Ctrl Pts',(207.947822886293,-5.91407209740434,
130.599880175086));
#140564=CARTESIAN_POINT('Ctrl Pts',(207.943099069957,-5.91669932500736,
130.700610864797));
#140565=CARTESIAN_POINT('Ctrl Pts',(207.938375253621,-5.91674927385308,
130.801429259683));
#140566=CARTESIAN_POINT('',(206.188375157632,-5.91498635325863,130.809335103955));
#140567=CARTESIAN_POINT('Ctrl Pts',(207.938375192211,-5.90834445110727,
130.801434732496));
#140568=CARTESIAN_POINT('Ctrl Pts',(207.88305646464,-5.90301392988973,131.980404529528));
#140569=CARTESIAN_POINT('Ctrl Pts',(207.734921862463,-4.98909168451827,
135.145083942105));
#140570=CARTESIAN_POINT('Ctrl Pts',(207.493971385684,0.173518526030102,
137.800670327432));
#140571=CARTESIAN_POINT('Ctrl Pts',(207.21552376187,5.97986291472846,134.440038130778));
#140572=CARTESIAN_POINT('Ctrl Pts',(206.937076138059,6.29112482667552,127.7385118325));
#140573=CARTESIAN_POINT('Ctrl Pts',(206.658628514245,0.821087121814331,
123.854289400871));
#140574=CARTESIAN_POINT('Ctrl Pts',(206.409061532297,-4.75784521223805,
126.09730669271));
#140575=CARTESIAN_POINT('Ctrl Pts',(206.252310424952,-5.90151704252715,
129.448939722285));
#140576=CARTESIAN_POINT('Ctrl Pts',(206.188375192211,-5.91227720962736,
130.809332089608));
#140577=CARTESIAN_POINT('',(204.438375192211,-5.92105141345348,130.805327648265));
#140578=CARTESIAN_POINT('Ctrl Pts',(206.188375135149,-5.91674790721062,
130.80933706396));
#140579=CARTESIAN_POINT('Ctrl Pts',(206.179566065341,-5.91659014051484,
130.996913839284));
#140580=CARTESIAN_POINT('Ctrl Pts',(206.170756995534,-5.90750858188079,
131.184105581818));
#140581=CARTESIAN_POINT('Ctrl Pts',(206.161947925727,-5.88963571160845,
131.370153642484));
#140582=CARTESIAN_POINT('Ctrl Pts',(206.153074186251,-5.87163163195439,
131.557567530276));
#140583=CARTESIAN_POINT('Ctrl Pts',(206.144200446775,-5.84470678641371,
131.74382085212));
#140584=CARTESIAN_POINT('Ctrl Pts',(206.135326707299,-5.80904529038186,
131.928159254686));
#140585=CARTESIAN_POINT('Ctrl Pts',(206.126381804847,-5.77309780689119,
132.113975959543));
#140586=CARTESIAN_POINT('Ctrl Pts',(206.117436902394,-5.72827303913071,
132.297846882214));
#140587=CARTESIAN_POINT('Ctrl Pts',(206.108491999942,-5.67480770886274,
132.479021189124));
#140588=CARTESIAN_POINT('Ctrl Pts',(206.106239088835,-5.66134164402378,
132.524652721779));
#140589=CARTESIAN_POINT('Ctrl Pts',(206.103986177728,-5.64732768966758,
132.570113299786));
#140590=CARTESIAN_POINT('Ctrl Pts',(206.101733266621,-5.63277009911369,
132.615391145478));
#140591=CARTESIAN_POINT('Ctrl Pts',(206.094310026419,-5.58480349665586,
132.764579599188));
#140592=CARTESIAN_POINT('Ctrl Pts',(206.086886786216,-5.53083319938669,
132.91208669215));
#140593=CARTESIAN_POINT('Ctrl Pts',(206.079463546014,-5.47099418136574,
133.057392625763));
#140594=CARTESIAN_POINT('Ctrl Pts',(206.072049079851,-5.41122589119732,
133.202526812296));
#140595=CARTESIAN_POINT('Ctrl Pts',(206.064634613687,-5.34560282846522,
133.345464676374));
#140596=CARTESIAN_POINT('Ctrl Pts',(206.057220147523,-5.274309902267,133.485700882685));
#140597=CARTESIAN_POINT('Ctrl Pts',(206.049812828053,-5.20308569425869,
133.625801917405));
#140598=CARTESIAN_POINT('Ctrl Pts',(206.042405508582,-5.12620267075052,
133.763206148049));
#140599=CARTESIAN_POINT('Ctrl Pts',(206.034998189112,-5.04389400946855,
133.897427668851));
#140600=CARTESIAN_POINT('Ctrl Pts',(206.027596394619,-4.96164674063805,
134.031549076396));
#140601=CARTESIAN_POINT('Ctrl Pts',(206.020194600126,-4.87398208622341,
134.162492184038));
#140602=CARTESIAN_POINT('Ctrl Pts',(206.012792805633,-4.78117932515222,
134.289795285328));
#140603=CARTESIAN_POINT('Ctrl Pts',(206.005394918777,-4.68842555753051,
134.417031179371));
#140604=CARTESIAN_POINT('Ctrl Pts',(205.99799703192,-4.59053930480269,134.540630593273));
#140605=CARTESIAN_POINT('Ctrl Pts',(205.990599145064,-4.48784330175735,
134.660160542533));
#140606=CARTESIAN_POINT('Ctrl Pts',(205.983202487927,-4.38516436944237,
134.779670622824));
#140607=CARTESIAN_POINT('Ctrl Pts',(205.975805830791,-4.27767751662466,
134.895112298157));
#140608=CARTESIAN_POINT('Ctrl Pts',(205.968409173654,-4.16574599834706,
135.0060853634));
#140609=CARTESIAN_POINT('Ctrl Pts',(205.961012844691,-4.05381944622384,
135.117053505014));
#140610=CARTESIAN_POINT('Ctrl Pts',(205.953616515728,-3.93744888583708,
135.223553167924));
#140611=CARTESIAN_POINT('Ctrl Pts',(205.946220186765,-3.81703449993298,
135.325220954805));
#140612=CARTESIAN_POINT('Ctrl Pts',(205.938822725573,-3.69660168102824,
135.426904304962));
#140613=CARTESIAN_POINT('Ctrl Pts',(205.931425264382,-3.5721240892894,135.523754065483));
#140614=CARTESIAN_POINT('Ctrl Pts',(205.924027803191,-3.44403492469912,
135.61544718922));
#140615=CARTESIAN_POINT('Ctrl Pts',(205.916627748971,-3.31590086107405,
135.707172454105));
#140616=CARTESIAN_POINT('Ctrl Pts',(205.909227694752,-3.18415300742791,
135.793737266225));
#140617=CARTESIAN_POINT('Ctrl Pts',(205.901827640532,-3.04925332393586,
135.874862045331));
#140618=CARTESIAN_POINT('Ctrl Pts',(205.894419449247,-2.9142053053851,135.956076028864));
#140619=CARTESIAN_POINT('Ctrl Pts',(205.887011257962,-2.77599885578924,
136.031837840764));
#140620=CARTESIAN_POINT('Ctrl Pts',(205.879603066678,-2.63512094888712,
136.10191365149));
#140621=CARTESIAN_POINT('Ctrl Pts',(205.872190315849,-2.49415633539396,
136.172032592006));
#140622=CARTESIAN_POINT('Ctrl Pts',(205.864777565021,-2.35051732811826,
136.236458405575));
#140623=CARTESIAN_POINT('Ctrl Pts',(205.857364814192,-2.20471013894131,
136.295005731371));
#140624=CARTESIAN_POINT('Ctrl Pts',(205.849941471535,-2.05869461081846,
136.353636713455));
#140625=CARTESIAN_POINT('Ctrl Pts',(205.842518128878,-1.91050506407407,
136.406372307113));
#140626=CARTESIAN_POINT('Ctrl Pts',(205.835094786222,-1.76066288435223,
136.453077000087));
#140627=CARTESIAN_POINT('Ctrl Pts',(205.831158405083,-1.68120596618447,
136.477843130523));
#140628=CARTESIAN_POINT('Ctrl Pts',(205.827222023945,-1.60128453480154,
136.500914311524));
#140629=CARTESIAN_POINT('Ctrl Pts',(205.823285642806,-1.5209772722179,136.52227620805));
#140630=CARTESIAN_POINT('Ctrl Pts',(205.815862363887,-1.36953278846232,
136.562560751281));
#140631=CARTESIAN_POINT('Ctrl Pts',(205.808439084968,-1.21625774237482,
136.596885322964));
#140632=CARTESIAN_POINT('Ctrl Pts',(205.801015806049,-1.06166241873887,
136.625082520486));
#140633=CARTESIAN_POINT('Ctrl Pts',(205.793601300696,-0.907249811172222,
136.653246391767));
#140634=CARTESIAN_POINT('Ctrl Pts',(205.786186795344,-0.751520395763363,
136.675297237676));
#140635=CARTESIAN_POINT('Ctrl Pts',(205.778772289991,-0.594999279427515,
136.691117485314));
#140636=CARTESIAN_POINT('Ctrl Pts',(205.771364930901,-0.438629021562489,
136.706922485052));
#140637=CARTESIAN_POINT('Ctrl Pts',(205.76395757181,-0.281468950781068,
136.716508804378));
#140638=CARTESIAN_POINT('Ctrl Pts',(205.75655021272,-0.124053917183144,
136.719809982418));
#140639=CARTESIAN_POINT('Ctrl Pts',(205.749148378216,0.0332437125062621,
136.723108698361));
#140640=CARTESIAN_POINT('Ctrl Pts',(205.741746543712,0.190795554774945,
136.720131598888));
#140641=CARTESIAN_POINT('Ctrl Pts',(205.734344709207,0.348062200778197,
136.710864089747));
#140642=CARTESIAN_POINT('Ctrl Pts',(205.726946781988,0.505245828778614,
136.701601472745));
#140643=CARTESIAN_POINT('Ctrl Pts',(205.719548854768,0.662144188633564,
136.686055081083));
#140644=CARTESIAN_POINT('Ctrl Pts',(205.712150927548,0.818218547581937,
136.664262406068));
#140645=CARTESIAN_POINT('Ctrl Pts',(205.704754229649,0.97426697149117,136.642473352365));
#140646=CARTESIAN_POINT('Ctrl Pts',(205.697357531751,1.12949129690173,136.614440126908));
#140647=CARTESIAN_POINT('Ctrl Pts',(205.689960833853,1.28335846744775,136.580252029853));
#140648=CARTESIAN_POINT('Ctrl Pts',(205.682564463884,1.43721881635304,136.546065448514));
#140649=CARTESIAN_POINT('Ctrl Pts',(205.675168093915,1.5897217656208,136.505724619111));
#140650=CARTESIAN_POINT('Ctrl Pts',(205.667771723946,1.74034526633639,136.459369805573));
#140651=CARTESIAN_POINT('Ctrl Pts',(205.66037422154,1.89099182858503,136.413007894781));
#140652=CARTESIAN_POINT('Ctrl Pts',(205.652976719135,2.03975801251326,136.360630276258));
#140653=CARTESIAN_POINT('Ctrl Pts',(205.645579216729,2.18613787059475,136.30242680244));
#140654=CARTESIAN_POINT('Ctrl Pts',(205.63817912112,2.3325690423081,136.244202925325));
#140655=CARTESIAN_POINT('Ctrl Pts',(205.630779025511,2.47661187598612,136.180149264629));
#140656=CARTESIAN_POINT('Ctrl Pts',(205.623378929902,2.61778144864533,136.110503364386));
#140657=CARTESIAN_POINT('Ctrl Pts',(205.61597069717,2.75910625094721,136.040780881718));
#140658=CARTESIAN_POINT('Ctrl Pts',(205.608562464438,2.89755114766472,135.965454044387));
#140659=CARTESIAN_POINT('Ctrl Pts',(205.601154231705,3.03265618688166,135.884806170337));
#140660=CARTESIAN_POINT('Ctrl Pts',(205.593741439334,3.16784438091394,135.804108658914));
#140661=CARTESIAN_POINT('Ctrl Pts',(205.586328646963,3.29968830944655,135.718083788424));
#140662=CARTESIAN_POINT('Ctrl Pts',(205.578915854592,3.4277584000582,135.627057260869));
#140663=CARTESIAN_POINT('Ctrl Pts',(205.571492470601,3.55601148104427,135.535900671891));
#140664=CARTESIAN_POINT('Ctrl Pts',(205.56406908661,3.68047966012121,135.439728380284));
#140665=CARTESIAN_POINT('Ctrl Pts',(205.55664570262,3.80076710215312,135.338905798473));
#140666=CARTESIAN_POINT('Ctrl Pts',(205.552709808078,3.86454376885181,135.285449443535));
#140667=CARTESIAN_POINT('Ctrl Pts',(205.548773913536,3.92714579463605,135.230686447014));
#140668=CARTESIAN_POINT('Ctrl Pts',(205.544838018994,3.98851860995265,135.174675235595));
#140669=CARTESIAN_POINT('Ctrl Pts',(205.537414752403,4.10427038243128,135.069035678946));
#140670=CARTESIAN_POINT('Ctrl Pts',(205.529991485813,4.21599734533866,134.958634520244));
#140671=CARTESIAN_POINT('Ctrl Pts',(205.522568219222,4.32328283706097,134.843810589193));
#140672=CARTESIAN_POINT('Ctrl Pts',(205.515153726284,4.43044152670348,134.729122369998));
#140673=CARTESIAN_POINT('Ctrl Pts',(205.507739233346,4.53316894181514,134.610022053583));
#140674=CARTESIAN_POINT('Ctrl Pts',(205.500324740408,4.63108233208609,134.486887874212));
#140675=CARTESIAN_POINT('Ctrl Pts',(205.492917393806,4.7289013501625,134.363872375674));
#140676=CARTESIAN_POINT('Ctrl Pts',(205.485510047204,4.82191534978399,134.236831044588));
#140677=CARTESIAN_POINT('Ctrl Pts',(205.478102700602,4.90977931610782,134.106177939833));
#140678=CARTESIAN_POINT('Ctrl Pts',(205.470700878647,4.99757775054161,133.975622280541));
#140679=CARTESIAN_POINT('Ctrl Pts',(205.463299056693,5.08023359234056,133.841460519697));
#140680=CARTESIAN_POINT('Ctrl Pts',(205.455897234738,5.15744299933014,133.704138586853));
#140681=CARTESIAN_POINT('Ctrl Pts',(205.448499320116,5.23461164839757,133.566889144614));
#140682=CARTESIAN_POINT('Ctrl Pts',(205.441101405494,5.30633940608169,133.426483177278));
#140683=CARTESIAN_POINT('Ctrl Pts',(205.433703490873,5.37236661664779,133.283394199192));
#140684=CARTESIAN_POINT('Ctrl Pts',(205.426306805605,5.4383828550952,133.140328999019));
#140685=CARTESIAN_POINT('Ctrl Pts',(205.418910120337,5.49870027026613,132.994582011598));
#140686=CARTESIAN_POINT('Ctrl Pts',(205.411513435069,5.55310586287155,132.846649979591));
#140687=CARTESIAN_POINT('Ctrl Pts',(205.40411707775,5.60750904328352,132.698724506482));
#140688=CARTESIAN_POINT('Ctrl Pts',(205.396720720431,5.6560007934494,132.548614531768));
#140689=CARTESIAN_POINT('Ctrl Pts',(205.389324363111,5.6984169411165,132.396835084456));
#140690=CARTESIAN_POINT('Ctrl Pts',(205.381926873363,5.74083958296442,132.245032398749));
#140691=CARTESIAN_POINT('Ctrl Pts',(205.374529383615,5.77718466965693,132.091560091043));
#140692=CARTESIAN_POINT('Ctrl Pts',(205.367131893866,5.80733845234025,131.936946447634));
#140693=CARTESIAN_POINT('Ctrl Pts',(205.359731810911,5.83750280549823,131.782278604073));
#140694=CARTESIAN_POINT('Ctrl Pts',(205.352331727957,5.8614714620337,131.626468994384));
#140695=CARTESIAN_POINT('Ctrl Pts',(205.344931645002,5.87918216165979,131.470053994821));
#140696=CARTESIAN_POINT('Ctrl Pts',(205.337523424855,5.89691233611661,131.313467000041));
#140697=CARTESIAN_POINT('Ctrl Pts',(205.330115204709,5.90837076922905,131.156273657112));
#140698=CARTESIAN_POINT('Ctrl Pts',(205.322706984562,5.91354720906745,130.999014075358));
#140699=CARTESIAN_POINT('Ctrl Pts',(205.315294204756,5.91872683493454,130.84165770246));
#140700=CARTESIAN_POINT('Ctrl Pts',(205.30788142495,5.91761676570394,130.684235381923));
#140701=CARTESIAN_POINT('Ctrl Pts',(205.300468645144,5.91025882921648,130.527284573548));
#140702=CARTESIAN_POINT('Ctrl Pts',(205.293045273578,5.90289037933228,130.370109505815));
#140703=CARTESIAN_POINT('Ctrl Pts',(205.285621902013,5.88925626469626,130.213407666724));
#140704=CARTESIAN_POINT('Ctrl Pts',(205.278198530447,5.86944995847761,130.057709596387));
#140705=CARTESIAN_POINT('Ctrl Pts',(205.274262485358,5.85894819204549,129.975154840818));
#140706=CARTESIAN_POINT('Ctrl Pts',(205.270326440269,5.84671205599,129.892882092421));
#140707=CARTESIAN_POINT('Ctrl Pts',(205.266390395181,5.8327612125786,129.810968852179));
#140708=CARTESIAN_POINT('Ctrl Pts',(205.258967132391,5.80645034102074,129.656482941948));
#140709=CARTESIAN_POINT('Ctrl Pts',(205.251543869601,5.77395789796265,129.502809451314));
#140710=CARTESIAN_POINT('Ctrl Pts',(205.244120606812,5.73534373383937,129.350482074768));
#140711=CARTESIAN_POINT('Ctrl Pts',(205.236706117758,5.69677520874019,129.198334737669));
#140712=CARTESIAN_POINT('Ctrl Pts',(205.229291628704,5.65209945553443,129.047530706073));
#140713=CARTESIAN_POINT('Ctrl Pts',(205.22187713965,5.60142780672731,128.898596443141));
#140714=CARTESIAN_POINT('Ctrl Pts',(205.214469797011,5.55080499751139,128.749805729682));
#140715=CARTESIAN_POINT('Ctrl Pts',(205.207062454371,5.49419791719723,128.602881548161));
#140716=CARTESIAN_POINT('Ctrl Pts',(205.199655111732,5.43176843551374,128.458337977979));
#140717=CARTESIAN_POINT('Ctrl Pts',(205.192253293815,5.36938551648445,128.313902214751));
#140718=CARTESIAN_POINT('Ctrl Pts',(205.184851475898,5.30118899017215,128.171843868699));
#140719=CARTESIAN_POINT('Ctrl Pts',(205.17744965798,5.22738979486144,128.03265960644));
#140720=CARTESIAN_POINT('Ctrl Pts',(205.170051747467,5.15362955798969,127.893548819258));
#140721=CARTESIAN_POINT('Ctrl Pts',(205.162653836954,5.07427271682429,127.757309423218));
#140722=CARTESIAN_POINT('Ctrl Pts',(205.155255926441,4.98957730139766,127.624415819951));
#140723=CARTESIAN_POINT('Ctrl Pts',(205.147859245375,4.90489596136757,127.491544302061));
#140724=CARTESIAN_POINT('Ctrl Pts',(205.140462564308,4.81487800835612,127.362017787878));
#140725=CARTESIAN_POINT('Ctrl Pts',(205.133065883242,4.7198262340098,127.236283981162));
#140726=CARTESIAN_POINT('Ctrl Pts',(205.125669530182,4.62477867473806,127.110555750117));
#140727=CARTESIAN_POINT('Ctrl Pts',(205.118273177122,4.52469796309431,126.988620189907));
#140728=CARTESIAN_POINT('Ctrl Pts',(205.110876824062,4.41992866778351,126.870893808985));
#140729=CARTESIAN_POINT('Ctrl Pts',(205.103479338627,4.31514333238748,126.753149404261));
#140730=CARTESIAN_POINT('Ctrl Pts',(205.096081853192,4.20566823223877,126.639615740833));
#140731=CARTESIAN_POINT('Ctrl Pts',(205.088684367756,4.0918863448901,126.53067407045));
#140732=CARTESIAN_POINT('Ctrl Pts',(205.081284289166,3.97806457180816,126.42169421105));
#140733=CARTESIAN_POINT('Ctrl Pts',(205.073884210575,3.85993327514114,126.317309807603));
#140734=CARTESIAN_POINT('Ctrl Pts',(205.066484131984,3.73791006961344,126.217863165917));
#140735=CARTESIAN_POINT('Ctrl Pts',(205.059075916258,3.61575268720724,126.118307172572));
#140736=CARTESIAN_POINT('Ctrl Pts',(205.051667700531,3.48969513894966,126.02370002017));
#140737=CARTESIAN_POINT('Ctrl Pts',(205.044259484804,3.36018629211852,125.93434227625));
#140738=CARTESIAN_POINT('Ctrl Pts',(205.036846709456,3.23059773496496,125.844929534275));
#140739=CARTESIAN_POINT('Ctrl Pts',(205.029433934108,3.09755396123104,125.76077283788));
#140740=CARTESIAN_POINT('Ctrl Pts',(205.02202115876,2.9615297594948,125.682127506302));
#140741=CARTESIAN_POINT('Ctrl Pts',(205.014597791674,2.82531119969063,125.603369802408));
#140742=CARTESIAN_POINT('Ctrl Pts',(205.007174424588,2.68610403603951,125.530139364625));
#140743=CARTESIAN_POINT('Ctrl Pts',(204.999751057502,2.5444051509773,125.462644321264));
#140744=CARTESIAN_POINT('Ctrl Pts',(204.995814962124,2.46927208532876,125.42685639307));
#140745=CARTESIAN_POINT('Ctrl Pts',(204.991878866746,2.39343879236606,125.39268011218));
#140746=CARTESIAN_POINT('Ctrl Pts',(204.987942771368,2.31698110677334,125.360140828344));
#140747=CARTESIAN_POINT('Ctrl Pts',(204.980519502944,2.17278594159917,125.298773454077));
#140748=CARTESIAN_POINT('Ctrl Pts',(204.97309623452,2.02593299682858,125.243045954815));
#140749=CARTESIAN_POINT('Ctrl Pts',(204.965672966097,1.87690363642786,125.193196451186));
#140750=CARTESIAN_POINT('Ctrl Pts',(204.958258471337,1.7280504158966,125.143405865378));
#140751=CARTESIAN_POINT('Ctrl Pts',(204.950843976577,1.57702625054469,125.099479563857));
#140752=CARTESIAN_POINT('Ctrl Pts',(204.943429481818,1.42433424764934,125.061608445177));
#140753=CARTESIAN_POINT('Ctrl Pts',(204.936022133407,1.27178941463677,125.023773828004));
#140754=CARTESIAN_POINT('Ctrl Pts',(204.928614784996,1.11758030422428,124.991982864216));
#140755=CARTESIAN_POINT('Ctrl Pts',(204.921207436585,0.962226921405626,
124.966377240215));
#140756=CARTESIAN_POINT('Ctrl Pts',(204.913805612837,0.80698940662729,124.940790713794));
#140757=CARTESIAN_POINT('Ctrl Pts',(204.906403789088,0.650609685497499,
124.921380402016));
#140758=CARTESIAN_POINT('Ctrl Pts',(204.899001965339,0.493619635819424,
124.908237296465));
#140759=CARTESIAN_POINT('Ctrl Pts',(204.89160404894,0.336712459641496,124.89510112903));
#140760=CARTESIAN_POINT('Ctrl Pts',(204.884206132541,0.179195967619653,
124.888225610057));
#140761=CARTESIAN_POINT('Ctrl Pts',(204.876808216143,0.0216087595666902,
124.887650076733));
#140762=CARTESIAN_POINT('Ctrl Pts',(204.869411529128,-0.135952260670864,
124.88707463905));
#140763=CARTESIAN_POINT('Ctrl Pts',(204.862014842114,-0.293583600686453,
124.89279711053));
#140764=CARTESIAN_POINT('Ctrl Pts',(204.854618155099,-0.450744927651624,
124.90480473829));
#140765=CARTESIAN_POINT('Ctrl Pts',(204.847221796053,-0.607899286109743,
124.916811833635));
#140766=CARTESIAN_POINT('Ctrl Pts',(204.839825437006,-0.764583300742472,
124.935103502707));
#140767=CARTESIAN_POINT('Ctrl Pts',(204.83242907796,-0.920260302747,124.95961498258));
#140768=CARTESIAN_POINT('Ctrl Pts',(204.825031586505,-1.07596113944049,
124.984130215246));
#140769=CARTESIAN_POINT('Ctrl Pts',(204.81763409505,-1.23065428774014,125.014867096753));
#140770=CARTESIAN_POINT('Ctrl Pts',(204.810236603595,-1.38381198042967,
125.051709492622));
#140771=CARTESIAN_POINT('Ctrl Pts',(204.802836518957,-1.53702336240519,
125.088564803558));
#140772=CARTESIAN_POINT('Ctrl Pts',(204.795436434318,-1.68869785439576,
125.131529802889));
#140773=CARTESIAN_POINT('Ctrl Pts',(204.78803634968,-1.83832173330245,125.180438163676));
#140774=CARTESIAN_POINT('Ctrl Pts',(204.780628127893,-1.98811013894526,
125.229400304201));
#140775=CARTESIAN_POINT('Ctrl Pts',(204.773219906105,-2.13584307336326,
125.284318741618));
#140776=CARTESIAN_POINT('Ctrl Pts',(204.765811684318,-2.2810250362999,125.344978294787));
#140777=CARTESIAN_POINT('Ctrl Pts',(204.758398902893,-2.42629635631982,
125.405675182902));
#140778=CARTESIAN_POINT('Ctrl Pts',(204.750986121469,-2.56901323864276,
125.47212007064));
#140779=CARTESIAN_POINT('Ctrl Pts',(204.743573340044,-2.70870424060689,
125.544051510734));
#140780=CARTESIAN_POINT('Ctrl Pts',(204.736149966909,-2.84859483927297,
125.616085729662));
#140781=CARTESIAN_POINT('Ctrl Pts',(204.728726593773,-2.98545059862428,
125.693621974519));
#140782=CARTESIAN_POINT('Ctrl Pts',(204.721303220637,-3.11882783680492,
125.77635470201));
#140783=CARTESIAN_POINT('Ctrl Pts',(204.717367196277,-3.18954717814477,
125.820221287307));
#140784=CARTESIAN_POINT('Ctrl Pts',(204.713431171916,-3.25928911964002,
125.865548075032));
#140785=CARTESIAN_POINT('Ctrl Pts',(204.709495147555,-3.3279913467505,125.912284968268));
#140786=CARTESIAN_POINT('Ctrl Pts',(204.702104411593,-3.45699461857756,
126.000043580996));
#140787=CARTESIAN_POINT('Ctrl Pts',(204.694713675631,-3.58272775527118,
126.093046915379));
#140788=CARTESIAN_POINT('Ctrl Pts',(204.68732293967,-3.70473253445668,126.191022627494));
#140789=CARTESIAN_POINT('Ctrl Pts',(204.679940958213,-3.82659279604236,
126.288882285019));
#140790=CARTESIAN_POINT('Ctrl Pts',(204.672558976756,-3.94473319850045,
126.391702364622));
#140791=CARTESIAN_POINT('Ctrl Pts',(204.665176995299,-4.05872330506565,
126.499166580659));
#140792=CARTESIAN_POINT('Ctrl Pts',(204.657802110667,-4.17260382482097,
126.60652748369));
#140793=CARTESIAN_POINT('Ctrl Pts',(204.650427226035,-4.28234171832161,
126.71852337928));
#140794=CARTESIAN_POINT('Ctrl Pts',(204.643052341403,-4.38753867962024,
126.83479705247));
#140795=CARTESIAN_POINT('Ctrl Pts',(204.635682901836,-4.49265797131831,
126.950984877841));
#140796=CARTESIAN_POINT('Ctrl Pts',(204.628313462269,-4.59324275370197,
127.071443914587));
#140797=CARTESIAN_POINT('Ctrl Pts',(204.620944022703,-4.68893086223868,
127.195779465417));
#140798=CARTESIAN_POINT('Ctrl Pts',(204.613336988099,-4.78770401129907,
127.324123667047));
#140799=CARTESIAN_POINT('Ctrl Pts',(204.605729953495,-4.88125914129115,
127.45659826124));
#140800=CARTESIAN_POINT('Ctrl Pts',(204.598122918891,-4.96924186267879,
127.592730833064));
#140801=CARTESIAN_POINT('Ctrl Pts',(204.590758398115,-5.05441967681546,
127.724523470504));
#140802=CARTESIAN_POINT('Ctrl Pts',(204.583393877339,-5.13437472757324,
127.859744080796));
#140803=CARTESIAN_POINT('Ctrl Pts',(204.576029356562,-5.20882895299715,
127.997933796692));
#140804=CARTESIAN_POINT('Ctrl Pts',(204.568664962593,-5.283281896423,128.136121133155));
#140805=CARTESIAN_POINT('Ctrl Pts',(204.561300568623,-5.35223402382612,
128.277277141798));
#140806=CARTESIAN_POINT('Ctrl Pts',(204.553936174654,-5.41545310427121,
128.420918099287));
#140807=CARTESIAN_POINT('Ctrl Pts',(204.54657042013,-5.47868386429348,128.564585594107));
#140808=CARTESIAN_POINT('Ctrl Pts',(204.539204665606,-5.53617931718692,
128.710738606591));
#140809=CARTESIAN_POINT('Ctrl Pts',(204.531838911082,-5.58775535548524,
128.858873365039));
#140810=CARTESIAN_POINT('Ctrl Pts',(204.524470308052,-5.63935133941324,
129.007065410574));
#140811=CARTESIAN_POINT('Ctrl Pts',(204.517101705023,-5.68502322819046,
129.157240371933));
#140812=CARTESIAN_POINT('Ctrl Pts',(204.509733101994,-5.7246368129675,129.308879450143));
#140813=CARTESIAN_POINT('Ctrl Pts',(204.502356410778,-5.76429387980796,
129.460684975799));
#140814=CARTESIAN_POINT('Ctrl Pts',(204.494979719562,-5.79787927133109,
129.613957462062));
#140815=CARTESIAN_POINT('Ctrl Pts',(204.487603028346,-5.82530980176946,
129.768167452221));
#140816=CARTESIAN_POINT('Ctrl Pts',(204.480221494494,-5.85275833974991,
129.922478677858));
#140817=CARTESIAN_POINT('Ctrl Pts',(204.472839960642,-5.87404391676752,
130.077728261269));
#140818=CARTESIAN_POINT('Ctrl Pts',(204.465458426791,-5.88913528604936,
130.233382382334));
#140819=CARTESIAN_POINT('Ctrl Pts',(204.458067024258,-5.90424683161207,
130.389244603885));
#140820=CARTESIAN_POINT('Ctrl Pts',(204.450675621726,-5.91314761819259,
130.545512068223));
#140821=CARTESIAN_POINT('Ctrl Pts',(204.443284219194,-5.91585846087386,
130.701651156428));
#140822=CARTESIAN_POINT('Ctrl Pts',(204.441647876866,-5.91645859956244,
130.736217938293));
#140823=CARTESIAN_POINT('Ctrl Pts',(204.440011534539,-5.91675556357633,
130.770778450004));
#140824=CARTESIAN_POINT('Ctrl Pts',(204.438375192211,-5.91674992108927,
130.805326945742));
#140825=CARTESIAN_POINT('',(202.688375192211,-5.91520709160217,130.79891930971));
#140826=CARTESIAN_POINT('Ctrl Pts',(204.438375192211,-5.92634035306676,
130.805328512059));
#140827=CARTESIAN_POINT('Ctrl Pts',(204.435932636055,-5.9264572190019,130.856982408026));
#140828=CARTESIAN_POINT('Ctrl Pts',(204.433490079899,-5.92584057372106,
130.908633442257));
#140829=CARTESIAN_POINT('Ctrl Pts',(204.338231649138,-5.87285210044721,
132.922235594029));
#140830=CARTESIAN_POINT('Ctrl Pts',(204.152599899928,-3.62660601729001,
136.789783698913));
#140831=CARTESIAN_POINT('Ctrl Pts',(203.874152276118,3.07543675800755,137.09079434209));
#140832=CARTESIAN_POINT('Ctrl Pts',(203.595704652303,6.95130345427144,131.614879558226));
#140833=CARTESIAN_POINT('Ctrl Pts',(203.317257028491,4.43926183532277,125.394137434058));
#140834=CARTESIAN_POINT('Ctrl Pts',(203.038809404678,-2.1522445239837,124.145126127266));
#140835=CARTESIAN_POINT('Ctrl Pts',(202.829182125918,-5.62563427618384,
127.811846704057));
#140836=CARTESIAN_POINT('Ctrl Pts',(202.712370721762,-5.91979598762536,
130.288990713325));
#140837=CARTESIAN_POINT('Ctrl Pts',(202.688375192211,-5.91520709160217,
130.79891930971));
#140838=CARTESIAN_POINT('',(200.938375192211,-5.90723919874194,130.805767413591));
#140839=CARTESIAN_POINT('Ctrl Pts',(202.688375192211,-5.91520709160217,
130.79891930971));
#140840=CARTESIAN_POINT('Ctrl Pts',(202.619554847158,-5.90204591476485,
132.26141930917));
#140841=CARTESIAN_POINT('Ctrl Pts',(202.457918627501,-4.61506249001968,
135.717037067151));
#140842=CARTESIAN_POINT('Ctrl Pts',(202.203466533238,1.18549267223545,137.701618597998));
#140843=CARTESIAN_POINT('Ctrl Pts',(201.925018909427,6.44364622673833,133.535108470905));
#140844=CARTESIAN_POINT('Ctrl Pts',(201.646571285612,5.78040368780743,126.859174470383));
#140845=CARTESIAN_POINT('Ctrl Pts',(201.368123661802,-0.194747451439191,
123.808673806412));
#140846=CARTESIAN_POINT('Ctrl Pts',(201.132058297333,-5.10870273655874,
126.672675766875));
#140847=CARTESIAN_POINT('Ctrl Pts',(200.98880880747,-5.90496142391559,129.730359660658));
#140848=CARTESIAN_POINT('Ctrl Pts',(200.938375192211,-5.90723919874194,
130.805767413591));
#140849=CARTESIAN_POINT('',(199.188375192211,-5.92038509218979,130.80931765918));
#140850=CARTESIAN_POINT('Ctrl Pts',(200.938375192211,-5.90723919874194,
130.805767413591));
#140851=CARTESIAN_POINT('Ctrl Pts',(200.895992932866,-5.90915334356233,
131.70949422463));
#140852=CARTESIAN_POINT('Ctrl Pts',(200.760794798915,-5.28885804543136,
134.58986393661));
#140853=CARTESIAN_POINT('Ctrl Pts',(200.532780790362,-0.799939293036777,
137.756889485374));
#140854=CARTESIAN_POINT('Ctrl Pts',(200.254333166548,5.41697271486199,135.235383878266));
#140855=CARTESIAN_POINT('Ctrl Pts',(199.975885542736,6.65595143161651,128.641984362081));
#140856=CARTESIAN_POINT('Ctrl Pts',(199.697437918923,1.77843594402775,124.035702986741));
#140857=CARTESIAN_POINT('Ctrl Pts',(199.434934468748,-4.36050283967217,
125.557080494142));
#140858=CARTESIAN_POINT('Ctrl Pts',(199.265246893177,-5.90575828303711,
129.179380091958));
#140859=CARTESIAN_POINT('Ctrl Pts',(199.188375192211,-5.92038509218979,
130.80931765918));
#140860=CARTESIAN_POINT('',(197.438375192211,-5.92351700154912,130.800613675003));
#140861=CARTESIAN_POINT('Ctrl Pts',(199.188375192211,-5.92038509218979,
130.80931765918));
#140862=CARTESIAN_POINT('Ctrl Pts',(199.172431018573,-5.92341887942187,
131.147387550494));
#140863=CARTESIAN_POINT('Ctrl Pts',(199.06367097033,-5.7429796640639,133.450227209526));
#140864=CARTESIAN_POINT('Ctrl Pts',(198.862095047485,-2.72093855833704,
137.252155115847));
#140865=CARTESIAN_POINT('Ctrl Pts',(198.583647423671,3.9539783690358,136.578753710139));
#140866=CARTESIAN_POINT('Ctrl Pts',(198.305199799859,6.99538233784591,130.598967147137));
#140867=CARTESIAN_POINT('Ctrl Pts',(198.026752176046,3.60837168160217,124.807927149431));
#140868=CARTESIAN_POINT('Ctrl Pts',(197.748304552233,-3.09455627127803,
124.527316566881));
#140869=CARTESIAN_POINT('Ctrl Pts',(197.552178890954,-5.81278598755467,
128.392589611084));
#140870=CARTESIAN_POINT('Ctrl Pts',(197.448869104281,-5.92515660607875,
130.578413788211));
#140871=CARTESIAN_POINT('Ctrl Pts',(197.438375192211,-5.92351700154912,
130.800613675003));
#140872=CARTESIAN_POINT('',(195.688375192211,-5.90858988324653,130.801212225252));
#140873=CARTESIAN_POINT('Ctrl Pts',(197.438375192211,-5.92351700154912,
130.800613675003));
#140874=CARTESIAN_POINT('Ctrl Pts',(197.356053229677,-5.91065473800382,
132.543712972427));
#140875=CARTESIAN_POINT('Ctrl Pts',(197.180915392537,-4.17421686252449,
136.274385756281));
#140876=CARTESIAN_POINT('Ctrl Pts',(196.912961680794,2.17250297652081,137.457013573142));
#140877=CARTESIAN_POINT('Ctrl Pts',(196.634514056981,6.77135626959459,132.57249375751));
#140878=CARTESIAN_POINT('Ctrl Pts',(196.356066433169,5.14766395005485,126.063145964373));
#140879=CARTESIAN_POINT('Ctrl Pts',(196.077618809355,-1.20648006222068,
123.910742816309));
#140880=CARTESIAN_POINT('Ctrl Pts',(195.85505506237,-5.39917704206329,127.253819372125));
#140881=CARTESIAN_POINT('Ctrl Pts',(195.725307189988,-5.91237200604756,
130.014152192806));
#140882=CARTESIAN_POINT('Ctrl Pts',(195.688375192211,-5.90858988324653,
130.801212225252));
#140883=CARTESIAN_POINT('',(193.938375192211,-5.91196518873725,130.809243212275));
#140884=CARTESIAN_POINT('Ctrl Pts',(195.688375192211,-5.90858988324653,
130.801212225252));
#140885=CARTESIAN_POINT('Ctrl Pts',(195.632491315384,-5.90286694115081,
131.992156895353));
#140886=CARTESIAN_POINT('Ctrl Pts',(195.483791563953,-4.97462506172764,
135.169312250667));
#140887=CARTESIAN_POINT('Ctrl Pts',(195.242275937916,0.216039013678407,
137.799422280975));
#140888=CARTESIAN_POINT('Ctrl Pts',(194.963828314104,6.00191785180767,134.403602569768));
#140889=CARTESIAN_POINT('Ctrl Pts',(194.685380690291,6.27232739411319,127.70025533723));
#140890=CARTESIAN_POINT('Ctrl Pts',(194.406933066478,0.778774481457,123.849429213348));
#140891=CARTESIAN_POINT('Ctrl Pts',(194.157931233786,-4.77381132895269,
126.121196694781));
#140892=CARTESIAN_POINT('Ctrl Pts',(194.001745275696,-5.90152936629919,
129.46069533092));
#140893=CARTESIAN_POINT('Ctrl Pts',(193.938375192211,-5.91196518873725,
130.809243212275));
#140894=CARTESIAN_POINT('',(192.188375873533,-5.92197168067619,130.805533319426));
#140895=CARTESIAN_POINT('Ctrl Pts',(193.938375192211,-5.91196518873725,
130.809243212275));
#140896=CARTESIAN_POINT('Ctrl Pts',(193.908929401091,-5.91681433885312,
131.435864751108));
#140897=CARTESIAN_POINT('Ctrl Pts',(193.78666773537,-5.53611148477146,134.031915457605));
#140898=CARTESIAN_POINT('Ctrl Pts',(193.571590195038,-1.75782624092181,
137.578399843691));
#140899=CARTESIAN_POINT('Ctrl Pts',(193.293142571227,4.74904303118782,135.944803285106));
#140900=CARTESIAN_POINT('Ctrl Pts',(193.014694947413,6.89177376128537,129.587391039638));
#140901=CARTESIAN_POINT('Ctrl Pts',(192.736247323601,2.70130108662762,124.348314384016));
#140902=CARTESIAN_POINT('Ctrl Pts',(192.46080781812,-3.8994475031143,125.034534503354));
#140903=CARTESIAN_POINT('Ctrl Pts',(192.278184187244,-5.92103596021112,
128.906232297951));
#140904=CARTESIAN_POINT('Ctrl Pts',(192.188376430972,-5.92624401559878,
130.805522386918));
#140905=CARTESIAN_POINT('',(190.438375193894,-5.91568182138061,130.798900870218));
#140906=CARTESIAN_POINT('Ctrl Pts',(192.188375192211,-5.91674988112158,
130.805546681526));
#140907=CARTESIAN_POINT('Ctrl Pts',(192.185367486799,-5.91673715075054,
130.869052886841));
#140908=CARTESIAN_POINT('Ctrl Pts',(192.182359781387,-5.91570200665032,
130.932547687523));
#140909=CARTESIAN_POINT('Ctrl Pts',(192.179352075975,-5.91364535475517,
130.996009204001));
#140910=CARTESIAN_POINT('Ctrl Pts',(192.17192880957,-5.90856936730653,131.152637489943));
#140911=CARTESIAN_POINT('Ctrl Pts',(192.164505543164,-5.89725874201999,
131.309300813403));
#140912=CARTESIAN_POINT('Ctrl Pts',(192.157082276759,-5.87970025871574,
131.465462296703));
#140913=CARTESIAN_POINT('Ctrl Pts',(192.149667784038,-5.86216252808058,
131.621439210099));
#140914=CARTESIAN_POINT('Ctrl Pts',(192.142253291317,-5.83839167951754,
131.776915096634));
#140915=CARTESIAN_POINT('Ctrl Pts',(192.134838798596,-5.80842648002977,
131.931353247794));
#140916=CARTESIAN_POINT('Ctrl Pts',(192.127431452242,-5.77849016212943,
132.08564254565));
#140917=CARTESIAN_POINT('Ctrl Pts',(192.120024105888,-5.74237144971965,
132.238895735347));
#140918=CARTESIAN_POINT('Ctrl Pts',(192.112616759534,-5.70016086098663,
132.390581510562));
#140919=CARTESIAN_POINT('Ctrl Pts',(192.105214937859,-5.65798175450327,
132.542154152802));
#140920=CARTESIAN_POINT('Ctrl Pts',(192.097813116184,-5.60971991816693,
132.692161350184));
#140921=CARTESIAN_POINT('Ctrl Pts',(192.090411294508,-5.55551684961682,
132.84008238051));
#140922=CARTESIAN_POINT('Ctrl Pts',(192.083013380197,-5.5013423944446,132.987925324475));
#140923=CARTESIAN_POINT('Ctrl Pts',(192.075615465886,-5.44123308132258,
133.133683944999));
#140924=CARTESIAN_POINT('Ctrl Pts',(192.068217551574,-5.37538008816079,
133.2768531798));
#140925=CARTESIAN_POINT('Ctrl Pts',(192.060820866662,-5.30953803857184,
133.419998622472));
#140926=CARTESIAN_POINT('Ctrl Pts',(192.05342418175,-5.23795435917514,133.560555194648));
#140927=CARTESIAN_POINT('Ctrl Pts',(192.046027496837,-5.16086820194777,
133.69803820234));
#140928=CARTESIAN_POINT('Ctrl Pts',(192.038631139902,-5.08378546280139,
133.835515113891));
#140929=CARTESIAN_POINT('Ctrl Pts',(192.031234782967,-5.00120091351712,
133.969918406331));
#140930=CARTESIAN_POINT('Ctrl Pts',(192.023838426031,-4.91339933435241,
134.100788615215));
#140931=CARTESIAN_POINT('Ctrl Pts',(192.016440936695,-4.82558431254177,
134.231678860662));
#140932=CARTESIAN_POINT('Ctrl Pts',(192.009043447358,-4.73255087844258,
134.359034635486));
#140933=CARTESIAN_POINT('Ctrl Pts',(192.001645958021,-4.63462665546448,
134.482426186171));
#140934=CARTESIAN_POINT('Ctrl Pts',(191.994245875506,-4.53666810530159,
134.605860991573));
#140935=CARTESIAN_POINT('Ctrl Pts',(191.986845792991,-4.43381558469625,
134.725328513823));
#140936=CARTESIAN_POINT('Ctrl Pts',(191.979445710476,-4.32643632479157,
134.840432877824));
#140937=CARTESIAN_POINT('Ctrl Pts',(191.97203749081,-4.21893899035197,134.955663810906));
#140938=CARTESIAN_POINT('Ctrl Pts',(191.964629271143,-4.10690523078763,
135.066521731207));
#140939=CARTESIAN_POINT('Ctrl Pts',(191.957221051477,-3.99073891115741,
135.172647868363));
#140940=CARTESIAN_POINT('Ctrl Pts',(191.949808272175,-3.8745010930958,135.278839324385));
#140941=CARTESIAN_POINT('Ctrl Pts',(191.942395492873,-3.75412593146085,
135.380292954059));
#140942=CARTESIAN_POINT('Ctrl Pts',(191.934982713571,-3.63004912034786,
135.476691293616));
#140943=CARTESIAN_POINT('Ctrl Pts',(191.927559342542,-3.50579502246853,
135.573227371642));
#140944=CARTESIAN_POINT('Ctrl Pts',(191.920135971513,-3.37782901450236,
135.664693516634));
#140945=CARTESIAN_POINT('Ctrl Pts',(191.912712600484,-3.24661509159063,
135.750816016087));
#140946=CARTESIAN_POINT('Ctrl Pts',(191.908776551044,-3.17704232122627,
135.796480231779));
#140947=CARTESIAN_POINT('Ctrl Pts',(191.904840501603,-3.10655685573822,
135.84064292555));
#140948=CARTESIAN_POINT('Ctrl Pts',(191.900904452162,-3.03523037952588,
135.883268679906));
#140949=CARTESIAN_POINT('Ctrl Pts',(191.893481185756,-2.90071087141565,
135.963659522316));
#140950=CARTESIAN_POINT('Ctrl Pts',(191.886057919351,-2.76279191120802,
136.038823925974));
#140951=CARTESIAN_POINT('Ctrl Pts',(191.878634652946,-2.62191804346816,
136.108460572868));
#140952=CARTESIAN_POINT('Ctrl Pts',(191.871220160225,-2.48121067694097,
136.178014915029));
#140953=CARTESIAN_POINT('Ctrl Pts',(191.863805667504,-2.33755568601003,
136.242054341289));
#140954=CARTESIAN_POINT('Ctrl Pts',(191.856391174783,-2.19142557325891,
136.300321363365));
#140955=CARTESIAN_POINT('Ctrl Pts',(191.848983828429,-2.04543630621208,
136.358532225492));
#140956=CARTESIAN_POINT('Ctrl Pts',(191.841576482075,-1.89697701105787,
136.410981622255));
#140957=CARTESIAN_POINT('Ctrl Pts',(191.834169135721,-1.74654361814439,
136.457458525122));
#140958=CARTESIAN_POINT('Ctrl Pts',(191.826767314046,-1.59622242413098,
136.503900763762));
#140959=CARTESIAN_POINT('Ctrl Pts',(191.819365492371,-1.44393041914754,
136.544379268321));
#140960=CARTESIAN_POINT('Ctrl Pts',(191.811963670695,-1.29018218445807,
136.578731621702));
#140961=CARTESIAN_POINT('Ctrl Pts',(191.804565756384,-1.1365151122651,136.613065840743));
#140962=CARTESIAN_POINT('Ctrl Pts',(191.797167842073,-0.981393704726121,
136.641280267975));
#140963=CARTESIAN_POINT('Ctrl Pts',(191.789769927761,-0.825346221371544,
136.663262748287));
#140964=CARTESIAN_POINT('Ctrl Pts',(191.782373242849,-0.669324670277544,
136.68524157551));
#140965=CARTESIAN_POINT('Ctrl Pts',(191.774976557937,-0.512377718094195,
136.700990459225));
#140966=CARTESIAN_POINT('Ctrl Pts',(191.767579873025,-0.355042419086338,
136.710448615822));
#140967=CARTESIAN_POINT('Ctrl Pts',(191.760183516089,-0.19771409649043,
136.719906353036));
#140968=CARTESIAN_POINT('Ctrl Pts',(191.752787159154,-0.0399978339334864,
136.723073895353));
#140969=CARTESIAN_POINT('Ctrl Pts',(191.745390802218,0.117565877448984,
136.719942484716));
#140970=CARTESIAN_POINT('Ctrl Pts',(191.737993312882,0.275153712237935,
136.716810594653));
#140971=CARTESIAN_POINT('Ctrl Pts',(191.730595823545,0.432588576099383,
136.707377838831));
#140972=CARTESIAN_POINT('Ctrl Pts',(191.723198334209,0.589331816772684,
136.691687563833));
#140973=CARTESIAN_POINT('Ctrl Pts',(191.715798251694,0.746130003545964,
136.675991788633));
#140974=CARTESIAN_POINT('Ctrl Pts',(191.708398169179,0.902235713210191,
136.654034164045));
#140975=CARTESIAN_POINT('Ctrl Pts',(191.700998086664,1.0571173874321,136.625909671872));
#140976=CARTESIAN_POINT('Ctrl Pts',(191.693589866998,1.21216936997707,136.597754253928));
#140977=CARTESIAN_POINT('Ctrl Pts',(191.686181647331,1.36599426160672,136.563418492823));
#140978=CARTESIAN_POINT('Ctrl Pts',(191.678773427665,1.51807191972469,136.523048247525));
#140979=CARTESIAN_POINT('Ctrl Pts',(191.671360648363,1.67024317910383,136.482653155014));
#140980=CARTESIAN_POINT('Ctrl Pts',(191.663947869061,1.82066470625482,136.43621628731));
#140981=CARTESIAN_POINT('Ctrl Pts',(191.656535089759,1.96883390661907,136.383932609274));
#140982=CARTESIAN_POINT('Ctrl Pts',(191.64911171873,2.11721481808522,136.331574225866));
#140983=CARTESIAN_POINT('Ctrl Pts',(191.641688347701,2.26333662937201,136.273352484731));
#140984=CARTESIAN_POINT('Ctrl Pts',(191.634264976672,2.40671825768975,136.209509809827));
#140985=CARTESIAN_POINT('Ctrl Pts',(191.630328927231,2.48274263741927,136.175658891709));
#140986=CARTESIAN_POINT('Ctrl Pts',(191.626392877791,2.55799707823944,136.140228488059));
#140987=CARTESIAN_POINT('Ctrl Pts',(191.62245682835,2.63241303524121,136.103259764973));
#140988=CARTESIAN_POINT('Ctrl Pts',(191.615033561944,2.77275920770318,136.033537906988));
#140989=CARTESIAN_POINT('Ctrl Pts',(191.607610295539,2.91054571611699,135.958130975866));
#140990=CARTESIAN_POINT('Ctrl Pts',(191.600187029134,3.04527876591065,135.877250109798));
#140991=CARTESIAN_POINT('Ctrl Pts',(191.592772536413,3.17985257242841,135.796464838196));
#140992=CARTESIAN_POINT('Ctrl Pts',(191.585358043692,3.31137978699819,135.710218699948));
#140993=CARTESIAN_POINT('Ctrl Pts',(191.577943550971,3.43938837824726,135.618770046154));
#140994=CARTESIAN_POINT('Ctrl Pts',(191.570536204617,3.56727358999668,135.527409534016));
#140995=CARTESIAN_POINT('Ctrl Pts',(191.563128858263,3.69164662828833,135.430856704515));
#140996=CARTESIAN_POINT('Ctrl Pts',(191.555721511909,3.81206188637452,135.329414731823));
#140997=CARTESIAN_POINT('Ctrl Pts',(191.548319690234,3.93238733421826,135.228048418381));
#140998=CARTESIAN_POINT('Ctrl Pts',(191.540917868558,4.04876059514704,135.121800461911));
#140999=CARTESIAN_POINT('Ctrl Pts',(191.533516046883,4.16076687931502,135.011016003796));
#141000=CARTESIAN_POINT('Ctrl Pts',(191.526118132572,4.27271403623751,134.900290027933));
#141001=CARTESIAN_POINT('Ctrl Pts',(191.51872021826,4.38029854276746,134.785032581598));
#141002=CARTESIAN_POINT('Ctrl Pts',(191.511322303949,4.48314050245561,134.665627481918));
#141003=CARTESIAN_POINT('Ctrl Pts',(191.503925619037,4.58596537167568,134.546242225199));
#141004=CARTESIAN_POINT('Ctrl Pts',(191.496528934124,4.68404901487392,134.422710965694));
#141005=CARTESIAN_POINT('Ctrl Pts',(191.489132249212,4.77705000213056,134.295452687341));
#141006=CARTESIAN_POINT('Ctrl Pts',(191.481735892277,4.87004686562598,134.168200051753));
#141007=CARTESIAN_POINT('Ctrl Pts',(191.474339535341,4.95796130103329,134.037221027301));
#141008=CARTESIAN_POINT('Ctrl Pts',(191.466943178406,5.04049379128799,133.902965610541));
#141009=CARTESIAN_POINT('Ctrl Pts',(191.459545689069,5.12303891747765,133.768689638933));
#141010=CARTESIAN_POINT('Ctrl Pts',(191.452148199733,5.20020026233308,133.63113659425));
#141011=CARTESIAN_POINT('Ctrl Pts',(191.444750710396,5.27172313985551,133.490783089779));
#141012=CARTESIAN_POINT('Ctrl Pts',(191.437350627881,5.34327108961184,133.350380384605));
#141013=CARTESIAN_POINT('Ctrl Pts',(191.429950545366,5.40917646734144,133.207175597486));
#141014=CARTESIAN_POINT('Ctrl Pts',(191.422550462851,5.4692318636611,133.061667283488));
#141015=CARTESIAN_POINT('Ctrl Pts',(191.415142243184,5.52935329706284,132.915998968139));
#141016=CARTESIAN_POINT('Ctrl Pts',(191.407734023518,5.58361176011364,132.768022412689));
#141017=CARTESIAN_POINT('Ctrl Pts',(191.400325803851,5.63184881831531,132.618254068169));
#141018=CARTESIAN_POINT('Ctrl Pts',(191.392913024549,5.68011556562145,132.468393543732));
#141019=CARTESIAN_POINT('Ctrl Pts',(191.385500245247,5.72235342333643,132.316739391503));
#141020=CARTESIAN_POINT('Ctrl Pts',(191.378087465945,5.75845475628461,132.163819841788));
#141021=CARTESIAN_POINT('Ctrl Pts',(191.370664094916,5.79460767251027,132.01068179345));
#141022=CARTESIAN_POINT('Ctrl Pts',(191.363240723888,5.82460648099202,131.856275102001));
#141023=CARTESIAN_POINT('Ctrl Pts',(191.355817352859,5.84839510287327,131.701135552089));
#141024=CARTESIAN_POINT('Ctrl Pts',(191.351881303418,5.86100840099461,131.618876840204));
#141025=CARTESIAN_POINT('Ctrl Pts',(191.347945253977,5.87187666241779,131.536412149219));
#141026=CARTESIAN_POINT('Ctrl Pts',(191.344009204537,5.88099747114688,131.453821399187));
#141027=CARTESIAN_POINT('Ctrl Pts',(191.336585938131,5.89819903175955,131.298057822193));
#141028=CARTESIAN_POINT('Ctrl Pts',(191.329162671726,5.90923401839223,131.14137484216));
#141029=CARTESIAN_POINT('Ctrl Pts',(191.32173940532,5.91401315955457,130.984302027795));
#141030=CARTESIAN_POINT('Ctrl Pts',(191.314324912599,5.91878665216895,130.827414860453));
#141031=CARTESIAN_POINT('Ctrl Pts',(191.306910419878,5.91731900564953,130.67013914539));
#141032=CARTESIAN_POINT('Ctrl Pts',(191.299495927157,5.90957243360595,130.513011661047));
#141033=CARTESIAN_POINT('Ctrl Pts',(191.292088580803,5.90183332800017,130.35603562209));
#141034=CARTESIAN_POINT('Ctrl Pts',(191.28468123445,5.88782736319993,130.199207899769));
#141035=CARTESIAN_POINT('Ctrl Pts',(191.277273888096,5.86756874689005,130.043067268706));
#141036=CARTESIAN_POINT('Ctrl Pts',(191.269872066421,5.84732524022051,129.887043093216));
#141037=CARTESIAN_POINT('Ctrl Pts',(191.262470244745,5.82083841545084,129.731705357212));
#141038=CARTESIAN_POINT('Ctrl Pts',(191.25506842307,5.78817444575804,129.577589592487));
#141039=CARTESIAN_POINT('Ctrl Pts',(191.247670508758,5.7555277191206,129.423555184274));
#141040=CARTESIAN_POINT('Ctrl Pts',(191.240272594447,5.71671041893551,129.270741826916));
#141041=CARTESIAN_POINT('Ctrl Pts',(191.232874680136,5.67184011811256,129.119676600586));
#141042=CARTESIAN_POINT('Ctrl Pts',(191.225477995223,5.6269772739196,128.968636478556));
#141043=CARTESIAN_POINT('Ctrl Pts',(191.218081310311,5.57606353168593,128.819344268479));
#141044=CARTESIAN_POINT('Ctrl Pts',(191.210684625399,5.51926684325338,128.672313696069));
#141045=CARTESIAN_POINT('Ctrl Pts',(191.203288268464,5.46247267324549,128.525289643149));
#141046=CARTESIAN_POINT('Ctrl Pts',(191.195891911528,5.39979621022294,128.380527376718));
#141047=CARTESIAN_POINT('Ctrl Pts',(191.188495554593,5.33145415274227,128.238522123095));
#141048=CARTESIAN_POINT('Ctrl Pts',(191.181098065256,5.26310163191814,128.096495128106));
#141049=CARTESIAN_POINT('Ctrl Pts',(191.17370057592,5.18908195138688,127.957226322785));
#141050=CARTESIAN_POINT('Ctrl Pts',(191.166303086583,5.10965843540239,127.821187602801));
#141051=CARTESIAN_POINT('Ctrl Pts',(191.158903004068,5.03020707762741,127.685101194655));
#141052=CARTESIAN_POINT('Ctrl Pts',(191.151502921553,4.94534830094565,127.552247448424));
#141053=CARTESIAN_POINT('Ctrl Pts',(191.144102839038,4.8553894440146,127.423070344689));
#141054=CARTESIAN_POINT('Ctrl Pts',(191.136694619372,4.7653316680724,127.293751197449));
#141055=CARTESIAN_POINT('Ctrl Pts',(191.129286399705,4.67016282567414,127.168117073055));
#141056=CARTESIAN_POINT('Ctrl Pts',(191.121878180039,4.5702317839837,127.046580421338));
#141057=CARTESIAN_POINT('Ctrl Pts',(191.114465400737,4.47023923640445,126.924968965839));
#141058=CARTESIAN_POINT('Ctrl Pts',(191.107052621435,4.3654788968777,126.807460286267));
#141059=CARTESIAN_POINT('Ctrl Pts',(191.099639842133,4.25633700107888,126.694430460526));
#141060=CARTESIAN_POINT('Ctrl Pts',(191.092216471104,4.14703915822113,126.58123913247));
#141061=CARTESIAN_POINT('Ctrl Pts',(191.084793100075,4.03334752442669,126.472539696962));
#141062=CARTESIAN_POINT('Ctrl Pts',(191.077369729046,3.91568255850171,126.368668939423));
#141063=CARTESIAN_POINT('Ctrl Pts',(191.073433679605,3.85329377023497,126.31359417143));
#141064=CARTESIAN_POINT('Ctrl Pts',(191.069497630165,3.78978845095696,126.259876215498));
#141065=CARTESIAN_POINT('Ctrl Pts',(191.065561580724,3.72523253376711,126.207560303014));
#141066=CARTESIAN_POINT('Ctrl Pts',(191.058138314318,3.60348208867042,126.108894124795));
#141067=CARTESIAN_POINT('Ctrl Pts',(191.050715047913,3.47762493989561,126.014919100111));
#141068=CARTESIAN_POINT('Ctrl Pts',(191.043291781507,3.34805837517246,125.925996580418));
#141069=CARTESIAN_POINT('Ctrl Pts',(191.035877288786,3.2186449473689,125.837179159759));
#141070=CARTESIAN_POINT('Ctrl Pts',(191.028462796065,3.08553113521307,125.753402566677));
#141071=CARTESIAN_POINT('Ctrl Pts',(191.021048303344,2.94914812114376,125.674988733792));
#141072=CARTESIAN_POINT('Ctrl Pts',(191.013640956991,2.81289655815807,125.596650479111));
#141073=CARTESIAN_POINT('Ctrl Pts',(191.006233610637,2.67338238768785,125.523664879322));
#141074=CARTESIAN_POINT('Ctrl Pts',(190.998826264283,2.53106657568212,125.456311201941));
#141075=CARTESIAN_POINT('Ctrl Pts',(190.991424442608,2.38885690817838,125.389007759474));
#141076=CARTESIAN_POINT('Ctrl Pts',(190.984022620932,2.24385009572029,125.327328034653));
#141077=CARTESIAN_POINT('Ctrl Pts',(190.976620799257,2.09653246459078,125.271505822127));
#141078=CARTESIAN_POINT('Ctrl Pts',(190.969222884945,1.94929260129213,125.215713077712));
#141079=CARTESIAN_POINT('Ctrl Pts',(190.961824970634,1.79974469693171,125.165771819394));
#141080=CARTESIAN_POINT('Ctrl Pts',(190.954427056323,1.64839575001803,125.121868029465));
#141081=CARTESIAN_POINT('Ctrl Pts',(190.94703037141,1.49707195455342,125.077971535549));
#141082=CARTESIAN_POINT('Ctrl Pts',(190.939633686498,1.34394806872582,125.040110622631));
#141083=CARTESIAN_POINT('Ctrl Pts',(190.932237001586,1.18954708660089,125.008421669366));
#141084=CARTESIAN_POINT('Ctrl Pts',(190.924840644651,1.03515295077734,124.976734121223));
#141085=CARTESIAN_POINT('Ctrl Pts',(190.917444287715,0.879482196927022,
124.951218063633));
#141086=CARTESIAN_POINT('Ctrl Pts',(190.91004793078,0.723068603840397,124.931958863885));
#141087=CARTESIAN_POINT('Ctrl Pts',(190.902650441443,0.566631063433394,
124.912696715504));
#141088=CARTESIAN_POINT('Ctrl Pts',(190.895252952107,0.409450827861063,
124.899693377976));
#141089=CARTESIAN_POINT('Ctrl Pts',(190.88785546277,0.252067249504715,124.892982380283));
#141090=CARTESIAN_POINT('Ctrl Pts',(190.880455380255,0.0946285005788653,
124.88626903006));
#141091=CARTESIAN_POINT('Ctrl Pts',(190.87305529774,-0.0630133603256108,
124.885852427237));
#141092=CARTESIAN_POINT('Ctrl Pts',(190.865655215225,-0.220318675722416,
124.891713981445));
#141093=CARTESIAN_POINT('Ctrl Pts',(190.858246995558,-0.377796964484852,
124.897581981035));
#141094=CARTESIAN_POINT('Ctrl Pts',(190.850838775892,-0.534937595424837,
124.909741910448));
#141095=CARTESIAN_POINT('Ctrl Pts',(190.843430556225,-0.691204991596928,
124.928123197065));
#141096=CARTESIAN_POINT('Ctrl Pts',(190.836017776923,-0.84756856774404,
124.946515797058));
#141097=CARTESIAN_POINT('Ctrl Pts',(190.828604997621,-1.00305747031484,
124.971137326051));
#141098=CARTESIAN_POINT('Ctrl Pts',(190.821192218319,-1.15714652449987,
125.001866112326));
#141099=CARTESIAN_POINT('Ctrl Pts',(190.81376884729,-1.31145574835155,125.032638805332));
#141100=CARTESIAN_POINT('Ctrl Pts',(190.806345476262,-1.46436076711051,
125.069536096735));
#141101=CARTESIAN_POINT('Ctrl Pts',(190.798922105233,-1.61535096541017,
125.112386283379));
#141102=CARTESIAN_POINT('Ctrl Pts',(190.794986055792,-1.69540959150786,
125.135106480513));
#141103=CARTESIAN_POINT('Ctrl Pts',(190.791050006351,-1.77493020547604,
125.15949943687));
#141104=CARTESIAN_POINT('Ctrl Pts',(190.787113956911,-1.85383911441731,
125.185534129735));
#141105=CARTESIAN_POINT('Ctrl Pts',(190.779690690505,-2.0026588540193,125.234634747963));
#141106=CARTESIAN_POINT('Ctrl Pts',(190.7722674241,-2.14975156694095,125.289726135378));
#141107=CARTESIAN_POINT('Ctrl Pts',(190.764844157694,-2.29459849424747,
125.350669361848));
#141108=CARTESIAN_POINT('Ctrl Pts',(190.757429664973,-2.4392742245148,125.411540558485));
#141109=CARTESIAN_POINT('Ctrl Pts',(190.750015172252,-2.58170911190695,
125.478249683713));
#141110=CARTESIAN_POINT('Ctrl Pts',(190.742600679531,-2.72139924075281,
125.550607983978));
#141111=CARTESIAN_POINT('Ctrl Pts',(190.735193333178,-2.86095473099336,
125.62289654259));
#141112=CARTESIAN_POINT('Ctrl Pts',(190.727785986824,-2.99777040011747,
125.700823265995));
#141113=CARTESIAN_POINT('Ctrl Pts',(190.72037864047,-3.13136212909958,125.784151281399));
#141114=CARTESIAN_POINT('Ctrl Pts',(190.712976818795,-3.26485422033005,
125.867417147625));
#141115=CARTESIAN_POINT('Ctrl Pts',(190.705574997119,-3.39512684380415,
125.956076087876));
#141116=CARTESIAN_POINT('Ctrl Pts',(190.698173175444,-3.5217204302287,126.049845313793));
#141117=CARTESIAN_POINT('Ctrl Pts',(190.690775261132,-3.6482471888842,126.143565039666));
#141118=CARTESIAN_POINT('Ctrl Pts',(190.683377346821,-3.77109847913389,
126.242389457018));
#141119=CARTESIAN_POINT('Ctrl Pts',(190.67597943251,-3.88984378373164,126.345992541614));
#141120=CARTESIAN_POINT('Ctrl Pts',(190.668582747597,-4.0085693550141,126.449578409258));
#141121=CARTESIAN_POINT('Ctrl Pts',(190.661186062685,-4.12319001387754,
126.557941122862));
#141122=CARTESIAN_POINT('Ctrl Pts',(190.653789377773,-4.23330833002912,
126.670714388701));
#141123=CARTESIAN_POINT('Ctrl Pts',(190.646393020838,-4.34342176341914,
126.783482654056));
#141124=CARTESIAN_POINT('Ctrl Pts',(190.638996663902,-4.44903299024769,
126.900660815703));
#141125=CARTESIAN_POINT('Ctrl Pts',(190.631600306967,-4.54978166812228,
127.021845933534));
#141126=CARTESIAN_POINT('Ctrl Pts',(190.62420281763,-4.65054577087687,127.143049605116));
#141127=CARTESIAN_POINT('Ctrl Pts',(190.616805328294,-4.7464456036807,127.268261167321));
#141128=CARTESIAN_POINT('Ctrl Pts',(190.609407838957,-4.83716142451464,
127.397044970948));
#141129=CARTESIAN_POINT('Ctrl Pts',(190.602007756442,-4.92790904563891,
127.525873919538));
#141130=CARTESIAN_POINT('Ctrl Pts',(190.594607673927,-5.01346882182785,
127.658277297765));
#141131=CARTESIAN_POINT('Ctrl Pts',(190.587207591412,-5.09356469563254,
127.793791027952));
#141132=CARTESIAN_POINT('Ctrl Pts',(190.579799371746,-5.17374864308446,
127.929453769417));
#141133=CARTESIAN_POINT('Ctrl Pts',(190.572391152079,-5.24845649947873,
128.068233371551));
#141134=CARTESIAN_POINT('Ctrl Pts',(190.564982932413,-5.31745814713684,
128.209641092078));
#141135=CARTESIAN_POINT('Ctrl Pts',(190.557570153111,-5.38650226415769,
128.351135846697));
#141136=CARTESIAN_POINT('Ctrl Pts',(190.550157373809,-5.44983302436487,
128.495261601939));
#141137=CARTESIAN_POINT('Ctrl Pts',(190.542744594507,-5.50726892380859,
128.641510746828));
#141138=CARTESIAN_POINT('Ctrl Pts',(190.535321223478,-5.56478689035895,
128.787968859353));
#141139=CARTESIAN_POINT('Ctrl Pts',(190.527897852449,-5.61639305166817,
128.9365560694));
#141140=CARTESIAN_POINT('Ctrl Pts',(190.52047448142,-5.66195586638615,129.086749972048));
#141141=CARTESIAN_POINT('Ctrl Pts',(190.516538431979,-5.68611436401442,
129.166386383086));
#141142=CARTESIAN_POINT('Ctrl Pts',(190.512602382539,-5.70857471323609,
129.246474316501));
#141143=CARTESIAN_POINT('Ctrl Pts',(190.508666333098,-5.72932318152839,
129.326935003837));
#141144=CARTESIAN_POINT('Ctrl Pts',(190.498971765574,-5.78042706879116,
129.525111266141));
#141145=CARTESIAN_POINT('Ctrl Pts',(190.48927719805,-5.82126881850071,129.726034303134));
#141146=CARTESIAN_POINT('Ctrl Pts',(190.479582630525,-5.85160626396125,
129.928783839625));
#141147=CARTESIAN_POINT('Ctrl Pts',(190.470087632604,-5.88131919141924,
130.127359631965));
#141148=CARTESIAN_POINT('Ctrl Pts',(190.460592634683,-5.90095589270113,
130.327687736164));
#141149=CARTESIAN_POINT('Ctrl Pts',(190.451097636761,-5.91033348368092,
130.528881627115));
#141150=CARTESIAN_POINT('Ctrl Pts',(190.446856827631,-5.91452185462971,
130.618742088053));
#141151=CARTESIAN_POINT('Ctrl Pts',(190.4426160185,-5.9166642962425,130.708774942494));
#141152=CARTESIAN_POINT('Ctrl Pts',(190.438375209369,-5.91674747976679,
130.798899557834));
#141153=CARTESIAN_POINT('',(188.688375158851,-5.91280930184219,130.805575254198));
#141154=CARTESIAN_POINT('Ctrl Pts',(190.438375192211,-5.91556591356672,
130.798901012961));
#141155=CARTESIAN_POINT('Ctrl Pts',(190.368989697902,-5.90218450277572,
132.273183331429));
#141156=CARTESIAN_POINT('Ctrl Pts',(190.206788328991,-4.59798200865986,
135.740709904657));
#141157=CARTESIAN_POINT('Ctrl Pts',(189.951771085471,1.22745627517318,137.694274377758));
#141158=CARTESIAN_POINT('Ctrl Pts',(189.673323461659,6.46014967796433,133.495833572777));
#141159=CARTESIAN_POINT('Ctrl Pts',(189.394875837845,5.75628112256356,126.824060607722));
#141160=CARTESIAN_POINT('Ctrl Pts',(189.116428214034,-0.237328574507486,
123.809988903246));
#141161=CARTESIAN_POINT('Ctrl Pts',(188.880927998822,-5.12203658652489,
126.696922428952));
#141162=CARTESIAN_POINT('Ctrl Pts',(188.738243658214,-5.90521979014647,
129.742180863919));
#141163=CARTESIAN_POINT('Ctrl Pts',(188.688375192211,-5.90715995150835,
130.805573381844));
#141164=CARTESIAN_POINT('',(186.938375192211,-5.91753456722523,130.809401790279));
#141165=CARTESIAN_POINT('Ctrl Pts',(188.688375135582,-5.9167498750567,130.805576560215));
#141166=CARTESIAN_POINT('Ctrl Pts',(188.680495520896,-5.916715288546,130.97387375165));
#141167=CARTESIAN_POINT('Ctrl Pts',(188.67261590621,-5.90949584186738,131.141986835927));
#141168=CARTESIAN_POINT('Ctrl Pts',(188.664736291524,-5.89516395080611,
131.309308689764));
#141169=CARTESIAN_POINT('Ctrl Pts',(188.656841930411,-5.88080523810475,
131.476943680682));
#141170=CARTESIAN_POINT('Ctrl Pts',(188.648947569298,-5.85930751799326,
131.643784192002));
#141171=CARTESIAN_POINT('Ctrl Pts',(188.641053208185,-5.83079446595158,
131.809231981636));
#141172=CARTESIAN_POINT('Ctrl Pts',(188.633135901846,-5.80219853976692,
131.975160650825));
#141173=CARTESIAN_POINT('Ctrl Pts',(188.625218595508,-5.76654654061531,
132.139688210389));
#141174=CARTESIAN_POINT('Ctrl Pts',(188.617301289169,-5.72401296888253,
132.30222779945));
#141175=CARTESIAN_POINT('Ctrl Pts',(188.609371641021,-5.68141309414261,
132.465020761625));
#141176=CARTESIAN_POINT('Ctrl Pts',(188.601441992874,-5.63191030844115,
132.625819284766));
#141177=CARTESIAN_POINT('Ctrl Pts',(188.593512344726,-5.5757279961427,132.784054501865));
#141178=CARTESIAN_POINT('Ctrl Pts',(188.585563505692,-5.51940971458834,
132.94267267089));
#141179=CARTESIAN_POINT('Ctrl Pts',(188.577614666658,-5.45637968482179,
133.098714854591));
#141180=CARTESIAN_POINT('Ctrl Pts',(188.569665827625,-5.38690907388433,
133.251632811704));
#141181=CARTESIAN_POINT('Ctrl Pts',(188.566288207219,-5.35738962430293,
133.316610704718));
#141182=CARTESIAN_POINT('Ctrl Pts',(188.562910586813,-5.32670783786975,
133.381024824207));
#141183=CARTESIAN_POINT('Ctrl Pts',(188.559532966408,-5.29488692684622,
133.444834626984));
#141184=CARTESIAN_POINT('Ctrl Pts',(188.552109700002,-5.22495156661437,
133.585074532128));
#141185=CARTESIAN_POINT('Ctrl Pts',(188.544686433597,-5.14933503520301,
133.722746124474));
#141186=CARTESIAN_POINT('Ctrl Pts',(188.537263167192,-5.06824922202705,
133.857355931339));
#141187=CARTESIAN_POINT('Ctrl Pts',(188.529848674471,-4.98725924554844,
133.991806640591));
#141188=CARTESIAN_POINT('Ctrl Pts',(188.52243418175,-4.90081304514209,134.123202450914));
#141189=CARTESIAN_POINT('Ctrl Pts',(188.515019689029,-4.80916968995939,
134.251071724647));
#141190=CARTESIAN_POINT('Ctrl Pts',(188.507612342675,-4.71761466409284,
134.37881775316));
#141191=CARTESIAN_POINT('Ctrl Pts',(188.500204996321,-4.62087267180682,
134.503043710459));
#141192=CARTESIAN_POINT('Ctrl Pts',(188.492797649967,-4.51924756505893,
134.623304451692));
#141193=CARTESIAN_POINT('Ctrl Pts',(188.485395828292,-4.41769825414966,
134.743475497927));
#141194=CARTESIAN_POINT('Ctrl Pts',(188.477994006617,-4.31127332042061,
134.859686932794));
#141195=CARTESIAN_POINT('Ctrl Pts',(188.470592184941,-4.2003185360947,134.971524492174));
#141196=CARTESIAN_POINT('Ctrl Pts',(188.46319427063,-4.08942232393587,135.083303013377));
#141197=CARTESIAN_POINT('Ctrl Pts',(188.455796356319,-3.97400128576268,
135.190711993113));
#141198=CARTESIAN_POINT('Ctrl Pts',(188.448398442007,-3.85443981639646,
135.293372119476));
#141199=CARTESIAN_POINT('Ctrl Pts',(188.441001757095,-3.73489821597734,
135.396015185588));
#141200=CARTESIAN_POINT('Ctrl Pts',(188.433605072183,-3.61121783291183,
135.493910721659));
#141201=CARTESIAN_POINT('Ctrl Pts',(188.426208387271,-3.483818170251,135.586717935786));
#141202=CARTESIAN_POINT('Ctrl Pts',(188.418812030335,-3.35642415662479,
135.679521034743));
#141203=CARTESIAN_POINT('Ctrl Pts',(188.4114156734,-3.22531149304034,135.767236040568));
#141204=CARTESIAN_POINT('Ctrl Pts',(188.404019316464,-3.09093063134526,
135.849564121362));
#141205=CARTESIAN_POINT('Ctrl Pts',(188.396621827128,-2.95652919559707,
135.931904806795));
#141206=CARTESIAN_POINT('Ctrl Pts',(188.389224337791,-2.81885888376706,
136.00885672998));
#141207=CARTESIAN_POINT('Ctrl Pts',(188.381826848455,-2.67839669617966,
136.080165930539));
#141208=CARTESIAN_POINT('Ctrl Pts',(188.37442676594,-2.53788526979019,136.151500128428));
#141209=CARTESIAN_POINT('Ctrl Pts',(188.367026683425,-2.39458035173523,
136.217187496532));
#141210=CARTESIAN_POINT('Ctrl Pts',(188.35962660091,-2.24898081214349,136.277021384424));
#141211=CARTESIAN_POINT('Ctrl Pts',(188.352218381243,-2.10322117088992,
136.336921065828));
#141212=CARTESIAN_POINT('Ctrl Pts',(188.344810161577,-1.95516221465031,
136.390954270921));
#141213=CARTESIAN_POINT('Ctrl Pts',(188.33740194191,-1.80532063496924,136.43896335134));
#141214=CARTESIAN_POINT('Ctrl Pts',(188.329989162608,-1.65538683029596,
136.487001980547));
#141215=CARTESIAN_POINT('Ctrl Pts',(188.322576383306,-1.50366857485122,
136.529008997548));
#141216=CARTESIAN_POINT('Ctrl Pts',(188.315163604004,-1.35069426213214,
136.564877571169));
#141217=CARTESIAN_POINT('Ctrl Pts',(188.307740232975,-1.19750137254131,
136.600797395489));
#141218=CARTESIAN_POINT('Ctrl Pts',(188.300316861946,-1.04304920681346,
136.630561188534));
#141219=CARTESIAN_POINT('Ctrl Pts',(188.292893490918,-0.887873634317857,
136.654113686883));
#141220=CARTESIAN_POINT('Ctrl Pts',(188.288957441477,-0.805595822389184,
136.666601786643));
#141221=CARTESIAN_POINT('Ctrl Pts',(188.285021392036,-0.72311468724722,
136.67734453826));
#141222=CARTESIAN_POINT('Ctrl Pts',(188.281085342595,-0.640510152529407,
136.686339647366));
#141223=CARTESIAN_POINT('Ctrl Pts',(188.273662076189,-0.484720578059533,
136.703304142411));
#141224=CARTESIAN_POINT('Ctrl Pts',(188.266238809784,-0.328020986091857,
136.714100671442));
#141225=CARTESIAN_POINT('Ctrl Pts',(188.258815543378,-0.170941080575582,
136.718640768985));
#141226=CARTESIAN_POINT('Ctrl Pts',(188.251401050657,-0.014046830462841,
136.72317550051));
#141227=CARTESIAN_POINT('Ctrl Pts',(188.243986557936,0.143226468969914,
136.721468508825));
#141228=CARTESIAN_POINT('Ctrl Pts',(188.236572065215,0.300341982397618,
136.713482824469));
#141229=CARTESIAN_POINT('Ctrl Pts',(188.229164718861,0.457306061978129,
136.705504837015));
#141230=CARTESIAN_POINT('Ctrl Pts',(188.221757372508,0.61411228800125,136.691260223337));
#141231=CARTESIAN_POINT('Ctrl Pts',(188.214350026154,0.770221908090596,
136.670764011026));
#141232=CARTESIAN_POINT('Ctrl Pts',(188.206948204478,0.926215095735712,
136.650283085563));
#141233=CARTESIAN_POINT('Ctrl Pts',(188.199546382803,1.08151234342266,136.623559893873));
#141234=CARTESIAN_POINT('Ctrl Pts',(188.192144561128,1.23557822068304,136.590661424046));
#141235=CARTESIAN_POINT('Ctrl Pts',(188.184746646816,1.38956276776613,136.557780321065));
#141236=CARTESIAN_POINT('Ctrl Pts',(188.177348732505,1.54231687484672,136.518730509913));
#141237=CARTESIAN_POINT('Ctrl Pts',(188.169950818194,1.69331364128615,136.473630365491));
#141238=CARTESIAN_POINT('Ctrl Pts',(188.162554133281,1.84428531480222,136.428537715894));
#141239=CARTESIAN_POINT('Ctrl Pts',(188.155157448369,1.99349986995265,136.377396835288));
#141240=CARTESIAN_POINT('Ctrl Pts',(188.147760763457,2.14044383721241,136.320376457123));
#141241=CARTESIAN_POINT('Ctrl Pts',(188.140364406522,2.28738128882264,136.263358607301));
#141242=CARTESIAN_POINT('Ctrl Pts',(188.132968049586,2.43204800471394,136.20046191333));
#141243=CARTESIAN_POINT('Ctrl Pts',(188.125571692651,2.57394908891939,136.131903827166));
#141244=CARTESIAN_POINT('Ctrl Pts',(188.118174203314,2.71587189854313,136.063335244583));
#141245=CARTESIAN_POINT('Ctrl Pts',(188.110776713978,2.85502789723953,135.989103706352));
#141246=CARTESIAN_POINT('Ctrl Pts',(188.103379224641,2.99094559062203,135.909473254564));
#141247=CARTESIAN_POINT('Ctrl Pts',(188.095979142126,3.12691092974114,135.829814888445));
#141248=CARTESIAN_POINT('Ctrl Pts',(188.088579059611,3.25963538151613,135.744754029243));
#141249=CARTESIAN_POINT('Ctrl Pts',(188.081178977096,3.38867543359986,135.65459869092));
#141250=CARTESIAN_POINT('Ctrl Pts',(188.07377075743,3.51785737848661,135.564344217535));
#141251=CARTESIAN_POINT('Ctrl Pts',(188.066362537763,3.64334652662018,135.46898429159));
#141252=CARTESIAN_POINT('Ctrl Pts',(188.058954318097,3.76473095956622,135.368868407524));
#141253=CARTESIAN_POINT('Ctrl Pts',(188.051541538795,3.88619010260547,135.268690903801));
#141254=CARTESIAN_POINT('Ctrl Pts',(188.044128759492,4.0035392187013,135.163751857378));
#141255=CARTESIAN_POINT('Ctrl Pts',(188.03671598019,4.11640281816916,135.054438075809));
#141256=CARTESIAN_POINT('Ctrl Pts',(188.029292609162,4.22942768244064,134.944968101584));
#141257=CARTESIAN_POINT('Ctrl Pts',(188.021869238133,4.33795397276301,134.831111177405));
#141258=CARTESIAN_POINT('Ctrl Pts',(188.014445867104,4.44164554397361,134.713288274123));
#141259=CARTESIAN_POINT('Ctrl Pts',(188.010509817663,4.49662530307466,134.650815743681));
#141260=CARTESIAN_POINT('Ctrl Pts',(188.006573768223,4.55024655251569,134.587228748358));
#141261=CARTESIAN_POINT('Ctrl Pts',(188.002637718782,4.60246416130131,134.522593290011));
#141262=CARTESIAN_POINT('Ctrl Pts',(187.995214452376,4.70094494181516,134.400692832772));
#141263=CARTESIAN_POINT('Ctrl Pts',(187.987791185971,4.79472832452141,134.274692815747));
#141264=CARTESIAN_POINT('Ctrl Pts',(187.980367919565,4.88345356298841,134.144991076123));
#141265=CARTESIAN_POINT('Ctrl Pts',(187.972953426844,4.9720739355918,134.015442633183));
#141266=CARTESIAN_POINT('Ctrl Pts',(187.965538934123,5.05564785509995,133.882201481457));
#141267=CARTESIAN_POINT('Ctrl Pts',(187.958124441402,5.13385404545199,133.745699292812));
#141268=CARTESIAN_POINT('Ctrl Pts',(187.950717095049,5.21198485773338,133.609328670115));
#141269=CARTESIAN_POINT('Ctrl Pts',(187.943309748695,5.28475805618814,133.469703589541));
#141270=CARTESIAN_POINT('Ctrl Pts',(187.935902402341,5.3518950751355,133.327285441504));
#141271=CARTESIAN_POINT('Ctrl Pts',(187.928500580666,5.41898202076117,133.184973514294));
#141272=CARTESIAN_POINT('Ctrl Pts',(187.92109875899,5.48044099847369,133.03987300371));
#141273=CARTESIAN_POINT('Ctrl Pts',(187.913696937315,5.53603895400241,132.892470591267));
#141274=CARTESIAN_POINT('Ctrl Pts',(187.906299023003,5.59160755980321,132.74514599141));
#141275=CARTESIAN_POINT('Ctrl Pts',(187.898901108692,5.64132117383657,132.595522258129));
#141276=CARTESIAN_POINT('Ctrl Pts',(187.891503194381,5.68499458559291,132.44410667238));
#141277=CARTESIAN_POINT('Ctrl Pts',(187.884106509468,5.72866073962051,132.292716249155));
#141278=CARTESIAN_POINT('Ctrl Pts',(187.876709824556,5.76628858020843,132.139534922778));
#141279=CARTESIAN_POINT('Ctrl Pts',(187.869313139644,5.79774252476681,131.985085894254));
#141280=CARTESIAN_POINT('Ctrl Pts',(187.861916782709,5.82919507462433,131.830643714162));
#141281=CARTESIAN_POINT('Ctrl Pts',(187.854520425773,5.85447419827982,131.67493430948));
#141282=CARTESIAN_POINT('Ctrl Pts',(187.847124068838,5.87349534086361,131.518491588294));
#141283=CARTESIAN_POINT('Ctrl Pts',(187.839726579501,5.8925193956329,131.362024915329));
#141284=CARTESIAN_POINT('Ctrl Pts',(187.832329090164,5.90528351654167,131.204825072902));
#141285=CARTESIAN_POINT('Ctrl Pts',(187.824931600828,5.91175499544869,131.047431463797));
#141286=CARTESIAN_POINT('Ctrl Pts',(187.817531518313,5.9182287429226,130.889982680606));
#141287=CARTESIAN_POINT('Ctrl Pts',(187.810131435798,5.91840544118585,130.73234036825));
#141288=CARTESIAN_POINT('Ctrl Pts',(187.802731353283,5.91230450185313,130.575044155298));
#141289=CARTESIAN_POINT('Ctrl Pts',(187.795323133616,5.90619685391042,130.417574978989));
#141290=CARTESIAN_POINT('Ctrl Pts',(187.78791491395,5.89379779728831,130.260453035358));
#141291=CARTESIAN_POINT('Ctrl Pts',(187.780506694283,5.87517871958054,130.10421379333));
#141292=CARTESIAN_POINT('Ctrl Pts',(187.773093914981,5.8565481821411,129.947878388655));
#141293=CARTESIAN_POINT('Ctrl Pts',(187.765681135679,5.83169005401839,129.792427135914));
#141294=CARTESIAN_POINT('Ctrl Pts',(187.758268356377,5.80072680601682,129.638385024143));
#141295=CARTESIAN_POINT('Ctrl Pts',(187.750844985348,5.76971931627449,129.484122809779));
#141296=CARTESIAN_POINT('Ctrl Pts',(187.74342161432,5.73258937218858,129.331274119478));
#141297=CARTESIAN_POINT('Ctrl Pts',(187.735998243291,5.68950945378594,129.180349306712));
#141298=CARTESIAN_POINT('Ctrl Pts',(187.73206219385,5.66666744736085,129.100325349594));
#141299=CARTESIAN_POINT('Ctrl Pts',(187.728126144409,5.64215350241321,129.020841949638));
#141300=CARTESIAN_POINT('Ctrl Pts',(187.724190094969,5.61599875376964,128.941972752443));
#141301=CARTESIAN_POINT('Ctrl Pts',(187.716766828563,5.56667171408872,128.793227907954));
#141302=CARTESIAN_POINT('Ctrl Pts',(187.709343562158,5.51135654039937,128.646219205077));
#141303=CARTESIAN_POINT('Ctrl Pts',(187.701920295752,5.45019295213473,128.501465190717));
#141304=CARTESIAN_POINT('Ctrl Pts',(187.694505803031,5.38910165415207,128.356882263581));
#141305=CARTESIAN_POINT('Ctrl Pts',(187.68709131031,5.32217584452053,128.214549061059));
#141306=CARTESIAN_POINT('Ctrl Pts',(187.679676817589,5.24960504344817,128.074969210988));
#141307=CARTESIAN_POINT('Ctrl Pts',(187.672269471236,5.17710418884611,127.935523893231));
#141308=CARTESIAN_POINT('Ctrl Pts',(187.664862124882,5.09896934552089,127.798826973745));
#141309=CARTESIAN_POINT('Ctrl Pts',(187.657454778528,5.01543812273929,127.665362210514));
#141310=CARTESIAN_POINT('Ctrl Pts',(187.650052956853,4.9319692006951,127.53199699034));
#141311=CARTESIAN_POINT('Ctrl Pts',(187.642651135177,4.84311211035346,127.401859441534));
#141312=CARTESIAN_POINT('Ctrl Pts',(187.635249313502,4.74915033913089,127.275408702502));
#141313=CARTESIAN_POINT('Ctrl Pts',(187.62785139919,4.65523816959588,127.149024715831));
#141314=CARTESIAN_POINT('Ctrl Pts',(187.620453484879,4.55622690793055,127.026323961781));
#141315=CARTESIAN_POINT('Ctrl Pts',(187.613055570568,4.45244323316465,126.907736460947));
#141316=CARTESIAN_POINT('Ctrl Pts',(187.605658885656,4.34867680536279,126.789168667204));
#141317=CARTESIAN_POINT('Ctrl Pts',(187.598262200743,4.24013978411027,126.674713050673));
#141318=CARTESIAN_POINT('Ctrl Pts',(187.590865515831,4.12719906752894,126.56476648375));
#141319=CARTESIAN_POINT('Ctrl Pts',(187.583469158896,4.01426335885729,126.454824791973));
#141320=CARTESIAN_POINT('Ctrl Pts',(187.57607280196,3.89692461059156,126.349392012655));
#141321=CARTESIAN_POINT('Ctrl Pts',(187.568676445025,3.77558631075384,126.248827874566));
#141322=CARTESIAN_POINT('Ctrl Pts',(187.561278955688,3.65422943371256,126.14824833985));
#141323=CARTESIAN_POINT('Ctrl Pts',(187.553881466352,3.52887207328063,126.05253916878));
#141324=CARTESIAN_POINT('Ctrl Pts',(187.546483977015,3.39995036474609,125.962019440019));
#141325=CARTESIAN_POINT('Ctrl Pts',(187.5390838945,3.27098346290651,125.871467979709));
#141326=CARTESIAN_POINT('Ctrl Pts',(187.531683811985,3.13845003058641,125.786109797999));
#141327=CARTESIAN_POINT('Ctrl Pts',(187.52428372947,3.00281456503668,125.706220245773));
#141328=CARTESIAN_POINT('Ctrl Pts',(187.516875509804,2.86702995434889,125.626242846772));
#141329=CARTESIAN_POINT('Ctrl Pts',(187.509467290137,2.72813682027947,125.551746275818));
#141330=CARTESIAN_POINT('Ctrl Pts',(187.502059070471,2.58662425473907,125.482959906541));
#141331=CARTESIAN_POINT('Ctrl Pts',(187.494646291169,2.44502459057584,125.414131200402));
#141332=CARTESIAN_POINT('Ctrl Pts',(187.487233511867,2.3008026235927,125.351019848396));
#141333=CARTESIAN_POINT('Ctrl Pts',(187.479820732564,2.15446624039682,125.293806581764));
#141334=CARTESIAN_POINT('Ctrl Pts',(187.472397361536,2.00792076491405,125.236511566134));
#141335=CARTESIAN_POINT('Ctrl Pts',(187.464973990507,1.85925519113648,125.185131589024));
#141336=CARTESIAN_POINT('Ctrl Pts',(187.457550619478,1.7089921235619,125.139797396619));
#141337=CARTESIAN_POINT('Ctrl Pts',(187.453614570037,1.62931903962022,125.115760120027));
#141338=CARTESIAN_POINT('Ctrl Pts',(187.449678520597,1.54919701811686,125.093421677015));
#141339=CARTESIAN_POINT('Ctrl Pts',(187.445742471156,1.46870484831581,125.072795680218));
#141340=CARTESIAN_POINT('Ctrl Pts',(187.43831920475,1.31689912814708,125.033895693975));
#141341=CARTESIAN_POINT('Ctrl Pts',(187.430895938345,1.1633173403862,125.000972121415));
#141342=CARTESIAN_POINT('Ctrl Pts',(187.423472671939,1.00847127499773,124.97418769989));
#141343=CARTESIAN_POINT('Ctrl Pts',(187.416058179218,0.853808224799215,
124.947434935327));
#141344=CARTESIAN_POINT('Ctrl Pts',(187.408643686497,0.697884235571734,
124.926806941762));
#141345=CARTESIAN_POINT('Ctrl Pts',(187.401229193776,0.541225463979645,
124.912416493625));
#141346=CARTESIAN_POINT('Ctrl Pts',(187.393821847423,0.384717686009742,
124.898039915544));
#141347=CARTESIAN_POINT('Ctrl Pts',(187.386414501069,0.227476904821062,
124.889888948137));
#141348=CARTESIAN_POINT('Ctrl Pts',(187.379007154715,0.0700385533196246,
124.888025167006));
#141349=CARTESIAN_POINT('Ctrl Pts',(187.37160533304,-0.0872823747195095,
124.886162775954));
#141350=CARTESIAN_POINT('Ctrl Pts',(187.364203511364,-0.244800208001704,
124.890578238706));
#141351=CARTESIAN_POINT('Ctrl Pts',(187.356801689689,-0.401975428509942,
124.901281224794));
#141352=CARTESIAN_POINT('Ctrl Pts',(187.349403775377,-0.559067677442723,
124.911978560858));
#141353=CARTESIAN_POINT('Ctrl Pts',(187.342005861066,-0.715817302305466,
124.928956784745));
#141354=CARTESIAN_POINT('Ctrl Pts',(187.334607946755,-0.871685936598251,
124.952173488771));
#141355=CARTESIAN_POINT('Ctrl Pts',(187.327211261842,-1.02752866835165,
124.975386334601));
#141356=CARTESIAN_POINT('Ctrl Pts',(187.31981457693,-1.18249033124199,125.00483554804));
#141357=CARTESIAN_POINT('Ctrl Pts',(187.312417892018,-1.33603870788574,
125.040426966531));
#141358=CARTESIAN_POINT('Ctrl Pts',(187.305021535083,-1.48958027603362,
125.076016806862));
#141359=CARTESIAN_POINT('Ctrl Pts',(187.297625178147,-1.64170831888113,
125.117748226424));
#141360=CARTESIAN_POINT('Ctrl Pts',(187.290228821212,-1.79190209129523,
125.165476201504));
#141361=CARTESIAN_POINT('Ctrl Pts',(187.282831331875,-1.94211885875933,
125.213211483858));
#141362=CARTESIAN_POINT('Ctrl Pts',(187.275433842538,-2.09040041034268,
125.266945036705));
#141363=CARTESIAN_POINT('Ctrl Pts',(187.268036353202,-2.2362425543513,125.326482396885));
#141364=CARTESIAN_POINT('Ctrl Pts',(187.260636270687,-2.38213582309748,
125.386040627795));
#141365=CARTESIAN_POINT('Ctrl Pts',(187.253236188172,-2.52558763631716,
125.451406575745));
#141366=CARTESIAN_POINT('Ctrl Pts',(187.245836105657,-2.66611526140484,
125.522338279919));
#141367=CARTESIAN_POINT('Ctrl Pts',(187.23842788599,-2.80679741106287,125.593347980794));
#141368=CARTESIAN_POINT('Ctrl Pts',(187.231019666324,-2.94454861767688,
125.669935491864));
#141369=CARTESIAN_POINT('Ctrl Pts',(187.223611446657,-3.07891153659171,
125.751813308303));
#141370=CARTESIAN_POINT('Ctrl Pts',(187.216198667355,-3.2133571536413,125.833741519172));
#141371=CARTESIAN_POINT('Ctrl Pts',(187.208785888053,-3.34441001746257,
125.920966317233));
#141372=CARTESIAN_POINT('Ctrl Pts',(187.201373108751,-3.47164354862595,
126.013158092752));
#141373=CARTESIAN_POINT('Ctrl Pts',(187.193949737723,-3.59905887702523,
126.105481596203));
#141374=CARTESIAN_POINT('Ctrl Pts',(187.186526366694,-3.72264368091018,
126.202786021196));
#141375=CARTESIAN_POINT('Ctrl Pts',(187.179102995665,-3.84200547931489,
126.304702357274));
#141376=CARTESIAN_POINT('Ctrl Pts',(187.175166946224,-3.90529396887533,
126.358740844111));
#141377=CARTESIAN_POINT('Ctrl Pts',(187.171230896784,-3.96739584334917,
126.414075295879));
#141378=CARTESIAN_POINT('Ctrl Pts',(187.167294847343,-4.02825706251959,
126.470646782902));
#141379=CARTESIAN_POINT('Ctrl Pts',(187.159982110724,-4.14133035410826,
126.57575023523));
#141380=CARTESIAN_POINT('Ctrl Pts',(187.152669374104,-4.25048290247324,
126.685464074864));
#141381=CARTESIAN_POINT('Ctrl Pts',(187.145356637485,-4.355306958856,126.799459637936));
#141382=CARTESIAN_POINT('Ctrl Pts',(187.138052644169,-4.4600056848014,126.913318904872));
#141383=CARTESIAN_POINT('Ctrl Pts',(187.130748650852,-4.56038595696257,
127.03144942948));
#141384=CARTESIAN_POINT('Ctrl Pts',(187.123444657536,-4.65607377997443,
127.153482980896));
#141385=CARTESIAN_POINT('Ctrl Pts',(187.11614769061,-4.75166955197894,127.275399136901));
#141386=CARTESIAN_POINT('Ctrl Pts',(187.108850723683,-4.84258162128955,
127.401210547057));
#141387=CARTESIAN_POINT('Ctrl Pts',(187.101553756756,-4.92847369766666,
127.530513099139));
#141388=CARTESIAN_POINT('Ctrl Pts',(187.094262461591,-5.01429901214382,
127.659715147376));
#141389=CARTESIAN_POINT('Ctrl Pts',(187.086971166426,-5.09511188989882,
127.792402615212));
#141390=CARTESIAN_POINT('Ctrl Pts',(187.079679871261,-5.1706173282255,127.92813965812));
#141391=CARTESIAN_POINT('Ctrl Pts',(187.072391625532,-5.24609118793796,
128.063819931771));
#141392=CARTESIAN_POINT('Ctrl Pts',(187.065103379803,-5.31626183691263,
128.202546907271));
#141393=CARTESIAN_POINT('Ctrl Pts',(187.057815134074,-5.38087854125002,
128.343857277431));
#141394=CARTESIAN_POINT('Ctrl Pts',(187.050528398168,-5.44548185967987,
128.48513837393));
#141395=CARTESIAN_POINT('Ctrl Pts',(187.043241662262,-5.50453336306754,
128.629001449778));
#141396=CARTESIAN_POINT('Ctrl Pts',(187.035954926356,-5.55782922554555,
128.774960493842));
#141397=CARTESIAN_POINT('Ctrl Pts',(187.028668162023,-5.61112529593695,
128.920920107308));
#141398=CARTESIAN_POINT('Ctrl Pts',(187.021381397691,-5.65866555016246,
129.068975342758));
#141399=CARTESIAN_POINT('Ctrl Pts',(187.014094633358,-5.7002951840503,129.218622500097));
#141400=CARTESIAN_POINT('Ctrl Pts',(187.006803471584,-5.74194994073617,
129.368359967031));
#141401=CARTESIAN_POINT('Ctrl Pts',(186.999512309809,-5.77768684994215,
129.519690902912));
#141402=CARTESIAN_POINT('Ctrl Pts',(186.992221148034,-5.80740158088912,
129.672098527418));
#141403=CARTESIAN_POINT('Ctrl Pts',(186.984927500083,-5.8371264441105,129.824558120621));
#141404=CARTESIAN_POINT('Ctrl Pts',(186.977633852133,-5.86082497829701,
129.97809475339));
#141405=CARTESIAN_POINT('Ctrl Pts',(186.970340204182,-5.87844452383703,
130.132184641597));
#141406=CARTESIAN_POINT('Ctrl Pts',(186.963039152689,-5.89608195439748,
130.286430941374));
#141407=CARTESIAN_POINT('Ctrl Pts',(186.955738101197,-5.90762804625571,
130.441231234208));
#141408=CARTESIAN_POINT('Ctrl Pts',(186.948437049704,-5.91308220639865,
130.596059434488));
#141409=CARTESIAN_POINT('Ctrl Pts',(186.945083097206,-5.91558773509581,
130.66718431692));
#141410=CARTESIAN_POINT('Ctrl Pts',(186.941729144709,-5.91680841145624,
130.738315114615));
#141411=CARTESIAN_POINT('Ctrl Pts',(186.938375192211,-5.91674785298769,
130.809401120074));
#141412=CARTESIAN_POINT('',(185.188375192211,-5.92379981193959,130.800775453898));
#141413=CARTESIAN_POINT('Ctrl Pts',(186.938375192211,-5.9200304115163,130.809403916499));
#141414=CARTESIAN_POINT('Ctrl Pts',(186.921865869317,-5.92320279675294,
131.159511089235));
#141415=CARTESIAN_POINT('Ctrl Pts',(186.812540671824,-5.73530460751272,
133.474529816069));
#141416=CARTESIAN_POINT('Ctrl Pts',(186.610399599713,-2.68163859043372,
137.268598778454));
#141417=CARTESIAN_POINT('Ctrl Pts',(186.331951975907,3.98905548069682,136.554577735401));
#141418=CARTESIAN_POINT('Ctrl Pts',(186.05350435209,6.99400244126163,130.556388074787));
#141419=CARTESIAN_POINT('Ctrl Pts',(185.775056728279,3.57180283432081,124.78607306685));
#141420=CARTESIAN_POINT('Ctrl Pts',(185.496609104465,-3.13270908509169,
124.546270308331));
#141421=CARTESIAN_POINT('Ctrl Pts',(185.301048592443,-5.81959460894973,
128.416832856216));
#141422=CARTESIAN_POINT('Ctrl Pts',(185.198303955025,-5.92529888389735,
130.590568476525));
#141423=CARTESIAN_POINT('Ctrl Pts',(185.188375192211,-5.92379981193959,
130.800775453898));
#141424=CARTESIAN_POINT('',(183.438375192211,-5.90878783959383,130.801050019915));
#141425=CARTESIAN_POINT('Ctrl Pts',(185.188375192211,-5.92379981193959,
130.800775453898));
#141426=CARTESIAN_POINT('Ctrl Pts',(185.105488080421,-5.9112852874943,132.555621405934));
#141427=CARTESIAN_POINT('Ctrl Pts',(184.929785094025,-4.15424292220225,
136.29728126716));
#141428=CARTESIAN_POINT('Ctrl Pts',(184.661266233027,2.21295931186131,137.443665672644));
#141429=CARTESIAN_POINT('Ctrl Pts',(184.382818609213,6.78199394032505,132.531241830544));
#141430=CARTESIAN_POINT('Ctrl Pts',(184.104370985402,5.11870745645332,126.031898516554));
#141431=CARTESIAN_POINT('Ctrl Pts',(183.825923361588,-1.24842111713792,
123.918214725658));
#141432=CARTESIAN_POINT('Ctrl Pts',(183.603924763859,-5.41009564609318,
127.278197857111));
#141433=CARTESIAN_POINT('Ctrl Pts',(183.474742040733,-5.91271172097454,
130.026098884935));
#141434=CARTESIAN_POINT('Ctrl Pts',(183.438375192211,-5.90878783959383,
130.801050019915));
#141435=CARTESIAN_POINT('',(181.688375192211,-5.9116597264178,130.809147953816));
#141436=CARTESIAN_POINT('Ctrl Pts',(183.438375192211,-5.90878783959383,
130.801050019915));
#141437=CARTESIAN_POINT('Ctrl Pts',(183.381926166128,-5.90269714734493,
132.003937776489));
#141438=CARTESIAN_POINT('Ctrl Pts',(183.232661265441,-4.96014564476939,
135.193432897632));
#141439=CARTESIAN_POINT('Ctrl Pts',(182.99058049015,0.258615936756311,137.79797758789));
#141440=CARTESIAN_POINT('Ctrl Pts',(182.712132866336,6.02371625752071,134.36700050664));
#141441=CARTESIAN_POINT('Ctrl Pts',(182.433685242524,6.2533156125226,127.662131411966));
#141442=CARTESIAN_POINT('Ctrl Pts',(182.155237618711,0.736423411067356,
123.844817450807));
#141443=CARTESIAN_POINT('Ctrl Pts',(181.906800935273,-4.78965977321783,
126.145110250613));
#141444=CARTESIAN_POINT('Ctrl Pts',(181.75118012644,-5.90155441818334,129.472452618097));
#141445=CARTESIAN_POINT('Ctrl Pts',(181.688375192211,-5.9116597264178,130.809147953816));
#141446=CARTESIAN_POINT('',(179.938376004444,-5.92191450869858,130.805748116515));
#141447=CARTESIAN_POINT('Ctrl Pts',(181.688375192211,-5.9116597264178,130.809147953816));
#141448=CARTESIAN_POINT('Ctrl Pts',(181.658364251836,-5.91648848400863,
131.447879361033));
#141449=CARTESIAN_POINT('Ctrl Pts',(181.535537436858,-5.52634643860716,
134.05629721562));
#141450=CARTESIAN_POINT('Ctrl Pts',(181.31989474727,-1.71655817300176,137.588974723689));
#141451=CARTESIAN_POINT('Ctrl Pts',(181.041447123461,4.78024637596874,135.91579927174));
#141452=CARTESIAN_POINT('Ctrl Pts',(180.762999499646,6.88423803344246,129.54546140426));
#141453=CARTESIAN_POINT('Ctrl Pts',(180.484551875834,2.66195125190711,124.331990413167));
#141454=CARTESIAN_POINT('Ctrl Pts',(180.209677598402,-3.92096128402385,
125.056887831312));
#141455=CARTESIAN_POINT('Ctrl Pts',(180.027619195576,-5.92009025890988,
128.918301208267));
#141456=CARTESIAN_POINT('Ctrl Pts',(179.938376667353,-5.92612969673344,
130.805735096168));
#141457=CARTESIAN_POINT('',(178.188375192211,-5.91592736650928,130.798890494443));
#141458=CARTESIAN_POINT('Ctrl Pts',(179.938375192211,-5.91674983355068,
130.805764069745));
#141459=CARTESIAN_POINT('Ctrl Pts',(179.934802337543,-5.91673193815412,
130.881208453364));
#141460=CARTESIAN_POINT('Ctrl Pts',(179.931229482876,-5.91527111751309,
130.956633994371));
#141461=CARTESIAN_POINT('Ctrl Pts',(179.927656628208,-5.91236916926149,
131.032003690964));
#141462=CARTESIAN_POINT('Ctrl Pts',(179.920233361803,-5.90633983502618,
131.18859817597));
#141463=CARTESIAN_POINT('Ctrl Pts',(179.912810095397,-5.89407576518302,
131.345189745836));
#141464=CARTESIAN_POINT('Ctrl Pts',(179.905386828992,-5.87556700792397,
131.501241452354));
#141465=CARTESIAN_POINT('Ctrl Pts',(179.897972336271,-5.85708012647892,
131.657108718716));
#141466=CARTESIAN_POINT('Ctrl Pts',(179.89055784355,-5.83236329248394,131.81243702474));
#141467=CARTESIAN_POINT('Ctrl Pts',(179.883143350829,-5.80145853932096,
131.966689907845));
#141468=CARTESIAN_POINT('Ctrl Pts',(179.875736004475,-5.77058357332259,
132.120794116214));
#141469=CARTESIAN_POINT('Ctrl Pts',(179.868328658121,-5.73353263444466,
132.27382460163));
#141470=CARTESIAN_POINT('Ctrl Pts',(179.860921311767,-5.69039947340868,
132.425250618624));
#141471=CARTESIAN_POINT('Ctrl Pts',(179.853519490092,-5.64729848271151,
132.576563696382));
#141472=CARTESIAN_POINT('Ctrl Pts',(179.846117668417,-5.59812440416739,
132.726274330983));
#141473=CARTESIAN_POINT('Ctrl Pts',(179.838715846741,-5.54302190257774,
132.873862671212));
#141474=CARTESIAN_POINT('Ctrl Pts',(179.83131793243,-5.48794848916994,133.021373100704));
#141475=CARTESIAN_POINT('Ctrl Pts',(179.823920018118,-5.42695301563993,
133.166763118208));
#141476=CARTESIAN_POINT('Ctrl Pts',(179.816522103807,-5.3602297308131,133.309528834554));
#141477=CARTESIAN_POINT('Ctrl Pts',(179.809125418895,-5.2935175341856,133.452270825829));
#141478=CARTESIAN_POINT('Ctrl Pts',(179.801728733983,-5.22107957331895,
133.592389043643));
#141479=CARTESIAN_POINT('Ctrl Pts',(179.79433204907,-5.1431579462292,133.729400258774));
#141480=CARTESIAN_POINT('Ctrl Pts',(179.786935692135,-5.06523977426604,
133.866405398685));
#141481=CARTESIAN_POINT('Ctrl Pts',(179.779539335199,-4.98183860409271,
134.000303485351));
#141482=CARTESIAN_POINT('Ctrl Pts',(179.772142978264,-4.89324200758084,
134.13063679638));
#141483=CARTESIAN_POINT('Ctrl Pts',(179.764745488927,-4.80463184670375,
134.260990061772));
#141484=CARTESIAN_POINT('Ctrl Pts',(179.757347999591,-4.71082488554907,
134.387777156069));
#141485=CARTESIAN_POINT('Ctrl Pts',(179.749950510254,-4.61215135748797,
134.510570328055));
#141486=CARTESIAN_POINT('Ctrl Pts',(179.742550427739,-4.51344323957483,
134.633406544996));
#141487=CARTESIAN_POINT('Ctrl Pts',(179.735150345224,-4.4098653918718,134.752245761303));
#141488=CARTESIAN_POINT('Ctrl Pts',(179.727750262709,-4.30178744852212,
134.866694344654));
#141489=CARTESIAN_POINT('Ctrl Pts',(179.720342043042,-4.19359066236287,
134.981268775988));
#141490=CARTESIAN_POINT('Ctrl Pts',(179.712933823376,-4.08088415489833,
135.091442661055));
#141491=CARTESIAN_POINT('Ctrl Pts',(179.70552560371,-3.96407396764172,135.19685969458));
#141492=CARTESIAN_POINT('Ctrl Pts',(179.698112824407,-3.84719188566385,
135.30234161053));
#141493=CARTESIAN_POINT('Ctrl Pts',(179.690700045105,-3.72620137726176,
135.403060602727));
#141494=CARTESIAN_POINT('Ctrl Pts',(179.683287265803,-3.60154006095042,
135.49870186548));
#141495=CARTESIAN_POINT('Ctrl Pts',(179.675863894774,-3.47670062270434,
135.594479784955));
#141496=CARTESIAN_POINT('Ctrl Pts',(179.668440523746,-3.34818020526591,
135.685165269879));
#141497=CARTESIAN_POINT('Ctrl Pts',(179.661017152717,-3.21644446134536,
135.77048743729));
#141498=CARTESIAN_POINT('Ctrl Pts',(179.657081103276,-3.14659500896289,
135.815727297728));
#141499=CARTESIAN_POINT('Ctrl Pts',(179.653145053835,-3.07584201855703,
135.859460108231));
#141500=CARTESIAN_POINT('Ctrl Pts',(179.649209004394,-3.00425738879533,
135.901650888324));
#141501=CARTESIAN_POINT('Ctrl Pts',(179.641785737989,-2.86925101114459,
135.981221382851));
#141502=CARTESIAN_POINT('Ctrl Pts',(179.634362471584,-2.73087705919654,
136.05554484203));
#141503=CARTESIAN_POINT('Ctrl Pts',(179.626939205178,-2.58958190348824,
136.124322659501));
#141504=CARTESIAN_POINT('Ctrl Pts',(179.619524712457,-2.44845374692,136.193019187303));
#141505=CARTESIAN_POINT('Ctrl Pts',(179.612110219736,-2.30441159141906,
136.256182958357));
#141506=CARTESIAN_POINT('Ctrl Pts',(179.604695727015,-2.15792949821889,
136.313559365407));
#141507=CARTESIAN_POINT('Ctrl Pts',(179.597288380661,-2.01158858997503,
136.370880470916));
#141508=CARTESIAN_POINT('Ctrl Pts',(179.589881034308,-1.86281277106264,
136.422425182046));
#141509=CARTESIAN_POINT('Ctrl Pts',(179.582473687954,-1.71209924723198,
136.467985493044));
#141510=CARTESIAN_POINT('Ctrl Pts',(179.575071866278,-1.5614981312336,136.513511823442));
#141511=CARTESIAN_POINT('Ctrl Pts',(179.567670044603,-1.40896254372182,
136.553062533368));
#141512=CARTESIAN_POINT('Ctrl Pts',(179.560268222928,-1.25500804510559,
136.586478341136));
#141513=CARTESIAN_POINT('Ctrl Pts',(179.552870308616,-1.10113481787052,
136.619876508959));
#141514=CARTESIAN_POINT('Ctrl Pts',(179.545472394305,-0.945844535144645,
136.647146145406));
#141515=CARTESIAN_POINT('Ctrl Pts',(179.538074479993,-0.789666129390942,
136.668178313112));
#141516=CARTESIAN_POINT('Ctrl Pts',(179.530677795081,-0.633513677655301,
136.689206985652));
#141517=CARTESIAN_POINT('Ctrl Pts',(179.523281110169,-0.476473765410261,
136.704000196932));
#141518=CARTESIAN_POINT('Ctrl Pts',(179.515884425257,-0.319083806977362,
136.712500433669));
#141519=CARTESIAN_POINT('Ctrl Pts',(179.508488068321,-0.161700827380124,
136.721000293498));
#141520=CARTESIAN_POINT('Ctrl Pts',(179.501091711386,-0.0039682052111765,
136.723207713473));
#141521=CARTESIAN_POINT('Ctrl Pts',(179.493695354451,0.153573525095219,
136.71911722582));
#141522=CARTESIAN_POINT('Ctrl Pts',(179.486297865114,0.311139375442765,
136.715026111904));
#141523=CARTESIAN_POINT('Ctrl Pts',(179.478900375777,0.468513902538733,
136.704635180148));
#141524=CARTESIAN_POINT('Ctrl Pts',(179.471502886441,0.625158727965406,
136.687991055259));
#141525=CARTESIAN_POINT('Ctrl Pts',(179.464102803926,0.781858464992578,
136.671341095798));
#141526=CARTESIAN_POINT('Ctrl Pts',(179.456702721411,0.937827620086148,
136.648433618271));
#141527=CARTESIAN_POINT('Ctrl Pts',(179.449302638896,1.09253522294258,136.619366838468));
#141528=CARTESIAN_POINT('Ctrl Pts',(179.44189441923,1.24741294271294,136.590268096752));
#141529=CARTESIAN_POINT('Ctrl Pts',(179.434486199563,1.40102597280012,136.554996596033));
#141530=CARTESIAN_POINT('Ctrl Pts',(179.427077979897,1.55285506812971,136.513701358832));
#141531=CARTESIAN_POINT('Ctrl Pts',(179.419665200595,1.70477761173422,136.472380705102));
#141532=CARTESIAN_POINT('Ctrl Pts',(179.412252421292,1.85491367752859,136.425029039235));
#141533=CARTESIAN_POINT('Ctrl Pts',(179.40483964199,2.0027618670726,136.371844381916));
#141534=CARTESIAN_POINT('Ctrl Pts',(179.397416270962,2.15082130904315,136.318583731865));
#141535=CARTESIAN_POINT('Ctrl Pts',(179.389992899933,2.29658600076753,136.259473584504));
#141536=CARTESIAN_POINT('Ctrl Pts',(179.382569528904,2.43957634407283,136.194759287789));
#141537=CARTESIAN_POINT('Ctrl Pts',(179.378633479463,2.51539325509978,136.160446214872));
#141538=CARTESIAN_POINT('Ctrl Pts',(179.374697430023,2.59043062670582,136.124558372525));
#141539=CARTESIAN_POINT('Ctrl Pts',(179.370761380582,2.66462016584161,136.087137343332));
#141540=CARTESIAN_POINT('Ctrl Pts',(179.363338114176,2.80453932127499,136.016562450144));
#141541=CARTESIAN_POINT('Ctrl Pts',(179.355914847771,2.94186425343108,135.940318170553));
#141542=CARTESIAN_POINT('Ctrl Pts',(179.348491581365,3.07610246214482,135.858618644704));
#141543=CARTESIAN_POINT('Ctrl Pts',(179.341077088644,3.21018201244378,135.777015680909));
#141544=CARTESIAN_POINT('Ctrl Pts',(179.333662595923,3.3411817853958,135.689970497116));
#141545=CARTESIAN_POINT('Ctrl Pts',(179.326248103202,3.46863133103027,135.597744313025));
#141546=CARTESIAN_POINT('Ctrl Pts',(179.318840756849,3.59595803599425,135.505607020003));
#141547=CARTESIAN_POINT('Ctrl Pts',(179.311433410495,3.71974102546335,135.408298885418));
#141548=CARTESIAN_POINT('Ctrl Pts',(179.304026064141,3.83953654645319,135.306125790357));
#141549=CARTESIAN_POINT('Ctrl Pts',(179.296624242466,3.95924271942392,135.204028899845));
#141550=CARTESIAN_POINT('Ctrl Pts',(179.28922242079,4.07496706275787,135.097074514833));
#141551=CARTESIAN_POINT('Ctrl Pts',(179.281820599115,4.18629689526787,134.985610295255));
#141552=CARTESIAN_POINT('Ctrl Pts',(179.274422684804,4.29756795762586,134.87420491677));
#141553=CARTESIAN_POINT('Ctrl Pts',(179.267024770492,4.40444886607418,134.758294708461));
#141554=CARTESIAN_POINT('Ctrl Pts',(179.259626856181,4.50656206760595,134.638265792882));
#141555=CARTESIAN_POINT('Ctrl Pts',(179.252230171269,4.6086582997761,134.518256823932));
#141556=CARTESIAN_POINT('Ctrl Pts',(179.244833486356,4.70598815587262,134.394130790199));
#141557=CARTESIAN_POINT('Ctrl Pts',(179.237436801444,4.79821276277581,134.266308746241));
#141558=CARTESIAN_POINT('Ctrl Pts',(179.230040444509,4.89043328034328,134.138492370046));
#141559=CARTESIAN_POINT('Ctrl Pts',(179.222644087573,4.97754878040159,134.006980612211));
#141560=CARTESIAN_POINT('Ctrl Pts',(179.215247730638,5.05926249069234,133.872225284199));
#141561=CARTESIAN_POINT('Ctrl Pts',(179.207850241301,5.14098871156078,133.737449324802));
#141562=CARTESIAN_POINT('Ctrl Pts',(179.200452751965,5.21731130237002,133.599429125651));
#141563=CARTESIAN_POINT('Ctrl Pts',(179.193055262628,5.28797848312044,133.45864284155));
#141564=CARTESIAN_POINT('Ctrl Pts',(179.185655180113,5.3586704361415,133.317807205035));
#141565=CARTESIAN_POINT('Ctrl Pts',(179.178255097598,5.42370286461153,133.174203886429));
#141566=CARTESIAN_POINT('Ctrl Pts',(179.170855015083,5.4828713978363,133.028332694119));
#141567=CARTESIAN_POINT('Ctrl Pts',(179.163446795416,5.54210499294605,132.882301101438));
#141568=CARTESIAN_POINT('Ctrl Pts',(179.15603857575,5.59546167541947,132.733997000985));
#141569=CARTESIAN_POINT('Ctrl Pts',(179.148630356084,5.64278615747782,132.583937798662));
#141570=CARTESIAN_POINT('Ctrl Pts',(179.141217576781,5.69013976696525,132.433786237403));
#141571=CARTESIAN_POINT('Ctrl Pts',(179.133804797479,5.73145368024142,132.281877781146));
#141572=CARTESIAN_POINT('Ctrl Pts',(179.126392018177,5.76662347961273,132.128741305616));
#141573=CARTESIAN_POINT('Ctrl Pts',(179.118968647149,5.80184353124267,131.975386021508));
#141574=CARTESIAN_POINT('Ctrl Pts',(179.11154527612,5.83090186655938,131.820799579596));
#141575=CARTESIAN_POINT('Ctrl Pts',(179.104121905091,5.85374566921849,131.665518095967));
#141576=CARTESIAN_POINT('Ctrl Pts',(179.10018585565,5.86585800151788,131.583184127419));
#141577=CARTESIAN_POINT('Ctrl Pts',(179.096249806209,5.87622407559727,131.50065480612));
#141578=CARTESIAN_POINT('Ctrl Pts',(179.092313756769,5.88484196200156,131.41801006535));
#141579=CARTESIAN_POINT('Ctrl Pts',(179.084890490363,5.90109502680501,131.262144663512));
#141580=CARTESIAN_POINT('Ctrl Pts',(179.077467223958,5.91117603521354,131.105397413357));
#141581=CARTESIAN_POINT('Ctrl Pts',(179.070043957552,5.91499894102585,130.948298417199));
#141582=CARTESIAN_POINT('Ctrl Pts',(179.062629464831,5.91881732848096,130.791385099008));
#141583=CARTESIAN_POINT('Ctrl Pts',(179.05521497211,5.91639232723587,130.63412123188));
#141584=CARTESIAN_POINT('Ctrl Pts',(179.047800479389,5.90768941912305,130.477043814329));
#141585=CARTESIAN_POINT('Ctrl Pts',(179.040393133036,5.89899489920073,130.320117793906));
#141586=CARTESIAN_POINT('Ctrl Pts',(179.032985786682,5.88403453903981,130.163378235523));
#141587=CARTESIAN_POINT('Ctrl Pts',(179.025578440328,5.8628258257359,130.007363817331));
#141588=CARTESIAN_POINT('Ctrl Pts',(179.018176618653,5.84163293069053,129.851465760579));
#141589=CARTESIAN_POINT('Ctrl Pts',(179.010774796977,5.81420101177123,129.696292135444));
#141590=CARTESIAN_POINT('Ctrl Pts',(179.003372975302,5.78059950086301,129.542378060982));
#141591=CARTESIAN_POINT('Ctrl Pts',(178.99597506099,5.74701572793086,129.388545236562));
#141592=CARTESIAN_POINT('Ctrl Pts',(178.988577146679,5.70726892866063,129.235971002404));
#141593=CARTESIAN_POINT('Ctrl Pts',(178.981179232368,5.66147988227038,129.08518171322));
#141594=CARTESIAN_POINT('Ctrl Pts',(178.973782547456,5.61569844518896,128.93441748248));
#141595=CARTESIAN_POINT('Ctrl Pts',(178.966385862543,5.56387686221214,128.785437964842));
#141596=CARTESIAN_POINT('Ctrl Pts',(178.958989177631,5.5061862092642,128.638755854132));
#141597=CARTESIAN_POINT('Ctrl Pts',(178.951592820696,5.44849811438028,128.49208024746));
#141598=CARTESIAN_POINT('Ctrl Pts',(178.94419646376,5.38494160360329,128.347702192559));
#141599=CARTESIAN_POINT('Ctrl Pts',(178.936800106825,5.31573638605803,128.206115587466));
#141600=CARTESIAN_POINT('Ctrl Pts',(178.929402617488,5.24652057301731,128.064507305103));
#141601=CARTESIAN_POINT('Ctrl Pts',(178.922005128152,5.17165449515218,127.925691658915));
#141602=CARTESIAN_POINT('Ctrl Pts',(178.914607638815,5.09140434440064,127.790138932899));
#141603=CARTESIAN_POINT('Ctrl Pts',(178.9072075563,5.01112606208312,127.654538689084));
#141604=CARTESIAN_POINT('Ctrl Pts',(178.899807473785,4.9254601391764,127.522203963786));
#141605=CARTESIAN_POINT('Ctrl Pts',(178.89240739127,4.8347166112795,127.393576858499));
#141606=CARTESIAN_POINT('Ctrl Pts',(178.884999171604,4.743873301545,127.264808314486));
#141607=CARTESIAN_POINT('Ctrl Pts',(178.877590951937,4.64794145183068,127.139755837558));
#141608=CARTESIAN_POINT('Ctrl Pts',(178.870182732271,4.54727243353588,127.018829746248));
#141609=CARTESIAN_POINT('Ctrl Pts',(178.862769952969,4.44654145513995,126.897829226946));
#141610=CARTESIAN_POINT('Ctrl Pts',(178.855357173667,4.34106774789423,126.780960430458));
#141611=CARTESIAN_POINT('Ctrl Pts',(178.847944394365,4.23123982961107,126.668597076596));
#141612=CARTESIAN_POINT('Ctrl Pts',(178.840521023336,4.12125498404791,126.556073172705));
#141613=CARTESIAN_POINT('Ctrl Pts',(178.833097652307,4.00690377237975,126.448067824391));
#141614=CARTESIAN_POINT('Ctrl Pts',(178.825674281278,3.88860869573101,126.344915251381));
#141615=CARTESIAN_POINT('Ctrl Pts',(178.821738231838,3.82588580763872,126.290221282058));
#141616=CARTESIAN_POINT('Ctrl Pts',(178.817802182397,3.76205466852198,126.236890896299));
#141617=CARTESIAN_POINT('Ctrl Pts',(178.813866132956,3.69718148559496,126.184968923298));
#141618=CARTESIAN_POINT('Ctrl Pts',(178.80644286655,3.57483268722024,126.08704570265));
#141619=CARTESIAN_POINT('Ctrl Pts',(178.799019600145,3.44840581763817,125.993838547293));
#141620=CARTESIAN_POINT('Ctrl Pts',(178.791596333739,3.31830035686659,125.905706383583));
#141621=CARTESIAN_POINT('Ctrl Pts',(178.784181841018,3.18834866994496,125.817678384771));
#141622=CARTESIAN_POINT('Ctrl Pts',(178.776767348297,3.05472735217882,125.734713645432));
#141623=CARTESIAN_POINT('Ctrl Pts',(178.769352855576,2.91786953771339,125.657131467491));
#141624=CARTESIAN_POINT('Ctrl Pts',(178.761945509222,2.7811436319621,125.579624066173));
#141625=CARTESIAN_POINT('Ctrl Pts',(178.754538162869,2.64118776230442,125.507489080993));
#141626=CARTESIAN_POINT('Ctrl Pts',(178.747130816515,2.49846458612938,125.441002968261));
#141627=CARTESIAN_POINT('Ctrl Pts',(178.73972899484,2.3558478582839,125.374566443381));
#141628=CARTESIAN_POINT('Ctrl Pts',(178.732327173164,2.2104682704742,125.313770558968));
#141629=CARTESIAN_POINT('Ctrl Pts',(178.724925351489,2.06281356314709,125.258846144932));
#141630=CARTESIAN_POINT('Ctrl Pts',(178.717527437177,1.91523680159044,125.203950725066));
#141631=CARTESIAN_POINT('Ctrl Pts',(178.710129522866,1.7653876613914,125.154920732585));
#141632=CARTESIAN_POINT('Ctrl Pts',(178.702731608555,1.61377426379196,125.11193906009));
#141633=CARTESIAN_POINT('Ctrl Pts',(178.695334923642,1.46218606158879,125.068964530368));
#141634=CARTESIAN_POINT('Ctrl Pts',(178.68793823873,1.30883454266877,125.03203642748));
#141635=CARTESIAN_POINT('Ctrl Pts',(178.680541553818,1.15424352158327,125.00128794394));
#141636=CARTESIAN_POINT('Ctrl Pts',(178.673145196882,0.999659355225655,
124.970540823821));
#141637=CARTESIAN_POINT('Ctrl Pts',(178.665748839947,0.84383616210872,124.945972851047));
#141638=CARTESIAN_POINT('Ctrl Pts',(178.658352483011,0.687308230788165,
124.927666142064));
#141639=CARTESIAN_POINT('Ctrl Pts',(178.650954993675,0.530756334641783,
124.909356630278));
#141640=CARTESIAN_POINT('Ctrl Pts',(178.643557504338,0.373499856248618,
124.897310334378));
#141641=CARTESIAN_POINT('Ctrl Pts',(178.636160015002,0.216078342097464,
124.891557499537));
#141642=CARTESIAN_POINT('Ctrl Pts',(178.628759932487,0.0586016440782505,
124.885802648048));
#141643=CARTESIAN_POINT('Ctrl Pts',(178.621359849972,-0.0990398320677371,
124.886345663696));
#141644=CARTESIAN_POINT('Ctrl Pts',(178.613959767457,-0.256306552017657,
124.893164671406));
#141645=CARTESIAN_POINT('Ctrl Pts',(178.60655154779,-0.413746202893404,
124.899991177317));
#141646=CARTESIAN_POINT('Ctrl Pts',(178.599143328124,-0.570809901440018,
124.913107441057));
#141647=CARTESIAN_POINT('Ctrl Pts',(178.591735108457,-0.726962510230612,
124.932439631107));
#141648=CARTESIAN_POINT('Ctrl Pts',(178.584322329155,-0.883211228346482,
124.951783719797));
#141649=CARTESIAN_POINT('Ctrl Pts',(178.576909549853,-1.0385473718329,124.977351297693));
#141650=CARTESIAN_POINT('Ctrl Pts',(178.569496770551,-1.19244651626097,
125.009017498444));
#141651=CARTESIAN_POINT('Ctrl Pts',(178.562073399522,-1.34656555900366,
125.040728945347));
#141652=CARTESIAN_POINT('Ctrl Pts',(178.554650028493,-1.49924314050149,
125.078556329378));
#141653=CARTESIAN_POINT('Ctrl Pts',(178.547226657465,-1.64996970005422,
125.1223248423));
#141654=CARTESIAN_POINT('Ctrl Pts',(178.543290608024,-1.72988853855967,
125.145531958061));
#141655=CARTESIAN_POINT('Ctrl Pts',(178.539354558583,-1.8092591923436,125.17040852702));
#141656=CARTESIAN_POINT('Ctrl Pts',(178.535418509143,-1.88800815871802,
125.196923078448));
#141657=CARTESIAN_POINT('Ctrl Pts',(178.527995242737,-2.0365262516354,125.246928694951));
#141658=CARTESIAN_POINT('Ctrl Pts',(178.520571976332,-2.18328088235783,
125.302914456743));
#141659=CARTESIAN_POINT('Ctrl Pts',(178.513148709927,-2.32775414726904,
125.364738278435));
#141660=CARTESIAN_POINT('Ctrl Pts',(178.505734217206,-2.47205665677897,
125.426489029504));
#141661=CARTESIAN_POINT('Ctrl Pts',(178.498319724485,-2.61408282780302,
125.494063960354));
#141662=CARTESIAN_POINT('Ctrl Pts',(178.490905231764,-2.7533299030029,125.567271253451));
#141663=CARTESIAN_POINT('Ctrl Pts',(178.48349788541,-2.89244276662918,125.640407986602));
#141664=CARTESIAN_POINT('Ctrl Pts',(178.476090539056,-3.02878153879216,
125.719166102016));
#141665=CARTESIAN_POINT('Ctrl Pts',(178.468683192702,-3.16186355134782,
125.803305784318));
#141666=CARTESIAN_POINT('Ctrl Pts',(178.461281371027,-3.29484630631761,
125.887382712069));
#141667=CARTESIAN_POINT('Ctrl Pts',(178.453879549352,-3.42457682400798,
125.97683301611));
#141668=CARTESIAN_POINT('Ctrl Pts',(178.446477727676,-3.55059726505351,
126.071371115793));
#141669=CARTESIAN_POINT('Ctrl Pts',(178.439079813365,-3.6765511808892,126.165859309549));
#141670=CARTESIAN_POINT('Ctrl Pts',(178.431681899054,-3.79879862271108,
126.265429726586));
#141671=CARTESIAN_POINT('Ctrl Pts',(178.424283984742,-3.91691106585152,
126.369753728031));
#141672=CARTESIAN_POINT('Ctrl Pts',(178.41688729983,-4.03500388084664,126.47406039272));
#141673=CARTESIAN_POINT('Ctrl Pts',(178.409490614918,-4.14896278146007,
126.583118827097));
#141674=CARTESIAN_POINT('Ctrl Pts',(178.402093930006,-4.25839257449629,
126.696560324955));
#141675=CARTESIAN_POINT('Ctrl Pts',(178.39469757307,-4.36781751530079,126.809996792698));
#141676=CARTESIAN_POINT('Ctrl Pts',(178.387301216135,-4.47271348866885,
126.927815668819));
#141677=CARTESIAN_POINT('Ctrl Pts',(178.379904859199,-4.57272261169512,
127.049611827168));
#141678=CARTESIAN_POINT('Ctrl Pts',(178.372507369863,-4.67274704637341,
127.171426632821));
#141679=CARTESIAN_POINT('Ctrl Pts',(178.365109880526,-4.76788290405682,
127.297219644647));
#141680=CARTESIAN_POINT('Ctrl Pts',(178.35771239119,-4.85781310057062,127.426553275158));
#141681=CARTESIAN_POINT('Ctrl Pts',(178.350312308675,-4.94777482197532,
127.555932243373));
#141682=CARTESIAN_POINT('Ctrl Pts',(178.34291222616,-5.03252703599572,127.688853995114));
#141683=CARTESIAN_POINT('Ctrl Pts',(178.335512143645,-5.11179651527014,
127.824852780863));
#141684=CARTESIAN_POINT('Ctrl Pts',(178.328103923978,-5.19115315948626,
127.961001111259));
#141685=CARTESIAN_POINT('Ctrl Pts',(178.320695704312,-5.26501484088846,
128.100232910055));
#141686=CARTESIAN_POINT('Ctrl Pts',(178.313287484645,-5.33315442117471,
128.242058043239));
#141687=CARTESIAN_POINT('Ctrl Pts',(178.305874705343,-5.40133594023571,
128.383970467425));
#141688=CARTESIAN_POINT('Ctrl Pts',(178.298461926041,-5.46378819269074,
128.528479064664));
#141689=CARTESIAN_POINT('Ctrl Pts',(178.291049146739,-5.52033276792493,
128.675075128517));
#141690=CARTESIAN_POINT('Ctrl Pts',(178.28362577571,-5.57695813669991,128.821880655701));
#141691=CARTESIAN_POINT('Ctrl Pts',(178.276202404682,-5.62765884934485,
128.970779254122));
#141692=CARTESIAN_POINT('Ctrl Pts',(178.268779033653,-5.67230654697386,
129.121247727812));
#141693=CARTESIAN_POINT('Ctrl Pts',(178.264842984212,-5.6959798275633,129.201029723002));
#141694=CARTESIAN_POINT('Ctrl Pts',(178.260906934771,-5.71795224266406,
129.281252895093));
#141695=CARTESIAN_POINT('Ctrl Pts',(178.256970885331,-5.73821053949377,
129.361838393494));
#141696=CARTESIAN_POINT('Ctrl Pts',(178.247172129819,-5.7886433657853,129.562455181598));
#141697=CARTESIAN_POINT('Ctrl Pts',(178.237373374307,-5.82857446158366,
129.765810079928));
#141698=CARTESIAN_POINT('Ctrl Pts',(178.227574618795,-5.85776135301345,
129.970956457724));
#141699=CARTESIAN_POINT('Ctrl Pts',(178.217994260588,-5.88629771913801,
130.171530477743));
#141700=CARTESIAN_POINT('Ctrl Pts',(178.208413902381,-5.90456354448022,
130.373817290485));
#141701=CARTESIAN_POINT('Ctrl Pts',(178.198833544173,-5.91237657174734,
130.576909883663));
#141702=CARTESIAN_POINT('Ctrl Pts',(178.195347434847,-5.91521958310837,
130.650811398403));
#141703=CARTESIAN_POINT('Ctrl Pts',(178.19186132552,-5.91667897563865,130.724819368428));
#141704=CARTESIAN_POINT('Ctrl Pts',(178.188375216193,-5.91674747022219,
130.798889226584));
#141705=CARTESIAN_POINT('',(176.438375192211,-5.90709253321605,130.805377784422));
#141706=CARTESIAN_POINT('Ctrl Pts',(178.188375192211,-5.91592736650928,
130.798890494443));
#141707=CARTESIAN_POINT('Ctrl Pts',(178.118424548647,-5.90234026736635,
132.284949550647));
#141708=CARTESIAN_POINT('Ctrl Pts',(177.955658030477,-4.58078385458697,
135.76435699672));
#141709=CARTESIAN_POINT('Ctrl Pts',(177.700075637705,1.26937439390032,137.686674848873));
#141710=CARTESIAN_POINT('Ctrl Pts',(177.421628013892,6.47641374616305,133.456458941318));
#141711=CARTESIAN_POINT('Ctrl Pts',(177.143180390079,5.73194525610269,126.789094236441));
#141712=CARTESIAN_POINT('Ctrl Pts',(176.864732766266,-0.279900903224888,
123.811563179148));
#141713=CARTESIAN_POINT('Ctrl Pts',(176.62979770031,-5.13526498310803,126.721178580489));
#141714=CARTESIAN_POINT('Ctrl Pts',(176.487678508958,-5.90548474499912,
129.754006561336));
#141715=CARTESIAN_POINT('Ctrl Pts',(176.438375192211,-5.90709253321605,
130.805377784422));
#141716=CARTESIAN_POINT('',(174.688376076494,-5.9186848337546,130.809462800912));
#141717=CARTESIAN_POINT('Ctrl Pts',(176.438375192211,-5.90709253321605,
130.805377784422));
#141718=CARTESIAN_POINT('Ctrl Pts',(176.394862634354,-5.90851148395661,
131.733263658879));
#141719=CARTESIAN_POINT('Ctrl Pts',(176.258534201893,-5.26482177762399,
134.63854442458));
#141720=CARTESIAN_POINT('Ctrl Pts',(176.029389894828,-0.715237544583954,
137.76611296774));
#141721=CARTESIAN_POINT('Ctrl Pts',(175.750942271015,5.47051605577885,135.169107415928));
#141722=CARTESIAN_POINT('Ctrl Pts',(175.472494647202,6.6291326504466,128.561112786155));
#141723=CARTESIAN_POINT('Ctrl Pts',(175.194047023389,1.69590019048836,124.0145533247));
#141724=CARTESIAN_POINT('Ctrl Pts',(174.932674316708,-4.3976998989599,125.603680783644));
#141725=CARTESIAN_POINT('Ctrl Pts',(174.764117484631,-5.9049897404614,129.202992274976));
#141726=CARTESIAN_POINT('Ctrl Pts',(174.688376527159,-5.91967202939123,
130.80945409654));
#141727=CARTESIAN_POINT('',(172.938373760814,-5.92088540128737,130.800975483928));
#141728=CARTESIAN_POINT('Ctrl Pts',(174.688375192211,-5.91674778536724,
130.809479880392));
#141729=CARTESIAN_POINT('Ctrl Pts',(174.677234495542,-5.91654344322708,
131.045654686463));
#141730=CARTESIAN_POINT('Ctrl Pts',(174.666093798872,-5.90219520381266,
131.281241271787));
#141731=CARTESIAN_POINT('Ctrl Pts',(174.654953102203,-5.8739315365935,131.514894829207));
#141732=CARTESIAN_POINT('Ctrl Pts',(174.649019326723,-5.85887769745775,
131.639343756504));
#141733=CARTESIAN_POINT('Ctrl Pts',(174.643085551242,-5.83987696246974,
131.763245004832));
#141734=CARTESIAN_POINT('Ctrl Pts',(174.637151775762,-5.81696862578434,
131.886398772688));
#141735=CARTESIAN_POINT('Ctrl Pts',(174.629728509357,-5.78830985925462,
132.040466487369));
#141736=CARTESIAN_POINT('Ctrl Pts',(174.622305242951,-5.7534825938637,132.193627803463));
#141737=CARTESIAN_POINT('Ctrl Pts',(174.614881976545,-5.71255479535126,
132.345349998649));
#141738=CARTESIAN_POINT('Ctrl Pts',(174.607467483824,-5.67167537009779,
132.496892870799));
#141739=CARTESIAN_POINT('Ctrl Pts',(174.600052991103,-5.6247098601858,132.64699965084));
#141740=CARTESIAN_POINT('Ctrl Pts',(174.592638498382,-5.57177759741108,
132.795145630441));
#141741=CARTESIAN_POINT('Ctrl Pts',(174.585231152028,-5.51889635274405,
132.94314882137));
#141742=CARTESIAN_POINT('Ctrl Pts',(174.577823805674,-5.46005992904419,
133.089194625093));
#141743=CARTESIAN_POINT('Ctrl Pts',(174.57041645932,-5.39543800101284,133.232771484723));
#141744=CARTESIAN_POINT('Ctrl Pts',(174.563014637645,-5.33086427045342,
133.376241259315));
#141745=CARTESIAN_POINT('Ctrl Pts',(174.555612815969,-5.26051377995737,
133.517245417411));
#141746=CARTESIAN_POINT('Ctrl Pts',(174.548210994294,-5.1846050020994,133.655290559656));
#141747=CARTESIAN_POINT('Ctrl Pts',(174.540813079983,-5.10873629589451,
133.793262828945));
#141748=CARTESIAN_POINT('Ctrl Pts',(174.533415165671,-5.0273153252958,133.928278866984));
#141749=CARTESIAN_POINT('Ctrl Pts',(174.52601725136,-4.94060731033035,134.059868253498));
#141750=CARTESIAN_POINT('Ctrl Pts',(174.518620566448,-4.85391370466393,
134.191435772243));
#141751=CARTESIAN_POINT('Ctrl Pts',(174.511223881535,-4.76193500360776,
134.31957745824));
#141752=CARTESIAN_POINT('Ctrl Pts',(174.503827196623,-4.66498077731926,
134.443850267193));
#141753=CARTESIAN_POINT('Ctrl Pts',(174.496430839688,-4.5680308500827,134.56811756576));
#141754=CARTESIAN_POINT('Ctrl Pts',(174.489034482753,-4.46610606590234,
134.688516034061));
#141755=CARTESIAN_POINT('Ctrl Pts',(174.481638125817,-4.35955729241333,
134.804634455276));
#141756=CARTESIAN_POINT('Ctrl Pts',(174.474240636481,-4.25299220603502,
134.920770654517));
#141757=CARTESIAN_POINT('Ctrl Pts',(174.466843147144,-4.14180197313662,
135.032625226841));
#141758=CARTESIAN_POINT('Ctrl Pts',(174.459445657808,-4.02637532920606,
135.139822792567));
#141759=CARTESIAN_POINT('Ctrl Pts',(174.452045575293,-3.91090822264448,
135.247057936233));
#141760=CARTESIAN_POINT('Ctrl Pts',(174.444645492778,-3.79120202165373,
135.349632569119));
#141761=CARTESIAN_POINT('Ctrl Pts',(174.437245410263,-3.6676795021956,135.447210780093));
#141762=CARTESIAN_POINT('Ctrl Pts',(174.429837190596,-3.54402115702884,
135.54489628834));
#141763=CARTESIAN_POINT('Ctrl Pts',(174.42242897093,-3.41653840594465,135.637574171094));
#141764=CARTESIAN_POINT('Ctrl Pts',(174.415020751264,-3.28568463866214,
135.724950726258));
#141765=CARTESIAN_POINT('Ctrl Pts',(174.407607971962,-3.15475033306937,
135.812381060234));
#141766=CARTESIAN_POINT('Ctrl Pts',(174.40019519266,-3.02044119471371,135.894503370643));
#141767=CARTESIAN_POINT('Ctrl Pts',(174.392782413358,-2.8832358430249,135.971069592919));
#141768=CARTESIAN_POINT('Ctrl Pts',(174.385359042329,-2.74583444589511,
136.047745216605));
#141769=CARTESIAN_POINT('Ctrl Pts',(174.3779356713,-2.60552890252608,136.118848728295));
#141770=CARTESIAN_POINT('Ctrl Pts',(174.370512300271,-2.462819205497,136.184179585109));
#141771=CARTESIAN_POINT('Ctrl Pts',(174.366576250831,-2.38715109986894,
136.21881957298));
#141772=CARTESIAN_POINT('Ctrl Pts',(174.362640201391,-2.31080738998295,
136.251837482137));
#141773=CARTESIAN_POINT('Ctrl Pts',(174.35870415195,-2.23386428477683,136.283209120646));
#141774=CARTESIAN_POINT('Ctrl Pts',(174.351280885545,-2.08875198965366,
136.342375051804));
#141775=CARTESIAN_POINT('Ctrl Pts',(174.34385761914,-1.94106804902361,136.395861319592));
#141776=CARTESIAN_POINT('Ctrl Pts',(174.336434352734,-1.79129739440587,
136.443437156087));
#141777=CARTESIAN_POINT('Ctrl Pts',(174.329019860013,-1.64170375626399,
136.490956761893));
#141778=CARTESIAN_POINT('Ctrl Pts',(174.321605367292,-1.49002866566799,
136.532579729446));
#141779=CARTESIAN_POINT('Ctrl Pts',(174.314190874571,-1.33677807634548,
136.568122838295));
#141780=CARTESIAN_POINT('Ctrl Pts',(174.306783528217,-1.18367519571074,
136.603631689358));
#141781=CARTESIAN_POINT('Ctrl Pts',(174.299376181864,-1.02900020063819,
136.633072264044));
#141782=CARTESIAN_POINT('Ctrl Pts',(174.29196883551,-0.873275191744421,
136.656310805493));
#141783=CARTESIAN_POINT('Ctrl Pts',(174.284567013834,-0.717666328437618,
136.679532014762));
#141784=CARTESIAN_POINT('Ctrl Pts',(174.277165192159,-0.561009378267391,
136.696560346347));
#141785=CARTESIAN_POINT('Ctrl Pts',(174.269763370484,-0.403837541848953,
136.70731291301));
#141786=CARTESIAN_POINT('Ctrl Pts',(174.262365456172,-0.246748675219313,
136.718059803478));
#141787=CARTESIAN_POINT('Ctrl Pts',(174.254967541861,-0.0891458351376757,
136.722537501462));
#141788=CARTESIAN_POINT('Ctrl Pts',(174.247569627549,0.0684318425907609,
136.720714870433));
#141789=CARTESIAN_POINT('Ctrl Pts',(174.240172942637,0.225983333767741,
136.718892542293));
#141790=CARTESIAN_POINT('Ctrl Pts',(174.232776257725,0.383509297983157,
136.710771967438));
#141791=CARTESIAN_POINT('Ctrl Pts',(174.225379572813,0.540469659291495,
136.696374119747));
#141792=CARTESIAN_POINT('Ctrl Pts',(174.217983215877,0.69742306081293,136.681976910472));
#141793=CARTESIAN_POINT('Ctrl Pts',(174.210586858942,0.853810537556758,
136.661303015894));
#141794=CARTESIAN_POINT('Ctrl Pts',(174.203190502006,1.00909646863808,136.634425358157));
#141795=CARTESIAN_POINT('Ctrl Pts',(174.195793012669,1.16440617439188,136.607543585382));
#141796=CARTESIAN_POINT('Ctrl Pts',(174.188395523333,1.31861363082728,136.574456221915));
#141797=CARTESIAN_POINT('Ctrl Pts',(174.180998033996,1.47119289936138,136.535287420045));
#141798=CARTESIAN_POINT('Ctrl Pts',(174.173597951481,1.62382565432149,136.496104887612));
#141799=CARTESIAN_POINT('Ctrl Pts',(174.166197868966,1.77482872365539,136.450836765063));
#141800=CARTESIAN_POINT('Ctrl Pts',(174.158797786451,1.92369097507765,136.399657177616));
#141801=CARTESIAN_POINT('Ctrl Pts',(174.151389566784,2.07271691584888,136.34842131295));
#141802=CARTESIAN_POINT('Ctrl Pts',(174.143981347118,2.21959698428384,136.291261123376));
#141803=CARTESIAN_POINT('Ctrl Pts',(174.136573127451,2.36383901227271,136.228399305348));
#141804=CARTESIAN_POINT('Ctrl Pts',(174.129160348149,2.5081698188232,136.16549879692));
#141805=CARTESIAN_POINT('Ctrl Pts',(174.121747568847,2.64985901435945,136.096889829714));
#141806=CARTESIAN_POINT('Ctrl Pts',(174.114334789545,2.78843918964349,136.022840994856));
#141807=CARTESIAN_POINT('Ctrl Pts',(174.106911418516,2.9272173747806,135.94868635555));
#141808=CARTESIAN_POINT('Ctrl Pts',(174.099488047487,3.0628773462658,135.869076513123));
#141809=CARTESIAN_POINT('Ctrl Pts',(174.092064676459,3.1949801234916,135.784323727168));
#141810=CARTESIAN_POINT('Ctrl Pts',(174.088128627018,3.26502418573835,135.73938576644));
#141811=CARTESIAN_POINT('Ctrl Pts',(174.084192577577,3.33406872782739,135.693002627549));
#141812=CARTESIAN_POINT('Ctrl Pts',(174.080256528136,3.40205220360581,135.6452253509));
#141813=CARTESIAN_POINT('Ctrl Pts',(174.072833261731,3.53026691723385,135.555118898219));
#141814=CARTESIAN_POINT('Ctrl Pts',(174.065409995325,3.65509320642557,135.459778850555));
#141815=CARTESIAN_POINT('Ctrl Pts',(174.05798672892,3.77607480225818,135.359488458829));
#141816=CARTESIAN_POINT('Ctrl Pts',(174.050572236199,3.89691340789153,135.259316602018));
#141817=CARTESIAN_POINT('Ctrl Pts',(174.043157743478,4.01391608065393,135.154206283297));
#141818=CARTESIAN_POINT('Ctrl Pts',(174.035743250757,4.12665519164441,135.04448414074));
#141819=CARTESIAN_POINT('Ctrl Pts',(174.028335904403,4.23928564043516,134.934867752515));
#141820=CARTESIAN_POINT('Ctrl Pts',(174.020928558049,4.34766044270246,134.820648648281));
#141821=CARTESIAN_POINT('Ctrl Pts',(174.013521211696,4.45138485687511,134.702193787224));
#141822=CARTESIAN_POINT('Ctrl Pts',(174.00611939002,4.55503190946633,134.583827274271));
#141823=CARTESIAN_POINT('Ctrl Pts',(173.998717568345,4.65403523522225,134.461231574499));
#141824=CARTESIAN_POINT('Ctrl Pts',(173.991315746669,4.7480368908042,134.334810482111));
#141825=CARTESIAN_POINT('Ctrl Pts',(173.983917832358,4.84198892364395,134.208456126432));
#141826=CARTESIAN_POINT('Ctrl Pts',(173.976519918047,4.93094432250053,134.078280698662));
#141827=CARTESIAN_POINT('Ctrl Pts',(173.969122003735,5.01458547525733,133.944720958966));
#141828=CARTESIAN_POINT('Ctrl Pts',(173.961725318823,5.09821272837186,133.811183414476));
#141829=CARTESIAN_POINT('Ctrl Pts',(173.954328633911,5.17652729020417,133.67426299035));
#141830=CARTESIAN_POINT('Ctrl Pts',(173.946931948999,5.24925488243041,133.534425404669));
#141831=CARTESIAN_POINT('Ctrl Pts',(173.939535592063,5.321979249839,133.394594019533));
#141832=CARTESIAN_POINT('Ctrl Pts',(173.932139235128,5.38911696797228,133.251846061218));
#141833=CARTESIAN_POINT('Ctrl Pts',(173.924742878193,5.4504398721223,133.106671578944));
#141834=CARTESIAN_POINT('Ctrl Pts',(173.917345388856,5.51177216496549,132.961474870085));
#141835=CARTESIAN_POINT('Ctrl Pts',(173.909947899519,5.56728772592756,132.813851241446));
#141836=CARTESIAN_POINT('Ctrl Pts',(173.902550410183,5.61680672519481,132.664310287398));
#141837=CARTESIAN_POINT('Ctrl Pts',(173.895150327668,5.6663430832705,132.514716911999));
#141838=CARTESIAN_POINT('Ctrl Pts',(173.887750245153,5.70987857714054,132.363205227167));
#141839=CARTESIAN_POINT('Ctrl Pts',(173.880350162638,5.747283423796,132.210299381901));
#141840=CARTESIAN_POINT('Ctrl Pts',(173.872941942972,5.78472940092567,132.057225400939));
#141841=CARTESIAN_POINT('Ctrl Pts',(173.865533723305,5.81603117931075,131.902754560826));
#141842=CARTESIAN_POINT('Ctrl Pts',(173.858125503639,5.84111009089988,131.747421309403));
#141843=CARTESIAN_POINT('Ctrl Pts',(173.850712724337,5.86620443814064,131.591992452956));
#141844=CARTESIAN_POINT('Ctrl Pts',(173.843299945035,5.88506824206225,131.435700497263));
#141845=CARTESIAN_POINT('Ctrl Pts',(173.835887165733,5.89767482987402,131.279083867018));
#141846=CARTESIAN_POINT('Ctrl Pts',(173.828463794704,5.91029943056965,131.122243455587));
#141847=CARTESIAN_POINT('Ctrl Pts',(173.821040423675,5.91664894373514,130.965077815077));
#141848=CARTESIAN_POINT('Ctrl Pts',(173.813617052647,5.91674880246757,130.808125056241));
#141849=CARTESIAN_POINT('Ctrl Pts',(173.809681003206,5.91680174996359,130.724904937476));
#141850=CARTESIAN_POINT('Ctrl Pts',(173.805744953765,5.91509856308171,130.64174458923));
#141851=CARTESIAN_POINT('Ctrl Pts',(173.801808904324,5.91164891636172,130.55872338061));
#141852=CARTESIAN_POINT('Ctrl Pts',(173.794385637919,5.90514299030768,130.402147972159));
#141853=CARTESIAN_POINT('Ctrl Pts',(173.786962371513,5.89240236639736,130.245594455225));
#141854=CARTESIAN_POINT('Ctrl Pts',(173.779539105108,5.87341872715443,130.089599805817));
#141855=CARTESIAN_POINT('Ctrl Pts',(173.772124612387,5.85445752499658,129.933789529131));
#141856=CARTESIAN_POINT('Ctrl Pts',(173.764710119666,5.82926803955538,129.778537172117));
#141857=CARTESIAN_POINT('Ctrl Pts',(173.757295626945,5.79789393682564,129.624379066939));
#141858=CARTESIAN_POINT('Ctrl Pts',(173.749888280591,5.76655007363732,129.470369545146));
#141859=CARTESIAN_POINT('Ctrl Pts',(173.742480934237,5.72903353421945,129.31745253887));
#141860=CARTESIAN_POINT('Ctrl Pts',(173.735073587884,5.68543968426595,129.166158505776));
#141861=CARTESIAN_POINT('Ctrl Pts',(173.727671766208,5.64187834825044,129.01497731348));
#141862=CARTESIAN_POINT('Ctrl Pts',(173.720269944533,5.59224882980388,128.865417041309));
#141863=CARTESIAN_POINT('Ctrl Pts',(173.712868122858,5.53669737530587,128.717997097759));
#141864=CARTESIAN_POINT('Ctrl Pts',(173.705470208546,5.4811752459883,128.57065497605));
#141865=CARTESIAN_POINT('Ctrl Pts',(173.698072294235,5.41973753778378,128.425451281223));
#141866=CARTESIAN_POINT('Ctrl Pts',(173.690674379924,5.35258003228326,128.282889308885));
#141867=CARTESIAN_POINT('Ctrl Pts',(173.683277695011,5.28543368714182,128.14035102776));
#141868=CARTESIAN_POINT('Ctrl Pts',(173.675881010099,5.21256959014646,128.000453935199));
#141869=CARTESIAN_POINT('Ctrl Pts',(173.668484325187,5.13423130897537,127.863680521323));
#141870=CARTESIAN_POINT('Ctrl Pts',(173.661087968252,5.05589650140576,127.726913172124));
#141871=CARTESIAN_POINT('Ctrl Pts',(173.653691611316,4.97208817782416,127.593269550138));
#141872=CARTESIAN_POINT('Ctrl Pts',(173.646295254381,4.88309530191968,127.463206500368));
#141873=CARTESIAN_POINT('Ctrl Pts',(173.638897765044,4.79408880097865,127.333123537613));
#141874=CARTESIAN_POINT('Ctrl Pts',(173.631500275708,4.69989637802937,127.206622546706));
#141875=CARTESIAN_POINT('Ctrl Pts',(173.624102786371,4.60084956684095,127.084130271768));
#141876=CARTESIAN_POINT('Ctrl Pts',(173.616702703856,4.50176803494637,126.961595057352));
#141877=CARTESIAN_POINT('Ctrl Pts',(173.609302621341,4.39782896131317,126.843071646839));
#141878=CARTESIAN_POINT('Ctrl Pts',(173.601902538826,4.28940317645384,126.728952545688));
#141879=CARTESIAN_POINT('Ctrl Pts',(173.59449431916,4.18085816629766,126.614707958854));
#141880=CARTESIAN_POINT('Ctrl Pts',(173.587086099493,4.06781684947402,126.504877623945));
#141881=CARTESIAN_POINT('Ctrl Pts',(173.579677879827,3.95068635008608,126.399816608733));
#141882=CARTESIAN_POINT('Ctrl Pts',(173.572265100525,3.83348375883016,126.29469093022));
#141883=CARTESIAN_POINT('Ctrl Pts',(173.564852321222,3.71218725688151,126.194340658035));
#141884=CARTESIAN_POINT('Ctrl Pts',(173.55743954192,3.5872354188883,126.099079264451));
#141885=CARTESIAN_POINT('Ctrl Pts',(173.550016170892,3.46210504384931,126.00368175692));
#141886=CARTESIAN_POINT('Ctrl Pts',(173.542592799863,3.33330920628706,125.913387863986));
#141887=CARTESIAN_POINT('Ctrl Pts',(173.535169428834,3.20131438122949,125.828467050071));
#141888=CARTESIAN_POINT('Ctrl Pts',(173.531233379393,3.13132755781107,125.783439996887));
#141889=CARTESIAN_POINT('Ctrl Pts',(173.527297329953,3.06044178749597,125.739922736716));
#141890=CARTESIAN_POINT('Ctrl Pts',(173.523361280512,2.98872907508726,125.697950031036));
#141891=CARTESIAN_POINT('Ctrl Pts',(173.515938014106,2.85348113756254,125.618790818047));
#141892=CARTESIAN_POINT('Ctrl Pts',(173.508514747701,2.71488161150959,125.544888865841));
#141893=CARTESIAN_POINT('Ctrl Pts',(173.501091481295,2.57337777425295,125.476541420795));
#141894=CARTESIAN_POINT('Ctrl Pts',(173.493676988574,2.43204118278068,125.408274756753));
#141895=CARTESIAN_POINT('Ctrl Pts',(173.486262495853,2.28780744568151,125.345549693042));
#141896=CARTESIAN_POINT('Ctrl Pts',(173.478848003132,2.14115139693,125.28861939286));
#141897=CARTESIAN_POINT('Ctrl Pts',(173.471440656779,1.99463670079973,125.231743964244));
#141898=CARTESIAN_POINT('Ctrl Pts',(173.464033310425,1.84570468663678,125.180652314282));
#141899=CARTESIAN_POINT('Ctrl Pts',(173.456625964071,1.69485319098633,125.13555093444));
#141900=CARTESIAN_POINT('Ctrl Pts',(173.449224142396,1.54411420607265,125.090483192909));
#141901=CARTESIAN_POINT('Ctrl Pts',(173.44182232072,1.3914589463391,125.051396932038));
#141902=CARTESIAN_POINT('Ctrl Pts',(173.434420499045,1.23740345460525,125.018449863585));
#141903=CARTESIAN_POINT('Ctrl Pts',(173.427022584733,1.08342928756632,124.985520187633));
#141904=CARTESIAN_POINT('Ctrl Pts',(173.419624670422,0.928056724741681,
124.958723327701));
#141905=CARTESIAN_POINT('Ctrl Pts',(173.412226756111,0.771815027712196,
124.938166610759));
#141906=CARTESIAN_POINT('Ctrl Pts',(173.404830071199,0.615599295218299,
124.917613309971));
#141907=CARTESIAN_POINT('Ctrl Pts',(173.397433386286,0.45851508492483,124.903298142686));
#141908=CARTESIAN_POINT('Ctrl Pts',(173.390036701374,0.301099983714709,
124.895276986214));
#141909=CARTESIAN_POINT('Ctrl Pts',(173.382640344439,0.143691862455135,
124.887256185409));
#141910=CARTESIAN_POINT('Ctrl Pts',(173.375243987503,-0.0140467477342156,
124.885528859503));
#141911=CARTESIAN_POINT('Ctrl Pts',(173.367847630568,-0.171575298280786,
124.890098831044));
#141912=CARTESIAN_POINT('Ctrl Pts',(173.360450141231,-0.329127966850539,
124.894669502258));
#141913=CARTESIAN_POINT('Ctrl Pts',(173.353052651895,-0.486470138576459,
124.90553937981));
#141914=CARTESIAN_POINT('Ctrl Pts',(173.345655162558,-0.643063579444112,
124.92266020057));
#141915=CARTESIAN_POINT('Ctrl Pts',(173.338255080043,-0.799711913899935,
124.939787023007));
#141916=CARTESIAN_POINT('Ctrl Pts',(173.330854997528,-0.955610624073656,
124.963169110885));
#141917=CARTESIAN_POINT('Ctrl Pts',(173.323454915013,-1.11022904105624,
124.992706632779));
#141918=CARTESIAN_POINT('Ctrl Pts',(173.316046695347,-1.26501747688335,
125.022276634214));
#141919=CARTESIAN_POINT('Ctrl Pts',(173.30863847568,-1.41852244113016,125.058015516781));
#141920=CARTESIAN_POINT('Ctrl Pts',(173.301230256014,-1.57022514470069,
125.099772678245));
#141921=CARTESIAN_POINT('Ctrl Pts',(173.293817476711,-1.72202121875402,
125.141555540544));
#141922=CARTESIAN_POINT('Ctrl Pts',(173.286404697409,-1.87201246694569,
125.189363949622));
#141923=CARTESIAN_POINT('Ctrl Pts',(173.278991918107,-2.01969809586478,
125.242998359624));
#141924=CARTESIAN_POINT('Ctrl Pts',(173.271568547079,-2.16759474493629,
125.296709404987));
#141925=CARTESIAN_POINT('Ctrl Pts',(173.26414517605,-2.31317885053309,125.356262936134));
#141926=CARTESIAN_POINT('Ctrl Pts',(173.256721805021,-2.45597156345851,
125.421412146516));
#141927=CARTESIAN_POINT('Ctrl Pts',(173.25278575558,-2.53168368611545,125.455955821094));
#141928=CARTESIAN_POINT('Ctrl Pts',(173.248849706139,-2.60661147990583,
125.492071885158));
#141929=CARTESIAN_POINT('Ctrl Pts',(173.244913656699,-2.68068677865969,
125.529718548457));
#141930=CARTESIAN_POINT('Ctrl Pts',(173.237490390293,-2.82039048029919,
125.600718980525));
#141931=CARTESIAN_POINT('Ctrl Pts',(173.230067123888,-2.95748271501561,
125.677380876813));
#141932=CARTESIAN_POINT('Ctrl Pts',(173.222643857482,-3.09147163669408,
125.759488599168));
#141933=CARTESIAN_POINT('Ctrl Pts',(173.215229364761,-3.22530219459432,
125.841499277013));
#141934=CARTESIAN_POINT('Ctrl Pts',(173.20781487204,-3.35603642516729,125.928942775866));
#141935=CARTESIAN_POINT('Ctrl Pts',(173.200400379319,-3.4832046756844,126.021556445348));
#141936=CARTESIAN_POINT('Ctrl Pts',(173.192993032965,-3.61025035665381,
126.114080850287));
#141937=CARTESIAN_POINT('Ctrl Pts',(173.185585686612,-3.73373660027955,
126.211765286989));
#141938=CARTESIAN_POINT('Ctrl Pts',(173.178178340258,-3.8532205866295,126.31430252515));
#141939=CARTESIAN_POINT('Ctrl Pts',(173.170776518582,-3.97261545731455,
126.416763287169));
#141940=CARTESIAN_POINT('Ctrl Pts',(173.163374696907,-4.08801373226404,
126.524069401869));
#141941=CARTESIAN_POINT('Ctrl Pts',(173.155972875232,-4.19900379035953,
126.635871954867));
#141942=CARTESIAN_POINT('Ctrl Pts',(173.14857496092,-4.30993525766733,126.747615488169));
#141943=CARTESIAN_POINT('Ctrl Pts',(173.141177046609,-4.41646288024796,
126.863850468309));
#141944=CARTESIAN_POINT('Ctrl Pts',(173.133779132297,-4.51821028206757,
126.984189625383));
#141945=CARTESIAN_POINT('Ctrl Pts',(173.126382447385,-4.61994077531485,
127.104508784271));
#141946=CARTESIAN_POINT('Ctrl Pts',(173.118985762473,-4.71689238363702,
127.228930481662));
#141947=CARTESIAN_POINT('Ctrl Pts',(173.111589077561,-4.80872751702927,
127.357032633538));
#141948=CARTESIAN_POINT('Ctrl Pts',(173.104192720625,-4.90055857835549,
127.485129105229));
#141949=CARTESIAN_POINT('Ctrl Pts',(173.09679636369,-4.98727339834807,127.616905403527));
#141950=CARTESIAN_POINT('Ctrl Pts',(173.089400006754,-5.06857658128193,
127.751908815788));
#141951=CARTESIAN_POINT('Ctrl Pts',(173.082002517418,-5.14989221194058,
127.886932897415));
#141952=CARTESIAN_POINT('Ctrl Pts',(173.074605028081,-5.22579436321945,
128.025184756979));
#141953=CARTESIAN_POINT('Ctrl Pts',(173.067207538745,-5.29603271162384,
128.166185475558));
#141954=CARTESIAN_POINT('Ctrl Pts',(173.05980745623,-5.36629568197261,128.30723562172));
#141955=CARTESIAN_POINT('Ctrl Pts',(173.052407373714,-5.43089073011257,
128.451036211508));
#141956=CARTESIAN_POINT('Ctrl Pts',(173.045007291199,-5.48961500754095,
128.597086816815));
#141957=CARTESIAN_POINT('Ctrl Pts',(173.037599071533,-5.5484038583492,128.743298019777));
#141958=CARTESIAN_POINT('Ctrl Pts',(173.030190851866,-5.6013089070106,128.891763832682));
#141959=CARTESIAN_POINT('Ctrl Pts',(173.0227826322,-5.6481764412713,129.041966379387));
#141960=CARTESIAN_POINT('Ctrl Pts',(173.015369852898,-5.69507282171727,
129.192261373252));
#141961=CARTESIAN_POINT('Ctrl Pts',(173.007957073596,-5.73592418654342,
129.34429487122));
#141962=CARTESIAN_POINT('Ctrl Pts',(173.000544294294,-5.77062772825557,
129.497537682204));
#141963=CARTESIAN_POINT('Ctrl Pts',(172.993120923265,-5.80538085601562,
129.650999453703));
#141964=CARTESIAN_POINT('Ctrl Pts',(172.985697552236,-5.8339685487822,129.805673623159));
#141965=CARTESIAN_POINT('Ctrl Pts',(172.978274181207,-5.85633962220855,
129.961023916212));
#141966=CARTESIAN_POINT('Ctrl Pts',(172.974338131767,-5.86820130212529,
130.043394369165));
#141967=CARTESIAN_POINT('Ctrl Pts',(172.970402082326,-5.87831613732414,
130.125954858955));
#141968=CARTESIAN_POINT('Ctrl Pts',(172.966466032885,-5.88668244164833,
130.208625446799));
#141969=CARTESIAN_POINT('Ctrl Pts',(172.957102419327,-5.90658535236688,
130.40529356514));
#141970=CARTESIAN_POINT('Ctrl Pts',(172.947738805769,-5.91663481636451,
130.602975526734));
#141971=CARTESIAN_POINT('Ctrl Pts',(172.938375192211,-5.91674901559961,
130.800947568913));
#141972=CARTESIAN_POINT('',(171.188376356001,-5.9123977248154,130.800865364339));
#141973=CARTESIAN_POINT('Ctrl Pts',(172.938372658076,-5.92407204290102,
130.800996989454));
#141974=CARTESIAN_POINT('Ctrl Pts',(172.854921241741,-5.9119229449166,132.567576623035));
#141975=CARTESIAN_POINT('Ctrl Pts',(172.678653950803,-4.13412436784543,
136.320139871475));
#141976=CARTESIAN_POINT('Ctrl Pts',(172.40957078526,2.25333364517889,137.430071750254));
#141977=CARTESIAN_POINT('Ctrl Pts',(172.131123161447,6.79238030177618,132.489925913362));
#141978=CARTESIAN_POINT('Ctrl Pts',(171.852675537634,5.08956128726442,126.000827914072));
#141979=CARTESIAN_POINT('Ctrl Pts',(171.574227913821,-1.29031591135152,
123.925941803677));
#141980=CARTESIAN_POINT('Ctrl Pts',(171.352795156532,-5.42090502035294,
127.302567481839));
#141981=CARTESIAN_POINT('Ctrl Pts',(171.224178273849,-5.91304630517759,
130.038021817468));
#141982=CARTESIAN_POINT('Ctrl Pts',(171.188377265769,-5.90899622223902,
130.800847976222));
#141983=CARTESIAN_POINT('',(169.438373999605,-5.91358019339441,130.809073357389));
#141984=CARTESIAN_POINT('Ctrl Pts',(171.188375192211,-5.91674898070731,
130.800887607493));
#141985=CARTESIAN_POINT('Ctrl Pts',(171.18090496395,-5.91684253313628,130.960267000919));
#141986=CARTESIAN_POINT('Ctrl Pts',(171.173434735688,-5.9104919442183,131.119659794272));
#141987=CARTESIAN_POINT('Ctrl Pts',(171.165964507427,-5.89772060551839,
131.278514834824));
#141988=CARTESIAN_POINT('Ctrl Pts',(171.158493173355,-5.88494737628981,
131.437393390531));
#141989=CARTESIAN_POINT('Ctrl Pts',(171.151021839283,-5.86575153204893,
131.595733673016));
#141990=CARTESIAN_POINT('Ctrl Pts',(171.143550505211,-5.84020840133279,
131.752989307572));
#141991=CARTESIAN_POINT('Ctrl Pts',(171.136076702404,-5.81465683046071,
131.910296903733));
#141992=CARTESIAN_POINT('Ctrl Pts',(171.128602899596,-5.78275385258358,
132.066518779791));
#141993=CARTESIAN_POINT('Ctrl Pts',(171.121129096789,-5.74462599973562,
132.22111842526));
#141994=CARTESIAN_POINT('Ctrl Pts',(171.113651461089,-5.7064785932572,132.375797356188));
#141995=CARTESIAN_POINT('Ctrl Pts',(171.106173825389,-5.66210003830098,
132.528852047103));
#141996=CARTESIAN_POINT('Ctrl Pts',(171.098696189689,-5.61166682707188,
132.67976083737));
#141997=CARTESIAN_POINT('Ctrl Pts',(171.091208645838,-5.56116678992481,
132.830869587509));
#141998=CARTESIAN_POINT('Ctrl Pts',(171.083721101987,-5.50459618557524,
132.979826412699));
#141999=CARTESIAN_POINT('Ctrl Pts',(171.076233558136,-5.44218016527434,
133.126128394755));
#142000=CARTESIAN_POINT('Ctrl Pts',(171.068740561995,-5.37971869479419,
133.27253691118));
#142001=CARTESIAN_POINT('Ctrl Pts',(171.061247565855,-5.31140347855277,
133.416286403861));
#142002=CARTESIAN_POINT('Ctrl Pts',(171.053754569714,-5.23750565751984,
133.55689854645));
#142003=CARTESIAN_POINT('Ctrl Pts',(171.046249473471,-5.1634885022134,133.697737757276));
#142004=CARTESIAN_POINT('Ctrl Pts',(171.038744377227,-5.08387091193248,
133.83542918238));
#142005=CARTESIAN_POINT('Ctrl Pts',(171.031239280983,-4.99896796735605,
133.969522512927));
#142006=CARTESIAN_POINT('Ctrl Pts',(171.026603742721,-4.94652748752451,
134.05234553669));
#142007=CARTESIAN_POINT('Ctrl Pts',(171.021968204458,-4.89207150365022,
134.133796524639));
#142008=CARTESIAN_POINT('Ctrl Pts',(171.017332666195,-4.83568178337217,
134.213775853712));
#142009=CARTESIAN_POINT('Ctrl Pts',(171.00990939979,-4.74538031406421,134.341853292187));
#142010=CARTESIAN_POINT('Ctrl Pts',(171.002486133384,-4.64985041243972,
134.466534345509));
#142011=CARTESIAN_POINT('Ctrl Pts',(170.995062866979,-4.54937602345474,
134.587363176343));
#142012=CARTESIAN_POINT('Ctrl Pts',(170.987648374258,-4.44902038685363,
134.708049197534));
#142013=CARTESIAN_POINT('Ctrl Pts',(170.980233881537,-4.34373213169881,
134.824891774797));
#142014=CARTESIAN_POINT('Ctrl Pts',(170.972819388816,-4.23383854646287,
134.937463776814));
#142015=CARTESIAN_POINT('Ctrl Pts',(170.965412042462,-4.12405088080163,
135.049927277698));
#142016=CARTESIAN_POINT('Ctrl Pts',(170.958004696108,-4.0096669808313,135.158128132436));
#142017=CARTESIAN_POINT('Ctrl Pts',(170.950597349755,-3.89105440604151,
135.261672158363));
#142018=CARTESIAN_POINT('Ctrl Pts',(170.943195528079,-3.7725302969849,135.36513895725));
#142019=CARTESIAN_POINT('Ctrl Pts',(170.935793706404,-3.64978407296881,
135.463955598576));
#142020=CARTESIAN_POINT('Ctrl Pts',(170.928391884729,-3.52322007245554,
135.557764753924));
#142021=CARTESIAN_POINT('Ctrl Pts',(170.920993970417,-3.39672288409311,
135.651524388149));
#142022=CARTESIAN_POINT('Ctrl Pts',(170.913596056106,-3.26641223208966,
135.740281579155));
#142023=CARTESIAN_POINT('Ctrl Pts',(170.906198141795,-3.13272535945786,
135.823719379869));
#142024=CARTESIAN_POINT('Ctrl Pts',(170.898801456882,-2.99906070315902,
135.907143314734));
#142025=CARTESIAN_POINT('Ctrl Pts',(170.89140477197,-2.86202125615291,135.985249416302));
#142026=CARTESIAN_POINT('Ctrl Pts',(170.884008087058,-2.72207315338673,
136.05776411531));
#142027=CARTESIAN_POINT('Ctrl Pts',(170.876611730123,-2.58213125606608,
136.130275598941));
#142028=CARTESIAN_POINT('Ctrl Pts',(170.869215373187,-2.43928129087289,
136.197196001237));
#142029=CARTESIAN_POINT('Ctrl Pts',(170.861819016252,-2.2940136536867,136.258297903527));
#142030=CARTESIAN_POINT('Ctrl Pts',(170.854421526915,-2.14872377565441,
136.319409160675));
#142031=CARTESIAN_POINT('Ctrl Pts',(170.847024037579,-2.00101583272812,
136.374699999318));
#142032=CARTESIAN_POINT('Ctrl Pts',(170.839626548242,-1.85139969235813,
136.423991365368));
#142033=CARTESIAN_POINT('Ctrl Pts',(170.832226465727,-1.70173110428202,
136.473300010429));
#142034=CARTESIAN_POINT('Ctrl Pts',(170.824826383212,-1.55015334128703,
136.516604878893));
#142035=CARTESIAN_POINT('Ctrl Pts',(170.817426300697,-1.39719074927454,
136.553776985567));
#142036=CARTESIAN_POINT('Ctrl Pts',(170.810018081031,-1.24405995916715,
136.590989966794));
#142037=CARTESIAN_POINT('Ctrl Pts',(170.802609861364,-1.08954166194996,
136.622056630609));
#142038=CARTESIAN_POINT('Ctrl Pts',(170.795201641698,-0.934170424566269,
136.646899122391));
#142039=CARTESIAN_POINT('Ctrl Pts',(170.787788862396,-0.778703558778695,
136.671756904312));
#142040=CARTESIAN_POINT('Ctrl Pts',(170.780376083094,-0.622383076571657,
136.690382836639));
#142041=CARTESIAN_POINT('Ctrl Pts',(170.772963303792,-0.465747442605949,
136.702751066002));
#142042=CARTESIAN_POINT('Ctrl Pts',(170.765539932763,-0.30888800030067,
136.715136967672));
#142043=CARTESIAN_POINT('Ctrl Pts',(170.758116561734,-0.151712878907354,
136.721247294134));
#142044=CARTESIAN_POINT('Ctrl Pts',(170.750693190705,0.00523985014762619,
136.72110829737));
#142045=CARTESIAN_POINT('Ctrl Pts',(170.746757141265,0.0884599531236234,
136.721034597951));
#142046=CARTESIAN_POINT('Ctrl Pts',(170.742821091824,0.171617613112122,
136.719204857148));
#142047=CARTESIAN_POINT('Ctrl Pts',(170.738885042383,0.254633475820528,
136.715628870276));
#142048=CARTESIAN_POINT('Ctrl Pts',(170.731461775977,0.411198802048661,
136.708884670637));
#142049=CARTESIAN_POINT('Ctrl Pts',(170.724038509572,0.567732748635394,
136.695905813678));
#142050=CARTESIAN_POINT('Ctrl Pts',(170.716615243167,0.723698327536533,
136.676684799116));
#142051=CARTESIAN_POINT('Ctrl Pts',(170.709200750446,0.879479568075601,
136.657486502198));
#142052=CARTESIAN_POINT('Ctrl Pts',(170.701786257724,1.03469341120078,136.632060778267));
#142053=CARTESIAN_POINT('Ctrl Pts',(170.694371765003,1.18880359182316,136.600452109474));
#142054=CARTESIAN_POINT('Ctrl Pts',(170.68696441865,1.34276523525142,136.568873906306));
#142055=CARTESIAN_POINT('Ctrl Pts',(170.679557072296,1.4956249706662,136.531124696679));
#142056=CARTESIAN_POINT('Ctrl Pts',(170.672149725942,1.64685248614557,136.487300653443));
#142057=CARTESIAN_POINT('Ctrl Pts',(170.664747904267,1.79796721043819,136.443509295832));
#142058=CARTESIAN_POINT('Ctrl Pts',(170.657346082591,1.94745178174247,136.393652229581));
#142059=CARTESIAN_POINT('Ctrl Pts',(170.649944260916,2.09478701472477,136.337876491352));
#142060=CARTESIAN_POINT('Ctrl Pts',(170.642546346605,2.24204447058444,136.282130196701));
#142061=CARTESIAN_POINT('Ctrl Pts',(170.635148432293,2.3871544995349,136.220471584335));
#142062=CARTESIAN_POINT('Ctrl Pts',(170.627750517982,2.52961410449764,136.153097201548));
#142063=CARTESIAN_POINT('Ctrl Pts',(170.62035383307,2.67205003525861,136.085734015161));
#142064=CARTESIAN_POINT('Ctrl Pts',(170.612957148157,2.81183607906894,136.012657102981));
#142065=CARTESIAN_POINT('Ctrl Pts',(170.605560463245,2.94849011703518,135.934110766671));
#142066=CARTESIAN_POINT('Ctrl Pts',(170.59816410631,3.08513809561822,135.855567913188));
#142067=CARTESIAN_POINT('Ctrl Pts',(170.590767749374,3.21865402084596,135.771556303813));
#142068=CARTESIAN_POINT('Ctrl Pts',(170.583371392439,3.34858148799712,135.682365597139));
#142069=CARTESIAN_POINT('Ctrl Pts',(170.575973903102,3.47852884737482,135.593161235141));
#142070=CARTESIAN_POINT('Ctrl Pts',(170.568576413766,3.60488634696185,135.498776408292));
#142071=CARTESIAN_POINT('Ctrl Pts',(170.561178924429,3.72722774767048,135.399543299407));
#142072=CARTESIAN_POINT('Ctrl Pts',(170.553778841914,3.84961203496816,135.30027540451));
#142073=CARTESIAN_POINT('Ctrl Pts',(170.546378759399,3.96797713065668,135.196156078782));
#142074=CARTESIAN_POINT('Ctrl Pts',(170.538978676884,4.08193109407247,135.087556749632));
#142075=CARTESIAN_POINT('Ctrl Pts',(170.531570457217,4.1960103615853,134.978838004356));
#142076=CARTESIAN_POINT('Ctrl Pts',(170.524162237551,4.30566853967162,134.865629675359));
#142077=CARTESIAN_POINT('Ctrl Pts',(170.516754017884,4.41055118054293,134.748339426626));
#142078=CARTESIAN_POINT('Ctrl Pts',(170.509341238582,4.51549837492998,134.630976987701));
#142079=CARTESIAN_POINT('Ctrl Pts',(170.50192845928,4.61566393828353,134.50952791018));
#142080=CARTESIAN_POINT('Ctrl Pts',(170.494515679978,4.7107350661301,134.384431245254));
#142081=CARTESIAN_POINT('Ctrl Pts',(170.487092308949,4.80594203606249,134.259155836346));
#142082=CARTESIAN_POINT('Ctrl Pts',(170.479668937921,4.89603981909766,134.130222735993));
#142083=CARTESIAN_POINT('Ctrl Pts',(170.472245566892,4.98075966102131,133.99809882876));
#142084=CARTESIAN_POINT('Ctrl Pts',(170.468309517451,5.02568015403342,133.928043562877));
#142085=CARTESIAN_POINT('Ctrl Pts',(170.46437346801,5.06908948773575,133.857091648785));
#142086=CARTESIAN_POINT('Ctrl Pts',(170.46043741857,5.11095301027064,133.785315144107));
#142087=CARTESIAN_POINT('Ctrl Pts',(170.453014152164,5.18990630725628,133.649946896351));
#142088=CARTESIAN_POINT('Ctrl Pts',(170.445590885759,5.26359724900008,133.511235064603));
#142089=CARTESIAN_POINT('Ctrl Pts',(170.438167619353,5.33172927014896,133.369627378029));
#142090=CARTESIAN_POINT('Ctrl Pts',(170.430753126632,5.39978076490694,133.228187059981));
#142091=CARTESIAN_POINT('Ctrl Pts',(170.423338633911,5.46228625678789,133.083858033033));
#142092=CARTESIAN_POINT('Ctrl Pts',(170.41592414119,5.51899330550528,132.937115515881));
#142093=CARTESIAN_POINT('Ctrl Pts',(170.408516794837,5.57564569783404,132.790514434693));
#142094=CARTESIAN_POINT('Ctrl Pts',(170.401109448483,5.62651063945996,132.641504840197));
#142095=CARTESIAN_POINT('Ctrl Pts',(170.393702102129,5.6713823967779,132.490584882608));
#142096=CARTESIAN_POINT('Ctrl Pts',(170.386300280454,5.71622068704628,132.339777486818));
#142097=CARTESIAN_POINT('Ctrl Pts',(170.378898458778,5.75507458733743,132.187062921222));
#142098=CARTESIAN_POINT('Ctrl Pts',(170.371496637103,5.7877871714044,132.032957468053));
#142099=CARTESIAN_POINT('Ctrl Pts',(170.364098722792,5.82048248675273,131.878933365954));
#142100=CARTESIAN_POINT('Ctrl Pts',(170.35670080848,5.84704286506366,131.72352020279));
#142101=CARTESIAN_POINT('Ctrl Pts',(170.349302894169,5.8673617849352,131.567247402864));
#142102=CARTESIAN_POINT('Ctrl Pts',(170.341906209257,5.88767732817102,131.41100057264));
#142103=CARTESIAN_POINT('Ctrl Pts',(170.334509524345,5.90175342345177,131.253894759001));
#142104=CARTESIAN_POINT('Ctrl Pts',(170.327112839432,5.90953501164803,131.09646763324));
#142105=CARTESIAN_POINT('Ctrl Pts',(170.319716482497,5.91731625480052,130.939047487964));
#142106=CARTESIAN_POINT('Ctrl Pts',(170.312320125562,5.9188035273941,130.781306431737));
#142107=CARTESIAN_POINT('Ctrl Pts',(170.304923768626,5.91399382950801,130.623785018325));
#142108=CARTESIAN_POINT('Ctrl Pts',(170.29752627929,5.90918339524489,130.466239487983));
#142109=CARTESIAN_POINT('Ctrl Pts',(170.290128789953,5.89807408227965,130.30891404056));
#142110=CARTESIAN_POINT('Ctrl Pts',(170.282731300617,5.88071497278581,130.152346835999));
#142111=CARTESIAN_POINT('Ctrl Pts',(170.275331218102,5.86334977808317,129.995724747049));
#142112=CARTESIAN_POINT('Ctrl Pts',(170.267931135587,5.83973046598384,129.839861800962));
#142113=CARTESIAN_POINT('Ctrl Pts',(170.260531053072,5.80995767538453,129.685288514107));
#142114=CARTESIAN_POINT('Ctrl Pts',(170.253122833405,5.78015214654102,129.530545258031));
#142115=CARTESIAN_POINT('Ctrl Pts',(170.245714613739,5.74417969693544,129.377094860036));
#142116=CARTESIAN_POINT('Ctrl Pts',(170.238306394072,5.70219171813597,129.225455879426));
#142117=CARTESIAN_POINT('Ctrl Pts',(170.23089361477,5.66017789643608,129.073723567553));
#142118=CARTESIAN_POINT('Ctrl Pts',(170.223480835468,5.61214128157387,128.923805249309));
#142119=CARTESIAN_POINT('Ctrl Pts',(170.216068056166,5.55828218129294,128.776201413849));
#142120=CARTESIAN_POINT('Ctrl Pts',(170.208644685137,5.50434612460392,128.628386675108));
#142121=CARTESIAN_POINT('Ctrl Pts',(170.201221314109,5.44457110819336,128.482893368432));
#142122=CARTESIAN_POINT('Ctrl Pts',(170.19379794308,5.3792046670526,128.340199966866));
#142123=CARTESIAN_POINT('Ctrl Pts',(170.189861893639,5.34454581151123,128.264540501469));
#142124=CARTESIAN_POINT('Ctrl Pts',(170.185925844198,5.30831576191901,128.18966775694));
#142125=CARTESIAN_POINT('Ctrl Pts',(170.181989794757,5.27055641221757,128.115649835773));
#142126=CARTESIAN_POINT('Ctrl Pts',(170.174566528351,5.199343457114,127.976054346479));
#142127=CARTESIAN_POINT('Ctrl Pts',(170.167143261946,5.122473018555,127.839078936869));
#142128=CARTESIAN_POINT('Ctrl Pts',(170.15971999554,5.04016148295009,127.705215124323));
#142129=CARTESIAN_POINT('Ctrl Pts',(170.152305502819,4.95794723274491,127.571509527688));
#142130=CARTESIAN_POINT('Ctrl Pts',(170.144891010098,4.87030487990625,127.440908522623));
#142131=CARTESIAN_POINT('Ctrl Pts',(170.137476517377,4.77749778924088,127.313881361604));
#142132=CARTESIAN_POINT('Ctrl Pts',(170.130069171024,4.68478014954309,127.186976634145));
#142133=CARTESIAN_POINT('Ctrl Pts',(170.12266182467,4.58690790091625,127.063639192598));
#142134=CARTESIAN_POINT('Ctrl Pts',(170.115254478316,4.48418894720447,126.94431138883));
#142135=CARTESIAN_POINT('Ctrl Pts',(170.107852656641,4.38154660516425,126.82507258424));
#142136=CARTESIAN_POINT('Ctrl Pts',(170.100450834965,4.27406499819322,126.70983774456));
#142137=CARTESIAN_POINT('Ctrl Pts',(170.09304901329,4.16209366668581,126.599017959442));
#142138=CARTESIAN_POINT('Ctrl Pts',(170.085651098978,4.05018144397212,126.488256675227));
#142139=CARTESIAN_POINT('Ctrl Pts',(170.078253184667,3.93378448152172,126.381906065856));
#142140=CARTESIAN_POINT('Ctrl Pts',(170.070855270356,3.8132906215737,126.28034191757));
#142141=CARTESIAN_POINT('Ctrl Pts',(170.063458585443,3.69281678551975,126.178794647402));
#142142=CARTESIAN_POINT('Ctrl Pts',(170.056061900531,3.568247688363,126.082032499992));
#142143=CARTESIAN_POINT('Ctrl Pts',(170.048665215619,3.44000592738821,125.990392422611));
#142144=CARTESIAN_POINT('Ctrl Pts',(170.041268858683,3.31176985278735,125.898756408648));
#142145=CARTESIAN_POINT('Ctrl Pts',(170.033872501748,3.17986174189001,125.812242230164));
#142146=CARTESIAN_POINT('Ctrl Pts',(170.026476144812,3.04473475635657,125.731144593589));
#142147=CARTESIAN_POINT('Ctrl Pts',(170.019078655476,2.90958708253732,125.65003454076));
#142148=CARTESIAN_POINT('Ctrl Pts',(170.011681166139,2.77121987291441,125.574342873171));
#142149=CARTESIAN_POINT('Ctrl Pts',(170.004283676803,2.63011242680299,125.504319185192));
#142150=CARTESIAN_POINT('Ctrl Pts',(169.996883594288,2.48895551569434,125.434270950519));
#142151=CARTESIAN_POINT('Ctrl Pts',(169.989483511773,2.34505678975826,125.369894817197));
#142152=CARTESIAN_POINT('Ctrl Pts',(169.982083429258,2.19891698522216,125.31139287193));
#142153=CARTESIAN_POINT('Ctrl Pts',(169.974675209591,2.05261648494759,125.252826597759));
#142154=CARTESIAN_POINT('Ctrl Pts',(169.967266989925,1.90407033148488,125.200147550055));
#142155=CARTESIAN_POINT('Ctrl Pts',(169.959858770258,1.75379663430364,125.153508652773));
#142156=CARTESIAN_POINT('Ctrl Pts',(169.952445990956,1.60343044616849,125.106841050028));
#142157=CARTESIAN_POINT('Ctrl Pts',(169.945033211654,1.45133495542855,125.06622110161));
#142158=CARTESIAN_POINT('Ctrl Pts',(169.937620432352,1.29803950901369,125.031750809555));
#142159=CARTESIAN_POINT('Ctrl Pts',(169.930197061323,1.14452502687665,124.997231264731));
#142160=CARTESIAN_POINT('Ctrl Pts',(169.922773690294,0.989807530928758,
124.968878992825));
#142161=CARTESIAN_POINT('Ctrl Pts',(169.915350319265,0.834423372802704,
124.946744362004));
#142162=CARTESIAN_POINT('Ctrl Pts',(169.911414269825,0.752034963776186,
124.935008049631));
#142163=CARTESIAN_POINT('Ctrl Pts',(169.907478220384,0.669459176533651,
124.925018869156));
#142164=CARTESIAN_POINT('Ctrl Pts',(169.903542170944,0.586775952330272,
124.916778385082));
#142165=CARTESIAN_POINT('Ctrl Pts',(169.896118904538,0.430837971931043,
124.901237089293));
#142166=CARTESIAN_POINT('Ctrl Pts',(169.888695638133,0.274046330774959,
124.891871811632));
#142167=CARTESIAN_POINT('Ctrl Pts',(169.881272371727,0.116931518494834,
124.888766177234));
#142168=CARTESIAN_POINT('Ctrl Pts',(169.873857879006,-0.0399975971249745,
124.885664213438));
#142169=CARTESIAN_POINT('Ctrl Pts',(169.866443386285,-0.197248753992104,
124.888807173698));
#142170=CARTESIAN_POINT('Ctrl Pts',(169.859028893564,-0.354284801597808,
124.898227124166));
#142171=CARTESIAN_POINT('Ctrl Pts',(169.85162154721,-0.511169491949031,
124.907637995332));
#142172=CARTESIAN_POINT('Ctrl Pts',(169.844214200856,-0.667839115666281,
124.923313790147));
#142173=CARTESIAN_POINT('Ctrl Pts',(169.836806854503,-0.823755080046966,
124.945234562377));
#142174=CARTESIAN_POINT('Ctrl Pts',(169.829405032827,-0.979554756418378,
124.967138985267));
#142175=CARTESIAN_POINT('Ctrl Pts',(169.822003211152,-1.13460152461393,
124.995279059635));
#142176=CARTESIAN_POINT('Ctrl Pts',(169.814601389476,-1.28836058814432,
125.029582911245));
#142177=CARTESIAN_POINT('Ctrl Pts',(169.807203475165,-1.44203848346232,
125.06386865412));
#142178=CARTESIAN_POINT('Ctrl Pts',(169.799805560854,-1.59442966448984,
125.10431161304));
#142179=CARTESIAN_POINT('Ctrl Pts',(169.792407646542,-1.74500833341729,
125.150788606987));
#142180=CARTESIAN_POINT('Ctrl Pts',(169.78501096163,-1.8955619789013,125.1972578773));
#142181=CARTESIAN_POINT('Ctrl Pts',(169.777614276718,-2.04430335374695,
125.249759082496));
#142182=CARTESIAN_POINT('Ctrl Pts',(169.770217591806,-2.19072055051497,
125.308118807743));
#142183=CARTESIAN_POINT('Ctrl Pts',(169.76282123487,-2.33713125499116,125.366475945258));
#142184=CARTESIAN_POINT('Ctrl Pts',(169.755424877935,-2.48121763953383,
125.43069094809));
#142185=CARTESIAN_POINT('Ctrl Pts',(169.748028520999,-2.62248681432916,
125.500541854527));
#142186=CARTESIAN_POINT('Ctrl Pts',(169.740631031663,-2.76377761779588,
125.570403455315));
#142187=CARTESIAN_POINT('Ctrl Pts',(169.733233542326,-2.90225001804727,
125.64590251233));
#142188=CARTESIAN_POINT('Ctrl Pts',(169.725836052989,-3.03743495128211,
125.726770689339));
#142189=CARTESIAN_POINT('Ctrl Pts',(169.718435970474,-3.17266727338555,
125.807667214562));
#142190=CARTESIAN_POINT('Ctrl Pts',(169.711035887959,-3.30460951386572,
125.893936415581));
#142191=CARTESIAN_POINT('Ctrl Pts',(169.703635805444,-3.43282099129518,
125.985266241625));
#142192=CARTESIAN_POINT('Ctrl Pts',(169.696227585778,-3.56117345042462,
126.076696494202));
#142193=CARTESIAN_POINT('Ctrl Pts',(169.688819366111,-3.68578664959458,
126.173198268115));
#142194=CARTESIAN_POINT('Ctrl Pts',(169.681411146445,-3.80625187872553,
126.274418322327));
#142195=CARTESIAN_POINT('Ctrl Pts',(169.673998367143,-3.92679125219456,
126.375700675793));
#142196=CARTESIAN_POINT('Ctrl Pts',(169.666585587841,-4.0431772930982,126.481706845402));
#142197=CARTESIAN_POINT('Ctrl Pts',(169.659172808539,-4.15503805928876,
126.592046611184));
#142198=CARTESIAN_POINT('Ctrl Pts',(169.65174943751,-4.2670586573882,126.702544035598));
#142199=CARTESIAN_POINT('Ctrl Pts',(169.644326066481,-4.37454081246608,
126.817387151258));
#142200=CARTESIAN_POINT('Ctrl Pts',(169.636902695452,-4.47715223719654,
126.93615193557));
#142201=CARTESIAN_POINT('Ctrl Pts',(169.632966646012,-4.5315592767123,126.999123873931));
#142202=CARTESIAN_POINT('Ctrl Pts',(169.629030596571,-4.58459768718307,
127.063197826358));
#142203=CARTESIAN_POINT('Ctrl Pts',(169.625094547131,-4.63622294214824,
127.128307381662));
#142204=CARTESIAN_POINT('Ctrl Pts',(169.617314574009,-4.73826512990403,
127.257002561406));
#142205=CARTESIAN_POINT('Ctrl Pts',(169.609534600887,-4.83511364716786,
127.390162962955));
#142206=CARTESIAN_POINT('Ctrl Pts',(169.601754627766,-4.92635568212228,
127.527326858857));
#142207=CARTESIAN_POINT('Ctrl Pts',(169.594350421438,-5.0131907960697,127.657865842737));
#142208=CARTESIAN_POINT('Ctrl Pts',(169.586946215111,-5.09494797384064,
127.792030342425));
#142209=CARTESIAN_POINT('Ctrl Pts',(169.579542008784,-5.17131070252216,
127.929386499338));
#142210=CARTESIAN_POINT('Ctrl Pts',(169.572144764004,-5.24760163379818,
128.066613511892));
#142211=CARTESIAN_POINT('Ctrl Pts',(169.564747519225,-5.31850802957858,
128.207025885231));
#142212=CARTESIAN_POINT('Ctrl Pts',(169.557350274446,-5.38375627541832,
128.350160354875));
#142213=CARTESIAN_POINT('Ctrl Pts',(169.549958517475,-5.4489561154119,128.493188637064));
#142214=CARTESIAN_POINT('Ctrl Pts',(169.542566760505,-5.50850600673006,
128.638934657115));
#142215=CARTESIAN_POINT('Ctrl Pts',(169.535175003534,-5.56217803209591,
128.786910221207));
#142216=CARTESIAN_POINT('Ctrl Pts',(169.527787264386,-5.61582088379647,
128.93480535253));
#142217=CARTESIAN_POINT('Ctrl Pts',(169.520399525237,-5.66359210391255,
129.084927264337));
#142218=CARTESIAN_POINT('Ctrl Pts',(169.513011786088,-5.70531179041672,
129.236767578339));
#142219=CARTESIAN_POINT('Ctrl Pts',(169.505625960535,-5.74702067055978,
129.388568562198));
#142220=CARTESIAN_POINT('Ctrl Pts',(169.498240134981,-5.78268103618175,
129.542086702717));
#142221=CARTESIAN_POINT('Ctrl Pts',(169.490854309427,-5.81216278083217,
129.696798261936));
#142222=CARTESIAN_POINT('Ctrl Pts',(169.483469578459,-5.84164015626333,
129.851486892771));
#142223=CARTESIAN_POINT('Ctrl Pts',(169.476084847491,-5.86494066769169,
130.007368222288));
#142224=CARTESIAN_POINT('Ctrl Pts',(169.468700116523,-5.88198533934066,
130.163908409918));
#142225=CARTESIAN_POINT('Ctrl Pts',(169.461313667309,-5.89903397686634,
130.320485020607));
#142226=CARTESIAN_POINT('Ctrl Pts',(169.453927218095,-5.90982382871627,
130.477720423684));
#142227=CARTESIAN_POINT('Ctrl Pts',(169.446540768881,-5.91432778501902,
130.635075609807));
#142228=CARTESIAN_POINT('Ctrl Pts',(169.443818909991,-5.9159874638645,130.693059980898));
#142229=CARTESIAN_POINT('Ctrl Pts',(169.441097051101,-5.91679410654643,
130.751060598256));
#142230=CARTESIAN_POINT('Ctrl Pts',(169.438375192211,-5.91674814130737,
130.80905048279));
#142231=CARTESIAN_POINT('',(167.688376105063,-5.921848643152,130.805960821993));
#142232=CARTESIAN_POINT('Ctrl Pts',(169.438373164445,-5.91136173808653,
130.809089376048));
#142233=CARTESIAN_POINT('Ctrl Pts',(169.407797750736,-5.91615588573312,
131.459917301021));
#142234=CARTESIAN_POINT('Ctrl Pts',(169.284406462423,-5.51647731895877,
134.080691029829));
#142235=CARTESIAN_POINT('Ctrl Pts',(169.068199299504,-1.67522649738779,
137.599298197324));
#142236=CARTESIAN_POINT('Ctrl Pts',(168.789751675692,4.81127258696239,135.886605852133));
#142237=CARTESIAN_POINT('Ctrl Pts',(168.51130405188,6.87644720762614,129.50357841786));
#142238=CARTESIAN_POINT('Ctrl Pts',(168.232856428066,2.6225027776035,124.315906278371));
#142239=CARTESIAN_POINT('Ctrl Pts',(167.958547360081,-3.94234836512363,
125.079289384233));
#142240=CARTESIAN_POINT('Ctrl Pts',(167.777054166701,-5.91917198462181,
128.930354853733));
#142241=CARTESIAN_POINT('Ctrl Pts',(167.688376847924,-5.92599799601691,
130.805946244722));
#142242=CARTESIAN_POINT('',(165.938375192211,-5.91629100133431,130.79888781122));
#142243=CARTESIAN_POINT('Ctrl Pts',(167.688375192211,-5.91674977873797,
130.805978735034));
#142244=CARTESIAN_POINT('Ctrl Pts',(167.684237188288,-5.91672588056883,
130.893363915518));
#142245=CARTESIAN_POINT('Ctrl Pts',(167.680099184364,-5.91476617950728,
130.980720247118));
#142246=CARTESIAN_POINT('Ctrl Pts',(167.67596118044,-5.91087389875397,131.06798974253));
#142247=CARTESIAN_POINT('Ctrl Pts',(167.668537914035,-5.90389144115121,
131.224544623933));
#142248=CARTESIAN_POINT('Ctrl Pts',(167.66111464763,-5.89067438120114,131.381058637645));
#142249=CARTESIAN_POINT('Ctrl Pts',(167.653691381224,-5.8712160358362,131.536994784828));
#142250=CARTESIAN_POINT('Ctrl Pts',(167.646276888503,-5.85178068861954,
131.692746628435));
#142251=CARTESIAN_POINT('Ctrl Pts',(167.638862395782,-5.82611878508409,
131.847921598201));
#142252=CARTESIAN_POINT('Ctrl Pts',(167.631447903061,-5.79427562343302,
132.001983497353));
#142253=CARTESIAN_POINT('Ctrl Pts',(167.624040556707,-5.76246315341997,
132.155896905847));
#142254=CARTESIAN_POINT('Ctrl Pts',(167.616633210354,-5.72448136101022,
132.308699016381));
#142255=CARTESIAN_POINT('Ctrl Pts',(167.609225864,-5.6804272259866,132.459859664008));
#142256=CARTESIAN_POINT('Ctrl Pts',(167.601824042324,-5.63640594819903,
132.61090757032));
#142257=CARTESIAN_POINT('Ctrl Pts',(167.594422220649,-5.58632144961113,
132.760316094556));
#142258=CARTESIAN_POINT('Ctrl Pts',(167.587020398974,-5.53032155682588,
132.907566275748));
#142259=CARTESIAN_POINT('Ctrl Pts',(167.579622484662,-5.47435122594817,
133.054738724714));
#142260=CARTESIAN_POINT('Ctrl Pts',(167.572224570351,-5.41247185221993,
133.199754751718));
#142261=CARTESIAN_POINT('Ctrl Pts',(167.56482665604,-5.34488074818397,133.342111659373));
#142262=CARTESIAN_POINT('Ctrl Pts',(167.557429971127,-5.27730087656324,
133.484444909893));
#142263=CARTESIAN_POINT('Ctrl Pts',(167.550033286215,-5.2040113184423,133.624119581212));
#142264=CARTESIAN_POINT('Ctrl Pts',(167.542636601303,-5.12525710890511,
133.760653926782));
#142265=CARTESIAN_POINT('Ctrl Pts',(167.535240244368,-5.04650639141215,
133.897182218276));
#142266=CARTESIAN_POINT('Ctrl Pts',(167.527843887432,-4.96229169081128,
134.030570137526));
#142267=CARTESIAN_POINT('Ctrl Pts',(167.520447530497,-4.87290335993222,
134.160361721151));
#142268=CARTESIAN_POINT('Ctrl Pts',(167.51305004116,-4.78350134347127,134.290173176198));
#142269=CARTESIAN_POINT('Ctrl Pts',(167.505652551824,-4.68892433131307,
134.416386891826));
#142270=CARTESIAN_POINT('Ctrl Pts',(167.498255062487,-4.58950515455338,
134.538577134967));
#142271=CARTESIAN_POINT('Ctrl Pts',(167.490854979972,-4.49005112655565,
134.660810211707));
#142272=CARTESIAN_POINT('Ctrl Pts',(167.483454897457,-4.38575178987019,
134.779016718441));
#142273=CARTESIAN_POINT('Ctrl Pts',(167.476054814942,-4.27697916794346,
134.892805280207));
#142274=CARTESIAN_POINT('Ctrl Pts',(167.468646595276,-4.1680869393367,135.006718964195));
#142275=CARTESIAN_POINT('Ctrl Pts',(167.461238375609,-4.05471186035349,
135.116204731494));
#142276=CARTESIAN_POINT('Ctrl Pts',(167.453830155943,-3.9372621339154,135.22090875512));
#142277=CARTESIAN_POINT('Ctrl Pts',(167.446417376641,-3.81974011913044,
135.325677222327));
#142278=CARTESIAN_POINT('Ctrl Pts',(167.439004597339,-3.69813874730967,
135.425657844868));
#142279=CARTESIAN_POINT('Ctrl Pts',(167.431591818037,-3.57289754517158,
135.520538486795));
#142280=CARTESIAN_POINT('Ctrl Pts',(167.424168447008,-3.4474773925306,135.615554698633));
#142281=CARTESIAN_POINT('Ctrl Pts',(167.416745075979,-3.3184073279918,135.705456163106));
#142282=CARTESIAN_POINT('Ctrl Pts',(167.409321704951,-3.18615464457944,
135.78997483683));
#142283=CARTESIAN_POINT('Ctrl Pts',(167.40538565551,-3.11603109847216,135.834788665638));
#142284=CARTESIAN_POINT('Ctrl Pts',(167.401449606069,-3.0450132049226,135.878089972339));
#142285=CARTESIAN_POINT('Ctrl Pts',(167.397513556628,-2.97317307420229,
135.919844214777));
#142286=CARTESIAN_POINT('Ctrl Pts',(167.390090290222,-2.83768482972203,
135.998591412907));
#142287=CARTESIAN_POINT('Ctrl Pts',(167.382667023817,-2.69886101353126,
136.072071173523));
#142288=CARTESIAN_POINT('Ctrl Pts',(167.375243757411,-2.55714980559849,
136.139987612983));
#142289=CARTESIAN_POINT('Ctrl Pts',(167.36782926469,-2.41560608854492,136.207823780852));
#142290=CARTESIAN_POINT('Ctrl Pts',(167.360414771969,-2.27118210600901,
136.270109556143));
#142291=CARTESIAN_POINT('Ctrl Pts',(167.353000279248,-2.1243534603076,136.326593222064));
#142292=CARTESIAN_POINT('Ctrl Pts',(167.345592932895,-1.97766633358292,
136.383022446901));
#142293=CARTESIAN_POINT('Ctrl Pts',(167.338185586541,-1.8285795038551,136.433660562389));
#142294=CARTESIAN_POINT('Ctrl Pts',(167.330778240187,-1.67759143385237,
136.478302593262));
#142295=CARTESIAN_POINT('Ctrl Pts',(167.323376418512,-1.5267159764487,136.522911328424));
#142296=CARTESIAN_POINT('Ctrl Pts',(167.315974596836,-1.37394245867082,
136.561532778151));
#142297=CARTESIAN_POINT('Ctrl Pts',(167.308572775161,-1.21978740096834,
136.594010802071));
#142298=CARTESIAN_POINT('Ctrl Pts',(167.301174860849,-1.06571372052088,
136.626471681095));
#142299=CARTESIAN_POINT('Ctrl Pts',(167.293776946538,-0.910260316947344,
136.652795516271));
#142300=CARTESIAN_POINT('Ctrl Pts',(167.286379032227,-0.753956776043483,
136.672876592015));
#142301=CARTESIAN_POINT('Ctrl Pts',(167.278982347315,-0.597679209952597,
136.692954330647));
#142302=CARTESIAN_POINT('Ctrl Pts',(167.271585662402,-0.440552156817429,
136.706791321324));
#142303=CARTESIAN_POINT('Ctrl Pts',(167.26418897749,-0.283113371102142,
136.714333323222));
#142304=CARTESIAN_POINT('Ctrl Pts',(167.256792620555,-0.125681566387597,
136.721874990701));
#142305=CARTESIAN_POINT('Ctrl Pts',(167.249396263619,0.0320615705531974,
136.723122206536));
#142306=CARTESIAN_POINT('Ctrl Pts',(167.241999906684,0.189575482016936,
136.718072793443));
#142307=CARTESIAN_POINT('Ctrl Pts',(167.234602417347,0.347113509262802,
136.713022607272));
#142308=CARTESIAN_POINT('Ctrl Pts',(167.227204928011,0.504421868022577,
136.701673884621));
#142309=CARTESIAN_POINT('Ctrl Pts',(167.219807438674,0.660962473671266,
136.684076526596));
#142310=CARTESIAN_POINT('Ctrl Pts',(167.212407356159,0.817557954386651,
136.666472999844));
#142311=CARTESIAN_POINT('Ctrl Pts',(167.205007273644,0.97338477541586,136.642616518223));
#142312=CARTESIAN_POINT('Ctrl Pts',(167.197607191129,1.12791257416039,136.61260852787));
#142313=CARTESIAN_POINT('Ctrl Pts',(167.190198971462,1.28261029210532,136.582567540647));
#142314=CARTESIAN_POINT('Ctrl Pts',(167.182790751796,1.43600576846275,136.546361607312));
#142315=CARTESIAN_POINT('Ctrl Pts',(167.175382532129,1.58758067492107,136.504142908419));
#142316=CARTESIAN_POINT('Ctrl Pts',(167.167969752827,1.73924887320532,136.46189822462));
#142317=CARTESIAN_POINT('Ctrl Pts',(167.160556973525,1.88909391429604,136.413633515224));
#142318=CARTESIAN_POINT('Ctrl Pts',(167.153144194223,2.03661561445089,136.359549849399));
#142319=CARTESIAN_POINT('Ctrl Pts',(167.145720823194,2.18434810052894,136.305388906297));
#142320=CARTESIAN_POINT('Ctrl Pts',(167.138297452166,2.32975027132682,136.245392543059));
#142321=CARTESIAN_POINT('Ctrl Pts',(167.130874081137,2.47234403106011,136.179809022544));
#142322=CARTESIAN_POINT('Ctrl Pts',(167.126938031696,2.54795066396015,136.145035066313));
#142323=CARTESIAN_POINT('Ctrl Pts',(167.123001982255,2.62276818581389,136.108691115105));
#142324=CARTESIAN_POINT('Ctrl Pts',(167.119065932815,2.69672855796225,136.070819166455));
#142325=CARTESIAN_POINT('Ctrl Pts',(167.111642666409,2.83621551161134,135.999393853244));
#142326=CARTESIAN_POINT('Ctrl Pts',(167.104219400004,2.97307377888389,135.922315050444));
#142327=CARTESIAN_POINT('Ctrl Pts',(167.096796133598,3.10681217227156,135.83979989222));
#142328=CARTESIAN_POINT('Ctrl Pts',(167.089381640877,3.24039249798464,135.75738226006));
#142329=CARTESIAN_POINT('Ctrl Pts',(167.081967148156,3.3708599750741,135.669541256212));
#142330=CARTESIAN_POINT('Ctrl Pts',(167.074552655435,3.49774575240416,135.576540959301));
#142331=CARTESIAN_POINT('Ctrl Pts',(167.067145309082,3.6245092324449,135.483630299577));
#142332=CARTESIAN_POINT('Ctrl Pts',(167.059737962728,3.74769758626735,135.385570465694));
#142333=CARTESIAN_POINT('Ctrl Pts',(167.052330616374,3.86686893109385,135.282670034326));
#142334=CARTESIAN_POINT('Ctrl Pts',(167.044928794699,3.98595139343525,135.179846349981));
#142335=CARTESIAN_POINT('Ctrl Pts',(167.037526973023,4.10102253096623,135.072189499663));
#142336=CARTESIAN_POINT('Ctrl Pts',(167.030125151348,4.21167178645031,134.960049648968));
#142337=CARTESIAN_POINT('Ctrl Pts',(167.022727237036,4.32226263105375,134.847968996028));
#142338=CARTESIAN_POINT('Ctrl Pts',(167.015329322725,4.42843598090915,134.731410320841));
#142339=CARTESIAN_POINT('Ctrl Pts',(167.007931408414,4.52981664044239,134.610762037079));
#142340=CARTESIAN_POINT('Ctrl Pts',(167.000534723502,4.63118045234922,134.490133802873));
#142341=CARTESIAN_POINT('Ctrl Pts',(166.993138038589,4.72775291475044,134.365417594449));
#142342=CARTESIAN_POINT('Ctrl Pts',(166.985741353677,4.81919772388348,134.237036521379));
#142343=CARTESIAN_POINT('Ctrl Pts',(166.978344996742,4.91063847825786,134.108661140859));
#142344=CARTESIAN_POINT('Ctrl Pts',(166.970948639806,4.9969518148703,133.976621522858));
#142345=CARTESIAN_POINT('Ctrl Pts',(166.963552282871,5.07784371726555,133.841371277002));
#142346=CARTESIAN_POINT('Ctrl Pts',(166.956154793534,5.15874800441759,133.706100323988));
#142347=CARTESIAN_POINT('Ctrl Pts',(166.948757304198,5.23422901301899,133.567618084759));
#142348=CARTESIAN_POINT('Ctrl Pts',(166.941359814861,5.30403787839899,133.426404237914));
#142349=CARTESIAN_POINT('Ctrl Pts',(166.933959732346,5.37387121516852,133.285140888775));
#142350=CARTESIAN_POINT('Ctrl Pts',(166.926559649831,5.43802828457844,133.141144359955));
#142351=CARTESIAN_POINT('Ctrl Pts',(166.919159567316,5.49630776219657,132.994915694645));
#142352=CARTESIAN_POINT('Ctrl Pts',(166.91175134765,5.55465132409161,132.848526235885));
#142353=CARTESIAN_POINT('Ctrl Pts',(166.904343127983,5.60710424883609,132.699900085894));
#142354=CARTESIAN_POINT('Ctrl Pts',(166.896934908317,5.65351440112497,132.549555586265));
#142355=CARTESIAN_POINT('Ctrl Pts',(166.889522129015,5.69995311808823,132.399118552105));
#142356=CARTESIAN_POINT('Ctrl Pts',(166.882109349713,5.7403415560233,132.246961420844));
#142357=CARTESIAN_POINT('Ctrl Pts',(166.87469657041,5.77457851858784,132.093613694027));
#142358=CARTESIAN_POINT('Ctrl Pts',(166.867273199382,5.80886440053004,131.940046856787));
#142359=CARTESIAN_POINT('Ctrl Pts',(166.859849828353,5.83698118591433,131.785286392668));
#142360=CARTESIAN_POINT('Ctrl Pts',(166.852426457324,5.85887932286573,131.629868729335));
#142361=CARTESIAN_POINT('Ctrl Pts',(166.848490407883,5.87049024051603,131.547462555039));
#142362=CARTESIAN_POINT('Ctrl Pts',(166.844554358443,5.88035374313279,131.464871661582));
#142363=CARTESIAN_POINT('Ctrl Pts',(166.840618309002,5.88846838787322,131.382175992507));
#142364=CARTESIAN_POINT('Ctrl Pts',(166.833195042596,5.90377235460417,131.226214541475));
#142365=CARTESIAN_POINT('Ctrl Pts',(166.825771776191,5.91289901123309,131.069408829523));
#142366=CARTESIAN_POINT('Ctrl Pts',(166.818348509785,5.91576554003616,130.912289472932));
#142367=CARTESIAN_POINT('Ctrl Pts',(166.810934017064,5.91862868084023,130.755355818374));
#142368=CARTESIAN_POINT('Ctrl Pts',(166.803519524343,5.91524641472873,130.598109626652));
#142369=CARTESIAN_POINT('Ctrl Pts',(166.796105031622,5.90558749303605,130.441088096452));
#142370=CARTESIAN_POINT('Ctrl Pts',(166.788697685269,5.89593788097574,130.284217909516));
#142371=CARTESIAN_POINT('Ctrl Pts',(166.781290338915,5.88002367981568,130.127572323112));
#142372=CARTESIAN_POINT('Ctrl Pts',(166.773882992561,5.85786565541429,129.971689898964));
#142373=CARTESIAN_POINT('Ctrl Pts',(166.766481170886,5.83572415730347,129.815923737809));
#142374=CARTESIAN_POINT('Ctrl Pts',(166.75907934921,5.80734816073423,129.660919973558));
#142375=CARTESIAN_POINT('Ctrl Pts',(166.751677527535,5.77281035372675,129.507213292701));
#142376=CARTESIAN_POINT('Ctrl Pts',(166.744279613223,5.73829077895876,129.353587752404));
#142377=CARTESIAN_POINT('Ctrl Pts',(166.736881698912,5.69761595343543,129.201258295142));
#142378=CARTESIAN_POINT('Ctrl Pts',(166.729483784601,5.65090985820759,129.050750530656));
#142379=CARTESIAN_POINT('Ctrl Pts',(166.722087099688,5.60421152468545,128.90026777783));
#142380=CARTESIAN_POINT('Ctrl Pts',(166.714690414776,5.55148402123303,128.751606473121));
#142381=CARTESIAN_POINT('Ctrl Pts',(166.707293729864,5.4929015415178,128.605278259469));
#142382=CARTESIAN_POINT('Ctrl Pts',(166.699897372929,5.43432165941111,128.458956534164));
#142383=CARTESIAN_POINT('Ctrl Pts',(166.692501015993,5.36988745598924,128.314968040774));
#142384=CARTESIAN_POINT('Ctrl Pts',(166.685104659058,5.29982164280383,128.173805330755));
#142385=CARTESIAN_POINT('Ctrl Pts',(166.677707169721,5.22974510236354,128.032621008365));
#142386=CARTESIAN_POINT('Ctrl Pts',(166.670309680384,5.15403540135419,127.894263665175));
#142387=CARTESIAN_POINT('Ctrl Pts',(166.662912191048,5.07296158953401,127.759201956082));
#142388=CARTESIAN_POINT('Ctrl Pts',(166.655512108533,4.99185935741483,127.624092901316));
#142389=CARTESIAN_POINT('Ctrl Pts',(166.648112026018,4.90538946266501,127.492282100661));
#142390=CARTESIAN_POINT('Ctrl Pts',(166.640711943503,4.81386462633662,127.364209760146));
#142391=CARTESIAN_POINT('Ctrl Pts',(166.633303723836,4.72223914904163,127.235996590927));
#142392=CARTESIAN_POINT('Ctrl Pts',(166.62589550417,4.62554784680075,127.11153039533));
#142393=CARTESIAN_POINT('Ctrl Pts',(166.618487284503,4.52414458222861,126.991219345387));
#142394=CARTESIAN_POINT('Ctrl Pts',(166.611074505201,4.42267890563909,126.870834246001));
#142395=CARTESIAN_POINT('Ctrl Pts',(166.603661725899,4.31649573904106,126.754609663215));
#142396=CARTESIAN_POINT('Ctrl Pts',(166.596248946597,4.20598586798708,126.642916944897));
#142397=CARTESIAN_POINT('Ctrl Pts',(166.588825575568,4.09531809524689,126.531064634786));
#142398=CARTESIAN_POINT('Ctrl Pts',(166.58140220454,3.98031154303065,126.423757375843));
#142399=CARTESIAN_POINT('Ctrl Pts',(166.573978833511,3.86139073912517,126.321326809719));
#142400=CARTESIAN_POINT('Ctrl Pts',(166.57004278407,3.79833607542974,126.267015665773));
#142401=CARTESIAN_POINT('Ctrl Pts',(166.566106734629,3.73418148176345,126.214074826365));
#142402=CARTESIAN_POINT('Ctrl Pts',(166.562170685189,3.66899343700182,126.162548716838));
#142403=CARTESIAN_POINT('Ctrl Pts',(166.554747418783,3.54605081902921,126.065372082344));
#142404=CARTESIAN_POINT('Ctrl Pts',(166.547324152378,3.41905891343449,125.972936250139));
#142405=CARTESIAN_POINT('Ctrl Pts',(166.539900885972,3.28841937772064,125.885597708182));
#142406=CARTESIAN_POINT('Ctrl Pts',(166.532486393251,3.15793424708902,125.798362393129));
#142407=CARTESIAN_POINT('Ctrl Pts',(166.52507190053,3.0238103751002,125.716212581821));
#142408=CARTESIAN_POINT('Ctrl Pts',(166.517657407809,2.88648283155587,125.63946493366));
#142409=CARTESIAN_POINT('Ctrl Pts',(166.510250061456,2.7492876494682,125.562791257771));
#142410=CARTESIAN_POINT('Ctrl Pts',(166.502842715102,2.6088952667398,125.491509560188));
#142411=CARTESIAN_POINT('Ctrl Pts',(166.495435368748,2.46577001505577,125.425893475773));
#142412=CARTESIAN_POINT('Ctrl Pts',(166.488033547073,2.3227515115844,125.360326330309));
#142413=CARTESIAN_POINT('Ctrl Pts',(166.480631725397,2.17700453551775,125.300416539118));
#142414=CARTESIAN_POINT('Ctrl Pts',(166.473229903722,2.0290182233931,125.246391958817));
#142415=CARTESIAN_POINT('Ctrl Pts',(166.46583198941,1.88111003209069,125.192395897671));
#142416=CARTESIAN_POINT('Ctrl Pts',(166.458434075099,1.7309652087691,125.144278987851));
#142417=CARTESIAN_POINT('Ctrl Pts',(166.451036160788,1.57909297857519,125.102221025491));
#142418=CARTESIAN_POINT('Ctrl Pts',(166.443639475876,1.42724598679064,125.0601700524));
#142419=CARTESIAN_POINT('Ctrl Pts',(166.436242790963,1.27367251727574,125.024176127926));
#142420=CARTESIAN_POINT('Ctrl Pts',(166.428846106051,1.11889718565743,124.994369253508));
#142421=CARTESIAN_POINT('Ctrl Pts',(166.421449749116,0.964128716939459,
124.964563700758));
#142422=CARTESIAN_POINT('Ctrl Pts',(166.41405339218,0.808158858642217,124.940944723177));
#142423=CARTESIAN_POINT('Ctrl Pts',(166.406657035245,0.65152238928837,124.923591183321));
#142424=CARTESIAN_POINT('Ctrl Pts',(166.399259545908,0.49486193849108,124.906234986593));
#142425=CARTESIAN_POINT('Ctrl Pts',(166.391862056572,0.337535044474101,
124.895146178702));
#142426=CARTESIAN_POINT('Ctrl Pts',(166.384464567235,0.180081427840616,
124.890351719885));
#142427=CARTESIAN_POINT('Ctrl Pts',(166.37706448472,0.0225726160860165,
124.885555580378));
#142428=CARTESIAN_POINT('Ctrl Pts',(166.369664402205,-0.135062633837593,
124.887058194374));
#142429=CARTESIAN_POINT('Ctrl Pts',(166.36226431969,-0.292284930763479,
124.894834402906));
#142430=CARTESIAN_POINT('Ctrl Pts',(166.354856100024,-0.449680109767736,
124.902619162179));
#142431=CARTESIAN_POINT('Ctrl Pts',(166.347447880357,-0.606661055867241,
124.916691274218));
#142432=CARTESIAN_POINT('Ctrl Pts',(166.340039660691,-0.76269309098338,
124.936973651338));
#142433=CARTESIAN_POINT('Ctrl Pts',(166.332626881389,-0.918821161213655,
124.957268511922));
#142434=CARTESIAN_POINT('Ctrl Pts',(166.325214102086,-1.07399878957714,
124.983781191305));
#142435=CARTESIAN_POINT('Ctrl Pts',(166.317801322784,-1.22770232145825,
125.016383633128));
#142436=CARTESIAN_POINT('Ctrl Pts',(166.310377951756,-1.38162547215363,
125.049032658848));
#142437=CARTESIAN_POINT('Ctrl Pts',(166.302954580727,-1.53406995886588,
125.087788733798));
#142438=CARTESIAN_POINT('Ctrl Pts',(166.295531209698,-1.68452729444312,
125.13247395114));
#142439=CARTESIAN_POINT('Ctrl Pts',(166.291595160257,-1.76430338394073,
125.156167125582));
#142440=CARTESIAN_POINT('Ctrl Pts',(166.287659110816,-1.84352113643791,
125.181526385335));
#142441=CARTESIAN_POINT('Ctrl Pts',(166.283723061376,-1.92210724217974,
125.20851981282));
#142442=CARTESIAN_POINT('Ctrl Pts',(166.27629979497,-2.07031818501966,125.259428574621));
#142443=CARTESIAN_POINT('Ctrl Pts',(166.268876528565,-2.21672929549576,
125.316306636218));
#142444=CARTESIAN_POINT('Ctrl Pts',(166.261453262159,-2.36082354450143,
125.379008762227));
#142445=CARTESIAN_POINT('Ctrl Pts',(166.254038769438,-2.50474748607107,
125.441636779531));
#142446=CARTESIAN_POINT('Ctrl Pts',(166.246624276717,-2.64635967789469,
125.510075011988));
#142447=CARTESIAN_POINT('Ctrl Pts',(166.239209783996,-2.78515853959671,
125.584128585193));
#142448=CARTESIAN_POINT('Ctrl Pts',(166.231802437643,-2.92382362173009,
125.658110782776));
#142449=CARTESIAN_POINT('Ctrl Pts',(166.224395091289,-3.05968044484829,
125.737697371788));
#142450=CARTESIAN_POINT('Ctrl Pts',(166.216987744935,-3.19224780957431,
125.822645603159));
#142451=CARTESIAN_POINT('Ctrl Pts',(166.20958592326,-3.32471630055828,125.907530476934));
#142452=CARTESIAN_POINT('Ctrl Pts',(166.202184101584,-3.45389990525267,
125.997768830151));
#142453=CARTESIAN_POINT('Ctrl Pts',(166.194782279909,-3.5793425311852,126.093072300455));
#142454=CARTESIAN_POINT('Ctrl Pts',(166.187384365598,-3.70471893693221,
126.188325460799));
#142455=CARTESIAN_POINT('Ctrl Pts',(166.179986451286,-3.82635800040218,
126.288638187903));
#142456=CARTESIAN_POINT('Ctrl Pts',(166.172588536975,-3.94383320538515,
126.393679240431));
#142457=CARTESIAN_POINT('Ctrl Pts',(166.165191852063,-4.06128888812006,
126.498702837042));
#142458=CARTESIAN_POINT('Ctrl Pts',(166.157795167151,-4.17458180769433,
126.608452950993));
#142459=CARTESIAN_POINT('Ctrl Pts',(166.150398482238,-4.28331902265383,
126.722558477252));
#142460=CARTESIAN_POINT('Ctrl Pts',(166.143002125303,-4.39205141609135,
126.836658943953));
#142461=CARTESIAN_POINT('Ctrl Pts',(166.135605768367,-4.49622824904004,
126.955114168725));
#142462=CARTESIAN_POINT('Ctrl Pts',(166.128209411432,-4.59549411134317,
127.077516854392));
#142463=CARTESIAN_POINT('Ctrl Pts',(166.120811922095,-4.69477517150308,
127.199938280222));
#142464=CARTESIAN_POINT('Ctrl Pts',(166.113414432759,-4.78914352877203,
127.326308080363));
#142465=CARTESIAN_POINT('Ctrl Pts',(166.106016943422,-4.87828476856935,
127.456186745252));
#142466=CARTESIAN_POINT('Ctrl Pts',(166.098616860907,-4.96745725669013,
127.586110938907));
#142467=CARTESIAN_POINT('Ctrl Pts',(166.091216778392,-5.05139876801785,
127.719546138697));
#142468=CARTESIAN_POINT('Ctrl Pts',(166.083816695877,-5.12983891540261,
127.856024940524));
#142469=CARTESIAN_POINT('Ctrl Pts',(166.076408476211,-5.20836531579331,
127.992653814823));
#142470=CARTESIAN_POINT('Ctrl Pts',(166.069000256545,-5.2813780852317,128.132332650995));
#142471=CARTESIAN_POINT('Ctrl Pts',(166.061592036878,-5.34865307320897,
128.274569941452));
#142472=CARTESIAN_POINT('Ctrl Pts',(166.054179257576,-5.41596946781898,
128.416894776589));
#142473=CARTESIAN_POINT('Ctrl Pts',(166.046766478274,-5.47754089833081,
128.561780861005));
#142474=CARTESIAN_POINT('Ctrl Pts',(166.039353698972,-5.53319205407562,
128.70871841165));
#142475=CARTESIAN_POINT('Ctrl Pts',(166.031930327943,-5.58892272680148,
128.855865913559));
#142476=CARTESIAN_POINT('Ctrl Pts',(166.024506956914,-5.63871611204877,
129.005070382862));
#142477=CARTESIAN_POINT('Ctrl Pts',(166.017083585886,-5.68244703815218,
129.155807851927));
#142478=CARTESIAN_POINT('Ctrl Pts',(166.013147536445,-5.70563422448215,
129.235732474924));
#142479=CARTESIAN_POINT('Ctrl Pts',(166.009211487004,-5.7271178912674,129.316087912996));
#142480=CARTESIAN_POINT('Ctrl Pts',(166.005275437563,-5.74688526595699,
129.39679523634));
#142481=CARTESIAN_POINT('Ctrl Pts',(165.99536581659,-5.79665272791137,129.599988564085));
#142482=CARTESIAN_POINT('Ctrl Pts',(165.985456195617,-5.8356617089951,129.805912698135));
#142483=CARTESIAN_POINT('Ctrl Pts',(165.975546574645,-5.86366917150755,
130.013592377427));
#142484=CARTESIAN_POINT('Ctrl Pts',(165.965876951706,-5.89099832997878,
130.216242327029));
#142485=CARTESIAN_POINT('Ctrl Pts',(165.956207328768,-5.90785247295491,
130.420564146172));
#142486=CARTESIAN_POINT('Ctrl Pts',(165.94653770583,-5.91404984588532,130.625629023034));
#142487=CARTESIAN_POINT('Ctrl Pts',(165.943816872408,-5.91579365942388,
130.683330070328));
#142488=CARTESIAN_POINT('Ctrl Pts',(165.941096038987,-5.91669400065677,
130.741089791547));
#142489=CARTESIAN_POINT('Ctrl Pts',(165.938375205566,-5.91674746826018,
130.798887105275));
#142490=CARTESIAN_POINT('',(164.188375192211,-5.90703701052902,130.805180874694));
#142491=CARTESIAN_POINT('Ctrl Pts',(165.938375192211,-5.91629100133431,
130.79888781122));
#142492=CARTESIAN_POINT('Ctrl Pts',(165.867859399391,-5.90251351537856,
132.296718260267));
#142493=CARTESIAN_POINT('Ctrl Pts',(165.704527731967,-4.56346770795856,
135.787977784439));
#142494=CARTESIAN_POINT('Ctrl Pts',(165.448380189937,1.31124547549227,137.678820293304));
#142495=CARTESIAN_POINT('Ctrl Pts',(165.169932566125,6.49243782846852,133.41698603538));
#142496=CARTESIAN_POINT('Ctrl Pts',(164.891484942312,5.70739699030252,126.754276652334));
#142497=CARTESIAN_POINT('Ctrl Pts',(164.613037318499,-0.322462860107947,
123.813396575733));
#142498=CARTESIAN_POINT('Ctrl Pts',(164.378667401798,-5.14838830328745,
126.745443838765));
#142499=CARTESIAN_POINT('Ctrl Pts',(164.237113359703,-5.9057559966609,129.765836853127));
#142500=CARTESIAN_POINT('Ctrl Pts',(164.188375192211,-5.90703701052902,
130.805180874694));
#142501=CARTESIAN_POINT('',(162.438375999696,-5.91850430126774,130.80953524169));
#142502=CARTESIAN_POINT('Ctrl Pts',(164.188375192211,-5.90703701052902,
130.805180874694));
#142503=CARTESIAN_POINT('Ctrl Pts',(164.144297485099,-5.90819553078106,
131.745140330083));
#142504=CARTESIAN_POINT('Ctrl Pts',(164.007403903381,-5.25265206602396,
134.662876630279));
#142505=CARTESIAN_POINT('Ctrl Pts',(163.777694447059,-0.672846130350174,
137.770337836536));
#142506=CARTESIAN_POINT('Ctrl Pts',(163.499246823248,5.49698415240917,135.13572596333));
#142507=CARTESIAN_POINT('Ctrl Pts',(163.220799199434,6.61535454171388,128.520800936328));
#142508=CARTESIAN_POINT('Ctrl Pts',(162.942351575622,1.65453728521643,124.004355698289));
#142509=CARTESIAN_POINT('Ctrl Pts',(162.681543965991,-4.41612301327428,
125.627031304092));
#142510=CARTESIAN_POINT('Ctrl Pts',(162.513552230965,-5.90464145011147,
129.214801166862));
#142511=CARTESIAN_POINT('Ctrl Pts',(162.438376370543,-5.91931103223556,
130.809528082525));
#142512=CARTESIAN_POINT('',(160.688373776686,-5.92101633406598,130.801148899096));
#142513=CARTESIAN_POINT('Ctrl Pts',(162.438375192211,-5.91674772355508,
130.809550830069));
#142514=CARTESIAN_POINT('Ctrl Pts',(162.42743056777,-5.91654415116547,131.041619646537));
#142515=CARTESIAN_POINT('Ctrl Pts',(162.41648594333,-5.90268400911373,131.273113435323));
#142516=CARTESIAN_POINT('Ctrl Pts',(162.405541318889,-5.87538811168766,
131.502748117124));
#142517=CARTESIAN_POINT('Ctrl Pts',(162.398846321925,-5.85869078676843,
131.643219222907));
#142518=CARTESIAN_POINT('Ctrl Pts',(162.39215132496,-5.83696670312851,131.782995481317));
#142519=CARTESIAN_POINT('Ctrl Pts',(162.385456327996,-5.81027417745911,
131.921788264106));
#142520=CARTESIAN_POINT('Ctrl Pts',(162.378033061591,-5.78067808800102,
132.075678670223));
#142521=CARTESIAN_POINT('Ctrl Pts',(162.370609795185,-5.74491913147518,
132.228625145143));
#142522=CARTESIAN_POINT('Ctrl Pts',(162.36318652878,-5.70306851519399,132.380095390141));
#142523=CARTESIAN_POINT('Ctrl Pts',(162.355772036059,-5.66126736286574,
132.531386609889));
#142524=CARTESIAN_POINT('Ctrl Pts',(162.348357543338,-5.61338898054029,
132.681204716409));
#142525=CARTESIAN_POINT('Ctrl Pts',(162.340943050617,-5.55955589185102,
132.829025737502));
#142526=CARTESIAN_POINT('Ctrl Pts',(162.333535704263,-5.50577468951937,
132.976704283129));
#142527=CARTESIAN_POINT('Ctrl Pts',(162.326128357909,-5.44605033366204,
133.12238922695));
#142528=CARTESIAN_POINT('Ctrl Pts',(162.318721011555,-5.38055560982868,
133.265570054416));
#142529=CARTESIAN_POINT('Ctrl Pts',(162.31131918988,-5.31510973443136,133.408644092219));
#142530=CARTESIAN_POINT('Ctrl Pts',(162.303917368204,-5.24390221503485,
133.549217394432));
#142531=CARTESIAN_POINT('Ctrl Pts',(162.296515546529,-5.16715452362796,
133.686797900743));
#142532=CARTESIAN_POINT('Ctrl Pts',(162.289117632217,-5.09044734672991,
133.824305779377));
#142533=CARTESIAN_POINT('Ctrl Pts',(162.281719717906,-5.0082060037273,133.958823683324));
#142534=CARTESIAN_POINT('Ctrl Pts',(162.274321803595,-4.92069857331505,
134.089882815494));
#142535=CARTESIAN_POINT('Ctrl Pts',(162.266925118682,-4.83320568505026,
134.220920168013));
#142536=CARTESIAN_POINT('Ctrl Pts',(162.25952843377,-4.74044865333258,134.348499579381));
#142537=CARTESIAN_POINT('Ctrl Pts',(162.252131748858,-4.64273973952022,
134.472179897953));
#142538=CARTESIAN_POINT('Ctrl Pts',(162.244735391922,-4.54503515822351,
134.59585473241));
#142539=CARTESIAN_POINT('Ctrl Pts',(162.237339034987,-4.44237936282352,
134.715630524915));
#142540=CARTESIAN_POINT('Ctrl Pts',(162.229942678051,-4.33512571764814,
134.831098202098));
#142541=CARTESIAN_POINT('Ctrl Pts',(162.222545188714,-4.22785565166576,
134.946583557678));
#142542=CARTESIAN_POINT('Ctrl Pts',(162.215147699378,-4.11598658833484,
135.057759211088));
#142543=CARTESIAN_POINT('Ctrl Pts',(162.207750210041,-3.99990954098363,
135.164252155947));
#142544=CARTESIAN_POINT('Ctrl Pts',(162.200350127526,-3.8837918030032,135.270782431743));
#142545=CARTESIAN_POINT('Ctrl Pts',(162.192950045011,-3.7634634189861,135.372626478538));
#142546=CARTESIAN_POINT('Ctrl Pts',(162.185549962496,-3.63934920184748,
135.469450964978));
#142547=CARTESIAN_POINT('Ctrl Pts',(162.178141742829,-3.51509850836809,
135.566381919893));
#142548=CARTESIAN_POINT('Ctrl Pts',(162.170733523163,-3.38705396266636,
135.658282061851));
#142549=CARTESIAN_POINT('Ctrl Pts',(162.163325303496,-3.25567073390916,
135.744860454108));
#142550=CARTESIAN_POINT('Ctrl Pts',(162.155912524194,-3.12420664096672,
135.83149213392));
#142551=CARTESIAN_POINT('Ctrl Pts',(162.148499744892,-2.98940008923525,
135.912795344946));
#142552=CARTESIAN_POINT('Ctrl Pts',(162.14108696559,-2.85173119931621,135.988524940709));
#142553=CARTESIAN_POINT('Ctrl Pts',(162.133663594561,-2.71386560163142,
136.064362742469));
#142554=CARTESIAN_POINT('Ctrl Pts',(162.126240223532,-2.57312983054176,
136.13461085711));
#142555=CARTESIAN_POINT('Ctrl Pts',(162.118816852503,-2.43002509012415,
136.199071789062));
#142556=CARTESIAN_POINT('Ctrl Pts',(162.114880803063,-2.35414752301458,
136.233250521898));
#142557=CARTESIAN_POINT('Ctrl Pts',(162.110944753623,-2.27760423821805,
136.265803093478));
#142558=CARTESIAN_POINT('Ctrl Pts',(162.107008704182,-2.20047159052352,
136.296705776221));
#142559=CARTESIAN_POINT('Ctrl Pts',(162.099585437777,-2.05500182417906,
136.354987271443));
#142560=CARTESIAN_POINT('Ctrl Pts',(162.092162171372,-1.90699503369736,
136.407573554191));
#142561=CARTESIAN_POINT('Ctrl Pts',(162.084738904966,-1.75693754636281,
136.45423681273));
#142562=CARTESIAN_POINT('Ctrl Pts',(162.077324412245,-1.60705741451664,
136.500844919173));
#142563=CARTESIAN_POINT('Ctrl Pts',(162.069909919524,-1.45513176329157,
136.541543826221));
#142564=CARTESIAN_POINT('Ctrl Pts',(162.062495426803,-1.30166765235591,
136.576153396704));
#142565=CARTESIAN_POINT('Ctrl Pts',(162.055088080449,-1.14835145590825,
136.61072960918));
#142566=CARTESIAN_POINT('Ctrl Pts',(162.047680734095,-0.993500113471112,
136.639228087804));
#142567=CARTESIAN_POINT('Ctrl Pts',(162.040273387742,-0.837636530203736,
136.661518256367));
#142568=CARTESIAN_POINT('Ctrl Pts',(162.032871566066,-0.681889195877158,
136.683791800082));
#142569=CARTESIAN_POINT('Ctrl Pts',(162.025469744391,-0.525131491909981,
136.699866200852));
#142570=CARTESIAN_POINT('Ctrl Pts',(162.018067922716,-0.367897113596595,
136.709661818716));
#142571=CARTESIAN_POINT('Ctrl Pts',(162.010670008404,-0.210745738087498,
136.71945226555));
#142572=CARTESIAN_POINT('Ctrl Pts',(162.003272094093,-0.0531185610031907,
136.722970507353));
#142573=CARTESIAN_POINT('Ctrl Pts',(161.995874179782,0.104445102303171,
136.720188690043));
#142574=CARTESIAN_POINT('Ctrl Pts',(161.988477494869,0.261982581387019,
136.717407335021));
#142575=CARTESIAN_POINT('Ctrl Pts',(161.981080809957,0.419456194766861,
136.708328005366));
#142576=CARTESIAN_POINT('Ctrl Pts',(161.973684125045,0.57632600417748,136.692974962164));
#142577=CARTESIAN_POINT('Ctrl Pts',(161.96628776811,0.733188857816362,136.677622599732));
#142578=CARTESIAN_POINT('Ctrl Pts',(161.958891411174,0.889447589197945,
136.655997113235));
#142579=CARTESIAN_POINT('Ctrl Pts',(161.951495054239,1.04456703125893,136.628174683941));
#142580=CARTESIAN_POINT('Ctrl Pts',(161.944097564902,1.19971022250251,136.600347994962));
#142581=CARTESIAN_POINT('Ctrl Pts',(161.936700075566,1.35371340965791,136.56632253997));
#142582=CARTESIAN_POINT('Ctrl Pts',(161.929302586229,1.5060514196369,136.526225670493));
#142583=CARTESIAN_POINT('Ctrl Pts',(161.921902503714,1.65844283146914,136.486114745121));
#142584=CARTESIAN_POINT('Ctrl Pts',(161.914502421199,1.80916754315514,136.439928262743));
#142585=CARTESIAN_POINT('Ctrl Pts',(161.907102338684,1.95771549182921,136.387843456758));
#142586=CARTESIAN_POINT('Ctrl Pts',(161.899694119018,2.106426784244,136.335701378175));
#142587=CARTESIAN_POINT('Ctrl Pts',(161.892285899351,2.25295618103334,136.277648146981));
#142588=CARTESIAN_POINT('Ctrl Pts',(161.884877679685,2.39681287882266,136.213909451472));
#142589=CARTESIAN_POINT('Ctrl Pts',(161.877464900383,2.5407581180093,136.150131525859));
#142590=CARTESIAN_POINT('Ctrl Pts',(161.870052121081,2.6820270461158,136.08066132747));
#142591=CARTESIAN_POINT('Ctrl Pts',(161.862639341779,2.82015389755464,136.005770287704));
#142592=CARTESIAN_POINT('Ctrl Pts',(161.85521597075,2.95847811111618,135.930772240109));
#142593=CARTESIAN_POINT('Ctrl Pts',(161.847792599721,3.09365096142933,135.850338071918));
#142594=CARTESIAN_POINT('Ctrl Pts',(161.840369228692,3.22523537683267,135.764782709135));
#142595=CARTESIAN_POINT('Ctrl Pts',(161.836433179252,3.29500459120555,135.719419202914));
#142596=CARTESIAN_POINT('Ctrl Pts',(161.832497129811,3.3637655067298,135.672616629669));
#142597=CARTESIAN_POINT('Ctrl Pts',(161.82856108037,3.43145688909021,135.624426403509));
#142598=CARTESIAN_POINT('Ctrl Pts',(161.821137813964,3.55912072364372,135.533541140937));
#142599=CARTESIAN_POINT('Ctrl Pts',(161.813714547559,3.68336433816243,135.437443006652));
#142600=CARTESIAN_POINT('Ctrl Pts',(161.806291281154,3.80373319640592,135.336418023762));
#142601=CARTESIAN_POINT('Ctrl Pts',(161.798876788433,3.92395978865511,135.235512444013));
#142602=CARTESIAN_POINT('Ctrl Pts',(161.791462295712,4.04032045728496,135.129691844265));
#142603=CARTESIAN_POINT('Ctrl Pts',(161.784047802991,4.15238956965613,135.019285459637));
#142604=CARTESIAN_POINT('Ctrl Pts',(161.776640456637,4.26435066559748,134.90898548884));
#142605=CARTESIAN_POINT('Ctrl Pts',(161.769233110283,4.37202817582391,134.79410879264));
#142606=CARTESIAN_POINT('Ctrl Pts',(161.761825763929,4.47502959986258,134.675024726327));
#142607=CARTESIAN_POINT('Ctrl Pts',(161.754423942254,4.57795420155314,134.556029477404));
#142608=CARTESIAN_POINT('Ctrl Pts',(161.747022120578,4.67620941818536,134.432833387703));
#142609=CARTESIAN_POINT('Ctrl Pts',(161.739620298903,4.76943977106237,134.305842422846));
#142610=CARTESIAN_POINT('Ctrl Pts',(161.732222384592,4.86262090836165,134.178918495531));
#142611=CARTESIAN_POINT('Ctrl Pts',(161.72482447028,4.95078224430348,134.048203982849));
#142612=CARTESIAN_POINT('Ctrl Pts',(161.717426555969,5.03360883133898,133.91413757027));
#142613=CARTESIAN_POINT('Ctrl Pts',(161.710029871057,5.11642165409845,133.780093437095));
#142614=CARTESIAN_POINT('Ctrl Pts',(161.702633186145,5.19390129145906,133.642698826822));
#142615=CARTESIAN_POINT('Ctrl Pts',(161.695236501232,5.26577630513684,133.502421118511));
#142616=CARTESIAN_POINT('Ctrl Pts',(161.687840144297,5.33764813180117,133.362149630261));
#142617=CARTESIAN_POINT('Ctrl Pts',(161.680443787362,5.40391565868912,133.218995630389));
#142618=CARTESIAN_POINT('Ctrl Pts',(161.673047430426,5.46435370838878,133.073450547938));
#142619=CARTESIAN_POINT('Ctrl Pts',(161.66564994109,5.52480101130816,132.927883182164));
#142620=CARTESIAN_POINT('Ctrl Pts',(161.658252451753,5.57941691676746,132.779924349673));
#142621=CARTESIAN_POINT('Ctrl Pts',(161.650854962416,5.62802470033038,132.630084730068));
#142622=CARTESIAN_POINT('Ctrl Pts',(161.643454879901,5.67664952327648,132.480192584417));
#142623=CARTESIAN_POINT('Ctrl Pts',(161.636054797386,5.71926191590507,132.328418693837));
#142624=CARTESIAN_POINT('Ctrl Pts',(161.628654714871,5.7557352882555,132.175287987645));
#142625=CARTESIAN_POINT('Ctrl Pts',(161.621246495205,5.79224876682841,132.021988898498));
#142626=CARTESIAN_POINT('Ctrl Pts',(161.613838275538,5.82260965741637,131.867330377562));
#142627=CARTESIAN_POINT('Ctrl Pts',(161.606430055872,5.84674254676127,131.711847341652));
#142628=CARTESIAN_POINT('Ctrl Pts',(161.59901727657,5.8708902894969,131.556268608527));
#142629=CARTESIAN_POINT('Ctrl Pts',(161.591604497268,5.88880235042085,131.399864719234));
#142630=CARTESIAN_POINT('Ctrl Pts',(161.584191717966,5.90045533478054,131.243174250855));
#142631=CARTESIAN_POINT('Ctrl Pts',(161.576768346937,5.91212496947076,131.086259895786));
#142632=CARTESIAN_POINT('Ctrl Pts',(161.569344975908,5.91751765313196,130.929058515902));
#142633=CARTESIAN_POINT('Ctrl Pts',(161.56192160488,5.91666209402293,130.772108057169));
#142634=CARTESIAN_POINT('Ctrl Pts',(161.557985555439,5.91620845605445,130.688889157971));
#142635=CARTESIAN_POINT('Ctrl Pts',(161.554049505998,5.91399908008518,130.605740718273));
#142636=CARTESIAN_POINT('Ctrl Pts',(161.550113456557,5.91004412361794,130.52274204682));
#142637=CARTESIAN_POINT('Ctrl Pts',(161.542690190151,5.902585199151,130.366209142766));
#142638=CARTESIAN_POINT('Ctrl Pts',(161.535266923746,5.88889182560213,130.2097360822));
#142639=CARTESIAN_POINT('Ctrl Pts',(161.52784365734,5.86895895437449,130.053859881812));
#142640=CARTESIAN_POINT('Ctrl Pts',(161.520429164619,5.8490496421453,129.898167914148));
#142641=CARTESIAN_POINT('Ctrl Pts',(161.513014671898,5.8229155582438,129.743071769148));
#142642=CARTESIAN_POINT('Ctrl Pts',(161.505600179177,5.79060363266186,129.58910750323));
#142643=CARTESIAN_POINT('Ctrl Pts',(161.498192832823,5.75832285053032,129.435291633868));
#142644=CARTESIAN_POINT('Ctrl Pts',(161.49078548647,5.71987615698665,129.282605834613));
#142645=CARTESIAN_POINT('Ctrl Pts',(161.483378140116,5.67536214500421,129.131579972785));
#142646=CARTESIAN_POINT('Ctrl Pts',(161.47597631844,5.63088133325133,128.980666751743));
#142647=CARTESIAN_POINT('Ctrl Pts',(161.468574496765,5.5803423184976,128.831411359542));
#142648=CARTESIAN_POINT('Ctrl Pts',(161.46117267509,5.52389450619997,128.684332304813));
#142649=CARTESIAN_POINT('Ctrl Pts',(161.453774760778,5.46747649226303,128.537330891972));
#142650=CARTESIAN_POINT('Ctrl Pts',(161.446376846467,5.40515602625247,128.392503876201));
#142651=CARTESIAN_POINT('Ctrl Pts',(161.438978932155,5.33713194983506,128.250353352003));
#142652=CARTESIAN_POINT('Ctrl Pts',(161.431582247243,5.26911917778517,128.108226450643));
#142653=CARTESIAN_POINT('Ctrl Pts',(161.424185562331,5.19540483748249,127.968775494491));
#142654=CARTESIAN_POINT('Ctrl Pts',(161.416788877419,5.11623542914677,127.832481482062));
#142655=CARTESIAN_POINT('Ctrl Pts',(161.409392520483,5.03706953126555,127.696193513052));
#142656=CARTESIAN_POINT('Ctrl Pts',(161.401996163548,4.95244923379804,127.563062532226));
#142657=CARTESIAN_POINT('Ctrl Pts',(161.394599806612,4.86266627602476,127.433543617118));
#142658=CARTESIAN_POINT('Ctrl Pts',(161.387202317276,4.77286957225141,127.304004872333));
#142659=CARTESIAN_POINT('Ctrl Pts',(161.379804827939,4.67790884703223,127.17807960121));
#142660=CARTESIAN_POINT('Ctrl Pts',(161.372407338603,4.57811822570637,127.056192521822));
#142661=CARTESIAN_POINT('Ctrl Pts',(161.365007256088,4.47829262293286,126.934262715107));
#142662=CARTESIAN_POINT('Ctrl Pts',(161.357607173573,4.37363398940875,126.816374207201));
#142663=CARTESIAN_POINT('Ctrl Pts',(161.350207091058,4.26451553806804,126.70291723894));
#142664=CARTESIAN_POINT('Ctrl Pts',(161.342798871391,4.15527709977247,126.589335513079));
#142665=CARTESIAN_POINT('Ctrl Pts',(161.335390651725,4.04156930891996,126.480195327652));
#142666=CARTESIAN_POINT('Ctrl Pts',(161.327982432058,3.92380144346892,126.375849265573));
#142667=CARTESIAN_POINT('Ctrl Pts',(161.320569652756,3.80596109386171,126.271438980234));
#142668=CARTESIAN_POINT('Ctrl Pts',(161.313156873454,3.68405597866619,126.171828933543));
#142669=CARTESIAN_POINT('Ctrl Pts',(161.305744094152,3.55852657259944,126.077329922235));
#142670=CARTESIAN_POINT('Ctrl Pts',(161.298320723123,3.43281780423052,125.982695886308));
#142671=CARTESIAN_POINT('Ctrl Pts',(161.290897352094,3.30347470840148,125.893187683131));
#142672=CARTESIAN_POINT('Ctrl Pts',(161.283473981066,3.17096539180398,125.809071932567));
#142673=CARTESIAN_POINT('Ctrl Pts',(161.279537931625,3.10070577263001,125.76447174329));
#142674=CARTESIAN_POINT('Ctrl Pts',(161.275601882185,3.02955641375347,125.721386791199));
#142675=CARTESIAN_POINT('Ctrl Pts',(161.271665832744,2.9575895302463,125.679851398814));
#142676=CARTESIAN_POINT('Ctrl Pts',(161.264242566338,2.82186223395502,125.601516945046));
#142677=CARTESIAN_POINT('Ctrl Pts',(161.256819299933,2.68281541367125,125.528460056726));
#142678=CARTESIAN_POINT('Ctrl Pts',(161.249396033528,2.54089814785558,125.460975252021));
#142679=CARTESIAN_POINT('Ctrl Pts',(161.241981540807,2.39914861646251,125.39357020875));
#142680=CARTESIAN_POINT('Ctrl Pts',(161.234567048086,2.25453572641405,125.331724298886));
#142681=CARTESIAN_POINT('Ctrl Pts',(161.227152555365,2.10753584396342,125.275687790484));
#142682=CARTESIAN_POINT('Ctrl Pts',(161.219745209011,1.96067764553395,125.21970529218));
#142683=CARTESIAN_POINT('Ctrl Pts',(161.212337862657,1.8114373813614,125.16952118027));
#142684=CARTESIAN_POINT('Ctrl Pts',(161.204930516303,1.66031413573936,125.125338911923));
#142685=CARTESIAN_POINT('Ctrl Pts',(161.197528694628,1.50930360353531,125.081189596379));
#142686=CARTESIAN_POINT('Ctrl Pts',(161.190126872953,1.35641324298605,125.04303331558));
#142687=CARTESIAN_POINT('Ctrl Pts',(161.182725051277,1.2021600473863,125.011024637065));
#142688=CARTESIAN_POINT('Ctrl Pts',(161.175327136966,1.04798828084787,124.979032855682));
#142689=CARTESIAN_POINT('Ctrl Pts',(161.167929222655,0.892455476624556,
124.953182289123));
#142690=CARTESIAN_POINT('Ctrl Pts',(161.160531308343,0.736091539820999,
124.933577040606));
#142691=CARTESIAN_POINT('Ctrl Pts',(161.153134623431,0.579753587867119,
124.913975050126));
#142692=CARTESIAN_POINT('Ctrl Pts',(161.145737938519,0.422585147493782,
124.900616364242));
#142693=CARTESIAN_POINT('Ctrl Pts',(161.138341253607,0.265124135764709,
124.893553586785));
#142694=CARTESIAN_POINT('Ctrl Pts',(161.130944896671,0.107670106021902,
124.886491122498));
#142695=CARTESIAN_POINT('Ctrl Pts',(161.123548539736,-0.0500760963594786,
124.885724028287));
#142696=CARTESIAN_POINT('Ctrl Pts',(161.1161521828,-0.207573909553045,124.891252836156));
#142697=CARTESIAN_POINT('Ctrl Pts',(161.108754693464,-0.365095836063884,
124.896782490499));
#142698=CARTESIAN_POINT('Ctrl Pts',(161.101357204127,-0.522368924573997,
124.908609953116));
#142699=CARTESIAN_POINT('Ctrl Pts',(161.093959714791,-0.67885524483256,
124.926683685388));
#142700=CARTESIAN_POINT('Ctrl Pts',(161.086559632276,-0.835396421127937,
124.944763753378));
#142701=CARTESIAN_POINT('Ctrl Pts',(161.079159549761,-0.991149909453824,
124.969094407738));
#142702=CARTESIAN_POINT('Ctrl Pts',(161.071759467246,-1.14558565843546,
124.99957258856));
#142703=CARTESIAN_POINT('Ctrl Pts',(161.064351247579,-1.30019122539966,
125.030084283276));
#142704=CARTESIAN_POINT('Ctrl Pts',(161.056943027913,-1.45347579283293,
125.066756931971));
#142705=CARTESIAN_POINT('Ctrl Pts',(161.049534808246,-1.60492149800979,
125.109436777186));
#142706=CARTESIAN_POINT('Ctrl Pts',(161.042122028944,-1.75646041549145,
125.152142891134));
#142707=CARTESIAN_POINT('Ctrl Pts',(161.034709249642,-1.9061578613372,125.200863453733));
#142708=CARTESIAN_POINT('Ctrl Pts',(161.02729647034,-2.05351426610689,125.255395874355));
#142709=CARTESIAN_POINT('Ctrl Pts',(161.019873099311,-2.20108122061784,
125.310006213458));
#142710=CARTESIAN_POINT('Ctrl Pts',(161.012449728283,-2.34630010963088,
125.370444852988));
#142711=CARTESIAN_POINT('Ctrl Pts',(161.005026357254,-2.48869359520285,
125.436462076079));
#142712=CARTESIAN_POINT('Ctrl Pts',(161.001090307813,-2.56419403793659,
125.471465991823));
#142713=CARTESIAN_POINT('Ctrl Pts',(160.997154258372,-2.63890059475449,
125.508037493488));
#142714=CARTESIAN_POINT('Ctrl Pts',(160.993218208932,-2.71274535513869,
125.546134376648));
#142715=CARTESIAN_POINT('Ctrl Pts',(160.985794942526,-2.85201426860962,
125.617983909328));
#142716=CARTESIAN_POINT('Ctrl Pts',(160.978371676121,-2.9886373006023,125.695478904593));
#142717=CARTESIAN_POINT('Ctrl Pts',(160.970948409715,-3.12212392676529,
125.778400734278));
#142718=CARTESIAN_POINT('Ctrl Pts',(160.963533916994,-3.25545278282157,
125.861224557247));
#142719=CARTESIAN_POINT('Ctrl Pts',(160.956119424273,-3.3856522977949,125.949462252342));
#142720=CARTESIAN_POINT('Ctrl Pts',(160.948704931552,-3.51225442648564,
126.042848315142));
#142721=CARTESIAN_POINT('Ctrl Pts',(160.941297585199,-3.63873453127822,
126.136144368939));
#142722=CARTESIAN_POINT('Ctrl Pts',(160.933890238845,-3.76162385409736,
126.234578691589));
#142723=CARTESIAN_POINT('Ctrl Pts',(160.926482892491,-3.88048145341341,
126.33784136291));
#142724=CARTESIAN_POINT('Ctrl Pts',(160.919081070816,-3.99925040424752,
126.441027017035));
#142725=CARTESIAN_POINT('Ctrl Pts',(160.91167924914,-4.11399333835672,126.549033605654));
#142726=CARTESIAN_POINT('Ctrl Pts',(160.904277427465,-4.22430076618984,
126.661509715196));
#142727=CARTESIAN_POINT('Ctrl Pts',(160.896879513154,-4.33454996359047,
126.773926449476));
#142728=CARTESIAN_POINT('Ctrl Pts',(160.889481598842,-4.44036805714527,
126.890807739926));
#142729=CARTESIAN_POINT('Ctrl Pts',(160.882083684531,-4.5413810352156,127.011764032707));
#142730=CARTESIAN_POINT('Ctrl Pts',(160.874686999619,-4.64237722676158,
127.132700224747));
#142731=CARTESIAN_POINT('Ctrl Pts',(160.867290314706,-4.73856964860784,
127.25770978885));
#142732=CARTESIAN_POINT('Ctrl Pts',(160.859893629794,-4.82962328634955,
127.386368593811));
#142733=CARTESIAN_POINT('Ctrl Pts',(160.852497272859,-4.92067288667764,
127.515021693907));
#142734=CARTESIAN_POINT('Ctrl Pts',(160.845100915923,-5.00658394031519,
127.647323408416));
#142735=CARTESIAN_POINT('Ctrl Pts',(160.837704558988,-5.08706381280048,
127.782819234928));
#142736=CARTESIAN_POINT('Ctrl Pts',(160.830307069651,-5.16755600695972,
127.918335806196));
#142737=CARTESIAN_POINT('Ctrl Pts',(160.822909580314,-5.24261517363796,
128.057047142211));
#142738=CARTESIAN_POINT('Ctrl Pts',(160.815512090978,-5.31199390929384,
128.198472809136));
#142739=CARTESIAN_POINT('Ctrl Pts',(160.808112008463,-5.38139696555798,
128.339948052609));
#142740=CARTESIAN_POINT('Ctrl Pts',(160.800711925948,-5.4451154618958,128.484139186497));
#142741=CARTESIAN_POINT('Ctrl Pts',(160.793311843433,-5.50294959981077,
128.630544557168));
#142742=CARTESIAN_POINT('Ctrl Pts',(160.785903623766,-5.56084733230582,
128.777110915596));
#142743=CARTESIAN_POINT('Ctrl Pts',(160.7784954041,-5.61284764721661,128.925896025821));
#142744=CARTESIAN_POINT('Ctrl Pts',(160.771087184433,-5.65879998759627,
129.076381085604));
#142745=CARTESIAN_POINT('Ctrl Pts',(160.763674405131,-5.70478061087473,
129.22695876643));
#142746=CARTESIAN_POINT('Ctrl Pts',(160.756261625829,-5.74470574776557,
129.379238121422));
#142747=CARTESIAN_POINT('Ctrl Pts',(160.748848846527,-5.77847581401576,
129.53268934348));
#142748=CARTESIAN_POINT('Ctrl Pts',(160.741425475498,-5.81229413252025,
129.68635982384));
#142749=CARTESIAN_POINT('Ctrl Pts',(160.734002104469,-5.83993975005202,
129.841205148942));
#142750=CARTESIAN_POINT('Ctrl Pts',(160.72657873344,-5.86136474766689,129.996688742788));
#142751=CARTESIAN_POINT('Ctrl Pts',(160.722642683999,-5.87272479548808,
130.079129875023));
#142752=CARTESIAN_POINT('Ctrl Pts',(160.718706634559,-5.88233687414806,
130.161750407033));
#142753=CARTESIAN_POINT('Ctrl Pts',(160.714770585118,-5.89019978413138,
130.244470391255));
#142754=CARTESIAN_POINT('Ctrl Pts',(160.705972120815,-5.90777617229443,
130.429378848125));
#142755=CARTESIAN_POINT('Ctrl Pts',(160.697173656513,-5.91664728421935,
130.615127793757));
#142756=CARTESIAN_POINT('Ctrl Pts',(160.688375192211,-5.91674911325059,
130.801121273744));
#142757=CARTESIAN_POINT('',(158.938376379574,-5.91250676172561,130.8007115422));
#142758=CARTESIAN_POINT('Ctrl Pts',(160.688372676203,-5.9243338325154,130.801170376087));
#142759=CARTESIAN_POINT('Ctrl Pts',(160.60435610457,-5.91260203390904,132.579506857946));
#142760=CARTESIAN_POINT('Ctrl Pts',(160.427523658333,-4.11390117656668,
136.342953783282));
#142761=CARTESIAN_POINT('Ctrl Pts',(160.157875337493,2.29362448039243,137.416232309703));
#142762=CARTESIAN_POINT('Ctrl Pts',(159.879427713679,6.80251496907736,132.448547536935));
#142763=CARTESIAN_POINT('Ctrl Pts',(159.600980089867,5.0602265225104,125.969935308263));
#142764=CARTESIAN_POINT('Ctrl Pts',(159.322532466054,-1.33216289243681,
123.933923764033));
#142765=CARTESIAN_POINT('Ctrl Pts',(159.101664869801,-5.43163117945458,
127.326948799706));
#142766=CARTESIAN_POINT('Ctrl Pts',(158.973613148154,-5.91338609833529,
130.049979290673));
#142767=CARTESIAN_POINT('Ctrl Pts',(158.93837730111,-5.90921436344405,130.800693926467));
#142768=CARTESIAN_POINT('',(157.188373977522,-5.91343480873076,130.808965839466));
#142769=CARTESIAN_POINT('Ctrl Pts',(158.938375192211,-5.91674888869566,
130.800734239386));
#142770=CARTESIAN_POINT('Ctrl Pts',(158.930915454658,-5.91684642256871,
130.959869168598));
#142771=CARTESIAN_POINT('Ctrl Pts',(158.923455717105,-5.91051955951184,
131.119024896707));
#142772=CARTESIAN_POINT('Ctrl Pts',(158.915995979553,-5.89778993384828,
131.27765171055));
#142773=CARTESIAN_POINT('Ctrl Pts',(158.908535435224,-5.88505893146643,
131.436295679998));
#142774=CARTESIAN_POINT('Ctrl Pts',(158.901074890895,-5.86592381531385,
131.594410257938));
#142775=CARTESIAN_POINT('Ctrl Pts',(158.893614346566,-5.84045817256563,
131.751450316069));
#142776=CARTESIAN_POINT('Ctrl Pts',(158.886151617577,-5.81498507275002,
131.908536360014));
#142777=CARTESIAN_POINT('Ctrl Pts',(158.878688888587,-5.78317781144301,
132.064546897695));
#142778=CARTESIAN_POINT('Ctrl Pts',(158.871226159598,-5.74516121293526,
132.218946493321));
#142779=CARTESIAN_POINT('Ctrl Pts',(158.863759867021,-5.70712646081542,
132.373419817541));
#142780=CARTESIAN_POINT('Ctrl Pts',(158.856293574443,-5.66287655157163,
132.526280313815));
#142781=CARTESIAN_POINT('Ctrl Pts',(158.848827281866,-5.61258631675067,
132.677007247212));
#142782=CARTESIAN_POINT('Ctrl Pts',(158.841351300495,-5.56223082172863,
132.827929774644));
#142783=CARTESIAN_POINT('Ctrl Pts',(158.833875319123,-5.50581945828213,
132.976712862554));
#142784=CARTESIAN_POINT('Ctrl Pts',(158.826399337751,-5.44357577420364,
133.122854385727));
#142785=CARTESIAN_POINT('Ctrl Pts',(158.818918114411,-5.38128844643688,
133.26909837962));
#142786=CARTESIAN_POINT('Ctrl Pts',(158.811436891071,-5.31316080199116,
133.412696788273));
#142787=CARTESIAN_POINT('Ctrl Pts',(158.803955667732,-5.23946244456385,
133.553171970588));
#142788=CARTESIAN_POINT('Ctrl Pts',(158.796462266502,-5.16564412139993,
133.693875817549));
#142789=CARTESIAN_POINT('Ctrl Pts',(158.788968865273,-5.08623714866151,
133.831445965049));
#142790=CARTESIAN_POINT('Ctrl Pts',(158.781475464043,-5.0015551708291,133.965432656551));
#142791=CARTESIAN_POINT('Ctrl Pts',(158.776196048838,-4.94189316853013,
134.059831895929));
#142792=CARTESIAN_POINT('Ctrl Pts',(158.770916633633,-4.87961366328841,
134.1524530099));
#142793=CARTESIAN_POINT('Ctrl Pts',(158.765637218427,-4.81483811113869,
134.24314885269));
#142794=CARTESIAN_POINT('Ctrl Pts',(158.758213952022,-4.72375867118721,
134.370674227512));
#142795=CARTESIAN_POINT('Ctrl Pts',(158.750790685616,-4.62747157055039,
134.494771453157));
#142796=CARTESIAN_POINT('Ctrl Pts',(158.743367419211,-4.52626352373467,
134.614986429189));
#142797=CARTESIAN_POINT('Ctrl Pts',(158.73595292649,-4.42517509642523,134.735059321103));
#142798=CARTESIAN_POINT('Ctrl Pts',(158.728538433769,-4.31917753808615,
134.85125881405));
#142799=CARTESIAN_POINT('Ctrl Pts',(158.721123941048,-4.20860073119569,
134.963159776924));
#142800=CARTESIAN_POINT('Ctrl Pts',(158.713716594694,-4.09813050239493,
135.074952885437));
#142801=CARTESIAN_POINT('Ctrl Pts',(158.70630924834,-3.98309007237963,135.182455448199));
#142802=CARTESIAN_POINT('Ctrl Pts',(158.698901901987,-3.86384939333115,
135.285275527286));
#142803=CARTESIAN_POINT('Ctrl Pts',(158.691500080311,-3.74469764847946,
135.38801891928));
#142804=CARTESIAN_POINT('Ctrl Pts',(158.684098258636,-3.62135217372323,
135.486086538658));
#142805=CARTESIAN_POINT('Ctrl Pts',(158.67669643696,-3.49421947519282,135.579123524945));
#142806=CARTESIAN_POINT('Ctrl Pts',(158.669298522649,-3.36715388902532,
135.672111397731));
#142807=CARTESIAN_POINT('Ctrl Pts',(158.661900608338,-3.23630536116322,
135.760073706346));
#142808=CARTESIAN_POINT('Ctrl Pts',(158.654502694027,-3.10211305586488,
135.842696171212));
#142809=CARTESIAN_POINT('Ctrl Pts',(158.647106009114,-2.96794305089252,
135.925304905723));
#142810=CARTESIAN_POINT('Ctrl Pts',(158.639709324202,-2.8304306889006,136.002575362156));
#142811=CARTESIAN_POINT('Ctrl Pts',(158.63231263929,-2.69004376149368,136.074236813811));
#142812=CARTESIAN_POINT('Ctrl Pts',(158.624916282355,-2.54966305899033,
136.145895087922));
#142813=CARTESIAN_POINT('Ctrl Pts',(158.617519925419,-2.40640837699323,
136.211944682055));
#142814=CARTESIAN_POINT('Ctrl Pts',(158.610123568484,-2.26077148665801,
136.272161166929));
#142815=CARTESIAN_POINT('Ctrl Pts',(158.602726079147,-2.11511229894314,
136.332386871101));
#142816=CARTESIAN_POINT('Ctrl Pts',(158.595328589811,-1.96707052167487,
136.38677754516));
#142817=CARTESIAN_POINT('Ctrl Pts',(158.587931100474,-1.81715710280992,
136.435157242042));
#142818=CARTESIAN_POINT('Ctrl Pts',(158.580531017959,-1.66719113202903,
136.483553898351));
#142819=CARTESIAN_POINT('Ctrl Pts',(158.573130935444,-1.51535256839407,
136.52593526761));
#142820=CARTESIAN_POINT('Ctrl Pts',(158.565730852929,-1.36216653326101,
136.562175558858));
#142821=CARTESIAN_POINT('Ctrl Pts',(158.558322633263,-1.2088120543336,136.598455700031));
#142822=CARTESIAN_POINT('Ctrl Pts',(158.550914413597,-1.0541075083823,136.628581191521));
#142823=CARTESIAN_POINT('Ctrl Pts',(158.54350619393,-0.898587926369288,
136.652477434207));
#142824=CARTESIAN_POINT('Ctrl Pts',(158.536093414628,-0.742972624648474,
136.676388384633));
#142825=CARTESIAN_POINT('Ctrl Pts',(158.528680635326,-0.586541657361018,
136.69406240472));
#142826=CARTESIAN_POINT('Ctrl Pts',(158.521267856024,-0.429833636567998,
136.705476919366));
#142827=CARTESIAN_POINT('Ctrl Pts',(158.513844484995,-0.272901704006047,
136.716907743607));
#142828=CARTESIAN_POINT('Ctrl Pts',(158.506421113967,-0.115692299412364,
136.722061187283));
#142829=CARTESIAN_POINT('Ctrl Pts',(158.498997742938,0.0412566755591604,
136.720966777285));
#142830=CARTESIAN_POINT('Ctrl Pts',(158.495061693497,0.12447478803224,136.720386494843));
#142831=CARTESIAN_POINT('Ctrl Pts',(158.491125644056,0.207619769152417,
136.718050583662));
#142832=CARTESIAN_POINT('Ctrl Pts',(158.487189594615,0.290612325724202,
136.713969321925));
#142833=CARTESIAN_POINT('Ctrl Pts',(158.47976632821,0.447133697301818,136.706272189662));
#142834=CARTESIAN_POINT('Ctrl Pts',(158.472343061804,0.603585737690694,
136.692340706608));
#142835=CARTESIAN_POINT('Ctrl Pts',(158.464919795399,0.759431423139469,
136.672170641421));
#142836=CARTESIAN_POINT('Ctrl Pts',(158.457505302678,0.915092911930112,
136.652024415575));
#142837=CARTESIAN_POINT('Ctrl Pts',(158.450090809957,1.07014910570366,136.625654332006));
#142838=CARTESIAN_POINT('Ctrl Pts',(158.442676317236,1.22406402008241,136.593108136437));
#142839=CARTESIAN_POINT('Ctrl Pts',(158.435268970882,1.37783058547173,136.560593310118));
#142840=CARTESIAN_POINT('Ctrl Pts',(158.427861624529,1.53045769859553,136.5219142993));
#142841=CARTESIAN_POINT('Ctrl Pts',(158.420454278175,1.68141564278876,136.477170503212));
#142842=CARTESIAN_POINT('Ctrl Pts',(158.413052456499,1.83226099685249,136.432460078735));
#142843=CARTESIAN_POINT('Ctrl Pts',(158.405650634824,1.98143930444071,136.381693981206));
#142844=CARTESIAN_POINT('Ctrl Pts',(158.398248813149,2.12843228489295,136.32502240499));
#142845=CARTESIAN_POINT('Ctrl Pts',(158.390850898837,2.27534766889573,136.268380745258));
#142846=CARTESIAN_POINT('Ctrl Pts',(158.383452984526,2.42007967582008,136.20583994935));
#142847=CARTESIAN_POINT('Ctrl Pts',(158.376055070214,2.56212651434601,136.137599622803));
#142848=CARTESIAN_POINT('Ctrl Pts',(158.368658385302,2.70414974726347,136.069370636562));
#142849=CARTESIAN_POINT('Ctrl Pts',(158.36126170039,2.84348836125589,135.995444161003));
#142850=CARTESIAN_POINT('Ctrl Pts',(158.353865015478,2.97966173349597,135.916067428059));
#142851=CARTESIAN_POINT('Ctrl Pts',(158.346468658543,3.11582906766606,135.836694214762));
#142852=CARTESIAN_POINT('Ctrl Pts',(158.339072301607,3.24883111664123,135.751871412594));
#142853=CARTESIAN_POINT('Ctrl Pts',(158.331675944672,3.37821324739038,135.661891453048));
#142854=CARTESIAN_POINT('Ctrl Pts',(158.324278455335,3.50761518687414,135.57189771734));
#142855=CARTESIAN_POINT('Ctrl Pts',(158.316880965998,3.63339579811905,135.476745465258));
#142856=CARTESIAN_POINT('Ctrl Pts',(158.309483476662,3.75513087202569,135.376769468102));
#142857=CARTESIAN_POINT('Ctrl Pts',(158.302083394147,3.87690861997383,135.276758424516));
#142858=CARTESIAN_POINT('Ctrl Pts',(158.294683311632,3.99463771874266,135.171920505944));
#142859=CARTESIAN_POINT('Ctrl Pts',(158.287283229117,4.10792849591445,135.062629518769));
#142860=CARTESIAN_POINT('Ctrl Pts',(158.279875009451,4.22134384794215,134.953218354919));
#142861=CARTESIAN_POINT('Ctrl Pts',(158.272466789784,4.33031086308549,134.839344602955));
#142862=CARTESIAN_POINT('Ctrl Pts',(158.265058570118,4.43447758168943,134.721418076934));
#142863=CARTESIAN_POINT('Ctrl Pts',(158.257645790816,4.53870841317052,134.603418969105));
#142864=CARTESIAN_POINT('Ctrl Pts',(158.250233011514,4.63813282568165,134.481362405539));
#142865=CARTESIAN_POINT('Ctrl Pts',(158.242820232211,4.73244069317407,134.355689333426));
#142866=CARTESIAN_POINT('Ctrl Pts',(158.235396861183,4.82688331217036,134.229836693733));
#142867=CARTESIAN_POINT('Ctrl Pts',(158.227973490154,4.91619457352484,134.100357531433));
#142868=CARTESIAN_POINT('Ctrl Pts',(158.220550119125,5.00010857006147,133.967720358427));
#142869=CARTESIAN_POINT('Ctrl Pts',(158.216614069684,5.04460178451412,133.897392946713));
#142870=CARTESIAN_POINT('Ctrl Pts',(158.212678020244,5.0875784095031,133.82617810226));
#142871=CARTESIAN_POINT('Ctrl Pts',(158.208741970803,5.12900423244793,133.754148092289));
#142872=CARTESIAN_POINT('Ctrl Pts',(158.201318704397,5.20713204166579,133.618301741464));
#142873=CARTESIAN_POINT('Ctrl Pts',(158.193895437992,5.27997723979626,133.479143902046));
#142874=CARTESIAN_POINT('Ctrl Pts',(158.186472171586,5.34724599243546,133.337124100184));
#142875=CARTESIAN_POINT('Ctrl Pts',(158.179057678865,5.41443523899529,133.195272153933));
#142876=CARTESIAN_POINT('Ctrl Pts',(158.171643186144,5.4760610010417,133.050565312398));
#142877=CARTESIAN_POINT('Ctrl Pts',(158.164228693423,5.53187373575638,132.903480322144));
#142878=CARTESIAN_POINT('Ctrl Pts',(158.15682134707,5.58763267605594,132.756537097942));
#142879=CARTESIAN_POINT('Ctrl Pts',(158.149414000716,5.63758961157662,132.607220634913));
#142880=CARTESIAN_POINT('Ctrl Pts',(158.142006654362,5.68154184490677,132.456030326398));
#142881=CARTESIAN_POINT('Ctrl Pts',(158.134604832687,5.72546129700346,132.304952781318));
#142882=CARTESIAN_POINT('Ctrl Pts',(158.127203011011,5.76338486051576,132.152004530449));
#142883=CARTESIAN_POINT('Ctrl Pts',(158.119801189336,5.7951587548607,131.997702801712));
#142884=CARTESIAN_POINT('Ctrl Pts',(158.112403275024,5.82691587601384,131.843482527657));
#142885=CARTESIAN_POINT('Ctrl Pts',(158.105005360713,5.85252971818674,131.687910563377));
#142886=CARTESIAN_POINT('Ctrl Pts',(158.097607446402,5.87189698470698,131.53151697179));
#142887=CARTESIAN_POINT('Ctrl Pts',(158.09021076149,5.89126103273897,131.375149369981));
#142888=CARTESIAN_POINT('Ctrl Pts',(158.082814076577,5.90438051954253,131.21796078196));
#142889=CARTESIAN_POINT('Ctrl Pts',(158.075417391665,5.91120365996612,131.060489204223));
#142890=CARTESIAN_POINT('Ctrl Pts',(158.06802103473,5.91802649784452,130.903024608941));
#142891=CARTESIAN_POINT('Ctrl Pts',(158.060624677794,5.91855352830065,130.745277421841));
#142892=CARTESIAN_POINT('Ctrl Pts',(158.053228320859,5.91278504197351,130.587788204932));
#142893=CARTESIAN_POINT('Ctrl Pts',(158.045830831522,5.90701567247639,130.430274876021));
#142894=CARTESIAN_POINT('Ctrl Pts',(158.038433342186,5.89494888068794,130.273019969015));
#142895=CARTESIAN_POINT('Ctrl Pts',(158.031035852849,5.87663702380465,130.116561335109));
#142896=CARTESIAN_POINT('Ctrl Pts',(158.023635770334,5.85831874772836,129.960047854871));
#142897=CARTESIAN_POINT('Ctrl Pts',(158.016235687819,5.83375109124769,129.80433157402));
#142898=CARTESIAN_POINT('Ctrl Pts',(158.008835605304,5.80303792079846,129.649942386475));
#142899=CARTESIAN_POINT('Ctrl Pts',(158.001427385638,5.77229097806086,129.495383432147));
#142900=CARTESIAN_POINT('Ctrl Pts',(157.994019165971,5.73538509881401,129.342154851743));
#142901=CARTESIAN_POINT('Ctrl Pts',(157.986610946305,5.69247482843885,129.190774273397));
#142902=CARTESIAN_POINT('Ctrl Pts',(157.979198167002,5.6495381475081,129.03930052283));
#142903=CARTESIAN_POINT('Ctrl Pts',(157.9717853877,5.60058982729749,128.889677394733));
#142904=CARTESIAN_POINT('Ctrl Pts',(157.964372608398,5.54583321845891,128.74240414966));
#142905=CARTESIAN_POINT('Ctrl Pts',(157.95694923737,5.49099837081001,128.594920473669));
#142906=CARTESIAN_POINT('Ctrl Pts',(157.949525866341,5.43033880283783,128.449793730138));
#142907=CARTESIAN_POINT('Ctrl Pts',(157.942102495312,5.36410495754869,128.307500876431));
#142908=CARTESIAN_POINT('Ctrl Pts',(157.938166445871,5.32898618351717,128.232053791125));
#142909=CARTESIAN_POINT('Ctrl Pts',(157.93423039643,5.29230103353882,128.157402976415));
#142910=CARTESIAN_POINT('Ctrl Pts',(157.93029434699,5.25409181533825,128.083616278512));
#142911=CARTESIAN_POINT('Ctrl Pts',(157.922871080584,5.18203042228066,127.94445686907));
#142912=CARTESIAN_POINT('Ctrl Pts',(157.915447814179,5.10432759975642,127.807951929475));
#142913=CARTESIAN_POINT('Ctrl Pts',(157.908024547773,5.02120272217172,127.674591650796));
#142914=CARTESIAN_POINT('Ctrl Pts',(157.900610055052,4.9381760912894,127.541388992892));
#142915=CARTESIAN_POINT('Ctrl Pts',(157.893195562331,4.84974035687387,127.411323911439));
#142916=CARTESIAN_POINT('Ctrl Pts',(157.88578106961,4.75616173532534,127.284864047042));
#142917=CARTESIAN_POINT('Ctrl Pts',(157.878373723257,4.66267330837544,127.158526069424));
#142918=CARTESIAN_POINT('Ctrl Pts',(157.870966376903,4.56405208308138,127.035786689192));
#142919=CARTESIAN_POINT('Ctrl Pts',(157.863559030549,4.4606086503039,126.917086375718));
#142920=CARTESIAN_POINT('Ctrl Pts',(157.856157208874,4.35724236954085,126.798474593416));
#142921=CARTESIAN_POINT('Ctrl Pts',(157.848755387198,4.24906128677821,126.683896159819));
#142922=CARTESIAN_POINT('Ctrl Pts',(157.841353565523,4.13641743835362,126.573760029212));
#142923=CARTESIAN_POINT('Ctrl Pts',(157.833955651211,4.02383305374083,126.463682038611));
#142924=CARTESIAN_POINT('Ctrl Pts',(157.8265577369,3.90679086151295,126.35804194102));
#142925=CARTESIAN_POINT('Ctrl Pts',(157.819159822589,3.78568098424077,126.257213154809));
#142926=CARTESIAN_POINT('Ctrl Pts',(157.811763137677,3.66459123323212,126.156401124512));
#142927=CARTESIAN_POINT('Ctrl Pts',(157.804366452764,3.53943542539678,126.060399057331));
#142928=CARTESIAN_POINT('Ctrl Pts',(157.796969767852,3.41063820128344,125.969541321827));
#142929=CARTESIAN_POINT('Ctrl Pts',(157.789573410917,3.2818466881739,125.878687615051));
#142930=CARTESIAN_POINT('Ctrl Pts',(157.782177053981,3.14941438486853,125.792978001585));
#142931=CARTESIAN_POINT('Ctrl Pts',(157.774780697046,3.01379623859334,125.712704423876));
#142932=CARTESIAN_POINT('Ctrl Pts',(157.767383207709,2.87815732883389,125.632418556078));
#142933=CARTESIAN_POINT('Ctrl Pts',(157.759985718373,2.73933192617019,125.557570571358));
#142934=CARTESIAN_POINT('Ctrl Pts',(157.752588229036,2.59780084038886,125.488407141831));
#142935=CARTESIAN_POINT('Ctrl Pts',(157.745188146521,2.45622014110446,125.419219467172));
#142936=CARTESIAN_POINT('Ctrl Pts',(157.737788064006,2.31193220548298,125.355720478979));
#142937=CARTESIAN_POINT('Ctrl Pts',(157.730387981491,2.16543899063345,125.298109212087));
#142938=CARTESIAN_POINT('Ctrl Pts',(157.722979761825,2.01878469143474,125.240434595684));
#142939=CARTESIAN_POINT('Ctrl Pts',(157.715571542158,1.86992061787313,125.188660766598));
#142940=CARTESIAN_POINT('Ctrl Pts',(157.708163322492,1.71936580071042,125.142937492075));
#142941=CARTESIAN_POINT('Ctrl Pts',(157.70075054319,1.56871831956924,125.097186075638));
#142942=CARTESIAN_POINT('Ctrl Pts',(157.693337763888,1.41637838165166,125.057492728236));
#142943=CARTESIAN_POINT('Ctrl Pts',(157.685924984585,1.26287594499535,125.023956227729));
#142944=CARTESIAN_POINT('Ctrl Pts',(157.678501613557,1.1091541768597,124.990371808697));
#142945=CARTESIAN_POINT('Ctrl Pts',(157.671078242528,0.95426695914299,124.962961871404));
#142946=CARTESIAN_POINT('Ctrl Pts',(157.663654871499,0.798750940145906,
124.94177351816));
#142947=CARTESIAN_POINT('Ctrl Pts',(157.659718822058,0.716292615317222,
124.930538944863));
#142948=CARTESIAN_POINT('Ctrl Pts',(157.655782772618,0.633657551031939,
124.921052611719));
#142949=CARTESIAN_POINT('Ctrl Pts',(157.651846723177,0.550925696587703,
124.913315596575));
#142950=CARTESIAN_POINT('Ctrl Pts',(157.644423456771,0.394896001079837,
124.898723827478));
#142951=CARTESIAN_POINT('Ctrl Pts',(157.637000190366,0.238050255806775,
124.890313158557));
#142952=CARTESIAN_POINT('Ctrl Pts',(157.62957692396,0.0809194496225133,
124.888163984156));
#142953=CARTESIAN_POINT('Ctrl Pts',(157.622162431239,-0.0760256409977402,
124.886017349901));
#142954=CARTESIAN_POINT('Ctrl Pts',(157.614747938518,-0.233254752273388,
124.890117484353));
#142955=CARTESIAN_POINT('Ctrl Pts',(157.607333445797,-0.390230548452075,
124.900493183286));
#142956=CARTESIAN_POINT('Ctrl Pts',(157.599926099444,-0.547055045447757,
124.910858881729));
#142957=CARTESIAN_POINT('Ctrl Pts',(157.59251875309,-0.703626343425722,
124.927488078575));
#142958=CARTESIAN_POINT('Ctrl Pts',(157.585111406736,-0.859405981080647,
124.950357549393));
#142959=CARTESIAN_POINT('Ctrl Pts',(157.577709585061,-1.01506943240597,
124.973209963296));
#142960=CARTESIAN_POINT('Ctrl Pts',(157.570307763385,-1.16994203132464,
125.002293329978));
#142961=CARTESIAN_POINT('Ctrl Pts',(157.56290594171,-1.32348942877478,125.03753252108));
#142962=CARTESIAN_POINT('Ctrl Pts',(157.555508027398,-1.47695576974743,
125.072753109686));
#142963=CARTESIAN_POINT('Ctrl Pts',(157.548110113087,-1.62909793954779,
125.114122967664));
#142964=CARTESIAN_POINT('Ctrl Pts',(157.540712198776,-1.7793908999459,125.161515715596));
#142965=CARTESIAN_POINT('Ctrl Pts',(157.533315513864,-1.92965888438154,
125.208900587713));
#142966=CARTESIAN_POINT('Ctrl Pts',(157.525918828951,-2.07807791365631,
125.26230625115));
#142967=CARTESIAN_POINT('Ctrl Pts',(157.518522144039,-2.22413714544071,
125.32155617816));
#142968=CARTESIAN_POINT('Ctrl Pts',(157.511125787104,-2.37018990080557,
125.380803477966));
#142969=CARTESIAN_POINT('Ctrl Pts',(157.503729430168,-2.51388272081235,
125.445894385763));
#142970=CARTESIAN_POINT('Ctrl Pts',(157.496333073233,-2.65472407592328,
125.516603943587));
#142971=CARTESIAN_POINT('Ctrl Pts',(157.488935583896,-2.79558699420534,
125.587324327225));
#142972=CARTESIAN_POINT('Ctrl Pts',(157.48153809456,-2.9335972446944,125.66366490622));
#142973=CARTESIAN_POINT('Ctrl Pts',(157.474140605223,-3.06828740571877,
125.745354493987));
#142974=CARTESIAN_POINT('Ctrl Pts',(157.466740522708,-3.2030247821701,125.827072717912));
#142975=CARTESIAN_POINT('Ctrl Pts',(157.459340440193,-3.33443943295326,
125.91414349043));
#142976=CARTESIAN_POINT('Ctrl Pts',(157.451940357678,-3.46209258434725,
126.006252083997));
#142977=CARTESIAN_POINT('Ctrl Pts',(157.444532138012,-3.58988610350434,
126.098461960432));
#142978=CARTESIAN_POINT('Ctrl Pts',(157.437123918345,-3.71390956019198,
126.195720502302));
#142979=CARTESIAN_POINT('Ctrl Pts',(157.429715698679,-3.83375640218153,
126.297671987182));
#142980=CARTESIAN_POINT('Ctrl Pts',(157.422302919377,-3.95367700790322,
126.3996862215));
#142981=CARTESIAN_POINT('Ctrl Pts',(157.414890140075,-4.06941560280145,
126.506398901927));
#142982=CARTESIAN_POINT('Ctrl Pts',(157.407477360772,-4.18060262699952,
126.617417551602));
#142983=CARTESIAN_POINT('Ctrl Pts',(157.400053989744,-4.29194852043124,
126.728594829929));
#142984=CARTESIAN_POINT('Ctrl Pts',(157.392630618715,-4.39872960147221,
126.844090092197));
#142985=CARTESIAN_POINT('Ctrl Pts',(157.385207247686,-4.50061617009897,
126.963477300939));
#142986=CARTESIAN_POINT('Ctrl Pts',(157.381271198245,-4.55463887352011,
127.026779263672));
#142987=CARTESIAN_POINT('Ctrl Pts',(157.377335148805,-4.60728626498116,
127.091174888821));
#142988=CARTESIAN_POINT('Ctrl Pts',(157.373399099364,-4.65851422311026,
127.15659749538));
#142989=CARTESIAN_POINT('Ctrl Pts',(157.365689769899,-4.75885168404861,
127.284737254798));
#142990=CARTESIAN_POINT('Ctrl Pts',(157.357980440434,-4.85406153169077,
127.41722862095));
#142991=CARTESIAN_POINT('Ctrl Pts',(157.35027111097,-4.94374546843798,127.553620500947));
#142992=CARTESIAN_POINT('Ctrl Pts',(157.342858577229,-5.02997673020698,
127.684761531701));
#142993=CARTESIAN_POINT('Ctrl Pts',(157.335446043488,-5.11109935062457,
127.819508015262));
#142994=CARTESIAN_POINT('Ctrl Pts',(157.328033509748,-5.18679860691237,
127.957423531181));
#142995=CARTESIAN_POINT('Ctrl Pts',(157.320628026987,-5.26242585625219,
128.095207858554));
#142996=CARTESIAN_POINT('Ctrl Pts',(157.313222544226,-5.33263983071511,
128.236154894347));
#142997=CARTESIAN_POINT('Ctrl Pts',(157.305817061465,-5.39716886407673,
128.37979904583));
#142998=CARTESIAN_POINT('Ctrl Pts',(157.298417163401,-5.4616492341606,128.523334870953));
#142999=CARTESIAN_POINT('Ctrl Pts',(157.291017265337,-5.52045304536111,
128.669563424275));
#143000=CARTESIAN_POINT('Ctrl Pts',(157.283617367272,-5.57335445625534,
128.817994420854));
#143001=CARTESIAN_POINT('Ctrl Pts',(157.276221591408,-5.62622639779663,
128.966342732202));
#143002=CARTESIAN_POINT('Ctrl Pts',(157.268825815544,-5.67320236126874,
129.116890693481));
#143003=CARTESIAN_POINT('Ctrl Pts',(157.26143003968,-5.71410461872065,129.269128072049));
#143004=CARTESIAN_POINT('Ctrl Pts',(157.254036397143,-5.75499507783323,
129.421321537436));
#143005=CARTESIAN_POINT('Ctrl Pts',(157.246642754605,-5.78981522071373,
129.575203090644));
#143006=CARTESIAN_POINT('Ctrl Pts',(157.239249112068,-5.81843719116697,
129.730247394975));
#143007=CARTESIAN_POINT('Ctrl Pts',(157.231856662052,-5.84705454517623,
129.885266692176));
#143008=CARTESIAN_POINT('Ctrl Pts',(157.224464212037,-5.8694756532606,130.041447999862));
#143009=CARTESIAN_POINT('Ctrl Pts',(157.217071762022,-5.8856238307037,130.198256100215));
#143010=CARTESIAN_POINT('Ctrl Pts',(157.209677888262,-5.90177511819504,
130.355094400928));
#143011=CARTESIAN_POINT('Ctrl Pts',(157.202284014502,-5.91165102567913,
130.512559364308));
#143012=CARTESIAN_POINT('Ctrl Pts',(157.194890140743,-5.91522675507618,
130.670110855812));
#143013=CARTESIAN_POINT('Ctrl Pts',(157.192718491232,-5.91627698006614,
130.716385194614));
#143014=CARTESIAN_POINT('Ctrl Pts',(157.190546841722,-5.91678406166311,
130.762666987724));
#143015=CARTESIAN_POINT('Ctrl Pts',(157.188375192211,-5.91674822587776,
130.808942546454));
#143016=CARTESIAN_POINT('',(155.438375192211,-5.9258497230187,130.806193117355));
#143017=CARTESIAN_POINT('Ctrl Pts',(157.188373110924,-5.9110709125586,130.808982457434));
#143018=CARTESIAN_POINT('Ctrl Pts',(157.157232565799,-5.91582530741731,
131.471921867218));
#143019=CARTESIAN_POINT('Ctrl Pts',(157.033276146074,-5.5065273811508,134.105074895486));
#143020=CARTESIAN_POINT('Ctrl Pts',(156.816503851736,-1.63383274564036,
137.60936988204));
#143021=CARTESIAN_POINT('Ctrl Pts',(156.538056227926,4.84212051448032,135.857224108064));
#143022=CARTESIAN_POINT('Ctrl Pts',(156.259608604111,6.86840157253082,129.461743632418));
#143023=CARTESIAN_POINT('Ctrl Pts',(155.981160980299,2.58295712549506,124.300062575641));
#143024=CARTESIAN_POINT('Ctrl Pts',(155.707416509666,-3.96362314909615,
125.101740191743));
#143025=CARTESIAN_POINT('Ctrl Pts',(155.526487913636,-5.91829371355799,
128.942418927956));
#143026=CARTESIAN_POINT('Ctrl Pts',(155.438375192211,-5.9258497230187,130.806193117355));
#143027=CARTESIAN_POINT('',(153.688375192211,-5.91665636044548,130.798893010347));
#143028=CARTESIAN_POINT('Ctrl Pts',(155.438375192211,-5.9258497230187,130.806193117355));
#143029=CARTESIAN_POINT('Ctrl Pts',(155.433672039032,-5.92625303674393,
130.905674955648));
#143030=CARTESIAN_POINT('Ctrl Pts',(155.428968885853,-5.92396577613154,
131.005137856645));
#143031=CARTESIAN_POINT('Ctrl Pts',(155.331449858069,-5.81954753850361,
133.064593445196));
#143032=CARTESIAN_POINT('Ctrl Pts',(155.145818108861,-3.47980464159975,
136.876305955482));
#143033=CARTESIAN_POINT('Ctrl Pts',(154.867370485047,3.22758017148122,137.014053586386));
#143034=CARTESIAN_POINT('Ctrl Pts',(154.588922861235,6.96897648302375,131.44539673931));
#143035=CARTESIAN_POINT('Ctrl Pts',(154.310475237422,4.30622386010103,125.287659012708));
#143036=CARTESIAN_POINT('Ctrl Pts',(154.032027613609,-2.31373811952758,
124.199500555112));
#143037=CARTESIAN_POINT('Ctrl Pts',(153.824660931872,-5.66034222041055,
127.909258680071));
#143038=CARTESIAN_POINT('Ctrl Pts',(153.710110124739,-5.92092250522073,
130.337292720254));
#143039=CARTESIAN_POINT('Ctrl Pts',(153.688375192211,-5.91665636044548,
130.798893010347));
#143040=CARTESIAN_POINT('',(151.938375192211,-5.9069934382874,130.80498290727));
#143041=CARTESIAN_POINT('Ctrl Pts',(153.688375192211,-5.91665636044548,
130.798893010347));
#143042=CARTESIAN_POINT('Ctrl Pts',(153.617294250135,-5.90270455317563,
132.308489759256));
#143043=CARTESIAN_POINT('Ctrl Pts',(153.453397433455,-4.5460332507832,135.811571704644));
#143044=CARTESIAN_POINT('Ctrl Pts',(153.196684742169,1.35306796840206,137.670711002101));
#143045=CARTESIAN_POINT('Ctrl Pts',(152.918237118358,6.50822133110401,133.377416317647));
#143046=CARTESIAN_POINT('Ctrl Pts',(152.639789494545,5.68263723480749,126.719609145577));
#143047=CARTESIAN_POINT('Ctrl Pts',(152.361341870732,-0.365012868011487,
123.81548902506));
#143048=CARTESIAN_POINT('Ctrl Pts',(152.127537103287,-5.16140692478195,
126.769717825966));
#143049=CARTESIAN_POINT('Ctrl Pts',(151.986548210447,-5.90603325491028,
129.777671834643));
#143050=CARTESIAN_POINT('Ctrl Pts',(151.938375192211,-5.9069934382874,130.80498290727));
#143051=CARTESIAN_POINT('',(150.188375920137,-5.91832258703425,130.809599870259));
#143052=CARTESIAN_POINT('Ctrl Pts',(151.938375192211,-5.9069934382874,130.80498290727));
#143053=CARTESIAN_POINT('Ctrl Pts',(151.893732335843,-5.90788325856775,
131.75701170556));
#143054=CARTESIAN_POINT('Ctrl Pts',(151.756273604869,-5.24038079272229,
134.687203035383));
#143055=CARTESIAN_POINT('Ctrl Pts',(151.525998999293,-0.63042978355948,
137.774304578484));
#143056=CARTESIAN_POINT('Ctrl Pts',(151.247551375479,5.52324855627425,135.102184010395));
#143057=CARTESIAN_POINT('Ctrl Pts',(150.969103751667,6.60133129858417,128.480573704642));
#143058=CARTESIAN_POINT('Ctrl Pts',(150.690656127853,1.61311307045599,123.994410048561));
#143059=CARTESIAN_POINT('Ctrl Pts',(150.430413613649,-4.43442532867792,
125.650413545519));
#143060=CARTESIAN_POINT('Ctrl Pts',(150.262986974047,-5.90431344697162,
129.226604649882));
#143061=CARTESIAN_POINT('Ctrl Pts',(150.188376209049,-5.91894766702673,
130.809594295568));
#143062=CARTESIAN_POINT('',(148.438373822973,-5.92114154475418,130.801327303241));
#143063=CARTESIAN_POINT('Ctrl Pts',(150.188375192211,-5.91674766787937,
130.809613915962));
#143064=CARTESIAN_POINT('Ctrl Pts',(150.177611091204,-5.91654497524426,
131.037904998178));
#143065=CARTESIAN_POINT('Ctrl Pts',(150.166846990196,-5.90312653602111,
131.265633413056));
#143066=CARTESIAN_POINT('Ctrl Pts',(150.156082889189,-5.87670615149839,
131.491569007678));
#143067=CARTESIAN_POINT('Ctrl Pts',(150.148642219535,-5.8584430979265,131.647746669091));
#143068=CARTESIAN_POINT('Ctrl Pts',(150.141201549882,-5.833968323526,131.803068599181));
#143069=CARTESIAN_POINT('Ctrl Pts',(150.133760880228,-5.80336442728749,
131.957136348831));
#143070=CARTESIAN_POINT('Ctrl Pts',(150.126337613823,-5.77283211159509,
132.110843743918));
#143071=CARTESIAN_POINT('Ctrl Pts',(150.118914347417,-5.73614278899573,
132.263569710176));
#143072=CARTESIAN_POINT('Ctrl Pts',(150.111491081012,-5.69337090573593,
132.414782392201));
#143073=CARTESIAN_POINT('Ctrl Pts',(150.104076588291,-5.65064957529008,
132.565816353394));
#143074=CARTESIAN_POINT('Ctrl Pts',(150.096662095569,-5.60186009470238,
132.715340234829));
#143075=CARTESIAN_POINT('Ctrl Pts',(150.089247602848,-5.54712817490362,
132.86283081985));
#143076=CARTESIAN_POINT('Ctrl Pts',(150.081840256495,-5.49244900778982,
133.010179247892));
#143077=CARTESIAN_POINT('Ctrl Pts',(150.074432910141,-5.43183893288328,
133.155497933402));
#143078=CARTESIAN_POINT('Ctrl Pts',(150.067025563787,-5.36547384017928,
133.298277423085));
#143079=CARTESIAN_POINT('Ctrl Pts',(150.059623742112,-5.29915824506516,
133.440950422439));
#143080=CARTESIAN_POINT('Ctrl Pts',(150.052221920436,-5.22709633538908,
133.581087659771));
#143081=CARTESIAN_POINT('Ctrl Pts',(150.044820098761,-5.14951257434729,
133.718198432054));
#143082=CARTESIAN_POINT('Ctrl Pts',(150.037422184449,-5.07196976916916,
133.855236824627));
#143083=CARTESIAN_POINT('Ctrl Pts',(150.030024270138,-4.98891110124634,
133.989251609871));
#143084=CARTESIAN_POINT('Ctrl Pts',(150.022626355827,-4.90060749800784,
134.119775631251));
#143085=CARTESIAN_POINT('Ctrl Pts',(150.015229670914,-4.81231856922621,
134.250277961907));
#143086=CARTESIAN_POINT('Ctrl Pts',(150.007832986002,-4.71878664399335,
134.377290371145));
#143087=CARTESIAN_POINT('Ctrl Pts',(150.00043630109,-4.62032666329727,134.500373616315));
#143088=CARTESIAN_POINT('Ctrl Pts',(149.993039944155,-4.52187104841988,
134.623451403846));
#143089=CARTESIAN_POINT('Ctrl Pts',(149.985643587219,-4.41848804574877,
134.742600082219));
#143090=CARTESIAN_POINT('Ctrl Pts',(149.978247230284,-4.31053350321053,
134.857412736673));
#143091=CARTESIAN_POINT('Ctrl Pts',(149.970849740947,-4.20256243255607,
134.972242969238));
#143092=CARTESIAN_POINT('Ctrl Pts',(149.963452251611,-4.0900186841422,135.08273558408));
#143093=CARTESIAN_POINT('Ctrl Pts',(149.956054762274,-3.97329553464828,
135.188519961938));
#143094=CARTESIAN_POINT('Ctrl Pts',(149.948654679759,-3.8565314680353,135.294341422345));
#143095=CARTESIAN_POINT('Ctrl Pts',(149.941254597244,-3.73558535980521,
135.395451109179));
#143096=CARTESIAN_POINT('Ctrl Pts',(149.933854514729,-3.61088404408494,
135.491518283217));
#143097=CARTESIAN_POINT('Ctrl Pts',(149.926446295062,-3.48604560644852,
135.587691092989));
#143098=CARTESIAN_POINT('Ctrl Pts',(149.919038075396,-3.35744401086744,
135.678810088757));
#143099=CARTESIAN_POINT('Ctrl Pts',(149.911629855729,-3.22553618908989,
135.764587109912));
#143100=CARTESIAN_POINT('Ctrl Pts',(149.904217076427,-3.09354718024895,
135.850416925392));
#143101=CARTESIAN_POINT('Ctrl Pts',(149.896804297125,-2.9582482104489,135.930898024315));
#143102=CARTESIAN_POINT('Ctrl Pts',(149.889391517823,-2.82012088367187,
136.005788187376));
#143103=CARTESIAN_POINT('Ctrl Pts',(149.881968146794,-2.68179619409281,
136.080785357013));
#143104=CARTESIAN_POINT('Ctrl Pts',(149.874544775766,-2.54063541029859,
136.150175471535));
#143105=CARTESIAN_POINT('Ctrl Pts',(149.867121404737,-2.39714092929154,
136.213764090003));
#143106=CARTESIAN_POINT('Ctrl Pts',(149.863185355297,-2.3210567123676,136.247480301299));
#143107=CARTESIAN_POINT('Ctrl Pts',(149.859249305856,-2.24431668899597,
136.279566329056));
#143108=CARTESIAN_POINT('Ctrl Pts',(149.855313256416,-2.16699735698748,
136.309998910926));
#143109=CARTESIAN_POINT('Ctrl Pts',(149.84788999001,-2.02117550985723,136.36739381057));
#143110=CARTESIAN_POINT('Ctrl Pts',(149.840466723605,-1.87285135396975,
136.419078159672));
#143111=CARTESIAN_POINT('Ctrl Pts',(149.8330434572,-1.72251259435359,136.464827111133));
#143112=CARTESIAN_POINT('Ctrl Pts',(149.825628964479,-1.57235152266629,
136.510521991132));
#143113=CARTESIAN_POINT('Ctrl Pts',(149.818214471758,-1.42018094047277,
136.550295329563));
#143114=CARTESIAN_POINT('Ctrl Pts',(149.810799979037,-1.2665089945928,136.583970079209));
#143115=CARTESIAN_POINT('Ctrl Pts',(149.803392632683,-1.11298516351992,
136.617612371864));
#143116=CARTESIAN_POINT('Ctrl Pts',(149.795985286329,-0.957963211791275,
136.645167698403));
#143117=CARTESIAN_POINT('Ctrl Pts',(149.788577939975,-0.80196682973234,
136.666508668111));
#143118=CARTESIAN_POINT('Ctrl Pts',(149.7811761183,-0.64608679566044,136.687833720919));
#143119=CARTESIAN_POINT('Ctrl Pts',(149.773774296625,-0.489234146610383,
136.70295359523));
#143120=CARTESIAN_POINT('Ctrl Pts',(149.766372474949,-0.331943052779465,
136.711791901315));
#143121=CARTESIAN_POINT('Ctrl Pts',(149.758974560638,-0.174734991692686,
136.720625541726));
#143122=CARTESIAN_POINT('Ctrl Pts',(149.751576646326,-0.0170893185384864,
136.723184196977));
#143123=CARTESIAN_POINT('Ctrl Pts',(149.744178732015,0.140454491766542,
136.719443296468));
#143124=CARTESIAN_POINT('Ctrl Pts',(149.736782047103,0.297972121148322,
136.715703017628));
#143125=CARTESIAN_POINT('Ctrl Pts',(149.729385362191,0.455387548450213,
136.705665269612));
#143126=CARTESIAN_POINT('Ctrl Pts',(149.721988677278,0.612160993094913,
136.689357599811));
#143127=CARTESIAN_POINT('Ctrl Pts',(149.714592320343,0.768927486240734,
136.673050653109));
#143128=CARTESIAN_POINT('Ctrl Pts',(149.707195963407,0.925051682035538,
136.650474376033));
#143129=CARTESIAN_POINT('Ctrl Pts',(149.699799606472,1.07999888706843,136.621708206152));
#143130=CARTESIAN_POINT('Ctrl Pts',(149.692402117135,1.23496981491403,136.592937632097));
#143131=CARTESIAN_POINT('Ctrl Pts',(149.685004627799,1.38876302614496,136.557975346407));
#143132=CARTESIAN_POINT('Ctrl Pts',(149.677607138462,1.54085413262811,136.516951895127));
#143133=CARTESIAN_POINT('Ctrl Pts',(149.670207055947,1.69299855441292,136.475914063139));
#143134=CARTESIAN_POINT('Ctrl Pts',(149.662806973432,1.84343932329165,136.428810932389));
#143135=CARTESIAN_POINT('Ctrl Pts',(149.655406890917,1.99166746471887,136.375822837888));
#143136=CARTESIAN_POINT('Ctrl Pts',(149.647998671251,2.14005859822582,136.322776477531));
#143137=CARTESIAN_POINT('Ctrl Pts',(149.640590451584,2.28623189366907,136.263832355901));
#143138=CARTESIAN_POINT('Ctrl Pts',(149.633182231918,2.42969793059621,136.199219144771));
#143139=CARTESIAN_POINT('Ctrl Pts',(149.625769452616,2.57325226847531,136.134566165288));
#143140=CARTESIAN_POINT('Ctrl Pts',(149.618356673314,2.71409569438009,136.064237309958));
#143141=CARTESIAN_POINT('Ctrl Pts',(149.610943894012,2.85176410363253,135.988506840401));
#143142=CARTESIAN_POINT('Ctrl Pts',(149.603520522983,2.98962921996412,135.912668163597));
#143143=CARTESIAN_POINT('Ctrl Pts',(149.596097151954,3.12430994022576,135.831412650158));
#143144=CARTESIAN_POINT('Ctrl Pts',(149.588673780925,3.25537111789792,135.745057880833));
#143145=CARTESIAN_POINT('Ctrl Pts',(149.584737731484,3.32486289907089,135.699270510082));
#143146=CARTESIAN_POINT('Ctrl Pts',(149.580801682043,3.39333764006722,135.652050236771));
#143147=CARTESIAN_POINT('Ctrl Pts',(149.576865632603,3.46073442067854,135.603448846806));
#143148=CARTESIAN_POINT('Ctrl Pts',(149.569442366197,3.58784264552746,135.511788142132));
#143149=CARTESIAN_POINT('Ctrl Pts',(149.562019099792,3.71149898148062,135.414935482176));
#143150=CARTESIAN_POINT('Ctrl Pts',(149.554595833386,3.83125064182295,135.31317965164));
#143151=CARTESIAN_POINT('Ctrl Pts',(149.547181340665,3.95086076564756,135.211544088046));
#143152=CARTESIAN_POINT('Ctrl Pts',(149.539766847944,4.06657511835765,135.105017128492));
#143153=CARTESIAN_POINT('Ctrl Pts',(149.532352355223,4.1779700793475,134.993930592943));
#143154=CARTESIAN_POINT('Ctrl Pts',(149.524945008869,4.28925767368004,134.882951126779));
#143155=CARTESIAN_POINT('Ctrl Pts',(149.517537662516,4.39623390183603,134.76742109541));
#143156=CARTESIAN_POINT('Ctrl Pts',(149.510130316162,4.49850851898521,134.647712236546));
#143157=CARTESIAN_POINT('Ctrl Pts',(149.502728494487,4.60070685586633,134.528092661065));
#143158=CARTESIAN_POINT('Ctrl Pts',(149.495326672811,4.69821032249184,134.40430074651));
#143159=CARTESIAN_POINT('Ctrl Pts',(149.487924851136,4.790665917979,134.276744614882));
#143160=CARTESIAN_POINT('Ctrl Pts',(149.480526936824,4.88307270687708,134.149255819142));
#143161=CARTESIAN_POINT('Ctrl Pts',(149.473129022513,4.97043671305392,134.018007065221));
#143162=CARTESIAN_POINT('Ctrl Pts',(149.465731108202,5.05244566519888,133.883438947637));
#143163=CARTESIAN_POINT('Ctrl Pts',(149.458334423289,5.13444098894366,133.748893192833));
#143164=CARTESIAN_POINT('Ctrl Pts',(149.450937738377,5.21108283079605,133.611029487619));
#143165=CARTESIAN_POINT('Ctrl Pts',(149.443541053465,5.28210260257023,133.47031685472));
#143166=CARTESIAN_POINT('Ctrl Pts',(149.43614469653,5.3531192252533,133.329610461167));
#143167=CARTESIAN_POINT('Ctrl Pts',(149.428748339594,5.41851410532828,133.186055724362));
#143168=CARTESIAN_POINT('Ctrl Pts',(149.421351982659,5.47806506102332,133.040145434961));
#143169=CARTESIAN_POINT('Ctrl Pts',(149.413954493322,5.53762513412174,132.894212806323));
#143170=CARTESIAN_POINT('Ctrl Pts',(149.406557003986,5.59133936026565,132.745924252647));
#143171=CARTESIAN_POINT('Ctrl Pts',(149.399159514649,5.63903412694477,132.595791519848));
#143172=CARTESIAN_POINT('Ctrl Pts',(149.391759432134,5.68674561295041,132.445606158253));
#143173=CARTESIAN_POINT('Ctrl Pts',(149.384359349619,5.72843332531943,132.293575685963));
#143174=CARTESIAN_POINT('Ctrl Pts',(149.376959267104,5.76397387183037,132.140225793157));
#143175=CARTESIAN_POINT('Ctrl Pts',(149.369551047438,5.79955349882585,131.98670727638));
#143176=CARTESIAN_POINT('Ctrl Pts',(149.362142827771,5.82897237658241,131.831866805549));
#143177=CARTESIAN_POINT('Ctrl Pts',(149.354734608105,5.85215834942968,131.676239746632));
#143178=CARTESIAN_POINT('Ctrl Pts',(149.347321828803,5.87535859285637,131.520516901856));
#143179=CARTESIAN_POINT('Ctrl Pts',(149.339909049501,5.89231824704431,131.364006874566));
#143180=CARTESIAN_POINT('Ctrl Pts',(149.332496270198,5.90301719614591,131.207248374275));
#143181=CARTESIAN_POINT('Ctrl Pts',(149.32507289917,5.91373143240772,131.050265890087));
#143182=CARTESIAN_POINT('Ctrl Pts',(149.317649528141,5.91816708673635,130.893034595984));
#143183=CARTESIAN_POINT('Ctrl Pts',(149.310226157112,5.91635614148846,130.73609225321));
#143184=CARTESIAN_POINT('Ctrl Pts',(149.306290107671,5.91539593486498,130.652877657291));
#143185=CARTESIAN_POINT('Ctrl Pts',(149.302354058231,5.91268045167756,130.569744207242));
#143186=CARTESIAN_POINT('Ctrl Pts',(149.29841800879,5.90822033201568,130.486771148508));
#143187=CARTESIAN_POINT('Ctrl Pts',(149.290994742384,5.89980868552901,130.330286549237));
#143188=CARTESIAN_POINT('Ctrl Pts',(149.283571475979,5.88516306975464,130.173899743206));
#143189=CARTESIAN_POINT('Ctrl Pts',(149.276148209573,5.86428170516227,130.018147767888));
#143190=CARTESIAN_POINT('Ctrl Pts',(149.268733716852,5.84342502060875,129.86257987847));
#143191=CARTESIAN_POINT('Ctrl Pts',(149.261319224131,5.81634730665521,129.707645692629));
#143192=CARTESIAN_POINT('Ctrl Pts',(149.25390473141,5.7830987555516,129.553880971175));
#143193=CARTESIAN_POINT('Ctrl Pts',(149.246497385057,5.74988225065333,129.400264453949));
#143194=CARTESIAN_POINT('Ctrl Pts',(149.239090038703,5.7105068276405,129.247815519545));
#143195=CARTESIAN_POINT('Ctrl Pts',(149.231682692349,5.66507430311255,129.097063425302));
#143196=CARTESIAN_POINT('Ctrl Pts',(149.224280870674,5.61967566387543,128.946423767658));
#143197=CARTESIAN_POINT('Ctrl Pts',(149.216879048998,5.56822902555666,128.797478786142));
#143198=CARTESIAN_POINT('Ctrl Pts',(149.209477227323,5.51088694715425,128.650746070303));
#143199=CARTESIAN_POINT('Ctrl Pts',(149.202079313011,5.45357513918877,128.504090813522));
#143200=CARTESIAN_POINT('Ctrl Pts',(149.1946813987,5.39037422468059,128.359645843425));
#143201=CARTESIAN_POINT('Ctrl Pts',(149.187283484389,5.32148609800419,128.217912034809));
#143202=CARTESIAN_POINT('Ctrl Pts',(149.179886799476,5.25260941928464,128.076201779779));
#143203=CARTESIAN_POINT('Ctrl Pts',(149.172490114564,5.17804756718716,127.937202127442));
#143204=CARTESIAN_POINT('Ctrl Pts',(149.165093429652,5.09804996533892,127.801392566885));
#143205=CARTESIAN_POINT('Ctrl Pts',(149.157697072717,5.01805591066821,127.665589028267));
#143206=CARTESIAN_POINT('Ctrl Pts',(149.150300715781,4.93262677495175,127.532975621818));
#143207=CARTESIAN_POINT('Ctrl Pts',(149.142904358846,4.84205706225094,127.404005640743));
#143208=CARTESIAN_POINT('Ctrl Pts',(149.135506869509,4.75147348309586,127.275015914035));
#143209=CARTESIAN_POINT('Ctrl Pts',(149.128109380173,4.65574797441214,127.149671028903));
#143210=CARTESIAN_POINT('Ctrl Pts',(149.120711890836,4.5552172407278,127.028393661636));
#143211=CARTESIAN_POINT('Ctrl Pts',(149.113311808321,4.45465126615065,126.907073780776));
#143212=CARTESIAN_POINT('Ctrl Pts',(149.105911725806,4.3492769509007,126.789824543879));
#143213=CARTESIAN_POINT('Ctrl Pts',(149.098511643291,4.23946987650391,126.677033912698));
#143214=CARTESIAN_POINT('Ctrl Pts',(149.091103423624,4.1295420579403,126.564119256623));
#143215=CARTESIAN_POINT('Ctrl Pts',(149.083695203958,4.0151720065438,126.455673264908));
#143216=CARTESIAN_POINT('Ctrl Pts',(149.076286984291,3.89677113896211,126.352046022543));
#143217=CARTESIAN_POINT('Ctrl Pts',(149.068874204989,3.77829739762201,126.24835499934));
#143218=CARTESIAN_POINT('Ctrl Pts',(149.061461425687,3.65578818641941,126.149488869229));
#143219=CARTESIAN_POINT('Ctrl Pts',(149.054048646385,3.52968586381837,126.055755741893));
#143220=CARTESIAN_POINT('Ctrl Pts',(149.046625275356,3.40340336030519,125.96188868427));
#143221=CARTESIAN_POINT('Ctrl Pts',(149.039201904328,3.27351779906642,125.873169487608));
#143222=CARTESIAN_POINT('Ctrl Pts',(149.031778533299,3.14049890111156,125.789861917335));
#143223=CARTESIAN_POINT('Ctrl Pts',(149.027842483858,3.06996908967165,125.745690244639));
#143224=CARTESIAN_POINT('Ctrl Pts',(149.023906434417,2.99855877869273,125.703039197153));
#143225=CARTESIAN_POINT('Ctrl Pts',(149.019970384977,2.92634039083971,125.661942657166));
#143226=CARTESIAN_POINT('Ctrl Pts',(149.012547118571,2.79013876520704,125.584435865331));
#143227=CARTESIAN_POINT('Ctrl Pts',(149.005123852166,2.65064980312381,125.512226748048));
#143228=CARTESIAN_POINT('Ctrl Pts',(148.99770058576,2.5083243675459,125.445607084357));
#143229=CARTESIAN_POINT('Ctrl Pts',(148.990286093039,2.3661671488134,125.379066159577));
#143230=CARTESIAN_POINT('Ctrl Pts',(148.982871600318,2.22118046449983,125.318101695282));
#143231=CARTESIAN_POINT('Ctrl Pts',(148.975457107597,2.07384219548515,125.262961055116));
#143232=CARTESIAN_POINT('Ctrl Pts',(148.968049761244,1.92664593664134,125.207873561574));
#143233=CARTESIAN_POINT('Ctrl Pts',(148.96064241489,1.77710295261238,125.158598847307));
#143234=CARTESIAN_POINT('Ctrl Pts',(148.953235068536,1.62571355694652,125.115337327645));
#143235=CARTESIAN_POINT('Ctrl Pts',(148.945833246861,1.47443707320333,125.072108074057));
#143236=CARTESIAN_POINT('Ctrl Pts',(148.938431425185,1.32131727724733,125.034883187226));
#143237=CARTESIAN_POINT('Ctrl Pts',(148.93102960351,1.16687209369101,125.003814084741));
#143238=CARTESIAN_POINT('Ctrl Pts',(148.923631689198,1.01250844054517,124.972761383394));
#143239=CARTESIAN_POINT('Ctrl Pts',(148.916233774887,0.856821158249057,
124.947858068111));
#143240=CARTESIAN_POINT('Ctrl Pts',(148.908835860576,0.700340775795215,
124.929205014498));
#143241=CARTESIAN_POINT('Ctrl Pts',(148.901439175664,0.543886397541983,
124.910555060685));
#143242=CARTESIAN_POINT('Ctrl Pts',(148.894042490751,0.386639551023458,
124.898153351213));
#143243=CARTESIAN_POINT('Ctrl Pts',(148.886645805839,0.229138463551447,
124.892049214483));
#143244=CARTESIAN_POINT('Ctrl Pts',(148.879249448904,0.0716443598427598,
124.885945348418));
#143245=CARTESIAN_POINT('Ctrl Pts',(148.871853091968,-0.0861035893867342,
124.886138514327));
#143246=CARTESIAN_POINT('Ctrl Pts',(148.864456735033,-0.243564829087545,
124.892625953651));
#143247=CARTESIAN_POINT('Ctrl Pts',(148.857059245696,-0.401050176506133,
124.899114386219));
#143248=CARTESIAN_POINT('Ctrl Pts',(148.84966175636,-0.558248353987908,
124.911898995629));
#143249=CARTESIAN_POINT('Ctrl Pts',(148.842264267023,-0.714621754978833,
124.930924969684));
#143250=CARTESIAN_POINT('Ctrl Pts',(148.834864184508,-0.871049972423344,
124.949957613264));
#143251=CARTESIAN_POINT('Ctrl Pts',(148.827464101993,-1.02665246739904,
124.975235932525));
#143252=CARTESIAN_POINT('Ctrl Pts',(148.820064019478,-1.1808998257067,125.006653642895));
#143253=CARTESIAN_POINT('Ctrl Pts',(148.812655799812,-1.33531679484166,
125.038105900268));
#143254=CARTESIAN_POINT('Ctrl Pts',(148.805247580145,-1.48837528544521,
125.075710956173));
#143255=CARTESIAN_POINT('Ctrl Pts',(148.797839360479,-1.63955838035195,
125.119311903622));
#143256=CARTESIAN_POINT('Ctrl Pts',(148.790426581177,-1.79083452593109,
125.162939686727));
#143257=CARTESIAN_POINT('Ctrl Pts',(148.783013801875,-1.94023262233649,
125.212570597488));
#143258=CARTESIAN_POINT('Ctrl Pts',(148.775601022573,-2.08725434261052,
125.267999008011));
#143259=CARTESIAN_POINT('Ctrl Pts',(148.768177651544,-2.23448613441307,
125.323506617247));
#143260=CARTESIAN_POINT('Ctrl Pts',(148.760754280515,-2.37933442570295,
125.384828125585));
#143261=CARTESIAN_POINT('Ctrl Pts',(148.753330909486,-2.52132340747843,
125.451710915091));
#143262=CARTESIAN_POINT('Ctrl Pts',(148.749394860046,-2.59660937259654,
125.487173774919));
#143263=CARTESIAN_POINT('Ctrl Pts',(148.745458810605,-2.67109192416717,
125.524199359016));
#143264=CARTESIAN_POINT('Ctrl Pts',(148.741522761164,-2.74470340984099,
125.562745050348));
#143265=CARTESIAN_POINT('Ctrl Pts',(148.734099494758,-2.88353237448325,
125.635441021227));
#143266=CARTESIAN_POINT('Ctrl Pts',(148.726676228353,-3.01968114113617,
125.713766243864));
#143267=CARTESIAN_POINT('Ctrl Pts',(148.719252961947,-3.15266052538826,
125.797499108181));
#143268=CARTESIAN_POINT('Ctrl Pts',(148.711838469226,-3.28548273905141,
125.881133007207));
#143269=CARTESIAN_POINT('Ctrl Pts',(148.704423976505,-3.41514271383474,
125.970161628865));
#143270=CARTESIAN_POINT('Ctrl Pts',(148.697009483784,-3.5411740294112,126.064316624529));
#143271=CARTESIAN_POINT('Ctrl Pts',(148.68960213743,-3.66708387126062,126.158380870064));
#143272=CARTESIAN_POINT('Ctrl Pts',(148.682194791077,-3.78937171956451,
126.257561431142));
#143273=CARTESIAN_POINT('Ctrl Pts',(148.674787444723,-3.90759852753498,
126.361545709188));
#143274=CARTESIAN_POINT('Ctrl Pts',(148.667385623047,-4.02573715749167,
126.465452431836));
#143275=CARTESIAN_POINT('Ctrl Pts',(148.659983801372,-4.13982049891955,
126.574155492152));
#143276=CARTESIAN_POINT('Ctrl Pts',(148.652581979697,-4.24944120900851,
126.687300990395));
#143277=CARTESIAN_POINT('Ctrl Pts',(148.645184065385,-4.35900405117806,
126.800386760011));
#143278=CARTESIAN_POINT('Ctrl Pts',(148.637786151074,-4.4641086945792,126.917910029692));
#143279=CARTESIAN_POINT('Ctrl Pts',(148.630388236762,-4.56438350582768,
127.039478976103));
#143280=CARTESIAN_POINT('Ctrl Pts',(148.62299155185,-4.66464165322159,127.161027719959));
#143281=CARTESIAN_POINT('Ctrl Pts',(148.615594866938,-4.76007132414656,
127.2866205185));
#143282=CARTESIAN_POINT('Ctrl Pts',(148.608198182026,-4.85034009221182,
127.415831209049));
#143283=CARTESIAN_POINT('Ctrl Pts',(148.60080182509,-4.94060485766535,127.545036170261));
#143284=CARTESIAN_POINT('Ctrl Pts',(148.593405468155,-5.02570896148213,
127.677858398495));
#143285=CARTESIAN_POINT('Ctrl Pts',(148.586009111219,-5.10536254130746,
127.81384161841));
#143286=CARTESIAN_POINT('Ctrl Pts',(148.578611621883,-5.18502831629924,
127.949845657703));
#143287=CARTESIAN_POINT('Ctrl Pts',(148.571214132546,-5.25924171703161,
128.08901133017));
#143288=CARTESIAN_POINT('Ctrl Pts',(148.56381664321,-5.32775826908414,128.230856704861));
#143289=CARTESIAN_POINT('Ctrl Pts',(148.556416560695,-5.39629883950763,
128.372751803229));
#143290=CARTESIAN_POINT('Ctrl Pts',(148.54901647818,-5.45913842293072,128.517328138161));
#143291=CARTESIAN_POINT('Ctrl Pts',(148.541616395665,-5.51608027826669,
128.664082849094));
#143292=CARTESIAN_POINT('Ctrl Pts',(148.534208175998,-5.57308474702654,
128.810998931918));
#143293=CARTESIAN_POINT('Ctrl Pts',(148.526799956332,-5.62417840129561,
128.960097826176));
#143294=CARTESIAN_POINT('Ctrl Pts',(148.519391736665,-5.66921384501301,
129.110859822759));
#143295=CARTESIAN_POINT('Ctrl Pts',(148.511978957363,-5.7142770072945,129.261714610834));
#143296=CARTESIAN_POINT('Ctrl Pts',(148.504566178061,-5.75327443680885,
129.414234180084));
#143297=CARTESIAN_POINT('Ctrl Pts',(148.497153398759,-5.78610977623428,
129.567888127024));
#143298=CARTESIAN_POINT('Ctrl Pts',(148.48973002773,-5.81899203233256,129.721761621931));
#143299=CARTESIAN_POINT('Ctrl Pts',(148.482306656701,-5.84569455021054,
129.876772364828));
#143300=CARTESIAN_POINT('Ctrl Pts',(148.474883285673,-5.86617267810224,
130.032383497965));
#143301=CARTESIAN_POINT('Ctrl Pts',(148.470947236232,-5.87703067287567,
130.114892254587));
#143302=CARTESIAN_POINT('Ctrl Pts',(148.467011186792,-5.88613963881658,
130.197569767277));
#143303=CARTESIAN_POINT('Ctrl Pts',(148.463075137351,-5.89349886309523,
130.280336082649));
#143304=CARTESIAN_POINT('Ctrl Pts',(148.454841822305,-5.90889267684155,
130.453464281364));
#143305=CARTESIAN_POINT('Ctrl Pts',(148.446608507258,-5.91665920916557,
130.627280655751));
#143306=CARTESIAN_POINT('Ctrl Pts',(148.438375192211,-5.91674920870991,
130.801300596218));
#143307=CARTESIAN_POINT('',(146.688376397846,-5.91262067511285,130.80056261765));
#143308=CARTESIAN_POINT('Ctrl Pts',(148.438372749788,-5.92458418098038,
130.801348235738));
#143309=CARTESIAN_POINT('Ctrl Pts',(148.353791004372,-5.91330618353133,
132.591447999183));
#143310=CARTESIAN_POINT('Ctrl Pts',(148.17639338435,-4.09355336934731,136.365725888165));
#143311=CARTESIAN_POINT('Ctrl Pts',(147.906179889726,2.33383032450629,137.402147863814));
#143312=CARTESIAN_POINT('Ctrl Pts',(147.627732265912,6.81239756668457,132.407108234558));
#143313=CARTESIAN_POINT('Ctrl Pts',(147.3492846421,5.03070424920177,125.939221843861));
#143314=CARTESIAN_POINT('Ctrl Pts',(147.070837018287,-1.3739605097317,123.942160310955));
#143315=CARTESIAN_POINT('Ctrl Pts',(146.850534579625,-5.44226183250563,
127.351331318721));
#143316=CARTESIAN_POINT('Ctrl Pts',(146.723048015568,-5.91372560248277,
130.061942539049));
#143317=CARTESIAN_POINT('Ctrl Pts',(146.688377326116,-5.90944225702956,
130.800544870309));
#143318=CARTESIAN_POINT('',(144.938373961035,-5.91329332165665,130.808852035354));
#143319=CARTESIAN_POINT('Ctrl Pts',(146.688375192211,-5.91674879577075,
130.800585667847));
#143320=CARTESIAN_POINT('Ctrl Pts',(146.680925564612,-5.91685017423445,
130.959483387732));
#143321=CARTESIAN_POINT('Ctrl Pts',(146.673475937013,-5.91054628583829,
131.118409240451));
#143322=CARTESIAN_POINT('Ctrl Pts',(146.666026309415,-5.89785702676342,
131.27681490568));
#143323=CARTESIAN_POINT('Ctrl Pts',(146.658576163893,-5.88516688548858,
131.435231583804));
#143324=CARTESIAN_POINT('Ctrl Pts',(146.651126018371,-5.86609051749853,
131.593127637726));
#143325=CARTESIAN_POINT('Ctrl Pts',(146.643675872849,-5.84069978669513,
131.749959139244));
#143326=CARTESIAN_POINT('Ctrl Pts',(146.636223817714,-5.81530254776845,
131.906830839634));
#143327=CARTESIAN_POINT('Ctrl Pts',(146.62877176258,-5.78358778015593,132.062637083029));
#143328=CARTESIAN_POINT('Ctrl Pts',(146.621319707445,-5.7456786176807,132.216843461648));
#143329=CARTESIAN_POINT('Ctrl Pts',(146.613864350142,-5.70775265683128,
132.371118172467));
#143330=CARTESIAN_POINT('Ctrl Pts',(146.60640899284,-5.66362692050174,132.523791251461));
#143331=CARTESIAN_POINT('Ctrl Pts',(146.598953635537,-5.6134745963873,132.674342841603));
#143332=CARTESIAN_POINT('Ctrl Pts',(146.591488802704,-5.56325853020448,
132.825085778207));
#143333=CARTESIAN_POINT('Ctrl Pts',(146.584023969871,-5.50700069033317,
132.973701492184));
#143334=CARTESIAN_POINT('Ctrl Pts',(146.576559137038,-5.44492303782663,
133.119688601815));
#143335=CARTESIAN_POINT('Ctrl Pts',(146.569089267876,-5.38280350314429,
133.265774205147));
#143336=CARTESIAN_POINT('Ctrl Pts',(146.561619398714,-5.31485648538662,
133.40922733926));
#143337=CARTESIAN_POINT('Ctrl Pts',(146.554149529553,-5.24135006816218,
133.549570996658));
#143338=CARTESIAN_POINT('Ctrl Pts',(146.54666740051,-5.16772300893682,133.690144992309));
#143339=CARTESIAN_POINT('Ctrl Pts',(146.539185271466,-5.08851850020001,
133.827598996989));
#143340=CARTESIAN_POINT('Ctrl Pts',(146.531703142423,-5.00404876843835,
133.961483751939));
#143341=CARTESIAN_POINT('Ctrl Pts',(146.525782685169,-4.93720957958121,
134.067424048357));
#143342=CARTESIAN_POINT('Ctrl Pts',(146.519862227915,-4.86707459463988,
134.171130098108));
#143343=CARTESIAN_POINT('Ctrl Pts',(146.513941770661,-4.79381602330894,
134.272394426105));
#143344=CARTESIAN_POINT('Ctrl Pts',(146.506518504255,-4.70196198769583,
134.399363011775));
#143345=CARTESIAN_POINT('Ctrl Pts',(146.49909523785,-4.60492125600033,134.522871811275));
#143346=CARTESIAN_POINT('Ctrl Pts',(146.491671971445,-4.50298330165497,
134.642468477895));
#143347=CARTESIAN_POINT('Ctrl Pts',(146.484257478724,-4.40116582950608,
134.761923791186));
#143348=CARTESIAN_POINT('Ctrl Pts',(146.476842986003,-4.29446289576129,
134.877475894003));
#143349=CARTESIAN_POINT('Ctrl Pts',(146.469428493282,-4.18320696468062,
134.988701671202));
#143350=CARTESIAN_POINT('Ctrl Pts',(146.462021146928,-4.07205826625514,
135.09982024481));
#143351=CARTESIAN_POINT('Ctrl Pts',(146.454613800574,-3.95636556906017,
135.206620532048));
#143352=CARTESIAN_POINT('Ctrl Pts',(146.44720645422,-3.83650120426009,135.30871285426));
#143353=CARTESIAN_POINT('Ctrl Pts',(146.439804632545,-3.7167262388252,135.410729032166));
#143354=CARTESIAN_POINT('Ctrl Pts',(146.432402810869,-3.59278608394093,
135.508043995664));
#143355=CARTESIAN_POINT('Ctrl Pts',(146.425000989194,-3.46508939834247,
135.600305365371));
#143356=CARTESIAN_POINT('Ctrl Pts',(146.417603074883,-3.33746012283026,
135.692518031019));
#143357=CARTESIAN_POINT('Ctrl Pts',(146.410205160571,-3.20607856774808,
135.779682197768));
#143358=CARTESIAN_POINT('Ctrl Pts',(146.40280724626,-3.0713858023266,135.861486265181));
#143359=CARTESIAN_POINT('Ctrl Pts',(146.395410561348,-2.93671542039964,
135.943276738242));
#143360=CARTESIAN_POINT('Ctrl Pts',(146.388013876436,-2.79873523899313,
136.019708686253));
#143361=CARTESIAN_POINT('Ctrl Pts',(146.380617191523,-2.65791468903476,
136.090514235114));
#143362=CARTESIAN_POINT('Ctrl Pts',(146.373220834588,-2.51710038320706,
136.161316644382));
#143363=CARTESIAN_POINT('Ctrl Pts',(146.365824477652,-2.37344629276073,
136.226492982859));
#143364=CARTESIAN_POINT('Ctrl Pts',(146.358428120717,-2.22744554590481,
136.285821818973));
#143365=CARTESIAN_POINT('Ctrl Pts',(146.35103063138,-2.08142244596171,136.345159738483));
#143366=CARTESIAN_POINT('Ctrl Pts',(146.343633142044,-1.93305232009356,
136.398648232491));
#143367=CARTESIAN_POINT('Ctrl Pts',(146.336235652707,-1.78284717783012,
136.446114467479));
#143368=CARTESIAN_POINT('Ctrl Pts',(146.328835570192,-1.63258938138722,
136.493597341681));
#143369=CARTESIAN_POINT('Ctrl Pts',(146.321435487677,-1.48049564354469,
136.535053641277));
#143370=CARTESIAN_POINT('Ctrl Pts',(146.314035405162,-1.32709184165449,
136.570360774201));
#143371=CARTESIAN_POINT('Ctrl Pts',(146.306627185496,-1.17351935651349,
136.605706730947));
#143372=CARTESIAN_POINT('Ctrl Pts',(146.299218965829,-1.01863429446173,
136.634889933799));
#143373=CARTESIAN_POINT('Ctrl Pts',(146.291810746163,-0.862972130654549,
136.657839041906));
#143374=CARTESIAN_POINT('Ctrl Pts',(146.284397966861,-0.707214159382685,
136.680802274806));
#143375=CARTESIAN_POINT('Ctrl Pts',(146.276985187559,-0.550678503621795,
136.697523727736));
#143376=CARTESIAN_POINT('Ctrl Pts',(146.269572408257,-0.393903902874796,
136.707984104697));
#143377=CARTESIAN_POINT('Ctrl Pts',(146.262149037228,-0.236905295226194,
136.718459427934));
#143378=CARTESIAN_POINT('Ctrl Pts',(146.254725666199,-0.0796674328840097,
136.722655797862));
#143379=CARTESIAN_POINT('Ctrl Pts',(146.24730229517,0.0772719722024892,
136.720606015182));
#143380=CARTESIAN_POINT('Ctrl Pts',(146.243366245729,0.16048501049027,136.719519171221));
#143381=CARTESIAN_POINT('Ctrl Pts',(146.239430196289,0.243614231769653,
136.716677176219));
#143382=CARTESIAN_POINT('Ctrl Pts',(146.235494146848,0.326580406880512,
136.712090790851));
#143383=CARTESIAN_POINT('Ctrl Pts',(146.228070880442,0.483052023851161,
136.703441011183));
#143384=CARTESIAN_POINT('Ctrl Pts',(146.220647614037,0.639416360654844,
136.688557418271));
#143385=CARTESIAN_POINT('Ctrl Pts',(146.213224347631,0.795136377732586,
136.667439049866));
#143386=CARTESIAN_POINT('Ctrl Pts',(146.20580985491,0.950672346682217,136.646345641619));
#143387=CARTESIAN_POINT('Ctrl Pts',(146.198395362189,1.10556514544094,136.619032175565));
#143388=CARTESIAN_POINT('Ctrl Pts',(146.190980869468,1.2592790902034,136.585549659232));
#143389=CARTESIAN_POINT('Ctrl Pts',(146.183573523114,1.41284487967899,136.552099414609));
#143390=CARTESIAN_POINT('Ctrl Pts',(146.176166176761,1.56523371485981,136.512492035865));
#143391=CARTESIAN_POINT('Ctrl Pts',(146.168758830407,1.71591649396653,136.466830144922));
#143392=CARTESIAN_POINT('Ctrl Pts',(146.161357008731,1.86648688817112,136.42120231034));
#143393=CARTESIAN_POINT('Ctrl Pts',(146.153955187056,2.01535340418601,136.369529062689));
#143394=CARTESIAN_POINT('Ctrl Pts',(146.146553365381,2.16199868522904,136.311963748472));
#143395=CARTESIAN_POINT('Ctrl Pts',(146.139155451069,2.30856655337047,136.254428822537));
#143396=CARTESIAN_POINT('Ctrl Pts',(146.131757536758,2.45291517517011,136.191008160558));
#143397=CARTESIAN_POINT('Ctrl Pts',(146.124359622446,2.59454398366055,136.121904418923));
#143398=CARTESIAN_POINT('Ctrl Pts',(146.116962937534,2.73614925601171,136.052812161077));
#143399=CARTESIAN_POINT('Ctrl Pts',(146.109566252622,2.87503527694299,135.978038861511));
#143400=CARTESIAN_POINT('Ctrl Pts',(146.10216956771,3.01072293750282,135.897834673267));
#143401=CARTESIAN_POINT('Ctrl Pts',(146.094773210774,3.14640458152964,135.817634041359));
#143402=CARTESIAN_POINT('Ctrl Pts',(146.087376853839,3.27888782581267,135.732003189538));
#143403=CARTESIAN_POINT('Ctrl Pts',(146.079980496903,3.40771982585763,135.641237311359));
#143404=CARTESIAN_POINT('Ctrl Pts',(146.072583007567,3.5365715504106,135.550457536692));
#143405=CARTESIAN_POINT('Ctrl Pts',(146.06518551823,3.6617706124662,135.454541385279));
#143406=CARTESIAN_POINT('Ctrl Pts',(146.057788028894,3.78289484863255,135.353826204499));
#143407=CARTESIAN_POINT('Ctrl Pts',(146.050387946379,3.90406154471191,135.253075718169));
#143408=CARTESIAN_POINT('Ctrl Pts',(146.042987863864,4.02115028406602,135.147523091562));
#143409=CARTESIAN_POINT('Ctrl Pts',(146.035587781349,4.13377367696238,135.037544496179));
#143410=CARTESIAN_POINT('Ctrl Pts',(146.028179561682,4.24652091085759,134.927444968025));
#143411=CARTESIAN_POINT('Ctrl Pts',(146.020771342016,4.35479272524531,134.812910012728));
#143412=CARTESIAN_POINT('Ctrl Pts',(146.013363122349,4.45823966164598,134.69435157923));
#143413=CARTESIAN_POINT('Ctrl Pts',(146.005950343047,4.56175026791007,134.575720174994));
#143414=CARTESIAN_POINT('Ctrl Pts',(145.998537563745,4.66042984537124,134.453060648234));
#143415=CARTESIAN_POINT('Ctrl Pts',(145.991124784443,4.75397095789735,134.326815825793));
#143416=CARTESIAN_POINT('Ctrl Pts',(145.983701413414,4.84764572635165,134.20039061883));
#143417=CARTESIAN_POINT('Ctrl Pts',(145.976278042385,4.93616715656382,134.070370192481));
#143418=CARTESIAN_POINT('Ctrl Pts',(145.968854671357,5.01927219824941,133.937224668619));
#143419=CARTESIAN_POINT('Ctrl Pts',(145.964918621916,5.06333648542698,133.866627717088));
#143420=CARTESIAN_POINT('Ctrl Pts',(145.960982572476,5.10587880918495,133.79515258117));
#143421=CARTESIAN_POINT('Ctrl Pts',(145.957046523035,5.14686539748783,133.72287173501));
#143422=CARTESIAN_POINT('Ctrl Pts',(145.949623256629,5.22416482388311,133.586552314953));
#143423=CARTESIAN_POINT('Ctrl Pts',(145.942199990224,5.29616157909455,133.446953624411));
#143424=CARTESIAN_POINT('Ctrl Pts',(145.934776723819,5.3625645705556,133.304526969856));
#143425=CARTESIAN_POINT('Ctrl Pts',(145.927362231098,5.42888907919511,133.162268651779));
#143426=CARTESIAN_POINT('Ctrl Pts',(145.919947738377,5.48963282784175,133.017189357821));
#143427=CARTESIAN_POINT('Ctrl Pts',(145.912533245656,5.54454918039234,132.869767344753));
#143428=CARTESIAN_POINT('Ctrl Pts',(145.905125899302,5.59941260249481,132.722487422573));
#143429=CARTESIAN_POINT('Ctrl Pts',(145.897718552948,5.64845968073772,132.572869623985));
#143430=CARTESIAN_POINT('Ctrl Pts',(145.890311206594,5.69149076141396,132.421414566957));
#143431=CARTESIAN_POINT('Ctrl Pts',(145.882909384919,5.73448974788684,132.270072470824));
#143432=CARTESIAN_POINT('Ctrl Pts',(145.875507563244,5.77148156934821,132.116896202237));
#143433=CARTESIAN_POINT('Ctrl Pts',(145.868105741568,5.80231559657743,131.96240391564));
#143434=CARTESIAN_POINT('Ctrl Pts',(145.860707827257,5.83313334676377,131.807993184319));
#143435=CARTESIAN_POINT('Ctrl Pts',(145.853309912946,5.85779970366842,131.652268183698));
#143436=CARTESIAN_POINT('Ctrl Pts',(145.845911998634,5.8762145991763,131.495759595673));
#143437=CARTESIAN_POINT('Ctrl Pts',(145.838515313722,5.89462643446256,131.339277016536));
#143438=CARTESIAN_POINT('Ctrl Pts',(145.83111862881,5.90678882664155,131.182011478816));
#143439=CARTESIAN_POINT('Ctrl Pts',(145.823721943898,5.91265326645856,131.02450128427));
#143440=CARTESIAN_POINT('Ctrl Pts',(145.816325586962,5.91851744624016,130.866998073892));
#143441=CARTESIAN_POINT('Ctrl Pts',(145.808929230027,5.9180842150296,130.709250601297));
#143442=CARTESIAN_POINT('Ctrl Pts',(145.801532873091,5.91135715401488,130.551799416711));
#143443=CARTESIAN_POINT('Ctrl Pts',(145.794135383755,5.90462906306994,130.394324125948));
#143444=CARTESIAN_POINT('Ctrl Pts',(145.786737894418,5.89160523959781,130.237145586498));
#143445=CARTESIAN_POINT('Ctrl Pts',(145.779340405082,5.87234131387779,130.080801320878));
#143446=CARTESIAN_POINT('Ctrl Pts',(145.771940322567,5.85307063521842,129.924402249017));
#143447=CARTESIAN_POINT('Ctrl Pts',(145.764540240052,5.82755554472008,129.768838403525));
#143448=CARTESIAN_POINT('Ctrl Pts',(145.757140157537,5.79590313250887,129.61463903624));
#143449=CARTESIAN_POINT('Ctrl Pts',(145.74973193787,5.76421591521665,129.460270110899));
#143450=CARTESIAN_POINT('Ctrl Pts',(145.742323718204,5.72637797388972,129.307269026028));
#143451=CARTESIAN_POINT('Ctrl Pts',(145.734915498537,5.682547001995,129.156152459408));
#143452=CARTESIAN_POINT('Ctrl Pts',(145.727502719235,5.63868905286833,129.004942883063));
#143453=CARTESIAN_POINT('Ctrl Pts',(145.720089939933,5.58883084110783,128.855620489456));
#143454=CARTESIAN_POINT('Ctrl Pts',(145.712677160631,5.53317875273848,128.708683292035));
#143455=CARTESIAN_POINT('Ctrl Pts',(145.705253789602,5.4774471460555,128.561536143857));
#143456=CARTESIAN_POINT('Ctrl Pts',(145.697830418573,5.41590527428469,128.416781341196));
#143457=CARTESIAN_POINT('Ctrl Pts',(145.690407047545,5.34880647916707,128.274894308061));
#143458=CARTESIAN_POINT('Ctrl Pts',(145.686470998104,5.3132290879834,128.199662398563));
#143459=CARTESIAN_POINT('Ctrl Pts',(145.682534948663,5.27609019699943,128.125236279882));
#143460=CARTESIAN_POINT('Ctrl Pts',(145.678598899223,5.23743252615506,128.051683539434));
#143461=CARTESIAN_POINT('Ctrl Pts',(145.671175632817,5.16452536540489,127.912965366447));
#143462=CARTESIAN_POINT('Ctrl Pts',(145.663752366412,5.0859930382221,127.776935955108));
#143463=CARTESIAN_POINT('Ctrl Pts',(145.656329100007,5.00205789888053,127.64408415201));
#143464=CARTESIAN_POINT('Ctrl Pts',(145.648914607286,4.91822196390334,127.511389368711));
#143465=CARTESIAN_POINT('Ctrl Pts',(145.641500114565,4.8289961249295,127.381865030479));
#143466=CARTESIAN_POINT('Ctrl Pts',(145.634085621844,4.73464944008796,127.255977148721));
#143467=CARTESIAN_POINT('Ctrl Pts',(145.62667827549,4.64039369013352,127.130210602443));
#143468=CARTESIAN_POINT('Ctrl Pts',(145.619270929136,4.5410271426175,127.008073831677));
#143469=CARTESIAN_POINT('Ctrl Pts',(145.611863582782,4.4368630639082,126.890005406982));
#143470=CARTESIAN_POINT('Ctrl Pts',(145.604461761107,4.3327766746982,126.772025042172));
#143471=CARTESIAN_POINT('Ctrl Pts',(145.597059939431,4.22390012483411,126.658107260404));
#143472=CARTESIAN_POINT('Ctrl Pts',(145.589658117756,4.11058793355197,126.548658865441));
#143473=CARTESIAN_POINT('Ctrl Pts',(145.582260203445,3.99733555889367,126.439268247435));
#143474=CARTESIAN_POINT('Ctrl Pts',(145.574862289133,3.87965247392742,126.334342576154));
#143475=CARTESIAN_POINT('Ctrl Pts',(145.567464374822,3.75793106709958,126.234252888264));
#143476=CARTESIAN_POINT('Ctrl Pts',(145.56006768991,3.63622988816143,126.134179833464));
#143477=CARTESIAN_POINT('Ctrl Pts',(145.552671004998,3.51049200734194,126.038941403905));
#143478=CARTESIAN_POINT('Ctrl Pts',(145.545274320085,3.3811440927185,125.948869377045));
#143479=CARTESIAN_POINT('Ctrl Pts',(145.53787796315,3.25180191351725,125.858801344073));
#143480=CARTESIAN_POINT('Ctrl Pts',(145.530481606214,3.11885032513162,125.773899471627));
#143481=CARTESIAN_POINT('Ctrl Pts',(145.523085249279,2.98274604349509,125.694452927351));
#143482=CARTESIAN_POINT('Ctrl Pts',(145.515687759942,2.84662092394524,125.614994219607));
#143483=CARTESIAN_POINT('Ctrl Pts',(145.508290270606,2.70734247246724,125.540992691276));
#143484=CARTESIAN_POINT('Ctrl Pts',(145.500892781269,2.56539299150256,125.472692083078));
#143485=CARTESIAN_POINT('Ctrl Pts',(145.493492698754,2.42339375036843,125.404367532208));
#143486=CARTESIAN_POINT('Ctrl Pts',(145.486092616239,2.27872195170525,125.341748042123));
#143487=CARTESIAN_POINT('Ctrl Pts',(145.478692533724,2.13188075490347,125.285029588413));
#143488=CARTESIAN_POINT('Ctrl Pts',(145.471284314058,1.98487809110943,125.228248766932));
#143489=CARTESIAN_POINT('Ctrl Pts',(145.463876094391,1.83570161366175,125.177382074964));
#143490=CARTESIAN_POINT('Ctrl Pts',(145.456467874725,1.68487125538148,125.132576117491));
#143491=CARTESIAN_POINT('Ctrl Pts',(145.449055095423,1.53394806353227,125.087742582699));
#143492=CARTESIAN_POINT('Ctrl Pts',(145.441642316121,1.38136932344967,125.048977307164));
#143493=CARTESIAN_POINT('Ctrl Pts',(145.434229536819,1.22766558464131,125.016375840911));
#143494=CARTESIAN_POINT('Ctrl Pts',(145.42680616579,1.07374222672317,124.983727792155));
#143495=CARTESIAN_POINT('Ctrl Pts',(145.419382794761,0.918691026639936,
124.957261205161));
#143496=CARTESIAN_POINT('Ctrl Pts',(145.411959423733,0.763048909474546,
124.937019914637));
#143497=CARTESIAN_POINT('Ctrl Pts',(145.408023374292,0.680523724368401,
124.926287496717));
#143498=CARTESIAN_POINT('Ctrl Pts',(145.404087324851,0.597832445114237,
124.917304362424));
#143499=CARTESIAN_POINT('Ctrl Pts',(145.40015127541,0.5150550260896,124.910071102909));
#143500=CARTESIAN_POINT('Ctrl Pts',(145.392728009004,0.358939397210291,
124.896429401206));
#143501=CARTESIAN_POINT('Ctrl Pts',(145.385304742599,0.202045359796482,
124.888973652685));
#143502=CARTESIAN_POINT('Ctrl Pts',(145.377881476193,0.0449043822473605,
124.887781017919));
#143503=CARTESIAN_POINT('Ctrl Pts',(145.370466983472,-0.112050867716212,
124.886589792749));
#143504=CARTESIAN_POINT('Ctrl Pts',(145.363052490751,-0.269252107218764,
124.891646949463));
#143505=CARTESIAN_POINT('Ctrl Pts',(145.35563799803,-0.426161835175479,
124.902978012384));
#143506=CARTESIAN_POINT('Ctrl Pts',(145.348230651676,-0.582920327628564,
124.914298154001));
#143507=CARTESIAN_POINT('Ctrl Pts',(145.340823305323,-0.739387498062542,
124.931880136678));
#143508=CARTESIAN_POINT('Ctrl Pts',(145.333415958969,-0.895025036522239,
124.955697458647));
#143509=CARTESIAN_POINT('Ctrl Pts',(145.326014137293,-1.05054649463355,
124.979497016758));
#143510=CARTESIAN_POINT('Ctrl Pts',(145.318612315618,-1.20523918541278,
125.009522598061));
#143511=CARTESIAN_POINT('Ctrl Pts',(145.311210493943,-1.35856922702592,
125.045695822852));
#143512=CARTESIAN_POINT('Ctrl Pts',(145.303812579631,-1.51181832690372,
125.081849952079));
#143513=CARTESIAN_POINT('Ctrl Pts',(145.29641466532,-1.663705847795,125.12414517614));
#143514=CARTESIAN_POINT('Ctrl Pts',(145.289016751009,-1.81370753050493,
125.172451921903));
#143515=CARTESIAN_POINT('Ctrl Pts',(145.281620066096,-1.96368428565677,
125.22075063996));
#143516=CARTESIAN_POINT('Ctrl Pts',(145.274223381184,-2.11177546963895,
125.275058782671));
#143517=CARTESIAN_POINT('Ctrl Pts',(145.266826696272,-2.25747132416115,
125.335196715918));
#143518=CARTESIAN_POINT('Ctrl Pts',(145.259430339337,-2.4031607183768,125.395331982586));
#143519=CARTESIAN_POINT('Ctrl Pts',(145.252033982401,-2.54645464925804,
125.461296383379));
#143520=CARTESIAN_POINT('Ctrl Pts',(145.244637625466,-2.68686296575698,
125.532861972423));
#143521=CARTESIAN_POINT('Ctrl Pts',(145.237240136129,-2.82729277912728,
125.604438518341));
#143522=CARTESIAN_POINT('Ctrl Pts',(145.229842646792,-2.96483576583358,
125.68161779049));
#143523=CARTESIAN_POINT('Ctrl Pts',(145.222445157456,-3.09902616365413,
125.764125761978));
#143524=CARTESIAN_POINT('Ctrl Pts',(145.215045074941,-3.23326360171076,
125.846662656507));
#143525=CARTESIAN_POINT('Ctrl Pts',(145.207644992426,-3.36414579317909,
125.934531774084));
#143526=CARTESIAN_POINT('Ctrl Pts',(145.200244909911,-3.49123588830347,
126.027415722058));
#143527=CARTESIAN_POINT('Ctrl Pts',(145.192836690244,-3.6184657320528,126.120401805481));
#143528=CARTESIAN_POINT('Ctrl Pts',(145.185428470578,-3.74189485052367,
126.218413511359));
#143529=CARTESIAN_POINT('Ctrl Pts',(145.178020250911,-3.86111886440333,
126.321092649058));
#143530=CARTESIAN_POINT('Ctrl Pts',(145.170607471609,-3.98041625867358,
126.423834984053));
#143531=CARTESIAN_POINT('Ctrl Pts',(145.163194692307,-4.09550311882838,
126.531250221017));
#143532=CARTESIAN_POINT('Ctrl Pts',(145.155781913005,-4.20601228095614,
126.642943640748));
#143533=CARTESIAN_POINT('Ctrl Pts',(145.148358541976,-4.31667934375759,
126.754796653276));
#143534=CARTESIAN_POINT('Ctrl Pts',(145.140935170948,-4.42275539394983,
126.870939782432));
#143535=CARTESIAN_POINT('Ctrl Pts',(145.133511799919,-4.52391333102896,
126.990944991669));
#143536=CARTESIAN_POINT('Ctrl Pts',(145.129575750478,-4.57754969651935,
127.054574633091));
#143537=CARTESIAN_POINT('Ctrl Pts',(145.125639701037,-4.6298041180975,127.119289544752));
#143538=CARTESIAN_POINT('Ctrl Pts',(145.121703651597,-4.68063288111521,
127.185022778303));
#143539=CARTESIAN_POINT('Ctrl Pts',(145.114064965789,-4.77927619251906,
127.312591175442));
#143540=CARTESIAN_POINT('Ctrl Pts',(145.106426279981,-4.87285827794634,
127.444399281556));
#143541=CARTESIAN_POINT('Ctrl Pts',(145.098787594173,-4.96099500290015,
127.580006551447));
#143542=CARTESIAN_POINT('Ctrl Pts',(145.091366378611,-5.04662251151985,
127.7117531381));
#143543=CARTESIAN_POINT('Ctrl Pts',(145.083945163049,-5.12711022034083,
127.847085199565));
#143544=CARTESIAN_POINT('Ctrl Pts',(145.076523947486,-5.20214519205127,
127.985563717589));
#143545=CARTESIAN_POINT('Ctrl Pts',(145.069109876635,-5.2771079244886,128.123908916612));
#143546=CARTESIAN_POINT('Ctrl Pts',(145.061695805784,-5.34662819244207,
128.265394218518));
#143547=CARTESIAN_POINT('Ctrl Pts',(145.054281734933,-5.41043627226524,
128.409551667721));
#143548=CARTESIAN_POINT('Ctrl Pts',(145.046873350587,-5.47419541204351,
128.553598549861));
#143549=CARTESIAN_POINT('Ctrl Pts',(145.039464966241,-5.53225093573288,
128.700313160822));
#143550=CARTESIAN_POINT('Ctrl Pts',(145.032056581895,-5.58437907086082,
128.849203090554));
#143551=CARTESIAN_POINT('Ctrl Pts',(145.024652429676,-5.63647742717881,
128.998007965163));
#143552=CARTESIAN_POINT('Ctrl Pts',(145.017248277456,-5.68265501508533,
129.148985333991));
#143553=CARTESIAN_POINT('Ctrl Pts',(145.009844125237,-5.72273627239586,
129.301623075909));
#143554=CARTESIAN_POINT('Ctrl Pts',(145.002442331162,-5.76280476424999,
129.454212204321));
#143555=CARTESIAN_POINT('Ctrl Pts',(144.995040537086,-5.79678069627863,
129.608460293921));
#143556=CARTESIAN_POINT('Ctrl Pts',(144.987638743011,-5.82453845256294,
129.763840374074));
#143557=CARTESIAN_POINT('Ctrl Pts',(144.980238245299,-5.85229134730386,
129.919193240681));
#143558=CARTESIAN_POINT('Ctrl Pts',(144.972837747588,-5.87382817296325,
130.075677336557));
#143559=CARTESIAN_POINT('Ctrl Pts',(144.965437249876,-5.88907452469448,
130.232756029503));
#143560=CARTESIAN_POINT('Ctrl Pts',(144.958035619644,-5.90432320962045,
130.389858760671));
#143561=CARTESIAN_POINT('Ctrl Pts',(144.950633989412,-5.91327946377241,
130.547555900412));
#143562=CARTESIAN_POINT('Ctrl Pts',(144.94323235918,-5.91592078837946,130.705306147098));
#143563=CARTESIAN_POINT('Ctrl Pts',(144.941613303524,-5.91649855995291,
130.73981292752));
#143564=CARTESIAN_POINT('Ctrl Pts',(144.939994247867,-5.91677436921867,
130.774322244405));
#143565=CARTESIAN_POINT('Ctrl Pts',(144.938375192211,-5.91674831314815,
130.808828431186));
#143566=CARTESIAN_POINT('',(143.188375192211,-5.92568524777546,130.806401493052));
#143567=CARTESIAN_POINT('Ctrl Pts',(144.938373068227,-5.91078788040133,
130.808869152286));
#143568=CARTESIAN_POINT('Ctrl Pts',(144.90666738808,-5.91549280454811,131.483920819572));
#143569=CARTESIAN_POINT('Ctrl Pts',(144.782145833326,-5.49648468611223,
134.129459311167));
#143570=CARTESIAN_POINT('Ctrl Pts',(144.564808403972,-1.59237845161755,
137.619189404644));
#143571=CARTESIAN_POINT('Ctrl Pts',(144.286360780157,4.87278901544506,135.827655128273));
#143572=CARTESIAN_POINT('Ctrl Pts',(144.007913156345,6.86010142628747,129.419958598146));
#143573=CARTESIAN_POINT('Ctrl Pts',(143.729465532532,2.54331576096232,124.284459892064));
#143574=CARTESIAN_POINT('Ctrl Pts',(143.456286211154,-3.98475800102683,
125.1242362306));
#143575=CARTESIAN_POINT('Ctrl Pts',(143.275922764381,-5.91742993572983,
128.954444514574));
#143576=CARTESIAN_POINT('Ctrl Pts',(143.188375192211,-5.92568524777546,
130.806401493052));
#143577=CARTESIAN_POINT('',(141.438375192211,-5.91702297748046,130.798906129064));
#143578=CARTESIAN_POINT('Ctrl Pts',(143.188375192211,-5.92568524777546,
130.806401493052));
#143579=CARTESIAN_POINT('Ctrl Pts',(143.183106889776,-5.92618202317967,
130.917845696673));
#143580=CARTESIAN_POINT('Ctrl Pts',(143.177838587341,-5.92331160393294,
131.02926379799));
#143581=CARTESIAN_POINT('Ctrl Pts',(143.079754410302,-5.80568103701415,
133.099976805968));
#143582=CARTESIAN_POINT('Ctrl Pts',(142.894122661094,-3.44277851418379,
136.897376014938));
#143583=CARTESIAN_POINT('Ctrl Pts',(142.615675037281,3.26532053551612,136.994291338557));
#143584=CARTESIAN_POINT('Ctrl Pts',(142.337227413468,6.97274953285437,131.402962724511));
#143585=CARTESIAN_POINT('Ctrl Pts',(142.058779789655,4.27256234724961,125.261548017523));
#143586=CARTESIAN_POINT('Ctrl Pts',(141.780332165842,-2.35390090920024,
124.213707308521));
#143587=CARTESIAN_POINT('Ctrl Pts',(141.57353063336,-5.66880166132113,127.933602662797));
#143588=CARTESIAN_POINT('Ctrl Pts',(141.459544975484,-5.92119195072286,
130.349379528659));
#143589=CARTESIAN_POINT('Ctrl Pts',(141.438375192211,-5.91702297748046,
130.798906129064));
#143590=CARTESIAN_POINT('',(139.688375192172,-5.9167499847919,130.804784840391));
#143591=CARTESIAN_POINT('Ctrl Pts',(141.438375192211,-5.91674748606238,
130.79890638302));
#143592=CARTESIAN_POINT('Ctrl Pts',(141.431065800626,-5.91689055543903,
130.954107881506));
#143593=CARTESIAN_POINT('Ctrl Pts',(141.423756409041,-5.91092284628539,
131.109486426606));
#143594=CARTESIAN_POINT('Ctrl Pts',(141.416447017456,-5.89882942285099,
131.264514942339));
#143595=CARTESIAN_POINT('Ctrl Pts',(141.409142780344,-5.88674452751565,
131.419434134311));
#143596=CARTESIAN_POINT('Ctrl Pts',(141.401838543231,-5.86854254517654,
131.574003406929));
#143597=CARTESIAN_POINT('Ctrl Pts',(141.394534306118,-5.84426061148494,
131.727696129471));
#143598=CARTESIAN_POINT('Ctrl Pts',(141.387232856437,-5.81998794422667,
131.881330200039));
#143599=CARTESIAN_POINT('Ctrl Pts',(141.379931406756,-5.78963999913602,
132.034088007126));
#143600=CARTESIAN_POINT('Ctrl Pts',(141.372629957075,-5.75330570620068,
132.185448599376));
#143601=CARTESIAN_POINT('Ctrl Pts',(141.365329820798,-5.71697794917513,
132.336781964477));
#143602=CARTESIAN_POINT('Ctrl Pts',(141.358029684521,-5.67466607556131,
132.486718241348));
#143603=CARTESIAN_POINT('Ctrl Pts',(141.350729548244,-5.6265099594955,132.634747526992));
#143604=CARTESIAN_POINT('Ctrl Pts',(141.34342919449,-5.57835240881922,132.782781222551));
#143605=CARTESIAN_POINT('Ctrl Pts',(141.336128840736,-5.52435038797274,
132.928907448565));
#143606=CARTESIAN_POINT('Ctrl Pts',(141.328828486982,-5.46469329765204,
133.07263258651));
#143607=CARTESIAN_POINT('Ctrl Pts',(141.321526384877,-5.40502192013949,
133.216392144984));
#143608=CARTESIAN_POINT('Ctrl Pts',(141.314224282772,-5.33969292580351,
133.357749116711));
#143609=CARTESIAN_POINT('Ctrl Pts',(141.306922180666,-5.26894327268043,
133.496231222141));
#143610=CARTESIAN_POINT('Ctrl Pts',(141.299612578507,-5.19812095195867,
133.634855563775));
#143611=CARTESIAN_POINT('Ctrl Pts',(141.292302976348,-5.12186702820574,
133.770598799663));
#143612=CARTESIAN_POINT('Ctrl Pts',(141.284993374188,-5.04046402047297,
133.903014038137));
#143613=CARTESIAN_POINT('Ctrl Pts',(141.277679838574,-4.95901720801798,
134.035500532121));
#143614=CARTESIAN_POINT('Ctrl Pts',(141.270366302959,-4.87241600671399,
134.164655143615));
#143615=CARTESIAN_POINT('Ctrl Pts',(141.263052767344,-4.78098497342835,
134.290061873605));
#143616=CARTESIAN_POINT('Ctrl Pts',(141.255728307744,-4.68941737264306,
134.415655919466));
#143617=CARTESIAN_POINT('Ctrl Pts',(141.248403848144,-4.59300576799819,
134.537490601409));
#143618=CARTESIAN_POINT('Ctrl Pts',(141.241079388544,-4.4921140771244,134.655184124376));
#143619=CARTESIAN_POINT('Ctrl Pts',(141.235198565101,-4.41110793424951,
134.749680492256));
#143620=CARTESIAN_POINT('Ctrl Pts',(141.229317741659,-4.32721448582552,
134.841507901096));
#143621=CARTESIAN_POINT('Ctrl Pts',(141.223436918216,-4.24063787803311,
134.930487245518));
#143622=CARTESIAN_POINT('Ctrl Pts',(141.216013651811,-4.13135365442037,
135.042804403935));
#143623=CARTESIAN_POINT('Ctrl Pts',(141.208590385405,-4.01743886492291,
135.150946661614));
#143624=CARTESIAN_POINT('Ctrl Pts',(141.201167119,-3.89924547964,135.254508396237));
#143625=CARTESIAN_POINT('Ctrl Pts',(141.193752626279,-3.78119178912335,
135.357947729489));
#143626=CARTESIAN_POINT('Ctrl Pts',(141.186338133558,-3.65886984672371,
135.456817072274));
#143627=CARTESIAN_POINT('Ctrl Pts',(141.178923640837,-3.53266992342586,
135.550745955339));
#143628=CARTESIAN_POINT('Ctrl Pts',(141.171516294483,-3.40659163636524,
135.64458430621));
#143629=CARTESIAN_POINT('Ctrl Pts',(141.164108948129,-3.2766431069661,135.733491455784));
#143630=CARTESIAN_POINT('Ctrl Pts',(141.156701601776,-3.14324920679138,
135.817135795699));
#143631=CARTESIAN_POINT('Ctrl Pts',(141.1492997801,-3.00995479681998,135.900717750509));
#143632=CARTESIAN_POINT('Ctrl Pts',(141.141897958425,-2.873220447571,135.979044513807));
#143633=CARTESIAN_POINT('Ctrl Pts',(141.134496136749,-2.73350156943249,
136.051826647224));
#143634=CARTESIAN_POINT('Ctrl Pts',(141.127098222438,-2.59385644780272,
136.124570359518));
#143635=CARTESIAN_POINT('Ctrl Pts',(141.119700308127,-2.45123026521982,
136.191775099103));
#143636=CARTESIAN_POINT('Ctrl Pts',(141.112302393815,-2.30610459091035,
136.253196472892));
#143637=CARTESIAN_POINT('Ctrl Pts',(141.104905708903,-2.16100303385463,
136.314607639563));
#143638=CARTESIAN_POINT('Ctrl Pts',(141.097509023991,-2.01340315289902,
136.370237202565));
#143639=CARTESIAN_POINT('Ctrl Pts',(141.090112339079,-1.86380824292428,
136.419888143641));
#143640=CARTESIAN_POINT('Ctrl Pts',(141.082715982143,-1.71421996614457,
136.469536883143));
#143641=CARTESIAN_POINT('Ctrl Pts',(141.075319625208,-1.56263719053038,
136.513207410233));
#143642=CARTESIAN_POINT('Ctrl Pts',(141.067923268272,-1.40957992781836,
136.550752093057));
#143643=CARTESIAN_POINT('Ctrl Pts',(141.060525778935,-1.25649923164864,
136.588302524067));
#143644=CARTESIAN_POINT('Ctrl Pts',(141.053128289599,-1.1019439614603,136.619725154422));
#143645=CARTESIAN_POINT('Ctrl Pts',(141.045730800262,-0.946445768353029,
136.644923173525));
#143646=CARTESIAN_POINT('Ctrl Pts',(141.038330717747,-0.790893065595329,
136.670130025753));
#143647=CARTESIAN_POINT('Ctrl Pts',(141.030930635232,-0.634397150076889,
136.689107862652));
#143648=CARTESIAN_POINT('Ctrl Pts',(141.023530552717,-0.47749611352947,
136.701811594392));
#143649=CARTESIAN_POINT('Ctrl Pts',(141.016122333051,-0.320422548162493,
136.714529295191));
#143650=CARTESIAN_POINT('Ctrl Pts',(141.008714113384,-0.162943344437875,
136.720959082884));
#143651=CARTESIAN_POINT('Ctrl Pts',(141.001305893718,-0.005598663443887,
136.721107968727));
#143652=CARTESIAN_POINT('Ctrl Pts',(140.993893114416,0.151842860575984,
136.721256946206));
#143653=CARTESIAN_POINT('Ctrl Pts',(140.986480335114,0.309149324733783,
136.715117333287));
#143654=CARTESIAN_POINT('Ctrl Pts',(140.979067555811,0.465784880194546,
136.702748109744));
#143655=CARTESIAN_POINT('Ctrl Pts',(140.971644184783,0.622644243882486,
136.690361212474));
#143656=CARTESIAN_POINT('Ctrl Pts',(140.964220813754,0.778830414595473,
136.671726971074));
#143657=CARTESIAN_POINT('Ctrl Pts',(140.956797442725,0.933816109861406,
136.646955763172));
#143658=CARTESIAN_POINT('Ctrl Pts',(140.952861393284,1.01599324432282,136.633821474366));
#143659=CARTESIAN_POINT('Ctrl Pts',(140.948925343844,1.09783309672732,136.618962708455));
#143660=CARTESIAN_POINT('Ctrl Pts',(140.944989294403,1.1792588336594,136.602401594115));
#143661=CARTESIAN_POINT('Ctrl Pts',(140.937566027997,1.33282523230163,136.571167849323));
#143662=CARTESIAN_POINT('Ctrl Pts',(140.930142761592,1.48538210268091,136.533781642481));
#143663=CARTESIAN_POINT('Ctrl Pts',(140.922719495186,1.63639793481917,136.490319847232));
#143664=CARTESIAN_POINT('Ctrl Pts',(140.915305002465,1.78723527878503,136.446909420215));
#143665=CARTESIAN_POINT('Ctrl Pts',(140.907890509744,1.93653485474148,136.397437800529));
#143666=CARTESIAN_POINT('Ctrl Pts',(140.900476017023,2.08377402541546,136.342033086528));
#143667=CARTESIAN_POINT('Ctrl Pts',(140.89306867067,2.23087128143318,136.286681773677));
#143668=CARTESIAN_POINT('Ctrl Pts',(140.885661324316,2.37591173866099,136.225408881583));
#143669=CARTESIAN_POINT('Ctrl Pts',(140.878253977962,2.51838675213341,136.158392624304));
#143670=CARTESIAN_POINT('Ctrl Pts',(140.870852156287,2.66075550236602,136.091426350279));
#143671=CARTESIAN_POINT('Ctrl Pts',(140.863450334611,2.80056228234905,136.018725398538));
#143672=CARTESIAN_POINT('Ctrl Pts',(140.856048512936,2.93731741894727,135.940516470229));
#143673=CARTESIAN_POINT('Ctrl Pts',(140.848650598625,3.0740003635726,135.862348827806));
#143674=CARTESIAN_POINT('Ctrl Pts',(140.841252684313,3.20763454984633,135.778679184328));
#143675=CARTESIAN_POINT('Ctrl Pts',(140.833854770002,3.33775406301456,135.689780597192));
#143676=CARTESIAN_POINT('Ctrl Pts',(140.82645808509,3.46785195268059,135.600896783388));
#143677=CARTESIAN_POINT('Ctrl Pts',(140.819061400178,3.59443602052922,135.506785960925));
#143678=CARTESIAN_POINT('Ctrl Pts',(140.811664715266,3.71706846634464,135.407765072858));
#143679=CARTESIAN_POINT('Ctrl Pts',(140.80426835833,3.83969547450895,135.308748575482));
#143680=CARTESIAN_POINT('Ctrl Pts',(140.796872001395,3.95837091859831,135.204822679915));
#143681=CARTESIAN_POINT('Ctrl Pts',(140.789475644459,4.07268951270544,135.096345088134));
#143682=CARTESIAN_POINT('Ctrl Pts',(140.782078155123,4.18702560928126,134.987850888157));
#143683=CARTESIAN_POINT('Ctrl Pts',(140.774680665786,4.29700325689377,134.874803861363));
#143684=CARTESIAN_POINT('Ctrl Pts',(140.76728317645,4.40225363563843,134.757598972385));
#143685=CARTESIAN_POINT('Ctrl Pts',(140.759883093935,4.50754090974044,134.640352997414));
#143686=CARTESIAN_POINT('Ctrl Pts',(140.75248301142,4.60809736636642,134.518946535896));
#143687=CARTESIAN_POINT('Ctrl Pts',(140.745082928905,4.70359421844273,134.393807927492));
#143688=CARTESIAN_POINT('Ctrl Pts',(140.737674709238,4.79919607912508,134.268531716323));
#143689=CARTESIAN_POINT('Ctrl Pts',(140.730266489572,4.88972699786911,134.139515459491));
#143690=CARTESIAN_POINT('Ctrl Pts',(140.722858269905,4.97490090317974,134.007217399572));
#143691=CARTESIAN_POINT('Ctrl Pts',(140.715445490603,5.06012723160788,133.874837912405));
#143692=CARTESIAN_POINT('Ctrl Pts',(140.708032711301,5.13998978767766,133.739172918207));
#143693=CARTESIAN_POINT('Ctrl Pts',(140.700619931999,5.21424855335885,133.600705121788));
#143694=CARTESIAN_POINT('Ctrl Pts',(140.693196560971,5.28861342344689,133.462039476089));
#143695=CARTESIAN_POINT('Ctrl Pts',(140.685773189942,5.35735834873741,133.320563364602));
#143696=CARTESIAN_POINT('Ctrl Pts',(140.678349818913,5.42029118399987,133.17678006681));
#143697=CARTESIAN_POINT('Ctrl Pts',(140.674413769472,5.45365968330849,133.100542712289));
#143698=CARTESIAN_POINT('Ctrl Pts',(140.670477720031,5.48539502199948,133.023657000717));
#143699=CARTESIAN_POINT('Ctrl Pts',(140.666541670591,5.51547428721513,132.946199535311));
#143700=CARTESIAN_POINT('Ctrl Pts',(140.659118404185,5.57220284267034,132.800117172921));
#143701=CARTESIAN_POINT('Ctrl Pts',(140.65169513778,5.62320948287038,132.651558599229));
#143702=CARTESIAN_POINT('Ctrl Pts',(140.644271871374,5.66827158966255,132.501012540715));
#143703=CARTESIAN_POINT('Ctrl Pts',(140.636857378653,5.71328043678675,132.35064441514));
#143704=CARTESIAN_POINT('Ctrl Pts',(140.629442885932,5.7523586296856,132.198293834652));
#143705=CARTESIAN_POINT('Ctrl Pts',(140.622028393211,5.7853314429195,132.044469749081));
#143706=CARTESIAN_POINT('Ctrl Pts',(140.614621046857,5.81827247571454,131.890793924955));
#143707=CARTESIAN_POINT('Ctrl Pts',(140.607213700504,5.84511976619896,131.73564778568));
#143708=CARTESIAN_POINT('Ctrl Pts',(140.59980635415,5.86574831587934,131.579555597722));
#143709=CARTESIAN_POINT('Ctrl Pts',(140.592404532474,5.88636148000912,131.423579829206));
#143710=CARTESIAN_POINT('Ctrl Pts',(140.585002710799,5.90076508986235,131.266659785438));
#143711=CARTESIAN_POINT('Ctrl Pts',(140.577600889124,5.90888519524603,131.109329979801));
#143712=CARTESIAN_POINT('Ctrl Pts',(140.570202974812,5.91700101408927,130.952083227345));
#143713=CARTESIAN_POINT('Ctrl Pts',(140.562805060501,5.91883991526116,130.794427515672));
#143714=CARTESIAN_POINT('Ctrl Pts',(140.555407146189,5.9143797913781,130.636902426251));
#143715=CARTESIAN_POINT('Ctrl Pts',(140.548010461277,5.9099204086867,130.479403514643));
#143716=CARTESIAN_POINT('Ctrl Pts',(140.540613776365,5.89916408905104,130.322035554988));
#143717=CARTESIAN_POINT('Ctrl Pts',(140.533217091453,5.88214084393088,130.165338196473));
#143718=CARTESIAN_POINT('Ctrl Pts',(140.525820734517,5.86511835363928,130.008647786082));
#143719=CARTESIAN_POINT('Ctrl Pts',(140.518424377582,5.84182953070357,129.852628288822));
#143720=CARTESIAN_POINT('Ctrl Pts',(140.511028020646,5.81235625299531,129.697814029859));
#143721=CARTESIAN_POINT('Ctrl Pts',(140.50363053131,5.78287846285299,129.542976068438));
#143722=CARTESIAN_POINT('Ctrl Pts',(140.496233041973,5.74721440244067,129.389344079463));
#143723=CARTESIAN_POINT('Ctrl Pts',(140.488835552636,5.70549701052338,129.237441849598));
#143724=CARTESIAN_POINT('Ctrl Pts',(140.481435470121,5.66376499463898,129.085486370643));
#143725=CARTESIAN_POINT('Ctrl Pts',(140.474035387606,5.61597552118902,128.935262217809));
#143726=CARTESIAN_POINT('Ctrl Pts',(140.466635305091,5.56231124701649,128.787277537023));
#143727=CARTESIAN_POINT('Ctrl Pts',(140.459227085425,5.50858796345766,128.639130131867));
#143728=CARTESIAN_POINT('Ctrl Pts',(140.451818865758,5.44897710557661,128.493227467744));
#143729=CARTESIAN_POINT('Ctrl Pts',(140.444410646092,5.38370957720002,128.35005791601));
#143730=CARTESIAN_POINT('Ctrl Pts',(140.43699786679,5.31840187774888,128.206800245806));
#143731=CARTESIAN_POINT('Ctrl Pts',(140.429585087488,5.24743073820561,128.066279372394));
#143732=CARTESIAN_POINT('Ctrl Pts',(140.422172308186,5.17107253618896,127.928958143481));
#143733=CARTESIAN_POINT('Ctrl Pts',(140.414748937157,5.09460522999219,127.791440703556));
#143734=CARTESIAN_POINT('Ctrl Pts',(140.407325566128,5.01273568189467,127.657132356947));
#143735=CARTESIAN_POINT('Ctrl Pts',(140.399902195099,4.92578345598751,127.526466795732));
#143736=CARTESIAN_POINT('Ctrl Pts',(140.395966145658,4.87967929942065,127.457184779897));
#143737=CARTESIAN_POINT('Ctrl Pts',(140.392030096218,4.83214689849864,127.38892633552));
#143738=CARTESIAN_POINT('Ctrl Pts',(140.388094046777,4.78323831671844,127.321752145748));
#143739=CARTESIAN_POINT('Ctrl Pts',(140.380670780371,4.69099825786723,127.195063720275));
#143740=CARTESIAN_POINT('Ctrl Pts',(140.373247513966,4.59358205735704,127.071850851466));
#143741=CARTESIAN_POINT('Ctrl Pts',(140.36582424756,4.49128056406732,126.952565002878));
#143742=CARTESIAN_POINT('Ctrl Pts',(140.358409754839,4.38909998264718,126.833420140257));
#143743=CARTESIAN_POINT('Ctrl Pts',(140.350995262118,4.2820458422903,126.718193339696));
#143744=CARTESIAN_POINT('Ctrl Pts',(140.343580769397,4.17045189353369,126.60730670247));
#143745=CARTESIAN_POINT('Ctrl Pts',(140.336173423044,4.05896550322618,126.49652694196));
#143746=CARTESIAN_POINT('Ctrl Pts',(140.32876607669,3.94294827857493,126.390079278187));
#143747=CARTESIAN_POINT('Ctrl Pts',(140.321358730336,3.8227737350675,126.288352254755));
#143748=CARTESIAN_POINT('Ctrl Pts',(140.313956908661,3.70268882226875,126.186701103175));
#143749=CARTESIAN_POINT('Ctrl Pts',(140.306555086985,3.57845304819304,126.089763821632));
#143750=CARTESIAN_POINT('Ctrl Pts',(140.29915326531,3.45047614220427,125.997891544059));
#143751=CARTESIAN_POINT('Ctrl Pts',(140.291755350999,3.32256679422905,125.906067765147));
#143752=CARTESIAN_POINT('Ctrl Pts',(140.284357436688,3.19092054995827,125.819303882397));
#143753=CARTESIAN_POINT('Ctrl Pts',(140.276959522376,3.05597942498416,125.737910152342));
#143754=CARTESIAN_POINT('Ctrl Pts',(140.269562837464,2.92106072477569,125.656529948447));
#143755=CARTESIAN_POINT('Ctrl Pts',(140.262166152552,2.7828485499254,125.580518318672));
#143756=CARTESIAN_POINT('Ctrl Pts',(140.25476946764,2.64181314450327,125.510141707091));
#143757=CARTESIAN_POINT('Ctrl Pts',(140.247373110704,2.50078399273881,125.439768216083));
#143758=CARTESIAN_POINT('Ctrl Pts',(140.239976753769,2.35693219333363,125.375029413135));
#143759=CARTESIAN_POINT('Ctrl Pts',(140.232580396834,2.2107515461741,125.31614522788));
#143760=CARTESIAN_POINT('Ctrl Pts',(140.225182907497,2.06454851838484,125.257252027305));
#143761=CARTESIAN_POINT('Ctrl Pts',(140.217785418161,1.9160162791809,125.204215368678));
#143762=CARTESIAN_POINT('Ctrl Pts',(140.210387928824,1.76566736176624,125.157206526336));
#143763=CARTESIAN_POINT('Ctrl Pts',(140.202987846309,1.61526573977063,125.110181205117));
#143764=CARTESIAN_POINT('Ctrl Pts',(140.195587763794,1.46304652769936,125.069188018563));
#143765=CARTESIAN_POINT('Ctrl Pts',(140.188187681279,1.30953597359666,125.034347957584));
#143766=CARTESIAN_POINT('Ctrl Pts',(140.180779461613,1.15585661885894,124.999469586376));
#143767=CARTESIAN_POINT('Ctrl Pts',(140.173371241946,1.00088345059321,124.970757935549));
#143768=CARTESIAN_POINT('Ctrl Pts',(140.16596302228,0.845152158611476,124.948282715822));
#143769=CARTESIAN_POINT('Ctrl Pts',(140.158550242978,0.689325016618268,
124.925793662972));
#143770=CARTESIAN_POINT('Ctrl Pts',(140.151137463676,0.532739191569369,
124.909548728185));
#143771=CARTESIAN_POINT('Ctrl Pts',(140.143724684374,0.375933479202662,
124.899565567633));
#143772=CARTESIAN_POINT('Ctrl Pts',(140.136301313345,0.218903715480498,
124.889568142673));
#143773=CARTESIAN_POINT('Ctrl Pts',(140.128877942316,0.06165380914696,124.885850370148));
#143774=CARTESIAN_POINT('Ctrl Pts',(140.121454571288,-0.0952786301733748,
124.888377812898));
#143775=CARTESIAN_POINT('Ctrl Pts',(140.117518521847,-0.17848797504547,
124.889717923689));
#143776=CARTESIAN_POINT('Ctrl Pts',(140.113582472406,-0.261608161221388,
124.892812922281));
#143777=CARTESIAN_POINT('Ctrl Pts',(140.109646422965,-0.344559992659762,
124.897651806903));
#143778=CARTESIAN_POINT('Ctrl Pts',(140.10222315656,-0.501004557910546,
124.906777792284));
#143779=CARTESIAN_POINT('Ctrl Pts',(140.094799890154,-0.657322869908095,
124.922137235511));
#143780=CARTESIAN_POINT('Ctrl Pts',(140.087376623749,-0.812977888652229,
124.943729464263));
#143781=CARTESIAN_POINT('Ctrl Pts',(140.079962131028,-0.96844893609033,
124.965296172795));
#143782=CARTESIAN_POINT('Ctrl Pts',(140.072547638307,-1.1232578846003,124.993080952733));
#143783=CARTESIAN_POINT('Ctrl Pts',(140.065133145586,-1.2768692081074,125.02703116635));
#143784=CARTESIAN_POINT('Ctrl Pts',(140.057725799232,-1.43033247523699,
125.060948657473));
#143785=CARTESIAN_POINT('Ctrl Pts',(140.050318452878,-1.5826000533251,125.101019671952));
#143786=CARTESIAN_POINT('Ctrl Pts',(140.042911106524,-1.73314315538902,
125.147139977938));
#143787=CARTESIAN_POINT('Ctrl Pts',(140.035509284849,-1.88357397672872,
125.193225885661));
#143788=CARTESIAN_POINT('Ctrl Pts',(140.028107463174,-2.03228252761314,
125.245351992432));
#143789=CARTESIAN_POINT('Ctrl Pts',(140.020705641498,-2.17875192039045,
125.303363377802));
#143790=CARTESIAN_POINT('Ctrl Pts',(140.013307727187,-2.32514399311632,
125.361344139413));
#143791=CARTESIAN_POINT('Ctrl Pts',(140.005909812875,-2.46929891562388,
125.425203855182));
#143792=CARTESIAN_POINT('Ctrl Pts',(139.998511898564,-2.61071674008065,
125.494738346108));
#143793=CARTESIAN_POINT('Ctrl Pts',(139.991115213652,-2.75211106345952,
125.564261281663));
#143794=CARTESIAN_POINT('Ctrl Pts',(139.983718528739,-2.8907688568771,125.639456956156));
#143795=CARTESIAN_POINT('Ctrl Pts',(139.976321843827,-3.02621177498084,
125.720073759464));
#143796=CARTESIAN_POINT('Ctrl Pts',(139.968925486892,-3.16164868740332,
125.800686988139));
#143797=CARTESIAN_POINT('Ctrl Pts',(139.961529129956,-3.29387068717532,
125.886720676746));
#143798=CARTESIAN_POINT('Ctrl Pts',(139.954132773021,-3.42242583036773,
125.977878254796));
#143799=CARTESIAN_POINT('Ctrl Pts',(139.946735283684,-3.5510006556812,126.069049789303));
#143800=CARTESIAN_POINT('Ctrl Pts',(139.939337794348,-3.67590720205223,
126.165346559318));
#143801=CARTESIAN_POINT('Ctrl Pts',(139.931940305011,-3.79672433481373,
126.266429934101));
#143802=CARTESIAN_POINT('Ctrl Pts',(139.924540222496,-3.9175838198334,126.367548743504));
#143803=CARTESIAN_POINT('Ctrl Pts',(139.917140139981,-4.03435075095351,
126.473457259045));
#143804=CARTESIAN_POINT('Ctrl Pts',(139.909740057466,-4.14663888517259,
126.583778131881));
#143805=CARTESIAN_POINT('Ctrl Pts',(139.902331837799,-4.25905049173922,
126.694220313858));
#143806=CARTESIAN_POINT('Ctrl Pts',(139.894923618133,-4.36697319961371,
126.809084280795));
#143807=CARTESIAN_POINT('Ctrl Pts',(139.887515398466,-4.47005880576604,
126.927957022029));
#143808=CARTESIAN_POINT('Ctrl Pts',(139.880102619164,-4.57320785938891,
127.046902927451));
#143809=CARTESIAN_POINT('Ctrl Pts',(139.872689839862,-4.67151364636655,
127.169862232749));
#143810=CARTESIAN_POINT('Ctrl Pts',(139.86527706056,-4.7646700798034,127.296391177402));
#143811=CARTESIAN_POINT('Ctrl Pts',(139.857853689531,-4.85795961952092,
127.423100912544));
#143812=CARTESIAN_POINT('Ctrl Pts',(139.850430318503,-4.94608490225515,
127.55339016543));
#143813=CARTESIAN_POINT('Ctrl Pts',(139.843006947474,-5.02878430982933,
127.686788015731));
#143814=CARTESIAN_POINT('Ctrl Pts',(139.839070898033,-5.07263352006995,
127.757518756797));
#143815=CARTESIAN_POINT('Ctrl Pts',(139.835134848592,-5.11495810104929,
127.82912304585));
#143816=CARTESIAN_POINT('Ctrl Pts',(139.831198799151,-5.15572450147464,
127.901528306289));
#143817=CARTESIAN_POINT('Ctrl Pts',(139.823436577619,-5.23611928206174,
128.044317587796));
#143818=CARTESIAN_POINT('Ctrl Pts',(139.815674356087,-5.31067601333723,
128.190622135892));
#143819=CARTESIAN_POINT('Ctrl Pts',(139.807912134555,-5.37908850597535,
128.339946405753));
#143820=CARTESIAN_POINT('Ctrl Pts',(139.800162163852,-5.44739302568525,
128.489035002596));
#143821=CARTESIAN_POINT('Ctrl Pts',(139.79241219315,-5.5095724986194,128.641133529821));
#143822=CARTESIAN_POINT('Ctrl Pts',(139.784662222447,-5.5653656799586,128.795720428075));
#143823=CARTESIAN_POINT('Ctrl Pts',(139.776638303261,-5.62313105680892,
128.955771714261));
#143824=CARTESIAN_POINT('Ctrl Pts',(139.768614384074,-5.67405018060018,
129.11849024006));
#143825=CARTESIAN_POINT('Ctrl Pts',(139.760590464888,-5.71788537890809,
129.283269773412));
#143826=CARTESIAN_POINT('Ctrl Pts',(139.752866423857,-5.7600823231272,129.441890996669));
#143827=CARTESIAN_POINT('Ctrl Pts',(139.745142382826,-5.79571510917827,
129.602421614688));
#143828=CARTESIAN_POINT('Ctrl Pts',(139.737418341795,-5.82462070112284,
129.764300883439));
#143829=CARTESIAN_POINT('Ctrl Pts',(139.729702869658,-5.85349422579409,
129.926000566637));
#143830=CARTESIAN_POINT('Ctrl Pts',(139.721987397521,-5.87565537091717,
130.089045600889));
#143831=CARTESIAN_POINT('Ctrl Pts',(139.714271925383,-5.89099142555501,
130.252862125694));
#143832=CARTESIAN_POINT('Ctrl Pts',(139.706566454259,-5.90630760116474,
130.416466306882));
#143833=CARTESIAN_POINT('Ctrl Pts',(139.698860983135,-5.91481629810642,
130.580839661933));
#143834=CARTESIAN_POINT('Ctrl Pts',(139.691155512011,-5.91645622347929,
130.745400307584));
#143835=CARTESIAN_POINT('Ctrl Pts',(139.690228738744,-5.9166534650198,130.765192790701));
#143836=CARTESIAN_POINT('Ctrl Pts',(139.689301965478,-5.91675140419712,
130.784987974349));
#143837=CARTESIAN_POINT('Ctrl Pts',(139.688375192211,-5.91674998479196,
130.804784839551));
#143838=CARTESIAN_POINT('',(137.938375192211,-5.917008063288,130.809669329993));
#143839=CARTESIAN_POINT('Ctrl Pts',(139.688375192172,-5.9167499847919,130.80478484039));
#143840=CARTESIAN_POINT('Ctrl Pts',(139.680584137911,-5.91673805233238,
130.971210067061));
#143841=CARTESIAN_POINT('Ctrl Pts',(139.672793083651,-5.90970006480498,
131.137483867577));
#143842=CARTESIAN_POINT('Ctrl Pts',(139.665002029391,-5.89569994840646,
131.303011478249));
#143843=CARTESIAN_POINT('Ctrl Pts',(139.657199697439,-5.88167956658594,
131.468778693135));
#143844=CARTESIAN_POINT('Ctrl Pts',(139.649397365486,-5.86067696226432,
131.633797253035));
#143845=CARTESIAN_POINT('Ctrl Pts',(139.641595033534,-5.83280745341976,
131.797480838804));
#143846=CARTESIAN_POINT('Ctrl Pts',(139.633773170766,-5.80486818155786,
131.961574157693));
#143847=CARTESIAN_POINT('Ctrl Pts',(139.625951307999,-5.77002767955835,
132.124325512147));
#143848=CARTESIAN_POINT('Ctrl Pts',(139.618129445232,-5.72845218244328,
132.285159778817));
#143849=CARTESIAN_POINT('Ctrl Pts',(139.610297413009,-5.68682263168829,
132.446203151285));
#143850=CARTESIAN_POINT('Ctrl Pts',(139.602465380787,-5.63844069455175,
132.605324163508));
#143851=CARTESIAN_POINT('Ctrl Pts',(139.594633348564,-5.58352163616306,
132.761965455371));
#143852=CARTESIAN_POINT('Ctrl Pts',(139.586782860964,-5.5284731666656,132.918975856317));
#143853=CARTESIAN_POINT('Ctrl Pts',(139.578932373364,-5.46685688233304,
133.073494561328));
#143854=CARTESIAN_POINT('Ctrl Pts',(139.571081885763,-5.39893602997023,
133.224984567458));
#143855=CARTESIAN_POINT('Ctrl Pts',(139.564971648955,-5.34607148024038,
133.342893143161));
#143856=CARTESIAN_POINT('Ctrl Pts',(139.558861412147,-5.28938863651094,
133.458967410419));
#143857=CARTESIAN_POINT('Ctrl Pts',(139.552751175339,-5.22903006457896,
133.572965888497));
#143858=CARTESIAN_POINT('Ctrl Pts',(139.545327908933,-5.15570103112815,
133.711461514633));
#143859=CARTESIAN_POINT('Ctrl Pts',(139.537904642528,-5.07675504096567,
133.847251270503));
#143860=CARTESIAN_POINT('Ctrl Pts',(139.530481376123,-4.99241593521631,
133.979846988549));
#143861=CARTESIAN_POINT('Ctrl Pts',(139.523066883402,-4.90817651128592,
134.112285989467));
#143862=CARTESIAN_POINT('Ctrl Pts',(139.515652390681,-4.81855685806873,
134.24153815499));
#143863=CARTESIAN_POINT('Ctrl Pts',(139.50823789796,-4.72382745082585,134.36713829479));
#143864=CARTESIAN_POINT('Ctrl Pts',(139.500830551606,-4.62918934735203,
134.492617376446));
#143865=CARTESIAN_POINT('Ctrl Pts',(139.493423205252,-4.52945151777752,
134.614451143893));
#143866=CARTESIAN_POINT('Ctrl Pts',(139.486015858898,-4.4249285618775,134.732201982079));
#143867=CARTESIAN_POINT('Ctrl Pts',(139.478614037223,-4.32048356314145,
134.849864997248));
#143868=CARTESIAN_POINT('Ctrl Pts',(139.471212215547,-4.21126079104434,
134.96345086859));
#143869=CARTESIAN_POINT('Ctrl Pts',(139.463810393872,-4.09761600135079,
135.072553873263));
#143870=CARTESIAN_POINT('Ctrl Pts',(139.456412479561,-3.98403120385755,
135.181599283308));
#143871=CARTESIAN_POINT('Ctrl Pts',(139.449014565249,-3.86602930634111,
135.28616628175));
#143872=CARTESIAN_POINT('Ctrl Pts',(139.441616650938,-3.74400382473826,
135.385885027939));
#143873=CARTESIAN_POINT('Ctrl Pts',(139.434219966026,-3.62199862155639,
135.485587202682));
#143874=CARTESIAN_POINT('Ctrl Pts',(139.426823281113,-3.49597145012708,
135.580442488246));
#143875=CARTESIAN_POINT('Ctrl Pts',(139.419426596201,-3.36634998636792,
135.67012040734));
#143876=CARTESIAN_POINT('Ctrl Pts',(139.412030239266,-3.23673427016026,
135.759794350021));
#143877=CARTESIAN_POINT('Ctrl Pts',(139.40463388233,-3.10352488550231,135.844291170306));
#143878=CARTESIAN_POINT('Ctrl Pts',(139.397237525395,-2.96717942633891,
135.923323091975));
#143879=CARTESIAN_POINT('Ctrl Pts',(139.389840036058,-2.83081309233788,
136.002367113633));
#143880=CARTESIAN_POINT('Ctrl Pts',(139.382442546722,-2.69131005079165,
136.075944383498));
#143881=CARTESIAN_POINT('Ctrl Pts',(139.375045057385,-2.54915334377066,
136.14381262994));
#143882=CARTESIAN_POINT('Ctrl Pts',(139.36764497487,-2.40694680393599,136.211704667491));
#143883=CARTESIAN_POINT('Ctrl Pts',(139.360244892355,-2.26208508319391,
136.273883536337));
#143884=CARTESIAN_POINT('Ctrl Pts',(139.35284480984,-2.11507193508654,136.33015479324));
#143885=CARTESIAN_POINT('Ctrl Pts',(139.345436590174,-1.96789713090972,
136.386487926174));
#143886=CARTESIAN_POINT('Ctrl Pts',(139.338028370507,-1.81856652372409,
136.436900340648));
#143887=CARTESIAN_POINT('Ctrl Pts',(139.330620150841,-1.66760049015753,
136.481247014855));
#143888=CARTESIAN_POINT('Ctrl Pts',(139.323207371539,-1.51654153951631,
136.525620983701));
#143889=CARTESIAN_POINT('Ctrl Pts',(139.315794592236,-1.36384551800387,
136.563921682478));
#143890=CARTESIAN_POINT('Ctrl Pts',(139.308381812934,-1.2100432634918,136.596055176413));
#143891=CARTESIAN_POINT('Ctrl Pts',(139.300958441906,-1.05602124910576,
136.628234584191));
#143892=CARTESIAN_POINT('Ctrl Pts',(139.293535070877,-0.900890212021972,
136.654229126076));
#143893=CARTESIAN_POINT('Ctrl Pts',(139.286111699848,-0.745187208254172,
136.673996601778));
#143894=CARTESIAN_POINT('Ctrl Pts',(139.282175650407,-0.662629739613447,
136.684477791709));
#143895=CARTESIAN_POINT('Ctrl Pts',(139.278239600966,-0.579911501811691,
136.693209200584));
#143896=CARTESIAN_POINT('Ctrl Pts',(139.274303551526,-0.497112450655344,
136.700190480605));
#143897=CARTESIAN_POINT('Ctrl Pts',(139.26688028512,-0.34095602424579,136.713356956847));
#143898=CARTESIAN_POINT('Ctrl Pts',(139.259457018715,-0.184040020820868,
136.720335139353));
#143899=CARTESIAN_POINT('Ctrl Pts',(139.252033752309,-0.0268961411683008,
136.721049485513));
#143900=CARTESIAN_POINT('Ctrl Pts',(139.244619259588,0.130062007468616,
136.721762987375));
#143901=CARTESIAN_POINT('Ctrl Pts',(139.237204766867,0.287247126580009,
136.716227387588));
#143902=CARTESIAN_POINT('Ctrl Pts',(139.229790274146,0.444121639883464,
136.704418797914));
#143903=CARTESIAN_POINT('Ctrl Pts',(139.222382927792,0.600844951624832,
136.692621589803));
#143904=CARTESIAN_POINT('Ctrl Pts',(139.214975581439,0.757257883806268,
136.67456345632));
#143905=CARTESIAN_POINT('Ctrl Pts',(139.207568235085,0.912822209628291,
136.650272537541));
#143906=CARTESIAN_POINT('Ctrl Pts',(139.200166413409,1.06827050970707,136.625999735846));
#143907=CARTESIAN_POINT('Ctrl Pts',(139.192764591734,1.22287109641961,136.595503462281));
#143908=CARTESIAN_POINT('Ctrl Pts',(139.185362770059,1.37609032896568,136.558863721139));
#143909=CARTESIAN_POINT('Ctrl Pts',(139.177964855747,1.5292286782716,136.52224332183));
#143910=CARTESIAN_POINT('Ctrl Pts',(139.170566941436,1.68098676351751,136.479486000311));
#143911=CARTESIAN_POINT('Ctrl Pts',(139.163169027125,1.83084072231294,136.430722924778));
#143912=CARTESIAN_POINT('Ctrl Pts',(139.155772342212,1.98066977809889,136.381967952784));
#143913=CARTESIAN_POINT('Ctrl Pts',(139.1483756573,2.12859498082751,136.327209323002));
#143914=CARTESIAN_POINT('Ctrl Pts',(139.140978972388,2.27410712131415,136.266628220246));
#143915=CARTESIAN_POINT('Ctrl Pts',(139.133582615453,2.41961280963993,136.20604980372));
#143916=CARTESIAN_POINT('Ctrl Pts',(139.126186258517,2.5627053038478,136.139649571035));
#143917=CARTESIAN_POINT('Ctrl Pts',(139.118789901582,2.70289514894905,136.067656958861));
#143918=CARTESIAN_POINT('Ctrl Pts',(139.111392412245,2.84310645747352,135.995653324434));
#143919=CARTESIAN_POINT('Ctrl Pts',(139.103994922909,2.98041389993418,135.918055776236));
#143920=CARTESIAN_POINT('Ctrl Pts',(139.096597433572,3.11435255031025,135.835139757508));
#143921=CARTESIAN_POINT('Ctrl Pts',(139.089197351057,3.24833815267259,135.752194672698));
#143922=CARTESIAN_POINT('Ctrl Pts',(139.081797268542,3.37895229453517,135.663927601756));
#143923=CARTESIAN_POINT('Ctrl Pts',(139.074397186027,3.50575909419982,135.570657265482));
#143924=CARTESIAN_POINT('Ctrl Pts',(139.066988966361,3.63270533097677,135.477284368885));
#143925=CARTESIAN_POINT('Ctrl Pts',(139.059580746694,3.75583556381397,135.378897441212));
#143926=CARTESIAN_POINT('Ctrl Pts',(139.052172527028,3.87474650548079,135.275855902229));
#143927=CARTESIAN_POINT('Ctrl Pts',(139.044759747726,3.99373063484815,135.172750942898));
#143928=CARTESIAN_POINT('Ctrl Pts',(139.037346968424,4.10849002689675,135.064985918659));
#143929=CARTESIAN_POINT('Ctrl Pts',(139.029934189121,4.21865872080517,134.952956664408));
#143930=CARTESIAN_POINT('Ctrl Pts',(139.022510818093,4.32898482890984,134.840767337505));
#143931=CARTESIAN_POINT('Ctrl Pts',(139.015087447064,4.43470688803128,134.724301887308));
#143932=CARTESIAN_POINT('Ctrl Pts',(139.007664076035,4.53549910197673,134.603989343964));
#143933=CARTESIAN_POINT('Ctrl Pts',(139.003728026594,4.58894155228695,134.540196746623));
#143934=CARTESIAN_POINT('Ctrl Pts',(138.999791977154,4.64099876189668,134.475323090231));
#143935=CARTESIAN_POINT('Ctrl Pts',(138.995855927713,4.69162722012794,134.409435455881));
#143936=CARTESIAN_POINT('Ctrl Pts',(138.988432661307,4.78711091229139,134.285173433781));
#143937=CARTESIAN_POINT('Ctrl Pts',(138.981009394902,4.87779878760417,134.156927434104));
#143938=CARTESIAN_POINT('Ctrl Pts',(138.973586128496,4.96333989266453,134.025103959154));
#143939=CARTESIAN_POINT('Ctrl Pts',(138.966171635775,5.04877989524251,133.893436288605));
#143940=CARTESIAN_POINT('Ctrl Pts',(138.958757143054,5.12908503470471,133.758199869283));
#143941=CARTESIAN_POINT('Ctrl Pts',(138.951342650333,5.2039446400889,133.619834067164));
#143942=CARTESIAN_POINT('Ctrl Pts',(138.94393530398,5.278732092967,133.481601627214));
#143943=CARTESIAN_POINT('Ctrl Pts',(138.936527957626,5.34808428427725,133.340246135284));
#143944=CARTESIAN_POINT('Ctrl Pts',(138.929120611272,5.41173396433075,133.19623562722));
#143945=CARTESIAN_POINT('Ctrl Pts',(138.921718789597,5.47533617205153,133.052332527627));
#143946=CARTESIAN_POINT('Ctrl Pts',(138.914316967921,5.53324418684925,132.905778694735));
#143947=CARTESIAN_POINT('Ctrl Pts',(138.906915146246,5.58523687271368,132.757066339937));
#143948=CARTESIAN_POINT('Ctrl Pts',(138.899517231935,5.63720211204399,132.608432489233));
#143949=CARTESIAN_POINT('Ctrl Pts',(138.892119317623,5.68325811847254,132.457642737417));
#143950=CARTESIAN_POINT('Ctrl Pts',(138.884721403312,5.72323208709994,132.305208724368));
#143951=CARTESIAN_POINT('Ctrl Pts',(138.8773247184,5.7631994127789,132.152800043086));
#143952=CARTESIAN_POINT('Ctrl Pts',(138.869928033487,5.79708661204707,131.99874800362));
#143953=CARTESIAN_POINT('Ctrl Pts',(138.862531348575,5.82477088081715,131.843578952895));
#143954=CARTESIAN_POINT('Ctrl Pts',(138.85513499164,5.85245392203775,131.688416782529));
#143955=CARTESIAN_POINT('Ctrl Pts',(138.847738634704,5.87393451407551,131.53213806688));
#143956=CARTESIAN_POINT('Ctrl Pts',(138.840342277769,5.88914112612127,131.375278614416));
#143957=CARTESIAN_POINT('Ctrl Pts',(138.832944788432,5.90435006633816,131.218395146369));
#143958=CARTESIAN_POINT('Ctrl Pts',(138.825547299096,5.91328307793312,131.060931136052));
#143959=CARTESIAN_POINT('Ctrl Pts',(138.818149809759,5.91592059523523,130.903426622692));
#143960=CARTESIAN_POINT('Ctrl Pts',(138.810749727244,5.91855903711495,130.745866896369));
#143961=CARTESIAN_POINT('Ctrl Pts',(138.803349644729,5.91489758458202,130.588267011748));
#143962=CARTESIAN_POINT('Ctrl Pts',(138.795949562214,5.90496878176886,130.431165964824));
#143963=CARTESIAN_POINT('Ctrl Pts',(138.788541342548,5.8950290612163,130.273892169149));
#143964=CARTESIAN_POINT('Ctrl Pts',(138.781133122881,5.8788082509739,130.117118679392));
#143965=CARTESIAN_POINT('Ctrl Pts',(138.773724903215,5.85639075447156,129.961379067685));
#143966=CARTESIAN_POINT('Ctrl Pts',(138.766312123912,5.83395946037415,129.805543600845));
#143967=CARTESIAN_POINT('Ctrl Pts',(138.75889934461,5.80532394797405,129.650743646252));
#143968=CARTESIAN_POINT('Ctrl Pts',(138.751486565308,5.77061943361669,129.497501055537));
#143969=CARTESIAN_POINT('Ctrl Pts',(138.74406319428,5.73586533182175,129.344039504623));
#143970=CARTESIAN_POINT('Ctrl Pts',(138.736639823251,5.6950250054579,129.192140121422));
#143971=CARTESIAN_POINT('Ctrl Pts',(138.729216452222,5.64828330893846,129.042308908771));
#143972=CARTESIAN_POINT('Ctrl Pts',(138.725280402781,5.62349973989224,128.962864804673));
#143973=CARTESIAN_POINT('Ctrl Pts',(138.72134435334,5.597057888815,128.884001803985));
#143974=CARTESIAN_POINT('Ctrl Pts',(138.7174083039,5.56899067434469,128.805792772442));
#143975=CARTESIAN_POINT('Ctrl Pts',(138.709985037494,5.51605678380148,128.658292979773));
#143976=CARTESIAN_POINT('Ctrl Pts',(138.702561771089,5.45717880393865,128.51267460645));
#143977=CARTESIAN_POINT('Ctrl Pts',(138.695138504683,5.39250903777161,128.369452643935));
#143978=CARTESIAN_POINT('Ctrl Pts',(138.687724011962,5.32791570589757,128.226399957886));
#143979=CARTESIAN_POINT('Ctrl Pts',(138.680309519241,5.25754436566888,128.08573838172));
#143980=CARTESIAN_POINT('Ctrl Pts',(138.67289502652,5.18159674288067,127.947966779758));
#143981=CARTESIAN_POINT('Ctrl Pts',(138.665487680167,5.10572232127067,127.810327967253));
#143982=CARTESIAN_POINT('Ctrl Pts',(138.658080333813,5.02428249593846,127.675573908359));
#143983=CARTESIAN_POINT('Ctrl Pts',(138.650672987459,4.93752658371395,127.544182432617));
#143984=CARTESIAN_POINT('Ctrl Pts',(138.643271165784,4.8508353773219,127.412888953594));
#143985=CARTESIAN_POINT('Ctrl Pts',(138.635869344108,4.75883618356946,127.28495337425));
#143986=CARTESIAN_POINT('Ctrl Pts',(138.628467522433,4.66182358442672,127.160827794854));
#143987=CARTESIAN_POINT('Ctrl Pts',(138.621069608121,4.56486219748007,127.036767740384));
#143988=CARTESIAN_POINT('Ctrl Pts',(138.61367169381,4.46289290514456,126.916513973701));
#143989=CARTESIAN_POINT('Ctrl Pts',(138.606273779499,4.35625275927245,126.800488434312));
#143990=CARTESIAN_POINT('Ctrl Pts',(138.598877094586,4.24963033505785,126.684482176264));
#143991=CARTESIAN_POINT('Ctrl Pts',(138.591480409674,4.13833885021982,126.572703025522));
#143992=CARTESIAN_POINT('Ctrl Pts',(138.584083724762,4.02275475672535,126.465538804015));
#143993=CARTESIAN_POINT('Ctrl Pts',(138.576687367827,3.90717578835071,126.358379334282));
#143994=CARTESIAN_POINT('Ctrl Pts',(138.569291010891,3.78730486352086,126.255834640711));
#143995=CARTESIAN_POINT('Ctrl Pts',(138.561894653956,3.66355410892532,126.158254521761));
#143996=CARTESIAN_POINT('Ctrl Pts',(138.554497164619,3.53978440777332,126.060659463046));
#143997=CARTESIAN_POINT('Ctrl Pts',(138.547099675283,3.41213398724868,125.968030723546));
#143998=CARTESIAN_POINT('Ctrl Pts',(138.539702185946,3.28104662192607,125.880676668809));
#143999=CARTESIAN_POINT('Ctrl Pts',(138.532302103431,3.14991330413065,125.793291992243));
#144000=CARTESIAN_POINT('Ctrl Pts',(138.524902020916,3.01534095320797,125.711185888728));
#144001=CARTESIAN_POINT('Ctrl Pts',(138.517501938401,2.8778006326532,125.634622318464));
#144002=CARTESIAN_POINT('Ctrl Pts',(138.510093718734,2.74010907237648,125.557974558684));
#144003=CARTESIAN_POINT('Ctrl Pts',(138.502685499068,2.59944335123651,125.486881685119));
#144004=CARTESIAN_POINT('Ctrl Pts',(138.495277279402,2.45629800069497,125.421561095544));
#144005=CARTESIAN_POINT('Ctrl Pts',(138.487864500099,2.31306454657868,125.356200302236));
#144006=CARTESIAN_POINT('Ctrl Pts',(138.480451720797,2.16734876670303,125.296619013161));
#144007=CARTESIAN_POINT('Ctrl Pts',(138.473038941495,2.01966279736456,125.242985540533));
#144008=CARTESIAN_POINT('Ctrl Pts',(138.465615570467,1.87176580738731,125.189275433885));
#144009=CARTESIAN_POINT('Ctrl Pts',(138.458192199438,1.7218933603057,125.141530230144));
#144010=CARTESIAN_POINT('Ctrl Pts',(138.450768828409,1.57057108896393,125.099867912951));
#144011=CARTESIAN_POINT('Ctrl Pts',(138.446832778968,1.49033638977069,125.077777552701));
#144012=CARTESIAN_POINT('Ctrl Pts',(138.442896729527,1.40969424739082,125.057396452677));
#144013=CARTESIAN_POINT('Ctrl Pts',(138.438960680087,1.32872375915806,125.038736303205));
#144014=CARTESIAN_POINT('Ctrl Pts',(138.431537413681,1.1760159453532,125.003543843664));
#144015=CARTESIAN_POINT('Ctrl Pts',(138.424114147276,1.02167809745959,124.974369267926));
#144016=CARTESIAN_POINT('Ctrl Pts',(138.41669088087,0.866225815879054,124.951362804615));
#144017=CARTESIAN_POINT('Ctrl Pts',(138.409276388149,0.710957265985616,
124.928383533034));
#144018=CARTESIAN_POINT('Ctrl Pts',(138.401861895428,0.554577269905189,
124.91155791682));
#144019=CARTESIAN_POINT('Ctrl Pts',(138.394447402707,0.397614574039386,
124.900985886701));
#144020=CARTESIAN_POINT('Ctrl Pts',(138.387040056354,0.240803164729622,
124.890424046303));
#144021=CARTESIAN_POINT('Ctrl Pts',(138.37963271,0.0834105436789232,124.886103817468));
#144022=CARTESIAN_POINT('Ctrl Pts',(138.372225363646,-0.0740265157508794,
124.888073721424));
#144023=CARTESIAN_POINT('Ctrl Pts',(138.364823541971,-0.231346152682223,
124.890042156151));
#144024=CARTESIAN_POINT('Ctrl Pts',(138.357421720295,-0.388709790336678,
124.898291377771));
#144025=CARTESIAN_POINT('Ctrl Pts',(138.35001989862,-0.545577835203225,
124.91281791737));
#144026=CARTESIAN_POINT('Ctrl Pts',(138.342621984309,-0.702363070649498,
124.927336788521));
#144027=CARTESIAN_POINT('Ctrl Pts',(138.335224069997,-0.858652863569166,
124.948126343829));
#144028=CARTESIAN_POINT('Ctrl Pts',(138.327826155686,-1.01391003954467,
124.975131080637));
#144029=CARTESIAN_POINT('Ctrl Pts',(138.320429470774,-1.1691414145945,125.002131329746));
#144030=CARTESIAN_POINT('Ctrl Pts',(138.313032785861,-1.32334014586377,
125.035344646546));
#144031=CARTESIAN_POINT('Ctrl Pts',(138.305636100949,-1.47597646629815,
125.074663938558));
#144032=CARTESIAN_POINT('Ctrl Pts',(138.298239744014,-1.62860601867814,
125.113981487112));
#144033=CARTESIAN_POINT('Ctrl Pts',(138.290843387078,-1.77967293647711,
125.159404379423));
#144034=CARTESIAN_POINT('Ctrl Pts',(138.283447030143,-1.92866015980101,
125.210774956249));
#144035=CARTESIAN_POINT('Ctrl Pts',(138.276049540806,-2.07767019344926,
125.26215339804));
#144036=CARTESIAN_POINT('Ctrl Pts',(138.26865205147,-2.2245995457011,125.319481215793));
#144037=CARTESIAN_POINT('Ctrl Pts',(138.261254562133,-2.36894890889079,
125.382551728499));
#144038=CARTESIAN_POINT('Ctrl Pts',(138.253854479618,-2.51334887352568,
125.445644350475));
#144039=CARTESIAN_POINT('Ctrl Pts',(138.246454397103,-2.6551667065646,125.51448352609));
#144040=CARTESIAN_POINT('Ctrl Pts',(138.239054314588,-2.79392570948898,
125.58881561322));
#144041=CARTESIAN_POINT('Ctrl Pts',(138.231646094922,-2.93283729220205,
125.663229436122));
#144042=CARTESIAN_POINT('Ctrl Pts',(138.224237875255,-3.0686829984143,125.743148056475));
#144043=CARTESIAN_POINT('Ctrl Pts',(138.216829655589,-3.20101261888635,
125.828272919763));
#144044=CARTESIAN_POINT('Ctrl Pts',(138.209416876287,-3.33342368603194,
125.913450175983));
#144045=CARTESIAN_POINT('Ctrl Pts',(138.202004096985,-3.46231405028907,
126.003839846379));
#144046=CARTESIAN_POINT('Ctrl Pts',(138.194591317683,-3.58726528364737,
126.099102033042));
#144047=CARTESIAN_POINT('Ctrl Pts',(138.187167946654,-3.71239505318744,
126.194500334784));
#144048=CARTESIAN_POINT('Ctrl Pts',(138.179744575625,-3.83357416379487,
126.294784820258));
#144049=CARTESIAN_POINT('Ctrl Pts',(138.172321204596,-3.9504192350998,126.399577032706));
#144050=CARTESIAN_POINT('Ctrl Pts',(138.168385155156,-4.01237329556604,
126.455140378201));
#144051=CARTESIAN_POINT('Ctrl Pts',(138.164449105715,-4.07310953999066,
126.511970414092));
#144052=CARTESIAN_POINT('Ctrl Pts',(138.160513056274,-4.13257537892972,
126.570006912458));
#144053=CARTESIAN_POINT('Ctrl Pts',(138.15319622246,-4.24311811160658,126.67789260345));
#144054=CARTESIAN_POINT('Ctrl Pts',(138.145879388645,-4.34962365026246,
126.79029608547));
#144055=CARTESIAN_POINT('Ctrl Pts',(138.138562554831,-4.4516921232071,126.906878378649));
#144056=CARTESIAN_POINT('Ctrl Pts',(138.131254509615,-4.55363799684109,
127.023320639275));
#144057=CARTESIAN_POINT('Ctrl Pts',(138.123946464399,-4.65115715751967,
127.143931437888));
#144058=CARTESIAN_POINT('Ctrl Pts',(138.116638419182,-4.74388446255217,
127.268333076885));
#144059=CARTESIAN_POINT('Ctrl Pts',(138.109210784725,-4.83812916213939,
127.394770430923));
#144060=CARTESIAN_POINT('Ctrl Pts',(138.101783150268,-4.92742349399904,
127.525123525742));
#144061=CARTESIAN_POINT('Ctrl Pts',(138.094355515811,-5.01142397125429,
127.65895756822));
#144062=CARTESIAN_POINT('Ctrl Pts',(138.087060421163,-5.09392553154876,
127.790403456215));
#144063=CARTESIAN_POINT('Ctrl Pts',(138.079765326516,-5.17132035816477,
127.925206767697));
#144064=CARTESIAN_POINT('Ctrl Pts',(138.072470231869,-5.2433247161891,128.062923679918));
#144065=CARTESIAN_POINT('Ctrl Pts',(138.065178223667,-5.31529861023819,
128.200582326158));
#144066=CARTESIAN_POINT('Ctrl Pts',(138.057886215466,-5.38188639496685,
128.341151780288));
#144067=CARTESIAN_POINT('Ctrl Pts',(138.050594207265,-5.4428493125588,128.484161935712));
#144068=CARTESIAN_POINT('Ctrl Pts',(138.043303748025,-5.50379928046742,
128.627141713059));
#144069=CARTESIAN_POINT('Ctrl Pts',(138.036013288785,-5.55912660869075,
128.772560805855));
#144070=CARTESIAN_POINT('Ctrl Pts',(138.028722829545,-5.60864002550062,
128.919927645329));
#144071=CARTESIAN_POINT('Ctrl Pts',(138.021193859767,-5.65977329522876,
129.07211565491));
#144072=CARTESIAN_POINT('Ctrl Pts',(138.013664889989,-5.7047055945997,129.226380625873));
#144073=CARTESIAN_POINT('Ctrl Pts',(138.006135920212,-5.74328164631964,
129.382162848777));
#144074=CARTESIAN_POINT('Ctrl Pts',(137.998841500885,-5.78065593596289,
129.533091978651));
#144075=CARTESIAN_POINT('Ctrl Pts',(137.991547081559,-5.81206404154171,
129.685444843784));
#144076=CARTESIAN_POINT('Ctrl Pts',(137.984252662233,-5.83741664668609,
129.838701539272));
#144077=CARTESIAN_POINT('Ctrl Pts',(137.97660641723,-5.86399206300757,129.999350137845));
#144078=CARTESIAN_POINT('Ctrl Pts',(137.968960172226,-5.88391324967551,
130.160991447785));
#144079=CARTESIAN_POINT('Ctrl Pts',(137.961313927222,-5.89713851398654,
130.323020914906));
#144080=CARTESIAN_POINT('Ctrl Pts',(137.953667682218,-5.91036377829757,
130.485050382027));
#144081=CARTESIAN_POINT('Ctrl Pts',(137.946021437215,-5.91689314513619,
130.647467521529));
#144082=CARTESIAN_POINT('Ctrl Pts',(137.938375192211,-5.91674761862911,
130.809669096323));
#144083=CARTESIAN_POINT('',(136.188375192211,-5.92482275393929,130.801481359489));
#144084=CARTESIAN_POINT('Ctrl Pts',(137.938375192211,-5.91858262641488,
130.809670742684));
#144085=CARTESIAN_POINT('Ctrl Pts',(137.919605272295,-5.92227655107304,
131.20796854486));
#144086=CARTESIAN_POINT('Ctrl Pts',(137.808019477772,-5.70376707825749,
133.571789017959));
#144087=CARTESIAN_POINT('Ctrl Pts',(137.60361780865,-2.52345964543731,137.331972121637));
#144088=CARTESIAN_POINT('Ctrl Pts',(137.325170184835,4.12787285265972,136.455752149097));
#144089=CARTESIAN_POINT('Ctrl Pts',(137.046722561023,6.98589185696212,130.386179444888));
#144090=CARTESIAN_POINT('Ctrl Pts',(136.768274937209,3.42421752450535,124.700894809093));
#144091=CARTESIAN_POINT('Ctrl Pts',(136.489827313397,-3.28414543064536,
124.624397080398));
#144092=CARTESIAN_POINT('Ctrl Pts',(136.296527398397,-5.84603763581142,
128.513744555582));
#144093=CARTESIAN_POINT('Ctrl Pts',(136.196043358002,-5.92579277232221,
130.639208488848));
#144094=CARTESIAN_POINT('Ctrl Pts',(136.188375192211,-5.92482275393929,
130.801481359489));
#144095=CARTESIAN_POINT('',(134.438375192211,-5.90967939056383,130.800446782654));
#144096=CARTESIAN_POINT('Ctrl Pts',(136.188375192211,-5.92482275393929,
130.801481359489));
#144097=CARTESIAN_POINT('Ctrl Pts',(136.103227483398,-5.91405161973785,
132.603367692488));
#144098=CARTESIAN_POINT('Ctrl Pts',(135.925263899979,-4.07309906563022,
136.388452668));
#144099=CARTESIAN_POINT('Ctrl Pts',(135.654484441958,2.37394968768175,137.387818934492));
#144100=CARTESIAN_POINT('Ctrl Pts',(135.376036818145,6.82202772839269,132.365609541781));
#144101=CARTESIAN_POINT('Ctrl Pts',(135.097589194333,5.00099556129847,125.908688658965));
#144102=CARTESIAN_POINT('Ctrl Pts',(134.819141570519,-1.41570721441751,
123.950651139233));
#144103=CARTESIAN_POINT('Ctrl Pts',(134.599403569813,-5.45281051817537,
127.375725945688));
#144104=CARTESIAN_POINT('Ctrl Pts',(134.47248144371,-5.91406978814998,130.073942001419));
#144105=CARTESIAN_POINT('Ctrl Pts',(134.438375192211,-5.90967939056383,
130.800446782654));
#144106=CARTESIAN_POINT('',(132.688375175112,-5.91363808545199,130.808706388299));
#144107=CARTESIAN_POINT('Ctrl Pts',(134.438375192211,-5.90967939056383,
130.800446782654));
#144108=CARTESIAN_POINT('Ctrl Pts',(134.379665569105,-5.90212187321015,
132.051033405842));
#144109=CARTESIAN_POINT('Ctrl Pts',(134.228140071397,-4.90112661354537,
135.289767902303));
#144110=CARTESIAN_POINT('Ctrl Pts',(133.98379869908,0.428812026623837,137.789607984421));
#144111=CARTESIAN_POINT('Ctrl Pts',(133.705351075268,6.10866981692772,134.219285740918));
#144112=CARTESIAN_POINT('Ctrl Pts',(133.426903451454,6.17495847058624,127.510814137418));
#144113=CARTESIAN_POINT('Ctrl Pts',(133.148455827642,0.566761953268891,
123.828950850487));
#144114=CARTESIAN_POINT('Ctrl Pts',(132.902279741227,-4.85191927268251,
126.240955591494));
#144115=CARTESIAN_POINT('Ctrl Pts',(132.748919529417,-5.90178715204232,
129.519491859617));
#144116=CARTESIAN_POINT('Ctrl Pts',(132.688375192211,-5.91051263528418,
130.808703727191));
#144117=CARTESIAN_POINT('',(130.938375192211,-5.92111984587309,130.806604383885));
#144118=CARTESIAN_POINT('Ctrl Pts',(132.688375158095,-5.91674840209997,
130.808709036521));
#144119=CARTESIAN_POINT('Ctrl Pts',(132.679863463167,-5.91661505896896,
130.990144580226));
#144120=CARTESIAN_POINT('Ctrl Pts',(132.671351768239,-5.90813228569475,
131.171242140953));
#144121=CARTESIAN_POINT('Ctrl Pts',(132.662840073311,-5.89141688080036,
131.351295439204));
#144122=CARTESIAN_POINT('Ctrl Pts',(132.654286777509,-5.87461977943247,
131.532228747219));
#144123=CARTESIAN_POINT('Ctrl Pts',(132.645733481707,-5.84950948183229,
131.71210743218));
#144124=CARTESIAN_POINT('Ctrl Pts',(132.637180185905,-5.8162539680182,131.89023369579));
#144125=CARTESIAN_POINT('Ctrl Pts',(132.628572394587,-5.78278657372961,
132.069494853226));
#144126=CARTESIAN_POINT('Ctrl Pts',(132.619964603269,-5.74106992332052,
132.246981060688));
#144127=CARTESIAN_POINT('Ctrl Pts',(132.611356811951,-5.69132379711266,
132.42200211027));
#144128=CARTESIAN_POINT('Ctrl Pts',(132.604758067973,-5.65318835230238,
132.556173473667));
#144129=CARTESIAN_POINT('Ctrl Pts',(132.598159323995,-5.61033516103908,
132.688896533316));
#144130=CARTESIAN_POINT('Ctrl Pts',(132.591560580017,-5.56288192611719,
132.819869297423));
#144131=CARTESIAN_POINT('Ctrl Pts',(132.584137313612,-5.50949934212925,
132.967207294329));
#144132=CARTESIAN_POINT('Ctrl Pts',(132.576714047206,-5.45017842274767,
133.112645788839));
#144133=CARTESIAN_POINT('Ctrl Pts',(132.569290780801,-5.38507303773925,
133.255670255436));
#144134=CARTESIAN_POINT('Ctrl Pts',(132.56187628808,-5.32004460188919,133.398525678991));
#144135=CARTESIAN_POINT('Ctrl Pts',(132.554461795359,-5.24924546216386,
133.538972417469));
#144136=CARTESIAN_POINT('Ctrl Pts',(132.547047302638,-5.17287886179537,
133.676512222842));
#144137=CARTESIAN_POINT('Ctrl Pts',(132.539639956284,-5.09658586643148,
133.813919462173));
#144138=CARTESIAN_POINT('Ctrl Pts',(132.53223260993,-5.01473627332167,133.948425022081));
#144139=CARTESIAN_POINT('Ctrl Pts',(132.524825263577,-4.92758085248979,
134.079551834072));
#144140=CARTESIAN_POINT('Ctrl Pts',(132.517423441901,-4.84049043545895,
134.210580846739));
#144141=CARTESIAN_POINT('Ctrl Pts',(132.510021620226,-4.74810227594555,
134.338235819595));
#144142=CARTESIAN_POINT('Ctrl Pts',(132.502619798551,-4.65071233059291,
134.462065551069));
#144143=CARTESIAN_POINT('Ctrl Pts',(132.495221884239,-4.55337379663426,
134.585829913792));
#144144=CARTESIAN_POINT('Ctrl Pts',(132.487823969928,-4.45103896551377,
134.705772764018));
#144145=CARTESIAN_POINT('Ctrl Pts',(132.480426055617,-4.34404617176119,
134.821473190062));
#144146=CARTESIAN_POINT('Ctrl Pts',(132.473029370704,-4.23707115826996,
134.937154388795));
#144147=CARTESIAN_POINT('Ctrl Pts',(132.465632685792,-4.12543997164268,
135.048594288785));
#144148=CARTESIAN_POINT('Ctrl Pts',(132.45823600088,-4.00953024249916,135.155406215693));
#144149=CARTESIAN_POINT('Ctrl Pts',(132.450839643945,-3.8936256529145,135.262213406449));
#144150=CARTESIAN_POINT('Ctrl Pts',(132.443443287009,-3.77344317254592,
135.364392779179));
#144151=CARTESIAN_POINT('Ctrl Pts',(132.436046930074,-3.64939599084017,
135.461595791415));
#144152=CARTESIAN_POINT('Ctrl Pts',(132.428649440737,-3.52532981719431,
135.558813685681));
#144153=CARTESIAN_POINT('Ctrl Pts',(132.4212519514,-3.39739805791841,135.651053472161));
#144154=CARTESIAN_POINT('Ctrl Pts',(132.413854462064,-3.26604542409023,
135.738008137432));
#144155=CARTESIAN_POINT('Ctrl Pts',(132.406454379549,-3.13464674480017,
135.824993284526));
#144156=CARTESIAN_POINT('Ctrl Pts',(132.399054297034,-2.99982511447287,
135.906689415786));
#144157=CARTESIAN_POINT('Ctrl Pts',(132.391654214519,-2.86205239782559,
135.982834005989));
#144158=CARTESIAN_POINT('Ctrl Pts',(132.384245994852,-2.72412818591259,
136.059062324996));
#144159=CARTESIAN_POINT('Ctrl Pts',(132.376837775186,-2.58324673407528,
136.129726731196));
#144160=CARTESIAN_POINT('Ctrl Pts',(132.36942955552,-2.43990323316877,136.194611333003));
#144161=CARTESIAN_POINT('Ctrl Pts',(132.362016776217,-2.29647150672927,
136.259535870201));
#144162=CARTESIAN_POINT('Ctrl Pts',(132.354603996915,-2.15057505685119,
136.31867337459));
#144163=CARTESIAN_POINT('Ctrl Pts',(132.347191217613,-2.00272652974338,
136.371857093502));
#144164=CARTESIAN_POINT('Ctrl Pts',(132.339767846585,-1.85466674972663,
136.425116803806));
#144165=CARTESIAN_POINT('Ctrl Pts',(132.332344475556,-1.7046496768683,136.47240562622));
#144166=CARTESIAN_POINT('Ctrl Pts',(132.324921104527,-1.55320130067954,
136.513607177496));
#144167=CARTESIAN_POINT('Ctrl Pts',(132.320985055086,-1.47289973766145,
136.535453228602));
#144168=CARTESIAN_POINT('Ctrl Pts',(132.317049005645,-1.39219593574406,
136.555588787283));
#144169=CARTESIAN_POINT('Ctrl Pts',(132.313112956203,-1.31116902747609,
136.574002404011));
#144170=CARTESIAN_POINT('Ctrl Pts',(132.305689689798,-1.15835480726222,
136.608729910486));
#144171=CARTESIAN_POINT('Ctrl Pts',(132.298266423393,-1.00392887687804,
136.637434599771));
#144172=CARTESIAN_POINT('Ctrl Pts',(132.290843156987,-0.848407291581399,
136.659967813245));
#144173=CARTESIAN_POINT('Ctrl Pts',(132.283428664266,-0.693069519883096,
136.682474394333));
#144174=CARTESIAN_POINT('Ctrl Pts',(132.276014171545,-0.536639036756118,
136.698823965696));
#144175=CARTESIAN_POINT('Ctrl Pts',(132.268599678824,-0.37964489030772,
136.708918206392));
#144176=CARTESIAN_POINT('Ctrl Pts',(132.26119233247,-0.222802060728393,
136.719002717879));
#144177=CARTESIAN_POINT('Ctrl Pts',(132.253784986117,-0.0653970194188368,
136.722843877706));
#144178=CARTESIAN_POINT('Ctrl Pts',(132.246377639763,0.0920333150634869,
136.720394798622));
#144179=CARTESIAN_POINT('Ctrl Pts',(132.238975818087,0.249346232062847,
136.717947546153));
#144180=CARTESIAN_POINT('Ctrl Pts',(132.231573996412,0.40668403302671,136.70921940196));
#144181=CARTESIAN_POINT('Ctrl Pts',(132.224172174737,0.563507137501594,
136.694215477279));
#144182=CARTESIAN_POINT('Ctrl Pts',(132.216774260425,0.720247456280445,
136.679219473053));
#144183=CARTESIAN_POINT('Ctrl Pts',(132.209376346114,0.876473249021992,
136.657954321672));
#144184=CARTESIAN_POINT('Ctrl Pts',(132.201978431803,1.03164751272782,136.630477160511));
#144185=CARTESIAN_POINT('Ctrl Pts',(132.19458174689,1.18679598928595,136.603004565556));
#144186=CARTESIAN_POINT('Ctrl Pts',(132.187185061978,1.3408929164058,136.569322074703));
#144187=CARTESIAN_POINT('Ctrl Pts',(132.179788377066,1.49340885543957,136.52953839236));
#144188=CARTESIAN_POINT('Ctrl Pts',(132.17239202013,1.64591803175678,136.489756474067));
#144189=CARTESIAN_POINT('Ctrl Pts',(132.164995663195,1.79684599816473,136.443873996419));
#144190=CARTESIAN_POINT('Ctrl Pts',(132.15759930626,1.94567617702488,136.39205019168));
#144191=CARTESIAN_POINT('Ctrl Pts',(132.150201816923,2.09452914216546,136.340218452584));
#144192=CARTESIAN_POINT('Ctrl Pts',(132.142804327586,2.24128332769327,136.282443697963));
#144193=CARTESIAN_POINT('Ctrl Pts',(132.13540683825,2.38544005732124,136.218934127588));
#144194=CARTESIAN_POINT('Ctrl Pts',(132.128006755735,2.52964732086721,136.155402294031));
#144195=CARTESIAN_POINT('Ctrl Pts',(132.12060667322,2.67125497424492,136.086131792574));
#144196=CARTESIAN_POINT('Ctrl Pts',(132.113206590705,2.8097870931432,136.011377715071));
#144197=CARTESIAN_POINT('Ctrl Pts',(132.105798371039,2.94847154234775,135.936541437775));
#144198=CARTESIAN_POINT('Ctrl Pts',(132.098390151372,3.08407337454253,135.856209719998));
#144199=CARTESIAN_POINT('Ctrl Pts',(132.090981931706,3.21614329127075,135.770682485157));
#144200=CARTESIAN_POINT('Ctrl Pts',(132.083569152404,3.3482944948291,135.68510260973));
#144201=CARTESIAN_POINT('Ctrl Pts',(132.076156373101,3.47690914701088,135.594321060081));
#144202=CARTESIAN_POINT('Ctrl Pts',(132.068743593799,3.60156985627617,135.498679006093));
#144203=CARTESIAN_POINT('Ctrl Pts',(132.061320222771,3.72640868660878,135.402900294253));
#144204=CARTESIAN_POINT('Ctrl Pts',(132.053896851742,3.84728200444542,135.302247445761));
#144205=CARTESIAN_POINT('Ctrl Pts',(132.046473480713,3.96380758308421,135.1971000825));
#144206=CARTESIAN_POINT('Ctrl Pts',(132.042537431272,4.02559224087191,135.141348427522));
#144207=CARTESIAN_POINT('Ctrl Pts',(132.038601381832,4.08615523288903,135.084333794629));
#144208=CARTESIAN_POINT('Ctrl Pts',(132.034665332391,4.14544415324828,135.026116571526));
#144209=CARTESIAN_POINT('Ctrl Pts',(132.027242065985,4.25726120670123,134.916320705653));
#144210=CARTESIAN_POINT('Ctrl Pts',(132.01981879958,4.36488226219099,134.80191338256));
#144211=CARTESIAN_POINT('Ctrl Pts',(132.012395533174,4.46790330853993,134.683248420537));
#144212=CARTESIAN_POINT('Ctrl Pts',(132.004981040453,4.57080259256751,134.564723710644));
#144213=CARTESIAN_POINT('Ctrl Pts',(131.997566547732,4.66911244715607,134.44195165753));
#144214=CARTESIAN_POINT('Ctrl Pts',(131.990152055011,4.76246418868836,134.315324219479));
#144215=CARTESIAN_POINT('Ctrl Pts',(131.982744708658,4.85572595429752,134.188818829721));
#144216=CARTESIAN_POINT('Ctrl Pts',(131.975337362304,4.94403890050665,134.058465751236));
#144217=CARTESIAN_POINT('Ctrl Pts',(131.96793001595,5.02707336214907,133.92469136511));
#144218=CARTESIAN_POINT('Ctrl Pts',(131.960528194275,5.11004589355733,133.791016752969));
#144219=CARTESIAN_POINT('Ctrl Pts',(131.953126372599,5.18774758326425,133.653926229846));
#144220=CARTESIAN_POINT('Ctrl Pts',(131.945724550924,5.25989107508295,133.513876522809));
#144221=CARTESIAN_POINT('Ctrl Pts',(131.938326636612,5.33199648291384,133.373900746921));
#144222=CARTESIAN_POINT('Ctrl Pts',(131.930928722301,5.39854936580052,133.230969229192));
#144223=CARTESIAN_POINT('Ctrl Pts',(131.92353080799,5.45930753179741,133.085564649598));
#144224=CARTESIAN_POINT('Ctrl Pts',(131.916134123077,5.52005560088938,132.940184233608));
#144225=CARTESIAN_POINT('Ctrl Pts',(131.908737438165,5.57501072053143,132.792331915523));
#144226=CARTESIAN_POINT('Ctrl Pts',(131.901340753253,5.62397817230058,132.642511884461));
#144227=CARTESIAN_POINT('Ctrl Pts',(131.893944396317,5.67294345280161,132.492698496576));
#144228=CARTESIAN_POINT('Ctrl Pts',(131.886548039382,5.71592147736038,132.340917924023));
#144229=CARTESIAN_POINT('Ctrl Pts',(131.879151682447,5.75276698976015,132.18769084713));
#144230=CARTESIAN_POINT('Ctrl Pts',(131.87175419311,5.78961814330195,132.03444031078));
#144231=CARTESIAN_POINT('Ctrl Pts',(131.864356703773,5.82033482792118,131.879743192101));
#144232=CARTESIAN_POINT('Ctrl Pts',(131.856959214437,5.84482266126758,131.724131578639));
#144233=CARTESIAN_POINT('Ctrl Pts',(131.849559131922,5.86931907878599,131.568465415767));
#144234=CARTESIAN_POINT('Ctrl Pts',(131.842159049407,5.8875822396772,131.411884488379));
#144235=CARTESIAN_POINT('Ctrl Pts',(131.834758966892,5.89956951122791,131.254927088456));
#144236=CARTESIAN_POINT('Ctrl Pts',(131.827350747225,5.91156996401602,131.097797097736));
#144237=CARTESIAN_POINT('Ctrl Pts',(131.819942527559,5.91728071729803,130.940290180197));
#144238=CARTESIAN_POINT('Ctrl Pts',(131.812534307892,5.91671124834779,130.782946459289));
#144239=CARTESIAN_POINT('Ctrl Pts',(131.80512152859,5.91614142889891,130.625505895945));
#144240=CARTESIAN_POINT('Ctrl Pts',(131.797708749288,5.90928370120321,130.46822910146));
#144241=CARTESIAN_POINT('Ctrl Pts',(131.790295969986,5.89619949082419,130.311651649813));
#144242=CARTESIAN_POINT('Ctrl Pts',(131.782872598957,5.8830965851118,130.15485047296));
#144243=CARTESIAN_POINT('Ctrl Pts',(131.775449227928,5.86374947382362,129.998751004161));
#144244=CARTESIAN_POINT('Ctrl Pts',(131.7680258569,5.83827094073324,129.843880016466));
#144245=CARTESIAN_POINT('Ctrl Pts',(131.764089807459,5.82476161114022,129.761763702715));
#144246=CARTESIAN_POINT('Ctrl Pts',(131.760153758018,5.80952936226843,129.679992540563));
#144247=CARTESIAN_POINT('Ctrl Pts',(131.756217708578,5.79259667334227,129.598643261597));
#144248=CARTESIAN_POINT('Ctrl Pts',(131.748794442172,5.76066215047756,129.445221060287));
#144249=CARTESIAN_POINT('Ctrl Pts',(131.741371175767,5.72257983865848,129.292836465631));
#144250=CARTESIAN_POINT('Ctrl Pts',(131.733947909361,5.67842903732282,129.142020631104));
#144251=CARTESIAN_POINT('Ctrl Pts',(131.72653341664,5.63433041856781,128.991383048369));
#144252=CARTESIAN_POINT('Ctrl Pts',(131.719118923919,5.58417769095449,128.842310889842));
#144253=CARTESIAN_POINT('Ctrl Pts',(131.711704431198,5.52810133758869,128.69532620252));
#144254=CARTESIAN_POINT('Ctrl Pts',(131.704297084845,5.47207903272345,128.548483184572));
#144255=CARTESIAN_POINT('Ctrl Pts',(131.696889738491,5.41014460059332,128.403723978802));
#144256=CARTESIAN_POINT('Ctrl Pts',(131.689482392137,5.34247857560552,128.261556411243));
#144257=CARTESIAN_POINT('Ctrl Pts',(131.682080570462,5.2748630184921,128.119494877619));
#144258=CARTESIAN_POINT('Ctrl Pts',(131.674678748786,5.20152454004015,127.980021469073));
#144259=CARTESIAN_POINT('Ctrl Pts',(131.667276927111,5.12269207462701,127.843624818638));
#144260=CARTESIAN_POINT('Ctrl Pts',(131.6598790128,5.04390122425867,127.707300170934));
#144261=CARTESIAN_POINT('Ctrl Pts',(131.652481098488,4.95962234920705,127.574049369056));
#144262=CARTESIAN_POINT('Ctrl Pts',(131.645083184177,4.87013063114568,127.444337076268));
#144263=CARTESIAN_POINT('Ctrl Pts',(131.637686499265,4.78065378498436,127.31464633931));
#144264=CARTESIAN_POINT('Ctrl Pts',(131.630289814352,4.68596602690469,127.188493251327));
#144265=CARTESIAN_POINT('Ctrl Pts',(131.62289312944,4.5863862954267,127.066314160976));
#144266=CARTESIAN_POINT('Ctrl Pts',(131.615496772505,4.48681097941837,126.944140488175));
#144267=CARTESIAN_POINT('Ctrl Pts',(131.608100415569,4.38234435715202,126.825940752002));
#144268=CARTESIAN_POINT('Ctrl Pts',(131.600704058634,4.27334597719978,126.712118601061));
#144269=CARTESIAN_POINT('Ctrl Pts',(131.593306569297,4.16433090931738,126.598279023658));
#144270=CARTESIAN_POINT('Ctrl Pts',(131.585909079961,4.05078296045702,126.488818635613));
#144271=CARTESIAN_POINT('Ctrl Pts',(131.578511590624,3.93309877497434,126.384104449786));
#144272=CARTESIAN_POINT('Ctrl Pts',(131.571111508109,3.8153733354828,126.279353556564));
#144273=CARTESIAN_POINT('Ctrl Pts',(131.563711425594,3.69350905123402,126.179352426111));
#144274=CARTESIAN_POINT('Ctrl Pts',(131.556311343079,3.56793575849341,126.084427886503));
#144275=CARTESIAN_POINT('Ctrl Pts',(131.548903123413,3.44222438500809,125.989398967604));
#144276=CARTESIAN_POINT('Ctrl Pts',(131.541494903746,3.31279615609758,125.899458012881));
#144277=CARTESIAN_POINT('Ctrl Pts',(131.53408668408,3.18011061561469,125.814888998752));
#144278=CARTESIAN_POINT('Ctrl Pts',(131.526673904778,3.04734340939542,125.730267933805));
#144279=CARTESIAN_POINT('Ctrl Pts',(131.519261125476,2.91131521855655,125.651025585218));
#144280=CARTESIAN_POINT('Ctrl Pts',(131.511848346174,2.77250983867293,125.577399764741));
#144281=CARTESIAN_POINT('Ctrl Pts',(131.504424975145,2.6335061271533,125.50366874424));
#144282=CARTESIAN_POINT('Ctrl Pts',(131.497001604116,2.49171763685584,125.435570441078));
#144283=CARTESIAN_POINT('Ctrl Pts',(131.489578233088,2.34764851925148,125.373294700772));
#144284=CARTESIAN_POINT('Ctrl Pts',(131.485642183647,2.27125961620314,125.340274608975));
#144285=CARTESIAN_POINT('Ctrl Pts',(131.481706134206,2.19422981901554,125.308890620834));
#144286=CARTESIAN_POINT('Ctrl Pts',(131.477770084765,2.11663583471571,125.279165299236));
#144287=CARTESIAN_POINT('Ctrl Pts',(131.470346818359,1.97029600195762,125.2231042704));
#144288=CARTESIAN_POINT('Ctrl Pts',(131.462923551954,1.82150610696681,125.172776402269));
#144289=CARTESIAN_POINT('Ctrl Pts',(131.455500285548,1.67075588748716,125.128402079405));
#144290=CARTESIAN_POINT('Ctrl Pts',(131.448085792827,1.52018384224779,125.084080203305));
#144291=CARTESIAN_POINT('Ctrl Pts',(131.440671300106,1.36765643901191,125.045697970471));
#144292=CARTESIAN_POINT('Ctrl Pts',(131.433256807385,1.21368342000861,125.013427780924));
#144293=CARTESIAN_POINT('Ctrl Pts',(131.425849461032,1.059858805998,124.981188694601));
#144294=CARTESIAN_POINT('Ctrl Pts',(131.418442114678,0.90459171299056,124.955049999767));
#144295=CARTESIAN_POINT('Ctrl Pts',(131.411034768324,0.748406972666796,
124.935134300089));
#144296=CARTESIAN_POINT('Ctrl Pts',(131.403632946648,0.592338720814656,
124.915233454291));
#144297=CARTESIAN_POINT('Ctrl Pts',(131.396231124973,0.435354553116601,
124.90154640912));
#144298=CARTESIAN_POINT('Ctrl Pts',(131.388829303298,0.277989315005478,
124.89414467369));
#144299=CARTESIAN_POINT('Ctrl Pts',(131.381431388986,0.120707148778738,
124.886746845579));
#144300=CARTESIAN_POINT('Ctrl Pts',(131.374033474675,-0.036955315291354,
124.885627736816));
#144301=CARTESIAN_POINT('Ctrl Pts',(131.366635560363,-0.194458400426787,
124.890806991107));
#144302=CARTESIAN_POINT('Ctrl Pts',(131.359238875451,-0.351935311406643,
124.895985384701));
#144303=CARTESIAN_POINT('Ctrl Pts',(131.351842190539,-0.509252523287558,
124.907460051755));
#144304=CARTESIAN_POINT('Ctrl Pts',(131.344445505627,-0.665870529525372,
124.925198517368));
#144305=CARTESIAN_POINT('Ctrl Pts',(131.337049148691,-0.822481591156665,
124.942936196438));
#144306=CARTESIAN_POINT('Ctrl Pts',(131.329652791756,-0.978393137864227,
124.966937079809));
#144307=CARTESIAN_POINT('Ctrl Pts',(131.32225643482,-1.13307122385995,124.997116851014));
#144308=CARTESIAN_POINT('Ctrl Pts',(131.314858945484,-1.28777299146552,
125.027301242818));
#144309=CARTESIAN_POINT('Ctrl Pts',(131.307461456147,-1.44124055592927,
125.063666334583));
#144310=CARTESIAN_POINT('Ctrl Pts',(131.300063966811,-1.59295074297537,
125.106076797594));
#144311=CARTESIAN_POINT('Ctrl Pts',(131.292663884296,-1.74471411179257,
125.148502127527));
#144312=CARTESIAN_POINT('Ctrl Pts',(131.285263801781,-1.89471851735897,
125.196976947569));
#144313=CARTESIAN_POINT('Ctrl Pts',(131.277863719266,-2.0424566529597,125.251316282854));
#144314=CARTESIAN_POINT('Ctrl Pts',(131.270455499599,-2.19035724182826,
125.305715369823));
#144315=CARTESIAN_POINT('Ctrl Pts',(131.263047279933,-2.33598623348387,
125.365991721447));
#144316=CARTESIAN_POINT('Ctrl Pts',(131.255639060266,-2.4788563158455,125.431912206656));
#144317=CARTESIAN_POINT('Ctrl Pts',(131.248226280964,-2.62181433235911,
125.497873264823));
#144318=CARTESIAN_POINT('Ctrl Pts',(131.240813501662,-2.76200972430766,
125.569485209282));
#144319=CARTESIAN_POINT('Ctrl Pts',(131.23340072236,-2.89898091060348,125.646469552173));
#144320=CARTESIAN_POINT('Ctrl Pts',(131.225977351331,-3.0361478077535,125.723563893904));
#144321=CARTESIAN_POINT('Ctrl Pts',(131.218553980302,-3.17008098123058,
125.806045770198));
#144322=CARTESIAN_POINT('Ctrl Pts',(131.211130609274,-3.30034820243907,
125.893593640285));
#144323=CARTESIAN_POINT('Ctrl Pts',(131.207194559833,-3.3694190088398,125.940013621685));
#144324=CARTESIAN_POINT('Ctrl Pts',(131.203258510392,-3.43745973383563,
125.987857159465));
#144325=CARTESIAN_POINT('Ctrl Pts',(131.199322460952,-3.50440993260739,
126.037071913623));
#144326=CARTESIAN_POINT('Ctrl Pts',(131.191967172959,-3.62951963982809,
126.129039429726));
#144327=CARTESIAN_POINT('Ctrl Pts',(131.184611884967,-3.7512127270936,126.226086955291));
#144328=CARTESIAN_POINT('Ctrl Pts',(131.177256596974,-3.86904358294745,
126.327929861288));
#144329=CARTESIAN_POINT('Ctrl Pts',(131.169910034406,-3.98673465851265,
126.429651953168));
#144330=CARTESIAN_POINT('Ctrl Pts',(131.162563471839,-4.10057233439905,
126.536157859477));
#144331=CARTESIAN_POINT('Ctrl Pts',(131.155216909271,-4.21014017975913,
126.647119918583));
#144332=CARTESIAN_POINT('Ctrl Pts',(131.147877385571,-4.319603046289,126.757975663039));
#144333=CARTESIAN_POINT('Ctrl Pts',(131.140537861871,-4.42480395838242,
126.87327879409));
#144334=CARTESIAN_POINT('Ctrl Pts',(131.133198338171,-4.52535995253196,
126.992661801746));
#144335=CARTESIAN_POINT('Ctrl Pts',(131.125864173213,-4.62584252861205,
127.11195764533));
#144336=CARTESIAN_POINT('Ctrl Pts',(131.118530008255,-4.72168669313732,
127.23532714599));
#144337=CARTESIAN_POINT('Ctrl Pts',(131.111195843297,-4.81254688099806,
127.362366561689));
#144338=CARTESIAN_POINT('Ctrl Pts',(131.10386482153,-4.90336812906279,127.489351532321));
#144339=CARTESIAN_POINT('Ctrl Pts',(131.096533799763,-4.98920942880024,
127.620002979867));
#144340=CARTESIAN_POINT('Ctrl Pts',(131.089202777995,-5.06976607935129,
127.753884841042));
#144341=CARTESIAN_POINT('Ctrl Pts',(131.081873298667,-5.15030578086776,
127.887738533614));
#144342=CARTESIAN_POINT('Ctrl Pts',(131.074543819339,-5.22556284885647,
128.024820961599));
#144343=CARTESIAN_POINT('Ctrl Pts',(131.067214340011,-5.29527657013599,
128.164668096027));
#144344=CARTESIAN_POINT('Ctrl Pts',(131.059884890251,-5.36499001018411,
128.304514666299));
#144345=CARTESIAN_POINT('Ctrl Pts',(131.052555440491,-5.42915997803113,
128.447125579991));
#144346=CARTESIAN_POINT('Ctrl Pts',(131.045225990731,-5.48757240378098,
128.592013520983));
#144347=CARTESIAN_POINT('Ctrl Pts',(131.037895057908,-5.5459966488725,128.736930779025));
#144348=CARTESIAN_POINT('Ctrl Pts',(131.030564125085,-5.59866089133872,
128.884125627996));
#144349=CARTESIAN_POINT('Ctrl Pts',(131.023233192263,-5.64539984928383,
129.033092398406));
#144350=CARTESIAN_POINT('Ctrl Pts',(131.015895152461,-5.69218411835187,
129.18220358478));
#144351=CARTESIAN_POINT('Ctrl Pts',(131.008557112659,-5.73303151523554,
129.33308975983));
#144352=CARTESIAN_POINT('Ctrl Pts',(131.001219072857,-5.76782697643615,
129.485231157507));
#144353=CARTESIAN_POINT('Ctrl Pts',(130.993877359742,-5.80263985572723,
129.637448714906));
#144354=CARTESIAN_POINT('Ctrl Pts',(130.986535646627,-5.83139469385814,
129.790922372803));
#144355=CARTESIAN_POINT('Ctrl Pts',(130.979193933511,-5.85402801498565,
129.945124583485));
#144356=CARTESIAN_POINT('Ctrl Pts',(130.971841575104,-5.87669415383726,
130.099550383342));
#144357=CARTESIAN_POINT('Ctrl Pts',(130.964489216696,-5.89322100286484,
130.254706467999));
#144358=CARTESIAN_POINT('Ctrl Pts',(130.957136858289,-5.90359711718267,
130.410061694802));
#144359=CARTESIAN_POINT('Ctrl Pts',(130.950882969596,-5.91242300139681,
130.542206272419));
#144360=CARTESIAN_POINT('Ctrl Pts',(130.944629080904,-5.91679963655113,
130.674494784546));
#144361=CARTESIAN_POINT('Ctrl Pts',(130.938375192211,-5.91674957518414,
130.806602727802));
#144362=CARTESIAN_POINT('',(129.188375192211,-5.91739037745531,130.798927194587));
#144363=CARTESIAN_POINT('Ctrl Pts',(130.938375192211,-5.92550534701643,
130.80660604574));
#144364=CARTESIAN_POINT('Ctrl Pts',(130.932541740521,-5.9261030892962,130.930015222463));
#144365=CARTESIAN_POINT('Ctrl Pts',(130.92670828883,-5.92258319844409,131.053389657062));
#144366=CARTESIAN_POINT('Ctrl Pts',(130.828058962535,-5.79159940387876,
133.135275101838));
#144367=CARTESIAN_POINT('Ctrl Pts',(130.642427213325,-3.40562481334391,
136.918220295468));
#144368=CARTESIAN_POINT('Ctrl Pts',(130.363979589513,3.30293990190001,136.97429972057));
#144369=CARTESIAN_POINT('Ctrl Pts',(130.085531965701,6.97626420488279,131.360506528292));
#144370=CARTESIAN_POINT('Ctrl Pts',(129.807084341888,4.23874251303069,125.235642413295));
#144371=CARTESIAN_POINT('Ctrl Pts',(129.528636718075,-2.39397647421211,
124.228158281014));
#144372=CARTESIAN_POINT('Ctrl Pts',(129.322400334849,-5.67717480651475,
127.95794273319));
#144373=CARTESIAN_POINT('Ctrl Pts',(129.208979826228,-5.92145620834998,
130.361470692854));
#144374=CARTESIAN_POINT('Ctrl Pts',(129.188375192211,-5.91739037745531,
130.798927194587));
#144375=CARTESIAN_POINT('',(127.438375192169,-5.91674999573792,130.804585195673));
#144376=CARTESIAN_POINT('Ctrl Pts',(129.188375192211,-5.91674750575255,
130.79892778488));
#144377=CARTESIAN_POINT('Ctrl Pts',(129.181067794371,-5.91688994338944,
130.954052667514));
#144378=CARTESIAN_POINT('Ctrl Pts',(129.173760396532,-5.91092763526548,
131.109359430848));
#144379=CARTESIAN_POINT('Ctrl Pts',(129.166452998692,-5.89884451512316,
131.26432142992));
#144380=CARTESIAN_POINT('Ctrl Pts',(129.159150918755,-5.88677018837911,
131.419170656582));
#144381=CARTESIAN_POINT('Ctrl Pts',(129.151848838819,-5.86858394450736,
131.573675236878));
#144382=CARTESIAN_POINT('Ctrl Pts',(129.144546758882,-5.84432178705686,
131.727308834874));
#144383=CARTESIAN_POINT('Ctrl Pts',(129.137247681465,-5.8200696058889,131.88087926074));
#144384=CARTESIAN_POINT('Ctrl Pts',(129.129948604049,-5.7897465394639,132.033579037759));
#144385=CARTESIAN_POINT('Ctrl Pts',(129.122649526632,-5.75344039640455,
132.184887389317));
#144386=CARTESIAN_POINT('Ctrl Pts',(129.115351907255,-5.71714150574178,
132.336165516012));
#144387=CARTESIAN_POINT('Ctrl Pts',(129.108054287878,-5.67486200501293,
132.486052396529));
#144388=CARTESIAN_POINT('Ctrl Pts',(129.100756668501,-5.62674067312069,
132.634038173845));
#144389=CARTESIAN_POINT('Ctrl Pts',(129.09345897469,-5.57861885040187,132.782025460581));
#144390=CARTESIAN_POINT('Ctrl Pts',(129.086161280879,-5.52465519666547,
132.928111239962));
#144391=CARTESIAN_POINT('Ctrl Pts',(129.078863587068,-5.46503805690862,
133.071801818356));
#144392=CARTESIAN_POINT('Ctrl Pts',(129.071564286455,-5.40540779068163,
133.215524034465));
#144393=CARTESIAN_POINT('Ctrl Pts',(129.064264985841,-5.34012170915914,
133.356849645448));
#144394=CARTESIAN_POINT('Ctrl Pts',(129.056965685228,-5.26941576627111,
133.495306184588));
#144395=CARTESIAN_POINT('Ctrl Pts',(129.049658966624,-5.19863796772325,
133.633903431645));
#144396=CARTESIAN_POINT('Ctrl Pts',(129.042352248019,-5.1224294819203,133.769625440692));
#144397=CARTESIAN_POINT('Ctrl Pts',(129.035045529415,-5.04107189146871,
133.902025019586));
#144398=CARTESIAN_POINT('Ctrl Pts',(129.027735001506,-4.95967188583252,
134.034493624032));
#144399=CARTESIAN_POINT('Ctrl Pts',(129.020424473597,-4.87311764274452,
134.163636029777));
#144400=CARTESIAN_POINT('Ctrl Pts',(129.013113945688,-4.78173285762243,
134.28903584502));
#144401=CARTESIAN_POINT('Ctrl Pts',(129.005792346453,-4.69020967609837,
134.414625570249));
#144402=CARTESIAN_POINT('Ctrl Pts',(128.998470747218,-4.59384157672553,
134.536461081353));
#144403=CARTESIAN_POINT('Ctrl Pts',(128.991149147983,-4.49299173791707,
134.654160067603));
#144404=CARTESIAN_POINT('Ctrl Pts',(128.984679922138,-4.40388273826438,
134.758156653506));
#144405=CARTESIAN_POINT('Ctrl Pts',(128.978210696293,-4.31127545703475,
134.858924203103));
#144406=CARTESIAN_POINT('Ctrl Pts',(128.971741470448,-4.21544240491636,
134.956224764348));
#144407=CARTESIAN_POINT('Ctrl Pts',(128.964318204043,-4.10547649966461,
135.067874597701));
#144408=CARTESIAN_POINT('Ctrl Pts',(128.956894937638,-3.99090552812758,
135.175321420097));
#144409=CARTESIAN_POINT('Ctrl Pts',(128.949471671232,-3.87208392302154,
135.278161759277));
#144410=CARTESIAN_POINT('Ctrl Pts',(128.942057178511,-3.7534027551848,135.380880549717));
#144411=CARTESIAN_POINT('Ctrl Pts',(128.93464268579,-3.63048123337495,135.4790034523));
#144412=CARTESIAN_POINT('Ctrl Pts',(128.927228193069,-3.50371187649744,
135.572162380327));
#144413=CARTESIAN_POINT('Ctrl Pts',(128.919820846715,-3.37706470469924,
135.665231518273));
#144414=CARTESIAN_POINT('Ctrl Pts',(128.912413500361,-3.24657737989109,
135.753345987021));
#144415=CARTESIAN_POINT('Ctrl Pts',(128.905006154008,-3.11267678435826,
135.836176770668));
#144416=CARTESIAN_POINT('Ctrl Pts',(128.897604332332,-2.97887605694135,
135.918945775991));
#144417=CARTESIAN_POINT('Ctrl Pts',(128.890202510657,-2.84166744382333,
135.996438747281));
#144418=CARTESIAN_POINT('Ctrl Pts',(128.882800688982,-2.70150810884803,
136.068369023746));
#144419=CARTESIAN_POINT('Ctrl Pts',(128.87540277467,-2.56142276289497,136.140261328777));
#144420=CARTESIAN_POINT('Ctrl Pts',(128.868004860359,-2.41839012851996,
136.206596617157));
#144421=CARTESIAN_POINT('Ctrl Pts',(128.860606946048,-2.27289325371729,
136.267133431779));
#144422=CARTESIAN_POINT('Ctrl Pts',(128.853210261135,-2.12742055785532,
136.327660186281));
#144423=CARTESIAN_POINT('Ctrl Pts',(128.845813576223,-1.97948477864414,
136.382390236227));
#144424=CARTESIAN_POINT('Ctrl Pts',(128.838416891311,-1.82959040094573,
136.431129630709));
#144425=CARTESIAN_POINT('Ctrl Pts',(128.831020534376,-1.67970266972099,
136.479866864036));
#144426=CARTESIAN_POINT('Ctrl Pts',(128.82362417744,-1.52785686769099,136.522613854633));
#144427=CARTESIAN_POINT('Ctrl Pts',(128.816227820505,-1.37457389563478,
136.559226138839));
#144428=CARTESIAN_POINT('Ctrl Pts',(128.808830331168,-1.22126745556424,
136.59584402848));
#144429=CARTESIAN_POINT('Ctrl Pts',(128.801432841832,-1.06652377045739,
136.626325254849));
#144430=CARTESIAN_POINT('Ctrl Pts',(128.794035352495,-0.910875070877245,
136.650576245453));
#144431=CARTESIAN_POINT('Ctrl Pts',(128.78663526998,-0.75517180888686,136.674835737205));
#144432=CARTESIAN_POINT('Ctrl Pts',(128.779235187465,-0.598563269395612,
136.692860587431));
#144433=CARTESIAN_POINT('Ctrl Pts',(128.77183510495,-0.441587808640241,
136.704608982657));
#144434=CARTESIAN_POINT('Ctrl Pts',(128.764426885284,-0.284439737228188,
136.716370296452));
#144435=CARTESIAN_POINT('Ctrl Pts',(128.757018665617,-0.126924311285822,
136.721841344405));
#144436=CARTESIAN_POINT('Ctrl Pts',(128.749610445951,0.0304183607859964,
136.721032425756));
#144437=CARTESIAN_POINT('Ctrl Pts',(128.742197666649,0.187857874647408,
136.720223009231));
#144438=CARTESIAN_POINT('Ctrl Pts',(128.734784887347,0.345124050714408,
136.713125940969));
#144439=CARTESIAN_POINT('Ctrl Pts',(128.727372108045,0.501681409106723,
136.699803461514));
#144440=CARTESIAN_POINT('Ctrl Pts',(128.719948737016,0.658462463994298,
136.686461946276));
#144441=CARTESIAN_POINT('Ctrl Pts',(128.712525365987,0.814532309022712,
136.666877300573));
#144442=CARTESIAN_POINT('Ctrl Pts',(128.705101994958,0.969364343389114,
136.641163109707));
#144443=CARTESIAN_POINT('Ctrl Pts',(128.701165945517,1.0514600031544,136.627528828707));
#144444=CARTESIAN_POINT('Ctrl Pts',(128.697229896077,1.13320788973021,136.612172155684));
#144445=CARTESIAN_POINT('Ctrl Pts',(128.693293846636,1.21453130582814,136.59511568661));
#144446=CARTESIAN_POINT('Ctrl Pts',(128.68587058023,1.36790473057144,136.562947718252));
#144447=CARTESIAN_POINT('Ctrl Pts',(128.678447313825,1.52023119397322,136.524633547119));
#144448=CARTESIAN_POINT('Ctrl Pts',(128.671024047419,1.67097966385473,136.480253280882));
#144449=CARTESIAN_POINT('Ctrl Pts',(128.663609554698,1.82154996156415,136.435925468434));
#144450=CARTESIAN_POINT('Ctrl Pts',(128.656195061977,1.97054562355525,136.385545936448));
#144451=CARTESIAN_POINT('Ctrl Pts',(128.648780569256,2.11744480200929,136.329245962344));
#144452=CARTESIAN_POINT('Ctrl Pts',(128.641373222902,2.26420239350458,136.273000252275));
#144453=CARTESIAN_POINT('Ctrl Pts',(128.633965876549,2.40886717798405,136.210845592995));
#144454=CARTESIAN_POINT('Ctrl Pts',(128.626558530195,2.55093160474578,136.142963291526));
#144455=CARTESIAN_POINT('Ctrl Pts',(128.619156708519,2.69289007449794,136.075131619238));
#144456=CARTESIAN_POINT('Ctrl Pts',(128.611754886844,2.83225171285692,136.001580970925));
#144457=CARTESIAN_POINT('Ctrl Pts',(128.604353065169,2.96852823575426,135.922541024315));
#144458=CARTESIAN_POINT('Ctrl Pts',(128.596955150857,3.10473281933593,135.843542802277));
#144459=CARTESIAN_POINT('Ctrl Pts',(128.589557236546,3.23785520881031,135.759061239781));
#144460=CARTESIAN_POINT('Ctrl Pts',(128.582159322234,3.36743116023369,135.669372225321));
#144461=CARTESIAN_POINT('Ctrl Pts',(128.574762637322,3.49698557848459,135.579698115547));
#144462=CARTESIAN_POINT('Ctrl Pts',(128.56736595241,3.62299442173573,135.484818483589));
#144463=CARTESIAN_POINT('Ctrl Pts',(128.559969267498,3.74502182720505,135.385052931644));
#144464=CARTESIAN_POINT('Ctrl Pts',(128.552572910562,3.86704382185134,135.28529180341));
#144465=CARTESIAN_POINT('Ctrl Pts',(128.545176553627,3.98508444073574,135.180645422236));
#144466=CARTESIAN_POINT('Ctrl Pts',(128.537780196691,4.09874058289344,135.071473950563));
#144467=CARTESIAN_POINT('Ctrl Pts',(128.530382707355,4.21241412609649,134.96228576446));
#144468=CARTESIAN_POINT('Ctrl Pts',(128.522985218018,4.3217015867391,134.848571367008));
#144469=CARTESIAN_POINT('Ctrl Pts',(128.515587728681,4.42623655601193,134.730727960636));
#144470=CARTESIAN_POINT('Ctrl Pts',(128.508187646166,4.53080816985605,134.61284324444));
#144471=CARTESIAN_POINT('Ctrl Pts',(128.500787563651,4.63062372781277,134.49082691661));
#144472=CARTESIAN_POINT('Ctrl Pts',(128.493387481136,4.72535705632517,134.36510931029));
#144473=CARTESIAN_POINT('Ctrl Pts',(128.48597926147,4.82019455387149,134.239253464538));
#144474=CARTESIAN_POINT('Ctrl Pts',(128.478571041803,4.90993843671278,134.10968851068));
#144475=CARTESIAN_POINT('Ctrl Pts',(128.471162822137,4.99430542810679,133.9768744242));
#144476=CARTESIAN_POINT('Ctrl Pts',(128.463750042835,5.07872434597632,133.843978592866));
#144477=CARTESIAN_POINT('Ctrl Pts',(128.456337263533,5.15775959105189,133.707829966179));
#144478=CARTESIAN_POINT('Ctrl Pts',(128.448924484231,5.23117408811143,133.568912701064));
#144479=CARTESIAN_POINT('Ctrl Pts',(128.441501113202,5.30469348324712,133.429796944445));
#144480=CARTESIAN_POINT('Ctrl Pts',(128.434077742173,5.37257592960687,133.28790498431));
#144481=CARTESIAN_POINT('Ctrl Pts',(128.426654371144,5.4346323491252,133.143741260459));
#144482=CARTESIAN_POINT('Ctrl Pts',(128.422718321704,5.4675361517749,133.067302194917));
#144483=CARTESIAN_POINT('Ctrl Pts',(128.418782272263,5.49880287733247,132.99022472585));
#144484=CARTESIAN_POINT('Ctrl Pts',(128.414846222823,5.52841007967023,132.912585594531));
#144485=CARTESIAN_POINT('Ctrl Pts',(128.407422956417,5.58424833927361,132.76616061589));
#144486=CARTESIAN_POINT('Ctrl Pts',(128.399999690012,5.63434971623466,132.617294302748));
#144487=CARTESIAN_POINT('Ctrl Pts',(128.392576423606,5.67849457154205,132.46647672767));
#144488=CARTESIAN_POINT('Ctrl Pts',(128.385161930885,5.7225872512966,132.31583740644));
#144489=CARTESIAN_POINT('Ctrl Pts',(128.377747438164,5.76073731894136,132.163251768604));
#144490=CARTESIAN_POINT('Ctrl Pts',(128.370332945443,5.79277315039603,132.009229818164));
#144491=CARTESIAN_POINT('Ctrl Pts',(128.362925599089,5.82477810451019,131.855356319879));
#144492=CARTESIAN_POINT('Ctrl Pts',(128.355518252736,5.85068047899101,131.700049628025));
#144493=CARTESIAN_POINT('Ctrl Pts',(128.348110906382,5.87035846901979,131.543834760256));
#144494=CARTESIAN_POINT('Ctrl Pts',(128.340709084707,5.89002178246118,131.38773640343));
#144495=CARTESIAN_POINT('Ctrl Pts',(128.333307263031,5.90346990860321,131.230731588165));
#144496=CARTESIAN_POINT('Ctrl Pts',(128.325905441356,5.91063215235769,131.073355268099));
#144497=CARTESIAN_POINT('Ctrl Pts',(128.318507527044,5.91779061521941,130.916062025769));
#144498=CARTESIAN_POINT('Ctrl Pts',(128.311109612733,5.91866978725571,130.758398041177));
#144499=CARTESIAN_POINT('Ctrl Pts',(128.303711698422,5.91325084607816,130.600903020372));
#144500=CARTESIAN_POINT('Ctrl Pts',(128.29631501351,5.90783280543032,130.443434172382));
#144501=CARTESIAN_POINT('Ctrl Pts',(128.288918328597,5.8961187416476,130.286134605162));
#144502=CARTESIAN_POINT('Ctrl Pts',(128.281521643685,5.8781419506315,130.129543775211));
#144503=CARTESIAN_POINT('Ctrl Pts',(128.27412528675,5.86016595672518,129.972959888661));
#144504=CARTESIAN_POINT('Ctrl Pts',(128.266728929814,5.83592783031404,129.817085047756));
#144505=CARTESIAN_POINT('Ctrl Pts',(128.259332572879,5.8055127003416,129.66245306935));
#144506=CARTESIAN_POINT('Ctrl Pts',(128.251935083542,5.77509291373494,129.507797416392));
#144507=CARTESIAN_POINT('Ctrl Pts',(128.244537594206,5.73849431257206,129.354385371121));
#144508=CARTESIAN_POINT('Ctrl Pts',(128.237140104869,5.69585302159305,129.202739901257));
#144509=CARTESIAN_POINT('Ctrl Pts',(128.229740022354,5.65319678277553,129.051041272309));
#144510=CARTESIAN_POINT('Ctrl Pts',(128.222339939839,5.60449373769657,128.90111081087));
#144511=CARTESIAN_POINT('Ctrl Pts',(128.214939857324,5.54992963304343,128.753455541565));
#144512=CARTESIAN_POINT('Ctrl Pts',(128.207531637658,5.49530552954812,128.605637910113));
#144513=CARTESIAN_POINT('Ctrl Pts',(128.200123417991,5.4348076251895,128.46010081744));
#144514=CARTESIAN_POINT('Ctrl Pts',(128.192715198325,5.36866979237122,128.317331220277));
#144515=CARTESIAN_POINT('Ctrl Pts',(128.185302419023,5.30249125282027,128.174473750808));
#144516=CARTESIAN_POINT('Ctrl Pts',(128.177889639721,5.23066603776645,128.034387502393));
#144517=CARTESIAN_POINT('Ctrl Pts',(128.170476860419,5.15347333719323,127.897533631772));
#144518=CARTESIAN_POINT('Ctrl Pts',(128.16305348939,5.07617034006962,127.760484217924));
#144519=CARTESIAN_POINT('Ctrl Pts',(128.155630118361,4.99348473579819,127.626676722914));
#144520=CARTESIAN_POINT('Ctrl Pts',(128.148206747332,4.90573872255601,127.496542885508));
#144521=CARTESIAN_POINT('Ctrl Pts',(128.144270697892,4.8592136808981,127.427542802397));
#144522=CARTESIAN_POINT('Ctrl Pts',(128.140334648451,4.81126665211715,127.359574965908));
#144523=CARTESIAN_POINT('Ctrl Pts',(128.13639859901,4.76195006814101,127.292699741138));
#144524=CARTESIAN_POINT('Ctrl Pts',(128.128975332605,4.66894052988033,127.166575154328));
#144525=CARTESIAN_POINT('Ctrl Pts',(128.121552066199,4.57077610256248,127.043957568431));
#144526=CARTESIAN_POINT('Ctrl Pts',(128.114128799794,4.46775037786499,126.925296668159));
#144527=CARTESIAN_POINT('Ctrl Pts',(128.106714307073,4.36484642101827,126.806776015218));
#144528=CARTESIAN_POINT('Ctrl Pts',(128.099299814352,4.25709284588642,126.69220301848));
#144529=CARTESIAN_POINT('Ctrl Pts',(128.091885321631,4.14482596627309,126.581997739768));
#144530=CARTESIAN_POINT('Ctrl Pts',(128.084477975277,4.03266729370517,126.471898681052));
#144531=CARTESIAN_POINT('Ctrl Pts',(128.077070628923,3.91600424144183,126.366159219284));
#144532=CARTESIAN_POINT('Ctrl Pts',(128.06966328257,3.79521268322544,126.265165617174));
#144533=CARTESIAN_POINT('Ctrl Pts',(128.062261460894,3.67451121591021,126.164247339902));
#144534=CARTESIAN_POINT('Ctrl Pts',(128.054859639219,3.54968765888871,126.068068112802));
#144535=CARTESIAN_POINT('Ctrl Pts',(128.047457817543,3.42115387138544,125.97697656916));
#144536=CARTESIAN_POINT('Ctrl Pts',(128.040059903232,3.29268793586909,125.885933112036));
#144537=CARTESIAN_POINT('Ctrl Pts',(128.032661988921,3.16051597431732,125.799972204874));
#144538=CARTESIAN_POINT('Ctrl Pts',(128.02526407461,3.02508188275239,125.719401407784));
#144539=CARTESIAN_POINT('Ctrl Pts',(128.017867389697,2.88967029787569,125.638844000099));
#144540=CARTESIAN_POINT('Ctrl Pts',(128.010470704785,2.75099797941207,125.563675115381));
#144541=CARTESIAN_POINT('Ctrl Pts',(128.003074019873,2.60953678463971,125.49415833026));
#144542=CARTESIAN_POINT('Ctrl Pts',(127.995677662938,2.46808186240486,125.424644627585));
#144543=CARTESIAN_POINT('Ctrl Pts',(127.988281306002,2.32383864477195,125.360782690831));
#144544=CARTESIAN_POINT('Ctrl Pts',(127.980884949067,2.17730226125249,125.302789439653));
#144545=CARTESIAN_POINT('Ctrl Pts',(127.97348745973,2.03074344263884,125.24478730956));
#144546=CARTESIAN_POINT('Ctrl Pts',(127.966089970394,1.88189110619851,125.192655791478));
#144547=CARTESIAN_POINT('Ctrl Pts',(127.958692481057,1.73125881823492,125.146563036635));
#144548=CARTESIAN_POINT('Ctrl Pts',(127.951292398542,1.58057372635705,125.100454124049));
#144549=CARTESIAN_POINT('Ctrl Pts',(127.943892316027,1.42810779739511,125.060388298553));
#144550=CARTESIAN_POINT('Ctrl Pts',(127.936492233512,1.27438800614917,125.026483345394));
#144551=CARTESIAN_POINT('Ctrl Pts',(127.929084013846,1.12049918418889,124.992541110253));
#144552=CARTESIAN_POINT('Ctrl Pts',(127.92167579418,0.965354111249209,124.964773357049));
#144553=CARTESIAN_POINT('Ctrl Pts',(127.914267574513,0.809488891566029,
124.943246534311));
#144554=CARTESIAN_POINT('Ctrl Pts',(127.906854795211,0.653527739440219,
124.921706462173));
#144555=CARTESIAN_POINT('Ctrl Pts',(127.899442015909,0.496845928034274,
124.906415010728));
#144556=CARTESIAN_POINT('Ctrl Pts',(127.892029236607,0.339982350581597,
124.897386556019));
#144557=CARTESIAN_POINT('Ctrl Pts',(127.884605865578,0.182894639093508,
124.88834520103));
#144558=CARTESIAN_POINT('Ctrl Pts',(127.877182494549,0.0256250150995326,
124.885584722199));
#144559=CARTESIAN_POINT('Ctrl Pts',(127.869759123521,-0.131289131365203,
124.889067410422));
#144560=CARTESIAN_POINT('Ctrl Pts',(127.86582307408,-0.214488776927516,
124.890914015284));
#144561=CARTESIAN_POINT('Ctrl Pts',(127.861887024639,-0.297588582945411,
124.894514932699));
#144562=CARTESIAN_POINT('Ctrl Pts',(127.857950975198,-0.380509421815742,
124.89985867901));
#144563=CARTESIAN_POINT('Ctrl Pts',(127.850527708792,-0.536895536047933,
124.909936817781));
#144564=CARTESIAN_POINT('Ctrl Pts',(127.843104442387,-0.693117454538892,
124.926247530366));
#144565=CARTESIAN_POINT('Ctrl Pts',(127.835681175981,-0.848638151331146,
124.948786875344));
#144566=CARTESIAN_POINT('Ctrl Pts',(127.82826668326,-1.00397503557443,124.971299580687));
#144567=CARTESIAN_POINT('Ctrl Pts',(127.82085219054,-1.15861198199119,125.000026211848));
#144568=CARTESIAN_POINT('Ctrl Pts',(127.813437697819,-1.31201379484953,
125.034910872172));
#144569=CARTESIAN_POINT('Ctrl Pts',(127.806030351465,-1.4652677532656,125.069761909347));
#144570=CARTESIAN_POINT('Ctrl Pts',(127.798623005111,-1.61728858655028,
125.11075907737));
#144571=CARTESIAN_POINT('Ctrl Pts',(127.791215658757,-1.76754815200689,
125.157794927446));
#144572=CARTESIAN_POINT('Ctrl Pts',(127.783813837082,-1.91769564821019,
125.204795696411));
#144573=CARTESIAN_POINT('Ctrl Pts',(127.776412015406,-2.06608413746188,
125.257826068563));
#144574=CARTESIAN_POINT('Ctrl Pts',(127.769010193731,-2.21219768473163,
125.316727979883));
#144575=CARTESIAN_POINT('Ctrl Pts',(127.76161227942,-2.35823409979941,125.375598797342));
#144576=CARTESIAN_POINT('Ctrl Pts',(127.754214365108,-2.50199761923544,
125.440334841869));
#144577=CARTESIAN_POINT('Ctrl Pts',(127.746816450797,-2.64298954736569,
125.510728894919));
#144578=CARTESIAN_POINT('Ctrl Pts',(127.739419765884,-2.78395804519353,
125.581111249753));
#144579=CARTESIAN_POINT('Ctrl Pts',(127.732023080972,-2.92215553218961,
125.657149580389));
#144580=CARTESIAN_POINT('Ctrl Pts',(127.72462639606,-3.05710520348624,125.738589369541));
#144581=CARTESIAN_POINT('Ctrl Pts',(127.717230039125,-3.19204889097331,
125.820025547567));
#144582=CARTESIAN_POINT('Ctrl Pts',(127.709833682189,-3.32374472949663,
125.906862515012));
#144583=CARTESIAN_POINT('Ctrl Pts',(127.702437325254,-3.45174258880932,
125.998800955768));
#144584=CARTESIAN_POINT('Ctrl Pts',(127.695039835917,-3.57976004492076,
126.090753472534));
#144585=CARTESIAN_POINT('Ctrl Pts',(127.68764234658,-3.70407809129121,126.187808799992));
#144586=CARTESIAN_POINT('Ctrl Pts',(127.680244857244,-3.82427766239768,
126.289625750114));
#144587=CARTESIAN_POINT('Ctrl Pts',(127.672844774729,-3.94451936927671,
126.391478392009));
#144588=CARTESIAN_POINT('Ctrl Pts',(127.665444692214,-4.06063944178101,
126.498095738762));
#144589=CARTESIAN_POINT('Ctrl Pts',(127.658044609699,-4.17225394109482,
126.609098097351));
#144590=CARTESIAN_POINT('Ctrl Pts',(127.650636390032,-4.28399117202575,
126.720222514446));
#144591=CARTESIAN_POINT('Ctrl Pts',(127.643228170366,-4.39121267077332,
126.835741309375));
#144592=CARTESIAN_POINT('Ctrl Pts',(127.635819950699,-4.49357275487206,
126.955239359516));
#144593=CARTESIAN_POINT('Ctrl Pts',(127.628407171397,-4.59599583989401,
127.074810958712));
#144594=CARTESIAN_POINT('Ctrl Pts',(127.620994392095,-4.69355131730112,
127.198366401086));
#144595=CARTESIAN_POINT('Ctrl Pts',(127.613581612793,-4.78593580716516,
127.325460071101));
#144596=CARTESIAN_POINT('Ctrl Pts',(127.606158241765,-4.87845230032126,
127.452735338512));
#144597=CARTESIAN_POINT('Ctrl Pts',(127.598734870736,-4.96578284263531,
127.583558621049));
#144598=CARTESIAN_POINT('Ctrl Pts',(127.591311499707,-5.04766868740341,
127.717457414563));
#144599=CARTESIAN_POINT('Ctrl Pts',(127.587375450266,-5.09108652712324,
127.788453767742));
#144600=CARTESIAN_POINT('Ctrl Pts',(127.583439400825,-5.13297444829509,
127.860314371871));
#144601=CARTESIAN_POINT('Ctrl Pts',(127.579503351385,-5.17329934204225,
127.932966447459));
#144602=CARTESIAN_POINT('Ctrl Pts',(127.571720884375,-5.25303084948161,
128.076616162733));
#144603=CARTESIAN_POINT('Ctrl Pts',(127.563938417365,-5.32687085259762,
128.223760860196));
#144604=CARTESIAN_POINT('Ctrl Pts',(127.556155950355,-5.39451514061434,
128.373900381277));
#144605=CARTESIAN_POINT('Ctrl Pts',(127.548386021547,-5.4620504480527,128.523798015092));
#144606=CARTESIAN_POINT('Ctrl Pts',(127.540616092739,-5.52340980383546,
128.676680565061));
#144607=CARTESIAN_POINT('Ctrl Pts',(127.532846163931,-5.57833413430794,
128.83202219617));
#144608=CARTESIAN_POINT('Ctrl Pts',(127.524973582954,-5.63398409583541,
128.989416118326));
#144609=CARTESIAN_POINT('Ctrl Pts',(127.517101001978,-5.68302759259376,
129.149334291285));
#144610=CARTESIAN_POINT('Ctrl Pts',(127.509228421001,-5.72524371990631,
129.31120459418));
#144611=CARTESIAN_POINT('Ctrl Pts',(127.501485147885,-5.76676644347643,
129.470416162583));
#144612=CARTESIAN_POINT('Ctrl Pts',(127.493741874769,-5.80168422650777,
129.631515907992));
#144613=CARTESIAN_POINT('Ctrl Pts',(127.485998601653,-5.82983536458688,
129.793939821901));
#144614=CARTESIAN_POINT('Ctrl Pts',(127.478061366746,-5.85869166249726,
129.960432303816));
#144615=CARTESIAN_POINT('Ctrl Pts',(127.470124131839,-5.88043772876022,
130.128315857805));
#144616=CARTESIAN_POINT('Ctrl Pts',(127.462186896932,-5.89495394412328,
130.296966728004));
#144617=CARTESIAN_POINT('Ctrl Pts',(127.454249662025,-5.90947015948635,
130.465617598202));
#144618=CARTESIAN_POINT('Ctrl Pts',(127.446312427118,-5.91675643119916,
130.635035426966));
#144619=CARTESIAN_POINT('Ctrl Pts',(127.438375192211,-5.91674999573795,
130.804585194783));
#144620=CARTESIAN_POINT('',(125.688375192211,-5.91687709322784,130.809716457862));
#144621=CARTESIAN_POINT('Ctrl Pts',(127.438375192169,-5.91674999573792,
130.804585195673));
#144622=CARTESIAN_POINT('Ctrl Pts',(127.430604669703,-5.91674369542117,
130.970573766693));
#144623=CARTESIAN_POINT('Ctrl Pts',(127.422834147236,-5.90974812859556,
131.136419067381));
#144624=CARTESIAN_POINT('Ctrl Pts',(127.415063624769,-5.89582513269253,
131.301529167669));
#144625=CARTESIAN_POINT('Ctrl Pts',(127.407282577955,-5.88188327957108,
131.466862892042));
#144626=CARTESIAN_POINT('Ctrl Pts',(127.399501531142,-5.86099529452708,
131.6314591157));
#144627=CARTESIAN_POINT('Ctrl Pts',(127.391720484328,-5.83327443974951,
131.794734220337));
#144628=CARTESIAN_POINT('Ctrl Pts',(127.383920661007,-5.80548669155154,
131.958403325458));
#144629=CARTESIAN_POINT('Ctrl Pts',(127.376120837686,-5.77083315191996,
132.120744625218));
#144630=CARTESIAN_POINT('Ctrl Pts',(127.368321014365,-5.72947802711713,
132.281185623883));
#144631=CARTESIAN_POINT('Ctrl Pts',(127.360511508761,-5.68807156627945,
132.441825785402));
#144632=CARTESIAN_POINT('Ctrl Pts',(127.352702003157,-5.63994700459161,
132.600560636575));
#144633=CARTESIAN_POINT('Ctrl Pts',(127.344892497554,-5.58531762056006,
132.756835365152));
#144634=CARTESIAN_POINT('Ctrl Pts',(127.337064695576,-5.53056024895637,
132.913476219459));
#144635=CARTESIAN_POINT('Ctrl Pts',(127.329236893598,-5.4692676909672,133.067645130788));
#144636=CARTESIAN_POINT('Ctrl Pts',(127.32140909162,-5.4017012640059,133.218807555674));
#144637=CARTESIAN_POINT('Ctrl Pts',(127.314624636937,-5.34314058974658,
133.349821935478));
#144638=CARTESIAN_POINT('Ctrl Pts',(127.307840182254,-5.27986784560114,
133.478578151947));
#144639=CARTESIAN_POINT('Ctrl Pts',(127.301055727571,-5.21207989665515,
133.604745182833));
#144640=CARTESIAN_POINT('Ctrl Pts',(127.293632461166,-5.13790915963536,
133.742791868326));
#144641=CARTESIAN_POINT('Ctrl Pts',(127.28620919476,-5.05813804137341,133.878098541676));
#144642=CARTESIAN_POINT('Ctrl Pts',(127.278785928355,-4.97299335046132,
134.010178406956));
#144643=CARTESIAN_POINT('Ctrl Pts',(127.271371435634,-4.88794929350306,
134.142102164803));
#144644=CARTESIAN_POINT('Ctrl Pts',(127.263956942913,-4.79754450611277,
134.270806395316));
#144645=CARTESIAN_POINT('Ctrl Pts',(127.256542450192,-4.70205229028583,
134.395827563247));
#144646=CARTESIAN_POINT('Ctrl Pts',(127.249135103838,-4.60665211345173,
134.520728231069));
#144647=CARTESIAN_POINT('Ctrl Pts',(127.241727757484,-4.50617449506531,
134.64195260874));
#144648=CARTESIAN_POINT('Ctrl Pts',(127.234320411131,-4.40093669295999,
134.759065004377));
#144649=CARTESIAN_POINT('Ctrl Pts',(127.226918589455,-4.29577738117766,
134.87609005317));
#144650=CARTESIAN_POINT('Ctrl Pts',(127.21951676778,-4.18586520328702,134.989008950014));
#144651=CARTESIAN_POINT('Ctrl Pts',(127.212114946104,-4.07155837821149,
135.09741814517));
#144652=CARTESIAN_POINT('Ctrl Pts',(127.204717031793,-3.95731189481916,
135.205770111955));
#144653=CARTESIAN_POINT('Ctrl Pts',(127.197319117482,-3.83867565460476,
135.309616861971));
#144654=CARTESIAN_POINT('Ctrl Pts',(127.18992120317,-3.71604541753918,135.408590956861));
#144655=CARTESIAN_POINT('Ctrl Pts',(127.182524518258,-3.59343555939452,
135.507548604052));
#144656=CARTESIAN_POINT('Ctrl Pts',(127.175127833346,-3.46683331191033,
135.601634969004));
#144657=CARTESIAN_POINT('Ctrl Pts',(127.167731148434,-3.33666835478942,
135.690522183933));
#144658=CARTESIAN_POINT('Ctrl Pts',(127.160334791498,-3.20650916931911,
135.77940545751));
#144659=CARTESIAN_POINT('Ctrl Pts',(127.152938434563,-3.07278789659433,
135.863089828931));
#144660=CARTESIAN_POINT('Ctrl Pts',(127.145542077627,-2.93596387385731,
135.941290312812));
#144661=CARTESIAN_POINT('Ctrl Pts',(127.138144588291,-2.79911890301292,
136.019502769387));
#144662=CARTESIAN_POINT('Ctrl Pts',(127.130747098954,-2.65917056040906,
136.092229481426));
#144663=CARTESIAN_POINT('Ctrl Pts',(127.123349609618,-2.51660335394268,
136.159231122202));
#144664=CARTESIAN_POINT('Ctrl Pts',(127.115949527103,-2.37398617076349,
136.2262562503));
#144665=CARTESIAN_POINT('Ctrl Pts',(127.108549444588,-2.22874863355076,
136.287552152705));
#144666=CARTESIAN_POINT('Ctrl Pts',(127.101149362073,-2.0813956701444,136.342927456271));
#144667=CARTESIAN_POINT('Ctrl Pts',(127.093741142406,-1.93388067700622,
136.398363650677));
#144668=CARTESIAN_POINT('Ctrl Pts',(127.08633292274,-1.78424596189502,136.447866113334));
#144669=CARTESIAN_POINT('Ctrl Pts',(127.078924703073,-1.63301277458622,
136.491292992805));
#144670=CARTESIAN_POINT('Ctrl Pts',(127.071511923771,-1.48168650577378,
136.534746600795));
#144671=CARTESIAN_POINT('Ctrl Pts',(127.064099144469,-1.32876016613994,
136.572117085926));
#144672=CARTESIAN_POINT('Ctrl Pts',(127.056686365167,-1.17476515552874,
136.603313746524));
#144673=CARTESIAN_POINT('Ctrl Pts',(127.049262994138,-1.02055010962506,
136.634554982375));
#144674=CARTESIAN_POINT('Ctrl Pts',(127.04183962311,-0.865263710605422,
136.659604715986));
#144675=CARTESIAN_POINT('Ctrl Pts',(127.034416252081,-0.709443261418309,
136.678424017065));
#144676=CARTESIAN_POINT('Ctrl Pts',(127.03048020264,-0.626823520400057,
136.688402462059));
#144677=CARTESIAN_POINT('Ctrl Pts',(127.0265441532,-0.544053664613397,136.696630179769));
#144678=CARTESIAN_POINT('Ctrl Pts',(127.022608103759,-0.461213650500511,
136.703107309118));
#144679=CARTESIAN_POINT('Ctrl Pts',(127.015184837353,-0.304979969229936,
136.715322972925));
#144680=CARTESIAN_POINT('Ctrl Pts',(127.007761570948,-0.148024394917613,
136.721345833891));
#144681=CARTESIAN_POINT('Ctrl Pts',(127.000338304543,0.00912092165060211,
136.721103587418));
#144682=CARTESIAN_POINT('Ctrl Pts',(126.992923811822,0.166080505504851,
136.720861627259));
#144683=CARTESIAN_POINT('Ctrl Pts',(126.985509319101,0.323229015572892,
136.714369299599));
#144684=CARTESIAN_POINT('Ctrl Pts',(126.97809482638,0.480028740117872,136.701605989022));
#144685=CARTESIAN_POINT('Ctrl Pts',(126.970687480026,0.63667733518493,136.688854980204));
#144686=CARTESIAN_POINT('Ctrl Pts',(126.963280133672,0.792977444412863,
136.669845051384));
#144687=CARTESIAN_POINT('Ctrl Pts',(126.955872787318,0.948391022270923,
136.644607618454));
#144688=CARTESIAN_POINT('Ctrl Pts',(126.948470965643,1.1036886868192,136.619389008553));
#144689=CARTESIAN_POINT('Ctrl Pts',(126.941069143967,1.2581007696677,136.587952202361));
#144690=CARTESIAN_POINT('Ctrl Pts',(126.933667322292,1.41109412691216,136.550380451111));
#144691=CARTESIAN_POINT('Ctrl Pts',(126.926269407981,1.56400672015455,136.512828533696));
#144692=CARTESIAN_POINT('Ctrl Pts',(126.918871493669,1.71550171772267,136.469148209832));
#144693=CARTESIAN_POINT('Ctrl Pts',(126.911473579358,1.86505606539004,136.419473834185));
#144694=CARTESIAN_POINT('Ctrl Pts',(126.904076894446,2.01458555983769,136.369807713518));
#144695=CARTESIAN_POINT('Ctrl Pts',(126.896680209533,2.16217469053301,136.314149635592));
#144696=CARTESIAN_POINT('Ctrl Pts',(126.889283524621,2.30731536064919,136.252683881563));
#144697=CARTESIAN_POINT('Ctrl Pts',(126.881887167686,2.45244959507596,136.19122085299));
#144698=CARTESIAN_POINT('Ctrl Pts',(126.87449081075,2.59513524104833,136.123950805921));
#144699=CARTESIAN_POINT('Ctrl Pts',(126.867094453815,2.73488424929218,136.051106152226));
#144700=CARTESIAN_POINT('Ctrl Pts',(126.859696964478,2.87465465346605,135.978250345828));
#144701=CARTESIAN_POINT('Ctrl Pts',(126.852299475142,3.01148719363715,135.899818405958));
#144702=CARTESIAN_POINT('Ctrl Pts',(126.844901985805,3.14491862909991,135.816088600891));
#144703=CARTESIAN_POINT('Ctrl Pts',(126.83750190329,3.27839683874543,135.73232944447));
#144704=CARTESIAN_POINT('Ctrl Pts',(126.830101820775,3.40847125391639,135.643268923558));
#144705=CARTESIAN_POINT('Ctrl Pts',(126.82270173826,3.53470794113451,135.549228406386));
#144706=CARTESIAN_POINT('Ctrl Pts',(126.815293518594,3.66108343856776,135.455084481998));
#144707=CARTESIAN_POINT('Ctrl Pts',(126.807885298927,3.78361248093266,135.355949848531));
#144708=CARTESIAN_POINT('Ctrl Pts',(126.800477079261,3.9018939763607,135.252186374016));
#144709=CARTESIAN_POINT('Ctrl Pts',(126.793064299959,4.02024827207562,135.148359034814));
#144710=CARTESIAN_POINT('Ctrl Pts',(126.785651520657,4.1343495416086,135.039897434219));
#144711=CARTESIAN_POINT('Ctrl Pts',(126.778238741354,4.24383424047797,134.927199627502));
#144712=CARTESIAN_POINT('Ctrl Pts',(126.770815370326,4.35347537621934,134.814340792873));
#144713=CARTESIAN_POINT('Ctrl Pts',(126.763391999297,4.45848651830365,134.697233940329));
#144714=CARTESIAN_POINT('Ctrl Pts',(126.755968628268,4.55854448820266,134.576310075284));
#144715=CARTESIAN_POINT('Ctrl Pts',(126.752032578827,4.61159762470175,134.512193340508));
#144716=CARTESIAN_POINT('Ctrl Pts',(126.748096529387,4.66325896545235,134.447003999064));
#144717=CARTESIAN_POINT('Ctrl Pts',(126.744160479946,4.7134854089243,134.380809395664));
#144718=CARTESIAN_POINT('Ctrl Pts',(126.73673721354,4.80821091379789,134.255968439515));
#144719=CARTESIAN_POINT('Ctrl Pts',(126.729313947135,4.89811643907389,134.127172773102));
#144720=CARTESIAN_POINT('Ctrl Pts',(126.721890680729,4.9828535123478,133.99483102755));
#144721=CARTESIAN_POINT('Ctrl Pts',(126.714476188008,5.06749043343813,133.862645698951));
#144722=CARTESIAN_POINT('Ctrl Pts',(126.707061695287,5.14697086256309,133.726922945069));
#144723=CARTESIAN_POINT('Ctrl Pts',(126.699647202566,5.22098680906185,133.588104014882));
#144724=CARTESIAN_POINT('Ctrl Pts',(126.692239856213,5.29493141620472,133.449418883607));
#144725=CARTESIAN_POINT('Ctrl Pts',(126.684832509859,5.36342185157869,133.307643844193));
#144726=CARTESIAN_POINT('Ctrl Pts',(126.677425163505,5.42619371951346,133.163248550642));
#144727=CARTESIAN_POINT('Ctrl Pts',(126.67002334183,5.48891876982088,133.018960952549));
#144728=CARTESIAN_POINT('Ctrl Pts',(126.662621520154,5.54593359693948,132.872057332438));
#144729=CARTESIAN_POINT('Ctrl Pts',(126.655219698479,5.59702006518662,132.723031238699));
#144730=CARTESIAN_POINT('Ctrl Pts',(126.647821784167,5.64807956528488,132.574083814675));
#144731=CARTESIAN_POINT('Ctrl Pts',(126.640423869856,5.69321681838378,132.42301650066));
#144732=CARTESIAN_POINT('Ctrl Pts',(126.633025955545,5.73226213728277,132.270341978967));
#144733=CARTESIAN_POINT('Ctrl Pts',(126.625629270632,5.77130096755809,132.117692829009));
#144734=CARTESIAN_POINT('Ctrl Pts',(126.61823258572,5.80424978048555,131.96343736277));
#144735=CARTESIAN_POINT('Ctrl Pts',(126.610835900808,5.83098897827627,131.808102664967));
#144736=CARTESIAN_POINT('Ctrl Pts',(126.603439543872,5.85772699042292,131.652774854867));
#144737=CARTESIAN_POINT('Ctrl Pts',(126.596043186937,5.87825587157571,131.49636827624));
#144738=CARTESIAN_POINT('Ctrl Pts',(126.588646830002,5.89250735386897,131.339419163054));
#144739=CARTESIAN_POINT('Ctrl Pts',(126.581249340665,5.90676101810057,131.182446020559));
#144740=CARTESIAN_POINT('Ctrl Pts',(126.573851851328,5.91473533606307,131.024930549908));
#144741=CARTESIAN_POINT('Ctrl Pts',(126.566454361992,5.91641402982012,130.867412899425));
#144742=CARTESIAN_POINT('Ctrl Pts',(126.559054279477,5.91809331204067,130.709840031374));
#144743=CARTESIAN_POINT('Ctrl Pts',(126.551654196962,5.91347257211605,130.552265355014));
#144744=CARTESIAN_POINT('Ctrl Pts',(126.544254114447,5.90258763459732,130.39522765825));
#144745=CARTESIAN_POINT('Ctrl Pts',(126.53684589478,5.8916907279708,130.238017282394));
#144746=CARTESIAN_POINT('Ctrl Pts',(126.529437675114,5.87451589353259,130.081345437962));
#144747=CARTESIAN_POINT('Ctrl Pts',(126.522029455447,5.85115078115382,129.925745173414));
#144748=CARTESIAN_POINT('Ctrl Pts',(126.514616676145,5.82777128793821,129.770049139498));
#144749=CARTESIAN_POINT('Ctrl Pts',(126.507203896843,5.79819399482663,129.615426365481));
#144750=CARTESIAN_POINT('Ctrl Pts',(126.499791117541,5.7625572923183,129.462397870226));
#144751=CARTESIAN_POINT('Ctrl Pts',(126.492367746512,5.72686967041826,129.309150720681));
#144752=CARTESIAN_POINT('Ctrl Pts',(126.484944375484,5.6851054460712,129.157502758481));
#144753=CARTESIAN_POINT('Ctrl Pts',(126.477521004455,5.6374525504484,129.007958851829));
#144754=CARTESIAN_POINT('Ctrl Pts',(126.473584955014,5.6121858417739,128.928667084266));
#144755=CARTESIAN_POINT('Ctrl Pts',(126.469648905573,5.58526441913393,128.849966503781));
#144756=CARTESIAN_POINT('Ctrl Pts',(126.465712856133,5.55672164411094,128.771929774371));
#144757=CARTESIAN_POINT('Ctrl Pts',(126.458289589727,5.50289086120658,128.624754938147));
#144758=CARTESIAN_POINT('Ctrl Pts',(126.450866323322,5.44312755184637,128.47949766977));
#144759=CARTESIAN_POINT('Ctrl Pts',(126.443443056916,5.37758715112309,128.336672024049));
#144760=CARTESIAN_POINT('Ctrl Pts',(126.436028564195,5.31212421371066,128.194015186379));
#144761=CARTESIAN_POINT('Ctrl Pts',(126.428614071474,5.24089793036124,128.053784586668));
#144762=CARTESIAN_POINT('Ctrl Pts',(126.421199578753,5.16411305986116,127.916477852031));
#144763=CARTESIAN_POINT('Ctrl Pts',(126.413792232399,5.08740219751015,127.779303458795));
#144764=CARTESIAN_POINT('Ctrl Pts',(126.406384886046,5.005143594865,127.645047643914));
#144765=CARTESIAN_POINT('Ctrl Pts',(126.398977539692,4.9175894728204,127.514186710414));
#144766=CARTESIAN_POINT('Ctrl Pts',(126.391575718017,4.83010065194325,127.383423377935));
#144767=CARTESIAN_POINT('Ctrl Pts',(126.384173896341,4.73732438253885,127.256050194145));
#144768=CARTESIAN_POINT('Ctrl Pts',(126.376772074666,4.63955799318205,127.132517457735));
#144769=CARTESIAN_POINT('Ctrl Pts',(126.369374160354,4.5418432139411,127.009049933294));
#144770=CARTESIAN_POINT('Ctrl Pts',(126.361976246043,4.43914379205028,126.889419110659));
#144771=CARTESIAN_POINT('Ctrl Pts',(126.354578331732,4.33179934158259,126.774044869791));
#144772=CARTESIAN_POINT('Ctrl Pts',(126.347181646819,4.22447272981522,126.658689802029));
#144773=CARTESIAN_POINT('Ctrl Pts',(126.339784961907,4.11250287553328,126.547590185152));
#144774=CARTESIAN_POINT('Ctrl Pts',(126.332388276995,3.99626858451111,126.441131542334));
#144775=CARTESIAN_POINT('Ctrl Pts',(126.324991920059,3.88003944743921,126.334677620003));
#144776=CARTESIAN_POINT('Ctrl Pts',(126.317595563124,3.75954652488443,126.23286451469));
#144777=CARTESIAN_POINT('Ctrl Pts',(126.310199206189,3.63520406522306,126.136039509642));
#144778=CARTESIAN_POINT('Ctrl Pts',(126.302801716852,3.5108425684136,126.039199680439));
#144779=CARTESIAN_POINT('Ctrl Pts',(126.295404227515,3.3826306555269,125.947349701476));
#144780=CARTESIAN_POINT('Ctrl Pts',(126.288006738179,3.25101397002412,125.860795231207));
#144781=CARTESIAN_POINT('Ctrl Pts',(126.280606655664,3.11935114649618,125.774210419402));
#144782=CARTESIAN_POINT('Ctrl Pts',(126.273206573149,2.98428148573068,125.692925017219));
#144783=CARTESIAN_POINT('Ctrl Pts',(126.265806490634,2.84627764929576,125.617200112471));
#144784=CARTESIAN_POINT('Ctrl Pts',(126.258398270967,2.70812206345563,125.541391940405));
#144785=CARTESIAN_POINT('Ctrl Pts',(126.250990051301,2.56702618602561,125.471156656197));
#144786=CARTESIAN_POINT('Ctrl Pts',(126.243581831634,2.42348586266683,125.406708643239));
#144787=CARTESIAN_POINT('Ctrl Pts',(126.236169052332,2.27985719263392,125.342220963605));
#144788=CARTESIAN_POINT('Ctrl Pts',(126.22875627303,2.13378142431607,125.283527791744));
#144789=CARTESIAN_POINT('Ctrl Pts',(126.221343493728,1.98577170908535,125.230794319235));
#144790=CARTESIAN_POINT('Ctrl Pts',(126.213920122699,1.83755051063265,125.177985498666));
#144791=CARTESIAN_POINT('Ctrl Pts',(126.20649675167,1.68739020173327,125.131153495658));
#144792=CARTESIAN_POINT('Ctrl Pts',(126.199073380642,1.53581712369258,125.090413091987));
#144793=CARTESIAN_POINT('Ctrl Pts',(126.195137331201,1.45544944077159,125.068811552409));
#144794=CARTESIAN_POINT('Ctrl Pts',(126.19120128176,1.3746847269651,125.048921721609));
#144795=CARTESIAN_POINT('Ctrl Pts',(126.18726523232,1.29360214930372,125.030754808211));
#144796=CARTESIAN_POINT('Ctrl Pts',(126.179841965914,1.14068293833117,124.996492576511));
#144797=CARTESIAN_POINT('Ctrl Pts',(126.172418699509,0.986170356037416,
124.968258039597));
#144798=CARTESIAN_POINT('Ctrl Pts',(126.164995433103,0.83058090775567,124.946198284703));
#144799=CARTESIAN_POINT('Ctrl Pts',(126.157580940382,0.675175353280782,
124.924164602608));
#144800=CARTESIAN_POINT('Ctrl Pts',(126.150166447661,0.518695832258268,
124.908291227556));
#144801=CARTESIAN_POINT('Ctrl Pts',(126.14275195494,0.361671689599985,124.898674869794));
#144802=CARTESIAN_POINT('Ctrl Pts',(126.135344608587,0.204798892722251,
124.889067780639));
#144803=CARTESIAN_POINT('Ctrl Pts',(126.127937262233,0.0473828893332454,
124.885705725405));
#144804=CARTESIAN_POINT('Ctrl Pts',(126.120529915879,-0.110039261787883,
124.88863395693));
#144805=CARTESIAN_POINT('Ctrl Pts',(126.113128094204,-0.267344001529506,
124.891560004469));
#144806=CARTESIAN_POINT('Ctrl Pts',(126.105726272528,-0.4246545082465,124.900766990378));
#144807=CARTESIAN_POINT('Ctrl Pts',(126.098324450853,-0.581431219541534,
124.916248161147));
#144808=CARTESIAN_POINT('Ctrl Pts',(126.090926536542,-0.738125169631245,
124.931721159526));
#144809=CARTESIAN_POINT('Ctrl Pts',(126.08352862223,-0.894285514939462,
124.953461709982));
#144810=CARTESIAN_POINT('Ctrl Pts',(126.076130707919,-1.04937542886165,
124.981411040951));
#144811=CARTESIAN_POINT('Ctrl Pts',(126.068734023007,-1.20443956965344,
125.009355727248));
#144812=CARTESIAN_POINT('Ctrl Pts',(126.061337338095,-1.35843326509065,
125.043507080126));
#144813=CARTESIAN_POINT('Ctrl Pts',(126.053940653182,-1.51082740983665,
125.083754784248));
#144814=CARTESIAN_POINT('Ctrl Pts',(126.046544296247,-1.66321479726657,
125.124000703746));
#144815=CARTESIAN_POINT('Ctrl Pts',(126.039147939311,-1.81400241410713,
125.170342341682));
#144816=CARTESIAN_POINT('Ctrl Pts',(126.031751582376,-1.96267416976077,
125.222618894246));
#144817=CARTESIAN_POINT('Ctrl Pts',(126.024354093039,-2.11136868743985,
125.274903450483));
#144818=CARTESIAN_POINT('Ctrl Pts',(126.016956603703,-2.25794634673264,
125.333124606754));
#144819=CARTESIAN_POINT('Ctrl Pts',(126.009559114366,-2.40190910735036,
125.397072646454));
#144820=CARTESIAN_POINT('Ctrl Pts',(126.002159031851,-2.54592233389065,
125.461043103041));
#144821=CARTESIAN_POINT('Ctrl Pts',(125.994758949336,-2.68731849577285,
125.530744288628));
#144822=CARTESIAN_POINT('Ctrl Pts',(125.987358866821,-2.82562244730206,
125.605919663991));
#144823=CARTESIAN_POINT('Ctrl Pts',(125.979950647155,-2.96407847824398,
125.681177702409));
#144824=CARTESIAN_POINT('Ctrl Pts',(125.972542427489,-3.09943518022415,
125.761921773426));
#144825=CARTESIAN_POINT('Ctrl Pts',(125.965134207822,-3.2312441697306,125.847850587506));
#144826=CARTESIAN_POINT('Ctrl Pts',(125.95772142852,-3.36313428547102,125.933832289338));
#144827=CARTESIAN_POINT('Ctrl Pts',(125.950308649218,-3.49147203410891,
126.025004877253));
#144828=CARTESIAN_POINT('Ctrl Pts',(125.942895869916,-3.61584106444145,
126.121025912551));
#144829=CARTESIAN_POINT('Ctrl Pts',(125.935472498887,-3.74038779907668,
126.217184147207));
#144830=CARTESIAN_POINT('Ctrl Pts',(125.928049127858,-3.86095420438861,
126.318204426282));
#144831=CARTESIAN_POINT('Ctrl Pts',(125.92062575683,-3.97715921088422,126.423705966286));
#144832=CARTESIAN_POINT('Ctrl Pts',(125.916689707389,-4.03877389363215,
126.479645414274));
#144833=CARTESIAN_POINT('Ctrl Pts',(125.912753657948,-4.09916307219774,
126.536844115996));
#144834=CARTESIAN_POINT('Ctrl Pts',(125.908817608507,-4.15827452473585,
126.595241524521));
#144835=CARTESIAN_POINT('Ctrl Pts',(125.90149902863,-4.26818470079762,126.703824027184));
#144836=CARTESIAN_POINT('Ctrl Pts',(125.894180448753,-4.37402795947477,
126.816901451091));
#144837=CARTESIAN_POINT('Ctrl Pts',(125.886861868876,-4.47540639748585,
126.934132182468));
#144838=CARTESIAN_POINT('Ctrl Pts',(125.879552092185,-4.57666289199929,
127.051221902347));
#144839=CARTESIAN_POINT('Ctrl Pts',(125.872242315493,-4.67346500209269,
127.172454701838));
#144840=CARTESIAN_POINT('Ctrl Pts',(125.864932538802,-4.76544979670491,
127.297450467935));
#144841=CARTESIAN_POINT('Ctrl Pts',(125.857575982694,-4.85802325431277,
127.423246153001));
#144842=CARTESIAN_POINT('Ctrl Pts',(125.850219426586,-4.94571721874585,
127.552852884212));
#144843=CARTESIAN_POINT('Ctrl Pts',(125.842862870478,-5.02820048573112,
127.685846478141));
#144844=CARTESIAN_POINT('Ctrl Pts',(125.835566061488,-5.11001385535975,
127.817759949273));
#144845=CARTESIAN_POINT('Ctrl Pts',(125.828269252498,-5.18670063628449,
127.953005146424));
#144846=CARTESIAN_POINT('Ctrl Pts',(125.820972443509,-5.25797928195931,
128.091136625156));
#144847=CARTESIAN_POINT('Ctrl Pts',(125.8136787567,-5.32922742870997,128.229208999771));
#144848=CARTESIAN_POINT('Ctrl Pts',(125.806385069891,-5.39507186801401,
128.37016485772));
#144849=CARTESIAN_POINT('Ctrl Pts',(125.799091383082,-5.45527616356596,
128.513532701347));
#144850=CARTESIAN_POINT('Ctrl Pts',(125.791799281877,-5.51546737106253,
128.656869377658));
#144851=CARTESIAN_POINT('Ctrl Pts',(125.784507180672,-5.57002072663485,
128.802616641396));
#144852=CARTESIAN_POINT('Ctrl Pts',(125.777215079467,-5.61874738739333,
128.95028177373));
#144853=CARTESIAN_POINT('Ctrl Pts',(125.769811755529,-5.66821725127364,
129.100199167673));
#144854=CARTESIAN_POINT('Ctrl Pts',(125.762408431591,-5.71168106557502,
129.252093037716));
#144855=CARTESIAN_POINT('Ctrl Pts',(125.755005107653,-5.7489934610278,129.405430759582));
#144856=CARTESIAN_POINT('Ctrl Pts',(125.747709255647,-5.7857642031293,129.556542521685));
#144857=CARTESIAN_POINT('Ctrl Pts',(125.740413403641,-5.81656087769184,
129.709056107196));
#144858=CARTESIAN_POINT('Ctrl Pts',(125.733117551634,-5.84129583934044,
129.862451131573));
#144859=CARTESIAN_POINT('Ctrl Pts',(125.725660491731,-5.86657734047008,
130.019235546166));
#144860=CARTESIAN_POINT('Ctrl Pts',(125.718203431827,-5.88552606068901,
130.176940386491));
#144861=CARTESIAN_POINT('Ctrl Pts',(125.710746371923,-5.89810441933159,
130.335004866391));
#144862=CARTESIAN_POINT('Ctrl Pts',(125.703289312019,-5.91068277797417,
130.493069346291));
#144863=CARTESIAN_POINT('Ctrl Pts',(125.695832252115,-5.91689079666146,
130.6514930386));
#144864=CARTESIAN_POINT('Ctrl Pts',(125.688375192211,-5.91674757605312,
130.809716340626));
#144865=CARTESIAN_POINT('',(123.938375192211,-5.92504829577756,130.801671299475));
#144866=CARTESIAN_POINT('Ctrl Pts',(125.688375192211,-5.91821605979866,
130.809717669868));
#144867=CARTESIAN_POINT('Ctrl Pts',(125.669040123039,-5.92203015439028,
131.220073233809));
#144868=CARTESIAN_POINT('Ctrl Pts',(125.556889179265,-5.69567161983018,
133.596115399124));
#144869=CARTESIAN_POINT('Ctrl Pts',(125.351922360878,-2.48367746759114,
137.347212195226));
#144870=CARTESIAN_POINT('Ctrl Pts',(125.07347473707,4.16219799704592,136.430519908213));
#144871=CARTESIAN_POINT('Ctrl Pts',(124.795027113255,6.98321683707467,130.343662086251));
#144872=CARTESIAN_POINT('Ctrl Pts',(124.516579489443,3.38700055293948,124.680163708199));
#144873=CARTESIAN_POINT('Ctrl Pts',(124.238131865629,-3.32170377516985,
124.644503106196));
#144874=CARTESIAN_POINT('Ctrl Pts',(124.045397099886,-5.8524521295715,128.537956850714));
#144875=CARTESIAN_POINT('Ctrl Pts',(123.945478208746,-5.92589711076374,
130.651373189507));
#144876=CARTESIAN_POINT('Ctrl Pts',(123.938375192211,-5.92504829577756,
130.801671299475));
#144877=CARTESIAN_POINT('',(122.188375192211,-5.90992605862746,130.800308419121));
#144878=CARTESIAN_POINT('Ctrl Pts',(123.938375192211,-5.92504829577756,
130.801671299475));
#144879=CARTESIAN_POINT('Ctrl Pts',(123.852662334142,-5.91480555481291,
132.615334621827));
#144880=CARTESIAN_POINT('Ctrl Pts',(123.674133601469,-4.05249985999765,
136.411139468064));
#144881=CARTESIAN_POINT('Ctrl Pts',(123.40278899419,2.4139810832736,137.373246052702));
#144882=CARTESIAN_POINT('Ctrl Pts',(123.124341370378,6.83140509735844,132.324052996348));
#144883=CARTESIAN_POINT('Ctrl Pts',(122.845893746565,4.97110155966289,125.878336884994));
#144884=CARTESIAN_POINT('Ctrl Pts',(122.567446122753,-1.45740145955266,
123.959395934234));
#144885=CARTESIAN_POINT('Ctrl Pts',(122.348273271301,-5.4632512585378,127.400110204618));
#144886=CARTESIAN_POINT('Ctrl Pts',(122.221916294454,-5.91440793099423,
130.08591681752));
#144887=CARTESIAN_POINT('Ctrl Pts',(122.188375192211,-5.90992605862746,
130.800308419121));
#144888=CARTESIAN_POINT('',(120.438375158672,-5.91341329990167,130.808580694715));
#144889=CARTESIAN_POINT('Ctrl Pts',(122.188375192211,-5.90992605862746,
130.800308419121));
#144890=CARTESIAN_POINT('Ctrl Pts',(122.12910041985,-5.90200556864557,132.062801203515));
#144891=CARTESIAN_POINT('Ctrl Pts',(121.977009772883,-4.8860947069906,135.313812493445));
#144892=CARTESIAN_POINT('Ctrl Pts',(121.732103251314,0.471325265101819,
137.786868263448));
#144893=CARTESIAN_POINT('Ctrl Pts',(121.4536556275,6.12934425592135,134.182037263242));
#144894=CARTESIAN_POINT('Ctrl Pts',(121.175208003688,6.15479531066329,127.473286434335));
#144895=CARTESIAN_POINT('Ctrl Pts',(120.896760379875,0.524290153371079,
123.825630047797));
#144896=CARTESIAN_POINT('Ctrl Pts',(120.651149442716,-4.86720232846028,
126.264962262151));
#144897=CARTESIAN_POINT('Ctrl Pts',(120.498354380162,-5.90187691199983,
129.531255255228));
#144898=CARTESIAN_POINT('Ctrl Pts',(120.438375192211,-5.91024609870193,
130.808577719811));
#144899=CARTESIAN_POINT('',(118.688375192211,-5.92111403471271,130.806804712595));
#144900=CARTESIAN_POINT('Ctrl Pts',(120.438375123354,-5.91674849279557,
130.80858382741));
#144901=CARTESIAN_POINT('Ctrl Pts',(120.429906845386,-5.91661962929804,
130.989122548634));
#144902=CARTESIAN_POINT('Ctrl Pts',(120.421438567417,-5.90822361023152,
131.16933121331));
#144903=CARTESIAN_POINT('Ctrl Pts',(120.412970289449,-5.89167472838423,
131.348510833424));
#144904=CARTESIAN_POINT('Ctrl Pts',(120.404463212892,-5.87505002554334,
131.528511389778));
#144905=CARTESIAN_POINT('Ctrl Pts',(120.395956136335,-5.85019768804956,
131.707473309596));
#144906=CARTESIAN_POINT('Ctrl Pts',(120.387449059779,-5.81728316216418,
131.884706475938));
#144907=CARTESIAN_POINT('Ctrl Pts',(120.378889667413,-5.78416622243705,
132.063029569755));
#144908=CARTESIAN_POINT('Ctrl Pts',(120.370330275048,-5.74288771416499,
132.239602441887));
#144909=CARTESIAN_POINT('Ctrl Pts',(120.361770882682,-5.69366480443984,
132.413743001334));
#144910=CARTESIAN_POINT('Ctrl Pts',(120.354468965871,-5.6516733199206,132.562300261501));
#144911=CARTESIAN_POINT('Ctrl Pts',(120.34716704906,-5.60390106750741,132.709087690254));
#144912=CARTESIAN_POINT('Ctrl Pts',(120.339865132249,-5.55050988539579,
132.853694795933));
#144913=CARTESIAN_POINT('Ctrl Pts',(120.332441865844,-5.49623140225706,
133.000705108066));
#144914=CARTESIAN_POINT('Ctrl Pts',(120.325018599438,-5.43602625655856,
133.145779804663));
#144915=CARTESIAN_POINT('Ctrl Pts',(120.317595333033,-5.3700514472791,133.28840530639));
#144916=CARTESIAN_POINT('Ctrl Pts',(120.310180840312,-5.30415461474539,
133.430862236618));
#144917=CARTESIAN_POINT('Ctrl Pts',(120.302766347591,-5.23250184760396,
133.570875398483));
#144918=CARTESIAN_POINT('Ctrl Pts',(120.29535185487,-5.15529941829848,133.707947790391));
#144919=CARTESIAN_POINT('Ctrl Pts',(120.287944508517,-5.07817139960087,
133.844888066766));
#144920=CARTESIAN_POINT('Ctrl Pts',(120.280537162163,-4.9955045494545,133.978892892891));
#144921=CARTESIAN_POINT('Ctrl Pts',(120.273129815809,-4.90755253728837,
134.109486735622));
#144922=CARTESIAN_POINT('Ctrl Pts',(120.265727994134,-4.81966612305121,
134.239983176537));
#144923=CARTESIAN_POINT('Ctrl Pts',(120.258326172459,-4.72650260322443,
134.367073391291));
#144924=CARTESIAN_POINT('Ctrl Pts',(120.250924350783,-4.62836067555996,
134.490307988247));
#144925=CARTESIAN_POINT('Ctrl Pts',(120.243526436472,-4.53027055625502,
134.613477530618));
#144926=CARTESIAN_POINT('Ctrl Pts',(120.236128522161,-4.42720749498932,
134.732795217418));
#144927=CARTESIAN_POINT('Ctrl Pts',(120.228730607849,-4.31951238223295,
134.847842204297));
#144928=CARTESIAN_POINT('Ctrl Pts',(120.221333922937,-4.21183516645075,
134.962870072455));
#144929=CARTESIAN_POINT('Ctrl Pts',(120.213937238025,-4.09952768178991,
135.073628377004));
#144930=CARTESIAN_POINT('Ctrl Pts',(120.206540553113,-3.98296990567007,
135.179732749514));
#144931=CARTESIAN_POINT('Ctrl Pts',(120.199144196178,-3.86641729784416,
135.285832417245));
#144932=CARTESIAN_POINT('Ctrl Pts',(120.191747839242,-3.74561504933562,
135.387278311958));
#144933=CARTESIAN_POINT('Ctrl Pts',(120.184351482307,-3.62097846361268,
135.483724412843));
#144934=CARTESIAN_POINT('Ctrl Pts',(120.17695399297,-3.4963227957102,135.580185279874));
#144935=CARTESIAN_POINT('Ctrl Pts',(120.169556503634,-3.36783191695308,
135.671644600433));
#144936=CARTESIAN_POINT('Ctrl Pts',(120.162159014297,-3.23595239905746,
135.757798073872));
#144937=CARTESIAN_POINT('Ctrl Pts',(120.154758931782,-3.10402665100148,
135.843981748277));
#144938=CARTESIAN_POINT('Ctrl Pts',(120.147358849268,-2.96871021106818,
135.924855668366));
#144939=CARTESIAN_POINT('Ctrl Pts',(120.139958766753,-2.83047653329784,
136.000160186155));
#144940=CARTESIAN_POINT('Ctrl Pts',(120.132550547086,-2.69209085338783,
136.075547509003));
#144941=CARTESIAN_POINT('Ctrl Pts',(120.12514232742,-2.55078185746082,136.145353020571));
#144942=CARTESIAN_POINT('Ctrl Pts',(120.117734107753,-2.40704604139051,
136.209363847641));
#144943=CARTESIAN_POINT('Ctrl Pts',(120.110321328452,-2.26322175832377,
136.273414072308));
#144944=CARTESIAN_POINT('Ctrl Pts',(120.10290854915,-2.11696802479533,136.331662367916));
#144945=CARTESIAN_POINT('Ctrl Pts',(120.095495769848,-1.96879849258671,
136.383945105508));
#144946=CARTESIAN_POINT('Ctrl Pts',(120.088072398819,-1.82041724880191,
136.436302547129));
#144947=CARTESIAN_POINT('Ctrl Pts',(120.08064902779,-1.67011509492895,136.482677296888));
#144948=CARTESIAN_POINT('Ctrl Pts',(120.073225656761,-1.51841871919148,
136.522956175543));
#144949=CARTESIAN_POINT('Ctrl Pts',(120.06928960732,-1.43798566085437,136.544313003488));
#144950=CARTESIAN_POINT('Ctrl Pts',(120.065353557878,-1.35716078332332,
136.563956922157));
#144951=CARTESIAN_POINT('Ctrl Pts',(120.061417508437,-1.27602328737747,
136.581876963936));
#144952=CARTESIAN_POINT('Ctrl Pts',(120.053994242031,-1.1230005022684,136.615673603459));
#144953=CARTESIAN_POINT('Ctrl Pts',(120.046570975626,-0.968402699448,136.643437726442));
#144954=CARTESIAN_POINT('Ctrl Pts',(120.03914770922,-0.812746829540018,
136.665023818397));
#144955=CARTESIAN_POINT('Ctrl Pts',(120.031733216499,-0.657274931943631,
136.686584397383));
#144956=CARTESIAN_POINT('Ctrl Pts',(120.024318723778,-0.500747822629744,
136.701981429075));
#144957=CARTESIAN_POINT('Ctrl Pts',(120.016904231057,-0.343695138411051,
136.711119814819));
#144958=CARTESIAN_POINT('Ctrl Pts',(120.009496884704,-0.186793827482337,
136.720249392643));
#144959=CARTESIAN_POINT('Ctrl Pts',(120.00208953835,-0.0293683202935072,
136.723132312138));
#144960=CARTESIAN_POINT('Ctrl Pts',(119.994682191996,0.128044189129835,
136.7197249553));
#144961=CARTESIAN_POINT('Ctrl Pts',(119.987280370321,0.285339294364816,
136.716320139796));
#144962=CARTESIAN_POINT('Ctrl Pts',(119.979878548645,0.442621049532602,
136.706634397463));
#144963=CARTESIAN_POINT('Ctrl Pts',(119.97247672697,0.599349915290433,136.690676124022));
#144964=CARTESIAN_POINT('Ctrl Pts',(119.965078812659,0.755996045100118,
136.674726274828));
#144965=CARTESIAN_POINT('Ctrl Pts',(119.957680898347,0.912089496327345,
136.652510526699));
#144966=CARTESIAN_POINT('Ctrl Pts',(119.950282984036,1.06709362373455,136.624089284839));
#144967=CARTESIAN_POINT('Ctrl Pts',(119.942886299124,1.22207199226762,136.595672766075));
#144968=CARTESIAN_POINT('Ctrl Pts',(119.935489614211,1.37596102944626,136.561052867546));
#144969=CARTESIAN_POINT('Ctrl Pts',(119.928092929299,1.52823196814656,136.520341514493));
#144970=CARTESIAN_POINT('Ctrl Pts',(119.920696572364,1.68049615499387,136.479631966624));
#144971=CARTESIAN_POINT('Ctrl Pts',(119.913300215428,1.83114202539174,136.432831597701));
#144972=CARTESIAN_POINT('Ctrl Pts',(119.905903858493,1.97965398056459,136.380102781595));
#144973=CARTESIAN_POINT('Ctrl Pts',(119.898506369156,2.12818867329702,136.327365892573));
#144974=CARTESIAN_POINT('Ctrl Pts',(119.89110887982,2.27458844847988,136.268698874004));
#144975=CARTESIAN_POINT('Ctrl Pts',(119.883711390483,2.4183559064365,136.204312957384));
#144976=CARTESIAN_POINT('Ctrl Pts',(119.876311307968,2.56217376185254,136.139904470381));
#144977=CARTESIAN_POINT('Ctrl Pts',(119.868911225453,2.70335712236475,136.069773246366));
#144978=CARTESIAN_POINT('Ctrl Pts',(119.861511142938,2.84143162529623,135.994177269555));
#144979=CARTESIAN_POINT('Ctrl Pts',(119.854102923272,2.97965795533809,135.918498167197));
#144980=CARTESIAN_POINT('Ctrl Pts',(119.846694703605,3.11476827317795,135.83734249094));
#144981=CARTESIAN_POINT('Ctrl Pts',(119.839286483939,3.24631511440242,135.751012893652));
#144982=CARTESIAN_POINT('Ctrl Pts',(119.831873704637,3.37794292051287,135.664630161937));
#144983=CARTESIAN_POINT('Ctrl Pts',(119.824460925334,3.50600257670346,135.573067380366));
#144984=CARTESIAN_POINT('Ctrl Pts',(119.817048146032,3.63007877596548,135.476668253284));
#144985=CARTESIAN_POINT('Ctrl Pts',(119.809624775004,3.75433226111951,135.380131386608));
#144986=CARTESIAN_POINT('Ctrl Pts',(119.802201403975,3.87459063699609,135.278744612786));
#144987=CARTESIAN_POINT('Ctrl Pts',(119.794778032946,3.99047399484126,135.172889873391));
#144988=CARTESIAN_POINT('Ctrl Pts',(119.790841983505,4.05191813175439,135.116763150613));
#144989=CARTESIAN_POINT('Ctrl Pts',(119.786905934064,4.11213293742652,135.059380909947));
#144990=CARTESIAN_POINT('Ctrl Pts',(119.782969884624,4.17106637453843,135.000803856989));
#144991=CARTESIAN_POINT('Ctrl Pts',(119.775546618218,4.2822129976811,134.890329363237));
#144992=CARTESIAN_POINT('Ctrl Pts',(119.768123351813,4.38913562935371,134.775269039935));
#144993=CARTESIAN_POINT('Ctrl Pts',(119.760700085407,4.49143241965637,134.655979158149));
#144994=CARTESIAN_POINT('Ctrl Pts',(119.753285592686,4.59360830364818,134.536830267096));
#144995=CARTESIAN_POINT('Ctrl Pts',(119.745871099965,4.69116898844872,134.413462048675));
#144996=CARTESIAN_POINT('Ctrl Pts',(119.738456607244,4.78374818323294,134.28626869819));
#144997=CARTESIAN_POINT('Ctrl Pts',(119.73104926089,4.87623814670367,134.159197941445));
#144998=CARTESIAN_POINT('Ctrl Pts',(119.723641914537,4.96375596049115,134.028309692132));
#144999=CARTESIAN_POINT('Ctrl Pts',(119.716234568183,5.04597456103929,133.894032330199));
#145000=CARTESIAN_POINT('Ctrl Pts',(119.708832746507,5.12813183985327,133.759855117389));
#145001=CARTESIAN_POINT('Ctrl Pts',(119.701430924832,5.2049975810027,133.622294141996));
#145002=CARTESIAN_POINT('Ctrl Pts',(119.694029103157,5.27628721385202,133.481807871844));
#145003=CARTESIAN_POINT('Ctrl Pts',(119.686631188845,5.34753921345904,133.3413957633));
#145004=CARTESIAN_POINT('Ctrl Pts',(119.679233274534,5.41322079855772,133.198061767473));
#145005=CARTESIAN_POINT('Ctrl Pts',(119.671835360222,5.4730927198998,133.052290029687));
#145006=CARTESIAN_POINT('Ctrl Pts',(119.66443867531,5.53295469161473,132.90654251652));
#145007=CARTESIAN_POINT('Ctrl Pts',(119.657041990398,5.58700877404001,132.758358410385));
#145008=CARTESIAN_POINT('Ctrl Pts',(119.649645305486,5.63506332150261,132.608243076363));
#145009=CARTESIAN_POINT('Ctrl Pts',(119.64224894855,5.68311573817622,132.458134398613));
#145010=CARTESIAN_POINT('Ctrl Pts',(119.634852591615,5.72516903502612,132.306095018769));
#145011=CARTESIAN_POINT('Ctrl Pts',(119.627456234679,5.76108112805576,132.152646491726));
#145012=CARTESIAN_POINT('Ctrl Pts',(119.620058745343,5.79699871931853,131.999174471322));
#145013=CARTESIAN_POINT('Ctrl Pts',(119.612661256006,5.826773149559,131.844293237645));
#145014=CARTESIAN_POINT('Ctrl Pts',(119.60526376667,5.85031327714352,131.688535442913));
#145015=CARTESIAN_POINT('Ctrl Pts',(119.597863684155,5.87386165668326,131.532723047528));
#145016=CARTESIAN_POINT('Ctrl Pts',(119.59046360164,5.89117132665236,131.376033848179));
#145017=CARTESIAN_POINT('Ctrl Pts',(119.583063519125,5.90220293186348,131.219006386388));
#145018=CARTESIAN_POINT('Ctrl Pts',(119.575655299458,5.91324666745862,131.061806256761));
#145019=CARTESIAN_POINT('Ctrl Pts',(119.568247079792,5.91799852562069,130.904267494484));
#145020=CARTESIAN_POINT('Ctrl Pts',(119.560838860125,5.91647127133269,130.74693015531));
#145021=CARTESIAN_POINT('Ctrl Pts',(119.553426080823,5.91494307704515,130.589495977628));
#145022=CARTESIAN_POINT('Ctrl Pts',(119.546013301521,5.90712808791871,130.432263842053));
#145023=CARTESIAN_POINT('Ctrl Pts',(119.538600522219,5.89309098856959,130.275768938725));
#145024=CARTESIAN_POINT('Ctrl Pts',(119.53117715119,5.87903383235464,130.119050428141));
#145025=CARTESIAN_POINT('Ctrl Pts',(119.523753780161,5.85873685775066,129.963071622861));
#145026=CARTESIAN_POINT('Ctrl Pts',(119.516330409133,5.83231605305868,129.808358599629));
#145027=CARTESIAN_POINT('Ctrl Pts',(119.512394359692,5.81830710845317,129.726326042428));
#145028=CARTESIAN_POINT('Ctrl Pts',(119.508458310251,5.80257737752639,129.64464911833));
#145029=CARTESIAN_POINT('Ctrl Pts',(119.504522260811,5.78514980617318,129.563404420662));
#145030=CARTESIAN_POINT('Ctrl Pts',(119.497098994405,5.75228195049539,129.410179456414));
#145031=CARTESIAN_POINT('Ctrl Pts',(119.489675728,5.71327273597372,129.258029502933));
#145032=CARTESIAN_POINT('Ctrl Pts',(119.482252461594,5.66820469385868,129.107485221133));
#145033=CARTESIAN_POINT('Ctrl Pts',(119.474837968873,5.62318991842674,128.957118870173));
#145034=CARTESIAN_POINT('Ctrl Pts',(119.467423476152,5.57213067548659,128.808354767496));
#145035=CARTESIAN_POINT('Ctrl Pts',(119.460008983431,5.51516062357471,128.661714156138));
#145036=CARTESIAN_POINT('Ctrl Pts',(119.452601637078,5.45824548154374,128.515214882522));
#145037=CARTESIAN_POINT('Ctrl Pts',(119.445194290724,5.39543100654209,128.370835371273));
#145038=CARTESIAN_POINT('Ctrl Pts',(119.43778694437,5.3269008209133,128.229082340049));
#145039=CARTESIAN_POINT('Ctrl Pts',(119.430385122695,5.25842174768234,128.087435033583));
#145040=CARTESIAN_POINT('Ctrl Pts',(119.422983301019,5.18423561379725,127.94841064129));
#145041=CARTESIAN_POINT('Ctrl Pts',(119.415581479344,5.10457432384171,127.812496393562));
#145042=CARTESIAN_POINT('Ctrl Pts',(119.408183565033,5.02495508646112,127.676653893907));
#145043=CARTESIAN_POINT('Ctrl Pts',(119.400785650721,4.93986663744964,127.543918590292));
#145044=CARTESIAN_POINT('Ctrl Pts',(119.39338773641,4.84958698191946,127.414753462261));
#145045=CARTESIAN_POINT('Ctrl Pts',(119.385991051498,4.75932232923027,127.28560979913));
#145046=CARTESIAN_POINT('Ctrl Pts',(119.378594366585,4.66386839584224,127.160035439731));
#145047=CARTESIAN_POINT('Ctrl Pts',(119.371197681673,4.56354677054439,127.038464783166));
#145048=CARTESIAN_POINT('Ctrl Pts',(119.363801324738,4.46322959361246,126.916899517171));
#145049=CARTESIAN_POINT('Ctrl Pts',(119.356404967802,4.35804539152727,126.799337888946));
#145050=CARTESIAN_POINT('Ctrl Pts',(119.349008610867,4.24835616332295,126.686181350942));
#145051=CARTESIAN_POINT('Ctrl Pts',(119.34161112153,4.13865014141778,126.573007488382));
#145052=CARTESIAN_POINT('Ctrl Pts',(119.334213632194,4.02443797988699,126.464240326978));
#145053=CARTESIAN_POINT('Ctrl Pts',(119.326816142857,3.90611854984878,126.360244458302));
#145054=CARTESIAN_POINT('Ctrl Pts',(119.319416060342,3.78775764311796,126.256212134036));
#145055=CARTESIAN_POINT('Ctrl Pts',(119.312015977827,3.66528688146725,126.156954678861));
#145056=CARTESIAN_POINT('Ctrl Pts',(119.304615895312,3.53913808269339,126.062796298259));
#145057=CARTESIAN_POINT('Ctrl Pts',(119.297207675646,3.4128505703467,125.968534380837));
#145058=CARTESIAN_POINT('Ctrl Pts',(119.289799455979,3.2828772433216,125.879382958877));
#145059=CARTESIAN_POINT('Ctrl Pts',(119.282391236313,3.14967936560169,125.795623206162));
#145060=CARTESIAN_POINT('Ctrl Pts',(119.274978457011,3.01639950681047,125.711811900716));
#145061=CARTESIAN_POINT('Ctrl Pts',(119.267565677709,2.87989146559127,125.633399062513));
#145062=CARTESIAN_POINT('Ctrl Pts',(119.260152898407,2.74064047618298,125.560619553897));
#145063=CARTESIAN_POINT('Ctrl Pts',(119.252729527378,2.60119051843079,125.487736054507));
#145064=CARTESIAN_POINT('Ctrl Pts',(119.245306156349,2.45899012144547,125.420502119833));
#145065=CARTESIAN_POINT('Ctrl Pts',(119.23788278532,2.31454458300072,125.359104522964));
#145066=CARTESIAN_POINT('Ctrl Pts',(119.233946735879,2.2379560925923,125.326550043888));
#145067=CARTESIAN_POINT('Ctrl Pts',(119.230010686439,2.16073667934626,125.295635539458));
#145068=CARTESIAN_POINT('Ctrl Pts',(119.226074636998,2.08296318621513,125.266383105209));
#145069=CARTESIAN_POINT('Ctrl Pts',(119.218651370592,1.93628480540107,125.211213927153));
#145070=CARTESIAN_POINT('Ctrl Pts',(119.211228104187,1.78719130712475,125.161792717803));
#145071=CARTESIAN_POINT('Ctrl Pts',(119.203804837781,1.63617376159973,125.118336876466));
#145072=CARTESIAN_POINT('Ctrl Pts',(119.19639034506,1.48533470627207,125.074932396325));
#145073=CARTESIAN_POINT('Ctrl Pts',(119.188975852339,1.33257648547059,125.037479352221));
#145074=CARTESIAN_POINT('Ctrl Pts',(119.181561359618,1.17840988142788,125.006147038035));
#145075=CARTESIAN_POINT('Ctrl Pts',(119.174154013265,1.02439186896254,124.974844923114));
#145076=CARTESIAN_POINT('Ctrl Pts',(119.166746666911,0.868968539040656,
124.949651867435));
#145077=CARTESIAN_POINT('Ctrl Pts',(119.159339320557,0.712665459942137,
124.930687277593));
#145078=CARTESIAN_POINT('Ctrl Pts',(119.151937498882,0.556478957576876,
124.911736832258));
#145079=CARTESIAN_POINT('Ctrl Pts',(119.144535677206,0.399414381503607,
124.899005647863));
#145080=CARTESIAN_POINT('Ctrl Pts',(119.137133855531,0.242007002542,124.89256197644));
#145081=CARTESIAN_POINT('Ctrl Pts',(119.129735941219,0.0846827177107159,
124.886121706581));
#145082=CARTESIAN_POINT('Ctrl Pts',(119.122338026908,-0.072983637571102,
124.885962354721));
#145083=CARTESIAN_POINT('Ctrl Pts',(119.114940112597,-0.230452276947585,
124.892100279036));
#145084=CARTESIAN_POINT('Ctrl Pts',(119.107543427685,-0.387894747893087,
124.89823718334));
#145085=CARTESIAN_POINT('Ctrl Pts',(119.100146742772,-0.545139195494856,
124.910669272316));
#145086=CARTESIAN_POINT('Ctrl Pts',(119.09275005786,-0.701646320888489,
124.929360787533));
#145087=CARTESIAN_POINT('Ctrl Pts',(119.085353700925,-0.858146506592173,
124.948051473949));
#145088=CARTESIAN_POINT('Ctrl Pts',(119.077957343989,-1.01390906443024,
124.973000990477));
#145089=CARTESIAN_POINT('Ctrl Pts',(119.070560987054,-1.16840057176563,
125.004121771932));
#145090=CARTESIAN_POINT('Ctrl Pts',(119.063163497717,-1.32291573214497,
125.035247318059));
#145091=CARTESIAN_POINT('Ctrl Pts',(119.055766008381,-1.47615908857449,
125.072545936687));
#145092=CARTESIAN_POINT('Ctrl Pts',(119.048368519044,-1.62760830025584,
125.115879116898));
#145093=CARTESIAN_POINT('Ctrl Pts',(119.040968436529,-1.77911060222412,
125.159227487489));
#145094=CARTESIAN_POINT('Ctrl Pts',(119.033568354014,-1.92881714856776,
125.208614528798));
#145095=CARTESIAN_POINT('Ctrl Pts',(119.026168271499,-2.07622176796565,
125.263852181265));
#145096=CARTESIAN_POINT('Ctrl Pts',(119.018760051833,-2.22378847389583,
125.319150573209));
#145097=CARTESIAN_POINT('Ctrl Pts',(119.011351832166,-2.36904784812238,
125.380312293057));
#145098=CARTESIAN_POINT('Ctrl Pts',(119.0039436125,-2.51151400672803,125.447101247654));
#145099=CARTESIAN_POINT('Ctrl Pts',(118.996530833198,-2.65406785087714,
125.513931309738));
#145100=CARTESIAN_POINT('Ctrl Pts',(118.989118053896,-2.79382472309748,
125.586395336536));
#145101=CARTESIAN_POINT('Ctrl Pts',(118.981705274593,-2.93032474608807,
125.664212035573));
#145102=CARTESIAN_POINT('Ctrl Pts',(118.974281903565,-3.06701980671292,
125.742139922759));
#145103=CARTESIAN_POINT('Ctrl Pts',(118.966858532536,-3.20044840812621,
125.825435560096));
#145104=CARTESIAN_POINT('Ctrl Pts',(118.959435161507,-3.33018028705042,
125.913774781673));
#145105=CARTESIAN_POINT('Ctrl Pts',(118.955499112066,-3.39896724213075,
125.960614356624));
#145106=CARTESIAN_POINT('Ctrl Pts',(118.951563062626,-3.46671546929933,
126.008871191182));
#145107=CARTESIAN_POINT('Ctrl Pts',(118.947627013185,-3.53336484346536,
126.05849257837));
#145108=CARTESIAN_POINT('Ctrl Pts',(118.940276572164,-3.65783032623298,
126.151158863527));
#145109=CARTESIAN_POINT('Ctrl Pts',(118.932926131144,-3.77885418607313,
126.248878586329));
#145110=CARTESIAN_POINT('Ctrl Pts',(118.925575690124,-3.89599287290778,
126.351364985775));
#145111=CARTESIAN_POINT('Ctrl Pts',(118.918233970298,-4.01299257634084,
126.453729786551));
#145112=CARTESIAN_POINT('Ctrl Pts',(118.910892250472,-4.12611599515914,
126.560849761971));
#145113=CARTESIAN_POINT('Ctrl Pts',(118.903550530647,-4.23494899655388,
126.672395279003));
#145114=CARTESIAN_POINT('Ctrl Pts',(118.896215841812,-4.34367777115461,
126.783833971529));
#145115=CARTESIAN_POINT('Ctrl Pts',(118.888881152978,-4.44812404099511,
126.899689499942));
#145116=CARTESIAN_POINT('Ctrl Pts',(118.881546464144,-4.54790736508967,
127.019592571693));
#145117=CARTESIAN_POINT('Ctrl Pts',(118.874217122619,-4.64761794278351,
127.139408228868));
#145118=CARTESIAN_POINT('Ctrl Pts',(118.866887781093,-4.74267209858175,
127.263265263788));
#145119=CARTESIAN_POINT('Ctrl Pts',(118.859558439568,-4.83272699882416,
127.390758368133));
#145120=CARTESIAN_POINT('Ctrl Pts',(118.852232235997,-4.92274334332396,
127.518196888093));
#145121=CARTESIAN_POINT('Ctrl Pts',(118.844906032426,-5.00776447083573,
127.649268069622));
#145122=CARTESIAN_POINT('Ctrl Pts',(118.837579828855,-5.08748860375037,
127.783534527039));
#145123=CARTESIAN_POINT('Ctrl Pts',(118.830255153022,-5.16719611173853,
127.917772985782));
#145124=CARTESIAN_POINT('Ctrl Pts',(118.82293047719,-5.24160862790158,128.05520506719));
#145125=CARTESIAN_POINT('Ctrl Pts',(118.815605801357,-5.31046853091582,
128.195365687588));
#145126=CARTESIAN_POINT('Ctrl Pts',(118.808281137258,-5.37932832362041,
128.335526083456));
#145127=CARTESIAN_POINT('Ctrl Pts',(118.800956473159,-5.44263535269792,
128.478414667306));
#145128=CARTESIAN_POINT('Ctrl Pts',(118.79363180906,-5.50017878311434,128.623543358766));
#145129=CARTESIAN_POINT('Ctrl Pts',(118.786305640915,-5.5577340294947,128.768701850942));
#145130=CARTESIAN_POINT('Ctrl Pts',(118.77897947277,-5.60952318185033,128.916101011511));
#145131=CARTESIAN_POINT('Ctrl Pts',(118.771653304625,-5.65538430752652,
129.065234717384));
#145132=CARTESIAN_POINT('Ctrl Pts',(118.764320097234,-5.70128949822011,
129.214511716281));
#145133=CARTESIAN_POINT('Ctrl Pts',(118.756986889844,-5.74125517395969,
129.365526224171));
#145134=CARTESIAN_POINT('Ctrl Pts',(118.749653682453,-5.7751697130392,129.517758368192));
#145135=CARTESIAN_POINT('Ctrl Pts',(118.742316774607,-5.80910136594485,
129.67006733102));
#145136=CARTESIAN_POINT('Ctrl Pts',(118.734979866761,-5.8369757312481,129.82359477925));
#145137=CARTESIAN_POINT('Ctrl Pts',(118.727642958916,-5.85873282046703,
129.9778134012));
#145138=CARTESIAN_POINT('Ctrl Pts',(118.720295637506,-5.88052079038378,
130.132250911744));
#145139=CARTESIAN_POINT('Ctrl Pts',(118.712948316096,-5.89617410202407,
130.287381176658));
#145140=CARTESIAN_POINT('Ctrl Pts',(118.705600994687,-5.90568481511976,
130.442673699135));
#145141=CARTESIAN_POINT('Ctrl Pts',(118.699859060528,-5.91311744061035,
130.564034857805));
#145142=CARTESIAN_POINT('Ctrl Pts',(118.69411712637,-5.91679956894418,130.685495037937));
#145143=CARTESIAN_POINT('Ctrl Pts',(118.688375192211,-5.9167494959397,130.806802911017));
#145144=CARTESIAN_POINT('',(116.938375192211,-5.91775807691223,130.798956223901));
#145145=CARTESIAN_POINT('Ctrl Pts',(118.688375192211,-5.92531066698449,
130.806806444865));
#145146=CARTESIAN_POINT('Ctrl Pts',(118.681976591265,-5.92601627665423,
130.942183404842));
#145147=CARTESIAN_POINT('Ctrl Pts',(118.675577990318,-5.92178053373525,
131.077515423935));
#145148=CARTESIAN_POINT('Ctrl Pts',(118.576363514767,-5.7773031608978,133.170487024815));
#145149=CARTESIAN_POINT('Ctrl Pts',(118.390731765559,-3.36834491582461,
136.938838024679));
#145150=CARTESIAN_POINT('Ctrl Pts',(118.112284141745,3.34043687663362,136.95407947322));
#145151=CARTESIAN_POINT('Ctrl Pts',(117.833836517933,6.9795203688748,131.318029723882));
#145152=CARTESIAN_POINT('Ctrl Pts',(117.55538889412,4.20476561065067,125.209943159972));
#145153=CARTESIAN_POINT('Ctrl Pts',(117.276941270308,-2.43396332954512,
124.242852937102));
#145154=CARTESIAN_POINT('Ctrl Pts',(117.071270036338,-5.68546201478638,
127.982278744742));
#145155=CARTESIAN_POINT('Ctrl Pts',(116.958414676972,-5.92171512746286,
130.37356612518));
#145156=CARTESIAN_POINT('Ctrl Pts',(116.938375192211,-5.91775807691223,
130.798956223901));
#145157=CARTESIAN_POINT('',(115.188375192211,-5.90693479489549,130.80438521844));
#145158=CARTESIAN_POINT('Ctrl Pts',(116.938375192211,-5.91775807691223,
130.798956223901));
#145159=CARTESIAN_POINT('Ctrl Pts',(116.865598802368,-5.90338745526516,
132.343824070018));
#145160=CARTESIAN_POINT('Ctrl Pts',(116.700006537921,-4.49301687389813,
135.882186555631));
#145161=CARTESIAN_POINT('Ctrl Pts',(116.441598398868,1.4782284268974,137.64485776677));
#145162=CARTESIAN_POINT('Ctrl Pts',(116.163150775056,6.55412255704564,133.258140973988));
#145163=CARTESIAN_POINT('Ctrl Pts',(115.884703151243,5.60709824395641,126.616519907489));
#145164=CARTESIAN_POINT('Ctrl Pts',(115.60625552743,-0.492575433349502,
123.823319866161));
#145165=CARTESIAN_POINT('Ctrl Pts',(115.374146207752,-5.19983838450488,
126.842588456896));
#145166=CARTESIAN_POINT('Ctrl Pts',(115.23485276268,-5.90689819190348,129.813205798887));
#145167=CARTESIAN_POINT('Ctrl Pts',(115.188375192211,-5.90693479489549,
130.80438521844));
#145168=CARTESIAN_POINT('',(113.438375192211,-5.91784867649587,130.809756633416));
#145169=CARTESIAN_POINT('Ctrl Pts',(115.188375192211,-5.90693479489549,
130.80438521844));
#145170=CARTESIAN_POINT('Ctrl Pts',(115.142036888076,-5.90697128820956,
131.79259464792));
#145171=CARTESIAN_POINT('Ctrl Pts',(115.002882709335,-5.20295378394123,
134.760144048991));
#145172=CARTESIAN_POINT('Ctrl Pts',(114.770912655992,-0.503046869620426,
137.78465462121));
#145173=CARTESIAN_POINT('Ctrl Pts',(114.492465032178,5.60080991683228,135.000607608133));
#145174=CARTESIAN_POINT('Ctrl Pts',(114.214017408366,6.55779600449193,128.360414608787));
#145175=CARTESIAN_POINT('Ctrl Pts',(113.935569784553,1.48848793016878,123.96608859811));
#145176=CARTESIAN_POINT('Ctrl Pts',(113.677022379168,-4.48861432852338,
125.720745735417));
#145177=CARTESIAN_POINT('Ctrl Pts',(113.511290848388,-5.90345104083902,
129.261993258066));
#145178=CARTESIAN_POINT('Ctrl Pts',(113.438375192211,-5.91784867649587,
130.809756633416));
#145179=CARTESIAN_POINT('',(111.688375192211,-5.92147968542167,130.801867673062));
#145180=CARTESIAN_POINT('Ctrl Pts',(113.438375192211,-5.91784867649587,
130.809756633416));
#145181=CARTESIAN_POINT('Ctrl Pts',(113.418474973783,-5.92177809453099,
131.232173859838));
#145182=CARTESIAN_POINT('Ctrl Pts',(113.305758880752,-5.68749102524069,
133.620446152917));
#145183=CARTESIAN_POINT('Ctrl Pts',(113.100226913113,-2.44380325616413,
137.36220982104));
#145184=CARTESIAN_POINT('Ctrl Pts',(112.821779289301,4.19636890965415,136.40507918793));
#145185=CARTESIAN_POINT('Ctrl Pts',(112.543331665489,6.98028305151762,130.30116179897));
#145186=CARTESIAN_POINT('Ctrl Pts',(112.264884041676,3.34965807482215,124.65965954167));
#145187=CARTESIAN_POINT('Ctrl Pts',(111.986436417863,-3.35913903274104,
124.664837387781));
#145188=CARTESIAN_POINT('Ctrl Pts',(111.794266801375,-5.85878875116337,
128.562162782962));
#145189=CARTESIAN_POINT('Ctrl Pts',(111.694913059491,-5.92599367912675,
130.663539518991));
#145190=CARTESIAN_POINT('Ctrl Pts',(111.688375192211,-5.92526049744177,
130.801866081339));
#145191=CARTESIAN_POINT('',(109.938375221708,-5.91299038747931,130.800172818778));
#145192=CARTESIAN_POINT('Ctrl Pts',(111.688375192211,-5.91674947565407,
130.801869664481));
#145193=CARTESIAN_POINT('Ctrl Pts',(111.681028256843,-5.91681482372276,
130.957090633337));
#145194=CARTESIAN_POINT('Ctrl Pts',(111.673681321476,-5.91076783778976,
131.112561170285));
#145195=CARTESIAN_POINT('Ctrl Pts',(111.666334386108,-5.89857585866385,
131.267753973246));
#145196=CARTESIAN_POINT('Ctrl Pts',(111.658995738555,-5.88639763287252,
131.422771708769));
#145197=CARTESIAN_POINT('Ctrl Pts',(111.651657091002,-5.86808823697625,
131.577511957074));
#145198=CARTESIAN_POINT('Ctrl Pts',(111.644318443448,-5.8436669866875,131.731445679035));
#145199=CARTESIAN_POINT('Ctrl Pts',(111.636986394494,-5.81926769494539,
131.885240990358));
#145200=CARTESIAN_POINT('Ctrl Pts',(111.62965434554,-5.78876754528707,132.038230844198));
#145201=CARTESIAN_POINT('Ctrl Pts',(111.622322296585,-5.75223777418,132.189889813143));
#145202=CARTESIAN_POINT('Ctrl Pts',(111.614995163127,-5.71573249308259,
132.341447108042));
#145203=CARTESIAN_POINT('Ctrl Pts',(111.607668029669,-5.6732057261156,132.491674924627));
#145204=CARTESIAN_POINT('Ctrl Pts',(111.600340896211,-5.62478001587141,
132.640056762235));
#145205=CARTESIAN_POINT('Ctrl Pts',(111.59301624978,-5.57637074262402,132.788388235031));
#145206=CARTESIAN_POINT('Ctrl Pts',(111.585691603349,-5.52206662529805,
132.934874612607));
#145207=CARTESIAN_POINT('Ctrl Pts',(111.578366956918,-5.46204039978975,
133.079013389653));
#145208=CARTESIAN_POINT('Ctrl Pts',(111.571043435937,-5.40202339745138,
133.223130019439));
#145209=CARTESIAN_POINT('Ctrl Pts',(111.563719914955,-5.3362861823376,133.364899414094));
#145210=CARTESIAN_POINT('Ctrl Pts',(111.556396393973,-5.26504997945334,
133.503838210797));
#145211=CARTESIAN_POINT('Ctrl Pts',(111.549072481829,-5.19380997170936,
133.642784428484));
#145212=CARTESIAN_POINT('Ctrl Pts',(111.541748569684,-5.11707056565635,
133.778899407751));
#145213=CARTESIAN_POINT('Ctrl Pts',(111.534424657539,-5.03509924458978,
133.911723834126));
#145214=CARTESIAN_POINT('Ctrl Pts',(111.52709883756,-4.95310657048997,134.044582860461));
#145215=CARTESIAN_POINT('Ctrl Pts',(111.51977301758,-4.86587946962067,134.174149303627));
#145216=CARTESIAN_POINT('Ctrl Pts',(111.5124471976,-4.77372894444798,134.299992538613));
#145217=CARTESIAN_POINT('Ctrl Pts',(111.505113740359,-4.68148235115796,
134.425966966802));
#145218=CARTESIAN_POINT('Ctrl Pts',(111.497780283117,-4.58430230842726,
134.548210126812));
#145219=CARTESIAN_POINT('Ctrl Pts',(111.490446825875,-4.48254073891411,
134.666323730605));
#145220=CARTESIAN_POINT('Ctrl Pts',(111.483109318504,-4.38072296842701,
134.784502566289));
#145221=CARTESIAN_POINT('Ctrl Pts',(111.475771811134,-4.27431889094365,
134.898547024507));
#145222=CARTESIAN_POINT('Ctrl Pts',(111.468434303764,-4.16371701420639,
135.008096002686));
#145223=CARTESIAN_POINT('Ctrl Pts',(111.46108589296,-4.05295078462652,135.117807769115));
#145224=CARTESIAN_POINT('Ctrl Pts',(111.453737482156,-3.93797457691017,
135.223010454999));
#145225=CARTESIAN_POINT('Ctrl Pts',(111.446389071352,-3.81921032087068,
135.323382977264));
#145226=CARTESIAN_POINT('Ctrl Pts',(111.440773104314,-3.72844564194221,
135.40009191361));
#145227=CARTESIAN_POINT('Ctrl Pts',(111.435157137275,-3.63546917588325,
135.473980540481));
#145228=CARTESIAN_POINT('Ctrl Pts',(111.429541170237,-3.54047996203196,
135.544923052652));
#145229=CARTESIAN_POINT('Ctrl Pts',(111.422117903832,-3.41492184617205,
135.638695890656));
#145230=CARTESIAN_POINT('Ctrl Pts',(111.414694637426,-3.28544581013673,
135.727618796898));
#145231=CARTESIAN_POINT('Ctrl Pts',(111.407271371021,-3.15246312477616,
135.811346418367));
#145232=CARTESIAN_POINT('Ctrl Pts',(111.3998568783,-3.01963761390607,135.894975080742));
#145233=CARTESIAN_POINT('Ctrl Pts',(111.392442385579,-2.88331401631127,
135.973420483882));
#145234=CARTESIAN_POINT('Ctrl Pts',(111.385027892858,-2.74393591172043,
136.046378003542));
#145235=CARTESIAN_POINT('Ctrl Pts',(111.377620546504,-2.60469214499458,
136.119265203997));
#145236=CARTESIAN_POINT('Ctrl Pts',(111.37021320015,-2.46240006080196,136.186674879226));
#145237=CARTESIAN_POINT('Ctrl Pts',(111.362805853797,-2.31753131135518,
136.248346214846));
#145238=CARTESIAN_POINT('Ctrl Pts',(111.355404032121,-2.1727706104869,136.309971553657));
#145239=CARTESIAN_POINT('Ctrl Pts',(111.348002210446,-2.02543741286825,
136.365866929071));
#145240=CARTESIAN_POINT('Ctrl Pts',(111.34060038877,-1.87602691241399,136.415817967168));
#145241=CARTESIAN_POINT('Ctrl Pts',(111.333202474459,-1.72669528459959,
136.465742636501));
#145242=CARTESIAN_POINT('Ctrl Pts',(111.325804560148,-1.57528889100536,
136.509729099871));
#145243=CARTESIAN_POINT('Ctrl Pts',(111.318406645836,-1.42232169026551,
136.54761157603));
#145244=CARTESIAN_POINT('Ctrl Pts',(111.311009960924,-1.26937990989975,
136.585487756809));
#145245=CARTESIAN_POINT('Ctrl Pts',(111.303613276012,-1.11487819917337,
136.617261873957));
#145246=CARTESIAN_POINT('Ctrl Pts',(111.296216591099,-0.959344537573924,
136.642818343775));
#145247=CARTESIAN_POINT('Ctrl Pts',(111.288820234164,-0.803817772499801,
136.668373680392));
#145248=CARTESIAN_POINT('Ctrl Pts',(111.281423877228,-0.647259515892521,
136.687711857333));
#145249=CARTESIAN_POINT('Ctrl Pts',(111.274027520293,-0.490206505653107,
136.700768688953));
#145250=CARTESIAN_POINT('Ctrl Pts',(111.266630030956,-0.333129450197,136.713827519607));
#145251=CARTESIAN_POINT('Ctrl Pts',(111.25923254162,-0.175557862322717,
136.720603059159));
#145252=CARTESIAN_POINT('Ctrl Pts',(111.251835052283,-0.0180319985780747,
136.721083140173));
#145253=CARTESIAN_POINT('Ctrl Pts',(111.244434969768,0.139549085614132,
136.721563389479));
#145254=CARTESIAN_POINT('Ctrl Pts',(111.237034887253,0.297084040700731,
136.715743785263));
#145255=CARTESIAN_POINT('Ctrl Pts',(111.229634804738,0.454034366966793,
136.703664250717));
#145256=CARTESIAN_POINT('Ctrl Pts',(111.222226585072,0.611157276251357,
136.691571433482));
#145257=CARTESIAN_POINT('Ctrl Pts',(111.214818365405,0.767693900457209,
136.673204967905));
#145258=CARTESIAN_POINT('Ctrl Pts',(111.207410145739,0.923111873492083,
136.648656557328));
#145259=CARTESIAN_POINT('Ctrl Pts',(111.199997366436,1.07862550369607,136.624093037614));
#145260=CARTESIAN_POINT('Ctrl Pts',(111.192584587134,1.23301874552727,136.593340063945));
#145261=CARTESIAN_POINT('Ctrl Pts',(111.185171807832,1.38577164822839,136.556539987289));
#145262=CARTESIAN_POINT('Ctrl Pts',(111.177748436803,1.53874281144028,136.519687328957));
#145263=CARTESIAN_POINT('Ctrl Pts',(111.170325065775,1.69006859625799,136.476770412435));
#145264=CARTESIAN_POINT('Ctrl Pts',(111.162901694746,1.8392455790784,136.427981005034));
#145265=CARTESIAN_POINT('Ctrl Pts',(111.158965645305,1.91834279482255,136.402111690544));
#145266=CARTESIAN_POINT('Ctrl Pts',(111.155029595864,1.99683624975567,136.37459220838));
#145267=CARTESIAN_POINT('Ctrl Pts',(111.151093546423,2.07465353583313,136.345456472066));
#145268=CARTESIAN_POINT('Ctrl Pts',(111.143670280018,2.2214145087805,136.290507382672));
#145269=CARTESIAN_POINT('Ctrl Pts',(111.136247013613,2.36621282833455,136.22964052949));
#145270=CARTESIAN_POINT('Ctrl Pts',(111.128823747207,2.50853563728656,136.163015254596));
#145271=CARTESIAN_POINT('Ctrl Pts',(111.121409254486,2.65069023249767,136.096468725244));
#145272=CARTESIAN_POINT('Ctrl Pts',(111.113994761765,2.79037480623799,136.024177478235));
#145273=CARTESIAN_POINT('Ctrl Pts',(111.106580269044,2.92709330382308,135.946350052912));
#145274=CARTESIAN_POINT('Ctrl Pts',(111.09917292269,3.06368002697254,135.868597640592));
#145275=CARTESIAN_POINT('Ctrl Pts',(111.091765576337,3.19730604306728,135.785319856274));
#145276=CARTESIAN_POINT('Ctrl Pts',(111.084358229983,3.32749698203934,135.696772537777));
#145277=CARTESIAN_POINT('Ctrl Pts',(111.076956408307,3.45759081969766,135.60829126121));
#145278=CARTESIAN_POINT('Ctrl Pts',(111.069554586632,3.58425437419898,135.514548485092));
#145279=CARTESIAN_POINT('Ctrl Pts',(111.062152764957,3.70703962228686,135.415844955748));
#145280=CARTESIAN_POINT('Ctrl Pts',(111.054754850645,3.82976005299812,135.317193531228));
#145281=CARTESIAN_POINT('Ctrl Pts',(111.047356936334,3.9486059644373,135.213586802126));
#145282=CARTESIAN_POINT('Ctrl Pts',(111.039959022022,4.0631600729491,135.105367567583));
#145283=CARTESIAN_POINT('Ctrl Pts',(111.03256233711,4.1776951446462,134.997166317113));
#145284=CARTESIAN_POINT('Ctrl Pts',(111.025165652198,4.28793955785393,134.884354338607));
#145285=CARTESIAN_POINT('Ctrl Pts',(111.017768967286,4.39351068292429,134.767313360349));
#145286=CARTESIAN_POINT('Ctrl Pts',(111.01037261035,4.4990771268601,134.650277571811));
#145287=CARTESIAN_POINT('Ctrl Pts',(111.002976253415,4.59997044464968,134.529013433565));
#145288=CARTESIAN_POINT('Ctrl Pts',(110.99557989648,4.69584651514763,134.4039378245));
#145289=CARTESIAN_POINT('Ctrl Pts',(110.988182407143,4.79173726451681,134.278843066039));
#145290=CARTESIAN_POINT('Ctrl Pts',(110.980784917806,4.88260900998074,134.149935971131));
#145291=CARTESIAN_POINT('Ctrl Pts',(110.97338742847,4.96815949287188,134.017664496113));
#145292=CARTESIAN_POINT('Ctrl Pts',(110.965987345955,5.05373996535192,133.885346653536));
#145293=CARTESIAN_POINT('Ctrl Pts',(110.95858726344,5.13399525873404,133.749662395969));
#145294=CARTESIAN_POINT('Ctrl Pts',(110.951187180925,5.20866788928199,133.611086357937));
#145295=CARTESIAN_POINT('Ctrl Pts',(110.943778961259,5.28342263006397,133.472357941305));
#145296=CARTESIAN_POINT('Ctrl Pts',(110.936370741592,5.35258227141165,133.330731722743));
#145297=CARTESIAN_POINT('Ctrl Pts',(110.928962521926,5.41593620906649,133.186705164818));
#145298=CARTESIAN_POINT('Ctrl Pts',(110.921549742624,5.47932914001303,133.04258996095));
#145299=CARTESIAN_POINT('Ctrl Pts',(110.914136963322,5.5369091107708,132.896071820502));
#145300=CARTESIAN_POINT('Ctrl Pts',(110.906724184019,5.5885148391545,132.747665136948));
#145301=CARTESIAN_POINT('Ctrl Pts',(110.899300812991,5.64019430422286,132.599046402965));
#145302=CARTESIAN_POINT('Ctrl Pts',(110.891877441962,5.68588236991391,132.448534092744));
#145303=CARTESIAN_POINT('Ctrl Pts',(110.884454070933,5.72546826274446,132.296655405738));
#145304=CARTESIAN_POINT('Ctrl Pts',(110.880518021492,5.74645765297392,132.216125681608));
#145305=CARTESIAN_POINT('Ctrl Pts',(110.876581972052,5.76573236293829,132.135211962611));
#145306=CARTESIAN_POINT('Ctrl Pts',(110.872645922611,5.78328178672794,132.053993498776));
#145307=CARTESIAN_POINT('Ctrl Pts',(110.865222656205,5.81637945229606,131.900818010725));
#145308=CARTESIAN_POINT('Ctrl Pts',(110.8577993898,5.84343747348966,131.746095062683));
#145309=CARTESIAN_POINT('Ctrl Pts',(110.850376123395,5.86431269746181,131.590342264227));
#145310=CARTESIAN_POINT('Ctrl Pts',(110.842961630674,5.88516324865282,131.434773552645));
#145311=CARTESIAN_POINT('Ctrl Pts',(110.835547137953,5.89984549924196,131.278177779864));
#145312=CARTESIAN_POINT('Ctrl Pts',(110.828132645232,5.90826676961038,131.12108501135));
#145313=CARTESIAN_POINT('Ctrl Pts',(110.820725298878,5.91667992324135,130.96414365476));
#145314=CARTESIAN_POINT('Ctrl Pts',(110.813317952524,5.91884409044083,130.806706626337));
#145315=CARTESIAN_POINT('Ctrl Pts',(110.80591060617,5.91471810620367,130.649311313645));
#145316=CARTESIAN_POINT('Ctrl Pts',(110.798508784495,5.91059519928123,130.492033392315));
#145317=CARTESIAN_POINT('Ctrl Pts',(110.791106962819,5.90019149193709,130.334797496329));
#145318=CARTESIAN_POINT('Ctrl Pts',(110.783705141144,5.88351784305867,130.178143121076));
#145319=CARTESIAN_POINT('Ctrl Pts',(110.776307226833,5.86685299606959,130.021571442447));
#145320=CARTESIAN_POINT('Ctrl Pts',(110.768909312521,5.84392483868674,129.865581043447));
#145321=CARTESIAN_POINT('Ctrl Pts',(110.76151139821,5.81479622552752,129.710708287943));
#145322=CARTESIAN_POINT('Ctrl Pts',(110.754114713298,5.78567245301547,129.555861269481));
#145323=CARTESIAN_POINT('Ctrl Pts',(110.746718028385,5.75035033870547,129.402131892397));
#145324=CARTESIAN_POINT('Ctrl Pts',(110.739321343473,5.7089442207431,129.250048407312));
#145325=CARTESIAN_POINT('Ctrl Pts',(110.731924986538,5.66753993877138,129.097971665769));
#145326=CARTESIAN_POINT('Ctrl Pts',(110.724528629602,5.62005228760751,128.947541031302));
#145327=CARTESIAN_POINT('Ctrl Pts',(110.717132272667,5.56664599338309,128.799271355999));
#145328=CARTESIAN_POINT('Ctrl Pts',(110.70973478333,5.51323152251866,128.65097898023));
#145329=CARTESIAN_POINT('Ctrl Pts',(110.702337293994,5.4538967308225,128.504848573621));
#145330=CARTESIAN_POINT('Ctrl Pts',(110.694939804657,5.38885511845664,128.361376566291));
#145331=CARTESIAN_POINT('Ctrl Pts',(110.687539722142,5.32379070585452,128.217854265072));
#145332=CARTESIAN_POINT('Ctrl Pts',(110.680139639627,5.25301564360368,128.076992558315));
#145333=CARTESIAN_POINT('Ctrl Pts',(110.672739557112,5.17679007892136,127.939264625931));
#145334=CARTESIAN_POINT('Ctrl Pts',(110.665331337446,5.10048069639449,127.801385247528));
#145335=CARTESIAN_POINT('Ctrl Pts',(110.657923117779,5.01870902312205,127.666646852014));
#145336=CARTESIAN_POINT('Ctrl Pts',(110.650514898113,4.93177975170426,127.535495517385));
#145337=CARTESIAN_POINT('Ctrl Pts',(110.643102118811,4.84479697677027,127.404263461299));
#145338=CARTESIAN_POINT('Ctrl Pts',(110.635689339509,4.75265049626616,127.276623167334));
#145339=CARTESIAN_POINT('Ctrl Pts',(110.628276560207,4.65568590702782,127.152988368999));
#145340=CARTESIAN_POINT('Ctrl Pts',(110.620853189178,4.55858277023719,127.029176915467));
#145341=CARTESIAN_POINT('Ctrl Pts',(110.613429818149,4.4566480164177,126.909382671706));
#145342=CARTESIAN_POINT('Ctrl Pts',(110.60600644712,4.35026531762562,126.793983798767));
#145343=CARTESIAN_POINT('Ctrl Pts',(110.602070397679,4.29385865810708,126.732796547375));
#145344=CARTESIAN_POINT('Ctrl Pts',(110.598134348239,4.23620210626621,126.672844346448));
#145345=CARTESIAN_POINT('Ctrl Pts',(110.594198298798,4.1773566046412,126.614178955614));
#145346=CARTESIAN_POINT('Ctrl Pts',(110.586775032392,4.0663758250838,126.503537859386));
#145347=CARTESIAN_POINT('Ctrl Pts',(110.579351765987,3.9508285482978,126.397141647097));
#145348=CARTESIAN_POINT('Ctrl Pts',(110.571928499581,3.831072876271,126.295390537914));
#145349=CARTESIAN_POINT('Ctrl Pts',(110.56451400686,3.71145874550318,126.193759690091));
#145350=CARTESIAN_POINT('Ctrl Pts',(110.557099514139,3.58764640191728,126.096763256595));
#145351=CARTESIAN_POINT('Ctrl Pts',(110.549685021418,3.46003170900208,126.004765724744));
#145352=CARTESIAN_POINT('Ctrl Pts',(110.542277675064,3.33254001593298,125.912856863579));
#145353=CARTESIAN_POINT('Ctrl Pts',(110.534870328711,3.20125357030618,125.825937528946));
#145354=CARTESIAN_POINT('Ctrl Pts',(110.527462982357,3.06660224080808,125.744332825234));
#145355=CARTESIAN_POINT('Ctrl Pts',(110.520061160682,2.93205133935162,125.662788985389));
#145356=CARTESIAN_POINT('Ctrl Pts',(110.512659339006,2.79414086896212,125.586552076545));
#145357=CARTESIAN_POINT('Ctrl Pts',(110.505257517331,2.65333059188378,125.515904573249));
#145358=CARTESIAN_POINT('Ctrl Pts',(110.497859603019,2.51259464745525,125.44529436422));
#145359=CARTESIAN_POINT('Ctrl Pts',(110.490461688708,2.36896227778349,125.380267851449));
#145360=CARTESIAN_POINT('Ctrl Pts',(110.483063774397,2.22291871543582,125.321062071338));
#145361=CARTESIAN_POINT('Ctrl Pts',(110.475667089485,2.07689942287797,125.261866130153));
#145362=CARTESIAN_POINT('Ctrl Pts',(110.468270404572,1.9284700785201,125.208489141934));
#145363=CARTESIAN_POINT('Ctrl Pts',(110.46087371966,1.77813691713127,125.161120443124));
#145364=CARTESIAN_POINT('Ctrl Pts',(110.453477362725,1.62781042167225,125.113753844692));
#145365=CARTESIAN_POINT('Ctrl Pts',(110.446081005789,1.47558063307365,125.072395118134));
#145366=CARTESIAN_POINT('Ctrl Pts',(110.438684648854,1.32196974947645,125.037183964821));
#145367=CARTESIAN_POINT('Ctrl Pts',(110.431287159517,1.16833534766071,125.00196742059));
#145368=CARTESIAN_POINT('Ctrl Pts',(110.423889670181,1.01331979370737,124.972900407086));
#145369=CARTESIAN_POINT('Ctrl Pts',(110.416492180844,0.857456150389222,
124.950071633184));
#145370=CARTESIAN_POINT('Ctrl Pts',(110.409092098329,0.7015378693113,124.92723485669));
#145371=CARTESIAN_POINT('Ctrl Pts',(110.401692015814,0.544771276080293,
124.910640727774));
#145372=CARTESIAN_POINT('Ctrl Pts',(110.394291933299,0.3876950862832,124.900326142517));
#145373=CARTESIAN_POINT('Ctrl Pts',(110.386883713632,0.230446175068722,
124.890000215312));
#145374=CARTESIAN_POINT('Ctrl Pts',(110.379475493966,0.0728873601448385,
124.885967645987));
#145375=CARTESIAN_POINT('Ctrl Pts',(110.372067274299,-0.084441366644023,
124.88821320408));
#145376=CARTESIAN_POINT('Ctrl Pts',(110.364654494997,-0.241866926639501,
124.890460144276));
#145377=CARTESIAN_POINT('Ctrl Pts',(110.357241715695,-0.399061744428589,
124.898992891373));
#145378=CARTESIAN_POINT('Ctrl Pts',(110.349828936393,-0.555490930763011,
124.913744318032));
#145379=CARTESIAN_POINT('Ctrl Pts',(110.342405565364,-0.712143630454446,
124.92851682222));
#145380=CARTESIAN_POINT('Ctrl Pts',(110.334982194336,-0.868028144814353,
124.949525702661));
#145381=CARTESIAN_POINT('Ctrl Pts',(110.327558823307,-1.02261893212332,
124.976652570472));
#145382=CARTESIAN_POINT('Ctrl Pts',(110.323622773866,-1.10458667690795,
124.991035886685));
#145383=CARTESIAN_POINT('Ctrl Pts',(110.319686724425,-1.18619093608855,
125.007138347652));
#145384=CARTESIAN_POINT('Ctrl Pts',(110.315750674985,-1.26735522189452,
125.024936658032));
#145385=CARTESIAN_POINT('Ctrl Pts',(110.308327408579,-1.42042853187652,
125.058503715942));
#145386=CARTESIAN_POINT('Ctrl Pts',(110.300904142174,-1.57239880407388,
125.098207160757));
#145387=CARTESIAN_POINT('Ctrl Pts',(110.293480875768,-1.72273575989662,
125.143962039367));
#145388=CARTESIAN_POINT('Ctrl Pts',(110.286066383047,-1.87289502992315,
125.189662839511));
#145389=CARTESIAN_POINT('Ctrl Pts',(110.278651890326,-2.02142447249822,
125.241400729143));
#145390=CARTESIAN_POINT('Ctrl Pts',(110.271237397605,-2.16780346023257,
125.299039671399));
#145391=CARTESIAN_POINT('Ctrl Pts',(110.263830051251,-2.31404136238737,
125.356623059072));
#145392=CARTESIAN_POINT('Ctrl Pts',(110.256422704898,-2.45813259100948,
125.420096040512));
#145393=CARTESIAN_POINT('Ctrl Pts',(110.249015358544,-2.59957127204351,
125.489272681881));
#145394=CARTESIAN_POINT('Ctrl Pts',(110.241613536868,-2.74090446277334,
125.558397728701));
#145395=CARTESIAN_POINT('Ctrl Pts',(110.234211715193,-2.87958871122211,
125.633217801848));
#145396=CARTESIAN_POINT('Ctrl Pts',(110.226809893518,-3.01513785083059,
125.713498774716));
#145397=CARTESIAN_POINT('Ctrl Pts',(110.219411979206,-3.15061543510308,
125.793737367883));
#145398=CARTESIAN_POINT('Ctrl Pts',(110.212014064895,-3.28296088616804,
125.879430929855));
#145399=CARTESIAN_POINT('Ctrl Pts',(110.204616150583,-3.41171249853264,
125.970299344697));
#145400=CARTESIAN_POINT('Ctrl Pts',(110.197219465671,-3.54044271471451,
126.061152658855));
#145401=CARTESIAN_POINT('Ctrl Pts',(110.189822780759,-3.66557997283185,
126.157178904063));
#145402=CARTESIAN_POINT('Ctrl Pts',(110.182426095847,-3.78669134651391,
126.258054511645));
#145403=CARTESIAN_POINT('Ctrl Pts',(110.175029738911,-3.90779734999058,
126.358925646296));
#145404=CARTESIAN_POINT('Ctrl Pts',(110.167633381976,-4.02487753714001,
126.464645476868));
#145405=CARTESIAN_POINT('Ctrl Pts',(110.16023702504,-4.13753211239265,126.574850175278));
#145406=CARTESIAN_POINT('Ctrl Pts',(110.152839535704,-4.25020393534867,
126.68507174631));
#145407=CARTESIAN_POINT('Ctrl Pts',(110.145442046367,-4.35844853040673,
126.79977929132));
#145408=CARTESIAN_POINT('Ctrl Pts',(110.138044557031,-4.46190313082993,
126.918572278813));
#145409=CARTESIAN_POINT('Ctrl Pts',(110.130644474516,-4.565393997103,127.037406909004));
#145410=CARTESIAN_POINT('Ctrl Pts',(110.123244392001,-4.66409128060714,
127.160329551736));
#145411=CARTESIAN_POINT('Ctrl Pts',(110.115844309486,-4.75767275069233,
127.286906913561));
#145412=CARTESIAN_POINT('Ctrl Pts',(110.108436089819,-4.85135712322395,
127.413623460207));
#145413=CARTESIAN_POINT('Ctrl Pts',(110.101027870153,-4.93991422605951,
127.544002451278));
#145414=CARTESIAN_POINT('Ctrl Pts',(110.093619650486,-5.02306499423533,
127.677581343906));
#145415=CARTESIAN_POINT('Ctrl Pts',(110.086206871184,-5.10626694032159,
127.811242452114));
#145416=CARTESIAN_POINT('Ctrl Pts',(110.078794091882,-5.18405573724024,
127.948107062538));
#145417=CARTESIAN_POINT('Ctrl Pts',(110.07138131258,-5.25619874041902,128.087688873737));
#145418=CARTESIAN_POINT('Ctrl Pts',(110.063957941551,-5.32844482490401,
128.227470125975));
#145419=CARTESIAN_POINT('Ctrl Pts',(110.056534570523,-5.39502884648885,
128.369975995833));
#145420=CARTESIAN_POINT('Ctrl Pts',(110.049111199494,-5.45576634095696,
128.514700338096));
#145421=CARTESIAN_POINT('Ctrl Pts',(110.045175150053,-5.48797081789958,
128.591436656976));
#145422=CARTESIAN_POINT('Ctrl Pts',(110.041239100613,-5.51853245682477,
128.668796404854));
#145423=CARTESIAN_POINT('Ctrl Pts',(110.037303051172,-5.54742951325403,
128.746702638703));
#145424=CARTESIAN_POINT('Ctrl Pts',(110.028756344549,-5.61017635301933,
128.915867618672));
#145425=CARTESIAN_POINT('Ctrl Pts',(110.020209637926,-5.66522896920832,
129.088032641139));
#145426=CARTESIAN_POINT('Ctrl Pts',(110.011662931303,-5.71232982365823,
129.262537492741));
#145427=CARTESIAN_POINT('Ctrl Pts',(110.003146762702,-5.75926238323207,
129.436418825455));
#145428=CARTESIAN_POINT('Ctrl Pts',(109.994630594102,-5.79829980958457,
129.612623168292));
#145429=CARTESIAN_POINT('Ctrl Pts',(109.986114425501,-5.82923382386852,
129.790475225045));
#145430=CARTESIAN_POINT('Ctrl Pts',(109.977658406563,-5.85994935133939,
129.967071113468));
#145431=CARTESIAN_POINT('Ctrl Pts',(109.969202387625,-5.88267545579212,
130.145291379479));
#145432=CARTESIAN_POINT('Ctrl Pts',(109.960746368688,-5.89725540094682,
130.324455107592));
#145433=CARTESIAN_POINT('Ctrl Pts',(109.953289332851,-5.91011289030673,
130.482452665433));
#145434=CARTESIAN_POINT('Ctrl Pts',(109.945832297014,-5.91663589330626,
130.641183591745));
#145435=CARTESIAN_POINT('Ctrl Pts',(109.938375261177,-5.9167485154848,130.800169316047));
#145436=CARTESIAN_POINT('',(108.188375192211,-5.90998823786883,130.808446092953));
#145437=CARTESIAN_POINT('Ctrl Pts',(109.938375192211,-5.91018173940183,
130.800175436554));
#145438=CARTESIAN_POINT('Ctrl Pts',(109.878535270594,-5.90190088737836,
132.074566921819));
#145439=CARTESIAN_POINT('Ctrl Pts',(109.725879474373,-4.87095122287221,
135.337840497513));
#145440=CARTESIAN_POINT('Ctrl Pts',(109.480407803546,0.513821038447506,
137.783869803085));
#145441=CARTESIAN_POINT('Ctrl Pts',(109.201960179734,6.14979156980978,134.144663624517));
#145442=CARTESIAN_POINT('Ctrl Pts',(108.923512555921,6.13440408253642,127.435882165428));
#145443=CARTESIAN_POINT('Ctrl Pts',(108.645064932108,0.481798925711525,
123.822567844538));
#145444=CARTESIAN_POINT('Ctrl Pts',(108.400019144205,-4.8823733627542,126.288986106739));
#145445=CARTESIAN_POINT('Ctrl Pts',(108.247789230906,-5.9019786814506,129.543020490365));
#145446=CARTESIAN_POINT('Ctrl Pts',(108.188375192211,-5.90998823786883,
130.808446092953));
#145447=CARTESIAN_POINT('',(106.438375192211,-5.92510185054946,130.807002374807));
#145448=CARTESIAN_POINT('Ctrl Pts',(108.188375192211,-5.90998823786883,
130.808446092953));
#145449=CARTESIAN_POINT('Ctrl Pts',(108.154973356302,-5.91449111118078,
131.519852677365));
#145450=CARTESIAN_POINT('Ctrl Pts',(108.028755645787,-5.4658095909918,134.202602094435));
#145451=CARTESIAN_POINT('Ctrl Pts',(107.809722060669,-1.46766768783018,
137.647131407855));
#145452=CARTESIAN_POINT('Ctrl Pts',(107.531274436856,4.96370662816406,135.737835765966));
#145453=CARTESIAN_POINT('Ctrl Pts',(107.252826813044,6.83367704342109,129.294917476357));
#145454=CARTESIAN_POINT('Ctrl Pts',(106.97437918923,2.42383209946288,124.239103693122));
#145455=CARTESIAN_POINT('Ctrl Pts',(106.70289531562,-4.04740441513389,125.191997893739));
#145456=CARTESIAN_POINT('Ctrl Pts',(106.524227316613,-5.91499524236282,
128.990435688002));
#145457=CARTESIAN_POINT('Ctrl Pts',(106.438375192211,-5.92510185054946,
130.807002374807));
#145458=CARTESIAN_POINT('',(104.688375192211,-5.91791127406073,130.79899341794));
#145459=CARTESIAN_POINT('Ctrl Pts',(106.438375192211,-5.92510185054946,
130.807002374807));
#145460=CARTESIAN_POINT('Ctrl Pts',(106.431411442009,-5.92592163101843,
130.954350116296));
#145461=CARTESIAN_POINT('Ctrl Pts',(106.424447691807,-5.92090358124783,
131.101641088351));
#145462=CARTESIAN_POINT('Ctrl Pts',(106.324668067,-5.76279283782334,133.205611270108));
#145463=CARTESIAN_POINT('Ctrl Pts',(106.139036317792,-3.33094020304525,
136.959228438572));
#145464=CARTESIAN_POINT('Ctrl Pts',(105.860588693979,3.37781007024566,136.933631345777));
#145465=CARTESIAN_POINT('Ctrl Pts',(105.582141070166,6.98251790417742,131.275533885272));
#145466=CARTESIAN_POINT('Ctrl Pts',(105.303693446353,4.17063289913194,125.184451209843));
#145467=CARTESIAN_POINT('Ctrl Pts',(105.02524582254,-2.47385999346925,124.257790732271));
#145468=CARTESIAN_POINT('Ctrl Pts',(104.820139737826,-5.69366364351441,
128.006610555169));
#145469=CARTESIAN_POINT('Ctrl Pts',(104.707849527717,-5.9219685611791,130.385665735681));
#145470=CARTESIAN_POINT('Ctrl Pts',(104.688375192211,-5.91812558406999,
130.798993223573));
#145471=CARTESIAN_POINT('',(102.938375192243,-5.91674999740235,130.804185291264));
#145472=CARTESIAN_POINT('Ctrl Pts',(104.688375192211,-5.91674756661093,
130.798994473354));
#145473=CARTESIAN_POINT('Ctrl Pts',(104.681070929629,-5.91688813321788,
130.95398418232));
#145474=CARTESIAN_POINT('Ctrl Pts',(104.673766667046,-5.91093459052331,
131.109165024354));
#145475=CARTESIAN_POINT('Ctrl Pts',(104.666462404463,-5.89886870365173,
131.264011114768));
#145476=CARTESIAN_POINT('Ctrl Pts',(104.659163775948,-5.88681212367718,
131.418737766252));
#145477=CARTESIAN_POINT('Ctrl Pts',(104.651865147433,-5.86865261192464,
131.573129798245));
#145478=CARTESIAN_POINT('Ctrl Pts',(104.644566518918,-5.84442399892119,
131.726661372924));
#145479=CARTESIAN_POINT('Ctrl Pts',(104.637224187918,-5.82005031063467,
131.881112258859));
#145480=CARTESIAN_POINT('Ctrl Pts',(104.629881856918,-5.78953459696489,
132.03469195511));
#145481=CARTESIAN_POINT('Ctrl Pts',(104.622539525918,-5.75296435337207,
132.186869825973));
#145482=CARTESIAN_POINT('Ctrl Pts',(104.615246064261,-5.716637515284,132.338034826047));
#145483=CARTESIAN_POINT('Ctrl Pts',(104.607952602604,-5.67433660502426,
132.487816229281));
#145484=CARTESIAN_POINT('Ctrl Pts',(104.600659140947,-5.62619862320037,
132.635704281327));
#145485=CARTESIAN_POINT('Ctrl Pts',(104.593365872807,-5.5780619186232,132.783588409455));
#145486=CARTESIAN_POINT('Ctrl Pts',(104.586072604668,-5.52408856948681,
132.92957892035));
#145487=CARTESIAN_POINT('Ctrl Pts',(104.578779336528,-5.46446520768868,
133.07318202007));
#145488=CARTESIAN_POINT('Ctrl Pts',(104.571484727083,-5.40483088054543,
133.216811529867));
#145489=CARTESIAN_POINT('Ctrl Pts',(104.564190117637,-5.33954462106144,
133.358052399635));
#145490=CARTESIAN_POINT('Ctrl Pts',(104.556895508191,-5.26884075583047,
133.496431874461));
#145491=CARTESIAN_POINT('Ctrl Pts',(104.549516763751,-5.19732140221541,
133.636407398583));
#145492=CARTESIAN_POINT('Ctrl Pts',(104.542138019311,-5.12025887064447,
133.773454747819));
#145493=CARTESIAN_POINT('Ctrl Pts',(104.534759274872,-5.03794240410383,
133.907112121543));
#145494=CARTESIAN_POINT('Ctrl Pts',(104.527453780949,-4.956443112324,134.039442647348));
#145495=CARTESIAN_POINT('Ctrl Pts',(104.520148287026,-4.86979399565266,
134.168449915169));
#145496=CARTESIAN_POINT('Ctrl Pts',(104.512842793103,-4.77831778963543,
134.293717243615));
#145497=CARTESIAN_POINT('Ctrl Pts',(104.505427423405,-4.68546576712084,
134.420868612344));
#145498=CARTESIAN_POINT('Ctrl Pts',(104.498012053707,-4.58764055265885,
134.544166319473));
#145499=CARTESIAN_POINT('Ctrl Pts',(104.490596684009,-4.48521962585023,
134.663212191595));
#145500=CARTESIAN_POINT('Ctrl Pts',(104.48318131431,-4.38279869904161,134.782258063717));
#145501=CARTESIAN_POINT('Ctrl Pts',(104.475765944612,-4.27578238614007,
134.897051848695));
#145502=CARTESIAN_POINT('Ctrl Pts',(104.468350574914,-4.16458378379214,
135.007237307439));
#145503=CARTESIAN_POINT('Ctrl Pts',(104.460927308509,-4.05326676485245,
135.117540103867));
#145504=CARTESIAN_POINT('Ctrl Pts',(104.453504042103,-3.93739618980244,
135.223584137171));
#145505=CARTESIAN_POINT('Ctrl Pts',(104.446080775698,-3.81733137710063,
135.324970279979));
#145506=CARTESIAN_POINT('Ctrl Pts',(104.438666282977,-3.69740847103641,
135.426236592786));
#145507=CARTESIAN_POINT('Ctrl Pts',(104.431251790256,-3.57330147716299,
135.522855734817));
#145508=CARTESIAN_POINT('Ctrl Pts',(104.423837297535,-3.44540736650959,
135.614464425313));
#145509=CARTESIAN_POINT('Ctrl Pts',(104.416429951181,-3.31763652501516,
135.705984819904));
#145510=CARTESIAN_POINT('Ctrl Pts',(104.409022604827,-3.18608613494249,
135.792504161153));
#145511=CARTESIAN_POINT('Ctrl Pts',(104.401615258474,-3.05118705249279,
135.873698654549));
#145512=CARTESIAN_POINT('Ctrl Pts',(104.394213436798,-2.91638858286824,
135.954832590028));
#145513=CARTESIAN_POINT('Ctrl Pts',(104.386811615123,-2.77824671234438,
136.030649393715));
#145514=CARTESIAN_POINT('Ctrl Pts',(104.379409793448,-2.63722206079119,
136.10086799173));
#145515=CARTESIAN_POINT('Ctrl Pts',(104.372011879136,-2.49627185505403,
136.171049521894));
#145516=CARTESIAN_POINT('Ctrl Pts',(104.364613964825,-2.35244223234035,
136.235638565941));
#145517=CARTESIAN_POINT('Ctrl Pts',(104.357216050514,-2.20621914442719,
136.294399565448));
#145518=CARTESIAN_POINT('Ctrl Pts',(104.349819365601,-2.06002035613838,
136.353150799943));
#145519=CARTESIAN_POINT('Ctrl Pts',(104.342422680689,-1.91142923810393,
136.406075773057));
#145520=CARTESIAN_POINT('Ctrl Pts',(104.335025995777,-1.76095259902307,
136.452986690028));
#145521=CARTESIAN_POINT('Ctrl Pts',(104.327629638842,-1.61048263223418,
136.499895526919));
#145522=CARTESIAN_POINT('Ctrl Pts',(104.320233281906,-1.458127667017,136.540790726794));
#145523=CARTESIAN_POINT('Ctrl Pts',(104.312836924971,-1.30441032429665,
136.575534178322));
#145524=CARTESIAN_POINT('Ctrl Pts',(104.305439435634,-1.15066944705815,
136.610282949161));
#145525=CARTESIAN_POINT('Ctrl Pts',(104.298041946298,-0.995566141135667,
136.638878014005));
#145526=CARTESIAN_POINT('Ctrl Pts',(104.290644456961,-0.839633736832117,
136.661232286851));
#145527=CARTESIAN_POINT('Ctrl Pts',(104.283244374446,-0.683646670666186,
136.683594395953));
#145528=CARTESIAN_POINT('Ctrl Pts',(104.275844291931,-0.526830296748347,
136.699711304421));
#145529=CARTESIAN_POINT('Ctrl Pts',(104.268444209416,-0.369723440469288,
136.709547756012));
#145530=CARTESIAN_POINT('Ctrl Pts',(104.26103598975,-0.212443829050997,
136.719395023793));
#145531=CARTESIAN_POINT('Ctrl Pts',(104.253627770083,-0.0548734701753229,
136.722948019605));
#145532=CARTESIAN_POINT('Ctrl Pts',(104.246219550417,0.10244769317082,136.720223617388));
#145533=CARTESIAN_POINT('Ctrl Pts',(104.238806771115,0.259865685068295,
136.717497538347));
#145534=CARTESIAN_POINT('Ctrl Pts',(104.231393991813,0.41703380399418,136.708486383821));
#145535=CARTESIAN_POINT('Ctrl Pts',(104.223981212511,0.573417367490317,
136.693258908856));
#145536=CARTESIAN_POINT('Ctrl Pts',(104.216557841482,0.730024379155305,
136.678009676161));
#145537=CARTESIAN_POINT('Ctrl Pts',(104.209134470453,0.885844227662873,
136.656526434193));
#145538=CARTESIAN_POINT('Ctrl Pts',(104.201711099424,1.04035173406291,136.628929170852));
#145539=CARTESIAN_POINT('Ctrl Pts',(104.197775049984,1.12227532131508,136.614296439642));
#145540=CARTESIAN_POINT('Ctrl Pts',(104.193839000543,1.20383019216157,136.597945677965));
#145541=CARTESIAN_POINT('Ctrl Pts',(104.189902951102,1.28493993008904,136.579900413859));
#145542=CARTESIAN_POINT('Ctrl Pts',(104.182479684696,1.43791036446801,136.545867608928));
#145543=CARTESIAN_POINT('Ctrl Pts',(104.175056418291,1.58975908912062,136.505701802784));
#145544=CARTESIAN_POINT('Ctrl Pts',(104.167633151886,1.73995608648117,136.459489562127));
#145545=CARTESIAN_POINT('Ctrl Pts',(104.160218659165,1.88997556346436,136.413331940502));
#145546=CARTESIAN_POINT('Ctrl Pts',(104.152804166444,2.03834684572162,136.361142217985));
#145547=CARTESIAN_POINT('Ctrl Pts',(104.145389673722,2.18454972232464,136.303058015422));
#145548=CARTESIAN_POINT('Ctrl Pts',(104.137982327369,2.33061168309022,136.245029796601));
#145549=CARTESIAN_POINT('Ctrl Pts',(104.130574981015,2.4745090543689,136.18111854503));
#145550=CARTESIAN_POINT('Ctrl Pts',(104.123167634661,2.61573653036711,136.111511733391));
#145551=CARTESIAN_POINT('Ctrl Pts',(104.115765812986,2.75685867358603,136.041956837138));
#145552=CARTESIAN_POINT('Ctrl Pts',(104.10836399131,2.89531455309249,135.966715003406));
#145553=CARTESIAN_POINT('Ctrl Pts',(104.100962169635,3.03061871718004,135.886021837441));
#145554=CARTESIAN_POINT('Ctrl Pts',(104.093564255324,3.16585145525257,135.805371268769));
#145555=CARTESIAN_POINT('Ctrl Pts',(104.086166341012,3.2979354715768,135.719275289696));
#145556=CARTESIAN_POINT('Ctrl Pts',(104.078768426701,3.42640991537508,135.628015420132));
#145557=CARTESIAN_POINT('Ctrl Pts',(104.071371741789,3.55486300905146,135.536770716303));
#145558=CARTESIAN_POINT('Ctrl Pts',(104.063975056876,3.67970741668296,135.440364041114));
#145559=CARTESIAN_POINT('Ctrl Pts',(104.056578371964,3.80051119873585,135.339120279421));
#145560=CARTESIAN_POINT('Ctrl Pts',(104.049182015029,3.92130962422245,135.237881006982));
#145561=CARTESIAN_POINT('Ctrl Pts',(104.041785658093,4.03806749426662,135.131805314281));
#145562=CARTESIAN_POINT('Ctrl Pts',(104.034389301158,4.15038612251815,135.021258244555));
#145563=CARTESIAN_POINT('Ctrl Pts',(104.026991811821,4.26272194703856,134.910694249791));
#145564=CARTESIAN_POINT('Ctrl Pts',(104.019594322485,4.37061691040595,134.795657776786));
#145565=CARTESIAN_POINT('Ctrl Pts',(104.012196833148,4.47370946664381,134.676550459317));
#145566=CARTESIAN_POINT('Ctrl Pts',(104.004796750633,4.57683816181694,134.557401388963));
#145567=CARTESIAN_POINT('Ctrl Pts',(103.997396668118,4.67516085392078,134.434178915021));
#145568=CARTESIAN_POINT('Ctrl Pts',(103.989996585603,4.76835663259408,134.30731730969));
#145569=CARTESIAN_POINT('Ctrl Pts',(103.982588365937,4.86165488960713,134.180316206982));
#145570=CARTESIAN_POINT('Ctrl Pts',(103.97518014627,4.94981475345225,134.049668282459));
#145571=CARTESIAN_POINT('Ctrl Pts',(103.967771926604,5.03255856827978,133.915836926223));
#145572=CARTESIAN_POINT('Ctrl Pts',(103.960359147302,5.1153533105451,133.78192319902));
#145573=CARTESIAN_POINT('Ctrl Pts',(103.952946368,5.19272517835729,133.644822460204));
#145574=CARTESIAN_POINT('Ctrl Pts',(103.945533588698,5.264443008356,133.505021717051));
#145575=CARTESIAN_POINT('Ctrl Pts',(103.938110217669,5.33626331215313,133.365021220041));
#145576=CARTESIAN_POINT('Ctrl Pts',(103.93068684664,5.40241328647759,133.222313351403));
#145577=CARTESIAN_POINT('Ctrl Pts',(103.923263475611,5.46271000849914,133.077404815452));
#145578=CARTESIAN_POINT('Ctrl Pts',(103.91932742617,5.49468077731558,133.000570832657));
#145579=CARTESIAN_POINT('Ctrl Pts',(103.915391376729,5.52500681822054,132.923118423985));
#145580=CARTESIAN_POINT('Ctrl Pts',(103.911455327289,5.55366662102438,132.84512459829));
#145581=CARTESIAN_POINT('Ctrl Pts',(103.904032060883,5.60771811466959,132.698030677136));
#145582=CARTESIAN_POINT('Ctrl Pts',(103.896608794478,5.65600342919169,132.548565445181));
#145583=CARTESIAN_POINT('Ctrl Pts',(103.889185528072,5.69830890816788,132.397221612629));
#145584=CARTESIAN_POINT('Ctrl Pts',(103.881771035351,5.74056438558124,132.24605665592));
#145585=CARTESIAN_POINT('Ctrl Pts',(103.87435654263,5.77685399616787,132.093017874238));
#145586=CARTESIAN_POINT('Ctrl Pts',(103.866942049909,5.80701233752974,131.938617323201));
#145587=CARTESIAN_POINT('Ctrl Pts',(103.859534703555,5.83714161114672,131.784365589228));
#145588=CARTESIAN_POINT('Ctrl Pts',(103.852127357202,5.86115130920403,131.628755062792));
#145589=CARTESIAN_POINT('Ctrl Pts',(103.844720010848,5.87892602765447,131.472312205532));
#145590=CARTESIAN_POINT('Ctrl Pts',(103.837318189173,5.89668748904934,131.315986029258));
#145591=CARTESIAN_POINT('Ctrl Pts',(103.829916367497,5.90822318821751,131.158829127538));
#145592=CARTESIAN_POINT('Ctrl Pts',(103.822514545822,5.91346894801861,131.001377275033));
#145593=CARTESIAN_POINT('Ctrl Pts',(103.81511663151,5.91871193862392,130.844008540137));
#145594=CARTESIAN_POINT('Ctrl Pts',(103.807718717199,5.91767159021922,130.686345536689));
#145595=CARTESIAN_POINT('Ctrl Pts',(103.800320802888,5.91033565237705,130.528928159891));
#145596=CARTESIAN_POINT('Ctrl Pts',(103.792924117975,5.90300093363465,130.371536943005));
#145597=CARTESIAN_POINT('Ctrl Pts',(103.785527433063,5.88937271923794,130.214391644283));
#145598=CARTESIAN_POINT('Ctrl Pts',(103.778130748151,5.86949087014882,130.05803127489));
#145599=CARTESIAN_POINT('Ctrl Pts',(103.770734391216,5.84960990264173,129.901677838679));
#145600=CARTESIAN_POINT('Ctrl Pts',(103.76333803428,5.82347589888097,129.746109632908));
#145601=CARTESIAN_POINT('Ctrl Pts',(103.755941677345,5.79118048037017,129.591859398482));
#145602=CARTESIAN_POINT('Ctrl Pts',(103.748544188008,5.75888011734825,129.437585547951));
#145603=CARTESIAN_POINT('Ctrl Pts',(103.741146698671,5.72041653778777,129.284630435945));
#145604=CARTESIAN_POINT('Ctrl Pts',(103.733749209335,5.67593222312858,129.133515334199));
#145605=CARTESIAN_POINT('Ctrl Pts',(103.72634912682,5.63143231456174,128.982347259288));
#145606=CARTESIAN_POINT('Ctrl Pts',(103.718949044305,5.5809075741387,128.833020836734));
#145607=CARTESIAN_POINT('Ctrl Pts',(103.71154896179,5.52454990747228,128.686040792245));
#145608=CARTESIAN_POINT('Ctrl Pts',(103.704140742123,5.4681302697579,128.538899128088));
#145609=CARTESIAN_POINT('Ctrl Pts',(103.696732522457,5.40586503054713,128.39410934336));
#145610=CARTESIAN_POINT('Ctrl Pts',(103.68932430279,5.33799397328917,128.252155511461));
#145611=CARTESIAN_POINT('Ctrl Pts',(103.681911523488,5.27008114252791,128.110114309347));
#145612=CARTESIAN_POINT('Ctrl Pts',(103.674498744186,5.19655579253233,127.97091286747));
#145613=CARTESIAN_POINT('Ctrl Pts',(103.667085964884,5.11770270687505,127.835008909441));
#145614=CARTESIAN_POINT('Ctrl Pts',(103.659662593855,5.03873695223119,127.698910765464));
#145615=CARTESIAN_POINT('Ctrl Pts',(103.652239222827,4.9544284575738,127.566119829768));
#145616=CARTESIAN_POINT('Ctrl Pts',(103.644815851798,4.86510465333724,127.43706388657));
#145617=CARTESIAN_POINT('Ctrl Pts',(103.640879802357,4.81774302903664,127.368635328833));
#145618=CARTESIAN_POINT('Ctrl Pts',(103.636943752916,4.76897208992012,127.301256252977));
#145619=CARTESIAN_POINT('Ctrl Pts',(103.633007703476,4.71884499893512,127.234986381299));
#145620=CARTESIAN_POINT('Ctrl Pts',(103.62558443707,4.62430686974852,127.110003471525));
#145621=CARTESIAN_POINT('Ctrl Pts',(103.618161170665,4.52465692896269,126.988590060143));
#145622=CARTESIAN_POINT('Ctrl Pts',(103.610737904259,4.42019422111259,126.871192224255));
#145623=CARTESIAN_POINT('Ctrl Pts',(103.603323411538,4.31585497950823,126.753933142859));
#145624=CARTESIAN_POINT('Ctrl Pts',(103.595908918817,4.20671453914133,126.640680466018));
#145625=CARTESIAN_POINT('Ctrl Pts',(103.588494426096,4.0931143028676,126.531850130023));
#145626=CARTESIAN_POINT('Ctrl Pts',(103.581087079743,3.97962355877872,126.423124688804));
#145627=CARTESIAN_POINT('Ctrl Pts',(103.573679733389,3.8616818440389,126.318813359302));
#145628=CARTESIAN_POINT('Ctrl Pts',(103.566272387035,3.73966970702886,126.219297799585));
#145629=CARTESIAN_POINT('Ctrl Pts',(103.55887056536,3.61774857127317,126.119856462327));
#145630=CARTESIAN_POINT('Ctrl Pts',(103.551468743684,3.49176334611748,126.025204007759));
#145631=CARTESIAN_POINT('Ctrl Pts',(103.544066922009,3.36213010464429,125.935684029216));
#145632=CARTESIAN_POINT('Ctrl Pts',(103.536669007698,3.23256529555132,125.846211307574));
#145633=CARTESIAN_POINT('Ctrl Pts',(103.529271093386,3.09935661177866,125.761865877655));
#145634=CARTESIAN_POINT('Ctrl Pts',(103.521873179075,2.96295166079344,125.682949872634));
#145635=CARTESIAN_POINT('Ctrl Pts',(103.514476494163,2.82656937783547,125.604046982021));
#145636=CARTESIAN_POINT('Ctrl Pts',(103.50707980925,2.68699220466574,125.530571912318));
#145637=CARTESIAN_POINT('Ctrl Pts',(103.499683124338,2.54469517246507,125.462782476068));
#145638=CARTESIAN_POINT('Ctrl Pts',(103.492286767403,2.40240444986392,125.394996045672));
#145639=CARTESIAN_POINT('Ctrl Pts',(103.484890410467,2.25739444503718,125.332894908006));
#145640=CARTESIAN_POINT('Ctrl Pts',(103.477494053532,2.11016289165644,125.276689938774));
#145641=CARTESIAN_POINT('Ctrl Pts',(103.470096564195,1.96290879674932,125.220476364418));
#145642=CARTESIAN_POINT('Ctrl Pts',(103.462699074859,1.81343282482721,125.170160889072));
#145643=CARTESIAN_POINT('Ctrl Pts',(103.455301585522,1.66225055126366,125.12590539917));
#145644=CARTESIAN_POINT('Ctrl Pts',(103.447901503007,1.51101528098924,125.081634395576));
#145645=CARTESIAN_POINT('Ctrl Pts',(103.440501420492,1.35807287621826,125.043427711738));
#145646=CARTESIAN_POINT('Ctrl Pts',(103.433101337977,1.20395170665455,125.011396708603));
#145647=CARTESIAN_POINT('Ctrl Pts',(103.425693118311,1.04966106501999,124.979330484088));
#145648=CARTESIAN_POINT('Ctrl Pts',(103.418284898644,0.894189435762269,
124.953453577946));
#145649=CARTESIAN_POINT('Ctrl Pts',(103.410876678978,0.738073692353686,
124.933825907069));
#145650=CARTESIAN_POINT('Ctrl Pts',(103.403463899676,0.581861862309744,
124.914186155687));
#145651=CARTESIAN_POINT('Ctrl Pts',(103.396051120374,0.425005499239751,
124.900803335466));
#145652=CARTESIAN_POINT('Ctrl Pts',(103.388638341072,0.268043631458563,
124.893685260711));
#145653=CARTESIAN_POINT('Ctrl Pts',(103.381214970043,0.110857489199907,
124.886557015317));
#145654=CARTESIAN_POINT('Ctrl Pts',(103.373791599014,-0.0464340865480609,
124.88571139527));
#145655=CARTESIAN_POINT('Ctrl Pts',(103.366368227985,-0.203294204659716,
124.891104151891));
#145656=CARTESIAN_POINT('Ctrl Pts',(103.362432178544,-0.286465203090883,
124.893963520848));
#145657=CARTESIAN_POINT('Ctrl Pts',(103.358496129104,-0.369515011775571,
124.898575856866));
#145658=CARTESIAN_POINT('Ctrl Pts',(103.354560079663,-0.452364648780765,
124.904928713812));
#145659=CARTESIAN_POINT('Ctrl Pts',(103.347136813257,-0.608616478520997,
124.916910003745));
#145660=CARTESIAN_POINT('Ctrl Pts',(103.339713546852,-0.764628247202771,
124.935121406622));
#145661=CARTESIAN_POINT('Ctrl Pts',(103.332290280446,-0.919863016651839,
124.959552443374));
#145662=CARTESIAN_POINT('Ctrl Pts',(103.324875787725,-1.07491431149509,
124.98395460467));
#145663=CARTESIAN_POINT('Ctrl Pts',(103.317461295004,-1.22919006992554,
125.014561709986));
#145664=CARTESIAN_POINT('Ctrl Pts',(103.310046802283,-1.38215581637968,
125.051311351155));
#145665=CARTESIAN_POINT('Ctrl Pts',(103.30263945593,-1.53497412868833,125.088025571637));
#145666=CARTESIAN_POINT('Ctrl Pts',(103.295232109576,-1.68648458215299,
125.130870454988));
#145667=CARTESIAN_POINT('Ctrl Pts',(103.287824763222,-1.83616038133609,
125.179732130589));
#145668=CARTESIAN_POINT('Ctrl Pts',(103.280422941547,-1.985724546661,125.228557363309));
#145669=CARTESIAN_POINT('Ctrl Pts',(103.273021119871,-2.13345642894244,
125.28339033761));
#145670=CARTESIAN_POINT('Ctrl Pts',(103.265619298196,-2.27884205571151,
125.344066720016));
#145671=CARTESIAN_POINT('Ctrl Pts',(103.258221383884,-2.42415093453936,
125.404711071832));
#145672=CARTESIAN_POINT('Ctrl Pts',(103.250823469573,-2.56711568089916,
125.471192545033));
#145673=CARTESIAN_POINT('Ctrl Pts',(103.243425555262,-2.70724015882465,
125.543297865142));
#145674=CARTESIAN_POINT('Ctrl Pts',(103.23602887035,-2.84734135060463,125.615391202654));
#145675=CARTESIAN_POINT('Ctrl Pts',(103.228632185437,-2.98460287912828,
125.69310636157));
#145676=CARTESIAN_POINT('Ctrl Pts',(103.221235500525,-3.11855107344445,
125.776183038679));
#145677=CARTESIAN_POINT('Ctrl Pts',(103.21383914359,-3.25249332835751,125.859256032082));
#145678=CARTESIAN_POINT('Ctrl Pts',(103.206442786654,-3.38312222394707,
125.947689874226));
#145679=CARTESIAN_POINT('Ctrl Pts',(103.199046429719,-3.50999130730211,
126.041179791147));
#145680=CARTESIAN_POINT('Ctrl Pts',(103.191648940382,-3.63687981463743,
126.134684021613));
#145681=CARTESIAN_POINT('Ctrl Pts',(103.184251451046,-3.76000706303217,
126.233245646722));
#145682=CARTESIAN_POINT('Ctrl Pts',(103.176853961709,-3.87895817176008,
126.336518401883));
#145683=CARTESIAN_POINT('Ctrl Pts',(103.169453879194,-3.99795097861475,
126.439827359149));
#145684=CARTESIAN_POINT('Ctrl Pts',(103.162053796679,-4.11276444940223,
126.547850489973));
#145685=CARTESIAN_POINT('Ctrl Pts',(103.154653714164,-4.22301929627321,
126.660203455271));
#145686=CARTESIAN_POINT('Ctrl Pts',(103.147245494498,-4.33339537968287,
126.772679964204));
#145687=CARTESIAN_POINT('Ctrl Pts',(103.139837274831,-4.43920256691127,
126.889495549236));
#145688=CARTESIAN_POINT('Ctrl Pts',(103.132429055165,-4.54010025495626,
127.010230910051));
#145689=CARTESIAN_POINT('Ctrl Pts',(103.125016275863,-4.64106004384467,
127.131040581467));
#145690=CARTESIAN_POINT('Ctrl Pts',(103.117603496561,-4.7371040851871,127.255774540897));
#145691=CARTESIAN_POINT('Ctrl Pts',(103.110190717259,-4.82793444661485,
127.383983512379));
#145692=CARTESIAN_POINT('Ctrl Pts',(103.10276734623,-4.91889459072227,127.512375674851));
#145693=CARTESIAN_POINT('Ctrl Pts',(103.095343975201,-5.00462597356885,
127.644252453965));
#145694=CARTESIAN_POINT('Ctrl Pts',(103.087920604172,-5.08487562005356,
127.77913823052));
#145695=CARTESIAN_POINT('Ctrl Pts',(103.083984554731,-5.12742590818442,
127.85065790579));
#145696=CARTESIAN_POINT('Ctrl Pts',(103.080048505291,-5.16843586946286,
127.92302314221));
#145697=CARTESIAN_POINT('Ctrl Pts',(103.07611245585,-5.20787328350828,127.996160762602));
#145698=CARTESIAN_POINT('Ctrl Pts',(103.068287579489,-5.28627496354613,
128.141558539092));
#145699=CARTESIAN_POINT('Ctrl Pts',(103.060462703129,-5.35867507229847,
128.290410856979));
#145700=CARTESIAN_POINT('Ctrl Pts',(103.052637826769,-5.42477333902216,
128.442208043592));
#145701=CARTESIAN_POINT('Ctrl Pts',(103.044826119433,-5.49076036440746,
128.593749760234));
#145702=CARTESIAN_POINT('Ctrl Pts',(103.037014412098,-5.550466563893,128.74822618012));
#145703=CARTESIAN_POINT('Ctrl Pts',(103.029202704763,-5.60363718529675,
128.905102641919));
#145704=CARTESIAN_POINT('Ctrl Pts',(103.021408952776,-5.65668559307875,
129.061618520372));
#145705=CARTESIAN_POINT('Ctrl Pts',(103.013615200789,-5.7032282856301,129.220523141253));
#145706=CARTESIAN_POINT('Ctrl Pts',(103.005821448802,-5.74305852531664,
129.381262118766));
#145707=CARTESIAN_POINT('Ctrl Pts',(102.998038259748,-5.78283478276906,
129.54178324549));
#145708=CARTESIAN_POINT('Ctrl Pts',(102.990255070694,-5.81591664255203,
129.704133471243));
#145709=CARTESIAN_POINT('Ctrl Pts',(102.98247188164,-5.84214646079905,129.867741541808));
#145710=CARTESIAN_POINT('Ctrl Pts',(102.974703271238,-5.86832714810848,
130.031043158938));
#145711=CARTESIAN_POINT('Ctrl Pts',(102.966934660835,-5.88768134387658,
130.195597612681));
#145712=CARTESIAN_POINT('Ctrl Pts',(102.959166050433,-5.90010205343943,
130.360822207166));
#145713=CARTESIAN_POINT('Ctrl Pts',(102.95223576437,-5.91118242250353,130.508217126603));
#145714=CARTESIAN_POINT('Ctrl Pts',(102.945305478307,-5.91674561064366,
130.656145013206));
#145715=CARTESIAN_POINT('Ctrl Pts',(102.938375192243,-5.91674999740235,
130.804185291264));
#145716=CARTESIAN_POINT('',(101.188375192211,-5.91674751171398,130.809786953944));
#145717=CARTESIAN_POINT('Ctrl Pts',(102.938375192211,-5.91674999740237,
130.804185291958));
#145718=CARTESIAN_POINT('Ctrl Pts',(102.930643930825,-5.91675489114609,
130.969335485603));
#145719=CARTESIAN_POINT('Ctrl Pts',(102.922912669439,-5.90984088281348,
131.134358686294));
#145720=CARTESIAN_POINT('Ctrl Pts',(102.915181408053,-5.89606567339422,
131.298668353215));
#145721=CARTESIAN_POINT('Ctrl Pts',(102.90744101397,-5.88227419175061,131.46317211401));
#145722=CARTESIAN_POINT('Ctrl Pts',(102.899700619886,-5.86160536074397,
131.626960339075));
#145723=CARTESIAN_POINT('Ctrl Pts',(102.891960225803,-5.83416837114592,
131.789454511375));
#145724=CARTESIAN_POINT('Ctrl Pts',(102.884102276323,-5.80631468878351,
131.954416525332));
#145725=CARTESIAN_POINT('Ctrl Pts',(102.876244326842,-5.77148569305193,
132.118044524203));
#145726=CARTESIAN_POINT('Ctrl Pts',(102.868386377361,-5.72984819340822,
132.279748784455));
#145727=CARTESIAN_POINT('Ctrl Pts',(102.860619727974,-5.68869447234087,
132.439574232159));
#145728=CARTESIAN_POINT('Ctrl Pts',(102.852853078587,-5.6408897815955,132.597520124815));
#145729=CARTESIAN_POINT('Ctrl Pts',(102.8450864292,-5.5866440981802,132.753036650869));
#145730=CARTESIAN_POINT('Ctrl Pts',(102.837182829673,-5.53144189496007,
132.911295416079));
#145731=CARTESIAN_POINT('Ctrl Pts',(102.829279230146,-5.46956958395598,
133.067038018644));
#145732=CARTESIAN_POINT('Ctrl Pts',(102.821375630618,-5.40129765077299,
133.219710333498));
#145733=CARTESIAN_POINT('Ctrl Pts',(102.813472031091,-5.33302571758999,
133.372382648353));
#145734=CARTESIAN_POINT('Ctrl Pts',(102.805568431564,-5.25835437312984,
133.521984396406));
#145735=CARTESIAN_POINT('Ctrl Pts',(102.797664832036,-5.17760078944642,
133.667991289916));
#145736=CARTESIAN_POINT('Ctrl Pts',(102.790241565631,-5.10175492164865,
133.805124764836));
#145737=CARTESIAN_POINT('Ctrl Pts',(102.782818299225,-5.02034244549844,
133.939450249718));
#145738=CARTESIAN_POINT('Ctrl Pts',(102.77539503282,-4.93359607919921,134.070483745957));
#145739=CARTESIAN_POINT('Ctrl Pts',(102.767980540099,-4.84695223990111,
134.201362371485));
#145740=CARTESIAN_POINT('Ctrl Pts',(102.760566047378,-4.75498726308215,
134.328956444911));
#145741=CARTESIAN_POINT('Ctrl Pts',(102.753151554657,-4.65798007372,134.452805792614));
#145742=CARTESIAN_POINT('Ctrl Pts',(102.745744208303,-4.561066383539,134.576535769652));
#145743=CARTESIAN_POINT('Ctrl Pts',(102.738336861949,-4.45912038450908,
134.696527914479));
#145744=CARTESIAN_POINT('Ctrl Pts',(102.730929515596,-4.35246461521372,
134.812350429905));
#145745=CARTESIAN_POINT('Ctrl Pts',(102.72352769392,-4.24588839381515,134.928086560529));
#145746=CARTESIAN_POINT('Ctrl Pts',(102.716125872245,-4.13460964824198,
135.039658980494));
#145747=CARTESIAN_POINT('Ctrl Pts',(102.708724050569,-4.0189914838226,135.146668531045));
#145748=CARTESIAN_POINT('Ctrl Pts',(102.701326136258,-3.90343435333242,
135.253621592087));
#145749=CARTESIAN_POINT('Ctrl Pts',(102.693928221947,-3.78354263939548,
135.356016327841));
#145750=CARTESIAN_POINT('Ctrl Pts',(102.686530307636,-3.65971654597314,
135.453490145298));
#145751=CARTESIAN_POINT('Ctrl Pts',(102.679133622723,-3.53591103020099,
135.550947764375));
#145752=CARTESIAN_POINT('Ctrl Pts',(102.671736937811,-3.40817272562196,
135.64348585751));
#145753=CARTESIAN_POINT('Ctrl Pts',(102.664340252899,-3.2769352716698,135.730781812286));
#145754=CARTESIAN_POINT('Ctrl Pts',(102.656943895964,-3.14570363692396,
135.818073896267));
#145755=CARTESIAN_POINT('Ctrl Pts',(102.649547539028,-3.01097347212354,
135.900124097315));
#145756=CARTESIAN_POINT('Ctrl Pts',(102.642151182093,-2.87320754997878,
135.976653043294));
#145757=CARTESIAN_POINT('Ctrl Pts',(102.634753692756,-2.73542053551983,
136.05319370605));
#145758=CARTESIAN_POINT('Ctrl Pts',(102.62735620342,-2.59459716462314,136.124211249309));
#145759=CARTESIAN_POINT('Ctrl Pts',(102.619958714083,-2.45122482292418,
136.189472262646));
#145760=CARTESIAN_POINT('Ctrl Pts',(102.612558631568,-2.30780222227279,
136.254756153131));
#145761=CARTESIAN_POINT('Ctrl Pts',(102.605158549053,-2.16182921133596,
136.31427934143));
#145762=CARTESIAN_POINT('Ctrl Pts',(102.597758466538,-2.01381301037555,
136.367856615744));
#145763=CARTESIAN_POINT('Ctrl Pts',(102.590350246872,-1.86563405038554,
136.421492803779));
#145764=CARTESIAN_POINT('Ctrl Pts',(102.582942027205,-1.71540776479546,
136.469169893595));
#145765=CARTESIAN_POINT('Ctrl Pts',(102.575533807539,-1.5636570916988,136.510752390138));
#145766=CARTESIAN_POINT('Ctrl Pts',(102.568121028237,-1.41181301859527,
136.552360480014));
#145767=CARTESIAN_POINT('Ctrl Pts',(102.560708248935,-1.25844305127042,
136.587866418042));
#145768=CARTESIAN_POINT('Ctrl Pts',(102.553295469633,-1.10407965441939,
136.617185978713));
#145769=CARTESIAN_POINT('Ctrl Pts',(102.545872098604,-0.949495695907687,
136.646547432548));
#145770=CARTESIAN_POINT('Ctrl Pts',(102.538448727576,-0.793915841144419,
136.669704799978));
#145771=CARTESIAN_POINT('Ctrl Pts',(102.531025356547,-0.637877827209255,
136.686625694903));
#145772=CARTESIAN_POINT('Ctrl Pts',(102.527089307106,-0.555142728135863,
136.695597559403));
#145773=CARTESIAN_POINT('Ctrl Pts',(102.523153257665,-0.472278839371946,
136.702816998817));
#145774=CARTESIAN_POINT('Ctrl Pts',(102.519217208224,-0.389366109742821,
136.708285125475));
#145775=CARTESIAN_POINT('Ctrl Pts',(102.511793941818,-0.232995289287956,
136.718597841695));
#145776=CARTESIAN_POINT('Ctrl Pts',(102.504370675413,-0.0759780225912232,
136.72270942545));
#145777=CARTESIAN_POINT('Ctrl Pts',(102.496947409008,0.08115269873832,136.720554056086));
#145778=CARTESIAN_POINT('Ctrl Pts',(102.489532916287,0.238097704604704,
136.718401234189));
#145779=CARTESIAN_POINT('Ctrl Pts',(102.482118423566,0.395155528571331,
136.709996207954));
#145780=CARTESIAN_POINT('Ctrl Pts',(102.474703930845,0.551788247772069,
136.695324909778));
#145781=CARTESIAN_POINT('Ctrl Pts',(102.467296584491,0.708269998460256,
136.680667752353));
#145782=CARTESIAN_POINT('Ctrl Pts',(102.459889238137,0.864327090902323,
136.659756381358));
#145783=CARTESIAN_POINT('Ctrl Pts',(102.452481891783,1.01942190190995,136.632628760712));
#145784=CARTESIAN_POINT('Ctrl Pts',(102.445080070108,1.17440103735679,136.605521372868));
#145785=CARTESIAN_POINT('Ctrl Pts',(102.437678248432,1.32841895428545,136.572207030938));
#145786=CARTESIAN_POINT('Ctrl Pts',(102.430276426757,1.48094356183199,136.532775470662));
#145787=CARTESIAN_POINT('Ctrl Pts',(102.422878512446,1.63338765282512,136.493364725999));
#145788=CARTESIAN_POINT('Ctrl Pts',(102.415480598134,1.78433964388543,136.44784328736));
#145789=CARTESIAN_POINT('Ctrl Pts',(102.408082683823,1.93327815522968,136.396351867292));
#145790=CARTESIAN_POINT('Ctrl Pts',(102.400685998911,2.08219191569537,136.344869004164));
#145791=CARTESIAN_POINT('Ctrl Pts',(102.393289313998,2.22909250807164,136.287418250493));
#145792=CARTESIAN_POINT('Ctrl Pts',(102.385892629086,2.37347411668863,136.224190059523));
#145793=CARTESIAN_POINT('Ctrl Pts',(102.378496272151,2.51784932327399,136.160964672158));
#145794=CARTESIAN_POINT('Ctrl Pts',(102.371099915215,2.6597054262402,136.091962506608));
#145795=CARTESIAN_POINT('Ctrl Pts',(102.36370355828,2.79855724194409,136.017421899199));
#145796=CARTESIAN_POINT('Ctrl Pts',(102.356306068943,2.93743031621535,135.942869879433));
#145797=CARTESIAN_POINT('Ctrl Pts',(102.348908579607,3.07329785845258,135.862777906003));
#145798=CARTESIAN_POINT('Ctrl Pts',(102.34151109027,3.2057000500142,135.777429866213));
#145799=CARTESIAN_POINT('Ctrl Pts',(102.334111007755,3.33814865495844,135.6920519078));
#145800=CARTESIAN_POINT('Ctrl Pts',(102.32671092524,3.46712917705859,135.601414416739));
#145801=CARTESIAN_POINT('Ctrl Pts',(102.319310842725,3.592211627442,135.505844020299));
#145802=CARTESIAN_POINT('Ctrl Pts',(102.311902623059,3.71743161883874,135.410168534382));
#145803=CARTESIAN_POINT('Ctrl Pts',(102.304494403392,3.83874468162846,135.309549537309));
#145804=CARTESIAN_POINT('Ctrl Pts',(102.297086183726,3.95575415917278,135.204353753321));
#145805=CARTESIAN_POINT('Ctrl Pts',(102.289673404424,4.07283565409778,135.099093223083));
#145806=CARTESIAN_POINT('Ctrl Pts',(102.282260625122,4.18560801894928,134.989250552694));
#145807=CARTESIAN_POINT('Ctrl Pts',(102.27484784582,4.29371258224892,134.875228193837));
#145808=CARTESIAN_POINT('Ctrl Pts',(102.267424474791,4.40197161041875,134.761042914487));
#145809=CARTESIAN_POINT('Ctrl Pts',(102.260001103762,4.50554927123721,134.64266629917));
#145810=CARTESIAN_POINT('Ctrl Pts',(102.252577732733,4.60412765733418,134.520533255842));
#145811=CARTESIAN_POINT('Ctrl Pts',(102.248641683293,4.65639628299939,134.455775385726));
#145812=CARTESIAN_POINT('Ctrl Pts',(102.244705633852,4.70726015778164,134.389961932632));
#145813=CARTESIAN_POINT('Ctrl Pts',(102.240769584411,4.75667700322258,134.323160761012));
#145814=CARTESIAN_POINT('Ctrl Pts',(102.233346318005,4.84987563147594,134.19717583613));
#145815=CARTESIAN_POINT('Ctrl Pts',(102.2259230516,4.93820649134497,134.067295174149));
#145816=CARTESIAN_POINT('Ctrl Pts',(102.218499785195,5.02132611106557,133.933931618331));
#145817=CARTESIAN_POINT('Ctrl Pts',(102.211085292474,5.10434749029832,133.800725687162));
#145818=CARTESIAN_POINT('Ctrl Pts',(102.203670799753,5.18216969388803,133.664045369766));
#145819=CARTESIAN_POINT('Ctrl Pts',(102.196256307032,5.25449012591507,133.524335632003));
#145820=CARTESIAN_POINT('Ctrl Pts',(102.188848960678,5.32674085278701,133.384760551745));
#145821=CARTESIAN_POINT('Ctrl Pts',(102.181441614324,5.39350019450025,133.242162193296));
#145822=CARTESIAN_POINT('Ctrl Pts',(102.17403426797,5.45450949270733,133.097013394692));
#145823=CARTESIAN_POINT('Ctrl Pts',(102.166632446295,5.51547328787797,132.95197285354));
#145824=CARTESIAN_POINT('Ctrl Pts',(102.15923062462,5.57069543469773,132.804386002453));
#145825=CARTESIAN_POINT('Ctrl Pts',(102.151828802944,5.61996382227698,132.654749008904));
#145826=CARTESIAN_POINT('Ctrl Pts',(102.144430888633,5.66920620145778,132.50519100756));
#145827=CARTESIAN_POINT('Ctrl Pts',(102.137032974322,5.71250096427134,132.353585372791));
#145828=CARTESIAN_POINT('Ctrl Pts',(102.12963506001,5.74968467766248,132.200446814745));
#145829=CARTESIAN_POINT('Ctrl Pts',(102.122238375098,5.78686221179517,132.047333705549));
#145830=CARTESIAN_POINT('Ctrl Pts',(102.114841690186,5.81793062406755,131.892688541069));
#145831=CARTESIAN_POINT('Ctrl Pts',(102.107445005274,5.84277674246381,131.737039822987));
#145832=CARTESIAN_POINT('Ctrl Pts',(102.100048648338,5.86762175915711,131.581398006531));
#145833=CARTESIAN_POINT('Ctrl Pts',(102.092652291403,5.88624497171845,131.424753093581));
#145834=CARTESIAN_POINT('Ctrl Pts',(102.085255934467,5.89858464563732,131.267642109482));
#145835=CARTESIAN_POINT('Ctrl Pts',(102.077858445131,5.91092620879179,131.110507071289));
#145836=CARTESIAN_POINT('Ctrl Pts',(102.070460955794,5.91698228855131,130.952906192042));
#145837=CARTESIAN_POINT('Ctrl Pts',(102.063063466458,5.91674318413639,130.795379778208));
#145838=CARTESIAN_POINT('Ctrl Pts',(102.055663383943,5.91650399590379,130.637798143734));
#145839=CARTESIAN_POINT('Ctrl Pts',(102.048263301428,5.90996523040597,130.480291399709));
#145840=CARTESIAN_POINT('Ctrl Pts',(102.040863218913,5.89716926892732,130.323397857969));
#145841=CARTESIAN_POINT('Ctrl Pts',(102.033454999246,5.88435923697359,130.166331795651));
#145842=CARTESIAN_POINT('Ctrl Pts',(102.02604677958,5.86527829873151,130.009880654487));
#145843=CARTESIAN_POINT('Ctrl Pts',(102.018638559913,5.84002058709075,129.854576376353));
#145844=CARTESIAN_POINT('Ctrl Pts',(102.011225780611,5.81474732974995,129.699176511027));
#145845=CARTESIAN_POINT('Ctrl Pts',(102.003813001309,5.78328979806562,129.544925280196));
#145846=CARTESIAN_POINT('Ctrl Pts',(101.996400222007,5.74579271534276,129.392341979299));
#145847=CARTESIAN_POINT('Ctrl Pts',(101.988976850979,5.70824205502964,129.239540660225));
#145848=CARTESIAN_POINT('Ctrl Pts',(101.98155347995,5.66463471166064,129.088412388619));
#145849=CARTESIAN_POINT('Ctrl Pts',(101.974130108921,5.61516474891769,128.939459707326));
#145850=CARTESIAN_POINT('Ctrl Pts',(101.97019405948,5.58893458765602,128.860481421635));
#145851=CARTESIAN_POINT('Ctrl Pts',(101.96625801004,5.56105703237352,128.782114424262));
#145852=CARTESIAN_POINT('Ctrl Pts',(101.962321960599,5.5315663268166,128.704430967666));
#145853=CARTESIAN_POINT('Ctrl Pts',(101.954898694193,5.47594777650948,128.557922392943));
#145854=CARTESIAN_POINT('Ctrl Pts',(101.947475427788,5.41442048453332,128.413403468563));
#145855=CARTESIAN_POINT('Ctrl Pts',(101.940052161383,5.3471461327407,128.271386318917));
#145856=CARTESIAN_POINT('Ctrl Pts',(101.932637668662,5.27995129364506,128.129537021748));
#145857=CARTESIAN_POINT('Ctrl Pts',(101.925223175941,5.20702307358521,127.990183947674));
#145858=CARTESIAN_POINT('Ctrl Pts',(101.91780868322,5.12857227445554,127.853822194128));
#145859=CARTESIAN_POINT('Ctrl Pts',(101.910401336866,5.05019708915963,127.717591871173));
#145860=CARTESIAN_POINT('Ctrl Pts',(101.902993990512,4.96631010648422,127.584347450367));
#145861=CARTESIAN_POINT('Ctrl Pts',(101.895586644158,4.87716932730788,127.454562128811));
#145862=CARTESIAN_POINT('Ctrl Pts',(101.888184822483,4.78809503268775,127.324873606044));
#145863=CARTESIAN_POINT('Ctrl Pts',(101.880783000807,4.69377495422336,127.19863935193));
#145864=CARTESIAN_POINT('Ctrl Pts',(101.873381179132,4.5945118805448,127.076306012007));
#145865=CARTESIAN_POINT('Ctrl Pts',(101.865983264821,4.49530120707003,126.954037250901));
#145866=CARTESIAN_POINT('Ctrl Pts',(101.858585350509,4.39115296967782,126.835665592008));
#145867=CARTESIAN_POINT('Ctrl Pts',(101.851187436198,4.28241186903464,126.721606749593));
#145868=CARTESIAN_POINT('Ctrl Pts',(101.843790751286,4.17368883918985,126.607566861688));
#145869=CARTESIAN_POINT('Ctrl Pts',(101.836394066373,4.06037471825631,126.497838637721));
#145870=CARTESIAN_POINT('Ctrl Pts',(101.828997381461,3.94285297742602,126.392802960581));
#145871=CARTESIAN_POINT('Ctrl Pts',(101.821601024526,3.82533644763288,126.287771940833));
#145872=CARTESIAN_POINT('Ctrl Pts',(101.81420466759,3.70361294724021,126.187433302954));
#145873=CARTESIAN_POINT('Ctrl Pts',(101.806808310655,3.5781009218694,126.092129261253));
#145874=CARTESIAN_POINT('Ctrl Pts',(101.799410821318,3.45256968028745,125.996810628261));
#145875=CARTESIAN_POINT('Ctrl Pts',(101.792013331982,3.32324905612667,125.906528351994));
#145876=CARTESIAN_POINT('Ctrl Pts',(101.784615842645,3.19058838101215,125.821582642836));
#145877=CARTESIAN_POINT('Ctrl Pts',(101.77721576013,3.05788120190286,125.736607156092));
#145878=CARTESIAN_POINT('Ctrl Pts',(101.769815677615,2.92183195486256,125.656972162231));
#145879=CARTESIAN_POINT('Ctrl Pts',(101.7624155951,2.78291644500274,125.582932975375));
#145880=CARTESIAN_POINT('Ctrl Pts',(101.755007375434,2.64384818325936,125.508812374822));
#145881=CARTESIAN_POINT('Ctrl Pts',(101.747599155767,2.5019076940745,125.440300045235));
#145882=CARTESIAN_POINT('Ctrl Pts',(101.740190936101,2.35759339633895,125.377604317525));
#145883=CARTESIAN_POINT('Ctrl Pts',(101.732778156799,2.21319027556084,125.31487000164));
#145884=CARTESIAN_POINT('Ctrl Pts',(101.725365377496,2.06641078217233,125.257959555909));
#145885=CARTESIAN_POINT('Ctrl Pts',(101.717952598194,1.91777004061455,125.207031912387));
#145886=CARTESIAN_POINT('Ctrl Pts',(101.710529227166,1.76891691419489,125.156031501059));
#145887=CARTESIAN_POINT('Ctrl Pts',(101.703105856137,1.61819758485778,125.111031071743));
#145888=CARTESIAN_POINT('Ctrl Pts',(101.695682485108,1.46613975229401,125.072138989851));
#145889=CARTESIAN_POINT('Ctrl Pts',(101.691746435667,1.38551504089039,125.051517474829));
#145890=CARTESIAN_POINT('Ctrl Pts',(101.687810386226,1.30451416695347,125.032612375321));
#145891=CARTESIAN_POINT('Ctrl Pts',(101.683874336786,1.2232164281044,125.015433935312));
#145892=CARTESIAN_POINT('Ctrl Pts',(101.67645107038,1.06989142985194,124.983035933576));
#145893=CARTESIAN_POINT('Ctrl Pts',(101.669027803975,0.915046561581508,
124.95668457816));
#145894=CARTESIAN_POINT('Ctrl Pts',(101.661604537569,0.759200081038398,
124.936520657287));
#145895=CARTESIAN_POINT('Ctrl Pts',(101.654190044848,0.603537798092602,
124.916380568493));
#145896=CARTESIAN_POINT('Ctrl Pts',(101.646775552127,0.446876625876293,
124.902413405039));
#145897=CARTESIAN_POINT('Ctrl Pts',(101.639361059406,0.289747047455172,
124.894709425576));
#145898=CARTESIAN_POINT('Ctrl Pts',(101.631953713052,0.132768916437669,
124.887012871498));
#145899=CARTESIAN_POINT('Ctrl Pts',(101.624546366699,-0.024676351654649,
124.885567501704));
#145900=CARTESIAN_POINT('Ctrl Pts',(101.617139020345,-0.182051186920557,
124.89041202734));
#145901=CARTESIAN_POINT('Ctrl Pts',(101.609737198669,-0.339308646096463,
124.895252939745));
#145902=CARTESIAN_POINT('Ctrl Pts',(101.602335376994,-0.496495405527897,
124.906374395249));
#145903=CARTESIAN_POINT('Ctrl Pts',(101.594933555319,-0.653072025024084,
124.923763072024));
#145904=CARTESIAN_POINT('Ctrl Pts',(101.587535641007,-0.809565988942297,
124.941142569453));
#145905=CARTESIAN_POINT('Ctrl Pts',(101.580137726696,-0.965450084301358,
124.964782658182));
#145906=CARTESIAN_POINT('Ctrl Pts',(101.572739812385,-1.1201882397861,124.994618035494));
#145907=CARTESIAN_POINT('Ctrl Pts',(101.565343127472,-1.27490068059598,
125.024448454707));
#145908=CARTESIAN_POINT('Ctrl Pts',(101.55794644256,-1.42846719329978,125.060472048556));
#145909=CARTESIAN_POINT('Ctrl Pts',(101.550549757648,-1.58036005478951,
125.102572068371));
#145910=CARTESIAN_POINT('Ctrl Pts',(101.543153400713,-1.7322461811907,125.144670221428));
#145911=CARTESIAN_POINT('Ctrl Pts',(101.535757043777,-1.88245844419995,
125.192844165016));
#145912=CARTESIAN_POINT('Ctrl Pts',(101.528360686842,-2.03048274914784,
125.246926824176));
#145913=CARTESIAN_POINT('Ctrl Pts',(101.520963197505,-2.17852971699439,
125.301017763529));
#145914=CARTESIAN_POINT('Ctrl Pts',(101.513565708169,-2.32438770913538,
125.361019091596));
#145915=CARTESIAN_POINT('Ctrl Pts',(101.506168218832,-2.46756127535356,
125.426715044002));
#145916=CARTESIAN_POINT('Ctrl Pts',(101.498768136317,-2.61078503084301,
125.492434026021));
#145917=CARTESIAN_POINT('Ctrl Pts',(101.491368053802,-2.75132214776985,
125.563851451296));
#145918=CARTESIAN_POINT('Ctrl Pts',(101.483967971287,-2.88870063884851,
125.640705015029));
#145919=CARTESIAN_POINT('Ctrl Pts',(101.476559751621,-3.02623019170205,
125.717643087156));
#145920=CARTESIAN_POINT('Ctrl Pts',(101.469151531954,-3.16059385644758,
125.800029053022));
#145921=CARTESIAN_POINT('Ctrl Pts',(101.461743312288,-3.29134695080476,
125.887556186645));
#145922=CARTESIAN_POINT('Ctrl Pts',(101.454330532986,-3.42218052150978,
125.975137191757));
#145923=CARTESIAN_POINT('Ctrl Pts',(101.446917753684,-3.54939879275536,
126.067865450524));
#145924=CARTESIAN_POINT('Ctrl Pts',(101.439504974382,-3.67258961316041,
126.16539348082));
#145925=CARTESIAN_POINT('Ctrl Pts',(101.432081603353,-3.79595645438663,
126.26306086374));
#145926=CARTESIAN_POINT('Ctrl Pts',(101.424658232324,-3.91528406907986,
126.365541472862));
#145927=CARTESIAN_POINT('Ctrl Pts',(101.417234861295,-4.03019605177665,
126.472449913645));
#145928=CARTESIAN_POINT('Ctrl Pts',(101.413298811855,-4.09112514227896,
126.529135334182));
#145929=CARTESIAN_POINT('Ctrl Pts',(101.409362762414,-4.15081348883542,
126.587064995423));
#145930=CARTESIAN_POINT('Ctrl Pts',(101.405426712973,-4.2092096105901,126.646177719158));
#145931=CARTESIAN_POINT('Ctrl Pts',(101.398103766296,-4.31785450750161,
126.756155840706));
#145932=CARTESIAN_POINT('Ctrl Pts',(101.390780819619,-4.42237227151351,
126.870583452434));
#145933=CARTESIAN_POINT('Ctrl Pts',(101.383457872942,-4.52236893674723,
126.989113605583));
#145934=CARTESIAN_POINT('Ctrl Pts',(101.37614376298,-4.62224493444518,127.107500726547));
#145935=CARTESIAN_POINT('Ctrl Pts',(101.368829653017,-4.71761044316818,
127.229980248052));
#145936=CARTESIAN_POINT('Ctrl Pts',(101.361515543054,-4.80810695455015,
127.356167166481));
#145937=CARTESIAN_POINT('Ctrl Pts',(101.35420977717,-4.89850022574951,127.482210128415));
#145938=CARTESIAN_POINT('Ctrl Pts',(101.346904011286,-4.98403533882533,
127.611951754446));
#145939=CARTESIAN_POINT('Ctrl Pts',(101.339598245403,-5.06439317574481,
127.744973044216));
#145940=CARTESIAN_POINT('Ctrl Pts',(101.332297196746,-5.14469912677806,
127.877908444074));
#145941=CARTESIAN_POINT('Ctrl Pts',(101.324996148089,-5.21983425330153,
128.01411896797));
#145942=CARTESIAN_POINT('Ctrl Pts',(101.317695099432,-5.2895219147003,128.153155518671));
#145943=CARTESIAN_POINT('Ctrl Pts',(101.310397231159,-5.35917921969485,
128.292131504136));
#145944=CARTESIAN_POINT('Ctrl Pts',(101.303099362887,-5.42339360907288,
128.433930724259));
#145945=CARTESIAN_POINT('Ctrl Pts',(101.295801494615,-5.48193384866948,
128.578078550686));
#145946=CARTESIAN_POINT('Ctrl Pts',(101.288505272512,-5.54046088343661,
128.722193861915));
#145947=CARTESIAN_POINT('Ctrl Pts',(101.281209050408,-5.59331617186153,
128.868656369036));
#145948=CARTESIAN_POINT('Ctrl Pts',(101.273912828305,-5.64031631067929,
129.016970766978));
#145949=CARTESIAN_POINT('Ctrl Pts',(101.266614230649,-5.68733175211061,
129.165333454095));
#145950=CARTESIAN_POINT('Ctrl Pts',(101.259315632994,-5.72848811293174,
129.315548871925));
#145951=CARTESIAN_POINT('Ctrl Pts',(101.252017035339,-5.76365158385039,
129.467105599823));
#145952=CARTESIAN_POINT('Ctrl Pts',(101.244717423453,-5.79881994116889,
129.618683388405));
#145953=CARTESIAN_POINT('Ctrl Pts',(101.237417811567,-5.82799367149967,
129.771602481803));
#145954=CARTESIAN_POINT('Ctrl Pts',(101.230118199681,-5.8510901061574,129.925341202464));
#145955=CARTESIAN_POINT('Ctrl Pts',(101.222812013546,-5.87420734215359,
130.079218384805));
#145956=CARTESIAN_POINT('Ctrl Pts',(101.215505827412,-5.89123629851133,
130.233916287517));
#145957=CARTESIAN_POINT('Ctrl Pts',(101.208199641278,-5.90214615682664,
130.388907484281));
#145958=CARTESIAN_POINT('Ctrl Pts',(101.201591491589,-5.91201368216852,
130.529090749511));
#145959=CARTESIAN_POINT('Ctrl Pts',(101.1949833419,-5.91687615839487,130.669513687404));
#145960=CARTESIAN_POINT('Ctrl Pts',(101.188375192211,-5.91674751171398,
130.809786953944));
#145961=CARTESIAN_POINT('',(99.4383751922114,-5.92157883723614,130.802066910743));
#145962=CARTESIAN_POINT('Ctrl Pts',(101.188375192211,-5.91748097844663,
130.809787626617));
#145963=CARTESIAN_POINT('Ctrl Pts',(101.167909824527,-5.92152051365936,
131.244270330207));
#145964=CARTESIAN_POINT('Ctrl Pts',(101.054628582244,-5.67922493894598,
133.644781142275));
#145965=CARTESIAN_POINT('Ctrl Pts',(100.848531465343,-2.40383848871005,
137.376964443327));
#145966=CARTESIAN_POINT('Ctrl Pts',(100.570083841535,4.23038432426813,136.379430930968));
#145967=CARTESIAN_POINT('Ctrl Pts',(100.29163621772,6.97709060900665,130.258680157901));
#145968=CARTESIAN_POINT('Ctrl Pts',(100.013188593908,3.3121914738928,124.6393830693));
#145969=CARTESIAN_POINT('Ctrl Pts',(99.7347409700951,-3.39644981617912,
124.685399171656));
#145970=CARTESIAN_POINT('Ctrl Pts',(99.543136502863,-5.86504781316068,128.586362303126));
#145971=CARTESIAN_POINT('Ctrl Pts',(99.444347910235,-5.92608242641807,130.675707350711));
#145972=CARTESIAN_POINT('Ctrl Pts',(99.4383751922114,-5.92545872057778,
130.802065407881));
#145973=CARTESIAN_POINT('',(97.688375206741,-5.91312254842892,130.800045764439));
#145974=CARTESIAN_POINT('Ctrl Pts',(99.4383751922114,-5.91674955613188,
130.802068781351));
#145975=CARTESIAN_POINT('Ctrl Pts',(99.431023129912,-5.91680971516,130.95737913934));
#145976=CARTESIAN_POINT('Ctrl Pts',(99.4236710676126,-5.91075049538843,
131.112939264388));
#145977=CARTESIAN_POINT('Ctrl Pts',(99.4163190053132,-5.89853912438324,
131.268221330087));
#145978=CARTESIAN_POINT('Ctrl Pts',(99.408975301965,-5.88634163713612,131.423326847334));
#145979=CARTESIAN_POINT('Ctrl Pts',(99.4016315986168,-5.86800594686994,
131.578154558207));
#145980=CARTESIAN_POINT('Ctrl Pts',(99.3942878952686,-5.84355125337422,
131.732174883294));
#145981=CARTESIAN_POINT('Ctrl Pts',(99.3869508649334,-5.8191187811586,131.88605525452));
#145982=CARTESIAN_POINT('Ctrl Pts',(99.3796138345983,-5.78857843098604,
132.039129326219));
#145983=CARTESIAN_POINT('Ctrl Pts',(99.3722768042632,-5.75200132330698,
132.190871107672));
#145984=CARTESIAN_POINT('Ctrl Pts',(99.3649447671003,-5.71544910796076,
132.34250962216));
#145985=CARTESIAN_POINT('Ctrl Pts',(99.3576127299374,-5.6728684020007,132.492817282297));
#145986=CARTESIAN_POINT('Ctrl Pts',(99.3502806927746,-5.62438163597361,
132.641276994384));
#145987=CARTESIAN_POINT('Ctrl Pts',(99.3429512462964,-5.57591200214526,
132.789684250069));
#145988=CARTESIAN_POINT('Ctrl Pts',(99.3356217998181,-5.52154057596112,
132.936244494583));
#145989=CARTESIAN_POINT('Ctrl Pts',(99.3282923533399,-5.46143998898768,
133.080454598312));
#145990=CARTESIAN_POINT('Ctrl Pts',(99.3209641084283,-5.40134925471783,
133.224641060683));
#145991=CARTESIAN_POINT('Ctrl Pts',(99.3136358635168,-5.33553137435344,
133.36647779707));
#145992=CARTESIAN_POINT('Ctrl Pts',(99.3063076186053,-5.2642074849828,133.505480777343));
#145993=CARTESIAN_POINT('Ctrl Pts',(99.2989790617049,-5.19288055910685,
133.644489675454));
#145994=CARTESIAN_POINT('Ctrl Pts',(99.2916505048046,-5.11604733151058,
133.780664238252));
#145995=CARTESIAN_POINT('Ctrl Pts',(99.2843219479042,-5.0339752224617,133.913544436857));
#145996=CARTESIAN_POINT('Ctrl Pts',(99.2769915654631,-4.9518826692811,134.04645773587));
#145997=CARTESIAN_POINT('Ctrl Pts',(99.269661183022,-4.86454883783369,134.176074713569));
#145998=CARTESIAN_POINT('Ctrl Pts',(99.2623308005808,-4.77228470195073,
134.301963980732));
#145999=CARTESIAN_POINT('Ctrl Pts',(99.2549928040885,-4.67992473152374,
134.427984008784));
#146000=CARTESIAN_POINT('Ctrl Pts',(99.2476548075961,-4.58262445388987,
134.550268285244));
#146001=CARTESIAN_POINT('Ctrl Pts',(99.2403168111037,-4.48073581656695,
134.668417695901));
#146002=CARTESIAN_POINT('Ctrl Pts',(99.2329748443228,-4.37879205148796,
134.786631032352));
#146003=CARTESIAN_POINT('Ctrl Pts',(99.225632877542,-4.27225524109257,134.900704768478));
#146004=CARTESIAN_POINT('Ctrl Pts',(99.2182909107612,-4.16151397634769,
135.010276925241));
#146005=CARTESIAN_POINT('Ctrl Pts',(99.2109378862937,-4.05060592493055,
135.12001410789));
#146006=CARTESIAN_POINT('Ctrl Pts',(99.2035848618261,-3.93548105011751,
135.225235910576));
#146007=CARTESIAN_POINT('Ctrl Pts',(99.1962318373586,-3.81656147570949,
135.325620294319));
#146008=CARTESIAN_POINT('Ctrl Pts',(99.1901031323955,-3.71744267240554,
135.40929011938));
#146009=CARTESIAN_POINT('Ctrl Pts',(99.1839744274325,-3.61568830166646,
135.489600015005));
#146010=CARTESIAN_POINT('Ctrl Pts',(99.1778457224694,-3.51155721606452,
135.566387127447));
#146011=CARTESIAN_POINT('Ctrl Pts',(99.1704224560639,-3.38543060462471,
135.659393920168));
#146012=CARTESIAN_POINT('Ctrl Pts',(99.1629991896585,-3.25541566851069,
135.747527021494));
#146013=CARTESIAN_POINT('Ctrl Pts',(99.1555759232531,-3.12192577321451,
135.830443588334));
#146014=CARTESIAN_POINT('Ctrl Pts',(99.148161430532,-2.98859365188864,135.913262154677));
#146015=CARTESIAN_POINT('Ctrl Pts',(99.140746937811,-2.85179506061965,135.990876263974));
#146016=CARTESIAN_POINT('Ctrl Pts',(99.13333244509,-2.71197542525192,136.062983997818));
#146017=CARTESIAN_POINT('Ctrl Pts',(99.1259250987362,-2.57229055331288,
136.135022231512));
#146018=CARTESIAN_POINT('Ctrl Pts',(99.1185177523824,-2.42959076363607,
136.201564485492));
#146019=CARTESIAN_POINT('Ctrl Pts',(99.1111104060286,-2.28434928734665,
136.262352821289));
#146020=CARTESIAN_POINT('Ctrl Pts',(99.1037085843533,-2.13921613763021,
136.323095818851));
#146021=CARTESIAN_POINT('Ctrl Pts',(99.0963067626779,-1.99154541873936,
136.378093299661));
#146022=CARTESIAN_POINT('Ctrl Pts',(99.0889049410025,-1.84183362036898,
136.427133908157));
#146023=CARTESIAN_POINT('Ctrl Pts',(99.0815070266911,-1.69220085369213,
136.476148628497));
#146024=CARTESIAN_POINT('Ctrl Pts',(99.0741091123798,-1.54052950722125,
136.519212623207));
#146025=CARTESIAN_POINT('Ctrl Pts',(99.0667111980685,-1.38733453922557,
136.556163242724));
#146026=CARTESIAN_POINT('Ctrl Pts',(99.0593145131563,-1.23416502945379,
136.593107721718));
#146027=CARTESIAN_POINT('Ctrl Pts',(99.0519178282441,-1.07947276321659,
136.623940754398));
#146028=CARTESIAN_POINT('Ctrl Pts',(99.0445211433319,-0.923786413810061,
136.64854997317));
#146029=CARTESIAN_POINT('Ctrl Pts',(99.0371247863964,-0.768106967699302,
136.673158100744));
#146030=CARTESIAN_POINT('Ctrl Pts',(99.029728429461,-0.611433894782134,
136.691542904848));
#146031=CARTESIAN_POINT('Ctrl Pts',(99.0223320725256,-0.454304313731296,
136.703643468305));
#146032=CARTESIAN_POINT('Ctrl Pts',(99.014934583189,-0.297150675740802,
136.715745884389));
#146033=CARTESIAN_POINT('Ctrl Pts',(99.0075370938524,-0.139540762671032,
136.721562115426));
#146034=CARTESIAN_POINT('Ctrl Pts',(99.0001396045159,0.0179851048732815,
136.721083282902));
#146035=CARTESIAN_POINT('Ctrl Pts',(98.9927395220009,0.175566192866603,
136.720604282524));
#146036=CARTESIAN_POINT('Ctrl Pts',(98.9853394394859,0.333062803612473,
136.713825826146));
#146037=CARTESIAN_POINT('Ctrl Pts',(98.9779393569709,0.489936690396937,
136.700791114223));
#146038=CARTESIAN_POINT('Ctrl Pts',(98.9705311373045,0.646983076146948,
136.687742069293));
#146039=CARTESIAN_POINT('Ctrl Pts',(98.963122917638,0.803404998202632,136.668423061143));
#146040=CARTESIAN_POINT('Ctrl Pts',(98.9557146979715,0.958670658559488,
136.642929032076));
#146041=CARTESIAN_POINT('Ctrl Pts',(98.9483019186694,1.11403188233977,136.61741931186));
#146042=CARTESIAN_POINT('Ctrl Pts',(98.9408891393674,1.26823506154246,136.585727072488));
#146043=CARTESIAN_POINT('Ctrl Pts',(98.9334763600653,1.42076112157449,136.547997827377));
#146044=CARTESIAN_POINT('Ctrl Pts',(98.9260529890365,1.57350511799364,136.510214672951));
#146045=CARTESIAN_POINT('Ctrl Pts',(98.9186296180078,1.72456685164282,136.466377388575));
#146046=CARTESIAN_POINT('Ctrl Pts',(98.911206246979,1.87344407558823,136.416680802493));
#146047=CARTESIAN_POINT('Ctrl Pts',(98.9072701975382,1.95238235198493,136.390330480099));
#146048=CARTESIAN_POINT('Ctrl Pts',(98.9033341480973,2.03070683371787,136.362333695868));
#146049=CARTESIAN_POINT('Ctrl Pts',(98.8993980986565,2.10834532052523,136.332724803464));
#146050=CARTESIAN_POINT('Ctrl Pts',(98.8919748322511,2.25476908362792,136.276883356452));
#146051=CARTESIAN_POINT('Ctrl Pts',(98.8845515658457,2.39919420659289,136.215136202522));
#146052=CARTESIAN_POINT('Ctrl Pts',(98.8771282994402,2.54110881167391,136.147645802706));
#146053=CARTESIAN_POINT('Ctrl Pts',(98.8697138067192,2.68285568547721,136.080235170937));
#146054=CARTESIAN_POINT('Ctrl Pts',(98.8622993139982,2.82209761384657,136.007094963671));
#146055=CARTESIAN_POINT('Ctrl Pts',(98.8548848212772,2.95833982072648,135.92843673601));
#146056=CARTESIAN_POINT('Ctrl Pts',(98.8474774749235,3.09445071223768,135.84985432211));
#146057=CARTESIAN_POINT('Ctrl Pts',(98.8400701285697,3.22756731704156,135.765764661248));
#146058=CARTESIAN_POINT('Ctrl Pts',(98.832662782216,3.35721683121657,135.67642647413));
#146059=CARTESIAN_POINT('Ctrl Pts',(98.8252609605406,3.48676964789279,135.587154918802));
#146060=CARTESIAN_POINT('Ctrl Pts',(98.8178591388652,3.61286021672606,135.492642842513));
#146061=CARTESIAN_POINT('Ctrl Pts',(98.8104573171898,3.73504235348902,135.393193713261));
#146062=CARTESIAN_POINT('Ctrl Pts',(98.8030594028784,3.85715999125305,135.29379708243));
#146063=CARTESIAN_POINT('Ctrl Pts',(98.7956614885671,3.97537301718541,135.189468824126));
#146064=CARTESIAN_POINT('Ctrl Pts',(98.7882635742557,4.08926624207776,135.080554271261));
#146065=CARTESIAN_POINT('Ctrl Pts',(98.7808668893435,4.20314053998237,134.97165781802));
#146066=CARTESIAN_POINT('Ctrl Pts',(98.7734702044313,4.31269619208334,134.858176840624));
#146067=CARTESIAN_POINT('Ctrl Pts',(98.7660735195191,4.41755289951034,134.740495389462));
#146068=CARTESIAN_POINT('Ctrl Pts',(98.7586771625837,4.52240495748097,134.622819156418));
#146069=CARTESIAN_POINT('Ctrl Pts',(98.7512808056482,4.62255823672275,134.500943098654));
#146070=CARTESIAN_POINT('Ctrl Pts',(98.7438844487128,4.71767116012618,134.375286182096));
#146071=CARTESIAN_POINT('Ctrl Pts',(98.7364869593762,4.81279864556113,134.249610027143));
#146072=CARTESIAN_POINT('Ctrl Pts',(98.7290894700397,4.90288401330732,134.120152158478));
#146073=CARTESIAN_POINT('Ctrl Pts',(98.7216919807031,4.98762773713472,133.987362364073));
#146074=CARTESIAN_POINT('Ctrl Pts',(98.7142918981881,5.07240116774308,133.854526020411));
#146075=CARTESIAN_POINT('Ctrl Pts',(98.7068918156731,5.15182902559318,133.71835574001));
#146076=CARTESIAN_POINT('Ctrl Pts',(98.6994917331581,5.22565672095441,133.579327715973));
#146077=CARTESIAN_POINT('Ctrl Pts',(98.6920835134917,5.29956559745636,133.440146816332));
#146078=CARTESIAN_POINT('Ctrl Pts',(98.6846752938252,5.3678618384454,133.29810222741));
#146079=CARTESIAN_POINT('Ctrl Pts',(98.6772670741587,5.43033787176085,133.153692684563));
#146080=CARTESIAN_POINT('Ctrl Pts',(98.6698542948567,5.49285235803233,133.009194260052));
#146081=CARTESIAN_POINT('Ctrl Pts',(98.6624415155546,5.54953936445879,132.862328328622));
#146082=CARTESIAN_POINT('Ctrl Pts',(98.6550287362526,5.60024074310215,132.713610255984));
#146083=CARTESIAN_POINT('Ctrl Pts',(98.6476053652238,5.65101456625302,132.564679687989));
#146084=CARTESIAN_POINT('Ctrl Pts',(98.6401819941951,5.6957855742973,132.41389205019));
#146085=CARTESIAN_POINT('Ctrl Pts',(98.6327586231663,5.73444620501691,132.261775206579));
#146086=CARTESIAN_POINT('Ctrl Pts',(98.6288225737255,5.75494499907408,132.1811192061));
#146087=CARTESIAN_POINT('Ctrl Pts',(98.6248865242845,5.77372680714943,132.100089655617));
#146088=CARTESIAN_POINT('Ctrl Pts',(98.6209504748437,5.79078150594723,132.018765868246));
#146089=CARTESIAN_POINT('Ctrl Pts',(98.6135272084382,5.82294613562024,131.865391743297));
#146090=CARTESIAN_POINT('Ctrl Pts',(98.6061039420328,5.84906181299111,131.710506952057));
#146091=CARTESIAN_POINT('Ctrl Pts',(98.5986806756273,5.86898853870163,131.554629965926));
#146092=CARTESIAN_POINT('Ctrl Pts',(98.5912661829063,5.88889171267715,131.398937213448));
#146093=CARTESIAN_POINT('Ctrl Pts',(98.5838516901853,5.90262044832208,131.242254966998));
#146094=CARTESIAN_POINT('Ctrl Pts',(98.5764371974642,5.91008529439362,131.085113846385));
#146095=CARTESIAN_POINT('Ctrl Pts',(98.5690298511104,5.91754294556548,130.9281241843));
#146096=CARTESIAN_POINT('Ctrl Pts',(98.5616225047566,5.91874870878988,130.77067689892));
#146097=CARTESIAN_POINT('Ctrl Pts',(98.5542151584028,5.913664691055,130.613309618434));
#146098=CARTESIAN_POINT('Ctrl Pts',(98.5468133367274,5.90858446517237,130.456059708404));
#146099=CARTESIAN_POINT('Ctrl Pts',(98.539411515052,5.89722381105688,130.298890055954));
#146100=CARTESIAN_POINT('Ctrl Pts',(98.5320096933766,5.87959687145631,130.142340080376));
#146101=CARTESIAN_POINT('Ctrl Pts',(98.5246117790652,5.86197923697987,129.985872746311));
#146102=CARTESIAN_POINT('Ctrl Pts',(98.5172138647539,5.83810194656837,129.830024807654));
#146103=CARTESIAN_POINT('Ctrl Pts',(98.5098159504425,5.80803111867375,129.675332235718));
#146104=CARTESIAN_POINT('Ctrl Pts',(98.5024192655302,5.77796528800529,129.520665370882));
#146105=CARTESIAN_POINT('Ctrl Pts',(98.495022580618,5.74170803378008,129.367153857783));
#146106=CARTESIAN_POINT('Ctrl Pts',(98.4876258957058,5.69937690763675,129.215325241246));
#146107=CARTESIAN_POINT('Ctrl Pts',(98.4802295387703,5.65704765849982,129.063503356948));
#146108=CARTESIAN_POINT('Ctrl Pts',(98.4728331818348,5.60864517320242,128.913364580423));
#146109=CARTESIAN_POINT('Ctrl Pts',(98.4654368248993,5.55433730887498,128.765422751485));
#146110=CARTESIAN_POINT('Ctrl Pts',(98.4580393355627,5.50002112987499,128.617458272275));
#146111=CARTESIAN_POINT('Ctrl Pts',(98.4506418462262,5.43979790025302,128.471691760842));
#146112=CARTESIAN_POINT('Ctrl Pts',(98.4432443568896,5.37388413812647,128.328618338472));
#146113=CARTESIAN_POINT('Ctrl Pts',(98.4358442743745,5.30794727003245,128.185494761935));
#146114=CARTESIAN_POINT('Ctrl Pts',(98.4284441918595,5.23631605388839,128.04506649291));
#146115=CARTESIAN_POINT('Ctrl Pts',(98.4210441093444,5.15925351247204,127.907805118953));
#146116=CARTESIAN_POINT('Ctrl Pts',(98.4136358896779,5.08210623286946,127.770392812005));
#146117=CARTESIAN_POINT('Ctrl Pts',(98.4062276700114,4.99951588377923,127.636154680266));
#146118=CARTESIAN_POINT('Ctrl Pts',(98.398819450345,4.9117898675597,127.505534938716));
#146119=CARTESIAN_POINT('Ctrl Pts',(98.3914066710429,4.82400985744078,127.374834802895));
#146120=CARTESIAN_POINT('Ctrl Pts',(98.3839938917408,4.73108810149869,127.247757795591));
#146121=CARTESIAN_POINT('Ctrl Pts',(98.3765811124387,4.63337270867953,127.124715538898));
#146122=CARTESIAN_POINT('Ctrl Pts',(98.3691577414099,4.53551769552477,127.00149747366));
#146123=CARTESIAN_POINT('Ctrl Pts',(98.3617343703811,4.43285560875591,126.882325955187));
#146124=CARTESIAN_POINT('Ctrl Pts',(98.3543109993523,4.32577241529428,126.767576802005));
#146125=CARTESIAN_POINT('Ctrl Pts',(98.3503749499117,4.26899433669849,126.706734047623));
#146126=CARTESIAN_POINT('Ctrl Pts',(98.3464389004712,4.21097390704092,126.647133929272));
#146127=CARTESIAN_POINT('Ctrl Pts',(98.3425028510307,4.15177238280614,126.588827834647));
#146128=CARTESIAN_POINT('Ctrl Pts',(98.3350795846252,4.0401201557092,126.478864359847));
#146129=CARTESIAN_POINT('Ctrl Pts',(98.3276563182197,3.92392735580368,126.373173487904));
#146130=CARTESIAN_POINT('Ctrl Pts',(98.3202330518143,3.80355451469021,126.272153250699));
#146131=CARTESIAN_POINT('Ctrl Pts',(98.3128185590933,3.68332394427833,126.171252411025));
#146132=CARTESIAN_POINT('Ctrl Pts',(98.3054040663723,3.55892344982694,126.075011455526));
#146133=CARTESIAN_POINT('Ctrl Pts',(98.2979895736513,3.43075110622816,125.983792455034));
#146134=CARTESIAN_POINT('Ctrl Pts',(98.2905822272975,3.30270229995984,125.892661374849));
#146135=CARTESIAN_POINT('Ctrl Pts',(98.2831748809437,3.17088918410599,125.806542828488));
#146136=CARTESIAN_POINT('Ctrl Pts',(98.27576753459,3.0357435983912,125.725759297584));
#146137=CARTESIAN_POINT('Ctrl Pts',(98.2683657129146,2.90069880935358,125.645036018085));
#146138=CARTESIAN_POINT('Ctrl Pts',(98.2609638912392,2.76232681842323,125.569640021911));
#146139=CARTESIAN_POINT('Ctrl Pts',(98.2535620695638,2.62108909882881,125.499850979673));
#146140=CARTESIAN_POINT('Ctrl Pts',(98.2461641552525,2.47992593752656,125.430098778526));
#146141=CARTESIAN_POINT('Ctrl Pts',(98.2387662409411,2.33590039418907,125.365947801548));
#146142=CARTESIAN_POINT('Ctrl Pts',(98.2313683266298,2.18949913530127,125.307632126999));
#146143=CARTESIAN_POINT('Ctrl Pts',(98.2239716417176,2.0431222056468,125.249326143457));
#146144=CARTESIAN_POINT('Ctrl Pts',(98.2165749568053,1.89437069046328,125.196853675738));
#146145=CARTESIAN_POINT('Ctrl Pts',(98.2091782718931,1.74375196768514,125.150400975183));
#146146=CARTESIAN_POINT('Ctrl Pts',(98.2017819149577,1.59313992349878,125.10395033439));
#146147=CARTESIAN_POINT('Ctrl Pts',(98.1943855580222,1.44066119305779,125.063519040045));
#146148=CARTESIAN_POINT('Ctrl Pts',(98.1869892010868,1.28683881522993,125.029243612161));
#146149=CARTESIAN_POINT('Ctrl Pts',(98.1795917117502,1.13299288680343,124.994962936622));
#146150=CARTESIAN_POINT('Ctrl Pts',(98.1721942224136,0.977803265767891,
124.966840085338));
#146151=CARTESIAN_POINT('Ctrl Pts',(98.164796733077,0.82180354501573,124.944960520636));
#146152=CARTESIAN_POINT('Ctrl Pts',(98.157396650562,0.665749138803402,124.923073286087));
#146153=CARTESIAN_POINT('Ctrl Pts',(98.149996568047,0.508884436922934,124.907433747371));
#146154=CARTESIAN_POINT('Ctrl Pts',(98.142596485532,0.351748369577102,124.89807552057));
#146155=CARTESIAN_POINT('Ctrl Pts',(98.1351882658656,0.194439514970794,
124.888707003436));
#146156=CARTESIAN_POINT('Ctrl Pts',(98.1277800461991,0.036859071852575,
124.885633614052));
#146157=CARTESIAN_POINT('Ctrl Pts',(98.1203718265326,-0.120453070650101,
124.888836835155));
#146158=CARTESIAN_POINT('Ctrl Pts',(98.1129590472305,-0.277862036151929,
124.892042027787));
#146159=CARTESIAN_POINT('Ctrl Pts',(98.1055462679284,-0.435002000231745,
124.901531506265));
#146160=CARTESIAN_POINT('Ctrl Pts',(98.0981334886263,-0.591338492174717,
124.917234888471));
#146161=CARTESIAN_POINT('Ctrl Pts',(98.0907101175975,-0.747898365028274,
124.932960708406));
#146162=CARTESIAN_POINT('Ctrl Pts',(98.0832867465688,-0.903652104190678,
124.954918112885));
#146163=CARTESIAN_POINT('Ctrl Pts',(98.07586337554,-1.05807489834628,124.982985516098));
#146164=CARTESIAN_POINT('Ctrl Pts',(98.0719273260993,-1.13995356913028,
124.99786752675));
#146165=CARTESIAN_POINT('Ctrl Pts',(98.0679912766585,-1.22145829612271,
125.014466437663));
#146166=CARTESIAN_POINT('Ctrl Pts',(98.0640552272178,-1.3025127347755,125.032758488326));
#146167=CARTESIAN_POINT('Ctrl Pts',(98.0566319608124,-1.4553788764545,125.067256725002));
#146168=CARTESIAN_POINT('Ctrl Pts',(98.049208694407,-1.60710464685679,125.107884520385));
#146169=CARTESIAN_POINT('Ctrl Pts',(98.0417854280016,-1.75716029435094,
125.154553694984));
#146170=CARTESIAN_POINT('Ctrl Pts',(98.0343709352805,-1.90703858853163,
125.201167710494));
#146171=CARTESIAN_POINT('Ctrl Pts',(98.0269564425595,-2.05525033598057,
125.253808782418));
#146172=CARTESIAN_POINT('Ctrl Pts',(98.0195419498385,-2.2012757470495,125.312337707203));
#146173=CARTESIAN_POINT('Ctrl Pts',(98.0121346034847,-2.34716041332917,
125.370810219607));
#146174=CARTESIAN_POINT('Ctrl Pts',(98.0047272571309,-2.49086259422015,
125.435159149245));
#146175=CARTESIAN_POINT('Ctrl Pts',(97.9973199107772,-2.63187755687176,
125.505195486327));
#146176=CARTESIAN_POINT('Ctrl Pts',(97.9899180891017,-2.77278734524423,
125.575179587667));
#146177=CARTESIAN_POINT('Ctrl Pts',(97.9825162674263,-2.91101357317273,
125.650842484954));
#146178=CARTESIAN_POINT('Ctrl Pts',(97.9751144457509,-3.0460715083007,125.731947096488));
#146179=CARTESIAN_POINT('Ctrl Pts',(97.9677165314396,-3.18105814739561,
125.813008893528));
#146180=CARTESIAN_POINT('Ctrl Pts',(97.9603186171283,-3.31287950537079,
125.899506492121));
#146181=CARTESIAN_POINT('Ctrl Pts',(97.9529207028169,-3.44107559043296,
125.991156970989));
#146182=CARTESIAN_POINT('Ctrl Pts',(97.9455240179047,-3.5692503716316,126.082792219209));
#146183=CARTESIAN_POINT('Ctrl Pts',(97.9381273329925,-3.69380077223537,
126.179578431282));
#146184=CARTESIAN_POINT('Ctrl Pts',(97.9307306480803,-3.81429584354901,
126.281189409179));
#146185=CARTESIAN_POINT('Ctrl Pts',(97.9233342911449,-3.934785571985,126.382795881538));
#146186=CARTESIAN_POINT('Ctrl Pts',(97.9159379342095,-4.05122004329452,
126.489226453697));
#146187=CARTESIAN_POINT('Ctrl Pts',(97.908541577274,-4.16320168404008,126.600114870645));
#146188=CARTESIAN_POINT('Ctrl Pts',(97.9011440879375,-4.27520046946032,
126.711020264891));
#146189=CARTESIAN_POINT('Ctrl Pts',(97.8937465986009,-4.38274480161207,
126.826384600209));
#146190=CARTESIAN_POINT('Ctrl Pts',(97.8863491092644,-4.48547435862851,
126.945805144259));
#146191=CARTESIAN_POINT('Ctrl Pts',(97.8789490267493,-4.58823992733302,
127.065267550997));
#146192=CARTESIAN_POINT('Ctrl Pts',(97.8715489442343,-4.68618711718988,
127.188788714636));
#146193=CARTESIAN_POINT('Ctrl Pts',(97.8641488617193,-4.77899634109947,
127.315933388246));
#146194=CARTESIAN_POINT('Ctrl Pts',(97.8567406420528,-4.87190761829117,
127.443217870495));
#146195=CARTESIAN_POINT('Ctrl Pts',(97.8493324223863,-4.95966942644447,
127.574133518166));
#146196=CARTESIAN_POINT('Ctrl Pts',(97.8419242027199,-5.04200552139587,
127.708216098214));
#146197=CARTESIAN_POINT('Ctrl Pts',(97.8345114234178,-5.12439229284004,
127.842381203853));
#146198=CARTESIAN_POINT('Ctrl Pts',(97.8270986441157,-5.20134651478244,
127.979716800978));
#146199=CARTESIAN_POINT('Ctrl Pts',(97.8196858648136,-5.27263850721605,
128.119735180988));
#146200=CARTESIAN_POINT('Ctrl Pts',(97.8122624937849,-5.34403236499151,
128.259953625824));
#146201=CARTESIAN_POINT('Ctrl Pts',(97.8048391227562,-5.40974767925094,
128.402862171217));
#146202=CARTESIAN_POINT('Ctrl Pts',(97.7974157517274,-5.46960307024504,
128.547953558442));
#146203=CARTESIAN_POINT('Ctrl Pts',(97.7934797022866,-5.50133983476077,
128.624884493369));
#146204=CARTESIAN_POINT('Ctrl Pts',(97.7895436528458,-5.53142999670768,
128.702428845323));
#146205=CARTESIAN_POINT('Ctrl Pts',(97.785607603405,-5.55985228038424,128.780509540336));
#146206=CARTESIAN_POINT('Ctrl Pts',(97.7770139152604,-5.62190745675972,
128.950985331644));
#146207=CARTESIAN_POINT('Ctrl Pts',(97.7684202271159,-5.67616396084671,
129.124443100668));
#146208=CARTESIAN_POINT('Ctrl Pts',(97.7598265389713,-5.72236577378178,
129.300212847714));
#146209=CARTESIAN_POINT('Ctrl Pts',(97.7512653268184,-5.768392987678,129.475318351802));
#146210=CARTESIAN_POINT('Ctrl Pts',(97.7427041146655,-5.80642618331576,
129.65271827668));
#146211=CARTESIAN_POINT('Ctrl Pts',(97.7341429025126,-5.83625879841363,
129.831728209901));
#146212=CARTESIAN_POINT('Ctrl Pts',(97.7256452108506,-5.86587006841195,
130.009409966851));
#146213=CARTESIAN_POINT('Ctrl Pts',(97.7171475191885,-5.88740192283493,
130.188677798431));
#146214=CARTESIAN_POINT('Ctrl Pts',(97.7086498275265,-5.9006995006581,130.368842574962));
#146215=CARTESIAN_POINT('Ctrl Pts',(97.7018916271594,-5.91127504268765,
130.512127328907));
#146216=CARTESIAN_POINT('Ctrl Pts',(97.6951334267924,-5.91664328977992,
130.65597899437));
#146217=CARTESIAN_POINT('Ctrl Pts',(97.6883752264253,-5.91674842443727,
130.800042699191));
#146218=CARTESIAN_POINT('',(95.9383751922114,-5.90973932447518,130.808309037287));
#146219=CARTESIAN_POINT('Ctrl Pts',(97.6883751922114,-5.91044616388941,
130.800048027004));
#146220=CARTESIAN_POINT('Ctrl Pts',(97.6279701213383,-5.90180813919648,
132.086330752508));
#146221=CARTESIAN_POINT('Ctrl Pts',(97.4747491758607,-4.85569580484173,
135.361851444278));
#146222=CARTESIAN_POINT('Ctrl Pts',(97.2287123557792,0.556297771968347,
137.780612714447));
#146223=CARTESIAN_POINT('Ctrl Pts',(96.9502647319661,6.17001100091076,134.107166209633));
#146224=CARTESIAN_POINT('Ctrl Pts',(96.6718171081533,6.11378554181002,127.398602716729));
#146225=CARTESIAN_POINT('Ctrl Pts',(96.3933694843406,0.439289844815531,
123.819764354175));
#146226=CARTESIAN_POINT('Ctrl Pts',(96.1488888456932,-4.89743273152406,
126.313026653818));
#146227=CARTESIAN_POINT('Ctrl Pts',(95.9972240816501,-5.90209215049429,
129.554787758123));
#146228=CARTESIAN_POINT('Ctrl Pts',(95.9383751922114,-5.90973932447518,
130.808309037287));
#146229=CARTESIAN_POINT('',(94.1883751922115,-5.92487953698549,130.807193534747));
#146230=CARTESIAN_POINT('Ctrl Pts',(95.9383751922114,-5.90973932447518,
130.808309037287));
#146231=CARTESIAN_POINT('Ctrl Pts',(95.9044082070458,-5.91415319613265,
131.531828870885));
#146232=CARTESIAN_POINT('Ctrl Pts',(95.7776253472764,-5.45539215556061,
134.226986472583));
#146233=CARTESIAN_POINT('Ctrl Pts',(95.5580266129015,-1.42598660733677,
137.655938736953));
#146234=CARTESIAN_POINT('Ctrl Pts',(95.2795789890891,4.99364612569024,135.707528868983));
#146235=CARTESIAN_POINT('Ctrl Pts',(95.0011313652761,6.82436202238293,129.25334691105));
#146236=CARTESIAN_POINT('Ctrl Pts',(94.7226837414632,2.38382260912524,124.224470778171));
#146237=CARTESIAN_POINT('Ctrl Pts',(94.4517650171081,-4.06803459211089,
125.214673966664));
#146238=CARTESIAN_POINT('Ctrl Pts',(94.2736621673578,-5.91423505740828,
129.002405790779));
#146239=CARTESIAN_POINT('Ctrl Pts',(94.1883751922115,-5.92487953698549,
130.807193534747));
#146240=CARTESIAN_POINT('',(92.4383751922114,-5.91809470196727,130.799038547181));
#146241=CARTESIAN_POINT('Ctrl Pts',(94.1883751922115,-5.92487953698549,
130.807193534747));
#146242=CARTESIAN_POINT('Ctrl Pts',(94.1808462927535,-5.92581920234919,
130.966515230048));
#146243=CARTESIAN_POINT('Ctrl Pts',(94.0805015186906,-5.84762556849407,
133.089009600992));
#146244=CARTESIAN_POINT('Ctrl Pts',(93.8873408700248,-3.29341206105117,
136.979390781575));
#146245=CARTESIAN_POINT('Ctrl Pts',(93.6088932462115,3.41505809786538,136.912956095953));
#146246=CARTESIAN_POINT('Ctrl Pts',(93.3304456223988,6.98525669970749,131.233020587166));
#146247=CARTESIAN_POINT('Ctrl Pts',(93.0519979985858,4.1363456432787,125.159167507523));
#146248=CARTESIAN_POINT('Ctrl Pts',(92.7735503747728,-2.51366498760439,
124.272971112994));
#146249=CARTESIAN_POINT('Ctrl Pts',(92.5690094393148,-5.70178004860599,
128.030938026362));
#146250=CARTESIAN_POINT('Ctrl Pts',(92.457284378461,-5.9222163663983,130.397769432159));
#146251=CARTESIAN_POINT('Ctrl Pts',(92.4383751922115,-5.91849239897776,
130.799038189537));
#146252=CARTESIAN_POINT('',(90.6883751922462,-5.91674998811213,130.803985550795));
#146253=CARTESIAN_POINT('Ctrl Pts',(92.4383751922115,-5.9167476075087,130.799039758607));
#146254=CARTESIAN_POINT('Ctrl Pts',(92.431072074229,-5.91688693521948,130.953970927748));
#146255=CARTESIAN_POINT('Ctrl Pts',(92.4237689562464,-5.91093675709542,
131.109097642124));
#146256=CARTESIAN_POINT('Ctrl Pts',(92.4164658382639,-5.89887780130397,
131.263894346234));
#146257=CARTESIAN_POINT('Ctrl Pts',(92.4091685072242,-5.88682840095014,
131.418568390449));
#146258=CARTESIAN_POINT('Ctrl Pts',(92.4018711761846,-5.86867988553666,
131.572912562971));
#146259=CARTESIAN_POINT('Ctrl Pts',(92.3945738451449,-5.84446504588668,
131.72640122942));
#146260=CARTESIAN_POINT('Ctrl Pts',(92.3871605652284,-5.8198654513932,131.882328710609));
#146261=CARTESIAN_POINT('Ctrl Pts',(92.3797472853118,-5.7890051060506,132.037372864326));
#146262=CARTESIAN_POINT('Ctrl Pts',(92.3723340053952,-5.75197330847544,
132.190987323311));
#146263=CARTESIAN_POINT('Ctrl Pts',(92.3650421934528,-5.71554828381093,
132.342084780733));
#146264=CARTESIAN_POINT('Ctrl Pts',(92.3577503815105,-5.67315260666512,
132.491798652156));
#146265=CARTESIAN_POINT('Ctrl Pts',(92.3504585695681,-5.62492277146484,
132.639619285317));
#146266=CARTESIAN_POINT('Ctrl Pts',(92.3431670707937,-5.5766950076346,132.787433569893));
#146267=CARTESIAN_POINT('Ctrl Pts',(92.3358755720193,-5.52263370339903,
132.933354411886));
#146268=CARTESIAN_POINT('Ctrl Pts',(92.3285840732449,-5.46292500449768,
133.076888055846));
#146269=CARTESIAN_POINT('Ctrl Pts',(92.3212913518392,-5.40320629370073,
133.220445767385));
#146270=CARTESIAN_POINT('Ctrl Pts',(92.3139986304335,-5.33783845222892,
133.361615129123));
#146271=CARTESIAN_POINT('Ctrl Pts',(92.3067059090278,-5.26705534710743,
133.49992336642));
#146272=CARTESIAN_POINT('Ctrl Pts',(92.2992016772044,-5.19421932328822,
133.642242950292));
#146273=CARTESIAN_POINT('Ctrl Pts',(92.291697445381,-5.11564935180377,133.781532541102));
#146274=CARTESIAN_POINT('Ctrl Pts',(92.2841932135576,-5.03164988115286,
133.917306173787));
#146275=CARTESIAN_POINT('Ctrl Pts',(92.276889709559,-4.94989728019178,134.049448049538));
#146276=CARTESIAN_POINT('Ctrl Pts',(92.2695862055604,-4.86300220249854,
134.178259375424));
#146277=CARTESIAN_POINT('Ctrl Pts',(92.2622827015618,-4.77128770943318,
134.303323914932));
#146278=CARTESIAN_POINT('Ctrl Pts',(92.254678105826,-4.67579222630446,134.433544322017));
#146279=CARTESIAN_POINT('Ctrl Pts',(92.2470735100902,-4.57507179766996,
134.559702064348));
#146280=CARTESIAN_POINT('Ctrl Pts',(92.2394689143544,-4.46953475600557,
134.681368436408));
#146281=CARTESIAN_POINT('Ctrl Pts',(92.2318643186186,-4.36399771434125,
134.803034808467));
#146282=CARTESIAN_POINT('Ctrl Pts',(92.2242597228828,-4.25364443123981,
134.920209524872));
#146283=CARTESIAN_POINT('Ctrl Pts',(92.216655127147,-4.13892252036997,135.03251044141));
#146284=CARTESIAN_POINT('Ctrl Pts',(92.2092318607415,-4.02693611944722,
135.142133575893));
#146285=CARTESIAN_POINT('Ctrl Pts',(92.2018085943361,-3.91042217108091,
135.247470307369));
#146286=CARTESIAN_POINT('Ctrl Pts',(92.1943853279307,-3.78974241667382,
135.348123703133));
#146287=CARTESIAN_POINT('Ctrl Pts',(92.1869708352097,-3.66920529571444,
135.448658134942));
#146288=CARTESIAN_POINT('Ctrl Pts',(92.1795563424887,-3.54451245311485,
135.544520012347));
#146289=CARTESIAN_POINT('Ctrl Pts',(92.1721418497677,-3.4160630639424,135.635348477794));
#146290=CARTESIAN_POINT('Ctrl Pts',(92.1647345034139,-3.28773747912728,
135.726089399346));
#146291=CARTESIAN_POINT('Ctrl Pts',(92.1573271570602,-3.15566285859136,
135.811806353029));
#146292=CARTESIAN_POINT('Ctrl Pts',(92.1499198107064,-3.02027202158217,
135.892178173075));
#146293=CARTESIAN_POINT('Ctrl Pts',(92.142517989031,-2.88498216416675,135.972490048786));
#146294=CARTESIAN_POINT('Ctrl Pts',(92.1351161673556,-2.74638133468789,
136.047464538988));
#146295=CARTESIAN_POINT('Ctrl Pts',(92.1277143456801,-2.60493185545782,
136.116823378934));
#146296=CARTESIAN_POINT('Ctrl Pts',(92.1203164313688,-2.4635570463081,136.186145604888));
#146297=CARTESIAN_POINT('Ctrl Pts',(92.1129185170575,-2.31933691658116,
136.249857920511));
#146298=CARTESIAN_POINT('Ctrl Pts',(92.1055206027462,-2.17275884296142,
136.307727729874));
#146299=CARTESIAN_POINT('Ctrl Pts',(92.098123917834,-2.0262051279577,136.365587922324));
#146300=CARTESIAN_POINT('Ctrl Pts',(92.0907272329219,-1.87729459363938,
136.41760739855));
#146301=CARTESIAN_POINT('Ctrl Pts',(92.0833305480097,-1.72653518247573,
136.463601452358));
#146302=CARTESIAN_POINT('Ctrl Pts',(92.0759341910742,-1.57578245614237,
136.50959346674));
#146303=CARTESIAN_POINT('Ctrl Pts',(92.0685378341388,-1.42318137302075,
136.549560481005));
#146304=CARTESIAN_POINT('Ctrl Pts',(92.0611414772034,-1.26925538507593,
136.583367567722));
#146305=CARTESIAN_POINT('Ctrl Pts',(92.0537439878668,-1.11530583066928,
136.617179830391));
#146306=CARTESIAN_POINT('Ctrl Pts',(92.0463464985303,-0.960031332176321,
136.644830207587));
#146307=CARTESIAN_POINT('Ctrl Pts',(92.0389490091937,-0.803965740135812,
136.666234861457));
#146308=CARTESIAN_POINT('Ctrl Pts',(92.0315489266788,-0.647845439544837,
136.687647018694));
#146309=CARTESIAN_POINT('Ctrl Pts',(92.0241488441638,-0.490933862875954,
136.702809042775));
#146310=CARTESIAN_POINT('Ctrl Pts',(92.0167487616488,-0.333770040151441,
136.711688958093));
#146311=CARTESIAN_POINT('Ctrl Pts',(92.0093405419824,-0.176433399646112,
136.720578637791));
#146312=CARTESIAN_POINT('Ctrl Pts',(92.001932322316,-0.0188443320902763,
136.723172392277));
#146313=CARTESIAN_POINT('Ctrl Pts',(91.9945241026495,0.138457332249514,
136.719490381962));
#146314=CARTESIAN_POINT('Ctrl Pts',(91.9871113233474,0.29585581313921,136.715806105432));
#146315=CARTESIAN_POINT('Ctrl Pts',(91.9796985440454,0.452966166648504,
136.705838390912));
#146316=CARTESIAN_POINT('Ctrl Pts',(91.9722857647433,0.609254138757135,
136.68965924694));
#146317=CARTESIAN_POINT('Ctrl Pts',(91.9648623937146,0.765765422449383,
136.673456985448));
#146318=CARTESIAN_POINT('Ctrl Pts',(91.9574390226858,0.92145160938465,136.651025621869));
#146319=CARTESIAN_POINT('Ctrl Pts',(91.9500156516571,1.0757882607436,136.622488338796));
#146320=CARTESIAN_POINT('Ctrl Pts',(91.9460796022161,1.15762125655496,136.607357186567));
#146321=CARTESIAN_POINT('Ctrl Pts',(91.9421435527752,1.239075084653,136.590510280186));
#146322=CARTESIAN_POINT('Ctrl Pts',(91.9382075033342,1.32007347316205,136.571971612419));
#146323=CARTESIAN_POINT('Ctrl Pts',(91.9307842369288,1.4728339060101,136.537008263585));
#146324=CARTESIAN_POINT('Ctrl Pts',(91.9233609705233,1.62443531659534,136.495918855334));
#146325=CARTESIAN_POINT('Ctrl Pts',(91.9159377041179,1.77434822412814,136.448793179129));
#146326=CARTESIAN_POINT('Ctrl Pts',(91.9085232113969,1.92408394705383,136.40172320156));
#146327=CARTESIAN_POINT('Ctrl Pts',(91.9011087186759,2.0721347866806,136.34863126789));
#146328=CARTESIAN_POINT('Ctrl Pts',(91.8936942259549,2.21798137945556,136.289658163086));
#146329=CARTESIAN_POINT('Ctrl Pts',(91.8862868796011,2.36368739979317,136.230741898781));
#146330=CARTESIAN_POINT('Ctrl Pts',(91.8788795332474,2.50719305905855,136.165955887195));
#146331=CARTESIAN_POINT('Ctrl Pts',(91.8714721868936,2.6479942020197,136.095490673478));
#146332=CARTESIAN_POINT('Ctrl Pts',(91.8640703652182,2.788690330177,136.025078015374));
#146333=CARTESIAN_POINT('Ctrl Pts',(91.8566685435428,2.92668562601896,135.948994755462));
#146334=CARTESIAN_POINT('Ctrl Pts',(91.8492667218674,3.06149608102939,135.867479449703));
#146335=CARTESIAN_POINT('Ctrl Pts',(91.841868807556,3.19623537064901,135.78600717524));
#146336=CARTESIAN_POINT('Ctrl Pts',(91.8344708932447,3.32779284910019,135.699108758429));
#146337=CARTESIAN_POINT('Ctrl Pts',(91.8270729789334,3.45570938783534,135.607068519295));
#146338=CARTESIAN_POINT('Ctrl Pts',(91.8196762940212,3.58360466916295,135.515043575578));
#146339=CARTESIAN_POINT('Ctrl Pts',(91.812279609109,3.70785990892144,135.417878723237));
#146340=CARTESIAN_POINT('Ctrl Pts',(91.8048829241967,3.82804515324628,135.315901470446));
#146341=CARTESIAN_POINT('Ctrl Pts',(91.7974865672613,3.94822506843153,135.213928739434));
#146342=CARTESIAN_POINT('Ctrl Pts',(91.7900902103259,4.06433506237359,135.107144273775));
#146343=CARTESIAN_POINT('Ctrl Pts',(91.7826938533904,4.17597867823078,134.995915536861));
#146344=CARTESIAN_POINT('Ctrl Pts',(91.7752963640539,4.28763938701026,134.884669770543));
#146345=CARTESIAN_POINT('Ctrl Pts',(91.7678988747173,4.39483209167113,134.768978641631));
#146346=CARTESIAN_POINT('Ctrl Pts',(91.7605013853807,4.49719769779428,134.649245977294));
#146347=CARTESIAN_POINT('Ctrl Pts',(91.7531013028658,4.59959918802175,134.529471340858));
#146348=CARTESIAN_POINT('Ctrl Pts',(91.7457012203508,4.69716996826024,134.405652631808));
#146349=CARTESIAN_POINT('Ctrl Pts',(91.7383011378358,4.78959177763234,134.278226067772));
#146350=CARTESIAN_POINT('Ctrl Pts',(91.7308929181693,4.8821152142855,134.150659385129));
#146351=CARTESIAN_POINT('Ctrl Pts',(91.7234846985029,4.96947815373376,134.019477227095));
#146352=CARTESIAN_POINT('Ctrl Pts',(91.7160764788364,5.05140576605887,133.885144665358));
#146353=CARTESIAN_POINT('Ctrl Pts',(91.7086636995343,5.13338380346227,133.75072942417));
#146354=CARTESIAN_POINT('Ctrl Pts',(91.7012509202323,5.20991966664164,133.613160240993));
#146355=CARTESIAN_POINT('Ctrl Pts',(91.6938381409302,5.28078516107104,133.472925521238));
#146356=CARTESIAN_POINT('Ctrl Pts',(91.6864147699014,5.35175191144219,133.332490427539));
#146357=CARTESIAN_POINT('Ctrl Pts',(91.6789913988727,5.41703195685918,133.189382529278));
#146358=CARTESIAN_POINT('Ctrl Pts',(91.671568027844,5.47644546233392,133.044109634885));
#146359=CARTESIAN_POINT('Ctrl Pts',(91.6676319784031,5.50794792854484,132.967082460501));
#146360=CARTESIAN_POINT('Ctrl Pts',(91.6636959289622,5.53780193278343,132.889446883624));
#146361=CARTESIAN_POINT('Ctrl Pts',(91.6597598795213,5.56598643403332,132.81128004262));
#146362=CARTESIAN_POINT('Ctrl Pts',(91.6523366131159,5.61914152378125,132.663859819992));
#146363=CARTESIAN_POINT('Ctrl Pts',(91.6449133467104,5.66651610639811,132.514103430867));
#146364=CARTESIAN_POINT('Ctrl Pts',(91.637490080305,5.70789952868653,132.362504876908));
#146365=CARTESIAN_POINT('Ctrl Pts',(91.630075587584,5.74923403920651,132.21108549985));
#146366=CARTESIAN_POINT('Ctrl Pts',(91.622661094863,5.78459138692901,132.057828648463));
#146367=CARTESIAN_POINT('Ctrl Pts',(91.615246602142,5.81380928954839,131.903247375727));
#146368=CARTESIAN_POINT('Ctrl Pts',(91.6078392557882,5.84299903085316,131.748815094241));
#146369=CARTESIAN_POINT('Ctrl Pts',(91.6004319094344,5.86606103862443,131.593061297061));
#146370=CARTESIAN_POINT('Ctrl Pts',(91.5930245630806,5.88288311567461,131.436513138569));
#146371=CARTESIAN_POINT('Ctrl Pts',(91.5856227414052,5.89969264618515,131.280081739599));
#146372=CARTESIAN_POINT('Ctrl Pts',(91.5782209197298,5.91027147295635,131.122857528558));
#146373=CARTESIAN_POINT('Ctrl Pts',(91.5708190980544,5.91455868144933,130.965376660842));
#146374=CARTESIAN_POINT('Ctrl Pts',(91.563421183743,5.91884362675829,130.807978926052));
#146375=CARTESIAN_POINT('Ctrl Pts',(91.5560232694317,5.91684355817676,130.650325176631));
#146376=CARTESIAN_POINT('Ctrl Pts',(91.5486253551204,5.90854951199959,130.492955372348));
#146377=CARTESIAN_POINT('Ctrl Pts',(91.5412286702081,5.9002568441424,130.335611720071));
#146378=CARTESIAN_POINT('Ctrl Pts',(91.5338319852959,5.88567229420846,130.178552291697));
#146379=CARTESIAN_POINT('Ctrl Pts',(91.5264353003837,5.86483900353505,130.022315845757));
#146380=CARTESIAN_POINT('Ctrl Pts',(91.5190389434483,5.84400663663162,129.866086327505));
#146381=CARTESIAN_POINT('Ctrl Pts',(91.5116425865128,5.81692612924937,129.710680089151));
#146382=CARTESIAN_POINT('Ctrl Pts',(91.5042462295773,5.78369234413948,129.556629304004));
#146383=CARTESIAN_POINT('Ctrl Pts',(91.4968487402407,5.7504534708521,129.402554933288));
#146384=CARTESIAN_POINT('Ctrl Pts',(91.4894512509041,5.71105952275197,129.249836793911));
#146385=CARTESIAN_POINT('Ctrl Pts',(91.4820537615675,5.6656561517681,129.098995280627));
#146386=CARTESIAN_POINT('Ctrl Pts',(91.4746536790525,5.6202368647031,128.948100890085));
#146387=CARTESIAN_POINT('Ctrl Pts',(91.4672535965375,5.56880406806876,128.799084792641));
#146388=CARTESIAN_POINT('Ctrl Pts',(91.4598535140225,5.51155273633097,128.652450536465));
#146389=CARTESIAN_POINT('Ctrl Pts',(91.4524452943561,5.45423845086832,128.505655040851));
#146390=CARTESIAN_POINT('Ctrl Pts',(91.4450370746896,5.39109298877237,128.361246964927));
#146391=CARTESIAN_POINT('Ctrl Pts',(91.4376288550231,5.32235907574186,128.219708913493));
#146392=CARTESIAN_POINT('Ctrl Pts',(91.430216075721,5.25358285813457,128.07808374775));
#146393=CARTESIAN_POINT('Ctrl Pts',(91.4228032964189,5.1792115117065,127.939332454627));
#146394=CARTESIAN_POINT('Ctrl Pts',(91.4153905171168,5.09953260104743,127.803911015697));
#146395=CARTESIAN_POINT('Ctrl Pts',(91.4079671460881,5.01973984142452,127.668296080265));
#146396=CARTESIAN_POINT('Ctrl Pts',(91.4005437750593,4.93462457269217,127.536020814614));
#146397=CARTESIAN_POINT('Ctrl Pts',(91.3931204040306,4.84451682326219,127.407511001874));
#146398=CARTESIAN_POINT('Ctrl Pts',(91.3891843545899,4.79673953240945,127.339372015609));
#146399=CARTESIAN_POINT('Ctrl Pts',(91.3852483051492,4.74755934134621,127.27229107068));
#146400=CARTESIAN_POINT('Ctrl Pts',(91.3813122557084,4.6970297755815,127.20632756466));
#146401=CARTESIAN_POINT('Ctrl Pts',(91.373888989303,4.60173259152136,127.081922450956));
#146402=CARTESIAN_POINT('Ctrl Pts',(91.3664657228975,4.50134541912187,126.961117886557));
#146403=CARTESIAN_POINT('Ctrl Pts',(91.3590424564921,4.39617001277534,126.844358119931));
#146404=CARTESIAN_POINT('Ctrl Pts',(91.3516279637711,4.29111891502469,126.727736353653));
#146405=CARTESIAN_POINT('Ctrl Pts',(91.3442134710501,4.18129109558825,126.61515014396));
#146406=CARTESIAN_POINT('Ctrl Pts',(91.3367989783291,4.06703048291858,126.507013341221));
#146407=CARTESIAN_POINT('Ctrl Pts',(91.3293916319753,3.95287999892924,126.398980764803));
#146408=CARTESIAN_POINT('Ctrl Pts',(91.3219842856215,3.834305496706,126.295389312641));
#146409=CARTESIAN_POINT('Ctrl Pts',(91.3145769392677,3.71168984083991,126.196618319227));
#146410=CARTESIAN_POINT('Ctrl Pts',(91.3071751175923,3.58916563635607,126.097920992945));
#146411=CARTESIAN_POINT('Ctrl Pts',(91.2997732959169,3.4626065690586,126.004037199892));
#146412=CARTESIAN_POINT('Ctrl Pts',(91.2923714742415,3.33243079587129,125.915307994283));
#146413=CARTESIAN_POINT('Ctrl Pts',(91.2849735599302,3.20232374146136,125.826625628131));
#146414=CARTESIAN_POINT('Ctrl Pts',(91.2775756456189,3.06860409116429,125.743092640004));
#146415=CARTESIAN_POINT('Ctrl Pts',(91.2701777313075,2.93172128332445,125.665008432767));
#146416=CARTESIAN_POINT('Ctrl Pts',(91.2627810463953,2.79486122292416,125.586937201708));
#146417=CARTESIAN_POINT('Ctrl Pts',(91.2553843614831,2.65483937219252,125.514313139197));
#146418=CARTESIAN_POINT('Ctrl Pts',(91.2479876765709,2.51213232288727,125.447391161352));
#146419=CARTESIAN_POINT('Ctrl Pts',(91.2405913196355,2.36943160136182,125.380472150898));
#146420=CARTESIAN_POINT('Ctrl Pts',(91.2331949627,2.2240462559833,125.31925488088));
#146421=CARTESIAN_POINT('Ctrl Pts',(91.2257986057645,2.07647529486173,125.263947193251));
#146422=CARTESIAN_POINT('Ctrl Pts',(91.218401116428,1.9288817402496,125.208631037874));
#146423=CARTESIAN_POINT('Ctrl Pts',(91.2110036270914,1.77910225319146,125.159226397424));
#146424=CARTESIAN_POINT('Ctrl Pts',(91.2036061377549,1.62765338495715,125.115892016885));
#146425=CARTESIAN_POINT('Ctrl Pts',(91.1962060552398,1.47615142655567,125.072542445545));
#146426=CARTESIAN_POINT('Ctrl Pts',(91.1888059727248,1.32297928052248,125.035267473416));
#146427=CARTESIAN_POINT('Ctrl Pts',(91.1814058902097,1.16866598465761,125.004175243045));
#146428=CARTESIAN_POINT('Ctrl Pts',(91.1739976705433,1.01418300546115,124.973048823571));
#146429=CARTESIAN_POINT('Ctrl Pts',(91.1665894508768,0.858556736660159,
124.948118796804));
#146430=CARTESIAN_POINT('Ctrl Pts',(91.1591812312104,0.702324406511077,
124.929441810423));
#146431=CARTESIAN_POINT('Ctrl Pts',(91.1517684519083,0.545995917969107,
124.910753328669));
#146432=CARTESIAN_POINT('Ctrl Pts',(91.1443556726062,0.389060996058686,
124.898325585603));
#146433=CARTESIAN_POINT('Ctrl Pts',(91.1369428933041,0.232058706675651,
124.892163114171));
#146434=CARTESIAN_POINT('Ctrl Pts',(91.1295195222753,0.0748320850588696,
124.88599183751));
#146435=CARTESIAN_POINT('Ctrl Pts',(91.1220961512465,-0.0824617239700671,
124.886103711596));
#146436=CARTESIAN_POINT('Ctrl Pts',(91.1146727802177,-0.239286108587151,
124.892451220363));
#146437=CARTESIAN_POINT('Ctrl Pts',(91.110736730777,-0.322438160258785,
124.895816821817));
#146438=CARTESIAN_POINT('Ctrl Pts',(91.1068006813363,-0.405458353621252,
124.900934620137));
#146439=CARTESIAN_POINT('Ctrl Pts',(91.1028646318956,-0.488267783968064,
124.907791688635));
#146440=CARTESIAN_POINT('Ctrl Pts',(91.0954413654902,-0.644443785211036,
124.92072390582));
#146441=CARTESIAN_POINT('Ctrl Pts',(91.0880180990847,-0.800341805377526,
124.939884659199));
#146442=CARTESIAN_POINT('Ctrl Pts',(91.0805948326793,-0.955424980030571,
124.965260201403));
#146443=CARTESIAN_POINT('Ctrl Pts',(91.0731803399583,-1.11032485925025,
124.990605751824));
#146444=CARTESIAN_POINT('Ctrl Pts',(91.0657658472373,-1.26441144517061,
125.022151410391));
#146445=CARTESIAN_POINT('Ctrl Pts',(91.0583513545163,-1.41715065202697,
125.05983151659));
#146446=CARTESIAN_POINT('Ctrl Pts',(91.0509440081626,-1.56974264308468,
125.097475305284));
#146447=CARTESIAN_POINT('Ctrl Pts',(91.0435366618088,-1.72098948044506,
125.141241681953));
#146448=CARTESIAN_POINT('Ctrl Pts',(91.036129315455,-1.87036507159359,125.191013571332));
#146449=CARTESIAN_POINT('Ctrl Pts',(91.0287274937796,-2.01962925279147,
125.240748338959));
#146450=CARTESIAN_POINT('Ctrl Pts',(91.0213256721042,-2.16702461406562,
125.296479583231));
#146451=CARTESIAN_POINT('Ctrl Pts',(91.0139238504288,-2.31203819281439,
125.35803984502));
#146452=CARTESIAN_POINT('Ctrl Pts',(91.0065259361174,-2.45697522002445,
125.419567609626));
#146453=CARTESIAN_POINT('Ctrl Pts',(90.999128021806,-2.5995326259831,125.486918118069));
#146454=CARTESIAN_POINT('Ctrl Pts',(90.9917301074946,-2.73921558217862,
125.559875079703));
#146455=CARTESIAN_POINT('Ctrl Pts',(90.9843334225824,-2.87887532560003,
125.632819917213));
#146456=CARTESIAN_POINT('Ctrl Pts',(90.9769367376702,-3.01566123675495,
125.711369186131));
#146457=CARTESIAN_POINT('Ctrl Pts',(90.969540052758,-3.14910123800777,125.7952597047));
#146458=CARTESIAN_POINT('Ctrl Pts',(90.9621436958225,-3.28253532239091,
125.879146503475));
#146459=CARTESIAN_POINT('Ctrl Pts',(90.9547473388871,-3.41262347583157,
125.968373882309));
#146460=CARTESIAN_POINT('Ctrl Pts',(90.9473509819516,-3.53892110893609,
126.062634355198));
#146461=CARTESIAN_POINT('Ctrl Pts',(90.9399534926151,-3.66523807853076,
126.156909259607));
#146462=CARTESIAN_POINT('Ctrl Pts',(90.9325560032785,-3.7877630730756,126.256218569106));
#146463=CARTESIAN_POINT('Ctrl Pts',(90.9251585139419,-3.90608332734201,
126.360213500024));
#146464=CARTESIAN_POINT('Ctrl Pts',(90.917758431427,-4.02444505858962,126.464244886203));
#146465=CARTESIAN_POINT('Ctrl Pts',(90.910358348912,-4.13859883469101,126.572964917792));
#146466=CARTESIAN_POINT('Ctrl Pts',(90.902958266397,-4.24816771440527,126.685986953996));
#146467=CARTESIAN_POINT('Ctrl Pts',(90.8955500467306,-4.3578570763672,126.799133269549));
#146468=CARTESIAN_POINT('Ctrl Pts',(90.8881418270641,-4.46295121361114,
126.916590768638));
#146469=CARTESIAN_POINT('Ctrl Pts',(90.8807336073976,-4.56311208184558,
127.037938085373));
#146470=CARTESIAN_POINT('Ctrl Pts',(90.8733208280956,-4.66333459742306,
127.159360089355));
#146471=CARTESIAN_POINT('Ctrl Pts',(90.8659080487935,-4.75861756827702,
127.284676385094));
#146472=CARTESIAN_POINT('Ctrl Pts',(90.8584952694914,-4.84866580242902,
127.413435891351));
#146473=CARTESIAN_POINT('Ctrl Pts',(90.8510718984627,-4.93884270172108,
127.542379375229));
#146474=CARTESIAN_POINT('Ctrl Pts',(90.843648527434,-5.02376972477853,127.674775582234));
#146475=CARTESIAN_POINT('Ctrl Pts',(90.8362251564052,-5.10319679641646,
127.810147362044));
#146476=CARTESIAN_POINT('Ctrl Pts',(90.8322891069644,-5.14531093562596,
127.881924727902));
#146477=CARTESIAN_POINT('Ctrl Pts',(90.8283530575235,-5.18587962935102,
127.954538262835));
#146478=CARTESIAN_POINT('Ctrl Pts',(90.8244170080826,-5.22487110325824,
128.027914594889));
#146479=CARTESIAN_POINT('Ctrl Pts',(90.8165699274292,-5.30260621434947,
128.174200866019));
#146480=CARTESIAN_POINT('Ctrl Pts',(90.8087228467758,-5.37428305171831,
128.323921525479));
#146481=CARTESIAN_POINT('Ctrl Pts',(90.8008757661224,-5.4396033048784,128.476561990525));
#146482=CARTESIAN_POINT('Ctrl Pts',(90.7930422008072,-5.50481105437651,
128.628939556845));
#146483=CARTESIAN_POINT('Ctrl Pts',(90.7852086354919,-5.56368392285292,
128.784226620248));
#146484=CARTESIAN_POINT('Ctrl Pts',(90.7773750701766,-5.61596930729451,
128.94188395945));
#146485=CARTESIAN_POINT('Ctrl Pts',(90.7695601035074,-5.66813055447299,
129.099166984667));
#146486=CARTESIAN_POINT('Ctrl Pts',(90.7617451368382,-5.71373541680176,
129.258808767443));
#146487=CARTESIAN_POINT('Ctrl Pts',(90.753930170169,-5.75257945854759,129.42025074635));
#146488=CARTESIAN_POINT('Ctrl Pts',(90.7461262213542,-5.79136873640084,
129.581465117862));
#146489=CARTESIAN_POINT('Ctrl Pts',(90.7383222725393,-5.82341611818608,
129.744474327453));
#146490=CARTESIAN_POINT('Ctrl Pts',(90.7305183237245,-5.84856635671517,
129.90870324245));
#146491=CARTESIAN_POINT('Ctrl Pts',(90.7227297011632,-5.87366720243783,
130.072609626629));
#146492=CARTESIAN_POINT('Ctrl Pts',(90.7149410786019,-5.89189787549124,
130.237730632963));
#146493=CARTESIAN_POINT('Ctrl Pts',(90.7071524560406,-5.90315384345051,
130.403480008088));
#146494=CARTESIAN_POINT('Ctrl Pts',(90.7008933681091,-5.91219935729549,
130.536679415985));
#146495=CARTESIAN_POINT('Ctrl Pts',(90.6946342801777,-5.91674151269891,
130.670284287664));
#146496=CARTESIAN_POINT('Ctrl Pts',(90.6883751922462,-5.91674998811213,
130.803985550795));
#146497=CARTESIAN_POINT('',(88.9383751922115,-5.91674749024185,130.809810316349));
#146498=CARTESIAN_POINT('Ctrl Pts',(90.6883751922114,-5.91674998811218,
130.803985551538));
#146499=CARTESIAN_POINT('Ctrl Pts',(90.6806626928907,-5.91676043156495,
130.96873334105));
#146500=CARTESIAN_POINT('Ctrl Pts',(90.67295019357,-5.90988562066363,131.133362254122));
#146501=CARTESIAN_POINT('Ctrl Pts',(90.6652376942492,-5.89618120901639,
131.297288313016));
#146502=CARTESIAN_POINT('Ctrl Pts',(90.6575167057358,-5.88246171284378,
131.461394806274));
#146503=CARTESIAN_POINT('Ctrl Pts',(90.6497957172224,-5.86189764216194,
131.624796578391));
#146504=CARTESIAN_POINT('Ctrl Pts',(90.6420747287089,-5.83459617221082,
131.786917521629));
#146505=CARTESIAN_POINT('Ctrl Pts',(90.6340659500057,-5.80627707411455,
131.955081320255));
#146506=CARTESIAN_POINT('Ctrl Pts',(90.6260571713024,-5.77070874452146,
132.121866580596));
#146507=CARTESIAN_POINT('Ctrl Pts',(90.6180483925991,-5.72806756474608,
132.286646870691));
#146508=CARTESIAN_POINT('Ctrl Pts',(90.6103020467591,-5.68682365755272,
132.446027615496));
#146509=CARTESIAN_POINT('Ctrl Pts',(90.602555700919,-5.63896326188491,132.603532434554));
#146510=CARTESIAN_POINT('Ctrl Pts',(90.5948093550789,-5.58469548427981,
132.758614160575));
#146511=CARTESIAN_POINT('Ctrl Pts',(90.586669359944,-5.52766995833463,132.921576739497));
#146512=CARTESIAN_POINT('Ctrl Pts',(90.5785293648092,-5.46356904828496,
133.081863137164));
#146513=CARTESIAN_POINT('Ctrl Pts',(90.5703893696743,-5.39269046322379,
133.238866754415));
#146514=CARTESIAN_POINT('Ctrl Pts',(90.5622493745395,-5.32181187816262,
133.395870371666));
#146515=CARTESIAN_POINT('Ctrl Pts',(90.5541093794046,-5.24415586832495,
133.549590877696));
#146516=CARTESIAN_POINT('Ctrl Pts',(90.5459693842698,-5.1600731277978,133.699455759056));
#146517=CARTESIAN_POINT('Ctrl Pts',(90.5385461178643,-5.08339389486299,
133.836124997886));
#146518=CARTESIAN_POINT('Ctrl Pts',(90.5311228514589,-5.00116524974444,
133.969952413179));
#146519=CARTESIAN_POINT('Ctrl Pts',(90.5236995850534,-4.91362285257071,
134.100455431918));
#146520=CARTESIAN_POINT('Ctrl Pts',(90.5162850923324,-4.82618392324049,
134.230804206926));
#146521=CARTESIAN_POINT('Ctrl Pts',(90.5088705996114,-4.73344394897865,
134.357836099414));
#146522=CARTESIAN_POINT('Ctrl Pts',(90.5014561068903,-4.63568465080247,
134.481092642179));
#146523=CARTESIAN_POINT('Ctrl Pts',(90.4940487605366,-4.53801957671838,
134.604230385648));
#146524=CARTESIAN_POINT('Ctrl Pts',(90.4866414141827,-4.43534504026797,
134.723599733067));
#146525=CARTESIAN_POINT('Ctrl Pts',(90.479234067829,-4.32798620253089,134.83877085863));
#146526=CARTESIAN_POINT('Ctrl Pts',(90.4718322461535,-4.22070743706488,
134.953856085223));
#146527=CARTESIAN_POINT('Ctrl Pts',(90.4644304244781,-4.10875158023966,
135.064749052701));
#146528=CARTESIAN_POINT('Ctrl Pts',(90.4570286028026,-3.99248416044879,
135.171052820031));
#146529=CARTESIAN_POINT('Ctrl Pts',(90.4496306884912,-3.87627811732363,
135.277300470429));
#146530=CARTESIAN_POINT('Ctrl Pts',(90.4422327741798,-3.75576531888127,
135.378963494154));
#146531=CARTESIAN_POINT('Ctrl Pts',(90.4348348598683,-3.63134816887476,
135.475681741072));
#146532=CARTESIAN_POINT('Ctrl Pts',(90.4274381749561,-3.50695169474222,
135.57238391517));
#146533=CARTESIAN_POINT('Ctrl Pts',(90.4200414900439,-3.37865245121897,
135.664142714472));
#146534=CARTESIAN_POINT('Ctrl Pts',(90.4126448051317,-3.24688603353782,
135.750638172224));
#146535=CARTESIAN_POINT('Ctrl Pts',(90.4052484481962,-3.11512545851761,
135.837129794677));
#146536=CARTESIAN_POINT('Ctrl Pts',(90.3978520912607,-2.9798983270917,135.918358334771));
#146537=CARTESIAN_POINT('Ctrl Pts',(90.3904557343252,-2.84166910401371,
135.994047242575));
#146538=CARTESIAN_POINT('Ctrl Pts',(90.3830582449886,-2.70341871768888,
136.069747738544));
#146539=CARTESIAN_POINT('Ctrl Pts',(90.375660755652,-2.56216565197898,136.139906734183));
#146540=CARTESIAN_POINT('Ctrl Pts',(90.3682632663154,-2.41839870432485,
136.204293790247));
#146541=CARTESIAN_POINT('Ctrl Pts',(90.3608631838004,-2.27458135939049,
136.268703417093));
#146542=CARTESIAN_POINT('Ctrl Pts',(90.3534631012855,-2.12824871845321,
136.327336923415));
#146543=CARTESIAN_POINT('Ctrl Pts',(90.3460630187705,-1.97990911981401,
136.380012188439));
#146544=CARTESIAN_POINT('Ctrl Pts',(90.338654799104,-1.831406406536,136.432745375332));
#146545=CARTESIAN_POINT('Ctrl Pts',(90.3312465794375,-1.68089268031238,
136.479507111761));
#146546=CARTESIAN_POINT('Ctrl Pts',(90.323838359771,-1.52889169434468,136.520165088458));
#146547=CARTESIAN_POINT('Ctrl Pts',(90.3164255804689,-1.37679715430617,
136.56084808946));
#146548=CARTESIAN_POINT('Ctrl Pts',(90.3090128011668,-1.22321389384794,
136.595419763122));
#146549=CARTESIAN_POINT('Ctrl Pts',(90.3016000218647,-1.06867488050435,
136.623799126759));
#146550=CARTESIAN_POINT('Ctrl Pts',(90.2941766508359,-0.913915054571438,
136.652219040162));
#146551=CARTESIAN_POINT('Ctrl Pts',(90.2867532798072,-0.758197116873509,
136.674428919804));
#146552=CARTESIAN_POINT('Ctrl Pts',(90.2793299087784,-0.602058991670594,
136.690399653543));
#146553=CARTESIAN_POINT('Ctrl Pts',(90.2753938593379,-0.51927081121063,
136.698867719784));
#146554=CARTESIAN_POINT('Ctrl Pts',(90.2714578098973,-0.43636451095525,
136.705582609427));
#146555=CARTESIAN_POINT('Ctrl Pts',(90.2675217604568,-0.353420031477407,
136.710545921453));
#146556=CARTESIAN_POINT('Ctrl Pts',(90.2600984940514,-0.196989331781025,
136.719906573035));
#146557=CARTESIAN_POINT('Ctrl Pts',(90.252675227646,-0.0399499458733333,
136.723062271943));
#146558=CARTESIAN_POINT('Ctrl Pts',(90.2452519612405,0.1171647438427,136.719950443213));
#146559=CARTESIAN_POINT('Ctrl Pts',(90.2378374685195,0.274093737043611,
136.716842292406));
#146560=CARTESIAN_POINT('Ctrl Pts',(90.2304229757985,0.4310974873121,136.707481366344));
#146561=CARTESIAN_POINT('Ctrl Pts',(90.2230084830775,0.587637996115035,
136.691856872174));
#146562=CARTESIAN_POINT('Ctrl Pts',(90.2156011367237,0.744027625281383,
136.67624743748));
#146563=CARTESIAN_POINT('Ctrl Pts',(90.20819379037,0.899954532896394,136.654386490109));
#146564=CARTESIAN_POINT('Ctrl Pts',(90.2007864440162,1.05488133682979,136.626315265939));
#146565=CARTESIAN_POINT('Ctrl Pts',(90.1933846223408,1.20969259050831,136.598264978346));
#146566=CARTESIAN_POINT('Ctrl Pts',(90.1859828006654,1.36350485998654,136.564013702878));
#146567=CARTESIAN_POINT('Ctrl Pts',(90.17858097899,1.51578661050585,136.5236544126));
#146568=CARTESIAN_POINT('Ctrl Pts',(90.1711830646786,1.6679879726742,136.483316427676));
#146569=CARTESIAN_POINT('Ctrl Pts',(90.1637851503673,1.81866006502622,136.436876944829));
#146570=CARTESIAN_POINT('Ctrl Pts',(90.1563872360559,1.96728237399586,136.384479847785));
#146571=CARTESIAN_POINT('Ctrl Pts',(90.1489905511438,2.11587998463392,136.332091458189));
#146572=CARTESIAN_POINT('Ctrl Pts',(90.1415938662316,2.26242813623829,136.273747543346));
#146573=CARTESIAN_POINT('Ctrl Pts',(90.1341971813194,2.40642218185364,136.209641632017));
#146574=CARTESIAN_POINT('Ctrl Pts',(90.1268008243839,2.55040984262232,136.145538563211));
#146575=CARTESIAN_POINT('Ctrl Pts',(90.1194044674485,2.69184328155654,136.075674157749));
#146576=CARTESIAN_POINT('Ctrl Pts',(90.1120081105131,2.83023877482334,136.000289700991));
#146577=CARTESIAN_POINT('Ctrl Pts',(90.1046106211765,2.96865545679327,135.924893702681));
#146578=CARTESIAN_POINT('Ctrl Pts',(90.0972131318399,3.10403293914437,135.843976148877));
#146579=CARTESIAN_POINT('Ctrl Pts',(90.0898156425034,3.23591313985699,135.757823720669));
#146580=CARTESIAN_POINT('Ctrl Pts',(90.0824155599884,3.36783957096878,135.671641091861));
#146581=CARTESIAN_POINT('Ctrl Pts',(90.0750154774735,3.49626596722398,135.580220139055));
#146582=CARTESIAN_POINT('Ctrl Pts',(90.0676153949586,3.62076433598955,135.483890100936));
#146583=CARTESIAN_POINT('Ctrl Pts',(90.0602071752921,3.74539960351103,135.387454138036));
#146584=CARTESIAN_POINT('Ctrl Pts',(90.0527989556256,3.86609792225628,135.286098538153));
#146585=CARTESIAN_POINT('Ctrl Pts',(90.0453907359591,3.98246487529061,135.180192433298));
#146586=CARTESIAN_POINT('Ctrl Pts',(90.0379779566571,4.09890345024309,135.074221145003));
#146587=CARTESIAN_POINT('Ctrl Pts',(90.030565177355,4.21100508217256,134.96369403235));
#146588=CARTESIAN_POINT('Ctrl Pts',(90.023152398053,4.31841355608367,134.849015722904));
#146589=CARTESIAN_POINT('Ctrl Pts',(90.0157290270242,4.42597550025919,134.73417355571));
#146590=CARTESIAN_POINT('Ctrl Pts',(90.0083056559955,4.5288306499666,134.615168627018));
#146591=CARTESIAN_POINT('Ctrl Pts',(90.0008822849668,4.626663751134,134.492437771917));
#146592=CARTESIAN_POINT('Ctrl Pts',(89.9969462355258,4.67853720884777,134.427362927653));
#146593=CARTESIAN_POINT('Ctrl Pts',(89.9930101860849,4.72899951607211,134.361241071086));
#146594=CARTESIAN_POINT('Ctrl Pts',(89.989074136644,4.77800880824216,134.294140322771));
#146595=CARTESIAN_POINT('Ctrl Pts',(89.9816508702386,4.87043880374435,134.167590405595));
#146596=CARTESIAN_POINT('Ctrl Pts',(89.9742276038331,4.95797740659319,134.037174454986));
#146597=CARTESIAN_POINT('Ctrl Pts',(89.9668043374277,5.04028366448247,133.903307397369));
#146598=CARTESIAN_POINT('Ctrl Pts',(89.9593898447067,5.12249264320998,133.769598559497));
#146599=CARTESIAN_POINT('Ctrl Pts',(89.9519753519856,5.19948139304801,133.632447048629));
#146600=CARTESIAN_POINT('Ctrl Pts',(89.9445608592646,5.27095003231685,133.492299664367));
#146601=CARTESIAN_POINT('Ctrl Pts',(89.9371535129108,5.34234978742056,133.352287359431));
#146602=CARTESIAN_POINT('Ctrl Pts',(89.929746166557,5.40823985555575,133.209285259937));
#146603=CARTESIAN_POINT('Ctrl Pts',(89.9223388202033,5.46836446146664,133.06376776969));
#146604=CARTESIAN_POINT('Ctrl Pts',(89.9149369985278,5.52844422417803,132.918358811877));
#146605=CARTESIAN_POINT('Ctrl Pts',(89.9075351768524,5.58276694480667,132.770438542351));
#146606=CARTESIAN_POINT('Ctrl Pts',(89.900133355177,5.63112353670508,132.62050441057));
#146607=CARTESIAN_POINT('Ctrl Pts',(89.8927354408656,5.6794546015352,132.470649427849));
#146608=CARTESIAN_POINT('Ctrl Pts',(89.8853375265543,5.72182569566769,132.31878305447));
#146609=CARTESIAN_POINT('Ctrl Pts',(89.8779396122429,5.75807652226219,132.165420985909));
#146610=CARTESIAN_POINT('Ctrl Pts',(89.8705429273306,5.79432132462683,132.012084403341));
#146611=CARTESIAN_POINT('Ctrl Pts',(89.8631462424184,5.82444779226367,131.857252981835));
#146612=CARTESIAN_POINT('Ctrl Pts',(89.8557495575062,5.84834597239345,131.701455902187));
#146613=CARTESIAN_POINT('Ctrl Pts',(89.8483532005708,5.87224309285286,131.545665730745));
#146614=CARTESIAN_POINT('Ctrl Pts',(89.8409568436353,5.88991241832283,131.388910355282));
#146615=CARTESIAN_POINT('Ctrl Pts',(89.8335604866999,5.90129548446236,131.231727166987));
#146616=CARTESIAN_POINT('Ctrl Pts',(89.8261629973633,5.9126802933784,131.074519913545));
#146617=CARTESIAN_POINT('Ctrl Pts',(89.8187655080266,5.9177768996482,130.9168850892));
#146618=CARTESIAN_POINT('Ctrl Pts',(89.81136801869,5.91657889167082,130.759363049462));
#146619=CARTESIAN_POINT('Ctrl Pts',(89.803967936175,5.9153804637336,130.601785790617));
#146620=CARTESIAN_POINT('Ctrl Pts',(89.79656785366,5.90788303112719,130.444321768149));
#146621=CARTESIAN_POINT('Ctrl Pts',(89.789167771145,5.89413225120764,130.287509025933));
#146622=CARTESIAN_POINT('Ctrl Pts',(89.7817595514785,5.88036635089195,130.130523851985));
#146623=CARTESIAN_POINT('Ctrl Pts',(89.7743513318121,5.86033340367287,129.974191760586));
#146624=CARTESIAN_POINT('Ctrl Pts',(89.7669431121456,5.83413077877718,129.819044110739));
#146625=CARTESIAN_POINT('Ctrl Pts',(89.7595303328435,5.80791202660307,129.663800970104));
#146626=CARTESIAN_POINT('Ctrl Pts',(89.7521175535414,5.77551610672988,129.509744088114));
#146627=CARTESIAN_POINT('Ctrl Pts',(89.7447047742394,5.73709090087995,129.357391869617));
#146628=CARTESIAN_POINT('Ctrl Pts',(89.7372814032106,5.69861079129397,129.204821963126));
#146629=CARTESIAN_POINT('Ctrl Pts',(89.7298580321818,5.65408429518321,129.053961941852));
#146630=CARTESIAN_POINT('Ctrl Pts',(89.7224346611531,5.60370853175498,128.905313158013));
#146631=CARTESIAN_POINT('Ctrl Pts',(89.7184986117124,5.57699809323635,128.826496006045));
#146632=CARTESIAN_POINT('Ctrl Pts',(89.7145625622717,5.54864401230487,128.748300159224));
#146633=CARTESIAN_POINT('Ctrl Pts',(89.7106265128311,5.51868097189372,128.67079766022));
#146634=CARTESIAN_POINT('Ctrl Pts',(89.7032032464256,5.46217161279101,128.524630365864));
#146635=CARTESIAN_POINT('Ctrl Pts',(89.6957799800202,5.39976573306095,128.380488653174));
#146636=CARTESIAN_POINT('Ctrl Pts',(89.6883567136147,5.33162812900701,128.238883652851));
#146637=CARTESIAN_POINT('Ctrl Pts',(89.6809422208937,5.26357105794249,128.097446017879));
#146638=CARTESIAN_POINT('Ctrl Pts',(89.6735277281727,5.18979590735851,127.958539460469));
#146639=CARTESIAN_POINT('Ctrl Pts',(89.6661132354517,5.11051648904238,127.822657785672));
#146640=CARTESIAN_POINT('Ctrl Pts',(89.6587058890979,5.03131348321451,127.686907078748));
#146641=CARTESIAN_POINT('Ctrl Pts',(89.6512985427442,4.94661695816185,127.554175770526));
#146642=CARTESIAN_POINT('Ctrl Pts',(89.6438911963904,4.8566877904679,127.424935478815));
#146643=CARTESIAN_POINT('Ctrl Pts',(89.636489374715,4.76682569534005,127.29579157939));
#146644=CARTESIAN_POINT('Ctrl Pts',(89.6290875530396,4.6717389406739,127.170133817194));
#146645=CARTESIAN_POINT('Ctrl Pts',(89.6216857313642,4.57173302834773,127.048406986327));
#146646=CARTESIAN_POINT('Ctrl Pts',(89.6142878170529,4.47177990836459,126.926744414108));
#146647=CARTESIAN_POINT('Ctrl Pts',(89.6068899027416,4.36691303871298,126.80900892825));
#146648=CARTESIAN_POINT('Ctrl Pts',(89.5994919884303,4.25747964424359,126.695614137026));
#146649=CARTESIAN_POINT('Ctrl Pts',(89.5920953035181,4.14806443561865,126.582238189958));
#146650=CARTESIAN_POINT('Ctrl Pts',(89.5846986186058,4.03408446728941,126.473201774218));
#146651=CARTESIAN_POINT('Ctrl Pts',(89.5773019336936,3.91592552188532,126.368883431338));
#146652=CARTESIAN_POINT('Ctrl Pts',(89.5699055767581,3.79777181577235,126.264569714043));
#146653=CARTESIAN_POINT('Ctrl Pts',(89.5625092198227,3.67543978086556,126.164973900703));
#146654=CARTESIAN_POINT('Ctrl Pts',(89.5551128628872,3.54934993818911,126.070435652088));
#146655=CARTESIAN_POINT('Ctrl Pts',(89.5477153735506,3.42324079083603,125.975882929426));
#146656=CARTESIAN_POINT('Ctrl Pts',(89.540317884214,3.29337298884547,125.886389537225));
#146657=CARTESIAN_POINT('Ctrl Pts',(89.5329203948774,3.16019768298323,125.802252945098));
#146658=CARTESIAN_POINT('Ctrl Pts',(89.5255203123625,3.02697569272453,125.718086859018));
#146659=CARTESIAN_POINT('Ctrl Pts',(89.5181202298475,2.89044420555162,125.639281510992));
#146660=CARTESIAN_POINT('Ctrl Pts',(89.5107201473325,2.75108057192996,125.566089314049));
#146661=CARTESIAN_POINT('Ctrl Pts',(89.503311927666,2.6115636936656,125.49281663476));
#146662=CARTESIAN_POINT('Ctrl Pts',(89.4959037079995,2.46920878031269,125.425169606593));
#146663=CARTESIAN_POINT('Ctrl Pts',(89.4884954883331,2.32451550969679,125.363353522581));
#146664=CARTESIAN_POINT('Ctrl Pts',(89.481082709031,2.17973318278706,125.3014993918));
#146665=CARTESIAN_POINT('Ctrl Pts',(89.4736699297289,2.03260997884623,125.245483488926));
#146666=CARTESIAN_POINT('Ctrl Pts',(89.4662571504268,1.88366198023594,125.195461607358));
#146667=CARTESIAN_POINT('Ctrl Pts',(89.458833779398,1.73450115774015,125.14536825218));
#146668=CARTESIAN_POINT('Ctrl Pts',(89.4514104083693,1.58351069049682,125.101286127954));
#146669=CARTESIAN_POINT('Ctrl Pts',(89.4439870373405,1.43121892807072,125.063320385828));
#146670=CARTESIAN_POINT('Ctrl Pts',(89.4400509878997,1.35047018144233,125.043190038378));
#146671=CARTESIAN_POINT('Ctrl Pts',(89.436114938459,1.2693557275585,125.024778364448));
#146672=CARTESIAN_POINT('Ctrl Pts',(89.4321788890182,1.18795492492918,125.008095125127));
#146673=CARTESIAN_POINT('Ctrl Pts',(89.4247556226128,1.03443555160173,124.976631056434));
#146674=CARTESIAN_POINT('Ctrl Pts',(89.4173323562074,0.879433144068388,
124.951222773912));
#146675=CARTESIAN_POINT('Ctrl Pts',(89.4099090898019,0.72346680749017,124.932007908391));
#146676=CARTESIAN_POINT('Ctrl Pts',(89.4024945970809,0.567684810169257,
124.912815753245));
#146677=CARTESIAN_POINT('Ctrl Pts',(89.3950801043599,0.410941518433562,
124.89980248959));
#146678=CARTESIAN_POINT('Ctrl Pts',(89.3876656116389,0.253767954950186,
124.893055145207));
#146679=CARTESIAN_POINT('Ctrl Pts',(89.3802582652851,0.0967458812652225,
124.886314304168));
#146680=CARTESIAN_POINT('Ctrl Pts',(89.3728509189314,-0.0607052681065663,
124.885827375188));
#146681=CARTESIAN_POINT('Ctrl Pts',(89.3654435725776,-0.218047697578145,
124.891629796356));
#146682=CARTESIAN_POINT('Ctrl Pts',(89.3580417509023,-0.375272775129521,
124.89742788986));
#146683=CARTESIAN_POINT('Ctrl Pts',(89.3506399292269,-0.532388922797885,
124.909505979728));
#146684=CARTESIAN_POINT('Ctrl Pts',(89.3432381075515,-0.688856791480747,
124.927847460656));
#146685=CARTESIAN_POINT('Ctrl Pts',(89.3358401932401,-0.845242061994901,
124.94617925926));
#146686=CARTESIAN_POINT('Ctrl Pts',(89.3284422789287,-1.00097936525315,
124.970767820726));
#146687=CARTESIAN_POINT('Ctrl Pts',(89.3210443646174,-1.15553303738866,
125.00154458033));
#146688=CARTESIAN_POINT('Ctrl Pts',(89.3136476797051,-1.3100610255072,125.032316225394));
#146689=CARTESIAN_POINT('Ctrl Pts',(89.3062509947929,-1.46340540713921,
125.06927395476));
#146690=CARTESIAN_POINT('Ctrl Pts',(89.2988543098807,-1.61503917963648,
125.11229780952));
#146691=CARTESIAN_POINT('Ctrl Pts',(89.2914579529453,-1.76666622853337,
125.155319756558));
#146692=CARTESIAN_POINT('Ctrl Pts',(89.2840615960098,-1.91658245998966,
125.204407192274));
#146693=CARTESIAN_POINT('Ctrl Pts',(89.2766652390744,-2.06427480589359,
125.259389915366));
#146694=CARTESIAN_POINT('Ctrl Pts',(89.2692677497378,-2.21198976387168,
125.314381056453));
#146695=CARTESIAN_POINT('Ctrl Pts',(89.2618702604013,-2.35747980848721,
125.375269151832));
#146696=CARTESIAN_POINT('Ctrl Pts',(89.2544727710648,-2.50025081212146,
125.441835425179));
#146697=CARTESIAN_POINT('Ctrl Pts',(89.2470726885498,-2.64307186391052,
125.50842503323));
#146698=CARTESIAN_POINT('Ctrl Pts',(89.2396726060348,-2.78317163887261,
125.580696624625));
#146699=CARTESIAN_POINT('Ctrl Pts',(89.2322725235198,-2.92007975519077,
125.658385026308));
#146700=CARTESIAN_POINT('Ctrl Pts',(89.2248643038533,-3.05713841605742,
125.736158854375));
#146701=CARTESIAN_POINT('Ctrl Pts',(89.2174560841868,-3.19099808459716,
125.819361203584));
#146702=CARTESIAN_POINT('Ctrl Pts',(89.2100478645204,-3.32121595389669,
125.907682646729));
#146703=CARTESIAN_POINT('Ctrl Pts',(89.2026350852183,-3.45151397012132,
125.996058450248));
#146704=CARTESIAN_POINT('Ctrl Pts',(89.1952223059163,-3.57816542107575,
126.0895594047));
#146705=CARTESIAN_POINT('Ctrl Pts',(89.1878095266143,-3.70076027823738,
126.187835525517));
#146706=CARTESIAN_POINT('Ctrl Pts',(89.1803861555856,-3.82353030468065,
126.286252067864));
#146707=CARTESIAN_POINT('Ctrl Pts',(89.1729627845568,-3.94223187995439,
126.389457159318));
#146708=CARTESIAN_POINT('Ctrl Pts',(89.1655394135281,-4.05649095157504,
126.49706312119));
#146709=CARTESIAN_POINT('Ctrl Pts',(89.1616033640871,-4.11707385295909,
126.554118384145));
#146710=CARTESIAN_POINT('Ctrl Pts',(89.1576673146462,-4.17640845933906,
126.612410311992));
#146711=CARTESIAN_POINT('Ctrl Pts',(89.1537312652053,-4.23444366322195,
126.671877414273));
#146712=CARTESIAN_POINT('Ctrl Pts',(89.1464056947544,-4.34245576547198,
126.782554491329));
#146713=CARTESIAN_POINT('Ctrl Pts',(89.1390801243036,-4.44631023157514,
126.897658490166));
#146714=CARTESIAN_POINT('Ctrl Pts',(89.1317545538528,-4.54561506504811,
127.016839760474));
#146715=CARTESIAN_POINT('Ctrl Pts',(89.1244378391925,-4.64479985014911,
127.135876954034));
#146716=CARTESIAN_POINT('Ctrl Pts',(89.1171211245321,-4.73944570272937,
127.25898131977));
#146717=CARTESIAN_POINT('Ctrl Pts',(89.1098044098719,-4.82919632579842,
127.385765378379));
#146718=CARTESIAN_POINT('Ctrl Pts',(89.1024960821167,-4.91884407073205,
127.512404108664));
#146719=CARTESIAN_POINT('Ctrl Pts',(89.0951877543616,-5.0036075403914,127.642713820679));
#146720=CARTESIAN_POINT('Ctrl Pts',(89.0878794266064,-5.08317004454765,
127.776273290438));
#146721=CARTESIAN_POINT('Ctrl Pts',(89.080575841019,-5.16268092283848,127.909746097224));
#146722=CARTESIAN_POINT('Ctrl Pts',(89.0732722554317,-5.23699735301651,
128.046464138771));
#146723=CARTESIAN_POINT('Ctrl Pts',(89.0659686698443,-5.30584530870804,
128.185976359562));
#146724=CARTESIAN_POINT('Ctrl Pts',(89.0586682910363,-5.37466303538422,
128.325427324838));
#146725=CARTESIAN_POINT('Ctrl Pts',(89.0513679122282,-5.43801689537401,
128.467669684678));
#146726=CARTESIAN_POINT('Ctrl Pts',(89.0440675334202,-5.49567842461156,
128.612227132634));
#146727=CARTESIAN_POINT('Ctrl Pts',(89.0367688286363,-5.55332673168708,
128.756751432632));
#146728=CARTESIAN_POINT('Ctrl Pts',(89.0294701238524,-5.60528516440204,
128.903589407486));
#146729=CARTESIAN_POINT('Ctrl Pts',(89.0221714190685,-5.65137321380395,
129.052244365487));
#146730=CARTESIAN_POINT('Ctrl Pts',(89.0148704812603,-5.69747536375345,
129.200944804179));
#146731=CARTESIAN_POINT('Ctrl Pts',(89.0075695434521,-5.73770342247987,
129.351462971357));
#146732=CARTESIAN_POINT('Ctrl Pts',(89.0002686056439,-5.77192657573628,
129.503286381863));
#146733=CARTESIAN_POINT('Ctrl Pts',(88.9929666749589,-5.80615438310364,
129.655130439298));
#146734=CARTESIAN_POINT('Ctrl Pts',(88.9856647442739,-5.83437558247517,
129.808279716939));
#146735=CARTESIAN_POINT('Ctrl Pts',(88.9783628135889,-5.85651055570804,
129.962211774795));
#146736=CARTESIAN_POINT('Ctrl Pts',(88.9710546158251,-5.87866452687827,
130.116275948988));
#146737=CARTESIAN_POINT('Ctrl Pts',(88.9637464180612,-5.89472179038301,
130.271123863905));
#146738=CARTESIAN_POINT('Ctrl Pts',(88.9564382202974,-5.90465460925057,
130.426227693906));
#146739=CARTESIAN_POINT('Ctrl Pts',(88.9504172109355,-5.91283796680676,
130.554013181203));
#146740=CARTESIAN_POINT('Ctrl Pts',(88.9443962015735,-5.91686523723295,
130.681972202389));
#146741=CARTESIAN_POINT('Ctrl Pts',(88.9383751922115,-5.91674749024185,
130.809810316349));
#146742=CARTESIAN_POINT('',(87.1883751922115,-5.92167067617498,130.802270369068));
#146743=CARTESIAN_POINT('Ctrl Pts',(88.9383751922115,-5.91711345945967,
130.80981065343));
#146744=CARTESIAN_POINT('Ctrl Pts',(88.9173446752718,-5.92125755772848,
131.2563625544));
#146745=CARTESIAN_POINT('Ctrl Pts',(88.8034982837279,-5.67087300393402,
133.669120225896));
#146746=CARTESIAN_POINT('Ctrl Pts',(88.5968360175794,-2.36378464613456,
137.391475515387));
#146747=CARTESIAN_POINT('Ctrl Pts',(88.3183883937666,4.26424298043648,136.353576087713));
#146748=CARTESIAN_POINT('Ctrl Pts',(88.0399407699536,6.97363962783762,130.216218737225));
#146749=CARTESIAN_POINT('Ctrl Pts',(87.7614931461409,3.27460213849075,124.619335042443));
#146750=CARTESIAN_POINT('Ctrl Pts',(87.483045522328,-3.43363474291932,124.706187695898));
#146751=CARTESIAN_POINT('Ctrl Pts',(87.2920062043515,-5.8712296258447,128.610555365562));
#146752=CARTESIAN_POINT('Ctrl Pts',(87.1937827609793,-5.92616330583837,
130.687876557329));
#146753=CARTESIAN_POINT('Ctrl Pts',(87.1883751922115,-5.92564232318124,
130.802268967144));
#146754=CARTESIAN_POINT('',(85.4383751922433,-5.91674833501214,130.799921852979));
#146755=CARTESIAN_POINT('Ctrl Pts',(87.1883751922115,-5.9167496313956,130.802272106112));
#146756=CARTESIAN_POINT('Ctrl Pts',(87.181017727412,-5.9168044873817,130.957679027627));
#146757=CARTESIAN_POINT('Ctrl Pts',(87.1736602626125,-5.91073235004027,
131.113335685801));
#146758=CARTESIAN_POINT('Ctrl Pts',(87.166302797813,-5.89850038482534,131.268713686594));
#146759=CARTESIAN_POINT('Ctrl Pts',(87.158953758399,-5.88628242701996,131.423913756591));
#146760=CARTESIAN_POINT('Ctrl Pts',(87.151604718985,-5.86791870763707,131.578835428669));
#146761=CARTESIAN_POINT('Ctrl Pts',(87.144255679571,-5.84342836198335,131.732948546019));
#146762=CARTESIAN_POINT('Ctrl Pts',(87.1369133832024,-5.81896048722727,
131.886920258257));
#146763=CARTESIAN_POINT('Ctrl Pts',(87.1295710868338,-5.78837723357423,
132.04008451902));
#146764=CARTESIAN_POINT('Ctrl Pts',(87.1222287904652,-5.75174965655959,
132.191914742913));
#146765=CARTESIAN_POINT('Ctrl Pts',(87.1148915608766,-5.71514735554355,
132.343640191638));
#146766=CARTESIAN_POINT('Ctrl Pts',(87.1075543312879,-5.67250912311375,
132.494033067684));
#146767=CARTESIAN_POINT('Ctrl Pts',(87.1002171016993,-5.62395732798598,
132.642575658167));
#146768=CARTESIAN_POINT('Ctrl Pts',(87.0928825618798,-5.57542333155484,
132.791063794134));
#146769=CARTESIAN_POINT('Ctrl Pts',(87.0855480220604,-5.52098020160226,
132.937702632535));
#146770=CARTESIAN_POINT('Ctrl Pts',(87.0782134822409,-5.4608005143236,133.081988397793));
#146771=CARTESIAN_POINT('Ctrl Pts',(87.0708802169912,-5.40063128485238,
133.226249089595));
#146772=CARTESIAN_POINT('Ctrl Pts',(87.0635469517414,-5.33472762736758,
133.368157170652));
#146773=CARTESIAN_POINT('Ctrl Pts',(87.0562136864917,-5.2633106383249,133.507227925999));
#146774=CARTESIAN_POINT('Ctrl Pts',(87.0488801855783,-5.19189135420766,
133.646303150559));
#146775=CARTESIAN_POINT('Ctrl Pts',(87.0415466846648,-5.1149585595205,133.782540529362));
#146776=CARTESIAN_POINT('Ctrl Pts',(87.0342131837514,-5.03277965687032,
133.915479305095));
#146777=CARTESIAN_POINT('Ctrl Pts',(87.0268779370043,-4.95058119048251,
134.048449728602));
#146778=CARTESIAN_POINT('Ctrl Pts',(87.0195426902574,-4.86313433070873,
134.178119662737));
#146779=CARTESIAN_POINT('Ctrl Pts',(87.0122074435103,-4.77075006606631,
134.30405694291));
#146780=CARTESIAN_POINT('Ctrl Pts',(87.0048646043054,-4.67827017769559,
134.430124576367));
#146781=CARTESIAN_POINT('Ctrl Pts',(86.9975217651005,-4.58084290189408,
134.55245153159));
#146782=CARTESIAN_POINT('Ctrl Pts',(86.9901789258955,-4.47882025222901,
134.6706378594));
#146783=CARTESIAN_POINT('Ctrl Pts',(86.9828321944078,-4.37674352252813,
134.788886835267));
#146784=CARTESIAN_POINT('Ctrl Pts',(86.97548546292,-4.27006682580401,134.902990533726));
#146785=CARTESIAN_POINT('Ctrl Pts',(86.9681387314323,-4.15917887539443,
135.012586092154));
#146786=CARTESIAN_POINT('Ctrl Pts',(86.9607807868572,-4.04812168016111,
135.122348922868));
#146787=CARTESIAN_POINT('Ctrl Pts',(86.953422842282,-3.93284067045875,135.22758961038));
#146788=CARTESIAN_POINT('Ctrl Pts',(86.9460648977068,-3.81375820132093,
135.327985153749));
#146789=CARTESIAN_POINT('Ctrl Pts',(86.9394266900386,-3.70632410043697,
135.41856024018));
#146790=CARTESIAN_POINT('Ctrl Pts',(86.9327884823704,-3.59579644350382,
135.505192137477));
#146791=CARTESIAN_POINT('Ctrl Pts',(86.9261502747022,-3.48250434805229,
135.587674743598));
#146792=CARTESIAN_POINT('Ctrl Pts',(86.9187270082967,-3.35581391470071,
135.679912044636));
#146793=CARTESIAN_POINT('Ctrl Pts',(86.9113037418913,-3.22526489625941,
135.767252075241));
#146794=CARTESIAN_POINT('Ctrl Pts',(86.9038804754859,-3.09127273754494,
135.849354514947));
#146795=CARTESIAN_POINT('Ctrl Pts',(86.8964659827649,-2.95743894643452,
135.931359916388));
#146796=CARTESIAN_POINT('Ctrl Pts',(86.8890514900438,-2.82017043061389,
136.008139855822));
#146797=CARTESIAN_POINT('Ctrl Pts',(86.8816369973228,-2.67991444553776,
136.07939513187));
#146798=CARTESIAN_POINT('Ctrl Pts',(86.874229650969,-2.53979364446059,136.1505817294));
#146799=CARTESIAN_POINT('Ctrl Pts',(86.8668223046153,-2.39669143709357,
136.216254096383));
#146800=CARTESIAN_POINT('Ctrl Pts',(86.8594149582615,-2.25108261593864,
136.276157179822));
#146801=CARTESIAN_POINT('Ctrl Pts',(86.8520131365861,-2.10558239533646,
136.336015585281));
#146802=CARTESIAN_POINT('Ctrl Pts',(86.8446113149108,-1.9575796271664,136.390113133535));
#146803=CARTESIAN_POINT('Ctrl Pts',(86.8372094932354,-1.80757207850582,
136.438241495212));
#146804=CARTESIAN_POINT('Ctrl Pts',(86.829811578924,-1.65764371766262,136.486344450301));
#146805=CARTESIAN_POINT('Ctrl Pts',(86.8224136646127,-1.50571303855146,
136.528484380601));
#146806=CARTESIAN_POINT('Ctrl Pts',(86.8150157503013,-1.35229597999468,
136.564501774256));
#146807=CARTESIAN_POINT('Ctrl Pts',(86.8076190653891,-1.19890441656933,
136.600513182473));
#146808=CARTESIAN_POINT('Ctrl Pts',(86.8002223804769,-1.04402732700005,
136.630403988158));
#146809=CARTESIAN_POINT('Ctrl Pts',(86.7928256955647,-0.888194058801287,
136.65406504398));
#146810=CARTESIAN_POINT('Ctrl Pts',(86.7854293386293,-0.732367700412934,
136.677725050647));
#146811=CARTESIAN_POINT('Ctrl Pts',(86.7780329816938,-0.575585616764118,
136.695155800659));
#146812=CARTESIAN_POINT('Ctrl Pts',(86.7706366247584,-0.418385287396174,
136.706299647562));
#146813=CARTESIAN_POINT('Ctrl Pts',(86.7632391354218,-0.261160890256827,
136.717445200616));
#146814=CARTESIAN_POINT('Ctrl Pts',(86.7558416460852,-0.103518492284539,
136.722301907616));
#146815=CARTESIAN_POINT('Ctrl Pts',(86.7484441567487,0.054001541880814,
136.720864179297));
#146816=CARTESIAN_POINT('Ctrl Pts',(86.7410440742336,0.211576794450855,
136.719425946984));
#146817=CARTESIAN_POINT('Ctrl Pts',(86.7336439917187,0.369029224761944,
136.711688889623));
#146818=CARTESIAN_POINT('Ctrl Pts',(86.7262439092036,0.525820859046008,
136.697699483327));
#146819=CARTESIAN_POINT('Ctrl Pts',(86.7188356895372,0.682784901850091,
136.683694694241));
#146820=CARTESIAN_POINT('Ctrl Pts',(86.7114274698707,0.839086325483952,
136.66342385939));
#146821=CARTESIAN_POINT('Ctrl Pts',(86.7040192502042,0.99419391973684,136.636985156524));
#146822=CARTESIAN_POINT('Ctrl Pts',(86.6966064709022,1.14939698012588,136.610530181078));
#146823=CARTESIAN_POINT('Ctrl Pts',(86.6891936916001,1.30340438264431,136.57789985037));
#146824=CARTESIAN_POINT('Ctrl Pts',(86.681780912298,1.45569794809776,136.539242834875));
#146825=CARTESIAN_POINT('Ctrl Pts',(86.6743575412692,1.60820911773939,136.500530584423));
#146826=CARTESIAN_POINT('Ctrl Pts',(86.6669341702405,1.75900120257212,136.455774556602));
#146827=CARTESIAN_POINT('Ctrl Pts',(86.6595107992117,1.90757315094241,136.405172633364));
#146828=CARTESIAN_POINT('Ctrl Pts',(86.6555747497709,1.98634956290362,136.378342279486));
#146829=CARTESIAN_POINT('Ctrl Pts',(86.6516387003301,2.06450216909274,136.34986923062));
#146830=CARTESIAN_POINT('Ctrl Pts',(86.6477026508893,2.14195897970616,136.319788279294));
#146831=CARTESIAN_POINT('Ctrl Pts',(86.6402793844839,2.28804010717831,136.263056543888));
#146832=CARTESIAN_POINT('Ctrl Pts',(86.6328561180785,2.43208668182863,136.200431377274));
#146833=CARTESIAN_POINT('Ctrl Pts',(86.625432851673,2.57358782434125,136.132078353417));
#146834=CARTESIAN_POINT('Ctrl Pts',(86.618018358952,2.71492172425416,136.063806117158));
#146835=CARTESIAN_POINT('Ctrl Pts',(86.610603866231,2.85371584759169,135.989819659871));
#146836=CARTESIAN_POINT('Ctrl Pts',(86.60318937351,2.9894767152613,135.910333544581));
#146837=CARTESIAN_POINT('Ctrl Pts',(86.5957820271562,3.12510673149553,135.830924041002));
#146838=CARTESIAN_POINT('Ctrl Pts',(86.5883746808025,3.25770899232424,135.74602561957));
#146839=CARTESIAN_POINT('Ctrl Pts',(86.5809673344487,3.38681227749217,135.655899874289));
#146840=CARTESIAN_POINT('Ctrl Pts',(86.5735655127733,3.51581927255932,135.56584134819));
#146841=CARTESIAN_POINT('Ctrl Pts',(86.5661636910979,3.64133218339242,135.470563473909));
#146842=CARTESIAN_POINT('Ctrl Pts',(86.5587618694225,3.76290668132671,135.370372429873));
#146843=CARTESIAN_POINT('Ctrl Pts',(86.5513639551112,3.88441700102952,135.27023427591));
#146844=CARTESIAN_POINT('Ctrl Pts',(86.5439660407998,4.00199276102789,135.165188354324));
#146845=CARTESIAN_POINT('Ctrl Pts',(86.5365681264885,4.11522088194545,135.055582519008));
#146846=CARTESIAN_POINT('Ctrl Pts',(86.5291714415763,4.22843018640389,134.945994898192));
#146847=CARTESIAN_POINT('Ctrl Pts',(86.5217747566641,4.3372930177734,134.831849126987));
#146848=CARTESIAN_POINT('Ctrl Pts',(86.5143780717518,4.44143142205343,134.713531563649));
#146849=CARTESIAN_POINT('Ctrl Pts',(86.5069817148164,4.54556520872726,134.595219246636));
#146850=CARTESIAN_POINT('Ctrl Pts',(86.4995853578809,4.64497473820458,134.472735785514));
#146851=CARTESIAN_POINT('Ctrl Pts',(86.4921890009455,4.73932099006906,134.346502217727));
#146852=CARTESIAN_POINT('Ctrl Pts',(86.4847915116089,4.83368168658562,134.220249323258));
#146853=CARTESIAN_POINT('Ctrl Pts',(86.4773940222723,4.92297733846744,134.090245477944));
#146854=CARTESIAN_POINT('Ctrl Pts',(86.4699965329358,5.00691116302107,133.956942284726));
#146855=CARTESIAN_POINT('Ctrl Pts',(86.4625964504208,5.0908744104469,133.82359236228));
#146856=CARTESIAN_POINT('Ctrl Pts',(86.4551963679058,5.16947188953632,133.686941104884));
#146857=CARTESIAN_POINT('Ctrl Pts',(86.4477962853908,5.24245191399824,133.547466246578));
#146858=CARTESIAN_POINT('Ctrl Pts',(86.4403880657243,5.31551218749959,133.407838021327));
#146859=CARTESIAN_POINT('Ctrl Pts',(86.4329798460578,5.38294249738766,133.265380325557));
#146860=CARTESIAN_POINT('Ctrl Pts',(86.4255716263913,5.44453831129131,133.120593148937));
#146861=CARTESIAN_POINT('Ctrl Pts',(86.4181588470893,5.50617203639054,132.975716858225));
#146862=CARTESIAN_POINT('Ctrl Pts',(86.4107460677872,5.56196397792784,132.828508577983));
#146863=CARTESIAN_POINT('Ctrl Pts',(86.4033332884852,5.61175912807262,132.679484627063));
#146864=CARTESIAN_POINT('Ctrl Pts',(86.3959099174564,5.66162542786313,132.530247743734));
#146865=CARTESIAN_POINT('Ctrl Pts',(86.3884865464276,5.7054777192543,132.379190365847));
#146866=CARTESIAN_POINT('Ctrl Pts',(86.3810631753989,5.74321165527887,132.226841002376));
#146867=CARTESIAN_POINT('Ctrl Pts',(86.3771271259581,5.76321909357249,132.146061714291));
#146868=CARTESIAN_POINT('Ctrl Pts',(86.3731910765173,5.78150730379123,132.064919334902));
#146869=CARTESIAN_POINT('Ctrl Pts',(86.3692550270765,5.7980666456284,131.983493237483));
#146870=CARTESIAN_POINT('Ctrl Pts',(86.3618317606711,5.82929704753391,131.829926158971));
#146871=CARTESIAN_POINT('Ctrl Pts',(86.3544084942657,5.85446941335588,131.674885263847));
#146872=CARTESIAN_POINT('Ctrl Pts',(86.3469852278602,5.87344690241255,131.518889866121));
#146873=CARTESIAN_POINT('Ctrl Pts',(86.3395707351392,5.89240196165317,131.363078842));
#146874=CARTESIAN_POINT('Ctrl Pts',(86.3321562424181,5.90517667363057,131.206315927798));
#146875=CARTESIAN_POINT('Ctrl Pts',(86.3247417496971,5.91168481879268,131.049132278009));
#146876=CARTESIAN_POINT('Ctrl Pts',(86.3173344033434,5.91818669115943,130.892100127741));
#146877=CARTESIAN_POINT('Ctrl Pts',(86.3099270569896,5.9184340057289,130.734648419672));
#146878=CARTESIAN_POINT('Ctrl Pts',(86.3025197106359,5.91239214288674,130.577315002697));
#146879=CARTESIAN_POINT('Ctrl Pts',(86.2951178889605,5.90635478629382,130.420098930921));
#146880=CARTESIAN_POINT('Ctrl Pts',(86.287716067285,5.8940376063805,130.263001345986));
#146881=CARTESIAN_POINT('Ctrl Pts',(86.2803142456096,5.87545802923088,130.106561571102));
#146882=CARTESIAN_POINT('Ctrl Pts',(86.2729163312983,5.85688826009538,129.950204379556));
#146883=CARTESIAN_POINT('Ctrl Pts',(86.2655184169869,5.83206272143745,129.794504676245));
#146884=CARTESIAN_POINT('Ctrl Pts',(86.2581205026755,5.80105079309351,129.639998020069));
#146885=CARTESIAN_POINT('Ctrl Pts',(86.2507238177633,5.77004401836949,129.485517040097));
#146886=CARTESIAN_POINT('Ctrl Pts',(86.2433271328511,5.73285296775542,129.332229079408));
#146887=CARTESIAN_POINT('Ctrl Pts',(86.2359304479389,5.68959840202705,129.180660957484));
#146888=CARTESIAN_POINT('Ctrl Pts',(86.2285340910034,5.64634575425143,129.029099556248));
#146889=CARTESIAN_POINT('Ctrl Pts',(86.221137734068,5.5970302283931,128.879258201114));
#146890=CARTESIAN_POINT('Ctrl Pts',(86.2137413771325,5.54182280636129,128.73164970058));
#146891=CARTESIAN_POINT('Ctrl Pts',(86.2063438877959,5.48660693193224,128.584018600808));
#146892=CARTESIAN_POINT('Ctrl Pts',(86.1989463984593,5.42549749597888,128.438621385983));
#146893=CARTESIAN_POINT('Ctrl Pts',(86.1915489091227,5.35871402655086,128.29595185021));
#146894=CARTESIAN_POINT('Ctrl Pts',(86.1841488266077,5.29190714628125,128.153232301854));
#146895=CARTESIAN_POINT('Ctrl Pts',(86.1767487440927,5.2194224305666,128.013242674184));
#146896=CARTESIAN_POINT('Ctrl Pts',(86.1693486615777,5.14152576799876,127.876452944926));
#146897=CARTESIAN_POINT('Ctrl Pts',(86.1619404419113,5.06354345004241,127.739512801298));
#146898=CARTESIAN_POINT('Ctrl Pts',(86.1545322222448,4.98013748555134,127.605779907578));
#146899=CARTESIAN_POINT('Ctrl Pts',(86.1471240025784,4.89161797525111,127.47569659927));
#146900=CARTESIAN_POINT('Ctrl Pts',(86.1397112232763,4.80304398266932,127.345533226856));
#146901=CARTESIAN_POINT('Ctrl Pts',(86.1322984439742,4.7093503945407,127.219024215098));
#146902=CARTESIAN_POINT('Ctrl Pts',(86.1248856646721,4.61088781902221,127.096579059425));
#146903=CARTESIAN_POINT('Ctrl Pts',(86.1174622936434,4.51228455555823,126.973958948371));
#146904=CARTESIAN_POINT('Ctrl Pts',(86.1100389226146,4.40889894002283,126.855414571132));
#146905=CARTESIAN_POINT('Ctrl Pts',(86.1026155515859,4.30111921990029,126.741319389778));
#146906=CARTESIAN_POINT('Ctrl Pts',(86.0986795021451,4.24397182615247,126.680823386948));
#146907=CARTESIAN_POINT('Ctrl Pts',(86.0947434527043,4.18558966863885,126.621577559669));
#146908=CARTESIAN_POINT('Ctrl Pts',(86.0908074032635,4.12603431552053,126.563632921799));
#146909=CARTESIAN_POINT('Ctrl Pts',(86.0833841368581,4.01371477819838,126.454351143165));
#146910=CARTESIAN_POINT('Ctrl Pts',(86.0759608704526,3.89688076074025,126.349369527982));
#146911=CARTESIAN_POINT('Ctrl Pts',(86.0685376040472,3.77589521099997,126.249083906097));
#146912=CARTESIAN_POINT('Ctrl Pts',(86.0611231113261,3.65505265613192,126.14891681349));
#146913=CARTESIAN_POINT('Ctrl Pts',(86.0537086186051,3.53006862052098,126.053434902231));
#146914=CARTESIAN_POINT('Ctrl Pts',(86.0462941258841,3.40134337571183,125.962997813251));
#146915=CARTESIAN_POINT('Ctrl Pts',(86.0388867795303,3.27274220114004,125.872647890943));
#146916=CARTESIAN_POINT('Ctrl Pts',(86.0314794331765,3.14040729944275,125.787333324008));
#146917=CARTESIAN_POINT('Ctrl Pts',(86.0240720868227,3.00477246538082,125.707373959374));
#146918=CARTESIAN_POINT('Ctrl Pts',(86.0166702651474,2.86923879289573,125.627474231451));
#146919=CARTESIAN_POINT('Ctrl Pts',(86.009268443472,2.73041040884894,125.552921941774));
#146920=CARTESIAN_POINT('Ctrl Pts',(86.0018666217966,2.5887504803534,125.483993946652));
#146921=CARTESIAN_POINT('Ctrl Pts',(85.9944687074853,2.44716533303143,125.415102338082));
#146922=CARTESIAN_POINT('Ctrl Pts',(85.9870707931739,2.30275195294887,125.351829274035));
#146923=CARTESIAN_POINT('Ctrl Pts',(85.9796728788626,2.15599842247466,125.294405865956));
#146924=CARTESIAN_POINT('Ctrl Pts',(85.9722761939504,2.00926927977482,125.236992000607));
#146925=CARTESIAN_POINT('Ctrl Pts',(85.9648795090382,1.86020110580809,125.185425997775));
#146926=CARTESIAN_POINT('Ctrl Pts',(85.957482824126,1.70930240287311,125.139891016797));
#146927=CARTESIAN_POINT('Ctrl Pts',(85.9500864671905,1.55841039094474,125.094358054889));
#146928=CARTESIAN_POINT('Ctrl Pts',(85.9426901102551,1.40568836881746,125.054855690953));
#146929=CARTESIAN_POINT('Ctrl Pts',(85.9352937533197,1.25166019670436,125.021517258587));
#146930=CARTESIAN_POINT('Ctrl Pts',(85.9278962639831,1.09760844248501,124.988173722022));
#146931=CARTESIAN_POINT('Ctrl Pts',(85.9204987746466,0.942250504976168,
124.960996075062));
#146932=CARTESIAN_POINT('Ctrl Pts',(85.91310128531,0.786120487417467,124.940066530315));
#146933=CARTESIAN_POINT('Ctrl Pts',(85.905701202795,0.629935738723143,124.91912964875));
#146934=CARTESIAN_POINT('Ctrl Pts',(85.8983011202801,0.472978740871434,
124.904445279762));
#146935=CARTESIAN_POINT('Ctrl Pts',(85.8909010377651,0.315788618710606,
124.896043758189));
#146936=CARTESIAN_POINT('Ctrl Pts',(85.8834928180986,0.158425649850476,
124.88763299828));
#146937=CARTESIAN_POINT('Ctrl Pts',(85.8760845984321,0.000829417739716704,
124.885518902723));
#146938=CARTESIAN_POINT('Ctrl Pts',(85.8686763787657,-0.156460311216934,
124.889679668139));
#146939=CARTESIAN_POINT('Ctrl Pts',(85.8612635994636,-0.313846849377126,
124.893842994437));
#146940=CARTESIAN_POINT('Ctrl Pts',(85.8538508201616,-0.470926136867647,
124.90428885266));
#146941=CARTESIAN_POINT('Ctrl Pts',(85.8464380408595,-0.627164141312106,
124.920943608518));
#146942=CARTESIAN_POINT('Ctrl Pts',(85.8390146698307,-0.78362538594404,
124.937622161473));
#146943=CARTESIAN_POINT('Ctrl Pts',(85.831591298802,-0.939242578396752,
124.96052727635));
#146944=CARTESIAN_POINT('Ctrl Pts',(85.8241679277732,-1.09349165720549,
124.989534174918));
#146945=CARTESIAN_POINT('Ctrl Pts',(85.8202318783324,-1.17527821994747,
125.004914328549));
#146946=CARTESIAN_POINT('Ctrl Pts',(85.8162958288915,-1.25668039456697,
125.022009074331));
#146947=CARTESIAN_POINT('Ctrl Pts',(85.8123597794507,-1.33762198256737,
125.040794187459));
#146948=CARTESIAN_POINT('Ctrl Pts',(85.8049365130452,-1.4902752914328,125.076222324556));
#146949=CARTESIAN_POINT('Ctrl Pts',(85.7975132466398,-1.64175093778632,
125.11777296503));
#146950=CARTESIAN_POINT('Ctrl Pts',(85.7900899802343,-1.79151971658515,
125.165354706274));
#146951=CARTESIAN_POINT('Ctrl Pts',(85.7826754875133,-1.94111148112497,
125.212880209852));
#146952=CARTESIAN_POINT('Ctrl Pts',(85.7752609947923,-2.08900004140721,
125.266422513432));
#146953=CARTESIAN_POINT('Ctrl Pts',(85.7678465020713,-2.23466646478566,
125.325839251936));
#146954=CARTESIAN_POINT('Ctrl Pts',(85.7604391557175,-2.38019248938183,
125.385198722351));
#146955=CARTESIAN_POINT('Ctrl Pts',(85.7530318093637,-2.52350029760603,
125.450421215716));
#146956=CARTESIAN_POINT('Ctrl Pts',(85.7456244630099,-2.66408631651537,
125.52131465329));
#146957=CARTESIAN_POINT('Ctrl Pts',(85.7382226413345,-2.8045674810671,125.592155215863));
#146958=CARTESIAN_POINT('Ctrl Pts',(85.7308208196591,-2.94233056645227,
125.668658133575));
#146959=CARTESIAN_POINT('Ctrl Pts',(85.7234189979836,-3.07689229247884,
125.750583378413));
#146960=CARTESIAN_POINT('Ctrl Pts',(85.7160210836722,-3.21138298441854,
125.832465375552));
#146961=CARTESIAN_POINT('Ctrl Pts',(85.7086231693608,-3.34267536461682,
125.919763805567));
#146962=CARTESIAN_POINT('Ctrl Pts',(85.7012252550494,-3.47031117202516,
126.012192952321));
#146963=CARTESIAN_POINT('Ctrl Pts',(85.6938285701372,-3.59792576867703,
126.104606739027));
#146964=CARTESIAN_POINT('Ctrl Pts',(85.686431885225,-3.72188469650641,126.202149331515));
#146965=CARTESIAN_POINT('Ctrl Pts',(85.6790352003128,-3.84175900046248,
126.304491914496));
#146966=CARTESIAN_POINT('Ctrl Pts',(85.6716388433773,-3.96162798906637,
126.4068299595));
#146967=CARTESIAN_POINT('Ctrl Pts',(85.6642424864419,-4.07741243001356,
126.513967329422));
#146968=CARTESIAN_POINT('Ctrl Pts',(85.6568461295064,-4.18871698673091,
126.625535355896));
#146969=CARTESIAN_POINT('Ctrl Pts',(85.6494486401698,-4.30003858445971,
126.737120463719));
#146970=CARTESIAN_POINT('Ctrl Pts',(85.6420511508333,-4.40687866861079,
126.853137314478));
#146971=CARTESIAN_POINT('Ctrl Pts',(85.6346536614967,-4.50887937553932,
126.973180989914));
#146972=CARTESIAN_POINT('Ctrl Pts',(85.6272535789817,-4.61091583865813,
127.093266746475));
#146973=CARTESIAN_POINT('Ctrl Pts',(85.6198534964666,-4.70810930539743,
127.217381853899));
#146974=CARTESIAN_POINT('Ctrl Pts',(85.6124534139516,-4.80014284405043,
127.345089127901));
#146975=CARTESIAN_POINT('Ctrl Pts',(85.6050451942851,-4.89227758304025,
127.472936829179));
#146976=CARTESIAN_POINT('Ctrl Pts',(85.5976369746186,-4.97924084446482,
127.604384282323));
#146977=CARTESIAN_POINT('Ctrl Pts',(85.5902287549521,-5.06075921519709,
127.738965581311));
#146978=CARTESIAN_POINT('Ctrl Pts',(85.58281597565,-5.14232775912674,127.873629712844));
#146979=CARTESIAN_POINT('Ctrl Pts',(85.5754031963479,-5.21844455452554,
128.011431207651));
#146980=CARTESIAN_POINT('Ctrl Pts',(85.5679904170458,-5.28888289446262,
128.151880968038));
#146981=CARTESIAN_POINT('Ctrl Pts',(85.560567046017,-5.35942188000269,128.292531409628));
#146982=CARTESIAN_POINT('Ctrl Pts',(85.5531436749882,-5.4242660518313,128.435837335027));
#146983=CARTESIAN_POINT('Ctrl Pts',(85.5457203039595,-5.48323712138758,
128.581290390799));
#146984=CARTESIAN_POINT('Ctrl Pts',(85.5417842545189,-5.51450499745621,
128.658413091064));
#146985=CARTESIAN_POINT('Ctrl Pts',(85.5378482050782,-5.54412256742039,
128.736139173653));
#146986=CARTESIAN_POINT('Ctrl Pts',(85.5339121556376,-5.57206902514388,
128.814391436515));
#146987=CARTESIAN_POINT('Ctrl Pts',(85.5252696428826,-5.6334319782717,128.986212494686));
#146988=CARTESIAN_POINT('Ctrl Pts',(85.5166271301276,-5.68688789089793,
129.160997686617));
#146989=CARTESIAN_POINT('Ctrl Pts',(85.5079846173726,-5.73218221780913,
129.338066791509));
#146990=CARTESIAN_POINT('Ctrl Pts',(85.4993767151302,-5.77729515535862,
129.514426790998));
#146991=CARTESIAN_POINT('Ctrl Pts',(85.4907688128877,-5.81431165938518,
129.693052344244));
#146992=CARTESIAN_POINT('Ctrl Pts',(85.4821609106453,-5.84302684476834,
129.873249531918));
#146993=CARTESIAN_POINT('Ctrl Pts',(85.4736201635406,-5.87151800666975,
130.052040898914));
#146994=CARTESIAN_POINT('Ctrl Pts',(85.465079416436,-5.89183680036727,130.232379354862));
#146995=CARTESIAN_POINT('Ctrl Pts',(85.4565386693314,-5.90383020450548,
130.413567220912));
#146996=CARTESIAN_POINT('Ctrl Pts',(85.4504841769687,-5.9123322679512,130.542010381418));
#146997=CARTESIAN_POINT('Ctrl Pts',(85.444429684606,-5.91665152736383,130.670879980918));
#146998=CARTESIAN_POINT('Ctrl Pts',(85.4383751922433,-5.91674833501214,
130.799921852979));
#146999=CARTESIAN_POINT('',(83.6883739829004,-5.91264948157148,130.808194539386));
#147000=CARTESIAN_POINT('Ctrl Pts',(85.4383751922114,-5.91674833501265,
130.799921853659));
#147001=CARTESIAN_POINT('Ctrl Pts',(85.4307539146953,-5.91687019458339,
130.962357258523));
#147002=CARTESIAN_POINT('Ctrl Pts',(85.4231326371792,-5.91029809451247,
131.124860175597));
#147003=CARTESIAN_POINT('Ctrl Pts',(85.4155113596631,-5.8970454115672,131.286839608211));
#147004=CARTESIAN_POINT('Ctrl Pts',(85.4081075734955,-5.88417092556854,
131.444196571015));
#147005=CARTESIAN_POINT('Ctrl Pts',(85.400703787328,-5.86499199036885,131.601059130023));
#147006=CARTESIAN_POINT('Ctrl Pts',(85.3933000011605,-5.83957365415491,
131.756888884968));
#147007=CARTESIAN_POINT('Ctrl Pts',(85.3858955184429,-5.81415292657773,
131.912733300414));
#147008=CARTESIAN_POINT('Ctrl Pts',(85.3784910357254,-5.78249168839217,
132.067544351286));
#147009=CARTESIAN_POINT('Ctrl Pts',(85.3710865530078,-5.74470638305384,
132.220792449671));
#147010=CARTESIAN_POINT('Ctrl Pts',(85.3636799272186,-5.70691014155405,
132.374084902494));
#147011=CARTESIAN_POINT('Ctrl Pts',(85.3562733014294,-5.66298639222918,
132.525813141182));
#147012=CARTESIAN_POINT('Ctrl Pts',(85.3488666756402,-5.61310181538212,
132.675461516143));
#147013=CARTESIAN_POINT('Ctrl Pts',(85.3410831636556,-5.56067886155875,
132.832724749514));
#147014=CARTESIAN_POINT('Ctrl Pts',(85.3332996516709,-5.50167272599804,
132.987690471323));
#147015=CARTESIAN_POINT('Ctrl Pts',(85.3255161396863,-5.43633420588795,
133.139783697951));
#147016=CARTESIAN_POINT('Ctrl Pts',(85.3180966545036,-5.37405150075683,
133.284763681742));
#147017=CARTESIAN_POINT('Ctrl Pts',(85.3106771693208,-5.30601546554471,
133.427133436658));
#147018=CARTESIAN_POINT('Ctrl Pts',(85.303257684138,-5.23249040253982,133.566420491977));
#147019=CARTESIAN_POINT('Ctrl Pts',(85.2958327199148,-5.15891104374737,
133.705810406103));
#147020=CARTESIAN_POINT('Ctrl Pts',(85.2884077556916,-5.07983476653098,
133.84211276473));
#147021=CARTESIAN_POINT('Ctrl Pts',(85.2809827914684,-4.99556937636149,
133.974883787085));
#147022=CARTESIAN_POINT('Ctrl Pts',(85.2735474374655,-4.91118607332156,
134.107840596421));
#147023=CARTESIAN_POINT('Ctrl Pts',(85.2661120834625,-4.82159937344177,
134.237255901933));
#147024=CARTESIAN_POINT('Ctrl Pts',(85.2586767294596,-4.7271578877185,134.36271822566));
#147025=CARTESIAN_POINT('Ctrl Pts',(85.2576059969147,-4.71355778578472,
134.380785501693));
#147026=CARTESIAN_POINT('Ctrl Pts',(85.2565352643698,-4.69985707014519,
134.398770864142));
#147027=CARTESIAN_POINT('Ctrl Pts',(85.2554645318249,-4.68605684431754,
134.416673147556));
#147028=CARTESIAN_POINT('Ctrl Pts',(85.2480412654194,-4.59038145529484,
134.540787633177));
#147029=CARTESIAN_POINT('Ctrl Pts',(85.240617999014,-4.48962706034283,134.661286093997));
#147030=CARTESIAN_POINT('Ctrl Pts',(85.2331947326086,-4.38409676459561,
134.777725202041));
#147031=CARTESIAN_POINT('Ctrl Pts',(85.2257802398875,-4.27869119689414,
134.89402668873));
#147032=CARTESIAN_POINT('Ctrl Pts',(85.2183657471666,-4.16852121247841,
135.006278098828));
#147033=CARTESIAN_POINT('Ctrl Pts',(85.2109512544455,-4.0539319978261,135.114066630684));
#147034=CARTESIAN_POINT('Ctrl Pts',(85.2035439080918,-3.93945322857323,
135.221751271894));
#147035=CARTESIAN_POINT('Ctrl Pts',(85.196136561738,-3.82056397883278,135.324981344231));
#147036=CARTESIAN_POINT('Ctrl Pts',(85.1887292153843,-3.6976482659861,135.423378680266));
#147037=CARTESIAN_POINT('Ctrl Pts',(85.1813273937089,-3.57482422831567,
135.521702627856));
#147038=CARTESIAN_POINT('Ctrl Pts',(85.1739255720335,-3.4479799972602,135.615200783779));
#147039=CARTESIAN_POINT('Ctrl Pts',(85.1665237503581,-3.31753476585832,
135.703533368125));
#147040=CARTESIAN_POINT('Ctrl Pts',(85.1591258360468,-3.18715839547835,
135.791819322388));
#147041=CARTESIAN_POINT('Ctrl Pts',(85.1517279217354,-3.05318511887992,
135.874944926978));
#147042=CARTESIAN_POINT('Ctrl Pts',(85.1443300074241,-2.916065283605,135.952612148353));
#147043=CARTESIAN_POINT('Ctrl Pts',(85.1369333225119,-2.77896823515908,
136.030266462846));
#147044=CARTESIAN_POINT('Ctrl Pts',(85.1295366375997,-2.63872599033432,
136.102464010618));
#147045=CARTESIAN_POINT('Ctrl Pts',(85.1221399526875,-2.49581591455787,
136.168951327316));
#147046=CARTESIAN_POINT('Ctrl Pts',(85.114743595752,-2.35291217556375,136.235435695897));
#147047=CARTESIAN_POINT('Ctrl Pts',(85.1073472388166,-2.20734117928812,
136.29621017938));
#147048=CARTESIAN_POINT('Ctrl Pts',(85.0999508818811,-2.05960256412904,
136.351068455584));
#147049=CARTESIAN_POINT('Ctrl Pts',(85.0925533925445,-1.91184132981071,
136.405935130731));
#147050=CARTESIAN_POINT('Ctrl Pts',(85.085155903208,-1.76191216578942,136.454883665105));
#147051=CARTESIAN_POINT('Ctrl Pts',(85.0777584138714,-1.61033210410749,
136.497756886664));
#147052=CARTESIAN_POINT('Ctrl Pts',(85.0703583313564,-1.45869890627057,
136.540645137364));
#147053=CARTESIAN_POINT('Ctrl Pts',(85.0629582488414,-1.30541401752857,
136.577453733514));
#147054=CARTESIAN_POINT('Ctrl Pts',(85.0555581663265,-1.1510068023798,136.608076143277));
#147055=CARTESIAN_POINT('Ctrl Pts',(85.04814994666,-0.996429800624187,136.638732225527));
#147056=CARTESIAN_POINT('Ctrl Pts',(85.0407417269935,-0.840728374247625,
136.663188463991));
#147057=CARTESIAN_POINT('Ctrl Pts',(85.0333335073271,-0.68443992143418,
136.68138984639));
#147058=CARTESIAN_POINT('Ctrl Pts',(85.025920728025,-0.52805527568584,136.699602431436));
#147059=CARTESIAN_POINT('Ctrl Pts',(85.0185079487229,-0.371083254912988,
136.711552461018));
#147060=CARTESIAN_POINT('Ctrl Pts',(85.0110951694209,-0.214062936311232,
136.717237042945));
#147061=CARTESIAN_POINT('Ctrl Pts',(85.0036717983921,-0.0568182597147348,
136.722929747268));
#147062=CARTESIAN_POINT('Ctrl Pts',(84.9962484273634,0.100474480233154,
136.722339125452));
#147063=CARTESIAN_POINT('Ctrl Pts',(84.9888250563346,0.257278818816543,
136.715514326605));
#147064=CARTESIAN_POINT('Ctrl Pts',(84.9848890068938,0.340420241603923,
136.711895654498));
#147065=CARTESIAN_POINT('Ctrl Pts',(84.9809529574529,0.423424473608377,
136.706525194973));
#147066=CARTESIAN_POINT('Ctrl Pts',(84.977016908012,0.506212649833241,136.699416114815));
#147067=CARTESIAN_POINT('Ctrl Pts',(84.9695936416066,0.662348566459157,
136.686008611506));
#147068=CARTESIAN_POINT('Ctrl Pts',(84.9621703752011,0.818187545774523,
136.666373446931));
#147069=CARTESIAN_POINT('Ctrl Pts',(84.9547471087957,0.97319276767137,136.640526002427));
#147070=CARTESIAN_POINT('Ctrl Pts',(84.9473326160747,1.12801478626865,136.614709107456));
#147071=CARTESIAN_POINT('Ctrl Pts',(84.9399181233537,1.28200464433728,136.582694608442));
#147072=CARTESIAN_POINT('Ctrl Pts',(84.9325036306326,1.43462845843442,136.544549791169));
#147073=CARTESIAN_POINT('Ctrl Pts',(84.9250962842789,1.58710516795292,136.506441739307));
#147074=CARTESIAN_POINT('Ctrl Pts',(84.9176889379251,1.73821809495301,136.462215222015));
#147075=CARTESIAN_POINT('Ctrl Pts',(84.9102815915713,1.88744150569384,136.411988915259));
#147076=CARTESIAN_POINT('Ctrl Pts',(84.9028797698959,2.03655361998528,136.361800069177));
#147077=CARTESIAN_POINT('Ctrl Pts',(84.8954779482205,2.18377867179703,136.30562046227));
#147078=CARTESIAN_POINT('Ctrl Pts',(84.8880761265451,2.32860421059144,136.243619114173));
#147079=CARTESIAN_POINT('Ctrl Pts',(84.8806782122337,2.47335329711207,136.181650496105));
#147080=CARTESIAN_POINT('Ctrl Pts',(84.8732802979223,2.61570505097423,136.113866403918));
#147081=CARTESIAN_POINT('Ctrl Pts',(84.865882383611,2.75516530427255,136.040484633346));
#147082=CARTESIAN_POINT('Ctrl Pts',(84.8584856986987,2.89460238180624,135.967115057494));
#147083=CARTESIAN_POINT('Ctrl Pts',(84.8510890137866,3.03114858242346,135.88814982315));
#147084=CARTESIAN_POINT('Ctrl Pts',(84.8436923288743,3.16433263170998,135.803853547694));
#147085=CARTESIAN_POINT('Ctrl Pts',(84.8362959719389,3.2975107754758,135.719561010023));
#147086=CARTESIAN_POINT('Ctrl Pts',(84.8288996150035,3.42732674890866,135.629938100893));
#147087=CARTESIAN_POINT('Ctrl Pts',(84.821503258068,3.55333690055581,135.535293658061));
#147088=CARTESIAN_POINT('Ctrl Pts',(84.8141057687314,3.67936634467932,135.440634724923));
#147089=CARTESIAN_POINT('Ctrl Pts',(84.8067082793948,3.80158850831983,135.340952951481));
#147090=CARTESIAN_POINT('Ctrl Pts',(84.7993107900582,3.91959168973813,135.236598376107));
#147091=CARTESIAN_POINT('Ctrl Pts',(84.7919107075432,4.03763623698866,135.132207219398));
#147092=CARTESIAN_POINT('Ctrl Pts',(84.7845106250282,4.15145857796007,135.023140246564));
#147093=CARTESIAN_POINT('Ctrl Pts',(84.7771105425132,4.260682949959,134.90978524389));
#147094=CARTESIAN_POINT('Ctrl Pts',(84.7697023228468,4.37002742538333,134.796305595737));
#147095=CARTESIAN_POINT('Ctrl Pts',(84.7622941031803,4.47476357561472,134.6785287703));
#147096=CARTESIAN_POINT('Ctrl Pts',(84.7548858835139,4.57455464042029,134.556877160409));
#147097=CARTESIAN_POINT('Ctrl Pts',(84.7474731042118,4.67440712496108,134.435150675982));
#147098=CARTESIAN_POINT('Ctrl Pts',(84.7400603249097,4.76930823477344,134.309544952112));
#147099=CARTESIAN_POINT('Ctrl Pts',(84.7326475456077,4.85896415218238,134.180511966411));
#147100=CARTESIAN_POINT('Ctrl Pts',(84.7252241745789,4.94874817417062,134.051294612328));
#147101=CARTESIAN_POINT('Ctrl Pts',(84.7178008035501,5.03327183533983,133.91864052993));
#147102=CARTESIAN_POINT('Ctrl Pts',(84.7103774325214,5.11228651394487,133.783027628468));
#147103=CARTESIAN_POINT('Ctrl Pts',(84.7064413830806,5.15418199247268,133.711122414126));
#147104=CARTESIAN_POINT('Ctrl Pts',(84.7025053336398,5.19452948766344,133.638385738386));
#147105=CARTESIAN_POINT('Ctrl Pts',(84.698569284199,5.23329744864993,133.564891069572));
#147106=CARTESIAN_POINT('Ctrl Pts',(84.6911460177936,5.30641261316367,133.42628241788));
#147107=CARTESIAN_POINT('Ctrl Pts',(84.6837227513881,5.37412776800918,133.284557384925));
#147108=CARTESIAN_POINT('Ctrl Pts',(84.6762994849827,5.43616568955871,133.140175926653));
#147109=CARTESIAN_POINT('Ctrl Pts',(84.6688849922617,5.49813028743685,132.995965115275));
#147110=CARTESIAN_POINT('Ctrl Pts',(84.6614704995407,5.55443086241595,132.849104467748));
#147111=CARTESIAN_POINT('Ctrl Pts',(84.6540560068196,5.60483544689032,132.700079524942));
#147112=CARTESIAN_POINT('Ctrl Pts',(84.6466486604658,5.65519144952862,132.551198217986));
#147113=CARTESIAN_POINT('Ctrl Pts',(84.639241314112,5.69966265615239,132.40015711987));
#147114=CARTESIAN_POINT('Ctrl Pts',(84.6318339677582,5.73806474028561,132.247462692539));
#147115=CARTESIAN_POINT('Ctrl Pts',(84.6244321460828,5.77643818269558,132.094882150473));
#147116=CARTESIAN_POINT('Ctrl Pts',(84.6170303244074,5.80875142499177,131.940651094957));
#147117=CARTESIAN_POINT('Ctrl Pts',(84.609628502732,5.83486967614705,131.785292024383));
#147118=CARTESIAN_POINT('Ctrl Pts',(84.6022305884206,5.86097413968081,131.630014966653));
#147119=CARTESIAN_POINT('Ctrl Pts',(84.5948326741093,5.88089006327614,131.473611446973));
#147120=CARTESIAN_POINT('Ctrl Pts',(84.5874347597979,5.89453357482782,131.316614946711));
#147121=CARTESIAN_POINT('Ctrl Pts',(84.5800380748857,5.9081748190754,131.159644536419));
#147122=CARTESIAN_POINT('Ctrl Pts',(84.5726413899735,5.91554568777026,131.002081712654));
#147123=CARTESIAN_POINT('Ctrl Pts',(84.5652447050612,5.91661407567471,130.844466004086));
#147124=CARTESIAN_POINT('Ctrl Pts',(84.5578483481258,5.91768241620572,130.686857284363));
#147125=CARTESIAN_POINT('Ctrl Pts',(84.5504519911903,5.9124488290741,130.529196057789));
#147126=CARTESIAN_POINT('Ctrl Pts',(84.5430556342549,5.90093334378395,130.372022515245));
#147127=CARTESIAN_POINT('Ctrl Pts',(84.5356581449183,5.88941609544361,130.21482490903));
#147128=CARTESIAN_POINT('Ctrl Pts',(84.5282606555817,5.87161506120222,130.05811550784));
#147129=CARTESIAN_POINT('Ctrl Pts',(84.5208631662451,5.84760220340926,129.902429892298));
#147130=CARTESIAN_POINT('Ctrl Pts',(84.5134630837301,5.82358092794618,129.746689701403));
#147131=CARTESIAN_POINT('Ctrl Pts',(84.5060630012151,5.79334355032403,129.591974379402));
#147132=CARTESIAN_POINT('Ctrl Pts',(84.4986629187001,5.75701321721257,129.438809674049));
#147133=CARTESIAN_POINT('Ctrl Pts',(84.4912546990337,5.72064293516506,129.285476548357));
#147134=CARTESIAN_POINT('Ctrl Pts',(84.4838464793672,5.67816640383382,129.133697807877));
#147135=CARTESIAN_POINT('Ctrl Pts',(84.4764382597007,5.62975696713954,128.983985092175));
#147136=CARTESIAN_POINT('Ctrl Pts',(84.4690254803986,5.58131773524458,128.834180230793));
#147137=CARTESIAN_POINT('Ctrl Pts',(84.4616127010965,5.52693845035551,128.686444277526));
#147138=CARTESIAN_POINT('Ctrl Pts',(84.4541999217945,5.46684055840752,128.541268734444));
#147139=CARTESIAN_POINT('Ctrl Pts',(84.4467765507657,5.40665679577329,128.395885757739));
#147140=CARTESIAN_POINT('Ctrl Pts',(84.4393531797369,5.34073826275935,128.25307083597));
#147141=CARTESIAN_POINT('Ctrl Pts',(84.4319298087082,5.26935265182927,128.113291463278));
#147142=CARTESIAN_POINT('Ctrl Pts',(84.4279937592675,5.23150228804109,128.039177085919));
#147143=CARTESIAN_POINT('Ctrl Pts',(84.4240577098268,5.19211566942541,127.965915645588));
#147144=CARTESIAN_POINT('Ctrl Pts',(84.4201216603861,5.15123755295005,127.893573398346));
#147145=CARTESIAN_POINT('Ctrl Pts',(84.4126983939807,5.07414270103757,127.757138177767));
#147146=CARTESIAN_POINT('Ctrl Pts',(84.4052751275753,4.99150711217917,127.623561658064));
#147147=CARTESIAN_POINT('Ctrl Pts',(84.3978518611698,4.90356791419812,127.493325692751));
#147148=CARTESIAN_POINT('Ctrl Pts',(84.3904373684488,4.81573265304605,127.363243655533));
#147149=CARTESIAN_POINT('Ctrl Pts',(84.3830228757278,4.72260646696588,127.236494620028));
#147150=CARTESIAN_POINT('Ctrl Pts',(84.3756083830068,4.62447247108644,127.113536193855));
#147151=CARTESIAN_POINT('Ctrl Pts',(84.368201036653,4.52643306044697,126.990696279642));
#147152=CARTESIAN_POINT('Ctrl Pts',(84.3607936902993,4.423395680346,126.871639991104));
#147153=CARTESIAN_POINT('Ctrl Pts',(84.3533863439455,4.31568679859894,126.756796162378));
#147154=CARTESIAN_POINT('Ctrl Pts',(84.3459845222701,4.20805825019905,126.642037988512));
#147155=CARTESIAN_POINT('Ctrl Pts',(84.3385827005946,4.09576539189862,126.5314862898));
#147156=CARTESIAN_POINT('Ctrl Pts',(84.3311808789192,3.97917495855005,126.425536892894));
#147157=CARTESIAN_POINT('Ctrl Pts',(84.3237829646078,3.86264607238379,126.31964342585));
#147158=CARTESIAN_POINT('Ctrl Pts',(84.3163850502965,3.74182440487551,126.218347672525));
#147159=CARTESIAN_POINT('Ctrl Pts',(84.3089871359851,3.61711345408748,126.122008556608));
#147160=CARTESIAN_POINT('Ctrl Pts',(84.3015904510729,3.49242322799751,126.025685450504));
#147161=CARTESIAN_POINT('Ctrl Pts',(84.2941937661606,3.36384529652664,125.934317574987));
#147162=CARTESIAN_POINT('Ctrl Pts',(84.2867970812484,3.23181622675876,125.848223569526));
#147163=CARTESIAN_POINT('Ctrl Pts',(84.279400724313,3.0997930112981,125.762133381563));
#147164=CARTESIAN_POINT('Ctrl Pts',(84.2720043673776,2.96431927450088,125.681316802586));
#147165=CARTESIAN_POINT('Ctrl Pts',(84.2646080104421,2.82586032069221,125.606048967575));
#147166=CARTESIAN_POINT('Ctrl Pts',(84.2572105211056,2.68738016846453,125.530769608865));
#147167=CARTESIAN_POINT('Ctrl Pts',(84.249813031769,2.54591421718082,125.461040863941));
#147168=CARTESIAN_POINT('Ctrl Pts',(84.2424155424324,2.40195196339562,125.397091683248));
#147169=CARTESIAN_POINT('Ctrl Pts',(84.2350154599174,2.25793924386471,125.333120085269));
#147170=CARTESIAN_POINT('Ctrl Pts',(84.2276153774024,2.11142882050549,125.274932236756));
#147171=CARTESIAN_POINT('Ctrl Pts',(84.2202152948874,1.96292958357739,125.222708710432));
#147172=CARTESIAN_POINT('Ctrl Pts',(84.2128070752209,1.81426705647262,125.170427758972));
#147173=CARTESIAN_POINT('Ctrl Pts',(84.2053988555544,1.66361170077824,125.124124351147));
#147174=CARTESIAN_POINT('Ctrl Pts',(84.197990635888,1.51148766997368,125.083929201491));
#147175=CARTESIAN_POINT('Ctrl Pts',(84.1905778565859,1.35927000936616,125.043709312391));
#147176=CARTESIAN_POINT('Ctrl Pts',(84.1831650772838,1.20558223601278,125.009605253477));
#147177=CARTESIAN_POINT('Ctrl Pts',(84.1757522979817,1.05095756146268,124.981696384888));
#147178=CARTESIAN_POINT('Ctrl Pts',(84.1683289269529,0.896111951926617,
124.953747638799));
#147179=CARTESIAN_POINT('Ctrl Pts',(84.1609055559242,0.740327136270051,
124.932011813869));
#147180=CARTESIAN_POINT('Ctrl Pts',(84.1534821848955,0.584141124868732,
124.916516384849));
#147181=CARTESIAN_POINT('Ctrl Pts',(84.1495461354548,0.501327553993802,
124.908300336575));
#147182=CARTESIAN_POINT('Ctrl Pts',(84.145610086014,0.418401199937062,124.901837816294));
#147183=CARTESIAN_POINT('Ctrl Pts',(84.1416740365733,0.335441998034453,
124.897126981721));
#147184=CARTESIAN_POINT('Ctrl Pts',(84.1342507701679,0.178983532310491,
124.888242494737));
#147185=CARTESIAN_POINT('Ctrl Pts',(84.1268275037625,0.0219352689361514,
124.885564784318));
#147186=CARTESIAN_POINT('Ctrl Pts',(84.119404237357,-0.135169221699544,
124.889154801704));
#147187=CARTESIAN_POINT('Ctrl Pts',(84.111989744636,-0.292088027874135,
124.892740575988));
#147188=CARTESIAN_POINT('Ctrl Pts',(84.104575251915,-0.449062559473018,
124.902579324101));
#147189=CARTESIAN_POINT('Ctrl Pts',(84.097160759194,-0.605554787605303,
124.91868020136));
#147190=CARTESIAN_POINT('Ctrl Pts',(84.0897534128402,-0.761896182635618,
124.934765559988));
#147191=CARTESIAN_POINT('Ctrl Pts',(84.0823460664865,-0.917755830803735,
124.957100993971));
#147192=CARTESIAN_POINT('Ctrl Pts',(84.0749387201327,-1.07259647797631,
124.985643632016));
#147193=CARTESIAN_POINT('Ctrl Pts',(84.0675368984573,-1.22732163915297,
125.014164981884));
#147194=CARTESIAN_POINT('Ctrl Pts',(84.0601350767819,-1.38102894708251,
125.048884250342));
#147195=CARTESIAN_POINT('Ctrl Pts',(84.0527332551065,-1.53318715244639,
125.089706846945));
#147196=CARTESIAN_POINT('Ctrl Pts',(84.0453353407952,-1.68526503467741,
125.130507893617));
#147197=CARTESIAN_POINT('Ctrl Pts',(84.0379374264838,-1.83579508331474,
125.17740575538));
#147198=CARTESIAN_POINT('Ctrl Pts',(84.0305395121725,-1.98425722513587,
125.230254964908));
#147199=CARTESIAN_POINT('Ctrl Pts',(84.0231428272603,-2.13269469524325,
125.283095391856));
#147200=CARTESIAN_POINT('Ctrl Pts',(84.0157461423481,-2.27906458923966,
125.341885078617));
#147201=CARTESIAN_POINT('Ctrl Pts',(84.0083494574359,-2.4228628515422,125.406428961356));
#147202=CARTESIAN_POINT('Ctrl Pts',(84.0009531005004,-2.56665473767931,
125.470969982151));
#147203=CARTESIAN_POINT('Ctrl Pts',(83.9935567435649,-2.70787487828596,
125.541264538743));
#147204=CARTESIAN_POINT('Ctrl Pts',(83.9861603866295,-2.84604028615942,
125.6170698746));
#147205=CARTESIAN_POINT('Ctrl Pts',(83.9787628972929,-2.98422684750905,
125.692886816448));
#147206=CARTESIAN_POINT('Ctrl Pts',(83.9713654079563,-3.11935741760163,
125.774216037936));
#147207=CARTESIAN_POINT('Ctrl Pts',(83.9639679186197,-3.25097478909792,
125.860769465059));
#147208=CARTESIAN_POINT('Ctrl Pts',(83.9565678361047,-3.38263829885985,
125.947353233351));
#147209=CARTESIAN_POINT('Ctrl Pts',(83.9491677535897,-3.51078584632074,
126.039164648475));
#147210=CARTESIAN_POINT('Ctrl Pts',(83.9417676710747,-3.63499044291924,
126.13587317061));
#147211=CARTESIAN_POINT('Ctrl Pts',(83.9343594514083,-3.75933161524051,
126.232688033707));
#147212=CARTESIAN_POINT('Ctrl Pts',(83.9269512317417,-3.87972088333852,
126.334410528282));
#147213=CARTESIAN_POINT('Ctrl Pts',(83.9195430120753,-3.99576495561633,
126.440670323564));
#147214=CARTESIAN_POINT('Ctrl Pts',(83.9121302327732,-4.11188045108458,
126.546995519977));
#147215=CARTESIAN_POINT('Ctrl Pts',(83.9047174534711,-4.22364515725599,
126.657863319483));
#147216=CARTESIAN_POINT('Ctrl Pts',(83.897304674169,-4.33070409233231,126.772868012196));
#147217=CARTESIAN_POINT('Ctrl Pts',(83.8898813031402,-4.43791599823532,
126.888037029007));
#147218=CARTESIAN_POINT('Ctrl Pts',(83.8824579321115,-4.54040846145767,
127.007354462172));
#147219=CARTESIAN_POINT('Ctrl Pts',(83.8750345610827,-4.63786755896348,
127.130382519099));
#147220=CARTESIAN_POINT('Ctrl Pts',(83.8710985116419,-4.68954271095976,
127.195614946899));
#147221=CARTESIAN_POINT('Ctrl Pts',(83.8671624622012,-4.73980353225777,
127.261890087097));
#147222=CARTESIAN_POINT('Ctrl Pts',(83.8632264127604,-4.78860836582211,
127.329139692031));
#147223=CARTESIAN_POINT('Ctrl Pts',(83.8557474286246,-4.88134362778165,
127.456922316716));
#147224=CARTESIAN_POINT('Ctrl Pts',(83.8482684444889,-4.96909931432236,
127.588610453369));
#147225=CARTESIAN_POINT('Ctrl Pts',(83.8407894603531,-5.05153140075413,
127.723782576079));
#147226=CARTESIAN_POINT('Ctrl Pts',(83.833319537821,-5.13386361173786,127.858790923043));
#147227=CARTESIAN_POINT('Ctrl Pts',(83.8258496152888,-5.21088487347303,
127.99727454451));
#147228=CARTESIAN_POINT('Ctrl Pts',(83.8183796927567,-5.2822922066956,128.138780079375));
#147229=CARTESIAN_POINT('Ctrl Pts',(83.8109174203979,-5.35362640951029,
128.280140694145));
#147230=CARTESIAN_POINT('Ctrl Pts',(83.8034551480392,-5.41935796657825,
128.424516736713));
#147231=CARTESIAN_POINT('Ctrl Pts',(83.7959928756804,-5.4792279555501,128.571427216495));
#147232=CARTESIAN_POINT('Ctrl Pts',(83.7885368470923,-5.53904785060169,
128.71821477456));
#147233=CARTESIAN_POINT('Ctrl Pts',(83.7810808185041,-5.59301580618984,
128.867532210053));
#147234=CARTESIAN_POINT('Ctrl Pts',(83.7736247899159,-5.64091952462577,
129.018875395226));
#147235=CARTESIAN_POINT('Ctrl Pts',(83.766173990919,-5.68878964382549,129.170112429653));
#147236=CARTESIAN_POINT('Ctrl Pts',(83.7587231919221,-5.73060389010518,
129.323372035202));
#147237=CARTESIAN_POINT('Ctrl Pts',(83.7512723929252,-5.76619871155417,
129.478131760479));
#147238=CARTESIAN_POINT('Ctrl Pts',(83.7438247346584,-5.80177852874236,
129.632826249994));
#147239=CARTESIAN_POINT('Ctrl Pts',(83.7363770763917,-5.83114406078232,
129.789019243894));
#147240=CARTESIAN_POINT('Ctrl Pts',(83.728929418125,-5.85418205790248,129.946174742925));
#147241=CARTESIAN_POINT('Ctrl Pts',(83.7214825419909,-5.8772176356355,130.103313737918));
#147242=CARTESIAN_POINT('Ctrl Pts',(83.7140356658568,-5.89392694270054,
130.261414675845));
#147243=CARTESIAN_POINT('Ctrl Pts',(83.7065887897227,-5.90424811944369,
130.41993285251));
#147244=CARTESIAN_POINT('Ctrl Pts',(83.7005175905523,-5.9126626436754,130.549167635705));
#147245=CARTESIAN_POINT('Ctrl Pts',(83.6944463913818,-5.91683217465459,
130.67867949077));
#147246=CARTESIAN_POINT('Ctrl Pts',(83.6883751922114,-5.91674877278903,
130.808171417949));
#147247=CARTESIAN_POINT('',(81.9383765539627,-5.9211714837301,130.807349049409));
#147248=CARTESIAN_POINT('Ctrl Pts',(83.6883730537543,-5.90949988628817,
130.808212304205));
#147249=CARTESIAN_POINT('Ctrl Pts',(83.6538416321521,-5.91380919305711,
131.543829778501));
#147250=CARTESIAN_POINT('Ctrl Pts',(83.5264943359454,-5.4448668572003,134.25138132363));
#147251=CARTESIAN_POINT('Ctrl Pts',(83.3063311651348,-1.38425268638609,
137.664492178298));
#147252=CARTESIAN_POINT('Ctrl Pts',(83.0278835413217,5.02340058182423,135.677040283301));
#147253=CARTESIAN_POINT('Ctrl Pts',(82.7494359175088,6.81479412209936,129.211833819126));
#147254=CARTESIAN_POINT('Ctrl Pts',(82.4709882936959,2.34372478536503,124.210081683459));
#147255=CARTESIAN_POINT('Ctrl Pts',(82.2006355289506,-4.08851989451056,
125.237390232203));
#147256=CARTESIAN_POINT('Ctrl Pts',(82.0230986388097,-5.91348347804172,
129.014328708923));
#147257=CARTESIAN_POINT('Ctrl Pts',(81.9383776232731,-5.92464404173536,
130.807328188564));
#147258=CARTESIAN_POINT('',(80.1883744842576,-5.91827765709797,130.799106644454));
#147259=CARTESIAN_POINT('Ctrl Pts',(81.9383751922115,-5.91674923182385,
130.807375615392));
#147260=CARTESIAN_POINT('Ctrl Pts',(81.9302811434977,-5.91666205962317,
130.97844573922));
#147261=CARTESIAN_POINT('Ctrl Pts',(81.9221870947839,-5.90915640203312,
131.149321703326));
#147262=CARTESIAN_POINT('Ctrl Pts',(81.9140930460701,-5.8942783013915,131.319543952162));
#147263=CARTESIAN_POINT('Ctrl Pts',(81.9066697796646,-5.88063320132161,
131.475659284047));
#147264=CARTESIAN_POINT('Ctrl Pts',(81.8992465132592,-5.86076089908632,
131.631468201526));
#147265=CARTESIAN_POINT('Ctrl Pts',(81.8918232468537,-5.83467759295216,
131.786433908518));
#147266=CARTESIAN_POINT('Ctrl Pts',(81.8844087541327,-5.80862511511972,
131.941216458915));
#147267=CARTESIAN_POINT('Ctrl Pts',(81.8769942614116,-5.77637630682767,
132.095157418048));
#147268=CARTESIAN_POINT('Ctrl Pts',(81.8695797686906,-5.73799926626215,
132.24772300549));
#147269=CARTESIAN_POINT('Ctrl Pts',(81.8621724223368,-5.69965921493319,
132.400141544476));
#147270=CARTESIAN_POINT('Ctrl Pts',(81.854765075983,-5.65520278070317,132.551186991259));
#147271=CARTESIAN_POINT('Ctrl Pts',(81.8473577296292,-5.60474943947957,
132.700333793313));
#147272=CARTESIAN_POINT('Ctrl Pts',(81.8399559079538,-5.55433372826142,
132.849369356055));
#147273=CARTESIAN_POINT('Ctrl Pts',(81.8325540862784,-5.49793013494314,
132.996508741584));
#147274=CARTESIAN_POINT('Ctrl Pts',(81.825152264603,-5.43570845882643,133.141239757176));
#147275=CARTESIAN_POINT('Ctrl Pts',(81.8177543502917,-5.37351962904817,
133.285894370391));
#147276=CARTESIAN_POINT('Ctrl Pts',(81.8103564359804,-5.30551898021813,
133.428142803561));
#147277=CARTESIAN_POINT('Ctrl Pts',(81.802958521669,-5.23192505985641,133.567491220803));
#147278=CARTESIAN_POINT('Ctrl Pts',(81.7955618367569,-5.15834336946914,
133.706816480866));
#147279=CARTESIAN_POINT('Ctrl Pts',(81.7881651518447,-5.07917042649308,
133.843242351721));
#147280=CARTESIAN_POINT('Ctrl Pts',(81.7807684669325,-4.99467156519957,
133.9762979622));
#147281=CARTESIAN_POINT('Ctrl Pts',(81.7733721099971,-4.91017645067413,
134.109347672855));
#147282=CARTESIAN_POINT('Ctrl Pts',(81.7659757530617,-4.82035608751353,
134.239027105152));
#147283=CARTESIAN_POINT('Ctrl Pts',(81.7585793961263,-4.72551998827836,
134.364893078151));
#147284=CARTESIAN_POINT('Ctrl Pts',(81.7511819067897,-4.63066936939443,
134.490778321552));
#147285=CARTESIAN_POINT('Ctrl Pts',(81.7437844174532,-4.53080171005563,
134.61284864497));
#147286=CARTESIAN_POINT('Ctrl Pts',(81.7363869281167,-4.42626767476855,
134.730692879843));
#147287=CARTESIAN_POINT('Ctrl Pts',(81.7289868456017,-4.32169699523714,
134.84857842483));
#147288=CARTESIAN_POINT('Ctrl Pts',(81.7215867630867,-4.21245693047433,
134.962234652631));
#147289=CARTESIAN_POINT('Ctrl Pts',(81.7141866805717,-4.09893583816266,
135.071286391132));
#147290=CARTESIAN_POINT('Ctrl Pts',(81.7067784609053,-3.98528991773983,
135.180458043231));
#147291=CARTESIAN_POINT('Ctrl Pts',(81.6993702412389,-3.86735383809443,
135.285014835901));
#147292=CARTESIAN_POINT('Ctrl Pts',(81.6919620215724,-3.74555050406112,
135.384620652109));
#147293=CARTESIAN_POINT('Ctrl Pts',(81.6845492422704,-3.62367220210819,
135.484287774034));
#147294=CARTESIAN_POINT('Ctrl Pts',(81.6771364629684,-3.49792220035367,
135.578997623423));
#147295=CARTESIAN_POINT('Ctrl Pts',(81.6697236836664,-3.36875292302638,
135.668457070773));
#147296=CARTESIAN_POINT('Ctrl Pts',(81.6623003126377,-3.23939908257802,
135.758044341977));
#147297=CARTESIAN_POINT('Ctrl Pts',(81.6548769416089,-3.10661652316693,
135.842366028338));
#147298=CARTESIAN_POINT('Ctrl Pts',(81.6474535705802,-2.97088353185277,
135.921174235695));
#147299=CARTESIAN_POINT('Ctrl Pts',(81.6435175211393,-2.89891464298731,
135.962960238214));
#147300=CARTESIAN_POINT('Ctrl Pts',(81.6395814716984,-2.82611664945376,
136.003196993845));
#147301=CARTESIAN_POINT('Ctrl Pts',(81.6356454222575,-2.75256306750672,
136.041853063565));
#147302=CARTESIAN_POINT('Ctrl Pts',(81.6282221558521,-2.61384330748768,
136.11475720464));
#147303=CARTESIAN_POINT('Ctrl Pts',(81.6207988894467,-2.47201538770909,
136.182256599698));
#147304=CARTESIAN_POINT('Ctrl Pts',(81.6133756230412,-2.32753968547343,
136.244074725407));
#147305=CARTESIAN_POINT('Ctrl Pts',(81.6059611303202,-2.18323474151975,
136.305819787225));
#147306=CARTESIAN_POINT('Ctrl Pts',(81.5985466375992,-2.03628858416384,
136.361896800104));
#147307=CARTESIAN_POINT('Ctrl Pts',(81.5911321448782,-1.88718710672944,
136.412074535616));
#147308=CARTESIAN_POINT('Ctrl Pts',(81.5837247985244,-1.73822933891236,
136.462203907938));
#147309=CARTESIAN_POINT('Ctrl Pts',(81.5763174521706,-1.58712073809383,
136.506445204225));
#147310=CARTESIAN_POINT('Ctrl Pts',(81.5689101058169,-1.43436804614598,
136.544614868964));
#147311=CARTESIAN_POINT('Ctrl Pts',(81.5615082841415,-1.28172928291891,
136.582756065327));
#147312=CARTESIAN_POINT('Ctrl Pts',(81.5541064624661,-1.12744923074613,
136.614834556794));
#147313=CARTESIAN_POINT('Ctrl Pts',(81.5467046407907,-0.972050592543462,
136.640716347646));
#147314=CARTESIAN_POINT('Ctrl Pts',(81.5393067264793,-0.81673398807239,
136.666584475702));
#147315=CARTESIAN_POINT('Ctrl Pts',(81.5319088121679,-0.660300340859842,
136.686262356703));
#147316=CARTESIAN_POINT('Ctrl Pts',(81.5245108978566,-0.503283259295052,
136.699666930508));
#147317=CARTESIAN_POINT('Ctrl Pts',(81.5171142129443,-0.346292271120638,
136.713069276716));
#147318=CARTESIAN_POINT('Ctrl Pts',(81.5097175280321,-0.188718412604161,
136.72020035308));
#147319=CARTESIAN_POINT('Ctrl Pts',(81.5023208431199,-0.031101260648081,
136.72102887547));
#147320=CARTESIAN_POINT('Ctrl Pts',(81.4949244861845,0.12650890239831,136.721857361122));
#147321=CARTESIAN_POINT('Ctrl Pts',(81.487528129249,0.28416198177493,136.716383846503));
#147322=CARTESIAN_POINT('Ctrl Pts',(81.4801317723135,0.441317817705747,
136.704629183172));
#147323=CARTESIAN_POINT('Ctrl Pts',(81.4727342829769,0.598497714596358,
136.692872720172));
#147324=CARTESIAN_POINT('Ctrl Pts',(81.4653367936403,0.755179844175743,
136.674833221512));
#147325=CARTESIAN_POINT('Ctrl Pts',(81.4579393043037,0.91082873595516,136.650583464521));
#147326=CARTESIAN_POINT('Ctrl Pts',(81.4505392217887,1.06653219021208,136.626325206816));
#147327=CARTESIAN_POINT('Ctrl Pts',(81.4431391392738,1.22120131691355,136.595852413825));
#147328=CARTESIAN_POINT('Ctrl Pts',(81.4357390567588,1.37431055632145,136.559289032176));
#147329=CARTESIAN_POINT('Ctrl Pts',(81.4283308370923,1.5275881550782,136.522685445329));
#147330=CARTESIAN_POINT('Ctrl Pts',(81.4209226174258,1.67930207775057,136.47997798178));
#147331=CARTESIAN_POINT('Ctrl Pts',(81.4135143977593,1.82894094916629,136.431340763876));
#147332=CARTESIAN_POINT('Ctrl Pts',(81.4061016184573,1.9786719208105,136.382673610575));
#147333=CARTESIAN_POINT('Ctrl Pts',(81.3986888391551,2.12632494698645,136.328069559685));
#147334=CARTESIAN_POINT('Ctrl Pts',(81.3912760598531,2.2714088631957,136.267750804867));
#147335=CARTESIAN_POINT('Ctrl Pts',(81.3838526888243,2.4167000821083,136.207345863783));
#147336=CARTESIAN_POINT('Ctrl Pts',(81.3764293177956,2.55941452171377,136.141210067103));
#147337=CARTESIAN_POINT('Ctrl Pts',(81.3690059467669,2.69908509579542,136.069611818426));
#147338=CARTESIAN_POINT('Ctrl Pts',(81.365069897326,2.77314178552418,136.031648709));
#147339=CARTESIAN_POINT('Ctrl Pts',(81.3611338478852,2.84634320129484,135.992150644551));
#147340=CARTESIAN_POINT('Ctrl Pts',(81.3571977984443,2.91862315523441,135.951162482825));
#147341=CARTESIAN_POINT('Ctrl Pts',(81.3497745320389,3.05494089258252,135.873860089006));
#147342=CARTESIAN_POINT('Ctrl Pts',(81.3423512656334,3.18839150030732,135.791021315114));
#147343=CARTESIAN_POINT('Ctrl Pts',(81.3349279992279,3.31849348632067,135.702884021996));
#147344=CARTESIAN_POINT('Ctrl Pts',(81.3275135065069,3.44844170259093,135.614850899839));
#147345=CARTESIAN_POINT('Ctrl Pts',(81.3200990137859,3.57504886911983,135.521531931141));
#147346=CARTESIAN_POINT('Ctrl Pts',(81.3126845210649,3.69785780967332,135.423210927106));
#147347=CARTESIAN_POINT('Ctrl Pts',(81.3052771747111,3.82054838234622,135.324984688556));
#147348=CARTESIAN_POINT('Ctrl Pts',(81.2978698283573,3.93944772766662,135.221766244366));
#147349=CARTESIAN_POINT('Ctrl Pts',(81.2904624820035,4.05412750882253,135.113882714587));
#147350=CARTESIAN_POINT('Ctrl Pts',(81.2830606603281,4.16872175747112,135.006079648414));
#147351=CARTESIAN_POINT('Ctrl Pts',(81.2756588386526,4.27910243755128,134.89361867928));
#147352=CARTESIAN_POINT('Ctrl Pts',(81.2682570169772,4.38487428097723,134.776867143995));
#147353=CARTESIAN_POINT('Ctrl Pts',(81.2608591026659,4.49059028827021,134.660177240937));
#147354=CARTESIAN_POINT('Ctrl Pts',(81.2534611883546,4.5917020542855,134.539201558446));
#147355=CARTESIAN_POINT('Ctrl Pts',(81.2460632740432,4.68785126980622,134.414344140337));
#147356=CARTESIAN_POINT('Ctrl Pts',(81.238666589131,4.78398450707171,134.289507471265));
#147357=CARTESIAN_POINT('Ctrl Pts',(81.2312699042187,4.87515660306296,134.160790642332));
#147358=CARTESIAN_POINT('Ctrl Pts',(81.2238732193065,4.96104958305994,134.028630705031));
#147359=CARTESIAN_POINT('Ctrl Pts',(81.2164768623711,5.04693875447212,133.89647662784));
#147360=CARTESIAN_POINT('Ctrl Pts',(81.2090805054357,5.12754907189866,133.760880058843));
#147361=CARTESIAN_POINT('Ctrl Pts',(81.2016841485002,5.20260610879401,133.622306720535));
#147362=CARTESIAN_POINT('Ctrl Pts',(81.1942866591636,5.27767463711337,133.483712166296));
#147363=CARTESIAN_POINT('Ctrl Pts',(81.186889169827,5.34718801419711,133.342140263547));
#147364=CARTESIAN_POINT('Ctrl Pts',(81.1794916804904,5.41091803479427,133.1980808567));
#147365=CARTESIAN_POINT('Ctrl Pts',(81.1720915979754,5.4746703958513,133.053970950051));
#147366=CARTESIAN_POINT('Ctrl Pts',(81.1646915154604,5.53263521305975,132.907372144349));
#147367=CARTESIAN_POINT('Ctrl Pts',(81.1572914329454,5.58463268835026,132.758793604064));
#147368=CARTESIAN_POINT('Ctrl Pts',(81.149883213279,5.63668734021036,132.610051686399));
#147369=CARTESIAN_POINT('Ctrl Pts',(81.1424749936125,5.68276142261082,132.459326039256));
#147370=CARTESIAN_POINT('Ctrl Pts',(81.1350667739461,5.722725018843,132.307141014433));
#147371=CARTESIAN_POINT('Ctrl Pts',(81.127653994644,5.76271321200183,132.154862322267));
#147372=CARTESIAN_POINT('Ctrl Pts',(81.1202412153419,5.79658334479457,132.001122826309));
#147373=CARTESIAN_POINT('Ctrl Pts',(81.1128284360398,5.82425686863249,131.846455858265));
#147374=CARTESIAN_POINT('Ctrl Pts',(81.1054050650111,5.85196993369905,131.691567894803));
#147375=CARTESIAN_POINT('Ctrl Pts',(81.0979816939823,5.87346865548916,131.535750181317));
#147376=CARTESIAN_POINT('Ctrl Pts',(81.0905583229536,5.88872637804382,131.379540769371));
#147377=CARTESIAN_POINT('Ctrl Pts',(81.0866222735129,5.89681638864603,131.296714790967));
#147378=CARTESIAN_POINT('Ctrl Pts',(81.0826862240723,5.90315270164919,131.213778698083));
#147379=CARTESIAN_POINT('Ctrl Pts',(81.0787501746316,5.90773728098375,131.130812423159));
#147380=CARTESIAN_POINT('Ctrl Pts',(81.0713269082262,5.91638365452921,130.974340617934));
#147381=CARTESIAN_POINT('Ctrl Pts',(81.0639036418207,5.91882236112527,130.8172884614));
#147382=CARTESIAN_POINT('Ctrl Pts',(81.0564803754153,5.91499326160493,130.660189616084));
#147383=CARTESIAN_POINT('Ctrl Pts',(81.0490658826943,5.91116868776223,130.503276448557));
#147384=CARTESIAN_POINT('Ctrl Pts',(81.0416513899733,5.90109106252754,130.346317071632));
#147385=CARTESIAN_POINT('Ctrl Pts',(81.0342368972523,5.8847520493813,130.189849527509));
#147386=CARTESIAN_POINT('Ctrl Pts',(81.0268295508985,5.86842878439108,130.033532792697));
#147387=CARTESIAN_POINT('Ctrl Pts',(81.0194222045447,5.84585618441963,129.877707315739));
#147388=CARTESIAN_POINT('Ctrl Pts',(81.0120148581909,5.8170779383199,129.722910284905));
#147389=CARTESIAN_POINT('Ctrl Pts',(81.0046130365155,5.78832115612185,129.568228707537));
#147390=CARTESIAN_POINT('Ctrl Pts',(80.99721121484,5.75336801151136,129.414574414414));
#147391=CARTESIAN_POINT('Ctrl Pts',(80.9898093931646,5.71231390329363,129.26247851029));
#147392=CARTESIAN_POINT('Ctrl Pts',(80.9824114788533,5.67128146722006,129.110462896409));
#147393=CARTESIAN_POINT('Ctrl Pts',(80.9750135645419,5.62415457865414,128.960004392645));
#147394=CARTESIAN_POINT('Ctrl Pts',(80.9676156502305,5.5710794962173,128.81162285024));
#147395=CARTESIAN_POINT('Ctrl Pts',(80.9602189653183,5.51801323389632,128.663265966156));
#147396=CARTESIAN_POINT('Ctrl Pts',(80.9528222804061,5.45900086515061,128.516985709549));
#147397=CARTESIAN_POINT('Ctrl Pts',(80.9454255954939,5.39423822067638,128.373285838565));
#147398=CARTESIAN_POINT('Ctrl Pts',(80.9380292385584,5.32947844784568,128.229592339384));
#147399=CARTESIAN_POINT('Ctrl Pts',(80.930632881623,5.25896905963994,128.088479338657));
#147400=CARTESIAN_POINT('Ctrl Pts',(80.9232365246875,5.18295354733297,127.950429453594));
#147401=CARTESIAN_POINT('Ctrl Pts',(80.9158390353509,5.10692639685695,127.812358432742));
#147402=CARTESIAN_POINT('Ctrl Pts',(80.9084415460144,5.02539162382225,127.677351788358));
#147403=CARTESIAN_POINT('Ctrl Pts',(80.9010440566778,4.93863799769287,127.545866288855));
#147404=CARTESIAN_POINT('Ctrl Pts',(80.8936439741628,4.85185396021446,127.414334697313));
#147405=CARTESIAN_POINT('Ctrl Pts',(80.8862438916478,4.75984763265399,127.28632701959));
#147406=CARTESIAN_POINT('Ctrl Pts',(80.8788438091327,4.66295020425295,127.162269740727));
#147407=CARTESIAN_POINT('Ctrl Pts',(80.8714355894663,4.56594622716795,127.038076048131));
#147408=CARTESIAN_POINT('Ctrl Pts',(80.8640273697998,4.46404063841445,126.917841723763));
#147409=CARTESIAN_POINT('Ctrl Pts',(80.8566191501333,4.35760436685586,126.801959495182));
#147410=CARTESIAN_POINT('Ctrl Pts',(80.8492063708312,4.25110258554804,126.686005943023));
#147411=CARTESIAN_POINT('Ctrl Pts',(80.8417935915291,4.14006482756889,126.574410088192));
#147412=CARTESIAN_POINT('Ctrl Pts',(80.834380812227,4.02489734255513,126.467526294653));
#147413=CARTESIAN_POINT('Ctrl Pts',(80.8269574411983,3.90956530083796,126.360489780538));
#147414=CARTESIAN_POINT('Ctrl Pts',(80.8195340701695,3.79009202975858,126.258179016823));
#147415=CARTESIAN_POINT('Ctrl Pts',(80.8121106991407,3.66691579913976,126.160907259932));
#147416=CARTESIAN_POINT('Ctrl Pts',(80.8081746496999,3.60160480609316,126.109331440426));
#147417=CARTESIAN_POINT('Ctrl Pts',(80.8042386002592,3.53525325422705,126.059171536811));
#147418=CARTESIAN_POINT('Ctrl Pts',(80.8003025508184,3.46792945451917,126.010469102212));
#147419=CARTESIAN_POINT('Ctrl Pts',(80.792879284413,3.34095886937311,125.918617830511));
#147420=CARTESIAN_POINT('Ctrl Pts',(80.7854560180076,3.21014462261667,125.831675550765));
#147421=CARTESIAN_POINT('Ctrl Pts',(80.7780327516022,3.07590319296048,125.749981317391));
#147422=CARTESIAN_POINT('Ctrl Pts',(80.7706182588811,2.94182042552591,125.668383639817));
#147423=CARTESIAN_POINT('Ctrl Pts',(80.7632037661601,2.80431885379939,125.592021854166));
#147424=CARTESIAN_POINT('Ctrl Pts',(80.7557892734391,2.66384664183009,125.521193799141));
#147425=CARTESIAN_POINT('Ctrl Pts',(80.7483819270854,2.52350982226747,125.450434010861));
#147426=CARTESIAN_POINT('Ctrl Pts',(80.7409745807316,2.38020839364564,125.385197501962));
#147427=CARTESIAN_POINT('Ctrl Pts',(80.7335672343779,2.23441792256095,125.325737879155));
#147428=CARTESIAN_POINT('Ctrl Pts',(80.7261654127025,2.08873618750994,125.266322603577));
#147429=CARTESIAN_POINT('Ctrl Pts',(80.7187635910271,1.94056945055037,125.212675775415));
#147430=CARTESIAN_POINT('Ctrl Pts',(80.7113617693517,1.7904161105369,125.165004208043));
#147431=CARTESIAN_POINT('Ctrl Pts',(80.7039638550404,1.64034203530273,125.11735780612));
#147432=CARTESIAN_POINT('Ctrl Pts',(80.696565940729,1.48828380047146,125.075680495735));
#147433=CARTESIAN_POINT('Ctrl Pts',(80.6891680264177,1.33475782797484,125.040130217664));
#147434=CARTESIAN_POINT('Ctrl Pts',(80.6817713415055,1.18125736870972,125.004585847403));
#147435=CARTESIAN_POINT('Ctrl Pts',(80.6743746565933,1.02629001919024,124.975166572756));
#147436=CARTESIAN_POINT('Ctrl Pts',(80.6669779716811,0.870385456685874,
124.951979929394));
#147437=CARTESIAN_POINT('Ctrl Pts',(80.6595816147457,0.714487807153293,
124.928794314152));
#147438=CARTESIAN_POINT('Ctrl Pts',(80.6521852578102,0.557653396501586,
124.91184083561));
#147439=CARTESIAN_POINT('Ctrl Pts',(80.6447889008748,0.4004198772385,124.901175504052));
#147440=CARTESIAN_POINT('Ctrl Pts',(80.6373914115382,0.243162285121993,
124.890508539605));
#147441=CARTESIAN_POINT('Ctrl Pts',(80.6299939222017,0.0855058351928214,
124.886131664334));
#147442=CARTESIAN_POINT('Ctrl Pts',(80.6225964328652,-0.0720090934002857,
124.888048822793));
#147443=CARTESIAN_POINT('Ctrl Pts',(80.6151963503502,-0.229579238607319,
124.889966653309));
#147444=CARTESIAN_POINT('Ctrl Pts',(80.6077962678352,-0.387007390667567,
124.89818290587));
#147445=CARTESIAN_POINT('Ctrl Pts',(80.6003961853202,-0.543755719762117,
124.912649467168));
#147446=CARTESIAN_POINT('Ctrl Pts',(80.5929879656537,-0.700676409758626,
124.927131935937));
#147447=CARTESIAN_POINT('Ctrl Pts',(80.5855797459873,-0.856915411966237,
124.947878404664));
#147448=CARTESIAN_POINT('Ctrl Pts',(80.5781715263208,-1.01194181745404,
124.974789079229));
#147449=CARTESIAN_POINT('Ctrl Pts',(80.5707587470188,-1.1670636391079,125.001716316865));
#147450=CARTESIAN_POINT('Ctrl Pts',(80.5633459677167,-1.32097101277216,
125.034815241989));
#147451=CARTESIAN_POINT('Ctrl Pts',(80.5559331884147,-1.47314621415442,
125.073935607654));
#147452=CARTESIAN_POINT('Ctrl Pts',(80.5485098173859,-1.62553885060062,
125.113111870332));
#147453=CARTESIAN_POINT('Ctrl Pts',(80.5410864463572,-1.77619401502127,
125.158326650082));
#147454=CARTESIAN_POINT('Ctrl Pts',(80.5336630753285,-1.92461126036826,
125.20938054084));
#147455=CARTESIAN_POINT('Ctrl Pts',(80.5297270258876,-2.00330564507659,
125.236450538742));
#147456=CARTESIAN_POINT('Ctrl Pts',(80.5257909764466,-2.08137122710373,
125.265161325373));
#147457=CARTESIAN_POINT('Ctrl Pts',(80.5218549270057,-2.15873612287603,
125.295477889254));
#147458=CARTESIAN_POINT('Ctrl Pts',(80.5144316606003,-2.30464390182277,
125.352653982585));
#147459=CARTESIAN_POINT('Ctrl Pts',(80.5070083941949,-2.44849919979424,
125.415717287347));
#147460=CARTESIAN_POINT('Ctrl Pts',(80.4995851277895,-2.58979164379113,
125.484500675401));
#147461=CARTESIAN_POINT('Ctrl Pts',(80.4921706350684,-2.73091709185292,
125.553202767203));
#147462=CARTESIAN_POINT('Ctrl Pts',(80.4847561423474,-2.86948538298017,
125.627611323359));
#147463=CARTESIAN_POINT('Ctrl Pts',(80.4773416496263,-3.00500369342217,
125.707510279856));
#147464=CARTESIAN_POINT('Ctrl Pts',(80.4699343032726,-3.14039138621438,
125.78733222673));
#147465=CARTESIAN_POINT('Ctrl Pts',(80.4625269569188,-3.27273463124757,
125.872633850587));
#147466=CARTESIAN_POINT('Ctrl Pts',(80.455119610565,-3.40156300665132,125.963152124402));
#147467=CARTESIAN_POINT('Ctrl Pts',(80.4477177888896,-3.53029529699237,
126.053602886274));
#147468=CARTESIAN_POINT('Ctrl Pts',(80.4403159672142,-3.65551763338324,
126.14926233736));
#147469=CARTESIAN_POINT('Ctrl Pts',(80.4329141455387,-3.77678662111905,
126.24982294827));
#147470=CARTESIAN_POINT('Ctrl Pts',(80.4255162312274,-3.89799159190011,
126.350330474016));
#147471=CARTESIAN_POINT('Ctrl Pts',(80.418118316916,-4.01524708364486,126.455733769205));
#147472=CARTESIAN_POINT('Ctrl Pts',(80.4107204026046,-4.12814107763788,
126.565683724287));
#147473=CARTESIAN_POINT('Ctrl Pts',(80.4033237176924,-4.24101631069721,
126.675615407681));
#147474=CARTESIAN_POINT('Ctrl Pts',(80.3959270327802,-4.34953121735832,
126.790091991183));
#147475=CARTESIAN_POINT('Ctrl Pts',(80.388530347868,-4.45330902131296,126.908725967962));
#147476=CARTESIAN_POINT('Ctrl Pts',(80.3811339909325,-4.55708222365094,
127.027354684387));
#147477=CARTESIAN_POINT('Ctrl Pts',(80.3737376339971,-4.65611849514698,
127.150140146586));
#147478=CARTESIAN_POINT('Ctrl Pts',(80.3663412770616,-4.75008009844821,
127.276660287205));
#147479=CARTESIAN_POINT('Ctrl Pts',(80.358943787725,-4.84405608751084,127.403199798381));
#147480=CARTESIAN_POINT('Ctrl Pts',(80.3515462983884,-4.93295563879555,
127.533474826775));
#147481=CARTESIAN_POINT('Ctrl Pts',(80.3441488090518,-5.01648334550757,
127.667032868231));
#147482=CARTESIAN_POINT('Ctrl Pts',(80.3367487265368,-5.10004033272776,
127.800637728253));
#147483=CARTESIAN_POINT('Ctrl Pts',(80.3293486440218,-5.17822152833742,
127.937527576381));
#147484=CARTESIAN_POINT('Ctrl Pts',(80.3219485615068,-5.25077670126935,
128.077223914739));
#147485=CARTESIAN_POINT('Ctrl Pts',(80.3145403418403,-5.32341165607266,
128.217073863582));
#147486=CARTESIAN_POINT('Ctrl Pts',(80.3071321221738,-5.39040806140536,
128.359736134166));
#147487=CARTESIAN_POINT('Ctrl Pts',(80.2997239025073,-5.45156290764021,
128.504710116611));
#147488=CARTESIAN_POINT('Ctrl Pts',(80.2923111232052,-5.51275539366258,
128.649773328124));
#147489=CARTESIAN_POINT('Ctrl Pts',(80.2848983439031,-5.56809902540777,
128.797150737987));
#147490=CARTESIAN_POINT('Ctrl Pts',(80.2774855646011,-5.61744036726017,
128.946325557946));
#147491=CARTESIAN_POINT('Ctrl Pts',(80.2700621935723,-5.66685221033565,
129.095713525884));
#147492=CARTESIAN_POINT('Ctrl Pts',(80.2626388225435,-5.71024453190905,
129.246903675374));
#147493=CARTESIAN_POINT('Ctrl Pts',(80.2552154515147,-5.74751459409594,
129.399367182295));
#147494=CARTESIAN_POINT('Ctrl Pts',(80.251279402074,-5.76727607534973,129.480206991974));
#147495=CARTESIAN_POINT('Ctrl Pts',(80.2473433526334,-5.78531723136706,
129.561404658535));
#147496=CARTESIAN_POINT('Ctrl Pts',(80.2434073031927,-5.80162866347082,
129.642880779733));
#147497=CARTESIAN_POINT('Ctrl Pts',(80.2326855063625,-5.8460609968706,129.864821695657));
#147498=CARTESIAN_POINT('Ctrl Pts',(80.2219637095323,-5.87776907583713,
130.089387932859));
#147499=CARTESIAN_POINT('Ctrl Pts',(80.2112419127021,-5.89651005129167,
130.315382317929));
#147500=CARTESIAN_POINT('Ctrl Pts',(80.2036196725385,-5.90983321139959,
130.476044145968));
#147501=CARTESIAN_POINT('Ctrl Pts',(80.195997432375,-5.9166037256679,130.637427484151));
#147502=CARTESIAN_POINT('Ctrl Pts',(80.1883751922114,-5.9167476551358,130.799092985738));
#147503=CARTESIAN_POINT('',(78.4383751922115,-5.90698454152535,130.803787244568));
#147504=CARTESIAN_POINT('Ctrl Pts',(80.1883742158069,-5.91885782199598,
130.799111823733));
#147505=CARTESIAN_POINT('Ctrl Pts',(80.1139027036646,-5.9042356999513,132.379208715788));
#147506=CARTESIAN_POINT('Ctrl Pts',(79.946615316918,-4.43891693990135,135.952540942315));
#147507=CARTESIAN_POINT('Ctrl Pts',(79.686512055567,1.60289591088837,137.616723293554));
#147508=CARTESIAN_POINT('Ctrl Pts',(79.4080644317542,6.59783804819266,133.138047318943));
#147509=CARTESIAN_POINT('Ctrl Pts',(79.1296168079412,5.52968934151192,126.514827272704));
#147510=CARTESIAN_POINT('Ctrl Pts',(78.8511691841285,-0.619973729671027,
123.833478815034));
#147511=CARTESIAN_POINT('Ctrl Pts',(78.6207553122183,-5.23734121523145,
126.915524519283));
#147512=CARTESIAN_POINT('Ctrl Pts',(78.4831573149128,-5.90780690404512,
129.84878494448));
#147513=CARTESIAN_POINT('Ctrl Pts',(78.4383751922115,-5.90698454152535,
130.803787244568));
#147514=CARTESIAN_POINT('',(76.6883751922115,-5.91674660505805,130.809825728295));
#147515=CARTESIAN_POINT('Ctrl Pts',(78.4383751922115,-5.90698454152535,
130.803787244568));
#147516=CARTESIAN_POINT('Ctrl Pts',(78.3903414403085,-5.90610246727639,
131.828132246147));
#147517=CARTESIAN_POINT('Ctrl Pts',(78.2494918138015,-5.16459899004978,
134.833020418668));
#147518=CARTESIAN_POINT('Ctrl Pts',(78.0158263126896,-0.375496194544659,
137.79267680519));
#147519=CARTESIAN_POINT('Ctrl Pts',(77.7373786888769,5.67650346289202,134.897631799166));
#147520=CARTESIAN_POINT('Ctrl Pts',(77.4589310650639,6.5120737505428,128.241070544663));
#147521=CARTESIAN_POINT('Ctrl Pts',(77.180483441251,1.36336639393345,123.940047643478));
#147522=CARTESIAN_POINT('Ctrl Pts',(76.9236314836335,-4.5417187762996,125.791339613774));
#147523=CARTESIAN_POINT('Ctrl Pts',(76.7595954006204,-5.90275439660642,
129.297330232585));
#147524=CARTESIAN_POINT('Ctrl Pts',(76.6883751922115,-5.91674660505805,
130.809825728295));
#147525=CARTESIAN_POINT('',(74.9383751922115,-5.92581065981966,130.802476432268));
#147526=CARTESIAN_POINT('Ctrl Pts',(76.6883751922115,-5.91674660505805,
130.809825728295));
#147527=CARTESIAN_POINT('Ctrl Pts',(76.6667795260161,-5.92098937645411,
131.268450444188));
#147528=CARTESIAN_POINT('Ctrl Pts',(76.5523679852163,-5.66243486174998,
133.693463258362));
#147529=CARTESIAN_POINT('Ctrl Pts',(76.3451405698123,-2.32364321265071,
137.405742499465));
#147530=CARTESIAN_POINT('Ctrl Pts',(76.0666929459994,4.29794362351234,136.327515616246));
#147531=CARTESIAN_POINT('Ctrl Pts',(75.7882453221866,6.96993023588617,130.173779110365));
#147532=CARTESIAN_POINT('Ctrl Pts',(75.5097976983735,3.23689146150164,124.599516203979));
#147533=CARTESIAN_POINT('Ctrl Pts',(75.2313500745608,-3.47069243506588,
124.72720219018));
#147534=CARTESIAN_POINT('Ctrl Pts',(75.04087590584,-5.87733449716643,128.63474192815));
#147535=CARTESIAN_POINT('Ctrl Pts',(74.9432176117236,-5.9262362747903,130.700047010826));
#147536=CARTESIAN_POINT('Ctrl Pts',(74.9383751922115,-5.92581065981966,
130.802476432268));
#147537=CARTESIAN_POINT('',(73.1883764114855,-5.91339957507466,130.799782862282));
#147538=CARTESIAN_POINT('Ctrl Pts',(74.9383751922115,-5.92581065981966,
130.802476432268));
#147539=CARTESIAN_POINT('Ctrl Pts',(74.8504017371193,-5.91807840543484,
132.663337533789));
#147540=CARTESIAN_POINT('Ctrl Pts',(74.6696124074228,-3.96884304173467,
136.501441794556));
#147541=CARTESIAN_POINT('Ctrl Pts',(74.3960072031221,2.57319737235008,137.312525936093));
#147542=CARTESIAN_POINT('Ctrl Pts',(74.1175595793092,6.86637983689192,132.15727911691));
#147543=CARTESIAN_POINT('Ctrl Pts',(73.8391119554963,4.84969467263334,125.758766290573));
#147544=CARTESIAN_POINT('Ctrl Pts',(73.5606643316834,-1.62362297501932,
123.996908159756));
#147545=CARTESIAN_POINT('Ctrl Pts',(73.3437527748612,-5.50406124702534,
127.497637476799));
#147546=CARTESIAN_POINT('Ctrl Pts',(73.2196570926434,-5.91574354109244,
130.13384201527));
#147547=CARTESIAN_POINT('Ctrl Pts',(73.1883772850298,-5.91100043112035,
130.79976611199));
#147548=CARTESIAN_POINT('',(71.4383739998493,-5.91253438439088,130.808046854168));
#147549=CARTESIAN_POINT('Ctrl Pts',(73.1883751922115,-5.91674824715087,
130.799806241969));
#147550=CARTESIAN_POINT('Ctrl Pts',(73.1806832710384,-5.91687441850351,
130.963719848506));
#147551=CARTESIAN_POINT('Ctrl Pts',(73.1729913498653,-5.91018413384904,
131.127709820108));
#147552=CARTESIAN_POINT('Ctrl Pts',(73.1652994286922,-5.89668968518873,
131.291167888556));
#147553=CARTESIAN_POINT('Ctrl Pts',(73.1579038379578,-5.88371510871657,
131.448328752439));
#147554=CARTESIAN_POINT('Ctrl Pts',(73.1505082472235,-5.86445090490816,
131.604997533534));
#147555=CARTESIAN_POINT('Ctrl Pts',(73.1431126564891,-5.83896106797313,
131.7606368377));
#147556=CARTESIAN_POINT('Ctrl Pts',(73.1357165832859,-5.81346956814847,
131.916286295364));
#147557=CARTESIAN_POINT('Ctrl Pts',(73.1283205100827,-5.78175168615157,
132.070905774352));
#147558=CARTESIAN_POINT('Ctrl Pts',(73.1209244368795,-5.74392283019527,
132.223966578127));
#147559=CARTESIAN_POINT('Ctrl Pts',(73.1135264262367,-5.70608406477466,
132.377067476971));
#147560=CARTESIAN_POINT('Ctrl Pts',(73.1061284155939,-5.66213122723873,
132.528608525751));
#147561=CARTESIAN_POINT('Ctrl Pts',(73.0987304049511,-5.61222999085755,
132.678074867984));
#147562=CARTESIAN_POINT('Ctrl Pts',(73.091329001014,-5.56230586594768,132.827609766928));
#147563=CARTESIAN_POINT('Ctrl Pts',(73.0839275970769,-5.5064280273273,132.975067711307));
#147564=CARTESIAN_POINT('Ctrl Pts',(73.0765261931398,-5.44481073729842,
133.119952679545));
#147565=CARTESIAN_POINT('Ctrl Pts',(73.0691159044766,-5.38311948120155,
133.265011569282));
#147566=CARTESIAN_POINT('Ctrl Pts',(73.0617056158135,-5.31567516287439,
133.407490972847));
#147567=CARTESIAN_POINT('Ctrl Pts',(73.0542953271503,-5.24273888727034,
133.546917731357));
#147568=CARTESIAN_POINT('Ctrl Pts',(73.0468797846426,-5.16975090034057,
133.686443342494));
#147569=CARTESIAN_POINT('Ctrl Pts',(73.0394642421349,-5.09126338328313,
133.822911674498));
#147570=CARTESIAN_POINT('Ctrl Pts',(73.0320486996272,-5.00758113594549,
133.955877986933));
#147571=CARTESIAN_POINT('Ctrl Pts',(73.0246225841321,-4.92377957550955,
134.089033881069));
#147572=CARTESIAN_POINT('Ctrl Pts',(73.0171964686369,-4.83476870784311,
134.218677481322));
#147573=CARTESIAN_POINT('Ctrl Pts',(73.0097703531418,-4.74089440338404,
134.344396043725));
#147574=CARTESIAN_POINT('Ctrl Pts',(73.0077699301137,-4.71560684618082,
134.378261704372));
#147575=CARTESIAN_POINT('Ctrl Pts',(73.0057695070856,-4.68996659012072,
134.41184275205));
#147576=CARTESIAN_POINT('Ctrl Pts',(73.0037690840576,-4.6639808508712,134.445131577844));
#147577=CARTESIAN_POINT('Ctrl Pts',(72.9963458176522,-4.56755171438989,
134.568661360663));
#147578=CARTESIAN_POINT('Ctrl Pts',(72.9889225512467,-4.46606567785079,
134.688544268325));
#147579=CARTESIAN_POINT('Ctrl Pts',(72.9814992848412,-4.35982853943538,
134.80433882616));
#147580=CARTESIAN_POINT('Ctrl Pts',(72.9740847921202,-4.25371696449499,
134.919996524443));
#147581=CARTESIAN_POINT('Ctrl Pts',(72.9666702993992,-4.14286571507969,
135.031575218817));
#147582=CARTESIAN_POINT('Ctrl Pts',(72.9592558066782,-4.02762248411247,
135.138664216528));
#147583=CARTESIAN_POINT('Ctrl Pts',(72.9518484603244,-3.91249032891033,
135.24564999783));
#147584=CARTESIAN_POINT('Ctrl Pts',(72.9444411139707,-3.79297489116168,
135.348154444944));
#147585=CARTESIAN_POINT('Ctrl Pts',(72.9370337676169,-3.6694624831454,135.445801735073));
#147586=CARTESIAN_POINT('Ctrl Pts',(72.9296319459415,-3.54604219534296,
135.54337619617));
#147587=CARTESIAN_POINT('Ctrl Pts',(72.9222301242662,-3.41863116460394,
135.636100482951));
#147588=CARTESIAN_POINT('Ctrl Pts',(72.9148283025908,-3.28765064453706,
135.723637373551));
#147589=CARTESIAN_POINT('Ctrl Pts',(72.9074303882794,-3.15673926806736,
135.811128054108));
#147590=CARTESIAN_POINT('Ctrl Pts',(72.9000324739681,-3.02226246453471,
135.893436585211));
#147591=CARTESIAN_POINT('Ctrl Pts',(72.8926345596568,-2.88467238735192,
135.970267680237));
#147592=CARTESIAN_POINT('Ctrl Pts',(72.8852378747446,-2.74710517514343,
136.047086007328));
#147593=CARTESIAN_POINT('Ctrl Pts',(72.8778411898323,-2.60642604171713,
136.118428523097));
#147594=CARTESIAN_POINT('Ctrl Pts',(72.8704445049201,-2.46311388656519,
136.184044673745));
#147595=CARTESIAN_POINT('Ctrl Pts',(72.8630481479847,-2.31980808602419,
136.249657914904));
#147596=CARTESIAN_POINT('Ctrl Pts',(72.8556517910492,-2.17386983531104,
136.309545140405));
#147597=CARTESIAN_POINT('Ctrl Pts',(72.8482554341138,-2.02580001950833,
136.363503073328));
#147598=CARTESIAN_POINT('Ctrl Pts',(72.8408579447772,-1.87770753383881,
136.417469267349));
#147599=CARTESIAN_POINT('Ctrl Pts',(72.8334604554406,-1.7274831840357,136.465504233444));
#147600=CARTESIAN_POINT('Ctrl Pts',(72.826062966104,-1.57564494931275,136.507453949803));
#147601=CARTESIAN_POINT('Ctrl Pts',(72.8186628835891,-1.42375348793298,
136.549418371569));
#147602=CARTESIAN_POINT('Ctrl Pts',(72.8112628010742,-1.27024737483301,
136.585293197116));
#147603=CARTESIAN_POINT('Ctrl Pts',(72.8038627185592,-1.11565661319277,
136.614975118971));
#147604=CARTESIAN_POINT('Ctrl Pts',(72.7964544988927,-0.960895863117023,
136.644689679151));
#147605=CARTESIAN_POINT('Ctrl Pts',(72.7890462792262,-0.805048449462165,
136.668197665722));
#147606=CARTESIAN_POINT('Ctrl Pts',(72.7816380595598,-0.648652095330869,
136.685447338719));
#147607=CARTESIAN_POINT('Ctrl Pts',(72.7742252802577,-0.492159481853218,
136.702707628602));
#147608=CARTESIAN_POINT('Ctrl Pts',(72.7668125009557,-0.335117626186382,
136.713701903534));
#147609=CARTESIAN_POINT('Ctrl Pts',(72.7593997216537,-0.17806561314373,
136.718430552891));
#147610=CARTESIAN_POINT('Ctrl Pts',(72.7519763506249,-0.0207891968196094,
136.723165958764));
#147611=CARTESIAN_POINT('Ctrl Pts',(72.7445529795961,0.136497033575762,
136.721617862338));
#147612=CARTESIAN_POINT('Ctrl Pts',(72.7371296085674,0.29325692245052,136.713838677423));
#147613=CARTESIAN_POINT('Ctrl Pts',(72.7331935591265,0.376374776934647,
136.709713966923));
#147614=CARTESIAN_POINT('Ctrl Pts',(72.7292575096857,0.459344779550445,
136.70383833658));
#147615=CARTESIAN_POINT('Ctrl Pts',(72.7253214602449,0.542088146912409,
136.696225433011));
#147616=CARTESIAN_POINT('Ctrl Pts',(72.7178981938394,0.698139555423767,
136.68186773447));
#147617=CARTESIAN_POINT('Ctrl Pts',(72.710474927434,0.85385612258439,136.66128429759));
#147618=CARTESIAN_POINT('Ctrl Pts',(72.7030516610285,1.00870113186288,136.634493771198));
#147619=CARTESIAN_POINT('Ctrl Pts',(72.6956371683075,1.16336312719937,136.607734908983));
#147620=CARTESIAN_POINT('Ctrl Pts',(72.6882226755865,1.31715525085031,136.57478362315));
#147621=CARTESIAN_POINT('Ctrl Pts',(72.6808081828655,1.46954403885216,136.535710448136));
#147622=CARTESIAN_POINT('Ctrl Pts',(72.6734008365117,1.62178594880344,136.496674933319));
#147623=CARTESIAN_POINT('Ctrl Pts',(72.6659934901579,1.77262685666831,136.451529368163));
#147624=CARTESIAN_POINT('Ctrl Pts',(72.6585861438041,1.92154176086084,136.400395626728));
#147625=CARTESIAN_POINT('Ctrl Pts',(72.6511843221286,2.07034559869916,136.349300022767));
#147626=CARTESIAN_POINT('Ctrl Pts',(72.6437825004533,2.21722594155913,136.29222525606));
#147627=CARTESIAN_POINT('Ctrl Pts',(72.6363806787778,2.36167137726813,136.229343462543));
#147628=CARTESIAN_POINT('Ctrl Pts',(72.6289827644665,2.50604056135599,136.166494863835));
#147629=CARTESIAN_POINT('Ctrl Pts',(72.6215848501551,2.64797705676082,136.097845492001));
#147630=CARTESIAN_POINT('Ctrl Pts',(72.6141869358437,2.78698803051749,136.023616146878));
#147631=CARTESIAN_POINT('Ctrl Pts',(72.6067902509315,2.92597590317223,135.949399137325));
#147632=CARTESIAN_POINT('Ctrl Pts',(72.5993935660192,3.06203889011029,135.869604170545));
#147633=CARTESIAN_POINT('Ctrl Pts',(72.591996881107,3.1947073364501,135.784498727793));
#147634=CARTESIAN_POINT('Ctrl Pts',(72.5846005241715,3.32736990013198,135.699397058705));
#147635=CARTESIAN_POINT('Ctrl Pts',(72.5772041672361,3.45663790829007,135.608985583404));
#147636=CARTESIAN_POINT('Ctrl Pts',(72.5698078103006,3.58206959767457,135.513575834554));
#147637=CARTESIAN_POINT('Ctrl Pts',(72.562410320964,3.70752049097066,135.418151478229));
#147638=CARTESIAN_POINT('Ctrl Pts',(72.5550128316274,3.82913359886926,135.317727550659));
#147639=CARTESIAN_POINT('Ctrl Pts',(72.5476153422908,3.94649935804197,135.212656589875));
#147640=CARTESIAN_POINT('Ctrl Pts',(72.5402152597758,4.0639062596002,135.107548796628));
#147641=CARTESIAN_POINT('Ctrl Pts',(72.5328151772608,4.17706257008706,134.997790975656));
#147642=CARTESIAN_POINT('Ctrl Pts',(72.5254150947457,4.2855948943364,134.883773193433));
#147643=CARTESIAN_POINT('Ctrl Pts',(72.5180068750793,4.39424656103326,134.769630036937));
#147644=CARTESIAN_POINT('Ctrl Pts',(72.5105986554128,4.49826382978093,134.651217834956));
#147645=CARTESIAN_POINT('Ctrl Pts',(72.5031904357463,4.59731251781099,134.528961022452));
#147646=CARTESIAN_POINT('Ctrl Pts',(72.4957776564442,4.69642216865595,134.40662896292));
#147647=CARTESIAN_POINT('Ctrl Pts',(72.4883648771421,4.79055692247838,134.280447876241));
#147648=CARTESIAN_POINT('Ctrl Pts',(72.48095209784,4.87942571836309,134.150871520204));
#147649=CARTESIAN_POINT('Ctrl Pts',(72.4735287268113,4.96842149415095,134.021110019394));
#147650=CARTESIAN_POINT('Ctrl Pts',(72.4661053557825,5.05213608624131,133.887943875251));
#147651=CARTESIAN_POINT('Ctrl Pts',(72.4586819847537,5.13032378666469,133.751852501606));
#147652=CARTESIAN_POINT('Ctrl Pts',(72.4547459353131,5.17178078151535,133.679693589835));
#147653=CARTESIAN_POINT('Ctrl Pts',(72.4508098858724,5.21168476036814,133.606712655085));
#147654=CARTESIAN_POINT('Ctrl Pts',(72.4468738364318,5.25000462016293,133.532983356379));
#147655=CARTESIAN_POINT('Ctrl Pts',(72.4394505700264,5.32227467981709,133.393932200026));
#147656=CARTESIAN_POINT('Ctrl Pts',(72.432027303621,5.38912585955543,133.25179759154));
#147657=CARTESIAN_POINT('Ctrl Pts',(72.4246040372155,5.45028374076894,133.107041165886));
#147658=CARTESIAN_POINT('Ctrl Pts',(72.4171895444945,5.51136933844579,132.962455830305));
#147659=CARTESIAN_POINT('Ctrl Pts',(72.4097750517735,5.56677488786008,132.815255186186));
#147660=CARTESIAN_POINT('Ctrl Pts',(72.4023605590525,5.61627138132904,132.665926177455));
#147661=CARTESIAN_POINT('Ctrl Pts',(72.3949532126988,5.66572016821398,132.516741097645));
#147662=CARTESIAN_POINT('Ctrl Pts',(72.387545866345,5.70927112085429,132.365432089115));
#147663=CARTESIAN_POINT('Ctrl Pts',(72.3801385199912,5.7467429991667,132.212506726472));
#147664=CARTESIAN_POINT('Ctrl Pts',(72.3727366983158,5.78418692953865,132.059695421335));
#147665=CARTESIAN_POINT('Ctrl Pts',(72.3653348766404,5.81556072493446,131.905270523486));
#147666=CARTESIAN_POINT('Ctrl Pts',(72.357933054965,5.84073277742038,131.749755342148));
#147667=CARTESIAN_POINT('Ctrl Pts',(72.3505351406537,5.8658915417755,131.594322256065));
#147668=CARTESIAN_POINT('Ctrl Pts',(72.3431372263424,5.88485502375799,131.437800400301));
#147669=CARTESIAN_POINT('Ctrl Pts',(72.3357393120311,5.8975426002691,131.280723756895));
#147670=CARTESIAN_POINT('Ctrl Pts',(72.3283426271189,5.91022806833525,131.123673216776));
#147671=CARTESIAN_POINT('Ctrl Pts',(72.3209459422067,5.91663967083529,130.966068443716));
#147672=CARTESIAN_POINT('Ctrl Pts',(72.3135492572945,5.91674858739051,130.808449151822));
#147673=CARTESIAN_POINT('Ctrl Pts',(72.3061529003591,5.91685749911626,130.650836848932));
#147674=CARTESIAN_POINT('Ctrl Pts',(72.2987565434237,5.91066428031545,130.493210401786));
#147675=CARTESIAN_POINT('Ctrl Pts',(72.2913601864883,5.89819224841629,130.336109869332));
#147676=CARTESIAN_POINT('Ctrl Pts',(72.2839626971517,5.88571830701719,130.178985284385));
#147677=CARTESIAN_POINT('Ctrl Pts',(72.2765652078152,5.86696366798362,130.022387146605));
#147678=CARTESIAN_POINT('Ctrl Pts',(72.2691677184786,5.84200355256304,129.866850588638));
#147679=CARTESIAN_POINT('Ctrl Pts',(72.2617676359636,5.8170346874127,129.711259507571));
#147680=CARTESIAN_POINT('Ctrl Pts',(72.2543675534486,5.78585607394117,129.556731115587));
#147681=CARTESIAN_POINT('Ctrl Pts',(72.2469674709336,5.7485940569124,129.403790401072));
#147682=CARTESIAN_POINT('Ctrl Pts',(72.2395592512672,5.7112910664652,129.250681512517));
#147683=CARTESIAN_POINT('Ctrl Pts',(72.2321510316007,5.66789140185292,129.099164150849));
#147684=CARTESIAN_POINT('Ctrl Pts',(72.2247428119342,5.61857151827982,128.949748890957));
#147685=CARTESIAN_POINT('Ctrl Pts',(72.2173300326322,5.56922127914133,128.800241668467));
#147686=CARTESIAN_POINT('Ctrl Pts',(72.2099172533302,5.51394369109511,128.652839474547));
#147687=CARTESIAN_POINT('Ctrl Pts',(72.2025044740281,5.45296318788609,128.508032454158));
#147688=CARTESIAN_POINT('Ctrl Pts',(72.1950811029994,5.39189555287429,128.363018526708));
#147689=CARTESIAN_POINT('Ctrl Pts',(72.1876577319706,5.32510888621411,128.220607515789));
#147690=CARTESIAN_POINT('Ctrl Pts',(72.1802343609418,5.25287372117891,128.081265277361));
#147691=CARTESIAN_POINT('Ctrl Pts',(72.1762983115009,5.21457290341656,128.007382679071));
#147692=CARTESIAN_POINT('Ctrl Pts',(72.1723622620599,5.1747410513595,127.934362353626));
#147693=CARTESIAN_POINT('Ctrl Pts',(72.168426212619,5.13342332446577,127.862270283411));
#147694=CARTESIAN_POINT('Ctrl Pts',(72.1610029462135,5.05549938102976,127.726306888907));
#147695=CARTESIAN_POINT('Ctrl Pts',(72.1535796798081,4.97205220502848,127.593235870351));
#147696=CARTESIAN_POINT('Ctrl Pts',(72.1461564134027,4.88332185307086,127.463537628867));
#147697=CARTESIAN_POINT('Ctrl Pts',(72.1387419206817,4.79469637302071,127.333992679933));
#147698=CARTESIAN_POINT('Ctrl Pts',(72.1313274279606,4.70080035499852,127.207812878322));
#147699=CARTESIAN_POINT('Ctrl Pts',(72.1239129352396,4.60191969447509,127.08545409977));
#147700=CARTESIAN_POINT('Ctrl Pts',(72.1165055888859,4.50313433885499,126.963213255216));
#147701=CARTESIAN_POINT('Ctrl Pts',(72.1090982425321,4.3993741383776,126.844786390294));
#147702=CARTESIAN_POINT('Ctrl Pts',(72.1016908961784,4.29096816524474,126.730600343893));
#147703=CARTESIAN_POINT('Ctrl Pts',(72.0942890745029,4.18264304537642,126.616499461753));
#147704=CARTESIAN_POINT('Ctrl Pts',(72.0868872528275,4.06967930803466,126.50663336981));
#147705=CARTESIAN_POINT('Ctrl Pts',(72.0794854311521,3.95244609078626,126.401395654961));
#147706=CARTESIAN_POINT('Ctrl Pts',(72.0720875168408,3.83527476004097,126.296213494283));
#147707=CARTESIAN_POINT('Ctrl Pts',(72.0646896025295,3.71383871507738,126.195655093518));
#147708=CARTESIAN_POINT('Ctrl Pts',(72.0572916882181,3.58854363135225,126.100076913496));
#147709=CARTESIAN_POINT('Ctrl Pts',(72.0498950033059,3.46326936939703,126.004514616833));
#147710=CARTESIAN_POINT('Ctrl Pts',(72.0424983183937,3.33413763798613,125.913931124515));
#147711=CARTESIAN_POINT('Ctrl Pts',(72.0351016334815,3.20158693576376,125.828642412598));
#147712=CARTESIAN_POINT('Ctrl Pts',(72.0277052765461,3.06904211097796,125.743357482472));
#147713=CARTESIAN_POINT('Ctrl Pts',(72.0203089196106,2.93307893074048,125.663367067928));
#147714=CARTESIAN_POINT('Ctrl Pts',(72.0129125626752,2.79416436558012,125.588943466405));
#147715=CARTESIAN_POINT('Ctrl Pts',(72.0055150733386,2.655228532246,125.51450847044));
#147716=CARTESIAN_POINT('Ctrl Pts',(71.9981175840021,2.51334074333734,125.445642160826));
#147717=CARTESIAN_POINT('Ctrl Pts',(71.9907200946655,2.36899188002583,125.382570504064));
#147718=CARTESIAN_POINT('Ctrl Pts',(71.9833200121505,2.22459241544302,125.319476737629));
#147719=CARTESIAN_POINT('Ctrl Pts',(71.9759199296355,2.07773050063319,125.262181817734));
#147720=CARTESIAN_POINT('Ctrl Pts',(71.9685198471205,1.92891611562463,125.210863215995));
#147721=CARTESIAN_POINT('Ctrl Pts',(71.961111627454,1.77993809390178,125.159488184178));
#147722=CARTESIAN_POINT('Ctrl Pts',(71.9537034077875,1.62900366751656,125.114102716159));
#147723=CARTESIAN_POINT('Ctrl Pts',(71.9462951881211,1.47663777593351,125.074834333379));
#147724=CARTESIAN_POINT('Ctrl Pts',(71.938882408819,1.32417810568568,125.035541781565));
#147725=CARTESIAN_POINT('Ctrl Pts',(71.9314696295169,1.17028557872398,125.002373895618));
#147726=CARTESIAN_POINT('Ctrl Pts',(71.9240568502148,1.01549387980607,124.975406788398));
#147727=CARTESIAN_POINT('Ctrl Pts',(71.916633479186,0.860481007250513,124.94840114931));
#147728=CARTESIAN_POINT('Ctrl Pts',(71.9092101081573,0.704566765790298,
124.927614033484));
#147729=CARTESIAN_POINT('Ctrl Pts',(71.9017867371286,0.548289323079683,
124.91306964014));
#147730=CARTESIAN_POINT('Ctrl Pts',(71.8978506876878,0.465427273128251,
124.905357853802));
#147731=CARTESIAN_POINT('Ctrl Pts',(71.8939146382469,0.382463116307205,
124.89940024951));
#147732=CARTESIAN_POINT('Ctrl Pts',(71.8899785888061,0.299476775256987,
124.895194498427));
#147733=CARTESIAN_POINT('Ctrl Pts',(71.8825553224006,0.142967125951911,
124.88726258314));
#147734=CARTESIAN_POINT('Ctrl Pts',(71.8751320559953,-0.0140945276653115,
124.885540919688));
#147735=CARTESIAN_POINT('Ctrl Pts',(71.8677087895898,-0.171174254063978,
124.890087210186));
#147736=CARTESIAN_POINT('Ctrl Pts',(71.8602942968688,-0.328068325271036,
124.894628127346));
#147737=CARTESIAN_POINT('Ctrl Pts',(71.8528798041477,-0.484980057243426,
124.905422241698));
#147738=CARTESIAN_POINT('Ctrl Pts',(71.8454653114267,-0.641371375327656,
124.922475433256));
#147739=CARTESIAN_POINT('Ctrl Pts',(71.8380579650729,-0.797611957571487,
124.939512188305));
#147740=CARTESIAN_POINT('Ctrl Pts',(71.8306506187191,-0.953332755896087,
124.962795970381));
#147741=CARTESIAN_POINT('Ctrl Pts',(71.8232432723653,-1.10799678709192,
124.992280638566));
#147742=CARTESIAN_POINT('Ctrl Pts',(71.8158414506899,-1.26254546401804,
125.021743315973));
#147743=CARTESIAN_POINT('Ctrl Pts',(71.8084396290145,-1.41603857806588,
125.057397601174));
#147744=CARTESIAN_POINT('Ctrl Pts',(71.8010378073391,-1.56794546555856,
125.099145671612));
#147745=CARTESIAN_POINT('Ctrl Pts',(71.7936398930277,-1.71977216258702,
125.140871703569));
#147746=CARTESIAN_POINT('Ctrl Pts',(71.7862419787163,-1.8700139416556,125.188685015556));
#147747=CARTESIAN_POINT('Ctrl Pts',(71.778844064405,-2.01815162467847,125.242436977106));
#147748=CARTESIAN_POINT('Ctrl Pts',(71.7714473794928,-2.16626468990654,
125.296180006056));
#147749=CARTESIAN_POINT('Ctrl Pts',(71.7640506945806,-2.31227400249792,
125.35585959867));
#147750=CARTESIAN_POINT('Ctrl Pts',(71.7566540096684,-2.45567670361769,
125.421277626397));
#147751=CARTESIAN_POINT('Ctrl Pts',(71.7492576527329,-2.59907304611172,
125.486692753421));
#147752=CARTESIAN_POINT('Ctrl Pts',(71.7418612957974,-2.73986266731835,
125.557845654697));
#147753=CARTESIAN_POINT('Ctrl Pts',(71.7344649388619,-2.87756406671134,
125.634490638111));
#147754=CARTESIAN_POINT('Ctrl Pts',(71.7270674495253,-3.01528654854002,
125.711147356068));
#147755=CARTESIAN_POINT('Ctrl Pts',(71.7196699601888,-3.1499195409213,125.793297648849));
#147756=CARTESIAN_POINT('Ctrl Pts',(71.7122724708522,-3.28100759857521,
125.880650664635));
#147757=CARTESIAN_POINT('Ctrl Pts',(71.7048723883372,-3.41214160894424,
125.968034301885));
#147758=CARTESIAN_POINT('Ctrl Pts',(71.6974723058222,-3.5397278999848,126.060624086451));
#147759=CARTESIAN_POINT('Ctrl Pts',(71.6900722233072,-3.66334150313637,
126.158086885434));
#147760=CARTESIAN_POINT('Ctrl Pts',(71.6826640036407,-3.78709103215239,
126.255656854785));
#147761=CARTESIAN_POINT('Ctrl Pts',(71.6752557839742,-3.90685885601902,
126.358110308322));
#147762=CARTESIAN_POINT('Ctrl Pts',(71.6678475643077,-4.02225394473465,
126.465074528062));
#147763=CARTESIAN_POINT('Ctrl Pts',(71.6604347850057,-4.13772005720158,
126.572104582493));
#147764=CARTESIAN_POINT('Ctrl Pts',(71.6530220057036,-4.24880780886742,
126.683650671363));
#147765=CARTESIAN_POINT('Ctrl Pts',(71.6456092264016,-4.3551646941821,126.79930493143));
#147766=CARTESIAN_POINT('Ctrl Pts',(71.6381858553728,-4.46167354720263,
126.915124443728));
#147767=CARTESIAN_POINT('Ctrl Pts',(71.6307624843441,-4.56343779239502,
127.035063566932));
#147768=CARTESIAN_POINT('Ctrl Pts',(71.6233391133153,-4.66014617750741,
127.158682605623));
#147769=CARTESIAN_POINT('Ctrl Pts',(71.6194030638746,-4.71142328377854,
127.224228386134));
#147770=CARTESIAN_POINT('Ctrl Pts',(71.6154670144339,-4.7612797382694,127.29080825029));
#147771=CARTESIAN_POINT('Ctrl Pts',(71.6115309649932,-4.80967430015931,
127.358353698117));
#147772=CARTESIAN_POINT('Ctrl Pts',(71.6040410472673,-4.90176442565088,
127.486886089441));
#147773=CARTESIAN_POINT('Ctrl Pts',(71.5965511295414,-4.98883527277445,
127.619302996982));
#147774=CARTESIAN_POINT('Ctrl Pts',(71.5890612118156,-5.07054482348986,
127.755179456093));
#147775=CARTESIAN_POINT('Ctrl Pts',(71.5815804528749,-5.15215445852537,
127.890889763406));
#147776=CARTESIAN_POINT('Ctrl Pts',(71.5740996939342,-5.22841566190887,
128.030050891975));
#147777=CARTESIAN_POINT('Ctrl Pts',(71.5666189349935,-5.29902767983761,
128.172206326721));
#147778=CARTESIAN_POINT('Ctrl Pts',(71.5591459364582,-5.36956644612311,
128.314214291964));
#147779=CARTESIAN_POINT('Ctrl Pts',(71.5516729379229,-5.43446753397698,
128.459210054913));
#147780=CARTESIAN_POINT('Ctrl Pts',(71.5441999393877,-5.49347442677738,
128.606709761574));
#147781=CARTESIAN_POINT('Ctrl Pts',(71.5367333079833,-5.55243104462984,
128.754083795797));
#147782=CARTESIAN_POINT('Ctrl Pts',(71.5292666765789,-5.60550333329829,
128.903957188612));
#147783=CARTESIAN_POINT('Ctrl Pts',(71.5218000451745,-5.65248154376742,
129.055823240251));
#147784=CARTESIAN_POINT('Ctrl Pts',(71.5143389009662,-5.69942523014719,
129.207577686167));
#147785=CARTESIAN_POINT('Ctrl Pts',(71.5068777567579,-5.74028365480453,
129.361321525862));
#147786=CARTESIAN_POINT('Ctrl Pts',(71.4994166125495,-5.77489592895132,
129.516530049408));
#147787=CARTESIAN_POINT('Ctrl Pts',(71.4919587331199,-5.80949305777818,
129.67167065824));
#147788=CARTESIAN_POINT('Ctrl Pts',(71.4845008536903,-5.8378494005576,129.828274319361));
#147789=CARTESIAN_POINT('Ctrl Pts',(71.4770429742607,-5.85985444105077,
129.985803049525));
#147790=CARTESIAN_POINT('Ctrl Pts',(71.4695862429928,-5.88185609380548,
130.143307527693));
#147791=CARTESIAN_POINT('Ctrl Pts',(71.4621295117249,-5.89750833699887,
130.301736431149));
#147792=CARTESIAN_POINT('Ctrl Pts',(71.454672780457,-5.90675209166039,130.4605433839));
#147793=CARTESIAN_POINT('Ctrl Pts',(71.4492402510418,-5.91348653967805,
130.576240652738));
#147794=CARTESIAN_POINT('Ctrl Pts',(71.4438077216267,-5.91682061820416,
130.692138378587));
#147795=CARTESIAN_POINT('Ctrl Pts',(71.4383751922115,-5.91674886586254,
130.808024060528));
#147796=CARTESIAN_POINT('',(69.688376602423,-5.92104773189643,130.807528757205));
#147797=CARTESIAN_POINT('Ctrl Pts',(71.4383730761828,-5.90926962530269,
130.80806451132));
#147798=CARTESIAN_POINT('Ctrl Pts',(71.4032764978486,-5.91346979626751,
131.55579444876));
#147799=CARTESIAN_POINT('Ctrl Pts',(71.27536404491,-5.43425968048745,134.275764099217));
#147800=CARTESIAN_POINT('Ctrl Pts',(71.0546357173675,-1.34246747144102,
137.67279141495));
#147801=CARTESIAN_POINT('Ctrl Pts',(70.7761880935544,5.05296889400591,135.646371138679));
#147802=CARTESIAN_POINT('Ctrl Pts',(70.4977404697419,6.8049736971114,129.170379738871));
#147803=CARTESIAN_POINT('Ctrl Pts',(70.2192928459285,2.30354011402361,124.195936942177));
#147804=CARTESIAN_POINT('Ctrl Pts',(69.9495052563708,-4.10889852220346,
125.260151943503));
#147805=CARTESIAN_POINT('Ctrl Pts',(69.7725335414168,-5.91277317614864,
129.026272740359));
#147806=CARTESIAN_POINT('Ctrl Pts',(69.6883777010673,-5.92439661000214,
130.807507312234));
#147807=CARTESIAN_POINT('',(67.9383744040955,-5.9184596220467,130.79916933959));
#147808=CARTESIAN_POINT('Ctrl Pts',(69.6883751922115,-5.91674913700228,
130.807556283809));
#147809=CARTESIAN_POINT('Ctrl Pts',(69.679715994242,-5.91665027484425,130.99059873685));
#147810=CARTESIAN_POINT('Ctrl Pts',(69.6710567962725,-5.90805820439472,
131.173407171725));
#147811=CARTESIAN_POINT('Ctrl Pts',(69.662397598303,-5.89103302688227,131.355414552025));
#147812=CARTESIAN_POINT('Ctrl Pts',(69.6549743318976,-5.87643786128845,
131.511443929858));
#147813=CARTESIAN_POINT('Ctrl Pts',(69.6475510654921,-5.85561747413632,
131.667128992214));
#147814=CARTESIAN_POINT('Ctrl Pts',(69.6401277990867,-5.82859133102236,
131.821933051563));
#147815=CARTESIAN_POINT('Ctrl Pts',(69.6327133063656,-5.80159713056516,
131.97655414537));
#147816=CARTESIAN_POINT('Ctrl Pts',(69.6252988136446,-5.7684118374569,132.130295944685));
#147817=CARTESIAN_POINT('Ctrl Pts',(69.6178843209236,-5.72910679789495,
132.282625093502));
#147818=CARTESIAN_POINT('Ctrl Pts',(69.6104769745698,-5.68983964200995,
132.43480742175));
#147819=CARTESIAN_POINT('Ctrl Pts',(69.6030696282161,-5.64446457494824,
132.585579451078));
#147820=CARTESIAN_POINT('Ctrl Pts',(69.5956622818623,-5.59310426959112,
132.734416365979));
#147821=CARTESIAN_POINT('Ctrl Pts',(69.5882604601869,-5.5417822706874,132.883142272693));
#147822=CARTESIAN_POINT('Ctrl Pts',(69.5808586385115,-5.48448404319401,
133.029935587389));
#147823=CARTESIAN_POINT('Ctrl Pts',(69.5734568168361,-5.42138250112914,
133.174285160447));
#147824=CARTESIAN_POINT('Ctrl Pts',(69.5660589025248,-5.35831426987715,
133.318558532489));
#147825=CARTESIAN_POINT('Ctrl Pts',(69.5586609882133,-5.28944897435379,
133.460390390876));
#147826=CARTESIAN_POINT('Ctrl Pts',(69.551263073902,-5.21500816414918,133.599288239233));
#147827=CARTESIAN_POINT('Ctrl Pts',(69.5438663889898,-5.14057972465685,
133.738163005287));
#147828=CARTESIAN_POINT('Ctrl Pts',(69.5364697040776,-5.06057778557375,
133.87410440031));
#147829=CARTESIAN_POINT('Ctrl Pts',(69.5290730191654,-4.97527054258163,
134.006643177026));
#147830=CARTESIAN_POINT('Ctrl Pts',(69.52167666223,-4.88996708220199,134.139176076833));
#147831=CARTESIAN_POINT('Ctrl Pts',(69.5142803052945,-4.79935898769267,
134.268306344426));
#147832=CARTESIAN_POINT('Ctrl Pts',(69.506883948359,-4.70375846364788,134.393592691166));
#147833=CARTESIAN_POINT('Ctrl Pts',(69.4994864590224,-4.60814330291887,
134.518898219566));
#147834=CARTESIAN_POINT('Ctrl Pts',(69.492088969686,-4.50753441718986,134.640358358516));
#147835=CARTESIAN_POINT('Ctrl Pts',(69.4846914803494,-4.40228496737017,
134.757564081665));
#147836=CARTESIAN_POINT('Ctrl Pts',(69.4772913978344,-4.29699862251869,
134.874810891099));
#147837=CARTESIAN_POINT('Ctrl Pts',(69.4698913153193,-4.18706872400283,
134.987800037833));
#147838=CARTESIAN_POINT('Ctrl Pts',(69.4624912328043,-4.07288590608889,
135.096158720749));
#147839=CARTESIAN_POINT('Ctrl Pts',(69.4550830131379,-3.95857753242862,
135.204636555175));
#147840=CARTESIAN_POINT('Ctrl Pts',(69.4476747934714,-3.8400071709917,135.308473500258));
#147841=CARTESIAN_POINT('Ctrl Pts',(69.4402665738049,-3.71759976481711,
135.407336019535));
#147842=CARTESIAN_POINT('Ctrl Pts',(69.4328537945029,-3.59511701892641,
135.506259387043));
#147843=CARTESIAN_POINT('Ctrl Pts',(69.4254410152008,-3.46879282129271,
135.600202005724));
#147844=CARTESIAN_POINT('Ctrl Pts',(69.4180282358987,-3.33908137212494,
135.688873505545));
#147845=CARTESIAN_POINT('Ctrl Pts',(69.41060486487,-3.20918458515573,135.777671703362));
#147846=CARTESIAN_POINT('Ctrl Pts',(69.4031814938412,-3.0758911958595,135.86118354231));
#147847=CARTESIAN_POINT('Ctrl Pts',(69.3957581228125,-2.93968099143647,
135.939164044289));
#147848=CARTESIAN_POINT('Ctrl Pts',(69.3918220733717,-2.86745907273259,
135.980511177555));
#147849=CARTESIAN_POINT('Ctrl Pts',(69.3878860239309,-2.79441749542759,
136.020304045642));
#147850=CARTESIAN_POINT('Ctrl Pts',(69.3839499744901,-2.72062996579226,
136.058511657623));
#147851=CARTESIAN_POINT('Ctrl Pts',(69.3765267080847,-2.58146898772969,
136.130570021401));
#147852=CARTESIAN_POINT('Ctrl Pts',(69.3691034416792,-2.43923280771762,
136.197204819048));
#147853=CARTESIAN_POINT('Ctrl Pts',(69.3616801752738,-2.29438347780483,
136.258142334804));
#147854=CARTESIAN_POINT('Ctrl Pts',(69.3542656825528,-2.1497053477709,136.319007827476));
#147855=CARTESIAN_POINT('Ctrl Pts',(69.3468511898318,-2.00242055629298,
136.37418929841));
#147856=CARTESIAN_POINT('Ctrl Pts',(69.3394366971108,-1.85301639524541,
136.423458481232));
#147857=CARTESIAN_POINT('Ctrl Pts',(69.332029350757,-1.70375623555302,136.47268017656));
#147858=CARTESIAN_POINT('Ctrl Pts',(69.3246220044032,-1.55238112509918,
136.516000812216));
#147859=CARTESIAN_POINT('Ctrl Pts',(69.3172146580494,-1.39939891372179,
136.553239920767));
#147860=CARTESIAN_POINT('Ctrl Pts',(69.309812836374,-1.24653080224944,136.590451254986));
#147861=CARTESIAN_POINT('Ctrl Pts',(69.3024110146986,-1.09205833764615,
136.621590005645));
#147862=CARTESIAN_POINT('Ctrl Pts',(69.2950091930232,-0.936505028813258,
136.64652536135));
#147863=CARTESIAN_POINT('Ctrl Pts',(69.2876112787119,-0.781033835361272,
136.671447553874));
#147864=CARTESIAN_POINT('Ctrl Pts',(69.2802133644006,-0.624483301654845,
136.690172814277));
#147865=CARTESIAN_POINT('Ctrl Pts',(69.2728154500892,-0.46738753180734,
136.702621332184));
#147866=CARTESIAN_POINT('Ctrl Pts',(69.265418765177,-0.310317868426777,
136.715067781374));
#147867=CARTESIAN_POINT('Ctrl Pts',(69.2580220802647,-0.152703520502925,
136.721239528814));
#147868=CARTESIAN_POINT('Ctrl Pts',(69.2506253953525,0.00491575462348875,
136.721108575512));
#147869=CARTESIAN_POINT('Ctrl Pts',(69.2432290384171,0.162528040745957,
136.720977628017));
#147870=CARTESIAN_POINT('Ctrl Pts',(69.2358326814816,0.320144880339142,
136.714544535768));
#147871=CARTESIAN_POINT('Ctrl Pts',(69.2284363245462,0.477226250564283,
136.701833438044));
#147872=CARTESIAN_POINT('Ctrl Pts',(69.2210388352096,0.634331670348327,
136.689120394218));
#147873=CARTESIAN_POINT('Ctrl Pts',(69.213641345873,0.790901085422228,136.670127461194));
#147874=CARTESIAN_POINT('Ctrl Pts',(69.2062438565364,0.946399478234522,
136.644930674512));
#147875=CARTESIAN_POINT('Ctrl Pts',(69.1988437740214,1.10195238076725,136.619725055136));
#147876=CARTESIAN_POINT('Ctrl Pts',(69.1914436915064,1.25643314526804,136.588311311862));
#147877=CARTESIAN_POINT('Ctrl Pts',(69.1840436089914,1.40931697623449,136.550816588249));
#147878=CARTESIAN_POINT('Ctrl Pts',(69.176635389325,1.56236891869003,136.513280635333));
#147879=CARTESIAN_POINT('Ctrl Pts',(69.1692271696585,1.7138200580025,136.469650437345));
#147880=CARTESIAN_POINT('Ctrl Pts',(69.161818949992,1.86316008840639,136.420103226293));
#147881=CARTESIAN_POINT('Ctrl Pts',(69.15440617069,2.01259203510712,136.370525519759));
#147882=CARTESIAN_POINT('Ctrl Pts',(69.1469933913879,2.15990993525838,136.315023674676));
#147883=CARTESIAN_POINT('Ctrl Pts',(69.1395806120859,2.30462398601776,136.253822870447));
#147884=CARTESIAN_POINT('Ctrl Pts',(69.1321572410571,2.44954481099938,136.192534619638));
#147885=CARTESIAN_POINT('Ctrl Pts',(69.1247338700283,2.59185401907099,136.125531305));
#147886=CARTESIAN_POINT('Ctrl Pts',(69.1173104989996,2.73108616651883,136.053084168445));
#147887=CARTESIAN_POINT('Ctrl Pts',(69.1133744495587,2.80491039192578,136.014670958298));
#147888=CARTESIAN_POINT('Ctrl Pts',(69.1094384001179,2.87787001551399,135.974728027862));
#147889=CARTESIAN_POINT('Ctrl Pts',(69.1055023506771,2.94989912369862,135.933300636956));
#147890=CARTESIAN_POINT('Ctrl Pts',(69.0980790842717,3.08574377378226,135.855169870613));
#147891=CARTESIAN_POINT('Ctrl Pts',(69.0906558178662,3.21868764584694,135.771520279805));
#147892=CARTESIAN_POINT('Ctrl Pts',(69.0832325514608,3.34825070465196,135.682592651951));
#147893=CARTESIAN_POINT('Ctrl Pts',(69.0758180587398,3.47766063068111,135.593770129168));
#147894=CARTESIAN_POINT('Ctrl Pts',(69.0684035660188,3.60369739242263,135.499682195697));
#147895=CARTESIAN_POINT('Ctrl Pts',(69.0609890732977,3.72590554975223,135.400615440444));
#147896=CARTESIAN_POINT('Ctrl Pts',(69.053581726944,3.84799591825892,135.301644169459));
#147897=CARTESIAN_POINT('Ctrl Pts',(69.0461743805902,3.96626474068308,135.197703863605));
#147898=CARTESIAN_POINT('Ctrl Pts',(69.0387670342364,4.08028567942142,135.08912424428));
#147899=CARTESIAN_POINT('Ctrl Pts',(69.031365212561,4.19422157704181,134.980625607731));
#147900=CARTESIAN_POINT('Ctrl Pts',(69.0239633908856,4.30391563018407,134.86749480371));
#147901=CARTESIAN_POINT('Ctrl Pts',(69.0165615692102,4.40897481416923,134.750101568328));
#147902=CARTESIAN_POINT('Ctrl Pts',(69.0091636548988,4.51397853822902,134.632770303922));
#147903=CARTESIAN_POINT('Ctrl Pts',(69.0017657405875,4.61435201756119,134.511181366811));
#147904=CARTESIAN_POINT('Ctrl Pts',(68.9943678262761,4.70973940911688,134.385740974455));
#147905=CARTESIAN_POINT('Ctrl Pts',(68.9869711413639,4.80511094901846,134.260321428017));
#147906=CARTESIAN_POINT('Ctrl Pts',(68.9795744564518,4.89549781992989,134.131051993483));
#147907=CARTESIAN_POINT('Ctrl Pts',(68.9721777715395,4.98058471347895,133.998371649851));
#147908=CARTESIAN_POINT('Ctrl Pts',(68.9647814146041,5.06566783418599,133.865697189405));
#147909=CARTESIAN_POINT('Ctrl Pts',(68.9573850576686,5.14545124328763,133.729612434816));
#147910=CARTESIAN_POINT('Ctrl Pts',(68.9499887007332,5.21966335430782,133.590584770465));
#147911=CARTESIAN_POINT('Ctrl Pts',(68.9425912113966,5.29388682739167,133.451535820623));
#147912=CARTESIAN_POINT('Ctrl Pts',(68.93519372206,5.36253712819855,133.309543393217));
#147913=CARTESIAN_POINT('Ctrl Pts',(68.9277962327235,5.4253890375276,133.165098712734));
#147914=CARTESIAN_POINT('Ctrl Pts',(68.9203961502085,5.48826297949603,133.020603397391));
#147915=CARTESIAN_POINT('Ctrl Pts',(68.9129960676935,5.54533433421071,132.873654459531));
#147916=CARTESIAN_POINT('Ctrl Pts',(68.9055959851785,5.59642640636216,132.724762148671));
#147917=CARTESIAN_POINT('Ctrl Pts',(68.898187765512,5.64757465949938,132.57570611541));
#147918=CARTESIAN_POINT('Ctrl Pts',(68.8907795458456,5.6927303784587,132.424702794848));
#147919=CARTESIAN_POINT('Ctrl Pts',(68.8833713261791,5.73176684081676,132.272277319908));
#147920=CARTESIAN_POINT('Ctrl Pts',(68.875958546877,5.77082732946607,132.119758029631));
#147921=CARTESIAN_POINT('Ctrl Pts',(68.868545767575,5.80376097877548,131.965815204999));
#147922=CARTESIAN_POINT('Ctrl Pts',(68.8611329882729,5.83049248815307,131.810982645981));
#147923=CARTESIAN_POINT('Ctrl Pts',(68.8537096172442,5.85726219276484,131.655928854942));
#147924=CARTESIAN_POINT('Ctrl Pts',(68.8462862462154,5.87781200958529,131.499983159576));
#147925=CARTESIAN_POINT('Ctrl Pts',(68.8388628751866,5.89211855842186,131.343683763742));
#147926=CARTESIAN_POINT('Ctrl Pts',(68.8349268257459,5.89970423389587,131.260810073718));
#147927=CARTESIAN_POINT('Ctrl Pts',(68.8309907763051,5.9055355739646,131.17783694651));
#147928=CARTESIAN_POINT('Ctrl Pts',(68.8270547268644,5.90961502909356,131.094844301121));
#147929=CARTESIAN_POINT('Ctrl Pts',(68.819631460459,5.91730875415144,130.938322762026));
#147930=CARTESIAN_POINT('Ctrl Pts',(68.8122081940535,5.91879139451045,130.781258670205));
#147931=CARTESIAN_POINT('Ctrl Pts',(68.804784927648,5.91400606067311,130.624186044383));
#147932=CARTESIAN_POINT('Ctrl Pts',(68.797370434927,5.90922638270297,130.46729906536));
#147933=CARTESIAN_POINT('Ctrl Pts',(68.789955942206,5.89819348790567,130.310403941893));
#147934=CARTESIAN_POINT('Ctrl Pts',(68.782541449485,5.8809023151317,130.154038756963));
#147935=CARTESIAN_POINT('Ctrl Pts',(68.7751341031312,5.86362780824105,129.997824282684));
#147936=CARTESIAN_POINT('Ctrl Pts',(68.7677267567775,5.84010707258086,129.842139098635));
#147937=CARTESIAN_POINT('Ctrl Pts',(68.7603194104237,5.8103870662121,129.687520117183));
#147938=CARTESIAN_POINT('Ctrl Pts',(68.7529175887483,5.78068922614536,129.533016456402));
#147939=CARTESIAN_POINT('Ctrl Pts',(68.7455157670729,5.7448013918412,129.379577779849));
#147940=CARTESIAN_POINT('Ctrl Pts',(68.7381139453975,5.70282219332268,129.227734601719));
#147941=CARTESIAN_POINT('Ctrl Pts',(68.7307160310861,5.66086515529631,129.07597158042));
#147942=CARTESIAN_POINT('Ctrl Pts',(68.7233181167747,5.61282325626493,128.92580273905));
#147943=CARTESIAN_POINT('Ctrl Pts',(68.7159202024634,5.55884591662218,128.777747028903));
#147944=CARTESIAN_POINT('Ctrl Pts',(68.7085235175512,5.50487754703404,128.629715922929));
#147945=CARTESIAN_POINT('Ctrl Pts',(68.7011268326389,5.44497582220963,128.483797601595));
#147946=CARTESIAN_POINT('Ctrl Pts',(68.6937301477267,5.37933963573566,128.340494621635));
#147947=CARTESIAN_POINT('Ctrl Pts',(68.6863337907913,5.31370635963893,128.19719799588));
#147948=CARTESIAN_POINT('Ctrl Pts',(68.6789374338559,5.24233928292074,128.056516820309));
#147949=CARTESIAN_POINT('Ctrl Pts',(68.6715410769204,5.16548483017149,127.91893222099));
#147950=CARTESIAN_POINT('Ctrl Pts',(68.6641435875838,5.08861861080932,127.781326557117));
#147951=CARTESIAN_POINT('Ctrl Pts',(68.6567460982472,5.0062635246613,127.6468187394));
#147952=CARTESIAN_POINT('Ctrl Pts',(68.6493486089106,4.91871111632016,127.515863769964));
#147953=CARTESIAN_POINT('Ctrl Pts',(68.6419485263956,4.83112801661799,127.384862894466));
#147954=CARTESIAN_POINT('Ctrl Pts',(68.6345484438806,4.7383441746543,127.257417657059));
#147955=CARTESIAN_POINT('Ctrl Pts',(68.6271483613656,4.64069336966992,127.133952518839));
#147956=CARTESIAN_POINT('Ctrl Pts',(68.6197401416991,4.54293518758671,127.010351618007));
#147957=CARTESIAN_POINT('Ctrl Pts',(68.6123319220326,4.44029958644868,126.890739849545));
#147958=CARTESIAN_POINT('Ctrl Pts',(68.6049237023661,4.33315987889097,126.775507675788));
#147959=CARTESIAN_POINT('Ctrl Pts',(68.597510923064,4.22595422863083,126.660204578552));
#147960=CARTESIAN_POINT('Ctrl Pts',(68.590098143762,4.11423921228098,126.549286709682));
#147961=CARTESIAN_POINT('Ctrl Pts',(68.5826853644599,3.99842322906532,126.443105953622));
#147962=CARTESIAN_POINT('Ctrl Pts',(68.5752619934312,3.8824417625417,126.336773481519));
#147963=CARTESIAN_POINT('Ctrl Pts',(68.5678386224024,3.76234791036724,126.235191881096));
#147964=CARTESIAN_POINT('Ctrl Pts',(68.5604152513737,3.6385818411254,126.138671735104));
#147965=CARTESIAN_POINT('Ctrl Pts',(68.5564792019329,3.57295810148776,126.08749443773));
#147966=CARTESIAN_POINT('Ctrl Pts',(68.5525431524921,3.50630244139167,126.03773936419));
#147967=CARTESIAN_POINT('Ctrl Pts',(68.5486071030514,3.43868342349489,125.989447651013));
#147968=CARTESIAN_POINT('Ctrl Pts',(68.5411838366459,3.31115606605807,125.898370987093));
#147969=CARTESIAN_POINT('Ctrl Pts',(68.5337605702405,3.17981500065238,125.812226621635));
#147970=CARTESIAN_POINT('Ctrl Pts',(68.526337303835,3.04507876219255,125.731351067551));
#147971=CARTESIAN_POINT('Ctrl Pts',(68.518922811114,2.91050177077733,125.650571101655));
#147972=CARTESIAN_POINT('Ctrl Pts',(68.511508318393,2.77253791077296,125.575047741906));
#147973=CARTESIAN_POINT('Ctrl Pts',(68.504093825672,2.63163715095387,125.505076093385));
#147974=CARTESIAN_POINT('Ctrl Pts',(68.4966864793182,2.49087219659181,125.435171886174));
#147975=CARTESIAN_POINT('Ctrl Pts',(68.4892791329644,2.34717630986715,125.370808902426));
#147976=CARTESIAN_POINT('Ctrl Pts',(68.4818717866106,2.20102659234113,125.312237849245));
#147977=CARTESIAN_POINT('Ctrl Pts',(68.4744699649352,2.05498587878835,125.253710480566));
#147978=CARTESIAN_POINT('Ctrl Pts',(68.4670681432598,1.90649532354502,125.200966579338));
#147979=CARTESIAN_POINT('Ctrl Pts',(68.4596663215844,1.75605457516337,125.154209921209));
#147980=CARTESIAN_POINT('Ctrl Pts',(68.452268407273,1.60569324328165,125.107477945556));
#147981=CARTESIAN_POINT('Ctrl Pts',(68.4448704929616,1.45338412411913,125.06672702899));
#147982=CARTESIAN_POINT('Ctrl Pts',(68.4374725786503,1.29964459146979,125.032111965752));
#147983=CARTESIAN_POINT('Ctrl Pts',(68.4300758937381,1.14593060754188,124.997502654911));
#147984=CARTESIAN_POINT('Ctrl Pts',(68.4226792088259,0.990787045733209,
124.969027255577));
#147985=CARTESIAN_POINT('Ctrl Pts',(68.4152825239136,0.8347442280997,124.946790077133));
#147986=CARTESIAN_POINT('Ctrl Pts',(68.4078861669782,0.678708329568245,
124.924553884708));
#147987=CARTESIAN_POINT('Ctrl Pts',(68.4004898100427,0.521773624058667,
124.908555415847));
#147988=CARTESIAN_POINT('Ctrl Pts',(68.3930934531073,0.364478095067757,
124.898847406954));
#147989=CARTESIAN_POINT('Ctrl Pts',(68.3856959637707,0.207158483729802,
124.889137911739));
#147990=CARTESIAN_POINT('Ctrl Pts',(68.3782984744341,0.0494783115272505,
124.885720817121));
#147991=CARTESIAN_POINT('Ctrl Pts',(68.3709009850975,-0.108022028391509,
124.888596778138));
#147992=CARTESIAN_POINT('Ctrl Pts',(68.3635009025825,-0.26557757981027,
124.891473747319));
#147993=CARTESIAN_POINT('Ctrl Pts',(68.3561008200676,-0.422952800430353,
124.900648157497));
#147994=CARTESIAN_POINT('Ctrl Pts',(68.3487007375525,-0.579610163276937,
124.916068622333));
#147995=CARTESIAN_POINT('Ctrl Pts',(68.3412925178861,-0.73643978699885,
124.931506043556));
#147996=CARTESIAN_POINT('Ctrl Pts',(68.3338842982196,-0.892549604816276,
124.953203199051));
#147997=CARTESIAN_POINT('Ctrl Pts',(68.3264760785531,-1.04740932510994,
124.981057064756));
#147998=CARTESIAN_POINT('Ctrl Pts',(68.3190632992511,-1.20236435897748,
125.00892807405));
#147999=CARTESIAN_POINT('Ctrl Pts',(68.311650519949,-1.35606739854285,125.042963263795));
#148000=CARTESIAN_POINT('Ctrl Pts',(68.3042377406469,-1.50800164370169,
125.083009238294));
#148001=CARTESIAN_POINT('Ctrl Pts',(68.2968143696182,-1.66015297963503,
125.12311243236));
#148002=CARTESIAN_POINT('Ctrl Pts',(68.2893909985894,-1.81053011756679,
125.169243455132));
#148003=CARTESIAN_POINT('Ctrl Pts',(68.2819676275606,-1.95863383356228,
125.221199857878));
#148004=CARTESIAN_POINT('Ctrl Pts',(68.2780315781199,-2.03716197748134,
125.24874838929));
#148005=CARTESIAN_POINT('Ctrl Pts',(68.2740955286792,-2.11505134242283,
125.277933851331));
#148006=CARTESIAN_POINT('Ctrl Pts',(68.2701594792385,-2.19223025926975,
125.308720795594));
#148007=CARTESIAN_POINT('Ctrl Pts',(68.2627362128331,-2.33778728777455,
125.366784011648));
#148008=CARTESIAN_POINT('Ctrl Pts',(68.2553129464276,-2.48125603620484,
125.430721836023));
#148009=CARTESIAN_POINT('Ctrl Pts',(68.2478896800222,-2.62212715837375,
125.50036403689));
#148010=CARTESIAN_POINT('Ctrl Pts',(68.2404751873012,-2.76283178257508,
125.56992392646));
#148011=CARTESIAN_POINT('Ctrl Pts',(68.2330606945801,-2.90094456035185,
125.645174608516));
#148012=CARTESIAN_POINT('Ctrl Pts',(68.2256462018591,-3.03597399232721,
125.725897023091));
#148013=CARTESIAN_POINT('Ctrl Pts',(68.2182388555054,-3.17087327785188,
125.806541634363));
#148014=CARTESIAN_POINT('Ctrl Pts',(68.2108315091516,-3.30269481567501,
125.892647288674));
#148015=CARTESIAN_POINT('Ctrl Pts',(68.2034241627978,-3.43096979376216,
125.983948100282));
#148016=CARTESIAN_POINT('Ctrl Pts',(68.1960223411224,-3.55914909953138,
126.0751808163));
#148017=CARTESIAN_POINT('Ctrl Pts',(68.188620519447,-3.6837868096121,126.171600758942));
#148018=CARTESIAN_POINT('Ctrl Pts',(68.1812186977716,-3.80444140953322,
126.272897705445));
#148019=CARTESIAN_POINT('Ctrl Pts',(68.1738207834603,-3.92503231683004,
126.374141178078));
#148020=CARTESIAN_POINT('Ctrl Pts',(68.1664228691489,-4.04164401632709,
126.480256287848));
#148021=CARTESIAN_POINT('Ctrl Pts',(68.1590249548376,-4.15386662207163,
126.590891423595));
#148022=CARTESIAN_POINT('Ctrl Pts',(68.1516282699254,-4.26607057845517,
126.701508173791));
#148023=CARTESIAN_POINT('Ctrl Pts',(68.1442315850131,-4.37388662313031,
126.816643197344));
#148024=CARTESIAN_POINT('Ctrl Pts',(68.1368349001009,-4.47694034563364,
126.935906701059));
#148025=CARTESIAN_POINT('Ctrl Pts',(68.1294385431655,-4.57998949862684,
127.055164916505));
#148026=CARTESIAN_POINT('Ctrl Pts',(68.12204218623,-4.67827650525111,127.178550965669));
#148027=CARTESIAN_POINT('Ctrl Pts',(68.1146458292945,-4.77146620365485,
127.305640733111));
#148028=CARTESIAN_POINT('Ctrl Pts',(68.1072483399579,-4.86467016963959,
127.432749958322));
#148029=CARTESIAN_POINT('Ctrl Pts',(68.0998508506213,-4.95277505274746,
127.563563729822));
#148030=CARTESIAN_POINT('Ctrl Pts',(68.0924533612847,-5.03548820617812,
127.697627753617));
#148031=CARTESIAN_POINT('Ctrl Pts',(68.0850532787697,-5.11823035457643,
127.831738773347));
#148032=CARTESIAN_POINT('Ctrl Pts',(68.0776531962548,-5.19557681431019,
127.969101996351));
#148033=CARTESIAN_POINT('Ctrl Pts',(68.0702531137398,-5.26728027170078,
128.109237410391));
#148034=CARTESIAN_POINT('Ctrl Pts',(68.0628448940733,-5.33906257441396,
128.249526917725));
#148035=CARTESIAN_POINT('Ctrl Pts',(68.0554366744068,-5.40518931272512,
128.392594371242));
#148036=CARTESIAN_POINT('Ctrl Pts',(68.0480284547403,-5.46546052812274,
128.537937934563));
#148037=CARTESIAN_POINT('Ctrl Pts',(68.0406156754382,-5.52576883944781,
128.683370954421));
#148038=CARTESIAN_POINT('Ctrl Pts',(68.0332028961361,-5.58021431767922,
128.831082526117));
#148039=CARTESIAN_POINT('Ctrl Pts',(68.0257901168341,-5.62864667588095,
128.980554936964));
#148040=CARTESIAN_POINT('Ctrl Pts',(68.0183667458053,-5.67714823650737,
129.130240921002));
#148041=CARTESIAN_POINT('Ctrl Pts',(68.0109433747765,-5.71961941676884,
129.281692410668));
#148042=CARTESIAN_POINT('Ctrl Pts',(68.0035200037478,-5.75596069978699,
129.43437996624));
#148043=CARTESIAN_POINT('Ctrl Pts',(67.999583954307,-5.77522972003999,129.515338571891));
#148044=CARTESIAN_POINT('Ctrl Pts',(67.9956479048663,-5.79277626855372,
129.596644555686));
#148045=CARTESIAN_POINT('Ctrl Pts',(67.9917118554256,-5.80859143016921,
129.678218459637));
#148046=CARTESIAN_POINT('Ctrl Pts',(67.9808130884996,-5.85238299400481,
129.904093408566));
#148047=CARTESIAN_POINT('Ctrl Pts',(67.9699143215737,-5.88300986694146,
130.132596655975));
#148048=CARTESIAN_POINT('Ctrl Pts',(67.9590155546477,-5.90022621487157,
130.362476949796));
#148049=CARTESIAN_POINT('Ctrl Pts',(67.9521354338356,-5.91109446762949,
130.507594668574));
#148050=CARTESIAN_POINT('Ctrl Pts',(67.9452553130236,-5.91661932922891,
130.65326080399));
#148051=CARTESIAN_POINT('Ctrl Pts',(67.9383751922115,-5.91674770925342,
130.799154126957));
#148052=CARTESIAN_POINT('',(66.1883751922116,-5.90702516183033,130.803589055723));
#148053=CARTESIAN_POINT('Ctrl Pts',(67.9383740532611,-5.91922168982187,
130.79917611158));
#148054=CARTESIAN_POINT('Ctrl Pts',(67.8633374460449,-5.90455875036985,
132.391010917394));
#148055=CARTESIAN_POINT('Ctrl Pts',(67.6954849642247,-4.42064434812357,
135.975930907562));
#148056=CARTESIAN_POINT('Ctrl Pts',(67.4348166077997,1.6443349981276,137.606839793888));
#148057=CARTESIAN_POINT('Ctrl Pts',(67.156368983987,6.61192161886336,133.097841168245));
#148058=CARTESIAN_POINT('Ctrl Pts',(66.8779213601741,5.50347528219203,126.481245959285));
#148059=CARTESIAN_POINT('Ctrl Pts',(66.599473736361,-0.662395979099899,
123.837381925391));
#148060=CARTESIAN_POINT('Ctrl Pts',(66.369625013707,-5.24963757446116,126.939849443361));
#148061=CARTESIAN_POINT('Ctrl Pts',(66.2325921656571,-5.90811822702256,
129.860655023505));
#148062=CARTESIAN_POINT('Ctrl Pts',(66.1883751922116,-5.90702516183033,
130.803589055723));
#148063=CARTESIAN_POINT('',(64.4383751922115,-5.91638089232767,130.809832875924));
#148064=CARTESIAN_POINT('Ctrl Pts',(66.1883751922116,-5.90702516183033,
130.803589055723));
#148065=CARTESIAN_POINT('Ctrl Pts',(66.1397762910528,-5.90582377324359,
131.839968397412));
#148066=CARTESIAN_POINT('Ctrl Pts',(65.9983615152899,-5.15160611073396,
134.857296499428));
#148067=CARTESIAN_POINT('Ctrl Pts',(65.7641308649225,-0.332949373316311,
137.794833079793));
#148068=CARTESIAN_POINT('Ctrl Pts',(65.4856832411095,5.7013151939231,134.863001472567));
#148069=CARTESIAN_POINT('Ctrl Pts',(65.2072356172968,6.49634962267588,128.201477195226));
#148070=CARTESIAN_POINT('Ctrl Pts',(64.9287879934838,1.32155611251496,123.931875625089));
#148071=CARTESIAN_POINT('Ctrl Pts',(64.6725011851222,-4.55918243657943,
125.814926826125));
#148072=CARTESIAN_POINT('Ctrl Pts',(64.5090302513647,-5.9025589280303,129.309102465528));
#148073=CARTESIAN_POINT('Ctrl Pts',(64.4383751922115,-5.91638089232767,
130.809832875924));
#148074=CARTESIAN_POINT('',(62.6883751922116,-5.92596308185693,130.80268746135));
#148075=CARTESIAN_POINT('Ctrl Pts',(64.4383751922115,-5.91638089232767,
130.809832875924));
#148076=CARTESIAN_POINT('Ctrl Pts',(64.4162143767604,-5.92071612328831,
131.280533913689));
#148077=CARTESIAN_POINT('Ctrl Pts',(64.3012376867048,-5.65391015254493,
133.717810089976));
#148078=CARTESIAN_POINT('Ctrl Pts',(64.0934451220452,-2.28341567571408,
137.419764866907));
#148079=CARTESIAN_POINT('Ctrl Pts',(63.8149974982322,4.33148500470616,136.30125048224));
#148080=CARTESIAN_POINT('Ctrl Pts',(63.5365498744195,6.96596257060751,130.13136284993));
#148081=CARTESIAN_POINT('Ctrl Pts',(63.2581022506065,3.19906084031009,124.579927288311));
#148082=CARTESIAN_POINT('Ctrl Pts',(62.9796546267936,-3.50762151942191,
124.748441875803));
#148083=CARTESIAN_POINT('Ctrl Pts',(62.7897456073286,-5.88336273271958,
128.658921952266));
#148084=CARTESIAN_POINT('Ctrl Pts',(62.6926524624679,-5.92630129488592,
130.712218582565));
#148085=CARTESIAN_POINT('Ctrl Pts',(62.6883751922116,-5.92596308185693,
130.80268746135));
#148086=CARTESIAN_POINT('',(60.9383763907753,-5.91354401369683,130.799673779747));
#148087=CARTESIAN_POINT('Ctrl Pts',(62.6883751922116,-5.92596308185693,
130.80268746135));
#148088=CARTESIAN_POINT('Ctrl Pts',(62.5998365878636,-5.91896214252789,
132.675374428599));
#148089=CARTESIAN_POINT('Ctrl Pts',(62.4184821089114,-3.94761271390423,
136.523902656696));
#148090=CARTESIAN_POINT('Ctrl Pts',(62.1443117553548,2.61276674649605,137.296741572097));
#148091=CARTESIAN_POINT('Ctrl Pts',(61.8658641315421,6.87448821768475,132.115456447487));
#148092=CARTESIAN_POINT('Ctrl Pts',(61.5874165077291,4.81889085424591,125.729338305771));
#148093=CARTESIAN_POINT('Ctrl Pts',(61.3089688839162,-1.66503178834267,
124.006917739971));
#148094=CARTESIAN_POINT('Ctrl Pts',(61.0926224593943,-5.51403400753928,
127.522021498947));
#148095=CARTESIAN_POINT('Ctrl Pts',(60.9690919094768,-5.91607461361271,
130.14584520162));
#148096=CARTESIAN_POINT('Ctrl Pts',(60.9383772341634,-5.91128936499411,
130.799657604163));
#148097=CARTESIAN_POINT('',(59.1883740221267,-5.91242413515847,130.807894219129));
#148098=CARTESIAN_POINT('Ctrl Pts',(60.9383751922115,-5.91674816187077,
130.799696767348));
#148099=CARTESIAN_POINT('Ctrl Pts',(60.9306126273815,-5.91687853020878,
130.965087289821));
#148100=CARTESIAN_POINT('Ctrl Pts',(60.9228500625514,-5.91006894075129,
131.130563255582));
#148101=CARTESIAN_POINT('Ctrl Pts',(60.9150874977214,-5.89633053957049,
131.295498816679));
#148102=CARTESIAN_POINT('Ctrl Pts',(60.90769975758,-5.88325551345419,131.452470267759));
#148103=CARTESIAN_POINT('Ctrl Pts',(60.9003120174386,-5.86390512345827,
131.608951866011));
#148104=CARTESIAN_POINT('Ctrl Pts',(60.8929242772972,-5.83834232962341,
131.764407181347));
#148105=CARTESIAN_POINT('Ctrl Pts',(60.8855362623704,-5.81277858498592,
131.91986827881));
#148106=CARTESIAN_POINT('Ctrl Pts',(60.8781482474435,-5.78100203643834,
132.074302648395));
#148107=CARTESIAN_POINT('Ctrl Pts',(60.8707602325167,-5.74312707618287,
132.227182443838));
#148108=CARTESIAN_POINT('Ctrl Pts',(60.8633704800293,-5.70524320825183,
132.38009819453));
#148109=CARTESIAN_POINT('Ctrl Pts',(60.8559807275417,-5.66125816267149,
132.531458280336));
#148110=CARTESIAN_POINT('Ctrl Pts',(60.8485909750543,-5.61133662443686,
132.680748597104));
#148111=CARTESIAN_POINT('Ctrl Pts',(60.8411980214569,-5.56139346107563,
132.830103583794));
#148112=CARTESIAN_POINT('Ctrl Pts',(60.8338050678595,-5.50550880325984,
132.977386662192));
#148113=CARTESIAN_POINT('Ctrl Pts',(60.8264121142621,-5.44389595922857,
133.122102481449));
#148114=CARTESIAN_POINT('Ctrl Pts',(60.8190104148024,-5.38221022721806,
133.266989499484));
#148115=CARTESIAN_POINT('Ctrl Pts',(60.8116087153427,-5.31478292445014,
133.409302850196));
#148116=CARTESIAN_POINT('Ctrl Pts',(60.804207015883,-5.2418742434211,133.54856997158));
#148117=CARTESIAN_POINT('Ctrl Pts',(60.7968002188792,-5.16891535024621,
133.68793300611));
#148118=CARTESIAN_POINT('Ctrl Pts',(60.7893934218755,-5.09046774340257,
133.824245308697));
#148119=CARTESIAN_POINT('Ctrl Pts',(60.7819866248717,-5.00683535243619,
133.957062683429));
#148120=CARTESIAN_POINT('Ctrl Pts',(60.7745691702738,-4.92308262334171,
134.090071168256));
#148121=CARTESIAN_POINT('Ctrl Pts',(60.7671517156758,-4.83413042530598,
134.219574377895));
#148122=CARTESIAN_POINT('Ctrl Pts',(60.7597342610779,-4.74032383136926,
134.345160038072));
#148123=CARTESIAN_POINT('Ctrl Pts',(60.7571807194821,-4.70802986361868,
134.388394304337));
#148124=CARTESIAN_POINT('Ctrl Pts',(60.7546271778862,-4.67516090251069,
134.431164592743));
#148125=CARTESIAN_POINT('Ctrl Pts',(60.7520736362904,-4.64173203189925,
134.473455098026));
#148126=CARTESIAN_POINT('Ctrl Pts',(60.744650369885,-4.54455272117663,134.5963956006));
#148127=CARTESIAN_POINT('Ctrl Pts',(60.7372271034796,-4.44233880365307,
134.7156585128));
#148128=CARTESIAN_POINT('Ctrl Pts',(60.7298038370742,-4.33539875922592,
134.830804229614));
#148129=CARTESIAN_POINT('Ctrl Pts',(60.7223893443532,-4.22858510905032,
134.945813853753));
#148130=CARTESIAN_POINT('Ctrl Pts',(60.7149748516321,-4.11705670226956,
135.056715697814));
#148131=CARTESIAN_POINT('Ctrl Pts',(60.7075603589111,-4.00116372536805,
135.163101193156));
#148132=CARTESIAN_POINT('Ctrl Pts',(60.7001530125573,-3.88538245048097,
135.269384150153));
#148133=CARTESIAN_POINT('Ctrl Pts',(60.6927456662036,-3.76524525341261,
135.371159173705));
#148134=CARTESIAN_POINT('Ctrl Pts',(60.6853383198498,-3.64114072702438,
135.468052799572));
#148135=CARTESIAN_POINT('Ctrl Pts',(60.6779364981744,-3.51712876247431,
135.564874158517));
#148136=CARTESIAN_POINT('Ctrl Pts',(60.670534676499,-3.38915565331457,135.656821140224));
#148137=CARTESIAN_POINT('Ctrl Pts',(60.6631328548236,-3.25764469811424,
135.743559093366));
#148138=CARTESIAN_POINT('Ctrl Pts',(60.6557349405123,-3.12620316652367,
135.830251258218));
#148139=CARTESIAN_POINT('Ctrl Pts',(60.6483370262009,-2.99122781914384,
135.911739665863));
#148140=CARTESIAN_POINT('Ctrl Pts',(60.6409391118896,-2.85317259850371,
135.987731787533));
#148141=CARTESIAN_POINT('Ctrl Pts',(60.6335424269774,-2.71514032013647,
136.063711280692));
#148142=CARTESIAN_POINT('Ctrl Pts',(60.6261457420651,-2.57402951102585,
136.134196120835));
#148143=CARTESIAN_POINT('Ctrl Pts',(60.6187490571529,-2.43032058698322,
136.198938674002));
#148144=CARTESIAN_POINT('Ctrl Pts',(60.6113527002175,-2.28661803514468,
136.263678356417));
#148145=CARTESIAN_POINT('Ctrl Pts',(60.603956343282,-2.14031793778975,136.322676104791));
#148146=CARTESIAN_POINT('Ctrl Pts',(60.5965599863466,-1.99192240812506,
136.375731695004));
#148147=CARTESIAN_POINT('Ctrl Pts',(60.58916249701,-1.84350415872615,136.428795408162));
#148148=CARTESIAN_POINT('Ctrl Pts',(60.5817650076735,-1.69299018976002,
136.475915026024));
#148149=CARTESIAN_POINT('Ctrl Pts',(60.5743675183369,-1.54089940841796,
136.51693968272));
#148150=CARTESIAN_POINT('Ctrl Pts',(60.5669674358219,-1.38875531188827,
136.557978720546));
#148151=CARTESIAN_POINT('Ctrl Pts',(60.5595673533069,-1.23503366265474,
136.592918446134));
#148152=CARTESIAN_POINT('Ctrl Pts',(60.552167270792,-1.08026508293948,136.621658780208));
#148153=CARTESIAN_POINT('Ctrl Pts',(60.5447590511255,-0.92532631926001,
136.650430717234));
#148154=CARTESIAN_POINT('Ctrl Pts',(60.537350831459,-0.769338693309987,
136.672989580815));
#148155=CARTESIAN_POINT('Ctrl Pts',(60.5299426117925,-0.612840233185152,
136.689286905217));
#148156=CARTESIAN_POINT('Ctrl Pts',(60.5225298324904,-0.456245450869427,
136.705594260351));
#148157=CARTESIAN_POINT('Ctrl Pts',(60.5151170531884,-0.299139579552217,
136.715632373235));
#148158=CARTESIAN_POINT('Ctrl Pts',(60.5077042738863,-0.14206169168865,
136.719404914801));
#148159=CARTESIAN_POINT('Ctrl Pts',(60.5002809028576,0.0152406364275426,
136.723182846752));
#148160=CARTESIAN_POINT('Ctrl Pts',(60.4928575318288,0.172514528971182,
136.72067733308));
#148161=CARTESIAN_POINT('Ctrl Pts',(60.4854341608,0.329224159341883,136.711944050359));
#148162=CARTESIAN_POINT('Ctrl Pts',(60.4814981113592,0.412315365560495,
136.707313454307));
#148163=CARTESIAN_POINT('Ctrl Pts',(60.4775620619184,0.495248064304087,
136.700932870871));
#148164=CARTESIAN_POINT('Ctrl Pts',(60.4736260124776,0.577943556717647,
136.692816425989));
#148165=CARTESIAN_POINT('Ctrl Pts',(60.4662027460722,0.733904674571259,
136.677509064247));
#148166=CARTESIAN_POINT('Ctrl Pts',(60.4587794796667,0.88949305944162,136.655978117788));
#148167=CARTESIAN_POINT('Ctrl Pts',(60.4513562132613,1.04417211826217,136.628245502241));
#148168=CARTESIAN_POINT('Ctrl Pts',(60.4439417205403,1.19866835928114,136.600545664342));
#148169=CARTESIAN_POINT('Ctrl Pts',(60.4365272278193,1.35225704969109,136.566658812711));
#148170=CARTESIAN_POINT('Ctrl Pts',(60.4291127350982,1.50440516477545,136.526658727827));
#148171=CARTESIAN_POINT('Ctrl Pts',(60.4217053887444,1.656406633778,136.486697196531));
#148172=CARTESIAN_POINT('Ctrl Pts',(60.4142980423906,1.80696993304082,136.440634256398));
#148173=CARTESIAN_POINT('Ctrl Pts',(60.4068906960368,1.95557081258704,136.388594975064));
#148174=CARTESIAN_POINT('Ctrl Pts',(60.3994888743614,2.10406085999091,136.336594506589));
#148175=CARTESIAN_POINT('Ctrl Pts',(60.392087052686,2.25059105119362,136.278626695009));
#148176=CARTESIAN_POINT('Ctrl Pts',(60.3846852310106,2.39465103133813,136.21486678618));
#148177=CARTESIAN_POINT('Ctrl Pts',(60.3772873166992,2.53863496334027,136.151140535711));
#148178=CARTESIAN_POINT('Ctrl Pts',(60.3698894023878,2.68015094077902,136.081628428057));
#148179=CARTESIAN_POINT('Ctrl Pts',(60.3624914880765,2.81870748389155,136.006554258979));
#148180=CARTESIAN_POINT('Ctrl Pts',(60.3550948031642,2.95724100142048,135.931492565865));
#148181=CARTESIAN_POINT('Ctrl Pts',(60.347698118252,3.09281573281521,135.85087082348));
#148182=CARTESIAN_POINT('Ctrl Pts',(60.3403014333398,3.22496366013016,135.764959367046));
#148183=CARTESIAN_POINT('Ctrl Pts',(60.3329050764043,3.35710572786734,135.679051720016));
#148184=CARTESIAN_POINT('Ctrl Pts',(60.3255087194688,3.48582098067647,135.587855028773));
#148185=CARTESIAN_POINT('Ctrl Pts',(60.3181123625334,3.61066955988036,135.491683509351));
#148186=CARTESIAN_POINT('Ctrl Pts',(60.3107148731968,3.73553725372099,135.395497265823));
#148187=CARTESIAN_POINT('Ctrl Pts',(60.3033173838602,3.85653679946014,135.294334905369));
#148188=CARTESIAN_POINT('Ctrl Pts',(60.2959198945235,3.97326078735673,135.188551452618));
#148189=CARTESIAN_POINT('Ctrl Pts',(60.2885198120085,4.09002569266584,135.082730917641));
#148190=CARTESIAN_POINT('Ctrl Pts',(60.2811197294935,4.20251177961862,134.972286315649));
#148191=CARTESIAN_POINT('Ctrl Pts',(60.2737196469785,4.31034803441242,134.857609978849));
#148192=CARTESIAN_POINT('Ctrl Pts',(60.266311427312,4.4183028662545,134.742807543627));
#148193=CARTESIAN_POINT('Ctrl Pts',(60.2589032076455,4.52159739912048,134.623764352912));
#148194=CARTESIAN_POINT('Ctrl Pts',(60.251494987979,4.61990004008962,134.500906868065));
#148195=CARTESIAN_POINT('Ctrl Pts',(60.2440822086769,4.71826318469429,134.377973766487));
#148196=CARTESIAN_POINT('Ctrl Pts',(60.2366694293748,4.81162809432899,134.251221992685));
#148197=CARTESIAN_POINT('Ctrl Pts',(60.2292566500727,4.89970647562366,134.121107067814));
#148198=CARTESIAN_POINT('Ctrl Pts',(60.2218332790439,4.98791070743961,133.990806228636));
#148199=CARTESIAN_POINT('Ctrl Pts',(60.2144099080152,5.07081312837586,133.857132957271));
#148200=CARTESIAN_POINT('Ctrl Pts',(60.2069865369864,5.14817095334338,133.72056815436));
#148201=CARTESIAN_POINT('Ctrl Pts',(60.2030504875458,5.18918792831466,133.648158219032));
#148202=CARTESIAN_POINT('Ctrl Pts',(60.1991144381052,5.22864691217467,133.574935729605));
#148203=CARTESIAN_POINT('Ctrl Pts',(60.1951783886646,5.26651725082294,133.500974533069));
#148204=CARTESIAN_POINT('Ctrl Pts',(60.1877551222592,5.33793952762424,133.361486024646));
#148205=CARTESIAN_POINT('Ctrl Pts',(60.1803318558537,5.40392425506068,133.218947107479));
#148206=CARTESIAN_POINT('Ctrl Pts',(60.1729085894483,5.46419982971065,133.073821078444));
#148207=CARTESIAN_POINT('Ctrl Pts',(60.1654940967273,5.52440416363705,132.928866576324));
#148208=CARTESIAN_POINT('Ctrl Pts',(60.1580796040063,5.57891263441363,132.781331390186));
#148209=CARTESIAN_POINT('Ctrl Pts',(60.1506651112852,5.62749920276649,132.631703848971));
#148210=CARTESIAN_POINT('Ctrl Pts',(60.1432577649315,5.67603894155552,132.482220524414));
#148211=CARTESIAN_POINT('Ctrl Pts',(60.1358504185777,5.71866802641614,132.330649212279));
#148212=CARTESIAN_POINT('Ctrl Pts',(60.1284430722239,5.75520831037373,132.17749858103));
#148213=CARTESIAN_POINT('Ctrl Pts',(60.1210412505485,5.79172134120881,132.0244621753));
#148214=CARTESIAN_POINT('Ctrl Pts',(60.1136394288732,5.82215452713652,131.86984915739));
#148215=CARTESIAN_POINT('Ctrl Pts',(60.1062376071978,5.84637944819327,131.714183627961));
#148216=CARTESIAN_POINT('Ctrl Pts',(60.0988396928864,5.87059158110293,131.558600273151));
#148217=CARTESIAN_POINT('Ctrl Pts',(60.0914417785751,5.88860191877396,131.401965881276));
#148218=CARTESIAN_POINT('Ctrl Pts',(60.0840438642637,5.90033309010159,131.244814915254));
#148219=CARTESIAN_POINT('Ctrl Pts',(60.0766471793515,5.91206231192133,131.087690064873));
#148220=CARTESIAN_POINT('Ctrl Pts',(60.0692504944393,5.91751441064191,130.93004918262));
#148221=CARTESIAN_POINT('Ctrl Pts',(60.0618538095271,5.91666385181157,130.77243214804));
#148222=CARTESIAN_POINT('Ctrl Pts',(60.0544574525917,5.9158133306959,130.614822102365));
#148223=CARTESIAN_POINT('Ctrl Pts',(60.0470610956562,5.90866070971744,130.457236275552));
#148224=CARTESIAN_POINT('Ctrl Pts',(60.0396647387208,5.89523259336448,130.300214574605));
#148225=CARTESIAN_POINT('Ctrl Pts',(60.0322672493842,5.88180242113266,130.143168833235));
#148226=CARTESIAN_POINT('Ctrl Pts',(60.0248697600477,5.86209487226647,129.986687761667));
#148227=CARTESIAN_POINT('Ctrl Pts',(60.0174722707112,5.83618842412403,129.83130602474));
#148228=CARTESIAN_POINT('Ctrl Pts',(60.0100721881962,5.81027289451631,129.675869818984));
#148229=CARTESIAN_POINT('Ctrl Pts',(60.0026721056812,5.77815420052971,129.521534083123));
#148230=CARTESIAN_POINT('Ctrl Pts',(59.9952720231662,5.73996188034063,129.368823026718));
#148231=CARTESIAN_POINT('Ctrl Pts',(59.9878638034998,5.70172756376917,129.215944048808));
#148232=CARTESIAN_POINT('Ctrl Pts',(59.9804555838333,5.65740637406578,129.064693680482));
#148233=CARTESIAN_POINT('Ctrl Pts',(59.9730473641668,5.60717787117967,128.915581413039));
#148234=CARTESIAN_POINT('Ctrl Pts',(59.9656345848648,5.55691845348793,128.766377369483));
#148235=CARTESIAN_POINT('Ctrl Pts',(59.9582218055627,5.50074461061487,128.619314396953));
#148236=CARTESIAN_POINT('Ctrl Pts',(59.9508090262606,5.43888375579863,128.474881265133));
#148237=CARTESIAN_POINT('Ctrl Pts',(59.9433856552319,5.3769345112923,128.330241760483));
#148238=CARTESIAN_POINT('Ctrl Pts',(59.9359622842031,5.30928218578974,128.188239937507));
#148239=CARTESIAN_POINT('Ctrl Pts',(59.9285389131744,5.23620014334941,128.04933999672));
#148240=CARTESIAN_POINT('Ctrl Pts',(59.9246028637335,5.19745029086743,127.975691915255));
#148241=CARTESIAN_POINT('Ctrl Pts',(59.9206668142927,5.1571746813569,127.902915410499));
#148242=CARTESIAN_POINT('Ctrl Pts',(59.9167307648518,5.11541887509268,127.831076188715));
#148243=CARTESIAN_POINT('Ctrl Pts',(59.9093074984464,5.03666872763349,127.695589658459));
#148244=CARTESIAN_POINT('Ctrl Pts',(59.901884232041,4.95241305665509,127.563029072047));
#148245=CARTESIAN_POINT('Ctrl Pts',(59.8944609656355,4.86289483865671,127.433873360408));
#148246=CARTESIAN_POINT('Ctrl Pts',(59.8870464729145,4.77348242375785,127.304870300094));
#148247=CARTESIAN_POINT('Ctrl Pts',(59.8796319801935,4.67882005314467,127.179264408014));
#148248=CARTESIAN_POINT('Ctrl Pts',(59.8722174874725,4.57919639203602,127.057509811133));
#148249=CARTESIAN_POINT('Ctrl Pts',(59.8648101411187,4.47966875196327,126.935872565918));
#148250=CARTESIAN_POINT('Ctrl Pts',(59.857402794765,4.37518957598218,126.818079512962));
#148251=CARTESIAN_POINT('Ctrl Pts',(59.8499954484113,4.2660905284871,126.704555480093));
#148252=CARTESIAN_POINT('Ctrl Pts',(59.8425936267359,4.15707285117726,126.591116117729));
#148253=CARTESIAN_POINT('Ctrl Pts',(59.8351918050605,4.0434424207067,126.481939703682));
#148254=CARTESIAN_POINT('Ctrl Pts',(59.8277899833851,3.92557076367819,126.377417570513));
#148255=CARTESIAN_POINT('Ctrl Pts',(59.8203920690737,3.80776133017958,126.272950613763));
#148256=CARTESIAN_POINT('Ctrl Pts',(59.8129941547624,3.68571540761689,126.173133291785));
#148257=CARTESIAN_POINT('Ctrl Pts',(59.805596240451,3.5598408338089,126.078319589343));
#148258=CARTESIAN_POINT('Ctrl Pts',(59.7981995555388,3.43398717807202,125.983521643218));
#148259=CARTESIAN_POINT('Ctrl Pts',(59.7908028706266,3.30430643174462,125.893725890703));
#148260=CARTESIAN_POINT('Ctrl Pts',(59.7834061857144,3.17123900878252,125.809245632736));
#148261=CARTESIAN_POINT('Ctrl Pts',(59.7760098287789,3.03817748616901,125.724769120711));
#148262=CARTESIAN_POINT('Ctrl Pts',(59.7686134718435,2.90172990065716,125.645607834673));
#148263=CARTESIAN_POINT('Ctrl Pts',(59.761217114908,2.76236487167567,125.572031224434));
#148264=CARTESIAN_POINT('Ctrl Pts',(59.7538196255715,2.62297850555287,125.498443349429));
#148265=CARTESIAN_POINT('Ctrl Pts',(59.7464221362348,2.4806741367228,125.430442026992));
#148266=CARTESIAN_POINT('Ctrl Pts',(59.7390246468983,2.33594401278453,125.368250231303));
#148267=CARTESIAN_POINT('Ctrl Pts',(59.7316245643832,2.19116315392443,125.306036634376));
#148268=CARTESIAN_POINT('Ctrl Pts',(59.7242244818682,2.04395518968559,125.249636766183));
#148269=CARTESIAN_POINT('Ctrl Pts',(59.7168243993532,1.89483117096766,125.199224990658));
#148270=CARTESIAN_POINT('Ctrl Pts',(59.7094161796867,1.74554317506188,125.148757782205));
#148271=CARTESIAN_POINT('Ctrl Pts',(59.7020079600203,1.59433527091627,125.104291935768));
#148272=CARTESIAN_POINT('Ctrl Pts',(59.6945997403538,1.44173316452865,125.065951774969));
#148273=CARTESIAN_POINT('Ctrl Pts',(59.6871869610517,1.28903713409041,125.02758801644));
#148274=CARTESIAN_POINT('Ctrl Pts',(59.6797741817496,1.13494555606537,124.99535753251));
#148275=CARTESIAN_POINT('Ctrl Pts',(59.6723614024475,0.979992568643787,
124.969333185934));
#148276=CARTESIAN_POINT('Ctrl Pts',(59.6649380314188,0.824818177127207,
124.943271654551));
#148277=CARTESIAN_POINT('Ctrl Pts',(59.6575146603901,0.668780287322377,
124.923434018103));
#148278=CARTESIAN_POINT('Ctrl Pts',(59.6500912893613,0.512417204220075,
124.909841199384));
#148279=CARTESIAN_POINT('Ctrl Pts',(59.6461552399205,0.429509745678901,
124.902633960745));
#148280=CARTESIAN_POINT('Ctrl Pts',(59.6422191904797,0.346510860363946,
124.897181493204));
#148281=CARTESIAN_POINT('Ctrl Pts',(59.6382831410389,0.263500455258547,
124.893480981456));
#148282=CARTESIAN_POINT('Ctrl Pts',(59.6308598746335,0.106945421894931,
124.886501931788));
#148283=CARTESIAN_POINT('Ctrl Pts',(59.623436608228,-0.0501238019878781,
124.885736379098));
#148284=CARTESIAN_POINT('Ctrl Pts',(59.6160133418226,-0.207172943502528,
124.891238774243));
#148285=CARTESIAN_POINT('Ctrl Pts',(59.6085988491015,-0.364036465974028,
124.896734666014));
#148286=CARTESIAN_POINT('Ctrl Pts',(59.6011843563805,-0.520879583897477,
124.908483746625));
#148287=CARTESIAN_POINT('Ctrl Pts',(59.5937698636595,-0.677164196795334,
124.926488620569));
#148288=CARTESIAN_POINT('Ctrl Pts',(59.5863625173057,-0.833298176699715,
124.944476140738));
#148289=CARTESIAN_POINT('Ctrl Pts',(59.5789551709519,-0.988874354888629,
124.968707408117));
#148290=CARTESIAN_POINT('Ctrl Pts',(59.5715478245981,-1.14335603897445,
124.999133013876));
#148291=CARTESIAN_POINT('Ctrl Pts',(59.5641460029227,-1.29772250479158,
125.02953592707));
#148292=CARTESIAN_POINT('Ctrl Pts',(59.5567441812472,-1.45099573721353,
125.066123907832));
#148293=CARTESIAN_POINT('Ctrl Pts',(59.5493423595718,-1.60264567786908,
125.108795905116));
#148294=CARTESIAN_POINT('Ctrl Pts',(59.5419444452604,-1.75421556370291,
125.151445376185));
#148295=CARTESIAN_POINT('Ctrl Pts',(59.5345465309489,-1.90416350594036,
125.200172366655));
#148296=CARTESIAN_POINT('Ctrl Pts',(59.5271486166375,-2.05197124087056,
125.25482508843));
#148297=CARTESIAN_POINT('Ctrl Pts',(59.5197519317252,-2.19975441283546,
125.309468727914));
#148298=CARTESIAN_POINT('Ctrl Pts',(59.5123552468131,-2.34539773359331,
125.370036014932));
#148299=CARTESIAN_POINT('Ctrl Pts',(59.5049585619008,-2.48839955969069,
125.436325763559));
#148300=CARTESIAN_POINT('Ctrl Pts',(59.4975622049654,-2.63139504493705,
125.50261257283));
#148301=CARTESIAN_POINT('Ctrl Pts',(59.4901658480299,-2.77174892973205,
125.574621182192));
#148302=CARTESIAN_POINT('Ctrl Pts',(59.4827694910944,-2.90898121806823,
125.652102973055));
#148303=CARTESIAN_POINT('Ctrl Pts',(59.4753720017579,-3.04623451701808,
125.729596626577));
#148304=CARTESIAN_POINT('Ctrl Pts',(59.4679745124212,-3.18036494281243,
125.812564946542));
#148305=CARTESIAN_POINT('Ctrl Pts',(59.4605770230846,-3.31091882910719,
125.900714314093));
#148306=CARTESIAN_POINT('Ctrl Pts',(59.4531769405696,-3.44151848086477,
125.988894582269));
#148307=CARTESIAN_POINT('Ctrl Pts',(59.4457768580546,-3.56853878772847,
126.082259305327));
#148308=CARTESIAN_POINT('Ctrl Pts',(59.4383767755396,-3.69155681688597,
126.180472769639));
#148309=CARTESIAN_POINT('Ctrl Pts',(59.4309685558731,-3.81471011701257,
126.278794229752));
#148310=CARTESIAN_POINT('Ctrl Pts',(59.4235603362066,-3.93385205860722,
126.381974845803));
#148311=CARTESIAN_POINT('Ctrl Pts',(59.4161521165401,-4.04859388775333,
126.489639526401));
#148312=CARTESIAN_POINT('Ctrl Pts',(59.408739337238,-4.1634063385812,126.597370472814));
#148313=CARTESIAN_POINT('Ctrl Pts',(59.401326557936,-4.27381301934535,126.709590717669));
#148314=CARTESIAN_POINT('Ctrl Pts',(59.3939137786339,-4.37946391380618,
126.82589025948));
#148315=CARTESIAN_POINT('Ctrl Pts',(59.3864904076051,-4.48526576721925,
126.942355975529));
#148316=CARTESIAN_POINT('Ctrl Pts',(59.3790670365763,-4.58629802346991,
127.062912344384));
#148317=CARTESIAN_POINT('Ctrl Pts',(59.3716436655476,-4.68225211262389,
127.187117784091));
#148318=CARTESIAN_POINT('Ctrl Pts',(59.367707616107,-4.73312927307716,127.252974488488));
#148319=CARTESIAN_POINT('Ctrl Pts',(59.3637715666664,-4.78257951331099,
127.319856609461));
#148320=CARTESIAN_POINT('Ctrl Pts',(59.3598355172259,-4.83056201024757,
127.387695397259));
#148321=CARTESIAN_POINT('Ctrl Pts',(59.3523342649679,-4.92200619023678,
127.516981339379));
#148322=CARTESIAN_POINT('Ctrl Pts',(59.3448330127099,-5.00839086364624,
127.650130842641));
#148323=CARTESIAN_POINT('Ctrl Pts',(59.3373317604519,-5.08937601999078,
127.786715461216));
#148324=CARTESIAN_POINT('Ctrl Pts',(59.3298397696976,-5.17026118711969,
127.923131444087));
#148325=CARTESIAN_POINT('Ctrl Pts',(59.3223477789434,-5.24575992574497,
128.062973789982));
#148326=CARTESIAN_POINT('Ctrl Pts',(59.3148557881892,-5.31557370710274,
128.205782789819));
#148327=CARTESIAN_POINT('Ctrl Pts',(59.307371674703,-5.38531408448924,128.34844163667));
#148328=CARTESIAN_POINT('Ctrl Pts',(59.2998875612169,-5.44938124783879,
128.49406060307));
#148329=CARTESIAN_POINT('Ctrl Pts',(59.2924034477308,-5.50752108409904,
128.642152933114));
#148330=CARTESIAN_POINT('Ctrl Pts',(59.2849258324734,-5.5656104393027,128.790116679079));
#148331=CARTESIAN_POINT('Ctrl Pts',(59.2774482172161,-5.61778258458526,
128.940549175663));
#148332=CARTESIAN_POINT('Ctrl Pts',(59.2699706019587,-5.6638303154753,129.092941113177));
#148333=CARTESIAN_POINT('Ctrl Pts',(59.262498739361,-5.70984262104381,129.245215812919));
#148334=CARTESIAN_POINT('Ctrl Pts',(59.2550268767634,-5.74973979688954,
129.399446603185));
#148335=CARTESIAN_POINT('Ctrl Pts',(59.2475550141657,-5.7833636108455,129.555106477189));
#148336=CARTESIAN_POINT('Ctrl Pts',(59.2400865491107,-5.81697213566247,
129.71069557084));
#148337=CARTESIAN_POINT('Ctrl Pts',(59.2326180840558,-5.84431290373922,
129.867712099814));
#148338=CARTESIAN_POINT('Ctrl Pts',(59.2251496190009,-5.86527812398675,
130.02561605689));
#148339=CARTESIAN_POINT('Ctrl Pts',(59.2176826651325,-5.88623910208314,
130.183488063315));
#148340=CARTESIAN_POINT('Ctrl Pts',(59.210215711264,-5.90082705133702,130.342246780994));
#148341=CARTESIAN_POINT('Ctrl Pts',(59.2027487573956,-5.90898566277173,
130.501344116929));
#148342=CARTESIAN_POINT('Ctrl Pts',(59.1979575690009,-5.91422065485974,
130.603429294231));
#148343=CARTESIAN_POINT('Ctrl Pts',(59.1931663806062,-5.91680961849877,
130.705653731667));
#148344=CARTESIAN_POINT('Ctrl Pts',(59.1883751922115,-5.91674895814525,
130.807871854834));
#148345=CARTESIAN_POINT('',(57.4383766205357,-5.92091818089423,130.807703535762));
#148346=CARTESIAN_POINT('Ctrl Pts',(59.1883731089969,-5.90904905956648,
130.807911672142));
#148347=CARTESIAN_POINT('Ctrl Pts',(59.152711370469,-5.91313005239658,131.56775334573));
#148348=CARTESIAN_POINT('Ctrl Pts',(59.0242337573369,-5.42355709184765,
134.300145737045));
#148349=CARTESIAN_POINT('Ctrl Pts',(58.8029402696001,-1.30063251087169,
137.680836139373));
#148350=CARTESIAN_POINT('Ctrl Pts',(58.5244926457873,5.08234996656148,135.615522571577));
#148351=CARTESIAN_POINT('Ctrl Pts',(58.2460450219744,6.79490111132396,129.128986206374));
#148352=CARTESIAN_POINT('Ctrl Pts',(57.9675973981615,2.26327008415277,124.182037078465));
#148353=CARTESIAN_POINT('Ctrl Pts',(57.6983749653315,-4.12915247357771,
125.282955627744));
#148354=CARTESIAN_POINT('Ctrl Pts',(57.521968407106,-5.91208800052518,129.038205754648));
#148355=CARTESIAN_POINT('Ctrl Pts',(57.4383777234847,-5.92413758308925,
130.807682022349));
#148356=CARTESIAN_POINT('',(55.688374326571,-5.91864047034299,130.799239860638));
#148357=CARTESIAN_POINT('Ctrl Pts',(57.4383751922116,-5.91674903983214,
130.807731395733));
#148358=CARTESIAN_POINT('Ctrl Pts',(57.4291508449863,-5.91663793686835,
131.002751157247));
#148359=CARTESIAN_POINT('Ctrl Pts',(57.419926497761,-5.90688570138042,131.19749249288));
#148360=CARTESIAN_POINT('Ctrl Pts',(57.4107021505358,-5.88756945797795,
131.39126473238));
#148361=CARTESIAN_POINT('Ctrl Pts',(57.4032788841304,-5.87202476768945,
131.547202374434));
#148362=CARTESIAN_POINT('Ctrl Pts',(57.3958556177249,-5.85025706712759,
131.702757812701));
#148363=CARTESIAN_POINT('Ctrl Pts',(57.3884323513195,-5.82228908849752,
131.857394488086));
#148364=CARTESIAN_POINT('Ctrl Pts',(57.3810178585985,-5.79435416569555,
132.011848395763));
#148365=CARTESIAN_POINT('Ctrl Pts',(57.3736033658774,-5.76023361746424,
132.1653853383));
#148366=CARTESIAN_POINT('Ctrl Pts',(57.3661888731564,-5.72000203536849,
132.317472403879));
#148367=CARTESIAN_POINT('Ctrl Pts',(57.3587815268026,-5.67980922998637,
132.469412882218));
#148368=CARTESIAN_POINT('Ctrl Pts',(57.3513741804489,-5.63351721148281,
132.619905907178));
#148369=CARTESIAN_POINT('Ctrl Pts',(57.3439668340951,-5.58125184516721,
132.768427419719));
#148370=CARTESIAN_POINT('Ctrl Pts',(57.3365650124197,-5.52902546033351,
132.916838159313));
#148371=CARTESIAN_POINT('Ctrl Pts',(57.3291631907442,-5.47083472187195,
133.063279963694));
#148372=CARTESIAN_POINT('Ctrl Pts',(57.3217613690688,-5.40685565210983,
133.207242745293));
#148373=CARTESIAN_POINT('Ctrl Pts',(57.3143634547574,-5.3429103564008,133.351129530059));
#148374=CARTESIAN_POINT('Ctrl Pts',(57.3069655404461,-5.2731829660132,133.492539558029));
#148375=CARTESIAN_POINT('Ctrl Pts',(57.2995676261347,-5.19789802439756,
133.63098169059));
#148376=CARTESIAN_POINT('Ctrl Pts',(57.2921709412225,-5.1226255937733,133.76940081658));
#148377=CARTESIAN_POINT('Ctrl Pts',(57.2847742563103,-5.04179762308435,
133.904852698414));
#148378=CARTESIAN_POINT('Ctrl Pts',(57.2773775713981,-4.95568515948476,
134.036869730092));
#148379=CARTESIAN_POINT('Ctrl Pts',(57.2699812144626,-4.86957651420206,
134.168880907996));
#148380=CARTESIAN_POINT('Ctrl Pts',(57.2625848575272,-4.7781840458603,134.297457225916));
#148381=CARTESIAN_POINT('Ctrl Pts',(57.2551885005917,-4.68182263951849,
134.422159303866));
#148382=CARTESIAN_POINT('Ctrl Pts',(57.2477910112551,-4.58544647999936,
134.546880474022));
#148383=CARTESIAN_POINT('Ctrl Pts',(57.2403935219185,-4.48410009597941,
134.667725927754));
#148384=CARTESIAN_POINT('Ctrl Pts',(57.232996032582,-4.37813913168417,134.784288796078));
#148385=CARTESIAN_POINT('Ctrl Pts',(57.2255959500669,-4.27214102293702,
134.900892525335));
#148386=CARTESIAN_POINT('Ctrl Pts',(57.218195867552,-4.16152536416108,135.013210404148));
#148387=CARTESIAN_POINT('Ctrl Pts',(57.2107957850369,-4.04668505173136,
135.120872016207));
#148388=CARTESIAN_POINT('Ctrl Pts',(57.2033875653705,-3.93171846057242,
135.228652013275));
#148389=CARTESIAN_POINT('Ctrl Pts',(57.1959793457039,-3.81251821101225,
135.331765263056));
#148390=CARTESIAN_POINT('Ctrl Pts',(57.1885711260375,-3.68951126854774,
135.429880822014));
#148391=CARTESIAN_POINT('Ctrl Pts',(57.1811583467354,-3.56642861736263,
135.528056769462));
#148392=CARTESIAN_POINT('Ctrl Pts',(57.1737455674333,-3.43953490483952,
135.621228676359));
#148393=CARTESIAN_POINT('Ctrl Pts',(57.1663327881313,-3.30928609033689,
135.709108942893));
#148394=CARTESIAN_POINT('Ctrl Pts',(57.1589094171025,-3.17885117022004,
135.797114776874));
#148395=CARTESIAN_POINT('Ctrl Pts',(57.1514860460737,-3.04505189027421,
135.879813673847));
#148396=CARTESIAN_POINT('Ctrl Pts',(57.144062675045,-2.90836952006152,135.956963580853));
#148397=CARTESIAN_POINT('Ctrl Pts',(57.1401266256043,-2.83589724772816,
135.997870312733));
#148398=CARTESIAN_POINT('Ctrl Pts',(57.1361905761636,-2.76261479323338,
136.037217818737));
#148399=CARTESIAN_POINT('Ctrl Pts',(57.1322545267229,-2.68859605013294,
136.074975557183));
#148400=CARTESIAN_POINT('Ctrl Pts',(57.1248312603175,-2.5489990106882,136.146185473513));
#148401=CARTESIAN_POINT('Ctrl Pts',(57.117407993912,-2.40635984105677,136.211953204573));
#148402=CARTESIAN_POINT('Ctrl Pts',(57.1099847275066,-2.26114225091217,
136.272007852313));
#148403=CARTESIAN_POINT('Ctrl Pts',(57.1025702347856,-2.11609629589936,
136.331991520447));
#148404=CARTESIAN_POINT('Ctrl Pts',(57.0951557420646,-1.96847832799159,
136.386275404666));
#148405=CARTESIAN_POINT('Ctrl Pts',(57.0877412493436,-1.81877701955703,
136.434634209109));
#148406=CARTESIAN_POINT('Ctrl Pts',(57.0803339029898,-1.66921999887947,
136.482946403517));
#148407=CARTESIAN_POINT('Ctrl Pts',(57.0729265566361,-1.51758398805077,
136.525344773279));
#148408=CARTESIAN_POINT('Ctrl Pts',(57.0655192102823,-1.364377926056,136.561651945733));
#148409=CARTESIAN_POINT('Ctrl Pts',(57.0581173886069,-1.21128613092261,
136.597932038929));
#148410=CARTESIAN_POINT('Ctrl Pts',(57.0507155669315,-1.05662697792297,
136.628129894922));
#148411=CARTESIAN_POINT('Ctrl Pts',(57.0433137452561,-0.90092476254508,
136.65211789149));
#148412=CARTESIAN_POINT('Ctrl Pts',(57.0359158309448,-0.745304741154928,
136.676093224981));
#148413=CARTESIAN_POINT('Ctrl Pts',(57.0285179166334,-0.588643121992735,
136.693865170916));
#148414=CARTESIAN_POINT('Ctrl Pts',(57.021120002322,-0.431474485104551,
136.705357171641));
#148415=CARTESIAN_POINT('Ctrl Pts',(57.0137233174098,-0.274331966792264,
136.716847262604));
#148416=CARTESIAN_POINT('Ctrl Pts',(57.0063266324977,-0.116682969918951,
136.722059452423));
#148417=CARTESIAN_POINT('Ctrl Pts',(56.9989299475855,0.0409325877373028,
136.720969028282));
#148418=CARTESIAN_POINT('Ctrl Pts',(56.99153359065,0.198541156554561,136.719878652492));
#148419=CARTESIAN_POINT('Ctrl Pts',(56.9841372337145,0.356115915814296,
136.712486220994));
#148420=CARTESIAN_POINT('Ctrl Pts',(56.9767408767791,0.513116999625759,
136.698819159892));
#148421=CARTESIAN_POINT('Ctrl Pts',(56.9693433874425,0.670142120704182,
136.685150006327));
#148422=CARTESIAN_POINT('Ctrl Pts',(56.961945898106,0.826593019535393,136.665204342729));
#148423=CARTESIAN_POINT('Ctrl Pts',(56.9545484087694,0.981935151330484,
136.639061460033));
#148424=CARTESIAN_POINT('Ctrl Pts',(56.9471483262544,1.13733173806884,136.61290941299));
#148425=CARTESIAN_POINT('Ctrl Pts',(56.9397482437394,1.29161841602725,136.580555883478));
#148426=CARTESIAN_POINT('Ctrl Pts',(56.9323481612244,1.44427117338549,136.542131207284));
#148427=CARTESIAN_POINT('Ctrl Pts',(56.924939941558,1.59709178814353,136.503664279207));
#148428=CARTESIAN_POINT('Ctrl Pts',(56.9175317218915,1.74827453201818,136.459112963514));
#148429=CARTESIAN_POINT('Ctrl Pts',(56.910123502225,1.89731018756023,136.408657595304));
#148430=CARTESIAN_POINT('Ctrl Pts',(56.902710722923,2.04643757206169,136.358171172656));
#148431=CARTESIAN_POINT('Ctrl Pts',(56.8952979436209,2.19341488726924,136.301773590022));
#148432=CARTESIAN_POINT('Ctrl Pts',(56.8878851643188,2.33775371014633,136.2396930042));
#148433=CARTESIAN_POINT('Ctrl Pts',(56.8804617932901,2.48229877110237,136.177523714726));
#148434=CARTESIAN_POINT('Ctrl Pts',(56.8730384222613,2.62419747431995,136.109655364962));
#148435=CARTESIAN_POINT('Ctrl Pts',(56.8656150512325,2.76298603583541,136.036362025085));
#148436=CARTESIAN_POINT('Ctrl Pts',(56.8616790017917,2.83657506133772,135.997500137632));
#148437=CARTESIAN_POINT('Ctrl Pts',(56.8577429523508,2.90929018919875,135.957113821308));
#148438=CARTESIAN_POINT('Ctrl Pts',(56.85380690291,2.98106578256428,135.91524873633));
#148439=CARTESIAN_POINT('Ctrl Pts',(56.8463836365046,3.11643231161008,135.836292492627));
#148440=CARTESIAN_POINT('Ctrl Pts',(56.8389603700992,3.24886452173071,135.751835184569));
#148441=CARTESIAN_POINT('Ctrl Pts',(56.8315371036937,3.37788385232074,135.662120517225));
#148442=CARTESIAN_POINT('Ctrl Pts',(56.8241226109727,3.50675069277659,135.572511885166));
#148443=CARTESIAN_POINT('Ctrl Pts',(56.8167081182517,3.63221237939239,135.477658473385));
#148444=CARTESIAN_POINT('Ctrl Pts',(56.8092936255307,3.7538152250301,135.377849637869));
#148445=CARTESIAN_POINT('Ctrl Pts',(56.801886279177,3.87530086526675,135.278137001867));
#148446=CARTESIAN_POINT('Ctrl Pts',(56.7944789328232,3.99293478229969,135.173478685896));
#148447=CARTESIAN_POINT('Ctrl Pts',(56.7870715864694,4.1062926535324,135.064207000482));
#148448=CARTESIAN_POINT('Ctrl Pts',(56.779669764794,4.21956597818814,134.955016814015));
#148449=CARTESIAN_POINT('Ctrl Pts',(56.7722679431187,4.32856933963917,134.841220367209));
#148450=CARTESIAN_POINT('Ctrl Pts',(56.7648661214433,4.432911971177,134.72318978178));
#148451=CARTESIAN_POINT('Ctrl Pts',(56.7574682071319,4.53719952105183,134.605221503779));
#148452=CARTESIAN_POINT('Ctrl Pts',(56.7500702928206,4.63683099432456,134.483023817571));
#148453=CARTESIAN_POINT('Ctrl Pts',(56.7426723785092,4.73145302730025,134.357005099209));
#148454=CARTESIAN_POINT('Ctrl Pts',(56.735275693597,4.82605933581067,134.231007322872));
#148455=CARTESIAN_POINT('Ctrl Pts',(56.7278790086848,4.91565763232375,134.101190072864));
#148456=CARTESIAN_POINT('Ctrl Pts',(56.7204823237726,4.99993528649898,133.96799423942));
#148457=CARTESIAN_POINT('Ctrl Pts',(56.7130859668372,5.0842092037147,133.834804312018));
#148458=CARTESIAN_POINT('Ctrl Pts',(56.7056896099017,5.16316274808802,133.698236414509));
#148459=CARTESIAN_POINT('Ctrl Pts',(56.6982932529663,5.23652718327612,133.558759575834));
#148460=CARTESIAN_POINT('Ctrl Pts',(56.6908957636297,5.30990285074653,133.4192613829));
#148461=CARTESIAN_POINT('Ctrl Pts',(56.6834982742931,5.37768753141459,133.276853692419));
#148462=CARTESIAN_POINT('Ctrl Pts',(56.6761007849565,5.43965900047506,133.132029090749));
#148463=CARTESIAN_POINT('Ctrl Pts',(56.6687007024415,5.50165219353794,132.98715372104));
#148464=CARTESIAN_POINT('Ctrl Pts',(56.6613006199266,5.55782797095889,132.839860096268));
#148465=CARTESIAN_POINT('Ctrl Pts',(56.6539005374116,5.60801274673584,132.690659532094));
#148466=CARTESIAN_POINT('Ctrl Pts',(56.6464923177451,5.65825270583287,132.541294906561));
#148467=CARTESIAN_POINT('Ctrl Pts',(56.6390840980787,5.70248838808931,132.390019508063));
#148468=CARTESIAN_POINT('Ctrl Pts',(56.6316758784122,5.74059627006279,132.237359231188));
#148469=CARTESIAN_POINT('Ctrl Pts',(56.6242630991101,5.77872760680182,132.084604994459));
#148470=CARTESIAN_POINT('Ctrl Pts',(56.616850319808,5.81072355225942,131.93046454556));
#148471=CARTESIAN_POINT('Ctrl Pts',(56.609437540506,5.83651205663076,131.775472132946));
#148472=CARTESIAN_POINT('Ctrl Pts',(56.6020141694772,5.86233740882646,131.620258259905));
#148473=CARTESIAN_POINT('Ctrl Pts',(56.5945907984485,5.88193755919618,131.464190361284));
#148474=CARTESIAN_POINT('Ctrl Pts',(56.5871674274198,5.8952924041802,131.307806773292));
#148475=CARTESIAN_POINT('Ctrl Pts',(56.5832313779789,5.90237346343602,131.224888442564));
#148476=CARTESIAN_POINT('Ctrl Pts',(56.579295328538,5.90769961448785,131.14188135563));
#148477=CARTESIAN_POINT('Ctrl Pts',(56.5753592790971,5.91127379424545,131.058865415098));
#148478=CARTESIAN_POINT('Ctrl Pts',(56.5679360126917,5.9180145857218,130.902299942097));
#148479=CARTESIAN_POINT('Ctrl Pts',(56.5605127462863,5.91854110490386,130.745229735058));
#148480=CARTESIAN_POINT('Ctrl Pts',(56.5530894798808,5.91279971407171,130.588189149112));
#148481=CARTESIAN_POINT('Ctrl Pts',(56.5456749871598,5.90706510908673,130.431334172098));
#148482=CARTESIAN_POINT('Ctrl Pts',(56.5382604944388,5.89507735355469,130.274509115897));
#148483=CARTESIAN_POINT('Ctrl Pts',(56.5308460017177,5.87683466188365,130.118252084327));
#148484=CARTESIAN_POINT('Ctrl Pts',(56.523438655364,5.85860955320567,129.962145659168));
#148485=CARTESIAN_POINT('Ctrl Pts',(56.5160313090102,5.83414155342617,129.806606536998));
#148486=CARTESIAN_POINT('Ctrl Pts',(56.5086239626564,5.80348088807406,129.652171334393));
#148487=CARTESIAN_POINT('Ctrl Pts',(56.501222140981,5.77284309060293,129.497851315388));
#148488=CARTESIAN_POINT('Ctrl Pts',(56.4938203193056,5.73602189644192,129.344633941132));
#148489=CARTESIAN_POINT('Ctrl Pts',(56.4864184976302,5.69311916317717,129.193049115601));
#148490=CARTESIAN_POINT('Ctrl Pts',(56.4790205833188,5.65023907793129,129.041544310519));
#148491=CARTESIAN_POINT('Ctrl Pts',(56.4716226690074,5.60128394864446,128.891670696105));
#148492=CARTESIAN_POINT('Ctrl Pts',(56.4642247546961,5.54640635194575,128.743946304474));
#148493=CARTESIAN_POINT('Ctrl Pts',(56.4568280697838,5.49153787490811,128.596246461957));
#148494=CARTESIAN_POINT('Ctrl Pts',(56.4494313848717,5.4307490136853,128.450695482952));
#148495=CARTESIAN_POINT('Ctrl Pts',(56.4420346999594,5.3642417173845,128.307794704162));
#148496=CARTESIAN_POINT('Ctrl Pts',(56.434638343024,5.29773737008691,128.164900261742));
#148497=CARTESIAN_POINT('Ctrl Pts',(56.4272419860885,5.22551524938953,128.02465612432));
#148498=CARTESIAN_POINT('Ctrl Pts',(56.4198456291531,5.14782470406803,127.887541908992));
#148499=CARTESIAN_POINT('Ctrl Pts',(56.4124481398165,5.0701222641257,127.750406701128));
#148500=CARTESIAN_POINT('Ctrl Pts',(56.4050506504799,4.98694991656233,127.616402694314));
#148501=CARTESIAN_POINT('Ctrl Pts',(56.3976531611433,4.89860197029609,127.48598310753));
#148502=CARTESIAN_POINT('Ctrl Pts',(56.3902530786283,4.81022305379425,127.355517802362));
#148503=CARTESIAN_POINT('Ctrl Pts',(56.3828529961133,4.71666513556686,127.228639727802));
#148504=CARTESIAN_POINT('Ctrl Pts',(56.3754529135983,4.61826457248577,127.105771305271));
#148505=CARTESIAN_POINT('Ctrl Pts',(56.3680446939318,4.51975580786975,126.982767776279));
#148506=CARTESIAN_POINT('Ctrl Pts',(56.3606364742654,4.41639399754719,126.863782995981));
#148507=CARTESIAN_POINT('Ctrl Pts',(56.3532282545989,4.30855482409166,126.74920514702));
#148508=CARTESIAN_POINT('Ctrl Pts',(56.3458154752968,4.20064927742411,126.634556777305));
#148509=CARTESIAN_POINT('Ctrl Pts',(56.3384026959947,4.08826114234471,126.524321004499));
#148510=CARTESIAN_POINT('Ctrl Pts',(56.3309899166927,3.97180095253115,126.418847220485));
#148511=CARTESIAN_POINT('Ctrl Pts',(56.3235665456639,3.85517435893695,126.313222730583));
#148512=CARTESIAN_POINT('Ctrl Pts',(56.3161431746351,3.73446437578927,126.212374057597));
#148513=CARTESIAN_POINT('Ctrl Pts',(56.3087198036064,3.61011305412161,126.116609099091));
#148514=CARTESIAN_POINT('Ctrl Pts',(56.3047837541656,3.54417899960593,126.065832220244));
#148515=CARTESIAN_POINT('Ctrl Pts',(56.3008477047249,3.47722170123107,126.016483820474));
#148516=CARTESIAN_POINT('Ctrl Pts',(56.2969116552842,3.40930997079423,125.968604618186));
#148517=CARTESIAN_POINT('Ctrl Pts',(56.2894883888788,3.28123056664013,125.878305936926));
#148518=CARTESIAN_POINT('Ctrl Pts',(56.2820651224733,3.14936754947702,125.792962677869));
#148519=CARTESIAN_POINT('Ctrl Pts',(56.2746418560679,3.01414149491475,125.712908799947));
#148520=CARTESIAN_POINT('Ctrl Pts',(56.2672273633469,2.87907526631916,125.632949539062));
#148521=CARTESIAN_POINT('Ctrl Pts',(56.2598128706259,2.74065423033887,125.55826740376));
#148522=CARTESIAN_POINT('Ctrl Pts',(56.2523983779049,2.59933014379981,125.489154754569));
#148523=CARTESIAN_POINT('Ctrl Pts',(56.2449910315511,2.45814227073612,125.420108718752));
#148524=CARTESIAN_POINT('Ctrl Pts',(56.2375836851973,2.31405725061324,125.356621645149));
#148525=CARTESIAN_POINT('Ctrl Pts',(56.2301763388435,2.16755370227811,125.298941331967));
#148526=CARTESIAN_POINT('Ctrl Pts',(56.2227745171681,2.02115942181659,125.241304038939));
#148527=CARTESIAN_POINT('Ctrl Pts',(56.2153726954928,1.87235055066234,125.18946501909));
#148528=CARTESIAN_POINT('Ctrl Pts',(56.2079708738174,1.72162796855045,125.143625002789));
#148529=CARTESIAN_POINT('Ctrl Pts',(56.2005729595061,1.57098495171644,125.097809185076));
#148530=CARTESIAN_POINT('Ctrl Pts',(56.1931750451947,1.41843059209391,125.057986172369));
#148531=CARTESIAN_POINT('Ctrl Pts',(56.1857771308833,1.26448319616759,125.02430760664));
#148532=CARTESIAN_POINT('Ctrl Pts',(56.1783804459711,1.11056138350559,124.990634637679));
#148533=CARTESIAN_POINT('Ctrl Pts',(56.1709837610589,0.95524735830994,124.963104168823));
#148534=CARTESIAN_POINT('Ctrl Pts',(56.1635870761467,0.799072067771759,
124.941817279303));
#148535=CARTESIAN_POINT('Ctrl Pts',(56.1561907192113,0.642903702209399,
124.920531333667));
#148536=CARTESIAN_POINT('Ctrl Pts',(56.1487943622758,0.485874517115526,
124.905488467316));
#148537=CARTESIAN_POINT('Ctrl Pts',(56.1413980053404,0.32852280704081,124.89673814082));
#148538=CARTESIAN_POINT('Ctrl Pts',(56.1340005160038,0.171147006017805,
124.887986474627));
#148539=CARTESIAN_POINT('Ctrl Pts',(56.1266030266673,0.0134489544389833,
124.885529287282));
#148540=CARTESIAN_POINT('Ctrl Pts',(56.1192055373307,-0.14403096057209,
124.889363944287));
#148541=CARTESIAN_POINT('Ctrl Pts',(56.1118054548157,-0.301566079923245,
124.893199945526));
#148542=CARTESIAN_POINT('Ctrl Pts',(56.1044053723007,-0.458882537506066,
124.903332173359));
#148543=CARTESIAN_POINT('Ctrl Pts',(56.0970052897857,-0.615443129108086,
124.919705970322));
#148544=CARTESIAN_POINT('Ctrl Pts',(56.0895970701192,-0.772175875175615,
124.936097771958));
#148545=CARTESIAN_POINT('Ctrl Pts',(56.0821888504527,-0.92815072389576,
124.958744810225));
#148546=CARTESIAN_POINT('Ctrl Pts',(56.0747806307862,-1.08283802061103,
124.987540834934));
#148547=CARTESIAN_POINT('Ctrl Pts',(56.0673678514841,-1.23762052477633,
125.016354583116));
#148548=CARTESIAN_POINT('Ctrl Pts',(56.0599550721821,-1.39111353472003,
125.051324776295));
#148549=CARTESIAN_POINT('Ctrl Pts',(56.05254229288,-1.542801193676,125.092294875709));
#148550=CARTESIAN_POINT('Ctrl Pts',(56.0451189218513,-1.69470559107253,
125.133323515123));
#148551=CARTESIAN_POINT('Ctrl Pts',(56.0376955508226,-1.84479913023503,
125.180369071514));
#148552=CARTESIAN_POINT('Ctrl Pts',(56.0302721797938,-1.99258382884118,
125.233226060984));
#148553=CARTESIAN_POINT('Ctrl Pts',(56.026336130353,-2.07094282208795,125.261252105087));
#148554=CARTESIAN_POINT('Ctrl Pts',(56.0224000809121,-2.14865308373086,
125.290911161063));
#148555=CARTESIAN_POINT('Ctrl Pts',(56.0184640314713,-2.22564316176527,
125.322167344889));
#148556=CARTESIAN_POINT('Ctrl Pts',(56.0110407650659,-2.37084404615895,
125.381115532112));
#148557=CARTESIAN_POINT('Ctrl Pts',(56.0036174986605,-2.51392092876084,
125.445925506861));
#148558=CARTESIAN_POINT('Ctrl Pts',(55.996194232255,-2.65436550907055,125.516423939924));
#148559=CARTESIAN_POINT('Ctrl Pts',(55.988779739534,-2.79464409554954,125.586839049693));
#148560=CARTESIAN_POINT('Ctrl Pts',(55.981365246813,-2.93229624215579,125.662929069208));
#148561=CARTESIAN_POINT('Ctrl Pts',(55.973950754092,-3.06683179209899,125.744471950661));
#148562=CARTESIAN_POINT('Ctrl Pts',(55.9665434077382,-3.20123767161417,
125.825936238016));
#148563=CARTESIAN_POINT('Ctrl Pts',(55.9591360613844,-3.33253261753232,
125.912842732105));
#148564=CARTESIAN_POINT('Ctrl Pts',(55.9517287150307,-3.46024944502699,
126.004922698321));
#148565=CARTESIAN_POINT('Ctrl Pts',(55.9443268933553,-3.58787101649304,
126.096933987824));
#148566=CARTESIAN_POINT('Ctrl Pts',(55.9369250716799,-3.7119194817674,126.194110849145));
#148567=CARTESIAN_POINT('Ctrl Pts',(55.9295232500045,-3.8319552229732,126.296140377646));
#148568=CARTESIAN_POINT('Ctrl Pts',(55.9221253356931,-3.95192759824541,
126.398116045552));
#148569=CARTESIAN_POINT('Ctrl Pts',(55.9147274213818,-4.06789118440539,
126.504939037767));
#148570=CARTESIAN_POINT('Ctrl Pts',(55.9073295070704,-4.17943824345153,
126.616255254556));
#148571=CARTESIAN_POINT('Ctrl Pts',(55.8999328221582,-4.29096676540029,
126.727552972609));
#148572=CARTESIAN_POINT('Ctrl Pts',(55.892536137246,-4.39807995292613,126.843342169842));
#148573=CARTESIAN_POINT('Ctrl Pts',(55.8851394523338,-4.50040577528442,
126.963230781139));
#148574=CARTESIAN_POINT('Ctrl Pts',(55.8777430953984,-4.60272706040851,
127.08311407645));
#148575=CARTESIAN_POINT('Ctrl Pts',(55.870346738463,-4.70026116009976,127.207096140462));
#148576=CARTESIAN_POINT('Ctrl Pts',(55.8629503815275,-4.79267550042741,
127.33475082537));
#148577=CARTESIAN_POINT('Ctrl Pts',(55.855552892191,-4.88510398962636,127.462425054536));
#148578=CARTESIAN_POINT('Ctrl Pts',(55.8481554028543,-4.97241093979794,
127.59377272179));
#148579=CARTESIAN_POINT('Ctrl Pts',(55.8407579135178,-5.05430647498039,
127.72833776013));
#148580=CARTESIAN_POINT('Ctrl Pts',(55.8333578310028,-5.13623071851609,
127.862949970035));
#148581=CARTESIAN_POINT('Ctrl Pts',(55.8259577484878,-5.21273957627244,
128.000781477871));
#148582=CARTESIAN_POINT('Ctrl Pts',(55.8185576659728,-5.28358866112371,
128.141350774823));
#148583=CARTESIAN_POINT('Ctrl Pts',(55.8111494463063,-5.35451565182703,
128.282074642168));
#148584=CARTESIAN_POINT('Ctrl Pts',(55.8037412266398,-5.41977027276596,
128.425541977201));
#148585=CARTESIAN_POINT('Ctrl Pts',(55.7963330069734,-5.47915562395426,
128.571249735637));
#148586=CARTESIAN_POINT('Ctrl Pts',(55.7889202276713,-5.53857752583539,
128.717047174767));
#148587=CARTESIAN_POINT('Ctrl Pts',(55.7815074483693,-5.59212283305584,
128.865087434788));
#148588=CARTESIAN_POINT('Ctrl Pts',(55.7740946690672,-5.63964441292811,
129.014851897769));
#148589=CARTESIAN_POINT('Ctrl Pts',(55.7666712980385,-5.68723389386225,
129.164830351238));
#148590=CARTESIAN_POINT('Ctrl Pts',(55.7592479270097,-5.72878235902658,
129.316537568987));
#148591=CARTESIAN_POINT('Ctrl Pts',(55.7518245559809,-5.7641935162364,129.469443515316));
#148592=CARTESIAN_POINT('Ctrl Pts',(55.7478885065401,-5.78296936146829,
129.550517916989));
#148593=CARTESIAN_POINT('Ctrl Pts',(55.7439524570992,-5.80002065228488,
129.631929205196));
#148594=CARTESIAN_POINT('Ctrl Pts',(55.7400164076584,-5.81533895737569,
129.713597869152));
#148595=CARTESIAN_POINT('Ctrl Pts',(55.7289255750963,-5.85850222538121,
129.943720353922));
#148596=CARTESIAN_POINT('Ctrl Pts',(55.7178347425342,-5.88801578371597,
130.176477191147));
#148597=CARTESIAN_POINT('Ctrl Pts',(55.7067439099721,-5.90363014035041,
130.410556442314));
#148598=CARTESIAN_POINT('Ctrl Pts',(55.7006210040519,-5.91225034412153,
130.539784363187));
#148599=CARTESIAN_POINT('Ctrl Pts',(55.6944980981317,-5.91663505796375,
130.669414956629));
#148600=CARTESIAN_POINT('Ctrl Pts',(55.6883751922115,-5.91674776958239,
130.799223143303));
#148601=CARTESIAN_POINT('',(53.9383751922116,-5.90707774427615,130.803391861671));
#148602=CARTESIAN_POINT('Ctrl Pts',(55.6883738953519,-5.91958331968349,
130.799248188382));
#148603=CARTESIAN_POINT('Ctrl Pts',(55.6127721915164,-5.90490201336922,
132.402818445112));
#148604=CARTESIAN_POINT('Ctrl Pts',(55.4443546130767,-4.40225102814146,
135.999289301185));
#148605=CARTESIAN_POINT('Ctrl Pts',(55.1831211600325,1.68571315393122,137.596704225852));
#148606=CARTESIAN_POINT('Ctrl Pts',(54.90467353622,6.62576018234721,133.057550031782));
#148607=CARTESIAN_POINT('Ctrl Pts',(54.6262259124067,5.47705728957188,126.447824840472));
#148608=CARTESIAN_POINT('Ctrl Pts',(54.3477782885941,-0.704793683201028,
123.841543199704));
#148609=CARTESIAN_POINT('Ctrl Pts',(54.1184947151954,-5.26183227781015,
126.964180250712));
#148610=CARTESIAN_POINT('Ctrl Pts',(53.9820270164014,-5.9084332985456,129.872530384689));
#148611=CARTESIAN_POINT('Ctrl Pts',(53.9383751922116,-5.90707774427615,
130.803391861671));
#148612=CARTESIAN_POINT('',(52.1883751922116,-5.91601678976896,130.809832131107));
#148613=CARTESIAN_POINT('Ctrl Pts',(53.9383751922116,-5.90707774427615,
130.803391861671));
#148614=CARTESIAN_POINT('Ctrl Pts',(53.8892111417971,-5.9055510145305,131.851799836197));
#148615=CARTESIAN_POINT('Ctrl Pts',(53.7472312167785,-5.13850862592351,
134.881563943613));
#148616=CARTESIAN_POINT('Ctrl Pts',(53.5124354171551,-0.290390214522944,
137.796730319866));
#148617=CARTESIAN_POINT('Ctrl Pts',(53.2339877933425,5.72591566061874,134.828220751543));
#148618=CARTESIAN_POINT('Ctrl Pts',(52.9555401695295,6.48038477018695,128.16198029659));
#148619=CARTESIAN_POINT('Ctrl Pts',(52.6770925457166,1.27969686034724,123.923958269158));
#148620=CARTESIAN_POINT('Ctrl Pts',(52.4213708866106,-4.57652770833536,
125.838541045522));
#148621=CARTESIAN_POINT('Ctrl Pts',(52.258465102109,-5.90238132460186,129.320871834531));
#148622=CARTESIAN_POINT('Ctrl Pts',(52.1883751922116,-5.91601678976896,
130.809832131107));
#148623=CARTESIAN_POINT('',(50.4383743543751,-5.92189907249208,130.802920451297));
#148624=CARTESIAN_POINT('Ctrl Pts',(52.1883751708118,-5.91674746906338,
130.809833261547));
#148625=CARTESIAN_POINT('Ctrl Pts',(52.1787920763061,-5.91655914876486,
131.013435698233));
#148626=CARTESIAN_POINT('Ctrl Pts',(52.1692089818004,-5.90585813140058,
131.21656877425));
#148627=CARTESIAN_POINT('Ctrl Pts',(52.1596258872947,-5.88480997411137,
131.418316748816));
#148628=CARTESIAN_POINT('Ctrl Pts',(52.1498159990139,-5.86326369055945,
131.624839296434));
#148629=CARTESIAN_POINT('Ctrl Pts',(52.1400061107331,-5.83087469838739,
131.829910702615));
#148630=CARTESIAN_POINT('Ctrl Pts',(52.1301962224523,-5.78786844693692,
132.032574525422));
#148631=CARTESIAN_POINT('Ctrl Pts',(52.1268632476651,-5.77325678698019,
132.1014309071));
#148632=CARTESIAN_POINT('Ctrl Pts',(52.123530272878,-5.75741993033894,132.170009565731));
#148633=CARTESIAN_POINT('Ctrl Pts',(52.1201972980909,-5.74036795552583,
132.238273549955));
#148634=CARTESIAN_POINT('Ctrl Pts',(52.1127740316855,-5.70238946488,132.390312426081));
#148635=CARTESIAN_POINT('Ctrl Pts',(52.1053507652801,-5.6583090420052,132.54107131796));
#148636=CARTESIAN_POINT('Ctrl Pts',(52.0979274988747,-5.60822693525101,
132.69002262472));
#148637=CARTESIAN_POINT('Ctrl Pts',(52.0905130061538,-5.55820402138787,
132.838797883405));
#148638=CARTESIAN_POINT('Ctrl Pts',(52.0830985134328,-5.50219366108803,
132.98576945914));
#148639=CARTESIAN_POINT('Ctrl Pts',(52.0756840207118,-5.44034688608054,
133.130420875086));
#148640=CARTESIAN_POINT('Ctrl Pts',(52.0682766743581,-5.37855972132337,
133.274932870551));
#148641=CARTESIAN_POINT('Ctrl Pts',(52.0608693280044,-5.31094748660528,
133.417128817239));
#148642=CARTESIAN_POINT('Ctrl Pts',(52.0534619816507,-5.23771066323937,
133.556508428039));
#148643=CARTESIAN_POINT('Ctrl Pts',(52.0460601599753,-5.1645284626593,133.695784084266));
#148644=CARTESIAN_POINT('Ctrl Pts',(52.0386583382999,-5.08573019919347,
133.832247258008));
#148645=CARTESIAN_POINT('Ctrl Pts',(52.0312565166245,-5.00156395702014,
133.965418754699));
#148646=CARTESIAN_POINT('Ctrl Pts',(52.0238586023132,-4.9174421455509,134.098519951195));
#148647=CARTESIAN_POINT('Ctrl Pts',(52.0164606880019,-4.82795819778345,
134.228332616496));
#148648=CARTESIAN_POINT('Ctrl Pts',(52.0090627736906,-4.73340546081606,
134.354403336466));
#148649=CARTESIAN_POINT('Ctrl Pts',(52.0016660887784,-4.63886843679818,
134.48045310577));
#148650=CARTESIAN_POINT('Ctrl Pts',(51.9942694038662,-4.53926451913656,
134.602761865571));
#148651=CARTESIAN_POINT('Ctrl Pts',(51.986872718954,-4.43492965747943,134.720906225076));
#148652=CARTESIAN_POINT('Ctrl Pts',(51.9794763620186,-4.3305994221394,134.839045345937));
#148653=CARTESIAN_POINT('Ctrl Pts',(51.9720800050832,-4.2215389070088,134.953020153849));
#148654=CARTESIAN_POINT('Ctrl Pts',(51.9646836481478,-4.10812334647795,
135.062441538899));
#148655=CARTESIAN_POINT('Ctrl Pts',(51.9572861588113,-3.99469042173525,
135.171879676643));
#148656=CARTESIAN_POINT('Ctrl Pts',(51.9498886694747,-3.87690139263427,
135.276762744222));
#148657=CARTESIAN_POINT('Ctrl Pts',(51.9424911801381,-3.75516711110429,
135.3767397062));
#148658=CARTESIAN_POINT('Ctrl Pts',(51.9350910976232,-3.63339015581062,
135.476751714948));
#148659=CARTESIAN_POINT('Ctrl Pts',(51.9276910151082,-3.50766548284016,
135.571853957159));
#148660=CARTESIAN_POINT('Ctrl Pts',(51.9202909325932,-3.37843552045251,
135.661736863714));
#148661=CARTESIAN_POINT('Ctrl Pts',(51.9128827129268,-3.24906345643605,
135.751718605766));
#148662=CARTESIAN_POINT('Ctrl Pts',(51.9054744932604,-3.11617871210872,
135.836469337328));
#148663=CARTESIAN_POINT('Ctrl Pts',(51.8980662735939,-2.98025170497133,
135.915723482548));
#148664=CARTESIAN_POINT('Ctrl Pts',(51.8906534942919,-2.8442410370291,135.995026407372));
#148665=CARTESIAN_POINT('Ctrl Pts',(51.8832407149899,-2.7051847041352,136.068825830096));
#148666=CARTESIAN_POINT('Ctrl Pts',(51.8758279356878,-2.56357553038275,
136.136903262733));
#148667=CARTESIAN_POINT('Ctrl Pts',(51.8684045646591,-2.42176401880202,
136.205077967598));
#148668=CARTESIAN_POINT('Ctrl Pts',(51.8609811936304,-2.27739272297172,
136.267514205589));
#148669=CARTESIAN_POINT('Ctrl Pts',(51.8535578226017,-2.13097290953555,
136.324042222634));
#148670=CARTESIAN_POINT('Ctrl Pts',(51.8496217731604,-2.05333761114648,
136.354014733646));
#148671=CARTESIAN_POINT('Ctrl Pts',(51.8456857237191,-1.97512664002955,
136.382327069553));
#148672=CARTESIAN_POINT('Ctrl Pts',(51.8417496742778,-1.89641753569978,
136.408959719446));
#148673=CARTESIAN_POINT('Ctrl Pts',(51.8343264078724,-1.74797462137917,
136.459188065961));
#148674=CARTESIAN_POINT('Ctrl Pts',(51.826903141467,-1.59731035063802,136.503590821326));
#148675=CARTESIAN_POINT('Ctrl Pts',(51.8194798750616,-1.44492279571566,
136.541967146156));
#148676=CARTESIAN_POINT('Ctrl Pts',(51.8120653823406,-1.292715350228,136.580298113358));
#148677=CARTESIAN_POINT('Ctrl Pts',(51.8046508896195,-1.13878903323905,
136.612616737607));
#148678=CARTESIAN_POINT('Ctrl Pts',(51.7972363968985,-0.983660007678643,
136.638770917827));
#148679=CARTESIAN_POINT('Ctrl Pts',(51.7898290505447,-0.828680501313577,
136.664899889664));
#148680=CARTESIAN_POINT('Ctrl Pts',(51.782421704191,-0.672500959779303,
136.684876184232));
#148681=CARTESIAN_POINT('Ctrl Pts',(51.7750143578372,-0.515650653838979,
136.698598054733));
#148682=CARTESIAN_POINT('Ctrl Pts',(51.7676125361618,-0.358917332774448,
136.712309690944));
#148683=CARTESIAN_POINT('Ctrl Pts',(51.7602107144864,-0.201514613708668,
136.719776158913));
#148684=CARTESIAN_POINT('Ctrl Pts',(51.752808892811,-0.0439797521587122,
136.720947162517));
#148685=CARTESIAN_POINT('Ctrl Pts',(51.7454109784996,0.11347194796408,136.722117547958));
#148686=CARTESIAN_POINT('Ctrl Pts',(51.7380130641883,0.271055279303985,
136.716999084829));
#148687=CARTESIAN_POINT('Ctrl Pts',(51.7306151498769,0.428230210433925,
136.705593492938));
#148688=CARTESIAN_POINT('Ctrl Pts',(51.7232184649647,0.585379021941531,
136.694189796449));
#148689=CARTESIAN_POINT('Ctrl Pts',(51.7158217800525,0.742119195984115,
136.67650107182));
#148690=CARTESIAN_POINT('Ctrl Pts',(51.7084250951403,0.897912932904884,
136.65258110994));
#148691=CARTESIAN_POINT('Ctrl Pts',(51.7010287382049,1.05369976176832,136.628662208695));
#148692=CARTESIAN_POINT('Ctrl Pts',(51.6936323812694,1.20853986797863,136.598512676227));
#148693=CARTESIAN_POINT('Ctrl Pts',(51.6862360243339,1.36190305899322,136.562237884442));
#148694=CARTESIAN_POINT('Ctrl Pts',(51.6788385349974,1.51528973030366,136.525957538894));
#148695=CARTESIAN_POINT('Ctrl Pts',(51.6714410456609,1.66719867288674,136.483550152689));
#148696=CARTESIAN_POINT('Ctrl Pts',(51.6640435563243,1.81711247518638,136.435171643965));
#148697=CARTESIAN_POINT('Ctrl Pts',(51.6566434738093,1.96707882953745,136.386776176231));
#148698=CARTESIAN_POINT('Ctrl Pts',(51.6492433912943,2.11504829608217,136.332405533068));
#148699=CARTESIAN_POINT('Ctrl Pts',(51.6418433087793,2.26052128227204,136.272264612233));
#148700=CARTESIAN_POINT('Ctrl Pts',(51.6344350891128,2.406154230965,136.212057560273));
#148701=CARTESIAN_POINT('Ctrl Pts',(51.6270268694463,2.54928487189358,136.146067701939));
#148702=CARTESIAN_POINT('Ctrl Pts',(51.6196186497799,2.68943549642102,136.074547262562));
#148703=CARTESIAN_POINT('Ctrl Pts',(51.6122058704778,2.82967238131952,136.002982803547));
#148704=CARTESIAN_POINT('Ctrl Pts',(51.6047930911757,2.96692527033519,135.925881163036));
#148705=CARTESIAN_POINT('Ctrl Pts',(51.5973803118736,3.10074395987572,135.843538869801));
#148706=CARTESIAN_POINT('Ctrl Pts',(51.5899569408449,3.23475385583515,135.761078922035));
#148707=CARTESIAN_POINT('Ctrl Pts',(51.5825335698162,3.36531944300499,135.673363573769));
#148708=CARTESIAN_POINT('Ctrl Pts',(51.5751101987874,3.49202155036641,135.580731211885));
#148709=CARTESIAN_POINT('Ctrl Pts',(51.5711741493467,3.55920204786404,135.531615310932));
#148710=CARTESIAN_POINT('Ctrl Pts',(51.5672380999059,3.62529695819835,135.481117715013));
#148711=CARTESIAN_POINT('Ctrl Pts',(51.5633020504651,3.69024795428735,135.429293114195));
#148712=CARTESIAN_POINT('Ctrl Pts',(51.5558787840597,3.81274350586153,135.331553534442));
#148713=CARTESIAN_POINT('Ctrl Pts',(51.5484555176542,3.93153852001657,135.228796190306));
#148714=CARTESIAN_POINT('Ctrl Pts',(51.5410322512488,4.04619480467912,135.121331565475));
#148715=CARTESIAN_POINT('Ctrl Pts',(51.5336177585278,4.16071557513481,135.013993954905));
#148716=CARTESIAN_POINT('Ctrl Pts',(51.5262032658068,4.27110708321817,134.901960390835));
#148717=CARTESIAN_POINT('Ctrl Pts',(51.5187887730858,4.37696236331513,134.78558292141));
#148718=CARTESIAN_POINT('Ctrl Pts',(51.511381426732,4.48271561610775,134.669317620971));
#148719=CARTESIAN_POINT('Ctrl Pts',(51.5039740803782,4.58394109558224,134.548717024605));
#148720=CARTESIAN_POINT('Ctrl Pts',(51.4965667340244,4.68026711550046,134.424171426167));
#148721=CARTESIAN_POINT('Ctrl Pts',(51.489164912349,4.77652129183885,134.299718718535));
#148722=CARTESIAN_POINT('Ctrl Pts',(51.4817630906735,4.86788305723269,134.171327161424));
#148723=CARTESIAN_POINT('Ctrl Pts',(51.4743612689981,4.9540196963999,134.039421576834));
#148724=CARTESIAN_POINT('Ctrl Pts',(51.4669633546868,5.0401108647059,133.907585624176));
#148725=CARTESIAN_POINT('Ctrl Pts',(51.4595654403754,5.12098219648986,133.772239650181));
#148726=CARTESIAN_POINT('Ctrl Pts',(51.452167526064,5.19634323849538,133.633838928181));
#148727=CARTESIAN_POINT('Ctrl Pts',(51.4447708411518,5.2716917568628,133.495461205871));
#148728=CARTESIAN_POINT('Ctrl Pts',(51.4373741562396,5.34153162452368,133.354030070604));
#148729=CARTESIAN_POINT('Ctrl Pts',(51.4299774713274,5.40561740342432,133.21002706375));
#148730=CARTESIAN_POINT('Ctrl Pts',(51.4225811143919,5.46970034069436,133.066030442141));
#148731=CARTESIAN_POINT('Ctrl Pts',(51.4151847574565,5.5280295447358,132.919462516744));
#148732=CARTESIAN_POINT('Ctrl Pts',(51.407788400521,5.58040708589907,132.770826309651));
#148733=CARTESIAN_POINT('Ctrl Pts',(51.4003909111844,5.63279264619761,132.622167345976));
#148734=CARTESIAN_POINT('Ctrl Pts',(51.3929934218478,5.67922460519249,132.471439822194));
#148735=CARTESIAN_POINT('Ctrl Pts',(51.3855959325112,5.71955446764392,132.319163328864));
#148736=CARTESIAN_POINT('Ctrl Pts',(51.3781958499962,5.75989846766612,132.166833455245));
#148737=CARTESIAN_POINT('Ctrl Pts',(51.3707957674812,5.79413601673944,132.012953891622));
#148738=CARTESIAN_POINT('Ctrl Pts',(51.3633956849662,5.82216945917212,131.858055711596));
#148739=CARTESIAN_POINT('Ctrl Pts',(51.3559874652997,5.85023372725667,131.702987205098));
#148740=CARTESIAN_POINT('Ctrl Pts',(51.3485792456332,5.87208019809251,131.546898212893));
#148741=CARTESIAN_POINT('Ctrl Pts',(51.3411710259668,5.88766286280675,131.390326978739));
#148742=CARTESIAN_POINT('Ctrl Pts',(51.3337582466647,5.90325511839111,131.233659377603));
#148743=CARTESIAN_POINT('Ctrl Pts',(51.3263454673626,5.91257586369814,131.076509314862));
#148744=CARTESIAN_POINT('Ctrl Pts',(51.3189326880606,5.91563123074403,130.919415840593));
#148745=CARTESIAN_POINT('Ctrl Pts',(51.3115093170318,5.91869096344165,130.762097903802));
#148746=CARTESIAN_POINT('Ctrl Pts',(51.304085946003,5.91546744582428,130.604837089201));
#148747=CARTESIAN_POINT('Ctrl Pts',(51.2966625749742,5.90601880018665,130.448168963618));
#148748=CARTESIAN_POINT('Ctrl Pts',(51.2927265255335,5.90100890155253,130.365099764236));
#148749=CARTESIAN_POINT('Ctrl Pts',(51.2887904760928,5.8942497574333,130.282197060201));
#148750=CARTESIAN_POINT('Ctrl Pts',(51.2848544266521,5.88575585291891,130.199539485056));
#148751=CARTESIAN_POINT('Ctrl Pts',(51.2774311602467,5.86973661409017,130.043649877984));
#148752=CARTESIAN_POINT('Ctrl Pts',(51.2700078938412,5.84749555710952,129.888161413633));
#148753=CARTESIAN_POINT('Ctrl Pts',(51.2625846274358,5.81905704717815,129.733610579422));
#148754=CARTESIAN_POINT('Ctrl Pts',(51.2551701347148,5.79065214920381,129.579242411461));
#148755=CARTESIAN_POINT('Ctrl Pts',(51.2477556419938,5.75606444537802,129.425810031309));
#148756=CARTESIAN_POINT('Ctrl Pts',(51.2403411492728,5.71537014892045,129.273846121284));
#148757=CARTESIAN_POINT('Ctrl Pts',(51.232933802919,5.67471507515792,129.122028679797));
#148758=CARTESIAN_POINT('Ctrl Pts',(51.2255264565653,5.62796522207529,128.971677248892));
#148759=CARTESIAN_POINT('Ctrl Pts',(51.2181191102115,5.57524804945439,128.823315502089));
#148760=CARTESIAN_POINT('Ctrl Pts',(51.2107172885361,5.52257019528973,128.675064409074));
#148761=CARTESIAN_POINT('Ctrl Pts',(51.2033154668607,5.46393400788523,128.528800395592));
#148762=CARTESIAN_POINT('Ctrl Pts',(51.1959136451853,5.39951706128397,128.385033011101));
#148763=CARTESIAN_POINT('Ctrl Pts',(51.1885157308739,5.3351341198874,128.241341520293));
#148764=CARTESIAN_POINT('Ctrl Pts',(51.1811178165626,5.26497664899024,128.100144373515));
#148765=CARTESIAN_POINT('Ctrl Pts',(51.1737199022513,5.18927068585997,127.961932023674));
#148766=CARTESIAN_POINT('Ctrl Pts',(51.1663232173391,5.11357730368743,127.823742642219));
#148767=CARTESIAN_POINT('Ctrl Pts',(51.1589265324269,5.03233743845365,127.688537400328));
#148768=CARTESIAN_POINT('Ctrl Pts',(51.1515298475147,4.94582355928902,127.556783076863));
#148769=CARTESIAN_POINT('Ctrl Pts',(51.1441334905793,4.85931351624045,127.425034595522));
#148770=CARTESIAN_POINT('Ctrl Pts',(51.1367371336438,4.76753012913943,127.296737040395));
#148771=CARTESIAN_POINT('Ctrl Pts',(51.1293407767083,4.67078961890795,127.172328831031));
#148772=CARTESIAN_POINT('Ctrl Pts',(51.1219432873718,4.57403429745725,127.047901574452));
#148773=CARTESIAN_POINT('Ctrl Pts',(51.1145457980352,4.4723205708751,126.927365144));
#148774=CARTESIAN_POINT('Ctrl Pts',(51.1071483086987,4.36600532010895,126.811125324313));
#148775=CARTESIAN_POINT('Ctrl Pts',(51.0997482261837,4.25965280069645,126.694844756938));
#148776=CARTESIAN_POINT('Ctrl Pts',(51.0923481436687,4.14869579729786,126.582864074389));
#148777=CARTESIAN_POINT('Ctrl Pts',(51.0849480611537,4.03352833188814,126.47555249542));
#148778=CARTESIAN_POINT('Ctrl Pts',(51.0775398414873,3.9182342280107,126.368122916338));
#148779=CARTESIAN_POINT('Ctrl Pts',(51.0701316218208,3.79872068931553,126.265372948727));
#148780=CARTESIAN_POINT('Ctrl Pts',(51.0627234021543,3.67541568660011,126.167632235054));
#148781=CARTESIAN_POINT('Ctrl Pts',(51.0553106228523,3.55203479171279,126.069831363602));
#148782=CARTESIAN_POINT('Ctrl Pts',(51.0478978435503,3.4248580837182,125.977046109082));
#148783=CARTESIAN_POINT('Ctrl Pts',(51.0404850642482,3.2943423952177,125.889562682191));
#148784=CARTESIAN_POINT('Ctrl Pts',(51.0330616932195,3.16364021978109,125.801954254876));
#148785=CARTESIAN_POINT('Ctrl Pts',(51.0256383221907,3.02958985258975,125.719662979942));
#148786=CARTESIAN_POINT('Ctrl Pts',(51.018214951162,2.89267329770254,125.642929444407));
#148787=CARTESIAN_POINT('Ctrl Pts',(51.0142789017211,2.82007685503185,125.602243482669));
#148788=CARTESIAN_POINT('Ctrl Pts',(51.0103428522802,2.7466749796996,125.563119205502));
#148789=CARTESIAN_POINT('Ctrl Pts',(51.0064068028393,2.67254165787765,125.525586929539));
#148790=CARTESIAN_POINT('Ctrl Pts',(50.9989835364339,2.53272852654616,125.454802228416));
#148791=CARTESIAN_POINT('Ctrl Pts',(50.9915602700284,2.38988984325885,125.389468946554));
#148792=CARTESIAN_POINT('Ctrl Pts',(50.9841370036229,2.24449014006184,125.329856569374));
#148793=CARTESIAN_POINT('Ctrl Pts',(50.9767225109019,2.09926228723931,125.270314649074));
#148794=CARTESIAN_POINT('Ctrl Pts',(50.9693080181809,1.95147978161683,125.216480314611));
#148795=CARTESIAN_POINT('Ctrl Pts',(50.9618935254599,1.80163197902212,125.168577373449));
#148796=CARTESIAN_POINT('Ctrl Pts',(50.9544861791061,1.65192860538102,125.120720602946));
#148797=CARTESIAN_POINT('Ctrl Pts',(50.9470788327523,1.50016425086646,125.078783957427));
#148798=CARTESIAN_POINT('Ctrl Pts',(50.9396714863985,1.34684839196752,125.042943259697));
#148799=CARTESIAN_POINT('Ctrl Pts',(50.9322696647231,1.19364688182042,125.007129293311));
#148800=CARTESIAN_POINT('Ctrl Pts',(50.9248678430477,1.03889653330481,124.977402306454));
#148801=CARTESIAN_POINT('Ctrl Pts',(50.9174660213723,0.883122027918332,
124.953888324981));
#148802=CARTESIAN_POINT('Ctrl Pts',(50.9100681070609,0.727429754680704,
124.930386756356));
#148803=CARTESIAN_POINT('Ctrl Pts',(50.9026701927495,0.57071476947349,124.913091716819));
#148804=CARTESIAN_POINT('Ctrl Pts',(50.8952722784381,0.413511882881774,
124.902078136592));
#148805=CARTESIAN_POINT('Ctrl Pts',(50.8878755935259,0.256335120558084,
124.891066386622));
#148806=CARTESIAN_POINT('Ctrl Pts',(50.8804789086137,0.0986709897909217,
124.886334050262));
#148807=CARTESIAN_POINT('Ctrl Pts',(50.8730822237015,-0.0589405189251695,
124.887904196892));
#148808=CARTESIAN_POINT('Ctrl Pts',(50.865685866766,-0.216545038981799,
124.889474273901));
#148809=CARTESIAN_POINT('Ctrl Pts',(50.8582895098306,-0.374096568347735,
124.897346274522));
#148810=CARTESIAN_POINT('Ctrl Pts',(50.8508931528951,-0.531055327108481,
124.911491129613));
#148811=CARTESIAN_POINT('Ctrl Pts',(50.8434956635586,-0.688038116655891,
124.925638150317));
#148812=CARTESIAN_POINT('Ctrl Pts',(50.8360981742219,-0.844427583078323,
124.946059904248));
#148813=CARTESIAN_POINT('Ctrl Pts',(50.8287006848853,-0.999689425397175,
124.972675473866));
#148814=CARTESIAN_POINT('Ctrl Pts',(50.8213006023703,-1.15500569451439,
124.999300373531));
#148815=CARTESIAN_POINT('Ctrl Pts',(50.8139005198553,-1.30919318481324,
125.032123348759));
#148816=CARTESIAN_POINT('Ctrl Pts',(50.8065004373403,-1.461728283598,125.071012469457));
#148817=CARTESIAN_POINT('Ctrl Pts',(50.7990922176738,-1.61443111040486,
125.109944352741));
#148818=CARTESIAN_POINT('Ctrl Pts',(50.7916839980073,-1.76547755513184,
125.154955610344));
#148819=CARTESIAN_POINT('Ctrl Pts',(50.7842757783408,-1.91435895156643,
125.205864358118));
#148820=CARTESIAN_POINT('Ctrl Pts',(50.7768629990387,-2.0633319820163,125.256804439376));
#148821=CARTESIAN_POINT('Ctrl Pts',(50.7694502197367,-2.21013696159357,
125.313649109171));
#148822=CARTESIAN_POINT('Ctrl Pts',(50.7620374404346,-2.35428616395485,
125.376168725167));
#148823=CARTESIAN_POINT('Ctrl Pts',(50.7546140694058,-2.49864133345638,
125.438777672122));
#148824=CARTESIAN_POINT('Ctrl Pts',(50.747190698377,-2.64033281149806,125.507077598366));
#148825=CARTESIAN_POINT('Ctrl Pts',(50.7397673273483,-2.77889765043978,
125.580793023394));
#148826=CARTESIAN_POINT('Ctrl Pts',(50.7358312779076,-2.85236805286118,
125.61987871052));
#148827=CARTESIAN_POINT('Ctrl Pts',(50.731895228467,-2.92495992185215,125.660486159611));
#148828=CARTESIAN_POINT('Ctrl Pts',(50.7279591790264,-2.99660775983645,
125.702569510887));
#148829=CARTESIAN_POINT('Ctrl Pts',(50.7205359126209,-3.13173334622803,
125.781937398021));
#148830=CARTESIAN_POINT('Ctrl Pts',(50.7131126462155,-3.26390788393835,
125.866797392972));
#148831=CARTESIAN_POINT('Ctrl Pts',(50.7056893798101,-3.39265355633307,
125.956904335226));
#148832=CARTESIAN_POINT('Ctrl Pts',(50.6982748870891,-3.52124706203486,
126.046904778557));
#148833=CARTESIAN_POINT('Ctrl Pts',(50.690860394368,-3.64641946636367,126.142139613201));
#148834=CARTESIAN_POINT('Ctrl Pts',(50.683445901647,-3.767717964983,126.242318103643));
#148835=CARTESIAN_POINT('Ctrl Pts',(50.6760385552932,-3.88889955154256,
126.342400038283));
#148836=CARTESIAN_POINT('Ctrl Pts',(50.6686312089394,-4.00621437979071,
126.447415906663));
#148837=CARTESIAN_POINT('Ctrl Pts',(50.6612238625856,-4.11923914053527,
126.557032108305));
#148838=CARTESIAN_POINT('Ctrl Pts',(50.6538220409102,-4.23217960314893,
126.666566554047));
#148839=CARTESIAN_POINT('Ctrl Pts',(50.6464202192348,-4.34083610246405,
126.780694242492));
#148840=CARTESIAN_POINT('Ctrl Pts',(50.6390183975594,-4.44481900619264,
126.89904186429));
#148841=CARTESIAN_POINT('Ctrl Pts',(50.6316204832481,-4.54874701815576,
127.017327011299));
#148842=CARTESIAN_POINT('Ctrl Pts',(50.6242225689366,-4.64800610221966,
127.139827375428));
#148843=CARTESIAN_POINT('Ctrl Pts',(50.6168246546253,-4.74224413928239,
127.266133507));
#148844=CARTESIAN_POINT('Ctrl Pts',(50.6094279697131,-4.83646651569314,
127.392418648785));
#148845=CARTESIAN_POINT('Ctrl Pts',(50.6020312848009,-4.92566927813927,
127.522508003883));
#148846=CARTESIAN_POINT('Ctrl Pts',(50.5946345998886,-5.00954113964657,
127.655959732563));
#148847=CARTESIAN_POINT('Ctrl Pts',(50.5872382429532,-5.09340928218753,
127.789405543853));
#148848=CARTESIAN_POINT('Ctrl Pts',(50.5798418860178,-5.17194679515063,
127.926213116219));
#148849=CARTESIAN_POINT('Ctrl Pts',(50.5724455290823,-5.24488637100059,
128.065912604952));
#148850=CARTESIAN_POINT('Ctrl Pts',(50.5650480397457,-5.31783711408582,
128.205633482032));
#148851=CARTESIAN_POINT('Ctrl Pts',(50.5576505504091,-5.38518804075603,
128.348246826142));
#148852=CARTESIAN_POINT('Ctrl Pts',(50.5502530610725,-5.44671842649877,
128.493259376828));
#148853=CARTESIAN_POINT('Ctrl Pts',(50.5428529785575,-5.50827038162302,
128.63832276144));
#148854=CARTESIAN_POINT('Ctrl Pts',(50.5354528960425,-5.56399758771458,
128.785786683702));
#148855=CARTESIAN_POINT('Ctrl Pts',(50.5280528135274,-5.61372801584443,
128.935139301985));
#148856=CARTESIAN_POINT('Ctrl Pts',(50.520644593861,-5.66351312769235,129.084656148825));
#148857=CARTESIAN_POINT('Ctrl Pts',(50.5132363741945,-5.7072881747754,129.236065484827));
#148858=CARTESIAN_POINT('Ctrl Pts',(50.505828154528,-5.74493123486562,129.388841041875));
#148859=CARTESIAN_POINT('Ctrl Pts',(50.4984153752259,-5.78259746363116,
129.541710629728));
#148860=CARTESIAN_POINT('Ctrl Pts',(50.4910025959238,-5.81412411038098,
129.695947749312));
#148861=CARTESIAN_POINT('Ctrl Pts',(50.4835898166218,-5.83944075171248,
129.851017935347));
#148862=CARTESIAN_POINT('Ctrl Pts',(50.476166445593,-5.86479356664839,130.006309692938));
#148863=CARTESIAN_POINT('Ctrl Pts',(50.4687430745643,-5.8839186092329,130.162436524779));
#148864=CARTESIAN_POINT('Ctrl Pts',(50.4613197035355,-5.89679741450964,
130.318860035968));
#148865=CARTESIAN_POINT('Ctrl Pts',(50.4573836540948,-5.90362606608985,
130.401799534928));
#148866=CARTESIAN_POINT('Ctrl Pts',(50.4534476046541,-5.90869954745151,
130.484822448345));
#148867=CARTESIAN_POINT('Ctrl Pts',(50.4495115552134,-5.91202103868685,
130.567848882922));
#148868=CARTESIAN_POINT('Ctrl Pts',(50.4457994342128,-5.91515356472693,
130.646151804683));
#148869=CARTESIAN_POINT('Ctrl Pts',(50.4420873132122,-5.91673052304171,
130.724517373101));
#148870=CARTESIAN_POINT('Ctrl Pts',(50.4383751922116,-5.91674982070073,
130.802903998923));
#148871=CARTESIAN_POINT('',(48.6883751922117,-5.91158553941399,130.799597756573));
#148872=CARTESIAN_POINT('Ctrl Pts',(50.438373671031,-5.92609883128946,130.802933869946));
#148873=CARTESIAN_POINT('Ctrl Pts',(50.3492704244875,-5.91986146368452,
132.687448269669));
#148874=CARTESIAN_POINT('Ctrl Pts',(50.1673513033397,-3.92624335915797,
136.546317570673));
#148875=CARTESIAN_POINT('Ctrl Pts',(49.8926163075878,2.65223930360469,137.280716630537));
#148876=CARTESIAN_POINT('Ctrl Pts',(49.6141686837748,6.88234186179267,132.073585194923));
#148877=CARTESIAN_POINT('Ctrl Pts',(49.3357210599618,4.78790847008234,125.700098377784));
#148878=CARTESIAN_POINT('Ctrl Pts',(49.0572734361491,-1.70637890329801,
124.017179201934));
#148879=CARTESIAN_POINT('Ctrl Pts',(48.8414914802322,-5.52392597259,127.546415598653));
#148880=CARTESIAN_POINT('Ctrl Pts',(48.7185253989198,-5.9164078143733,130.157882010726));
#148881=CARTESIAN_POINT('Ctrl Pts',(48.6883751922117,-5.91158553941399,
130.799597756573));
#148882=CARTESIAN_POINT('',(46.9383751922116,-5.90883819398982,130.807710527577));
#148883=CARTESIAN_POINT('Ctrl Pts',(48.6883751922117,-5.91158553941399,
130.799597756573));
#148884=CARTESIAN_POINT('Ctrl Pts',(48.6257095243155,-5.90156268670095,
132.133371226262));
#148885=CARTESIAN_POINT('Ctrl Pts',(48.4702279818151,-4.79354772380148,
135.457715080396));
#148886=CARTESIAN_POINT('Ctrl Pts',(48.2219305647104,0.725982839758202,
137.765000634599));
#148887=CARTESIAN_POINT('Ctrl Pts',(47.9434829408974,6.24859503990529,133.955966645865));
#148888=CARTESIAN_POINT('Ctrl Pts',(47.6650353170847,6.02905365921741,127.250760681639));
#148889=CARTESIAN_POINT('Ctrl Pts',(47.3865876932715,0.269106501353806,
123.81113945552));
#148890=CARTESIAN_POINT('Ctrl Pts',(47.1443676516474,-4.95656072458745,
126.409346611893));
#148891=CARTESIAN_POINT('Ctrl Pts',(46.9949634846273,-5.90265684270682,
129.601880827053));
#148892=CARTESIAN_POINT('Ctrl Pts',(46.9383751922116,-5.90883819398982,
130.807710527577));
#148893=CARTESIAN_POINT('',(45.1883751922116,-5.92386795880746,130.807904967694));
#148894=CARTESIAN_POINT('Ctrl Pts',(46.9383751922116,-5.90883819398982,
130.807710527577));
#148895=CARTESIAN_POINT('Ctrl Pts',(46.902147610023,-5.91279546857935,131.579677531993));
#148896=CARTESIAN_POINT('Ctrl Pts',(46.7731041532299,-5.41277144263418,
134.324515665972));
#148897=CARTESIAN_POINT('Ctrl Pts',(46.5512448218333,-1.25874935488714,
137.688626053462));
#148898=CARTESIAN_POINT('Ctrl Pts',(46.27279719802,5.11154271077221,135.584495725102));
#148899=CARTESIAN_POINT('Ctrl Pts',(45.9943495742072,6.78457673797554,129.087654755492));
#148900=CARTESIAN_POINT('Ctrl Pts',(45.7159019503944,2.22291618797788,124.168382607389));
#148901=CARTESIAN_POINT('Ctrl Pts',(45.4472438230623,-4.14930174401023,
125.305804141896));
#148902=CARTESIAN_POINT('Ctrl Pts',(45.2714015703349,-5.9114443679371,129.050163660677));
#148903=CARTESIAN_POINT('Ctrl Pts',(45.1883751922116,-5.92386795880746,
130.807904967694));
#148904=CARTESIAN_POINT('',(43.4383751922116,-5.91881984665077,130.799298212246));
#148905=CARTESIAN_POINT('Ctrl Pts',(45.1883751922116,-5.92386795880746,
130.807904967694));
#148906=CARTESIAN_POINT('Ctrl Pts',(45.1785856957306,-5.92533280289505,
131.015157201605));
#148907=CARTESIAN_POINT('Ctrl Pts',(45.1687961992496,-5.91540331898639,
131.222267486992));
#148908=CARTESIAN_POINT('Ctrl Pts',(45.0661908281642,-5.68704911656536,
133.379871893754));
#148909=CARTESIAN_POINT('Ctrl Pts',(44.8805590789556,-3.14209308084078,
137.057744629576));
#148910=CARTESIAN_POINT('Ctrl Pts',(44.6021114551428,3.56277101426011,136.827999321065));
#148911=CARTESIAN_POINT('Ctrl Pts',(44.32366383133,6.9936225982931,131.06282431515));
#148912=CARTESIAN_POINT('Ctrl Pts',(44.045216207517,3.99767667195677,125.060133797806));
#148913=CARTESIAN_POINT('Ctrl Pts',(43.7667685837041,-2.67193881854835,
124.336107106742));
#148914=CARTESIAN_POINT('Ctrl Pts',(43.564488245269,-5.73340049741501,128.128201901887));
#148915=CARTESIAN_POINT('Ctrl Pts',(43.4550237814381,-5.92314857408724,
130.446223158808));
#148916=CARTESIAN_POINT('Ctrl Pts',(43.4383751922116,-5.91994246001312,
130.799297252068));
#148917=CARTESIAN_POINT('',(41.6883752167573,-5.91147118309346,130.803194539491));
#148918=CARTESIAN_POINT('Ctrl Pts',(43.4383751922116,-5.9167478358041,130.799299984451));
#148919=CARTESIAN_POINT('Ctrl Pts',(43.4310738632198,-5.91688020106165,
130.954057666618));
#148920=CARTESIAN_POINT('Ctrl Pts',(43.423772534228,-5.91093669250362,131.109027043208));
#148921=CARTESIAN_POINT('Ctrl Pts',(43.4164712052362,-5.89889422020681,
131.263683533727));
#148922=CARTESIAN_POINT('Ctrl Pts',(43.4091762411837,-5.8868622459447,131.418205202329));
#148923=CARTESIAN_POINT('Ctrl Pts',(43.4018812771311,-5.86874191729228,
131.572414145738));
#148924=CARTESIAN_POINT('Ctrl Pts',(43.3945863130785,-5.84456219308604,
131.725785239361));
#148925=CARTESIAN_POINT('Ctrl Pts',(43.3872960069955,-5.82039790808101,
131.879058402702));
#148926=CARTESIAN_POINT('Ctrl Pts',(43.3800057009126,-5.790181987833,132.031494401671));
#148927=CARTESIAN_POINT('Ctrl Pts',(43.3727153948296,-5.75399524481711,
132.18257296881));
#148928=CARTESIAN_POINT('Ctrl Pts',(43.365427232522,-5.71781914281539,132.333607110034));
#148929=CARTESIAN_POINT('Ctrl Pts',(43.3581390702143,-5.6756757968219,132.483284238412));
#148930=CARTESIAN_POINT('Ctrl Pts',(43.3508509079067,-5.62769715383045,
132.631094125024));
#148931=CARTESIAN_POINT('Ctrl Pts',(43.3435635977204,-5.57972412043198,
132.778886729919));
#148932=CARTESIAN_POINT('Ctrl Pts',(43.3362762875341,-5.52591726582878,
132.924812160688));
#148933=CARTESIAN_POINT('Ctrl Pts',(43.3289889773478,-5.46645834994697,
133.06837556248));
#148934=CARTESIAN_POINT('Ctrl Pts',(43.3217009811613,-5.40699383682384,
133.211952478798));
#148935=CARTESIAN_POINT('Ctrl Pts',(43.3144129849747,-5.34187635144991,
133.35316656767));
#148936=CARTESIAN_POINT('Ctrl Pts',(43.3071249887881,-5.27133559294232,
133.491543460076));
#148937=CARTESIAN_POINT('Ctrl Pts',(43.2998347680968,-5.20077330337891,
133.629962589065));
#148938=CARTESIAN_POINT('Ctrl Pts',(43.2925445474055,-5.12478462248862,
133.765542455605));
#148939=CARTESIAN_POINT('Ctrl Pts',(43.2852543267141,-5.04364477738988,
133.897834057246));
#148940=CARTESIAN_POINT('Ctrl Pts',(43.2779564503192,-4.96241972463731,
134.030264582705));
#148941=CARTESIAN_POINT('Ctrl Pts',(43.2706585739243,-4.87603291001786,
134.159399620895));
#148942=CARTESIAN_POINT('Ctrl Pts',(43.2633606975294,-4.78480268829636,
134.284819466134));
#148943=CARTESIAN_POINT('Ctrl Pts',(43.2560584445036,-4.6935177546307,134.410314527276));
#148944=CARTESIAN_POINT('Ctrl Pts',(43.2487561914779,-4.5973838684373,134.53208965766));
#148945=CARTESIAN_POINT('Ctrl Pts',(43.2414539384521,-4.4967585403759,134.64975958153));
#148946=CARTESIAN_POINT('Ctrl Pts',(43.2341415377505,-4.39599337695109,
134.767593027019));
#148947=CARTESIAN_POINT('Ctrl Pts',(43.2268291370489,-4.290724572944,134.881309596506));
#148948=CARTESIAN_POINT('Ctrl Pts',(43.2195167363474,-4.18134561707234,
134.990561686924));
#148949=CARTESIAN_POINT('Ctrl Pts',(43.216302269591,-4.13326359423922,135.038587940823));
#148950=CARTESIAN_POINT('Ctrl Pts',(43.2130878028346,-4.08438774511687,
135.085752009502));
#148951=CARTESIAN_POINT('Ctrl Pts',(43.2098733360782,-4.03475336763297,
135.132026943067));
#148952=CARTESIAN_POINT('Ctrl Pts',(43.2024500696728,-3.92013118148087,
135.238891062617));
#148953=CARTESIAN_POINT('Ctrl Pts',(43.1950268032674,-3.80108715052099,
135.341359818122));
#148954=CARTESIAN_POINT('Ctrl Pts',(43.187603536862,-3.67799257299818,135.439045201814));
#148955=CARTESIAN_POINT('Ctrl Pts',(43.180189044141,-3.55504348304345,135.536615129496));
#148956=CARTESIAN_POINT('Ctrl Pts',(43.17277455142,-3.4280536654459,135.629412708999));
#148957=CARTESIAN_POINT('Ctrl Pts',(43.165360058699,-3.29743096270113,135.717086908407));
#148958=CARTESIAN_POINT('Ctrl Pts',(43.1579527123452,-3.16693415903493,
135.804676604121));
#148959=CARTESIAN_POINT('Ctrl Pts',(43.1505453659914,-3.03281174891307,
135.887152543895));
#148960=CARTESIAN_POINT('Ctrl Pts',(43.1431380196376,-2.89550424266712,
135.964204194962));
#148961=CARTESIAN_POINT('Ctrl Pts',(43.1357361979622,-2.75829914553965,
136.041198378001));
#148962=CARTESIAN_POINT('Ctrl Pts',(43.1283343762869,-2.61791400650058,
136.112776145849));
#148963=CARTESIAN_POINT('Ctrl Pts',(43.1209325546114,-2.47481778569465,
136.178670572352));
#148964=CARTESIAN_POINT('Ctrl Pts',(43.1135346403001,-2.33179710427043,
136.244530213699));
#148965=CARTESIAN_POINT('Ctrl Pts',(43.1061367259887,-2.18606852951715,
136.30471233298));
#148966=CARTESIAN_POINT('Ctrl Pts',(43.0987388116774,-2.03812495663172,
136.358996269313));
#148967=CARTESIAN_POINT('Ctrl Pts',(43.0913421267652,-1.89020596928393,
136.41327118464));
#148968=CARTESIAN_POINT('Ctrl Pts',(43.0839454418531,-1.74007306446702,
136.461649733906));
#148969=CARTESIAN_POINT('Ctrl Pts',(43.0765487569409,-1.5882385311008,136.503959632482));
#148970=CARTESIAN_POINT('Ctrl Pts',(43.0691524000054,-1.43641073023689,
136.546267654992));
#148971=CARTESIAN_POINT('Ctrl Pts',(43.0617560430699,-1.28288181044486,
136.582507461651));
#148972=CARTESIAN_POINT('Ctrl Pts',(43.0543596861345,-1.12817835358521,
136.612556909445));
#148973=CARTESIAN_POINT('Ctrl Pts',(43.0469621967979,-0.97345121123072,
136.642610957887));
#148974=CARTESIAN_POINT('Ctrl Pts',(43.0395647074613,-0.817549540226447,
136.666472689166));
#148975=CARTESIAN_POINT('Ctrl Pts',(43.0321672181248,-0.661009074052499,
136.684071287873));
#148976=CARTESIAN_POINT('Ctrl Pts',(43.0247671356097,-0.504413732859909,
136.701676055741));
#148977=CARTESIAN_POINT('Ctrl Pts',(43.0173670530946,-0.34717952138695,
136.713013278072));
#148978=CARTESIAN_POINT('Ctrl Pts',(43.0099669705796,-0.189846088377888,
136.718064112435));
#148979=CARTESIAN_POINT('Ctrl Pts',(43.0025587509131,-0.032339651086311,
136.72312050071));
#148980=CARTESIAN_POINT('Ctrl Pts',(42.9951505312467,0.125265852295126,
136.721876684258));
#148981=CARTESIAN_POINT('Ctrl Pts',(42.9877423115802,0.282431242364485,
136.714365960697));
#148982=CARTESIAN_POINT('Ctrl Pts',(42.9803295322782,0.439693365108987,
136.706850614411));
#148983=CARTESIAN_POINT('Ctrl Pts',(42.9729167529761,0.59651446377348,136.693060707733));
#148984=CARTESIAN_POINT('Ctrl Pts',(42.9655039736741,0.752362195889403,
136.673081235273));
#148985=CARTESIAN_POINT('Ctrl Pts',(42.9580806026453,0.908432610553728,
136.653073215205));
#148986=CARTESIAN_POINT('Ctrl Pts',(42.9506572316165,1.06352651384456,136.62685802807));
#148987=CARTESIAN_POINT('Ctrl Pts',(42.9432338605878,1.21712262151333,136.594571588394));
#148988=CARTESIAN_POINT('Ctrl Pts',(42.939297811147,1.29856296328754,136.577452543376));
#148989=CARTESIAN_POINT('Ctrl Pts',(42.9353617617062,1.37958247648485,136.558627484354));
#148990=CARTESIAN_POINT('Ctrl Pts',(42.9314257122654,1.46010549598786,136.538122253969));
#148991=CARTESIAN_POINT('Ctrl Pts',(42.92400244586,1.61196939773252,136.499450029408));
#148992=CARTESIAN_POINT('Ctrl Pts',(42.9165791794545,1.76252547035062,136.454681779949));
#148993=CARTESIAN_POINT('Ctrl Pts',(42.9091559130491,1.9112465761481,136.403920161643));
#148994=CARTESIAN_POINT('Ctrl Pts',(42.9017414203281,2.05979190594948,136.353218539354));
#148995=CARTESIAN_POINT('Ctrl Pts',(42.8943269276071,2.20650623605967,136.296537767699));
#148996=CARTESIAN_POINT('Ctrl Pts',(42.8869124348861,2.350873784555,136.234031234794));
#148997=CARTESIAN_POINT('Ctrl Pts',(42.8795050885323,2.49510218617154,136.171584948039));
#148998=CARTESIAN_POINT('Ctrl Pts',(42.8720977421785,2.6369879689361,136.103324225895));
#148999=CARTESIAN_POINT('Ctrl Pts',(42.8646903958248,2.77603176624284,136.029451831632));
#149000=CARTESIAN_POINT('Ctrl Pts',(42.8572885741494,2.91497185943954,135.955634534188));
#149001=CARTESIAN_POINT('Ctrl Pts',(42.849886752474,3.05107385946634,135.876214072708));
#149002=CARTESIAN_POINT('Ctrl Pts',(42.8424849307986,3.1838597093746,135.791440716534));
#149003=CARTESIAN_POINT('Ctrl Pts',(42.8350870164872,3.31657546266687,135.706712111554));
#149004=CARTESIAN_POINT('Ctrl Pts',(42.8276891021759,3.44597823833732,135.616636439868));
#149005=CARTESIAN_POINT('Ctrl Pts',(42.8202911878645,3.57161596624295,135.521509115565));
#149006=CARTESIAN_POINT('Ctrl Pts',(42.8128945029523,3.69723281543698,135.426397599699));
#149007=CARTESIAN_POINT('Ctrl Pts',(42.8054978180401,3.8190855613395,135.326236322482));
#149008=CARTESIAN_POINT('Ctrl Pts',(42.7981011331279,3.936752351339,135.22136316304));
#149009=CARTESIAN_POINT('Ctrl Pts',(42.7907047761925,4.05441392387007,135.116494653784));
#149010=CARTESIAN_POINT('Ctrl Pts',(42.783308419257,4.16788963087681,135.006914926103));
#149011=CARTESIAN_POINT('Ctrl Pts',(42.7759120623216,4.27679207962592,134.893000986949));
#149012=CARTESIAN_POINT('Ctrl Pts',(42.768514572985,4.38571120161748,134.77906960728));
#149013=CARTESIAN_POINT('Ctrl Pts',(42.7611170836484,4.49005541322899,134.660802964712));
#149014=CARTESIAN_POINT('Ctrl Pts',(42.7537195943119,4.58947555841892,134.538613509535));
#149015=CARTESIAN_POINT('Ctrl Pts',(42.7463195117969,4.68893055518748,134.416381221032));
#149016=CARTESIAN_POINT('Ctrl Pts',(42.7389194292818,4.78345781338101,134.290223671413));
#149017=CARTESIAN_POINT('Ctrl Pts',(42.7315193467668,4.87274978700204,134.160584697655));
#149018=CARTESIAN_POINT('Ctrl Pts',(42.7241111271003,4.96213994632701,134.03080317252));
#149019=CARTESIAN_POINT('Ctrl Pts',(42.7167029074339,5.04628311262473,133.897532885731));
#149020=CARTESIAN_POINT('Ctrl Pts',(42.7092946877674,5.12491586048902,133.761245462366));
#149021=CARTESIAN_POINT('Ctrl Pts',(42.7018819084654,5.20359700549757,133.624874156366));
#149022=CARTESIAN_POINT('Ctrl Pts',(42.6944691291633,5.27676080085523,133.485482343259));
#149023=CARTESIAN_POINT('Ctrl Pts',(42.6870563498613,5.34419101082741,133.343563839502));
#149024=CARTESIAN_POINT('Ctrl Pts',(42.6796329788325,5.41171756824586,133.201442555932));
#149025=CARTESIAN_POINT('Ctrl Pts',(42.6722096078038,5.47349403196441,133.056787713618));
#149026=CARTESIAN_POINT('Ctrl Pts',(42.664786236775,5.52935298385414,132.910111348883));
#149027=CARTESIAN_POINT('Ctrl Pts',(42.6608501873342,5.55897074046346,132.832340020849));
#149028=CARTESIAN_POINT('Ctrl Pts',(42.6569141378934,5.58692571105045,132.754000605576));
#149029=CARTESIAN_POINT('Ctrl Pts',(42.6529780884526,5.61319873891446,132.675170730846));
#149030=CARTESIAN_POINT('Ctrl Pts',(42.6455548220471,5.66274884951259,132.526500047301));
#149031=CARTESIAN_POINT('Ctrl Pts',(42.6381315556416,5.70646328812605,132.375634627079));
#149032=CARTESIAN_POINT('Ctrl Pts',(42.6307082892362,5.74414349140036,132.223073454155));
#149033=CARTESIAN_POINT('Ctrl Pts',(42.6232937965152,5.78177915980349,132.070692595868));
#149034=CARTESIAN_POINT('Ctrl Pts',(42.6158793037942,5.8133947004483,131.916620333196));
#149035=CARTESIAN_POINT('Ctrl Pts',(42.6084648110732,5.83884037037358,131.761373518104));
#149036=CARTESIAN_POINT('Ctrl Pts',(42.6010574647194,5.86426151480434,131.606276335736));
#149037=CARTESIAN_POINT('Ctrl Pts',(42.5936501183655,5.88352456735708,131.4500072206));
#149038=CARTESIAN_POINT('Ctrl Pts',(42.5862427720117,5.89653019866703,131.293095902467));
#149039=CARTESIAN_POINT('Ctrl Pts',(42.5788409503363,5.90952612988641,131.136301614717));
#149040=CARTESIAN_POINT('Ctrl Pts',(42.5714391286609,5.91627390182893,130.978866448102));
#149041=CARTESIAN_POINT('Ctrl Pts',(42.5640373069855,5.91672567172351,130.821327882166));
#149042=CARTESIAN_POINT('Ctrl Pts',(42.5566393926741,5.91717720313227,130.663872479614));
#149043=CARTESIAN_POINT('Ctrl Pts',(42.5492414783628,5.91133935055484,130.506314158799));
#149044=CARTESIAN_POINT('Ctrl Pts',(42.5418435640514,5.89921629927872,130.349192937667));
#149045=CARTESIAN_POINT('Ctrl Pts',(42.5344468791392,5.88709526263374,130.192097827232));
#149046=CARTESIAN_POINT('Ctrl Pts',(42.5270501942269,5.8686911289748,130.035440044143));
#149047=CARTESIAN_POINT('Ctrl Pts',(42.5196535093147,5.84406014394001,129.879757136872));
#149048=CARTESIAN_POINT('Ctrl Pts',(42.5122571523792,5.81943025106894,129.724081132744));
#149049=CARTESIAN_POINT('Ctrl Pts',(42.5048607954438,5.78857411414706,129.569380287195));
#149050=CARTESIAN_POINT('Ctrl Pts',(42.4974644385084,5.75159952456495,129.416184306169));
#149051=CARTESIAN_POINT('Ctrl Pts',(42.4900669491718,5.71461927407879,129.262964870447));
#149052=CARTESIAN_POINT('Ctrl Pts',(42.4826694598351,5.67151879332518,129.111251120904));
#149053=CARTESIAN_POINT('Ctrl Pts',(42.4752719704985,5.62245636104609,128.961559751864));
#149054=CARTESIAN_POINT('Ctrl Pts',(42.4678718879835,5.57337673000736,128.811815908746));
#149055=CARTESIAN_POINT('Ctrl Pts',(42.4604718054685,5.51833110255527,128.664096212138));
#149056=CARTESIAN_POINT('Ctrl Pts',(42.4530717229535,5.45752665518637,128.518899313927));
#149057=CARTESIAN_POINT('Ctrl Pts',(42.445663503287,5.39665534707674,128.3735427568));
#149058=CARTESIAN_POINT('Ctrl Pts',(42.4382552836205,5.3300127170849,128.230714882618));
#149059=CARTESIAN_POINT('Ctrl Pts',(42.430847063954,5.25785316887965,128.09089224351));
#149060=CARTESIAN_POINT('Ctrl Pts',(42.4234342846519,5.18564920767632,127.950983545901));
#149061=CARTESIAN_POINT('Ctrl Pts',(42.4160215053498,5.10792174604282,127.81408409294));
#149062=CARTESIAN_POINT('Ctrl Pts',(42.4086087260477,5.02496936505489,127.680642729734));
#149063=CARTESIAN_POINT('Ctrl Pts',(42.4011853550189,4.94189845781504,127.547010699251));
#149064=CARTESIAN_POINT('Ctrl Pts',(42.3937619839902,4.85358792975135,127.416846935062));
#149065=CARTESIAN_POINT('Ctrl Pts',(42.3863386129614,4.76037807793621,127.290569058921));
#149066=CARTESIAN_POINT('Ctrl Pts',(42.3824025635208,4.71095597796659,127.223613498998));
#149067=CARTESIAN_POINT('Ctrl Pts',(42.3784665140802,4.66015715365228,127.157749823019));
#149068=CARTESIAN_POINT('Ctrl Pts',(42.3745304646396,4.60803656078139,127.093036107771));
#149069=CARTESIAN_POINT('Ctrl Pts',(42.3671071982341,4.50973874925041,126.970988060455));
#149070=CARTESIAN_POINT('Ctrl Pts',(42.3596839318287,4.40644012034219,126.852663420469));
#149071=CARTESIAN_POINT('Ctrl Pts',(42.3522606654233,4.29845315506421,126.738498957817));
#149072=CARTESIAN_POINT('Ctrl Pts',(42.3448461727022,4.19059382141112,126.624469428078));
#149073=CARTESIAN_POINT('Ctrl Pts',(42.3374316799813,4.07805743524288,126.514590556936));
#149074=CARTESIAN_POINT('Ctrl Pts',(42.3300171872602,3.96119789902671,126.409267698497));
#149075=CARTESIAN_POINT('Ctrl Pts',(42.3226098409065,3.8444509964314,126.304046354195));
#149076=CARTESIAN_POINT('Ctrl Pts',(42.3152024945526,3.7233895145285,126.203372528709));
#149077=CARTESIAN_POINT('Ctrl Pts',(42.3077951481988,3.59840544002805,126.107616122527));
#149078=CARTESIAN_POINT('Ctrl Pts',(42.3003933265235,3.47351458336627,126.011931135086));
#149079=CARTESIAN_POINT('Ctrl Pts',(42.2929915048481,3.34470725445664,125.921156490321));
#149080=CARTESIAN_POINT('Ctrl Pts',(42.2855896831728,3.21240978987496,125.835622960533));
#149081=CARTESIAN_POINT('Ctrl Pts',(42.2781917688614,3.08018216409485,125.750134583229));
#149082=CARTESIAN_POINT('Ctrl Pts',(42.2707938545501,2.94446838459398,125.669882012963));
#149083=CARTESIAN_POINT('Ctrl Pts',(42.2633959402388,2.80572504601558,125.595153621423));
#149084=CARTESIAN_POINT('Ctrl Pts',(42.2559992553266,2.66700476406279,125.520437648387));
#149085=CARTESIAN_POINT('Ctrl Pts',(42.2486025704143,2.52525625058312,125.451244208928));
#149086=CARTESIAN_POINT('Ctrl Pts',(42.2412058855021,2.38096216247064,125.387816540077));
#149087=CARTESIAN_POINT('Ctrl Pts',(42.2338095285666,2.23667447250883,125.324391683675));
#149088=CARTESIAN_POINT('Ctrl Pts',(42.2264131716312,2.08984177408347,125.266732239761));
#149089=CARTESIAN_POINT('Ctrl Pts',(42.2190168146957,1.94096798768702,125.215033839387));
#149090=CARTESIAN_POINT('Ctrl Pts',(42.2116193253592,1.79207140833466,125.163327523855));
#149091=CARTESIAN_POINT('Ctrl Pts',(42.2042218360226,1.64113347145343,125.11758419154));
#149092=CARTESIAN_POINT('Ctrl Pts',(42.1968243466861,1.48867444013729,125.077949963956));
#149093=CARTESIAN_POINT('Ctrl Pts',(42.1894242641711,1.33616196454341,125.038301842654));
#149094=CARTESIAN_POINT('Ctrl Pts',(42.1820241816561,1.18212769394658,125.004767183732));
#149095=CARTESIAN_POINT('Ctrl Pts',(42.1746240991411,1.02710314225816,124.97744121726));
#149096=CARTESIAN_POINT('Ctrl Pts',(42.1672158794746,0.871908125138678,
124.950085203079));
#149097=CARTESIAN_POINT('Ctrl Pts',(42.1598076598081,0.715721020147045,
124.928951580348));
#149098=CARTESIAN_POINT('Ctrl Pts',(42.1523994401417,0.559080275483776,
124.914083900122));
#149099=CARTESIAN_POINT('Ctrl Pts',(42.1449866608396,0.402343121054518,
124.899207069086));
#149100=CARTESIAN_POINT('Ctrl Pts',(42.1375738815375,0.245152142473199,
124.890603885634));
#149101=CARTESIAN_POINT('Ctrl Pts',(42.1301611022354,0.0880463562037916,
124.888265756793));
#149102=CARTESIAN_POINT('Ctrl Pts',(42.1227377312066,-0.0692839101796727,
124.885924287124));
#149103=CARTESIAN_POINT('Ctrl Pts',(42.1153143601779,-0.226528368943481,
124.889865741497));
#149104=CARTESIAN_POINT('Ctrl Pts',(42.1078909891491,-0.383151724199011,
124.900029553106));
#149105=CARTESIAN_POINT('Ctrl Pts',(42.1039549397083,-0.466197185281535,
124.905418649899));
#149106=CARTESIAN_POINT('Ctrl Pts',(42.1000188902675,-0.549068166615232,
124.912556213816));
#149107=CARTESIAN_POINT('Ctrl Pts',(42.0960828408267,-0.631686101607738,
124.921427400918));
#149108=CARTESIAN_POINT('Ctrl Pts',(42.0886595744213,-0.787500948585284,
124.938158182934));
#149109=CARTESIAN_POINT('Ctrl Pts',(42.0812363080159,-0.942886251466519,
124.961108886852));
#149110=CARTESIAN_POINT('Ctrl Pts',(42.0738130416105,-1.09730563966232,
124.990252698404));
#149111=CARTESIAN_POINT('Ctrl Pts',(42.0663985488895,-1.25154251696522,
125.019362064391));
#149112=CARTESIAN_POINT('Ctrl Pts',(42.0589840561685,-1.40481538876541,
125.054649899477));
#149113=CARTESIAN_POINT('Ctrl Pts',(42.0515695634475,-1.55659192624549,
125.09603755929));
#149114=CARTESIAN_POINT('Ctrl Pts',(42.0441622170937,-1.70822217578466,
125.137385328118));
#149115=CARTESIAN_POINT('Ctrl Pts',(42.03675487074,-1.85835860445632,125.184821119712));
#149116=CARTESIAN_POINT('Ctrl Pts',(42.0293475243862,-2.00647812611256,
125.2382150848));
#149117=CARTESIAN_POINT('Ctrl Pts',(42.0219457027108,-2.15448717464132,
125.291569226655));
#149118=CARTESIAN_POINT('Ctrl Pts',(42.0145438810354,-2.30048196172353,
125.35087256769));
#149119=CARTESIAN_POINT('Ctrl Pts',(42.00714205936,-2.44395375392194,125.415945209379));
#149120=CARTESIAN_POINT('Ctrl Pts',(41.9997441450487,-2.58734980847783,
125.480983499726));
#149121=CARTESIAN_POINT('Ctrl Pts',(41.9923462307374,-2.72822518152775,
125.551784871527));
#149122=CARTESIAN_POINT('Ctrl Pts',(41.984948316426,-2.866090457244,125.628121050719));
#149123=CARTESIAN_POINT('Ctrl Pts',(41.9775516315138,-3.00393282225275,
125.704444544223));
#149124=CARTESIAN_POINT('Ctrl Pts',(41.9701549466016,-3.1387657564655,125.786300838968));
#149125=CARTESIAN_POINT('Ctrl Pts',(41.9627582616894,-3.27012372983875,
125.873415337597));
#149126=CARTESIAN_POINT('Ctrl Pts',(41.955361904754,-3.40147587866162,125.960525973478));
#149127=CARTESIAN_POINT('Ctrl Pts',(41.9479655478186,-3.52935306191335,
126.052894143335));
#149128=CARTESIAN_POINT('Ctrl Pts',(41.9405691908831,-3.65331830831435,
126.150201627949));
#149129=CARTESIAN_POINT('Ctrl Pts',(41.9331717015466,-3.77730253411086,
126.247524010587));
#149130=CARTESIAN_POINT('Ctrl Pts',(41.92577421221,-3.89737333685454,126.34978698321));
#149131=CARTESIAN_POINT('Ctrl Pts',(41.9183767228735,-4.01312656546657,
126.456631815991));
#149132=CARTESIAN_POINT('Ctrl Pts',(41.9109766403586,-4.12892037119295,
126.563514103062));
#149133=CARTESIAN_POINT('Ctrl Pts',(41.9035765578436,-4.24039331524811,
126.674981195114));
#149134=CARTESIAN_POINT('Ctrl Pts',(41.8961764753286,-4.34717798162448,
126.79063738862));
#149135=CARTESIAN_POINT('Ctrl Pts',(41.8887682556622,-4.45408006872018,
126.906420758002));
#149136=CARTESIAN_POINT('Ctrl Pts',(41.8813600359958,-4.55628332938965,
127.026402153576));
#149137=CARTESIAN_POINT('Ctrl Pts',(41.8739518163293,-4.65346007849235,
127.150152104033));
#149138=CARTESIAN_POINT('Ctrl Pts',(41.8665390370272,-4.75069663826223,
127.273978220518));
#149139=CARTESIAN_POINT('Ctrl Pts',(41.8591262577252,-4.84290030368096,
127.401577211877));
#149140=CARTESIAN_POINT('Ctrl Pts',(41.8517134784232,-4.9297869526943,127.532490943581));
#149141=CARTESIAN_POINT('Ctrl Pts',(41.8442901073945,-5.01679774942646,
127.663591730964));
#149142=CARTESIAN_POINT('Ctrl Pts',(41.8368667363657,-5.09847616310607,
127.79801639988));
#149143=CARTESIAN_POINT('Ctrl Pts',(41.829443365337,-5.17458380979925,127.935281852899));
#149144=CARTESIAN_POINT('Ctrl Pts',(41.8255073158959,-5.21493791025638,
128.008063289734));
#149145=CARTESIAN_POINT('Ctrl Pts',(41.8215712664549,-5.25372666523621,
128.081643021004));
#149146=CARTESIAN_POINT('Ctrl Pts',(41.8176352170139,-5.29092009620234,
128.155946922899));
#149147=CARTESIAN_POINT('Ctrl Pts',(41.8096921274624,-5.36597777962749,
128.305894873405));
#149148=CARTESIAN_POINT('Ctrl Pts',(41.8017490379109,-5.43473806517258,
128.459197098472));
#149149=CARTESIAN_POINT('Ctrl Pts',(41.7938059483595,-5.49691040210597,
128.615318225624));
#149150=CARTESIAN_POINT('Ctrl Pts',(41.7858780055998,-5.55896418171488,
128.77114164315));
#149151=CARTESIAN_POINT('Ctrl Pts',(41.7779500628403,-5.61445495316443,
128.929772973799));
#149152=CARTESIAN_POINT('Ctrl Pts',(41.7700221200806,-5.66313861815877,
129.090653654862));
#149153=CARTESIAN_POINT('Ctrl Pts',(41.7621157324991,-5.7116899177838,129.251096919582));
#149154=CARTESIAN_POINT('Ctrl Pts',(41.7542093449176,-5.7534709436117,129.413777056059));
#149155=CARTESIAN_POINT('Ctrl Pts',(41.7463029573361,-5.78828636125568,
129.578117753121));
#149156=CARTESIAN_POINT('Ctrl Pts',(41.7384097906993,-5.82304356107211,
129.742183642095));
#149157=CARTESIAN_POINT('Ctrl Pts',(41.7305166240624,-5.8508583106983,129.907904271569));
#149158=CARTESIAN_POINT('Ctrl Pts',(41.7226234574255,-5.87158482744633,
130.074687967262));
#149159=CARTESIAN_POINT('Ctrl Pts',(41.7147488404953,-5.89226263487094,
130.241079705103));
#149160=CARTESIAN_POINT('Ctrl Pts',(41.7068742235651,-5.90588539747435,
130.408529236549));
#149161=CARTESIAN_POINT('Ctrl Pts',(41.698999606635,-5.91235828421885,130.576435012316));
#149162=CARTESIAN_POINT('Ctrl Pts',(41.6954581533194,-5.91526933708988,
130.651947316161));
#149163=CARTESIAN_POINT('Ctrl Pts',(41.6919167000038,-5.91673495586757,
130.727551735458));
#149164=CARTESIAN_POINT('Ctrl Pts',(41.6883752466882,-5.91674988476282,
130.803192859412));
#149165=CARTESIAN_POINT('',(39.9383751911717,-5.91572623955714,130.809823626609));
#149166=CARTESIAN_POINT('Ctrl Pts',(41.6883751922116,-5.90714223694013,
130.803195917287));
#149167=CARTESIAN_POINT('Ctrl Pts',(41.6386459925414,-5.90528448095996,
131.86362665666));
#149168=CARTESIAN_POINT('Ctrl Pts',(41.496100918267,-5.12530615771963,134.905822374616));
#149169=CARTESIAN_POINT('Ctrl Pts',(41.2607399693881,-0.247820295217642,
137.79836845511));
#149170=CARTESIAN_POINT('Ctrl Pts',(40.9822923455752,5.75030395140879,134.793290924898));
#149171=CARTESIAN_POINT('Ctrl Pts',(40.7038447217622,6.4641797846552,128.122581312326));
#149172=CARTESIAN_POINT('Ctrl Pts',(40.4253970979495,1.23779018854298,123.916295869069));
#149173=CARTESIAN_POINT('Ctrl Pts',(40.1702405880992,-4.59375490894458,
125.86218170759));
#149174=CARTESIAN_POINT('Ctrl Pts',(40.0078999528533,-5.90222128016794,
129.332638640001));
#149175=CARTESIAN_POINT('Ctrl Pts',(39.9383751922116,-5.91565475715166,
130.809823538498));
#149176=CARTESIAN_POINT('',(38.1883744840812,-5.92195841769095,130.803134636241));
#149177=CARTESIAN_POINT('Ctrl Pts',(39.9383751763149,-5.91674747680489,
130.809824885406));
#149178=CARTESIAN_POINT('Ctrl Pts',(39.9288809276006,-5.91656114752689,
131.011583532271));
#149179=CARTESIAN_POINT('Ctrl Pts',(39.9193866788863,-5.90605155807218,
131.212880654709));
#149180=CARTESIAN_POINT('Ctrl Pts',(39.909892430172,-5.88538083791949,131.412820111));
#149181=CARTESIAN_POINT('Ctrl Pts',(39.9001899609273,-5.86425678349646,
131.617144485033));
#149182=CARTESIAN_POINT('Ctrl Pts',(39.8904874916825,-5.83252101133659,
131.820051237144));
#149183=CARTESIAN_POINT('Ctrl Pts',(39.8807850224378,-5.79039458226029,
132.020609417866));
#149184=CARTESIAN_POINT('Ctrl Pts',(39.8766906317331,-5.77261745199748,
132.105243909375));
#149185=CARTESIAN_POINT('Ctrl Pts',(39.8725962410283,-5.75299053662962,
132.189460452012));
#149186=CARTESIAN_POINT('Ctrl Pts',(39.8685018503236,-5.73153296479048,
132.273190231926));
#149187=CARTESIAN_POINT('Ctrl Pts',(39.8610785839182,-5.69262967400549,
132.424995105271));
#149188=CARTESIAN_POINT('Ctrl Pts',(39.8536553175129,-5.64763235567367,
132.575482873891));
#149189=CARTESIAN_POINT('Ctrl Pts',(39.8462320511075,-5.59664446794347,
132.724126556929));
#149190=CARTESIAN_POINT('Ctrl Pts',(39.8388175583866,-5.54571684366221,
132.872594555478));
#149191=CARTESIAN_POINT('Ctrl Pts',(39.8314030656656,-5.48881286340787,
133.019222457208));
#149192=CARTESIAN_POINT('Ctrl Pts',(39.8239885729446,-5.42608670005231,
133.163494714224));
#149193=CARTESIAN_POINT('Ctrl Pts',(39.8165812265909,-5.36342099453469,
133.307627916207));
#149194=CARTESIAN_POINT('Ctrl Pts',(39.8091738802373,-5.2949444254275,133.44940965347));
#149195=CARTESIAN_POINT('Ctrl Pts',(39.8017665338836,-5.22086051571906,
133.588340868557));
#149196=CARTESIAN_POINT('Ctrl Pts',(39.7943647122082,-5.1468318605854,133.727168463501));
#149197=CARTESIAN_POINT('Ctrl Pts',(39.7869628905328,-5.06720436699781,
133.863149441501));
#149198=CARTESIAN_POINT('Ctrl Pts',(39.7795610688575,-4.98222903153145,
133.995806127028));
#149199=CARTESIAN_POINT('Ctrl Pts',(39.7721631545462,-4.89729855388323,
134.128392784123));
#149200=CARTESIAN_POINT('Ctrl Pts',(39.7647652402349,-4.80702605750756,
134.257658330108));
#149201=CARTESIAN_POINT('Ctrl Pts',(39.7573673259236,-4.71170764412821,
134.383151144932));
#149202=CARTESIAN_POINT('Ctrl Pts',(39.7499706410115,-4.61640507094005,
134.508623105127));
#149203=CARTESIAN_POINT('Ctrl Pts',(39.7425739560993,-4.51605847057263,
134.630323281512));
#149204=CARTESIAN_POINT('Ctrl Pts',(39.7351772711872,-4.41100636374977,
134.747830336159));
#149205=CARTESIAN_POINT('Ctrl Pts',(39.7277809142518,-4.30595891504757,
134.86533218042));
#149206=CARTESIAN_POINT('Ctrl Pts',(39.7203845573165,-4.19620662355086,
134.978640994331));
#149207=CARTESIAN_POINT('Ctrl Pts',(39.7129882003811,-4.08212708532021,
135.087369959348));
#149208=CARTESIAN_POINT('Ctrl Pts',(39.7055907110446,-3.96803008122102,
135.196115571048));
#149209=CARTESIAN_POINT('Ctrl Pts',(39.6981932217081,-3.84960478147709,
135.300279680133));
#149210=CARTESIAN_POINT('Ctrl Pts',(39.6907957323716,-3.72726416725788,
135.399513758646));
#149211=CARTESIAN_POINT('Ctrl Pts',(39.6833956498567,-3.60488066672601,
135.498782623511));
#149212=CARTESIAN_POINT('Ctrl Pts',(39.6759955673418,-3.4785794088019,135.593117781928));
#149213=CARTESIAN_POINT('Ctrl Pts',(39.6685954848269,-3.34880469798308,
135.6822123637));
#149214=CARTESIAN_POINT('Ctrl Pts',(39.6611872651605,-3.21888728652836,
135.771404914125));
#149215=CARTESIAN_POINT('Ctrl Pts',(39.6537790454941,-3.0854891024902,135.855345168296));
#149216=CARTESIAN_POINT('Ctrl Pts',(39.6463708258277,-2.94908217128925,
135.933770418848));
#149217=CARTESIAN_POINT('Ctrl Pts',(39.6389580465257,-2.81259128389822,
136.012243938832));
#149218=CARTESIAN_POINT('Ctrl Pts',(39.6315452672237,-2.67308828936398,
136.085195518857));
#149219=CARTESIAN_POINT('Ctrl Pts',(39.6241324879217,-2.5310673326472,136.152409674943));
#149220=CARTESIAN_POINT('Ctrl Pts',(39.616709116893,-2.38884344972733,136.219719869767));
#149221=CARTESIAN_POINT('Ctrl Pts',(39.6092857458643,-2.24409476166139,
136.281276121904));
#149222=CARTESIAN_POINT('Ctrl Pts',(39.6018623748356,-2.09733355896172,
136.336911792653));
#149223=CARTESIAN_POINT('Ctrl Pts',(39.5979263253939,-2.01951724778617,
136.36641116025));
#149224=CARTESIAN_POINT('Ctrl Pts',(39.5939902759524,-1.94113538050561,
136.394246879217));
#149225=CARTESIAN_POINT('Ctrl Pts',(39.5900542265107,-1.86226561396691,
136.420399911013));
#149226=CARTESIAN_POINT('Ctrl Pts',(39.5826309601053,-1.71351969574773,
136.46972371276));
#149227=CARTESIAN_POINT('Ctrl Pts',(39.5752076936998,-1.56258792429142,
136.513208509265));
#149228=CARTESIAN_POINT('Ctrl Pts',(39.5677844272944,-1.40996958517554,
136.550656496772));
#149229=CARTESIAN_POINT('Ctrl Pts',(39.5603699345734,-1.25753162826233,
136.588060223867));
#149230=CARTESIAN_POINT('Ctrl Pts',(39.5529554418523,-1.10341143053259,
136.619441256146));
#149231=CARTESIAN_POINT('Ctrl Pts',(39.5455409491313,-0.948126071235282,
136.64465063738));
#149232=CARTESIAN_POINT('Ctrl Pts',(39.5381336027775,-0.792990381813435,
136.669835720864));
#149233=CARTESIAN_POINT('Ctrl Pts',(39.5307262564237,-0.636692132549131,
136.688860936119));
#149234=CARTESIAN_POINT('Ctrl Pts',(39.5233189100699,-0.479761203760998,
136.701627760054));
#149235=CARTESIAN_POINT('Ctrl Pts',(39.5159170883945,-0.32294731998022,
136.714385062009));
#149236=CARTESIAN_POINT('Ctrl Pts',(39.5085152667191,-0.165502066712273,
136.720893236615));
#149237=CARTESIAN_POINT('Ctrl Pts',(39.5011134450436,-0.0079629956869028,
136.721105259107));
#149238=CARTESIAN_POINT('Ctrl Pts',(39.4937155307323,0.14949291168893,136.721317169674));
#149239=CARTESIAN_POINT('Ctrl Pts',(39.4863176164209,0.307042165836828,
136.715239546913));
#149240=CARTESIAN_POINT('Ctrl Pts',(39.4789197021096,0.464144755804185,
136.702877397924));
#149241=CARTESIAN_POINT('Ctrl Pts',(39.4715230171974,0.62122123817122,136.690517303299));
#149242=CARTESIAN_POINT('Ctrl Pts',(39.4641263322851,0.777850831894141,
136.671874784474));
#149243=CARTESIAN_POINT('Ctrl Pts',(39.4567296473729,0.933496074720745,
136.647006905078));
#149244=CARTESIAN_POINT('Ctrl Pts',(39.4493332904375,1.08913441607418,136.622140128351));
#149245=CARTESIAN_POINT('Ctrl Pts',(39.4419369335021,1.24378812469433,136.591048598808));
#149246=CARTESIAN_POINT('Ctrl Pts',(39.4345405765666,1.39692765929057,136.553840913837));
#149247=CARTESIAN_POINT('Ctrl Pts',(39.42714308723,1.55009063994051,136.516627532275));
#149248=CARTESIAN_POINT('Ctrl Pts',(39.4197455978935,1.70173862220643,136.47329621893));
#149249=CARTESIAN_POINT('Ctrl Pts',(39.4123481085569,1.85135515323665,136.424006038683));
#149250=CARTESIAN_POINT('Ctrl Pts',(39.4049480260419,2.0010241321101,136.37469857984));
#149251=CARTESIAN_POINT('Ctrl Pts',(39.3975479435268,2.14865988758613,136.319428211898));
#149252=CARTESIAN_POINT('Ctrl Pts',(39.3901478610118,2.2937640836433,136.258402869977));
#149253=CARTESIAN_POINT('Ctrl Pts',(39.3827396413453,2.4390278366809,136.19731042442));
#149254=CARTESIAN_POINT('Ctrl Pts',(39.3753314216789,2.58175412673234,136.130450511889));
#149255=CARTESIAN_POINT('Ctrl Pts',(39.3679232020125,2.72146678937886,136.058078260988));
#149256=CARTESIAN_POINT('Ctrl Pts',(39.3605104227104,2.86126544283821,135.985661466175));
#149257=CARTESIAN_POINT('Ctrl Pts',(39.3530976434082,2.99804644930585,135.907725756886));
#149258=CARTESIAN_POINT('Ctrl Pts',(39.3456848641062,3.1313614185855,135.824570396917));
#149259=CARTESIAN_POINT('Ctrl Pts',(39.3382614930774,3.26486687454492,135.74129622067));
#149260=CARTESIAN_POINT('Ctrl Pts',(39.3308381220487,3.3948960944153,135.652787707778));
#149261=CARTESIAN_POINT('Ctrl Pts',(39.3234147510199,3.52103197480109,135.559385790468));
#149262=CARTESIAN_POINT('Ctrl Pts',(39.3194787015792,3.58791224516892,135.509861852763));
#149263=CARTESIAN_POINT('Ctrl Pts',(39.3155426521385,3.65369853771744,135.458962853969));
#149264=CARTESIAN_POINT('Ctrl Pts',(39.3116066026978,3.7183328593593,135.406743838193));
#149265=CARTESIAN_POINT('Ctrl Pts',(39.3041833362924,3.84023117281087,135.308260404137));
#149266=CARTESIAN_POINT('Ctrl Pts',(39.296760069887,3.95839847284968,135.204781824887));
#149267=CARTESIAN_POINT('Ctrl Pts',(39.2893368034815,4.07239846552338,135.096621245778));
#149268=CARTESIAN_POINT('Ctrl Pts',(39.2819223107605,4.18626371967286,134.988588503492));
#149269=CARTESIAN_POINT('Ctrl Pts',(39.2745078180395,4.29597120235384,134.875885030702));
#149270=CARTESIAN_POINT('Ctrl Pts',(39.2670933253185,4.40111609850937,134.758865346346));
#149271=CARTESIAN_POINT('Ctrl Pts',(39.2596859789647,4.5061596520555,134.641958449967));
#149272=CARTESIAN_POINT('Ctrl Pts',(39.2522786326109,4.60664912599584,134.520743899827));
#149273=CARTESIAN_POINT('Ctrl Pts',(39.2448712862571,4.70221521680818,134.395614245106));
#149274=CARTESIAN_POINT('Ctrl Pts',(39.2374694645817,4.79771003082449,134.270577916802));
#149275=CARTESIAN_POINT('Ctrl Pts',(39.2300676429062,4.88828854764652,134.141632593492));
#149276=CARTESIAN_POINT('Ctrl Pts',(39.2226658212308,4.97362064416872,134.009205114636));
#149277=CARTESIAN_POINT('Ctrl Pts',(39.2152679069195,5.05890769454127,133.876847543215));
#149278=CARTESIAN_POINT('Ctrl Pts',(39.2078699926081,5.13895363860715,133.741011790118));
#149279=CARTESIAN_POINT('Ctrl Pts',(39.2004720782968,5.21347079986936,133.60215488831));
#149280=CARTESIAN_POINT('Ctrl Pts',(39.1930753933846,5.28797557773124,133.463321062001));
#149281=CARTESIAN_POINT('Ctrl Pts',(39.1856787084723,5.3569532199578,133.321467412027));
#149282=CARTESIAN_POINT('Ctrl Pts',(39.1782820235601,5.42016122432172,133.17707696489));
#149283=CARTESIAN_POINT('Ctrl Pts',(39.1708856666247,5.48336642597648,133.032692920177));
#149284=CARTESIAN_POINT('Ctrl Pts',(39.1634893096892,5.54080234875001,132.885772643923));
#149285=CARTESIAN_POINT('Ctrl Pts',(39.1560929527538,5.59227412869818,132.736820353755));
#149286=CARTESIAN_POINT('Ctrl Pts',(39.1486954634172,5.64375378910726,132.587845258612));
#149287=CARTESIAN_POINT('Ctrl Pts',(39.1412979740807,5.68926736660663,132.436837882949));
#149288=CARTESIAN_POINT('Ctrl Pts',(39.1339004847441,5.72866953160297,132.284318711629));
#149289=CARTESIAN_POINT('Ctrl Pts',(39.1265004022291,5.76808550896718,132.131746074951));
#149290=CARTESIAN_POINT('Ctrl Pts',(39.1191003197141,5.80138571511799,131.977660948681));
#149291=CARTESIAN_POINT('Ctrl Pts',(39.1117002371991,5.82847572896873,131.822594991039));
#149292=CARTESIAN_POINT('Ctrl Pts',(39.1042920175326,5.85559553107463,131.667358522436));
#149293=CARTESIAN_POINT('Ctrl Pts',(39.0968837978661,5.87649143914705,131.51113943653));
#149294=CARTESIAN_POINT('Ctrl Pts',(39.0894755781997,5.89112072160808,131.354476247175));
#149295=CARTESIAN_POINT('Ctrl Pts',(39.0820627988976,5.90575900814838,131.197716634241));
#149296=CARTESIAN_POINT('Ctrl Pts',(39.0746500195955,5.91412296372715,131.040512745104));
#149297=CARTESIAN_POINT('Ctrl Pts',(39.0672372402934,5.91622200159782,130.883403582527));
#149298=CARTESIAN_POINT('Ctrl Pts',(39.0598138692646,5.91832403867224,130.726069935011));
#149299=CARTESIAN_POINT('Ctrl Pts',(39.0523904982359,5.91414328956474,130.568831656556));
#149300=CARTESIAN_POINT('Ctrl Pts',(39.0449671272071,5.90374113564045,130.412223950259));
#149301=CARTESIAN_POINT('Ctrl Pts',(39.0410310777664,5.89822566403367,130.329186786632));
#149302=CARTESIAN_POINT('Ctrl Pts',(39.0370950283257,5.8909619928557,130.246326763421));
#149303=CARTESIAN_POINT('Ctrl Pts',(39.033158978885,5.88196508559281,130.163722424537));
#149304=CARTESIAN_POINT('Ctrl Pts',(39.0257357124796,5.86499719927847,130.007933219393));
#149305=CARTESIAN_POINT('Ctrl Pts',(39.0183124460742,5.8418100519577,129.852583023509));
#149306=CARTESIAN_POINT('Ctrl Pts',(39.0108891796687,5.81243127413145,129.698208166048));
#149307=CARTESIAN_POINT('Ctrl Pts',(39.0034746869477,5.78308721958079,129.544015766849));
#149308=CARTESIAN_POINT('Ctrl Pts',(38.9960601942267,5.74756617013776,129.390796774614));
#149309=CARTESIAN_POINT('Ctrl Pts',(38.9886457015057,5.70594758019843,129.239083397861));
#149310=CARTESIAN_POINT('Ctrl Pts',(38.981238355152,5.66436910382299,129.087516248173));
#149311=CARTESIAN_POINT('Ctrl Pts',(38.9738310087982,5.61670488507211,128.937452182556));
#149312=CARTESIAN_POINT('Ctrl Pts',(38.9664236624444,5.56308556911545,128.789414088946));
#149313=CARTESIAN_POINT('Ctrl Pts',(38.959021840769,5.50950624446756,128.64148640773));
#149314=CARTESIAN_POINT('Ctrl Pts',(38.9516200190936,5.44998079289106,128.495582039298));
#149315=CARTESIAN_POINT('Ctrl Pts',(38.9442181974182,5.38468988691117,128.35220944272));
#149316=CARTESIAN_POINT('Ctrl Pts',(38.9368202831068,5.31943344749233,128.208912531421));
#149317=CARTESIAN_POINT('Ctrl Pts',(38.9294223687955,5.24841776934164,128.068145069138));
#149318=CARTESIAN_POINT('Ctrl Pts',(38.9220244544841,5.17187187106469,127.930396123737));
#149319=CARTESIAN_POINT('Ctrl Pts',(38.9146277695719,5.09533869332735,127.792670069712));
#149320=CARTESIAN_POINT('Ctrl Pts',(38.9072310846597,5.01327730059677,127.65796186298));
#149321=CARTESIAN_POINT('Ctrl Pts',(38.8998343997475,4.92596299837052,127.526736615154));
#149322=CARTESIAN_POINT('Ctrl Pts',(38.8924380428121,4.83865256775205,127.395517185994));
#149323=CARTESIAN_POINT('Ctrl Pts',(38.8850416858767,4.74608989755134,127.267780719453));
#149324=CARTESIAN_POINT('Ctrl Pts',(38.8776453289412,4.64859387161577,127.143963702029));
#149325=CARTESIAN_POINT('Ctrl Pts',(38.8702478396046,4.55108291878959,127.020127727903));
#149326=CARTESIAN_POINT('Ctrl Pts',(38.8628503502681,4.44863733726269,126.900212691035));
#149327=CARTESIAN_POINT('Ctrl Pts',(38.8554528609315,4.34161647149663,126.78462219611));
#149328=CARTESIAN_POINT('Ctrl Pts',(38.8480527784165,4.23455808973198,126.668991181117));
#149329=CARTESIAN_POINT('Ctrl Pts',(38.8406526959015,4.12292148391106,126.557688000084));
#149330=CARTESIAN_POINT('Ctrl Pts',(38.8332526133865,4.00710291624785,126.4510794664));
#149331=CARTESIAN_POINT('Ctrl Pts',(38.82584439372,3.89115699416305,126.344353705674));
#149332=CARTESIAN_POINT('Ctrl Pts',(38.8184361740536,3.77102020156013,126.242333154614));
#149333=CARTESIAN_POINT('Ctrl Pts',(38.8110279543871,3.64712250793451,126.145344844399));
#149334=CARTESIAN_POINT('Ctrl Pts',(38.803615175085,3.52314855734582,126.048296839498));
#149335=CARTESIAN_POINT('Ctrl Pts',(38.796202395783,3.39540939546134,125.956287464793));
#149336=CARTESIAN_POINT('Ctrl Pts',(38.7887896164809,3.26436358866415,125.869600144807));
#149337=CARTESIAN_POINT('Ctrl Pts',(38.7813662454522,3.13313053747277,125.782788961913));
#149338=CARTESIAN_POINT('Ctrl Pts',(38.7739428744234,2.99858172357663,125.701315214279));
#149339=CARTESIAN_POINT('Ctrl Pts',(38.7665195033946,2.86120060662562,125.62541655037));
#149340=CARTESIAN_POINT('Ctrl Pts',(38.7625834539538,2.78835784200169,125.585173257601));
#149341=CARTESIAN_POINT('Ctrl Pts',(38.7586474045129,2.71471916605623,125.546496523365));
#149342=CARTESIAN_POINT('Ctrl Pts',(38.754711355072,2.64035874813627,125.509416213359));
#149343=CARTESIAN_POINT('Ctrl Pts',(38.7472880886666,2.50011732065159,125.439483905927));
#149344=CARTESIAN_POINT('Ctrl Pts',(38.7398648222612,2.35688358160388,125.375021334148));
#149345=CARTESIAN_POINT('Ctrl Pts',(38.7324415558557,2.21112369486684,125.31629515071));
#149346=CARTESIAN_POINT('Ctrl Pts',(38.7250270631347,2.0655360842111,125.257638376744));
#149347=CARTESIAN_POINT('Ctrl Pts',(38.7176125704137,1.9174286117822,125.204704633764));
#149348=CARTESIAN_POINT('Ctrl Pts',(38.7101980776927,1.76729198672081,125.157714746239));
#149349=CARTESIAN_POINT('Ctrl Pts',(38.7027907313389,1.6173000689914,125.110770149337));
#149350=CARTESIAN_POINT('Ctrl Pts',(38.6953833849851,1.46528324605487,125.069758113509));
#149351=CARTESIAN_POINT('Ctrl Pts',(38.6879760386313,1.31175205524416,125.034851356973));
#149352=CARTESIAN_POINT('Ctrl Pts',(38.6805742169559,1.15833537378774,124.999970635214));
#149353=CARTESIAN_POINT('Ctrl Pts',(38.6731723952805,1.00340693583127,124.971186208423));
#149354=CARTESIAN_POINT('Ctrl Pts',(38.6657705736051,0.847492180306439,
124.948620906238));
#149355=CARTESIAN_POINT('Ctrl Pts',(38.6583726592937,0.691659730967629,
124.926067516101));
#149356=CARTESIAN_POINT('Ctrl Pts',(38.6509747449823,0.5348423695119,124.909726765597));
#149357=CARTESIAN_POINT('Ctrl Pts',(38.643576830671,0.377575352737061,124.899670328016));
#149358=CARTESIAN_POINT('Ctrl Pts',(38.6361801457588,0.220334470887072,
124.889615561632));
#149359=CARTESIAN_POINT('Ctrl Pts',(38.6287834608465,0.0626444541963754,
124.885843059267));
#149360=CARTESIAN_POINT('Ctrl Pts',(38.6213867759343,-0.0949545764154013,
124.888372602795));
#149361=CARTESIAN_POINT('Ctrl Pts',(38.6139904189989,-0.252546618921009,
124.89090203416));
#149362=CARTESIAN_POINT('Ctrl Pts',(38.6065940620634,-0.41004731011999,
124.899732949809));
#149363=CARTESIAN_POINT('Ctrl Pts',(38.5991977051279,-0.566917057050841,
124.914832995343));
#149364=CARTESIAN_POINT('Ctrl Pts',(38.5918002157913,-0.723810821140417,
124.929935352733));
#149365=CARTESIAN_POINT('Ctrl Pts',(38.5844027264547,-0.880073077015787,
124.951308715367));
#149366=CARTESIAN_POINT('Ctrl Pts',(38.5770052371182,-1.03517002616573,
124.978868914763));
#149367=CARTESIAN_POINT('Ctrl Pts',(38.5696051546031,-1.190321344311,125.006438775344));
#149368=CARTESIAN_POINT('Ctrl Pts',(38.5622050720881,-1.34430617510638,
125.040199725455));
#149369=CARTESIAN_POINT('Ctrl Pts',(38.5548049895731,-1.4966017186534,125.080016650069));
#149370=CARTESIAN_POINT('Ctrl Pts',(38.5473967699066,-1.64906472680669,
125.119877357484));
#149371=CARTESIAN_POINT('Ctrl Pts',(38.5399885502401,-1.79983437669202,
125.165807243714));
#149372=CARTESIAN_POINT('Ctrl Pts',(38.5325803305736,-1.94840311870171,
125.217621331584));
#149373=CARTESIAN_POINT('Ctrl Pts',(38.5251675512716,-2.0970633022931,125.269467310161));
#149374=CARTESIAN_POINT('Ctrl Pts',(38.5177547719695,-2.24351953227452,
125.327204570334));
#149375=CARTESIAN_POINT('Ctrl Pts',(38.5103419926675,-2.38728548923707,
125.390600505095));
#149376=CARTESIAN_POINT('Ctrl Pts',(38.5029186216387,-2.53125686574089,
125.454087022941));
#149377=CARTESIAN_POINT('Ctrl Pts',(38.4954952506099,-2.67252995753066,
125.52324819999));
#149378=CARTESIAN_POINT('Ctrl Pts',(38.4880718795811,-2.81064350247165,
125.597805742746));
#149379=CARTESIAN_POINT('Ctrl Pts',(38.4841358301405,-2.88387461798553,
125.637337940897));
#149380=CARTESIAN_POINT('Ctrl Pts',(38.4801997806998,-2.95621795294915,
125.678386524937));
#149381=CARTESIAN_POINT('Ctrl Pts',(38.4762637312592,-3.0276082901613,125.720905237232));
#149382=CARTESIAN_POINT('Ctrl Pts',(38.4688404648538,-3.16224823813214,
125.80109420166));
#149383=CARTESIAN_POINT('Ctrl Pts',(38.4614171984484,-3.29390376007871,
125.886757208278));
#149384=CARTESIAN_POINT('Ctrl Pts',(38.4539939320429,-3.42209854058113,
125.977646192509));
#149385=CARTESIAN_POINT('Ctrl Pts',(38.4465794393219,-3.5501418054991,126.068427753509));
#149386=CARTESIAN_POINT('Ctrl Pts',(38.439164946601,-3.67473216920356,126.164422783625));
#149387=CARTESIAN_POINT('Ctrl Pts',(38.4317504538799,-3.79541860553706,
126.26533779638));
#149388=CARTESIAN_POINT('Ctrl Pts',(38.4243431075262,-3.91598871973946,
126.366155543447));
#149389=CARTESIAN_POINT('Ctrl Pts',(38.4169357611724,-4.03266211301745,
126.471883594784));
#149390=CARTESIAN_POINT('Ctrl Pts',(38.4095284148186,-4.14501751474261,
126.582185779289));
#149391=CARTESIAN_POINT('Ctrl Pts',(38.4021265931432,-4.2572891175704,126.692405696264));
#149392=CARTESIAN_POINT('Ctrl Pts',(38.3947247714678,-4.36524887609951,
126.807192693139));
#149393=CARTESIAN_POINT('Ctrl Pts',(38.3873229497923,-4.46850943770092,
126.926171095679));
#149394=CARTESIAN_POINT('Ctrl Pts',(38.379925035481,-4.5717154888555,127.045086690445));
#149395=CARTESIAN_POINT('Ctrl Pts',(38.3725271211697,-4.67022703939225,
127.168189003144));
#149396=CARTESIAN_POINT('Ctrl Pts',(38.3651292068583,-4.76369446916959,
127.295066448235));
#149397=CARTESIAN_POINT('Ctrl Pts',(38.3577325219461,-4.85714636635578,
127.421922808596));
#149398=CARTESIAN_POINT('Ctrl Pts',(38.3503358370339,-4.94555558525297,
127.552552755974));
#149399=CARTESIAN_POINT('Ctrl Pts',(38.3429391521217,-5.02861353425828,
127.686512563928));
#149400=CARTESIAN_POINT('Ctrl Pts',(38.3355427951862,-5.11166780038709,
127.820466431964));
#149401=CARTESIAN_POINT('Ctrl Pts',(38.3281464382508,-5.18937107170843,
127.957749549736));
#149402=CARTESIAN_POINT('Ctrl Pts',(38.3207500813153,-5.2614589057177,128.097890454061));
#149403=CARTESIAN_POINT('Ctrl Pts',(38.3133525919788,-5.33355777655829,
128.238052814316));
#149404=CARTESIAN_POINT('Ctrl Pts',(38.3059551026421,-5.40003932746775,
128.381073500337));
#149405=CARTESIAN_POINT('Ctrl Pts',(38.2985576133056,-5.46068584063949,
128.526457917199));
#149406=CARTESIAN_POINT('Ctrl Pts',(38.2911575307906,-5.52135361335258,
128.671893298343));
#149407=CARTESIAN_POINT('Ctrl Pts',(38.2837574482756,-5.5761821321981,128.81969371576));
#149408=CARTESIAN_POINT('Ctrl Pts',(38.2763573657606,-5.62500248715958,
128.969346290116));
#149409=CARTESIAN_POINT('Ctrl Pts',(38.2689491460942,-5.67387652512014,
129.119163422861));
#149410=CARTESIAN_POINT('Ctrl Pts',(38.2615409264277,-5.71672908954976,
129.270836424734));
#149411=CARTESIAN_POINT('Ctrl Pts',(38.2541327067612,-5.75344146402281,
129.423838295196));
#149412=CARTESIAN_POINT('Ctrl Pts',(38.2467199274591,-5.79017643434988,
129.576934335755));
#149413=CARTESIAN_POINT('Ctrl Pts',(38.2393071481571,-5.82076361185966,
129.731360509329));
#149414=CARTESIAN_POINT('Ctrl Pts',(38.231894368855,-5.84513582789617,129.886581931855));
#149415=CARTESIAN_POINT('Ctrl Pts',(38.2244709978262,-5.86954286809787,
130.042025142029));
#149416=CARTESIAN_POINT('Ctrl Pts',(38.2170476267974,-5.88771716800039,
130.198265500764));
#149417=CARTESIAN_POINT('Ctrl Pts',(38.2096242557687,-5.89964354035209,
130.35476451073));
#149418=CARTESIAN_POINT('Ctrl Pts',(38.2056882063279,-5.90596718914241,
130.437744040958));
#149419=CARTESIAN_POINT('Ctrl Pts',(38.2017521568871,-5.9105351924658,130.520796299877));
#149420=CARTESIAN_POINT('Ctrl Pts',(38.1978161074462,-5.91335121668874,
130.60384141503));
#149421=CARTESIAN_POINT('Ctrl Pts',(38.1946691357013,-5.91560269975465,
130.670238099032));
#149422=CARTESIAN_POINT('Ctrl Pts',(38.1915221639564,-5.91673594582547,
130.73667291686));
#149423=CARTESIAN_POINT('Ctrl Pts',(38.1883751922115,-5.91674987009191,
130.80312075171));
#149424=CARTESIAN_POINT('',(36.4383751922116,-5.91188926911274,130.799500886255));
#149425=CARTESIAN_POINT('Ctrl Pts',(38.1883739050364,-5.92621749523645,
130.803145989751));
#149426=CARTESIAN_POINT('Ctrl Pts',(38.0987054312354,-5.92080046752888,
132.699513211106));
#149427=CARTESIAN_POINT('Ctrl Pts',(37.9162210828302,-3.90476091023743,
136.568682839027));
#149428=CARTESIAN_POINT('Ctrl Pts',(37.6409208598204,2.69161358101603,137.264451705223));
#149429=CARTESIAN_POINT('Ctrl Pts',(37.3624732360077,6.88994047818806,132.031666910778));
#149430=CARTESIAN_POINT('Ctrl Pts',(37.0840256121947,4.75674866821361,125.671047590115));
#149431=CARTESIAN_POINT('Ctrl Pts',(36.8055779883818,-1.74766278776102,
124.027692165396));
#149432=CARTESIAN_POINT('Ctrl Pts',(36.5903611817208,-5.53371367076097,
127.570797637055));
#149433=CARTESIAN_POINT('Ctrl Pts',(36.4679602496641,-5.91673427114246,
130.169895298242));
#149434=CARTESIAN_POINT('Ctrl Pts',(36.4383751922116,-5.91188926911274,
130.799500886255));
#149435=CARTESIAN_POINT('',(34.6883751922117,-5.90863770699821,130.807549372269));
#149436=CARTESIAN_POINT('Ctrl Pts',(36.4383751922116,-5.91188926911274,
130.799500886255));
#149437=CARTESIAN_POINT('Ctrl Pts',(36.3751443750598,-5.90153426345037,
132.145128687637));
#149438=CARTESIAN_POINT('Ctrl Pts',(36.2190976833036,-4.77772734883998,
135.481633513835));
#149439=CARTESIAN_POINT('Ctrl Pts',(35.970235116943,0.768340780429054,137.760452406458));
#149440=CARTESIAN_POINT('Ctrl Pts',(35.6917874931303,6.26766398833651,133.917871282335));
#149441=CARTESIAN_POINT('Ctrl Pts',(35.4133398693173,6.00731018337622,127.214125960743));
#149442=CARTESIAN_POINT('Ctrl Pts',(35.1348922455045,0.226531793307069,
123.809630896056));
#149443=CARTESIAN_POINT('Ctrl Pts',(34.8932373531359,-4.97106715849222,
126.433463773508));
#149444=CARTESIAN_POINT('Ctrl Pts',(34.7443983353716,-5.90282418023302,
129.613660964501));
#149445=CARTESIAN_POINT('Ctrl Pts',(34.6883751922117,-5.90863770699821,
130.807549372269));
#149446=CARTESIAN_POINT('',(32.9383751922116,-5.9235876075816,130.808068272843));
#149447=CARTESIAN_POINT('Ctrl Pts',(34.6883751922117,-5.90863770699821,
130.807549372269));
#149448=CARTESIAN_POINT('Ctrl Pts',(34.6515824607673,-5.9124556921549,131.591625614405));
#149449=CARTESIAN_POINT('Ctrl Pts',(34.5219738547188,-5.40187661372055,
134.348894589915));
#149450=CARTESIAN_POINT('Ctrl Pts',(34.2995493740658,-1.21681955547966,
137.696160868569));
#149451=CARTESIAN_POINT('Ctrl Pts',(34.0211017502528,5.14054604489025,135.553291748959));
#149452=CARTESIAN_POINT('Ctrl Pts',(33.7426541264402,6.77400095963935,129.046386917784));
#149453=CARTESIAN_POINT('Ctrl Pts',(33.4642065026269,2.18247992082522,124.154974034912));
#149454=CARTESIAN_POINT('Ctrl Pts',(33.196113524551,-4.16930635618508,125.328689761559));
#149455=CARTESIAN_POINT('Ctrl Pts',(33.0208364210792,-5.91080789301554,
129.062074719763));
#149456=CARTESIAN_POINT('Ctrl Pts',(32.9383751922116,-5.9235876075816,130.808068272843));
#149457=CARTESIAN_POINT('',(31.1883751922117,-5.91899767233231,130.79938269648));
#149458=CARTESIAN_POINT('Ctrl Pts',(32.9383751922116,-5.9235876075816,130.808068272843));
#149459=CARTESIAN_POINT('Ctrl Pts',(32.9280205464749,-5.92519235467021,
131.02731245522));
#149460=CARTESIAN_POINT('Ctrl Pts',(32.8248500261334,-5.81447119154423,
133.21015694754));
#149461=CARTESIAN_POINT('Ctrl Pts',(32.6288636311887,-3.10396874173013,
137.076755581275));
#149462=CARTESIAN_POINT('Ctrl Pts',(32.3504160073755,3.5993726028644,136.806200118591));
#149463=CARTESIAN_POINT('Ctrl Pts',(32.0719683835628,6.99506636455412,131.020247360633));
#149464=CARTESIAN_POINT('Ctrl Pts',(31.7935207597497,3.96263586520661,125.035905232443));
#149465=CARTESIAN_POINT('Ctrl Pts',(31.515073135937,-2.71126340873828,124.352491798475));
#149466=CARTESIAN_POINT('Ctrl Pts',(31.3133579467576,-5.74109606907425,
128.152505750201));
#149467=CARTESIAN_POINT('Ctrl Pts',(31.2044586321825,-5.92336622444082,
130.458345827985));
#149468=CARTESIAN_POINT('Ctrl Pts',(31.1883751922117,-5.92029803960656,
130.799381602861));
#149469=CARTESIAN_POINT('',(29.4383752206225,-5.91150934056856,130.802999882248));
#149470=CARTESIAN_POINT('Ctrl Pts',(31.1883751922117,-5.91674790756165,
130.799384588548));
#149471=CARTESIAN_POINT('Ctrl Pts',(31.1810736186236,-5.91687803629541,
130.954114175227));
#149472=CARTESIAN_POINT('Ctrl Pts',(31.1737720450354,-5.91093449718433,
131.109059102874));
#149473=CARTESIAN_POINT('Ctrl Pts',(31.1664704714473,-5.89889333136726,
131.263694948583));
#149474=CARTESIAN_POINT('Ctrl Pts',(31.1591753990885,-5.88686288685281,
131.41819310848));
#149475=CARTESIAN_POINT('Ctrl Pts',(31.1518803267297,-5.86874564859868,
131.572382352231));
#149476=CARTESIAN_POINT('Ctrl Pts',(31.1445852543709,-5.84456970245775,
131.725737606433));
#149477=CARTESIAN_POINT('Ctrl Pts',(31.1372949755956,-5.82040964230286,
131.878992091076));
#149478=CARTESIAN_POINT('Ctrl Pts',(31.1300046968204,-5.79019885757158,
132.031413297529));
#149479=CARTESIAN_POINT('Ctrl Pts',(31.1227144180451,-5.75401729566393,
132.182480903934));
#149480=CARTESIAN_POINT('Ctrl Pts',(31.1154264573996,-5.71784723860511,
132.333500474548));
#149481=CARTESIAN_POINT('Ctrl Pts',(31.108138496754,-5.67571026758409,132.483166926363));
#149482=CARTESIAN_POINT('Ctrl Pts',(31.1008505361085,-5.62773748163055,
132.63096988075));
#149483=CARTESIAN_POINT('Ctrl Pts',(31.0935635496382,-5.57977110815652,
132.778753078448));
#149484=CARTESIAN_POINT('Ctrl Pts',(31.0862765631679,-5.52597059006752,
132.924672907551));
#149485=CARTESIAN_POINT('Ctrl Pts',(31.0789895766976,-5.46651687014971,
133.068234260433));
#149486=CARTESIAN_POINT('Ctrl Pts',(31.0717020260758,-5.40705854738212,
133.211806727697));
#149487=CARTESIAN_POINT('Ctrl Pts',(31.064414475454,-5.34194629960161,133.353019999323));
#149488=CARTESIAN_POINT('Ctrl Pts',(31.0571269248322,-5.27140905118794,
133.491399355202));
#149489=CARTESIAN_POINT('Ctrl Pts',(31.0498372714414,-5.20085144977045,
133.629818639424));
#149490=CARTESIAN_POINT('Ctrl Pts',(31.0425476180504,-5.12486590861082,
133.765402037925));
#149491=CARTESIAN_POINT('Ctrl Pts',(31.0352579646596,-5.04372693339733,
133.897700104887));
#149492=CARTESIAN_POINT('Ctrl Pts',(31.0279607119279,-4.96250337216937,
134.030136090356));
#149493=CARTESIAN_POINT('Ctrl Pts',(31.0206634591962,-4.87611585245031,
134.15927957765));
#149494=CARTESIAN_POINT('Ctrl Pts',(31.0133662064645,-4.78488207870418,
134.284710320598));
#149495=CARTESIAN_POINT('Ctrl Pts',(31.0060646862501,-4.69359495083073,
134.410214416292));
#149496=CARTESIAN_POINT('Ctrl Pts',(30.9987631660356,-4.59745616387367,
134.532001142695));
#149497=CARTESIAN_POINT('Ctrl Pts',(30.9914616458212,-4.49682265436147,
134.64968460622));
#149498=CARTESIAN_POINT('Ctrl Pts',(30.9841498323878,-4.39604727812509,
134.767533972411));
#149499=CARTESIAN_POINT('Ctrl Pts',(30.9768380189543,-4.29076478995553,
134.881268245521));
#149500=CARTESIAN_POINT('Ctrl Pts',(30.9695262055209,-4.18136822975938,
134.990539100342));
#149501=CARTESIAN_POINT('Ctrl Pts',(30.9657434331176,-4.12477183370912,
135.047070462619));
#149502=CARTESIAN_POINT('Ctrl Pts',(30.9619606607143,-4.06707483665724,
135.102407846852));
#149503=CARTESIAN_POINT('Ctrl Pts',(30.958177888311,-4.00833487973587,135.156507450382));
#149504=CARTESIAN_POINT('Ctrl Pts',(30.9507546219056,-3.89306430504004,
135.262671852207));
#149505=CARTESIAN_POINT('Ctrl Pts',(30.9433313555002,-3.77339872329145,
135.364414054398));
#149506=CARTESIAN_POINT('Ctrl Pts',(30.9359080890948,-3.64971178776911,
135.461348316575));
#149507=CARTESIAN_POINT('Ctrl Pts',(30.9284935963738,-3.52617103993263,
135.558168010504));
#149508=CARTESIAN_POINT('Ctrl Pts',(30.9210791036528,-3.39861868995656,
135.650190847619));
#149509=CARTESIAN_POINT('Ctrl Pts',(30.9136646109318,-3.26746470961103,
135.737068285161));
#149510=CARTESIAN_POINT('Ctrl Pts',(30.906257264578,-3.13643714040962,135.823861986957));
#149511=CARTESIAN_POINT('Ctrl Pts',(30.8988499182242,-3.00181516081051,
135.905519957464));
#149512=CARTESIAN_POINT('Ctrl Pts',(30.8914425718704,-2.86404116328473,
135.981734351179));
#149513=CARTESIAN_POINT('Ctrl Pts',(30.8840407501951,-2.7263699228048,136.057891901324));
#149514=CARTESIAN_POINT('Ctrl Pts',(30.8766389285197,-2.58555167058872,
136.128613778815));
#149515=CARTESIAN_POINT('Ctrl Pts',(30.8692371068443,-2.4420569829478,136.193635917134));
#149516=CARTESIAN_POINT('Ctrl Pts',(30.8618391925329,-2.29863804503449,
136.258623730773));
#149517=CARTESIAN_POINT('Ctrl Pts',(30.8544412782215,-2.15254582465138,
136.317917643822));
#149518=CARTESIAN_POINT('Ctrl Pts',(30.8470433639101,-2.00427455108857,
136.37129999988));
#149519=CARTESIAN_POINT('Ctrl Pts',(30.8396466789979,-1.85602791752194,
136.424673484759));
#149520=CARTESIAN_POINT('Ctrl Pts',(30.8322499940857,-1.70560330035875,
136.472137236077));
#149521=CARTESIAN_POINT('Ctrl Pts',(30.8248533091735,-1.55351402777272,
136.513522090849));
#149522=CARTESIAN_POINT('Ctrl Pts',(30.8174569522381,-1.40143149898463,
136.554905110572));
#149523=CARTESIAN_POINT('Ctrl Pts',(30.8100605953026,-1.24768482173847,
136.590209671679));
#149524=CARTESIAN_POINT('Ctrl Pts',(30.8026642383672,-1.09280131165758,
136.619316838875));
#149525=CARTESIAN_POINT('Ctrl Pts',(30.7952667490306,-0.937894088515456,
136.648428462453));
#149526=CARTESIAN_POINT('Ctrl Pts',(30.787869259694,-0.781850052877025,
136.671340733907));
#149527=CARTESIAN_POINT('Ctrl Pts',(30.7804717703574,-0.625205359369967,
136.687986100303));
#149528=CARTESIAN_POINT('Ctrl Pts',(30.7730716878424,-0.468505754308653,
136.704637301707));
#149529=CARTESIAN_POINT('Ctrl Pts',(30.7656716053274,-0.311205443132389,
136.715017184711));
#149530=CARTESIAN_POINT('Ctrl Pts',(30.7582715228124,-0.153844179286222,
136.719110192231));
#149531=CARTESIAN_POINT('Ctrl Pts',(30.750863303146,0.00369011944644976,
136.723207700434));
#149532=CARTESIAN_POINT('Ctrl Pts',(30.7434550834795,0.161285131299126,
136.721004517593));
#149533=CARTESIAN_POINT('Ctrl Pts',(30.736046863813,0.31840188955168,136.71253722285));
#149534=CARTESIAN_POINT('Ctrl Pts',(30.728634084511,0.475615350547304,136.704064716629));
#149535=CARTESIAN_POINT('Ctrl Pts',(30.7212213052089,0.632349600604035,
136.689320450907));
#149536=CARTESIAN_POINT('Ctrl Pts',(30.7138085259068,0.788072824502699,
136.66839265924));
#149537=CARTESIAN_POINT('Ctrl Pts',(30.7063851548781,0.944018553046586,
136.647434964963));
#149538=CARTESIAN_POINT('Ctrl Pts',(30.6989617838493,1.09895000352174,136.620276162924));
#149539=CARTESIAN_POINT('Ctrl Pts',(30.6915384128206,1.25234672868807,136.587055338338));
#149540=CARTESIAN_POINT('Ctrl Pts',(30.6876023633798,1.33368135307515,136.56944086002));
#149541=CARTESIAN_POINT('Ctrl Pts',(30.683666313939,1.41458477169084,136.55012296101));
#149542=CARTESIAN_POINT('Ctrl Pts',(30.6797302644982,1.49498147813114,136.529127944064));
#149543=CARTESIAN_POINT('Ctrl Pts',(30.6723069980928,1.64660715738226,136.489531997337));
#149544=CARTESIAN_POINT('Ctrl Pts',(30.6648837316873,1.79688792350402,136.443848099782));
#149545=CARTESIAN_POINT('Ctrl Pts',(30.6574604652819,1.94529727346557,136.392182114388));
#149546=CARTESIAN_POINT('Ctrl Pts',(30.6500459725609,2.0935312159003,136.340577193899));
#149547=CARTESIAN_POINT('Ctrl Pts',(30.6426314798399,2.23989779578875,136.283004380637));
#149548=CARTESIAN_POINT('Ctrl Pts',(30.6352169871188,2.38388217448049,136.219620199589));
#149549=CARTESIAN_POINT('Ctrl Pts',(30.6278096407651,2.52772777560693,136.156297110602));
#149550=CARTESIAN_POINT('Ctrl Pts',(30.6204022944114,2.66919540716613,136.087173954138));
#149551=CARTESIAN_POINT('Ctrl Pts',(30.6129949480576,2.80778694608197,136.012456529501));
#149552=CARTESIAN_POINT('Ctrl Pts',(30.6055931263822,2.94627511819893,135.937794831938));
#149553=CARTESIAN_POINT('Ctrl Pts',(30.5981913047068,3.08189114167944,135.85754735043));
#149554=CARTESIAN_POINT('Ctrl Pts',(30.5907894830314,3.21415849189268,135.771967259752));
#149555=CARTESIAN_POINT('Ctrl Pts',(30.58339156872,3.34635601920263,135.686432346138));
#149556=CARTESIAN_POINT('Ctrl Pts',(30.5759936544085,3.47520808115981,135.59557063192));
#149557=CARTESIAN_POINT('Ctrl Pts',(30.5685957400972,3.60026441426646,135.499680277596));
#149558=CARTESIAN_POINT('Ctrl Pts',(30.5611990551849,3.72529996527858,135.403805858511));
#149559=CARTESIAN_POINT('Ctrl Pts',(30.5538023702728,3.84654074340866,135.302904684799));
#149560=CARTESIAN_POINT('Ctrl Pts',(30.5464056853606,3.96356696062728,135.197317197265));
#149561=CARTESIAN_POINT('Ctrl Pts',(30.5390093284251,4.08058798878063,135.091734391592));
#149562=CARTESIAN_POINT('Ctrl Pts',(30.5316129714896,4.19339455044032,134.981465935333));
#149563=CARTESIAN_POINT('Ctrl Pts',(30.5242166145542,4.30160155499882,134.866891186624));
#149564=CARTESIAN_POINT('Ctrl Pts',(30.5168191252176,4.40982512632628,134.752298896229));
#149565=CARTESIAN_POINT('Ctrl Pts',(30.509421635881,4.51344748206035,134.633399272034));
#149566=CARTESIAN_POINT('Ctrl Pts',(30.5020241465444,4.61212198333057,134.510606882101));
#149567=CARTESIAN_POINT('Ctrl Pts',(30.4946240640294,4.71083107479424,134.387771447486));
#149568=CARTESIAN_POINT('Ctrl Pts',(30.4872239815144,4.80458862480395,134.261040821023));
#149569=CARTESIAN_POINT('Ctrl Pts',(30.4798238989994,4.89308979482202,134.130860703589));
#149570=CARTESIAN_POINT('Ctrl Pts',(30.472415679333,4.98168828097442,134.000537439732));
#149571=CARTESIAN_POINT('Ctrl Pts',(30.4650074596664,5.0650186342318,133.866757418797));
#149572=CARTESIAN_POINT('Ctrl Pts',(30.45759924,5.14282030498432,133.729993860668));
#149573=CARTESIAN_POINT('Ctrl Pts',(30.4501864606979,5.22066986136723,133.59314612685));
#149574=CARTESIAN_POINT('Ctrl Pts',(30.4427736813959,5.29298378363884,133.453311527561));
#149575=CARTESIAN_POINT('Ctrl Pts',(30.4353609020938,5.35954884607186,133.310985186398));
#149576=CARTESIAN_POINT('Ctrl Pts',(30.427937531065,5.42620901978758,133.168455482684));
#149577=CARTESIAN_POINT('Ctrl Pts',(30.4205141600363,5.48710378384813,133.02342726962));
#149578=CARTESIAN_POINT('Ctrl Pts',(30.4130907890076,5.54206884013689,132.876413593164));
#149579=CARTESIAN_POINT('Ctrl Pts',(30.4091547395668,5.57121263184922,132.798463414363));
#149580=CARTESIAN_POINT('Ctrl Pts',(30.405218690126,5.5986902102386,132.719955280698));
#149581=CARTESIAN_POINT('Ctrl Pts',(30.4012826406853,5.62448289150163,132.640966935127));
#149582=CARTESIAN_POINT('Ctrl Pts',(30.3938593742799,5.67312708340229,132.49199738052));
#149583=CARTESIAN_POINT('Ctrl Pts',(30.3864361078745,5.71592235145471,132.34086865329));
#149584=CARTESIAN_POINT('Ctrl Pts',(30.3790128414691,5.75267317344041,132.188080936879));
#149585=CARTESIAN_POINT('Ctrl Pts',(30.3715983487481,5.78938055900654,132.03547380286));
#149586=CARTESIAN_POINT('Ctrl Pts',(30.3641838560271,5.82005763229482,131.881211942021));
#149587=CARTESIAN_POINT('Ctrl Pts',(30.3567693633061,5.84455779934302,131.725813108278));
#149588=CARTESIAN_POINT('Ctrl Pts',(30.3493620169523,5.86903435220777,131.570564053781));
#149589=CARTESIAN_POINT('Ctrl Pts',(30.3419546705985,5.88734579340239,131.414180574283));
#149590=CARTESIAN_POINT('Ctrl Pts',(30.3345473242447,5.89939602001794,131.257192994386));
#149591=CARTESIAN_POINT('Ctrl Pts',(30.3271455025693,5.91143725911992,131.100322501748));
#149592=CARTESIAN_POINT('Ctrl Pts',(30.319743680894,5.91722655349739,130.942849176438));
#149593=CARTESIAN_POINT('Ctrl Pts',(30.3123418592185,5.91671933305621,130.785310779276));
#149594=CARTESIAN_POINT('Ctrl Pts',(30.3049439449072,5.91621238037276,130.627855545408));
#149595=CARTESIAN_POINT('Ctrl Pts',(30.2975460305958,5.90941553373817,130.470335680449));
#149596=CARTESIAN_POINT('Ctrl Pts',(30.2901481162845,5.89633626560493,130.313291166865));
#149597=CARTESIAN_POINT('Ctrl Pts',(30.2827514313723,5.88325917100875,130.156272751229));
#149598=CARTESIAN_POINT('Ctrl Pts',(30.2753547464601,5.86390175794559,129.999729901832));
#149599=CARTESIAN_POINT('Ctrl Pts',(30.2679580615479,5.83832354322159,129.844199814802));
#149600=CARTESIAN_POINT('Ctrl Pts',(30.2605617046125,5.81274646266239,129.688676624139));
#149601=CARTESIAN_POINT('Ctrl Pts',(30.253165347677,5.78094918947733,129.534166474902));
#149602=CARTESIAN_POINT('Ctrl Pts',(30.2457689907415,5.74304273753031,129.381198407064));
#149603=CARTESIAN_POINT('Ctrl Pts',(30.238371501405,5.70513048200873,129.228206919425));
#149604=CARTESIAN_POINT('Ctrl Pts',(30.2309740120684,5.66110727515254,129.076758345647));
#149605=CARTESIAN_POINT('Ctrl Pts',(30.2235765227319,5.61113453803621,128.927368406992));
#149606=CARTESIAN_POINT('Ctrl Pts',(30.2161764402169,5.56114428305427,128.777926099925));
#149607=CARTESIAN_POINT('Ctrl Pts',(30.2087763577018,5.50520046374941,128.630544218579));
#149608=CARTESIAN_POINT('Ctrl Pts',(30.2013762751868,5.44351328821527,128.48572014446));
#149609=CARTESIAN_POINT('Ctrl Pts',(30.1939680555204,5.38175828129011,128.340736821384));
#149610=CARTESIAN_POINT('Ctrl Pts',(30.1865598358539,5.31424745222283,128.198317266076));
#149611=CARTESIAN_POINT('Ctrl Pts',(30.1791516161874,5.24123810087678,128.058936473209));
#149612=CARTESIAN_POINT('Ctrl Pts',(30.1717388368853,5.168183813493,127.91946989379));
#149613=CARTESIAN_POINT('Ctrl Pts',(30.1643260575833,5.08962444614304,127.78304612638));
#149614=CARTESIAN_POINT('Ctrl Pts',(30.1569132782812,5.00586130661822,127.650112190222));
#149615=CARTESIAN_POINT('Ctrl Pts',(30.1494899072524,4.92197848239179,127.516988311822));
#149616=CARTESIAN_POINT('Ctrl Pts',(30.1420665362237,4.83287724674095,127.387364530517));
#149617=CARTESIAN_POINT('Ctrl Pts',(30.134643165195,4.73890043261532,127.261656388836));
#149618=CARTESIAN_POINT('Ctrl Pts',(30.1307071157541,4.68907167082233,127.195002915791));
#149619=CARTESIAN_POINT('Ctrl Pts',(30.1267710663133,4.63787285679946,127.129449686971));
#149620=CARTESIAN_POINT('Ctrl Pts',(30.1228350168724,4.58535929884655,127.065054443557));
#149621=CARTESIAN_POINT('Ctrl Pts',(30.115411750467,4.48632036744083,126.943607024187));
#149622=CARTESIAN_POINT('Ctrl Pts',(30.1079884840615,4.38230337674868,126.825913384557));
#149623=CARTESIAN_POINT('Ctrl Pts',(30.1005652176561,4.27362346073099,126.712408384415));
#149624=CARTESIAN_POINT('Ctrl Pts',(30.0931507249351,4.16507199534872,126.599037537757));
#149625=CARTESIAN_POINT('Ctrl Pts',(30.085736232214,4.05186883034323,126.489845743341));
#149626=CARTESIAN_POINT('Ctrl Pts',(30.078321739493,3.93437032913027,126.385236193457));
#149627=CARTESIAN_POINT('Ctrl Pts',(30.0709143931392,3.81698507739635,126.280727470195));
#149628=CARTESIAN_POINT('Ctrl Pts',(30.0635070467855,3.69531300833176,126.180792445563));
#149629=CARTESIAN_POINT('Ctrl Pts',(30.0560997004317,3.56974835307321,126.085798627062));
#149630=CARTESIAN_POINT('Ctrl Pts',(30.0486978787563,3.44427734867218,125.990875658534));
#149631=CARTESIAN_POINT('Ctrl Pts',(30.0412960570808,3.31491983523602,125.900886782384));
#149632=CARTESIAN_POINT('Ctrl Pts',(30.0338942354055,3.1821041549464,125.816160169551));
#149633=CARTESIAN_POINT('Ctrl Pts',(30.0264963210942,3.04935858702152,125.731478283239));
#149634=CARTESIAN_POINT('Ctrl Pts',(30.0190984067829,2.91315880180979,125.652053328163));
#149635=CARTESIAN_POINT('Ctrl Pts',(30.0117004924716,2.77396314089516,125.57817089125));
#149636=CARTESIAN_POINT('Ctrl Pts',(30.0043038075593,2.63479061177271,125.504300732257));
#149637=CARTESIAN_POINT('Ctrl Pts',(29.9969071226471,2.49262352445887,125.435971438226));
#149638=CARTESIAN_POINT('Ctrl Pts',(29.9895104377349,2.34794600755799,125.373423303612));
#149639=CARTESIAN_POINT('Ctrl Pts',(29.9821140807995,2.20327490581003,125.310877942449));
#149640=CARTESIAN_POINT('Ctrl Pts',(29.974717723864,2.05609393845387,125.254113379142));
#149641=CARTESIAN_POINT('Ctrl Pts',(29.9673213669285,1.90690820750723,125.203322173613));
#149642=CARTESIAN_POINT('Ctrl Pts',(29.9599238775919,1.75769963584433,125.15252319182));
#149643=CARTESIAN_POINT('Ctrl Pts',(29.9525263882554,1.6064860428455,125.107699509086));
#149644=CARTESIAN_POINT('Ctrl Pts',(29.9451288989188,1.45378857144856,125.068994077228));
#149645=CARTESIAN_POINT('Ctrl Pts',(29.9377288164038,1.3010375721893,125.030275077241));
#149646=CARTESIAN_POINT('Ctrl Pts',(29.9303287338888,1.14680202050313,124.997678689964));
#149647=CARTESIAN_POINT('Ctrl Pts',(29.9229286513738,0.991614000146153,
124.971296908226));
#149648=CARTESIAN_POINT('Ctrl Pts',(29.9155204317073,0.836255334607523,
124.944886117008));
#149649=CARTESIAN_POINT('Ctrl Pts',(29.9081122120408,0.679942477040716,
124.924703641073));
#149650=CARTESIAN_POINT('Ctrl Pts',(29.9007039923743,0.523214130777668,
124.910789752984));
#149651=CARTESIAN_POINT('Ctrl Pts',(29.8932912130722,0.366389320832201,
124.896867301128));
#149652=CARTESIAN_POINT('Ctrl Pts',(29.8858784337702,0.209148884616497,
124.889221143176));
#149653=CARTESIAN_POINT('Ctrl Pts',(29.8784656544681,0.052031776299944,
124.887839405168));
#149654=CARTESIAN_POINT('Ctrl Pts',(29.8710422834393,-0.105309828308809,
124.886455692868));
#149655=CARTESIAN_POINT('Ctrl Pts',(29.8636189124105,-0.262527380945767,
124.891354265867));
#149656=CARTESIAN_POINT('Ctrl Pts',(29.8561955413817,-0.419085964327446,
124.902471299983));
#149657=CARTESIAN_POINT('Ctrl Pts',(29.852259491941,-0.502097081807044,
124.90836581822));
#149658=CARTESIAN_POINT('Ctrl Pts',(29.8483234425003,-0.584923079354862,
124.91600770908));
#149659=CARTESIAN_POINT('Ctrl Pts',(29.8443873930595,-0.667485482193467,
124.92538165064));
#149660=CARTESIAN_POINT('Ctrl Pts',(29.8369641266541,-0.823195597264386,
124.943060611872));
#149661=CARTESIAN_POINT('Ctrl Pts',(29.8295408602487,-0.978438313767397,
124.966956765008));
#149662=CARTESIAN_POINT('Ctrl Pts',(29.8221175938432,-1.13267743427713,
124.997040031239));
#149663=CARTESIAN_POINT('Ctrl Pts',(29.8147031011222,-1.28673425695539,
125.027087741547));
#149664=CARTESIAN_POINT('Ctrl Pts',(29.8072886084012,-1.43978948189665,
125.063307938306));
#149665=CARTESIAN_POINT('Ctrl Pts',(29.7998741156802,-1.59131126887694,
125.105618738164));
#149666=CARTESIAN_POINT('Ctrl Pts',(29.7924667693264,-1.74268701345381,
125.14788875728));
#149667=CARTESIAN_POINT('Ctrl Pts',(29.7850594229726,-1.89253190531764,
125.196237593054));
#149668=CARTESIAN_POINT('Ctrl Pts',(29.7776520766189,-2.04032365844145,
125.250532214446));
#149669=CARTESIAN_POINT('Ctrl Pts',(29.7702502549434,-2.18800518290161,
125.304786340861));
#149670=CARTESIAN_POINT('Ctrl Pts',(29.7628484332679,-2.33363626877076,
125.364977294851));
#149671=CARTESIAN_POINT('Ctrl Pts',(29.7554466115925,-2.47670928713071,
125.430922084416));
#149672=CARTESIAN_POINT('Ctrl Pts',(29.7480486972811,-2.61970677835692,
125.49683206224));
#149673=CARTESIAN_POINT('Ctrl Pts',(29.7406507829698,-2.76014855326697,
125.568489670636));
#149674=CARTESIAN_POINT('Ctrl Pts',(29.7332528686584,-2.89754659466987,
125.645663660561));
#149675=CARTESIAN_POINT('Ctrl Pts',(29.7258561837462,-3.03492180301074,
125.722824825567));
#149676=CARTESIAN_POINT('Ctrl Pts',(29.7184594988339,-3.1692539565818,125.805500370047));
#149677=CARTESIAN_POINT('Ctrl Pts',(29.7110628139217,-3.30007920551684,
125.893412867914));
#149678=CARTESIAN_POINT('Ctrl Pts',(29.7036664569863,-3.43089865352306,
125.981321467648));
#149679=CARTESIAN_POINT('Ctrl Pts',(29.6962701000508,-3.55821119623962,
126.074466350848));
#149680=CARTESIAN_POINT('Ctrl Pts',(29.6888737431154,-3.68158180757366,
126.17252664422));
#149681=CARTESIAN_POINT('Ctrl Pts',(29.6814762537788,-3.80497130726343,
126.270601950873));
#149682=CARTESIAN_POINT('Ctrl Pts',(29.6740787644423,-3.92441738163343,
126.373593933858));
#149683=CARTESIAN_POINT('Ctrl Pts',(29.6666812751057,-4.03951807078312,
126.481141409809));
#149684=CARTESIAN_POINT('Ctrl Pts',(29.6592811925907,-4.15465910829997,
126.588726586361));
#149685=CARTESIAN_POINT('Ctrl Pts',(29.6518811100758,-4.26545145519191,
126.700870180637));
#149686=CARTESIAN_POINT('Ctrl Pts',(29.6444810275608,-4.37153011101842,
126.817174259875));
#149687=CARTESIAN_POINT('Ctrl Pts',(29.6370728078944,-4.47772541123308,
126.933606227405));
#149688=CARTESIAN_POINT('Ctrl Pts',(29.6296645882279,-4.5791964175029,127.054207540259));
#149689=CARTESIAN_POINT('Ctrl Pts',(29.6222563685614,-4.67561806507234,
127.17854674037));
#149690=CARTESIAN_POINT('Ctrl Pts',(29.6148435892594,-4.77209905855644,
127.302962469182));
#149691=CARTESIAN_POINT('Ctrl Pts',(29.6074308099574,-4.86352428437705,
127.431120366309));
#149692=CARTESIAN_POINT('Ctrl Pts',(29.6000180306554,-4.94961241453897,
127.562560576178));
#149693=CARTESIAN_POINT('Ctrl Pts',(29.5925946596266,-5.03582355145902,
127.694188593984));
#149694=CARTESIAN_POINT('Ctrl Pts',(29.5851712885978,-5.11668217071284,
127.82910797201));
#149695=CARTESIAN_POINT('Ctrl Pts',(29.5777479175691,-5.19195283353445,
127.966834170667));
#149696=CARTESIAN_POINT('Ctrl Pts',(29.5738118681283,-5.23186314505729,
128.039859905889));
#149697=CARTESIAN_POINT('Ctrl Pts',(29.5698758186875,-5.27020328066042,
128.113674392054));
#149698=CARTESIAN_POINT('Ctrl Pts',(29.5659397692467,-5.30694371357554,
128.188203324237));
#149699=CARTESIAN_POINT('Ctrl Pts',(29.5579707528573,-5.38132924060183,
128.339096317574));
#149700=CARTESIAN_POINT('Ctrl Pts',(29.5500017364678,-5.44935422305597,
128.493323694942));
#149701=CARTESIAN_POINT('Ctrl Pts',(29.5420327200784,-5.51073002588949,
128.650344567426));
#149702=CARTESIAN_POINT('Ctrl Pts',(29.5340793302799,-5.5719854757813,128.807057534791));
#149703=CARTESIAN_POINT('Ctrl Pts',(29.5261259404815,-5.6266176400274,128.966552807321));
#149704=CARTESIAN_POINT('Ctrl Pts',(29.518172550683,-5.67438451996701,129.128266681637));
#149705=CARTESIAN_POINT('Ctrl Pts',(29.5102415681632,-5.72201682511289,
129.289524955518));
#149706=CARTESIAN_POINT('Ctrl Pts',(29.5023105856434,-5.76282234525453,
129.45298908768));
#149707=CARTESIAN_POINT('Ctrl Pts',(29.4943796031236,-5.79660799173531,
129.6180780405));
#149708=CARTESIAN_POINT('Ctrl Pts',(29.4864625062504,-5.8303344859551,129.782877953866));
#149709=CARTESIAN_POINT('Ctrl Pts',(29.4785454093773,-5.85706554950225,
129.949296736362));
#149710=CARTESIAN_POINT('Ctrl Pts',(29.4706283125042,-5.87665773256306,
130.116738296225));
#149711=CARTESIAN_POINT('Ctrl Pts',(29.4627306403779,-5.89620184583215,
130.283769035054));
#149712=CARTESIAN_POINT('Ctrl Pts',(29.4548329682517,-5.90864197837242,
130.451817261117));
#149713=CARTESIAN_POINT('Ctrl Pts',(29.4469352961255,-5.91388568523945,
130.620277309197));
#149714=CARTESIAN_POINT('Ctrl Pts',(29.444081949191,-5.91578018208298,130.68114017538));
#149715=CARTESIAN_POINT('Ctrl Pts',(29.4412286022565,-5.91673580774773,
130.742056685041));
#149716=CARTESIAN_POINT('Ctrl Pts',(29.438375255322,-5.91674984308085,130.8029979354));
#149717=CARTESIAN_POINT('',(27.6883751922116,-5.91529524537258,130.809807152419));
#149718=CARTESIAN_POINT('Ctrl Pts',(29.4383751922116,-5.90721857606676,
130.803001476268));
#149719=CARTESIAN_POINT('Ctrl Pts',(29.3880808432857,-5.90502446395126,
131.875448957813));
#149720=CARTESIAN_POINT('Ctrl Pts',(29.2449706197554,-5.11199832894571,
134.930071410922));
#149721=CARTESIAN_POINT('Ctrl Pts',(29.009044521621,-0.205241192839764,
137.799747424816));
#149722=CARTESIAN_POINT('Ctrl Pts',(28.730596897808,5.77447916256885,134.758213286979));
#149723=CARTESIAN_POINT('Ctrl Pts',(28.4521492739951,6.44773526656473,128.083281702383));
#149724=CARTESIAN_POINT('Ctrl Pts',(28.1737016501822,1.195837649966,123.90888870875));
#149725=CARTESIAN_POINT('Ctrl Pts',(27.9191102895877,-4.61086435825437,
125.885848252815));
#149726=CARTESIAN_POINT('Ctrl Pts',(27.7573348035975,-5.90207848774965,
129.344403176503));
#149727=CARTESIAN_POINT('Ctrl Pts',(27.6883751922116,-5.91529524537258,
130.809807152419));
#149728=CARTESIAN_POINT('',(25.9383751922117,-5.92200882025382,130.803339028211));
#149729=CARTESIAN_POINT('Ctrl Pts',(27.6883751922116,-5.91529524537258,
130.809807152419));
#149730=CARTESIAN_POINT('Ctrl Pts',(27.6645189289932,-5.9198675224259,131.316756978095));
#149731=CARTESIAN_POINT('Ctrl Pts',(27.5478467911706,-5.62781300415635,
133.790871818885));
#149732=CARTESIAN_POINT('Ctrl Pts',(27.3383587787435,-2.16223136626054,
137.460359118851));
#149733=CARTESIAN_POINT('Ctrl Pts',(27.0599111549305,4.4311411779048,136.22123687532));
#149734=CARTESIAN_POINT('Ctrl Pts',(26.7814635311178,6.95251145285309,130.004269980034));
#149735=CARTESIAN_POINT('Ctrl Pts',(26.503015907305,3.08486335170113,124.522547294034));
#149736=CARTESIAN_POINT('Ctrl Pts',(26.224568283492,-3.61762346571424,124.813504168722));
#149737=CARTESIAN_POINT('Ctrl Pts',(26.0363547117943,-5.90099064463134,
128.731422459272));
#149738=CARTESIAN_POINT('Ctrl Pts',(25.9409570147008,-5.92644834143233,
130.748738712938));
#149739=CARTESIAN_POINT('Ctrl Pts',(25.9383751922117,-5.9263183307278,130.803338284789));
#149740=CARTESIAN_POINT('',(24.1883752150562,-5.91399912579995,130.799408621223));
#149741=CARTESIAN_POINT('Ctrl Pts',(25.9383751922117,-5.91674991196247,
130.80333993541));
#149742=CARTESIAN_POINT('Ctrl Pts',(25.9309865517842,-5.91677682314269,
130.959340236106));
#149743=CARTESIAN_POINT('Ctrl Pts',(25.9235979113567,-5.91062985096164,
131.115586525969));
#149744=CARTESIAN_POINT('Ctrl Pts',(25.9162092709292,-5.89827665873343,
131.271546896838));
#149745=CARTESIAN_POINT('Ctrl Pts',(25.9088293095786,-5.88593797719979,
131.42732406864));
#149746=CARTESIAN_POINT('Ctrl Pts',(25.9014493482279,-5.86740761380681,
131.582815617648));
#149747=CARTESIAN_POINT('Ctrl Pts',(25.8940693868772,-5.8427051950539,131.737487921952));
#149748=CARTESIAN_POINT('Ctrl Pts',(25.8866964457628,-5.81802627463759,
131.892013093219));
#149749=CARTESIAN_POINT('Ctrl Pts',(25.8793235046484,-5.78718704453997,
132.045720201084));
#149750=CARTESIAN_POINT('Ctrl Pts',(25.871950563534,-5.75025904433928,132.198079199452));
#149751=CARTESIAN_POINT('Ctrl Pts',(25.8645829896906,-5.71335792657033,
132.350327285224));
#149752=CARTESIAN_POINT('Ctrl Pts',(25.8572154158473,-5.67037695146818,
132.501228850292));
#149753=CARTESIAN_POINT('Ctrl Pts',(25.8498478420039,-5.62143897356322,
132.650262681329));
#149754=CARTESIAN_POINT('Ctrl Pts',(25.8422572250815,-5.5710194662557,132.803808304886));
#149755=CARTESIAN_POINT('Ctrl Pts',(25.8346666081591,-5.51427664135492,
132.955370916967));
#149756=CARTESIAN_POINT('Ctrl Pts',(25.8270759912367,-5.45140084465804,
133.104395268036));
#149757=CARTESIAN_POINT('Ctrl Pts',(25.8197131383383,-5.39041169889071,
133.248947994962));
#149758=CARTESIAN_POINT('Ctrl Pts',(25.81235028544,-5.3236525039499,133.391112229823));
#149759=CARTESIAN_POINT('Ctrl Pts',(25.8049874325417,-5.25134636247009,
133.530400225472));
#149760=CARTESIAN_POINT('Ctrl Pts',(25.7976246335066,-5.17904074994853,
133.669687202154));
#149761=CARTESIAN_POINT('Ctrl Pts',(25.7902618344715,-5.1011884450187,133.806097646521));
#149762=CARTESIAN_POINT('Ctrl Pts',(25.7828990354363,-5.01805886634146,
133.93916775301));
#149763=CARTESIAN_POINT('Ctrl Pts',(25.7755348016019,-4.93491308808304,
134.072263791063));
#149764=CARTESIAN_POINT('Ctrl Pts',(25.7681705677676,-4.84648818882913,
134.20201787566));
#149765=CARTESIAN_POINT('Ctrl Pts',(25.7608063339332,-4.75309721281873,
134.327994742726));
#149766=CARTESIAN_POINT('Ctrl Pts',(25.7534391759961,-4.65966915422614,
134.454021631195));
#149767=CARTESIAN_POINT('Ctrl Pts',(25.7460720180589,-4.56127131814642,
134.576268013992));
#149768=CARTESIAN_POINT('Ctrl Pts',(25.7387048601218,-4.45825721635506,
134.694331460043));
#149769=CARTESIAN_POINT('Ctrl Pts',(25.731329522749,-4.35512874247756,134.812525986813));
#149770=CARTESIAN_POINT('Ctrl Pts',(25.7239541853762,-4.24737401883896,
134.926528021219));
#149771=CARTESIAN_POINT('Ctrl Pts',(25.7165788480033,-4.13538404176333,
135.035971349856));
#149772=CARTESIAN_POINT('Ctrl Pts',(25.7091985999226,-4.02331949859767,
135.145487548952));
#149773=CARTESIAN_POINT('Ctrl Pts',(25.7018183518418,-3.90701436365152,
135.250438744274));
#149774=CARTESIAN_POINT('Ctrl Pts',(25.694438103761,-3.7868924195254,135.350499239016));
#149775=CARTESIAN_POINT('Ctrl Pts',(25.6870479415286,-3.66660911128828,
135.450694148606));
#149776=CARTESIAN_POINT('Ctrl Pts',(25.6796577792962,-3.54249905746435,
135.545985015808));
#149777=CARTESIAN_POINT('Ctrl Pts',(25.6722676170638,-3.41501511222522,
135.636089329505));
#149778=CARTESIAN_POINT('Ctrl Pts',(25.6707360899979,-3.38859551459576,
135.654762423659));
#149779=CARTESIAN_POINT('Ctrl Pts',(25.6692045629321,-3.36203109940731,
135.673212924242));
#149780=CARTESIAN_POINT('Ctrl Pts',(25.6676730358662,-3.33532602361916,
135.691438566471));
#149781=CARTESIAN_POINT('Ctrl Pts',(25.6602497694608,-3.20588731086571,
135.779777715472));
#149782=CARTESIAN_POINT('Ctrl Pts',(25.6528265030553,-3.0727408334396,135.863104438142));
#149783=CARTESIAN_POINT('Ctrl Pts',(25.6454032366499,-2.93631220034191,
135.941091214417));
#149784=CARTESIAN_POINT('Ctrl Pts',(25.6379887439289,-2.80004481455865,
136.018985816799));
#149785=CARTESIAN_POINT('Ctrl Pts',(25.6305742512079,-2.66050331566374,
136.091552852161));
#149786=CARTESIAN_POINT('Ctrl Pts',(25.6231597584869,-2.51814385723093,
136.158506868537));
#149787=CARTESIAN_POINT('Ctrl Pts',(25.6157524121331,-2.37592161020409,
136.225396352112));
#149788=CARTESIAN_POINT('Ctrl Pts',(25.6083450657794,-2.23088714630567,
136.286683429217));
#149789=CARTESIAN_POINT('Ctrl Pts',(25.6009377194256,-2.08352279988314,
136.342127613826));
#149790=CARTESIAN_POINT('Ctrl Pts',(25.5935358977502,-1.93626836334992,
136.39753044607));
#149791=CARTESIAN_POINT('Ctrl Pts',(25.5861340760748,-1.78668785219971,
136.447098931998));
#149792=CARTESIAN_POINT('Ctrl Pts',(25.5787322543995,-1.63528514282548,
136.490639986728));
#149793=CARTESIAN_POINT('Ctrl Pts',(25.5713343400881,-1.4839623577628,136.534158056474));
#149794=CARTESIAN_POINT('Ctrl Pts',(25.5639364257767,-1.33081964804332,
136.571654928886));
#149795=CARTESIAN_POINT('Ctrl Pts',(25.5565385114654,-1.17637756777835,
136.602986866992));
#149796=CARTESIAN_POINT('Ctrl Pts',(25.5491418265532,-1.02196115298549,
136.634313598298));
#149797=CARTESIAN_POINT('Ctrl Pts',(25.541745141641,-0.866246161694955,
136.65947735448));
#149798=CARTESIAN_POINT('Ctrl Pts',(25.5343484567288,-0.70976501781126,
136.678385147817));
#149799=CARTESIAN_POINT('Ctrl Pts',(25.5269520997934,-0.553290812465243,
136.697292102763));
#149800=CARTESIAN_POINT('Ctrl Pts',(25.5195557428579,-0.396050892675834,
136.70994360164));
#149801=CARTESIAN_POINT('Ctrl Pts',(25.5121593859225,-0.238584243338168,
136.716298381221));
#149802=CARTESIAN_POINT('Ctrl Pts',(25.5047618965859,-0.0810934854544955,
136.722654133735));
#149803=CARTESIAN_POINT('Ctrl Pts',(25.4973644072494,0.0766236980771254,
136.722711232359));
#149804=CARTESIAN_POINT('Ctrl Pts',(25.4899669179128,0.234027022798936,
136.716480534745));
#149805=CARTESIAN_POINT('Ctrl Pts',(25.4825668353979,0.391485525011773,
136.710247652969));
#149806=CARTESIAN_POINT('Ctrl Pts',(25.4751667528829,0.548629576587278,
136.69772260121));
#149807=CARTESIAN_POINT('Ctrl Pts',(25.467766670368,0.704922867280941,136.678968205625));
#149808=CARTESIAN_POINT('Ctrl Pts',(25.4603584507015,0.86138801851551,136.660193187654));
#149809=CARTESIAN_POINT('Ctrl Pts',(25.452950231035,1.01700016974872,136.635175190851));
#149810=CARTESIAN_POINT('Ctrl Pts',(25.4455420113686,1.17123134454028,136.604028513236));
#149811=CARTESIAN_POINT('Ctrl Pts',(25.4381292320665,1.32555744604644,136.572862665361));
#149812=CARTESIAN_POINT('Ctrl Pts',(25.4307164527644,1.47850051561693,136.535560708537));
#149813=CARTESIAN_POINT('Ctrl Pts',(25.4233036734624,1.62954713838233,136.492287013564));
#149814=CARTESIAN_POINT('Ctrl Pts',(25.4158803024336,1.78080958364573,136.448951487106));
#149815=CARTESIAN_POINT('Ctrl Pts',(25.4084569314049,1.93016981663079,136.399627297533));
#149816=CARTESIAN_POINT('Ctrl Pts',(25.4010335603761,2.07713303967526,136.344527483103));
#149817=CARTESIAN_POINT('Ctrl Pts',(25.3970975109352,2.1550564668704,136.315312239389));
#149818=CARTESIAN_POINT('Ctrl Pts',(25.3931614614943,2.23230638687109,136.284474045113));
#149819=CARTESIAN_POINT('Ctrl Pts',(25.3892254120534,2.30881190201944,136.252049867477));
#149820=CARTESIAN_POINT('Ctrl Pts',(25.3818021456479,2.45309891592922,136.190898880381));
#149821=CARTESIAN_POINT('Ctrl Pts',(25.3743788792425,2.5951729709797,136.12391910699));
#149822=CARTESIAN_POINT('Ctrl Pts',(25.3669556128371,2.73452846320441,136.051291591614));
#149823=CARTESIAN_POINT('Ctrl Pts',(25.3595411201161,2.87371924880987,135.97874991593));
#149824=CARTESIAN_POINT('Ctrl Pts',(25.352126627395,3.01019753950847,135.900573956051));
#149825=CARTESIAN_POINT('Ctrl Pts',(25.344712134674,3.14347661432864,135.816993193136));
#149826=CARTESIAN_POINT('Ctrl Pts',(25.3373047883202,3.27662722975921,135.733492988507));
#149827=CARTESIAN_POINT('Ctrl Pts',(25.3298974419664,3.40658445386946,135.644598548635));
#149828=CARTESIAN_POINT('Ctrl Pts',(25.3224900956126,3.53288524545814,135.550585686494));
#149829=CARTESIAN_POINT('Ctrl Pts',(25.3150882739371,3.65909183715158,135.456642942693));
#149830=CARTESIAN_POINT('Ctrl Pts',(25.3076864522617,3.78164712819944,135.357589599743));
#149831=CARTESIAN_POINT('Ctrl Pts',(25.3002846305863,3.90011631332493,135.253745216029));
#149832=CARTESIAN_POINT('Ctrl Pts',(25.2928867162749,4.01852295948891,135.149955650957));
#149833=CARTESIAN_POINT('Ctrl Pts',(25.2854888019636,4.13284751553753,135.041380327494));
#149834=CARTESIAN_POINT('Ctrl Pts',(25.2780908876523,4.24268767927291,134.928379509211));
#149835=CARTESIAN_POINT('Ctrl Pts',(25.27069420274,4.3525095895661,134.815397469614));
#149836=CARTESIAN_POINT('Ctrl Pts',(25.2632975178278,4.45784832665976,134.697991662238));
#149837=CARTESIAN_POINT('Ctrl Pts',(25.2559008329156,4.55833786922462,134.57655976826));
#149838=CARTESIAN_POINT('Ctrl Pts',(25.2485044759801,4.65882295597786,134.455133258698));
#149839=CARTESIAN_POINT('Ctrl Pts',(25.2411081190446,4.75445903773717,134.329681305086));
#149840=CARTESIAN_POINT('Ctrl Pts',(25.2337117621092,4.8449200640789,134.200635066898));
#149841=CARTESIAN_POINT('Ctrl Pts',(25.2263142727726,4.93539494023456,134.071569071402));
#149842=CARTESIAN_POINT('Ctrl Pts',(25.218916783436,5.02069296907916,133.938908001315));
#149843=CARTESIAN_POINT('Ctrl Pts',(25.2115192940994,5.10053124851564,133.803112282078));
#149844=CARTESIAN_POINT('Ctrl Pts',(25.2041192115844,5.18039751513722,133.667268959863));
#149845=CARTESIAN_POINT('Ctrl Pts',(25.1967191290695,5.25480003269814,133.528289122304));
#149846=CARTESIAN_POINT('Ctrl Pts',(25.1893190465545,5.32350176983622,133.386657941472));
#149847=CARTESIAN_POINT('Ctrl Pts',(25.181910826888,5.39227905159728,133.244871022595));
#149848=CARTESIAN_POINT('Ctrl Pts',(25.1745026072214,5.45534287111988,133.100427274226));
#149849=CARTESIAN_POINT('Ctrl Pts',(25.1670943875549,5.51250400640318,132.953832678768));
#149850=CARTESIAN_POINT('Ctrl Pts',(25.1596816082528,5.56970032341163,132.807147856783));
#149851=CARTESIAN_POINT('Ctrl Pts',(25.1522688289507,5.6209865956346,132.658309901965));
#149852=CARTESIAN_POINT('Ctrl Pts',(25.1448560496486,5.66622359960249,132.507839611216));
#149853=CARTESIAN_POINT('Ctrl Pts',(25.1374326786198,5.71152524032286,132.357154321461));
#149854=CARTESIAN_POINT('Ctrl Pts',(25.130009307591,5.75076025695564,132.204832398073));
#149855=CARTESIAN_POINT('Ctrl Pts',(25.1225859365622,5.78384043439918,132.051405280723));
#149856=CARTESIAN_POINT('Ctrl Pts',(25.1186498871216,5.80138033822696,131.970054541675));
#149857=CARTESIAN_POINT('Ctrl Pts',(25.114713837681,5.81719076069269,131.888393198882));
#149858=CARTESIAN_POINT('Ctrl Pts',(25.1107777882404,5.83126448143482,131.806500882228));
#149859=CARTESIAN_POINT('Ctrl Pts',(25.1033545218349,5.85780707952975,131.652054528784));
#149860=CARTESIAN_POINT('Ctrl Pts',(25.0959312554294,5.87824959631605,131.496319398934));
#149861=CARTESIAN_POINT('Ctrl Pts',(25.088507989024,5.89247105820696,131.339818730487));
#149862=CARTESIAN_POINT('Ctrl Pts',(25.081093496303,5.90667571151096,131.183503032834));
#149863=CARTESIAN_POINT('Ctrl Pts',(25.073679003582,5.91467391219624,131.026423965734));
#149864=CARTESIAN_POINT('Ctrl Pts',(25.066264510861,5.91639564468866,130.869115061499));
#149865=CARTESIAN_POINT('Ctrl Pts',(25.0588571645073,5.91811571771047,130.711957777509));
#149866=CARTESIAN_POINT('Ctrl Pts',(25.0514498181535,5.91357136183765,130.554571468168));
#149867=CARTESIAN_POINT('Ctrl Pts',(25.0440424717997,5.90274434125828,130.397494786802));
#149868=CARTESIAN_POINT('Ctrl Pts',(25.0366406501243,5.89192539587927,130.24053525915));
#149869=CARTESIAN_POINT('Ctrl Pts',(25.0292388284488,5.87483314150947,130.083885270469));
#149870=CARTESIAN_POINT('Ctrl Pts',(25.0218370067734,5.85150140879616,129.928083363863));
#149871=CARTESIAN_POINT('Ctrl Pts',(25.0144390924621,5.8281819927232,129.772363703874));
#149872=CARTESIAN_POINT('Ctrl Pts',(25.0070411781508,5.79862971315761,129.6174916026));
#149873=CARTESIAN_POINT('Ctrl Pts',(24.9996432638395,5.76293021588128,129.464000259534));
#149874=CARTESIAN_POINT('Ctrl Pts',(24.9922465789273,5.72723665121354,129.310534423945));
#149875=CARTESIAN_POINT('Ctrl Pts',(24.9848498940151,5.68539798080428,129.158449254398));
#149876=CARTESIAN_POINT('Ctrl Pts',(24.9774532091029,5.63755094161994,129.008267651392));
#149877=CARTESIAN_POINT('Ctrl Pts',(24.9700568521675,5.58970602402332,128.858092707595));
#149878=CARTESIAN_POINT('Ctrl Pts',(24.962660495232,5.5358533806978,128.709821518195));
#149879=CARTESIAN_POINT('Ctrl Pts',(24.9552641382965,5.4761795201021,128.563961450874));
#149880=CARTESIAN_POINT('Ctrl Pts',(24.9478666489599,5.41649652328609,128.418079052005));
#149881=CARTESIAN_POINT('Ctrl Pts',(24.9404691596234,5.35099067597582,128.274608855763));
#149882=CARTESIAN_POINT('Ctrl Pts',(24.9330716702868,5.2798964316416,128.134037746893));
#149883=CARTESIAN_POINT('Ctrl Pts',(24.9256715877718,5.20877726533044,127.99341736104));
#149884=CARTESIAN_POINT('Ctrl Pts',(24.9182715052568,5.1320659700031,127.855698418855));
#149885=CARTESIAN_POINT('Ctrl Pts',(24.9108714227418,5.05004261342194,127.721342588893));
#149886=CARTESIAN_POINT('Ctrl Pts',(24.9034632030753,4.96792906372778,127.586839020883));
#149887=CARTESIAN_POINT('Ctrl Pts',(24.8960549834089,4.8804919822371,127.455706269231));
#149888=CARTESIAN_POINT('Ctrl Pts',(24.8886467637424,4.78805478716329,127.328377027613));
#149889=CARTESIAN_POINT('Ctrl Pts',(24.8812339844403,4.69556069853792,127.200969416971));
#149890=CARTESIAN_POINT('Ctrl Pts',(24.8738212051382,4.59806059471343,127.077370273499));
#149891=CARTESIAN_POINT('Ctrl Pts',(24.8664084258361,4.49591738318717,126.957978233292));
#149892=CARTESIAN_POINT('Ctrl Pts',(24.8589850548074,4.39362822465067,126.838415600139));
#149893=CARTESIAN_POINT('Ctrl Pts',(24.8515616837786,4.28668296138282,126.723072349192));
#149894=CARTESIAN_POINT('Ctrl Pts',(24.8441383127499,4.17548102621142,126.612309954436));
#149895=CARTESIAN_POINT('Ctrl Pts',(24.8402022633091,4.11651909192989,126.553581075029));
#149896=CARTESIAN_POINT('Ctrl Pts',(24.8362662138683,4.05636101100038,126.496139368364));
#149897=CARTESIAN_POINT('Ctrl Pts',(24.8323301644275,3.99506987551722,126.44003395103));
#149898=CARTESIAN_POINT('Ctrl Pts',(24.8249068980221,3.87947670682649,126.334220884929));
#149899=CARTESIAN_POINT('Ctrl Pts',(24.8174836316166,3.75950201109489,126.232843374869));
#149900=CARTESIAN_POINT('Ctrl Pts',(24.8100603652112,3.63552061393169,126.13628602217));
#149901=CARTESIAN_POINT('Ctrl Pts',(24.8026458724902,3.51168575248375,126.039842792244));
#149902=CARTESIAN_POINT('Ctrl Pts',(24.7952313797692,3.38385390745977,125.94820860685));
#149903=CARTESIAN_POINT('Ctrl Pts',(24.7878168870482,3.25243610957519,125.861730759319));
#149904=CARTESIAN_POINT('Ctrl Pts',(24.7804095406944,3.12114497711258,125.775336262395));
#149905=CARTESIAN_POINT('Ctrl Pts',(24.7730021943407,2.98627508230078,125.69408841312));
#149906=CARTESIAN_POINT('Ctrl Pts',(24.7655948479869,2.84826975253751,125.618293709081));
#149907=CARTESIAN_POINT('Ctrl Pts',(24.7581930263115,2.71036735235504,125.542555535592));
#149908=CARTESIAN_POINT('Ctrl Pts',(24.7507912046361,2.56933449933088,125.472262588));
#149909=CARTESIAN_POINT('Ctrl Pts',(24.7433893829607,2.42564257132432,125.407677499328));
#149910=CARTESIAN_POINT('Ctrl Pts',(24.7359914686493,2.28202649716826,125.343126504621));
#149911=CARTESIAN_POINT('Ctrl Pts',(24.7285935543379,2.13575448319964,125.284277520683));
#149912=CARTESIAN_POINT('Ctrl Pts',(24.7211956400266,1.98732141889056,125.231346698642));
#149913=CARTESIAN_POINT('Ctrl Pts',(24.7137989551144,1.83891302146392,125.178424672744));
#149914=CARTESIAN_POINT('Ctrl Pts',(24.7064022702022,1.6883446377251,125.131418982065));
#149915=CARTESIAN_POINT('Ctrl Pts',(24.6990055852899,1.53613010834403,125.090497226415));
#149916=CARTESIAN_POINT('Ctrl Pts',(24.6916092283545,1.38392232831514,125.049577285278));
#149917=CARTESIAN_POINT('Ctrl Pts',(24.6842128714191,1.23006890827354,125.014740839698));
#149918=CARTESIAN_POINT('Ctrl Pts',(24.6768165144836,1.07509752339819,124.986105219452));
#149919=CARTESIAN_POINT('Ctrl Pts',(24.6694190251471,0.920102412008413,
124.957465215019));
#149920=CARTESIAN_POINT('Ctrl Pts',(24.6620215358105,0.763989362083347,
124.93502799406));
#149921=CARTESIAN_POINT('Ctrl Pts',(24.654624046474,0.607294731375145,124.918859477328));
#149922=CARTESIAN_POINT('Ctrl Pts',(24.647223963959,0.450545171606831,124.902685292747));
#149923=CARTESIAN_POINT('Ctrl Pts',(24.639823881444,0.293213996241964,124.89278422586));
#149924=CARTESIAN_POINT('Ctrl Pts',(24.632423798929,0.135841003575897,124.889170190856));
#149925=CARTESIAN_POINT('Ctrl Pts',(24.6250155792626,-0.0217050368741682,
124.885552181848));
#149926=CARTESIAN_POINT('Ctrl Pts',(24.6176073595961,-0.179292613026846,
124.888235019489));
#149927=CARTESIAN_POINT('Ctrl Pts',(24.6101991399296,-0.336382871992765,
124.897180484378));
#149928=CARTESIAN_POINT('Ctrl Pts',(24.6027863606276,-0.493569817392334,
124.906131455051));
#149929=CARTESIAN_POINT('Ctrl Pts',(24.5953735813255,-0.650258464994145,
124.921352697622));
#149930=CARTESIAN_POINT('Ctrl Pts',(24.5879608020234,-0.805917270594964,
124.94275436028));
#149931=CARTESIAN_POINT('Ctrl Pts',(24.5805374309947,-0.961798488796456,
124.964186602637));
#149932=CARTESIAN_POINT('Ctrl Pts',(24.5731140599659,-1.11664655958836,
124.991816836919));
#149933=CARTESIAN_POINT('Ctrl Pts',(24.5656906889372,-1.26994146146879,
125.025504394494));
#149934=CARTESIAN_POINT('Ctrl Pts',(24.5617546394963,-1.35122209670789,
125.043366345842));
#149935=CARTESIAN_POINT('Ctrl Pts',(24.5578185900555,-1.43206634354629,
125.062930397549));
#149936=CARTESIAN_POINT('Ctrl Pts',(24.5538825406146,-1.51239877598623,
125.084170017167));
#149937=CARTESIAN_POINT('Ctrl Pts',(24.5464592742092,-1.66390323647658,
125.1242272769));
#149938=CARTESIAN_POINT('Ctrl Pts',(24.5390360078037,-1.81404426043895,
125.170368365808));
#149939=CARTESIAN_POINT('Ctrl Pts',(24.5316127413982,-1.96229566949174,
125.222485818899));
#149940=CARTESIAN_POINT('Ctrl Pts',(24.5241982486772,-2.11037185769075,
125.274541673489));
#149941=CARTESIAN_POINT('Ctrl Pts',(24.5167837559562,-2.25656252778023,
125.332559709599));
#149942=CARTESIAN_POINT('Ctrl Pts',(24.5093692632351,-2.40035331990266,
125.396381835976));
#149943=CARTESIAN_POINT('Ctrl Pts',(24.5019619168813,-2.54400552104704,
125.460142448185));
#149944=CARTESIAN_POINT('Ctrl Pts',(24.4945545705274,-2.68526211022845,
125.529695863283));
#149945=CARTESIAN_POINT('Ctrl Pts',(24.4871472241736,-2.82362559306031,
125.604834766807));
#149946=CARTESIAN_POINT('Ctrl Pts',(24.4797454024982,-2.96188587918515,
125.6799176289));
#149947=CARTESIAN_POINT('Ctrl Pts',(24.4723435808227,-3.09725702877218,
125.760577507234));
#149948=CARTESIAN_POINT('Ctrl Pts',(24.4649417591473,-3.22926328997477,
125.846559777827));
#149949=CARTESIAN_POINT('Ctrl Pts',(24.457543844836,-3.36119986609922,125.932496659048));
#149950=CARTESIAN_POINT('Ctrl Pts',(24.4501459305247,-3.48977477941823,
126.023750133753));
#149951=CARTESIAN_POINT('Ctrl Pts',(24.4427480162133,-3.61453867601762,
126.120020672379));
#149952=CARTESIAN_POINT('Ctrl Pts',(24.4353513313011,-3.73928183912138,
126.216275212588));
#149953=CARTESIAN_POINT('Ctrl Pts',(24.4279546463888,-3.86021494720823,
126.317544934156));
#149954=CARTESIAN_POINT('Ctrl Pts',(24.4205579614766,-3.97691925037793,
126.423488120166));
#149955=CARTESIAN_POINT('Ctrl Pts',(24.4131616045412,-4.0936183787562,126.529426608544));
#149956=CARTESIAN_POINT('Ctrl Pts',(24.4057652476058,-4.20608879865333,
126.640037898417));
#149957=CARTESIAN_POINT('Ctrl Pts',(24.3983688906703,-4.3139465758812,126.754941461324));
#149958=CARTESIAN_POINT('Ctrl Pts',(24.3909714013337,-4.42182086641042,
126.869862616259));
#149959=CARTESIAN_POINT('Ctrl Pts',(24.3835739119972,-4.52508085261635,
126.989077080526));
#149960=CARTESIAN_POINT('Ctrl Pts',(24.3761764226606,-4.62338115903669,
127.112169232932));
#149961=CARTESIAN_POINT('Ctrl Pts',(24.3687763401456,-4.72171592447677,
127.235304535101));
#149962=CARTESIAN_POINT('Ctrl Pts',(24.3613762576305,-4.81508731577404,
127.362319940287));
#149963=CARTESIAN_POINT('Ctrl Pts',(24.3539761751155,-4.90319185236293,
127.492768821855));
#149964=CARTESIAN_POINT('Ctrl Pts',(24.3465679554491,-4.99139326894742,
127.623361145378));
#149965=CARTESIAN_POINT('Ctrl Pts',(24.3391597357826,-5.07431605585901,
127.757394175585));
#149966=CARTESIAN_POINT('Ctrl Pts',(24.3317515161161,-5.15170110501327,
127.894393901759));
#149967=CARTESIAN_POINT('Ctrl Pts',(24.324338736814,-5.22913378337383,128.031477948978));
#149968=CARTESIAN_POINT('Ctrl Pts',(24.316925957512,-5.30102176227275,128.171531999267));
#149969=CARTESIAN_POINT('Ctrl Pts',(24.3095131782099,-5.36715332395629,
128.314060282336));
#149970=CARTESIAN_POINT('Ctrl Pts',(24.3020898071812,-5.4333793775166,128.456792216501));
#149971=CARTESIAN_POINT('Ctrl Pts',(24.2946664361524,-5.4938324435237,128.60200510052));
#149972=CARTESIAN_POINT('Ctrl Pts',(24.2872430651236,-5.54834978615739,
128.749185390743));
#149973=CARTESIAN_POINT('Ctrl Pts',(24.283307015683,-5.57725618934632,128.827223912159));
#149974=CARTESIAN_POINT('Ctrl Pts',(24.2793709662423,-5.60449468870749,
128.905815314474));
#149975=CARTESIAN_POINT('Ctrl Pts',(24.2754349168017,-5.63004683714687,
128.984881798224));
#149976=CARTESIAN_POINT('Ctrl Pts',(24.2665164093745,-5.68794423632163,
129.164034787332));
#149977=CARTESIAN_POINT('Ctrl Pts',(24.2575979019474,-5.73732328000852,
129.34606681738));
#149978=CARTESIAN_POINT('Ctrl Pts',(24.2486793945203,-5.77793595100518,
129.530238681258));
#149979=CARTESIAN_POINT('Ctrl Pts',(24.2398101565805,-5.81832426097514,
129.713393104336));
#149980=CARTESIAN_POINT('Ctrl Pts',(24.2309409186407,-5.85004272511329,
129.898663761957));
#149981=CARTESIAN_POINT('Ctrl Pts',(24.222071680701,-5.87289414555811,130.085302262793));
#149982=CARTESIAN_POINT('Ctrl Pts',(24.2132929185469,-5.89551245688669,
130.270036849773));
#149983=CARTESIAN_POINT('Ctrl Pts',(24.2045141563928,-5.90944364635717,
130.456111473033));
#149984=CARTESIAN_POINT('Ctrl Pts',(24.1957353942387,-5.91454328238171,
130.642779915335));
#149985=CARTESIAN_POINT('Ctrl Pts',(24.1932820128116,-5.91596846648941,
130.69494773596));
#149986=CARTESIAN_POINT('Ctrl Pts',(24.1908286313845,-5.91670417310227,
130.747161813275));
#149987=CARTESIAN_POINT('Ctrl Pts',(24.1883752499575,-5.91674792517552,
130.799405576576));
#149988=CARTESIAN_POINT('',(22.4383751628218,-5.91238909884781,130.807386683679));
#149989=CARTESIAN_POINT('Ctrl Pts',(24.1883751922117,-5.91219990274765,
130.799410614093));
#149990=CARTESIAN_POINT('Ctrl Pts',(24.1245792258041,-5.90151963868852,
132.156885527756));
#149991=CARTESIAN_POINT('Ctrl Pts',(23.9679673847923,-4.76179293726462,
135.505531964573));
#149992=CARTESIAN_POINT('Ctrl Pts',(23.718539669176,0.810670249943998,137.755646417775));
#149993=CARTESIAN_POINT('Ctrl Pts',(23.4400920453631,6.28650068617809,133.879660546521));
#149994=CARTESIAN_POINT('Ctrl Pts',(23.1616444215502,5.98534410444456,127.177624277308));
#149995=CARTESIAN_POINT('Ctrl Pts',(22.8831967977373,0.183948691041906,
123.808381528874));
#149996=CARTESIAN_POINT('Ctrl Pts',(22.6421070546244,-4.98546409398633,
126.457594913206));
#149997=CARTESIAN_POINT('Ctrl Pts',(22.4938331861159,-5.90300137026986,
129.625444179626));
#149998=CARTESIAN_POINT('Ctrl Pts',(22.4383751922117,-5.90844756488801,
130.807384039503));
#149999=CARTESIAN_POINT('',(20.6883751922117,-5.92023233031357,130.808223305572));
#150000=CARTESIAN_POINT('Ctrl Pts',(22.4383751303106,-5.91674922467675,
130.807389608667));
#150001=CARTESIAN_POINT('Ctrl Pts',(22.4302244668188,-5.9166601718607,130.981342968942));
#150002=CARTESIAN_POINT('Ctrl Pts',(22.4220738033269,-5.90889565774037,
131.155031843747));
#150003=CARTESIAN_POINT('Ctrl Pts',(22.413923139835,-5.89355001080322,131.327809595654));
#150004=CARTESIAN_POINT('Ctrl Pts',(22.4057305305205,-5.87812539044425,
131.501476515046));
#150005=CARTESIAN_POINT('Ctrl Pts',(22.3975379212059,-5.85504148845746,
131.674222681994));
#150006=CARTESIAN_POINT('Ctrl Pts',(22.3893453118913,-5.82444442124337,
131.845407084515));
#150007=CARTESIAN_POINT('Ctrl Pts',(22.3811313931613,-5.79376776941935,
132.017036746832));
#150008=CARTESIAN_POINT('Ctrl Pts',(22.3729174744312,-5.75553892972251,
132.187096296581));
#150009=CARTESIAN_POINT('Ctrl Pts',(22.3647035557012,-5.7099541235859,132.354958717992));
#150010=CARTESIAN_POINT('Ctrl Pts',(22.3564598853453,-5.66420420477377,
132.523429153692));
#150011=CARTESIAN_POINT('Ctrl Pts',(22.3482162149894,-5.61104504834546,
132.689686306487));
#150012=CARTESIAN_POINT('Ctrl Pts',(22.3399725446335,-5.55072257989809,
132.85311863244));
#150013=CARTESIAN_POINT('Ctrl Pts',(22.3354155464595,-5.51737707156257,
132.943461984223));
#150014=CARTESIAN_POINT('Ctrl Pts',(22.3308585482854,-5.48184347136795,
133.032942554786));
#150015=CARTESIAN_POINT('Ctrl Pts',(22.3263015501114,-5.44416932289011,
133.121460301697));
#150016=CARTESIAN_POINT('Ctrl Pts',(22.318878283706,-5.3827988263333,133.265654087132));
#150017=CARTESIAN_POINT('Ctrl Pts',(22.3114550173006,-5.31560291797675,
133.40762604585));
#150018=CARTESIAN_POINT('Ctrl Pts',(22.3040317508951,-5.24276341136604,
133.546870849988));
#150019=CARTESIAN_POINT('Ctrl Pts',(22.2966172581741,-5.1700099950031,133.685951078332));
#150020=CARTESIAN_POINT('Ctrl Pts',(22.2892027654531,-5.0916264289242,133.822310240488));
#150021=CARTESIAN_POINT('Ctrl Pts',(22.281788272732,-5.00784293473085,133.95546196528));
#150022=CARTESIAN_POINT('Ctrl Pts',(22.2743809263782,-4.92414019422371,
134.088485353427));
#150023=CARTESIAN_POINT('Ctrl Pts',(22.2669735800244,-4.83504808451739,
134.218307144843));
#150024=CARTESIAN_POINT('Ctrl Pts',(22.2595662336707,-4.74084312293794,
134.344464718605));
#150025=CARTESIAN_POINT('Ctrl Pts',(22.2521644119952,-4.64670842297286,
134.470528199288));
#150026=CARTESIAN_POINT('Ctrl Pts',(22.2447625903198,-4.54746868643463,
134.592932606093));
#150027=CARTESIAN_POINT('Ctrl Pts',(22.2373607686444,-4.44344413303837,
134.711243620558));
#150028=CARTESIAN_POINT('Ctrl Pts',(22.229962854333,-4.33947449339412,134.829492179559));
#150029=CARTESIAN_POINT('Ctrl Pts',(22.2225649400217,-4.23072531314612,
134.943651370063));
#150030=CARTESIAN_POINT('Ctrl Pts',(22.2151670257103,-4.11755746768501,
135.053319438596));
#150031=CARTESIAN_POINT('Ctrl Pts',(22.2077703407981,-4.00440842866689,
135.162969282286));
#150032=CARTESIAN_POINT('Ctrl Pts',(22.2003736558859,-3.88684244961945,
135.268129225746));
#150033=CARTESIAN_POINT('Ctrl Pts',(22.1929769709737,-3.76525776827935,
135.368433853275));
#150034=CARTESIAN_POINT('Ctrl Pts',(22.1855806140382,-3.64367847813143,
135.468734033191));
#150035=CARTESIAN_POINT('Ctrl Pts',(22.1781842571028,-3.51808112795462,
135.564179087687));
#150036=CARTESIAN_POINT('Ctrl Pts',(22.1707879001673,-3.38889737291734,
135.65444362287));
#150037=CARTESIAN_POINT('Ctrl Pts',(22.1633904108308,-3.25969383951737,
135.744721977783));
#150038=CARTESIAN_POINT('Ctrl Pts',(22.1559929214942,-3.12690311396992,
135.829818020288));
#150039=CARTESIAN_POINT('Ctrl Pts',(22.1485954321576,-2.99098605171237,
135.909449549305));
#150040=CARTESIAN_POINT('Ctrl Pts',(22.1411953496426,-2.85502134393895,
135.989108993031));
#150041=CARTESIAN_POINT('Ctrl Pts',(22.1337952671276,-2.71592843934977,
136.063299920781));
#150042=CARTESIAN_POINT('Ctrl Pts',(22.1263951846125,-2.57419287017456,
136.131786039817));
#150043=CARTESIAN_POINT('Ctrl Pts',(22.1189869649461,-2.43230144817048,
136.20034746638));
#150044=CARTESIAN_POINT('Ctrl Pts',(22.1115787452796,-2.28776189466713,
136.26319139408));
#150045=CARTESIAN_POINT('Ctrl Pts',(22.1041705256131,-2.14108047944648,
136.320129371152));
#150046=CARTESIAN_POINT('Ctrl Pts',(22.096757746311,-1.99430878426228,136.377102392599));
#150047=CARTESIAN_POINT('Ctrl Pts',(22.089344967009,-1.84539295282117,136.428162099402));
#150048=CARTESIAN_POINT('Ctrl Pts',(22.0819321877069,-1.69485399329648,
136.473170060818));
#150049=CARTESIAN_POINT('Ctrl Pts',(22.0745088166781,-1.54409993664685,
136.51824233172));
#150050=CARTESIAN_POINT('Ctrl Pts',(22.0670854456493,-1.39171848062952,
136.557245494882));
#150051=CARTESIAN_POINT('Ctrl Pts',(22.0596620746206,-1.23824119854686,
136.590092144065));
#150052=CARTESIAN_POINT('Ctrl Pts',(22.0557260251799,-1.15686386095275,
136.607508225605));
#150053=CARTESIAN_POINT('Ctrl Pts',(22.0517899757393,-1.07517855195031,
136.6231943551));
#150054=CARTESIAN_POINT('Ctrl Pts',(22.0478539262986,-0.993264912318842,
136.63714343338));
#150055=CARTESIAN_POINT('Ctrl Pts',(22.0404306598932,-0.838778344405665,
136.663450959681));
#150056=CARTESIAN_POINT('Ctrl Pts',(22.0330073934877,-0.683012284863759,
136.683656450438));
#150057=CARTESIAN_POINT('Ctrl Pts',(22.0255841270823,-0.526490154997762,
136.697639728485));
#150058=CARTESIAN_POINT('Ctrl Pts',(22.0181696343613,-0.37015302129069,
136.711606479458));
#150059=CARTESIAN_POINT('Ctrl Pts',(22.0107551416403,-0.213061964186039,
136.719365623281));
#150060=CARTESIAN_POINT('Ctrl Pts',(22.0033406489193,-0.0557506219285824,
136.720847956406));
#150061=CARTESIAN_POINT('Ctrl Pts',(21.9959333025655,0.101409097734539,
136.722328860803));
#150062=CARTESIAN_POINT('Ctrl Pts',(21.9885259562117,0.25878830908947,136.717544995021));
#150063=CARTESIAN_POINT('Ctrl Pts',(21.981118609858,0.415848331681116,136.70647894301));
#150064=CARTESIAN_POINT('Ctrl Pts',(21.9737167881825,0.572791212982378,
136.695421144477));
#150065=CARTESIAN_POINT('Ctrl Pts',(21.9663149665071,0.729415008763857,
136.678090515284));
#150066=CARTESIAN_POINT('Ctrl Pts',(21.9589131448317,0.885181228026921,
136.654521705609));
#150067=CARTESIAN_POINT('Ctrl Pts',(21.9515152305203,1.04086521951532,136.630965337725));
#150068=CARTESIAN_POINT('Ctrl Pts',(21.944117316209,1.19569216791252,136.601177403406));
#150069=CARTESIAN_POINT('Ctrl Pts',(21.9367194018976,1.34912900468063,136.565244359773));
#150070=CARTESIAN_POINT('Ctrl Pts',(21.9293227169854,1.50254034302988,136.529317287561));
#150071=CARTESIAN_POINT('Ctrl Pts',(21.9219260320732,1.65456166513102,136.487247217862));
#150072=CARTESIAN_POINT('Ctrl Pts',(21.914529347161,1.80467027918037,136.439171683249));
#150073=CARTESIAN_POINT('Ctrl Pts',(21.9071329902256,1.95477223725647,136.391098280356));
#150074=CARTESIAN_POINT('Ctrl Pts',(21.8997366332901,2.10296130040508,136.337020055881));
#150075=CARTESIAN_POINT('Ctrl Pts',(21.8923402763547,2.24873038536462,136.277124290194));
#150076=CARTESIAN_POINT('Ctrl Pts',(21.8849427870181,2.39452178794319,136.217219354313));
#150077=CARTESIAN_POINT('Ctrl Pts',(21.8775452976815,2.53789212930005,136.151495245641));
#150078=CARTESIAN_POINT('Ctrl Pts',(21.870147808345,2.67835488205304,136.080187158335));
#150079=CARTESIAN_POINT('Ctrl Pts',(21.86274772583,2.81886687380627,136.008854074089));
#150080=CARTESIAN_POINT('Ctrl Pts',(21.8553476433149,2.95646891498172,135.931933282806));
#150081=CARTESIAN_POINT('Ctrl Pts',(21.8479475608,3.09069976377644,135.849705554505));
#150082=CARTESIAN_POINT('Ctrl Pts',(21.8405393411335,3.22507821318868,135.767387408363));
#150083=CARTESIAN_POINT('Ctrl Pts',(21.8331311214671,3.35607774863777,135.679750866398));
#150084=CARTESIAN_POINT('Ctrl Pts',(21.8257229018006,3.4832661691351,135.587120004934));
#150085=CARTESIAN_POINT('Ctrl Pts',(21.8183101224985,3.61053287198317,135.494432130721));
#150086=CARTESIAN_POINT('Ctrl Pts',(21.8108973431965,3.73398349376836,135.396744042944));
#150087=CARTESIAN_POINT('Ctrl Pts',(21.8034845638944,3.85321995114101,135.294419255338));
#150088=CARTESIAN_POINT('Ctrl Pts',(21.7960611928656,3.9726267791556,135.191948261276));
#150089=CARTESIAN_POINT('Ctrl Pts',(21.7886378218369,4.08780714405189,135.084827589056));
#150090=CARTESIAN_POINT('Ctrl Pts',(21.7812144508081,4.1984001801314,134.973457221145));
#150091=CARTESIAN_POINT('Ctrl Pts',(21.7772784013673,4.25703926150438,134.914405979783));
#150092=CARTESIAN_POINT('Ctrl Pts',(21.7733423519265,4.31438935129554,134.854160552016));
#150093=CARTESIAN_POINT('Ctrl Pts',(21.7694063024857,4.37040142898546,134.792784104612));
#150094=CARTESIAN_POINT('Ctrl Pts',(21.7619830360803,4.47603845943128,134.677030040302));
#150095=CARTESIAN_POINT('Ctrl Pts',(21.7545597696748,4.57723327103468,134.556901204187));
#150096=CARTESIAN_POINT('Ctrl Pts',(21.7471365032694,4.67360183334036,134.432773006738));
#150097=CARTESIAN_POINT('Ctrl Pts',(21.7397220105484,4.7698564960083,134.308791518511));
#150098=CARTESIAN_POINT('Ctrl Pts',(21.7323075178274,4.86129603698431,134.180820369883));
#150099=CARTESIAN_POINT('Ctrl Pts',(21.7248930251064,4.9475737888576,134.049271119615));
#150100=CARTESIAN_POINT('Ctrl Pts',(21.7174856787526,5.03376838298534,133.917848661468));
#150101=CARTESIAN_POINT('Ctrl Pts',(21.7100783323988,5.1148108891555,133.782855277437));
#150102=CARTESIAN_POINT('Ctrl Pts',(21.7026709860451,5.19039548480622,133.644734760844));
#150103=CARTESIAN_POINT('Ctrl Pts',(21.6952691643697,5.26592370661386,133.506717259744));
#150104=CARTESIAN_POINT('Ctrl Pts',(21.6878673426943,5.33600194481329,133.365577596133));
#150105=CARTESIAN_POINT('Ctrl Pts',(21.6804655210189,5.40036828404338,133.221787547009));
#150106=CARTESIAN_POINT('Ctrl Pts',(21.6730676067075,5.46470064478401,133.078073403533));
#150107=CARTESIAN_POINT('Ctrl Pts',(21.6656696923962,5.52332695947045,132.93171200081));
#150108=CARTESIAN_POINT('Ctrl Pts',(21.6582717780849,5.57603183036203,132.783198556683));
#150109=CARTESIAN_POINT('Ctrl Pts',(21.6508750931727,5.62872794266023,132.634709792797));
#150110=CARTESIAN_POINT('Ctrl Pts',(21.6434784082604,5.67550443945883,132.484070048754));
#150111=CARTESIAN_POINT('Ctrl Pts',(21.6360817233482,5.71619450311981,132.331793419689));
#150112=CARTESIAN_POINT('Ctrl Pts',(21.6286853664128,5.75688276254074,132.17952354273));
#150113=CARTESIAN_POINT('Ctrl Pts',(21.6212890094774,5.79148502906606,132.025617285708));
#150114=CARTESIAN_POINT('Ctrl Pts',(21.6138926525419,5.81988477608601,131.870602501747));
#150115=CARTESIAN_POINT('Ctrl Pts',(21.6064951632054,5.84828887117973,131.715563984627));
#150116=CARTESIAN_POINT('Ctrl Pts',(21.5990976738687,5.87048848866989,131.559416969847));
#150117=CARTESIAN_POINT('Ctrl Pts',(21.5917001845322,5.88641852412558,131.402697914858));
#150118=CARTESIAN_POINT('Ctrl Pts',(21.5843001020172,5.90235414383049,131.245923922248));
#150119=CARTESIAN_POINT('Ctrl Pts',(21.5769000195022,5.9120157679861,131.088577861331));
#150120=CARTESIAN_POINT('Ctrl Pts',(21.5694999369872,5.91539030390024,130.931199550954));
#150121=CARTESIAN_POINT('Ctrl Pts',(21.5620917173207,5.91876855046352,130.773648186946));
#150122=CARTESIAN_POINT('Ctrl Pts',(21.5546834976543,5.91584589446426,130.616064876099));
#150123=CARTESIAN_POINT('Ctrl Pts',(21.5472752779878,5.90666137530154,130.458988412516));
#150124=CARTESIAN_POINT('Ctrl Pts',(21.5398624986857,5.89747120322051,130.30181527099));
#150125=CARTESIAN_POINT('Ctrl Pts',(21.5324497193837,5.88201152482766,130.145149968972));
#150126=CARTESIAN_POINT('Ctrl Pts',(21.5250369400816,5.86037300074793,129.989523913309));
#150127=CARTESIAN_POINT('Ctrl Pts',(21.5176135690529,5.83870355853024,129.833675491839));
#150128=CARTESIAN_POINT('Ctrl Pts',(21.5101901980241,5.81083770383978,129.678869648872));
#150129=CARTESIAN_POINT('Ctrl Pts',(21.5027668269954,5.77691689652957,129.525626191232));
#150130=CARTESIAN_POINT('Ctrl Pts',(21.4988307775545,5.75893127057486,129.444372832964));
#150131=CARTESIAN_POINT('Ctrl Pts',(21.4948947281136,5.73924421034106,129.363558452899));
#150132=CARTESIAN_POINT('Ctrl Pts',(21.4909586786728,5.71788236303121,129.283258436568));
#150133=CARTESIAN_POINT('Ctrl Pts',(21.4835354122674,5.67759458568581,129.131815111848));
#150134=CARTESIAN_POINT('Ctrl Pts',(21.476112145862,5.63122506112857,128.98174448063));
#150135=CARTESIAN_POINT('Ctrl Pts',(21.4686888794565,5.57888205498102,128.833572557142));
#150136=CARTESIAN_POINT('Ctrl Pts',(21.4612743867355,5.52660091391984,128.685575760562));
#150137=CARTESIAN_POINT('Ctrl Pts',(21.4538598940145,5.46836046768032,128.539473553334));
#150138=CARTESIAN_POINT('Ctrl Pts',(21.4464454012935,5.40431959010051,128.395780054131));
#150139=CARTESIAN_POINT('Ctrl Pts',(21.4390380549397,5.34034043752962,128.252225052133));
#150140=CARTESIAN_POINT('Ctrl Pts',(21.4316307085859,5.27057213449128,128.111074474983));
#150141=CARTESIAN_POINT('Ctrl Pts',(21.4242233622321,5.19522275231093,127.972825500996));
#150142=CARTESIAN_POINT('Ctrl Pts',(21.4168215405567,5.11992956854257,127.834679638309));
#150143=CARTESIAN_POINT('Ctrl Pts',(21.4094197188813,5.03906377176702,127.699431396083));
#150144=CARTESIAN_POINT('Ctrl Pts',(21.4020178972059,4.95288070968222,127.567556138121));
#150145=CARTESIAN_POINT('Ctrl Pts',(21.3946199828945,4.86674314296504,127.43575049608));
#150146=CARTESIAN_POINT('Ctrl Pts',(21.3872220685832,4.77529410479863,127.307314603903));
#150147=CARTESIAN_POINT('Ctrl Pts',(21.3798241542719,4.67883380824042,127.182697359149));
#150148=CARTESIAN_POINT('Ctrl Pts',(21.3724274693596,4.58238954163353,127.058100823521));
#150149=CARTESIAN_POINT('Ctrl Pts',(21.3650307844474,4.48093589773038,126.93732197075));
#150150=CARTESIAN_POINT('Ctrl Pts',(21.3576340995352,4.37481523031845,126.820779030216));
#150151=CARTESIAN_POINT('Ctrl Pts',(21.3502377425997,4.26869926840813,126.704241257319));
#150152=CARTESIAN_POINT('Ctrl Pts',(21.3428413856643,4.15791694578784,126.591939299214));
#150153=CARTESIAN_POINT('Ctrl Pts',(21.3354450287288,4.0428493747614,126.484256510546));
#150154=CARTESIAN_POINT('Ctrl Pts',(21.3280475393922,3.92776418659609,126.376557235368));
#150155=CARTESIAN_POINT('Ctrl Pts',(21.3206500500557,3.80839271625744,126.273478792856));
#150156=CARTESIAN_POINT('Ctrl Pts',(21.3132525607191,3.68515111005727,126.175365925568));
#150157=CARTESIAN_POINT('Ctrl Pts',(21.3058524782041,3.5618663017031,126.077218664966));
#150158=CARTESIAN_POINT('Ctrl Pts',(21.2984523956891,3.43470894823616,125.984040677616));
#150159=CARTESIAN_POINT('Ctrl Pts',(21.2910523131741,3.30412613761959,125.896134764042));
#150160=CARTESIAN_POINT('Ctrl Pts',(21.2836440935076,3.1733997377785,125.808132188879));
#150161=CARTESIAN_POINT('Ctrl Pts',(21.2762358738411,3.03924066841423,125.725413473446));
#150162=CARTESIAN_POINT('Ctrl Pts',(21.2688276541746,2.90212333401301,125.648237004164));
#150163=CARTESIAN_POINT('Ctrl Pts',(21.2614148748726,2.76492160618038,125.571013034053));
#150164=CARTESIAN_POINT('Ctrl Pts',(21.2540020955705,2.62475831680516,125.499338276822));
#150165=CARTESIAN_POINT('Ctrl Pts',(21.2465893162685,2.48212955780155,125.433423695502));
#150166=CARTESIAN_POINT('Ctrl Pts',(21.2391659452397,2.33929700413846,125.367414932337));
#150167=CARTESIAN_POINT('Ctrl Pts',(21.231742574211,2.193992288999,125.307182925623));
#150168=CARTESIAN_POINT('Ctrl Pts',(21.2243192031822,2.04672920309351,125.252889629467));
#150169=CARTESIAN_POINT('Ctrl Pts',(21.2203831537414,1.9686467814178,125.224102021095));
#150170=CARTESIAN_POINT('Ctrl Pts',(21.2164471043007,1.8900140177486,125.196983156011));
#150171=CARTESIAN_POINT('Ctrl Pts',(21.2125110548599,1.81090873953358,125.171551362888));
#150172=CARTESIAN_POINT('Ctrl Pts',(21.2050877884545,1.66171865361026,125.123587794758));
#150173=CARTESIAN_POINT('Ctrl Pts',(21.1976645220491,1.51039612068351,125.081482947169));
#150174=CARTESIAN_POINT('Ctrl Pts',(21.1902412556437,1.35744221163455,125.045430056726));
#150175=CARTESIAN_POINT('Ctrl Pts',(21.1828267629226,1.20466908140384,125.009419777806));
#150176=CARTESIAN_POINT('Ctrl Pts',(21.1754122702017,1.05026877283904,124.979447302931));
#150177=CARTESIAN_POINT('Ctrl Pts',(21.1679977774807,0.894759703731321,
124.955656860743));
#150178=CARTESIAN_POINT('Ctrl Pts',(21.1605904311269,0.739400520119218,
124.931889348678));
#150179=CARTESIAN_POINT('Ctrl Pts',(21.1531830847731,0.582935069993669,
124.914292063222));
#150180=CARTESIAN_POINT('Ctrl Pts',(21.1457757384193,0.425894111184199,
124.902958685096));
#150181=CARTESIAN_POINT('Ctrl Pts',(21.1383739167439,0.268970279446402,
124.891633759832));
#150182=CARTESIAN_POINT('Ctrl Pts',(21.1309720950685,0.111472164418757,
124.886563466352));
#150183=CARTESIAN_POINT('Ctrl Pts',(21.1235702733931,-0.0460622752016699,
124.887789919154));
#150184=CARTESIAN_POINT('Ctrl Pts',(21.1161723590817,-0.203513553617891,
124.889015724522));
#150185=CARTESIAN_POINT('Ctrl Pts',(21.1087744447703,-0.36100074609635,
124.896531653359));
#150186=CARTESIAN_POINT('Ctrl Pts',(21.101376530459,-0.51798390991503,124.910327768016));
#150187=CARTESIAN_POINT('Ctrl Pts',(21.0939798455468,-0.6749409859794,124.92412159001));
#150188=CARTESIAN_POINT('Ctrl Pts',(21.0865831606345,-0.831393828123101,
124.944193493831));
#150189=CARTESIAN_POINT('Ctrl Pts',(21.0791864757223,-0.986805517538934,
124.970481510741));
#150190=CARTESIAN_POINT('Ctrl Pts',(21.0717901187869,-1.1422103158376,124.996768362011));
#150191=CARTESIAN_POINT('Ctrl Pts',(21.0643937618515,-1.2965736851325,125.029270716067));
#150192=CARTESIAN_POINT('Ctrl Pts',(21.0569974049161,-1.4493670977951,125.067875144881));
#150193=CARTESIAN_POINT('Ctrl Pts',(21.0495999155795,-1.60218390351925,
125.106485484131));
#150194=CARTESIAN_POINT('Ctrl Pts',(21.0422024262429,-1.75342991206571,
125.151199666894));
#150195=CARTESIAN_POINT('Ctrl Pts',(21.0348049369063,-1.90259014451064,
125.201853919265));
#150196=CARTESIAN_POINT('Ctrl Pts',(21.0274048543914,-2.05180266484361,
125.252525928405));
#150197=CARTESIAN_POINT('Ctrl Pts',(21.0200047718764,-2.19892760007851,
125.309142032998));
#150198=CARTESIAN_POINT('Ctrl Pts',(21.0126046893614,-2.34346853359358,
125.371489756359));
#150199=CARTESIAN_POINT('Ctrl Pts',(21.005196469695,-2.48816840472444,125.433906037451));
#150200=CARTESIAN_POINT('Ctrl Pts',(20.9977882500285,-2.63027825674252,
125.50206637588));
#150201=CARTESIAN_POINT('Ctrl Pts',(20.990380030362,-2.76932427462137,125.57571130589));
#150202=CARTESIAN_POINT('Ctrl Pts',(20.98296725106,-2.90845587300412,125.649401563125));
#150203=CARTESIAN_POINT('Ctrl Pts',(20.9755544717579,-3.04451955778293,
125.72858295107));
#150204=CARTESIAN_POINT('Ctrl Pts',(20.9681416924559,-3.17706968998805,
125.812952124219));
#150205=CARTESIAN_POINT('Ctrl Pts',(20.9607183214271,-3.30980921603823,
125.897441847999));
#150206=CARTESIAN_POINT('Ctrl Pts',(20.9532949503983,-3.43902485694339,
125.987133949212));
#150207=CARTESIAN_POINT('Ctrl Pts',(20.9458715793696,-3.56430263969862,
126.081683701331));
#150208=CARTESIAN_POINT('Ctrl Pts',(20.9419355299287,-3.63072792611547,
126.131816248596));
#150209=CARTESIAN_POINT('Ctrl Pts',(20.9379994804879,-3.69604672483393,
126.183313810674));
#150210=CARTESIAN_POINT('Ctrl Pts',(20.9340634310471,-3.76020154778401,
126.236120816226));
#150211=CARTESIAN_POINT('Ctrl Pts',(20.9267412047266,-3.87954865971624,
126.334357602062));
#150212=CARTESIAN_POINT('Ctrl Pts',(20.9194189784062,-3.99524768171368,
126.437442896164));
#150213=CARTESIAN_POINT('Ctrl Pts',(20.9120967520858,-4.10687126251552,
126.545072062464));
#150214=CARTESIAN_POINT('Ctrl Pts',(20.9047832287334,-4.21836217103901,
126.65257330412));
#150215=CARTESIAN_POINT('Ctrl Pts',(20.8974697053809,-4.32578700190047,
126.764607409021));
#150216=CARTESIAN_POINT('Ctrl Pts',(20.8901561820285,-4.42874974390157,
126.880828246298));
#150217=CARTESIAN_POINT('Ctrl Pts',(20.8828496514327,-4.5316140390448,126.996937960113));
#150218=CARTESIAN_POINT('Ctrl Pts',(20.8755431208368,-4.63002448194077,
127.117226154788));
#150219=CARTESIAN_POINT('Ctrl Pts',(20.868236590241,-4.723620555289,127.24130863757));
#150220=CARTESIAN_POINT('Ctrl Pts',(20.8607423653231,-4.81962097791119,
127.368578621887));
#150221=CARTESIAN_POINT('Ctrl Pts',(20.8532481404052,-4.91055603775388,
127.499840194328));
#150222=CARTESIAN_POINT('Ctrl Pts',(20.8457539154873,-4.99607891110555,
127.634640428574));
#150223=CARTESIAN_POINT('Ctrl Pts',(20.8384559082725,-5.07936258000908,
127.765911252823));
#150224=CARTESIAN_POINT('Ctrl Pts',(20.8311579010577,-5.15751371329181,
127.900537404431));
#150225=CARTESIAN_POINT('Ctrl Pts',(20.823859893843,-5.23025478183218,128.038069692948));
#150226=CARTESIAN_POINT('Ctrl Pts',(20.816563307892,-5.3029816842792,128.175575197487));
#150227=CARTESIAN_POINT('Ctrl Pts',(20.809266721941,-5.37030043851679,128.315985373361));
#150228=CARTESIAN_POINT('Ctrl Pts',(20.8019701359901,-5.43197903761385,
128.458825647154));
#150229=CARTESIAN_POINT('Ctrl Pts',(20.7946734383954,-5.49365858044433,
128.601668106521));
#150230=CARTESIAN_POINT('Ctrl Pts',(20.7873767408008,-5.54969764470332,
128.746940384638));
#150231=CARTESIAN_POINT('Ctrl Pts',(20.7800800432061,-5.59991214306054,
128.894147395828));
#150232=CARTESIAN_POINT('Ctrl Pts',(20.7724379722899,-5.65250343555768,
129.048322130943));
#150233=CARTESIAN_POINT('Ctrl Pts',(20.7647959013736,-5.69870515924171,
129.204618785034));
#150234=CARTESIAN_POINT('Ctrl Pts',(20.7571538304574,-5.73836449839119,
129.362450965021));
#150235=CARTESIAN_POINT('Ctrl Pts',(20.7498489476912,-5.77627396380313,
129.513319176554));
#150236=CARTESIAN_POINT('Ctrl Pts',(20.742544064925,-5.80820598129173,129.665589919651));
#150237=CARTESIAN_POINT('Ctrl Pts',(20.7352391821588,-5.83407966707298,
129.818741522405));
#150238=CARTESIAN_POINT('Ctrl Pts',(20.7279303509646,-5.85996733807322,
129.971975906512));
#150239=CARTESIAN_POINT('Ctrl Pts',(20.7206215197703,-5.87979010731257,
130.126091718317));
#150240=CARTESIAN_POINT('Ctrl Pts',(20.7133126885761,-5.89351903032862,
130.280562945125));
#150241=CARTESIAN_POINT('Ctrl Pts',(20.7059954531342,-5.9072637399002,130.435211794649));
#150242=CARTESIAN_POINT('Ctrl Pts',(20.6986782176923,-5.91490060277359,
130.590216492637));
#150243=CARTESIAN_POINT('Ctrl Pts',(20.6913609822504,-5.91645273702643,
130.74505148646));
#150244=CARTESIAN_POINT('Ctrl Pts',(20.6903657189042,-5.91666385259631,
130.766111570599));
#150245=CARTESIAN_POINT('Ctrl Pts',(20.6893704555579,-5.9167624764504,130.787168523725));
#150246=CARTESIAN_POINT('Ctrl Pts',(20.6883751922117,-5.91674874062564,
130.808221032684));
#150247=CARTESIAN_POINT('',(18.9383751922117,-5.92064976466596,130.799473661469));
#150248=CARTESIAN_POINT('Ctrl Pts',(20.6883751922117,-5.92329750720146,
130.808225305463));
#150249=CARTESIAN_POINT('Ctrl Pts',(20.6774553972192,-5.92504451074842,
131.039465369392));
#150250=CARTESIAN_POINT('Ctrl Pts',(20.6665356022267,-5.91268190666388,
131.270516923428));
#150251=CARTESIAN_POINT('Ctrl Pts',(20.5627999326298,-5.65527249371549,
133.448917103978));
#150252=CARTESIAN_POINT('Ctrl Pts',(20.3771681834213,-3.06572938391748,
137.09553410706));
#150253=CARTESIAN_POINT('Ctrl Pts',(20.0987205596083,3.63584081539465,136.784178515751));
#150254=CARTESIAN_POINT('Ctrl Pts',(19.8202729357954,6.99625092605647,130.977662406353));
#150255=CARTESIAN_POINT('Ctrl Pts',(19.5418253119827,3.92744822153119,125.011890419323));
#150256=CARTESIAN_POINT('Ctrl Pts',(19.2633776881697,-2.75048753206931,
124.369115566576));
#150257=CARTESIAN_POINT('Ctrl Pts',(19.062227648246,-5.74870851970597,128.176804517244));
#150258=CARTESIAN_POINT('Ctrl Pts',(18.9538934829267,-5.92357746849997,
130.470471986277));
#150259=CARTESIAN_POINT('Ctrl Pts',(18.9383751922117,-5.92064976466596,
130.799473661469));
#150260=CARTESIAN_POINT('',(17.1883751922117,-5.90730668608647,130.802808790882));
#150261=CARTESIAN_POINT('Ctrl Pts',(18.9383751922117,-5.92064976466596,
130.799473661469));
#150262=CARTESIAN_POINT('Ctrl Pts',(18.8610776083224,-5.90606668738842,
132.438251736634));
#150263=CARTESIAN_POINT('Ctrl Pts',(18.6909641498289,-4.34635737984644,
136.069165665711));
#150264=CARTESIAN_POINT('Ctrl Pts',(18.428034816731,1.80946671150537,137.564788913929));
#150265=CARTESIAN_POINT('Ctrl Pts',(18.1495871929181,6.665800747261,132.936181653243));
#150266=CARTESIAN_POINT('Ctrl Pts',(17.8711395691052,5.39658953875396,126.348535006014));
#150267=CARTESIAN_POINT('Ctrl Pts',(17.5926919452923,-0.831823817814186,
123.855574416618));
#150268=CARTESIAN_POINT('Ctrl Pts',(17.3651038196611,-5.29781027684818,
127.037204659635));
#150269=CARTESIAN_POINT('Ctrl Pts',(17.2303315686343,-5.90939828044888,
129.908188672729));
#150270=CARTESIAN_POINT('Ctrl Pts',(17.1883751922117,-5.90730668608647,
130.802808790882));
#150271=CARTESIAN_POINT('',(15.4383751922118,-5.91493869631653,130.809783036639));
#150272=CARTESIAN_POINT('Ctrl Pts',(17.1883751922117,-5.90730668608647,
130.802808790882));
#150273=CARTESIAN_POINT('Ctrl Pts',(17.13751569403,-5.90477125646307,131.887266843558));
#150274=CARTESIAN_POINT('Ctrl Pts',(16.993840321244,-5.09858476319956,134.954310666059));
#150275=CARTESIAN_POINT('Ctrl Pts',(16.7573490738536,-0.162654485168709,
137.8008671779));
#150276=CARTESIAN_POINT('Ctrl Pts',(16.4789014500409,5.79844039827919,134.722989137587));
#150277=CARTESIAN_POINT('Ctrl Pts',(16.2004538262279,6.43105182527334,128.044082923024));
#150278=CARTESIAN_POINT('Ctrl Pts',(15.922006202415,1.1538407991874,123.901737062677));
#150279=CARTESIAN_POINT('Ctrl Pts',(15.6679799910763,-4.62785637852258,
125.90954012655));
#150280=CARTESIAN_POINT('Ctrl Pts',(15.5067696543419,-5.90195263961237,
129.356165732764));
#150281=CARTESIAN_POINT('Ctrl Pts',(15.4383751922118,-5.91493869631653,
130.809783036639));
#150282=CARTESIAN_POINT('',(13.6883751922117,-5.92204994786472,130.803560432901));
#150283=CARTESIAN_POINT('Ctrl Pts',(15.4383751922118,-5.91493869631653,
130.809783036639));
#150284=CARTESIAN_POINT('Ctrl Pts',(15.4139537797376,-5.9195755899671,131.328821956632));
#150285=CARTESIAN_POINT('Ctrl Pts',(15.2967164926591,-5.61893840176707,
133.815232264866));
#150286=CARTESIAN_POINT('Ctrl Pts',(15.0866633309763,-2.12167435304641,
137.473397914658));
#150287=CARTESIAN_POINT('Ctrl Pts',(14.8082157071634,4.46403314239369,136.194162899092));
#150288=CARTESIAN_POINT('Ctrl Pts',(14.5297680833506,6.94751226011757,129.961962893285));
#150289=CARTESIAN_POINT('Ctrl Pts',(14.2513204595376,3.04656701563547,124.503885242677));
#150290=CARTESIAN_POINT('Ctrl Pts',(13.9728728357247,-3.65402448314156,
124.835636666255));
#150291=CARTESIAN_POINT('Ctrl Pts',(13.7852244132827,-5.90671534475003,
128.755576012039));
#150292=CARTESIAN_POINT('Ctrl Pts',(13.6903918654451,-5.92648126663072,
130.760913461161));
#150293=CARTESIAN_POINT('Ctrl Pts',(13.6883751922117,-5.92640055191772,
130.803559845049));
#150294=CARTESIAN_POINT('',(11.9383752134708,-5.91415767949116,130.799325238322));
#150295=CARTESIAN_POINT('Ctrl Pts',(13.6883751922117,-5.91674994598809,
130.803561149034));
#150296=CARTESIAN_POINT('Ctrl Pts',(13.6809794773941,-5.91677104378405,
130.959702858383));
#150297=CARTESIAN_POINT('Ctrl Pts',(13.6735837625766,-5.91060705855891,
131.116089056026));
#150298=CARTESIAN_POINT('Ctrl Pts',(13.666188047759,-5.89822592375295,131.272186990132));
#150299=CARTESIAN_POINT('Ctrl Pts',(13.6588010451561,-5.88585937402858,
131.428101039551));
#150300=CARTESIAN_POINT('Ctrl Pts',(13.6514140425531,-5.86729028044803,
131.583727129818));
#150301=CARTESIAN_POINT('Ctrl Pts',(13.6440270399501,-5.84253853942223,
131.738530825754));
#150302=CARTESIAN_POINT('Ctrl Pts',(13.6366470966912,-5.81781045224694,
131.893186584481));
#150303=CARTESIAN_POINT('Ctrl Pts',(13.6292671534324,-5.7869115376568,132.047021144144));
#150304=CARTESIAN_POINT('Ctrl Pts',(13.6218872101735,-5.74991360270379,
132.199503665408));
#150305=CARTESIAN_POINT('Ctrl Pts',(13.6145126792117,-5.71294280126818,
132.351874359156));
#150306=CARTESIAN_POINT('Ctrl Pts',(13.60713814825,-5.66988197294389,132.502894624388));
#150307=CARTESIAN_POINT('Ctrl Pts',(13.5997636172883,-5.62085423726775,
132.652042464067));
#150308=CARTESIAN_POINT('Ctrl Pts',(13.592105866072,-5.56994358214264,132.806918354699));
#150309=CARTESIAN_POINT('Ctrl Pts',(13.5844481148558,-5.51259864495505,
132.959774724882));
#150310=CARTESIAN_POINT('Ctrl Pts',(13.5767903636396,-5.44901484055608,
133.110042258621));
#150311=CARTESIAN_POINT('Ctrl Pts',(13.5694206793814,-5.38782291238791,
133.254657073942));
#150312=CARTESIAN_POINT('Ctrl Pts',(13.5620509951233,-5.32085313439952,
133.39687391235));
#150313=CARTESIAN_POINT('Ctrl Pts',(13.5546813108651,-5.24832926401106,
133.536204408676));
#150314=CARTESIAN_POINT('Ctrl Pts',(13.5473117254542,-5.17580636636187,
133.675533036206));
#150315=CARTESIAN_POINT('Ctrl Pts',(13.5399421400432,-5.09772969793309,
133.811975064591));
#150316=CARTESIAN_POINT('Ctrl Pts',(13.5325725546323,-5.01436932318016,
133.945066088197));
#150317=CARTESIAN_POINT('Ctrl Pts',(13.5252015847893,-4.93099328855467,
134.078182113951));
#150318=CARTESIAN_POINT('Ctrl Pts',(13.5178306149464,-4.84233177149242,
134.207945562806));
#150319=CARTESIAN_POINT('Ctrl Pts',(13.5104596451035,-4.74869845760246,
134.333920578987));
#150320=CARTESIAN_POINT('Ctrl Pts',(13.5030858069555,-4.65502870767952,
134.4599446165));
#150321=CARTESIAN_POINT('Ctrl Pts',(13.4957119688076,-4.55638353394629,
134.5821769849));
#150322=CARTESIAN_POINT('Ctrl Pts',(13.4883381306597,-4.45311709156444,
134.700214661459));
#150323=CARTESIAN_POINT('Ctrl Pts',(13.480956116768,-4.34973615250395,134.818383212304));
#150324=CARTESIAN_POINT('Ctrl Pts',(13.4735741028763,-4.24172396280241,
134.93234750252));
#150325=CARTESIAN_POINT('Ctrl Pts',(13.4661920889845,-4.12947218201619,
135.041740711498));
#150326=CARTESIAN_POINT('Ctrl Pts',(13.4588052247392,-4.01714664617641,
135.151205797306));
#150327=CARTESIAN_POINT('Ctrl Pts',(13.4514183604939,-3.90057624880907,
135.256093567857));
#150328=CARTESIAN_POINT('Ctrl Pts',(13.4440314962486,-3.78018545722401,
135.356077708016));
#150329=CARTESIAN_POINT('Ctrl Pts',(13.4366345987805,-3.6596311446114,135.456197651828));
#150330=CARTESIAN_POINT('Ctrl Pts',(13.4292377013124,-3.53524637667355,
135.551400441991));
#150331=CARTESIAN_POINT('Ctrl Pts',(13.4218408038443,-3.4074847590033,135.641402914224));
#150332=CARTESIAN_POINT('Ctrl Pts',(13.4198863985959,-3.37372763620945,
135.665183330928));
#150333=CARTESIAN_POINT('Ctrl Pts',(13.4179319933474,-3.33973490196413,
135.688600951994));
#150334=CARTESIAN_POINT('Ctrl Pts',(13.415977588099,-3.3055151971596,135.71165109642));
#150335=CARTESIAN_POINT('Ctrl Pts',(13.4085543216936,-3.17554113713192,
135.799200678518));
#150336=CARTESIAN_POINT('Ctrl Pts',(13.4011310552881,-3.04188989318962,
135.881715356937));
#150337=CARTESIAN_POINT('Ctrl Pts',(13.3937077888826,-2.90498906015586,
135.958870208485));
#150338=CARTESIAN_POINT('Ctrl Pts',(13.3862932961616,-2.76825003253783,
136.035933869406));
#150339=CARTESIAN_POINT('Ctrl Pts',(13.3788788034407,-2.62826938288247,
136.107650131558));
#150340=CARTESIAN_POINT('Ctrl Pts',(13.3714643107197,-2.4855049939392,136.173736325002));
#150341=CARTESIAN_POINT('Ctrl Pts',(13.3640569643659,-2.34287820668858,
136.239758822085));
#150342=CARTESIAN_POINT('Ctrl Pts',(13.3566496180121,-2.19747335810855,
136.300161897735));
#150343=CARTESIAN_POINT('Ctrl Pts',(13.3492422716583,-2.04977423751675,
136.354708006488));
#150344=CARTESIAN_POINT('Ctrl Pts',(13.3418404499829,-1.90218527650209,
136.409213432695));
#150345=CARTESIAN_POINT('Ctrl Pts',(13.3344386283075,-1.75230579928924,
136.457870461206));
#150346=CARTESIAN_POINT('Ctrl Pts',(13.3270368066322,-1.60064084829797,
136.500489077956));
#150347=CARTESIAN_POINT('Ctrl Pts',(13.3196388923208,-1.44905596005355,
136.54308519667));
#150348=CARTESIAN_POINT('Ctrl Pts',(13.3122409780095,-1.2956878336085,136.57964915121));
#150349=CARTESIAN_POINT('Ctrl Pts',(13.3048430636982,-1.14105788839725,
136.610040376029));
#150350=CARTESIAN_POINT('Ctrl Pts',(13.297446378786,-0.98645363987762,136.640426550378));
#150351=CARTESIAN_POINT('Ctrl Pts',(13.2900496938737,-0.830588354698773,
136.664641958985));
#150352=CARTESIAN_POINT('Ctrl Pts',(13.2826530089615,-0.673995012943288,
136.682596856867));
#150353=CARTESIAN_POINT('Ctrl Pts',(13.275256652026,-0.517408614700673,
136.70055095861));
#150354=CARTESIAN_POINT('Ctrl Pts',(13.2678602950906,-0.360094594938191,
136.712245059062));
#150355=CARTESIAN_POINT('Ctrl Pts',(13.2604639381552,-0.202592179745797,
136.717641176715));
#150356=CARTESIAN_POINT('Ctrl Pts',(13.2530664488187,-0.045065650532001,
136.723038120526));
#150357=CARTESIAN_POINT('Ctrl Pts',(13.245668959482,0.112648958440613,136.722135148831));
#150358=CARTESIAN_POINT('Ctrl Pts',(13.2382714701455,0.270011438818095,
136.714946407943));
#150359=CARTESIAN_POINT('Ctrl Pts',(13.2308713876305,0.427429082370029,
136.707755147053));
#150360=CARTESIAN_POINT('Ctrl Pts',(13.2234713051155,0.584493978886043,
136.69427374691));
#150361=CARTESIAN_POINT('Ctrl Pts',(13.2160712226005,0.740670210498876,
136.674568297178));
#150362=CARTESIAN_POINT('Ctrl Pts',(13.2086630029341,0.897018173933227,
136.654841179279));
#150363=CARTESIAN_POINT('Ctrl Pts',(13.2012547832676,1.05247515038622,136.628876390669));
#150364=CARTESIAN_POINT('Ctrl Pts',(13.1938465636011,1.20651386896422,136.596791441192));
#150365=CARTESIAN_POINT('Ctrl Pts',(13.186433784299,1.36064739580324,136.564686743965));
#150366=CARTESIAN_POINT('Ctrl Pts',(13.179021004997,1.51336056409415,136.526454470385));
#150367=CARTESIAN_POINT('Ctrl Pts',(13.1716082256949,1.66414096905166,136.482262113508));
#150368=CARTESIAN_POINT('Ctrl Pts',(13.1641848546662,1.81513681612266,136.43800661252));
#150369=CARTESIAN_POINT('Ctrl Pts',(13.1567614836374,1.96419403146673,136.387774138677));
#150370=CARTESIAN_POINT('Ctrl Pts',(13.1493381126087,2.11081912341345,136.331780738267));
#150371=CARTESIAN_POINT('Ctrl Pts',(13.1454020631678,2.18856326538575,136.302091693826));
#150372=CARTESIAN_POINT('Ctrl Pts',(13.141466013727,2.26562403328145,136.270783828722));
#150373=CARTESIAN_POINT('Ctrl Pts',(13.1375299642861,2.34193075578605,136.237894541046));
#150374=CARTESIAN_POINT('Ctrl Pts',(13.1301066978807,2.48584285297614,136.175866370929));
#150375=CARTESIAN_POINT('Ctrl Pts',(13.1226834314752,2.62750655083135,136.108022993419));
#150376=CARTESIAN_POINT('Ctrl Pts',(13.1152601650698,2.76641735682101,136.034548527228));
#150377=CARTESIAN_POINT('Ctrl Pts',(13.1078456723488,2.90516398177401,135.961160901755));
#150378=CARTESIAN_POINT('Ctrl Pts',(13.1004311796278,3.04116386458929,135.882155608202));
#150379=CARTESIAN_POINT('Ctrl Pts',(13.0930166869068,3.17393169023008,135.797765086288));
#150380=CARTESIAN_POINT('Ctrl Pts',(13.085609340553,3.3065715492417,135.713455903136));
#150381=CARTESIAN_POINT('Ctrl Pts',(13.0782019941992,3.43598523985819,135.623772023763));
#150382=CARTESIAN_POINT('Ctrl Pts',(13.0707946478455,3.56171140840925,135.528992074697));
#150383=CARTESIAN_POINT('Ctrl Pts',(13.0633928261701,3.68734380564007,135.434282816092));
#150384=CARTESIAN_POINT('Ctrl Pts',(13.0559910044947,3.80929386020798,135.33448527953));
#150385=CARTESIAN_POINT('Ctrl Pts',(13.0485891828193,3.92712872013466,135.229921664258));
#150386=CARTESIAN_POINT('Ctrl Pts',(13.0411912685079,4.04490137595686,135.125413247303));
#150387=CARTESIAN_POINT('Ctrl Pts',(13.0337933541966,4.15856288502563,135.016144009467));
#150388=CARTESIAN_POINT('Ctrl Pts',(13.0263954398852,4.26771314562347,134.902476656574));
#150389=CARTESIAN_POINT('Ctrl Pts',(13.018998754973,4.37684526742787,134.788828193133));
#150390=CARTESIAN_POINT('Ctrl Pts',(13.0116020700607,4.48146737036548,134.670783334224));
#150391=CARTESIAN_POINT('Ctrl Pts',(13.0042053851485,4.58121586068676,134.548741981729));
#150392=CARTESIAN_POINT('Ctrl Pts',(12.9968090282131,4.68095992805517,134.426706040676));
#150393=CARTESIAN_POINT('Ctrl Pts',(12.9894126712777,4.77583057625002,134.300674247424));
#150394=CARTESIAN_POINT('Ctrl Pts',(12.9820163143422,4.86550438547872,134.171079738222));
#150395=CARTESIAN_POINT('Ctrl Pts',(12.9746188250056,4.95519192399667,134.041465387768));
#150396=CARTESIAN_POINT('Ctrl Pts',(12.9672213356691,5.03968082687911,133.908287542272));
#150397=CARTESIAN_POINT('Ctrl Pts',(12.9598238463325,5.11869100001087,133.772008340748));
#150398=CARTESIAN_POINT('Ctrl Pts',(12.9524237638176,5.19772887003601,133.635681366762));
#150399=CARTESIAN_POINT('Ctrl Pts',(12.9450236813026,5.27128399937201,133.496251194936));
#150400=CARTESIAN_POINT('Ctrl Pts',(12.9376235987876,5.33912231442844,133.354204431228));
#150401=CARTESIAN_POINT('Ctrl Pts',(12.9302153791212,5.40703522468662,133.2120014725));
#150402=CARTESIAN_POINT('Ctrl Pts',(12.9228071594547,5.46921860568836,133.067176512971));
#150403=CARTESIAN_POINT('Ctrl Pts',(12.9153989397882,5.52548631899722,132.920236677517));
#150404=CARTESIAN_POINT('Ctrl Pts',(12.9079861604861,5.5817886641449,132.773206403046));
#150405=CARTESIAN_POINT('Ctrl Pts',(12.900573381184,5.63216796727591,132.624059011756));
#150406=CARTESIAN_POINT('Ctrl Pts',(12.8931606018819,5.6764881777387,132.473316138391));
#150407=CARTESIAN_POINT('Ctrl Pts',(12.8857372308532,5.72087171499654,132.32235787654));
#150408=CARTESIAN_POINT('Ctrl Pts',(12.8783138598244,5.75917877791385,132.169799940643));
#150409=CARTESIAN_POINT('Ctrl Pts',(12.8708904887957,5.7913243880475,132.016174297513));
#150410=CARTESIAN_POINT('Ctrl Pts',(12.8669544393548,5.80836876186376,131.934718295328));
#150411=CARTESIAN_POINT('Ctrl Pts',(12.863018389914,5.82368179562796,131.852962222998));
#150412=CARTESIAN_POINT('Ctrl Pts',(12.8590823404732,5.837256753842,131.770985752883));
#150413=CARTESIAN_POINT('Ctrl Pts',(12.8516590740678,5.86285870137356,131.616380688644));
#150414=CARTESIAN_POINT('Ctrl Pts',(12.8442358076623,5.88235283546909,131.460524004804));
#150415=CARTESIAN_POINT('Ctrl Pts',(12.8368125412569,5.89562136988027,131.303939665877));
#150416=CARTESIAN_POINT('Ctrl Pts',(12.8293980485359,5.90887422198572,131.147540396634));
#150417=CARTESIAN_POINT('Ctrl Pts',(12.8219835558149,5.91591608961713,130.990415552528));
#150418=CARTESIAN_POINT('Ctrl Pts',(12.8145690630939,5.91668020626019,130.833099082188));
#150419=CARTESIAN_POINT('Ctrl Pts',(12.8071617167401,5.91744358641887,130.675934239386));
#150420=CARTESIAN_POINT('Ctrl Pts',(12.7997543703864,5.91194125960596,130.518578508832));
#150421=CARTESIAN_POINT('Ctrl Pts',(12.7923470240326,5.9001582692831,130.361570644881));
#150422=CARTESIAN_POINT('Ctrl Pts',(12.7849452023572,5.88838406715895,130.204679883318));
#150423=CARTESIAN_POINT('Ctrl Pts',(12.7775433806818,5.8703385565255,130.048136842402));
#150424=CARTESIAN_POINT('Ctrl Pts',(12.7701415590064,5.84605884566799,129.892479849325));
#150425=CARTESIAN_POINT('Ctrl Pts',(12.762743644695,5.82179195188082,129.736905026364));
#150426=CARTESIAN_POINT('Ctrl Pts',(12.7553457303837,5.79129746941189,129.582215687623));
#150427=CARTESIAN_POINT('Ctrl Pts',(12.7479478160723,5.75466428819294,129.428944501368));
#150428=CARTESIAN_POINT('Ctrl Pts',(12.7405511311601,5.71803719474423,129.275698786004));
#150429=CARTESIAN_POINT('Ctrl Pts',(12.7331544462478,5.67527351391464,129.123871118105));
#150430=CARTESIAN_POINT('Ctrl Pts',(12.7257577613356,5.62651316318096,128.973983556124));
#150431=CARTESIAN_POINT('Ctrl Pts',(12.7183614044002,5.57775497453233,128.824102640316));
#150432=CARTESIAN_POINT('Ctrl Pts',(12.7109650474648,5.52300076015743,128.676162014362));
#150433=CARTESIAN_POINT('Ctrl Pts',(12.7035686905293,5.46244011355051,128.530667901218));
#150434=CARTESIAN_POINT('Ctrl Pts',(12.6961712011927,5.40187019495374,128.385151512553));
#150435=CARTESIAN_POINT('Ctrl Pts',(12.6887737118561,5.33549221750866,128.242082727166));
#150436=CARTESIAN_POINT('Ctrl Pts',(12.6813762225195,5.26354359414734,128.101946993598));
#150437=CARTESIAN_POINT('Ctrl Pts',(12.6739761400045,5.19156974930774,127.961762135665));
#150438=CARTESIAN_POINT('Ctrl Pts',(12.6665760574895,5.11402154097226,127.824512708521));
#150439=CARTESIAN_POINT('Ctrl Pts',(12.6591759749745,5.03118184202175,127.690658667313));
#150440=CARTESIAN_POINT('Ctrl Pts',(12.651767755308,4.94825105230635,127.556657439826));
#150441=CARTESIAN_POINT('Ctrl Pts',(12.6443595356415,4.86001734854309,127.426059372093));
#150442=CARTESIAN_POINT('Ctrl Pts',(12.6369513159751,4.76680677688238,127.299295181034));
#150443=CARTESIAN_POINT('Ctrl Pts',(12.629538536673,4.67353883567012,127.172452968731));
#150444=CARTESIAN_POINT('Ctrl Pts',(12.622125757371,4.57528815522929,127.049449626072));
#150445=CARTESIAN_POINT('Ctrl Pts',(12.6147129780689,4.47242006294447,126.930681572643));
#150446=CARTESIAN_POINT('Ctrl Pts',(12.6072896070402,4.3694049879052,126.811743817851));
#150447=CARTESIAN_POINT('Ctrl Pts',(12.5998662360114,4.26175957897851,126.697053710119));
#150448=CARTESIAN_POINT('Ctrl Pts',(12.5924428649826,4.14988546198636,126.586970285276));
#150449=CARTESIAN_POINT('Ctrl Pts',(12.5885068155419,4.0905671207747,126.528601412009));
#150450=CARTESIAN_POINT('Ctrl Pts',(12.5845707661011,4.03006049046271,126.471526968918));
#150451=CARTESIAN_POINT('Ctrl Pts',(12.5806347166603,3.96842896096237,126.415795687626));
#150452=CARTESIAN_POINT('Ctrl Pts',(12.5732114502549,3.85219381977877,126.310688230424));
#150453=CARTESIAN_POINT('Ctrl Pts',(12.5657881838495,3.73160423322244,126.21004291868));
#150454=CARTESIAN_POINT('Ctrl Pts',(12.5583649174441,3.60703736113541,126.11424206492));
#150455=CARTESIAN_POINT('Ctrl Pts',(12.5509504247231,3.48261771674637,126.018554439814));
#150456=CARTESIAN_POINT('Ctrl Pts',(12.543535932002,3.35423043685518,125.927700100912));
#150457=CARTESIAN_POINT('Ctrl Pts',(12.536121439281,3.22228865863494,125.842023833053));
#150458=CARTESIAN_POINT('Ctrl Pts',(12.5287140929273,3.09047405086807,125.756430143206));
#150459=CARTESIAN_POINT('Ctrl Pts',(12.5213067465734,2.95511207616322,125.676004790596));
#150460=CARTESIAN_POINT('Ctrl Pts',(12.5138994002197,2.81664791944207,125.60105156847));
#150461=CARTESIAN_POINT('Ctrl Pts',(12.5064975785442,2.67828703451217,125.526154249285));
#150462=CARTESIAN_POINT('Ctrl Pts',(12.4990957568688,2.53682890137621,125.456721111065));
#150463=CARTESIAN_POINT('Ctrl Pts',(12.4916939351934,2.39274648788165,125.393011912554));
#150464=CARTESIAN_POINT('Ctrl Pts',(12.484296020882,2.24874013437307,125.329336345635));
#150465=CARTESIAN_POINT('Ctrl Pts',(12.4768981065708,2.10211260001836,125.271378851299));
#150466=CARTESIAN_POINT('Ctrl Pts',(12.4695001922595,1.95336008089372,125.219352564137));
#150467=CARTESIAN_POINT('Ctrl Pts',(12.4621035073473,1.80463228173848,125.167334922799));
#150468=CARTESIAN_POINT('Ctrl Pts',(12.4547068224351,1.65378055070234,125.121246655515));
#150469=CARTESIAN_POINT('Ctrl Pts',(12.4473101375229,1.50131973916258,125.081252231094));
#150470=CARTESIAN_POINT('Ctrl Pts',(12.4399137805874,1.34886568789498,125.041259580069));
#150471=CARTESIAN_POINT('Ctrl Pts',(12.432517423652,1.1948030590687,125.007360329364));
#150472=CARTESIAN_POINT('Ctrl Pts',(12.4251210667166,1.0396602323058,124.979668594475));
#150473=CARTESIAN_POINT('Ctrl Pts',(12.41772357738,0.884493652779841,124.951972619911));
#150474=CARTESIAN_POINT('Ctrl Pts',(12.4103260880433,0.728246913534963,
124.930486119106));
#150475=CARTESIAN_POINT('Ctrl Pts',(12.4029285987067,0.571456763664193,
124.915271746632));
#150476=CARTESIAN_POINT('Ctrl Pts',(12.3955285161917,0.414611651249442,
124.900052040782));
#150477=CARTESIAN_POINT('Ctrl Pts',(12.3881284336768,0.257223120262054,
124.891108876859));
#150478=CARTESIAN_POINT('Ctrl Pts',(12.3807283511618,0.0998310436957964,
124.888452882889));
#150479=CARTESIAN_POINT('Ctrl Pts',(12.3733201314954,-0.057734101638944,
124.88579396838));
#150480=CARTESIAN_POINT('Ctrl Pts',(12.3659119118288,-0.215302426864783,
124.889436036619));
#150481=CARTESIAN_POINT('Ctrl Pts',(12.3585036921623,-0.37233532172839,
124.899337588763));
#150482=CARTESIAN_POINT('Ctrl Pts',(12.3510909128603,-0.529464867718775,
124.909245235147));
#150483=CARTESIAN_POINT('Ctrl Pts',(12.3436781335582,-0.686057956218949,
124.925420003975));
#150484=CARTESIAN_POINT('Ctrl Pts',(12.3362653542561,-0.84158359982742,
124.947768809441));
#150485=CARTESIAN_POINT('Ctrl Pts',(12.3288419832274,-0.997331465768686,
124.970149547928));
#150486=CARTESIAN_POINT('Ctrl Pts',(12.3214186121986,-1.15200847450612,
124.998721874444));
#150487=CARTESIAN_POINT('Ctrl Pts',(12.3139952411698,-1.30509547046255,
125.033341957444));
#150488=CARTESIAN_POINT('Ctrl Pts',(12.310059191729,-1.38626586899091,125.051698356148));
#150489=CARTESIAN_POINT('Ctrl Pts',(12.3061231422882,-1.46698952603585,
125.071754167255));
#150490=CARTESIAN_POINT('Ctrl Pts',(12.3021870928474,-1.54719117850762,
125.093482399669));
#150491=CARTESIAN_POINT('Ctrl Pts',(12.294763826442,-1.69844899206153,125.134461167887));
#150492=CARTESIAN_POINT('Ctrl Pts',(12.2873405600365,-1.8483063603538,125.181515352935));
#150493=CARTESIAN_POINT('Ctrl Pts',(12.2799172936311,-1.99623776892161,
125.234534288817));
#150494=CARTESIAN_POINT('Ctrl Pts',(12.2725028009101,-2.14399433484879,
125.287490560718));
#150495=CARTESIAN_POINT('Ctrl Pts',(12.2650883081892,-2.28982912410956,
125.34639742599));
#150496=CARTESIAN_POINT('Ctrl Pts',(12.2576738154682,-2.43322874872264,
125.411093665255));
#150497=CARTESIAN_POINT('Ctrl Pts',(12.2502664691144,-2.57649015937863,
125.475727547848));
#150498=CARTESIAN_POINT('Ctrl Pts',(12.2428591227606,-2.7173207400215,125.546139543234));
#150499=CARTESIAN_POINT('Ctrl Pts',(12.2354517764069,-2.85522426746406,
125.622119312398));
#150500=CARTESIAN_POINT('Ctrl Pts',(12.2280499547315,-2.99302494125285,
125.698042412985));
#150501=CARTESIAN_POINT('Ctrl Pts',(12.2206481330561,-3.1279025831521,125.779524839487));
#150502=CARTESIAN_POINT('Ctrl Pts',(12.2132463113807,-3.25938300009817,
125.866309076607));
#150503=CARTESIAN_POINT('Ctrl Pts',(12.2058483970694,-3.39079400955632,
125.953047501004));
#150504=CARTESIAN_POINT('Ctrl Pts',(12.198450482758,-3.51881105487927,126.045081956985));
#150505=CARTESIAN_POINT('Ctrl Pts',(12.1910525684467,-3.6429866137998,126.142110185192));
#150506=CARTESIAN_POINT('Ctrl Pts',(12.1836558835344,-3.7671415369954,126.239122289067));
#150507=CARTESIAN_POINT('Ctrl Pts',(12.1762591986222,-3.8874559469332,126.341126288495));
#150508=CARTESIAN_POINT('Ctrl Pts',(12.1688625137099,-4.00351318159925,
126.447777923841));
#150509=CARTESIAN_POINT('Ctrl Pts',(12.1614661567745,-4.11956527016589,
126.554424830142));
#150510=CARTESIAN_POINT('Ctrl Pts',(12.154069799839,-4.23136028393053,126.665718710013));
#150511=CARTESIAN_POINT('Ctrl Pts',(12.1466734429035,-4.33851661220324,
126.781276704927));
#150512=CARTESIAN_POINT('Ctrl Pts',(12.1392759535669,-4.44568934638351,
126.896852392065));
#150513=CARTESIAN_POINT('Ctrl Pts',(12.1318784642303,-4.54822172714036,
127.016693220408));
#150514=CARTESIAN_POINT('Ctrl Pts',(12.1244809748937,-4.64577091541466,
127.140381474068));
#150515=CARTESIAN_POINT('Ctrl Pts',(12.1170808923787,-4.74335429940568,
127.264113086454));
#150516=CARTESIAN_POINT('Ctrl Pts',(12.1096808098637,-4.8359507819253,127.3916945165));
#150517=CARTESIAN_POINT('Ctrl Pts',(12.1022807273486,-4.92325960677384,
127.522677298474));
#150518=CARTESIAN_POINT('Ctrl Pts',(12.0948725076822,-5.01066443665062,
127.653804109481));
#150519=CARTESIAN_POINT('Ctrl Pts',(12.0874642880157,-5.09276979009712,
127.788339430907));
#150520=CARTESIAN_POINT('Ctrl Pts',(12.0800560683492,-5.16931944926736,
127.925807683551));
#150521=CARTESIAN_POINT('Ctrl Pts',(12.0726432890471,-5.2459162234752,128.063360545611));
#150522=CARTESIAN_POINT('Ctrl Pts',(12.0652305097451,-5.31695032170018,
128.203849603554));
#150523=CARTESIAN_POINT('Ctrl Pts',(12.057817730443,-5.38221304800567,128.346777807491));
#150524=CARTESIAN_POINT('Ctrl Pts',(12.0503943594142,-5.44756902475539,
128.489910233949));
#150525=CARTESIAN_POINT('Ctrl Pts',(12.0429709883855,-5.50713701866604,
128.63548842248));
#150526=CARTESIAN_POINT('Ctrl Pts',(12.0355476173567,-5.5607574230185,128.782997848332));
#150527=CARTESIAN_POINT('Ctrl Pts',(12.0316115679159,-5.58918824800988,
128.861210885358));
#150528=CARTESIAN_POINT('Ctrl Pts',(12.0276755184751,-5.61594783453282,
128.939966640036));
#150529=CARTESIAN_POINT('Ctrl Pts',(12.0237394690344,-5.64101820942251,
129.01918720205));
#150530=CARTESIAN_POINT('Ctrl Pts',(12.0147583710996,-5.69822264639261,
129.199949064065));
#150531=CARTESIAN_POINT('Ctrl Pts',(12.0057772731648,-5.74676996117718,
129.38357397859));
#150532=CARTESIAN_POINT('Ctrl Pts',(11.99679617523,-5.78641323558252,129.569309027722));
#150533=CARTESIAN_POINT('Ctrl Pts',(11.9878683594006,-5.8258213185738,129.753942167653));
#150534=CARTESIAN_POINT('Ctrl Pts',(11.9789405435712,-5.85643063877623,
129.940660477226));
#150535=CARTESIAN_POINT('Ctrl Pts',(11.9700127277418,-5.87804537080221,
130.128703025815));
#150536=CARTESIAN_POINT('Ctrl Pts',(11.9611813895651,-5.8994265251368,130.314713509222));
#150537=CARTESIAN_POINT('Ctrl Pts',(11.9523500513883,-5.9120063782527,130.502019741965));
#150538=CARTESIAN_POINT('Ctrl Pts',(11.9435187132116,-5.91564207791684,
130.689864467064));
#150539=CARTESIAN_POINT('Ctrl Pts',(11.9418042244861,-5.91634790142387,
130.726332061996));
#150540=CARTESIAN_POINT('Ctrl Pts',(11.9400897357606,-5.91671677188543,
130.762819889619));
#150541=CARTESIAN_POINT('Ctrl Pts',(11.9383752470351,-5.9167478548645,130.799322318615));
#150542=CARTESIAN_POINT('',(10.1883751630607,-5.91241648564898,130.807217379792));
#150543=CARTESIAN_POINT('Ctrl Pts',(11.9383751922117,-5.91251709691396,
130.799327087625));
#150544=CARTESIAN_POINT('Ctrl Pts',(11.8740140765483,-5.90151912380169,
132.168641977221));
#150545=CARTESIAN_POINT('Ctrl Pts',(11.7168370862809,-4.74574414496558,
135.529409927722));
#150546=CARTESIAN_POINT('Ctrl Pts',(11.4668442214086,0.852969679778676,
137.750582846644));
#150547=CARTESIAN_POINT('Ctrl Pts',(11.188396597596,6.3051044354217,133.841335854337));
#150548=CARTESIAN_POINT('Ctrl Pts',(10.9099489737828,5.96315623638791,127.141256983926));
#150549=CARTESIAN_POINT('Ctrl Pts',(10.6315013499702,0.14135877248956,123.807391400271));
#150550=CARTESIAN_POINT('Ctrl Pts',(10.390976756113,-4.99975189704023,126.481739594297));
#150551=CARTESIAN_POINT('Ctrl Pts',(10.2432680368602,-5.90318810762329,
129.637230627951));
#150552=CARTESIAN_POINT('Ctrl Pts',(10.1883751922117,-5.90826796113811,
130.807214753531));
#150553=CARTESIAN_POINT('',(8.43837519221174,-5.91996550474033,130.808373808165));
#150554=CARTESIAN_POINT('Ctrl Pts',(10.1883751326147,-5.91674930901506,
130.807220122726));
#150555=CARTESIAN_POINT('Ctrl Pts',(10.1802557825323,-5.91666555315848,
130.980523676609));
#150556=CARTESIAN_POINT('Ctrl Pts',(10.17213643245,-5.90896352231583,131.153570801375));
#150557=CARTESIAN_POINT('Ctrl Pts',(10.1640170823676,-5.89373526771853,
131.325719569298));
#150558=CARTESIAN_POINT('Ctrl Pts',(10.1558579373264,-5.87843237564924,
131.498712081246));
#150559=CARTESIAN_POINT('Ctrl Pts',(10.1476987922851,-5.8555293843832,131.670797173441));
#150560=CARTESIAN_POINT('Ctrl Pts',(10.1395396472439,-5.82517011905515,
131.841338749721));
#150561=CARTESIAN_POINT('Ctrl Pts',(10.1313603771817,-5.79473597077675,
132.012300977036));
#150562=CARTESIAN_POINT('Ctrl Pts',(10.1231811071196,-5.75680883326587,
132.181711843681));
#150563=CARTESIAN_POINT('Ctrl Pts',(10.1150018370573,-5.71158264529618,
132.348949316363));
#150564=CARTESIAN_POINT('Ctrl Pts',(10.1067934972637,-5.66619572010589,
132.516781163406));
#150565=CARTESIAN_POINT('Ctrl Pts',(10.0985851574701,-5.61345788464016,
132.68242392312));
#150566=CARTESIAN_POINT('Ctrl Pts',(10.0903768176765,-5.55361278413328,
132.84527110223));
#150567=CARTESIAN_POINT('Ctrl Pts',(10.0851199125658,-5.51528590895333,
132.949564076162));
#150568=CARTESIAN_POINT('Ctrl Pts',(10.079863007455,-5.47404489903722,133.052710882648));
#150569=CARTESIAN_POINT('Ctrl Pts',(10.0746061023443,-5.42996361159411,
133.154557575113));
#150570=CARTESIAN_POINT('Ctrl Pts',(10.0671828359389,-5.36771650359163,
133.298375109339));
#150571=CARTESIAN_POINT('Ctrl Pts',(10.0597595695335,-5.29965761661069,
133.439935397079));
#150572=CARTESIAN_POINT('Ctrl Pts',(10.052336303128,-5.2259718369024,133.578734226582));
#150573=CARTESIAN_POINT('Ctrl Pts',(10.044921810407,-5.1523731476664,133.717369007395));
#150574=CARTESIAN_POINT('Ctrl Pts',(10.037507317686,-5.07316097693031,133.853248500117));
#150575=CARTESIAN_POINT('Ctrl Pts',(10.030092824965,-4.98856850270957,133.985887744006));
#150576=CARTESIAN_POINT('Ctrl Pts',(10.0226854786113,-4.90405756190033,
134.118399145198));
#150577=CARTESIAN_POINT('Ctrl Pts',(10.0152781322575,-4.81417684077245,
134.247676202358));
#150578=CARTESIAN_POINT('Ctrl Pts',(10.0078707859037,-4.71920566763366,
134.373257986373));
#150579=CARTESIAN_POINT('Ctrl Pts',(10.0004689642283,-4.62430532757886,
134.498746106754));
#150580=CARTESIAN_POINT('Ctrl Pts',(9.9930671425529,-4.52432231935671,134.620544145244));
#150581=CARTESIAN_POINT('Ctrl Pts',(9.9856653208775,-4.41957950056913,134.738219740698));
#150582=CARTESIAN_POINT('Ctrl Pts',(9.97826740656617,-4.31489197470057,
134.855833216121));
#150583=CARTESIAN_POINT('Ctrl Pts',(9.97086949225485,-4.20544988992888,
134.969328304391));
#150584=CARTESIAN_POINT('Ctrl Pts',(9.96347157794352,-4.09161656054591,
135.078305456233));
#150585=CARTESIAN_POINT('Ctrl Pts',(9.95607489303133,-3.97780214819697,
135.187264498049));
#150586=CARTESIAN_POINT('Ctrl Pts',(9.94867820811911,-3.85959820895147,
135.291706835655));
#150587=CARTESIAN_POINT('Ctrl Pts',(9.94128152320692,-3.73740519755676,
135.391269484306));
#150588=CARTESIAN_POINT('Ctrl Pts',(9.93388516627149,-3.61521760432805,
135.490827718244));
#150589=CARTESIAN_POINT('Ctrl Pts',(9.92648880933602,-3.48904158004227,
135.585506457646));
#150590=CARTESIAN_POINT('Ctrl Pts',(9.91909245240058,-3.35931075263528,
135.674982942252));
#150591=CARTESIAN_POINT('Ctrl Pts',(9.91169496306401,-3.22956006310742,
135.764473125936));
#150592=CARTESIAN_POINT('Ctrl Pts',(9.90429747372752,-3.09625379410099,
135.848759256972));
#150593=CARTESIAN_POINT('Ctrl Pts',(9.89689998439096,-2.95985451035286,
135.927561944866));
#150594=CARTESIAN_POINT('Ctrl Pts',(9.88949990187597,-2.82340741204725,
136.006392256919));
#150595=CARTESIAN_POINT('Ctrl Pts',(9.88209981936093,-2.68386546329304,
136.079735112094));
#150596=CARTESIAN_POINT('Ctrl Pts',(9.87469973684594,-2.54171562570514,
136.147357177601));
#150597=CARTESIAN_POINT('Ctrl Pts',(9.86729151717948,-2.39940947975746,
136.215053600521));
#150598=CARTESIAN_POINT('Ctrl Pts',(9.85988329751304,-2.25449005541267,
136.277016510581));
#150599=CARTESIAN_POINT('Ctrl Pts',(9.85247507784658,-2.1074647602321,136.333060541317));
#150600=CARTESIAN_POINT('Ctrl Pts',(9.84506229854452,-1.9603489734356,136.389139066218));
#150601=CARTESIAN_POINT('Ctrl Pts',(9.8376495192424,-1.81112508613271,136.439291334071));
#150602=CARTESIAN_POINT('Ctrl Pts',(9.83023673994035,-1.66031493951092,
136.483382088219));
#150603=CARTESIAN_POINT('Ctrl Pts',(9.8228133689116,-1.50928930827934,136.527535841304));
#150604=CARTESIAN_POINT('Ctrl Pts',(9.8153899978829,-1.35667325221345,136.565610692654));
#150605=CARTESIAN_POINT('Ctrl Pts',(9.80796662685415,-1.20299886683335,
136.597522473487));
#150606=CARTESIAN_POINT('Ctrl Pts',(9.80403057741325,-1.12151702033605,
136.614442865398));
#150607=CARTESIAN_POINT('Ctrl Pts',(9.80009452797233,-1.03973773884549,
136.629631462605));
#150608=CARTESIAN_POINT('Ctrl Pts',(9.79615847853142,-0.957740704880099,
136.643081650867));
#150609=CARTESIAN_POINT('Ctrl Pts',(9.78873521212603,-0.803096857865298,
136.668448286163));
#150610=CARTESIAN_POINT('Ctrl Pts',(9.78131194572057,-0.647210687750097,
136.687705210344));
#150611=CARTESIAN_POINT('Ctrl Pts',(9.77388867931512,-0.490606337693888,
136.700735434682));
#150612=CARTESIAN_POINT('Ctrl Pts',(9.76647418659409,-0.334187080974039,
136.713750258377));
#150613=CARTESIAN_POINT('Ctrl Pts',(9.75905969387298,-0.177051702291723,
136.720553000588));
#150614=CARTESIAN_POINT('Ctrl Pts',(9.75164520115194,-0.0197342512662653,
136.721077707459));
#150615=CARTESIAN_POINT('Ctrl Pts',(9.74423785479816,0.137431571276773,
136.721601908597));
#150616=CARTESIAN_POINT('Ctrl Pts',(9.73683050844441,0.294778746010715,
136.71586011952));
#150617=CARTESIAN_POINT('Ctrl Pts',(9.72942316209063,0.451768496444515,
136.7038382036));
#150618=CARTESIAN_POINT('Ctrl Pts',(9.72202134041521,0.608641157999782,
136.691825254079));
#150619=CARTESIAN_POINT('Ctrl Pts',(9.71461951873975,0.7651565554465,136.673541532482));
#150620=CARTESIAN_POINT('Ctrl Pts',(9.70721769706432,0.920776418688503,
136.649024966294));
#150621=CARTESIAN_POINT('Ctrl Pts',(9.69981978275297,1.0763141314156,136.62452134221));
#150622=CARTESIAN_POINT('Ctrl Pts',(9.69242186844165,1.2309568836169,136.593791484212));
#150623=CARTESIAN_POINT('Ctrl Pts',(9.68502395413029,1.38417214292008,136.55692509276));
#150624=CARTESIAN_POINT('Ctrl Pts',(9.67762726921806,1.53736194062699,136.520064827833));
#150625=CARTESIAN_POINT('Ctrl Pts',(9.67023058430588,1.68912435367026,136.477070140658));
#150626=CARTESIAN_POINT('Ctrl Pts',(9.66283389939366,1.83893753713031,136.428081743034));
#150627=CARTESIAN_POINT('Ctrl Pts',(9.6554375424582,1.98874407771681,136.379095517607));
#150628=CARTESIAN_POINT('Ctrl Pts',(9.64804118552274,2.13660120576398,136.324116226187));
#150629=CARTESIAN_POINT('Ctrl Pts',(9.64064482858728,2.28200298743408,136.263334232436));
#150630=CARTESIAN_POINT('Ctrl Pts',(9.6332473392507,2.42742703048815,136.202542932805));
#150631=CARTESIAN_POINT('Ctrl Pts',(9.62584984991406,2.57039463422069,136.135947305888));
#150632=CARTESIAN_POINT('Ctrl Pts',(9.61845236057746,2.71042071195736,136.063785503111));
#150633=CARTESIAN_POINT('Ctrl Pts',(9.61105227806245,2.85049587561852,135.991598404126));
#150634=CARTESIAN_POINT('Ctrl Pts',(9.60365219554746,2.98762712865781,135.913841415326));
#150635=CARTESIAN_POINT('Ctrl Pts',(9.59625211303245,3.12135494694482,135.830798109238));
#150636=CARTESIAN_POINT('Ctrl Pts',(9.58884389336597,3.2552298127156,135.747663488497));
#150637=CARTESIAN_POINT('Ctrl Pts',(9.58143567369948,3.38569345254174,135.65923113888));
#150638=CARTESIAN_POINT('Ctrl Pts',(9.574027454033,3.51231564618689,135.565827761635));
#150639=CARTESIAN_POINT('Ctrl Pts',(9.56661467473092,3.6390157736796,135.472366896171));
#150640=CARTESIAN_POINT('Ctrl Pts',(9.5592018954289,3.76186945309335,135.373929139353));
#150641=CARTESIAN_POINT('Ctrl Pts',(9.55178911612683,3.88048082126535,135.270880421428));
#150642=CARTESIAN_POINT('Ctrl Pts',(9.54436574509806,3.9992616669225,135.167684462662));
#150643=CARTESIAN_POINT('Ctrl Pts',(9.53694237406926,4.11378782385723,135.059864639566));
#150644=CARTESIAN_POINT('Ctrl Pts',(9.52951900304049,4.22370086786386,134.947823123889));
#150645=CARTESIAN_POINT('Ctrl Pts',(9.52558295359982,4.28197940112157,134.88841602388));
#150646=CARTESIAN_POINT('Ctrl Pts',(9.52164690415912,4.33896169732797,134.827822606048));
#150647=CARTESIAN_POINT('Ctrl Pts',(9.51771085471844,4.39459912138594,134.766106334395));
#150648=CARTESIAN_POINT('Ctrl Pts',(9.510287588313,4.49952956677796,134.649711372152));
#150649=CARTESIAN_POINT('Ctrl Pts',(9.50286432190755,4.59999124515387,134.528968760205));
#150650=CARTESIAN_POINT('Ctrl Pts',(9.49544105550211,4.69560241840369,134.404256239772));
#150651=CARTESIAN_POINT('Ctrl Pts',(9.4880265627811,4.79110058718675,134.279691119183));
#150652=CARTESIAN_POINT('Ctrl Pts',(9.48061207006012,4.88175943729564,134.151165723124));
#150653=CARTESIAN_POINT('Ctrl Pts',(9.47319757733911,4.96723481301753,134.019093712995));
#150654=CARTESIAN_POINT('Ctrl Pts',(9.46579023098533,5.05262780435421,133.887148998842));
#150655=CARTESIAN_POINT('Ctrl Pts',(9.45838288463151,5.13284706595016,133.751664787188));
#150656=CARTESIAN_POINT('Ctrl Pts',(9.45097553827773,5.2075894824056,133.613086724761));
#150657=CARTESIAN_POINT('Ctrl Pts',(9.44357371660233,5.28227615314697,133.474612019081));
#150658=CARTESIAN_POINT('Ctrl Pts',(9.43617189492692,5.35149393576633,133.333048384335));
#150659=CARTESIAN_POINT('Ctrl Pts',(9.42877007325151,5.4149837915957,133.188869183132));
#150660=CARTESIAN_POINT('Ctrl Pts',(9.42137215894014,5.47844013162446,133.044766093006));
#150661=CARTESIAN_POINT('Ctrl Pts',(9.41397424462879,5.53617441670041,132.898050527002));
#150662=CARTESIAN_POINT('Ctrl Pts',(9.40657633031742,5.58797426760525,132.749219004977));
#150663=CARTESIAN_POINT('Ctrl Pts',(9.39917964540521,5.63976551031455,132.60041221605));
#150664=CARTESIAN_POINT('Ctrl Pts',(9.39178296049298,5.68562415357426,132.449490521201));
#150665=CARTESIAN_POINT('Ctrl Pts',(9.38438627558077,5.72538651228013,132.296969021502));
#150666=CARTESIAN_POINT('Ctrl Pts',(9.37698991864532,5.76514710788134,132.144454284767));
#150667=CARTESIAN_POINT('Ctrl Pts',(9.3695935617099,5.79881186223639,131.990340245453));
#150668=CARTESIAN_POINT('Ctrl Pts',(9.36219720477445,5.82626746408627,131.835155456237));
#150669=CARTESIAN_POINT('Ctrl Pts',(9.35479971543785,5.85372726945892,131.679946907832));
#150670=CARTESIAN_POINT('Ctrl Pts',(9.34740222610125,5.87497596444269,131.523667650722));
#150671=CARTESIAN_POINT('Ctrl Pts',(9.34000473676466,5.88995171138167,131.366854528726));
#150672=CARTESIAN_POINT('Ctrl Pts',(9.33260465424964,5.90493270804553,131.209986436134));
#150673=CARTESIAN_POINT('Ctrl Pts',(9.32520457173462,5.9136363430605,131.052584477426));
#150674=CARTESIAN_POINT('Ctrl Pts',(9.31780448921961,5.91605281000753,130.895188541147));
#150675=CARTESIAN_POINT('Ctrl Pts',(9.31039626955313,5.9184719341084,130.737619531854));
#150676=CARTESIAN_POINT('Ctrl Pts',(9.30298804988662,5.91459007791834,130.580056931698));
#150677=CARTESIAN_POINT('Ctrl Pts',(9.29557983022013,5.90444955990576,130.423039287152));
#150678=CARTESIAN_POINT('Ctrl Pts',(9.28816705091806,5.89430280057356,130.265925000866));
#150679=CARTESIAN_POINT('Ctrl Pts',(9.28075427161598,5.87788974245218,130.109356708943));
#150680=CARTESIAN_POINT('Ctrl Pts',(9.2733414923139,5.85530427931114,129.953865256508));
#150681=CARTESIAN_POINT('Ctrl Pts',(9.26591812128514,5.83268654500121,129.798151630594));
#150682=CARTESIAN_POINT('Ctrl Pts',(9.25849475025642,5.80387885949493,129.643518283187));
#150683=CARTESIAN_POINT('Ctrl Pts',(9.25107137922765,5.76902584423608,129.490484150376));
#150684=CARTESIAN_POINT('Ctrl Pts',(9.24713532978698,5.75054593925979,129.409341781158));
#150685=CARTESIAN_POINT('Ctrl Pts',(9.24319928034628,5.73036730371311,129.328648739123));
#150686=CARTESIAN_POINT('Ctrl Pts',(9.23926323090561,5.7085170431985,129.248480246197));
#150687=CARTESIAN_POINT('Ctrl Pts',(9.23183996450018,5.66730813379008,129.097284970507));
#150688=CARTESIAN_POINT('Ctrl Pts',(9.22441669809475,5.62002594582548,128.947499384207));
#150689=CARTESIAN_POINT('Ctrl Pts',(9.21699343168933,5.56678194491824,128.799648832737));
#150690=CARTESIAN_POINT('Ctrl Pts',(9.20957893896833,5.51360087399835,128.65197302834));
#150691=CARTESIAN_POINT('Ctrl Pts',(9.20216444624736,5.45447214121539,128.506228054175));
#150692=CARTESIAN_POINT('Ctrl Pts',(9.19474995352635,5.38955774705014,128.362927052279));
#150693=CARTESIAN_POINT('Ctrl Pts',(9.18734260717259,5.32470591982197,128.219764169283));
#150694=CARTESIAN_POINT('Ctrl Pts',(9.17993526081881,5.25407968580243,128.07904090679));
#150695=CARTESIAN_POINT('Ctrl Pts',(9.17252791446504,5.17789013892738,127.941253167312));
#150696=CARTESIAN_POINT('Ctrl Pts',(9.16512609278965,5.10175741709096,127.803568195129));
#150697=CARTESIAN_POINT('Ctrl Pts',(9.15772427111429,5.02006982413318,127.668814711798));
#150698=CARTESIAN_POINT('Ctrl Pts',(9.1503224494389,4.93308559669535,127.537466517939));
#150699=CARTESIAN_POINT('Ctrl Pts',(9.14292453512756,4.84614728755411,127.40618766177));
#150700=CARTESIAN_POINT('Ctrl Pts',(9.13552662081615,4.75391811799677,127.278310825464));
#150701=CARTESIAN_POINT('Ctrl Pts',(9.12812870650481,4.65670102808541,127.154283070783));
#150702=CARTESIAN_POINT('Ctrl Pts',(9.12073202159262,4.55950009389069,127.030275927265));
#150703=CARTESIAN_POINT('Ctrl Pts',(9.11333533668043,4.45731311453102,126.910116889373));
#150704=CARTESIAN_POINT('Ctrl Pts',(9.10593865176824,4.35048498333183,126.794222094734));
#150705=CARTESIAN_POINT('Ctrl Pts',(9.09854229483281,4.24366158900391,126.678332438991));
#150706=CARTESIAN_POINT('Ctrl Pts',(9.09114593789743,4.13219770502983,126.566706925023));
#150707=CARTESIAN_POINT('Ctrl Pts',(9.08374958096201,4.01647677024077,126.459726580433));
#150708=CARTESIAN_POINT('Ctrl Pts',(9.07635209162545,3.90073811828117,126.352729856879));
#150709=CARTESIAN_POINT('Ctrl Pts',(9.06895460228889,3.78074139188313,126.250379972193));
#150710=CARTESIAN_POINT('Ctrl Pts',(9.06155711295233,3.65690482819401,126.153019129347));
#150711=CARTESIAN_POINT('Ctrl Pts',(9.05415703043734,3.53302485378928,126.055624156807));
#150712=CARTESIAN_POINT('Ctrl Pts',(9.04675694792233,3.40530265539782,125.963221938731));
#150713=CARTESIAN_POINT('Ctrl Pts',(9.03935686540734,3.27418715593197,125.876112548482));
#150714=CARTESIAN_POINT('Ctrl Pts',(9.03194864574089,3.14292748149564,125.788907372503));
#150715=CARTESIAN_POINT('Ctrl Pts',(9.02454042607443,3.00826736548948,125.707006853991));
#150716=CARTESIAN_POINT('Ctrl Pts',(9.01713220640798,2.87068277648156,125.630666486743));
#150717=CARTESIAN_POINT('Ctrl Pts',(9.00971942710593,2.73301350645463,125.554279133273));
#150718=CARTESIAN_POINT('Ctrl Pts',(9.00230664780383,2.59241650938984,125.483458917735));
#150719=CARTESIAN_POINT('Ctrl Pts',(8.99489386850178,2.4493891522018,125.418413779398));
#150720=CARTESIAN_POINT('Ctrl Pts',(8.98747049747303,2.30615743081849,125.353275701517));
#150721=CARTESIAN_POINT('Ctrl Pts',(8.9800471264443,2.16048875851841,125.293929321806));
#150722=CARTESIAN_POINT('Ctrl Pts',(8.97262375541555,2.01289790235313,125.24053346378));
#150723=CARTESIAN_POINT('Ctrl Pts',(8.96868770597461,1.93464168901706,125.212221698638));
#150724=CARTESIAN_POINT('Ctrl Pts',(8.96475165653366,1.85584530199803,125.185581995953));
#150725=CARTESIAN_POINT('Ctrl Pts',(8.96081560709271,1.77658667887363,125.160632210303));
#150726=CARTESIAN_POINT('Ctrl Pts',(8.95339234068728,1.62710738924394,125.113577693225));
#150727=CARTESIAN_POINT('Ctrl Pts',(8.94596907428184,1.47553135581495,125.072394768949));
#150728=CARTESIAN_POINT('Ctrl Pts',(8.93854580787641,1.32236081647028,125.037273620341));
#150729=CARTESIAN_POINT('Ctrl Pts',(8.93113131515539,1.16937131198288,125.002193982013));
#150730=CARTESIAN_POINT('Ctrl Pts',(8.92371682243439,1.0147914131362,124.973161940961));
#150731=CARTESIAN_POINT('Ctrl Pts',(8.91630232971337,0.859140406076983,
124.950318567397));
#150732=CARTESIAN_POINT('Ctrl Pts',(8.9088949833596,0.703639421318752,124.927497211137));
#150733=CARTESIAN_POINT('Ctrl Pts',(8.90148763700586,0.547069750464317,
124.910852701322));
#150734=CARTESIAN_POINT('Ctrl Pts',(8.89408029065208,0.389962711770638,
124.900475486068));
#150735=CARTESIAN_POINT('Ctrl Pts',(8.88667846897668,0.232972849433727,
124.890106010532));
#150736=CARTESIAN_POINT('Ctrl Pts',(8.87927664730127,0.075446788166063,
124.885994546723));
#150737=CARTESIAN_POINT('Ctrl Pts',(8.87187482562587,-0.082077266939525,
124.888179933649));
#150738=CARTESIAN_POINT('Ctrl Pts',(8.86447691131451,-0.239518166322587,
124.890364166927));
#150739=CARTESIAN_POINT('Ctrl Pts',(8.85707899700321,-0.396956689335564,
124.898838625752));
#150740=CARTESIAN_POINT('Ctrl Pts',(8.84968108269186,-0.553852963753639,
124.913590085875));
#150741=CARTESIAN_POINT('Ctrl Pts',(8.84228439777964,-0.710723164857518,
124.928339094572));
#150742=CARTESIAN_POINT('Ctrl Pts',(8.83488771286733,-0.867050924916991,
124.949362999365));
#150743=CARTESIAN_POINT('Ctrl Pts',(8.82749102795512,-1.02229971229404,
124.976596564282));
#150744=CARTESIAN_POINT('Ctrl Pts',(8.82009467101968,-1.17754161577694,
125.003828921635));
#150745=CARTESIAN_POINT('Ctrl Pts',(8.81269831408429,-1.33170427402173,
125.03727032714));
#150746=CARTESIAN_POINT('Ctrl Pts',(8.80530195714886,-1.48425985966084,
125.076804137574));
#150747=CARTESIAN_POINT('Ctrl Pts',(8.79790446781229,-1.63683880194958,
125.116344000735));
#150748=CARTESIAN_POINT('Ctrl Pts',(8.79050697847572,-1.78780982033592,
125.161978032431));
#150749=CARTESIAN_POINT('Ctrl Pts',(8.78310948913915,-1.93665894237565,
125.213539326967));
#150750=CARTESIAN_POINT('Ctrl Pts',(8.77570940662415,-2.08556024324458,
125.265118696235));
#150751=CARTESIAN_POINT('Ctrl Pts',(8.76830932410908,-2.23233781429737,
125.322629343103));
#150752=CARTESIAN_POINT('Ctrl Pts',(8.76090924159408,-2.37649654151563,
125.385855772993));
#150753=CARTESIAN_POINT('Ctrl Pts',(8.7535010219276,-2.52081378607435,125.449151726842));
#150754=CARTESIAN_POINT('Ctrl Pts',(8.74609280226119,-2.66250609379996,
125.518175865424));
#150755=CARTESIAN_POINT('Ctrl Pts',(8.73868458259471,-2.80110123788644,
125.59266584354));
#150756=CARTESIAN_POINT('Ctrl Pts',(8.73127180329265,-2.93978168497152,
125.667201668995));
#150757=CARTESIAN_POINT('Ctrl Pts',(8.72385902399058,-3.07536084922278,
125.747209848161));
#150758=CARTESIAN_POINT('Ctrl Pts',(8.71644624468851,-3.20739494647732,
125.832384328422));
#150759=CARTESIAN_POINT('Ctrl Pts',(8.70902287365976,-3.3396177002418,125.917680509974));
#150760=CARTESIAN_POINT('Ctrl Pts',(8.70159950263096,-3.46828496580264,
126.008157521682));
#150761=CARTESIAN_POINT('Ctrl Pts',(8.69417613160221,-3.59298487627311,
126.103468123435));
#150762=CARTESIAN_POINT('Ctrl Pts',(8.69024008216141,-3.65910376093801,
126.154004091432));
#150763=CARTESIAN_POINT('Ctrl Pts',(8.68630403272065,-3.7241078691726,126.205898313446));
#150764=CARTESIAN_POINT('Ctrl Pts',(8.68236798327985,-3.78794005225051,
126.259094869223));
#150765=CARTESIAN_POINT('Ctrl Pts',(8.67504798366789,-3.90665084650963,
126.35802624026));
#150766=CARTESIAN_POINT('Ctrl Pts',(8.66772798405598,-4.02168689880861,
126.461781356428));
#150767=CARTESIAN_POINT('Ctrl Pts',(8.66040798444402,-4.13262285489824,
126.570053247798));
#150768=CARTESIAN_POINT('Ctrl Pts',(8.65309668814274,-4.24342691069527,
126.678196406387));
#150769=CARTESIAN_POINT('Ctrl Pts',(8.6457853918414,-4.35014029680781,126.790845389904));
#150770=CARTESIAN_POINT('Ctrl Pts',(8.63847409554012,-4.45236924206574,
126.90765191729));
#150771=CARTESIAN_POINT('Ctrl Pts',(8.63116979082812,-4.55450042862692,
127.024346745843));
#150772=CARTESIAN_POINT('Ctrl Pts',(8.62386548611617,-4.65215545616205,
127.145190919551));
#150773=CARTESIAN_POINT('Ctrl Pts',(8.61656118140417,-4.74497627253956,
127.269798305831));
#150774=CARTESIAN_POINT('Ctrl Pts',(8.60913676518781,-4.83932342829229,
127.396454727743));
#150775=CARTESIAN_POINT('Ctrl Pts',(8.60171234897144,-4.92867568711041,
127.526998947513));
#150776=CARTESIAN_POINT('Ctrl Pts',(8.59428793275509,-5.0126981313822,127.66098854189));
#150777=CARTESIAN_POINT('Ctrl Pts',(8.58699214256618,-5.0952649092545,127.792656802341));
#150778=CARTESIAN_POINT('Ctrl Pts',(8.57969635237722,-5.17268483853595,
127.927651684691));
#150779=CARTESIAN_POINT('Ctrl Pts',(8.57240056218831,-5.24468283714531,
128.065522816554));
#150780=CARTESIAN_POINT('Ctrl Pts',(8.56510620557832,-5.31666668858055,
128.203366857568));
#150781=CARTESIAN_POINT('Ctrl Pts',(8.55781184896839,-5.38323055104187,
128.344085682939));
#150782=CARTESIAN_POINT('Ctrl Pts',(8.55051749235841,-5.44414499442681,
128.487203773035));
#150783=CARTESIAN_POINT('Ctrl Pts',(8.54322303516512,-5.50506027777294,
128.630323836614));
#150784=CARTESIAN_POINT('Ctrl Pts',(8.53592857797181,-5.56032583716038,
128.775842876562));
#150785=CARTESIAN_POINT('Ctrl Pts',(8.52863412077852,-5.60976026776962,
128.923265112108));
#150786=CARTESIAN_POINT('Ctrl Pts',(8.52111254339796,-5.6607338885941,129.075277485736));
#150787=CARTESIAN_POINT('Ctrl Pts',(8.51359096601739,-5.70550721491024,
129.229313086705));
#150788=CARTESIAN_POINT('Ctrl Pts',(8.50606938863683,-5.74393698777221,
129.384811941753));
#150789=CARTESIAN_POINT('Ctrl Pts',(8.4987669129632,-5.7812473107628,129.535781153238));
#150790=CARTESIAN_POINT('Ctrl Pts',(8.49146443728962,-5.81257846859075,
129.688129167305));
#150791=CARTESIAN_POINT('Ctrl Pts',(8.484161961616,-5.83785156299875,129.841334298667));
#150792=CARTESIAN_POINT('Ctrl Pts',(8.47653083338196,-5.86426208908855,
130.001434524369));
#150793=CARTESIAN_POINT('Ctrl Pts',(8.46889970514792,-5.88405653739746,
130.162470332057));
#150794=CARTESIAN_POINT('Ctrl Pts',(8.46126857691388,-5.89720552610408,
130.323842620622));
#150795=CARTESIAN_POINT('Ctrl Pts',(8.45363744867984,-5.91035451481071,
130.485214909186));
#150796=CARTESIAN_POINT('Ctrl Pts',(8.44600632044577,-5.91685808759334,
130.646923203604));
#150797=CARTESIAN_POINT('Ctrl Pts',(8.43837519221174,-5.91674864045279,
130.808371627427));
#150798=CARTESIAN_POINT('',(6.68837519221171,-5.92099708260688,130.799573344013));
#150799=CARTESIAN_POINT('Ctrl Pts',(8.43837519221174,-5.92299826574412,
130.808375864097));
#150800=CARTESIAN_POINT('Ctrl Pts',(8.42689024796347,-5.92488935017588,
131.051615824253));
#150801=CARTESIAN_POINT('Ctrl Pts',(8.32258942911039,-5.80065370683978,
133.258658416759));
#150802=CARTESIAN_POINT('Ctrl Pts',(8.12547273565442,-3.02737642437282,
137.114079511095));
#150803=CARTESIAN_POINT('Ctrl Pts',(7.84702511184098,3.67217430050631,136.761935328562));
#150804=CARTESIAN_POINT('Ctrl Pts',(7.56857748802829,6.99717623890907,130.935071030307));
#150805=CARTESIAN_POINT('Ctrl Pts',(7.29012986421539,3.8921150448166,124.988090248315));
#150806=CARTESIAN_POINT('Ctrl Pts',(7.01168224040252,-2.78960973507063,
124.38597779505));
#150807=CARTESIAN_POINT('Ctrl Pts',(6.81109734973462,-5.75623819392495,
128.201098093543));
#150808=CARTESIAN_POINT('Ctrl Pts',(6.70332833367101,-5.92378219031308,
130.482601527499));
#150809=CARTESIAN_POINT('Ctrl Pts',(6.68837519221171,-5.92099708260688,
130.799573344013));
#150810=CARTESIAN_POINT('',(4.93837519221179,-5.90740647963781,130.802618111737));
#150811=CARTESIAN_POINT('Ctrl Pts',(6.68837519221171,-5.92099708260688,
130.799573344013));
#150812=CARTESIAN_POINT('Ctrl Pts',(6.6105124590667,-5.9064947053841,132.450082170598));
#150813=CARTESIAN_POINT('Ctrl Pts',(6.4398338513174,-4.32747935093831,136.092391492262));
#150814=CARTESIAN_POINT('Ctrl Pts',(6.17633936896388,1.85058583215606,137.553648921391));
#150815=CARTESIAN_POINT('Ctrl Pts',(5.89789174515079,6.67865424514227,132.895565534405));
#150816=CARTESIAN_POINT('Ctrl Pts',(5.61944412133808,5.36936567723543,126.315766989886));
#150817=CARTESIAN_POINT('Ctrl Pts',(5.34099649752515,-0.874107639948943,
123.860766709212));
#150818=CARTESIAN_POINT('Ctrl Pts',(5.1139735211497,-5.30960218217041,127.061555711575));
#150819=CARTESIAN_POINT('Ctrl Pts',(4.97976641937861,-5.90972563308018,
129.920085651997));
#150820=CARTESIAN_POINT('Ctrl Pts',(4.93837519221179,-5.90740647963781,
130.802618111737));
#150821=CARTESIAN_POINT('',(3.18837519221176,-5.9145855427205,130.809751264182));
#150822=CARTESIAN_POINT('Ctrl Pts',(4.93837519221179,-5.90740647963781,
130.802618111737));
#150823=CARTESIAN_POINT('Ctrl Pts',(4.88695054477432,-5.90452515293428,
131.899080422732));
#150824=CARTESIAN_POINT('Ctrl Pts',(4.74271002273249,-5.08506508489207,
134.97853974863));
#150825=CARTESIAN_POINT('Ctrl Pts',(4.50565362608645,-0.120061750281574,
137.801727672856));
#150826=CARTESIAN_POINT('Ctrl Pts',(4.22720600227359,5.82218677065032,134.68761978198));
#150827=CARTESIAN_POINT('Ctrl Pts',(3.9487583784607,6.41413007899093,128.004986426763));
#150828=CARTESIAN_POINT('Ctrl Pts',(3.67031075464771,1.1118011924118,123.894841195861));
#150829=CARTESIAN_POINT('Ctrl Pts',(3.41684969256491,-4.6447312943842,125.933256779022));
#150830=CARTESIAN_POINT('Ctrl Pts',(3.25620450508613,-5.90184342734158,
129.367926591703));
#150831=CARTESIAN_POINT('Ctrl Pts',(3.18837519221176,-5.9145855427205,130.809751264182));
#150832=CARTESIAN_POINT('',(1.43837519221172,-5.9220814725113,130.803783456464));
#150833=CARTESIAN_POINT('Ctrl Pts',(3.18837519221176,-5.9145855427205,130.809751264182));
#150834=CARTESIAN_POINT('Ctrl Pts',(3.16338863048184,-5.91927940793884,
131.340882122744));
#150835=CARTESIAN_POINT('Ctrl Pts',(3.04558619414775,-5.6099754134907,133.839595697384));
#150836=CARTESIAN_POINT('Ctrl Pts',(2.83496788320905,-2.0810387204088,137.486189586833));
#150837=CARTESIAN_POINT('Ctrl Pts',(2.55652025939625,4.49675969049486,136.166889201757));
#150838=CARTESIAN_POINT('Ctrl Pts',(2.27807263558332,6.94225562475717,129.9196870219));
#150839=CARTESIAN_POINT('Ctrl Pts',(1.99962501177045,3.00815778790935,124.485456657748));
#150840=CARTESIAN_POINT('Ctrl Pts',(1.72117738795757,-3.69029009934919,
124.857990337051));
#150841=CARTESIAN_POINT('Ctrl Pts',(1.53409411477124,-5.91236490058832,
128.779722884542));
#150842=CARTESIAN_POINT('Ctrl Pts',(1.43982671618935,-5.9265061143831,130.773088677422));
#150843=CARTESIAN_POINT('Ctrl Pts',(1.43837519221171,-5.92646357529495,
130.803783029388));
#150844=CARTESIAN_POINT('',(-0.311624788304493,-5.91431933878038,130.799248754294));
#150845=CARTESIAN_POINT('Ctrl Pts',(1.43837519221174,-5.9167499719005,130.803783976068));
#150846=CARTESIAN_POINT('Ctrl Pts',(1.43097212084849,-5.91676520388193,
130.960074888071));
#150847=CARTESIAN_POINT('Ctrl Pts',(1.42356904948527,-5.91058352531488,
131.116608525822));
#150848=CARTESIAN_POINT('Ctrl Pts',(1.41616597812202,-5.89817319978246,
131.272851244866));
#150849=CARTESIAN_POINT('Ctrl Pts',(1.40877164548738,-5.88577752363829,
131.428909531983));
#150850=CARTESIAN_POINT('Ctrl Pts',(1.40137731285276,-5.86716786357436,
131.584677213211));
#150851=CARTESIAN_POINT('Ctrl Pts',(1.39398298021811,-5.84236444631937,
131.73961899838));
#150852=CARTESIAN_POINT('Ctrl Pts',(1.38659573990202,-5.817584819411,131.894412170206));
#150853=CARTESIAN_POINT('Ctrl Pts',(1.37920849958587,-5.78662332010163,
132.04838065453));
#150854=CARTESIAN_POINT('Ctrl Pts',(1.37182125926978,-5.74955208297358,
132.200992783769));
#150855=CARTESIAN_POINT('Ctrl Pts',(1.36443947063227,-5.71250820389276,
132.353492287422));
#150856=CARTESIAN_POINT('Ctrl Pts',(1.35705768199478,-5.66936365231962,
132.50463706549));
#150857=CARTESIAN_POINT('Ctrl Pts',(1.34967589335727,-5.62024187187363,
132.653904308355));
#150858=CARTESIAN_POINT('Ctrl Pts',(1.34195115364788,-5.56883793894613,
132.810106369251));
#150859=CARTESIAN_POINT('Ctrl Pts',(1.33422641393849,-5.51088814896009,
132.964251841321));
#150860=CARTESIAN_POINT('Ctrl Pts',(1.32650167422909,-5.44659310119009,
133.115757198114));
#150861=CARTESIAN_POINT('Ctrl Pts',(1.31912484760139,-5.38519382584074,
133.260438933974));
#150862=CARTESIAN_POINT('Ctrl Pts',(1.31174802097365,-5.31800851899369,
133.40271278799));
#150863=CARTESIAN_POINT('Ctrl Pts',(1.30437119434595,-5.24526164482172,
133.542089756809));
#150864=CARTESIAN_POINT('Ctrl Pts',(1.2969945080438,-5.17251615447596,133.681464074332));
#150865=CARTESIAN_POINT('Ctrl Pts',(1.28961782174171,-5.09420948069823,
133.817941283128));
#150866=CARTESIAN_POINT('Ctrl Pts',(1.28224113543956,-5.01061238377904,
133.951056361044));
#150867=CARTESIAN_POINT('Ctrl Pts',(1.27486311199148,-4.92700013350854,
134.084195568261));
#150868=CARTESIAN_POINT('Ctrl Pts',(1.26748508854335,-4.83809575072785,
134.213971113281));
#150869=CARTESIAN_POINT('Ctrl Pts',(1.26010706509527,-4.74421361042342,
134.339946535228));
#150870=CARTESIAN_POINT('Ctrl Pts',(1.25272622647908,-4.65029564832886,
134.46597002452));
#150871=CARTESIAN_POINT('Ctrl Pts',(1.24534538786292,-4.55139637189808,
134.588190203319));
#150872=CARTESIAN_POINT('Ctrl Pts',(1.23796454924673,-4.44787062566144,
134.706203446266));
#150873=CARTESIAN_POINT('Ctrl Pts',(1.23057553704002,-4.34423023431447,
134.824347377875));
#150874=CARTESIAN_POINT('Ctrl Pts',(1.22318652483326,-4.2359533912951,134.93827478933));
#150875=CARTESIAN_POINT('Ctrl Pts',(1.21579751262655,-4.12343246340871,
135.047618243755));
#150876=CARTESIAN_POINT('Ctrl Pts',(1.20840370882591,-4.01083856844906,
135.157032604738));
#150877=CARTESIAN_POINT('Ctrl Pts',(1.20100990502526,-3.89399538428133,
135.261856836618));
#150878=CARTESIAN_POINT('Ctrl Pts',(1.19361610122462,-3.7733281051864,135.361763998123));
#150879=CARTESIAN_POINT('Ctrl Pts',(1.18621214497658,-3.65249513759912,
135.46180834236));
#150880=CARTESIAN_POINT('Ctrl Pts',(1.17880818872853,-3.52782788922118,
135.556921910029));
#150881=CARTESIAN_POINT('Ctrl Pts',(1.17140423248048,-3.3997807577748,135.646820876728));
#150882=CARTESIAN_POINT('Ctrl Pts',(1.16903020176424,-3.35872327269568,
135.675646399348));
#150883=CARTESIAN_POINT('Ctrl Pts',(1.16665617104802,-3.31731848458099,
135.703936150045));
#150884=CARTESIAN_POINT('Ctrl Pts',(1.16428214033178,-3.27558188361879,
135.731681784915));
#150885=CARTESIAN_POINT('Ctrl Pts',(1.15685887392635,-3.14507729255366,
135.818438555928));
#150886=CARTESIAN_POINT('Ctrl Pts',(1.14943560752094,-3.01092623459139,
135.900138132485));
#150887=CARTESIAN_POINT('Ctrl Pts',(1.1420123411155,-2.87355827453246,135.976458200304));
#150888=CARTESIAN_POINT('Ctrl Pts',(1.13459784839449,-2.73635267199463,
136.052688064141));
#150889=CARTESIAN_POINT('Ctrl Pts',(1.12718335567345,-2.59593805861329,
136.123550895612));
#150890=CARTESIAN_POINT('Ctrl Pts',(1.11976886295244,-2.45277402934651,
136.188766817275));
#150891=CARTESIAN_POINT('Ctrl Pts',(1.11236151659866,-2.30974798696096,
136.253919881377));
#150892=CARTESIAN_POINT('Ctrl Pts',(1.10495417024496,-2.16397814173031,
136.313436717314));
#150893=CARTESIAN_POINT('Ctrl Pts',(1.09754682389118,-2.01594972001534,
136.367082728985));
#150894=CARTESIAN_POINT('Ctrl Pts',(1.09014500221579,-1.8680317034825,136.420688729436));
#150895=CARTESIAN_POINT('Ctrl Pts',(1.08274318054034,-1.71785881404619,
136.468432497526));
#150896=CARTESIAN_POINT('Ctrl Pts',(1.07534135886496,-1.56593724143843,
136.510127097048));
#150897=CARTESIAN_POINT('Ctrl Pts',(1.06794344455362,-1.4140958670463,136.551799686314));
#150898=CARTESIAN_POINT('Ctrl Pts',(1.06054553024226,-1.26050800698827,
136.587429368093));
#150899=CARTESIAN_POINT('Ctrl Pts',(1.05314761593092,-1.10569592670047,
136.616878753467));
#150900=CARTESIAN_POINT('Ctrl Pts',(1.04575093101872,-0.95090957337161,
136.646323244888));
#150901=CARTESIAN_POINT('Ctrl Pts',(1.0383542461065,-0.794899769950169,
136.669589408608));
#150902=CARTESIAN_POINT('Ctrl Pts',(1.0309575611943,-0.638200032947009,
136.68659074571));
#150903=CARTESIAN_POINT('Ctrl Pts',(1.02356120425885,-0.481507244174174,
136.703591328955));
#150904=CARTESIAN_POINT('Ctrl Pts',(1.01616484732343,-0.324124953767255,
136.714327597653));
#150905=CARTESIAN_POINT('Ctrl Pts',(1.00876849038798,-0.166592609029845,
136.718764853422));
#150906=CARTESIAN_POINT('Ctrl Pts',(1.00137100105141,-0.00903614568851985,
136.723202788547));
#150907=CARTESIAN_POINT('Ctrl Pts',(0.993973511714845,0.148670044553117,
136.721339779992));
#150908=CARTESIAN_POINT('Ctrl Pts',(0.986576022378273,0.305985849462564,
136.713193262212));
#150909=CARTESIAN_POINT('Ctrl Pts',(0.979175939863302,0.463356801183101,
136.705043888682));
#150910=CARTESIAN_POINT('Ctrl Pts',(0.971775857348313,0.620336722540329,
136.690606639713));
#150911=CARTESIAN_POINT('Ctrl Pts',(0.964375774833343,0.776390107902843,
136.669950866028));
#150912=CARTESIAN_POINT('Ctrl Pts',(0.95696755516688,0.932615090005686,
136.649272379196));
#150913=CARTESIAN_POINT('Ctrl Pts',(0.949559335500442,1.087911131163,136.622361760914));
#150914=CARTESIAN_POINT('Ctrl Pts',(0.94215111583398,1.24175168556608,136.589339728496));
#150915=CARTESIAN_POINT('Ctrl Pts',(0.934738336531926,1.39568692626342,
136.556297371568));
#150916=CARTESIAN_POINT('Ctrl Pts',(0.927325557229862,1.54816453443217,
136.517136197943));
#150917=CARTESIAN_POINT('Ctrl Pts',(0.919912777927806,1.69867313435842,
136.472026816727));
#150918=CARTESIAN_POINT('Ctrl Pts',(0.912489406899048,1.84939678803061,
136.426852981111));
#150919=CARTESIAN_POINT('Ctrl Pts',(0.905066035870255,1.99814546236399,
136.375714084383));
#150920=CARTESIAN_POINT('Ctrl Pts',(0.897642664841499,2.14442698996647,
136.318829172849));
#150921=CARTESIAN_POINT('Ctrl Pts',(0.893706615400625,2.22198896588004,
136.288667427818));
#150922=CARTESIAN_POINT('Ctrl Pts',(0.889770565959759,2.29885772615748,
136.256891052009));
#150923=CARTESIAN_POINT('Ctrl Pts',(0.885834516518884,2.37496282844648,
136.223537873017));
#150924=CARTESIAN_POINT('Ctrl Pts',(0.87841125011346,2.51849467620134,136.160634818356));
#150925=CARTESIAN_POINT('Ctrl Pts',(0.870987983708066,2.659742767461,136.091930350689));
#150926=CARTESIAN_POINT('Ctrl Pts',(0.863564717302637,2.79820373982473,
136.017611656307));
#150927=CARTESIAN_POINT('Ctrl Pts',(0.856150224581625,2.93650106281779,
135.943380800449));
#150928=CARTESIAN_POINT('Ctrl Pts',(0.848735731860612,3.07201749822384,
135.863549100793));
#150929=CARTESIAN_POINT('Ctrl Pts',(0.841321239139603,3.20426915492438,
135.778351947002));
#150930=CARTESIAN_POINT('Ctrl Pts',(0.833913892785829,3.33639334249901,
135.693236909434));
#150931=CARTESIAN_POINT('Ctrl Pts',(0.826506546432057,3.46525870415051,
135.602766913829));
#150932=CARTESIAN_POINT('Ctrl Pts',(0.819099200078284,3.59040559083518,
135.507223389942));
#150933=CARTESIAN_POINT('Ctrl Pts',(0.811697378402865,3.71545913825058,
135.41175112602));
#150934=CARTESIAN_POINT('Ctrl Pts',(0.804295556727454,3.83679943743615,
135.311213093878));
#150935=CARTESIAN_POINT('Ctrl Pts',(0.796893735052038,3.95399560575159,
135.205934121689));
#150936=CARTESIAN_POINT('Ctrl Pts',(0.789495820740721,4.0711299071212,135.10071072545));
#150937=CARTESIAN_POINT('Ctrl Pts',(0.782097906429348,4.18412415743951,
134.990751622254));
#150938=CARTESIAN_POINT('Ctrl Pts',(0.77469999211803,4.29258047029525,134.876421946738));
#150939=CARTESIAN_POINT('Ctrl Pts',(0.767303307205828,4.40101875967986,
134.76211127074));
#150940=CARTESIAN_POINT('Ctrl Pts',(0.759906622293692,4.50492035165083,
134.643431734493));
#150941=CARTESIAN_POINT('Ctrl Pts',(0.75250993738149,4.60392409351145,134.520785445769));
#150942=CARTESIAN_POINT('Ctrl Pts',(0.745113580446058,4.70292344544226,
134.398144595311));
#150943=CARTESIAN_POINT('Ctrl Pts',(0.737717223510577,4.79702514460619,
134.271537632573));
#150944=CARTESIAN_POINT('Ctrl Pts',(0.730320866575141,4.88590841382615,
134.141399654527));
#150945=CARTESIAN_POINT('Ctrl Pts',(0.722923377238545,4.97480529130192,
134.011241752024));
#150946=CARTESIAN_POINT('Ctrl Pts',(0.715525887901973,5.05848193745507,
133.877552066072));
#150947=CARTESIAN_POINT('Ctrl Pts',(0.708128398565378,5.13666107653126,
133.740794432136));
#150948=CARTESIAN_POINT('Ctrl Pts',(0.700728316050354,5.21486762118357,
133.603988858023));
#150949=CARTESIAN_POINT('Ctrl Pts',(0.693328233535386,5.2875726366831,133.464113518565));
#150950=CARTESIAN_POINT('Ctrl Pts',(0.685928151020363,5.35454501588482,
133.321656435574));
#150951=CARTESIAN_POINT('Ctrl Pts',(0.6785199313539,5.42159103810212,133.179042706377));
#150952=CARTESIAN_POINT('Ctrl Pts',(0.671111711687377,5.48289167635482,
133.033841902229));
#150953=CARTESIAN_POINT('Ctrl Pts',(0.663703492020915,5.53826388266825,
132.886562271689));
#150954=CARTESIAN_POINT('Ctrl Pts',(0.65629071271885,5.5936701696508,132.739191992994));
#150955=CARTESIAN_POINT('Ctrl Pts',(0.648877933416802,5.64314063686597,
132.589740691942));
#150956=CARTESIAN_POINT('Ctrl Pts',(0.641465154114741,5.68654241152167,
132.438730821793));
#150957=CARTESIAN_POINT('Ctrl Pts',(0.634041783085998,5.73000620066828,
132.287505181661));
#150958=CARTESIAN_POINT('Ctrl Pts',(0.626618412057289,5.76738389038742,
132.134716886344));
#150959=CARTESIAN_POINT('Ctrl Pts',(0.619195041028547,5.79859374204342,
131.980898410089));
#150960=CARTESIAN_POINT('Ctrl Pts',(0.615258991587718,5.81514195426174,
131.899340163154));
#150961=CARTESIAN_POINT('Ctrl Pts',(0.611322942146822,5.82995703189355,
131.817492390791));
#150962=CARTESIAN_POINT('Ctrl Pts',(0.607386892705989,5.84303272455383,
131.735434804886));
#150963=CARTESIAN_POINT('Ctrl Pts',(0.599963626300545,5.86769307283249,
131.580676758799));
#150964=CARTESIAN_POINT('Ctrl Pts',(0.592540359895133,5.88623810187495,
131.424704296294));
#150965=CARTESIAN_POINT('Ctrl Pts',(0.585117093489686,5.89855321713593,
131.268042089177));
#150966=CARTESIAN_POINT('Ctrl Pts',(0.577702600768656,5.91085377695339,
131.111565043778));
#150967=CARTESIAN_POINT('Ctrl Pts',(0.570288108047624,5.91693905059183,
130.954400244984));
#150968=CARTESIAN_POINT('Ctrl Pts',(0.562873615326595,5.91674552307085,
130.79708203796));
#150969=CARTESIAN_POINT('Ctrl Pts',(0.555466268972801,5.91655218207898,
130.639915460146));
#150970=CARTESIAN_POINT('Ctrl Pts',(0.548058922619009,5.91009208821658,
130.482596139254));
#150971=CARTESIAN_POINT('Ctrl Pts',(0.540651576265219,5.89735356477309,
130.325662910701));
#150972=CARTESIAN_POINT('Ctrl Pts',(0.533249754589813,5.88462454220099,
130.16884672887));
#150973=CARTESIAN_POINT('Ctrl Pts',(0.525847932914469,5.8656264439867,130.012416436479));
#150974=CARTESIAN_POINT('Ctrl Pts',(0.518446111239058,5.84039965467834,
129.856910124858));
#150975=CARTESIAN_POINT('Ctrl Pts',(0.511048196927705,5.81518618239572,
129.701485903808));
#150976=CARTESIAN_POINT('Ctrl Pts',(0.503650282616284,5.78375062700797,
129.546985059673));
#150977=CARTESIAN_POINT('Ctrl Pts',(0.496252368304937,5.7461851193028,129.393939709751));
#150978=CARTESIAN_POINT('Ctrl Pts',(0.488855683392715,5.7086258543034,129.240919793188));
#150979=CARTESIAN_POINT('Ctrl Pts',(0.481458998480501,5.66493874767725,
129.089355252966));
#150980=CARTESIAN_POINT('Ctrl Pts',(0.474062313568282,5.61526689222679,
128.93976728615));
#150981=CARTESIAN_POINT('Ctrl Pts',(0.466665956632824,5.56559723927845,
128.79018595222));
#150982=CARTESIAN_POINT('Ctrl Pts',(0.459269599697343,5.50994348279135,
128.642581371708));
#150983=CARTESIAN_POINT('Ctrl Pts',(0.451873242761877,5.44849829426981,
128.497458604077));
#150984=CARTESIAN_POINT('Ctrl Pts',(0.444475753425283,5.38704369833305,
128.35231361778));
#150985=CARTESIAN_POINT('Ctrl Pts',(0.437078264088703,5.31979605041375,
128.209651544716));
#150986=CARTESIAN_POINT('Ctrl Pts',(0.429680774752114,5.24699571410832,
128.06995637923));
#150987=CARTESIAN_POINT('Ctrl Pts',(0.422280692237107,5.17416985775784,
127.93021224382));
#150988=CARTESIAN_POINT('Ctrl Pts',(0.414880609722111,5.09578760999192,
127.793437417545));
#150989=CARTESIAN_POINT('Ctrl Pts',(0.407480527207099,5.01213463832796,
127.660090125103));
#150990=CARTESIAN_POINT('Ctrl Pts',(0.400072307540625,4.92838968162203,
127.526596203605));
#150991=CARTESIAN_POINT('Ctrl Pts',(0.392664087874122,4.83936262511829,
127.396537659149));
#150992=CARTESIAN_POINT('Ctrl Pts',(0.385255868207651,4.74538213082243,
127.270343215943));
#150993=CARTESIAN_POINT('Ctrl Pts',(0.377843088905566,4.65134379310021,
127.144071102163));
#150994=CARTESIAN_POINT('Ctrl Pts',(0.370430309603479,4.55234617675713,
127.021668118249));
#150995=CARTESIAN_POINT('Ctrl Pts',(0.363017530301391,4.44875701552763,
126.903528452592));
#150996=CARTESIAN_POINT('Ctrl Pts',(0.355594159272623,4.34501984124686,
126.785219983441));
#150997=CARTESIAN_POINT('Ctrl Pts',(0.348170788243878,4.2366782755013,126.671187268809));
#150998=CARTESIAN_POINT('Ctrl Pts',(0.340747417215113,4.12413612222472,
126.561786893061));
#150999=CARTESIAN_POINT('Ctrl Pts',(0.336811367774451,4.06446357214758,
126.503780188815));
#151000=CARTESIAN_POINT('Ctrl Pts',(0.332875318333758,4.00361063455032,
126.447075124216));
#151001=CARTESIAN_POINT('Ctrl Pts',(0.328939268893095,3.94164099481367,
126.391720044111));
#151002=CARTESIAN_POINT('Ctrl Pts',(0.321516002487664,3.82476818827281,
126.287322090601));
#151003=CARTESIAN_POINT('Ctrl Pts',(0.314092736082256,3.7035681793829,126.187412706623));
#151004=CARTESIAN_POINT('Ctrl Pts',(0.30666946967682,3.57842044824294,126.092371901737));
#151005=CARTESIAN_POINT('Ctrl Pts',(0.29925497695581,3.45342063132831,125.997443427191));
#151006=CARTESIAN_POINT('Ctrl Pts',(0.291840484234759,3.32448267400762,
125.907372301423));
#151007=CARTESIAN_POINT('Ctrl Pts',(0.284425991513757,3.19202180460264,
125.822500788));
#151008=CARTESIAN_POINT('Ctrl Pts',(0.27701864515998,3.05968860597046,125.737711076937));
#151009=CARTESIAN_POINT('Ctrl Pts',(0.269611298806304,2.9238395672605,125.658111201183));
#151010=CARTESIAN_POINT('Ctrl Pts',(0.262203952452523,2.7849217144219,125.584002238389));
#151011=CARTESIAN_POINT('Ctrl Pts',(0.254802130777138,2.64610747175942,
125.509948548856));
#151012=CARTESIAN_POINT('Ctrl Pts',(0.247400309101722,2.5042293002962,125.441377792879));
#151013=CARTESIAN_POINT('Ctrl Pts',(0.239998487426334,2.35976174034193,
125.378546845299));
#151014=CARTESIAN_POINT('Ctrl Pts',(0.232600573114961,2.21537044368741,
125.315749065688));
#151015=CARTESIAN_POINT('Ctrl Pts',(0.225202658803554,2.0683928222819,125.258685208589));
#151016=CARTESIAN_POINT('Ctrl Pts',(0.217804744492184,1.91932636041903,
125.207565384158));
#151017=CARTESIAN_POINT('Ctrl Pts',(0.210408059579972,1.770284670698,125.156454054914));
#151018=CARTESIAN_POINT('Ctrl Pts',(0.203011374667773,1.61915518223042,
125.111284918842));
#151019=CARTESIAN_POINT('Ctrl Pts',(0.195614689755558,1.4664537380229,125.072219307659));
#151020=CARTESIAN_POINT('Ctrl Pts',(0.188218332820104,1.31375906475744,
125.033155428686));
#151021=CARTESIAN_POINT('Ctrl Pts',(0.180821975884583,1.15949293599379,
125.000194629006));
#151022=CARTESIAN_POINT('Ctrl Pts',(0.173425618949125,1.00418441621774,
124.973447805602));
#151023=CARTESIAN_POINT('Ctrl Pts',(0.166028129612527,0.848852118310616,
124.946696887191));
#151024=CARTESIAN_POINT('Ctrl Pts',(0.158630640275958,0.692477479526676,
124.926161902732));
#151025=CARTESIAN_POINT('Ctrl Pts',(0.151233150939362,0.535597620410355,
124.911902238289));
#151026=CARTESIAN_POINT('Ctrl Pts',(0.143833068424346,0.378662767302617,
124.897637575143));
#151027=CARTESIAN_POINT('Ctrl Pts',(0.136432985909389,0.221222712782735,
124.889652645576));
#151028=CARTESIAN_POINT('Ctrl Pts',(0.129032903394375,0.0638173845376825,
124.887954791059));
#151029=CARTESIAN_POINT('Ctrl Pts',(0.121624683727909,-0.0937610270469865,
124.886255069575));
#151030=CARTESIAN_POINT('Ctrl Pts',(0.114216464061448,-0.251304262593419,
124.890856233454));
#151031=CARTESIAN_POINT('Ctrl Pts',(0.106808244394983,-0.40827397444272,
124.901713505948));
#151032=CARTESIAN_POINT('Ctrl Pts',(0.0993954650929377,-0.565340298530262,
124.912577460912));
#151033=CARTESIAN_POINT('Ctrl Pts',(0.0919826857909391,-0.72183202531378,
124.929705156634));
#151034=CARTESIAN_POINT('Ctrl Pts',(0.0845699064888947,-0.877218743869465,
124.953000276765));
#151035=CARTESIAN_POINT('Ctrl Pts',(0.0771465354601375,-1.03282748625598,
124.976328682055));
#151036=CARTESIAN_POINT('Ctrl Pts',(0.069723164431318,-1.18732770132546,
125.005842042047));
#151037=CARTESIAN_POINT('Ctrl Pts',(0.0622997934025591,-1.34020111866291,
125.041393367613));
#151038=CARTESIAN_POINT('Ctrl Pts',(0.058363743961779,-1.42125827268231,
125.06024353347));
#151039=CARTESIAN_POINT('Ctrl Pts',(0.0544276945210084,-1.50185834868971,
125.080790360802));
#151040=CARTESIAN_POINT('Ctrl Pts',(0.0504916450802284,-1.58192624929231,
125.103006400865));
#151041=CARTESIAN_POINT('Ctrl Pts',(0.0430683786747836,-1.73293181099582,
125.144905159084));
#151042=CARTESIAN_POINT('Ctrl Pts',(0.0356451122694012,-1.88249997059805,
125.192870696663));
#151043=CARTESIAN_POINT('Ctrl Pts',(0.0282218458639534,-2.03010589702807,
125.246789150697));
#151044=CARTESIAN_POINT('Ctrl Pts',(0.0208073531429645,-2.17753736551032,
125.300643877597));
#151045=CARTESIAN_POINT('Ctrl Pts',(0.0133928604218992,-2.32301086998142,
125.360437389217));
#151046=CARTESIAN_POINT('Ctrl Pts',(0.00597836770091931,-2.46601401336008,
125.426005344026));
#151047=CARTESIAN_POINT('Ctrl Pts',(-0.00142897865282537,-2.60887932492519,
125.491510101973));
#151048=CARTESIAN_POINT('Ctrl Pts',(-0.00883632500662208,-2.74927867850225,
125.562778068504));
#151049=CARTESIAN_POINT('Ctrl Pts',(-0.0162436713603711,-2.88671714049119,
125.639595887852));
#151050=CARTESIAN_POINT('Ctrl Pts',(-0.0236454930357674,-3.02405309569032,
125.716356413574));
#151051=CARTESIAN_POINT('Ctrl Pts',(-0.0310473147111037,-3.15843223196212,
125.798658368884));
#151052=CARTESIAN_POINT('Ctrl Pts',(-0.0384491363865038,-3.28938193259737,
125.88624135671));
#151053=CARTESIAN_POINT('Ctrl Pts',(-0.0458470506978888,-3.42026250590552,
125.973778110159));
#151054=CARTESIAN_POINT('Ctrl Pts',(-0.0532449650092701,-3.54771693951329,
126.066590137045));
#151055=CARTESIAN_POINT('Ctrl Pts',(-0.0606428793206533,-3.67129955938354,
126.164372459416));
#151056=CARTESIAN_POINT('Ctrl Pts',(-0.0680395642328581,-3.79486164206386,
126.262138532139));
#151057=CARTESIAN_POINT('Ctrl Pts',(-0.0754362491450449,-3.91455289555713,
126.364873029631));
#151058=CARTESIAN_POINT('Ctrl Pts',(-0.0828329340572509,-4.02995876117528,
126.472229162298));
#151059=CARTESIAN_POINT('Ctrl Pts',(-0.0902292909927178,-4.14535950957674,
126.579580534681));
#151060=CARTESIAN_POINT('Ctrl Pts',(-0.097625647928219,-4.25647497460286,
126.691552880514));
#151061=CARTESIAN_POINT('Ctrl Pts',(-0.105022004863685,-4.36292588320257,
126.80776102539));
#151062=CARTESIAN_POINT('Ctrl Pts',(-0.112419494200237,-4.46939308970754,
126.923986962029));
#151063=CARTESIAN_POINT('Ctrl Pts',(-0.119816983536782,-4.57119406563906,
127.044449713702));
#151064=CARTESIAN_POINT('Ctrl Pts',(-0.127214472873334,-4.66798852104518,
127.168729485302));
#151065=CARTESIAN_POINT('Ctrl Pts',(-0.134614555388326,-4.76481690759787,
127.293052822982));
#151066=CARTESIAN_POINT('Ctrl Pts',(-0.142014637903356,-4.85663505014213,
127.42119555031));
#151067=CARTESIAN_POINT('Ctrl Pts',(-0.149414720418349,-4.94314492798882,
127.552707379074));
#151068=CARTESIAN_POINT('Ctrl Pts',(-0.156822940084836,-5.02974993233988,
127.684363818613));
#151069=CARTESIAN_POINT('Ctrl Pts',(-0.164231159751286,-5.11103480987731,
127.819396446001));
#151070=CARTESIAN_POINT('Ctrl Pts',(-0.171639379417769,-5.18674624248784,
127.95732813118));
#151071=CARTESIAN_POINT('Ctrl Pts',(-0.179052158719834,-5.26250427422172,
128.095344711009));
#151072=CARTESIAN_POINT('Ctrl Pts',(-0.186464938021906,-5.33268185957847,
128.236263570734));
#151073=CARTESIAN_POINT('Ctrl Pts',(-0.193877717323971,-5.39707333217188,
128.379586399281));
#151074=CARTESIAN_POINT('Ctrl Pts',(-0.201301088352739,-5.46155681032108,
128.523114014207));
#151075=CARTESIAN_POINT('Ctrl Pts',(-0.208724459381482,-5.5202375248212,
128.669052112798));
#151076=CARTESIAN_POINT('Ctrl Pts',(-0.21614783041025,-5.57295900396849,
128.816885208262));
#151077=CARTESIAN_POINT('Ctrl Pts',(-0.220083879851061,-5.60091319724702,
128.895269862684));
#151078=CARTESIAN_POINT('Ctrl Pts',(-0.224019929291911,-5.62719287934486,
128.9741870514));
#151079=CARTESIAN_POINT('Ctrl Pts',(-0.227955978732723,-5.6517805516924,
129.053558756129));
#151080=CARTESIAN_POINT('Ctrl Pts',(-0.237002541632423,-5.7082925258925,
129.235985610793));
#151081=CARTESIAN_POINT('Ctrl Pts',(-0.246049104532169,-5.75600204132922,
129.421259959019));
#151082=CARTESIAN_POINT('Ctrl Pts',(-0.255095667431874,-5.79466319391346,
129.608614393819));
#151083=CARTESIAN_POINT('Ctrl Pts',(-0.264517182244824,-5.83492673110393,
129.803734087598));
#151084=CARTESIAN_POINT('Ctrl Pts',(-0.273938697057761,-5.86537581948693,
130.001110085161));
#151085=CARTESIAN_POINT('Ctrl Pts',(-0.283360211870729,-5.88578779369038,
130.199850394207));
#151086=CARTESIAN_POINT('Ctrl Pts',(-0.292243301940128,-5.90503325569336,
130.387233007377));
#151087=CARTESIAN_POINT('Ctrl Pts',(-0.30112639200945,-5.91535635260079,
130.575828272977));
#151088=CARTESIAN_POINT('Ctrl Pts',(-0.31000948207884,-5.9166181911593,
130.764867041597));
#151089=CARTESIAN_POINT('Ctrl Pts',(-0.310547906822408,-5.91669467412829,
130.776325120905));
#151090=CARTESIAN_POINT('Ctrl Pts',(-0.311086331566016,-5.91673788194359,
130.787784823116));
#151091=CARTESIAN_POINT('Ctrl Pts',(-0.311624756309584,-5.91674778936248,
130.799245974448));
#151092=CARTESIAN_POINT('',(-2.06162483645605,-5.91244912682104,130.807044328504));
#151093=CARTESIAN_POINT('Ctrl Pts',(-0.311624807788274,-5.91284049796445,
130.799250447123));
#151094=CARTESIAN_POINT('Ctrl Pts',(-0.376551072707372,-5.90153303013459,
132.180398272274));
#151095=CARTESIAN_POINT('Ctrl Pts',(-0.53429321223076,-4.72958062977401,
135.55326689347));
#151096=CARTESIAN_POINT('Ctrl Pts',(-0.784851226358526,0.895237502509812,
137.745261880691));
#151097=CARTESIAN_POINT('Ctrl Pts',(-1.06329885017127,6.32347454670116,
133.80289862592));
#151098=CARTESIAN_POINT('Ctrl Pts',(-1.34174647398429,5.94074740138417,
127.105025428197));
#151099=CARTESIAN_POINT('Ctrl Pts',(-1.62019409779717,0.0987636158356631,
123.806660546933));
#151100=CARTESIAN_POINT('Ctrl Pts',(-1.86015354239845,-5.01393093486658,
126.505897385061));
#151101=CARTESIAN_POINT('Ctrl Pts',(-2.00729711239547,-5.90338408802778,
129.649020459756));
#151102=CARTESIAN_POINT('Ctrl Pts',(-2.0616248077882,-5.90809907779839,
130.807041742467));
#151103=CARTESIAN_POINT('',(-3.81162480778819,-5.91969451445794,130.808517656963));
#151104=CARTESIAN_POINT('Ctrl Pts',(-2.06162486479582,-5.916749390203,130.807046884944));
#151105=CARTESIAN_POINT('Ctrl Pts',(-2.06971386832509,-5.91667099475305,
130.979720027814));
#151106=CARTESIAN_POINT('Ctrl Pts',(-2.07780287185427,-5.90902959923856,
131.152144819403));
#151107=CARTESIAN_POINT('Ctrl Pts',(-2.08589187538357,-5.89391499210028,
131.323683858328));
#151108=CARTESIAN_POINT('Ctrl Pts',(-2.09401865753072,-5.87872979419454,
131.496024047578));
#151109=CARTESIAN_POINT('Ctrl Pts',(-2.10214543967794,-5.85600149689041,
131.66746994883));
#151110=CARTESIAN_POINT('Ctrl Pts',(-2.11027222182508,-5.82587165323201,
131.837390163401));
#151111=CARTESIAN_POINT('Ctrl Pts',(-2.11841801499163,-5.79567132668976,
132.007707873122));
#151112=CARTESIAN_POINT('Ctrl Pts',(-2.12656380815816,-5.75803489747663,
132.176492521182));
#151113=CARTESIAN_POINT('Ctrl Pts',(-2.13470960132469,-5.71315404569664,
132.343126815739));
#151114=CARTESIAN_POINT('Ctrl Pts',(-2.14288381330348,-5.66811661487335,
132.510342459299));
#151115=CARTESIAN_POINT('Ctrl Pts',(-2.1510580252823,-5.61578424161571,
132.675392494474));
#151116=CARTESIAN_POINT('Ctrl Pts',(-2.15923223726111,-5.55639832036391,
132.83767521889));
#151117=CARTESIAN_POINT('Ctrl Pts',(-2.16518460664839,-5.51315415926175,
132.955847676786));
#151118=CARTESIAN_POINT('Ctrl Pts',(-2.17113697603566,-5.46617079334389,
133.07255319289));
#151119=CARTESIAN_POINT('Ctrl Pts',(-2.17708934542293,-5.41555669099828,
133.187567761119));
#151120=CARTESIAN_POINT('Ctrl Pts',(-2.18451261182834,-5.352435278139,133.331003714926));
#151121=CARTESIAN_POINT('Ctrl Pts',(-2.19193587823382,-5.28351593448006,
133.47214708612));
#151122=CARTESIAN_POINT('Ctrl Pts',(-2.19935914463929,-5.20898661212708,
133.610494797747));
#151123=CARTESIAN_POINT('Ctrl Pts',(-2.20677363736034,-5.13454537724375,
133.748678993869));
#151124=CARTESIAN_POINT('Ctrl Pts',(-2.21418813008139,-5.05450753708574,
133.884073782093));
#151125=CARTESIAN_POINT('Ctrl Pts',(-2.22160262280244,-4.96910921744193,
134.016195630084));
#151126=CARTESIAN_POINT('Ctrl Pts',(-2.22900996915625,-4.88379320791378,
134.148190134063));
#151127=CARTESIAN_POINT('Ctrl Pts',(-2.23641731551008,-4.79312720592667,
134.276917666559));
#151128=CARTESIAN_POINT('Ctrl Pts',(-2.2438246618639,-4.69739334041939,
134.401919007347));
#151129=CARTESIAN_POINT('Ctrl Pts',(-2.25122648353934,-4.60173087684083,
134.526827117419));
#151130=CARTESIAN_POINT('Ctrl Pts',(-2.25862830521476,-4.50100830184079,
134.648014274325));
#151131=CARTESIAN_POINT('Ctrl Pts',(-2.2660301268902,-4.39555109894441,
134.765050090255));
#151132=CARTESIAN_POINT('Ctrl Pts',(-2.27342804120158,-4.2901495660847,
134.882024123889));
#151133=CARTESIAN_POINT('Ctrl Pts',(-2.28082595551296,-4.18001863220431,
134.994850904326));
#151134=CARTESIAN_POINT('Ctrl Pts',(-2.28822386982435,-4.06552403703358,
135.103133101288));
#151135=CARTESIAN_POINT('Ctrl Pts',(-2.2956205547366,-3.95104846878726,
135.211397303713));
#151136=CARTESIAN_POINT('Ctrl Pts',(-2.30301723964884,-3.83221094943262,
135.315118165317));
#151137=CARTESIAN_POINT('Ctrl Pts',(-2.31041392456109,-3.70941413588868,
135.413935145759));
#151138=CARTESIAN_POINT('Ctrl Pts',(-2.31781028149657,-3.58662276728415,
135.512747744554));
#151139=CARTESIAN_POINT('Ctrl Pts',(-2.32520663843209,-3.45987274438713,
135.606656660505));
#151140=CARTESIAN_POINT('Ctrl Pts',(-2.33260299536758,-3.32959965183265,
135.69534177895));
#151141=CARTESIAN_POINT('Ctrl Pts',(-2.34000048470418,-3.19930661413532,
135.784040475314));
#151142=CARTESIAN_POINT('Ctrl Pts',(-2.34739797404077,-3.06548974138161,
135.867513571626));
#151143=CARTESIAN_POINT('Ctrl Pts',(-2.35479546337737,-2.92861329046739,
135.945484498333));
#151144=CARTESIAN_POINT('Ctrl Pts',(-2.36219554589239,-2.79168885772548,
136.023482757628));
#151145=CARTESIAN_POINT('Ctrl Pts',(-2.36959562840737,-2.65170303558292,
136.09597482248));
#151146=CARTESIAN_POINT('Ctrl Pts',(-2.37699571092239,-2.50914419699526,
136.162730328699));
#151147=CARTESIAN_POINT('Ctrl Pts',(-2.38440393058889,-2.36642860030897,
136.229559239459));
#151148=CARTESIAN_POINT('Ctrl Pts',(-2.39181215025541,-2.2211346751637,
136.29063883582));
#151149=CARTESIAN_POINT('Ctrl Pts',(-2.39922036992192,-2.07377094809798,
136.345786843487));
#151150=CARTESIAN_POINT('Ctrl Pts',(-2.40663314922402,-1.92631652111715,
136.400968793832));
#151151=CARTESIAN_POINT('Ctrl Pts',(-2.41404592852614,-1.77679010749687,
136.450211764322));
#151152=CARTESIAN_POINT('Ctrl Pts',(-2.42145870782824,-1.62571436210178,
136.493383677403));
#151153=CARTESIAN_POINT('Ctrl Pts',(-2.42888207885702,-1.47442275259691,
136.536617276538));
#151154=CARTESIAN_POINT('Ctrl Pts',(-2.43630544988579,-1.32157775172488,
136.573762405197));
#151155=CARTESIAN_POINT('Ctrl Pts',(-2.44372882091457,-1.16771195750656,
136.604738135176));
#151156=CARTESIAN_POINT('Ctrl Pts',(-2.44766487035497,-1.08612862146141,
136.621162210462));
#151157=CARTESIAN_POINT('Ctrl Pts',(-2.45160091979537,-1.00425839785975,
136.635852712559));
#151158=CARTESIAN_POINT('Ctrl Pts',(-2.45553696923577,-0.922181008006428,
136.6488035124));
#151159=CARTESIAN_POINT('Ctrl Pts',(-2.46296023564119,-0.767385612275549,
136.67322831672));
#151160=CARTESIAN_POINT('Ctrl Pts',(-2.47038350204662,-0.611385108007345,
136.691535960751));
#151161=CARTESIAN_POINT('Ctrl Pts',(-2.47780676845204,-0.454704340793631,
136.703612648541));
#151162=CARTESIAN_POINT('Ctrl Pts',(-2.48522126117303,-0.298208757235235,
136.715675062689));
#151163=CARTESIAN_POINT('Ctrl Pts',(-2.49263575389405,-0.141034879685641,
136.721521151211));
#151164=CARTESIAN_POINT('Ctrl Pts',(-2.50005024661505,0.0162828506506795,
136.721088212383));
#151165=CARTESIAN_POINT('Ctrl Pts',(-2.50745759296882,0.173448952235817,
136.720655690839));
#151166=CARTESIAN_POINT('Ctrl Pts',(-2.51486493932254,0.330758259790891,
136.713956191231));
#151167=CARTESIAN_POINT('Ctrl Pts',(-2.52227228567631,0.487671920753468,
136.70097885688));
#151168=CARTESIAN_POINT('Ctrl Pts',(-2.52967410735171,0.644468549587685,
136.688011201514));
#151169=CARTESIAN_POINT('Ctrl Pts',(-2.53707592902713,0.800869748963157,
136.668775065024));
#151170=CARTESIAN_POINT('Ctrl Pts',(-2.54447775070253,0.956337489631983,
136.643311650793));
#151171=CARTESIAN_POINT('Ctrl Pts',(-2.55187566501387,1.11172316009045,
136.617861678501));
#151172=CARTESIAN_POINT('Ctrl Pts',(-2.55927357932525,1.26617598575162,
136.586191035531));
#151173=CARTESIAN_POINT('Ctrl Pts',(-2.56667149363659,1.41916399014193,
136.548392662357));
#151174=CARTESIAN_POINT('Ctrl Pts',(-2.57406817854878,1.57212657070138,
136.510600570586));
#151175=CARTESIAN_POINT('Ctrl Pts',(-2.58146486346097,1.72362445107397,
136.46668285912));
#151176=CARTESIAN_POINT('Ctrl Pts',(-2.58886154837316,1.87313665256134,
136.416783413768));
#151177=CARTESIAN_POINT('Ctrl Pts',(-2.59625790530859,2.02264222452102,
136.36688618101));
#151178=CARTESIAN_POINT('Ctrl Pts',(-2.60365426224399,2.17016193856577,
136.311007859925));
#151179=CARTESIAN_POINT('Ctrl Pts',(-2.61105061917942,2.31519102902924,
136.249341890408));
#151180=CARTESIAN_POINT('Ctrl Pts',(-2.61844810851598,2.4602423238167,136.187666479674));
#151181=CARTESIAN_POINT('Ctrl Pts',(-2.62584559785254,2.60280189220714,
136.120201802237));
#151182=CARTESIAN_POINT('Ctrl Pts',(-2.6332430871891,2.74238610620907,136.047188957973));
#151183=CARTESIAN_POINT('Ctrl Pts',(-2.64064316970409,2.88201925124103,
135.974150519168));
#151184=CARTESIAN_POINT('Ctrl Pts',(-2.64804325221907,3.01867463469476,
135.895560214166));
#151185=CARTESIAN_POINT('Ctrl Pts',(-2.65544333473406,3.15189446714023,
135.811704407492));
#151186=CARTESIAN_POINT('Ctrl Pts',(-2.66285155440052,3.28526078848681,
135.727756392738));
#151187=CARTESIAN_POINT('Ctrl Pts',(-2.67025977406701,3.41518369831154,
135.638531512362));
#151188=CARTESIAN_POINT('Ctrl Pts',(-2.67766799373348,3.54123497307229,
135.544359080434));
#151189=CARTESIAN_POINT('Ctrl Pts',(-2.68508077303554,3.66736383028937,
135.450128686945));
#151190=CARTESIAN_POINT('Ctrl Pts',(-2.69249355233754,3.78961601494304,
135.350944908736));
#151191=CARTESIAN_POINT('Ctrl Pts',(-2.6999063316396,3.90759789872617,135.247176079002));
#151192=CARTESIAN_POINT('Ctrl Pts',(-2.70732970266834,4.02574836055765,
135.143258979497));
#151193=CARTESIAN_POINT('Ctrl Pts',(-2.71475307369716,4.13961606572169,
135.03474400083));
#151194=CARTESIAN_POINT('Ctrl Pts',(-2.7221764447259,4.24884504478696,134.922035489128));
#151195=CARTESIAN_POINT('Ctrl Pts',(-2.72611249416683,4.30676087040284,
134.862274731817));
#151196=CARTESIAN_POINT('Ctrl Pts',(-2.73004854360773,4.36337326153021,
134.801335569227));
#151197=CARTESIAN_POINT('Ctrl Pts',(-2.73398459304866,4.41863397029641,
134.739281760237));
#151198=CARTESIAN_POINT('Ctrl Pts',(-2.7414078594541,4.52285394239833,134.62225021312));
#151199=CARTESIAN_POINT('Ctrl Pts',(-2.74883112585958,4.62257876490229,
134.500898299503));
#151200=CARTESIAN_POINT('Ctrl Pts',(-2.75625439226502,4.71742900618905,
134.375606077355));
#151201=CARTESIAN_POINT('Ctrl Pts',(-2.76366888498604,4.81216714236757,
134.25046194021));
#151202=CARTESIAN_POINT('Ctrl Pts',(-2.77108337770697,4.90204194221244,
134.121387059276));
#151203=CARTESIAN_POINT('Ctrl Pts',(-2.778497870428,4.98671177446159,133.988797183263));
#151204=CARTESIAN_POINT('Ctrl Pts',(-2.78590521678178,5.07129999873854,
133.856335102364));
#151205=CARTESIAN_POINT('Ctrl Pts',(-2.7933125631356,5.15069304320606,133.720365083504));
#151206=CARTESIAN_POINT('Ctrl Pts',(-2.80071990948937,5.22459051085855,
133.581334610305));
#151207=CARTESIAN_POINT('Ctrl Pts',(-2.80812173116479,5.29843286299177,
133.442407831277));
#151208=CARTESIAN_POINT('Ctrl Pts',(-2.81552355284021,5.36678762514084,
133.300425471088));
#151209=CARTESIAN_POINT('Ctrl Pts',(-2.82292537451562,5.42939864492969,
133.155862460418));
#151210=CARTESIAN_POINT('Ctrl Pts',(-2.83032328882698,5.49197661284856,
133.011375763436));
#151211=CARTESIAN_POINT('Ctrl Pts',(-2.83772120313832,5.54881672894887,
132.864311470751));
#151212=CARTESIAN_POINT('Ctrl Pts',(-2.84511911744968,5.59970964040452,
132.715167385835));
#151213=CARTESIAN_POINT('Ctrl Pts',(-2.85251580236189,5.6505940943815,132.566048085959));
#151214=CARTESIAN_POINT('Ctrl Pts',(-2.85991248727416,5.69553318479359,
132.414850032761));
#151215=CARTESIAN_POINT('Ctrl Pts',(-2.86730917218637,5.73436636513568,
132.262089314169));
#151216=CARTESIAN_POINT('Ctrl Pts',(-2.87470552912181,5.77319782357385,
132.109335369148));
#151217=CARTESIAN_POINT('Ctrl Pts',(-2.88210188605724,5.80592381829896,
131.955019258296));
#151218=CARTESIAN_POINT('Ctrl Pts',(-2.88949824299269,5.83243425760153,
131.799670214252));
#151219=CARTESIAN_POINT('Ctrl Pts',(-2.89689573232926,5.85894875572004,
131.644297385874));
#151220=CARTESIAN_POINT('Ctrl Pts',(-2.90429322166587,5.87924574081938,
131.487891677419));
#151221=CARTESIAN_POINT('Ctrl Pts',(-2.91169071100245,5.89326664431007,
131.330990299185));
#151222=CARTESIAN_POINT('Ctrl Pts',(-2.91909079351746,5.90729246280676,
131.174033919417));
#151223=CARTESIAN_POINT('Ctrl Pts',(-2.92649087603246,5.91503778616497,
131.016581895506));
#151224=CARTESIAN_POINT('Ctrl Pts',(-2.93389095854747,5.91649609460213,
130.859174165688));
#151225=CARTESIAN_POINT('Ctrl Pts',(-2.94129917821394,5.91795600659933,
130.70159334989));
#151226=CARTESIAN_POINT('Ctrl Pts',(-2.94870739788036,5.91311509406243,
130.544057298964));
#151227=CARTESIAN_POINT('Ctrl Pts',(-2.95611561754683,5.90201895296102,
130.387104291803));
#151228=CARTESIAN_POINT('Ctrl Pts',(-2.9635283968489,5.8909159823699,130.230054682686));
#151229=CARTESIAN_POINT('Ctrl Pts',(-2.97094117615101,5.87355015271227,
130.073589202554));
#151230=CARTESIAN_POINT('Ctrl Pts',(-2.97835395545309,5.85001858742294,
129.91823811514));
#151231=CARTESIAN_POINT('Ctrl Pts',(-2.98577732648185,5.82645339912962,
129.762665054807));
#151232=CARTESIAN_POINT('Ctrl Pts',(-2.99320069751052,5.79670495028728,
129.608209932956));
#151233=CARTESIAN_POINT('Ctrl Pts',(-3.00062406853928,5.7609210185715,129.455390795709));
#151234=CARTESIAN_POINT('Ctrl Pts',(-3.00456011798005,5.74194751935226,
129.374362422296));
#151235=CARTESIAN_POINT('Ctrl Pts',(-3.00849616742082,5.72127805621818,
129.293793708396));
#151236=CARTESIAN_POINT('Ctrl Pts',(-3.01243221686158,5.69894019216676,
129.213759709542));
#151237=CARTESIAN_POINT('Ctrl Pts',(-3.01985548326705,5.65681167770635,
129.062818085478));
#151238=CARTESIAN_POINT('Ctrl Pts',(-3.0272787496725,5.60861857839295,128.913323094456));
#151239=CARTESIAN_POINT('Ctrl Pts',(-3.03470201607794,5.5544755557017,128.76579939366));
#151240=CARTESIAN_POINT('Ctrl Pts',(-3.04211650879897,5.50039652556691,
128.618450053627));
#151241=CARTESIAN_POINT('Ctrl Pts',(-3.04953100151999,5.44038169727705,
128.473067713157));
#151242=CARTESIAN_POINT('Ctrl Pts',(-3.05694549424101,5.37459619195267,
128.330164518639));
#151243=CARTESIAN_POINT('Ctrl Pts',(-3.06435284059479,5.30887409317512,
128.187399059599));
#151244=CARTESIAN_POINT('Ctrl Pts',(-3.07176018694859,5.23739254525498,
128.047108326315));
#151245=CARTESIAN_POINT('Ctrl Pts',(-3.07916753330238,5.16036565691642,
127.909786927121));
#151246=CARTESIAN_POINT('Ctrl Pts',(-3.0865693549778,5.08339621813723,127.772567947407));
#151247=CARTESIAN_POINT('Ctrl Pts',(-3.09397117665318,5.00088985596024,
127.63831421631));
#151248=CARTESIAN_POINT('Ctrl Pts',(-3.1013729983286,4.91310768640109,127.50749795371));
#151249=CARTESIAN_POINT('Ctrl Pts',(-3.10877091263997,4.82537185636597,
127.376750747997));
#151250=CARTESIAN_POINT('Ctrl Pts',(-3.11616882695138,4.73236597300262,
127.249437706085));
#151251=CARTESIAN_POINT('Ctrl Pts',(-3.12356674126275,4.63439569215218,
127.126004037371));
#151252=CARTESIAN_POINT('Ctrl Pts',(-3.13096342617496,4.5364416921852,127.002590881094));
#151253=CARTESIAN_POINT('Ctrl Pts',(-3.13836011108717,4.43352516394429,
126.883056110618));
#151254=CARTESIAN_POINT('Ctrl Pts',(-3.14575679599938,4.32599352751265,
126.767813756396));
#151255=CARTESIAN_POINT('Ctrl Pts',(-3.15315315293482,4.21846665914646,
126.652576512142));
#151256=CARTESIAN_POINT('Ctrl Pts',(-3.16054950987033,4.10632534415289,
126.541631578635));
#151257=CARTESIAN_POINT('Ctrl Pts',(-3.16794586680578,3.98995533368209,
126.435357642318));
#151258=CARTESIAN_POINT('Ctrl Pts',(-3.17534335614237,3.87356750666544,
126.329067435191));
#151259=CARTESIAN_POINT('Ctrl Pts',(-3.18274084547889,3.75294997072971,
126.227449900944));
#151260=CARTESIAN_POINT('Ctrl Pts',(-3.19013833481549,3.62852303835991,
126.13084469028));
#151261=CARTESIAN_POINT('Ctrl Pts',(-3.1975384173305,3.50405248832185,126.03420561481));
#151262=CARTESIAN_POINT('Ctrl Pts',(-3.20493849984549,3.37577017779809,
125.942582590007));
#151263=CARTESIAN_POINT('Ctrl Pts',(-3.2123385823605,3.24412684801521,125.856272950953));
#151264=CARTESIAN_POINT('Ctrl Pts',(-3.21974680202699,3.11233876285798,
125.769868405579));
#151265=CARTESIAN_POINT('Ctrl Pts',(-3.22715502169347,2.97718259008883,
125.68878911884));
#151266=CARTESIAN_POINT('Ctrl Pts',(-3.23456324135995,2.83913584472054,
125.613287682447));
#151267=CARTESIAN_POINT('Ctrl Pts',(-3.24197602066203,2.70100413388391,
125.53773977618));
#151268=CARTESIAN_POINT('Ctrl Pts',(-3.24938879996411,2.55997863900215,
125.467776726604));
#151269=CARTESIAN_POINT('Ctrl Pts',(-3.25680157926618,2.41655798356017,
125.403603441522));
#151270=CARTESIAN_POINT('Ctrl Pts',(-3.26422495029494,2.27293240195994,
125.339338462641));
#151271=CARTESIAN_POINT('Ctrl Pts',(-3.27164832132375,2.12690517030463,
125.280879909035));
#151272=CARTESIAN_POINT('Ctrl Pts',(-3.27907169235252,1.97899201291219,
125.228383467745));
#151273=CARTESIAN_POINT('Ctrl Pts',(-3.28300774179317,1.90056490773808,
125.200548594938));
#151274=CARTESIAN_POINT('Ctrl Pts',(-3.28694379123385,1.82160781720802,
125.1743890418));
#151275=CARTESIAN_POINT('Ctrl Pts',(-3.29087984067451,1.74219878614146,
125.149922188149));
#151276=CARTESIAN_POINT('Ctrl Pts',(-3.29830310707993,1.59243583181593,
125.103778465746));
#151277=CARTESIAN_POINT('Ctrl Pts',(-3.30572637348536,1.44061191459084,
125.063518990832));
#151278=CARTESIAN_POINT('Ctrl Pts',(-3.31314963989078,1.28723042074159,
125.029330885485));
#151279=CARTESIAN_POINT('Ctrl Pts',(-3.32056413261178,1.13403021108032,
124.99518318764));
#151280=CARTESIAN_POINT('Ctrl Pts',(-3.32797862533272,0.979276449967203,
124.967092656203));
#151281=CARTESIAN_POINT('Ctrl Pts',(-3.33539311805373,0.823489272662264,
124.945197197733));
#151282=CARTESIAN_POINT('Ctrl Pts',(-3.3428004644075,0.667852248904096,
124.92332284293));
#151283=CARTESIAN_POINT('Ctrl Pts',(-3.35020781076128,0.511184159067502,
124.907631725526));
#151284=CARTESIAN_POINT('Ctrl Pts',(-3.35761515711505,0.354016862148698,
124.898211057674));
#151285=CARTESIAN_POINT('Ctrl Pts',(-3.36501697879046,0.196966786529296,
124.888797416111));
#151286=CARTESIAN_POINT('Ctrl Pts',(-3.37241880046591,0.0394186162072712,
124.885644934324));
#151287=CARTESIAN_POINT('Ctrl Pts',(-3.37982062214132,-0.11808921727217,
124.888789174395));
#151288=CARTESIAN_POINT('Ctrl Pts',(-3.38721853645269,-0.275513903592357,
124.891931754645));
#151289=CARTESIAN_POINT('Ctrl Pts',(-3.39461645076402,-0.432897923198201,
124.901364429435));
#151290=CARTESIAN_POINT('Ctrl Pts',(-3.40201436507539,-0.589701494367243,
124.917070688402));
#151291=CARTESIAN_POINT('Ctrl Pts',(-3.40941104998759,-0.746479007627239,
124.932774337273));
#151292=CARTESIAN_POINT('Ctrl Pts',(-3.41680773489981,-0.902675892819454,
124.954749463988));
#151293=CARTESIAN_POINT('Ctrl Pts',(-3.42420441981201,-1.05775602535642,
124.982927567764));
#151294=CARTESIAN_POINT('Ctrl Pts',(-3.43160077674746,-1.2128292814778,
125.011104422094));
#151295=CARTESIAN_POINT('Ctrl Pts',(-3.43899713368289,-1.36678551611854,
125.045483639864));
#151296=CARTESIAN_POINT('Ctrl Pts',(-3.44639349061833,-1.51909762173092,
125.085945366979));
#151297=CARTESIAN_POINT('Ctrl Pts',(-3.4537909799549,-1.67143304671528,
125.126413288887));
#151298=CARTESIAN_POINT('Ctrl Pts',(-3.46118846929145,-1.82212348065478,
125.172965478529));
#151299=CARTESIAN_POINT('Ctrl Pts',(-3.46858595862801,-1.97065597663022,
125.225431904608));
#151300=CARTESIAN_POINT('Ctrl Pts',(-3.475986041143,-2.11924054044208,125.277916722711));
#151301=CARTESIAN_POINT('Ctrl Pts',(-3.48338612365803,-2.26566530841536,
125.336319780775));
#151302=CARTESIAN_POINT('Ctrl Pts',(-3.49078620617303,-2.40943648748165,
125.400422574315));
#151303=CARTESIAN_POINT('Ctrl Pts',(-3.49819442583949,-2.55336575773936,
125.464595855467));
#151304=CARTESIAN_POINT('Ctrl Pts',(-3.50560264550593,-2.69463527071165,
125.534481236485));
#151305=CARTESIAN_POINT('Ctrl Pts',(-3.51301086517239,-2.83277440531145,
125.609813502455));
#151306=CARTESIAN_POINT('Ctrl Pts',(-3.52042364447445,-2.97099856224363,
125.685192134177));
#151307=CARTESIAN_POINT('Ctrl Pts',(-3.52783642377653,-3.1060881820313,
125.766024139831));
#151308=CARTESIAN_POINT('Ctrl Pts',(-3.53524920307859,-3.23760135176302,
125.852000771032));
#151309=CARTESIAN_POINT('Ctrl Pts',(-3.54267257410736,-3.36930243367918,
125.938100249675));
#151310=CARTESIAN_POINT('Ctrl Pts',(-3.55009594513606,-3.49741655608301,
126.029358819219));
#151311=CARTESIAN_POINT('Ctrl Pts',(-3.55751931616481,-3.62153397346784,
126.125426738837));
#151312=CARTESIAN_POINT('Ctrl Pts',(-3.56145536560567,-3.68734400632288,
126.176364254937));
#151313=CARTESIAN_POINT('Ctrl Pts',(-3.56539141504655,-3.75203101532407,
126.22865321393));
#151314=CARTESIAN_POINT('Ctrl Pts',(-3.5693274644874,-3.81553819320636,
126.282237348715));
#151315=CARTESIAN_POINT('Ctrl Pts',(-3.57664552322221,-3.93361324912388,
126.381863090592));
#151316=CARTESIAN_POINT('Ctrl Pts',(-3.58396358195698,-4.04798671406309,
126.486287983218));
#151317=CARTESIAN_POINT('Ctrl Pts',(-3.59128164069176,-4.15823522630859,
126.595202701167));
#151318=CARTESIAN_POINT('Ctrl Pts',(-3.59859099504814,-4.26835260476512,
126.703987871793));
#151319=CARTESIAN_POINT('Ctrl Pts',(-3.6059003494045,-4.37435452104216,
126.817251975381));
#151320=CARTESIAN_POINT('Ctrl Pts',(-3.61320970376087,-4.47584943989803,
126.934644561592));
#151321=CARTESIAN_POINT('Ctrl Pts',(-3.62051206677417,-4.57724727961884,
127.051924862667));
#151322=CARTESIAN_POINT('Ctrl Pts',(-3.62781442978749,-4.67414645020482,
127.173325499512));
#151323=CARTESIAN_POINT('Ctrl Pts',(-3.63511679280077,-4.76619136037824,
127.29845838294));
#151324=CARTESIAN_POINT('Ctrl Pts',(-3.64247129342525,-4.85889345531905,
127.424484693552));
#151325=CARTESIAN_POINT('Ctrl Pts',(-3.64982579404971,-4.94667140748425,
127.554296489972));
#151326=CARTESIAN_POINT('Ctrl Pts',(-3.65718029467419,-5.02920194550765,
127.687461781575));
#151327=CARTESIAN_POINT('Ctrl Pts',(-3.66447414910763,-5.11105192572958,
127.819528974459));
#151328=CARTESIAN_POINT('Ctrl Pts',(-3.67176800354105,-5.18774050561212,
127.954894228281));
#151329=CARTESIAN_POINT('Ctrl Pts',(-3.67906185797449,-5.25899503833872,
128.093105972715));
#151330=CARTESIAN_POINT('Ctrl Pts',(-3.68635426495622,-5.33023543073724,
128.231290289287));
#151331=CARTESIAN_POINT('Ctrl Pts',(-3.69364667193797,-5.39604374529136,
128.372319630748));
#151332=CARTESIAN_POINT('Ctrl Pts',(-3.7009390789197,-5.45619311560956,
128.51571751571));
#151333=CARTESIAN_POINT('Ctrl Pts',(-3.70823157369812,-5.5163432100941,
128.659117127105));
#151334=CARTESIAN_POINT('Ctrl Pts',(-3.71552406847653,-5.57083407676291,
128.804884983558));
#151335=CARTESIAN_POINT('Ctrl Pts',(-3.72281656325495,-5.61948697861811,
128.952524593605));
#151336=CARTESIAN_POINT('Ctrl Pts',(-3.73021725029939,-5.66886170035249,
129.102354601375));
#151337=CARTESIAN_POINT('Ctrl Pts',(-3.73761793734379,-5.71222370981426,
129.254111961045));
#151338=CARTESIAN_POINT('Ctrl Pts',(-3.74501862438822,-5.74943886994097,
129.407262466643));
#151339=CARTESIAN_POINT('Ctrl Pts',(-3.75231896663071,-5.7861494353118,
129.558336427582));
#151340=CARTESIAN_POINT('Ctrl Pts',(-3.75961930887324,-5.81687876911714,
129.710765601758));
#151341=CARTESIAN_POINT('Ctrl Pts',(-3.76691965111573,-5.84154993401416,
129.864028266257));
#151342=CARTESIAN_POINT('Ctrl Pts',(-3.77437051056114,-5.86672976475309,
130.020450874058));
#151343=CARTESIAN_POINT('Ctrl Pts',(-3.7818213700065,-5.88559883849026,
130.177741294122));
#151344=CARTESIAN_POINT('Ctrl Pts',(-3.78927222945191,-5.89813120227993,
130.335341552717));
#151345=CARTESIAN_POINT('Ctrl Pts',(-3.79672308889732,-5.9106635660696,
130.492941811312));
#151346=CARTESIAN_POINT('Ctrl Pts',(-3.80417394834277,-5.91685925896518,
130.650851486073));
#151347=CARTESIAN_POINT('Ctrl Pts',(-3.81162480778818,-5.91674854110931,
130.808515588187));
#151348=CARTESIAN_POINT('',(-5.56162480778817,-5.92133943401158,130.799680554466));
#151349=CARTESIAN_POINT('Ctrl Pts',(-3.81162480778818,-5.92269048599951,
130.808519760851));
#151350=CARTESIAN_POINT('Ctrl Pts',(-3.82367490129221,-5.92472695610432,
131.063763701174));
#151351=CARTESIAN_POINT('Ctrl Pts',(-3.92854086940023,-5.79362457393622,
133.282917976605));
#151352=CARTESIAN_POINT('Ctrl Pts',(-4.1262227121134,-2.98891128428301,
137.132391106201));
#151353=CARTESIAN_POINT('Ctrl Pts',(-4.40467033592598,3.70837171184995,
136.739471381239));
#151354=CARTESIAN_POINT('Ctrl Pts',(-4.68311795973906,6.997842268822,130.892474810749));
#151355=CARTESIAN_POINT('Ctrl Pts',(-4.96156558355173,3.85663764434708,
124.96450560134));
#151356=CARTESIAN_POINT('Ctrl Pts',(-5.24001320736476,-2.82862856805823,
124.403077859063));
#151357=CARTESIAN_POINT('Ctrl Pts',(-5.44003294877681,-5.76368543459087,
128.225386373625));
#151358=CARTESIAN_POINT('Ctrl Pts',(-5.54723681558465,-5.92398027789449,
130.494734343713));
#151359=CARTESIAN_POINT('Ctrl Pts',(-5.56162480778817,-5.92133943401158,
130.799680554466));
#151360=CARTESIAN_POINT('',(-7.31162406064559,-5.91165886957557,130.802412404394));
#151361=CARTESIAN_POINT('Ctrl Pts',(-5.56162480778817,-5.92133943401158,
130.799680554466));
#151362=CARTESIAN_POINT('Ctrl Pts',(-5.64005269018895,-5.90694438913263,
132.4619198174));
#151363=CARTESIAN_POINT('Ctrl Pts',(-5.811296447194,-4.3084791224879,136.1155826924));
#151364=CARTESIAN_POINT('Ctrl Pts',(-6.0753560788034,1.89163637866986,137.542258831492));
#151365=CARTESIAN_POINT('Ctrl Pts',(-6.3538037026163,6.6912602630285,132.854871925206));
#151366=CARTESIAN_POINT('Ctrl Pts',(-6.63225132642916,5.34194285190056,
126.283165300243));
#151367=CARTESIAN_POINT('Ctrl Pts',(-6.91069895024212,-0.916359071709015,
123.86621629923));
#151368=CARTESIAN_POINT('Ctrl Pts',(-7.13715632573601,-5.32128556064457,
127.085904605724));
#151369=CARTESIAN_POINT('Ctrl Pts',(-7.27079782662573,-5.91005140945893,
129.93196890033));
#151370=CARTESIAN_POINT('Ctrl Pts',(-7.31162345291109,-5.90751794173804,
130.80240080057));
#151371=CARTESIAN_POINT('',(-9.06162556537631,-5.91501731293399,130.809728729937));
#151372=CARTESIAN_POINT('Ctrl Pts',(-7.31162480778818,-5.91674968393517,
130.802426670017));
#151373=CARTESIAN_POINT('Ctrl Pts',(-7.31920618702081,-5.91680260022219,
130.964319594534));
#151374=CARTESIAN_POINT('Ctrl Pts',(-7.32678756625346,-5.91020663906297,
131.126157705063));
#151375=CARTESIAN_POINT('Ctrl Pts',(-7.33436894548609,-5.89700160063828,
131.287374783579));
#151376=CARTESIAN_POINT('Ctrl Pts',(-7.34195464930973,-5.88378902975958,
131.448683823981));
#151377=CARTESIAN_POINT('Ctrl Pts',(-7.34954035313338,-5.86395989318124,
131.60937078082));
#151378=CARTESIAN_POINT('Ctrl Pts',(-7.35712605695701,-5.83760574229044,
131.768875915567));
#151379=CARTESIAN_POINT('Ctrl Pts',(-7.36471724504278,-5.81123253804941,
131.928496368285));
#151380=CARTESIAN_POINT('Ctrl Pts',(-7.37230843312853,-5.77832497003735,
132.086932953921));
#151381=CARTESIAN_POINT('Ctrl Pts',(-7.37989962121429,-5.73902546356901,
132.243637273045));
#151382=CARTESIAN_POINT('Ctrl Pts',(-7.3875031414854,-5.6996621134978,132.400596164534));
#151383=CARTESIAN_POINT('Ctrl Pts',(-7.39510666175654,-5.65388615734692,
132.555816829051));
#151384=CARTESIAN_POINT('Ctrl Pts',(-7.40271018202765,-5.60189000088908,
132.708765768903));
#151385=CARTESIAN_POINT('Ctrl Pts',(-7.41032018911973,-5.54984948474697,
132.861845194682));
#151386=CARTESIAN_POINT('Ctrl Pts',(-7.41793019621185,-5.49157830818657,
133.012648707527));
#151387=CARTESIAN_POINT('Ctrl Pts',(-7.42554020330394,-5.42731662350922,
133.160663830372));
#151388=CARTESIAN_POINT('Ctrl Pts',(-7.43316447032582,-5.36293452276646,
133.30895630976));
#151389=CARTESIAN_POINT('Ctrl Pts',(-7.44078873734768,-5.2925396253266,
133.45444964239));
#151390=CARTESIAN_POINT('Ctrl Pts',(-7.44841300436957,-5.21641829709212,
133.596655500322));
#151391=CARTESIAN_POINT('Ctrl Pts',(-7.45480673553567,-5.15258274315095,
133.715909721514));
#151392=CARTESIAN_POINT('Ctrl Pts',(-7.46120046670169,-5.08472090197207,
133.832852405316));
#151393=CARTESIAN_POINT('Ctrl Pts',(-7.46759419786778,-5.01302437116272,
133.947212382545));
#151394=CARTESIAN_POINT('Ctrl Pts',(-7.47501746427324,-4.92978307829047,
134.079986901058));
#151395=CARTESIAN_POINT('Ctrl Pts',(-7.48244073067869,-4.84113729034282,
134.209652823494));
#151396=CARTESIAN_POINT('Ctrl Pts',(-7.48986399708411,-4.7473458793924,
134.33573962072));
#151397=CARTESIAN_POINT('Ctrl Pts',(-7.49727848980512,-4.65366532210083,
134.461677393822));
#151398=CARTESIAN_POINT('Ctrl Pts',(-7.50469298252618,-4.55485146808713,
134.584044165415));
#151399=CARTESIAN_POINT('Ctrl Pts',(-7.51210747524718,-4.45120802225076,
134.702395725816));
#151400=CARTESIAN_POINT('Ctrl Pts',(-7.51951482160097,-4.34766447186931,
134.820633214528));
#151401=CARTESIAN_POINT('Ctrl Pts',(-7.52692216795465,-4.23930084102183,
134.934862917531));
#151402=CARTESIAN_POINT('Ctrl Pts',(-7.53432951430844,-4.12646282892634,
135.044671347217));
#151403=CARTESIAN_POINT('Ctrl Pts',(-7.54173133598383,-4.01370897567789,
135.154397877632));
#151404=CARTESIAN_POINT('Ctrl Pts',(-7.54913315765924,-3.89648765229909,
135.259709441377));
#151405=CARTESIAN_POINT('Ctrl Pts',(-7.55653497933463,-3.77518327665619,
135.360227361683));
#151406=CARTESIAN_POINT('Ctrl Pts',(-7.56393289364595,-3.6539429366493,
135.460692219362));
#151407=CARTESIAN_POINT('Ctrl Pts',(-7.57133080795728,-3.52862412369346,
135.556368235688));
#151408=CARTESIAN_POINT('Ctrl Pts',(-7.57872872226861,-3.39964629634104,
135.646915276243));
#151409=CARTESIAN_POINT('Ctrl Pts',(-7.58612540718083,-3.27068990276289,
135.737447269523));
#151410=CARTESIAN_POINT('Ctrl Pts',(-7.59352209209302,-3.13807600683679,
135.8228517644));
#151411=CARTESIAN_POINT('Ctrl Pts',(-7.60091877700523,-3.00225526314517,
135.902830377937));
#151412=CARTESIAN_POINT('Ctrl Pts',(-7.60831513394069,-2.86644054188765,
135.982805445138));
#151413=CARTESIAN_POINT('Ctrl Pts',(-7.6157114908761,-2.72741957726719,
136.057354919954));
#151414=CARTESIAN_POINT('Ctrl Pts',(-7.62310784781155,-2.58566974565933,
136.126225190146));
#151415=CARTESIAN_POINT('Ctrl Pts',(-7.63050533714813,-2.44389821179039,
136.195106004553));
#151416=CARTESIAN_POINT('Ctrl Pts',(-7.63790282648476,-2.29939731483277,
136.258305719899));
#151417=CARTESIAN_POINT('Ctrl Pts',(-7.64530031582134,-2.15266649036484,
136.315617964466));
#151418=CARTESIAN_POINT('Ctrl Pts',(-7.65270039833633,-2.00588422963427,
136.372950299751));
#151419=CARTESIAN_POINT('Ctrl Pts',(-7.66010048085135,-1.85687083253691,
136.424390919428));
#151420=CARTESIAN_POINT('Ctrl Pts',(-7.66750056336633,-1.70614290023417,
136.469782664199));
#151421=CARTESIAN_POINT('Ctrl Pts',(-7.67490878303281,-1.55524922707422,
136.515224321861));
#151422=CARTESIAN_POINT('Ctrl Pts',(-7.68231700269922,-1.40263761128612,
136.554603713706));
#151423=CARTESIAN_POINT('Ctrl Pts',(-7.68972522236569,-1.24883762586639,
136.587814183276));
#151424=CARTESIAN_POINT('Ctrl Pts',(-7.69713800166776,-1.09494297912192,
136.621045093335));
#151425=CARTESIAN_POINT('Ctrl Pts',(-7.70455078096983,-0.939858872187931,
136.648099451377));
#151426=CARTESIAN_POINT('Ctrl Pts',(-7.7119635602719,-0.784121582926229,
136.668922315228));
#151427=CARTESIAN_POINT('Ctrl Pts',(-7.71938693130066,-0.628161768922276,
136.689774931764));
#151428=CARTESIAN_POINT('Ctrl Pts',(-7.72681030232945,-0.471547279287036,
136.704378236555));
#151429=CARTESIAN_POINT('Ctrl Pts',(-7.7342336733582,-0.314816817708669,
136.712729337762));
#151430=CARTESIAN_POINT('Ctrl Pts',(-7.73816972279904,-0.231714566283128,
136.717157292004));
#151431=CARTESIAN_POINT('Ctrl Pts',(-7.74210577223987,-0.148579678551725,
136.719828398119));
#151432=CARTESIAN_POINT('Ctrl Pts',(-7.74604182168071,-0.0654919224773062,
136.720748144646));
#151433=CARTESIAN_POINT('Ctrl Pts',(-7.75346508808615,0.091208992397516,
136.722482757892));
#151434=CARTESIAN_POINT('Ctrl Pts',(-7.76088835449162,0.2482158189521,136.717990144255));
#151435=CARTESIAN_POINT('Ctrl Pts',(-7.76831162089707,0.40499276102326,
136.707233767653));
#151436=CARTESIAN_POINT('Ctrl Pts',(-7.77572611361809,0.56158440576863,
136.696490104195));
#151437=CARTESIAN_POINT('Ctrl Pts',(-7.78314060633911,0.717946338073995,
136.67949743928));
#151438=CARTESIAN_POINT('Ctrl Pts',(-7.79055509906013,0.873540671836888,
136.656271182257));
#151439=CARTESIAN_POINT('Ctrl Pts',(-7.7979624454139,1.02898503792266,136.633067311576));
#151440=CARTESIAN_POINT('Ctrl Pts',(-7.80536979176764,1.18366291161396,
136.603641864615));
#151441=CARTESIAN_POINT('Ctrl Pts',(-7.81277713812142,1.33703955520385,
136.568062187766));
#151442=CARTESIAN_POINT('Ctrl Pts',(-7.82017895979682,1.49030180470616,
136.532509047581));
#151443=CARTESIAN_POINT('Ctrl Pts',(-7.82758078147224,1.64226439443974,
136.490810900925));
#151444=CARTESIAN_POINT('Ctrl Pts',(-7.83498260314764,1.79240094566833,
136.44308648539));
#151445=CARTESIAN_POINT('Ctrl Pts',(-7.84238051745899,1.94245824098018,
136.395387263203));
#151446=CARTESIAN_POINT('Ctrl Pts',(-7.84977843177032,2.09069106268633,
136.341668220491));
#151447=CARTESIAN_POINT('Ctrl Pts',(-7.85717634608167,2.23658651847378,
136.282098408651));
#151448=CARTESIAN_POINT('Ctrl Pts',(-7.86457303099389,2.38245772908351,
136.222538496234));
#151449=CARTESIAN_POINT('Ctrl Pts',(-7.87196971590612,2.52599199942731,
136.157129885372));
#151450=CARTESIAN_POINT('Ctrl Pts',(-7.87936640081833,2.66669470167901,
136.086090441264));
#151451=CARTESIAN_POINT('Ctrl Pts',(-7.88676275775377,2.80739116502525,
136.015054147119));
#151452=CARTESIAN_POINT('Ctrl Pts',(-7.89415911468924,2.94525597669146,
135.938387684415));
#151453=CARTESIAN_POINT('Ctrl Pts',(-7.90155547162468,3.07981773192763,
135.856355599809));
#151454=CARTESIAN_POINT('Ctrl Pts',(-7.90895296096127,3.21440008891243,
135.77431095588));
#151455=CARTESIAN_POINT('Ctrl Pts',(-7.91635045029784,3.34567806377901,
135.686899248675));
#151456=CARTESIAN_POINT('Ctrl Pts',(-7.92374793963444,3.47320807302478,
135.594429118535));
#151457=CARTESIAN_POINT('Ctrl Pts',(-7.93114802214946,3.60078278771778,
135.501926573134));
#151458=CARTESIAN_POINT('Ctrl Pts',(-7.93854810466452,3.724606618912,135.404362293319));
#151459=CARTESIAN_POINT('Ctrl Pts',(-7.94594818717954,3.84426810849415,
135.302085961839));
#151460=CARTESIAN_POINT('Ctrl Pts',(-7.95335640684601,3.96406117818525,
135.199697167019));
#151461=CARTESIAN_POINT('Ctrl Pts',(-7.96076462651248,4.07968248190624,
135.092586215658));
#151462=CARTESIAN_POINT('Ctrl Pts',(-7.96817284617896,4.19075603941705,
134.981141002095));
#151463=CARTESIAN_POINT('Ctrl Pts',(-7.97558562548104,4.30189796084931,
134.869627195863));
#151464=CARTESIAN_POINT('Ctrl Pts',(-7.982998404783,4.40848630642737,134.753774085851));
#151465=CARTESIAN_POINT('Ctrl Pts',(-7.99041118408508,4.51018498046012,
134.634003160223));
#151466=CARTESIAN_POINT('Ctrl Pts',(-7.99783455511383,4.61202896632739,
134.514061100281));
#151467=CARTESIAN_POINT('Ctrl Pts',(-8.00525792614263,4.70896909740414,
134.390190337543));
#151468=CARTESIAN_POINT('Ctrl Pts',(-8.01268129717138,4.80071175820258,
134.262842535569));
#151469=CARTESIAN_POINT('Ctrl Pts',(-8.01661734661211,4.84935591829206,
134.195319675295));
#151470=CARTESIAN_POINT('Ctrl Pts',(-8.02055339605287,4.89653963301674,
134.126819737847));
#151471=CARTESIAN_POINT('Ctrl Pts',(-8.0244894454936,4.94222440350663,134.05741280096));
#151472=CARTESIAN_POINT('Ctrl Pts',(-8.03191271189902,5.02838445487897,
133.926513484105));
#151473=CARTESIAN_POINT('Ctrl Pts',(-8.03933597830439,5.10947071664635,
133.791990826852));
#151474=CARTESIAN_POINT('Ctrl Pts',(-8.04675924470982,5.18516283905393,
133.654275861042));
#151475=CARTESIAN_POINT('Ctrl Pts',(-8.05417373743083,5.26076549965877,
133.516723662884));
#151476=CARTESIAN_POINT('Ctrl Pts',(-8.06158823015184,5.33098653317177,
133.375986990381));
#151477=CARTESIAN_POINT('Ctrl Pts',(-8.06900272287285,5.39554816333842,
133.232526711472));
#151478=CARTESIAN_POINT('Ctrl Pts',(-8.07641006922662,5.46004756657512,
133.089204704982));
#151479=CARTESIAN_POINT('Ctrl Pts',(-8.08381741558041,5.51889827362221,
132.943164656302));
#151480=CARTESIAN_POINT('Ctrl Pts',(-8.09122476193417,5.57186790611307,
132.794892857779));
#151481=CARTESIAN_POINT('Ctrl Pts',(-8.09862658360956,5.62479803185367,
132.646731645957));
#151482=CARTESIAN_POINT('Ctrl Pts',(-8.10602840528499,5.671855691762,132.496342348608));
#151483=CARTESIAN_POINT('Ctrl Pts',(-8.11343022696039,5.71285626257538,
132.344232003641));
#151484=CARTESIAN_POINT('Ctrl Pts',(-8.12082814127174,5.75383518950658,
132.192201956542));
#151485=CARTESIAN_POINT('Ctrl Pts',(-8.12822605558308,5.78876329839053,
132.038453030722));
#151486=CARTESIAN_POINT('Ctrl Pts',(-8.13562396989443,5.8175055861331,131.883508113421));
#151487=CARTESIAN_POINT('Ctrl Pts',(-8.14302065480663,5.84624309742888,
131.728588945155));
#151488=CARTESIAN_POINT('Ctrl Pts',(-8.15041733971876,5.86879675978339,
131.572474546548));
#151489=CARTESIAN_POINT('Ctrl Pts',(-8.15781402463097,5.88508251093504,
131.415698823461));
#151490=CARTESIAN_POINT('Ctrl Pts',(-8.16521038156641,5.90136753995942,
131.258930051973));
#151491=CARTESIAN_POINT('Ctrl Pts',(-8.17260673850193,5.91138517182087,
131.10150038561));
#151492=CARTESIAN_POINT('Ctrl Pts',(-8.18000309543737,5.91510317133079,
130.943949424468));
#151493=CARTESIAN_POINT('Ctrl Pts',(-8.18740058477395,5.91882174007594,
130.786374341872));
#151494=CARTESIAN_POINT('Ctrl Pts',(-8.19479807411057,5.9162387472346,130.628678300737));
#151495=CARTESIAN_POINT('Ctrl Pts',(-8.20219556344716,5.90737409294855,
130.471401328072));
#151496=CARTESIAN_POINT('Ctrl Pts',(-8.20959564596219,5.89850633117166,
130.314069222208));
#151497=CARTESIAN_POINT('Ctrl Pts',(-8.21699572847713,5.88335254472493,
130.157156849771));
#151498=CARTESIAN_POINT('Ctrl Pts',(-8.22439581099215,5.86198452844846,
130.001199394192));
#151499=CARTESIAN_POINT('Ctrl Pts',(-8.23180403065861,5.8405930158415,129.84507044736));
#151500=CARTESIAN_POINT('Ctrl Pts',(-8.23921225032514,5.81297367779061,
129.689898884433));
#151501=CARTESIAN_POINT('Ctrl Pts',(-8.2466204699916,5.77924963428516,129.536210694602));
#151502=CARTESIAN_POINT('Ctrl Pts',(-8.25403324929363,5.74550483419375,
129.382427912254));
#151503=CARTESIAN_POINT('Ctrl Pts',(-8.26144602859567,5.70564793595996,
129.23013068255));
#151504=CARTESIAN_POINT('Ctrl Pts',(-8.26885880789771,5.65985188158431,
129.079829596962));
#151505=CARTESIAN_POINT('Ctrl Pts',(-8.27628217892648,5.61399039165835,
128.929313754133));
#151506=CARTESIAN_POINT('Ctrl Pts',(-8.2837055499552,5.56217291950594,128.7808001034));
#151507=CARTESIAN_POINT('Ctrl Pts',(-8.29112892098397,5.50462075612902,
128.634779806973));
#151508=CARTESIAN_POINT('Ctrl Pts',(-8.29506497042482,5.47410521816088,
128.557356342097));
#151509=CARTESIAN_POINT('Ctrl Pts',(-8.29900101986567,5.4419782311007,128.48063345719));
#151510=CARTESIAN_POINT('Ctrl Pts',(-8.30293706930652,5.40827794375211,
128.404681421168));
#151511=CARTESIAN_POINT('Ctrl Pts',(-8.31036033571196,5.34472025356365,
128.261438251615));
#151512=CARTESIAN_POINT('Ctrl Pts',(-8.31778360211739,5.27537163726404,
128.120505300964));
#151513=CARTESIAN_POINT('Ctrl Pts',(-8.32520686852283,5.20042157728153,
127.982385071775));
#151514=CARTESIAN_POINT('Ctrl Pts',(-8.33262136124384,5.12556010204561,
127.844428089226));
#151515=CARTESIAN_POINT('Ctrl Pts',(-8.34003585396484,5.04511053745627,
127.709277535795));
#151516=CARTESIAN_POINT('Ctrl Pts',(-8.34745034668586,4.95931047991477,
127.577416222894));
#151517=CARTESIAN_POINT('Ctrl Pts',(-8.35485769303963,4.87359311969916,
127.44568200289));
#151518=CARTESIAN_POINT('Ctrl Pts',(-8.36226503939338,4.78253573534287,
127.317231022774));
#151519=CARTESIAN_POINT('Ctrl Pts',(-8.36967238574715,4.68642185218623,
127.19252164194));
#151520=CARTESIAN_POINT('Ctrl Pts',(-8.37707420742253,4.59037965439009,
127.067905274067));
#151521=CARTESIAN_POINT('Ctrl Pts',(-8.384476029098,4.48928869391211,126.947025243365));
#151522=CARTESIAN_POINT('Ctrl Pts',(-8.39187785077337,4.38347576272227,
126.830310944987));
#151523=CARTESIAN_POINT('Ctrl Pts',(-8.39927576508479,4.27771868935379,
126.713658259177));
#151524=CARTESIAN_POINT('Ctrl Pts',(-8.40667367939615,4.16724485968297,
126.601167202025));
#151525=CARTESIAN_POINT('Ctrl Pts',(-8.41407159370758,4.05242122108274,
126.493233988781));
#151526=CARTESIAN_POINT('Ctrl Pts',(-8.42146827861979,3.93761666408912,
126.38531871208));
#151527=CARTESIAN_POINT('Ctrl Pts',(-8.42886496353199,3.81846400455809,
126.281960031435));
#151528=CARTESIAN_POINT('Ctrl Pts',(-8.4362616484442,3.69536699490435,126.183517259966));
#151529=CARTESIAN_POINT('Ctrl Pts',(-8.44365800537966,3.57227544350102,
126.085078853553));
#151530=CARTESIAN_POINT('Ctrl Pts',(-8.45105436231505,3.44524018126523,
125.991556156052));
#151531=CARTESIAN_POINT('Ctrl Pts',(-8.45845071925049,3.31469776513331,
125.903267954871));
#151532=CARTESIAN_POINT('Ctrl Pts',(-8.46584820858705,3.18413536262459,
125.814966236542));
#151533=CARTESIAN_POINT('Ctrl Pts',(-8.47324569792369,3.0500650463107,125.731900819401));
#151534=CARTESIAN_POINT('Ctrl Pts',(-8.48064318726026,2.9129519127197,125.654346858683));
#151535=CARTESIAN_POINT('Ctrl Pts',(-8.48804326977528,2.77579071433149,
125.576765711544));
#151536=CARTESIAN_POINT('Ctrl Pts',(-8.49544335229031,2.6355848996846,125.504700051159));
#151537=CARTESIAN_POINT('Ctrl Pts',(-8.50284343480533,2.49282354062182,
125.438378754214));
#151538=CARTESIAN_POINT('Ctrl Pts',(-8.51025165447179,2.34990520076914,
125.371984530185));
#151539=CARTESIAN_POINT('Ctrl Pts',(-8.51765987413826,2.20442604333549,
125.31134744147));
#151540=CARTESIAN_POINT('Ctrl Pts',(-8.52506809380472,2.05689514728419,
125.256648213739));
#151541=CARTESIAN_POINT('Ctrl Pts',(-8.53248087310678,1.90927344842785,
125.201915319546));
#151542=CARTESIAN_POINT('Ctrl Pts',(-8.53989365240889,1.75959784874113,
125.153127684114));
#151543=CARTESIAN_POINT('Ctrl Pts',(-8.54730643171095,1.6083914026664,125.110415793604));
#151544=CARTESIAN_POINT('Ctrl Pts',(-8.55472980273972,1.45696890573042,
125.067642874341));
#151545=CARTESIAN_POINT('Ctrl Pts',(-8.56215317376846,1.30401155583226,
125.030963125341));
#151546=CARTESIAN_POINT('Ctrl Pts',(-8.56957654479723,1.15005219484346,
125.000455853389));
#151547=CARTESIAN_POINT('Ctrl Pts',(-8.57351259423796,1.06841924744448,
124.984280165789));
#151548=CARTESIAN_POINT('Ctrl Pts',(-8.57744864367869,0.986504690218252,
124.969838916533));
#151549=CARTESIAN_POINT('Ctrl Pts',(-8.58138469311942,0.904388262755151,
124.957137992021));
#151550=CARTESIAN_POINT('Ctrl Pts',(-8.58880795952485,0.749519243323195,
124.933184444771));
#151551=CARTESIAN_POINT('Ctrl Pts',(-8.59623122593032,0.593463739467604,
124.915351697413));
#151552=CARTESIAN_POINT('Ctrl Pts',(-8.60365449233575,0.436746940704876,
124.903751947921));
#151553=CARTESIAN_POINT('Ctrl Pts',(-8.61106898505675,0.280215368183765,
124.89216590837));
#151554=CARTESIAN_POINT('Ctrl Pts',(-8.61848347777772,0.123024425170152,
124.886798230144));
#151555=CARTESIAN_POINT('Ctrl Pts',(-8.62589797049873,-0.0342912587645142,
124.887709988023));
#151556=CARTESIAN_POINT('Ctrl Pts',(-8.63330531685251,-0.191455315920397,
124.888620867115));
#151557=CARTESIAN_POINT('Ctrl Pts',(-8.6407126632062,-0.348743503857413,
124.895799131111));
#151558=CARTESIAN_POINT('Ctrl Pts',(-8.64812000955999,-0.505616939465063,
124.90925399656));
#151559=CARTESIAN_POINT('Ctrl Pts',(-8.65552183123537,-0.66237337294527,
124.922698826863));
#151560=CARTESIAN_POINT('Ctrl Pts',(-8.66292365291083,-0.818715299698069,
124.942410905705));
#151561=CARTESIAN_POINT('Ctrl Pts',(-8.67032547458621,-0.974104818376584,
124.968347392314));
#151562=CARTESIAN_POINT('Ctrl Pts',(-8.67772338889763,-1.12941230813973,
124.994270187255));
#151563=CARTESIAN_POINT('Ctrl Pts',(-8.68512130320901,-1.28376802384472,
125.0264107848));
#151564=CARTESIAN_POINT('Ctrl Pts',(-8.69251921752044,-1.43664027436086,
125.064674625756));
#151565=CARTESIAN_POINT('Ctrl Pts',(-8.69991590243266,-1.58948712028103,
125.102932107954));
#151566=CARTESIAN_POINT('Ctrl Pts',(-8.70731258734491,-1.74085062851949,
125.147310723432));
#151567=CARTESIAN_POINT('Ctrl Pts',(-8.71470927225712,-1.89021026072991,
125.197665001365));
#151568=CARTESIAN_POINT('Ctrl Pts',(-8.72210562919258,-2.03956327017773,
125.248017046536));
#151569=CARTESIAN_POINT('Ctrl Pts',(-8.72950198612796,-2.18691222653348,
125.304344108062));
#151570=CARTESIAN_POINT('Ctrl Pts',(-8.73689834306342,-2.33175295523339,
125.36645121061));
#151571=CARTESIAN_POINT('Ctrl Pts',(-8.74429583239997,-2.476615859418,125.428567821914));
#151572=CARTESIAN_POINT('Ctrl Pts',(-8.75169332173665,-2.61896942821068,
125.496466089147));
#151573=CARTESIAN_POINT('Ctrl Pts',(-8.75909081107321,-2.75833076968514,
125.569903441554));
#151574=CARTESIAN_POINT('Ctrl Pts',(-8.76649089358819,-2.89774096406203,
125.643366537311));
#151575=CARTESIAN_POINT('Ctrl Pts',(-8.7738909761031,-3.03415651268254,
125.722372410268));
#151576=CARTESIAN_POINT('Ctrl Pts',(-8.78129105861808,-3.16712049983219,
125.806633303872));
#151577=CARTESIAN_POINT('Ctrl Pts',(-8.78869927828456,-3.30023069455512,
125.890986850991));
#151578=CARTESIAN_POINT('Ctrl Pts',(-8.79610749795097,-3.42988143274203,
125.98060675873));
#151579=CARTESIAN_POINT('Ctrl Pts',(-8.80351571761744,-3.55564549515307,
126.075162411179));
#151580=CARTESIAN_POINT('Ctrl Pts',(-8.81092849691953,-3.6814869632464,
126.169776261054));
#151581=CARTESIAN_POINT('Ctrl Pts',(-8.81834127622162,-3.80343670033355,
126.269331673449));
#151582=CARTESIAN_POINT('Ctrl Pts',(-8.8257540555237,-3.92110220101021,
126.373459118804));
#151583=CARTESIAN_POINT('Ctrl Pts',(-8.83317742655246,-4.03893582767187,
126.477735346336));
#151584=CARTESIAN_POINT('Ctrl Pts',(-8.84060079758134,-4.15247272314095,
126.586596396495));
#151585=CARTESIAN_POINT('Ctrl Pts',(-8.8480241686101,-4.26135815032544,
126.699636841579));
#151586=CARTESIAN_POINT('Ctrl Pts',(-8.85196021805085,-4.31909181648815,
126.75957359793));
#151587=CARTESIAN_POINT('Ctrl Pts',(-8.85589626749153,-4.37551846753956,
126.820684786896));
#151588=CARTESIAN_POINT('Ctrl Pts',(-8.85983231693228,-4.43059004989061,
126.882906503043));
#151589=CARTESIAN_POINT('Ctrl Pts',(-8.86718970865023,-4.53353164398957,
126.999213359942));
#151590=CARTESIAN_POINT('Ctrl Pts',(-8.87454710036816,-4.63206126020542,
127.119769697859));
#151591=CARTESIAN_POINT('Ctrl Pts',(-8.88190449208611,-4.7258026946892,
127.244203394441));
#151592=CARTESIAN_POINT('Ctrl Pts',(-8.8893928385737,-4.82121264002974,
127.370851895766));
#151593=CARTESIAN_POINT('Ctrl Pts',(-8.89688118506131,-4.91166201865871,
127.501516857651));
#151594=CARTESIAN_POINT('Ctrl Pts',(-8.90436953154889,-4.9967929033199,
127.635766095726));
#151595=CARTESIAN_POINT('Ctrl Pts',(-8.91170891505276,-5.08023030990724,
127.767344761988));
#151596=CARTESIAN_POINT('Ctrl Pts',(-8.91904829855669,-5.15855859255118,
127.902366116144));
#151597=CARTESIAN_POINT('Ctrl Pts',(-8.92638768206055,-5.23148127387495,
128.04038987901));
#151598=CARTESIAN_POINT('Ctrl Pts',(-8.93372207269983,-5.30435434707122,
128.178319746529));
#151599=CARTESIAN_POINT('Ctrl Pts',(-8.94105646333905,-5.3718289589588,
128.319247623731));
#151600=CARTESIAN_POINT('Ctrl Pts',(-8.94839085397834,-5.43365278803803,
128.462705659732));
#151601=CARTESIAN_POINT('Ctrl Pts',(-8.95572176758381,-5.49544730813234,
128.606095686206));
#151602=CARTESIAN_POINT('Ctrl Pts',(-8.96305268118929,-5.55159622698705,
128.75201313542));
#151603=CARTESIAN_POINT('Ctrl Pts',(-8.97038359479475,-5.60189401281919,
128.899967267535));
#151604=CARTESIAN_POINT('Ctrl Pts',(-8.97798702921087,-5.65406157834139,
129.053421475385));
#151605=CARTESIAN_POINT('Ctrl Pts',(-8.98559046362695,-5.69993441543101,
129.209066325241));
#151606=CARTESIAN_POINT('Ctrl Pts',(-8.99319389804307,-5.73933868459386,
129.366333487772));
#151607=CARTESIAN_POINT('Ctrl Pts',(-9.00052389561581,-5.77732588636504,
129.517944964445));
#151608=CARTESIAN_POINT('Ctrl Pts',(-9.0078538931886,-5.80930162471794,
129.671063696745));
#151609=CARTESIAN_POINT('Ctrl Pts',(-9.01518389076134,-5.83516163910139,
129.82516747622));
#151610=CARTESIAN_POINT('Ctrl Pts',(-9.02251469196999,-5.86102448868856,
129.979288151107));
#151611=CARTESIAN_POINT('Ctrl Pts',(-9.02984549317875,-5.88077022376458,
130.13439371172));
#151612=CARTESIAN_POINT('Ctrl Pts',(-9.03717629438742,-5.89434619599635,
130.289954664798));
#151613=CARTESIAN_POINT('Ctrl Pts',(-9.0445110515798,-5.90792949434753,
130.445599564579));
#151614=CARTESIAN_POINT('Ctrl Pts',(-9.05184580877206,-5.91533636109181,
130.601699967749));
#151615=CARTESIAN_POINT('Ctrl Pts',(-9.05918056596443,-5.91656619986861,
130.757724096767));
#151616=CARTESIAN_POINT('Ctrl Pts',(-9.05999531323902,-5.91670281077001,
130.775055309042));
#151617=CARTESIAN_POINT('Ctrl Pts',(-9.06081006051364,-5.91676325721273,
130.792385582182));
#151618=CARTESIAN_POINT('Ctrl Pts',(-9.06162480778823,-5.91674757799995,
130.80971418943));
#151619=CARTESIAN_POINT('',(-10.8116248077882,-5.92210306258463,130.804007665308));
#151620=CARTESIAN_POINT('Ctrl Pts',(-9.06162590728991,-5.91423641208638,
130.809735292338));
#151621=CARTESIAN_POINT('Ctrl Pts',(-9.087177251775,-5.91897718201145,131.352952955589));
#151622=CARTESIAN_POINT('Ctrl Pts',(-9.20554447086439,-5.6009174926255,
133.863968248938));
#151623=CARTESIAN_POINT('Ctrl Pts',(-9.41672756455816,-2.040325974115,137.498733661377));
#151624=CARTESIAN_POINT('Ctrl Pts',(-9.69517518837099,4.52931960951324,
136.139416793954));
#151625=CARTESIAN_POINT('Ctrl Pts',(-9.9736228121838,6.93674174156142,129.877443932418));
#151626=CARTESIAN_POINT('Ctrl Pts',(-10.2520704359968,2.96963709179157,
124.467262222132));
#151627=CARTESIAN_POINT('Ctrl Pts',(-10.5305180598095,-3.72641897050015,
124.880564352784));
#151628=CARTESIAN_POINT('Ctrl Pts',(-10.7170361837401,-5.91793960293745,
128.803863058467));
#151629=CARTESIAN_POINT('Ctrl Pts',(-10.8107384330663,-5.92652287167294,
130.785264230727));
#151630=CARTESIAN_POINT('Ctrl Pts',(-10.8116248077882,-5.92650673784803,
130.804007402853));
#151631=CARTESIAN_POINT('',(-12.5616247901692,-5.91448392200524,130.799179299216));
#151632=CARTESIAN_POINT('Ctrl Pts',(-10.8116248077882,-5.91674998949168,
130.804007984347));
#151633=CARTESIAN_POINT('Ctrl Pts',(-10.8190355189351,-5.91675931365845,
130.960455989369));
#151634=CARTESIAN_POINT('Ctrl Pts',(-10.826446230082,-5.91055926251472,
131.117144690899));
#151635=CARTESIAN_POINT('Ctrl Pts',(-10.833856941229,-5.89811849125637,
131.273539502001));
#151636=CARTESIAN_POINT('Ctrl Pts',(-10.8412588941427,-5.88569242292915,
131.429749480339));
#151637=CARTESIAN_POINT('Ctrl Pts',(-10.8486608470566,-5.86704034398258,
131.585665889726));
#151638=CARTESIAN_POINT('Ctrl Pts',(-10.8560627999703,-5.84218287332432,
131.740752542529));
#151639=CARTESIAN_POINT('Ctrl Pts',(-10.8634576340751,-5.81734930927392,
131.895690041146));
#151640=CARTESIAN_POINT('Ctrl Pts',(-10.8708524681798,-5.78632229287438,
132.049799004285));
#151641=CARTESIAN_POINT('Ctrl Pts',(-10.8782473022846,-5.74917434773922,
132.202546900504));
#151642=CARTESIAN_POINT('Ctrl Pts',(-10.8856366512894,-5.71205395700066,
132.355181496349));
#151643=CARTESIAN_POINT('Ctrl Pts',(-10.8930260002943,-5.66882176532332,
132.506456672812));
#151644=CARTESIAN_POINT('Ctrl Pts',(-10.9004153492991,-5.61960160090809,
132.655848778363));
#151645=CARTESIAN_POINT('Ctrl Pts',(-10.9078008424935,-5.57040711989483,
132.805162930142));
#151646=CARTESIAN_POINT('Ctrl Pts',(-10.9151863356879,-5.5152310055336,
132.952595612798));
#151647=CARTESIAN_POINT('Ctrl Pts',(-10.9225718288824,-5.45424725585621,
133.097637189305));
#151648=CARTESIAN_POINT('Ctrl Pts',(-10.9299561642655,-5.39327306649797,
133.242656027888));
#151649=CARTESIAN_POINT('Ctrl Pts',(-10.9373404996487,-5.32649319331895,
133.38528415894));
#151650=CARTESIAN_POINT('Ctrl Pts',(-10.9447248350319,-5.25413024738925,
133.525030738321));
#151651=CARTESIAN_POINT('Ctrl Pts',(-10.9521089113768,-5.18176983991028,
133.664772415472));
#151652=CARTESIAN_POINT('Ctrl Pts',(-10.9594929877217,-5.10382692130971,
133.801632409126));
#151653=CARTESIAN_POINT('Ctrl Pts',(-10.9668770640667,-5.0205705190883,
133.93514362272));
#151654=CARTESIAN_POINT('Ctrl Pts',(-10.9742623525782,-4.93730044953324,
134.068676753455));
#151655=CARTESIAN_POINT('Ctrl Pts',(-10.9816476410899,-4.84871535804594,
134.198859691677));
#151656=CARTESIAN_POINT('Ctrl Pts',(-10.9890329296015,-4.75512803777965,
134.325253672861));
#151657=CARTESIAN_POINT('Ctrl Pts',(-10.996420901947,-4.66150670762611,
134.451693585961));
#151658=CARTESIAN_POINT('Ctrl Pts',(-11.0038088742926,-4.5628797525375,
134.574341499877));
#151659=CARTESIAN_POINT('Ctrl Pts',(-11.0111968466382,-4.45960061714789,
134.69279126476));
#151660=CARTESIAN_POINT('Ctrl Pts',(-11.0185929605209,-4.356207668269,134.811371561148));
#151661=CARTESIAN_POINT('Ctrl Pts',(-11.0259890744035,-4.24815254817928,
134.925744187803));
#151662=CARTESIAN_POINT('Ctrl Pts',(-11.0333851882862,-4.13582645113043,
135.035538955645));
#151663=CARTESIAN_POINT('Ctrl Pts',(-11.0407859638256,-4.02342955667067,
135.14540292544));
#151664=CARTESIAN_POINT('Ctrl Pts',(-11.0481867393651,-3.90675659927995,
135.250683037295));
#151665=CARTESIAN_POINT('Ctrl Pts',(-11.0555875149045,-3.78623184874473,
135.351049407229));
#151666=CARTESIAN_POINT('Ctrl Pts',(-11.0629986690587,-3.66553807809285,
135.451556527802));
#151667=CARTESIAN_POINT('Ctrl Pts',(-11.0704098232127,-3.54098202428191,
135.547135919064));
#151668=CARTESIAN_POINT('Ctrl Pts',(-11.0778209773669,-3.41301750281109,
135.637500599814));
#151669=CARTESIAN_POINT('Ctrl Pts',(-11.081018420723,-3.35780892119289,
135.676487232947));
#151670=CARTESIAN_POINT('Ctrl Pts',(-11.0842158640792,-3.30196621716772,
135.714503788482));
#151671=CARTESIAN_POINT('Ctrl Pts',(-11.0874133074354,-3.24552719218759,
135.751529889713));
#151672=CARTESIAN_POINT('Ctrl Pts',(-11.0948365738408,-3.11449690598059,
135.837490634836));
#151673=CARTESIAN_POINT('Ctrl Pts',(-11.1022598402462,-2.97985100501508,
135.918372082122));
#151674=CARTESIAN_POINT('Ctrl Pts',(-11.1096831066517,-2.84202100815124,
135.993854538145));
#151675=CARTESIAN_POINT('Ctrl Pts',(-11.1170975993727,-2.70435391489762,
136.069247780173));
#151676=CARTESIAN_POINT('Ctrl Pts',(-11.1245120920937,-2.5635105409054,
136.139254555114));
#151677=CARTESIAN_POINT('Ctrl Pts',(-11.1319265848147,-2.41995217631083,
136.203597788396));
#151678=CARTESIAN_POINT('Ctrl Pts',(-11.1393339311685,-2.27653217867294,
136.267879005247));
#151679=CARTESIAN_POINT('Ctrl Pts',(-11.1467412775222,-2.13040273834685,
136.326507396052));
#151680=CARTESIAN_POINT('Ctrl Pts',(-11.154148623876,-1.9820505007563,136.379251322768));
#151681=CARTESIAN_POINT('Ctrl Pts',(-11.1615504455514,-1.83380890986177,
136.431955911074));
#151682=CARTESIAN_POINT('Ctrl Pts',(-11.1689522672268,-1.68334817291361,
136.47878464958));
#151683=CARTESIAN_POINT('Ctrl Pts',(-11.1763540889022,-1.53117560819909,
136.519553686864));
#151684=CARTESIAN_POINT('Ctrl Pts',(-11.1837520032136,-1.37908337419568,
136.560301202491));
#151685=CARTESIAN_POINT('Ctrl Pts',(-11.191149917525,-1.22528147177775,
136.594995291237));
#151686=CARTESIAN_POINT('Ctrl Pts',(-11.1985478318364,-1.07029299303037,
136.623501745909));
#151687=CARTESIAN_POINT('Ctrl Pts',(-11.2059445167486,-0.915330270557275,
136.652003463325));
#151688=CARTESIAN_POINT('Ctrl Pts',(-11.2133412016608,-0.759181729893625,
136.674319520023));
#151689=CARTESIAN_POINT('Ctrl Pts',(-11.220737886573,-0.602381404208926,
136.690366666354));
#151690=CARTESIAN_POINT('Ctrl Pts',(-11.2281342435084,-0.445588031215432,
136.706413101137));
#151691=CARTESIAN_POINT('Ctrl Pts',(-11.2355306004439,-0.288143302023389,
136.716191140245));
#151692=CARTESIAN_POINT('Ctrl Pts',(-11.2429269573793,-0.130586865160602,
136.719669369706));
#151693=CARTESIAN_POINT('Ctrl Pts',(-11.2503244467159,0.0269936939955663,
136.723148131694));
#151694=CARTESIAN_POINT('Ctrl Pts',(-11.2577219360525,0.184685621645346,
136.720325155313));
#151695=CARTESIAN_POINT('Ctrl Pts',(-11.2651194253891,0.341948921691745,
136.711221162513));
#151696=CARTESIAN_POINT('Ctrl Pts',(-11.2725195079042,0.499267350144185,
136.702113978323));
#151697=CARTESIAN_POINT('Ctrl Pts',(-11.2799195904191,0.656156479395662,
136.686721415504));
#151698=CARTESIAN_POINT('Ctrl Pts',(-11.2873196729341,0.812081235894015,
136.665116083273));
#151699=CARTESIAN_POINT('Ctrl Pts',(-11.2947278926006,0.968177447691148,
136.643486993757));
#151700=CARTESIAN_POINT('Ctrl Pts',(-11.3021361122671,1.12330679900085,
136.615631542985));
#151701=CARTESIAN_POINT('Ctrl Pts',(-11.3095443319335,1.27694348861063,
136.581673651269));
#151702=CARTESIAN_POINT('Ctrl Pts',(-11.3169571112356,1.43067473903929,
136.547694859037));
#151703=CARTESIAN_POINT('Ctrl Pts',(-11.3243698905376,1.58291113697194,
136.507606236499));
#151704=CARTESIAN_POINT('Ctrl Pts',(-11.3317826698397,1.73314235471533,
136.461581502487));
#151705=CARTESIAN_POINT('Ctrl Pts',(-11.3392060408685,1.883588229868,136.415491006178));
#151706=CARTESIAN_POINT('Ctrl Pts',(-11.3466294118972,2.03202285125357,
136.363447581534));
#151707=CARTESIAN_POINT('Ctrl Pts',(-11.354052782926,2.1779553939957,136.305673266768));
#151708=CARTESIAN_POINT('Ctrl Pts',(-11.3579888323667,2.25533232976046,
136.275039938803));
#151709=CARTESIAN_POINT('Ctrl Pts',(-11.3619248818075,2.33200623401698,
136.242796229776));
#151710=CARTESIAN_POINT('Ctrl Pts',(-11.3658609312483,2.40790689598538,
136.208980395383));
#151711=CARTESIAN_POINT('Ctrl Pts',(-11.3732841976537,2.55105317568001,
136.145204787073));
#151712=CARTESIAN_POINT('Ctrl Pts',(-11.3807074640591,2.69188042634453,
136.075641775118));
#151713=CARTESIAN_POINT('Ctrl Pts',(-11.3881307304646,2.82988643436045,
136.00048160645));
#151714=CARTESIAN_POINT('Ctrl Pts',(-11.3955452231856,2.96772933073578,
135.92541027086));
#151715=CARTESIAN_POINT('Ctrl Pts',(-11.4029597159066,3.10275729712157,
135.844755123294));
#151716=CARTESIAN_POINT('Ctrl Pts',(-11.4103742086276,3.23448788424841,
135.758754494636));
#151717=CARTESIAN_POINT('Ctrl Pts',(-11.4177815549814,3.36609150447582,
135.672836756622));
#151718=CARTESIAN_POINT('Ctrl Pts',(-11.4251889013352,3.49440376200909,
135.581583997183));
#151719=CARTESIAN_POINT('Ctrl Pts',(-11.432596247689,3.61896672946355,135.485280438876));
#151720=CARTESIAN_POINT('Ctrl Pts',(-11.4399980693644,3.74343679315774,
135.389048707396));
#151721=CARTESIAN_POINT('Ctrl Pts',(-11.4473998910398,3.86416284065097,
135.28777390515));
#151722=CARTESIAN_POINT('Ctrl Pts',(-11.4548017127152,3.9807159746075,135.181783477195));
#151723=CARTESIAN_POINT('Ctrl Pts',(-11.4621996270266,4.09720758107121,
135.075849000763));
#151724=CARTESIAN_POINT('Ctrl Pts',(-11.4695975413379,4.20953038559673,
134.965204106781));
#151725=CARTESIAN_POINT('Ctrl Pts',(-11.4769954556492,4.31728873182291,
134.850216345169));
#151726=CARTESIAN_POINT('Ctrl Pts',(-11.4843921405615,4.42502917056719,
134.735247692436));
#151727=CARTESIAN_POINT('Ctrl Pts',(-11.4917888254737,4.52820640145996,
134.615937876565));
#151728=CARTESIAN_POINT('Ctrl Pts',(-11.4991855103859,4.62646172623994,
134.492691196315));
#151729=CARTESIAN_POINT('Ctrl Pts',(-11.5065818673213,4.72471269427572,
134.369449980953));
#151730=CARTESIAN_POINT('Ctrl Pts',(-11.5139782242569,4.81804195743561,
134.242272540197));
#151731=CARTESIAN_POINT('Ctrl Pts',(-11.5213745811923,4.90613139304453,
134.111595915618));
#151732=CARTESIAN_POINT('Ctrl Pts',(-11.5287720705289,4.99423431537117,
133.980899284115));
#151733=CARTESIAN_POINT('Ctrl Pts',(-11.5361695598654,5.07709560412569,
133.846702711627));
#151734=CARTESIAN_POINT('Ctrl Pts',(-11.543567049202,5.15444081218917,133.709471712884));
#151735=CARTESIAN_POINT('Ctrl Pts',(-11.550967131717,5.23181313349533,133.572192608027));
#151736=CARTESIAN_POINT('Ctrl Pts',(-11.558367214232,5.30366534104637,133.431877284069));
#151737=CARTESIAN_POINT('Ctrl Pts',(-11.565767296747,5.36976930270644,133.289015160598));
#151738=CARTESIAN_POINT('Ctrl Pts',(-11.5731755164135,5.43594595246811,
133.145995945536));
#151739=CARTESIAN_POINT('Ctrl Pts',(-11.58058373608,5.49636157645428,133.000424677238));
#151740=CARTESIAN_POINT('Ctrl Pts',(-11.5879919557464,5.55083622393497,
132.852810709111));
#151741=CARTESIAN_POINT('Ctrl Pts',(-11.5954047350485,5.60534439965208,
132.705105887051));
#151742=CARTESIAN_POINT('Ctrl Pts',(-11.6028175143506,5.65390419780506,
132.55535621421));
#151743=CARTESIAN_POINT('Ctrl Pts',(-11.6102302936526,5.69638592838495,
132.404084943004));
#151744=CARTESIAN_POINT('Ctrl Pts',(-11.6176536646814,5.73892835885381,
132.252597528311));
#151745=CARTESIAN_POINT('Ctrl Pts',(-11.6250770357102,5.77537529033085,
132.099584535201));
#151746=CARTESIAN_POINT('Ctrl Pts',(-11.632500406739,5.8056482270167,131.94557892562));
#151747=CARTESIAN_POINT('Ctrl Pts',(-11.6364364561797,5.82169966443649,
131.863921456107));
#151748=CARTESIAN_POINT('Ctrl Pts',(-11.6403725056204,5.83601623695736,
131.781985016613));
#151749=CARTESIAN_POINT('Ctrl Pts',(-11.6443085550612,5.84859217953896,
131.699849355594));
#151750=CARTESIAN_POINT('Ctrl Pts',(-11.6517318214666,5.87231001476642,
131.544944062277));
#151751=CARTESIAN_POINT('Ctrl Pts',(-11.659155087872,5.88990525156296,131.388861600725));
#151752=CARTESIAN_POINT('Ctrl Pts',(-11.6665783542775,5.90126649133266,
131.232127330594));
#151753=CARTESIAN_POINT('Ctrl Pts',(-11.6739928469985,5.91261430306044,
131.075578307353));
#151754=CARTESIAN_POINT('Ctrl Pts',(-11.6814073397195,5.91774275721396,
130.918379377672));
#151755=CARTESIAN_POINT('Ctrl Pts',(-11.6888218324405,5.91659159270028,
130.761065263446));
#151756=CARTESIAN_POINT('Ctrl Pts',(-11.6962291787943,5.9154415377223,130.603902774486));
#151757=CARTESIAN_POINT('Ctrl Pts',(-11.7036365251481,5.90802391619174,
130.446625692782));
#151758=CARTESIAN_POINT('Ctrl Pts',(-11.7110438715019,5.8943303316585,130.289772914846));
#151759=CARTESIAN_POINT('Ctrl Pts',(-11.7184456931773,5.88064696031722,
130.133037123629));
#151760=CARTESIAN_POINT('Ctrl Pts',(-11.7258475148528,5.86069697850371,
129.976725376345));
#151761=CARTESIAN_POINT('Ctrl Pts',(-11.7332493365282,5.8345240455325,129.821375508522));
#151762=CARTESIAN_POINT('Ctrl Pts',(-11.7406472508396,5.80836492904881,
129.666107648684));
#151763=CARTESIAN_POINT('Ctrl Pts',(-11.7480451651509,5.77598946559807,
129.511801024239));
#151764=CARTESIAN_POINT('Ctrl Pts',(-11.7554430794623,5.73749302341003,
129.358987181799));
#151765=CARTESIAN_POINT('Ctrl Pts',(-11.7628397643745,5.69900297863251,
129.206198734248));
#151766=CARTESIAN_POINT('Ctrl Pts',(-11.7702364492867,5.65439406505184,
129.054902937985));
#151767=CARTESIAN_POINT('Ctrl Pts',(-11.7776331341989,5.60381254549375,
128.905620109369));
#151768=CARTESIAN_POINT('Ctrl Pts',(-11.7850294911344,5.55323326877324,
128.756343900111));
#151769=CARTESIAN_POINT('Ctrl Pts',(-11.7924258480699,5.49668203244469,
128.609080834582));
#151770=CARTESIAN_POINT('Ctrl Pts',(-11.7998222050053,5.43435457888297,
128.464334790043));
#151771=CARTESIAN_POINT('Ctrl Pts',(-11.8072196943419,5.37201758282882,
128.319566584515));
#151772=CARTESIAN_POINT('Ctrl Pts',(-11.8146171836785,5.30390275632155,
128.177316510169));
#151773=CARTESIAN_POINT('Ctrl Pts',(-11.8220146730151,5.23025340471511,
128.038067089221));
#151774=CARTESIAN_POINT('Ctrl Pts',(-11.8294147555301,5.15657823544275,
127.898768854604));
#151775=CARTESIAN_POINT('Ctrl Pts',(-11.8368148380451,5.07736485272949,
127.762473697439));
#151776=CARTESIAN_POINT('Ctrl Pts',(-11.8442149205601,4.99290170814379,
127.629638094996));
#151777=CARTESIAN_POINT('Ctrl Pts',(-11.8516231402266,4.90834568764772,
127.496656426152));
#151778=CARTESIAN_POINT('Ctrl Pts',(-11.859031359893,4.81852857733406,127.367142224342));
#151779=CARTESIAN_POINT('Ctrl Pts',(-11.8664395795595,4.72378164288507,
127.24152220517));
#151780=CARTESIAN_POINT('Ctrl Pts',(-11.8738523588615,4.628976393279,127.115824868973));
#151781=CARTESIAN_POINT('Ctrl Pts',(-11.8812651381636,4.52923550942774,
126.994026779493));
#151782=CARTESIAN_POINT('Ctrl Pts',(-11.8886779174657,4.42492911778911,
126.876519879318));
#151783=CARTESIAN_POINT('Ctrl Pts',(-11.8961012884944,4.32047368828646,
126.758845079773));
#151784=CARTESIAN_POINT('Ctrl Pts',(-11.9035246595232,4.21143998035911,
126.645473983765));
#151785=CARTESIAN_POINT('Ctrl Pts',(-11.9109480305519,4.09823396108951,
126.536760710982));
#151786=CARTESIAN_POINT('Ctrl Pts',(-11.9148840799927,4.03820941333243,
126.479118325215));
#151787=CARTESIAN_POINT('Ctrl Pts',(-11.9188201294334,3.977012423375,126.422784740331));
#151788=CARTESIAN_POINT('Ctrl Pts',(-11.9227561788741,3.91470696970683,
126.367807912613));
#151789=CARTESIAN_POINT('Ctrl Pts',(-11.9301794452796,3.79720082857353,
126.264123331302));
#151790=CARTESIAN_POINT('Ctrl Pts',(-11.937602711685,3.67539488846097,126.164953577267));
#151791=CARTESIAN_POINT('Ctrl Pts',(-11.9450259780904,3.54967093566331,
126.070676343028));
#151792=CARTESIAN_POINT('Ctrl Pts',(-11.9524404708114,3.42409557813748,
125.976510536651));
#151793=CARTESIAN_POINT('Ctrl Pts',(-11.9598549635325,3.29461172123091,
125.887225961637));
#151794=CARTESIAN_POINT('Ctrl Pts',(-11.9672694562535,3.16163666902764,
125.803162347595));
#151795=CARTESIAN_POINT('Ctrl Pts',(-11.9746768026073,3.02878978318536,
125.719179757229));
#151796=CARTESIAN_POINT('Ctrl Pts',(-11.982084148961,2.89245871440621,125.640408307933));
#151797=CARTESIAN_POINT('Ctrl Pts',(-11.9894914953148,2.75309231310214,
125.567146350607));
#151798=CARTESIAN_POINT('Ctrl Pts',(-11.9968933169902,2.61382985651876,
125.493939034813));
#151799=CARTESIAN_POINT('Ctrl Pts',(-12.0042951386656,2.47153690407494,
125.426233201992));
#151800=CARTESIAN_POINT('Ctrl Pts',(-12.011696960341,2.3266895509583,125.364282833567));
#151801=CARTESIAN_POINT('Ctrl Pts',(-12.0190948746524,2.18191866163187,
125.302365168259));
#151802=CARTESIAN_POINT('Ctrl Pts',(-12.0264927889637,2.03459639948691,
125.24619706292));
#151803=CARTESIAN_POINT('Ctrl Pts',(-12.0338907032751,1.88522151859995,
125.195985595485));
#151804=CARTESIAN_POINT('Ctrl Pts',(-12.0412873881873,1.73587146110804,
125.145782472284));
#151805=CARTESIAN_POINT('Ctrl Pts',(-12.0486840730995,1.58446981536809,
125.101534141184));
#151806=CARTESIAN_POINT('Ctrl Pts',(-12.0560807580117,1.43153339690129,
125.063398790829));
#151807=CARTESIAN_POINT('Ctrl Pts',(-12.0634771149471,1.27860375979576,
125.025265131435));
#151808=CARTESIAN_POINT('Ctrl Pts',(-12.0708734718826,1.1241398474834,124.993244004154));
#151809=CARTESIAN_POINT('Ctrl Pts',(-12.0782698288181,0.968671389709072,
124.967443083348));
#151810=CARTESIAN_POINT('Ctrl Pts',(-12.0856673181547,0.813179129316302,
124.941638212356));
#151811=CARTESIAN_POINT('Ctrl Pts',(-12.0930648074912,0.656682385513134,
124.922055505173));
#151812=CARTESIAN_POINT('Ctrl Pts',(-12.1004622968278,0.499718630392232,
124.908751077159));
#151813=CARTESIAN_POINT('Ctrl Pts',(-12.1078623793428,0.342699851870522,
124.895441985298));
#151814=CARTESIAN_POINT('Ctrl Pts',(-12.1152624618578,0.185214107817576,
124.888415585973));
#151815=CARTESIAN_POINT('Ctrl Pts',(-12.1226625443728,0.0278013606063731,
124.887675933822));
#151816=CARTESIAN_POINT('Ctrl Pts',(-12.1300707640393,-0.129784478102812,
124.886935468348));
#151817=CARTESIAN_POINT('Ctrl Pts',(-12.1374789837059,-0.287296786147881,
124.892495557369));
#151818=CARTESIAN_POINT('Ctrl Pts',(-12.1448872033723,-0.444197498413058,
124.904308147892));
#151819=CARTESIAN_POINT('Ctrl Pts',(-12.1522999826744,-0.601194780448383,
124.916128008867));
#151820=CARTESIAN_POINT('Ctrl Pts',(-12.1597127619765,-0.757579346657777,
124.934207996812));
#151821=CARTESIAN_POINT('Ctrl Pts',(-12.1671255412786,-0.91282138224968,
124.958448568398));
#151822=CARTESIAN_POINT('Ctrl Pts',(-12.1745489123073,-1.06828523494239,
124.982723776049));
#151823=CARTESIAN_POINT('Ctrl Pts',(-12.1819722833361,-1.22260293128174,
125.013177075888));
#151824=CARTESIAN_POINT('Ctrl Pts',(-12.1893956543649,-1.37525710521962,
125.049658326653));
#151825=CARTESIAN_POINT('Ctrl Pts',(-12.1933317038056,-1.45619801112647,
125.069001561163));
#151826=CARTESIAN_POINT('Ctrl Pts',(-12.1972677532463,-1.53667151942998,
125.090038643349));
#151827=CARTESIAN_POINT('Ctrl Pts',(-12.201203802687,-1.61660270121701,
125.112741667837));
#151828=CARTESIAN_POINT('Ctrl Pts',(-12.2086270690924,-1.76735041550362,
125.155558863484));
#151829=CARTESIAN_POINT('Ctrl Pts',(-12.2160503354979,-1.91662382411278,
125.204433976212));
#151830=CARTESIAN_POINT('Ctrl Pts',(-12.2234736019033,-2.06389879881326,
125.259249950433));
#151831=CARTESIAN_POINT('Ctrl Pts',(-12.2308880946243,-2.21099970672385,
125.314001136724));
#151832=CARTESIAN_POINT('Ctrl Pts',(-12.2383025873453,-2.3561065358316,
125.37467907902));
#151833=CARTESIAN_POINT('Ctrl Pts',(-12.2457170800663,-2.49870789894229,
125.441116319731));
#151834=CARTESIAN_POINT('Ctrl Pts',(-12.2531244264201,-2.64117181749058,
125.507489525727));
#151835=CARTESIAN_POINT('Ctrl Pts',(-12.2605317727739,-2.78113474145283,
125.579610822543));
#151836=CARTESIAN_POINT('Ctrl Pts',(-12.2679391191276,-2.91810304515607,
125.657263845564));
#151837=CARTESIAN_POINT('Ctrl Pts',(-12.275340940803,-3.05496919273051,
125.734858952031));
#151838=CARTESIAN_POINT('Ctrl Pts',(-12.2827427624784,-3.18884484390587,
125.817977386421));
#151839=CARTESIAN_POINT('Ctrl Pts',(-12.2901445841538,-3.31925897584034,
125.906355879532));
#151840=CARTESIAN_POINT('Ctrl Pts',(-12.2975424984651,-3.44960426316988,
125.994687718325));
#151841=CARTESIAN_POINT('Ctrl Pts',(-12.3049404127765,-3.57649136219079,
126.088273876933));
#151842=CARTESIAN_POINT('Ctrl Pts',(-12.3123383270878,-3.6994764636106,
126.186806670107));
#151843=CARTESIAN_POINT('Ctrl Pts',(-12.3197350120001,-3.82244112713774,
126.285323088919));
#151844=CARTESIAN_POINT('Ctrl Pts',(-12.3271316969122,-3.94150478898354,
126.388784277612));
#151845=CARTESIAN_POINT('Ctrl Pts',(-12.3345283818244,-4.05625500914746,
126.496840929478));
#151846=CARTESIAN_POINT('Ctrl Pts',(-12.3419247387599,-4.17100014116654,
126.604892789999));
#151847=CARTESIAN_POINT('Ctrl Pts',(-12.3493210956954,-4.28143194002967,
126.717539452618));
#151848=CARTESIAN_POINT('Ctrl Pts',(-12.3567174526308,-4.3871734843788,
126.834393441321));
#151849=CARTESIAN_POINT('Ctrl Pts',(-12.3641149419674,-4.49293121802787,
126.951265320668));
#151850=CARTESIAN_POINT('Ctrl Pts',(-12.371512431304,-4.59399701686227,
127.07234553188));
#151851=CARTESIAN_POINT('Ctrl Pts',(-12.3789099206405,-4.69003315264681,
127.197212216187));
#151852=CARTESIAN_POINT('Ctrl Pts',(-12.3863100031555,-4.78610295375015,
127.322122672316));
#151853=CARTESIAN_POINT('Ctrl Pts',(-12.3937100856705,-4.87713935396442,
127.450821948551));
#151854=CARTESIAN_POINT('Ctrl Pts',(-12.4011101681855,-4.96284707915426,
127.582857950885));
#151855=CARTESIAN_POINT('Ctrl Pts',(-12.4085183878519,-5.04864904879892,
127.715039140378));
#151856=CARTESIAN_POINT('Ctrl Pts',(-12.4159266075184,-5.12911043838591,
127.850564070045));
#151857=CARTESIAN_POINT('Ctrl Pts',(-12.4233348271848,-5.20398083892142,
127.988954076649));
#151858=CARTESIAN_POINT('Ctrl Pts',(-12.4307476064869,-5.27889732093917,
128.127429259992));
#151859=CARTESIAN_POINT('Ctrl Pts',(-12.438160385789,-5.34821579297108,
128.268772699698));
#151860=CARTESIAN_POINT('Ctrl Pts',(-12.445573165091,-5.41173362580237,
128.412484841975));
#151861=CARTESIAN_POINT('Ctrl Pts',(-12.4529965361198,-5.47534221589199,
128.556402326901));
#151862=CARTESIAN_POINT('Ctrl Pts',(-12.4604199071485,-5.53313347654608,
128.702694927761));
#151863=CARTESIAN_POINT('Ctrl Pts',(-12.4678432781772,-5.58495407687434,
128.850846214828));
#151864=CARTESIAN_POINT('Ctrl Pts',(-12.4717793276181,-5.61243060258706,
128.929399582073));
#151865=CARTESIAN_POINT('Ctrl Pts',(-12.475715377059,-5.63822940645647,
129.008475280521));
#151866=CARTESIAN_POINT('Ctrl Pts',(-12.4796514264999,-5.66233346515659,
129.087995186818));
#151867=CARTESIAN_POINT('Ctrl Pts',(-12.4887665432281,-5.71815372655736,
129.272147657207));
#151868=CARTESIAN_POINT('Ctrl Pts',(-12.4978816599562,-5.76501905627374,
129.459132538451));
#151869=CARTESIAN_POINT('Ctrl Pts',(-12.5069967766844,-5.80268447077341,
129.648167080504));
#151870=CARTESIAN_POINT('Ctrl Pts',(-12.5161014405401,-5.84030669199463,
129.836984844864));
#151871=CARTESIAN_POINT('Ctrl Pts',(-12.5252061043959,-5.86874999000234,
130.027847637754));
#151872=CARTESIAN_POINT('Ctrl Pts',(-12.5343107682516,-5.88781784875314,
130.21995361692));
#151873=CARTESIAN_POINT('Ctrl Pts',(-12.5434154321073,-5.90688570750392,
130.412059596086));
#151874=CARTESIAN_POINT('Ctrl Pts',(-12.5525200959631,-5.9165779597188,
130.605408827073));
#151875=CARTESIAN_POINT('Ctrl Pts',(-12.5616247598188,-5.91674772904762,
130.799176670249));
#151876=CARTESIAN_POINT('',(-14.3116248077882,-5.90794108543601,130.806865238042));
#151877=CARTESIAN_POINT('Ctrl Pts',(-12.5616248077882,-5.91316974211598,
130.799180825377));
#151878=CARTESIAN_POINT('Ctrl Pts',(-12.627116221963,-5.90156166892063,
132.192154654826));
#151879=CARTESIAN_POINT('Ctrl Pts',(-12.7854235107422,-4.71330205150837,
135.577102347049));
#151880=CARTESIAN_POINT('Ctrl Pts',(-13.0365466741257,0.937472151881782,
137.739683717091));
#151881=CARTESIAN_POINT('Ctrl Pts',(-13.3149942979386,6.34161033930907,
133.764350285572));
#151882=CARTESIAN_POINT('Ctrl Pts',(-13.5934419217515,5.91811842979897,
127.068930952691));
#151883=CARTESIAN_POINT('Ctrl Pts',(-13.8718895455643,0.056164799462427,
123.806188995947));
#151884=CARTESIAN_POINT('Ctrl Pts',(-14.11128384091,-5.02800157587884,126.530067858737));
#151885=CARTESIAN_POINT('Ctrl Pts',(-14.2578622616512,-5.90358900820754,
129.660813820107));
#151886=CARTESIAN_POINT('Ctrl Pts',(-14.3116248077882,-5.90794108543601,
130.806865238042));
#151887=CARTESIAN_POINT('',(-16.0616248077882,-5.92237476527066,130.808656821232));
#151888=CARTESIAN_POINT('Ctrl Pts',(-14.3116248077882,-5.90794108543601,
130.806865238042));
#151889=CARTESIAN_POINT('Ctrl Pts',(-14.3506781362555,-5.91110245173523,
131.639361570173));
#151890=CARTESIAN_POINT('Ctrl Pts',(-14.482547339327,-5.35732722362217,
134.446388667616));
#151891=CARTESIAN_POINT('Ctrl Pts',(-14.707232417003,-1.04866502285217,
137.723743697016));
#151892=CARTESIAN_POINT('Ctrl Pts',(-14.9856800408159,5.25464389193611,
135.4267277708));
#151893=CARTESIAN_POINT('Ctrl Pts',(-15.2641276646288,6.72919177365889,
128.881982245949));
#151894=CARTESIAN_POINT('Ctrl Pts',(-15.5425752884417,2.01994115468555,
124.103808531212));
#151895=CARTESIAN_POINT('Ctrl Pts',(-15.8084076694948,-4.24808364837976,
125.420624513406));
#151896=CARTESIAN_POINT('Ctrl Pts',(-15.9814241759437,-5.90849869859571,
129.109618236687));
#151897=CARTESIAN_POINT('Ctrl Pts',(-16.0616248077882,-5.92237476527066,
130.808656821232));
#151898=CARTESIAN_POINT('',(-17.8116248077883,-5.92167625280914,130.799795184471));
#151899=CARTESIAN_POINT('Ctrl Pts',(-16.0616248077882,-5.92237476527066,
130.808656821232));
#151900=CARTESIAN_POINT('Ctrl Pts',(-16.074240050548,-5.92455741577639,
131.075908882834));
#151901=CARTESIAN_POINT('Ctrl Pts',(-16.1796711679109,-5.7865147396121,
133.307183312521));
#151902=CARTESIAN_POINT('Ctrl Pts',(-16.3779181598812,-2.95033538898635,
137.150468213798));
#151903=CARTESIAN_POINT('Ctrl Pts',(-16.6563657836929,3.74443170811431,
136.716787506209));
#151904=CARTESIAN_POINT('Ctrl Pts',(-16.9348134075062,6.99824899111522,
130.849875326086));
#151905=CARTESIAN_POINT('Ctrl Pts',(-17.2132610313189,3.82101733475201,
124.941137352339));
#151906=CARTESIAN_POINT('Ctrl Pts',(-17.4917086551319,-2.86754258517585,
124.420415124962));
#151907=CARTESIAN_POINT('Ctrl Pts',(-17.6911632472883,-5.77105058276818,
128.249669255985));
#151908=CARTESIAN_POINT('Ctrl Pts',(-17.7978019648404,-5.92417162324444,
130.506870325296));
#151909=CARTESIAN_POINT('Ctrl Pts',(-17.8116248077883,-5.92167625280914,
130.799795184471));
#151910=CARTESIAN_POINT('',(-19.5616239976484,-5.91172027463249,130.802225031155));
#151911=CARTESIAN_POINT('Ctrl Pts',(-17.8116248077883,-5.92167625280914,
130.799795184471));
#151912=CARTESIAN_POINT('Ctrl Pts',(-17.8906178394447,-5.90741602598498,
132.473765058911));
#151913=CARTESIAN_POINT('Ctrl Pts',(-18.0624267457055,-4.28935641582584,
136.138738636046));
#151914=CARTESIAN_POINT('Ctrl Pts',(-18.3270515265707,1.93261682990332,
137.530619066297));
#151915=CARTESIAN_POINT('Ctrl Pts',(-18.6054991503834,6.70361833380628,
132.814102333552));
#151916=CARTESIAN_POINT('Ctrl Pts',(-18.8839467741964,5.31432207890837,
126.25073114516));
#151917=CARTESIAN_POINT('Ctrl Pts',(-19.1623943980091,-0.958576547442623,
123.871922984737));
#151918=CARTESIAN_POINT('Ctrl Pts',(-19.3882865867831,-5.33287767884445,
127.110263284248));
#151919=CARTESIAN_POINT('Ctrl Pts',(-19.5213629009526,-5.91038304027362,
129.943875328412));
#151920=CARTESIAN_POINT('Ctrl Pts',(-19.5616233405177,-5.90764080910516,
130.80221248317));
#151921=CARTESIAN_POINT('',(-21.3116256300176,-5.91484479357845,130.809683424605));
#151922=CARTESIAN_POINT('Ctrl Pts',(-19.5616248077881,-5.91674962015507,
130.802240500865));
#151923=CARTESIAN_POINT('Ctrl Pts',(-19.5691919858151,-5.91680751748068,
130.963818389114));
#151924=CARTESIAN_POINT('Ctrl Pts',(-19.5767591638421,-5.91024237122003,
131.125349323677));
#151925=CARTESIAN_POINT('Ctrl Pts',(-19.5843263418691,-5.89709206905609,
131.28626900261));
#151926=CARTESIAN_POINT('Ctrl Pts',(-19.591897422316,-5.88393498523593,
131.447271668378));
#151927=CARTESIAN_POINT('Ctrl Pts',(-19.5994685027628,-5.86418600343569,
131.607662102599));
#151928=CARTESIAN_POINT('Ctrl Pts',(-19.6070395832096,-5.83793478736771,
131.766882295733));
#151929=CARTESIAN_POINT('Ctrl Pts',(-19.6146157566898,-5.81166591221945,
131.926209595608));
#151930=CARTESIAN_POINT('Ctrl Pts',(-19.6221919301698,-5.77888613908945,
132.084364741324));
#151931=CARTESIAN_POINT('Ctrl Pts',(-19.62976810365,-5.73973604494925,132.240800904111));
#151932=CARTESIAN_POINT('Ctrl Pts',(-19.6373562482108,-5.70052408990546,
132.397484251039));
#151933=CARTESIAN_POINT('Ctrl Pts',(-19.6449443927717,-5.65492178265798,
132.552442848179));
#151934=CARTESIAN_POINT('Ctrl Pts',(-19.6525325373325,-5.60311972573027,
132.705144640445));
#151935=CARTESIAN_POINT('Ctrl Pts',(-19.6601268842168,-5.55127532734408,
132.857971246608));
#151936=CARTESIAN_POINT('Ctrl Pts',(-19.667721231101,-5.49322119737034,
133.008537043984));
#151937=CARTESIAN_POINT('Ctrl Pts',(-19.6753155779852,-5.42919574204391,
133.156330888865));
#151938=CARTESIAN_POINT('Ctrl Pts',(-19.6829241974717,-5.36504995907494,
133.304402493347));
#151939=CARTESIAN_POINT('Ctrl Pts',(-19.6905328169581,-5.29491056763434,
133.449691416725));
#151940=CARTESIAN_POINT('Ctrl Pts',(-19.6981414364445,-5.21906227235888,
133.591710534555));
#151941=CARTESIAN_POINT('Ctrl Pts',(-19.705190839508,-5.14878865622799,
133.72329156658));
#151942=CARTESIAN_POINT('Ctrl Pts',(-19.7122402425716,-5.07361507784861,
133.852065885224));
#151943=CARTESIAN_POINT('Ctrl Pts',(-19.7192896456351,-4.99380006069075,
133.977669854994));
#151944=CARTESIAN_POINT('Ctrl Pts',(-19.7267129120405,-4.90975207390692,
134.109935200127));
#151945=CARTESIAN_POINT('Ctrl Pts',(-19.7341361784459,-4.82031861508711,
134.239059108081));
#151946=CARTESIAN_POINT('Ctrl Pts',(-19.7415594448514,-4.72576141575207,
134.364572634271));
#151947=CARTESIAN_POINT('Ctrl Pts',(-19.7489739375724,-4.63131597517402,
134.489937813896));
#151948=CARTESIAN_POINT('Ctrl Pts',(-19.7563884302934,-4.53175907068169,
134.611700810339));
#151949=CARTESIAN_POINT('Ctrl Pts',(-19.7638029230144,-4.42739710557802,
134.729419270888));
#151950=CARTESIAN_POINT('Ctrl Pts',(-19.7712102693681,-4.32313572846548,
134.847024269953));
#151951=CARTESIAN_POINT('Ctrl Pts',(-19.7786176157219,-4.21407875672101,
134.960592216365));
#151952=CARTESIAN_POINT('Ctrl Pts',(-19.7860249620757,-4.10057440017407,
135.069711734548));
#151953=CARTESIAN_POINT('Ctrl Pts',(-19.7934267837511,-3.98715469945836,
135.178749867277));
#151954=CARTESIAN_POINT('Ctrl Pts',(-19.8008286054265,-3.86929448653938,
135.283345920376));
#151955=CARTESIAN_POINT('Ctrl Pts',(-19.8082304271019,-3.74738047727398,
135.383123564154));
#151956=CARTESIAN_POINT('Ctrl Pts',(-19.8156283414133,-3.62553082546509,
135.48284853609));
#151957=CARTESIAN_POINT('Ctrl Pts',(-19.8230262557246,-3.49963192730841,
135.577759928578));
#151958=CARTESIAN_POINT('Ctrl Pts',(-19.830424170036,-3.37010530407945,
135.667520166863));
#151959=CARTESIAN_POINT('Ctrl Pts',(-19.8378208549482,-3.2406002058258,
135.757265488624));
#151960=CARTESIAN_POINT('Ctrl Pts',(-19.8452175398604,-3.1074688855274,
135.841861142729));
#151961=CARTESIAN_POINT('Ctrl Pts',(-19.8526142247726,-2.97116380575872,
135.92101149503));
#151962=CARTESIAN_POINT('Ctrl Pts',(-19.860010581708,-2.83486476989991,
136.000158337721));
#151963=CARTESIAN_POINT('Ctrl Pts',(-19.8674069386435,-2.69539257720325,
136.073860171237));
#151964=CARTESIAN_POINT('Ctrl Pts',(-19.8748032955789,-2.55322613900928,
136.141866293964));
#151965=CARTESIAN_POINT('Ctrl Pts',(-19.8822007849155,-2.41103793477069,
136.209882828602));
#151966=CARTESIAN_POINT('Ctrl Pts',(-19.889598274252,-2.26615500047468,
136.272201755031));
#151967=CARTESIAN_POINT('Ctrl Pts',(-19.8969957635886,-2.11907801868945,
136.328619745558));
#151968=CARTESIAN_POINT('Ctrl Pts',(-19.9043958461036,-1.97194947929667,
136.385057513325));
#151969=CARTESIAN_POINT('Ctrl Pts',(-19.9117959286186,-1.82262570942006,
136.435590093083));
#151970=CARTESIAN_POINT('Ctrl Pts',(-19.9191960111336,-1.67162425732287,
136.480063473145));
#151971=CARTESIAN_POINT('Ctrl Pts',(-19.9266042308,-1.52045676360534,136.524585756261));
#151972=CARTESIAN_POINT('Ctrl Pts',(-19.9340124504665,-1.36760826182186,
136.563035428276));
#151973=CARTESIAN_POINT('Ctrl Pts',(-19.9414206701329,-1.21360896440533,
136.595309058367));
#151974=CARTESIAN_POINT('Ctrl Pts',(-19.948833449435,-1.05951488299108,
136.627602552339));
#151975=CARTESIAN_POINT('Ctrl Pts',(-19.956246228737,-0.904268961850489,
136.65371236815));
#151976=CARTESIAN_POINT('Ctrl Pts',(-19.9636590080391,-0.748407803357998,
136.673586829118));
#151977=CARTESIAN_POINT('Ctrl Pts',(-19.9710823790678,-0.592323943132867,
136.693489687649));
#151978=CARTESIAN_POINT('Ctrl Pts',(-19.9785057500965,-0.43562346074044,
136.707139365023));
#151979=CARTESIAN_POINT('Ctrl Pts',(-19.9859291211253,-0.278845067491367,
136.714536248699));
#151980=CARTESIAN_POINT('Ctrl Pts',(-19.9898651705661,-0.195717401542456,
136.71845825391));
#151981=CARTESIAN_POINT('Ctrl Pts',(-19.9938012200071,-0.112567794325544,
136.720623244878));
#151982=CARTESIAN_POINT('Ctrl Pts',(-19.997737269448,-0.0294759789153038,
136.721037195609));
#151983=CARTESIAN_POINT('Ctrl Pts',(-20.0051605358534,0.127232591737446,
136.72181789377));
#151984=CARTESIAN_POINT('Ctrl Pts',(-20.0125838022589,0.284209161504598,
136.716369618254));
#151985=CARTESIAN_POINT('Ctrl Pts',(-20.0200070686643,0.440917721744524,
136.704659095198));
#151986=CARTESIAN_POINT('Ctrl Pts',(-20.0274215613853,0.597441065480305,
136.692962413008));
#151987=CARTESIAN_POINT('Ctrl Pts',(-20.0348360541062,0.753696661586576,
136.675018243465));
#151988=CARTESIAN_POINT('Ctrl Pts',(-20.0422505468273,0.909146727727743,
136.650845269899));
#151989=CARTESIAN_POINT('Ctrl Pts',(-20.049657893181,1.06444696524235,136.626695595154));
#151990=CARTESIAN_POINT('Ctrl Pts',(-20.0570652395348,1.21894285206313,
136.596329125259));
#151991=CARTESIAN_POINT('Ctrl Pts',(-20.0644725858886,1.37210007034716,
136.559816460456));
#151992=CARTESIAN_POINT('Ctrl Pts',(-20.071874407564,1.52514305819995,136.523331028175));
#151993=CARTESIAN_POINT('Ctrl Pts',(-20.0792762292395,1.67684900396512,
136.480708614672));
#151994=CARTESIAN_POINT('Ctrl Pts',(-20.0866780509149,1.82669226144844,
136.432071159559));
#151995=CARTESIAN_POINT('Ctrl Pts',(-20.0940759652263,1.97645641784294,
136.38345937978));
#151996=CARTESIAN_POINT('Ctrl Pts',(-20.1014738795376,2.12435949007881,
136.328838997098));
#151997=CARTESIAN_POINT('Ctrl Pts',(-20.108871793849,2.26988962440962,136.268382181899));
#151998=CARTESIAN_POINT('Ctrl Pts',(-20.1162684787612,2.41539557427146,
136.207935413527));
#151999=CARTESIAN_POINT('Ctrl Pts',(-20.1236651636734,2.55852902447798,
136.141654280692));
#152000=CARTESIAN_POINT('Ctrl Pts',(-20.1310618485856,2.69879668257461,
136.069759655495));
#152001=CARTESIAN_POINT('Ctrl Pts',(-20.138458205521,2.8390581210563,135.997868218181));
#152002=CARTESIAN_POINT('Ctrl Pts',(-20.1458545624565,2.97645368788785,
135.92036395369));
#152003=CARTESIAN_POINT('Ctrl Pts',(-20.1532509193919,3.11051359742387,
135.837514273351));
#152004=CARTESIAN_POINT('Ctrl Pts',(-20.1606484087285,3.24459403187428,
135.754651908514));
#152005=CARTESIAN_POINT('Ctrl Pts',(-20.168045898065,3.37533747459153,135.666442694552));
#152006=CARTESIAN_POINT('Ctrl Pts',(-20.1754433874016,3.50230222907294,
135.573197966305));
#152007=CARTESIAN_POINT('Ctrl Pts',(-20.1828434699166,3.62931149085276,
135.479920551264));
#152008=CARTESIAN_POINT('Ctrl Pts',(-20.1902435524317,3.75253912641491,
135.381604328283));
#152009=CARTESIAN_POINT('Ctrl Pts',(-20.1976436349467,3.87157581388762,
135.278601478295));
#152010=CARTESIAN_POINT('Ctrl Pts',(-20.2050518546132,3.99074339443513,
135.175485366086));
#152011=CARTESIAN_POINT('Ctrl Pts',(-20.2124600742796,4.10571054119851,
135.06767257955));
#152012=CARTESIAN_POINT('Ctrl Pts',(-20.2198682939461,4.21610364212668,
134.955553294538));
#152013=CARTESIAN_POINT('Ctrl Pts',(-20.2272810732482,4.32656468816663,
134.843365001977));
#152014=CARTESIAN_POINT('Ctrl Pts',(-20.2346938525502,4.43244582814584,
134.726865204941));
#152015=CARTESIAN_POINT('Ctrl Pts',(-20.2421066318523,4.53341353831838,
134.606477429697));
#152016=CARTESIAN_POINT('Ctrl Pts',(-20.249530002881,4.63452551588983,134.485917638755));
#152017=CARTESIAN_POINT('Ctrl Pts',(-20.2569533739098,4.73070981439883,
134.361459068963));
#152018=CARTESIAN_POINT('Ctrl Pts',(-20.2643767449386,4.8216755732019,134.233555162833));
#152019=CARTESIAN_POINT('Ctrl Pts',(-20.2683127943793,4.86990780121213,
134.165737442792));
#152020=CARTESIAN_POINT('Ctrl Pts',(-20.27224884382,4.91667366317013,134.096951553825));
#152021=CARTESIAN_POINT('Ctrl Pts',(-20.2761848932607,4.96193508750228,
134.027267806722));
#152022=CARTESIAN_POINT('Ctrl Pts',(-20.2836081596662,5.04729672123318,
133.89584643444));
#152023=CARTESIAN_POINT('Ctrl Pts',(-20.2910314260716,5.12756260306324,
133.76083267449));
#152024=CARTESIAN_POINT('Ctrl Pts',(-20.298454692477,5.20241501298613,133.622659500786));
#152025=CARTESIAN_POINT('Ctrl Pts',(-20.305869185198,5.2771789535767,133.484649636298));
#152026=CARTESIAN_POINT('Ctrl Pts',(-20.3132836779191,5.34654198198527,
133.343488115957));
#152027=CARTESIAN_POINT('Ctrl Pts',(-20.3206981706401,5.41022913253789,
133.199637490067));
#152028=CARTESIAN_POINT('Ctrl Pts',(-20.3281055169939,5.47385489901702,
133.055925512827));
#152029=CARTESIAN_POINT('Ctrl Pts',(-20.3355128633477,5.53181552846948,
132.909529928972));
#152030=CARTESIAN_POINT('Ctrl Pts',(-20.3429202097014,5.58388160703363,
132.760938436394));
#152031=CARTESIAN_POINT('Ctrl Pts',(-20.3503220313768,5.63590885275183,
132.612457768958));
#152032=CARTESIAN_POINT('Ctrl Pts',(-20.3577238530522,5.68205017845196,
132.461784804643));
#152033=CARTESIAN_POINT('Ctrl Pts',(-20.3651256747276,5.72212405077568,
132.309427695817));
#152034=CARTESIAN_POINT('Ctrl Pts',(-20.3725235890389,5.7621767684143,132.157151015122));
#152035=CARTESIAN_POINT('Ctrl Pts',(-20.3799215033503,5.79616831681066,
132.003192320601));
#152036=CARTESIAN_POINT('Ctrl Pts',(-20.3873194176616,5.82396687833496,
131.848075311607));
#152037=CARTESIAN_POINT('Ctrl Pts',(-20.3947161025738,5.8517608202426,131.692984080246));
#152038=CARTESIAN_POINT('Ctrl Pts',(-20.4021127874861,5.87336375207505,
131.536735283534));
#152039=CARTESIAN_POINT('Ctrl Pts',(-20.4095094723983,5.88869486316469,
131.379863329148));
#152040=CARTESIAN_POINT('Ctrl Pts',(-20.4169058293338,5.9040252944568,131.222998330629));
#152041=CARTESIAN_POINT('Ctrl Pts',(-20.4243021862691,5.91308442165166,
131.065510600904));
#152042=CARTESIAN_POINT('Ctrl Pts',(-20.4316985432046,5.91584329485683,
130.907939926298));
#152043=CARTESIAN_POINT('Ctrl Pts',(-20.4390960325412,5.91860259045253,
130.75034512722));
#152044=CARTESIAN_POINT('Ctrl Pts',(-20.4464935218778,5.91505970490617,
130.592667731239));
#152045=CARTESIAN_POINT('Ctrl Pts',(-20.4538910112144,5.90523782528847,
130.435447634219));
#152046=CARTESIAN_POINT('Ctrl Pts',(-20.4612910937293,5.8954125026261,130.278172423937));
#152047=CARTESIAN_POINT('Ctrl Pts',(-20.4686911762443,5.87930382679594,
130.121355204123));
#152048=CARTESIAN_POINT('Ctrl Pts',(-20.4760912587593,5.85698684912133,
129.965530711256));
#152049=CARTESIAN_POINT('Ctrl Pts',(-20.4834994784258,5.8346453316355,129.80953487334));
#152050=CARTESIAN_POINT('Ctrl Pts',(-20.4909076980923,5.80608193196049,
129.654534312133));
#152051=CARTESIAN_POINT('Ctrl Pts',(-20.4983159177588,5.77142296965002,
129.501054257612));
#152052=CARTESIAN_POINT('Ctrl Pts',(-20.5057286970609,5.73674267532657,
129.347479738679));
#152053=CARTESIAN_POINT('Ctrl Pts',(-20.5131414763629,5.6959594390843,129.195427950941));
#152054=CARTESIAN_POINT('Ctrl Pts',(-20.520554255665,5.64924930783475,129.045408423665));
#152055=CARTESIAN_POINT('Ctrl Pts',(-20.5279776266938,5.60247243495918,
128.895174541453));
#152056=CARTESIAN_POINT('Ctrl Pts',(-20.5354009977225,5.54975187811928,
128.746979069994));
#152057=CARTESIAN_POINT('Ctrl Pts',(-20.5428243687512,5.4913119140608,128.601311815339));
#152058=CARTESIAN_POINT('Ctrl Pts',(-20.546760418192,5.46032564286905,128.524075541682));
#152059=CARTESIAN_POINT('Ctrl Pts',(-20.5506964676328,5.42773221707083,
128.447549644362));
#152060=CARTESIAN_POINT('Ctrl Pts',(-20.5546325170737,5.3935702125098,128.371804158771));
#152061=CARTESIAN_POINT('Ctrl Pts',(-20.5620557834791,5.32914173806776,
128.228950536882));
#152062=CARTESIAN_POINT('Ctrl Pts',(-20.5694790498846,5.25893650776519,
128.088442342102));
#152063=CARTESIAN_POINT('Ctrl Pts',(-20.57690231629,5.18314705939539,127.950780914249));
#152064=CARTESIAN_POINT('Ctrl Pts',(-20.584316809011,5.10744718785952,127.813282190772));
#152065=CARTESIAN_POINT('Ctrl Pts',(-20.591731301732,5.0261764140352,127.678623860702));
#152066=CARTESIAN_POINT('Ctrl Pts',(-20.5991457944531,4.93957526893164,
127.547287280188));
#152067=CARTESIAN_POINT('Ctrl Pts',(-20.6065531408069,4.85305759327196,
127.416077286815));
#152068=CARTESIAN_POINT('Ctrl Pts',(-20.6139604871607,4.76121997842291,
127.288182978741));
#152069=CARTESIAN_POINT('Ctrl Pts',(-20.6213678335145,4.66434873463549,
127.16406098097));
#152070=CARTESIAN_POINT('Ctrl Pts',(-20.6287696551899,4.56754974107713,
127.040031558067));
#152071=CARTESIAN_POINT('Ctrl Pts',(-20.6361714768653,4.46572482252367,
126.919769136361));
#152072=CARTESIAN_POINT('Ctrl Pts',(-20.6435732985407,4.35920337874054,
126.803701113775));
#152073=CARTESIAN_POINT('Ctrl Pts',(-20.650971212852,4.25273816679812,126.687694362593));
#152074=CARTESIAN_POINT('Ctrl Pts',(-20.6583691271634,4.14158161895885,
126.575877875198));
#152075=CARTESIAN_POINT('Ctrl Pts',(-20.6657670414748,4.0261030876717,126.468645625787));
#152076=CARTESIAN_POINT('Ctrl Pts',(-20.673163726387,3.91064374682128,126.36143119643));
#152077=CARTESIAN_POINT('Ctrl Pts',(-20.6805604112992,3.79086412128721,
126.25879974684));
#152078=CARTESIAN_POINT('Ctrl Pts',(-20.6879570962114,3.66717014324457,
126.161108125724));
#152079=CARTESIAN_POINT('Ctrl Pts',(-20.6953534531469,3.54348164992218,
126.063420836357));
#152080=CARTESIAN_POINT('Ctrl Pts',(-20.7027498100824,3.41587944215051,
125.970673171312));
#152081=CARTESIAN_POINT('Ctrl Pts',(-20.7101461670179,3.28480200932697,
125.883181254647));
#152082=CARTESIAN_POINT('Ctrl Pts',(-20.7175436563545,3.15370450821347,
125.795675942745));
#152083=CARTESIAN_POINT('Ctrl Pts',(-20.7249411456912,3.01913103313984,
125.713428188682));
#152084=CARTESIAN_POINT('Ctrl Pts',(-20.7323386350278,2.88154834696496,
125.636710311421));
#152085=CARTESIAN_POINT('Ctrl Pts',(-20.7397387175428,2.74391743139351,
125.559965540827));
#152086=CARTESIAN_POINT('Ctrl Pts',(-20.7471388000578,2.60327553030642,
125.488754688241));
#152087=CARTESIAN_POINT('Ctrl Pts',(-20.7545388825728,2.4601130997225,125.423303648989));
#152088=CARTESIAN_POINT('Ctrl Pts',(-20.7619471022393,2.31679324732848,
125.35778063959));
#152089=CARTESIAN_POINT('Ctrl Pts',(-20.7693553219058,2.17094767011622,
125.298030247263));
#152090=CARTESIAN_POINT('Ctrl Pts',(-20.7767635415723,2.02308653774545,
125.244230095421));
#152091=CARTESIAN_POINT('Ctrl Pts',(-20.7841763208744,1.87513439931468,
125.190396830482));
#152092=CARTESIAN_POINT('Ctrl Pts',(-20.7915891001764,1.72516458858511,
125.142521216831));
#152093=CARTESIAN_POINT('Ctrl Pts',(-20.7990018794785,1.57370094461438,
125.100730554227));
#152094=CARTESIAN_POINT('Ctrl Pts',(-20.8064252505072,1.42202088228663,
125.058880179166));
#152095=CARTESIAN_POINT('Ctrl Pts',(-20.8138486215361,1.26884308629081,
125.02313220456));
#152096=CARTESIAN_POINT('Ctrl Pts',(-20.8212719925648,1.11470087138906,
124.993562692167));
#152097=CARTESIAN_POINT('Ctrl Pts',(-20.8252080420055,1.03297097045967,
124.977884227186));
#152098=CARTESIAN_POINT('Ctrl Pts',(-20.8291440914461,0.950970022939117,
124.963941882654));
#152099=CARTESIAN_POINT('Ctrl Pts',(-20.8330801408867,0.868777802772557,
124.951741059461));
#152100=CARTESIAN_POINT('Ctrl Pts',(-20.8405034072921,0.71376584066374,
124.928730687694));
#152101=CARTESIAN_POINT('Ctrl Pts',(-20.8479266736976,0.557604675160329,
124.911848224881));
#152102=CARTESIAN_POINT('Ctrl Pts',(-20.855349940103,0.400820169029187,
124.901202669942));
#152103=CARTESIAN_POINT('Ctrl Pts',(-20.862764432824,0.244220969164372,
124.890569697164));
#152104=CARTESIAN_POINT('Ctrl Pts',(-20.870178925545,0.0870002639540167,
124.886158984275));
#152105=CARTESIAN_POINT('Ctrl Pts',(-20.877593418266,-0.0703069551563289,
124.888028350481));
#152106=CARTESIAN_POINT('Ctrl Pts',(-20.8850007646198,-0.227462555646608,
124.88989591492));
#152107=CARTESIAN_POINT('Ctrl Pts',(-20.8924081109736,-0.384704133267359,
124.898031503764));
#152108=CARTESIAN_POINT('Ctrl Pts',(-20.8998154573273,-0.541492758788583,
124.912441053054));
#152109=CARTESIAN_POINT('Ctrl Pts',(-20.9072172790027,-0.698164445437596,
124.926839855159));
#152110=CARTESIAN_POINT('Ctrl Pts',(-20.9146191006782,-0.854383482518331,
124.947503266464));
#152111=CARTESIAN_POINT('Ctrl Pts',(-20.9220209223536,-1.00961223943391,
124.974385172636));
#152112=CARTESIAN_POINT('Ctrl Pts',(-20.9294188366649,-1.16475905229657,
125.001252888059));
#152113=CARTESIAN_POINT('Ctrl Pts',(-20.9368167509762,-1.31891625920597,
125.034332497166));
#152114=CARTESIAN_POINT('Ctrl Pts',(-20.9442146652875,-1.47155275449112,
125.07352620596));
#152115=CARTESIAN_POINT('Ctrl Pts',(-20.9516113501998,-1.62416388436031,
125.11271340147));
#152116=CARTESIAN_POINT('Ctrl Pts',(-20.959008035112,-1.77525444295494,
125.158012587351));
#152117=CARTESIAN_POINT('Ctrl Pts',(-20.9664047200242,-1.92430478709526,
125.209275126811));
#152118=CARTESIAN_POINT('Ctrl Pts',(-20.9738010769597,-2.07334852218692,
125.260535393235));
#152119=CARTESIAN_POINT('Ctrl Pts',(-20.9811974338951,-2.22035186969653,
125.317758366071));
#152120=CARTESIAN_POINT('Ctrl Pts',(-20.9885937908305,-2.36481185127169,
125.380746004544));
#152121=CARTESIAN_POINT('Ctrl Pts',(-20.9959912801671,-2.50929395003902,
125.443743286586));
#152122=CARTESIAN_POINT('Ctrl Pts',(-21.0033887695036,-2.6512315653259,
125.512506842399));
#152123=CARTESIAN_POINT('Ctrl Pts',(-21.0107862588402,-2.79014329074996,
125.586791166223));
#152124=CARTESIAN_POINT('Ctrl Pts',(-21.0181863413553,-2.92910371146462,
125.661101530302));
#152125=CARTESIAN_POINT('Ctrl Pts',(-21.0255864238703,-3.06503580144865,
125.740936339628));
#152126=CARTESIAN_POINT('Ctrl Pts',(-21.0329865063853,-3.19748440510901,
125.826005061603));
#152127=CARTESIAN_POINT('Ctrl Pts',(-21.0403947260518,-3.33007864962458,
125.911167325383));
#152128=CARTESIAN_POINT('Ctrl Pts',(-21.0478029457183,-3.459181443868,126.001574793515));
#152129=CARTESIAN_POINT('Ctrl Pts',(-21.0552111653848,-3.58436758906766,
126.096894255611));
#152130=CARTESIAN_POINT('Ctrl Pts',(-21.0626239446869,-3.70963078425137,
126.192272385245));
#152131=CARTESIAN_POINT('Ctrl Pts',(-21.0700367239889,-3.83097223984001,
126.292568295772));
#152132=CARTESIAN_POINT('Ctrl Pts',(-21.077449503291,-3.94800170713282,
126.397410075187));
#152133=CARTESIAN_POINT('Ctrl Pts',(-21.0848728743198,-4.06519839161614,
126.502401657452));
#152134=CARTESIAN_POINT('Ctrl Pts',(-21.0922962453486,-4.17807051539867,
126.611951821977));
#152135=CARTESIAN_POINT('Ctrl Pts',(-21.0997196163774,-4.28626581591441,
126.725652989184));
#152136=CARTESIAN_POINT('Ctrl Pts',(-21.1036556658181,-4.34363356035738,
126.785940076258));
#152137=CARTESIAN_POINT('Ctrl Pts',(-21.1075917152587,-4.39968716480038,
126.847393618015));
#152138=CARTESIAN_POINT('Ctrl Pts',(-21.1115277646994,-4.45437896555516,
126.90994941769));
#152139=CARTESIAN_POINT('Ctrl Pts',(-21.1188905251277,-4.55668525830135,
127.026966079533));
#152140=CARTESIAN_POINT('Ctrl Pts',(-21.1262532855559,-4.65454638571701,
127.148210387153));
#152141=CARTESIAN_POINT('Ctrl Pts',(-21.1336160459842,-4.74758812446407,
127.273307295546));
#152142=CARTESIAN_POINT('Ctrl Pts',(-21.141033077726,-4.84131567900425,
127.399326300157));
#152143=CARTESIAN_POINT('Ctrl Pts',(-21.1484501094678,-4.93015219722535,
127.529254695775));
#152144=CARTESIAN_POINT('Ctrl Pts',(-21.1558671412097,-5.01375270467083,
127.662670884491));
#152145=CARTESIAN_POINT('Ctrl Pts',(-21.1632118482149,-5.09653800936527,
127.794786109286));
#152146=CARTESIAN_POINT('Ctrl Pts',(-21.1705565552201,-5.17418873204522,
127.930321095861));
#152147=CARTESIAN_POINT('Ctrl Pts',(-21.1779012622253,-5.24641037403859,
128.068833474641));
#152148=CARTESIAN_POINT('Ctrl Pts',(-21.1852409137826,-5.31858230502862,
128.207250513726));
#152149=CARTESIAN_POINT('Ctrl Pts',(-21.1925805653399,-5.38533241623092,
128.348640531718));
#152150=CARTESIAN_POINT('Ctrl Pts',(-21.1999202168971,-5.44641050684016,
128.492533817505));
#152151=CARTESIAN_POINT('Ctrl Pts',(-21.2072563252452,-5.50745911206495,
128.636357638959));
#152152=CARTESIAN_POINT('Ctrl Pts',(-21.2145924335934,-5.56284099861111,
128.782681973944));
#152153=CARTESIAN_POINT('Ctrl Pts',(-21.2219285419415,-5.61235286949372,
128.931014458741));
#152154=CARTESIAN_POINT('Ctrl Pts',(-21.229403230762,-5.6628000289697,129.082148972194));
#152155=CARTESIAN_POINT('Ctrl Pts',(-21.2368779195825,-5.70715300054209,
129.235367901247));
#152156=CARTESIAN_POINT('Ctrl Pts',(-21.2443526084031,-5.74524894773119,
129.390131113174));
#152157=CARTESIAN_POINT('Ctrl Pts',(-21.2516875524619,-5.78263266338919,
129.542000913923));
#152158=CARTESIAN_POINT('Ctrl Pts',(-21.2590224965208,-5.81399119400866,
129.695357374521));
#152159=CARTESIAN_POINT('Ctrl Pts',(-21.2663574405796,-5.83922173065768,
129.849677349296));
#152160=CARTESIAN_POINT('Ctrl Pts',(-21.273902001781,-5.86517330252611,
130.008407461612));
#152161=CARTESIAN_POINT('Ctrl Pts',(-21.2814465629825,-5.88464130933544,
130.168156564734));
#152162=CARTESIAN_POINT('Ctrl Pts',(-21.2889911241839,-5.89757087839648,
130.328347700945));
#152163=CARTESIAN_POINT('Ctrl Pts',(-21.2965356853853,-5.91050044745754,
130.488538837157));
#152164=CARTESIAN_POINT('Ctrl Pts',(-21.3040802465867,-5.91689157699635,
130.649171569774));
#152165=CARTESIAN_POINT('Ctrl Pts',(-21.3116248077882,-5.91674761992799,
130.809667648422));
#152166=CARTESIAN_POINT('',(-23.0616248077882,-5.9221143857238,130.804232609979));
#152167=CARTESIAN_POINT('Ctrl Pts',(-21.3116260420174,-5.91389133234292,
130.809691329677));
#152168=CARTESIAN_POINT('Ctrl Pts',(-21.337742490849,-5.91867273821186,
131.365005195582));
#152169=CARTESIAN_POINT('Ctrl Pts',(-21.4566748142849,-5.59177582902208,
133.888337854231));
#152170=CARTESIAN_POINT('Ctrl Pts',(-21.6684230123253,-1.999537622794,137.511029673468));
#152171=CARTESIAN_POINT('Ctrl Pts',(-21.9468706361382,4.56171169292535,
136.111746693683));
#152172=CARTESIAN_POINT('Ctrl Pts',(-22.2253182599512,6.93097081485253,
129.835235190171));
#152173=CARTESIAN_POINT('Ctrl Pts',(-22.5037658837639,2.93100635467636,
124.449302610028));
#152174=CARTESIAN_POINT('Ctrl Pts',(-22.7822135075769,-3.76240975782294,
124.903357876965));
#152175=CARTESIAN_POINT('Ctrl Pts',(-22.9681664822516,-5.92343974002014,
128.827996518787));
#152176=CARTESIAN_POINT('Ctrl Pts',(-23.061303582322,-5.92653152972454,
130.79743998992));
#152177=CARTESIAN_POINT('Ctrl Pts',(-23.0616248077882,-5.92652937499865,
130.804232514548));
#152178=CARTESIAN_POINT('',(-24.8116247921649,-5.91465124248381,130.799116998419));
#152179=CARTESIAN_POINT('Ctrl Pts',(-23.0616248077882,-5.9167499986178,
130.804232725931));
#152180=CARTESIAN_POINT('Ctrl Pts',(-23.06904344305,-5.91675338383835,130.960845812215));
#152181=CARTESIAN_POINT('Ctrl Pts',(-23.0764620783118,-5.91053428214121,
131.11769729394));
#152182=CARTESIAN_POINT('Ctrl Pts',(-23.0838807135736,-5.89806180331044,
131.27425159091));
#152183=CARTESIAN_POINT('Ctrl Pts',(-23.0912905785281,-5.88560406943866,
131.430620809459));
#152184=CARTESIAN_POINT('Ctrl Pts',(-23.0987004434825,-5.86690770278589,
131.586693173578));
#152185=CARTESIAN_POINT('Ctrl Pts',(-23.106110308437,-5.84199377780407,
131.741931554935));
#152186=CARTESIAN_POINT('Ctrl Pts',(-23.1135130349591,-5.81710385411908,
131.897020384486));
#152187=CARTESIAN_POINT('Ctrl Pts',(-23.1209157614812,-5.78600835519952,
132.051276464101));
#152188=CARTESIAN_POINT('Ctrl Pts',(-23.1283184880033,-5.7487802566815,
132.204166362264));
#152189=CARTESIAN_POINT('Ctrl Pts',(-23.1357157023083,-5.71157987894451,
132.356942415574));
#152190=CARTESIAN_POINT('Ctrl Pts',(-23.1431129166133,-5.66825608191381,
132.508353951294));
#152191=CARTESIAN_POINT('Ctrl Pts',(-23.1505101309183,-5.61893314033713,
132.65787644618));
#152192=CARTESIAN_POINT('Ctrl Pts',(-23.1579034548305,-5.56963613901479,
132.807320303185));
#152193=CARTESIAN_POINT('Ctrl Pts',(-23.1652967787427,-5.51434639340068,
132.954876743804));
#152194=CARTESIAN_POINT('Ctrl Pts',(-23.1726901026549,-5.45323834317587,
133.100035275486));
#152195=CARTESIAN_POINT('Ctrl Pts',(-23.180082221126,-5.39214025628437,
133.245170139863));
#152196=CARTESIAN_POINT('Ctrl Pts',(-23.187474339597,-5.32522589225838,
133.387907526963));
#152197=CARTESIAN_POINT('Ctrl Pts',(-23.1948664580682,-5.25271830153739,
133.527755742625));
#152198=CARTESIAN_POINT('Ctrl Pts',(-23.202258272332,-5.18021369471566,
133.667598203123));
#152199=CARTESIAN_POINT('Ctrl Pts',(-23.2096500865959,-5.10211649090185,
133.8045513967));
#152200=CARTESIAN_POINT('Ctrl Pts',(-23.2170419008597,-5.01869616088841,
133.938147369594));
#152201=CARTESIAN_POINT('Ctrl Pts',(-23.2244348753669,-4.93526273694747,
134.071764312148));
#152202=CARTESIAN_POINT('Ctrl Pts',(-23.231827849874,-4.84650472121751,
134.202022667709));
#152203=CARTESIAN_POINT('Ctrl Pts',(-23.2392208243811,-4.75273536194316,
134.328482797888));
#152204=CARTESIAN_POINT('Ctrl Pts',(-23.2466164240032,-4.65893270682275,
134.454987831829));
#152205=CARTESIAN_POINT('Ctrl Pts',(-23.2540120236253,-4.56011538792318,
134.577691655166));
#152206=CARTESIAN_POINT('Ctrl Pts',(-23.2614076232473,-4.45663732663343,
134.696187219736));
#152207=CARTESIAN_POINT('Ctrl Pts',(-23.2688113610781,-4.35304539681253,
134.814813178282));
#152208=CARTESIAN_POINT('Ctrl Pts',(-23.276215098909,-4.24478272858463,
134.929221348638));
#152209=CARTESIAN_POINT('Ctrl Pts',(-23.2836188367398,-4.1322410363748,
135.03904060309));
#152210=CARTESIAN_POINT('Ctrl Pts',(-23.2910271706411,-4.01962948086737,
135.148928030813));
#152211=CARTESIAN_POINT('Ctrl Pts',(-23.2984355045423,-3.90273388561915,
135.254220616916));
#152212=CARTESIAN_POINT('Ctrl Pts',(-23.3058438384435,-3.78197908895288,
135.35458750567));
#152213=CARTESIAN_POINT('Ctrl Pts',(-23.3132626868675,-3.66105290704956,
135.455096843448));
#152214=CARTESIAN_POINT('Ctrl Pts',(-23.3206815352914,-3.53625688098093,
135.550666295677));
#152215=CARTESIAN_POINT('Ctrl Pts',(-23.3281003837154,-3.40804549595954,
135.641007850926));
#152216=CARTESIAN_POINT('Ctrl Pts',(-23.3317698408778,-3.34463050778605,
135.685691937731));
#152217=CARTESIAN_POINT('Ctrl Pts',(-23.3354392980403,-3.28038037848562,
135.729097762255));
#152218=CARTESIAN_POINT('Ctrl Pts',(-23.3391087552027,-3.21535223655167,
135.771194675334));
#152219=CARTESIAN_POINT('Ctrl Pts',(-23.3465320216081,-3.08380111057824,
135.856356209261));
#152220=CARTESIAN_POINT('Ctrl Pts',(-23.3539552880136,-2.9486653559629,
135.936416530185));
#152221=CARTESIAN_POINT('Ctrl Pts',(-23.361378554419,-2.81037842963538,
136.011058577381));
#152222=CARTESIAN_POINT('Ctrl Pts',(-23.36879304714,-2.67225494697077,136.085612403876));
#152223=CARTESIAN_POINT('Ctrl Pts',(-23.376207539861,-2.5309880313707,136.154760528159));
#152224=CARTESIAN_POINT('Ctrl Pts',(-23.383622032582,-2.38704065105636,
136.218228688798));
#152225=CARTESIAN_POINT('Ctrl Pts',(-23.3910293789357,-2.24323201264648,
136.281635676434));
#152226=CARTESIAN_POINT('Ctrl Pts',(-23.3984367252895,-2.0967483921047,
136.339373449612));
#152227=CARTESIAN_POINT('Ctrl Pts',(-23.4058440716433,-1.94807783588486,
136.391213336927));
#152228=CARTESIAN_POINT('Ctrl Pts',(-23.4132458933187,-1.79951816377508,
136.443014560099));
#152229=CARTESIAN_POINT('Ctrl Pts',(-23.4206477149941,-1.64877515469279,
136.488926533766));
#152230=CARTESIAN_POINT('Ctrl Pts',(-23.4280495366695,-1.49635723668165,
136.528768498101));
#152231=CARTESIAN_POINT('Ctrl Pts',(-23.4354474509808,-1.34401977890322,
136.568589430173));
#152232=CARTESIAN_POINT('Ctrl Pts',(-23.4428453652921,-1.19000953331409,
136.602346640283));
#152233=CARTESIAN_POINT('Ctrl Pts',(-23.4502432796035,-1.03485039926491,
136.629909107935));
#152234=CARTESIAN_POINT('Ctrl Pts',(-23.4576399645157,-0.879717049848722,
136.657466995205));
#152235=CARTESIAN_POINT('Ctrl Pts',(-23.4650366494279,-0.723435558084921,
136.678832117951));
#152236=CARTESIAN_POINT('Ctrl Pts',(-23.4724333343401,-0.566540454012888,
136.693924478878));
#152237=CARTESIAN_POINT('Ctrl Pts',(-23.4798296912756,-0.409652306833961,
136.709016170593));
#152238=CARTESIAN_POINT('Ctrl Pts',(-23.487226048211,-0.252150973028266,
136.717835617782));
#152239=CARTESIAN_POINT('Ctrl Pts',(-23.4946224051465,-0.0945762823509183,
136.720354692049));
#152240=CARTESIAN_POINT('Ctrl Pts',(-23.502019894483,0.0630225334133913,
136.722874151993));
#152241=CARTESIAN_POINT('Ctrl Pts',(-23.5094173838196,0.220694355137821,
136.719091312394));
#152242=CARTESIAN_POINT('Ctrl Pts',(-23.5168148731562,0.377899322870641,
136.709030181926));
#152243=CARTESIAN_POINT('Ctrl Pts',(-23.5242149556712,0.535159398561426,
136.698965524544));
#152244=CARTESIAN_POINT('Ctrl Pts',(-23.5316150381861,0.691951922121476,
136.682618218254));
#152245=CARTESIAN_POINT('Ctrl Pts',(-23.5390151207011,0.847742271905184,
136.66006412807));
#152246=CARTESIAN_POINT('Ctrl Pts',(-23.5464233403676,1.00370392919434,
136.637485237345));
#152247=CARTESIAN_POINT('Ctrl Pts',(-23.5538315600341,1.15866084228152,
136.608685986277));
#152248=CARTESIAN_POINT('Ctrl Pts',(-23.5612397797006,1.31208797403423,
136.573793493586));
#152249=CARTESIAN_POINT('Ctrl Pts',(-23.5686525590026,1.46560953762647,
136.538879525147));
#152250=CARTESIAN_POINT('Ctrl Pts',(-23.5760653383046,1.61759908414759,
136.497864939193));
#152251=CARTESIAN_POINT('Ctrl Pts',(-23.5834781176067,1.76754735283541,
136.450926557851));
#152252=CARTESIAN_POINT('Ctrl Pts',(-23.5909014886354,1.91770987464118,
136.403921108748));
#152253=CARTESIAN_POINT('Ctrl Pts',(-23.5983248596642,2.06582494277933,
136.350975084677));
#152254=CARTESIAN_POINT('Ctrl Pts',(-23.605748230693,2.21140309307698,136.292313507527));
#152255=CARTESIAN_POINT('Ctrl Pts',(-23.6096842801338,2.2885921214657,136.261209731756));
#152256=CARTESIAN_POINT('Ctrl Pts',(-23.6136203295746,2.36506832852509,
136.228499884312));
#152257=CARTESIAN_POINT('Ctrl Pts',(-23.6175563790155,2.4407617376494,136.194222647574));
#152258=CARTESIAN_POINT('Ctrl Pts',(-23.6249796454209,2.58351714494553,
136.129576848845));
#152259=CARTESIAN_POINT('Ctrl Pts',(-23.6324029118264,2.72391833660915,
136.059157870285));
#152260=CARTESIAN_POINT('Ctrl Pts',(-23.6398261782318,2.86146426641368,
135.98315901242));
#152261=CARTESIAN_POINT('Ctrl Pts',(-23.6472406709528,2.99884762835166,
135.907249978892));
#152262=CARTESIAN_POINT('Ctrl Pts',(-23.6546551636738,3.13338212220588,
135.825774372123));
#152263=CARTESIAN_POINT('Ctrl Pts',(-23.6620696563948,3.26458675843334,
135.738973455384));
#152264=CARTESIAN_POINT('Ctrl Pts',(-23.6694770027486,3.395664934693,135.652256200637));
#152265=CARTESIAN_POINT('Ctrl Pts',(-23.6768843491024,3.52341933345018,
135.560224058769));
#152266=CARTESIAN_POINT('Ctrl Pts',(-23.6842916954562,3.6473937659479,135.463164034606));
#152267=CARTESIAN_POINT('Ctrl Pts',(-23.6916935171316,3.77127573363693,
135.366176401471));
#152268=CARTESIAN_POINT('Ctrl Pts',(-23.6990953388071,3.89138305588978,
135.264168581894));
#152269=CARTESIAN_POINT('Ctrl Pts',(-23.7064971604825,4.00728883656822,
135.157470625688));
#152270=CARTESIAN_POINT('Ctrl Pts',(-23.7138950747938,4.12313343148609,
135.050828994504));
#152271=CARTESIAN_POINT('Ctrl Pts',(-23.7212929891051,4.23478062805544,
134.939502409724));
#152272=CARTESIAN_POINT('Ctrl Pts',(-23.7286909034164,4.34183701462641,
134.82386082293));
#152273=CARTESIAN_POINT('Ctrl Pts',(-23.7360875883286,4.44887561036875,
134.708238453669));
#152274=CARTESIAN_POINT('Ctrl Pts',(-23.7434842732408,4.55132465691304,
134.588302779243));
#152275=CARTESIAN_POINT('Ctrl Pts',(-23.7508809581531,4.6488279237252,134.464460274419));
#152276=CARTESIAN_POINT('Ctrl Pts',(-23.7582773150885,4.74632686714018,
134.340623260901));
#152277=CARTESIAN_POINT('Ctrl Pts',(-23.765673672024,4.83888023594587,134.212880054734));
#152278=CARTESIAN_POINT('Ctrl Pts',(-23.7730700289595,4.92617257375734,
134.081669625893));
#152279=CARTESIAN_POINT('Ctrl Pts',(-23.7804675182961,5.01347827624883,
133.9504391084));
#152280=CARTESIAN_POINT('Ctrl Pts',(-23.7878650076327,5.09552113714935,
133.815740622081));
#152281=CARTESIAN_POINT('Ctrl Pts',(-23.7952624969693,5.17202954814514,
133.678041343676));
#152282=CARTESIAN_POINT('Ctrl Pts',(-23.8026625794843,5.2485647790457,133.540293795002));
#152283=CARTESIAN_POINT('Ctrl Pts',(-23.8100626619992,5.3195615161386,133.399543685981));
#152284=CARTESIAN_POINT('Ctrl Pts',(-23.8174627445142,5.38479461075073,
133.256281815837));
#152285=CARTESIAN_POINT('Ctrl Pts',(-23.8248709641806,5.4500994358565,133.112862414539));
#152286=CARTESIAN_POINT('Ctrl Pts',(-23.8322791838472,5.50962780685286,
132.966926076288));
#152287=CARTESIAN_POINT('Ctrl Pts',(-23.8396874035136,5.56320287692264,
132.818983240466));
#152288=CARTESIAN_POINT('Ctrl Pts',(-23.8471001828157,5.61681092155418,
132.670949348296));
#152289=CARTESIAN_POINT('Ctrl Pts',(-23.8545129621178,5.66445825124413,
132.520906852696));
#152290=CARTESIAN_POINT('Ctrl Pts',(-23.8619257414199,5.70601836357232,
132.369379785843));
#152291=CARTESIAN_POINT('Ctrl Pts',(-23.8693491124487,5.74763785893798,
132.217636210012));
#152292=CARTESIAN_POINT('Ctrl Pts',(-23.8767724834774,5.78315268161847,
132.064404189062));
#152293=CARTESIAN_POINT('Ctrl Pts',(-23.8841958545062,5.81248758155938,
131.91021715289));
#152294=CARTESIAN_POINT('Ctrl Pts',(-23.8881319039469,5.82804164938912,
131.828463486645));
#152295=CARTESIAN_POINT('Ctrl Pts',(-23.8920679533876,5.84185918629352,
131.746441416203));
#152296=CARTESIAN_POINT('Ctrl Pts',(-23.8960040028284,5.85393491279052,
131.664230723636));
#152297=CARTESIAN_POINT('Ctrl Pts',(-23.9034272692338,5.87670935609358,
131.50918392316));
#152298=CARTESIAN_POINT('Ctrl Pts',(-23.9108505356393,5.89335414864615,
131.352997246254));
#152299=CARTESIAN_POINT('Ctrl Pts',(-23.9182738020448,5.90376109192957,
131.196196720954));
#152300=CARTESIAN_POINT('Ctrl Pts',(-23.9256882947658,5.91415573507031,
131.039581520854));
#152301=CARTESIAN_POINT('Ctrl Pts',(-23.9331027874867,5.91832717970208,
130.882354285348));
#152302=CARTESIAN_POINT('Ctrl Pts',(-23.9405172802078,5.9162184208524,130.725050093253));
#152303=CARTESIAN_POINT('Ctrl Pts',(-23.9479246265615,5.91411169450389,
130.567897516862));
#152304=CARTESIAN_POINT('Ctrl Pts',(-23.9553319729153,5.90573682016777,
130.410668502306));
#152305=CARTESIAN_POINT('Ctrl Pts',(-23.9627393192691,5.89108868196553,
130.253901987224));
#152306=CARTESIAN_POINT('Ctrl Pts',(-23.9701411409445,5.87645146889744,
130.097252394525));
#152307=CARTESIAN_POINT('Ctrl Pts',(-23.9775429626198,5.85555034273875,
129.941064984538));
#152308=CARTESIAN_POINT('Ctrl Pts',(-23.9849447842952,5.82843223595262,
129.785877317061));
#152309=CARTESIAN_POINT('Ctrl Pts',(-23.9923426986066,5.80132844460386,
129.630771571944));
#152310=CARTESIAN_POINT('Ctrl Pts',(-23.9997406129179,5.76801427277528,
129.47666488508));
#152311=CARTESIAN_POINT('Ctrl Pts',(-24.0071385272293,5.72858832260481,
129.324088212697));
#152312=CARTESIAN_POINT('Ctrl Pts',(-24.0145352121415,5.68916892431204,
129.17153689579));
#152313=CARTESIAN_POINT('Ctrl Pts',(-24.0219318970538,5.64363985677666,
129.020515449806));
#152314=CARTESIAN_POINT('Ctrl Pts',(-24.029328581966,5.59215054742784,128.871543291122));
#152315=CARTESIAN_POINT('Ctrl Pts',(-24.0367249389014,5.54066352116895,
128.72257773802));
#152316=CARTESIAN_POINT('Ctrl Pts',(-24.0441212958367,5.48321690052589,
128.575661644361));
#152317=CARTESIAN_POINT('Ctrl Pts',(-24.0515176527722,5.42000949149078,
128.431297686532));
#152318=CARTESIAN_POINT('Ctrl Pts',(-24.0589151421087,5.35679240524017,
128.286911626212));
#152319=CARTESIAN_POINT('Ctrl Pts',(-24.0663126314454,5.28781292416555,
128.145078821713));
#152320=CARTESIAN_POINT('Ctrl Pts',(-24.0737101207819,5.2133172863627,128.006280305243));
#152321=CARTESIAN_POINT('Ctrl Pts',(-24.081110203297,5.13879553422885,127.867433133166));
#152322=CARTESIAN_POINT('Ctrl Pts',(-24.088510285812,5.05875395184917,127.731622695578));
#152323=CARTESIAN_POINT('Ctrl Pts',(-24.095910368327,4.97348376415447,127.599303705405));
#152324=CARTESIAN_POINT('Ctrl Pts',(-24.1033185879935,4.88811981312278,
127.466839216899));
#152325=CARTESIAN_POINT('Ctrl Pts',(-24.1107268076599,4.7975159772053,127.337874156931));
#152326=CARTESIAN_POINT('Ctrl Pts',(-24.1181350273264,4.70200611348575,
127.21283321669));
#152327=CARTESIAN_POINT('Ctrl Pts',(-24.1255478066285,4.60643746503847,
127.087715315836));
#152328=CARTESIAN_POINT('Ctrl Pts',(-24.1329605859306,4.50595700961332,
126.966526634061));
#152329=CARTESIAN_POINT('Ctrl Pts',(-24.1403733652327,4.40093725267633,
126.849656853628));
#152330=CARTESIAN_POINT('Ctrl Pts',(-24.1477967362615,4.29576743858598,
126.732620084172));
#152331=CARTESIAN_POINT('Ctrl Pts',(-24.1552201072901,4.18604562876078,
126.619914807795));
#152332=CARTESIAN_POINT('Ctrl Pts',(-24.1626434783189,4.07217993838861,
126.511892666389));
#152333=CARTESIAN_POINT('Ctrl Pts',(-24.1665795277597,4.01180561718372,
126.454616735059));
#152334=CARTESIAN_POINT('Ctrl Pts',(-24.1705155772005,3.95026684254355,
126.398656717354));
#152335=CARTESIAN_POINT('Ctrl Pts',(-24.1744516266413,3.88762788369584,
126.344060179209));
#152336=CARTESIAN_POINT('Ctrl Pts',(-24.1818748930467,3.7694927622037,126.241092812166));
#152337=CARTESIAN_POINT('Ctrl Pts',(-24.1892981594522,3.64708540443271,
126.142666362847));
#152338=CARTESIAN_POINT('Ctrl Pts',(-24.1967214258576,3.52078988872497,
126.049156192733));
#152339=CARTESIAN_POINT('Ctrl Pts',(-24.2041359185786,3.39464364382862,
125.955756543874));
#152340=CARTESIAN_POINT('Ctrl Pts',(-24.2115504112996,3.26461868540771,
125.867261828084));
#152341=CARTESIAN_POINT('Ctrl Pts',(-24.2189649040206,3.13113437784517,
125.784009228432));
#152342=CARTESIAN_POINT('Ctrl Pts',(-24.2263722503744,2.99777872748367,
125.70083687077));
#152343=CARTESIAN_POINT('Ctrl Pts',(-24.2337795967281,2.86097068043396,
125.622896766838));
#152344=CARTESIAN_POINT('Ctrl Pts',(-24.2411869430819,2.72116089493841,
125.550484529728));
#152345=CARTESIAN_POINT('Ctrl Pts',(-24.2485887647573,2.58145538485581,
125.478126300396));
#152346=CARTESIAN_POINT('Ctrl Pts',(-24.2559905864327,2.4387529241492,125.411287899597));
#152347=CARTESIAN_POINT('Ctrl Pts',(-24.2633924081081,2.29353114524227,
125.350220405919));
#152348=CARTESIAN_POINT('Ctrl Pts',(-24.2707903224195,2.14838602778201,
125.289185149296));
#152349=CARTESIAN_POINT('Ctrl Pts',(-24.2781882367308,2.0007245839777,125.233914877047));
#152350=CARTESIAN_POINT('Ctrl Pts',(-24.2855861510422,1.85104681920726,
125.184613627211));
#152351=CARTESIAN_POINT('Ctrl Pts',(-24.2929828359544,1.70139392816611,
125.135320570349));
#152352=CARTESIAN_POINT('Ctrl Pts',(-24.3003795208666,1.54972573539777,
125.091994683858));
#152353=CARTESIAN_POINT('Ctrl Pts',(-24.3077762057788,1.39656000978726,
125.054791007451));
#152354=CARTESIAN_POINT('Ctrl Pts',(-24.3151725627142,1.24340107570508,
125.017588980693));
#152355=CARTESIAN_POINT('Ctrl Pts',(-24.3225689196496,1.08874510356055,
124.986508712365));
#152356=CARTESIAN_POINT('Ctrl Pts',(-24.3299652765851,0.933122468728264,
124.961654650221));
#152357=CARTESIAN_POINT('Ctrl Pts',(-24.3373627659216,0.777476007673962,
124.936796782856));
#152358=CARTESIAN_POINT('Ctrl Pts',(-24.3447602552583,0.620862957897172,
124.918167078594));
#152359=CARTESIAN_POINT('Ctrl Pts',(-24.3521577445949,0.463821123122597,
124.905818380009));
#152360=CARTESIAN_POINT('Ctrl Pts',(-24.3595578271099,0.306724237574495,
124.893465352607));
#152361=CARTESIAN_POINT('Ctrl Pts',(-24.366957909625,0.149198639679638,
124.887397743888));
#152362=CARTESIAN_POINT('Ctrl Pts',(-24.37435799214,-0.00821569351148752,
124.887616321513));
#152363=CARTESIAN_POINT('Ctrl Pts',(-24.3817662118065,-0.165803119943195,
124.887835139486));
#152364=CARTESIAN_POINT('Ctrl Pts',(-24.3891744314729,-0.32327866380961,
124.894353947618));
#152365=CARTESIAN_POINT('Ctrl Pts',(-24.3965826511394,-0.480104562476285,
124.90712141845));
#152366=CARTESIAN_POINT('Ctrl Pts',(-24.4039954304414,-0.637026984867033,
124.919896747447));
#152367=CARTESIAN_POINT('Ctrl Pts',(-24.4114082097436,-0.793298595614365,
124.938928357654));
#152368=CARTESIAN_POINT('Ctrl Pts',(-24.4188209890456,-0.948390195691438,
124.964113482451));
#152369=CARTESIAN_POINT('Ctrl Pts',(-24.4262443600744,-1.10370339792,124.989334592936));
#152370=CARTESIAN_POINT('Ctrl Pts',(-24.4336677311031,-1.25783285723011,
125.020726704164));
#152371=CARTESIAN_POINT('Ctrl Pts',(-24.4410911021318,-1.41026213111176,
125.058136528301));
#152372=CARTESIAN_POINT('Ctrl Pts',(-24.4450271515726,-1.4910837896137,
125.077972114694));
#152373=CARTESIAN_POINT('Ctrl Pts',(-24.4489632010134,-1.57142774824051,
125.099498672198));
#152374=CARTESIAN_POINT('Ctrl Pts',(-24.4528992504542,-1.65121924933523,
125.122687839842));
#152375=CARTESIAN_POINT('Ctrl Pts',(-24.4603225168596,-1.80170353019258,
125.16642188631));
#152376=CARTESIAN_POINT('Ctrl Pts',(-24.467745783265,-1.95067665642722,
125.216204763103));
#152377=CARTESIAN_POINT('Ctrl Pts',(-24.4751690496705,-2.09761522206942,
125.271916226283));
#152378=CARTESIAN_POINT('Ctrl Pts',(-24.4825835423915,-2.24438011852973,
125.32756184314));
#152379=CARTESIAN_POINT('Ctrl Pts',(-24.4899980351125,-2.38911489528683,
125.38912196767));
#152380=CARTESIAN_POINT('Ctrl Pts',(-24.4974125278335,-2.53130919398322,
125.456426032424));
#152381=CARTESIAN_POINT('Ctrl Pts',(-24.5048198741873,-2.67336644046101,
125.523665226987));
#152382=CARTESIAN_POINT('Ctrl Pts',(-24.512227220541,-2.81288774843008,
125.596637181607));
#152383=CARTESIAN_POINT('Ctrl Pts',(-24.5196345668948,-2.94938081843602,
125.675122530838));
#152384=CARTESIAN_POINT('Ctrl Pts',(-24.5270363885702,-3.08577208676019,
125.753549342734));
#152385=CARTESIAN_POINT('Ctrl Pts',(-24.5344382102455,-3.21913929202749,
125.837481176219));
#152386=CARTESIAN_POINT('Ctrl Pts',(-24.5418400319209,-3.34901302271742,
125.926651899718));
#152387=CARTESIAN_POINT('Ctrl Pts',(-24.5492379462323,-3.47881819407678,
126.015775550687));
#152388=CARTESIAN_POINT('Ctrl Pts',(-24.5566358605436,-3.60513325666363,
126.110132373147));
#152389=CARTESIAN_POINT('Ctrl Pts',(-24.564033774855,-3.72751628237571,
126.209411985957));
#152390=CARTESIAN_POINT('Ctrl Pts',(-24.5714304597672,-3.84987897024865,
126.308675100296));
#152391=CARTESIAN_POINT('Ctrl Pts',(-24.5788271446794,-3.96831062849901,
126.412859146397));
#152392=CARTESIAN_POINT('Ctrl Pts',(-24.5862238295915,-4.08240095109692,
126.521612313383));
#152393=CARTESIAN_POINT('Ctrl Pts',(-24.593620186527,-4.19648621481037,
126.63036065814));
#152394=CARTESIAN_POINT('Ctrl Pts',(-24.6010165434625,-4.30623025541946,
126.74367746338));
#152395=CARTESIAN_POINT('Ctrl Pts',(-24.608412900398,-4.41125851722605,
126.861172965843));
#152396=CARTESIAN_POINT('Ctrl Pts',(-24.6158103897346,-4.5163028591284,
126.978686457168));
#152397=CARTESIAN_POINT('Ctrl Pts',(-24.6232078790711,-4.61662973583615,
127.100379641249));
#152398=CARTESIAN_POINT('Ctrl Pts',(-24.6306053684077,-4.71190399334551,
127.225828611283));
#152399=CARTESIAN_POINT('Ctrl Pts',(-24.6380054509227,-4.80721164909733,
127.351321557257));
#152400=CARTESIAN_POINT('Ctrl Pts',(-24.6454055334377,-4.897462933594,127.480572613399));
#152401=CARTESIAN_POINT('Ctrl Pts',(-24.6528056159527,-4.98236533019543,
127.613127896662));
#152402=CARTESIAN_POINT('Ctrl Pts',(-24.6602138356191,-5.06736108571047,
127.745828938087));
#152403=CARTESIAN_POINT('Ctrl Pts',(-24.6676220552856,-5.14699600582089,
127.881841148107));
#152404=CARTESIAN_POINT('Ctrl Pts',(-24.675030274952,-5.22102259993138,
128.020684348043));
#152405=CARTESIAN_POINT('Ctrl Pts',(-24.6824430542541,-5.29509475617545,
128.159613003652));
#152406=CARTESIAN_POINT('Ctrl Pts',(-24.6898558335562,-5.36355154626121,
128.301375785805));
#152407=CARTESIAN_POINT('Ctrl Pts',(-24.6972686128583,-5.42619338565387,
128.445471916507));
#152408=CARTESIAN_POINT('Ctrl Pts',(-24.704691983887,-5.48892473064418,
128.589773938517));
#152409=CARTESIAN_POINT('Ctrl Pts',(-24.7121153549158,-5.54582439597577,
128.736415620721));
#152410=CARTESIAN_POINT('Ctrl Pts',(-24.7195387259445,-5.59674219725355,
128.88487960959));
#152411=CARTESIAN_POINT('Ctrl Pts',(-24.7234747753854,-5.62374003724726,
128.963598778834));
#152412=CARTESIAN_POINT('Ctrl Pts',(-24.7274108248262,-5.64905700690369,
129.042830056833));
#152413=CARTESIAN_POINT('Ctrl Pts',(-24.731346874267,-5.67267655877129,
129.122495218057));
#152414=CARTESIAN_POINT('Ctrl Pts',(-24.7405338723611,-5.72780614523887,
129.308438940391));
#152415=CARTESIAN_POINT('Ctrl Pts',(-24.7497208704551,-5.77382055480966,
129.49720052025));
#152416=CARTESIAN_POINT('Ctrl Pts',(-24.7589078685492,-5.81047562116316,
129.687980924823));
#152417=CARTESIAN_POINT('Ctrl Pts',(-24.7679691199866,-5.84662897281139,
129.876150030497));
#152418=CARTESIAN_POINT('Ctrl Pts',(-24.777030371424,-5.87367744459647,
130.066283120076));
#152419=CARTESIAN_POINT('Ctrl Pts',(-24.7860916228615,-5.89143236350679,
130.257592596624));
#152420=CARTESIAN_POINT('Ctrl Pts',(-24.7946026697757,-5.90810919328551,
130.4372856491));
#152421=CARTESIAN_POINT('Ctrl Pts',(-24.80311371669,-5.91658710362847,130.618016443981));
#152422=CARTESIAN_POINT('Ctrl Pts',(-24.8116247636042,-5.91674767427923,
130.799114532234));
#152423=CARTESIAN_POINT('',(-26.5616248077882,-5.90779414308507,130.806685475366));
#152424=CARTESIAN_POINT('Ctrl Pts',(-24.8116248077882,-5.91350445555948,
130.799118347467));
#152425=CARTESIAN_POINT('Ctrl Pts',(-24.8776813712188,-5.90160535121287,
132.203911372475));
#152426=CARTESIAN_POINT('Ctrl Pts',(-25.0365538092536,-4.69690807201577,
135.600915768792));
#152427=CARTESIAN_POINT('Ctrl Pts',(-25.2882421218929,0.97967206287985,
137.733848562542));
#152428=CARTESIAN_POINT('Ctrl Pts',(-25.5666897457058,6.3595111412122,133.72569226172));
#152429=CARTESIAN_POINT('Ctrl Pts',(-25.8451373695187,5.89527016016011,
127.032974894907));
#152430=CARTESIAN_POINT('Ctrl Pts',(-26.1235849933315,0.0135639018792721,
123.805976764782));
#152431=CARTESIAN_POINT('Ctrl Pts',(-26.3624141394214,-5.04196418963154,
126.554250593529));
#152432=CARTESIAN_POINT('Ctrl Pts',(-26.5084274109069,-5.90380256593809,
129.672610848885));
#152433=CARTESIAN_POINT('Ctrl Pts',(-26.5616248077882,-5.90779414308507,
130.806685475366));
#152434=CARTESIAN_POINT('',(-28.3116248077882,-5.92205169517661,130.808786883972));
#152435=CARTESIAN_POINT('Ctrl Pts',(-26.5616248077882,-5.90779414308507,
130.806685475366));
#152436=CARTESIAN_POINT('Ctrl Pts',(-26.6012432855112,-5.91076684888552,
131.651281507495));
#152437=CARTESIAN_POINT('Ctrl Pts',(-26.7336776378389,-5.34594544265701,
134.470755369925));
#152438=CARTESIAN_POINT('Ctrl Pts',(-26.9589278647701,-1.00652534475882,
137.729999018512));
#152439=CARTESIAN_POINT('Ctrl Pts',(-27.2373754885831,5.28268419639938,
135.394655620227));
#152440=CARTESIAN_POINT('Ctrl Pts',(-27.515823112396,6.71736503453805,128.841055362868));
#152441=CARTESIAN_POINT('Ctrl Pts',(-27.7942707362089,1.97911556745978,
124.091636721785));
#152442=CARTESIAN_POINT('Ctrl Pts',(-28.0595379680061,-4.26746898338629,
125.443702988462));
#152443=CARTESIAN_POINT('Ctrl Pts',(-28.2319893251994,-5.90797919871711,
129.121481013772));
#152444=CARTESIAN_POINT('Ctrl Pts',(-28.3116248077882,-5.92205169517661,
130.808786883972));
#152445=CARTESIAN_POINT('',(-30.0616248077881,-5.92200696645842,130.799917113144));
#152446=CARTESIAN_POINT('Ctrl Pts',(-28.3116248077882,-5.92205169517661,
130.808786883972));
#152447=CARTESIAN_POINT('Ctrl Pts',(-28.3248051998037,-5.92438082051049,
131.088051253275));
#152448=CARTESIAN_POINT('Ctrl Pts',(-28.4308014664233,-5.77932387060202,
133.33145433914));
#152449=CARTESIAN_POINT('Ctrl Pts',(-28.6296136076478,-2.91165016792604,
137.168310164028));
#152450=CARTESIAN_POINT('Ctrl Pts',(-28.9080612314604,3.7803529530868,136.693884544035));
#152451=CARTESIAN_POINT('Ctrl Pts',(-29.1865088552733,6.99839639071874,
130.807274154852));
#152452=CARTESIAN_POINT('Ctrl Pts',(-29.4649564790863,3.78525543595478,
124.917986367238));
#152453=CARTESIAN_POINT('Ctrl Pts',(-29.743404102899,-2.90635034444604,
124.437988950305));
#152454=CARTESIAN_POINT('Ctrl Pts',(-29.9422935457997,-5.77833397768845,
128.273946643054));
#152455=CARTESIAN_POINT('Ctrl Pts',(-30.0483671140961,-5.92435612236718,
130.519009360987));
#152456=CARTESIAN_POINT('Ctrl Pts',(-30.0616248077881,-5.92200696645842,
130.799917113144));
#152457=CARTESIAN_POINT('',(-31.8116248077882,-5.90777491155152,130.802060587744));
#152458=CARTESIAN_POINT('Ctrl Pts',(-30.0616248077881,-5.92200696645842,
130.799917113144));
#152459=CARTESIAN_POINT('Ctrl Pts',(-30.1411829887004,-5.90790990137895,
132.485618282964));
#152460=CARTESIAN_POINT('Ctrl Pts',(-30.3135570442171,-4.27011095544813,
136.161858688443));
#152461=CARTESIAN_POINT('Ctrl Pts',(-30.5787469743377,1.97352566730395,
137.51873005712));
#152462=CARTESIAN_POINT('Ctrl Pts',(-30.8571945981506,6.71572799954466,
132.773258270183));
#152463=CARTESIAN_POINT('Ctrl Pts',(-31.1356422219637,5.28650438175435,
126.218465726483));
#152464=CARTESIAN_POINT('Ctrl Pts',(-31.4140898457764,-1.00075850276986,
123.877886554275));
#152465=CARTESIAN_POINT('Ctrl Pts',(-31.6394173743847,-5.34438097876868,
127.134633213779));
#152466=CARTESIAN_POINT('Ctrl Pts',(-31.7719290283886,-5.91072106251254,
129.955809741519));
#152467=CARTESIAN_POINT('Ctrl Pts',(-31.8116248077882,-5.90777491155152,
130.802060587744));
#152468=CARTESIAN_POINT('',(-33.5616248231286,-5.91467433100452,130.809612195234));
#152469=CARTESIAN_POINT('Ctrl Pts',(-31.8116248077882,-5.90777491155152,
130.802060587744));
#152470=CARTESIAN_POINT('Ctrl Pts',(-31.8647449029928,-5.90383243147168,
131.934496483914));
#152471=CARTESIAN_POINT('Ctrl Pts',(-32.0106808728018,-5.04386563195127,
135.051161972767));
#152472=CARTESIAN_POINT('Ctrl Pts',(-32.2494327172153,0.00773683405587478,
137.802753338164));
#152473=CARTESIAN_POINT('Ctrl Pts',(-32.5278803410281,5.89212794841245,
134.580653610686));
#152474=CARTESIAN_POINT('Ctrl Pts',(-32.8063279648409,6.36194132462962,
127.888325104698));
#152475=CARTESIAN_POINT('Ctrl Pts',(-33.0847755886539,0.985441421623745,
123.875690778778));
#152476=CARTESIAN_POINT('Ctrl Pts',(-33.3365412029694,-4.69465669647055,
126.004549984482));
#152477=CARTESIAN_POINT('Ctrl Pts',(-33.495490942681,-5.90161251282196,
129.403201726833));
#152478=CARTESIAN_POINT('Ctrl Pts',(-33.5616248077881,-5.91355064207631,
130.809610871177));
#152479=CARTESIAN_POINT('',(-35.3116248077882,-5.92211511787841,130.804457825077));
#152480=CARTESIAN_POINT('Ctrl Pts',(-33.5616248514337,-5.91674766723801,
130.809614638272));
#152481=CARTESIAN_POINT('Ctrl Pts',(-33.5706680044378,-5.91657680444688,
131.002029567238));
#152482=CARTESIAN_POINT('Ctrl Pts',(-33.5797111574419,-5.90701618416332,
131.194029392853));
#152483=CARTESIAN_POINT('Ctrl Pts',(-33.5887543104459,-5.88820921070805,
131.38481117828));
#152484=CARTESIAN_POINT('Ctrl Pts',(-33.5979300201283,-5.86912656018184,
131.5783894883));
#152485=CARTESIAN_POINT('Ctrl Pts',(-33.6071057298108,-5.84052454621328,
131.7707138291));
#152486=CARTESIAN_POINT('Ctrl Pts',(-33.6162814394932,-5.80260190920715,
131.960968436045));
#152487=CARTESIAN_POINT('Ctrl Pts',(-33.6247445717553,-5.7676243103274,
132.136448040104));
#152488=CARTESIAN_POINT('Ctrl Pts',(-33.6332077040174,-5.72471811545822,
132.310167201927));
#152489=CARTESIAN_POINT('Ctrl Pts',(-33.6416708362795,-5.67407496370947,
132.481502194388));
#152490=CARTESIAN_POINT('Ctrl Pts',(-33.6490941026849,-5.62965434077741,
132.631785240217));
#152491=CARTESIAN_POINT('Ctrl Pts',(-33.6565173690903,-5.57919184969903,
132.780529531387));
#152492=CARTESIAN_POINT('Ctrl Pts',(-33.6639406354957,-5.5228101227562,
132.927212216355));
#152493=CARTESIAN_POINT('Ctrl Pts',(-33.6713551282167,-5.46649503433241,
133.07372153457));
#152494=CARTESIAN_POINT('Ctrl Pts',(-33.6787696209375,-5.40427476833725,
133.218173751702));
#152495=CARTESIAN_POINT('Ctrl Pts',(-33.6861841136585,-5.33632222046923,
133.360059293433));
#152496=CARTESIAN_POINT('Ctrl Pts',(-33.6935914600122,-5.26843516782522,
133.501808080536));
#152497=CARTESIAN_POINT('Ctrl Pts',(-33.700998806366,-5.19482699263484,
133.640994782786));
#152498=CARTESIAN_POINT('Ctrl Pts',(-33.7084061527197,-5.11571930563854,
133.777128107367));
#152499=CARTESIAN_POINT('Ctrl Pts',(-33.7158079743951,-5.03667062013976,
133.913159898578));
#152500=CARTESIAN_POINT('Ctrl Pts',(-33.7232097960704,-4.95213077670942,
134.046142525209));
#152501=CARTESIAN_POINT('Ctrl Pts',(-33.7306116177458,-4.86236804723507,
134.175607795648));
#152502=CARTESIAN_POINT('Ctrl Pts',(-33.7380095320571,-4.77265270280689,
134.305004722379));
#152503=CARTESIAN_POINT('Ctrl Pts',(-33.7454074463684,-4.67772017543241,
134.430887684796));
#152504=CARTESIAN_POINT('Ctrl Pts',(-33.7528053606797,-4.57788286062919,
134.552816176441));
#152505=CARTESIAN_POINT('Ctrl Pts',(-33.7602020455918,-4.47806213697645,
134.674724405781));
#152506=CARTESIAN_POINT('Ctrl Pts',(-33.767598730504,-4.37333847986577,
134.792679180076));
#152507=CARTESIAN_POINT('Ctrl Pts',(-33.7749954154162,-4.26406556974834,
134.906271803756));
#152508=CARTESIAN_POINT('Ctrl Pts',(-33.7823917723516,-4.1547975049064,
135.019859390619));
#152509=CARTESIAN_POINT('Ctrl Pts',(-33.7897881292869,-4.04098084693891,
135.129084942428));
#152510=CARTESIAN_POINT('Ctrl Pts',(-33.7971844862223,-3.9230070650703,
135.233575686843));
#152511=CARTESIAN_POINT('Ctrl Pts',(-33.8045819755589,-3.80501522111433,
135.338082429058));
#152512=CARTESIAN_POINT('Ctrl Pts',(-33.8119794648955,-3.68286526543293,
135.437852672959));
#152513=CARTESIAN_POINT('Ctrl Pts',(-33.819376954232,-3.5569826305485,135.532553203373));
#152514=CARTESIAN_POINT('Ctrl Pts',(-33.826777036747,-3.43105586770155,
135.62728693091));
#152515=CARTESIAN_POINT('Ctrl Pts',(-33.8341771192619,-3.30139411859141,
135.71694718233));
#152516=CARTESIAN_POINT('Ctrl Pts',(-33.8415772017769,-3.16845259701143,
135.801243516233));
#152517=CARTESIAN_POINT('Ctrl Pts',(-33.8489854214433,-3.03536489256176,
135.885632542621));
#152518=CARTESIAN_POINT('Ctrl Pts',(-33.8563936411097,-2.89899052878617,
135.964645672416));
#152519=CARTESIAN_POINT('Ctrl Pts',(-33.8638018607762,-2.75981080927196,
136.038037609846));
#152520=CARTESIAN_POINT('Ctrl Pts',(-33.8712146400782,-2.62054542696272,
136.111474718789));
#152521=CARTESIAN_POINT('Ctrl Pts',(-33.8786274193802,-2.47847158446133,
136.179283580962));
#152522=CARTESIAN_POINT('Ctrl Pts',(-33.8860401986822,-2.33409096574279,
136.241266900199));
#152523=CARTESIAN_POINT('Ctrl Pts',(-33.8934635697109,-2.18950404922545,
136.30333878411));
#152524=CARTESIAN_POINT('Ctrl Pts',(-33.9008869407397,-2.04260412128661,
136.359568367478));
#152525=CARTESIAN_POINT('Ctrl Pts',(-33.9083103117684,-1.8939092157265,
136.409807829438));
#152526=CARTESIAN_POINT('Ctrl Pts',(-33.9122463612098,-1.81506760890063,
136.436445997653));
#152527=CARTESIAN_POINT('Ctrl Pts',(-33.9161824106512,-1.73572157262807,
136.461400975028));
#152528=CARTESIAN_POINT('Ctrl Pts',(-33.9201184600926,-1.65594940717217,
136.484656571421));
#152529=CARTESIAN_POINT('Ctrl Pts',(-33.927541726498,-1.50550159274937,
136.52851590043));
#152530=CARTESIAN_POINT('Ctrl Pts',(-33.9349649929035,-1.35308259888669,
136.566460300172));
#152531=CARTESIAN_POINT('Ctrl Pts',(-33.9423882593089,-1.19919860113999,
136.598310330631));
#152532=CARTESIAN_POINT('Ctrl Pts',(-33.9498027520299,-1.04549648149914,
136.630122716998));
#152533=CARTESIAN_POINT('Ctrl Pts',(-33.9572172447509,-0.89033316654087,
136.655854996848));
#152534=CARTESIAN_POINT('Ctrl Pts',(-33.9646317374719,-0.734230829918383,
136.675377194863));
#152535=CARTESIAN_POINT('Ctrl Pts',(-33.9720390838257,-0.578278950605082,
136.694880576649));
#152536=CARTESIAN_POINT('Ctrl Pts',(-33.9794464301795,-0.421390219358522,
136.708185746559));
#152537=CARTESIAN_POINT('Ctrl Pts',(-33.9868537765333,-0.264097760757492,
136.71521359622));
#152538=CARTESIAN_POINT('Ctrl Pts',(-33.9942555982087,-0.106922616806393,
136.722236204245));
#152539=CARTESIAN_POINT('Ctrl Pts',(-34.0016574198841,0.0506552836175792,
136.722990797649));
#152540=CARTESIAN_POINT('Ctrl Pts',(-34.0090592415595,0.208097030143856,
136.717450012167));
#152541=CARTESIAN_POINT('Ctrl Pts',(-34.0164571558708,0.365455664397442,
136.711912151622));
#152542=CARTESIAN_POINT('Ctrl Pts',(-34.0238550701822,0.522677915772416,
136.700085543762));
#152543=CARTESIAN_POINT('Ctrl Pts',(-34.0312529844935,0.679224316300961,
136.68199491128));
#152544=CARTESIAN_POINT('Ctrl Pts',(-34.0386496694057,0.835744701658003,
136.663907285134));
#152545=CARTESIAN_POINT('Ctrl Pts',(-34.0460463543179,0.991589088612023,
136.63955774319));
#152546=CARTESIAN_POINT('Ctrl Pts',(-34.0534430392301,1.14622245708218,
136.60902293689));
#152547=CARTESIAN_POINT('Ctrl Pts',(-34.0608393961656,1.30084896894674,
136.578489484536));
#152548=CARTESIAN_POINT('Ctrl Pts',(-34.0682357531011,1.45426420287109,
136.541771385467));
#152549=CARTESIAN_POINT('Ctrl Pts',(-34.0756321100365,1.60594293625012,
136.498996501273));
#152550=CARTESIAN_POINT('Ctrl Pts',(-34.0830295993731,1.75764489203024,
136.456215068136));
#152551=CARTESIAN_POINT('Ctrl Pts',(-34.0904270887096,1.90760945858968,
136.407375104806));
#152552=CARTESIAN_POINT('Ctrl Pts',(-34.0978245780462,2.05532633589457,
136.352654428773));
#152553=CARTESIAN_POINT('Ctrl Pts',(-34.1052246605612,2.20309499512202,
136.297914570491));
#152554=CARTESIAN_POINT('Ctrl Pts',(-34.1126247430762,2.34861404651103,
136.237290024718));
#152555=CARTESIAN_POINT('Ctrl Pts',(-34.1200248255912,2.49139307931174,
136.171006785039));
#152556=CARTESIAN_POINT('Ctrl Pts',(-34.1274330452576,2.63432911233706,
136.104650660124));
#152557=CARTESIAN_POINT('Ctrl Pts',(-34.1348412649241,2.77451877095215,
136.032623572213));
#152558=CARTESIAN_POINT('Ctrl Pts',(-34.1422494845906,2.91149552453135,
135.955197867289));
#152559=CARTESIAN_POINT('Ctrl Pts',(-34.1496622638926,3.0485565850168,135.877724508135));
#152560=CARTESIAN_POINT('Ctrl Pts',(-34.1570750431947,3.18240048342844,
135.794846107025));
#152561=CARTESIAN_POINT('Ctrl Pts',(-34.1644878224968,3.31259005647194,
135.706878101498));
#152562=CARTESIAN_POINT('Ctrl Pts',(-34.1719111935255,3.44296565048269,
135.61878440316));
#152563=CARTESIAN_POINT('Ctrl Pts',(-34.1793345645543,3.56967619075622,
135.525586796656));
#152564=CARTESIAN_POINT('Ctrl Pts',(-34.186757935583,3.69231730148945,135.427641217705));
#152565=CARTESIAN_POINT('Ctrl Pts',(-34.1906939850238,3.75734456113292,
135.375708121573));
#152566=CARTESIAN_POINT('Ctrl Pts',(-34.1946300344646,3.82122836109007,
135.3224408289));
#152567=CARTESIAN_POINT('Ctrl Pts',(-34.1985660839053,3.88391275693069,
135.267896464745));
#152568=CARTESIAN_POINT('Ctrl Pts',(-34.2059893503108,4.00213357117372,
135.16502749622));
#152569=CARTESIAN_POINT('Ctrl Pts',(-34.2134126167162,4.11644345854232,
135.057302954858));
#152570=CARTESIAN_POINT('Ctrl Pts',(-34.2208358831217,4.22641785081445,
134.945051708775));
#152571=CARTESIAN_POINT('Ctrl Pts',(-34.2282503758427,4.33626226248787,
134.832933134343));
#152572=CARTESIAN_POINT('Ctrl Pts',(-34.2356648685636,4.44178112011132,
134.71629876882));
#152573=CARTESIAN_POINT('Ctrl Pts',(-34.2430793612847,4.54258282415461,
134.595517676855));
#152574=CARTESIAN_POINT('Ctrl Pts',(-34.2504867076384,4.64328737172043,
134.474852998253));
#152575=CARTESIAN_POINT('Ctrl Pts',(-34.2578940539922,4.73928357944742,
134.350049834669));
#152576=CARTESIAN_POINT('Ctrl Pts',(-34.265301400346,4.83021672436177,134.221513958901));
#152577=CARTESIAN_POINT('Ctrl Pts',(-34.2727032220214,4.92108204790593,
134.093073950038));
#152578=CARTESIAN_POINT('Ctrl Pts',(-34.2801050436968,5.00689161294138,
133.96090707574));
#152579=CARTESIAN_POINT('Ctrl Pts',(-34.2875068653722,5.08733110291786,
133.825451945511));
#152580=CARTESIAN_POINT('Ctrl Pts',(-34.2949047796836,5.16772812951372,
133.690068320991));
#152581=CARTESIAN_POINT('Ctrl Pts',(-34.302302693995,5.24276053660876,133.551400217714));
#152582=CARTESIAN_POINT('Ctrl Pts',(-34.3097006083064,5.31215752849287,
133.40991486858));
#152583=CARTESIAN_POINT('Ctrl Pts',(-34.3170972932186,5.38154298785591,
133.268453031744));
#152584=CARTESIAN_POINT('Ctrl Pts',(-34.3244939781307,5.44529472646293,
133.124175213066));
#152585=CARTESIAN_POINT('Ctrl Pts',(-34.3318906630429,5.50318804192056,
132.977572972069));
#152586=CARTESIAN_POINT('Ctrl Pts',(-34.3392870199784,5.56107879032792,
132.830977231568));
#152587=CARTESIAN_POINT('Ctrl Pts',(-34.3466833769139,5.61311149498209,
132.682057620886));
#152588=CARTESIAN_POINT('Ctrl Pts',(-34.3540797338494,5.65910983381282,
132.531325136988));
#152589=CARTESIAN_POINT('Ctrl Pts',(-34.361477223186,5.70511521510666,132.380569575562));
#152590=CARTESIAN_POINT('Ctrl Pts',(-34.3688747125226,5.74508428205129,
132.228000945336));
#152591=CARTESIAN_POINT('Ctrl Pts',(-34.3762722018592,5.77889080790296,
132.074144690877));
#152592=CARTESIAN_POINT('Ctrl Pts',(-34.3836722843742,5.81270918457986,
131.920234502347));
#152593=CARTESIAN_POINT('Ctrl Pts',(-34.3910723668891,5.84036063902073,
131.765036155272));
#152594=CARTESIAN_POINT('Ctrl Pts',(-34.3984724494041,5.86177022704046,
131.60908440116));
#152595=CARTESIAN_POINT('Ctrl Pts',(-34.4058806690706,5.88320335710317,
131.452961162062));
#152596=CARTESIAN_POINT('Ctrl Pts',(-34.4132888887371,5.89838086293466,
131.296083231517));
#152597=CARTESIAN_POINT('Ctrl Pts',(-34.4206971084036,5.90727970572456,
131.138990324608));
#152598=CARTESIAN_POINT('Ctrl Pts',(-34.4281098877057,5.91618402560374,
130.981800729635));
#152599=CARTESIAN_POINT('Ctrl Pts',(-34.4355226670077,5.91880197592184,
130.824396267028));
#152600=CARTESIAN_POINT('Ctrl Pts',(-34.4429354463098,5.91516264577609,
130.667315236341));
#152601=CARTESIAN_POINT('Ctrl Pts',(-34.4503588173386,5.91151811558477,
130.510009760911));
#152602=CARTESIAN_POINT('Ctrl Pts',(-34.4577821883674,5.90159847183417,
130.353029011956));
#152603=CARTESIAN_POINT('Ctrl Pts',(-34.4652055593961,5.88548459832653,
130.196905594242));
#152604=CARTESIAN_POINT('Ctrl Pts',(-34.4691416088369,5.87694063594584,
130.114125212042));
#152605=CARTESIAN_POINT('Ctrl Pts',(-34.4730776582776,5.86665610833664,
130.03158568904));
#152606=CARTESIAN_POINT('Ctrl Pts',(-34.4770137077183,5.85464883710015,
129.94936497036));
#152607=CARTESIAN_POINT('Ctrl Pts',(-34.4844369741237,5.8320034982819,129.794299260948));
#152608=CARTESIAN_POINT('Ctrl Pts',(-34.4918602405292,5.80315907701315,
129.639899369356));
#152609=CARTESIAN_POINT('Ctrl Pts',(-34.4992835069346,5.7681627698604,129.486700258104));
#152610=CARTESIAN_POINT('Ctrl Pts',(-34.5066979996556,5.7332078254364,129.33368221548));
#152611=CARTESIAN_POINT('Ctrl Pts',(-34.5141124923766,5.69211555045192,
129.181862488594));
#152612=CARTESIAN_POINT('Ctrl Pts',(-34.5215269850976,5.64498478033734,
129.031770029681));
#152613=CARTESIAN_POINT('Ctrl Pts',(-34.5289343314514,5.59789943663343,
128.88182223553));
#152614=CARTESIAN_POINT('Ctrl Pts',(-34.5363416778052,5.54478729561533,
128.733598748812));
#152615=CARTESIAN_POINT('Ctrl Pts',(-34.543749024159,5.48579800899795,128.587617338119));
#152616=CARTESIAN_POINT('Ctrl Pts',(-34.5511508458343,5.42685271881607,
128.44174480587));
#152617=CARTESIAN_POINT('Ctrl Pts',(-34.5585526675098,5.36203915022589,
128.298111364639));
#152618=CARTESIAN_POINT('Ctrl Pts',(-34.5659544891851,5.29155642205193,
128.157218536993));
#152619=CARTESIAN_POINT('Ctrl Pts',(-34.5733524034965,5.22111090116154,
128.016400085574));
#152620=CARTESIAN_POINT('Ctrl Pts',(-34.5807503178078,5.14500234739315,
127.878319699479));
#152621=CARTESIAN_POINT('Ctrl Pts',(-34.5881482321192,5.06347748532286,
127.743457757603));
#152622=CARTESIAN_POINT('Ctrl Pts',(-34.5955449170314,4.98196617120563,
127.608618227336));
#152623=CARTESIAN_POINT('Ctrl Pts',(-34.6029416019435,4.89504052813163,
127.476996398926));
#152624=CARTESIAN_POINT('Ctrl Pts',(-34.6103382868558,4.80299266191712,
127.349047020789));
#152625=CARTESIAN_POINT('Ctrl Pts',(-34.6177346437912,4.71094887720146,
127.221103316062));
#152626=CARTESIAN_POINT('Ctrl Pts',(-34.6251310007266,4.61378353894749,
127.096832040857));
#152627=CARTESIAN_POINT('Ctrl Pts',(-34.6325273576621,4.51183125698855,
126.976657746266));
#152628=CARTESIAN_POINT('Ctrl Pts',(-34.6399248469986,4.40986336587497,
126.856465052683));
#152629=CARTESIAN_POINT('Ctrl Pts',(-34.6473223363352,4.30310731328024,
126.740370873347));
#152630=CARTESIAN_POINT('Ctrl Pts',(-34.6547198256718,4.19193694196172,
126.628765422014));
#152631=CARTESIAN_POINT('Ctrl Pts',(-34.6621199081868,4.08072760004171,
126.517120847563));
#152632=CARTESIAN_POINT('Ctrl Pts',(-34.6695199907018,3.9651011217521,126.409968398288));
#152633=CARTESIAN_POINT('Ctrl Pts',(-34.6769200732168,3.84546689951739,
126.307660173105));
#152634=CARTESIAN_POINT('Ctrl Pts',(-34.6843282928833,3.72570112715681,
126.205239449511));
#152635=CARTESIAN_POINT('Ctrl Pts',(-34.6917365125497,3.60191909380826,
126.107673830589));
#152636=CARTESIAN_POINT('Ctrl Pts',(-34.6991447322162,3.47456242401793,
126.01527442873));
#152637=CARTESIAN_POINT('Ctrl Pts',(-34.7065575115182,3.34712736832223,
125.92281815658));
#152638=CARTESIAN_POINT('Ctrl Pts',(-34.7139702908203,3.2161136020986,125.835534643976));
#152639=CARTESIAN_POINT('Ctrl Pts',(-34.7213830701224,3.08198973537656,
125.753690381495));
#152640=CARTESIAN_POINT('Ctrl Pts',(-34.7288064411511,2.94767422618397,
125.671729176094));
#152641=CARTESIAN_POINT('Ctrl Pts',(-34.7362298121799,2.81024006641469,
125.595222924042));
#152642=CARTESIAN_POINT('Ctrl Pts',(-34.7436531832087,2.67017907121341,
125.524391461392));
#152643=CARTESIAN_POINT('Ctrl Pts',(-34.7475892326495,2.59591537083926,
125.486834920316));
#152644=CARTESIAN_POINT('Ctrl Pts',(-34.7515252820903,2.52091349410799,
125.450872956343));
#152645=CARTESIAN_POINT('Ctrl Pts',(-34.7554613315312,2.44524865147138,
125.416532706898));
#152646=CARTESIAN_POINT('Ctrl Pts',(-34.7628845979366,2.30254711967953,
125.351768068167));
#152647=CARTESIAN_POINT('Ctrl Pts',(-34.770307864342,2.15705500379107,125.292578783864));
#152648=CARTESIAN_POINT('Ctrl Pts',(-34.7777311307475,2.00924789382214,
125.239214306491));
#152649=CARTESIAN_POINT('Ctrl Pts',(-34.7851456234685,1.86161547958236,
125.185912901498));
#152650=CARTESIAN_POINT('Ctrl Pts',(-34.7925601161895,1.71167386523139,
125.138422725452));
#152651=CARTESIAN_POINT('Ctrl Pts',(-34.7999746089105,1.55992149622803,
125.096946536907));
#152652=CARTESIAN_POINT('Ctrl Pts',(-34.8073819552643,1.40831539187129,
125.055510324674));
#152653=CARTESIAN_POINT('Ctrl Pts',(-34.814789301618,1.25490236503129,125.020076657996));
#152654=CARTESIAN_POINT('Ctrl Pts',(-34.8221966479718,1.10019891949657,
124.990799497217));
#152655=CARTESIAN_POINT('Ctrl Pts',(-34.8295984696472,0.945610857628153,
124.961544172449));
#152656=CARTESIAN_POINT('Ctrl Pts',(-34.8370002913226,0.789734658627721,
124.938436279892));
#152657=CARTESIAN_POINT('Ctrl Pts',(-34.844402112998,0.633099896222334,
124.921579380438));
#152658=CARTESIAN_POINT('Ctrl Pts',(-34.8518000273094,0.476547820088555,
124.90473137961));
#152659=CARTESIAN_POINT('Ctrl Pts',(-34.8591979416207,0.31923834825994,
124.894127839917));
#152660=CARTESIAN_POINT('Ctrl Pts',(-34.8665958559321,0.16170899776651,
124.889820841511));
#152661=CARTESIAN_POINT('Ctrl Pts',(-34.8739925408443,0.00420582579348278,
124.88551455885));
#152662=CARTESIAN_POINT('Ctrl Pts',(-34.8813892257565,-0.153516779530488,
124.887502750932));
#152663=CARTESIAN_POINT('Ctrl Pts',(-34.8887859106687,-0.310918335154468,
124.89578546349));
#152664=CARTESIAN_POINT('Ctrl Pts',(-34.8961822676042,-0.468312911428527,
124.904067808783));
#152665=CARTESIAN_POINT('Ctrl Pts',(-34.9035786245396,-0.625386093526133,
124.918644099979));
#152666=CARTESIAN_POINT('Ctrl Pts',(-34.9109749814751,-0.781599829800576,
124.939462300583));
#152667=CARTESIAN_POINT('Ctrl Pts',(-34.9183724708116,-0.937837482796614,
124.960283688506));
#152668=CARTESIAN_POINT('Ctrl Pts',(-34.9257699601482,-1.09321505791928,
124.987348839353));
#152669=CARTESIAN_POINT('Ctrl Pts',(-34.9331674494848,-1.24720218614087,
125.020554148692));
#152670=CARTESIAN_POINT('Ctrl Pts',(-34.9405675319998,-1.40124329431176,
125.053771098101));
#152671=CARTESIAN_POINT('Ctrl Pts',(-34.9479676145148,-1.55389262045127,
125.093132412821));
#152672=CARTESIAN_POINT('Ctrl Pts',(-34.9553676970298,-1.70463264716345,
125.138483977475));
#152673=CARTESIAN_POINT('Ctrl Pts',(-34.9627759166963,-1.85553842803146,
125.183885410838));
#152674=CARTESIAN_POINT('Ctrl Pts',(-34.9701841363628,-2.00453035900149,
125.235290140983));
#152675=CARTESIAN_POINT('Ctrl Pts',(-34.9775923560292,-2.15110798355421,
125.29249478052));
#152676=CARTESIAN_POINT('Ctrl Pts',(-34.9850051353313,-2.29777582418927,
125.349734628559));
#152677=CARTESIAN_POINT('Ctrl Pts',(-34.9924179146334,-2.44202605617368,
125.412781350005));
#152678=CARTESIAN_POINT('Ctrl Pts',(-34.9998306939355,-2.58338117826988,
125.481384734635));
#152679=CARTESIAN_POINT('Ctrl Pts',(-35.0072540649642,-2.72493827519343,
125.550086142999));
#152680=CARTESIAN_POINT('Ctrl Pts',(-35.014677435993,-2.86359167218565,
125.624359895948));
#152681=CARTESIAN_POINT('Ctrl Pts',(-35.0221008070218,-2.99889057685087,
125.703911042227));
#152682=CARTESIAN_POINT('Ctrl Pts',(-35.0260368564625,-3.07062930255596,
125.746090968787));
#152683=CARTESIAN_POINT('Ctrl Pts',(-35.0299729059032,-3.14142546773644,
125.789753851896));
#152684=CARTESIAN_POINT('Ctrl Pts',(-35.0339089553439,-3.21121558782093,
125.834851083313));
#152685=CARTESIAN_POINT('Ctrl Pts',(-35.0413287007412,-3.34277514520565,
125.919862712426));
#152686=CARTESIAN_POINT('Ctrl Pts',(-35.0487484461384,-3.47115642993611,
126.01023134199));
#152687=CARTESIAN_POINT('Ctrl Pts',(-35.0561681915356,-3.59589276206859,
126.10569210338));
#152688=CARTESIAN_POINT('Ctrl Pts',(-35.0635791648688,-3.72048162349532,
126.201040005384));
#152689=CARTESIAN_POINT('Ctrl Pts',(-35.070990138202,-3.84143381596459,
126.301467831249));
#152690=CARTESIAN_POINT('Ctrl Pts',(-35.0784011115352,-3.95830956914989,
126.406666231041));
#152691=CARTESIAN_POINT('Ctrl Pts',(-35.0858049436034,-4.0750727000542,
126.511763260929));
#152692=CARTESIAN_POINT('Ctrl Pts',(-35.0932087756717,-4.18776693570188,
126.621621464936));
#152693=CARTESIAN_POINT('Ctrl Pts',(-35.1006126077399,-4.29598378439776,
126.735889911429));
#152694=CARTESIAN_POINT('Ctrl Pts',(-35.1080109236896,-4.40412000768699,
126.850073223861));
#152695=CARTESIAN_POINT('Ctrl Pts',(-35.1154092396391,-4.50778523011824,
126.96865996627));
#152696=CARTESIAN_POINT('Ctrl Pts',(-35.1228075555888,-4.60660628734779,
127.091260958808));
#152697=CARTESIAN_POINT('Ctrl Pts',(-35.1302019761786,-4.70537531333374,
127.213797399496));
#152698=CARTESIAN_POINT('Ctrl Pts',(-35.1375963967684,-4.79930501966338,
127.340343590851));
#152699=CARTESIAN_POINT('Ctrl Pts',(-35.1449908173582,-4.88806125469121,
127.470475836581));
#152700=CARTESIAN_POINT('Ctrl Pts',(-35.1523840254788,-4.9768029362871,
127.60058674442));
#152701=CARTESIAN_POINT('Ctrl Pts',(-35.1597772335994,-5.06037261971129,
127.734282231269));
#152702=CARTESIAN_POINT('Ctrl Pts',(-35.1671704417201,-5.1384783258287,
127.871107976301));
#152703=CARTESIAN_POINT('Ctrl Pts',(-35.1745633391319,-5.21658074945654,
128.00792797106));
#152704=CARTESIAN_POINT('Ctrl Pts',(-35.1819562365439,-5.28921946707104,
128.147877637899));
#152705=CARTESIAN_POINT('Ctrl Pts',(-35.1893491339557,-5.35614763294323,
128.2904765517));
#152706=CARTESIAN_POINT('Ctrl Pts',(-35.1967431841452,-5.42308623495231,
128.433097701009));
#152707=CARTESIAN_POINT('Ctrl Pts',(-35.2041372343345,-5.48431235348562,
128.578368581476));
#152708=CARTESIAN_POINT('Ctrl Pts',(-35.2115312845239,-5.53962668377834,
128.725787364859));
#152709=CARTESIAN_POINT('Ctrl Pts',(-35.2189279513926,-5.59496058925036,
128.87325831825));
#152710=CARTESIAN_POINT('Ctrl Pts',(-35.2263246182613,-5.6443784099813,
129.022878338263));
#152711=CARTESIAN_POINT('Ctrl Pts',(-35.2337212851299,-5.68773028758663,
129.174129119229));
#152712=CARTESIAN_POINT('Ctrl Pts',(-35.2411260889127,-5.7311298556597,
129.325546287925));
#152713=CARTESIAN_POINT('Ctrl Pts',(-35.2485308926954,-5.76845005152466,
129.478597440704));
#152714=CARTESIAN_POINT('Ctrl Pts',(-35.2559356964781,-5.79959169685811,
129.632752017293));
#152715=CARTESIAN_POINT('Ctrl Pts',(-35.2633450869446,-5.83075263195026,
129.787002080313));
#152716=CARTESIAN_POINT('Ctrl Pts',(-35.270754477411,-5.85572733156779,
129.94235656096));
#152717=CARTESIAN_POINT('Ctrl Pts',(-35.2781638678775,-5.8744684193152,
130.098278927555));
#152718=CARTESIAN_POINT('Ctrl Pts',(-35.2855837906031,-5.89323614703997,
130.25442293381));
#152719=CARTESIAN_POINT('Ctrl Pts',(-35.2930037133287,-5.9057525368752,
130.411136066717));
#152720=CARTESIAN_POINT('Ctrl Pts',(-35.3004236360544,-5.91202228871884,
130.567880131708));
#152721=CARTESIAN_POINT('Ctrl Pts',(-35.3041573599656,-5.91517724372873,
130.646754142266));
#152722=CARTESIAN_POINT('Ctrl Pts',(-35.3078910838769,-5.91675129300788,
130.725636030376));
#152723=CARTESIAN_POINT('Ctrl Pts',(-35.3116248077882,-5.91674999920293,
130.804457737012));
#152724=CARTESIAN_POINT('',(-37.0616239770217,-5.91482137216616,130.799044590469));
#152725=CARTESIAN_POINT('Ctrl Pts',(-35.3116248077882,-5.92653083872268,
130.804457897558));
#152726=CARTESIAN_POINT('Ctrl Pts',(-35.3118687315778,-5.92653208400454,
130.809615823741));
#152727=CARTESIAN_POINT('Ctrl Pts',(-35.3121126553674,-5.9265259352798,
130.814773746866));
#152728=CARTESIAN_POINT('Ctrl Pts',(-35.312356579157,-5.9265123836523,130.819931650541));
#152729=CARTESIAN_POINT('Ctrl Pts',(-35.4051724537613,-5.92135582979253,
132.782574742726));
#152730=CARTESIAN_POINT('Ctrl Pts',(-35.5908042029699,-3.76732180451587,
136.702228618086));
#152731=CARTESIAN_POINT('Ctrl Pts',(-35.8692518267827,2.92571392784882,
137.161856865519));
#152732=CARTESIAN_POINT('Ctrl Pts',(-36.1476994505958,6.93016148959074,
131.77925664204));
#152733=CARTESIAN_POINT('Ctrl Pts',(-36.4261470744084,4.5661291996099,125.500774598388));
#152734=CARTESIAN_POINT('Ctrl Pts',(-36.7045946982214,-1.99395275700014,
124.096029011779));
#152735=CARTESIAN_POINT('Ctrl Pts',(-36.9164201919863,-5.59051847633362,
127.717049891396));
#152736=CARTESIAN_POINT('Ctrl Pts',(-37.0354298111468,-5.91863080344013,
130.242067918483));
#152737=CARTESIAN_POINT('Ctrl Pts',(-37.0616235557032,-5.91384448342225,
130.79903650694));
#152738=CARTESIAN_POINT('',(-38.8116256262763,-5.91172911628527,130.806521618407));
#152739=CARTESIAN_POINT('Ctrl Pts',(-37.0616248077882,-5.9167476261515,
130.799060529776));
#152740=CARTESIAN_POINT('Ctrl Pts',(-37.0689647505484,-5.91688749960742,
130.955208120347));
#152741=CARTESIAN_POINT('Ctrl Pts',(-37.0763046933087,-5.91084185943447,
131.111484207038));
#152742=CARTESIAN_POINT('Ctrl Pts',(-37.083644636069,-5.89860708023356,
131.267356379446));
#152743=CARTESIAN_POINT('Ctrl Pts',(-37.0910548573097,-5.88625515547447,
131.424720996657));
#152744=CARTESIAN_POINT('Ctrl Pts',(-37.0984650785504,-5.86759492024982,
131.581673532812));
#152745=CARTESIAN_POINT('Ctrl Pts',(-37.1058752997912,-5.84267655759526,
131.737667215543));
#152746=CARTESIAN_POINT('Ctrl Pts',(-37.113211006174,-5.81800876617095,
131.892092274784));
#152747=CARTESIAN_POINT('Ctrl Pts',(-37.1205467125568,-5.78720820846725,
132.045577296126));
#152748=CARTESIAN_POINT('Ctrl Pts',(-37.1278824189397,-5.75037550520156,
132.197598612913));
#152749=CARTESIAN_POINT('Ctrl Pts',(-37.1352182544506,-5.71354215358158,
132.349622605682));
#152750=CARTESIAN_POINT('Ctrl Pts',(-37.1425540899616,-5.6706765341907,
132.500182473154));
#152751=CARTESIAN_POINT('Ctrl Pts',(-37.1498899254725,-5.62192992566291,
132.648766883397));
#152752=CARTESIAN_POINT('Ctrl Pts',(-37.1572273971942,-5.57317244451913,
132.797384434432));
#152753=CARTESIAN_POINT('Ctrl Pts',(-37.1645648689158,-5.51853148208788,
132.944025290296));
#152754=CARTESIAN_POINT('Ctrl Pts',(-37.1719023406374,-5.45820743073228,
133.088195595317));
#152755=CARTESIAN_POINT('Ctrl Pts',(-37.1793679744049,-5.39682971210151,
133.234884092155));
#152756=CARTESIAN_POINT('Ctrl Pts',(-37.1868336081724,-5.32956868366509,
133.379014551005));
#152757=CARTESIAN_POINT('Ctrl Pts',(-37.1942992419399,-5.25668503500476,
133.520091275282));
#152758=CARTESIAN_POINT('Ctrl Pts',(-37.201648244731,-5.18494000248497,
133.658964045198));
#152759=CARTESIAN_POINT('Ctrl Pts',(-37.2089972475221,-5.10774699201546,
133.794877500466));
#152760=CARTESIAN_POINT('Ctrl Pts',(-37.2163462503132,-5.02539905273462,
133.927387182178));
#152761=CARTESIAN_POINT('Ctrl Pts',(-37.2238701995689,-4.94109078206554,
134.063051319128));
#152762=CARTESIAN_POINT('Ctrl Pts',(-37.2313941488245,-4.85137933113472,
134.195147248156));
#152763=CARTESIAN_POINT('Ctrl Pts',(-37.2389180980802,-4.75662316941709,
134.323233531819));
#152764=CARTESIAN_POINT('Ctrl Pts',(-37.2464420473359,-4.66186700769946,
134.451319815483));
#152765=CARTESIAN_POINT('Ctrl Pts',(-37.2539659965916,-4.56206645123366,
134.575396169357));
#152766=CARTESIAN_POINT('Ctrl Pts',(-37.2614899458473,-4.45762002442124,
134.69506161872));
#152767=CARTESIAN_POINT('Ctrl Pts',(-37.2689132122526,-4.35457126306258,
134.813125747006));
#152768=CARTESIAN_POINT('Ctrl Pts',(-37.2763364786581,-4.24667288625402,
134.927271563592));
#152769=CARTESIAN_POINT('Ctrl Pts',(-37.2837597450635,-4.13425440785265,
135.037075001227));
#152770=CARTESIAN_POINT('Ctrl Pts',(-37.2911742377845,-4.02196879875681,
135.146748660318));
#152771=CARTESIAN_POINT('Ctrl Pts',(-37.2985887305055,-3.90517398655583,
135.252089898103));
#152772=CARTESIAN_POINT('Ctrl Pts',(-37.3060032232265,-3.7842396314193,
135.352707677158));
#152773=CARTESIAN_POINT('Ctrl Pts',(-37.3134105695803,-3.66342183736735,
135.453228477009));
#152774=CARTESIAN_POINT('Ctrl Pts',(-37.3208179159341,-3.53847272841698,
135.549034644404));
#152775=CARTESIAN_POINT('Ctrl Pts',(-37.3282252622878,-3.40979861672405,
135.639772074297));
#152776=CARTESIAN_POINT('Ctrl Pts',(-37.3356270839632,-3.28122047503841,
135.730441828791));
#152777=CARTESIAN_POINT('Ctrl Pts',(-37.3430289056386,-3.14892316623746,
135.816050158977));
#152778=CARTESIAN_POINT('Ctrl Pts',(-37.350430727314,-3.0133457776533,135.896283416156));
#152779=CARTESIAN_POINT('Ctrl Pts',(-37.3578286416254,-2.87783995931628,
135.976474318824));
#152780=CARTESIAN_POINT('Ctrl Pts',(-37.3652265559368,-2.73905783006307,
136.051295609785));
#152781=CARTESIAN_POINT('Ctrl Pts',(-37.3726244702482,-2.59746703435814,
136.120477204693));
#152782=CARTESIAN_POINT('Ctrl Pts',(-37.3800211551604,-2.45589976847555,
136.189647302874));
#152783=CARTESIAN_POINT('Ctrl Pts',(-37.3874178400726,-2.31152509757524,
136.253179401378));
#152784=CARTESIAN_POINT('Ctrl Pts',(-37.3948145249848,-2.16483492256999,
136.310849546141));
#152785=CARTESIAN_POINT('Ctrl Pts',(-37.4022108819203,-2.01815125196061,
136.36851713375));
#152786=CARTESIAN_POINT('Ctrl Pts',(-37.4096072388557,-1.86915262880618,
136.420323147854));
#152787=CARTESIAN_POINT('Ctrl Pts',(-37.4170035957912,-1.71835031781262,
136.466092044239));
#152788=CARTESIAN_POINT('Ctrl Pts',(-37.4244010851277,-1.56752491860069,
136.511867947958));
#152789=CARTESIAN_POINT('Ctrl Pts',(-37.4317985744642,-1.41489563893112,
136.551604785135));
#152790=CARTESIAN_POINT('Ctrl Pts',(-37.4391960638008,-1.26098811485812,
136.585177128811));
#152791=CARTESIAN_POINT('Ctrl Pts',(-37.4465961463158,-1.10702663874159,
136.61876124122));
#152792=CARTESIAN_POINT('Ctrl Pts',(-37.4539962288307,-0.9517863905786,
136.646176478176));
#152793=CARTESIAN_POINT('Ctrl Pts',(-37.4613963113457,-0.795802235308524,
136.667348709382));
#152794=CARTESIAN_POINT('Ctrl Pts',(-37.4688045310121,-0.639646559423499,
136.688544221633));
#152795=CARTESIAN_POINT('Ctrl Pts',(-37.4762127506786,-0.482745712959932,
136.703482968384));
#152796=CARTESIAN_POINT('Ctrl Pts',(-37.4836209703451,-0.325639445438268,
136.712142732207));
#152797=CARTESIAN_POINT('Ctrl Pts',(-37.4910337496472,-0.168436481629955,
136.72080782597));
#152798=CARTESIAN_POINT('Ctrl Pts',(-37.4984465289492,-0.0110282172193689,
136.72318623046));
#152799=CARTESIAN_POINT('Ctrl Pts',(-37.5058593082513,0.146047093129462,
136.71930785394));
#152800=CARTESIAN_POINT('Ctrl Pts',(-37.51328267928,0.303346840047373,136.715423935814));
#152801=CARTESIAN_POINT('Ctrl Pts',(-37.5207060503087,0.460312311211555,
136.705265405573));
#152802=CARTESIAN_POINT('Ctrl Pts',(-37.5281294213375,0.616411025564011,
136.68891395746));
#152803=CARTESIAN_POINT('Ctrl Pts',(-37.5320654707783,0.699178309452366,
136.680244027323));
#152804=CARTESIAN_POINT('Ctrl Pts',(-37.5360015202192,0.78170208557782,
136.66983390052));
#152805=CARTESIAN_POINT('Ctrl Pts',(-37.5399375696601,0.863904436027291,
136.65770151725));
#152806=CARTESIAN_POINT('Ctrl Pts',(-37.5473608360655,1.01893550352477,
136.634820221042));
#152807=CARTESIAN_POINT('Ctrl Pts',(-37.554784102471,1.17329132002504,136.605740862823));
#152808=CARTESIAN_POINT('Ctrl Pts',(-37.5622073688764,1.32643699545262,
136.570511453227));
#152809=CARTESIAN_POINT('Ctrl Pts',(-37.5696218615974,1.47940166541024,
136.535323681868));
#152810=CARTESIAN_POINT('Ctrl Pts',(-37.5770363543184,1.63115868104402,
136.494000410687));
#152811=CARTESIAN_POINT('Ctrl Pts',(-37.5844508470394,1.78117924114398,
136.446641279977));
#152812=CARTESIAN_POINT('Ctrl Pts',(-37.5918581933932,1.93105520577973,
136.39932779578));
#152813=CARTESIAN_POINT('Ctrl Pts',(-37.5992655397469,2.07919769322025,
136.34599014535));
#152814=CARTESIAN_POINT('Ctrl Pts',(-37.6066728861007,2.22508916321667,
136.286778768185));
#152815=CARTESIAN_POINT('Ctrl Pts',(-37.6140747077761,2.3708718218508,136.227611553098));
#152816=CARTESIAN_POINT('Ctrl Pts',(-37.6214765294515,2.51440646153834,
136.162579473914));
#152817=CARTESIAN_POINT('Ctrl Pts',(-37.6288783511269,2.65519186331895,
136.091882412459));
#152818=CARTESIAN_POINT('Ctrl Pts',(-37.6362762654382,2.79590294558063,
136.021222671432));
#152819=CARTESIAN_POINT('Ctrl Pts',(-37.6436741797496,2.93386734751713,
135.944904070954));
#152820=CARTESIAN_POINT('Ctrl Pts',(-37.6510720940609,3.06860506626174,
135.863174066371));
#152821=CARTESIAN_POINT('Ctrl Pts',(-37.658468778973,3.20332039404266,135.781457643832));
#152822=CARTESIAN_POINT('Ctrl Pts',(-37.6658654638852,3.33480978400542,
135.694331795399));
#152823=CARTESIAN_POINT('Ctrl Pts',(-37.6732621487974,3.46261893279522,
135.602089318602));
#152824=CARTESIAN_POINT('Ctrl Pts',(-37.6806585057328,3.59042241439342,
135.509850931933));
#152825=CARTESIAN_POINT('Ctrl Pts',(-37.6880548626682,3.71454567659037,
135.412496586469));
#152826=CARTESIAN_POINT('Ctrl Pts',(-37.6954512196036,3.83456467800391,
135.310361537751));
#152827=CARTESIAN_POINT('Ctrl Pts',(-37.7028487089402,3.95460205463261,
135.208210851896));
#152828=CARTESIAN_POINT('Ctrl Pts',(-37.7102461982768,4.0705336349945,135.101278247345));
#152829=CARTESIAN_POINT('Ctrl Pts',(-37.7176436876134,4.18196977470881,
134.989938160262));
#152830=CARTESIAN_POINT('Ctrl Pts',(-37.7250437701284,4.2934449781901,134.878559043083));
#152831=CARTESIAN_POINT('Ctrl Pts',(-37.7324438526433,4.4004213395681,134.7627696309));
#152832=CARTESIAN_POINT('Ctrl Pts',(-37.7398439351583,4.50254738335946,
134.642979851497));
#152833=CARTESIAN_POINT('Ctrl Pts',(-37.7472521548248,4.60478572523436,
134.523058350917));
#152834=CARTESIAN_POINT('Ctrl Pts',(-37.7546603744913,4.70216285599346,
134.399127982643));
#152835=CARTESIAN_POINT('Ctrl Pts',(-37.7620685941578,4.79436833568445,
134.271630844169));
#152836=CARTESIAN_POINT('Ctrl Pts',(-37.7694813734598,4.88663056630966,
134.144055233334));
#152837=CARTESIAN_POINT('Ctrl Pts',(-37.7768941527619,4.97371459719107,
134.012908788174));
#152838=CARTESIAN_POINT('Ctrl Pts',(-37.7843069320639,5.05535465120457,
133.878660523731));
#152839=CARTESIAN_POINT('Ctrl Pts',(-37.7917303030927,5.13711135635579,
133.744220439071));
#152840=CARTESIAN_POINT('Ctrl Pts',(-37.7991536741214,5.21340836841894,
133.606670008957));
#152841=CARTESIAN_POINT('Ctrl Pts',(-37.8065770451502,5.28402660005538,
133.466501382516));
#152842=CARTESIAN_POINT('Ctrl Pts',(-37.8105130945911,5.3214700809316,133.392180613474));
#152843=CARTESIAN_POINT('Ctrl Pts',(-37.814449144032,5.35731786317353,133.317124095605));
#152844=CARTESIAN_POINT('Ctrl Pts',(-37.8183851934729,5.39154292384411,
133.241407080571));
#152845=CARTESIAN_POINT('Ctrl Pts',(-37.8258084598784,5.45609032013927,
133.09860715327));
#152846=CARTESIAN_POINT('Ctrl Pts',(-37.8332317262838,5.51505812166864,
132.953025129843));
#152847=CARTESIAN_POINT('Ctrl Pts',(-37.8406549926893,5.56819759998688,
132.805136979382));
#152848=CARTESIAN_POINT('Ctrl Pts',(-37.8480694854103,5.62127427185471,
132.657423620433));
#152849=CARTESIAN_POINT('Ctrl Pts',(-37.8554839781313,5.66853620729608,
132.507409907748));
#152850=CARTESIAN_POINT('Ctrl Pts',(-37.8628984708523,5.70978140653925,
132.355594594772));
#152851=CARTESIAN_POINT('Ctrl Pts',(-37.8703058172061,5.75098685210641,
132.203925607112));
#152852=CARTESIAN_POINT('Ctrl Pts',(-37.8777131635599,5.78618700924205,
132.050458833913));
#152853=CARTESIAN_POINT('Ctrl Pts',(-37.8851205099137,5.81522870380972,
131.895711012667));
#152854=CARTESIAN_POINT('Ctrl Pts',(-37.8925223315891,5.84424873798604,
131.741078608184));
#152855=CARTESIAN_POINT('Ctrl Pts',(-37.8999241532645,5.86711938674388,
131.585167423407));
#152856=CARTESIAN_POINT('Ctrl Pts',(-37.90732597494,5.88373789523335,131.42850718905));
#152857=CARTESIAN_POINT('Ctrl Pts',(-37.9147238892513,5.90034763094142,
131.271929654412));
#152858=CARTESIAN_POINT('Ctrl Pts',(-37.9221218035627,5.91071176011901,
131.114604227964));
#152859=CARTESIAN_POINT('Ctrl Pts',(-37.929519717874,5.91477902068223,130.957068505369));
#152860=CARTESIAN_POINT('Ctrl Pts',(-37.9369164027863,5.91884560534056,
130.799558962353));
#152861=CARTESIAN_POINT('Ctrl Pts',(-37.9443130876985,5.91661738860387,
130.641839565358));
#152862=CARTESIAN_POINT('Ctrl Pts',(-37.9517097726107,5.90809514726439,
130.484450796881));
#152863=CARTESIAN_POINT('Ctrl Pts',(-37.9591061295462,5.89957328381004,
130.327069007186));
#152864=CARTESIAN_POINT('Ctrl Pts',(-37.9665024864817,5.88475797084915,
130.17001818961));
#152865=CARTESIAN_POINT('Ctrl Pts',(-37.9738988434171,5.86370206363789,
130.013836315986));
#152866=CARTESIAN_POINT('Ctrl Pts',(-37.9812963327537,5.84264293271358,
129.857630530519));
#152867=CARTESIAN_POINT('Ctrl Pts',(-37.9886938220903,5.81534135498785,
129.702294323873));
#152868=CARTESIAN_POINT('Ctrl Pts',(-37.9960913114268,5.78190174190415,
129.548357906794));
#152869=CARTESIAN_POINT('Ctrl Pts',(-38.0034913939418,5.74845040661577,
129.394367527543));
#152870=CARTESIAN_POINT('Ctrl Pts',(-38.0108914764569,5.70885683118664,
129.241778279389));
#152871=CARTESIAN_POINT('Ctrl Pts',(-38.0182915589719,5.66327591838806,
129.091107444592));
#152872=CARTESIAN_POINT('Ctrl Pts',(-38.0256997786384,5.61764488469003,
128.940270931723));
#152873=CARTESIAN_POINT('Ctrl Pts',(-38.0331079983049,5.56601347371388,
128.791357402531));
#152874=CARTESIAN_POINT('Ctrl Pts',(-38.0405162179713,5.50858583422576,
128.644867003436));
#152875=CARTESIAN_POINT('Ctrl Pts',(-38.0479289972734,5.45112284898393,
128.498286441945));
#152876=CARTESIAN_POINT('Ctrl Pts',(-38.0553417765755,5.38785667624764,
128.354132323378));
#152877=CARTESIAN_POINT('Ctrl Pts',(-38.0627545558775,5.31903825262584,
128.212881767642));
#152878=CARTESIAN_POINT('Ctrl Pts',(-38.0701779269063,5.25012149801281,
128.071429386487));
#152879=CARTESIAN_POINT('Ctrl Pts',(-38.0776012979351,5.17563682420441,
127.932889182062));
#152880=CARTESIAN_POINT('Ctrl Pts',(-38.0850246689639,5.09587986814256,
127.797711497373));
#152881=CARTESIAN_POINT('Ctrl Pts',(-38.0889607184045,5.05359081629822,
127.726037045409));
#152882=CARTESIAN_POINT('Ctrl Pts',(-38.0928967678452,5.00982024403914,
127.655307409686));
#152883=CARTESIAN_POINT('Ctrl Pts',(-38.0968328172858,4.96461685616323,
127.585586000728));
#152884=CARTESIAN_POINT('Ctrl Pts',(-38.1042560836913,4.87936467737595,
127.45409359936));
#152885=CARTESIAN_POINT('Ctrl Pts',(-38.1116793500968,4.78875593506575,
127.325791678178));
#152886=CARTESIAN_POINT('Ctrl Pts',(-38.1191026165022,4.69305663170765,
127.201146772388));
#152887=CARTESIAN_POINT('Ctrl Pts',(-38.1265171092232,4.59747043697866,
127.076649186525));
#152888=CARTESIAN_POINT('Ctrl Pts',(-38.1339316019442,4.49680588243088,
126.955800305716));
#152889=CARTESIAN_POINT('Ctrl Pts',(-38.1413460946652,4.39137339765278,
126.83903966651));
#152890=CARTESIAN_POINT('Ctrl Pts',(-38.1487534410189,4.28604253267327,
126.722391565604));
#152891=CARTESIAN_POINT('Ctrl Pts',(-38.1561607873727,4.17595313471987,
126.609824136937));
#152892=CARTESIAN_POINT('Ctrl Pts',(-38.1635681337265,4.06145715531702,
126.501745559485));
#152893=CARTESIAN_POINT('Ctrl Pts',(-38.1709699554019,3.94704657133514,
126.393747591114));
#152894=CARTESIAN_POINT('Ctrl Pts',(-38.1783717770773,3.82823622024836,
126.290232062869));
#152895=CARTESIAN_POINT('Ctrl Pts',(-38.1857735987527,3.70541623800441,
126.191571757708));
#152896=CARTESIAN_POINT('Ctrl Pts',(-38.1931715130641,3.58266109147218,
126.092963534553));
#152897=CARTESIAN_POINT('Ctrl Pts',(-38.2005694273755,3.45590081949079,
125.999205663265));
#152898=CARTESIAN_POINT('Ctrl Pts',(-38.2079673416869,3.32556000811,125.910631855675));
#152899=CARTESIAN_POINT('Ctrl Pts',(-38.2153640265991,3.19524085700837,
125.822072767446));
#152900=CARTESIAN_POINT('Ctrl Pts',(-38.2227607115113,3.0613426558988,125.738696242707));
#152901=CARTESIAN_POINT('Ctrl Pts',(-38.2301573964235,2.92432054788648,
125.660793771912));
#152902=CARTESIAN_POINT('Ctrl Pts',(-38.237553753359,2.7873045155782,125.582894755395));
#152903=CARTESIAN_POINT('Ctrl Pts',(-38.2449501102944,2.64716517630255,
125.510469494701));
#152904=CARTESIAN_POINT('Ctrl Pts',(-38.2523464672299,2.50438371055579,
125.443764308124));
#152905=CARTESIAN_POINT('Ctrl Pts',(-38.2597439565665,2.36158038460171,
125.377048908812));
#152906=CARTESIAN_POINT('Ctrl Pts',(-38.267141445903,2.21613446496167,125.316055485384));
#152907=CARTESIAN_POINT('Ctrl Pts',(-38.2745389352396,2.06854846988755,
125.260982785393));
#152908=CARTESIAN_POINT('Ctrl Pts',(-38.2819390177546,1.92091073877228,
125.205890779753));
#152909=CARTESIAN_POINT('Ctrl Pts',(-38.2893391002695,1.77113178810304,
125.156723760283));
#152910=CARTESIAN_POINT('Ctrl Pts',(-38.2967391827845,1.6197305508264,125.113631006592));
#152911=CARTESIAN_POINT('Ctrl Pts',(-38.3041474024509,1.46816283232451,
125.070490867988));
#152912=CARTESIAN_POINT('Ctrl Pts',(-38.3115556221174,1.31496962396608,
125.033438436376));
#152913=CARTESIAN_POINT('Ctrl Pts',(-38.3189638417839,1.16068206049287,
125.002572296975));
#152914=CARTESIAN_POINT('Ctrl Pts',(-38.3263766210859,1.00629953559833,
124.971687159979));
#152915=CARTESIAN_POINT('Ctrl Pts',(-38.3337894003881,0.850821681264618,
124.946995960648));
#152916=CARTESIAN_POINT('Ctrl Pts',(-38.3412021796902,0.694785549349044,
124.928545473868));
#152917=CARTESIAN_POINT('Ctrl Pts',(-38.3486255507189,0.538526465691044,
124.910068624167));
#152918=CARTESIAN_POINT('Ctrl Pts',(-38.3560489217477,0.381707882463004,
124.897850325232));
#152919=CARTESIAN_POINT('Ctrl Pts',(-38.3634722927764,0.224868484980453,
124.891885270728));
#152920=CARTESIAN_POINT('Ctrl Pts',(-38.3674083422172,0.1417084731253,124.888722455701));
#152921=CARTESIAN_POINT('Ctrl Pts',(-38.371344391658,0.0585425639595697,
124.887316782014));
#152922=CARTESIAN_POINT('Ctrl Pts',(-38.3752804410988,-0.0245495673137258,
124.887661547878));
#152923=CARTESIAN_POINT('Ctrl Pts',(-38.3827037075042,-0.181258733677899,
124.888311765539));
#152924=CARTESIAN_POINT('Ctrl Pts',(-38.3901269739097,-0.338179012127287,
124.89519314427));
#152925=CARTESIAN_POINT('Ctrl Pts',(-38.3975502403151,-0.494774112546116,
124.908334062329));
#152926=CARTESIAN_POINT('Ctrl Pts',(-38.4049647330361,-0.651184130560886,
124.921459448915));
#152927=CARTESIAN_POINT('Ctrl Pts',(-38.4123792257571,-0.807269367205017,
124.940829617649));
#152928=CARTESIAN_POINT('Ctrl Pts',(-38.4197937184781,-0.962492233156298,
124.966420975568));
#152929=CARTESIAN_POINT('Ctrl Pts',(-38.4272010648318,-1.11756548946534,
124.991987667572));
#152930=CARTESIAN_POINT('Ctrl Pts',(-38.4346084111856,-1.2717776639549,
125.023763551158));
#152931=CARTESIAN_POINT('Ctrl Pts',(-38.4420157575394,-1.42459510569688,
125.061673150245));
#152932=CARTESIAN_POINT('Ctrl Pts',(-38.4494175792147,-1.57729857042446,
125.099554474923));
#152933=CARTESIAN_POINT('Ctrl Pts',(-38.4568194008902,-1.72860901291464,
125.143560316652));
#152934=CARTESIAN_POINT('Ctrl Pts',(-38.4642212225655,-1.87800192229878,
125.193563941305));
#152935=CARTESIAN_POINT('Ctrl Pts',(-38.4716191368769,-2.02731596833021,
125.243541169434));
#152936=CARTESIAN_POINT('Ctrl Pts',(-38.4790170511881,-2.17471414410284,
125.299509756694));
#152937=CARTESIAN_POINT('Ctrl Pts',(-38.4864149654995,-2.31968618927086,
125.361292866214));
#152938=CARTESIAN_POINT('Ctrl Pts',(-38.4938116504117,-2.46463414271443,
125.423065708502));
#152939=CARTESIAN_POINT('Ctrl Pts',(-38.501208335324,-2.60715642266795,
125.490651009083));
#152940=CARTESIAN_POINT('Ctrl Pts',(-38.5086050202362,-2.74676177399196,
125.563823400883));
#152941=CARTESIAN_POINT('Ctrl Pts',(-38.5160013771716,-2.8863609350686,
125.636992548143));
#152942=CARTESIAN_POINT('Ctrl Pts',(-38.5233977341069,-3.02304309405251,
125.715748120738));
#152943=CARTESIAN_POINT('Ctrl Pts',(-38.5307940910424,-3.15634092657646,
125.799818428942));
#152944=CARTESIAN_POINT('Ctrl Pts',(-38.5381915803789,-3.28965916733866,
125.883901608525));
#152945=CARTESIAN_POINT('Ctrl Pts',(-38.5455890697155,-3.41959173417185,
125.97330094475));
#152946=CARTESIAN_POINT('Ctrl Pts',(-38.552986559052,-3.54569979173979,
126.067701082687));
#152947=CARTESIAN_POINT('Ctrl Pts',(-38.560386641567,-3.67185205629075,
126.162134312446));
#152948=CARTESIAN_POINT('Ctrl Pts',(-38.5677867240819,-3.79417684364332,
126.261571610609));
#152949=CARTESIAN_POINT('Ctrl Pts',(-38.5751868065969,-3.9122680647023,
126.365657073465));
#152950=CARTESIAN_POINT('Ctrl Pts',(-38.5825950262633,-4.03048913920025,
126.46985698899));
#152951=CARTESIAN_POINT('Ctrl Pts',(-38.5900032459298,-4.14446707036462,
126.578715029497));
#152952=CARTESIAN_POINT('Ctrl Pts',(-38.5974114655962,-4.25383182435837,
126.691837624004));
#152953=CARTESIAN_POINT('Ctrl Pts',(-38.6048242448983,-4.36326389053382,
126.805029843581));
#152954=CARTESIAN_POINT('Ctrl Pts',(-38.6122370242004,-4.46807687384833,
126.922491569439));
#152955=CARTESIAN_POINT('Ctrl Pts',(-38.6196498035025,-4.56794113161665,
127.04379624761));
#152956=CARTESIAN_POINT('Ctrl Pts',(-38.6270731745312,-4.66794808011922,
127.165274251593));
#152957=CARTESIAN_POINT('Ctrl Pts',(-38.6344965455601,-4.76299195579472,
127.290605877973));
#152958=CARTESIAN_POINT('Ctrl Pts',(-38.6419199165888,-4.8527860504428,
127.419335047334));
#152959=CARTESIAN_POINT('Ctrl Pts',(-38.6458559660298,-4.90039703400673,
127.487590341745));
#152960=CARTESIAN_POINT('Ctrl Pts',(-38.6497920154706,-4.94653287243654,
127.556800375546));
#152961=CARTESIAN_POINT('Ctrl Pts',(-38.6537280649116,-4.99115613774335,
127.626894493251));
#152962=CARTESIAN_POINT('Ctrl Pts',(-38.6613354298912,-5.07740136175988,
127.762368283485));
#152963=CARTESIAN_POINT('Ctrl Pts',(-38.668942794871,-5.15824413217771,
127.901539367087));
#152964=CARTESIAN_POINT('Ctrl Pts',(-38.6765501598506,-5.23336050802567,
128.043949714179));
#152965=CARTESIAN_POINT('Ctrl Pts',(-38.6841471984717,-5.30837491970684,
128.186166751195));
#152966=CARTESIAN_POINT('Ctrl Pts',(-38.6917442370928,-5.37767825823327,
128.331613988293));
#152967=CARTESIAN_POINT('Ctrl Pts',(-38.6993412757139,-5.44098975463447,
128.479804519628));
#152968=CARTESIAN_POINT('Ctrl Pts',(-38.706929205525,-5.5042253408787,128.627817371281));
#152969=CARTESIAN_POINT('Ctrl Pts',(-38.7145171353361,-5.56148326037924,
128.778566646554));
#152970=CARTESIAN_POINT('Ctrl Pts',(-38.7221050651471,-5.61252852435859,
128.931540784864));
#152971=CARTESIAN_POINT('Ctrl Pts',(-38.729682813662,-5.66350529706784,
129.084309666267));
#152972=CARTESIAN_POINT('Ctrl Pts',(-38.7372605621768,-5.70828592504904,
129.239297129655));
#152973=CARTESIAN_POINT('Ctrl Pts',(-38.7448383106917,-5.74668354628789,
129.395971899447));
#152974=CARTESIAN_POINT('Ctrl Pts',(-38.7524101067497,-5.78505100550889,
129.552523598408));
#152975=CARTESIAN_POINT('Ctrl Pts',(-38.7599819028078,-5.81704536229033,
129.710759626737));
#152976=CARTESIAN_POINT('Ctrl Pts',(-38.7675536988658,-5.8425293624966,
129.870133016355));
#152977=CARTESIAN_POINT('Ctrl Pts',(-38.7751197874821,-5.86799415346311,
130.029386274061));
#152978=CARTESIAN_POINT('Ctrl Pts',(-38.7826858760982,-5.88695831494093,
130.189774840909));
#152979=CARTESIAN_POINT('Ctrl Pts',(-38.7902519647145,-5.89933554312272,
130.350741049923));
#152980=CARTESIAN_POINT('Ctrl Pts',(-38.797376245739,-5.91099002621745,
130.502307938262));
#152981=CARTESIAN_POINT('Ctrl Pts',(-38.8045005267636,-5.91680476845105,
130.654386640099));
#152982=CARTESIAN_POINT('Ctrl Pts',(-38.8116248077881,-5.91674961105175,
130.806505989098));
#152983=CARTESIAN_POINT('',(-40.5616248077881,-5.92172186145805,130.808909800869));
#152984=CARTESIAN_POINT('Ctrl Pts',(-38.8116262899063,-5.90765850045092,
130.806534290646));
#152985=CARTESIAN_POINT('Ctrl Pts',(-38.8518094228458,-5.9104285553906,
131.66321689387));
#152986=CARTESIAN_POINT('Ctrl Pts',(-38.9848084303895,-5.33445556096476,
134.495125854073));
#152987=CARTESIAN_POINT('Ctrl Pts',(-39.2106233125373,-0.964348369497292,
137.735997707935));
#152988=CARTESIAN_POINT('Ctrl Pts',(-39.4890709363504,5.31052874905888,
135.362413374583));
#152989=CARTESIAN_POINT('Ctrl Pts',(-39.7675185601631,6.70528938098473,
128.800201230786));
#152990=CARTESIAN_POINT('Ctrl Pts',(-40.0459661839761,1.9382166433815,124.079713654814));
#152991=CARTESIAN_POINT('Ctrl Pts',(-40.3106682665177,-4.28673125538328,
125.466818082008));
#152992=CARTESIAN_POINT('Ctrl Pts',(-40.4825544744551,-5.90748225943271,
129.133335360171));
#152993=CARTESIAN_POINT('Ctrl Pts',(-40.5616248077881,-5.92172186145805,
130.808909800869));
#152994=CARTESIAN_POINT('',(-42.3116248077881,-5.92233099613373,130.800046206929));
#152995=CARTESIAN_POINT('Ctrl Pts',(-40.5616248077881,-5.92172186145805,
130.808909800869));
#152996=CARTESIAN_POINT('Ctrl Pts',(-40.5753703490593,-5.92419726568458,
131.100190697975));
#152997=CARTESIAN_POINT('Ctrl Pts',(-40.6819317649349,-5.77205163170407,
133.35573096718));
#152998=CARTESIAN_POINT('Ctrl Pts',(-40.8813090554146,-2.87285705459878,
137.185916295787));
#152999=CARTESIAN_POINT('Ctrl Pts',(-41.1597566792278,3.8161341156876,136.670763343377));
#153000=CARTESIAN_POINT('Ctrl Pts',(-41.4382043030406,6.99828446217392,
130.764672875656));
#153001=CARTESIAN_POINT('Ctrl Pts',(-41.7166519268534,3.74935327312268,
124.895053503897));
#153002=CARTESIAN_POINT('Ctrl Pts',(-41.9950995506663,-2.94505040783266,
124.455798683895));
#153003=CARTESIAN_POINT('Ctrl Pts',(-42.1934238443113,-5.78553595672184,
128.298218441183));
#153004=CARTESIAN_POINT('Ctrl Pts',(-42.2989322633518,-5.92453367529058,
130.531151337971));
#153005=CARTESIAN_POINT('Ctrl Pts',(-42.3116248077881,-5.92233099613373,
130.800046206929));
#153006=CARTESIAN_POINT('',(-44.0616248077881,-5.9079203307475,130.801880397855));
#153007=CARTESIAN_POINT('Ctrl Pts',(-42.3116248077881,-5.92233099613373,
130.800046206929));
#153008=CARTESIAN_POINT('Ctrl Pts',(-42.3917481379561,-5.90842629875613,
132.497479883376));
#153009=CARTESIAN_POINT('Ctrl Pts',(-42.5646873427284,-4.25074246905246,
136.184942210171));
#153010=CARTESIAN_POINT('Ctrl Pts',(-42.830442422105,2.01436137498844,137.506592244515));
#153011=CARTESIAN_POINT('Ctrl Pts',(-43.1088900459179,6.72758881151127,
132.732341248584));
#153012=CARTESIAN_POINT('Ctrl Pts',(-43.3873376697308,5.25849079123855,
126.186370239837));
#153013=CARTESIAN_POINT('Ctrl Pts',(-43.6657852935438,-1.04290337462631,
123.884106786848));
#153014=CARTESIAN_POINT('Ctrl Pts',(-43.890547672896,-5.35577621547134,
127.158999481025));
#153015=CARTESIAN_POINT('Ctrl Pts',(-44.0224941776442,-5.91105646319498,
129.967728913076));
#153016=CARTESIAN_POINT('Ctrl Pts',(-44.0616248077881,-5.9079203307475,
130.801880397855));
#153017=CARTESIAN_POINT('',(-45.8116248406311,-5.91565936145396,130.80955222336));
#153018=CARTESIAN_POINT('Ctrl Pts',(-44.0616248077881,-5.9079203307475,
130.801880397855));
#153019=CARTESIAN_POINT('Ctrl Pts',(-44.1153100522485,-5.90361771572484,
131.946294025052));
#153020=CARTESIAN_POINT('Ctrl Pts',(-44.2618111713132,-5.02991776548405,
135.075346352124));
#153021=CARTESIAN_POINT('Ctrl Pts',(-44.5011281649824,0.0503378935809273,
137.802576577854));
#153022=CARTESIAN_POINT('Ctrl Pts',(-44.7795757887951,5.91500614821685,
134.544716589515));
#153023=CARTESIAN_POINT('Ctrl Pts',(-45.0580234126083,6.34407271675586,
127.849652189506));
#153024=CARTESIAN_POINT('Ctrl Pts',(-45.3364710364209,0.943246383778656,
123.869820489349));
#153025=CARTESIAN_POINT('Ctrl Pts',(-45.5876715014812,-4.71106648683667,
126.028360352011));
#153026=CARTESIAN_POINT('Ctrl Pts',(-45.7460560919367,-5.90156674869486,
129.414958509883));
#153027=CARTESIAN_POINT('Ctrl Pts',(-45.8116248077881,-5.9132152101497,
130.809549379698));
#153028=CARTESIAN_POINT('',(-47.5616248077881,-5.9209525136144,130.804682771848));
#153029=CARTESIAN_POINT('Ctrl Pts',(-45.8116248552558,-5.9167477212215,
130.809553489618));
#153030=CARTESIAN_POINT('Ctrl Pts',(-45.8206040918004,-5.9165800069701,
131.000646762258));
#153031=CARTESIAN_POINT('Ctrl Pts',(-45.829583328345,-5.9071510035541,131.191332648828));
#153032=CARTESIAN_POINT('Ctrl Pts',(-45.8385625648896,-5.88860123260384,
131.380820577907));
#153033=CARTESIAN_POINT('Ctrl Pts',(-45.8476965180825,-5.8697318400051,
131.573573476911));
#153034=CARTESIAN_POINT('Ctrl Pts',(-45.8568304712754,-5.84142468682038,
131.765086783783));
#153035=CARTESIAN_POINT('Ctrl Pts',(-45.8659644244682,-5.8038773369655,
131.954551219144));
#153036=CARTESIAN_POINT('Ctrl Pts',(-45.8750983776611,-5.76632998711067,
132.144015654505));
#153037=CARTESIAN_POINT('Ctrl Pts',(-45.8842323308539,-5.71954254678255,
132.331431292939));
#153038=CARTESIAN_POINT('Ctrl Pts',(-45.8933662840467,-5.66376059943453,
132.516010825638));
#153039=CARTESIAN_POINT('Ctrl Pts',(-45.9007895504522,-5.61842598395795,
132.666020686132));
#153040=CARTESIAN_POINT('Ctrl Pts',(-45.9082128168576,-5.56705897911314,
132.81445504191));
#153041=CARTESIAN_POINT('Ctrl Pts',(-45.9156360832631,-5.50978539765564,
132.960791797613));
#153042=CARTESIAN_POINT('Ctrl Pts',(-45.9230505759841,-5.45257950881506,
133.106955595424));
#153043=CARTESIAN_POINT('Ctrl Pts',(-45.9304650687051,-5.38948107397045,
133.251026383773));
#153044=CARTESIAN_POINT('Ctrl Pts',(-45.9378795614261,-5.32066608754048,
133.392495650248));
#153045=CARTESIAN_POINT('Ctrl Pts',(-45.9452869077799,-5.25191742758537,
133.533828563318));
#153046=CARTESIAN_POINT('Ctrl Pts',(-45.9526942541338,-5.17746334722068,
133.672564612907));
#153047=CARTESIAN_POINT('Ctrl Pts',(-45.9601016004875,-5.09752844371975,
133.808213864309));
#153048=CARTESIAN_POINT('Ctrl Pts',(-45.967503422163,-5.0176531586855,133.943761943382));
#153049=CARTESIAN_POINT('Ctrl Pts',(-45.9749052438384,-4.93230537858831,
134.076227488131));
#153050=CARTESIAN_POINT('Ctrl Pts',(-45.9823070655138,-4.84175622036051,
134.205143948668));
#153051=CARTESIAN_POINT('Ctrl Pts',(-45.9897049798252,-4.75125486232863,
134.333992355208));
#153052=CARTESIAN_POINT('Ctrl Pts',(-45.9971028941366,-4.65555780851086,
134.459295104067));
#153053=CARTESIAN_POINT('Ctrl Pts',(-46.0045008084479,-4.55498013012467,
134.580613598587));
#153054=CARTESIAN_POINT('Ctrl Pts',(-46.0118974933601,-4.45441916592382,
134.701911932174));
#153055=CARTESIAN_POINT('Ctrl Pts',(-46.0192941782724,-4.34897942490795,
134.819227038416));
#153056=CARTESIAN_POINT('Ctrl Pts',(-46.0266908631846,-4.23901706882133,
134.932152382268));
#153057=CARTESIAN_POINT('Ctrl Pts',(-46.0340872201201,-4.12905958858097,
135.045072718892));
#153058=CARTESIAN_POINT('Ctrl Pts',(-46.0414835770555,-4.01458015243537,
135.153603412703));
#153059=CARTESIAN_POINT('Ctrl Pts',(-46.048879933991,-3.89597249152699,
135.257374081252));
#153060=CARTESIAN_POINT('Ctrl Pts',(-46.0562774233276,-3.77734667148276,
135.361160637355));
#153061=CARTESIAN_POINT('Ctrl Pts',(-46.0636749126641,-3.65459164916284,
135.460185471294));
#153062=CARTESIAN_POINT('Ctrl Pts',(-46.0710724020007,-3.52813487758272,
135.554117963798));
#153063=CARTESIAN_POINT('Ctrl Pts',(-46.0784724845157,-3.40163377677754,
135.648083384191));
#153064=CARTESIAN_POINT('Ctrl Pts',(-46.0858725670307,-3.27142864259895,
135.736952686545));
#153065=CARTESIAN_POINT('Ctrl Pts',(-46.0932726495457,-3.13797644840548,
135.820438205857));
#153066=CARTESIAN_POINT('Ctrl Pts',(-46.1006808692122,-3.00437750980528,
135.90401552608));
#153067=CARTESIAN_POINT('Ctrl Pts',(-46.1080890888787,-2.86752469738175,
135.982197042484));
#153068=CARTESIAN_POINT('Ctrl Pts',(-46.1154973085452,-2.72790079898975,
136.054740393675));
#153069=CARTESIAN_POINT('Ctrl Pts',(-46.1229100878472,-2.58819096441784,
136.127328394087));
#153070=CARTESIAN_POINT('Ctrl Pts',(-46.1303228671493,-2.4457069824236,
136.194271156114));
#153071=CARTESIAN_POINT('Ctrl Pts',(-46.1377356464513,-2.30095172868477,
136.255374441137));
#153072=CARTESIAN_POINT('Ctrl Pts',(-46.1451590174801,-2.15598964185105,
136.316565033399));
#153073=CARTESIAN_POINT('Ctrl Pts',(-46.1525823885089,-2.00875015019221,
136.371899353406));
#153074=CARTESIAN_POINT('Ctrl Pts',(-46.1600057595377,-1.85975217773808,
136.42123273645));
#153075=CARTESIAN_POINT('Ctrl Pts',(-46.1639418089784,-1.78074987758808,
136.447390479878));
#153076=CARTESIAN_POINT('Ctrl Pts',(-46.167877858419,-1.70125340339786,
136.471861993046));
#153077=CARTESIAN_POINT('Ctrl Pts',(-46.1718139078597,-1.62134115253402,
136.49463156275));
#153078=CARTESIAN_POINT('Ctrl Pts',(-46.1792371742651,-1.47062914137653,
136.537574260597));
#153079=CARTESIAN_POINT('Ctrl Pts',(-46.1866604406705,-1.31798199315385,
136.574590139641));
#153080=CARTESIAN_POINT('Ctrl Pts',(-46.1940837070759,-1.16390696634591,
136.60550284442));
#153081=CARTESIAN_POINT('Ctrl Pts',(-46.201498199797,-1.0100140434243,136.63637901295));
#153082=CARTESIAN_POINT('Ctrl Pts',(-46.208912692518,-0.854696963591946,
136.661166292901));
#153083=CARTESIAN_POINT('Ctrl Pts',(-46.216327185239,-0.698478682024039,
136.679737889985));
#153084=CARTESIAN_POINT('Ctrl Pts',(-46.2237345315928,-0.542410969517422,
136.698291587064));
#153085=CARTESIAN_POINT('Ctrl Pts',(-46.2311418779465,-0.385444152710189,
136.710641484224));
#153086=CARTESIAN_POINT('Ctrl Pts',(-46.2385492243003,-0.228111827858697,
136.716711719834));
#153087=CARTESIAN_POINT('Ctrl Pts',(-46.2459510459757,-0.0708968473911126,
136.722777428034));
#153088=CARTESIAN_POINT('Ctrl Pts',(-46.2533528676511,0.0866827269031233,
136.722572786051));
#153089=CARTESIAN_POINT('Ctrl Pts',(-46.2607546893265,0.24408782806416,
136.716073710629));
#153090=CARTESIAN_POINT('Ctrl Pts',(-46.2681526036379,0.401409836297532,
136.709578066018));
#153091=CARTESIAN_POINT('Ctrl Pts',(-46.2755505179492,0.558557182789278,
136.696794620807));
#153092=CARTESIAN_POINT('Ctrl Pts',(-46.2829484322605,0.714990560060742,
136.67775138113));
#153093=CARTESIAN_POINT('Ctrl Pts',(-46.2903451171727,0.871397940942893,
136.658711306094));
#153094=CARTESIAN_POINT('Ctrl Pts',(-46.2977418020848,1.02709121788791,
136.633413546274));
#153095=CARTESIAN_POINT('Ctrl Pts',(-46.305138486997,1.18153584732672,136.60193800851));
#153096=CARTESIAN_POINT('Ctrl Pts',(-46.3125348439324,1.33597362852904,
136.570463866404));
#153097=CARTESIAN_POINT('Ctrl Pts',(-46.3199312008679,1.48916250653336,
136.532812565563));
#153098=CARTESIAN_POINT('Ctrl Pts',(-46.3273275578034,1.64057804679553,
136.489115162388));
#153099=CARTESIAN_POINT('Ctrl Pts',(-46.3347250471399,1.79201676916325,
136.445411069029));
#153100=CARTESIAN_POINT('Ctrl Pts',(-46.3421225364765,1.94168125450721,
136.395659133709));
#153101=CARTESIAN_POINT('Ctrl Pts',(-46.349520025813,2.08906229467371,136.340040276964));
#153102=CARTESIAN_POINT('Ctrl Pts',(-46.356920108328,2.23649499903559,136.284401923115));
#153103=CARTESIAN_POINT('Ctrl Pts',(-46.364320190843,2.38164231547602,136.222892684806));
#153104=CARTESIAN_POINT('Ctrl Pts',(-46.371720273358,2.52401521801844,136.155741536704));
#153105=CARTESIAN_POINT('Ctrl Pts',(-46.3791284930245,2.66654467420348,
136.088516549011));
#153106=CARTESIAN_POINT('Ctrl Pts',(-46.3865367126909,2.80629328610091,
136.015637421353));
#153107=CARTESIAN_POINT('Ctrl Pts',(-46.3939449323574,2.94279618957607,
135.93737933457));
#153108=CARTESIAN_POINT('Ctrl Pts',(-46.4013577116595,3.07938310831084,
135.859073081241));
#153109=CARTESIAN_POINT('Ctrl Pts',(-46.4087704909616,3.21272002255385,
135.775381469877));
#153110=CARTESIAN_POINT('Ctrl Pts',(-46.4161832702636,3.34237169726821,
135.68662259331));
#153111=CARTESIAN_POINT('Ctrl Pts',(-46.4236066412924,3.47220862437528,
135.597736893899));
#153112=CARTESIAN_POINT('Ctrl Pts',(-46.431030012321,3.59834949671244,135.503769691108));
#153113=CARTESIAN_POINT('Ctrl Pts',(-46.4384533833498,3.7203921126505,135.405079375611));
#153114=CARTESIAN_POINT('Ctrl Pts',(-46.4423894327907,3.78510203599523,
135.352751402291));
#153115=CARTESIAN_POINT('Ctrl Pts',(-46.4463254822316,3.84866039920618,
135.299096217713));
#153116=CARTESIAN_POINT('Ctrl Pts',(-46.4502615316725,3.91101160662611,
135.244171286427));
#153117=CARTESIAN_POINT('Ctrl Pts',(-46.457684798078,4.02860403790226,135.140584580175));
#153118=CARTESIAN_POINT('Ctrl Pts',(-46.4651080644834,4.14225605751435,
135.032166197969));
#153119=CARTESIAN_POINT('Ctrl Pts',(-46.4725313308888,4.25154510702018,
134.919247586302));
#153120=CARTESIAN_POINT('Ctrl Pts',(-46.4799458236099,4.36070498594555,
134.806462435056));
#153121=CARTESIAN_POINT('Ctrl Pts',(-46.4873603163309,4.46551190206133,
134.689187907262));
#153122=CARTESIAN_POINT('Ctrl Pts',(-46.4947748090519,4.56557650969404,
134.567795444507));
#153123=CARTESIAN_POINT('Ctrl Pts',(-46.5021821554057,4.66554467129055,
134.446519984378));
#153124=CARTESIAN_POINT('Ctrl Pts',(-46.5095895017595,4.76077938815014,
134.321134776944));
#153125=CARTESIAN_POINT('Ctrl Pts',(-46.5169968481133,4.85092841392537,
134.192047746784));
#153126=CARTESIAN_POINT('Ctrl Pts',(-46.5243986697887,4.94101020315604,
134.063056994602));
#153127=CARTESIAN_POINT('Ctrl Pts',(-46.5318004914641,5.02601364106179,
133.930370221872));
#153128=CARTESIAN_POINT('Ctrl Pts',(-46.5392023131395,5.10562708685644,
133.794427943306));
#153129=CARTESIAN_POINT('Ctrl Pts',(-46.5466002274509,5.18519850533277,
133.658557427611));
#153130=CARTESIAN_POINT('Ctrl Pts',(-46.5539981417623,5.2593854101478,133.519435149973));
#153131=CARTESIAN_POINT('Ctrl Pts',(-46.5613960560736,5.32791985478793,
133.377529983048));
#153132=CARTESIAN_POINT('Ctrl Pts',(-46.5687927409858,5.3964429102466,133.235648398188));
#153133=CARTESIAN_POINT('Ctrl Pts',(-46.576189425898,5.4593152076483,133.090985177716));
#153134=CARTESIAN_POINT('Ctrl Pts',(-46.5835861108102,5.51631504102523,
132.944033239875));
#153135=CARTESIAN_POINT('Ctrl Pts',(-46.5909824677457,5.57331234696981,
132.797087818037));
#153136=CARTESIAN_POINT('Ctrl Pts',(-46.5983788246811,5.62443757163981,
132.647854228649));
#153137=CARTESIAN_POINT('Ctrl Pts',(-46.6057751816165,5.66951750681539,
132.496844532531));
#153138=CARTESIAN_POINT('Ctrl Pts',(-46.6131726709531,5.71460434384419,
132.345811716442));
#153139=CARTESIAN_POINT('Ctrl Pts',(-46.6205701602898,5.7536439416983,132.193002609904));
#153140=CARTESIAN_POINT('Ctrl Pts',(-46.6279676496264,5.78651327450287,
132.038943416127));
#153141=CARTESIAN_POINT('Ctrl Pts',(-46.6353677321414,5.81939412960106,
131.884830217138));
#153142=CARTESIAN_POINT('Ctrl Pts',(-46.6427678146564,5.84610033533533,
131.729466423278));
#153143=CARTESIAN_POINT('Ctrl Pts',(-46.6501678971714,5.86656020409331,
131.573387232352));
#153144=CARTESIAN_POINT('Ctrl Pts',(-46.6575761168379,5.88704257058034,
131.417136416309));
#153145=CARTESIAN_POINT('Ctrl Pts',(-46.6649843365043,5.90126483471731,
131.260169002562));
#153146=CARTESIAN_POINT('Ctrl Pts',(-46.6723925561708,5.90920724351964,
131.103024836439));
#153147=CARTESIAN_POINT('Ctrl Pts',(-46.6798053354729,5.91715454074205,
130.945783950704));
#153148=CARTESIAN_POINT('Ctrl Pts',(-46.6872181147749,5.91881427691498,
130.78836646823));
#153149=CARTESIAN_POINT('Ctrl Pts',(-46.694630894077,5.91421881737888,130.631310501526));
#153150=CARTESIAN_POINT('Ctrl Pts',(-46.7020542651057,5.9096167916347,130.474030125892));
#153151=CARTESIAN_POINT('Ctrl Pts',(-46.7094776361345,5.89874174529678,
130.317112669114));
#153152=CARTESIAN_POINT('Ctrl Pts',(-46.7169010071633,5.88167780278516,
130.161090233727));
#153153=CARTESIAN_POINT('Ctrl Pts',(-46.720837056604,5.87263009102193,130.078363394779));
#153154=CARTESIAN_POINT('Ctrl Pts',(-46.7247731060448,5.86184331245711,
129.995888005881));
#153155=CARTESIAN_POINT('Ctrl Pts',(-46.7287091554855,5.84933576283583,
129.913741902228));
#153156=CARTESIAN_POINT('Ctrl Pts',(-46.736132421891,5.82574691459707,129.75881691443));
#153157=CARTESIAN_POINT('Ctrl Pts',(-46.7435556882964,5.79596315178447,
129.604595467689));
#153158=CARTESIAN_POINT('Ctrl Pts',(-46.7509789547018,5.76003492655879,
129.451612227316));
#153159=CARTESIAN_POINT('Ctrl Pts',(-46.7583934474228,5.72414916551163,
129.298809800429));
#153160=CARTESIAN_POINT('Ctrl Pts',(-46.7658079401439,5.68213348210251,
129.147243026752));
#153161=CARTESIAN_POINT('Ctrl Pts',(-46.7732224328649,5.63408992981298,
128.997440247079));
#153162=CARTESIAN_POINT('Ctrl Pts',(-46.7806297792187,5.58609268370796,
128.847781852965));
#153163=CARTESIAN_POINT('Ctrl Pts',(-46.7880371255726,5.53207924830008,
128.699884421162));
#153164=CARTESIAN_POINT('Ctrl Pts',(-46.7954444719264,5.47220242433592,
128.554264799697));
#153165=CARTESIAN_POINT('Ctrl Pts',(-46.8028462936018,5.41237025876611,
128.408753786839));
#153166=CARTESIAN_POINT('Ctrl Pts',(-46.8102481152771,5.34668355349613,
128.265517545392));
#153167=CARTESIAN_POINT('Ctrl Pts',(-46.8176499369525,5.27534447657152,
128.125056376535));
#153168=CARTESIAN_POINT('Ctrl Pts',(-46.8250478512639,5.20404305899032,
127.984669356036));
#153169=CARTESIAN_POINT('Ctrl Pts',(-46.8324457655753,5.12709538083476,
127.847054822619));
#153170=CARTESIAN_POINT('Ctrl Pts',(-46.8398436798867,5.0447510863124,127.712691644398));
#153171=CARTESIAN_POINT('Ctrl Pts',(-46.8472403647989,4.96242047591803,
127.578350794899));
#153172=CARTESIAN_POINT('Ctrl Pts',(-46.854637049711,4.87469522394634,127.447260546199));
#153173=CARTESIAN_POINT('Ctrl Pts',(-46.8620337346233,4.78187019898427,
127.319873860156));
#153174=CARTESIAN_POINT('Ctrl Pts',(-46.8694300915587,4.68904928998107,
127.192492822572));
#153175=CARTESIAN_POINT('Ctrl Pts',(-46.8768264484943,4.59112927745094,
127.068815322819));
#153176=CARTESIAN_POINT('Ctrl Pts',(-46.8842228054297,4.48844734939068,
126.949263867256));
#153177=CARTESIAN_POINT('Ctrl Pts',(-46.8916202947663,4.38574970046495,
126.829694108061));
#153178=CARTESIAN_POINT('Ctrl Pts',(-46.8990177841029,4.27828892759111,
126.714251934074));
#153179=CARTESIAN_POINT('Ctrl Pts',(-46.9064152734394,4.16644124194198,
126.603325276136));
#153180=CARTESIAN_POINT('Ctrl Pts',(-46.9138153559545,4.05455434826004,
126.49235973303));
#153181=CARTESIAN_POINT('Ctrl Pts',(-46.9212154384694,3.93827774488875,
126.385913120234));
#153182=CARTESIAN_POINT('Ctrl Pts',(-46.9286155209844,3.81802295999359,
126.284335038052));
#153183=CARTESIAN_POINT('Ctrl Pts',(-46.9360237406509,3.69763594259994,
126.182645260326));
#153184=CARTESIAN_POINT('Ctrl Pts',(-46.9434319603175,3.57326229303051,
126.08583494544));
#153185=CARTESIAN_POINT('Ctrl Pts',(-46.950840179984,3.44534552147863,125.994212511725));
#153186=CARTESIAN_POINT('Ctrl Pts',(-46.9582529592861,3.31735001928808,
125.90253368593));
#153187=CARTESIAN_POINT('Ctrl Pts',(-46.9656657385881,3.18580736093037,
125.816049308469));
#153188=CARTESIAN_POINT('Ctrl Pts',(-46.9730785178902,3.05118776995655,
125.735023012418));
#153189=CARTESIAN_POINT('Ctrl Pts',(-46.980501888919,2.91637582819831,125.653880942196));
#153190=CARTESIAN_POINT('Ctrl Pts',(-46.9879252599477,2.77847849949409,
125.578212708367));
#153191=CARTESIAN_POINT('Ctrl Pts',(-46.9953486309765,2.63798892808085,
125.508235149092));
#153192=CARTESIAN_POINT('Ctrl Pts',(-46.9992846804171,2.56349798631965,
125.471131368077));
#153193=CARTESIAN_POINT('Ctrl Pts',(-47.0032207298578,2.48827858852154,
125.435626628109));
#153194=CARTESIAN_POINT('Ctrl Pts',(-47.0071567792984,2.41240610893801,
125.401747608284));
#153195=CARTESIAN_POINT('Ctrl Pts',(-47.0145800457038,2.26931298033693,
125.33785283422));
#153196=CARTESIAN_POINT('Ctrl Pts',(-47.0220033121093,2.12346325810717,
125.279550298363));
#153197=CARTESIAN_POINT('Ctrl Pts',(-47.0294265785147,1.97533404194146,
125.227086553541));
#153198=CARTESIAN_POINT('Ctrl Pts',(-47.0368410712357,1.8273799022079,125.174684816508));
#153199=CARTESIAN_POINT('Ctrl Pts',(-47.0442555639566,1.67715197974729,
125.12810825751));
#153200=CARTESIAN_POINT('Ctrl Pts',(-47.0516700566776,1.52514994503228,
125.087556597165));
#153201=CARTESIAN_POINT('Ctrl Pts',(-47.0590774030314,1.37329441560132,
125.047044022038));
#153202=CARTESIAN_POINT('Ctrl Pts',(-47.0664847493851,1.2196685363637,125.012544880502));
#153203=CARTESIAN_POINT('Ctrl Pts',(-47.0738920957389,1.06478973873867,
124.984209985943));
#153204=CARTESIAN_POINT('Ctrl Pts',(-47.0812939174143,0.910026455563924,
124.955896224619));
#153205=CARTESIAN_POINT('Ctrl Pts',(-47.0886957390897,0.754012480288078,
124.933737622864));
#153206=CARTESIAN_POINT('Ctrl Pts',(-47.0960975607651,0.597278007230945,
124.917834515986));
#153207=CARTESIAN_POINT('Ctrl Pts',(-47.1034954750764,0.440626273082122,
124.901939804235));
#153208=CARTESIAN_POINT('Ctrl Pts',(-47.1108933893877,0.283255169078555,
124.892294048405));
#153209=CARTESIAN_POINT('Ctrl Pts',(-47.118291303699,0.125702519317995,
124.888946055666));
#153210=CARTESIAN_POINT('Ctrl Pts',(-47.1256879886112,-0.0318239480504715,
124.885598619303));
#153211=CARTESIAN_POINT('Ctrl Pts',(-47.1330846735234,-0.189531528449952,
124.888546876815));
#153212=CARTESIAN_POINT('Ctrl Pts',(-47.1404813584356,-0.346879748565037,
124.897787583857));
#153213=CARTESIAN_POINT('Ctrl Pts',(-47.147877715371,-0.504220991695153,
124.907027881157));
#153214=CARTESIAN_POINT('Ctrl Pts',(-47.1552740723065,-0.661202533568382,
124.92256005133));
#153215=CARTESIAN_POINT('Ctrl Pts',(-47.1626704292419,-0.817286649267769,
124.944328783572));
#153216=CARTESIAN_POINT('Ctrl Pts',(-47.1700679185785,-0.973394661843957,
124.966100848662));
#153217=CARTESIAN_POINT('Ctrl Pts',(-47.1774654079151,-1.12860460492493,
124.994111325456));
#153218=CARTESIAN_POINT('Ctrl Pts',(-47.1848628972517,-1.28238674997907,
125.028253382933));
#153219=CARTESIAN_POINT('Ctrl Pts',(-47.1922629797666,-1.43622280312554,
125.062407408856));
#153220=CARTESIAN_POINT('Ctrl Pts',(-47.1996630622816,-1.58862969753152,
125.102697214077));
#153221=CARTESIAN_POINT('Ctrl Pts',(-47.2070631447966,-1.7390908635335,
125.148965535799));
#153222=CARTESIAN_POINT('Ctrl Pts',(-47.214471364463,-1.88971747705528,
125.195284734298));
#153223=CARTESIAN_POINT('Ctrl Pts',(-47.2218795841295,-2.03839373236685,
125.247595468205));
#153224=CARTESIAN_POINT('Ctrl Pts',(-47.229287803796,-2.18462042029797,
125.305691307477));
#153225=CARTESIAN_POINT('Ctrl Pts',(-47.236700583098,-2.33093710831559,
125.363822903768));
#153226=CARTESIAN_POINT('Ctrl Pts',(-47.2441133624,-2.47480088438865,125.427746549209));
#153227=CARTESIAN_POINT('Ctrl Pts',(-47.2515261417021,-2.61573577922724,
125.497209131527));
#153228=CARTESIAN_POINT('Ctrl Pts',(-47.2589495127308,-2.75687204845277,
125.566770965239));
#153229=CARTESIAN_POINT('Ctrl Pts',(-47.2663728837596,-2.89507075110273,
125.641887364649));
#153230=CARTESIAN_POINT('Ctrl Pts',(-47.2737962547883,-3.02988289858559,
125.722260639864));
#153231=CARTESIAN_POINT('Ctrl Pts',(-47.2777323042293,-3.10136353395812,
125.764876478916));
#153232=CARTESIAN_POINT('Ctrl Pts',(-47.2816683536703,-3.17189259909195,
125.808969509407));
#153233=CARTESIAN_POINT('Ctrl Pts',(-47.2856044031113,-3.24140690648408,
125.854490737549));
#153234=CARTESIAN_POINT('Ctrl Pts',(-47.2930162254636,-3.37230660809053,
125.940210000303));
#153235=CARTESIAN_POINT('Ctrl Pts',(-47.3004280478159,-3.50000465181596,
126.031256948241));
#153236=CARTESIAN_POINT('Ctrl Pts',(-47.3078398701682,-3.62403655674368,
126.127364829896));
#153237=CARTESIAN_POINT('Ctrl Pts',(-47.3152429245292,-3.74792173518232,
126.223359018448));
#153238=CARTESIAN_POINT('Ctrl Pts',(-47.3226459788901,-3.86814911387529,
126.324401997154));
#153239=CARTESIAN_POINT('Ctrl Pts',(-47.330049033251,-3.98428134418833,
126.430182668185));
#153240=CARTESIAN_POINT('Ctrl Pts',(-47.3374449580763,-4.10030173297716,
126.535861466795));
#153241=CARTESIAN_POINT('Ctrl Pts',(-47.3448408829016,-4.21223454932345,
126.646268624337));
#153242=CARTESIAN_POINT('Ctrl Pts',(-47.3522368077269,-4.31967394087877,
126.761051625293));
#153243=CARTESIAN_POINT('Ctrl Pts',(-47.3596272357581,-4.42703348140647,
126.87574931731));
#153244=CARTESIAN_POINT('Ctrl Pts',(-47.3670176637894,-4.52990599151765,
126.994816105166));
#153245=CARTESIAN_POINT('Ctrl Pts',(-47.3744080918207,-4.62792115513288,
127.117861418546));
#153246=CARTESIAN_POINT('Ctrl Pts',(-47.3817946513783,-4.72588501331898,
127.240842324621));
#153247=CARTESIAN_POINT('Ctrl Pts',(-47.389181210936,-4.81899635557964,
127.367797316666));
#153248=CARTESIAN_POINT('Ctrl Pts',(-47.3965677704936,-4.90692407484567,
127.498301530647));
#153249=CARTESIAN_POINT('Ctrl Pts',(-47.4039531539833,-4.99483779449974,
127.628784966102));
#153250=CARTESIAN_POINT('Ctrl Pts',(-47.4113385374729,-5.07756931966951,
127.76281619184));
#153251=CARTESIAN_POINT('Ctrl Pts',(-47.4187239209626,-5.1548298966107,
127.899939969742));
#153252=CARTESIAN_POINT('Ctrl Pts',(-47.4261090319252,-5.23208762256904,
128.037058687656));
#153253=CARTESIAN_POINT('Ctrl Pts',(-47.4334941428878,-5.30387461774855,
128.177269404505));
#153254=CARTESIAN_POINT('Ctrl Pts',(-47.4408792538504,-5.36994742205108,
128.320091057533));
#153255=CARTESIAN_POINT('Ctrl Pts',(-47.448265562596,-5.43603094262898,
128.462935874648));
#153256=CARTESIAN_POINT('Ctrl Pts',(-47.4556518713417,-5.49639826988397,
128.608392131039));
#153257=CARTESIAN_POINT('Ctrl Pts',(-47.4630381800873,-5.55085362025247,
128.755957666721));
#153258=CARTESIAN_POINT('Ctrl Pts',(-47.4704271573781,-5.60532864439423,
128.903576515271));
#153259=CARTESIAN_POINT('Ctrl Pts',(-47.4778161346689,-5.65388730982331,
129.053305809042));
#153260=CARTESIAN_POINT('Ctrl Pts',(-47.4852051119597,-5.69638338638967,
129.20462724048));
#153261=CARTESIAN_POINT('Ctrl Pts',(-47.4926022196446,-5.73892622312777,
129.35611517708));
#153262=CARTESIAN_POINT('Ctrl Pts',(-47.4999993273293,-5.77539304871202,
129.509198388863));
#153263=CARTESIAN_POINT('Ctrl Pts',(-47.5073964350142,-5.80568839616147,
129.663346678485));
#153264=CARTESIAN_POINT('Ctrl Pts',(-47.5147981891878,-5.83600277361541,
129.817591796265));
#153265=CARTESIAN_POINT('Ctrl Pts',(-47.5221999433615,-5.86013789172212,
129.972902955716));
#153266=CARTESIAN_POINT('Ctrl Pts',(-47.5296016975352,-5.87805012173235,
130.128744358953));
#153267=CARTESIAN_POINT('Ctrl Pts',(-47.5370138398728,-5.89598749107826,
130.284804481431));
#153268=CARTESIAN_POINT('Ctrl Pts',(-47.5444259822105,-5.90768450440213,
130.441395961452));
#153269=CARTESIAN_POINT('Ctrl Pts',(-47.5518381245481,-5.91314961196789,
130.597981769367));
#153270=CARTESIAN_POINT('Ctrl Pts',(-47.5551003522948,-5.91555491191055,
130.666898223484));
#153271=CARTESIAN_POINT('Ctrl Pts',(-47.5583625800414,-5.91675373834474,
130.735813626156));
#153272=CARTESIAN_POINT('Ctrl Pts',(-47.5616248077881,-5.91674999124214,
130.804682543192));
#153273=CARTESIAN_POINT('',(-49.3116240411325,-5.91499358592128,130.798998257019));
#153274=CARTESIAN_POINT('Ctrl Pts',(-47.5616248077881,-5.92651106080092,
130.804683074284));
#153275=CARTESIAN_POINT('Ctrl Pts',(-47.5624338808334,-5.92652453422277,
130.821791600891));
#153276=CARTESIAN_POINT('Ctrl Pts',(-47.5632429538788,-5.92645688555592,
130.838900017864));
#153277=CARTESIAN_POINT('Ctrl Pts',(-47.5640520269241,-5.92630779380708,
130.856007725069));
#153278=CARTESIAN_POINT('Ctrl Pts',(-47.6568679015285,-5.90920416991987,
132.818583064616));
#153279=CARTESIAN_POINT('Ctrl Pts',(-47.8424996507371,-3.73135000823455,
136.72505210137));
#153280=CARTESIAN_POINT('Ctrl Pts',(-48.1209472745499,2.96435960527904,
137.143929424743));
#153281=CARTESIAN_POINT('Ctrl Pts',(-48.3993948983631,6.93596755856032,
131.737052719471));
#153282=CARTESIAN_POINT('Ctrl Pts',(-48.6778425221754,4.53376016637594,
125.473077537096));
#153283=CARTESIAN_POINT('Ctrl Pts',(-48.9562901459887,-2.03475133220846,
124.108291058007));
#153284=CARTESIAN_POINT('Ctrl Pts',(-49.1675505350751,-5.59967235445915,
127.741419835367));
#153285=CARTESIAN_POINT('Ctrl Pts',(-49.2859950495572,-5.91893576568948,
130.254119462179));
#153286=CARTESIAN_POINT('Ctrl Pts',(-49.3116236894351,-5.9141889528215,
130.798991507132));
#153287=CARTESIAN_POINT('',(-51.0616255637457,-5.91166693131237,130.806334617391));
#153288=CARTESIAN_POINT('Ctrl Pts',(-49.311624807788,-5.91674758335821,
130.799012970911));
#153289=CARTESIAN_POINT('Ctrl Pts',(-49.3189601365017,-5.91688859414086,
130.955030236323));
#153290=CARTESIAN_POINT('Ctrl Pts',(-49.3262954652154,-5.91085441233806,
131.111181924842));
#153291=CARTESIAN_POINT('Ctrl Pts',(-49.333630793929,-5.89864003330865,
131.266936362659));
#153292=CARTESIAN_POINT('Ctrl Pts',(-49.3411122355826,-5.88618235518545,
131.425793284318));
#153293=CARTESIAN_POINT('Ctrl Pts',(-49.3485936772361,-5.8672956371023,
131.584236560695));
#153294=CARTESIAN_POINT('Ctrl Pts',(-49.3560751188896,-5.84203044944819,
131.741703025771));
#153295=CARTESIAN_POINT('Ctrl Pts',(-49.3634057495404,-5.81727455779103,
131.895995279699));
#153296=CARTESIAN_POINT('Ctrl Pts',(-49.3707363801912,-5.78639498403716,
132.049349339782));
#153297=CARTESIAN_POINT('Ctrl Pts',(-49.378067010842,-5.74949152254786,
132.201242070893));
#153298=CARTESIAN_POINT('Ctrl Pts',(-49.3853976119527,-5.7125882097672,
132.353134189928));
#153299=CARTESIAN_POINT('Ctrl Pts',(-49.3927282130636,-5.66966114701411,
132.503564621729));
#153300=CARTESIAN_POINT('Ctrl Pts',(-49.4000588141744,-5.62086080807607,
132.652022474815));
#153301=CARTESIAN_POINT('Ctrl Pts',(-49.4073908965377,-5.57205060833313,
132.80051032593));
#153302=CARTESIAN_POINT('Ctrl Pts',(-49.414722978901,-5.51736488940606,
132.947024443542));
#153303=CARTESIAN_POINT('Ctrl Pts',(-49.4220550612644,-5.4570032682094,
133.091071332381));
#153304=CARTESIAN_POINT('Ctrl Pts',(-49.4296492556269,-5.39448380093025,
133.24026770211));
#153305=CARTESIAN_POINT('Ctrl Pts',(-49.4372434499894,-5.32587525907213,
133.386816757951));
#153306=CARTESIAN_POINT('Ctrl Pts',(-49.4448376443519,-5.25145229250738,
133.530196155895));
#153307=CARTESIAN_POINT('Ctrl Pts',(-49.4521810926983,-5.1794866323373,
133.668841435762));
#153308=CARTESIAN_POINT('Ctrl Pts',(-49.4595245410447,-5.10208465192191,
133.804522744505));
#153309=CARTESIAN_POINT('Ctrl Pts',(-49.4668679893912,-5.01953949060683,
133.936796389412));
#153310=CARTESIAN_POINT('Ctrl Pts',(-49.4745875567617,-4.93276650551575,
134.075844867052));
#153311=CARTESIAN_POINT('Ctrl Pts',(-49.4823071241322,-4.84030990417987,
134.211127013296));
#153312=CARTESIAN_POINT('Ctrl Pts',(-49.4900266915027,-4.7425584360818,
134.342166440792));
#153313=CARTESIAN_POINT('Ctrl Pts',(-49.4977462588732,-4.64480696798372,
134.473205868288));
#153314=CARTESIAN_POINT('Ctrl Pts',(-49.5054658262438,-4.54176099529537,
134.600002253022));
#153315=CARTESIAN_POINT('Ctrl Pts',(-49.5131853936143,-4.43385363374095,
134.722124331353));
#153316=CARTESIAN_POINT('Ctrl Pts',(-49.5206086600197,-4.33008809177773,
134.839558985125));
#153317=CARTESIAN_POINT('Ctrl Pts',(-49.5280319264252,-4.22149687609221,
134.953045878808));
#153318=CARTESIAN_POINT('Ctrl Pts',(-49.5354551928306,-4.10841207585408,
135.062162958854));
#153319=CARTESIAN_POINT('Ctrl Pts',(-49.5428696855516,-3.99546093245856,
135.171151071573));
#153320=CARTESIAN_POINT('Ctrl Pts',(-49.5502841782725,-3.87802704218116,
135.275779394456));
#153321=CARTESIAN_POINT('Ctrl Pts',(-49.5576986709935,-3.75648243869832,
135.375659147552));
#153322=CARTESIAN_POINT('Ctrl Pts',(-49.5651060173473,-3.63505498448056,
135.475442632781));
#153323=CARTESIAN_POINT('Ctrl Pts',(-49.5725133637012,-3.50952499121401,
135.570486424419));
#153324=CARTESIAN_POINT('Ctrl Pts',(-49.5799207100549,-3.38030091906444,
135.660438897317));
#153325=CARTESIAN_POINT('Ctrl Pts',(-49.5873225317303,-3.25117322710323,
135.750324280268));
#153326=CARTESIAN_POINT('Ctrl Pts',(-49.5947243534057,-3.11835724726064,
135.83512569306));
#153327=CARTESIAN_POINT('Ctrl Pts',(-49.6021261750811,-2.98229396800212,
135.914532165657));
#153328=CARTESIAN_POINT('Ctrl Pts',(-49.6095240893924,-2.84630251548943,
135.993896720195));
#153329=CARTESIAN_POINT('Ctrl Pts',(-49.6169220037039,-2.70706749911355,
136.067871818679));
#153330=CARTESIAN_POINT('Ctrl Pts',(-49.6243199180152,-2.5650581987547,
136.13619022845));
#153331=CARTESIAN_POINT('Ctrl Pts',(-49.6317166029274,-2.42307249776545,
136.204497284941));
#153332=CARTESIAN_POINT('Ctrl Pts',(-49.6391132878395,-2.27831376387749,
136.267149356742));
#153333=CARTESIAN_POINT('Ctrl Pts',(-49.6465099727517,-2.13127525216176,
136.32392548828));
#153334=CARTESIAN_POINT('Ctrl Pts',(-49.6539063296872,-1.98424326028772,
136.380699102305));
#153335=CARTESIAN_POINT('Ctrl Pts',(-49.6613026866226,-1.83493203982097,
136.431597159654));
#153336=CARTESIAN_POINT('Ctrl Pts',(-49.668699043558,-1.68385391458236,
136.476447231577));
#153337=CARTESIAN_POINT('Ctrl Pts',(-49.6760965328946,-1.53275265889687,
136.521304170161));
#153338=CARTESIAN_POINT('Ctrl Pts',(-49.6834940222311,-1.37988431768758,
136.56011117336));
#153339=CARTESIAN_POINT('Ctrl Pts',(-49.6908915115677,-1.2257752807794,
136.592746016236));
#153340=CARTESIAN_POINT('Ctrl Pts',(-49.6982915940827,-1.07161222118723,
136.625392299204));
#153341=CARTESIAN_POINT('Ctrl Pts',(-49.7056916765978,-0.916207964937106,
136.651862036767));
#153342=CARTESIAN_POINT('Ctrl Pts',(-49.7130917591128,-0.760097818310723,
136.672084355874));
#153343=CARTESIAN_POINT('Ctrl Pts',(-49.7204999787792,-0.603816012530057,
136.692328911499));
#153344=CARTESIAN_POINT('Ctrl Pts',(-49.7279081984456,-0.446827136684607,
136.706312281484));
#153345=CARTESIAN_POINT('Ctrl Pts',(-49.7353164181121,-0.289671065538309,
136.714015534419));
#153346=CARTESIAN_POINT('Ctrl Pts',(-49.7427291974141,-0.132418267451838,
136.721723528578));
#153347=CARTESIAN_POINT('Ctrl Pts',(-49.7501419767162,0.0250015585711839,
136.723143700219));
#153348=CARTESIAN_POINT('Ctrl Pts',(-49.7575547560182,0.18205034989943,
136.718309233559));
#153349=CARTESIAN_POINT('Ctrl Pts',(-49.764978127047,0.339323539905137,
136.713467859186));
#153350=CARTESIAN_POINT('Ctrl Pts',(-49.7724014980757,0.496224265005591,
136.702354023785));
#153351=CARTESIAN_POINT('Ctrl Pts',(-49.7798248691045,0.652220551304472,
136.685052661446));
#153352=CARTESIAN_POINT('Ctrl Pts',(-49.7837609185454,0.734933525382986,
136.675879063994));
#153353=CARTESIAN_POINT('Ctrl Pts',(-49.7876969679864,0.81739240313919,
136.664966784417));
#153354=CARTESIAN_POINT('Ctrl Pts',(-49.7916330174273,0.899519377310721,
136.652334236893));
#153355=CARTESIAN_POINT('Ctrl Pts',(-49.7990562838328,1.0544082874971,136.628509646511));
#153356=CARTESIAN_POINT('Ctrl Pts',(-49.8064795502382,1.20858422983443,
136.598491219399));
#153357=CARTESIAN_POINT('Ctrl Pts',(-49.8139028166436,1.36151261641186,
136.562330221328));
#153358=CARTESIAN_POINT('Ctrl Pts',(-49.8213173093646,1.51426025433648,
136.526211962554));
#153359=CARTESIAN_POINT('Ctrl Pts',(-49.8287318020855,1.66576291178343,
136.483965668971));
#153360=CARTESIAN_POINT('Ctrl Pts',(-49.8361462948066,1.81549240387893,
136.435694197985));
#153361=CARTESIAN_POINT('Ctrl Pts',(-49.8435536411603,1.96507758105295,
136.387469252861));
#153362=CARTESIAN_POINT('Ctrl Pts',(-49.8509609875141,2.11289264233934,
136.333230805285));
#153363=CARTESIAN_POINT('Ctrl Pts',(-49.8583683338679,2.25842097284595,
136.273132442383));
#153364=CARTESIAN_POINT('Ctrl Pts',(-49.8657701555433,2.403840762833,136.213078903107));
#153365=CARTESIAN_POINT('Ctrl Pts',(-49.8731719772188,2.54697687443162,
136.147174292725));
#153366=CARTESIAN_POINT('Ctrl Pts',(-49.8805737988941,2.68732931470535,
136.075621540422));
#153367=CARTESIAN_POINT('Ctrl Pts',(-49.8879717132055,2.82760766401857,
136.004106560259));
#153368=CARTESIAN_POINT('Ctrl Pts',(-49.8953696275168,2.96510493681251,
135.926949545315));
#153369=CARTESIAN_POINT('Ctrl Pts',(-49.9027675418282,3.09934264544475,
135.844400868261));
#153370=CARTESIAN_POINT('Ctrl Pts',(-49.9101642267403,3.23355804620476,
135.761865909301));
#153371=CARTESIAN_POINT('Ctrl Pts',(-49.9175609116526,3.36451464020499,
135.673941261871));
#153372=CARTESIAN_POINT('Ctrl Pts',(-49.9249575965648,3.49175991484945,
135.580922483548));
#153373=CARTESIAN_POINT('Ctrl Pts',(-49.9323539535002,3.61899954730527,
135.487907829775));
#153374=CARTESIAN_POINT('Ctrl Pts',(-49.9397503104356,3.74252788625252,
135.389799714534));
#153375=CARTESIAN_POINT('Ctrl Pts',(-49.947146667371,3.86192293896113,135.286935968414));
#153376=CARTESIAN_POINT('Ctrl Pts',(-49.9545441567076,3.98133627135712,
135.184056473591));
#153377=CARTESIAN_POINT('Ctrl Pts',(-49.9619416460442,4.09661477466076,
135.076420141819));
#153378=CARTESIAN_POINT('Ctrl Pts',(-49.9693391353808,4.20737109100973,
134.964403774197));
#153379=CARTESIAN_POINT('Ctrl Pts',(-49.9767392178958,4.3181662328137,134.852348139412));
#153380=CARTESIAN_POINT('Ctrl Pts',(-49.9841393004108,4.42443576915005,
134.735909677063));
#153381=CARTESIAN_POINT('Ctrl Pts',(-49.9915393829258,4.52583072639426,
134.615500446872));
#153382=CARTESIAN_POINT('Ctrl Pts',(-49.9989476025923,4.6273371778176,134.494958814354));
#153383=CARTESIAN_POINT('Ctrl Pts',(-50.0063558222587,4.72395810507664,
134.370437979989));
#153384=CARTESIAN_POINT('Ctrl Pts',(-50.0137640419251,4.81538576514369,
134.242381922816));
#153385=CARTESIAN_POINT('Ctrl Pts',(-50.0211768212272,4.9068696974101,134.114247049276));
#153386=CARTESIAN_POINT('Ctrl Pts',(-50.0285896005293,4.99315378919068,
133.982572928743));
#153387=CARTESIAN_POINT('Ctrl Pts',(-50.0360023798314,5.07397512331324,
133.847830185427));
#153388=CARTESIAN_POINT('Ctrl Pts',(-50.0434257508601,5.15491193874802,
133.712894915362));
#153389=CARTESIAN_POINT('Ctrl Pts',(-50.0508491218888,5.23037022869458,
133.57488259217));
#153390=CARTESIAN_POINT('Ctrl Pts',(-50.0582724929176,5.30013390572492,
133.434286689509));
#153391=CARTESIAN_POINT('Ctrl Pts',(-50.0622085423584,5.3371242812435,133.359739368364));
#153392=CARTESIAN_POINT('Ctrl Pts',(-50.0661445917993,5.37251450898053,
133.284466025495));
#153393=CARTESIAN_POINT('Ctrl Pts',(-50.0700806412402,5.40627802457782,
133.208542075665));
#153394=CARTESIAN_POINT('Ctrl Pts',(-50.0775039076456,5.46995496127022,
133.065351875793));
#153395=CARTESIAN_POINT('Ctrl Pts',(-50.0849271740511,5.52803547116503,
132.91941359592));
#153396=CARTESIAN_POINT('Ctrl Pts',(-50.0923504404565,5.58027372778425,
132.771204710396));
#153397=CARTESIAN_POINT('Ctrl Pts',(-50.0997649331775,5.63245024312219,
132.623170995467));
#153398=CARTESIAN_POINT('Ctrl Pts',(-50.1071794258986,5.67879812686119,
132.472872365374));
#153399=CARTESIAN_POINT('Ctrl Pts',(-50.1145939186196,5.71911841902588,
132.32080879395));
#153400=CARTESIAN_POINT('Ctrl Pts',(-50.1220012649734,5.75939984897513,
132.168891787121));
#153401=CARTESIAN_POINT('Ctrl Pts',(-50.1294086113271,5.79366515812602,
132.015213583958));
#153402=CARTESIAN_POINT('Ctrl Pts',(-50.1368159576809,5.82176432070789,
131.860291844793));
#153403=CARTESIAN_POINT('Ctrl Pts',(-50.1442177793563,5.84984252587406,
131.705485652106));
#153404=CARTESIAN_POINT('Ctrl Pts',(-50.1516196010318,5.87176367525707,
131.549438135872));
#153405=CARTESIAN_POINT('Ctrl Pts',(-50.1590214227072,5.88742824053203,
131.392679642489));
#153406=CARTESIAN_POINT('Ctrl Pts',(-50.1664193370186,5.903084536605,131.236003900693));
#153407=CARTESIAN_POINT('Ctrl Pts',(-50.1738172513299,5.91249078923427,
131.078618299723));
#153408=CARTESIAN_POINT('Ctrl Pts',(-50.1812151656413,5.91559900978313,
130.92106073733));
#153409=CARTESIAN_POINT('Ctrl Pts',(-50.1886118505536,5.9187067138021,130.763529358145));
#153410=CARTESIAN_POINT('Ctrl Pts',(-50.1960085354658,5.91551845561344,
130.605826447114));
#153411=CARTESIAN_POINT('Ctrl Pts',(-50.203405220378,5.90603830206536,130.448492471988));
#153412=CARTESIAN_POINT('Ctrl Pts',(-50.2108015773135,5.89655856887723,
130.291165473216));
#153413=CARTESIAN_POINT('Ctrl Pts',(-50.2181979342489,5.88078751750683,
130.134207750443));
#153414=CARTESIAN_POINT('Ctrl Pts',(-50.2255942911844,5.85878127701831,
129.978156943791));
#153415=CARTESIAN_POINT('Ctrl Pts',(-50.232991780521,5.83677166731826,129.822082245362));
#153416=CARTESIAN_POINT('Ctrl Pts',(-50.2403892698575,5.80852501984798,
129.666915109189));
#153417=CARTESIAN_POINT('Ctrl Pts',(-50.2477867591941,5.7741489716597,129.513185100612));
#153418=CARTESIAN_POINT('Ctrl Pts',(-50.2551868417091,5.73976087300087,
129.359401202218));
#153419=CARTESIAN_POINT('Ctrl Pts',(-50.2625869242241,5.69923917708544,
129.207055798521));
#153420=CARTESIAN_POINT('Ctrl Pts',(-50.2699870067391,5.65274193265868,
129.056665219259));
#153421=CARTESIAN_POINT('Ctrl Pts',(-50.2773952264056,5.60619355973164,
128.906109270095));
#153422=CARTESIAN_POINT('Ctrl Pts',(-50.2848034460721,5.55365662644702,
128.75751279498));
#153423=CARTESIAN_POINT('Ctrl Pts',(-50.2922116657386,5.49533832232179,
128.611374688354));
#153424=CARTESIAN_POINT('Ctrl Pts',(-50.2996244450407,5.43698412425355,
128.465146636162));
#153425=CARTESIAN_POINT('Ctrl Pts',(-50.3070372243427,5.37284161665725,
128.321380307587));
#153426=CARTESIAN_POINT('Ctrl Pts',(-50.3144500036448,5.30316463585685,
128.180551286174));
#153427=CARTESIAN_POINT('Ctrl Pts',(-50.3218733746735,5.23338809731875,
128.039521041652));
#153428=CARTESIAN_POINT('Ctrl Pts',(-50.3292967457023,5.15806146999229,
127.901436813406));
#153429=CARTESIAN_POINT('Ctrl Pts',(-50.3367201167311,5.07748312670762,
127.766747136476));
#153430=CARTESIAN_POINT('Ctrl Pts',(-50.3406561661718,5.03475855564861,
127.695331437936));
#153431=CARTESIAN_POINT('Ctrl Pts',(-50.3445922156124,4.99055824298862,
127.624869556566));
#153432=CARTESIAN_POINT('Ctrl Pts',(-50.3485282650531,4.94493127862104,
127.555424605236));
#153433=CARTESIAN_POINT('Ctrl Pts',(-50.3559515314586,4.85888024779004,
127.424453594327));
#153434=CARTESIAN_POINT('Ctrl Pts',(-50.363374797864,4.76749217403929,127.296705611415));
#153435=CARTESIAN_POINT('Ctrl Pts',(-50.3707980642694,4.67103589484764,
127.172645563828));
#153436=CARTESIAN_POINT('Ctrl Pts',(-50.3782125569904,4.57469361896752,
127.048732144915));
#153437=CARTESIAN_POINT('Ctrl Pts',(-50.3856270497114,4.47329528806214,
126.928498276871));
#153438=CARTESIAN_POINT('Ctrl Pts',(-50.3930415424325,4.36715400155214,
126.812381598429));
#153439=CARTESIAN_POINT('Ctrl Pts',(-50.4004488887862,4.26111501801069,
126.696376837614));
#153440=CARTESIAN_POINT('Ctrl Pts',(-50.40785623514,4.15034242987009,126.584481639974));
#153441=CARTESIAN_POINT('Ctrl Pts',(-50.4152635814937,4.03519066683523,
126.477102034492));
#153442=CARTESIAN_POINT('Ctrl Pts',(-50.4226654031691,3.92012478832934,
126.369802516771));
#153443=CARTESIAN_POINT('Ctrl Pts',(-50.4300672248445,3.80068651012137,
126.267012138759));
#153444=CARTESIAN_POINT('Ctrl Pts',(-50.4374690465199,3.67726823016638,
126.169101301637));
#153445=CARTESIAN_POINT('Ctrl Pts',(-50.4448669608312,3.55391510176157,
126.071242150884));
#153446=CARTESIAN_POINT('Ctrl Pts',(-50.4522648751426,3.4265864475819,125.978257642468));
#153447=CARTESIAN_POINT('Ctrl Pts',(-50.4596627894539,3.29570887720916,
125.890478897461));
#153448=CARTESIAN_POINT('Ctrl Pts',(-50.4670594743661,3.16485305631352,
125.802714739688));
#153449=CARTESIAN_POINT('Ctrl Pts',(-50.4744561592783,3.03044979945639,
125.720154836078));
#153450=CARTESIAN_POINT('Ctrl Pts',(-50.4818528441905,2.89295601569535,
125.643087901098));
#153451=CARTESIAN_POINT('Ctrl Pts',(-50.4892492011259,2.75546832855256,
125.566024383347));
#153452=CARTESIAN_POINT('Ctrl Pts',(-50.4966455580614,2.61489071261536,
125.49445353246));
#153453=CARTESIAN_POINT('Ctrl Pts',(-50.5040419149969,2.47170583887421,
125.428618733084));
#153454=CARTESIAN_POINT('Ctrl Pts',(-50.5114394043335,2.32849904316315,
125.362773854232));
#153455=CARTESIAN_POINT('Ctrl Pts',(-50.5188368936701,2.18268453401855,
125.302666931465));
#153456=CARTESIAN_POINT('Ctrl Pts',(-50.5262343830067,2.03476603021457,
125.248493649686));
#153457=CARTESIAN_POINT('Ctrl Pts',(-50.5336344655217,1.88679567380839,
125.194301377546));
#153458=CARTESIAN_POINT('Ctrl Pts',(-50.5410345480367,1.7367202045926,125.146047016012));
#153459=CARTESIAN_POINT('Ctrl Pts',(-50.5484346305517,1.58505945460646,
125.103876683034));
#153460=CARTESIAN_POINT('Ctrl Pts',(-50.5558428502182,1.43323193803482,
125.061659979439));
#153461=CARTESIAN_POINT('Ctrl Pts',(-50.5632510698847,1.27981601932356,
125.025540764864));
#153462=CARTESIAN_POINT('Ctrl Pts',(-50.5706592895511,1.12534342348995,
124.995614389531));
#153463=CARTESIAN_POINT('Ctrl Pts',(-50.5780720688532,0.970775752350672,
124.965669595014));
#153464=CARTESIAN_POINT('Ctrl Pts',(-50.5854848481553,0.815150476322736,
124.941925290982));
#153465=CARTESIAN_POINT('Ctrl Pts',(-50.5928976274574,0.659004922045166,
124.92442498227));
#153466=CARTESIAN_POINT('Ctrl Pts',(-50.6003209984861,0.502636259677368,
124.906899668297));
#153467=CARTESIAN_POINT('Ctrl Pts',(-50.607744369515,0.345746205680676,
124.895636194966));
#153468=CARTESIAN_POINT('Ctrl Pts',(-50.6151677405438,0.188873403088834,
124.890625976909));
#153469=CARTESIAN_POINT('Ctrl Pts',(-50.6191037899845,0.105695679043978,
124.887969439077));
#153470=CARTESIAN_POINT('Ctrl Pts',(-50.6230398394252,0.0225227540158833,
124.887070045928));
#153471=CARTESIAN_POINT('Ctrl Pts',(-50.626975888866,-0.0605657390643266,
124.887920610792));
#153472=CARTESIAN_POINT('Ctrl Pts',(-50.6343991552714,-0.217268043911369,
124.889524749581));
#153473=CARTESIAN_POINT('Ctrl Pts',(-50.6418224216769,-0.37414352608616,
124.89736121909));
#153474=CARTESIAN_POINT('Ctrl Pts',(-50.6492456880823,-0.530655732662615,
124.911455132502));
#153475=CARTESIAN_POINT('Ctrl Pts',(-50.6566601808033,-0.686982954808871,
124.925532388079));
#153476=CARTESIAN_POINT('Ctrl Pts',(-50.6640746735243,-0.842947387840515,
124.945852333067));
#153477=CARTESIAN_POINT('Ctrl Pts',(-50.6714891662454,-0.998011596012674,
124.97238810248));
#153478=CARTESIAN_POINT('Ctrl Pts',(-50.6788965125992,-1.15292634746315,
124.998898295719));
#153479=CARTESIAN_POINT('Ctrl Pts',(-50.686303858953,-1.30694223593648,
125.031612323848));
#153480=CARTESIAN_POINT('Ctrl Pts',(-50.6937112053068,-1.45952607983614,
125.070451463701));
#153481=CARTESIAN_POINT('Ctrl Pts',(-50.7011130269822,-1.61199612094792,
125.109261635858));
#153482=CARTESIAN_POINT('Ctrl Pts',(-50.7085148486576,-1.76303588395808,
125.154187731872));
#153483=CARTESIAN_POINT('Ctrl Pts',(-50.715916670333,-1.91212163918262,
125.205099827116));
#153484=CARTESIAN_POINT('Ctrl Pts',(-50.7233145846443,-2.06112869319554,
125.255985046261));
#153485=CARTESIAN_POINT('Ctrl Pts',(-50.7307124989556,-2.20818344134278,
125.312849851085));
#153486=CARTESIAN_POINT('Ctrl Pts',(-50.7381104132668,-2.3527767091887,
125.375514301893));
#153487=CARTESIAN_POINT('Ctrl Pts',(-50.745507098179,-2.49734594825835,
125.438168339007));
#153488=CARTESIAN_POINT('Ctrl Pts',(-50.7529037830912,-2.63945417669665,
125.50661996096));
#153489=CARTESIAN_POINT('Ctrl Pts',(-50.7603004680034,-2.77861152033932,
125.580640814443));
#153490=CARTESIAN_POINT('Ctrl Pts',(-50.7676968249389,-2.91776269359994,
125.654658385765));
#153491=CARTESIAN_POINT('Ctrl Pts',(-50.7750931818743,-3.05396291265647,
125.734244522298));
#153492=CARTESIAN_POINT('Ctrl Pts',(-50.7824895388098,-3.18674651565259,
125.819124694616));
#153493=CARTESIAN_POINT('Ctrl Pts',(-50.7898870281463,-3.31955044815674,
125.904017862304));
#153494=CARTESIAN_POINT('Ctrl Pts',(-50.797284517483,-3.44893640850621,
125.99420647858));
#153495=CARTESIAN_POINT('Ctrl Pts',(-50.8046820068195,-3.57446748915029,
126.089372523042));
#153496=CARTESIAN_POINT('Ctrl Pts',(-50.8120820893346,-3.70004257452118,
126.184571927813));
#153497=CARTESIAN_POINT('Ctrl Pts',(-50.8194821718496,-3.82175979242311,
126.284752009336));
#153498=CARTESIAN_POINT('Ctrl Pts',(-50.8268822543646,-3.93921522777169,
126.389554398513));
#153499=CARTESIAN_POINT('Ctrl Pts',(-50.8342904740311,-4.05679981744515,
126.49447202869));
#153500=CARTESIAN_POINT('Ctrl Pts',(-50.8416986936975,-4.17011298707178,
126.604021868327));
#153501=CARTESIAN_POINT('Ctrl Pts',(-50.849106913364,-4.27878710544865,
126.717808101233));
#153502=CARTESIAN_POINT('Ctrl Pts',(-50.856519692666,-4.38752811093222,
126.831664367667));
#153503=CARTESIAN_POINT('Ctrl Pts',(-50.8639324719681,-4.49162412943925,
126.94976194361));
#153504=CARTESIAN_POINT('Ctrl Pts',(-50.8713452512702,-4.59074812094708,
127.071672276367));
#153505=CARTESIAN_POINT('Ctrl Pts',(-50.8787686222989,-4.69001374546256,
127.193756800325));
#153506=CARTESIAN_POINT('Ctrl Pts',(-50.8861919933277,-4.78429293101191,
127.319664663649));
#153507=CARTESIAN_POINT('Ctrl Pts',(-50.8936153643564,-4.87330175099166,
127.448938050097));
#153508=CARTESIAN_POINT('Ctrl Pts',(-50.8975514137973,-4.92049636308275,
127.517481901465));
#153509=CARTESIAN_POINT('Ctrl Pts',(-50.9014874632381,-4.96621004560118,
127.586971494906));
#153510=CARTESIAN_POINT('Ctrl Pts',(-50.9054235126789,-5.0104058013515,
127.657335948409));
#153511=CARTESIAN_POINT('Ctrl Pts',(-50.9130462144203,-5.09599696817618,
127.793606401897));
#153512=CARTESIAN_POINT('Ctrl Pts',(-50.9206689161617,-5.17613985804444,
127.933553529582));
#153513=CARTESIAN_POINT('Ctrl Pts',(-50.9282916179031,-5.25051253618389,
128.076715356562));
#153514=CARTESIAN_POINT('Ctrl Pts',(-50.9359038231383,-5.32478280269742,
128.219680048845));
#153515=CARTESIAN_POINT('Ctrl Pts',(-50.9435160283734,-5.39329852644854,
128.365850318301));
#153516=CARTESIAN_POINT('Ctrl Pts',(-50.9511282336086,-5.45578114959963,
128.514735624216));
#153517=CARTESIAN_POINT('Ctrl Pts',(-50.9587311300378,-5.51818736406292,
128.663438861417));
#153518=CARTESIAN_POINT('Ctrl Pts',(-50.966334026467,-5.57457504267055,
128.814850203501));
#153519=CARTESIAN_POINT('Ctrl Pts',(-50.9739369228963,-5.62471157029013,
128.968454761171));
#153520=CARTESIAN_POINT('Ctrl Pts',(-50.9815292619871,-5.67477847861519,
129.121846024434));
#153521=CARTESIAN_POINT('Ctrl Pts',(-50.9891216010781,-5.71861143700816,
129.277424103212));
#153522=CARTESIAN_POINT('Ctrl Pts',(-50.9967139401689,-5.75602608788787,
129.434654722837));
#153523=CARTESIAN_POINT('Ctrl Pts',(-51.0043001049327,-5.79341031200569,
129.591757477616));
#153524=CARTESIAN_POINT('Ctrl Pts',(-51.0118862696965,-5.82438654572741,
129.750509760866));
#153525=CARTESIAN_POINT('Ctrl Pts',(-51.0194724344602,-5.84882012205448,
129.910361880234));
#153526=CARTESIAN_POINT('Ctrl Pts',(-51.0270524158079,-5.87323378278868,
130.070083705549));
#153527=CARTESIAN_POINT('Ctrl Pts',(-51.0346323971556,-5.89111536534244,
130.230903238429));
#153528=CARTESIAN_POINT('Ctrl Pts',(-51.0422123785033,-5.90238121170339,
130.392260394039));
#153529=CARTESIAN_POINT('Ctrl Pts',(-51.0486831882649,-5.91199853729579,
130.530006307879));
#153530=CARTESIAN_POINT('Ctrl Pts',(-51.0551539980265,-5.91679543811377,
130.668143704449));
#153531=CARTESIAN_POINT('Ctrl Pts',(-51.0616248077881,-5.91674967550615,
130.806320183304));
#153532=CARTESIAN_POINT('',(-52.8116248077881,-5.92138584378568,130.809025436609));
#153533=CARTESIAN_POINT('Ctrl Pts',(-51.0616261784267,-5.90753407287618,
130.806346353971));
#153534=CARTESIAN_POINT('Ctrl Pts',(-51.1023744977817,-5.91009664804197,
131.675124094495));
#153535=CARTESIAN_POINT('Ctrl Pts',(-51.2359386917411,-5.32287699652367,
134.519485052779));
#153536=CARTESIAN_POINT('Ctrl Pts',(-51.4623187603045,-0.922135659953538,
137.741739542996));
#153537=CARTESIAN_POINT('Ctrl Pts',(-51.7407663841177,5.33817651812515,
135.330002228618));
#153538=CARTESIAN_POINT('Ctrl Pts',(-52.0192140079303,6.69296526046545,
128.759421363569));
#153539=CARTESIAN_POINT('Ctrl Pts',(-52.2976616317434,1.89724589797152,
124.068039772106));
#153540=CARTESIAN_POINT('Ctrl Pts',(-52.5617985650291,-4.30587073622864,
125.489969153991));
#153541=CARTESIAN_POINT('Ctrl Pts',(-52.7331196237108,-5.90700759757791,
129.145181670511));
#153542=CARTESIAN_POINT('Ctrl Pts',(-52.8116248077881,-5.92138584378568,
130.809025436609));
#153543=CARTESIAN_POINT('',(-54.561624807788,-5.92017284106423,130.80018406539));
#153544=CARTESIAN_POINT('Ctrl Pts',(-52.8116248077881,-5.92138584378568,
130.809025436609));
#153545=CARTESIAN_POINT('Ctrl Pts',(-52.8259354983151,-5.92400685071941,
131.112327103904));
#153546=CARTESIAN_POINT('Ctrl Pts',(-52.9330620634458,-5.76469768580607,
133.380013103561));
#153547=CARTESIAN_POINT('Ctrl Pts',(-53.1330045031822,-2.83395748649668,
137.203285956645));
#153548=CARTESIAN_POINT('Ctrl Pts',(-53.4114521269948,3.85177387003691,
136.647424761012));
#153549=CARTESIAN_POINT('Ctrl Pts',(-53.6898997508079,6.99791320962053,
130.722073067109));
#153550=CARTESIAN_POINT('Ctrl Pts',(-53.9683473746205,3.71331217662896,
124.872339612104));
#153551=CARTESIAN_POINT('Ctrl Pts',(-54.2467949984337,-2.98364134130034,
124.473843665782));
#153552=CARTESIAN_POINT('Ctrl Pts',(-54.4445541428227,-5.79265685533358,
128.322484560607));
#153553=CARTESIAN_POINT('Ctrl Pts',(-54.5494974126075,-5.92470418608257,
130.543296141923));
#153554=CARTESIAN_POINT('Ctrl Pts',(-54.561624807788,-5.92264775691338,
130.800182319391));
#153555=CARTESIAN_POINT('',(-56.3116247825725,-5.9119383046366,130.801701158817));
#153556=CARTESIAN_POINT('Ctrl Pts',(-54.561624807788,-5.91674852761932,
130.800186481168));
#153557=CARTESIAN_POINT('Ctrl Pts',(-54.5689357564989,-5.91685767039822,
130.954894021801));
#153558=CARTESIAN_POINT('Ctrl Pts',(-54.5762467052098,-5.91089487079683,
131.109837684137));
#153559=CARTESIAN_POINT('Ctrl Pts',(-54.5835576539206,-5.89883112223607,
131.264493156993));
#153560=CARTESIAN_POINT('Ctrl Pts',(-54.5908612387532,-5.8867795247627,
131.418992854704));
#153561=CARTESIAN_POINT('Ctrl Pts',(-54.5981648235857,-5.86863923493353,
131.573204559887));
#153562=CARTESIAN_POINT('Ctrl Pts',(-54.6054684084182,-5.84443325961165,
131.726602687982));
#153563=CARTESIAN_POINT('Ctrl Pts',(-54.6127663366966,-5.82024603157801,
131.879882010746));
#153564=CARTESIAN_POINT('Ctrl Pts',(-54.6200642649749,-5.79000252674056,
132.032348632106));
#153565=CARTESIAN_POINT('Ctrl Pts',(-54.6273621932533,-5.75377765361574,
132.18348108919));
#153566=CARTESIAN_POINT('Ctrl Pts',(-54.6347091954536,-5.71730919127959,
132.335629815838));
#153567=CARTESIAN_POINT('Ctrl Pts',(-54.6420561976538,-5.67477864734158,
132.486425974986));
#153568=CARTESIAN_POINT('Ctrl Pts',(-54.649403199854,-5.62631510966825,
132.635346376445));
#153569=CARTESIAN_POINT('Ctrl Pts',(-54.6566959102122,-5.57820970101953,
132.783166306898));
#153570=CARTESIAN_POINT('Ctrl Pts',(-54.6639886205705,-5.52425882523823,
132.929137742254));
#153571=CARTESIAN_POINT('Ctrl Pts',(-54.6712813309288,-5.46463902029307,
133.072763346446));
#153572=CARTESIAN_POINT('Ctrl Pts',(-54.6785738299039,-5.40502094345963,
133.216384787573));
#153573=CARTESIAN_POINT('Ctrl Pts',(-54.6858663288789,-5.33973441171662,
133.35766017723));
#153574=CARTESIAN_POINT('Ctrl Pts',(-54.693158827854,-5.26900418996104,
133.496111982138));
#153575=CARTESIAN_POINT('Ctrl Pts',(-54.7004526507512,-5.19826112743533,
133.63458892238));
#153576=CARTESIAN_POINT('Ctrl Pts',(-54.7077464736486,-5.12207258387678,
133.770240915353));
#153577=CARTESIAN_POINT('Ctrl Pts',(-54.7150402965458,-5.04070922180969,
133.902615142886));
#153578=CARTESIAN_POINT('Ctrl Pts',(-54.7224277923386,-4.95830092873383,
134.036689422279));
#153579=CARTESIAN_POINT('Ctrl Pts',(-54.7298152881314,-4.87058418760669,
134.167400813144));
#153580=CARTESIAN_POINT('Ctrl Pts',(-54.7372027839241,-4.77788483902664,
134.294310048073));
#153581=CARTESIAN_POINT('Ctrl Pts',(-54.7445074650968,-4.68622466008602,
134.419796616869));
#153582=CARTESIAN_POINT('Ctrl Pts',(-54.7518121462695,-4.58969330068087,
134.541565574923));
#153583=CARTESIAN_POINT('Ctrl Pts',(-54.7591168274421,-4.48864520973242,
134.659226989264));
#153584=CARTESIAN_POINT('Ctrl Pts',(-54.766545730545,-4.38587871539249,
134.778889329813));
#153585=CARTESIAN_POINT('Ctrl Pts',(-54.7739746336478,-4.27844077059429,
134.89430285753));
#153586=CARTESIAN_POINT('Ctrl Pts',(-54.7814035367507,-4.16674134915281,
135.005098301802));
#153587=CARTESIAN_POINT('Ctrl Pts',(-54.7888324398536,-4.05504192771117,
135.115893746075));
#153588=CARTESIAN_POINT('Ctrl Pts',(-54.7962613429565,-3.93908137815843,
135.222070878999));
#153589=CARTESIAN_POINT('Ctrl Pts',(-54.8036902460594,-3.81930212530724,
135.323305387988));
#153590=CARTESIAN_POINT('Ctrl Pts',(-54.8111135124648,-3.69961375524164,
135.424463085059));
#153591=CARTESIAN_POINT('Ctrl Pts',(-54.8185367788702,-3.5757227460027,
135.521015376547));
#153592=CARTESIAN_POINT('Ctrl Pts',(-54.8259600452757,-3.44801884360224,
135.612592789234));
#153593=CARTESIAN_POINT('Ctrl Pts',(-54.8333745379967,-3.32046587660907,
135.704061965024));
#153594=CARTESIAN_POINT('Ctrl Pts',(-54.8407890307177,-3.18910928711066,
135.790567750556));
#153595=CARTESIAN_POINT('Ctrl Pts',(-54.8482035234387,-3.05437352208537,
135.871779383573));
#153596=CARTESIAN_POINT('Ctrl Pts',(-54.8556108697925,-2.91976762046351,
135.952912741761));
#153597=CARTESIAN_POINT('Ctrl Pts',(-54.8630182161462,-2.78178934487982,
136.028761914501));
#153598=CARTESIAN_POINT('Ctrl Pts',(-54.8704255625,-2.64089379994834,136.099038180921));
#153599=CARTESIAN_POINT('Ctrl Pts',(-54.8778273841754,-2.50010334022915,
136.16926203265));
#153600=CARTESIAN_POINT('Ctrl Pts',(-54.8852292058509,-2.35640027610511,
136.233921088279));
#153601=CARTESIAN_POINT('Ctrl Pts',(-54.8926310275263,-2.21026600553464,
136.292771566764));
#153602=CARTESIAN_POINT('Ctrl Pts',(-54.9000289418376,-2.06420887810892,
136.35159097854));
#153603=CARTESIAN_POINT('Ctrl Pts',(-54.9074268561489,-1.9157234456159,
136.404607780765));
#153604=CARTESIAN_POINT('Ctrl Pts',(-54.9148247704603,-1.76531276052781,
136.451625567966));
#153605=CARTESIAN_POINT('Ctrl Pts',(-54.9222214553725,-1.61492707096665,
136.498635541664));
#153606=CARTESIAN_POINT('Ctrl Pts',(-54.9296181402848,-1.46261711974746,
136.539648367676));
#153607=CARTESIAN_POINT('Ctrl Pts',(-54.937014825197,-1.30890297514993,
136.574516903503));
#153608=CARTESIAN_POINT('Ctrl Pts',(-54.9444111821324,-1.15519564639844,
136.609383893224));
#153609=CARTESIAN_POINT('Ctrl Pts',(-54.9518075390678,-1.00008461211801,
136.638107051889));
#153610=CARTESIAN_POINT('Ctrl Pts',(-54.9592038960033,-0.844101775724089,
136.660590014944));
#153611=CARTESIAN_POINT('Ctrl Pts',(-54.9666013853398,-0.688095057960154,
136.683076420198));
#153612=CARTESIAN_POINT('Ctrl Pts',(-54.9739988746763,-0.531216641819291,
136.699320674274));
#153613=CARTESIAN_POINT('Ctrl Pts',(-54.9813963640128,-0.374005072893866,
136.70927812486));
#153614=CARTESIAN_POINT('Ctrl Pts',(-54.9887964465278,-0.216738393696886,
136.719239066015));
#153615=CARTESIAN_POINT('Ctrl Pts',(-54.9961965290429,-0.0591387015138569,
136.722908792292));
#153616=CARTESIAN_POINT('Ctrl Pts',(-55.0035966115578,0.0982540774499587,
136.720294753336));
#153617=CARTESIAN_POINT('Ctrl Pts',(-55.0110048312243,0.255819925955066,
136.717677839975));
#153618=CARTESIAN_POINT('Ctrl Pts',(-55.0184130508907,0.413178033388422,
136.708763368567));
#153619=CARTESIAN_POINT('Ctrl Pts',(-55.0258212705572,0.569791480473101,
136.693610844147));
#153620=CARTESIAN_POINT('Ctrl Pts',(-55.0332340498593,0.726501320521672,
136.6784489936));
#153621=CARTESIAN_POINT('Ctrl Pts',(-55.0406468291613,0.882465217976646,
136.657041490165));
#153622=CARTESIAN_POINT('Ctrl Pts',(-55.0480596084634,1.03715559896363,
136.629499141759));
#153623=CARTESIAN_POINT('Ctrl Pts',(-55.0554829794922,1.19206700882078,
136.601917439554));
#153624=CARTESIAN_POINT('Ctrl Pts',(-55.0629063505209,1.34570090429466,
136.568183465048));
#153625=CARTESIAN_POINT('Ctrl Pts',(-55.0703297215497,1.49754323536802,
136.528458347401));
#153626=CARTESIAN_POINT('Ctrl Pts',(-55.0742657709905,1.57805368271103,
136.507395136833));
#153627=CARTESIAN_POINT('Ctrl Pts',(-55.0782018204313,1.65806075277631,
136.484648420463));
#153628=CARTESIAN_POINT('Ctrl Pts',(-55.0821378698722,1.73749012815274,
136.46024769362));
#153629=CARTESIAN_POINT('Ctrl Pts',(-55.0895611362776,1.88729145120475,
136.414228684314));
#153630=CARTESIAN_POINT('Ctrl Pts',(-55.096984402683,2.03548974523695,136.362184541436));
#153631=CARTESIAN_POINT('Ctrl Pts',(-55.1044076690885,2.1815634947261,136.304243460044));
#153632=CARTESIAN_POINT('Ctrl Pts',(-55.1118221618095,2.32746459717403,
136.246370860198));
#153633=CARTESIAN_POINT('Ctrl Pts',(-55.1192366545305,2.4712458096998,136.182615331342));
#153634=CARTESIAN_POINT('Ctrl Pts',(-55.1266511472515,2.61239942869045,
136.113155187662));
#153635=CARTESIAN_POINT('Ctrl Pts',(-55.1340584936053,2.75341699850918,
136.043761992283));
#153636=CARTESIAN_POINT('Ctrl Pts',(-55.1414658399591,2.89181168395572,
135.968675291871));
#153637=CARTESIAN_POINT('Ctrl Pts',(-55.1488731863129,3.02709458082315,
135.888121918144));
#153638=CARTESIAN_POINT('Ctrl Pts',(-55.1562750079882,3.1622765786014,135.807628624162));
#153639=CARTESIAN_POINT('Ctrl Pts',(-55.1636768296637,3.29435108964162,
135.721676965385));
#153640=CARTESIAN_POINT('Ctrl Pts',(-55.171078651339,3.42285280669413,135.630540185942));
#153641=CARTESIAN_POINT('Ctrl Pts',(-55.1784765656504,3.55128668869137,
135.539451516894));
#153642=CARTESIAN_POINT('Ctrl Pts',(-55.1858744799618,3.67615122913889,
135.443183393821));
#153643=CARTESIAN_POINT('Ctrl Pts',(-55.1932723942732,3.79700927440007,
135.342052887059));
#153644=CARTESIAN_POINT('Ctrl Pts',(-55.2006690791854,3.91784723524655,
135.240939186353));
#153645=CARTESIAN_POINT('Ctrl Pts',(-55.2080657640976,4.03467973632571,
135.134964945004));
#153646=CARTESIAN_POINT('Ctrl Pts',(-55.2154624490098,4.14710187287758,
135.024488177069));
#153647=CARTESIAN_POINT('Ctrl Pts',(-55.2228588059452,4.25951902451362,
134.91401630779));
#153648=CARTESIAN_POINT('Ctrl Pts',(-55.2302551628807,4.36752593420728,
134.799042570538));
#153649=CARTESIAN_POINT('Ctrl Pts',(-55.2376515198162,4.47075402093921,
134.679962383325));
#153650=CARTESIAN_POINT('Ctrl Pts',(-55.2450490091528,4.57399791215519,
134.560863964631));
#153651=CARTESIAN_POINT('Ctrl Pts',(-55.2524464984893,4.6724612790629,134.437658126219));
#153652=CARTESIAN_POINT('Ctrl Pts',(-55.2598439878259,4.76581545736149,
134.310773826085));
#153653=CARTESIAN_POINT('Ctrl Pts',(-55.267244070341,4.85920236082283,134.183845046855));
#153654=CARTESIAN_POINT('Ctrl Pts',(-55.274644152856,4.94747628868341,134.053235539056));
#153655=CARTESIAN_POINT('Ctrl Pts',(-55.282044235371,5.03035166523881,133.91940358461));
#153656=CARTESIAN_POINT('Ctrl Pts',(-55.2894524550375,5.11331817179017,
133.785424468172));
#153657=CARTESIAN_POINT('Ctrl Pts',(-55.296860674704,5.19087407527716,133.648216146231));
#153658=CARTESIAN_POINT('Ctrl Pts',(-55.3042688943705,5.26277922098575,
133.508262508105));
#153659=CARTESIAN_POINT('Ctrl Pts',(-55.3116816736725,5.33472862311183,
133.36822273085));
#153660=CARTESIAN_POINT('Ctrl Pts',(-55.3190944529746,5.40102018038405,
133.22543460828));
#153661=CARTESIAN_POINT('Ctrl Pts',(-55.3265072322767,5.46146195207614,
133.080401897623));
#153662=CARTESIAN_POINT('Ctrl Pts',(-55.3339306033054,5.52199008580589,
132.935161957429));
#153663=CARTESIAN_POINT('Ctrl Pts',(-55.3413539743342,5.57665161087823,
132.78767137281));
#153664=CARTESIAN_POINT('Ctrl Pts',(-55.348777345363,5.62530423322799,132.638449722852));
#153665=CARTESIAN_POINT('Ctrl Pts',(-55.3527133948037,5.6511010210011,132.55932882352));
#153666=CARTESIAN_POINT('Ctrl Pts',(-55.3566494442444,5.67520933994965,
132.479721453742));
#153667=CARTESIAN_POINT('Ctrl Pts',(-55.3605854936851,5.69761383495216,
132.399706081803));
#153668=CARTESIAN_POINT('Ctrl Pts',(-55.3680087600905,5.73986801330723,
132.248799587519));
#153669=CARTESIAN_POINT('Ctrl Pts',(-55.375432026496,5.77618659980623,132.095985035081));
#153670=CARTESIAN_POINT('Ctrl Pts',(-55.3828552929015,5.8063955567029,131.94177048283));
#153671=CARTESIAN_POINT('Ctrl Pts',(-55.3902697856225,5.83656880912125,
131.787738199373));
#153672=CARTESIAN_POINT('Ctrl Pts',(-55.3976842783434,5.86064673446612,
131.632309572518));
#153673=CARTESIAN_POINT('Ctrl Pts',(-55.4050987710644,5.87850492730756,
131.476008130865));
#153674=CARTESIAN_POINT('Ctrl Pts',(-55.4125061174182,5.89634590775034,
131.319857338427));
#153675=CARTESIAN_POINT('Ctrl Pts',(-55.419913463772,5.90797904808998,131.162835774353));
#153676=CARTESIAN_POINT('Ctrl Pts',(-55.4273208101258,5.91333092360849,
131.005477375683));
#153677=CARTESIAN_POINT('Ctrl Pts',(-55.4347226318012,5.91867880749633,
130.848236340844));
#153678=CARTESIAN_POINT('Ctrl Pts',(-55.4421244534765,5.91775474200638,
130.690659343106));
#153679=CARTESIAN_POINT('Ctrl Pts',(-55.4495262751519,5.91053710522861,
130.533285553763));
#153680=CARTESIAN_POINT('Ctrl Pts',(-55.4569241894632,5.90332327858513,
130.375994840819));
#153681=CARTESIAN_POINT('Ctrl Pts',(-55.4643221037745,5.88982251428714,
130.218907494594));
#153682=CARTESIAN_POINT('Ctrl Pts',(-55.4717200180858,5.87006528036957,
130.062562689084));
#153683=CARTESIAN_POINT('Ctrl Pts',(-55.479116702998,5.85031132974576,129.906243865245));
#153684=CARTESIAN_POINT('Ctrl Pts',(-55.4865133879103,5.82430301977792,
129.750667707205));
#153685=CARTESIAN_POINT('Ctrl Pts',(-55.4939100728225,5.79212269691946,
129.59636838815));
#153686=CARTESIAN_POINT('Ctrl Pts',(-55.501306429758,5.75994380097016,129.442075910888));
#153687=CARTESIAN_POINT('Ctrl Pts',(-55.5087027866934,5.72159351249984,
129.289060525473));
#153688=CARTESIAN_POINT('Ctrl Pts',(-55.5160991436289,5.67720528083589,
129.137846062649));
#153689=CARTESIAN_POINT('Ctrl Pts',(-55.5234966329654,5.63281025322056,
128.986608448506));
#153690=CARTESIAN_POINT('Ctrl Pts',(-55.530894122302,5.58237554690949,128.837172664168));
#153691=CARTESIAN_POINT('Ctrl Pts',(-55.5382916116386,5.52608440532971,
128.690047086495));
#153692=CARTESIAN_POINT('Ctrl Pts',(-55.5456916941536,5.46977353097736,
128.542869934177));
#153693=CARTESIAN_POINT('Ctrl Pts',(-55.5530917766685,5.40760226723185,
128.398004949341));
#153694=CARTESIAN_POINT('Ctrl Pts',(-55.5604918591835,5.3398018190108,128.255940107487));
#153695=CARTESIAN_POINT('Ctrl Pts',(-55.56790007885,5.27192681722698,128.113719050736));
#153696=CARTESIAN_POINT('Ctrl Pts',(-55.5753082985164,5.19841043027967,
127.974304623126));
#153697=CARTESIAN_POINT('Ctrl Pts',(-55.5827165181829,5.11952995846776,
127.838160427617));
#153698=CARTESIAN_POINT('Ctrl Pts',(-55.590129297485,5.04060093704142,127.701932437627));
#153699=CARTESIAN_POINT('Ctrl Pts',(-55.5975420767871,4.95630145152058,
127.568979004977));
#153700=CARTESIAN_POINT('Ctrl Pts',(-55.6049548560891,4.86695157847769,
127.439733907921));
#153701=CARTESIAN_POINT('Ctrl Pts',(-55.6123782271179,4.77747403814637,
127.310304139411));
#153702=CARTESIAN_POINT('Ctrl Pts',(-55.6198015981466,4.68293192163988,
127.184593586628));
#153703=CARTESIAN_POINT('Ctrl Pts',(-55.6272249691754,4.58368545213959,
127.063002810787));
#153704=CARTESIAN_POINT('Ctrl Pts',(-55.6311610186162,4.53106259262298,
126.998532463904));
#153705=CARTESIAN_POINT('Ctrl Pts',(-55.6350970680571,4.47711779309835,
126.935219724504));
#153706=CARTESIAN_POINT('Ctrl Pts',(-55.639033117498,4.42190877134034,126.873119925311));
#153707=CARTESIAN_POINT('Ctrl Pts',(-55.6464563839034,4.31778627932138,
126.756001642103));
#153708=CARTESIAN_POINT('Ctrl Pts',(-55.6538796503089,4.20885015155603,
126.64284578839));
#153709=CARTESIAN_POINT('Ctrl Pts',(-55.6613029167144,4.09543376026158,
126.534073404999));
#153710=CARTESIAN_POINT('Ctrl Pts',(-55.6687174094354,3.98215141772317,
126.425429581533));
#153711=CARTESIAN_POINT('Ctrl Pts',(-55.6761319021563,3.8643996187672,126.321159171647));
#153712=CARTESIAN_POINT('Ctrl Pts',(-55.6835463948773,3.74255157865935,
126.221649821151));
#153713=CARTESIAN_POINT('Ctrl Pts',(-55.6909537412311,3.6208209802804,126.122236381514));
#153714=CARTESIAN_POINT('Ctrl Pts',(-55.6983610875849,3.49500228785228,
126.027575100232));
#153715=CARTESIAN_POINT('Ctrl Pts',(-55.7057684339386,3.36550502987478,
125.938016357612));
#153716=CARTESIAN_POINT('Ctrl Pts',(-55.713170255614,3.23610435583737,125.848524411281));
#153717=CARTESIAN_POINT('Ctrl Pts',(-55.7205720772894,3.10303088485882,
125.764127637438));
#153718=CARTESIAN_POINT('Ctrl Pts',(-55.7279738989648,2.96672654984779,
125.685135662465));
#153719=CARTESIAN_POINT('Ctrl Pts',(-55.7353718132762,2.83049416883345,
125.60618538674));
#153720=CARTESIAN_POINT('Ctrl Pts',(-55.7427697275877,2.69103464263019,
125.532634414398));
#153721=CARTESIAN_POINT('Ctrl Pts',(-55.7501676418991,2.54881806230884,
125.464748548534));
#153722=CARTESIAN_POINT('Ctrl Pts',(-55.7575643268113,2.40662511580368,
125.39687396407));
#153723=CARTESIAN_POINT('Ctrl Pts',(-55.7649610117235,2.26167636107247,
125.33466277826));
#153724=CARTESIAN_POINT('Ctrl Pts',(-55.7723576966357,2.11446572341416,
125.278334444356));
#153725=CARTESIAN_POINT('Ctrl Pts',(-55.7797540535712,1.96726161323,125.222008608108));
#153726=CARTESIAN_POINT('Ctrl Pts',(-55.7871504105066,1.81779616818379,
125.17156523851));
#153727=CARTESIAN_POINT('Ctrl Pts',(-55.7945467674421,1.66658223453711,
125.127175204174));
#153728=CARTESIAN_POINT('Ctrl Pts',(-55.8019442567786,1.51534514965138,
125.082778373611));
#153729=CARTESIAN_POINT('Ctrl Pts',(-55.8093417461152,1.36235940134909,
125.04443682881));
#153730=CARTESIAN_POINT('Ctrl Pts',(-55.8167392354518,1.20815174902764,
125.012271191994));
#153731=CARTESIAN_POINT('Ctrl Pts',(-55.8241393179668,1.05389003945249,
124.980094279564));
#153732=CARTESIAN_POINT('Ctrl Pts',(-55.8315394004817,0.898405938248125,
124.954097661707));
#153733=CARTESIAN_POINT('Ctrl Pts',(-55.8389394829967,0.742234964929896,
124.934350581856));
#153734=CARTESIAN_POINT('Ctrl Pts',(-55.8463477026632,0.585892265571738,
124.91458178806));
#153735=CARTESIAN_POINT('Ctrl Pts',(-55.8537559223297,0.428861556319229,
124.901076302982));
#153736=CARTESIAN_POINT('Ctrl Pts',(-55.8611641419962,0.271682767056356,
124.893851414749));
#153737=CARTESIAN_POINT('Ctrl Pts',(-55.8685769212983,0.114407236871135,
124.886622079718));
#153738=CARTESIAN_POINT('Ctrl Pts',(-55.8759897006004,-0.0430161825081487,
124.885681046457));
#153739=CARTESIAN_POINT('Ctrl Pts',(-55.8834024799025,-0.200049531943761,
124.890993493222));
#153740=CARTESIAN_POINT('Ctrl Pts',(-55.8908258509313,-0.35730725799318,
124.896313530661));
#153741=CARTESIAN_POINT('Ctrl Pts',(-55.8982492219599,-0.514173429648822,
124.90790486642));
#153742=CARTESIAN_POINT('Ctrl Pts',(-55.9056725929887,-0.670116333988602,
124.925680947655));
#153743=CARTESIAN_POINT('Ctrl Pts',(-55.9096086424294,-0.752801003666507,
124.935106252457));
#153744=CARTESIAN_POINT('Ctrl Pts',(-55.9135446918702,-0.835226286248772,
124.946269457947));
#153745=CARTESIAN_POINT('Ctrl Pts',(-55.9174807413109,-0.917314430879882,
124.959151913217));
#153746=CARTESIAN_POINT('Ctrl Pts',(-55.9249040077163,-1.07213010977379,
124.983447821808));
#153747=CARTESIAN_POINT('Ctrl Pts',(-55.9323272741218,-1.22621397221266,
125.013935368411));
#153748=CARTESIAN_POINT('Ctrl Pts',(-55.9397505405272,-1.37903158879716,
125.05056166039));
#153749=CARTESIAN_POINT('Ctrl Pts',(-55.9471650332482,-1.53166858765001,
125.087144663134));
#153750=CARTESIAN_POINT('Ctrl Pts',(-55.9545795259692,-1.68304196016181,
125.12985188301));
#153751=CARTESIAN_POINT('Ctrl Pts',(-55.9619940186902,-1.83262383696791,
125.178578855475));
#153752=CARTESIAN_POINT('Ctrl Pts',(-55.969401365044,-1.98206154112907,
125.227258863049));
#153753=CARTESIAN_POINT('Ctrl Pts',(-55.9768087113978,-2.12971083456876,
125.281946957596));
#153754=CARTESIAN_POINT('Ctrl Pts',(-55.9842160577516,-2.27505557225412,
125.342487980305));
#153755=CARTESIAN_POINT('Ctrl Pts',(-55.991617879427,-2.42029190635057,
125.402983849236));
#153756=CARTESIAN_POINT('Ctrl Pts',(-55.9990197011024,-2.56322676398866,
125.469323811439));
#153757=CARTESIAN_POINT('Ctrl Pts',(-56.0064215227778,-2.70336077219452,
125.541303416864));
#153758=CARTESIAN_POINT('Ctrl Pts',(-56.0138194370891,-2.84342080474805,
125.613245024815));
#153759=CARTESIAN_POINT('Ctrl Pts',(-56.0212173514004,-2.98068260125099,
125.690820176775));
#153760=CARTESIAN_POINT('Ctrl Pts',(-56.0286152657118,-3.11466843832551,
125.773777044878));
#153761=CARTESIAN_POINT('Ctrl Pts',(-56.036011950624,-3.24863200938505,
125.856720127054));
#153762=CARTESIAN_POINT('Ctrl Pts',(-56.0434086355363,-3.37932038442163,
125.945042954049));
#153763=CARTESIAN_POINT('Ctrl Pts',(-56.0508053204485,-3.50628195251088,
126.038448592361));
#153764=CARTESIAN_POINT('Ctrl Pts',(-56.0582016773839,-3.63323789099132,
126.131850088969));
#153765=CARTESIAN_POINT('Ctrl Pts',(-56.0655980343194,-3.75646705040901,
126.230333727552));
#153766=CARTESIAN_POINT('Ctrl Pts',(-56.0729943912549,-3.8755484682286,
126.333560394685));
#153767=CARTESIAN_POINT('Ctrl Pts',(-56.0803918805915,-3.99464811771743,
126.436802866085));
#153768=CARTESIAN_POINT('Ctrl Pts',(-56.087789369928,-4.10959847909074,
126.544789567404));
#153769=CARTESIAN_POINT('Ctrl Pts',(-56.0951868592646,-4.22001334313334,
126.657142520302));
#153770=CARTESIAN_POINT('Ctrl Pts',(-56.1025869417797,-4.33046691293567,
126.769534858354));
#153771=CARTESIAN_POINT('Ctrl Pts',(-56.1099870242948,-4.43638155841314,
126.886296229282));
#153772=CARTESIAN_POINT('Ctrl Pts',(-56.1173871068098,-4.53740956172568,
127.007013513118));
#153773=CARTESIAN_POINT('Ctrl Pts',(-56.1247953264763,-4.63854865571322,
127.127863538017));
#153774=CARTESIAN_POINT('Ctrl Pts',(-56.1322035461427,-4.7347901368442,
127.252677876477));
#153775=CARTESIAN_POINT('Ctrl Pts',(-56.1396117658091,-4.82582761483588,
127.381011614851));
#153776=CARTESIAN_POINT('Ctrl Pts',(-56.1470245451112,-4.91692112487597,
127.5094243405));
#153777=CARTESIAN_POINT('Ctrl Pts',(-56.1544373244133,-5.00280404626517,
127.641360470222));
#153778=CARTESIAN_POINT('Ctrl Pts',(-56.1618501037154,-5.08321489546729,
127.776348581758));
#153779=CARTESIAN_POINT('Ctrl Pts',(-56.1692734747441,-5.16374063946177,
127.911529570638));
#153780=CARTESIAN_POINT('Ctrl Pts',(-56.1766968457729,-5.23877851785293,
128.049770923644));
#153781=CARTESIAN_POINT('Ctrl Pts',(-56.1841202168016,-5.30811394617773,
128.19057851171));
#153782=CARTESIAN_POINT('Ctrl Pts',(-56.1880562662423,-5.34487725395585,
128.265238073533));
#153783=CARTESIAN_POINT('Ctrl Pts',(-56.1919923156831,-5.38003821160391,
128.340618783419));
#153784=CARTESIAN_POINT('Ctrl Pts',(-56.1959283651238,-5.41357048442335,
128.4166451461));
#153785=CARTESIAN_POINT('Ctrl Pts',(-56.2041038846963,-5.48321995323033,
128.57455856296));
#153786=CARTESIAN_POINT('Ctrl Pts',(-56.2122794042688,-5.54602121981847,
128.735669095438));
#153787=CARTESIAN_POINT('Ctrl Pts',(-56.2204549238413,-5.60169867752389,
128.899392773027));
#153788=CARTESIAN_POINT('Ctrl Pts',(-56.2285995869807,-5.65716599473232,
129.06249851696));
#153789=CARTESIAN_POINT('Ctrl Pts',(-56.2367442501201,-5.70556305390394,
129.228197500401));
#153790=CARTESIAN_POINT('Ctrl Pts',(-56.2448889132596,-5.74666302753057,
129.395888178889));
#153791=CARTESIAN_POINT('Ctrl Pts',(-56.2530141703147,-5.78766507328249,
129.563179305009));
#153792=CARTESIAN_POINT('Ctrl Pts',(-56.2611394273701,-5.82140464485385,
129.732452425879));
#153793=CARTESIAN_POINT('Ctrl Pts',(-56.2692646844253,-5.84770389665012,
129.903089459921));
#153794=CARTESIAN_POINT('Ctrl Pts',(-56.2773578624664,-5.87389931738443,
130.073052808468));
#153795=CARTESIAN_POINT('Ctrl Pts',(-56.2854510405073,-5.89271295735898,
130.244369089194));
#153796=CARTESIAN_POINT('Ctrl Pts',(-56.2935442185484,-5.90401770404672,
130.41641021764));
#153797=CARTESIAN_POINT('Ctrl Pts',(-56.2995710627509,-5.91243614568859,
130.544526153346));
#153798=CARTESIAN_POINT('Ctrl Pts',(-56.3055979069536,-5.91669151175424,
130.673043678158));
#153799=CARTESIAN_POINT('Ctrl Pts',(-56.3116247511561,-5.91674940103896,
130.801698324359));
#153800=CARTESIAN_POINT('',(-58.061624841459,-5.91543455321711,130.809483652149));
#153801=CARTESIAN_POINT('Ctrl Pts',(-56.311624807788,-5.9080768208085,130.80170343381));
#153802=CARTESIAN_POINT('Ctrl Pts',(-56.3658752015043,-5.90341159627506,
131.958087879031));
#153803=CARTESIAN_POINT('Ctrl Pts',(-56.5129414698247,-5.01586192239143,
135.099518527684));
#153804=CARTESIAN_POINT('Ctrl Pts',(-56.7528236127496,0.092937087818058,
137.802140496073));
#153805=CARTESIAN_POINT('Ctrl Pts',(-57.0312712365624,5.9376651652947,134.508640968079));
#153806=CARTESIAN_POINT('Ctrl Pts',(-57.3097188603752,6.3259690269338,127.811088762121));
#153807=CARTESIAN_POINT('Ctrl Pts',(-57.5881664841882,0.901016393590843,
123.864207161853));
#153808=CARTESIAN_POINT('Ctrl Pts',(-57.8388017999925,-4.72736082987953,
126.052192822845));
#153809=CARTESIAN_POINT('Ctrl Pts',(-57.9966212411924,-5.90153607060214,
129.426714923525));
#153810=CARTESIAN_POINT('Ctrl Pts',(-58.061624807788,-5.91288519561185,
130.809480727883));
#153811=CARTESIAN_POINT('',(-59.8116248077881,-5.9209921477642,130.804907070087));
#153812=CARTESIAN_POINT('Ctrl Pts',(-58.0616248588036,-5.91674778079818,
130.8094851585));
#153813=CARTESIAN_POINT('Ctrl Pts',(-58.0705428481065,-5.91658336994005,
130.999312421554));
#153814=CARTESIAN_POINT('Ctrl Pts',(-58.0794608374095,-5.90727989835948,
131.188740026179));
#153815=CARTESIAN_POINT('Ctrl Pts',(-58.0883788267124,-5.88897505791403,
131.376989057103));
#153816=CARTESIAN_POINT('Ctrl Pts',(-58.0978259775627,-5.86958407379152,
131.576408111347));
#153817=CARTESIAN_POINT('Ctrl Pts',(-58.1072731284129,-5.84009146292724,
131.774504383113));
#153818=CARTESIAN_POINT('Ctrl Pts',(-58.1167202792632,-5.80071843205518,
131.970377870661));
#153819=CARTESIAN_POINT('Ctrl Pts',(-58.1261674301134,-5.76134540118317,
132.166251358209));
#153820=CARTESIAN_POINT('Ctrl Pts',(-58.1356145809637,-5.71209208476659,
132.359902120265));
#153821=CARTESIAN_POINT('Ctrl Pts',(-58.1450617318139,-5.65323636242812,
132.550456031059));
#153822=CARTESIAN_POINT('Ctrl Pts',(-58.1524849982193,-5.60698943429867,
132.700187147544));
#153823=CARTESIAN_POINT('Ctrl Pts',(-58.1599082646247,-5.55471981911166,
132.848306067638));
#153824=CARTESIAN_POINT('Ctrl Pts',(-58.1673315310301,-5.49655650543425,
132.994291471513));
#153825=CARTESIAN_POINT('Ctrl Pts',(-58.174746023751,-5.43846193596345,
133.140104332764));
#153826=CARTESIAN_POINT('Ctrl Pts',(-58.182160516472,-5.3744876704066,133.28378835373));
#153827=CARTESIAN_POINT('Ctrl Pts',(-58.1895750091929,-5.30481279538097,
133.424836102752));
#153828=CARTESIAN_POINT('Ctrl Pts',(-58.1969823555467,-5.23520507562311,
133.565747904643));
#153829=CARTESIAN_POINT('Ctrl Pts',(-58.2043897019004,-5.15990784900905,
133.704028160654));
#153830=CARTESIAN_POINT('Ctrl Pts',(-58.2117970482541,-5.07914869102246,
133.839188312343));
#153831=CARTESIAN_POINT('Ctrl Pts',(-58.2191988699295,-4.99844976626266,
133.974247656492));
#153832=CARTESIAN_POINT('Ctrl Pts',(-58.2266006916049,-4.91229721209398,
134.106191210799));
#153833=CARTESIAN_POINT('Ctrl Pts',(-58.2340025132802,-4.82096498044718,
134.234554084384));
#153834=CARTESIAN_POINT('Ctrl Pts',(-58.2414004275915,-4.7296809623748,
134.362849196208));
#153835=CARTESIAN_POINT('Ctrl Pts',(-58.2487983419028,-4.63322292820549,
134.487567088367));
#153836=CARTESIAN_POINT('Ctrl Pts',(-58.2561962562141,-4.53190861318151,
134.60827109026));
#153837=CARTESIAN_POINT('Ctrl Pts',(-58.2635929411263,-4.43061113475851,
134.728955033338));
#153838=CARTESIAN_POINT('Ctrl Pts',(-58.2709896260384,-4.32445921694841,
134.845626124371));
#153839=CARTESIAN_POINT('Ctrl Pts',(-58.2783863109506,-4.21381148959082,
134.957880003905));
#153840=CARTESIAN_POINT('Ctrl Pts',(-58.285782667886,-4.10316866846942,
135.070128905984));
#153841=CARTESIAN_POINT('Ctrl Pts',(-58.2931790248215,-3.98803069622591,
135.177960720152));
#153842=CARTESIAN_POINT('Ctrl Pts',(-58.3005753817569,-3.86879355133091,
135.281007467573));
#153843=CARTESIAN_POINT('Ctrl Pts',(-58.3079728710934,-3.74953815092462,
135.384069991715));
#153844=CARTESIAN_POINT('Ctrl Pts',(-58.3153703604299,-3.62618261070159,
135.482345746291));
#153845=CARTESIAN_POINT('Ctrl Pts',(-58.3227678497665,-3.49915638833094,
135.575506720181));
#153846=CARTESIAN_POINT('Ctrl Pts',(-58.3301679322814,-3.3720856371153,
135.668700351507));
#153847=CARTESIAN_POINT('Ctrl Pts',(-58.3375680147963,-3.24134194267041,
135.75677541171));
#153848=CARTESIAN_POINT('Ctrl Pts',(-58.3449680973113,-3.10738402098666,
135.839447022844));
#153849=CARTESIAN_POINT('Ctrl Pts',(-58.3523763169777,-2.97327879879642,
135.922209539914));
#153850=CARTESIAN_POINT('Ctrl Pts',(-58.3597845366441,-2.83595260885898,
135.999556545884));
#153851=CARTESIAN_POINT('Ctrl Pts',(-58.3671927563105,-2.69588970540682,
136.071248622715));
#153852=CARTESIAN_POINT('Ctrl Pts',(-58.3746055356126,-2.55574059557467,
136.142984824823));
#153853=CARTESIAN_POINT('Ctrl Pts',(-58.3820183149145,-2.4128517538871,
136.209059006115));
#153854=CARTESIAN_POINT('Ctrl Pts',(-58.3894310942165,-2.2677272290903,
136.269279992721));
#153855=CARTESIAN_POINT('Ctrl Pts',(-58.3968544652452,-2.12239534356681,
136.329587025896));
#153856=CARTESIAN_POINT('Ctrl Pts',(-58.4042778362741,-1.97482174420468,
136.384024032109));
#153857=CARTESIAN_POINT('Ctrl Pts',(-58.4117012073028,-1.82552622603439,
136.432449508172));
#153858=CARTESIAN_POINT('Ctrl Pts',(-58.4156372567442,-1.74636615999106,
136.458125857538));
#153859=CARTESIAN_POINT('Ctrl Pts',(-58.4195733061856,-1.66672219362542,
136.482112999708));
#153860=CARTESIAN_POINT('Ctrl Pts',(-58.4235093556269,-1.58667281850235,
136.504395698995));
#153861=CARTESIAN_POINT('Ctrl Pts',(-58.4309326220324,-1.43570219529896,
136.546420174425));
#153862=CARTESIAN_POINT('Ctrl Pts',(-58.4383558884377,-1.28283254911229,
136.582506161133));
#153863=CARTESIAN_POINT('Ctrl Pts',(-58.4457791548431,-1.12857220254967,
136.612480394751));
#153864=CARTESIAN_POINT('Ctrl Pts',(-58.4531936475642,-0.974494178905941,
136.642419201315));
#153865=CARTESIAN_POINT('Ctrl Pts',(-58.4606081402852,-0.819029089530808,
136.666260562867));
#153866=CARTESIAN_POINT('Ctrl Pts',(-58.4680226330062,-0.662700651743137,
136.683880870842));
#153867=CARTESIAN_POINT('Ctrl Pts',(-58.47542997936,-0.506522889189468,
136.7014841957));
#153868=CARTESIAN_POINT('Ctrl Pts',(-58.4828373257138,-0.349483803284461,
136.712878362478));
#153869=CARTESIAN_POINT('Ctrl Pts',(-58.4902446720675,-0.192117442189441,
136.717990759104));
#153870=CARTESIAN_POINT('Ctrl Pts',(-58.4976464937429,-0.0348684508638419,
136.723099342711));
#153871=CARTESIAN_POINT('Ctrl Pts',(-58.5050483154183,0.122706958132031,
136.721935472925));
#153872=CARTESIAN_POINT('Ctrl Pts',(-58.5124501370937,0.280069581224368,
136.714478348388));
#153873=CARTESIAN_POINT('Ctrl Pts',(-58.519848051405,0.437349133812882,
136.707025160408));
#153874=CARTESIAN_POINT('Ctrl Pts',(-58.5272459657164,0.594415752268915,
136.693285351544));
#153875=CARTESIAN_POINT('Ctrl Pts',(-58.5346438800277,0.750730309587199,
136.673290210325));
#153876=CARTESIAN_POINT('Ctrl Pts',(-58.5420405649399,0.907018890261891,
136.653298391937));
#153877=CARTESIAN_POINT('Ctrl Pts',(-58.5494372498521,1.06255528792672,
136.627053351657));
#153878=CARTESIAN_POINT('Ctrl Pts',(-58.5568339347643,1.21680545533208,
136.594638248766));
#153879=CARTESIAN_POINT('Ctrl Pts',(-58.5642302916997,1.3710487831236,136.562224583194));
#153880=CARTESIAN_POINT('Ctrl Pts',(-58.5716266486352,1.5240056287379,136.523641475764));
#153881=CARTESIAN_POINT('Ctrl Pts',(-58.5790230055706,1.6751523651249,136.47902317283));
#153882=CARTESIAN_POINT('Ctrl Pts',(-58.5864204949072,1.82632224246288,
136.43439803872));
#153883=CARTESIAN_POINT('Ctrl Pts',(-58.5938179842437,1.97568110071901,
136.383735974986));
#153884=CARTESIAN_POINT('Ctrl Pts',(-58.6012154735802,2.12272084248869,
136.327220998507));
#153885=CARTESIAN_POINT('Ctrl Pts',(-58.6086155560952,2.26981212881212,
136.27068621079));
#153886=CARTESIAN_POINT('Ctrl Pts',(-58.6160156386103,2.41458233181698,
136.208294559191));
#153887=CARTESIAN_POINT('Ctrl Pts',(-58.6234157211252,2.55654382842102,
136.140277990976));
#153888=CARTESIAN_POINT('Ctrl Pts',(-58.6308239407917,2.69866142628457,
136.072186631553));
#153889=CARTESIAN_POINT('Ctrl Pts',(-58.6382321604582,2.8379638130283,135.99845816471));
#153890=CARTESIAN_POINT('Ctrl Pts',(-58.6456403801246,2.97398780823429,
135.919370595951));
#153891=CARTESIAN_POINT('Ctrl Pts',(-58.6530531594267,3.11009552393966,
135.840234350112));
#153892=CARTESIAN_POINT('Ctrl Pts',(-58.6604659387287,3.24292051316542,
135.755732629717));
#153893=CARTESIAN_POINT('Ctrl Pts',(-58.6678787180307,3.37202948525996,
135.666186171104));
#153894=CARTESIAN_POINT('Ctrl Pts',(-58.6753020890595,3.50132293430843,
135.576511764312));
#153895=CARTESIAN_POINT('Ctrl Pts',(-58.6827254600882,3.62688946451295,
135.481778447222));
#153896=CARTESIAN_POINT('Ctrl Pts',(-58.690148831117,3.74832906332195,135.382347052185));
#153897=CARTESIAN_POINT('Ctrl Pts',(-58.6940848805579,3.81271925251582,
135.329626140711));
#153898=CARTESIAN_POINT('Ctrl Pts',(-58.6980209299988,3.87594982380001,
135.275585052442));
#153899=CARTESIAN_POINT('Ctrl Pts',(-58.7019569794397,3.93796553235037,
135.220281589291));
#153900=CARTESIAN_POINT('Ctrl Pts',(-58.7093802458452,4.05492522322926,
135.115980983754));
#153901=CARTESIAN_POINT('Ctrl Pts',(-58.7168035122506,4.16791516366784,
135.006872778187));
#153902=CARTESIAN_POINT('Ctrl Pts',(-58.7242267786561,4.27651482066179,
134.893290985176));
#153903=CARTESIAN_POINT('Ctrl Pts',(-58.7316412713771,4.38498612187981,
134.779843436411));
#153904=CARTESIAN_POINT('Ctrl Pts',(-58.7390557640981,4.48907721282924,
134.661933091995));
#153905=CARTESIAN_POINT('Ctrl Pts',(-58.7464702568192,4.58840101612065,
134.539933756692));
#153906=CARTESIAN_POINT('Ctrl Pts',(-58.753877603173,4.68762908739097,134.418052008943));
#153907=CARTESIAN_POINT('Ctrl Pts',(-58.7612849495269,4.78209878442577,
134.292089403853));
#153908=CARTESIAN_POINT('Ctrl Pts',(-58.7686922958807,4.87146035055661,
134.16245600267));
#153909=CARTESIAN_POINT('Ctrl Pts',(-58.7760941175561,4.96075526746001,
134.032919286967));
#153910=CARTESIAN_POINT('Ctrl Pts',(-58.7834959392316,5.04494942840241,
133.899717532562));
#153911=CARTESIAN_POINT('Ctrl Pts',(-58.7908977609071,5.1237338799097,133.76329314305));
#153912=CARTESIAN_POINT('Ctrl Pts',(-58.7982956752184,5.2024767417183,133.62694077091));
#153913=CARTESIAN_POINT('Ctrl Pts',(-58.8056935895297,5.27581539523022,
133.48736947414));
#153914=CARTESIAN_POINT('Ctrl Pts',(-58.8130915038411,5.34348475305723,
133.345049747772));
#153915=CARTESIAN_POINT('Ctrl Pts',(-58.8204881887534,5.41114286546462,
133.20275367236));
#153916=CARTESIAN_POINT('Ctrl Pts',(-58.8278848736657,5.47313339190495,
133.057710410642));
#153917=CARTESIAN_POINT('Ctrl Pts',(-58.8352815585779,5.52923763105137,
132.910414221315));
#153918=CARTESIAN_POINT('Ctrl Pts',(-58.8426779155134,5.58533938247696,
132.763124563256));
#153919=CARTESIAN_POINT('Ctrl Pts',(-58.8500742724488,5.63555523269865,
132.613582525067));
#153920=CARTESIAN_POINT('Ctrl Pts',(-58.8574706293843,5.67971509376531,
132.462301212447));
#153921=CARTESIAN_POINT('Ctrl Pts',(-58.8648681187209,5.7238817158195,132.310996738272));
#153922=CARTESIAN_POINT('Ctrl Pts',(-58.8722656080576,5.76199039795617,
132.15795281782));
#153923=CARTESIAN_POINT('Ctrl Pts',(-58.8796630973942,5.79392131972813,
132.003696393444));
#153924=CARTESIAN_POINT('Ctrl Pts',(-58.8870631799092,5.82586343483522,
131.849385894717));
#153925=CARTESIAN_POINT('Ctrl Pts',(-58.8944632624243,5.85162340225436,
131.693862411133));
#153926=CARTESIAN_POINT('Ctrl Pts',(-58.9018633449393,5.87113279360231,
131.537661566964));
#153927=CARTESIAN_POINT('Ctrl Pts',(-58.9092715646058,5.89066363753166,
131.381288963908));
#153928=CARTESIAN_POINT('Ctrl Pts',(-58.9166797842723,5.90393013296248,
131.224237883445));
#153929=CARTESIAN_POINT('Ctrl Pts',(-58.9240880039388,5.91091581346791,
131.067048281142));
#153930=CARTESIAN_POINT('Ctrl Pts',(-58.9315007832409,5.91790579354315,
130.909761931261));
#153931=CARTESIAN_POINT('Ctrl Pts',(-58.938913562543,5.91860725406831,130.752337262083));
#153932=CARTESIAN_POINT('Ctrl Pts',(-58.9463263418451,5.91305583542779,
130.595312179128));
#153933=CARTESIAN_POINT('Ctrl Pts',(-58.9537497128739,5.90749648465999,
130.438062731372));
#153934=CARTESIAN_POINT('Ctrl Pts',(-58.9611730839027,5.89566643871305,
130.281214381404));
#153935=CARTESIAN_POINT('Ctrl Pts',(-58.9685964549315,5.87765305950754,
130.125298709813));
#153936=CARTESIAN_POINT('Ctrl Pts',(-58.972532504372,5.86810193362853,130.042628479597));
#153937=CARTESIAN_POINT('Ctrl Pts',(-58.9764685538124,5.85681330381691,
129.960220280966));
#153938=CARTESIAN_POINT('Ctrl Pts',(-58.9804046032529,5.84380593928373,
129.878151836301));
#153939=CARTESIAN_POINT('Ctrl Pts',(-58.9878278696583,5.81927445571807,
129.723373310919));
#153940=CARTESIAN_POINT('Ctrl Pts',(-58.9952511360636,5.78855245501014,
129.569336023763));
#153941=CARTESIAN_POINT('Ctrl Pts',(-59.002674402469,5.75169364304545,129.416574323121));
#153942=CARTESIAN_POINT('Ctrl Pts',(-59.01008889519,5.71487839513551,129.263993174122));
#153943=CARTESIAN_POINT('Ctrl Pts',(-59.0175033879111,5.67194086020873,
129.112684970017));
#153944=CARTESIAN_POINT('Ctrl Pts',(-59.0249178806321,5.62298630601622,
128.963177420583));
#153945=CARTESIAN_POINT('Ctrl Pts',(-59.0323252269858,5.57407893606622,
128.813813972153));
#153946=CARTESIAN_POINT('Ctrl Pts',(-59.0397325733396,5.51916620775687,
128.666248075659));
#153947=CARTESIAN_POINT('Ctrl Pts',(-59.0471399196933,5.45840406520437,
128.520995639412));
#153948=CARTESIAN_POINT('Ctrl Pts',(-59.0545417413687,5.3976872413502,128.375851537911));
#153949=CARTESIAN_POINT('Ctrl Pts',(-59.0619435630441,5.33112983344623,
128.233017803919));
#153950=CARTESIAN_POINT('Ctrl Pts',(-59.0693453847194,5.25893705126755,
128.092993498693));
#153951=CARTESIAN_POINT('Ctrl Pts',(-59.0767432990308,5.18678237909663,
127.953043111208));
#153952=CARTESIAN_POINT('Ctrl Pts',(-59.0841412133421,5.10899842787934,
127.815899529827));
#153953=CARTESIAN_POINT('Ctrl Pts',(-59.0915391276534,5.02583775220401,
127.682040094138));
#153954=CARTESIAN_POINT('Ctrl Pts',(-59.0989358125656,4.94269089632428,
127.548202903458));
#153955=CARTESIAN_POINT('Ctrl Pts',(-59.1063324974779,4.85416928614718,
127.417649092064));
#153956=CARTESIAN_POINT('Ctrl Pts',(-59.11372918239,4.7605705421038,127.290829818476));
#153957=CARTESIAN_POINT('Ctrl Pts',(-59.1211255393255,4.66697594832682,
127.164016168187));
#153958=CARTESIAN_POINT('Ctrl Pts',(-59.1285218962608,4.56830488998346,
127.040937026801));
#153959=CARTESIAN_POINT('Ctrl Pts',(-59.1359182531963,4.46489712073938,
126.922012840291));
#153960=CARTESIAN_POINT('Ctrl Pts',(-59.1433157425328,4.36147351950169,
126.803070446184));
#153961=CARTESIAN_POINT('Ctrl Pts',(-59.1507132318694,4.25331200834828,
126.688284555299));
#153962=CARTESIAN_POINT('Ctrl Pts',(-59.158110721206,4.14079115292679,126.578040801184));
#153963=CARTESIAN_POINT('Ctrl Pts',(-59.1655108037209,4.02823085349386,
126.467758401292));
#153964=CARTESIAN_POINT('Ctrl Pts',(-59.1729108862359,3.9113084337142,126.362021569393));
#153965=CARTESIAN_POINT('Ctrl Pts',(-59.1803109687509,3.79043754224487,
126.261177394226));
#153966=CARTESIAN_POINT('Ctrl Pts',(-59.1877191884174,3.66943374080454,
126.160222330521));
#153967=CARTESIAN_POINT('Ctrl Pts',(-59.1951274080838,3.54447308372678,
126.064170907012));
#153968=CARTESIAN_POINT('Ctrl Pts',(-59.2025356277503,3.41600095041762,
125.973328836544));
#153969=CARTESIAN_POINT('Ctrl Pts',(-59.2099484070524,3.28744974465408,
125.882430854297));
#153970=CARTESIAN_POINT('Ctrl Pts',(-59.2173611863543,3.15538306852536,
125.796748816688));
#153971=CARTESIAN_POINT('Ctrl Pts',(-59.2247739656563,3.02027274167973,
125.716543489527));
#153972=CARTESIAN_POINT('Ctrl Pts',(-59.232197336685,2.88496936286306,125.636223561233));
#153973=CARTESIAN_POINT('Ctrl Pts',(-59.2396207077139,2.74661397506129,
125.561396149541));
#153974=CARTESIAN_POINT('Ctrl Pts',(-59.2470440787426,2.60570103332997,
125.492275086684));
#153975=CARTESIAN_POINT('Ctrl Pts',(-59.2509801281836,2.53098561046079,
125.455625440619));
#153976=CARTESIAN_POINT('Ctrl Pts',(-59.2549161776246,2.45555147886789,
125.420579240293));
#153977=CARTESIAN_POINT('Ctrl Pts',(-59.2588522270655,2.37947417380949,
125.387162705483));
#153978=CARTESIAN_POINT('Ctrl Pts',(-59.266275493471,2.23599475076708,125.32414016373));
#153979=CARTESIAN_POINT('Ctrl Pts',(-59.2736987598764,2.08979282671053,
125.266726536739));
#153980=CARTESIAN_POINT('Ctrl Pts',(-59.2811220262819,1.94134699333004,
125.215165468532));
#153981=CARTESIAN_POINT('Ctrl Pts',(-59.2885365190029,1.79307661059673,
125.163665341225));
#153982=CARTESIAN_POINT('Ctrl Pts',(-59.2959510117239,1.64256794677638,
125.118004125186));
#153983=CARTESIAN_POINT('Ctrl Pts',(-59.3033655044449,1.49032187883998,
125.078378495698));
#153984=CARTESIAN_POINT('Ctrl Pts',(-59.3107728507987,1.33822255139582,
125.038791058884));
#153985=CARTESIAN_POINT('Ctrl Pts',(-59.3181801971524,1.18438951242256,
125.005227720868));
#153986=CARTESIAN_POINT('Ctrl Pts',(-59.3255875435062,1.02934110179654,
124.977836142491));
#153987=CARTESIAN_POINT('Ctrl Pts',(-59.3329893651816,0.874408332124798,
124.950464993786));
#153988=CARTESIAN_POINT('Ctrl Pts',(-59.3403911868572,0.718262361727727,
124.929256503929));
#153989=CARTESIAN_POINT('Ctrl Pts',(-59.3477930085326,0.561433985871367,
124.914307778923));
#153990=CARTESIAN_POINT('Ctrl Pts',(-59.3551909228439,0.404688398493871,
124.899366945233));
#153991=CARTESIAN_POINT('Ctrl Pts',(-59.3625888371553,0.247261493758251,
124.890679330693));
#153992=CARTESIAN_POINT('Ctrl Pts',(-59.3699867514666,0.0896913829007215,
124.888290467683));
#153993=CARTESIAN_POINT('Ctrl Pts',(-59.3773834363788,-0.0678525426627713,
124.885902001659));
#153994=CARTESIAN_POINT('Ctrl Pts',(-59.384780121291,-0.22553925422612,
124.889810215351));
#153995=CARTESIAN_POINT('Ctrl Pts',(-59.3921768062032,-0.382828308236872,
124.900008574461));
#153996=CARTESIAN_POINT('Ctrl Pts',(-59.3995731631387,-0.540110387886141,
124.910206481366));
#153997=CARTESIAN_POINT('Ctrl Pts',(-59.4069695200742,-0.696994472526925,
124.926693954966));
#153998=CARTESIAN_POINT('Ctrl Pts',(-59.4143658770096,-0.85294318389762,
124.949412412198));
#153999=CARTESIAN_POINT('Ctrl Pts',(-59.4217633663462,-1.00891577141414,
124.972134347684));
#154000=CARTESIAN_POINT('Ctrl Pts',(-59.4291608556827,-1.16395233109188,
125.001089112486));
#154001=CARTESIAN_POINT('Ctrl Pts',(-59.4365583450193,-1.3175237945246,
125.036166652956));
#154002=CARTESIAN_POINT('Ctrl Pts',(-59.4439584275343,-1.47114909219575,
125.071256489804));
#154003=CARTESIAN_POINT('Ctrl Pts',(-59.4513585100493,-1.62330790737527,
125.112473292572));
#154004=CARTESIAN_POINT('Ctrl Pts',(-59.4587585925643,-1.77348463727377,
125.159656656874));
#154005=CARTESIAN_POINT('Ctrl Pts',(-59.4661668122308,-1.92382650192533,
125.206891904135));
#154006=CARTESIAN_POINT('Ctrl Pts',(-59.4735750318972,-2.07218157232565,
125.260106703411));
#154007=CARTESIAN_POINT('Ctrl Pts',(-59.4809832515637,-2.21805190515195,
125.319091589656));
#154008=CARTESIAN_POINT('Ctrl Pts',(-59.4883960308658,-2.36401201873434,
125.378112780113));
#154009=CARTESIAN_POINT('Ctrl Pts',(-59.4958088101678,-2.50748400797178,
125.442910980836));
#154010=CARTESIAN_POINT('Ctrl Pts',(-59.5032215894699,-2.64799345315919,
125.513230186881));
#154011=CARTESIAN_POINT('Ctrl Pts',(-59.5106449604987,-2.78870366483113,
125.583649868304));
#154012=CARTESIAN_POINT('Ctrl Pts',(-59.5180683315274,-2.92644255213581,
125.65960613071));
#154013=CARTESIAN_POINT('Ctrl Pts',(-59.5254917025562,-3.06076294692327,
125.740798556601));
#154014=CARTESIAN_POINT('Ctrl Pts',(-59.5294277519969,-3.13198284321272,
125.783848728994));
#154015=CARTESIAN_POINT('Ctrl Pts',(-59.5333638014378,-3.20224219481042,
125.828370272979));
#154016=CARTESIAN_POINT('Ctrl Pts',(-59.5372998508785,-3.27147811362319,
125.874313811035));
#154017=CARTESIAN_POINT('Ctrl Pts',(-59.5447040751354,-3.40171994041827,
125.960739620477));
#154018=CARTESIAN_POINT('Ctrl Pts',(-59.5521082993922,-3.52873656741033,
126.052464121099));
#154019=CARTESIAN_POINT('Ctrl Pts',(-59.5595125236491,-3.65206569474598,
126.14921865155));
#154020=CARTESIAN_POINT('Ctrl Pts',(-59.5669079843502,-3.77524885112543,
126.245858664437));
#154021=CARTESIAN_POINT('Ctrl Pts',(-59.5743034450512,-3.89475290211312,
126.347516628378));
#154022=CARTESIAN_POINT('Ctrl Pts',(-59.5816989057523,-4.01014290459188,
126.453879673205));
#154023=CARTESIAN_POINT('Ctrl Pts',(-59.5890872484693,-4.12542184648628,
126.560140345714));
#154024=CARTESIAN_POINT('Ctrl Pts',(-59.5964755911865,-4.23659434794291,
126.671096831731));
#154025=CARTESIAN_POINT('Ctrl Pts',(-59.6038639339035,-4.3432571807991,
126.786395009956));
#154026=CARTESIAN_POINT('Ctrl Pts',(-59.6112467984276,-4.4498409269638,
126.901607698688));
#154027=CARTESIAN_POINT('Ctrl Pts',(-59.6186296629518,-4.55192140798027,
127.021155395861));
#154028=CARTESIAN_POINT('Ctrl Pts',(-59.626012527476,-4.64913114114335,
127.144646121195));
#154029=CARTESIAN_POINT('Ctrl Pts',(-59.633746372489,-4.7509622132949,127.274007580714));
#154030=CARTESIAN_POINT('Ctrl Pts',(-59.6414802175019,-4.8474477724383,
127.407695866079));
#154031=CARTESIAN_POINT('Ctrl Pts',(-59.6492140625149,-4.93821123908698,
127.545219577253));
#154032=CARTESIAN_POINT('Ctrl Pts',(-59.6565918955248,-5.02479659206562,
127.67641266093));
#154033=CARTESIAN_POINT('Ctrl Pts',(-59.6639697285347,-5.10617465032543,
127.811095611072));
#154034=CARTESIAN_POINT('Ctrl Pts',(-59.6713475615446,-5.18206199385268,
127.94881092366));
#154035=CARTESIAN_POINT('Ctrl Pts',(-59.6787252287696,-5.25794763213975,
128.086523141691));
#154036=CARTESIAN_POINT('Ctrl Pts',(-59.6861028959945,-5.32834261959897,
128.227267257946));
#154037=CARTESIAN_POINT('Ctrl Pts',(-59.6934805632195,-5.39300911312665,
128.370560447414));
#154038=CARTESIAN_POINT('Ctrl Pts',(-59.7008595412986,-5.45768709651109,
128.513879097025));
#154039=CARTESIAN_POINT('Ctrl Pts',(-59.7082385193777,-5.51663440523919,
128.659747379284));
#154040=CARTESIAN_POINT('Ctrl Pts',(-59.7156174974568,-5.56966110690731,
128.807661913028));
#154041=CARTESIAN_POINT('Ctrl Pts',(-59.7229992635616,-5.62270784384367,
128.955632333849));
#154042=CARTESIAN_POINT('Ctrl Pts',(-59.7303810296664,-5.66982939381967,
129.105650192144));
#154043=CARTESIAN_POINT('Ctrl Pts',(-59.7377627957712,-5.71088555804053,
129.257196532711));
#154044=CARTESIAN_POINT('Ctrl Pts',(-59.7451527055776,-5.7519870161851,
129.40891006202));
#154045=CARTESIAN_POINT('Ctrl Pts',(-59.7525426153839,-5.78700962983586,
129.562155078025));
#154046=CARTESIAN_POINT('Ctrl Pts',(-59.7599325251903,-5.81586409879498,
129.716401359667));
#154047=CARTESIAN_POINT('Ctrl Pts',(-59.7673272013841,-5.84473717847892,
129.870747127982));
#154048=CARTESIAN_POINT('Ctrl Pts',(-59.7747218775778,-5.8674341334322,
130.026095078201));
#154049=CARTESIAN_POINT('Ctrl Pts',(-59.7821165537716,-5.88391755623333,
130.181910013944));
#154050=CARTESIAN_POINT('Ctrl Pts',(-59.7895213737257,-5.90042359042213,
130.337938691211));
#154051=CARTESIAN_POINT('Ctrl Pts',(-59.7969261936799,-5.91069905083801,
130.494435259889));
#154052=CARTESIAN_POINT('Ctrl Pts',(-59.804331013634,-5.91475860492403,
130.650864011815));
#154053=CARTESIAN_POINT('Ctrl Pts',(-59.806762278352,-5.91609150034639,
130.7022251128));
#154054=CARTESIAN_POINT('Ctrl Pts',(-59.8091935430701,-5.91675471187478,
130.753578940631));
#154055=CARTESIAN_POINT('Ctrl Pts',(-59.8116248077881,-5.91674997480182,
130.804906678574));
#154056=CARTESIAN_POINT('',(-61.5616241089946,-5.91516794619516,130.798959479098));
#154057=CARTESIAN_POINT('Ctrl Pts',(-59.8116248077881,-5.92647066646659,
130.804907575703));
#154058=CARTESIAN_POINT('Ctrl Pts',(-59.8129990300892,-5.9265088843322,
130.833967190104));
#154059=CARTESIAN_POINT('Ctrl Pts',(-59.8143732523903,-5.92631371465216,
130.863026276885));
#154060=CARTESIAN_POINT('Ctrl Pts',(-59.9085633492957,-5.89683354231334,
132.854516748754));
#154061=CARTESIAN_POINT('Ctrl Pts',(-60.0941950985041,-3.69523994540662,
136.747656191254));
#154062=CARTESIAN_POINT('Ctrl Pts',(-60.3726427223173,3.00289543727563,
137.125767068913));
#154063=CARTESIAN_POINT('Ctrl Pts',(-60.6510903461299,6.94151661269781,
131.694814235658));
#154064=CARTESIAN_POINT('Ctrl Pts',(-60.929537969943,4.5012231329918,125.445578028453));
#154065=CARTESIAN_POINT('Ctrl Pts',(-61.2079855937559,-2.07547450896312,
124.12080122956));
#154066=CARTESIAN_POINT('Ctrl Pts',(-61.4186808805036,-5.60873709036134,
127.765787223005));
#154067=CARTESIAN_POINT('Ctrl Pts',(-61.5365602926472,-5.9192368584348,
130.266176064463));
#154068=CARTESIAN_POINT('Ctrl Pts',(-61.5616238301864,-5.91453770888721,
130.798954126379));
#154069=CARTESIAN_POINT('',(-63.3116254755953,-5.91161047281451,130.806144527447));
#154070=CARTESIAN_POINT('Ctrl Pts',(-61.561624807788,-5.91674754700121,
130.798972894932));
#154071=CARTESIAN_POINT('Ctrl Pts',(-61.5689558267893,-5.91688950142237,
130.95486593736));
#154072=CARTESIAN_POINT('Ctrl Pts',(-61.5762868457905,-5.91086609325577,
131.11089921841));
#154073=CARTESIAN_POINT('Ctrl Pts',(-61.5836178647918,-5.89867096461179,
131.26654176576));
#154074=CARTESIAN_POINT('Ctrl Pts',(-61.5911704888164,-5.88610719666045,
131.426889139317));
#154075=CARTESIAN_POINT('Ctrl Pts',(-61.598723112841,-5.86699266002491,
131.586821372375));
#154076=CARTESIAN_POINT('Ctrl Pts',(-61.6062757368655,-5.84137829381317,
131.745758615794));
#154077=CARTESIAN_POINT('Ctrl Pts',(-61.6136016021555,-5.8165329690963,
131.899923953704));
#154078=CARTESIAN_POINT('Ctrl Pts',(-61.6209274674455,-5.78557257107751,
132.053152789232));
#154079=CARTESIAN_POINT('Ctrl Pts',(-61.6282533327354,-5.74859609097896,
132.204922485275));
#154080=CARTESIAN_POINT('Ctrl Pts',(-61.6355790136,-5.71162054174657,132.356688360586));
#154081=CARTESIAN_POINT('Ctrl Pts',(-61.6429046944647,-5.66862930161556,
132.506994799048));
#154082=CARTESIAN_POINT('Ctrl Pts',(-61.6502303753293,-5.61977206211482,
132.655331317597));
#154083=CARTESIAN_POINT('Ctrl Pts',(-61.6575573859683,-5.57090595393626,
132.80369476253));
#154084=CARTESIAN_POINT('Ctrl Pts',(-61.6648843966073,-5.51617184659786,
132.950087213911));
#154085=CARTESIAN_POINT('Ctrl Pts',(-61.6722114072463,-5.45576860355499,
133.094015505745));
#154086=CARTESIAN_POINT('Ctrl Pts',(-61.6795412625481,-5.39534190935679,
133.237999676777));
#154087=CARTESIAN_POINT('Ctrl Pts',(-61.6868711178499,-5.32924184664861,
133.379517433259));
#154088=CARTESIAN_POINT('Ctrl Pts',(-61.6942009731517,-5.25771438357038,
133.518097897278));
#154089=CARTESIAN_POINT('Ctrl Pts',(-61.7015389587674,-5.18610758185615,
133.656832075471));
#154090=CARTESIAN_POINT('Ctrl Pts',(-61.7088769443831,-5.10906153733858,
133.792622118929));
#154091=CARTESIAN_POINT('Ctrl Pts',(-61.7162149299988,-5.0268671996667,
133.925023482955));
#154092=CARTESIAN_POINT('Ctrl Pts',(-61.7235578007166,-4.9446181429269,
134.057512990269));
#154093=CARTESIAN_POINT('Ctrl Pts',(-61.7309006714343,-4.8572141803491,
134.186609011208));
#154094=CARTESIAN_POINT('Ctrl Pts',(-61.7382435421521,-4.76498766214409,
134.311898663278));
#154095=CARTESIAN_POINT('Ctrl Pts',(-61.7455963441718,-4.67263640670414,
134.437357770783));
#154096=CARTESIAN_POINT('Ctrl Pts',(-61.7529491461915,-4.57544981514295,
134.558999939309));
#154097=CARTESIAN_POINT('Ctrl Pts',(-61.7603019482111,-4.47379861883439,
134.676447455515));
#154098=CARTESIAN_POINT('Ctrl Pts',(-61.7618282459346,-4.45269782092106,
134.70082726013));
#154099=CARTESIAN_POINT('Ctrl Pts',(-61.763354543658,-4.43140476358562,
134.725026452925));
#154100=CARTESIAN_POINT('Ctrl Pts',(-61.7648808413815,-4.40992294498366,
134.74904186981));
#154101=CARTESIAN_POINT('Ctrl Pts',(-61.772304107787,-4.3054444674859,134.865842697485));
#154102=CARTESIAN_POINT('Ctrl Pts',(-61.7797273741924,-4.19616443681054,
134.978666462967));
#154103=CARTESIAN_POINT('Ctrl Pts',(-61.7871506405979,-4.08241750513419,
135.08709314205));
#154104=CARTESIAN_POINT('Ctrl Pts',(-61.7945651333189,-3.96880501288466,
135.195391669803));
#154105=CARTESIAN_POINT('Ctrl Pts',(-61.80197962604,-3.85073639608633,135.299303200744));
#154106=CARTESIAN_POINT('Ctrl Pts',(-61.809394118761,-3.72858604813662,
135.3984412268));
#154107=CARTESIAN_POINT('Ctrl Pts',(-61.8168014651148,-3.60655343329133,
135.497483699894));
#154108=CARTESIAN_POINT('Ctrl Pts',(-61.8242088114686,-3.48044720726796,
135.591761593892));
#154109=CARTESIAN_POINT('Ctrl Pts',(-61.8316161578223,-3.35067796310653,
135.680925776574));
#154110=CARTESIAN_POINT('Ctrl Pts',(-61.8390179794977,-3.22100550574349,
135.770023457245));
#154111=CARTESIAN_POINT('Ctrl Pts',(-61.8464198011732,-3.08767577640384,
135.854014810297));
#154112=CARTESIAN_POINT('Ctrl Pts',(-61.8538216228486,-2.95113164834545,
135.932591555875));
#154113=CARTESIAN_POINT('Ctrl Pts',(-61.8612195371599,-2.81465960086883,
136.011126821402));
#154114=CARTESIAN_POINT('Ctrl Pts',(-61.8686174514713,-2.67497685677345,
136.084252986235));
#154115=CARTESIAN_POINT('Ctrl Pts',(-61.8760153657827,-2.53255431396588,
136.151705679306));
#154116=CARTESIAN_POINT('Ctrl Pts',(-61.8834120506949,-2.39015543920132,
136.219147162963));
#154117=CARTESIAN_POINT('Ctrl Pts',(-61.8908087356072,-2.24501800641278,
136.280916886466));
#154118=CARTESIAN_POINT('Ctrl Pts',(-61.8982054205194,-2.09763660655163,
136.336796900918));
#154119=CARTESIAN_POINT('Ctrl Pts',(-61.9056017774548,-1.95026174173641,
136.392674437593));
#154120=CARTESIAN_POINT('Ctrl Pts',(-61.9129981343903,-1.80064345673848,
136.44266265214));
#154121=CARTESIAN_POINT('Ctrl Pts',(-61.9203944913257,-1.64929511550924,
136.486592237665));
#154122=CARTESIAN_POINT('Ctrl Pts',(-61.9277919806623,-1.4979236024628,
136.530528548922));
#154123=CARTESIAN_POINT('Ctrl Pts',(-61.9351894699989,-1.34482186430642,
136.568404280136));
#154124=CARTESIAN_POINT('Ctrl Pts',(-61.9425869593355,-1.19051702513014,
136.600100412914));
#154125=CARTESIAN_POINT('Ctrl Pts',(-61.9499870418505,-1.03615809463147,
136.631807656722));
#154126=CARTESIAN_POINT('Ctrl Pts',(-61.9573871243655,-0.880595588856351,
136.657330914044));
#154127=CARTESIAN_POINT('Ctrl Pts',(-61.9647872068805,-0.724365235592859,
136.676602571706));
#154128=CARTESIAN_POINT('Ctrl Pts',(-61.972195426547,-0.567963090995085,
136.695895420537));
#154129=CARTESIAN_POINT('Ctrl Pts',(-61.9796036462135,-0.410892003047028,
136.708922895596));
#154130=CARTESIAN_POINT('Ctrl Pts',(-61.98701186588,-0.253691951750863,
136.715669352196));
#154131=CARTESIAN_POINT('Ctrl Pts',(-61.9944246451821,-0.0963951464457003,
136.722419961128));
#154132=CARTESIAN_POINT('Ctrl Pts',(-62.0018374244841,0.0610304079409894,
136.722881847293));
#154133=CARTESIAN_POINT('Ctrl Pts',(-62.0092502037862,0.218046860748704,
136.717091469636));
#154134=CARTESIAN_POINT('Ctrl Pts',(-62.0166735748149,0.375287666027083,
136.711292818415));
#154135=CARTESIAN_POINT('Ctrl Pts',(-62.0240969458437,0.532117831050493,
136.699224089679));
#154136=CARTESIAN_POINT('Ctrl Pts',(-62.0315203168725,0.688005908796778,
136.680973454223));
#154137=CARTESIAN_POINT('Ctrl Pts',(-62.0354563663132,0.77066150809838,
136.671296529386));
#154138=CARTESIAN_POINT('Ctrl Pts',(-62.0393924157538,0.853052431933938,
136.659882501396));
#154139=CARTESIAN_POINT('Ctrl Pts',(-62.0433284651945,0.93510098657501,
136.646750257722));
#154140=CARTESIAN_POINT('Ctrl Pts',(-62.0507517316,1.08984199998493,136.621983255996));
#154141=CARTESIAN_POINT('Ctrl Pts',(-62.0581749980054,1.24383235511324,
136.591026872334));
#154142=CARTESIAN_POINT('Ctrl Pts',(-62.0655982644109,1.39653778602307,
136.553935625748));
#154143=CARTESIAN_POINT('Ctrl Pts',(-62.0730127571319,1.54906273179517,
136.516888217935));
#154144=CARTESIAN_POINT('Ctrl Pts',(-62.0804272498529,1.70030541706897,
136.473720467399));
#154145=CARTESIAN_POINT('Ctrl Pts',(-62.0878417425739,1.84973829287897,
136.424538444856));
#154146=CARTESIAN_POINT('Ctrl Pts',(-62.0952490889277,1.99902713965721,
136.375403825797));
#154147=CARTESIAN_POINT('Ctrl Pts',(-62.1026564352815,2.14650929744772,
136.320266590901));
#154148=CARTESIAN_POINT('Ctrl Pts',(-62.1100637816352,2.29166909585843,
136.259283469228));
#154149=CARTESIAN_POINT('Ctrl Pts',(-62.1174656033106,2.43672062861471,
136.198345831068));
#154150=CARTESIAN_POINT('Ctrl Pts',(-62.1248674249859,2.5794529081633,136.131571131608));
#154151=CARTESIAN_POINT('Ctrl Pts',(-62.1322692466613,2.71936718611896,
136.059165339871));
#154152=CARTESIAN_POINT('Ctrl Pts',(-62.1396671609727,2.85920760441578,
135.986797770588));
#154153=CARTESIAN_POINT('Ctrl Pts',(-62.147065075284,2.99623265305317,135.908805200259));
#154154=CARTESIAN_POINT('Ctrl Pts',(-62.1544629895953,3.12996537734346,
135.825440909608));
#154155=CARTESIAN_POINT('Ctrl Pts',(-62.1618596745075,3.2636758776817,135.742090472589));
#154156=CARTESIAN_POINT('Ctrl Pts',(-62.1692563594197,3.39409482307481,
135.653370284242));
#154157=CARTESIAN_POINT('Ctrl Pts',(-62.1766530443319,3.52077150845368,
135.559578651238));
#154158=CARTESIAN_POINT('Ctrl Pts',(-62.1840494012674,3.64744257685557,
135.465791177054));
#154159=CARTESIAN_POINT('Ctrl Pts',(-62.1914457582028,3.77037141516492,
135.366932927468));
#154160=CARTESIAN_POINT('Ctrl Pts',(-62.1988421151383,3.88913809494087,
135.263344295601));
#154161=CARTESIAN_POINT('Ctrl Pts',(-62.2062396044749,4.00792295819904,
135.159739804049));
#154162=CARTESIAN_POINT('Ctrl Pts',(-62.2136370938114,4.12254411275699,
135.051403733558));
#154163=CARTESIAN_POINT('Ctrl Pts',(-62.221034583148,4.23261650162447,134.938715236207));
#154164=CARTESIAN_POINT('Ctrl Pts',(-62.228434665663,4.34272747619692,134.825987236077));
#154165=CARTESIAN_POINT('Ctrl Pts',(-62.235834748178,4.44828624963538,134.708904038233));
#154166=CARTESIAN_POINT('Ctrl Pts',(-62.243234830693,4.54894636310545,134.587879819062));
#154167=CARTESIAN_POINT('Ctrl Pts',(-62.2506430503594,4.6497171627184,134.466722521321));
#154168=CARTESIAN_POINT('Ctrl Pts',(-62.258051270026,4.7455783061534,134.341615835029));
#154169=CARTESIAN_POINT('Ctrl Pts',(-62.2654594896924,4.836224758711,134.213005604321));
#154170=CARTESIAN_POINT('Ctrl Pts',(-62.2728722689945,4.92692700264789,
134.084316216162));
#154171=CARTESIAN_POINT('Ctrl Pts',(-62.2802850482965,5.01240795803893,
133.952119299488));
#154172=CARTESIAN_POINT('Ctrl Pts',(-62.2876978275986,5.09240757740633,
133.816887070242));
#154173=CARTESIAN_POINT('Ctrl Pts',(-62.2951211986274,5.17252150398149,
133.681461614846));
#154174=CARTESIAN_POINT('Ctrl Pts',(-62.3025445696562,5.24713827567704,
133.542992512674));
#154175=CARTESIAN_POINT('Ctrl Pts',(-62.3099679406849,5.31604481298278,
133.401974543626));
#154176=CARTESIAN_POINT('Ctrl Pts',(-62.3139039901258,5.3525807124521,133.327203432756));
#154177=CARTESIAN_POINT('Ctrl Pts',(-62.3178400395665,5.38751207428662,
133.251716054167));
#154178=CARTESIAN_POINT('Ctrl Pts',(-62.3217760890074,5.42081279369141,
133.17558798293));
#154179=CARTESIAN_POINT('Ctrl Pts',(-62.3291993554128,5.48361691120855,
133.032012816455));
#154180=CARTESIAN_POINT('Ctrl Pts',(-62.3366226218183,5.54080797727401,
132.885723687931));
#154181=CARTESIAN_POINT('Ctrl Pts',(-62.3440458882237,5.59214307648628,
132.73719955928));
#154182=CARTESIAN_POINT('Ctrl Pts',(-62.3514603809447,5.64341750187446,
132.588850973815));
#154183=CARTESIAN_POINT('Ctrl Pts',(-62.3588748736656,5.6888496164733,132.438272995684));
#154184=CARTESIAN_POINT('Ctrl Pts',(-62.3662893663866,5.72824350747633,
132.285966800583));
#154185=CARTESIAN_POINT('Ctrl Pts',(-62.3736967127404,5.76759942916395,
132.133807403929));
#154186=CARTESIAN_POINT('Ctrl Pts',(-62.3811040590942,5.80092862061613,
131.979923465405));
#154187=CARTESIAN_POINT('Ctrl Pts',(-62.388511405448,5.82808420998719,131.824833549004));
#154188=CARTESIAN_POINT('Ctrl Pts',(-62.3959132271233,5.85521954569522,
131.669859304514));
#154189=CARTESIAN_POINT('Ctrl Pts',(-62.4033150487987,5.87619038340733,
131.51368123922));
#154190=CARTESIAN_POINT('Ctrl Pts',(-62.4107168704741,5.89090042501172,
131.356830295555));
#154191=CARTESIAN_POINT('Ctrl Pts',(-62.4181147847854,5.90560270129963,
131.200062152281));
#154192=CARTESIAN_POINT('Ctrl Pts',(-62.4255126990967,5.91405072882852,
131.042622208774));
#154193=CARTESIAN_POINT('Ctrl Pts',(-62.432910613408,5.91619979418705,130.885048644938));
#154194=CARTESIAN_POINT('Ctrl Pts',(-62.4403072983202,5.91834850240991,
130.727501266969));
#154195=CARTESIAN_POINT('Ctrl Pts',(-62.4477039832325,5.91420032091174,
130.569820685641));
#154196=CARTESIAN_POINT('Ctrl Pts',(-62.4551006681447,5.90376260644601,
130.412547333935));
#154197=CARTESIAN_POINT('Ctrl Pts',(-62.4624970250802,5.89332535479948,
130.255280955894));
#154198=CARTESIAN_POINT('Ctrl Pts',(-62.4698933820155,5.87659914942211,
130.098422144051));
#154199=CARTESIAN_POINT('Ctrl Pts',(-62.477289738951,5.85364339110611,129.942508186891));
#154200=CARTESIAN_POINT('Ctrl Pts',(-62.4846872282875,5.83068411820494,
129.786570358907));
#154201=CARTESIAN_POINT('Ctrl Pts',(-62.4920847176241,5.80149344768047,
129.631578042983));
#154202=CARTESIAN_POINT('Ctrl Pts',(-62.4994822069606,5.76618223820521,
129.478060139429));
#154203=CARTESIAN_POINT('Ctrl Pts',(-62.5068822894756,5.73085865044005,
129.324488420411));
#154204=CARTESIAN_POINT('Ctrl Pts',(-62.5142823719906,5.68941033558519,
129.172392506387));
#154205=CARTESIAN_POINT('Ctrl Pts',(-62.5216824545057,5.64199848250326,
129.022287755439));
#154206=CARTESIAN_POINT('Ctrl Pts',(-62.5290906741721,5.59453449521489,
128.872017948886));
#154207=CARTESIAN_POINT('Ctrl Pts',(-62.5364988938385,5.54109398639783,
128.723744034144));
#154208=CARTESIAN_POINT('Ctrl Pts',(-62.543907113505,5.48188717864237,128.577963635189));
#154209=CARTESIAN_POINT('Ctrl Pts',(-62.551319892807,5.42264393008474,128.432093510831));
#154210=CARTESIAN_POINT('Ctrl Pts',(-62.5587326721091,5.35762746445342,
128.288720299563));
#154211=CARTESIAN_POINT('Ctrl Pts',(-62.5661454514112,5.28709450838142,
128.148318030945));
#154212=CARTESIAN_POINT('Ctrl Pts',(-62.5735688224399,5.21646077151412,
128.007715148981));
#154213=CARTESIAN_POINT('Ctrl Pts',(-62.5809921934686,5.14029498192602,
127.870092013678));
#154214=CARTESIAN_POINT('Ctrl Pts',(-62.5884155644974,5.05889823727925,
127.735895335482));
#154215=CARTESIAN_POINT('Ctrl Pts',(-62.5923516139384,5.01573973017724,
127.664741036694));
#154216=CARTESIAN_POINT('Ctrl Pts',(-62.5962876633793,4.97111131497194,
127.594549520663));
#154217=CARTESIAN_POINT('Ctrl Pts',(-62.6002237128203,4.92506246483318,
127.525383600265));
#154218=CARTESIAN_POINT('Ctrl Pts',(-62.6076469792258,4.83821577061095,
127.394938832994));
#154219=CARTESIAN_POINT('Ctrl Pts',(-62.6150702456312,4.74605175183823,
127.2677495221));
#154220=CARTESIAN_POINT('Ctrl Pts',(-62.6224935120366,4.64884207103577,
127.144278929807));
#154221=CARTESIAN_POINT('Ctrl Pts',(-62.6299080047576,4.55174728400325,
127.020954269501));
#154222=CARTESIAN_POINT('Ctrl Pts',(-62.6373224974786,4.449618934093,126.901339869533));
#154223=CARTESIAN_POINT('Ctrl Pts',(-62.6447369901996,4.34277277895584,
126.785871454602));
#154224=CARTESIAN_POINT('Ctrl Pts',(-62.6521443365534,4.23602960616584,
126.670514332476));
#154225=CARTESIAN_POINT('Ctrl Pts',(-62.6595516829072,4.12457793255688,
126.55929551218));
#154226=CARTESIAN_POINT('Ctrl Pts',(-62.666959029261,4.00877465288077,126.452618857659));
#154227=CARTESIAN_POINT('Ctrl Pts',(-62.6743608509365,3.89305774365899,
126.346021766611));
#154228=CARTESIAN_POINT('Ctrl Pts',(-62.6817626726119,3.7729959641588,126.243960347766));
#154229=CARTESIAN_POINT('Ctrl Pts',(-62.6891644942873,3.64898395980213,
126.146802606805));
#154230=CARTESIAN_POINT('Ctrl Pts',(-62.6965624085986,3.5250374204192,126.04969615466));
#154231=CARTESIAN_POINT('Ctrl Pts',(-62.7039603229099,3.39714510225023,
125.95748845469));
#154232=CARTESIAN_POINT('Ctrl Pts',(-62.7113582372212,3.26573562260086,
125.870508024939));
#154233=CARTESIAN_POINT('Ctrl Pts',(-62.7187549221334,3.13434798082131,
125.783542049755));
#154234=CARTESIAN_POINT('Ctrl Pts',(-62.7261516070456,2.99944464857826,
125.701801826562));
#154235=CARTESIAN_POINT('Ctrl Pts',(-62.7335482919578,2.86148428395073,
125.625573283141));
#154236=CARTESIAN_POINT('Ctrl Pts',(-62.7409446488932,2.72353003663054,
125.549348119774));
#154237=CARTESIAN_POINT('Ctrl Pts',(-62.7483410058287,2.58251935318737,
125.478634330778));
#154238=CARTESIAN_POINT('Ctrl Pts',(-62.7557373627642,2.43893637722032,
125.413672358135));
#154239=CARTESIAN_POINT('Ctrl Pts',(-62.7631348521008,2.2953314183329,125.348700439648));
#154240=CARTESIAN_POINT('Ctrl Pts',(-62.7705323414373,2.14915372289414,
125.289482244828));
#154241=CARTESIAN_POINT('Ctrl Pts',(-62.7779298307739,2.00090819153502,
125.236210388671));
#154242=CARTESIAN_POINT('Ctrl Pts',(-62.7853299132889,1.85261069293574,
125.182919858147));
#154243=CARTESIAN_POINT('Ctrl Pts',(-62.7927299958039,1.70224426627697,
125.135579942633));
#154244=CARTESIAN_POINT('Ctrl Pts',(-62.8001300783188,1.55032962342813,
125.094333593005));
#154245=CARTESIAN_POINT('Ctrl Pts',(-62.8075382979853,1.3982479348112,125.053041888775));
#154246=CARTESIAN_POINT('Ctrl Pts',(-62.8149465176518,1.24461499063038,
125.017857229647));
#154247=CARTESIAN_POINT('Ctrl Pts',(-62.8223547373183,1.08996308647519,
124.988871727316));
#154248=CARTESIAN_POINT('Ctrl Pts',(-62.8297675166204,0.935215996652834,
124.959868384892));
#154249=CARTESIAN_POINT('Ctrl Pts',(-62.8371802959225,0.779449065682284,
124.937071856014));
#154250=CARTESIAN_POINT('Ctrl Pts',(-62.8445930752246,0.623199875073401,
124.920522373851));
#154251=CARTESIAN_POINT('Ctrl Pts',(-62.8520164462534,0.466727428294285,
124.903949245011));
#154252=CARTESIAN_POINT('Ctrl Pts',(-62.8594398172821,0.309771717147762,
124.893641014655));
#154253=CARTESIAN_POINT('Ctrl Pts',(-62.8668631883109,0.152871322426201,
124.889585818702));
#154254=CARTESIAN_POINT('Ctrl Pts',(-62.8707992377517,0.0696789683721043,
124.887435656504));
#154255=CARTESIAN_POINT('Ctrl Pts',(-62.8747352871924,-0.0134978905157239,
124.887042577221));
#154256=CARTESIAN_POINT('Ctrl Pts',(-62.8786713366332,-0.0965796665288729,
124.888398909567));
#154257=CARTESIAN_POINT('Ctrl Pts',(-62.8860946030386,-0.253269303196848,
124.890956910042));
#154258=CARTESIAN_POINT('Ctrl Pts',(-62.8935178694441,-0.410094176017949,
124.899748179946));
#154259=CARTESIAN_POINT('Ctrl Pts',(-62.9009411358495,-0.566517689134258,
124.914794566455));
#154260=CARTESIAN_POINT('Ctrl Pts',(-62.9083556285705,-0.72275632264845,
124.929823169385));
#154261=CARTESIAN_POINT('Ctrl Pts',(-62.9157701212915,-0.878594172747348,
124.951092137663));
#154262=CARTESIAN_POINT('Ctrl Pts',(-62.9231846140125,-1.0334939771783,
124.978571335277));
#154263=CARTESIAN_POINT('Ctrl Pts',(-62.9305919603663,-1.18824448334631,
125.006024047406));
#154264=CARTESIAN_POINT('Ctrl Pts',(-62.93799930672,-1.34205837868717,125.039675007847));
#154265=CARTESIAN_POINT('Ctrl Pts',(-62.9454066530738,-1.49440297069326,
125.079442249267));
#154266=CARTESIAN_POINT('Ctrl Pts',(-62.9528084747492,-1.64663393835414,
125.119179830778));
#154267=CARTESIAN_POINT('Ctrl Pts',(-62.9602102964246,-1.79739742504874,
125.165024516323));
#154268=CARTESIAN_POINT('Ctrl Pts',(-62.9676121181,-1.94617050168461,125.216843195591));
#154269=CARTESIAN_POINT('Ctrl Pts',(-62.9750100324113,-2.09486504217244,
125.268634520182));
#154270=CARTESIAN_POINT('Ctrl Pts',(-62.9824079467227,-2.24157091353098,
125.326393435425));
#154271=CARTESIAN_POINT('Ctrl Pts',(-62.9898058610341,-2.38578004610241,
125.389936905469));
#154272=CARTESIAN_POINT('Ctrl Pts',(-62.9972025459463,-2.5299652137316,
125.453469815741));
#154273=CARTESIAN_POINT('Ctrl Pts',(-63.0045992308585,-2.67165412478181,
125.522785222565));
#154274=CARTESIAN_POINT('Ctrl Pts',(-63.0119959157707,-2.81035830421638,
125.597651794862));
#154275=CARTESIAN_POINT('Ctrl Pts',(-63.0193922727061,-2.94905633336247,
125.672515047497));
#154276=CARTESIAN_POINT('Ctrl Pts',(-63.0267886296416,-3.08476956554182,
125.752928798875));
#154277=CARTESIAN_POINT('Ctrl Pts',(-63.034184986577,-3.21703401866431,
125.838615690039));
#154278=CARTESIAN_POINT('Ctrl Pts',(-63.0415824759136,-3.34931872181129,
125.924315700085));
#154279=CARTESIAN_POINT('Ctrl Pts',(-63.0489799652501,-3.47815328123212,
126.015290254439));
#154280=CARTESIAN_POINT('Ctrl Pts',(-63.0563774545867,-3.60310273335147,
126.111218679012));
#154281=CARTESIAN_POINT('Ctrl Pts',(-63.0637775371017,-3.72809598630953,
126.207180731147));
#154282=CARTESIAN_POINT('Ctrl Pts',(-63.0711776196167,-3.8492011244829,
126.308099883817));
#154283=CARTESIAN_POINT('Ctrl Pts',(-63.0785777021317,-3.96601642176519,
126.413615315822));
#154284=CARTESIAN_POINT('Ctrl Pts',(-63.0859859217982,-4.08296016947491,
126.51924677289));
#154285=CARTESIAN_POINT('Ctrl Pts',(-63.0933941414647,-4.19560437870349,
126.629484352249));
#154286=CARTESIAN_POINT('Ctrl Pts',(-63.1008023611312,-4.30358383450491,
126.743930007164));
#154287=CARTESIAN_POINT('Ctrl Pts',(-63.1082151404333,-4.41162974985904,
126.85844610147));
#154288=CARTESIAN_POINT('Ctrl Pts',(-63.1156279197354,-4.5150049462427,
126.977175151348));
#154289=CARTESIAN_POINT('Ctrl Pts',(-63.1230406990374,-4.6133849984144,
127.09968662126));
#154290=CARTESIAN_POINT('Ctrl Pts',(-63.1304640700662,-4.71190562061876,
127.222373141306));
#154291=CARTESIAN_POINT('Ctrl Pts',(-63.1378874410948,-4.80541662249223,
127.348852576011));
#154292=CARTESIAN_POINT('Ctrl Pts',(-63.1453108121236,-4.89363686954924,
127.478665389273));
#154293=CARTESIAN_POINT('Ctrl Pts',(-63.1492468615643,-4.94041336135445,
127.547495257681));
#154294=CARTESIAN_POINT('Ctrl Pts',(-63.1531829110052,-4.9857031940248,
127.6172618358));
#154295=CARTESIAN_POINT('Ctrl Pts',(-63.157118960446,-5.02946980252924,
127.687894017721));
#154296=CARTESIAN_POINT('Ctrl Pts',(-63.1647574958261,-5.11440592758521,
127.8249670979));
#154297=CARTESIAN_POINT('Ctrl Pts',(-63.1723960312061,-5.19384721590906,
127.965696268982));
#154298=CARTESIAN_POINT('Ctrl Pts',(-63.1800345665862,-5.26747373740206,
128.10961554831));
#154299=CARTESIAN_POINT('Ctrl Pts',(-63.1876624252813,-5.34099734817427,
128.253333665931));
#154300=CARTESIAN_POINT('Ctrl Pts',(-63.1952902839764,-5.40872222743115,
128.400232705789));
#154301=CARTESIAN_POINT('Ctrl Pts',(-63.2029181426715,-5.47037202551696,
128.549818432345));
#154302=CARTESIAN_POINT('Ctrl Pts',(-63.2105364798587,-5.53194486897401,
128.699217437867));
#154303=CARTESIAN_POINT('Ctrl Pts',(-63.2181548170458,-5.58745760920087,
128.851296132596));
#154304=CARTESIAN_POINT('Ctrl Pts',(-63.2257731542331,-5.63667999997509,
129.005536240263));
#154305=CARTESIAN_POINT('Ctrl Pts',(-63.2333805424304,-5.6858316488739,
129.159554675753));
#154306=CARTESIAN_POINT('Ctrl Pts',(-63.2409879306277,-5.7287108711197,
129.315728003917));
#154307=CARTESIAN_POINT('Ctrl Pts',(-63.248595318825,-5.76513580658427,
129.473518893641));
#154308=CARTESIAN_POINT('Ctrl Pts',(-63.2561962949227,-5.80153004027449,
129.631176784905));
#154309=CARTESIAN_POINT('Ctrl Pts',(-63.2637972710204,-5.83148074705281,
129.790449188093));
#154310=CARTESIAN_POINT('Ctrl Pts',(-63.2713982471181,-5.85485583816483,
129.950783628181));
#154311=CARTESIAN_POINT('Ctrl Pts',(-63.2789925608585,-5.87821044069677,
130.110977532987));
#154312=CARTESIAN_POINT('Ctrl Pts',(-63.286586874599,-5.8950008692544,130.272231279304));
#154313=CARTESIAN_POINT('Ctrl Pts',(-63.2941811883394,-5.90514610021885,
130.433982300746));
#154314=CARTESIAN_POINT('Ctrl Pts',(-63.2999957281556,-5.91291373418863,
130.55782597993));
#154315=CARTESIAN_POINT('Ctrl Pts',(-63.3058102679718,-5.91678690610155,
130.681960891403));
#154316=CARTESIAN_POINT('Ctrl Pts',(-63.311624807788,-5.91674973488962,
130.806131827204));
#154317=CARTESIAN_POINT('',(-65.0616248077881,-5.92104421557129,130.809133668594));
#154318=CARTESIAN_POINT('Ctrl Pts',(-63.3116260199717,-5.90742110137121,
130.806154880301));
#154319=CARTESIAN_POINT('Ctrl Pts',(-63.3529395414009,-5.90976699514064,
131.687025087133));
#154320=CARTESIAN_POINT('Ctrl Pts',(-63.4870689374345,-5.31119943819695,
134.543840127222));
#154321=CARTESIAN_POINT('Ctrl Pts',(-63.7140142080715,-0.879888780334608,
137.747224310923));
#154322=CARTESIAN_POINT('Ctrl Pts',(-63.9924618318848,5.36562647909369,
135.297423383343));
#154323=CARTESIAN_POINT('Ctrl Pts',(-64.2709094556975,6.68039312965957,
128.718717272324));
#154324=CARTESIAN_POINT('Ctrl Pts',(-64.5493570795105,1.85620484941623,
124.056615506246));
#154325=CARTESIAN_POINT('Ctrl Pts',(-64.8129288635406,-4.32488770099073,
125.513155569012));
#154326=CARTESIAN_POINT('Ctrl Pts',(-64.9836847729665,-5.9065549279853,
129.157020333449));
#154327=CARTESIAN_POINT('Ctrl Pts',(-65.0616248077881,-5.92104421557129,
130.809133668594));
#154328=CARTESIAN_POINT('',(-66.811624807788,-5.92032734119191,130.800327082424));
#154329=CARTESIAN_POINT('Ctrl Pts',(-65.0616248077881,-5.92104421557129,
130.809133668594));
#154330=CARTESIAN_POINT('Ctrl Pts',(-65.0765006475708,-5.92380967906112,
131.124460359592));
#154331=CARTESIAN_POINT('Ctrl Pts',(-65.1841923619582,-5.75726169392666,
133.404300651249));
#154332=CARTESIAN_POINT('Ctrl Pts',(-65.3846999509489,-2.7949529050576,
137.220418502967));
#154333=CARTESIAN_POINT('Ctrl Pts',(-65.6631475747624,3.88727089549114,
136.623869661759));
#154334=CARTESIAN_POINT('Ctrl Pts',(-65.9415951985748,6.99728264681958,
130.679476307755));
#154335=CARTESIAN_POINT('Ctrl Pts',(-66.2200428223878,3.67713348198754,
124.849845533531));
#154336=CARTESIAN_POINT('Ctrl Pts',(-66.4984904462009,-3.022121714838,124.492123227301));
#154337=CARTESIAN_POINT('Ctrl Pts',(-66.6956844413341,-5.79969700705658,
128.346744915426));
#154338=CARTESIAN_POINT('Ctrl Pts',(-66.8000625618632,-5.92486756286859,
130.555443657081));
#154339=CARTESIAN_POINT('Ctrl Pts',(-66.811624807788,-5.92295665797096,
130.800325291063));
#154340=CARTESIAN_POINT('',(-68.5616247814665,-5.91202197454765,130.801527559385));
#154341=CARTESIAN_POINT('Ctrl Pts',(-66.811624807788,-5.91674862680149,
130.800329520612));
#154342=CARTESIAN_POINT('Ctrl Pts',(-66.8189381851903,-5.91685404465674,
130.955059351555));
#154343=CARTESIAN_POINT('Ctrl Pts',(-66.8262515625927,-5.91088576872365,
131.11002755393));
#154344=CARTESIAN_POINT('Ctrl Pts',(-66.833564939995,-5.89881422802683,
131.264709686999));
#154345=CARTESIAN_POINT('Ctrl Pts',(-66.8408708436195,-5.88675502362949,
131.419233745374));
#154346=CARTESIAN_POINT('Ctrl Pts',(-66.8481767472438,-5.86860499411473,
131.57347193579));
#154347=CARTESIAN_POINT('Ctrl Pts',(-66.8554826508682,-5.84438657742092,
131.726898473788));
#154348=CARTESIAN_POINT('Ctrl Pts',(-66.8627827872296,-5.82018727868801,
131.880203897239));
#154349=CARTESIAN_POINT('Ctrl Pts',(-66.8700829235912,-5.7899291856031,
132.032698565328));
#154350=CARTESIAN_POINT('Ctrl Pts',(-66.8773830599525,-5.75368664151171,
132.183860742173));
#154351=CARTESIAN_POINT('Ctrl Pts',(-66.884799836364,-5.71686502164054,
132.337438156623));
#154352=CARTESIAN_POINT('Ctrl Pts',(-66.8922166127753,-5.67386610235044,
132.489639732482));
#154353=CARTESIAN_POINT('Ctrl Pts',(-66.8996333891867,-5.62482223672649,
132.639927387729));
#154354=CARTESIAN_POINT('Ctrl Pts',(-66.9069280459753,-5.57658589421485,
132.787740508117));
#154355=CARTESIAN_POINT('Ctrl Pts',(-66.914222702764,-5.52250227479232,
132.933701875274));
#154356=CARTESIAN_POINT('Ctrl Pts',(-66.9215173595526,-5.46274784021575,
133.077313893971));
#154357=CARTESIAN_POINT('Ctrl Pts',(-66.928811716405,-5.40299586257673,
133.220920007737));
#154358=CARTESIAN_POINT('Ctrl Pts',(-66.9361060732575,-5.33757368119745,
133.362176609946));
#154359=CARTESIAN_POINT('Ctrl Pts',(-66.9434004301099,-5.26670599742825,
133.500605877025));
#154360=CARTESIAN_POINT('Ctrl Pts',(-66.9506960212525,-5.19582632202199,
133.639058567947));
#154361=CARTESIAN_POINT('Ctrl Pts',(-66.9579916123949,-5.11949948634783,
133.774682629542));
#154362=CARTESIAN_POINT('Ctrl Pts',(-66.9652872035375,-5.03799610746026,
133.90702492163));
#154363=CARTESIAN_POINT('Ctrl Pts',(-66.9727954110615,-4.9541174647778,
134.043224082713));
#154364=CARTESIAN_POINT('Ctrl Pts',(-66.9803036185857,-4.86475618760571,
134.175946905039));
#154365=CARTESIAN_POINT('Ctrl Pts',(-66.9878118261097,-4.77025445314744,
134.304732457061));
#154366=CARTESIAN_POINT('Ctrl Pts',(-66.9951182219343,-4.6782928130569,
134.430056406423));
#154367=CARTESIAN_POINT('Ctrl Pts',(-67.0024246177587,-4.58146379742863,
134.5516517656));
#154368=CARTESIAN_POINT('Ctrl Pts',(-67.0097310135832,-4.48012248870291,
134.669128792854));
#154369=CARTESIAN_POINT('Ctrl Pts',(-67.0173401269571,-4.37458242133302,
134.791473111539));
#154370=CARTESIAN_POINT('Ctrl Pts',(-67.024949240331,-4.26414848190876,
134.909350187863));
#154371=CARTESIAN_POINT('Ctrl Pts',(-67.0325583537049,-4.14926203807001,
135.022364304375));
#154372=CARTESIAN_POINT('Ctrl Pts',(-67.0401674670787,-4.03437559423109,
135.135378420887));
#154373=CARTESIAN_POINT('Ctrl Pts',(-67.0477765804526,-3.91503703897663,
135.243529322294));
#154374=CARTESIAN_POINT('Ctrl Pts',(-67.0553856938265,-3.79172326303862,
135.346470838491));
#154375=CARTESIAN_POINT('Ctrl Pts',(-67.0628089602319,-3.6714213349072,
135.446898084264));
#154376=CARTESIAN_POINT('Ctrl Pts',(-67.0702322266374,-3.54694487987857,
135.542694427125));
#154377=CARTESIAN_POINT('Ctrl Pts',(-67.0776554930429,-3.4186858858318,
135.633492773193));
#154378=CARTESIAN_POINT('Ctrl Pts',(-67.0850699857639,-3.29057848326456,
135.724183803158));
#154379=CARTESIAN_POINT('Ctrl Pts',(-67.0924844784849,-3.15869774222967,
135.809888381094));
#154380=CARTESIAN_POINT('Ctrl Pts',(-67.0998989712059,-3.02347011528522,
135.890278334604));
#154381=CARTESIAN_POINT('Ctrl Pts',(-67.1073063175597,-2.88837282581884,
135.97059080525));
#154382=CARTESIAN_POINT('Ctrl Pts',(-67.1147136639134,-2.74993539120956,
136.045598659754));
#154383=CARTESIAN_POINT('Ctrl Pts',(-67.1221210102672,-2.60861466516525,
136.115015952945));
#154384=CARTESIAN_POINT('Ctrl Pts',(-67.1295228319425,-2.46739934145076,
136.184381472099));
#154385=CARTESIAN_POINT('Ctrl Pts',(-67.136924653618,-2.32330534178862,
136.248164568405));
#154386=CARTESIAN_POINT('Ctrl Pts',(-67.1443264752933,-2.17681553918244,
136.306124395744));
#154387=CARTESIAN_POINT('Ctrl Pts',(-67.1517243896047,-2.03040306740153,
136.364053626542));
#154388=CARTESIAN_POINT('Ctrl Pts',(-67.1591223039162,-1.88159765767546,
136.416165573517));
#154389=CARTESIAN_POINT('Ctrl Pts',(-67.1665202182276,-1.73090354873195,
136.462266897056));
#154390=CARTESIAN_POINT('Ctrl Pts',(-67.1739169031398,-1.58023448241613,
136.508360559391));
#154391=CARTESIAN_POINT('Ctrl Pts',(-67.1813135880519,-1.42767769643456,
136.548445471626));
#154392=CARTESIAN_POINT('Ctrl Pts',(-67.1887102729642,-1.2737541451294,
136.582377659793));
#154393=CARTESIAN_POINT('Ctrl Pts',(-67.1961066298996,-1.11983741895603,
136.616308343371));
#154394=CARTESIAN_POINT('Ctrl Pts',(-67.2035029868351,-0.964554412504578,
136.644086764972));
#154395=CARTESIAN_POINT('Ctrl Pts',(-67.2108993437705,-0.808437605933992,
136.665619799671));
#154396=CARTESIAN_POINT('Ctrl Pts',(-67.2182968331071,-0.652296897481104,
136.687156131133));
#154397=CARTESIAN_POINT('Ctrl Pts',(-67.2256943224437,-0.495322504547796,
136.702445120794));
#154398=CARTESIAN_POINT('Ctrl Pts',(-67.2330918117803,-0.338053234559719,
136.71144539545));
#154399=CARTESIAN_POINT('Ctrl Pts',(-67.2404918942953,-0.180728834072846,
136.720448825138));
#154400=CARTESIAN_POINT('Ctrl Pts',(-67.2478919768104,-0.0231097231805228,
136.723159129364));
#154401=CARTESIAN_POINT('Ctrl Pts',(-67.2552920593254,0.134264227263688,
136.719587044321));
#154402=CARTESIAN_POINT('Ctrl Pts',(-67.2627002789918,0.291811226544174,
136.716011031403));
#154403=CARTESIAN_POINT('Ctrl Pts',(-67.2701084986582,0.449112153578574,
136.706138841696));
#154404=CARTESIAN_POINT('Ctrl Pts',(-67.2775167183247,0.605630461261856,
136.690033247512));
#154405=CARTESIAN_POINT('Ctrl Pts',(-67.2849294976268,0.76224510335187,
136.673917740603));
#154406=CARTESIAN_POINT('Ctrl Pts',(-67.2923422769288,0.918075797607008,
136.651561237288));
#154407=CARTESIAN_POINT('Ctrl Pts',(-67.2997550562309,1.07259565444685,
136.623077754922));
#154408=CARTESIAN_POINT('Ctrl Pts',(-67.3071784272596,1.22733629650462,
136.594553574021));
#154409=CARTESIAN_POINT('Ctrl Pts',(-67.3146017982884,1.38076199722079,
136.559885011399));
#154410=CARTESIAN_POINT('Ctrl Pts',(-67.3220251693172,1.53235969694117,
136.519236322399));
#154411=CARTESIAN_POINT('Ctrl Pts',(-67.3259612187579,1.6127404348687,136.497683412139));
#154412=CARTESIAN_POINT('Ctrl Pts',(-67.3298972681987,1.69260755686729,
136.47445009147));
#154413=CARTESIAN_POINT('Ctrl Pts',(-67.3338333176394,1.77188692644919,
136.449566307563));
#154414=CARTESIAN_POINT('Ctrl Pts',(-67.3412565840448,1.92140534325825,
136.402636267711));
#154415=CARTESIAN_POINT('Ctrl Pts',(-67.3486798504503,2.06928408404975,
136.349690964011));
#154416=CARTESIAN_POINT('Ctrl Pts',(-67.3561031168558,2.21500242332258,
136.290861763759));
#154417=CARTESIAN_POINT('Ctrl Pts',(-67.3635176095768,2.36054853561976,
136.232102094736));
#154418=CARTESIAN_POINT('Ctrl Pts',(-67.3709321022978,2.50393898621277,
136.167472510072));
#154419=CARTESIAN_POINT('Ctrl Pts',(-67.3783465950188,2.64466716634428,
136.097154411184));
#154420=CARTESIAN_POINT('Ctrl Pts',(-67.3857539413726,2.78525970735704,
136.026904087527));
#154421=CARTESIAN_POINT('Ctrl Pts',(-67.3931612877263,2.92319475461249,
135.950976330567));
#154422=CARTESIAN_POINT('Ctrl Pts',(-67.4005686340801,3.05798479375098,
135.869600943917));
#154423=CARTESIAN_POINT('Ctrl Pts',(-67.4079704557555,3.19267430139371,
135.788286250099));
#154424=CARTESIAN_POINT('Ctrl Pts',(-67.4153722774309,3.32422315325712,
135.701532208771));
#154425=CARTESIAN_POINT('Ctrl Pts',(-67.4227740991063,3.45216771402715,
135.609614891455));
#154426=CARTESIAN_POINT('Ctrl Pts',(-67.4301720134176,3.5800447338582,135.517746096577));
#154427=CARTESIAN_POINT('Ctrl Pts',(-67.4375699277289,3.70432094946446,
135.420719671232));
#154428=CARTESIAN_POINT('Ctrl Pts',(-67.4449678420402,3.82456114540592,
135.31885534096));
#154429=CARTESIAN_POINT('Ctrl Pts',(-67.4523645269524,3.94478135960889,
135.217007938691));
#154430=CARTESIAN_POINT('Ctrl Pts',(-67.4597612118647,4.06096660076599,
135.110324468204));
#154431=CARTESIAN_POINT('Ctrl Pts',(-67.4671578967769,4.17271415095235,
134.999165401694));
#154432=CARTESIAN_POINT('Ctrl Pts',(-67.4745542537123,4.28445674613523,
134.888011264093));
#154433=CARTESIAN_POINT('Ctrl Pts',(-67.4819506106478,4.39176177693915,
134.772382188323));
#154434=CARTESIAN_POINT('Ctrl Pts',(-67.4893469675832,4.49426307619539,
134.652675828726));
#154435=CARTESIAN_POINT('Ctrl Pts',(-67.4967444569198,4.59678006866222,
134.53295114178));
#154436=CARTESIAN_POINT('Ctrl Pts',(-67.5041419462564,4.6944916223632,134.409148211626));
#154437=CARTESIAN_POINT('Ctrl Pts',(-67.511539435593,4.78707169027595,134.281697988984));
#154438=CARTESIAN_POINT('Ctrl Pts',(-67.518939518108,4.87968421198824,134.154203088863));
#154439=CARTESIAN_POINT('Ctrl Pts',(-67.5263396006229,4.96716144719189,
134.023058652502));
#154440=CARTESIAN_POINT('Ctrl Pts',(-67.5337396831379,5.04922061516566,
133.888724691713));
#154441=CARTESIAN_POINT('Ctrl Pts',(-67.5411479028044,5.13137001563016,
133.754243016924));
#154442=CARTESIAN_POINT('Ctrl Pts',(-67.5485561224709,5.20808925618579,
133.616565132338));
#154443=CARTESIAN_POINT('Ctrl Pts',(-67.5559643421374,5.27914113213969,
133.476176380198));
#154444=CARTESIAN_POINT('Ctrl Pts',(-67.5633771214394,5.35023673933787,
133.335701221124));
#154445=CARTESIAN_POINT('Ctrl Pts',(-67.5707899007415,5.41565787655098,
133.192512208562));
#154446=CARTESIAN_POINT('Ctrl Pts',(-67.5782026800435,5.47521567312217,
133.047114258806));
#154447=CARTESIAN_POINT('Ctrl Pts',(-67.5856260510723,5.53485856866601,
132.901508557642));
#154448=CARTESIAN_POINT('Ctrl Pts',(-67.593049422101,5.58862126393568,132.753687965464));
#154449=CARTESIAN_POINT('Ctrl Pts',(-67.6004727931298,5.63636463032776,
132.604172917916));
#154450=CARTESIAN_POINT('Ctrl Pts',(-67.6044088425706,5.66167930877564,
132.52489645214));
#154451=CARTESIAN_POINT('Ctrl Pts',(-67.6083448920115,5.68530258839858,
132.445143803118));
#154452=CARTESIAN_POINT('Ctrl Pts',(-67.6122809414524,5.70721959201832,
132.364993531157));
#154453=CARTESIAN_POINT('Ctrl Pts',(-67.6197042078578,5.74855437683823,
132.213832619643));
#154454=CARTESIAN_POINT('Ctrl Pts',(-67.6271274742632,5.78394206488328,
132.060799816961));
#154455=CARTESIAN_POINT('Ctrl Pts',(-67.6345507406687,5.81321171432706,
131.906404231454));
#154456=CARTESIAN_POINT('Ctrl Pts',(-67.6419652333897,5.84244676947592,
131.752191128706));
#154457=CARTESIAN_POINT('Ctrl Pts',(-67.6493797261106,5.865578110545,131.596618812418));
#154458=CARTESIAN_POINT('Ctrl Pts',(-67.6567942188316,5.88248452127648,
131.44021155878));
#154459=CARTESIAN_POINT('Ctrl Pts',(-67.6642015651854,5.89937463697273,
131.283955056342));
#154460=CARTESIAN_POINT('Ctrl Pts',(-67.6716089115392,5.91005172694864,
131.126865587287));
#154461=CARTESIAN_POINT('Ctrl Pts',(-67.679016257893,5.91444561807293,130.969477525719));
#154462=CARTESIAN_POINT('Ctrl Pts',(-67.6864180795684,5.91883623206746,
130.812206850104));
#154463=CARTESIAN_POINT('Ctrl Pts',(-67.6938199012438,5.91695296778733,
130.654638396951));
#154464=CARTESIAN_POINT('Ctrl Pts',(-67.7012217229192,5.90877748581179,
130.497311459183));
#154465=CARTESIAN_POINT('Ctrl Pts',(-67.7086196372306,5.90060631960951,
130.34006757308));
#154466=CARTESIAN_POINT('Ctrl Pts',(-67.716017551542,5.88614957018592,130.183065320302));
#154467=CARTESIAN_POINT('Ctrl Pts',(-67.7234154658534,5.8654409871166,130.026843679389));
#154468=CARTESIAN_POINT('Ctrl Pts',(-67.7308121507656,5.84473584543821,
129.870647999679));
#154469=CARTESIAN_POINT('Ctrl Pts',(-67.7382088356779,5.81778098111208,
129.715233044069));
#154470=CARTESIAN_POINT('Ctrl Pts',(-67.7456055205901,5.78466199072975,
129.561132474582));
#154471=CARTESIAN_POINT('Ctrl Pts',(-67.7530018775255,5.75154446887815,
129.407038738076));
#154472=CARTESIAN_POINT('Ctrl Pts',(-67.7603982344609,5.71226344286773,
129.254259636773));
#154473=CARTESIAN_POINT('Ctrl Pts',(-67.7677945913964,5.66695554825979,
129.103318179369));
#154474=CARTESIAN_POINT('Ctrl Pts',(-67.7751920807329,5.62164071689778,
128.952353612443));
#154475=CARTESIAN_POINT('Ctrl Pts',(-67.7825895700695,5.57029728699078,
128.803227607177));
#154476=CARTESIAN_POINT('Ctrl Pts',(-67.7899870594061,5.51311159320498,
128.656447415556));
#154477=CARTESIAN_POINT('Ctrl Pts',(-67.7973871419211,5.45590585306255,
128.509615770366));
#154478=CARTESIAN_POINT('Ctrl Pts',(-67.8047872244359,5.39285390692614,
128.365131923671));
#154479=CARTESIAN_POINT('Ctrl Pts',(-67.8121873069509,5.32418992587507,
128.223482434522));
#154480=CARTESIAN_POINT('Ctrl Pts',(-67.8195955266174,5.2554504417182,128.081677187199));
#154481=CARTESIAN_POINT('Ctrl Pts',(-67.8270037462839,5.18108676166788,
127.94271285773));
#154482=CARTESIAN_POINT('Ctrl Pts',(-67.8344119659504,5.10137900296805,
127.807051352479));
#154483=CARTESIAN_POINT('Ctrl Pts',(-67.8418247452524,5.02162218547251,
127.671306349835));
#154484=CARTESIAN_POINT('Ctrl Pts',(-67.8492375245545,4.93651493654471,
127.538868535399));
#154485=CARTESIAN_POINT('Ctrl Pts',(-67.8566503038566,4.84637996735821,
127.410169730994));
#154486=CARTESIAN_POINT('Ctrl Pts',(-67.8640736748853,4.75611620910082,
127.281287035702));
#154487=CARTESIAN_POINT('Ctrl Pts',(-67.871497045914,4.66081060842491,127.156154316742));
#154488=CARTESIAN_POINT('Ctrl Pts',(-67.8789204169428,4.56082582016753,
127.035169935126));
#154489=CARTESIAN_POINT('Ctrl Pts',(-67.8828564663836,4.50781148633142,
126.971021113013));
#154490=CARTESIAN_POINT('Ctrl Pts',(-67.8867925158244,4.45348228366514,
126.908037923958));
#154491=CARTESIAN_POINT('Ctrl Pts',(-67.8907285652652,4.39789626569995,
126.846275348317));
#154492=CARTESIAN_POINT('Ctrl Pts',(-67.8981518316706,4.29306277059753,
126.729793058203));
#154493=CARTESIAN_POINT('Ctrl Pts',(-67.905575098076,4.18343984936724,126.617302426135));
#154494=CARTESIAN_POINT('Ctrl Pts',(-67.9129983644815,4.06936343104479,
126.50922245581));
#154495=CARTESIAN_POINT('Ctrl Pts',(-67.9204128572025,3.95542184157551,
126.401270227034));
#154496=CARTESIAN_POINT('Ctrl Pts',(-67.9278273499235,3.83703750070714,
126.29771853766));
#154497=CARTESIAN_POINT('Ctrl Pts',(-67.9352418426445,3.71458597650059,
126.198952754446));
#154498=CARTESIAN_POINT('Ctrl Pts',(-67.9426491889983,3.59225247568294,
126.100282165413));
#154499=CARTESIAN_POINT('Ctrl Pts',(-67.9500565353522,3.46585988429572,
126.006388532077));
#154500=CARTESIAN_POINT('Ctrl Pts',(-67.957463881706,3.33581985611548,125.917619735337));
#154501=CARTESIAN_POINT('Ctrl Pts',(-67.9648657033814,3.20587681669476,
125.828917145716));
#154502=CARTESIAN_POINT('Ctrl Pts',(-67.9722675250568,3.07229206414244,
125.745331991539));
#154503=CARTESIAN_POINT('Ctrl Pts',(-67.9796693467322,2.93550940796286,
125.667171203279));
#154504=CARTESIAN_POINT('Ctrl Pts',(-67.9870672610436,2.79879895828218,
125.589051675491));
#154505=CARTESIAN_POINT('Ctrl Pts',(-67.994465175355,2.65889429029634,125.516350995597));
#154506=CARTESIAN_POINT('Ctrl Pts',(-68.0018630896664,2.51626710438533,
125.449332100192));
#154507=CARTESIAN_POINT('Ctrl Pts',(-68.0092597745786,2.37366362052509,
125.382324342111));
#154508=CARTESIAN_POINT('Ctrl Pts',(-68.0166564594908,2.22833885421258,
125.320996653142));
#154509=CARTESIAN_POINT('Ctrl Pts',(-68.0240531444031,2.08078805746974,
125.265565475805));
#154510=CARTESIAN_POINT('Ctrl Pts',(-68.0314495013385,1.93324380328427,
125.210136756346));
#154511=CARTESIAN_POINT('Ctrl Pts',(-68.0388458582739,1.78347406437819,
125.160604159934));
#154512=CARTESIAN_POINT('Ctrl Pts',(-68.0462422152094,1.63199271763696,
125.117135430176));
#154513=CARTESIAN_POINT('Ctrl Pts',(-68.0536397045459,1.48048817871504,
125.073660045246));
#154514=CARTESIAN_POINT('Ctrl Pts',(-68.0610371938826,1.32727186901836,
125.036250478496));
#154515=CARTESIAN_POINT('Ctrl Pts',(-68.0684346832192,1.17287127244642,
125.005024143385));
#154516=CARTESIAN_POINT('Ctrl Pts',(-68.0758347657342,1.01841655098383,
124.97378686193));
#154517=CARTESIAN_POINT('Ctrl Pts',(-68.0832348482492,0.862777081747325,
124.948737201585));
#154518=CARTESIAN_POINT('Ctrl Pts',(-68.0906349307642,0.70648879583477,
124.929941144643));
#154519=CARTESIAN_POINT('Ctrl Pts',(-68.0980431504307,0.550028654885474,
124.911124419503));
#154520=CARTESIAN_POINT('Ctrl Pts',(-68.1054513700972,0.392918643326962,
124.898575075148));
#154521=CARTESIAN_POINT('Ctrl Pts',(-68.1128595897637,0.235698786277303,
124.892307112679));
#154522=CARTESIAN_POINT('Ctrl Pts',(-68.1202723690658,0.0783821630289842,
124.886035292383));
#154523=CARTESIAN_POINT('Ctrl Pts',(-68.1276851483679,-0.0790440679956438,
124.886052557593));
#154524=CARTESIAN_POINT('Ctrl Pts',(-68.13509792767,-0.236042169595822,
124.892320812501));
#154525=CARTESIAN_POINT('Ctrl Pts',(-68.1425212986987,-0.393264597446046,
124.898598023786));
#154526=CARTESIAN_POINT('Ctrl Pts',(-68.1499446697275,-0.550057302984203,
124.911144033695));
#154527=CARTESIAN_POINT('Ctrl Pts',(-68.1573680407563,-0.705889110011352,
124.929869054301));
#154528=CARTESIAN_POINT('Ctrl Pts',(-68.1613040901969,-0.788514873226247,
124.939797509527));
#154529=CARTESIAN_POINT('Ctrl Pts',(-68.1652401396375,-0.870870675056604,
124.951462254279));
#154530=CARTESIAN_POINT('Ctrl Pts',(-68.1691761890781,-0.952878879620812,
124.964844164702));
#154531=CARTESIAN_POINT('Ctrl Pts',(-68.1765994554835,-1.10754379404624,
124.990082030125));
#154532=CARTESIAN_POINT('Ctrl Pts',(-68.184022721889,-1.26143921531752,
125.021506964069));
#154533=CARTESIAN_POINT('Ctrl Pts',(-68.1914459882944,-1.41403104590956,
125.059062821655));
#154534=CARTESIAN_POINT('Ctrl Pts',(-68.1988604810154,-1.56644252563046,
125.096574291335));
#154535=CARTESIAN_POINT('Ctrl Pts',(-68.2062749737363,-1.71755312257445,
125.140202172629));
#154536=CARTESIAN_POINT('Ctrl Pts',(-68.2136894664573,-1.86683561306241,
125.189838789636));
#154537=CARTESIAN_POINT('Ctrl Pts',(-68.2210968128109,-2.01597421946437,
125.239427565002));
#154538=CARTESIAN_POINT('Ctrl Pts',(-68.2285041591646,-2.16328787534932,
125.295013429462));
#154539=CARTESIAN_POINT('Ctrl Pts',(-68.2359115055183,-2.30826138974307,
125.356438085158));
#154540=CARTESIAN_POINT('Ctrl Pts',(-68.2433133271937,-2.45312677742169,
125.417816928029));
#154541=CARTESIAN_POINT('Ctrl Pts',(-68.2507151488692,-2.5956551566285,
125.485025746154));
#154542=CARTESIAN_POINT('Ctrl Pts',(-68.2581169705446,-2.7353484081873,
125.557857053446));
#154543=CARTESIAN_POINT('Ctrl Pts',(-68.2655148848559,-2.87496791676578,
125.630649913657));
#154544=CARTESIAN_POINT('Ctrl Pts',(-68.2729127991672,-3.01175494815713,
125.709059179844));
#154545=CARTESIAN_POINT('Ctrl Pts',(-68.2803107134786,-3.14523332078233,
125.792830120768));
#154546=CARTESIAN_POINT('Ctrl Pts',(-68.2877073983907,-3.27868951172316,
125.87658714048));
#154547=CARTESIAN_POINT('Ctrl Pts',(-68.2951040833029,-3.4088378192892,
125.965703868289));
#154548=CARTESIAN_POINT('Ctrl Pts',(-68.3025007682151,-3.53522844844189,
126.059880627111));
#154549=CARTESIAN_POINT('Ctrl Pts',(-68.3098971251504,-3.66161347330128,
126.154053210037));
#154550=CARTESIAN_POINT('Ctrl Pts',(-68.3172934820858,-3.78424085170587,
126.253285154815));
#154551=CARTESIAN_POINT('Ctrl Pts',(-68.3246898390212,-3.9026916931995,
126.357234791785));
#154552=CARTESIAN_POINT('Ctrl Pts',(-68.3320873283577,-4.02116066981935,
126.461200343709));
#154553=CARTESIAN_POINT('Ctrl Pts',(-68.3394848176942,-4.13545155572639,
126.56988477976));
#154554=CARTESIAN_POINT('Ctrl Pts',(-68.3468823070307,-4.24518044972245,
126.682907777633));
#154555=CARTESIAN_POINT('Ctrl Pts',(-68.3542823895456,-4.35494780901156,
126.795970395542));
#154556=CARTESIAN_POINT('Ctrl Pts',(-68.3616824720604,-4.46014973252857,
126.913374335658));
#154557=CARTESIAN_POINT('Ctrl Pts',(-68.3690825545753,-4.56044102365434,
127.034704369011));
#154558=CARTESIAN_POINT('Ctrl Pts',(-68.3764907742417,-4.66084259536575,
127.156167817209));
#154559=CARTESIAN_POINT('Ctrl Pts',(-68.3838989939082,-4.75632251306026,
127.28156569236));
#154560=CARTESIAN_POINT('Ctrl Pts',(-68.3913072135746,-4.84657710044748,
127.410451223973));
#154561=CARTESIAN_POINT('Ctrl Pts',(-68.3987199928767,-4.93688723802791,
127.539416082482));
#154562=CARTESIAN_POINT('Ctrl Pts',(-68.4061327721787,-5.02196543553689,
127.671872561452));
#154563=CARTESIAN_POINT('Ctrl Pts',(-68.4135455514808,-5.10155308396407,
127.807347655633));
#154564=CARTESIAN_POINT('Ctrl Pts',(-68.4209689225095,-5.18125445095527,
127.943016322981));
#154565=CARTESIAN_POINT('Ctrl Pts',(-68.4283922935382,-5.25544942471556,
128.081711891558));
#154566=CARTESIAN_POINT('Ctrl Pts',(-68.4358156645669,-5.32392643266154,
128.222938935216));
#154567=CARTESIAN_POINT('Ctrl Pts',(-68.4397517140082,-5.36023458536214,
128.297820902469));
#154568=CARTESIAN_POINT('Ctrl Pts',(-68.4436877634495,-5.39493602778715,
128.373414250463));
#154569=CARTESIAN_POINT('Ctrl Pts',(-68.4476238128907,-5.42800488528706,
128.449643325023));
#154570=CARTESIAN_POINT('Ctrl Pts',(-68.4558328600923,-5.49697348341427,
128.608627118429));
#154571=CARTESIAN_POINT('Ctrl Pts',(-68.464041907294,-5.55901664151482,
128.770788760264));
#154572=CARTESIAN_POINT('Ctrl Pts',(-68.4722509544957,-5.61386054495428,
128.935537366345));
#154573=CARTESIAN_POINT('Ctrl Pts',(-68.4804279058865,-5.66849001917829,
129.099641836758));
#154574=CARTESIAN_POINT('Ctrl Pts',(-68.4886048572773,-5.71597630648745,
129.266312870272));
#154575=CARTESIAN_POINT('Ctrl Pts',(-68.4967818086681,-5.75609457352925,
129.434942557554));
#154576=CARTESIAN_POINT('Ctrl Pts',(-68.5049382975006,-5.79611244589609,
129.603150254459));
#154577=CARTESIAN_POINT('Ctrl Pts',(-68.5130947863331,-5.82879901029771,
129.773306600435));
#154578=CARTESIAN_POINT('Ctrl Pts',(-68.5212512751656,-5.85397853701506,
129.944787554548));
#154579=CARTESIAN_POINT('Ctrl Pts',(-68.5293741259582,-5.87905422126489,
130.115561306908));
#154580=CARTESIAN_POINT('Ctrl Pts',(-68.5374969767507,-5.89668456597095,
130.287648538314));
#154581=CARTESIAN_POINT('Ctrl Pts',(-68.5456198275432,-5.90674465531011,
130.460415651815));
#154582=CARTESIAN_POINT('Ctrl Pts',(-68.550954801205,-5.91335197988504,
130.573886651554));
#154583=CARTESIAN_POINT('Ctrl Pts',(-68.5562897748668,-5.91669473803662,
130.687650583833));
#154584=CARTESIAN_POINT('Ctrl Pts',(-68.5616247485286,-5.91674932031565,
130.801524591425));
#154585=CARTESIAN_POINT('',(-70.3116248421866,-5.91520845600957,130.809408030844));
#154586=CARTESIAN_POINT('Ctrl Pts',(-68.561624807788,-5.90824422428163,
130.801529931163));
#154587=CARTESIAN_POINT('Ctrl Pts',(-68.61644035076,-5.9032143751984,131.969878185027));
#154588=CARTESIAN_POINT('Ctrl Pts',(-68.7640717683365,-5.00169773296238,
135.123678078319));
#154589=CARTESIAN_POINT('Ctrl Pts',(-69.0045190605167,0.135532838237384,
137.801445108984));
#154590=CARTESIAN_POINT('Ctrl Pts',(-69.2829666843298,5.96010416000349,
134.472428083174));
#154591=CARTESIAN_POINT('Ctrl Pts',(-69.5614143081424,6.30763092600427,
127.772636251522));
#154592=CARTESIAN_POINT('Ctrl Pts',(-69.8398619319555,0.858753015907526,
123.858851004297));
#154593=CARTESIAN_POINT('Ctrl Pts',(-70.0899320985043,-4.74354006348326,
126.076046876634));
#154594=CARTESIAN_POINT('Ctrl Pts',(-70.2471863904481,-5.9015201675211,
129.438471216138));
#154595=CARTESIAN_POINT('Ctrl Pts',(-70.311624807788,-5.91256097363447,
130.809405039745));
#154596=CARTESIAN_POINT('',(-72.061624807788,-5.92102598959136,130.805130248854));
#154597=CARTESIAN_POINT('Ctrl Pts',(-70.3116248621877,-5.91674784561244,
130.809409770031));
#154598=CARTESIAN_POINT('Ctrl Pts',(-70.3204841076535,-5.91658688933848,
130.998023145018));
#154599=CARTESIAN_POINT('Ctrl Pts',(-70.3293433531193,-5.90740330510671,
131.186244603552));
#154600=CARTESIAN_POINT('Ctrl Pts',(-70.338202598585,-5.88933200357266,
131.373306233767));
#154601=CARTESIAN_POINT('Ctrl Pts',(-70.3471311539176,-5.87111932210882,
131.561831331354));
#154602=CARTESIAN_POINT('Ctrl Pts',(-70.3560597092502,-5.84387940990915,
131.749178369704));
#154603=CARTESIAN_POINT('Ctrl Pts',(-70.3649882645828,-5.80779893960273,
131.934582737173));
#154604=CARTESIAN_POINT('Ctrl Pts',(-70.3739910897327,-5.77141834348192,
132.121529341657));
#154605=CARTESIAN_POINT('Ctrl Pts',(-70.3829939148826,-5.72604955131969,
132.306500814378));
#154606=CARTESIAN_POINT('Ctrl Pts',(-70.3919967400325,-5.671932023571,132.488735184724));
#154607=CARTESIAN_POINT('Ctrl Pts',(-70.3935835532154,-5.66239341707536,
132.520855313286));
#154608=CARTESIAN_POINT('Ctrl Pts',(-70.3951703663982,-5.65258313575233,
132.552890463939));
#154609=CARTESIAN_POINT('Ctrl Pts',(-70.3967571795811,-5.64250264266975,
132.584836534271));
#154610=CARTESIAN_POINT('Ctrl Pts',(-70.4041804459868,-5.59534511558212,
132.734283358413));
#154611=CARTESIAN_POINT('Ctrl Pts',(-70.4116037123924,-5.54217482691998,
132.882081354229));
#154612=CARTESIAN_POINT('Ctrl Pts',(-70.4190269787981,-5.48312393628243,
133.027709996739));
#154613=CARTESIAN_POINT('Ctrl Pts',(-70.4264414715193,-5.42414283889365,
133.173166518287));
#154614=CARTESIAN_POINT('Ctrl Pts',(-70.4338559642406,-5.35929511321063,
133.316458447614));
#154615=CARTESIAN_POINT('Ctrl Pts',(-70.4412704569618,-5.28876293141317,
133.457079452612));
#154616=CARTESIAN_POINT('Ctrl Pts',(-70.4486778033158,-5.21829873118802,
133.597564921792));
#154617=CARTESIAN_POINT('Ctrl Pts',(-70.4560851496698,-5.14216114848641,
133.735384260204));
#154618=CARTESIAN_POINT('Ctrl Pts',(-70.4634924960238,-5.0605807285695,
133.870050303775));
#154619=CARTESIAN_POINT('Ctrl Pts',(-70.4708943176995,-4.9790611544075,
134.004615908331));
#154620=CARTESIAN_POINT('Ctrl Pts',(-70.4782961393752,-4.89210701857658,
134.136032582983));
#154621=CARTESIAN_POINT('Ctrl Pts',(-70.4856979610508,-4.79999509785458,
134.263837113088));
#154622=CARTESIAN_POINT('Ctrl Pts',(-70.4930958753624,-4.70793180229853,
134.391574176177));
#154623=CARTESIAN_POINT('Ctrl Pts',(-70.500493789674,-4.61071636205924,
134.515702590174));
#154624=CARTESIAN_POINT('Ctrl Pts',(-70.5078917039855,-4.50866916463,134.635787626712));
#154625=CARTESIAN_POINT('Ctrl Pts',(-70.5152883888979,-4.40663892559379,
134.755852707296));
#154626=CARTESIAN_POINT('Ctrl Pts',(-70.5226850738102,-4.29977876448117,
134.871875459832));
#154627=CARTESIAN_POINT('Ctrl Pts',(-70.5300817587226,-4.18844976593796,
134.983453715442));
#154628=CARTESIAN_POINT('Ctrl Pts',(-70.5374781156583,-4.07712570383905,
135.095027023555));
#154629=CARTESIAN_POINT('Ctrl Pts',(-70.544874472594,-3.96133346197043,
135.202155962333));
#154630=CARTESIAN_POINT('Ctrl Pts',(-70.5522708295296,-3.8414712514578,
135.304474970193));
#154631=CARTESIAN_POINT('Ctrl Pts',(-70.5596683188664,-3.72159068973457,
135.406809643356));
#154632=CARTESIAN_POINT('Ctrl Pts',(-70.5670658082032,-3.59763920258552,
135.504332676924));
#154633=CARTESIAN_POINT('Ctrl Pts',(-70.57446329754,-3.47004823641974,135.596718680088));
#154634=CARTESIAN_POINT('Ctrl Pts',(-70.5818633800552,-3.34241254343875,
135.689137069022));
#154635=CARTESIAN_POINT('Ctrl Pts',(-70.5892634625704,-3.21113513347473,
135.776414623421));
#154636=CARTESIAN_POINT('Ctrl Pts',(-70.5966635450856,-3.07667644815211,
135.85826926295));
#154637=CARTESIAN_POINT('Ctrl Pts',(-70.6040717647522,-2.9420699116821,
135.94021391007));
#154638=CARTESIAN_POINT('Ctrl Pts',(-70.611479984419,-2.80427543289505,
136.016723539482));
#154639=CARTESIAN_POINT('Ctrl Pts',(-70.6188882040856,-2.66377871445692,
136.087561685376));
#154640=CARTESIAN_POINT('Ctrl Pts',(-70.6263009833879,-2.52319552263271,
136.158443430966));
#154641=CARTESIAN_POINT('Ctrl Pts',(-70.6337137626902,-2.37990711604169,
136.223646583119));
#154642=CARTESIAN_POINT('Ctrl Pts',(-70.6411265419925,-2.23441869782084,
136.282983039793));
#154643=CARTESIAN_POINT('Ctrl Pts',(-70.6485499130215,-2.08872239892553,
136.342404279179));
#154644=CARTESIAN_POINT('Ctrl Pts',(-70.6559732840504,-1.94082016024555,
136.395941954412));
#154645=CARTESIAN_POINT('Ctrl Pts',(-70.6633966550793,-1.79123262855091,
136.443457729065));
#154646=CARTESIAN_POINT('Ctrl Pts',(-70.6673327045175,-1.71191772999733,
136.468651732894));
#154647=CARTESIAN_POINT('Ctrl Pts',(-70.6712687539558,-1.63212922277147,
136.492153615189));
#154648=CARTESIAN_POINT('Ctrl Pts',(-70.675204803394,-1.55194568972767,
136.513948618345));
#154649=CARTESIAN_POINT('Ctrl Pts',(-70.6826280697994,-1.4007220487503,
136.555053314124));
#154650=CARTESIAN_POINT('Ctrl Pts',(-70.6900513362048,-1.24763556924053,
136.590208071316));
#154651=CARTESIAN_POINT('Ctrl Pts',(-70.6974746026102,-1.09319561909706,
136.619242723068));
#154652=CARTESIAN_POINT('Ctrl Pts',(-70.7048890953312,-0.938938204148988,
136.648243058273));
#154653=CARTESIAN_POINT('Ctrl Pts',(-70.7123035880522,-0.783330866047083,
136.671137617974));
#154654=CARTESIAN_POINT('Ctrl Pts',(-70.7197180807732,-0.626898064847358,
136.687805983913));
#154655=CARTESIAN_POINT('Ctrl Pts',(-70.727125427127,-0.470616039471021,
136.704458284254));
#154656=CARTESIAN_POINT('Ctrl Pts',(-70.7345327734807,-0.313510503609283,
136.714896298435));
#154657=CARTESIAN_POINT('Ctrl Pts',(-70.7419401198345,-0.156115937539085,
136.719050666634));
#154658=CARTESIAN_POINT('Ctrl Pts',(-70.7493419415099,0.00116123772535637,
136.723201936348));
#154659=CARTESIAN_POINT('Ctrl Pts',(-70.7567437631853,0.158726642408166,
136.721078881886));
#154660=CARTESIAN_POINT('Ctrl Pts',(-70.7641455848607,0.316040956301952,
136.712663984561));
#154661=CARTESIAN_POINT('Ctrl Pts',(-70.7715434991721,0.473272225193966,
136.704253529394));
#154662=CARTESIAN_POINT('Ctrl Pts',(-70.7789414134834,0.630252295452986,
136.689557866009));
#154663=CARTESIAN_POINT('Ctrl Pts',(-70.7863393277948,0.786442240524691,
136.668611564176));
#154664=CARTESIAN_POINT('Ctrl Pts',(-70.793736012707,0.942606229661098,
136.647668743239));
#154665=CARTESIAN_POINT('Ctrl Pts',(-70.8011326976192,1.09797998458732,
136.62047739502));
#154666=CARTESIAN_POINT('Ctrl Pts',(-70.8085293825314,1.25202997416255,
136.587123928155));
#154667=CARTESIAN_POINT('Ctrl Pts',(-70.8159257394668,1.40607313300003,
136.553771940218));
#154668=CARTESIAN_POINT('Ctrl Pts',(-70.8233220964023,1.55879227835214,
136.51425845591));
#154669=CARTESIAN_POINT('Ctrl Pts',(-70.8307184533377,1.70966461006603,
136.468720906565));
#154670=CARTESIAN_POINT('Ctrl Pts',(-70.8381159426743,1.86056004071886,
136.423176385305));
#154671=CARTESIAN_POINT('Ctrl Pts',(-70.8455134320108,2.00960773733972,
136.371606070458));
#154672=CARTESIAN_POINT('Ctrl Pts',(-70.8529109213474,2.15630073210085,
136.314197068427));
#154673=CARTESIAN_POINT('Ctrl Pts',(-70.8603110038624,2.3030451498641,136.25676794176));
#154674=CARTESIAN_POINT('Ctrl Pts',(-70.8677110863775,2.44743287492025,
136.193496188818));
#154675=CARTESIAN_POINT('Ctrl Pts',(-70.8751111688925,2.58897770515041,
136.124616720869));
#154676=CARTESIAN_POINT('Ctrl Pts',(-70.882519388559,2.73067817847258,136.055661512865));
#154677=CARTESIAN_POINT('Ctrl Pts',(-70.8899276082255,2.8695291781614,135.981086438873));
#154678=CARTESIAN_POINT('Ctrl Pts',(-70.8973358278919,3.00506922467902,
135.901172318756));
#154679=CARTESIAN_POINT('Ctrl Pts',(-70.904748607194,3.14069269383387,135.821209012832));
#154680=CARTESIAN_POINT('Ctrl Pts',(-70.912161386496,3.27300083616388,135.735900314648));
#154681=CARTESIAN_POINT('Ctrl Pts',(-70.9195741657981,3.40156232145845,
135.645569592165));
#154682=CARTESIAN_POINT('Ctrl Pts',(-70.9269975368269,3.53030750143197,
135.555109800909));
#154683=CARTESIAN_POINT('Ctrl Pts',(-70.9344209078556,3.65529503658982,
135.459613879899));
#154684=CARTESIAN_POINT('Ctrl Pts',(-70.9418442788844,3.7761271182807,135.359445089789));
#154685=CARTESIAN_POINT('Ctrl Pts',(-70.9457803283253,3.84019518732119,
135.306333193754));
#154686=CARTESIAN_POINT('Ctrl Pts',(-70.9497163777662,3.90309562364617,
135.251908204306));
#154687=CARTESIAN_POINT('Ctrl Pts',(-70.9536524272071,3.96477353531171,
135.196228258581));
#154688=CARTESIAN_POINT('Ctrl Pts',(-70.9610756936125,4.08109615180713,
135.091217618658));
#154689=CARTESIAN_POINT('Ctrl Pts',(-70.9684989600179,4.1934198261867,134.981423632777));
#154690=CARTESIAN_POINT('Ctrl Pts',(-70.9759222264233,4.30132606646703,
134.867182867238));
#154691=CARTESIAN_POINT('Ctrl Pts',(-70.9833367191443,4.40910477053255,
134.753077124797));
#154692=CARTESIAN_POINT('Ctrl Pts',(-70.9907512118652,4.51247617918092,
134.634535332972));
#154693=CARTESIAN_POINT('Ctrl Pts',(-70.9981657045862,4.61105549765007,
134.511933645854));
#154694=CARTESIAN_POINT('Ctrl Pts',(-71.0055730509399,4.70953980166063,
134.389450126858));
#154695=CARTESIAN_POINT('Ctrl Pts',(-71.0129803972937,4.80324097826053,
134.262914791706));
#154696=CARTESIAN_POINT('Ctrl Pts',(-71.0203877436475,4.8918117734207,134.132739823114));
#154697=CARTESIAN_POINT('Ctrl Pts',(-71.0277895653228,4.98031650914026,
134.002661943924));
#154698=CARTESIAN_POINT('Ctrl Pts',(-71.0351913869981,5.06369827327327,
133.868950143686));
#154699=CARTESIAN_POINT('Ctrl Pts',(-71.0425932086735,5.14165081110609,
133.732048698484));
#154700=CARTESIAN_POINT('Ctrl Pts',(-71.0499911229848,5.21956219840097,
133.595219522491));
#154701=CARTESIAN_POINT('Ctrl Pts',(-71.0573890372961,5.29204988301889,
133.455204378455));
#154702=CARTESIAN_POINT('Ctrl Pts',(-71.0647869516075,5.35885164651987,
133.312475366355));
#154703=CARTESIAN_POINT('Ctrl Pts',(-71.0721836365196,5.42564230877956,
133.169770073227));
#154704=CARTESIAN_POINT('Ctrl Pts',(-71.0795803214317,5.48674876717679,
133.024352144898));
#154705=CARTESIAN_POINT('Ctrl Pts',(-71.0869770063439,5.5419553331297,132.876717162202));
#154706=CARTESIAN_POINT('Ctrl Pts',(-71.0943733632793,5.5971594511657,132.729088725796));
#154707=CARTESIAN_POINT('Ctrl Pts',(-71.1017697202147,5.64646406617286,
132.579243780142));
#154708=CARTESIAN_POINT('Ctrl Pts',(-71.1091660771501,5.68970221677142,
132.427696456808));
#154709=CARTESIAN_POINT('Ctrl Pts',(-71.1165635664867,5.73294698724122,
132.276125931191));
#154710=CARTESIAN_POINT('Ctrl Pts',(-71.1239610558232,5.77012334153,132.122852867925));
#154711=CARTESIAN_POINT('Ctrl Pts',(-71.1313585451597,5.80111466905825,
131.968404928981));
#154712=CARTESIAN_POINT('Ctrl Pts',(-71.1387586276746,5.83211686054832,
131.813902848551));
#154713=CARTESIAN_POINT('Ctrl Pts',(-71.1461587101896,5.85692963510831,
131.658225438225));
#154714=CARTESIAN_POINT('Ctrl Pts',(-71.1535587927045,5.87548782611979,
131.501908728895));
#154715=CARTESIAN_POINT('Ctrl Pts',(-71.1609670123709,5.8940664237701,131.345420133272));
#154716=CARTESIAN_POINT('Ctrl Pts',(-71.1683752320374,5.90637665890132,
131.18829120568));
#154717=CARTESIAN_POINT('Ctrl Pts',(-71.1757834517039,5.91240535225445,
131.031061991918));
#154718=CARTESIAN_POINT('Ctrl Pts',(-71.1831962310059,5.91843775616775,
130.873736006198));
#154719=CARTESIAN_POINT('Ctrl Pts',(-71.1906090103079,5.91818091505398,
130.716309983746));
#154720=CARTESIAN_POINT('Ctrl Pts',(-71.1980217896099,5.91167374302079,
130.559321603165));
#154721=CARTESIAN_POINT('Ctrl Pts',(-71.2054451606386,5.90515727323503,
130.402108910224));
#154722=CARTESIAN_POINT('Ctrl Pts',(-71.2128685316673,5.89237266604779,
130.245335479142));
#154723=CARTESIAN_POINT('Ctrl Pts',(-71.220291902696,5.87341051764293,130.08953234886));
#154724=CARTESIAN_POINT('Ctrl Pts',(-71.2242279521373,5.8633563315669,130.006921790729));
#154725=CARTESIAN_POINT('Ctrl Pts',(-71.2281640015786,5.85156626881008,
129.924583836008));
#154726=CARTESIAN_POINT('Ctrl Pts',(-71.2321000510199,5.83805957135399,
129.842596091384));
#154727=CARTESIAN_POINT('Ctrl Pts',(-71.2395233174253,5.81258636148441,
129.687969763792));
#154728=CARTESIAN_POINT('Ctrl Pts',(-71.2469465838308,5.78092726129591,
129.534122344127));
#154729=CARTESIAN_POINT('Ctrl Pts',(-71.2543698502362,5.74313922840864,
129.381587843855));
#154730=CARTESIAN_POINT('Ctrl Pts',(-71.2617843429573,5.70539585783808,
129.229233626694));
#154731=CARTESIAN_POINT('Ctrl Pts',(-71.2691988356783,5.66153806245929,
129.078189598941));
#154732=CARTESIAN_POINT('Ctrl Pts',(-71.2766133283993,5.61167432039221,
128.928982819801));
#154733=CARTESIAN_POINT('Ctrl Pts',(-71.2840206747531,5.56185863887714,
128.779919851772));
#154734=CARTESIAN_POINT('Ctrl Pts',(-71.2914280211068,5.50604865247688,
128.632690958695));
#154735=CARTESIAN_POINT('Ctrl Pts',(-71.2988353674606,5.44440344289867,
128.487811090046));
#154736=CARTESIAN_POINT('Ctrl Pts',(-71.306237189136,5.38280421064341,128.343039278269));
#154737=CARTESIAN_POINT('Ctrl Pts',(-71.3136390108115,5.31537856641355,
128.200613344487));
#154738=CARTESIAN_POINT('Ctrl Pts',(-71.321040832487,5.24233475410965,128.061031091542));
#154739=CARTESIAN_POINT('Ctrl Pts',(-71.3284387467984,5.16932950106569,
127.921522522982));
#154740=CARTESIAN_POINT('Ctrl Pts',(-71.3358366611097,5.09071215909823,
127.784854975543));
#154741=CARTESIAN_POINT('Ctrl Pts',(-71.3432345754211,5.00673818381789,
127.651504242594));
#154742=CARTESIAN_POINT('Ctrl Pts',(-71.3506312603333,4.92277816348892,
127.518175670119));
#154743=CARTESIAN_POINT('Ctrl Pts',(-71.3580279452456,4.83346347530592,
127.388163133751));
#154744=CARTESIAN_POINT('Ctrl Pts',(-71.3654246301578,4.73909448051574,
127.261915971951));
#154745=CARTESIAN_POINT('Ctrl Pts',(-71.3728209870933,4.64472967014569,
127.135674408083));
#154746=CARTESIAN_POINT('Ctrl Pts',(-71.3802173440287,4.54531122228001,
127.013198185805));
#154747=CARTESIAN_POINT('Ctrl Pts',(-71.3876137009642,4.4411814436635,126.894905675127));
#154748=CARTESIAN_POINT('Ctrl Pts',(-71.3950111903008,4.33703572251192,
126.776595053563));
#154749=CARTESIAN_POINT('Ctrl Pts',(-71.4024086796374,4.22817748104193,
126.662469699213));
#154750=CARTESIAN_POINT('Ctrl Pts',(-71.4098061689741,4.11498762534811,
126.552912934043));
#154751=CARTESIAN_POINT('Ctrl Pts',(-71.4172062514891,4.00175809112585,
126.443317763919));
#154752=CARTESIAN_POINT('Ctrl Pts',(-71.424606334004,3.88419418753936,126.338294631034));
#154753=CARTESIAN_POINT('Ctrl Pts',(-71.432006416519,3.76271166840945,126.2381880997));
#154754=CARTESIAN_POINT('Ctrl Pts',(-71.4394146361855,3.64109556676105,
126.137971490943));
#154755=CARTESIAN_POINT('Ctrl Pts',(-71.4468228558521,3.51555253263624,
126.042682518032));
#154756=CARTESIAN_POINT('Ctrl Pts',(-71.4542310755186,3.38652979815007,
125.952624176997));
#154757=CARTESIAN_POINT('Ctrl Pts',(-71.4616438548207,3.25742765232351,
125.862510406556));
#154758=CARTESIAN_POINT('Ctrl Pts',(-71.4690566341228,3.12484185220072,
125.77763388378));
#154759=CARTESIAN_POINT('Ctrl Pts',(-71.4764694134249,2.98924579604377,
125.698252497546));
#154760=CARTESIAN_POINT('Ctrl Pts',(-71.4838927844536,2.85345599388315,
125.618757687465));
#154761=CARTESIAN_POINT('Ctrl Pts',(-71.4913161554824,2.71464767379158,
125.544773870667));
#154762=CARTESIAN_POINT('Ctrl Pts',(-71.4987395265112,2.57331658332102,
125.476511865536));
#154763=CARTESIAN_POINT('Ctrl Pts',(-71.5026755759517,2.49837944796581,
125.440317712494));
#154764=CARTESIAN_POINT('Ctrl Pts',(-71.5066116253922,2.42273337783236,
125.405731350467));
#154765=CARTESIAN_POINT('Ctrl Pts',(-71.5105476748328,2.34645406638664,
125.372778538941));
#154766=CARTESIAN_POINT('Ctrl Pts',(-71.5179709412382,2.20259366558696,
125.310630564822));
#154767=CARTESIAN_POINT('Ctrl Pts',(-71.5253942076436,2.05604495727097,
125.254107974183));
#154768=CARTESIAN_POINT('Ctrl Pts',(-71.532817474049,1.90728800739199,125.203451493204));
#154769=CARTESIAN_POINT('Ctrl Pts',(-71.5402319667699,1.75870687587426,
125.15285488398));
#154770=CARTESIAN_POINT('Ctrl Pts',(-71.5476464594908,1.60792304784986,
125.108110702893));
#154771=CARTESIAN_POINT('Ctrl Pts',(-71.5550609522118,1.45543858822795,
125.069412572605));
#154772=CARTESIAN_POINT('Ctrl Pts',(-71.5624682985656,1.30310109886895,
125.030751741032));
#154773=CARTESIAN_POINT('Ctrl Pts',(-71.5698756449194,1.14906660050176,
124.998125450238));
#154774=CARTESIAN_POINT('Ctrl Pts',(-71.5772829912731,0.993854322252511,
124.971678203047));
#154775=CARTESIAN_POINT('Ctrl Pts',(-71.5846848129485,0.838757807176206,
124.94525068121));
#154776=CARTESIAN_POINT('Ctrl Pts',(-71.5920866346238,0.682485627705961,
124.924993089139));
#154777=CARTESIAN_POINT('Ctrl Pts',(-71.5994884562992,0.52556916038521,
124.910999299935));
#154778=CARTESIAN_POINT('Ctrl Pts',(-71.6068863706105,0.368735528046346,
124.897012897943));
#154779=CARTESIAN_POINT('Ctrl Pts',(-71.6142842849218,0.211258656092448,
124.889283746618));
#154780=CARTESIAN_POINT('Ctrl Pts',(-71.6216821992331,0.0536769229582773,
124.887854101856));
#154781=CARTESIAN_POINT('Ctrl Pts',(-71.6290788841453,-0.103878622950895,
124.886424694675));
#154782=CARTESIAN_POINT('Ctrl Pts',(-71.6364755690574,-0.261538622537786,
124.891292719726));
#154783=CARTESIAN_POINT('Ctrl Pts',(-71.6438722539696,-0.418762682039236,
124.902448353));
#154784=CARTESIAN_POINT('Ctrl Pts',(-71.651268610905,-0.575979770061128,
124.913603491622));
#154785=CARTESIAN_POINT('Ctrl Pts',(-71.6586649678404,-0.732760584070799,
124.931045657698));
#154786=CARTESIAN_POINT('Ctrl Pts',(-71.6660613247758,-0.888568112374757,
124.954712998079));
#154787=CARTESIAN_POINT('Ctrl Pts',(-71.6734588141123,-1.04439949520928,
124.97838396199));
#154788=CARTESIAN_POINT('Ctrl Pts',(-71.6808563034489,-1.19925692654631,
125.00828194187));
#154789=CARTESIAN_POINT('Ctrl Pts',(-71.6882537927854,-1.35261201770984,
125.04429366552));
#154790=CARTESIAN_POINT('Ctrl Pts',(-71.6956538753004,-1.5060208672624,
125.080318013025));
#154791=CARTESIAN_POINT('Ctrl Pts',(-71.7030539578153,-1.65792596491327,
125.122460286036));
#154792=CARTESIAN_POINT('Ctrl Pts',(-71.7104540403303,-1.80781269385303,
125.170556944518));
#154793=CARTESIAN_POINT('Ctrl Pts',(-71.7178622599967,-1.95786423866042,
125.218706490221));
#154794=CARTESIAN_POINT('Ctrl Pts',(-71.7252704796631,-2.10589262679697,
125.272823382971));
#154795=CARTESIAN_POINT('Ctrl Pts',(-71.7326786993295,-2.25140119923883,
125.33269513048));
#154796=CARTESIAN_POINT('Ctrl Pts',(-71.7400914786316,-2.39699932977909,
125.392603728051));
#154797=CARTESIAN_POINT('Ctrl Pts',(-71.7475042579336,-2.54007421577242,
125.458274082932));
#154798=CARTESIAN_POINT('Ctrl Pts',(-71.7549170372357,-2.68015300467841,
125.529447306997));
#154799=CARTESIAN_POINT('Ctrl Pts',(-71.7623404082644,-2.82043194472722,
125.600722226703));
#154800=CARTESIAN_POINT('Ctrl Pts',(-71.7697637792931,-2.95770591272066,
125.677515537516));
#154801=CARTESIAN_POINT('Ctrl Pts',(-71.7771871503218,-3.09152957752034,
125.759524105466));
#154802=CARTESIAN_POINT('Ctrl Pts',(-71.781123199763,-3.16248609566007,
125.803007015967));
#154803=CARTESIAN_POINT('Ctrl Pts',(-71.7850592492042,-3.23247313024798,
125.847955423691));
#154804=CARTESIAN_POINT('Ctrl Pts',(-71.7889952986454,-3.30142809493104,
125.894319569214));
#154805=CARTESIAN_POINT('Ctrl Pts',(-71.7963922461212,-3.43101392955234,
125.981450880523));
#154806=CARTESIAN_POINT('Ctrl Pts',(-71.8037891935969,-3.55735086442155,
126.073852199481));
#154807=CARTESIAN_POINT('Ctrl Pts',(-71.8111861410727,-3.67997876379524,
126.171252928281));
#154808=CARTESIAN_POINT('Ctrl Pts',(-71.8185743296968,-3.80246145738337,
126.268538323217));
#154809=CARTESIAN_POINT('Ctrl Pts',(-71.8259625183209,-3.9212435648374,
126.37081111428));
#154810=CARTESIAN_POINT('Ctrl Pts',(-71.8333507069451,-4.03589253330437,
126.477756634981));
#154811=CARTESIAN_POINT('Ctrl Pts',(-71.8407317889035,-4.15043122143831,
126.584599285262));
#154812=CARTESIAN_POINT('Ctrl Pts',(-71.8481128708618,-4.26084441107513,
126.696105463363));
#154813=CARTESIAN_POINT('Ctrl Pts',(-71.8554939528202,-4.36673148392284,
126.811919420777));
#154814=CARTESIAN_POINT('Ctrl Pts',(-71.8628695744455,-4.47254022426022,
126.927647702029));
#154815=CARTESIAN_POINT('Ctrl Pts',(-71.870245196071,-4.5738292611642,127.047677141507));
#154816=CARTESIAN_POINT('Ctrl Pts',(-71.8776208176963,-4.67023393119619,
127.17161432992));
#154817=CARTESIAN_POINT('Ctrl Pts',(-71.8852876506168,-4.77044494193312,
127.300444924067));
#154818=CARTESIAN_POINT('Ctrl Pts',(-71.8929544835373,-4.86537769775476,
127.433497869516));
#154819=CARTESIAN_POINT('Ctrl Pts',(-71.9006213164578,-4.95466745374232,
127.570291820319));
#154820=CARTESIAN_POINT('Ctrl Pts',(-71.9079919684677,-5.04050781654442,
127.701801221775));
#154821=CARTESIAN_POINT('Ctrl Pts',(-71.9153626204778,-5.12113281117333,
127.836767641905));
#154822=CARTESIAN_POINT('Ctrl Pts',(-71.9227332724877,-5.19626186138799,
127.974732862828));
#154823=CARTESIAN_POINT('Ctrl Pts',(-71.9301037804294,-5.27138944311522,
128.112695387055));
#154824=CARTESIAN_POINT('Ctrl Pts',(-71.937474288371,-5.34102111385726,
128.253656265171));
#154825=CARTESIAN_POINT('Ctrl Pts',(-71.9448447963127,-5.40492200940477,
128.397132204068));
#154826=CARTESIAN_POINT('Ctrl Pts',(-71.9522166426895,-5.46883450892819,
128.540634197237));
#154827=CARTESIAN_POINT('Ctrl Pts',(-71.9595884890663,-5.52701400855252,
128.686651816637));
#154828=CARTESIAN_POINT('Ctrl Pts',(-71.966960335443,-5.57927366816981,
128.834681481725));
#154829=CARTESIAN_POINT('Ctrl Pts',(-71.9743350033206,-5.6315533296523,
128.982767803696));
#154830=CARTESIAN_POINT('Ctrl Pts',(-71.9817096711983,-5.67790851565975,
129.132867349833));
#154831=CARTESIAN_POINT('Ctrl Pts',(-71.9890843390759,-5.718202207928,129.284461255191));
#154832=CARTESIAN_POINT('Ctrl Pts',(-71.9964671243711,-5.75854025212212,
129.43622202244));
#154833=CARTESIAN_POINT('Ctrl Pts',(-72.0038499096662,-5.79280338507631,
129.589480069292));
#154834=CARTESIAN_POINT('Ctrl Pts',(-72.0112326949614,-5.82090555401294,
129.743705587049));
#154835=CARTESIAN_POINT('Ctrl Pts',(-72.0186202885717,-5.84902602553843,
129.898031549944));
#154836=CARTESIAN_POINT('Ctrl Pts',(-72.0260078821819,-5.87097748700464,
130.053325867692));
#154837=CARTESIAN_POINT('Ctrl Pts',(-72.0333954757921,-5.88672580388552,
130.209054081092));
#154838=CARTESIAN_POINT('Ctrl Pts',(-72.0407930705532,-5.90249544046816,
130.364993115692));
#154839=CARTESIAN_POINT('Ctrl Pts',(-72.0481906653144,-5.91204514566992,
130.521366844748));
#154840=CARTESIAN_POINT('Ctrl Pts',(-72.0555882600755,-5.91539285414198,
130.677640675702));
#154841=CARTESIAN_POINT('Ctrl Pts',(-72.0576004426463,-5.91630344749795,
130.720147935031));
#154842=CARTESIAN_POINT('Ctrl Pts',(-72.0596126252172,-5.91675547192607,
130.762647832883));
#154843=CARTESIAN_POINT('Ctrl Pts',(-72.061624807788,-5.91674995001673,
130.805129693042));
#154844=CARTESIAN_POINT('',(-73.811624807788,-5.91489018159219,130.798942093786));
#154845=CARTESIAN_POINT('Ctrl Pts',(-72.061624807788,-5.92641032049353,
130.805130948724));
#154846=CARTESIAN_POINT('Ctrl Pts',(-72.0635641793449,-5.92648514252835,
130.846142460203));
#154847=CARTESIAN_POINT('Ctrl Pts',(-72.0655035509017,-5.92609641746022,
130.887152515512));
#154848=CARTESIAN_POINT('Ctrl Pts',(-72.0674429224586,-5.92523982529112,
130.928152795978));
#154849=CARTESIAN_POINT('Ctrl Pts',(-72.1602587970629,-5.88424440537134,
132.890374463603));
#154850=CARTESIAN_POINT('Ctrl Pts',(-72.3458905462715,-3.65899295410281,
136.770040050133));
#154851=CARTESIAN_POINT('Ctrl Pts',(-72.6243381700844,3.04131999587715,
137.107370471042));
#154852=CARTESIAN_POINT('Ctrl Pts',(-72.9027857938972,6.94680844638694,
131.652542755755));
#154853=CARTESIAN_POINT('Ctrl Pts',(-73.1812334177101,4.46851930512866,
125.418277091475));
#154854=CARTESIAN_POINT('Ctrl Pts',(-73.459681041523,-2.11612077824121,
124.133559062861));
#154855=CARTESIAN_POINT('Ctrl Pts',(-73.6698115048829,-5.61771766134115,
127.790156687924));
#154856=CARTESIAN_POINT('Ctrl Pts',(-73.7871260936373,-5.91953532486225,
130.27824939099));
#154857=CARTESIAN_POINT('Ctrl Pts',(-73.811624807788,-5.91489018159219,
130.798942093786));
#154858=CARTESIAN_POINT('',(-75.5616248077879,-5.90731964829396,130.80593864926));
#154859=CARTESIAN_POINT('Ctrl Pts',(-73.811624807788,-5.91489018159219,
130.798942093786));
#154860=CARTESIAN_POINT('Ctrl Pts',(-73.8799419682416,-5.90193672631452,
132.250946746161));
#154861=CARTESIAN_POINT('Ctrl Pts',(-74.0410750033003,-4.63017145259677,
135.695938571682));
#154862=CARTESIAN_POINT('Ctrl Pts',(-74.2950239129616,1.14809306898754,
137.707942502008));
#154863=CARTESIAN_POINT('Ctrl Pts',(-74.5734715367747,6.4287513065015,133.569992040856));
#154864=CARTESIAN_POINT('Ctrl Pts',(-74.8519191605875,5.80170115531016,
126.890561410293));
#154865=CARTESIAN_POINT('Ctrl Pts',(-75.1303667844004,-0.156828928757731,
123.8077210515));
#154866=CARTESIAN_POINT('Ctrl Pts',(-75.366935333467,-5.09674180081162,
126.651095881476));
#154867=CARTESIAN_POINT('Ctrl Pts',(-75.5106880079297,-5.90473716813048,
129.719838266436));
#154868=CARTESIAN_POINT('Ctrl Pts',(-75.5616248077879,-5.90731964829396,
130.80593864926));
#154869=CARTESIAN_POINT('',(-77.311624807788,-5.92069754378162,130.809234386756));
#154870=CARTESIAN_POINT('Ctrl Pts',(-75.5616248077879,-5.90731964829396,
130.80593864926));
#154871=CARTESIAN_POINT('Ctrl Pts',(-75.603503882534,-5.90944290456639,
131.698905605187));
#154872=CARTESIAN_POINT('Ctrl Pts',(-75.738198831884,-5.29942908797976,
134.568186077309));
#154873=CARTESIAN_POINT('Ctrl Pts',(-75.9657096558394,-0.837609296111783,
137.752451808497));
#154874=CARTESIAN_POINT('Ctrl Pts',(-76.2441572796519,5.3928776148045,135.264678045965));
#154875=CARTESIAN_POINT('Ctrl Pts',(-76.522604903465,6.66757345442674,128.678090465366));
#154876=CARTESIAN_POINT('Ctrl Pts',(-76.8010525272776,1.81509501850905,
124.04544128056));
#154877=CARTESIAN_POINT('Ctrl Pts',(-77.0640591620522,-4.34378242790828,
125.536376696356));
#154878=CARTESIAN_POINT('Ctrl Pts',(-77.2342499222222,-5.90612396355947,
129.168851731668));
#154879=CARTESIAN_POINT('Ctrl Pts',(-77.311624807788,-5.92069754378162,
130.809234386756));
#154880=CARTESIAN_POINT('',(-79.0616248077881,-5.92047761364803,130.800476772624));
#154881=CARTESIAN_POINT('Ctrl Pts',(-77.311624807788,-5.92069754378162,
130.809234386756));
#154882=CARTESIAN_POINT('Ctrl Pts',(-77.3270657968265,-5.92360585816317,
131.136590355181));
#154883=CARTESIAN_POINT('Ctrl Pts',(-77.4353226604685,-5.74974331525388,
133.428593509251));
#154884=CARTESIAN_POINT('Ctrl Pts',(-77.636395398717,-2.75584475561056,
137.237313299921));
#154885=CARTESIAN_POINT('Ctrl Pts',(-77.914843022529,3.92262387668917,136.600098918449));
#154886=CARTESIAN_POINT('Ctrl Pts',(-78.1932906463423,6.99639279714031,
130.636884176034));
#154887=CARTESIAN_POINT('Ctrl Pts',(-78.4717382701551,3.64081852980919,
124.827572101703));
#154888=CARTESIAN_POINT('Ctrl Pts',(-78.750185893968,-3.06049010254254,
124.510636691099));
#154889=CARTESIAN_POINT('Ctrl Pts',(-78.9468147398456,-5.80665674345474,
128.370999423577));
#154890=CARTESIAN_POINT('Ctrl Pts',(-79.0506277111191,-5.92502371784771,
130.567593766307));
#154891=CARTESIAN_POINT('Ctrl Pts',(-79.0616248077881,-5.92325710276932,
130.800474949274));
#154892=CARTESIAN_POINT('',(-80.8116247804992,-5.91211101482029,130.801357666489));
#154893=CARTESIAN_POINT('Ctrl Pts',(-79.0616248077881,-5.91674872689752,
130.800479218781));
#154894=CARTESIAN_POINT('Ctrl Pts',(-79.0689408856106,-5.91685024886036,
130.955237845168));
#154895=CARTESIAN_POINT('Ctrl Pts',(-79.0762569634331,-5.91087581439112,
131.110236902362));
#154896=CARTESIAN_POINT('Ctrl Pts',(-79.0835730412556,-5.89879532966383,
131.264951782523));
#154897=CARTESIAN_POINT('Ctrl Pts',(-79.0908815388731,-5.88672736155428,
131.419506362244));
#154898=CARTESIAN_POINT('Ctrl Pts',(-79.0981900364905,-5.86856596065094,
131.573776970751));
#154899=CARTESIAN_POINT('Ctrl Pts',(-79.1054985341081,-5.84433303758537,
131.727237591105));
#154900=CARTESIAN_POINT('Ctrl Pts',(-79.1128011570195,-5.82011959339369,
131.88057485696));
#154901=CARTESIAN_POINT('Ctrl Pts',(-79.1201037799308,-5.78984439899684,
132.033103052641));
#154902=CARTESIAN_POINT('Ctrl Pts',(-79.1274064028422,-5.75358127374173,
132.184300141222));
#154903=CARTESIAN_POINT('Ctrl Pts',(-79.1348928502902,-5.71640531863396,
132.339303223223));
#154904=CARTESIAN_POINT('Ctrl Pts',(-79.1423792977382,-5.67293600697595,
132.492906886673));
#154905=CARTESIAN_POINT('Ctrl Pts',(-79.1498657451862,-5.62330902356941,
132.644557940666));
#154906=CARTESIAN_POINT('Ctrl Pts',(-79.1571626313433,-5.57493862482498,
132.792369100001));
#154907=CARTESIAN_POINT('Ctrl Pts',(-79.1644595175005,-5.5207187620526,
132.938324956991));
#154908=CARTESIAN_POINT('Ctrl Pts',(-79.1717564036576,-5.46082585735375,
133.081927634836));
#154909=CARTESIAN_POINT('Ctrl Pts',(-79.1790529036736,-5.40093612210465,
133.225522713426));
#154910=CARTESIAN_POINT('Ctrl Pts',(-79.1863494036894,-5.33537408989546,
133.366764505674));
#154911=CARTESIAN_POINT('Ctrl Pts',(-79.1936459037054,-5.2643644339058,
133.50517487803));
#154912=CARTESIAN_POINT('Ctrl Pts',(-79.2009435505635,-5.19334361683021,
133.643607005316));
#154913=CARTESIAN_POINT('Ctrl Pts',(-79.2082411974216,-5.11687364797293,
133.77920648526));
#154914=CARTESIAN_POINT('Ctrl Pts',(-79.2155388442796,-5.03522513301774,
133.911519838193));
#154915=CARTESIAN_POINT('Ctrl Pts',(-79.2231673690558,-4.94987464519807,
134.049832325861));
#154916=CARTESIAN_POINT('Ctrl Pts',(-79.230795893832,-4.85886527367793,
134.184553327272));
#154917=CARTESIAN_POINT('Ctrl Pts',(-79.2384244186081,-4.76255600949217,
134.31519966528));
#154918=CARTESIAN_POINT('Ctrl Pts',(-79.2457328170896,-4.67028830364041,
134.44036351102));
#154919=CARTESIAN_POINT('Ctrl Pts',(-79.2530412155711,-4.57315675802231,
134.561787455097));
#154920=CARTESIAN_POINT('Ctrl Pts',(-79.2603496140526,-4.47151711635527,
134.679081928918));
#154921=CARTESIAN_POINT('Ctrl Pts',(-79.2676628513618,-4.36981017995708,
134.796454062398));
#154922=CARTESIAN_POINT('Ctrl Pts',(-79.274976088671,-4.26358946657629,
134.909691002896));
#154923=CARTESIAN_POINT('Ctrl Pts',(-79.2822893259802,-4.15324649538433,
135.018441076109));
#154924=CARTESIAN_POINT('Ctrl Pts',(-79.2896121733775,-4.04275852607044,
135.127334054269));
#154925=CARTESIAN_POINT('Ctrl Pts',(-79.2969350207748,-3.92813777357985,
135.231728144505));
#154926=CARTESIAN_POINT('Ctrl Pts',(-79.3042578681721,-3.80980790028127,
135.331312608194));
#154927=CARTESIAN_POINT('Ctrl Pts',(-79.3051989593126,-3.79460081082798,
135.344110643088));
#154928=CARTESIAN_POINT('Ctrl Pts',(-79.3061400504532,-3.77933249924615,
135.35682930223));
#154929=CARTESIAN_POINT('Ctrl Pts',(-79.3070811415938,-3.76400389706835,
135.369467979431));
#154930=CARTESIAN_POINT('Ctrl Pts',(-79.3145044079992,-3.64309286870323,
135.469161052537));
#154931=CARTESIAN_POINT('Ctrl Pts',(-79.3219276744046,-3.51803558040563,
135.564197897001));
#154932=CARTESIAN_POINT('Ctrl Pts',(-79.32935094081,-3.38922624739663,135.654213811886));
#154933=CARTESIAN_POINT('Ctrl Pts',(-79.336765433531,-3.2605691563223,135.744123335435));
#154934=CARTESIAN_POINT('Ctrl Pts',(-79.3441799262521,-3.12816915064036,
135.829023529961));
#154935=CARTESIAN_POINT('Ctrl Pts',(-79.3515944189731,-2.99245467268624,
135.908588825084));
#154936=CARTESIAN_POINT('Ctrl Pts',(-79.3590017653269,-2.85687100145592,
135.988077432179));
#154937=CARTESIAN_POINT('Ctrl Pts',(-79.3664091116806,-2.71797953767195,
136.062241189004));
#154938=CARTESIAN_POINT('Ctrl Pts',(-79.3738164580344,-2.57623886720719,
136.130796936681));
#154939=CARTESIAN_POINT('Ctrl Pts',(-79.3812182797097,-2.43460391228202,
136.199301552896));
#154940=CARTESIAN_POINT('Ctrl Pts',(-79.3886201013852,-2.29012431653675,
136.262206326375));
#154941=CARTESIAN_POINT('Ctrl Pts',(-79.3960219230606,-2.14328441012716,
136.319273354845));
#154942=CARTESIAN_POINT('Ctrl Pts',(-79.4034198373719,-1.99652201936074,
136.376310258076));
#154943=CARTESIAN_POINT('Ctrl Pts',(-79.4108177516832,-1.84740214644256,
136.427515418772));
#154944=CARTESIAN_POINT('Ctrl Pts',(-79.4182156659946,-1.69643019767104,
136.472698570346));
#154945=CARTESIAN_POINT('Ctrl Pts',(-79.4256123509068,-1.54548333769871,
136.517874213301));
#154946=CARTESIAN_POINT('Ctrl Pts',(-79.433009035819,-1.39268537000304,
136.557029726399));
#154947=CARTESIAN_POINT('Ctrl Pts',(-79.4404057207312,-1.23855811568455,
136.590024309535));
#154948=CARTESIAN_POINT('Ctrl Pts',(-79.4478020776667,-1.08443769553003,
136.623017429657));
#154949=CARTESIAN_POINT('Ctrl Pts',(-79.4551984346021,-0.92898847097632,
136.649850084854));
#154950=CARTESIAN_POINT('Ctrl Pts',(-79.4625947915375,-0.772743479194567,
136.670432393283));
#154951=CARTESIAN_POINT('Ctrl Pts',(-79.4699922808741,-0.616474565906143,
136.691017852916));
#154952=CARTESIAN_POINT('Ctrl Pts',(-79.4773897702108,-0.459410012926293,
136.705351011623));
#154953=CARTESIAN_POINT('Ctrl Pts',(-79.4847872595473,-0.302088869548253,
136.71339377684));
#154954=CARTESIAN_POINT('Ctrl Pts',(-79.4921873420623,-0.144712577487056,
136.721439361435));
#154955=CARTESIAN_POINT('Ctrl Pts',(-79.4995874245773,0.0129201114784148,
136.723190143181));
#154956=CARTESIAN_POINT('Ctrl Pts',(-79.5069875070923,0.170269401851392,
136.718660144416));
#154957=CARTESIAN_POINT('Ctrl Pts',(-79.5143957267587,0.32779171394526,
136.714125164451));
#154958=CARTESIAN_POINT('Ctrl Pts',(-79.5218039464251,0.485029631737011,
136.703295622263));
#154959=CARTESIAN_POINT('Ctrl Pts',(-79.5292121660916,0.641447000175478,
136.686237555115));
#154960=CARTESIAN_POINT('Ctrl Pts',(-79.5366249453937,0.797960640894256,
136.66916898901));
#154961=CARTESIAN_POINT('Ctrl Pts',(-79.5440377246957,0.95365235758637,
136.645864314243));
#154962=CARTESIAN_POINT('Ctrl Pts',(-79.5514505039978,1.10799596448945,
136.616440753384));
#154963=CARTESIAN_POINT('Ctrl Pts',(-79.5588738750265,1.26256010477585,
136.586975150762));
#154964=CARTESIAN_POINT('Ctrl Pts',(-79.5662972460552,1.41577192548795,
136.551373284681));
#154965=CARTESIAN_POINT('Ctrl Pts',(-79.5737206170839,1.56711937634628,
136.50980253058));
#154966=CARTESIAN_POINT('Ctrl Pts',(-79.5776566665248,1.64736742632598,
136.487760719279));
#154967=CARTESIAN_POINT('Ctrl Pts',(-79.5815927159658,1.72709164075768,
136.464041655228));
#154968=CARTESIAN_POINT('Ctrl Pts',(-79.5855287654067,1.80621806682415,
136.438675736334));
#154969=CARTESIAN_POINT('Ctrl Pts',(-79.5929520318121,1.95544803693053,
136.390836404945));
#154970=CARTESIAN_POINT('Ctrl Pts',(-79.6003752982176,2.10300174478034,
136.33699190233));
#154971=CARTESIAN_POINT('Ctrl Pts',(-79.607798564623,2.24835927419038,136.277276763156));
#154972=CARTESIAN_POINT('Ctrl Pts',(-79.615213057344,2.39354500307185,136.217632202318));
#154973=CARTESIAN_POINT('Ctrl Pts',(-79.622627550065,2.53653937834598,136.152130956718));
#154974=CARTESIAN_POINT('Ctrl Pts',(-79.630042042786,2.67683690488364,136.080957508286));
#154975=CARTESIAN_POINT('Ctrl Pts',(-79.6374493891398,2.81699920738231,
136.009852659503));
#154976=CARTESIAN_POINT('Ctrl Pts',(-79.6448567354935,2.95446950521293,
135.933086659525));
#154977=CARTESIAN_POINT('Ctrl Pts',(-79.6522640818472,3.08876169192816,
135.850892275346));
#154978=CARTESIAN_POINT('Ctrl Pts',(-79.6596659035226,3.22295371846438,
135.76875919484));
#154979=CARTESIAN_POINT('Ctrl Pts',(-79.6670677251981,3.35397203655822,
135.681205985664));
#154980=CARTESIAN_POINT('Ctrl Pts',(-79.6744695468735,3.48135470001146,
135.588511536507));
#154981=CARTESIAN_POINT('Ctrl Pts',(-79.6818674611848,3.6086701191482,135.495866020029));
#154982=CARTESIAN_POINT('Ctrl Pts',(-79.6892653754961,3.73235340481413,
135.398084887761));
#154983=CARTESIAN_POINT('Ctrl Pts',(-79.6966632898075,3.85197129589288,
135.295490508598));
#154984=CARTESIAN_POINT('Ctrl Pts',(-79.7040599747197,3.97156930864839,
135.192913178759));
#154985=CARTESIAN_POINT('Ctrl Pts',(-79.7114566596317,4.08710298459685,
135.085524432329));
#154986=CARTESIAN_POINT('Ctrl Pts',(-79.7188533445439,4.19817180757139,
134.973687186283));
#154987=CARTESIAN_POINT('Ctrl Pts',(-79.7262497014793,4.30923570563794,
134.861854899218));
#154988=CARTESIAN_POINT('Ctrl Pts',(-79.7336460584149,4.41583488132454,
134.745574769608));
#154989=CARTESIAN_POINT('Ctrl Pts',(-79.7410424153504,4.51760559488155,
134.625246673391));
#154990=CARTESIAN_POINT('Ctrl Pts',(-79.7484399046869,4.61939188979462,
134.504900154635));
#154991=CARTESIAN_POINT('Ctrl Pts',(-79.7558373940235,4.71634800955154,
134.380504720301));
#154992=CARTESIAN_POINT('Ctrl Pts',(-79.76323488336,4.80815053649018,134.252493297865));
#154993=CARTESIAN_POINT('Ctrl Pts',(-79.770634965875,4.89998524466245,134.124437001224));
#154994=CARTESIAN_POINT('Ctrl Pts',(-79.7780350483901,4.9866625457081,133.992762495906));
#154995=CARTESIAN_POINT('Ctrl Pts',(-79.7854351309051,5.06790246436763,
133.857931506567));
#154996=CARTESIAN_POINT('Ctrl Pts',(-79.7928433505715,5.1492317146695,133.722952256695));
#154997=CARTESIAN_POINT('Ctrl Pts',(-79.800251570238,5.22511144943452,133.584809911168));
#154998=CARTESIAN_POINT('Ctrl Pts',(-79.8076597899044,5.29530742278066,
133.44399124717));
#154999=CARTESIAN_POINT('Ctrl Pts',(-79.8150725692065,5.36554660057672,
133.303085911635));
#155000=CARTESIAN_POINT('Ctrl Pts',(-79.8224853485085,5.43009489352607,
133.159501315004));
#155001=CARTESIAN_POINT('Ctrl Pts',(-79.8298981278106,5.48876650804002,
133.013743513924));
#155002=CARTESIAN_POINT('Ctrl Pts',(-79.8373214988393,5.54752195530829,
132.867777447262));
#155003=CARTESIAN_POINT('Ctrl Pts',(-79.844744869868,5.60038382857864,132.719632325072));
#155004=CARTESIAN_POINT('Ctrl Pts',(-79.8521682408967,5.64721616986486,
132.569829420269));
#155005=CARTESIAN_POINT('Ctrl Pts',(-79.8561042903376,5.67204780094216,
132.490400325668));
#155006=CARTESIAN_POINT('Ctrl Pts',(-79.8600403397786,5.69518516586961,
132.41050535267));
#155007=CARTESIAN_POINT('Ctrl Pts',(-79.8639763892195,5.71661386596347,
132.330223150684));
#155008=CARTESIAN_POINT('Ctrl Pts',(-79.8713996556249,5.75702772557264,
132.178813423265));
#155009=CARTESIAN_POINT('Ctrl Pts',(-79.8788229220304,5.79148320386002,
132.025568041024));
#155010=CARTESIAN_POINT('Ctrl Pts',(-79.8862461884358,5.81981246125332,
131.870997143446));
#155011=CARTESIAN_POINT('Ctrl Pts',(-79.8936606811569,5.84810823581706,
131.716608935831));
#155012=CARTESIAN_POINT('Ctrl Pts',(-79.9010751738779,5.87029213547004,
131.560898694898));
#155013=CARTESIAN_POINT('Ctrl Pts',(-79.9084896665989,5.88624613761831,
131.404391425003));
#155014=CARTESIAN_POINT('Ctrl Pts',(-79.9158970129527,5.90218476269859,
131.248035002708));
#155015=CARTESIAN_POINT('Ctrl Pts',(-79.9233043593065,5.91190540666725,
131.090883449679));
#155016=CARTESIAN_POINT('Ctrl Pts',(-79.9307117056603,5.91534115058,130.933471557284));
#155017=CARTESIAN_POINT('Ctrl Pts',(-79.9381135273357,5.91877433198531,
130.776177068617));
#155018=CARTESIAN_POINT('Ctrl Pts',(-79.9455153490112,5.91593193870001,
130.618622998807));
#155019=CARTESIAN_POINT('Ctrl Pts',(-79.9529171706866,5.90679891447224,
130.461348742422));
#155020=CARTESIAN_POINT('Ctrl Pts',(-79.960315084998,5.89767071149682,130.304157509892));
#155021=CARTESIAN_POINT('Ctrl Pts',(-79.9677129993094,5.88225851264802,
130.147246168339));
#155022=CARTESIAN_POINT('Ctrl Pts',(-79.9751109136208,5.86059934779146,
129.991153480874));
#155023=CARTESIAN_POINT('Ctrl Pts',(-79.982507598533,5.83894378229526,129.835086733183));
#155024=CARTESIAN_POINT('Ctrl Pts',(-79.9899042834451,5.81104336243338,
129.679838738962));
#155025=CARTESIAN_POINT('Ctrl Pts',(-79.9973009683574,5.77698693176365,
129.525942629296));
#155026=CARTESIAN_POINT('Ctrl Pts',(-80.0046973252928,5.74293201119174,
129.372053343545));
#155027=CARTESIAN_POINT('Ctrl Pts',(-80.0120936822283,5.70272170321407,
129.21951618764));
#155028=CARTESIAN_POINT('Ctrl Pts',(-80.0194900391638,5.65649582456277,
129.068853328845));
#155029=CARTESIAN_POINT('Ctrl Pts',(-80.0268875285004,5.61026286861157,
128.918167403182));
#155030=CARTESIAN_POINT('Ctrl Pts',(-80.034285017837,5.55801261765797,128.769356702906));
#155031=CARTESIAN_POINT('Ctrl Pts',(-80.0416825071736,5.49993449070261,
128.622927336331));
#155032=CARTESIAN_POINT('Ctrl Pts',(-80.0490825896886,5.44183600454979,
128.476446639168));
#155033=CARTESIAN_POINT('Ctrl Pts',(-80.0564826722035,5.37790571243548,
128.332349284517));
#155034=CARTESIAN_POINT('Ctrl Pts',(-80.0638827547185,5.30838074292339,
128.191120396947));
#155035=CARTESIAN_POINT('Ctrl Pts',(-80.071290974385,5.23877932355988,128.049736213697));
#155036=CARTESIAN_POINT('Ctrl Pts',(-80.0786991940516,5.16357110597951,
127.911227131742));
#155037=CARTESIAN_POINT('Ctrl Pts',(-80.0861074137181,5.08303901399145,
127.776053343735));
#155038=CARTESIAN_POINT('Ctrl Pts',(-80.0935201930202,5.0024573558443,127.640796358516));
#155039=CARTESIAN_POINT('Ctrl Pts',(-80.1009329723223,4.91654549718926,
127.508879069826));
#155040=CARTESIAN_POINT('Ctrl Pts',(-80.1083457516244,4.82562877184278,
127.380731327052));
#155041=CARTESIAN_POINT('Ctrl Pts',(-80.1157691226531,4.7345821404157,127.252400480774));
#155042=CARTESIAN_POINT('Ctrl Pts',(-80.123192493682,4.63851658715403,127.127850232476));
#155043=CARTESIAN_POINT('Ctrl Pts',(-80.1306158647108,4.53779718511222,
127.007476728205));
#155044=CARTESIAN_POINT('Ctrl Pts',(-80.1345519141514,4.48439334142351,
126.943651807922));
#155045=CARTESIAN_POINT('Ctrl Pts',(-80.1384879635919,4.4296817488055,126.88100050308));
#155046=CARTESIAN_POINT('Ctrl Pts',(-80.1424240130325,4.37372079439489,
126.819577439628));
#155047=CARTESIAN_POINT('Ctrl Pts',(-80.1498472794379,4.26818018085312,
126.703735458901));
#155048=CARTESIAN_POINT('Ctrl Pts',(-80.1572705458433,4.15787452827597,
126.591914216861));
#155049=CARTESIAN_POINT('Ctrl Pts',(-80.1646938122487,4.0431423100696,126.484530664544));
#155050=CARTESIAN_POINT('Ctrl Pts',(-80.1721083049697,3.92854569581723,
126.377274030669));
#155051=CARTESIAN_POINT('Ctrl Pts',(-80.1795227976908,3.80953319981205,
126.274444898952));
#155052=CARTESIAN_POINT('Ctrl Pts',(-80.1869372904118,3.68648272899339,
126.176426342824));
#155053=CARTESIAN_POINT('Ctrl Pts',(-80.1943446367656,3.56355085885057,
126.07850226067));
#155054=CARTESIAN_POINT('Ctrl Pts',(-80.2017519831193,3.4365890520289,125.985379754543));
#155055=CARTESIAN_POINT('Ctrl Pts',(-80.2091593294731,3.30601107232773,
125.897404193045));
#155056=CARTESIAN_POINT('Ctrl Pts',(-80.2165611511485,3.17553048261099,
125.80949424704));
#155057=CARTESIAN_POINT('Ctrl Pts',(-80.2239629728239,3.04143939851723,
125.726723809808));
#155058=CARTESIAN_POINT('Ctrl Pts',(-80.2313647944993,2.90418348970092,
125.649397104538));
#155059=CARTESIAN_POINT('Ctrl Pts',(-80.2387627088107,2.76700003720969,
125.572111219434));
#155060=CARTESIAN_POINT('Ctrl Pts',(-80.246160623122,2.62665541165997,125.50026352594));
#155061=CARTESIAN_POINT('Ctrl Pts',(-80.2535585374334,2.48362290526187,
125.434114084402));
#155062=CARTESIAN_POINT('Ctrl Pts',(-80.2609552223456,2.34061416827208,
125.367975635702));
#155063=CARTESIAN_POINT('Ctrl Pts',(-80.2683519072578,2.194918775442,125.307533716093));
#155064=CARTESIAN_POINT('Ctrl Pts',(-80.27574859217,2.04703328716472,125.253001749348));
#155065=CARTESIAN_POINT('Ctrl Pts',(-80.2831449491054,1.89915435628538,
125.198472200608));
#155066=CARTESIAN_POINT('Ctrl Pts',(-80.2905413060408,1.74908587329303,
125.149852212831));
#155067=CARTESIAN_POINT('Ctrl Pts',(-80.2979376629762,1.59734272665514,
125.107306398401));
#155068=CARTESIAN_POINT('Ctrl Pts',(-80.3053351523128,1.44557634775411,
125.064754070099));
#155069=CARTESIAN_POINT('Ctrl Pts',(-80.3127326416494,1.29213515415045,
125.028277867628));
#155070=CARTESIAN_POINT('Ctrl Pts',(-80.3201301309859,1.1375473346996,124.997991991323));
#155071=CARTESIAN_POINT('Ctrl Pts',(-80.3275302135009,0.982905324727631,
124.967695498351));
#155072=CARTESIAN_POINT('Ctrl Pts',(-80.3349302960158,0.827116254738348,
124.943593723744));
#155073=CARTESIAN_POINT('Ctrl Pts',(-80.3423303785308,0.670716447552981,
124.925749386205));
#155074=CARTESIAN_POINT('Ctrl Pts',(-80.3497385981973,0.514144662701546,
124.907885426983));
#155075=CARTESIAN_POINT('Ctrl Pts',(-80.3571468178638,0.356961170607229,
124.896292688371));
#155076=CARTESIAN_POINT('Ctrl Pts',(-80.3645550375302,0.199706071611347,
124.890981883926));
#155077=CARTESIAN_POINT('Ctrl Pts',(-80.3719678168323,0.0423541847264234,
124.88566781077));
#155078=CARTESIAN_POINT('Ctrl Pts',(-80.3793805961343,-0.11506902445551,
124.886643373811));
#155079=CARTESIAN_POINT('Ctrl Pts',(-80.3867933754363,-0.272026060596711,
124.893867204588));
#155080=CARTESIAN_POINT('Ctrl Pts',(-80.3942167464651,-0.429207364312377,
124.901101357113));
#155081=CARTESIAN_POINT('Ctrl Pts',(-80.4016401174939,-0.585920793721219,
124.914601576276));
#155082=CARTESIAN_POINT('Ctrl Pts',(-80.4090634885226,-0.741635729030356,
124.93427484239));
#155083=CARTESIAN_POINT('Ctrl Pts',(-80.4129995379635,-0.824199524061613,
124.944706080137));
#155084=CARTESIAN_POINT('Ctrl Pts',(-80.4169355874043,-0.906482793422893,
124.95687193191));
#155085=CARTESIAN_POINT('Ctrl Pts',(-80.4208716368452,-0.988408019083317,
124.970752801616));
#155086=CARTESIAN_POINT('Ctrl Pts',(-80.4282949032507,-1.14291643787704,
124.996931688674));
#155087=CARTESIAN_POINT('Ctrl Pts',(-80.4357181696561,-1.29661771533132,
125.029292845497));
#155088=CARTESIAN_POINT('Ctrl Pts',(-80.4431414360616,-1.44897810558652,
125.067776877043));
#155089=CARTESIAN_POINT('Ctrl Pts',(-80.4505559287826,-1.60115841851317,
125.10621542366));
#155090=CARTESIAN_POINT('Ctrl Pts',(-80.4579704215036,-1.75200064043173,
125.150762349724));
#155091=CARTESIAN_POINT('Ctrl Pts',(-80.4653849142246,-1.90097821288504,
125.201306771971));
#155092=CARTESIAN_POINT('Ctrl Pts',(-80.4727922605784,-2.04981219514426,
125.2518024776));
#155093=CARTESIAN_POINT('Ctrl Pts',(-80.4801996069321,-2.19678475471506,
125.308284052219));
#155094=CARTESIAN_POINT('Ctrl Pts',(-80.4876069532858,-2.34138167377254,
125.370590064789));
#155095=CARTESIAN_POINT('Ctrl Pts',(-80.4950087749612,-2.48587074699286,
125.432849607185));
#155096=CARTESIAN_POINT('Ctrl Pts',(-80.5024105966367,-2.62798736632663,
125.500924790785));
#155097=CARTESIAN_POINT('Ctrl Pts',(-80.509812418312,-2.76723468485333,
125.574605101154));
#155098=CARTESIAN_POINT('Ctrl Pts',(-80.5172103326234,-2.90640849580527,
125.64824651626));
#155099=CARTESIAN_POINT('Ctrl Pts',(-80.5246082469348,-3.04271569339197,
125.72748699119));
#155100=CARTESIAN_POINT('Ctrl Pts',(-80.5320061612462,-3.17568165547834,
125.812068900773));
#155101=CARTESIAN_POINT('Ctrl Pts',(-80.5394028461584,-3.30862552103311,
125.896636754376));
#155102=CARTESIAN_POINT('Ctrl Pts',(-80.5467995310706,-3.43822893843607,
125.986544080748));
#155103=CARTESIAN_POINT('Ctrl Pts',(-80.5541962159828,-3.56404394520174,
126.081488470326));
#155104=CARTESIAN_POINT('Ctrl Pts',(-80.5615925729183,-3.68985337319888,
126.176428649972));
#155105=CARTESIAN_POINT('Ctrl Pts',(-80.5689889298536,-3.81187442659001,
126.276405223872));
#155106=CARTESIAN_POINT('Ctrl Pts',(-80.5763852867891,-3.92969030252024,
126.38107397879));
#155107=CARTESIAN_POINT('Ctrl Pts',(-80.5837827761256,-4.04752421636084,
126.48575875876));
#155108=CARTESIAN_POINT('Ctrl Pts',(-80.5911802654623,-4.16115139171191,
126.595136902202));
#155109=CARTESIAN_POINT('Ctrl Pts',(-80.5985777547988,-4.27019024961786,
126.708825756944));
#155110=CARTESIAN_POINT('Ctrl Pts',(-80.6059778373138,-4.37926733092688,
126.822554465138));
#155111=CARTESIAN_POINT('Ctrl Pts',(-80.6133779198288,-4.48375263419014,
126.940596624002));
#155112=CARTESIAN_POINT('Ctrl Pts',(-80.6207780023437,-4.58330349680079,
127.062534910947));
#155113=CARTESIAN_POINT('Ctrl Pts',(-80.6281862220102,-4.68296382581909,
127.184607281575));
#155114=CARTESIAN_POINT('Ctrl Pts',(-80.6355944416767,-4.77767864203371,
127.310584046753));
#155115=CARTESIAN_POINT('Ctrl Pts',(-80.6430026613431,-4.86714699439943,
127.440016595708));
#155116=CARTESIAN_POINT('Ctrl Pts',(-80.6504154406452,-4.95667041304343,
127.569528808238));
#155117=CARTESIAN_POINT('Ctrl Pts',(-80.6578282199473,-5.04094073406692,
127.702500728233));
#155118=CARTESIAN_POINT('Ctrl Pts',(-80.6652409992494,-5.11970223256816,
127.838457784981));
#155119=CARTESIAN_POINT('Ctrl Pts',(-80.6726643702781,-5.1985762691919,
127.974609103547));
#155120=CARTESIAN_POINT('Ctrl Pts',(-80.6800877413068,-5.27192558899847,
128.113753748281));
#155121=CARTESIAN_POINT('Ctrl Pts',(-80.6875111123356,-5.339541639124,128.255395014314));
#155122=CARTESIAN_POINT('Ctrl Pts',(-80.6914471617765,-5.37539329132617,
128.330496612202));
#155123=CARTESIAN_POINT('Ctrl Pts',(-80.6953832112174,-5.40963393264518,
128.406299797149));
#155124=CARTESIAN_POINT('Ctrl Pts',(-80.6993192606582,-5.44223814943938,
128.482728758876));
#155125=CARTESIAN_POINT('Ctrl Pts',(-80.7075629756018,-5.51052486007303,
128.642802605347));
#155126=CARTESIAN_POINT('Ctrl Pts',(-80.7158066905453,-5.57180668670428,
128.806035138289));
#155127=CARTESIAN_POINT('Ctrl Pts',(-80.7240504054889,-5.62581158504579,
128.971828333522));
#155128=CARTESIAN_POINT('Ctrl Pts',(-80.7322607000411,-5.67959754509978,
129.136949395682));
#155129=CARTESIAN_POINT('Ctrl Pts',(-80.7404709945934,-5.7261653457546,
129.304610194852));
#155130=CARTESIAN_POINT('Ctrl Pts',(-80.7486812891456,-5.76529212749997,
129.474196249119));
#155131=CARTESIAN_POINT('Ctrl Pts',(-80.7568699712177,-5.80431591333105,
129.643335891237));
#155132=CARTESIAN_POINT('Ctrl Pts',(-80.7650586532899,-5.83593768790586,
129.814390458695));
#155133=CARTESIAN_POINT('Ctrl Pts',(-80.773247335362,-5.85998381724229,
129.986729756995));
#155134=CARTESIAN_POINT('Ctrl Pts',(-80.7814007344187,-5.88392633772643,
130.15832648768));
#155135=CARTESIAN_POINT('Ctrl Pts',(-80.7895541334754,-5.90035826308932,
130.331196682838));
#155136=CARTESIAN_POINT('Ctrl Pts',(-80.7977075325322,-5.90915685221338,
130.504701046653));
#155137=CARTESIAN_POINT('Ctrl Pts',(-80.8023466037498,-5.91416301973651,
130.603420500307));
#155138=CARTESIAN_POINT('Ctrl Pts',(-80.8069856749674,-5.91669893396806,
130.702344957279));
#155139=CARTESIAN_POINT('Ctrl Pts',(-80.811624746185,-5.91674923638228,
130.801354578692));
#155140=CARTESIAN_POINT('',(-82.5616248426584,-5.91498137599263,130.809325487812));
#155141=CARTESIAN_POINT('Ctrl Pts',(-80.8116248077882,-5.9084223721743,
130.801360122124));
#155142=CARTESIAN_POINT('Ctrl Pts',(-80.8670055000158,-5.90302635562967,
131.981665087397));
#155143=CARTESIAN_POINT('Ctrl Pts',(-81.015202066848,-4.98742482863156,
135.147824577937));
#155144=CARTESIAN_POINT('Ctrl Pts',(-81.2562145082839,0.178123566435826,
137.800490442363));
#155145=CARTESIAN_POINT('Ctrl Pts',(-81.5346621320968,5.98232230086394,
134.436079276676));
#155146=CARTESIAN_POINT('Ctrl Pts',(-81.8131097559099,6.28905909348952,
127.734296082587));
#155147=CARTESIAN_POINT('Ctrl Pts',(-82.0915573797235,0.816457816798208,
123.853752215139));
#155148=CARTESIAN_POINT('Ctrl Pts',(-82.3410623970142,-4.75960452750159,
126.09992199794));
#155149=CARTESIAN_POINT('Ctrl Pts',(-82.497751539704,-5.90151872823958,
129.450227630412));
#155150=CARTESIAN_POINT('Ctrl Pts',(-82.5616248077882,-5.9122429093786,
130.809322447035));
#155151=CARTESIAN_POINT('',(-84.3116248077883,-5.92105424700558,130.805351872892));
#155152=CARTESIAN_POINT('Ctrl Pts',(-82.5616248651526,-5.91674791528943,
130.809327449367));
#155153=CARTESIAN_POINT('Ctrl Pts',(-82.5704277186159,-5.91659056117995,
130.996775834263));
#155154=CARTESIAN_POINT('Ctrl Pts',(-82.5792305720792,-5.90752161874744,
131.183840062295));
#155155=CARTESIAN_POINT('Ctrl Pts',(-82.5880334255424,-5.88967326213172,
131.369762623072));
#155156=CARTESIAN_POINT('Ctrl Pts',(-82.596900390002,-5.87169491631084,
131.557039253943));
#155157=CARTESIAN_POINT('Ctrl Pts',(-82.6057673544616,-5.84480890847867,
131.743157495007));
#155158=CARTESIAN_POINT('Ctrl Pts',(-82.6146343189213,-5.80919903321914,
131.927364248435));
#155159=CARTESIAN_POINT('Ctrl Pts',(-82.6235720648078,-5.77330489858391,
132.113041450618));
#155160=CARTESIAN_POINT('Ctrl Pts',(-82.6325098106944,-5.7285471183117,
132.296776497412));
#155161=CARTESIAN_POINT('Ctrl Pts',(-82.6414475565809,-5.67516207160035,
132.477819916016));
#155162=CARTESIAN_POINT('Ctrl Pts',(-82.6437825801703,-5.66121500430027,
132.525118268252));
#155163=CARTESIAN_POINT('Ctrl Pts',(-82.6461176037597,-5.64667934482961,
132.572233022749));
#155164=CARTESIAN_POINT('Ctrl Pts',(-82.6484526273491,-5.63155983789489,
132.619151061311));
#155165=CARTESIAN_POINT('Ctrl Pts',(-82.6558758937544,-5.58349345929223,
132.768308055291));
#155166=CARTESIAN_POINT('Ctrl Pts',(-82.6632991601597,-5.52942446740412,
132.915779650107));
#155167=CARTESIAN_POINT('Ctrl Pts',(-82.6707224265651,-5.46948818796429,
133.061046134916));
#155168=CARTESIAN_POINT('Ctrl Pts',(-82.678136919286,-5.40962274822936,
133.206140926805));
#155169=CARTESIAN_POINT('Ctrl Pts',(-82.6855514120068,-5.3439039653829,
133.349035454746));
#155170=CARTESIAN_POINT('Ctrl Pts',(-82.6929659047278,-5.2725170904167,
133.489224504947));
#155171=CARTESIAN_POINT('Ctrl Pts',(-82.7003732510815,-5.20119902080825,
133.629278435664));
#155172=CARTESIAN_POINT('Ctrl Pts',(-82.7077805974352,-5.1242239033331,
133.766631749521));
#155173=CARTESIAN_POINT('Ctrl Pts',(-82.7151879437889,-5.04182524448686,
133.900798694866));
#155174=CARTESIAN_POINT('Ctrl Pts',(-82.7225897654642,-4.95948804166888,
134.034865573442));
#155175=CARTESIAN_POINT('Ctrl Pts',(-82.7299915871396,-4.87173554630225,
134.165750498738));
#155176=CARTESIAN_POINT('Ctrl Pts',(-82.7373934088149,-4.77884734975571,
134.292991949512));
#155177=CARTESIAN_POINT('Ctrl Pts',(-82.7447913231262,-4.68600818816535,
134.420166230513));
#155178=CARTESIAN_POINT('Ctrl Pts',(-82.7521892374374,-4.58803894422062,
134.543700566717));
#155179=CARTESIAN_POINT('Ctrl Pts',(-82.7595871517487,-4.48526264579371,
134.663162188099));
#155180=CARTESIAN_POINT('Ctrl Pts',(-82.7669838366608,-4.3825034269229,
134.782603957127));
#155181=CARTESIAN_POINT('Ctrl Pts',(-82.774380521573,-4.27493898226133,
134.897974071897));
#155182=CARTESIAN_POINT('Ctrl Pts',(-82.7817772064852,-4.16293283788085,
135.008872569005));
#155183=CARTESIAN_POINT('Ctrl Pts',(-82.7891735634205,-4.0509316599705,
135.119766148757));
#155184=CARTESIAN_POINT('Ctrl Pts',(-82.7965699203559,-3.93448943921327,
135.22618824244));
#155185=CARTESIAN_POINT('Ctrl Pts',(-82.8039662772913,-3.814006604634,135.327775719268));
#155186=CARTESIAN_POINT('Ctrl Pts',(-82.8113637666278,-3.69350532382517,
135.429378749399));
#155187=CARTESIAN_POINT('Ctrl Pts',(-82.8187612559642,-3.56896248283143,
135.526145448207));
#155188=CARTESIAN_POINT('Ctrl Pts',(-82.8261587453007,-3.44081150081433,
135.617753057246));
#155189=CARTESIAN_POINT('Ctrl Pts',(-82.8335588278157,-3.31261559566933,
135.70939277919));
#155190=CARTESIAN_POINT('Ctrl Pts',(-82.8409589103306,-3.18080933473297,
135.795869593682));
#155191=CARTESIAN_POINT('Ctrl Pts',(-82.8483589928455,-3.04585486820177,
135.876904228453));
#155192=CARTESIAN_POINT('Ctrl Pts',(-82.8557672125119,-2.91075200536077,
135.958027969136));
#155193=CARTESIAN_POINT('Ctrl Pts',(-82.8631754321783,-2.77249434376342,
136.0336973869));
#155194=CARTESIAN_POINT('Ctrl Pts',(-82.8705836518447,-2.63156901651121,
136.103678976925));
#155195=CARTESIAN_POINT('Ctrl Pts',(-82.8779964311467,-2.49055695207155,
136.173703639451));
#155196=CARTESIAN_POINT('Ctrl Pts',(-82.8854092104487,-2.34687429019651,
136.238033346342));
#155197=CARTESIAN_POINT('Ctrl Pts',(-82.8928219897506,-2.20102736969333,
136.296483074355));
#155198=CARTESIAN_POINT('Ctrl Pts',(-82.9002453607793,-2.05497205627038,
136.35501631808));
#155199=CARTESIAN_POINT('Ctrl Pts',(-82.9076687318081,-1.90674665885866,
136.407652678481));
#155200=CARTESIAN_POINT('Ctrl Pts',(-82.9150921028368,-1.75687265667485,
136.454256991016));
#155201=CARTESIAN_POINT('Ctrl Pts',(-82.9190281522783,-1.67740586452409,
136.478967715783));
#155202=CARTESIAN_POINT('Ctrl Pts',(-82.9229642017198,-1.59747577289914,
136.501983467373));
#155203=CARTESIAN_POINT('Ctrl Pts',(-82.9269002511613,-1.51716105303232,
136.523289966812));
#155204=CARTESIAN_POINT('Ctrl Pts',(-82.9343235175668,-1.36568999792873,
136.563473359791));
#155205=CARTESIAN_POINT('Ctrl Pts',(-82.9417467839723,-1.21239235777182,
136.597695584795));
#155206=CARTESIAN_POINT('Ctrl Pts',(-82.9491700503777,-1.05777852687676,
136.62578957879));
#155207=CARTESIAN_POINT('Ctrl Pts',(-82.9565845430987,-0.903347436689951,
136.653850368017));
#155208=CARTESIAN_POINT('Ctrl Pts',(-82.9639990358196,-0.747603615948766,
136.675797277501));
#155209=CARTESIAN_POINT('Ctrl Pts',(-82.9714135285406,-0.59107224801231,
136.691513083753));
#155210=CARTESIAN_POINT('Ctrl Pts',(-82.9788208748944,-0.434691750901128,
136.707213742518));
#155211=CARTESIAN_POINT('Ctrl Pts',(-82.9862282212481,-0.277525586685956,
136.716695217319));
#155212=CARTESIAN_POINT('Ctrl Pts',(-82.9936355676019,-0.120108647953987,
136.71989140315));
#155213=CARTESIAN_POINT('Ctrl Pts',(-83.0010373892773,0.0371908832860754,
136.723085205144));
#155214=CARTESIAN_POINT('Ctrl Pts',(-83.0084392109528,0.194740445012163,
136.720003044677));
#155215=CARTESIAN_POINT('Ctrl Pts',(-83.0158410326282,0.35200062036801,
136.710630686379));
#155216=CARTESIAN_POINT('Ctrl Pts',(-83.0232389469396,0.509177779301398,
136.701263275677));
#155217=CARTESIAN_POINT('Ctrl Pts',(-83.0306368612509,0.66606548440955,
136.685612302325));
#155218=CARTESIAN_POINT('Ctrl Pts',(-83.0380347755622,0.822125029559199,
136.663715616051));
#155219=CARTESIAN_POINT('Ctrl Pts',(-83.0454314604744,0.978158640443431,
136.641822568609));
#155220=CARTESIAN_POINT('Ctrl Pts',(-83.0528281453866,1.13336399519958,
136.613685920037));
#155221=CARTESIAN_POINT('Ctrl Pts',(-83.0602248302988,1.28720809856583,
136.579395325123));
#155222=CARTESIAN_POINT('Ctrl Pts',(-83.0676211872343,1.44104538032332,
136.54510625069));
#155223=CARTESIAN_POINT('Ctrl Pts',(-83.0750175441697,1.59352116634909,
136.504663853691));
#155224=CARTESIAN_POINT('Ctrl Pts',(-83.0824139011051,1.74411350276013,
136.458208745345));
#155225=CARTESIAN_POINT('Ctrl Pts',(-83.0898113904417,1.89472889524231,
136.411746524604));
#155226=CARTESIAN_POINT('Ctrl Pts',(-83.0972088797783,2.04345990721087,
136.359269869601));
#155227=CARTESIAN_POINT('Ctrl Pts',(-83.1046063691148,2.18980071920077,
136.300968969331));
#155228=CARTESIAN_POINT('Ctrl Pts',(-83.1120064516298,2.33619283073524,
136.24264763177));
#155229=CARTESIAN_POINT('Ctrl Pts',(-83.1194065341448,2.48019272750221,
136.178498122042));
#155230=CARTESIAN_POINT('Ctrl Pts',(-83.1268066166598,2.62131564636256,
136.108758306714));
#155231=CARTESIAN_POINT('Ctrl Pts',(-83.1342148363263,2.76259374438019,
136.038941805289));
#155232=CARTESIAN_POINT('Ctrl Pts',(-83.1416230559927,2.90098821183925,
135.963522887555));
#155233=CARTESIAN_POINT('Ctrl Pts',(-83.1490312756591,3.03603928718225,
135.882785177327));
#155234=CARTESIAN_POINT('Ctrl Pts',(-83.1564440549612,3.17117348420867,
135.801997774386));
#155235=CARTESIAN_POINT('Ctrl Pts',(-83.1638568342633,3.30295987691573,
135.71588525956));
#155236=CARTESIAN_POINT('Ctrl Pts',(-83.1712696135653,3.4309691115169,135.624773620444));
#155237=CARTESIAN_POINT('Ctrl Pts',(-83.1786929845941,3.55916125171568,
135.533531796746));
#155238=CARTESIAN_POINT('Ctrl Pts',(-83.1861163556228,3.68356516036802,
135.437276810452));
#155239=CARTESIAN_POINT('Ctrl Pts',(-83.1935397266516,3.80378524746377,
135.336374337059));
#155240=CARTESIAN_POINT('Ctrl Pts',(-83.1974757760924,3.86752882228469,
135.282873424544));
#155241=CARTESIAN_POINT('Ctrl Pts',(-83.2014118255333,3.93009679285136,
135.228066550657));
#155242=CARTESIAN_POINT('Ctrl Pts',(-83.2053478749742,3.9914346221341,135.172012185598));
#155243=CARTESIAN_POINT('Ctrl Pts',(-83.2127711413796,4.10711585387093,
135.066295402495));
#155244=CARTESIAN_POINT('Ctrl Pts',(-83.2201944077851,4.21876909999845,
134.955819704755));
#155245=CARTESIAN_POINT('Ctrl Pts',(-83.2276176741905,4.32597792506152,
134.840924199919));
#155246=CARTESIAN_POINT('Ctrl Pts',(-83.2350321669115,4.43306003819651,
134.726164492029));
#155247=CARTESIAN_POINT('Ctrl Pts',(-83.2424466596325,4.53570793407956,
134.606995645404));
#155248=CARTESIAN_POINT('Ctrl Pts',(-83.2498611523535,4.63353911483465,
134.483796149519));
#155249=CARTESIAN_POINT('Ctrl Pts',(-83.2572684987073,4.73127600221445,
134.360715397946));
#155250=CARTESIAN_POINT('Ctrl Pts',(-83.2646758450611,4.82420518624881,
134.233612021542));
#155251=CARTESIAN_POINT('Ctrl Pts',(-83.2720831914149,4.91198192841564,
134.10290030922));
#155252=CARTESIAN_POINT('Ctrl Pts',(-83.2794850130903,4.99969320337655,
133.972286086625));
#155253=CARTESIAN_POINT('Ctrl Pts',(-83.2868868347657,5.08225948095878,
133.83806919529));
#155254=CARTESIAN_POINT('Ctrl Pts',(-83.2942886564411,5.15937721655751,
133.700695767332));
#155255=CARTESIAN_POINT('Ctrl Pts',(-83.3016865707524,5.23645424230368,
133.563394857737));
#155256=CARTESIAN_POINT('Ctrl Pts',(-83.3090844850638,5.30808827196975,
133.422941054746));
#155257=CARTESIAN_POINT('Ctrl Pts',(-83.3164823993751,5.37401996578059,
133.279808045788));
#155258=CARTESIAN_POINT('Ctrl Pts',(-83.3238790842873,5.43994070294013,
133.13669882294));
#155259=CARTESIAN_POINT('Ctrl Pts',(-83.3312757691996,5.50016082897185,
132.99091161651));
#155260=CARTESIAN_POINT('Ctrl Pts',(-83.3386724541118,5.55446767603133,
132.842943311111));
#155261=CARTESIAN_POINT('Ctrl Pts',(-83.3460688110472,5.6087721150683,132.694981566783));
#155262=CARTESIAN_POINT('Ctrl Pts',(-83.3534651679826,5.65716366785959,
132.544839266222));
#155263=CARTESIAN_POINT('Ctrl Pts',(-83.3608615249181,5.69947850578363,
132.393031547813));
#155264=CARTESIAN_POINT('Ctrl Pts',(-83.3682590142546,5.74179982221738,
132.241200587254));
#155265=CARTESIAN_POINT('Ctrl Pts',(-83.3756565035912,5.77804247107385,
132.087704060762));
#155266=CARTESIAN_POINT('Ctrl Pts',(-83.3830539929277,5.80809305596224,
131.933070330372));
#155267=CARTESIAN_POINT('Ctrl Pts',(-83.3904540754427,5.83815417503662,
131.778382393368));
#155268=CARTESIAN_POINT('Ctrl Pts',(-83.3978541579579,5.86201883728974,
131.622556824982));
#155269=CARTESIAN_POINT('Ctrl Pts',(-83.4052542404729,5.87962514028273,
131.466130042861));
#155270=CARTESIAN_POINT('Ctrl Pts',(-83.4126624601393,5.8972508032158,131.309531253412));
#155271=CARTESIAN_POINT('Ctrl Pts',(-83.4200706798058,5.90860432188552,
131.152330301159));
#155272=CARTESIAN_POINT('Ctrl Pts',(-83.4274788994722,5.91367580468914,
130.995067302122));
#155273=CARTESIAN_POINT('Ctrl Pts',(-83.4348916787743,5.91875040890583,
130.837707510332));
#155274=CARTESIAN_POINT('Ctrl Pts',(-83.4423044580764,5.91753527566853,
130.680285968084));
#155275=CARTESIAN_POINT('Ctrl Pts',(-83.4497172373785,5.91007259136617,
130.523340107136));
#155276=CARTESIAN_POINT('Ctrl Pts',(-83.4571406084072,5.90259924403053,
130.366169994582));
#155277=CARTESIAN_POINT('Ctrl Pts',(-83.4645639794359,5.88886054933901,
130.209477291681));
#155278=CARTESIAN_POINT('Ctrl Pts',(-83.4719873504646,5.86895033438173,
130.053792476049));
#155279=CARTESIAN_POINT('Ctrl Pts',(-83.4759233999054,5.85839346067233,
129.971244651195));
#155280=CARTESIAN_POINT('Ctrl Pts',(-83.4798594493463,5.84610240185867,
129.888979991474));
#155281=CARTESIAN_POINT('Ctrl Pts',(-83.4837954987871,5.83209687197968,
129.807075985004));
#155282=CARTESIAN_POINT('Ctrl Pts',(-83.4912187651925,5.80568287972549,
129.652607584938));
#155283=CARTESIAN_POINT('Ctrl Pts',(-83.4986420315979,5.77308785319627,
129.498955733639));
#155284=CARTESIAN_POINT('Ctrl Pts',(-83.5060652980034,5.73437199963621,
129.346654085959));
#155285=CARTESIAN_POINT('Ctrl Pts',(-83.5134797907244,5.6957019049999,129.19453244618));
#155286=CARTESIAN_POINT('Ctrl Pts',(-83.5208942834454,5.65092547433633,
129.043758191772));
#155287=CARTESIAN_POINT('Ctrl Pts',(-83.5283087761665,5.60015439211455,
128.894857711839));
#155288=CARTESIAN_POINT('Ctrl Pts',(-83.5357161225202,5.54943224497331,
128.746100747794));
#155289=CARTESIAN_POINT('Ctrl Pts',(-83.543123468874,5.4927270685423,128.599214313756));
#155290=CARTESIAN_POINT('Ctrl Pts',(-83.5505308152278,5.43020107622494,
128.454712381283));
#155291=CARTESIAN_POINT('Ctrl Pts',(-83.5579326369032,5.36772171815161,
128.310318223804));
#155292=CARTESIAN_POINT('Ctrl Pts',(-83.5653344585786,5.29943033607883,
128.168305367879));
#155293=CARTESIAN_POINT('Ctrl Pts',(-83.572736280254,5.22553820031607,128.029170339488));
#155294=CARTESIAN_POINT('Ctrl Pts',(-83.5801341945653,5.1516850716366,127.890108759396));
#155295=CARTESIAN_POINT('Ctrl Pts',(-83.5875321088768,5.0722372521146,127.753922310164));
#155296=CARTESIAN_POINT('Ctrl Pts',(-83.5949300231882,4.98745308891698,
127.621085221319));
#155297=CARTESIAN_POINT('Ctrl Pts',(-83.6023267081004,4.90268301530926,
127.488270207588));
#155298=CARTESIAN_POINT('Ctrl Pts',(-83.6097233930125,4.81257855871012,
127.358803763909));
#155299=CARTESIAN_POINT('Ctrl Pts',(-83.6171200779247,4.71744281005215,
127.233133392033));
#155300=CARTESIAN_POINT('Ctrl Pts',(-83.6245164348601,4.62231127981298,
127.107468592513));
#155301=CARTESIAN_POINT('Ctrl Pts',(-83.6319127917957,4.52214912641339,
126.985599827747));
#155302=CARTESIAN_POINT('Ctrl Pts',(-83.6393091487311,4.41730119699303,
126.867943376274));
#155303=CARTESIAN_POINT('Ctrl Pts',(-83.6467066380677,4.31243721508671,
126.750268911296));
#155304=CARTESIAN_POINT('Ctrl Pts',(-83.6541041274043,4.20288627708352,
126.636808322438));
#155305=CARTESIAN_POINT('Ctrl Pts',(-83.6615016167408,4.08903161541035,
126.52794260588));
#155306=CARTESIAN_POINT('Ctrl Pts',(-83.6689016992559,3.9751370421622,126.419038726614));
#155307=CARTESIAN_POINT('Ctrl Pts',(-83.6763017817709,3.85693601114403,
126.314733184414));
#155308=CARTESIAN_POINT('Ctrl Pts',(-83.6837018642859,3.73484636593445,
126.215368006397));
#155309=CARTESIAN_POINT('Ctrl Pts',(-83.6911100839524,3.61262247060866,
126.115893566151));
#155310=CARTESIAN_POINT('Ctrl Pts',(-83.6985183036188,3.48650171148146,
126.021370574806));
#155311=CARTESIAN_POINT('Ctrl Pts',(-83.7059265232853,3.35693315680455,
125.932099300349));
#155312=CARTESIAN_POINT('Ctrl Pts',(-83.7133393025874,3.2272848548442,125.842773080913));
#155313=CARTESIAN_POINT('Ctrl Pts',(-83.7207520818894,3.09418484374474,
125.758705218099));
#155314=CARTESIAN_POINT('Ctrl Pts',(-83.7281648611915,2.95810808284002,
125.680150714299));
#155315=CARTESIAN_POINT('Ctrl Pts',(-83.7355882322202,2.82183688907815,
125.60148396814));
#155316=CARTESIAN_POINT('Ctrl Pts',(-83.7430116032491,2.6825807802918,125.528346487734));
#155317=CARTESIAN_POINT('Ctrl Pts',(-83.7504349742778,2.54083677815922,
125.460946069802));
#155318=CARTESIAN_POINT('Ctrl Pts',(-83.7543710237185,2.46568070712909,
125.425208750965));
#155319=CARTESIAN_POINT('Ctrl Pts',(-83.7583070731592,2.38982550153584,
125.39108350884));
#155320=CARTESIAN_POINT('Ctrl Pts',(-83.7622431226,2.31334701024829,125.358595641672));
#155321=CARTESIAN_POINT('Ctrl Pts',(-83.7696663890055,2.16911096248821,
125.297324538102));
#155322=CARTESIAN_POINT('Ctrl Pts',(-83.777089655411,2.02222090032576,125.241695078277));
#155323=CARTESIAN_POINT('Ctrl Pts',(-83.7845129218165,1.87315834618837,
125.191945061622));
#155324=CARTESIAN_POINT('Ctrl Pts',(-83.7919274145376,1.7242719716111,125.142253845354));
#155325=CARTESIAN_POINT('Ctrl Pts',(-83.7993419072586,1.57321856672915,
125.098428357233));
#155326=CARTESIAN_POINT('Ctrl Pts',(-83.8067563999797,1.4205013657857,125.060659160117));
#155327=CARTESIAN_POINT('Ctrl Pts',(-83.8141637463335,1.26793135943022,
125.022926366376));
#155328=CARTESIAN_POINT('Ctrl Pts',(-83.8215710926874,1.11370110947068,
124.991238331783));
#155329=CARTESIAN_POINT('Ctrl Pts',(-83.8289784390413,0.958330715042835,
124.96573639579));
#155330=CARTESIAN_POINT('Ctrl Pts',(-83.8363802607168,0.803076201716939,
124.940253480104));
#155331=CARTESIAN_POINT('Ctrl Pts',(-83.8437820823923,0.646683603893124,
124.92094753647));
#155332=CARTESIAN_POINT('Ctrl Pts',(-83.8511839040678,0.489684859701897,
124.907909201614));
#155333=CARTESIAN_POINT('Ctrl Pts',(-83.8585818183792,0.332768993925651,
124.894877749594));
#155334=CARTESIAN_POINT('Ctrl Pts',(-83.8659797326906,0.175247990112921,
124.888107347889));
#155335=CARTESIAN_POINT('Ctrl Pts',(-83.873377647002,0.0176604739472239,
124.887636974353));
#155336=CARTESIAN_POINT('Ctrl Pts',(-83.8807743319143,-0.139900854031991,
124.887166678984));
#155337=CARTESIAN_POINT('Ctrl Pts',(-83.8881710168266,-0.297528299496211,
124.89299433501));
#155338=CARTESIAN_POINT('Ctrl Pts',(-83.8955677017389,-0.454681538496048,
124.905106829073));
#155339=CARTESIAN_POINT('Ctrl Pts',(-83.9029640586744,-0.611827809156583,
124.917218786055));
#155340=CARTESIAN_POINT('Ctrl Pts',(-83.9103604156099,-0.768499542967437,
124.935614998284));
#155341=CARTESIAN_POINT('Ctrl Pts',(-83.9177567725454,-0.924160114702367,
124.960230344814));
#155342=CARTESIAN_POINT('Ctrl Pts',(-83.925154261882,-1.07984451846821,
124.984849460016));
#155343=CARTESIAN_POINT('Ctrl Pts',(-83.9325517512187,-1.23451708316797,
125.015689547096));
#155344=CARTESIAN_POINT('Ctrl Pts',(-83.9399492405553,-1.38765011943543,
125.052634119502));
#155345=CARTESIAN_POINT('Ctrl Pts',(-83.9473493230704,-1.54083683625116,
125.08959164277));
#155346=CARTESIAN_POINT('Ctrl Pts',(-83.9547494055855,-1.69248258747714,
125.132657824431));
#155347=CARTESIAN_POINT('Ctrl Pts',(-83.9621494881005,-1.84207376135324,
125.181665994858));
#155348=CARTESIAN_POINT('Ctrl Pts',(-83.9695577077671,-1.99182942610357,
125.230728054806));
#155349=CARTESIAN_POINT('Ctrl Pts',(-83.9769659274336,-2.1395256467322,
125.285745035712));
#155350=CARTESIAN_POINT('Ctrl Pts',(-83.9843741471001,-2.28466706691807,
125.34650142592));
#155351=CARTESIAN_POINT('Ctrl Pts',(-83.9917869264023,-2.42989781922626,
125.407295210671));
#155352=CARTESIAN_POINT('Ctrl Pts',(-83.9991997057044,-2.57257030028518,
125.473835286277));
#155353=CARTESIAN_POINT('Ctrl Pts',(-84.0066124850065,-2.71221324224078,
125.545859891017));
#155354=CARTESIAN_POINT('Ctrl Pts',(-84.0140358560354,-2.85205571258064,
125.617987407891));
#155355=CARTESIAN_POINT('Ctrl Pts',(-84.0214592270643,-2.98885967452723,
125.695614921511));
#155356=CARTESIAN_POINT('Ctrl Pts',(-84.0288825980931,-3.1221816504556,
125.778436592667));
#155357=CARTESIAN_POINT('Ctrl Pts',(-84.0328186475332,-3.19287216109585,
125.822350629984));
#155358=CARTESIAN_POINT('Ctrl Pts',(-84.0367546969732,-3.26258428524958,
125.86772423585));
#155359=CARTESIAN_POINT('Ctrl Pts',(-84.0406907464133,-3.33125574062314,
125.914507270781));
#155360=CARTESIAN_POINT('Ctrl Pts',(-84.0480807349862,-3.46018737073213,
126.002343081487));
#155361=CARTESIAN_POINT('Ctrl Pts',(-84.0554707235591,-3.58584624170242,
126.09542051636));
#155362=CARTESIAN_POINT('Ctrl Pts',(-84.0628607121321,-3.70777436591683,
126.193467015025));
#155363=CARTESIAN_POINT('Ctrl Pts',(-84.0702419467397,-3.82955805762495,
126.291397370663));
#155364=CARTESIAN_POINT('Ctrl Pts',(-84.0776231813473,-3.94761950699797,
126.394284841588));
#155365=CARTESIAN_POINT('Ctrl Pts',(-84.0850044159549,-4.06152853707728,
126.501812941478));
#155366=CARTESIAN_POINT('Ctrl Pts',(-84.0923785549292,-4.17532806559606,
126.609237673842));
#155367=CARTESIAN_POINT('Ctrl Pts',(-84.0997526939036,-4.28498284807336,
126.721293898398));
#155368=CARTESIAN_POINT('Ctrl Pts',(-84.1071268328779,-4.39009486258093,
126.837624218454));
#155369=CARTESIAN_POINT('Ctrl Pts',(-84.1144955286214,-4.49512928851112,
126.953868669125));
#155370=CARTESIAN_POINT('Ctrl Pts',(-84.1218642243649,-4.59562737058503,
127.07438065576));
#155371=CARTESIAN_POINT('Ctrl Pts',(-84.1292329201084,-4.69122725126851,
127.198765321439));
#155372=CARTESIAN_POINT('Ctrl Pts',(-84.1368325820951,-4.78982363853225,
127.3270487312));
#155373=CARTESIAN_POINT('Ctrl Pts',(-84.1444322440818,-4.88320944683711,
127.459451278672));
#155374=CARTESIAN_POINT('Ctrl Pts',(-84.1520319060684,-4.97103155000614,
127.595501647255));
#155375=CARTESIAN_POINT('Ctrl Pts',(-84.1593956889991,-5.05612782210165,
127.727329271121));
#155376=CARTESIAN_POINT('Ctrl Pts',(-84.1667594719297,-5.13600040644814,
127.862581303961));
#155377=CARTESIAN_POINT('Ctrl Pts',(-84.1741232548603,-5.21037154955868,
128.000798797657));
#155378=CARTESIAN_POINT('Ctrl Pts',(-84.1814869129748,-5.28474143207755,
128.139013948566));
#155379=CARTESIAN_POINT('Ctrl Pts',(-84.1888505710893,-5.35360987989874,
128.280194128444));
#155380=CARTESIAN_POINT('Ctrl Pts',(-84.1962142292037,-5.4167449851209,
128.42385556009));
#155381=CARTESIAN_POINT('Ctrl Pts',(-84.2035792504389,-5.47989177757308,
128.567543585565));
#155382=CARTESIAN_POINT('Ctrl Pts',(-84.2109442716741,-5.53730296312743,
128.713713431915));
#155383=CARTESIAN_POINT('Ctrl Pts',(-84.2183092929092,-5.58879476948356,
128.861861302999));
#155384=CARTESIAN_POINT('Ctrl Pts',(-84.2256771657943,-5.6403065128644,
129.010066535204));
#155385=CARTESIAN_POINT('Ctrl Pts',(-84.2330450386795,-5.68589419122215,
129.16025096082));
#155386=CARTESIAN_POINT('Ctrl Pts',(-84.2404129115646,-5.72542394021127,
129.311895788045));
#155387=CARTESIAN_POINT('Ctrl Pts',(-84.247788868667,-5.76499706224492,
129.463707003827));
#155388=CARTESIAN_POINT('Ctrl Pts',(-84.2551648257693,-5.79849888988038,
129.616981455431));
#155389=CARTESIAN_POINT('Ctrl Pts',(-84.2625407828717,-5.8258465888192,
129.771189728485));
#155390=CARTESIAN_POINT('Ctrl Pts',(-84.269921586644,-5.85321225766608,
129.925499330302));
#155391=CARTESIAN_POINT('Ctrl Pts',(-84.2773023904166,-5.87441569162345,
130.080743603662));
#155392=CARTESIAN_POINT('Ctrl Pts',(-84.2846831941889,-5.8894259978173,
130.236388806));
#155393=CARTESIAN_POINT('Ctrl Pts',(-84.2920738499913,-5.90445634003871,
130.392241766362));
#155394=CARTESIAN_POINT('Ctrl Pts',(-84.2994645057937,-5.91327703278537,
130.548496349418));
#155395=CARTESIAN_POINT('Ctrl Pts',(-84.3068551615961,-5.91590924399315,
130.704619054833));
#155396=CARTESIAN_POINT('Ctrl Pts',(-84.3084450436602,-5.91647548675968,
130.738204259687));
#155397=CARTESIAN_POINT('Ctrl Pts',(-84.3100349257242,-5.91675553673264,
130.771783382383));
#155398=CARTESIAN_POINT('Ctrl Pts',(-84.3116248077882,-5.91674991708632,
130.805351152296));
#155399=CARTESIAN_POINT('',(-86.0616248077884,-5.91524629155455,130.798916926214));
#155400=CARTESIAN_POINT('Ctrl Pts',(-84.3116248077882,-5.92633068612177,
130.805352756231));
#155401=CARTESIAN_POINT('Ctrl Pts',(-84.3141293286007,-5.92645332124771,
130.858317280176));
#155402=CARTESIAN_POINT('Ctrl Pts',(-84.3166338494132,-5.92580498622787,
130.911278725251));
#155403=CARTESIAN_POINT('Ctrl Pts',(-84.3191383702257,-5.92437648619433,
130.964219118996));
#155404=CARTESIAN_POINT('Ctrl Pts',(-84.4119542448301,-5.87143722558873,
132.926154880442));
#155405=CARTESIAN_POINT('Ctrl Pts',(-84.5975859940389,-3.62261037746975,
136.79220284857));
#155406=CARTESIAN_POINT('Ctrl Pts',(-84.8760336178514,3.07963185724678,
137.088740312823));
#155407=CARTESIAN_POINT('Ctrl Pts',(-85.1544812416647,6.95184286353423,
131.610239846154));
#155408=CARTESIAN_POINT('Ctrl Pts',(-85.4329288654772,4.43564989463864,
125.391175737797));
#155409=CARTESIAN_POINT('Ctrl Pts',(-85.7113764892903,-2.15668863388649,
124.146564085169));
#155410=CARTESIAN_POINT('Ctrl Pts',(-85.9209418033934,-5.62660433157627,
127.814517552592));
#155411=CARTESIAN_POINT('Ctrl Pts',(-86.0376912428933,-5.9198278487999,
130.290313715552));
#155412=CARTESIAN_POINT('Ctrl Pts',(-86.0616248077884,-5.91524629155455,
130.798916926214));
#155413=CARTESIAN_POINT('',(-87.8116248459704,-5.91288564422817,130.805748365634));
#155414=CARTESIAN_POINT('Ctrl Pts',(-86.0616248077884,-5.91524629155455,
130.798916926214));
#155415=CARTESIAN_POINT('Ctrl Pts',(-86.1305071174976,-5.90206028075724,
132.262709053696));
#155416=CARTESIAN_POINT('Ctrl Pts',(-86.2922053018102,-4.61319546921273,
135.719633866992));
#155417=CARTESIAN_POINT('Ctrl Pts',(-86.546719360729,1.19009585987408,137.70082582626));
#155418=CARTESIAN_POINT('Ctrl Pts',(-86.8251669845419,6.44546738008766,
133.530807166203));
#155419=CARTESIAN_POINT('Ctrl Pts',(-87.1036146083547,5.77776925657911,
126.855317322279));
#155420=CARTESIAN_POINT('Ctrl Pts',(-87.3820622321676,-0.199416554002256,
123.808805345226));
#155421=CARTESIAN_POINT('Ctrl Pts',(-87.6180656319783,-5.11016985858347,
126.675333768416));
#155422=CARTESIAN_POINT('Ctrl Pts',(-87.7612531571857,-5.9049894213493,
129.731655556594));
#155423=CARTESIAN_POINT('Ctrl Pts',(-87.8116248077884,-5.90722993476821,
130.805746223546));
#155424=CARTESIAN_POINT('',(-89.5616248077884,-5.91765122622102,130.809325232297));
#155425=CARTESIAN_POINT('Ctrl Pts',(-87.8116248720577,-5.9167498369114,
130.805749829188));
#155426=CARTESIAN_POINT('Ctrl Pts',(-87.8195256863451,-5.91671021723652,
130.974492806248));
#155427=CARTESIAN_POINT('Ctrl Pts',(-87.8274265006325,-5.90944765888795,
131.143044400043));
#155428=CARTESIAN_POINT('Ctrl Pts',(-87.8353273149198,-5.89503649630339,
131.310794492569));
#155429=CARTESIAN_POINT('Ctrl Pts',(-87.8432437624533,-5.88059681852492,
131.478876510184));
#155430=CARTESIAN_POINT('Ctrl Pts',(-87.8511602099868,-5.85898030346369,
131.646153571259));
#155431=CARTESIAN_POINT('Ctrl Pts',(-87.8590766575203,-5.83031251647461,
131.812024511302));
#155432=CARTESIAN_POINT('Ctrl Pts',(-87.8670169080892,-5.80155853168713,
131.978394189175));
#155433=CARTESIAN_POINT('Ctrl Pts',(-87.874957158658,-5.76571090722074,
132.14334900184));
#155434=CARTESIAN_POINT('Ctrl Pts',(-87.8828974092269,-5.72294601732455,
132.306299179988));
#155435=CARTESIAN_POINT('Ctrl Pts',(-87.8908505397602,-5.68011175804805,
132.469513681343));
#155436=CARTESIAN_POINT('Ctrl Pts',(-87.8988036702936,-5.63033790661179,
132.630716778108));
#155437=CARTESIAN_POINT('Ctrl Pts',(-87.9067568008269,-5.57384969476232,
132.789336723895));
#155438=CARTESIAN_POINT('Ctrl Pts',(-87.9147293056713,-5.51722387418352,
132.948343077545));
#155439=CARTESIAN_POINT('Ctrl Pts',(-87.9227018105157,-5.45385108760204,
133.104753426786));
#155440=CARTESIAN_POINT('Ctrl Pts',(-87.9306743153601,-5.38400431265361,
133.258016690415));
#155441=CARTESIAN_POINT('Ctrl Pts',(-87.9334353701712,-5.35981482920035,
133.311095149403));
#155442=CARTESIAN_POINT('Ctrl Pts',(-87.9361964249824,-5.33484925618582,
133.363796385668));
#155443=CARTESIAN_POINT('Ctrl Pts',(-87.9389574797935,-5.30912016458389,
133.416098284429));
#155444=CARTESIAN_POINT('Ctrl Pts',(-87.9463807461987,-5.23994591257194,
133.55671516984));
#155445=CARTESIAN_POINT('Ctrl Pts',(-87.9538040126041,-5.16507665292041,
133.694794571345));
#155446=CARTESIAN_POINT('Ctrl Pts',(-87.9612272790093,-5.08472159737783,
133.829841875095));
#155447=CARTESIAN_POINT('Ctrl Pts',(-87.9686417717301,-5.00446151483783,
133.964729564147));
#155448=CARTESIAN_POINT('Ctrl Pts',(-87.9760562644508,-4.91872873137602,
134.096591971124));
#155449=CARTESIAN_POINT('Ctrl Pts',(-87.9834707571716,-4.82777975612728,
134.224956061173));
#155450=CARTESIAN_POINT('Ctrl Pts',(-87.9908781035252,-4.73691844092507,
134.35319642908));
#155451=CARTESIAN_POINT('Ctrl Pts',(-87.9982854498788,-4.64085115718459,
134.477944890121));
#155452=CARTESIAN_POINT('Ctrl Pts',(-88.0056927962324,-4.53987933977658,
134.598754659145));
#155453=CARTESIAN_POINT('Ctrl Pts',(-88.0130946179076,-4.43898283095945,
134.719474323686));
#155454=CARTESIAN_POINT('Ctrl Pts',(-88.0204964395829,-4.33318931038353,
134.836260860222));
#155455=CARTESIAN_POINT('Ctrl Pts',(-88.0278982612581,-4.22284229993852,
134.948698136682));
#155456=CARTESIAN_POINT('Ctrl Pts',(-88.0352961755693,-4.11255354082138,
135.061076058378));
#155457=CARTESIAN_POINT('Ctrl Pts',(-88.0426940898805,-3.99771633983363,
135.169109026722));
#155458=CARTESIAN_POINT('Ctrl Pts',(-88.0500920041917,-3.87871303033228,
135.272415652011));
#155459=CARTESIAN_POINT('Ctrl Pts',(-88.0574886891037,-3.7597294970222,
135.375705109613));
#155460=CARTESIAN_POINT('Ctrl Pts',(-88.0648853740157,-3.63658151089322,
135.474269538537));
#155461=CARTESIAN_POINT('Ctrl Pts',(-88.0722820589278,-3.50968672178958,
135.567765878238));
#155462=CARTESIAN_POINT('Ctrl Pts',(-88.0796784158631,-3.38279755933387,
135.661258072212));
#155463=CARTESIAN_POINT('Ctrl Pts',(-88.0870747727984,-3.25216222477146,
135.749682402359));
#155464=CARTESIAN_POINT('Ctrl Pts',(-88.0944711297337,-3.118229543706,135.83273759978));
#155465=CARTESIAN_POINT('Ctrl Pts',(-88.1018686190701,-2.98427635720516,
135.915805513164));
#155466=CARTESIAN_POINT('Ctrl Pts',(-88.1092661084065,-2.84702513628258,
135.993502460308));
#155467=CARTESIAN_POINT('Ctrl Pts',(-88.1166635977429,-2.70695149782632,
136.065571899288));
#155468=CARTESIAN_POINT('Ctrl Pts',(-88.1240636802577,-2.56682875677344,
136.137666602097));
#155469=CARTESIAN_POINT('Ctrl Pts',(-88.1314637627726,-2.42388196004227,
136.204129698402));
#155470=CARTESIAN_POINT('Ctrl Pts',(-88.1388638452875,-2.27860885041737,
136.264751837003));
#155471=CARTESIAN_POINT('Ctrl Pts',(-88.1462720649538,-2.1331759980738,
136.325440635877));
#155472=CARTESIAN_POINT('Ctrl Pts',(-88.1536802846201,-1.98541206901908,
136.380275506577));
#155473=CARTESIAN_POINT('Ctrl Pts',(-88.1610885042865,-1.83583289277636,
136.429096002658));
#155474=CARTESIAN_POINT('Ctrl Pts',(-88.1685012835884,-1.68616165304652,
136.477946546939));
#155475=CARTESIAN_POINT('Ctrl Pts',(-88.1759140628902,-1.53467329824412,
136.520775239082));
#155476=CARTESIAN_POINT('Ctrl Pts',(-88.1833268421921,-1.38189563509513,
136.557472385662));
#155477=CARTESIAN_POINT('Ctrl Pts',(-88.1907502132206,-1.22889967605669,
136.594221966846));
#155478=CARTESIAN_POINT('Ctrl Pts',(-88.1981735842493,-1.07461109453228,
136.624822432275));
#155479=CARTESIAN_POINT('Ctrl Pts',(-88.2055969552779,-0.919565452500392,
136.649215615003));
#155480=CARTESIAN_POINT('Ctrl Pts',(-88.2095330047208,-0.837356532780662,
136.662149465799));
#155481=CARTESIAN_POINT('Ctrl Pts',(-88.2134690541636,-0.754934833286352,
136.67333909607));
#155482=CARTESIAN_POINT('Ctrl Pts',(-88.2174051036064,-0.672380264045972,
136.682781778305));
#155483=CARTESIAN_POINT('Ctrl Pts',(-88.2248283700119,-0.51668492298055,
136.700590382294));
#155484=CARTESIAN_POINT('Ctrl Pts',(-88.2322516364172,-0.360046148254001,
136.712236043032));
#155485=CARTESIAN_POINT('Ctrl Pts',(-88.2396749028227,-0.202993156564742,
136.717627425422));
#155486=CARTESIAN_POINT('Ctrl Pts',(-88.2470893955437,-0.0461257884692195,
136.723012435645));
#155487=CARTESIAN_POINT('Ctrl Pts',(-88.2545038882647,0.111154452662149,
136.722157868729));
#155488=CARTESIAN_POINT('Ctrl Pts',(-88.2619183809857,0.268310939758517,
136.715023846181));
#155489=CARTESIAN_POINT('Ctrl Pts',(-88.2693257273395,0.425315953515783,
136.707896699674));
#155490=CARTESIAN_POINT('Ctrl Pts',(-88.2767330736932,0.582197080288214,
136.694502163438));
#155491=CARTESIAN_POINT('Ctrl Pts',(-88.284140420047,0.738415494164904,
136.674852344881));
#155492=CARTESIAN_POINT('Ctrl Pts',(-88.2915422417224,0.89451739445474,
136.655217181901));
#155493=CARTESIAN_POINT('Ctrl Pts',(-88.2989440633977,1.0499571972343,136.629336072478));
#155494=CARTESIAN_POINT('Ctrl Pts',(-88.3063458850731,1.2041991168331,136.597273101759));
#155495=CARTESIAN_POINT('Ctrl Pts',(-88.3137437993844,1.35835961332359,
136.565227056832));
#155496=CARTESIAN_POINT('Ctrl Pts',(-88.3211417136959,1.51132312143541,
136.527005725522));
#155497=CARTESIAN_POINT('Ctrl Pts',(-88.3285396280072,1.66256210669305,
136.482724625261));
#155498=CARTESIAN_POINT('Ctrl Pts',(-88.3359363129194,1.81377595877445,
136.438450883716));
#155499=CARTESIAN_POINT('Ctrl Pts',(-88.3433329978315,1.96326549888,136.388119476654));
#155500=CARTESIAN_POINT('Ctrl Pts',(-88.3507296827437,2.11051635051412,
136.331896352115));
#155501=CARTESIAN_POINT('Ctrl Pts',(-88.3581260396791,2.25776067289117,
136.275675720567));
#155502=CARTESIAN_POINT('Ctrl Pts',(-88.3655223966145,2.40276615542933,
136.213564024141));
#155503=CARTESIAN_POINT('Ctrl Pts',(-88.3729187535499,2.54503673087071,
136.145776029329));
#155504=CARTESIAN_POINT('Ctrl Pts',(-88.3803162428864,2.6873290883008,136.077977656002));
#155505=CARTESIAN_POINT('Ctrl Pts',(-88.387713732223,2.82688536788368,136.004501414465));
#155506=CARTESIAN_POINT('Ctrl Pts',(-88.3951112215596,2.96323265108595,
135.925608787499));
#155507=CARTESIAN_POINT('Ctrl Pts',(-88.4025113040746,3.0996277306168,135.846688504844));
#155508=CARTESIAN_POINT('Ctrl Pts',(-88.4099113865895,3.2328112511753,135.762348243291));
#155509=CARTESIAN_POINT('Ctrl Pts',(-88.4173114691045,3.36233803753505,
135.672893608503));
#155510=CARTESIAN_POINT('Ctrl Pts',(-88.4247196887709,3.49200725191227,
135.583340609148));
#155511=CARTESIAN_POINT('Ctrl Pts',(-88.4321279084374,3.61801139462666,
135.488662217768));
#155512=CARTESIAN_POINT('Ctrl Pts',(-88.4395361281039,3.73993665908209,
135.389205691127));
#155513=CARTESIAN_POINT('Ctrl Pts',(-88.4469489074059,3.86193696650301,
135.289687950653));
#155514=CARTESIAN_POINT('Ctrl Pts',(-88.4543616867079,3.97985311425477,
135.185386461633));
#155515=CARTESIAN_POINT('Ctrl Pts',(-88.4617744660099,4.09330752172398,
135.076685990837));
#155516=CARTESIAN_POINT('Ctrl Pts',(-88.4691978370386,4.20692403817123,
134.967830203711));
#155517=CARTESIAN_POINT('Ctrl Pts',(-88.4766212080673,4.31606582340914,
134.854563149413));
#155518=CARTESIAN_POINT('Ctrl Pts',(-88.4840445790961,4.42039445560797,
134.737303970747));
#155519=CARTESIAN_POINT('Ctrl Pts',(-88.487980628537,4.47571199973378,134.67513034062));
#155520=CARTESIAN_POINT('Ctrl Pts',(-88.4919166779781,4.52967709439935,
134.611834899044));
#155521=CARTESIAN_POINT('Ctrl Pts',(-88.495852727419,4.58224425155113,134.547483402304));
#155522=CARTESIAN_POINT('Ctrl Pts',(-88.5032759938245,4.68138426937022,
134.4261184878));
#155523=CARTESIAN_POINT('Ctrl Pts',(-88.51069926023,4.77584917742638,134.300628614471));
#155524=CARTESIAN_POINT('Ctrl Pts',(-88.5181225266355,4.8652760783635,134.171409658463));
#155525=CARTESIAN_POINT('Ctrl Pts',(-88.5255370193565,4.95459728413016,
134.04234342853));
#155526=CARTESIAN_POINT('Ctrl Pts',(-88.5329515120776,5.03889212489643,
133.909557192965));
#155527=CARTESIAN_POINT('Ctrl Pts',(-88.5403660047986,5.11783698971795,
133.773480876022));
#155528=CARTESIAN_POINT('Ctrl Pts',(-88.5477733511524,5.19670576450654,
133.637535714556));
#155529=CARTESIAN_POINT('Ctrl Pts',(-88.5551806975061,5.27023464287378,
133.498307105482));
#155530=CARTESIAN_POINT('Ctrl Pts',(-88.5625880438599,5.33814256255764,
133.356254922648));
#155531=CARTESIAN_POINT('Ctrl Pts',(-88.5699898655354,5.40599983395298,
133.214308687691));
#155532=CARTESIAN_POINT('Ctrl Pts',(-88.5773916872109,5.46824433383542,
133.069543407504));
#155533=CARTESIAN_POINT('Ctrl Pts',(-88.5847935088863,5.52464037361033,
132.922444493331));
#155534=CARTESIAN_POINT('Ctrl Pts',(-88.5921914231977,5.58100664235498,
132.775423231529));
#155535=CARTESIAN_POINT('Ctrl Pts',(-88.5995893375091,5.6315304663153,132.626071136821));
#155536=CARTESIAN_POINT('Ctrl Pts',(-88.6069872518206,5.67602388830884,
132.474894478895));
#155537=CARTESIAN_POINT('Ctrl Pts',(-88.6143839367328,5.72050991630278,
132.323742943787));
#155538=CARTESIAN_POINT('Ctrl Pts',(-88.621780621645,5.75896742599438,132.170767805002));
#155539=CARTESIAN_POINT('Ctrl Pts',(-88.6291773065572,5.79125800110753,
132.01649152102));
#155540=CARTESIAN_POINT('Ctrl Pts',(-88.6365736634927,5.82354714442264,
131.862222077811));
#155541=CARTESIAN_POINT('Ctrl Pts',(-88.6439700204282,5.84966982039167,
131.706651969501));
#155542=CARTESIAN_POINT('Ctrl Pts',(-88.6513663773637,5.86953858167827,
131.550314638059));
#155543=CARTESIAN_POINT('Ctrl Pts',(-88.6587638667003,5.88941038492301,
131.393953370973));
#155544=CARTESIAN_POINT('Ctrl Pts',(-88.666161356037,5.90302631992822,131.236825017212));
#155545=CARTESIAN_POINT('Ctrl Pts',(-88.6735588453736,5.910350755544,131.079468794363));
#155546=CARTESIAN_POINT('Ctrl Pts',(-88.6809589278886,5.91767775872933,
130.922057410534));
#155547=CARTESIAN_POINT('Ctrl Pts',(-88.6883590104036,5.9187088540938,130.764418371239));
#155548=CARTESIAN_POINT('Ctrl Pts',(-88.6957590929186,5.9134605282542,130.607091402331));
#155549=CARTESIAN_POINT('Ctrl Pts',(-88.7031673125851,5.90820643134079,
130.449591436246));
#155550=CARTESIAN_POINT('Ctrl Pts',(-88.7105755322517,5.89665913619996,
130.292404599168));
#155551=CARTESIAN_POINT('Ctrl Pts',(-88.7179837519182,5.87888712720884,
130.136066739068));
#155552=CARTESIAN_POINT('Ctrl Pts',(-88.7253965312203,5.86110417984273,
129.979632655623));
#155553=CARTESIAN_POINT('Ctrl Pts',(-88.7328093105224,5.83708894127932,
129.824048958439));
#155554=CARTESIAN_POINT('Ctrl Pts',(-88.7402220898245,5.80696103515571,
129.669841292617));
#155555=CARTESIAN_POINT('Ctrl Pts',(-88.7476454608533,5.77679008086693,
129.51541328765));
#155556=CARTESIAN_POINT('Ctrl Pts',(-88.7550688318821,5.74048910105205,
129.362365603122));
#155557=CARTESIAN_POINT('Ctrl Pts',(-88.7624922029109,5.69822780715882,
129.211209519829));
#155558=CARTESIAN_POINT('Ctrl Pts',(-88.7664282523514,5.67581985509309,
129.131062937534));
#155559=CARTESIAN_POINT('Ctrl Pts',(-88.7703643017918,5.65173705931615,
129.051447842784));
#155560=CARTESIAN_POINT('Ctrl Pts',(-88.7743003512322,5.62601015504827,
128.972438048844));
#155561=CARTESIAN_POINT('Ctrl Pts',(-88.7817236176376,5.57749001650363,
128.82342804327));
#155562=CARTESIAN_POINT('Ctrl Pts',(-88.7891468840431,5.52297242225242,
128.676121698943));
#155563=CARTESIAN_POINT('Ctrl Pts',(-88.7965701504485,5.46259427922258,
128.531038312413));
#155564=CARTESIAN_POINT('Ctrl Pts',(-88.8039846431695,5.40228749814371,
128.386126402398));
#155565=CARTESIAN_POINT('Ctrl Pts',(-88.8113991358904,5.33613409791209,
128.243432561701));
#155566=CARTESIAN_POINT('Ctrl Pts',(-88.8188136286114,5.26432086635844,
128.103461437937));
#155567=CARTESIAN_POINT('Ctrl Pts',(-88.8262209749652,5.19257685110109,
127.963625223611));
#155568=CARTESIAN_POINT('Ctrl Pts',(-88.833628321319,5.11518403392875,127.826506831742));
#155569=CARTESIAN_POINT('Ctrl Pts',(-88.8410356676727,5.03237739871642,
127.692591301021));
#155570=CARTESIAN_POINT('Ctrl Pts',(-88.8484374893481,4.94963252381674,
127.558775649556));
#155571=CARTESIAN_POINT('Ctrl Pts',(-88.8558393110234,4.86148206622286,
127.428158418919));
#155572=CARTESIAN_POINT('Ctrl Pts',(-88.8632411326988,4.76820702072042,
127.301200277237));
#155573=CARTESIAN_POINT('Ctrl Pts',(-88.8706390470101,4.67498121438846,
127.17430915577));
#155574=CARTESIAN_POINT('Ctrl Pts',(-88.8780369613215,4.57663642820413,
127.051073576446));
#155575=CARTESIAN_POINT('Ctrl Pts',(-88.8854348756328,4.47349700574649,
126.931925324101));
#155576=CARTESIAN_POINT('Ctrl Pts',(-88.892831560545,4.37037472318987,126.812796872033));
#155577=CARTESIAN_POINT('Ctrl Pts',(-88.9002282454572,4.26245962981492,
126.697754680818));
#155578=CARTESIAN_POINT('Ctrl Pts',(-88.9076249303694,4.15011646736071,
126.587197605559));
#155579=CARTESIAN_POINT('Ctrl Pts',(-88.9150212873048,4.03777828632004,
126.476645432517));
#155580=CARTESIAN_POINT('Ctrl Pts',(-88.9224176442402,3.92101269266855,
126.370578241839));
#155581=CARTESIAN_POINT('Ctrl Pts',(-88.9298140011756,3.8002212188215,126.26935794386));
#155582=CARTESIAN_POINT('Ctrl Pts',(-88.9372114905122,3.6794112514911,126.168122148795));
#155583=CARTESIAN_POINT('Ctrl Pts',(-88.9446089798487,3.5545744628249,126.071734963771));
#155584=CARTESIAN_POINT('Ctrl Pts',(-88.9520064691853,3.42614525234258,
125.980517826559));
#155585=CARTESIAN_POINT('Ctrl Pts',(-88.9594065517003,3.29767102119944,
125.889268713321));
#155586=CARTESIAN_POINT('Ctrl Pts',(-88.9668066342152,3.16560216510214,
125.803193472302));
#155587=CARTESIAN_POINT('Ctrl Pts',(-88.9742067167302,3.03040168211528,
125.722569967851));
#155588=CARTESIAN_POINT('Ctrl Pts',(-88.9816149363967,2.89505253229862,
125.641857809569));
#155589=CARTESIAN_POINT('Ctrl Pts',(-88.9890231560632,2.75656519942118,
125.566609551064));
#155590=CARTESIAN_POINT('Ctrl Pts',(-88.9964313757297,2.61542752503644,
125.497057213409));
#155591=CARTESIAN_POINT('Ctrl Pts',(-89.0038441550317,2.47420298276853,
125.42746206745));
#155592=CARTESIAN_POINT('Ctrl Pts',(-89.0112569343337,2.33032518892126,
125.363569979129));
#155593=CARTESIAN_POINT('Ctrl Pts',(-89.0186697136357,2.18430104310365,
125.305564429708));
#155594=CARTESIAN_POINT('Ctrl Pts',(-89.0260930846645,2.03806825113843,
125.247475999239));
#155595=CARTESIAN_POINT('Ctrl Pts',(-89.0335164556932,1.88968333332055,
125.195291029769));
#155596=CARTESIAN_POINT('Ctrl Pts',(-89.0409398267219,1.73966817784561,
125.14914309801));
#155597=CARTESIAN_POINT('Ctrl Pts',(-89.0448758761629,1.66012654284449,
125.124674357286));
#155598=CARTESIAN_POINT('Ctrl Pts',(-89.0488119256039,1.58012676943059,
125.10190199201));
#155599=CARTESIAN_POINT('Ctrl Pts',(-89.0527479750449,1.4997475719321,125.080840041646));
#155600=CARTESIAN_POINT('Ctrl Pts',(-89.0601712414504,1.34815491400506,
125.04111786058));
#155601=CARTESIAN_POINT('Ctrl Pts',(-89.0675945078558,1.19475382323004,
125.007362379376));
#155602=CARTESIAN_POINT('Ctrl Pts',(-89.0750177742613,1.04005520004056,
124.979739106827));
#155603=CARTESIAN_POINT('Ctrl Pts',(-89.0824322669823,0.885539417776762,
124.952148482692));
#155604=CARTESIAN_POINT('Ctrl Pts',(-89.0898467597034,0.729729519585911,
124.930675705481));
#155605=CARTESIAN_POINT('Ctrl Pts',(-89.0972612524245,0.573151043182486,
124.915436399663));
#155606=CARTESIAN_POINT('Ctrl Pts',(-89.1046685987783,0.416723483009693,
124.900211782063));
#155607=CARTESIAN_POINT('Ctrl Pts',(-89.1120759451322,0.25952918842875,
124.891208710921));
#155608=CARTESIAN_POINT('Ctrl Pts',(-89.1194832914861,0.102103250750166,
124.888491662908));
#155609=CARTESIAN_POINT('Ctrl Pts',(-89.1268851131615,-0.0552052727252053,
124.885776641372));
#155610=CARTESIAN_POINT('Ctrl Pts',(-89.134286934837,-0.212744723657578,
124.889338314234));
#155611=CARTESIAN_POINT('Ctrl Pts',(-89.1416887565125,-0.369975644361653,
124.899189274999));
#155612=CARTESIAN_POINT('Ctrl Pts',(-89.1490866708239,-0.527123564086124,
124.909035035517));
#155613=CARTESIAN_POINT('Ctrl Pts',(-89.1564845851353,-0.683962906322821,
124.925163448583));
#155614=CARTESIAN_POINT('Ctrl Pts',(-89.1638824994467,-0.839955082635276,
124.947535025007));
#155615=CARTESIAN_POINT('Ctrl Pts',(-89.1712791843589,-0.995921335877792,
124.969902883681));
#155616=CARTESIAN_POINT('Ctrl Pts',(-89.1786758692712,-1.1510403334545,
124.998511793638));
#155617=CARTESIAN_POINT('Ctrl Pts',(-89.1860725541835,-1.3047793554507,
125.033270478252));
#155618=CARTESIAN_POINT('Ctrl Pts',(-89.1934689111189,-1.45851156049757,
125.068027621629));
#155619=CARTESIAN_POINT('Ctrl Pts',(-89.2008652680544,-1.61086354752181,
125.108933915146));
#155620=CARTESIAN_POINT('Ctrl Pts',(-89.2082616249899,-1.76131379303023,
125.155847159586));
#155621=CARTESIAN_POINT('Ctrl Pts',(-89.2156591143265,-1.91178707285532,
125.202767586564));
#155622=CARTESIAN_POINT('Ctrl Pts',(-89.2230566036631,-2.06035767502607,
125.255696684538));
#155623=CARTESIAN_POINT('Ctrl Pts',(-89.2304540929998,-2.20652036129021,
125.314442725857));
#155624=CARTESIAN_POINT('Ctrl Pts',(-89.2378541755148,-2.35273428465765,
125.373209360509));
#155625=CARTESIAN_POINT('Ctrl Pts',(-89.2452542580299,-2.49653826538684,
125.437796859254));
#155626=CARTESIAN_POINT('Ctrl Pts',(-89.252654340545,-2.63744826656805,
125.507965881174));
#155627=CARTESIAN_POINT('Ctrl Pts',(-89.2600625602115,-2.77851321278125,
125.578212061148));
#155628=CARTESIAN_POINT('Ctrl Pts',(-89.267470779878,-2.91667748996452,
125.654051854702));
#155629=CARTESIAN_POINT('Ctrl Pts',(-89.2748789995446,-3.05148220194328,
125.735200239976));
#155630=CARTESIAN_POINT('Ctrl Pts',(-89.2822917788467,-3.18636988397292,
125.816398570729));
#155631=CARTESIAN_POINT('Ctrl Pts',(-89.2897045581488,-3.31789356938112,
125.902911799136));
#155632=CARTESIAN_POINT('Ctrl Pts',(-89.2971173374509,-3.4456248985642,
125.994412632307));
#155633=CARTESIAN_POINT('Ctrl Pts',(-89.3045407084797,-3.57353873626059,
126.08604420616));
#155634=CARTESIAN_POINT('Ctrl Pts',(-89.3119640795085,-3.69764910161482,
126.182677389314));
#155635=CARTESIAN_POINT('Ctrl Pts',(-89.3193874505374,-3.81756151943951,
126.283945303926));
#155636=CARTESIAN_POINT('Ctrl Pts',(-89.3233234999776,-3.88114196062024,
126.337639982135));
#155637=CARTESIAN_POINT('Ctrl Pts',(-89.3272595494179,-3.94354282809521,
126.392637037533));
#155638=CARTESIAN_POINT('Ctrl Pts',(-89.3311955988581,-4.00470976305055,
126.448877834197));
#155639=CARTESIAN_POINT('Ctrl Pts',(-89.3385080480173,-4.11834657297179,
126.553362793676));
#155640=CARTESIAN_POINT('Ctrl Pts',(-89.3458204971765,-4.22808804895773,
126.662479011971));
#155641=CARTESIAN_POINT('Ctrl Pts',(-89.3531329463357,-4.33352468703351,
126.775900074211));
#155642=CARTESIAN_POINT('Ctrl Pts',(-89.3604366596762,-4.43883536521067,
126.889185637958));
#155643=CARTESIAN_POINT('Ctrl Pts',(-89.3677403730167,-4.53985117746494,
127.006765534692));
#155644=CARTESIAN_POINT('Ctrl Pts',(-89.3750440863571,-4.63619615567382,
127.128273598926));
#155645=CARTESIAN_POINT('Ctrl Pts',(-89.3823407809178,-4.73244854752861,
127.249664895386));
#155646=CARTESIAN_POINT('Ctrl Pts',(-89.3896374754785,-4.82403879937958,
127.374976547731));
#155647=CARTESIAN_POINT('Ctrl Pts',(-89.3969341700392,-4.9106284511203,
127.503806303887));
#155648=CARTESIAN_POINT('Ctrl Pts',(-89.4042252189038,-4.99715110555869,
127.632536380162));
#155649=CARTESIAN_POINT('Ctrl Pts',(-89.4115162677685,-5.07868064890465,
127.764778822264));
#155650=CARTESIAN_POINT('Ctrl Pts',(-89.4188073166332,-5.15491973223651,
127.90009941776));
#155651=CARTESIAN_POINT('Ctrl Pts',(-89.4260953266394,-5.23112703964872,
128.035363612573));
#155652=CARTESIAN_POINT('Ctrl Pts',(-89.4333833366456,-5.3020480845713,
128.17370307362));
#155653=CARTESIAN_POINT('Ctrl Pts',(-89.4406713466518,-5.36742963650288,
128.314655884131));
#155654=CARTESIAN_POINT('Ctrl Pts',(-89.4479578575399,-5.43279773967874,
128.455579701142));
#155655=CARTESIAN_POINT('Ctrl Pts',(-89.4552443684281,-5.49262845538774,
128.599115448444));
#155656=CARTESIAN_POINT('Ctrl Pts',(-89.4625308793163,-5.54671533715024,
128.744778249433));
#155657=CARTESIAN_POINT('Ctrl Pts',(-89.4698174294749,-5.60080251041268,
128.890441835469));
#155658=CARTESIAN_POINT('Ctrl Pts',(-89.4771039796335,-5.6491456554883,
129.038232136214));
#155659=CARTESIAN_POINT('Ctrl Pts',(-89.4843905297921,-5.69158725130675,
129.187646318977));
#155660=CARTESIAN_POINT('Ctrl Pts',(-89.4916815851253,-5.73405508818516,
129.337152882492));
#155661=CARTESIAN_POINT('Ctrl Pts',(-89.4989726404585,-5.77061398263426,
129.488284962247));
#155662=CARTESIAN_POINT('Ctrl Pts',(-89.5062636957917,-5.80115681224227,
129.640526350037));
#155663=CARTESIAN_POINT('Ctrl Pts',(-89.5135572427252,-5.8317100793684,
129.792819763859));
#155664=CARTESIAN_POINT('Ctrl Pts',(-89.5208507896587,-5.85624312395901,
129.946222860742));
#155665=CARTESIAN_POINT('Ctrl Pts',(-89.5281443365922,-5.87470046014896,
130.100212148828));
#155666=CARTESIAN_POINT('Ctrl Pts',(-89.5354455288377,-5.89317714386569,
130.25436285305));
#155667=CARTESIAN_POINT('Ctrl Pts',(-89.5427467210833,-5.90556537004156,
130.409100591828));
#155668=CARTESIAN_POINT('Ctrl Pts',(-89.5500479133288,-5.9118617108521,
130.563899239667));
#155669=CARTESIAN_POINT('Ctrl Pts',(-89.5539068781487,-5.9151895725033,
130.645716361596));
#155670=CARTESIAN_POINT('Ctrl Pts',(-89.5577658429685,-5.91681652206415,
130.727550517598));
#155671=CARTESIAN_POINT('Ctrl Pts',(-89.5616248077884,-5.91674791778598,
130.809324474466));
#155672=CARTESIAN_POINT('',(-91.3116248077885,-5.92354848925726,130.800631107972));
#155673=CARTESIAN_POINT('Ctrl Pts',(-89.5616248077884,-5.92034638875527,
130.809327493404));
#155674=CARTESIAN_POINT('Ctrl Pts',(-89.5776309460825,-5.92339549946666,
131.148716982508));
#155675=CARTESIAN_POINT('Ctrl Pts',(-89.5936370843766,-5.89673577148018,
131.487627614299));
#155676=CARTESIAN_POINT('Ctrl Pts',(-89.702459097275,-5.50197556203136,
133.754623470739));
#155677=CARTESIAN_POINT('Ctrl Pts',(-89.8880908464838,-2.71663448732176,
137.253969721429));
#155678=CARTESIAN_POINT('Ctrl Pts',(-90.1665384702964,3.95783150361734,
136.576113411936));
#155679=CARTESIAN_POINT('Ctrl Pts',(-90.4449860941093,6.99524369355141,
130.594298250215));
#155680=CARTESIAN_POINT('Ctrl Pts',(-90.7234337179224,3.60436866576331,
124.805520141973));
#155681=CARTESIAN_POINT('Ctrl Pts',(-91.001881341735,-3.09874508266306,
124.529383371151));
#155682=CARTESIAN_POINT('Ctrl Pts',(-91.1979450383571,-5.81353639408446,
128.395248006798));
#155683=CARTESIAN_POINT('Ctrl Pts',(-91.3011928603751,-5.92517256730769,
130.579746351147));
#155684=CARTESIAN_POINT('Ctrl Pts',(-91.3116248077885,-5.92354848925726,
130.800631107972));
#155685=CARTESIAN_POINT('',(-93.0616248077885,-5.90861108400418,130.801194235313));
#155686=CARTESIAN_POINT('Ctrl Pts',(-91.3116248077885,-5.92354848925726,
130.800631107972));
#155687=CARTESIAN_POINT('Ctrl Pts',(-91.3940087349794,-5.91072270299169,
132.545018133961));
#155688=CARTESIAN_POINT('Ctrl Pts',(-91.569208536774,-4.17203293217058,
136.276898039585));
#155689=CARTESIAN_POINT('Ctrl Pts',(-91.837224213174,2.17694268671267,137.455562093173));
#155690=CARTESIAN_POINT('Ctrl Pts',(-92.1156718369866,6.77253487019274,
132.567973943205));
#155691=CARTESIAN_POINT('Ctrl Pts',(-92.3941194608,5.1444983646849,126.059711304276));
#155692=CARTESIAN_POINT('Ctrl Pts',(-92.6725670846125,-1.21108081525124,
123.911549595256));
#155693=CARTESIAN_POINT('Ctrl Pts',(-92.895068866942,-5.40037890449579,
127.256492211878));
#155694=CARTESIAN_POINT('Ctrl Pts',(-93.0247547746675,-5.91240923823485,
130.015461788493));
#155695=CARTESIAN_POINT('Ctrl Pts',(-93.0616248077885,-5.90861108400418,
130.801194235313));
#155696=CARTESIAN_POINT('',(-94.8116248077886,-5.91193135788434,130.809233089015));
#155697=CARTESIAN_POINT('Ctrl Pts',(-93.0616248077885,-5.90861108400418,
130.801194235313));
#155698=CARTESIAN_POINT('Ctrl Pts',(-93.1175706492718,-5.90284784170329,
131.993448735702));
#155699=CARTESIAN_POINT('Ctrl Pts',(-93.2663323653589,-4.97304284201653,
135.171957595505));
#155700=CARTESIAN_POINT('Ctrl Pts',(-93.5079099560513,0.220707694199726,
137.799276531578));
#155701=CARTESIAN_POINT('Ctrl Pts',(-93.7863575798639,6.00431876457061,
134.399595895508));
#155702=CARTESIAN_POINT('Ctrl Pts',(-94.0648052036771,6.27025421757813,
127.696069676023));
#155703=CARTESIAN_POINT('Ctrl Pts',(-94.3432528274898,0.774132363579867,
123.848910983356));
#155704=CARTESIAN_POINT('Ctrl Pts',(-94.592192695527,-4.77555456394825,
126.123817676288));
#155705=CARTESIAN_POINT('Ctrl Pts',(-94.74831668896,-5.90153144142422,129.461984403364));
#155706=CARTESIAN_POINT('Ctrl Pts',(-94.8116248077886,-5.91193135788434,
130.809233089015));
#155707=CARTESIAN_POINT('',(-96.5616241144883,-5.921965846863,130.805557042125));
#155708=CARTESIAN_POINT('Ctrl Pts',(-94.8116248077886,-5.91193135788434,
130.809233089015));
#155709=CARTESIAN_POINT('Ctrl Pts',(-94.8411325635643,-5.9167787329236,
131.437182330294));
#155710=CARTESIAN_POINT('Ctrl Pts',(-94.963456193944,-5.53504529805508,
134.034588688322));
#155711=CARTESIAN_POINT('Ctrl Pts',(-95.1785956989288,-1.75330463822294,
137.579571564541));
#155712=CARTESIAN_POINT('Ctrl Pts',(-95.4570433227414,4.752472869827,135.94163247643));
#155713=CARTESIAN_POINT('Ctrl Pts',(-95.7354909465543,6.89095998170769,
129.582791519719));
#155714=CARTESIAN_POINT('Ctrl Pts',(-96.0139385703672,2.69699151251502,
124.346512886951));
#155715=CARTESIAN_POINT('Ctrl Pts',(-96.289316103979,-3.90181258504973,
125.036983019214));
#155716=CARTESIAN_POINT('Ctrl Pts',(-96.4718777629867,-5.92093097606058,
128.907556428895));
#155717=CARTESIAN_POINT('Ctrl Pts',(-96.56162354739,-5.9262323504286,130.80554592138));
#155718=CARTESIAN_POINT('',(-98.3116248063916,-5.9157015749469,130.798899360433));
#155719=CARTESIAN_POINT('Ctrl Pts',(-96.5616248077887,-5.91674987627087,
130.80557063768));
#155720=CARTESIAN_POINT('Ctrl Pts',(-96.5646944778568,-5.91673662110768,
130.870385663671));
#155721=CARTESIAN_POINT('Ctrl Pts',(-96.5677641479249,-5.91565837655804,
130.935188584664));
#155722=CARTESIAN_POINT('Ctrl Pts',(-96.570833817993,-5.91351612517523,
130.999956118006));
#155723=CARTESIAN_POINT('Ctrl Pts',(-96.5782570843985,-5.90833560011258,
131.156580981185));
#155724=CARTESIAN_POINT('Ctrl Pts',(-96.5856803508038,-5.89692041521548,
131.313236720677));
#155725=CARTESIAN_POINT('Ctrl Pts',(-96.5931036172093,-5.87925770863647,
131.469386450101));
#155726=CARTESIAN_POINT('Ctrl Pts',(-96.6005181099303,-5.86161587790978,
131.625351623512));
#155727=CARTESIAN_POINT('Ctrl Pts',(-96.6079326026514,-5.83774126504488,
131.78081160999));
#155728=CARTESIAN_POINT('Ctrl Pts',(-96.6153470953724,-5.80767299525278,
131.935229727017));
#155729=CARTESIAN_POINT('Ctrl Pts',(-96.6227544417262,-5.77763370639124,
132.089499010049));
#155730=CARTESIAN_POINT('Ctrl Pts',(-96.63016178808,-5.74141271592911,132.242728058824));
#155731=CARTESIAN_POINT('Ctrl Pts',(-96.6375691344338,-5.69910089664331,
132.394385627552));
#155732=CARTESIAN_POINT('Ctrl Pts',(-96.6449709561092,-5.65682063510867,
132.545930084343));
#155733=CARTESIAN_POINT('Ctrl Pts',(-96.6523727777846,-5.60845868990398,
132.695905036815));
#155734=CARTESIAN_POINT('Ctrl Pts',(-96.65977459946,-5.55415690618363,132.843789857327));
#155735=CARTESIAN_POINT('Ctrl Pts',(-96.6671725137713,-5.49988378795238,
132.991596610593));
#155736=CARTESIAN_POINT('Ctrl Pts',(-96.6745704280827,-5.43967720423761,
133.137315079766));
#155737=CARTESIAN_POINT('Ctrl Pts',(-96.681968342394,-5.37372867000152,
133.280440330278));
#155738=CARTESIAN_POINT('Ctrl Pts',(-96.6893650273062,-5.30779109521531,
133.42354179597));
#155739=CARTESIAN_POINT('Ctrl Pts',(-96.6967617122184,-5.23611361979543,
133.564050559594));
#155740=CARTESIAN_POINT('Ctrl Pts',(-96.7041583971306,-5.15893571916605,
133.701482086889));
#155741=CARTESIAN_POINT('Ctrl Pts',(-96.711554754066,-5.08176124068567,
133.838907520326));
#155742=CARTESIAN_POINT('Ctrl Pts',(-96.7189511110015,-4.99908700472486,
133.973255663251));
#155743=CARTESIAN_POINT('Ctrl Pts',(-96.726347467937,-4.91119809813897,
134.104067241394));
#155744=CARTESIAN_POINT('Ctrl Pts',(-96.7337449572736,-4.82329573553686,
134.234898847124));
#155745=CARTESIAN_POINT('Ctrl Pts',(-96.7411424466101,-4.73017732082761,
134.362192500083));
#155746=CARTESIAN_POINT('Ctrl Pts',(-96.7485399359467,-4.63217076417917,
134.485518665516));
#155747=CARTESIAN_POINT('Ctrl Pts',(-96.7559400184617,-4.53412985148437,
134.608888062744));
#155748=CARTESIAN_POINT('Ctrl Pts',(-96.7633401009766,-4.43119761732927,
134.728286911311));
#155749=CARTESIAN_POINT('Ctrl Pts',(-96.7707401834916,-4.32374155699493,
134.843319581311));
#155750=CARTESIAN_POINT('Ctrl Pts',(-96.7781484031581,-4.21616733767535,
134.958478741557));
#155751=CARTESIAN_POINT('Ctrl Pts',(-96.7855566228246,-4.10405961293047,
135.069261862239));
#155752=CARTESIAN_POINT('Ctrl Pts',(-96.7929648424911,-3.98782248718409,
135.175310442628));
#155753=CARTESIAN_POINT('Ctrl Pts',(-96.8003776217932,-3.87151381942633,
135.281424294148));
#155754=CARTESIAN_POINT('Ctrl Pts',(-96.8077904010953,-3.75107097119409,
135.382797558979));
#155755=CARTESIAN_POINT('Ctrl Pts',(-96.8152031803974,-3.62692984837114,
135.47911306422));
#155756=CARTESIAN_POINT('Ctrl Pts',(-96.8226265514261,-3.50261134689007,
135.575566189572));
#155757=CARTESIAN_POINT('Ctrl Pts',(-96.8300499224549,-3.37458431998493,
135.666946905571));
#155758=CARTESIAN_POINT('Ctrl Pts',(-96.8374732934836,-3.24331294537814,
135.752981809458));
#155759=CARTESIAN_POINT('Ctrl Pts',(-96.8414093429244,-3.17370971274992,
135.798599579877));
#155760=CARTESIAN_POINT('Ctrl Pts',(-96.8453453923651,-3.1031947873653,
135.842715219548));
#155761=CARTESIAN_POINT('Ctrl Pts',(-96.8492814418058,-3.03183987724647,
135.885293358829));
#155762=CARTESIAN_POINT('Ctrl Pts',(-96.8567047082112,-2.89726674366976,
135.965594400697));
#155763=CARTESIAN_POINT('Ctrl Pts',(-96.8641279746166,-2.75929764704575,
136.040666736073));
#155764=CARTESIAN_POINT('Ctrl Pts',(-96.8715512410221,-2.61837733294993,
136.110209343717));
#155765=CARTESIAN_POINT('Ctrl Pts',(-96.8789657337431,-2.47762357496266,
136.179669757773));
#155766=CARTESIAN_POINT('Ctrl Pts',(-96.8863802264642,-2.33392587406002,
136.243613289819));
#155767=CARTESIAN_POINT('Ctrl Pts',(-96.8937947191852,-2.18775690457629,
136.30178276699));
#155768=CARTESIAN_POINT('Ctrl Pts',(-96.9012020655389,-2.04172881824852,
136.359896178229));
#155769=CARTESIAN_POINT('Ctrl Pts',(-96.9086094118927,-1.8932345497504,
136.412246476812));
#155770=CARTESIAN_POINT('Ctrl Pts',(-96.9160167582465,-1.7427701701668,
136.458622965254));
#155771=CARTESIAN_POINT('Ctrl Pts',(-96.9234185799219,-1.59241801259418,
136.50496486436));
#155772=CARTESIAN_POINT('Ctrl Pts',(-96.9308204015973,-1.44009902487803,
136.545341715331));
#155773=CARTESIAN_POINT('Ctrl Pts',(-96.9382222232727,-1.28632789657008,
136.579591444555));
#155774=CARTESIAN_POINT('Ctrl Pts',(-96.9456201375841,-1.13263794284381,
136.613823093614));
#155775=CARTESIAN_POINT('Ctrl Pts',(-96.9530180518955,-0.977497738640905,
136.641933981555));
#155776=CARTESIAN_POINT('Ctrl Pts',(-96.9604159662068,-0.821435618230036,
136.663812305873));
#155777=CARTESIAN_POINT('Ctrl Pts',(-96.967812651119,-0.665399432512547,
136.68568699441));
#155778=CARTESIAN_POINT('Ctrl Pts',(-96.9752093360312,-0.508442003976059,
136.701331123184));
#155779=CARTESIAN_POINT('Ctrl Pts',(-96.9826060209434,-0.351100427334726,
136.710684267048));
#155780=CARTESIAN_POINT('Ctrl Pts',(-96.9900023778789,-0.193765827383783,
136.720036996183));
#155781=CARTESIAN_POINT('Ctrl Pts',(-96.9973987348144,-0.0360474858361569,
136.7230992729));
#155782=CARTESIAN_POINT('Ctrl Pts',(-97.0047950917498,0.121514100447624,
136.719862699883));
#155783=CARTESIAN_POINT('Ctrl Pts',(-97.0121925810864,0.2790998098125,136.716625631338));
#155784=CARTESIAN_POINT('Ctrl Pts',(-97.0195900704229,0.436528342883927,
136.707087800537));
#155785=CARTESIAN_POINT('Ctrl Pts',(-97.0269875597595,0.593261076452136,
136.691292913564));
#155786=CARTESIAN_POINT('Ctrl Pts',(-97.0343876422745,0.750048752436907,
136.675492489718));
#155787=CARTESIAN_POINT('Ctrl Pts',(-97.0417877247895,0.906139772107623,
136.653430680061));
#155788=CARTESIAN_POINT('Ctrl Pts',(-97.0491878073045,1.06100264064333,
136.625202821152));
#155789=CARTESIAN_POINT('Ctrl Pts',(-97.0565960269709,1.21603579682349,
136.59694392281));
#155790=CARTESIAN_POINT('Ctrl Pts',(-97.0640042466373,1.36983773740229,
136.562505501684));
#155791=CARTESIAN_POINT('Ctrl Pts',(-97.0714124663038,1.52188841725016,
136.522033763868));
#155792=CARTESIAN_POINT('Ctrl Pts',(-97.0788252456059,1.67403268175481,
136.481537116372));
#155793=CARTESIAN_POINT('Ctrl Pts',(-97.086238024908,1.82442318194635,136.434999862856));
#155794=CARTESIAN_POINT('Ctrl Pts',(-97.0936508042101,1.97255745350397,
136.382617303586));
#155795=CARTESIAN_POINT('Ctrl Pts',(-97.1010741752388,2.12090338625538,
136.330159897659));
#155796=CARTESIAN_POINT('Ctrl Pts',(-97.1084975462676,2.2669863059375,136.271840643105));
#155797=CARTESIAN_POINT('Ctrl Pts',(-97.1159209172964,2.41032529166931,
136.207902284921));
#155798=CARTESIAN_POINT('Ctrl Pts',(-97.1198569667372,2.48632706127606,
136.174000633232));
#155799=CARTESIAN_POINT('Ctrl Pts',(-97.1237930161779,2.56155783794563,
136.138520010245));
#155800=CARTESIAN_POINT('Ctrl Pts',(-97.1277290656187,2.63594910425982,
136.101501627795));
#155801=CARTESIAN_POINT('Ctrl Pts',(-97.1351523320242,2.77624871085666,
136.031686113799));
#155802=CARTESIAN_POINT('Ctrl Pts',(-97.1425755984296,2.91398485957519,
135.956187236336));
#155803=CARTESIAN_POINT('Ctrl Pts',(-97.1499988648351,3.04866389687383,
135.875216463121));
#155804=CARTESIAN_POINT('Ctrl Pts',(-97.1574133575561,3.18318375473478,
135.794341390635));
#155805=CARTESIAN_POINT('Ctrl Pts',(-97.164827850277,3.31465337656868,135.708007486114));
#155806=CARTESIAN_POINT('Ctrl Pts',(-97.1722423429981,3.44260090353974,
135.616473415646));
#155807=CARTESIAN_POINT('Ctrl Pts',(-97.1796496893518,3.57042510986717,
135.525027569162));
#155808=CARTESIAN_POINT('Ctrl Pts',(-97.1870570357057,3.69473367799984,
135.42839175061));
#155809=CARTESIAN_POINT('Ctrl Pts',(-97.1944643820595,3.81508120363753,
135.326869431505));
#155810=CARTESIAN_POINT('Ctrl Pts',(-97.2018662037349,3.93533896955015,
135.225422831575));
#155811=CARTESIAN_POINT('Ctrl Pts',(-97.2092680254103,4.05164129126286,
135.119097227521));
#155812=CARTESIAN_POINT('Ctrl Pts',(-97.2166698470857,4.16357360938068,
135.008238037493));
#155813=CARTESIAN_POINT('Ctrl Pts',(-97.2240677613971,4.27544683929903,
134.897437369168));
#155814=CARTESIAN_POINT('Ctrl Pts',(-97.2314656757085,4.38295439534775,
134.782108143152));
#155815=CARTESIAN_POINT('Ctrl Pts',(-97.2388635900198,4.48571663733404,
134.662634430043));
#155816=CARTESIAN_POINT('Ctrl Pts',(-97.246260274932,4.58846180209986,134.543180571298));
#155817=CARTESIAN_POINT('Ctrl Pts',(-97.2536569598442,4.68646297472457,
134.419583875136));
#155818=CARTESIAN_POINT('Ctrl Pts',(-97.2610536447564,4.77937900500779,
134.292263553284));
#155819=CARTESIAN_POINT('Ctrl Pts',(-97.2684500016918,4.87229091529686,
134.164948876949));
#155820=CARTESIAN_POINT('Ctrl Pts',(-97.2758463586274,4.96011791151835,
134.033911204755));
#155821=CARTESIAN_POINT('Ctrl Pts',(-97.2832427155628,5.04256077701662,
133.899600733065));
#155822=CARTESIAN_POINT('Ctrl Pts',(-97.2906402048994,5.1250162647283,133.765269698098));
#155823=CARTESIAN_POINT('Ctrl Pts',(-97.298037694236,5.20208578508113,133.627665184095));
#155824=CARTESIAN_POINT('Ctrl Pts',(-97.3054351835726,5.27351497024009,
133.487263974222));
#155825=CARTESIAN_POINT('Ctrl Pts',(-97.3128352660876,5.34496919478907,
133.346813546922));
#155826=CARTESIAN_POINT('Ctrl Pts',(-97.3202353486026,5.41077897836871,
133.203564804336));
#155827=CARTESIAN_POINT('Ctrl Pts',(-97.3276354311176,5.47073724439364,
133.058016439848));
#155828=CARTESIAN_POINT('Ctrl Pts',(-97.3350436507841,5.530761440696,132.91230802997));
#155829=CARTESIAN_POINT('Ctrl Pts',(-97.3424518704505,5.58492112735976,
132.764295293639));
#155830=CARTESIAN_POINT('Ctrl Pts',(-97.349860090117,5.63305821461801,132.614494787517));
#155831=CARTESIAN_POINT('Ctrl Pts',(-97.3572728694191,5.68122492945026,
132.464602081683));
#155832=CARTESIAN_POINT('Ctrl Pts',(-97.3646856487212,5.72336155890942,
132.31291977233));
#155833=CARTESIAN_POINT('Ctrl Pts',(-97.3720984280233,5.75936082040169,
132.159976161488));
#155834=CARTESIAN_POINT('Ctrl Pts',(-97.379521799052,5.79541151932693,132.006814017642));
#155835=CARTESIAN_POINT('Ctrl Pts',(-97.3869451700808,5.82530726514585,
131.852387338417));
#155836=CARTESIAN_POINT('Ctrl Pts',(-97.3943685411096,5.84899233661424,
131.69723194577));
#155837=CARTESIAN_POINT('Ctrl Pts',(-97.3983045905503,5.86155072982207,
131.614964833687));
#155838=CARTESIAN_POINT('Ctrl Pts',(-97.402240639991,5.87236394924333,131.532492907243));
#155839=CARTESIAN_POINT('Ctrl Pts',(-97.4061766894317,5.88142963222386,
131.449896088086));
#155840=CARTESIAN_POINT('Ctrl Pts',(-97.4135999558372,5.89852722739512,
131.294121064911));
#155841=CARTESIAN_POINT('Ctrl Pts',(-97.4210232222426,5.9094576363208,131.137430754673));
#155842=CARTESIAN_POINT('Ctrl Pts',(-97.428446488648,5.91413194098158,130.980354785542));
#155843=CARTESIAN_POINT('Ctrl Pts',(-97.435860981369,5.91880072100244,130.823464467161));
#155844=CARTESIAN_POINT('Ctrl Pts',(-97.44327547409,5.9172281039504,130.666189766683));
#155845=CARTESIAN_POINT('Ctrl Pts',(-97.450689966811,5.90937666170668,130.509067487649));
#155846=CARTESIAN_POINT('Ctrl Pts',(-97.4580973131647,5.90153278697858,
130.352096648982));
#155847=CARTESIAN_POINT('Ctrl Pts',(-97.4655046595185,5.88742215344312,
130.195278309622));
#155848=CARTESIAN_POINT('Ctrl Pts',(-97.4729120058723,5.86705932837742,
130.039151234587));
#155849=CARTESIAN_POINT('Ctrl Pts',(-97.4803138275477,5.84671169067495,
129.883140605015));
#155850=CARTESIAN_POINT('Ctrl Pts',(-97.4877156492232,5.8201211944147,129.727820581767));
#155851=CARTESIAN_POINT('Ctrl Pts',(-97.4951174708985,5.78735437019004,
129.57372665235));
#155852=CARTESIAN_POINT('Ctrl Pts',(-97.5025153852099,5.75460484331674,
129.419714067919));
#155853=CARTESIAN_POINT('Ctrl Pts',(-97.5099132995212,5.71568555923869,
129.266926652509));
#155854=CARTESIAN_POINT('Ctrl Pts',(-97.5173112138326,5.67071444262972,
129.115891407704));
#155855=CARTESIAN_POINT('Ctrl Pts',(-97.5247078987448,5.62575079940453,
128.964881262218));
#155856=CARTESIAN_POINT('Ctrl Pts',(-97.532104583657,5.57473742609889,128.815623066859));
#155857=CARTESIAN_POINT('Ctrl Pts',(-97.5395012685692,5.51784261739424,
128.66863043513));
#155858=CARTESIAN_POINT('Ctrl Pts',(-97.5468976255047,5.46095033146503,
128.521644321209));
#155859=CARTESIAN_POINT('Ctrl Pts',(-97.5542939824401,5.39817726342021,
128.376923919304));
#155860=CARTESIAN_POINT('Ctrl Pts',(-97.5616903393755,5.32974044229802,
128.234964310993));
#155861=CARTESIAN_POINT('Ctrl Pts',(-97.5690878287121,5.2612931433238,128.092982968303));
#155862=CARTESIAN_POINT('Ctrl Pts',(-97.5764853180487,5.18718052680902,
127.953763597112));
#155863=CARTESIAN_POINT('Ctrl Pts',(-97.5838828073852,5.10766623190721,
127.817777917232));
#155864=CARTESIAN_POINT('Ctrl Pts',(-97.5912828899002,5.02812406339271,
127.681744567782));
#155865=CARTESIAN_POINT('Ctrl Pts',(-97.5986829724152,4.94317663475815,
127.548947488614));
#155866=CARTESIAN_POINT('Ctrl Pts',(-97.6060830549301,4.85313158091947,
127.419830455079));
#155867=CARTESIAN_POINT('Ctrl Pts',(-97.6134912745966,4.76298751328711,
127.290571444092));
#155868=CARTESIAN_POINT('Ctrl Pts',(-97.620899494263,4.66773483983959,127.165000866421));
#155869=CARTESIAN_POINT('Ctrl Pts',(-97.6283077139295,4.56772270294536,
127.043530938958));
#155870=CARTESIAN_POINT('Ctrl Pts',(-97.6357204932315,4.46764901024965,
126.921986248781));
#155871=CARTESIAN_POINT('Ctrl Pts',(-97.6431332725336,4.36281026499271,
126.804547515795));
#155872=CARTESIAN_POINT('Ctrl Pts',(-97.6505460518356,4.25359295377042,
126.691590560034));
#155873=CARTESIAN_POINT('Ctrl Pts',(-97.6579694228644,4.14421958773192,
126.578472206077));
#155874=CARTESIAN_POINT('Ctrl Pts',(-97.6653927938932,4.03045542976861,
126.469848676225));
#155875=CARTESIAN_POINT('Ctrl Pts',(-97.672816164922,3.91272116337437,126.366056475196));
#155876=CARTESIAN_POINT('Ctrl Pts',(-97.6767522143629,3.85029563033586,
126.311023359749));
#155877=CARTESIAN_POINT('Ctrl Pts',(-97.6806882638037,3.78675447211467,
126.25734780127));
#155878=CARTESIAN_POINT('Ctrl Pts',(-97.6846243132446,3.72216365198443,
126.205074987129));
#155879=CARTESIAN_POINT('Ctrl Pts',(-97.69204757965,3.60034738103171,126.10649009104));
#155880=CARTESIAN_POINT('Ctrl Pts',(-97.6994708460555,3.47442753834198,
126.012599088388));
#155881=CARTESIAN_POINT('Ctrl Pts',(-97.7068941124609,3.34480165273408,
125.923763065384));
#155882=CARTESIAN_POINT('Ctrl Pts',(-97.7143086051819,3.21532897415821,
125.835032039182));
#155883=CARTESIAN_POINT('Ctrl Pts',(-97.7217230979029,3.08215927646435,
125.751344309189));
#155884=CARTESIAN_POINT('Ctrl Pts',(-97.7291375906239,2.94572395686344,
125.67302152017));
#155885=CARTESIAN_POINT('Ctrl Pts',(-97.7365449369777,2.80942013876025,
125.594774221604));
#155886=CARTESIAN_POINT('Ctrl Pts',(-97.7439522833314,2.66985728643288,
125.521881754306));
#155887=CARTESIAN_POINT('Ctrl Pts',(-97.7513596296852,2.52749655211978,
125.454623078067));
#155888=CARTESIAN_POINT('Ctrl Pts',(-97.7587614513606,2.38524199581328,
125.387414565886));
#155889=CARTESIAN_POINT('Ctrl Pts',(-97.7661632730361,2.24019404862509,
125.325831637004));
#155890=CARTESIAN_POINT('Ctrl Pts',(-97.7735650947115,2.09283919277186,
125.270107761426));
#155891=CARTESIAN_POINT('Ctrl Pts',(-97.7809630090228,1.94556212440044,
125.214413302048));
#155892=CARTESIAN_POINT('Ctrl Pts',(-97.7883609233342,1.79598092095095,
125.164571867925));
#155893=CARTESIAN_POINT('Ctrl Pts',(-97.7957588376455,1.64460270494951,
125.120769102919));
#155894=CARTESIAN_POINT('Ctrl Pts',(-97.8031555225577,1.49324964526107,
125.076973617137));
#155895=CARTESIAN_POINT('Ctrl Pts',(-97.8105522074699,1.34010052395105,
125.039214912448));
#155896=CARTESIAN_POINT('Ctrl Pts',(-97.8179488923821,1.1856784259921,125.007629018411));
#155897=CARTESIAN_POINT('Ctrl Pts',(-97.8253452493176,1.03126317527079,
124.976044524927));
#155898=CARTESIAN_POINT('Ctrl Pts',(-97.832741606253,0.875575425857908,
124.950632372677));
#155899=CARTESIAN_POINT('Ctrl Pts',(-97.8401379631885,0.719149013401902,
124.93147757267));
#155900=CARTESIAN_POINT('Ctrl Pts',(-97.847535452525,0.56269865166281,124.912319840015));
#155901=CARTESIAN_POINT('Ctrl Pts',(-97.8549329418616,0.405509772255039,
124.899421412516));
#155902=CARTESIAN_POINT('Ctrl Pts',(-97.8623304311981,0.248121749818079,
124.892815459169));
#155903=CARTESIAN_POINT('Ctrl Pts',(-97.8697305137131,0.0906785552540618,
124.886207190115));
#155904=CARTESIAN_POINT('Ctrl Pts',(-97.8771305962281,-0.0669635485920499,
124.885895802622));
#155905=CARTESIAN_POINT('Ctrl Pts',(-97.8845306787431,-0.224264916761973,
124.89186234614));
#155906=CARTESIAN_POINT('Ctrl Pts',(-97.8919388984096,-0.381739253957398,
124.897835450487));
#155907=CARTESIAN_POINT('Ctrl Pts',(-97.8993471180761,-0.538871733969701,
124.910100257891));
#155908=CARTESIAN_POINT('Ctrl Pts',(-97.9067553377425,-0.695126827075153,
124.92858583829));
#155909=CARTESIAN_POINT('Ctrl Pts',(-97.9141681170446,-0.8514780925836,
124.947082796254));
#155910=CARTESIAN_POINT('Ctrl Pts',(-97.9215808963467,-1.00695052732344,
124.971808098047));
#155911=CARTESIAN_POINT('Ctrl Pts',(-97.9289936756488,-1.1610190378098,
125.002639721457));
#155912=CARTESIAN_POINT('Ctrl Pts',(-97.9364170466775,-1.31530768860881,
125.033515398537));
#155913=CARTESIAN_POINT('Ctrl Pts',(-97.9438404177062,-1.46818804687434,
125.070514735438));
#155914=CARTESIAN_POINT('Ctrl Pts',(-97.9512637887349,-1.61914961195375,
125.113465688242));
#155915=CARTESIAN_POINT('Ctrl Pts',(-97.9551998381757,-1.69919305603231,
125.136239314012));
#155916=CARTESIAN_POINT('Ctrl Pts',(-97.9591358876166,-1.778697371648,125.160685339546));
#155917=CARTESIAN_POINT('Ctrl Pts',(-97.9630719370574,-1.85758888662536,
125.18677269295));
#155918=CARTESIAN_POINT('Ctrl Pts',(-97.9704952034628,-2.00637582175179,
125.235972627313));
#155919=CARTESIAN_POINT('Ctrl Pts',(-97.9779184698683,-2.15343173215094,
125.291162176854));
#155920=CARTESIAN_POINT('Ctrl Pts',(-97.9853417362737,-2.29823795172998,
125.352202065238));
#155921=CARTESIAN_POINT('Ctrl Pts',(-97.9927562289947,-2.44287302238289,
125.413169809542));
#155922=CARTESIAN_POINT('Ctrl Pts',(-98.0001707217156,-2.58526335423886,
125.479973985526));
#155923=CARTESIAN_POINT('Ctrl Pts',(-98.0075852144366,-2.72490515771916,
125.55242550335));
#155924=CARTESIAN_POINT('Ctrl Pts',(-98.0149925607904,-2.86441236917224,
125.624807189673));
#155925=CARTESIAN_POINT('Ctrl Pts',(-98.0223999071442,-3.00117599702698,
125.70282521089));
#155926=CARTESIAN_POINT('Ctrl Pts',(-98.029807253498,-3.1347120804622,125.786242371141));
#155927=CARTESIAN_POINT('Ctrl Pts',(-98.0372090751734,-3.26814856764799,
125.869597315727));
#155928=CARTESIAN_POINT('Ctrl Pts',(-98.0446108968488,-3.39836198828382,
125.95834318436));
#155929=CARTESIAN_POINT('Ctrl Pts',(-98.0520127185242,-3.5248929619209,
126.052196882013));
#155930=CARTESIAN_POINT('Ctrl Pts',(-98.0594106328356,-3.65135714084228,
126.146001035031));
#155931=CARTESIAN_POINT('Ctrl Pts',(-98.0668085471469,-3.77414244514158,
126.244907425265));
#155932=CARTESIAN_POINT('Ctrl Pts',(-98.0742064614583,-3.89281857526756,
126.348589741213));
#155933=CARTESIAN_POINT('Ctrl Pts',(-98.0816031463705,-4.01147498357355,
126.452254827042));
#155934=CARTESIAN_POINT('Ctrl Pts',(-98.0889998312827,-4.12602329215452,
126.560694018016));
#155935=CARTESIAN_POINT('Ctrl Pts',(-98.0963965161949,-4.23606631528235,
126.673540755235));
#155936=CARTESIAN_POINT('Ctrl Pts',(-98.1037928731303,-4.34610445898721,
126.786382488711));
#155937=CARTESIAN_POINT('Ctrl Pts',(-98.1111892300658,-4.45163745382707,
126.903631112581));
#155938=CARTESIAN_POINT('Ctrl Pts',(-98.1185855870013,-4.55230522642488,
127.024883446321));
#155939=CARTESIAN_POINT('Ctrl Pts',(-98.1259830763379,-4.65298841151566,
127.146154344102));
#155940=CARTESIAN_POINT('Ctrl Pts',(-98.1333805656745,-4.74880465274432,
127.271429885044));
#155941=CARTESIAN_POINT('Ctrl Pts',(-98.140778055011,-4.83943449892919,
127.400274206637));
#155942=CARTESIAN_POINT('Ctrl Pts',(-98.148178137526,-4.93009611526602,
127.529163694407));
#155943=CARTESIAN_POINT('Ctrl Pts',(-98.155578220041,-5.015567502134,127.661624148483));
#155944=CARTESIAN_POINT('Ctrl Pts',(-98.1629783025559,-5.09557291188604,
127.797191307043));
#155945=CARTESIAN_POINT('Ctrl Pts',(-98.1703865222224,-5.17566629581097,
127.93290753563));
#155946=CARTESIAN_POINT('Ctrl Pts',(-98.1777947418888,-5.25028150960514,
128.071736969274));
#155947=CARTESIAN_POINT('Ctrl Pts',(-98.1852029615553,-5.31918876184357,
128.213190712219));
#155948=CARTESIAN_POINT('Ctrl Pts',(-98.1926157408573,-5.38813842534596,
128.354731517582));
#155949=CARTESIAN_POINT('Ctrl Pts',(-98.2000285201593,-5.451372977293,128.498899509704));
#155950=CARTESIAN_POINT('Ctrl Pts',(-98.2074412994613,-5.50871125257117,
128.64518695658));
#155951=CARTESIAN_POINT('Ctrl Pts',(-98.21486467049,-5.56613145546588,128.79168342582));
#155952=CARTESIAN_POINT('Ctrl Pts',(-98.2222880415189,-5.61763843340822,
128.940305046379));
#155953=CARTESIAN_POINT('Ctrl Pts',(-98.2297114125476,-5.66310099374721,
129.090529325659));
#155954=CARTESIAN_POINT('Ctrl Pts',(-98.2336474619885,-5.68720633409882,
129.170181843118));
#155955=CARTESIAN_POINT('Ctrl Pts',(-98.2375835114293,-5.70961322506146,
129.250284749454));
#155956=CARTESIAN_POINT('Ctrl Pts',(-98.2415195608702,-5.730307986688,129.330759267065));
#155957=CARTESIAN_POINT('Ctrl Pts',(-98.2512252464837,-5.78133804949806,
129.529196908549));
#155958=CARTESIAN_POINT('Ctrl Pts',(-98.2609309320973,-5.82208048302636,
129.73038031375));
#155959=CARTESIAN_POINT('Ctrl Pts',(-98.2706366177106,-5.85229309841448,
129.933386420043));
#155960=CARTESIAN_POINT('Ctrl Pts',(-98.2801407901906,-5.88187842799923,
130.132177636403));
#155961=CARTESIAN_POINT('Ctrl Pts',(-98.2896449626705,-5.90136670172385,
130.332716894857));
#155962=CARTESIAN_POINT('Ctrl Pts',(-98.2991491351504,-5.91057510998828,
130.534115484979));
#155963=CARTESIAN_POINT('Ctrl Pts',(-98.303307687164,-5.91460425032748,
130.622237466587));
#155964=CARTESIAN_POINT('Ctrl Pts',(-98.3074662391774,-5.91666588808329,
130.710523658734));
#155965=CARTESIAN_POINT('Ctrl Pts',(-98.311624791191,-5.91674747839506,
130.798898071854));
#155966=CARTESIAN_POINT('',(-100.061624840552,-5.91280015844335,130.805553846743));
#155967=CARTESIAN_POINT('Ctrl Pts',(-98.3116248077888,-5.91560542397323,
130.798899478893));
#155968=CARTESIAN_POINT('Ctrl Pts',(-98.3810722667536,-5.90220073733502,
132.274473302428));
#155969=CARTESIAN_POINT('Ctrl Pts',(-98.5433356003227,-4.59610210103513,
135.743303909333));
#155970=CARTESIAN_POINT('Ctrl Pts',(-98.7984148084961,1.23205455133509,
137.693453599436));
#155971=CARTESIAN_POINT('Ctrl Pts',(-99.076862432309,6.46194461450306,133.491521262083));
#155972=CARTESIAN_POINT('Ctrl Pts',(-99.3553100561219,5.75362326048721,
126.820219567513));
#155973=CARTESIAN_POINT('Ctrl Pts',(-99.6337576799348,-0.241996789793268,
123.81014886183));
#155974=CARTESIAN_POINT('Ctrl Pts',(-99.8691959304905,-5.12349212797977,
126.699581489776));
#155975=CARTESIAN_POINT('Ctrl Pts',(-100.011818306442,-5.9052485242762,
129.743477247566));
#155976=CARTESIAN_POINT('Ctrl Pts',(-100.061624807789,-5.90715198088181,
130.805552007816));
#155977=CARTESIAN_POINT('',(-101.811624807789,-5.91752016895145,130.809410794066));
#155978=CARTESIAN_POINT('Ctrl Pts',(-100.061624863462,-5.91674987942144,
130.805555132688));
#155979=CARTESIAN_POINT('Ctrl Pts',(-100.069501906503,-5.91671591332789,
130.973798193149));
#155980=CARTESIAN_POINT('Ctrl Pts',(-100.077378949543,-5.90950170403371,
131.141858042596));
#155981=CARTESIAN_POINT('Ctrl Pts',(-100.085255992583,-5.89517943177854,
131.309127920029));
#155982=CARTESIAN_POINT('Ctrl Pts',(-100.093147676019,-5.88083053992256,
131.47670868789));
#155983=CARTESIAN_POINT('Ctrl Pts',(-100.101039359456,-5.85934722133416,
131.643496259084));
#155984=CARTESIAN_POINT('Ctrl Pts',(-100.108931042892,-5.83085291951967,
131.808892744195));
#155985=CARTESIAN_POINT('Ctrl Pts',(-100.116845568588,-5.80227614173708,
131.974767964854));
#155986=CARTESIAN_POINT('Ctrl Pts',(-100.124760094284,-5.76664783455927,
132.139243754121));
#155987=CARTESIAN_POINT('Ctrl Pts',(-100.13267461998,-5.72414226850208,
132.30173360131));
#155988=CARTESIAN_POINT('Ctrl Pts',(-100.140601422694,-5.68157076777453,
132.46447550289));
#155989=CARTESIAN_POINT('Ctrl Pts',(-100.148528225409,-5.63210078849964,
132.62522503003));
#155990=CARTESIAN_POINT('Ctrl Pts',(-100.156455028124,-5.57595548860646,
132.783413661721));
#155991=CARTESIAN_POINT('Ctrl Pts',(-100.164400999593,-5.51967441701875,
132.941984828346));
#155992=CARTESIAN_POINT('Ctrl Pts',(-100.172346971061,-5.45668584942095,
133.09798244126));
#155993=CARTESIAN_POINT('Ctrl Pts',(-100.18029294253,-5.38726073115559,
133.250858599795));
#155994=CARTESIAN_POINT('Ctrl Pts',(-100.183746270873,-5.35708849487361,
133.317298754201));
#155995=CARTESIAN_POINT('Ctrl Pts',(-100.187199599217,-5.32570110981252,
133.383149672588));
#155996=CARTESIAN_POINT('Ctrl Pts',(-100.19065292756,-5.293123410409,133.448368016323));
#155997=CARTESIAN_POINT('Ctrl Pts',(-100.198076193966,-5.22309446513999,
133.588561213128));
#155998=CARTESIAN_POINT('Ctrl Pts',(-100.205499460371,-5.14738606413112,
133.726182305912));
#155999=CARTESIAN_POINT('Ctrl Pts',(-100.212922726777,-5.06621042610964,
133.860737963523));
#156000=CARTESIAN_POINT('Ctrl Pts',(-100.220337219498,-4.98513073095086,
133.99513458752));
#156001=CARTESIAN_POINT('Ctrl Pts',(-100.227751712219,-4.89859685201709,
134.12647267161));
#156002=CARTESIAN_POINT('Ctrl Pts',(-100.23516620494,-4.80686817318816,
134.254280751147));
#156003=CARTESIAN_POINT('Ctrl Pts',(-100.242573551294,-4.71522790591366,
134.381965644446));
#156004=CARTESIAN_POINT('Ctrl Pts',(-100.249980897647,-4.61840302278341,
134.506127005366));
#156005=CARTESIAN_POINT('Ctrl Pts',(-100.257388244001,-4.51669767279131,
134.626319891957));
#156006=CARTESIAN_POINT('Ctrl Pts',(-100.264790065677,-4.41506817848608,
134.746423134158));
#156007=CARTESIAN_POINT('Ctrl Pts',(-100.272191887352,-4.30856570521863,
134.862563511726));
#156008=CARTESIAN_POINT('Ctrl Pts',(-100.279593709028,-4.19753630162808,
134.974326991413));
#156009=CARTESIAN_POINT('Ctrl Pts',(-100.286991623339,-4.08656550959543,
135.086031472029));
#156010=CARTESIAN_POINT('Ctrl Pts',(-100.294389537651,-3.97107280892837,
135.193363392137));
#156011=CARTESIAN_POINT('Ctrl Pts',(-100.301787451962,-3.85144284752758,
135.295943696474));
#156012=CARTESIAN_POINT('Ctrl Pts',(-100.309184136874,-3.73183276645624,
135.398506953824));
#156013=CARTESIAN_POINT('Ctrl Pts',(-100.316580821787,-3.60808707231421,
135.496319919834));
#156014=CARTESIAN_POINT('Ctrl Pts',(-100.323977506699,-3.48062549551459,
135.589042082666));
#156015=CARTESIAN_POINT('Ctrl Pts',(-100.331373863634,-3.35316957049486,
135.681760134101));
#156016=CARTESIAN_POINT('Ctrl Pts',(-100.33877022057,-3.22199839230176,
135.76938761159));
#156017=CARTESIAN_POINT('Ctrl Pts',(-100.346166577505,-3.08756261213258,
135.851625983946));
#156018=CARTESIAN_POINT('Ctrl Pts',(-100.353564066842,-2.95310624950226,
135.933876947208));
#156019=CARTESIAN_POINT('Ctrl Pts',(-100.360961556179,-2.81538460815103,
136.010736967669));
#156020=CARTESIAN_POINT('Ctrl Pts',(-100.368359045515,-2.67487485779842,
136.081952403373));
#156021=CARTESIAN_POINT('Ctrl Pts',(-100.37575912803,-2.53431585197084,
136.153192803537));
#156022=CARTESIAN_POINT('Ctrl Pts',(-100.383159210546,-2.39096712397539,
136.218784510709));
#156023=CARTESIAN_POINT('Ctrl Pts',(-100.390559293061,-2.24532768175479,
136.278521207469));
#156024=CARTESIAN_POINT('Ctrl Pts',(-100.397967512727,-2.09952809399517,
136.338323590868));
#156025=CARTESIAN_POINT('Ctrl Pts',(-100.405375732394,-1.95143310723619,
136.392257964627));
#156026=CARTESIAN_POINT('Ctrl Pts',(-100.41278395206,-1.80155951812696,
136.440167025273));
#156027=CARTESIAN_POINT('Ctrl Pts',(-100.420196731362,-1.6515936843244,
136.488105573146));
#156028=CARTESIAN_POINT('Ctrl Pts',(-100.427609510665,-1.49984742583941,
136.530011319157));
#156029=CARTESIAN_POINT('Ctrl Pts',(-100.435022289967,-1.34684920735396,
136.565777784822));
#156030=CARTESIAN_POINT('Ctrl Pts',(-100.442445660996,-1.19363237783882,
136.60159535529));
#156031=CARTESIAN_POINT('Ctrl Pts',(-100.449869032024,-1.03916038119999,
136.631256055372));
#156032=CARTESIAN_POINT('Ctrl Pts',(-100.457292403053,-0.883969123571974,
136.654704979317));
#156033=CARTESIAN_POINT('Ctrl Pts',(-100.461228452493,-0.801682995029756,
136.66713816144));
#156034=CARTESIAN_POINT('Ctrl Pts',(-100.465164501933,-0.719194708221002,
136.677825860104));
#156035=CARTESIAN_POINT('Ctrl Pts',(-100.469100551373,-0.636584188296631,
136.686765834287));
#156036=CARTESIAN_POINT('Ctrl Pts',(-100.476523817779,-0.480783325877515,
136.703626346592));
#156037=CARTESIAN_POINT('Ctrl Pts',(-100.483947084184,-0.324076562861753,
136.714318286882));
#156038=CARTESIAN_POINT('Ctrl Pts',(-100.49137035059,-0.166993662125266,
136.718753543244));
#156039=CARTESIAN_POINT('Ctrl Pts',(-100.498784843311,-0.0100964203325258,
136.723183557501));
#156040=CARTESIAN_POINT('Ctrl Pts',(-100.506199336032,0.147175704769412,
136.721371596949));
#156041=CARTESIAN_POINT('Ctrl Pts',(-100.513613828753,0.30428585330045,
136.713281050435));
#156042=CARTESIAN_POINT('Ctrl Pts',(-100.521021175107,0.461244573155242,
136.705198301895));
#156043=CARTESIAN_POINT('Ctrl Pts',(-100.52842852146,0.618041256940341,
136.690849033882));
#156044=CARTESIAN_POINT('Ctrl Pts',(-100.535835867814,0.774137162429258,
136.670248633565));
#156045=CARTESIAN_POINT('Ctrl Pts',(-100.54323768949,0.930116645703146,
136.649663597805));
#156046=CARTESIAN_POINT('Ctrl Pts',(-100.550639511165,1.08539602288506,
136.6228367617));
#156047=CARTESIAN_POINT('Ctrl Pts',(-100.55804133284,1.23943990833583,136.58983547069));
#156048=CARTESIAN_POINT('Ctrl Pts',(-100.565439247152,1.39340247521811,
136.556851600804));
#156049=CARTESIAN_POINT('Ctrl Pts',(-100.572837161463,1.54613048517815,
136.517699845356));
#156050=CARTESIAN_POINT('Ctrl Pts',(-100.580235075774,1.69709711670182,
136.472498930891));
#156051=CARTESIAN_POINT('Ctrl Pts',(-100.587631760687,1.84803866030994,
136.427305527998));
#156052=CARTESIAN_POINT('Ctrl Pts',(-100.595028445599,1.99721904916031,
136.3760650682));
#156053=CARTESIAN_POINT('Ctrl Pts',(-100.602425130511,2.14412492646037,
136.318946627615));
#156054=CARTESIAN_POINT('Ctrl Pts',(-100.609821487447,2.29102428979989,
136.261830719722));
#156055=CARTESIAN_POINT('Ctrl Pts',(-100.617217844382,2.435648994197,136.198837484552));
#156056=CARTESIAN_POINT('Ctrl Pts',(-100.624614201317,2.5775042889294,136.13018470432));
#156057=CARTESIAN_POINT('Ctrl Pts',(-100.632011690654,2.71938130206996,
136.061521413172));
#156058=CARTESIAN_POINT('Ctrl Pts',(-100.639409179991,2.8584877252611,135.987197014295));
#156059=CARTESIAN_POINT('Ctrl Pts',(-100.646806669327,2.99435224045142,
135.907475864413));
#156060=CARTESIAN_POINT('Ctrl Pts',(-100.654206751842,3.13026438273712,
135.827726768406));
#156061=CARTESIAN_POINT('Ctrl Pts',(-100.661606834357,3.26293203260323,
135.74257734359));
#156062=CARTESIAN_POINT('Ctrl Pts',(-100.669006916872,3.39191188337985,
135.652335899876));
#156063=CARTESIAN_POINT('Ctrl Pts',(-100.676415136539,3.52103356076166,
135.561995226417));
#156064=CARTESIAN_POINT('Ctrl Pts',(-100.683823356205,3.64645903466989,
135.466551566227));
#156065=CARTESIAN_POINT('Ctrl Pts',(-100.691231575872,3.76777662002576,
135.366354688593));
#156066=CARTESIAN_POINT('Ctrl Pts',(-100.698644355174,3.88916887433146,
135.266096141453));
#156067=CARTESIAN_POINT('Ctrl Pts',(-100.706057134476,4.00644792460274,
135.161078795836));
#156068=CARTESIAN_POINT('Ctrl Pts',(-100.713469913778,4.11923853940647,
135.051689709827));
#156069=CARTESIAN_POINT('Ctrl Pts',(-100.720893284807,4.23219031472949,
134.942144323563));
#156070=CARTESIAN_POINT('Ctrl Pts',(-100.728316655835,4.3406405891142,134.828214990815));
#156071=CARTESIAN_POINT('Ctrl Pts',(-100.735740026864,4.44425349844226,
134.710322906693));
#156072=CARTESIAN_POINT('Ctrl Pts',(-100.739676076305,4.49919154912415,
134.647813694912));
#156073=CARTESIAN_POINT('Ctrl Pts',(-100.743612125746,4.55277034661906,
134.584190925211));
#156074=CARTESIAN_POINT('Ctrl Pts',(-100.747548175186,4.60494480399341,
134.519520629554));
#156075=CARTESIAN_POINT('Ctrl Pts',(-100.754971441592,4.70334420229488,
134.397554470233));
#156076=CARTESIAN_POINT('Ctrl Pts',(-100.762394707997,4.79704346765728,
134.271491887234));
#156077=CARTESIAN_POINT('Ctrl Pts',(-100.769817974403,4.88568211925863,
134.141730958427));
#156078=CARTESIAN_POINT('Ctrl Pts',(-100.777232467124,4.97421600733476,
134.012123396261));
#156079=CARTESIAN_POINT('Ctrl Pts',(-100.784646959845,5.05770097880735,
133.878826494297));
#156080=CARTESIAN_POINT('Ctrl Pts',(-100.792061452566,5.13581604579875,
133.742272138735));
#156081=CARTESIAN_POINT('Ctrl Pts',(-100.799468798919,5.21385582254761,
133.605849399401));
#156082=CARTESIAN_POINT('Ctrl Pts',(-100.806876145273,5.28653581453356,
133.466175778759));
#156083=CARTESIAN_POINT('Ctrl Pts',(-100.814283491627,5.35357776408466,
133.323712853042));
#156084=CARTESIAN_POINT('Ctrl Pts',(-100.821685313302,5.42056971122043,
133.18135618155));
#156085=CARTESIAN_POINT('Ctrl Pts',(-100.829087134978,5.48193183050659,
133.036214683591));
#156086=CARTESIAN_POINT('Ctrl Pts',(-100.836488956653,5.53743139255126,
132.88877519612));
#156087=CARTESIAN_POINT('Ctrl Pts',(-100.843886870964,5.5929016568093,132.741413540806));
#156088=CARTESIAN_POINT('Ctrl Pts',(-100.851284785276,5.64251539608859,
132.591756660391));
#156089=CARTESIAN_POINT('Ctrl Pts',(-100.858682699587,5.68608773849637,
132.440311959331));
#156090=CARTESIAN_POINT('Ctrl Pts',(-100.866079384499,5.72965283997126,
132.288892425632));
#156091=CARTESIAN_POINT('Ctrl Pts',(-100.873476069411,5.7671784340452,132.135686019346));
#156092=CARTESIAN_POINT('Ctrl Pts',(-100.880872754324,5.79852928735964,
131.981216031851));
#156093=CARTESIAN_POINT('Ctrl Pts',(-100.888269111259,5.82987875054439,
131.826752893718));
#156094=CARTESIAN_POINT('Ctrl Pts',(-100.895665468195,5.85505394311581,
131.671026651619));
#156095=CARTESIAN_POINT('Ctrl Pts',(-100.90306182513,5.87397066657043,131.514571269957));
#156096=CARTESIAN_POINT('Ctrl Pts',(-100.910459314467,5.89289028622365,
131.358091934578));
#156097=CARTESIAN_POINT('Ctrl Pts',(-100.917856803803,5.90554948406987,
131.200883607982));
#156098=CARTESIAN_POINT('Ctrl Pts',(-100.92525429314,5.91191591198988,131.043485714661));
#156099=CARTESIAN_POINT('Ctrl Pts',(-100.932654375655,5.91828457165133,
130.886032645754));
#156100=CARTESIAN_POINT('Ctrl Pts',(-100.94005445817,5.91835605433714,130.728390250576));
#156101=CARTESIAN_POINT('Ctrl Pts',(-100.947454540685,5.9121501318231,130.571098144622));
#156102=CARTESIAN_POINT('Ctrl Pts',(-100.954862760351,5.90593738525926,
130.413633079827));
#156103=CARTESIAN_POINT('Ctrl Pts',(-100.962270980018,5.89343346317159,
130.25651944672));
#156104=CARTESIAN_POINT('Ctrl Pts',(-100.969679199684,5.87471011052705,
130.100292666462));
#156105=CARTESIAN_POINT('Ctrl Pts',(-100.977091978986,5.85597523397138,
129.943969731228));
#156106=CARTESIAN_POINT('Ctrl Pts',(-100.984504758288,5.83101335823092,
129.788535104223));
#156107=CARTESIAN_POINT('Ctrl Pts',(-100.99191753759,5.79994730447737,129.634513692629));
#156108=CARTESIAN_POINT('Ctrl Pts',(-100.999340908619,5.76883686208931,
129.480272208018));
#156109=CARTESIAN_POINT('Ctrl Pts',(-101.006764279648,5.73160491015267,
129.327448333477));
#156110=CARTESIAN_POINT('Ctrl Pts',(-101.014187650677,5.68842426928217,
129.176552307248));
#156111=CARTESIAN_POINT('Ctrl Pts',(-101.018123700118,5.66552885738664,
129.096543613438));
#156112=CARTESIAN_POINT('Ctrl Pts',(-101.022059749558,5.64096186812597,
129.017076592574));
#156113=CARTESIAN_POINT('Ctrl Pts',(-101.025995798999,5.61475448547331,
128.93822486946));
#156114=CARTESIAN_POINT('Ctrl Pts',(-101.033419065405,5.5653281796963,128.789512980551));
#156115=CARTESIAN_POINT('Ctrl Pts',(-101.04084233181,5.50991490000123,128.64254122954));
#156116=CARTESIAN_POINT('Ctrl Pts',(-101.048265598216,5.44865471188496,
128.497828069963));
#156117=CARTESIAN_POINT('Ctrl Pts',(-101.055680090937,5.38746692822353,
128.353285949322));
#156118=CARTESIAN_POINT('Ctrl Pts',(-101.063094583658,5.3204461357511,128.210997446935));
#156119=CARTESIAN_POINT('Ctrl Pts',(-101.070509076379,5.24778219077092,
128.071466064034));
#156120=CARTESIAN_POINT('Ctrl Pts',(-101.077916422733,5.17518828203687,
127.932069166733));
#156121=CARTESIAN_POINT('Ctrl Pts',(-101.085323769086,5.09696222020373,
127.795424427395));
#156122=CARTESIAN_POINT('Ctrl Pts',(-101.09273111544,5.01334193736096,127.66201544531));
#156123=CARTESIAN_POINT('Ctrl Pts',(-101.100132937116,4.92978402167995,
127.528705964678));
#156124=CARTESIAN_POINT('Ctrl Pts',(-101.107534758791,4.84084009315306,
127.398627750931));
#156125=CARTESIAN_POINT('Ctrl Pts',(-101.114936580466,4.74679394557737,
127.272239753166));
#156126=CARTESIAN_POINT('Ctrl Pts',(-101.122334494778,4.65279744423093,
127.145918474641));
#156127=CARTESIAN_POINT('Ctrl Pts',(-101.129732409089,4.55370431019756,
127.023283831214));
#156128=CARTESIAN_POINT('Ctrl Pts',(-101.137130323401,4.44984150944379,
126.904765625348));
#156129=CARTESIAN_POINT('Ctrl Pts',(-101.144527008313,4.34599596880339,
126.786267115058));
#156130=CARTESIAN_POINT('Ctrl Pts',(-101.151923693225,4.23738258037395,
126.671883965111));
#156131=CARTESIAN_POINT('Ctrl Pts',(-101.159320378137,4.12436850708096,
126.562012802936));
#156132=CARTESIAN_POINT('Ctrl Pts',(-101.166716735073,4.01135944495008,
126.452146512562));
#156133=CARTESIAN_POINT('Ctrl Pts',(-101.174113092008,3.89395035359867,
126.346792072374));
#156134=CARTESIAN_POINT('Ctrl Pts',(-101.181509448944,3.77254496105348,
126.246308941759));
#156135=CARTESIAN_POINT('Ctrl Pts',(-101.18890693828,3.65112098103277,126.14581042692));
#156136=CARTESIAN_POINT('Ctrl Pts',(-101.196304427617,3.52569976914942,
126.050184944692));
#156137=CARTESIAN_POINT('Ctrl Pts',(-101.203701916953,3.39671767355769,
125.959751282579));
#156138=CARTESIAN_POINT('Ctrl Pts',(-101.211101999468,3.26769036349247,
125.869285919086));
#156139=CARTESIAN_POINT('Ctrl Pts',(-101.218502081983,3.1350999899019,125.784016213455));
#156140=CARTESIAN_POINT('Ctrl Pts',(-101.225902164498,2.99941123371145,
125.704217206486));
#156141=CARTESIAN_POINT('Ctrl Pts',(-101.233310384165,2.86357327378423,
125.624330452304));
#156142=CARTESIAN_POINT('Ctrl Pts',(-101.240718603831,2.72463044924826,
125.549926599678));
#156143=CARTESIAN_POINT('Ctrl Pts',(-101.248126823498,2.58307200499659,
125.481234695751));
#156144=CARTESIAN_POINT('Ctrl Pts',(-101.2555396028,2.44142643388451,125.412500513102));
#156145=CARTESIAN_POINT('Ctrl Pts',(-101.262952382102,2.29716237648222,
125.349485433522));
#156146=CARTESIAN_POINT('Ctrl Pts',(-101.270365161404,2.15078783990958,
125.292369849232));
#156147=CARTESIAN_POINT('Ctrl Pts',(-101.277788532433,2.00420415653501,
125.235172655517));
#156148=CARTESIAN_POINT('Ctrl Pts',(-101.285211903462,1.85550432322439,
125.183891914026));
#156149=CARTESIAN_POINT('Ctrl Pts',(-101.29263527449,1.7052110316233,125.138658022112));
#156150=CARTESIAN_POINT('Ctrl Pts',(-101.296571323931,1.62552192218051,
125.114673927248));
#156151=CARTESIAN_POINT('Ctrl Pts',(-101.300507373372,1.54538500913211,
125.092388965221));
#156152=CARTESIAN_POINT('Ctrl Pts',(-101.304443422812,1.46487909081005,
125.071816696076));
#156153=CARTESIAN_POINT('Ctrl Pts',(-101.311866689218,1.3130474413549,125.033018038507));
#156154=CARTESIAN_POINT('Ctrl Pts',(-101.319289955623,1.1594437135535,125.000196978694));
#156155=CARTESIAN_POINT('Ctrl Pts',(-101.326713222029,1.00457980587252,
124.973515912368));
#156156=CARTESIAN_POINT('Ctrl Pts',(-101.334127714749,0.849898934469772,
124.946866380847));
#156157=CARTESIAN_POINT('Ctrl Pts',(-101.34154220747,0.693961212187642,
124.926342460551));
#156158=CARTESIAN_POINT('Ctrl Pts',(-101.348956700191,0.537292870842562,
124.912056574711));
#156159=CARTESIAN_POINT('Ctrl Pts',(-101.356364046545,0.38077553234333,
124.897784458146));
#156160=CARTESIAN_POINT('Ctrl Pts',(-101.363771392899,0.223529345960948,
124.889738440098));
#156161=CARTESIAN_POINT('Ctrl Pts',(-101.371178739253,0.0660897855796993,
124.88797973879));
#156162=CARTESIAN_POINT('Ctrl Pts',(-101.378580560928,-0.0912323504380104,
124.886222349189));
#156163=CARTESIAN_POINT('Ctrl Pts',(-101.385982382603,-0.248747201613833,
124.890742943414));
#156164=CARTESIAN_POINT('Ctrl Pts',(-101.393384204279,-0.405915243597154,
124.901550830904));
#156165=CARTESIAN_POINT('Ctrl Pts',(-101.40078211859,-0.563000317794506,
124.912353012994));
#156166=CARTESIAN_POINT('Ctrl Pts',(-101.408180032902,-0.71973857593204,
124.929435852829));
#156167=CARTESIAN_POINT('Ctrl Pts',(-101.415577947213,-0.875591679933997,
124.952756583412));
#156168=CARTESIAN_POINT('Ctrl Pts',(-101.422974632125,-1.03141888397731,
124.976073438512));
#156169=CARTESIAN_POINT('Ctrl Pts',(-101.430371317037,-1.18636085700193,
125.005626071778));
#156170=CARTESIAN_POINT('Ctrl Pts',(-101.437768001949,-1.33988544459,125.041319965456));
#156171=CARTESIAN_POINT('Ctrl Pts',(-101.445164358885,-1.49340322473696,
125.077012276429));
#156172=CARTESIAN_POINT('Ctrl Pts',(-101.45256071582,-1.64550338081134,
125.118845221833));
#156173=CARTESIAN_POINT('Ctrl Pts',(-101.459957072756,-1.79566526458957,
125.166673430426));
#156174=CARTESIAN_POINT('Ctrl Pts',(-101.467354562092,-1.94585013853554,
125.214508961639));
#156175=CARTESIAN_POINT('Ctrl Pts',(-101.474752051429,-2.09409579359361,
125.268341470383));
#156176=CARTESIAN_POINT('Ctrl Pts',(-101.482149540765,-2.23989816797303,
125.327976157029));
#156177=CARTESIAN_POINT('Ctrl Pts',(-101.48954962328,-2.38575165314857,
125.387631748522));
#156178=CARTESIAN_POINT('Ctrl Pts',(-101.496949705795,-2.52915980708469,
125.453093426255));
#156179=CARTESIAN_POINT('Ctrl Pts',(-101.50434978831,-2.66964005877586,
125.524118907277));
#156180=CARTESIAN_POINT('Ctrl Pts',(-101.511758007977,-2.81027478294568,
125.595222488116));
#156181=CARTESIAN_POINT('Ctrl Pts',(-101.519166227643,-2.94797484191478,
125.671901921703));
#156182=CARTESIAN_POINT('Ctrl Pts',(-101.526574447309,-3.08228308301985,
125.753869398028));
#156183=CARTESIAN_POINT('Ctrl Pts',(-101.533987226611,-3.21667398860627,
125.835887323967));
#156184=CARTESIAN_POINT('Ctrl Pts',(-101.541400005913,-3.34766860660781,
125.923199571487));
#156185=CARTESIAN_POINT('Ctrl Pts',(-101.548812785215,-3.47484057768205,
126.015476246212));
#156186=CARTESIAN_POINT('Ctrl Pts',(-101.556236156244,-3.60219425803251,
126.107884770178));
#156187=CARTESIAN_POINT('Ctrl Pts',(-101.563659527273,-3.72571409029497,
126.205271657962));
#156188=CARTESIAN_POINT('Ctrl Pts',(-101.571082898302,-3.84500783988038,
126.307267637233));
#156189=CARTESIAN_POINT('Ctrl Pts',(-101.575018947743,-3.9082602483304,
126.361348352808));
#156190=CARTESIAN_POINT('Ctrl Pts',(-101.578954997184,-3.9703251769893,
126.416724241041));
#156191=CARTESIAN_POINT('Ctrl Pts',(-101.582891046625,-4.03114862498385,
126.473336336199));
#156192=CARTESIAN_POINT('Ctrl Pts',(-101.590203834316,-4.14415253117462,
126.578515968421));
#156193=CARTESIAN_POINT('Ctrl Pts',(-101.597516622007,-4.25323255256093,
126.68830342459));
#156194=CARTESIAN_POINT('Ctrl Pts',(-101.604829409697,-4.35798115646332,
126.802369762703));
#156195=CARTESIAN_POINT('Ctrl Pts',(-101.612133453102,-4.46260450693228,
126.916299705675));
#156196=CARTESIAN_POINT('Ctrl Pts',(-101.619437496507,-4.56290648635817,
127.034498070333));
#156197=CARTESIAN_POINT('Ctrl Pts',(-101.626741539911,-4.65851334223814,
127.156596370429));
#156198=CARTESIAN_POINT('Ctrl Pts',(-101.634038555917,-4.75402821242929,
127.278577196772));
#156199=CARTESIAN_POINT('Ctrl Pts',(-101.641335571924,-4.84485671208898,
127.404450190631));
#156200=CARTESIAN_POINT('Ctrl Pts',(-101.64863258793,-4.9306628180773,127.533811009789));
#156201=CARTESIAN_POINT('Ctrl Pts',(-101.655923928853,-5.01640219037763,
127.663071221602));
#156202=CARTESIAN_POINT('Ctrl Pts',(-101.663215269776,-5.09712673366964,
127.795813538242));
#156203=CARTESIAN_POINT('Ctrl Pts',(-101.670506610699,-5.17254173400305,
127.931601913376));
#156204=CARTESIAN_POINT('Ctrl Pts',(-101.677794900797,-5.24792517937439,
128.067333472267));
#156205=CARTESIAN_POINT('Ctrl Pts',(-101.685083190895,-5.31800331445087,
128.206108218088));
#156206=CARTESIAN_POINT('Ctrl Pts',(-101.692371480993,-5.3825257125239,
128.347462671676));
#156207=CARTESIAN_POINT('Ctrl Pts',(-101.699658259854,-5.44703473179476,
128.488787815236));
#156208=CARTESIAN_POINT('Ctrl Pts',(-101.706945038716,-5.50599014677343,
128.632691251676));
#156209=CARTESIAN_POINT('Ctrl Pts',(-101.714231817577,-5.55918845395391,
128.778686829434));
#156210=CARTESIAN_POINT('Ctrl Pts',(-101.721518623426,-5.61238695816111,
128.924682947905));
#156211=CARTESIAN_POINT('Ctrl Pts',(-101.728805429276,-5.65982818182036,
129.072770860525));
#156212=CARTESIAN_POINT('Ctrl Pts',(-101.736092235125,-5.70135765486742,
129.222446759676));
#156213=CARTESIAN_POINT('Ctrl Pts',(-101.74338342505,-5.74291211395053,
129.372212710714));
#156214=CARTESIAN_POINT('Ctrl Pts',(-101.750674614976,-5.77854761592046,
129.523568184695));
#156215=CARTESIAN_POINT('Ctrl Pts',(-101.757965804902,-5.80816017317679,
129.675996330103));
#156216=CARTESIAN_POINT('Ctrl Pts',(-101.765259480235,-5.83778282470643,
129.828476434932));
#156217=CARTESIAN_POINT('Ctrl Pts',(-101.772553155568,-5.86137838176501,
129.982029559142));
#156218=CARTESIAN_POINT('Ctrl Pts',(-101.779846830901,-5.87889453206986,
130.136131881803));
#156219=CARTESIAN_POINT('Ctrl Pts',(-101.787147880188,-5.89642839132037,
130.290390002948));
#156220=CARTESIAN_POINT('Ctrl Pts',(-101.794448929476,-5.90787054262023,
130.445198047472));
#156221=CARTESIAN_POINT('Ctrl Pts',(-101.801749978764,-5.91322074119755,
130.600029933695));
#156222=CARTESIAN_POINT('Ctrl Pts',(-101.805041588439,-5.91563282810543,
130.669834439132));
#156223=CARTESIAN_POINT('Ctrl Pts',(-101.808333198114,-5.91680738581963,
130.73964381692));
#156224=CARTESIAN_POINT('Ctrl Pts',(-101.811624807789,-5.91674784530102,
130.809410134943));
#156225=CARTESIAN_POINT('',(-103.561624807789,-5.92383021006907,130.800793567564));
#156226=CARTESIAN_POINT('Ctrl Pts',(-101.811624807789,-5.91999130402177,
130.809412903001));
#156227=CARTESIAN_POINT('Ctrl Pts',(-101.828196095339,-5.92317871838217,
131.16084013514));
#156228=CARTESIAN_POINT('Ctrl Pts',(-101.844767382888,-5.89458903006583,
131.511749486344));
#156229=CARTESIAN_POINT('Ctrl Pts',(-101.954154545042,-5.48391453579545,
133.788060896094));
#156230=CARTESIAN_POINT('Ctrl Pts',(-102.139786294252,-2.67732355314469,
137.270387150308));
#156231=CARTESIAN_POINT('Ctrl Pts',(-102.418233918063,3.99289247164586,
136.551914030995));
#156232=CARTESIAN_POINT('Ctrl Pts',(-102.696681541877,6.99383537863429,
130.551720108334));
#156233=CARTESIAN_POINT('Ctrl Pts',(-102.975129165689,3.56778524051166,
124.783690471483));
#156234=CARTESIAN_POINT('Ctrl Pts',(-103.253576789502,-3.13688523764292,
124.548362572792));
#156235=CARTESIAN_POINT('Ctrl Pts',(-103.449075336869,-5.82033628648036,
128.419490590634));
#156236=CARTESIAN_POINT('Ctrl Pts',(-103.551758009631,-5.9253140316399,
130.591901291897));
#156237=CARTESIAN_POINT('Ctrl Pts',(-103.561624807789,-5.92383021006907,
130.800793567564));
#156238=CARTESIAN_POINT('',(-105.311624807789,-5.90881016785237,130.801032495528));
#156239=CARTESIAN_POINT('Ctrl Pts',(-103.561624807789,-5.92383021006907,
130.800793567564));
#156240=CARTESIAN_POINT('Ctrl Pts',(-103.644573884235,-5.91135588689535,
132.556927732469));
#156241=CARTESIAN_POINT('Ctrl Pts',(-103.820338835288,-4.15204534669574,
136.299789154536));
#156242=CARTESIAN_POINT('Ctrl Pts',(-104.08891966094,2.21739010421207,137.442187193775));
#156243=CARTESIAN_POINT('Ctrl Pts',(-104.367367284755,6.78314500569334,
132.526714925521));
#156244=CARTESIAN_POINT('Ctrl Pts',(-104.645814908566,5.11552102198397,
126.028483189903));
#156245=CARTESIAN_POINT('Ctrl Pts',(-104.924262532381,-1.25301687383302,
123.919049495752));
#156246=CARTESIAN_POINT('Ctrl Pts',(-105.146199165453,-5.41128692724257,
127.280870894205));
#156247=CARTESIAN_POINT('Ctrl Pts',(-105.275319923923,-5.91274898233932,
130.027409099224));
#156248=CARTESIAN_POINT('Ctrl Pts',(-105.311624807789,-5.90881016785237,
130.801032495528));
#156249=CARTESIAN_POINT('',(-107.061624807789,-5.91162666396341,130.809137112237));
#156250=CARTESIAN_POINT('Ctrl Pts',(-105.311624807789,-5.90881016785237,
130.801032495528));
#156251=CARTESIAN_POINT('Ctrl Pts',(-105.368135798528,-5.90267913848951,
132.005229284751));
#156252=CARTESIAN_POINT('Ctrl Pts',(-105.517462663871,-4.95855140697165,
135.196076695011));
#156253=CARTESIAN_POINT('Ctrl Pts',(-105.759605403818,0.263283643556469,
137.797803421612));
#156254=CARTESIAN_POINT('Ctrl Pts',(-106.038053027631,6.02609273603925,
134.362979291574));
#156255=CARTESIAN_POINT('Ctrl Pts',(-106.316500651444,6.25121699508972,
127.657958448323));
#156256=CARTESIAN_POINT('Ctrl Pts',(-106.594948275257,0.731778224585158,
123.844327488307));
#156257=CARTESIAN_POINT('Ctrl Pts',(-106.843322994039,-4.79139051656404,
126.147733406097));
#156258=CARTESIAN_POINT('Ctrl Pts',(-106.998881838216,-5.90155799568876,
129.473741766361));
#156259=CARTESIAN_POINT('Ctrl Pts',(-107.061624807789,-5.91162666396341,
130.809137112237));
#156260=CARTESIAN_POINT('',(-108.811623984105,-5.9219077054752,130.805771569576));
#156261=CARTESIAN_POINT('Ctrl Pts',(-107.061624807789,-5.91162666396341,
130.809137112237));
#156262=CARTESIAN_POINT('Ctrl Pts',(-107.09169771282,-5.91645260871668,
131.449196352165));
#156263=CARTESIAN_POINT('Ctrl Pts',(-107.214586492457,-5.52527017600959,
134.058970572693));
#156264=CARTESIAN_POINT('Ctrl Pts',(-107.430291146694,-1.71202952148277,
137.590118898561));
#156265=CARTESIAN_POINT('Ctrl Pts',(-107.708738770509,4.78365684944718,
135.912607643408));
#156266=CARTESIAN_POINT('Ctrl Pts',(-107.987186394321,6.88339627035972,
129.540866923268));
#156267=CARTESIAN_POINT('Ctrl Pts',(-108.265634018135,2.65763079141432,
124.330215183077));
#156268=CARTESIAN_POINT('Ctrl Pts',(-108.540446324043,-3.9233124235248,
125.059341665262));
#156269=CARTESIAN_POINT('Ctrl Pts',(-108.722442755349,-5.9199882563494,
128.919623569311));
#156270=CARTESIAN_POINT('Ctrl Pts',(-108.811623312048,-5.92611609334515,
130.805758370925));
#156271=CARTESIAN_POINT('',(-110.561624807789,-5.91596713820667,130.798889816873));
#156272=CARTESIAN_POINT('Ctrl Pts',(-108.811624807789,-5.91674982788728,
130.805787746087));
#156273=CARTESIAN_POINT('Ctrl Pts',(-108.815259627113,-5.91673131483953,
130.882541220298));
#156274=CARTESIAN_POINT('Ctrl Pts',(-108.818894446437,-5.9152193692786,
130.959274886021));
#156275=CARTESIAN_POINT('Ctrl Pts',(-108.822529265761,-5.91221591608982,
131.035949745191));
#156276=CARTESIAN_POINT('Ctrl Pts',(-108.829952532166,-5.90608206701258,
131.192540171146));
#156277=CARTESIAN_POINT('Ctrl Pts',(-108.837375798572,-5.89371348566192,
131.349123520698));
#156278=CARTESIAN_POINT('Ctrl Pts',(-108.844799064977,-5.87510057860846,
131.50516283912));
#156279=CARTESIAN_POINT('Ctrl Pts',(-108.852213557698,-5.85650967046538,
131.661017732025));
#156280=CARTESIAN_POINT('Ctrl Pts',(-108.859628050419,-5.83168917087945,
131.816329506644));
#156281=CARTESIAN_POINT('Ctrl Pts',(-108.86704254314,-5.80068147127559,
131.970561728567));
#156282=CARTESIAN_POINT('Ctrl Pts',(-108.874449889494,-5.76970365806003,
132.124645295668));
#156283=CARTESIAN_POINT('Ctrl Pts',(-108.881857235847,-5.73255058997771,
132.277651018013));
#156284=CARTESIAN_POINT('Ctrl Pts',(-108.889264582201,-5.68931637196582,
132.429048212823));
#156285=CARTESIAN_POINT('Ctrl Pts',(-108.896666403877,-5.64611439966498,
132.580332489893));
#156286=CARTESIAN_POINT('Ctrl Pts',(-108.904068225552,-5.59684041039193,
132.730010270789));
#156287=CARTESIAN_POINT('Ctrl Pts',(-108.911470047227,-5.54163941588126,
132.877561800966));
#156288=CARTESIAN_POINT('Ctrl Pts',(-108.918867961539,-5.4864675615459,
133.025035439839));
#156289=CARTESIAN_POINT('Ctrl Pts',(-108.92626587585,-5.42537506363842,
133.170384714623));
#156290=CARTESIAN_POINT('Ctrl Pts',(-108.933663790161,-5.35855650725274,
133.313105865908));
#156291=CARTESIAN_POINT('Ctrl Pts',(-108.941060475073,-5.29174905489902,
133.455803299527));
#156292=CARTESIAN_POINT('Ctrl Pts',(-108.948457159985,-5.21921759077214,
133.595873138712));
#156293=CARTESIAN_POINT('Ctrl Pts',(-108.955853844898,-5.14120453535692,
133.732832315931));
#156294=CARTESIAN_POINT('Ctrl Pts',(-108.963250201833,-5.0631949391221,
133.869785420237));
#156295=CARTESIAN_POINT('Ctrl Pts',(-108.970646558768,-4.97970441964543,
134.003627812462));
#156296=CARTESIAN_POINT('Ctrl Pts',(-108.978042915704,-4.89102085423309,
134.13390196225));
#156297=CARTESIAN_POINT('Ctrl Pts',(-108.98544040504,-4.80232371114049,
134.264196057341));
#156298=CARTESIAN_POINT('Ctrl Pts',(-108.992837894377,-4.70843214910487,
134.390920513623));
#156299=CARTESIAN_POINT('Ctrl Pts',(-109.000235383713,-4.60967668691873,
134.513647800379));
#156300=CARTESIAN_POINT('Ctrl Pts',(-109.007635466228,-4.51088660615854,
134.636418108995));
#156301=CARTESIAN_POINT('Ctrl Pts',(-109.015035548743,-4.40722946441964,
134.755188167652));
#156302=CARTESIAN_POINT('Ctrl Pts',(-109.022435631258,-4.29907515848576,
134.869564590824));
#156303=CARTESIAN_POINT('Ctrl Pts',(-109.029843850925,-4.19080192577381,
134.984066782631));
#156304=CARTESIAN_POINT('Ctrl Pts',(-109.037252070591,-4.07802190982685,
135.094165419218));
#156305=CARTESIAN_POINT('Ctrl Pts',(-109.044660290258,-3.96114138987724,
135.199504466395));
#156306=CARTESIAN_POINT('Ctrl Pts',(-109.05207306956,-3.84418893191785,
135.304908347998));
#156307=CARTESIAN_POINT('Ctrl Pts',(-109.059485848862,-3.72313122737752,
135.405546564814));
#156308=CARTESIAN_POINT('Ctrl Pts',(-109.066898628164,-3.59840610478514,
135.501104603302));
#156309=CARTESIAN_POINT('Ctrl Pts',(-109.074321999192,-3.47350276908874,
135.596799179596));
#156310=CARTESIAN_POINT('Ctrl Pts',(-109.081745370221,-3.34492185387414,
135.687398865671));
#156311=CARTESIAN_POINT('Ctrl Pts',(-109.08916874125,-3.21312919254382,
135.772633089414));
#156312=CARTESIAN_POINT('Ctrl Pts',(-109.093104790691,-3.14324956117784,
135.817826320014));
#156313=CARTESIAN_POINT('Ctrl Pts',(-109.097040840132,-3.07246739784303,
135.861511897964));
#156314=CARTESIAN_POINT('Ctrl Pts',(-109.100976889573,-3.00085462453805,
135.903654890785));
#156315=CARTESIAN_POINT('Ctrl Pts',(-109.108400155979,-2.86579516905582,
135.98313526));
#156316=CARTESIAN_POINT('Ctrl Pts',(-109.115823422384,-2.72737164206612,
136.057366347408));
#156317=CARTESIAN_POINT('Ctrl Pts',(-109.12324668879,-2.58603061330607,
136.126049844639));
#156318=CARTESIAN_POINT('Ctrl Pts',(-109.130661181511,-2.44485663790436,
136.19465216368));
#156319=CARTESIAN_POINT('Ctrl Pts',(-109.138075674232,-2.30077235695841,
136.257719782308));
#156320=CARTESIAN_POINT('Ctrl Pts',(-109.145490166953,-2.15425200152916,
136.314998409728));
#156321=CARTESIAN_POINT('Ctrl Pts',(-109.152897513306,-2.00787286793487,
136.372221829852));
#156322=CARTESIAN_POINT('Ctrl Pts',(-109.16030485966,-1.85906267956538,
136.423667231745));
#156323=CARTESIAN_POINT('Ctrl Pts',(-109.167712206014,-1.70831878088991,
136.469126941551));
#156324=CARTESIAN_POINT('Ctrl Pts',(-109.175114027689,-1.55768731270089,
136.514552745792));
#156325=CARTESIAN_POINT('Ctrl Pts',(-109.182515849365,-1.40512536175021,
136.554001639762));
#156326=CARTESIAN_POINT('Ctrl Pts',(-109.18991767104,-1.25114859464169,
136.587314685914));
#156327=CARTESIAN_POINT('Ctrl Pts',(-109.197315585352,-1.09725311067041,
136.620610146369));
#156328=CARTESIAN_POINT('Ctrl Pts',(-109.204713499663,-0.941944661902468,
136.647776131024));
#156329=CARTESIAN_POINT('Ctrl Pts',(-109.212111413974,-0.785752253391338,
136.668704055564));
#156330=CARTESIAN_POINT('Ctrl Pts',(-109.219508098887,-0.629585801224661,
136.689628502263));
#156331=CARTESIAN_POINT('Ctrl Pts',(-109.226904783799,-0.472536050493206,
136.704316896771));
#156332=CARTESIAN_POINT('Ctrl Pts',(-109.234301468711,-0.315140453785023,
136.712712084506));
#156333=CARTESIAN_POINT('Ctrl Pts',(-109.241697825646,-0.157751836162537,
136.721106899989));
#156334=CARTESIAN_POINT('Ctrl Pts',(-109.249094182582,-1.77758225209934E-5,
136.723209043659));
#156335=CARTESIAN_POINT('Ctrl Pts',(-109.256490539517,0.157521189271796,
136.719013408511));
#156336=CARTESIAN_POINT('Ctrl Pts',(-109.263888028854,0.315084273983848,
136.714817131));
#156337=CARTESIAN_POINT('Ctrl Pts',(-109.271285518191,0.472451830786333,
136.704321164749));
#156338=CARTESIAN_POINT('Ctrl Pts',(-109.278683007527,0.629085512500264,
136.687572493783));
#156339=CARTESIAN_POINT('Ctrl Pts',(-109.286083090042,0.785774101908284,
136.670817951597));
#156340=CARTESIAN_POINT('Ctrl Pts',(-109.293483172557,0.941727933077042,
136.647806380353));
#156341=CARTESIAN_POINT('Ctrl Pts',(-109.300883255072,1.09641610137364,
136.618636350204));
#156342=CARTESIAN_POINT('Ctrl Pts',(-109.308291474739,1.2512743652134,136.589434244609));
#156343=CARTESIAN_POINT('Ctrl Pts',(-109.315699694405,1.4048638197542,136.55406022548));
#156344=CARTESIAN_POINT('Ctrl Pts',(-109.323107914072,1.55666531949973,
136.512663661866));
#156345=CARTESIAN_POINT('Ctrl Pts',(-109.330520693374,1.70856025053627,
136.471241619358));
#156346=CARTESIAN_POINT('Ctrl Pts',(-109.337933472676,1.85866467886952,
136.423789758408));
#156347=CARTESIAN_POINT('Ctrl Pts',(-109.345346251978,2.00647733833629,
136.370506434309));
#156348=CARTESIAN_POINT('Ctrl Pts',(-109.352769623007,2.15450119946242,
136.317146976497));
#156349=CARTESIAN_POINT('Ctrl Pts',(-109.360192994036,2.30022640671125,
136.257939554269));
#156350=CARTESIAN_POINT('Ctrl Pts',(-109.367616365064,2.4431735257698,136.193129835623));
#156351=CARTESIAN_POINT('Ctrl Pts',(-109.371552414505,2.51896751826102,
136.15876616771));
#156352=CARTESIAN_POINT('Ctrl Pts',(-109.375488463946,2.59398092045337,
136.122828251008));
#156353=CARTESIAN_POINT('Ctrl Pts',(-109.379424513386,2.66814546706626,
136.085357713671));
#156354=CARTESIAN_POINT('Ctrl Pts',(-109.386847779792,2.80801748738663,
136.014689449668));
#156355=CARTESIAN_POINT('Ctrl Pts',(-109.394271046197,2.94529150107708,
135.938353531993));
#156356=CARTESIAN_POINT('Ctrl Pts',(-109.401694312603,3.07947515100627,
135.856564429452));
#156357=CARTESIAN_POINT('Ctrl Pts',(-109.409108805324,3.21350020700451,
135.774871994838));
#156358=CARTESIAN_POINT('Ctrl Pts',(-109.416523298045,3.3444418540295,135.68773939698));
#156359=CARTESIAN_POINT('Ctrl Pts',(-109.423937790766,3.47182981656182,
135.595428169514));
#156360=CARTESIAN_POINT('Ctrl Pts',(-109.43134513712,3.59909499777978,135.503205915085));
#156361=CARTESIAN_POINT('Ctrl Pts',(-109.438752483473,3.72281301310655,
135.405815185433));
#156362=CARTESIAN_POINT('Ctrl Pts',(-109.446159829827,3.84254031381146,
135.303562157754));
#156363=CARTESIAN_POINT('Ctrl Pts',(-109.453561651503,3.96217831737845,
135.201385394241));
#156364=CARTESIAN_POINT('Ctrl Pts',(-109.460963473178,4.07783125014783,
135.094353794911));
#156365=CARTESIAN_POINT('Ctrl Pts',(-109.468365294853,4.18908666306373,
134.982815295056));
#156366=CARTESIAN_POINT('Ctrl Pts',(-109.475763209165,4.30028334511317,
134.871335675507));
#156367=CARTESIAN_POINT('Ctrl Pts',(-109.483161123476,4.40708686756276,
134.755354157267));
#156368=CARTESIAN_POINT('Ctrl Pts',(-109.490559037787,4.50911993520033,
134.635257114795));
#156369=CARTESIAN_POINT('Ctrl Pts',(-109.4979557227,4.61113604679298,134.515180030272));
#156370=CARTESIAN_POINT('Ctrl Pts',(-109.505352407612,4.70838303551247,
134.390989063117));
#156371=CARTESIAN_POINT('Ctrl Pts',(-109.512749092524,4.8005223093399,134.263105493967));
#156372=CARTESIAN_POINT('Ctrl Pts',(-109.520145449459,4.89265749761539,
134.135227595308));
#156373=CARTESIAN_POINT('Ctrl Pts',(-109.527541806395,4.97968520310246,
134.003657723085));
#156374=CARTESIAN_POINT('Ctrl Pts',(-109.53493816333,5.06130895516232,133.868847886734));
#156375=CARTESIAN_POINT('Ctrl Pts',(-109.542335652667,5.142945204027,133.734017410654));
#156376=CARTESIAN_POINT('Ctrl Pts',(-109.549733142003,5.21917565872633,
133.595946302098));
#156377=CARTESIAN_POINT('Ctrl Pts',(-109.55713063134,5.28974885845261,133.45511288381));
#156378=CARTESIAN_POINT('Ctrl Pts',(-109.564530713855,5.36034679750456,
133.314230096586));
#156379=CARTESIAN_POINT('Ctrl Pts',(-109.57193079637,5.4252833660262,133.170583405236));
#156380=CARTESIAN_POINT('Ctrl Pts',(-109.579330878885,5.484354526957,133.024672754439));
#156381=CARTESIAN_POINT('Ctrl Pts',(-109.586739098551,5.54349064270199,
132.878601659882));
#156382=CARTESIAN_POINT('Ctrl Pts',(-109.594147318218,5.59674833037502,
132.730261980499));
#156383=CARTESIAN_POINT('Ctrl Pts',(-109.601555537884,5.64397264756525,
132.580171225721));
#156384=CARTESIAN_POINT('Ctrl Pts',(-109.608968317186,5.69122603053486,
132.429988092587));
#156385=CARTESIAN_POINT('Ctrl Pts',(-109.616381096488,5.73243854603033,
132.278052095933));
#156386=CARTESIAN_POINT('Ctrl Pts',(-109.623793875791,5.76750612936996,
132.124892181059));
#156387=CARTESIAN_POINT('Ctrl Pts',(-109.631217246819,5.80262381891711,
131.971513424115));
#156388=CARTESIAN_POINT('Ctrl Pts',(-109.638640617848,5.83157897180921,
131.816907622169));
#156389=CARTESIAN_POINT('Ctrl Pts',(-109.646063988877,5.85431912953475,
131.661610926439));
#156390=CARTESIAN_POINT('Ctrl Pts',(-109.650000038318,5.86637650680343,
131.57926889207));
#156391=CARTESIAN_POINT('Ctrl Pts',(-109.653936087758,5.87668749585636,
131.496732670503));
#156392=CARTESIAN_POINT('Ctrl Pts',(-109.657872137199,5.88525022058892,
131.414082196287));
#156393=CARTESIAN_POINT('Ctrl Pts',(-109.665295403604,5.90139925220106,
131.258205981348));
#156394=CARTESIAN_POINT('Ctrl Pts',(-109.67271867001,5.91137564021911,131.101452037716));
#156395=CARTESIAN_POINT('Ctrl Pts',(-109.680141936415,5.91509369226822,
130.944350525019));
#156396=CARTESIAN_POINT('Ctrl Pts',(-109.687556429136,5.91880734988857,
130.787434693263));
#156397=CARTESIAN_POINT('Ctrl Pts',(-109.694970921857,5.91627738623169,
130.630172479687));
#156398=CARTESIAN_POINT('Ctrl Pts',(-109.702385414578,5.90746964154779,
130.473100905722));
#156399=CARTESIAN_POINT('Ctrl Pts',(-109.709792760932,5.89867038609981,
130.316180723253));
#156400=CARTESIAN_POINT('Ctrl Pts',(-109.717200107286,5.88360541625958,
130.159451184805));
#156401=CARTESIAN_POINT('Ctrl Pts',(-109.72460745364,5.86229257864988,130.003450956739));
#156402=CARTESIAN_POINT('Ctrl Pts',(-109.732009275315,5.84099563695856,
129.847567079528));
#156403=CARTESIAN_POINT('Ctrl Pts',(-109.73941109699,5.81346015629185,129.692411797898));
#156404=CARTESIAN_POINT('Ctrl Pts',(-109.746812918666,5.7797559256749,129.538520184444));
#156405=CARTESIAN_POINT('Ctrl Pts',(-109.754210832977,5.74606948725895,
129.384709809175));
#156406=CARTESIAN_POINT('Ctrl Pts',(-109.761608747288,5.70622086390113,
129.23216213729));
#156407=CARTESIAN_POINT('Ctrl Pts',(-109.7690066616,5.66033118609864,129.081403442771));
#156408=CARTESIAN_POINT('Ctrl Pts',(-109.776403346512,5.61444913432814,
128.930669801611));
#156409=CARTESIAN_POINT('Ctrl Pts',(-109.783800031424,5.56252812918237,
128.781724904543));
#156410=CARTESIAN_POINT('Ctrl Pts',(-109.791196716336,5.50473958873584,
128.635081331097));
#156411=CARTESIAN_POINT('Ctrl Pts',(-109.798593073272,5.44695361069374,
128.48844425998));
#156412=CARTESIAN_POINT('Ctrl Pts',(-109.805989430207,5.38330075152544,
128.344108656892));
#156413=CARTESIAN_POINT('Ctrl Pts',(-109.813385787143,5.31400104995022,
128.202568273118));
#156414=CARTESIAN_POINT('Ctrl Pts',(-109.820783276479,5.24469073841357,
128.06100621915));
#156415=CARTESIAN_POINT('Ctrl Pts',(-109.828180765816,5.16973202720599,
127.922240571904));
#156416=CARTESIAN_POINT('Ctrl Pts',(-109.835578255152,5.0893914220888,127.786741437605));
#156417=CARTESIAN_POINT('Ctrl Pts',(-109.842978337667,5.00902265369714,
127.651194804295));
#156418=CARTESIAN_POINT('Ctrl Pts',(-109.850378420182,4.92326842542812,
127.518917284658));
#156419=CARTESIAN_POINT('Ctrl Pts',(-109.857778502697,4.83243906788443,
127.390350773162));
#156420=CARTESIAN_POINT('Ctrl Pts',(-109.865186722364,4.74150983412451,
127.261642889571));
#156421=CARTESIAN_POINT('Ctrl Pts',(-109.87259494203,4.64549454174053,127.136654468491));
#156422=CARTESIAN_POINT('Ctrl Pts',(-109.880003161697,4.54474483591337,
127.015795593848));
#156423=CARTESIAN_POINT('Ctrl Pts',(-109.887415940999,4.44393312032338,
126.894862332585));
#156424=CARTESIAN_POINT('Ctrl Pts',(-109.894828720301,4.33838143458433,
126.778063958665));
#156425=CARTESIAN_POINT('Ctrl Pts',(-109.902241499603,4.22847854585466,
126.665773932507));
#156426=CARTESIAN_POINT('Ctrl Pts',(-109.909664870632,4.11841862272379,
126.553323461094));
#156427=CARTESIAN_POINT('Ctrl Pts',(-109.91708824166,4.00399535028944,126.445394458505));
#156428=CARTESIAN_POINT('Ctrl Pts',(-109.924511612689,3.88563145265092,
126.342320862401));
#156429=CARTESIAN_POINT('Ctrl Pts',(-109.92844766213,3.82287207402125,126.287668768531));
#156430=CARTESIAN_POINT('Ctrl Pts',(-109.93238371157,3.75900535471351,126.234380997603));
#156431=CARTESIAN_POINT('Ctrl Pts',(-109.936319761011,3.69409753184754,
126.182502334613));
#156432=CARTESIAN_POINT('Ctrl Pts',(-109.943743027417,3.57168340362395,
126.084660795291));
#156433=CARTESIAN_POINT('Ctrl Pts',(-109.951166293822,3.44519435275468,
125.991538042044));
#156434=CARTESIAN_POINT('Ctrl Pts',(-109.958589560228,3.31503009872752,
125.903492734524));
#156435=CARTESIAN_POINT('Ctrl Pts',(-109.966004052949,3.18501968803915,
125.815551489246));
#156436=CARTESIAN_POINT('Ctrl Pts',(-109.97341854567,3.05134302670548,125.732675951541));
#156437=CARTESIAN_POINT('Ctrl Pts',(-109.980833038391,2.91443346188762,
125.655185134177));
#156438=CARTESIAN_POINT('Ctrl Pts',(-109.988240384744,2.77765585566289,
125.577769005381));
#156439=CARTESIAN_POINT('Ctrl Pts',(-109.995647731098,2.63765187197414,
125.505727447306));
#156440=CARTESIAN_POINT('Ctrl Pts',(-110.003055077452,2.49488435262316,
125.439336607411));
#156441=CARTESIAN_POINT('Ctrl Pts',(-110.010456899127,2.35222331467443,
125.372995284309));
#156442=CARTESIAN_POINT('Ctrl Pts',(-110.017858720803,2.20680318212132,
125.31229644444));
#156443=CARTESIAN_POINT('Ctrl Pts',(-110.025260542478,2.05911184936531,
125.257470592128));
#156444=CARTESIAN_POINT('Ctrl Pts',(-110.03265845679,1.91149848171465,125.202673681957));
#156445=CARTESIAN_POINT('Ctrl Pts',(-110.040056371101,1.76161665070222,
125.153743714522));
#156446=CARTESIAN_POINT('Ctrl Pts',(-110.047454285412,1.60997459952522,
125.110863243246));
#156447=CARTESIAN_POINT('Ctrl Pts',(-110.054850970324,1.45835774850584,
125.067989897928));
#156448=CARTESIAN_POINT('Ctrl Pts',(-110.062247655237,1.30498161674168,
125.031164154989));
#156449=CARTESIAN_POINT('Ctrl Pts',(-110.069644340149,1.1503701075644,125.000518857307));
#156450=CARTESIAN_POINT('Ctrl Pts',(-110.077040697084,0.99576545402345,
124.96987491847));
#156451=CARTESIAN_POINT('Ctrl Pts',(-110.08443705402,0.839925898160404,
124.945410952568));
#156452=CARTESIAN_POINT('Ctrl Pts',(-110.091833410955,0.683385783219098,
124.927208719427));
#156453=CARTESIAN_POINT('Ctrl Pts',(-110.099230900292,0.526821701586567,
124.909003699478));
#156454=CARTESIAN_POINT('Ctrl Pts',(-110.106628389628,0.36955721813547,
124.897062364282));
#156455=CARTESIAN_POINT('Ctrl Pts',(-110.114025878965,0.21213189942102,
124.891414598892));
#156456=CARTESIAN_POINT('Ctrl Pts',(-110.12142596148,0.0546513955053594,
124.885764853687));
#156457=CARTESIAN_POINT('Ctrl Pts',(-110.128826043995,-0.102989683101735,
124.886413084194));
#156458=CARTESIAN_POINT('Ctrl Pts',(-110.13622612651,-0.260251816797729,
124.893337055242));
#156459=CARTESIAN_POINT('Ctrl Pts',(-110.143634346176,-0.417686876376887,
124.900268639907));
#156460=CARTESIAN_POINT('Ctrl Pts',(-110.151042565843,-0.574741785724433,
124.913489730079));
#156461=CARTESIAN_POINT('Ctrl Pts',(-110.158450785509,-0.730881456810193,
124.932926137084));
#156462=CARTESIAN_POINT('Ctrl Pts',(-110.165863564811,-0.887117229258178,
124.952374506874));
#156463=CARTESIAN_POINT('Ctrl Pts',(-110.173276344113,-1.04243627352356,
124.978045755402));
#156464=CARTESIAN_POINT('Ctrl Pts',(-110.180689123416,-1.19631424863407,
125.009814666327));
#156465=CARTESIAN_POINT('Ctrl Pts',(-110.188112494444,-1.35041209181179,
125.041628970162));
#156466=CARTESIAN_POINT('Ctrl Pts',(-110.195535865473,-1.503064392093,125.079558247685));
#156467=CARTESIAN_POINT('Ctrl Pts',(-110.202959236502,-1.65376170556361,
125.123427350601));
#156468=CARTESIAN_POINT('Ctrl Pts',(-110.206895285943,-1.73366503709898,
125.146687801592));
#156469=CARTESIAN_POINT('Ctrl Pts',(-110.210831335383,-1.81301906978824,
125.171617339533));
#156470=CARTESIAN_POINT('Ctrl Pts',(-110.214767384824,-1.89175032196432,
125.198184444643));
#156471=CARTESIAN_POINT('Ctrl Pts',(-110.22219065123,-2.04023500644922,
125.24828917575));
#156472=CARTESIAN_POINT('Ctrl Pts',(-110.229613917635,-2.18695223779104,
125.304372873823));
#156473=CARTESIAN_POINT('Ctrl Pts',(-110.237037184041,-2.33138420732124,
125.366293107839));
#156474=CARTESIAN_POINT('Ctrl Pts',(-110.244451676762,-2.47564547025819,
125.42814015728));
#156475=CARTESIAN_POINT('Ctrl Pts',(-110.251866169483,-2.61762650797175,
125.495809865903));
#156476=CARTESIAN_POINT('Ctrl Pts',(-110.259280662204,-2.75682469126078,
125.569110080662));
#156477=CARTESIAN_POINT('Ctrl Pts',(-110.266688008558,-2.89588871009964,
125.642339645914));
#156478=CARTESIAN_POINT('Ctrl Pts',(-110.274095354912,-3.03217488620213,
125.721188740658));
#156479=CARTESIAN_POINT('Ctrl Pts',(-110.281502701265,-3.16520071159223,
125.805417227425));
#156480=CARTESIAN_POINT('Ctrl Pts',(-110.288904522941,-3.29812732130297,
125.889582893409));
#156481=CARTESIAN_POINT('Ctrl Pts',(-110.296306344616,-3.42779810809489,
125.979119763837));
#156482=CARTESIAN_POINT('Ctrl Pts',(-110.303708166292,-3.5537554233102,
126.07374195255));
#156483=CARTESIAN_POINT('Ctrl Pts',(-110.311106080603,-3.67964624663961,
126.168314190947));
#156484=CARTESIAN_POINT('Ctrl Pts',(-110.318503994915,-3.80182720474181,
126.267966177674));
#156485=CARTESIAN_POINT('Ctrl Pts',(-110.325901909226,-3.91986999238874,
126.372368987918));
#156486=CARTESIAN_POINT('Ctrl Pts',(-110.333298594138,-4.0378931634657,
126.476754448309));
#156487=CARTESIAN_POINT('Ctrl Pts',(-110.340695279051,-4.15177924959809,
126.585888918224));
#156488=CARTESIAN_POINT('Ctrl Pts',(-110.348091963963,-4.26113330376478,
126.699403427771));
#156489=CARTESIAN_POINT('Ctrl Pts',(-110.355488320898,-4.37048250905812,
126.812912903966));
#156490=CARTESIAN_POINT('Ctrl Pts',(-110.362884677834,-4.47529982296371,
126.930801764785));
#156491=CARTESIAN_POINT('Ctrl Pts',(-110.370281034769,-4.57522763305013,
127.052664645306));
#156492=CARTESIAN_POINT('Ctrl Pts',(-110.377678524106,-4.67517074233938,
127.174546183344));
#156493=CARTESIAN_POINT('Ctrl Pts',(-110.385076013442,-4.77022262054007,
127.300402663878));
#156494=CARTESIAN_POINT('Ctrl Pts',(-110.392473502779,-4.86006647560802,
127.429796287883));
#156495=CARTESIAN_POINT('Ctrl Pts',(-110.399873585294,-4.94994182529971,
127.559235270621));
#156496=CARTESIAN_POINT('Ctrl Pts',(-110.407273667809,-5.03460530419998,
127.692213559104));
#156497=CARTESIAN_POINT('Ctrl Pts',(-110.414673750324,-5.11378399586417,
127.828265221557));
#156498=CARTESIAN_POINT('Ctrl Pts',(-110.422081969991,-5.19304975263995,
127.9644664868));
#156499=CARTESIAN_POINT('Ctrl Pts',(-110.429490189657,-5.26681848981989,
128.103747552243));
#156500=CARTESIAN_POINT('Ctrl Pts',(-110.436898409324,-5.33486339628371,
128.245618132381));
#156501=CARTESIAN_POINT('Ctrl Pts',(-110.444311188626,-5.40295018325208,
128.387576031494));
#156502=CARTESIAN_POINT('Ctrl Pts',(-110.451723967928,-5.46530597212129,
128.532126279184));
#156503=CARTESIAN_POINT('Ctrl Pts',(-110.45913674723,-5.52175269184324,
128.678760050051));
#156504=CARTESIAN_POINT('Ctrl Pts',(-110.466560118259,-5.57828006528533,
128.825603338125));
#156505=CARTESIAN_POINT('Ctrl Pts',(-110.473983489287,-5.62888138693405,
128.974535742665));
#156506=CARTESIAN_POINT('Ctrl Pts',(-110.481406860316,-5.67342864712985,
129.125033982147));
#156507=CARTESIAN_POINT('Ctrl Pts',(-110.485342909757,-5.69704867338016,
129.204831759869));
#156508=CARTESIAN_POINT('Ctrl Pts',(-110.489278959197,-5.71896754006529,
129.28506957918));
#156509=CARTESIAN_POINT('Ctrl Pts',(-110.493215008638,-5.73917204703325,
129.365668580662));
#156510=CARTESIAN_POINT('Ctrl Pts',(-110.503025581335,-5.78953162392232,
129.56656096664));
#156511=CARTESIAN_POINT('Ctrl Pts',(-110.512836154033,-5.82936219324129,
129.770190592286));
#156512=CARTESIAN_POINT('Ctrl Pts',(-110.522646726731,-5.85842123244092,
129.975607804126));
#156513=CARTESIAN_POINT('Ctrl Pts',(-110.532236678111,-5.88682678853453,
130.176405569441));
#156514=CARTESIAN_POINT('Ctrl Pts',(-110.541826629492,-5.90493989260881,
130.378911712314));
#156515=CARTESIAN_POINT('Ctrl Pts',(-110.551416580872,-5.91257834870321,
130.582216896192));
#156516=CARTESIAN_POINT('Ctrl Pts',(-110.554819315566,-5.91528864811252,
130.65435423821));
#156517=CARTESIAN_POINT('Ctrl Pts',(-110.55822205026,-5.91668060726454,
130.726591950347));
#156518=CARTESIAN_POINT('Ctrl Pts',(-110.561624784954,-5.91674746965208,
130.798888610095));
#156519=CARTESIAN_POINT('',(-112.311624807789,-5.90708586381852,130.805356254123));
#156520=CARTESIAN_POINT('Ctrl Pts',(-110.561624807789,-5.91596713820667,
130.798889816873));
#156521=CARTESIAN_POINT('Ctrl Pts',(-110.63163741601,-5.90235840387917,
132.286239780293));
#156522=CARTESIAN_POINT('Ctrl Pts',(-110.794465898833,-4.57889102550224,
135.766948144642));
#156523=CARTESIAN_POINT('Ctrl Pts',(-111.050110256264,1.27396758855394,
137.685826094749));
#156524=CARTESIAN_POINT('Ctrl Pts',(-111.328557880076,6.47818239918729,
133.452135784232));
#156525=CARTESIAN_POINT('Ctrl Pts',(-111.607005503889,5.72926406176812,
126.785269446559));
#156526=CARTESIAN_POINT('Ctrl Pts',(-111.885453127702,-0.284568058305057,
123.811751551519));
#156527=CARTESIAN_POINT('Ctrl Pts',(-112.120326229002,-5.13670898525614,
126.723838658395));
#156528=CARTESIAN_POINT('Ctrl Pts',(-112.262383455698,-5.90551418374586,
129.755303443924));
#156529=CARTESIAN_POINT('Ctrl Pts',(-112.311624807789,-5.90708586381852,
130.805356254123));
#156530=CARTESIAN_POINT('',(-114.061623931777,-5.91866510547899,130.80947112303));
#156531=CARTESIAN_POINT('Ctrl Pts',(-112.311624807789,-5.90708586381852,
130.805356254123));
#156532=CARTESIAN_POINT('Ctrl Pts',(-112.355199330302,-5.90847667064653,
131.734566112796));
#156533=CARTESIAN_POINT('Ctrl Pts',(-112.491589727419,-5.26349239955701,
134.641212553306));
#156534=CARTESIAN_POINT('Ctrl Pts',(-112.72079599914,-0.710590888339653,
137.766588789623));
#156535=CARTESIAN_POINT('Ctrl Pts',(-112.999243622954,5.47342800940259,
135.165455245776));
#156536=CARTESIAN_POINT('Ctrl Pts',(-113.277691246766,6.62763395832767,
128.556688789929));
#156537=CARTESIAN_POINT('Ctrl Pts',(-113.556138870579,1.69136807746817,
124.013422938799));
#156538=CARTESIAN_POINT('Ctrl Pts',(-113.817449618239,-4.39972576943155,
125.606239437587));
#156539=CARTESIAN_POINT('Ctrl Pts',(-113.985944491294,-5.90495055333275,
129.204287311635));
#156540=CARTESIAN_POINT('Ctrl Pts',(-114.061623489744,-5.91963258048528,
130.809462585875));
#156541=CARTESIAN_POINT('',(-115.811626237887,-5.92090002699625,130.800994224613));
#156542=CARTESIAN_POINT('Ctrl Pts',(-114.061624807789,-5.9167477783002,
130.809488041834));
#156543=CARTESIAN_POINT('Ctrl Pts',(-114.072743188688,-5.91654351548332,
131.045195388206));
#156544=CARTESIAN_POINT('Ctrl Pts',(-114.083861569587,-5.90225126763551,
131.280316005178));
#156545=CARTESIAN_POINT('Ctrl Pts',(-114.094979950486,-5.8740986305719,
131.513512111122));
#156546=CARTESIAN_POINT('Ctrl Pts',(-114.100998006393,-5.8588604276985,
131.639734374552));
#156547=CARTESIAN_POINT('Ctrl Pts',(-114.107016062299,-5.83956221767358,
131.765393514612));
#156548=CARTESIAN_POINT('Ctrl Pts',(-114.113034118206,-5.81624514316456,
131.890280963224));
#156549=CARTESIAN_POINT('Ctrl Pts',(-114.120457384612,-5.78748355328094,
132.044329515808));
#156550=CARTESIAN_POINT('Ctrl Pts',(-114.127880651017,-5.75255407086956,
132.197467552954));
#156551=CARTESIAN_POINT('Ctrl Pts',(-114.135303917423,-5.71152501721092,
132.349162397819));
#156552=CARTESIAN_POINT('Ctrl Pts',(-114.142718410144,-5.67054445648646,
132.500677951976));
#156553=CARTESIAN_POINT('Ctrl Pts',(-114.150132902865,-5.62347877095304,
132.650753352294));
#156554=CARTESIAN_POINT('Ctrl Pts',(-114.157547395586,-5.57044764258701,
132.798863970207));
#156555=CARTESIAN_POINT('Ctrl Pts',(-114.16495474194,-5.51746762761925,
132.94683183353));
#156556=CARTESIAN_POINT('Ctrl Pts',(-114.172362088294,-5.45853374136815,
133.092838335406));
#156557=CARTESIAN_POINT('Ctrl Pts',(-114.179769434648,-5.39381599992676,
133.236372032308));
#156558=CARTESIAN_POINT('Ctrl Pts',(-114.187171256323,-5.3291465274186,
133.379798676363));
#156559=CARTESIAN_POINT('Ctrl Pts',(-114.194573077999,-5.25870194189213,
133.520755848878));
#156560=CARTESIAN_POINT('Ctrl Pts',(-114.201974899674,-5.18270104518394,
133.65875029642));
#156561=CARTESIAN_POINT('Ctrl Pts',(-114.209372813985,-5.10674026875731,
133.796671897768));
#156562=CARTESIAN_POINT('Ctrl Pts',(-114.216770728297,-5.02522920225714,
133.931633562767));
#156563=CARTESIAN_POINT('Ctrl Pts',(-114.224168642608,-4.93843337962503,
134.063165048259));
#156564=CARTESIAN_POINT('Ctrl Pts',(-114.23156532752,-4.85165198088412,
134.194674675605));
#156565=CARTESIAN_POINT('Ctrl Pts',(-114.238962012432,-4.75958777444136,
134.322754943523));
#156566=CARTESIAN_POINT('Ctrl Pts',(-114.246358697344,-4.66255062608722,
134.446963014435));
#156567=CARTESIAN_POINT('Ctrl Pts',(-114.25375505428,-4.56551778046164,
134.57116557783));
#156568=CARTESIAN_POINT('Ctrl Pts',(-114.261151411215,-4.46351266118179,
134.691495991443));
#156569=CARTESIAN_POINT('Ctrl Pts',(-114.268547768151,-4.356886410264,134.807543272724));
#156570=CARTESIAN_POINT('Ctrl Pts',(-114.275945257487,-4.25024383459528,
134.923608321139));
#156571=CARTESIAN_POINT('Ctrl Pts',(-114.283342746824,-4.13897897113188,
135.035388656619));
#156572=CARTESIAN_POINT('Ctrl Pts',(-114.29074023616,-4.02348080581559,
135.142509159022));
#156573=CARTESIAN_POINT('Ctrl Pts',(-114.298140318675,-3.90794215279632,
135.24966721235));
#156574=CARTESIAN_POINT('Ctrl Pts',(-114.30554040119,-3.78816751686652,
135.35216192663));
#156575=CARTESIAN_POINT('Ctrl Pts',(-114.312940483705,-3.6645798980917,
135.449657672976));
#156576=CARTESIAN_POINT('Ctrl Pts',(-114.320348703371,-3.5408563820251,
135.547260625918));
#156577=CARTESIAN_POINT('Ctrl Pts',(-114.327756923038,-3.41331180314285,
135.63985340195));
#156578=CARTESIAN_POINT('Ctrl Pts',(-114.335165142704,-3.2823997470893,
135.727142601649));
#156579=CARTESIAN_POINT('Ctrl Pts',(-114.342577922006,-3.15140711684963,
135.814485526393));
#156580=CARTESIAN_POINT('Ctrl Pts',(-114.349990701308,-3.01704319734404,
135.896518176282));
#156581=CARTESIAN_POINT('Ctrl Pts',(-114.35740348061,-2.87978677346191,
135.972992806249));
#156582=CARTESIAN_POINT('Ctrl Pts',(-114.364826851639,-2.74233423116445,
136.049576706755));
#156583=CARTESIAN_POINT('Ctrl Pts',(-114.372250222667,-2.60198126228096,
136.120586558186));
#156584=CARTESIAN_POINT('Ctrl Pts',(-114.379673593696,-2.45922799312802,
136.185822151417));
#156585=CARTESIAN_POINT('Ctrl Pts',(-114.383609643136,-2.38353678451015,
136.220411628252));
#156586=CARTESIAN_POINT('Ctrl Pts',(-114.387545692577,-2.30717105441215,
136.253378575815));
#156587=CARTESIAN_POINT('Ctrl Pts',(-114.391481742018,-2.23020702790131,
136.28469885304));
#156588=CARTESIAN_POINT('Ctrl Pts',(-114.398905008423,-2.08505527585811,
136.343767918417));
#156589=CARTESIAN_POINT('Ctrl Pts',(-114.406328274828,-1.93733566967042,
136.397155605291));
#156590=CARTESIAN_POINT('Ctrl Pts',(-114.413751541234,-1.78753329477134,
136.444631469448));
#156591=CARTESIAN_POINT('Ctrl Pts',(-114.421166033955,-1.63790797383908,
136.492051221075));
#156592=CARTESIAN_POINT('Ctrl Pts',(-114.428580526676,-1.48620513652192,
136.533572946533));
#156593=CARTESIAN_POINT('Ctrl Pts',(-114.435995019397,-1.33293085872197,
136.569013763104));
#156594=CARTESIAN_POINT('Ctrl Pts',(-114.44340236575,-1.17980431244164,
136.604420420482));
#156595=CARTESIAN_POINT('Ctrl Pts',(-114.450809712104,-1.02510970223607,
136.633757753556));
#156596=CARTESIAN_POINT('Ctrl Pts',(-114.458217058458,-0.869369217879168,
136.65689235396));
#156597=CARTESIAN_POINT('Ctrl Pts',(-114.465618880134,-0.713744890651249,
136.680009699707));
#156598=CARTESIAN_POINT('Ctrl Pts',(-114.473020701809,-0.557076610118659,
136.696933469624));
#156599=CARTESIAN_POINT('Ctrl Pts',(-114.480422523484,-0.39989763209945,
136.707581132365));
#156600=CARTESIAN_POINT('Ctrl Pts',(-114.487820437796,-0.242801627639259,
136.718223174287));
#156601=CARTESIAN_POINT('Ctrl Pts',(-114.495218352107,-0.085195834101807,
136.722595682081));
#156602=CARTESIAN_POINT('Ctrl Pts',(-114.502616266419,0.0723805920462764,
136.720667879059));
#156603=CARTESIAN_POINT('Ctrl Pts',(-114.510012951331,0.229930831850837,
136.718740396403));
#156604=CARTESIAN_POINT('Ctrl Pts',(-114.517409636243,0.387451341047541,
136.710514685474));
#156605=CARTESIAN_POINT('Ctrl Pts',(-114.524806321155,0.544402057809802,
136.696012080607));
#156606=CARTESIAN_POINT('Ctrl Pts',(-114.532202678091,0.701345815212809,
136.681510118801));
#156607=CARTESIAN_POINT('Ctrl Pts',(-114.539599035026,0.857719458703056,
136.660731850808));
#156608=CARTESIAN_POINT('Ctrl Pts',(-114.546995391962,1.01298741618553,
136.633750556243));
#156609=CARTESIAN_POINT('Ctrl Pts',(-114.554392881299,1.16827914558912,
136.606765130773));
#156610=CARTESIAN_POINT('Ctrl Pts',(-114.561790370635,1.32246448410944,
136.573574851671));
#156611=CARTESIAN_POINT('Ctrl Pts',(-114.569187859972,1.47501757614395,
136.534304222224));
#156612=CARTESIAN_POINT('Ctrl Pts',(-114.576587942487,1.62762414542817,
136.49501982652));
#156613=CARTESIAN_POINT('Ctrl Pts',(-114.583988025002,1.77859696773102,
136.44965092976));
#156614=CARTESIAN_POINT('Ctrl Pts',(-114.591388107517,1.92742502709768,
136.398371998267));
#156615=CARTESIAN_POINT('Ctrl Pts',(-114.598796327184,2.07641673821573,
136.347036680318));
#156616=CARTESIAN_POINT('Ctrl Pts',(-114.60620454685,2.2232586233909,136.289778471005));
#156617=CARTESIAN_POINT('Ctrl Pts',(-114.613612766517,2.36745866325774,
136.226820395219));
#156618=CARTESIAN_POINT('Ctrl Pts',(-114.621025545819,2.51174745584301,
136.163823569789));
#156619=CARTESIAN_POINT('Ctrl Pts',(-114.628438325121,2.65339082799382,
136.095120049948));
#156620=CARTESIAN_POINT('Ctrl Pts',(-114.635851104423,2.79192154984266,
136.020978738727));
#156621=CARTESIAN_POINT('Ctrl Pts',(-114.643274475452,2.93065021088314,
135.946731490923));
#156622=CARTESIAN_POINT('Ctrl Pts',(-114.650697846481,3.0662570179886,135.86703112241));
#156623=CARTESIAN_POINT('Ctrl Pts',(-114.658121217509,3.19830319906141,
135.782190185698));
#156624=CARTESIAN_POINT('Ctrl Pts',(-114.66205726695,3.2683172526697,135.737205485325));
#156625=CARTESIAN_POINT('Ctrl Pts',(-114.665993316391,3.33733082178464,
135.690776274222));
#156626=CARTESIAN_POINT('Ctrl Pts',(-114.669929365832,3.405282394333,135.642953633862));
#156627=CARTESIAN_POINT('Ctrl Pts',(-114.677352632237,3.53343693946514,
135.552761626635));
#156628=CARTESIAN_POINT('Ctrl Pts',(-114.684775898643,3.65819956784641,
135.457338287135));
#156629=CARTESIAN_POINT('Ctrl Pts',(-114.692199165048,3.77911419970643,
135.356967170748));
#156630=CARTESIAN_POINT('Ctrl Pts',(-114.699613657769,3.89988592051292,
135.256714684685));
#156631=CARTESIAN_POINT('Ctrl Pts',(-114.70702815049,4.01681841321489,135.151526298038));
#156632=CARTESIAN_POINT('Ctrl Pts',(-114.714442643211,4.12948426701537,
135.041728934219));
#156633=CARTESIAN_POINT('Ctrl Pts',(-114.721849989565,4.24204152922415,
134.932037397233));
#156634=CARTESIAN_POINT('Ctrl Pts',(-114.729257335919,4.350340073857,134.817745985618));
#156635=CARTESIAN_POINT('Ctrl Pts',(-114.736664682272,4.45398540435096,
134.699221921942));
#156636=CARTESIAN_POINT('Ctrl Pts',(-114.744066503948,4.55755343224713,
134.580786257985));
#156637=CARTESIAN_POINT('Ctrl Pts',(-114.751468325623,4.65647491164731,
134.458124507523));
#156638=CARTESIAN_POINT('Ctrl Pts',(-114.758870147299,4.75039216879779,
134.331640703571));
#156639=CARTESIAN_POINT('Ctrl Pts',(-114.76626806161,4.84425984775953,134.205223669434));
#156640=CARTESIAN_POINT('Ctrl Pts',(-114.773665975921,4.93312834354486,
134.07498889897));
#156641=CARTESIAN_POINT('Ctrl Pts',(-114.781063890233,5.01668033561569,
133.941373364232));
#156642=CARTESIAN_POINT('Ctrl Pts',(-114.788460575145,5.10021844286086,
133.807780033974));
#156643=CARTESIAN_POINT('Ctrl Pts',(-114.795857260057,5.17844160216471,
133.670807370693));
#156644=CARTESIAN_POINT('Ctrl Pts',(-114.803253944969,5.25107584609969,
133.530921275429));
#156645=CARTESIAN_POINT('Ctrl Pts',(-114.810650301904,5.32370686935617,
133.391041382862));
#156646=CARTESIAN_POINT('Ctrl Pts',(-114.81804665884,5.39074929796717,133.248248646475));
#156647=CARTESIAN_POINT('Ctrl Pts',(-114.825443015775,5.45197529435011,
133.103033267661));
#156648=CARTESIAN_POINT('Ctrl Pts',(-114.832840505112,5.51321066458958,
132.957795656002));
#156649=CARTESIAN_POINT('Ctrl Pts',(-114.840237994448,5.56862768443936,
132.810135007377));
#156650=CARTESIAN_POINT('Ctrl Pts',(-114.847635483785,5.61804686424543,
132.660561036067));
#156651=CARTESIAN_POINT('Ctrl Pts',(-114.8550355663,5.66748336786831,132.510934631833));
#156652=CARTESIAN_POINT('Ctrl Pts',(-114.862435648815,5.71091772828087,
132.359393923761));
#156653=CARTESIAN_POINT('Ctrl Pts',(-114.86983573133,5.74822051233694,132.206463147358));
#156654=CARTESIAN_POINT('Ctrl Pts',(-114.877243950996,5.78556431463894,
132.053364207844));
#156655=CARTESIAN_POINT('Ctrl Pts',(-114.884652170662,5.81676298725624,
131.898872510325));
#156656=CARTESIAN_POINT('Ctrl Pts',(-114.892060390329,5.84173821886264,
131.743522555029));
#156657=CARTESIAN_POINT('Ctrl Pts',(-114.899473169631,5.86672882230735,
131.588076984428));
#156658=CARTESIAN_POINT('Ctrl Pts',(-114.906885948933,5.88548830776054,
131.431772473239));
#156659=CARTESIAN_POINT('Ctrl Pts',(-114.914298728235,5.89799036179937,
131.275147463837));
#156660=CARTESIAN_POINT('Ctrl Pts',(-114.921722099264,5.91051027935928,
131.118298661276));
#156661=CARTESIAN_POINT('Ctrl Pts',(-114.929145470292,5.91675489371841,
130.961128817903));
#156662=CARTESIAN_POINT('Ctrl Pts',(-114.936568841321,5.91674999712059,
130.804176027378));
#156663=CARTESIAN_POINT('Ctrl Pts',(-114.940504890762,5.91674740082693,
130.720955891807));
#156664=CARTESIAN_POINT('Ctrl Pts',(-114.944440940203,5.91498871043917,
130.637796698842));
#156665=CARTESIAN_POINT('Ctrl Pts',(-114.948376989644,5.91148365346844,
130.554777811116));
#156666=CARTESIAN_POINT('Ctrl Pts',(-114.955800256049,5.90487322541099,
130.398206779802));
#156667=CARTESIAN_POINT('Ctrl Pts',(-114.963223522455,5.89202811549701,
130.241661801239));
#156668=CARTESIAN_POINT('Ctrl Pts',(-114.97064678886,5.87294036464704,130.085679856867));
#156669=CARTESIAN_POINT('Ctrl Pts',(-114.978061281581,5.85387517393344,
129.929882270199));
#156670=CARTESIAN_POINT('Ctrl Pts',(-114.985475774302,5.82858207369721,
129.774646760036));
#156671=CARTESIAN_POINT('Ctrl Pts',(-114.992890267023,5.79710508788874,
129.620509629276));
#156672=CARTESIAN_POINT('Ctrl Pts',(-115.000297613377,5.76565844078429,
129.466521061687));
#156673=CARTESIAN_POINT('Ctrl Pts',(-115.007704959731,5.72803984800505,
129.313629129212));
#156674=CARTESIAN_POINT('Ctrl Pts',(-115.015112306084,5.68434502926818,
129.162364225751));
#156675=CARTESIAN_POINT('Ctrl Pts',(-115.02251412776,5.64068279977563,129.011212141361));
#156676=CARTESIAN_POINT('Ctrl Pts',(-115.029915949435,5.5909534710577,128.861685026835));
#156677=CARTESIAN_POINT('Ctrl Pts',(-115.037317771111,5.53530363613135,
128.714302192945));
#156678=CARTESIAN_POINT('Ctrl Pts',(-115.044715685422,5.47968317831968,
128.566997161305));
#156679=CARTESIAN_POINT('Ctrl Pts',(-115.052113599733,5.41814857019337,
128.421834504317));
#156680=CARTESIAN_POINT('Ctrl Pts',(-115.059511514045,5.35089592921541,
128.279317386806));
#156681=CARTESIAN_POINT('Ctrl Pts',(-115.066908198957,5.28365446440639,
128.136823953055));
#156682=CARTESIAN_POINT('Ctrl Pts',(-115.074304883869,5.21069701183099,
127.996975523491));
#156683=CARTESIAN_POINT('Ctrl Pts',(-115.081701568781,5.13226746114255,
127.860254425562));
#156684=CARTESIAN_POINT('Ctrl Pts',(-115.089097925717,5.05384138810257,
127.72353938999));
#156685=CARTESIAN_POINT('Ctrl Pts',(-115.096494282652,4.96994388514552,
127.589951734135));
#156686=CARTESIAN_POINT('Ctrl Pts',(-115.103890639587,4.88086422080918,
127.459948110036));
#156687=CARTESIAN_POINT('Ctrl Pts',(-115.111288128924,4.79177091814857,
127.32992458205));
#156688=CARTESIAN_POINT('Ctrl Pts',(-115.118685618261,4.69749408535773,
127.203486486365));
#156689=CARTESIAN_POINT('Ctrl Pts',(-115.126083107597,4.59836554095464,
127.081060345729));
#156690=CARTESIAN_POINT('Ctrl Pts',(-115.133483190112,4.49920224719412,
126.9585912888));
#156691=CARTESIAN_POINT('Ctrl Pts',(-115.140883272627,4.39518409038359,
126.84013727696));
#156692=CARTESIAN_POINT('Ctrl Pts',(-115.148283355142,4.28668216292368,
126.726090568075));
#156693=CARTESIAN_POINT('Ctrl Pts',(-115.155691574809,4.17806092644011,
126.61191845311));
#156694=CARTESIAN_POINT('Ctrl Pts',(-115.163099794475,4.06494633050394,
126.502163590066));
#156695=CARTESIAN_POINT('Ctrl Pts',(-115.170508014142,3.94774573611127,
126.39718077491));
#156696=CARTESIAN_POINT('Ctrl Pts',(-115.177920793444,3.83047300670836,
126.292133344582));
#156697=CARTESIAN_POINT('Ctrl Pts',(-115.185333572746,3.709109554784,126.191864051927));
#156698=CARTESIAN_POINT('Ctrl Pts',(-115.192746352048,3.58409416411012,
126.096686076427));
#156699=CARTESIAN_POINT('Ctrl Pts',(-115.200169723077,3.45890014558359,
126.001372106172));
#156700=CARTESIAN_POINT('Ctrl Pts',(-115.207593094105,3.33004407166639,
125.911164195825));
#156701=CARTESIAN_POINT('Ctrl Pts',(-115.215016465134,3.19799259713175,
125.826331498407));
#156702=CARTESIAN_POINT('Ctrl Pts',(-115.218952514575,3.12797573680298,
125.781351166705));
#156703=CARTESIAN_POINT('Ctrl Pts',(-115.222888564016,3.0570609374621,125.737881227666));
#156704=CARTESIAN_POINT('Ctrl Pts',(-115.226824613456,2.98532022709708,
125.695956394701));
#156705=CARTESIAN_POINT('Ctrl Pts',(-115.234247879862,2.85001948629717,
125.616887468158));
#156706=CARTESIAN_POINT('Ctrl Pts',(-115.241671146267,2.71137066658009,
125.543078038184));
#156707=CARTESIAN_POINT('Ctrl Pts',(-115.249094412673,2.56982124356253,
125.474825052563));
#156708=CARTESIAN_POINT('Ctrl Pts',(-115.256508905394,2.42843912020803,
125.406652736303));
#156709=CARTESIAN_POINT('Ctrl Pts',(-115.263923398115,2.28416355051382,
125.344023952788));
#156710=CARTESIAN_POINT('Ctrl Pts',(-115.271337890836,2.13746953731795,
125.287191548239));
#156711=CARTESIAN_POINT('Ctrl Pts',(-115.278745237189,1.99091691333493,
125.230413920901));
#156712=CARTESIAN_POINT('Ctrl Pts',(-115.286152583543,1.84195083213713,
125.179421684325));
#156713=CARTESIAN_POINT('Ctrl Pts',(-115.293559929897,1.69106926797789,
125.134420997658));
#156714=CARTESIAN_POINT('Ctrl Pts',(-115.300961751572,1.54030023698164,
125.089453874201));
#156715=CARTESIAN_POINT('Ctrl Pts',(-115.308363573248,1.3876189238245,125.050469509055));
#156716=CARTESIAN_POINT('Ctrl Pts',(-115.315765394923,1.23354147647298,
125.01762526952));
#156717=CARTESIAN_POINT('Ctrl Pts',(-115.323163309235,1.07954536540657,
124.984798368204));
#156718=CARTESIAN_POINT('Ctrl Pts',(-115.330561223546,0.924154952104155,
124.958105214874));
#156719=CARTESIAN_POINT('Ctrl Pts',(-115.337959137857,0.767899569662173,
124.937652783234));
#156720=CARTESIAN_POINT('Ctrl Pts',(-115.34535582277,0.611670154030214,
124.917203750417));
#156721=CARTESIAN_POINT('Ctrl Pts',(-115.352752507682,0.454576424322626,
124.902993429364));
#156722=CARTESIAN_POINT('Ctrl Pts',(-115.360149192594,0.297156004596891,
124.895077338569));
#156723=CARTESIAN_POINT('Ctrl Pts',(-115.367545549529,0.139742565057531,
124.887161598782));
#156724=CARTESIAN_POINT('Ctrl Pts',(-115.374941906465,-0.0179971628708776,
124.885539553071));
#156725=CARTESIAN_POINT('Ctrl Pts',(-115.3823382634,-0.175522628184875,
124.890214663204));
#156726=CARTESIAN_POINT('Ctrl Pts',(-115.389735752737,-0.333072211050205,
124.894890489108));
#156727=CARTESIAN_POINT('Ctrl Pts',(-115.397133242073,-0.490407092826112,
124.905865379454));
#156728=CARTESIAN_POINT('Ctrl Pts',(-115.40453073141,-0.646989071830415,
124.923090711888));
#156729=CARTESIAN_POINT('Ctrl Pts',(-115.411930813925,-0.803625940404501,
124.940322082636));
#156730=CARTESIAN_POINT('Ctrl Pts',(-115.41933089644,-0.959509009898548,
124.963808217108));
#156731=CARTESIAN_POINT('Ctrl Pts',(-115.426730978955,-1.11410767815242,
124.993448929717));
#156732=CARTESIAN_POINT('Ctrl Pts',(-115.434139198622,-1.26887634353538,
125.023122235336));
#156733=CARTESIAN_POINT('Ctrl Pts',(-115.441547418288,-1.42235742031468,
125.058963564082));
#156734=CARTESIAN_POINT('Ctrl Pts',(-115.448955637955,-1.57403222002663,
125.100821967498));
#156735=CARTESIAN_POINT('Ctrl Pts',(-115.456368417257,-1.72580037304697,
125.142706134063));
#156736=CARTESIAN_POINT('Ctrl Pts',(-115.463781196559,-1.87575967896434,
125.190614641464));
#156737=CARTESIAN_POINT('Ctrl Pts',(-115.471193975861,-2.02340947766266,
125.244347609649));
#156738=CARTESIAN_POINT('Ctrl Pts',(-115.47861734689,-2.17127024531725,
125.298157354019));
#156739=CARTESIAN_POINT('Ctrl Pts',(-115.486040717918,-2.31681457054969,
125.357808039406));
#156740=CARTESIAN_POINT('Ctrl Pts',(-115.493464088947,-2.45956376899659,
125.423052539715));
#156741=CARTESIAN_POINT('Ctrl Pts',(-115.497400138388,-2.53525281923191,
125.4576467393));
#156742=CARTESIAN_POINT('Ctrl Pts',(-115.501336187829,-2.61015649131219,
125.493812804534));
#156743=CARTESIAN_POINT('Ctrl Pts',(-115.505272237269,-2.6842066469748,
125.531508899678));
#156744=CARTESIAN_POINT('Ctrl Pts',(-115.512695503675,-2.8238629295303,
125.602602558666));
#156745=CARTESIAN_POINT('Ctrl Pts',(-115.52011877008,-2.96090396710151,
125.679355937636));
#156746=CARTESIAN_POINT('Ctrl Pts',(-115.527542036486,-3.09483805760692,
125.761553070208));
#156747=CARTESIAN_POINT('Ctrl Pts',(-115.534956529207,-3.22861384913951,
125.843653052596));
#156748=CARTESIAN_POINT('Ctrl Pts',(-115.542371021928,-3.35928968799544,
125.931183788193));
#156749=CARTESIAN_POINT('Ctrl Pts',(-115.549785514649,-3.48639609685202,
126.023882313217));
#156750=CARTESIAN_POINT('Ctrl Pts',(-115.557192861002,-3.61337999576663,
126.116491491912));
#156751=CARTESIAN_POINT('Ctrl Pts',(-115.564600207356,-3.73680101415961,
126.214258325538));
#156752=CARTESIAN_POINT('Ctrl Pts',(-115.57200755371,-3.85621653725284,
126.316875288307));
#156753=CARTESIAN_POINT('Ctrl Pts',(-115.579409375385,-3.97554299574364,
126.419415715473));
#156754=CARTESIAN_POINT('Ctrl Pts',(-115.586811197061,-4.09086962544521,
126.526798826783));
#156755=CARTESIAN_POINT('Ctrl Pts',(-115.594213018736,-4.20178503820745,
126.638675433206));
#156756=CARTESIAN_POINT('Ctrl Pts',(-115.601610933047,-4.31264189958634,
126.750492980839));
#156757=CARTESIAN_POINT('Ctrl Pts',(-115.609008847359,-4.41909191948323,
126.866799035043));
#156758=CARTESIAN_POINT('Ctrl Pts',(-115.61640676167,-4.52075898042449,
126.987206074793));
#156759=CARTESIAN_POINT('Ctrl Pts',(-115.623803446582,-4.6224091461448,
127.107593105078));
#156760=CARTESIAN_POINT('Ctrl Pts',(-115.631200131494,-4.71927768983861,
127.23207948337));
#156761=CARTESIAN_POINT('Ctrl Pts',(-115.638596816407,-4.81102730328872,
127.360242900427));
#156762=CARTESIAN_POINT('Ctrl Pts',(-115.645993173342,-4.90277284846483,
127.488400634584));
#156763=CARTESIAN_POINT('Ctrl Pts',(-115.653389530277,-4.98939969741253,
127.620234779783));
#156764=CARTESIAN_POINT('Ctrl Pts',(-115.660785887213,-5.07061275662749,
127.755292426327));
#156765=CARTESIAN_POINT('Ctrl Pts',(-115.668183376549,-5.15183824976914,
127.890370750541));
#156766=CARTESIAN_POINT('Ctrl Pts',(-115.675580865886,-5.22764811041424,
128.028673238842));
#156767=CARTESIAN_POINT('Ctrl Pts',(-115.682978355222,-5.29779233476972,
128.169720805342));
#156768=CARTESIAN_POINT('Ctrl Pts',(-115.690378437737,-5.36796114807441,
128.310817815848));
#156769=CARTESIAN_POINT('Ctrl Pts',(-115.697778520252,-5.43246020469847,
128.454661486414));
#156770=CARTESIAN_POINT('Ctrl Pts',(-115.705178602767,-5.49108699018608,
128.600751253657));
#156771=CARTESIAN_POINT('Ctrl Pts',(-115.712586822434,-5.5497782418514,
128.747001661617));
#156772=CARTESIAN_POINT('Ctrl Pts',(-115.7199950421,-5.60258418788139,128.895502751981));
#156773=CARTESIAN_POINT('Ctrl Pts',(-115.727403261767,-5.6493514617036,
129.045736546126));
#156774=CARTESIAN_POINT('Ctrl Pts',(-115.734816041069,-5.69614752000235,
129.196062806664));
#156775=CARTESIAN_POINT('Ctrl Pts',(-115.742228820371,-5.73689740369434,
129.348123536281));
#156776=CARTESIAN_POINT('Ctrl Pts',(-115.749641599673,-5.77149865850742,
129.501389475389));
#156777=CARTESIAN_POINT('Ctrl Pts',(-115.757064970702,-5.80614935321605,
129.654874408058));
#156778=CARTESIAN_POINT('Ctrl Pts',(-115.76448834173,-5.83463380511123,
129.809567623405));
#156779=CARTESIAN_POINT('Ctrl Pts',(-115.771911712759,-5.85690118778432,
129.964932813029));
#156780=CARTESIAN_POINT('Ctrl Pts',(-115.7758477622,-5.86870788837696,130.047311164509));
#156781=CARTESIAN_POINT('Ctrl Pts',(-115.779783811641,-5.87876761780374,
130.129878386884));
#156782=CARTESIAN_POINT('Ctrl Pts',(-115.783719861082,-5.88707874326198,
130.212554540263));
#156783=CARTESIAN_POINT('Ctrl Pts',(-115.793021509985,-5.90671954609073,
130.407934339944));
#156784=CARTESIAN_POINT('Ctrl Pts',(-115.802323158887,-5.91663620857664,
130.604307906375));
#156785=CARTESIAN_POINT('Ctrl Pts',(-115.811624807789,-5.91674902639369,
130.800966332757));
#156786=CARTESIAN_POINT('',(-117.561623641159,-5.91240943842373,130.800848266352));
#156787=CARTESIAN_POINT('Ctrl Pts',(-115.811627340781,-5.92410128582936,
130.80101573486));
#156788=CARTESIAN_POINT('Ctrl Pts',(-115.895140722153,-5.91199619999421,
132.568884144565));
#156789=CARTESIAN_POINT('Ctrl Pts',(-116.071469978128,-4.13191312647295,
136.322643274555));
#156790=CARTESIAN_POINT('Ctrl Pts',(-116.340615108709,2.25775535553418,
137.428566327301));
#156791=CARTESIAN_POINT('Ctrl Pts',(-116.619062732521,6.79350378926132,
132.485392085333));
#156792=CARTESIAN_POINT('Ctrl Pts',(-116.897510356334,5.08635412177019,
125.997432047439));
#156793=CARTESIAN_POINT('Ctrl Pts',(-117.175957980147,-1.29490650141688,
123.926804533975));
#156794=CARTESIAN_POINT('Ctrl Pts',(-117.397328771323,-5.42208574202265,
127.305240655926));
#156795=CARTESIAN_POINT('Ctrl Pts',(-117.525883687893,-5.91308356794792,
130.03933258855));
#156796=CARTESIAN_POINT('Ctrl Pts',(-117.561622729858,-5.90901965686141,
130.800830848655));
#156797=CARTESIAN_POINT('',(-119.311626003087,-5.91356406754834,130.809061880768));
#156798=CARTESIAN_POINT('Ctrl Pts',(-117.561624807789,-5.91674897067867,
130.800870564149));
#156799=CARTESIAN_POINT('Ctrl Pts',(-117.569093867034,-5.9168429661827,
130.960222796103));
#156800=CARTESIAN_POINT('Ctrl Pts',(-117.576562926279,-5.91049501553312,
131.119589242322));
#156801=CARTESIAN_POINT('Ctrl Pts',(-117.584031985525,-5.89772831670426,
131.278418910231));
#156802=CARTESIAN_POINT('Ctrl Pts',(-117.591502117278,-5.88495978466076,
131.437271385045));
#156803=CARTESIAN_POINT('Ctrl Pts',(-117.598972249032,-5.8657706965315,
131.595586565996));
#156804=CARTESIAN_POINT('Ctrl Pts',(-117.606442380785,-5.84023618905349,
131.75281821734));
#156805=CARTESIAN_POINT('Ctrl Pts',(-117.613914949671,-5.81469335093576,
131.910101165552));
#156806=CARTESIAN_POINT('Ctrl Pts',(-117.621387518557,-5.78280102702624,
132.066299521576));
#156807=CARTESIAN_POINT('Ctrl Pts',(-117.628860087442,-5.74468556128407,
132.220876895084));
#156808=CARTESIAN_POINT('Ctrl Pts',(-117.636336459297,-5.70655069767341,
132.3755329367));
#156809=CARTESIAN_POINT('Ctrl Pts',(-117.643812831151,-5.66218646917605,
132.528566000158));
#156810=CARTESIAN_POINT('Ctrl Pts',(-117.651289203005,-5.61176918510571,
132.679454528707));
#156811=CARTESIAN_POINT('Ctrl Pts',(-117.658775458655,-5.56128524917017,
132.830542532536));
#156812=CARTESIAN_POINT('Ctrl Pts',(-117.666261714304,-5.50473238764771,
132.979479993584));
#156813=CARTESIAN_POINT('Ctrl Pts',(-117.673747969954,-5.44233557517172,
133.125764083084));
#156814=CARTESIAN_POINT('Ctrl Pts',(-117.681239654599,-5.37989351283663,
133.272154257081));
#156815=CARTESIAN_POINT('Ctrl Pts',(-117.688731339244,-5.3115992067413,
133.415886896698));
#156816=CARTESIAN_POINT('Ctrl Pts',(-117.696223023889,-5.23772362846842,
133.556483753308));
#156817=CARTESIAN_POINT('Ctrl Pts',(-117.703726816965,-5.16372864883794,
133.697307849499));
#156818=CARTESIAN_POINT('Ctrl Pts',(-117.711230610041,-5.08413455551827,
133.834985723117));
#156819=CARTESIAN_POINT('Ctrl Pts',(-117.718734403117,-4.99925627082989,
133.969067128614));
#156820=CARTESIAN_POINT('Ctrl Pts',(-117.723440678002,-4.94602178855046,
134.05316112546));
#156821=CARTESIAN_POINT('Ctrl Pts',(-117.728146952887,-4.89070954258863,
134.135841027791));
#156822=CARTESIAN_POINT('Ctrl Pts',(-117.732853227772,-4.83340515316376,
134.217002583532));
#156823=CARTESIAN_POINT('Ctrl Pts',(-117.740276494178,-4.74301822097579,
134.345019723382));
#156824=CARTESIAN_POINT('Ctrl Pts',(-117.747699760583,-4.64740512449227,
134.469636989212));
#156825=CARTESIAN_POINT('Ctrl Pts',(-117.755123026989,-4.54685011284645,
134.590398733302));
#156826=CARTESIAN_POINT('Ctrl Pts',(-117.76253751971,-4.44641394887382,
134.71101774704));
#156827=CARTESIAN_POINT('Ctrl Pts',(-117.76995201243,-4.34104773268394,
134.827790025518));
#156828=CARTESIAN_POINT('Ctrl Pts',(-117.777366505151,-4.23107903775765,
134.940288655957));
#156829=CARTESIAN_POINT('Ctrl Pts',(-117.784773851505,-4.12121633479946,
135.05267885598));
#156830=CARTESIAN_POINT('Ctrl Pts',(-117.792181197859,-4.00676024358271,
135.160803343133));
#156831=CARTESIAN_POINT('Ctrl Pts',(-117.799588544213,-3.88807858660534,
135.26426818016));
#156832=CARTESIAN_POINT('Ctrl Pts',(-117.806990365888,-3.76948544688534,
135.367655849207));
#156833=CARTESIAN_POINT('Ctrl Pts',(-117.814392187564,-3.64667329681064,
135.466390543755));
#156834=CARTESIAN_POINT('Ctrl Pts',(-117.821794009239,-3.52004671324594,
135.560115205333));
#156835=CARTESIAN_POINT('Ctrl Pts',(-117.829191923551,-3.39348697486942,
135.653790390391));
#156836=CARTESIAN_POINT('Ctrl Pts',(-117.836589837862,-3.2631171124924,
135.742460588118));
#156837=CARTESIAN_POINT('Ctrl Pts',(-117.843987752173,-3.12937458057083,
135.825809143338));
#156838=CARTESIAN_POINT('Ctrl Pts',(-117.851384437086,-2.99565427423154,
135.909143847541));
#156839=CARTESIAN_POINT('Ctrl Pts',(-117.858781121998,-2.85856272722925,
135.987158467187));
#156840=CARTESIAN_POINT('Ctrl Pts',(-117.86617780691,-2.71856625699627,
136.059579744189));
#156841=CARTESIAN_POINT('Ctrl Pts',(-117.873574163846,-2.57857599435348,
136.131997809955));
#156842=CARTESIAN_POINT('Ctrl Pts',(-117.880970520781,-2.43568139615297,
136.198822854695));
#156843=CARTESIAN_POINT('Ctrl Pts',(-117.888366877716,-2.29037300995161,
136.259827787093));
#156844=CARTESIAN_POINT('Ctrl Pts',(-117.895764367053,-2.14504237666494,
136.320842059502));
#156845=CARTESIAN_POINT('Ctrl Pts',(-117.90316185639,-1.99729756375695,
136.376034300808));
#156846=CARTESIAN_POINT('Ctrl Pts',(-117.910559345726,-1.84764855807082,
136.425225797266));
#156847=CARTESIAN_POINT('Ctrl Pts',(-117.917959428241,-1.69794709315796,
136.474434537725));
#156848=CARTESIAN_POINT('Ctrl Pts',(-117.925359510757,-1.54634046086461,
136.517638228681));
#156849=CARTESIAN_POINT('Ctrl Pts',(-117.932759593272,-1.39335309306427,
136.554708234932));
#156850=CARTESIAN_POINT('Ctrl Pts',(-117.940167812938,-1.24019749992534,
136.591819003466));
#156851=CARTESIAN_POINT('Ctrl Pts',(-117.947576032605,-1.08565850223514,
136.622782529891));
#156852=CARTESIAN_POINT('Ctrl Pts',(-117.954984252271,-0.930270718780585,
136.64752131639));
#156853=CARTESIAN_POINT('Ctrl Pts',(-117.962397031573,-0.774787296738102,
136.672275329199));
#156854=CARTESIAN_POINT('Ctrl Pts',(-117.969809810875,-0.618454417802717,
136.69079692407));
#156855=CARTESIAN_POINT('Ctrl Pts',(-117.977222590177,-0.461810563770643,
136.703060607029));
#156856=CARTESIAN_POINT('Ctrl Pts',(-117.984645961206,-0.304942889654284,
136.715341812913));
#156857=CARTESIAN_POINT('Ctrl Pts',(-117.992069332235,-0.147763725040503,
136.721347234294));
#156858=CARTESIAN_POINT('Ctrl Pts',(-117.999492703264,0.00918887628557559,
136.721103482272));
#156859=CARTESIAN_POINT('Ctrl Pts',(-118.003428752704,0.0924089115290399,
136.720974239102));
#156860=CARTESIAN_POINT('Ctrl Pts',(-118.007364802145,0.175565331760546,
136.719088996615));
#156861=CARTESIAN_POINT('Ctrl Pts',(-118.011300851585,0.258578789242901,
136.715457603089));
#156862=CARTESIAN_POINT('Ctrl Pts',(-118.018724117991,0.415139579303627,
136.708608908229));
#156863=CARTESIAN_POINT('Ctrl Pts',(-118.026147384396,0.57166482851955,
136.695525578381));
#156864=CARTESIAN_POINT('Ctrl Pts',(-118.033570650802,0.727617543960155,
136.676200471668));
#156865=CARTESIAN_POINT('Ctrl Pts',(-118.040985143523,0.88338593624262,
136.656898205626));
#156866=CARTESIAN_POINT('Ctrl Pts',(-118.048399636244,1.03858277485292,
136.631368892658));
#156867=CARTESIAN_POINT('Ctrl Pts',(-118.055814128965,1.1926718245104,136.599657372825));
#156868=CARTESIAN_POINT('Ctrl Pts',(-118.063221475319,1.34661235734003,
136.567976417749));
#156869=CARTESIAN_POINT('Ctrl Pts',(-118.070628821672,1.49944686367386,
136.530125193037));
#156870=CARTESIAN_POINT('Ctrl Pts',(-118.078036168026,1.65064509589691,
136.486200225465));
#156871=CARTESIAN_POINT('Ctrl Pts',(-118.085437989702,1.80173055877441,
136.442308018791));
#156872=CARTESIAN_POINT('Ctrl Pts',(-118.092839811377,1.95118182057804,
136.392351192844));
#156873=CARTESIAN_POINT('Ctrl Pts',(-118.100241633053,2.09847979422678,
136.336477130775));
#156874=CARTESIAN_POINT('Ctrl Pts',(-118.107639547364,2.24570001042137,
136.280632564189));
#156875=CARTESIAN_POINT('Ctrl Pts',(-118.115037461675,2.39076885411446,
136.218877114466));
#156876=CARTESIAN_POINT('Ctrl Pts',(-118.122435375987,2.53318345952155,
136.151407664573));
#156877=CARTESIAN_POINT('Ctrl Pts',(-118.129832060899,2.67557439820509,
136.083949426879));
#156878=CARTESIAN_POINT('Ctrl Pts',(-118.137228745811,2.81531163700423,
136.010779233283));
#156879=CARTESIAN_POINT('Ctrl Pts',(-118.144625430723,2.95191322018767,
135.932141707178));
#156880=CARTESIAN_POINT('Ctrl Pts',(-118.152021787659,3.08850874631415,
135.853507667942));
#156881=CARTESIAN_POINT('Ctrl Pts',(-118.159418144594,3.22196856975973,
135.769406964465));
#156882=CARTESIAN_POINT('Ctrl Pts',(-118.16681450153,3.35183647923222,135.680129559896));
#156883=CARTESIAN_POINT('Ctrl Pts',(-118.174211990866,3.48172427181245,
135.590838486728));
#156884=CARTESIAN_POINT('Ctrl Pts',(-118.181609480203,3.60801874779308,
135.496369345851));
#156885=CARTESIAN_POINT('Ctrl Pts',(-118.189006969539,3.73029388989078,
135.397054604492));
#156886=CARTESIAN_POINT('Ctrl Pts',(-118.196407052054,3.85261189534983,
135.297705048504));
#156887=CARTESIAN_POINT('Ctrl Pts',(-118.203807134569,3.97090747209434,
135.193506745304));
#156888=CARTESIAN_POINT('Ctrl Pts',(-118.211207217084,4.08478892745061,
135.084831383811));
#156889=CARTESIAN_POINT('Ctrl Pts',(-118.218615436751,4.19879560717483,
134.976036522585));
#156890=CARTESIAN_POINT('Ctrl Pts',(-118.226023656417,4.30837820196499,
134.862755029416));
#156891=CARTESIAN_POINT('Ctrl Pts',(-118.233431876084,4.41318253619956,
134.745394804767));
#156892=CARTESIAN_POINT('Ctrl Pts',(-118.240844655386,4.51805137575309,
134.627962346857));
#156893=CARTESIAN_POINT('Ctrl Pts',(-118.248257434688,4.61813585778442,
134.506446442675));
#156894=CARTESIAN_POINT('Ctrl Pts',(-118.25567021399,4.71312347092657,134.38128635209));
#156895=CARTESIAN_POINT('Ctrl Pts',(-118.263093585019,4.80824680682499,
134.255947426898));
#156896=CARTESIAN_POINT('Ctrl Pts',(-118.270516956048,4.89825851570351,
134.126954221111));
#156897=CARTESIAN_POINT('Ctrl Pts',(-118.277940327076,4.98289015502144,
133.994773798565));
#156898=CARTESIAN_POINT('Ctrl Pts',(-118.281876376517,5.02776388089454,
133.924688566908));
#156899=CARTESIAN_POINT('Ctrl Pts',(-118.285812425958,5.07112584934273,
133.853707695839));
#156900=CARTESIAN_POINT('Ctrl Pts',(-118.289748475398,5.11294145660963,
133.781903266091));
#156901=CARTESIAN_POINT('Ctrl Pts',(-118.297171741804,5.19180438689723,
133.64648235252));
#156902=CARTESIAN_POINT('Ctrl Pts',(-118.304595008209,5.26540273149978,
133.507721367969));
#156903=CARTESIAN_POINT('Ctrl Pts',(-118.312018274615,5.33344022395911,
133.366068239438));
#156904=CARTESIAN_POINT('Ctrl Pts',(-118.319432767336,5.40139730175232,
133.224582533141));
#156905=CARTESIAN_POINT('Ctrl Pts',(-118.326847260057,5.46380644988677,
133.080211820169));
#156906=CARTESIAN_POINT('Ctrl Pts',(-118.334261752778,5.52041554530835,
132.933431487598));
#156907=CARTESIAN_POINT('Ctrl Pts',(-118.341669099131,5.57697007875264,
132.786792627437));
#156908=CARTESIAN_POINT('Ctrl Pts',(-118.349076445485,5.62773555526403,
132.637749117236));
#156909=CARTESIAN_POINT('Ctrl Pts',(-118.356483791839,5.67250657376463,
132.48679924441));
#156910=CARTESIAN_POINT('Ctrl Pts',(-118.363885613514,5.71724420035027,
132.335961955696));
#156911=CARTESIAN_POINT('Ctrl Pts',(-118.37128743519,5.75599616538529,132.183221491774));
#156912=CARTESIAN_POINT('Ctrl Pts',(-118.378689256865,5.78860588724099,
132.029094239501));
#156913=CARTESIAN_POINT('Ctrl Pts',(-118.386087171176,5.82119839467855,
131.875048349804));
#156914=CARTESIAN_POINT('Ctrl Pts',(-118.393485085488,5.84765503934111,
131.719617494006));
#156915=CARTESIAN_POINT('Ctrl Pts',(-118.400882999799,5.86786965320518,
131.563331167386));
#156916=CARTESIAN_POINT('Ctrl Pts',(-118.408279684711,5.88808090776712,
131.407070812718));
#156917=CARTESIAN_POINT('Ctrl Pts',(-118.415676369624,5.90205214245062,
131.249955639233));
#156918=CARTESIAN_POINT('Ctrl Pts',(-118.423073054536,5.90972865699758,
131.092523354855));
#156919=CARTESIAN_POINT('Ctrl Pts',(-118.430469411471,5.91740483115983,
130.935098051189));
#156920=CARTESIAN_POINT('Ctrl Pts',(-118.437865768407,5.91878682197877,
130.777356037443));
#156921=CARTESIAN_POINT('Ctrl Pts',(-118.445262125342,5.91387199031722,
130.619837869263));
#156922=CARTESIAN_POINT('Ctrl Pts',(-118.452659614679,5.9089564061824,130.462295584649));
#156923=CARTESIAN_POINT('Ctrl Pts',(-118.460057104015,5.89774209163881,
130.304977586979));
#156924=CARTESIAN_POINT('Ctrl Pts',(-118.467454593352,5.88027848803428,
130.148422003318));
#156925=CARTESIAN_POINT('Ctrl Pts',(-118.474854675867,5.8628087625905,129.991811539339));
#156926=CARTESIAN_POINT('Ctrl Pts',(-118.482254758382,5.83908542781921,
129.835964392254));
#156927=CARTESIAN_POINT('Ctrl Pts',(-118.489654840897,5.80920947667834,
129.681411011141));
#156928=CARTESIAN_POINT('Ctrl Pts',(-118.497063060563,5.77930067385799,
129.526687682698));
#156929=CARTESIAN_POINT('Ctrl Pts',(-118.50447128023,5.74322581454411,129.373261328048));
#156930=CARTESIAN_POINT('Ctrl Pts',(-118.511879499896,5.7011366363743,129.221650405338));
#156931=CARTESIAN_POINT('Ctrl Pts',(-118.519292279198,5.65902155301762,
129.069946168635));
#156932=CARTESIAN_POINT('Ctrl Pts',(-118.5267050585,5.61088488855768,128.920059944961));
#156933=CARTESIAN_POINT('Ctrl Pts',(-118.534117837803,5.55692728473598,
128.772492089669));
#156934=CARTESIAN_POINT('Ctrl Pts',(-118.541541208831,5.50289258375951,
128.624713382506));
#156935=CARTESIAN_POINT('Ctrl Pts',(-118.54896457986,5.44302047376027,128.479260004));
#156936=CARTESIAN_POINT('Ctrl Pts',(-118.556387950889,5.37755880902272,
128.336610261877));
#156937=CARTESIAN_POINT('Ctrl Pts',(-118.56032400033,5.34284946364741,128.260973945769));
#156938=CARTESIAN_POINT('Ctrl Pts',(-118.56426004977,5.30656944965414,128.186125399019));
#156939=CARTESIAN_POINT('Ctrl Pts',(-118.568196099211,5.26876070642898,
128.112132696143));
#156940=CARTESIAN_POINT('Ctrl Pts',(-118.575619365617,5.19745459667746,
127.972584767753));
#156941=CARTESIAN_POINT('Ctrl Pts',(-118.583042632022,5.12049275345589,
127.83566069445));
#156942=CARTESIAN_POINT('Ctrl Pts',(-118.590465898428,5.03809189118005,
127.701851849081));
#156943=CARTESIAN_POINT('Ctrl Pts',(-118.597880391149,4.95578841988069,
127.568201154656));
#156944=CARTESIAN_POINT('Ctrl Pts',(-118.60529488387,4.86805891926092,127.437658673999));
#156945=CARTESIAN_POINT('Ctrl Pts',(-118.612709376591,4.77516706726302,
127.310693483704));
#156946=CARTESIAN_POINT('Ctrl Pts',(-118.620116722944,4.68236474792912,
127.18385066724));
#156947=CARTESIAN_POINT('Ctrl Pts',(-118.627524069298,4.58441020173542,
127.060578576244));
#156948=CARTESIAN_POINT('Ctrl Pts',(-118.634931415652,4.48161162769726,
126.94131935698));
#156949=CARTESIAN_POINT('Ctrl Pts',(-118.642333237327,4.37888972471427,
126.822149085742));
#156950=CARTESIAN_POINT('Ctrl Pts',(-118.649735059003,4.27133123025304,
126.706986008402));
#156951=CARTESIAN_POINT('Ctrl Pts',(-118.657136880678,4.15928595900455,
126.596240981229));
#156952=CARTESIAN_POINT('Ctrl Pts',(-118.66453479499,4.04729983558228,126.485554415492));
#156953=CARTESIAN_POINT('Ctrl Pts',(-118.671932709301,3.93083191724816,
126.379281516878));
#156954=CARTESIAN_POINT('Ctrl Pts',(-118.679330623612,3.81027029696671,
126.277797812683));
#156955=CARTESIAN_POINT('Ctrl Pts',(-118.686727308524,3.68972871183952,
126.176330973238));
#156956=CARTESIAN_POINT('Ctrl Pts',(-118.694123993437,3.56509506026617,
126.079651988793));
#156957=CARTESIAN_POINT('Ctrl Pts',(-118.701520678349,3.43679216432674,
125.98809752449));
#156958=CARTESIAN_POINT('Ctrl Pts',(-118.708917035284,3.30849495747179,
125.896547119809));
#156959=CARTESIAN_POINT('Ctrl Pts',(-118.71631339222,3.17652913361562,125.8101210003));
#156960=CARTESIAN_POINT('Ctrl Pts',(-118.723709749155,3.04134805101419,
125.729113569875));
#156961=CARTESIAN_POINT('Ctrl Pts',(-118.731107238492,2.9061462718443,125.648093737007));
#156962=CARTESIAN_POINT('Ctrl Pts',(-118.738504727828,2.76772857399205,
125.572494436992));
#156963=CARTESIAN_POINT('Ctrl Pts',(-118.745902217165,2.6265744232531,125.502564944248));
#156964=CARTESIAN_POINT('Ctrl Pts',(-118.75330229968,2.48537079114643,125.432610937829));
#156965=CARTESIAN_POINT('Ctrl Pts',(-118.760702382195,2.34142913056556,
125.368330861475));
#156966=CARTESIAN_POINT('Ctrl Pts',(-118.76810246471,2.19525031250549,125.309926467634));
#156967=CARTESIAN_POINT('Ctrl Pts',(-118.775510684376,2.04891075580638,
125.251457852157));
#156968=CARTESIAN_POINT('Ctrl Pts',(-118.782918904043,1.90032947574322,
125.198877960655));
#156969=CARTESIAN_POINT('Ctrl Pts',(-118.790327123709,1.75002468373652,
125.15233937125));
#156970=CARTESIAN_POINT('Ctrl Pts',(-118.797739903011,1.59962738163832,
125.105772138118));
#156971=CARTESIAN_POINT('Ctrl Pts',(-118.805152682313,1.44750481371909,
125.065253712159));
#156972=CARTESIAN_POINT('Ctrl Pts',(-118.812565461615,1.29418639487025,
125.030885742083));
#156973=CARTESIAN_POINT('Ctrl Pts',(-118.819988832644,1.14064890747486,
124.996468665439));
#156974=CARTESIAN_POINT('Ctrl Pts',(-118.827412203673,0.985912522772439,
124.968219663269));
#156975=CARTESIAN_POINT('Ctrl Pts',(-118.834835574702,0.83051362589355,
124.946188745753));
#156976=CARTESIAN_POINT('Ctrl Pts',(-118.838771624143,0.748117402020576,
124.93450742466));
#156977=CARTESIAN_POINT('Ctrl Pts',(-118.842707673583,0.665534966065186,
124.92457336014));
#156978=CARTESIAN_POINT('Ctrl Pts',(-118.846643723024,0.582846260308975,
124.916388063338));
#156979=CARTESIAN_POINT('Ctrl Pts',(-118.85406698943,0.426897941883304,
124.900950849024));
#156980=CARTESIAN_POINT('Ctrl Pts',(-118.861490255835,0.270100084963614,
124.891690221222));
#156981=CARTESIAN_POINT('Ctrl Pts',(-118.868913522241,0.112983234878659,
124.888689450983));
#156982=CARTESIAN_POINT('Ctrl Pts',(-118.876328014962,-0.0439479161367905,
124.885692227406));
#156983=CARTESIAN_POINT('Ctrl Pts',(-118.883742507683,-0.201196940265092,
124.888940141434));
#156984=CARTESIAN_POINT('Ctrl Pts',(-118.891157000404,-0.358226665715189,
124.898464900702));
#156985=CARTESIAN_POINT('Ctrl Pts',(-118.898564346757,-0.515105040003833,
124.907980479649));
#156986=CARTESIAN_POINT('Ctrl Pts',(-118.905971693111,-0.671764166295322,
124.923760837307));
#156987=CARTESIAN_POINT('Ctrl Pts',(-118.913379039465,-0.827665465319788,
124.945785667971));
#156988=CARTESIAN_POINT('Ctrl Pts',(-118.92078086114,-0.983450487274067,
124.967794071686));
#156989=CARTESIAN_POINT('Ctrl Pts',(-118.928182682815,-1.13847843934629,
124.996037622975));
#156990=CARTESIAN_POINT('Ctrl Pts',(-118.935584504491,-1.29221457313743,
125.030444090678));
#156991=CARTESIAN_POINT('Ctrl Pts',(-118.942982418802,-1.44586955081935,
125.064832395474));
#156992=CARTESIAN_POINT('Ctrl Pts',(-118.950380333114,-1.59823370497385,
125.10537705615));
#156993=CARTESIAN_POINT('Ctrl Pts',(-118.957778247425,-1.7487813201234,
125.15195454078));
#156994=CARTESIAN_POINT('Ctrl Pts',(-118.965174932337,-1.89930391699073,
125.198524285077));
#156995=CARTESIAN_POINT('Ctrl Pts',(-118.972571617249,-2.04801021771648,
125.251124753345));
#156996=CARTESIAN_POINT('Ctrl Pts',(-118.979968302161,-2.19438843071803,
125.309582189128));
#156997=CARTESIAN_POINT('Ctrl Pts',(-118.987364659097,-2.34076015315663,
125.368037032846));
#156998=CARTESIAN_POINT('Ctrl Pts',(-118.994761016032,-2.48480364645216,
125.432348189252));
#156999=CARTESIAN_POINT('Ctrl Pts',(-119.002157372968,-2.62602616904493,
125.50229336771));
#157000=CARTESIAN_POINT('Ctrl Pts',(-119.009554862304,-2.76727031316644,
125.572249254954));
#157001=CARTESIAN_POINT('Ctrl Pts',(-119.016952351641,-2.90569229208119,
125.647840716076));
#157002=CARTESIAN_POINT('Ctrl Pts',(-119.024349840977,-3.04082322118871,
125.728799101834));
#157003=CARTESIAN_POINT('Ctrl Pts',(-119.031749923492,-3.17600152023414,
125.809785867429));
#157004=CARTESIAN_POINT('Ctrl Pts',(-119.039150006007,-3.30788615249289,
125.896143111718));
#157005=CARTESIAN_POINT('Ctrl Pts',(-119.046550088522,-3.43603664490841,
125.987558489873));
#157006=CARTESIAN_POINT('Ctrl Pts',(-119.053958308189,-3.56432805196397,
126.079074388634));
#157007=CARTESIAN_POINT('Ctrl Pts',(-119.061366527855,-3.68887681499692,
126.175659311899));
#157008=CARTESIAN_POINT('Ctrl Pts',(-119.068774747521,-3.80927445978313,
126.276959745924));
#157009=CARTESIAN_POINT('Ctrl Pts',(-119.076187526823,-3.92974620731146,
126.378322528676));
#157010=CARTESIAN_POINT('Ctrl Pts',(-119.083600306125,-4.04606147037299,
126.484406354453));
#157011=CARTESIAN_POINT('Ctrl Pts',(-119.091013085428,-4.15784856734825,
126.594820755123));
#157012=CARTESIAN_POINT('Ctrl Pts',(-119.098436456456,-4.2697953909698,
126.705392921066));
#157013=CARTESIAN_POINT('Ctrl Pts',(-119.105859827485,-4.37720087212692,
126.820307748184));
#157014=CARTESIAN_POINT('Ctrl Pts',(-119.113283198514,-4.47973300657406,
126.9391409922));
#157015=CARTESIAN_POINT('Ctrl Pts',(-119.117219247955,-4.53409800448784,
127.002149229548));
#157016=CARTESIAN_POINT('Ctrl Pts',(-119.121155297396,-4.58709363814147,
127.066258567251));
#157017=CARTESIAN_POINT('Ctrl Pts',(-119.125091346837,-4.63867542540924,
127.131402564415));
#157018=CARTESIAN_POINT('Ctrl Pts',(-119.132863574377,-4.74053018956919,
127.260037627662));
#157019=CARTESIAN_POINT('Ctrl Pts',(-119.140635801916,-4.83719850919677,
127.393125371721));
#157020=CARTESIAN_POINT('Ctrl Pts',(-119.148408029456,-4.92826918109601,
127.53020523928));
#157021=CARTESIAN_POINT('Ctrl Pts',(-119.155813131687,-5.01503808128868,
127.660810066263));
#157022=CARTESIAN_POINT('Ctrl Pts',(-119.163218233918,-5.09672570044091,
127.795038205085));
#157023=CARTESIAN_POINT('Ctrl Pts',(-119.170623336149,-5.17301572214231,
127.93245551799));
#157024=CARTESIAN_POINT('Ctrl Pts',(-119.17802146723,-5.24923392454755,
128.069743466472));
#157025=CARTESIAN_POINT('Ctrl Pts',(-119.18541959831,-5.32006446199202,
128.210214289691));
#157026=CARTESIAN_POINT('Ctrl Pts',(-119.192817729391,-5.38523393391365,
128.353404469544));
#157027=CARTESIAN_POINT('Ctrl Pts',(-119.200210362271,-5.45035497268593,
128.496488232219));
#157028=CARTESIAN_POINT('Ctrl Pts',(-119.207602995152,-5.50982316662364,
128.642286989992));
#157029=CARTESIAN_POINT('Ctrl Pts',(-119.214995628032,-5.56341082638834,
128.790312321391));
#157030=CARTESIAN_POINT('Ctrl Pts',(-119.222384231907,-5.61696928073043,
128.938256978576));
#157031=CARTESIAN_POINT('Ctrl Pts',(-119.229772835783,-5.66465345539427,
129.088425442635));
#157032=CARTESIAN_POINT('Ctrl Pts',(-119.237161439658,-5.70628368712896,
129.240309133597));
#157033=CARTESIAN_POINT('Ctrl Pts',(-119.244548106085,-5.74790300253594,
129.392152997441));
#157034=CARTESIAN_POINT('Ctrl Pts',(-119.251934772511,-5.78347143426546,
129.545710833374));
#157035=CARTESIAN_POINT('Ctrl Pts',(-119.259321438938,-5.81285912307789,
129.700458729829));
#157036=CARTESIAN_POINT('Ctrl Pts',(-119.266707000318,-5.84224241548663,
129.855183475969));
#157037=CARTESIAN_POINT('Ctrl Pts',(-119.274092561699,-5.86544674003761,
130.011097560354));
#157038=CARTESIAN_POINT('Ctrl Pts',(-119.281478123079,-5.88239337269882,
130.167666993184));
#157039=CARTESIAN_POINT('Ctrl Pts',(-119.288865370254,-5.8993438735216,
130.324272163843));
#157040=CARTESIAN_POINT('Ctrl Pts',(-119.296252617429,-5.91003379119672,
130.48153260989));
#157041=CARTESIAN_POINT('Ctrl Pts',(-119.303639864604,-5.91443626993552,
130.638909200615));
#157042=CARTESIAN_POINT('Ctrl Pts',(-119.306301512332,-5.91602249647667,
130.695612467109));
#157043=CARTESIAN_POINT('Ctrl Pts',(-119.30896316006,-5.91679298923901,
130.75233079368));
#157044=CARTESIAN_POINT('Ctrl Pts',(-119.311624807789,-5.91674815043348,
130.809038955094));
#157045=CARTESIAN_POINT('',(-121.061624807789,-5.92598265696487,130.806004651264));
#157046=CARTESIAN_POINT('Ctrl Pts',(-119.311626841947,-5.91132948029671,
130.809077969991));
#157047=CARTESIAN_POINT('Ctrl Pts',(-119.342264218181,-5.9161197406693,
131.461233790425));
#157048=CARTESIAN_POINT('Ctrl Pts',(-119.465717469021,-5.51539089397821,
134.083364516096));
#157049=CARTESIAN_POINT('Ctrl Pts',(-119.681986594463,-1.67069096485224,
137.600414783785));
#157050=CARTESIAN_POINT('Ctrl Pts',(-119.960434218276,4.8146635689039,135.883393522426));
#157051=CARTESIAN_POINT('Ctrl Pts',(-120.238881842088,6.87557749223074,
129.498989146037));
#157052=CARTESIAN_POINT('Ctrl Pts',(-120.517329465902,2.61817159083127,
124.314157381049));
#157053=CARTESIAN_POINT('Ctrl Pts',(-120.791577121135,-3.9446989483673,
125.081750020864));
#157054=CARTESIAN_POINT('Ctrl Pts',(-120.973008901765,-5.91908509112532,
128.931699198858));
#157055=CARTESIAN_POINT('Ctrl Pts',(-121.061624807789,-5.92598265696487,
130.806004651264));
#157056=CARTESIAN_POINT('',(-122.81162480779,-5.91633098458257,130.798887995784));
#157057=CARTESIAN_POINT('Ctrl Pts',(-121.061624807789,-5.92598265696487,
130.806004651264));
#157058=CARTESIAN_POINT('Ctrl Pts',(-121.065824776369,-5.92630956847657,
130.894837732832));
#157059=CARTESIAN_POINT('Ctrl Pts',(-121.070024744948,-5.92448577112936,
130.983657094296));
#157060=CARTESIAN_POINT('Ctrl Pts',(-121.074224713527,-5.92046945784547,
131.0723772017));
#157061=CARTESIAN_POINT('Ctrl Pts',(-121.167040588132,-5.8317122152397,
133.033019098945));
#157062=CARTESIAN_POINT('Ctrl Pts',(-121.35267233734,-3.51266264211408,
136.857356709837));
#157063=CARTESIAN_POINT('Ctrl Pts',(-121.631119961154,3.19387708256752,
137.031455422673));
#157064=CARTESIAN_POINT('Ctrl Pts',(-121.909567584966,6.96539979793815,
131.48315822011));
#157065=CARTESIAN_POINT('Ctrl Pts',(-122.188015208779,4.3360603777024,125.311079181914));
#157066=CARTESIAN_POINT('Ctrl Pts',(-122.466462832592,-2.27790670131724,
124.187057421366));
#157067=CARTESIAN_POINT('Ctrl Pts',(-122.674332698929,-5.65273738408376,
127.887580674196));
#157068=CARTESIAN_POINT('Ctrl Pts',(-122.789386690661,-5.92067836177203,
130.326534880517));
#157069=CARTESIAN_POINT('Ctrl Pts',(-122.81162480779,-5.91633098458257,
130.798887995784));
#157070=CARTESIAN_POINT('',(-124.56162480779,-5.90703164895106,130.80515921599));
#157071=CARTESIAN_POINT('Ctrl Pts',(-122.81162480779,-5.91633098458257,
130.798887995784));
#157072=CARTESIAN_POINT('Ctrl Pts',(-122.882202565266,-5.9025335874754,
132.298008781056));
#157073=CARTESIAN_POINT('Ctrl Pts',(-123.045596197347,-4.5615619224176,
135.790566014123));
#157074=CARTESIAN_POINT('Ctrl Pts',(-123.30180570403,1.31583341844267,137.677943594819));
#157075=CARTESIAN_POINT('Ctrl Pts',(-123.580253327844,6.49418013243721,
133.412652192102));
#157076=CARTESIAN_POINT('Ctrl Pts',(-123.858700951656,5.70469256306374,
126.750468254505));
#157077=CARTESIAN_POINT('Ctrl Pts',(-124.137148575469,-0.327128782042009,
123.813613354913));
#157078=CARTESIAN_POINT('Ctrl Pts',(-124.371456527514,-5.14982080752232,
126.748104892097));
#157079=CARTESIAN_POINT('Ctrl Pts',(-124.512948604954,-5.90578610812664,
129.767134245352));
#157080=CARTESIAN_POINT('Ctrl Pts',(-124.56162480779,-5.90703164895106,
130.80515921599));
#157081=CARTESIAN_POINT('',(-126.311624008903,-5.91848443048205,130.80954271012));
#157082=CARTESIAN_POINT('Ctrl Pts',(-124.56162480779,-5.90703164895106,
130.80515921599));
#157083=CARTESIAN_POINT('Ctrl Pts',(-124.605764479558,-5.90816110770012,
131.746442200737));
#157084=CARTESIAN_POINT('Ctrl Pts',(-124.742720025934,-5.25131157107666,
134.665544139357));
#157085=CARTESIAN_POINT('Ctrl Pts',(-124.972491446908,-0.668196663714802,
137.770785364084));
#157086=CARTESIAN_POINT('Ctrl Pts',(-125.25093907072,5.49987382026564,135.132056134964));
#157087=CARTESIAN_POINT('Ctrl Pts',(-125.529386694533,6.61382894724947,
128.516386145036));
#157088=CARTESIAN_POINT('Ctrl Pts',(-125.807834318346,1.64999837518252,
124.003252921589));
#157089=CARTESIAN_POINT('Ctrl Pts',(-126.068579969149,-4.41813562501859,
125.629593465656));
#157090=CARTESIAN_POINT('Ctrl Pts',(-126.236509745349,-5.9046045021028,
129.216095594019));
#157091=CARTESIAN_POINT('Ctrl Pts',(-126.311623646944,-5.91927129782895,
130.809535722935));
#157092=CARTESIAN_POINT('',(-128.061626221021,-5.9210303473077,130.801168248253));
#157093=CARTESIAN_POINT('Ctrl Pts',(-126.31162480779,-5.91674771714553,
130.809558131701));
#157094=CARTESIAN_POINT('Ctrl Pts',(-126.322548913763,-5.91654423567127,
131.04119743407));
#157095=CARTESIAN_POINT('Ctrl Pts',(-126.333473019736,-5.90273466878703,
131.272263102242));
#157096=CARTESIAN_POINT('Ctrl Pts',(-126.344397125709,-5.87553903220174,
131.501477281815));
#157097=CARTESIAN_POINT('Ctrl Pts',(-126.351174605797,-5.85866644913645,
131.64368521552));
#157098=CARTESIAN_POINT('Ctrl Pts',(-126.357952085885,-5.83664222687754,
131.785181319252));
#157099=CARTESIAN_POINT('Ctrl Pts',(-126.364729565973,-5.80952707624724,
131.925665978674));
#157100=CARTESIAN_POINT('Ctrl Pts',(-126.372152832378,-5.7798282819857,
132.079536597133));
#157101=CARTESIAN_POINT('Ctrl Pts',(-126.379576098784,-5.74396725203922,
132.232459171309));
#157102=CARTESIAN_POINT('Ctrl Pts',(-126.386999365189,-5.70201554897757,
132.383901450124));
#157103=CARTESIAN_POINT('Ctrl Pts',(-126.39441385791,-5.66011342934495,
132.535164736742));
#157104=CARTESIAN_POINT('Ctrl Pts',(-126.401828350631,-5.6121350642719,
132.684950854323));
#157105=CARTESIAN_POINT('Ctrl Pts',(-126.409242843352,-5.55820332708034,
132.832735912558));
#157106=CARTESIAN_POINT('Ctrl Pts',(-126.416650189706,-5.50432357132758,
132.98037852999));
#157107=CARTESIAN_POINT('Ctrl Pts',(-126.42405753606,-5.44450199396681,
133.126023579409));
#157108=CARTESIAN_POINT('Ctrl Pts',(-126.431464882413,-5.37891172124297,
133.269160661702));
#157109=CARTESIAN_POINT('Ctrl Pts',(-126.438866704089,-5.31337036821911,
133.412190986959));
#157110=CARTESIAN_POINT('Ctrl Pts',(-126.446268525764,-5.24206904155062,
133.552716731677));
#157111=CARTESIAN_POINT('Ctrl Pts',(-126.453670347439,-5.16522954159385,
133.690245983471));
#157112=CARTESIAN_POINT('Ctrl Pts',(-126.461068261751,-5.08843060461076,
133.827702634645));
#157113=CARTESIAN_POINT('Ctrl Pts',(-126.468466176062,-5.00609949836088,
133.962165618118));
#157114=CARTESIAN_POINT('Ctrl Pts',(-126.475864090373,-4.91850461436961,
134.093166315829));
#157115=CARTESIAN_POINT('Ctrl Pts',(-126.483260775286,-4.83092428705931,
134.224145243599));
#157116=CARTESIAN_POINT('Ctrl Pts',(-126.490657460198,-4.73808212540959,
134.351662717531));
#157117=CARTESIAN_POINT('Ctrl Pts',(-126.49805414511,-4.64029068514787,
134.475277794489));
#157118=CARTESIAN_POINT('Ctrl Pts',(-126.505450502045,-4.54250358106108,
134.598887390226));
#157119=CARTESIAN_POINT('Ctrl Pts',(-126.512846858981,-4.43976786631959,
134.71859464028));
#157120=CARTESIAN_POINT('Ctrl Pts',(-126.520243215916,-4.33243717820127,
134.833990707219));
#157121=CARTESIAN_POINT('Ctrl Pts',(-126.527640705253,-4.22509005748029,
134.949404441591));
#157122=CARTESIAN_POINT('Ctrl Pts',(-126.535038194589,-4.11314681686869,
135.060505405236));
#157123=CARTESIAN_POINT('Ctrl Pts',(-126.542435683926,-3.99699871856404,
135.166920852829));
#157124=CARTESIAN_POINT('Ctrl Pts',(-126.549835766441,-3.88080990472375,
135.273373604192));
#157125=CARTESIAN_POINT('Ctrl Pts',(-126.557235848956,-3.76041357352431,
135.375137317277));
#157126=CARTESIAN_POINT('Ctrl Pts',(-126.564635931471,-3.6362347602623,
135.471878944339));
#157127=CARTESIAN_POINT('Ctrl Pts',(-126.572044151137,-3.51191939962938,
135.568726948764));
#157128=CARTESIAN_POINT('Ctrl Pts',(-126.579452370804,-3.38381354534519,
135.660541609214));
#157129=CARTESIAN_POINT('Ctrl Pts',(-126.58686059047,-3.25237256065573,
135.747032292803));
#157130=CARTESIAN_POINT('Ctrl Pts',(-126.594273369772,-3.12085067623341,
135.833576209965));
#157131=CARTESIAN_POINT('Ctrl Pts',(-126.601686149074,-2.98598989015763,
135.914789428664));
#157132=CARTESIAN_POINT('Ctrl Pts',(-126.609098928376,-2.84827048654154,
135.990427122924));
#157133=CARTESIAN_POINT('Ctrl Pts',(-126.616522299405,-2.71035430298296,
136.066172891869));
#157134=CARTESIAN_POINT('Ctrl Pts',(-126.623945670433,-2.56957167739537,
136.136327059293));
#157135=CARTESIAN_POINT('Ctrl Pts',(-126.631369041462,-2.42642394555893,
136.200692464193));
#157136=CARTESIAN_POINT('Ctrl Pts',(-126.635305090903,-2.35052358335188,
136.234820546299));
#157137=CARTESIAN_POINT('Ctrl Pts',(-126.639241140344,-2.27395858895807,
136.267322023191));
#157138=CARTESIAN_POINT('Ctrl Pts',(-126.643177189785,-2.19680533298606,
136.298173218253));
#157139=CARTESIAN_POINT('Ctrl Pts',(-126.650600456191,-2.05129670010231,
136.356357609303));
#157140=CARTESIAN_POINT('Ctrl Pts',(-126.658023722596,-1.90325484481399,
136.408845095856));
#157141=CARTESIAN_POINT('Ctrl Pts',(-126.665446989002,-1.75316624634602,
136.455408190819));
#157142=CARTESIAN_POINT('Ctrl Pts',(-126.672861481723,-1.60325504013736,
136.501916252071));
#157143=CARTESIAN_POINT('Ctrl Pts',(-126.680275974443,-1.45130225899473,
136.542513749999));
#157144=CARTESIAN_POINT('Ctrl Pts',(-126.687690467164,-1.29781508270283,
136.577020885901));
#157145=CARTESIAN_POINT('Ctrl Pts',(-126.695097813518,-1.14447584312969,
136.611494762526));
#157146=CARTESIAN_POINT('Ctrl Pts',(-126.702505159872,-0.989605514383623,
136.639889882046));
#157147=CARTESIAN_POINT('Ctrl Pts',(-126.709912506226,-0.833727088658144,
136.662076017288));
#157148=CARTESIAN_POINT('Ctrl Pts',(-126.717314327901,-0.677964922943527,
136.684245605273));
#157149=CARTESIAN_POINT('Ctrl Pts',(-126.724716149577,-0.521196525320297,
136.70021537734));
#157150=CARTESIAN_POINT('Ctrl Pts',(-126.732117971252,-0.363955644118238,
136.709906049752));
#157151=CARTESIAN_POINT('Ctrl Pts',(-126.739515885563,-0.206797769153853,
136.719591606534));
#157152=CARTESIAN_POINT('Ctrl Pts',(-126.746913799875,-0.0491682789911599,
136.723004642116));
#157153=CARTESIAN_POINT('Ctrl Pts',(-126.754311714186,0.108393492546098,
136.720117662381));
#157154=CARTESIAN_POINT('Ctrl Pts',(-126.761708399098,0.265929080175612,
136.717231162409));
#157155=CARTESIAN_POINT('Ctrl Pts',(-126.769105084011,0.42339659864496,
136.708046731834));
#157156=CARTESIAN_POINT('Ctrl Pts',(-126.776501768923,0.580256126001817,
136.692588992106));
#157157=CARTESIAN_POINT('Ctrl Pts',(-126.783898125858,0.737108698042853,
136.677131937791));
#157158=CARTESIAN_POINT('Ctrl Pts',(-126.791294482794,0.893352961076833,
136.655402164018));
#157159=CARTESIAN_POINT('Ctrl Pts',(-126.798690839729,1.04845379900548,
136.627476209227));
#157160=CARTESIAN_POINT('Ctrl Pts',(-126.806088329066,1.20357838326837,
136.599545978902));
#157161=CARTESIAN_POINT('Ctrl Pts',(-126.813485818402,1.35755882644164,
136.565417744819));
#157162=CARTESIAN_POINT('Ctrl Pts',(-126.820883307739,1.50987004055252,
136.525219208996));
#157163=CARTESIAN_POINT('Ctrl Pts',(-126.828283390254,1.66223464712361,
136.485006581639));
#157164=CARTESIAN_POINT('Ctrl Pts',(-126.835683472769,1.81292849889796,
136.438719511039));
#157165=CARTESIAN_POINT('Ctrl Pts',(-126.843083555284,1.96144165141475,
136.386535570987));
#157166=CARTESIAN_POINT('Ctrl Pts',(-126.85049177495,2.11011810941004,136.334294249328));
#157167=CARTESIAN_POINT('Ctrl Pts',(-126.857899994617,2.25660872697291,
136.276143232643));
#157168=CARTESIAN_POINT('Ctrl Pts',(-126.865308214283,2.40042285146972,
136.212308536753));
#157169=CARTESIAN_POINT('Ctrl Pts',(-126.872720993585,2.54432549116049,
136.148434551674));
#157170=CARTESIAN_POINT('Ctrl Pts',(-126.880133772887,2.68554802116171,
136.078870081342));
#157171=CARTESIAN_POINT('Ctrl Pts',(-126.88754655219,2.82362485715162,136.003886867964));
#157172=CARTESIAN_POINT('Ctrl Pts',(-126.894969923218,2.96189898380015,
135.928796515054));
#157173=CARTESIAN_POINT('Ctrl Pts',(-126.902393294247,3.09701811966087,
135.848272146079));
#157174=CARTESIAN_POINT('Ctrl Pts',(-126.909816665276,3.2285454033614,135.762628978691));
#157175=CARTESIAN_POINT('Ctrl Pts',(-126.913752714717,3.29828432513476,
135.717218916361));
#157176=CARTESIAN_POINT('Ctrl Pts',(-126.917688764158,3.36701398780455,
135.670370460299));
#157177=CARTESIAN_POINT('Ctrl Pts',(-126.921624813598,3.43467319138462,
135.622135065471));
#157178=CARTESIAN_POINT('Ctrl Pts',(-126.929048080004,3.56227633776266,
135.531164616202));
#157179=CARTESIAN_POINT('Ctrl Pts',(-126.936471346409,3.68645578562979,
135.434983579145));
#157180=CARTESIAN_POINT('Ctrl Pts',(-126.943894612815,3.80675718974784,
135.333878280718));
#157181=CARTESIAN_POINT('Ctrl Pts',(-126.951309105536,3.92691640759664,
135.232892480357));
#157182=CARTESIAN_POINT('Ctrl Pts',(-126.958723598257,4.04320642224506,
135.126994241334));
#157183=CARTESIAN_POINT('Ctrl Pts',(-126.966138090978,4.15520182089066,
135.016513082775));
#157184=CARTESIAN_POINT('Ctrl Pts',(-126.973545437332,4.26708927415449,
134.906138410116));
#157185=CARTESIAN_POINT('Ctrl Pts',(-126.980952783685,4.37469008800407,
134.791189872077));
#157186=CARTESIAN_POINT('Ctrl Pts',(-126.988360130039,4.47761200857355,
134.672037085832));
#157187=CARTESIAN_POINT('Ctrl Pts',(-126.995761951715,4.58045716609164,
134.55297316823));
#157188=CARTESIAN_POINT('Ctrl Pts',(-127.00316377339,4.67863013581545,134.429711527284));
#157189=CARTESIAN_POINT('Ctrl Pts',(-127.010565595065,4.77177571008174,
134.302658365782));
#157190=CARTESIAN_POINT('Ctrl Pts',(-127.017963509377,4.86487211352442,
134.175672274655));
#157191=CARTESIAN_POINT('Ctrl Pts',(-127.025361423688,4.95294618676935,
134.044898949382));
#157192=CARTESIAN_POINT('Ctrl Pts',(-127.032759338,5.03568327513056,133.910777285541));
#157193=CARTESIAN_POINT('Ctrl Pts',(-127.040156022912,5.11840661408858,
133.776677910287));
#157194=CARTESIAN_POINT('Ctrl Pts',(-127.047552707824,5.19579453261965,
133.639231618218));
#157195=CARTESIAN_POINT('Ctrl Pts',(-127.054949392736,5.26757590444405,
133.498905969461));
#157196=CARTESIAN_POINT('Ctrl Pts',(-127.062345749671,5.33935409340721,
133.35858654289));
#157197=CARTESIAN_POINT('Ctrl Pts',(-127.069742106607,5.40552605996147,
133.215388345829));
#157198=CARTESIAN_POINT('Ctrl Pts',(-127.077138463542,5.46586695474059,
133.069802957502));
#157199=CARTESIAN_POINT('Ctrl Pts',(-127.084535952879,5.52621708786491,
132.92419527968));
#157200=CARTESIAN_POINT('Ctrl Pts',(-127.091933442216,5.58073422868631,
132.776200027735));
#157201=CARTESIAN_POINT('Ctrl Pts',(-127.099330931552,5.62924199365182,
132.626327999109));
#157202=CARTESIAN_POINT('Ctrl Pts',(-127.106731014067,5.67776676293907,
132.476403433076));
#157203=CARTESIAN_POINT('Ctrl Pts',(-127.114131096582,5.72027784731098,
132.324601135423));
#157204=CARTESIAN_POINT('Ctrl Pts',(-127.121531179097,5.75664900718979,
132.171446119837));
#157205=CARTESIAN_POINT('Ctrl Pts',(-127.128939398764,5.79306016089797,
132.018122694568));
#157206=CARTESIAN_POINT('Ctrl Pts',(-127.13634761843,5.82331782066315,131.863443944246));
#157207=CARTESIAN_POINT('Ctrl Pts',(-127.143755838097,5.84734693026466,
131.707944835901));
#157208=CARTESIAN_POINT('Ctrl Pts',(-127.151168617399,5.87139082938217,
131.55235002045));
#157209=CARTESIAN_POINT('Ctrl Pts',(-127.158581396701,5.88919849734115,
131.395934210909));
#157210=CARTESIAN_POINT('Ctrl Pts',(-127.165994176003,5.90074689885786,
131.239235999853));
#157211=CARTESIAN_POINT('Ctrl Pts',(-127.173417547032,5.91231180127221,
131.082313891045));
#157212=CARTESIAN_POINT('Ctrl Pts',(-127.18084091806,5.91759956248604,130.925108946925));
#157213=CARTESIAN_POINT('Ctrl Pts',(-127.188264289089,5.91663924979412,
130.768159094178));
#157214=CARTESIAN_POINT('Ctrl Pts',(-127.19220033853,5.91613006896249,130.684940516292));
#157215=CARTESIAN_POINT('Ctrl Pts',(-127.196136387971,5.91386519754827,
130.601793569727));
#157216=CARTESIAN_POINT('Ctrl Pts',(-127.200072437411,5.90985484598521,
130.51879755643));
#157217=CARTESIAN_POINT('Ctrl Pts',(-127.207495703817,5.90229144809595,
130.362269665567));
#157218=CARTESIAN_POINT('Ctrl Pts',(-127.214918970222,5.88849364245485,
130.20580577925));
#157219=CARTESIAN_POINT('Ctrl Pts',(-127.222342236628,5.86845673888837,
130.049942917419));
#157220=CARTESIAN_POINT('Ctrl Pts',(-127.229756729349,5.84844351727795,
129.894264272546));
#157221=CARTESIAN_POINT('Ctrl Pts',(-127.23717122207,5.82220592305286,129.739185604818));
#157222=CARTESIAN_POINT('Ctrl Pts',(-127.244585714791,5.78979124397579,
129.58524293921));
#157223=CARTESIAN_POINT('Ctrl Pts',(-127.251993061144,5.75740780738681,
129.431448649338));
#157224=CARTESIAN_POINT('Ctrl Pts',(-127.259400407498,5.71885921500412,
129.278788544648));
#157225=CARTESIAN_POINT('Ctrl Pts',(-127.266807753852,5.67424441342958,
129.127792426539));
#157226=CARTESIAN_POINT('Ctrl Pts',(-127.274209575527,5.62966288725728,
128.976908927031));
#157227=CARTESIAN_POINT('Ctrl Pts',(-127.281611397203,5.57902426592168,
128.827687299435));
#157228=CARTESIAN_POINT('Ctrl Pts',(-127.289013218878,5.52247830091577,
128.680645952548));
#157229=CARTESIAN_POINT('Ctrl Pts',(-127.29641113319,5.46596218608463,128.533682227642));
#157230=CARTESIAN_POINT('Ctrl Pts',(-127.303809047501,5.40354507175694,
128.388896838808));
#157231=CARTESIAN_POINT('Ctrl Pts',(-127.311206961812,5.33542613466919,
128.246791747723));
#157232=CARTESIAN_POINT('Ctrl Pts',(-127.318603646725,5.26731851771308,
128.104710271927));
#157233=CARTESIAN_POINT('Ctrl Pts',(-127.326000331637,5.19351111978584,
127.965308546152));
#157234=CARTESIAN_POINT('Ctrl Pts',(-127.333397016549,5.11425076208616,
127.829067404284));
#157235=CARTESIAN_POINT('Ctrl Pts',(-127.340793373484,5.03499391887379,
127.692832303491));
#157236=CARTESIAN_POINT('Ctrl Pts',(-127.34818973042,4.95028478436528,127.55975783062));
#157237=CARTESIAN_POINT('Ctrl Pts',(-127.355586087355,4.86041540150948,
127.430298868388));
#157238=CARTESIAN_POINT('Ctrl Pts',(-127.362983576692,4.77053225942149,
127.300820085657));
#157239=CARTESIAN_POINT('Ctrl Pts',(-127.370381066029,4.67548750878616,
127.174958222417));
#157240=CARTESIAN_POINT('Ctrl Pts',(-127.377778555365,4.57561555833868,
127.05313777364));
#157241=CARTESIAN_POINT('Ctrl Pts',(-127.38517863788,4.47570859793393,126.931274620894));
#157242=CARTESIAN_POINT('Ctrl Pts',(-127.392578720395,4.3709713051476,126.813455991777));
#157243=CARTESIAN_POINT('Ctrl Pts',(-127.39997880291,4.26177715328981,126.700071877943));
#157244=CARTESIAN_POINT('Ctrl Pts',(-127.407387022576,4.15246293123678,
126.58656308662));
#157245=CARTESIAN_POINT('Ctrl Pts',(-127.414795242243,4.03868232204893,
126.477498817731));
#157246=CARTESIAN_POINT('Ctrl Pts',(-127.422203461909,3.92084483891866,
126.373231380946));
#157247=CARTESIAN_POINT('Ctrl Pts',(-127.429616241211,3.80293482878374,
126.268899769295));
#157248=CARTESIAN_POINT('Ctrl Pts',(-127.437029020513,3.68096325779922,
126.169371108176));
#157249=CARTESIAN_POINT('Ctrl Pts',(-127.444441799816,3.55537080801979,
126.07495590027));
#157250=CARTESIAN_POINT('Ctrl Pts',(-127.451865170844,3.42959890585823,
125.980405787488));
#157251=CARTESIAN_POINT('Ctrl Pts',(-127.459288541873,3.30019609819134,
125.89098393198));
#157252=CARTESIAN_POINT('Ctrl Pts',(-127.466711912902,3.16763066955715,
125.806956641122));
#157253=CARTESIAN_POINT('Ctrl Pts',(-127.470647962343,3.09734129843189,
125.762403355302));
#157254=CARTESIAN_POINT('Ctrl Pts',(-127.474584011783,3.02616319912008,
125.719365900171));
#157255=CARTESIAN_POINT('Ctrl Pts',(-127.478520061224,2.95416860958555,
125.677878550043));
#157256=CARTESIAN_POINT('Ctrl Pts',(-127.485943327629,2.8183890605967,125.599634702476));
#157257=CARTESIAN_POINT('Ctrl Pts',(-127.493366594035,2.67929351077128,
125.526670634738));
#157258=CARTESIAN_POINT('Ctrl Pts',(-127.50078986044,2.53733123504071,125.459280565201));
#157259=CARTESIAN_POINT('Ctrl Pts',(-127.508204353161,2.39553674693082,
125.39197014513));
#157260=CARTESIAN_POINT('Ctrl Pts',(-127.515618845882,2.25088261114735,
125.330220768325));
#157261=CARTESIAN_POINT('Ctrl Pts',(-127.523033338603,2.10384536087433,
125.274282384844));
#157262=CARTESIAN_POINT('Ctrl Pts',(-127.530440684957,1.95694983063899,
125.218397916883));
#157263=CARTESIAN_POINT('Ctrl Pts',(-127.537848031311,1.80767610522029,
125.168313423892));
#157264=CARTESIAN_POINT('Ctrl Pts',(-127.545255377665,1.65652340459452,
125.12423202989));
#157265=CARTESIAN_POINT('Ctrl Pts',(-127.55265719934,1.50548343935553,125.080183513455));
#157266=CARTESIAN_POINT('Ctrl Pts',(-127.560059021015,1.35256764613377,
125.042129285089));
#157267=CARTESIAN_POINT('Ctrl Pts',(-127.567460842691,1.19829312127212,
125.010223567236));
#157268=CARTESIAN_POINT('Ctrl Pts',(-127.574858757002,1.04410003673127,
124.978334692163));
#157269=CARTESIAN_POINT('Ctrl Pts',(-127.582256671313,0.888550013652561,
124.952587938946));
#157270=CARTESIAN_POINT('Ctrl Pts',(-127.589654585625,0.732173026504409,
124.933087057106));
#157271=CARTESIAN_POINT('Ctrl Pts',(-127.597051270537,0.575822026374777,
124.913589415958));
#157272=CARTESIAN_POINT('Ctrl Pts',(-127.604447955449,0.418644704992514,
124.90033563231));
#157273=CARTESIAN_POINT('Ctrl Pts',(-127.611844640361,0.26117901441101,
124.893377950959));
#157274=CARTESIAN_POINT('Ctrl Pts',(-127.619240997297,0.103720306023239,
124.886420578118));
#157275=CARTESIAN_POINT('Ctrl Pts',(-127.626637354232,-0.0540263732060113,
124.885758768956));
#157276=CARTESIAN_POINT('Ctrl Pts',(-127.634033711168,-0.211520461215678,
124.891392694688));
#157277=CARTESIAN_POINT('Ctrl Pts',(-127.641431200504,-0.369038661972731,
124.897027482988));
#157278=CARTESIAN_POINT('Ctrl Pts',(-127.648828689841,-0.526303821425139,
124.908959912077));
#157279=CARTESIAN_POINT('Ctrl Pts',(-127.656226179177,-0.682778043840405,
124.927138084315));
#157280=CARTESIAN_POINT('Ctrl Pts',(-127.663626261692,-0.839307118051996,
124.945322628884));
#157281=CARTESIAN_POINT('Ctrl Pts',(-127.671026344207,-0.995044332627594,
124.969757232701));
#157282=CARTESIAN_POINT('Ctrl Pts',(-127.678426426722,-1.14945970509599,
125.00033848211));
#157283=CARTESIAN_POINT('Ctrl Pts',(-127.685834646389,-1.30404487314005,
125.030953358747));
#157284=CARTESIAN_POINT('Ctrl Pts',(-127.693242866055,-1.45730492992901,
125.067728306313));
#157285=CARTESIAN_POINT('Ctrl Pts',(-127.700651085722,-1.6087221154754,
125.110509221746));
#157286=CARTESIAN_POINT('Ctrl Pts',(-127.708063865024,-1.76023249577339,
125.153316468119));
#157287=CARTESIAN_POINT('Ctrl Pts',(-127.715476644326,-1.90989739060958,
125.202136932745));
#157288=CARTESIAN_POINT('Ctrl Pts',(-127.722889423628,-2.05721736587058,
125.256767691615));
#157289=CARTESIAN_POINT('Ctrl Pts',(-127.730312794657,-2.20474783882064,
125.311476509475));
#157290=CARTESIAN_POINT('Ctrl Pts',(-127.737736165686,-2.34992635680104,
125.372012059291));
#157291=CARTESIAN_POINT('Ctrl Pts',(-127.745159536714,-2.49227574864398,
125.43812430566));
#157292=CARTESIAN_POINT('Ctrl Pts',(-127.749095586155,-2.56775281182466,
125.473178605025));
#157293=CARTESIAN_POINT('Ctrl Pts',(-127.753031635596,-2.64243494300916,
125.509799960098));
#157294=CARTESIAN_POINT('Ctrl Pts',(-127.756967685036,-2.71625425986335,
125.547946121137));
#157295=CARTESIAN_POINT('Ctrl Pts',(-127.764390951442,-2.85547518763159,
125.619888590356));
#157296=CARTESIAN_POINT('Ctrl Pts',(-127.771814217847,-2.99204646654796,
125.697474754956));
#157297=CARTESIAN_POINT('Ctrl Pts',(-127.779237484253,-3.1254777182897,
125.780485659431));
#157298=CARTESIAN_POINT('Ctrl Pts',(-127.786651976974,-3.25875126537266,
125.86339845191));
#157299=CARTESIAN_POINT('Ctrl Pts',(-127.794066469695,-3.38889185867762,
125.951723026688));
#157300=CARTESIAN_POINT('Ctrl Pts',(-127.801480962416,-3.51543163031537,
126.045193567012));
#157301=CARTESIAN_POINT('Ctrl Pts',(-127.80888830877,-3.64184943815671,
126.13857401691));
#157302=CARTESIAN_POINT('Ctrl Pts',(-127.816295655124,-3.76467303537882,
126.237090337914));
#157303=CARTESIAN_POINT('Ctrl Pts',(-127.823703001478,-3.88346168740095,
126.340432315612));
#157304=CARTESIAN_POINT('Ctrl Pts',(-127.831104823153,-4.00216174236476,
126.443697216964));
#157305=CARTESIAN_POINT('Ctrl Pts',(-127.838506644829,-4.11683256385394,
126.551780364644));
#157306=CARTESIAN_POINT('Ctrl Pts',(-127.845908466504,-4.22706489695321,
126.664330071852));
#157307=CARTESIAN_POINT('Ctrl Pts',(-127.853306380816,-4.33723903926251,
126.776820364946));
#157308=CARTESIAN_POINT('Ctrl Pts',(-127.860704295127,-4.44297909892476,
126.893772255756));
#157309=CARTESIAN_POINT('Ctrl Pts',(-127.868102209438,-4.54391132438536,
127.014795940902));
#157310=CARTESIAN_POINT('Ctrl Pts',(-127.875498894351,-4.64482677674047,
127.135799514105));
#157311=CARTESIAN_POINT('Ctrl Pts',(-127.882895579263,-4.74093574176654,
127.260873252274));
#157312=CARTESIAN_POINT('Ctrl Pts',(-127.890292264175,-4.83190348821213,
127.3895928007));
#157313=CARTESIAN_POINT('Ctrl Pts',(-127.897688621111,-4.92286720105278,
127.518306641566));
#157314=CARTESIAN_POINT('Ctrl Pts',(-127.905084978046,-5.00868993314501,
127.650665666403));
#157315=CARTESIAN_POINT('Ctrl Pts',(-127.912481334982,-5.08907935344174,
127.786215177586));
#157316=CARTESIAN_POINT('Ctrl Pts',(-127.919878824318,-5.16948108156372,
127.921785441744));
#157317=CARTESIAN_POINT('Ctrl Pts',(-127.927276313655,-5.24444765112627,
128.060546843761));
#157318=CARTESIAN_POINT('Ctrl Pts',(-127.934673802992,-5.31373197930008,
128.202018784781));
#157319=CARTESIAN_POINT('Ctrl Pts',(-127.942073885507,-5.38304059498783,
128.343540318571));
#157320=CARTESIAN_POINT('Ctrl Pts',(-127.949473968022,-5.44666283934295,
128.487773948112));
#157321=CARTESIAN_POINT('Ctrl Pts',(-127.956874050537,-5.50439924873311,
128.634217886535));
#157322=CARTESIAN_POINT('Ctrl Pts',(-127.964282270203,-5.56219914524093,
128.780822855123));
#157323=CARTESIAN_POINT('Ctrl Pts',(-127.97169048987,-5.6141001446118,128.929642638889));
#157324=CARTESIAN_POINT('Ctrl Pts',(-127.979098709536,-5.65995203619768,
129.080158335222));
#157325=CARTESIAN_POINT('Ctrl Pts',(-127.986511488838,-5.70583214885774,
129.230766671454));
#157326=CARTESIAN_POINT('Ctrl Pts',(-127.99392426814,-5.74565564072694,
129.383072639847));
#157327=CARTESIAN_POINT('Ctrl Pts',(-128.001337047443,-5.77932328118467,
129.536546366953));
#157328=CARTESIAN_POINT('Ctrl Pts',(-128.008760418471,-5.81303902754589,
129.690239384518));
#157329=CARTESIAN_POINT('Ctrl Pts',(-128.0161837895,-5.84058129018013,129.845103126703));
#157330=CARTESIAN_POINT('Ctrl Pts',(-128.023607160529,-5.86190250828191,
130.00060098565));
#157331=CARTESIAN_POINT('Ctrl Pts',(-128.027543209969,-5.87320752971389,
130.083049681574));
#157332=CARTESIAN_POINT('Ctrl Pts',(-128.03147925941,-5.88276446263719,
130.165676610584));
#157333=CARTESIAN_POINT('Ctrl Pts',(-128.03541530885,-5.89057216089617,
130.248401824331));
#157334=CARTESIAN_POINT('Ctrl Pts',(-128.044151808496,-5.90790221584405,
130.432019640013));
#157335=CARTESIAN_POINT('Ctrl Pts',(-128.052888308143,-5.9166486189631,
130.6164602422));
#157336=CARTESIAN_POINT('Ctrl Pts',(-128.06162480779,-5.91674912383553,
130.801140665471));
#157337=CARTESIAN_POINT('',(-129.811623618163,-5.91251901558631,130.800694970794));
#157338=CARTESIAN_POINT('Ctrl Pts',(-128.061627320749,-5.92436185088451,
130.801189712243));
#157339=CARTESIAN_POINT('Ctrl Pts',(-128.145705858053,-5.91267799511827,
132.58081561286));
#157340=CARTESIAN_POINT('Ctrl Pts',(-128.322600269963,-4.11167625071623,
136.345452640801));
#157341=CARTESIAN_POINT('Ctrl Pts',(-128.592310556475,2.29803694488353,
137.414699998437));
#157342=CARTESIAN_POINT('Ctrl Pts',(-128.870758180289,6.80361083705033,
132.444006953921));
#157343=CARTESIAN_POINT('Ctrl Pts',(-129.149205804101,5.05699874483257,
125.966559027475));
#157344=CARTESIAN_POINT('Ctrl Pts',(-129.427653427914,-1.33674814576103,
123.934814422572));
#157345=CARTESIAN_POINT('Ctrl Pts',(-129.648459058428,-5.43280141090012,
127.329622118098));
#157346=CARTESIAN_POINT('Ctrl Pts',(-129.776448814336,-5.91342334095441,
130.051290695285));
#157347=CARTESIAN_POINT('Ctrl Pts',(-129.811622695641,-5.90923887852463,
130.80067733591));
#157348=CARTESIAN_POINT('',(-131.561626024561,-5.91341910262869,130.808953665459));
#157349=CARTESIAN_POINT('Ctrl Pts',(-129.81162480779,-5.91674887854272,
130.800717711655));
#157350=CARTESIAN_POINT('Ctrl Pts',(-129.819083418388,-5.9168468407104,
130.959826280473));
#157351=CARTESIAN_POINT('Ctrl Pts',(-129.826542028985,-5.91052253319917,
131.118956455526));
#157352=CARTESIAN_POINT('Ctrl Pts',(-129.834000639583,-5.89779739881852,
131.277558678624));
#157353=CARTESIAN_POINT('Ctrl Pts',(-129.841460024799,-5.88507094286057,
131.436177373463));
#157354=CARTESIAN_POINT('Ctrl Pts',(-129.848919410016,-5.86594236406024,
131.594267643675));
#157355=CARTESIAN_POINT('Ctrl Pts',(-129.856378795233,-5.84048505975837,
131.751284494781));
#157356=CARTESIAN_POINT('Ctrl Pts',(-129.863840334521,-5.81502040406574,
131.908346688166));
#157357=CARTESIAN_POINT('Ctrl Pts',(-129.871301873809,-5.78322344019467,
132.06433448515));
#157358=CARTESIAN_POINT('Ctrl Pts',(-129.878763413097,-5.74521880623851,
132.218712564906));
#157359=CARTESIAN_POINT('Ctrl Pts',(-129.886228486933,-5.70719616940552,
132.37316377389));
#157360=CARTESIAN_POINT('Ctrl Pts',(-129.893693560768,-5.66296009141423,
132.52600339301));
#157361=CARTESIAN_POINT('Ctrl Pts',(-129.901158634603,-5.61268522274912,
132.676710785893));
#157362=CARTESIAN_POINT('Ctrl Pts',(-129.908633373557,-5.56234526262317,
132.827613301401));
#157363=CARTESIAN_POINT('Ctrl Pts',(-129.916108112511,-5.50595100864783,
132.976377729922));
#157364=CARTESIAN_POINT('Ctrl Pts',(-129.923582851465,-5.44372583382088,
133.12250203014));
#157365=CARTESIAN_POINT('Ctrl Pts',(-129.931062809614,-5.38145721060622,
133.268728360851));
#157366=CARTESIAN_POINT('Ctrl Pts',(-129.938542767764,-5.31334970658557,
133.412310560036));
#157367=CARTESIAN_POINT('Ctrl Pts',(-129.946022725913,-5.23967275794865,
133.55277105855));
#157368=CARTESIAN_POINT('Ctrl Pts',(-129.953514870734,-5.16587577163415,
133.693460401395));
#157369=CARTESIAN_POINT('Ctrl Pts',(-129.961007015556,-5.08649139201798,
133.831017566116));
#157370=CARTESIAN_POINT('Ctrl Pts',(-129.968499160377,-5.00183310721932,
133.964992853373));
#157371=CARTESIAN_POINT('Ctrl Pts',(-129.973848998765,-4.94138204111693,
134.060659201508));
#157372=CARTESIAN_POINT('Ctrl Pts',(-129.979198837152,-4.878242813534,134.154499841785));
#157373=CARTESIAN_POINT('Ctrl Pts',(-129.98454867554,-4.81254188109021,
134.246361664232));
#157374=CARTESIAN_POINT('Ctrl Pts',(-129.991971941945,-4.7213773468976,
134.373826221309));
#157375=CARTESIAN_POINT('Ctrl Pts',(-129.999395208351,-4.62500744123637,
134.497859154213));
#157376=CARTESIAN_POINT('Ctrl Pts',(-130.006818474756,-4.52371918163029,
134.61800655397));
#157377=CARTESIAN_POINT('Ctrl Pts',(-130.014232967477,-4.4225506363356,
134.738011949478));
#157378=CARTESIAN_POINT('Ctrl Pts',(-130.021647460198,-4.31647554633551,
134.854140670372));
#157379=CARTESIAN_POINT('Ctrl Pts',(-130.029061952919,-4.20582407778094,
134.965967805812));
#157380=CARTESIAN_POINT('Ctrl Pts',(-130.036469299273,-4.0952792592774,
135.077687158049));
#157381=CARTESIAN_POINT('Ctrl Pts',(-130.043876645626,-3.98016710422518,
135.185112915191));
#157382=CARTESIAN_POINT('Ctrl Pts',(-130.05128399198,-3.8608578263152,135.287853386321));
#157383=CARTESIAN_POINT('Ctrl Pts',(-130.058685813656,-3.7416375337663,
135.390517229732));
#157384=CARTESIAN_POINT('Ctrl Pts',(-130.066087635331,-3.61822663300769,
135.488502502538));
#157385=CARTESIAN_POINT('Ctrl Pts',(-130.073489457006,-3.49103186692444,
135.581454615659));
#157386=CARTESIAN_POINT('Ctrl Pts',(-130.080887371318,-3.36390424596741,
135.674357660084));
#157387=CARTESIAN_POINT('Ctrl Pts',(-130.088285285629,-3.23299703838111,
135.762232616602));
#157388=CARTESIAN_POINT('Ctrl Pts',(-130.09568319994,-3.09874961808637,
135.844765498814));
#157389=CARTESIAN_POINT('Ctrl Pts',(-130.103079884852,-2.96452450727796,
135.927284665559));
#157390=CARTESIAN_POINT('Ctrl Pts',(-130.110476569765,-2.82696060313257,
136.004463324617));
#157391=CARTESIAN_POINT('Ctrl Pts',(-130.117873254677,-2.68652587784223,
136.07603106157));
#157392=CARTESIAN_POINT('Ctrl Pts',(-130.125269611612,-2.54609737957438,
136.147595625135));
#157393=CARTESIAN_POINT('Ctrl Pts',(-130.132665968548,-2.40279864586589,
136.213549591784));
#157394=CARTESIAN_POINT('Ctrl Pts',(-130.140062325483,-2.25712159755419,
136.273668860512));
#157395=CARTESIAN_POINT('Ctrl Pts',(-130.14745981482,-2.11142224571491,
136.333797333653));
#157396=CARTESIAN_POINT('Ctrl Pts',(-130.154857304156,-1.96334419933927,
136.388089187764));
#157397=CARTESIAN_POINT('Ctrl Pts',(-130.162254793493,-1.8133985237029,
136.436368816844));
#157398=CARTESIAN_POINT('Ctrl Pts',(-130.169654876008,-1.66340028484216,
136.484665370273));
#157399=CARTESIAN_POINT('Ctrl Pts',(-130.177054958522,-1.51153346834006,
136.526945388162));
#157400=CARTESIAN_POINT('Ctrl Pts',(-130.184455041037,-1.35832327939251,
136.563083430062));
#157401=CARTESIAN_POINT('Ctrl Pts',(-130.191863260704,-1.20494462009204,
136.599261209454));
#157402=CARTESIAN_POINT('Ctrl Pts',(-130.19927148037,-1.05022000187908,
136.629283439454));
#157403=CARTESIAN_POINT('Ctrl Pts',(-130.206679700037,-0.894684505386521,
136.653075878059));
#157404=CARTESIAN_POINT('Ctrl Pts',(-130.214092479339,-0.739053279390232,
136.676882960512));
#157405=CARTESIAN_POINT('Ctrl Pts',(-130.221505258641,-0.582610550736434,
136.694452569615));
#157406=CARTESIAN_POINT('Ctrl Pts',(-130.228918037943,-0.425894946433585,
136.705762489757));
#157407=CARTESIAN_POINT('Ctrl Pts',(-130.236341408972,-0.268955419526746,
136.717088570043));
#157408=CARTESIAN_POINT('Ctrl Pts',(-130.24376478,-0.111742610375219,136.722137085971));
#157409=CARTESIAN_POINT('Ctrl Pts',(-130.251188151029,0.0452055991941102,
136.720937923433));
#157410=CARTESIAN_POINT('Ctrl Pts',(-130.25512420047,0.128423305833506,
136.720302098682));
#157411=CARTESIAN_POINT('Ctrl Pts',(-130.259060249911,0.211566709373327,
136.717910694392));
#157412=CARTESIAN_POINT('Ctrl Pts',(-130.262996299352,0.294556523495727,
136.713774041669));
#157413=CARTESIAN_POINT('Ctrl Pts',(-130.270419565758,0.451072722897707,
136.705972443734));
#157414=CARTESIAN_POINT('Ctrl Pts',(-130.277842832163,0.607515430120606,
136.69193654267));
#157415=CARTESIAN_POINT('Ctrl Pts',(-130.285266098569,0.763347618708535,
136.671662465563));
#157416=CARTESIAN_POINT('Ctrl Pts',(-130.29268059129,0.91899562659061,136.651412350732));
#157417=CARTESIAN_POINT('Ctrl Pts',(-130.30009508401,1.07403418558803,136.624938783556));
#157418=CARTESIAN_POINT('Ctrl Pts',(-130.307509576731,1.22792734330951,
136.592289867484));
#157419=CARTESIAN_POINT('Ctrl Pts',(-130.314916923085,1.38167217301248,
136.559672419666));
#157420=CARTESIAN_POINT('Ctrl Pts',(-130.322324269439,1.53427343652915,
136.520891549229));
#157421=CARTESIAN_POINT('Ctrl Pts',(-130.329731615793,1.68520148365469,
136.47604700893));
#157422=CARTESIAN_POINT('Ctrl Pts',(-130.337133437468,1.83601696294807,
136.431235915382));
#157423=CARTESIAN_POINT('Ctrl Pts',(-130.344535259144,1.9851613543867,136.38037026277));
#157424=CARTESIAN_POINT('Ctrl Pts',(-130.351937080819,2.13211647767011,
136.323600591344));
#157425=CARTESIAN_POINT('Ctrl Pts',(-130.35933499513,2.27899402448742,136.266860888186));
#157426=CARTESIAN_POINT('Ctrl Pts',(-130.366732909442,2.42368425743984,
136.204223507422));
#157427=CARTESIAN_POINT('Ctrl Pts',(-130.374130823753,2.5656855185423,136.135888389457));
#157428=CARTESIAN_POINT('Ctrl Pts',(-130.381527508665,2.70766318161153,
136.067564627549));
#157429=CARTESIAN_POINT('Ctrl Pts',(-130.388924193578,2.84695242366649,
135.993545169393));
#157430=CARTESIAN_POINT('Ctrl Pts',(-130.39632087849,2.9830727869974,135.91407756765));
#157431=CARTESIAN_POINT('Ctrl Pts',(-130.403717235425,3.11918711460876,
135.834613489584));
#157432=CARTESIAN_POINT('Ctrl Pts',(-130.411113592361,3.25213252049968,
135.749701936473));
#157433=CARTESIAN_POINT('Ctrl Pts',(-130.418509949296,3.38145456691855,
135.659635643182));
#157434=CARTESIAN_POINT('Ctrl Pts',(-130.425907438633,3.51079641287212,
135.569555560511));
#157435=CARTESIAN_POINT('Ctrl Pts',(-130.433304927969,3.63651348843412,
135.474319379607));
#157436=CARTESIAN_POINT('Ctrl Pts',(-130.440702417306,3.75818180803671,
135.374262154825));
#157437=CARTESIAN_POINT('Ctrl Pts',(-130.448102499821,3.87989277828064,
135.274169855138));
#157438=CARTESIAN_POINT('Ctrl Pts',(-130.455502582336,3.99755187863581,
135.169253383738));
#157439=CARTESIAN_POINT('Ctrl Pts',(-130.462902664851,4.11076968626162,
135.059886807006));
#157440=CARTESIAN_POINT('Ctrl Pts',(-130.470310884517,4.22411198850615,
134.95039997048));
#157441=CARTESIAN_POINT('Ctrl Pts',(-130.477719104184,4.33300297638259,
134.836453515797));
#157442=CARTESIAN_POINT('Ctrl Pts',(-130.48512732385,4.43709096383735,134.718457491831));
#157443=CARTESIAN_POINT('Ctrl Pts',(-130.492540103152,4.54124301571189,
134.600388843281));
#157444=CARTESIAN_POINT('Ctrl Pts',(-130.499952882454,4.64058594161079,
134.478265947858));
#157445=CARTESIAN_POINT('Ctrl Pts',(-130.507365661756,4.73480990985672,
134.352529959638));
#157446=CARTESIAN_POINT('Ctrl Pts',(-130.514789032785,4.82916850972674,
134.226614313943));
#157447=CARTESIAN_POINT('Ctrl Pts',(-130.522212403814,4.91839333264034,
134.097075571281));
#157448=CARTESIAN_POINT('Ctrl Pts',(-130.529635774843,5.00221878418057,
133.964382420923));
#157449=CARTESIAN_POINT('Ctrl Pts',(-130.533571824284,5.04666504995262,
133.894025328673));
#157450=CARTESIAN_POINT('Ctrl Pts',(-130.537507873725,5.08959413429763,
133.822781816101));
#157451=CARTESIAN_POINT('Ctrl Pts',(-130.541443923165,5.13097187287621,
133.750724173248));
#157452=CARTESIAN_POINT('Ctrl Pts',(-130.548867189571,5.20900899647822,
133.614825707674));
#157453=CARTESIAN_POINT('Ctrl Pts',(-130.556290455976,5.28176129997569,
133.475619280029));
#157454=CARTESIAN_POINT('Ctrl Pts',(-130.563713722382,5.34893524905838,
133.333554612474));
#157455=CARTESIAN_POINT('Ctrl Pts',(-130.571128215103,5.4160298041117,133.191657853559));
#157456=CARTESIAN_POINT('Ctrl Pts',(-130.578542707824,5.47755897044204,
133.046909913244));
#157457=CARTESIAN_POINT('Ctrl Pts',(-130.585957200545,5.53327352348262,
132.89978770454));
#157458=CARTESIAN_POINT('Ctrl Pts',(-130.593364546899,5.58893437673969,
132.75280729776));
#157459=CARTESIAN_POINT('Ctrl Pts',(-130.600771893252,5.63879164253432,
132.603457525125));
#157460=CARTESIAN_POINT('Ctrl Pts',(-130.608179239606,5.68264295681117,
132.452237915154));
#157461=CARTESIAN_POINT('Ctrl Pts',(-130.615581061281,5.72646156512317,
132.301131090473));
#157462=CARTESIAN_POINT('Ctrl Pts',(-130.622982882957,5.76428303761727,
132.148157562268));
#157463=CARTESIAN_POINT('Ctrl Pts',(-130.630384704632,5.79595393895926,
131.993834660983));
#157464=CARTESIAN_POINT('Ctrl Pts',(-130.637782618944,5.82760812147905,
131.839593225556));
#157465=CARTESIAN_POINT('Ctrl Pts',(-130.645180533255,5.85311812422539,
131.684004200426));
#157466=CARTESIAN_POINT('Ctrl Pts',(-130.652578447566,5.87238100432991,
131.527597717337));
#157467=CARTESIAN_POINT('Ctrl Pts',(-130.659975132479,5.8916406832932,131.371217226169));
#157468=CARTESIAN_POINT('Ctrl Pts',(-130.667371817391,5.90465525446638,
131.214019916792));
#157469=CARTESIAN_POINT('Ctrl Pts',(-130.674768502303,5.91137329178559,
131.056543820147));
#157470=CARTESIAN_POINT('Ctrl Pts',(-130.682164859238,5.91809103121999,
130.899074706157));
#157471=CARTESIAN_POINT('Ctrl Pts',(-130.689561216174,5.91851277602355,
130.741327202434));
#157472=CARTESIAN_POINT('Ctrl Pts',(-130.696957573109,5.91263917762366,
130.583841870676));
#157473=CARTESIAN_POINT('Ctrl Pts',(-130.704355062446,5.90676467996086,
130.426332427512));
#157474=CARTESIAN_POINT('Ctrl Pts',(-130.711752551782,5.89459293388846,
130.269085609296));
#157475=CARTESIAN_POINT('Ctrl Pts',(-130.719150041119,5.87617665557045,
130.112639232159));
#157476=CARTESIAN_POINT('Ctrl Pts',(-130.726550123634,5.85775392145465,
129.956138012988));
#157477=CARTESIAN_POINT('Ctrl Pts',(-130.733950206149,5.83308234040288,
129.800438164062));
#157478=CARTESIAN_POINT('Ctrl Pts',(-130.741350288664,5.80226613249603,
129.646069509861));
#157479=CARTESIAN_POINT('Ctrl Pts',(-130.74875850833,5.77141603900056,129.491531111454));
#157480=CARTESIAN_POINT('Ctrl Pts',(-130.756166727997,5.73440789830192,
129.338327197348));
#157481=CARTESIAN_POINT('Ctrl Pts',(-130.763574947663,5.69139660122823,
129.186975292411));
#157482=CARTESIAN_POINT('Ctrl Pts',(-130.770987726965,5.64835883141875,
129.035530232901));
#157483=CARTESIAN_POINT('Ctrl Pts',(-130.778400506268,5.59931065883326,
128.885939807811));
#157484=CARTESIAN_POINT('Ctrl Pts',(-130.78581328557,5.54445576730088,128.738703141859));
#157485=CARTESIAN_POINT('Ctrl Pts',(-130.793236656598,5.48952249652728,
128.591256097255));
#157486=CARTESIAN_POINT('Ctrl Pts',(-130.800660027627,5.42876607982015,
128.446169872191));
#157487=CARTESIAN_POINT('Ctrl Pts',(-130.808083398656,5.36243727846669,
128.303921256771));
#157488=CARTESIAN_POINT('Ctrl Pts',(-130.812019448097,5.32726815645068,
128.228497627666));
#157489=CARTESIAN_POINT('Ctrl Pts',(-130.815955497538,5.29053319029321,
128.153871314428));
#157490=CARTESIAN_POINT('Ctrl Pts',(-130.819891546978,5.25227473299223,
128.080110135016));
#157491=CARTESIAN_POINT('Ctrl Pts',(-130.827314813384,5.18012047652921,
127.940998852656));
#157492=CARTESIAN_POINT('Ctrl Pts',(-130.834738079789,5.10232656353443,
127.804545804823));
#157493=CARTESIAN_POINT('Ctrl Pts',(-130.842161346195,5.01911269553447,
127.671241036059));
#157494=CARTESIAN_POINT('Ctrl Pts',(-130.849575838916,4.93599717941601,
127.538093822461));
#157495=CARTESIAN_POINT('Ctrl Pts',(-130.856990331637,4.8474746550883,127.408087794825));
#157496=CARTESIAN_POINT('Ctrl Pts',(-130.864404824358,4.75381165101063,
127.28169041597));
#157497=CARTESIAN_POINT('Ctrl Pts',(-130.871812170712,4.66023892286264,
127.155414863667));
#157498=CARTESIAN_POINT('Ctrl Pts',(-130.879219517065,4.56153579933309,
127.032741333743));
#157499=CARTESIAN_POINT('Ctrl Pts',(-130.886626863419,4.45801316519695,
126.914110088175));
#157500=CARTESIAN_POINT('Ctrl Pts',(-130.894028685094,4.35456774214733,
126.795567322265));
#157501=CARTESIAN_POINT('Ctrl Pts',(-130.90143050677,4.24631021015695,126.681061117715));
#157502=CARTESIAN_POINT('Ctrl Pts',(-130.908832328445,4.13359287843425,
126.571000193759));
#157503=CARTESIAN_POINT('Ctrl Pts',(-130.916230242757,4.02093504931325,
126.460997370107));
#157504=CARTESIAN_POINT('Ctrl Pts',(-130.923628157068,3.90382237556222,
126.35543541376));
#157505=CARTESIAN_POINT('Ctrl Pts',(-130.931026071379,3.78264522889645,
126.254687482625));
#157506=CARTESIAN_POINT('Ctrl Pts',(-130.938422756292,3.6614882196739,126.153956293968));
#157507=CARTESIAN_POINT('Ctrl Pts',(-130.945819441204,3.53626836485406,
126.058037781172));
#157508=CARTESIAN_POINT('Ctrl Pts',(-130.953216126116,3.40741052805931,
125.967266029306));
#157509=CARTESIAN_POINT('Ctrl Pts',(-130.960612483051,3.27855840495609,
125.876498302355));
#157510=CARTESIAN_POINT('Ctrl Pts',(-130.968008839987,3.14606892580091,
125.790877097548));
#157511=CARTESIAN_POINT('Ctrl Pts',(-130.975405196922,3.01039723257024,
125.710694053623));
#157512=CARTESIAN_POINT('Ctrl Pts',(-130.982802686259,2.87470476765698,
125.630498733468));
#157513=CARTESIAN_POINT('Ctrl Pts',(-130.990200175596,2.73582943996688,
125.555743421948));
#157514=CARTESIAN_POINT('Ctrl Pts',(-130.997597664932,2.59425222381635,
125.486674470215));
#157515=CARTESIAN_POINT('Ctrl Pts',(-131.004997747447,2.45262537799198,
125.417581306469));
#157516=CARTESIAN_POINT('Ctrl Pts',(-131.012397829962,2.30829509324542,
125.354178634818));
#157517=CARTESIAN_POINT('Ctrl Pts',(-131.019797912477,2.16176345941615,
125.296665155031));
#157518=CARTESIAN_POINT('Ctrl Pts',(-131.027206132144,2.01507069899187,
125.23908843326));
#157519=CARTESIAN_POINT('Ctrl Pts',(-131.03461435181,1.86617210307173,125.187413972366));
#157520=CARTESIAN_POINT('Ctrl Pts',(-131.042022571477,1.71558680226133,
125.141791193143));
#157521=CARTESIAN_POINT('Ctrl Pts',(-131.049435350779,1.56490881871051,
125.096140333861));
#157522=CARTESIAN_POINT('Ctrl Pts',(-131.056848130081,1.41254242210993,
125.056548671863));
#157523=CARTESIAN_POINT('Ctrl Pts',(-131.064260909383,1.25901763630676,
125.023114631278));
#157524=CARTESIAN_POINT('Ctrl Pts',(-131.071684280412,1.10527348709026,
124.989632818568));
#157525=CARTESIAN_POINT('Ctrl Pts',(-131.079107651441,0.950368009599541,
124.96232626408));
#157526=CARTESIAN_POINT('Ctrl Pts',(-131.086531022469,0.794837883453356,
124.941241711938));
#157527=CARTESIAN_POINT('Ctrl Pts',(-131.09046707191,0.712372078679832,
124.930062176476));
#157528=CARTESIAN_POINT('Ctrl Pts',(-131.094403121351,0.629730701320683,
124.920630998739));
#157529=CARTESIAN_POINT('Ctrl Pts',(-131.098339170791,0.546993701375111,
124.912949203214));
#157530=CARTESIAN_POINT('Ctrl Pts',(-131.105762437197,0.390954301605477,
124.898461576593));
#157531=CARTESIAN_POINT('Ctrl Pts',(-131.113185703602,0.234102977717035,
124.890155593429));
#157532=CARTESIAN_POINT('Ctrl Pts',(-131.120608970008,0.0769707721032721,
124.88811129365));
#157533=CARTESIAN_POINT('Ctrl Pts',(-131.128023462729,-0.0799757162929195,
124.886069410063));
#157534=CARTESIAN_POINT('Ctrl Pts',(-131.13543795545,-0.237202055987336,
124.890274483356));
#157535=CARTESIAN_POINT('Ctrl Pts',(-131.142852448171,-0.394170892128082,
124.900754950662));
#157536=CARTESIAN_POINT('Ctrl Pts',(-131.150259794524,-0.55098843579523,
124.911225316499));
#157537=CARTESIAN_POINT('Ctrl Pts',(-131.157667140878,-0.707548600041204,
124.927959010351));
#157538=CARTESIAN_POINT('Ctrl Pts',(-131.165074487232,-0.863312939181342,
124.950932448404));
#157539=CARTESIAN_POINT('Ctrl Pts',(-131.172476308907,-1.01896110339981,
124.973888752));
#157540=CARTESIAN_POINT('Ctrl Pts',(-131.179878130583,-1.17381425664995,
125.003075479147));
#157541=CARTESIAN_POINT('Ctrl Pts',(-131.187279952258,-1.32733810013195,
125.03841714486));
#157542=CARTESIAN_POINT('Ctrl Pts',(-131.19467786657,-1.48078089957244,
125.073740153983));
#157543=CARTESIAN_POINT('Ctrl Pts',(-131.202075780881,-1.63289542391584,
125.115211547313));
#157544=CARTESIAN_POINT('Ctrl Pts',(-131.209473695192,-1.7831567193988,
125.162704595035));
#157545=CARTESIAN_POINT('Ctrl Pts',(-131.216870380105,-1.93339304418024,
125.210189750273));
#157546=CARTESIAN_POINT('Ctrl Pts',(-131.224267065017,-2.0817763957433,
125.263694461438));
#157547=CARTESIAN_POINT('Ctrl Pts',(-131.231663749929,-2.22779604969253,
125.32304185987));
#157548=CARTESIAN_POINT('Ctrl Pts',(-131.239060106864,-2.37380922897729,
125.382386626776));
#157549=CARTESIAN_POINT('Ctrl Pts',(-131.2464564638,-2.51745857321808,125.447573425274));
#157550=CARTESIAN_POINT('Ctrl Pts',(-131.253852820735,-2.65825270313081,
125.518376969389));
#157551=CARTESIAN_POINT('Ctrl Pts',(-131.261250310072,-2.79906838898466,
125.589191353707));
#157552=CARTESIAN_POINT('Ctrl Pts',(-131.268647799409,-2.93702765658215,
125.66562402817));
#157553=CARTESIAN_POINT('Ctrl Pts',(-131.276045288745,-3.07166326535431,
125.747403494278));
#157554=CARTESIAN_POINT('Ctrl Pts',(-131.28344537126,-3.20634607043021,
125.829211628051));
#157555=CARTESIAN_POINT('Ctrl Pts',(-131.290845453775,-3.3377025781153,
125.916370091531));
#157556=CARTESIAN_POINT('Ctrl Pts',(-131.29824553629,-3.46529422484557,
126.008563864392));
#157557=CARTESIAN_POINT('Ctrl Pts',(-131.305653755957,-3.59302617170761,
126.100859013785));
#157558=CARTESIAN_POINT('Ctrl Pts',(-131.313061975623,-3.71698468729859,
126.198200311227));
#157559=CARTESIAN_POINT('Ctrl Pts',(-131.320470195289,-3.83676345690102,
126.300231763027));
#157560=CARTESIAN_POINT('Ctrl Pts',(-131.327882974592,-3.95661594833819,
126.402326013484));
#157561=CARTESIAN_POINT('Ctrl Pts',(-131.335295753894,-4.0722832939897,
126.509115917794));
#157562=CARTESIAN_POINT('Ctrl Pts',(-131.342708533196,-4.18339619601278,
126.62020875253));
#157563=CARTESIAN_POINT('Ctrl Pts',(-131.350131904224,-4.29466786136111,
126.731460321918));
#157564=CARTESIAN_POINT('Ctrl Pts',(-131.357555275253,-4.40137183337431,
126.847026827581));
#157565=CARTESIAN_POINT('Ctrl Pts',(-131.364978646282,-4.50317869645347,
126.966482012098));
#157566=CARTESIAN_POINT('Ctrl Pts',(-131.368914695723,-4.55715913808003,
127.029820017217));
#157567=CARTESIAN_POINT('Ctrl Pts',(-131.372850745164,-4.60976353810745,
127.094250766581));
#157568=CARTESIAN_POINT('Ctrl Pts',(-131.376786794604,-4.66094781967877,
127.159707549751));
#157569=CARTESIAN_POINT('Ctrl Pts',(-131.384488378487,-4.76109901034053,
127.287785439489));
#157570=CARTESIAN_POINT('Ctrl Pts',(-131.39218996237,-4.85612985087017,
127.420202583377));
#157571=CARTESIAN_POINT('Ctrl Pts',(-131.399891546253,-4.94564361363236,
127.556509049308));
#157572=CARTESIAN_POINT('Ctrl Pts',(-131.4073050145,-5.03180867370954,127.687716301281));
#157573=CARTESIAN_POINT('Ctrl Pts',(-131.414718482747,-5.11286169848056,
127.822526811496));
#157574=CARTESIAN_POINT('Ctrl Pts',(-131.422131950995,-5.18848816115942,
127.960503876447));
#157575=CARTESIAN_POINT('Ctrl Pts',(-131.429538358199,-5.26404259254646,
128.098349523559));
#157576=CARTESIAN_POINT('Ctrl Pts',(-131.436944765404,-5.33418057081548,
128.239355398321));
#157577=CARTESIAN_POINT('Ctrl Pts',(-131.444351172609,-5.39863064300834,
128.383055650638));
#157578=CARTESIAN_POINT('Ctrl Pts',(-131.451751984199,-5.46303202253433,
128.526647335993));
#157579=CARTESIAN_POINT('Ctrl Pts',(-131.45915279579,-5.52175389857244,
128.672929008114));
#157580=CARTESIAN_POINT('Ctrl Pts',(-131.46655360738,-5.57457065688352,
128.821410150733));
#157581=CARTESIAN_POINT('Ctrl Pts',(-131.473950284995,-5.62735791258903,
128.969808354135));
#157582=CARTESIAN_POINT('Ctrl Pts',(-131.481346962609,-5.67424649400309,
129.120403231358));
#157583=CARTESIAN_POINT('Ctrl Pts',(-131.488743640224,-5.71505891104223,
129.272684344388));
#157584=CARTESIAN_POINT('Ctrl Pts',(-131.496138160116,-5.75585942248531,
129.424921034726));
#157585=CARTESIAN_POINT('Ctrl Pts',(-131.503532680008,-5.79058720060037,
129.578842622291));
#157586=CARTESIAN_POINT('Ctrl Pts',(-131.510927199901,-5.81911463531049,
129.733923592975));
#157587=CARTESIAN_POINT('Ctrl Pts',(-131.51832051618,-5.84763742658413,
129.888979320988));
#157588=CARTESIAN_POINT('Ctrl Pts',(-131.52571383246,-5.86996182017713,
130.045193689219));
#157589=CARTESIAN_POINT('Ctrl Pts',(-131.533107148739,-5.88601138189131,
130.202031326608));
#157590=CARTESIAN_POINT('Ctrl Pts',(-131.540501856673,-5.90206396463677,
130.358898485763));
#157591=CARTESIAN_POINT('Ctrl Pts',(-131.547896564607,-5.91183932033364,
130.516388777382));
#157592=CARTESIAN_POINT('Ctrl Pts',(-131.555291272541,-5.91531290361354,
130.673961941027));
#157593=CARTESIAN_POINT('Ctrl Pts',(-131.557402450957,-5.91630460661441,
130.718948851272));
#157594=CARTESIAN_POINT('Ctrl Pts',(-131.559513629373,-5.91678298102441,
130.763942507053));
#157595=CARTESIAN_POINT('Ctrl Pts',(-131.56162480779,-5.9167482353232,130.808930333076));
#157596=CARTESIAN_POINT('',(-133.31162480779,-5.9258324623384,130.806216140417));
#157597=CARTESIAN_POINT('Ctrl Pts',(-131.561626894289,-5.91103949408356,
130.808970343057));
#157598=CARTESIAN_POINT('Ctrl Pts',(-131.592829402331,-5.9157889408592,
131.473237742977));
#157599=CARTESIAN_POINT('Ctrl Pts',(-131.71684778498,-5.50543080433528,
134.107748453049));
#157600=CARTESIAN_POINT('Ctrl Pts',(-131.933682042229,-1.62929050015997,
137.610458838751));
#157601=CARTESIAN_POINT('Ctrl Pts',(-132.212129666044,4.8454918792327,135.853991195998));
#157602=CARTESIAN_POINT('Ctrl Pts',(-132.490577289856,6.86750393704832,
129.457159739833));
#157603=CARTESIAN_POINT('Ctrl Pts',(-132.769024913669,2.57861537293547,
124.298340075881));
#157604=CARTESIAN_POINT('Ctrl Pts',(-133.042707419646,-3.96594661910167,
125.104204454854));
#157605=CARTESIAN_POINT('Ctrl Pts',(-133.223574051021,-5.91819771649719,
128.943738175882));
#157606=CARTESIAN_POINT('Ctrl Pts',(-133.31162480779,-5.9258324623384,130.806216140417));
#157607=CARTESIAN_POINT('',(-135.06162480779,-5.91669650453655,130.79889406161));
#157608=CARTESIAN_POINT('Ctrl Pts',(-133.31162480779,-5.9258324623384,130.806216140417));
#157609=CARTESIAN_POINT('Ctrl Pts',(-133.316389925625,-5.92624563838489,
130.907009447499));
#157610=CARTESIAN_POINT('Ctrl Pts',(-133.32115504346,-5.92389767337334,
131.007783100793));
#157611=CARTESIAN_POINT('Ctrl Pts',(-133.418736035899,-5.8180376903742,
133.068477094558));
#157612=CARTESIAN_POINT('Ctrl Pts',(-133.604367785107,-3.47575125535195,
136.878627136354));
#157613=CARTESIAN_POINT('Ctrl Pts',(-133.882815408921,3.23172400096065,
137.011898012697));
#157614=CARTESIAN_POINT('Ctrl Pts',(-134.161263032733,6.96940277888598,
131.440745277975));
#157615=CARTESIAN_POINT('Ctrl Pts',(-134.439710656546,4.30254087726768,
125.284786129456));
#157616=CARTESIAN_POINT('Ctrl Pts',(-134.718158280359,-2.31814589975123,
124.201046289305));
#157617=CARTESIAN_POINT('Ctrl Pts',(-134.925462997441,-5.6612739620627,
127.911928013576));
#157618=CARTESIAN_POINT('Ctrl Pts',(-135.039951839917,-5.92095229654158,
130.338617738869));
#157619=CARTESIAN_POINT('Ctrl Pts',(-135.06162480779,-5.91669650453655,
130.79889406161));
#157620=CARTESIAN_POINT('',(-136.81162480779,-5.90698938982151,130.80496114814));
#157621=CARTESIAN_POINT('Ctrl Pts',(-135.06162480779,-5.91669650453655,
130.79889406161));
#157622=CARTESIAN_POINT('Ctrl Pts',(-135.132767714522,-5.90272659439496,
132.309780604324));
#157623=CARTESIAN_POINT('Ctrl Pts',(-135.296726495857,-4.54411447408175,
135.814156954017));
#157624=CARTESIAN_POINT('Ctrl Pts',(-135.553501151798,1.35765048963333,
137.669806391752));
#157625=CARTESIAN_POINT('Ctrl Pts',(-135.83194877561,6.50993722145643,133.373071948767));
#157626=CARTESIAN_POINT('Ctrl Pts',(-136.110396399423,5.67990967487751,
126.715817280924));
#157627=CARTESIAN_POINT('Ctrl Pts',(-136.388844023236,-0.369677383902886,
123.815734203013));
#157628=CARTESIAN_POINT('Ctrl Pts',(-136.622586826026,-5.16282797254495,
126.77237981359));
#157629=CARTESIAN_POINT('Ctrl Pts',(-136.76351375421,-5.90606400737249,
129.778969746663));
#157630=CARTESIAN_POINT('Ctrl Pts',(-136.81162480779,-5.90698938982151,
130.80496114814));
#157631=CARTESIAN_POINT('',(-138.561624088733,-5.91830260272839,130.809606478819));
#157632=CARTESIAN_POINT('Ctrl Pts',(-136.81162480779,-5.90698938982151,
130.80496114814));
#157633=CARTESIAN_POINT('Ctrl Pts',(-136.856329628814,-5.90784925577088,
131.758312998952));
#157634=CARTESIAN_POINT('Ctrl Pts',(-136.993850324443,-5.23902913899845,
134.689869888022));
#157635=CARTESIAN_POINT('Ctrl Pts',(-137.224186894675,-0.625777678858699,
137.774723795112));
#157636=CARTESIAN_POINT('Ctrl Pts',(-137.502634518488,5.52611583132312,
135.098496659793));
#157637=CARTESIAN_POINT('Ctrl Pts',(-137.781082142301,6.59977885829072,
128.476168281864));
#157638=CARTESIAN_POINT('Ctrl Pts',(-138.059529766113,1.60856753160757,
123.993334921931));
#157639=CARTESIAN_POINT('Ctrl Pts',(-138.319710321652,-4.43642471316069,
125.652979148224));
#157640=CARTESIAN_POINT('Ctrl Pts',(-138.487075002584,-5.90427870488731,
129.227898504401));
#157641=CARTESIAN_POINT('Ctrl Pts',(-138.561623808914,-5.9189077050571,
130.809601079842));
#157642=CARTESIAN_POINT('',(-140.311626173768,-5.92115491125036,130.801347234396));
#157643=CARTESIAN_POINT('Ctrl Pts',(-138.56162480779,-5.91674766216093,
130.80962035265));
#157644=CARTESIAN_POINT('Ctrl Pts',(-138.572369984272,-5.91654507308181,
131.03751556811));
#157645=CARTESIAN_POINT('Ctrl Pts',(-138.583115160753,-5.90317251244182,
131.264849426288));
#157646=CARTESIAN_POINT('Ctrl Pts',(-138.593860337235,-5.87684304778801,
131.490397317871));
#157647=CARTESIAN_POINT('Ctrl Pts',(-138.60138189607,-5.85841258107345,
131.648279483841));
#157648=CARTESIAN_POINT('Ctrl Pts',(-138.608903454904,-5.83363427395434,
131.805287471932));
#157649=CARTESIAN_POINT('Ctrl Pts',(-138.616425013739,-5.80259373517108,
131.961009443724));
#157650=CARTESIAN_POINT('Ctrl Pts',(-138.623848280145,-5.77195883703105,
132.114696426328));
#157651=CARTESIAN_POINT('Ctrl Pts',(-138.63127154655,-5.73516758839248,
132.267397870938));
#157652=CARTESIAN_POINT('Ctrl Pts',(-138.638694812956,-5.69229479046269,
132.418581971957));
#157653=CARTESIAN_POINT('Ctrl Pts',(-138.646109305677,-5.64947266461969,
132.569587385923));
#157654=CARTESIAN_POINT('Ctrl Pts',(-138.653523798398,-5.6005833978621,
132.719078670389));
#157655=CARTESIAN_POINT('Ctrl Pts',(-138.660938291119,-5.5457530503043,
132.866532692719));
#157656=CARTESIAN_POINT('Ctrl Pts',(-138.668345637473,-5.4909755502998,
133.013844593311));
#157657=CARTESIAN_POINT('Ctrl Pts',(-138.675752983826,-5.43026849853887,
133.159122793345));
#157658=CARTESIAN_POINT('Ctrl Pts',(-138.68316033018,-5.36380812500308,
133.301857957034));
#157659=CARTESIAN_POINT('Ctrl Pts',(-138.690562151856,-5.29739732012109,
133.444486663454));
#157660=CARTESIAN_POINT('Ctrl Pts',(-138.697963973531,-5.22524189440597,
133.584575773143));
#157661=CARTESIAN_POINT('Ctrl Pts',(-138.705365795207,-5.14756663851491,
133.721634732994));
#157662=CARTESIAN_POINT('Ctrl Pts',(-138.712763709518,-5.06993238678681,
133.858621340488));
#157663=CARTESIAN_POINT('Ctrl Pts',(-138.72016162383,-4.98678429159512,
133.992580659863));
#157664=CARTESIAN_POINT('Ctrl Pts',(-138.727559538141,-4.89839359210376,
134.123045715513));
#157665=CARTESIAN_POINT('Ctrl Pts',(-138.734956223053,-4.81001758154322,
134.253489090238));
#157666=CARTESIAN_POINT('Ctrl Pts',(-138.742352907966,-4.71640090498478,
134.380439044978));
#157667=CARTESIAN_POINT('Ctrl Pts',(-138.749749592878,-4.61785879651094,
134.503456547383));
#157668=CARTESIAN_POINT('Ctrl Pts',(-138.757145949813,-4.51932105749745,
134.626468595063));
#157669=CARTESIAN_POINT('Ctrl Pts',(-138.764542306749,-4.41585855420128,
134.745548245764));
#157670=CARTESIAN_POINT('Ctrl Pts',(-138.771938663684,-4.30782740605772,
134.86028882232));
#157671=CARTESIAN_POINT('Ctrl Pts',(-138.779336153021,-4.1997797180699,
134.97504696595));
#157672=CARTESIAN_POINT('Ctrl Pts',(-138.786733642357,-4.08716224840645,
135.085464440872));
#157673=CARTESIAN_POINT('Ctrl Pts',(-138.794131131694,-3.97036852102234,
135.191170890392));
#157674=CARTESIAN_POINT('Ctrl Pts',(-138.801531214209,-3.85353385177799,
135.296914395145));
#157675=CARTESIAN_POINT('Ctrl Pts',(-138.808931296724,-3.73252028663693,
135.397943336143));
#157676=CARTESIAN_POINT('Ctrl Pts',(-138.816331379239,-3.60775488037699,
135.493927259124));
#157677=CARTESIAN_POINT('Ctrl Pts',(-138.823739598905,-3.48285228172649,
135.590016726296));
#157678=CARTESIAN_POINT('Ctrl Pts',(-138.831147818572,-3.35418989904718,
135.681049868937));
#157679=CARTESIAN_POINT('Ctrl Pts',(-138.838556038238,-3.2222248563131,
135.766738831473));
#157680=CARTESIAN_POINT('Ctrl Pts',(-138.845968817541,-3.09017859129717,
135.852480534136));
#157681=CARTESIAN_POINT('Ctrl Pts',(-138.853381596843,-2.95482593596447,
135.932871312259));
#157682=CARTESIAN_POINT('Ctrl Pts',(-138.860794376145,-2.8166486558548,
136.007669268028));
#157683=CARTESIAN_POINT('Ctrl Pts',(-138.868217747174,-2.67827394156724,
136.082574098624));
#157684=CARTESIAN_POINT('Ctrl Pts',(-138.875641118202,-2.53706687602473,
136.151869982453));
#157685=CARTESIAN_POINT('Ctrl Pts',(-138.883064489231,-2.39352998589385,
136.215362813937));
#157686=CARTESIAN_POINT('Ctrl Pts',(-138.887000538672,-2.31742328263425,
136.249028236675));
#157687=CARTESIAN_POINT('Ctrl Pts',(-138.890936588112,-2.24066186110984,
136.281063038531));
#157688=CARTESIAN_POINT('Ctrl Pts',(-138.894872637552,-2.16332223464045,
136.311444008219));
#157689=CARTESIAN_POINT('Ctrl Pts',(-138.902295903958,-2.01746211279161,
136.368741568899));
#157690=CARTESIAN_POINT('Ctrl Pts',(-138.909719170363,-1.86910349414759,
136.420326910188));
#157691=CARTESIAN_POINT('Ctrl Pts',(-138.917142436769,-1.71873423369849,
136.465975510546));
#157692=CARTESIAN_POINT('Ctrl Pts',(-138.92455692949,-1.56854269722742,
136.511570158049));
#157693=CARTESIAN_POINT('Ctrl Pts',(-138.931971422211,-1.4163456029246,
136.551241924091));
#157694=CARTESIAN_POINT('Ctrl Pts',(-138.939385914932,-1.2626512156636,
136.584814100649));
#157695=CARTESIAN_POINT('Ctrl Pts',(-138.946793261285,-1.10910496483953,
136.618353919078));
#157696=CARTESIAN_POINT('Ctrl Pts',(-138.954200607639,-0.954064656329923,
136.645805772855));
#157697=CARTESIAN_POINT('Ctrl Pts',(-138.961607953993,-0.798054065368237,
136.667042620818));
#157698=CARTESIAN_POINT('Ctrl Pts',(-138.969009775668,-0.642159832991233,
136.688263629538));
#157699=CARTESIAN_POINT('Ctrl Pts',(-138.976411597344,-0.485297127387972,
136.70327881199));
#157700=CARTESIAN_POINT('Ctrl Pts',(-138.983813419019,-0.328000169621734,
136.712012134982));
#157701=CARTESIAN_POINT('Ctrl Pts',(-138.99121133333,-0.170786247695105,
136.720740847721));
#157702=CARTESIAN_POINT('Ctrl Pts',(-138.998609247642,-0.0131389019250054,
136.723194284621));
#157703=CARTESIAN_POINT('Ctrl Pts',(-139.006007161953,0.144402376492931,
136.719348235149));
#157704=CARTESIAN_POINT('Ctrl Pts',(-139.013403846865,0.301917474408259,
136.715502824822));
#157705=CARTESIAN_POINT('Ctrl Pts',(-139.020800531778,0.459326167133431,
136.705360014933));
#157706=CARTESIAN_POINT('Ctrl Pts',(-139.02819721669,0.616088692597387,
136.688947713136));
#157707=CARTESIAN_POINT('Ctrl Pts',(-139.035593573625,0.772844267046688,
136.672536139078));
#157708=CARTESIAN_POINT('Ctrl Pts',(-139.042989930561,0.928953359935741,
136.649855664732));
#157709=CARTESIAN_POINT('Ctrl Pts',(-139.050386287496,1.08388133099193,
136.620986084521));
#157710=CARTESIAN_POINT('Ctrl Pts',(-139.057783776833,1.238833021916,136.592112084303));
#157711=CARTESIAN_POINT('Ctrl Pts',(-139.065181266169,1.39260286394066,
136.557047159876));
#157712=CARTESIAN_POINT('Ctrl Pts',(-139.072578755506,1.54466655618022,
136.515922207247));
#157713=CARTESIAN_POINT('Ctrl Pts',(-139.079978838021,1.69678355411159,
136.47478283833));
#157714=CARTESIAN_POINT('Ctrl Pts',(-139.087378920536,1.84719285134129,
136.427579309074));
#157715=CARTESIAN_POINT('Ctrl Pts',(-139.094779003051,1.99538559379863,
136.374492294157));
#157716=CARTESIAN_POINT('Ctrl Pts',(-139.102187222718,2.14374128941111,
136.321346904609));
#157717=CARTESIAN_POINT('Ctrl Pts',(-139.109595442384,2.28987521109871,
136.262305235359));
#157718=CARTESIAN_POINT('Ctrl Pts',(-139.11700366205,2.43329809114091,136.197596284784));
#157719=CARTESIAN_POINT('Ctrl Pts',(-139.124416441352,2.57680924557264,
136.132847506929));
#157720=CARTESIAN_POINT('Ctrl Pts',(-139.131829220655,2.71760570037214,
136.062424663841));
#157721=CARTESIAN_POINT('Ctrl Pts',(-139.139241999957,2.85522353401579,
135.986602326836));
#157722=CARTESIAN_POINT('Ctrl Pts',(-139.146665370985,2.99303800247359,
135.910671651321));
#157723=CARTESIAN_POINT('Ctrl Pts',(-139.154088742014,3.12766446020009,
135.829326265745));
#157724=CARTESIAN_POINT('Ctrl Pts',(-139.161512113043,3.25866797273628,
135.742884041218));
#157725=CARTESIAN_POINT('Ctrl Pts',(-139.165448162484,3.32812917846873,
135.697050299622));
#157726=CARTESIAN_POINT('Ctrl Pts',(-139.169384211925,3.39657238788596,
135.649784334589));
#157727=CARTESIAN_POINT('Ctrl Pts',(-139.173320261365,3.46393671535675,
135.601137972677));
#157728=CARTESIAN_POINT('Ctrl Pts',(-139.180743527771,3.59098373459849,
135.50939245231));
#157729=CARTESIAN_POINT('Ctrl Pts',(-139.188166794176,3.71457540043574,
135.412457281719));
#157730=CARTESIAN_POINT('Ctrl Pts',(-139.195590060582,3.83425911899848,
135.310621547747));
#157731=CARTESIAN_POINT('Ctrl Pts',(-139.203004553303,3.95380138134499,
135.208906175156));
#157732=CARTESIAN_POINT('Ctrl Pts',(-139.210419046024,4.06944460877007,
135.102302007856));
#157733=CARTESIAN_POINT('Ctrl Pts',(-139.217833538745,4.18076540222964,
134.991141148478));
#157734=CARTESIAN_POINT('Ctrl Pts',(-139.225240885098,4.29197890051763,
134.88008743012));
#157735=CARTESIAN_POINT('Ctrl Pts',(-139.232648231452,4.3988779963961,134.764486025116));
#157736=CARTESIAN_POINT('Ctrl Pts',(-139.240055577806,4.50107269323137,
134.644708931554));
#157737=CARTESIAN_POINT('Ctrl Pts',(-139.247457399481,4.60319116940617,
134.525021172266));
#157738=CARTESIAN_POINT('Ctrl Pts',(-139.254859221157,4.70061199161803,
134.401164208341));
#157739=CARTESIAN_POINT('Ctrl Pts',(-139.262261042832,4.7929824314566,134.273546397291));
#157740=CARTESIAN_POINT('Ctrl Pts',(-139.269658957144,4.88530410965899,
134.145995954691));
#157741=CARTESIAN_POINT('Ctrl Pts',(-139.277056871455,4.97258049674658,
134.014688920462));
#157742=CARTESIAN_POINT('Ctrl Pts',(-139.284454785766,5.05449961554519,
133.880066097444));
#157743=CARTESIAN_POINT('Ctrl Pts',(-139.291851470678,5.1364051208723,133.745465646297));
#157744=CARTESIAN_POINT('Ctrl Pts',(-139.299248155591,5.21295493099283,
133.607550818565));
#157745=CARTESIAN_POINT('Ctrl Pts',(-139.306644840503,5.28388077082161,
133.466790816133));
#157746=CARTESIAN_POINT('Ctrl Pts',(-139.314041197438,5.35480346572432,
133.326037055147));
#157747=CARTESIAN_POINT('Ctrl Pts',(-139.321437554374,5.42010251819538,
133.182438703674));
#157748=CARTESIAN_POINT('Ctrl Pts',(-139.328833911309,5.47955607541675,
133.036488700554));
#157749=CARTESIAN_POINT('Ctrl Pts',(-139.336231400646,5.53901873512951,
132.890516352115));
#157750=CARTESIAN_POINT('Ctrl Pts',(-139.343628889982,5.59263397676986,
132.74219198087));
#157751=CARTESIAN_POINT('Ctrl Pts',(-139.351026379319,5.64022852942182,
132.592027448493));
#157752=CARTESIAN_POINT('Ctrl Pts',(-139.358426461834,5.68783976627049,
132.441810276171));
#157753=CARTESIAN_POINT('Ctrl Pts',(-139.365826544349,5.72942599933814,
132.289752014026));
#157754=CARTESIAN_POINT('Ctrl Pts',(-139.373226626864,5.76486418729327,
132.136378434475));
#157755=CARTESIAN_POINT('Ctrl Pts',(-139.38063484653,5.80034134317913,131.982836204907));
#157756=CARTESIAN_POINT('Ctrl Pts',(-139.388043066197,5.82965686888374,
131.827976133461));
#157757=CARTESIAN_POINT('Ctrl Pts',(-139.395451285863,5.85273896607318,
131.672333634145));
#157758=CARTESIAN_POINT('Ctrl Pts',(-139.402864065165,5.87583526990836,
131.516595339467));
#157759=CARTESIAN_POINT('Ctrl Pts',(-139.410276844468,5.89269046050387,
131.360074027619));
#157760=CARTESIAN_POINT('Ctrl Pts',(-139.41768962377,5.90328478156865,131.20330842142));
#157761=CARTESIAN_POINT('Ctrl Pts',(-139.425112994798,5.91389424029617,
131.046318821172));
#157762=CARTESIAN_POINT('Ctrl Pts',(-139.432536365827,5.91822495242524,
130.889084601592));
#157763=CARTESIAN_POINT('Ctrl Pts',(-139.439959736856,5.91630925922449,
130.732143502458));
#157764=CARTESIAN_POINT('Ctrl Pts',(-139.443895786297,5.91529351272302,
130.648929565946));
#157765=CARTESIAN_POINT('Ctrl Pts',(-139.447831835738,5.91252254420794,
130.565797946815));
#157766=CARTESIAN_POINT('Ctrl Pts',(-139.451767885178,5.9080070466573,130.482827883388));
#157767=CARTESIAN_POINT('Ctrl Pts',(-139.459191151584,5.89949095920072,
130.326348933175));
#157768=CARTESIAN_POINT('Ctrl Pts',(-139.466614417989,5.88474096911531,
130.16997193693));
#157769=CARTESIAN_POINT('Ctrl Pts',(-139.474037684395,5.86375565530722,
130.014233933197));
#157770=CARTESIAN_POINT('Ctrl Pts',(-139.481452177116,5.84279514439733,
129.85867999885));
#157771=CARTESIAN_POINT('Ctrl Pts',(-139.488866669837,5.81561402842719,
129.703763920054));
#157772=CARTESIAN_POINT('Ctrl Pts',(-139.496281162558,5.78226285721951,
129.550021423998));
#157773=CARTESIAN_POINT('Ctrl Pts',(-139.503688508911,5.74894383112621,
129.396427110749));
#157774=CARTESIAN_POINT('Ctrl Pts',(-139.511095855265,5.70946666757237,
129.244004490721));
#157775=CARTESIAN_POINT('Ctrl Pts',(-139.518503201619,5.6639335363781,129.09328275318));
#157776=CARTESIAN_POINT('Ctrl Pts',(-139.525905023294,5.61843436551095,
128.942673429598));
#157777=CARTESIAN_POINT('Ctrl Pts',(-139.53330684497,5.56688832799046,128.793762818394));
#157778=CARTESIAN_POINT('Ctrl Pts',(-139.540708666645,5.50944832823656,
128.64706840718));
#157779=CARTESIAN_POINT('Ctrl Pts',(-139.548106580957,5.45203865061142,
128.500451434804));
#157780=CARTESIAN_POINT('Ctrl Pts',(-139.555504495268,5.38874134297153,
128.356048679199));
#157781=CARTESIAN_POINT('Ctrl Pts',(-139.562902409579,5.31975863394631,
128.214360880297));
#157782=CARTESIAN_POINT('Ctrl Pts',(-139.570299094491,5.25078738859596,
128.072696627337));
#157783=CARTESIAN_POINT('Ctrl Pts',(-139.577695779404,5.17613278027719,
127.933746770933));
#157784=CARTESIAN_POINT('Ctrl Pts',(-139.585092464316,5.09604455258802,
127.797990633592));
#157785=CARTESIAN_POINT('Ctrl Pts',(-139.592488821251,5.0159598760948,127.662240515821));
#157786=CARTESIAN_POINT('Ctrl Pts',(-139.599885178187,4.930442248963,127.529684157056));
#157787=CARTESIAN_POINT('Ctrl Pts',(-139.607281535122,4.83978647773083,
127.40077465384));
#157788=CARTESIAN_POINT('Ctrl Pts',(-139.614679024459,4.74911682686866,
127.27184541425));
#157789=CARTESIAN_POINT('Ctrl Pts',(-139.622076513795,4.65330768030736,
127.146564447313));
#157790=CARTESIAN_POINT('Ctrl Pts',(-139.629474003132,4.5526960246077,127.025354204496));
#157791=CARTESIAN_POINT('Ctrl Pts',(-139.636874085647,4.45204909964796,
126.904101471617));
#157792=CARTESIAN_POINT('Ctrl Pts',(-139.644274168162,4.3465965519648,126.786922591035));
#157793=CARTESIAN_POINT('Ctrl Pts',(-139.651674250677,4.23671422193866,
126.674205273741));
#157794=CARTESIAN_POINT('Ctrl Pts',(-139.659082470343,4.12671106499463,
126.56136401217));
#157795=CARTESIAN_POINT('Ctrl Pts',(-139.66649069001,4.01226865873714,126.452994378852));
#157796=CARTESIAN_POINT('Ctrl Pts',(-139.673898909676,3.89379865338024,
126.349446184108));
#157797=CARTESIAN_POINT('Ctrl Pts',(-139.681311688978,3.77525573171182,
126.245834257177));
#157798=CARTESIAN_POINT('Ctrl Pts',(-139.68872446828,3.65268056136824,126.147049915666));
#157799=CARTESIAN_POINT('Ctrl Pts',(-139.696137247583,3.52651570635732,
126.053400973945));
#157800=CARTESIAN_POINT('Ctrl Pts',(-139.703560618611,3.40017058108484,
125.959618222224));
#157801=CARTESIAN_POINT('Ctrl Pts',(-139.71098398964,3.2702258347369,125.870985735115));
#157802=CARTESIAN_POINT('Ctrl Pts',(-139.718407360669,3.13715136426387,
125.787766964479));
#157803=CARTESIAN_POINT('Ctrl Pts',(-139.72234341011,3.06659208694024,125.74364237548));
#157804=CARTESIAN_POINT('Ctrl Pts',(-139.726279459551,2.99515332518775,
125.701038999026));
#157805=CARTESIAN_POINT('Ctrl Pts',(-139.730215508991,2.9229075242693,125.659990669062));
#157806=CARTESIAN_POINT('Ctrl Pts',(-139.737638775397,2.78665419845301,
125.582574799826));
#157807=CARTESIAN_POINT('Ctrl Pts',(-139.745062041802,2.64711707275638,
125.510458798036));
#157808=CARTESIAN_POINT('Ctrl Pts',(-139.752485308208,2.50474720477755,
125.443934141747));
#157809=CARTESIAN_POINT('Ctrl Pts',(-139.759899800929,2.36254560615918,
125.377488112078));
#157810=CARTESIAN_POINT('Ctrl Pts',(-139.76731429365,2.21751826449865,125.316620430127));
#157811=CARTESIAN_POINT('Ctrl Pts',(-139.774728786371,2.07014322566789,
125.261578140531));
#157812=CARTESIAN_POINT('Ctrl Pts',(-139.782136132724,1.92291023244813,
125.206588902767));
#157813=CARTESIAN_POINT('Ctrl Pts',(-139.789543479078,1.77333439420133,
125.157414009261));
#157814=CARTESIAN_POINT('Ctrl Pts',(-139.796950825432,1.62191615812796,
125.114253541376));
#157815=CARTESIAN_POINT('Ctrl Pts',(-139.804352647107,1.47061085548815,
125.071125264197));
#157816=CARTESIAN_POINT('Ctrl Pts',(-139.811754468783,1.31746624855318,
125.034002582723));
#157817=CARTESIAN_POINT('Ctrl Pts',(-139.819156290458,1.16300036288113,
125.00303656883));
#157818=CARTESIAN_POINT('Ctrl Pts',(-139.82655420477,1.00861601854733,124.972086901655));
#157819=CARTESIAN_POINT('Ctrl Pts',(-139.833952119081,0.852912149655667,
124.947287502607));
#157820=CARTESIAN_POINT('Ctrl Pts',(-139.841350033392,0.696419352408148,
124.928738893179));
#157821=CARTESIAN_POINT('Ctrl Pts',(-139.848746718304,0.539952561424241,
124.910193366193));
#157822=CARTESIAN_POINT('Ctrl Pts',(-139.856143403217,0.382697472630334,
124.897896611074));
#157823=CARTESIAN_POINT('Ctrl Pts',(-139.863540088129,0.225192346141724,
124.891897596985));
#157824=CARTESIAN_POINT('Ctrl Pts',(-139.870936445064,0.0676942035959251,
124.885898848898));
#157825=CARTESIAN_POINT('Ctrl Pts',(-139.878332802,-0.0900535815729142,
124.886197300808));
#157826=CARTESIAN_POINT('Ctrl Pts',(-139.885729158935,-0.247510456276855,
124.892789833372));
#157827=CARTESIAN_POINT('Ctrl Pts',(-139.893126648272,-0.404991438030731,
124.89938337527));
#157828=CARTESIAN_POINT('Ctrl Pts',(-139.900524137608,-0.562181047641271,
124.912272900941));
#157829=CARTESIAN_POINT('Ctrl Pts',(-139.907921626945,-0.718541715257594,
124.931403239385));
#157830=CARTESIAN_POINT('Ctrl Pts',(-139.91532170946,-0.874957194863338,
124.950540283938));
#157831=CARTESIAN_POINT('Ctrl Pts',(-139.922721791975,-1.03054278361979,
124.975922451668));
#157832=CARTESIAN_POINT('Ctrl Pts',(-139.93012187449,-1.18476913838338,
125.007443104677));
#157833=CARTESIAN_POINT('Ctrl Pts',(-139.937530094157,-1.33916508087868,
125.038998417885));
#157834=CARTESIAN_POINT('Ctrl Pts',(-139.944938313823,-1.49219843856993,
125.076705621563));
#157835=CARTESIAN_POINT('Ctrl Pts',(-139.952346533489,-1.64335239913165,
125.120407463751));
#157836=CARTESIAN_POINT('Ctrl Pts',(-139.959759312791,-1.79459939243439,
125.164136203693));
#157837=CARTESIAN_POINT('Ctrl Pts',(-139.967172092094,-1.94396433030163,
125.213866816484));
#157838=CARTESIAN_POINT('Ctrl Pts',(-139.974584871396,-2.0909490231294,
125.269393341676));
#157839=CARTESIAN_POINT('Ctrl Pts',(-139.982008242424,-2.23814373457897,
125.324999205771));
#157840=CARTESIAN_POINT('Ctrl Pts',(-139.989431613453,-2.38295106566392,
125.386417376849));
#157841=CARTESIAN_POINT('Ctrl Pts',(-139.996854984482,-2.52489537609378,
125.453394919463));
#157842=CARTESIAN_POINT('Ctrl Pts',(-140.000791033923,-2.60015765539067,
125.48890801966));
#157843=CARTESIAN_POINT('Ctrl Pts',(-140.004727083364,-2.67461547830674,
125.525983307554));
#157844=CARTESIAN_POINT('Ctrl Pts',(-140.008663132804,-2.7482012209517,
125.564578120968));
#157845=CARTESIAN_POINT('Ctrl Pts',(-140.01608639921,-2.88698163504634,
125.637366734561));
#157846=CARTESIAN_POINT('Ctrl Pts',(-140.023509665615,-3.0230780946054,
125.715782809807));
#157847=CARTESIAN_POINT('Ctrl Pts',(-140.03093293202,-3.15600156323604,
125.799604410182));
#157848=CARTESIAN_POINT('Ctrl Pts',(-140.038347424741,-3.28876792736536,
125.883326940386));
#157849=CARTESIAN_POINT('Ctrl Pts',(-140.045761917462,-3.41836845270827,
125.972442081442));
#157850=CARTESIAN_POINT('Ctrl Pts',(-140.053176410183,-3.5443368981461,
126.066681173477));
#157851=CARTESIAN_POINT('Ctrl Pts',(-140.060583756537,-3.67018393045359,
126.160829434328));
#157852=CARTESIAN_POINT('Ctrl Pts',(-140.067991102891,-3.79240555522919,
126.260091592148));
#157853=CARTESIAN_POINT('Ctrl Pts',(-140.075398449244,-3.91056293442113,
126.364154755398));
#157854=CARTESIAN_POINT('Ctrl Pts',(-140.08280027092,-4.02863218738185,
126.468140304414));
#157855=CARTESIAN_POINT('Ctrl Pts',(-140.090202092595,-4.14264295148744,
126.576919483399));
#157856=CARTESIAN_POINT('Ctrl Pts',(-140.09760391427,-4.25218812022256,
126.690138120819));
#157857=CARTESIAN_POINT('Ctrl Pts',(-140.105001828581,-4.3616754609155,
126.803296991001));
#157858=CARTESIAN_POINT('Ctrl Pts',(-140.112399742893,-4.46670164210321,
126.920890384716));
#157859=CARTESIAN_POINT('Ctrl Pts',(-140.119797657204,-4.56689529199973,
127.042526230673));
#157860=CARTESIAN_POINT('Ctrl Pts',(-140.127194342116,-4.66707229152975,
127.16414186296));
#157861=CARTESIAN_POINT('Ctrl Pts',(-140.134591027028,-4.76241811653455,
127.289798326349));
#157862=CARTESIAN_POINT('Ctrl Pts',(-140.14198771194,-4.85260062513205,
127.419069236389));
#157863=CARTESIAN_POINT('Ctrl Pts',(-140.149384068876,-4.94277913494261,
127.548334414422));
#157864=CARTESIAN_POINT('Ctrl Pts',(-140.156780425811,-5.02779456998593,
127.681213414279));
#157865=CARTESIAN_POINT('Ctrl Pts',(-140.164176782746,-5.10735737250467,
127.817249767259));
#157866=CARTESIAN_POINT('Ctrl Pts',(-140.171574272083,-5.1869323562916,
127.953306947751));
#157867=CARTESIAN_POINT('Ctrl Pts',(-140.178971761419,-5.26105285685825,
128.092522121625));
#157868=CARTESIAN_POINT('Ctrl Pts',(-140.186369250756,-5.32947472149487,
128.234413194865));
#157869=CARTESIAN_POINT('Ctrl Pts',(-140.193769333271,-5.39792057130996,
128.376354007801));
#157870=CARTESIAN_POINT('Ctrl Pts',(-140.201169415786,-5.4606636458513,
128.520972251684));
#157871=CARTESIAN_POINT('Ctrl Pts',(-140.208569498301,-5.51750753970128,
128.667764934747));
#157872=CARTESIAN_POINT('Ctrl Pts',(-140.215977717967,-5.57441393925632,
128.814719031457));
#157873=CARTESIAN_POINT('Ctrl Pts',(-140.223385937633,-5.62540806875892,
128.963851994048));
#157874=CARTESIAN_POINT('Ctrl Pts',(-140.2307941573,-5.67034287905158,129.114644015147));
#157875=CARTESIAN_POINT('Ctrl Pts',(-140.238206936602,-5.7153053459702,
129.26552884622));
#157876=CARTESIAN_POINT('Ctrl Pts',(-140.245619715903,-5.75420097034454,
129.418074409631));
#157877=CARTESIAN_POINT('Ctrl Pts',(-140.253032495205,-5.78693374888261,
129.571750237704));
#157878=CARTESIAN_POINT('Ctrl Pts',(-140.260455866234,-5.81971329754973,
129.725645645007));
#157879=CARTESIAN_POINT('Ctrl Pts',(-140.267879237263,-5.84631235033739,
129.880674175493));
#157880=CARTESIAN_POINT('Ctrl Pts',(-140.275302608291,-5.86668661380568,
130.036298941727));
#157881=CARTESIAN_POINT('Ctrl Pts',(-140.279238657733,-5.8774895371729,
130.118814926968));
#157882=CARTESIAN_POINT('Ctrl Pts',(-140.283174707175,-5.88654331946295,
130.201498500882));
#157883=CARTESIAN_POINT('Ctrl Pts',(-140.287110756616,-5.89384730120973,
130.284269709625));
#157884=CARTESIAN_POINT('Ctrl Pts',(-140.295282107008,-5.90901057468745,
130.456105088978));
#157885=CARTESIAN_POINT('Ctrl Pts',(-140.303453457399,-5.91666048185143,
130.628613165077));
#157886=CARTESIAN_POINT('Ctrl Pts',(-140.31162480779,-5.91674921901585,
130.801320588729));
#157887=CARTESIAN_POINT('',(-142.061623600479,-5.91263345657567,130.80054659611));
#157888=CARTESIAN_POINT('Ctrl Pts',(-140.311627245294,-5.92461090629068,
130.801368136286));
#157889=CARTESIAN_POINT('Ctrl Pts',(-140.396270957006,-5.91338488009951,
132.59275803674));
#157890=CARTESIAN_POINT('Ctrl Pts',(-140.573730543324,-4.09131473212171,
136.368220126305));
#157891=CARTESIAN_POINT('Ctrl Pts',(-140.844006004241,2.33823337963563,
137.400588721007));
#157892=CARTESIAN_POINT('Ctrl Pts',(-141.122453628056,6.81346577453316,
132.402561064817));
#157893=CARTESIAN_POINT('Ctrl Pts',(-141.400901251868,5.02745597894928,
125.935865274023));
#157894=CARTESIAN_POINT('Ctrl Pts',(-141.679348875681,-1.3785402564146,
123.94307886473));
#157895=CARTESIAN_POINT('Ctrl Pts',(-141.899589348986,-5.443421615627,127.354004753196));
#157896=CARTESIAN_POINT('Ctrl Pts',(-142.027013947685,-5.91376279909305,
130.06325457639));
#157897=CARTESIAN_POINT('Ctrl Pts',(-142.061622671781,-5.90946782723236,
130.800528840258));
#157898=CARTESIAN_POINT('',(-143.811626040432,-5.91327805224815,130.808839182428));
#157899=CARTESIAN_POINT('Ctrl Pts',(-142.06162480779,-5.91674878554795,
130.800569678778));
#157900=CARTESIAN_POINT('Ctrl Pts',(-142.069073349795,-5.91685057702334,
130.959441826839));
#157901=CARTESIAN_POINT('Ctrl Pts',(-142.0765218918,-5.91054916224425,131.118342907778));
#157902=CARTESIAN_POINT('Ctrl Pts',(-142.083970433805,-5.89786424799386,
131.276724751192));
#157903=CARTESIAN_POINT('Ctrl Pts',(-142.091419462658,-5.8851785046396,
131.435116946666));
#157904=CARTESIAN_POINT('Ctrl Pts',(-142.09886849151,-5.86610845896061,
131.592989472193));
#157905=CARTESIAN_POINT('Ctrl Pts',(-142.106317520362,-5.84072578702984,
131.749798528391));
#157906=CARTESIAN_POINT('Ctrl Pts',(-142.113768429199,-5.81533670902553,
131.906647160026));
#157907=CARTESIAN_POINT('Ctrl Pts',(-142.121219338036,-5.78363188935134,
132.062431426492));
#157908=CARTESIAN_POINT('Ctrl Pts',(-142.128670246872,-5.74573427754804,
132.216617029946));
#157909=CARTESIAN_POINT('Ctrl Pts',(-142.136124429677,-5.70782001333851,
132.370870383351));
#157910=CARTESIAN_POINT('Ctrl Pts',(-142.143578612481,-5.66370762371264,
132.523523319449));
#157911=CARTESIAN_POINT('Ctrl Pts',(-142.151032795286,-5.61357011716365,
132.674056074636));
#157912=CARTESIAN_POINT('Ctrl Pts',(-142.158496430599,-5.56336903218619,
132.824779717576));
#157913=CARTESIAN_POINT('Ctrl Pts',(-142.165960065912,-5.5071276828603,
132.973377461212));
#157914=CARTESIAN_POINT('Ctrl Pts',(-142.173423701226,-5.44506785729073,
133.119348002413));
#157915=CARTESIAN_POINT('Ctrl Pts',(-142.180892350598,-5.38296634002241,
133.265416606406));
#157916=CARTESIAN_POINT('Ctrl Pts',(-142.188360999971,-5.31503871128872,
133.40885415989));
#157917=CARTESIAN_POINT('Ctrl Pts',(-142.195829649343,-5.24155288908102,
133.549183721787));
#157918=CARTESIAN_POINT('Ctrl Pts',(-142.203310567848,-5.16794634795429,
133.689743810233));
#157919=CARTESIAN_POINT('Ctrl Pts',(-142.210791486353,-5.08876355043455,
133.827185388102));
#157920=CARTESIAN_POINT('Ctrl Pts',(-142.218272404858,-5.0043165686423,
133.961059247989));
#157921=CARTESIAN_POINT('Ctrl Pts',(-142.224262977674,-4.93669308187295,
134.068262809332));
#157922=CARTESIAN_POINT('Ctrl Pts',(-142.23025355049,-4.86569481696976,
134.173179102954));
#157923=CARTESIAN_POINT('Ctrl Pts',(-142.236244123306,-4.79150027851089,
134.275593200314));
#157924=CARTESIAN_POINT('Ctrl Pts',(-142.243667389712,-4.69956152044658,
134.402500451375));
#157925=CARTESIAN_POINT('Ctrl Pts',(-142.251090656117,-4.60243837662734,
134.525944455269));
#157926=CARTESIAN_POINT('Ctrl Pts',(-142.258513922523,-4.50042062233194,
134.64547305859));
#157927=CARTESIAN_POINT('Ctrl Pts',(-142.265928415244,-4.39852344454978,
134.764860389029));
#157928=CARTESIAN_POINT('Ctrl Pts',(-142.273342907965,-4.2917434113877,
134.880341249147));
#157929=CARTESIAN_POINT('Ctrl Pts',(-142.280757400686,-4.18041326943229,
134.991492745796));
#157930=CARTESIAN_POINT('Ctrl Pts',(-142.28816474704,-4.06919043165921,
135.102537110447));
#157931=CARTESIAN_POINT('Ctrl Pts',(-142.295572093394,-3.95342647829153,
135.20926015688));
#157932=CARTESIAN_POINT('Ctrl Pts',(-142.302979439748,-3.83349400049477,
135.31127245503));
#157933=CARTESIAN_POINT('Ctrl Pts',(-142.310381261424,-3.71365097286441,
135.413208668559));
#157934=CARTESIAN_POINT('Ctrl Pts',(-142.317783083099,-3.58964589445368,
135.510440888746));
#157935=CARTESIAN_POINT('Ctrl Pts',(-142.325184904775,-3.46188765909607,
135.602617009038));
#157936=CARTESIAN_POINT('Ctrl Pts',(-142.332582819086,-3.33419686631753,
135.694744470272));
#157937=CARTESIAN_POINT('Ctrl Pts',(-142.339980733398,-3.20275716433496,
135.781820929342));
#157938=CARTESIAN_POINT('Ctrl Pts',(-142.347378647709,-3.06800983025294,
135.86353508026));
#157939=CARTESIAN_POINT('Ctrl Pts',(-142.354775332621,-2.93328488873232,
135.945235651769));
#157940=CARTESIAN_POINT('Ctrl Pts',(-142.362172017534,-2.79525372492089,
136.021575490356));
#157941=CARTESIAN_POINT('Ctrl Pts',(-142.369568702446,-2.65438594842956,
136.092287035292));
#157942=CARTESIAN_POINT('Ctrl Pts',(-142.376965059382,-2.51352441816346,
136.162995444803));
#157943=CARTESIAN_POINT('Ctrl Pts',(-142.384361416317,-2.36982685893144,
136.228075889413));
#157944=CARTESIAN_POINT('Ctrl Pts',(-142.391757773253,-2.22378654662323,
136.287307266728));
#157945=CARTESIAN_POINT('Ctrl Pts',(-142.399155262589,-2.07772387517038,
136.346547712518));
#157946=CARTESIAN_POINT('Ctrl Pts',(-142.406552751926,-1.92931808240953,
136.399937167629));
#157947=CARTESIAN_POINT('Ctrl Pts',(-142.413950241263,-1.77908129311106,
136.447303140311));
#157948=CARTESIAN_POINT('Ctrl Pts',(-142.421350323778,-1.62879183853878,
136.494685717061));
#157949=CARTESIAN_POINT('Ctrl Pts',(-142.428750406293,-1.47667046530508,
136.536040495182));
#157950=CARTESIAN_POINT('Ctrl Pts',(-142.436150488808,-1.3232431324667,
136.57124523362));
#157951=CARTESIAN_POINT('Ctrl Pts',(-142.443558708475,-1.16964709050294,
136.606488683287));
#157952=CARTESIAN_POINT('Ctrl Pts',(-142.450966928141,-1.01474258514053,
136.635568504377));
#157953=CARTESIAN_POINT('Ctrl Pts',(-142.458375147808,-0.859065139030692,
136.658413713448));
#157954=CARTESIAN_POINT('Ctrl Pts',(-142.46578792711,-0.703291876050397,
136.681272983363));
#157955=CARTESIAN_POINT('Ctrl Pts',(-142.473200706412,-0.546745094718591,
136.697889955647));
#157956=CARTESIAN_POINT('Ctrl Pts',(-142.480613485715,-0.389963547296973,
136.708245693876));
#157957=CARTESIAN_POINT('Ctrl Pts',(-142.488036856744,-0.232957983047854,
136.71861622887));
#157958=CARTESIAN_POINT('Ctrl Pts',(-142.495460227772,-0.0757173549334295,
136.722707652266));
#157959=CARTESIAN_POINT('Ctrl Pts',(-142.502883598801,0.0812206471090248,
136.720553123645));
#157960=CARTESIAN_POINT('Ctrl Pts',(-142.506819648241,0.164432941444102,
136.719410740873));
#157961=CARTESIAN_POINT('Ctrl Pts',(-142.510755697681,0.247560247345356,
136.716513263394));
#157962=CARTESIAN_POINT('Ctrl Pts',(-142.514691747121,0.330523342852393,
136.711871504761));
#157963=CARTESIAN_POINT('Ctrl Pts',(-142.522115013526,0.486989151831294,
136.703117292841));
#157964=CARTESIAN_POINT('Ctrl Pts',(-142.529538279931,0.643343520020078,
136.688129340668));
#157965=CARTESIAN_POINT('Ctrl Pts',(-142.536961546337,0.799049407337154,
136.66690704443));
#157966=CARTESIAN_POINT('Ctrl Pts',(-142.544376039058,0.954571263226434,
136.645709831184));
#157967=CARTESIAN_POINT('Ctrl Pts',(-142.551790531779,1.10944579760184,
136.618292990788));
#157968=CARTESIAN_POINT('Ctrl Pts',(-142.5592050245,1.2631373608214,136.584707888293));
#157969=CARTESIAN_POINT('Ctrl Pts',(-142.566612370854,1.41668079032637,
136.551155156384));
#157970=CARTESIAN_POINT('Ctrl Pts',(-142.574019717208,1.56904315632977,
136.511446077262));
#157971=CARTESIAN_POINT('Ctrl Pts',(-142.581427063561,1.71969542566331,
136.465683625967));
#157972=CARTESIAN_POINT('Ctrl Pts',(-142.588828885237,1.87023533284973,
136.419955306035));
#157973=CARTESIAN_POINT('Ctrl Pts',(-142.596230706912,2.01906732732325,
136.368182711602));
#157974=CARTESIAN_POINT('Ctrl Pts',(-142.603632528588,2.16567415476532,
136.310519534441));
#157975=CARTESIAN_POINT('Ctrl Pts',(-142.611030442899,2.31220358960521,
136.252886797221));
#157976=CARTESIAN_POINT('Ctrl Pts',(-142.61842835721,2.45650985026844,136.189369806466));
#157977=CARTESIAN_POINT('Ctrl Pts',(-142.625826271522,2.59809250515853,
136.120171552611));
#157978=CARTESIAN_POINT('Ctrl Pts',(-142.633222956434,2.73965163157933,
136.05098479825));
#157979=CARTESIAN_POINT('Ctrl Pts',(-142.640619641346,2.87848771547634,
135.976118818351));
#157980=CARTESIAN_POINT('Ctrl Pts',(-142.648016326259,3.01412181496487,
135.895824085672));
#157981=CARTESIAN_POINT('Ctrl Pts',(-142.655412683194,3.14974990029569,
135.815532913344));
#157982=CARTESIAN_POINT('Ctrl Pts',(-142.662809040129,3.28217596229204,
135.729813657026));
#157983=CARTESIAN_POINT('Ctrl Pts',(-142.670205397065,3.41094735358215,
135.638961812452));
#157984=CARTESIAN_POINT('Ctrl Pts',(-142.677602886402,3.539738460101,135.548096058228));
#157985=CARTESIAN_POINT('Ctrl Pts',(-142.685000375738,3.66487347675334,
135.452096366306));
#157986=CARTESIAN_POINT('Ctrl Pts',(-142.692397865075,3.78593046539778,
135.351300365756));
#157987=CARTESIAN_POINT('Ctrl Pts',(-142.69979794759,3.90702989038176,135.250469031325));
#157988=CARTESIAN_POINT('Ctrl Pts',(-142.707198030105,4.02404815444621,
135.144838279445));
#157989=CARTESIAN_POINT('Ctrl Pts',(-142.71459811262,4.13659811901385,135.034784540091));
#157990=CARTESIAN_POINT('Ctrl Pts',(-142.722006332286,4.24927184383811,
134.924609785337));
#157991=CARTESIAN_POINT('Ctrl Pts',(-142.729414551953,4.35746718980525,
134.810002591467));
#157992=CARTESIAN_POINT('Ctrl Pts',(-142.736822771619,4.46083497346151,
134.69137514057));
#157993=CARTESIAN_POINT('Ctrl Pts',(-142.744235550921,4.56426637826441,
134.572674676456));
#157994=CARTESIAN_POINT('Ctrl Pts',(-142.751648330223,4.66286406684211,
134.449949315099));
#157995=CARTESIAN_POINT('Ctrl Pts',(-142.759061109526,4.7563208986878,134.323642088436));
#157996=CARTESIAN_POINT('Ctrl Pts',(-142.766484480554,4.84991126603712,
134.197154388084));
#157997=CARTESIAN_POINT('Ctrl Pts',(-142.773907851583,4.93834589672733,
134.067074908652));
#157998=CARTESIAN_POINT('Ctrl Pts',(-142.781331222612,5.02136205430695,
133.933873947473));
#157999=CARTESIAN_POINT('Ctrl Pts',(-142.785267272052,5.06537921299629,
133.863247601751));
#158000=CARTESIAN_POINT('Ctrl Pts',(-142.789203321493,5.10787382247675,
133.791744087645));
#158001=CARTESIAN_POINT('Ctrl Pts',(-142.793139370933,5.14881215909193,
133.719435901823));
#158002=CARTESIAN_POINT('Ctrl Pts',(-142.800562637338,5.22602058431397,
133.583064920012));
#158003=CARTESIAN_POINT('Ctrl Pts',(-142.807985903744,5.29792415084296,
133.443418207619));
#158004=CARTESIAN_POINT('Ctrl Pts',(-142.815409170149,5.36423206739362,
133.3009472653));
#158005=CARTESIAN_POINT('Ctrl Pts',(-142.82282366287,5.43046161349344,133.158644711804));
#158006=CARTESIAN_POINT('Ctrl Pts',(-142.830238155591,5.49110851803365,
133.013524907833));
#158007=CARTESIAN_POINT('Ctrl Pts',(-142.837652648312,5.5459264641699,132.866066274666));
#158008=CARTESIAN_POINT('Ctrl Pts',(-142.845059994666,5.60069157470595,
132.718749767682));
#158009=CARTESIAN_POINT('Ctrl Pts',(-142.852467341019,5.64963878230422,
132.569099266825));
#158010=CARTESIAN_POINT('Ctrl Pts',(-142.859874687373,5.69256876743057,
132.417615523207));
#158011=CARTESIAN_POINT('Ctrl Pts',(-142.867276509049,5.73546673375435,
132.26624476188));
#158012=CARTESIAN_POINT('Ctrl Pts',(-142.874678330724,5.77235631221911,
132.113043837882));
#158013=CARTESIAN_POINT('Ctrl Pts',(-142.882080152399,5.80308721947066,
131.958531006077));
#158014=CARTESIAN_POINT('Ctrl Pts',(-142.889478066711,5.83380190411557,
131.804099740393));
#158015=CARTESIAN_POINT('Ctrl Pts',(-142.896875981022,5.85836431966345,
131.64835831134));
#158016=CARTESIAN_POINT('Ctrl Pts',(-142.904273895333,5.87667475221561,
131.491837467483));
#158017=CARTESIAN_POINT('Ctrl Pts',(-142.911670580245,5.89498214190599,
131.335342634551));
#158018=CARTESIAN_POINT('Ctrl Pts',(-142.919067265158,5.90703956730942,
131.178069014288));
#158019=CARTESIAN_POINT('Ctrl Pts',(-142.92646395007,5.91279887846187,131.020554940711));
#158020=CARTESIAN_POINT('Ctrl Pts',(-142.933860307005,5.91855793424043,
130.863047851472));
#158021=CARTESIAN_POINT('Ctrl Pts',(-142.941256663941,5.91801941740107,
130.705300703166));
#158022=CARTESIAN_POINT('Ctrl Pts',(-142.948653020876,5.91118726991158,
130.547854043507));
#158023=CARTESIAN_POINT('Ctrl Pts',(-142.956050510213,5.90435407640287,
130.390383278363));
#158024=CARTESIAN_POINT('Ctrl Pts',(-142.963447999549,5.89122534983063,
130.23321346644));
#158025=CARTESIAN_POINT('Ctrl Pts',(-142.970845488886,5.87185707922157,
130.076882093006));
#158026=CARTESIAN_POINT('Ctrl Pts',(-142.978245571401,5.8524820190953,129.920495917852));
#158027=CARTESIAN_POINT('Ctrl Pts',(-142.985645653916,5.82686310597789,
129.7649491366));
#158028=CARTESIAN_POINT('Ctrl Pts',(-142.993045736431,5.79510778321126,
129.610770929497));
#158029=CARTESIAN_POINT('Ctrl Pts',(-143.000453956097,5.76331754220268,
129.456423187605));
#158030=CARTESIAN_POINT('Ctrl Pts',(-143.007862175763,5.72537749147001,
129.303447391069));
#158031=CARTESIAN_POINT('Ctrl Pts',(-143.01527039543,5.68144566929237,129.152360112306));
#158032=CARTESIAN_POINT('Ctrl Pts',(-143.022683174732,5.63748680781111,
129.001179841843));
#158033=CARTESIAN_POINT('Ctrl Pts',(-143.030095954034,5.58752894459882,
128.851890758466));
#158034=CARTESIAN_POINT('Ctrl Pts',(-143.037508733336,5.53177879802467,
128.704990737763));
#158035=CARTESIAN_POINT('Ctrl Pts',(-143.044932104365,5.47594899302675,
128.557880819422));
#158036=CARTESIAN_POINT('Ctrl Pts',(-143.052355475393,5.41431052096332,
128.413167124023));
#158037=CARTESIAN_POINT('Ctrl Pts',(-143.059778846422,5.34711704083224,
128.27132490638));
#158038=CARTESIAN_POINT('Ctrl Pts',(-143.063714895863,5.31148944537873,
128.196116759124));
#158039=CARTESIAN_POINT('Ctrl Pts',(-143.067650945304,5.27430088828306,
128.1217154447));
#158040=CARTESIAN_POINT('Ctrl Pts',(-143.071586994745,5.23559413458562,
128.048188521997));
#158041=CARTESIAN_POINT('Ctrl Pts',(-143.079010261151,5.16259440511387,
127.909519040486));
#158042=CARTESIAN_POINT('Ctrl Pts',(-143.086433527556,5.08397130502822,
127.773542074441));
#158043=CARTESIAN_POINT('Ctrl Pts',(-143.093856793961,4.99994751482491,
127.640746321939));
#158044=CARTESIAN_POINT('Ctrl Pts',(-143.101271286683,4.91602303376388,
127.508107522989));
#158045=CARTESIAN_POINT('Ctrl Pts',(-143.108685779404,4.82671076596348,
127.378642765794));
#158046=CARTESIAN_POINT('Ctrl Pts',(-143.116100272125,4.73228008052372,
127.252817882081));
#158047=CARTESIAN_POINT('Ctrl Pts',(-143.123507618478,4.63794041093303,
127.127114273126));
#158048=CARTESIAN_POINT('Ctrl Pts',(-143.130914964832,4.53849236754767,
127.005043849986));
#158049=CARTESIAN_POINT('Ctrl Pts',(-143.138322311186,4.43424950938221,
126.887044974036));
#158050=CARTESIAN_POINT('Ctrl Pts',(-143.145724132861,4.33008439947413,
126.769134106101));
#158051=CARTESIAN_POINT('Ctrl Pts',(-143.153125954537,4.22113184147722,
126.65528901741));
#158052=CARTESIAN_POINT('Ctrl Pts',(-143.160527776212,4.10774662606244,
126.545916275019));
#158053=CARTESIAN_POINT('Ctrl Pts',(-143.167925690523,3.99442126582092,
126.436601269647));
#158054=CARTESIAN_POINT('Ctrl Pts',(-143.175323604835,3.87666817630713,
126.331754167205));
#158055=CARTESIAN_POINT('Ctrl Pts',(-143.182721519146,3.7548799935218,126.231745742382));
#158056=CARTESIAN_POINT('Ctrl Pts',(-143.190118204058,3.63311204972211,
126.131753937145));
#158057=CARTESIAN_POINT('Ctrl Pts',(-143.19751488897,3.50731063172423,126.036599450295));
#158058=CARTESIAN_POINT('Ctrl Pts',(-143.204911573883,3.37790262894944,
125.946613774447));
#158059=CARTESIAN_POINT('Ctrl Pts',(-143.212307930818,3.2485003642611,125.856632088657));
#158060=CARTESIAN_POINT('Ctrl Pts',(-143.219704287754,3.11549213925364,
125.771818971278));
#158061=CARTESIAN_POINT('Ctrl Pts',(-143.227100644689,2.97933486275858,
125.692463285063));
#158062=CARTESIAN_POINT('Ctrl Pts',(-143.234498134026,2.84315674023651,
125.61309544929));
#158063=CARTESIAN_POINT('Ctrl Pts',(-143.241895623362,2.70382892878528,
125.539186896349));
#158064=CARTESIAN_POINT('Ctrl Pts',(-143.249293112699,2.56183389341936,
125.470981045003));
#158065=CARTESIAN_POINT('Ctrl Pts',(-143.256693195214,2.4197890819129,125.402751284202));
#158066=CARTESIAN_POINT('Ctrl Pts',(-143.264093277729,2.27507552121324,
125.340228366664));
#158067=CARTESIAN_POINT('Ctrl Pts',(-143.271493360244,2.12819650139914,
125.283607932113));
#158068=CARTESIAN_POINT('Ctrl Pts',(-143.278901579911,1.9811559730047,125.226925237575));
#158069=CARTESIAN_POINT('Ctrl Pts',(-143.286309799577,1.83194557872065,
125.176158122105));
#158070=CARTESIAN_POINT('Ctrl Pts',(-143.293718019244,1.68108534910109,
125.131452843634));
#158071=CARTESIAN_POINT('Ctrl Pts',(-143.301130798546,1.53013226752743,
125.08672004981));
#158072=CARTESIAN_POINT('Ctrl Pts',(-143.308543577848,1.37752768824008,
125.048056618857));
#158073=CARTESIAN_POINT('Ctrl Pts',(-143.31595635715,1.22380222440171,125.015557746674));
#158074=CARTESIAN_POINT('Ctrl Pts',(-143.323379728179,1.06985711041137,
124.983012438578));
#158075=CARTESIAN_POINT('Ctrl Pts',(-143.330803099207,0.914788280213099,
124.956649343626));
#158076=CARTESIAN_POINT('Ctrl Pts',(-143.338226470236,0.759132688026945,
124.936511938155));
#158077=CARTESIAN_POINT('Ctrl Pts',(-143.342162519677,0.676600358145183,
124.925834602583));
#158078=CARTESIAN_POINT('Ctrl Pts',(-143.346098569118,0.593903101680449,
124.916906661104));
#158079=CARTESIAN_POINT('Ctrl Pts',(-143.350034618558,0.511120873387011,
124.909728651507));
#158080=CARTESIAN_POINT('Ctrl Pts',(-143.357457884964,0.354996174372463,
124.896191149424));
#158081=CARTESIAN_POINT('Ctrl Pts',(-143.364881151369,0.198097195700472,
124.888840118679));
#158082=CARTESIAN_POINT('Ctrl Pts',(-143.372304417774,0.0409554571512921,
124.88775236511));
#158083=CARTESIAN_POINT('Ctrl Pts',(-143.379718910495,-0.116000552913623,
124.886665897176));
#158084=CARTESIAN_POINT('Ctrl Pts',(-143.387133403216,-0.273198382092143,
124.891827973915));
#158085=CARTESIAN_POINT('Ctrl Pts',(-143.394547895937,-0.430100512383416,
124.903263760901));
#158086=CARTESIAN_POINT('Ctrl Pts',(-143.401955242291,-0.586851414494252,
124.914688525644));
#158087=CARTESIAN_POINT('Ctrl Pts',(-143.409362588645,-0.743306815297192,
124.932374935615));
#158088=CARTESIAN_POINT('Ctrl Pts',(-143.416769934999,-0.89892842264511,
124.956296129767));
#158089=CARTESIAN_POINT('Ctrl Pts',(-143.424171756674,-1.054433961527,124.980199482589));
#158090=CARTESIAN_POINT('Ctrl Pts',(-143.431573578349,-1.20910657781373,
125.01032830407));
#158091=CARTESIAN_POINT('Ctrl Pts',(-143.438975400025,-1.36241244210333,
125.046603858193));
#158092=CARTESIAN_POINT('Ctrl Pts',(-143.446373314336,-1.5156373774205,
125.082860262734));
#158093=CARTESIAN_POINT('Ctrl Pts',(-143.453771228647,-1.66749663529066,
125.12525685198));
#158094=CARTESIAN_POINT('Ctrl Pts',(-143.461169142958,-1.81746604311702,
125.173663702919));
#158095=CARTESIAN_POINT('Ctrl Pts',(-143.46856582787,-1.96741052874832,
125.222062509518));
#158096=CARTESIAN_POINT('Ctrl Pts',(-143.475962512783,-2.11546543274709,
125.27646948094));
#158097=CARTESIAN_POINT('Ctrl Pts',(-143.483359197695,-2.26112111683015,
125.33670464288));
#158098=CARTESIAN_POINT('Ctrl Pts',(-143.49075555463,-2.40677034238755,
125.396937133929));
#158099=CARTESIAN_POINT('Ctrl Pts',(-143.498151911566,-2.55002021459294,
125.462997158996));
#158100=CARTESIAN_POINT('Ctrl Pts',(-143.505548268501,-2.69038073464604,
125.534656445115));
#158101=CARTESIAN_POINT('Ctrl Pts',(-143.512945757837,-2.83076274425348,
125.606326702454));
#158102=CARTESIAN_POINT('Ctrl Pts',(-143.520343247174,-2.96825418840066,
125.683597758014));
#158103=CARTESIAN_POINT('Ctrl Pts',(-143.52774073651,-3.10238948786392,
125.766195274101));
#158104=CARTESIAN_POINT('Ctrl Pts',(-143.535140819025,-3.23657180824789,
125.848821744619));
#158105=CARTESIAN_POINT('Ctrl Pts',(-143.54254090154,-3.36739532389419,
125.936778197598));
#158106=CARTESIAN_POINT('Ctrl Pts',(-143.549940984055,-3.49442339698252,
126.029746948889));
#158107=CARTESIAN_POINT('Ctrl Pts',(-143.557349203721,-3.62159115049655,
126.122817928879));
#158108=CARTESIAN_POINT('Ctrl Pts',(-143.564757423388,-3.74495482531704,
126.22091199348));
#158109=CARTESIAN_POINT('Ctrl Pts',(-143.572165643054,-3.86411028128924,
126.32367068224));
#158110=CARTESIAN_POINT('Ctrl Pts',(-143.579578422356,-3.98333907545603,
126.426492617258));
#158111=CARTESIAN_POINT('Ctrl Pts',(-143.586991201658,-4.09835421760054,
126.533984642959));
#158112=CARTESIAN_POINT('Ctrl Pts',(-143.59440398096,-4.20878880734122,
126.645751795171));
#158113=CARTESIAN_POINT('Ctrl Pts',(-143.601827351989,-4.31938119120306,
126.757678645532));
#158114=CARTESIAN_POINT('Ctrl Pts',(-143.609250723018,-4.42537970011683,
126.873892547378));
#158115=CARTESIAN_POINT('Ctrl Pts',(-143.616674094046,-4.52645751933683,
126.993965245936));
#158116=CARTESIAN_POINT('Ctrl Pts',(-143.620610143488,-4.58005140442691,
127.057630671829));
#158117=CARTESIAN_POINT('Ctrl Pts',(-143.624546192929,-4.63226262156781,
127.122380445366));
#158118=CARTESIAN_POINT('Ctrl Pts',(-143.628482242371,-4.68304750080456,
127.188147589036));
#158119=CARTESIAN_POINT('Ctrl Pts',(-143.636113182597,-4.78150570962224,
127.315652375148));
#158120=CARTESIAN_POINT('Ctrl Pts',(-143.643744122823,-4.87490999056476,
127.447384705789));
#158121=CARTESIAN_POINT('Ctrl Pts',(-143.651375063048,-4.96287774080348,
127.582905186812));
#158122=CARTESIAN_POINT('Ctrl Pts',(-143.658797252299,-5.04843905709521,
127.714718387778));
#158123=CARTESIAN_POINT('Ctrl Pts',(-143.666219441551,-5.12885712916795,
127.850114878207));
#158124=CARTESIAN_POINT('Ctrl Pts',(-143.673641630802,-5.20381921518821,
127.988655352781));
#158125=CARTESIAN_POINT('Ctrl Pts',(-143.681056664793,-5.27870903503637,
128.127062269308));
#158126=CARTESIAN_POINT('Ctrl Pts',(-143.688471698784,-5.34815316205252,
128.268606812903));
#158127=CARTESIAN_POINT('Ctrl Pts',(-143.695886732775,-5.41188208523512,
128.412820766756));
#158128=CARTESIAN_POINT('Ctrl Pts',(-143.703296068788,-5.47556203682004,
128.556923901418));
#158129=CARTESIAN_POINT('Ctrl Pts',(-143.7107054048,-5.53353537798816,128.703692024345));
#158130=CARTESIAN_POINT('Ctrl Pts',(-143.718114740812,-5.58557856269081,
128.852632490365));
#158131=CARTESIAN_POINT('Ctrl Pts',(-143.725907246394,-5.64031313089013,
129.0092753273));
#158132=CARTESIAN_POINT('Ctrl Pts',(-143.733699751975,-5.68848768069859,
129.168320795676));
#158133=CARTESIAN_POINT('Ctrl Pts',(-143.741492257557,-5.72989940319255,
129.329171344356));
#158134=CARTESIAN_POINT('Ctrl Pts',(-143.748894865279,-5.7692390909901,
129.48197373909));
#158135=CARTESIAN_POINT('Ctrl Pts',(-143.756297473002,-5.80247610360676,
129.636404580094));
#158136=CARTESIAN_POINT('Ctrl Pts',(-143.763700080724,-5.82948772392865,
129.791936082568));
#158137=CARTESIAN_POINT('Ctrl Pts',(-143.771101448252,-5.85649481886142,
129.947441528088));
#158138=CARTESIAN_POINT('Ctrl Pts',(-143.778502815779,-5.87727853829152,
130.104046901191));
#158139=CARTESIAN_POINT('Ctrl Pts',(-143.785904183306,-5.89176743063363,
130.261215051603));
#158140=CARTESIAN_POINT('Ctrl Pts',(-143.793306662413,-5.90625849899951,
130.418406806418));
#158141=CARTESIAN_POINT('Ctrl Pts',(-143.800709141519,-5.91445282034711,
130.576161137043));
#158142=CARTESIAN_POINT('Ctrl Pts',(-143.808111620626,-5.9163308740846,
130.733936538919));
#158143=CARTESIAN_POINT('Ctrl Pts',(-143.809282683014,-5.91662797969786,
130.758896398477));
#158144=CARTESIAN_POINT('Ctrl Pts',(-143.810453745402,-5.91676711521594,
130.783856783679));
#158145=CARTESIAN_POINT('Ctrl Pts',(-143.81162480779,-5.91674832286034,
130.808815550709));
#158146=CARTESIAN_POINT('',(-145.56162480779,-5.92566626415315,130.806424113553));
#158147=CARTESIAN_POINT('Ctrl Pts',(-143.811626935791,-5.91075733511084,
130.808856347913));
#158148=CARTESIAN_POINT('Ctrl Pts',(-143.843394579256,-5.91545624009792,
131.485236077572));
#158149=CARTESIAN_POINT('Ctrl Pts',(-143.87516222272,-5.80834015743627,
132.160170260916));
#158150=CARTESIAN_POINT('Ctrl Pts',(-143.999745740789,-4.92438460180809,
134.641836647651));
#158151=CARTESIAN_POINT('Ctrl Pts',(-144.185377489997,-1.58782966150643,
137.620250691237));
#158152=CARTESIAN_POINT('Ctrl Pts',(-144.46382511381,4.87614063807827,135.824401753654));
#158153=CARTESIAN_POINT('Ctrl Pts',(-144.742272737623,6.85917590398193,
129.415380254652));
#158154=CARTESIAN_POINT('Ctrl Pts',(-145.020720361436,2.53896360349993,
124.282763853699));
#158155=CARTESIAN_POINT('Ctrl Pts',(-145.29383771816,-3.98706758988356,
125.126705578275));
#158156=CARTESIAN_POINT('Ctrl Pts',(-145.474139200277,-5.91733683117123,
128.955762140162));
#158157=CARTESIAN_POINT('Ctrl Pts',(-145.56162480779,-5.92566626415315,
130.806424113553));
#158158=CARTESIAN_POINT('',(-147.31162480779,-5.91706323075389,130.7989080505));
#158159=CARTESIAN_POINT('Ctrl Pts',(-145.56162480779,-5.92566626415315,
130.806424113553));
#158160=CARTESIAN_POINT('Ctrl Pts',(-145.566955074881,-5.92617375451377,
130.919180061563));
#158161=CARTESIAN_POINT('Ctrl Pts',(-145.572285341971,-5.92323536319911,
131.031909033594));
#158162=CARTESIAN_POINT('Ctrl Pts',(-145.577615609062,-5.91676776598012,
131.144435159557));
#158163=CARTESIAN_POINT('Ctrl Pts',(-145.670431483666,-5.80414757598299,
133.1038511925));
#158164=CARTESIAN_POINT('Ctrl Pts',(-145.856063232874,-3.43871107334941,
136.89967247869));
#158165=CARTESIAN_POINT('Ctrl Pts',(-146.134510856688,3.26945116665681,
136.992110580141));
#158166=CARTESIAN_POINT('Ctrl Pts',(-146.412958480499,6.97314750603267,
131.398308754382));
#158167=CARTESIAN_POINT('Ctrl Pts',(-146.691406104313,4.26886194461242,
125.258697606868));
#158168=CARTESIAN_POINT('Ctrl Pts',(-146.969853728126,-2.35829919844555,
124.215279845482));
#158169=CARTESIAN_POINT('Ctrl Pts',(-147.176593295952,-5.66972392369356,
127.936271574623));
#158170=CARTESIAN_POINT('Ctrl Pts',(-147.290516989173,-5.92122118069781,
130.350705029069));
#158171=CARTESIAN_POINT('Ctrl Pts',(-147.31162480779,-5.91706323075389,
130.7989080505));
#158172=CARTESIAN_POINT('',(-149.061624807827,-5.91674998631937,130.804762972876));
#158173=CARTESIAN_POINT('Ctrl Pts',(-147.31162480779,-5.9167474878674,130.798908341457));
#158174=CARTESIAN_POINT('Ctrl Pts',(-147.318933966831,-5.91689049786105,
130.954101146018));
#158175=CARTESIAN_POINT('Ctrl Pts',(-147.326243125871,-5.91092341403555,
131.10947153384));
#158176=CARTESIAN_POINT('Ctrl Pts',(-147.333552284912,-5.89883117521154,
131.264492477854));
#158177=CARTESIAN_POINT('Ctrl Pts',(-147.340856271384,-5.88674749386184,
131.419403716151));
#158178=CARTESIAN_POINT('Ctrl Pts',(-147.348160257856,-5.86854731442905,
131.573965621545));
#158179=CARTESIAN_POINT('Ctrl Pts',(-147.355464244328,-5.84426764698183,
131.727651597128));
#158180=CARTESIAN_POINT('Ctrl Pts',(-147.362765419609,-5.81999732440011,
131.881278421376));
#158181=CARTESIAN_POINT('Ctrl Pts',(-147.37006659489,-5.78965222652408,
132.03402960761));
#158182=CARTESIAN_POINT('Ctrl Pts',(-147.377367770171,-5.75332115896855,
132.185384224991));
#158183=CARTESIAN_POINT('Ctrl Pts',(-147.384667616045,-5.71699670662247,
132.33671128352));
#158184=CARTESIAN_POINT('Ctrl Pts',(-147.391967461918,-5.67468854189339,
132.486641905648));
#158185=CARTESIAN_POINT('Ctrl Pts',(-147.399267307792,-5.62653641745565,
132.634666194661));
#158186=CARTESIAN_POINT('Ctrl Pts',(-147.406567355322,-5.57838296282187,
132.782694572826));
#158187=CARTESIAN_POINT('Ctrl Pts',(-147.413867402853,-5.52438534596461,
132.928816147779));
#158188=CARTESIAN_POINT('Ctrl Pts',(-147.421167450384,-5.46473285050311,
133.072537293915));
#158189=CARTESIAN_POINT('Ctrl Pts',(-147.428469230619,-5.40506619621038,
133.216292553015));
#158190=CARTESIAN_POINT('Ctrl Pts',(-147.435771010854,-5.33974214007272,
133.35764589509));
#158191=CARTESIAN_POINT('Ctrl Pts',(-147.443072791089,-5.26899752875663,
133.49612502116));
#158192=CARTESIAN_POINT('Ctrl Pts',(-147.4503820623,-5.19818033977865,133.634746214464));
#158193=CARTESIAN_POINT('Ctrl Pts',(-147.45769133351,-5.12193166448401,
133.770486960439));
#158194=CARTESIAN_POINT('Ctrl Pts',(-147.465000604721,-5.04053391802298,
133.902900335523));
#158195=CARTESIAN_POINT('Ctrl Pts',(-147.472313795679,-4.95909252033,134.03538472003));
#158196=CARTESIAN_POINT('Ctrl Pts',(-147.479626986638,-4.8724967655997,
134.164537861454));
#158197=CARTESIAN_POINT('Ctrl Pts',(-147.486940177597,-4.78107111505981,
134.289943718747));
#158198=CARTESIAN_POINT('Ctrl Pts',(-147.494264308553,-4.68950869845622,
134.415537174));
#158199=CARTESIAN_POINT('Ctrl Pts',(-147.501588439509,-4.59310219201926,
134.537371847386));
#158200=CARTESIAN_POINT('Ctrl Pts',(-147.508912570465,-4.49221543116387,
134.655065888359));
#158201=CARTESIAN_POINT('Ctrl Pts',(-147.514858038894,-4.41031915497808,
134.750605715421));
#158202=CARTESIAN_POINT('Ctrl Pts',(-147.520803507323,-4.32547134683653,
134.843417653146));
#158203=CARTESIAN_POINT('Ctrl Pts',(-147.526748975753,-4.23788302417541,
134.933316664305));
#158204=CARTESIAN_POINT('Ctrl Pts',(-147.534172242158,-4.12852386082811,
135.045560857908));
#158205=CARTESIAN_POINT('Ctrl Pts',(-147.541595508563,-4.01453691909021,
135.153627061113));
#158206=CARTESIAN_POINT('Ctrl Pts',(-147.549018774969,-3.89627443970795,
135.257109886611));
#158207=CARTESIAN_POINT('Ctrl Pts',(-147.55643326769,-3.77815173675523,
135.360470404002));
#158208=CARTESIAN_POINT('Ctrl Pts',(-147.563847760411,-3.65576383302849,
135.459258083175));
#158209=CARTESIAN_POINT('Ctrl Pts',(-147.571262253132,-3.52950124668865,
135.55310271544));
#158210=CARTESIAN_POINT('Ctrl Pts',(-147.578669599486,-3.40336035698288,
135.646856896716));
#158211=CARTESIAN_POINT('Ctrl Pts',(-147.586076945839,-3.2733525170426,
135.735677294669));
#158212=CARTESIAN_POINT('Ctrl Pts',(-147.593484292193,-3.13990281966218,
135.819232584583));
#158213=CARTESIAN_POINT('Ctrl Pts',(-147.600886113869,-3.00655265410045,
135.902725555811));
#158214=CARTESIAN_POINT('Ctrl Pts',(-147.608287935544,-2.86976605751078,
135.98096104077));
#158215=CARTESIAN_POINT('Ctrl Pts',(-147.61568975722,-2.72999863336022,
136.053649905113));
#158216=CARTESIAN_POINT('Ctrl Pts',(-147.623087671531,-2.59030499134612,
136.126300397569));
#158217=CARTESIAN_POINT('Ctrl Pts',(-147.630485585842,-2.447633985931,136.193409928893));
#158218=CARTESIAN_POINT('Ctrl Pts',(-147.637883500153,-2.30246734934998,
136.254734427469));
#158219=CARTESIAN_POINT('Ctrl Pts',(-147.645280185066,-2.15732483683016,
136.316048735026));
#158220=CARTESIAN_POINT('Ctrl Pts',(-147.652676869978,-2.00968785979474,
136.37157977274));
#158221=CARTESIAN_POINT('Ctrl Pts',(-147.66007355489,-1.86005984450871,
136.421130858313));
#158222=CARTESIAN_POINT('Ctrl Pts',(-147.667469911825,-1.71043846388568,
136.47067974674));
#158223=CARTESIAN_POINT('Ctrl Pts',(-147.674866268761,-1.55882657492322,
136.514249092895));
#158224=CARTESIAN_POINT('Ctrl Pts',(-147.682262625696,-1.40574428777643,
136.551691612026));
#158225=CARTESIAN_POINT('Ctrl Pts',(-147.689660115033,-1.25263856334024,
136.589139863703));
#158226=CARTESIAN_POINT('Ctrl Pts',(-147.697057604369,-1.09806235510469,
136.620459331913));
#158227=CARTESIAN_POINT('Ctrl Pts',(-147.704455093706,-0.942547378665527,
136.645553560918));
#158228=CARTESIAN_POINT('Ctrl Pts',(-147.711855176221,-0.786977886693119,
136.670656586667));
#158229=CARTESIAN_POINT('Ctrl Pts',(-147.719255258736,-0.630469339614789,
136.689529968942));
#158230=CARTESIAN_POINT('Ctrl Pts',(-147.726655341251,-0.473559859136847,
136.702128977066));
#158231=CARTESIAN_POINT('Ctrl Pts',(-147.734063560917,-0.316477840554209,
136.714741839094));
#158232=CARTESIAN_POINT('Ctrl Pts',(-147.741471780584,-0.158994380459275,
136.721066518681));
#158233=CARTESIAN_POINT('Ctrl Pts',(-147.74888000025,-0.00164963514046322,
136.721110387601));
#158234=CARTESIAN_POINT('Ctrl Pts',(-147.756292779552,0.155791953244103,
136.721154283521));
#158235=CARTESIAN_POINT('Ctrl Pts',(-147.763705558854,0.313094284589634,
136.714909680587));
#158236=CARTESIAN_POINT('Ctrl Pts',(-147.771118338156,0.469721549545526,
136.702435916203));
#158237=CARTESIAN_POINT('Ctrl Pts',(-147.778541709185,0.626572610882453,
136.689944328719));
#158238=CARTESIAN_POINT('Ctrl Pts',(-147.785965080214,0.782746309716429,
136.671205847807));
#158239=CARTESIAN_POINT('Ctrl Pts',(-147.793388451242,0.93771543736235,
136.646331202996));
#158240=CARTESIAN_POINT('Ctrl Pts',(-147.797324500683,1.01988378727759,
136.633142069458));
#158241=CARTESIAN_POINT('Ctrl Pts',(-147.801260550124,1.10171370423964,
136.618228684312));
#158242=CARTESIAN_POINT('Ctrl Pts',(-147.805196599565,1.18312836961951,
136.60161322751));
#158243=CARTESIAN_POINT('Ctrl Pts',(-147.812619865971,1.33667388765318,
136.570276994533));
#158244=CARTESIAN_POINT('Ctrl Pts',(-147.820043132376,1.48920577129814,
136.532788974667));
#158245=CARTESIAN_POINT('Ctrl Pts',(-147.827466398781,1.64019256200267,
136.489226396285));
#158246=CARTESIAN_POINT('Ctrl Pts',(-147.834880891502,1.79100089885968,
136.445715305253));
#158247=CARTESIAN_POINT('Ctrl Pts',(-147.842295384223,1.9402674226153,136.396144049259));
#158248=CARTESIAN_POINT('Ctrl Pts',(-147.849709876944,2.08746958160983,
136.34064107545));
#158249=CARTESIAN_POINT('Ctrl Pts',(-147.857117223298,2.23452986162189,
136.285191597498));
#158250=CARTESIAN_POINT('Ctrl Pts',(-147.864524569652,2.37952939105012,
136.223821914395));
#158251=CARTESIAN_POINT('Ctrl Pts',(-147.871931916006,2.52195964398813,
136.156710579648));
#158252=CARTESIAN_POINT('Ctrl Pts',(-147.879333737681,2.66428366706951,
136.089649299065));
#158253=CARTESIAN_POINT('Ctrl Pts',(-147.886735559357,2.80404189296403,
136.016855051986));
#158254=CARTESIAN_POINT('Ctrl Pts',(-147.894137381032,2.94074479995316,
135.938554866331));
#158255=CARTESIAN_POINT('Ctrl Pts',(-147.901535295343,3.07737554254216,
135.860296014734));
#158256=CARTESIAN_POINT('Ctrl Pts',(-147.908933209655,3.21095385524653,
135.776537198147));
#158257=CARTESIAN_POINT('Ctrl Pts',(-147.916331123966,3.3410140056634,135.687551784873));
#158258=CARTESIAN_POINT('Ctrl Pts',(-147.923727808878,3.47105254244226,
135.59858115936));
#158259=CARTESIAN_POINT('Ctrl Pts',(-147.93112449379,3.59757376951305,135.504385871589));
#158260=CARTESIAN_POINT('Ctrl Pts',(-147.938521178703,3.72014009829545,
135.405283156748));
#158261=CARTESIAN_POINT('Ctrl Pts',(-147.945917535638,3.8427009923584,135.306184836226));
#158262=CARTESIAN_POINT('Ctrl Pts',(-147.953313892573,3.96130704653665,
135.202179756007));
#158263=CARTESIAN_POINT('Ctrl Pts',(-147.960710249509,4.07555321375501,
135.09362588849));
#158264=CARTESIAN_POINT('Ctrl Pts',(-147.968107738845,4.18981687235322,
134.985055401098));
#158265=CARTESIAN_POINT('Ctrl Pts',(-147.975505228182,4.2997190442562,134.871934996872));
#158266=CARTESIAN_POINT('Ctrl Pts',(-147.982902717519,4.40489117325363,
134.754659886519));
#158267=CARTESIAN_POINT('Ctrl Pts',(-147.990302800034,4.5101001701777,134.637343665558));
#158268=CARTESIAN_POINT('Ctrl Pts',(-147.997702882548,4.61057557383729,
134.515870116477));
#158269=CARTESIAN_POINT('Ctrl Pts',(-148.005102965063,4.70598888311962,
134.390667798282));
#158270=CARTESIAN_POINT('Ctrl Pts',(-148.01251118473,4.80150710914464,134.265327807267));
#158271=CARTESIAN_POINT('Ctrl Pts',(-148.019919404396,4.89195189813434,
134.136251155931));
#158272=CARTESIAN_POINT('Ctrl Pts',(-148.027327624063,4.97703748450313,
134.003896277682));
#158273=CARTESIAN_POINT('Ctrl Pts',(-148.034740403365,5.0621754396306,133.871459937213));
#158274=CARTESIAN_POINT('Ctrl Pts',(-148.042153182667,5.14194743074158,
133.7357416704));
#158275=CARTESIAN_POINT('Ctrl Pts',(-148.049565961969,5.21611376203199,
133.59722434214));
#158276=CARTESIAN_POINT('Ctrl Pts',(-148.056989332998,5.29038606565472,
133.458509093825));
#158277=CARTESIAN_POINT('Ctrl Pts',(-148.064412704026,5.35903654993662,
133.316987131281));
#158278=CARTESIAN_POINT('Ctrl Pts',(-148.071836075055,5.42187340559484,
133.173161862121));
#158279=CARTESIAN_POINT('Ctrl Pts',(-148.075772124496,5.45519101421609,
133.096902253368));
#158280=CARTESIAN_POINT('Ctrl Pts',(-148.079708173937,5.486875029849,133.019995377734));
#158281=CARTESIAN_POINT('Ctrl Pts',(-148.083644223378,5.51690259076839,
132.94251785371));
#158282=CARTESIAN_POINT('Ctrl Pts',(-148.091067489784,5.57353363353146,
132.796397661398));
#158283=CARTESIAN_POINT('Ctrl Pts',(-148.098490756189,5.62444110961093,
132.647805077326));
#158284=CARTESIAN_POINT('Ctrl Pts',(-148.105914022594,5.66940272709543,
132.497228976448));
#158285=CARTESIAN_POINT('Ctrl Pts',(-148.113328515315,5.71431120368202,
132.346830844015));
#158286=CARTESIAN_POINT('Ctrl Pts',(-148.120743008036,5.75328770421019,
132.194454215421));
#158287=CARTESIAN_POINT('Ctrl Pts',(-148.128157500757,5.78615784296867,
132.040608156998));
#158288=CARTESIAN_POINT('Ctrl Pts',(-148.135564847111,5.81899630024998,
131.886910381198));
#158289=CARTESIAN_POINT('Ctrl Pts',(-148.142972193465,5.84574003524237,
131.731746357735));
#158290=CARTESIAN_POINT('Ctrl Pts',(-148.150379539819,5.86626439939253,
131.575640436386));
#158291=CARTESIAN_POINT('Ctrl Pts',(-148.157781361494,5.88677345569757,
131.419650944724));
#158292=CARTESIAN_POINT('Ctrl Pts',(-148.16518318317,5.90107232886947,131.262721322474));
#158293=CARTESIAN_POINT('Ctrl Pts',(-148.172585004845,5.9090874254831,131.105386132261));
#158294=CARTESIAN_POINT('Ctrl Pts',(-148.179982919156,5.91709829098963,
130.94813399807));
#158295=CARTESIAN_POINT('Ctrl Pts',(-148.187380833468,5.91883196727027,
130.790477094168));
#158296=CARTESIAN_POINT('Ctrl Pts',(-148.194778747779,5.91426670708034,
130.632955016663));
#158297=CARTESIAN_POINT('Ctrl Pts',(-148.202175432691,5.90970220555385,
130.475459116469));
#158298=CARTESIAN_POINT('Ctrl Pts',(-148.209572117603,5.89884085588715,
130.318098370978));
#158299=CARTESIAN_POINT('Ctrl Pts',(-148.216968802516,5.88171302971251,
130.161412409224));
#158300=CARTESIAN_POINT('Ctrl Pts',(-148.224365159451,5.86458596300368,
130.00473339509));
#158301=CARTESIAN_POINT('Ctrl Pts',(-148.231761516386,5.84119301283541,
129.848729476288));
#158302=CARTESIAN_POINT('Ctrl Pts',(-148.239157873322,5.81161641368678,
129.693934923219));
#158303=CARTESIAN_POINT('Ctrl Pts',(-148.246555362658,5.78203528628523,
129.539116670708));
#158304=CARTESIAN_POINT('Ctrl Pts',(-148.253952851995,5.74626869489624,
129.38550851929));
#158305=CARTESIAN_POINT('Ctrl Pts',(-148.261350341332,5.70444992784726,
129.233634166785));
#158306=CARTESIAN_POINT('Ctrl Pts',(-148.268750423847,5.66261650129438,
129.081706574961));
#158307=CARTESIAN_POINT('Ctrl Pts',(-148.276150506362,5.61472677406775,
128.931514351815));
#158308=CARTESIAN_POINT('Ctrl Pts',(-148.283550588876,5.56096374212256,
128.783565521249));
#158309=CARTESIAN_POINT('Ctrl Pts',(-148.290958808543,5.50714159219669,
128.635454005734));
#158310=CARTESIAN_POINT('Ctrl Pts',(-148.298367028209,5.44743336747213,
128.489591160308));
#158311=CARTESIAN_POINT('Ctrl Pts',(-148.305775247876,5.38207029767888,
128.346465202105));
#158312=CARTESIAN_POINT('Ctrl Pts',(-148.313188027178,5.31666699800662,
128.203251152263));
#158313=CARTESIAN_POINT('Ctrl Pts',(-148.32060080648,5.2456020861296,128.062777678566));
#158314=CARTESIAN_POINT('Ctrl Pts',(-148.328013585782,5.16915224852444,
127.925507444152));
#158315=CARTESIAN_POINT('Ctrl Pts',(-148.335436956811,5.09259317580628,
127.788041071591));
#158316=CARTESIAN_POINT('Ctrl Pts',(-148.34286032784,5.01063400424249,127.65378739726));
#158317=CARTESIAN_POINT('Ctrl Pts',(-148.350283698868,4.92359458731299,
127.523179899854));
#158318=CARTESIAN_POINT('Ctrl Pts',(-148.354219748309,4.87744419997718,
127.453928670849));
#158319=CARTESIAN_POINT('Ctrl Pts',(-148.35815579775,4.82986625176899,127.385701966331));
#158320=CARTESIAN_POINT('Ctrl Pts',(-148.36209184719,4.78091284667562,127.318560434682));
#158321=CARTESIAN_POINT('Ctrl Pts',(-148.369515113596,4.68858825244866,
127.191933601403));
#158322=CARTESIAN_POINT('Ctrl Pts',(-148.376938380001,4.59108983741368,
127.068785778736));
#158323=CARTESIAN_POINT('Ctrl Pts',(-148.384361646406,4.48870875170665,
126.949568236016));
#158324=CARTESIAN_POINT('Ctrl Pts',(-148.391776139128,4.38644867194041,
126.830491598532));
#158325=CARTESIAN_POINT('Ctrl Pts',(-148.399190631849,4.27931764936329,
126.715336275004));
#158326=CARTESIAN_POINT('Ctrl Pts',(-148.40660512457,4.16764971616188,126.604524143859));
#158327=CARTESIAN_POINT('Ctrl Pts',(-148.414012470923,4.05608941271872,
126.493818817619));
#158328=CARTESIAN_POINT('Ctrl Pts',(-148.421419817277,3.94000116732137,
126.387448611174));
#158329=CARTESIAN_POINT('Ctrl Pts',(-148.428827163631,3.81975875470066,
126.285801818747));
#158330=CARTESIAN_POINT('Ctrl Pts',(-148.436228985306,3.69960602340812,
126.184230838332));
#158331=CARTESIAN_POINT('Ctrl Pts',(-148.443630806982,3.57530557795129,
126.087376497323));
#158332=CARTESIAN_POINT('Ctrl Pts',(-148.451032628657,3.44726738196088,
125.995589656107));
#158333=CARTESIAN_POINT('Ctrl Pts',(-148.458430542969,3.31929677633676,
125.90385126845));
#158334=CARTESIAN_POINT('Ctrl Pts',(-148.46582845728,3.1875926523864,125.817175269952));
#158335=CARTESIAN_POINT('Ctrl Pts',(-148.473226371591,3.05259723267876,
125.735871622062));
#158336=CARTESIAN_POINT('Ctrl Pts',(-148.480623056503,2.91762424676138,
125.654581485364));
#158337=CARTESIAN_POINT('Ctrl Pts',(-148.488019741416,2.77936137009441,
125.57866211976));
#158338=CARTESIAN_POINT('Ctrl Pts',(-148.495416426328,2.63827902447642,
125.508379655411));
#158339=CARTESIAN_POINT('Ctrl Pts',(-148.502812783263,2.49720293459748,
125.43810030746));
#158340=CARTESIAN_POINT('Ctrl Pts',(-148.510209140199,2.35330795847815,
125.373457530239));
#158341=CARTESIAN_POINT('Ctrl Pts',(-148.517605497134,2.20708804268295,
125.314670923754));
#158342=CARTESIAN_POINT('Ctrl Pts',(-148.525002986471,2.06084574024578,
125.25587531689));
#158343=CARTESIAN_POINT('Ctrl Pts',(-148.532400475807,1.91227813575677,
125.202937805259));
#158344=CARTESIAN_POINT('Ctrl Pts',(-148.539797965144,1.76189787661972,
125.15602932108));
#158345=CARTESIAN_POINT('Ctrl Pts',(-148.547198047659,1.61146490191573,
125.109104393205));
#158346=CARTESIAN_POINT('Ctrl Pts',(-148.554598130174,1.45921836358121,
125.068212811768));
#158347=CARTESIAN_POINT('Ctrl Pts',(-148.561998212689,1.30568459029637,
125.03347521642));
#158348=CARTESIAN_POINT('Ctrl Pts',(-148.569406432355,1.15198199084393,
124.998699423514));
#158349=CARTESIAN_POINT('Ctrl Pts',(-148.576814652022,0.996989694018722,
124.970091213148));
#158350=CARTESIAN_POINT('Ctrl Pts',(-148.584222871688,0.841243436040651,
124.947719938489));
#158351=CARTESIAN_POINT('Ctrl Pts',(-148.59163565099,0.685401318839116,
124.925334894684));
#158352=CARTESIAN_POINT('Ctrl Pts',(-148.599048430293,0.528804686275663,
124.909194473919));
#158353=CARTESIAN_POINT('Ctrl Pts',(-148.606461209595,0.371992345752456,
124.899315972756));
#158354=CARTESIAN_POINT('Ctrl Pts',(-148.613884580623,0.21495594440401,
124.889423356727));
#158355=CARTESIAN_POINT('Ctrl Pts',(-148.621307951652,0.0577035917347928,
124.885810538663));
#158356=CARTESIAN_POINT('Ctrl Pts',(-148.628731322681,-0.0992271257348289,
124.888442722597));
#158357=CARTESIAN_POINT('Ctrl Pts',(-148.632667372122,-0.182435557639672,
124.889838369677));
#158358=CARTESIAN_POINT('Ctrl Pts',(-148.636603421563,-0.265553659599762,
124.892988844659));
#158359=CARTESIAN_POINT('Ctrl Pts',(-148.640539471003,-0.348502242934304,
124.897883092918));
#158360=CARTESIAN_POINT('Ctrl Pts',(-148.647962737409,-0.504940682363872,
124.90711349239));
#158361=CARTESIAN_POINT('Ctrl Pts',(-148.655386003814,-0.661248708158524,
124.922577264053));
#158362=CARTESIAN_POINT('Ctrl Pts',(-148.66280927022,-0.816889280886414,
124.944273377151));
#158363=CARTESIAN_POINT('Ctrl Pts',(-148.670223762941,-0.972345899383371,
124.965943847245));
#158364=CARTESIAN_POINT('Ctrl Pts',(-148.677638255662,-1.12713626895924,
124.993831945456));
#158365=CARTESIAN_POINT('Ctrl Pts',(-148.685052748383,-1.2807248987907,
125.027884676638));
#158366=CARTESIAN_POINT('Ctrl Pts',(-148.692460094737,-1.43416549411733,
125.061904586516));
#158367=CARTESIAN_POINT('Ctrl Pts',(-148.69986744109,-1.58640629360985,
125.102077220338));
#158368=CARTESIAN_POINT('Ctrl Pts',(-148.707274787444,-1.73691857997097,
125.14829799335));
#158369=CARTESIAN_POINT('Ctrl Pts',(-148.714676609119,-1.88731860858998,
125.194484293166));
#158370=CARTESIAN_POINT('Ctrl Pts',(-148.722078430795,-2.03599233571464,
125.246709641185));
#158371=CARTESIAN_POINT('Ctrl Pts',(-148.72948025247,-2.18242297720716,
125.304818772007));
#158372=CARTESIAN_POINT('Ctrl Pts',(-148.736878166782,-2.32877631910385,
125.36289722747));
#158373=CARTESIAN_POINT('Ctrl Pts',(-148.744276081093,-2.47288858747791,
125.426853142636));
#158374=CARTESIAN_POINT('Ctrl Pts',(-148.751673995404,-2.61425997088384,
125.496482004868));
#158375=CARTESIAN_POINT('Ctrl Pts',(-148.759070680316,-2.7556078609312,
125.566099296047));
#158376=CARTESIAN_POINT('Ctrl Pts',(-148.766467365229,-2.89421543545877,
125.641387498452));
#158377=CARTESIAN_POINT('Ctrl Pts',(-148.773864050141,-3.02960451715323,
125.722094682755));
#158378=CARTESIAN_POINT('Ctrl Pts',(-148.781260407076,-3.16498759555432,
125.802798288416));
#158379=CARTESIAN_POINT('Ctrl Pts',(-148.788656764012,-3.29715214423205,
125.888920207067));
#158380=CARTESIAN_POINT('Ctrl Pts',(-148.796053120947,-3.42564641729864,
125.980163566641));
#158381=CARTESIAN_POINT('Ctrl Pts',(-148.803450610284,-3.55416036316647,
126.071420895807));
#158382=CARTESIAN_POINT('Ctrl Pts',(-148.81084809962,-3.67900261016223,
126.16780101101));
#158383=CARTESIAN_POINT('Ctrl Pts',(-148.818245588957,-3.79975224972568,
126.268965000511));
#158384=CARTESIAN_POINT('Ctrl Pts',(-148.825645671472,-3.92054421788826,
126.370164452891));
#158385=CARTESIAN_POINT('Ctrl Pts',(-148.833045753987,-4.03724043625919,
126.47615087884));
#158386=CARTESIAN_POINT('Ctrl Pts',(-148.840445836502,-4.14945491377776,
126.586546671809));
#158387=CARTESIAN_POINT('Ctrl Pts',(-148.847854056168,-4.26179278265012,
126.697063856301));
#158388=CARTESIAN_POINT('Ctrl Pts',(-148.855262275835,-4.36963880258899,
126.811999828733));
#158389=CARTESIAN_POINT('Ctrl Pts',(-148.862670495502,-4.47264504629845,
126.930941346131));
#158390=CARTESIAN_POINT('Ctrl Pts',(-148.870083274804,-4.57571468863245,
127.049956070049));
#158391=CARTESIAN_POINT('Ctrl Pts',(-148.877496054106,-4.67393838672805,
127.172980960398));
#158392=CARTESIAN_POINT('Ctrl Pts',(-148.884908833408,-4.76701034993793,
127.299572052462));
#158393=CARTESIAN_POINT('Ctrl Pts',(-148.892332204437,-4.86021529873281,
127.426344023814));
#158394=CARTESIAN_POINT('Ctrl Pts',(-148.899755575465,-4.94825360260969,
127.556692065321));
#158395=CARTESIAN_POINT('Ctrl Pts',(-148.907178946494,-5.03086395775739,
127.690145082148));
#158396=CARTESIAN_POINT('Ctrl Pts',(-148.911114995935,-5.07466595026532,
127.760905073831));
#158397=CARTESIAN_POINT('Ctrl Pts',(-148.915051045376,-5.11694273081757,
127.83253759572));
#158398=CARTESIAN_POINT('Ctrl Pts',(-148.918987094816,-5.15766079656884,
127.904970048837));
#158399=CARTESIAN_POINT('Ctrl Pts',(-148.926751505812,-5.23798290689435,
128.047853247807));
#158400=CARTESIAN_POINT('Ctrl Pts',(-148.934515916807,-5.31246115629263,
128.194249487309));
#158401=CARTESIAN_POINT('Ctrl Pts',(-148.942280327803,-5.38078957262255,
128.343662721103));
#158402=CARTESIAN_POINT('Ctrl Pts',(-148.950032457311,-5.44900990933353,
128.492839618008));
#158403=CARTESIAN_POINT('Ctrl Pts',(-148.957784586819,-5.51109966585383,
128.645023705493));
#158404=CARTESIAN_POINT('Ctrl Pts',(-148.965536716327,-5.56679783573118,
128.799692959674));
#158405=CARTESIAN_POINT('Ctrl Pts',(-148.973544057282,-5.62432967086496,
128.959454152033));
#158406=CARTESIAN_POINT('Ctrl Pts',(-148.981551398237,-5.67504168273002,
129.121866666269));
#158407=CARTESIAN_POINT('Ctrl Pts',(-148.989558739193,-5.71869808140008,
129.286328069729));
#158408=CARTESIAN_POINT('Ctrl Pts',(-148.997284861167,-5.76082126098831,
129.445013564739));
#158409=CARTESIAN_POINT('Ctrl Pts',(-149.005010983141,-5.79637585996302,
129.60560613198));
#158410=CARTESIAN_POINT('Ctrl Pts',(-149.012737105116,-5.82519898902617,
129.767544674041));
#158411=CARTESIAN_POINT('Ctrl Pts',(-149.020454611823,-5.85398997790732,
129.929302641181));
#158412=CARTESIAN_POINT('Ctrl Pts',(-149.028172118529,-5.87606439770469,
130.092403274386));
#158413=CARTESIAN_POINT('Ctrl Pts',(-149.035889625236,-5.89130968835139,
130.256272377921));
#158414=CARTESIAN_POINT('Ctrl Pts',(-149.043597068162,-5.90653509883906,
130.41992779292));
#158415=CARTESIAN_POINT('Ctrl Pts',(-149.051304511088,-5.91494910876179,
130.584349357764));
#158416=CARTESIAN_POINT('Ctrl Pts',(-149.059011954014,-5.91649057852451,
130.748954871197));
#158417=CARTESIAN_POINT('Ctrl Pts',(-149.059882905273,-5.91666476664925,
130.767555512222));
#158418=CARTESIAN_POINT('Ctrl Pts',(-149.060753856532,-5.91675125147269,
130.78615849435));
#158419=CARTESIAN_POINT('Ctrl Pts',(-149.06162480779,-5.91674998631942,
130.804762972079));
#158420=CARTESIAN_POINT('',(-150.81162480779,-5.91699367364741,130.809674885172));
#158421=CARTESIAN_POINT('Ctrl Pts',(-149.061624807827,-5.91674998631937,
130.804762972876));
#158422=CARTESIAN_POINT('Ctrl Pts',(-149.069413580783,-5.91673867224068,
130.971139738019));
#158423=CARTESIAN_POINT('Ctrl Pts',(-149.077202353739,-5.90970539075821,
131.137365971676));
#158424=CARTESIAN_POINT('Ctrl Pts',(-149.084991126695,-5.89571383838781,
131.302847225553));
#158425=CARTESIAN_POINT('Ctrl Pts',(-149.09279109274,-5.88170217903905,
131.46856628921));
#158426=CARTESIAN_POINT('Ctrl Pts',(-149.100591058784,-5.86071231162993,
131.633537926564));
#158427=CARTESIAN_POINT('Ctrl Pts',(-149.108391024829,-5.83285932808322,
131.797176119708));
#158428=CARTESIAN_POINT('Ctrl Pts',(-149.116210437207,-5.80493690341401,
131.96122228422));
#158429=CARTESIAN_POINT('Ctrl Pts',(-149.124029849585,-5.77011719447778,
132.123928048353));
#158430=CARTESIAN_POINT('Ctrl Pts',(-149.131849261963,-5.72856621314113,
132.284718582437));
#158431=CARTESIAN_POINT('Ctrl Pts',(-149.139678789375,-5.68696148229353,
132.445717111912));
#158432=CARTESIAN_POINT('Ctrl Pts',(-149.147508316787,-5.6386081857672,
132.604795168376));
#158433=CARTESIAN_POINT('Ctrl Pts',(-149.155337844199,-5.58372137006321,
132.761395677037));
#158434=CARTESIAN_POINT('Ctrl Pts',(-149.163185809046,-5.52870530363394,
132.918364957854));
#158435=CARTESIAN_POINT('Ctrl Pts',(-149.171033773893,-5.46712506161874,
133.072844732718));
#158436=CARTESIAN_POINT('Ctrl Pts',(-149.17888173874,-5.39924367833758,
133.224298274703));
#158437=CARTESIAN_POINT('Ctrl Pts',(-149.18506606537,-5.34575202100989,
133.343646180968));
#158438=CARTESIAN_POINT('Ctrl Pts',(-149.191250392,-5.28834849034848,133.461115324402));
#158439=CARTESIAN_POINT('Ctrl Pts',(-149.19743471863,-5.22718104389468,
133.576455294313));
#158440=CARTESIAN_POINT('Ctrl Pts',(-149.204857985035,-5.15375959035101,
133.714901947451));
#158441=CARTESIAN_POINT('Ctrl Pts',(-149.212281251441,-5.07472298733138,
133.850638981989));
#158442=CARTESIAN_POINT('Ctrl Pts',(-149.219704517846,-4.99029540172941,
133.983178379876));
#158443=CARTESIAN_POINT('Ctrl Pts',(-149.227119010567,-4.90596760252235,
134.115561127201));
#158444=CARTESIAN_POINT('Ctrl Pts',(-149.234533503288,-4.81626170222304,
134.244753448903));
#158445=CARTESIAN_POINT('Ctrl Pts',(-149.241947996009,-4.7214484865153,
134.370290335281));
#158446=CARTESIAN_POINT('Ctrl Pts',(-149.249355342363,-4.62672665535452,
134.495706224481));
#158447=CARTESIAN_POINT('Ctrl Pts',(-149.256762688717,-4.5269075322286,
134.617473396564));
#158448=CARTESIAN_POINT('Ctrl Pts',(-149.264170035071,-4.42230600892101,
134.735154446548));
#158449=CARTESIAN_POINT('Ctrl Pts',(-149.271571856746,-4.31778250137589,
134.852747725565));
#158450=CARTESIAN_POINT('Ctrl Pts',(-149.278973678421,-4.20848394275051,
134.966260672825));
#158451=CARTESIAN_POINT('Ctrl Pts',(-149.286375500097,-4.0947663595227,
135.075287803017));
#158452=CARTESIAN_POINT('Ctrl Pts',(-149.293773414408,-3.98110880692223,
135.184257378635));
#158453=CARTESIAN_POINT('Ctrl Pts',(-149.301171328719,-3.863037144318,135.288745595534));
#158454=CARTESIAN_POINT('Ctrl Pts',(-149.308569243031,-3.74094513440269,
135.38838287579));
#158455=CARTESIAN_POINT('Ctrl Pts',(-149.315965927943,-3.61887341396427,
135.488003598137));
#158456=CARTESIAN_POINT('Ctrl Pts',(-149.323362612855,-3.49278296114364,
135.582774747995));
#158457=CARTESIAN_POINT('Ctrl Pts',(-149.330759297767,-3.36310167233426,
135.67236613359));
#158458=CARTESIAN_POINT('Ctrl Pts',(-149.338155654703,-3.23342613372912,
135.761953546609));
#158459=CARTESIAN_POINT('Ctrl Pts',(-149.345552011638,-3.10016038285177,
135.846361439856));
#158460=CARTESIAN_POINT('Ctrl Pts',(-149.352948368573,-2.96376220561619,
135.925302342587));
#158461=CARTESIAN_POINT('Ctrl Pts',(-149.36034585791,-2.82734314547147,
136.004255331372));
#158462=CARTESIAN_POINT('Ctrl Pts',(-149.367743347247,-2.68779102716578,
136.077739476041));
#158463=CARTESIAN_POINT('Ctrl Pts',(-149.375140836583,-2.54558905436183,
136.145512827419));
#158464=CARTESIAN_POINT('Ctrl Pts',(-149.382540919098,-2.40333723287655,
136.213309936639));
#158465=CARTESIAN_POINT('Ctrl Pts',(-149.389941001613,-2.2584340442274,
136.275392106275));
#158466=CARTESIAN_POINT('Ctrl Pts',(-149.397341084128,-2.11138337162196,
136.331565229351));
#158467=CARTESIAN_POINT('Ctrl Pts',(-149.404749303795,-1.96417100168503,
136.387800120551));
#158468=CARTESIAN_POINT('Ctrl Pts',(-149.412157523461,-1.81480678089696,
136.438112855756));
#158469=CARTESIAN_POINT('Ctrl Pts',(-149.419565743127,-1.66381118256195,
136.482358760511));
#158470=CARTESIAN_POINT('Ctrl Pts',(-149.426978522429,-1.51272264895524,
136.526631897881));
#158471=CARTESIAN_POINT('Ctrl Pts',(-149.434391301732,-1.36000109833726,
136.564830673902));
#158472=CARTESIAN_POINT('Ctrl Pts',(-149.441804081034,-1.20617743115649,
136.59686150812));
#158473=CARTESIAN_POINT('Ctrl Pts',(-149.449227452062,-1.05213397350665,
136.628938109496));
#158474=CARTESIAN_POINT('Ctrl Pts',(-149.456650823091,-0.896985621384072,
136.654829106158));
#158475=CARTESIAN_POINT('Ctrl Pts',(-149.46407419412,-0.741269458848689,
136.674492656275));
#158476=CARTESIAN_POINT('Ctrl Pts',(-149.468010243561,-0.6587050131144,
136.684918742367));
#158477=CARTESIAN_POINT('Ctrl Pts',(-149.471946293001,-0.575980966114923,
136.693594940491));
#158478=CARTESIAN_POINT('Ctrl Pts',(-149.475882342442,-0.49317727387102,
136.700520956213));
#158479=CARTESIAN_POINT('Ctrl Pts',(-149.483305608848,-0.337012094513541,
136.713583205712));
#158480=CARTESIAN_POINT('Ctrl Pts',(-149.490728875253,-0.18009146857571,
136.720456655888));
#158481=CARTESIAN_POINT('Ctrl Pts',(-149.498152141658,-0.0229471471463872,
136.72106611902));
#158482=CARTESIAN_POINT('Ctrl Pts',(-149.505566634379,0.13401144274503,
136.721674861818));
#158483=CARTESIAN_POINT('Ctrl Pts',(-149.5129811271,0.291192832209383,136.71603435287));
#158484=CARTESIAN_POINT('Ctrl Pts',(-149.520395619821,0.448059429140211,
136.704121062742));
#158485=CARTESIAN_POINT('Ctrl Pts',(-149.527802966175,0.604774832138994,
136.692219255091));
#158486=CARTESIAN_POINT('Ctrl Pts',(-149.535210312529,0.761175676904451,
136.674056730619));
#158487=CARTESIAN_POINT('Ctrl Pts',(-149.542617658883,0.916723755538576,
136.649661988627));
#158488=CARTESIAN_POINT('Ctrl Pts',(-149.550019480558,1.07215582054716,
136.625285441154));
#158489=CARTESIAN_POINT('Ctrl Pts',(-149.557421302234,1.22673601863348,
136.594685988989));
#158490=CARTESIAN_POINT('Ctrl Pts',(-149.564823123909,1.37993076251357,
136.557943992574));
#158491=CARTESIAN_POINT('Ctrl Pts',(-149.57222103822,1.53304463608083,136.521221391973));
#158492=CARTESIAN_POINT('Ctrl Pts',(-149.579618952532,1.68477414991668,
136.478362791761));
#158493=CARTESIAN_POINT('Ctrl Pts',(-149.587016866843,1.83459552929319,
136.429499709748));
#158494=CARTESIAN_POINT('Ctrl Pts',(-149.594413551755,1.98439201107428,
136.380644747893));
#158495=CARTESIAN_POINT('Ctrl Pts',(-149.601810236668,2.13228063318821,
136.32578740028));
#158496=CARTESIAN_POINT('Ctrl Pts',(-149.60920692158,2.27775230749229,136.265109191545));
#158497=CARTESIAN_POINT('Ctrl Pts',(-149.616603278515,2.4232175314299,136.204433673345));
#158498=CARTESIAN_POINT('Ctrl Pts',(-149.623999635451,2.56626567612014,
136.137937950927));
#158499=CARTESIAN_POINT('Ctrl Pts',(-149.631395992386,2.70640743981672,
136.065851787587));
#158500=CARTESIAN_POINT('Ctrl Pts',(-149.638793481723,2.84657065957509,
135.99375458767));
#158501=CARTESIAN_POINT('Ctrl Pts',(-149.646190971059,2.98382628035887,
135.916065413362));
#158502=CARTESIAN_POINT('Ctrl Pts',(-149.653588460396,3.1177095600905,135.833060018149));
#158503=CARTESIAN_POINT('Ctrl Pts',(-149.660988542911,3.25163977239809,
135.750025525523));
#158504=CARTESIAN_POINT('Ctrl Pts',(-149.668388625426,3.38219497289253,
135.66167129817));
#158505=CARTESIAN_POINT('Ctrl Pts',(-149.675788707941,3.50893949269723,
135.568316347743));
#158506=CARTESIAN_POINT('Ctrl Pts',(-149.683196927608,3.6358233811313,135.474858743951));
#158507=CARTESIAN_POINT('Ctrl Pts',(-149.690605147274,3.75888791995032,
135.376389657123));
#158508=CARTESIAN_POINT('Ctrl Pts',(-149.69801336694,3.87773006190177,135.273268776113));
#158509=CARTESIAN_POINT('Ctrl Pts',(-149.705426146243,3.99664534920893,
135.17008442592));
#158510=CARTESIAN_POINT('Ctrl Pts',(-149.712838925545,4.11133278986144,
135.062242831582));
#158511=CARTESIAN_POINT('Ctrl Pts',(-149.720251704847,4.22142668731228,
134.950140072162));
#158512=CARTESIAN_POINT('Ctrl Pts',(-149.727675075875,4.33167789208653,
134.837877135062));
#158513=CARTESIAN_POINT('Ctrl Pts',(-149.735098446904,4.43732219488111,
134.72134114851));
#158514=CARTESIAN_POINT('Ctrl Pts',(-149.742521817933,4.53803408592429,
134.600961360005));
#158515=CARTESIAN_POINT('Ctrl Pts',(-149.746457867374,4.59143394710403,
134.537133107667));
#158516=CARTESIAN_POINT('Ctrl Pts',(-149.750393916815,4.64344784635833,
134.472224721073));
#158517=CARTESIAN_POINT('Ctrl Pts',(-149.754329966255,4.69403231779098,
134.406303310341));
#158518=CARTESIAN_POINT('Ctrl Pts',(-149.761753232661,4.78943305222581,
134.281977587037));
#158519=CARTESIAN_POINT('Ctrl Pts',(-149.769176499066,4.88003531184366,
134.153671087926));
#158520=CARTESIAN_POINT('Ctrl Pts',(-149.776599765472,4.9654884146336,134.021790549459));
#158521=CARTESIAN_POINT('Ctrl Pts',(-149.784014258193,5.05084051895248,
133.890065882836));
#158522=CARTESIAN_POINT('Ctrl Pts',(-149.791428750914,5.13105537940183,
133.754775895408));
#158523=CARTESIAN_POINT('Ctrl Pts',(-149.798843243635,5.20582261833553,
133.616360160405));
#158524=CARTESIAN_POINT('Ctrl Pts',(-149.806250589989,5.28051779378942,
133.478077835698));
#158525=CARTESIAN_POINT('Ctrl Pts',(-149.813657936342,5.34977562446093,
133.336676087374));
#158526=CARTESIAN_POINT('Ctrl Pts',(-149.821065282696,5.41332917310285,
133.192623129547));
#158527=CARTESIAN_POINT('Ctrl Pts',(-149.828467104372,5.47683532111046,
133.048677611851));
#158528=CARTESIAN_POINT('Ctrl Pts',(-149.835868926047,5.53464550827882,
132.902085161934));
#158529=CARTESIAN_POINT('Ctrl Pts',(-149.843270747722,5.58653892716462,
132.753338138671));
#158530=CARTESIAN_POINT('Ctrl Pts',(-149.850668662034,5.63840495191854,
132.604669637805));
#158531=CARTESIAN_POINT('Ctrl Pts',(-149.858066576345,5.68436030616929,
132.453849180318));
#158532=CARTESIAN_POINT('Ctrl Pts',(-149.865464490657,5.72423252654085,
132.301388521311));
#158533=CARTESIAN_POINT('Ctrl Pts',(-149.872861175569,5.76409812087268,
132.1489531985));
#158534=CARTESIAN_POINT('Ctrl Pts',(-149.880257860481,5.79788249331798,
131.994878575943));
#158535=CARTESIAN_POINT('Ctrl Pts',(-149.887654545393,5.82546319111763,
131.83969108241));
#158536=CARTESIAN_POINT('Ctrl Pts',(-149.895050902328,5.85304266596024,
131.684510470053));
#158537=CARTESIAN_POINT('Ctrl Pts',(-149.902447259264,5.87441894778336,
131.528217452376));
#158538=CARTESIAN_POINT('Ctrl Pts',(-149.9098436162,5.88952086340951,131.371347885469));
#158539=CARTESIAN_POINT('Ctrl Pts',(-149.917241105536,5.90462509117755,
131.21445430143));
#158540=CARTESIAN_POINT('Ctrl Pts',(-149.924638594873,5.91345300424894,
131.056984364006));
#158541=CARTESIAN_POINT('Ctrl Pts',(-149.932036084209,5.91598539739665,
130.899478125364));
#158542=CARTESIAN_POINT('Ctrl Pts',(-149.939436166724,5.91851867827084,
130.741916673154));
#158543=CARTESIAN_POINT('Ctrl Pts',(-149.946836249239,5.91475203933263,
130.584319267406));
#158544=CARTESIAN_POINT('Ctrl Pts',(-149.954236331754,5.90471838445042,
130.427224882275));
#158545=CARTESIAN_POINT('Ctrl Pts',(-149.961644551421,5.89467369653317,
130.269957755718));
#158546=CARTESIAN_POINT('Ctrl Pts',(-149.969052771087,5.87834825424528,
130.113195127169));
#158547=CARTESIAN_POINT('Ctrl Pts',(-149.976460990754,5.85582681712102,
129.957470512307));
#158548=CARTESIAN_POINT('Ctrl Pts',(-149.983873770056,5.83329151842801,
129.801650051542));
#158549=CARTESIAN_POINT('Ctrl Pts',(-149.991286549358,5.80455269394827,
129.646869243687));
#158550=CARTESIAN_POINT('Ctrl Pts',(-149.99869932866,5.76974590829766,129.493649850012));
#158551=CARTESIAN_POINT('Ctrl Pts',(-150.006122699689,5.7348893890795,129.340211529282));
#158552=CARTESIAN_POINT('Ctrl Pts',(-150.013546070717,5.69394768928889,
129.188339438058));
#158553=CARTESIAN_POINT('Ctrl Pts',(-150.020969441746,5.64710600102051,
129.038539455687));
#158554=CARTESIAN_POINT('Ctrl Pts',(-150.024905491187,5.62226941395013,
128.959111910635));
#158555=CARTESIAN_POINT('Ctrl Pts',(-150.028841540628,5.59577493306521,
128.880266575654));
#158556=CARTESIAN_POINT('Ctrl Pts',(-150.032777590068,5.56765552562929,
128.802076294492));
#158557=CARTESIAN_POINT('Ctrl Pts',(-150.040200856474,5.51462320078087,
128.654611864452));
#158558=CARTESIAN_POINT('Ctrl Pts',(-150.047624122879,5.45564804365642,
128.509032820616));
#158559=CARTESIAN_POINT('Ctrl Pts',(-150.055047389285,5.39088270095922,
128.365854052679));
#158560=CARTESIAN_POINT('Ctrl Pts',(-150.062461882006,5.32619390551866,
128.222844510155));
#158561=CARTESIAN_POINT('Ctrl Pts',(-150.069876374727,5.25572869891388,
128.082229933409));
#158562=CARTESIAN_POINT('Ctrl Pts',(-150.077290867448,5.17968913985313,
127.944509052014));
#158563=CARTESIAN_POINT('Ctrl Pts',(-150.084698213801,5.10372287058223,
127.80692091119));
#158564=CARTESIAN_POINT('Ctrl Pts',(-150.092105560155,5.02219312420585,
127.672221237864));
#158565=CARTESIAN_POINT('Ctrl Pts',(-150.099512906509,4.93534953641716,
127.540887695067));
#158566=CARTESIAN_POINT('Ctrl Pts',(-150.106914728184,4.84857071985266,
127.409652105781));
#158567=CARTESIAN_POINT('Ctrl Pts',(-150.11431654986,4.75648615828004,127.281777958146));
#158568=CARTESIAN_POINT('Ctrl Pts',(-150.121718371535,4.65939073535001,
127.157717155719));
#158569=CARTESIAN_POINT('Ctrl Pts',(-150.129116285847,4.56234656833796,
127.033721844023));
#158570=CARTESIAN_POINT('Ctrl Pts',(-150.136514200158,4.46029703749109,
126.913536161702));
#158571=CARTESIAN_POINT('Ctrl Pts',(-150.143912114469,4.35357947620254,
126.797581823212));
#158572=CARTESIAN_POINT('Ctrl Pts',(-150.151308799382,4.24687964943678,
126.681646754229));
#158573=CARTESIAN_POINT('Ctrl Pts',(-150.158705484294,4.13551358439462,
126.569941907893));
#158574=CARTESIAN_POINT('Ctrl Pts',(-150.166102169206,4.019857991804,126.462854854789));
#158575=CARTESIAN_POINT('Ctrl Pts',(-150.173498526141,3.90420752750356,
126.355772550036));
#158576=CARTESIAN_POINT('Ctrl Pts',(-150.180894883077,3.78426818775358,
126.253307885007));
#158577=CARTESIAN_POINT('Ctrl Pts',(-150.188291240012,3.66045233261851,
126.155810383017));
#158578=CARTESIAN_POINT('Ctrl Pts',(-150.195688729349,3.53661752095957,
126.05829795391));
#158579=CARTESIAN_POINT('Ctrl Pts',(-150.203086218686,3.40890530547316,
125.965754433029));
#158580=CARTESIAN_POINT('Ctrl Pts',(-150.210483708022,3.27775966644817,
125.878487889662));
#158581=CARTESIAN_POINT('Ctrl Pts',(-150.217883790537,3.1465680545229,125.791190755145));
#158582=CARTESIAN_POINT('Ctrl Pts',(-150.225283873052,3.01194093332542,
125.709174487823));
#158583=CARTESIAN_POINT('Ctrl Pts',(-150.232683955567,2.87434954242147,
125.632702733436));
#158584=CARTESIAN_POINT('Ctrl Pts',(-150.240092175234,2.73660685563828,
125.556146890494));
#158585=CARTESIAN_POINT('Ctrl Pts',(-150.2475003949,2.5958937161636,125.485147917581));
#158586=CARTESIAN_POINT('Ctrl Pts',(-150.254908614567,2.45270480044723,
125.419922882355));
#158587=CARTESIAN_POINT('Ctrl Pts',(-150.262321393869,2.30942775434246,
125.354657702209));
#158588=CARTESIAN_POINT('Ctrl Pts',(-150.269734173171,2.16367224045783,
125.295173681792));
#158589=CARTESIAN_POINT('Ctrl Pts',(-150.277146952473,2.01595050731278,
125.241638791466));
#158590=CARTESIAN_POINT('Ctrl Pts',(-150.284570323502,1.86801770242816,
125.188027407978));
#158591=CARTESIAN_POINT('Ctrl Pts',(-150.29199369453,1.71811342204681,125.140382244553));
#158592=CARTESIAN_POINT('Ctrl Pts',(-150.299417065559,1.56676337764193,
125.09882093398));
#158593=CARTESIAN_POINT('Ctrl Pts',(-150.303353115,1.48651395250529,125.076784129864));
#158594=CARTESIAN_POINT('Ctrl Pts',(-150.307289164441,1.40585822508792,
125.056456857534));
#158595=CARTESIAN_POINT('Ctrl Pts',(-150.311225213881,1.32487530050843,
125.03785075452));
#158596=CARTESIAN_POINT('Ctrl Pts',(-150.318648480287,1.17214403213982,
125.002760224914));
#158597=CARTESIAN_POINT('Ctrl Pts',(-150.326071746692,1.01778674657429,
124.973688665707));
#158598=CARTESIAN_POINT('Ctrl Pts',(-150.333495013098,0.862319144366244,
124.950785961362));
#158599=CARTESIAN_POINT('Ctrl Pts',(-150.340909505819,0.707035291953226,
124.927910326111));
#158600=CARTESIAN_POINT('Ctrl Pts',(-150.34832399854,0.550644100747854,
124.911189086673));
#158601=CARTESIAN_POINT('Ctrl Pts',(-150.355738491261,0.393674383730942,
124.90072182085));
#158602=CARTESIAN_POINT('Ctrl Pts',(-150.363145837614,0.236855960037095,
124.890264643771));
#158603=CARTESIAN_POINT('Ctrl Pts',(-150.370553183968,0.079460490583632,
124.886049464784));
#158604=CARTESIAN_POINT('Ctrl Pts',(-150.377960530322,-0.077975219002551,
124.888124446847));
#158605=CARTESIAN_POINT('Ctrl Pts',(-150.385362351997,-0.235293507096815,
124.89019788131));
#158606=CARTESIAN_POINT('Ctrl Pts',(-150.392764173673,-0.392651603905657,
124.898552130635));
#158607=CARTESIAN_POINT('Ctrl Pts',(-150.400165995348,-0.549509918353506,
124.913183365766));
#158608=CARTESIAN_POINT('Ctrl Pts',(-150.407563909659,-0.70628542851814,
124.927806877181));
#158609=CARTESIAN_POINT('Ctrl Pts',(-150.414961823971,-0.862561311010674,
124.948700740682));
#158610=CARTESIAN_POINT('Ctrl Pts',(-150.422359738282,-1.01780042857745,
124.975809095096));
#158611=CARTESIAN_POINT('Ctrl Pts',(-150.429756423194,-1.17301374821898,
125.002912944593));
#158612=CARTESIAN_POINT('Ctrl Pts',(-150.437153108107,-1.32719027750919,
125.036229171177));
#158613=CARTESIAN_POINT('Ctrl Pts',(-150.444549793019,-1.47980032098872,
125.07565032881));
#158614=CARTESIAN_POINT('Ctrl Pts',(-150.451946149954,-1.632403597579,125.115069738467));
#158615=CARTESIAN_POINT('Ctrl Pts',(-150.459342506889,-1.78344016503396,
125.16059344757));
#158616=CARTESIAN_POINT('Ctrl Pts',(-150.466738863825,-1.93239306880156,
125.212063451808));
#158617=CARTESIAN_POINT('Ctrl Pts',(-150.474136353161,-2.08136877763899,
125.263541336234));
#158618=CARTESIAN_POINT('Ctrl Pts',(-150.481533842498,-2.22825983473902,
125.320967206583));
#158619=CARTESIAN_POINT('Ctrl Pts',(-150.488931331835,-2.37256707049267,
125.384134048638));
#158620=CARTESIAN_POINT('Ctrl Pts',(-150.496331414349,-2.51692489292431,
125.447323033732));
#158621=CARTESIAN_POINT('Ctrl Pts',(-150.503731496865,-2.65869674890081,
125.516256847787));
#158622=CARTESIAN_POINT('Ctrl Pts',(-150.511131579379,-2.79740610929864,
125.590681530572));
#158623=CARTESIAN_POINT('Ctrl Pts',(-150.518539799046,-2.93626799489769,
125.665188050947));
#158624=CARTESIAN_POINT('Ctrl Pts',(-150.525948018712,-3.07206033060034,
125.745197321283));
#158625=CARTESIAN_POINT('Ctrl Pts',(-150.533356238379,-3.20433310653234,
125.830410486646));
#158626=CARTESIAN_POINT('Ctrl Pts',(-150.540769017681,-3.33668729415122,
125.91567609929));
#158627=CARTESIAN_POINT('Ctrl Pts',(-150.548181796983,-3.46551730073332,
126.006151775118));
#158628=CARTESIAN_POINT('Ctrl Pts',(-150.555594576285,-3.59040492522026,
126.101497337026));
#158629=CARTESIAN_POINT('Ctrl Pts',(-150.563017947314,-3.71547099500153,
126.196979133143));
#158630=CARTESIAN_POINT('Ctrl Pts',(-150.570441318342,-3.8365831455343,
126.297344475108));
#158631=CARTESIAN_POINT('Ctrl Pts',(-150.577864689371,-3.95335824912827,
126.402214650364));
#158632=CARTESIAN_POINT('Ctrl Pts',(-150.581800738812,-4.01527521103776,
126.457819333614));
#158633=CARTESIAN_POINT('Ctrl Pts',(-150.585736788253,-4.07597351174698,
126.514689894168));
#158634=CARTESIAN_POINT('Ctrl Pts',(-150.589672837694,-4.13540060202172,
126.572766069018));
#158635=CARTESIAN_POINT('Ctrl Pts',(-150.596989848785,-4.24587398026017,
126.680728131459));
#158636=CARTESIAN_POINT('Ctrl Pts',(-150.604306859877,-4.35230691777609,
126.793205472225));
#158637=CARTESIAN_POINT('Ctrl Pts',(-150.611623870968,-4.45429975870204,
126.909858823738));
#158638=CARTESIAN_POINT('Ctrl Pts',(-150.618932091929,-4.55617007278003,
127.026372036323));
#158639=CARTESIAN_POINT('Ctrl Pts',(-150.626240312891,-4.65361065207637,
127.147050991511));
#158640=CARTESIAN_POINT('Ctrl Pts',(-150.633548533852,-4.74625659640716,
127.27151772783));
#158641=CARTESIAN_POINT('Ctrl Pts',(-150.6409683786,-4.84031758977789,127.397885535339));
#158642=CARTESIAN_POINT('Ctrl Pts',(-150.648388223347,-4.92943597383426,
127.528157526693));
#158643=CARTESIAN_POINT('Ctrl Pts',(-150.655808068095,-5.01326962268013,
127.661900076396));
#158644=CARTESIAN_POINT('Ctrl Pts',(-150.663103336763,-5.09569573974858,
127.793397144824));
#158645=CARTESIAN_POINT('Ctrl Pts',(-150.670398605431,-5.17301295976667,
127.928248814312));
#158646=CARTESIAN_POINT('Ctrl Pts',(-150.6776938741,-5.24493778813581,128.066011085259));
#158647=CARTESIAN_POINT('Ctrl Pts',(-150.684986052498,-5.31683214920228,
128.203715000213));
#158648=CARTESIAN_POINT('Ctrl Pts',(-150.692278230896,-5.38333848524696,
128.344326723231));
#158649=CARTESIAN_POINT('Ctrl Pts',(-150.699570409294,-5.44421829342693,
128.48737599612));
#158650=CARTESIAN_POINT('Ctrl Pts',(-150.706861034815,-5.50508513719152,
128.630394806526));
#158651=CARTESIAN_POINT('Ctrl Pts',(-150.714151660337,-5.56032768742805,
128.775849779635));
#158652=CARTESIAN_POINT('Ctrl Pts',(-150.721442285858,-5.60975493921973,
128.923249221503));
#158653=CARTESIAN_POINT('Ctrl Pts',(-150.728957496019,-5.66070477662374,
129.075189240912));
#158654=CARTESIAN_POINT('Ctrl Pts',(-150.73647270618,-5.7054751140223,129.229195055014));
#158655=CARTESIAN_POINT('Ctrl Pts',(-150.743987916341,-5.74391178353263,
129.38470996142));
#158656=CARTESIAN_POINT('Ctrl Pts',(-150.751282479144,-5.78121994839688,
129.535658933872));
#158657=CARTESIAN_POINT('Ctrl Pts',(-150.758577041947,-5.81256108288044,
129.688029234886));
#158658=CARTESIAN_POINT('Ctrl Pts',(-150.76587160475,-5.83784605474345,
129.841300908298));
#158659=CARTESIAN_POINT('Ctrl Pts',(-150.77349713859,-5.86427826374589,
130.001526868908));
#158660=CARTESIAN_POINT('Ctrl Pts',(-150.78112267243,-5.88409180770352,
130.162737444565));
#158661=CARTESIAN_POINT('Ctrl Pts',(-150.78874820627,-5.89724546106289,
130.324332978286));
#158662=CARTESIAN_POINT('Ctrl Pts',(-150.79637374011,-5.91039911442222,
130.485928512005));
#158663=CARTESIAN_POINT('Ctrl Pts',(-150.80399927395,-5.91689290169413,
130.647908525579));
#158664=CARTESIAN_POINT('Ctrl Pts',(-150.81162480779,-5.91674761363104,
130.809674664177));
#158665=CARTESIAN_POINT('',(-152.561624807791,-5.92484811461594,130.801501939966));
#158666=CARTESIAN_POINT('Ctrl Pts',(-150.81162480779,-5.91854249043319,
130.809676276221));
#158667=CARTESIAN_POINT('Ctrl Pts',(-150.830456692362,-5.92224981611246,
131.209295934625));
#158668=CARTESIAN_POINT('Ctrl Pts',(-150.942104451545,-5.70288361260892,
133.574456017664));
#158669=CARTESIAN_POINT('Ctrl Pts',(-151.146568085314,-2.5191023459754,
137.333654905673));
#158670=CARTESIAN_POINT('Ctrl Pts',(-151.425015709135,4.13164385332104,
136.452995815532));
#158671=CARTESIAN_POINT('Ctrl Pts',(-151.703463332944,6.98561119344034,
130.381516929611));
#158672=CARTESIAN_POINT('Ctrl Pts',(-151.981910956759,3.42014311286449,
124.69861073587));
#158673=CARTESIAN_POINT('Ctrl Pts',(-152.260358580571,-3.28826940515126,
124.626590400934));
#158674=CARTESIAN_POINT('Ctrl Pts',(-152.453596530916,-5.84674475077773,
128.516399573093));
#158675=CARTESIAN_POINT('Ctrl Pts',(-152.554018606655,-5.92580458990376,
130.640542179685));
#158676=CARTESIAN_POINT('Ctrl Pts',(-152.561624807791,-5.92484811461594,
130.801501939966));
#158677=CARTESIAN_POINT('',(-154.311624807791,-5.90970598804176,130.800431355485));
#158678=CARTESIAN_POINT('Ctrl Pts',(-152.561624807791,-5.92484811461594,
130.801501939966));
#158679=CARTESIAN_POINT('Ctrl Pts',(-152.646834481259,-5.91413304864473,
132.604679159562));
#158680=CARTESIAN_POINT('Ctrl Pts',(-152.824860029333,-4.07084663883969,
136.390942232934));
#158681=CARTESIAN_POINT('Ctrl Pts',(-153.095701452011,2.37834317028329,
137.386233017932));
#158682=CARTESIAN_POINT('Ctrl Pts',(-153.374149075822,6.82306823653916,
132.3610559538));
#158683=CARTESIAN_POINT('Ctrl Pts',(-153.652596699636,4.99772691883392,
125.90535192446));
#158684=CARTESIAN_POINT('Ctrl Pts',(-153.931044323448,-1.4202812847494,
123.951597554207));
#158685=CARTESIAN_POINT('Ctrl Pts',(-154.1507203595,-5.45395989307253,127.378399482155));
#158686=CARTESIAN_POINT('Ctrl Pts',(-154.277580520948,-5.91410690545322,
130.075254683052));
#158687=CARTESIAN_POINT('Ctrl Pts',(-154.311624807791,-5.90970598804176,
130.800431355485));
#158688=CARTESIAN_POINT('',(-156.061624824859,-5.91361334729715,130.808692848313));
#158689=CARTESIAN_POINT('Ctrl Pts',(-154.311624807791,-5.90970598804176,
130.800431355485));
#158690=CARTESIAN_POINT('Ctrl Pts',(-154.370396395552,-5.90210856339691,
132.052323769702));
#158691=CARTESIAN_POINT('Ctrl Pts',(-154.521983857917,-4.89948390548452,
135.292405018535));
#158692=CARTESIAN_POINT('Ctrl Pts',(-154.766387194888,0.433474109379777,
137.789320225665));
#158693=CARTESIAN_POINT('Ctrl Pts',(-155.0448348187,6.11094768694514,134.215207858028));
#158694=CARTESIAN_POINT('Ctrl Pts',(-155.323282442513,6.17275887660265,
127.506693505547));
#158695=CARTESIAN_POINT('Ctrl Pts',(-155.601730066326,0.562106214696297,
123.828574129024));
#158696=CARTESIAN_POINT('Ctrl Pts',(-155.847844188085,-4.85360043142605,
126.243586901841));
#158697=CARTESIAN_POINT('Ctrl Pts',(-156.00114243524,-5.90179639786853,
129.520781549821));
#158698=CARTESIAN_POINT('Ctrl Pts',(-156.061624807791,-5.91048299654473,
130.808690191434));
#158699=CARTESIAN_POINT('',(-157.811624807791,-5.92111944829027,130.806626556176));
#158700=CARTESIAN_POINT('Ctrl Pts',(-156.061624841952,-5.9167484120262,
130.808695509193));
#158701=CARTESIAN_POINT('Ctrl Pts',(-156.070131700184,-5.91661555689736,
130.990031154992));
#158702=CARTESIAN_POINT('Ctrl Pts',(-156.078638558416,-5.90814245645985,
131.171029685701));
#158703=CARTESIAN_POINT('Ctrl Pts',(-156.087145416648,-5.89144563320417,
131.350985638489));
#158704=CARTESIAN_POINT('Ctrl Pts',(-156.095693557071,-5.87466778338968,
131.531814883841));
#158705=CARTESIAN_POINT('Ctrl Pts',(-156.104241697494,-5.84958630670668,
131.711591278413));
#158706=CARTESIAN_POINT('Ctrl Pts',(-156.112789837917,-5.81636890357933,
131.889617886593));
#158707=CARTESIAN_POINT('Ctrl Pts',(-156.121392227815,-5.78294069124846,
132.068774313601));
#158708=CARTESIAN_POINT('Ctrl Pts',(-156.129994617713,-5.74127304004691,
132.246158545632));
#158709=CARTESIAN_POINT('Ctrl Pts',(-156.138597007611,-5.691585441371,132.421081287958));
#158710=CARTESIAN_POINT('Ctrl Pts',(-156.145273109725,-5.65302412451932,
132.556834503472));
#158711=CARTESIAN_POINT('Ctrl Pts',(-156.151949211838,-5.60963343823935,
132.69110558819));
#158712=CARTESIAN_POINT('Ctrl Pts',(-156.158625313952,-5.56153547190469,
132.823581694429));
#158713=CARTESIAN_POINT('Ctrl Pts',(-156.166048580357,-5.50805456170145,
132.970884029261));
#158714=CARTESIAN_POINT('Ctrl Pts',(-156.173471846762,-5.44863658521653,
133.116282898686));
#158715=CARTESIAN_POINT('Ctrl Pts',(-156.180895113167,-5.38343575559325,
133.259263879998));
#158716=CARTESIAN_POINT('Ctrl Pts',(-156.188309605888,-5.31831198793581,
133.402075869664));
#158717=CARTESIAN_POINT('Ctrl Pts',(-156.195724098609,-5.2474191253225,
133.542475323237));
#158718=CARTESIAN_POINT('Ctrl Pts',(-156.20313859133,-5.17096074348685,
133.679964128452));
#158719=CARTESIAN_POINT('Ctrl Pts',(-156.210545937683,-5.09457605511823,
133.817320416779));
#158720=CARTESIAN_POINT('Ctrl Pts',(-156.217953284037,-5.01263670691561,
133.951771317679));
#158721=CARTESIAN_POINT('Ctrl Pts',(-156.22536063039,-4.92539378725776,
134.082839930135));
#158722=CARTESIAN_POINT('Ctrl Pts',(-156.232762452065,-4.83821593666113,
134.213810786675));
#158723=CARTESIAN_POINT('Ctrl Pts',(-156.24016427374,-4.74574259670467,
134.341404068271));
#158724=CARTESIAN_POINT('Ctrl Pts',(-156.247566095415,-4.64827002511213,
134.465168770986));
#158725=CARTESIAN_POINT('Ctrl Pts',(-156.254964009726,-4.55084890853113,
134.588868139278));
#158726=CARTESIAN_POINT('Ctrl Pts',(-156.262361924037,-4.44843404650144,
134.708742661235));
#158727=CARTESIAN_POINT('Ctrl Pts',(-156.269759838349,-4.34136405440738,
134.824371651083));
#158728=CARTESIAN_POINT('Ctrl Pts',(-156.27715652326,-4.23431185540402,
134.93998142549));
#158729=CARTESIAN_POINT('Ctrl Pts',(-156.284553208172,-4.12260631508079,
135.051346794421));
#158730=CARTESIAN_POINT('Ctrl Pts',(-156.291949893084,-4.00662532205224,
135.158081335663));
#158731=CARTESIAN_POINT('Ctrl Pts',(-156.299346250019,-3.89064947174247,
135.264811144185));
#158732=CARTESIAN_POINT('Ctrl Pts',(-156.306742606954,-3.77039882035604,
135.36691028051));
#158733=CARTESIAN_POINT('Ctrl Pts',(-156.314138963889,-3.64628678987608,
135.464030478026));
#158734=CARTESIAN_POINT('Ctrl Pts',(-156.321536453226,-3.52215575752705,
135.561165544891));
#158735=CARTESIAN_POINT('Ctrl Pts',(-156.328933942562,-3.39416246295797,
135.653319925064));
#158736=CARTESIAN_POINT('Ctrl Pts',(-156.336331431898,-3.26275182205814,
135.740186902005));
#158737=CARTESIAN_POINT('Ctrl Pts',(-156.343731514413,-3.13129511536205,
135.827084330029));
#158738=CARTESIAN_POINT('Ctrl Pts',(-156.351131596928,-2.99641898845008,
135.908690458811));
#158739=CARTESIAN_POINT('Ctrl Pts',(-156.358531679442,-2.85859548115215,
135.984743078122));
#158740=CARTESIAN_POINT('Ctrl Pts',(-156.365939899109,-2.72062042273954,
136.060879325106));
#158741=CARTESIAN_POINT('Ctrl Pts',(-156.373348118775,-2.57969183859533,
136.131449686766));
#158742=CARTESIAN_POINT('Ctrl Pts',(-156.380756338441,-2.43630506355726,
136.196238602071));
#158743=CARTESIAN_POINT('Ctrl Pts',(-156.388169117743,-2.29283003635168,
136.261067393872));
#158744=CARTESIAN_POINT('Ctrl Pts',(-156.395581897044,-2.14689414870795,
136.320107509118));
#158745=CARTESIAN_POINT('Ctrl Pts',(-156.402994676346,-1.99901015801677,
136.373192537336));
#158746=CARTESIAN_POINT('Ctrl Pts',(-156.410418047374,-1.8509148637444,
136.426353415931));
#158747=CARTESIAN_POINT('Ctrl Pts',(-156.417841418403,-1.7008662622286,
136.473542101607));
#158748=CARTESIAN_POINT('Ctrl Pts',(-156.425264789431,-1.54939042054123,
136.514642562202));
#158749=CARTESIAN_POINT('Ctrl Pts',(-156.429200838876,-1.46907429459182,
136.536435012622));
#158750=CARTESIAN_POINT('Ctrl Pts',(-156.43313688832,-1.38835707146956,
136.556516702527));
#158751=CARTESIAN_POINT('Ctrl Pts',(-156.437072937764,-1.30731789134756,
136.574876235209));
#158752=CARTESIAN_POINT('Ctrl Pts',(-156.44449620417,-1.1544805269183,136.609501740835));
#158753=CARTESIAN_POINT('Ctrl Pts',(-156.451919470575,-1.00003547249919,
136.638103354904));
#158754=CARTESIAN_POINT('Ctrl Pts',(-156.45934273698,-0.844498882452665,
136.660532763263));
#158755=CARTESIAN_POINT('Ctrl Pts',(-156.466757229701,-0.689146123739063,
136.682935661924));
#158756=CARTESIAN_POINT('Ctrl Pts',(-156.474171722423,-0.532704763226046,
136.69918082292));
#158757=CARTESIAN_POINT('Ctrl Pts',(-156.481586215144,-0.375703914525576,
136.709170278437));
#158758=CARTESIAN_POINT('Ctrl Pts',(-156.488993561497,-0.218854389154062,
136.71915010574));
#158759=CARTESIAN_POINT('Ctrl Pts',(-156.496400907851,-0.0614468191907923,
136.722886207535));
#158760=CARTESIAN_POINT('Ctrl Pts',(-156.503808254205,0.0959818456323094,
136.720332054939));
#158761=CARTESIAN_POINT('Ctrl Pts',(-156.51121007588,0.253293094217742,
136.717779807326));
#158762=CARTESIAN_POINT('Ctrl Pts',(-156.518611897556,0.410625034693445,
136.708946652779));
#158763=CARTESIAN_POINT('Ctrl Pts',(-156.526013719231,0.567438090137523,
136.693838062668));
#158764=CARTESIAN_POINT('Ctrl Pts',(-156.533411633542,0.724168365190709,
136.678737448263));
#158765=CARTESIAN_POINT('Ctrl Pts',(-156.540809547854,0.880379930091205,
136.657368031511));
#158766=CARTESIAN_POINT('Ctrl Pts',(-156.548207462165,1.03553582009553,
136.629787308187));
#158767=CARTESIAN_POINT('Ctrl Pts',(-156.555604147077,1.19066592600552,
136.602211168279));
#158768=CARTESIAN_POINT('Ctrl Pts',(-156.563000831989,1.34474033802766,
136.568425835693));
#158769=CARTESIAN_POINT('Ctrl Pts',(-156.570397516902,1.49722969018486,
136.528540368179));
#158770=CARTESIAN_POINT('Ctrl Pts',(-156.577793873837,1.64971228080395,
136.488656669229));
#158771=CARTESIAN_POINT('Ctrl Pts',(-156.585190230773,1.80060959015691,
136.442673467631));
#158772=CARTESIAN_POINT('Ctrl Pts',(-156.592586587708,1.94940514699695,
136.390750340398));
#158773=CARTESIAN_POINT('Ctrl Pts',(-156.599984077045,2.09822348481703,
136.338819263601));
#158774=CARTESIAN_POINT('Ctrl Pts',(-156.607381566381,2.24493907693255,
136.280946573395));
#158775=CARTESIAN_POINT('Ctrl Pts',(-156.614779055718,2.38905338612669,
136.217340802338));
#158776=CARTESIAN_POINT('Ctrl Pts',(-156.622179138233,2.53321821436831,
136.153712734377));
#158777=CARTESIAN_POINT('Ctrl Pts',(-156.629579220748,2.67477960284958,
136.084347734856));
#158778=CARTESIAN_POINT('Ctrl Pts',(-156.636979303263,2.81326179762183,
136.009501213222));
#158779=CARTESIAN_POINT('Ctrl Pts',(-156.644387522929,2.95189626780375,
135.934572390142));
#158780=CARTESIAN_POINT('Ctrl Pts',(-156.651795742596,3.08744445382917,
135.854150185243));
#158781=CARTESIAN_POINT('Ctrl Pts',(-156.659203962262,3.21945725751989,
135.768534821752));
#158782=CARTESIAN_POINT('Ctrl Pts',(-156.666616741564,3.35155131288852,
135.682866763432));
#158783=CARTESIAN_POINT('Ctrl Pts',(-156.674029520866,3.480105345904,135.591999392457));
#158784=CARTESIAN_POINT('Ctrl Pts',(-156.681442300168,3.6047021928271,135.496274157213));
#158785=CARTESIAN_POINT('Ctrl Pts',(-156.688865671197,3.72947706956828,
135.400412145265));
#158786=CARTESIAN_POINT('Ctrl Pts',(-156.696289042226,3.85028318154151,
135.29967864446));
#158787=CARTESIAN_POINT('Ctrl Pts',(-156.703712413255,3.96673855550187,
135.194453531707));
#158788=CARTESIAN_POINT('Ctrl Pts',(-156.707648462696,4.02848598908599,
135.138660652082));
#158789=CARTESIAN_POINT('Ctrl Pts',(-156.711584512136,4.08901091421956,
135.081605610203));
#158790=CARTESIAN_POINT('Ctrl Pts',(-156.715520561577,4.14826096533169,
135.023348828738));
#158791=CARTESIAN_POINT('Ctrl Pts',(-156.722943827983,4.26000471259557,
134.913478357029));
#158792=CARTESIAN_POINT('Ctrl Pts',(-156.730367094388,4.36754938499623,
134.798999229671));
#158793=CARTESIAN_POINT('Ctrl Pts',(-156.737790360794,4.47049120759569,
134.680265534525));
#158794=CARTESIAN_POINT('Ctrl Pts',(-156.745204853515,4.57331136150992,
134.561672172747));
#158795=CARTESIAN_POINT('Ctrl Pts',(-156.752619346236,4.67153925219407,
134.438834531824));
#158796=CARTESIAN_POINT('Ctrl Pts',(-156.760033838957,4.76480645771854,
134.312144816029));
#158797=CARTESIAN_POINT('Ctrl Pts',(-156.767441185311,4.85798376879888,
134.185577208551));
#158798=CARTESIAN_POINT('Ctrl Pts',(-156.774848531665,4.94620969351042,
134.055165216204));
#158799=CARTESIAN_POINT('Ctrl Pts',(-156.782255878019,5.0291548513403,133.921335440008));
#158800=CARTESIAN_POINT('Ctrl Pts',(-156.789657699694,5.11203814554214,
133.787605479109));
#158801=CARTESIAN_POINT('Ctrl Pts',(-156.79705952137,5.18964831932791,133.650463125918));
#158802=CARTESIAN_POINT('Ctrl Pts',(-156.804461343045,5.26169832140905,
133.510365299192));
#158803=CARTESIAN_POINT('Ctrl Pts',(-156.811859257356,5.33371028885493,
133.370341429017));
#158804=CARTESIAN_POINT('Ctrl Pts',(-156.819257171668,5.40016775983627,
133.227365523592));
#158805=CARTESIAN_POINT('Ctrl Pts',(-156.826655085979,5.46082886461755,
133.081920424434));
#158806=CARTESIAN_POINT('Ctrl Pts',(-156.834051770892,5.52147988862363,
132.936499495612));
#158807=CARTESIAN_POINT('Ctrl Pts',(-156.841448455804,5.57633631464319,
132.788610531647));
#158808=CARTESIAN_POINT('Ctrl Pts',(-156.848845140716,5.62520376080864,
132.638757851505));
#158809=CARTESIAN_POINT('Ctrl Pts',(-156.856241497652,5.67406904014033,
132.488911815988));
#158810=CARTESIAN_POINT('Ctrl Pts',(-156.863637854587,5.71694575190104,
132.337102592328));
#158811=CARTESIAN_POINT('Ctrl Pts',(-156.871034211523,5.75368898742517,
132.183850957685));
#158812=CARTESIAN_POINT('Ctrl Pts',(-156.878431700859,5.79043784843245,
132.030575859826));
#158813=CARTESIAN_POINT('Ctrl Pts',(-156.885829190196,5.82105127638797,
131.875858274301));
#158814=CARTESIAN_POINT('Ctrl Pts',(-156.893226679533,5.8454352440948,131.720230351532));
#158815=CARTESIAN_POINT('Ctrl Pts',(-156.900626762048,5.86982775956375,
131.564547873635));
#158816=CARTESIAN_POINT('Ctrl Pts',(-156.908026844563,5.88798640925056,
131.407954791702));
#158817=CARTESIAN_POINT('Ctrl Pts',(-156.915426927078,5.89986891972477,
131.250989426048));
#158818=CARTESIAN_POINT('Ctrl Pts',(-156.922835146744,5.91176449624079,
131.093851460837));
#158819=CARTESIAN_POINT('Ctrl Pts',(-156.930243366411,5.91737012307851,
130.93634076684));
#158820=CARTESIAN_POINT('Ctrl Pts',(-156.937651586077,5.91669563800539,
130.778997461058));
#158821=CARTESIAN_POINT('Ctrl Pts',(-156.945064365379,5.91602073779795,
130.621557313097));
#158822=CARTESIAN_POINT('Ctrl Pts',(-156.952477144682,5.90905804004873,
130.464285130708));
#158823=CARTESIAN_POINT('Ctrl Pts',(-156.959889923984,5.89586932776679,
130.307716446757));
#158824=CARTESIAN_POINT('Ctrl Pts',(-156.967313295012,5.88266177083427,
130.150924050127));
#158825=CARTESIAN_POINT('Ctrl Pts',(-156.974736666041,5.86321047805915,
129.994837528979));
#158826=CARTESIAN_POINT('Ctrl Pts',(-156.98216003707,5.83762858477514,129.839983580969));
#158827=CARTESIAN_POINT('Ctrl Pts',(-156.98609608651,5.82406445112959,129.757876302081));
#158828=CARTESIAN_POINT('Ctrl Pts',(-156.99003213595,5.80877762895482,129.676115324647));
#158829=CARTESIAN_POINT('Ctrl Pts',(-156.99396818539,5.79179064868332,129.594777365233));
#158830=CARTESIAN_POINT('Ctrl Pts',(-157.001391451796,5.75975373403073,
129.441376512221));
#158831=CARTESIAN_POINT('Ctrl Pts',(-157.008814718201,5.7215697243251,129.289017368863));
#158832=CARTESIAN_POINT('Ctrl Pts',(-157.016237984607,5.67731827349541,
129.13823103559));
#158833=CARTESIAN_POINT('Ctrl Pts',(-157.023652477327,5.63311912420575,
128.987622919241));
#158834=CARTESIAN_POINT('Ctrl Pts',(-157.031066970048,5.58286691222061,
128.838584267457));
#158835=CARTESIAN_POINT('Ctrl Pts',(-157.038481462769,5.52669246904767,
128.691637040031));
#158836=CARTESIAN_POINT('Ctrl Pts',(-157.045888809123,5.47057216891798,
128.544831445875));
#158837=CARTESIAN_POINT('Ctrl Pts',(-157.053296155477,5.40854113364339,
128.400113609376));
#158838=CARTESIAN_POINT('Ctrl Pts',(-157.060703501831,5.34078023653029,
128.257991235959));
#158839=CARTESIAN_POINT('Ctrl Pts',(-157.068105323506,5.27306987805073,
128.115974862769));
#158840=CARTESIAN_POINT('Ctrl Pts',(-157.075507145181,5.19963832690507,
127.976550433743));
#158841=CARTESIAN_POINT('Ctrl Pts',(-157.082908966857,5.12071484354904,
127.840206429006));
#158842=CARTESIAN_POINT('Ctrl Pts',(-157.090306881168,5.04183302328554,
127.703934399208));
#158843=CARTESIAN_POINT('Ctrl Pts',(-157.097704795479,4.9574652311445,127.570739877437));
#158844=CARTESIAN_POINT('Ctrl Pts',(-157.105102709791,4.86788695886932,
127.441087343184));
#158845=CARTESIAN_POINT('Ctrl Pts',(-157.112499394703,4.77832357287775,
127.311456354831));
#158846=CARTESIAN_POINT('Ctrl Pts',(-157.119896079615,4.68355163726892,
127.185366492595));
#158847=CARTESIAN_POINT('Ctrl Pts',(-157.127292764527,4.58389038172495,
127.063253892166));
#158848=CARTESIAN_POINT('Ctrl Pts',(-157.134689121463,4.48423354526548,
126.941146706339));
#158849=CARTESIAN_POINT('Ctrl Pts',(-157.142085478398,4.3796880559703,126.823016720869));
#158850=CARTESIAN_POINT('Ctrl Pts',(-157.149481835334,4.27061373173946,
126.709267344296));
#158851=CARTESIAN_POINT('Ctrl Pts',(-157.15687932467,4.16152270795112,126.595500552404));
#158852=CARTESIAN_POINT('Ctrl Pts',(-157.164276814007,4.04790172700596,
126.486115974285));
#158853=CARTESIAN_POINT('Ctrl Pts',(-157.171674303343,3.93014767812742,
126.381480357983));
#158854=CARTESIAN_POINT('Ctrl Pts',(-157.179074385858,3.81235235074976,
126.276808061828));
#158855=CARTESIAN_POINT('Ctrl Pts',(-157.186474468373,3.69042134968084,
126.176888289784));
#158856=CARTESIAN_POINT('Ctrl Pts',(-157.193874550888,3.56478472922586,
126.082047582963));
#158857=CARTESIAN_POINT('Ctrl Pts',(-157.201282770555,3.43900995839112,
125.987102589036));
#158858=CARTESIAN_POINT('Ctrl Pts',(-157.208690990221,3.30952172882964,
125.897248038899));
#158859=CARTESIAN_POINT('Ctrl Pts',(-157.216099209887,3.17677977382686,
125.812767602195));
#158860=CARTESIAN_POINT('Ctrl Pts',(-157.22351198919,3.04395611836533,125.72823516919));
#158861=CARTESIAN_POINT('Ctrl Pts',(-157.230924768492,2.90787506893844,
125.649083627833));
#158862=CARTESIAN_POINT('Ctrl Pts',(-157.238337547794,2.76902057973649,
125.57555046692));
#158863=CARTESIAN_POINT('Ctrl Pts',(-157.245760918822,2.62996768872893,
125.501912238379));
#158864=CARTESIAN_POINT('Ctrl Pts',(-157.253184289851,2.48813377902014,
125.433908584573));
#158865=CARTESIAN_POINT('Ctrl Pts',(-157.26060766088,2.34402312867773,125.371729014491));
#158866=CARTESIAN_POINT('Ctrl Pts',(-157.264543710321,2.26761220396997,
125.338759914452));
#158867=CARTESIAN_POINT('Ctrl Pts',(-157.268479759762,2.1905614772537,125.307427345457));
#158868=CARTESIAN_POINT('Ctrl Pts',(-157.272415809203,2.11294767059808,
125.277753819194));
#158869=CARTESIAN_POINT('Ctrl Pts',(-157.279839075609,1.96657045350461,
125.221790474746));
#158870=CARTESIAN_POINT('Ctrl Pts',(-157.287262342014,1.81774700121957,
125.171561924975));
#158871=CARTESIAN_POINT('Ctrl Pts',(-157.29468560842,1.66696719846948,125.127288227528));
#158872=CARTESIAN_POINT('Ctrl Pts',(-157.302100101141,1.5163656049239,125.083066857916));
#158873=CARTESIAN_POINT('Ctrl Pts',(-157.309514593862,1.36381261812584,
125.044786435315));
#158874=CARTESIAN_POINT('Ctrl Pts',(-157.316929086583,1.20981809525616,
125.012619019489));
#158875=CARTESIAN_POINT('Ctrl Pts',(-157.324336432937,1.05597199810628,
124.980482607831));
#158876=CARTESIAN_POINT('Ctrl Pts',(-157.331743779291,0.900687493877916,
124.95444754906));
#158877=CARTESIAN_POINT('Ctrl Pts',(-157.339151125644,0.744489495964291,
124.934636096526));
#158878=CARTESIAN_POINT('Ctrl Pts',(-157.34655294732,0.588407996410522,
124.914839420121));
#158879=CARTESIAN_POINT('Ctrl Pts',(-157.353954768995,0.431414728504796,
124.90125715427));
#158880=CARTESIAN_POINT('Ctrl Pts',(-157.361356590671,0.274044585288307,
124.893960451099));
#158881=CARTESIAN_POINT('Ctrl Pts',(-157.368754504982,0.116757516545007,
124.886667599801));
#158882=CARTESIAN_POINT('Ctrl Pts',(-157.376152419294,-0.0409056593381581,
124.885653720275));
#158883=CARTESIAN_POINT('Ctrl Pts',(-157.383550333605,-0.198405252592531,
124.890938096027));
#158884=CARTESIAN_POINT('Ctrl Pts',(-157.390947018517,-0.355878672271614,
124.896221593611));
#158885=CARTESIAN_POINT('Ctrl Pts',(-157.398343703429,-0.513188190552356,
124.907801256666));
#158886=CARTESIAN_POINT('Ctrl Pts',(-157.405740388342,-0.669794322685559,
124.925644250212));
#158887=CARTESIAN_POINT('Ctrl Pts',(-157.413136745277,-0.826393510738753,
124.943486452581));
#158888=CARTESIAN_POINT('Ctrl Pts',(-157.420533102213,-0.982289003760471,
124.967591390976));
#158889=CARTESIAN_POINT('Ctrl Pts',(-157.427929459148,-1.13694691235704,
124.997874392577));
#158890=CARTESIAN_POINT('Ctrl Pts',(-157.435326948485,-1.29162849947469,
125.028162030584));
#158891=CARTESIAN_POINT('Ctrl Pts',(-157.442724437821,-1.44507175852789,
125.064629543427));
#158892=CARTESIAN_POINT('Ctrl Pts',(-157.450121927158,-1.59675360568007,
125.10714125324));
#158893=CARTESIAN_POINT('Ctrl Pts',(-157.457522009673,-1.74848862466842,
125.149667865467));
#158894=CARTESIAN_POINT('Ctrl Pts',(-157.464922092188,-1.89846064317388,
125.198242792467));
#158895=CARTESIAN_POINT('Ctrl Pts',(-157.472322174703,-2.04616247805276,
125.252680720822));
#158896=CARTESIAN_POINT('Ctrl Pts',(-157.47973039437,-2.194026726283,125.307178509276));
#158897=CARTESIAN_POINT('Ctrl Pts',(-157.487138614036,-2.33961545513118,
125.367552044937));
#158898=CARTESIAN_POINT('Ctrl Pts',(-157.494546833703,-2.48244150822397,
125.433567871542));
#158899=CARTESIAN_POINT('Ctrl Pts',(-157.501959613005,-2.62535546836926,
125.499624329787));
#158900=CARTESIAN_POINT('Ctrl Pts',(-157.509372392307,-2.76550303298194,
125.571329829199));
#158901=CARTESIAN_POINT('Ctrl Pts',(-157.516785171609,-2.9024228069489,
125.64840557391));
#158902=CARTESIAN_POINT('Ctrl Pts',(-157.524208542638,-3.03953821831,125.725591448059));
#158903=CARTESIAN_POINT('Ctrl Pts',(-157.531631913667,-3.17341631090493,
125.808162697281));
#158904=CARTESIAN_POINT('Ctrl Pts',(-157.539055284696,-3.30362507084091,
125.895797492393));
#158905=CARTESIAN_POINT('Ctrl Pts',(-157.542991334136,-3.37266487966637,
125.942263563523));
#158906=CARTESIAN_POINT('Ctrl Pts',(-157.546927383576,-3.4406736571893,
125.990152503206));
#158907=CARTESIAN_POINT('Ctrl Pts',(-157.550863433017,-3.50759099353742,
126.03941193111));
#158908=CARTESIAN_POINT('Ctrl Pts',(-157.558218175006,-3.63263000813877,
126.131456095763));
#158909=CARTESIAN_POINT('Ctrl Pts',(-157.565572916995,-3.75424966978868,
126.228577345023));
#158910=CARTESIAN_POINT('Ctrl Pts',(-157.572927658984,-3.87200459353564,
126.330490817255));
#158911=CARTESIAN_POINT('Ctrl Pts',(-157.580273676026,-3.98961982435429,
126.432283389307));
#158912=CARTESIAN_POINT('Ctrl Pts',(-157.587619693069,-4.10337915519362,
126.538856625361));
#158913=CARTESIAN_POINT('Ctrl Pts',(-157.594965710111,-4.21286640760883,
126.649882648658));
#158914=CARTESIAN_POINT('Ctrl Pts',(-157.602304689178,-4.32224876391778,
126.760802301603));
#158915=CARTESIAN_POINT('Ctrl Pts',(-157.609643668245,-4.42736692186733,
126.876165982255));
#158916=CARTESIAN_POINT('Ctrl Pts',(-157.616982647312,-4.52783819494831,
126.99560598608));
#158917=CARTESIAN_POINT('Ctrl Pts',(-157.624316268933,-4.62823612412295,
127.114958798848));
#158918=CARTESIAN_POINT('Ctrl Pts',(-157.631649890554,-4.72399367667982,
127.238381721226));
#158919=CARTESIAN_POINT('Ctrl Pts',(-157.638983512176,-4.8147655874284,
127.365470840237));
#158920=CARTESIAN_POINT('Ctrl Pts',(-157.646313991294,-4.90549860184631,
127.492505500767));
#158921=CARTESIAN_POINT('Ctrl Pts',(-157.653644470413,-4.99125000375958,
127.62320292324));
#158922=CARTESIAN_POINT('Ctrl Pts',(-157.660974949531,-5.07171541329371,
127.757126900068));
#158923=CARTESIAN_POINT('Ctrl Pts',(-157.668303887895,-5.15216391022401,
127.891022728115));
#158924=CARTESIAN_POINT('Ctrl Pts',(-157.675632826258,-5.2273284289208,
128.028143435116));
#158925=CARTESIAN_POINT('Ctrl Pts',(-157.682961764622,-5.29694859574216,
128.16802487708));
#158926=CARTESIAN_POINT('Ctrl Pts',(-157.690290675458,-5.36656850107277,
128.307905793654));
#158927=CARTESIAN_POINT('Ctrl Pts',(-157.697619586294,-5.43064392617252,
128.450547083563));
#158928=CARTESIAN_POINT('Ctrl Pts',(-157.704948497131,-5.48896115645343,
128.595461347467));
#158929=CARTESIAN_POINT('Ctrl Pts',(-157.712278893428,-5.54729020677008,
128.740404983338));
#158930=CARTESIAN_POINT('Ctrl Pts',(-157.719609289726,-5.59985859777098,
128.887622156598));
#158931=CARTESIAN_POINT('Ctrl Pts',(-157.726939686023,-5.64650141551444,
129.036607148585));
#158932=CARTESIAN_POINT('Ctrl Pts',(-157.734277182083,-5.69318940856624,
129.185736438093));
#158933=CARTESIAN_POINT('Ctrl Pts',(-157.741614678143,-5.73394025124491,
129.336636602246));
#158934=CARTESIAN_POINT('Ctrl Pts',(-157.748952174202,-5.76863925827811,
129.488787863838));
#158935=CARTESIAN_POINT('Ctrl Pts',(-157.756293346656,-5.80335565097007,
129.641015359596));
#158936=CARTESIAN_POINT('Ctrl Pts',(-157.763634519109,-5.83201409738659,
129.79449482759));
#158937=CARTESIAN_POINT('Ctrl Pts',(-157.770975691562,-5.8545515050313,
129.948698746594));
#158938=CARTESIAN_POINT('Ctrl Pts',(-157.778327484036,-5.87712151615164,
130.103125742883));
#158939=CARTESIAN_POINT('Ctrl Pts',(-157.78567927651,-5.89355275828968,
130.258278905398));
#158940=CARTESIAN_POINT('Ctrl Pts',(-157.793031068984,-5.90383417195853,
130.413627163003));
#158941=CARTESIAN_POINT('Ctrl Pts',(-157.799228981919,-5.91250189578266,
130.544593179627));
#158942=CARTESIAN_POINT('Ctrl Pts',(-157.805426894855,-5.9167996709415,
130.675697717311));
#158943=CARTESIAN_POINT('Ctrl Pts',(-157.811624807791,-5.91674956674677,
130.806624883877));
#158944=CARTESIAN_POINT('',(-159.561624807791,-5.91743068731423,130.798929988566));
#158945=CARTESIAN_POINT('Ctrl Pts',(-157.811624807791,-5.9254847114659,
130.806628226708));
#158946=CARTESIAN_POINT('Ctrl Pts',(-157.817520224137,-5.92609395467479,
130.931349446311));
#158947=CARTESIAN_POINT('Ctrl Pts',(-157.823415640483,-5.92249881701993,
131.056034883051));
#158948=CARTESIAN_POINT('Ctrl Pts',(-157.829311056829,-5.91458801171559,
131.180445903534));
#158949=CARTESIAN_POINT('Ctrl Pts',(-157.922126931433,-5.7900423867684,
133.139140081975));
#158950=CARTESIAN_POINT('Ctrl Pts',(-158.107758680643,-3.4015434686423,
136.920491957005));
#158951=CARTESIAN_POINT('Ctrl Pts',(-158.386206304455,3.30705718159266,
136.972093858232));
#158952=CARTESIAN_POINT('Ctrl Pts',(-158.664653928267,6.97663384066779,
131.355850221806));
#158953=CARTESIAN_POINT('Ctrl Pts',(-158.943101552081,4.23502482768286,
125.232814580849));
#158954=CARTESIAN_POINT('Ctrl Pts',(-159.221549175893,-2.39836510947921,
124.229757562476));
#158955=CARTESIAN_POINT('Ctrl Pts',(-159.427723594463,-5.67808762901621,
127.960611207063));
#158956=CARTESIAN_POINT('Ctrl Pts',(-159.541082138429,-5.92148486028014,
130.362796665562));
#158957=CARTESIAN_POINT('Ctrl Pts',(-159.561624807791,-5.91743068731423,
130.798929988566));
#158958=CARTESIAN_POINT('',(-161.311624807829,-5.91674999652905,130.804563283626));
#158959=CARTESIAN_POINT('Ctrl Pts',(-159.561624807791,-5.91674750835102,
130.798930615543));
#158960=CARTESIAN_POINT('Ctrl Pts',(-159.568932004374,-5.91688986440021,
130.954047463703));
#158961=CARTESIAN_POINT('Ctrl Pts',(-159.576239200957,-5.91092810715701,
131.109346714272));
#158962=CARTESIAN_POINT('Ctrl Pts',(-159.58354639754,-5.89884604826352,
131.264301767482));
#158963=CARTESIAN_POINT('Ctrl Pts',(-159.590848258521,-5.88677281150266,
131.419143674908));
#158964=CARTESIAN_POINT('Ctrl Pts',(-159.598150119502,-5.86858819695825,
131.573641503703));
#158965=CARTESIAN_POINT('Ctrl Pts',(-159.605451980483,-5.84432808587817,
131.727268948396));
#158966=CARTESIAN_POINT('Ctrl Pts',(-159.612750815579,-5.82007802816727,
131.880832730009));
#158967=CARTESIAN_POINT('Ctrl Pts',(-159.620049650675,-5.78975754077517,
132.033526466032));
#158968=CARTESIAN_POINT('Ctrl Pts',(-159.627348485771,-5.75345431116056,
132.184829397325));
#158969=CARTESIAN_POINT('Ctrl Pts',(-159.634645847149,-5.71715841158406,
132.336101778821));
#158970=CARTESIAN_POINT('Ctrl Pts',(-159.641943208527,-5.67488226185732,
132.485983540557));
#158971=CARTESIAN_POINT('Ctrl Pts',(-159.649240569904,-5.62676452252715,
132.633964829009));
#158972=CARTESIAN_POINT('Ctrl Pts',(-159.656537990201,-5.57864639469371,
132.781947312264));
#158973=CARTESIAN_POINT('Ctrl Pts',(-159.663835410497,-5.52468670211461,
132.928028926103));
#158974=CARTESIAN_POINT('Ctrl Pts',(-159.671132830794,-5.46507367570252,
133.071715967229));
#158975=CARTESIAN_POINT('Ctrl Pts',(-159.678431842531,-5.40544764873038,
133.215434343989));
#158976=CARTESIAN_POINT('Ctrl Pts',(-159.685730854267,-5.34016598231529,
133.356756754134));
#158977=CARTESIAN_POINT('Ctrl Pts',(-159.693029866004,-5.26946452189638,
133.495210709075));
#158978=CARTESIAN_POINT('Ctrl Pts',(-159.700336286835,-5.19869129370716,
133.633805206115));
#158979=CARTESIAN_POINT('Ctrl Pts',(-159.707642707666,-5.1224874584411,
133.769525089707));
#158980=CARTESIAN_POINT('Ctrl Pts',(-159.714949128497,-5.04113449756899,
133.901923133468));
#158981=CARTESIAN_POINT('Ctrl Pts',(-159.722259345137,-4.95973927245551,
134.034389960255));
#158982=CARTESIAN_POINT('Ctrl Pts',(-159.729569561777,-4.87318980763445,
134.163531191305));
#158983=CARTESIAN_POINT('Ctrl Pts',(-159.736879778418,-4.78180970556107,
134.288930390479));
#158984=CARTESIAN_POINT('Ctrl Pts',(-159.744201082717,-4.69029100411616,
134.41451978697));
#158985=CARTESIAN_POINT('Ctrl Pts',(-159.751522387017,-4.59392726697723,
134.53635551228));
#158986=CARTESIAN_POINT('Ctrl Pts',(-159.758843691317,-4.49308159296783,
134.654055197846));
#158987=CARTESIAN_POINT('Ctrl Pts',(-159.765377268717,-4.40308628752762,
134.759091127812));
#158988=CARTESIAN_POINT('Ctrl Pts',(-159.771910846118,-4.30952228015494,
134.860833538824));
#158989=CARTESIAN_POINT('Ctrl Pts',(-159.778444423519,-4.21267037862175,
134.959037361139));
#158990=CARTESIAN_POINT('Ctrl Pts',(-159.785867689924,-4.10262997918174,
135.070613774849));
#158991=CARTESIAN_POINT('Ctrl Pts',(-159.79329095633,-3.98798731970659,
135.177984104969));
#158992=CARTESIAN_POINT('Ctrl Pts',(-159.800714222735,-3.86909710212392,
135.28074511589));
#158993=CARTESIAN_POINT('Ctrl Pts',(-159.808128715456,-3.75034740290522,
135.38338467183));
#158994=CARTESIAN_POINT('Ctrl Pts',(-159.815543208177,-3.62736041810098,
135.481425510788));
#158995=CARTESIAN_POINT('Ctrl Pts',(-159.822957700898,-3.5005289122021,
135.574499808128));
#158996=CARTESIAN_POINT('Ctrl Pts',(-159.830365047252,-3.37381965128336,
135.667484396957));
#158997=CARTESIAN_POINT('Ctrl Pts',(-159.837772393605,-3.24327354511521,
135.755511754651));
#158998=CARTESIAN_POINT('Ctrl Pts',(-159.845179739959,-3.10931769548364,
135.838253150294));
#158999=CARTESIAN_POINT('Ctrl Pts',(-159.852581561635,-2.97546175517859,
135.920932834282));
#159000=CARTESIAN_POINT('Ctrl Pts',(-159.85998338331,-2.83820145132589,
135.99833421088));
#159001=CARTESIAN_POINT('Ctrl Pts',(-159.867385204985,-2.69799413899417,
136.070170924485));
#159002=CARTESIAN_POINT('Ctrl Pts',(-159.874783119297,-2.55786084101086,
136.141969716048));
#159003=CARTESIAN_POINT('Ctrl Pts',(-159.882181033608,-2.41478396419327,
136.208209525083));
#159004=CARTESIAN_POINT('Ctrl Pts',(-159.889578947919,-2.26924671758432,
136.268649216939));
#159005=CARTESIAN_POINT('Ctrl Pts',(-159.896975632832,-2.12373365662606,
136.329078864813));
#159006=CARTESIAN_POINT('Ctrl Pts',(-159.904372317744,-1.97576138177387,
136.383710165482));
#159007=CARTESIAN_POINT('Ctrl Pts',(-159.911769002656,-1.82583450722637,
136.43234950479));
#159008=CARTESIAN_POINT('Ctrl Pts',(-159.919165359592,-1.6759142805936,
136.480986687379));
#159009=CARTESIAN_POINT('Ctrl Pts',(-159.926561716527,-1.52403998167192,
136.523632321694));
#159010=CARTESIAN_POINT('Ctrl Pts',(-159.933958073463,-1.37073260754405,
136.560142291771));
#159011=CARTESIAN_POINT('Ctrl Pts',(-159.941355562799,-1.21740176166583,
136.596657851618));
#159012=CARTESIAN_POINT('Ctrl Pts',(-159.948753052136,-1.06263776687743,
136.627035790296));
#159013=CARTESIAN_POINT('Ctrl Pts',(-159.956150541472,-0.90697291607658,
136.651182890562));
#159014=CARTESIAN_POINT('Ctrl Pts',(-159.963550623987,-0.751253497203818,
136.675338455556));
#159015=CARTESIAN_POINT('Ctrl Pts',(-159.970950706502,-0.594632962231653,
136.693258776203));
#159016=CARTESIAN_POINT('Ctrl Pts',(-159.978350789017,-0.437649695184568,
136.704902398352));
#159017=CARTESIAN_POINT('Ctrl Pts',(-159.985759008684,-0.280493808897315,
136.716558823861));
#159018=CARTESIAN_POINT('Ctrl Pts',(-159.99316722835,-0.122974766486851,
136.721924739746));
#159019=CARTESIAN_POINT('Ctrl Pts',(-160.000575448017,0.0343673306403178,
136.721010805729));
#159020=CARTESIAN_POINT('Ctrl Pts',(-160.007988227319,0.191806269203324,
136.7200963092));
#159021=CARTESIAN_POINT('Ctrl Pts',(-160.015401006621,0.349067673429993,
136.712894278026));
#159022=CARTESIAN_POINT('Ctrl Pts',(-160.022813785923,0.505616105100663,
136.699467310134));
#159023=CARTESIAN_POINT('Ctrl Pts',(-160.030237156952,0.662388220511676,
136.686021157161));
#159024=CARTESIAN_POINT('Ctrl Pts',(-160.03766052798,0.818444959356333,
136.666332349798));
#159025=CARTESIAN_POINT('Ctrl Pts',(-160.045083899009,0.973259796759561,
136.640514824791));
#159026=CARTESIAN_POINT('Ctrl Pts',(-160.04901994845,1.05534633828929,136.626825753548));
#159027=CARTESIAN_POINT('Ctrl Pts',(-160.052955997891,1.13708395712726,
136.611414522782));
#159028=CARTESIAN_POINT('Ctrl Pts',(-160.056892047333,1.21839597108338,
136.594303779649));
#159029=CARTESIAN_POINT('Ctrl Pts',(-160.064315313738,1.37174789172974,
136.56203345211));
#159030=CARTESIAN_POINT('Ctrl Pts',(-160.071738580143,1.52404874909483,
136.52361762194));
#159031=CARTESIAN_POINT('Ctrl Pts',(-160.079161846549,1.67476756458465,
136.479136751222));
#159032=CARTESIAN_POINT('Ctrl Pts',(-160.08657633927,1.82530824295054,136.4347084532));
#159033=CARTESIAN_POINT('Ctrl Pts',(-160.093990831991,1.9742702468371,136.384229487949));
#159034=CARTESIAN_POINT('Ctrl Pts',(-160.101405324712,2.12113181616055,
136.32783148116));
#159035=CARTESIAN_POINT('Ctrl Pts',(-160.108812671065,2.26785183477466,
136.271487832893));
#159036=CARTESIAN_POINT('Ctrl Pts',(-160.116220017419,2.41247510301682,
136.209236633538));
#159037=CARTESIAN_POINT('Ctrl Pts',(-160.123627363773,2.55449419130832,
136.141259528832));
#159038=CARTESIAN_POINT('Ctrl Pts',(-160.131029185448,2.69640735640609,
136.073333124015));
#159039=CARTESIAN_POINT('Ctrl Pts',(-160.138431007124,2.83571987366102,
135.999689477655));
#159040=CARTESIAN_POINT('Ctrl Pts',(-160.145832828799,2.97194361240766,
135.920558593326));
#159041=CARTESIAN_POINT('Ctrl Pts',(-160.15323074311,3.10809543970221,135.841469481575));
#159042=CARTESIAN_POINT('Ctrl Pts',(-160.160628657422,3.24116141381868,
135.756899087742));
#159043=CARTESIAN_POINT('Ctrl Pts',(-160.168026571733,3.3706774750536,135.667123610111));
#159044=CARTESIAN_POINT('Ctrl Pts',(-160.175423256645,3.50017201306936,
135.577363051535));
#159045=CARTESIAN_POINT('Ctrl Pts',(-160.182819941557,3.62611750254257,
135.482399338365));
#159046=CARTESIAN_POINT('Ctrl Pts',(-160.190216626469,3.74807829410105,
135.382552363637));
#159047=CARTESIAN_POINT('Ctrl Pts',(-160.197612983405,3.87003367779022,
135.282709816228));
#159048=CARTESIAN_POINT('Ctrl Pts',(-160.20500934034,3.98800442602976,135.177984674266));
#159049=CARTESIAN_POINT('Ctrl Pts',(-160.212405697276,4.10158767832863,
135.068737369154));
#159050=CARTESIAN_POINT('Ctrl Pts',(-160.219803186612,4.21518832051307,
134.959473338001));
#159051=CARTESIAN_POINT('Ctrl Pts',(-160.227200675949,4.32439986017536,
134.84568602392));
#159052=CARTESIAN_POINT('Ctrl Pts',(-160.234598165285,4.42885615369344,
134.727772873803));
#159053=CARTESIAN_POINT('Ctrl Pts',(-160.2419982478,4.53334906420314,134.609818389415));
#159054=CARTESIAN_POINT('Ctrl Pts',(-160.249398330315,4.63308316231466,
134.487735468656));
#159055=CARTESIAN_POINT('Ctrl Pts',(-160.25679841283,4.72773256176189,134.361954662276));
#159056=CARTESIAN_POINT('Ctrl Pts',(-160.264206632496,4.82248603795442,
134.236035546968));
#159057=CARTESIAN_POINT('Ctrl Pts',(-160.271614852163,4.91214342499873,
134.106410724022));
#159058=CARTESIAN_POINT('Ctrl Pts',(-160.279023071829,4.99642175321808,
133.973540357888));
#159059=CARTESIAN_POINT('Ctrl Pts',(-160.286435851131,5.08075195334219,
133.840588212261));
#159060=CARTESIAN_POINT('Ctrl Pts',(-160.293848630433,5.15969631085155,
133.704386865242));
#159061=CARTESIAN_POINT('Ctrl Pts',(-160.301261409735,5.23301807371878,
133.565420631878));
#159062=CARTESIAN_POINT('Ctrl Pts',(-160.308684780764,5.30644460215935,
133.426255837043));
#159063=CARTESIAN_POINT('Ctrl Pts',(-160.316108151793,5.37423233015227,
133.28431860159));
#159064=CARTESIAN_POINT('Ctrl Pts',(-160.323531522822,5.43619251635348,
133.140113491404));
#159065=CARTESIAN_POINT('Ctrl Pts',(-160.327467572263,5.46904529379542,
133.06365248182));
#159066=CARTESIAN_POINT('Ctrl Pts',(-160.331403621704,5.50026056841827,
132.986554161491));
#159067=CARTESIAN_POINT('Ctrl Pts',(-160.335339671145,5.52981594531894,
132.908895286655));
#159068=CARTESIAN_POINT('Ctrl Pts',(-160.342762937551,5.58555646375567,
132.76243307238));
#159069=CARTESIAN_POINT('Ctrl Pts',(-160.350186203956,5.63555847140281,
132.613533353129));
#159070=CARTESIAN_POINT('Ctrl Pts',(-160.357609470362,5.67960265638814,
132.462686347949));
#159071=CARTESIAN_POINT('Ctrl Pts',(-160.365023963083,5.72359478480446,
132.312017631402));
#159072=CARTESIAN_POINT('Ctrl Pts',(-160.372438455803,5.76164300340042,
132.159406564972));
#159073=CARTESIAN_POINT('Ctrl Pts',(-160.379852948525,5.793576028527,132.005363267096));
#159074=CARTESIAN_POINT('Ctrl Pts',(-160.387260294878,5.82547827540171,
131.851468441949));
#159075=CARTESIAN_POINT('Ctrl Pts',(-160.394667641232,5.85127698744293,
131.696144496611));
#159076=CARTESIAN_POINT('Ctrl Pts',(-160.402074987586,5.87085071027271,
131.539916529914));
#159077=CARTESIAN_POINT('Ctrl Pts',(-160.409476809261,5.89040983428153,
131.383805083929));
#159078=CARTESIAN_POINT('Ctrl Pts',(-160.416878630937,5.90375316737584,
131.226791327923));
#159079=CARTESIAN_POINT('Ctrl Pts',(-160.424280452612,5.91081037152842,
131.069410262599));
#159080=CARTESIAN_POINT('Ctrl Pts',(-160.431678366924,5.91786385023786,
130.912112277514));
#159081=CARTESIAN_POINT('Ctrl Pts',(-160.439076281235,5.91863779207514,
130.754447741251));
#159082=CARTESIAN_POINT('Ctrl Pts',(-160.446474195546,5.91311373487316,
130.5969563723));
#159083=CARTESIAN_POINT('Ctrl Pts',(-160.453870880459,5.90759059566927,
130.439491175557));
#159084=CARTESIAN_POINT('Ctrl Pts',(-160.461267565371,5.89577154771621,
130.282199461714));
#159085=CARTESIAN_POINT('Ctrl Pts',(-160.468664250283,5.87769024695864,
130.125620664928));
#159086=CARTESIAN_POINT('Ctrl Pts',(-160.476060607218,5.85960974794489,
129.969048811009));
#159087=CARTESIAN_POINT('Ctrl Pts',(-160.483456964154,5.83526759106086,
129.813190182125));
#159088=CARTESIAN_POINT('Ctrl Pts',(-160.490853321089,5.80474926151761,
129.658578538194));
#159089=CARTESIAN_POINT('Ctrl Pts',(-160.498250810426,5.7742262595402,129.503943222825));
#159090=CARTESIAN_POINT('Ctrl Pts',(-160.505648299763,5.73752527440648,
129.350555638804));
#159091=CARTESIAN_POINT('Ctrl Pts',(-160.513045789099,5.69478277987167,
129.198938662883));
#159092=CARTESIAN_POINT('Ctrl Pts',(-160.520445871614,5.65202530202185,
129.047268537867));
#159093=CARTESIAN_POINT('Ctrl Pts',(-160.527845954129,5.60322219938922,
128.897370615798));
#159094=CARTESIAN_POINT('Ctrl Pts',(-160.535246036644,5.54855955702418,
128.749751797217));
#159095=CARTESIAN_POINT('Ctrl Pts',(-160.542654256311,5.49383680746418,
128.601970656568));
#159096=CARTESIAN_POINT('Ctrl Pts',(-160.550062475977,5.43324178045389,
128.456473974554));
#159097=CARTESIAN_POINT('Ctrl Pts',(-160.557470695644,5.36700867335544,
128.313748551702));
#159098=CARTESIAN_POINT('Ctrl Pts',(-160.564883474946,5.30073480088472,
128.170935283734));
#159099=CARTESIAN_POINT('Ctrl Pts',(-160.572296254248,5.2288161037707,128.030897004974));
#159100=CARTESIAN_POINT('Ctrl Pts',(-160.57970903355,5.15153207972547,127.894094685721));
#159101=CARTESIAN_POINT('Ctrl Pts',(-160.587132404579,5.07413762864232,
127.757096896898));
#159102=CARTESIAN_POINT('Ctrl Pts',(-160.594555775608,4.99136273537086,
127.623344618718));
#159103=CARTESIAN_POINT('Ctrl Pts',(-160.601979146636,4.90352988617272,
127.493269374802));
#159104=CARTESIAN_POINT('Ctrl Pts',(-160.605915196077,4.85695880200896,
127.424300359367));
#159105=CARTESIAN_POINT('Ctrl Pts',(-160.609851245518,4.80896641999349,
127.356364539404));
#159106=CARTESIAN_POINT('Ctrl Pts',(-160.613787294958,4.75960521233209,
127.289522245003));
#159107=CARTESIAN_POINT('Ctrl Pts',(-160.621210561364,4.66651151519086,
127.163459763835));
#159108=CARTESIAN_POINT('Ctrl Pts',(-160.628633827769,4.56826527082558,
127.040907723338));
#159109=CARTESIAN_POINT('Ctrl Pts',(-160.636057094175,4.46516037098241,
126.922315612172));
#159110=CARTESIAN_POINT('Ctrl Pts',(-160.643471586896,4.36217733256824,
126.803863667031));
#159111=CARTESIAN_POINT('Ctrl Pts',(-160.650886079617,4.25434731174153,
126.689362614007));
#159112=CARTESIAN_POINT('Ctrl Pts',(-160.658300572338,4.14200690259376,
126.579232290359));
#159113=CARTESIAN_POINT('Ctrl Pts',(-160.665707918692,4.02977477136156,
126.469208114463));
#159114=CARTESIAN_POINT('Ctrl Pts',(-160.673115265045,3.91304117117206,
126.363546540911));
#159115=CARTESIAN_POINT('Ctrl Pts',(-160.680522611399,3.79218223348808,
126.262633581458));
#159116=CARTESIAN_POINT('Ctrl Pts',(-160.687924433075,3.67141343695992,
126.161795886697));
#159117=CARTESIAN_POINT('Ctrl Pts',(-160.69532625475,3.54652571463779,126.065699992266));
#159118=CARTESIAN_POINT('Ctrl Pts',(-160.702728076425,3.41793115834349,
125.974694256488));
#159119=CARTESIAN_POINT('Ctrl Pts',(-160.710125990737,3.28940448611521,
125.883736561931));
#159120=CARTESIAN_POINT('Ctrl Pts',(-160.717523905048,3.15717518093391,
125.797863889724));
#159121=CARTESIAN_POINT('Ctrl Pts',(-160.724921819359,3.02168734399846,
125.717383503639));
#159122=CARTESIAN_POINT('Ctrl Pts',(-160.732318504271,2.88622202268293,
125.636916491934));
#159123=CARTESIAN_POINT('Ctrl Pts',(-160.739715189184,2.74749956497993,
125.561840178314));
#159124=CARTESIAN_POINT('Ctrl Pts',(-160.747111874096,2.60599200398201,
125.492417824418));
#159125=CARTESIAN_POINT('Ctrl Pts',(-160.754508231031,2.46449071757763,
125.422998548781));
#159126=CARTESIAN_POINT('Ctrl Pts',(-160.761904587967,2.32020490856619,
125.359232898803));
#159127=CARTESIAN_POINT('Ctrl Pts',(-160.769300944902,2.17362985112807,
125.301337463627));
#159128=CARTESIAN_POINT('Ctrl Pts',(-160.776698434239,2.02703235267489,
125.243433164513));
#159129=CARTESIAN_POINT('Ctrl Pts',(-160.784095923575,1.87814525514074,
125.191401006869));
#159130=CARTESIAN_POINT('Ctrl Pts',(-160.791493412912,1.72748223694418,
125.145408799116));
#159131=CARTESIAN_POINT('Ctrl Pts',(-160.798893495427,1.57676640405821,
125.099400468865));
#159132=CARTESIAN_POINT('Ctrl Pts',(-160.806293577942,1.42427376783506,
125.059436412946));
#159133=CARTESIAN_POINT('Ctrl Pts',(-160.813693660457,1.27053138157105,
125.025634064861));
#159134=CARTESIAN_POINT('Ctrl Pts',(-160.821101880124,1.11661993974935,
124.991794547618));
#159135=CARTESIAN_POINT('Ctrl Pts',(-160.82851009979,0.961456368275483,
124.9641303494));
#159136=CARTESIAN_POINT('Ctrl Pts',(-160.835918319456,0.805576815615801,
124.942707560907));
#159137=CARTESIAN_POINT('Ctrl Pts',(-160.843331098758,0.649601321692446,
124.921271587045));
#159138=CARTESIAN_POINT('Ctrl Pts',(-160.850743878061,0.492909339179487,
124.906084713475));
#159139=CARTESIAN_POINT('Ctrl Pts',(-160.858156657363,0.336039770785305,
124.897160956563));
#159140=CARTESIAN_POINT('Ctrl Pts',(-160.865580028391,0.178946059795572,
124.888224448969));
#159141=CARTESIAN_POINT('Ctrl Pts',(-160.87300339942,0.0216746283987935,
124.885568937547));
#159142=CARTESIAN_POINT('Ctrl Pts',(-160.880426770449,-0.135237158657845,
124.889156354532));
#159143=CARTESIAN_POINT('Ctrl Pts',(-160.88436281989,-0.218435553201027,
124.891058489096));
#159144=CARTESIAN_POINT('Ctrl Pts',(-160.88829886933,-0.301532937337538,
124.894714869186));
#159145=CARTESIAN_POINT('Ctrl Pts',(-160.892234918771,-0.384450191146429,
124.900113958336));
#159146=CARTESIAN_POINT('Ctrl Pts',(-160.899658185177,-0.540829544073461,
124.910296471973));
#159147=CARTESIAN_POINT('Ctrl Pts',(-160.907081451582,-0.69704054147606,
124.926711448447));
#159148=CARTESIAN_POINT('Ctrl Pts',(-160.914504717987,-0.852546160146982,
124.949354587909));
#159149=CARTESIAN_POINT('Ctrl Pts',(-160.921919210708,-1.00786798409102,
124.971970965061));
#159150=CARTESIAN_POINT('Ctrl Pts',(-160.929333703429,-1.1624857229909,
125.000800799484));
#159151=CARTESIAN_POINT('Ctrl Pts',(-160.93674819615,-1.31586421854117,
125.035787837331));
#159152=CARTESIAN_POINT('Ctrl Pts',(-160.944155542504,-1.46909488212195,
125.070741153354));
#159153=CARTESIAN_POINT('Ctrl Pts',(-160.951562888858,-1.62108831872102,
125.111839775829));
#159154=CARTESIAN_POINT('Ctrl Pts',(-160.958970235212,-1.77131645747413,
125.158975903485));
#159155=CARTESIAN_POINT('Ctrl Pts',(-160.966372056887,-1.92143255041314,
125.206076875238));
#159156=CARTESIAN_POINT('Ctrl Pts',(-160.973773878562,-2.06978561244166,
125.259206274819));
#159157=CARTESIAN_POINT('Ctrl Pts',(-160.981175700238,-2.21585981414128,
125.31820569389));
#159158=CARTESIAN_POINT('Ctrl Pts',(-160.988573614549,-2.36185690440853,
125.377173967627));
#159159=CARTESIAN_POINT('Ctrl Pts',(-160.995971528861,-2.50557718490952,
125.442005950122));
#159160=CARTESIAN_POINT('Ctrl Pts',(-161.003369443172,-2.64652209838561,
125.51249409003));
#159161=CARTESIAN_POINT('Ctrl Pts',(-161.010766128084,-2.78744358937308,
125.582970516088));
#159162=CARTESIAN_POINT('Ctrl Pts',(-161.018162812996,-2.92559029516622,
125.659101067226));
#159163=CARTESIAN_POINT('Ctrl Pts',(-161.025559497909,-3.06048558087654,
125.74063090798));
#159164=CARTESIAN_POINT('Ctrl Pts',(-161.032955854844,-3.19537488518891,
125.822157133616));
#159165=CARTESIAN_POINT('Ctrl Pts',(-161.04035221178,-3.32701273660073,
125.909081979748));
#159166=CARTESIAN_POINT('Ctrl Pts',(-161.047748568715,-3.45494920473856,
126.001105829906));
#159167=CARTESIAN_POINT('Ctrl Pts',(-161.055146058052,-3.58290526027554,
126.09314376915));
#159168=CARTESIAN_POINT('Ctrl Pts',(-161.062543547388,-3.70715850111594,
126.190282048845));
#159169=CARTESIAN_POINT('Ctrl Pts',(-161.069941036725,-3.82729008954988,
126.29217920134));
#159170=CARTESIAN_POINT('Ctrl Pts',(-161.07734111924,-3.94746378992712,
126.394112073725));
#159171=CARTESIAN_POINT('Ctrl Pts',(-161.084741201755,-4.06351267673059,
126.500806898996));
#159172=CARTESIAN_POINT('Ctrl Pts',(-161.09214128427,-4.17505306464934,
126.611883727962));
#159173=CARTESIAN_POINT('Ctrl Pts',(-161.099549503937,-4.28671610269077,
126.723082697321));
#159174=CARTESIAN_POINT('Ctrl Pts',(-161.106957723603,-4.39386047660583,
126.83867302959));
#159175=CARTESIAN_POINT('Ctrl Pts',(-161.11436594327,-4.49614078107216,
126.958239371521));
#159176=CARTESIAN_POINT('Ctrl Pts',(-161.121778722572,-4.59848403735984,
127.077879304541));
#159177=CARTESIAN_POINT('Ctrl Pts',(-161.129191501874,-4.69595702817189,
127.201499831054));
#159178=CARTESIAN_POINT('Ctrl Pts',(-161.136604281176,-4.7882566710658,
127.328655133136));
#159179=CARTESIAN_POINT('Ctrl Pts',(-161.144027652205,-4.88068819601723,
127.455992120677));
#159180=CARTESIAN_POINT('Ctrl Pts',(-161.151451023234,-4.9679314032225,
127.586873661283));
#159181=CARTESIAN_POINT('Ctrl Pts',(-161.158874394263,-5.04972786139977,
127.720827078215));
#159182=CARTESIAN_POINT('Ctrl Pts',(-161.162810443703,-5.09309830620011,
127.791852394034));
#159183=CARTESIAN_POINT('Ctrl Pts',(-161.166746493143,-5.13493825596471,
127.863740939493));
#159184=CARTESIAN_POINT('Ctrl Pts',(-161.170682542584,-5.17521465039959,
127.93641991302));
#159185=CARTESIAN_POINT('Ctrl Pts',(-161.178467267524,-5.25487336836381,
128.080164504248));
#159186=CARTESIAN_POINT('Ctrl Pts',(-161.186251992465,-5.32863465868597,
128.22740185616));
#159187=CARTESIAN_POINT('Ctrl Pts',(-161.194036717405,-5.39619452720069,
128.377631298687));
#159188=CARTESIAN_POINT('Ctrl Pts',(-161.201808871549,-5.46364529984529,
128.527618150277));
#159189=CARTESIAN_POINT('Ctrl Pts',(-161.209581025693,-5.52491447891031,
128.680587171784));
#159190=CARTESIAN_POINT('Ctrl Pts',(-161.217353179838,-5.57974322839213,
128.836012053995));
#159191=CARTESIAN_POINT('Ctrl Pts',(-161.225209148834,-5.63516325069629,
128.993113036967));
#159192=CARTESIAN_POINT('Ctrl Pts',(-161.23306511783,-5.68400292496206,
129.152722890867));
#159193=CARTESIAN_POINT('Ctrl Pts',(-161.240921086826,-5.72604313071144,
129.314273161162));
#159194=CARTESIAN_POINT('Ctrl Pts',(-161.248666503456,-5.76749172972071,
129.473550030862));
#159195=CARTESIAN_POINT('Ctrl Pts',(-161.256411920086,-5.8023308548413,
129.634712746245));
#159196=CARTESIAN_POINT('Ctrl Pts',(-161.264157336717,-5.83039894683897,
129.797196935139));
#159197=CARTESIAN_POINT('Ctrl Pts',(-161.272068581896,-5.85906797371045,
129.963159893291));
#159198=CARTESIAN_POINT('Ctrl Pts',(-161.279979827075,-5.88067262040033,
130.130501244622));
#159199=CARTESIAN_POINT('Ctrl Pts',(-161.287891072254,-5.89509459606671,
130.298603496089));
#159200=CARTESIAN_POINT('Ctrl Pts',(-161.295802317433,-5.90951657173305,
130.466705747554));
#159201=CARTESIAN_POINT('Ctrl Pts',(-161.303713562612,-5.916755785072,130.635568548246));
#159202=CARTESIAN_POINT('Ctrl Pts',(-161.311624807791,-5.91674999652907,
130.804563282823));
#159203=CARTESIAN_POINT('',(-163.061624807791,-5.91686277527085,130.809721141343));
#159204=CARTESIAN_POINT('Ctrl Pts',(-161.311624807829,-5.91674999652905,
130.804563283627));
#159205=CARTESIAN_POINT('Ctrl Pts',(-161.31939311633,-5.91674431254827,
130.970504700389));
#159206=CARTESIAN_POINT('Ctrl Pts',(-161.327161424832,-5.90975332908639,
131.13630374045));
#159207=CARTESIAN_POINT('Ctrl Pts',(-161.334929733334,-5.89583865538439,
131.301368778641));
#159208=CARTESIAN_POINT('Ctrl Pts',(-161.342708486022,-5.88190527394895,
131.466655740307));
#159209=CARTESIAN_POINT('Ctrl Pts',(-161.35048723871,-5.86102964709646,
131.631206417196));
#159210=CARTESIAN_POINT('Ctrl Pts',(-161.358265991398,-5.83332481242634,
131.794437480861));
#159211=CARTESIAN_POINT('Ctrl Pts',(-161.366063440059,-5.80555339010722,
131.95806086496));
#159212=CARTESIAN_POINT('Ctrl Pts',(-161.37386088872,-5.77091998786326,
132.120357981835));
#159213=CARTESIAN_POINT('Ctrl Pts',(-161.381658337382,-5.7295885904063,
132.280756617014));
#159214=CARTESIAN_POINT('Ctrl Pts',(-161.389465416141,-5.68820614735775,
132.441353349613));
#159215=CARTESIAN_POINT('Ctrl Pts',(-161.397272494899,-5.64010928699573,
132.600046619344));
#159216=CARTESIAN_POINT('Ctrl Pts',(-161.405079573658,-5.5855110710074,
132.756281885997));
#159217=CARTESIAN_POINT('Ctrl Pts',(-161.412904931998,-5.53078501815113,
132.912882963635));
#159218=CARTESIAN_POINT('Ctrl Pts',(-161.420730290337,-5.46952728045612,
133.067014234323));
#159219=CARTESIAN_POINT('Ctrl Pts',(-161.428555648677,-5.40199896495129,
133.218141416472));
#159220=CARTESIAN_POINT('Ctrl Pts',(-161.43541382125,-5.34281690309353,
133.350589829784));
#159221=CARTESIAN_POINT('Ctrl Pts',(-161.442271993823,-5.27881928973841,
133.480731107596));
#159222=CARTESIAN_POINT('Ctrl Pts',(-161.449130166396,-5.21020966922348,
133.608223268487));
#159223=CARTESIAN_POINT('Ctrl Pts',(-161.456553432802,-5.135946811937,133.7462204193));
#159224=CARTESIAN_POINT('Ctrl Pts',(-161.463976699207,-5.05608540342793,
133.881473820707));
#159225=CARTESIAN_POINT('Ctrl Pts',(-161.471399965612,-4.97085257714099,
134.013496828267));
#159226=CARTESIAN_POINT('Ctrl Pts',(-161.478814458333,-4.88572048897633,
134.145363795596));
#159227=CARTESIAN_POINT('Ctrl Pts',(-161.486228951054,-4.79522982038961,
134.274007658384));
#159228=CARTESIAN_POINT('Ctrl Pts',(-161.493643443775,-4.69965418269364,
134.398965063898));
#159229=CARTESIAN_POINT('Ctrl Pts',(-161.501050790129,-4.60417066439565,
134.52380203076));
#159230=CARTESIAN_POINT('Ctrl Pts',(-161.508458136482,-4.50361215935036,
134.644959319442));
#159231=CARTESIAN_POINT('Ctrl Pts',(-161.515865482836,-4.39829621611526,
134.762001449906));
#159232=CARTESIAN_POINT('Ctrl Pts',(-161.523267304511,-4.29305882148397,
134.878956285933));
#159233=CARTESIAN_POINT('Ctrl Pts',(-161.530669126187,-4.18307130238067,
134.991801798711));
#159234=CARTESIAN_POINT('Ctrl Pts',(-161.538070947862,-4.06869214699103,
135.100134677676));
#159235=CARTESIAN_POINT('Ctrl Pts',(-161.545468862173,-3.95437337146752,
135.208410368557));
#159236=CARTESIAN_POINT('Ctrl Pts',(-161.552866776484,-3.83566784702602,
135.312177913807));
#159237=CARTESIAN_POINT('Ctrl Pts',(-161.560264690796,-3.71297157878944,
135.411070139296));
#159238=CARTESIAN_POINT('Ctrl Pts',(-161.567661375708,-3.59029570044652,
135.509945930692));
#159239=CARTESIAN_POINT('Ctrl Pts',(-161.57505806062,-3.46363068490344,
135.603947776284));
#159240=CARTESIAN_POINT('Ctrl Pts',(-161.582454745532,-3.3334064305968,
135.692748095146));
#159241=CARTESIAN_POINT('Ctrl Pts',(-161.589851102467,-3.20318795057005,
135.781544476507));
#159242=CARTESIAN_POINT('Ctrl Pts',(-161.597247459403,-3.06941085399642,
135.86513957942));
#159243=CARTESIAN_POINT('Ctrl Pts',(-161.604643816338,-2.93253466822418,
135.94324872514));
#159244=CARTESIAN_POINT('Ctrl Pts',(-161.612041305675,-2.79563752635846,
136.021369829569));
#159245=CARTESIAN_POINT('Ctrl Pts',(-161.619438795011,-2.65564067478649,
136.094003119394));
#159246=CARTESIAN_POINT('Ctrl Pts',(-161.626836284348,-2.51302878103162,
136.160909591318));
#159247=CARTESIAN_POINT('Ctrl Pts',(-161.634236366863,-2.37036689489867,
136.227839517203));
#159248=CARTESIAN_POINT('Ctrl Pts',(-161.641636449378,-2.22508847918491,
136.289038469762));
#159249=CARTESIAN_POINT('Ctrl Pts',(-161.649036531892,-2.07769858934638,
136.344315412899));
#159250=CARTESIAN_POINT('Ctrl Pts',(-161.656444751559,-1.93014662917171,
136.399653138717));
#159251=CARTESIAN_POINT('Ctrl Pts',(-161.663852971225,-1.78047890785916,
136.449055719338));
#159252=CARTESIAN_POINT('Ctrl Pts',(-161.671261190892,-1.62921676974423,
136.492381651255));
#159253=CARTESIAN_POINT('Ctrl Pts',(-161.678673970194,-1.47786153230723,
136.535734249559));
#159254=CARTESIAN_POINT('Ctrl Pts',(-161.686086749496,-1.32491028447664,
136.57300265842));
#159255=CARTESIAN_POINT('Ctrl Pts',(-161.693499528798,-1.17089448651533,
136.60409653086));
#159256=CARTESIAN_POINT('Ctrl Pts',(-161.700922899826,-1.01665862355904,
136.635234831682));
#159257=CARTESIAN_POINT('Ctrl Pts',(-161.708346270855,-0.861355540132692,
136.66018091659));
#159258=CARTESIAN_POINT('Ctrl Pts',(-161.715769641884,-0.705522565048401,
136.67889621391));
#159259=CARTESIAN_POINT('Ctrl Pts',(-161.719705691326,-0.622896182474263,
136.688819513619));
#159260=CARTESIAN_POINT('Ctrl Pts',(-161.723641740768,-0.540120853656633,
136.696991986241));
#159261=CARTESIAN_POINT('Ctrl Pts',(-161.727577790209,-0.457276534927223,
136.703413824065));
#159262=CARTESIAN_POINT('Ctrl Pts',(-161.735001056615,-0.301034735329166,
136.715525209779));
#159263=CARTESIAN_POINT('Ctrl Pts',(-161.74242432302,-0.1440751761255,136.721443312216));
#159264=CARTESIAN_POINT('Ctrl Pts',(-161.749847589426,0.0130699437580426,
136.721096181969));
#159265=CARTESIAN_POINT('Ctrl Pts',(-161.757262082147,0.170029331159972,
136.720749462001));
#159266=CARTESIAN_POINT('Ctrl Pts',(-161.764676574868,0.327173473037769,
136.714152249828));
#159267=CARTESIAN_POINT('Ctrl Pts',(-161.772091067589,0.483964644014953,
136.701284288926));
#159268=CARTESIAN_POINT('Ctrl Pts',(-161.779498413943,0.640604693758912,
136.688428730649));
#159269=CARTESIAN_POINT('Ctrl Pts',(-161.786905760296,0.796892080337304,
136.669314486353));
#159270=CARTESIAN_POINT('Ctrl Pts',(-161.79431310665,0.952288779307195,
136.643973331035));
#159271=CARTESIAN_POINT('Ctrl Pts',(-161.801714928326,1.10756957755577,
136.618651076106));
#159272=CARTESIAN_POINT('Ctrl Pts',(-161.809116750001,1.26196064407807,
136.587111217337));
#159273=CARTESIAN_POINT('Ctrl Pts',(-161.816518571676,1.41492889065313,
136.549437361779));
#159274=CARTESIAN_POINT('Ctrl Pts',(-161.823916485988,1.56781638648196,
136.511783393956));
#159275=CARTESIAN_POINT('Ctrl Pts',(-161.831314400299,1.71928219665713,
136.468001967198));
#159276=CARTESIAN_POINT('Ctrl Pts',(-161.83871231461,1.86880335674129,136.418227785244));
#159277=CARTESIAN_POINT('Ctrl Pts',(-161.846108999522,2.01829966912103,
136.368461874856));
#159278=CARTESIAN_POINT('Ctrl Pts',(-161.853505684435,2.16585161895605,
136.312705303604));
#159279=CARTESIAN_POINT('Ctrl Pts',(-161.860902369347,2.31095123252788,
136.251142691725));
#159280=CARTESIAN_POINT('Ctrl Pts',(-161.868298726282,2.45604441223079,
136.189582809596));
#159281=CARTESIAN_POINT('Ctrl Pts',(-161.875695083218,2.59868512823418,
136.122217544531));
#159282=CARTESIAN_POINT('Ctrl Pts',(-161.883091440153,2.73838548649179,
136.049279634088));
#159283=CARTESIAN_POINT('Ctrl Pts',(-161.89048892949,2.87810723323088,135.976330556664));
#159284=CARTESIAN_POINT('Ctrl Pts',(-161.897886418826,3.01488739493115,
135.897807307835));
#159285=CARTESIAN_POINT('Ctrl Pts',(-161.905283908163,3.14826291671537,
135.813988464995));
#159286=CARTESIAN_POINT('Ctrl Pts',(-161.912683990678,3.2816851930818,135.73014023959));
#159287=CARTESIAN_POINT('Ctrl Pts',(-161.920084073193,3.41170013743103,
135.640992922675));
#159288=CARTESIAN_POINT('Ctrl Pts',(-161.927484155708,3.5378740308729,135.546868172033));
#159289=CARTESIAN_POINT('Ctrl Pts',(-161.934892375374,3.66418666548178,
135.452639921551));
#159290=CARTESIAN_POINT('Ctrl Pts',(-161.942300595041,3.78664951491966,
135.35342353035));
#159291=CARTESIAN_POINT('Ctrl Pts',(-161.949708814707,3.90486172892967,
135.24958113408));
#159292=CARTESIAN_POINT('Ctrl Pts',(-161.957121594009,4.02314670058528,
135.145674824549));
#159293=CARTESIAN_POINT('Ctrl Pts',(-161.964534373311,4.13717555395143,
135.037137093263));
#159294=CARTESIAN_POINT('Ctrl Pts',(-161.971947152613,4.24658501030232,
134.924366238045));
#159295=CARTESIAN_POINT('Ctrl Pts',(-161.979370523642,4.35615079601509,
134.81143425054));
#159296=CARTESIAN_POINT('Ctrl Pts',(-161.986793894671,4.46108375383855,
134.694257336274));
#159297=CARTESIAN_POINT('Ctrl Pts',(-161.9942172657,4.5610609929833,134.573266716262));
#159298=CARTESIAN_POINT('Ctrl Pts',(-161.998153315141,4.61407132409991,
134.5091145864));
#159299=CARTESIAN_POINT('Ctrl Pts',(-162.002089364581,4.66568914388588,
134.443890779039));
#159300=CARTESIAN_POINT('Ctrl Pts',(-162.006025414022,4.71587139576867,
134.377662667641));
#159301=CARTESIAN_POINT('Ctrl Pts',(-162.013448680428,4.81051355668355,
134.252758516456));
#159302=CARTESIAN_POINT('Ctrl Pts',(-162.020871946833,4.9003330995738,134.123902872896));
#159303=CARTESIAN_POINT('Ctrl Pts',(-162.028295213239,4.98498182484608,
133.991504600579));
#159304=CARTESIAN_POINT('Ctrl Pts',(-162.03570970596,5.06953050235472,133.859262812024));
#159305=CARTESIAN_POINT('Ctrl Pts',(-162.043124198681,5.1489203280553,133.723487040583));
#159306=CARTESIAN_POINT('Ctrl Pts',(-162.050538691402,5.22284360585934,
133.584618740697));
#159307=CARTESIAN_POINT('Ctrl Pts',(-162.057946037756,5.29669563362507,
133.445884287307));
#159308=CARTESIAN_POINT('Ctrl Pts',(-162.065353384109,5.36509142853283,
133.304063566756));
#159309=CARTESIAN_POINT('Ctrl Pts',(-162.072760730463,5.42776690843336,
133.159626409407));
#159310=CARTESIAN_POINT('Ctrl Pts',(-162.080162552139,5.49039564259637,
133.015296978739));
#159311=CARTESIAN_POINT('Ctrl Pts',(-162.087564373814,5.54731240882532,
132.868355337822));
#159312=CARTESIAN_POINT('Ctrl Pts',(-162.094966195489,5.59829940089622,
132.719295180528));
#159313=CARTESIAN_POINT('Ctrl Pts',(-162.102364109801,5.64925947733088,
132.57031371093));
#159314=CARTESIAN_POINT('Ctrl Pts',(-162.109762024112,5.69429589320263,
132.419216304511));
#159315=CARTESIAN_POINT('Ctrl Pts',(-162.117159938424,5.73323930352933,
132.266515756724));
#159316=CARTESIAN_POINT('Ctrl Pts',(-162.124556623336,5.7721762421678,132.113840584998));
#159317=CARTESIAN_POINT('Ctrl Pts',(-162.131953308248,5.80502209270777,
131.959563162021));
#159318=CARTESIAN_POINT('Ctrl Pts',(-162.13934999316,5.83165760918026,131.804210652216));
#159319=CARTESIAN_POINT('Ctrl Pts',(-162.146746350096,5.85829194460595,
131.648865030905));
#159320=CARTESIAN_POINT('Ctrl Pts',(-162.154142707031,5.878716430416,131.49244478548));
#159321=CARTESIAN_POINT('Ctrl Pts',(-162.161539063967,5.89286315665971,
131.335486195356));
#159322=CARTESIAN_POINT('Ctrl Pts',(-162.168936553303,5.90701204880337,
131.17850357447));
#159323=CARTESIAN_POINT('Ctrl Pts',(-162.17633404264,5.91488123410928,131.020982816586));
#159324=CARTESIAN_POINT('Ctrl Pts',(-162.183731531977,5.91645479515706,
130.863464080773));
#159325=CARTESIAN_POINT('Ctrl Pts',(-162.191131614492,5.91802890781421,
130.705890127012));
#159326=CARTESIAN_POINT('Ctrl Pts',(-162.198531697007,5.91330299852247,
130.548318569779));
#159327=CARTESIAN_POINT('Ctrl Pts',(-162.205931779522,5.90231325142926,
130.391288172948));
#159328=CARTESIAN_POINT('Ctrl Pts',(-162.213339999188,5.89131141997936,
130.234085105053));
#159329=CARTESIAN_POINT('Ctrl Pts',(-162.220748218855,5.87403202154923,
130.077424758553));
#159330=CARTESIAN_POINT('Ctrl Pts',(-162.228156438521,5.85056306176411,
129.921840123288));
#159331=CARTESIAN_POINT('Ctrl Pts',(-162.235569217823,5.82707965722577,
129.766159728274));
#159332=CARTESIAN_POINT('Ctrl Pts',(-162.242981997125,5.79739917049999,
129.611556729531));
#159333=CARTESIAN_POINT('Ctrl Pts',(-162.250394776428,5.76166033979989,
129.458552053439));
#159334=CARTESIAN_POINT('Ctrl Pts',(-162.257818147456,5.72587044378254,
129.305328757091));
#159335=CARTESIAN_POINT('Ctrl Pts',(-162.265241518485,5.68400501402058,
129.153708703452));
#159336=CARTESIAN_POINT('Ctrl Pts',(-162.272664889514,5.63625231860867,
129.00419663518));
#159337=CARTESIAN_POINT('Ctrl Pts',(-162.276600938954,5.61093269369319,
128.924921749096));
#159338=CARTESIAN_POINT('Ctrl Pts',(-162.280536988395,5.58395874975827,
128.846239154367));
#159339=CARTESIAN_POINT('Ctrl Pts',(-162.284473037835,5.5553638968772,128.768221492709));
#159340=CARTESIAN_POINT('Ctrl Pts',(-162.291896304241,5.50143489675405,
128.621082617658));
#159341=CARTESIAN_POINT('Ctrl Pts',(-162.299319570646,5.44157465134277,
128.475865269586));
#159342=CARTESIAN_POINT('Ctrl Pts',(-162.306742837052,5.37593893879817,
128.333083399443));
#159343=CARTESIAN_POINT('Ctrl Pts',(-162.314157329773,5.3103808022151,128.190470285614));
#159344=CARTESIAN_POINT('Ctrl Pts',(-162.321571822494,5.23906094032782,
128.050287255844));
#159345=CARTESIAN_POINT('Ctrl Pts',(-162.328986315215,5.16218444400936,
127.913031800477));
#159346=CARTESIAN_POINT('Ctrl Pts',(-162.336393661568,5.0853820441524,127.775908637086));
#159347=CARTESIAN_POINT('Ctrl Pts',(-162.343801007922,5.00303385318983,
127.641707754139));
#159348=CARTESIAN_POINT('Ctrl Pts',(-162.351208354276,4.9153924098601,127.510905286217));
#159349=CARTESIAN_POINT('Ctrl Pts',(-162.358610175951,4.82781633282532,
127.38020037571));
#159350=CARTESIAN_POINT('Ctrl Pts',(-162.366011997627,4.73495507113505,
127.252889142151));
#159351=CARTESIAN_POINT('Ctrl Pts',(-162.373413819302,4.63710625384166,
127.129421685681));
#159352=CARTESIAN_POINT('Ctrl Pts',(-162.380811733613,4.53930909017728,
127.00601940672));
#159353=CARTESIAN_POINT('Ctrl Pts',(-162.388209647925,4.4365298457112,126.886457155622));
#159354=CARTESIAN_POINT('Ctrl Pts',(-162.395607562236,4.32910841468215,
126.771154585582));
#159355=CARTESIAN_POINT('Ctrl Pts',(-162.403004247148,4.22170483514626,
126.655871176739));
#159356=CARTESIAN_POINT('Ctrl Pts',(-162.41040093206,4.10966085435452,126.544846316883));
#159357=CARTESIAN_POINT('Ctrl Pts',(-162.417797616973,3.99335553530743,
126.438465276272));
#159358=CARTESIAN_POINT('Ctrl Pts',(-162.425193973908,3.87705537336007,
126.332088952709));
#159359=CARTESIAN_POINT('Ctrl Pts',(-162.432590330844,3.75649452430975,
126.230356290917));
#159360=CARTESIAN_POINT('Ctrl Pts',(-162.439986687779,3.63208746822846,
126.133614297583));
#159361=CARTESIAN_POINT('Ctrl Pts',(-162.447384177116,3.5076613651093,126.036857492803));
#159362=CARTESIAN_POINT('Ctrl Pts',(-162.454781666452,3.37938817715672,
125.945093107044));
#159363=CARTESIAN_POINT('Ctrl Pts',(-162.462179155789,3.24771375173889,
125.858626501253));
#159364=CARTESIAN_POINT('Ctrl Pts',(-162.469579238304,3.11599316805516,
125.772129584727));
#159365=CARTESIAN_POINT('Ctrl Pts',(-162.476979320819,2.98086928488876,
125.690934350475));
#159366=CARTESIAN_POINT('Ctrl Pts',(-162.484379403334,2.84281493796091,
125.615301570782));
#159367=CARTESIAN_POINT('Ctrl Pts',(-162.491787623,2.70460878608648,125.539585625074));
#159368=CARTESIAN_POINT('Ctrl Pts',(-162.499195842666,2.56346606280127,
125.469444528426));
#159369=CARTESIAN_POINT('Ctrl Pts',(-162.506604062333,2.41988275674233,
125.405092333241));
#159370=CARTESIAN_POINT('Ctrl Pts',(-162.514016841635,2.27621107755392,
125.340700530353));
#159371=CARTESIAN_POINT('Ctrl Pts',(-162.521429620937,2.13009616806607,
125.282104867221));
#159372=CARTESIAN_POINT('Ctrl Pts',(-162.528842400239,1.98205128979071,
125.22947019289));
#159373=CARTESIAN_POINT('Ctrl Pts',(-162.536265771268,1.83379487805087,
125.176760311669));
#159374=CARTESIAN_POINT('Ctrl Pts',(-162.543689142297,1.6836033454161,125.1300285409));
#159375=CARTESIAN_POINT('Ctrl Pts',(-162.551112513325,1.53200310968357,
125.08938931104));
#159376=CARTESIAN_POINT('Ctrl Pts',(-162.555048562766,1.45162102709549,
125.067841416241));
#159377=CARTESIAN_POINT('Ctrl Pts',(-162.558984612207,1.37084305615965,
125.048005494832));
#159378=CARTESIAN_POINT('Ctrl Pts',(-162.562920661648,1.28974837137003,
125.029892702593));
#159379=CARTESIAN_POINT('Ctrl Pts',(-162.570343928054,1.13680632674361,
124.995732541714));
#159380=CARTESIAN_POINT('Ctrl Pts',(-162.577767194459,0.982274934227822,
124.967601137744));
#159381=CARTESIAN_POINT('Ctrl Pts',(-162.585190460865,0.826670797211579,
124.945645233155));
#159382=CARTESIAN_POINT('Ctrl Pts',(-162.592604953586,0.671250571362725,
124.923715278621));
#159383=CARTESIAN_POINT('Ctrl Pts',(-162.600019446307,0.514760490792069,
124.907946346559));
#159384=CARTESIAN_POINT('Ctrl Pts',(-162.607433939028,0.357729964841097,
124.898434793891));
#159385=CARTESIAN_POINT('Ctrl Pts',(-162.614841285382,0.200850790823578,
124.888932408815));
#159386=CARTESIAN_POINT('Ctrl Pts',(-162.622248631736,0.0434325785518419,
124.885675418823));
#159387=CARTESIAN_POINT('Ctrl Pts',(-162.629655978089,-0.113987583111378,
124.888708718291));
#159388=CARTESIAN_POINT('Ctrl Pts',(-162.637057799765,-0.271290334878907,
124.89173975541));
#159389=CARTESIAN_POINT('Ctrl Pts',(-162.64445962144,-0.428594661520668,
124.90105173335));
#159390=CARTESIAN_POINT('Ctrl Pts',(-162.651861443116,-0.585361005267014,
124.916637538479));
#159391=CARTESIAN_POINT('Ctrl Pts',(-162.659259357427,-0.742044593280763,
124.932215115983));
#159392=CARTESIAN_POINT('Ctrl Pts',(-162.666657271738,-0.898190393466454,
124.954059888023));
#159393=CARTESIAN_POINT('Ctrl Pts',(-162.67405518605,-1.05326161856515,
124.982112724754));
#159394=CARTESIAN_POINT('Ctrl Pts',(-162.681451870962,-1.20830707363929,
125.010160899611));
#159395=CARTESIAN_POINT('Ctrl Pts',(-162.688848555874,-1.3622779410688,
125.044415025217));
#159396=CARTESIAN_POINT('Ctrl Pts',(-162.696245240786,-1.51464518926287,
125.084764433119));
#159397=CARTESIAN_POINT('Ctrl Pts',(-162.703641597722,-1.66700568133349,
125.125112051885));
#159398=CARTESIAN_POINT('Ctrl Pts',(-162.711037954657,-1.81776233469293,
125.171554319996));
#159399=CARTESIAN_POINT('Ctrl Pts',(-162.718434311593,-1.9663991661842,
125.223930089217));
#159400=CARTESIAN_POINT('Ctrl Pts',(-162.725831800929,-2.11505875435425,
125.276313877302));
#159401=CARTESIAN_POINT('Ctrl Pts',(-162.733229290266,-2.26159752233207,
125.334632851241));
#159402=CARTESIAN_POINT('Ctrl Pts',(-162.740626779603,-2.40551756991143,
125.398676962065));
#159403=CARTESIAN_POINT('Ctrl Pts',(-162.748026862118,-2.54948806844015,
125.462743523453));
#159404=CARTESIAN_POINT('Ctrl Pts',(-162.755426944633,-2.6908376780212,
125.532539065852));
#159405=CARTESIAN_POINT('Ctrl Pts',(-162.762827027148,-2.82909142428802,
125.607806732969));
#159406=CARTESIAN_POINT('Ctrl Pts',(-162.770235246814,-2.9674971947615,
125.683157164623));
#159407=CARTESIAN_POINT('Ctrl Pts',(-162.777643466481,-3.1027999754093,
125.763991559064));
#159408=CARTESIAN_POINT('Ctrl Pts',(-162.785051686147,-3.23455158390961,
125.850008327556));
#159409=CARTESIAN_POINT('Ctrl Pts',(-162.792464465449,-3.36638428332694,
125.936078037934));
#159410=CARTESIAN_POINT('Ctrl Pts',(-162.799877244751,-3.49466115186897,
126.027336262275));
#159411=CARTESIAN_POINT('Ctrl Pts',(-162.807290024053,-3.61896606698017,
126.123440284069));
#159412=CARTESIAN_POINT('Ctrl Pts',(-162.814713395082,-3.74344859478323,
126.219681623796));
#159413=CARTESIAN_POINT('Ctrl Pts',(-162.822136766111,-3.863947549065,126.320782350261));
#159414=CARTESIAN_POINT('Ctrl Pts',(-162.82956013714,-3.98008211456447,
126.426361425718));
#159415=CARTESIAN_POINT('Ctrl Pts',(-162.83349618658,-4.04165944779781,
126.482341984856));
#159416=CARTESIAN_POINT('Ctrl Pts',(-162.837432236021,-4.10201043665572,
126.539580979506));
#159417=CARTESIAN_POINT('Ctrl Pts',(-162.841368285461,-4.16108289971568,
126.598017827898));
#159418=CARTESIAN_POINT('Ctrl Pts',(-162.848687074464,-4.27092371841971,
126.706676768753));
#159419=CARTESIAN_POINT('Ctrl Pts',(-162.856005863466,-4.37669434539834,
126.819828129737));
#159420=CARTESIAN_POINT('Ctrl Pts',(-162.863324652469,-4.47799709319613,
126.937130006932));
#159421=CARTESIAN_POINT('Ctrl Pts',(-162.870634636601,-4.57917796869682,
127.054290764072));
#159422=CARTESIAN_POINT('Ctrl Pts',(-162.877944620732,-4.67590141054578,
127.175591814463));
#159423=CARTESIAN_POINT('Ctrl Pts',(-162.885254604864,-4.76780473015378,
127.300652779058));
#159424=CARTESIAN_POINT('Ctrl Pts',(-162.892603363319,-4.86019553222356,
127.426377104097));
#159425=CARTESIAN_POINT('Ctrl Pts',(-162.899952121774,-4.94771462715774,
127.555901093354));
#159426=CARTESIAN_POINT('Ctrl Pts',(-162.90730088023,-5.03003213962764,
127.688801721186));
#159427=CARTESIAN_POINT('Ctrl Pts',(-162.914597894588,-5.1117700378161,
127.820766568774));
#159428=CARTESIAN_POINT('Ctrl Pts',(-162.921894908946,-5.18837915329614,
127.956060330833));
#159429=CARTESIAN_POINT('Ctrl Pts',(-162.929191923305,-5.2595781789961,
128.094237383924));
#159430=CARTESIAN_POINT('Ctrl Pts',(-162.936485811445,-5.33074670130998,
128.23235523862));
#159431=CARTESIAN_POINT('Ctrl Pts',(-162.943779699586,-5.39650956936092,
128.373353585452));
#159432=CARTESIAN_POINT('Ctrl Pts',(-162.951073587727,-5.45663060084042,
128.516760773084));
#159433=CARTESIAN_POINT('Ctrl Pts',(-162.958365886117,-5.51673852854785,
128.660136704182));
#159434=CARTESIAN_POINT('Ctrl Pts',(-162.965658184507,-5.57120691878873,
128.805920076421));
#159435=CARTESIAN_POINT('Ctrl Pts',(-162.972950482897,-5.61984719435055,
128.953618043719));
#159436=CARTESIAN_POINT('Ctrl Pts',(-162.980340009971,-5.66913599384149,
129.103285277534));
#159437=CARTESIAN_POINT('Ctrl Pts',(-162.987729537046,-5.71243999132663,
129.254918155311));
#159438=CARTESIAN_POINT('Ctrl Pts',(-162.99511906412,-5.74961487539809,
129.407986975914));
#159439=CARTESIAN_POINT('Ctrl Pts',(-163.002415090189,-5.78631937902255,
129.559118989394));
#159440=CARTESIAN_POINT('Ctrl Pts',(-163.009711116258,-5.81704892816231,
129.711650428953));
#159441=CARTESIAN_POINT('Ctrl Pts',(-163.017007142327,-5.84171605951823,
129.865060855793));
#159442=CARTESIAN_POINT('Ctrl Pts',(-163.024443419904,-5.86685736713843,
130.021420291257));
#159443=CARTESIAN_POINT('Ctrl Pts',(-163.031879697481,-5.88570073750554,
130.178692438175));
#159444=CARTESIAN_POINT('Ctrl Pts',(-163.039315975059,-5.89820902089197,
130.336321187209));
#159445=CARTESIAN_POINT('Ctrl Pts',(-163.046752252636,-5.91071730427839,
130.493949936243));
#159446=CARTESIAN_POINT('Ctrl Pts',(-163.054188530214,-5.91689052196692,
130.651934866212));
#159447=CARTESIAN_POINT('Ctrl Pts',(-163.061624807791,-5.91674757180022,
130.809721036972));
#159448=CARTESIAN_POINT('',(-164.811624807791,-5.92507222483892,130.801692424892));
#159449=CARTESIAN_POINT('Ctrl Pts',(-163.061624807791,-5.91817580952646,
130.809722330918));
#159450=CARTESIAN_POINT('Ctrl Pts',(-163.081021841618,-5.92200279167935,
131.221400182703));
#159451=CARTESIAN_POINT('Ctrl Pts',(-163.193234750051,-5.69477883690624,
133.5987828848));
#159452=CARTESIAN_POINT('Ctrl Pts',(-163.398263533087,-2.47931000527729,
137.348868423979));
#159453=CARTESIAN_POINT('Ctrl Pts',(-163.676711156899,4.16595214925394,
136.42774067056));
#159454=CARTESIAN_POINT('Ctrl Pts',(-163.955158780713,6.98290779669783,
130.339001365844));
#159455=CARTESIAN_POINT('Ctrl Pts',(-164.233606404525,3.3829123129869,124.677904479389));
#159456=CARTESIAN_POINT('Ctrl Pts',(-164.512054028338,-3.3258143219058,
124.6467214899));
#159457=CARTESIAN_POINT('Ctrl Pts',(-164.704726829427,-5.85315069107131,
128.540611173087));
#159458=CARTESIAN_POINT('Ctrl Pts',(-164.804583755911,-5.92590807902851,
130.652707065092));
#159459=CARTESIAN_POINT('Ctrl Pts',(-164.811624807791,-5.92507222483892,
130.801692424892));
#159460=CARTESIAN_POINT('',(-166.561624807791,-5.90995365707892,130.800293572401));
#159461=CARTESIAN_POINT('Ctrl Pts',(-164.811624807791,-5.92507222483892,
130.801692424892));
#159462=CARTESIAN_POINT('Ctrl Pts',(-164.897399630515,-5.9148897625933,
132.616647497437));
#159463=CARTESIAN_POINT('Ctrl Pts',(-165.075990327845,-4.05023365468494,
136.413624265273));
#159464=CARTESIAN_POINT('Ctrl Pts',(-165.347396899777,2.41836483055078,
137.371633421151));
#159465=CARTESIAN_POINT('Ctrl Pts',(-165.625844523591,6.83241786724281,
132.319493158866));
#159466=CARTESIAN_POINT('Ctrl Pts',(-165.904292147403,4.96781266611051,
125.875020109467));
#159467=CARTESIAN_POINT('Ctrl Pts',(-166.182739771216,-1.46196968404082,
123.960370175338));
#159468=CARTESIAN_POINT('Ctrl Pts',(-166.401850658011,-5.46439026136785,
127.402783795988));
#159469=CARTESIAN_POINT('Ctrl Pts',(-166.528145670204,-5.91444494865032,
130.087230112169));
#159470=CARTESIAN_POINT('Ctrl Pts',(-166.561624807791,-5.90995365707892,
130.800293572401));
#159471=CARTESIAN_POINT('',(-168.311624841251,-5.9133887742954,130.808566527428));
#159472=CARTESIAN_POINT('Ctrl Pts',(-166.561624807791,-5.90995365707892,
130.800293572401));
#159473=CARTESIAN_POINT('Ctrl Pts',(-166.620961544808,-5.90199351813743,
132.0640913302));
#159474=CARTESIAN_POINT('Ctrl Pts',(-166.77311415643,-4.88443978267444,
135.316447813812));
#159475=CARTESIAN_POINT('Ctrl Pts',(-167.018082642654,0.475985509809786,
137.786552130608));
#159476=CARTESIAN_POINT('Ctrl Pts',(-167.296530266468,6.13159726050651,
134.17794558986));
#159477=CARTESIAN_POINT('Ctrl Pts',(-167.57497789028,6.15257067397626,127.469179268363));
#159478=CARTESIAN_POINT('Ctrl Pts',(-167.853425514094,0.51963220783115,
123.825281674103));
#159479=CARTESIAN_POINT('Ctrl Pts',(-168.098974486596,-4.86887118749209,
126.267595478663));
#159480=CARTESIAN_POINT('Ctrl Pts',(-168.251707584496,-5.90188748972451,
129.532545137536));
#159481=CARTESIAN_POINT('Ctrl Pts',(-168.311624807791,-5.91021739760105,
130.808563558795));
#159482=CARTESIAN_POINT('',(-170.061624807791,-5.92111310252186,130.806826412176));
#159483=CARTESIAN_POINT('Ctrl Pts',(-168.311624876699,-5.91674850288211,
130.808569672372));
#159484=CARTESIAN_POINT('Ctrl Pts',(-168.320088487823,-5.91662013988444,
130.989011982903));
#159485=CARTESIAN_POINT('Ctrl Pts',(-168.328552098947,-5.90823344174668,
131.169125107682));
#159486=CARTESIAN_POINT('Ctrl Pts',(-168.337015710071,-5.89170242808678,
131.348210837182));
#159487=CARTESIAN_POINT('Ctrl Pts',(-168.345517826292,-5.875096206779,131.528111315055));
#159488=CARTESIAN_POINT('Ctrl Pts',(-168.354019942514,-5.85027150266959,
131.70697488581));
#159489=CARTESIAN_POINT('Ctrl Pts',(-168.362522058735,-5.81739348635992,
131.884112249821));
#159490=CARTESIAN_POINT('Ctrl Pts',(-168.371076260356,-5.78431405377052,
132.062334787236));
#159491=CARTESIAN_POINT('Ctrl Pts',(-168.379630461977,-5.743082419642,132.238809761398));
#159492=CARTESIAN_POINT('Ctrl Pts',(-168.388184663598,-5.69391546743878,
132.412855943068));
#159493=CARTESIAN_POINT('Ctrl Pts',(-168.395563362972,-5.65150494504025,
132.562985026839));
#159494=CARTESIAN_POINT('Ctrl Pts',(-168.402942062346,-5.60319098766957,
132.711307263188));
#159495=CARTESIAN_POINT('Ctrl Pts',(-168.41032076172,-5.54914085771267,
132.857398927916));
#159496=CARTESIAN_POINT('Ctrl Pts',(-168.417744028125,-5.49476426726326,
133.004372980102));
#159497=CARTESIAN_POINT('Ctrl Pts',(-168.42516729453,-5.43446230746612,
133.14940746154));
#159498=CARTESIAN_POINT('Ctrl Pts',(-168.432590560936,-5.36839232004439,
133.291988897794));
#159499=CARTESIAN_POINT('Ctrl Pts',(-168.440005053656,-5.30240042186101,
133.43440181463));
#159500=CARTESIAN_POINT('Ctrl Pts',(-168.447419546377,-5.23065422140141,
133.574367121954));
#159501=CARTESIAN_POINT('Ctrl Pts',(-168.454834039098,-5.15336032277811,
133.711387955951));
#159502=CARTESIAN_POINT('Ctrl Pts',(-168.462241385452,-5.07614092292436,
133.848276724109));
#159503=CARTESIAN_POINT('Ctrl Pts',(-168.469648731806,-4.99338465206927,
133.982226345878));
#159504=CARTESIAN_POINT('Ctrl Pts',(-168.477056078159,-4.90534549697139,
134.112761457525));
#159505=CARTESIAN_POINT('Ctrl Pts',(-168.484457899835,-4.81737200479691,
134.243199211161));
#159506=CARTESIAN_POINT('Ctrl Pts',(-168.49185972151,-4.72412368163286,
134.370227217285));
#159507=CARTESIAN_POINT('Ctrl Pts',(-168.499261543185,-4.62589952510303,
134.493396283719));
#159508=CARTESIAN_POINT('Ctrl Pts',(-168.506659457496,-4.52772722034086,
134.616500330163));
#159509=CARTESIAN_POINT('Ctrl Pts',(-168.514057371808,-4.4245845455776,
134.735749202791));
#159510=CARTESIAN_POINT('Ctrl Pts',(-168.521455286119,-4.31681267075757,
134.850724284871));
#159511=CARTESIAN_POINT('Ctrl Pts',(-168.528851971031,-4.20905870566811,
134.965680260178));
#159512=CARTESIAN_POINT('Ctrl Pts',(-168.536248655943,-4.09667732237509,
135.076363582438));
#159513=CARTESIAN_POINT('Ctrl Pts',(-168.543645340855,-3.98004875475335,
135.182390136914));
#159514=CARTESIAN_POINT('Ctrl Pts',(-168.551041697791,-3.86342535856451,
135.288411990062));
#159515=CARTESIAN_POINT('Ctrl Pts',(-168.558438054726,-3.74255542871703,
135.389777234882));
#159516=CARTESIAN_POINT('Ctrl Pts',(-168.565834411661,-3.61785449953204,
135.486140127829));
#159517=CARTESIAN_POINT('Ctrl Pts',(-168.573231900998,-3.49313447831644,
135.58251777418));
#159518=CARTESIAN_POINT('Ctrl Pts',(-168.580629390334,-3.36458258529304,
135.673891315433));
#159519=CARTESIAN_POINT('Ctrl Pts',(-168.588026879671,-3.23264559517856,
135.759956749059));
#159520=CARTESIAN_POINT('Ctrl Pts',(-168.595426962186,-3.10066235475653,
135.84605235279));
#159521=CARTESIAN_POINT('Ctrl Pts',(-168.6028270447,-2.96529196711281,135.926835940332));
#159522=CARTESIAN_POINT('Ctrl Pts',(-168.610227127215,-2.82700805947962,
136.002048179755));
#159523=CARTESIAN_POINT('Ctrl Pts',(-168.617635346882,-2.68857209447425,
136.077343122768));
#159524=CARTESIAN_POINT('Ctrl Pts',(-168.625043566548,-2.54721653958297,
136.147054304629));
#159525=CARTESIAN_POINT('Ctrl Pts',(-168.632451786215,-2.4034380326473,
136.210969183546));
#159526=CARTESIAN_POINT('Ctrl Pts',(-168.639864565517,-2.25957103243927,
136.274923401004));
#159527=CARTESIAN_POINT('Ctrl Pts',(-168.647277344819,-2.11327845470429,
136.333074069203));
#159528=CARTESIAN_POINT('Ctrl Pts',(-168.654690124121,-1.96507406032067,
136.385257902049));
#159529=CARTESIAN_POINT('Ctrl Pts',(-168.662113495149,-1.81665790454848,
136.437516297604));
#159530=CARTESIAN_POINT('Ctrl Pts',(-168.669536866178,-1.6663248321565,
136.483790720553));
#159531=CARTESIAN_POINT('Ctrl Pts',(-168.676960237207,-1.51460160679054,
136.523968343207));
#159532=CARTESIAN_POINT('Ctrl Pts',(-168.680896286648,-1.43415431213647,
136.545271482791));
#159533=CARTESIAN_POINT('Ctrl Pts',(-168.68483233609,-1.35331634162635,
136.564861451967));
#159534=CARTESIAN_POINT('Ctrl Pts',(-168.688768385531,-1.27216690334182,
136.582727335986));
#159535=CARTESIAN_POINT('Ctrl Pts',(-168.696191651937,-1.1191215953542,
136.616421835664));
#159536=CARTESIAN_POINT('Ctrl Pts',(-168.703614918342,-0.96450529630121,
136.644082768928));
#159537=CARTESIAN_POINT('Ctrl Pts',(-168.711038184747,-0.808835053812479,
136.665564966352));
#159538=CARTESIAN_POINT('Ctrl Pts',(-168.718452677468,-0.653348800622317,
136.687021773602));
#159539=CARTESIAN_POINT('Ctrl Pts',(-168.72586717019,-0.496811449698955,
136.702314330648));
#159540=CARTESIAN_POINT('Ctrl Pts',(-168.733281662911,-0.339752701209014,
136.711347892355));
#159541=CARTESIAN_POINT('Ctrl Pts',(-168.740689009264,-0.182845331854025,
136.720372747175));
#159542=CARTESIAN_POINT('Ctrl Pts',(-168.748096355618,-0.0254179355759166,
136.723150595193));
#159543=CARTESIAN_POINT('Ctrl Pts',(-168.755503701972,0.131992264607301,
136.719638176953));
#159544=CARTESIAN_POINT('Ctrl Pts',(-168.762905523647,0.289285062324475,
136.716128378407));
#159545=CARTESIAN_POINT('Ctrl Pts',(-168.770307345323,0.446560317885286,
136.70633766334));
#159546=CARTESIAN_POINT('Ctrl Pts',(-168.777709166998,0.603278497670724,
136.690274787578));
#159547=CARTESIAN_POINT('Ctrl Pts',(-168.785107081309,0.759913947148946,
136.674220391283));
#159548=CARTESIAN_POINT('Ctrl Pts',(-168.792504995621,0.915992536105768,
136.651900466323));
#159549=CARTESIAN_POINT('Ctrl Pts',(-168.799902909932,1.07097765973953,
136.623375776065));
#159550=CARTESIAN_POINT('Ctrl Pts',(-168.807299594844,1.22593702765723,
136.594855826093));
#159551=CARTESIAN_POINT('Ctrl Pts',(-168.814696279757,1.37980292412841,
136.560133224793));
#159552=CARTESIAN_POINT('Ctrl Pts',(-168.822092964669,1.5320466568494,136.519320250296));
#159553=CARTESIAN_POINT('Ctrl Pts',(-168.829489321604,1.68428363892374,
136.478509085489));
#159554=CARTESIAN_POINT('Ctrl Pts',(-168.83688567854,1.83489823969964,136.431608181102));
#159555=CARTESIAN_POINT('Ctrl Pts',(-168.844282035475,1.98337496888992,
136.378780255096));
#159556=CARTESIAN_POINT('Ctrl Pts',(-168.851679524812,2.13187443024648,
136.325944241));
#159557=CARTESIAN_POINT('Ctrl Pts',(-168.859077014148,2.27823501657022,
136.267179523589));
#159558=CARTESIAN_POINT('Ctrl Pts',(-168.866474503485,2.42195946927794,
136.202697666295));
#159559=CARTESIAN_POINT('Ctrl Pts',(-168.873874586,2.56573430436995,136.138193204985));
#159560=CARTESIAN_POINT('Ctrl Pts',(-168.881274668515,2.70687082560657,
136.067967766285));
#159561=CARTESIAN_POINT('Ctrl Pts',(-168.88867475103,2.84489484260351,135.992279650958));
#159562=CARTESIAN_POINT('Ctrl Pts',(-168.896082970697,2.98307063119655,
135.916508308766));
#159563=CARTESIAN_POINT('Ctrl Pts',(-168.903491190363,3.11812675304043,
135.835262473623));
#159564=CARTESIAN_POINT('Ctrl Pts',(-168.91089941003,3.24961594582166,135.74884509698));
#159565=CARTESIAN_POINT('Ctrl Pts',(-168.918312189332,3.38118606800704,
135.662374531883));
#159566=CARTESIAN_POINT('Ctrl Pts',(-168.925724968634,3.50918458373577,
135.570726299582));
#159567=CARTESIAN_POINT('Ctrl Pts',(-168.933137747936,3.63319641549096,
135.474244381533));
#159568=CARTESIAN_POINT('Ctrl Pts',(-168.940561118964,3.75738544116676,
135.377624605596));
#159569=CARTESIAN_POINT('Ctrl Pts',(-168.947984489993,3.87757612147127,
135.276157590056));
#159570=CARTESIAN_POINT('Ctrl Pts',(-168.955407861022,3.99338880265521,
135.170225529966));
#159571=CARTESIAN_POINT('Ctrl Pts',(-168.959343910463,4.05479546510575,
135.114057809902));
#159572=CARTESIAN_POINT('Ctrl Pts',(-168.963279959904,4.1149719586162,135.056635392724));
#159573=CARTESIAN_POINT('Ctrl Pts',(-168.967216009344,4.17386628639581,
134.998019018746));
#159574=CARTESIAN_POINT('Ctrl Pts',(-168.97463927575,4.28493915055956,134.887470366778));
#159575=CARTESIAN_POINT('Ctrl Pts',(-168.982062542155,4.3917849634643,134.772338705508));
#159576=CARTESIAN_POINT('Ctrl Pts',(-168.989485808561,4.49400211308639,
134.652980574132));
#159577=CARTESIAN_POINT('Ctrl Pts',(-168.996900301282,4.59609845052623,
134.533763514154));
#159578=CARTESIAN_POINT('Ctrl Pts',(-169.004314794003,4.69357677368831,
134.410330208079));
#159579=CARTESIAN_POINT('Ctrl Pts',(-169.011729286724,4.78607105492777,
134.2830750956));
#159580=CARTESIAN_POINT('Ctrl Pts',(-169.019136633077,4.87847618669688,
134.155942636388));
#159581=CARTESIAN_POINT('Ctrl Pts',(-169.026543979431,4.96590662197317,
134.02499600403));
#159582=CARTESIAN_POINT('Ctrl Pts',(-169.033951325785,5.04803558318792,
133.890663796673));
#159583=CARTESIAN_POINT('Ctrl Pts',(-169.04135314746,5.13010328952486,133.756431779345));
#159584=CARTESIAN_POINT('Ctrl Pts',(-169.048754969136,5.20687720094412,
133.61881953193));
#159585=CARTESIAN_POINT('Ctrl Pts',(-169.056156790811,5.27807305286969,
133.47828571208));
#159586=CARTESIAN_POINT('Ctrl Pts',(-169.063554705123,5.34923132105902,
133.33782607894));
#159587=CARTESIAN_POINT('Ctrl Pts',(-169.070952619434,5.41481722581945,
133.19444827704));
#159588=CARTESIAN_POINT('Ctrl Pts',(-169.078350533745,5.4745918410901,133.048636611282));
#159589=CARTESIAN_POINT('Ctrl Pts',(-169.085747218657,5.5343565229042,132.902849176777));
#159590=CARTESIAN_POINT('Ctrl Pts',(-169.09314390357,5.58831169046194,132.754629026218));
#159591=CARTESIAN_POINT('Ctrl Pts',(-169.100540588482,5.63626603542987,
132.604481652486));
#159592=CARTESIAN_POINT('Ctrl Pts',(-169.107936945417,5.68421825405189,
132.454340936445));
#159593=CARTESIAN_POINT('Ctrl Pts',(-169.115333302353,5.7261700655739,132.302273522745));
#159594=CARTESIAN_POINT('Ctrl Pts',(-169.122729659288,5.76197973413347,
132.148801060998));
#159595=CARTESIAN_POINT('Ctrl Pts',(-169.130127148625,5.79779488524471,
131.995305102225));
#159596=CARTESIAN_POINT('Ctrl Pts',(-169.137524637961,5.82746593614781,
131.840404030635));
#159597=CARTESIAN_POINT('Ctrl Pts',(-169.144922127298,5.8509021007386,131.684630559159));
#159598=CARTESIAN_POINT('Ctrl Pts',(-169.152322209813,5.87434648084059,
131.528802481535));
#159599=CARTESIAN_POINT('Ctrl Pts',(-169.159722292328,5.8915515675544,131.372101764055));
#159600=CARTESIAN_POINT('Ctrl Pts',(-169.167122374843,5.90247836514137,
131.215066974393));
#159601=CARTESIAN_POINT('Ctrl Pts',(-169.174530594509,5.91341717786557,
131.057859508836));
#159602=CARTESIAN_POINT('Ctrl Pts',(-169.181938814176,5.91806388854385,
130.900317610106));
#159603=CARTESIAN_POINT('Ctrl Pts',(-169.189347033842,5.91643162260689,
130.742981325315));
#159604=CARTESIAN_POINT('Ctrl Pts',(-169.196759813144,5.91479835203747,
130.585548202665));
#159605=CARTESIAN_POINT('Ctrl Pts',(-169.204172592446,5.90687842287881,
130.428321318085));
#159606=CARTESIAN_POINT('Ctrl Pts',(-169.211585371748,5.8927368769358,130.271835818424));
#159607=CARTESIAN_POINT('Ctrl Pts',(-169.219008742777,5.8785751248888,130.115126724944));
#159608=CARTESIAN_POINT('Ctrl Pts',(-169.226432113806,5.85817404954565,
129.959161501258));
#159609=CARTESIAN_POINT('Ctrl Pts',(-169.233855484835,5.83164999030207,
129.804466146579));
#159610=CARTESIAN_POINT('Ctrl Pts',(-169.237791534276,5.8175862976549,129.722442957664));
#159611=CARTESIAN_POINT('Ctrl Pts',(-169.241727583717,5.80180205643049,
129.64077655028));
#159612=CARTESIAN_POINT('Ctrl Pts',(-169.245663633157,5.7843202636394,129.559543502424));
#159613=CARTESIAN_POINT('Ctrl Pts',(-169.253086899563,5.75135014802388,
129.406340509366));
#159614=CARTESIAN_POINT('Ctrl Pts',(-169.260510165968,5.71223939242906,
129.254216625775));
#159615=CARTESIAN_POINT('Ctrl Pts',(-169.267933432374,5.66707088226718,
129.103702457365));
#159616=CARTESIAN_POINT('Ctrl Pts',(-169.275347925095,5.62195575753318,
128.953366184201));
#159617=CARTESIAN_POINT('Ctrl Pts',(-169.282762417816,5.57079723602915,
128.804636193235));
#159618=CARTESIAN_POINT('Ctrl Pts',(-169.290176910537,5.51372932415616,
128.65803363818));
#159619=CARTESIAN_POINT('Ctrl Pts',(-169.297584256891,5.4567164164852,128.511572384187));
#159620=CARTESIAN_POINT('Ctrl Pts',(-169.304991603244,5.39380559195493,
128.367234829491));
#159621=CARTESIAN_POINT('Ctrl Pts',(-169.312398949598,5.32518081106764,
128.225527569085));
#159622=CARTESIAN_POINT('Ctrl Pts',(-169.319800771273,5.256607213131,128.0839259993));
#159623=CARTESIAN_POINT('Ctrl Pts',(-169.327202592949,5.18232830642846,
127.944951152179));
#159624=CARTESIAN_POINT('Ctrl Pts',(-169.334604414624,5.10257632068526,
127.809090103225));
#159625=CARTESIAN_POINT('Ctrl Pts',(-169.342002328936,5.02286643539454,
127.67330077426));
#159626=CARTESIAN_POINT('Ctrl Pts',(-169.349400243247,4.93768941353346,
127.540622290972));
#159627=CARTESIAN_POINT('Ctrl Pts',(-169.356798157558,4.84732356915969,
127.411517447249));
#159628=CARTESIAN_POINT('Ctrl Pts',(-169.364194842471,4.75697274194998,
127.282434058409));
#159629=CARTESIAN_POINT('Ctrl Pts',(-169.371591527383,4.66143501746512,
127.156923435997));
#159630=CARTESIAN_POINT('Ctrl Pts',(-169.378988212295,4.56103227435438,
127.035419764382));
#159631=CARTESIAN_POINT('Ctrl Pts',(-169.386384569231,4.46063398320649,
126.913921480367));
#159632=CARTESIAN_POINT('Ctrl Pts',(-169.393780926166,4.35537134014572,
126.796430081639));
#159633=CARTESIAN_POINT('Ctrl Pts',(-169.401177283101,4.24560661206784,
126.68334677895));
#159634=CARTESIAN_POINT('Ctrl Pts',(-169.408574772438,4.13582507872986,
126.570246162918));
#159635=CARTESIAN_POINT('Ctrl Pts',(-169.415972261774,4.02154034794373,
126.461555254602));
#159636=CARTESIAN_POINT('Ctrl Pts',(-169.423369751111,3.90315153407888,
126.357638379274));
#159637=CARTESIAN_POINT('Ctrl Pts',(-169.430769833626,3.78472121919869,
126.253685076047));
#159638=CARTESIAN_POINT('Ctrl Pts',(-169.438169916141,3.66218423721486,
126.154509383896));
#159639=CARTESIAN_POINT('Ctrl Pts',(-169.445569998656,3.5359726222131,126.060435220022));
#159640=CARTESIAN_POINT('Ctrl Pts',(-169.452978218323,3.4096222245656,125.966257611935));
#159641=CARTESIAN_POINT('Ctrl Pts',(-169.460386437989,3.27958942396931,
125.877192958201));
#159642=CARTESIAN_POINT('Ctrl Pts',(-169.467794657656,3.1463356719695,125.79352212468));
#159643=CARTESIAN_POINT('Ctrl Pts',(-169.475207436958,3.01299990450878,
125.709799793156));
#159644=CARTESIAN_POINT('Ctrl Pts',(-169.48262021626,2.87643955844939,125.631478082266));
#159645=CARTESIAN_POINT('Ctrl Pts',(-169.490032995562,2.73714002467679,
125.55879153044));
#159646=CARTESIAN_POINT('Ctrl Pts',(-169.497456366591,2.59764145319803,
125.48600112066));
#159647=CARTESIAN_POINT('Ctrl Pts',(-169.504879737619,2.45539621379955,
125.41886211007));
#159648=CARTESIAN_POINT('Ctrl Pts',(-169.512303108648,2.31090972880087,
125.357560934465));
#159649=CARTESIAN_POINT('Ctrl Pts',(-169.516239158089,2.23429952754937,
125.325057580257));
#159650=CARTESIAN_POINT('Ctrl Pts',(-169.52017520753,2.15705949817252,125.294194621429));
#159651=CARTESIAN_POINT('Ctrl Pts',(-169.52411125697,2.07926649835301,125.264994102221));
#159652=CARTESIAN_POINT('Ctrl Pts',(-169.531534523376,1.93255132852796,
125.209922834311));
#159653=CARTESIAN_POINT('Ctrl Pts',(-169.538957789781,1.78342487815733,
125.160601145754));
#159654=CARTESIAN_POINT('Ctrl Pts',(-169.546381056187,1.63237836244457,
125.117246108052));
#159655=CARTESIAN_POINT('Ctrl Pts',(-169.553795548908,1.48151037116932,
125.073942312405));
#159656=CARTESIAN_POINT('Ctrl Pts',(-169.561210041629,1.32872718702708,
125.036591232382));
#159657=CARTESIAN_POINT('Ctrl Pts',(-169.56862453435,1.17453970512887,125.005361820914));
#159658=CARTESIAN_POINT('Ctrl Pts',(-169.576031880704,1.02050083493077,
124.974162509528));
#159659=CARTESIAN_POINT('Ctrl Pts',(-169.583439227058,0.865060724971309,
124.949073193979));
#159660=CARTESIAN_POINT('Ctrl Pts',(-169.590846573412,0.708745023109134,
124.930212930053));
#159661=CARTESIAN_POINT('Ctrl Pts',(-169.598248395087,0.552545907394415,
124.911366732823));
#159662=CARTESIAN_POINT('Ctrl Pts',(-169.605650216763,0.395472869101588,
124.898740381201));
#159663=CARTESIAN_POINT('Ctrl Pts',(-169.613052038438,0.238061224484711,
124.892401769951));
#159664=CARTESIAN_POINT('Ctrl Pts',(-169.62044995275,0.0807326762501853,
124.886066504803));
#159665=CARTESIAN_POINT('Ctrl Pts',(-169.627847867061,-0.0769337502724467,
124.886012384565));
#159666=CARTESIAN_POINT('Ctrl Pts',(-169.635245781372,-0.234398257929557,
124.892255407137));
#159667=CARTESIAN_POINT('Ctrl Pts',(-169.642642466285,-0.391836597841968,
124.898497392233));
#159668=CARTESIAN_POINT('Ctrl Pts',(-169.650039151197,-0.549072712846464,
124.911034428431));
#159669=CARTESIAN_POINT('Ctrl Pts',(-169.657435836109,-0.705567328065082,
124.929830397364));
#159670=CARTESIAN_POINT('Ctrl Pts',(-169.664832193045,-0.862055004148467,
124.948625532864));
#159671=CARTESIAN_POINT('Ctrl Pts',(-169.67222854998,-1.01780087518644,
124.973679004766));
#159672=CARTESIAN_POINT('Ctrl Pts',(-169.679624906916,-1.17227157710454,
125.004902891881));
#159673=CARTESIAN_POINT('Ctrl Pts',(-169.687022396252,-1.32676592888146,
125.036131559452));
#159674=CARTESIAN_POINT('Ctrl Pts',(-169.694419885589,-1.47998435688509,
125.073532449308));
#159675=CARTESIAN_POINT('Ctrl Pts',(-169.701817374926,-1.63140461288007,
125.116966701934));
#159676=CARTESIAN_POINT('Ctrl Pts',(-169.709217457441,-1.78287794901085,
125.160416180369));
#159677=CARTESIAN_POINT('Ctrl Pts',(-169.716617539956,-1.93255149951431,
125.209903129633));
#159678=CARTESIAN_POINT('Ctrl Pts',(-169.724017622471,-2.07991921869906,
125.265239152371));
#159679=CARTESIAN_POINT('Ctrl Pts',(-169.731425842137,-2.22744898384103,
125.320636022755));
#159680=CARTESIAN_POINT('Ctrl Pts',(-169.738834061804,-2.37266750442005,
125.38189467975));
#159681=CARTESIAN_POINT('Ctrl Pts',(-169.74624228147,-2.51508905420318,
125.448778705959));
#159682=CARTESIAN_POINT('Ctrl Pts',(-169.753655060772,-2.65759826207378,
125.515703898171));
#159683=CARTESIAN_POINT('Ctrl Pts',(-169.761067840075,-2.79730673834968,
125.588261187052));
#159684=CARTESIAN_POINT('Ctrl Pts',(-169.768480619377,-2.93375479357592,
125.666168973255));
#159685=CARTESIAN_POINT('Ctrl Pts',(-169.775903990406,-3.07039781218206,
125.744188077756));
#159686=CARTESIAN_POINT('Ctrl Pts',(-169.783327361434,-3.20377078969541,
125.827572751073));
#159687=CARTESIAN_POINT('Ctrl Pts',(-169.790750732463,-3.33344367929301,
125.915998540195));
#159688=CARTESIAN_POINT('Ctrl Pts',(-169.794686781903,-3.402199356803,125.962884015326));
#159689=CARTESIAN_POINT('Ctrl Pts',(-169.798622831343,-3.46991536070847,
126.011186056468));
#159690=CARTESIAN_POINT('Ctrl Pts',(-169.802558880784,-3.53653160111034,
126.060851916525));
#159691=CARTESIAN_POINT('Ctrl Pts',(-169.809908808481,-3.66092651989311,
126.153594776088));
#159692=CARTESIAN_POINT('Ctrl Pts',(-169.817258736178,-3.78187706383077,
126.251388173978));
#159693=CARTESIAN_POINT('Ctrl Pts',(-169.824608663876,-3.89893990826541,
126.353945114016));
#159694=CARTESIAN_POINT('Ctrl Pts',(-169.831949870823,-4.01586385667119,
126.4563803694));
#159695=CARTESIAN_POINT('Ctrl Pts',(-169.839291077771,-4.12890900020466,
126.563567671924));
#159696=CARTESIAN_POINT('Ctrl Pts',(-169.846632284719,-4.23766145748654,
126.675177171141));
#159697=CARTESIAN_POINT('Ctrl Pts',(-169.853966461502,-4.3463097700869,
126.786679789685));
#159698=CARTESIAN_POINT('Ctrl Pts',(-169.861300638285,-4.45067331315389,
126.902595905783));
#159699=CARTESIAN_POINT('Ctrl Pts',(-169.868634815068,-4.55037192176472,
127.02255603032));
#159700=CARTESIAN_POINT('Ctrl Pts',(-169.875963645743,-4.64999785697112,
127.142428712206));
#159701=CARTESIAN_POINT('Ctrl Pts',(-169.883292476417,-4.74496538355266,
127.266339242789));
#159702=CARTESIAN_POINT('Ctrl Pts',(-169.890621307092,-4.83493196680158,
127.393882141032));
#159703=CARTESIAN_POINT('Ctrl Pts',(-169.897947000245,-4.92486003475322,
127.521370437306));
#159704=CARTESIAN_POINT('Ctrl Pts',(-169.905272693398,-5.00979119925454,
127.652487696564));
#159705=CARTESIAN_POINT('Ctrl Pts',(-169.912598386551,-5.08942400263278,
127.786796387276));
#159706=CARTESIAN_POINT('Ctrl Pts',(-169.919922553488,-5.16904021552028,
127.921077096466));
#159707=CARTESIAN_POINT('Ctrl Pts',(-169.927246720425,-5.24336006876812,
128.058547586537));
#159708=CARTESIAN_POINT('Ctrl Pts',(-169.934570887362,-5.31212627938997,
128.198742657405));
#159709=CARTESIAN_POINT('Ctrl Pts',(-169.941895044416,-5.38089239721408,
128.338937539084));
#159710=CARTESIAN_POINT('Ctrl Pts',(-169.949219201469,-5.44410471934802,
128.481856651774));
#159711=CARTESIAN_POINT('Ctrl Pts',(-169.956543358523,-5.50155276466311,
128.627011830594));
#159712=CARTESIAN_POINT('Ctrl Pts',(-169.963869021802,-5.55901262426792,
128.772196860828));
#159713=CARTESIAN_POINT('Ctrl Pts',(-169.971194685081,-5.61070570805527,
128.919618517567));
#159714=CARTESIAN_POINT('Ctrl Pts',(-169.97852034836,-5.65647044968558,
129.068770627294));
#159715=CARTESIAN_POINT('Ctrl Pts',(-169.985853043202,-5.70227911876219,
129.218065901191));
#159716=CARTESIAN_POINT('Ctrl Pts',(-169.993185738044,-5.74214796873194,
129.369094580373));
#159717=CARTESIAN_POINT('Ctrl Pts',(-170.000518432887,-5.7759657541962,
129.521336779575));
#159718=CARTESIAN_POINT('Ctrl Pts',(-170.007854831032,-5.80980061899016,
129.673655867156));
#159719=CARTESIAN_POINT('Ctrl Pts',(-170.015191229178,-5.83757826355815,
129.827189320821));
#159720=CARTESIAN_POINT('Ctrl Pts',(-170.022527627323,-5.85923908056783,
129.981409854004));
#159721=CARTESIAN_POINT('Ctrl Pts',(-170.029874413467,-5.88093056828681,
130.135848756289));
#159722=CARTESIAN_POINT('Ctrl Pts',(-170.037221199612,-5.8964878893391,
130.290976302403));
#159723=CARTESIAN_POINT('Ctrl Pts',(-170.044567985756,-5.90590348629985,
130.446262065473));
#159724=CARTESIAN_POINT('Ctrl Pts',(-170.050253593101,-5.91319012649709,
130.566436228403));
#159725=CARTESIAN_POINT('Ctrl Pts',(-170.055939200446,-5.91679950964778,
130.686705078958));
#159726=CARTESIAN_POINT('Ctrl Pts',(-170.061624807791,-5.91674948694934,
130.806824594987));
#159727=CARTESIAN_POINT('',(-171.811624807791,-5.91779838983984,130.798959891652));
#159728=CARTESIAN_POINT('Ctrl Pts',(-170.061624807791,-5.92528845016055,
130.806828150962));
#159729=CARTESIAN_POINT('Ctrl Pts',(-170.068085373393,-5.92600628089009,
130.943517473629));
#159730=CARTESIAN_POINT('Ctrl Pts',(-170.074545938994,-5.92168800861787,
131.080160639199));
#159731=CARTESIAN_POINT('Ctrl Pts',(-170.081006504596,-5.91218909021727,
131.216442711532));
#159732=CARTESIAN_POINT('Ctrl Pts',(-170.1738223792,-5.77572264540439,133.174342455337));
#159733=CARTESIAN_POINT('Ctrl Pts',(-170.35945412841,-3.36424981849401,
136.941084799823));
#159734=CARTESIAN_POINT('Ctrl Pts',(-170.637901752222,3.34454065233045,
136.951848588703));
#159735=CARTESIAN_POINT('Ctrl Pts',(-170.916349376035,6.97986165355384,
131.313371253588));
#159736=CARTESIAN_POINT('Ctrl Pts',(-171.194796999848,4.20103078036093,
125.207138010521));
#159737=CARTESIAN_POINT('Ctrl Pts',(-171.47324462366,-2.43834214822045,
124.244478903803));
#159738=CARTESIAN_POINT('Ctrl Pts',(-171.678853892974,-5.68636543667235,
127.98494676486));
#159739=CARTESIAN_POINT('Ctrl Pts',(-171.791647287685,-5.92174318505954,
130.374892560432));
#159740=CARTESIAN_POINT('Ctrl Pts',(-171.811624807791,-5.91779838983984,
130.798959891652));
#159741=CARTESIAN_POINT('',(-173.561624807791,-5.90693470452075,130.804363326736));
#159742=CARTESIAN_POINT('Ctrl Pts',(-171.811624807791,-5.91779838983984,
130.798959891652));
#159743=CARTESIAN_POINT('Ctrl Pts',(-171.88446316229,-5.90341560403291,
132.345116093169));
#159744=CARTESIAN_POINT('Ctrl Pts',(-172.050117391391,-4.49105891822915,
135.884762486509));
#159745=CARTESIAN_POINT('Ctrl Pts',(-172.3085874951,1.48279366496714,137.643869626081));
#159746=CARTESIAN_POINT('Ctrl Pts',(-172.587035118912,6.55575882898706,
133.253765995716));
#159747=CARTESIAN_POINT('Ctrl Pts',(-172.865482742725,5.60430189578342,
126.612778482949));
#159748=CARTESIAN_POINT('Ctrl Pts',(-173.143930366538,-0.49723469427191,
123.823650181717));
#159749=CARTESIAN_POINT('Ctrl Pts',(-173.37597772156,-5.20122531230544,
126.845253006048));
#159750=CARTESIAN_POINT('Ctrl Pts',(-173.515209201978,-5.90693067888632,
129.814505326009));
#159751=CARTESIAN_POINT('Ctrl Pts',(-173.561624807791,-5.90693470452075,
130.804363326736));
#159752=CARTESIAN_POINT('',(-175.311624807791,-5.91780836735944,130.809760420718));
#159753=CARTESIAN_POINT('Ctrl Pts',(-173.561624807791,-5.90693470452075,
130.804363326736));
#159754=CARTESIAN_POINT('Ctrl Pts',(-173.608025076582,-5.90693872882499,
131.793894250518));
#159755=CARTESIAN_POINT('Ctrl Pts',(-173.747241219977,-5.20156840285358,
134.762808706442));
#159756=CARTESIAN_POINT('Ctrl Pts',(-173.979273237976,-0.498387885347994,
137.784988816106));
#159757=CARTESIAN_POINT('Ctrl Pts',(-174.257720861789,5.6036093792587,134.996868513205));
#159758=CARTESIAN_POINT('Ctrl Pts',(-174.536168485602,6.55616337585614,
128.356038269631));
#159759=CARTESIAN_POINT('Ctrl Pts',(-174.814616109415,1.48392351643239,
123.965096656601));
#159760=CARTESIAN_POINT('Ctrl Pts',(-175.073101550145,-4.49057407776603,
125.723321227789));
#159761=CARTESIAN_POINT('Ctrl Pts',(-175.23877111627,-5.90342260648341,
129.263285342462));
#159762=CARTESIAN_POINT('Ctrl Pts',(-175.311624807791,-5.91780836735944,
130.809760420718));
#159763=CARTESIAN_POINT('',(-177.061624807791,-5.92149090377293,130.801889302419));
#159764=CARTESIAN_POINT('Ctrl Pts',(-175.311624807791,-5.91780836735944,
130.809760420718));
#159765=CARTESIAN_POINT('Ctrl Pts',(-175.331586990875,-5.92175011947117,
131.233500357588));
#159766=CARTESIAN_POINT('Ctrl Pts',(-175.351549173958,-5.8801256076613,
131.656471884122));
#159767=CARTESIAN_POINT('Ctrl Pts',(-175.464327231645,-5.37130495022946,
133.986320566974));
#159768=CARTESIAN_POINT('Ctrl Pts',(-175.649958980855,-2.43942579283476,
137.363839433112));
#159769=CARTESIAN_POINT('Ctrl Pts',(-175.928406604667,4.20010607429807,
136.402277149186));
#159770=CARTESIAN_POINT('Ctrl Pts',(-176.206854228481,6.97994564573954,
130.296503046127));
#159771=CARTESIAN_POINT('Ctrl Pts',(-176.485301852292,3.34555615804791,
124.657425240999));
#159772=CARTESIAN_POINT('Ctrl Pts',(-176.763749476106,-3.36323599938494,
124.667080752447));
#159773=CARTESIAN_POINT('Ctrl Pts',(-176.955857127938,-5.85947879357928,
128.56481640463));
#159774=CARTESIAN_POINT('Ctrl Pts',(-177.055148905167,-5.92600379227935,
130.664873565487));
#159775=CARTESIAN_POINT('Ctrl Pts',(-177.061624807791,-5.92528292508171,
130.801887719831));
#159776=CARTESIAN_POINT('',(-178.811624778335,-5.91300466705327,130.800158578124));
#159777=CARTESIAN_POINT('Ctrl Pts',(-177.061624807791,-5.91674948471524,
130.801891281235));
#159778=CARTESIAN_POINT('Ctrl Pts',(-177.068972291863,-5.91681426963166,
130.957121703259));
#159779=CARTESIAN_POINT('Ctrl Pts',(-177.076319775935,-5.91076597571889,
131.112601726254));
#159780=CARTESIAN_POINT('Ctrl Pts',(-177.083667260007,-5.89857192890814,
131.267803992745));
#159781=CARTESIAN_POINT('Ctrl Pts',(-177.091006448241,-5.88639165005279,
131.42283102472));
#159782=CARTESIAN_POINT('Ctrl Pts',(-177.098345636476,-5.86807945544121,
131.577580547625));
#159783=CARTESIAN_POINT('Ctrl Pts',(-177.10568482471,-5.84365464559986,
131.731523464891));
#159784=CARTESIAN_POINT('Ctrl Pts',(-177.113017405978,-5.81925182373462,
131.885327797937));
#159785=CARTESIAN_POINT('Ctrl Pts',(-177.120349987246,-5.78874739755558,
132.038326596132));
#159786=CARTESIAN_POINT('Ctrl Pts',(-177.127682568514,-5.75221258835055,
132.189994371818));
#159787=CARTESIAN_POINT('Ctrl Pts',(-177.135010225576,-5.71570231415444,
132.341560294768));
#159788=CARTESIAN_POINT('Ctrl Pts',(-177.142337882637,-5.67316980720683,
132.491796605054));
#159789=CARTESIAN_POINT('Ctrl Pts',(-177.149665539699,-5.62473759539901,
132.640186738255));
#159790=CARTESIAN_POINT('Ctrl Pts',(-177.156990698151,-5.5763218981673,
132.788526272897));
#159791=CARTESIAN_POINT('Ctrl Pts',(-177.164315856604,-5.52201061408288,
132.935020520132));
#159792=CARTESIAN_POINT('Ctrl Pts',(-177.171641015057,-5.46197646524778,
133.079166907249));
#159793=CARTESIAN_POINT('Ctrl Pts',(-177.178965039566,-5.4019516097736,
133.223290980325));
#159794=CARTESIAN_POINT('Ctrl Pts',(-177.186289064075,-5.33620579825766,
133.365067564186));
#159795=CARTESIAN_POINT('Ctrl Pts',(-177.193613088584,-5.26496024379123,
133.504013223698));
#159796=CARTESIAN_POINT('Ctrl Pts',(-177.200937495439,-5.1937109699983,
133.642966136776));
#159797=CARTESIAN_POINT('Ctrl Pts',(-177.208261902294,-5.11696155583199,
133.779087491855));
#159798=CARTESIAN_POINT('Ctrl Pts',(-177.215586309148,-5.03497947549541,
133.911917896819));
#159799=CARTESIAN_POINT('Ctrl Pts',(-177.222912614691,-4.95297614314753,
134.04478273508));
#159800=CARTESIAN_POINT('Ctrl Pts',(-177.230238920234,-4.86573764564598,
134.174354601081));
#159801=CARTESIAN_POINT('Ctrl Pts',(-177.237565225776,-4.77357498023392,
134.30020278657));
#159802=CARTESIAN_POINT('Ctrl Pts',(-177.24489916596,-4.68131627339521,
134.426182116695));
#159803=CARTESIAN_POINT('Ctrl Pts',(-177.252233106143,-4.58412337606316,
134.548429708487));
#159804=CARTESIAN_POINT('Ctrl Pts',(-177.259567046327,-4.48234821164094,
134.666547183761));
#159805=CARTESIAN_POINT('Ctrl Pts',(-177.266905027796,-4.38051696514717,
134.784729746356));
#159806=CARTESIAN_POINT('Ctrl Pts',(-177.274243009266,-4.27409868182224,
134.898777380797));
#159807=CARTESIAN_POINT('Ctrl Pts',(-177.281580990735,-4.16348187665067,
135.008328888771));
#159808=CARTESIAN_POINT('Ctrl Pts',(-177.288929892491,-4.05270045301331,
135.11804342985));
#159809=CARTESIAN_POINT('Ctrl Pts',(-177.296278794248,-3.93770830787742,
135.223248222139));
#159810=CARTESIAN_POINT('Ctrl Pts',(-177.303627696004,-3.81892739053334,
135.323622078063));
#159811=CARTESIAN_POINT('Ctrl Pts',(-177.30930003858,-3.72724484027508,
135.401096905637));
#159812=CARTESIAN_POINT('Ctrl Pts',(-177.314972381156,-3.63330573039015,
135.475694413771));
#159813=CARTESIAN_POINT('Ctrl Pts',(-177.320644723731,-3.53731516994476,
135.547285026723));
#159814=CARTESIAN_POINT('Ctrl Pts',(-177.328067990137,-3.41169449504985,
135.640974042324));
#159815=CARTESIAN_POINT('Ctrl Pts',(-177.335491256542,-3.28215913785233,
135.729810512298));
#159816=CARTESIAN_POINT('Ctrl Pts',(-177.342914522947,-3.14912059961039,
135.813449358206));
#159817=CARTESIAN_POINT('Ctrl Pts',(-177.350329015668,-3.0162393018725,
135.896989349945));
#159818=CARTESIAN_POINT('Ctrl Pts',(-177.35774350839,-2.87986337766262,
135.975343748868));
#159819=CARTESIAN_POINT('Ctrl Pts',(-177.365158001111,-2.7404366099266,
136.048208226858));
#159820=CARTESIAN_POINT('Ctrl Pts',(-177.372565347464,-2.60114422695826,
136.12100247532));
#159821=CARTESIAN_POINT('Ctrl Pts',(-177.379972693818,-2.45880718307821,
136.188317165231));
#159822=CARTESIAN_POINT('Ctrl Pts',(-177.387380040172,-2.3138973044699,
136.249891797062));
#159823=CARTESIAN_POINT('Ctrl Pts',(-177.394781861847,-2.16909550511661,
136.31142050421));
#159824=CARTESIAN_POINT('Ctrl Pts',(-177.402183683522,-2.02172503394739,
136.367217532269));
#159825=CARTESIAN_POINT('Ctrl Pts',(-177.409585505198,-1.87228122784675,
136.417068837878));
#159826=CARTESIAN_POINT('Ctrl Pts',(-177.416983419509,-1.72291631196724,
136.46689382737));
#159827=CARTESIAN_POINT('Ctrl Pts',(-177.424381333821,-1.57148059411923,
136.510779227457));
#159828=CARTESIAN_POINT('Ctrl Pts',(-177.431779248132,-1.41848814347019,
136.54855959996));
#159829=CARTESIAN_POINT('Ctrl Pts',(-177.439175933044,-1.26552111739154,
136.58633369405));
#159830=CARTESIAN_POINT('Ctrl Pts',(-177.446572617956,-1.11099823401281,
136.61800468472));
#159831=CARTESIAN_POINT('Ctrl Pts',(-177.453969302868,-0.955447549848219,
136.643457340689));
#159832=CARTESIAN_POINT('Ctrl Pts',(-177.461365659804,-0.799903762963973,
136.668908868061));
#159833=CARTESIAN_POINT('Ctrl Pts',(-177.468762016739,-0.643332634308196,
136.688142548689));
#159834=CARTESIAN_POINT('Ctrl Pts',(-177.476158373675,-0.486270944501928,
136.701094555182));
#159835=CARTESIAN_POINT('Ctrl Pts',(-177.483555863011,-0.329185208149992,
136.71404854466));
#159836=CARTESIAN_POINT('Ctrl Pts',(-177.490953352348,-0.171609133160149,
136.720718914368));
#159837=CARTESIAN_POINT('Ctrl Pts',(-177.498350841684,-0.0140829840808063,
136.721093857459));
#159838=CARTESIAN_POINT('Ctrl Pts',(-177.505750924199,0.143498385546124,
136.721468931986));
#159839=CARTESIAN_POINT('Ctrl Pts',(-177.513151006714,0.301029421353311,
136.715544185182));
#159840=CARTESIAN_POINT('Ctrl Pts',(-177.520551089229,0.457971650391806,
136.703359899642));
#159841=CARTESIAN_POINT('Ctrl Pts',(-177.527959308896,0.615086453544958,
136.691162216229));
#159842=CARTESIAN_POINT('Ctrl Pts',(-177.535367528562,0.77161078451577,
136.672691277176));
#159843=CARTESIAN_POINT('Ctrl Pts',(-177.542775748229,0.927012338536299,
136.648039141125));
#159844=CARTESIAN_POINT('Ctrl Pts',(-177.550188527531,1.08250953962031,
136.623371832095));
#159845=CARTESIAN_POINT('Ctrl Pts',(-177.557601306833,1.23688222154091,
136.592515818272));
#159846=CARTESIAN_POINT('Ctrl Pts',(-177.565014086135,1.3896105286662,136.555613797623));
#159847=CARTESIAN_POINT('Ctrl Pts',(-177.572437457163,1.54255706115918,
136.518659049637));
#159848=CARTESIAN_POINT('Ctrl Pts',(-177.579860828192,1.69385416814397,
136.475641142989));
#159849=CARTESIAN_POINT('Ctrl Pts',(-177.587284199221,1.84299855412119,
136.42675218095));
#159850=CARTESIAN_POINT('Ctrl Pts',(-177.591220248662,1.9220784862429,136.4008300802));
#159851=CARTESIAN_POINT('Ctrl Pts',(-177.595156298103,2.00055355631309,
136.373258215113));
#159852=CARTESIAN_POINT('Ctrl Pts',(-177.599092347544,2.07835137893825,
136.344070547532));
#159853=CARTESIAN_POINT('Ctrl Pts',(-177.60651561395,2.22507564441075,136.289023517395));
#159854=CARTESIAN_POINT('Ctrl Pts',(-177.613938880355,2.36983330722165,
136.228060034725));
#159855=CARTESIAN_POINT('Ctrl Pts',(-177.62136214676,2.51211161662649,136.16133978386));
#159856=CARTESIAN_POINT('Ctrl Pts',(-177.628776639481,2.65422176488509,
136.094698390792));
#159857=CARTESIAN_POINT('Ctrl Pts',(-177.636191132203,2.79385805801418,
136.022313929918));
#159858=CARTESIAN_POINT('Ctrl Pts',(-177.643605624924,2.93052458062564,
135.944395271617));
#159859=CARTESIAN_POINT('Ctrl Pts',(-177.651012971277,3.0670593788972,135.866551714253));
#159860=CARTESIAN_POINT('Ctrl Pts',(-177.658420317631,3.20062978296294,
135.783184762192));
#159861=CARTESIAN_POINT('Ctrl Pts',(-177.665827663985,3.33076159361491,
135.694550569807));
#159862=CARTESIAN_POINT('Ctrl Pts',(-177.67322948566,3.46079634705327,135.605982484146));
#159863=CARTESIAN_POINT('Ctrl Pts',(-177.680631307335,3.58739730640505,
135.512155189587));
#159864=CARTESIAN_POINT('Ctrl Pts',(-177.688033129011,3.71011664924135,
135.413369731413));
#159865=CARTESIAN_POINT('Ctrl Pts',(-177.695431043322,3.83277120949215,
135.314636421313));
#159866=CARTESIAN_POINT('Ctrl Pts',(-177.702828957634,3.95154794400457,
135.210950393712));
#159867=CARTESIAN_POINT('Ctrl Pts',(-177.710226871945,4.0660297980114,135.102654726184));
#159868=CARTESIAN_POINT('Ctrl Pts',(-177.717623556857,4.18049262721051,
134.994377055432));
#159869=CARTESIAN_POINT('Ctrl Pts',(-177.725020241769,4.29066172152809,
134.881491521395));
#159870=CARTESIAN_POINT('Ctrl Pts',(-177.732416926681,4.3961547061791,134.764380107649));
#159871=CARTESIAN_POINT('Ctrl Pts',(-177.739813283617,4.50164301316061,
134.647273886747));
#159872=CARTESIAN_POINT('Ctrl Pts',(-177.747209640552,4.60245537290049,
134.525942436072));
#159873=CARTESIAN_POINT('Ctrl Pts',(-177.754605997488,4.69824794256832,
134.4008028641));
#159874=CARTESIAN_POINT('Ctrl Pts',(-177.762003486824,4.79405517832313,
134.275644132939));
#159875=CARTESIAN_POINT('Ctrl Pts',(-177.769400976161,4.88484086681493,
134.146676416024));
#159876=CARTESIAN_POINT('Ctrl Pts',(-177.776798465497,4.97030304842392,
134.01434787133));
#159877=CARTESIAN_POINT('Ctrl Pts',(-177.784198548012,5.05579518866831,
133.88197293907));
#159878=CARTESIAN_POINT('Ctrl Pts',(-177.791598630527,5.13595990414746,
133.746235146767));
#159879=CARTESIAN_POINT('Ctrl Pts',(-177.798998713042,5.21054002796877,
133.60760930069));
#159880=CARTESIAN_POINT('Ctrl Pts',(-177.806406932709,5.28520216030313,
133.468831021244));
#159881=CARTESIAN_POINT('Ctrl Pts',(-177.813815152375,5.35426726036343,
133.327158674864));
#159882=CARTESIAN_POINT('Ctrl Pts',(-177.821223372042,5.41752505596053,
133.183089864567));
#159883=CARTESIAN_POINT('Ctrl Pts',(-177.828636151344,5.4808217856753,133.038932382322));
#159884=CARTESIAN_POINT('Ctrl Pts',(-177.836048930646,5.53830395269912,
132.89237584379));
#159885=CARTESIAN_POINT('Ctrl Pts',(-177.843461709948,5.58981061820532,
132.743934749972));
#159886=CARTESIAN_POINT('Ctrl Pts',(-177.850885080977,5.64139087885053,
132.595281556559));
#159887=CARTESIAN_POINT('Ctrl Pts',(-177.858308452005,5.68697847761942,
132.444738786182));
#159888=CARTESIAN_POINT('Ctrl Pts',(-177.865731823034,5.72646299292331,
132.292833712109));
#159889=CARTESIAN_POINT('Ctrl Pts',(-177.869667872475,5.74739863035717,
132.212289996917));
#159890=CARTESIAN_POINT('Ctrl Pts',(-177.873603921916,5.76661933161712,
132.131363431378));
#159891=CARTESIAN_POINT('Ctrl Pts',(-177.877539971357,5.78411454368991,
132.050133272578));
#159892=CARTESIAN_POINT('Ctrl Pts',(-177.884963237763,5.8171099676497,131.8969357282));
#159893=CARTESIAN_POINT('Ctrl Pts',(-177.892386504168,5.84406471575569,
131.742194755227));
#159894=CARTESIAN_POINT('Ctrl Pts',(-177.899809770574,5.8648359806621,131.586428058668));
#159895=CARTESIAN_POINT('Ctrl Pts',(-177.907224263295,5.88558269565833,
131.430845465408));
#159896=CARTESIAN_POINT('Ctrl Pts',(-177.914638756016,5.90016042593295,
131.274239928101));
#159897=CARTESIAN_POINT('Ctrl Pts',(-177.922053248737,5.90847684567043,
131.11714157395));
#159898=CARTESIAN_POINT('Ctrl Pts',(-177.92946059509,5.91678524972947,130.960194637107));
#159899=CARTESIAN_POINT('Ctrl Pts',(-177.936867941444,5.91884433792153,
130.802756199315));
#159900=CARTESIAN_POINT('Ctrl Pts',(-177.944275287798,5.91461330392035,
130.645363675493));
#159901=CARTESIAN_POINT('Ctrl Pts',(-177.951677109473,5.91038542558397,
130.488088540955));
#159902=CARTESIAN_POINT('Ctrl Pts',(-177.959078931149,5.89987677627389,
130.330859623758));
#159903=CARTESIAN_POINT('Ctrl Pts',(-177.966480752824,5.88309857495163,
130.174216411926));
#159904=CARTESIAN_POINT('Ctrl Pts',(-177.973878667135,5.86632923071125,
130.017655890825));
#159905=CARTESIAN_POINT('Ctrl Pts',(-177.981276581447,5.8432969654369,129.861680829558));
#159906=CARTESIAN_POINT('Ctrl Pts',(-177.988674495758,5.81406499171843,
129.706827549921));
#159907=CARTESIAN_POINT('Ctrl Pts',(-177.99607118067,5.78483787582355,129.552000004089));
#159908=CARTESIAN_POINT('Ctrl Pts',(-178.003467865583,5.74941316546099,
129.398294236358));
#159909=CARTESIAN_POINT('Ctrl Pts',(-178.010864550495,5.70790555132229,
129.246238420919));
#159910=CARTESIAN_POINT('Ctrl Pts',(-178.01826090743,5.66639977767482,129.094189347795));
#159911=CARTESIAN_POINT('Ctrl Pts',(-178.025657264366,5.61881173485485,
128.943790441616));
#159912=CARTESIAN_POINT('Ctrl Pts',(-178.033053621301,5.56530649258613,
128.795556444413));
#159913=CARTESIAN_POINT('Ctrl Pts',(-178.040451110638,5.51179305852807,
128.647299752205));
#159914=CARTESIAN_POINT('Ctrl Pts',(-178.047848599974,5.45236074792454,
128.501208980088));
#159915=CARTESIAN_POINT('Ctrl Pts',(-178.055246089311,5.38722339222336,
128.357780415574));
#159916=CARTESIAN_POINT('Ctrl Pts',(-178.062646171826,5.32206320272322,
128.214301572398));
#159917=CARTESIAN_POINT('Ctrl Pts',(-178.070046254341,5.2511941406124,128.073487134563));
#159918=CARTESIAN_POINT('Ctrl Pts',(-178.077446336856,5.17487666886568,
127.935810108244));
#159919=CARTESIAN_POINT('Ctrl Pts',(-178.084854556523,5.09847527821303,
127.797981691881));
#159920=CARTESIAN_POINT('Ctrl Pts',(-178.092262776189,5.0166136944242,127.663297903417));
#159921=CARTESIAN_POINT('Ctrl Pts',(-178.099670995855,4.92959690775829,
127.532204617385));
#159922=CARTESIAN_POINT('Ctrl Pts',(-178.107083775158,4.84252656371214,
127.401030645623));
#159923=CARTESIAN_POINT('Ctrl Pts',(-178.11449655446,4.75029491250327,127.273451881607));
#159924=CARTESIAN_POINT('Ctrl Pts',(-178.121909333762,4.65324782702965,
127.149881828088));
#159925=CARTESIAN_POINT('Ctrl Pts',(-178.129332704791,4.55606207612909,
127.026135211882));
#159926=CARTESIAN_POINT('Ctrl Pts',(-178.136756075819,4.45404739049054,
126.906409029329));
#159927=CARTESIAN_POINT('Ctrl Pts',(-178.144179446848,4.34758769448162,
126.79108118532));
#159928=CARTESIAN_POINT('Ctrl Pts',(-178.148115496289,4.29114020919341,
126.729931595174));
#159929=CARTESIAN_POINT('Ctrl Pts',(-178.15205154573,4.2334436561737,126.670017889436));
#159930=CARTESIAN_POINT('Ctrl Pts',(-178.15598759517,4.17455901249309,126.611391787046));
#159931=CARTESIAN_POINT('Ctrl Pts',(-178.163410861576,4.06350441223662,
126.500824787596));
#159932=CARTESIAN_POINT('Ctrl Pts',(-178.170834127981,3.94788614894046,
126.394505718966));
#159933=CARTESIAN_POINT('Ctrl Pts',(-178.178257394387,3.82806259163174,
126.292834561224));
#159934=CARTESIAN_POINT('Ctrl Pts',(-178.185671887108,3.70838065581702,
126.191283570348));
#159935=CARTESIAN_POINT('Ctrl Pts',(-178.193086379829,3.58450360127617,
126.094369794788));
#159936=CARTESIAN_POINT('Ctrl Pts',(-178.20050087255,3.45682753468036,126.00245745757));
#159937=CARTESIAN_POINT('Ctrl Pts',(-178.207908218903,3.32927452708373,
125.910633708923));
#159938=CARTESIAN_POINT('Ctrl Pts',(-178.215315565257,3.19793009794471,
125.823802018436));
#159939=CARTESIAN_POINT('Ctrl Pts',(-178.222722911611,3.06322433283905,
125.742287203519));
#159940=CARTESIAN_POINT('Ctrl Pts',(-178.230124733286,2.92861903637594,
125.660833185426));
#159941=CARTESIAN_POINT('Ctrl Pts',(-178.237526554962,2.79065771374413,
125.584688339437));
#159942=CARTESIAN_POINT('Ctrl Pts',(-178.244928376637,2.64980031561801,
125.514134833174));
#159943=CARTESIAN_POINT('Ctrl Pts',(-178.252326290949,2.50901727501513,
125.443618571557));
#159944=CARTESIAN_POINT('Ctrl Pts',(-178.25972420526,2.36534153655218,125.378687938122));
#159945=CARTESIAN_POINT('Ctrl Pts',(-178.267122119571,2.21925849089409,
125.319579645358));
#159946=CARTESIAN_POINT('Ctrl Pts',(-178.274518804484,2.0731997215886,125.26048117532));
#159947=CARTESIAN_POINT('Ctrl Pts',(-178.281915489396,1.92473478477583,
125.207203265498));
#159948=CARTESIAN_POINT('Ctrl Pts',(-178.289312174308,1.77437004148133,
125.159934914415));
#159949=CARTESIAN_POINT('Ctrl Pts',(-178.296708531243,1.62401196551712,
125.11266865926));
#159950=CARTESIAN_POINT('Ctrl Pts',(-178.304104888179,1.47175460668375,
125.071411544961));
#159951=CARTESIAN_POINT('Ctrl Pts',(-178.311501245114,1.31812025624708,
125.036302924324));
#159952=CARTESIAN_POINT('Ctrl Pts',(-178.318898734451,1.16446238399872,
125.001188928467));
#159953=CARTESIAN_POINT('Ctrl Pts',(-178.326296223788,1.00942746431455,
124.972225383793));
#159954=CARTESIAN_POINT('Ctrl Pts',(-178.333693713124,0.853548619055772,
124.949500643373));
#159955=CARTESIAN_POINT('Ctrl Pts',(-178.341093795639,0.697615130709651,
124.92676793683));
#159956=CARTESIAN_POINT('Ctrl Pts',(-178.348493878154,0.540837496942744,
124.910278442666));
#159957=CARTESIAN_POINT('Ctrl Pts',(-178.355893960669,0.383754457847682,
124.900068697396));
#159958=CARTESIAN_POINT('Ctrl Pts',(-178.363302180336,0.22649868980283,
124.889847725462));
#159959=CARTESIAN_POINT('Ctrl Pts',(-178.370710400002,0.068937218506624,
124.885920316844));
#159960=CARTESIAN_POINT('Ctrl Pts',(-178.378118619668,-0.0883899744820926,
124.888270880678));
#159961=CARTESIAN_POINT('Ctrl Pts',(-178.385531398971,-0.245813999732949,
124.890622891245));
#159962=CARTESIAN_POINT('Ctrl Pts',(-178.392944178273,-0.403003087479562,
124.899260553307));
#159963=CARTESIAN_POINT('Ctrl Pts',(-178.400356957575,-0.559422393395732,
124.914116382539));
#159964=CARTESIAN_POINT('Ctrl Pts',(-178.407780328604,-0.7160651985522,
124.928993438476));
#159965=CARTESIAN_POINT('Ctrl Pts',(-178.415203699632,-0.871935656190584,
124.950106356566));
#159966=CARTESIAN_POINT('Ctrl Pts',(-178.422627070661,-1.02650830372507,
124.977336397187));
#159967=CARTESIAN_POINT('Ctrl Pts',(-178.426563120102,-1.10846643036695,
124.9917744181));
#159968=CARTESIAN_POINT('Ctrl Pts',(-178.430499169543,-1.19005992407337,
125.007931340782));
#159969=CARTESIAN_POINT('Ctrl Pts',(-178.434435218983,-1.27121231263882,
125.025783818847));
#159970=CARTESIAN_POINT('Ctrl Pts',(-178.441858485389,-1.42426318479541,
125.05945303532));
#159971=CARTESIAN_POINT('Ctrl Pts',(-178.449281751794,-1.57620692379148,
125.099257901129));
#159972=CARTESIAN_POINT('Ctrl Pts',(-178.4567050182,-1.72651330785561,125.145113109257));
#159973=CARTESIAN_POINT('Ctrl Pts',(-178.464119510921,-1.87664204225593,
125.190914120338));
#159974=CARTESIAN_POINT('Ctrl Pts',(-178.471534003642,-2.02513692022056,
125.242751131763));
#159975=CARTESIAN_POINT('Ctrl Pts',(-178.478948496363,-2.17147740527155,
125.300487759215));
#159976=CARTESIAN_POINT('Ctrl Pts',(-178.486355842717,-2.31767684185384,
125.358168737931));
#159977=CARTESIAN_POINT('Ctrl Pts',(-178.493763189071,-2.46172567447768,
125.421737876344));
#159978=CARTESIAN_POINT('Ctrl Pts',(-178.501170535424,-2.60311815329856,
125.49100890302));
#159979=CARTESIAN_POINT('Ctrl Pts',(-178.5085723571,-2.74440517627349,125.560228264751));
#159980=CARTESIAN_POINT('Ctrl Pts',(-178.515974178775,-2.88303945651406,
125.63514088355));
#159981=CARTESIAN_POINT('Ctrl Pts',(-178.523376000451,-3.01853498383293,
125.715512308383));
#159982=CARTESIAN_POINT('Ctrl Pts',(-178.530773914762,-3.15395898411763,
125.795841305766));
#159983=CARTESIAN_POINT('Ctrl Pts',(-178.538171829073,-3.28624721107121,
125.881623180252));
#159984=CARTESIAN_POINT('Ctrl Pts',(-178.545569743385,-3.41493814626204,
125.972577507812));
#159985=CARTESIAN_POINT('Ctrl Pts',(-178.552966428297,-3.54360769535433,
126.063516720413));
#159986=CARTESIAN_POINT('Ctrl Pts',(-178.560363113209,-3.66868083460214,
126.159626464855));
#159987=CARTESIAN_POINT('Ctrl Pts',(-178.567759798121,-3.78972485369128,
126.260582883586));
#159988=CARTESIAN_POINT('Ctrl Pts',(-178.575156155057,-3.91076350556178,
126.361534825803));
#159989=CARTESIAN_POINT('Ctrl Pts',(-178.582552511992,-4.02777310582645,
126.467332775903));
#159990=CARTESIAN_POINT('Ctrl Pts',(-178.589948868928,-4.14035410183528,
126.577612639047));
#159991=CARTESIAN_POINT('Ctrl Pts',(-178.597346358264,-4.25295233428265,
126.68790938632));
#159992=CARTESIAN_POINT('Ctrl Pts',(-178.604743847601,-4.3611203457351,
126.802689151698));
#159993=CARTESIAN_POINT('Ctrl Pts',(-178.612141336938,-4.46449563686406,
126.921551161654));
#159994=CARTESIAN_POINT('Ctrl Pts',(-178.619541419453,-4.56790716604064,
127.040454838502));
#159995=CARTESIAN_POINT('Ctrl Pts',(-178.626941501968,-4.66652238504518,
127.163443327591));
#159996=CARTESIAN_POINT('Ctrl Pts',(-178.634341584483,-4.7600193524934,
127.290083120499));
#159997=CARTESIAN_POINT('Ctrl Pts',(-178.641749804149,-4.85361912946892,
127.416862166879));
#159998=CARTESIAN_POINT('Ctrl Pts',(-178.649158023815,-4.94208919345739,
127.547300234764));
#159999=CARTESIAN_POINT('Ctrl Pts',(-178.656566243482,-5.02515078827324,
127.680934595132));
#160000=CARTESIAN_POINT('Ctrl Pts',(-178.663979022784,-5.10826350611499,
127.814651205219));
#160001=CARTESIAN_POINT('Ctrl Pts',(-178.671391802086,-5.18596093787455,
127.9515677039));
#160002=CARTESIAN_POINT('Ctrl Pts',(-178.678804581388,-5.25801076360465,
128.091197634567));
#160003=CARTESIAN_POINT('Ctrl Pts',(-178.686227952417,-5.33016353750426,
128.231027075026));
#160004=CARTESIAN_POINT('Ctrl Pts',(-178.693651323446,-5.39665243126757,
128.373577353457));
#160005=CARTESIAN_POINT('Ctrl Pts',(-178.701074694474,-5.45729331853665,
128.518342201639));
#160006=CARTESIAN_POINT('Ctrl Pts',(-178.705010743915,-5.48944657202259,
128.595099997725));
#160007=CARTESIAN_POINT('Ctrl Pts',(-178.708946793355,-5.51995657176065,
128.672480126188));
#160008=CARTESIAN_POINT('Ctrl Pts',(-178.712882842796,-5.54880162463143,
128.750405629503));
#160009=CARTESIAN_POINT('Ctrl Pts',(-178.721434613827,-5.6114726584305,
128.919712715677));
#160010=CARTESIAN_POINT('Ctrl Pts',(-178.729986384858,-5.66643819996979,
129.092017853483));
#160011=CARTESIAN_POINT('Ctrl Pts',(-178.738538155888,-5.71344087978109,
129.266659776783));
#160012=CARTESIAN_POINT('Ctrl Pts',(-178.747059185309,-5.76027459598887,
129.440673903352));
#160013=CARTESIAN_POINT('Ctrl Pts',(-178.75558021473,-5.79920250282132,
129.617007918382));
#160014=CARTESIAN_POINT('Ctrl Pts',(-178.764101244151,-5.8300165114818,
129.79498554439));
#160015=CARTESIAN_POINT('Ctrl Pts',(-178.772561766365,-5.86061171212024,
129.971699364291));
#160016=CARTESIAN_POINT('Ctrl Pts',(-178.781022288579,-5.88320776267889,
130.150033394038));
#160017=CARTESIAN_POINT('Ctrl Pts',(-178.789482810793,-5.89764813416431,
130.329305833264));
#160018=CARTESIAN_POINT('Ctrl Pts',(-178.796863453485,-5.91024537338753,
130.485696394638));
#160019=CARTESIAN_POINT('Ctrl Pts',(-178.804244096178,-5.91663666015527,
130.642800748586));
#160020=CARTESIAN_POINT('Ctrl Pts',(-178.811624738871,-5.91674850538075,
130.800155076613));
#160021=CARTESIAN_POINT('',(-180.561624807791,-5.90996050472777,130.808431327307));
#160022=CARTESIAN_POINT('Ctrl Pts',(-178.811624807791,-5.91021030986751,
130.800161191611));
#160023=CARTESIAN_POINT('Ctrl Pts',(-178.871526694064,-5.90189013011824,
132.075856832088));
#160024=CARTESIAN_POINT('Ctrl Pts',(-179.024244454939,-4.86928404315109,
135.340473970702));
#160025=CARTESIAN_POINT('Ctrl Pts',(-179.269778090423,0.518479272423054,
137.783525307874));
#160026=CARTESIAN_POINT('Ctrl Pts',(-179.548225714233,6.15201962547423,
134.140558312264));
#160027=CARTESIAN_POINT('Ctrl Pts',(-179.826673338048,6.13215448558245,
127.431788617551));
#160028=CARTESIAN_POINT('Ctrl Pts',(-180.10512096186,0.477138945842835,
123.822247831545));
#160029=CARTESIAN_POINT('Ctrl Pts',(-180.350104785108,-4.88402996107005,
126.29162117749));
#160030=CARTESIAN_POINT('Ctrl Pts',(-180.502272733752,-5.90199055707381,
129.544310586215));
#160031=CARTESIAN_POINT('Ctrl Pts',(-180.561624807791,-5.90996050472777,
130.808431327307));
#160032=CARTESIAN_POINT('',(-182.311624807792,-5.92507812272359,130.807023572335));
#160033=CARTESIAN_POINT('Ctrl Pts',(-180.561624807791,-5.90996050472777,
130.808431327307));
#160034=CARTESIAN_POINT('Ctrl Pts',(-180.595088608356,-5.9144541090899,
131.521166055697));
#160035=CARTESIAN_POINT('Ctrl Pts',(-180.721368283525,-5.46467200361853,
134.2052756912));
#160036=CARTESIAN_POINT('Ctrl Pts',(-180.9404638333,-1.46310027610978,137.648109452265));
#160037=CARTESIAN_POINT('Ctrl Pts',(-181.218911457112,4.96699828222215,
135.734521730019));
#160038=CARTESIAN_POINT('Ctrl Pts',(-181.497359080924,6.83266807054414,
129.290356797193));
#160039=CARTESIAN_POINT('Ctrl Pts',(-181.775806704738,2.41944969642949,
124.23748741209));
#160040=CARTESIAN_POINT('Ctrl Pts',(-182.047228613693,-4.04967250708035,
125.19448203293));
#160041=CARTESIAN_POINT('Ctrl Pts',(-182.225834648045,-5.91491065230807,
128.991748760208));
#160042=CARTESIAN_POINT('Ctrl Pts',(-182.311624807792,-5.92507812272359,
130.807023572335));
#160043=CARTESIAN_POINT('',(-184.061624807792,-5.91793140692411,130.798997977614));
#160044=CARTESIAN_POINT('Ctrl Pts',(-182.311624807792,-5.92507812272359,
130.807023572335));
#160045=CARTESIAN_POINT('Ctrl Pts',(-182.318650522649,-5.92591077938457,
130.955684016088));
#160046=CARTESIAN_POINT('Ctrl Pts',(-182.325676237506,-5.920802909146,131.104286291747));
#160047=CARTESIAN_POINT('Ctrl Pts',(-182.425517826968,-5.76118888251318,
133.209457008152));
#160048=CARTESIAN_POINT('Ctrl Pts',(-182.611149576176,-3.32683150482748,
136.961450244072));
#160049=CARTESIAN_POINT('Ctrl Pts',(-182.88959719999,3.38190018988211,136.931375521743));
#160050=CARTESIAN_POINT('Ctrl Pts',(-183.168044823802,6.98283082510118,
131.270873423793));
#160051=CARTESIAN_POINT('Ctrl Pts',(-183.446492447615,4.16688106229984,
125.181668847338));
#160052=CARTESIAN_POINT('Ctrl Pts',(-183.724940071428,-2.47822883329544,
124.259443323958));
#160053=CARTESIAN_POINT('Ctrl Pts',(-183.929984191486,-5.69455770389321,
128.0092781062));
#160054=CARTESIAN_POINT('Ctrl Pts',(-184.042212436941,-5.92199600856727,
130.386992623478));
#160055=CARTESIAN_POINT('Ctrl Pts',(-184.061624807792,-5.9181658456461,
130.798997765173));
#160056=CARTESIAN_POINT('',(-185.811624807754,-5.91674999671234,130.804163375351));
#160057=CARTESIAN_POINT('Ctrl Pts',(-184.061624807792,-5.91674757076024,
130.798999050368));
#160058=CARTESIAN_POINT('Ctrl Pts',(-184.068928931162,-5.91688801138847,
130.953982046063));
#160059=CARTESIAN_POINT('Ctrl Pts',(-184.076233054531,-5.91093487072381,
131.109156665659));
#160060=CARTESIAN_POINT('Ctrl Pts',(-184.083537177901,-5.89886979863471,
131.263997062221));
#160061=CARTESIAN_POINT('Ctrl Pts',(-184.090835650274,-5.88681406095517,
131.41871766309));
#160062=CARTESIAN_POINT('Ctrl Pts',(-184.098134122647,-5.86865583195702,
131.57310417378));
#160063=CARTESIAN_POINT('Ctrl Pts',(-184.10543259502,-5.84442882662681,
131.726630780259));
#160064=CARTESIAN_POINT('Ctrl Pts',(-184.112782708521,-5.8200304005078,
131.881243680798));
#160065=CARTESIAN_POINT('Ctrl Pts',(-184.120132822023,-5.78947697807806,
132.034984065929));
#160066=CARTESIAN_POINT('Ctrl Pts',(-184.127482935524,-5.75285625138199,
132.187319587831));
#160067=CARTESIAN_POINT('Ctrl Pts',(-184.134776202234,-5.71651875443688,
132.338476925796));
#160068=CARTESIAN_POINT('Ctrl Pts',(-184.142069468944,-5.67420758047763,
132.488250678532));
#160069=CARTESIAN_POINT('Ctrl Pts',(-184.149362735654,-5.62605967323285,
132.636131104205));
#160070=CARTESIAN_POINT('Ctrl Pts',(-184.1566557956,-5.57791313097582,132.784007337485));
#160071=CARTESIAN_POINT('Ctrl Pts',(-184.163948855547,-5.52393030354824,
132.929989984487));
#160072=CARTESIAN_POINT('Ctrl Pts',(-184.171241915494,-5.46429776820347,
133.073585256712));
#160073=CARTESIAN_POINT('Ctrl Pts',(-184.178536303616,-5.40465437287707,
133.217206679795));
#160074=CARTESIAN_POINT('Ctrl Pts',(-184.185830691739,-5.33935937028289,
133.358439507777));
#160075=CARTESIAN_POINT('Ctrl Pts',(-184.193125079861,-5.26864703532705,
133.49681098473));
#160076=CARTESIAN_POINT('Ctrl Pts',(-184.200517599794,-5.19698340338551,
133.637043980879));
#160077=CARTESIAN_POINT('Ctrl Pts',(-184.207910119727,-5.11975580564257,
133.774337715552));
#160078=CARTESIAN_POINT('Ctrl Pts',(-184.215302639659,-5.03725512909461,
133.908227774342));
#160079=CARTESIAN_POINT('Ctrl Pts',(-184.222607901079,-4.95572825936504,
134.040537445459));
#160080=CARTESIAN_POINT('Ctrl Pts',(-184.2299131625,-4.86905238698824,134.16952307254));
#160081=CARTESIAN_POINT('Ctrl Pts',(-184.23721842392,-4.7775502821432,134.294768024172));
#160082=CARTESIAN_POINT('Ctrl Pts',(-184.244654573109,-4.68440874160218,
134.422256979315));
#160083=CARTESIAN_POINT('Ctrl Pts',(-184.252090722298,-4.58626664978123,
134.545869616373));
#160084=CARTESIAN_POINT('Ctrl Pts',(-184.259526871487,-4.48350479392226,
134.665204479389));
#160085=CARTESIAN_POINT('Ctrl Pts',(-184.266963020676,-4.38074293806359,
134.784539342404));
#160086=CARTESIAN_POINT('Ctrl Pts',(-184.274399169865,-4.27336164917223,
134.899596175744));
#160087=CARTESIAN_POINT('Ctrl Pts',(-184.281835319054,-4.161777721421,135.010015948187));
#160088=CARTESIAN_POINT('Ctrl Pts',(-184.289258585459,-4.05038710764862,
135.120244423497));
#160089=CARTESIAN_POINT('Ctrl Pts',(-184.296681851865,-3.93444578121529,
135.226211097442));
#160090=CARTESIAN_POINT('Ctrl Pts',(-184.30410511827,-3.81431332688993,
135.327517082559));
#160091=CARTESIAN_POINT('Ctrl Pts',(-184.311519610991,-3.6943228591492,
135.428703332415));
#160092=CARTESIAN_POINT('Ctrl Pts',(-184.318934103712,-3.57015140620211,
135.525239619935));
#160093=CARTESIAN_POINT('Ctrl Pts',(-184.326348596433,-3.44219618145469,
135.616762929393));
#160094=CARTESIAN_POINT('Ctrl Pts',(-184.333755942787,-3.31436428477031,
135.70819802524));
#160095=CARTESIAN_POINT('Ctrl Pts',(-184.341163289141,-3.18275617821301,
135.794629546266));
#160096=CARTESIAN_POINT('Ctrl Pts',(-184.348570635494,-3.04780293399889,
135.8757339856));
#160097=CARTESIAN_POINT('Ctrl Pts',(-184.35597245717,-2.91295034300579,
135.956777934184));
#160098=CARTESIAN_POINT('Ctrl Pts',(-184.363374278845,-2.77475790068248,
136.032502520666));
#160099=CARTESIAN_POINT('Ctrl Pts',(-184.370776100521,-2.63368641439405,
136.102626978663));
#160100=CARTESIAN_POINT('Ctrl Pts',(-184.378174014832,-2.49268939864553,
136.172714418505));
#160101=CARTESIAN_POINT('Ctrl Pts',(-184.385571929143,-2.34881669916657,
136.237207451659));
#160102=CARTESIAN_POINT('Ctrl Pts',(-184.392969843455,-2.20255442484518,
136.295870844097));
#160103=CARTESIAN_POINT('Ctrl Pts',(-184.400366528367,-2.05631645666011,
136.354524487743));
#160104=CARTESIAN_POINT('Ctrl Pts',(-184.407763213279,-1.90769004789607,
136.407350274588));
#160105=CARTESIAN_POINT('Ctrl Pts',(-184.415159898191,-1.75718213247968,
136.454160748172));
#160106=CARTESIAN_POINT('Ctrl Pts',(-184.422556255127,-1.60668089074197,
136.50096914613));
#160107=CARTESIAN_POINT('Ctrl Pts',(-184.429952612062,-1.45429866469017,
136.541762650303));
#160108=CARTESIAN_POINT('Ctrl Pts',(-184.437348968997,-1.30055816731291,
136.576403498205));
#160109=CARTESIAN_POINT('Ctrl Pts',(-184.444746458334,-1.14679413187302,
136.611049649709));
#160110=CARTESIAN_POINT('Ctrl Pts',(-184.45214394767,-0.991671775233469,
136.63954118726));
#160111=CARTESIAN_POINT('Ctrl Pts',(-184.459541437007,-0.835724485702392,
136.661791380836));
#160112=CARTESIAN_POINT('Ctrl Pts',(-184.466941519522,-0.679722529091387,
136.684049374182));
#160113=CARTESIAN_POINT('Ctrl Pts',(-184.474341602037,-0.522895433160513,
136.70006161478));
#160114=CARTESIAN_POINT('Ctrl Pts',(-184.481741684552,-0.365782046711605,
136.709793206022));
#160115=CARTESIAN_POINT('Ctrl Pts',(-184.489149904218,-0.208495897941526,
136.71953549815));
#160116=CARTESIAN_POINT('Ctrl Pts',(-184.496558123885,-0.0509232027779254,
136.722983325656));
#160117=CARTESIAN_POINT('Ctrl Pts',(-184.503966343551,0.106396107174741,
136.720153922853));
#160118=CARTESIAN_POINT('Ctrl Pts',(-184.511379122853,0.263812244537669,
136.717322778599));
#160119=CARTESIAN_POINT('Ctrl Pts',(-184.518791902155,0.420974314123582,
136.708206727033));
#160120=CARTESIAN_POINT('Ctrl Pts',(-184.526204681458,0.577347679482734,
136.692874880052));
#160121=CARTESIAN_POINT('Ctrl Pts',(-184.533628052486,0.733944478439272,
136.677521126208));
#160122=CARTESIAN_POINT('Ctrl Pts',(-184.541051423515,0.889749953635859,
136.655933889856));
#160123=CARTESIAN_POINT('Ctrl Pts',(-184.548474794544,1.04423900632314,
136.628233509394));
#160124=CARTESIAN_POINT('Ctrl Pts',(-184.552410843985,1.1261528089723,136.613546103012));
#160125=CARTESIAN_POINT('Ctrl Pts',(-184.556346893425,1.20769674862925,
136.59714091264));
#160126=CARTESIAN_POINT('Ctrl Pts',(-184.560282942866,1.28879442450105,
136.579041517311));
#160127=CARTESIAN_POINT('Ctrl Pts',(-184.567706209272,1.44174211022288,
136.544906622583));
#160128=CARTESIAN_POINT('Ctrl Pts',(-184.575129475677,1.59356399310633,
136.504639476673));
#160129=CARTESIAN_POINT('Ctrl Pts',(-184.582552742083,1.74373011348117,
136.458327000013));
#160130=CARTESIAN_POINT('Ctrl Pts',(-184.589967234804,1.89371874997225,
136.412069260854));
#160131=CARTESIAN_POINT('Ctrl Pts',(-184.597381727525,2.04205516608679,
136.359780522206));
#160132=CARTESIAN_POINT('Ctrl Pts',(-184.604796220246,2.18821924286488,
136.301598752089));
#160133=CARTESIAN_POINT('Ctrl Pts',(-184.612203566599,2.33424244120238,
136.243473059753));
#160134=CARTESIAN_POINT('Ctrl Pts',(-184.619610912953,2.47809712401023,
136.179465780693));
#160135=CARTESIAN_POINT('Ctrl Pts',(-184.627018259307,2.6192781107327,136.109764724808));
#160136=CARTESIAN_POINT('Ctrl Pts',(-184.634420080982,2.76035379934881,
136.040115654599));
#160137=CARTESIAN_POINT('Ctrl Pts',(-184.641821902658,2.89875942920178,
135.964781427729));
#160138=CARTESIAN_POINT('Ctrl Pts',(-184.649223724333,3.03400970594374,
135.883997973396));
#160139=CARTESIAN_POINT('Ctrl Pts',(-184.656621638644,3.16918858511778,
135.803257164018));
#160140=CARTESIAN_POINT('Ctrl Pts',(-184.664019552956,3.30121510880317,
135.71707304701));
#160141=CARTESIAN_POINT('Ctrl Pts',(-184.671417467267,3.42962861422033,
135.625727449806));
#160142=CARTESIAN_POINT('Ctrl Pts',(-184.678814152179,3.55802077964237,
135.534397032583));
#160143=CARTESIAN_POINT('Ctrl Pts',(-184.686210837092,3.68280081455794,
135.437907053702));
#160144=CARTESIAN_POINT('Ctrl Pts',(-184.693607522004,3.80353699636812,
135.336582686238));
#160145=CARTESIAN_POINT('Ctrl Pts',(-184.701003878939,3.92426782460947,
135.235262811603));
#160146=CARTESIAN_POINT('Ctrl Pts',(-184.708400235875,4.04095487032625,
135.129109214579));
#160147=CARTESIAN_POINT('Ctrl Pts',(-184.71579659281,4.15319969089864,135.018487204419));
#160148=CARTESIAN_POINT('Ctrl Pts',(-184.723194082147,4.2654616964396,134.907848257747));
#160149=CARTESIAN_POINT('Ctrl Pts',(-184.730591571483,4.37327985674116,
134.792739797803));
#160150=CARTESIAN_POINT('Ctrl Pts',(-184.73798906082,4.47629289397063,134.673563699583));
#160151=CARTESIAN_POINT('Ctrl Pts',(-184.745389143335,4.57934204226076,
134.554345824366));
#160152=CARTESIAN_POINT('Ctrl Pts',(-184.75278922585,4.67758246983172,134.431057754148));
#160153=CARTESIAN_POINT('Ctrl Pts',(-184.760189308365,4.77069355624095,
134.304133975219));
#160154=CARTESIAN_POINT('Ctrl Pts',(-184.767597528031,4.86390702786161,
134.177070630548));
#160155=CARTESIAN_POINT('Ctrl Pts',(-184.775005747698,4.95197967345292,
134.046363894402));
#160156=CARTESIAN_POINT('Ctrl Pts',(-184.782413967364,5.03463414650848,
133.912477342097));
#160157=CARTESIAN_POINT('Ctrl Pts',(-184.789826746667,5.11733949201328,
133.778508384854));
#160158=CARTESIAN_POINT('Ctrl Pts',(-184.797239525968,5.194619837159,133.641356036106));
#160159=CARTESIAN_POINT('Ctrl Pts',(-184.804652305271,5.26624434368106,
133.501507457311));
#160160=CARTESIAN_POINT('Ctrl Pts',(-184.812075676299,5.3379711906568,133.361459056308));
#160161=CARTESIAN_POINT('Ctrl Pts',(-184.819499047328,5.4040259024361,133.21870706884));
#160162=CARTESIAN_POINT('Ctrl Pts',(-184.826922418357,5.46422589442022,
133.073758321197));
#160163=CARTESIAN_POINT('Ctrl Pts',(-184.830858467798,5.49614537464935,
132.9969030172));
#160164=CARTESIAN_POINT('Ctrl Pts',(-184.834794517239,5.52641971457611,
132.919430385207));
#160165=CARTESIAN_POINT('Ctrl Pts',(-184.838730566679,5.55502745541382,
132.841417448413));
#160166=CARTESIAN_POINT('Ctrl Pts',(-184.846153833085,5.60898076181651,
132.69428748432));
#160167=CARTESIAN_POINT('Ctrl Pts',(-184.85357709949,5.65716630769147,132.544790058487));
#160168=CARTESIAN_POINT('Ctrl Pts',(-184.861000365896,5.69937076551409,
132.39341802361));
#160169=CARTESIAN_POINT('Ctrl Pts',(-184.868414858617,5.74152534117242,
132.242224897908));
#160170=CARTESIAN_POINT('Ctrl Pts',(-184.875829351338,5.7777128006819,132.089161929462));
#160171=CARTESIAN_POINT('Ctrl Pts',(-184.883243844059,5.80776808344369,
131.93474128417));
#160172=CARTESIAN_POINT('Ctrl Pts',(-184.890651190412,5.83779439779231,
131.78046947531));
#160173=CARTESIAN_POINT('Ctrl Pts',(-184.898058536766,5.86170023104261,
131.624842958691));
#160174=CARTESIAN_POINT('Ctrl Pts',(-184.90546588312,5.87937053055049,131.468388272859));
#160175=CARTESIAN_POINT('Ctrl Pts',(-184.912867704795,5.89702765088234,
131.312050276835));
#160176=CARTESIAN_POINT('Ctrl Pts',(-184.920269526471,5.9084584559214,131.154885710824));
#160177=CARTESIAN_POINT('Ctrl Pts',(-184.927671348146,5.91359912613479,
130.997430392202));
#160178=CARTESIAN_POINT('Ctrl Pts',(-184.935069262458,5.91873708262841,
130.840058193015));
#160179=CARTESIAN_POINT('Ctrl Pts',(-184.942467176769,5.91759150510721,
130.682395919046));
#160180=CARTESIAN_POINT('Ctrl Pts',(-184.94986509108,5.91015050348987,130.52498347355));
#160181=CARTESIAN_POINT('Ctrl Pts',(-184.957261775993,5.90271073843201,
130.367597187147));
#160182=CARTESIAN_POINT('Ctrl Pts',(-184.964658460905,5.88897764325531,
130.210461019335));
#160183=CARTESIAN_POINT('Ctrl Pts',(-184.972055145817,5.86899143866611,
130.054113954552));
#160184=CARTESIAN_POINT('Ctrl Pts',(-184.979451502752,5.84900612028617,
129.897773822362));
#160185=CARTESIAN_POINT('Ctrl Pts',(-184.986847859688,5.82276829113332,
129.742223093914));
#160186=CARTESIAN_POINT('Ctrl Pts',(-184.994244216623,5.79036992825915,
129.587994448844));
#160187=CARTESIAN_POINT('Ctrl Pts',(-185.00164170596,5.75796660511301,129.433742190975));
#160188=CARTESIAN_POINT('Ctrl Pts',(-185.009039195297,5.71940094696954,
129.280812784864));
#160189=CARTESIAN_POINT('Ctrl Pts',(-185.016436684633,5.67481578315034,
129.129727407037));
#160190=CARTESIAN_POINT('Ctrl Pts',(-185.023836767148,5.63021499007076,
128.978589066463));
#160191=CARTESIAN_POINT('Ctrl Pts',(-185.031236849663,5.57959059565481,
128.829296399002));
#160192=CARTESIAN_POINT('Ctrl Pts',(-185.038636932178,5.52313484234269,
128.682354002166));
#160193=CARTESIAN_POINT('Ctrl Pts',(-185.046045151844,5.46661701012626,
128.535250027059));
#160194=CARTESIAN_POINT('Ctrl Pts',(-185.053453371511,5.40425514743527,
128.3905018324));
#160195=CARTESIAN_POINT('Ctrl Pts',(-185.060861591177,5.33628936075163,
128.248593331441));
#160196=CARTESIAN_POINT('Ctrl Pts',(-185.06827437048,5.26828174226036,128.106597488167));
#160197=CARTESIAN_POINT('Ctrl Pts',(-185.075687149781,5.19466350113199,
127.967445150473));
#160198=CARTESIAN_POINT('Ctrl Pts',(-185.083099929084,5.11571972637515,
127.831593851794));
#160199=CARTESIAN_POINT('Ctrl Pts',(-185.090523300112,5.03666315305096,
127.69554844241));
#160200=CARTESIAN_POINT('Ctrl Pts',(-185.097946671141,4.95226604824019,
127.562813806486));
#160201=CARTESIAN_POINT('Ctrl Pts',(-185.10537004217,4.86285612782121,127.433817509607));
#160202=CARTESIAN_POINT('Ctrl Pts',(-185.109306091611,4.81544884265258,
127.365420577777));
#160203=CARTESIAN_POINT('Ctrl Pts',(-185.113242141051,4.76663294343972,
127.298074068215));
#160204=CARTESIAN_POINT('Ctrl Pts',(-185.117178190492,4.71646163297881,
127.231837667725));
#160205=CARTESIAN_POINT('Ctrl Pts',(-185.124601456898,4.62184010724392,
127.10691788357));
#160206=CARTESIAN_POINT('Ctrl Pts',(-185.132024723303,4.52210915344613,
126.9855710088));
#160207=CARTESIAN_POINT('Ctrl Pts',(-185.139447989709,4.41756811377999,
126.868242920823));
#160208=CARTESIAN_POINT('Ctrl Pts',(-185.14686248243,4.31315063294114,126.751053504903));
#160209=CARTESIAN_POINT('Ctrl Pts',(-185.154276975151,4.20393462841209,
126.637873697119));
#160210=CARTESIAN_POINT('Ctrl Pts',(-185.161691467872,4.09026178058174,
126.529119205808));
#160211=CARTESIAN_POINT('Ctrl Pts',(-185.169098814225,3.97669849492183,
126.420469536169));
#160212=CARTESIAN_POINT('Ctrl Pts',(-185.176506160579,3.85868718572215,
126.316236947986));
#160213=CARTESIAN_POINT('Ctrl Pts',(-185.183913506933,3.73660865600951,
126.21680284525));
#160214=CARTESIAN_POINT('Ctrl Pts',(-185.191315328609,3.61462117706974,
126.11744290422));
#160215=CARTESIAN_POINT('Ctrl Pts',(-185.198717150284,3.48857280588916,
126.022874557316));
#160216=CARTESIAN_POINT('Ctrl Pts',(-185.206118971959,3.35887984478284,
125.933441120098));
#160217=CARTESIAN_POINT('Ctrl Pts',(-185.213516886271,3.2292553475808,125.844054894095));
#160218=CARTESIAN_POINT('Ctrl Pts',(-185.220914800582,3.09599039862963,
125.759798390713));
#160219=CARTESIAN_POINT('Ctrl Pts',(-185.228312714894,2.95953280695017,
125.68097344431));
#160220=CARTESIAN_POINT('Ctrl Pts',(-185.235709399806,2.82309789204744,
125.602161597183));
#160221=CARTESIAN_POINT('Ctrl Pts',(-185.243106084718,2.68347171034644,
125.52877970213));
#160222=CARTESIAN_POINT('Ctrl Pts',(-185.25050276963,2.54112946499453,125.461085254585));
#160223=CARTESIAN_POINT('Ctrl Pts',(-185.257899126566,2.39879353124695,
125.393393808683));
#160224=CARTESIAN_POINT('Ctrl Pts',(-185.265295483501,2.25374211042627,
125.33138946918));
#160225=CARTESIAN_POINT('Ctrl Pts',(-185.272691840437,2.10647307683844,
125.275282779531));
#160226=CARTESIAN_POINT('Ctrl Pts',(-185.280089329773,1.95918149598603,
125.219167499804));
#160227=CARTESIAN_POINT('Ctrl Pts',(-185.28748681911,1.80967197519407,125.168951800726));
#160228=CARTESIAN_POINT('Ctrl Pts',(-185.294884308446,1.65846019776952,
125.124797224583));
#160229=CARTESIAN_POINT('Ctrl Pts',(-185.302284390961,1.50719541329015,
125.080627170122));
#160230=CARTESIAN_POINT('Ctrl Pts',(-185.309684473476,1.35422754221607,
125.042522573463));
#160231=CARTESIAN_POINT('Ctrl Pts',(-185.317084555991,1.2000850284593,125.010594442877));
#160232=CARTESIAN_POINT('Ctrl Pts',(-185.324492775658,1.04577301916263,
124.97863120403));
#160233=CARTESIAN_POINT('Ctrl Pts',(-185.331900995324,0.890284153455571,
124.952858070407));
#160234=CARTESIAN_POINT('Ctrl Pts',(-185.339309214991,0.734155344681294,
124.933334600559));
#160235=CARTESIAN_POINT('Ctrl Pts',(-185.346721994293,0.577930441230811,
124.913799114341));
#160236=CARTESIAN_POINT('Ctrl Pts',(-185.354134773595,0.421065180974498,
124.900520988071));
#160237=CARTESIAN_POINT('Ctrl Pts',(-185.361547552897,0.264098597322687,
124.89350767629));
#160238=CARTESIAN_POINT('Ctrl Pts',(-185.368970923926,0.106907732454928,
124.88648434356));
#160239=CARTESIAN_POINT('Ctrl Pts',(-185.376394294955,-0.0503843726528677,
124.885743705147));
#160240=CARTESIAN_POINT('Ctrl Pts',(-185.383817665983,-0.207240856527645,
124.891241154044));
#160241=CARTESIAN_POINT('Ctrl Pts',(-185.387753715424,-0.290409927994593,
124.894156033358));
#160242=CARTESIAN_POINT('Ctrl Pts',(-185.391689764865,-0.373456639755591,
124.898823798456));
#160243=CARTESIAN_POINT('Ctrl Pts',(-185.395625814305,-0.456302018202181,
124.905231950493));
#160244=CARTESIAN_POINT('Ctrl Pts',(-185.403049080711,-0.612545816442367,
124.917317525243));
#160245=CARTESIAN_POINT('Ctrl Pts',(-185.410472347116,-0.768545395500247,
124.935633051325));
#160246=CARTESIAN_POINT('Ctrl Pts',(-185.417895613522,-0.923763824315242,
124.960167691303));
#160247=CARTESIAN_POINT('Ctrl Pts',(-185.425310106243,-1.07879879783747,
124.984673333373));
#160248=CARTESIAN_POINT('Ctrl Pts',(-185.432724598964,-1.23305409374088,
125.015383400464));
#160249=CARTESIAN_POINT('Ctrl Pts',(-185.440139091685,-1.38599527823421,
125.052235127696));
#160250=CARTESIAN_POINT('Ctrl Pts',(-185.447546438038,-1.53878905225622,
125.089051335846));
#160251=CARTESIAN_POINT('Ctrl Pts',(-185.454953784392,-1.69027087592442,
125.131997332593));
#160252=CARTESIAN_POINT('Ctrl Pts',(-185.462361130746,-1.83991402991944,
125.180958895743));
#160253=CARTESIAN_POINT('Ctrl Pts',(-185.469762952421,-1.98944557440407,
125.229883941511));
#160254=CARTESIAN_POINT('Ctrl Pts',(-185.477164774097,-2.1371408264938,
125.284815504598));
#160255=CARTESIAN_POINT('Ctrl Pts',(-185.484566595772,-2.28248592351566,
125.345588908523));
#160256=CARTESIAN_POINT('Ctrl Pts',(-185.491964510084,-2.42775429399301,
125.40633023064));
#160257=CARTESIAN_POINT('Ctrl Pts',(-185.499362424395,-2.57067463664222,
125.472907108294));
#160258=CARTESIAN_POINT('Ctrl Pts',(-185.506760338706,-2.7107509579538,
125.545105935916));
#160259=CARTESIAN_POINT('Ctrl Pts',(-185.514157023618,-2.85080400112102,
125.617292765403));
#160260=CARTESIAN_POINT('Ctrl Pts',(-185.521553708531,-2.98801362948039,
125.695099519758));
#160261=CARTESIAN_POINT('Ctrl Pts',(-185.528950393443,-3.12190634592099,
125.778265579686));
#160262=CARTESIAN_POINT('Ctrl Pts',(-185.536346750378,-3.25579312541823,
125.861427951945));
#160263=CARTESIAN_POINT('Ctrl Pts',(-185.543743107314,-3.38636296832752,
125.949948960309));
#160264=CARTESIAN_POINT('Ctrl Pts',(-185.551139464249,-3.51316962525318,
126.043523532903));
#160265=CARTESIAN_POINT('Ctrl Pts',(-185.558536953586,-3.6399956966021,
126.137112432005));
#160266=CARTESIAN_POINT('Ctrl Pts',(-185.565934442922,-3.7630571343807,
126.235756214237));
#160267=CARTESIAN_POINT('Ctrl Pts',(-185.573331932259,-3.88193928906325,
126.339108338184));
#160268=CARTESIAN_POINT('Ctrl Pts',(-185.580732014774,-4.00086311770033,
126.442496692057));
#160269=CARTESIAN_POINT('Ctrl Pts',(-185.588132097289,-4.1156044648104,
126.550596429015));
#160270=CARTESIAN_POINT('Ctrl Pts',(-185.595532179804,-4.22578429914888,
126.66302295691));
#160271=CARTESIAN_POINT('Ctrl Pts',(-185.60294039947,-4.33608528754245,
126.775573109331));
#160272=CARTESIAN_POINT('Ctrl Pts',(-185.610348619137,-4.44181448473375,
126.892459287456));
#160273=CARTESIAN_POINT('Ctrl Pts',(-185.617756838803,-4.54263156765102,
127.013261963735));
#160274=CARTESIAN_POINT('Ctrl Pts',(-185.625169618105,-4.64351070180004,
127.134138992044));
#160275=CARTESIAN_POINT('Ctrl Pts',(-185.632582397407,-4.73947147030228,
127.258937026566));
#160276=CARTESIAN_POINT('Ctrl Pts',(-185.639995176709,-4.8302162407166,
127.387206592589));
#160277=CARTESIAN_POINT('Ctrl Pts',(-185.647418547738,-4.92109067151479,
127.515659436183));
#160278=CARTESIAN_POINT('Ctrl Pts',(-185.654841918766,-5.00673401647177,
127.6475934058));
#160279=CARTESIAN_POINT('Ctrl Pts',(-185.662265289795,-5.08689361798639,
127.7825327135));
#160280=CARTESIAN_POINT('Ctrl Pts',(-185.666201339236,-5.12939616211485,
127.854080772271));
#160281=CARTESIAN_POINT('Ctrl Pts',(-185.670137388677,-5.17035781537923,
127.926473363939));
#160282=CARTESIAN_POINT('Ctrl Pts',(-185.674073438118,-5.20974640624689,
127.999637289839));
#160283=CARTESIAN_POINT('Ctrl Pts',(-185.681900715772,-5.288075055757,128.145131997376));
#160284=CARTESIAN_POINT('Ctrl Pts',(-185.689727993426,-5.36039597288839,
128.294079034415));
#160285=CARTESIAN_POINT('Ctrl Pts',(-185.69755527108,-5.42640910216598,
128.445968195082));
#160286=CARTESIAN_POINT('Ctrl Pts',(-185.705369342796,-5.49231085616024,
128.597601093116));
#160287=CARTESIAN_POINT('Ctrl Pts',(-185.713183414512,-5.55192591167538,
128.752165934091));
#160288=CARTESIAN_POINT('Ctrl Pts',(-185.720997486229,-5.60499975256745,
128.909127561655));
#160289=CARTESIAN_POINT('Ctrl Pts',(-185.728793533698,-5.6579511712372,
129.065727135315));
#160290=CARTESIAN_POINT('Ctrl Pts',(-185.736589581167,-5.70439137034077,
129.22471217246));
#160291=CARTESIAN_POINT('Ctrl Pts',(-185.744385628636,-5.7441138651048,
129.38552783418));
#160292=CARTESIAN_POINT('Ctrl Pts',(-185.752171064916,-5.78378229363978,
129.54612460994));
#160293=CARTESIAN_POINT('Ctrl Pts',(-185.759956501197,-5.81675116516731,
129.708546741938));
#160294=CARTESIAN_POINT('Ctrl Pts',(-185.767741937477,-5.842863099156,129.872222555356));
#160295=CARTESIAN_POINT('Ctrl Pts',(-185.775512714118,-5.86892586550339,
130.035590174303));
#160296=CARTESIAN_POINT('Ctrl Pts',(-185.783283490759,-5.88815739778654,
130.200206457726));
#160297=CARTESIAN_POINT('Ctrl Pts',(-185.7910542674,-5.90045097199386,130.365488324528));
#160298=CARTESIAN_POINT('Ctrl Pts',(-185.797911114185,-5.9112986849928,
130.511331203479));
#160299=CARTESIAN_POINT('Ctrl Pts',(-185.804767960969,-5.91674511390588,
130.657691966486));
#160300=CARTESIAN_POINT('Ctrl Pts',(-185.811624807754,-5.91674999671234,
130.804163375351));
#160301=CARTESIAN_POINT('',(-187.561624807792,-5.91674750900767,130.809789904034));
#160302=CARTESIAN_POINT('Ctrl Pts',(-185.811624807791,-5.91674999671237,
130.804163376133));
#160303=CARTESIAN_POINT('Ctrl Pts',(-185.819353984328,-5.91675550068887,
130.969268914026));
#160304=CARTESIAN_POINT('Ctrl Pts',(-185.827083160864,-5.90984584058032,
131.134248349692));
#160305=CARTESIAN_POINT('Ctrl Pts',(-185.834812337401,-5.89607849221174,
131.298515427497));
#160306=CARTESIAN_POINT('Ctrl Pts',(-185.84255057446,-5.88229500507678,
131.462975067292));
#160307=CARTESIAN_POINT('Ctrl Pts',(-185.85028881152,-5.86163781335462,
131.626720362507));
#160308=CARTESIAN_POINT('Ctrl Pts',(-185.858027048579,-5.83421588616898,
131.789173064722));
#160309=CARTESIAN_POINT('Ctrl Pts',(-185.865901549692,-5.80631108117604,
131.954486426734));
#160310=CARTESIAN_POINT('Ctrl Pts',(-185.873776050805,-5.77140116501924,
132.118460904788));
#160311=CARTESIAN_POINT('Ctrl Pts',(-185.881650551917,-5.72965398230494,
132.28050282127));
#160312=CARTESIAN_POINT('Ctrl Pts',(-185.889414944337,-5.68849054802612,
132.44027891503));
#160313=CARTESIAN_POINT('Ctrl Pts',(-185.897179336757,-5.64067998075974,
132.59817586172));
#160314=CARTESIAN_POINT('Ctrl Pts',(-185.904943729177,-5.58643216126939,
132.753644144925));
#160315=CARTESIAN_POINT('Ctrl Pts',(-185.912873284636,-5.53103038996559,
132.91241952709));
#160316=CARTESIAN_POINT('Ctrl Pts',(-185.920802840095,-5.46891459747241,
133.068661436369));
#160317=CARTESIAN_POINT('Ctrl Pts',(-185.928732395554,-5.40035816938212,
133.221810142352));
#160318=CARTESIAN_POINT('Ctrl Pts',(-185.936661951013,-5.33180174129202,
133.374958848335));
#160319=CARTESIAN_POINT('Ctrl Pts',(-185.944591506471,-5.25680489255712,
133.525014066598));
#160320=CARTESIAN_POINT('Ctrl Pts',(-185.95252106193,-5.17568835721522,
133.671446349016));
#160321=CARTESIAN_POINT('Ctrl Pts',(-185.959944328336,-5.09975097902817,
133.808529171427));
#160322=CARTESIAN_POINT('Ctrl Pts',(-185.967367594741,-5.01824886787116,
133.942800289093));
#160323=CARTESIAN_POINT('Ctrl Pts',(-185.974790861147,-4.93141506493196,
134.073775858838));
#160324=CARTESIAN_POINT('Ctrl Pts',(-185.982205353868,-4.84468389233649,
134.204596626337));
#160325=CARTESIAN_POINT('Ctrl Pts',(-185.989619846589,-4.75263377562075,
134.332129290969));
#160326=CARTESIAN_POINT('Ctrl Pts',(-185.99703433931,-4.65554394683494,
134.455913865376));
#160327=CARTESIAN_POINT('Ctrl Pts',(-186.004441685664,-4.55854769688175,
134.579579131549));
#160328=CARTESIAN_POINT('Ctrl Pts',(-186.011849032018,-4.45652163394964,
134.699503207619));
#160329=CARTESIAN_POINT('Ctrl Pts',(-186.019256378371,-4.34978858474558,
134.815254511764));
#160330=CARTESIAN_POINT('Ctrl Pts',(-186.026658200047,-4.24313514107611,
134.930919484221));
#160331=CARTESIAN_POINT('Ctrl Pts',(-186.034060021722,-4.13178195327352,
135.042417608329));
#160332=CARTESIAN_POINT('Ctrl Pts',(-186.041461843398,-4.0160923929967,
135.149349967773));
#160333=CARTESIAN_POINT('Ctrl Pts',(-186.048859757709,-3.90046390433854,
135.256225878457));
#160334=CARTESIAN_POINT('Ctrl Pts',(-186.056257672021,-3.78050387557164,
135.358540571827));
#160335=CARTESIAN_POINT('Ctrl Pts',(-186.063655586332,-3.65661275257442,
135.455931722065));
#160336=CARTESIAN_POINT('Ctrl Pts',(-186.071052271244,-3.53274221803405,
135.553306687661));
#160337=CARTESIAN_POINT('Ctrl Pts',(-186.078448956157,-3.4049421790122,
135.645759503541));
#160338=CARTESIAN_POINT('Ctrl Pts',(-186.085845641069,-3.27364649016796,
135.732967846785));
#160339=CARTESIAN_POINT('Ctrl Pts',(-186.093241998004,-3.14235662311216,
135.820172323119));
#160340=CARTESIAN_POINT('Ctrl Pts',(-186.10063835494,-3.00757172538186,
135.902132582656));
#160341=CARTESIAN_POINT('Ctrl Pts',(-186.108034711876,-2.86975475604621,
135.978569562192));
#160342=CARTESIAN_POINT('Ctrl Pts',(-186.115432201212,-2.73191668658033,
136.055018244425));
#160343=CARTESIAN_POINT('Ctrl Pts',(-186.122829690549,-2.59104594766015,
136.125941781829));
#160344=CARTESIAN_POINT('Ctrl Pts',(-186.130227179886,-2.44763008059823,
136.191107089329));
#160345=CARTESIAN_POINT('Ctrl Pts',(-186.137627262401,-2.30416393932624,
136.256295240426));
#160346=CARTESIAN_POINT('Ctrl Pts',(-186.145027344916,-2.15815123321437,
136.315720988395));
#160347=CARTESIAN_POINT('Ctrl Pts',(-186.152427427431,-2.01009930602779,
136.369199460013));
#160348=CARTESIAN_POINT('Ctrl Pts',(-186.159835647097,-1.8618845805278,
136.422736736708));
#160349=CARTESIAN_POINT('Ctrl Pts',(-186.167243866764,-1.71162650717714,
136.47031355006));
#160350=CARTESIAN_POINT('Ctrl Pts',(-186.174652086431,-1.5598481143866,
136.511794754071));
#160351=CARTESIAN_POINT('Ctrl Pts',(-186.182064865733,-1.40797630452743,
136.553301489072));
#160352=CARTESIAN_POINT('Ctrl Pts',(-186.189477645035,-1.25458267355879,
136.588705055152));
#160353=CARTESIAN_POINT('Ctrl Pts',(-186.196890424337,-1.10019974227204,
136.617921582208));
#160354=CARTESIAN_POINT('Ctrl Pts',(-186.204313795366,-0.94559622141344,
136.647179855207));
#160355=CARTESIAN_POINT('Ctrl Pts',(-186.211737166394,-0.790000945331487,
136.67023337849));
#160356=CARTESIAN_POINT('Ctrl Pts',(-186.219160537423,-0.633951672601608,
136.687050124867));
#160357=CARTESIAN_POINT('Ctrl Pts',(-186.223096586864,-0.551210603860005,
136.695966767307));
#160358=CARTESIAN_POINT('Ctrl Pts',(-186.227032636304,-0.468341915081361,
136.703130899092));
#160359=CARTESIAN_POINT('Ctrl Pts',(-186.230968685744,-0.385425554330736,
136.708543685914));
#160360=CARTESIAN_POINT('Ctrl Pts',(-186.23839195215,-0.229047885666553,
136.718752032934));
#160361=CARTESIAN_POINT('Ctrl Pts',(-186.245815218555,-0.0720279097393259,
136.72275881741));
#160362=CARTESIAN_POINT('Ctrl Pts',(-186.253238484961,0.0851013380298015,
136.72049857444));
#160363=CARTESIAN_POINT('Ctrl Pts',(-186.260652977682,0.242044872077285,
136.718241002889));
#160364=CARTESIAN_POINT('Ctrl Pts',(-186.268067470403,0.399097051278048,
136.709731153093));
#160365=CARTESIAN_POINT('Ctrl Pts',(-186.275481963124,0.555719943496593,
136.694955316482));
#160366=CARTESIAN_POINT('Ctrl Pts',(-186.282889309477,0.712191876675316,
136.680193721379));
#160367=CARTESIAN_POINT('Ctrl Pts',(-186.290296655831,0.868234977439624,
136.65917819753));
#160368=CARTESIAN_POINT('Ctrl Pts',(-186.297704002185,1.02331164805928,
136.631947067671));
#160369=CARTESIAN_POINT('Ctrl Pts',(-186.30510582386,1.1782726566464,136.604736247816));
#160370=CARTESIAN_POINT('Ctrl Pts',(-186.312507645536,1.33226830420908,
136.571319116806));
#160371=CARTESIAN_POINT('Ctrl Pts',(-186.319909467211,1.48476655989437,
136.531785765494));
#160372=CARTESIAN_POINT('Ctrl Pts',(-186.327307381523,1.63718431293841,
136.492273283531));
#160373=CARTESIAN_POINT('Ctrl Pts',(-186.334705295834,1.78810588790865,
136.446651104826));
#160374=CARTESIAN_POINT('Ctrl Pts',(-186.342103210145,1.93700999905407,
136.395060289885));
#160375=CARTESIAN_POINT('Ctrl Pts',(-186.349499895057,2.08588936503698,
136.343478048401));
#160376=CARTESIAN_POINT('Ctrl Pts',(-186.35689657997,2.23275158021718,136.285929261356));
#160377=CARTESIAN_POINT('Ctrl Pts',(-186.364293264882,2.37709095615206,
136.22260471955));
#160378=CARTESIAN_POINT('Ctrl Pts',(-186.371689621817,2.52142393192816,
136.15928298562));
#160379=CARTESIAN_POINT('Ctrl Pts',(-186.379085978753,2.66323394903901,
136.090186156123));
#160380=CARTESIAN_POINT('Ctrl Pts',(-186.386482335688,2.80203598302284,
136.015552891158));
#160381=CARTESIAN_POINT('Ctrl Pts',(-186.393879825025,2.94085926795201,
135.94090819965));
#160382=CARTESIAN_POINT('Ctrl Pts',(-186.401277314361,3.07667332397372,
135.860725561701));
#160383=CARTESIAN_POINT('Ctrl Pts',(-186.408674803698,3.20901852202426,
135.775289171449));
#160384=CARTESIAN_POINT('Ctrl Pts',(-186.416074886213,3.34141011347863,
135.689822831602));
#160385=CARTESIAN_POINT('Ctrl Pts',(-186.423474968728,3.47033011248045,
135.599099274988));
#160386=CARTESIAN_POINT('Ctrl Pts',(-186.430875051243,3.59534874825436,
135.503445415793));
#160387=CARTESIAN_POINT('Ctrl Pts',(-186.438283270909,3.72050485487072,
135.407686375345));
#160388=CARTESIAN_POINT('Ctrl Pts',(-186.445691490576,3.84175073429224,
135.306986432451));
#160389=CARTESIAN_POINT('Ctrl Pts',(-186.453099710242,3.95868997473241,
135.201712576012));
#160390=CARTESIAN_POINT('Ctrl Pts',(-186.460512489544,4.07570118932416,
135.096373925272));
#160391=CARTESIAN_POINT('Ctrl Pts',(-186.467925268846,4.18840021653473,
134.986456011451));
#160392=CARTESIAN_POINT('Ctrl Pts',(-186.475338048148,4.29642865357484,
134.872361525536));
#160393=CARTESIAN_POINT('Ctrl Pts',(-186.482761419177,4.40461144671197,
134.758104016068));
#160394=CARTESIAN_POINT('Ctrl Pts',(-186.490184790206,4.50811007610825,
134.639658296061));
#160395=CARTESIAN_POINT('Ctrl Pts',(-186.497608161235,4.60660692473589,
134.517459485557));
#160396=CARTESIAN_POINT('Ctrl Pts',(-186.501544210675,4.65883231727349,
134.452666744113));
#160397=CARTESIAN_POINT('Ctrl Pts',(-186.505480260116,4.7096522547113,134.386819357501));
#160398=CARTESIAN_POINT('Ctrl Pts',(-186.509416309556,4.75902450389532,
134.319985218377));
#160399=CARTESIAN_POINT('Ctrl Pts',(-186.516839575961,4.85213902500785,
134.193938117801));
#160400=CARTESIAN_POINT('Ctrl Pts',(-186.524262842367,4.94038317868034,
134.063998529898));
#160401=CARTESIAN_POINT('Ctrl Pts',(-186.531686108772,5.02341376877007,
133.930579527085));
#160402=CARTESIAN_POINT('Ctrl Pts',(-186.539100601493,5.10634622359734,
133.797318214453));
#160403=CARTESIAN_POINT('Ctrl Pts',(-186.546515094214,5.18407718502282,
133.660585986465));
#160404=CARTESIAN_POINT('Ctrl Pts',(-186.553929586935,5.25630435417878,
133.520828010844));
#160405=CARTESIAN_POINT('Ctrl Pts',(-186.561336933289,5.3284619080698,133.381204739222));
#160406=CARTESIAN_POINT('Ctrl Pts',(-186.568744279642,5.39512606019245,
133.238561855208));
#160407=CARTESIAN_POINT('Ctrl Pts',(-186.576151625996,5.45603846784417,
133.093372369372));
#160408=CARTESIAN_POINT('Ctrl Pts',(-186.583553447672,5.51690544472435,
132.948291171332));
#160409=CARTESIAN_POINT('Ctrl Pts',(-186.590955269347,5.57202907504359,
132.800667496085));
#160410=CARTESIAN_POINT('Ctrl Pts',(-186.598357091022,5.6211975791176,132.650997652563));
#160411=CARTESIAN_POINT('Ctrl Pts',(-186.605755005334,5.67034012752104,
132.501406818586));
#160412=CARTESIAN_POINT('Ctrl Pts',(-186.613152919645,5.71353369422572,
132.349772321271));
#160413=CARTESIAN_POINT('Ctrl Pts',(-186.620550833956,5.75061518974696,
132.196608979731));
#160414=CARTESIAN_POINT('Ctrl Pts',(-186.627947518869,5.78769052299643,
132.043471091159));
#160415=CARTESIAN_POINT('Ctrl Pts',(-186.635344203781,5.81865571320347,
131.88880522507));
#160416=CARTESIAN_POINT('Ctrl Pts',(-186.642740888693,5.84339794111647,
131.733139958559));
#160417=CARTESIAN_POINT('Ctrl Pts',(-186.650137245628,5.86813907193316,
131.577481594409));
#160418=CARTESIAN_POINT('Ctrl Pts',(-186.657533602564,5.88665773050493,
131.42082428662));
#160419=CARTESIAN_POINT('Ctrl Pts',(-186.664929959499,5.89889254076296,
131.26370510162));
#160420=CARTESIAN_POINT('Ctrl Pts',(-186.672327448836,5.91112922420171,
131.106561861272));
#160421=CARTESIAN_POINT('Ctrl Pts',(-186.679724938173,5.91708011472825,
130.948956975106));
#160422=CARTESIAN_POINT('Ctrl Pts',(-186.687122427509,5.91673587218311,
130.791430755944));
#160423=CARTESIAN_POINT('Ctrl Pts',(-186.694522510024,5.91639150896428,
130.633849316211));
#160424=CARTESIAN_POINT('Ctrl Pts',(-186.701922592539,5.90974761986768,
130.47634697145));
#160425=CARTESIAN_POINT('Ctrl Pts',(-186.709322675054,5.89684694545481,
130.319462005091));
#160426=CARTESIAN_POINT('Ctrl Pts',(-186.716730894721,5.88393208542427,
130.162404527584));
#160427=CARTESIAN_POINT('Ctrl Pts',(-186.724139114387,5.86474673092027,
130.005966156498));
#160428=CARTESIAN_POINT('Ctrl Pts',(-186.731547334054,5.83938536984659,
129.850678770763));
#160429=CARTESIAN_POINT('Ctrl Pts',(-186.738960113356,5.81400839927836,
129.695295808233));
#160430=CARTESIAN_POINT('Ctrl Pts',(-186.746372892658,5.78244792237959,
129.541065607525));
#160431=CARTESIAN_POINT('Ctrl Pts',(-186.75378567196,5.7448490090175,129.38850736737));
#160432=CARTESIAN_POINT('Ctrl Pts',(-186.761209042988,5.70719637256474,
129.235731144846));
#160433=CARTESIAN_POINT('Ctrl Pts',(-186.768632414017,5.66348817105071,
129.084632011842));
#160434=CARTESIAN_POINT('Ctrl Pts',(-186.776055785046,5.61391880352735,
128.935712381567));
#160435=CARTESIAN_POINT('Ctrl Pts',(-186.779991834487,5.58763593546334,
128.856751620311));
#160436=CARTESIAN_POINT('Ctrl Pts',(-186.783927883928,5.55970608173856,
128.77840324676));
#160437=CARTESIAN_POINT('Ctrl Pts',(-186.787863933369,5.53016353431541,
128.700739490502));
#160438=CARTESIAN_POINT('Ctrl Pts',(-186.795287199775,5.47444721187183,
128.554268070017));
#160439=CARTESIAN_POINT('Ctrl Pts',(-186.80271046618,5.41282347703181,128.409790243116));
#160440=CARTESIAN_POINT('Ctrl Pts',(-186.810133732586,5.34545435342012,
128.267818026163));
#160441=CARTESIAN_POINT('Ctrl Pts',(-186.817548225307,5.27816485451769,
128.12601360858));
#160442=CARTESIAN_POINT('Ctrl Pts',(-186.824962718028,5.20514364198745,
127.986709240179));
#160443=CARTESIAN_POINT('Ctrl Pts',(-186.832377210749,5.12660184812075,
127.850399877586));
#160444=CARTESIAN_POINT('Ctrl Pts',(-186.839784557103,5.04813575579202,
127.714221895088));
#160445=CARTESIAN_POINT('Ctrl Pts',(-186.847191903456,4.96415986019837,
127.581033492824));
#160446=CARTESIAN_POINT('Ctrl Pts',(-186.85459924981,4.87493247798782,127.451307695592));
#160447=CARTESIAN_POINT('Ctrl Pts',(-186.862001071486,4.78577164492528,
127.321678652754));
#160448=CARTESIAN_POINT('Ctrl Pts',(-186.869402893161,4.69136733467664,
127.195507379004));
#160449=CARTESIAN_POINT('Ctrl Pts',(-186.876804714836,4.59202263391012,
127.073240317689));
#160450=CARTESIAN_POINT('Ctrl Pts',(-186.884202629148,4.4927303764384,126.951037800204));
#160451=CARTESIAN_POINT('Ctrl Pts',(-186.891600543459,4.38850315720013,
126.832735679553));
#160452=CARTESIAN_POINT('Ctrl Pts',(-186.89899845777,4.27968595424607,126.718749439844));
#160453=CARTESIAN_POINT('Ctrl Pts',(-186.906395142683,4.17088683473652,
126.604782142579));
#160454=CARTESIAN_POINT('Ctrl Pts',(-186.913791827595,4.05749950290368,
126.495129572533));
#160455=CARTESIAN_POINT('Ctrl Pts',(-186.921188512507,3.93990768406763,
126.390172356569));
#160456=CARTESIAN_POINT('Ctrl Pts',(-186.928584869443,3.82232107937571,
126.285219794517));
#160457=CARTESIAN_POINT('Ctrl Pts',(-186.935981226378,3.70053063686753,
126.184962421158));
#160458=CARTESIAN_POINT('Ctrl Pts',(-186.943377583313,3.57495503047606,
126.089742171438));
#160459=CARTESIAN_POINT('Ctrl Pts',(-186.95077507265,3.4493601981394,125.994507343255));
#160460=CARTESIAN_POINT('Ctrl Pts',(-186.958172561986,3.31997934549403,
125.904311399832));
#160461=CARTESIAN_POINT('Ctrl Pts',(-186.965570051323,3.18726200443501,
125.819454251586));
#160462=CARTESIAN_POINT('Ctrl Pts',(-186.972970133838,3.05449813951574,
125.734567356798));
#160463=CARTESIAN_POINT('Ctrl Pts',(-186.980370216353,2.91839577182612,
125.655023184307));
#160464=CARTESIAN_POINT('Ctrl Pts',(-186.987770298868,2.77943087677651,
125.581076730611));
#160465=CARTESIAN_POINT('Ctrl Pts',(-186.995178518535,2.64031317554104,
125.507048965188));
#160466=CARTESIAN_POINT('Ctrl Pts',(-187.002586738201,2.49832699064388,
125.438631386499));
#160467=CARTESIAN_POINT('Ctrl Pts',(-187.009994957867,2.35397087991152,
125.376031992747));
#160468=CARTESIAN_POINT('Ctrl Pts',(-187.017407737169,2.20952592040129,
125.313394070112));
#160469=CARTESIAN_POINT('Ctrl Pts',(-187.024820516472,2.06270847584779,
125.256581602402));
#160470=CARTESIAN_POINT('Ctrl Pts',(-187.032233295774,1.91403377665382,
125.205753177825));
#160471=CARTESIAN_POINT('Ctrl Pts',(-187.039656666802,1.76514664407727,
125.15485212721));
#160472=CARTESIAN_POINT('Ctrl Pts',(-187.047080037831,1.61439731357947,
125.109952302834));
#160473=CARTESIAN_POINT('Ctrl Pts',(-187.05450340886,1.46231355706026,125.071161717882));
#160474=CARTESIAN_POINT('Ctrl Pts',(-187.058439458301,1.38167510015412,
125.050594018973));
#160475=CARTESIAN_POINT('Ctrl Pts',(-187.062375507741,1.30066162638929,
125.031742986259));
#160476=CARTESIAN_POINT('Ctrl Pts',(-187.066311557182,1.21935244020638,
125.014618810796));
#160477=CARTESIAN_POINT('Ctrl Pts',(-187.073734823588,1.06600585263888,
124.9823231503));
#160478=CARTESIAN_POINT('Ctrl Pts',(-187.081158089993,0.911143431117751,
124.956075149189));
#160479=CARTESIAN_POINT('Ctrl Pts',(-187.088581356398,0.755283527239422,
124.936015249749));
#160480=CARTESIAN_POINT('Ctrl Pts',(-187.095995849119,0.599607836824118,
124.915979059444));
#160481=CARTESIAN_POINT('Ctrl Pts',(-187.10341034184,0.442937377369268,
124.902116459795));
#160482=CARTESIAN_POINT('Ctrl Pts',(-187.110824834561,0.285802692063943,
124.894517355371));
#160483=CARTESIAN_POINT('Ctrl Pts',(-187.118232180915,0.128819459083885,
124.88692557525));
#160484=CARTESIAN_POINT('Ctrl Pts',(-187.125639527269,-0.0286267386259374,
124.885585289803));
#160485=CARTESIAN_POINT('Ctrl Pts',(-187.133046873623,-0.185998305446971,
124.890534851374));
#160486=CARTESIAN_POINT('Ctrl Pts',(-187.140448695298,-0.343252498615732,
124.895480721376));
#160487=CARTESIAN_POINT('Ctrl Pts',(-187.147850516973,-0.500431800219757,
124.906707085891));
#160488=CARTESIAN_POINT('Ctrl Pts',(-187.155252338649,-0.656996779079823,
124.924200263054));
#160489=CARTESIAN_POINT('Ctrl Pts',(-187.16265025296,-0.813479108507141,
124.941684205705));
#160490=CARTESIAN_POINT('Ctrl Pts',(-187.170048167272,-0.969347390991606,
124.965428331216));
#160491=CARTESIAN_POINT('Ctrl Pts',(-187.177446081583,-1.12406559892257,
124.995366979093));
#160492=CARTESIAN_POINT('Ctrl Pts',(-187.184842766495,-1.27875809549403,
125.02530065171));
#160493=CARTESIAN_POINT('Ctrl Pts',(-187.192239451407,-1.43230053069113,
125.061426732754));
#160494=CARTESIAN_POINT('Ctrl Pts',(-187.199636136319,-1.58416525944525,
125.103628121363));
#160495=CARTESIAN_POINT('Ctrl Pts',(-187.207032493255,-1.73602325435815,
125.145827638718));
#160496=CARTESIAN_POINT('Ctrl Pts',(-187.21442885019,-1.88620333107437,
125.194101828061));
#160497=CARTESIAN_POINT('Ctrl Pts',(-187.221825207126,-2.03419150655014,
125.248283271346));
#160498=CARTESIAN_POINT('Ctrl Pts',(-187.229222696462,-2.18220233939295,
125.302473009948));
#160499=CARTESIAN_POINT('Ctrl Pts',(-187.236620185799,-2.32802025223464,
125.362571674956));
#160500=CARTESIAN_POINT('Ctrl Pts',(-187.244017675135,-2.4711499389764,
125.428363171362));
#160501=CARTESIAN_POINT('Ctrl Pts',(-187.25141775765,-2.61432979960858,
125.494177730874));
#160502=CARTESIAN_POINT('Ctrl Pts',(-187.258817840165,-2.75481921895261,
125.565688939224));
#160503=CARTESIAN_POINT('Ctrl Pts',(-187.26621792268,-2.89214638489867,
125.642634176653));
#160504=CARTESIAN_POINT('Ctrl Pts',(-187.273626142347,-3.02962455618108,
125.719664023281));
#160505=CARTESIAN_POINT('Ctrl Pts',(-187.281034362013,-3.16393320396151,
125.802139649419));
#160506=CARTESIAN_POINT('Ctrl Pts',(-187.28844258168,-3.29462785077745,
125.889754032357));
#160507=CARTESIAN_POINT('Ctrl Pts',(-187.295855360982,-3.42540293796775,
125.977422340486));
#160508=CARTESIAN_POINT('Ctrl Pts',(-187.303268140284,-3.55255929106162,
126.070235488155));
#160509=CARTESIAN_POINT('Ctrl Pts',(-187.310680919586,-3.67568499069044,
126.167845718236));
#160510=CARTESIAN_POINT('Ctrl Pts',(-187.318104290615,-3.79898661809308,
126.26559541839));
#160511=CARTESIAN_POINT('Ctrl Pts',(-187.325527661644,-3.91824580736076,
126.368155647766));
#160512=CARTESIAN_POINT('Ctrl Pts',(-187.332951032672,-4.03308641033856,
126.475140760682));
#160513=CARTESIAN_POINT('Ctrl Pts',(-187.336887082113,-4.09397765360244,
126.531866834624));
#160514=CARTESIAN_POINT('Ctrl Pts',(-187.340823131554,-4.1536273227506,
126.589836320882));
#160515=CARTESIAN_POINT('Ctrl Pts',(-187.344759180995,-4.21198397777087,
126.648988006897));
#160516=CARTESIAN_POINT('Ctrl Pts',(-187.352082400964,-4.32055949944319,
126.759042724129));
#160517=CARTESIAN_POINT('Ctrl Pts',(-187.359405620933,-4.42500455681407,
126.873544452405));
#160518=CARTESIAN_POINT('Ctrl Pts',(-187.366728840903,-4.52492539990628,
126.992145947878));
#160519=CARTESIAN_POINT('Ctrl Pts',(-187.374043222144,-4.62472564397862,
127.1106042978));
#160520=CARTESIAN_POINT('Ctrl Pts',(-187.381357603385,-4.72001229335793,
127.233152278661));
#160521=CARTESIAN_POINT('Ctrl Pts',(-187.388671984626,-4.81042708213411,
127.3594046164));
#160522=CARTESIAN_POINT('Ctrl Pts',(-187.395978017208,-4.90073867116098,
127.485512849288));
#160523=CARTESIAN_POINT('Ctrl Pts',(-187.403284049789,-4.98618925122516,
127.615316708677));
#160524=CARTESIAN_POINT('Ctrl Pts',(-187.410590082371,-5.06645997052641,
127.748396951297));
#160525=CARTESIAN_POINT('Ctrl Pts',(-187.417891395085,-5.14667883307661,
127.881391220987));
#160526=CARTESIAN_POINT('Ctrl Pts',(-187.4251927078,-5.22172429356674,128.017657336095));
#160527=CARTESIAN_POINT('Ctrl Pts',(-187.432494020514,-5.29131999812529,
128.156745985498));
#160528=CARTESIAN_POINT('Ctrl Pts',(-187.439792150053,-5.36088536083589,
128.295773996006));
#160529=CARTESIAN_POINT('Ctrl Pts',(-187.447090279593,-5.42500552334415,
128.437621749531));
#160530=CARTESIAN_POINT('Ctrl Pts',(-187.454388409132,-5.48344955540227,
128.581814434501));
#160531=CARTESIAN_POINT('Ctrl Pts',(-187.461684889562,-5.54188038124945,
128.725974537204));
#160532=CARTESIAN_POINT('Ctrl Pts',(-187.468981369991,-5.59463748570317,
128.87247816067));
#160533=CARTESIAN_POINT('Ctrl Pts',(-187.47627785042,-5.64153778312993,
129.020829848553));
#160534=CARTESIAN_POINT('Ctrl Pts',(-187.483576690867,-5.68845325027215,
129.169229520201));
#160535=CARTESIAN_POINT('Ctrl Pts',(-187.490875531314,-5.7295080036463,
129.319478085701));
#160536=CARTESIAN_POINT('Ctrl Pts',(-187.498174371761,-5.76456856275173,
129.471064008467));
#160537=CARTESIAN_POINT('Ctrl Pts',(-187.505474224208,-5.79963398307961,
129.62267094895));
#160538=CARTESIAN_POINT('Ctrl Pts',(-187.512774076655,-5.82870347565599,
129.775615239507));
#160539=CARTESIAN_POINT('Ctrl Pts',(-187.520073929102,-5.85169470676966,
129.929375119821));
#160540=CARTESIAN_POINT('Ctrl Pts',(-187.527380321913,-5.87470653706738,
130.083272762574));
#160541=CARTESIAN_POINT('Ctrl Pts',(-187.534686714723,-5.89162917731749,
130.237987073307));
#160542=CARTESIAN_POINT('Ctrl Pts',(-187.541993107533,-5.9024321476053,
130.392990582907));
#160543=CARTESIAN_POINT('Ctrl Pts',(-187.54853700762,-5.91210772350591,
130.531817977784));
#160544=CARTESIAN_POINT('Ctrl Pts',(-187.555080907706,-5.91687497723714,
130.670877114353));
#160545=CARTESIAN_POINT('Ctrl Pts',(-187.561624807792,-5.91674750900767,
130.809789904034));
#160546=CARTESIAN_POINT('',(-189.311624807792,-5.92158926949562,130.802089018337));
#160547=CARTESIAN_POINT('Ctrl Pts',(-187.561624807792,-5.91744066498834,
130.809790540083));
#160548=CARTESIAN_POINT('Ctrl Pts',(-187.582152140131,-5.92149194206913,
131.245596366776));
#160549=CARTESIAN_POINT('Ctrl Pts',(-187.695495347076,-5.67831340457064,
133.64744955503));
#160550=CARTESIAN_POINT('Ctrl Pts',(-187.90165442862,-2.39945118657061,
137.378567378342));
#160551=CARTESIAN_POINT('Ctrl Pts',(-188.180102052435,4.23410436286723,
136.376606194958));
#160552=CARTESIAN_POINT('Ctrl Pts',(-188.458549676247,6.97672485032798,
130.254023545258));
#160553=CARTESIAN_POINT('Ctrl Pts',(-188.73699730006,3.3080760322958,124.637173779559));
#160554=CARTESIAN_POINT('Ctrl Pts',(-189.015444923873,-3.40053305091948,
124.687667434156));
#160555=CARTESIAN_POINT('Ctrl Pts',(-189.20698742645,-5.86572937063765,
128.589015218929));
#160556=CARTESIAN_POINT('Ctrl Pts',(-189.305714054423,-5.92609167912231,
130.677041554188));
#160557=CARTESIAN_POINT('Ctrl Pts',(-189.311624807792,-5.92547957657923,
130.802087525964));
#160558=CARTESIAN_POINT('',(-191.061624793292,-5.91313729896144,130.80003214728));
#160559=CARTESIAN_POINT('Ctrl Pts',(-189.311624807792,-5.91674956464851,
130.802090874911));
#160560=CARTESIAN_POINT('Ctrl Pts',(-189.318977448973,-5.91680914766334,
130.957411468767));
#160561=CARTESIAN_POINT('Ctrl Pts',(-189.326330090154,-5.91074854494049,
131.112981837623));
#160562=CARTESIAN_POINT('Ctrl Pts',(-189.333682731335,-5.89853497471983,
131.268274094959));
#160563=CARTESIAN_POINT('Ctrl Pts',(-189.341027006048,-5.88633530215123,
131.42338964739));
#160564=CARTESIAN_POINT('Ctrl Pts',(-189.348371280761,-5.86799662359575,
131.578227341974));
#160565=CARTESIAN_POINT('Ctrl Pts',(-189.355715555474,-5.8435381292413,
131.732257537813));
#160566=CARTESIAN_POINT('Ctrl Pts',(-189.363053149278,-5.81910188418644,
131.886147616115));
#160567=CARTESIAN_POINT('Ctrl Pts',(-189.370390743082,-5.78855696232474,
132.039231283816));
#160568=CARTESIAN_POINT('Ctrl Pts',(-189.377728336886,-5.75197447447406,
132.190982486533));
#160569=CARTESIAN_POINT('Ctrl Pts',(-189.385060929245,-5.71541692194747,
132.342630252726));
#160570=CARTESIAN_POINT('Ctrl Pts',(-189.392393521605,-5.67283008434618,
132.492946992982));
#160571=CARTESIAN_POINT('Ctrl Pts',(-189.399726113965,-5.62433638296606,
132.641415546996));
#160572=CARTESIAN_POINT('Ctrl Pts',(-189.407056104548,-5.57585988828992,
132.789831420881));
#160573=CARTESIAN_POINT('Ctrl Pts',(-189.414386095132,-5.52148081560047,
132.936400051107));
#160574=CARTESIAN_POINT('Ctrl Pts',(-189.421716085716,-5.46137178798303,
133.080618238294));
#160575=CARTESIAN_POINT('Ctrl Pts',(-189.429044866575,-5.40127268062225,
133.224812624041));
#160576=CARTESIAN_POINT('Ctrl Pts',(-189.436373647433,-5.33544564582625,
133.366656986859));
#160577=CARTESIAN_POINT('Ctrl Pts',(-189.443702428292,-5.26411181390032,
133.505667222388));
#160578=CARTESIAN_POINT('Ctrl Pts',(-189.45103151263,-5.19277502809146,
133.644683214231));
#160579=CARTESIAN_POINT('Ctrl Pts',(-189.458360596969,-5.11593116510898,
133.780864506177));
#160580=CARTESIAN_POINT('Ctrl Pts',(-189.465689681307,-5.03384764105057,
133.913750990162));
#160581=CARTESIAN_POINT('Ctrl Pts',(-189.473020582319,-4.95174377079516,
134.046670412968));
#160582=CARTESIAN_POINT('Ctrl Pts',(-189.480351483332,-4.86439785503814,
134.176293078574));
#160583=CARTESIAN_POINT('Ctrl Pts',(-189.487682384344,-4.77212086708803,
134.302187513283));
#160584=CARTESIAN_POINT('Ctrl Pts',(-189.495020896959,-4.6797480688371,
134.428212662962));
#160585=CARTESIAN_POINT('Ctrl Pts',(-189.502359409575,-4.5824341979447,
134.550501542638));
#160586=CARTESIAN_POINT('Ctrl Pts',(-189.509697922191,-4.48053120714239,
134.668654946978));
#160587=CARTESIAN_POINT('Ctrl Pts',(-189.517040396452,-4.37857320471192,
134.78687213562));
#160588=CARTESIAN_POINT('Ctrl Pts',(-189.524382870713,-4.27202140698691,
134.900949123779));
#160589=CARTESIAN_POINT('Ctrl Pts',(-189.531725344974,-4.16126441642406,
135.010523835881));
#160590=CARTESIAN_POINT('Ctrl Pts',(-189.539078893906,-4.05034037083163,
135.120263819778));
#160591=CARTESIAN_POINT('Ctrl Pts',(-189.546432442839,-3.93519874240669,
135.225487704928));
#160592=CARTESIAN_POINT('Ctrl Pts',(-189.553785991771,-3.81626167847011,
135.325873347167));
#160593=CARTESIAN_POINT('Ctrl Pts',(-189.559970718347,-3.71622926868426,
135.410303022565));
#160594=CARTESIAN_POINT('Ctrl Pts',(-189.566155444922,-3.61351273278213,
135.491310933321));
#160595=CARTESIAN_POINT('Ctrl Pts',(-189.572340171498,-3.50837810462016,
135.568729792758));
#160596=CARTESIAN_POINT('Ctrl Pts',(-189.579763437904,-3.38218944555196,
135.661652383818));
#160597=CARTESIAN_POINT('Ctrl Pts',(-189.587186704309,-3.25211571553351,
135.749698689375));
#160598=CARTESIAN_POINT('Ctrl Pts',(-189.594609970715,-3.11857050878932,
135.832526142309));
#160599=CARTESIAN_POINT('Ctrl Pts',(-189.602024463436,-2.98518314138887,
135.915255700071));
#160600=CARTESIAN_POINT('Ctrl Pts',(-189.609438956157,-2.84833277843893,
135.992778488313));
#160601=CARTESIAN_POINT('Ctrl Pts',(-189.616853448878,-2.70846504719477,
136.064792885985));
#160602=CARTESIAN_POINT('Ctrl Pts',(-189.624260795232,-2.5687321257355,
136.13673787347));
#160603=CARTESIAN_POINT('Ctrl Pts',(-189.631668141586,-2.42598795540314,
136.203184870211));
#160604=CARTESIAN_POINT('Ctrl Pts',(-189.63907548794,-2.28070593937386,
136.263876253646));
#160605=CARTESIAN_POINT('Ctrl Pts',(-189.646477309616,-2.13553228015454,
136.324522371158));
#160606=CARTESIAN_POINT('Ctrl Pts',(-189.653879131291,-1.98782488706824,
136.379421279541));
#160607=CARTESIAN_POINT('Ctrl Pts',(-189.661280952967,-1.83808039076475,
136.428361954656));
#160608=CARTESIAN_POINT('Ctrl Pts',(-189.668678867278,-1.68841494341483,
136.477276794369));
#160609=CARTESIAN_POINT('Ctrl Pts',(-189.67607678159,-1.53671488843013,
136.520239549164));
#160610=CARTESIAN_POINT('Ctrl Pts',(-189.683474695901,-1.38349529252278,
136.557087913212));
#160611=CARTESIAN_POINT('Ctrl Pts',(-189.690871380814,-1.23030115893236,
136.59393015373));
#160612=CARTESIAN_POINT('Ctrl Pts',(-189.698268065726,-1.07558834819108,
136.62465993296));
#160613=CARTESIAN_POINT('Ctrl Pts',(-189.705664750638,-0.919885608475016,
136.649165236184));
#160614=CARTESIAN_POINT('Ctrl Pts',(-189.713061107574,-0.7641897727816,
136.673669452817));
#160615=CARTESIAN_POINT('Ctrl Pts',(-189.72045746451,-0.607504464148897,
136.691949684189));
#160616=CARTESIAN_POINT('Ctrl Pts',(-189.727853821445,-0.450366841788114,
136.703945371624));
#160617=CARTESIAN_POINT('Ctrl Pts',(-189.735251310782,-0.293205161256196,
136.71594289563));
#160618=CARTESIAN_POINT('Ctrl Pts',(-189.742648800119,-0.135591401348304,
136.721653931456));
#160619=CARTESIAN_POINT('Ctrl Pts',(-189.750046289455,0.021934111525369,
136.721069961217));
#160620=CARTESIAN_POINT('Ctrl Pts',(-189.75744637197,0.179514844723607,
136.720485786269));
#160621=CARTESIAN_POINT('Ctrl Pts',(-189.764846454486,0.337006896234077,
136.713602213106));
#160622=CARTESIAN_POINT('Ctrl Pts',(-189.772246537001,0.493872048296028,
136.700462801417));
#160623=CARTESIAN_POINT('Ctrl Pts',(-189.779654756667,0.650909689718572,
136.687308941594));
#160624=CARTESIAN_POINT('Ctrl Pts',(-189.787062976334,0.807318682811136,
136.667885536733));
#160625=CARTESIAN_POINT('Ctrl Pts',(-189.794471196001,0.962567293055188,
136.642287884057));
#160626=CARTESIAN_POINT('Ctrl Pts',(-189.801883975303,1.11791145622882,
136.616674476453));
#160627=CARTESIAN_POINT('Ctrl Pts',(-189.809296754605,1.27209344867101,
136.584879323986));
#160628=CARTESIAN_POINT('Ctrl Pts',(-189.816709533907,1.4245942930246,136.547048286487));
#160629=CARTESIAN_POINT('Ctrl Pts',(-189.824132904936,1.57731303773595,
136.509163194228));
#160630=CARTESIAN_POINT('Ctrl Pts',(-189.831556275965,1.72834547933129,
136.465225096164));
#160631=CARTESIAN_POINT('Ctrl Pts',(-189.838979646994,1.87718950102327,
136.41542915571));
#160632=CARTESIAN_POINT('Ctrl Pts',(-189.842915696433,1.95611017275407,
136.389026153255));
#160633=CARTESIAN_POINT('Ctrl Pts',(-189.846851745872,2.03441595105685,
136.360977098998));
#160634=CARTESIAN_POINT('Ctrl Pts',(-189.850787795312,2.11203465861468,
136.331316394783));
#160635=CARTESIAN_POINT('Ctrl Pts',(-189.858211061717,2.25842111873141,
136.275377232289));
#160636=CARTESIAN_POINT('Ctrl Pts',(-189.865634328123,2.40280499749717,
136.213533698149));
#160637=CARTESIAN_POINT('Ctrl Pts',(-189.873057594528,2.54467452571146,
136.145948595003));
#160638=CARTESIAN_POINT('Ctrl Pts',(-189.880472087249,2.68637637592454,
136.078443371836));
#160639=CARTESIAN_POINT('Ctrl Pts',(-189.88788657997,2.82556945715901,136.005210246327));
#160640=CARTESIAN_POINT('Ctrl Pts',(-189.895301072691,2.96175913466819,
135.926461103764));
#160641=CARTESIAN_POINT('Ctrl Pts',(-189.902708419045,3.09781754743913,
135.847787862589));
#160642=CARTESIAN_POINT('Ctrl Pts',(-189.910115765399,3.23087799845622,
135.763609374162));
#160643=CARTESIAN_POINT('Ctrl Pts',(-189.917523111753,3.36046785658173,
135.674184674694));
#160644=CARTESIAN_POINT('Ctrl Pts',(-189.924924933428,3.48996106170153,
135.584826671541));
#160645=CARTESIAN_POINT('Ctrl Pts',(-189.932326755103,3.61598852205761,
135.49023045941));
#160646=CARTESIAN_POINT('Ctrl Pts',(-189.939728576779,3.73810425606627,
135.390699804028));
#160647=CARTESIAN_POINT('Ctrl Pts',(-189.94712649109,3.86015552612914,135.291221690105));
#160648=CARTESIAN_POINT('Ctrl Pts',(-189.954524405402,3.97829889370356,
135.18681455587));
#160649=CARTESIAN_POINT('Ctrl Pts',(-189.961922319713,4.09211940015992,
135.077824011271));
#160650=CARTESIAN_POINT('Ctrl Pts',(-189.969319004625,4.20592099171351,
134.968851578922));
#160651=CARTESIAN_POINT('Ctrl Pts',(-189.976715689538,4.31540087856674,
134.855297505843));
#160652=CARTESIAN_POINT('Ctrl Pts',(-189.98411237445,4.42017901826155,134.73754609616));
#160653=CARTESIAN_POINT('Ctrl Pts',(-189.991508731385,4.52495251198384,
134.619799907697));
#160654=CARTESIAN_POINT('Ctrl Pts',(-189.998905088321,4.62502442492598,
134.497857031564));
#160655=CARTESIAN_POINT('Ctrl Pts',(-190.006301445256,4.72005345968584,
134.372136661575));
#160656=CARTESIAN_POINT('Ctrl Pts',(-190.013698934593,4.81509704363352,
134.246397043477));
#160657=CARTESIAN_POINT('Ctrl Pts',(-190.02109642393,4.90509598697833,134.11687907778));
#160658=CARTESIAN_POINT('Ctrl Pts',(-190.028493913266,4.98975106375987,
133.984032752269));
#160659=CARTESIAN_POINT('Ctrl Pts',(-190.035893995781,5.07443581624746,
133.851139857685));
#160660=CARTESIAN_POINT('Ctrl Pts',(-190.043294078296,5.15377277199098,
133.71491659491));
#160661=CARTESIAN_POINT('Ctrl Pts',(-190.050694160811,5.22750765914304,
133.575839326866));
#160662=CARTESIAN_POINT('Ctrl Pts',(-190.058102380478,5.30132362538356,
133.436609129067));
#160663=CARTESIAN_POINT('Ctrl Pts',(-190.065510600145,5.36952504604308,
133.294518988678));
#160664=CARTESIAN_POINT('Ctrl Pts',(-190.072918819811,5.43190468187914,
133.150067779485));
#160665=CARTESIAN_POINT('Ctrl Pts',(-190.080331599113,5.49432271134037,
133.005527662983));
#160666=CARTESIAN_POINT('Ctrl Pts',(-190.087744378416,5.55091168210434,
132.858623929535));
#160667=CARTESIAN_POINT('Ctrl Pts',(-190.095157157718,5.60151379023981,
132.709872050293));
#160668=CARTESIAN_POINT('Ctrl Pts',(-190.102580528747,5.65218820104032,
132.56090762739));
#160669=CARTESIAN_POINT('Ctrl Pts',(-190.110003899775,5.69685855860319,
132.410090141567));
#160670=CARTESIAN_POINT('Ctrl Pts',(-190.117427270804,5.73541765304766,
132.25794752849));
#160671=CARTESIAN_POINT('Ctrl Pts',(-190.121363320244,5.7558626101311,132.17727786444));
#160672=CARTESIAN_POINT('Ctrl Pts',(-190.125299369684,5.77459033229658,
132.096235796439));
#160673=CARTESIAN_POINT('Ctrl Pts',(-190.129235419124,5.79159074918677,
132.014900644345));
#160674=CARTESIAN_POINT('Ctrl Pts',(-190.13665868553,5.82365300488208,131.861505085854));
#160675=CARTESIAN_POINT('Ctrl Pts',(-190.144081951935,5.84966530135562,
131.706602898674));
#160676=CARTESIAN_POINT('Ctrl Pts',(-190.15150521834,5.86948798532478,131.550712647528));
#160677=CARTESIAN_POINT('Ctrl Pts',(-190.158919711061,5.88928724052766,
131.395006645713));
#160678=CARTESIAN_POINT('Ctrl Pts',(-190.166334203782,5.90291139835537,
131.238315271165));
#160679=CARTESIAN_POINT('Ctrl Pts',(-190.173748696503,5.9102713617377,131.081169203277));
#160680=CARTESIAN_POINT('Ctrl Pts',(-190.181156042857,5.91762423131021,
130.924174598686));
#160681=CARTESIAN_POINT('Ctrl Pts',(-190.18856338921,5.91872490889553,130.766726543612));
#160682=CARTESIAN_POINT('Ctrl Pts',(-190.195970735564,5.91353586032059,
130.609362691417));
#160683=CARTESIAN_POINT('Ctrl Pts',(-190.203372557239,5.90835068193385,
130.45211620712));
#160684=CARTESIAN_POINT('Ctrl Pts',(-190.210774378915,5.8968851302798,130.294954172144));
#160685=CARTESIAN_POINT('Ctrl Pts',(-190.21817620059,5.8791537081288,130.138415996223));
#160686=CARTESIAN_POINT('Ctrl Pts',(-190.225574114901,5.86143164625758,
129.981960455587));
#160687=CARTESIAN_POINT('Ctrl Pts',(-190.232972029212,5.83745034325019,
129.826128488115));
#160688=CARTESIAN_POINT('Ctrl Pts',(-190.240369943524,5.80727627526828,
129.671456020874));
#160689=CARTESIAN_POINT('Ctrl Pts',(-190.247766628436,5.77710722166901,
129.51680925739));
#160690=CARTESIAN_POINT('Ctrl Pts',(-190.255163313348,5.74074751701105,
129.36332197774));
#160691=CARTESIAN_POINT('Ctrl Pts',(-190.26255999826,5.69831506500718,129.211521648174));
#160692=CARTESIAN_POINT('Ctrl Pts',(-190.269956355195,5.6558844945027,129.059728049594));
#160693=CARTESIAN_POINT('Ctrl Pts',(-190.277352712131,5.60738181255083,
128.909621611885));
#160694=CARTESIAN_POINT('Ctrl Pts',(-190.284749069066,5.55297521919776,
128.761716062712));
#160695=CARTESIAN_POINT('Ctrl Pts',(-190.292146558402,5.49856029605635,
128.613787868822));
#160696=CARTESIAN_POINT('Ctrl Pts',(-190.299544047739,5.43823979060307,
128.468061584774));
#160697=CARTESIAN_POINT('Ctrl Pts',(-190.306941537075,5.37223055136691,
128.325032187232));
#160698=CARTESIAN_POINT('Ctrl Pts',(-190.31434161959,5.30619817269379,128.181952650957));
#160699=CARTESIAN_POINT('Ctrl Pts',(-190.321741702105,5.23447324617382,
128.041572222184));
#160700=CARTESIAN_POINT('Ctrl Pts',(-190.32914178462,5.15731910927882,127.904362312813));
#160701=CARTESIAN_POINT('Ctrl Pts',(-190.336550004286,5.08008013347921,
127.767001527043));
#160702=CARTESIAN_POINT('Ctrl Pts',(-190.343958223952,4.99740020795088,
127.632818548654));
#160703=CARTESIAN_POINT('Ctrl Pts',(-190.351366443619,4.90958703146701,
127.502257387358));
#160704=CARTESIAN_POINT('Ctrl Pts',(-190.358779222921,4.82171980743826,
127.371615867845));
#160705=CARTESIAN_POINT('Ctrl Pts',(-190.366192002223,4.72871325692401,
127.244600907808));
#160706=CARTESIAN_POINT('Ctrl Pts',(-190.373604781525,4.63091576352256,
127.121623896911));
#160707=CARTESIAN_POINT('Ctrl Pts',(-190.381028152553,4.53297853247616,
126.998471170694));
#160708=CARTESIAN_POINT('Ctrl Pts',(-190.388451523582,4.43023692968165,
126.879368198737));
#160709=CARTESIAN_POINT('Ctrl Pts',(-190.395874894611,4.32307717280776,
126.764690541873));
#160710=CARTESIAN_POINT('Ctrl Pts',(-190.399810944053,4.26625849842815,
126.703885696528));
#160711=CARTESIAN_POINT('Ctrl Pts',(-190.403746993495,4.20819830263757,
126.644324316123));
#160712=CARTESIAN_POINT('Ctrl Pts',(-190.407683042937,4.14895787620481,
126.586057747456));
#160713=CARTESIAN_POINT('Ctrl Pts',(-190.415106309343,4.03723228082388,
126.476168817428));
#160714=CARTESIAN_POINT('Ctrl Pts',(-190.422529575748,3.92096896531795,
126.370555519829));
#160715=CARTESIAN_POINT('Ctrl Pts',(-190.429952842154,3.80052872686658,
126.269615645822));
#160716=CARTESIAN_POINT('Ctrl Pts',(-190.437367334875,3.68023083877513,
126.168795074362));
#160717=CARTESIAN_POINT('Ctrl Pts',(-190.444781827596,3.55576613772917,
126.072637169181));
#160718=CARTESIAN_POINT('Ctrl Pts',(-190.452196320317,3.42753294018989,
125.981503735342));
#160719=CARTESIAN_POINT('Ctrl Pts',(-190.459603666671,3.29942333863392,
125.890458139337));
#160720=CARTESIAN_POINT('Ctrl Pts',(-190.467011013024,3.16755277385676,
125.804427588461));
#160721=CARTESIAN_POINT('Ctrl Pts',(-190.474418359378,3.03235330072144,
125.72373427605));
#160722=CARTESIAN_POINT('Ctrl Pts',(-190.481820181054,2.89725466445357,
125.643101147756));
#160723=CARTESIAN_POINT('Ctrl Pts',(-190.489222002729,2.75883238263387,
125.567797522283));
#160724=CARTESIAN_POINT('Ctrl Pts',(-190.496623824405,2.61754811504931,
125.498102762175));
#160725=CARTESIAN_POINT('Ctrl Pts',(-190.504021738716,2.47633843033066,
125.428444793389));
#160726=CARTESIAN_POINT('Ctrl Pts',(-190.511419653028,2.33227010265108,
125.364389957968));
#160727=CARTESIAN_POINT('Ctrl Pts',(-190.518817567339,2.18582995461846,
125.306172009307));
#160728=CARTESIAN_POINT('Ctrl Pts',(-190.526214252251,2.03941414228153,
125.247963735412));
#160729=CARTESIAN_POINT('Ctrl Pts',(-190.533610937163,1.89062763842013,
125.195590560915));
#160730=CARTESIAN_POINT('Ctrl Pts',(-190.541007622076,1.73997794516578,
125.149238398477));
#160731=CARTESIAN_POINT('Ctrl Pts',(-190.548403979011,1.58933493187669,
125.102888291342));
#160732=CARTESIAN_POINT('Ctrl Pts',(-190.555800335947,1.43682925025374,
125.0625587752));
#160733=CARTESIAN_POINT('Ctrl Pts',(-190.563196692882,1.28298403016603,
125.028386020943));
#160734=CARTESIAN_POINT('Ctrl Pts',(-190.570594182219,1.12911525598238,
124.994208034749));
#160735=CARTESIAN_POINT('Ctrl Pts',(-190.577991671555,0.97390689941849,
124.966188768263));
#160736=CARTESIAN_POINT('Ctrl Pts',(-190.585389160892,0.817892610288261,
124.944413327655));
#160737=CARTESIAN_POINT('Ctrl Pts',(-190.592789243407,0.661823630589273,
124.9226302537));
#160738=CARTESIAN_POINT('Ctrl Pts',(-190.600189325922,0.50494852531532,
124.907095415004));
#160739=CARTESIAN_POINT('Ctrl Pts',(-190.607589408437,0.347806246985612,
124.897842067942));
#160740=CARTESIAN_POINT('Ctrl Pts',(-190.614997628104,0.190491174567385,
124.888578545873));
#160741=CARTESIAN_POINT('Ctrl Pts',(-190.62240584777,0.0329087152680474,
124.885610331419));
#160742=CARTESIAN_POINT('Ctrl Pts',(-190.629814067437,-0.124401254264218,
124.888918546982));
#160743=CARTESIAN_POINT('Ctrl Pts',(-190.637226846739,-0.281808045457423,
124.892228798696));
#160744=CARTESIAN_POINT('Ctrl Pts',(-190.644639626041,-0.438941640954478,
124.901823155316));
#160745=CARTESIAN_POINT('Ctrl Pts',(-190.652052405343,-0.59526761713485,
124.917630878017));
#160746=CARTESIAN_POINT('Ctrl Pts',(-190.659475776372,-0.75181695920117,
124.933461187533));
#160747=CARTESIAN_POINT('Ctrl Pts',(-190.666899147401,-0.907556008596329,
124.955522542167));
#160748=CARTESIAN_POINT('Ctrl Pts',(-190.67432251843,-1.06196003527188,
124.983693005858));
#160749=CARTESIAN_POINT('Ctrl Pts',(-190.67825856787,-1.14382875507758,
124.998629661646));
#160750=CARTESIAN_POINT('Ctrl Pts',(-190.68219461731,-1.22532238526077,
125.015282967731));
#160751=CARTESIAN_POINT('Ctrl Pts',(-190.68613066675,-1.3063645971489,125.033629112651));
#160752=CARTESIAN_POINT('Ctrl Pts',(-190.693553933156,-1.45920767955153,
125.068229369412));
#160753=CARTESIAN_POINT('Ctrl Pts',(-190.700977199561,-1.61090629986719,
125.108958422396));
#160754=CARTESIAN_POINT('Ctrl Pts',(-190.708400465967,-1.76093076543627,
125.155727738555));
#160755=CARTESIAN_POINT('Ctrl Pts',(-190.715814958688,-1.91077791454581,
125.202441777267));
#160756=CARTESIAN_POINT('Ctrl Pts',(-190.723229451409,-2.05895449464387,
125.255181758744));
#160757=CARTESIAN_POINT('Ctrl Pts',(-190.73064394413,-2.20494080910687,
125.313808132539));
#160758=CARTESIAN_POINT('Ctrl Pts',(-190.738051290484,-2.35078641646454,
125.372378000029));
#160759=CARTESIAN_POINT('Ctrl Pts',(-190.745458636838,-2.49444561681005,
125.436822826783));
#160760=CARTESIAN_POINT('Ctrl Pts',(-190.752865983192,-2.63541380355637,
125.506953266179));
#160761=CARTESIAN_POINT('Ctrl Pts',(-190.760267804868,-2.7762768509102,
125.577031399648));
#160762=CARTESIAN_POINT('Ctrl Pts',(-190.767669626543,-2.91445254820704,
125.652786536705));
#160763=CARTESIAN_POINT('Ctrl Pts',(-190.775071448219,-3.04945632143417,
125.733981272175));
#160764=CARTESIAN_POINT('Ctrl Pts',(-190.78246936253,-3.18438882722145,
125.815133145578));
#160765=CARTESIAN_POINT('Ctrl Pts',(-190.789867276842,-3.31615242456538,
125.901718706713));
#160766=CARTESIAN_POINT('Ctrl Pts',(-190.797265191153,-3.44428731060594,
125.993454727352));
#160767=CARTESIAN_POINT('Ctrl Pts',(-190.804661876065,-3.5724009029514,
126.085175503127));
#160768=CARTESIAN_POINT('Ctrl Pts',(-190.812058560978,-3.69688667759057,
126.182044822578));
#160769=CARTESIAN_POINT('Ctrl Pts',(-190.81945524589,-3.81731390363919,
126.283736200123));
#160770=CARTESIAN_POINT('Ctrl Pts',(-190.826851602826,-3.9377357898191,
126.385423068566));
#160771=CARTESIAN_POINT('Ctrl Pts',(-190.834247959761,-4.05409920001659,
126.491931329125));
#160772=CARTESIAN_POINT('Ctrl Pts',(-190.841644316697,-4.16600680533306,
126.602894461518));
#160773=CARTESIAN_POINT('Ctrl Pts',(-190.849041806034,-4.27793154398928,
126.713874582649));
#160774=CARTESIAN_POINT('Ctrl Pts',(-190.85643929537,-4.38539885432859,
126.829310670813));
#160775=CARTESIAN_POINT('Ctrl Pts',(-190.863836784707,-4.48804868336094,
126.948799753271));
#160776=CARTESIAN_POINT('Ctrl Pts',(-190.871236867222,-4.59073449613216,
127.068330722442));
#160777=CARTESIAN_POINT('Ctrl Pts',(-190.878636949737,-4.68859922218421,
127.19191723167));
#160778=CARTESIAN_POINT('Ctrl Pts',(-190.886037032252,-4.78132356498639,
127.319123820818));
#160779=CARTESIAN_POINT('Ctrl Pts',(-190.893445251919,-4.87414986773537,
127.446470286688));
#160780=CARTESIAN_POINT('Ctrl Pts',(-190.900853471586,-4.9618242790364,
127.57744448025));
#160781=CARTESIAN_POINT('Ctrl Pts',(-190.908261691252,-5.04407086463152,
127.711581984189));
#160782=CARTESIAN_POINT('Ctrl Pts',(-190.915674470554,-5.12636807162771,
127.845802047523));
#160783=CARTESIAN_POINT('Ctrl Pts',(-190.923087249857,-5.20323061424422,
127.98318897578));
#160784=CARTESIAN_POINT('Ctrl Pts',(-190.930500029159,-5.27442913803752,
128.123254907169));
#160785=CARTESIAN_POINT('Ctrl Pts',(-190.937923400188,-5.3457293936204,
128.26352097133));
#160786=CARTESIAN_POINT('Ctrl Pts',(-190.945346771217,-5.41134931149239,
128.406473345405));
#160787=CARTESIAN_POINT('Ctrl Pts',(-190.952770142245,-5.47110785050535,
128.551604649726));
#160788=CARTESIAN_POINT('Ctrl Pts',(-190.956706191685,-5.50279326176559,
128.628556749628));
#160789=CARTESIAN_POINT('Ctrl Pts',(-190.960642241124,-5.53283166141068,
128.706121167425));
#160790=CARTESIAN_POINT('Ctrl Pts',(-190.964578290564,-5.56120182518544,
128.784220814965));
#160791=CARTESIAN_POINT('Ctrl Pts',(-190.973177240122,-5.62318112981626,
128.954842383627));
#160792=CARTESIAN_POINT('Ctrl Pts',(-190.98177618968,-5.67735007641122,
129.128443962409));
#160793=CARTESIAN_POINT('Ctrl Pts',(-190.990375139238,-5.72345280997876,
129.304354452763));
#160794=CARTESIAN_POINT('Ctrl Pts',(-190.998941388787,-5.76938022448008,
129.479595992265));
#160795=CARTESIAN_POINT('Ctrl Pts',(-191.007507638336,-5.80730256775135,
129.657128801406));
#160796=CARTESIAN_POINT('Ctrl Pts',(-191.016073887885,-5.83701346337239,
129.836267444927));
#160797=CARTESIAN_POINT('Ctrl Pts',(-191.024576231815,-5.8665027108652,
130.014069684944));
#160798=CARTESIAN_POINT('Ctrl Pts',(-191.033078575745,-5.88790249831863,
130.19345375926));
#160799=CARTESIAN_POINT('Ctrl Pts',(-191.041580919675,-5.90105816818685,
130.373729617549));
#160800=CARTESIAN_POINT('Ctrl Pts',(-191.048262204323,-5.91139611450565,
130.515393414546));
#160801=CARTESIAN_POINT('Ctrl Pts',(-191.054943488972,-5.9166441504911,
130.657607486087));
#160802=CARTESIAN_POINT('Ctrl Pts',(-191.06162477362,-5.91674841448608,
130.80002908476));
#160803=CARTESIAN_POINT('',(-192.811624807792,-5.9097125884178,130.808293688258));
#160804=CARTESIAN_POINT('Ctrl Pts',(-191.061624807792,-5.91047567621124,
130.800034404554));
#160805=CARTESIAN_POINT('Ctrl Pts',(-191.12209184332,-5.90179870917759,
132.087620467717));
#160806=CARTESIAN_POINT('Ctrl Pts',(-191.275374753451,-4.85401633074215,
135.36448301843));
#160807=CARTESIAN_POINT('Ctrl Pts',(-191.52147353819,0.560953822592365,
137.780239869629));
#160808=CARTESIAN_POINT('Ctrl Pts',(-191.799921162001,6.17221402509524,
134.103047410633));
#160809=CARTESIAN_POINT('Ctrl Pts',(-192.078368785815,6.11151106794695,
127.394522938632));
#160810=CARTESIAN_POINT('Ctrl Pts',(-192.356816409627,0.434628003272854,
123.819472713731));
#160811=CARTESIAN_POINT('Ctrl Pts',(-192.601235083619,-4.89907710821755,
126.315663527414));
#160812=CARTESIAN_POINT('Ctrl Pts',(-192.752837883008,-5.902105290066,129.556078088356));
#160813=CARTESIAN_POINT('Ctrl Pts',(-192.811624807792,-5.9097125884178,
130.808293688258));
#160814=CARTESIAN_POINT('',(-194.561624807792,-5.92485436802142,130.807214191615));
#160815=CARTESIAN_POINT('Ctrl Pts',(-192.811624807792,-5.9097125884178,
130.808293688258));
#160816=CARTESIAN_POINT('Ctrl Pts',(-192.845653757612,-5.91411609097954,
131.533141636508));
#160817=CARTESIAN_POINT('Ctrl Pts',(-192.972498582038,-5.45424420182938,
134.22966001815));
#160818=CARTESIAN_POINT('Ctrl Pts',(-193.192159281066,-1.42141332660588,
137.656888960118));
#160819=CARTESIAN_POINT('Ctrl Pts',(-193.47060690488,4.99691754528912,135.704194857198));
#160820=CARTESIAN_POINT('Ctrl Pts',(-193.749054528692,6.82332530604844,
129.248792458293));
#160821=CARTESIAN_POINT('Ctrl Pts',(-194.027502152505,2.37943044852847,
124.222881204015));
#160822=CARTESIAN_POINT('Ctrl Pts',(-194.298358912204,-4.07028890202498,
125.217162883923));
#160823=CARTESIAN_POINT('Ctrl Pts',(-194.476399797301,-5.91415325007818,
129.003717447568));
#160824=CARTESIAN_POINT('Ctrl Pts',(-194.561624807792,-5.92485436802142,
130.807214191615));
#160825=CARTESIAN_POINT('',(-196.311624807792,-5.91811478187531,130.799043979201));
#160826=CARTESIAN_POINT('Ctrl Pts',(-194.561624807792,-5.92485436802142,
130.807214191615));
#160827=CARTESIAN_POINT('Ctrl Pts',(-194.569215671905,-5.92580750057834,
130.96784894699));
#160828=CARTESIAN_POINT('Ctrl Pts',(-194.576806536018,-5.91984348713247,
131.128411830021));
#160829=CARTESIAN_POINT('Ctrl Pts',(-194.677213274735,-5.74644163664981,
133.244482439234));
#160830=CARTESIAN_POINT('Ctrl Pts',(-194.862845023943,-3.28928991419861,
136.981587535098));
#160831=CARTESIAN_POINT('Ctrl Pts',(-195.141292647756,3.41913440987934,
136.910675415994));
#160832=CARTESIAN_POINT('Ctrl Pts',(-195.419740271569,6.98554124528268,
131.228358307197));
#160833=CARTESIAN_POINT('Ctrl Pts',(-195.698187895382,4.13257693892937,
125.156408035065));
#160834=CARTESIAN_POINT('Ctrl Pts',(-195.976635519195,-2.5180236866903,
124.27465026843));
#160835=CARTESIAN_POINT('Ctrl Pts',(-196.181114489998,-5.70266478639503,
128.033605093401));
#160836=CARTESIAN_POINT('Ctrl Pts',(-196.292777586197,-5.92224318811939,
130.39909676226));
#160837=CARTESIAN_POINT('Ctrl Pts',(-196.311624807792,-5.91853255389597,
130.799043603888));
#160838=CARTESIAN_POINT('',(-198.061624807755,-5.91674998668501,130.803963675558));
#160839=CARTESIAN_POINT('Ctrl Pts',(-196.311624807792,-5.91674761240624,
130.79904520742));
#160840=CARTESIAN_POINT('Ctrl Pts',(-196.318927817343,-5.91688679200283,
130.953970325757));
#160841=CARTESIAN_POINT('Ctrl Pts',(-196.326230826894,-5.91093694148842,
131.109091464218));
#160842=CARTESIAN_POINT('Ctrl Pts',(-196.333533836445,-5.89887867729289,
131.263883101324));
#160843=CARTESIAN_POINT('Ctrl Pts',(-196.340831042499,-5.88682999546239,
131.41855172985));
#160844=CARTESIAN_POINT('Ctrl Pts',(-196.348128248553,-5.86868258965433,
131.572890996276));
#160845=CARTESIAN_POINT('Ctrl Pts',(-196.355425454607,-5.84446913863302,
131.726375286683));
#160846=CARTESIAN_POINT('Ctrl Pts',(-196.362846509282,-5.81984473545903,
131.882464521733));
#160847=CARTESIAN_POINT('Ctrl Pts',(-196.370267563958,-5.78894650617216,
132.037669091922));
#160848=CARTESIAN_POINT('Ctrl Pts',(-196.377688618634,-5.75186394852528,
132.191440889272));
#160849=CARTESIAN_POINT('Ctrl Pts',(-196.3849802672,-5.71542802531407,132.342531260482));
#160850=CARTESIAN_POINT('Ctrl Pts',(-196.392271915766,-5.67302179942338,
132.492238033825));
#160851=CARTESIAN_POINT('Ctrl Pts',(-196.399563564333,-5.62478171151197,
132.640051566593));
#160852=CARTESIAN_POINT('Ctrl Pts',(-196.40685488677,-5.57654378120929,
132.787858488184));
#160853=CARTESIAN_POINT('Ctrl Pts',(-196.414146209206,-5.52247262718137,
132.933771971568));
#160854=CARTESIAN_POINT('Ctrl Pts',(-196.421437531643,-5.46275434354564,
133.077298263999));
#160855=CARTESIAN_POINT('Ctrl Pts',(-196.428730063846,-5.40302615153141,
133.220848370123));
#160856=CARTESIAN_POINT('Ctrl Pts',(-196.43602259605,-5.3376491138028,133.362010141883));
#160857=CARTESIAN_POINT('Ctrl Pts',(-196.443315128253,-5.26685704862626,
133.500310801052));
#160858=CARTESIAN_POINT('Ctrl Pts',(-196.450833098134,-5.19387655310716,
133.642886817326));
#160859=CARTESIAN_POINT('Ctrl Pts',(-196.458351068014,-5.11514103364721,
133.782421580859));
#160860=CARTESIAN_POINT('Ctrl Pts',(-196.465869037895,-5.03095663489101,
133.918426432597));
#160861=CARTESIAN_POINT('Ctrl Pts',(-196.473172341532,-4.9491760165358,
134.050547835598));
#160862=CARTESIAN_POINT('Ctrl Pts',(-196.480475645169,-4.86225370657967,
134.179337872425));
#160863=CARTESIAN_POINT('Ctrl Pts',(-196.487778948806,-4.77051280347123,
134.304380353856));
#160864=CARTESIAN_POINT('Ctrl Pts',(-196.495404251808,-4.67472708529593,
134.434935901931));
#160865=CARTESIAN_POINT('Ctrl Pts',(-196.503029554811,-4.57368851682401,
134.561405546719));
#160866=CARTESIAN_POINT('Ctrl Pts',(-196.510654857813,-4.467808907599,134.683357153744));
#160867=CARTESIAN_POINT('Ctrl Pts',(-196.518280160816,-4.361929298374,134.805308760768));
#160868=CARTESIAN_POINT('Ctrl Pts',(-196.525905463818,-4.25120902523955,
134.922742040811));
#160869=CARTESIAN_POINT('Ctrl Pts',(-196.53353076682,-4.13609959561202,
135.035271949381));
#160870=CARTESIAN_POINT('Ctrl Pts',(-196.540954033226,-4.024040053635,135.144820316129));
#160871=CARTESIAN_POINT('Ctrl Pts',(-196.548377299631,-3.90745582610583,
135.250079258993));
#160872=CARTESIAN_POINT('Ctrl Pts',(-196.555800566037,-3.78670891927233,
135.350652086797));
#160873=CARTESIAN_POINT('Ctrl Pts',(-196.563215058758,-3.66610472525497,
135.451106045871));
#160874=CARTESIAN_POINT('Ctrl Pts',(-196.570629551479,-3.5413479291358,
135.546884677918));
#160875=CARTESIAN_POINT('Ctrl Pts',(-196.578044044199,-3.41283794674118,
135.63762739189));
#160876=CARTESIAN_POINT('Ctrl Pts',(-196.585451390553,-3.28445182710626,
135.728282644617));
#160877=CARTESIAN_POINT('Ctrl Pts',(-196.592858736907,-3.15232002574301,
135.813911428368));
#160878=CARTESIAN_POINT('Ctrl Pts',(-196.60026608326,-3.0168755761589,135.894192866322));
#160879=CARTESIAN_POINT('Ctrl Pts',(-196.607667904936,-2.88153214615492,
135.974414427351));
#160880=CARTESIAN_POINT('Ctrl Pts',(-196.615069726611,-2.74288130716737,
136.049296394212));
#160881=CARTESIAN_POINT('Ctrl Pts',(-196.622471548287,-2.60138556712834,
136.118560810788));
#160882=CARTESIAN_POINT('Ctrl Pts',(-196.629869462598,-2.45996452158867,
136.187788663217));
#160883=CARTESIAN_POINT('Ctrl Pts',(-196.637267376909,-2.31570190033966,
136.251404707507));
#160884=CARTESIAN_POINT('Ctrl Pts',(-196.644665291221,-2.1690852351992,
136.309176673071));
#160885=CARTESIAN_POINT('Ctrl Pts',(-196.652061976133,-2.02249293508921,
136.366939037981));
#160886=CARTESIAN_POINT('Ctrl Pts',(-196.659458661045,-1.87354771447102,
136.418859114951));
#160887=CARTESIAN_POINT('Ctrl Pts',(-196.666855345957,-1.72275763897961,
136.464752536845));
#160888=CARTESIAN_POINT('Ctrl Pts',(-196.674251702893,-1.57197424967773,
136.510643923776));
#160889=CARTESIAN_POINT('Ctrl Pts',(-196.681648059828,-1.41934652527773,
136.550509078279));
#160890=CARTESIAN_POINT('Ctrl Pts',(-196.689044416763,-1.26539800768293,
136.584213422323));
#160891=CARTESIAN_POINT('Ctrl Pts',(-196.6964419061,-1.11142592017751,136.617922926587));
#160892=CARTESIAN_POINT('Ctrl Pts',(-196.703839395436,-0.956133001520995,
136.645469662442));
#160893=CARTESIAN_POINT('Ctrl Pts',(-196.711236884773,-0.800053158089319,
136.666770148359));
#160894=CARTESIAN_POINT('Ctrl Pts',(-196.718636967288,-0.643918601110704,
136.688078101128));
#160895=CARTESIAN_POINT('Ctrl Pts',(-196.726037049803,-0.486996939769862,
136.703135394011));
#160896=CARTESIAN_POINT('Ctrl Pts',(-196.733437132318,-0.329827225310558,
136.711910411173));
#160897=CARTESIAN_POINT('Ctrl Pts',(-196.740845351984,-0.172484686592092,
136.720695077368));
#160898=CARTESIAN_POINT('Ctrl Pts',(-196.748253571651,-0.0148939229818671,
136.723183651275));
#160899=CARTESIAN_POINT('Ctrl Pts',(-196.755661791317,0.142405248829505,
136.719396653602));
#160900=CARTESIAN_POINT('Ctrl Pts',(-196.763074570619,0.299801235656451,
136.715607325096));
#160901=CARTESIAN_POINT('Ctrl Pts',(-196.770487349921,0.456904901399012,
136.705534752304));
#160902=CARTESIAN_POINT('Ctrl Pts',(-196.777900129223,0.613182040216748,
136.689251300328));
#160903=CARTESIAN_POINT('Ctrl Pts',(-196.785323500252,0.769682475138877,
136.672944581791));
#160904=CARTESIAN_POINT('Ctrl Pts',(-196.792746871281,0.925353655985176,
136.650409313252));
#160905=CARTESIAN_POINT('Ctrl Pts',(-196.80017024231,1.07967122626914,136.621769027302));
#160906=CARTESIAN_POINT('Ctrl Pts',(-196.804106291751,1.16149410484353,
136.606583260475));
#160907=CARTESIAN_POINT('Ctrl Pts',(-196.808042341192,1.24293667063961,
136.589681992946));
#160908=CARTESIAN_POINT('Ctrl Pts',(-196.811978390633,1.32392266781222,
136.571089268383));
#160909=CARTESIAN_POINT('Ctrl Pts',(-196.819401657039,1.47665973097384,
136.536023970121));
#160910=CARTESIAN_POINT('Ctrl Pts',(-196.826824923444,1.62823368340216,
136.494833387375));
#160911=CARTESIAN_POINT('Ctrl Pts',(-196.83424818985,1.7781151043552,136.447607664982));
#160912=CARTESIAN_POINT('Ctrl Pts',(-196.841662682571,1.92781937791556,
136.40043775947));
#160913=CARTESIAN_POINT('Ctrl Pts',(-196.849077175292,2.07583474930553,
136.347247023744));
#160914=CARTESIAN_POINT('Ctrl Pts',(-196.856491668013,2.22164194905233,
136.288176589379));
#160915=CARTESIAN_POINT('Ctrl Pts',(-196.863899014366,2.36730861433047,
136.229163089323));
#160916=CARTESIAN_POINT('Ctrl Pts',(-196.87130636072,2.51077100136879,136.164281311885));
#160917=CARTESIAN_POINT('Ctrl Pts',(-196.878713707074,2.65152508222352,
136.093722138661));
#160918=CARTESIAN_POINT('Ctrl Pts',(-196.886115528749,2.79217418337481,
136.02321559113));
#160919=CARTESIAN_POINT('Ctrl Pts',(-196.893517350425,2.93011866807073,
135.947040245676));
#160920=CARTESIAN_POINT('Ctrl Pts',(-196.9009191721,3.06487468712279,135.865434981249));
#160921=CARTESIAN_POINT('Ctrl Pts',(-196.908317086411,3.19955956952096,
135.783872795607));
#160922=CARTESIAN_POINT('Ctrl Pts',(-196.915715000723,3.33105901987783,
135.696886592468));
#160923=CARTESIAN_POINT('Ctrl Pts',(-196.923112915034,3.45891409951243,
135.604760998232));
#160924=CARTESIAN_POINT('Ctrl Pts',(-196.930509599946,3.5867479319525,135.512650713597));
#160925=CARTESIAN_POINT('Ctrl Pts',(-196.937906284858,3.7109382930943,135.415402950964));
#160926=CARTESIAN_POINT('Ctrl Pts',(-196.94530296977,3.83105544775849,135.313345505398));
#160927=CARTESIAN_POINT('Ctrl Pts',(-196.952699326706,3.95116727630217,
135.211292585167));
#160928=CARTESIAN_POINT('Ctrl Pts',(-196.960095683641,4.0672059730031,135.104430647757));
#160929=CARTESIAN_POINT('Ctrl Pts',(-196.967492040577,4.17877532636475,
134.993127421085));
#160930=CARTESIAN_POINT('Ctrl Pts',(-196.974889529913,4.29036176127955,
134.881807153605));
#160931=CARTESIAN_POINT('Ctrl Pts',(-196.98228701925,4.39747722609323,134.766044506611));
#160932=CARTESIAN_POINT('Ctrl Pts',(-196.989684508586,4.49976289599391,
134.646243546852));
#160933=CARTESIAN_POINT('Ctrl Pts',(-196.997084591101,4.60208442197746,
134.526400591052));
#160934=CARTESIAN_POINT('Ctrl Pts',(-197.004484673616,4.69957253990412,
134.40251678771));
#160935=CARTESIAN_POINT('Ctrl Pts',(-197.011884756131,4.79190928011303,
134.275028566775));
#160936=CARTESIAN_POINT('Ctrl Pts',(-197.019292975798,4.88434755406011,
134.147400159435));
#160937=CARTESIAN_POINT('Ctrl Pts',(-197.026701195464,4.97162291886746,
134.01615972179));
#160938=CARTESIAN_POINT('Ctrl Pts',(-197.034109415131,5.05346085508178,
133.881772508856));
#160939=CARTESIAN_POINT('Ctrl Pts',(-197.041522194433,5.13534916118031,
133.747302582836));
#160940=CARTESIAN_POINT('Ctrl Pts',(-197.048934973735,5.2117931892249,133.609682347809));
#160941=CARTESIAN_POINT('Ctrl Pts',(-197.056347753037,5.28256507071789,
133.469400361384));
#160942=CARTESIAN_POINT('Ctrl Pts',(-197.063771124065,5.35343807439412,
133.328917933479));
#160943=CARTESIAN_POINT('Ctrl Pts',(-197.071194495094,5.41862259046731,
133.185766497095));
#160944=CARTESIAN_POINT('Ctrl Pts',(-197.078617866123,5.47793912291705,
133.04045398058));
#160945=CARTESIAN_POINT('Ctrl Pts',(-197.082553915564,5.50939017170535,
132.963405797591));
#160946=CARTESIAN_POINT('Ctrl Pts',(-197.086489965005,5.53919235282093,
132.88575031248));
#160947=CARTESIAN_POINT('Ctrl Pts',(-197.090426014446,5.56732467673674,
132.80756467764));
#160948=CARTESIAN_POINT('Ctrl Pts',(-197.097849280852,5.62038136165785,
132.660109010435));
#160949=CARTESIAN_POINT('Ctrl Pts',(-197.105272547257,5.66765598150285,
132.510321035348));
#160950=CARTESIAN_POINT('Ctrl Pts',(-197.112695813663,5.70893821283385,
132.35869489453));
#160951=CARTESIAN_POINT('Ctrl Pts',(-197.120110306384,5.75017165199582,
132.207247963219));
#160952=CARTESIAN_POINT('Ctrl Pts',(-197.127524799105,5.7854267033022,132.053967547337));
#160953=CARTESIAN_POINT('Ctrl Pts',(-197.134939291826,5.81454142691153,
131.899366808064));
#160954=CARTESIAN_POINT('Ctrl Pts',(-197.14234663818,5.84362808865393,131.744915078805));
#160955=CARTESIAN_POINT('Ctrl Pts',(-197.149753984533,5.86658613620568,
131.589145923993));
#160956=CARTESIAN_POINT('Ctrl Pts',(-197.157161330887,5.88330372424391,
131.432586572775));
#160957=CARTESIAN_POINT('Ctrl Pts',(-197.164563152563,5.90000884367436,
131.276143989427));
#160958=CARTESIAN_POINT('Ctrl Pts',(-197.171964974238,5.91048273160501,
131.118912752756));
#160959=CARTESIAN_POINT('Ctrl Pts',(-197.179366795914,5.91466483135784,
130.961429058695));
#160960=CARTESIAN_POINT('Ctrl Pts',(-197.186764710225,5.91884472341276,
130.804028499051));
#160961=CARTESIAN_POINT('Ctrl Pts',(-197.194162624536,5.91673943210462,
130.646376119654));
#160962=CARTESIAN_POINT('Ctrl Pts',(-197.201560538848,5.90834035411677,
130.489011886135));
#160963=CARTESIAN_POINT('Ctrl Pts',(-197.20895722376,5.8999426719033,130.331673803696));
#160964=CARTESIAN_POINT('Ctrl Pts',(-197.216353908672,5.8852532987146,130.1746241445));
#160965=CARTESIAN_POINT('Ctrl Pts',(-197.223750593585,5.86431573546309,
130.018401638166));
#160966=CARTESIAN_POINT('Ctrl Pts',(-197.23114695052,5.84337910060514,129.862186058901));
#160967=CARTESIAN_POINT('Ctrl Pts',(-197.238543307455,5.81619487614345,
129.706797929561));
#160968=CARTESIAN_POINT('Ctrl Pts',(-197.245939664391,5.7828582799976,129.552769360021));
#160969=CARTESIAN_POINT('Ctrl Pts',(-197.253337153727,5.74951657993387,
129.398717208314));
#160970=CARTESIAN_POINT('Ctrl Pts',(-197.260734643064,5.71002071162072,
129.246025395738));
#160971=CARTESIAN_POINT('Ctrl Pts',(-197.268132132401,5.66451667428286,
129.09521421972));
#160972=CARTESIAN_POINT('Ctrl Pts',(-197.275532214916,5.61899668557493,
128.944350177076));
#160973=CARTESIAN_POINT('Ctrl Pts',(-197.282932297431,5.56746444227009,
128.79536844072));
#160974=CARTESIAN_POINT('Ctrl Pts',(-197.290332379946,5.51011525487502,
128.648772428581));
#160975=CARTESIAN_POINT('Ctrl Pts',(-197.297740599612,5.45270300615285,
128.502015219055));
#160976=CARTESIAN_POINT('Ctrl Pts',(-197.305148819279,5.38946117553666,
128.357649320603));
#160977=CARTESIAN_POINT('Ctrl Pts',(-197.312557038945,5.32063281077705,
128.216157175913));
#160978=CARTESIAN_POINT('Ctrl Pts',(-197.319969818248,5.2517620833074,128.07457794517));
#160979=CARTESIAN_POINT('Ctrl Pts',(-197.32738259755,5.17729814637798,127.935876320775));
#160980=CARTESIAN_POINT('Ctrl Pts',(-197.334795376852,5.09752886885128,
127.80050809227));
#160981=CARTESIAN_POINT('Ctrl Pts',(-197.34221874788,5.01764561323994,127.664946443292));
#160982=CARTESIAN_POINT('Ctrl Pts',(-197.349642118909,4.93244207870739,
127.532728015764));
#160983=CARTESIAN_POINT('Ctrl Pts',(-197.357065489938,4.84224857777326,
127.40427837245));
#160984=CARTESIAN_POINT('Ctrl Pts',(-197.361001539378,4.79442581941926,
127.336171289465));
#160985=CARTESIAN_POINT('Ctrl Pts',(-197.364937588819,4.74520086733818,
127.26912318392));
#160986=CARTESIAN_POINT('Ctrl Pts',(-197.368873638259,4.69462728667099,
127.203193417651));
#160987=CARTESIAN_POINT('Ctrl Pts',(-197.376296904665,4.59924709187124,
127.078851936054));
#160988=CARTESIAN_POINT('Ctrl Pts',(-197.38372017107,4.49877931298799,126.958114400183));
#160989=CARTESIAN_POINT('Ctrl Pts',(-197.391143437476,4.39352600085202,
126.841424857004));
#160990=CARTESIAN_POINT('Ctrl Pts',(-197.398557930197,4.28839708939024,
126.724873231176));
#160991=CARTESIAN_POINT('Ctrl Pts',(-197.405972422918,4.17849415076658,
126.612360349171));
#160992=CARTESIAN_POINT('Ctrl Pts',(-197.413386915639,4.06416138957402,
126.504299831717));
#160993=CARTESIAN_POINT('Ctrl Pts',(-197.420794261992,3.94993882660157,
126.396343467059));
#160994=CARTESIAN_POINT('Ctrl Pts',(-197.428201608346,3.83129521052947,
126.292831178398));
#160995=CARTESIAN_POINT('Ctrl Pts',(-197.4356089547,3.70861365904349,126.194142044607));
#160996=CARTESIAN_POINT('Ctrl Pts',(-197.443010776375,3.58602360808748,
126.095526516895));
#160997=CARTESIAN_POINT('Ctrl Pts',(-197.450412598051,3.45940190792309,
126.001727214337));
#160998=CARTESIAN_POINT('Ctrl Pts',(-197.457814419726,3.32916694301156,
125.91308491198));
#160999=CARTESIAN_POINT('Ctrl Pts',(-197.465212334038,3.19900072812314,
125.824489403203));
#161000=CARTESIAN_POINT('Ctrl Pts',(-197.472610248349,3.06522535501235,
125.741045682467));
#161001=CARTESIAN_POINT('Ctrl Pts',(-197.48000816266,2.92829046175452,125.6630528526));
#161002=CARTESIAN_POINT('Ctrl Pts',(-197.487404847572,2.79137832459229,
125.585072983727));
#161003=CARTESIAN_POINT('Ctrl Pts',(-197.494801532485,2.65130803341802,
125.512542392469));
#161004=CARTESIAN_POINT('Ctrl Pts',(-197.502198217397,2.50855635002252,
125.445715676794));
#161005=CARTESIAN_POINT('Ctrl Pts',(-197.509594574332,2.36581099638625,
125.378891924286));
#161006=CARTESIAN_POINT('Ctrl Pts',(-197.516990931268,2.22038482501944,
125.317771702748));
#161007=CARTESIAN_POINT('Ctrl Pts',(-197.524387288203,2.0727769826413,125.262562521033));
#161008=CARTESIAN_POINT('Ctrl Pts',(-197.53178477754,1.9251465411261,125.207344886652));
#161009=CARTESIAN_POINT('Ctrl Pts',(-197.539182266876,1.77533411318653,
125.158040224843));
#161010=CARTESIAN_POINT('Ctrl Pts',(-197.546579756213,1.62385635592891,
125.11480693579));
#161011=CARTESIAN_POINT('Ctrl Pts',(-197.553979838728,1.47232549837808,
125.071558491375));
#161012=CARTESIAN_POINT('Ctrl Pts',(-197.561379921243,1.31912850795002,
125.034385759555));
#161013=CARTESIAN_POINT('Ctrl Pts',(-197.568780003758,1.16479449450476,
125.003396529755));
#161014=CARTESIAN_POINT('Ctrl Pts',(-197.576188223424,1.01029077494556,
124.972373224112));
#161015=CARTESIAN_POINT('Ctrl Pts',(-197.583596443091,0.854647901707854,
124.947547072864));
#161016=CARTESIAN_POINT('Ctrl Pts',(-197.591004662757,0.698403140736846,
124.928974365113));
#161017=CARTESIAN_POINT('Ctrl Pts',(-197.598417442059,0.542062213722543,
124.910390226172));
#161018=CARTESIAN_POINT('Ctrl Pts',(-197.605830221361,0.38511903209279,
124.898067229277));
#161019=CARTESIAN_POINT('Ctrl Pts',(-197.613243000663,0.228112664648767,
124.892009547583));
#161020=CARTESIAN_POINT('Ctrl Pts',(-197.620666371692,0.0708819591442937,
124.88594321039));
#161021=CARTESIAN_POINT('Ctrl Pts',(-197.628089742721,-0.0864117401809329,
124.886160067387));
#161022=CARTESIAN_POINT('Ctrl Pts',(-197.63551311375,-0.243231853336173,
124.892612244367));
#161023=CARTESIAN_POINT('Ctrl Pts',(-197.639449163191,-0.326381640180508,
124.896033343419));
#161024=CARTESIAN_POINT('Ctrl Pts',(-197.643385212631,-0.409398399272633,
124.901206550941));
#161025=CARTESIAN_POINT('Ctrl Pts',(-197.647321262072,-0.492203234551277,
124.908118887583));
#161026=CARTESIAN_POINT('Ctrl Pts',(-197.654744528478,-0.64837056963286,
124.921155338763));
#161027=CARTESIAN_POINT('Ctrl Pts',(-197.662167794883,-0.804255766574924,
124.940420139216));
#161028=CARTESIAN_POINT('Ctrl Pts',(-197.669591061289,-0.959321970235522,
124.965899183256));
#161029=CARTESIAN_POINT('Ctrl Pts',(-197.67700555401,-1.11420489852084,
124.991348113182));
#161030=CARTESIAN_POINT('Ctrl Pts',(-197.684420046731,-1.26827039553683,
125.022996607056));
#161031=CARTESIAN_POINT('Ctrl Pts',(-197.691834539452,-1.42098441946168,
125.060778647911));
#161032=CARTESIAN_POINT('Ctrl Pts',(-197.699241885806,-1.57355125186026,
125.098524273012));
#161033=CARTESIAN_POINT('Ctrl Pts',(-197.706649232159,-1.72476884444938,
125.142391586927));
#161034=CARTESIAN_POINT('Ctrl Pts',(-197.714056578513,-1.87411118297151,
125.192263163284));
#161035=CARTESIAN_POINT('Ctrl Pts',(-197.721458400189,-2.02334213634406,
125.242097543538));
#161036=CARTESIAN_POINT('Ctrl Pts',(-197.728860221864,-2.17070026796815,
125.297927151792));
#161037=CARTESIAN_POINT('Ctrl Pts',(-197.73626204354,-2.31567272712397,
125.359584186586));
#161038=CARTESIAN_POINT('Ctrl Pts',(-197.743659957851,-2.46056865644708,
125.421208673112));
#161039=CARTESIAN_POINT('Ctrl Pts',(-197.751057872162,-2.60308107876267,
125.488654313942));
#161040=CARTESIAN_POINT('Ctrl Pts',(-197.758455786474,-2.74271531002859,
125.561704488214));
#161041=CARTESIAN_POINT('Ctrl Pts',(-197.765852471386,-2.88232633661789,
125.634742522872));
#161042=CARTESIAN_POINT('Ctrl Pts',(-197.773249156298,-3.01905979100342,
125.713383069601));
#161043=CARTESIAN_POINT('Ctrl Pts',(-197.780645841211,-3.15244377131063,
125.797362631624));
#161044=CARTESIAN_POINT('Ctrl Pts',(-197.788042198146,-3.28582183723238,
125.881338469906));
#161045=CARTESIAN_POINT('Ctrl Pts',(-197.795438555081,-3.41585040848234,
125.970652653875));
#161046=CARTESIAN_POINT('Ctrl Pts',(-197.802834912017,-3.54208510099192,
126.064997400864));
#161047=CARTESIAN_POINT('Ctrl Pts',(-197.810232401353,-3.66833912035446,
126.159356592273));
#161048=CARTESIAN_POINT('Ctrl Pts',(-197.81762989069,-3.79079780538828,
126.258747656766));
#161049=CARTESIAN_POINT('Ctrl Pts',(-197.825027380027,-3.90904862374609,
126.362821535256));
#161050=CARTESIAN_POINT('Ctrl Pts',(-197.832427462542,-4.02734089474615,
126.466931896683));
#161051=CARTESIAN_POINT('Ctrl Pts',(-197.839827545057,-4.14142208218471,
126.575728093952));
#161052=CARTESIAN_POINT('Ctrl Pts',(-197.847227627572,-4.2509155029613,
126.688823234771));
#161053=CARTESIAN_POINT('Ctrl Pts',(-197.854635847238,-4.36052932300976,
126.802042735323));
#161054=CARTESIAN_POINT('Ctrl Pts',(-197.862044066905,-4.46554504194146,
126.919570351452));
#161055=CARTESIAN_POINT('Ctrl Pts',(-197.869452286571,-4.56562489677327,
127.040984491736));
#161056=CARTESIAN_POINT('Ctrl Pts',(-197.876865065873,-4.66576634908582,
127.162473360399));
#161057=CARTESIAN_POINT('Ctrl Pts',(-197.884277845175,-4.76096565859968,
127.287853223139));
#161058=CARTESIAN_POINT('Ctrl Pts',(-197.891690624478,-4.8509279344683,
127.416672801799));
#161059=CARTESIAN_POINT('Ctrl Pts',(-197.899113995506,-4.94101875265536,
127.545676443914));
#161060=CARTESIAN_POINT('Ctrl Pts',(-197.906537366535,-5.02585739131891,
127.678129304451));
#161061=CARTESIAN_POINT('Ctrl Pts',(-197.913960737564,-5.10519409379517,
127.813554066286));
#161062=CARTESIAN_POINT('Ctrl Pts',(-197.917896787004,-5.14726031710364,
127.88535952448));
#161063=CARTESIAN_POINT('Ctrl Pts',(-197.921832836445,-5.18778053718604,
127.958000120082));
#161064=CARTESIAN_POINT('Ctrl Pts',(-197.925768885886,-5.22672302868686,
128.031402459949));
#161065=CARTESIAN_POINT('Ctrl Pts',(-197.933618442971,-5.30438498764153,
128.177786763732));
#161066=CARTESIAN_POINT('Ctrl Pts',(-197.941468000057,-5.37598238513895,
128.327603249052));
#161067=CARTESIAN_POINT('Ctrl Pts',(-197.949317557143,-5.44121712518422,
128.480336788277));
#161068=CARTESIAN_POINT('Ctrl Pts',(-197.957153559567,-5.50633921749837,
128.632806586333));
#161069=CARTESIAN_POINT('Ctrl Pts',(-197.964989561992,-5.56512043354741,
128.788183113502));
#161070=CARTESIAN_POINT('Ctrl Pts',(-197.972825564417,-5.6173084054525,
128.94592664227));
#161071=CARTESIAN_POINT('Ctrl Pts',(-197.98064289557,-5.66937202622657,
129.103294306917));
#161072=CARTESIAN_POINT('Ctrl Pts',(-197.988460226724,-5.71487364188634,
129.263017430468));
#161073=CARTESIAN_POINT('Ctrl Pts',(-197.996277557878,-5.75360906848479,
129.424536987695));
#161074=CARTESIAN_POINT('Ctrl Pts',(-198.004083819218,-5.79228964337747,
129.585827823465));
#161075=CARTESIAN_POINT('Ctrl Pts',(-198.011890080558,-5.82422305311737,
129.748909723495));
#161076=CARTESIAN_POINT('Ctrl Pts',(-198.019696341898,-5.84925431259238,
129.913207123986));
#161077=CARTESIAN_POINT('Ctrl Pts',(-198.027487193755,-5.87423616060821,
130.07718020303));
#161078=CARTESIAN_POINT('Ctrl Pts',(-198.035278045612,-5.89234298762165,
130.242363691703));
#161079=CARTESIAN_POINT('Ctrl Pts',(-198.04306889747,-5.90347053031272,
130.40817094048));
#161080=CARTESIAN_POINT('Ctrl Pts',(-198.049254200898,-5.91230489518304,
130.539808425459));
#161081=CARTESIAN_POINT('Ctrl Pts',(-198.055439504327,-5.91674112270733,
130.671838733572));
#161082=CARTESIAN_POINT('Ctrl Pts',(-198.061624807755,-5.91674998668501,
130.803963675558));
#161083=CARTESIAN_POINT('',(-199.811624807792,-5.91674748832781,130.809812394026));
#161084=CARTESIAN_POINT('Ctrl Pts',(-198.061624807792,-5.91674998668506,
130.803963676344));
#161085=CARTESIAN_POINT('Ctrl Pts',(-198.069335284224,-5.91676103632174,
130.96866800542));
#161086=CARTESIAN_POINT('Ctrl Pts',(-198.077045760657,-5.90989046074581,
131.133254346916));
#161087=CARTESIAN_POINT('Ctrl Pts',(-198.084756237089,-5.89619368993992,
131.297138999004));
#161088=CARTESIAN_POINT('Ctrl Pts',(-198.09247513413,-5.88248196089642,
131.461202629451));
#161089=CARTESIAN_POINT('Ctrl Pts',(-198.10019403117,-5.86192918777857,
131.624562717793));
#161090=CARTESIAN_POINT('Ctrl Pts',(-198.107912928211,-5.83464232566053,
131.786643414988));
#161091=CARTESIAN_POINT('Ctrl Pts',(-198.115938226668,-5.80627231226227,
131.955157901231));
#161092=CARTESIAN_POINT('Ctrl Pts',(-198.123963525126,-5.77062274114287,
132.122288952053));
#161093=CARTESIAN_POINT('Ctrl Pts',(-198.131988823583,-5.72787106095795,
132.287406021976));
#161094=CARTESIAN_POINT('Ctrl Pts',(-198.13973298131,-5.68661704950663,
132.446738742092));
#161095=CARTESIAN_POINT('Ctrl Pts',(-198.147477139037,-5.63875026118319,
132.604195921967));
#161096=CARTESIAN_POINT('Ctrl Pts',(-198.155221296764,-5.58447970808055,
132.759230677835));
#161097=CARTESIAN_POINT('Ctrl Pts',(-198.162974554244,-5.53014538450852,
132.914447606882));
#161098=CARTESIAN_POINT('Ctrl Pts',(-198.170727811723,-5.46939239828204,
133.067236130232));
#161099=CARTESIAN_POINT('Ctrl Pts',(-198.178481069202,-5.40247702272164,
133.217071247017));
#161100=CARTESIAN_POINT('Ctrl Pts',(-198.186248543322,-5.33543894881967,
133.367181106642));
#161101=CARTESIAN_POINT('Ctrl Pts',(-198.194016017441,-5.26221604894185,
133.514326447479));
#161102=CARTESIAN_POINT('Ctrl Pts',(-198.201783491561,-5.18311009938688,
133.658007452781));
#161103=CARTESIAN_POINT('Ctrl Pts',(-198.202594497607,-5.17485060571508,
133.673009261883));
#161104=CARTESIAN_POINT('Ctrl Pts',(-198.203405503652,-5.16652701566992,
133.687973331658));
#161105=CARTESIAN_POINT('Ctrl Pts',(-198.204216509698,-5.15813969907268,
133.702899112627));
#161106=CARTESIAN_POINT('Ctrl Pts',(-198.211639776104,-5.08136926578121,
133.839517142834));
#161107=CARTESIAN_POINT('Ctrl Pts',(-198.219063042509,-4.9990513182663,
133.973289646283));
#161108=CARTESIAN_POINT('Ctrl Pts',(-198.226486308914,-4.91142183868873,
134.103734207348));
#161109=CARTESIAN_POINT('Ctrl Pts',(-198.233900801635,-4.82389592987909,
134.234024593775));
#161110=CARTESIAN_POINT('Ctrl Pts',(-198.241315294356,-4.73107119111244,
134.360994560333));
#161111=CARTESIAN_POINT('Ctrl Pts',(-198.248729787077,-4.63322964933905,
134.484185827951));
#161112=CARTESIAN_POINT('Ctrl Pts',(-198.256137133431,-4.53548241092728,
134.607258359188));
#161113=CARTESIAN_POINT('Ctrl Pts',(-198.263544479785,-4.43272822641348,
134.726559151738));
#161114=CARTESIAN_POINT('Ctrl Pts',(-198.270951826138,-4.32529254368441,
134.841658596914));
#161115=CARTESIAN_POINT('Ctrl Pts',(-198.278353647814,-4.21793699054084,
134.956672196582));
#161116=CARTESIAN_POINT('Ctrl Pts',(-198.285755469489,-4.10590714512817,
135.067490416427));
#161117=CARTESIAN_POINT('Ctrl Pts',(-198.293157291165,-3.98956880068971,
135.173716559471));
#161118=CARTESIAN_POINT('Ctrl Pts',(-198.300555205476,-3.87329187035737,
135.279886626562));
#161119=CARTESIAN_POINT('Ctrl Pts',(-198.307953119787,-3.75271124559411,
135.381469193533));
#161120=CARTESIAN_POINT('Ctrl Pts',(-198.315351034099,-3.62822957043913,
135.478104378909));
#161121=CARTESIAN_POINT('Ctrl Pts',(-198.322747719011,-3.50376858188041,
135.57472350527));
#161122=CARTESIAN_POINT('Ctrl Pts',(-198.330144403923,-3.37540812416725,
135.666396653101));
#161123=CARTESIAN_POINT('Ctrl Pts',(-198.337541088835,-3.24358400599151,
135.752804146452));
#161124=CARTESIAN_POINT('Ctrl Pts',(-198.344937445771,-3.11176573303569,
135.839207808404));
#161125=CARTESIAN_POINT('Ctrl Pts',(-198.352333802706,-2.97648441719638,
135.920346075478));
#161126=CARTESIAN_POINT('Ctrl Pts',(-198.359730159642,-2.83820470770205,
135.995942707804));
#161127=CARTESIAN_POINT('Ctrl Pts',(-198.367127648978,-2.69990382723119,
136.071550914167));
#161128=CARTESIAN_POINT('Ctrl Pts',(-198.374525138315,-2.55860396661923,
136.141615617351));
#161129=CARTESIAN_POINT('Ctrl Pts',(-198.381922627651,-2.41479407700068,
136.205906704399));
#161130=CARTESIAN_POINT('Ctrl Pts',(-198.389322710166,-2.27093377504764,
136.270220328589));
#161131=CARTESIAN_POINT('Ctrl Pts',(-198.396722792681,-2.12456203282009,
136.328756154751));
#161132=CARTESIAN_POINT('Ctrl Pts',(-198.404122875196,-1.97618731005907,
136.381332401434));
#161133=CARTESIAN_POINT('Ctrl Pts',(-198.411531094863,-1.82764943403772,
136.433966461105));
#161134=CARTESIAN_POINT('Ctrl Pts',(-198.418939314529,-1.67710453105635,
136.480627729429));
#161135=CARTESIAN_POINT('Ctrl Pts',(-198.426347534195,-1.52507644250729,
136.521184246734));
#161136=CARTESIAN_POINT('Ctrl Pts',(-198.433760313498,-1.37295478320602,
136.561765725898));
#161137=CARTESIAN_POINT('Ctrl Pts',(-198.441173092799,-1.21934848271258,
136.596234885463));
#161138=CARTESIAN_POINT('Ctrl Pts',(-198.448585872102,-1.06479056249309,
136.624511098484));
#161139=CARTESIAN_POINT('Ctrl Pts',(-198.45600924313,-0.910011802669364,
136.652827713883));
#161140=CARTESIAN_POINT('Ctrl Pts',(-198.463432614159,-0.754279076069821,
136.67493365743));
#161141=CARTESIAN_POINT('Ctrl Pts',(-198.470855985188,-0.598130326265068,
136.690800176017));
#161142=CARTESIAN_POINT('Ctrl Pts',(-198.474792034629,-0.515336512371863,
136.699212984885));
#161143=CARTESIAN_POINT('Ctrl Pts',(-198.47872808407,-0.432425748835829,
136.705872538709));
#161144=CARTESIAN_POINT('Ctrl Pts',(-198.482664133511,-0.349477975144942,
136.710780489823));
#161145=CARTESIAN_POINT('Ctrl Pts',(-198.490087399917,-0.193041062691021,
136.720036732451));
#161146=CARTESIAN_POINT('Ctrl Pts',(-198.497510666322,-0.0359996055459115,
136.72308761753));
#161147=CARTESIAN_POINT('Ctrl Pts',(-198.504933932728,0.1211129722417,136.719870926107));
#161148=CARTESIAN_POINT('Ctrl Pts',(-198.512348425449,0.278039856009755,
136.716658036546));
#161149=CARTESIAN_POINT('Ctrl Pts',(-198.51976291817,0.435037323525875,
136.707192323227));
#161150=CARTESIAN_POINT('Ctrl Pts',(-198.527177410891,0.591567369173254,
136.691463352378));
#161151=CARTESIAN_POINT('Ctrl Pts',(-198.534584757244,0.74794654526894,
136.675749541703));
#161152=CARTESIAN_POINT('Ctrl Pts',(-198.541992103598,0.903858827456171,
136.653784528579));
#161153=CARTESIAN_POINT('Ctrl Pts',(-198.549399449952,1.05876686124651,
136.62560990754));
#161154=CARTESIAN_POINT('Ctrl Pts',(-198.556801271627,1.2135593587809,136.597456300197));
#161155=CARTESIAN_POINT('Ctrl Pts',(-198.564203093303,1.36734873359921,
136.563102373113));
#161156=CARTESIAN_POINT('Ctrl Pts',(-198.571604914978,1.5196035131144,136.522641454096));
#161157=CARTESIAN_POINT('Ctrl Pts',(-198.57900282929,1.67177791851663,136.482201894084));
#161158=CARTESIAN_POINT('Ctrl Pts',(-198.586400743601,1.82241898210764,
136.43566185819));
#161159=CARTESIAN_POINT('Ctrl Pts',(-198.593798657912,1.97100628646992,
136.383165577519));
#161160=CARTESIAN_POINT('Ctrl Pts',(-198.601195342825,2.11956889831808,
136.330678020777));
#161161=CARTESIAN_POINT('Ctrl Pts',(-198.608592027737,2.26607807668035,
136.27223630799));
#161162=CARTESIAN_POINT('Ctrl Pts',(-198.615988712649,2.41002930388112,
136.208034304692));
#161163=CARTESIAN_POINT('Ctrl Pts',(-198.623385069584,2.55397414813362,
136.143835148178));
#161164=CARTESIAN_POINT('Ctrl Pts',(-198.63078142652,2.6953609258196,136.073876361061));
#161165=CARTESIAN_POINT('Ctrl Pts',(-198.638177783455,2.83370607425544,
135.998399551501));
#161166=CARTESIAN_POINT('Ctrl Pts',(-198.645575272792,2.97207240368668,
135.922911186248));
#161167=CARTESIAN_POINT('Ctrl Pts',(-198.652972762128,3.10739584891269,
135.84190329519));
#161168=CARTESIAN_POINT('Ctrl Pts',(-198.660370251465,3.23921851935599,
135.755662865093));
#161169=CARTESIAN_POINT('Ctrl Pts',(-198.66777033398,3.37108740003226,135.669392203545));
#161170=CARTESIAN_POINT('Ctrl Pts',(-198.675170416495,3.49945275040591,
135.577885555203));
#161171=CARTESIAN_POINT('Ctrl Pts',(-198.68257049901,3.62388679768368,135.481472444332));
#161172=CARTESIAN_POINT('Ctrl Pts',(-198.689978718676,3.74845767298839,
135.384953317334));
#161173=CARTESIAN_POINT('Ctrl Pts',(-198.697386938343,3.86908831687014,
135.283517182095));
#161174=CARTESIAN_POINT('Ctrl Pts',(-198.704795158009,3.98538455885265,
135.17753343379));
#161175=CARTESIAN_POINT('Ctrl Pts',(-198.712207937311,4.10175237923126,
135.071484454256));
#161176=CARTESIAN_POINT('Ctrl Pts',(-198.719620716613,4.21378021684949,
134.960882545995));
#161177=CARTESIAN_POINT('Ctrl Pts',(-198.727033495915,4.32111212685275,
134.846132574229));
#161178=CARTESIAN_POINT('Ctrl Pts',(-198.734456866944,4.42859739772255,
134.731218642321));
#161179=CARTESIAN_POINT('Ctrl Pts',(-198.741880237973,4.53137309681198,
134.612145091307));
#161180=CARTESIAN_POINT('Ctrl Pts',(-198.749303609002,4.62912426167716,
134.489348966591));
#161181=CARTESIAN_POINT('Ctrl Pts',(-198.753239658442,4.68095427479721,
134.424239514812));
#161182=CARTESIAN_POINT('Ctrl Pts',(-198.757175707883,4.73137243893255,
134.35808399281));
#161183=CARTESIAN_POINT('Ctrl Pts',(-198.761111757324,4.78033693499349,
134.290950549066));
#161184=CARTESIAN_POINT('Ctrl Pts',(-198.76853502373,4.87268244643274,134.164338969331));
#161185=CARTESIAN_POINT('Ctrl Pts',(-198.775958290135,4.9601339859933,134.033864621697));
#161186=CARTESIAN_POINT('Ctrl Pts',(-198.783381556541,5.04235087838011,
133.899942660058));
#161187=CARTESIAN_POINT('Ctrl Pts',(-198.790796049262,5.12447059722781,
133.766178983056));
#161188=CARTESIAN_POINT('Ctrl Pts',(-198.798210541983,5.20136779059828,
133.628976117973));
#161189=CARTESIAN_POINT('Ctrl Pts',(-198.805625034704,5.27274287508696,
133.488781064463));
#161190=CARTESIAN_POINT('Ctrl Pts',(-198.813032381058,5.34404916558199,
133.348721136224));
#161191=CARTESIAN_POINT('Ctrl Pts',(-198.820439727411,5.40984377485081,
133.205675091435));
#161192=CARTESIAN_POINT('Ctrl Pts',(-198.827847073765,5.46987124432698,
133.060117504508));
#161193=CARTESIAN_POINT('Ctrl Pts',(-198.835248895441,5.52985394305153,
132.914668479921));
#161194=CARTESIAN_POINT('Ctrl Pts',(-198.842650717116,5.58407792484558,
132.766711986614));
#161195=CARTESIAN_POINT('Ctrl Pts',(-198.850052538791,5.63233443512196,
132.616745613487));
#161196=CARTESIAN_POINT('Ctrl Pts',(-198.857450453103,5.68056547116234,
132.46685840644));
#161197=CARTESIAN_POINT('Ctrl Pts',(-198.864848367414,5.7228351953659,132.314963787059));
#161198=CARTESIAN_POINT('Ctrl Pts',(-198.872246281726,5.7589836551197,132.161577557692));
#161199=CARTESIAN_POINT('Ctrl Pts',(-198.879642966638,5.79512610765524,
132.008216818333));
#161200=CARTESIAN_POINT('Ctrl Pts',(-198.88703965155,5.82514922912225,131.853365323941));
#161201=CARTESIAN_POINT('Ctrl Pts',(-198.894436336462,5.84894341995819,
131.697552328582));
#161202=CARTESIAN_POINT('Ctrl Pts',(-198.901832693398,5.87273655573477,
131.541746242135));
#161203=CARTESIAN_POINT('Ctrl Pts',(-198.909229050333,5.89030125370091,
131.384979108511));
#161204=CARTESIAN_POINT('Ctrl Pts',(-198.916625407269,5.90157940820071,
131.227788357802));
#161205=CARTESIAN_POINT('Ctrl Pts',(-198.924022896605,5.9128592894148,131.070573540788));
#161206=CARTESIAN_POINT('Ctrl Pts',(-198.931420385942,5.91785068400867,
130.912935349915));
#161207=CARTESIAN_POINT('Ctrl Pts',(-198.938817875279,5.91654754103343,
130.75541414485));
#161208=CARTESIAN_POINT('Ctrl Pts',(-198.946217957794,5.91524394124343,
130.597837720972));
#161209=CARTESIAN_POINT('Ctrl Pts',(-198.953618040309,5.90764141376477,
130.440378737603));
#161210=CARTESIAN_POINT('Ctrl Pts',(-198.961018122824,5.89378597505109,
130.283575208025));
#161211=CARTESIAN_POINT('Ctrl Pts',(-198.96842634249,5.87991530085824,130.126599256847));
#161212=CARTESIAN_POINT('Ctrl Pts',(-198.975834562157,5.85977801704612,
129.970280570899));
#161213=CARTESIAN_POINT('Ctrl Pts',(-198.983242781823,5.83347184746589,
129.815150444083));
#161214=CARTESIAN_POINT('Ctrl Pts',(-198.990655561125,5.80714948687722,
129.659924837261));
#161215=CARTESIAN_POINT('Ctrl Pts',(-198.998068340427,5.77465075171243,
129.505889611662));
#161216=CARTESIAN_POINT('Ctrl Pts',(-199.005481119729,5.73612386966094,
129.353563073315));
#161217=CARTESIAN_POINT('Ctrl Pts',(-199.012904490758,5.6975419385936,129.201018883665));
#161218=CARTESIAN_POINT('Ctrl Pts',(-199.020327861787,5.65291476358045,
129.050188614405));
#161219=CARTESIAN_POINT('Ctrl Pts',(-199.027751232816,5.60243979840348,
128.901573486076));
#161220=CARTESIAN_POINT('Ctrl Pts',(-199.031687282256,5.57567676073842,
128.82277417907));
#161221=CARTESIAN_POINT('Ctrl Pts',(-199.035623331697,5.54727049570574,
128.744597274093));
#161222=CARTESIAN_POINT('Ctrl Pts',(-199.039559381137,5.51725573431446,
128.667114790649));
#161223=CARTESIAN_POINT('Ctrl Pts',(-199.046982647543,5.46064883105527,
128.520985245009));
#161224=CARTESIAN_POINT('Ctrl Pts',(-199.054405913948,5.39814676042029,
128.376885216112));
#161225=CARTESIAN_POINT('Ctrl Pts',(-199.061829180354,5.32991465982133,
128.235325724552));
#161226=CARTESIAN_POINT('Ctrl Pts',(-199.069243673075,5.26176320389876,
128.093933544556));
#161227=CARTESIAN_POINT('Ctrl Pts',(-199.076658165796,5.18789535905273,
127.955076257988));
#161228=CARTESIAN_POINT('Ctrl Pts',(-199.084072658517,5.10852526660425,
127.819247527084));
#161229=CARTESIAN_POINT('Ctrl Pts',(-199.09148000487,5.02923167403911,127.683549713025));
#161230=CARTESIAN_POINT('Ctrl Pts',(-199.098887351224,4.94444657871635,
127.550874963544));
#161231=CARTESIAN_POINT('Ctrl Pts',(-199.106294697578,4.85443117193422,
127.421694722232));
#161232=CARTESIAN_POINT('Ctrl Pts',(-199.113696519254,4.7644829020383,127.292610828418));
#161233=CARTESIAN_POINT('Ctrl Pts',(-199.121098340929,4.66931230052762,
127.16701655816));
#161234=CARTESIAN_POINT('Ctrl Pts',(-199.128500162604,4.56922516608224,
127.045356501561));
#161235=CARTESIAN_POINT('Ctrl Pts',(-199.135898076916,4.46919086685664,
126.92376066836));
#161236=CARTESIAN_POINT('Ctrl Pts',(-199.143295991227,4.36424544012047,
126.806095200239));
#161237=CARTESIAN_POINT('Ctrl Pts',(-199.150693905538,4.25473638670253,
126.692773473631));
#161238=CARTESIAN_POINT('Ctrl Pts',(-199.158090590451,4.14524553170241,
126.579470579038));
#161239=CARTESIAN_POINT('Ctrl Pts',(-199.165487275363,4.0311928143572,126.470510261472));
#161240=CARTESIAN_POINT('Ctrl Pts',(-199.172883960275,3.91296426986117,
126.3662708049));
#161241=CARTESIAN_POINT('Ctrl Pts',(-199.18028031721,3.79474096774303,126.262035970415));
#161242=CARTESIAN_POINT('Ctrl Pts',(-199.187676674146,3.67234248664227,
126.162521827584));
#161243=CARTESIAN_POINT('Ctrl Pts',(-199.195073031081,3.5461895741899,126.068067756434));
#161244=CARTESIAN_POINT('Ctrl Pts',(-199.202470520418,3.42001734740458,
125.973599224125));
#161245=CARTESIAN_POINT('Ctrl Pts',(-199.209868009754,3.29008984357849,
125.884192529796));
#161246=CARTESIAN_POINT('Ctrl Pts',(-199.217265499091,3.15685841191773,
125.800144841882));
#161247=CARTESIAN_POINT('Ctrl Pts',(-199.224665581606,3.02358027618456,
125.716067691181));
#161248=CARTESIAN_POINT('Ctrl Pts',(-199.232065664121,2.8869962222029,125.637353486203));
#161249=CARTESIAN_POINT('Ctrl Pts',(-199.239465746636,2.74758376880045,
125.564254321323));
#161250=CARTESIAN_POINT('Ctrl Pts',(-199.246873966302,2.60801801707374,
125.491074776397));
#161251=CARTESIAN_POINT('Ctrl Pts',(-199.254282185969,2.4656179856307,125.423522775534));
#161252=CARTESIAN_POINT('Ctrl Pts',(-199.261690405635,2.32088348920477,
125.361803278223));
#161253=CARTESIAN_POINT('Ctrl Pts',(-199.269103184937,2.1760599111109,125.300045793591));
#161254=CARTESIAN_POINT('Ctrl Pts',(-199.276515964239,2.028899353128,125.24412809794));
#161255=CARTESIAN_POINT('Ctrl Pts',(-199.283928743541,1.87991800148424,
125.194205640188));
#161256=CARTESIAN_POINT('Ctrl Pts',(-199.29135211457,1.73072377829936,125.144211850888));
#161257=CARTESIAN_POINT('Ctrl Pts',(-199.298775485599,1.57970392286291,
125.100230512364));
#161258=CARTESIAN_POINT('Ctrl Pts',(-199.306198856628,1.42738685480326,
125.062366423104));
#161259=CARTESIAN_POINT('Ctrl Pts',(-199.310134906068,1.34662469051819,
125.042289974441));
#161260=CARTESIAN_POINT('Ctrl Pts',(-199.314070955509,1.26549796615698,
125.023932443002));
#161261=CARTESIAN_POINT('Ctrl Pts',(-199.31800700495,1.18408604672678,125.007303536905));
#161262=CARTESIAN_POINT('Ctrl Pts',(-199.325430271356,1.03054570746349,
124.975941938976));
#161263=CARTESIAN_POINT('Ctrl Pts',(-199.332853537761,0.875526376150656,
124.950637115694));
#161264=CARTESIAN_POINT('Ctrl Pts',(-199.340276804166,0.719547249692918,
124.931526351391));
#161265=CARTESIAN_POINT('Ctrl Pts',(-199.347691296887,0.563752477609392,
124.912438174424));
#161266=CARTESIAN_POINT('Ctrl Pts',(-199.355105789608,0.407000535315681,
124.899529529172));
#161267=CARTESIAN_POINT('Ctrl Pts',(-199.362520282329,0.24982250344574,
124.892887088972));
#161268=CARTESIAN_POINT('Ctrl Pts',(-199.369927628683,0.0927959656810105,
124.886251051005));
#161269=CARTESIAN_POINT('Ctrl Pts',(-199.377334975037,-0.0646554736133486,
124.885869210084));
#161270=CARTESIAN_POINT('Ctrl Pts',(-199.38474232139,-0.221993995317587,
124.891776645347));
#161271=CARTESIAN_POINT('Ctrl Pts',(-199.392144143066,-0.379215168016295,
124.897679674621));
#161272=CARTESIAN_POINT('Ctrl Pts',(-199.399545964741,-0.536323219385118,
124.909862626159));
#161273=CARTESIAN_POINT('Ctrl Pts',(-199.406947786417,-0.692778811524635,
124.928308534679));
#161274=CARTESIAN_POINT('Ctrl Pts',(-199.414345700728,-0.84915181197491,
124.946744705747));
#161275=CARTESIAN_POINT('Ctrl Pts',(-199.421743615039,-1.00487266934929,
124.971437205811));
#161276=CARTESIAN_POINT('Ctrl Pts',(-199.429141529351,-1.15940576566253,
125.00231711264));
#161277=CARTESIAN_POINT('Ctrl Pts',(-199.436538214263,-1.3139131813789,
125.033191887789));
#161278=CARTESIAN_POINT('Ctrl Pts',(-199.443934899175,-1.46723286208119,
125.070251955885));
#161279=CARTESIAN_POINT('Ctrl Pts',(-199.451331584087,-1.61883788530298,
125.113377006308));
#161280=CARTESIAN_POINT('Ctrl Pts',(-199.458727941023,-1.7704361861996,
125.156500144521));
#161281=CARTESIAN_POINT('Ctrl Pts',(-199.466124297958,-1.92031962173487,
125.205687628209));
#161282=CARTESIAN_POINT('Ctrl Pts',(-199.473520654893,-2.06797523750912,
125.260768913666));
#161283=CARTESIAN_POINT('Ctrl Pts',(-199.48091814423,-2.21565345973426,
125.315858632208));
#161284=CARTESIAN_POINT('Ctrl Pts',(-199.488315633567,-2.36110283327585,
125.376843818751));
#161285=CARTESIAN_POINT('Ctrl Pts',(-199.495713122903,-2.50382937664356,
125.443505367221));
#161286=CARTESIAN_POINT('Ctrl Pts',(-199.503113205418,-2.64660595258121,
125.510190283794));
#161287=CARTESIAN_POINT('Ctrl Pts',(-199.510513287933,-2.78665745995995,
125.582555366178));
#161288=CARTESIAN_POINT('Ctrl Pts',(-199.517913370448,-2.92351369405257,
125.660335127428));
#161289=CARTESIAN_POINT('Ctrl Pts',(-199.525321590115,-3.06052041564315,
125.738200415521));
#161290=CARTESIAN_POINT('Ctrl Pts',(-199.532729809781,-3.1943245224501,
125.821492088438));
#161291=CARTESIAN_POINT('Ctrl Pts',(-199.540138029447,-3.3244834141804,
125.909900423496));
#161292=CARTESIAN_POINT('Ctrl Pts',(-199.54755080875,-3.45472241653674,
125.998363172409));
#161293=CARTESIAN_POINT('Ctrl Pts',(-199.554963588052,-3.58131143374482,
126.091948637279));
#161294=CARTESIAN_POINT('Ctrl Pts',(-199.562376367354,-3.7038406709643,
126.190306559949));
#161295=CARTESIAN_POINT('Ctrl Pts',(-199.569799738382,-3.82654498370379,
126.288805021032));
#161296=CARTESIAN_POINT('Ctrl Pts',(-199.577223109411,-3.94517765014855,
126.39208931474));
#161297=CARTESIAN_POINT('Ctrl Pts',(-199.58464648044,-4.05936487664758,
126.499771512815));
#161298=CARTESIAN_POINT('Ctrl Pts',(-199.588582529881,-4.11990968402192,
126.556867198033));
#161299=CARTESIAN_POINT('Ctrl Pts',(-199.592518579321,-4.17920537128048,
126.615198714714));
#161300=CARTESIAN_POINT('Ctrl Pts',(-199.596454628762,-4.23720087198234,
126.674704538306));
#161301=CARTESIAN_POINT('Ctrl Pts',(-199.603780504856,-4.3451435842251,
126.785458302217));
#161302=CARTESIAN_POINT('Ctrl Pts',(-199.611106380951,-4.44892529945081,
126.900636519193));
#161303=CARTESIAN_POINT('Ctrl Pts',(-199.618432257045,-4.54815423714637,
127.01988924132));
#161304=CARTESIAN_POINT('Ctrl Pts',(-199.625749275158,-4.64726319356173,
127.138997770688));
#161305=CARTESIAN_POINT('Ctrl Pts',(-199.633066293272,-4.74183008260889,
127.262170710391));
#161306=CARTESIAN_POINT('Ctrl Pts',(-199.640383311386,-4.83149884976926,
127.389020308435));
#161307=CARTESIAN_POINT('Ctrl Pts',(-199.647691937754,-4.9210647775684,
127.515724425147));
#161308=CARTESIAN_POINT('Ctrl Pts',(-199.655000564122,-5.00574355056634,
127.646096491343));
#161309=CARTESIAN_POINT('Ctrl Pts',(-199.66230919049,-5.08521874467687,
127.779715038116));
#161310=CARTESIAN_POINT('Ctrl Pts',(-199.669613071836,-5.1646423406467,
127.913246834945));
#161311=CARTESIAN_POINT('Ctrl Pts',(-199.676916953183,-5.23886888252049,
128.050020591129));
#161312=CARTESIAN_POINT('Ctrl Pts',(-199.684220834529,-5.30762463042162,
128.18958503541));
#161313=CARTESIAN_POINT('Ctrl Pts',(-199.691521506071,-5.37635016253885,
128.329088145923));
#161314=CARTESIAN_POINT('Ctrl Pts',(-199.698822177613,-5.43960951509057,
128.471379160608));
#161315=CARTESIAN_POINT('Ctrl Pts',(-199.706122849155,-5.49717452749041,
128.615981588053));
#161316=CARTESIAN_POINT('Ctrl Pts',(-199.713421843476,-5.55472631518357,
128.760550795239));
#161317=CARTESIAN_POINT('Ctrl Pts',(-199.720720837798,-5.60658622516097,
128.907430001561));
#161318=CARTESIAN_POINT('Ctrl Pts',(-199.728019832119,-5.6525740654497,
129.05612236232));
#161319=CARTESIAN_POINT('Ctrl Pts',(-199.735321043721,-5.69857587587576,
129.204859892687));
#161320=CARTESIAN_POINT('Ctrl Pts',(-199.742622255322,-5.73870193341256,
129.355411312575));
#161321=CARTESIAN_POINT('Ctrl Pts',(-199.749923466924,-5.77282175169358,
129.50726401913));
#161322=CARTESIAN_POINT('Ctrl Pts',(-199.757225668922,-5.80694619826219,
129.659137324213));
#161323=CARTESIAN_POINT('Ctrl Pts',(-199.764527870919,-5.83506270707501,
129.81231189086));
#161324=CARTESIAN_POINT('Ctrl Pts',(-199.771830072916,-5.85709199383315,
129.966265194433));
#161325=CARTESIAN_POINT('Ctrl Pts',(-199.779138508574,-5.87914008630182,
130.120349923109));
#161326=CARTESIAN_POINT('Ctrl Pts',(-199.786446944231,-5.8950905299074,
130.275214335113));
#161327=CARTESIAN_POINT('Ctrl Pts',(-199.793755379889,-5.90491592475032,
130.430330559776));
#161328=CARTESIAN_POINT('Ctrl Pts',(-199.799711855857,-5.91292375720509,
130.556752424544));
#161329=CARTESIAN_POINT('Ctrl Pts',(-199.805668331824,-5.9168640205334,
130.683341391447));
#161330=CARTESIAN_POINT('Ctrl Pts',(-199.811624807792,-5.91674748832781,
130.809812394026));
#161331=CARTESIAN_POINT('',(-201.561624807792,-5.9216802870108,130.802292919862));
#161332=CARTESIAN_POINT('Ctrl Pts',(-199.811624807792,-5.91707319532089,
130.809812694137));
#161333=CARTESIAN_POINT('Ctrl Pts',(-199.832717289386,-5.92122840583984,
131.257688120002));
#161334=CARTESIAN_POINT('Ctrl Pts',(-199.946625645587,-5.66995203506684,
133.671789078785));
#161335=CARTESIAN_POINT('Ctrl Pts',(-200.153349876387,-2.35938766776408,
137.393051713948));
#161336=CARTESIAN_POINT('Ctrl Pts',(-200.431797500202,4.26794575514161,
136.350728759107));
#161337=CARTESIAN_POINT('Ctrl Pts',(-200.710245124014,6.97324552981307,
130.211564437336));
#161338=CARTESIAN_POINT('Ctrl Pts',(-200.988692747828,3.27047332456854,
124.617150845494));
#161339=CARTESIAN_POINT('Ctrl Pts',(-201.26714037164,-3.43770409444905,
124.708480772182));
#161340=CARTESIAN_POINT('Ctrl Pts',(-201.458117724962,-5.87190273225,128.613207570693));
#161341=CARTESIAN_POINT('Ctrl Pts',(-201.556279203679,-5.9261716932185,
130.689210903785));
#161342=CARTESIAN_POINT('Ctrl Pts',(-201.561624807792,-5.92566153694035,
130.802291529712));
#161343=CARTESIAN_POINT('',(-203.31162480776,-5.91674832526764,130.799908882784));
#161344=CARTESIAN_POINT('Ctrl Pts',(-201.561624807792,-5.91674963930729,
130.802294641516));
#161345=CARTESIAN_POINT('Ctrl Pts',(-201.568982881734,-5.91680390723813,
130.957712590457));
#161346=CARTESIAN_POINT('Ctrl Pts',(-201.576340955677,-5.91073031198679,
131.113380258586));
#161347=CARTESIAN_POINT('Ctrl Pts',(-201.583699029619,-5.89849601535624,
131.26876918696));
#161348=CARTESIAN_POINT('Ctrl Pts',(-201.591048671187,-5.88627573926641,
131.423980039155));
#161349=CARTESIAN_POINT('Ctrl Pts',(-201.598398312754,-5.86790884059778,
131.578912411785));
#161350=CARTESIAN_POINT('Ctrl Pts',(-201.605747954322,-5.84341445076555,
131.733036082454));
#161351=CARTESIAN_POINT('Ctrl Pts',(-201.61309084544,-5.81894255837628,
131.887018194647));
#161352=CARTESIAN_POINT('Ctrl Pts',(-201.620433736558,-5.78835443516488,
132.040192709969));
#161353=CARTESIAN_POINT('Ctrl Pts',(-201.627776627676,-5.75172113270748,
132.192032975893));
#161354=CARTESIAN_POINT('Ctrl Pts',(-201.635114444198,-5.71511314714554,
132.343768306585));
#161355=CARTESIAN_POINT('Ctrl Pts',(-201.64245226072,-5.67246838760474,
132.494170855111));
#161356=CARTESIAN_POINT('Ctrl Pts',(-201.649790077242,-5.62390921912543,
132.642722839093));
#161357=CARTESIAN_POINT('Ctrl Pts',(-201.65712519342,-5.57536792060671,
132.791220155373));
#161358=CARTESIAN_POINT('Ctrl Pts',(-201.664460309597,-5.52091665958435,
132.937867900585));
#161359=CARTESIAN_POINT('Ctrl Pts',(-201.671795425774,-5.46072800920963,
133.082162226999));
#161360=CARTESIAN_POINT('Ctrl Pts',(-201.679129259572,-5.40054988146438,
133.2264313268));
#161361=CARTESIAN_POINT('Ctrl Pts',(-201.68646309337,-5.33463650595489,
133.368347475309));
#161362=CARTESIAN_POINT('Ctrl Pts',(-201.693796927167,-5.2632089776057,
133.507425881401));
#161363=CARTESIAN_POINT('Ctrl Pts',(-201.701130988438,-5.19177923379931,
133.646508601267));
#161364=CARTESIAN_POINT('Ctrl Pts',(-201.708465049707,-5.11483517035096,
133.782753065024));
#161365=CARTESIAN_POINT('Ctrl Pts',(-201.715799110978,-5.03264419073689,
133.915698434638));
#161366=CARTESIAN_POINT('Ctrl Pts',(-201.723134909502,-4.95043374214518,
134.04867529567));
#161367=CARTESIAN_POINT('Ctrl Pts',(-201.730470708027,-4.86297410395734,
134.178351183875));
#161368=CARTESIAN_POINT('Ctrl Pts',(-201.737806506552,-4.77057626898022,
134.304293848978));
#161369=CARTESIAN_POINT('Ctrl Pts',(-201.745149895269,-4.67808283196083,
134.430366824234));
#161370=CARTESIAN_POINT('Ctrl Pts',(-201.752493283986,-4.58064121767003,
134.55269855382));
#161371=CARTESIAN_POINT('Ctrl Pts',(-201.759836672703,-4.4786034494646,
134.67088899648));
#161372=CARTESIAN_POINT('Ctrl Pts',(-201.767183945264,-4.3765117145283,
134.789141948854));
#161373=CARTESIAN_POINT('Ctrl Pts',(-201.774531217824,-4.26981924252526,
134.903248973441));
#161374=CARTESIAN_POINT('Ctrl Pts',(-201.781878490384,-4.15891476263121,
135.012847110317));
#161375=CARTESIAN_POINT('Ctrl Pts',(-201.789236993135,-4.04784076697534,
135.12261276623));
#161376=CARTESIAN_POINT('Ctrl Pts',(-201.796595495886,-3.93254218153233,
135.227855508902));
#161377=CARTESIAN_POINT('Ctrl Pts',(-201.803953998638,-3.81344138899068,
135.328252231567));
#161378=CARTESIAN_POINT('Ctrl Pts',(-201.81064787218,-3.70509792958346,
135.419580996176));
#161379=CARTESIAN_POINT('Ctrl Pts',(-201.817341745723,-3.5936086492963,
135.506900002018));
#161380=CARTESIAN_POINT('Ctrl Pts',(-201.824035619266,-3.47931103503038,
135.589998013359));
#161381=CARTESIAN_POINT('Ctrl Pts',(-201.831458885672,-3.35255906776189,
135.682150736593));
#161382=CARTESIAN_POINT('Ctrl Pts',(-201.838882152077,-3.22195178485856,
135.769403615139));
#161383=CARTESIAN_POINT('Ctrl Pts',(-201.846305418483,-3.0879048581852,
135.851416605892));
#161384=CARTESIAN_POINT('Ctrl Pts',(-201.853719911204,-2.95401636384689,
135.933332664101));
#161385=CARTESIAN_POINT('Ctrl Pts',(-201.861134403924,-2.8166966332044,
136.010020969021));
#161386=CARTESIAN_POINT('Ctrl Pts',(-201.868548896646,-2.67639312130945,
136.081182617852));
#161387=CARTESIAN_POINT('Ctrl Pts',(-201.875956242999,-2.53622483922201,
136.152275678408));
#161388=CARTESIAN_POINT('Ctrl Pts',(-201.883363589353,-2.39307883188319,
136.217852519758));
#161389=CARTESIAN_POINT('Ctrl Pts',(-201.890770935707,-2.24743006191977,
136.277658405854));
#161390=CARTESIAN_POINT('Ctrl Pts',(-201.898172757382,-2.10188992230359,
136.337419686464));
#161391=CARTESIAN_POINT('Ctrl Pts',(-201.905574579058,-1.95385108065789,
136.391418440872));
#161392=CARTESIAN_POINT('Ctrl Pts',(-201.912976400733,-1.80381144299486,
136.439446671977));
#161393=CARTESIAN_POINT('Ctrl Pts',(-201.920374315044,-1.65385101008865,
136.487449549353));
#161394=CARTESIAN_POINT('Ctrl Pts',(-201.927772229356,-1.50189223927456,
136.529488066856));
#161395=CARTESIAN_POINT('Ctrl Pts',(-201.935170143667,-1.34845117572333,
136.56540305702));
#161396=CARTESIAN_POINT('Ctrl Pts',(-201.942566828579,-1.19503561129339,
136.601312078765));
#161397=CARTESIAN_POINT('Ctrl Pts',(-201.949963513491,-1.04013860613695,
136.631099507851));
#161398=CARTESIAN_POINT('Ctrl Pts',(-201.957360198404,-0.884289580498989,
136.654656550279));
#161399=CARTESIAN_POINT('Ctrl Pts',(-201.964756555339,-0.728447465370143,
136.678212548163));
#161400=CARTESIAN_POINT('Ctrl Pts',(-201.972152912275,-0.571653782799518,
136.695538652899));
#161401=CARTESIAN_POINT('Ctrl Pts',(-201.97954926921,-0.414446050683824,
136.706577576775));
#161402=CARTESIAN_POINT('Ctrl Pts',(-201.986946758547,-0.25721424966346,
136.717618190738));
#161403=CARTESIAN_POINT('Ctrl Pts',(-201.994344247883,-0.0995686452809479,
136.722369681061));
#161404=CARTESIAN_POINT('Ctrl Pts',(-202.00174173722,0.0579503942137365,
136.720826819135));
#161405=CARTESIAN_POINT('Ctrl Pts',(-202.009141819735,0.215524651763755,
136.719283416362));
#161406=CARTESIAN_POINT('Ctrl Pts',(-202.016541902249,0.372971883044187,
136.711441271919));
#161407=CARTESIAN_POINT('Ctrl Pts',(-202.023941984764,0.529754145426437,
136.69734722097));
#161408=CARTESIAN_POINT('Ctrl Pts',(-202.031350204431,0.686708806024008,
136.683237672164));
#161409=CARTESIAN_POINT('Ctrl Pts',(-202.038758424097,0.842996665438895,
136.662862521241));
#161410=CARTESIAN_POINT('Ctrl Pts',(-202.046166643764,0.998086579105648,
136.636320300478));
#161411=CARTESIAN_POINT('Ctrl Pts',(-202.053579423066,1.15327194802645,
136.609761743421));
#161412=CARTESIAN_POINT('Ctrl Pts',(-202.060992202368,1.30725753771265,
136.577028630497));
#161413=CARTESIAN_POINT('Ctrl Pts',(-202.06840498167,1.45952526831276,136.538269977999));
#161414=CARTESIAN_POINT('Ctrl Pts',(-202.075828352699,1.61201056618677,
136.49945594532));
#161415=CARTESIAN_POINT('Ctrl Pts',(-202.083251723727,1.76277274582379,
136.454599283991));
#161416=CARTESIAN_POINT('Ctrl Pts',(-202.090675094756,1.91131088775466,
136.403898210337));
#161417=CARTESIAN_POINT('Ctrl Pts',(-202.094611144197,1.99006937472724,
136.377015284531));
#161418=CARTESIAN_POINT('Ctrl Pts',(-202.098547193638,2.06820295967937,
136.34849008045));
#161419=CARTESIAN_POINT('Ctrl Pts',(-202.102483243078,2.14563967604513,
136.318357438664));
#161420=CARTESIAN_POINT('Ctrl Pts',(-202.109906509484,2.29168290639948,
136.261528216662));
#161421=CARTESIAN_POINT('Ctrl Pts',(-202.117329775889,2.43568765092004,
136.198806922689));
#161422=CARTESIAN_POINT('Ctrl Pts',(-202.124753042294,2.5771431409141,136.130359471653));
#161423=CARTESIAN_POINT('Ctrl Pts',(-202.132167535015,2.71843144226654,
136.06199291982));
#161424=CARTESIAN_POINT('Ctrl Pts',(-202.139582027737,2.85717615375475,
135.987913843359));
#161425=CARTESIAN_POINT('Ctrl Pts',(-202.146996520458,2.99288393960237,
135.908337134613));
#161426=CARTESIAN_POINT('Ctrl Pts',(-202.154403866811,3.12846092517669,
135.828837124895));
#161427=CARTESIAN_POINT('Ctrl Pts',(-202.161811213165,3.26100649253989,
135.743850219369));
#161428=CARTESIAN_POINT('Ctrl Pts',(-202.169218559519,3.39004959613795,
135.653638326486));
#161429=CARTESIAN_POINT('Ctrl Pts',(-202.176620381194,3.51899645452082,
135.563493717036));
#161430=CARTESIAN_POINT('Ctrl Pts',(-202.18402220287,3.64444574588738,135.468132092632));
#161431=CARTESIAN_POINT('Ctrl Pts',(-202.191424024545,3.76595334602514,
135.36785992819));
#161432=CARTESIAN_POINT('Ctrl Pts',(-202.198821938857,3.88739680324591,
135.267640696643));
#161433=CARTESIAN_POINT('Ctrl Pts',(-202.206219853168,4.00490242603697,
135.16251632462));
#161434=CARTESIAN_POINT('Ctrl Pts',(-202.213617767479,4.11805736728282,
135.052834941634));
#161435=CARTESIAN_POINT('Ctrl Pts',(-202.221014452392,4.23119350423076,
134.943171785704));
#161436=CARTESIAN_POINT('Ctrl Pts',(-202.228411137304,4.33998012680202,
134.828953381375));
#161437=CARTESIAN_POINT('Ctrl Pts',(-202.235807822216,4.44403953894811,
134.710566339077));
#161438=CARTESIAN_POINT('Ctrl Pts',(-202.243204179152,4.54809433699053,
134.592184546185));
#161439=CARTESIAN_POINT('Ctrl Pts',(-202.250600536087,4.64742209493324,
134.469634763234));
#161440=CARTESIAN_POINT('Ctrl Pts',(-202.257996893022,4.74168407344933,
134.343338253847));
#161441=CARTESIAN_POINT('Ctrl Pts',(-202.265394382359,4.83596048371523,
134.217022408141));
#161442=CARTESIAN_POINT('Ctrl Pts',(-202.272791871696,4.92516934696955,
134.086958992999));
#161443=CARTESIAN_POINT('Ctrl Pts',(-202.280189361032,5.00901418199923,
133.953599809344));
#161444=CARTESIAN_POINT('Ctrl Pts',(-202.287589443547,5.09288840870597,
133.820193876833));
#161445=CARTESIAN_POINT('Ctrl Pts',(-202.294989526062,5.17139466485451,
133.683490191393));
#161446=CARTESIAN_POINT('Ctrl Pts',(-202.302389608577,5.24428158306487,
133.543966654942));
#161447=CARTESIAN_POINT('Ctrl Pts',(-202.309797828244,5.31724864793465,
133.40428969802));
#161448=CARTESIAN_POINT('Ctrl Pts',(-202.31720604791,5.3845838619657,133.261787028827));
#161449=CARTESIAN_POINT('Ctrl Pts',(-202.324614267577,5.44608302654156,
133.116958773432));
#161450=CARTESIAN_POINT('Ctrl Pts',(-202.332027046879,5.50762004282705,
132.972041378663));
#161451=CARTESIAN_POINT('Ctrl Pts',(-202.339439826181,5.56331372040708,
132.824795893876));
#161452=CARTESIAN_POINT('Ctrl Pts',(-202.346852605483,5.61300939609337,
132.675738741267));
#161453=CARTESIAN_POINT('Ctrl Pts',(-202.354275976512,5.66277607929151,
132.526468608809));
#161454=CARTESIAN_POINT('Ctrl Pts',(-202.361699347541,5.70652754037334,
132.375381996141));
#161455=CARTESIAN_POINT('Ctrl Pts',(-202.36912271857,5.74415978513868,132.223007481763));
#161456=CARTESIAN_POINT('Ctrl Pts',(-202.37305876801,5.76411330428583,132.142214858066));
#161457=CARTESIAN_POINT('Ctrl Pts',(-202.376994817451,5.78234735340238,
132.061060290616));
#161458=CARTESIAN_POINT('Ctrl Pts',(-202.380930866892,5.79885234516005,
131.9796231591));
#161459=CARTESIAN_POINT('Ctrl Pts',(-202.388354133297,5.82998024451299,
131.82603527062));
#161460=CARTESIAN_POINT('Ctrl Pts',(-202.395777399702,5.85504912545923,
131.670977609184));
#161461=CARTESIAN_POINT('Ctrl Pts',(-202.403200666108,5.87392249395432,
131.514969580018));
#161462=CARTESIAN_POINT('Ctrl Pts',(-202.410615158829,5.89277355569518,
131.359145939387));
#161463=CARTESIAN_POINT('Ctrl Pts',(-202.41802965155,5.90544363622744,131.202374533849));
#161464=CARTESIAN_POINT('Ctrl Pts',(-202.425444144271,5.91184687052777,
131.045186575326));
#161465=CARTESIAN_POINT('Ctrl Pts',(-202.432851490625,5.91824393314985,
130.888150120474));
#161466=CARTESIAN_POINT('Ctrl Pts',(-202.440258836978,5.91838615934132,
130.730698282408));
#161467=CARTESIAN_POINT('Ctrl Pts',(-202.447666183332,5.91223928847316,
130.573368933009));
#161468=CARTESIAN_POINT('Ctrl Pts',(-202.455068005008,5.90609700217325,
130.416156925776));
#161469=CARTESIAN_POINT('Ctrl Pts',(-202.462469826683,5.8936749730336,130.259067596714));
#161470=CARTESIAN_POINT('Ctrl Pts',(-202.469871648358,5.87499098709605,
130.10264025728));
#161471=CARTESIAN_POINT('Ctrl Pts',(-202.47726956267,5.85631686428913,129.94629549462));
#161472=CARTESIAN_POINT('Ctrl Pts',(-202.484667476981,5.83138741218186,
129.790612395348));
#161473=CARTESIAN_POINT('Ctrl Pts',(-202.492065391293,5.80027236804441,
129.636126471943));
#161474=CARTESIAN_POINT('Ctrl Pts',(-202.499462076205,5.76916249466294,
129.481666221295));
#161475=CARTESIAN_POINT('Ctrl Pts',(-202.506858761117,5.73186914302823,
129.328403117249));
#161476=CARTESIAN_POINT('Ctrl Pts',(-202.514255446029,5.68851342550535,
129.176863898569));
#161477=CARTESIAN_POINT('Ctrl Pts',(-202.521651802964,5.64515963042055,
129.025331399297));
#161478=CARTESIAN_POINT('Ctrl Pts',(-202.5290481599,5.59574410661747,128.875522992302));
#161479=CARTESIAN_POINT('Ctrl Pts',(-202.536444516835,5.54043817823208,
128.727951371852));
#161480=CARTESIAN_POINT('Ctrl Pts',(-202.543842006172,5.48512378236803,
128.580357157809));
#161481=CARTESIAN_POINT('Ctrl Pts',(-202.551239495508,5.42391731725896,
128.435000761769));
#161482=CARTESIAN_POINT('Ctrl Pts',(-202.558636984845,5.35703864047963,
128.292375831205));
#161483=CARTESIAN_POINT('Ctrl Pts',(-202.56603706736,5.29013651948354,128.149700903693));
#161484=CARTESIAN_POINT('Ctrl Pts',(-202.573437149875,5.21755838634373,
128.009759685829));
#161485=CARTESIAN_POINT('Ctrl Pts',(-202.58083723239,5.13957044327107,127.873021977771));
#161486=CARTESIAN_POINT('Ctrl Pts',(-202.588245452056,5.06149674443775,
127.736133912546));
#161487=CARTESIAN_POINT('Ctrl Pts',(-202.595653671723,4.9780015408993,127.60245671643));
#161488=CARTESIAN_POINT('Ctrl Pts',(-202.603061891389,4.8893952285411,127.472432517859));
#161489=CARTESIAN_POINT('Ctrl Pts',(-202.610474670691,4.80073438047586,
127.342328291562));
#161490=CARTESIAN_POINT('Ctrl Pts',(-202.617887449993,4.70695637704169,
127.215881842089));
#161491=CARTESIAN_POINT('Ctrl Pts',(-202.625300229295,4.60841209962781,
127.093502430771));
#161492=CARTESIAN_POINT('Ctrl Pts',(-202.632723600324,4.50972701752896,
126.970948158011));
#161493=CARTESIAN_POINT('Ctrl Pts',(-202.640146971353,4.40626230469941,
126.852472810054));
#161494=CARTESIAN_POINT('Ctrl Pts',(-202.647570342382,4.29840645779756,
126.738449589756));
#161495=CARTESIAN_POINT('Ctrl Pts',(-202.651506391822,4.24121869980284,
126.677991742403));
#161496=CARTESIAN_POINT('Ctrl Pts',(-202.655442441263,4.18279701272454,
126.618784894444));
#161497=CARTESIAN_POINT('Ctrl Pts',(-202.659378490704,4.12320299875834,
126.560880018632));
#161498=CARTESIAN_POINT('Ctrl Pts',(-202.66680175711,4.01081054828672,126.451673230002));
#161499=CARTESIAN_POINT('Ctrl Pts',(-202.674225023515,3.89390648875168,
126.346769616974));
#161500=CARTESIAN_POINT('Ctrl Pts',(-202.681648289921,3.77285403211578,
126.246564767065));
#161501=CARTESIAN_POINT('Ctrl Pts',(-202.689062782642,3.65194464943049,
126.146478350966));
#161502=CARTESIAN_POINT('Ctrl Pts',(-202.696477275363,3.52689691396513,
126.051079879331));
#161503=CARTESIAN_POINT('Ctrl Pts',(-202.703891768084,3.39811133721108,
125.960728725853));
#161504=CARTESIAN_POINT('Ctrl Pts',(-202.711299114438,3.2694498888457,125.87046465622));
#161505=CARTESIAN_POINT('Ctrl Pts',(-202.718706460791,3.13705807494424,
125.785238432848));
#161506=CARTESIAN_POINT('Ctrl Pts',(-202.726113807145,3.00136990364706,
125.705369613065));
#161507=CARTESIAN_POINT('Ctrl Pts',(-202.733515628821,2.86578293370648,
125.625560362461));
#161508=CARTESIAN_POINT('Ctrl Pts',(-202.740917450496,2.7269048219899,125.551100747908));
#161509=CARTESIAN_POINT('Ctrl Pts',(-202.748319272171,2.5851989202899,125.482267316521));
#161510=CARTESIAN_POINT('Ctrl Pts',(-202.755717186483,2.44356782403319,
125.413470221767));
#161511=CARTESIAN_POINT('Ctrl Pts',(-202.763115100794,2.29911224564274,
125.350293557936));
#161512=CARTESIAN_POINT('Ctrl Pts',(-202.770513015105,2.15232042163001,
125.292968110664));
#161513=CARTESIAN_POINT('Ctrl Pts',(-202.777909700018,2.00555299175515,
125.235652189841));
#161514=CARTESIAN_POINT('Ctrl Pts',(-202.78530638493,1.85645043418548,125.184185691378));
#161515=CARTESIAN_POINT('Ctrl Pts',(-202.792703069842,1.70552137335281,
125.13875143518));
#161516=CARTESIAN_POINT('Ctrl Pts',(-202.800099426778,1.55459900487243,
125.093319193584));
#161517=CARTESIAN_POINT('Ctrl Pts',(-202.807495783713,1.40185065161534,
125.053918770026));
#161518=CARTESIAN_POINT('Ctrl Pts',(-202.814892140649,1.2478002626691,125.020683148431));
#161519=CARTESIAN_POINT('Ctrl Pts',(-202.822289629985,1.09372628821504,
124.987442438377));
#161520=CARTESIAN_POINT('Ctrl Pts',(-202.829687119322,0.938350246075035,
124.960368488343));
#161521=CARTESIAN_POINT('Ctrl Pts',(-202.837084608658,0.782206294241051,
124.939543154443));
#161522=CARTESIAN_POINT('Ctrl Pts',(-202.844484691173,0.626007606387029,
124.918710520255));
#161523=CARTESIAN_POINT('Ctrl Pts',(-202.851884773688,0.469040842675188,
124.904130912675));
#161524=CARTESIAN_POINT('Ctrl Pts',(-202.859284856203,0.311845148080142,
124.895834306707));
#161525=CARTESIAN_POINT('Ctrl Pts',(-202.86669307587,0.154476600659004,
124.887528577766));
#161526=CARTESIAN_POINT('Ctrl Pts',(-202.874101295536,-0.00312100736494086,
124.885519667463));
#161527=CARTESIAN_POINT('Ctrl Pts',(-202.881509515203,-0.160407924259452,
124.889785412166));
#161528=CARTESIAN_POINT('Ctrl Pts',(-202.888922294505,-0.317791648627735,
124.894053782363));
#161529=CARTESIAN_POINT('Ctrl Pts',(-202.896335073807,-0.474863929231365,
124.904604478017));
#161530=CARTESIAN_POINT('Ctrl Pts',(-202.903747853109,-0.631090782958744,
124.921363508425));
#161531=CARTESIAN_POINT('Ctrl Pts',(-202.911171224138,-0.787540860940819,
124.938146484921));
#161532=CARTESIAN_POINT('Ctrl Pts',(-202.918594595167,-0.943142731124381,
124.961155458605));
#161533=CARTESIAN_POINT('Ctrl Pts',(-202.926017966195,-1.09737241544244,
124.990265301498));
#161534=CARTESIAN_POINT('Ctrl Pts',(-202.929954015636,-1.17914869475504,
125.00570003868));
#161535=CARTESIAN_POINT('Ctrl Pts',(-202.933890065077,-1.260539441657,125.022849111077));
#161536=CARTESIAN_POINT('Ctrl Pts',(-202.937826114517,-1.34146847383707,
125.041688243033));
#161537=CARTESIAN_POINT('Ctrl Pts',(-202.945249380923,-1.49409810282559,
125.077218257956));
#161538=CARTESIAN_POINT('Ctrl Pts',(-202.952672647328,-1.64554598320926,
125.118869988883));
#161539=CARTESIAN_POINT('Ctrl Pts',(-202.960095913734,-1.79528297106824,
125.166551680018));
#161540=CARTESIAN_POINT('Ctrl Pts',(-202.967510406455,-1.94484298224202,
125.214177015355));
#161541=CARTESIAN_POINT('Ctrl Pts',(-202.974924899176,-2.0926957737322,
125.267818012581));
#161542=CARTESIAN_POINT('Ctrl Pts',(-202.982339391897,-2.23832250802715,
125.327331960296));
#161543=CARTESIAN_POINT('Ctrl Pts',(-202.98974673825,-2.38380888179367,
125.386788546228));
#161544=CARTESIAN_POINT('Ctrl Pts',(-202.997154084604,-2.52707312651263,
125.452106673295));
#161545=CARTESIAN_POINT('Ctrl Pts',(-203.004561430958,-2.66761179755283,
125.523093926699));
#161546=CARTESIAN_POINT('Ctrl Pts',(-203.011963252633,-2.80804564954954,
125.594028235132));
#161547=CARTESIAN_POINT('Ctrl Pts',(-203.019365074309,-2.94575764374757,
125.670623083307));
#161548=CARTESIAN_POINT('Ctrl Pts',(-203.026766895984,-3.08026466026495,
125.752638120712));
#161549=CARTESIAN_POINT('Ctrl Pts',(-203.034164810295,-3.21470067157453,
125.834609863016));
#161550=CARTESIAN_POINT('Ctrl Pts',(-203.041562724607,-3.34593475675407,
125.921995902334));
#161551=CARTESIAN_POINT('Ctrl Pts',(-203.048960638918,-3.47350884555318,
126.014510216733));
#161552=CARTESIAN_POINT('Ctrl Pts',(-203.05635732383,-3.60106173385371,
126.107009156931));
#161553=CARTESIAN_POINT('Ctrl Pts',(-203.063754008742,-3.72495553101644,
126.20463446186));
#161554=CARTESIAN_POINT('Ctrl Pts',(-203.071150693655,-3.84476150154799,
126.307057030002));
#161555=CARTESIAN_POINT('Ctrl Pts',(-203.07854705059,-3.96456215975726,
126.409475056621));
#161556=CARTESIAN_POINT('Ctrl Pts',(-203.085943407525,-4.08027506799617,
126.516689680931));
#161557=CARTESIAN_POINT('Ctrl Pts',(-203.093339764461,-4.19150513584072,
126.628331970787));
#161558=CARTESIAN_POINT('Ctrl Pts',(-203.100737253797,-4.3027522332923,
126.739991353362));
#161559=CARTESIAN_POINT('Ctrl Pts',(-203.108134743134,-4.40951486027692,
126.85607948678));
#161560=CARTESIAN_POINT('Ctrl Pts',(-203.11553223247,-4.51143542348493,
126.976191214023));
#161561=CARTESIAN_POINT('Ctrl Pts',(-203.122932314985,-4.61339171478823,
127.096345046245));
#161562=CARTESIAN_POINT('Ctrl Pts',(-203.1303323975,-4.71050232147278,127.220524996061));
#161563=CARTESIAN_POINT('Ctrl Pts',(-203.137732480015,-4.80245060369318,
127.348293667753));
#161564=CARTESIAN_POINT('Ctrl Pts',(-203.145140699682,-4.89449999250279,
127.476202834236));
#161565=CARTESIAN_POINT('Ctrl Pts',(-203.152548919348,-4.98137550230915,
127.607708300172));
#161566=CARTESIAN_POINT('Ctrl Pts',(-203.159957139014,-5.06280403100677,
127.74234397716));
#161567=CARTESIAN_POINT('Ctrl Pts',(-203.167369918316,-5.14428267760486,
127.87706252016));
#161568=CARTESIAN_POINT('Ctrl Pts',(-203.174782697619,-5.22030748290961,
128.014914787064));
#161569=CARTESIAN_POINT('Ctrl Pts',(-203.182195476921,-5.29065206648016,
128.155411528975));
#161570=CARTESIAN_POINT('Ctrl Pts',(-203.189618847949,-5.36109716169105,
128.296109019219));
#161571=CARTESIAN_POINT('Ctrl Pts',(-203.197042218978,-5.42584567210385,
128.43945819178));
#161572=CARTESIAN_POINT('Ctrl Pts',(-203.204465590007,-5.48471964848875,
128.584950574338));
#161573=CARTESIAN_POINT('Ctrl Pts',(-203.208401639448,-5.51593604343254,
128.662094126619));
#161574=CARTESIAN_POINT('Ctrl Pts',(-203.212337688889,-5.54550172992229,
128.739839959623));
#161575=CARTESIAN_POINT('Ctrl Pts',(-203.21627373833,-5.5733959533535,128.818110857429));
#161576=CARTESIAN_POINT('Ctrl Pts',(-203.224921721089,-5.63468297906373,
128.990081607504));
#161577=CARTESIAN_POINT('Ctrl Pts',(-203.233569703848,-5.68805083248295,
129.165014549172));
#161578=CARTESIAN_POINT('Ctrl Pts',(-203.242217686606,-5.73324512702968,
129.342228313056));
#161579=CARTESIAN_POINT('Ctrl Pts',(-203.250830811819,-5.77825725629626,
129.518727778925));
#161580=CARTESIAN_POINT('Ctrl Pts',(-203.259443937031,-5.81516149890193,
129.697489615715));
#161581=CARTESIAN_POINT('Ctrl Pts',(-203.268057062243,-5.84375315109936,
129.877818836794));
#161582=CARTESIAN_POINT('Ctrl Pts',(-203.276602616523,-5.87212049858119,
130.056733354925));
#161583=CARTESIAN_POINT('Ctrl Pts',(-203.285148170803,-5.89230509977486,
130.237190643914));
#161584=CARTESIAN_POINT('Ctrl Pts',(-203.293693725083,-5.90415413278233,
130.418492066309));
#161585=CARTESIAN_POINT('Ctrl Pts',(-203.299670752642,-5.91244171653796,
130.545299943557));
#161586=CARTESIAN_POINT('Ctrl Pts',(-203.305647780201,-5.91665247871619,
130.672520358863));
#161587=CARTESIAN_POINT('Ctrl Pts',(-203.31162480776,-5.91674832526764,
130.799908882784));
#161588=CARTESIAN_POINT('',(-205.061626015508,-5.91263662896126,130.80817859488));
#161589=CARTESIAN_POINT('Ctrl Pts',(-203.311624807792,-5.91674832526815,
130.799908883463));
#161590=CARTESIAN_POINT('Ctrl Pts',(-203.31925383089,-5.91687066290775,
130.962506425771));
#161591=CARTESIAN_POINT('Ctrl Pts',(-203.326882853988,-5.91028565918037,
131.125172439786));
#161592=CARTESIAN_POINT('Ctrl Pts',(-203.334511877086,-5.8970065749038,
131.287314050147));
#161593=CARTESIAN_POINT('Ctrl Pts',(-203.341914747701,-5.88412113183752,
131.444649183011));
#161594=CARTESIAN_POINT('Ctrl Pts',(-203.349317618315,-5.86493289222459,
131.601490170919));
#161595=CARTESIAN_POINT('Ctrl Pts',(-203.35672048893,-5.83950678773434,
131.757298725999));
#161596=CARTESIAN_POINT('Ctrl Pts',(-203.364124032299,-5.81407837258119,
131.913121440585));
#161597=CARTESIAN_POINT('Ctrl Pts',(-203.371527575669,-5.78241102307281,
132.067911168375));
#161598=CARTESIAN_POINT('Ctrl Pts',(-203.378931119038,-5.7446210682295,
132.22113842123));
#161599=CARTESIAN_POINT('Ctrl Pts',(-203.386336782644,-5.70682029105092,
132.374409555499));
#161600=CARTESIAN_POINT('Ctrl Pts',(-203.39374244625,-5.66289350593888,
132.526116962837));
#161601=CARTESIAN_POINT('Ctrl Pts',(-203.401148109856,-5.61300728187641,
132.675745082635));
#161602=CARTESIAN_POINT('Ctrl Pts',(-203.40894588088,-5.56047973361094,
132.833295557386));
#161603=CARTESIAN_POINT('Ctrl Pts',(-203.416743651903,-5.5013446649065,
132.988540125356));
#161604=CARTESIAN_POINT('Ctrl Pts',(-203.424541422927,-5.43585428549973,
133.1409005272));
#161605=CARTESIAN_POINT('Ctrl Pts',(-203.431959917198,-5.37354930079099,
133.285850252536));
#161606=CARTESIAN_POINT('Ctrl Pts',(-203.439378411468,-5.305492808283,133.428189425049));
#161607=CARTESIAN_POINT('Ctrl Pts',(-203.446796905739,-5.23194910023918,
133.567445700405));
#161608=CARTESIAN_POINT('Ctrl Pts',(-203.454220864128,-5.15835122331424,
133.706804545468));
#161609=CARTESIAN_POINT('Ctrl Pts',(-203.461644822517,-5.07925826396159,
133.84307564888));
#161610=CARTESIAN_POINT('Ctrl Pts',(-203.469068780906,-4.99497801599823,
133.975815359825));
#161611=CARTESIAN_POINT('Ctrl Pts',(-203.47650313371,-4.91057976578007,
134.108740921968));
#161612=CARTESIAN_POINT('Ctrl Pts',(-203.483937486513,-4.82097993977899,
134.238124918073));
#161613=CARTESIAN_POINT('Ctrl Pts',(-203.491371839317,-4.72652713722884,
134.363556001854));
#161614=CARTESIAN_POINT('Ctrl Pts',(-203.492488346925,-4.71234200565376,
134.382393520477));
#161615=CARTESIAN_POINT('Ctrl Pts',(-203.493604854534,-4.69804748499611,
134.401141949454));
#161616=CARTESIAN_POINT('Ctrl Pts',(-203.494721362142,-4.68364482727004,
134.419799967699));
#161617=CARTESIAN_POINT('Ctrl Pts',(-203.502144628548,-4.58788662156608,
134.543850568851));
#161618=CARTESIAN_POINT('Ctrl Pts',(-203.509567894953,-4.48705182451503,
134.664281756115));
#161619=CARTESIAN_POINT('Ctrl Pts',(-203.516991161359,-4.38144383707481,
134.78065040392));
#161620=CARTESIAN_POINT('Ctrl Pts',(-203.52440565408,-4.27596066950554,
134.896881513646));
#161621=CARTESIAN_POINT('Ctrl Pts',(-203.531820146801,-4.16571578943428,
135.009059367759));
#161622=CARTESIAN_POINT('Ctrl Pts',(-203.539234639522,-4.05105465877887,
135.116771395088));
#161623=CARTESIAN_POINT('Ctrl Pts',(-203.546641985876,-3.93650404283811,
135.22437960551));
#161624=CARTESIAN_POINT('Ctrl Pts',(-203.55404933223,-3.81754592051431,
135.327530304353));
#161625=CARTESIAN_POINT('Ctrl Pts',(-203.561456678584,-3.69456456150438,
135.425845580581));
#161626=CARTESIAN_POINT('Ctrl Pts',(-203.568858500259,-3.57167492663218,
135.524087529567));
#161627=CARTESIAN_POINT('Ctrl Pts',(-203.576260321934,-3.44476832015857,
135.617501004755));
#161628=CARTESIAN_POINT('Ctrl Pts',(-203.58366214361,-3.31426416180886,
135.705746506093));
#161629=CARTESIAN_POINT('Ctrl Pts',(-203.591060057921,-3.18382889558812,
135.793945423318));
#161630=CARTESIAN_POINT('Ctrl Pts',(-203.598457972233,-3.04980016813304,
135.876981591329));
#161631=CARTESIAN_POINT('Ctrl Pts',(-203.605855886544,-2.91262852580243,
135.954557277227));
#161632=CARTESIAN_POINT('Ctrl Pts',(-203.613252571456,-2.77547967891002,
136.032120071453));
#161633=CARTESIAN_POINT('Ctrl Pts',(-203.620649256369,-2.63518927836053,
136.104224000971));
#161634=CARTESIAN_POINT('Ctrl Pts',(-203.628045941281,-2.49223485864503,
136.170615920089));
#161635=CARTESIAN_POINT('Ctrl Pts',(-203.635442298216,-2.3492867776783,
136.23700489532));
#161636=CARTESIAN_POINT('Ctrl Pts',(-203.642838655152,-2.20367525098471,
136.297682206512));
#161637=CARTESIAN_POINT('Ctrl Pts',(-203.650235012087,-2.05590005455707,
136.352441865004));
#161638=CARTESIAN_POINT('Ctrl Pts',(-203.657632501424,-1.90810223337002,
136.40720990734));
#161639=CARTESIAN_POINT('Ctrl Pts',(-203.665029990761,-1.75814043291998,
136.456058363276));
#161640=CARTESIAN_POINT('Ctrl Pts',(-203.672427480097,-1.60653179003577,
136.498830405887));
#161641=CARTESIAN_POINT('Ctrl Pts',(-203.679827562612,-1.45487000097703,
136.541617442172));
#161642=CARTESIAN_POINT('Ctrl Pts',(-203.687227645127,-1.30156057913766,
136.578323722869));
#161643=CARTESIAN_POINT('Ctrl Pts',(-203.694627727642,-1.14713296000083,
136.60884306948));
#161644=CARTESIAN_POINT('Ctrl Pts',(-203.702035947309,-0.992535531820553,
136.63939597525));
#161645=CARTESIAN_POINT('Ctrl Pts',(-203.709444166976,-0.836817817244495,
136.663748288138));
#161646=CARTESIAN_POINT('Ctrl Pts',(-203.716852386642,-0.680517251053971,
136.681845354553));
#161647=CARTESIAN_POINT('Ctrl Pts',(-203.724265165944,-0.524120484472526,
136.699953559411));
#161648=CARTESIAN_POINT('Ctrl Pts',(-203.731677945247,-0.367140522827894,
136.711798818167));
#161649=CARTESIAN_POINT('Ctrl Pts',(-203.739090724549,-0.210116445125973,
136.717378598427));
#161650=CARTESIAN_POINT('Ctrl Pts',(-203.746514095577,-0.0528680040588055,
136.722966351339));
#161651=CARTESIAN_POINT('Ctrl Pts',(-203.753937466606,0.104424306655523,
136.722270747431));
#161652=CARTESIAN_POINT('Ctrl Pts',(-203.761360837635,0.261224055224296,
136.715341293856));
#161653=CARTESIAN_POINT('Ctrl Pts',(-203.765296887076,0.344363044267299,
136.711667131301));
#161654=CARTESIAN_POINT('Ctrl Pts',(-203.769232936516,0.427363673358813,
136.706241273284));
#161655=CARTESIAN_POINT('Ctrl Pts',(-203.773168985957,0.510147086307701,
136.699076939225));
#161656=CARTESIAN_POINT('Ctrl Pts',(-203.780592252362,0.666274019559398,
136.68556522878));
#161657=CARTESIAN_POINT('Ctrl Pts',(-203.788015518767,0.822099859025682,
136.665826056643));
#161658=CARTESIAN_POINT('Ctrl Pts',(-203.795438785173,0.977087794984135,
136.639875162436));
#161659=CARTESIAN_POINT('Ctrl Pts',(-203.802853277894,1.13189254807323,
136.613954940032));
#161660=CARTESIAN_POINT('Ctrl Pts',(-203.810267770615,1.28586100433918,
136.581837670375));
#161661=CARTESIAN_POINT('Ctrl Pts',(-203.817682263336,1.43845932536675,
136.543590995567));
#161662=CARTESIAN_POINT('Ctrl Pts',(-203.82508960969,1.59091056638773,136.505381184343));
#161663=CARTESIAN_POINT('Ctrl Pts',(-203.832496956044,1.74199394153385,
136.461053819284));
#161664=CARTESIAN_POINT('Ctrl Pts',(-203.839904302397,1.8911837963895,136.410727927222));
#161665=CARTESIAN_POINT('Ctrl Pts',(-203.847306124073,2.04026237982279,
136.360439570108));
#161666=CARTESIAN_POINT('Ctrl Pts',(-203.854707945748,2.18744990277064,
136.30416171299));
#161667=CARTESIAN_POINT('Ctrl Pts',(-203.862109767424,2.33223402761866,
136.24206371749));
#161668=CARTESIAN_POINT('Ctrl Pts',(-203.869507681735,2.47694172205335,
136.179998503038));
#161669=CARTESIAN_POINT('Ctrl Pts',(-203.876905596046,2.61924820292951,
136.112119415821));
#161670=CARTESIAN_POINT('Ctrl Pts',(-203.884303510358,2.7586594478157,136.038644581345));
#161671=CARTESIAN_POINT('Ctrl Pts',(-203.89170019527,2.89804752508276,135.965181957054));
#161672=CARTESIAN_POINT('Ctrl Pts',(-203.899096880182,3.03454099135519,
135.886125604982));
#161673=CARTESIAN_POINT('Ctrl Pts',(-203.906493565094,3.16766874893783,
135.801740456992));
#161674=CARTESIAN_POINT('Ctrl Pts',(-203.91388992203,3.30079060349657,135.717359050728));
#161675=CARTESIAN_POINT('Ctrl Pts',(-203.921286278965,3.43054673081018,
135.627649518213));
#161676=CARTESIAN_POINT('Ctrl Pts',(-203.928682635901,3.55649368565297,
135.532920993242));
#161677=CARTESIAN_POINT('Ctrl Pts',(-203.936080125237,3.68245992329573,
135.438177965092));
#161678=CARTESIAN_POINT('Ctrl Pts',(-203.943477614574,3.80461552889866,
135.338414638858));
#161679=CARTESIAN_POINT('Ctrl Pts',(-203.95087510391,3.92254903444112,135.233981327616));
#161680=CARTESIAN_POINT('Ctrl Pts',(-203.958275186425,4.04052388139095,
135.12951140744));
#161681=CARTESIAN_POINT('Ctrl Pts',(-203.96567526894,4.15427340221235,135.020368490215));
#161682=CARTESIAN_POINT('Ctrl Pts',(-203.973075351455,4.26342209311666,
134.906940612938));
#161683=CARTESIAN_POINT('Ctrl Pts',(-203.980483571122,4.37269080422754,
134.793388010048));
#161684=CARTESIAN_POINT('Ctrl Pts',(-203.987891790788,4.47734832309786,
134.675541306575));
#161685=CARTESIAN_POINT('Ctrl Pts',(-203.995300010455,4.57705817148828,
134.55382312002));
#161686=CARTESIAN_POINT('Ctrl Pts',(-204.002712789757,4.6768293896272,134.432030017952));
#161687=CARTESIAN_POINT('Ctrl Pts',(-204.010125569059,4.77164664501153,
134.306360982011));
#161688=CARTESIAN_POINT('Ctrl Pts',(-204.017538348361,4.8612164216961,134.177268185812));
#161689=CARTESIAN_POINT('Ctrl Pts',(-204.02496171939,4.95091417987762,134.047990935772));
#161690=CARTESIAN_POINT('Ctrl Pts',(-204.032385090419,5.03534928462894,
133.915280469116));
#161691=CARTESIAN_POINT('Ctrl Pts',(-204.039808461447,5.11427343323228,
133.779614860926));
#161692=CARTESIAN_POINT('Ctrl Pts',(-204.043744510888,5.15612091057836,
133.707681700217));
#161693=CARTESIAN_POINT('Ctrl Pts',(-204.047680560328,5.19641984998835,
133.634918111469));
#161694=CARTESIAN_POINT('Ctrl Pts',(-204.051616609769,5.23513874963715,
133.561397584048));
#161695=CARTESIAN_POINT('Ctrl Pts',(-204.059039876174,5.30816138600291,
133.422740163822));
#161696=CARTESIAN_POINT('Ctrl Pts',(-204.06646314258,5.3757819339304,133.280969967167));
#161697=CARTESIAN_POINT('Ctrl Pts',(-204.073886408985,5.437723476843,133.136547134955));
#161698=CARTESIAN_POINT('Ctrl Pts',(-204.081300901706,5.49959180999563,
132.992294998537));
#161699=CARTESIAN_POINT('Ctrl Pts',(-204.088715394427,5.5557943529252,132.845396806912));
#161700=CARTESIAN_POINT('Ctrl Pts',(-204.096129887148,5.60609946214324,
132.696338255663));
#161701=CARTESIAN_POINT('Ctrl Pts',(-204.103537233502,5.65635608540307,
132.547423372657));
#161702=CARTESIAN_POINT('Ctrl Pts',(-204.110944579855,5.70072647244532,
132.396352626674));
#161703=CARTESIAN_POINT('Ctrl Pts',(-204.118351926209,5.73902663486398,
132.243632602572));
#161704=CARTESIAN_POINT('Ctrl Pts',(-204.125753747884,5.77729823157674,
132.091026482824));
#161705=CARTESIAN_POINT('Ctrl Pts',(-204.13315556956,5.80950852791993,131.936773894766));
#161706=CARTESIAN_POINT('Ctrl Pts',(-204.140557391235,5.83552308162863,
131.781397426637));
#161707=CARTESIAN_POINT('Ctrl Pts',(-204.147955305546,5.86152390245685,
131.626102980537));
#161708=CARTESIAN_POINT('Ctrl Pts',(-204.155353219858,5.88133543288823,
131.469686203167));
#161709=CARTESIAN_POINT('Ctrl Pts',(-204.162751134169,5.89487415689882,
131.312680631756));
#161710=CARTESIAN_POINT('Ctrl Pts',(-204.170147819081,5.90841063101912,
131.155701151823));
#161711=CARTESIAN_POINT('Ctrl Pts',(-204.177544503993,5.9156763355876,130.998133443599));
#161712=CARTESIAN_POINT('Ctrl Pts',(-204.184941188905,5.91663952547246,
130.840517057061));
#161713=CARTESIAN_POINT('Ctrl Pts',(-204.192337545841,5.91760267264848,
130.682907659399));
#161714=CARTESIAN_POINT('Ctrl Pts',(-204.199733902776,5.91226385852082,
130.525249961006));
#161715=CARTESIAN_POINT('Ctrl Pts',(-204.207130259712,5.90064347312982,
130.368084139275));
#161716=CARTESIAN_POINT('Ctrl Pts',(-204.214527749048,5.8890213086282,130.210894255055));
#161717=CARTESIAN_POINT('Ctrl Pts',(-204.221925238385,5.87111568546889,
130.054196769752));
#161718=CARTESIAN_POINT('Ctrl Pts',(-204.229322727721,5.84699892344906,
129.898527215838));
#161719=CARTESIAN_POINT('Ctrl Pts',(-204.236722810236,5.82287370733566,
129.742803092204));
#161720=CARTESIAN_POINT('Ctrl Pts',(-204.244122892751,5.79253307447818,
129.58810798606));
#161721=CARTESIAN_POINT('Ctrl Pts',(-204.251522975266,5.75610052241988,
129.434967562853));
#161722=CARTESIAN_POINT('Ctrl Pts',(-204.258931194933,5.71962790902519,
129.281658746007));
#161723=CARTESIAN_POINT('Ctrl Pts',(-204.266339414599,5.67705008515344,
129.129908389533));
#161724=CARTESIAN_POINT('Ctrl Pts',(-204.273747634265,5.62854073617138,
128.980228017189));
#161725=CARTESIAN_POINT('Ctrl Pts',(-204.281160413567,5.58000153049444,
128.830455519072));
#161726=CARTESIAN_POINT('Ctrl Pts',(-204.288573192869,5.52552365400217,
128.682755893192));
#161727=CARTESIAN_POINT('Ctrl Pts',(-204.295985972171,5.46532888062469,
128.537620493708));
#161728=CARTESIAN_POINT('Ctrl Pts',(-204.3034093432,5.40504809813207,128.392277717958));
#161729=CARTESIAN_POINT('Ctrl Pts',(-204.310832714229,5.33903426053937,
128.249506824144));
#161730=CARTESIAN_POINT('Ctrl Pts',(-204.318256085258,5.26755537227114,
128.109775127633));
#161731=CARTESIAN_POINT('Ctrl Pts',(-204.322192134699,5.22965555059476,
128.035686029319));
#161732=CARTESIAN_POINT('Ctrl Pts',(-204.32612818414,5.19022004371018,127.962450893188));
#161733=CARTESIAN_POINT('Ctrl Pts',(-204.330064233581,5.14929365279669,
127.890135945416));
#161734=CARTESIAN_POINT('Ctrl Pts',(-204.337487499987,5.07210775681115,
127.753752210805));
#161735=CARTESIAN_POINT('Ctrl Pts',(-204.344910766392,4.98938303310252,
127.620230874498));
#161736=CARTESIAN_POINT('Ctrl Pts',(-204.352334032798,4.90135693104575,
127.490053631635));
#161737=CARTESIAN_POINT('Ctrl Pts',(-204.359748525519,4.81343486853123,
127.360030247463));
#161738=CARTESIAN_POINT('Ctrl Pts',(-204.367163018239,4.72022410681939,
127.233343395595));
#161739=CARTESIAN_POINT('Ctrl Pts',(-204.374577510961,4.62200806639798,
127.110450494586));
#161740=CARTESIAN_POINT('Ctrl Pts',(-204.381984857314,4.52388669029411,
126.987676042383));
#161741=CARTESIAN_POINT('Ctrl Pts',(-204.389392203668,4.42076987115514,
126.868688550817));
#161742=CARTESIAN_POINT('Ctrl Pts',(-204.396799550022,4.31298436294144,
126.753916636035));
#161743=CARTESIAN_POINT('Ctrl Pts',(-204.404201371697,4.20527924522689,
126.639230322478));
#161744=CARTESIAN_POINT('Ctrl Pts',(-204.411603193373,4.09291262618729,
126.528753596247));
#161745=CARTESIAN_POINT('Ctrl Pts',(-204.419005015048,3.97625150478076,
126.422882039137));
#161746=CARTESIAN_POINT('Ctrl Pts',(-204.42640292936,3.85965196787114,126.317066370797));
#161747=CARTESIAN_POINT('Ctrl Pts',(-204.433800843671,3.73876271923734,
126.215851280293));
#161748=CARTESIAN_POINT('Ctrl Pts',(-204.441198757982,3.61398749640891,
126.119595421924));
#161749=CARTESIAN_POINT('Ctrl Pts',(-204.448595442894,3.48923300895941,
126.023355559533));
#161750=CARTESIAN_POINT('Ctrl Pts',(-204.455992127807,3.36059412427482,
125.932073521404));
#161751=CARTESIAN_POINT('Ctrl Pts',(-204.463388812719,3.22850762201203,
125.846067655557));
#161752=CARTESIAN_POINT('Ctrl Pts',(-204.470785169654,3.0964269766028,125.7600656033));
#161753=CARTESIAN_POINT('Ctrl Pts',(-204.47818152659,2.9608993304014,125.679339461843));
#161754=CARTESIAN_POINT('Ctrl Pts',(-204.485577883525,2.82239017126325,
125.604164055545));
#161755=CARTESIAN_POINT('Ctrl Pts',(-204.492975372862,2.68385980601923,
125.5289771397));
#161756=CARTESIAN_POINT('Ctrl Pts',(-204.500372862198,2.54234734704194,
125.459342829222));
#161757=CARTESIAN_POINT('Ctrl Pts',(-204.507770351535,2.39834244358581,
125.395489747801));
#161758=CARTESIAN_POINT('Ctrl Pts',(-204.51517043405,2.25428705943503,125.331614282781));
#161759=CARTESIAN_POINT('Ctrl Pts',(-204.522570516565,2.1077378322723,125.273524232987));
#161760=CARTESIAN_POINT('Ctrl Pts',(-204.52997059908,1.95920377276374,125.221399831452));
#161761=CARTESIAN_POINT('Ctrl Pts',(-204.537378818746,1.81050638478601,
125.169218113778));
#161762=CARTESIAN_POINT('Ctrl Pts',(-204.544787038413,1.65982015826697,
125.123015268486));
#161763=CARTESIAN_POINT('Ctrl Pts',(-204.552195258079,1.5076693338124,125.082921660242));
#161764=CARTESIAN_POINT('Ctrl Pts',(-204.559608037382,1.35542486306415,
125.042803375052));
#161765=CARTESIAN_POINT('Ctrl Pts',(-204.567020816684,1.2017143617988,125.008801899886));
#161766=CARTESIAN_POINT('Ctrl Pts',(-204.574433595986,1.04707109441425,
124.980996238984));
#161767=CARTESIAN_POINT('Ctrl Pts',(-204.581856967014,0.89220686547698,
124.953150848049));
#161768=CARTESIAN_POINT('Ctrl Pts',(-204.589280338043,0.73640757733136,
124.931519003745));
#161769=CARTESIAN_POINT('Ctrl Pts',(-204.596703709072,0.580211258570826,
124.916127821733));
#161770=CARTESIAN_POINT('Ctrl Pts',(-204.600639758513,0.497392222485452,
124.907967047723));
#161771=CARTESIAN_POINT('Ctrl Pts',(-204.604575807954,0.414461573604239,
124.901559876592));
#161772=CARTESIAN_POINT('Ctrl Pts',(-204.608511857394,0.331499246015727,
124.896904412702));
#161773=CARTESIAN_POINT('Ctrl Pts',(-204.6159351238,0.175034885349205,124.888124353097));
#161774=CARTESIAN_POINT('Ctrl Pts',(-204.623358390205,0.017984869765548,
124.885551462325));
#161775=CARTESIAN_POINT('Ctrl Pts',(-204.630781656611,-0.139117189784255,
124.889246335491));
#161776=CARTESIAN_POINT('Ctrl Pts',(-204.638196149331,-0.296033567746183,
124.892936841624));
#161777=CARTESIAN_POINT('Ctrl Pts',(-204.645610642053,-0.453001497684593,
124.902880357385));
#161778=CARTESIAN_POINT('Ctrl Pts',(-204.653025134774,-0.609482944717867,
124.919085678993));
#161779=CARTESIAN_POINT('Ctrl Pts',(-204.660432481127,-0.765813569041512,
124.935275381302));
#161780=CARTESIAN_POINT('Ctrl Pts',(-204.667839827481,-0.92165827510939,
124.957714836041));
#161781=CARTESIAN_POINT('Ctrl Pts',(-204.675247173835,-1.07647983752149,
124.986360813346));
#161782=CARTESIAN_POINT('Ctrl Pts',(-204.68264899551,-1.23118592817213,
125.0149854254));
#161783=CARTESIAN_POINT('Ctrl Pts',(-204.690050817186,-1.38487002911259,
125.049807275314));
#161784=CARTESIAN_POINT('Ctrl Pts',(-204.697452638861,-1.53700095427533,
125.090731418094));
#161785=CARTESIAN_POINT('Ctrl Pts',(-204.704850553172,-1.689051570706,125.131633957337));
#161786=CARTESIAN_POINT('Ctrl Pts',(-204.712248467484,-1.83955028467765,
125.17863227724));
#161787=CARTESIAN_POINT('Ctrl Pts',(-204.719646381795,-1.98797712017319,
125.231580563395));
#161788=CARTESIAN_POINT('Ctrl Pts',(-204.727043066707,-2.1363792898212,
125.284520050505));
#161789=CARTESIAN_POINT('Ctrl Pts',(-204.734439751619,-2.28270991309183,
125.343407416136));
#161790=CARTESIAN_POINT('Ctrl Pts',(-204.741836436532,-2.42646506470635,
125.408047260073));
#161791=CARTESIAN_POINT('Ctrl Pts',(-204.749232793467,-2.57021384206722,
125.472684237812));
#161792=CARTESIAN_POINT('Ctrl Pts',(-204.756629150402,-2.711387034376,125.5430730336));
#161793=CARTESIAN_POINT('Ctrl Pts',(-204.764025507338,-2.84950181656107,
125.6189705686));
#161794=CARTESIAN_POINT('Ctrl Pts',(-204.771422996674,-2.98763774447108,
125.694879723706));
#161795=CARTESIAN_POINT('Ctrl Pts',(-204.778820486011,-3.12271400273242,
125.776299117558));
#161796=CARTESIAN_POINT('Ctrl Pts',(-204.786217975348,-3.25427357637751,
125.862940371059));
#161797=CARTESIAN_POINT('Ctrl Pts',(-204.793618057863,-3.38587926802739,
125.949611996517));
#161798=CARTESIAN_POINT('Ctrl Pts',(-204.801018140377,-3.5139655090601,
126.041508920977));
#161799=CARTESIAN_POINT('Ctrl Pts',(-204.808418222892,-3.63810553162232,
126.138300319705));
#161800=CARTESIAN_POINT('Ctrl Pts',(-204.815826442559,-3.76238205890143,
126.235198150526));
#161801=CARTESIAN_POINT('Ctrl Pts',(-204.823234662225,-3.88270340732681,
126.337000974104));
#161802=CARTESIAN_POINT('Ctrl Pts',(-204.830642881892,-3.99867653255975,
126.443338197255));
#161803=CARTESIAN_POINT('Ctrl Pts',(-204.838055661194,-4.11472103731682,
126.549740869193));
#161804=CARTESIAN_POINT('Ctrl Pts',(-204.845468440496,-4.22641172186707,
126.660683239356));
#161805=CARTESIAN_POINT('Ctrl Pts',(-204.852881219798,-4.33339387527508,
126.775759361022));
#161806=CARTESIAN_POINT('Ctrl Pts',(-204.860304590827,-4.44052888980039,
126.890999908847));
#161807=CARTESIAN_POINT('Ctrl Pts',(-204.867727961855,-4.54294169391004,
127.010385722194));
#161808=CARTESIAN_POINT('Ctrl Pts',(-204.875151332884,-4.64031865683491,
127.133478799047));
#161809=CARTESIAN_POINT('Ctrl Pts',(-204.879087382325,-4.69195025910903,
127.198745701977));
#161810=CARTESIAN_POINT('Ctrl Pts',(-204.883023431766,-4.74216683506,127.265054373102));
#161811=CARTESIAN_POINT('Ctrl Pts',(-204.886959481207,-4.79092677321238,
127.332336536973));
#161812=CARTESIAN_POINT('Ctrl Pts',(-204.894439644792,-4.88359133935193,
127.460201188986));
#161813=CARTESIAN_POINT('Ctrl Pts',(-204.901919808376,-4.97127200205635,
127.591969048914));
#161814=CARTESIAN_POINT('Ctrl Pts',(-204.909399971961,-5.05362495660158,
127.727218215838));
#161815=CARTESIAN_POINT('Ctrl Pts',(-204.916871063548,-5.13587803287105,
127.862303351566));
#161816=CARTESIAN_POINT('Ctrl Pts',(-204.924342155134,-5.21281607482848,
128.000861080831));
#161817=CARTESIAN_POINT('Ctrl Pts',(-204.931813246721,-5.28413634723124,
128.142437698628));
#161818=CARTESIAN_POINT('Ctrl Pts',(-204.939276676359,-5.35538347741398,
128.28386912309));
#161819=CARTESIAN_POINT('Ctrl Pts',(-204.946740105998,-5.42102414483629,
128.428312948119));
#161820=CARTESIAN_POINT('Ctrl Pts',(-204.954203535636,-5.48079969101944,
128.575287871014));
#161821=CARTESIAN_POINT('Ctrl Pts',(-204.961660708341,-5.5405251246347,
128.722139578124));
#161822=CARTESIAN_POINT('Ctrl Pts',(-204.969117881046,-5.59439509099741,
128.871517820658));
#161823=CARTESIAN_POINT('Ctrl Pts',(-204.976575053751,-5.64219757205847,
129.022918190667));
#161824=CARTESIAN_POINT('Ctrl Pts',(-204.984026968987,-5.68996635133299,
129.174211820128));
#161825=CARTESIAN_POINT('Ctrl Pts',(-204.991478884223,-5.73167605837681,
129.327524388969));
#161826=CARTESIAN_POINT('Ctrl Pts',(-204.99893079946,-5.76716343358339,
129.482333199984));
#161827=CARTESIAN_POINT('Ctrl Pts',(-205.006379560772,-5.80263578923023,
129.637076490228));
#161828=CARTESIAN_POINT('Ctrl Pts',(-205.013828322084,-5.83189097662629,
129.793314405558));
#161829=CARTESIAN_POINT('Ctrl Pts',(-205.021277083396,-5.85481604611657,
129.95051073109));
#161830=CARTESIAN_POINT('Ctrl Pts',(-205.028725022292,-5.87773858445527,
130.107689700612));
#161831=CARTESIAN_POINT('Ctrl Pts',(-205.036172961189,-5.89433233816279,
130.265826508781));
#161832=CARTESIAN_POINT('Ctrl Pts',(-205.043620900085,-5.90453575298649,
130.424376270251));
#161833=CARTESIAN_POINT('Ctrl Pts',(-205.049622202654,-5.91275732682686,
130.552130418624));
#161834=CARTESIAN_POINT('Ctrl Pts',(-205.055623505223,-5.91683088167834,
130.680152436099));
#161835=CARTESIAN_POINT('Ctrl Pts',(-205.061624807792,-5.91674878301709,
130.808155504365));
#161836=CARTESIAN_POINT('',(-206.811623442643,-5.92115820836986,130.807369057892));
#161837=CARTESIAN_POINT('Ctrl Pts',(-205.061626944303,-5.90947417380247,
130.808196352657));
#161838=CARTESIAN_POINT('Ctrl Pts',(-205.096220331209,-5.91377200472859,
131.545141902329));
#161839=CARTESIAN_POINT('Ctrl Pts',(-205.223629592719,-5.44370849995411,
134.254054771831));
#161840=CARTESIAN_POINT('Ctrl Pts',(-205.443854728833,-1.37967370610466,
137.665414544981));
#161841=CARTESIAN_POINT('Ctrl Pts',(-205.722302352646,5.0266516457322,135.673686419238));
#161842=CARTESIAN_POINT('Ctrl Pts',(-206.000749976459,6.813729700728,129.207285761534));
#161843=CARTESIAN_POINT('Ctrl Pts',(-206.279197600272,2.3393230299546,124.208518875085));
#161844=CARTESIAN_POINT('Ctrl Pts',(-206.549488398635,-4.09076040919075,
125.239883832662));
#161845=CARTESIAN_POINT('Ctrl Pts',(-206.726963322394,-5.91340440505827,
129.015638925646));
#161846=CARTESIAN_POINT('Ctrl Pts',(-206.811622371547,-5.92461749863669,
130.807348163968));
#161847=CARTESIAN_POINT('',(-208.561625524649,-5.9182976546993,130.799113135042));
#161848=CARTESIAN_POINT('Ctrl Pts',(-206.811624807792,-5.91674922156144,
130.807395687932));
#161849=CARTESIAN_POINT('Ctrl Pts',(-206.819780821161,-5.91666079577132,
130.979778256311));
#161850=CARTESIAN_POINT('Ctrl Pts',(-206.827936834529,-5.90903961803116,
131.151962513016));
#161851=CARTESIAN_POINT('Ctrl Pts',(-206.836092847897,-5.89393313865187,
131.323477867907));
#161852=CARTESIAN_POINT('Ctrl Pts',(-206.843516114303,-5.88018384523864,
131.479584057844));
#161853=CARTESIAN_POINT('Ctrl Pts',(-206.850939380708,-5.86020755555771,
131.635379677207));
#161854=CARTESIAN_POINT('Ctrl Pts',(-206.858362647114,-5.83402082614694,
131.79032794085));
#161855=CARTESIAN_POINT('Ctrl Pts',(-206.865777139835,-5.80786504727567,
131.945093068512));
#161856=CARTESIAN_POINT('Ctrl Pts',(-206.873191632556,-5.77551350102985,
132.099012469469));
#161857=CARTESIAN_POINT('Ctrl Pts',(-206.880606125277,-5.73703464184265,
132.251552408863));
#161858=CARTESIAN_POINT('Ctrl Pts',(-206.888013471631,-5.69859287002863,
132.40394532452));
#161859=CARTESIAN_POINT('Ctrl Pts',(-206.895420817985,-5.6540356331216,
132.554961066011));
#161860=CARTESIAN_POINT('Ctrl Pts',(-206.902828164338,-5.60348275777306,
132.704074160667));
#161861=CARTESIAN_POINT('Ctrl Pts',(-206.910229986014,-5.55296758666621,
132.853076041151));
#161862=CARTESIAN_POINT('Ctrl Pts',(-206.917631807689,-5.49646580036238,
133.00017774834));
#161863=CARTESIAN_POINT('Ctrl Pts',(-206.925033629365,-5.43414753997931,
133.144867202952));
#161864=CARTESIAN_POINT('Ctrl Pts',(-206.932431543676,-5.37186217692081,
133.289480277128));
#161865=CARTESIAN_POINT('Ctrl Pts',(-206.939829457987,-5.30376660206674,
133.431683292801));
#161866=CARTESIAN_POINT('Ctrl Pts',(-206.947227372299,-5.23007969249045,
133.570982560062));
#161867=CARTESIAN_POINT('Ctrl Pts',(-206.954624057211,-5.15640502834161,
133.710258678312));
#161868=CARTESIAN_POINT('Ctrl Pts',(-206.962020742123,-5.07714104799469,
133.846631676217));
#161869=CARTESIAN_POINT('Ctrl Pts',(-206.969417427036,-4.99255339993645,
133.97963085981));
#161870=CARTESIAN_POINT('Ctrl Pts',(-206.976813783971,-4.90796950258341,
134.11262414608));
#161871=CARTESIAN_POINT('Ctrl Pts',(-206.984210140907,-4.81806260721323,
134.242243600501));
#161872=CARTESIAN_POINT('Ctrl Pts',(-206.991606497842,-4.72314252211075,
134.368046248809));
#161873=CARTESIAN_POINT('Ctrl Pts',(-206.999003987179,-4.62820790450037,
134.493868157825));
#161874=CARTESIAN_POINT('Ctrl Pts',(-207.006401476515,-4.52825879375254,
134.615871799175));
#161875=CARTESIAN_POINT('Ctrl Pts',(-207.013798965852,-4.4236461287228,
134.733646238431));
#161876=CARTESIAN_POINT('Ctrl Pts',(-207.021199048367,-4.31899679188596,
134.851461963334));
#161877=CARTESIAN_POINT('Ctrl Pts',(-207.028599130882,-4.20968089363974,
134.965045255495));
#161878=CARTESIAN_POINT('Ctrl Pts',(-207.035999213397,-4.09608704198211,
135.074021202086));
#161879=CARTESIAN_POINT('Ctrl Pts',(-207.043407433063,-3.98236828220669,
135.183116978934));
#161880=CARTESIAN_POINT('Ctrl Pts',(-207.05081565273,-3.86436244426953,
135.287595033992));
#161881=CARTESIAN_POINT('Ctrl Pts',(-207.058223872396,-3.74249265724638,
135.38711953256));
#161882=CARTESIAN_POINT('Ctrl Pts',(-207.065636651698,-3.62054786140282,
135.486705286797));
#161883=CARTESIAN_POINT('Ctrl Pts',(-207.073049431,-3.49473467526279,135.581331185504));
#161884=CARTESIAN_POINT('Ctrl Pts',(-207.080462210303,-3.36550571859837,
135.670704401207));
#161885=CARTESIAN_POINT('Ctrl Pts',(-207.087885581331,-3.23609211354025,
135.760205317552));
#161886=CARTESIAN_POINT('Ctrl Pts',(-207.09530895236,-3.10325330470338,
135.84443836179));
#161887=CARTESIAN_POINT('Ctrl Pts',(-207.102732323389,-2.96746774449341,
135.92315595904));
#161888=CARTESIAN_POINT('Ctrl Pts',(-207.106668372829,-2.89547098234766,
135.9648939179));
#161889=CARTESIAN_POINT('Ctrl Pts',(-207.11060442227,-2.82264614973579,
136.005082076847));
#161890=CARTESIAN_POINT('Ctrl Pts',(-207.11454047171,-2.74906678387943,
136.043689045931));
#161891=CARTESIAN_POINT('Ctrl Pts',(-207.121963738116,-2.61029839619412,
136.116500584748));
#161892=CARTESIAN_POINT('Ctrl Pts',(-207.129387004521,-2.46842545674248,
136.183905304267));
#161893=CARTESIAN_POINT('Ctrl Pts',(-207.136810270927,-2.32390852728499,
136.245626988487));
#161894=CARTESIAN_POINT('Ctrl Pts',(-207.144224763648,-2.17956240483674,
136.307275722802));
#161895=CARTESIAN_POINT('Ctrl Pts',(-207.151639256369,-2.0325788526123,
136.363254646609));
#161896=CARTESIAN_POINT('Ctrl Pts',(-207.15905374909,-1.88344391815646,
136.413332855834));
#161897=CARTESIAN_POINT('Ctrl Pts',(-207.166461095443,-1.73445272556529,
136.463362797795));
#161898=CARTESIAN_POINT('Ctrl Pts',(-207.173868441797,-1.58331463034264,
136.507503229499));
#161899=CARTESIAN_POINT('Ctrl Pts',(-207.181275788151,-1.4305364967586,
136.545570933688));
#161900=CARTESIAN_POINT('Ctrl Pts',(-207.188677609826,-1.27787231087058,
136.583610245546));
#161901=CARTESIAN_POINT('Ctrl Pts',(-207.196079431502,-1.12357088284622,
136.61558575841));
#161902=CARTESIAN_POINT('Ctrl Pts',(-207.203481253177,-0.96815500491798,
136.641363825459));
#161903=CARTESIAN_POINT('Ctrl Pts',(-207.210879167489,-0.812821169821938,
136.667128284467));
#161904=CARTESIAN_POINT('Ctrl Pts',(-207.2182770818,-0.656374423802763,
136.686701752249));
#161905=CARTESIAN_POINT('Ctrl Pts',(-207.225674996111,-0.499348430567841,
136.700001524829));
#161906=CARTESIAN_POINT('Ctrl Pts',(-207.233071681024,-0.342348532204476,
136.713299087228));
#161907=CARTESIAN_POINT('Ctrl Pts',(-207.240468365936,-0.184769949275625,
136.720324992153));
#161908=CARTESIAN_POINT('Ctrl Pts',(-207.247865050848,-0.027152279443601,
136.721048315613));
#161909=CARTESIAN_POINT('Ctrl Pts',(-207.255261407783,0.130458401455771,
136.721771607));
#161910=CARTESIAN_POINT('Ctrl Pts',(-207.262657764719,0.288107792518586,
136.716192870875));
#161911=CARTESIAN_POINT('Ctrl Pts',(-207.270054121654,0.445255748006126,
136.704333319314));
#161912=CARTESIAN_POINT('Ctrl Pts',(-207.277451610991,0.602427763247279,
136.692471952024));
#161913=CARTESIAN_POINT('Ctrl Pts',(-207.284849100328,0.759097817788442,
136.674327882701));
#161914=CARTESIAN_POINT('Ctrl Pts',(-207.292246589664,0.914730489834055,
136.649974246046));
#161915=CARTESIAN_POINT('Ctrl Pts',(-207.299646672179,1.07041771867137,
136.625612072261));
#161916=CARTESIAN_POINT('Ctrl Pts',(-207.307046754694,1.22506647240331,
136.595036054919));
#161917=CARTESIAN_POINT('Ctrl Pts',(-207.314446837209,1.37815127413479,
136.558370491393));
#161918=CARTESIAN_POINT('Ctrl Pts',(-207.321855056876,1.53140440834349,
136.521664610311));
#161919=CARTESIAN_POINT('Ctrl Pts',(-207.329263276542,1.68308979289289,
136.478855897533));
#161920=CARTESIAN_POINT('Ctrl Pts',(-207.336671496209,1.83269616893944,
136.430118816676));
#161921=CARTESIAN_POINT('Ctrl Pts',(-207.344084275511,1.98239462521413,
136.38135173896));
#161922=CARTESIAN_POINT('Ctrl Pts',(-207.351497054813,2.13001117400739,
136.326649151863));
#161923=CARTESIAN_POINT('Ctrl Pts',(-207.358909834115,2.27505479922936,
136.266233576818));
#161924=CARTESIAN_POINT('Ctrl Pts',(-207.366333205144,2.42030566958471,
136.205731677165));
#161925=CARTESIAN_POINT('Ctrl Pts',(-207.373756576173,2.56297593624992,
136.139500643018));
#161926=CARTESIAN_POINT('Ctrl Pts',(-207.381179947201,2.7025986922535,136.067809189665));
#161927=CARTESIAN_POINT('Ctrl Pts',(-207.385115996642,2.77663002768745,
136.029796660885));
#161928=CARTESIAN_POINT('Ctrl Pts',(-207.389052046083,2.84980506487561,
135.99024974826));
#161929=CARTESIAN_POINT('Ctrl Pts',(-207.392988095523,2.92205764589925,
135.949213353704));
#161930=CARTESIAN_POINT('Ctrl Pts',(-207.400411361929,3.05832375878637,
135.87181999427));
#161931=CARTESIAN_POINT('Ctrl Pts',(-207.407834628334,3.19171904753105,
135.788892169611));
#161932=CARTESIAN_POINT('Ctrl Pts',(-207.41525789474,3.32176217890836,135.700668061883));
#161933=CARTESIAN_POINT('Ctrl Pts',(-207.422672387461,3.4516516101038,135.612548227724));
#161934=CARTESIAN_POINT('Ctrl Pts',(-207.430086880182,3.57819646435842,
135.519144778126));
#161935=CARTESIAN_POINT('Ctrl Pts',(-207.437501372903,3.70093975496472,
135.420741829362));
#161936=CARTESIAN_POINT('Ctrl Pts',(-207.444908719256,3.82356474096634,
135.322433725065));
#161937=CARTESIAN_POINT('Ctrl Pts',(-207.45231606561,3.94239516850163,135.219135946626));
#161938=CARTESIAN_POINT('Ctrl Pts',(-207.459723411964,4.05700291918446,
135.11117589991));
#161939=CARTESIAN_POINT('Ctrl Pts',(-207.46712523364,4.17152519108292,135.003296373869));
#161940=CARTESIAN_POINT('Ctrl Pts',(-207.474527055315,4.28183078651756,
134.890761758177));
#161941=CARTESIAN_POINT('Ctrl Pts',(-207.48192887699,4.387524682663,134.773939653374));
#161942=CARTESIAN_POINT('Ctrl Pts',(-207.489326791302,4.49316278382338,
134.65717921805));
#161943=CARTESIAN_POINT('Ctrl Pts',(-207.496724705613,4.59419378426487,
134.536136077267));
#161944=CARTESIAN_POINT('Ctrl Pts',(-207.504122619924,4.69025964452218,
134.411214513895));
#161945=CARTESIAN_POINT('Ctrl Pts',(-207.511519304837,4.7863095403762,134.286313710222));
#161946=CARTESIAN_POINT('Ctrl Pts',(-207.518915989749,4.8773957063178,134.157536058776));
#161947=CARTESIAN_POINT('Ctrl Pts',(-207.526312674661,4.96320045939997,
134.02531882318));
#161948=CARTESIAN_POINT('Ctrl Pts',(-207.533709031597,5.04900140780948,
133.893107450235));
#161949=CARTESIAN_POINT('Ctrl Pts',(-207.541105388532,5.12952120577963,
133.757457109527));
#161950=CARTESIAN_POINT('Ctrl Pts',(-207.548501745467,5.20448573766415,
133.61883370661));
#161951=CARTESIAN_POINT('Ctrl Pts',(-207.555899234804,5.27946174681009,
133.480189080095));
#161952=CARTESIAN_POINT('Ctrl Pts',(-207.563296724141,5.34888061877977,
133.33857081342));
#161953=CARTESIAN_POINT('Ctrl Pts',(-207.570694213477,5.41251447531095,
133.194468903199));
#161954=CARTESIAN_POINT('Ctrl Pts',(-207.578094295992,5.4761706385918,133.050316478276));
#161955=CARTESIAN_POINT('Ctrl Pts',(-207.585494378507,5.53403759814204,
132.903679017647));
#161956=CARTESIAN_POINT('Ctrl Pts',(-207.592894461022,5.58593589576508,
132.755065805672));
#161957=CARTESIAN_POINT('Ctrl Pts',(-207.600302680689,5.6378912609017,132.606289178192));
#161958=CARTESIAN_POINT('Ctrl Pts',(-207.607710900355,5.68386473390605,
132.455532813299));
#161959=CARTESIAN_POINT('Ctrl Pts',(-207.615119120022,5.72372674806762,
132.303321149386));
#161960=CARTESIAN_POINT('Ctrl Pts',(-207.622531899324,5.76361329663376,
132.151015801734));
#161961=CARTESIAN_POINT('Ctrl Pts',(-207.629944678626,5.79738081120918,
131.997253734006));
#161962=CARTESIAN_POINT('Ctrl Pts',(-207.637357457928,5.82495109918533,
131.842568330213));
#161963=CARTESIAN_POINT('Ctrl Pts',(-207.644780828957,5.85256078088182,
131.687661904661));
#161964=CARTESIAN_POINT('Ctrl Pts',(-207.652204199985,5.87395550014103,
131.531829876945));
#161965=CARTESIAN_POINT('Ctrl Pts',(-207.659627571014,5.88910896012277,
131.375610316298));
#161966=CARTESIAN_POINT('Ctrl Pts',(-207.663563620455,5.89714368820723,
131.292778956808));
#161967=CARTESIAN_POINT('Ctrl Pts',(-207.667499669896,5.90342464558926,
131.209838653336));
#161968=CARTESIAN_POINT('Ctrl Pts',(-207.671435719336,5.90795384954832,
131.126869336994));
#161969=CARTESIAN_POINT('Ctrl Pts',(-207.678858985742,5.91649578686362,
130.970391795754));
#161970=CARTESIAN_POINT('Ctrl Pts',(-207.686282252147,5.9188296712671,130.81333804653));
#161971=CARTESIAN_POINT('Ctrl Pts',(-207.693705518553,5.91489571978865,
130.656241791869));
#161972=CARTESIAN_POINT('Ctrl Pts',(-207.701120011274,5.91096641791416,
130.499331211935));
#161973=CARTESIAN_POINT('Ctrl Pts',(-207.708534503995,5.90078403519882,
130.342378596101));
#161974=CARTESIAN_POINT('Ctrl Pts',(-207.715948996716,5.88434059423159,
130.185921992011));
#161975=CARTESIAN_POINT('Ctrl Pts',(-207.723356343069,5.86791300207183,
130.029616186687));
#161976=CARTESIAN_POINT('Ctrl Pts',(-207.730763689423,5.84523640420407,
129.873805810115));
#161977=CARTESIAN_POINT('Ctrl Pts',(-207.738171035777,5.8163548480082,129.719028021284));
#161978=CARTESIAN_POINT('Ctrl Pts',(-207.745572857452,5.78749483276658,
129.564365671568));
#161979=CARTESIAN_POINT('Ctrl Pts',(-207.752974679128,5.75243914213516,
129.41073474152));
#161980=CARTESIAN_POINT('Ctrl Pts',(-207.760376500803,5.71128352937423,
129.258666272102));
#161981=CARTESIAN_POINT('Ctrl Pts',(-207.767774415114,5.67014964234093,
129.106678078445));
#161982=CARTESIAN_POINT('Ctrl Pts',(-207.775172329426,5.622922343438,128.956251062191));
#161983=CARTESIAN_POINT('Ctrl Pts',(-207.782570243737,5.5697482382197,128.80790497685));
#161984=CARTESIAN_POINT('Ctrl Pts',(-207.789966928649,5.51658296957293,
128.659583543936));
#161985=CARTESIAN_POINT('Ctrl Pts',(-207.797363613561,5.45747298183366,
128.513342706659));
#161986=CARTESIAN_POINT('Ctrl Pts',(-207.804760298474,5.39261444187882,
128.369686092349));
#161987=CARTESIAN_POINT('Ctrl Pts',(-207.812156655409,5.32775877781979,
128.226035847924));
#161988=CARTESIAN_POINT('Ctrl Pts',(-207.819553012344,5.25715522197387,
128.084969938857));
#161989=CARTESIAN_POINT('Ctrl Pts',(-207.82694936928,5.18104758767484,127.946970819735));
#161990=CARTESIAN_POINT('Ctrl Pts',(-207.834346858616,5.1049283011025,127.808950572595));
#161991=CARTESIAN_POINT('Ctrl Pts',(-207.841744347953,5.0233034384614,127.673998377207));
#161992=CARTESIAN_POINT('Ctrl Pts',(-207.84914183729,4.93646207401314,127.542570809143));
#161993=CARTESIAN_POINT('Ctrl Pts',(-207.856541919805,4.84959026745932,
127.41109716935));
#161994=CARTESIAN_POINT('Ctrl Pts',(-207.86394200232,4.75749852395979,127.283150928114));
#161995=CARTESIAN_POINT('Ctrl Pts',(-207.871342084835,4.6605183173321,127.159158349336));
#161996=CARTESIAN_POINT('Ctrl Pts',(-207.878750304501,4.56343147099727,
127.03502942797));
#161997=CARTESIAN_POINT('Ctrl Pts',(-207.886158524168,4.4614456566951,126.914863145442));
#161998=CARTESIAN_POINT('Ctrl Pts',(-207.893566743834,4.35493206532541,
126.799051981655));
#161999=CARTESIAN_POINT('Ctrl Pts',(-207.900979523136,4.24835291661749,
126.68316953803));
#162000=CARTESIAN_POINT('Ctrl Pts',(-207.908392302438,4.13724070071562,
126.571647818218));
#162001=CARTESIAN_POINT('Ctrl Pts',(-207.91580508174,4.02200190367991,126.464840914961));
#162002=CARTESIAN_POINT('Ctrl Pts',(-207.923228452769,3.90659844804667,
126.357881400993));
#162003=CARTESIAN_POINT('Ctrl Pts',(-207.930651823798,3.78705691809108,
126.25565040036));
#162004=CARTESIAN_POINT('Ctrl Pts',(-207.938075194826,3.66381579261569,
126.158460876904));
#162005=CARTESIAN_POINT('Ctrl Pts',(-207.942011244267,3.59847039075598,
126.106928659536));
#162006=CARTESIAN_POINT('Ctrl Pts',(-207.945947293708,3.53208537533614,
126.056813052246));
#162007=CARTESIAN_POINT('Ctrl Pts',(-207.949883343149,3.46472908505259,
126.008155562557));
#162008=CARTESIAN_POINT('Ctrl Pts',(-207.957306609555,3.33769722370025,
125.916389055557));
#162009=CARTESIAN_POINT('Ctrl Pts',(-207.96472987596,3.20682497801239,125.829534104802));
#162010=CARTESIAN_POINT('Ctrl Pts',(-207.972153142366,3.0725290529027,125.747929486663));
#162011=CARTESIAN_POINT('Ctrl Pts',(-207.979567635087,2.9383918544239,125.666421318405));
#162012=CARTESIAN_POINT('Ctrl Pts',(-207.986982127808,2.80083934701695,
125.590151322724));
#162013=CARTESIAN_POINT('Ctrl Pts',(-207.994396620529,2.66031989341828,
125.519417039137));
#162014=CARTESIAN_POINT('Ctrl Pts',(-208.001803966883,2.51993587775946,
125.448750931915));
#162015=CARTESIAN_POINT('Ctrl Pts',(-208.009211313236,2.37659094011565,
125.383610081518));
#162016=CARTESIAN_POINT('Ctrl Pts',(-208.01661865959,2.23076081624254,125.324247777193));
#162017=CARTESIAN_POINT('Ctrl Pts',(-208.024020481265,2.08503945797724,
125.264929747515));
#162018=CARTESIAN_POINT('Ctrl Pts',(-208.031422302941,1.93683694840379,
125.211381822536));
#162019=CARTESIAN_POINT('Ctrl Pts',(-208.038824124616,1.78665182429972,
125.16381048294));
#162020=CARTESIAN_POINT('Ctrl Pts',(-208.046222038928,1.63654598175406,
125.116264255884));
#162021=CARTESIAN_POINT('Ctrl Pts',(-208.053619953239,1.48445996401649,
125.074688443328));
#162022=CARTESIAN_POINT('Ctrl Pts',(-208.06101786755,1.33091029831849,125.039240641336));
#162023=CARTESIAN_POINT('Ctrl Pts',(-208.068414552463,1.17738614978904,
125.003798730125));
#162024=CARTESIAN_POINT('Ctrl Pts',(-208.075811237375,1.02239919941734,
124.974482892213));
#162025=CARTESIAN_POINT('Ctrl Pts',(-208.083207922287,0.866479196127633,
124.951400309724));
#162026=CARTESIAN_POINT('Ctrl Pts',(-208.090604279223,0.710566106494265,
124.928318750741));
#162027=CARTESIAN_POINT('Ctrl Pts',(-208.098000636158,0.553720415478458,
124.911469952293));
#162028=CARTESIAN_POINT('Ctrl Pts',(-208.105396993094,0.39647981285127,
124.900909565808));
#162029=CARTESIAN_POINT('Ctrl Pts',(-208.11279448243,0.239215136286403,
124.890347562501));
#162030=CARTESIAN_POINT('Ctrl Pts',(-208.120191971767,0.0815558002050929,
124.886075913179));
#162031=CARTESIAN_POINT('Ctrl Pts',(-208.127589461103,-0.0759578137315606,
124.88809820173));
#162032=CARTESIAN_POINT('Ctrl Pts',(-208.134989543618,-0.233526643821177,
124.890121199191));
#162033=CARTESIAN_POINT('Ctrl Pts',(-208.142389626133,-0.390949277026624,
124.898442522523));
#162034=CARTESIAN_POINT('Ctrl Pts',(-208.149789708648,-0.547687915761142,
124.913013699464));
#162035=CARTESIAN_POINT('Ctrl Pts',(-208.157197928315,-0.704598904742296,
124.927600898913));
#162036=CARTESIAN_POINT('Ctrl Pts',(-208.164606147981,-0.860824025291776,
124.948451641943));
#162037=CARTESIAN_POINT('Ctrl Pts',(-208.172014367648,-1.01583243520272,
124.975465780113));
#162038=CARTESIAN_POINT('Ctrl Pts',(-208.17942714695,-1.17093625020352,
125.002496545034));
#162039=CARTESIAN_POINT('Ctrl Pts',(-208.186839926252,-1.32482149830291,
125.035698185506));
#162040=CARTESIAN_POINT('Ctrl Pts',(-208.194252705554,-1.47697055560345,
125.074920109071));
#162041=CARTESIAN_POINT('Ctrl Pts',(-208.201676076583,-1.62933701061236,
125.11419807476));
#162042=CARTESIAN_POINT('Ctrl Pts',(-208.209099447612,-1.77996196368261,
125.159513396531));
#162043=CARTESIAN_POINT('Ctrl Pts',(-208.21652281864,-1.92834510096755,
125.210666334351));
#162044=CARTESIAN_POINT('Ctrl Pts',(-208.220458868081,-2.00702140075778,
125.23778884938));
#162045=CARTESIAN_POINT('Ctrl Pts',(-208.224394917522,-2.0850678028919,
125.26655173309));
#162046=CARTESIAN_POINT('Ctrl Pts',(-208.228330966962,-2.16241244718007,
125.296919926031));
#162047=CARTESIAN_POINT('Ctrl Pts',(-208.235754233368,-2.30828203246709,
125.35419339016));
#162048=CARTESIAN_POINT('Ctrl Pts',(-208.243177499773,-2.45209520792221,
125.417352694518));
#162049=CARTESIAN_POINT('Ctrl Pts',(-208.250600766178,-2.59334171220647,
125.486230370362));
#162050=CARTESIAN_POINT('Ctrl Pts',(-208.258015258899,-2.73442127485285,
125.555026638513));
#162051=CARTESIAN_POINT('Ctrl Pts',(-208.26542975162,-2.87293987245686,
125.629527663019));
#162052=CARTESIAN_POINT('Ctrl Pts',(-208.272844244341,-3.00840482558562,
125.709517050989));
#162053=CARTESIAN_POINT('Ctrl Pts',(-208.280251590695,-3.14373921249238,
125.789429342175));
#162054=CARTESIAN_POINT('Ctrl Pts',(-208.287658937049,-3.276025495006,125.87481927716));
#162055=CARTESIAN_POINT('Ctrl Pts',(-208.295066283402,-3.40479342691352,
125.965423515004));
#162056=CARTESIAN_POINT('Ctrl Pts',(-208.302468105078,-3.53346531883929,
126.05596017679));
#162057=CARTESIAN_POINT('Ctrl Pts',(-208.309869926753,-3.65862378115038,
126.151703183975));
#162058=CARTESIAN_POINT('Ctrl Pts',(-208.317271748428,-3.77982562449569,
126.252344711299));
#162059=CARTESIAN_POINT('Ctrl Pts',(-208.32466966274,-3.90096348633133,
126.352933110745));
#162060=CARTESIAN_POINT('Ctrl Pts',(-208.332067577051,-4.01814860241678,
126.458414642534));
#162061=CARTESIAN_POINT('Ctrl Pts',(-208.339465491362,-4.13096918713531,
126.568439922199));
#162062=CARTESIAN_POINT('Ctrl Pts',(-208.346862176274,-4.24377102311959,
126.678446917659));
#162063=CARTESIAN_POINT('Ctrl Pts',(-208.354258861187,-4.35220950026474,
126.792995901993));
#162064=CARTESIAN_POINT('Ctrl Pts',(-208.361655546099,-4.45590810098091,
126.911699116984));
#162065=CARTESIAN_POINT('Ctrl Pts',(-208.369051903034,-4.55960210359245,
127.03039706855));
#162066=CARTESIAN_POINT('Ctrl Pts',(-208.37644825997,-4.65855640207167,
127.153248603385));
#162067=CARTESIAN_POINT('Ctrl Pts',(-208.383844616905,-4.75243354084222,
127.279831428812));
#162068=CARTESIAN_POINT('Ctrl Pts',(-208.391242106241,-4.84632505244239,
127.406433634393));
#162069=CARTESIAN_POINT('Ctrl Pts',(-208.398639595578,-4.93513763419133,
127.536767968181));
#162070=CARTESIAN_POINT('Ctrl Pts',(-208.406037084914,-5.01857618137592,
127.67038172896));
#162071=CARTESIAN_POINT('Ctrl Pts',(-208.413437167429,-5.10204397781375,
127.804042327836));
#162072=CARTESIAN_POINT('Ctrl Pts',(-208.420837249944,-5.18013379133206,
127.940984326111));
#162073=CARTESIAN_POINT('Ctrl Pts',(-208.428237332459,-5.25259571028425,
128.080729059002));
#162074=CARTESIAN_POINT('Ctrl Pts',(-208.435645552125,-5.32513730856569,
128.220627455594));
#162075=CARTESIAN_POINT('Ctrl Pts',(-208.443053771792,-5.39203848159874,
128.363334409951));
#162076=CARTESIAN_POINT('Ctrl Pts',(-208.450461991458,-5.45309655392448,
128.508349176811));
#162077=CARTESIAN_POINT('Ctrl Pts',(-208.45787477076,-5.51419220647511,
128.653453197841));
#162078=CARTESIAN_POINT('Ctrl Pts',(-208.465287550062,-5.56943746148115,
128.800867512992));
#162079=CARTESIAN_POINT('Ctrl Pts',(-208.472700329364,-5.61867922828225,
128.950075231718));
#162080=CARTESIAN_POINT('Ctrl Pts',(-208.480123700393,-5.66799135402889,
129.099496145429));
#162081=CARTESIAN_POINT('Ctrl Pts',(-208.487547071422,-5.71128275678052,
129.250715222671));
#162082=CARTESIAN_POINT('Ctrl Pts',(-208.49497044245,-5.74845105162981,
129.403203570866));
#162083=CARTESIAN_POINT('Ctrl Pts',(-208.498906491892,-5.76815857340318,
129.484056552001));
#162084=CARTESIAN_POINT('Ctrl Pts',(-208.502842541333,-5.78614553147746,
129.565266241738));
#162085=CARTESIAN_POINT('Ctrl Pts',(-208.506778590774,-5.80240258017325,
129.646753231576));
#162086=CARTESIAN_POINT('Ctrl Pts',(-208.517519108524,-5.84676409612494,
129.869111327882));
#162087=CARTESIAN_POINT('Ctrl Pts',(-208.528259626274,-5.87835505477374,
130.094094933894));
#162088=CARTESIAN_POINT('Ctrl Pts',(-208.539000144024,-5.89693230953219,
130.320501237895));
#162089=CARTESIAN_POINT('Ctrl Pts',(-208.546541698614,-5.90997650201339,
130.47947453329));
#162090=CARTESIAN_POINT('Ctrl Pts',(-208.554083253203,-5.91660542909776,
130.63914897901));
#162091=CARTESIAN_POINT('Ctrl Pts',(-208.561624807792,-5.91674766075738,
130.799099303841));
#162092=CARTESIAN_POINT('',(-210.311624807793,-5.90698841004286,130.803765473938));
#162093=CARTESIAN_POINT('Ctrl Pts',(-208.561625802215,-5.91889781063289,
130.799118490467));
#162094=CARTESIAN_POINT('Ctrl Pts',(-208.636159273006,-5.90427014288086,
132.380502494848));
#162095=CARTESIAN_POINT('Ctrl Pts',(-208.803508618402,-4.43691936218312,
135.955107010576));
#162096=CARTESIAN_POINT('Ctrl Pts',(-209.063673838401,1.60744234334904,
137.615651952041));
#162097=CARTESIAN_POINT('Ctrl Pts',(-209.342121462214,6.59939415603132,
133.133643190306));
#162098=CARTESIAN_POINT('Ctrl Pts',(-209.620569086027,5.526825137655,126.511137535992));
#162099=CARTESIAN_POINT('Ctrl Pts',(-209.899016709839,-0.624626181811619,
123.833894158043));
#162100=CARTESIAN_POINT('Ctrl Pts',(-210.129368617095,-5.23869439854464,
126.918191279253));
#162101=CARTESIAN_POINT('Ctrl Pts',(-210.266904649746,-5.90784084701446,
129.850086159445));
#162102=CARTESIAN_POINT('Ctrl Pts',(-210.311624807793,-5.90698841004286,
130.803765473938));
#162103=CARTESIAN_POINT('',(-212.061624807793,-5.9167064429625,130.809826898457));
#162104=CARTESIAN_POINT('Ctrl Pts',(-210.311624807793,-5.90698841004286,
130.803765473938));
#162105=CARTESIAN_POINT('Ctrl Pts',(-210.35972052435,-5.90607162958501,
131.829430230063));
#162106=CARTESIAN_POINT('Ctrl Pts',(-210.500632115514,-5.1631795060691,
134.835682530948));
#162107=CARTESIAN_POINT('Ctrl Pts',(-210.734359581277,-0.370831884411458,
137.792925866865));
#162108=CARTESIAN_POINT('Ctrl Pts',(-211.012807205092,5.67923417909519,
134.893842206882));
#162109=CARTESIAN_POINT('Ctrl Pts',(-211.291254828904,6.51036147803477,
128.236724748581));
#162110=CARTESIAN_POINT('Ctrl Pts',(-211.569702452717,1.3587846274958,123.939139217901));
#162111=CARTESIAN_POINT('Ctrl Pts',(-211.826492445681,-4.54363933266225,
125.793924450652));
#162112=CARTESIAN_POINT('Ctrl Pts',(-211.990466564038,-5.90273208346157,
129.298621124659));
#162113=CARTESIAN_POINT('Ctrl Pts',(-212.061624807793,-5.9167064429625,
130.809826898457));
#162114=CARTESIAN_POINT('',(-213.811624807793,-5.92582816037032,130.802499402571));
#162115=CARTESIAN_POINT('Ctrl Pts',(-212.061624807793,-5.9167064429625,
130.809826898457));
#162116=CARTESIAN_POINT('Ctrl Pts',(-212.083282438643,-5.92095966090986,
131.269775529293));
#162117=CARTESIAN_POINT('Ctrl Pts',(-212.104940069493,-5.87187244348729,
131.728826242693));
#162118=CARTESIAN_POINT('Ctrl Pts',(-212.219413574947,-5.31230370266279,
134.083875118018));
#162119=CARTESIAN_POINT('Ctrl Pts',(-212.405045324154,-2.31923672099176,
137.407291903154));
#162120=CARTESIAN_POINT('Ctrl Pts',(-212.683492947968,4.30162899711266,
136.324645800563));
#162121=CARTESIAN_POINT('Ctrl Pts',(-212.961940571781,6.96950781311999,
130.169127295691));
#162122=CARTESIAN_POINT('Ctrl Pts',(-213.240388195594,3.23274942825056,
124.597357180765));
#162123=CARTESIAN_POINT('Ctrl Pts',(-213.518835819407,-3.47474775259045,
124.729519995276));
#162124=CARTESIAN_POINT('Ctrl Pts',(-213.709248023473,-5.87799918612228,
128.637393418206));
#162125=CARTESIAN_POINT('Ctrl Pts',(-213.806844352935,-5.92624379243174,
130.701381486186));
#162126=CARTESIAN_POINT('Ctrl Pts',(-213.811624807793,-5.92582816037032,
130.802499402571));
#162127=CARTESIAN_POINT('',(-215.561623590517,-5.91341522243185,130.799770594371));
#162128=CARTESIAN_POINT('Ctrl Pts',(-213.811624807793,-5.92582816037032,
130.802499402571));
#162129=CARTESIAN_POINT('Ctrl Pts',(-213.899660227539,-5.91817400525774,
132.664656556716));
#162130=CARTESIAN_POINT('Ctrl Pts',(-214.08051152189,-3.96652147180024,
136.503906757722));
#162131=CARTESIAN_POINT('Ctrl Pts',(-214.354178690847,2.57754055760962,
137.310807052006));
#162132=CARTESIAN_POINT('Ctrl Pts',(-214.632626314659,6.86728128874809,
132.15269597331));
#162133=CARTESIAN_POINT('Ctrl Pts',(-214.911073938471,4.84632600086921,
125.755530572531));
#162134=CARTESIAN_POINT('Ctrl Pts',(-215.189521562285,-1.62816612562249,
123.997993334078));
#162135=CARTESIAN_POINT('Ctrl Pts',(-215.406371156135,-5.50515921563603,
127.500311042211));
#162136=CARTESIAN_POINT('Ctrl Pts',(-215.530404875382,-5.91577993612624,
130.13515780681));
#162137=CARTESIAN_POINT('Ctrl Pts',(-215.561622720024,-5.91103173213339,
130.799753902201));
#162138=CARTESIAN_POINT('',(-217.311625997971,-5.91252205760374,130.808030356679));
#162139=CARTESIAN_POINT('Ctrl Pts',(-215.561624807793,-5.91674823766587,
130.799793936299));
#162140=CARTESIAN_POINT('Ctrl Pts',(-215.569324474548,-5.91687487495898,
130.963869538927));
#162141=CARTESIAN_POINT('Ctrl Pts',(-215.577024141303,-5.91017156417642,
131.128022491076));
#162142=CARTESIAN_POINT('Ctrl Pts',(-215.584723808058,-5.89665047465998,
131.291642612095));
#162143=CARTESIAN_POINT('Ctrl Pts',(-215.592118521284,-5.88366490234,131.448782383406));
#162144=CARTESIAN_POINT('Ctrl Pts',(-215.599513234511,-5.86439129366342,
131.605430320925));
#162145=CARTESIAN_POINT('Ctrl Pts',(-215.606907947737,-5.83889352847738,
131.761049138248));
#162146=CARTESIAN_POINT('Ctrl Pts',(-215.614303120355,-5.81339417926048,
131.916677623282));
#162147=CARTESIAN_POINT('Ctrl Pts',(-215.621698292973,-5.78166996330471,
132.071276492695));
#162148=CARTESIAN_POINT('Ctrl Pts',(-215.629093465591,-5.74383617647952,
132.224317145163));
#162149=CARTESIAN_POINT('Ctrl Pts',(-215.636490553458,-5.70599259122162,
132.377397433064));
#162150=CARTESIAN_POINT('Ctrl Pts',(-215.643887641324,-5.66203637385671,
132.528918338521));
#162151=CARTESIAN_POINT('Ctrl Pts',(-215.651284729191,-5.61213308837605,
132.678365089507));
#162152=CARTESIAN_POINT('Ctrl Pts',(-215.658685189034,-5.56220705438438,
132.827879966089));
#162153=CARTESIAN_POINT('Ctrl Pts',(-215.666085648878,-5.5063286721697,
132.975318452261));
#162154=CARTESIAN_POINT('Ctrl Pts',(-215.673486108721,-5.44471209851916,
133.12018460197));
#162155=CARTESIAN_POINT('Ctrl Pts',(-215.680895437876,-5.38302167856777,
133.265224371026));
#162156=CARTESIAN_POINT('Ctrl Pts',(-215.688304767031,-5.3155794815067,
133.40768530491));
#162157=CARTESIAN_POINT('Ctrl Pts',(-215.695714096186,-5.24264651133644,
133.547094312198));
#162158=CARTESIAN_POINT('Ctrl Pts',(-215.703128661892,-5.16966199571579,
133.686601846943));
#162159=CARTESIAN_POINT('Ctrl Pts',(-215.710543227598,-5.09117916043528,
133.823052835578));
#162160=CARTESIAN_POINT('Ctrl Pts',(-215.717957793304,-5.00750270899136,
133.956002599445));
#162161=CARTESIAN_POINT('Ctrl Pts',(-215.725382941123,-4.92370683400875,
134.089142110021));
#162162=CARTESIAN_POINT('Ctrl Pts',(-215.732808088942,-4.83470275432093,
134.218770113668));
#162163=CARTESIAN_POINT('Ctrl Pts',(-215.740233236761,-4.74083625196273,
134.344473920071));
#162164=CARTESIAN_POINT('Ctrl Pts',(-215.742294427811,-4.71477928996594,
134.379368789104));
#162165=CARTESIAN_POINT('Ctrl Pts',(-215.74435561886,-4.68834785493428,
134.41396147569));
#162166=CARTESIAN_POINT('Ctrl Pts',(-215.74641680991,-4.66154984466891,
134.448243657424));
#162167=CARTESIAN_POINT('Ctrl Pts',(-215.753840076316,-4.56503828192443,
134.571709052828));
#162168=CARTESIAN_POINT('Ctrl Pts',(-215.761263342721,-4.46347225429003,
134.69152419875));
#162169=CARTESIAN_POINT('Ctrl Pts',(-215.768686609127,-4.35715785453345,
134.807247824718));
#162170=CARTESIAN_POINT('Ctrl Pts',(-215.776101101848,-4.25096910956851,
134.922834674969));
#162171=CARTESIAN_POINT('Ctrl Pts',(-215.783515594568,-4.1400434136425,
135.034339358809));
#162172=CARTESIAN_POINT('Ctrl Pts',(-215.790930087289,-4.02472873371046,
135.141351415636));
#162173=CARTESIAN_POINT('Ctrl Pts',(-215.798337433643,-3.90952519840813,
135.248260330214));
#162174=CARTESIAN_POINT('Ctrl Pts',(-215.805744779997,-3.78994137252184,
135.350684986059));
#162175=CARTESIAN_POINT('Ctrl Pts',(-215.813152126351,-3.66636381908059,
135.448249818294));
#162176=CARTESIAN_POINT('Ctrl Pts',(-215.820553948026,-3.54287843444136,
135.545741882996));
#162177=CARTESIAN_POINT('Ctrl Pts',(-215.827955769702,-3.41540554491641,
135.638381110914));
#162178=CARTESIAN_POINT('Ctrl Pts',(-215.835357591377,-3.28436662909331,
135.725830561414));
#162179=CARTESIAN_POINT('Ctrl Pts',(-215.842755505688,-3.1533968876935,
135.81323384803));
#162180=CARTESIAN_POINT('Ctrl Pts',(-215.85015342,-3.01886517875771,135.895452606667));
#162181=CARTESIAN_POINT('Ctrl Pts',(-215.857551334311,-2.88122385268178,
135.972191852546));
#162182=CARTESIAN_POINT('Ctrl Pts',(-215.864948019223,-2.74360540009777,
136.048918345755));
#162183=CARTESIAN_POINT('Ctrl Pts',(-215.872344704135,-2.60287868172131,
136.120166951866));
#162184=CARTESIAN_POINT('Ctrl Pts',(-215.879741389048,-2.45952276416553,
136.185687436767));
#162185=CARTESIAN_POINT('Ctrl Pts',(-215.887137745983,-2.31617320316135,
136.251205016421));
#162186=CARTESIAN_POINT('Ctrl Pts',(-215.894534102918,-2.17019501429799,
136.31099482471));
#162187=CARTESIAN_POINT('Ctrl Pts',(-215.901930459854,-2.02208921821998,
136.364853919069));
#162188=CARTESIAN_POINT('Ctrl Pts',(-215.909327949191,-1.87396074676607,
136.418721259392));
#162189=CARTESIAN_POINT('Ctrl Pts',(-215.916725438527,-1.72370437034527,
136.466655950236));
#162190=CARTESIAN_POINT('Ctrl Pts',(-215.924122927864,-1.57183817085506,
136.508504315541));
#162191=CARTESIAN_POINT('Ctrl Pts',(-215.931523010379,-1.41991873490469,
136.550367350724));
#162192=CARTESIAN_POINT('Ctrl Pts',(-215.938923092894,-1.26638871198569,
136.586139713374));
#162193=CARTESIAN_POINT('Ctrl Pts',(-215.946323175409,-1.11177817411067,
136.615718449783));
#162194=CARTESIAN_POINT('Ctrl Pts',(-215.953731395075,-0.956997626054681,
136.645329711054));
#162195=CARTESIAN_POINT('Ctrl Pts',(-215.961139614742,-0.801134557128024,
136.668733674823));
#162196=CARTESIAN_POINT('Ctrl Pts',(-215.968547834408,-0.644726724846512,
136.685878960032));
#162197=CARTESIAN_POINT('Ctrl Pts',(-215.97596061371,-0.488222626153588,
136.703034797879));
#162198=CARTESIAN_POINT('Ctrl Pts',(-215.983373393012,-0.331173467533277,
136.713924255588));
#162199=CARTESIAN_POINT('Ctrl Pts',(-215.990786172314,-0.174118333418985,
136.718548082338));
#162200=CARTESIAN_POINT('Ctrl Pts',(-215.998209543343,-0.0168387915641384,
136.723178515829));
#162201=CARTESIAN_POINT('Ctrl Pts',(-216.005632914372,0.140446370548699,
136.72152544187));
#162202=CARTESIAN_POINT('Ctrl Pts',(-216.0130562854,0.29720103242974,136.713641632108));
#162203=CARTESIAN_POINT('Ctrl Pts',(-216.016992334841,0.380316115439795,
136.709461447002));
#162204=CARTESIAN_POINT('Ctrl Pts',(-216.020928384282,0.463282177994346,
136.703530441126));
#162205=CARTESIAN_POINT('Ctrl Pts',(-216.024864433723,0.546020445833623,
136.695862313673));
#162206=CARTESIAN_POINT('Ctrl Pts',(-216.032287700129,0.702062236798269,
136.681400464612));
#162207=CARTESIAN_POINT('Ctrl Pts',(-216.039710966534,0.857765031229207,
136.660713102083));
#162208=CARTESIAN_POINT('Ctrl Pts',(-216.04713423294,1.01259212516141,136.633819233129));
#162209=CARTESIAN_POINT('Ctrl Pts',(-216.054548725661,1.16723622632573,
136.606957150495));
#162210=CARTESIAN_POINT('Ctrl Pts',(-216.061963218382,1.32100632297602,
136.573903226202));
#162211=CARTESIAN_POINT('Ctrl Pts',(-216.069377711103,1.47336899834449,
136.534728350724));
#162212=CARTESIAN_POINT('Ctrl Pts',(-216.076785057457,1.62558482083053,
136.495591233465));
#162213=CARTESIAN_POINT('Ctrl Pts',(-216.08419240381,1.77639556349853,136.450345002302));
#162214=CARTESIAN_POINT('Ctrl Pts',(-216.091599750164,1.9252763062222,136.399111881671));
#162215=CARTESIAN_POINT('Ctrl Pts',(-216.099001571839,2.07404600807014,
136.347916972633));
#162216=CARTESIAN_POINT('Ctrl Pts',(-216.106403393515,2.22088822468311,
136.290744185985));
#162217=CARTESIAN_POINT('Ctrl Pts',(-216.11380521519,2.36529165889142,136.227765998955));
#162218=CARTESIAN_POINT('Ctrl Pts',(-216.121203129502,2.50961886365209,
136.164821057619));
#162219=CARTESIAN_POINT('Ctrl Pts',(-216.128601043813,2.65150950864942,
136.096076968103));
#162220=CARTESIAN_POINT('Ctrl Pts',(-216.135998958124,2.79047090839696,
136.021754859129));
#162221=CARTESIAN_POINT('Ctrl Pts',(-216.143395643036,2.92940921527988,
135.947445101141));
#162222=CARTESIAN_POINT('Ctrl Pts',(-216.150792327949,3.06541891418995,
135.867559339329));
#162223=CARTESIAN_POINT('Ctrl Pts',(-216.158189012861,3.19803052887582,
135.782365368355));
#162224=CARTESIAN_POINT('Ctrl Pts',(-216.165585369796,3.33063626342411,
135.69717517497));
#162225=CARTESIAN_POINT('Ctrl Pts',(-216.172981726732,3.45984389926964,
135.60667744219));
#162226=CARTESIAN_POINT('Ctrl Pts',(-216.180378083667,3.58521188118791,
135.511183997457));
#162227=CARTESIAN_POINT('Ctrl Pts',(-216.187775573004,3.71059905726426,
135.415675932434));
#162228=CARTESIAN_POINT('Ctrl Pts',(-216.19517306234,3.83214511192364,135.315170858741));
#162229=CARTESIAN_POINT('Ctrl Pts',(-216.202570551677,3.94944071722406,
135.210021587685));
#162230=CARTESIAN_POINT('Ctrl Pts',(-216.209970634192,4.06677744031659,
135.104835456717));
#162231=CARTESIAN_POINT('Ctrl Pts',(-216.217370716707,4.17986046970684,
134.995002136039));
#162232=CARTESIAN_POINT('Ctrl Pts',(-216.224770799222,4.28831667065473,
134.880911941257));
#162233=CARTESIAN_POINT('Ctrl Pts',(-216.232179018888,4.39689213034528,
134.766696292576));
#162234=CARTESIAN_POINT('Ctrl Pts',(-216.239587238555,4.50083034382097,
134.648214692508));
#162235=CARTESIAN_POINT('Ctrl Pts',(-216.246995458221,4.59979741166932,
134.525891798962));
#162236=CARTESIAN_POINT('Ctrl Pts',(-216.254408237523,4.69882539209686,
134.403493617716));
#162237=CARTESIAN_POINT('Ctrl Pts',(-216.261821016825,4.79287590764574,
134.277249730586));
#162238=CARTESIAN_POINT('Ctrl Pts',(-216.269233796127,4.8816582003181,134.147614089525));
#162239=CARTESIAN_POINT('Ctrl Pts',(-216.276657167156,4.97056734929359,
134.017793218981));
#162240=CARTESIAN_POINT('Ctrl Pts',(-216.284080538185,5.05419304337971,
133.884571230695));
#162241=CARTESIAN_POINT('Ctrl Pts',(-216.291503909213,5.13228989463789,
133.748427702382));
#162242=CARTESIAN_POINT('Ctrl Pts',(-216.295439958654,5.17369871908487,
133.676241136949));
#162243=CARTESIAN_POINT('Ctrl Pts',(-216.299376008095,5.21355397923511,
133.603233585252));
#162244=CARTESIAN_POINT('Ctrl Pts',(-216.303312057536,5.25182462119782,
133.529478727058));
#162245=CARTESIAN_POINT('Ctrl Pts',(-216.310735323942,5.32400185755124,
133.390379366318));
#162246=CARTESIAN_POINT('Ctrl Pts',(-216.318158590347,5.39075815720084,
133.248200170866));
#162247=CARTESIAN_POINT('Ctrl Pts',(-216.325581856753,5.4518194097087,133.103402958721));
#162248=CARTESIAN_POINT('Ctrl Pts',(-216.332996349474,5.51280849288693,
132.958776884856));
#162249=CARTESIAN_POINT('Ctrl Pts',(-216.340410842195,5.56811578352684,
132.81153929408));
#162250=CARTESIAN_POINT('Ctrl Pts',(-216.347825334916,5.61751259899866,
132.662177283061));
#162251=CARTESIAN_POINT('Ctrl Pts',(-216.35523268127,5.66686180395983,132.512959232772));
#162252=CARTESIAN_POINT('Ctrl Pts',(-216.362640027623,5.71031175841179,
132.361621190639));
#162253=CARTESIAN_POINT('Ctrl Pts',(-216.370047373977,5.74768156108323,
132.208670852124));
#162254=CARTESIAN_POINT('Ctrl Pts',(-216.377449195653,5.78502349194605,
132.055834589741));
#162255=CARTESIAN_POINT('Ctrl Pts',(-216.384851017328,5.81629421222117,
131.901388786409));
#162256=CARTESIAN_POINT('Ctrl Pts',(-216.392252839003,5.8413624632775,131.745856839073));
#162257=CARTESIAN_POINT('Ctrl Pts',(-216.399650753315,5.86641748099923,
131.590406995842));
#162258=CARTESIAN_POINT('Ctrl Pts',(-216.407048667626,5.88527649104824,
131.433872518103));
#162259=CARTESIAN_POINT('Ctrl Pts',(-216.414446581938,5.89785922674048,
131.276787441584));
#162260=CARTESIAN_POINT('Ctrl Pts',(-216.42184326685,5.91043987141032,131.119728469756));
#162261=CARTESIAN_POINT('Ctrl Pts',(-216.429239951762,5.91674628199853,
130.962119452491));
#162262=CARTESIAN_POINT('Ctrl Pts',(-216.436636636674,5.91674999835537,
130.804500123008));
#162263=CARTESIAN_POINT('Ctrl Pts',(-216.44403299361,5.91675371454741,130.646887782532));
#162264=CARTESIAN_POINT('Ctrl Pts',(-216.451429350545,5.9104552921762,130.489265504047));
#162265=CARTESIAN_POINT('Ctrl Pts',(-216.458825707481,5.89787840911742,
130.332173330818));
#162266=CARTESIAN_POINT('Ctrl Pts',(-216.466223196817,5.8852996005057,130.175057106376));
#162267=CARTESIAN_POINT('Ctrl Pts',(-216.473620686154,5.86644044702607,
130.018471520923));
#162268=CARTESIAN_POINT('Ctrl Pts',(-216.481018175491,5.84137652707394,
129.862951656779));
#162269=CARTESIAN_POINT('Ctrl Pts',(-216.488418258006,5.81630382100349,
129.707377275388));
#162270=CARTESIAN_POINT('Ctrl Pts',(-216.495818340521,5.78502207726764,
129.552869727429));
#162271=CARTESIAN_POINT('Ctrl Pts',(-216.503218423036,5.74765799099632,
129.399953916843));
#162272=CARTESIAN_POINT('Ctrl Pts',(-216.510626642702,5.71025281907119,
129.246869959604));
#162273=CARTESIAN_POINT('Ctrl Pts',(-216.518034862369,5.666752036575,129.095381598012));
#162274=CARTESIAN_POINT('Ctrl Pts',(-216.525443082035,5.61733243944677,
128.945999289073));
#162275=CARTESIAN_POINT('Ctrl Pts',(-216.532855861337,5.56788242538113,
128.796525037816));
#162276=CARTESIAN_POINT('Ctrl Pts',(-216.540268640639,5.51250646869158,
128.649159770763));
#162277=CARTESIAN_POINT('Ctrl Pts',(-216.547681419941,5.45142933021152,
128.504393482973));
#162278=CARTESIAN_POINT('Ctrl Pts',(-216.55510479097,5.39026492185168,128.359420346321));
#162279=CARTESIAN_POINT('Ctrl Pts',(-216.562528161999,5.32338322038728,
128.217053942686));
#162280=CARTESIAN_POINT('Ctrl Pts',(-216.569951533028,5.25105506995864,
128.077759947361));
#162281=CARTESIAN_POINT('Ctrl Pts',(-216.573887582468,5.21270494911401,
128.003902928732));
#162282=CARTESIAN_POINT('Ctrl Pts',(-216.577823631909,5.17282436982461,
127.930909204615));
#162283=CARTESIAN_POINT('Ctrl Pts',(-216.581759681349,5.13145853557716,
127.858844727242));
#162284=CARTESIAN_POINT('Ctrl Pts',(-216.589182947755,5.05344386316463,
127.722933371962));
#162285=CARTESIAN_POINT('Ctrl Pts',(-216.59660621416,4.96990788988157,127.58991807837));
#162286=CARTESIAN_POINT('Ctrl Pts',(-216.604029480566,4.88109099291859,
127.460279087258));
#162287=CARTESIAN_POINT('Ctrl Pts',(-216.611443973287,4.79237907015178,
127.330793318667));
#162288=CARTESIAN_POINT('Ctrl Pts',(-216.618858466008,4.69839885659414,
127.204676214376));
#162289=CARTESIAN_POINT('Ctrl Pts',(-216.626272958729,4.59943655191889,
127.082383459203));
#162290=CARTESIAN_POINT('Ctrl Pts',(-216.633680305082,4.50056963083848,
126.960208574392));
#162291=CARTESIAN_POINT('Ctrl Pts',(-216.641087651436,4.39673041158119,
126.841850988735));
#162292=CARTESIAN_POINT('Ctrl Pts',(-216.64849499779,4.28824825116155,126.727737321392));
#162293=CARTESIAN_POINT('Ctrl Pts',(-216.655896819465,4.17984700083087,
126.613708764328));
#162294=CARTESIAN_POINT('Ctrl Pts',(-216.663298641141,4.06680996049485,
126.503918092479));
#162295=CARTESIAN_POINT('Ctrl Pts',(-216.670700462816,3.94950653033062,
126.398758646283));
#162296=CARTESIAN_POINT('Ctrl Pts',(-216.678098377128,3.83226502373242,
126.293654712937));
#162297=CARTESIAN_POINT('Ctrl Pts',(-216.685496291439,3.71076188991149,
126.193177384882));
#162298=CARTESIAN_POINT('Ctrl Pts',(-216.69289420575,3.58540304214761,126.097682852108));
#162299=CARTESIAN_POINT('Ctrl Pts',(-216.700290890663,3.46006502675123,
126.002204188793));
#162300=CARTESIAN_POINT('Ctrl Pts',(-216.707687575575,3.33087286577215,
125.911706903312));
#162301=CARTESIAN_POINT('Ctrl Pts',(-216.715084260487,3.19826526864947,
125.826506678985));
#162302=CARTESIAN_POINT('Ctrl Pts',(-216.722480617422,3.06566355148662,
125.741310232524));
#162303=CARTESIAN_POINT('Ctrl Pts',(-216.729876974358,2.92964701336309,
125.661410581986));
#162304=CARTESIAN_POINT('Ctrl Pts',(-216.737273331293,2.79068280644374,
125.58707971308));
#162305=CARTESIAN_POINT('Ctrl Pts',(-216.74467082063,2.65169732374956,125.512737463927));
#162306=CARTESIAN_POINT('Ctrl Pts',(-216.752068309967,2.50976360285831,
125.443965870116));
#162307=CARTESIAN_POINT('Ctrl Pts',(-216.759465799303,2.36537267564962,
125.380990570465));
#162308=CARTESIAN_POINT('Ctrl Pts',(-216.766865881818,2.22093113242585,
125.317993194921));
#162309=CARTESIAN_POINT('Ctrl Pts',(-216.774265964333,2.07403100985985,
125.260796308143));
#162310=CARTESIAN_POINT('Ctrl Pts',(-216.781666046848,1.92518240631656,
125.209577041331));
#162311=CARTESIAN_POINT('Ctrl Pts',(-216.789074266515,1.77617012843103,
125.158301453669));
#162312=CARTESIAN_POINT('Ctrl Pts',(-216.796482486181,1.62520544394597,
125.11301673424));
#162313=CARTESIAN_POINT('Ctrl Pts',(-216.803890705847,1.47281337732091,
125.073850054092));
#162314=CARTESIAN_POINT('Ctrl Pts',(-216.811303485149,1.32032751592122,
125.034659267506));
#162315=CARTESIAN_POINT('Ctrl Pts',(-216.818716264452,1.16641288592535,
125.001594101759));
#162316=CARTESIAN_POINT('Ctrl Pts',(-216.826129043754,1.01160322277228,
124.974730313492));
#162317=CARTESIAN_POINT('Ctrl Pts',(-216.833552414782,0.856572360312867,
124.947828140985));
#162318=CARTESIAN_POINT('Ctrl Pts',(-216.840975785811,0.700644279591562,
124.927145091957));
#162319=CARTESIAN_POINT('Ctrl Pts',(-216.84839915684,0.544357164294071,
124.912705006434));
#162320=CARTESIAN_POINT('Ctrl Pts',(-216.852335206281,0.461489985705045,
124.905048526604));
#162321=CARTESIAN_POINT('Ctrl Pts',(-216.856271255721,0.378521871066538,
124.899146296581));
#162322=CARTESIAN_POINT('Ctrl Pts',(-216.860207305162,0.295532741446856,
124.894995934181));
#162323=CARTESIAN_POINT('Ctrl Pts',(-216.867630571568,0.139017832987244,
124.887168480224));
#162324=CARTESIAN_POINT('Ctrl Pts',(-216.875053837973,-0.018044934740192,
124.885551645143));
#162325=CARTESIAN_POINT('Ctrl Pts',(-216.882477104379,-0.175121591811435,
124.890202774679));
#162326=CARTESIAN_POINT('Ctrl Pts',(-216.8898915971,-0.332012597318424,
124.894848406966));
#162327=CARTESIAN_POINT('Ctrl Pts',(-216.897306089821,-0.488917090002346,
124.905747246839));
#162328=CARTESIAN_POINT('Ctrl Pts',(-216.904720582542,-0.645296991405024,
124.922904815183));
#162329=CARTESIAN_POINT('Ctrl Pts',(-216.912127928895,-0.801526167972022,
124.940045846417));
#162330=CARTESIAN_POINT('Ctrl Pts',(-216.919535275249,-0.957231391269231,
124.963433556365));
#162331=CARTESIAN_POINT('Ctrl Pts',(-216.926942621603,-1.11187570900268,
124.99302144572));
#162332=CARTESIAN_POINT('Ctrl Pts',(-216.934344443278,-1.26640468716869,
125.022587267311));
#162333=CARTESIAN_POINT('Ctrl Pts',(-216.941746264954,-1.41987397021381,
125.058343990801));
#162334=CARTESIAN_POINT('Ctrl Pts',(-216.949148086629,-1.57175295986926,
125.100193439472));
#162335=CARTESIAN_POINT('Ctrl Pts',(-216.956546000941,-1.72355177379002,
125.142020796146));
#162336=CARTESIAN_POINT('Ctrl Pts',(-216.963943915252,-1.87376160725783,
125.189934373668));
#162337=CARTESIAN_POINT('Ctrl Pts',(-216.971341829563,-2.02186338150322,
125.243785195091));
#162338=CARTESIAN_POINT('Ctrl Pts',(-216.978738514476,-2.1699405439191,
125.297627067483));
#162339=CARTESIAN_POINT('Ctrl Pts',(-216.986135199388,-2.31590999191378,
125.357404098105));
#162340=CARTESIAN_POINT('Ctrl Pts',(-216.9935318843,-2.45926899900166,125.422917822827));
#162341=CARTESIAN_POINT('Ctrl Pts',(-217.000928241235,-2.60262164940094,
125.488428642601));
#162342=CARTESIAN_POINT('Ctrl Pts',(-217.008324598171,-2.74336374951875,
125.55967549554));
#162343=CARTESIAN_POINT('Ctrl Pts',(-217.015720955106,-2.88101396291893,
125.636412368215));
#162344=CARTESIAN_POINT('Ctrl Pts',(-217.023118444443,-3.01868525091819,
125.713160989502));
#162345=CARTESIAN_POINT('Ctrl Pts',(-217.03051593378,-3.1532633835701,125.795401122365));
#162346=CARTESIAN_POINT('Ctrl Pts',(-217.037913423116,-3.28429310981991,
125.882841611071));
#162347=CARTESIAN_POINT('Ctrl Pts',(-217.045313505631,-3.41536876833806,
125.970312751906));
#162348=CARTESIAN_POINT('Ctrl Pts',(-217.052713588146,-3.54289323356809,
126.062987671034));
#162349=CARTESIAN_POINT('Ctrl Pts',(-217.060113670661,-3.66644175938774,
126.160532951996));
#162350=CARTESIAN_POINT('Ctrl Pts',(-217.067521890328,-3.79012613951173,
126.258185494021));
#162351=CARTESIAN_POINT('Ctrl Pts',(-217.074930109994,-3.90982555597913,
126.360718861628));
#162352=CARTESIAN_POINT('Ctrl Pts',(-217.082338329661,-4.02514922763937,
126.467760075928));
#162353=CARTESIAN_POINT('Ctrl Pts',(-217.089751108963,-4.14054387909489,
126.574867172309));
#162354=CARTESIAN_POINT('Ctrl Pts',(-217.097163888265,-4.25155715657824,
126.686487379865));
#162355=CARTESIAN_POINT('Ctrl Pts',(-217.104576667567,-4.35783682683886,
126.80221260017));
#162356=CARTESIAN_POINT('Ctrl Pts',(-217.112000038595,-4.46426835447682,
126.918103174097));
#162357=CARTESIAN_POINT('Ctrl Pts',(-217.119423409624,-4.56595252578291,
127.03811019131));
#162358=CARTESIAN_POINT('Ctrl Pts',(-217.126846780653,-4.66257838204143,
127.161793748747));
#162359=CARTESIAN_POINT('Ctrl Pts',(-217.130782830094,-4.71381172953475,
127.227373738645));
#162360=CARTESIAN_POINT('Ctrl Pts',(-217.134718879534,-4.76362373538357,
127.293986863771));
#162361=CARTESIAN_POINT('Ctrl Pts',(-217.138654928975,-4.81197320449548,
127.361564596638));
#162362=CARTESIAN_POINT('Ctrl Pts',(-217.146146069748,-4.90399254643782,
127.490179421632));
#162363=CARTESIAN_POINT('Ctrl Pts',(-217.15363721052,-4.99098822520857,
127.622676463298));
#162364=CARTESIAN_POINT('Ctrl Pts',(-217.161128351292,-5.07261844284067,
127.758630377401));
#162365=CARTESIAN_POINT('Ctrl Pts',(-217.168610322293,-5.15414873838094,
127.894417872746));
#162366=CARTESIAN_POINT('Ctrl Pts',(-217.176092293294,-5.23032646158278,
128.033653507964));
#162367=CARTESIAN_POINT('Ctrl Pts',(-217.183574264295,-5.30085110262719,
128.175880419757));
#162368=CARTESIAN_POINT('Ctrl Pts',(-217.191048462408,-5.3713024768669,
128.317959574521));
#162369=CARTESIAN_POINT('Ctrl Pts',(-217.198522660521,-5.43611230127342,
128.463023494699));
#162370=CARTESIAN_POINT('Ctrl Pts',(-217.205996858634,-5.49502432286834,
128.610588010028));
#162371=CARTESIAN_POINT('Ctrl Pts',(-217.213464675629,-5.55388604815469,
128.758026541726));
#162372=CARTESIAN_POINT('Ctrl Pts',(-217.220932492624,-5.60685986334836,
128.907961080522));
#162373=CARTESIAN_POINT('Ctrl Pts',(-217.228400309619,-5.65373629863065,
129.059884642367));
#162374=CARTESIAN_POINT('Ctrl Pts',(-217.235862610705,-5.70057810985261,
129.211695989823));
#162375=CARTESIAN_POINT('Ctrl Pts',(-217.243324911791,-5.74133140817679,
129.365493085869));
#162376=CARTESIAN_POINT('Ctrl Pts',(-217.250787212877,-5.77583559641578,
129.520750970642));
#162377=CARTESIAN_POINT('Ctrl Pts',(-217.258246235064,-5.81032462368122,
129.675940635851));
#162378=CARTESIAN_POINT('Ctrl Pts',(-217.265705257251,-5.83856993091696,
129.832589456409));
#162379=CARTESIAN_POINT('Ctrl Pts',(-217.273164279438,-5.86046130109009,
129.990159229133));
#162380=CARTESIAN_POINT('Ctrl Pts',(-217.280622113517,-5.88234918430061,
130.147703903388));
#162381=CARTESIAN_POINT('Ctrl Pts',(-217.288079947595,-5.89788509194219,
130.306168877629));
#162382=CARTESIAN_POINT('Ctrl Pts',(-217.295537781673,-5.90701024927821,
130.465007589847));
#162383=CARTESIAN_POINT('Ctrl Pts',(-217.300900123713,-5.91357143236328,
130.579216017546));
#162384=CARTESIAN_POINT('Ctrl Pts',(-217.306262465753,-5.91681938424466,
130.693617469333));
#162385=CARTESIAN_POINT('Ctrl Pts',(-217.311624807793,-5.91674887602822,
130.808007605195));
#162386=CARTESIAN_POINT('',(-219.061623395149,-5.9210338050865,130.807548187548));
#162387=CARTESIAN_POINT('Ctrl Pts',(-217.311626920727,-5.90924496437867,
130.808047996124));
#162388=CARTESIAN_POINT('Ctrl Pts',(-217.346785464747,-5.91343255841384,
131.55710594002));
#162389=CARTESIAN_POINT('Ctrl Pts',(-217.474759883373,-5.4330908806276,
134.278437435159));
#162390=CARTESIAN_POINT('Ctrl Pts',(-217.6955501766,-1.337882961292,137.673685890998));
#162391=CARTESIAN_POINT('Ctrl Pts',(-217.973997800414,5.05619948175488,
135.642997546604));
#162392=CARTESIAN_POINT('Ctrl Pts',(-218.252445424226,6.80388161014486,
129.165838244978));
#162393=CARTESIAN_POINT('Ctrl Pts',(-218.530893048039,2.29912892690833,
124.194400957491));
#162394=CARTESIAN_POINT('Ctrl Pts',(-218.800618671839,-4.11112532191061,
125.262650173527));
#162395=CARTESIAN_POINT('Ctrl Pts',(-218.977528421034,-5.91269684251228,
129.027581667749));
#162396=CARTESIAN_POINT('Ctrl Pts',(-219.061622295625,-5.92436876444137,
130.807526727116));
#162397=CARTESIAN_POINT('',(-220.811625604547,-5.91847951006198,130.799176690814));
#162398=CARTESIAN_POINT('Ctrl Pts',(-219.061624807793,-5.91674912645136,
130.807575759414));
#162399=CARTESIAN_POINT('Ctrl Pts',(-219.070345970417,-5.9166489483197,
130.991931194124));
#162400=CARTESIAN_POINT('Ctrl Pts',(-219.079067133041,-5.90793327527812,
131.176047965864));
#162401=CARTESIAN_POINT('Ctrl Pts',(-219.087788295665,-5.8906639236756,
131.359346293784));
#162402=CARTESIAN_POINT('Ctrl Pts',(-219.09521156207,-5.87596462231853,
131.515365895582));
#162403=CARTESIAN_POINT('Ctrl Pts',(-219.102634828476,-5.85504033059687,
131.671037027068));
#162404=CARTESIAN_POINT('Ctrl Pts',(-219.110058094881,-5.82791087230526,
131.825823013823));
#162405=CARTESIAN_POINT('Ctrl Pts',(-219.117472587602,-5.80081347878032,
131.980426056395));
#162406=CARTESIAN_POINT('Ctrl Pts',(-219.124887080323,-5.76752558085258,
132.134145672538));
#162407=CARTESIAN_POINT('Ctrl Pts',(-219.132301573044,-5.72811888068246,
132.286448553982));
#162408=CARTESIAN_POINT('Ctrl Pts',(-219.139708919398,-5.68875016217372,
132.438604640174));
#162409=CARTESIAN_POINT('Ctrl Pts',(-219.147116265752,-5.64327447512745,
132.589346351144));
#162410=CARTESIAN_POINT('Ctrl Pts',(-219.154523612106,-5.59181484267633,
132.738148953379));
#162411=CARTESIAN_POINT('Ctrl Pts',(-219.161925433781,-5.54039359076056,
132.886840573018));
#162412=CARTESIAN_POINT('Ctrl Pts',(-219.169327255457,-5.48299740146014,
133.033595612342));
#162413=CARTESIAN_POINT('Ctrl Pts',(-219.176729077132,-5.41979952991243,
133.177903037255));
#162414=CARTESIAN_POINT('Ctrl Pts',(-219.184126991443,-5.35663502002935,
133.3221342834));
#162415=CARTESIAN_POINT('Ctrl Pts',(-219.191524905755,-5.2876750767107,
133.463920147288));
#162416=CARTESIAN_POINT('Ctrl Pts',(-219.198922820066,-5.21314157820515,
133.602768280522));
#162417=CARTESIAN_POINT('Ctrl Pts',(-219.206319504978,-5.13862046581477,
133.741593339715));
#162418=CARTESIAN_POINT('Ctrl Pts',(-219.21371618989,-5.05852781290098,
133.877481308598));
#162419=CARTESIAN_POINT('Ctrl Pts',(-219.221112874803,-4.97313212827649,
134.009963119001));
#162420=CARTESIAN_POINT('Ctrl Pts',(-219.228509231738,-4.88774023018615,
134.142439055021));
#162421=CARTESIAN_POINT('Ctrl Pts',(-219.235905588674,-4.79704597017358,
134.271508819103));
#162422=CARTESIAN_POINT('Ctrl Pts',(-219.243301945609,-4.70136184729367,
134.39673133108));
#162423=CARTESIAN_POINT('Ctrl Pts',(-219.250699434946,-4.60566307493001,
134.521973014944));
#162424=CARTESIAN_POINT('Ctrl Pts',(-219.258096924282,-4.5049731452149,
134.643365977242));
#162425=CARTESIAN_POINT('Ctrl Pts',(-219.265494413619,-4.39964549197633,
134.760501427425));
#162426=CARTESIAN_POINT('Ctrl Pts',(-219.272894496134,-4.29428091629235,
134.877677939259));
#162427=CARTESIAN_POINT('Ctrl Pts',(-219.280294578649,-4.18427562967898,
134.990593690084));
#162428=CARTESIAN_POINT('Ctrl Pts',(-219.287694661164,-4.07002051513498,
135.098876139587));
#162429=CARTESIAN_POINT('Ctrl Pts',(-219.295102880831,-3.95563976534666,
135.207277656775));
#162430=CARTESIAN_POINT('Ctrl Pts',(-219.302511100497,-3.83700012620945,
135.311035441066));
#162431=CARTESIAN_POINT('Ctrl Pts',(-219.309919320164,-3.7145267632806,
135.409816239692));
#162432=CARTESIAN_POINT('Ctrl Pts',(-219.317332099466,-3.59197802004045,
135.508657836251));
#162433=CARTESIAN_POINT('Ctrl Pts',(-219.324744878768,-3.46559115022453,
135.602516121185));
#162434=CARTESIAN_POINT('Ctrl Pts',(-219.33215765807,-3.33582054774286,
135.691101027671));
#162435=CARTESIAN_POINT('Ctrl Pts',(-219.339581029099,-3.20586452293891,
135.779812508426));
#162436=CARTESIAN_POINT('Ctrl Pts',(-219.347004400128,-3.07251542485004,
135.863235364487));
#162437=CARTESIAN_POINT('Ctrl Pts',(-219.354427771156,-2.93625320407586,
135.941124938036));
#162438=CARTESIAN_POINT('Ctrl Pts',(-219.358363820597,-2.86400370505544,
135.982423858866));
#162439=CARTESIAN_POINT('Ctrl Pts',(-219.362299870038,-2.79093558498296,
136.022167967796));
#162440=CARTESIAN_POINT('Ctrl Pts',(-219.366235919478,-2.71712257079711,
136.060326323101));
#162441=CARTESIAN_POINT('Ctrl Pts',(-219.373659185884,-2.57791352966545,
136.132291790327));
#162442=CARTESIAN_POINT('Ctrl Pts',(-219.381082452289,-2.43563290713131,
136.198831640141));
#162443=CARTESIAN_POINT('Ctrl Pts',(-219.388505718695,-2.29074293782725,
136.259672465233));
#162444=CARTESIAN_POINT('Ctrl Pts',(-219.395920211416,-2.14602421643454,
136.320441381522));
#162445=CARTESIAN_POINT('Ctrl Pts',(-219.403334704137,-1.99870262787695,
136.375524537568));
#162446=CARTESIAN_POINT('Ctrl Pts',(-219.410749196858,-1.84926561627258,
136.424693992284));
#162447=CARTESIAN_POINT('Ctrl Pts',(-219.418156543212,-1.6999726376862,
136.473816055629));
#162448=CARTESIAN_POINT('Ctrl Pts',(-219.425563889566,-1.54856864736606,
136.517035649029));
#162449=CARTESIAN_POINT('Ctrl Pts',(-219.432971235919,-1.39556161548667,
136.554172644048));
#162450=CARTESIAN_POINT('Ctrl Pts',(-219.440373057595,-1.24266870202429,
136.591281940896));
#162451=CARTESIAN_POINT('Ctrl Pts',(-219.44777487927,-1.08817548882546,
136.622317584739));
#162452=CARTESIAN_POINT('Ctrl Pts',(-219.455176700946,-0.932605571982637,
136.647149113619));
#162453=CARTESIAN_POINT('Ctrl Pts',(-219.462574615257,-0.777117779287963,
136.671967534128));
#162454=CARTESIAN_POINT('Ctrl Pts',(-219.469972529568,-0.62055478261063,
136.690588303511));
#162455=CARTESIAN_POINT('Ctrl Pts',(-219.47737044388,-0.463450739213037,
136.702931967887));
#162456=CARTESIAN_POINT('Ctrl Pts',(-219.484767128792,-0.306372803657523,
136.715273580969));
#162457=CARTESIAN_POINT('Ctrl Pts',(-219.492163813704,-0.148754371617358,
136.721340130161));
#162458=CARTESIAN_POINT('Ctrl Pts',(-219.499560498616,0.00886478099952192,
136.721103976725));
#162459=CARTESIAN_POINT('Ctrl Pts',(-219.506956855552,0.166476944618001,
136.720867833762));
#162460=CARTESIAN_POINT('Ctrl Pts',(-219.514353212487,0.324089455452518,
136.714329544408));
#162461=CARTESIAN_POINT('Ctrl Pts',(-219.521749569423,0.481162306895928,
136.701513608368));
#162462=CARTESIAN_POINT('Ctrl Pts',(-219.529147058759,0.638259206593881,
136.688695710175));
#162463=CARTESIAN_POINT('Ctrl Pts',(-219.536544548096,0.79481591030149,
136.669598281929));
#162464=CARTESIAN_POINT('Ctrl Pts',(-219.543942037432,0.950297451335014,
136.644297716241));
#162465=CARTESIAN_POINT('Ctrl Pts',(-219.551342119947,1.1058334961815,136.61898828148));
#162466=CARTESIAN_POINT('Ctrl Pts',(-219.558742202462,1.26029325973372,
136.587471439783));
#162467=CARTESIAN_POINT('Ctrl Pts',(-219.566142284977,1.41315203146586,
136.549874684946));
#162468=CARTESIAN_POINT('Ctrl Pts',(-219.573550504643,1.566178887132,136.512236588613));
#162469=CARTESIAN_POINT('Ctrl Pts',(-219.58095872431,1.71760087251689,136.468505316992));
#162470=CARTESIAN_POINT('Ctrl Pts',(-219.588366943976,1.866907800259,136.418858442646));
#162471=CARTESIAN_POINT('Ctrl Pts',(-219.595779723278,2.01630662392423,
136.369181011478));
#162472=CARTESIAN_POINT('Ctrl Pts',(-219.603192502581,2.16358744755067,
136.313580854063));
#162473=CARTESIAN_POINT('Ctrl Pts',(-219.610605281883,2.30826061869695,
136.252283476663));
#162474=CARTESIAN_POINT('Ctrl Pts',(-219.618028652911,2.45314050565446,
136.190898514696));
#162475=CARTESIAN_POINT('Ctrl Pts',(-219.62545202394,2.59540496186664,136.123800233249));
#162476=CARTESIAN_POINT('Ctrl Pts',(-219.632875394969,2.73458872475895,
136.051260184827));
#162477=CARTESIAN_POINT('Ctrl Pts',(-219.636811444409,2.80838729551299,
136.012797710579));
#162478=CARTESIAN_POINT('Ctrl Pts',(-219.64074749385,2.88132024365648,135.972806093445));
#162479=CARTESIAN_POINT('Ctrl Pts',(-219.644683543291,2.9533216858271,135.931330637229));
#162480=CARTESIAN_POINT('Ctrl Pts',(-219.652106809697,3.08911415867301,
135.853109221209));
#162481=CARTESIAN_POINT('Ctrl Pts',(-219.659530076102,3.22200217070551,
135.769370918026));
#162482=CARTESIAN_POINT('Ctrl Pts',(-219.666953342507,3.35150584750005,
135.680356835435));
#162483=CARTESIAN_POINT('Ctrl Pts',(-219.674367835228,3.48085646170323,
135.591447960098));
#162484=CARTESIAN_POINT('Ctrl Pts',(-219.681782327949,3.60683039806602,
135.497275926604));
#162485=CARTESIAN_POINT('Ctrl Pts',(-219.68919682067,3.72897240784421,135.39812762777));
#162486=CARTESIAN_POINT('Ctrl Pts',(-219.696604167024,3.85099669255481,
135.299074891799));
#162487=CARTESIAN_POINT('Ctrl Pts',(-219.704011513378,3.96919611554074,
135.195055672689));
#162488=CARTESIAN_POINT('Ctrl Pts',(-219.711418859732,4.0831445593603,135.086399976314));
#162489=CARTESIAN_POINT('Ctrl Pts',(-219.718820681407,4.19700801613143,
134.977825319457));
#162490=CARTESIAN_POINT('Ctrl Pts',(-219.726222503082,4.30662653771201,
134.864621327302));
#162491=CARTESIAN_POINT('Ctrl Pts',(-219.733624324758,4.41160734628434,
134.747157998197));
#162492=CARTESIAN_POINT('Ctrl Pts',(-219.741022239069,4.51653273630501,
134.629756677069));
#162493=CARTESIAN_POINT('Ctrl Pts',(-219.74842015338,4.61682504092196,134.508100774558));
#162494=CARTESIAN_POINT('Ctrl Pts',(-219.755818067692,4.71212868828817,
134.382596745536));
#162495=CARTESIAN_POINT('Ctrl Pts',(-219.763214752604,4.80741649791705,
134.257113573007));
#162496=CARTESIAN_POINT('Ctrl Pts',(-219.770611437516,4.89771707012715,
134.127783840167));
#162497=CARTESIAN_POINT('Ctrl Pts',(-219.778008122428,4.98271538960518,
133.995046736364));
#162498=CARTESIAN_POINT('Ctrl Pts',(-219.785404479364,5.06770994016866,
133.862315518264));
#162499=CARTESIAN_POINT('Ctrl Pts',(-219.792800836299,5.14740250416741,
133.726177543978));
#162500=CARTESIAN_POINT('Ctrl Pts',(-219.800197193235,5.22152180713321,
133.587100379048));
#162501=CARTESIAN_POINT('Ctrl Pts',(-219.807594682571,5.29565245795372,
133.448001921048));
#162502=CARTESIAN_POINT('Ctrl Pts',(-219.814992171908,5.36420797316718,
133.305963705855));
#162503=CARTESIAN_POINT('Ctrl Pts',(-219.822389661244,5.42696346148188,
133.161477108162));
#162504=CARTESIAN_POINT('Ctrl Pts',(-219.829789743759,5.48974094863562,
133.016939860917));
#162505=CARTESIAN_POINT('Ctrl Pts',(-219.837189826274,5.54671421220162,
132.869952864533));
#162506=CARTESIAN_POINT('Ctrl Pts',(-219.844589908789,5.59770689746666,
132.721026486348));
#162507=CARTESIAN_POINT('Ctrl Pts',(-219.851998128456,5.64875565443139,
132.5719363483));
#162508=CARTESIAN_POINT('Ctrl Pts',(-219.859406348122,5.69381057887091,
132.420902922995));
#162509=CARTESIAN_POINT('Ctrl Pts',(-219.866814567789,5.73274529888063,
132.268451427817));
#162510=CARTESIAN_POINT('Ctrl Pts',(-219.874227347091,5.77170398256086,
132.115906101288));
#162511=CARTESIAN_POINT('Ctrl Pts',(-219.881640126393,5.80453487815331,
131.961941329969));
#162512=CARTESIAN_POINT('Ctrl Pts',(-219.889052905695,5.83116304135805,
131.80709096397));
#162513=CARTESIAN_POINT('Ctrl Pts',(-219.896476276724,5.85782925213108,
131.652019340507));
#162514=CARTESIAN_POINT('Ctrl Pts',(-219.903899647752,5.87827498121259,
131.496059964268));
#162515=CARTESIAN_POINT('Ctrl Pts',(-219.911323018781,5.89247720762978,
131.339751054596));
#162516=CARTESIAN_POINT('Ctrl Pts',(-219.915259068222,5.90000756885379,
131.256872320109));
#162517=CARTESIAN_POINT('Ctrl Pts',(-219.919195117662,5.90578352869573,
131.173895319359));
#162518=CARTESIAN_POINT('Ctrl Pts',(-219.923131167103,5.90980759096107,
131.090899969696));
#162519=CARTESIAN_POINT('Ctrl Pts',(-219.930554433509,5.91739684680695,
130.934373330425));
#162520=CARTESIAN_POINT('Ctrl Pts',(-219.937977699914,5.91877465722026,
130.777308284025));
#162521=CARTESIAN_POINT('Ctrl Pts',(-219.945400966319,5.91388448913744,
130.620238887073));
#162522=CARTESIAN_POINT('Ctrl Pts',(-219.95281545904,5.90900010082718,130.463355133104));
#162523=CARTESIAN_POINT('Ctrl Pts',(-219.960229951761,5.89786249164671,
130.306467408292));
#162524=CARTESIAN_POINT('Ctrl Pts',(-219.967644444482,5.88046695958147,
130.150113798872));
#162525=CARTESIAN_POINT('Ctrl Pts',(-219.975051790836,5.86308819398497,
129.993910888948));
#162526=CARTESIAN_POINT('Ctrl Pts',(-219.98245913719,5.83946355427546,129.838241438069));
#162527=CARTESIAN_POINT('Ctrl Pts',(-219.989866483544,5.80964035685599,
129.683642327142));
#162528=CARTESIAN_POINT('Ctrl Pts',(-219.997268305219,5.77983940270232,
129.529158522065));
#162529=CARTESIAN_POINT('Ctrl Pts',(-220.004670126895,5.7438491664946,129.375743832381));
#162530=CARTESIAN_POINT('Ctrl Pts',(-220.01207194857,5.70176863231611,129.223928706335));
#162531=CARTESIAN_POINT('Ctrl Pts',(-220.019469862882,5.65971031212406,
129.072193722313));
#162532=CARTESIAN_POINT('Ctrl Pts',(-220.026867777193,5.61156819628912,
128.922056979096));
#162533=CARTESIAN_POINT('Ctrl Pts',(-220.034265691504,5.55749205153644,
128.774037328134));
#162534=CARTESIAN_POINT('Ctrl Pts',(-220.041662376417,5.50342489325805,
128.626042275353));
#162535=CARTESIAN_POINT('Ctrl Pts',(-220.049059061329,5.44342579120522,
128.480163966854));
#162536=CARTESIAN_POINT('Ctrl Pts',(-220.056455746241,5.37769397434287,
128.33690482651));
#162537=CARTESIAN_POINT('Ctrl Pts',(-220.063852103176,5.31196507209816,
128.193652038426));
#162538=CARTESIAN_POINT('Ctrl Pts',(-220.071248460112,5.2405041161445,128.053018526867));
#162539=CARTESIAN_POINT('Ctrl Pts',(-220.078644817047,5.16355785213638,
127.915485253321));
#162540=CARTESIAN_POINT('Ctrl Pts',(-220.086042306384,5.0865998074586,127.777930923079));
#162541=CARTESIAN_POINT('Ctrl Pts',(-220.093439795721,5.00415496481943,
127.643478101749));
#162542=CARTESIAN_POINT('Ctrl Pts',(-220.100837285057,4.91651517242971,
127.512581596768));
#162543=CARTESIAN_POINT('Ctrl Pts',(-220.108237367572,4.82884465804676,
127.38163920622));
#162544=CARTESIAN_POINT('Ctrl Pts',(-220.115637450087,4.73597577570763,
127.254255924113));
#162545=CARTESIAN_POINT('Ctrl Pts',(-220.123037532602,4.63824258787776,
127.130855988673));
#162546=CARTESIAN_POINT('Ctrl Pts',(-220.130445752269,4.54040193236052,
127.007320362319));
#162547=CARTESIAN_POINT('Ctrl Pts',(-220.137853971935,4.4376865213498,126.887777122792));
#162548=CARTESIAN_POINT('Ctrl Pts',(-220.145262191602,4.33046992800464,
126.772616483181));
#162549=CARTESIAN_POINT('Ctrl Pts',(-220.152674970904,4.22318734463529,
126.657384964118));
#162550=CARTESIAN_POINT('Ctrl Pts',(-220.160087750206,4.11139832302276,
126.54654168214));
#162551=CARTESIAN_POINT('Ctrl Pts',(-220.167500529508,3.99551149715896,
126.440438249034));
#162552=CARTESIAN_POINT('Ctrl Pts',(-220.174923900537,3.87945908676399,
126.334183210368));
#162553=CARTESIAN_POINT('Ctrl Pts',(-220.182347271566,3.75929746251838,
126.232681787062));
#162554=CARTESIAN_POINT('Ctrl Pts',(-220.189770642594,3.63546700020045,
126.136244268014));
#162555=CARTESIAN_POINT('Ctrl Pts',(-220.193706692035,3.56980911780938,
126.085110781429));
#162556=CARTESIAN_POINT('Ctrl Pts',(-220.197642741476,3.50312026442755,
126.035400207099));
#162557=CARTESIAN_POINT('Ctrl Pts',(-220.201578790916,3.4354690301533,125.987153635781));
#162558=CARTESIAN_POINT('Ctrl Pts',(-220.209002057322,3.30788091363256,
125.896162107997));
#162559=CARTESIAN_POINT('Ctrl Pts',(-220.216425323727,3.17648238196665,
125.810105422969));
#162560=CARTESIAN_POINT('Ctrl Pts',(-220.223848590133,3.04169219457659,
125.729319814188));
#162561=CARTESIAN_POINT('Ctrl Pts',(-220.231263082854,2.90706131799441,
125.648629687288));
#162562=CARTESIAN_POINT('Ctrl Pts',(-220.238677575575,2.76904708200507,
125.573198425868));
#162563=CARTESIAN_POINT('Ctrl Pts',(-220.246092068296,2.62809965224538,
125.503320834621));
#162564=CARTESIAN_POINT('Ctrl Pts',(-220.25349941465,2.48728807292547,125.433510594027));
#162565=CARTESIAN_POINT('Ctrl Pts',(-220.260906761003,2.34354926028618,
125.369243531862));
#162566=CARTESIAN_POINT('Ctrl Pts',(-220.268314107357,2.1973604831124,125.310770036739));
#162567=CARTESIAN_POINT('Ctrl Pts',(-220.275715929032,2.05128073904362,
125.252340153354));
#162568=CARTESIAN_POINT('Ctrl Pts',(-220.283117750708,1.90275501390172,
125.199695371236));
#162569=CARTESIAN_POINT('Ctrl Pts',(-220.290519572383,1.75228309213406,
125.153039132504));
#162570=CARTESIAN_POINT('Ctrl Pts',(-220.297917486695,1.60189060332305,
125.106407523238));
#162571=CARTESIAN_POINT('Ctrl Pts',(-220.305315401006,1.44955431961587,
125.065758271743));
#162572=CARTESIAN_POINT('Ctrl Pts',(-220.312713315317,1.29579171800591,
125.031245826914));
#162573=CARTESIAN_POINT('Ctrl Pts',(-220.32011000023,1.14205466895057,124.996739117427));
#162574=CARTESIAN_POINT('Ctrl Pts',(-220.327506685142,0.986892136302272,
124.968367272227));
#162575=CARTESIAN_POINT('Ctrl Pts',(-220.334903370054,0.830834511618251,
124.94623424672));
#162576=CARTESIAN_POINT('Ctrl Pts',(-220.34229972699,0.674783806692845,
124.924102202614));
#162577=CARTESIAN_POINT('Ctrl Pts',(-220.349696083925,0.517838458246394,
124.908208480575));
#162578=CARTESIAN_POINT('Ctrl Pts',(-220.35709244086,0.360536484853832,
124.898605457928));
#162579=CARTESIAN_POINT('Ctrl Pts',(-220.364489930197,0.203210428127571,
124.889000965034));
#162580=CARTESIAN_POINT('Ctrl Pts',(-220.371887419533,0.0455280103671136,
124.885689111983));
#162581=CARTESIAN_POINT('Ctrl Pts',(-220.37928490887,-0.111970374962323,
124.888670193141));
#162582=CARTESIAN_POINT('Ctrl Pts',(-220.386684991385,-0.269523971106809,
124.891652319313));
#162583=CARTESIAN_POINT('Ctrl Pts',(-220.3940850739,-0.426893033378565,
124.900931764719));
#162584=CARTESIAN_POINT('Ctrl Pts',(-220.401485156415,-0.583540069219387,
124.916456784272));
#162585=CARTESIAN_POINT('Ctrl Pts',(-220.408893376081,-0.740359354579599,
124.93199887518));
#162586=CARTESIAN_POINT('Ctrl Pts',(-220.416301595748,-0.896454656248115,
124.953800218545));
#162587=CARTESIAN_POINT('Ctrl Pts',(-220.423709815414,-1.05129575148534,
124.981757436393));
#162588=CARTESIAN_POINT('Ctrl Pts',(-220.431122594716,-1.20623214883302,
125.009731861442));
#162589=CARTESIAN_POINT('Ctrl Pts',(-220.438535374018,-1.35991243798555,
125.043869629947));
#162590=CARTESIAN_POINT('Ctrl Pts',(-220.445948153321,-1.51181992133489,
125.084017001318));
#162591=CARTESIAN_POINT('Ctrl Pts',(-220.453371524349,-1.6639444572204,
125.124221737135));
#162592=CARTESIAN_POINT('Ctrl Pts',(-220.460794895378,-1.81429077233319,
125.170453116159));
#162593=CARTESIAN_POINT('Ctrl Pts',(-220.468218266407,-1.96235977797054,
125.222508356506));
#162594=CARTESIAN_POINT('Ctrl Pts',(-220.472154315848,-2.04086951762733,
125.250109293986));
#162595=CARTESIAN_POINT('Ctrl Pts',(-220.476090365289,-2.11873938590875,
125.27934673539));
#162596=CARTESIAN_POINT('Ctrl Pts',(-220.480026414729,-2.19589773737316,
125.310185184482));
#162597=CARTESIAN_POINT('Ctrl Pts',(-220.487449681135,-2.34141598020358,
125.368345537036));
#162598=CARTESIAN_POINT('Ctrl Pts',(-220.49487294754,-2.4848420225225,125.432379102817));
#162599=CARTESIAN_POINT('Ctrl Pts',(-220.502296213946,-2.62566663187468,
125.50211531008));
#162600=CARTESIAN_POINT('Ctrl Pts',(-220.509710706667,-2.76632479823296,
125.571769094937));
#162601=CARTESIAN_POINT('Ctrl Pts',(-220.517125199388,-2.90438732052647,
125.647111941132));
#162602=CARTESIAN_POINT('Ctrl Pts',(-220.524539692109,-3.03936284569548,
125.727924460703));
#162603=CARTESIAN_POINT('Ctrl Pts',(-220.531947038462,-3.17420827637197,
125.808659090125));
#162604=CARTESIAN_POINT('Ctrl Pts',(-220.539354384816,-3.30597231515705,
125.894852707182));
#162605=CARTESIAN_POINT('Ctrl Pts',(-220.54676173117,-3.43418632758138,
125.986239113291));
#162606=CARTESIAN_POINT('Ctrl Pts',(-220.554163552845,-3.56230471315764,
126.077557359971));
#162607=CARTESIAN_POINT('Ctrl Pts',(-220.561565374521,-3.68687804171274,
126.174060468344));
#162608=CARTESIAN_POINT('Ctrl Pts',(-220.568967196196,-3.80746500592656,
126.275437921036));
#162609=CARTESIAN_POINT('Ctrl Pts',(-220.576365110507,-3.92798831322027,
126.37676185736));
#162610=CARTESIAN_POINT('Ctrl Pts',(-220.583763024818,-4.0445291621136,
126.482954773883));
#162611=CARTESIAN_POINT('Ctrl Pts',(-220.59116093913,-4.15667790142167,
126.593664785957));
#162612=CARTESIAN_POINT('Ctrl Pts',(-220.598557624042,-4.26880800364434,
126.704356400035));
#162613=CARTESIAN_POINT('Ctrl Pts',(-220.605954308954,-4.37654717949532,
126.819563357831));
#162614=CARTESIAN_POINT('Ctrl Pts',(-220.613350993866,-4.47952127875511,
126.938895616343));
#162615=CARTESIAN_POINT('Ctrl Pts',(-220.620747350802,-4.58249081203542,
127.058222583538));
#162616=CARTESIAN_POINT('Ctrl Pts',(-220.628143707737,-4.68069544495884,
127.18167420512));
#162617=CARTESIAN_POINT('Ctrl Pts',(-220.635540064673,-4.77380029881667,
127.30882614205));
#162618=CARTESIAN_POINT('Ctrl Pts',(-220.642937554009,-4.86691940726531,
127.435997546267));
#162619=CARTESIAN_POINT('Ctrl Pts',(-220.650335043346,-4.9549369614398,
127.566870092656));
#162620=CARTESIAN_POINT('Ctrl Pts',(-220.657732532682,-5.03756061781539,
127.700989292002));
#162621=CARTESIAN_POINT('Ctrl Pts',(-220.665132615197,-5.12021323778553,
127.835155506625));
#162622=CARTESIAN_POINT('Ctrl Pts',(-220.672532697712,-5.19746799966815,
127.972570322542));
#162623=CARTESIAN_POINT('Ctrl Pts',(-220.679932780227,-5.26907791021533,
128.112753562556));
#162624=CARTESIAN_POINT('Ctrl Pts',(-220.687340999893,-5.34076656322093,
128.253090948454));
#162625=CARTESIAN_POINT('Ctrl Pts',(-220.69474921956,-5.40679779899382,
128.396202505211));
#162626=CARTESIAN_POINT('Ctrl Pts',(-220.702157439226,-5.46697199400874,
128.541586263101));
#162627=CARTESIAN_POINT('Ctrl Pts',(-220.709570218528,-5.52718322523663,
128.687059502268));
#162628=CARTESIAN_POINT('Ctrl Pts',(-220.71698299783,-5.58153010389817,
128.834807379722));
#162629=CARTESIAN_POINT('Ctrl Pts',(-220.724395777132,-5.62986268862889,
128.984312082586));
#162630=CARTESIAN_POINT('Ctrl Pts',(-220.731819148161,-5.67826433322331,
129.13403040478));
#162631=CARTESIAN_POINT('Ctrl Pts',(-220.73924251919,-5.72063442044092,
129.28551020734));
#162632=CARTESIAN_POINT('Ctrl Pts',(-220.746665890219,-5.75687378679056,
129.438221984241));
#162633=CARTESIAN_POINT('Ctrl Pts',(-220.75060193966,-5.77608876838261,
129.51919343263));
#162634=CARTESIAN_POINT('Ctrl Pts',(-220.754537989101,-5.79358104676735,
129.600511109454));
#162635=CARTESIAN_POINT('Ctrl Pts',(-220.758474038542,-5.80934175982063,
129.682095550791));
#162636=CARTESIAN_POINT('Ctrl Pts',(-220.769393094443,-5.85306379874289,
129.90842021691));
#162637=CARTESIAN_POINT('Ctrl Pts',(-220.780312150343,-5.88357025894,130.137373687765));
#162638=CARTESIAN_POINT('Ctrl Pts',(-220.791231206244,-5.90061493995885,
130.36769839933));
#162639=CARTESIAN_POINT('Ctrl Pts',(-220.798029073427,-5.91122643227021,
130.511091455686));
#162640=CARTESIAN_POINT('Ctrl Pts',(-220.80482694061,-5.91662104841901,
130.655015641359));
#162641=CARTESIAN_POINT('Ctrl Pts',(-220.811624807793,-5.91674771557038,
130.799161310626));
#162642=CARTESIAN_POINT('',(-222.561624807793,-5.90703034408285,130.803567381702));
#162643=CARTESIAN_POINT('Ctrl Pts',(-220.811625964301,-5.91926145875612,
130.799183635355));
#162644=CARTESIAN_POINT('Ctrl Pts',(-220.886724530319,-5.90459539466751,
132.39230526411));
#162645=CARTESIAN_POINT('Ctrl Pts',(-221.05463897094,-4.41863354744595,
135.978493543736));
#162646=CARTESIAN_POINT('Ctrl Pts',(-221.315369286169,1.64887482479054,
137.605740796802));
#162647=CARTESIAN_POINT('Ctrl Pts',(-221.593816909981,6.61345088869389,
133.093427648732));
#162648=CARTESIAN_POINT('Ctrl Pts',(-221.872264533795,5.50058867092583,
126.477573726163));
#162649=CARTESIAN_POINT('Ctrl Pts',(-222.150712157606,-0.667045816727497,
123.837825581499));
#162650=CARTESIAN_POINT('Ctrl Pts',(-222.380498915606,-5.25097959326614,
126.942516864827));
#162651=CARTESIAN_POINT('Ctrl Pts',(-222.517469799002,-5.90815259440714,
129.861956814884));
#162652=CARTESIAN_POINT('Ctrl Pts',(-222.561624807793,-5.90703034408285,
130.803567381702));
#162653=CARTESIAN_POINT('',(-224.311624807793,-5.91634088406479,130.809833178867));
#162654=CARTESIAN_POINT('Ctrl Pts',(-222.561624807793,-5.90703034408285,
130.803567381702));
#162655=CARTESIAN_POINT('Ctrl Pts',(-222.610285673606,-5.90579357222084,
131.841265860195));
#162656=CARTESIAN_POINT('Ctrl Pts',(-222.751762414023,-5.15017517596034,
134.85995768299));
#162657=CARTESIAN_POINT('Ctrl Pts',(-222.986055029046,-0.328283633494095,
137.795053743877));
#162658=CARTESIAN_POINT('Ctrl Pts',(-223.264502652858,5.70402279120795,
134.85919532785));
#162659=CARTESIAN_POINT('Ctrl Pts',(-223.542950276671,6.49461092779884,
128.197141902751));
#162660=CARTESIAN_POINT('Ctrl Pts',(-223.821397900484,1.31696890112159,
123.930995106856));
#162661=CARTESIAN_POINT('Ctrl Pts',(-224.077622744192,-4.56108999705214,
125.817514651832));
#162662=CARTESIAN_POINT('Ctrl Pts',(-224.241031713294,-5.90253858859253,
129.310393028754));
#162663=CARTESIAN_POINT('Ctrl Pts',(-224.311624807793,-5.91634088406479,
130.809833178867));
#162664=CARTESIAN_POINT('',(-226.061624807793,-5.92597879789556,130.802710800977));
#162665=CARTESIAN_POINT('Ctrl Pts',(-224.311624807793,-5.91634088406479,
130.809833178867));
#162666=CARTESIAN_POINT('Ctrl Pts',(-224.333847587899,-5.92068586113956,
131.281858509026));
#162667=CARTESIAN_POINT('Ctrl Pts',(-224.356070368004,-5.86896945013117,
131.752943156795));
#162668=CARTESIAN_POINT('Ctrl Pts',(-224.471109022714,-5.29224194237738,
134.11615185666));
#162669=CARTESIAN_POINT('Ctrl Pts',(-224.656740771924,-2.27899983402202,
137.421287418344));
#162670=CARTESIAN_POINT('Ctrl Pts',(-224.935188395735,4.3351528406458,136.298358285803));
#162671=CARTESIAN_POINT('Ctrl Pts',(-225.213636019549,6.9655118387511,130.126713692855));
#162672=CARTESIAN_POINT('Ctrl Pts',(-225.492083643361,3.19490574121353,
124.577793518826));
#162673=CARTESIAN_POINT('Ctrl Pts',(-225.770531267174,-3.51166265267364,
124.750784323824));
#162674=CARTESIAN_POINT('Ctrl Pts',(-225.960378321985,-5.88401903759723,
128.661572723237));
#162675=CARTESIAN_POINT('Ctrl Pts',(-226.057409502191,-5.92630793883599,
130.713553172688));
#162676=CARTESIAN_POINT('Ctrl Pts',(-226.061624807793,-5.92597879789556,
130.802710800977));
#162677=CARTESIAN_POINT('',(-227.811623611839,-5.91356008316327,130.799662206759));
#162678=CARTESIAN_POINT('Ctrl Pts',(-226.061624807793,-5.92597879789556,
130.802710800977));
#162679=CARTESIAN_POINT('Ctrl Pts',(-226.150225376795,-5.91906065782266,
132.676695119892));
#162680=CARTESIAN_POINT('Ctrl Pts',(-226.331641820403,-3.945277242289,136.526362468158));
#162681=CARTESIAN_POINT('Ctrl Pts',(-226.605874138613,2.61709938795056,
137.29499628165));
#162682=CARTESIAN_POINT('Ctrl Pts',(-226.884321762427,6.87536175394465,
132.110867901409));
#162683=CARTESIAN_POINT('Ctrl Pts',(-227.162769386239,4.81550254815928,
125.726123153737));
#162684=CARTESIAN_POINT('Ctrl Pts',(-227.441217010051,-1.66956824900632,
124.008030549637));
#162685=CARTESIAN_POINT('Ctrl Pts',(-227.657501471997,-5.51512181869817,
127.524694996426));
#162686=CARTESIAN_POINT('Ctrl Pts',(-227.780970059337,-5.91611079036253,
130.147161607405));
#162687=CARTESIAN_POINT('Ctrl Pts',(-227.811622772073,-5.91132151002306,
130.799646100255));
#162688=CARTESIAN_POINT('',(-229.561625975116,-5.91241234693134,130.807877191858));
#162689=CARTESIAN_POINT('Ctrl Pts',(-227.811624807793,-5.916748152698,130.799685144877));
#162690=CARTESIAN_POINT('Ctrl Pts',(-227.819395118205,-5.91687897381839,
130.965237522987));
#162691=CARTESIAN_POINT('Ctrl Pts',(-227.827165428617,-5.9100562349648,
131.13087635323));
#162692=CARTESIAN_POINT('Ctrl Pts',(-227.834935739028,-5.89629095285145,
131.295973841373));
#162693=CARTESIAN_POINT('Ctrl Pts',(-227.842322639182,-5.88320489075527,
131.452924927735));
#162694=CARTESIAN_POINT('Ctrl Pts',(-227.849709539335,-5.86384499508312,
131.609386400109));
#162695=CARTESIAN_POINT('Ctrl Pts',(-227.857096439489,-5.83827411370623,
131.764821931585));
#162696=CARTESIAN_POINT('Ctrl Pts',(-227.864483592032,-5.81270235864333,
131.920262773862));
#162697=CARTESIAN_POINT('Ctrl Pts',(-227.871870744576,-5.7809192553894,
132.074677236392));
#162698=CARTESIAN_POINT('Ctrl Pts',(-227.879257897119,-5.74303908593296,
132.227537563679));
#162699=CARTESIAN_POINT('Ctrl Pts',(-227.886646765646,-5.70515011717909,
132.380433399346));
#162700=CARTESIAN_POINT('Ctrl Pts',(-227.894035634173,-5.66116135210173,
132.531774018092));
#162701=CARTESIAN_POINT('Ctrl Pts',(-227.9014245027,-5.61123736849344,132.681045395818));
#162702=CARTESIAN_POINT('Ctrl Pts',(-227.908816551567,-5.56129189644803,
132.830381023397));
#162703=CARTESIAN_POINT('Ctrl Pts',(-227.916208600434,-5.50540623786596,
132.97764528244));
#162704=CARTESIAN_POINT('Ctrl Pts',(-227.923600649301,-5.44379359751809,
133.122342893193));
#162705=CARTESIAN_POINT('Ctrl Pts',(-227.931001429038,-5.38210818547155,
133.267211408664));
#162706=CARTESIAN_POINT('Ctrl Pts',(-227.938402208775,-5.31468243151133,
133.40950687864));
#162707=CARTESIAN_POINT('Ctrl Pts',(-227.945802988512,-5.24177642922586,
133.548756804073));
#162708=CARTESIAN_POINT('Ctrl Pts',(-227.953208848849,-5.16882037732131,
133.688102323908));
#162709=CARTESIAN_POINT('Ctrl Pts',(-227.960614709185,-5.09037676739029,
133.824397810815));
#162710=CARTESIAN_POINT('Ctrl Pts',(-227.968020569522,-5.00674943471655,
133.957199126032));
#162711=CARTESIAN_POINT('Ctrl Pts',(-227.975437096918,-4.92300164908518,
134.090191722146));
#162712=CARTESIAN_POINT('Ctrl Pts',(-227.982853624315,-4.83405544377064,
134.21967979103));
#162713=CARTESIAN_POINT('Ctrl Pts',(-227.990270151711,-4.74025580559906,
134.345251107257));
#162714=CARTESIAN_POINT('Ctrl Pts',(-227.992884187033,-4.70719510828498,
134.389510076247));
#162715=CARTESIAN_POINT('Ctrl Pts',(-227.995498222355,-4.6735318185491,
134.433282798673));
#162716=CARTESIAN_POINT('Ctrl Pts',(-227.998112257678,-4.63928212662991,
134.476552321717));
#162717=CARTESIAN_POINT('Ctrl Pts',(-228.005535524083,-4.54202078311397,
134.599427936319));
#162718=CARTESIAN_POINT('Ctrl Pts',(-228.012958790489,-4.43972728846017,
134.718622601108));
#162719=CARTESIAN_POINT('Ctrl Pts',(-228.020382056894,-4.33271041590368,
134.83369691706));
#162720=CARTESIAN_POINT('Ctrl Pts',(-228.027796549615,-4.22582002840335,
134.948635224726));
#162721=CARTESIAN_POINT('Ctrl Pts',(-228.035211042337,-4.11421762701217,
135.059462606449));
#162722=CARTESIAN_POINT('Ctrl Pts',(-228.042625535058,-3.99825367082837,
135.165770727405));
#162723=CARTESIAN_POINT('Ctrl Pts',(-228.050032881411,-3.88240148507183,
135.271976384592));
#162724=CARTESIAN_POINT('Ctrl Pts',(-228.057440227765,-3.76219638684362,
135.373671202055));
#162725=CARTESIAN_POINT('Ctrl Pts',(-228.064847574119,-3.63802721818065,
135.470481974997));
#162726=CARTESIAN_POINT('Ctrl Pts',(-228.072249395795,-3.51395065956829,
135.567220542813));
#162727=CARTESIAN_POINT('Ctrl Pts',(-228.07965121747,-3.38591621054431,
135.659082090681));
#162728=CARTESIAN_POINT('Ctrl Pts',(-228.087053039145,-3.25434739294053,
135.745732249872));
#162729=CARTESIAN_POINT('Ctrl Pts',(-228.094450953457,-3.12284802949069,
135.832336667119));
#162730=CARTESIAN_POINT('Ctrl Pts',(-228.101848867768,-2.98781832419317,
135.913734969737));
#162731=CARTESIAN_POINT('Ctrl Pts',(-228.10924678208,-2.84971241471892,
135.989634931997));
#162732=CARTESIAN_POINT('Ctrl Pts',(-228.116643466992,-2.71162945594152,
136.06552228106));
#162733=CARTESIAN_POINT('Ctrl Pts',(-228.124040151905,-2.57047163441416,
136.135912923622));
#162734=CARTESIAN_POINT('Ctrl Pts',(-228.131436836817,-2.42671953112006,
136.200559546421));
#162735=CARTESIAN_POINT('Ctrl Pts',(-228.138833193752,-2.28297380194487,
136.265203302722));
#162736=CARTESIAN_POINT('Ctrl Pts',(-228.146229550688,-2.13663436018288,
136.324103392575));
#162737=CARTESIAN_POINT('Ctrl Pts',(-228.153625907623,-1.9882034525649,
136.377059927031));
#162738=CARTESIAN_POINT('Ctrl Pts',(-228.16102339696,-1.83974981979605,
136.430024569267));
#162739=CARTESIAN_POINT('Ctrl Pts',(-228.168420886297,-1.68920443520671,
136.477043718781));
#162740=CARTESIAN_POINT('Ctrl Pts',(-228.175818375633,-1.53708630656534,
136.51796685607));
#162741=CARTESIAN_POINT('Ctrl Pts',(-228.183218458149,-1.38491485315001,
136.558904338901));
#162742=CARTESIAN_POINT('Ctrl Pts',(-228.190618540663,-1.23116991825896,
136.593741457945));
#162743=CARTESIAN_POINT('Ctrl Pts',(-228.198018623179,-1.07638219079224,
136.622378488099));
#162744=CARTESIAN_POINT('Ctrl Pts',(-228.205426842845,-0.921424258306389,
136.651047007613));
#162745=CARTESIAN_POINT('Ctrl Pts',(-228.212835062512,-0.765421610588236,
136.67350175502));
#162746=CARTESIAN_POINT('Ctrl Pts',(-228.220243282178,-0.608912307961287,
136.689694623696));
#162747=CARTESIAN_POINT('Ctrl Pts',(-228.227656061481,-0.452306676469624,
136.705897458814));
#162748=CARTESIAN_POINT('Ctrl Pts',(-228.235068840783,-0.295194140383829,
136.71583071196));
#162749=CARTESIAN_POINT('Ctrl Pts',(-228.242481620085,-0.138113769588865,
136.71949841386));
#162750=CARTESIAN_POINT('Ctrl Pts',(-228.249904991114,0.0191910450060024,
136.723171356346));
#162751=CARTESIAN_POINT('Ctrl Pts',(-228.257328362142,0.176463230261345,
136.720560873587));
#162752=CARTESIAN_POINT('Ctrl Pts',(-228.264751733171,0.33316699685643,
136.711722999772));
#162753=CARTESIAN_POINT('Ctrl Pts',(-228.268687782611,0.416255093935163,
136.707036947015));
#162754=CARTESIAN_POINT('Ctrl Pts',(-228.272623832051,0.499183515576516,
136.700601013057));
#162755=CARTESIAN_POINT('Ctrl Pts',(-228.27655988149,0.581873572371184,
136.692429376359));
#162756=CARTESIAN_POINT('Ctrl Pts',(-228.283983147896,0.737824438863897,
136.677017924571));
#162757=CARTESIAN_POINT('Ctrl Pts',(-228.291406414301,0.893398418636188,
136.655383138227));
#162758=CARTESIAN_POINT('Ctrl Pts',(-228.298829680707,1.04805893336818,
136.627547291088));
#162759=CARTESIAN_POINT('Ctrl Pts',(-228.306244173428,1.20253665221508,
136.599744343609));
#162760=CARTESIAN_POINT('Ctrl Pts',(-228.313658666149,1.35610269124354,
136.565754989506));
#162761=CARTESIAN_POINT('Ctrl Pts',(-228.32107315887,1.5082240750992,136.525653364996));
#162762=CARTESIAN_POINT('Ctrl Pts',(-228.328480505224,1.6601988386374,136.485590391941));
#162763=CARTESIAN_POINT('Ctrl Pts',(-228.335887851577,1.8107313604801,136.43942697129));
#162764=CARTESIAN_POINT('Ctrl Pts',(-228.343295197931,1.95929747424139,
136.387288520551));
#162765=CARTESIAN_POINT('Ctrl Pts',(-228.350697019606,2.10775278179038,
136.335188956636));
#162766=CARTESIAN_POINT('Ctrl Pts',(-228.358098841282,2.25424425077843,
136.277123359014));
#162767=CARTESIAN_POINT('Ctrl Pts',(-228.365500662957,2.39826164342685,
136.213267314133));
#162768=CARTESIAN_POINT('Ctrl Pts',(-228.372898577269,2.54220301041555,
136.14944497836));
#162769=CARTESIAN_POINT('Ctrl Pts',(-228.38029649158,2.68367256172371,136.079838433883));
#162770=CARTESIAN_POINT('Ctrl Pts',(-228.387694405892,2.82217896706645,
136.004671804442));
#162771=CARTESIAN_POINT('Ctrl Pts',(-228.395091090804,2.9606623551568,135.929517666331));
#162772=CARTESIAN_POINT('Ctrl Pts',(-228.402487775716,3.09618324681663,
135.848805454976));
#162773=CARTESIAN_POINT('Ctrl Pts',(-228.409884460629,3.22827380463498,
135.762805817909));
#162774=CARTESIAN_POINT('Ctrl Pts',(-228.417280817564,3.36035850541957,
135.676809994157));
#162775=CARTESIAN_POINT('Ctrl Pts',(-228.424677174499,3.48901286196149,
135.585527414536));
#162776=CARTESIAN_POINT('Ctrl Pts',(-228.432073531435,3.61379722539937,
135.489272588585));
#162777=CARTESIAN_POINT('Ctrl Pts',(-228.439471020772,3.73860069364186,
135.393003025775));
#162778=CARTESIAN_POINT('Ctrl Pts',(-228.446868510108,3.85953269342429,
135.291759928873));
#162779=CARTESIAN_POINT('Ctrl Pts',(-228.454265999445,3.97618605205117,
135.185898594347));
#162780=CARTESIAN_POINT('Ctrl Pts',(-228.46166608196,4.09288030333158,135.080000150295));
#162781=CARTESIAN_POINT('Ctrl Pts',(-228.469066164475,4.20529265095796,
134.969480496077));
#162782=CARTESIAN_POINT('Ctrl Pts',(-228.47646624699,4.31305234306541,134.854732211442));
#162783=CARTESIAN_POINT('Ctrl Pts',(-228.483874466656,4.42093052803276,
134.739857749271));
#162784=CARTESIAN_POINT('Ctrl Pts',(-228.491282686323,4.52414558464567,
134.620745642984));
#162785=CARTESIAN_POINT('Ctrl Pts',(-228.498690905989,4.62236620469127,
134.497822575165));
#162786=CARTESIAN_POINT('Ctrl Pts',(-228.506103685292,4.72064727788989,
134.374823850248));
#162787=CARTESIAN_POINT('Ctrl Pts',(-228.513516464594,4.81392756852741,
134.248009789941));
#162788=CARTESIAN_POINT('Ctrl Pts',(-228.520929243896,4.9019190873274,134.117836107712));
#162789=CARTESIAN_POINT('Ctrl Pts',(-228.528352614925,4.99003633253573,
133.987476427221));
#162790=CARTESIAN_POINT('Ctrl Pts',(-228.535775985954,5.07284951717573,
133.853747853892));
#162791=CARTESIAN_POINT('Ctrl Pts',(-228.543199356982,5.15011617718097,
133.717131450302));
#162792=CARTESIAN_POINT('Ctrl Pts',(-228.547135406423,5.19108481429918,
133.644694155061));
#162793=CARTESIAN_POINT('Ctrl Pts',(-228.551071455863,5.23049491832864,
133.571445345756));
#162794=CARTESIAN_POINT('Ctrl Pts',(-228.555007505303,5.26831588446356,
133.497458889818));
#162795=CARTESIAN_POINT('Ctrl Pts',(-228.562430771709,5.33964504624945,
133.357922742945));
#162796=CARTESIAN_POINT('Ctrl Pts',(-228.569854038114,5.40553462394097,
133.215339817202));
#162797=CARTESIAN_POINT('Ctrl Pts',(-228.577277304519,5.46571332339622,
133.07017359064));
#162798=CARTESIAN_POINT('Ctrl Pts',(-228.58469179724,5.52582089662624,132.925178938502));
#162799=CARTESIAN_POINT('Ctrl Pts',(-228.592106289962,5.58023088554384,
132.777607404523));
#162800=CARTESIAN_POINT('Ctrl Pts',(-228.599520782683,5.62871757685187,
132.627947468401));
#162801=CARTESIAN_POINT('Ctrl Pts',(-228.606928129036,5.67715753486134,
132.47843178016));
#162802=CARTESIAN_POINT('Ctrl Pts',(-228.61433547539,5.71968544666903,132.326832049766));
#162803=CARTESIAN_POINT('Ctrl Pts',(-228.621742821744,5.7561235048417,132.173657064472));
#162804=CARTESIAN_POINT('Ctrl Pts',(-228.629144643419,5.79253438613595,
132.02059632286));
#162805=CARTESIAN_POINT('Ctrl Pts',(-228.636546465095,5.82286437159545,
131.865963027302));
#162806=CARTESIAN_POINT('Ctrl Pts',(-228.64394828677,5.84698539108677,131.710281364054));
#162807=CARTESIAN_POINT('Ctrl Pts',(-228.651346201081,5.87109367727974,
131.554681883944));
#162808=CARTESIAN_POINT('Ctrl Pts',(-228.658744115393,5.88899946811958,
131.39803550628));
#162809=CARTESIAN_POINT('Ctrl Pts',(-228.666142029704,5.90062574923648,
131.240876745501));
#162810=CARTESIAN_POINT('Ctrl Pts',(-228.673538714616,5.91225009827629,
131.083744101658));
#162811=CARTESIAN_POINT('Ctrl Pts',(-228.680935399529,5.91759698119891,
130.926099615613));
#162812=CARTESIAN_POINT('Ctrl Pts',(-228.688332084441,5.91664122389118,
130.76848318383));
#162813=CARTESIAN_POINT('Ctrl Pts',(-228.695728441376,5.91568550896273,
130.610873740925));
#162814=CARTESIAN_POINT('Ctrl Pts',(-228.703124798311,5.90842771173963,
130.453292723101));
#162815=CARTESIAN_POINT('Ctrl Pts',(-228.710521155247,5.89489479705551,
130.296280019483));
#162816=CARTESIAN_POINT('Ctrl Pts',(-228.717918644583,5.88135981044764,
130.139243276821));
#162817=CARTESIAN_POINT('Ctrl Pts',(-228.72531613392,5.86154782548237,129.982775393558));
#162818=CARTESIAN_POINT('Ctrl Pts',(-228.732713623256,5.83553767635279,
129.827410982033));
#162819=CARTESIAN_POINT('Ctrl Pts',(-228.740113705771,5.80951840940571,
129.671992107755));
#162820=CARTESIAN_POINT('Ctrl Pts',(-228.747513788286,5.77729671395034,
129.517677843317));
#162821=CARTESIAN_POINT('Ctrl Pts',(-228.754913870801,5.73900247800852,
129.364992311707));
#162822=CARTESIAN_POINT('Ctrl Pts',(-228.762322090468,5.70066613361748,
129.212138886657));
#162823=CARTESIAN_POINT('Ctrl Pts',(-228.769730310134,5.65624400443657,
129.060918133404));
#162824=CARTESIAN_POINT('Ctrl Pts',(-228.7771385298,5.60591599042587,128.911839423289));
#162825=CARTESIAN_POINT('Ctrl Pts',(-228.784551309102,5.5555570003626,128.762668957716));
#162826=CARTESIAN_POINT('Ctrl Pts',(-228.791964088405,5.49928501545498,
128.615643510168));
#162827=CARTESIAN_POINT('Ctrl Pts',(-228.799376867707,5.4373277751111,128.47125169844));
#162828=CARTESIAN_POINT('Ctrl Pts',(-228.806800238735,5.37528200735645,
128.32665357292));
#162829=CARTESIAN_POINT('Ctrl Pts',(-228.814223609764,5.30753492034926,
128.184696934905));
#162830=CARTESIAN_POINT('Ctrl Pts',(-228.821646980793,5.23436018790941,
128.045845802357));
#162831=CARTESIAN_POINT('Ctrl Pts',(-228.825583030234,5.19556118896182,
127.972223600184));
#162832=CARTESIAN_POINT('Ctrl Pts',(-228.829519079675,5.15523701504349,
127.899473992864));
#162833=CARTESIAN_POINT('Ctrl Pts',(-228.833455129116,5.11343327027361,
127.827662656241));
#162834=CARTESIAN_POINT('Ctrl Pts',(-228.840878395522,5.03459271229616,
127.692228716537));
#162835=CARTESIAN_POINT('Ctrl Pts',(-228.848301661927,4.95024858489456,
127.559724394589));
#162836=CARTESIAN_POINT('Ctrl Pts',(-228.855724928333,4.8606441841678,127.430628459048));
#162837=CARTESIAN_POINT('Ctrl Pts',(-228.863139421054,4.77114568840151,
127.301685104183));
#162838=CARTESIAN_POINT('Ctrl Pts',(-228.870553913775,4.67639950546935,
127.176142420784));
#162839=CARTESIAN_POINT('Ctrl Pts',(-228.877968406496,4.57669460362477,
127.05445434305));
#162840=CARTESIAN_POINT('Ctrl Pts',(-228.885375752849,4.47708580111841,
126.932883552868));
#162841=CARTESIAN_POINT('Ctrl Pts',(-228.892783099203,4.3725280295438,126.815160258903));
#162842=CARTESIAN_POINT('Ctrl Pts',(-228.900190445557,4.26335323676517,
126.701709067524));
#162843=CARTESIAN_POINT('Ctrl Pts',(-228.907592267232,4.15425987066592,
126.588342492323));
#162844=CARTESIAN_POINT('Ctrl Pts',(-228.914994088908,4.04055659766189,
126.479241943189));
#162845=CARTESIAN_POINT('Ctrl Pts',(-228.922395910583,3.92261520546097,
126.374798504627));
#162846=CARTESIAN_POINT('Ctrl Pts',(-228.929793824895,3.80473607360361,
126.270410200943));
#162847=CARTESIAN_POINT('Ctrl Pts',(-228.937191739206,3.68262355694131,
126.170674358564));
#162848=CARTESIAN_POINT('Ctrl Pts',(-228.944589653517,3.55668572946279,
126.075944689971));
#162849=CARTESIAN_POINT('Ctrl Pts',(-228.951986338429,3.43076883056591,
125.981230763729));
#162850=CARTESIAN_POINT('Ctrl Pts',(-228.959383023342,3.30102818055546,
125.891521584306));
#162851=CARTESIAN_POINT('Ctrl Pts',(-228.966779708254,3.16790440239628,
125.807130158624));
#162852=CARTESIAN_POINT('Ctrl Pts',(-228.974176065189,3.03478652708454,
125.722742474945));
#162853=CARTESIAN_POINT('Ctrl Pts',(-228.981572422125,2.89828613718103,
125.643672276036));
#162854=CARTESIAN_POINT('Ctrl Pts',(-228.98896877906,2.75887203184956,125.570188698878));
#162855=CARTESIAN_POINT('Ctrl Pts',(-228.996366268397,2.61943658186264,
125.496693871197));
#162856=CARTESIAN_POINT('Ctrl Pts',(-229.003763757733,2.47708685846287,
125.428787542409));
#162857=CARTESIAN_POINT('Ctrl Pts',(-229.01116124707,2.33231525795974,125.366692358101));
#162858=CARTESIAN_POINT('Ctrl Pts',(-229.018561329585,2.18749290799668,
125.304575406424));
#162859=CARTESIAN_POINT('Ctrl Pts',(-229.0259614121,2.04024733346464,125.248273802112));
#162860=CARTESIAN_POINT('Ctrl Pts',(-229.033361494615,1.89108970152551,
125.197961567972));
#162861=CARTESIAN_POINT('Ctrl Pts',(-229.040769714282,1.74176805543608,
125.147594010359));
#162862=CARTESIAN_POINT('Ctrl Pts',(-229.048177933948,1.59053050703603,
125.103229094834));
#162863=CARTESIAN_POINT('Ctrl Pts',(-229.055586153615,1.43790284518368,
125.064990794117));
#162864=CARTESIAN_POINT('Ctrl Pts',(-229.062998932917,1.28518124355305,
125.026728958365));
#162865=CARTESIAN_POINT('Ctrl Pts',(-229.070411712219,1.13106818819075,
124.994601327278));
#162866=CARTESIAN_POINT('Ctrl Pts',(-229.077824491521,0.976097865799036,
124.968680407095));
#162867=CARTESIAN_POINT('Ctrl Pts',(-229.08524786255,0.820906114542193,
124.942722449886));
#162868=CARTESIAN_POINT('Ctrl Pts',(-229.092671233578,0.664855019216633,
124.922988962552));
#162869=CARTESIAN_POINT('Ctrl Pts',(-229.100094604607,0.508482898657796,
124.909500508601));
#162870=CARTESIAN_POINT('Ctrl Pts',(-229.104030654048,0.425570648240655,
124.902348606664));
#162871=CARTESIAN_POINT('Ctrl Pts',(-229.107966703489,0.342568142260644,
124.896951536459));
#162872=CARTESIAN_POINT('Ctrl Pts',(-229.111902752929,0.259555285804272,
124.893306429343));
#162873=CARTESIAN_POINT('Ctrl Pts',(-229.119326019335,0.102995629270808,
124.886431871082));
#162874=CARTESIAN_POINT('Ctrl Pts',(-229.12674928574,-0.0540740705800281,
124.885771151604));
#162875=CARTESIAN_POINT('Ctrl Pts',(-229.134172552146,-0.211119504637652,
124.891378365161));
#162876=CARTESIAN_POINT('Ctrl Pts',(-229.141587044866,-0.36797932403403,
124.896978951456));
#162877=CARTESIAN_POINT('Ctrl Pts',(-229.149001537587,-0.52481456530801,
124.90883271158));
#162878=CARTESIAN_POINT('Ctrl Pts',(-229.156416030308,-0.681087126363573,
124.92694189088));
#162879=CARTESIAN_POINT('Ctrl Pts',(-229.163823376662,-0.837209066042122,
124.94503361587));
#162880=CARTESIAN_POINT('Ctrl Pts',(-229.171230723016,-0.992769036852196,
124.969368714386));
#162881=CARTESIAN_POINT('Ctrl Pts',(-229.17863806937,-1.14723037950276,
124.999897419402));
#162882=CARTESIAN_POINT('Ctrl Pts',(-229.186039891045,-1.30157651905693,
125.030403354957));
#162883=CARTESIAN_POINT('Ctrl Pts',(-229.19344171272,-1.45482529734682,
125.067093627042));
#162884=CARTESIAN_POINT('Ctrl Pts',(-229.200843534396,-1.60644672356402,
125.109866830858));
#162885=CARTESIAN_POINT('Ctrl Pts',(-229.208241448707,-1.75798811000924,
125.152617455033));
#162886=CARTESIAN_POINT('Ctrl Pts',(-229.215639363018,-1.90790349688792,
125.201444514717));
#162887=CARTESIAN_POINT('Ctrl Pts',(-229.22303727733,-2.05567472191291,
125.256195875943));
#162888=CARTESIAN_POINT('Ctrl Pts',(-229.230433962242,-2.20342139004135,
125.310938138486));
#162889=CARTESIAN_POINT('Ctrl Pts',(-229.237830647154,-2.34902425380694,
125.371602619038));
#162890=CARTESIAN_POINT('Ctrl Pts',(-229.245227332066,-2.49198180414596,
125.437987796907));
#162891=CARTESIAN_POINT('Ctrl Pts',(-229.252623689001,-2.6349330155974,
125.504370031188));
#162892=CARTESIAN_POINT('Ctrl Pts',(-229.260020045937,-2.77523880827291,
125.576472301197));
#162893=CARTESIAN_POINT('Ctrl Pts',(-229.267416402872,-2.91241935220797,
125.654045668033));
#162894=CARTESIAN_POINT('Ctrl Pts',(-229.274813892208,-3.04962089883412,
125.731630911549));
#162895=CARTESIAN_POINT('Ctrl Pts',(-229.282211381545,-3.18369591903235,
125.814688735983));
#162896=CARTESIAN_POINT('Ctrl Pts',(-229.289608870881,-3.31419094253027,
125.902925219751));
#162897=CARTESIAN_POINT('Ctrl Pts',(-229.297008953396,-3.44473171085695,
125.991192634683));
#162898=CARTESIAN_POINT('Ctrl Pts',(-229.304409035911,-3.57168967481552,
126.084642114373));
#162899=CARTESIAN_POINT('Ctrl Pts',(-229.311809118426,-3.69464212575393,
126.182937662988));
#162900=CARTESIAN_POINT('Ctrl Pts',(-229.319217338092,-3.81772977555214,
126.281341297663));
#162901=CARTESIAN_POINT('Ctrl Pts',(-229.326625557759,-3.93680282455531,
126.384601409885));
#162902=CARTESIAN_POINT('Ctrl Pts',(-229.334033777425,-4.05147276928151,
126.49234264888));
#162903=CARTESIAN_POINT('Ctrl Pts',(-229.341446556727,-4.16621329144531,
126.600150200809));
#162904=CARTESIAN_POINT('Ctrl Pts',(-229.348859336029,-4.27654504822498,
126.712444109629));
#162905=CARTESIAN_POINT('Ctrl Pts',(-229.356272115331,-4.38211829710703,
126.82881414033));
#162906=CARTESIAN_POINT('Ctrl Pts',(-229.36369548636,-4.48784239399783,
126.945350445989));
#162907=CARTESIAN_POINT('Ctrl Pts',(-229.371118857388,-4.58879416455572,
127.065974220159));
#162908=CARTESIAN_POINT('Ctrl Pts',(-229.378542228417,-4.68466533364117,
127.190243675036));
#162909=CARTESIAN_POINT('Ctrl Pts',(-229.382478277859,-4.73549852789738,
127.25613432183));
#162910=CARTESIAN_POINT('Ctrl Pts',(-229.3864143273,-4.78490411785535,127.323049432599));
#162911=CARTESIAN_POINT('Ctrl Pts',(-229.390350376742,-4.83284132633213,
127.390920230362));
#162912=CARTESIAN_POINT('Ctrl Pts',(-229.397852896466,-4.92421463286067,
127.520289031871));
#162913=CARTESIAN_POINT('Ctrl Pts',(-229.405355416191,-5.01052398939715,
127.653519099379));
#162914=CARTESIAN_POINT('Ctrl Pts',(-229.412857935915,-5.09142960561877,
127.790181602722));
#162915=CARTESIAN_POINT('Ctrl Pts',(-229.420351182523,-5.17223522247587,
127.926675191171));
#162916=CARTESIAN_POINT('Ctrl Pts',(-229.427844429131,-5.24765021274718,
128.066592460557));
#162917=CARTESIAN_POINT('Ctrl Pts',(-229.435337675739,-5.31737629159523,
128.209473349093));
#162918=CARTESIAN_POINT('Ctrl Pts',(-229.442823031844,-5.38702894782525,
128.352203781889));
#162919=CARTESIAN_POINT('Ctrl Pts',(-229.45030838795,-5.45100446252196,
128.497891296409));
#162920=CARTESIAN_POINT('Ctrl Pts',(-229.457793744055,-5.50904898602782,
128.64604881617));
#162921=CARTESIAN_POINT('Ctrl Pts',(-229.465272587066,-5.5670430043205,
128.794077422354));
#162922=CARTESIAN_POINT('Ctrl Pts',(-229.472751430076,-5.61911617704095,
128.944571417532));
#162923=CARTESIAN_POINT('Ctrl Pts',(-229.480230273087,-5.66506157844929,
129.097021203484));
#162924=CARTESIAN_POINT('Ctrl Pts',(-229.48770333383,-5.71097145716933,
129.24935312288));
#162925=CARTESIAN_POINT('Ctrl Pts',(-229.495176394572,-5.75076290159714,
129.403637473352));
#162926=CARTESIAN_POINT('Ctrl Pts',(-229.502649455315,-5.78427797044171,
129.55934699388));
#162927=CARTESIAN_POINT('Ctrl Pts',(-229.510119103402,-5.81777773425938,
129.714985407934));
#162928=CARTESIAN_POINT('Ctrl Pts',(-229.517588751489,-5.84500675505069,
129.872047341744));
#162929=CARTESIAN_POINT('Ctrl Pts',(-229.525058399576,-5.86585754000281,
130.029992563672));
#162930=CARTESIAN_POINT('Ctrl Pts',(-229.532526496849,-5.88670399601297,
130.187904993755));
#162931=CARTESIAN_POINT('Ctrl Pts',(-229.539994594123,-5.90117480371219,
130.346699987606));
#162932=CARTESIAN_POINT('Ctrl Pts',(-229.547462691397,-5.90921395717982,
130.505829261137));
#162933=CARTESIAN_POINT('Ctrl Pts',(-229.552183396862,-5.91429563653148,
130.606417456997));
#162934=CARTESIAN_POINT('Ctrl Pts',(-229.556904102328,-5.91680844807815,
130.707139070979));
#162935=CARTESIAN_POINT('Ctrl Pts',(-229.561624807793,-5.91674896819402,
130.80785488072));
#162936=CARTESIAN_POINT('',(-231.311623378035,-5.92090363694542,130.807722361332));
#162937=CARTESIAN_POINT('Ctrl Pts',(-229.561626886787,-5.90902547570768,
130.807894616703));
#162938=CARTESIAN_POINT('Ctrl Pts',(-229.597350591376,-5.91309279083499,
131.569064203554));
#162939=CARTESIAN_POINT('Ctrl Pts',(-229.72589017057,-5.42237780748865,
134.302818932609));
#162940=CARTESIAN_POINT('Ctrl Pts',(-229.947245624369,-1.2960426407277,
137.681702691617));
#162941=CARTESIAN_POINT('Ctrl Pts',(-230.22569324818,5.08555995844198,135.61212937651));
#162942=CARTESIAN_POINT('Ctrl Pts',(-230.504140871994,6.79378139922902,
129.124451444466));
#162943=CARTESIAN_POINT('Ctrl Pts',(-230.782588495806,2.25884962879145,
124.180527974388));
#162944=CARTESIAN_POINT('Ctrl Pts',(-231.051748963516,-4.13136558520875,
125.285458413445));
#162945=CARTESIAN_POINT('Ctrl Pts',(-231.228093556619,-5.91201437708188,
129.039513442124));
#162946=CARTESIAN_POINT('Ctrl Pts',(-231.311622275119,-5.92410850363469,
130.807700850245));
#162947=CARTESIAN_POINT('',(-233.061625681752,-5.91866021983708,130.79924806649));
#162948=CARTESIAN_POINT('Ctrl Pts',(-231.311624807793,-5.91674902906247,
130.807750247089));
#162949=CARTESIAN_POINT('Ctrl Pts',(-231.320911119673,-5.9166365522368,
131.004083546839));
#162950=CARTESIAN_POINT('Ctrl Pts',(-231.330197431552,-5.90675262271671,
131.200133270132));
#162951=CARTESIAN_POINT('Ctrl Pts',(-231.339483743431,-5.88717642798294,
131.395194154446));
#162952=CARTESIAN_POINT('Ctrl Pts',(-231.346907009837,-5.87152766337025,
131.551121386745));
#162953=CARTESIAN_POINT('Ctrl Pts',(-231.354330276242,-5.84965614496523,
131.706662261903));
#162954=CARTESIAN_POINT('Ctrl Pts',(-231.361753542648,-5.82158496308475,
131.861280236121));
#162955=CARTESIAN_POINT('Ctrl Pts',(-231.369168035369,-5.79354695901001,
132.015715464733));
#162956=CARTESIAN_POINT('Ctrl Pts',(-231.37658252809,-5.75932394289552,
132.169229599925));
#162957=CARTESIAN_POINT('Ctrl Pts',(-231.383997020811,-5.71899086197203,
132.321289779782));
#162958=CARTESIAN_POINT('Ctrl Pts',(-231.391404367165,-5.67869665559046,
132.473203398312));
#162959=CARTESIAN_POINT('Ctrl Pts',(-231.398811713519,-5.63230420352266,
132.623665492975));
#162960=CARTESIAN_POINT('Ctrl Pts',(-231.406219059873,-5.57993972082383,
132.772152088854));
#162961=CARTESIAN_POINT('Ctrl Pts',(-231.413620881548,-5.52761429353179,
132.920527937828));
#162962=CARTESIAN_POINT('Ctrl Pts',(-231.421022703224,-5.46932582807081,
133.066930871227));
#162963=CARTESIAN_POINT('Ctrl Pts',(-231.428424524899,-5.40525068717784,
133.210850919076));
#162964=CARTESIAN_POINT('Ctrl Pts',(-231.435822439211,-5.34120937105298,
133.354694992653));
#162965=CARTESIAN_POINT('Ctrl Pts',(-231.443220353522,-5.27138761460429,
133.49605845083));
#162966=CARTESIAN_POINT('Ctrl Pts',(-231.450618267833,-5.19601028903398,
133.63445030497));
#162967=CARTESIAN_POINT('Ctrl Pts',(-231.458014952746,-5.1206454898076,
133.772819160895));
#162968=CARTESIAN_POINT('Ctrl Pts',(-231.465411637658,-5.03972713218782,
133.908217065379));
#162969=CARTESIAN_POINT('Ctrl Pts',(-231.47280832257,-4.95352657536361,
134.040176593432));
#162970=CARTESIAN_POINT('Ctrl Pts',(-231.480204679506,-4.86732984076243,
134.17213027026));
#162971=CARTESIAN_POINT('Ctrl Pts',(-231.487601036442,-4.7758515768148,
134.300645561276));
#162972=CARTESIAN_POINT('Ctrl Pts',(-231.494997393377,-4.67940696176591,
134.425283296757));
#162973=CARTESIAN_POINT('Ctrl Pts',(-231.502394882714,-4.58294758080025,
134.549940114593));
#162974=CARTESIAN_POINT('Ctrl Pts',(-231.50979237205,-4.48152056321827,
134.670717899579));
#162975=CARTESIAN_POINT('Ctrl Pts',(-231.517189861387,-4.37548182472375,
134.787210020194));
#162976=CARTESIAN_POINT('Ctrl Pts',(-231.524589943902,-4.26940591451367,
134.90374297694));
#162977=CARTESIAN_POINT('Ctrl Pts',(-231.531990026417,-4.1587153158174,
135.015987002296));
#162978=CARTESIAN_POINT('Ctrl Pts',(-231.539390108932,-4.04380317215016,
135.123571942265));
#162979=CARTESIAN_POINT('Ctrl Pts',(-231.546798328599,-3.92876467076787,
135.231275182935));
#162980=CARTESIAN_POINT('Ctrl Pts',(-231.554206548266,-3.80949562666422,
135.334308851678));
#162981=CARTESIAN_POINT('Ctrl Pts',(-231.561614767932,-3.68642322612335,
135.432342290001));
#162982=CARTESIAN_POINT('Ctrl Pts',(-231.569027547234,-3.56327507657316,
135.530436066271));
#162983=CARTESIAN_POINT('Ctrl Pts',(-231.576440326536,-3.43631920639107,
135.623523259479));
#162984=CARTESIAN_POINT('Ctrl Pts',(-231.583853105839,-3.30601176678733,
135.711316574202));
#162985=CARTESIAN_POINT('Ctrl Pts',(-231.591276476867,-3.17551813780325,
135.799235332129));
#162986=CARTESIAN_POINT('Ctrl Pts',(-231.598699847896,-3.04166369175963,
135.881844908749));
#162987=CARTESIAN_POINT('Ctrl Pts',(-231.606123218925,-2.9049298596653,
135.958903572371));
#162988=CARTESIAN_POINT('Ctrl Pts',(-231.610059268365,-2.83243030101829,
135.999761924813));
#162989=CARTESIAN_POINT('Ctrl Pts',(-231.613995317805,-2.75912160106797,
136.039060510985));
#162990=CARTESIAN_POINT('Ctrl Pts',(-231.617931367245,-2.68507767373807,
136.07676883853));
#162991=CARTESIAN_POINT('Ctrl Pts',(-231.625354633651,-2.5454331376027,
136.147885567456));
#162992=CARTESIAN_POINT('Ctrl Pts',(-231.632777900056,-2.40275010424733,
136.213558081908));
#162993=CARTESIAN_POINT('Ctrl Pts',(-231.640201166462,-2.25749246404825,
136.273515793392));
#162994=CARTESIAN_POINT('Ctrl Pts',(-231.647615659183,-2.11240650631658,
136.333402639841));
#162995=CARTESIAN_POINT('Ctrl Pts',(-231.655030151904,-1.96475234048154,
136.387587986999));
#162996=CARTESIAN_POINT('Ctrl Pts',(-231.662444644625,-1.81501878917212,
136.435846865214));
#162997=CARTESIAN_POINT('Ctrl Pts',(-231.669851990979,-1.66542955669681,
136.484059229706));
#162998=CARTESIAN_POINT('Ctrl Pts',(-231.677259337332,-1.51376528160977,
136.526356383284));
#162999=CARTESIAN_POINT('Ctrl Pts',(-231.684666683686,-1.36053502116693,
136.56256129301));
#163000=CARTESIAN_POINT('Ctrl Pts',(-231.692068505362,-1.20741904563294,
136.598739199747));
#163001=CARTESIAN_POINT('Ctrl Pts',(-231.699470327037,-1.05273977206209,
136.628833824533));
#163002=CARTESIAN_POINT('Ctrl Pts',(-231.706872148713,-0.897021581004777,
136.652717895102));
#163003=CARTESIAN_POINT('Ctrl Pts',(-231.714270063024,-0.741385592368861,
136.676589357457));
#163004=CARTESIAN_POINT('Ctrl Pts',(-231.721667977335,-0.584712146532838,
136.694256738441));
#163005=CARTESIAN_POINT('Ctrl Pts',(-231.729065891647,-0.427535874520726,
136.705643837214));
#163006=CARTESIAN_POINT('Ctrl Pts',(-231.736462576559,-0.270385722353779,
136.717029043657));
#163007=CARTESIAN_POINT('Ctrl Pts',(-231.743859261471,-0.112733281811311,
136.722136012316));
#163008=CARTESIAN_POINT('Ctrl Pts',(-231.751255946383,0.044881512954716,
136.720940390737));
#163009=CARTESIAN_POINT('Ctrl Pts',(-231.758652303319,0.202489318916024,
136.719744822173));
#163010=CARTESIAN_POINT('Ctrl Pts',(-231.766048660254,0.360059109133106,
136.712247221869));
#163011=CARTESIAN_POINT('Ctrl Pts',(-231.773445017189,0.517051036140522,
136.698475376249));
#163012=CARTESIAN_POINT('Ctrl Pts',(-231.780842506526,0.674066999012743,
136.684701422124));
#163013=CARTESIAN_POINT('Ctrl Pts',(-231.788239995863,0.830504550621419,
136.664651342617));
#163014=CARTESIAN_POINT('Ctrl Pts',(-231.795637485199,0.985829199218018,
136.63840478542));
#163015=CARTESIAN_POINT('Ctrl Pts',(-231.803037567714,1.14120829662918,
136.612149027532));
#163016=CARTESIAN_POINT('Ctrl Pts',(-231.810437650229,1.29547334643917,
136.579692529347));
#163017=CARTESIAN_POINT('Ctrl Pts',(-231.817837732744,1.44810042393478,
136.541165976361));
#163018=CARTESIAN_POINT('Ctrl Pts',(-231.825245952411,1.60089533059276,
136.50259705947));
#163019=CARTESIAN_POINT('Ctrl Pts',(-231.832654172077,1.75204830581659,
136.457944849484));
#163020=CARTESIAN_POINT('Ctrl Pts',(-231.840062391744,1.9010502526319,136.407390021332));
#163021=CARTESIAN_POINT('Ctrl Pts',(-231.847475171046,2.05014390765883,
136.356804077527));
#163022=CARTESIAN_POINT('Ctrl Pts',(-231.854887950348,2.19708354857286,
136.300308410078));
#163023=CARTESIAN_POINT('Ctrl Pts',(-231.86230072965,2.34138090472541,136.238131501721));
#163024=CARTESIAN_POINT('Ctrl Pts',(-231.869724100679,2.48588443970751,
136.175865752081));
#163025=CARTESIAN_POINT('Ctrl Pts',(-231.877147471707,2.62773781380484,
136.107902709685));
#163026=CARTESIAN_POINT('Ctrl Pts',(-231.884570842736,2.76647742608029,
136.034516754192));
#163027=CARTESIAN_POINT('Ctrl Pts',(-231.888506892177,2.84004049751884,
135.995605759719));
#163028=CARTESIAN_POINT('Ctrl Pts',(-231.892442941618,2.91272865405808,
135.955170919982));
#163029=CARTESIAN_POINT('Ctrl Pts',(-231.896378991058,2.98447628933346,
135.913257938995));
#163030=CARTESIAN_POINT('Ctrl Pts',(-231.903802257464,3.11979009029819,
135.834211364913));
#163031=CARTESIAN_POINT('Ctrl Pts',(-231.911225523869,3.25216590140438,
135.749665686158));
#163032=CARTESIAN_POINT('Ctrl Pts',(-231.918648790275,3.38112532480981,
135.659864927154));
#163033=CARTESIAN_POINT('Ctrl Pts',(-231.926063282996,3.50993232888618,
135.57017030519));
#163034=CARTESIAN_POINT('Ctrl Pts',(-231.933477775717,3.63533067934663,
135.475233177379));
#163035=CARTESIAN_POINT('Ctrl Pts',(-231.940892268438,3.75686688227963,
135.375343202452));
#163036=CARTESIAN_POINT('Ctrl Pts',(-231.948299614791,3.87828594404449,
135.275549505243));
#163037=CARTESIAN_POINT('Ctrl Pts',(-231.955706961145,3.99584998255798,
135.170812699932));
#163038=CARTESIAN_POINT('Ctrl Pts',(-231.963114307499,4.1091348971128,135.061465380175));
#163039=CARTESIAN_POINT('Ctrl Pts',(-231.970516129175,4.22233531950435,
134.952199615775));
#163040=CARTESIAN_POINT('Ctrl Pts',(-231.97791795085,4.33126270527624,134.838330441974));
#163041=CARTESIAN_POINT('Ctrl Pts',(-231.985319772525,4.43552653617301,
134.720230241213));
#163042=CARTESIAN_POINT('Ctrl Pts',(-231.992717686837,4.53973532700504,
134.602192384629));
#163043=CARTESIAN_POINT('Ctrl Pts',(-232.000115601148,4.63928521942924,
134.479928228397));
#163044=CARTESIAN_POINT('Ctrl Pts',(-232.007513515459,4.73382312239265,
134.353846384322));
#163045=CARTESIAN_POINT('Ctrl Pts',(-232.014910200372,4.82834531487183,
134.227785492762));
#163046=CARTESIAN_POINT('Ctrl Pts',(-232.022306885284,4.91785694722976,
134.097908470888));
#163047=CARTESIAN_POINT('Ctrl Pts',(-232.029703570196,5.00204568345988,
133.9646564175));
#163048=CARTESIAN_POINT('Ctrl Pts',(-232.037099927131,5.08623068667297,
133.831410272648));
#163049=CARTESIAN_POINT('Ctrl Pts',(-232.044496284067,5.16509306366303,
133.694789709427));
#163050=CARTESIAN_POINT('Ctrl Pts',(-232.051892641002,5.23836439119204,
133.55526393604));
#163051=CARTESIAN_POINT('Ctrl Pts',(-232.059290130339,5.31164693674857,
133.4157168009));
#163052=CARTESIAN_POINT('Ctrl Pts',(-232.066687619676,5.37933655485596,
133.273263900467));
#163053=CARTESIAN_POINT('Ctrl Pts',(-232.074085109012,5.44121134952643,
133.128397969306));
#163054=CARTESIAN_POINT('Ctrl Pts',(-232.081485191527,5.50310783431035,
132.983481255619));
#163055=CARTESIAN_POINT('Ctrl Pts',(-232.088885274042,5.55918529072697,
132.836150170137));
#163056=CARTESIAN_POINT('Ctrl Pts',(-232.096285356557,5.60927047408139,
132.686916144263));
#163057=CARTESIAN_POINT('Ctrl Pts',(-232.103693576224,5.65941073124371,
132.537518020237));
#163058=CARTESIAN_POINT('Ctrl Pts',(-232.11110179589,5.70354543759155,132.386213131119));
#163059=CARTESIAN_POINT('Ctrl Pts',(-232.118510015557,5.74155142070898,
132.233527453822));
#163060=CARTESIAN_POINT('Ctrl Pts',(-232.125922794859,5.77958079587487,
132.080747801039));
#163061=CARTESIAN_POINT('Ctrl Pts',(-232.133335574161,5.81147385592338,
131.926586031351));
#163062=CARTESIAN_POINT('Ctrl Pts',(-232.140748353463,5.83715890764027,
131.771576441183));
#163063=CARTESIAN_POINT('Ctrl Pts',(-232.148171724492,5.86288065936353,
131.616345366044));
#163064=CARTESIAN_POINT('Ctrl Pts',(-232.15559509552,5.88237664064327,131.460264420415));
#163065=CARTESIAN_POINT('Ctrl Pts',(-232.163018466549,5.89562710722712,
131.303871953803));
#163066=CARTESIAN_POINT('Ctrl Pts',(-232.16695451599,5.9026528225503,131.220948915421));
#163067=CARTESIAN_POINT('Ctrl Pts',(-232.170890565431,5.90792357082179,
131.137938292135));
#163068=CARTESIAN_POINT('Ctrl Pts',(-232.174826614871,5.91144234228026,
131.054919984575));
#163069=CARTESIAN_POINT('Ctrl Pts',(-232.182249881277,5.91807863543398,
130.898350047427));
#163070=CARTESIAN_POINT('Ctrl Pts',(-232.189673147682,5.91850032080185,
130.741279523956));
#163071=CARTESIAN_POINT('Ctrl Pts',(-232.197096414088,5.9126541173217,130.584242804977));
#163072=CARTESIAN_POINT('Ctrl Pts',(-232.204510906809,5.90681482356856,
130.42739169036));
#163073=CARTESIAN_POINT('Ctrl Pts',(-232.21192539953,5.89472240063129,130.270574670102));
#163074=CARTESIAN_POINT('Ctrl Pts',(-232.219339892251,5.8763754220661,130.114329849094));
#163075=CARTESIAN_POINT('Ctrl Pts',(-232.226747238604,5.85804612700956,
129.958235622727));
#163076=CARTESIAN_POINT('Ctrl Pts',(-232.234154584958,5.8334743208782,129.80271286593));
#163077=CARTESIAN_POINT('Ctrl Pts',(-232.241561931312,5.80271058734489,
129.648298161634));
#163078=CARTESIAN_POINT('Ctrl Pts',(-232.248963752987,5.77196979856478,
129.493998625651));
#163079=CARTESIAN_POINT('Ctrl Pts',(-232.256365574663,5.73504635041257,
129.340805861169));
#163080=CARTESIAN_POINT('Ctrl Pts',(-232.263767396338,5.69204245412661,
129.189249704062));
#163081=CARTESIAN_POINT('Ctrl Pts',(-232.27116531065,5.64906125926263,129.03777355227));
#163082=CARTESIAN_POINT('Ctrl Pts',(-232.278563224961,5.60000611041983,
128.887932645462));
#163083=CARTESIAN_POINT('Ctrl Pts',(-232.285961139272,5.54502992994455,
128.740244913803));
#163084=CARTESIAN_POINT('Ctrl Pts',(-232.293357824184,5.49006288551317,
128.592581725167));
#163085=CARTESIAN_POINT('Ctrl Pts',(-232.300754509097,5.42917689243577,
128.447071351018));
#163086=CARTESIAN_POINT('Ctrl Pts',(-232.308151194009,5.36257423438275,
128.30421499316));
#163087=CARTESIAN_POINT('Ctrl Pts',(-232.315547550944,5.29597452956138,
128.161364969703));
#163088=CARTESIAN_POINT('Ctrl Pts',(-232.32294390788,5.22365882151237,128.021169066879));
#163089=CARTESIAN_POINT('Ctrl Pts',(-232.330340264815,5.1458767790677,127.884106735255));
#163090=CARTESIAN_POINT('Ctrl Pts',(-232.337737754152,5.06808282799377,
127.747023419038));
#163091=CARTESIAN_POINT('Ctrl Pts',(-232.345135243488,4.98482106038119,
127.613074953965));
#163092=CARTESIAN_POINT('Ctrl Pts',(-232.352532732825,4.8963860875755,127.482714362484));
#163093=CARTESIAN_POINT('Ctrl Pts',(-232.35993281534,4.80792011402731,127.352308073301));
#163094=CARTESIAN_POINT('Ctrl Pts',(-232.367332897855,4.71427753413996,
127.225492470557));
#163095=CARTESIAN_POINT('Ctrl Pts',(-232.37473298037,4.615794986648,127.102689751088));
#163096=CARTESIAN_POINT('Ctrl Pts',(-232.382141200036,4.51720414747067,
126.979751997403));
#163097=CARTESIAN_POINT('Ctrl Pts',(-232.389549419703,4.41376294590961,
126.860836230597));
#163098=CARTESIAN_POINT('Ctrl Pts',(-232.396957639369,4.30584732354023,
126.746330382481));
#163099=CARTESIAN_POINT('Ctrl Pts',(-232.404370418671,4.19786528090595,
126.631754057927));
#163100=CARTESIAN_POINT('Ctrl Pts',(-232.411783197973,4.08540359596706,
126.521593321123));
#163101=CARTESIAN_POINT('Ctrl Pts',(-232.419195977275,3.96887303550515,
126.41619728987));
#163102=CARTESIAN_POINT('Ctrl Pts',(-232.426619348304,3.85217597071355,
126.310650663824));
#163103=CARTESIAN_POINT('Ctrl Pts',(-232.434042719333,3.73139870481147,
126.209882579017));
#163104=CARTESIAN_POINT('Ctrl Pts',(-232.441466090361,3.60698349423465,
126.114200637904));
#163105=CARTESIAN_POINT('Ctrl Pts',(-232.445402139802,3.54101556428341,
126.063467776869));
#163106=CARTESIAN_POINT('Ctrl Pts',(-232.449338189243,3.47402534411361,
126.014164077538));
#163107=CARTESIAN_POINT('Ctrl Pts',(-232.453274238684,3.40608167268386,
125.96633021238));
#163108=CARTESIAN_POINT('Ctrl Pts',(-232.460697505089,3.27794202881931,
125.876117035537));
#163109=CARTESIAN_POINT('Ctrl Pts',(-232.468120771495,3.14602208019629,
125.790861805098));
#163110=CARTESIAN_POINT('Ctrl Pts',(-232.4755440379,3.01074262522589,125.710898199216));
#163111=CARTESIAN_POINT('Ctrl Pts',(-232.482958530621,2.875623059337,125.631029103675));
#163112=CARTESIAN_POINT('Ctrl Pts',(-232.490373023342,2.73715220893361,
125.556439371649));
#163113=CARTESIAN_POINT('Ctrl Pts',(-232.497787516063,2.59578202587182,
125.487421062083));
#163114=CARTESIAN_POINT('Ctrl Pts',(-232.505194862417,2.45454810071496,
125.418469274962));
#163115=CARTESIAN_POINT('Ctrl Pts',(-232.512602208771,2.31042073937398,
125.355078382466));
#163116=CARTESIAN_POINT('Ctrl Pts',(-232.520009555125,2.16387872597769,
125.297495863301));
#163117=CARTESIAN_POINT('Ctrl Pts',(-232.5274113768,2.0174460091437,125.239956291352));
#163118=CARTESIAN_POINT('Ctrl Pts',(-232.534813198475,1.86860257210839,
125.188216602865));
#163119=CARTESIAN_POINT('Ctrl Pts',(-232.542215020151,1.71784942846917,
125.142477193863));
#163120=CARTESIAN_POINT('Ctrl Pts',(-232.549612934462,1.56717586624146,
125.096761930338));
#163121=CARTESIAN_POINT('Ctrl Pts',(-232.557010848773,1.41459496144134,
125.057040746177));
#163122=CARTESIAN_POINT('Ctrl Pts',(-232.564408763085,1.26062512164881,
125.023464937382));
#163123=CARTESIAN_POINT('Ctrl Pts',(-232.571805447997,1.1066808688497,124.989894708278));
#163124=CARTESIAN_POINT('Ctrl Pts',(-232.579202132909,0.95134850352873,
124.962467907119));
#163125=CARTESIAN_POINT('Ctrl Pts',(-232.586598817821,0.795159040222278,
124.941285258742));
#163126=CARTESIAN_POINT('Ctrl Pts',(-232.593995174757,0.63897650252075,
124.920103549625));
#163127=CARTESIAN_POINT('Ctrl Pts',(-232.601391531692,0.481937312310916,
124.905165492943));
#163128=CARTESIAN_POINT('Ctrl Pts',(-232.608787888628,0.32457979703512,
124.896520189977));
#163129=CARTESIAN_POINT('Ctrl Pts',(-232.616185377964,0.167198189921571,
124.887873563393));
#163130=CARTESIAN_POINT('Ctrl Pts',(-232.623582867301,0.00949853346116747,
124.885521629336));
#163131=CARTESIAN_POINT('Ctrl Pts',(-232.630980356637,-0.147978787101232,
124.889461392637));
#163132=CARTESIAN_POINT('Ctrl Pts',(-232.638380439152,-0.305511311094459,
124.893402537015));
#163133=CARTESIAN_POINT('Ctrl Pts',(-232.645780521667,-0.462820971064362,
124.903639760644));
#163134=CARTESIAN_POINT('Ctrl Pts',(-232.653180604182,-0.619370599398267,
124.920118047523));
#163135=CARTESIAN_POINT('Ctrl Pts',(-232.660588823849,-0.776092370141994,
124.936614453973));
#163136=CARTESIAN_POINT('Ctrl Pts',(-232.667997043515,-0.932052068761462,
124.959365589816));
#163137=CARTESIAN_POINT('Ctrl Pts',(-232.675405263182,-1.08672011163195,
124.988264851378));
#163138=CARTESIAN_POINT('Ctrl Pts',(-232.682818042484,-1.24148335010205,
125.017181899952));
#163139=CARTESIAN_POINT('Ctrl Pts',(-232.690230821786,-1.39495298562878,
125.052254531504));
#163140=CARTESIAN_POINT('Ctrl Pts',(-232.697643601088,-1.54661326603992,
125.093325863005));
#163141=CARTESIAN_POINT('Ctrl Pts',(-232.705066972117,-1.69849024577166,
125.134455879149));
#163142=CARTESIAN_POINT('Ctrl Pts',(-232.712490343145,-1.8485523517892,
125.181601602307));
#163143=CARTESIAN_POINT('Ctrl Pts',(-232.719913714174,-1.99630173902771,
125.234557216255));
#163144=CARTESIAN_POINT('Ctrl Pts',(-232.723849763615,-2.07464200933777,
125.262635553422));
#163145=CARTESIAN_POINT('Ctrl Pts',(-232.727785813056,-2.15233245826397,
125.292346469113));
#163146=CARTESIAN_POINT('Ctrl Pts',(-232.731721862496,-2.22930165776773,
125.323654031625));
#163147=CARTESIAN_POINT('Ctrl Pts',(-232.739145128901,-2.37446316590539,
125.382699117448));
#163148=CARTESIAN_POINT('Ctrl Pts',(-232.746568395307,-2.51749676037933,
125.447604571862));
#163149=CARTESIAN_POINT('Ctrl Pts',(-232.753991661712,-2.65789425648788,
125.518196726441));
#163150=CARTESIAN_POINT('Ctrl Pts',(-232.761406154433,-2.7981258144153,
125.588705446956));
#163151=CARTESIAN_POINT('Ctrl Pts',(-232.768820647154,-2.93572714543821,
125.664887322981));
#163152=CARTESIAN_POINT('Ctrl Pts',(-232.776235139875,-3.07020824107732,
125.746519979614));
#163153=CARTESIAN_POINT('Ctrl Pts',(-232.783642486228,-3.20455971877371,
125.828073955619));
#163154=CARTESIAN_POINT('Ctrl Pts',(-232.791049832582,-3.33579663126267,
125.915068060809));
#163155=CARTESIAN_POINT('Ctrl Pts',(-232.798457178935,-3.46345197318393,
126.007233248822));
#163156=CARTESIAN_POINT('Ctrl Pts',(-232.805859000611,-3.59101210493502,
126.099329696561));
#163157=CARTESIAN_POINT('Ctrl Pts',(-232.813260822286,-3.71499568362199,
126.196589330162));
#163158=CARTESIAN_POINT('Ctrl Pts',(-232.820662643961,-3.83496330030851,
126.298698951641));
#163159=CARTESIAN_POINT('Ctrl Pts',(-232.828060558272,-3.95486758702402,
126.400754670245));
#163160=CARTESIAN_POINT('Ctrl Pts',(-232.835458472584,-4.07075985026051,
126.507655036483));
#163161=CARTESIAN_POINT('Ctrl Pts',(-232.842856386895,-4.18223258844476,
126.619045678562));
#163162=CARTESIAN_POINT('Ctrl Pts',(-232.850253071807,-4.29368680188208,
126.730417809537));
#163163=CARTESIAN_POINT('Ctrl Pts',(-232.857649756719,-4.40072268412277,
126.846278471755));
#163164=CARTESIAN_POINT('Ctrl Pts',(-232.865046441631,-4.50296846618191,
126.966235351883));
#163165=CARTESIAN_POINT('Ctrl Pts',(-232.872442798566,-4.60520971455621,
127.086186912998));
#163166=CARTESIAN_POINT('Ctrl Pts',(-232.879839155502,-4.70266104291436,
127.21023404678));
#163167=CARTESIAN_POINT('Ctrl Pts',(-232.887235512437,-4.7949901618244,
127.337950383548));
#163168=CARTESIAN_POINT('Ctrl Pts',(-232.894633001773,-4.88733341655824,
127.465686274013));
#163169=CARTESIAN_POINT('Ctrl Pts',(-232.90203049111,-4.97455268163518,
127.597092183468));
#163170=CARTESIAN_POINT('Ctrl Pts',(-232.909427980446,-5.05635838555179,
127.73171185154));
#163171=CARTESIAN_POINT('Ctrl Pts',(-232.916828062961,-5.13819276633097,
127.866378710328));
#163172=CARTESIAN_POINT('Ctrl Pts',(-232.924228145476,-5.2146096138745,
128.004261251926));
#163173=CARTESIAN_POINT('Ctrl Pts',(-232.931628227991,-5.28536486248556,
128.144877804517));
#163174=CARTESIAN_POINT('Ctrl Pts',(-232.939036447657,-5.35619791376658,
128.285648979464));
#163175=CARTESIAN_POINT('Ctrl Pts',(-232.946444667323,-5.42135676546849,
128.429159835566));
#163176=CARTESIAN_POINT('Ctrl Pts',(-232.95385288699,-5.4806448533968,128.574907197233));
#163177=CARTESIAN_POINT('Ctrl Pts',(-232.961265666291,-5.53996943215396,
128.720744263969));
#163178=CARTESIAN_POINT('Ctrl Pts',(-232.968678445593,-5.59341592062896,
128.868820228869));
#163179=CARTESIAN_POINT('Ctrl Pts',(-232.976091224895,-5.64083753230937,
129.018616375915));
#163180=CARTESIAN_POINT('Ctrl Pts',(-232.983514595924,-5.68832690221248,
129.168626558721));
#163181=CARTESIAN_POINT('Ctrl Pts',(-232.990937966952,-5.72977410385884,
129.320361473454));
#163182=CARTESIAN_POINT('Ctrl Pts',(-232.998361337981,-5.76508319884803,
129.473291020265));
#163183=CARTESIAN_POINT('Ctrl Pts',(-233.002297387423,-5.78380492824951,
129.554377935513));
#163184=CARTESIAN_POINT('Ctrl Pts',(-233.006233436866,-5.80080187876953,
129.635800586197));
#163185=CARTESIAN_POINT('Ctrl Pts',(-233.010169486308,-5.81606567216756,
129.717479455923));
#163186=CARTESIAN_POINT('Ctrl Pts',(-233.021282375884,-5.85916087537255,
129.948088413775));
#163187=CARTESIAN_POINT('Ctrl Pts',(-233.03239526546,-5.88855019482882,
130.181332592728));
#163188=CARTESIAN_POINT('Ctrl Pts',(-233.043508155036,-5.90398369189102,
130.415892950463));
#163189=CARTESIAN_POINT('Ctrl Pts',(-233.049547039289,-5.91237044870438,
130.543356005041));
#163190=CARTESIAN_POINT('Ctrl Pts',(-233.055585923541,-5.91663678834088,
130.671207350514));
#163191=CARTESIAN_POINT('Ctrl Pts',(-233.061624807793,-5.91674777656172,
130.799231187579));
#163192=CARTESIAN_POINT('',(-234.811624807793,-5.90708423514873,130.803370312258));
#163193=CARTESIAN_POINT('Ctrl Pts',(-233.061626121642,-5.9196228110901,
130.799256562163));
#163194=CARTESIAN_POINT('Ctrl Pts',(-233.137289784469,-5.9049408922486,
132.404113396264));
#163195=CARTESIAN_POINT('Ctrl Pts',(-233.305769321901,-4.40022697300252,
136.001848438897));
#163196=CARTESIAN_POINT('Ctrl Pts',(-233.567064733934,1.69024620653965,
137.595577613887));
#163197=CARTESIAN_POINT('Ctrl Pts',(-233.84551235775,6.62726255753125,133.053127284941));
#163198=CARTESIAN_POINT('Ctrl Pts',(-234.12395998156,5.47414837784594,126.444170247007));
#163199=CARTESIAN_POINT('Ctrl Pts',(-234.402407605374,-0.709440733999325,
123.84201515248));
#163200=CARTESIAN_POINT('Ctrl Pts',(-234.631629214118,-5.26316317401156,
126.966848296847));
#163201=CARTESIAN_POINT('Ctrl Pts',(-234.768034948258,-5.90846806025998,
129.873832758555));
#163202=CARTESIAN_POINT('Ctrl Pts',(-234.811624807793,-5.90708423514873,
130.803370312258));
#163203=CARTESIAN_POINT('',(-236.561624807793,-5.91597698617805,130.809831571247));
#163204=CARTESIAN_POINT('Ctrl Pts',(-234.811624807793,-5.90708423514873,
130.803370312258));
#163205=CARTESIAN_POINT('Ctrl Pts',(-234.860850822862,-5.90552148187296,
131.853096787939));
#163206=CARTESIAN_POINT('Ctrl Pts',(-235.002892712535,-5.13706619888831,
134.884224157401));
#163207=CARTESIAN_POINT('Ctrl Pts',(-235.237750476812,-0.285723217902968,
137.796922578187));
#163208=CARTESIAN_POINT('Ctrl Pts',(-235.516198100626,5.72860003865988,
134.824398195424));
#163209=CARTESIAN_POINT('Ctrl Pts',(-235.794645724438,6.47861971736538,
128.15765566837));
#163210=CARTESIAN_POINT('Ctrl Pts',(-236.073093348251,1.27510437398114,
123.923105690896));
#163211=CARTESIAN_POINT('Ctrl Pts',(-236.328753042703,-4.57842230759621,
125.841131797943));
#163212=CARTESIAN_POINT('Ctrl Pts',(-236.49159686255,-5.90236292534572,
129.322162102131));
#163213=CARTESIAN_POINT('Ctrl Pts',(-236.561624807793,-5.91597698617805,
130.809831571247));
#163214=CARTESIAN_POINT('',(-238.311625634305,-5.92190600550432,130.802943865459));
#163215=CARTESIAN_POINT('Ctrl Pts',(-236.561624830344,-5.91674746952458,
130.809832762891));
#163216=CARTESIAN_POINT('Ctrl Pts',(-236.571197958137,-5.91655935773222,
131.013228306209));
#163217=CARTESIAN_POINT('Ctrl Pts',(-236.580771085931,-5.9058798916068,
131.216155350628));
#163218=CARTESIAN_POINT('Ctrl Pts',(-236.590344213725,-5.88487424717071,
131.417700374542));
#163219=CARTESIAN_POINT('Ctrl Pts',(-236.600141982541,-5.86337568865675,
131.623974812015));
#163220=CARTESIAN_POINT('Ctrl Pts',(-236.609939751358,-5.83106062150952,
131.828801897574));
#163221=CARTESIAN_POINT('Ctrl Pts',(-236.619737520175,-5.78815400136439,
132.031228099811));
#163222=CARTESIAN_POINT('Ctrl Pts',(-236.623154545409,-5.77319008391645,
132.101825340267));
#163223=CARTESIAN_POINT('Ctrl Pts',(-236.626571570643,-5.75693833299246,
132.17213076509));
#163224=CARTESIAN_POINT('Ctrl Pts',(-236.629988595877,-5.73940963744891,
132.24210453637));
#163225=CARTESIAN_POINT('Ctrl Pts',(-236.637411862283,-5.70132967963608,
132.394118030572));
#163226=CARTESIAN_POINT('Ctrl Pts',(-236.644835128688,-5.6571486452557,
132.544847468187));
#163227=CARTESIAN_POINT('Ctrl Pts',(-236.652258395093,-5.60696713477279,
132.693765315368));
#163228=CARTESIAN_POINT('Ctrl Pts',(-236.659672887815,-5.55684493466795,
132.842507154021));
#163229=CARTESIAN_POINT('Ctrl Pts',(-236.667087380536,-5.50073649329569,
132.989441313911));
#163230=CARTESIAN_POINT('Ctrl Pts',(-236.674501873257,-5.43879318706466,
133.134051419119));
#163231=CARTESIAN_POINT('Ctrl Pts',(-236.681909219611,-5.37690958412411,
133.278522143663));
#163232=CARTESIAN_POINT('Ctrl Pts',(-236.689316565965,-5.30920245832512,
133.420672932107));
#163233=CARTESIAN_POINT('Ctrl Pts',(-236.696723912318,-5.23587262484384,
133.560003631258));
#163234=CARTESIAN_POINT('Ctrl Pts',(-236.704125733994,-5.16259748351916,
133.699230412317));
#163235=CARTESIAN_POINT('Ctrl Pts',(-236.711527555669,-5.08370815770051,
133.835640963176));
#163236=CARTESIAN_POINT('Ctrl Pts',(-236.718929377345,-4.99945305134075,
133.968756254957));
#163237=CARTESIAN_POINT('Ctrl Pts',(-236.726327291656,-4.9152424225958,
134.101801276212));
#163238=CARTESIAN_POINT('Ctrl Pts',(-236.733725205968,-4.82567185361808,
134.231554188142));
#163239=CARTESIAN_POINT('Ctrl Pts',(-236.741123120279,-4.73103499406368,
134.357561772503));
#163240=CARTESIAN_POINT('Ctrl Pts',(-236.748519805192,-4.63641386143831,
134.483548416689));
#163241=CARTESIAN_POINT('Ctrl Pts',(-236.755916490104,-4.53672833316742,
134.605790670398));
#163242=CARTESIAN_POINT('Ctrl Pts',(-236.763313175016,-4.43231464140906,
134.723865367155));
#163243=CARTESIAN_POINT('Ctrl Pts',(-236.770709531952,-4.3279055794632,
134.841934828356));
#163244=CARTESIAN_POINT('Ctrl Pts',(-236.778105888887,-4.21876901817637,
134.955836820395));
#163245=CARTESIAN_POINT('Ctrl Pts',(-236.785502245823,-4.10528045155975,
135.06518248389));
#163246=CARTESIAN_POINT('Ctrl Pts',(-236.79289973516,-3.99177450955385,
135.174544888485));
#163247=CARTESIAN_POINT('Ctrl Pts',(-236.800297224496,-3.87391550435985,
135.279349316525));
#163248=CARTESIAN_POINT('Ctrl Pts',(-236.807694713833,-3.75211452210784,
135.379245006869));
#163249=CARTESIAN_POINT('Ctrl Pts',(-236.815094796348,-3.63027084271049,
135.479175715492));
#163250=CARTESIAN_POINT('Ctrl Pts',(-236.822494878863,-3.50448272345132,
135.574194023839));
#163251=CARTESIAN_POINT('Ctrl Pts',(-236.829894961379,-3.37519279910778,
135.66399065815));
#163252=CARTESIAN_POINT('Ctrl Pts',(-236.837303181045,-3.24576070720091,
135.753886033092));
#163253=CARTESIAN_POINT('Ctrl Pts',(-236.844711400712,-3.11281942710979,
135.838548054235));
#163254=CARTESIAN_POINT('Ctrl Pts',(-236.852119620378,-2.9768395534843,
135.917711459755));
#163255=CARTESIAN_POINT('Ctrl Pts',(-236.859532399681,-2.84077598651554,
135.99692358903));
#163256=CARTESIAN_POINT('Ctrl Pts',(-236.866945178983,-2.70167042848735,
136.070630184656));
#163257=CARTESIAN_POINT('Ctrl Pts',(-236.874357958285,-2.56001584920902,
136.138613087622));
#163258=CARTESIAN_POINT('Ctrl Pts',(-236.881781329314,-2.41815886722468,
136.206693127748));
#163259=CARTESIAN_POINT('Ctrl Pts',(-236.889204700343,-2.27374593159784,
136.269032993795));
#163260=CARTESIAN_POINT('Ctrl Pts',(-236.896628071372,-2.12728842215766,
136.325463272965));
#163261=CARTESIAN_POINT('Ctrl Pts',(-236.900564120811,-2.04963313647679,
136.355383960998));
#163262=CARTESIAN_POINT('Ctrl Pts',(-236.904500170251,-1.97140328625092,
136.383644090074));
#163263=CARTESIAN_POINT('Ctrl Pts',(-236.90843621969,-1.89267642399992,
136.410224201041));
#163264=CARTESIAN_POINT('Ctrl Pts',(-236.915859486096,-1.74420001873219,
136.460353460804));
#163265=CARTESIAN_POINT('Ctrl Pts',(-236.923282752501,-1.59350614572517,
136.504655648109));
#163266=CARTESIAN_POINT('Ctrl Pts',(-236.930706018907,-1.44109301115393,
136.542930256048));
#163267=CARTESIAN_POINT('Ctrl Pts',(-236.938120511628,-1.28886001625062,
136.581159626578));
#163268=CARTESIAN_POINT('Ctrl Pts',(-236.945535004349,-1.13491216305952,
136.613375508264));
#163269=CARTESIAN_POINT('Ctrl Pts',(-236.95294949707,-0.979765715912632,
136.639426144569));
#163270=CARTESIAN_POINT('Ctrl Pts',(-236.960356843424,-0.824768804752221,
136.66545167229));
#163271=CARTESIAN_POINT('Ctrl Pts',(-236.967764189777,-0.668575965184154,
136.685323723171));
#163272=CARTESIAN_POINT('Ctrl Pts',(-236.975171536131,-0.511716535762781,
136.698940903687));
#163273=CARTESIAN_POINT('Ctrl Pts',(-236.982573357807,-0.354974098022284,
136.712547927997));
#163274=CARTESIAN_POINT('Ctrl Pts',(-236.989975179482,-0.197566430655348,
136.719909338676));
#163275=CARTESIAN_POINT('Ctrl Pts',(-236.997377001157,-0.040030822628623,
136.720975198197));
#163276=CARTESIAN_POINT('Ctrl Pts',(-237.004774915469,0.117421623577328,
136.722040495059));
#163277=CARTESIAN_POINT('Ctrl Pts',(-237.01217282978,0.275001503591715,
136.716816856899));
#163278=CARTESIAN_POINT('Ctrl Pts',(-237.019570744091,0.432168787255593,
136.705306363955));
#163279=CARTESIAN_POINT('Ctrl Pts',(-237.026967429004,0.589309952568007,
136.693797783846));
#163280=CARTESIAN_POINT('Ctrl Pts',(-237.034364113916,0.746038285676928,
136.676004449735));
#163281=CARTESIAN_POINT('Ctrl Pts',(-237.041760798828,0.901816022947122,
136.651980511442));
#163282=CARTESIAN_POINT('Ctrl Pts',(-237.049157155763,1.0575868528692,136.627957638396));
#163283=CARTESIAN_POINT('Ctrl Pts',(-237.056553512699,1.21240680182578,
136.597704767387));
#163284=CARTESIAN_POINT('Ctrl Pts',(-237.063949869634,1.36574574772098,
136.561327624166));
#163285=CARTESIAN_POINT('Ctrl Pts',(-237.071347358971,1.51910817020024,
136.524944911512));
#163286=CARTESIAN_POINT('Ctrl Pts',(-237.078744848307,1.67098877489771,
136.48243614585));
#163287=CARTESIAN_POINT('Ctrl Pts',(-237.086142337644,1.82087025443732,
136.433957590619));
#163288=CARTESIAN_POINT('Ctrl Pts',(-237.093542420159,1.97080427469704,
136.385462041306));
#163289=CARTESIAN_POINT('Ctrl Pts',(-237.100942502674,2.11873741957135,
136.330992650683));
#163290=CARTESIAN_POINT('Ctrl Pts',(-237.108342585189,2.26417023337838,
136.270754649904));
#163291=CARTESIAN_POINT('Ctrl Pts',(-237.115750804855,2.40976296551525,
136.210450411251));
#163292=CARTESIAN_POINT('Ctrl Pts',(-237.123159024522,2.55284953081454,
136.144365037632));
#163293=CARTESIAN_POINT('Ctrl Pts',(-237.130567244188,2.69295238908918,
136.07275107316));
#163294=CARTESIAN_POINT('Ctrl Pts',(-237.13798002349,2.83314147833533,136.001093031489));
#163295=CARTESIAN_POINT('Ctrl Pts',(-237.145392802792,2.97034287667068,
135.923899801168));
#163296=CARTESIAN_POINT('Ctrl Pts',(-237.152805582094,3.104106578516,135.841468211385));
#163297=CARTESIAN_POINT('Ctrl Pts',(-237.160228953123,3.23806140821161,
135.758918839482));
#163298=CARTESIAN_POINT('Ctrl Pts',(-237.167652324152,3.36856842226183,
135.671116367089));
#163299=CARTESIAN_POINT('Ctrl Pts',(-237.175075695181,3.49520867559148,
135.578399460786));
#163300=CARTESIAN_POINT('Ctrl Pts',(-237.179011744622,3.56235637659947,
135.529238732351));
#163301=CARTESIAN_POINT('Ctrl Pts',(-237.182947794062,3.62841756849829,
135.478697033813));
#163302=CARTESIAN_POINT('Ctrl Pts',(-237.186883843503,3.69333396072086,
135.426829094158));
#163303=CARTESIAN_POINT('Ctrl Pts',(-237.194307109909,3.81576425047862,
135.329007778713));
#163304=CARTESIAN_POINT('Ctrl Pts',(-237.201730376314,3.93449065462452,
135.22617116986));
#163305=CARTESIAN_POINT('Ctrl Pts',(-237.20915364272,4.0490751884096,135.11863004368));
#163306=CARTESIAN_POINT('Ctrl Pts',(-237.21656813544,4.1635242927914,135.011216022182));
#163307=CARTESIAN_POINT('Ctrl Pts',(-237.223982628162,4.27384100149055,
134.899108804231));
#163308=CARTESIAN_POINT('Ctrl Pts',(-237.231397120883,4.37961858395188,
134.782660709515));
#163309=CARTESIAN_POINT('Ctrl Pts',(-237.238804467236,4.48529421399707,
134.666324851858));
#163310=CARTESIAN_POINT('Ctrl Pts',(-237.24621181359,4.586439178217,134.54565672122));
#163311=CARTESIAN_POINT('Ctrl Pts',(-237.253619159944,4.68268205095096,
134.421046859446));
#163312=CARTESIAN_POINT('Ctrl Pts',(-237.261020981619,4.77885314211912,
134.296529936407));
#163313=CARTESIAN_POINT('Ctrl Pts',(-237.268422803295,4.87012919451791,
134.16807743012));
#163314=CARTESIAN_POINT('Ctrl Pts',(-237.27582462497,4.95617777647921,134.036114384553));
#163315=CARTESIAN_POINT('Ctrl Pts',(-237.283222539281,5.04218093406413,
133.90422100125));
#163316=CARTESIAN_POINT('Ctrl Pts',(-237.290620453593,5.12296191358878,
133.76882108128));
#163317=CARTESIAN_POINT('Ctrl Pts',(-237.298018367904,5.19823056572549,
133.630370091729));
#163318=CARTESIAN_POINT('Ctrl Pts',(-237.305415052816,5.27348670957762,
133.491942110221));
#163319=CARTESIAN_POINT('Ctrl Pts',(-237.312811737728,5.34323216600439,
133.350464393086));
#163320=CARTESIAN_POINT('Ctrl Pts',(-237.320208422641,5.40722181840293,
133.206418645401));
#163321=CARTESIAN_POINT('Ctrl Pts',(-237.327604779576,5.47120863343322,
133.062379284856));
#163322=CARTESIAN_POINT('Ctrl Pts',(-237.335001136512,5.52944000034581,
132.915772461322));
#163323=CARTESIAN_POINT('Ctrl Pts',(-237.342397493447,5.5817183252683,132.767101328884));
#163324=CARTESIAN_POINT('Ctrl Pts',(-237.349794982784,5.63400465413579,
132.618407434516));
#163325=CARTESIAN_POINT('Ctrl Pts',(-237.35719247212,5.68033600240231,132.467648954127));
#163326=CARTESIAN_POINT('Ctrl Pts',(-237.364589961457,5.72056422165255,
132.315345577269));
#163327=CARTESIAN_POINT('Ctrl Pts',(-237.371990043972,5.76080654284263,
132.162988810699));
#163328=CARTESIAN_POINT('Ctrl Pts',(-237.379390126487,5.79494138013114,
132.009086430112));
#163329=CARTESIAN_POINT('Ctrl Pts',(-237.386790209002,5.82287143230362,
131.854169574168));
#163330=CARTESIAN_POINT('Ctrl Pts',(-237.394198428668,5.85083219643978,
131.699082371216));
#163331=CARTESIAN_POINT('Ctrl Pts',(-237.401606648335,5.87257448360726,
131.542978832741));
#163332=CARTESIAN_POINT('Ctrl Pts',(-237.409014868001,5.88805264418454,
131.386397233091));
#163333=CARTESIAN_POINT('Ctrl Pts',(-237.416427647303,5.9035403313114,131.229719260078));
#163334=CARTESIAN_POINT('Ctrl Pts',(-237.423840426605,5.91275618754745,
131.072563011375));
#163335=CARTESIAN_POINT('Ctrl Pts',(-237.431253205907,5.91570670468684,
130.915467532847));
#163336=CARTESIAN_POINT('Ctrl Pts',(-237.438676576936,5.9186614376635,130.758147588931));
#163337=CARTESIAN_POINT('Ctrl Pts',(-237.446099947965,5.91533295984985,
130.600888960837));
#163338=CARTESIAN_POINT('Ctrl Pts',(-237.453523318994,5.90577975098215,
130.444227176479));
#163339=CARTESIAN_POINT('Ctrl Pts',(-237.457459368435,5.90071441041429,
130.361161339363));
#163340=CARTESIAN_POINT('Ctrl Pts',(-237.461395417875,5.89389993587512,
130.278263165059));
#163341=CARTESIAN_POINT('Ctrl Pts',(-237.465331467316,5.88535086493392,
130.195611277425));
#163342=CARTESIAN_POINT('Ctrl Pts',(-237.472754733722,5.86922758394652,
130.039732396829));
#163343=CARTESIAN_POINT('Ctrl Pts',(-237.480178000127,5.8468827539285,129.884258811505));
#163344=CARTESIAN_POINT('Ctrl Pts',(-237.487601266533,5.81834109814454,
129.729726992491));
#163345=CARTESIAN_POINT('Ctrl Pts',(-237.495015759254,5.78983317622748,
129.575377817253));
#163346=CARTESIAN_POINT('Ctrl Pts',(-237.502430251975,5.75514307441088,
129.421968556219));
#163347=CARTESIAN_POINT('Ctrl Pts',(-237.509844744696,5.71434736142671,
129.270031840721));
#163348=CARTESIAN_POINT('Ctrl Pts',(-237.517252091049,5.67359096888664,
129.118241567549));
#163349=CARTESIAN_POINT('Ctrl Pts',(-237.524659437403,5.62674077684647,
128.967921372484));
#163350=CARTESIAN_POINT('Ctrl Pts',(-237.532066783757,5.57392459457616,
128.819594843859));
#163351=CARTESIAN_POINT('Ctrl Pts',(-237.539468605433,5.52114780460723,
128.671378942755));
#163352=CARTESIAN_POINT('Ctrl Pts',(-237.546870427108,5.46241400896619,
128.525154097524));
#163353=CARTESIAN_POINT('Ctrl Pts',(-237.554272248783,5.39790112174626,
128.381429738991));
#163354=CARTESIAN_POINT('Ctrl Pts',(-237.561670163095,5.33342229037732,
128.237781251429));
#163355=CARTESIAN_POINT('Ctrl Pts',(-237.569068077406,5.26317059559922,
128.096630961448));
#163356=CARTESIAN_POINT('Ctrl Pts',(-237.576465991717,5.18737240197308,
127.958469170981));
#163357=CARTESIAN_POINT('Ctrl Pts',(-237.58386267663,5.11158680463171,127.820330340497));
#163358=CARTESIAN_POINT('Ctrl Pts',(-237.591259361542,5.03025671717498,
127.685179350814));
#163359=CARTESIAN_POINT('Ctrl Pts',(-237.598656046454,4.94365492021578,
127.553482798834));
#163360=CARTESIAN_POINT('Ctrl Pts',(-237.606052403389,4.85705696327102,
127.421792086416));
#163361=CARTESIAN_POINT('Ctrl Pts',(-237.613448760325,4.76518796670724,
127.293555819044));
#163362=CARTESIAN_POINT('Ctrl Pts',(-237.62084511726,4.66836444399128,127.16921220511));
#163363=CARTESIAN_POINT('Ctrl Pts',(-237.628242606597,4.57152609734655,
127.044849553852));
#163364=CARTESIAN_POINT('Ctrl Pts',(-237.635640095934,4.46973194353695,
126.924381037252));
#163365=CARTESIAN_POINT('Ctrl Pts',(-237.64303758527,4.36333913426416,126.808212201666));
#163366=CARTESIAN_POINT('Ctrl Pts',(-237.650437667785,4.25690902915715,
126.692002643275));
#163367=CARTESIAN_POINT('Ctrl Pts',(-237.6578377503,4.14587731097074,126.580096041933));
#163368=CARTESIAN_POINT('Ctrl Pts',(-237.665237832815,4.03063824802058,
126.472861353328));
#163369=CARTESIAN_POINT('Ctrl Pts',(-237.672646052481,3.91527246787367,
126.365508749159));
#163370=CARTESIAN_POINT('Ctrl Pts',(-237.680054272148,3.79569037717168,
126.262838571605));
#163371=CARTESIAN_POINT('Ctrl Pts',(-237.687462491814,3.67232016663075,
126.165180177417));
#163372=CARTESIAN_POINT('Ctrl Pts',(-237.694875271117,3.54887402378378,
126.067461676118));
#163373=CARTESIAN_POINT('Ctrl Pts',(-237.702288050419,3.42163541625867,
125.974761324081));
#163374=CARTESIAN_POINT('Ctrl Pts',(-237.709700829721,3.29106136758126,
125.887365027034));
#163375=CARTESIAN_POINT('Ctrl Pts',(-237.717124200749,3.16030074857997,
125.799843854059));
#163376=CARTESIAN_POINT('Ctrl Pts',(-237.724547571778,3.02619548740785,
125.717642066971));
#163377=CARTESIAN_POINT('Ctrl Pts',(-237.731970942807,2.88922774859188,
125.64099993103));
#163378=CARTESIAN_POINT('Ctrl Pts',(-237.735906992248,2.81660416697704,
125.600362431552));
#163379=CARTESIAN_POINT('Ctrl Pts',(-237.739843041688,2.7431761951985,125.561287153868));
#163380=CARTESIAN_POINT('Ctrl Pts',(-237.743779091129,2.66901783964593,
125.523804365224));
#163381=CARTESIAN_POINT('Ctrl Pts',(-237.751202357534,2.52915749547435,
125.453112995638));
#163382=CARTESIAN_POINT('Ctrl Pts',(-237.75862562394,2.38627523847299,125.387875063449));
#163383=CARTESIAN_POINT('Ctrl Pts',(-237.766048890345,2.24083578044774,
125.328359743975));
#163384=CARTESIAN_POINT('Ctrl Pts',(-237.773463383066,2.09556821978388,
125.268914766667));
#163385=CARTESIAN_POINT('Ctrl Pts',(-237.780877875787,1.94774981631503,
125.215179078981));
#163386=CARTESIAN_POINT('Ctrl Pts',(-237.788292368508,1.7978700751362,125.167376161722));
#163387=CARTESIAN_POINT('Ctrl Pts',(-237.795699714862,1.6481347936948,125.119619318714));
#163388=CARTESIAN_POINT('Ctrl Pts',(-237.803107061216,1.4963424831204,125.077783974936));
#163389=CARTESIAN_POINT('Ctrl Pts',(-237.81051440757,1.34300273713837,125.042045613113));
#163390=CARTESIAN_POINT('Ctrl Pts',(-237.817916229245,1.18977735772408,
125.006333906309));
#163391=CARTESIAN_POINT('Ctrl Pts',(-237.82531805092,1.03500720293174,124.976710211422));
#163392=CARTESIAN_POINT('Ctrl Pts',(-237.832719872596,0.879217038255834,
124.95330020409));
#163393=CARTESIAN_POINT('Ctrl Pts',(-237.840117786907,0.723509113995637,
124.92990255472));
#163394=CARTESIAN_POINT('Ctrl Pts',(-237.847515701218,0.566782620430349,
124.912712115646));
#163395=CARTESIAN_POINT('Ctrl Pts',(-237.85491361553,0.40957241803676,124.901803460123));
#163396=CARTESIAN_POINT('Ctrl Pts',(-237.862310300442,0.252388341126501,
124.890896617421));
#163397=CARTESIAN_POINT('Ctrl Pts',(-237.869706985354,0.0947210869634865,
124.886269512216));
#163398=CARTESIAN_POINT('Ctrl Pts',(-237.877103670266,-0.0628893386807736,
124.887944853475));
#163399=CARTESIAN_POINT('Ctrl Pts',(-237.884500027202,-0.220492775713597,
124.889620120448));
#163400=CARTESIAN_POINT('Ctrl Pts',(-237.891896384137,-0.378039015961473,
124.897597274263));
#163401=CARTESIAN_POINT('Ctrl Pts',(-237.899292741072,-0.534988299031808,
124.911846885516));
#163402=CARTESIAN_POINT('Ctrl Pts',(-237.906690230409,-0.691961611438055,
124.926098678421));
#163403=CARTESIAN_POINT('Ctrl Pts',(-237.914087719746,-0.848337412893152,
124.946624807152));
#163404=CARTESIAN_POINT('Ctrl Pts',(-237.921485209082,-1.00358145654447,
124.973343997578));
#163405=CARTESIAN_POINT('Ctrl Pts',(-237.928885291597,-1.15887992075442,
125.000072554375));
#163406=CARTESIAN_POINT('Ctrl Pts',(-237.936285374112,-1.3130454696029,
125.03299843197));
#163407=CARTESIAN_POINT('Ctrl Pts',(-237.943685456627,-1.46555457856517,
125.071989350826));
#163408=CARTESIAN_POINT('Ctrl Pts',(-237.951093676293,-1.61823138697129,
125.111023144205));
#163409=CARTESIAN_POINT('Ctrl Pts',(-237.95850189596,-1.76924775609696,
125.156135205027));
#163410=CARTESIAN_POINT('Ctrl Pts',(-237.965910115626,-1.91809514123826,
125.207143309684));
#163411=CARTESIAN_POINT('Ctrl Pts',(-237.973322894928,-2.0670341394619,
125.258182808978));
#163412=CARTESIAN_POINT('Ctrl Pts',(-237.980735674231,-2.21380114638396,
125.315125448465));
#163413=CARTESIAN_POINT('Ctrl Pts',(-237.988148453533,-2.35790858904034,
125.377741260339));
#163414=CARTESIAN_POINT('Ctrl Pts',(-237.995571824561,-2.50222193916855,
125.440446540621));
#163415=CARTESIAN_POINT('Ctrl Pts',(-238.00299519559,-2.643867800088,125.508841021092));
#163416=CARTESIAN_POINT('Ctrl Pts',(-238.010418566619,-2.78238340812622,
125.582648912322));
#163417=CARTESIAN_POINT('Ctrl Pts',(-238.014354616059,-2.85582770714487,
125.621783627248));
#163418=CARTESIAN_POINT('Ctrl Pts',(-238.0182906655,-2.92839245725591,125.662439517439));
#163419=CARTESIAN_POINT('Ctrl Pts',(-238.022226714941,-3.00001219150598,
125.70457067941));
#163420=CARTESIAN_POINT('Ctrl Pts',(-238.029649981347,-3.13508477512495,
125.784028736018));
#163421=CARTESIAN_POINT('Ctrl Pts',(-238.037073247752,-3.26720264511097,
125.868976929596));
#163422=CARTESIAN_POINT('Ctrl Pts',(-238.044496514157,-3.39588814856414,
125.959169780773));
#163423=CARTESIAN_POINT('Ctrl Pts',(-238.051911006878,-3.52442155643852,
126.04925603149));
#163424=CARTESIAN_POINT('Ctrl Pts',(-238.059325499599,-3.64953037010122,
126.144574389001));
#163425=CARTESIAN_POINT('Ctrl Pts',(-238.06673999232,-3.77076197936284,
126.244833815639));
#163426=CARTESIAN_POINT('Ctrl Pts',(-238.074147338674,-3.89187674103551,
126.344996608467));
#163427=CARTESIAN_POINT('Ctrl Pts',(-238.081554685028,-4.00912145219235,
126.450090753137));
#163428=CARTESIAN_POINT('Ctrl Pts',(-238.088962031382,-4.12207302639116,
126.559782366715));
#163429=CARTESIAN_POINT('Ctrl Pts',(-238.096363853057,-4.23494035704452,
126.669392168149));
#163430=CARTESIAN_POINT('Ctrl Pts',(-238.103765674732,-4.34352065967597,
126.783592352008));
#163431=CARTESIAN_POINT('Ctrl Pts',(-238.111167496408,-4.44742455124296,
126.902009348971));
#163432=CARTESIAN_POINT('Ctrl Pts',(-238.118565410719,-4.55127359275439,
127.020363834524));
#163433=CARTESIAN_POINT('Ctrl Pts',(-238.12596332503,-4.65045089403539,
127.142930420066));
#163434=CARTESIAN_POINT('Ctrl Pts',(-238.133361239342,-4.7446046093423,
127.269299420994));
#163435=CARTESIAN_POINT('Ctrl Pts',(-238.140757924254,-4.83874267800999,
127.395647421687));
#163436=CARTESIAN_POINT('Ctrl Pts',(-238.148154609166,-4.92785859477709,
127.525796284596));
#163437=CARTESIAN_POINT('Ctrl Pts',(-238.155551294078,-5.01164136763678,
127.659303962322));
#163438=CARTESIAN_POINT('Ctrl Pts',(-238.162947651014,-5.09542042548051,
127.792805720178));
#163439=CARTESIAN_POINT('Ctrl Pts',(-238.170344007949,-5.17386661118653,
127.929665680529));
#163440=CARTESIAN_POINT('Ctrl Pts',(-238.177740364884,-5.24671293086851,
128.069413820358));
#163441=CARTESIAN_POINT('Ctrl Pts',(-238.185137854221,-5.31957040350801,
128.209183355984));
#163442=CARTESIAN_POINT('Ctrl Pts',(-238.192535343558,-5.38682613045449,
128.351841620498));
#163443=CARTESIAN_POINT('Ctrl Pts',(-238.199932832894,-5.44825971646252,
128.496895206239));
#163444=CARTESIAN_POINT('Ctrl Pts',(-238.207332915409,-5.50971483791898,
128.641999640289));
#163445=CARTESIAN_POINT('Ctrl Pts',(-238.214732997924,-5.56534360944434,
128.78950072383));
#163446=CARTESIAN_POINT('Ctrl Pts',(-238.222133080439,-5.61497434376742,
128.938886500529));
#163447=CARTESIAN_POINT('Ctrl Pts',(-238.229541300106,-5.66465965218497,
129.088436542247));
#163448=CARTESIAN_POINT('Ctrl Pts',(-238.236949519772,-5.70833363406839,
129.239875061395));
#163449=CARTESIAN_POINT('Ctrl Pts',(-238.244357739438,-5.7458747184651,
129.3926757086));
#163450=CARTESIAN_POINT('Ctrl Pts',(-238.25177051874,-5.78343890877296,
129.545570402053));
#163451=CARTESIAN_POINT('Ctrl Pts',(-238.259183298043,-5.81486260569806,
129.699828529178));
#163452=CARTESIAN_POINT('Ctrl Pts',(-238.266596077345,-5.8400757425728,
129.854915577812));
#163453=CARTESIAN_POINT('Ctrl Pts',(-238.274019448373,-5.86532490515984,
130.010224222095));
#163454=CARTESIAN_POINT('Ctrl Pts',(-238.281442819402,-5.88434573942735,
130.166363783827));
#163455=CARTESIAN_POINT('Ctrl Pts',(-238.288866190431,-5.89712013976513,
130.322795855902));
#163456=CARTESIAN_POINT('Ctrl Pts',(-238.292802239872,-5.90389343334238,
130.40573989406));
#163457=CARTESIAN_POINT('Ctrl Pts',(-238.296738289313,-5.90891150141813,
130.488766175199));
#163458=CARTESIAN_POINT('Ctrl Pts',(-238.300674338754,-5.91217757740723,
130.571794808163));
#163459=CARTESIAN_POINT('Ctrl Pts',(-238.304324495101,-5.91520642350734,
130.648792695533));
#163460=CARTESIAN_POINT('Ctrl Pts',(-238.307974651447,-5.91673115899377,
130.725850138482));
#163461=CARTESIAN_POINT('Ctrl Pts',(-238.311624807793,-5.91674982647209,
130.802927633805));
#163462=CARTESIAN_POINT('',(-240.061624807793,-5.91161849392799,130.79958681816));
#163463=CARTESIAN_POINT('Ctrl Pts',(-238.311626308619,-5.92611269417211,
130.802957108117));
#163464=CARTESIAN_POINT('Ctrl Pts',(-238.400791526601,-5.91996305970325,
132.688770394391));
#163465=CARTESIAN_POINT('Ctrl Pts',(-238.582772619189,-3.92389412409859,
136.548772126044));
#163466=CARTESIAN_POINT('Ctrl Pts',(-238.857569586381,2.65656124071048,
137.27894499841));
#163467=CARTESIAN_POINT('Ctrl Pts',(-239.136017210193,6.8831874500826,132.068991416398));
#163468=CARTESIAN_POINT('Ctrl Pts',(-239.414464834006,4.78450065523404,
125.696903910905));
#163469=CARTESIAN_POINT('Ctrl Pts',(-239.692912457819,-1.71090850592639,
124.018319605701));
#163470=CARTESIAN_POINT('Ctrl Pts',(-239.908632449081,-5.52500361660484,
127.549088971211));
#163471=CARTESIAN_POINT('Ctrl Pts',(-240.031536565739,-5.91644372475995,
130.159198921121));
#163472=CARTESIAN_POINT('Ctrl Pts',(-240.061624807793,-5.91161849392799,
130.79958681816));
#163473=CARTESIAN_POINT('',(-241.811624807794,-5.90881571325937,130.807693068847));
#163474=CARTESIAN_POINT('Ctrl Pts',(-240.061624807793,-5.91161849392799,
130.79958681816));
#163475=CARTESIAN_POINT('Ctrl Pts',(-240.124352440344,-5.90155890633036,
132.13466038688));
#163476=CARTESIAN_POINT('Ctrl Pts',(-240.279895947497,-4.79181868608966,
135.460338528975));
#163477=CARTESIAN_POINT('Ctrl Pts',(-240.528255329258,0.730628432584491,
137.76451454));
#163478=CARTESIAN_POINT('Ctrl Pts',(-240.80670295307,6.25069713114807,133.95179543103));
#163479=CARTESIAN_POINT('Ctrl Pts',(-241.085150576883,6.02668052970619,
127.246737489248));
#163480=CARTESIAN_POINT('Ctrl Pts',(-241.363598200696,0.264438941185339,
123.810961402823));
#163481=CARTESIAN_POINT('Ctrl Pts',(-241.605756277667,-4.95815660938682,
126.411990193879));
#163482=CARTESIAN_POINT('Ctrl Pts',(-241.755098480032,-5.90267469980127,
129.603172291332));
#163483=CARTESIAN_POINT('Ctrl Pts',(-241.811624807794,-5.90881571325937,
130.807693068847));
#163484=CARTESIAN_POINT('',(-243.561624807793,-5.92383771494013,130.807923172733));
#163485=CARTESIAN_POINT('Ctrl Pts',(-241.811624807794,-5.90881571325937,
130.807693068847));
#163486=CARTESIAN_POINT('Ctrl Pts',(-241.847914354636,-5.9127582052693,
131.58098783095));
#163487=CARTESIAN_POINT('Ctrl Pts',(-241.977019776084,-5.41158160550046,
134.327188727802));
#163488=CARTESIAN_POINT('Ctrl Pts',(-242.198941072135,-1.25415429483498,
137.689464649819));
#163489=CARTESIAN_POINT('Ctrl Pts',(-242.477388695948,5.11473198784157,
135.581083052765));
#163490=CARTESIAN_POINT('Ctrl Pts',(-242.755836319761,6.78342944224106,
129.083126893611));
#163491=CARTESIAN_POINT('Ctrl Pts',(-243.034283943573,2.21848662817418,
124.166900439835));
#163492=CARTESIAN_POINT('Ctrl Pts',(-243.302880106251,-4.15150118806808,
125.308311422276));
#163493=CARTESIAN_POINT('Ctrl Pts',(-243.478660394324,-5.91137340593356,
129.0514701503));
#163494=CARTESIAN_POINT('Ctrl Pts',(-243.561624807793,-5.92383771494013,
130.807923172733));
#163495=CARTESIAN_POINT('',(-245.311624807793,-5.91883942950955,130.799307097317));
#163496=CARTESIAN_POINT('Ctrl Pts',(-243.561624807793,-5.92383771494013,
130.807923172733));
#163497=CARTESIAN_POINT('Ctrl Pts',(-243.571476268929,-5.92531776705672,
131.016490050542));
#163498=CARTESIAN_POINT('Ctrl Pts',(-243.581327730064,-5.91526185254255,
131.224912612235));
#163499=CARTESIAN_POINT('Ctrl Pts',(-243.591179191199,-5.89319859537182,
131.432056249349));
#163500=CARTESIAN_POINT('Ctrl Pts',(-243.683995065804,-5.6853288709936,
133.383667039193));
#163501=CARTESIAN_POINT('Ctrl Pts',(-243.869626815012,-3.13791867181878,
137.059840370501));
#163502=CARTESIAN_POINT('Ctrl Pts',(-244.148074438826,3.56679059049603,
136.825620071692));
#163503=CARTESIAN_POINT('Ctrl Pts',(-244.426522062638,6.99379354755183,
131.058156489415));
#163504=CARTESIAN_POINT('Ctrl Pts',(-244.70496968645,3.9938419002167,125.057466899528));
#163505=CARTESIAN_POINT('Ctrl Pts',(-244.983417310265,-2.67625534339352,
124.33789188515));
#163506=CARTESIAN_POINT('Ctrl Pts',(-245.185635684044,-5.7342483307801,
128.130866893151));
#163507=CARTESIAN_POINT('Ctrl Pts',(-245.295038183221,-5.92317274697103,
130.447552151081));
#163508=CARTESIAN_POINT('Ctrl Pts',(-245.311624807793,-5.91998161812495,
130.799306122113));
#163509=CARTESIAN_POINT('',(-247.061624782818,-5.9114750784464,130.803173118476));
#163510=CARTESIAN_POINT('Ctrl Pts',(-245.311624807793,-5.91674784340849,
130.799308883118));
#163511=CARTESIAN_POINT('Ctrl Pts',(-245.31892615016,-5.91687997302728,
130.954063184845));
#163512=CARTESIAN_POINT('Ctrl Pts',(-245.326227492527,-5.91093649428155,
131.109029588657));
#163513=CARTESIAN_POINT('Ctrl Pts',(-245.333528834894,-5.89889422026084,
131.263683533033));
#163514=CARTESIAN_POINT('Ctrl Pts',(-245.340823797219,-5.88686246899084,
131.418202338075));
#163515=CARTESIAN_POINT('Ctrl Pts',(-245.348118759545,-5.86874255656274,
131.572408845108));
#163516=CARTESIAN_POINT('Ctrl Pts',(-245.355413721871,-5.84456334439123,
131.725777936645));
#163517=CARTESIAN_POINT('Ctrl Pts',(-245.362704011208,-5.82039962087947,
131.87904878339));
#163518=CARTESIAN_POINT('Ctrl Pts',(-245.369994300544,-5.79018438262468,
132.031482902934));
#163519=CARTESIAN_POINT('Ctrl Pts',(-245.377284589881,-5.75399834557609,
132.18256002317));
#163520=CARTESIAN_POINT('Ctrl Pts',(-245.384572716181,-5.71782304496787,
132.333592318645));
#163521=CARTESIAN_POINT('Ctrl Pts',(-245.39186084248,-5.67568055576135,
132.483268040689));
#163522=CARTESIAN_POINT('Ctrl Pts',(-245.399148968779,-5.62770273034245,
132.631076945132));
#163523=CARTESIAN_POINT('Ctrl Pts',(-245.406436229452,-5.57973060335499,
132.778868293988));
#163524=CARTESIAN_POINT('Ctrl Pts',(-245.413723490124,-5.52592463746925,
132.924792899662));
#163525=CARTESIAN_POINT('Ctrl Pts',(-245.421010750797,-5.46646650143819,
133.068355880625));
#163526=CARTESIAN_POINT('Ctrl Pts',(-245.428298683994,-5.40700287815248,
133.211932110686));
#163527=CARTESIAN_POINT('Ctrl Pts',(-245.435586617191,-5.34188619451485,
133.35314592632));
#163528=CARTESIAN_POINT('Ctrl Pts',(-245.442874550388,-5.27134606317935,
133.491522920945));
#163529=CARTESIAN_POINT('Ctrl Pts',(-245.450164694634,-5.20078453103629,
133.629941897055));
#163530=CARTESIAN_POINT('Ctrl Pts',(-245.45745483888,-5.12479645279535,
133.765521996797));
#163531=CARTESIAN_POINT('Ctrl Pts',(-245.464744983125,-5.04365697501847,
133.897814169965));
#163532=CARTESIAN_POINT('Ctrl Pts',(-245.472042776834,-4.96243235853778,
134.03024515576));
#163533=CARTESIAN_POINT('Ctrl Pts',(-245.479340570542,-4.87604575298051,
134.159380998799));
#163534=CARTESIAN_POINT('Ctrl Pts',(-245.486638364251,-4.78481544041778,
134.284801934934));
#163535=CARTESIAN_POINT('Ctrl Pts',(-245.49394052254,-4.69353056587861,
134.410297881379));
#163536=CARTESIAN_POINT('Ctrl Pts',(-245.501242680829,-4.59739645440353,
134.532074195589));
#163537=CARTESIAN_POINT('Ctrl Pts',(-245.508544839119,-4.49677055236318,
134.649745534827));
#163538=CARTESIAN_POINT('Ctrl Pts',(-245.515857160924,-4.39600459406856,
134.767580655027));
#163539=CARTESIAN_POINT('Ctrl Pts',(-245.523169482728,-4.29073462575644,
134.881299113301));
#163540=CARTESIAN_POINT('Ctrl Pts',(-245.530481804533,-4.18135408563361,
134.990553228168));
#163541=CARTESIAN_POINT('Ctrl Pts',(-245.533758722319,-4.13233668091564,
135.039513977122));
#163542=CARTESIAN_POINT('Ctrl Pts',(-245.537035640105,-4.08249419958879,
135.087578716439));
#163543=CARTESIAN_POINT('Ctrl Pts',(-245.54031255789,-4.03186404556836,
135.134718903038));
#163544=CARTESIAN_POINT('Ctrl Pts',(-245.547735824296,-3.91717056040364,
135.24150649626));
#163545=CARTESIAN_POINT('Ctrl Pts',(-245.555159090701,-3.79805816502304,
135.343895775135));
#163546=CARTESIAN_POINT('Ctrl Pts',(-245.562582357107,-3.67489841655756,
135.441498979798));
#163547=CARTESIAN_POINT('Ctrl Pts',(-245.569996849828,-3.55188423268733,
135.538986825578));
#163548=CARTESIAN_POINT('Ctrl Pts',(-245.577411342549,-3.42483250729264,
135.631699627332));
#163549=CARTESIAN_POINT('Ctrl Pts',(-245.584825835269,-3.2941513170682,
135.719286625428));
#163550=CARTESIAN_POINT('Ctrl Pts',(-245.592233181623,-3.1635960822946,
135.806789203878));
#163551=CARTESIAN_POINT('Ctrl Pts',(-245.599640527977,-3.02941865495771,
135.889175607681));
#163552=CARTESIAN_POINT('Ctrl Pts',(-245.607047874331,-2.89205975255052,
135.966135598149));
#163553=CARTESIAN_POINT('Ctrl Pts',(-245.614449696006,-2.75480329759579,
136.043038188953));
#163554=CARTESIAN_POINT('Ctrl Pts',(-245.621851517681,-2.61437041652712,
136.114522243312));
#163555=CARTESIAN_POINT('Ctrl Pts',(-245.629253339357,-2.47123024753988,
136.180321148126));
#163556=CARTESIAN_POINT('Ctrl Pts',(-245.636651253668,-2.32816564113242,
136.246085318212));
#163557=CARTESIAN_POINT('Ctrl Pts',(-245.644049167979,-2.18239693135943,
136.306170160162));
#163558=CARTESIAN_POINT('Ctrl Pts',(-245.651447082291,-2.03441716058419,
136.360355342115));
#163559=CARTESIAN_POINT('Ctrl Pts',(-245.658843767203,-1.88646198136328,
136.414531519475));
#163560=CARTESIAN_POINT('Ctrl Pts',(-245.666240452115,-1.73629682059031,
136.462809854446));
#163561=CARTESIAN_POINT('Ctrl Pts',(-245.673637137027,-1.58443408205927,
136.505018404358));
#163562=CARTESIAN_POINT('Ctrl Pts',(-245.681033493962,-1.43257807728075,
136.547225082698));
#163563=CARTESIAN_POINT('Ctrl Pts',(-245.688429850898,-1.27902500407501,
136.583362411157));
#163564=CARTESIAN_POINT('Ctrl Pts',(-245.695826207833,-1.12430152570741,
136.613308598207));
#163565=CARTESIAN_POINT('Ctrl Pts',(-245.70322369717,-0.969554358780719,
136.643259370094));
#163566=CARTESIAN_POINT('Ctrl Pts',(-245.710621186506,-0.813636796417068,
136.66701704228));
#163567=CARTESIAN_POINT('Ctrl Pts',(-245.718018675843,-0.657084619241684,
136.684511156936));
#163568=CARTESIAN_POINT('Ctrl Pts',(-245.725418758358,-0.500477562943501,
136.702011404127));
#163569=CARTESIAN_POINT('Ctrl Pts',(-245.732818840872,-0.343235819668255,
136.713243680774));
#163570=CARTESIAN_POINT('Ctrl Pts',(-245.740218923387,-0.185899050616081,
136.718189504631));
#163571=CARTESIAN_POINT('Ctrl Pts',(-245.747627143054,-0.0283892736110474,
136.723140766929));
#163572=CARTESIAN_POINT('Ctrl Pts',(-245.75503536272,0.129215364502986,
136.721791759783));
#163573=CARTESIAN_POINT('Ctrl Pts',(-245.762443582386,0.286375706668068,
136.714176140671));
#163574=CARTESIAN_POINT('Ctrl Pts',(-245.769856361688,0.443632778401392,
136.706555834272));
#163575=CARTESIAN_POINT('Ctrl Pts',(-245.777269140991,0.600444638309981,
136.692661263232));
#163576=CARTESIAN_POINT('Ctrl Pts',(-245.784681920293,0.756279000772,136.672577777444));
#163577=CARTESIAN_POINT('Ctrl Pts',(-245.792105291321,0.912336026678791,
136.652465595431));
#163578=CARTESIAN_POINT('Ctrl Pts',(-245.79952866235,1.06741239856714,136.626146899487));
#163579=CARTESIAN_POINT('Ctrl Pts',(-245.806952033379,1.22098692301827,
136.593757952032));
#163580=CARTESIAN_POINT('Ctrl Pts',(-245.81088808282,1.30241582086114,136.576584554927));
#163581=CARTESIAN_POINT('Ctrl Pts',(-245.814824132261,1.38342275157227,
136.557705425074));
#163582=CARTESIAN_POINT('Ctrl Pts',(-245.818760181702,1.4639320672993,136.537146455606));
#163583=CARTESIAN_POINT('Ctrl Pts',(-245.826183448107,1.61577012413466,
136.498372880818));
#163584=CARTESIAN_POINT('Ctrl Pts',(-245.833606714513,1.76629628345212,
136.453504155375));
#163585=CARTESIAN_POINT('Ctrl Pts',(-245.841029980918,1.91498347619099,
136.402643287137));
#163586=CARTESIAN_POINT('Ctrl Pts',(-245.848444473639,2.06349493301575,
136.351842532221));
#163587=CARTESIAN_POINT('Ctrl Pts',(-245.85585896636,2.21017139988103,136.295063851339));
#163588=CARTESIAN_POINT('Ctrl Pts',(-245.863273459081,2.35449719735416,
136.232460976822));
#163589=CARTESIAN_POINT('Ctrl Pts',(-245.870680805435,2.49868388819033,
136.169918441312));
#163590=CARTESIAN_POINT('Ctrl Pts',(-245.878088151789,2.64052407995554,
136.101563035246));
#163591=CARTESIAN_POINT('Ctrl Pts',(-245.885495498143,2.77951854148591,
136.027597855145));
#163592=CARTESIAN_POINT('Ctrl Pts',(-245.892897319818,2.91840933570251,
135.953687841067));
#163593=CARTESIAN_POINT('Ctrl Pts',(-245.900299141493,3.05445829764989,
135.874176558433));
#163594=CARTESIAN_POINT('Ctrl Pts',(-245.907700963169,3.18718753752367,
135.789314595604));
#163595=CARTESIAN_POINT('Ctrl Pts',(-245.91509887748,3.31984671066527,135.704497430744));
#163596=CARTESIAN_POINT('Ctrl Pts',(-245.922496791791,3.44918933811908,
135.614335411555));
#163597=CARTESIAN_POINT('Ctrl Pts',(-245.929894706103,3.57476354701164,
135.51912425379));
#163598=CARTESIAN_POINT('Ctrl Pts',(-245.937291391015,3.7003168877483,135.423928918392));
#163599=CARTESIAN_POINT('Ctrl Pts',(-245.944688075927,3.82210275565909,
135.323686335051));
#163600=CARTESIAN_POINT('Ctrl Pts',(-245.952084760839,3.93969952373787,
135.218734664377));
#163601=CARTESIAN_POINT('Ctrl Pts',(-245.959481117775,4.05729107745271,
135.11378764737));
#163602=CARTESIAN_POINT('Ctrl Pts',(-245.96687747471,4.17069362215726,135.004132206769));
#163603=CARTESIAN_POINT('Ctrl Pts',(-245.974273831645,4.27952001683103,
134.890145607998));
#163604=CARTESIAN_POINT('Ctrl Pts',(-245.981671320982,4.38836307310365,
134.776141557589));
#163605=CARTESIAN_POINT('Ctrl Pts',(-245.989068810319,4.49262832652164,
134.657805298687));
#163606=CARTESIAN_POINT('Ctrl Pts',(-245.996466299655,4.59196689640381,
134.535549514531));
#163607=CARTESIAN_POINT('Ctrl Pts',(-246.00386638217,4.6913402892678,134.413250873798));
#163608=CARTESIAN_POINT('Ctrl Pts',(-246.011266464685,4.7857833248092,134.287030261754));
#163609=CARTESIAN_POINT('Ctrl Pts',(-246.0186665472,4.87498875333009,134.157331720544));
#163610=CARTESIAN_POINT('Ctrl Pts',(-246.026074766867,4.9642922723903,134.027490562454));
#163611=CARTESIAN_POINT('Ctrl Pts',(-246.033482986533,5.0483464710805,133.8941641455));
#163612=CARTESIAN_POINT('Ctrl Pts',(-246.0408912062,5.12688823883087,133.757824270472));
#163613=CARTESIAN_POINT('Ctrl Pts',(-246.048303985502,5.2054783477292,133.621400480525));
#163614=CARTESIAN_POINT('Ctrl Pts',(-246.055716764804,5.27854909222213,
133.4819598666));
#163615=CARTESIAN_POINT('Ctrl Pts',(-246.063129544106,5.34588456621218,
133.339996389367));
#163616=CARTESIAN_POINT('Ctrl Pts',(-246.070552915135,5.4133162522849,133.19783006806));
#163617=CARTESIAN_POINT('Ctrl Pts',(-246.077976286163,5.47499615496007,
133.053134026371));
#163618=CARTESIAN_POINT('Ctrl Pts',(-246.085399657192,5.53075719789552,
132.90642041225));
#163619=CARTESIAN_POINT('Ctrl Pts',(-246.089335706633,5.56032304083054,
132.828629333691));
#163620=CARTESIAN_POINT('Ctrl Pts',(-246.093271756074,5.58822571895365,
132.750271277815));
#163621=CARTESIAN_POINT('Ctrl Pts',(-246.097207805515,5.61444612737974,
132.671423885174));
#163622=CARTESIAN_POINT('Ctrl Pts',(-246.104631071921,5.6638969993561,132.522720163409));
#163623=CARTESIAN_POINT('Ctrl Pts',(-246.112054338326,5.70751073580989,
132.37182560037));
#163624=CARTESIAN_POINT('Ctrl Pts',(-246.119477604732,5.74508910646872,
132.219239312449));
#163625=CARTESIAN_POINT('Ctrl Pts',(-246.126892097453,5.78262306261424,
132.066833368848));
#163626=CARTESIAN_POINT('Ctrl Pts',(-246.134306590174,5.81413576344467,
131.912740039266));
#163627=CARTESIAN_POINT('Ctrl Pts',(-246.141721082895,5.83947781099574,
131.757476275494));
#163628=CARTESIAN_POINT('Ctrl Pts',(-246.149128429249,5.86479543292705,
131.602362160785));
#163629=CARTESIAN_POINT('Ctrl Pts',(-246.156535775603,5.88395418216651,
131.446080223678));
#163630=CARTESIAN_POINT('Ctrl Pts',(-246.163943121956,5.89685508293014,
131.28916026012));
#163631=CARTESIAN_POINT('Ctrl Pts',(-246.171344943632,5.90974636171538,
131.132357333391));
#163632=CARTESIAN_POINT('Ctrl Pts',(-246.178746765307,5.91638905487225,
130.974917698161));
#163633=CARTESIAN_POINT('Ctrl Pts',(-246.186148586983,5.91673567837141,
130.817378865788));
#163634=CARTESIAN_POINT('Ctrl Pts',(-246.193546501294,5.91708211889073,
130.659923196939));
#163635=CARTESIAN_POINT('Ctrl Pts',(-246.200944415605,5.91113910813369,
130.502368807587));
#163636=CARTESIAN_POINT('Ctrl Pts',(-246.208342329917,5.89891119181218,
130.345255712764));
#163637=CARTESIAN_POINT('Ctrl Pts',(-246.215739014829,5.88668530754854,
130.188168727288));
#163638=CARTESIAN_POINT('Ctrl Pts',(-246.223135699741,5.86817661955672,
130.031523262602));
#163639=CARTESIAN_POINT('Ctrl Pts',(-246.230532384653,5.84344173223939,
129.875856829516));
#163640=CARTESIAN_POINT('Ctrl Pts',(-246.237928741589,5.81870794169289,
129.720197298843));
#163641=CARTESIAN_POINT('Ctrl Pts',(-246.245325098525,5.78774855933448,
129.565517082127));
#163642=CARTESIAN_POINT('Ctrl Pts',(-246.25272145546,5.75067173007351,129.412345813251));
#163643=CARTESIAN_POINT('Ctrl Pts',(-246.260118944797,5.71358922425522,
129.259151093461));
#163644=CARTESIAN_POINT('Ctrl Pts',(-246.267516434133,5.6703874944759,129.107466144354));
#163645=CARTESIAN_POINT('Ctrl Pts',(-246.27491392347,5.62122516430065,128.957807554496));
#163646=CARTESIAN_POINT('Ctrl Pts',(-246.282314005985,5.57204560034683,
128.808096502052));
#163647=CARTESIAN_POINT('Ctrl Pts',(-246.2897140885,5.51690139228881,128.660413577564));
#163648=CARTESIAN_POINT('Ctrl Pts',(-246.297114171015,5.45600004939328,
128.515257294533));
#163649=CARTESIAN_POINT('Ctrl Pts',(-246.304522390681,5.39503173921034,
128.369941397246));
#163650=CARTESIAN_POINT('Ctrl Pts',(-246.311930610348,5.32829379615479,
128.227158034306));
#163651=CARTESIAN_POINT('Ctrl Pts',(-246.319338830014,5.25604094190495,
128.087383587939));
#163652=CARTESIAN_POINT('Ctrl Pts',(-246.326751609316,5.18374361722872,
127.947523112733));
#163653=CARTESIAN_POINT('Ctrl Pts',(-246.334164388619,5.10592480181901,
127.810675568067));
#163654=CARTESIAN_POINT('Ctrl Pts',(-246.341577167921,5.02288337625871,
127.677289599664));
#163655=CARTESIAN_POINT('Ctrl Pts',(-246.34900053895,4.93972329721543,127.543713043134));
#163656=CARTESIAN_POINT('Ctrl Pts',(-246.356423909978,4.85132591334758,
127.413608249218));
#163657=CARTESIAN_POINT('Ctrl Pts',(-246.363847281007,4.75803180038588,
127.287392612449));
#163658=CARTESIAN_POINT('Ctrl Pts',(-246.367783330447,4.70856502313687,
127.220470053338));
#163659=CARTESIAN_POINT('Ctrl Pts',(-246.371719379888,4.65772225060832,
127.154640296798));
#163660=CARTESIAN_POINT('Ctrl Pts',(-246.375655429328,4.60555847733841,
127.089961382923));
#163661=CARTESIAN_POINT('Ctrl Pts',(-246.383078695734,4.50717922891786,
126.967978969904));
#163662=CARTESIAN_POINT('Ctrl Pts',(-246.390501962139,4.40380164935547,
126.849723301093));
#163663=CARTESIAN_POINT('Ctrl Pts',(-246.397925228545,4.29573851110339,
126.735630937835));
#163664=CARTESIAN_POINT('Ctrl Pts',(-246.405339721266,4.18780309450695,
126.621673422276));
#163665=CARTESIAN_POINT('Ctrl Pts',(-246.412754213987,4.07519339671987,
126.511869686004));
#163666=CARTESIAN_POINT('Ctrl Pts',(-246.420168706708,3.95826359067691,
126.406624846829));
#163667=CARTESIAN_POINT('Ctrl Pts',(-246.427576053061,3.84144648598301,
126.301481446592));
#163668=CARTESIAN_POINT('Ctrl Pts',(-246.434983399415,3.72031783810252,
126.200888443848));
#163669=CARTESIAN_POINT('Ctrl Pts',(-246.442390745769,3.59526988054162,
126.105215477376));
#163670=CARTESIAN_POINT('Ctrl Pts',(-246.449792567444,3.47031518846561,
126.009613867413));
#163671=CARTESIAN_POINT('Ctrl Pts',(-246.45719438912,3.34144730233433,125.918925213011));
#163672=CARTESIAN_POINT('Ctrl Pts',(-246.464596210795,3.20909277939671,
125.833480001848));
#163673=CARTESIAN_POINT('Ctrl Pts',(-246.471994125107,3.07680812538038,
125.748079896545));
#163674=CARTESIAN_POINT('Ctrl Pts',(-246.479392039418,2.94104081296533,
125.667917923884));
#163675=CARTESIAN_POINT('Ctrl Pts',(-246.486789953729,2.80224762916167,
125.593282150746));
#163676=CARTESIAN_POINT('Ctrl Pts',(-246.494186638642,2.66347751026779,
125.518658780719));
#163677=CARTESIAN_POINT('Ctrl Pts',(-246.501583323554,2.52168284643765,
125.449559964178));
#163678=CARTESIAN_POINT('Ctrl Pts',(-246.508980008466,2.37734645680199,
125.38622861596));
#163679=CARTESIAN_POINT('Ctrl Pts',(-246.516376365401,2.23301646719352,
125.32290007592));
#163680=CARTESIAN_POINT('Ctrl Pts',(-246.523772722337,2.08614531770971,
125.265338645704));
#163681=CARTESIAN_POINT('Ctrl Pts',(-246.531169079272,1.93723705930119,
125.213739619987));
#163682=CARTESIAN_POINT('Ctrl Pts',(-246.538566568609,1.78830600265816,
125.162132694328));
#163683=CARTESIAN_POINT('Ctrl Pts',(-246.545964057946,1.63733756882728,
125.116490113025));
#163684=CARTESIAN_POINT('Ctrl Pts',(-246.553361547282,1.48485211831284,
125.076957650318));
#163685=CARTESIAN_POINT('Ctrl Pts',(-246.560761629797,1.33231321425946,
125.037411329568));
#163686=CARTESIAN_POINT('Ctrl Pts',(-246.568161712312,1.17825659586304,
125.00397948553));
#163687=CARTESIAN_POINT('Ctrl Pts',(-246.575561794827,1.0232138404762,124.976756993506));
#163688=CARTESIAN_POINT('Ctrl Pts',(-246.582970014494,0.868000599641695,
124.949504567553));
#163689=CARTESIAN_POINT('Ctrl Pts',(-246.59037823416,0.711799424179775,
124.928475193816));
#163690=CARTESIAN_POINT('Ctrl Pts',(-246.597786453827,0.555148791238356,
124.913712063961));
#163691=CARTESIAN_POINT('Ctrl Pts',(-246.605199233129,0.398401742445324,
124.898939847647));
#163692=CARTESIAN_POINT('Ctrl Pts',(-246.612612012431,0.241205056835051,
124.890441580415));
#163693=CARTESIAN_POINT('Ctrl Pts',(-246.620024791733,0.0840977450162274,
124.888208309538));
#163694=CARTESIAN_POINT('Ctrl Pts',(-246.627448162762,-0.0732340490966529,
124.88597184766));
#163695=CARTESIAN_POINT('Ctrl Pts',(-246.634871533791,-0.230475842183839,
124.890018251153));
#163696=CARTESIAN_POINT('Ctrl Pts',(-246.642294904819,-0.387092378900183,
124.900286595952));
#163697=CARTESIAN_POINT('Ctrl Pts',(-246.64623095426,-0.470134224627617,
124.90573111875));
#163698=CARTESIAN_POINT('Ctrl Pts',(-246.650167003701,-0.553000423662025,
124.912923991829));
#163699=CARTESIAN_POINT('Ctrl Pts',(-246.654103053141,-0.635612419335864,
124.921850318817));
#163700=CARTESIAN_POINT('Ctrl Pts',(-246.661526319547,-0.791416064948631,
124.938685092936));
#163701=CARTESIAN_POINT('Ctrl Pts',(-246.668949585952,-0.946786015185273,
124.961739500879));
#163702=CARTESIAN_POINT('Ctrl Pts',(-246.676372852358,-1.10118591747281,
124.990986370396));
#163703=CARTESIAN_POINT('Ctrl Pts',(-246.683787345079,-1.25540333189839,
125.020198672542));
#163704=CARTESIAN_POINT('Ctrl Pts',(-246.6912018378,-1.4086526173274,125.055588799002));
#163705=CARTESIAN_POINT('Ctrl Pts',(-246.698616330521,-1.56040149755077,
125.097077750129));
#163706=CARTESIAN_POINT('Ctrl Pts',(-246.706023676875,-1.71200411648926,
125.138526712642));
#163707=CARTESIAN_POINT('Ctrl Pts',(-246.713431023229,-1.86210885155117,
125.186062699542));
#163708=CARTESIAN_POINT('Ctrl Pts',(-246.720838369582,-2.01019270337069,
125.23955551246));
#163709=CARTESIAN_POINT('Ctrl Pts',(-246.728240191258,-2.15816610866622,
125.29300842842));
#163710=CARTESIAN_POINT('Ctrl Pts',(-246.735642012933,-2.30412128227739,
125.352409197853));
#163711=CARTESIAN_POINT('Ctrl Pts',(-246.743043834609,-2.44754961095031,
125.417577582726));
#163712=CARTESIAN_POINT('Ctrl Pts',(-246.75044174892,-2.59090222492619,
125.482711565717));
#163713=CARTESIAN_POINT('Ctrl Pts',(-246.757839663231,-2.731730311492,125.553606946494));
#163714=CARTESIAN_POINT('Ctrl Pts',(-246.765237577543,-2.86954460728643,
125.630035124394));
#163715=CARTESIAN_POINT('Ctrl Pts',(-246.772634262455,-3.00733600084452,
125.706450601317));
#163716=CARTESIAN_POINT('Ctrl Pts',(-246.780030947367,-3.14211427150775,
125.788396869658));
#163717=CARTESIAN_POINT('Ctrl Pts',(-246.787427632279,-3.27341407261145,
125.875599021411));
#163718=CARTESIAN_POINT('Ctrl Pts',(-246.794823989215,-3.40470805174401,
125.96279730653));
#163719=CARTESIAN_POINT('Ctrl Pts',(-246.80222034615,-3.5325235570325,126.05525080515));
#163720=CARTESIAN_POINT('Ctrl Pts',(-246.809616703086,-3.65642382968436,
126.152641006474));
#163721=CARTESIAN_POINT('Ctrl Pts',(-246.817014192422,-3.78034307178426,
126.250046118487));
#163722=CARTESIAN_POINT('Ctrl Pts',(-246.824411681759,-3.90034559419467,
126.352389207441));
#163723=CARTESIAN_POINT('Ctrl Pts',(-246.831809171096,-4.01602748535452,
126.459311273844));
#163724=CARTESIAN_POINT('Ctrl Pts',(-246.839209253611,-4.13174992862215,
126.566270821612));
#163725=CARTESIAN_POINT('Ctrl Pts',(-246.846609336125,-4.24314845113487,
126.677812289459));
#163726=CARTESIAN_POINT('Ctrl Pts',(-246.85400941864,-4.34985590107221,
126.79353972872));
#163727=CARTESIAN_POINT('Ctrl Pts',(-246.861417638307,-4.45668068682071,
126.909394422197));
#163728=CARTESIAN_POINT('Ctrl Pts',(-246.868825857974,-4.55880384529215,
127.029444004784));
#163729=CARTESIAN_POINT('Ctrl Pts',(-246.87623407764,-4.65589797806187,
127.153258786559));
#163730=CARTESIAN_POINT('Ctrl Pts',(-246.883646856942,-4.75305187065021,
127.277149774267));
#163731=CARTESIAN_POINT('Ctrl Pts',(-246.891059636244,-4.84517035187053,
127.404810276891));
#163732=CARTESIAN_POINT('Ctrl Pts',(-246.898472415546,-4.93196960550558,
127.535781970376));
#163733=CARTESIAN_POINT('Ctrl Pts',(-246.905895786575,-5.01889288198459,
127.666940802357));
#163734=CARTESIAN_POINT('Ctrl Pts',(-246.913319157604,-5.10048155813349,
127.801419956128));
#163735=CARTESIAN_POINT('Ctrl Pts',(-246.920742528633,-5.17649757250621,
127.938736175261));
#163736=CARTESIAN_POINT('Ctrl Pts',(-246.924678578073,-5.21680308730434,
128.0115445295));
#163737=CARTESIAN_POINT('Ctrl Pts',(-246.928614627514,-5.2555427241668,
128.085150133234));
#163738=CARTESIAN_POINT('Ctrl Pts',(-246.932550676955,-5.29268655403647,
128.159478842662));
#163739=CARTESIAN_POINT('Ctrl Pts',(-246.940496569803,-5.36767059490483,
128.309529793383));
#163740=CARTESIAN_POINT('Ctrl Pts',(-246.948442462651,-5.43635038415996,
128.462932834914));
#163741=CARTESIAN_POINT('Ctrl Pts',(-246.956388355499,-5.4984355816421,
128.619151996626));
#163742=CARTESIAN_POINT('Ctrl Pts',(-246.96431905051,-5.56040203089155,
128.775072363293));
#163743=CARTESIAN_POINT('Ctrl Pts',(-246.972249745521,-5.61579893021929,
128.933797839802));
#163744=CARTESIAN_POINT('Ctrl Pts',(-246.980180440532,-5.66438241210903,
129.094769306202));
#163745=CARTESIAN_POINT('Ctrl Pts',(-246.988089489402,-5.71283328961795,
129.25530141501));
#163746=CARTESIAN_POINT('Ctrl Pts',(-246.995998538272,-5.75450775997896,
129.418067006546));
#163747=CARTESIAN_POINT('Ctrl Pts',(-247.003907587142,-5.78921073565506,
129.582489257448));
#163748=CARTESIAN_POINT('Ctrl Pts',(-247.011803344685,-5.82385539223615,
129.746635193231));
#163749=CARTESIAN_POINT('Ctrl Pts',(-247.019699102229,-5.85155184801984,
129.912431954205));
#163750=CARTESIAN_POINT('Ctrl Pts',(-247.027594859772,-5.87215457678867,
130.079287387609));
#163751=CARTESIAN_POINT('Ctrl Pts',(-247.035471973177,-5.89270865663014,
130.245748827676));
#163752=CARTESIAN_POINT('Ctrl Pts',(-247.043349086582,-5.90620238177112,
130.413263665022));
#163753=CARTESIAN_POINT('Ctrl Pts',(-247.051226199987,-5.91254118359208,
130.58122990514));
#163754=CARTESIAN_POINT('Ctrl Pts',(-247.05469238411,-5.91533046097139,
130.655140471724));
#163755=CARTESIAN_POINT('Ctrl Pts',(-247.058158568234,-5.91673500055715,
130.729138285269));
#163756=CARTESIAN_POINT('Ctrl Pts',(-247.061624752358,-5.91674988049034,
130.803171408753));
#163757=CARTESIAN_POINT('',(-248.811624809121,-5.91570646661543,130.809822233771));
#163758=CARTESIAN_POINT('Ctrl Pts',(-247.061624807794,-5.90715003001972,
130.803174520355));
#163759=CARTESIAN_POINT('Ctrl Pts',(-247.111415972118,-5.90525564854376,
131.864923107975));
#163760=CARTESIAN_POINT('Ctrl Pts',(-247.254023011045,-5.1238521970333,
134.908481577047));
#163761=CARTESIAN_POINT('Ctrl Pts',(-247.489445924582,-0.243152214736913,
137.798532300536));
#163762=CARTESIAN_POINT('Ctrl Pts',(-247.767893548391,5.75296501072868,
134.789452099034));
#163763=CARTESIAN_POINT('Ctrl Pts',(-248.046341172206,6.46238843929711,
128.118267508609));
#163764=CARTESIAN_POINT('Ctrl Pts',(-248.324788796018,1.23319259737722,
123.915471262371));
#163765=CARTESIAN_POINT('Ctrl Pts',(-248.579883341214,-4.59563658194247,
125.864775325139));
#163766=CARTESIAN_POINT('Ctrl Pts',(-248.742162011806,-5.90220478747528,
129.333928644561));
#163767=CARTESIAN_POINT('Ctrl Pts',(-248.811624807794,-5.91561520810599,
130.809822121327));
#163768=CARTESIAN_POINT('',(-250.561625504064,-5.9219643862223,130.803158325684));
#163769=CARTESIAN_POINT('Ctrl Pts',(-248.811624824253,-5.916747478069,130.809823516448));
#163770=CARTESIAN_POINT('Ctrl Pts',(-248.821109605322,-5.9165613768173,
131.011385752081));
#163771=CARTESIAN_POINT('Ctrl Pts',(-248.83059438639,-5.90607209373853,
131.212487319424));
#163772=CARTESIAN_POINT('Ctrl Pts',(-248.840079167459,-5.88544138888699,
131.412234140987));
#163773=CARTESIAN_POINT('Ctrl Pts',(-248.849770269771,-5.864361906919,131.616326029925));
#163774=CARTESIAN_POINT('Ctrl Pts',(-248.859461372084,-5.83269498810474,
131.81900383568));
#163775=CARTESIAN_POINT('Ctrl Pts',(-248.869152474397,-5.79066122698276,
132.019339266275));
#163776=CARTESIAN_POINT('Ctrl Pts',(-248.873329664146,-5.772543267808,132.105690548099));
#163777=CARTESIAN_POINT('Ctrl Pts',(-248.877506853895,-5.75249985213029,
132.191606933873));
#163778=CARTESIAN_POINT('Ctrl Pts',(-248.881684043643,-5.7305513441666,
132.27701531381));
#163779=CARTESIAN_POINT('Ctrl Pts',(-248.889107310048,-5.69154674260298,
132.428794188036));
#163780=CARTESIAN_POINT('Ctrl Pts',(-248.896530576453,-5.646448993928,132.579251890481));
#163781=CARTESIAN_POINT('Ctrl Pts',(-248.903953842859,-5.59536190799099,
132.727861509456));
#163782=CARTESIAN_POINT('Ctrl Pts',(-248.911368335579,-5.5443352027469,
132.876295484204));
#163783=CARTESIAN_POINT('Ctrl Pts',(-248.9187828283,-5.48733337100067,133.022885373731));
#163784=CARTESIAN_POINT('Ctrl Pts',(-248.926197321021,-5.42451092968302,
133.167115733157));
#163785=CARTESIAN_POINT('Ctrl Pts',(-248.933604667374,-5.36174903899972,
133.311207077931));
#163786=CARTESIAN_POINT('Ctrl Pts',(-248.941012013728,-5.29317785546428,
133.452943080153));
#163787=CARTESIAN_POINT('Ctrl Pts',(-248.948419360082,-5.21900123510664,
133.591824818315));
#163788=CARTESIAN_POINT('Ctrl Pts',(-248.955821181757,-5.14487993847098,
133.730602973236));
#163789=CARTESIAN_POINT('Ctrl Pts',(-248.963223003432,-5.06516170455207,
133.866530775002));
#163790=CARTESIAN_POINT('Ctrl Pts',(-248.970624825107,-4.98009784868515,
133.999130715714));
#163791=CARTESIAN_POINT('Ctrl Pts',(-248.978022739419,-4.8950788973656,
134.13166065795));
#163792=CARTESIAN_POINT('Ctrl Pts',(-248.98542065373,-4.8047201451247,134.26086592438));
#163793=CARTESIAN_POINT('Ctrl Pts',(-248.992818568041,-4.70931799504596,
134.386295092684));
#163794=CARTESIAN_POINT('Ctrl Pts',(-249.000215252953,-4.61393169907366,
134.511703416935));
#163795=CARTESIAN_POINT('Ctrl Pts',(-249.007611937866,-4.51350389445523,
134.633336591671));
#163796=CARTESIAN_POINT('Ctrl Pts',(-249.015008622778,-4.40837338305349,
134.750773504998));
#163797=CARTESIAN_POINT('Ctrl Pts',(-249.022404979713,-4.30324753324909,
134.868205211047));
#163798=CARTESIAN_POINT('Ctrl Pts',(-249.029801336648,-4.19341964026121,
134.981440747519));
#163799=CARTESIAN_POINT('Ctrl Pts',(-249.037197693584,-4.0792675582414,
135.090093547974));
#163800=CARTESIAN_POINT('Ctrl Pts',(-249.04459518292,-3.96509799924608,
135.19876298345));
#163801=CARTESIAN_POINT('Ctrl Pts',(-249.051992672257,-3.846603203412,135.302848028488));
#163802=CARTESIAN_POINT('Ctrl Pts',(-249.059390161594,-3.72419638443535,
135.402000430846));
#163803=CARTESIAN_POINT('Ctrl Pts',(-249.066790244108,-3.60174665593858,
135.501187590925));
#163804=CARTESIAN_POINT('Ctrl Pts',(-249.074190326623,-3.47538246383626,
135.595438430817));
#163805=CARTESIAN_POINT('Ctrl Pts',(-249.081590409138,-3.34554831734197,
135.684446376939));
#163806=CARTESIAN_POINT('Ctrl Pts',(-249.088998628805,-3.21557140485613,
135.773552196447));
#163807=CARTESIAN_POINT('Ctrl Pts',(-249.096406848471,-3.08211722611327,
135.857403397694));
#163808=CARTESIAN_POINT('Ctrl Pts',(-249.103815068138,-2.9456579817682,
135.935737588414));
#163809=CARTESIAN_POINT('Ctrl Pts',(-249.11122784744,-2.80911474903517,
136.014119992521));
#163810=CARTESIAN_POINT('Ctrl Pts',(-249.118640626742,-2.66956309534981,
136.086978447522));
#163811=CARTESIAN_POINT('Ctrl Pts',(-249.126053406044,-2.52749730938361,
136.154097799294));
#163812=CARTESIAN_POINT('Ctrl Pts',(-249.133476777072,-2.38522853315999,
136.221313054343));
#163813=CARTESIAN_POINT('Ctrl Pts',(-249.140900148101,-2.24043879271867,
136.282772682851));
#163814=CARTESIAN_POINT('Ctrl Pts',(-249.14832351913,-2.0936404896779,136.338310388072));
#163815=CARTESIAN_POINT('Ctrl Pts',(-249.152259568573,-2.01580450698774,
136.367757812004));
#163816=CARTESIAN_POINT('Ctrl Pts',(-249.156195618015,-1.93740407869069,
136.395541210207));
#163817=CARTESIAN_POINT('Ctrl Pts',(-249.160131667458,-1.8585168743233,
136.421641595971));
#163818=CARTESIAN_POINT('Ctrl Pts',(-249.167554933864,-1.70973806894697,
136.470866108934));
#163819=CARTESIAN_POINT('Ctrl Pts',(-249.174978200269,-1.55877730795987,
136.514250159045));
#163820=CARTESIAN_POINT('Ctrl Pts',(-249.182401466675,-1.4061340088489,
136.551596275833));
#163821=CARTESIAN_POINT('Ctrl Pts',(-249.189815959396,-1.25367112144082,
136.588898252613));
#163822=CARTESIAN_POINT('Ctrl Pts',(-249.197230452117,-1.0995300133307,
136.620176413136));
#163823=CARTESIAN_POINT('Ctrl Pts',(-249.204644944838,-0.944227863070491,
136.645282146323));
#163824=CARTESIAN_POINT('Ctrl Pts',(-249.212052291192,-0.789075398869725,
136.67036368166));
#163825=CARTESIAN_POINT('Ctrl Pts',(-249.219459637545,-0.632764486379176,
136.68928457421));
#163826=CARTESIAN_POINT('Ctrl Pts',(-249.226866983899,-0.475825071556931,
136.701946654563));
#163827=CARTESIAN_POINT('Ctrl Pts',(-249.234268805574,-0.319002708071244,
136.714599291058));
#163828=CARTESIAN_POINT('Ctrl Pts',(-249.24167062725,-0.161553146107153,
136.721002380199));
#163829=CARTESIAN_POINT('Ctrl Pts',(-249.249072448925,-0.00401396866050681,
136.721109256012));
#163830=CARTESIAN_POINT('Ctrl Pts',(-249.256470363237,0.153442045080647,
136.721216075406));
#163831=CARTESIAN_POINT('Ctrl Pts',(-249.263868277548,0.310987207736695,
136.715033300571));
#163832=CARTESIAN_POINT('Ctrl Pts',(-249.271266191859,0.468081511817204,
136.702566299025));
#163833=CARTESIAN_POINT('Ctrl Pts',(-249.278662876771,0.625149709674131,
136.690101369268));
#163834=CARTESIAN_POINT('Ctrl Pts',(-249.286059561684,0.781766825894961,
136.671354314978));
#163835=CARTESIAN_POINT('Ctrl Pts',(-249.293456246596,0.9373954364333,136.646382558491));
#163836=CARTESIAN_POINT('Ctrl Pts',(-249.300852603531,1.09301714623596,
136.621411909279));
#163837=CARTESIAN_POINT('Ctrl Pts',(-249.308248960466,1.24765006892486,
136.590217165813));
#163838=CARTESIAN_POINT('Ctrl Pts',(-249.315645317402,1.40076473580871,
136.55290727889));
#163839=CARTESIAN_POINT('Ctrl Pts',(-249.323042806738,1.55390284493894,
136.515591679728));
#163840=CARTESIAN_POINT('Ctrl Pts',(-249.330440296075,1.7055218727186,136.472159161305));
#163841=CARTESIAN_POINT('Ctrl Pts',(-249.337837785411,1.85510547257604,
136.422769133162));
#163842=CARTESIAN_POINT('Ctrl Pts',(-249.345237867926,2.00474150873273,
136.373361791421));
#163843=CARTESIAN_POINT('Ctrl Pts',(-249.352637950441,2.15234034210798,
136.317992898949));
#163844=CARTESIAN_POINT('Ctrl Pts',(-249.360038032956,2.29740377557393,
136.256870723424));
#163845=CARTESIAN_POINT('Ctrl Pts',(-249.367446252623,2.44262672119807,
136.195681337783));
#163846=CARTESIAN_POINT('Ctrl Pts',(-249.374854472289,2.58530835500866,
136.128726180037));
#163847=CARTESIAN_POINT('Ctrl Pts',(-249.382262691955,2.72497268297404,
136.056260696542));
#163848=CARTESIAN_POINT('Ctrl Pts',(-249.389675471257,2.86472297200286,
135.983750611751));
#163849=CARTESIAN_POINT('Ctrl Pts',(-249.397088250559,3.00145193121146,
135.905723627787));
#163850=CARTESIAN_POINT('Ctrl Pts',(-249.404501029861,3.13471137024171,
135.822479307651));
#163851=CARTESIAN_POINT('Ctrl Pts',(-249.41192440089,3.2681612166075,135.739116044126));
#163852=CARTESIAN_POINT('Ctrl Pts',(-249.419347771919,3.39813133409427,
135.650520765273));
#163853=CARTESIAN_POINT('Ctrl Pts',(-249.426771142948,3.52420484694847,
135.557034681632));
#163854=CARTESIAN_POINT('Ctrl Pts',(-249.430707192388,3.59105204855583,
135.507466116918));
#163855=CARTESIAN_POINT('Ctrl Pts',(-249.434643241829,3.65680435482759,
135.456523221577));
#163856=CARTESIAN_POINT('Ctrl Pts',(-249.43857929127,3.72140380942754,135.404261078411));
#163857=CARTESIAN_POINT('Ctrl Pts',(-249.446002557675,3.84323636472394,
135.305696307444));
#163858=CARTESIAN_POINT('Ctrl Pts',(-249.453425824081,3.96133457351837,
135.202138882594));
#163859=CARTESIAN_POINT('Ctrl Pts',(-249.460849090486,4.07526235095892,
135.093902240322));
#163860=CARTESIAN_POINT('Ctrl Pts',(-249.468263583207,4.18905547522797,
134.985793524773));
#163861=CARTESIAN_POINT('Ctrl Pts',(-249.475678075928,4.29868771155913,
134.87301685479));
#163862=CARTESIAN_POINT('Ctrl Pts',(-249.483092568649,4.40375448160294,
134.75592701942));
#163863=CARTESIAN_POINT('Ctrl Pts',(-249.490499915003,4.50871998433807,
134.638950039641));
#163864=CARTESIAN_POINT('Ctrl Pts',(-249.497907261357,4.60912853341538,
134.517668446599));
#163865=CARTESIAN_POINT('Ctrl Pts',(-249.505314607711,4.70461108739482,
134.392475035873));
#163866=CARTESIAN_POINT('Ctrl Pts',(-249.512716429386,4.80002242688316,
134.267374999115));
#163867=CARTESIAN_POINT('Ctrl Pts',(-249.520118251061,4.8905148612835,134.138369249516));
#163868=CARTESIAN_POINT('Ctrl Pts',(-249.527520072737,4.97575855245018,
134.005884846776));
#163869=CARTESIAN_POINT('Ctrl Pts',(-249.534917987048,5.06095724413607,
133.87347038152));
#163870=CARTESIAN_POINT('Ctrl Pts',(-249.54231590136,5.14091250923251,133.737581233445));
#163871=CARTESIAN_POINT('Ctrl Pts',(-249.549713815671,5.21533697634506,
133.59867462742));
#163872=CARTESIAN_POINT('Ctrl Pts',(-249.557110500583,5.28974907546105,
133.459791105154));
#163873=CARTESIAN_POINT('Ctrl Pts',(-249.564507185496,5.35863202464555,
133.317891448883));
#163874=CARTESIAN_POINT('Ctrl Pts',(-249.571903870408,5.42174364411263,
133.173458846856));
#163875=CARTESIAN_POINT('Ctrl Pts',(-249.579300227344,5.48485246514455,
133.029032649121));
#163876=CARTESIAN_POINT('Ctrl Pts',(-249.586696584279,5.54219031581788,
132.882074071012));
#163877=CARTESIAN_POINT('Ctrl Pts',(-249.594092941215,5.5935626687629,132.733087460103));
#163878=CARTESIAN_POINT('Ctrl Pts',(-249.601490430551,5.64494288694615,
132.584078038963));
#163879=CARTESIAN_POINT('Ctrl Pts',(-249.608887919888,5.69035566713929,
132.433040319712));
#163880=CARTESIAN_POINT('Ctrl Pts',(-249.616285409224,5.72965602716966,
132.280494884094));
#163881=CARTESIAN_POINT('Ctrl Pts',(-249.623685491739,5.76897016388037,
132.12789597391));
#163882=CARTESIAN_POINT('Ctrl Pts',(-249.631085574254,5.80216752125575,
131.973788656333));
#163883=CARTESIAN_POINT('Ctrl Pts',(-249.63848565677,5.82915403307591,131.818704652485));
#163884=CARTESIAN_POINT('Ctrl Pts',(-249.645893876436,5.85617021934014,
131.66345011783));
#163885=CARTESIAN_POINT('Ctrl Pts',(-249.653302096103,5.87696185712679,
131.507217120119));
#163886=CARTESIAN_POINT('Ctrl Pts',(-249.660710315769,5.89148657428888,
131.350544201605));
#163887=CARTESIAN_POINT('Ctrl Pts',(-249.668123095071,5.90602023117203,
131.193774853524));
#163888=CARTESIAN_POINT('Ctrl Pts',(-249.675535874373,5.91427926196693,
131.036565417029));
#163889=CARTESIAN_POINT('Ctrl Pts',(-249.682948653676,5.91627343967264,
130.87945488848));
#163890=CARTESIAN_POINT('Ctrl Pts',(-249.690372024704,5.91827046675297,
130.72211987304));
#163891=CARTESIAN_POINT('Ctrl Pts',(-249.697795395733,5.91398477270314,
130.564884419973));
#163892=CARTESIAN_POINT('Ctrl Pts',(-249.705218766762,5.9034780960863,130.408283691289));
#163893=CARTESIAN_POINT('Ctrl Pts',(-249.709154816202,5.89790720404025,
130.325250227364));
#163894=CARTESIAN_POINT('Ctrl Pts',(-249.713090865643,5.89058823104175,
130.24239507062));
#163895=CARTESIAN_POINT('Ctrl Pts',(-249.717026915084,5.88153619299649,
130.159796754964));
#163896=CARTESIAN_POINT('Ctrl Pts',(-249.724450181489,5.86446433174631,
130.004018909431));
#163897=CARTESIAN_POINT('Ctrl Pts',(-249.731873447894,5.8411735038838,129.848684223995));
#163898=CARTESIAN_POINT('Ctrl Pts',(-249.7392967143,5.81169169786706,129.694329009258));
#163899=CARTESIAN_POINT('Ctrl Pts',(-249.746711207021,5.78224473689672,
129.540156229566));
#163900=CARTESIAN_POINT('Ctrl Pts',(-249.754125699742,5.74662143209289,
129.386960979346));
#163901=CARTESIAN_POINT('Ctrl Pts',(-249.761540192463,5.704901593047,129.235275413968));
#163902=CARTESIAN_POINT('Ctrl Pts',(-249.768947538817,5.66322196515258,
129.083736048848));
#163903=CARTESIAN_POINT('Ctrl Pts',(-249.77635488517,5.61545759944475,128.933703829285));
#163904=CARTESIAN_POINT('Ctrl Pts',(-249.783762231524,5.56173949005624,
128.785701555899));
#163905=CARTESIAN_POINT('Ctrl Pts',(-249.7911640532,5.50806144566054,128.637809668193));
#163906=CARTESIAN_POINT('Ctrl Pts',(-249.798565874875,5.44843862608452,
128.491945061455));
#163907=CARTESIAN_POINT('Ctrl Pts',(-249.80596769655,5.38305204317507,128.348616074058));
#163908=CARTESIAN_POINT('Ctrl Pts',(-249.813365610862,5.31769997733359,
128.205362748917));
#163909=CARTESIAN_POINT('Ctrl Pts',(-249.820763525173,5.24659036227847,
128.06464271613));
#163910=CARTESIAN_POINT('Ctrl Pts',(-249.828161439484,5.16995254298388,
127.926944890599));
#163911=CARTESIAN_POINT('Ctrl Pts',(-249.835558124397,5.09332745950461,
127.78926994795));
#163912=CARTESIAN_POINT('Ctrl Pts',(-249.842954809309,5.01117617647154,
127.654616541628));
#163913=CARTESIAN_POINT('Ctrl Pts',(-249.850351494221,4.92377430975135,
127.523449599399));
#163914=CARTESIAN_POINT('Ctrl Pts',(-249.857747851156,4.83637631852152,
127.392288473248));
#163915=CARTESIAN_POINT('Ctrl Pts',(-249.865144208092,4.74372841352031,
127.264613814455));
#163916=CARTESIAN_POINT('Ctrl Pts',(-249.872540565027,4.64614976984916,
127.140861896585));
#163917=CARTESIAN_POINT('Ctrl Pts',(-249.879938054364,4.54855618663856,
127.017091031981));
#163918=CARTESIAN_POINT('Ctrl Pts',(-249.887335543701,4.4460305927857,126.897244397291));
#163919=CARTESIAN_POINT('Ctrl Pts',(-249.894733033037,4.33893260205083,
126.781725357272));
#163920=CARTESIAN_POINT('Ctrl Pts',(-249.902133115552,4.23179706828147,
126.666165822233));
#163921=CARTESIAN_POINT('Ctrl Pts',(-249.909533198067,4.12008620001085,
126.554937175845));
#163922=CARTESIAN_POINT('Ctrl Pts',(-249.916933280582,4.00419650418772,
126.448405966935));
#163923=CARTESIAN_POINT('Ctrl Pts',(-249.924341500248,3.88817937573012,
126.34175761601));
#163924=CARTESIAN_POINT('Ctrl Pts',(-249.931749719915,3.76797451809576,
126.239817270824));
#163925=CARTESIAN_POINT('Ctrl Pts',(-249.939157939581,3.64401211895541,
126.142911675509));
#163926=CARTESIAN_POINT('Ctrl Pts',(-249.946570718883,3.51997342302683,
126.045946436417));
#163927=CARTESIAN_POINT('Ctrl Pts',(-249.953983498185,3.39217287958458,
125.954022339421));
#163928=CARTESIAN_POINT('Ctrl Pts',(-249.961396277487,3.26106924407624,
125.86742250292));
#163929=CARTESIAN_POINT('Ctrl Pts',(-249.968819648516,3.12977828154515,
125.780698928512));
#163930=CARTESIAN_POINT('Ctrl Pts',(-249.976243019545,2.9951751194234,125.699315001221));
#163931=CARTESIAN_POINT('Ctrl Pts',(-249.983666390574,2.85774337586741,
125.623508046783));
#163932=CARTESIAN_POINT('Ctrl Pts',(-249.987602440014,2.78487376780305,
125.583313380577));
#163933=CARTESIAN_POINT('Ctrl Pts',(-249.991538489455,2.71120929416588,
125.544685803771));
#163934=CARTESIAN_POINT('Ctrl Pts',(-249.995474538896,2.63682414421973,
125.507655132554));
#163935=CARTESIAN_POINT('Ctrl Pts',(-250.002897805302,2.49653607290554,
125.437816442327));
#163936=CARTESIAN_POINT('Ctrl Pts',(-250.010321071707,2.35325934137193,
125.3734494837));
#163937=CARTESIAN_POINT('Ctrl Pts',(-250.017744338112,2.20746029136132,
125.314820598169));
#163938=CARTESIAN_POINT('Ctrl Pts',(-250.025158830833,2.06183356371996,
125.256261007111));
#163939=CARTESIAN_POINT('Ctrl Pts',(-250.032573323555,1.91369079460125,
125.203426127602));
#163940=CARTESIAN_POINT('Ctrl Pts',(-250.039987816276,1.7635228404219,125.156536456545));
#163941=CARTESIAN_POINT('Ctrl Pts',(-250.047395162629,1.61349962377008,
125.109691979519));
#163942=CARTESIAN_POINT('Ctrl Pts',(-250.054802508983,1.46145546194378,
125.068781413732));
#163943=CARTESIAN_POINT('Ctrl Pts',(-250.062209855337,1.30790100743993,
125.033977136615));
#163944=CARTESIAN_POINT('Ctrl Pts',(-250.069611677012,1.15446107964197,
124.999198817841));
#163945=CARTESIAN_POINT('Ctrl Pts',(-250.077013498688,0.999513464543592,
124.970517801673));
#163946=CARTESIAN_POINT('Ctrl Pts',(-250.084415320363,0.843583682939877,
124.948056567025));
#163947=CARTESIAN_POINT('Ctrl Pts',(-250.091813234674,0.687736215453672,
124.925607189489));
#163948=CARTESIAN_POINT('Ctrl Pts',(-250.099211148986,0.530907982584985,
124.909371107564));
#163949=CARTESIAN_POINT('Ctrl Pts',(-250.106609063297,0.373634288849452,
124.899419637277));
#163950=CARTESIAN_POINT('Ctrl Pts',(-250.114005748209,0.216386731148808,
124.889469820744));
#163951=CARTESIAN_POINT('Ctrl Pts',(-250.121402433121,0.0586942316921057,
124.885802566596));
#163952=CARTESIAN_POINT('Ctrl Pts',(-250.128799118034,-0.0989030755182705,
124.888437296211));
#163953=CARTESIAN_POINT('Ctrl Pts',(-250.136195474969,-0.256493394698895,
124.891071909));
#163954=CARTESIAN_POINT('Ctrl Pts',(-250.143591831905,-0.413988156780406,
124.900007943697));
#163955=CARTESIAN_POINT('Ctrl Pts',(-250.15098818884,-0.570847790515854,
124.915212685771));
#163956=CARTESIAN_POINT('Ctrl Pts',(-250.158385678177,-0.72773143986167,
124.93041975573));
#163957=CARTESIAN_POINT('Ctrl Pts',(-250.165783167513,-0.883979395663796,
124.951897408047));
#163958=CARTESIAN_POINT('Ctrl Pts',(-250.17318065685,-1.03905791570666,
124.979561117986));
#163959=CARTESIAN_POINT('Ctrl Pts',(-250.180580739365,-1.1941907982841,
125.007234525395));
#163960=CARTESIAN_POINT('Ctrl Pts',(-250.18798082188,-1.34815306163966,
125.041098242404));
#163961=CARTESIAN_POINT('Ctrl Pts',(-250.195380904395,-1.50042199617141,
125.081016805081));
#163962=CARTESIAN_POINT('Ctrl Pts',(-250.202789124061,-1.65285836605051,
125.120979262323));
#163963=CARTESIAN_POINT('Ctrl Pts',(-250.210197343728,-1.80359732727412,
125.167009766825));
#163964=CARTESIAN_POINT('Ctrl Pts',(-250.217605563394,-1.95213145380731,
125.2189230027));
#163965=CARTESIAN_POINT('Ctrl Pts',(-250.225018342696,-2.10075700061695,
125.270868190306));
#163966=CARTESIAN_POINT('Ctrl Pts',(-250.232431121998,-2.24717466227714,
125.328703187207));
#163967=CARTESIAN_POINT('Ctrl Pts',(-250.2398439013,-2.39089827473667,125.392195061861));
#163968=CARTESIAN_POINT('Ctrl Pts',(-250.247267272329,-2.53482724623345,
125.455777656683));
#163969=CARTESIAN_POINT('Ctrl Pts',(-250.254690643358,-2.67605414616755,
125.525033108521));
#163970=CARTESIAN_POINT('Ctrl Pts',(-250.262114014387,-2.81411789824898,
125.599682816083));
#163971=CARTESIAN_POINT('Ctrl Pts',(-250.266050063827,-2.88732261239898,
125.639263882228));
#163972=CARTESIAN_POINT('Ctrl Pts',(-250.269986113268,-2.95963853411174,
125.680360741391));
#163973=CARTESIAN_POINT('Ctrl Pts',(-250.273922162709,-3.03100047707438,
125.72292709242));
#163974=CARTESIAN_POINT('Ctrl Pts',(-250.281345429115,-3.16558687436931,
125.80320590201));
#163975=CARTESIAN_POINT('Ctrl Pts',(-250.28876869552,-3.2971851927532,125.88895676067));
#163976=CARTESIAN_POINT('Ctrl Pts',(-250.296191961926,-3.42531928247853,
125.979931285968));
#163977=CARTESIAN_POINT('Ctrl Pts',(-250.303606454647,-3.55330192835068,
126.070798286933));
#163978=CARTESIAN_POINT('Ctrl Pts',(-250.311020947368,-3.67782819414175,
126.166876451276));
#163979=CARTESIAN_POINT('Ctrl Pts',(-250.318435440089,-3.79844724967701,
126.267871991556));
#163980=CARTESIAN_POINT('Ctrl Pts',(-250.325842786442,-3.91895004802533,
126.368770188531));
#163981=CARTESIAN_POINT('Ctrl Pts',(-250.333250132796,-4.03555284902245,
126.474576087887));
#163982=CARTESIAN_POINT('Ctrl Pts',(-250.34065747915,-4.14783460650516,
126.584953237426));
#163983=CARTESIAN_POINT('Ctrl Pts',(-250.348059300825,-4.26003262001699,
126.695248063523));
#163984=CARTESIAN_POINT('Ctrl Pts',(-250.355461122501,-4.36791574197479,
126.81010709064));
#163985=CARTESIAN_POINT('Ctrl Pts',(-250.362862944176,-4.47109687057285,
126.929154386092));
#163986=CARTESIAN_POINT('Ctrl Pts',(-250.370260858488,-4.57422353065627,
127.048138837404));
#163987=CARTESIAN_POINT('Ctrl Pts',(-250.377658772799,-4.67265289681752,
127.171306872455));
#163988=CARTESIAN_POINT('Ctrl Pts',(-250.38505668711,-4.76603562369825,
127.29824667245));
#163989=CARTESIAN_POINT('Ctrl Pts',(-250.392453372023,-4.85940283206378,
127.425165377352));
#163990=CARTESIAN_POINT('Ctrl Pts',(-250.399850056935,-4.94772484465036,
127.555854302785));
#163991=CARTESIAN_POINT('Ctrl Pts',(-250.407246741847,-5.03069336608107,
127.689869516444));
#163992=CARTESIAN_POINT('Ctrl Pts',(-250.414643098783,-5.1136582086006,
127.823878787728));
#163993=CARTESIAN_POINT('Ctrl Pts',(-250.422039455718,-5.19126983545631,
127.96121373658));
#163994=CARTESIAN_POINT('Ctrl Pts',(-250.429435812654,-5.26326411887217,
128.101402723426));
#163995=CARTESIAN_POINT('Ctrl Pts',(-250.43683330199,-5.33526942479662,
128.241613173564));
#163996=CARTESIAN_POINT('Ctrl Pts',(-250.444230791327,-5.40165550430265,
128.384678199652));
#163997=CARTESIAN_POINT('Ctrl Pts',(-250.451628280663,-5.46220496974072,
128.530103061562));
#163998=CARTESIAN_POINT('Ctrl Pts',(-250.459028363178,-5.52277566070012,
128.675578901933));
#163999=CARTESIAN_POINT('Ctrl Pts',(-250.466428445694,-5.57750552059136,
128.823415880744));
#164000=CARTESIAN_POINT('Ctrl Pts',(-250.473828528209,-5.62622598174772,
128.97310100604));
#164001=CARTESIAN_POINT('Ctrl Pts',(-250.481236747875,-5.67500001605964,
129.122950725519));
#164002=CARTESIAN_POINT('Ctrl Pts',(-250.488644967542,-5.71775133951511,
129.274652294788));
#164003=CARTESIAN_POINT('Ctrl Pts',(-250.496053187208,-5.75436158745201,
129.427678634188));
#164004=CARTESIAN_POINT('Ctrl Pts',(-250.50346596651,-5.79099436838565,
129.580799158748));
#164005=CARTESIAN_POINT('Ctrl Pts',(-250.510878745812,-5.82147847009779,
129.73524571279));
#164006=CARTESIAN_POINT('Ctrl Pts',(-250.518291525114,-5.84574708094623,
129.890483367544));
#164007=CARTESIAN_POINT('Ctrl Pts',(-250.525714896143,-5.8700503679239,
130.045942833138));
#164008=CARTESIAN_POINT('Ctrl Pts',(-250.533138267172,-5.88812038394804,
130.202195287184));
#164009=CARTESIAN_POINT('Ctrl Pts',(-250.540561638201,-5.89994230118079,
130.358702222338));
#164010=CARTESIAN_POINT('Ctrl Pts',(-250.544497687641,-5.90621056535981,
130.441685954678));
#164011=CARTESIAN_POINT('Ctrl Pts',(-250.548433737081,-5.91072313592196,
130.52474124392));
#164012=CARTESIAN_POINT('Ctrl Pts',(-250.552369786522,-5.91348373254231,
130.60778822007));
#164013=CARTESIAN_POINT('Ctrl Pts',(-250.555454793612,-5.91564744015758,
130.672878995519));
#164014=CARTESIAN_POINT('Ctrl Pts',(-250.558539800703,-5.91673648840975,
130.738005692603));
#164015=CARTESIAN_POINT('Ctrl Pts',(-250.561624807794,-5.91674987505615,
130.803144672231));
#164016=CARTESIAN_POINT('',(-252.311624807794,-5.91192299704699,130.799490663889));
#164017=CARTESIAN_POINT('Ctrl Pts',(-250.561626073556,-5.92622942976624,
130.803169493092));
#164018=CARTESIAN_POINT('Ctrl Pts',(-250.651356519148,-5.92090504172026,
132.700837097956));
#164019=CARTESIAN_POINT('Ctrl Pts',(-250.833902839346,-3.90239773599972,
136.571132087067));
#164020=CARTESIAN_POINT('Ctrl Pts',(-251.109265034147,2.69592465361927,
137.262653797056));
#164021=CARTESIAN_POINT('Ctrl Pts',(-251.387712657961,6.89075808716923,
132.027068070047));
#164022=CARTESIAN_POINT('Ctrl Pts',(-251.666160281773,4.75332147089434,
125.667873926718));
#164023=CARTESIAN_POINT('Ctrl Pts',(-251.944607905586,-1.75218536453816,
124.02886012108));
#164024=CARTESIAN_POINT('Ctrl Pts',(-252.159762747593,-5.53478123322217,
127.573470886404));
#164025=CARTESIAN_POINT('Ctrl Pts',(-252.282101714996,-5.91676991525287,
130.171212797355));
#164026=CARTESIAN_POINT('Ctrl Pts',(-252.311624807794,-5.91192299704699,
130.799490663889));
#164027=CARTESIAN_POINT('',(-254.061624807794,-5.90861635227361,130.807531447417));
#164028=CARTESIAN_POINT('Ctrl Pts',(-252.311624807794,-5.91192299704699,
130.799490663889));
#164029=CARTESIAN_POINT('Ctrl Pts',(-252.3749175896,-5.90153198081667,132.146417769118));
#164030=CARTESIAN_POINT('Ctrl Pts',(-252.53102624601,-4.77598582474867,
135.484254796133));
#164031=CARTESIAN_POINT('Ctrl Pts',(-252.779950777026,0.772983328442457,
137.759938041367));
#164032=CARTESIAN_POINT('Ctrl Pts',(-253.058398400838,6.26974064878271,
133.913687349603));
#164033=CARTESIAN_POINT('Ctrl Pts',(-253.33684602465,6.00491260842544,127.210117287218));
#164034=CARTESIAN_POINT('Ctrl Pts',(-253.615293648464,0.221863234051362,
123.809481262411));
#164035=CARTESIAN_POINT('Ctrl Pts',(-253.856886576178,-4.97265101715999,
126.436108905062));
#164036=CARTESIAN_POINT('Ctrl Pts',(-254.005663629288,-5.90284313340416,
129.614952760039));
#164037=CARTESIAN_POINT('Ctrl Pts',(-254.061624807794,-5.90861635227361,
130.807531447417));
#164038=CARTESIAN_POINT('',(-255.811624807794,-5.92355635148729,130.808085951784));
#164039=CARTESIAN_POINT('Ctrl Pts',(-254.061624807794,-5.90861635227361,
130.807531447417));
#164040=CARTESIAN_POINT('Ctrl Pts',(-254.098479503892,-5.91241845638623,
131.592935298274));
#164041=CARTESIAN_POINT('Ctrl Pts',(-254.228150074594,-5.40067620360337,
134.35156746288));
#164042=CARTESIAN_POINT('Ctrl Pts',(-254.450636519901,-1.21221946432122,
137.696971457865));
#164043=CARTESIAN_POINT('Ctrl Pts',(-254.729084143717,5.1437144673035,135.54985976376));
#164044=CARTESIAN_POINT('Ctrl Pts',(-255.007531767527,6.77282616373886,
129.041866052034));
#164045=CARTESIAN_POINT('Ctrl Pts',(-255.285979391341,2.17804134336251,
124.15351899416));
#164046=CARTESIAN_POINT('Ctrl Pts',(-255.554010404761,-4.17149201360333,
125.331201206967));
#164047=CARTESIAN_POINT('Ctrl Pts',(-255.729225543581,-5.91073967446976,
129.063380221612));
#164048=CARTESIAN_POINT('Ctrl Pts',(-255.811624807794,-5.92355635148729,
130.808085951784));
#164049=CARTESIAN_POINT('',(-257.561624807794,-5.92033794655308,130.799393324114));
#164050=CARTESIAN_POINT('Ctrl Pts',(-255.811624807794,-5.92355635148729,
130.808085951784));
#164051=CARTESIAN_POINT('Ctrl Pts',(-255.822041418185,-5.92517658841868,
131.028645200844));
#164052=CARTESIAN_POINT('Ctrl Pts',(-255.832458028576,-5.91393033387313,
131.249037543385));
#164053=CARTESIAN_POINT('Ctrl Pts',(-255.842874638967,-5.88926851932256,
131.467918319388));
#164054=CARTESIAN_POINT('Ctrl Pts',(-255.935690513571,-5.66952257501434,
133.418227479128));
#164055=CARTESIAN_POINT('Ctrl Pts',(-256.121322262779,-3.09978113180407,
137.078824961414));
#164056=CARTESIAN_POINT('Ctrl Pts',(-256.399769886593,3.60337663794395,
136.803798165417));
#164057=CARTESIAN_POINT('Ctrl Pts',(-256.678217510405,6.99521075334592,
131.015575332266));
#164058=CARTESIAN_POINT('Ctrl Pts',(-256.956665134218,3.95878142380252,
125.033267860759));
#164059=CARTESIAN_POINT('Ctrl Pts',(-257.235112758031,-2.71556236807722,
124.354291237798));
#164060=CARTESIAN_POINT('Ctrl Pts',(-257.436765982556,-5.74194199984043,
128.155182833242));
#164061=CARTESIAN_POINT('Ctrl Pts',(-257.545603332477,-5.92339174586805,
130.459678785459));
#164062=CARTESIAN_POINT('Ctrl Pts',(-257.561624807794,-5.92033794655308,
130.799393324114));
#164063=CARTESIAN_POINT('',(-259.311624331364,-5.91238880389048,130.802664157255));
#164064=CARTESIAN_POINT('Ctrl Pts',(-257.561624807794,-5.92033794655308,
130.799393324114));
#164065=CARTESIAN_POINT('Ctrl Pts',(-257.638419207082,-5.90570042539457,
132.427718644327));
#164066=CARTESIAN_POINT('Ctrl Pts',(-257.808029480972,-4.36304327368764,
136.048423324747));
#164067=CARTESIAN_POINT('Ctrl Pts',(-258.070455629471,1.77275496796904,
137.574574651028));
#164068=CARTESIAN_POINT('Ctrl Pts',(-258.348903253281,6.65423282923866,
132.972130842852));
#164069=CARTESIAN_POINT('Ctrl Pts',(-258.627350877096,5.42050131933435,
126.378127222952));
#164070=CARTESIAN_POINT('Ctrl Pts',(-258.905798500908,-0.79385004661475,
123.850643128868));
#164071=CARTESIAN_POINT('Ctrl Pts',(-259.133889458064,-5.2876300368704,
127.016239948135));
#164072=CARTESIAN_POINT('Ctrl Pts',(-259.269164540617,-5.90905021799741,
129.897487457751));
#164073=CARTESIAN_POINT('Ctrl Pts',(-259.311623748564,-5.90705419484729,
130.802653254356));
#164074=CARTESIAN_POINT('',(-260.000000000001,4.64033908871117,134.475216608242));
#164075=CARTESIAN_POINT('Ctrl Pts',(-259.311624807794,-5.91674975934287,
130.802673070197));
#164076=CARTESIAN_POINT('Ctrl Pts',(-259.319249567293,-5.91679619665931,
130.965488044112));
#164077=CARTESIAN_POINT('Ctrl Pts',(-259.326874326793,-5.91011785639963,
131.128231102469));
#164078=CARTESIAN_POINT('Ctrl Pts',(-259.334499086292,-5.8967587757839,
131.290330269618));
#164079=CARTESIAN_POINT('Ctrl Pts',(-259.342129178135,-5.88339035255241,
131.452542800124));
#164080=CARTESIAN_POINT('Ctrl Pts',(-259.349759269977,-5.86333189910214,
131.614110202848));
#164081=CARTESIAN_POINT('Ctrl Pts',(-259.357389361819,-5.83667914730406,
131.774467361139));
#164082=CARTESIAN_POINT('Ctrl Pts',(-259.3650258447,-5.81000407090589,131.934958836121));
#164083=CARTESIAN_POINT('Ctrl Pts',(-259.37266232758,-5.7767237359774,132.094237710268));
#164084=CARTESIAN_POINT('Ctrl Pts',(-259.38029881046,-5.73698466795682,
132.251750503578));
#164085=CARTESIAN_POINT('Ctrl Pts',(-259.387948278586,-5.69717802673954,
132.40953113515));
#164086=CARTESIAN_POINT('Ctrl Pts',(-259.395597746712,-5.65089078706961,
132.565539354429));
#164087=CARTESIAN_POINT('Ctrl Pts',(-259.403247214838,-5.59831936063122,
132.719236827372));
#164088=CARTESIAN_POINT('Ctrl Pts',(-259.410903777593,-5.54569917593195,
132.873076849643));
#164089=CARTESIAN_POINT('Ctrl Pts',(-259.418560340348,-5.48678329977216,
133.0246015341));
#164090=CARTESIAN_POINT('Ctrl Pts',(-259.426216903103,-5.42181579432039,
133.173293722353));
#164091=CARTESIAN_POINT('Ctrl Pts',(-259.433887329274,-5.35673065493482,
133.322255141307));
#164092=CARTESIAN_POINT('Ctrl Pts',(-259.441557755446,-5.28557213369624,
133.468373507889));
#164093=CARTESIAN_POINT('Ctrl Pts',(-259.449228181618,-5.2086303301978,
133.61115605825));
#164094=CARTESIAN_POINT('Ctrl Pts',(-259.453716703923,-5.16360610422695,
133.694708477349));
#164095=CARTESIAN_POINT('Ctrl Pts',(-259.458205226229,-5.11660235328243,
133.777119156976));
#164096=CARTESIAN_POINT('Ctrl Pts',(-259.462693748535,-5.06768388172451,
133.858294250998));
#164097=CARTESIAN_POINT('Ctrl Pts',(-259.47012929275,-4.98664708755365,
133.992766346643));
#164098=CARTESIAN_POINT('Ctrl Pts',(-259.477564836965,-4.90013544228489,
134.124207857881));
#164099=CARTESIAN_POINT('Ctrl Pts',(-259.48500038118,-4.80840170338421,
134.252143038397));
#164100=CARTESIAN_POINT('Ctrl Pts',(-259.492427278007,-4.71677464898281,
134.379929432863));
#164101=CARTESIAN_POINT('Ctrl Pts',(-259.499854174834,-4.61993780523473,
134.504217314733));
#164102=CARTESIAN_POINT('Ctrl Pts',(-259.50728107166,-4.51818913327925,
134.624556622801));
#164103=CARTESIAN_POINT('Ctrl Pts',(-259.514700934918,-4.41653682138671,
134.744781964731));
#164104=CARTESIAN_POINT('Ctrl Pts',(-259.522120798177,-4.30998218112583,
134.86106589582));
#164105=CARTESIAN_POINT('Ctrl Pts',(-259.529540661435,-4.19886561158322,
134.972988465955));
#164106=CARTESIAN_POINT('Ctrl Pts',(-259.536955099493,-4.08783028742268,
135.084829201383));
#164107=CARTESIAN_POINT('Ctrl Pts',(-259.544369537551,-3.97223993690416,
135.192314663084));
#164108=CARTESIAN_POINT('Ctrl Pts',(-259.551783975609,-3.85247419313978,
135.295059132685));
#164109=CARTESIAN_POINT('Ctrl Pts',(-259.559194592593,-3.73277017134383,
135.39775065233));
#164110=CARTESIAN_POINT('Ctrl Pts',(-259.566605209578,-3.6088953235766,
135.49570580466));
#164111=CARTESIAN_POINT('Ctrl Pts',(-259.574015826562,-3.48126490870701,
135.588576875001));
#164112=CARTESIAN_POINT('Ctrl Pts',(-259.581425300866,-3.35365417381794,
135.681433625081));
#164113=CARTESIAN_POINT('Ctrl Pts',(-259.58883477517,-3.22228932129518,
135.769207630182));
#164114=CARTESIAN_POINT('Ctrl Pts',(-259.596244249474,-3.08761745835792,
135.851592432466));
#164115=CARTESIAN_POINT('Ctrl Pts',(-259.603653447889,-2.95295060988279,
135.93397416718));
#164116=CARTESIAN_POINT('Ctrl Pts',(-259.611062646304,-2.81497731298843,
136.010966903991));
#164117=CARTESIAN_POINT('Ctrl Pts',(-259.618471844718,-2.67417210930629,
136.082308522984));
#164118=CARTESIAN_POINT('Ctrl Pts',(-259.625882215982,-2.53334461666666,
136.153661435099));
#164119=CARTESIAN_POINT('Ctrl Pts',(-259.633292587246,-2.38968465629391,
136.219361280047));
#164120=CARTESIAN_POINT('Ctrl Pts',(-259.640702958511,-2.24368959943131,
136.279192810785));
#164121=CARTESIAN_POINT('Ctrl Pts',(-259.648115951775,-2.09764288535344,
136.339045511624));
#164122=CARTESIAN_POINT('Ctrl Pts',(-259.65552894504,-1.94925977349594,
136.393025622985));
#164123=CARTESIAN_POINT('Ctrl Pts',(-259.662941938305,-1.79905562264375,
136.440966815371));
#164124=CARTESIAN_POINT('Ctrl Pts',(-259.670363046142,-1.64868705204678,
136.488960486191));
#164125=CARTESIAN_POINT('Ctrl Pts',(-259.67778415398,-1.49649381591127,
136.530901923211));
#164126=CARTESIAN_POINT('Ctrl Pts',(-259.685205261817,-1.34300510067358,
136.566675071157));
#164127=CARTESIAN_POINT('Ctrl Pts',(-259.692630935413,-1.18942195310739,
136.602470228159));
#164128=CARTESIAN_POINT('Ctrl Pts',(-259.700056609009,-1.03454210251154,
136.632089463809));
#164129=CARTESIAN_POINT('Ctrl Pts',(-259.707482282606,-0.878902344620537,
136.655468310227));
#164130=CARTESIAN_POINT('Ctrl Pts',(-259.714918445666,-0.723042730901533,
136.67888018147));
#164131=CARTESIAN_POINT('Ctrl Pts',(-259.722354608726,-0.566421434618302,
136.696034017051));
#164132=CARTESIAN_POINT('Ctrl Pts',(-259.729790771786,-0.409578588352051,
136.706917346854));
#164133=CARTESIAN_POINT('Ctrl Pts',(-259.733574305306,-0.329776658048363,
136.71245480519));
#164134=CARTESIAN_POINT('Ctrl Pts',(-259.737357838827,-0.249917354980275,
136.716369795289));
#164135=CARTESIAN_POINT('Ctrl Pts',(-259.741141372347,-0.170071456658404,
136.718665839833));
#164136=CARTESIAN_POINT('Ctrl Pts',(-259.748429931939,-0.0162571492104426,
136.723088916143));
#164137=CARTESIAN_POINT('Ctrl Pts',(-259.755718491532,0.138008324997689,
136.72151530412));
#164138=CARTESIAN_POINT('Ctrl Pts',(-259.763007051124,0.292206850264092,
136.713890693567));
#164139=CARTESIAN_POINT('Ctrl Pts',(-259.770286825596,0.446219515417705,
136.706275273185));
#164140=CARTESIAN_POINT('Ctrl Pts',(-259.777566600069,0.600165009584265,
136.692623380763));
#164141=CARTESIAN_POINT('Ctrl Pts',(-259.784846374541,0.753521181319539,
136.672932538554));
#164142=CARTESIAN_POINT('Ctrl Pts',(-259.792119092978,0.906728710185211,
136.653260782001));
#164143=CARTESIAN_POINT('Ctrl Pts',(-259.799391811415,1.05934767157003,
136.627561769673));
#164144=CARTESIAN_POINT('Ctrl Pts',(-259.806664529853,1.21085730663432,
136.595885040848));
#164145=CARTESIAN_POINT('Ctrl Pts',(-259.813931913241,1.36225579876186,
136.564231549123));
#164146=CARTESIAN_POINT('Ctrl Pts',(-259.821199296629,1.51254620623473,
136.526609145561));
#164147=CARTESIAN_POINT('Ctrl Pts',(-259.828466680018,1.66121458269763,
136.483118991782));
#164148=CARTESIAN_POINT('Ctrl Pts',(-259.835731084076,1.80982201119389,
136.439646667192));
#164149=CARTESIAN_POINT('Ctrl Pts',(-259.842995488133,1.95680835961825,
136.390311483737));
#164150=CARTESIAN_POINT('Ctrl Pts',(-259.850259892191,2.1016717106643,136.335265297914));
#164151=CARTESIAN_POINT('Ctrl Pts',(-259.857522856591,2.24650635271518,
136.280230021135));
#164152=CARTESIAN_POINT('Ctrl Pts',(-259.86478582099,2.3892184718474,136.219486130079));
#164153=CARTESIAN_POINT('Ctrl Pts',(-259.87204878539,2.52932344090061,136.153234657381));
#164154=CARTESIAN_POINT('Ctrl Pts',(-259.879311858217,2.66943050156796,
136.086982195621));
#164155=CARTESIAN_POINT('Ctrl Pts',(-259.886574931045,2.80692998421195,
136.01522215424));
#164156=CARTESIAN_POINT('Ctrl Pts',(-259.893838003872,2.9413596176415,135.938202664436));
#164157=CARTESIAN_POINT('Ctrl Pts',(-259.901102733218,3.07581991098706,
135.861165608482));
#164158=CARTESIAN_POINT('Ctrl Pts',(-259.908367462565,3.2072086261801,135.77886691071));
#164159=CARTESIAN_POINT('Ctrl Pts',(-259.915632191911,3.33509066003826,
135.691599188766));
#164160=CARTESIAN_POINT('Ctrl Pts',(-259.922904436531,3.46310498630635,
135.604241189424));
#164161=CARTESIAN_POINT('Ctrl Pts',(-259.930176681152,3.58760506608904,
135.511904118905));
#164162=CARTESIAN_POINT('Ctrl Pts',(-259.937448925772,3.70818675737722,
135.414922571917));
#164163=CARTESIAN_POINT('Ctrl Pts',(-259.944725048152,3.82883274610836,
135.317889311726));
#164164=CARTESIAN_POINT('Ctrl Pts',(-259.952001170531,3.9455558944256,135.216206898089));
#164165=CARTESIAN_POINT('Ctrl Pts',(-259.95927729291,4.05798808483907,135.110247665063));
#164166=CARTESIAN_POINT('Ctrl Pts',(-259.966564564679,4.17059255798621,
135.004126067982));
#164167=CARTESIAN_POINT('Ctrl Pts',(-259.973851836448,4.27889266917242,
134.893714837875));
#164168=CARTESIAN_POINT('Ctrl Pts',(-259.981139108216,4.38255926705988,
134.779420973486));
#164169=CARTESIAN_POINT('Ctrl Pts',(-259.987426072145,4.47199577802895,
134.680815977621));
#164170=CARTESIAN_POINT('Ctrl Pts',(-259.993713036073,4.55798411034979,
134.57932176143));
#164171=CARTESIAN_POINT('Ctrl Pts',(-260.000000000001,4.64033908871117,
134.475216608242));
#164172=CARTESIAN_POINT('',(-260.,-0.0185920708335255,136.72108140677));
#164173=CARTESIAN_POINT('Origin',(-260.,0.,130.804360617566));
#164174=CARTESIAN_POINT('',(-259.56337387439,-5.91070033503288,130.799418600708));
#164175=CARTESIAN_POINT('Ctrl Pts',(-260.,-0.0185920708348715,136.72108140677));
#164176=CARTESIAN_POINT('Ctrl Pts',(-259.991311830341,-0.203157853229185,
136.720501446988));
#164177=CARTESIAN_POINT('Ctrl Pts',(-259.982623660683,-0.387555641347291,
136.711281624755));
#164178=CARTESIAN_POINT('Ctrl Pts',(-259.973935491024,-0.571044165506732,
136.693489511005));
#164179=CARTESIAN_POINT('Ctrl Pts',(-259.965231695903,-0.754862689346968,
136.675665398568));
#164180=CARTESIAN_POINT('Ctrl Pts',(-259.95652790078,-0.93776857354042,
136.649238166263));
#164181=CARTESIAN_POINT('Ctrl Pts',(-259.947824105659,-1.1190256334236,
136.614327243481));
#164182=CARTESIAN_POINT('Ctrl Pts',(-259.939119990154,-1.30028936528833,
136.579415035644));
#164183=CARTESIAN_POINT('Ctrl Pts',(-259.93041587465,-1.47990405091075,
136.536018539262));
#164184=CARTESIAN_POINT('Ctrl Pts',(-259.921711759146,-1.65714402095923,
136.484308175097));
#164185=CARTESIAN_POINT('Ctrl Pts',(-259.913018683697,-1.83415918481704,
136.432663398902));
#164186=CARTESIAN_POINT('Ctrl Pts',(-259.904325608248,-2.00880554981633,
136.372725847947));
#164187=CARTESIAN_POINT('Ctrl Pts',(-259.895632532799,-2.18037229441418,
136.304715807938));
#164188=CARTESIAN_POINT('Ctrl Pts',(-259.886971363205,-2.35130934427719,
136.236955382527));
#164189=CARTESIAN_POINT('Ctrl Pts',(-259.878310193612,-2.5191892311127,
136.161181632495));
#164190=CARTESIAN_POINT('Ctrl Pts',(-259.869649024019,-2.68332250330789,
136.077662325769));
#164191=CARTESIAN_POINT('Ctrl Pts',(-259.866691412044,-2.73937065317332,
136.049142193578));
#164192=CARTESIAN_POINT('Ctrl Pts',(-259.863733800069,-2.79498204109144,
136.019719294179));
#164193=CARTESIAN_POINT('Ctrl Pts',(-259.860776188094,-2.85012961403489,
135.989405626599));
#164194=CARTESIAN_POINT('Ctrl Pts',(-259.853352615767,-2.98854939318207,
135.913318666693));
#164195=CARTESIAN_POINT('Ctrl Pts',(-259.84592904344,-3.1239691154349,135.831658168558));
#164196=CARTESIAN_POINT('Ctrl Pts',(-259.838505471113,-3.25591924795894,
135.744696680353));
#164197=CARTESIAN_POINT('Ctrl Pts',(-259.831082830257,-3.38785282406021,
135.657746103627));
#164198=CARTESIAN_POINT('Ctrl Pts',(-259.823660189402,-3.51631736824606,
135.565496065799));
#164199=CARTESIAN_POINT('Ctrl Pts',(-259.816237548546,-3.64087156035974,
135.468262936812));
#164200=CARTESIAN_POINT('Ctrl Pts',(-259.808814397566,-3.76543431253152,
135.371023125422));
#164201=CARTESIAN_POINT('Ctrl Pts',(-259.801391246585,-3.88608588625228,
135.268799770186));
#164202=CARTESIAN_POINT('Ctrl Pts',(-259.793968095604,-4.00241743025333,
135.161950005806));
#164203=CARTESIAN_POINT('Ctrl Pts',(-259.78654036091,-4.11882080769124,
135.055034262883));
#164204=CARTESIAN_POINT('Ctrl Pts',(-259.779112626216,-4.23089855479602,
134.943486656561));
#164205=CARTESIAN_POINT('Ctrl Pts',(-259.771684891523,-4.33827781733205,
134.827702032627));
#164206=CARTESIAN_POINT('Ctrl Pts',(-259.764254403954,-4.44569687687905,
134.711874496478));
#164207=CARTESIAN_POINT('Ctrl Pts',(-259.756823916385,-4.54841373821342,
134.59180709261));
#164208=CARTESIAN_POINT('Ctrl Pts',(-259.749393428817,-4.64609561235738,
134.467928021523));
#164209=CARTESIAN_POINT('Ctrl Pts',(-259.74195603147,-4.74386832308964,
134.34393375248));
#164210=CARTESIAN_POINT('Ctrl Pts',(-259.734518634122,-4.83659647863859,
134.216121037179));
#164211=CARTESIAN_POINT('Ctrl Pts',(-259.727081236775,-4.9239901424912,
134.084947705139));
#164212=CARTESIAN_POINT('Ctrl Pts',(-259.725238283246,-4.94564589835924,
134.052443544885));
#164213=CARTESIAN_POINT('Ctrl Pts',(-259.723395329716,-4.96697432049345,
134.019733157467));
#164214=CARTESIAN_POINT('Ctrl Pts',(-259.721552376187,-4.98797143306394,
133.986823743109));
#164215=CARTESIAN_POINT('Ctrl Pts',(-259.713932604088,-5.07478491477979,
133.850758327824));
#164216=CARTESIAN_POINT('Ctrl Pts',(-259.706312831988,-5.15611030533379,
133.711008123288));
#164217=CARTESIAN_POINT('Ctrl Pts',(-259.698693059889,-5.23163338743316,
133.568043425342));
#164218=CARTESIAN_POINT('Ctrl Pts',(-259.691080565604,-5.30708433575536,
133.425215276161));
#164219=CARTESIAN_POINT('Ctrl Pts',(-259.683468071318,-5.37674385685914,
133.279179054989));
#164220=CARTESIAN_POINT('Ctrl Pts',(-259.675855577033,-5.44034190027707,
133.130432536185));
#164221=CARTESIAN_POINT('Ctrl Pts',(-259.668249196025,-5.50388887075926,
132.981805469506));
#164222=CARTESIAN_POINT('Ctrl Pts',(-259.660642815016,-5.56138392811307,
132.83047275924));
#164223=CARTESIAN_POINT('Ctrl Pts',(-259.653036434007,-5.61260362325501,
132.676955376377));
#164224=CARTESIAN_POINT('Ctrl Pts',(-259.645435683464,-5.66378540408173,
132.523551631567));
#164225=CARTESIAN_POINT('Ctrl Pts',(-259.637834932921,-5.70870097555932,
132.367966765819));
#164226=CARTESIAN_POINT('Ctrl Pts',(-259.630234182378,-5.74717554453198,
132.210740304149));
#164227=CARTESIAN_POINT('Ctrl Pts',(-259.622636910555,-5.78563250442226,
132.053585802056));
#164228=CARTESIAN_POINT('Ctrl Pts',(-259.615039638731,-5.81765425465708,
131.894791536687));
#164229=CARTESIAN_POINT('Ctrl Pts',(-259.607442366908,-5.84311614749782,
131.734911126324));
#164230=CARTESIAN_POINT('Ctrl Pts',(-259.599846844175,-5.86857217834461,
131.575067524615));
#164231=CARTESIAN_POINT('Ctrl Pts',(-259.592251321443,-5.88747130420872,
131.414138617028));
#164232=CARTESIAN_POINT('Ctrl Pts',(-259.58465579871,-5.899740131173,131.252687448267));
#164233=CARTESIAN_POINT('Ctrl Pts',(-259.577562263208,-5.91119811276277,
131.101906568833));
#164234=CARTESIAN_POINT('Ctrl Pts',(-259.570468727707,-5.91687368214121,
130.950670495385));
#164235=CARTESIAN_POINT('Ctrl Pts',(-259.563375192205,-5.91674795525148,
130.799441620975));
#164236=CARTESIAN_POINT('',(-257.81337519221,-5.92178402722332,130.799850810543));
#164237=CARTESIAN_POINT('Ctrl Pts',(-259.563373045442,-5.90689618837314,
130.799404120224));
#164238=CARTESIAN_POINT('Ctrl Pts',(-259.52328361442,-5.91028116954653,
129.946147187527));
#164239=CARTESIAN_POINT('Ctrl Pts',(-259.39037830879,-5.33824730543968,
127.12303984211));
#164240=CARTESIAN_POINT('Ctrl Pts',(-259.164657128564,-0.969924417821122,
123.869831148738));
#164241=CARTESIAN_POINT('Ctrl Pts',(-258.886209504748,5.30519432384848,
126.242992475658));
#164242=CARTESIAN_POINT('Ctrl Pts',(-258.607761880936,6.70769697358496,
132.800694938907));
#164243=CARTESIAN_POINT('Ctrl Pts',(-258.329314257122,1.9447785293426,137.527620338931));
#164244=CARTESIAN_POINT('Ctrl Pts',(-258.064518694214,-4.28345898126671,
136.145471011969));
#164245=CARTESIAN_POINT('Ctrl Pts',(-257.89253900591,-5.90755031029441,
132.477311743359));
#164246=CARTESIAN_POINT('Ctrl Pts',(-257.81337519221,-5.92178402722332,
130.799850810543));
#164247=CARTESIAN_POINT('',(-256.06337519221,-5.92227829491472,130.80869798814));
#164248=CARTESIAN_POINT('Ctrl Pts',(-257.81337519221,-5.92178402722332,
130.799850810543));
#164249=CARTESIAN_POINT('Ctrl Pts',(-257.799723131306,-5.92423867867741,
130.510567137243));
#164250=CARTESIAN_POINT('Ctrl Pts',(-257.693255195793,-5.77329314096876,
128.257096185211));
#164251=CARTESIAN_POINT('Ctrl Pts',(-257.493971385687,-2.87925022698376,
124.425616511888));
#164252=CARTESIAN_POINT('Ctrl Pts',(-257.215523761869,3.81020896683791,
124.934163083578));
#164253=CARTESIAN_POINT('Ctrl Pts',(-256.937076138059,6.99832954735633,
130.836978163555));
#164254=CARTESIAN_POINT('Ctrl Pts',(-256.658628514244,3.7552968212212,136.709902062958));
#164255=CARTESIAN_POINT('Ctrl Pts',(-256.380180890433,-2.93865415896156,
137.155878050677));
#164256=CARTESIAN_POINT('Ctrl Pts',(-256.181763116421,-5.78435051408065,
133.314517757552));
#164257=CARTESIAN_POINT('Ctrl Pts',(-256.076161217013,-5.92450519214891,
131.079579575374));
#164258=CARTESIAN_POINT('Ctrl Pts',(-256.06337519221,-5.92227829491472,
130.80869798814));
#164259=CARTESIAN_POINT('',(-254.31337519221,-5.90789551585446,130.806811267338));
#164260=CARTESIAN_POINT('Ctrl Pts',(-256.06337519221,-5.92227829491472,
130.80869798814));
#164261=CARTESIAN_POINT('Ctrl Pts',(-255.983345342409,-5.90833977579574,
129.113205208021));
#164262=CARTESIAN_POINT('Ctrl Pts',(-255.810499618004,-4.25395404596283,
125.427592952043));
#164263=CARTESIAN_POINT('Ctrl Pts',(-255.544838018994,2.00761156116971,
124.100105126704));
#164264=CARTESIAN_POINT('Ctrl Pts',(-255.266390395181,6.72564432193871,
128.869606478615));
#164265=CARTESIAN_POINT('Ctrl Pts',(-254.987942771368,5.26313784737678,
135.417054192137));
#164266=CARTESIAN_POINT('Ctrl Pts',(-254.709495147555,-1.03593483579578,
137.725660886227));
#164267=CARTESIAN_POINT('Ctrl Pts',(-254.484639287835,-5.35389815067843,
134.453752389533));
#164268=CARTESIAN_POINT('Ctrl Pts',(-254.352599302721,-5.91100089308872,
131.642964263266));
#164269=CARTESIAN_POINT('Ctrl Pts',(-254.31337519221,-5.90789551585446,
130.806811267338));
#164270=CARTESIAN_POINT('',(-252.56337517516,-5.91453573035578,130.799159711326));
#164271=CARTESIAN_POINT('Ctrl Pts',(-254.31337519221,-5.90789551585446,
130.806811267338));
#164272=CARTESIAN_POINT('Ctrl Pts',(-254.259783428116,-5.90365264987245,
129.664378372864));
#164273=CARTESIAN_POINT('Ctrl Pts',(-254.113375789419,-5.03223228932717,
126.53737431623));
#164274=CARTESIAN_POINT('Ctrl Pts',(-253.874152276116,0.0432914040588217,
123.806097541657));
#164275=CARTESIAN_POINT('Ctrl Pts',(-253.595704652304,5.91123701504208,
127.058050750705));
#164276=CARTESIAN_POINT('Ctrl Pts',(-253.317257028491,6.34704457441364,
133.75267975028));
#164277=CARTESIAN_POINT('Ctrl Pts',(-253.038809404678,0.950228248086572,
137.737947478949));
#164278=CARTESIAN_POINT('Ctrl Pts',(-252.78751545925,-4.70836014979751,
135.584300855963));
#164279=CARTESIAN_POINT('Ctrl Pts',(-252.629037388428,-5.90157326896774,
132.195707362608));
#164280=CARTESIAN_POINT('Ctrl Pts',(-252.56337519221,-5.91327032966472,
130.799161186809));
#164281=CARTESIAN_POINT('',(-250.81337519221,-5.92210605632582,130.804075584904));
#164282=CARTESIAN_POINT('Ctrl Pts',(-252.563375145356,-5.91674771189706,
130.799157132112));
#164283=CARTESIAN_POINT('Ctrl Pts',(-252.554385525451,-5.91657946607099,
130.607849187631));
#164284=CARTESIAN_POINT('Ctrl Pts',(-252.545395905546,-5.90712912470598,
130.416949906316));
#164285=CARTESIAN_POINT('Ctrl Pts',(-252.536406285641,-5.88853768247511,
130.227251854359));
#164286=CARTESIAN_POINT('Ctrl Pts',(-252.527291320086,-5.86968701277697,
130.034908771158));
#164287=CARTESIAN_POINT('Ctrl Pts',(-252.518176354532,-5.84143860087722,
129.843800628979));
#164288=CARTESIAN_POINT('Ctrl Pts',(-252.509061388977,-5.80398847189683,
129.654730946503));
#164289=CARTESIAN_POINT('Ctrl Pts',(-252.500012311669,-5.76680905412209,
129.467027969111));
#164290=CARTESIAN_POINT('Ctrl Pts',(-252.490963234361,-5.72056062638132,
129.281333985984));
#164291=CARTESIAN_POINT('Ctrl Pts',(-252.481914157052,-5.66548117725332,
129.098414078929));
#164292=CARTESIAN_POINT('Ctrl Pts',(-252.474490890639,-5.62029762860797,
128.948358647194));
#164293=CARTESIAN_POINT('Ctrl Pts',(-252.467067624226,-5.56908010727519,
128.799872645413));
#164294=CARTESIAN_POINT('Ctrl Pts',(-252.459644357813,-5.51195390025377,
128.65347829536));
#164295=CARTESIAN_POINT('Ctrl Pts',(-252.452229865084,-5.4548952116643,
128.507256971271));
#164296=CARTESIAN_POINT('Ctrl Pts',(-252.444815372356,-5.39194187260987,
128.363122722427));
#164297=CARTESIAN_POINT('Ctrl Pts',(-252.437400879627,-5.32326936540353,
128.221584238191));
#164298=CARTESIAN_POINT('Ctrl Pts',(-252.429993533266,-5.25466304734425,
128.080182174074));
#164299=CARTESIAN_POINT('Ctrl Pts',(-252.422586186904,-5.18034869699358,
127.941371227381));
#164300=CARTESIAN_POINT('Ctrl Pts',(-252.415178840543,-5.10055041820027,
127.805641558718));
#164301=CARTESIAN_POINT('Ctrl Pts',(-252.407777018859,-5.02081165597293,
127.670013122361));
#164302=CARTESIAN_POINT('Ctrl Pts',(-252.400375197176,-4.9355972976652,
127.537461708557));
#164303=CARTESIAN_POINT('Ctrl Pts',(-252.392973375493,-4.84517799030723,
127.408454139946));
#164304=CARTESIAN_POINT('Ctrl Pts',(-252.385575461174,-4.75480641459697,
127.279514673425));
#164305=CARTESIAN_POINT('Ctrl Pts',(-252.378177546855,-4.65923557562838,
127.154115631288));
#164306=CARTESIAN_POINT('Ctrl Pts',(-252.370779632536,-4.55878010284036,
127.032695927214));
#164307=CARTESIAN_POINT('Ctrl Pts',(-252.363382947615,-4.45834132392844,
126.911296400891));
#164308=CARTESIAN_POINT('Ctrl Pts',(-252.355986262695,-4.35301975998355,
126.793875187499));
#164309=CARTESIAN_POINT('Ctrl Pts',(-252.348589577775,-4.24317116323312,
126.680839180492));
#164310=CARTESIAN_POINT('Ctrl Pts',(-252.341193220832,-4.13332743728395,
126.56780818562));
#164311=CARTESIAN_POINT('Ctrl Pts',(-252.333796863888,-4.01895733781476,
126.459162278221));
#164312=CARTESIAN_POINT('Ctrl Pts',(-252.326400506945,-3.9004542228339,
126.355272237001));
#164313=CARTESIAN_POINT('Ctrl Pts',(-252.3190030176,-3.78193296472295,126.251366289951));
#164314=CARTESIAN_POINT('Ctrl Pts',(-252.311605528256,-3.65927771187928,
126.152217904996));
#164315=CARTESIAN_POINT('Ctrl Pts',(-252.304208038911,-3.53291558420442,
126.058158131643));
#164316=CARTESIAN_POINT('Ctrl Pts',(-252.296807956388,-3.40650916048073,
125.964065385781));
#164317=CARTESIAN_POINT('Ctrl Pts',(-252.289407873865,-3.27639357401108,
125.875065025821));
#164318=CARTESIAN_POINT('Ctrl Pts',(-252.282007791342,-3.14302550827543,
125.791445176744));
#164319=CARTESIAN_POINT('Ctrl Pts',(-252.274599571667,-3.00951079064127,
125.707733379047));
#164320=CARTESIAN_POINT('Ctrl Pts',(-252.267191351993,-2.87273676783248,
125.629414106142));
#164321=CARTESIAN_POINT('Ctrl Pts',(-252.259783132318,-2.73318598342807,
125.556730205419));
#164322=CARTESIAN_POINT('Ctrl Pts',(-252.252370353008,-2.59354930784409,
125.484001568967));
#164323=CARTESIAN_POINT('Ctrl Pts',(-252.244957573698,-2.45113280209025,
125.416915374782));
#164324=CARTESIAN_POINT('Ctrl Pts',(-252.237544794388,-2.30643914601276,
125.355666367726));
#164325=CARTESIAN_POINT('Ctrl Pts',(-252.230121423351,-2.16153874485486,
125.294329845216));
#164326=CARTESIAN_POINT('Ctrl Pts',(-252.222698052315,-2.01435504338489,
125.238847298903));
#164327=CARTESIAN_POINT('Ctrl Pts',(-252.215274681278,-1.86540681970865,
125.189363915921));
#164328=CARTESIAN_POINT('Ctrl Pts',(-252.211338631931,-1.78643089953227,
125.163126639584));
#164329=CARTESIAN_POINT('Ctrl Pts',(-252.207402582585,-1.70695910773732,
125.138575094991));
#164330=CARTESIAN_POINT('Ctrl Pts',(-252.203466533239,-1.62706982582334,
125.115725074275));
#164331=CARTESIAN_POINT('Ctrl Pts',(-252.196043266835,-1.47640112981881,
125.072630647307));
#164332=CARTESIAN_POINT('Ctrl Pts',(-252.188620000432,-1.32379133005656,
125.035461087659));
#164333=CARTESIAN_POINT('Ctrl Pts',(-252.181196734029,-1.16974750718794,
125.004393261457));
#164334=CARTESIAN_POINT('Ctrl Pts',(-252.17378224131,-1.01588575132546,
124.973362154846));
#164335=CARTESIAN_POINT('Ctrl Pts',(-252.166367748591,-0.860593708413412,
124.948418499748));
#164336=CARTESIAN_POINT('Ctrl Pts',(-252.158953255872,-0.704394205693282,
124.929689616949));
#164337=CARTESIAN_POINT('Ctrl Pts',(-252.15154590952,-0.548345253934723,
124.910978785754));
#164338=CARTESIAN_POINT('Ctrl Pts',(-252.144138563168,-0.391390951766817,
124.898470846027));
#164339=CARTESIAN_POINT('Ctrl Pts',(-252.136731216816,-0.234064818790602,
124.892242196636));
#164340=CARTESIAN_POINT('Ctrl Pts',(-252.129329395143,-0.0768560255804177,
124.886018192806));
#164341=CARTESIAN_POINT('Ctrl Pts',(-252.12192757347,0.0807236748453837,
124.886064168869));
#164342=CARTESIAN_POINT('Ctrl Pts',(-252.114525751796,0.23813524004973,
124.892404750854));
#164343=CARTESIAN_POINT('Ctrl Pts',(-252.107127837487,0.395463708914521,
124.898741985696));
#164344=CARTESIAN_POINT('Ctrl Pts',(-252.099729923178,0.552623847270964,
124.911367193811));
#164345=CARTESIAN_POINT('Ctrl Pts',(-252.092332008868,0.709076319714843,
124.930252912108));
#164346=CARTESIAN_POINT('Ctrl Pts',(-252.084935323958,0.865502792595908,
124.949135491941));
#164347=CARTESIAN_POINT('Ctrl Pts',(-252.077538639048,1.0212214627234,124.97427647241));
#164348=CARTESIAN_POINT('Ctrl Pts',(-252.070141954138,1.17569770634179,
125.005596484942));
#164349=CARTESIAN_POINT('Ctrl Pts',(-252.062745597205,1.33016710032166,
125.036915108713));
#164350=CARTESIAN_POINT('Ctrl Pts',(-252.055349240271,1.48339381147729,
125.074412145596));
#164351=CARTESIAN_POINT('Ctrl Pts',(-252.047952883338,1.63485327357079,
125.117957067307));
#164352=CARTESIAN_POINT('Ctrl Pts',(-252.040555394003,1.78633592449418,
125.161508655857));
#164353=CARTESIAN_POINT('Ctrl Pts',(-252.033157904669,1.9360504288259,125.211109869767));
#164354=CARTESIAN_POINT('Ctrl Pts',(-252.025760415334,2.08348739650297,
125.26658030131));
#164355=CARTESIAN_POINT('Ctrl Pts',(-252.018360332821,2.23097604798114,
125.322070177927));
#164356=CARTESIAN_POINT('Ctrl Pts',(-252.010960250308,2.37618522405199,
125.383433237168));
#164357=CARTESIAN_POINT('Ctrl Pts',(-252.003560167795,2.51862566843399,
125.450440996876));
#164358=CARTESIAN_POINT('Ctrl Pts',(-251.996151948131,2.66122274072767,
125.517522438506));
#164359=CARTESIAN_POINT('Ctrl Pts',(-251.988743728467,2.80104466326066,
125.590260817245));
#164360=CARTESIAN_POINT('Ctrl Pts',(-251.981335508802,2.93762629505646,
125.668381420461));
#164361=CARTESIAN_POINT('Ctrl Pts',(-251.973922729502,3.07429199056805,
125.746550105606));
#164362=CARTESIAN_POINT('Ctrl Pts',(-251.966509950202,3.20771310571814,
125.83010741846));
#164363=CARTESIAN_POINT('Ctrl Pts',(-251.959097170902,3.3374540854052,125.918735704588));
#164364=CARTESIAN_POINT('Ctrl Pts',(-251.951673799875,3.46738044508888,
126.007490626968));
#164365=CARTESIAN_POINT('Ctrl Pts',(-251.944250428849,3.59361586841001,
126.101330771682));
#164366=CARTESIAN_POINT('Ctrl Pts',(-251.936827057822,3.71575779308237,
126.199898153212));
#164367=CARTESIAN_POINT('Ctrl Pts',(-251.932891008357,3.78052037272035,
126.252160944331));
#164368=CARTESIAN_POINT('Ctrl Pts',(-251.928954958891,3.84413272915417,
126.305752105551));
#164369=CARTESIAN_POINT('Ctrl Pts',(-251.925018909426,3.90653920889307,
126.360614228326));
#164370=CARTESIAN_POINT('Ctrl Pts',(-251.917595643021,4.02423588129208,
126.464082479034));
#164371=CARTESIAN_POINT('Ctrl Pts',(-251.910172376617,4.13799700900795,
126.572386370818));
#164372=CARTESIAN_POINT('Ctrl Pts',(-251.902749110212,4.24739970008144,
126.685194882827));
#164373=CARTESIAN_POINT('Ctrl Pts',(-251.895334617492,4.35667308625939,
126.797870064543));
#164374=CARTESIAN_POINT('Ctrl Pts',(-251.887920124772,4.46159803215885,
126.9150390035));
#164375=CARTESIAN_POINT('Ctrl Pts',(-251.880505632052,4.56178481830169,
127.036330650327));
#164376=CARTESIAN_POINT('Ctrl Pts',(-251.8730982857,4.66187504064777,127.157505391698));
#164377=CARTESIAN_POINT('Ctrl Pts',(-251.865690939347,4.7572359587348,127.282794644363));
#164378=CARTESIAN_POINT('Ctrl Pts',(-251.858283592994,4.84751491565739,
127.411790838626));
#164379=CARTESIAN_POINT('Ctrl Pts',(-251.85088177132,4.93772653912762,127.540690822659));
#164380=CARTESIAN_POINT('Ctrl Pts',(-251.843479949645,5.02286353534696,
127.673291938723));
#164381=CARTESIAN_POINT('Ctrl Pts',(-251.836078127971,5.10261382013593,
127.80915398612));
#164382=CARTESIAN_POINT('Ctrl Pts',(-251.828680213661,5.1823220053701,127.944944312999));
#164383=CARTESIAN_POINT('Ctrl Pts',(-251.82128229935,5.25664895385125,128.083991821801));
#164384=CARTESIAN_POINT('Ctrl Pts',(-251.81388438504,5.32532624709685,128.225827909904));
#164385=CARTESIAN_POINT('Ctrl Pts',(-251.806487700129,5.39399212742215,
128.367640427422));
#164386=CARTESIAN_POINT('Ctrl Pts',(-251.799091015218,5.45701005336667,
128.512240268852));
#164387=CARTESIAN_POINT('Ctrl Pts',(-251.791694330306,5.51415782275889,
128.659134739434));
#164388=CARTESIAN_POINT('Ctrl Pts',(-251.784297973372,5.57130305815897,
128.806022696561));
#164389=CARTESIAN_POINT('Ctrl Pts',(-251.776901616437,5.62257851920319,
128.955204732637));
#164390=CARTESIAN_POINT('Ctrl Pts',(-251.769505259503,5.66781048216889,
129.106168961505));
#164391=CARTESIAN_POINT('Ctrl Pts',(-251.762107770167,5.71304937026359,
129.257156303381));
#164392=CARTESIAN_POINT('Ctrl Pts',(-251.754710280832,5.7522428107855,129.40992602373));
#164393=CARTESIAN_POINT('Ctrl Pts',(-251.747312791497,5.78526724809163,
129.563952043483));
#164394=CARTESIAN_POINT('Ctrl Pts',(-251.739912708983,5.81830326206303,
129.718032056819));
#164395=CARTESIAN_POINT('Ctrl Pts',(-251.732512626469,5.84516588901763,
129.873368881604));
#164396=CARTESIAN_POINT('Ctrl Pts',(-251.725112543955,5.8657829024923,130.029427392488));
#164397=CARTESIAN_POINT('Ctrl Pts',(-251.717704324289,5.88642258649274,
130.185657505748));
#164398=CARTESIAN_POINT('Ctrl Pts',(-251.710296104624,5.90080289285541,
130.342610519604));
#164399=CARTESIAN_POINT('Ctrl Pts',(-251.702887884959,5.90890352503909,
130.499746608892));
#164400=CARTESIAN_POINT('Ctrl Pts',(-251.695475105658,5.91700914302668,
130.656979412819));
#164401=CARTESIAN_POINT('Ctrl Pts',(-251.688062326357,5.91882738096768,
130.814395144299));
#164402=CARTESIAN_POINT('Ctrl Pts',(-251.680649547056,5.91439006236425,
130.971455658507));
#164403=CARTESIAN_POINT('Ctrl Pts',(-251.673226176028,5.9099464035119,131.128740588143));
#164404=CARTESIAN_POINT('Ctrl Pts',(-251.665802805,5.89922936182667,131.285668915369));
#164405=CARTESIAN_POINT('Ctrl Pts',(-251.658379433973,5.88232252591546,
131.441708453216));
#164406=CARTESIAN_POINT('Ctrl Pts',(-251.65444338452,5.87335811581224,131.524444360569));
#164407=CARTESIAN_POINT('Ctrl Pts',(-251.650507335067,5.8626543865947,131.606930569052));
#164408=CARTESIAN_POINT('Ctrl Pts',(-251.646571285614,5.85022955562714,
131.689089225087));
#164409=CARTESIAN_POINT('Ctrl Pts',(-251.639148019207,5.82679671225734,
131.844037885828));
#164410=CARTESIAN_POINT('Ctrl Pts',(-251.631724752801,5.79716824906139,
131.998289243483));
#164411=CARTESIAN_POINT('Ctrl Pts',(-251.624301486394,5.76139407982381,
132.151308582215));
#164412=CARTESIAN_POINT('Ctrl Pts',(-251.616886993672,5.72566219268329,
132.304147064796));
#164413=CARTESIAN_POINT('Ctrl Pts',(-251.60947250095,5.68379914211561,132.455756066969));
#164414=CARTESIAN_POINT('Ctrl Pts',(-251.602058008228,5.63590644956803,
132.605607145451));
#164415=CARTESIAN_POINT('Ctrl Pts',(-251.594650661873,5.5880599178005,132.755313791822));
#164416=CARTESIAN_POINT('Ctrl Pts',(-251.587243315518,5.53419542667724,
132.903265534435));
#164417=CARTESIAN_POINT('Ctrl Pts',(-251.579835969163,5.47446525645678,
133.048945371668));
#164418=CARTESIAN_POINT('Ctrl Pts',(-251.572434147486,5.41477963525075,
133.194516555383));
#164419=CARTESIAN_POINT('Ctrl Pts',(-251.56503232581,5.34923718685904,133.337818863736));
#164420=CARTESIAN_POINT('Ctrl Pts',(-251.557630504133,5.27803957547498,
133.478351792237));
#164421=CARTESIAN_POINT('Ctrl Pts',(-251.550232589821,5.20687954875555,
133.6188105345));
#164422=CARTESIAN_POINT('Ctrl Pts',(-251.542834675508,5.13007047272427,
133.756502476267));
#164423=CARTESIAN_POINT('Ctrl Pts',(-251.535436761195,5.04786150929324,
133.8909484983));
#164424=CARTESIAN_POINT('Ctrl Pts',(-251.528040076282,4.96566620750038,
134.025372177845));
#164425=CARTESIAN_POINT('Ctrl Pts',(-251.520643391369,4.87807299385584,
134.156550690065));
#164426=CARTESIAN_POINT('Ctrl Pts',(-251.513246706455,4.78537628071299,
134.28403077643));
#164427=CARTESIAN_POINT('Ctrl Pts',(-251.505850349519,4.69268367783954,
134.411505210195));
#164428=CARTESIAN_POINT('Ctrl Pts',(-251.498453992582,4.59488824495589,
134.535281242258));
#164429=CARTESIAN_POINT('Ctrl Pts',(-251.491057635645,4.49232674446931,
134.654936026959));
#164430=CARTESIAN_POINT('Ctrl Pts',(-251.483660146308,4.38974954155489,
134.774609131115));
#164431=CARTESIAN_POINT('Ctrl Pts',(-251.47626265697,4.2824050610685,134.890159448109));
#164432=CARTESIAN_POINT('Ctrl Pts',(-251.468865167632,4.17066912338748,
135.001198668495));
#164433=CARTESIAN_POINT('Ctrl Pts',(-251.461465085116,4.05889401684656,
135.112276813507));
#164434=CARTESIAN_POINT('Ctrl Pts',(-251.4540650026,3.94272465276058,135.218840450467));
#164435=CARTESIAN_POINT('Ctrl Pts',(-251.446664920083,3.82257220707633,
135.320539564883));
#164436=CARTESIAN_POINT('Ctrl Pts',(-251.439256700416,3.70228764142629,
135.42235050793));
#164437=CARTESIAN_POINT('Ctrl Pts',(-251.431848480748,3.5780115325228,135.519286004722));
#164438=CARTESIAN_POINT('Ctrl Pts',(-251.42444026108,3.45018707979019,135.611037190516));
#164439=CARTESIAN_POINT('Ctrl Pts',(-251.417027481777,3.32228395323944,
135.702844847635));
#164440=CARTESIAN_POINT('Ctrl Pts',(-251.409614702474,3.19082844206446,
135.789461630659));
#164441=CARTESIAN_POINT('Ctrl Pts',(-251.402201923171,3.05629050412772,
135.870623433181));
#164442=CARTESIAN_POINT('Ctrl Pts',(-251.394778552141,2.92156033207666,
135.951901203491));
#164443=CARTESIAN_POINT('Ctrl Pts',(-251.387355181111,2.7837392630747,136.027708246836));
#164444=CARTESIAN_POINT('Ctrl Pts',(-251.379931810081,2.64332022277605,
136.097827228622));
#164445=CARTESIAN_POINT('Ctrl Pts',(-251.375995760654,2.56886667857348,
136.135005995111));
#164446=CARTESIAN_POINT('Ctrl Pts',(-251.372059711227,2.49368306864493,
136.170586454851));
#164447=CARTESIAN_POINT('Ctrl Pts',(-251.3681236618,2.41784474033988,136.204541852868));
#164448=CARTESIAN_POINT('Ctrl Pts',(-251.360700395395,2.27481601949637,
136.268580674038));
#164449=CARTESIAN_POINT('Ctrl Pts',(-251.35327712899,2.12902507563505,136.327030035431));
#164450=CARTESIAN_POINT('Ctrl Pts',(-251.345853862585,1.98094875995439,
136.379642903956));
#164451=CARTESIAN_POINT('Ctrl Pts',(-251.338439369864,1.8330474581819,136.43219358844));
#164452=CARTESIAN_POINT('Ctrl Pts',(-251.331024877143,1.68286650950291,
136.4789213873));
#164453=CARTESIAN_POINT('Ctrl Pts',(-251.323610384423,1.53090538303937,
136.519626076902));
#164454=CARTESIAN_POINT('Ctrl Pts',(-251.316203038069,1.37909072243075,
136.560291533792));
#164455=CARTESIAN_POINT('Ctrl Pts',(-251.308795691716,1.22549965802752,
136.594945342693));
#164456=CARTESIAN_POINT('Ctrl Pts',(-251.301388345363,1.07064946913359,
136.623436169296));
#164457=CARTESIAN_POINT('Ctrl Pts',(-251.293986523688,0.915914773352263,
136.651905746366));
#164458=CARTESIAN_POINT('Ctrl Pts',(-251.286584702013,0.759923188515468,
136.6742214263));
#164459=CARTESIAN_POINT('Ctrl Pts',(-251.279182880338,0.603204807647272,
136.690282339992));
#164460=CARTESIAN_POINT('Ctrl Pts',(-251.271784966027,0.446569157192895,
136.706334775254));
#164461=CARTESIAN_POINT('Ctrl Pts',(-251.264387051716,0.289207845217121,
136.716138982091));
#164462=CARTESIAN_POINT('Ctrl Pts',(-251.256989137405,0.131658646401416,
136.719645611827));
#164463=CARTESIAN_POINT('Ctrl Pts',(-251.249592452493,-0.0258643705954541,
136.723151658825));
#164464=CARTESIAN_POINT('Ctrl Pts',(-251.242195767581,-0.183574839623018,
136.720362197501));
#164465=CARTESIAN_POINT('Ctrl Pts',(-251.23479908267,-0.340932284373179,
136.711279927999));
#164466=CARTESIAN_POINT('Ctrl Pts',(-251.227402725735,-0.498282751729341,
136.702198061215));
#164467=CARTESIAN_POINT('Ctrl Pts',(-251.2200063688,-0.655279853255146,
136.686823962568));
#164468=CARTESIAN_POINT('Ctrl Pts',(-251.212610011865,-0.811385808614204,
136.665212401401));
#164469=CARTESIAN_POINT('Ctrl Pts',(-251.205212522529,-0.967515664193547,
136.643597531448));
#164470=CARTESIAN_POINT('Ctrl Pts',(-251.197815033193,-1.12275373214748,
136.615743348696));
#164471=CARTESIAN_POINT('Ctrl Pts',(-251.190417543856,-1.27657017664553,
136.581756150728));
#164472=CARTESIAN_POINT('Ctrl Pts',(-251.183017461342,-1.43044054125997,
136.547757038601));
#164473=CARTESIAN_POINT('Ctrl Pts',(-251.175617378827,-1.58288792593311,
136.507620711276));
#164474=CARTESIAN_POINT('Ctrl Pts',(-251.168217296313,-1.7333956029165,
136.46150391134));
#164475=CARTESIAN_POINT('Ctrl Pts',(-251.160809076647,-1.88406877856353,
136.415336401241));
#164476=CARTESIAN_POINT('Ctrl Pts',(-251.153400856981,-2.03279762982558,
136.363175394969));
#164477=CARTESIAN_POINT('Ctrl Pts',(-251.145992637315,-2.17908273993251,
136.305226819813));
#164478=CARTESIAN_POINT('Ctrl Pts',(-251.138579858013,-2.32545788608382,
136.247242578277));
#164479=CARTESIAN_POINT('Ctrl Pts',(-251.131167078711,-2.46938595350926,
136.183463820706));
#164480=CARTESIAN_POINT('Ctrl Pts',(-251.12375429941,-2.6103907183032,136.114143179997));
#164481=CARTESIAN_POINT('Ctrl Pts',(-251.116330928381,-2.75159695731775,
136.044723490705));
#164482=CARTESIAN_POINT('Ctrl Pts',(-251.108907557353,-2.88987122410066,
135.969746280717));
#164483=CARTESIAN_POINT('Ctrl Pts',(-251.101484186325,-3.0247642305461,
135.889508787689));
#164484=CARTESIAN_POINT('Ctrl Pts',(-251.097548136879,-3.0962877393667,
135.84696494356));
#164485=CARTESIAN_POINT('Ctrl Pts',(-251.093612087434,-3.16686116580283,
135.802942950607));
#164486=CARTESIAN_POINT('Ctrl Pts',(-251.089676037988,-3.23642127305177,
135.757491738972));
#164487=CARTESIAN_POINT('Ctrl Pts',(-251.082262927628,-3.36742998084501,
135.671889448529));
#164488=CARTESIAN_POINT('Ctrl Pts',(-251.074849817269,-3.49524090964866,
135.580954646384));
#164489=CARTESIAN_POINT('Ctrl Pts',(-251.067436706909,-3.61938921607638,
135.484953770688));
#164490=CARTESIAN_POINT('Ctrl Pts',(-251.060032365242,-3.74339067208673,
135.389066450859));
#164491=CARTESIAN_POINT('Ctrl Pts',(-251.052628023575,-3.86373783562373,
135.288125211725));
#164492=CARTESIAN_POINT('Ctrl Pts',(-251.045223681908,-3.97999295862695,
135.182440860296));
#164493=CARTESIAN_POINT('Ctrl Pts',(-251.037826471706,-4.0961361109251,
135.076858298371));
#164494=CARTESIAN_POINT('Ctrl Pts',(-251.030429261504,-4.20819479333491,
134.966541968504));
#164495=CARTESIAN_POINT('Ctrl Pts',(-251.023032051303,-4.31576271800789,
134.851844122703));
#164496=CARTESIAN_POINT('Ctrl Pts',(-251.015640341042,-4.42325066425436,
134.737231556535));
#164497=CARTESIAN_POINT('Ctrl Pts',(-251.008248630781,-4.5262542457145,
134.618244232668));
#164498=CARTESIAN_POINT('Ctrl Pts',(-251.00085692052,-4.62440267623168,
134.495272490066));
#164499=CARTESIAN_POINT('Ctrl Pts',(-250.993469083091,-4.72249968259949,
134.372365177605));
#164500=CARTESIAN_POINT('Ctrl Pts',(-250.986081245663,-4.81574637096713,
134.245477895747));
#164501=CARTESIAN_POINT('Ctrl Pts',(-250.978693408234,-4.90381113174446,
134.115035314162));
#164502=CARTESIAN_POINT('Ctrl Pts',(-250.971306752627,-4.99186180492488,
133.984613599294));
#164503=CARTESIAN_POINT('Ctrl Pts',(-250.963920097021,-5.07473198604866,
133.850638023283));
#164504=CARTESIAN_POINT('Ctrl Pts',(-250.956533441414,-5.1521323889978,
133.713563671452));
#164505=CARTESIAN_POINT('Ctrl Pts',(-250.949147064478,-5.22952987192629,
133.576494490911));
#164506=CARTESIAN_POINT('Ctrl Pts',(-250.941760687542,-5.30145780279621,
133.436327093028));
#164507=CARTESIAN_POINT('Ctrl Pts',(-250.934374310605,-5.36767216274448,
133.293542434107));
#164508=CARTESIAN_POINT('Ctrl Pts',(-250.926986743122,-5.43389719521569,
133.150734760955));
#164509=CARTESIAN_POINT('Ctrl Pts',(-250.919599175639,-5.49440666570941,
133.005309326591));
#164510=CARTESIAN_POINT('Ctrl Pts',(-250.912211608156,-5.54900420961933,
132.857768235193));
#164511=CARTESIAN_POINT('Ctrl Pts',(-250.904821380464,-5.60362141370727,
132.710174015321));
#164512=CARTESIAN_POINT('Ctrl Pts',(-250.897431152772,-5.65232232312268,
132.560462972647));
#164513=CARTESIAN_POINT('Ctrl Pts',(-250.89004092508,-5.69496010914035,
132.409153413475));
#164514=CARTESIAN_POINT('Ctrl Pts',(-250.882642565357,-5.73764481276505,
132.257677356857));
#164515=CARTESIAN_POINT('Ctrl Pts',(-250.875244205634,-5.7742529686653,
132.104599631833));
#164516=CARTESIAN_POINT('Ctrl Pts',(-250.867845845911,-5.80468849773136,
131.950450494847));
#164517=CARTESIAN_POINT('Ctrl Pts',(-250.860442849322,-5.83514310203205,
131.796204746069));
#164518=CARTESIAN_POINT('Ctrl Pts',(-250.853039852734,-5.85941731376475,
131.64088661638));
#164519=CARTESIAN_POINT('Ctrl Pts',(-250.845636856145,-5.87746688625184,
131.485032023983));
#164520=CARTESIAN_POINT('Ctrl Pts',(-250.838223446978,-5.89554184610583,
131.328958216547));
#164521=CARTESIAN_POINT('Ctrl Pts',(-250.830810037811,-5.9073746551586,
131.172346811769));
#164522=CARTESIAN_POINT('Ctrl Pts',(-250.823396628644,-5.91297314554463,
131.015735030795));
#164523=CARTESIAN_POINT('Ctrl Pts',(-250.820056149833,-5.91549582277577,
130.945165833253));
#164524=CARTESIAN_POINT('Ctrl Pts',(-250.816715671021,-5.91675338732688,
130.874596511954));
#164525=CARTESIAN_POINT('Ctrl Pts',(-250.81337519221,-5.91674999314685,
130.804075842693));
#164526=CARTESIAN_POINT('',(-249.063375969071,-5.91496647234029,130.809715820468));
#164527=CARTESIAN_POINT('Ctrl Pts',(-250.81337519221,-5.92651577310741,
130.804075372663));
#164528=CARTESIAN_POINT('Ctrl Pts',(-250.812659599531,-5.92652634227882,
130.788943599106));
#164529=CARTESIAN_POINT('Ctrl Pts',(-250.811944006853,-5.92647342300579,
130.773811901629));
#164530=CARTESIAN_POINT('Ctrl Pts',(-250.811228414174,-5.92635679277963,
130.758680695231));
#164531=CARTESIAN_POINT('Ctrl Pts',(-250.71841253957,-5.91122928131646,
128.79608912902));
#164532=CARTESIAN_POINT('Ctrl Pts',(-250.532780790362,-3.73730962072342,
124.887429206006));
#164533=CARTESIAN_POINT('Ctrl Pts',(-250.254333166549,2.95797483390075,
124.461810230503));
#164534=CARTESIAN_POINT('Ctrl Pts',(-249.975885542736,6.9350249212652,129.864685209915));
#164535=CARTESIAN_POINT('Ctrl Pts',(-249.697437918923,4.53912590079626,
136.131075983253));
#164536=CARTESIAN_POINT('Ctrl Pts',(-249.41899029511,-2.02800807388145,
137.502475560044));
#164537=CARTESIAN_POINT('Ctrl Pts',(-249.207636433196,-5.59816439000333,
133.871332218785));
#164538=CARTESIAN_POINT('Ctrl Pts',(-249.089098445888,-5.91888558459242,
131.356595549194));
#164539=CARTESIAN_POINT('Ctrl Pts',(-249.063376333184,-5.91413166792106,
130.809722808261));
#164540=CARTESIAN_POINT('',(-247.313374425905,-5.91167834912772,130.802355503486));
#164541=CARTESIAN_POINT('Ctrl Pts',(-249.06337519221,-5.91674758999916,
130.80970091149));
#164542=CARTESIAN_POINT('Ctrl Pts',(-249.056039121377,-5.91688842597513,
130.653662511114));
#164543=CARTESIAN_POINT('Ctrl Pts',(-249.048703050544,-5.91085239615979,
130.497490660387));
#164544=CARTESIAN_POINT('Ctrl Pts',(-249.041366979711,-5.89863472226865,
130.341717152523));
#164545=CARTESIAN_POINT('Ctrl Pts',(-249.033897315869,-5.88619455927311,
130.183106941982));
#164546=CARTESIAN_POINT('Ctrl Pts',(-249.026427652026,-5.86734539502519,
130.02491012295));
#164547=CARTESIAN_POINT('Ctrl Pts',(-249.018957988183,-5.84213773715391,
129.867687129833));
#164548=CARTESIAN_POINT('Ctrl Pts',(-249.01162653947,-5.81739650986932,
129.713373316668));
#164549=CARTESIAN_POINT('Ctrl Pts',(-249.004295090756,-5.7865301308496,
129.559997991909));
#164550=CARTESIAN_POINT('Ctrl Pts',(-248.996963642042,-5.74963852955144,
129.408084376274));
#164551=CARTESIAN_POINT('Ctrl Pts',(-248.989632196889,-5.71274694616648,
129.256170834402));
#164552=CARTESIAN_POINT('Ctrl Pts',(-248.982300751735,-5.66983023572421,
129.10571937014));
#164553=CARTESIAN_POINT('Ctrl Pts',(-248.974969306581,-5.62103900359289,
128.957240945594));
#164554=CARTESIAN_POINT('Ctrl Pts',(-248.967636354787,-5.5722377446736,
128.808732008153));
#164555=CARTESIAN_POINT('Ctrl Pts',(-248.960303402993,-5.51755968027065,
128.662197278831));
#164556=CARTESIAN_POINT('Ctrl Pts',(-248.952970451199,-5.45720455405735,
128.518130310341));
#164557=CARTESIAN_POINT('Ctrl Pts',(-248.945397500889,-5.39487407861425,
128.369348206731));
#164558=CARTESIAN_POINT('Ctrl Pts',(-248.93782455058,-5.32648877245105,
128.223198555189));
#164559=CARTESIAN_POINT('Ctrl Pts',(-248.93025160027,-5.25232094526869,
128.080199232774));
#164560=CARTESIAN_POINT('Ctrl Pts',(-248.922907255254,-5.18039202857906,
127.941516643039));
#164561=CARTESIAN_POINT('Ctrl Pts',(-248.915562910238,-5.10302489309629,
127.805797237635));
#164562=CARTESIAN_POINT('Ctrl Pts',(-248.908218565223,-5.02051266192647,
127.67348483371));
#164563=CARTESIAN_POINT('Ctrl Pts',(-248.900531312266,-4.93414792938501,
127.53499475515));
#164564=CARTESIAN_POINT('Ctrl Pts',(-248.89284405931,-4.84214637605896,
127.400237873611));
#164565=CARTESIAN_POINT('Ctrl Pts',(-248.885156806354,-4.74489163246716,
127.269684683531));
#164566=CARTESIAN_POINT('Ctrl Pts',(-248.877469553398,-4.64763688887508,
127.139131493451));
#164567=CARTESIAN_POINT('Ctrl Pts',(-248.869782300441,-4.54512930921572,
127.012782312023));
#164568=CARTESIAN_POINT('Ctrl Pts',(-248.862095047485,-4.43779615577289,
126.891063306818));
#164569=CARTESIAN_POINT('Ctrl Pts',(-248.85467178108,-4.33414891056291,
126.773524231756));
#164570=CARTESIAN_POINT('Ctrl Pts',(-248.847248514674,-4.22567201910399,
126.659928055844));
#164571=CARTESIAN_POINT('Ctrl Pts',(-248.839825248268,-4.11269714543466,
126.550697166794));
#164572=CARTESIAN_POINT('Ctrl Pts',(-248.832410755547,-3.9998557986837,
126.441595379584));
#164573=CARTESIAN_POINT('Ctrl Pts',(-248.824996262826,-3.88252731748045,
126.336848866352));
#164574=CARTESIAN_POINT('Ctrl Pts',(-248.817581770105,-3.76108334385289,
126.236846781452));
#164575=CARTESIAN_POINT('Ctrl Pts',(-248.810174423751,-3.63975642249939,
126.136941082326));
#164576=CARTESIAN_POINT('Ctrl Pts',(-248.802767077397,-3.51432219181145,
126.041770943571));
#164577=CARTESIAN_POINT('Ctrl Pts',(-248.795359731044,-3.38518875769885,
125.951688401431));
#164578=CARTESIAN_POINT('Ctrl Pts',(-248.787957909368,-3.25615163617297,
125.861673046249));
#164579=CARTESIAN_POINT('Ctrl Pts',(-248.780556087693,-3.12342110962033,
125.776737944937));
#164580=CARTESIAN_POINT('Ctrl Pts',(-248.773154266017,-2.98743785316926,
125.697194511402));
#164581=CARTESIAN_POINT('Ctrl Pts',(-248.765756351706,-2.85152638122117,
125.617693068226));
#164582=CARTESIAN_POINT('Ctrl Pts',(-248.758358437394,-2.71236592044747,
125.543577812451));
#164583=CARTESIAN_POINT('Ctrl Pts',(-248.750960523083,-2.57042548141573,
125.475116449113));
#164584=CARTESIAN_POINT('Ctrl Pts',(-248.74356383817,-2.4285086303101,125.406666462812));
#164585=CARTESIAN_POINT('Ctrl Pts',(-248.736167153258,-2.28381305374583,
125.343868666186));
#164586=CARTESIAN_POINT('Ctrl Pts',(-248.728770468346,-2.13683178406518,
125.286944511352));
#164587=CARTESIAN_POINT('Ctrl Pts',(-248.72137411141,-1.98985703168806,
125.230022880594));
#164588=CARTESIAN_POINT('Ctrl Pts',(-248.713977754475,-1.84059713581557,
125.178974508595));
#164589=CARTESIAN_POINT('Ctrl Pts',(-248.706581397539,-1.68956424639153,
125.133972339871));
#164590=CARTESIAN_POINT('Ctrl Pts',(-248.699183908203,-1.53850823344611,
125.088963281201));
#164591=CARTESIAN_POINT('Ctrl Pts',(-248.691786418866,-1.3856790442339,
125.050002375581));
#164592=CARTESIAN_POINT('Ctrl Pts',(-248.684388929529,-1.23160294524551,
125.017212377909));
#164593=CARTESIAN_POINT('Ctrl Pts',(-248.676988847014,-1.07747283512013,
124.984410885754));
#164594=CARTESIAN_POINT('Ctrl Pts',(-248.669588764499,-0.922095309844468,
124.957784686123));
#164595=CARTESIAN_POINT('Ctrl Pts',(-248.662188681984,-0.766005604067277,
124.937405191023));
#164596=CARTESIAN_POINT('Ctrl Pts',(-248.654780462318,-0.609744261611506,
124.917003286574));
#164597=CARTESIAN_POINT('Ctrl Pts',(-248.647372242651,-0.452769545104186,
124.902861852648));
#164598=CARTESIAN_POINT('Ctrl Pts',(-248.639964022985,-0.295621309973686,
124.89500036424));
#164599=CARTESIAN_POINT('Ctrl Pts',(-248.632551243682,-0.138376352727071,
124.887134037217));
#164600=CARTESIAN_POINT('Ctrl Pts',(-248.62513846438,0.0190419635371055,
124.885555361347));
#164601=CARTESIAN_POINT('Ctrl Pts',(-248.617725685078,0.176095543047275,
124.890231694198));
#164602=CARTESIAN_POINT('Ctrl Pts',(-248.610302314049,0.333373528077153,
124.894914708813));
#164603=CARTESIAN_POINT('Ctrl Pts',(-248.60287894302,0.490285364088859,
124.90587055631));
#164604=CARTESIAN_POINT('Ctrl Pts',(-248.595455571992,0.646298991936183,
124.92301483828));
#164605=CARTESIAN_POINT('Ctrl Pts',(-248.591519522552,0.729021160899325,
124.932105147951));
#164606=CARTESIAN_POINT('Ctrl Pts',(-248.587583473112,0.811490984336267,
124.94293439471));
#164607=CARTESIAN_POINT('Ctrl Pts',(-248.583647423672,0.893630636483042,
124.955484242736));
#164608=CARTESIAN_POINT('Ctrl Pts',(-248.576224157266,1.0485434569725,124.979152864451));
#164609=CARTESIAN_POINT('Ctrl Pts',(-248.568800890861,1.20274954650635,
125.00901603764));
#164610=CARTESIAN_POINT('Ctrl Pts',(-248.561377624455,1.35571426582556,
125.045023034828));
#164611=CARTESIAN_POINT('Ctrl Pts',(-248.553963131734,1.5084981935499,125.080987474736));
#164612=CARTESIAN_POINT('Ctrl Pts',(-248.546548639013,1.66004331170418,
125.12308119991));
#164613=CARTESIAN_POINT('Ctrl Pts',(-248.539134146292,1.80982133211593,
125.17120188482));
#164614=CARTESIAN_POINT('Ctrl Pts',(-248.531726799938,1.95945499083214,
125.219276189201));
#164615=CARTESIAN_POINT('Ctrl Pts',(-248.524319453584,2.10732458951269,
125.273365775303));
#164616=CARTESIAN_POINT('Ctrl Pts',(-248.516912107231,2.25291335888148,
125.333317576255));
#164617=CARTESIAN_POINT('Ctrl Pts',(-248.509510285555,2.39839354265291,
125.393224662892));
#164618=CARTESIAN_POINT('Ctrl Pts',(-248.50210846388,2.54159594059722,125.45898511709));
#164619=CARTESIAN_POINT('Ctrl Pts',(-248.494706642204,2.68202035570336,
125.530396513205));
#164620=CARTESIAN_POINT('Ctrl Pts',(-248.487308727893,2.82237064185423,
125.6017702118));
#164621=CARTESIAN_POINT('Ctrl Pts',(-248.479910813582,2.95994553382201,
125.678788742564));
#164622=CARTESIAN_POINT('Ctrl Pts',(-248.47251289927,3.09426629210827,125.761202214737));
#164623=CARTESIAN_POINT('Ctrl Pts',(-248.465116214358,3.22856472872152,
125.843601991286));
#164624=CARTESIAN_POINT('Ctrl Pts',(-248.457719529446,3.35960978706752,
125.931394734843));
#164625=CARTESIAN_POINT('Ctrl Pts',(-248.450322844533,3.48694865718476,
126.024285343613));
#164626=CARTESIAN_POINT('Ctrl Pts',(-248.442926487598,3.61428188096307,
126.117171833516));
#164627=CARTESIAN_POINT('Ctrl Pts',(-248.435530130662,3.73790894168576,
126.215155519181));
#164628=CARTESIAN_POINT('Ctrl Pts',(-248.428133773727,3.85740750667736,
126.317898995092));
#164629=CARTESIAN_POINT('Ctrl Pts',(-248.42073628439,3.97692436720433,126.420658201292));
#164630=CARTESIAN_POINT('Ctrl Pts',(-248.413338795054,4.09231119036169,
126.528178405362));
#164631=CARTESIAN_POINT('Ctrl Pts',(-248.405941305717,4.20318023908498,
126.64008319642));
#164632=CARTESIAN_POINT('Ctrl Pts',(-248.398541223202,4.31408815278158,
126.752027215529));
#164633=CARTESIAN_POINT('Ctrl Pts',(-248.391141140687,4.42047487634386,
126.868358616781));
#164634=CARTESIAN_POINT('Ctrl Pts',(-248.383741058172,4.52199102142404,
126.988665692043));
#164635=CARTESIAN_POINT('Ctrl Pts',(-248.376332838506,4.62361879394142,
127.109105057302));
#164636=CARTESIAN_POINT('Ctrl Pts',(-248.368924618839,4.72036505140227,
127.233528541592));
#164637=CARTESIAN_POINT('Ctrl Pts',(-248.361516399173,4.81192160389547,
127.361492475963));
#164638=CARTESIAN_POINT('Ctrl Pts',(-248.35410361987,4.90353450791928,127.489535170001));
#164639=CARTESIAN_POINT('Ctrl Pts',(-248.346690840568,4.98995113773683,
127.621122344922));
#164640=CARTESIAN_POINT('Ctrl Pts',(-248.339278061266,5.07090810244087,
127.755783641484));
#164641=CARTESIAN_POINT('Ctrl Pts',(-248.331854690237,5.1519807422527,127.890637348421));
#164642=CARTESIAN_POINT('Ctrl Pts',(-248.324431319209,5.22757795761725,
128.028573623214));
#164643=CARTESIAN_POINT('Ctrl Pts',(-248.31700794818,5.29748316434078,128.169099210034));
#164644=CARTESIAN_POINT('Ctrl Pts',(-248.31307189874,5.33454858229421,128.243609248024));
#164645=CARTESIAN_POINT('Ctrl Pts',(-248.309135849299,5.37001458430393,
128.318846918548));
#164646=CARTESIAN_POINT('Ctrl Pts',(-248.305199799859,5.40385453009061,
128.394736833628));
#164647=CARTESIAN_POINT('Ctrl Pts',(-248.297776533453,5.46767561174162,
128.537862845039));
#164648=CARTESIAN_POINT('Ctrl Pts',(-248.290353267048,5.52590303645513,
128.683742570062));
#164649=CARTESIAN_POINT('Ctrl Pts',(-248.282930000642,5.57829049711204,
128.83189878211));
#164650=CARTESIAN_POINT('Ctrl Pts',(-248.275515507921,5.63061604014097,
128.979879885819));
#164651=CARTESIAN_POINT('Ctrl Pts',(-248.268101015201,5.67711523505334,
129.130131772354));
#164652=CARTESIAN_POINT('Ctrl Pts',(-248.26068652248,5.71758861855437,129.282154668465));
#164653=CARTESIAN_POINT('Ctrl Pts',(-248.253279176126,5.75802299228471,
129.434031039186));
#164654=CARTESIAN_POINT('Ctrl Pts',(-248.245871829772,5.79244302160307,
129.58767466294));
#164655=CARTESIAN_POINT('Ctrl Pts',(-248.238464483418,5.82069815958615,
129.742568030716));
#164656=CARTESIAN_POINT('Ctrl Pts',(-248.231062661743,5.84893222382131,
129.897345873174));
#164657=CARTESIAN_POINT('Ctrl Pts',(-248.223660840068,5.8710104852747,130.053371238049));
#164658=CARTESIAN_POINT('Ctrl Pts',(-248.216259018392,5.88683288166969,
130.210113879424));
#164659=CARTESIAN_POINT('Ctrl Pts',(-248.208861104081,5.90264692554483,
130.366773777579));
#164660=CARTESIAN_POINT('Ctrl Pts',(-248.201463189769,5.91221164389696,
130.524149827675));
#164661=CARTESIAN_POINT('Ctrl Pts',(-248.194065275458,5.9154785065081,130.681704180553));
#164662=CARTESIAN_POINT('Ctrl Pts',(-248.186668590546,5.91874482622592,
130.839232350755));
#164663=CARTESIAN_POINT('Ctrl Pts',(-248.179271905634,5.91571535964195,
130.996938392079));
#164664=CARTESIAN_POINT('Ctrl Pts',(-248.171875220721,5.90639362940904,
131.154281832951));
#164665=CARTESIAN_POINT('Ctrl Pts',(-248.164478863786,5.89707231251142,
131.31161829705));
#164666=CARTESIAN_POINT('Ctrl Pts',(-248.157082506851,5.88145930879928,
131.468591820021));
#164667=CARTESIAN_POINT('Ctrl Pts',(-248.149686149915,5.85961020596212,
131.624664705502));
#164668=CARTESIAN_POINT('Ctrl Pts',(-248.142288660579,5.83775775797154,
131.78076148614));
#164669=CARTESIAN_POINT('Ctrl Pts',(-248.134891171242,5.80966736155416,
131.935956985013));
#164670=CARTESIAN_POINT('Ctrl Pts',(-248.127493681905,5.77544612049189,
132.08972152867));
#164671=CARTESIAN_POINT('Ctrl Pts',(-248.12009359939,5.74121288322676,132.24353997425));
#164672=CARTESIAN_POINT('Ctrl Pts',(-248.112693516876,5.70084460340386,
132.395926101739));
#164673=CARTESIAN_POINT('Ctrl Pts',(-248.105293434361,5.65449880979943,
132.546363422523));
#164674=CARTESIAN_POINT('Ctrl Pts',(-248.097885214694,5.60810205423026,
132.696966164607));
#164675=CARTESIAN_POINT('Ctrl Pts',(-248.090476995028,5.5557147683582,132.845615463476));
#164676=CARTESIAN_POINT('Ctrl Pts',(-248.083068775361,5.49754363926177,
132.991812216325));
#164677=CARTESIAN_POINT('Ctrl Pts',(-248.075655996059,5.43933670680584,
133.138098950836));
#164678=CARTESIAN_POINT('Ctrl Pts',(-248.068243216757,5.3753389890633,133.281929791188));
#164679=CARTESIAN_POINT('Ctrl Pts',(-248.060830437455,5.3058038433676,133.42282889849));
#164680=CARTESIAN_POINT('Ctrl Pts',(-248.053407066426,5.23616934259515,
133.563929329044));
#164681=CARTESIAN_POINT('Ctrl Pts',(-248.045983695398,5.16098178952406,
133.70208933316));
#164682=CARTESIAN_POINT('Ctrl Pts',(-248.038560324369,5.08053910520641,
133.836860075599));
#164683=CARTESIAN_POINT('Ctrl Pts',(-248.034624274928,5.0378864637818,133.908318757025));
#164684=CARTESIAN_POINT('Ctrl Pts',(-248.030688225487,4.99375712111194,
133.978825107679));
#164685=CARTESIAN_POINT('Ctrl Pts',(-248.026752176046,4.94820010351743,
134.048315965294));
#164686=CARTESIAN_POINT('Ctrl Pts',(-248.01932890964,4.86228099012706,134.179373554009));
#164687=CARTESIAN_POINT('Ctrl Pts',(-248.011905643235,4.77102159127743,
134.307213490192));
#164688=CARTESIAN_POINT('Ctrl Pts',(-248.004482376829,4.67469027619907,
134.431370596062));
#164689=CARTESIAN_POINT('Ctrl Pts',(-247.997067884108,4.57847281673531,
134.555380958543));
#164690=CARTESIAN_POINT('Ctrl Pts',(-247.989653391387,4.47719559989458,
134.675716862927));
#164691=CARTESIAN_POINT('Ctrl Pts',(-247.982238898666,4.37117128428337,
134.791940355447));
#164692=CARTESIAN_POINT('Ctrl Pts',(-247.974831552313,4.26524915889839,
134.908051827389));
#164693=CARTESIAN_POINT('Ctrl Pts',(-247.967424205959,4.15458929342252,
135.020058504474));
#164694=CARTESIAN_POINT('Ctrl Pts',(-247.960016859605,4.03954570855317,
135.127554001051));
#164695=CARTESIAN_POINT('Ctrl Pts',(-247.95261503793,3.92458792753074,135.23496932343));
#164696=CARTESIAN_POINT('Ctrl Pts',(-247.945213216254,3.8052532088006,135.337879910926));
#164697=CARTESIAN_POINT('Ctrl Pts',(-247.937811394579,3.68193357716447,
135.435914967441));
#164698=CARTESIAN_POINT('Ctrl Pts',(-247.930413480267,3.5586790450016,135.533898272014));
#164699=CARTESIAN_POINT('Ctrl Pts',(-247.923015565956,3.43144408083488,
135.627010939651));
#164700=CARTESIAN_POINT('Ctrl Pts',(-247.915617651645,3.30065496062629,
135.714921419897));
#164701=CARTESIAN_POINT('Ctrl Pts',(-247.908220966732,3.16988757519691,
135.802817291017));
#164702=CARTESIAN_POINT('Ctrl Pts',(-247.90082428182,3.03556751547619,135.8855124825));
#164703=CARTESIAN_POINT('Ctrl Pts',(-247.893427596908,2.89815139958546,
135.962717819969));
#164704=CARTESIAN_POINT('Ctrl Pts',(-247.886031239973,2.7607413768697,136.039919734071));
#164705=CARTESIAN_POINT('Ctrl Pts',(-247.878634883037,2.620235896397,136.111632095323));
#164706=CARTESIAN_POINT('Ctrl Pts',(-247.871238526102,2.47711738385079,
136.177611033201));
#164707=CARTESIAN_POINT('Ctrl Pts',(-247.863841036765,2.33397695949535,
136.243600072623));
#164708=CARTESIAN_POINT('Ctrl Pts',(-247.856443547429,2.18822304551935,
136.303853784557));
#164709=CARTESIAN_POINT('Ctrl Pts',(-247.849046058092,2.04035916340784,
136.35817597701));
#164710=CARTESIAN_POINT('Ctrl Pts',(-247.841645975577,1.89244344784061,
136.412517212024));
#164711=CARTESIAN_POINT('Ctrl Pts',(-247.834245893062,1.7424166416891,136.460922659066));
#164712=CARTESIAN_POINT('Ctrl Pts',(-247.826845810547,1.59079842960389,
136.503245676845));
#164713=CARTESIAN_POINT('Ctrl Pts',(-247.819437590881,1.43901349770798,
136.545615233133));
#164714=CARTESIAN_POINT('Ctrl Pts',(-247.812029371214,1.28563402495745,
136.581888902843));
#164715=CARTESIAN_POINT('Ctrl Pts',(-247.804621151548,1.1311916400925,136.611970800411));
#164716=CARTESIAN_POINT('Ctrl Pts',(-247.797208372246,0.976654198516669,
136.642071212885));
#164717=CARTESIAN_POINT('Ctrl Pts',(-247.789795592944,0.821052909356628,
136.665972202912));
#164718=CARTESIAN_POINT('Ctrl Pts',(-247.782382813641,0.664925055174279,
136.683629724649));
#164719=CARTESIAN_POINT('Ctrl Pts',(-247.774959442613,0.508574118191981,
136.701312476281));
#164720=CARTESIAN_POINT('Ctrl Pts',(-247.767536071584,0.351695484840332,
136.712733915431));
#164721=CARTESIAN_POINT('Ctrl Pts',(-247.760112700555,0.194827806524608,
136.717902085105));
#164722=CARTESIAN_POINT('Ctrl Pts',(-247.756176651114,0.111652799491557,
136.720642372675));
#164723=CARTESIAN_POINT('Ctrl Pts',(-247.752240601674,0.0284808222158047,
136.72162551162));
#164724=CARTESIAN_POINT('Ctrl Pts',(-247.748304552233,-0.0546084851756728,
136.720858608426));
#164725=CARTESIAN_POINT('Ctrl Pts',(-247.740881285827,-0.211312325782589,
136.719412252935));
#164726=CARTESIAN_POINT('Ctrl Pts',(-247.733458019422,-0.368195618920861,
136.711733744254));
#164727=CARTESIAN_POINT('Ctrl Pts',(-247.726034753017,-0.524721937222637,
136.697797429062));
#164728=CARTESIAN_POINT('Ctrl Pts',(-247.718620260296,-0.681063254415326,
136.683877585438));
#164729=CARTESIAN_POINT('Ctrl Pts',(-247.711205767575,-0.837048068398791,
136.663714690278));
#164730=CARTESIAN_POINT('Ctrl Pts',(-247.703791274854,-0.992138916650457,
136.637335067413));
#164731=CARTESIAN_POINT('Ctrl Pts',(-247.6963839285,-1.14708028250351,136.610980870222));
#164732=CARTESIAN_POINT('Ctrl Pts',(-247.688976582146,-1.30112903243422,
136.578421936227));
#164733=CARTESIAN_POINT('Ctrl Pts',(-247.681569235793,-1.45375190585053,
136.539736451697));
#164734=CARTESIAN_POINT('Ctrl Pts',(-247.674167414117,-1.60626094736971,
136.501079820261));
#164735=CARTESIAN_POINT('Ctrl Pts',(-247.666765592442,-1.75734586959446,
136.456305827931));
#164736=CARTESIAN_POINT('Ctrl Pts',(-247.659363770767,-1.90648281228602,
136.405543871929));
#164737=CARTESIAN_POINT('Ctrl Pts',(-247.651965856455,-2.05554102674641,
136.354808712768));
#164738=CARTESIAN_POINT('Ctrl Pts',(-247.644567942144,-2.20265295713487,
136.298092005196));
#164739=CARTESIAN_POINT('Ctrl Pts',(-247.637170027833,-2.34730924809386,
136.235573176131));
#164740=CARTESIAN_POINT('Ctrl Pts',(-247.62977334292,-2.49194149980182,
136.173064736561));
#164741=CARTESIAN_POINT('Ctrl Pts',(-247.622376658008,-2.63411857967471,
136.104756237117));
#164742=CARTESIAN_POINT('Ctrl Pts',(-247.614979973096,-2.77335038386919,
136.030875537739));
#164743=CARTESIAN_POINT('Ctrl Pts',(-247.607583616161,-2.91257601437956,
135.956998114309));
#164744=CARTESIAN_POINT('Ctrl Pts',(-247.600187259225,-3.04885629913221,
135.877549157195));
#164745=CARTESIAN_POINT('Ctrl Pts',(-247.59279090229,-3.18172530008505,
135.792802726812));
#164746=CARTESIAN_POINT('Ctrl Pts',(-247.585393412953,-3.31461464362113,
135.708043321535));
#164747=CARTESIAN_POINT('Ctrl Pts',(-247.577995923617,-3.44409134868632,
135.617985028821));
#164748=CARTESIAN_POINT('Ctrl Pts',(-247.57059843428,-3.56971818773886,
135.522945428993));
#164749=CARTESIAN_POINT('Ctrl Pts',(-247.563198351765,-3.6953890650849,
135.42787251318));
#164750=CARTESIAN_POINT('Ctrl Pts',(-247.55579826925,-3.81720709192725,
135.327815038682));
#164751=CARTESIAN_POINT('Ctrl Pts',(-247.548398186736,-3.93476799254689,
135.223130967712));
#164752=CARTESIAN_POINT('Ctrl Pts',(-247.540989967069,-4.05245816346248,
135.118331785844));
#164753=CARTESIAN_POINT('Ctrl Pts',(-247.533581747403,-4.16588158063674,
135.008896096001));
#164754=CARTESIAN_POINT('Ctrl Pts',(-247.526173527736,-4.27467021450847,
134.895219344006));
#164755=CARTESIAN_POINT('Ctrl Pts',(-247.518760748434,-4.38352580596943,
134.781472625868));
#164756=CARTESIAN_POINT('Ctrl Pts',(-247.511347969132,-4.4877406833542,
134.663479923365));
#164757=CARTESIAN_POINT('Ctrl Pts',(-247.50393518983,-4.58698737529911,
134.54166945968));
#164758=CARTESIAN_POINT('Ctrl Pts',(-247.496511818802,-4.68637587557155,
134.419684947493));
#164759=CARTESIAN_POINT('Ctrl Pts',(-247.489088447773,-4.78078178910005,
134.293872077067));
#164760=CARTESIAN_POINT('Ctrl Pts',(-247.481665076744,-4.86992072845301,
134.164688378527));
#164761=CARTESIAN_POINT('Ctrl Pts',(-247.477729027303,-4.91718433296531,
134.096192081829));
#164762=CARTESIAN_POINT('Ctrl Pts',(-247.473792977861,-4.96296796091647,
134.0267485524));
#164763=CARTESIAN_POINT('Ctrl Pts',(-247.46985692842,-5.0072345437592,133.956428634961));
#164764=CARTESIAN_POINT('Ctrl Pts',(-247.462236797479,-5.09293396461543,
133.820290360621));
#164765=CARTESIAN_POINT('Ctrl Pts',(-247.454616666537,-5.1731927381962,
133.680472003976));
#164766=CARTESIAN_POINT('Ctrl Pts',(-247.446996535596,-5.24768859798355,
133.537434883131));
#164767=CARTESIAN_POINT('Ctrl Pts',(-247.439386872341,-5.32208212365789,
133.394594250747));
#164768=CARTESIAN_POINT('Ctrl Pts',(-247.431777209087,-5.39072834575388,
133.248543966223));
#164769=CARTESIAN_POINT('Ctrl Pts',(-247.424167545832,-5.45334834088897,
133.099773964966));
#164770=CARTESIAN_POINT('Ctrl Pts',(-247.41656715745,-5.51589201301343,
132.95118528877));
#164771=CARTESIAN_POINT('Ctrl Pts',(-247.408966769067,-5.57242395691912,
132.799883816999));
#164772=CARTESIAN_POINT('Ctrl Pts',(-247.401366380684,-5.62271116517123,
132.6463838844));
#164773=CARTESIAN_POINT('Ctrl Pts',(-247.393776486392,-5.67292894032262,
132.493095893897));
#164774=CARTESIAN_POINT('Ctrl Pts',(-247.3861865921,-5.71691906458911,132.337615822874));
#164775=CARTESIAN_POINT('Ctrl Pts',(-247.378596697808,-5.75449676660908,
132.180477446031));
#164776=CARTESIAN_POINT('Ctrl Pts',(-247.371012940078,-5.79204408640011,
132.023466118313));
#164777=CARTESIAN_POINT('Ctrl Pts',(-247.363429182348,-5.82318923077531,
131.864799491174));
#164778=CARTESIAN_POINT('Ctrl Pts',(-247.355845424619,-5.8477971054084,
131.705026802385));
#164779=CARTESIAN_POINT('Ctrl Pts',(-247.348267771385,-5.87238517209377,
131.545382721577));
#164780=CARTESIAN_POINT('Ctrl Pts',(-247.340690118151,-5.89044640661716,
131.384634695695));
#164781=CARTESIAN_POINT('Ctrl Pts',(-247.333112464918,-5.90189671411097,
131.223342405316));
#164782=CARTESIAN_POINT('Ctrl Pts',(-247.326533374015,-5.9118381315317,
131.083304769971));
#164783=CARTESIAN_POINT('Ctrl Pts',(-247.319954283113,-5.91679692710892,
130.942857179328));
#164784=CARTESIAN_POINT('Ctrl Pts',(-247.31337519221,-5.91674966518615,
130.802370135328));
#164785=CARTESIAN_POINT('',(-245.56337519221,-5.92144182645146,130.799714417675));
#164786=CARTESIAN_POINT('Ctrl Pts',(-247.313373802672,-5.90755386651321,
130.802343603462));
#164787=CARTESIAN_POINT('Ctrl Pts',(-247.272718969984,-5.9101514079421,
129.935566300425));
#164788=CARTESIAN_POINT('Ctrl Pts',(-247.139248262692,-5.32479902775277,
127.093265132076));
#164789=CARTESIAN_POINT('Ctrl Pts',(-246.912961680793,-0.92912039214145,
123.867913700948));
#164790=CARTESIAN_POINT('Ctrl Pts',(-246.634514056983,5.3336169743627,126.273346327016));
#164791=CARTESIAN_POINT('Ctrl Pts',(-246.356066433168,6.6950209031102,132.842559733769));
#164792=CARTESIAN_POINT('Ctrl Pts',(-246.077618809355,1.90402769183364,
137.538767724297));
#164793=CARTESIAN_POINT('Ctrl Pts',(-245.813388395704,-4.30271337160949,
136.122583916631));
#164794=CARTESIAN_POINT('Ctrl Pts',(-245.641973856654,-5.90708458492476,
132.465498504199));
#164795=CARTESIAN_POINT('Ctrl Pts',(-245.56337519221,-5.92144182645146,
130.799714417675));
#164796=CARTESIAN_POINT('',(-243.813375192209,-5.9225958886547,130.808561907707));
#164797=CARTESIAN_POINT('Ctrl Pts',(-245.56337519221,-5.92144182645146,
130.799714417675));
#164798=CARTESIAN_POINT('Ctrl Pts',(-245.54915798205,-5.92403881612739,
130.498401378748));
#164799=CARTESIAN_POINT('Ctrl Pts',(-245.53494077189,-5.90303585155336,
130.197451465269));
#164800=CARTESIAN_POINT('Ctrl Pts',(-245.427907687125,-5.55779885964375,
127.96065567089));
#164801=CARTESIAN_POINT('Ctrl Pts',(-245.242275937917,-2.84039908430047,
124.408292014724));
#164802=CARTESIAN_POINT('Ctrl Pts',(-244.963828314104,3.84588857597675,
124.957421111165));
#164803=CARTESIAN_POINT('Ctrl Pts',(-244.685380690291,6.99799251703414,
130.879601975114));
#164804=CARTESIAN_POINT('Ctrl Pts',(-244.406933066478,3.71928320587602,
136.732639707219));
#164805=CARTESIAN_POINT('Ctrl Pts',(-244.128485442666,-2.97726567439561,
137.137878568468));
#164806=CARTESIAN_POINT('Ctrl Pts',(-243.930632817909,-5.79148458215932,
133.290250095944));
#164807=CARTESIAN_POINT('Ctrl Pts',(-243.825596067757,-5.92467647219331,
131.067434134564));
#164808=CARTESIAN_POINT('Ctrl Pts',(-243.813375192209,-5.9225958886547,
130.808561907707));
#164809=CARTESIAN_POINT('',(-242.06337519221,-5.90805017840298,130.806988762596));
#164810=CARTESIAN_POINT('Ctrl Pts',(-243.813375192209,-5.9225958886547,
130.808561907707));
#164811=CARTESIAN_POINT('Ctrl Pts',(-243.732780193153,-5.90887472541408,
129.101335056553));
#164812=CARTESIAN_POINT('Ctrl Pts',(-243.559369319492,-4.23448331121838,
125.404542141305));
#164813=CARTESIAN_POINT('Ctrl Pts',(-243.293142571227,2.04838543811749,
124.11244925927));
#164814=CARTESIAN_POINT('Ctrl Pts',(-243.014694947414,6.73729691441007,
128.910583751768));
#164815=CARTESIAN_POINT('Ctrl Pts',(-242.736247323601,5.23496166160834,
135.449006667785));
#164816=CARTESIAN_POINT('Ctrl Pts',(-242.457799699788,-1.07804761611268,
137.719226767226));
#164817=CARTESIAN_POINT('Ctrl Pts',(-242.233508989324,-5.3652113839518,
134.429383518755));
#164818=CARTESIAN_POINT('Ctrl Pts',(-242.102034153465,-5.91133744411979,
131.631040389034));
#164819=CARTESIAN_POINT('Ctrl Pts',(-242.06337519221,-5.90805017840298,
130.806988762596));
#164820=CARTESIAN_POINT('',(-240.313375158645,-5.91547317117931,130.799225748986));
#164821=CARTESIAN_POINT('Ctrl Pts',(-242.06337519221,-5.90805017840298,
130.806988762596));
#164822=CARTESIAN_POINT('Ctrl Pts',(-242.00921827886,-5.90344508403932,
129.652583908473));
#164823=CARTESIAN_POINT('Ctrl Pts',(-241.862245490907,-5.01819434382023,
126.513200125347));
#164824=CARTESIAN_POINT('Ctrl Pts',(-241.622456828348,0.0858910237578114,
123.80649070863));
#164825=CARTESIAN_POINT('Ctrl Pts',(-241.344009204537,5.93393234070992,
127.094103550159));
#164826=CARTESIAN_POINT('Ctrl Pts',(-241.065561580723,6.32897972525682,
133.791261380503));
#164827=CARTESIAN_POINT('Ctrl Pts',(-240.787113956911,0.908003930142733,
137.743603327918));
#164828=CARTESIAN_POINT('Ctrl Pts',(-240.536385160739,-4.72467356506664,
135.560472003922));
#164829=CARTESIAN_POINT('Ctrl Pts',(-240.378472239172,-5.9015401168494,
132.183950904784));
#164830=CARTESIAN_POINT('Ctrl Pts',(-240.313375192209,-5.91293939285975,
130.799228662519));
#164831=CARTESIAN_POINT('',(-238.56337519221,-5.92098466177766,130.803851200521));
#164832=CARTESIAN_POINT('Ctrl Pts',(-240.313375141761,-5.91674777057218,
130.799224283353));
#164833=CARTESIAN_POINT('Ctrl Pts',(-240.304447198716,-5.91658280276366,
130.609191300127));
#164834=CARTESIAN_POINT('Ctrl Pts',(-240.29551925567,-5.90725896805116,
130.419559254438));
#164835=CARTESIAN_POINT('Ctrl Pts',(-240.286591312625,-5.88891442289698,
130.231108943084));
#164836=CARTESIAN_POINT('Ctrl Pts',(-240.277195878735,-5.8696093085647,
130.032790872178));
#164837=CARTESIAN_POINT('Ctrl Pts',(-240.267800444845,-5.84031377300887,
129.835781692581));
#164838=CARTESIAN_POINT('Ctrl Pts',(-240.258405010955,-5.8012449903555,
129.640965962096));
#164839=CARTESIAN_POINT('Ctrl Pts',(-240.249009577065,-5.76217620770222,
129.446150231612));
#164840=CARTESIAN_POINT('Ctrl Pts',(-240.239614143174,-5.71333430736417,
129.25352788837));
#164841=CARTESIAN_POINT('Ctrl Pts',(-240.230218709284,-5.65499162829623,
129.063958294424));
#164842=CARTESIAN_POINT('Ctrl Pts',(-240.222795442879,-5.60889548685207,
128.914180688121));
#164843=CARTESIAN_POINT('Ctrl Pts',(-240.215372176473,-5.5567750380937,
128.76600921319));
#164844=CARTESIAN_POINT('Ctrl Pts',(-240.207948910068,-5.4987587456095,
128.619965319072));
#164845=CARTESIAN_POINT('Ctrl Pts',(-240.200534417347,-5.44081102356507,
128.474094036708));
#164846=CARTESIAN_POINT('Ctrl Pts',(-240.193119924626,-5.37698146490024,
128.330345673324));
#164847=CARTESIAN_POINT('Ctrl Pts',(-240.185705431904,-5.30744864521202,
128.189227840643));
#164848=CARTESIAN_POINT('Ctrl Pts',(-240.178298085551,-5.23798284387309,
128.048246022642));
#164849=CARTESIAN_POINT('Ctrl Pts',(-240.170890739197,-5.16282488887633,
127.909890020461));
#164850=CARTESIAN_POINT('Ctrl Pts',(-240.163483392843,-5.08220186366389,
127.77464862144));
#164851=CARTESIAN_POINT('Ctrl Pts',(-240.156081571168,-5.00163897014562,
127.639508090556));
#164852=CARTESIAN_POINT('Ctrl Pts',(-240.148679749492,-4.91561931271538,
127.507477856713));
#164853=CARTESIAN_POINT('Ctrl Pts',(-240.141277927817,-4.8244163750696,
127.379023086393));
#164854=CARTESIAN_POINT('Ctrl Pts',(-240.133880013506,-4.73326158274495,
127.250636126348));
#164855=CARTESIAN_POINT('Ctrl Pts',(-240.126482099194,-4.63692917506799,
127.125821174471));
#164856=CARTESIAN_POINT('Ctrl Pts',(-240.119084184883,-4.53573644743927,
127.005015221071));
#164857=CARTESIAN_POINT('Ctrl Pts',(-240.111687499971,-4.43456053620563,
126.884229343427));
#164858=CARTESIAN_POINT('Ctrl Pts',(-240.104290815059,-4.32852614753222,
126.767451427893));
#164859=CARTESIAN_POINT('Ctrl Pts',(-240.096894130146,-4.21799150393006,
126.655086194818));
#164860=CARTESIAN_POINT('Ctrl Pts',(-240.089497773211,-4.10746176154984,
126.542725944135));
#164861=CARTESIAN_POINT('Ctrl Pts',(-240.082101416275,-3.99243242279038,
126.434778252988));
#164862=CARTESIAN_POINT('Ctrl Pts',(-240.07470505934,-3.87329909540618,
126.331611498733));
#164863=CARTESIAN_POINT('Ctrl Pts',(-240.067307570004,-3.75414752840543,
126.228428949383));
#164864=CARTESIAN_POINT('Ctrl Pts',(-240.059910080667,-3.63089100390062,
126.130029038771));
#164865=CARTESIAN_POINT('Ctrl Pts',(-240.05251259133,-3.50395864907101,
126.036740210266));
#164866=CARTESIAN_POINT('Ctrl Pts',(-240.045112508815,-3.37698179830101,
125.943418679507));
#164867=CARTESIAN_POINT('Ctrl Pts',(-240.0377124263,-3.24632685230914,125.855212019014));
#164868=CARTESIAN_POINT('Ctrl Pts',(-240.030312343786,-3.1124522400116,
125.772405568468));
#164869=CARTESIAN_POINT('Ctrl Pts',(-240.022904124119,-2.97843041881538,
125.689508063716));
#164870=CARTESIAN_POINT('Ctrl Pts',(-240.015495904453,-2.84118217866342,
125.612022824149));
#164871=CARTESIAN_POINT('Ctrl Pts',(-240.008087684786,-2.70119153247436,
125.540189755275));
#164872=CARTESIAN_POINT('Ctrl Pts',(-240.000674905484,-2.56111472437804,
125.468312474347));
#164873=CARTESIAN_POINT('Ctrl Pts',(-239.993262126182,-2.41829248476486,
125.402094452746));
#164874=CARTESIAN_POINT('Ctrl Pts',(-239.98584934688,-2.27322866963384,
125.341727371772));
#164875=CARTESIAN_POINT('Ctrl Pts',(-239.978425975851,-2.12795758052115,
125.281274035481));
#164876=CARTESIAN_POINT('Ctrl Pts',(-239.971002604823,-1.98043886821596,
125.226688466011));
#164877=CARTESIAN_POINT('Ctrl Pts',(-239.963579233794,-1.83119218500668,
125.178112689855));
#164878=CARTESIAN_POINT('Ctrl Pts',(-239.959643184353,-1.75205801244773,
125.152356647779));
#164879=CARTESIAN_POINT('Ctrl Pts',(-239.955707134913,-1.67243823896076,
125.128289324805));
#164880=CARTESIAN_POINT('Ctrl Pts',(-239.951771085472,-1.59241134073006,
125.105926035647));
#164881=CARTESIAN_POINT('Ctrl Pts',(-239.944347819067,-1.44148310821466,
125.063749570226));
#164882=CARTESIAN_POINT('Ctrl Pts',(-239.936924552661,-1.28864987425473,
125.027509678405));
#164883=CARTESIAN_POINT('Ctrl Pts',(-239.929501286256,-1.13441978674124,
124.997380136287));
#164884=CARTESIAN_POINT('Ctrl Pts',(-239.922086793535,-0.980371986382731,
124.967286204787));
#164885=CARTESIAN_POINT('Ctrl Pts',(-239.914672300814,-0.824930981520049,
124.94328831858));
#164886=CARTESIAN_POINT('Ctrl Pts',(-239.907257808093,-0.668620364745964,
124.925510613497));
#164887=CARTESIAN_POINT('Ctrl Pts',(-239.899850461739,-0.512460406029317,
124.907750043235));
#164888=CARTESIAN_POINT('Ctrl Pts',(-239.892443115385,-0.355432872438929,
124.896197760646));
#164889=CARTESIAN_POINT('Ctrl Pts',(-239.885035769031,-0.198071738752809,
124.890926915493));
#164890=CARTESIAN_POINT('Ctrl Pts',(-239.877633947356,-0.0408279709366401,
124.885660001536));
#164891=CARTESIAN_POINT('Ctrl Pts',(-239.870232125681,0.11674853007498,
124.886665209125));
#164892=CARTESIAN_POINT('Ctrl Pts',(-239.862830304005,0.274118581926308,
124.893963882528));
#164893=CARTESIAN_POINT('Ctrl Pts',(-239.855432389694,0.431405559351781,
124.901258703019));
#164894=CARTESIAN_POINT('Ctrl Pts',(-239.848034475382,0.588485932708498,
124.914840355609));
#164895=CARTESIAN_POINT('Ctrl Pts',(-239.840636561071,0.744820543760275,
124.934678094627));
#164896=CARTESIAN_POINT('Ctrl Pts',(-239.833239876159,0.90112917483567,
124.954512536973));
#164897=CARTESIAN_POINT('Ctrl Pts',(-239.825843191246,1.05669191960906,
124.980600955408));
#164898=CARTESIAN_POINT('Ctrl Pts',(-239.818446506334,1.21097464736905,
125.012860728424));
#164899=CARTESIAN_POINT('Ctrl Pts',(-239.811050149399,1.36525053407166,
125.045119071008));
#164900=CARTESIAN_POINT('Ctrl Pts',(-239.803653792463,1.51824615121821,
125.083548147673));
#164901=CARTESIAN_POINT('Ctrl Pts',(-239.796257435528,1.66943773685229,
125.128014239369));
#164902=CARTESIAN_POINT('Ctrl Pts',(-239.788859946191,1.82065247030411,
125.172487138937));
#164903=CARTESIAN_POINT('Ctrl Pts',(-239.781462456855,1.97006226413546,
125.222998788572));
#164904=CARTESIAN_POINT('Ctrl Pts',(-239.774064967518,2.11715883591395,
125.279365683088));
#164905=CARTESIAN_POINT('Ctrl Pts',(-239.766664885003,2.26430697216745,
125.335752336931));
#164906=CARTESIAN_POINT('Ctrl Pts',(-239.759264802488,2.40913992351535,
125.39799818877));
#164907=CARTESIAN_POINT('Ctrl Pts',(-239.751864719973,2.55116983357646,
125.465871782441));
#164908=CARTESIAN_POINT('Ctrl Pts',(-239.744456500306,2.69335592012452,
125.533820010106));
#164909=CARTESIAN_POINT('Ctrl Pts',(-239.73704828064,2.83273247294492,125.60740817695));
#164910=CARTESIAN_POINT('Ctrl Pts',(-239.729640060973,2.96883603193272,
125.686358743983));
#164911=CARTESIAN_POINT('Ctrl Pts',(-239.722227281671,3.10502336039045,
125.765357903773));
#164912=CARTESIAN_POINT('Ctrl Pts',(-239.714814502369,3.23793336649246,
125.849725840755));
#164913=CARTESIAN_POINT('Ctrl Pts',(-239.707401723067,3.36713243685951,
125.939142255031));
#164914=CARTESIAN_POINT('Ctrl Pts',(-239.699978352038,3.49651611291696,
126.028686431672));
#164915=CARTESIAN_POINT('Ctrl Pts',(-239.69255498101,3.62217796580202,126.123293268655));
#164916=CARTESIAN_POINT('Ctrl Pts',(-239.685131609981,3.74371761984629,
126.222602336583));
#164917=CARTESIAN_POINT('Ctrl Pts',(-239.68119556054,3.80816086072349,126.275258387286));
#164918=CARTESIAN_POINT('Ctrl Pts',(-239.677259511099,3.87144581355598,
126.329235781727));
#164919=CARTESIAN_POINT('Ctrl Pts',(-239.673323461659,3.93351717534727,
126.384476773646));
#164920=CARTESIAN_POINT('Ctrl Pts',(-239.665900195253,4.05058182650684,
126.488659560394));
#164921=CARTESIAN_POINT('Ctrl Pts',(-239.658476928847,4.16368156997823,
126.597653941848));
#164922=CARTESIAN_POINT('Ctrl Pts',(-239.651053662442,4.27239553665532,
126.711126329027));
#164923=CARTESIAN_POINT('Ctrl Pts',(-239.643639169721,4.38098101245193,
126.824464601268));
#164924=CARTESIAN_POINT('Ctrl Pts',(-239.636224677,4.48519077375898,126.942270077301));
#164925=CARTESIAN_POINT('Ctrl Pts',(-239.628810184279,4.58463736700177,
127.064169342298));
#164926=CARTESIAN_POINT('Ctrl Pts',(-239.621402837925,4.6839881098739,127.185951116194));
#164927=CARTESIAN_POINT('Ctrl Pts',(-239.613995491571,4.77858458991015,
127.311818536534));
#164928=CARTESIAN_POINT('Ctrl Pts',(-239.606588145218,4.8680766377315,127.441361894451));
#164929=CARTESIAN_POINT('Ctrl Pts',(-239.599186323542,4.95750193900725,
127.570808634044));
#164930=CARTESIAN_POINT('Ctrl Pts',(-239.591784501867,5.04183017721024,
127.703925546399));
#164931=CARTESIAN_POINT('Ctrl Pts',(-239.584382680192,5.1207519535698,127.840270539226));
#164932=CARTESIAN_POINT('Ctrl Pts',(-239.57698476588,5.19963206773796,127.976543556594));
#164933=CARTESIAN_POINT('Ctrl Pts',(-239.569586851569,5.27311121746229,
128.116040938422));
#164934=CARTESIAN_POINT('Ctrl Pts',(-239.562188937258,5.34092384175067,
128.258292456829));
#164935=CARTESIAN_POINT('Ctrl Pts',(-239.554792252345,5.40872519681105,
128.400520335614));
#164936=CARTESIAN_POINT('Ctrl Pts',(-239.547395567433,5.47086173490065,
128.545501105967));
#164937=CARTESIAN_POINT('Ctrl Pts',(-239.539998882521,5.52711425713773,
128.692740729649));
#164938=CARTESIAN_POINT('Ctrl Pts',(-239.532602525585,5.5833642850792,128.839973824573));
#164939=CARTESIAN_POINT('Ctrl Pts',(-239.52520616865,5.63373068270668,128.989465224959));
#164940=CARTESIAN_POINT('Ctrl Pts',(-239.517809811715,5.67804284551261,
129.140701996627));
#164941=CARTESIAN_POINT('Ctrl Pts',(-239.510412322378,5.7223617926238,129.291961923032));
#164942=CARTESIAN_POINT('Ctrl Pts',(-239.503014833041,5.76062455432498,
129.444967394531));
#164943=CARTESIAN_POINT('Ctrl Pts',(-239.495617343705,5.79271077965507,
129.599191589683));
#164944=CARTESIAN_POINT('Ctrl Pts',(-239.48821726119,5.82480825276165,129.753469847888));
#164945=CARTESIAN_POINT('Ctrl Pts',(-239.480817178675,5.85072480266036,
129.908967315098));
#164946=CARTESIAN_POINT('Ctrl Pts',(-239.47341709616,5.87039146168622,130.065148436212));
#164947=CARTESIAN_POINT('Ctrl Pts',(-239.466008876493,5.89007974622549,
130.221501294526));
#164948=CARTESIAN_POINT('Ctrl Pts',(-239.458600656827,5.90350436859606,
130.378538937433));
#164949=CARTESIAN_POINT('Ctrl Pts',(-239.45119243716,5.91064831870181,130.535721426219));
#164950=CARTESIAN_POINT('Ctrl Pts',(-239.443779657858,5.91779666578963,
130.693000658204));
#164951=CARTESIAN_POINT('Ctrl Pts',(-239.436366878556,5.91865663578798,
130.850424541285));
#164952=CARTESIAN_POINT('Ctrl Pts',(-239.428954099254,5.91326332744977,
131.007455134325));
#164953=CARTESIAN_POINT('Ctrl Pts',(-239.421530728226,5.90786231289968,
131.164710100041));
#164954=CARTESIAN_POINT('Ctrl Pts',(-239.414107357197,5.89619020248658,
131.321570282092));
#164955=CARTESIAN_POINT('Ctrl Pts',(-239.406683986168,5.87833382284187,
131.477504012195));
#164956=CARTESIAN_POINT('Ctrl Pts',(-239.402747936727,5.86886594189645,
131.560183817473));
#164957=CARTESIAN_POINT('Ctrl Pts',(-239.398811887287,5.85766029406112,
131.642603340781));
#164958=CARTESIAN_POINT('Ctrl Pts',(-239.394875837846,5.84473557027929,
131.724684840876));
#164959=CARTESIAN_POINT('Ctrl Pts',(-239.38745257144,5.82035994459329,131.879487988383));
#164960=CARTESIAN_POINT('Ctrl Pts',(-239.380029305035,5.7897930585554,132.033556131228));
#164961=CARTESIAN_POINT('Ctrl Pts',(-239.372606038629,5.75308807999222,
132.186354867319));
#164962=CARTESIAN_POINT('Ctrl Pts',(-239.365191545909,5.71642648366544,
132.338973007995));
#164963=CARTESIAN_POINT('Ctrl Pts',(-239.357777053188,5.67364132170575,
132.49032436891));
#164964=CARTESIAN_POINT('Ctrl Pts',(-239.350362560467,5.62483733046353,
132.639881134565));
#164965=CARTESIAN_POINT('Ctrl Pts',(-239.342955214113,5.5760803783455,132.789293751778));
#164966=CARTESIAN_POINT('Ctrl Pts',(-239.335547867759,5.52131626096951,
132.936914864721));
#164967=CARTESIAN_POINT('Ctrl Pts',(-239.328140521405,5.46070040290813,
133.082228408325));
#164968=CARTESIAN_POINT('Ctrl Pts',(-239.32073869973,5.4001297544406,133.227433571607));
#164969=CARTESIAN_POINT('Ctrl Pts',(-239.313336878054,5.33371619859061,
133.370334249396));
#164970=CARTESIAN_POINT('Ctrl Pts',(-239.305935056379,5.26166444252784,
133.510431174063));
#164971=CARTESIAN_POINT('Ctrl Pts',(-239.298537142068,5.18965072202625,
133.650454142654));
#164972=CARTESIAN_POINT('Ctrl Pts',(-239.291139227756,5.11200489917788,
133.787675974645));
#164973=CARTESIAN_POINT('Ctrl Pts',(-239.283741313445,5.02897904781305,
133.921619076398));
#164974=CARTESIAN_POINT('Ctrl Pts',(-239.276344628533,4.94596699383835,
134.055539919237));
#164975=CARTESIAN_POINT('Ctrl Pts',(-239.268947943621,4.85757688227853,
134.186182796258));
#164976=CARTESIAN_POINT('Ctrl Pts',(-239.261551258708,4.76410587914538,
134.313096249498));
#164977=CARTESIAN_POINT('Ctrl Pts',(-239.254154901773,4.67063902061473,
134.440004075263));
#164978=CARTESIAN_POINT('Ctrl Pts',(-239.246758544838,4.57209193983944,
134.563182505476));
#164979=CARTESIAN_POINT('Ctrl Pts',(-239.239362187902,4.46880396696874,
134.68221075228));
#164980=CARTESIAN_POINT('Ctrl Pts',(-239.231964698566,4.36550018044543,
134.801257222613));
#164981=CARTESIAN_POINT('Ctrl Pts',(-239.224567209229,4.25745430125329,
134.916151962402));
#164982=CARTESIAN_POINT('Ctrl Pts',(-239.217169719892,4.14504450655627,
135.026508957116));
#164983=CARTESIAN_POINT('Ctrl Pts',(-239.209769637377,4.03259530678013,
135.136904637304));
#164984=CARTESIAN_POINT('Ctrl Pts',(-239.202369554862,3.91577941196701,
135.242759143993));
#164985=CARTESIAN_POINT('Ctrl Pts',(-239.194969472348,3.79501012108299,
135.343724972118));
#164986=CARTESIAN_POINT('Ctrl Pts',(-239.187561252681,3.67410803194808,
135.444801822551));
#164987=CARTESIAN_POINT('Ctrl Pts',(-239.180153033014,3.54924415173958,
135.540979019406));
#164988=CARTESIAN_POINT('Ctrl Pts',(-239.172744813348,3.42086355181755,
135.631950401542));
#164989=CARTESIAN_POINT('Ctrl Pts',(-239.165332034046,3.29240393577841,
135.722977775045));
#164990=CARTESIAN_POINT('Ctrl Pts',(-239.157919254744,3.16042359925697,
135.808792746258));
#164991=CARTESIAN_POINT('Ctrl Pts',(-239.150506475442,3.02539409909899,
135.889134074431));
#164992=CARTESIAN_POINT('Ctrl Pts',(-239.143083104413,2.89017166245913,
135.969590198061));
#164993=CARTESIAN_POINT('Ctrl Pts',(-239.135659733384,2.75189168800368,
136.04455688092));
#164994=CARTESIAN_POINT('Ctrl Pts',(-239.128236362356,2.61104841523133,
136.11381979302));
#164995=CARTESIAN_POINT('Ctrl Pts',(-239.124300312915,2.53636993251568,
136.150544650959));
#164996=CARTESIAN_POINT('Ctrl Pts',(-239.120364263474,2.46097112694201,
136.185666787633));
#164997=CARTESIAN_POINT('Ctrl Pts',(-239.116428214033,2.38492750732977,
136.219159907224));
#164998=CARTESIAN_POINT('Ctrl Pts',(-239.109004947627,2.24151161398831,
136.282326885485));
#164999=CARTESIAN_POINT('Ctrl Pts',(-239.101581681222,2.09536757343469,
136.339887693094));
#165000=CARTESIAN_POINT('Ctrl Pts',(-239.094158414816,1.94697373179301,
136.391598204264));
#165001=CARTESIAN_POINT('Ctrl Pts',(-239.086743922095,1.7987552793488,136.443247597904));
#165002=CARTESIAN_POINT('Ctrl Pts',(-239.079329429374,1.64829266779216,
136.489060336946));
#165003=CARTESIAN_POINT('Ctrl Pts',(-239.071914936653,1.49608657580917,
136.528839241876));
#165004=CARTESIAN_POINT('Ctrl Pts',(-239.0645075903,1.34402718578767,136.5685798064));
#165005=CARTESIAN_POINT('Ctrl Pts',(-239.057100243946,1.19022801949183,
136.602298020843));
#165006=CARTESIAN_POINT('Ctrl Pts',(-239.049692897592,1.03520726785652,
136.629845702525));
#165007=CARTESIAN_POINT('Ctrl Pts',(-239.042291075917,0.880302136546384,
136.657372838106));
#165008=CARTESIAN_POINT('Ctrl Pts',(-239.034889254241,0.72417759998665,
136.678738539528));
#165009=CARTESIAN_POINT('Ctrl Pts',(-239.027487432566,0.567364355398914,
136.69384516638));
#165010=CARTESIAN_POINT('Ctrl Pts',(-239.020089518254,0.410633891302364,
136.708943818562));
#165011=CARTESIAN_POINT('Ctrl Pts',(-239.012691603943,0.253215813869249,
136.717789940777));
#165012=CARTESIAN_POINT('Ctrl Pts',(-239.005293689632,0.0956481882167628,
136.720337458848));
#165013=CARTESIAN_POINT('Ctrl Pts',(-238.997897004719,-0.0618932525546835,
136.722884553569));
#165014=CARTESIAN_POINT('Ctrl Pts',(-238.990500319807,-0.219583819337571,
136.719135115535));
#165015=CARTESIAN_POINT('Ctrl Pts',(-238.983103634895,-0.376883062274058,
136.709095134873));
#165016=CARTESIAN_POINT('Ctrl Pts',(-238.97570727796,-0.534175330397275,
136.699055599393));
#165017=CARTESIAN_POINT('Ctrl Pts',(-238.968310921024,-0.691075936635662,
136.682726099669));
#165018=CARTESIAN_POINT('Ctrl Pts',(-238.960914564089,-0.847047444013144,
136.66016467765));
#165019=CARTESIAN_POINT('Ctrl Pts',(-238.953517074752,-1.00304283102658,
136.637599801419));
#165020=CARTESIAN_POINT('Ctrl Pts',(-238.946119585416,-1.15810846646915,
136.608801156552));
#165021=CARTESIAN_POINT('Ctrl Pts',(-238.938722096079,-1.31171517139054,
136.573878263925));
#165022=CARTESIAN_POINT('Ctrl Pts',(-238.931322013564,-1.46537572290444,
136.538943129132));
#165023=CARTESIAN_POINT('Ctrl Pts',(-238.923921931049,-1.61757596187038,
136.497879554932));
#165024=CARTESIAN_POINT('Ctrl Pts',(-238.916521848534,-1.76780012425026,
136.450847426477));
#165025=CARTESIAN_POINT('Ctrl Pts',(-238.909113628868,-1.91818947353988,
136.403763581361));
#165026=CARTESIAN_POINT('Ctrl Pts',(-238.901705409201,-2.06659805035564,
136.350698186771));
#165027=CARTESIAN_POINT('Ctrl Pts',(-238.894297189535,-2.21252770071824,
136.291860206273));
#165028=CARTESIAN_POINT('Ctrl Pts',(-238.886884410233,-2.35854716834568,
136.232986011979));
#165029=CARTESIAN_POINT('Ctrl Pts',(-238.879471630931,-2.50208432972178,
136.168332305074));
#165030=CARTESIAN_POINT('Ctrl Pts',(-238.872058851629,-2.64266450761232,
136.09815461268));
#165031=CARTESIAN_POINT('Ctrl Pts',(-238.8646354806,-2.7834455530538,136.027876647108));
#165032=CARTESIAN_POINT('Ctrl Pts',(-238.857212109571,-2.92126085037995,
135.952059111555));
#165033=CARTESIAN_POINT('Ctrl Pts',(-238.849788738542,-3.05566292917917,
135.871001973113));
#165034=CARTESIAN_POINT('Ctrl Pts',(-238.845852689102,-3.12692613629289,
135.828023533371));
#165035=CARTESIAN_POINT('Ctrl Pts',(-238.841916639661,-3.19723028071578,
135.783572755617));
#165036=CARTESIAN_POINT('Ctrl Pts',(-238.83798059022,-3.26651242466866,
135.737698954026));
#165037=CARTESIAN_POINT('Ctrl Pts',(-238.830575131449,-3.39686293686282,
135.651389940007));
#165038=CARTESIAN_POINT('Ctrl Pts',(-238.823169672677,-3.52399215415378,
135.559777460672));
#165039=CARTESIAN_POINT('Ctrl Pts',(-238.815764213906,-3.64743741711899,
135.463129859619));
#165040=CARTESIAN_POINT('Ctrl Pts',(-238.808367519445,-3.77073658344827,
135.36659664035));
#165041=CARTESIAN_POINT('Ctrl Pts',(-238.800970824984,-3.89036018059399,
135.265040388873));
#165042=CARTESIAN_POINT('Ctrl Pts',(-238.793574130524,-4.00587286862359,
135.158773680532));
#165043=CARTESIAN_POINT('Ctrl Pts',(-238.786184555943,-4.12127436692031,
135.052609261966));
#165044=CARTESIAN_POINT('Ctrl Pts',(-238.778794981362,-4.2325725588388,
134.941743664802));
#165045=CARTESIAN_POINT('Ctrl Pts',(-238.771405406781,-4.33936378316464,
134.826530743239));
#165046=CARTESIAN_POINT('Ctrl Pts',(-238.764021313419,-4.44607579506923,
134.711403280895));
#165047=CARTESIAN_POINT('Ctrl Pts',(-238.756637220058,-4.54828724127563,
134.591935188395));
#165048=CARTESIAN_POINT('Ctrl Pts',(-238.749253126696,-4.64563017140943,
134.468518211474));
#165049=CARTESIAN_POINT('Ctrl Pts',(-238.741508212759,-4.74772972233884,
134.339070516573));
#165050=CARTESIAN_POINT('Ctrl Pts',(-238.733763298822,-4.84447267690336,
134.205278594195));
#165051=CARTESIAN_POINT('Ctrl Pts',(-238.726018384885,-4.93548047736706,
134.067635509454));
#165052=CARTESIAN_POINT('Ctrl Pts',(-238.718639333783,-5.02218915041337,
133.936494561414));
#165053=CARTESIAN_POINT('Ctrl Pts',(-238.711260282681,-5.10369184030888,
133.801858290106));
#165054=CARTESIAN_POINT('Ctrl Pts',(-238.703881231578,-5.17970465458188,
133.664184083062));
#165055=CARTESIAN_POINT('Ctrl Pts',(-238.696502350099,-5.25571572154588,
133.52651304074));
#165056=CARTESIAN_POINT('Ctrl Pts',(-238.689123468619,-5.32623698218892,
133.385804530002));
#165057=CARTESIAN_POINT('Ctrl Pts',(-238.681744587139,-5.39103009844791,
133.242541299987));
#165058=CARTESIAN_POINT('Ctrl Pts',(-238.674364399656,-5.45583468256891,
133.099252713528));
#165059=CARTESIAN_POINT('Ctrl Pts',(-238.666984212174,-5.5149089492929,
132.953408849594));
#165060=CARTESIAN_POINT('Ctrl Pts',(-238.659604024691,-5.568062452315,132.805513057941));
#165061=CARTESIAN_POINT('Ctrl Pts',(-238.652221055053,-5.62123599294713,
132.657561513083));
#165062=CARTESIAN_POINT('Ctrl Pts',(-238.644838085415,-5.66848419968955,
132.507556853508));
#165063=CARTESIAN_POINT('Ctrl Pts',(-238.637455115776,-5.70966634504485,
132.35601805101));
#165064=CARTESIAN_POINT('Ctrl Pts',(-238.630063998789,-5.75089393624544,
132.204312020483));
#165065=CARTESIAN_POINT('Ctrl Pts',(-238.622672881802,-5.78604200163665,
132.051068828938));
#165066=CARTESIAN_POINT('Ctrl Pts',(-238.615281764816,-5.81502070102805,
131.896818767389));
#165067=CARTESIAN_POINT('Ctrl Pts',(-238.607885888735,-5.84401805961916,
131.74246938521));
#165068=CARTESIAN_POINT('Ctrl Pts',(-238.600490012655,-5.86683808367786,
131.58711221157));
#165069=CARTESIAN_POINT('Ctrl Pts',(-238.593094136575,-5.88344282135011,
131.431282566778));
#165070=CARTESIAN_POINT('Ctrl Pts',(-238.585688093829,-5.900070384558,131.275238712332));
#165071=CARTESIAN_POINT('Ctrl Pts',(-238.578282051082,-5.91046557869002,
131.118721462958));
#165072=CARTESIAN_POINT('Ctrl Pts',(-238.570876008335,-5.91464252743418,
130.962266713607));
#165073=CARTESIAN_POINT('Ctrl Pts',(-238.568375736293,-5.91605266082417,
130.909447759008));
#165074=CARTESIAN_POINT('Ctrl Pts',(-238.565875464252,-5.91675451944664,
130.856635888774));
#165075=CARTESIAN_POINT('Ctrl Pts',(-238.56337519221,-5.91674997810161,
130.803851564856));
#165076=CARTESIAN_POINT('',(-236.8133759018,-5.91514049166533,130.809755854059));
#165077=CARTESIAN_POINT('Ctrl Pts',(-238.56337519221,-5.92647874297726,
130.803850727833));
#165078=CARTESIAN_POINT('Ctrl Pts',(-238.562094450275,-5.92651203176314,
130.776767969747));
#165079=CARTESIAN_POINT('Ctrl Pts',(-238.560813708341,-5.92634251264235,
130.749685640048));
#165080=CARTESIAN_POINT('Ctrl Pts',(-238.559532966407,-5.92596892446363,
130.722606125681));
#165081=CARTESIAN_POINT('Ctrl Pts',(-238.466717091803,-5.89889484136622,
128.760143007206));
#165082=CARTESIAN_POINT('Ctrl Pts',(-238.281085342595,-3.70122233609977,
124.864788768594));
#165083=CARTESIAN_POINT('Ctrl Pts',(-238.002637718782,2.99652893391074,
124.479933775664));
#165084=CARTESIAN_POINT('Ctrl Pts',(-237.724190094969,6.94061650223621,
129.906918085011));
#165085=CARTESIAN_POINT('Ctrl Pts',(-237.445742471156,4.50661657297107,
136.158608239275));
#165086=CARTESIAN_POINT('Ctrl Pts',(-237.167294847343,-2.06874382639764,
137.490006398721));
#165087=CARTESIAN_POINT('Ctrl Pts',(-236.956506088141,-5.60724384558112,
133.846964395534));
#165088=CARTESIAN_POINT('Ctrl Pts',(-236.838533203544,-5.9191873299868,
131.344539778461));
#165089=CARTESIAN_POINT('Ctrl Pts',(-236.813376193551,-5.91447974316152,
130.80976145495));
#165090=CARTESIAN_POINT('',(-235.063374513861,-5.91162093914216,130.802545185735));
#165091=CARTESIAN_POINT('Ctrl Pts',(-236.813375192209,-5.91674755256041,
130.809742231672));
#165092=CARTESIAN_POINT('Ctrl Pts',(-236.806043481234,-5.91688936434239,
130.653829061879));
#165093=CARTESIAN_POINT('Ctrl Pts',(-236.79871177026,-5.91086422133638,
130.497776607582));
#165094=CARTESIAN_POINT('Ctrl Pts',(-236.791380059285,-5.89866598767684,
130.342115954726));
#165095=CARTESIAN_POINT('Ctrl Pts',(-236.783839206803,-5.88611979199543,
130.182014987229));
#165096=CARTESIAN_POINT('Ctrl Pts',(-236.776298354321,-5.86704303141833,
130.022328917354));
#165097=CARTESIAN_POINT('Ctrl Pts',(-236.768757501839,-5.84148658530926,
129.863634814714));
#165098=CARTESIAN_POINT('Ctrl Pts',(-236.761430869615,-5.816656145774,129.709448888259));
#165099=CARTESIAN_POINT('Ctrl Pts',(-236.754104237391,-5.78570924155664,
129.556199733322));
#165100=CARTESIAN_POINT('Ctrl Pts',(-236.746777605167,-5.74874499510395,
129.404410067094));
#165101=CARTESIAN_POINT('Ctrl Pts',(-236.739451132004,-5.71178155114529,
129.25262369622));
#165102=CARTESIAN_POINT('Ctrl Pts',(-236.732124658841,-5.66880111465606,
129.102297121385));
#165103=CARTESIAN_POINT('Ctrl Pts',(-236.724798185678,-5.61995350497976,
128.953940891027));
#165104=CARTESIAN_POINT('Ctrl Pts',(-236.71747035792,-5.57109686384674,
128.805557231018));
#165105=CARTESIAN_POINT('Ctrl Pts',(-236.710142530162,-5.51637100990835,
128.659145002411));
#165106=CARTESIAN_POINT('Ctrl Pts',(-236.702814702404,-5.45597492971321,
128.515197423549));
#165107=CARTESIAN_POINT('Ctrl Pts',(-236.695113443847,-5.39250102656027,
128.363914183805));
#165108=CARTESIAN_POINT('Ctrl Pts',(-236.68741218529,-5.32276401191484,
128.215353818769));
#165109=CARTESIAN_POINT('Ctrl Pts',(-236.679710926733,-5.24705053215068,
128.07006157109));
#165110=CARTESIAN_POINT('Ctrl Pts',(-236.67237187002,-5.17489797191598,
127.931602637689));
#165111=CARTESIAN_POINT('Ctrl Pts',(-236.665032813306,-5.09731849324256,
127.796111745667));
#165112=CARTESIAN_POINT('Ctrl Pts',(-236.657693756593,-5.01460532544673,
127.664031973538));
#165113=CARTESIAN_POINT('Ctrl Pts',(-236.650349725213,-4.93183609179975,
127.531862673163));
#165114=CARTESIAN_POINT('Ctrl Pts',(-236.643005693833,-4.84392645314405,
127.403109410562));
#165115=CARTESIAN_POINT('Ctrl Pts',(-236.635661662453,-4.75121086146454,
127.278183379763));
#165116=CARTESIAN_POINT('Ctrl Pts',(-236.6283078109,-4.65837129385027,127.153090302395));
#165117=CARTESIAN_POINT('Ctrl Pts',(-236.620953959347,-4.56071318704533,
127.031834963828));
#165118=CARTESIAN_POINT('Ctrl Pts',(-236.613600107794,-4.45860914621786,
126.914793155269));
#165119=CARTESIAN_POINT('Ctrl Pts',(-236.612533271768,-4.44379673556223,
126.897813696687));
#165120=CARTESIAN_POINT('Ctrl Pts',(-236.611466435743,-4.42889081546524,
126.880922847802));
#165121=CARTESIAN_POINT('Ctrl Pts',(-236.610399599717,-4.41389258223086,
126.864121686355));
#165122=CARTESIAN_POINT('Ctrl Pts',(-236.602976333312,-4.30953176365291,
126.74721571922));
#165123=CARTESIAN_POINT('Ctrl Pts',(-236.595553066906,-4.20036538985445,
126.63428197761));
#165124=CARTESIAN_POINT('Ctrl Pts',(-236.588129800501,-4.08672768992291,
126.525740822478));
#165125=CARTESIAN_POINT('Ctrl Pts',(-236.58071530778,-3.97322430031599,
126.417327953978));
#165126=CARTESIAN_POINT('Ctrl Pts',(-236.573300815059,-3.8552603711819,
126.313297593224));
#165127=CARTESIAN_POINT('Ctrl Pts',(-236.565886322338,-3.73320990655597,
126.214036625069));
#165128=CARTESIAN_POINT('Ctrl Pts',(-236.558478975984,-3.61127707876331,
126.114871328372));
#165129=CARTESIAN_POINT('Ctrl Pts',(-236.55107162963,-3.4852658444353,126.020466506665));
#165130=CARTESIAN_POINT('Ctrl Pts',(-236.543664283276,-3.35558644486496,
125.931171705412));
#165131=CARTESIAN_POINT('Ctrl Pts',(-236.536262461601,-3.22600376508298,
125.841943503591));
#165132=CARTESIAN_POINT('Ctrl Pts',(-236.528860639926,-3.09275867365177,
125.757817944319));
#165133=CARTESIAN_POINT('Ctrl Pts',(-236.52145881825,-2.95629373319983,
125.679103753218));
#165134=CARTESIAN_POINT('Ctrl Pts',(-236.514060903939,-2.81990083152731,
125.600431114726));
#165135=CARTESIAN_POINT('Ctrl Pts',(-236.506662989627,-2.68029178847692,
125.527164341358));
#165136=CARTESIAN_POINT('Ctrl Pts',(-236.499265075316,-2.53793723552307,
125.459568278191));
#165137=CARTESIAN_POINT('Ctrl Pts',(-236.491868390404,-2.39560633931356,
125.391983448263));
#165138=CARTESIAN_POINT('Ctrl Pts',(-236.484471705492,-2.25053117561159,
125.330067618179));
#165139=CARTESIAN_POINT('Ctrl Pts',(-236.477075020579,-2.10320611566655,
125.274039234724));
#165140=CARTESIAN_POINT('Ctrl Pts',(-236.469678663644,-1.95588758826947,
125.218013335626));
#165141=CARTESIAN_POINT('Ctrl Pts',(-236.462282306708,-1.80631971190855,
125.167874496786));
#165142=CARTESIAN_POINT('Ctrl Pts',(-236.454885949773,-1.65501567980099,
125.123792541914));
#165143=CARTESIAN_POINT('Ctrl Pts',(-236.447488460436,-1.50368848265942,
125.079703837983));
#165144=CARTESIAN_POINT('Ctrl Pts',(-236.4400909711,-1.35062495892817,125.041673968871));
#165145=CARTESIAN_POINT('Ctrl Pts',(-236.432693481763,-1.19635211259129,
125.009822483668));
#165146=CARTESIAN_POINT('Ctrl Pts',(-236.425293399248,-1.04202518614662,
124.977959832976));
#165147=CARTESIAN_POINT('Ctrl Pts',(-236.417893316733,-0.886488458421695,
124.952279953763));
#165148=CARTESIAN_POINT('Ctrl Pts',(-236.410493234218,-0.730277588853789,
124.932850998591));
#165149=CARTESIAN_POINT('Ctrl Pts',(-236.403085014552,-0.573894949376595,
124.913400679285));
#165150=CARTESIAN_POINT('Ctrl Pts',(-236.395676794885,-0.416837058326022,
124.90021505702));
#165151=CARTESIAN_POINT('Ctrl Pts',(-236.388268575219,-0.259643879677973,
124.893310320178));
#165152=CARTESIAN_POINT('Ctrl Pts',(-236.380855795916,-0.102353951251823,
124.886401333586));
#165153=CARTESIAN_POINT('Ctrl Pts',(-236.373443016614,0.0550710582627565,
124.885780936936));
#165154=CARTESIAN_POINT('Ctrl Pts',(-236.366030237312,0.212093261767607,
124.891413212861));
#165155=CARTESIAN_POINT('Ctrl Pts',(-236.358606866284,0.369339825961107,
124.897053536445));
#165156=CARTESIAN_POINT('Ctrl Pts',(-236.351183495255,0.526182063406159,
124.908964347838));
#165157=CARTESIAN_POINT('Ctrl Pts',(-236.343760124226,0.682088438571443,
124.927058011398));
#165158=CARTESIAN_POINT('Ctrl Pts',(-236.339824074786,0.7647537395973,124.936651705968));
#165159=CARTESIAN_POINT('Ctrl Pts',(-236.335888025345,0.847156114368657,
124.947982769311));
#165160=CARTESIAN_POINT('Ctrl Pts',(-236.331951975905,0.929217850178815,
124.961032392196));
#165161=CARTESIAN_POINT('Ctrl Pts',(-236.324528709499,1.08398372287413,
124.985643573694));
#165162=CARTESIAN_POINT('Ctrl Pts',(-236.317105443094,1.23800516971489,
125.016444889822));
#165163=CARTESIAN_POINT('Ctrl Pts',(-236.309682176688,1.39074787014024,
125.053382359548));
#165164=CARTESIAN_POINT('Ctrl Pts',(-236.302267683967,1.54331004137817,
125.090276172251));
#165165=CARTESIAN_POINT('Ctrl Pts',(-236.294853191246,1.69459611529923,
125.133291615673));
#165166=CARTESIAN_POINT('Ctrl Pts',(-236.287438698525,1.84407843640344,
125.18232315034));
#165167=CARTESIAN_POINT('Ctrl Pts',(-236.280031352172,1.99341668081866,
125.231307426568));
#165168=CARTESIAN_POINT('Ctrl Pts',(-236.272624005818,2.14095428115501,
125.286296134733));
#165169=CARTESIAN_POINT('Ctrl Pts',(-236.265216659464,2.2861754094724,125.347133065079));
#165170=CARTESIAN_POINT('Ctrl Pts',(-236.257814837788,2.431288226393,125.407924620947));
#165171=CARTESIAN_POINT('Ctrl Pts',(-236.250413016113,2.57408766857886,
125.474555570397));
#165172=CARTESIAN_POINT('Ctrl Pts',(-236.243011194438,2.71407478050877,
125.546820446697));
#165173=CARTESIAN_POINT('Ctrl Pts',(-236.235613280126,2.85398799433195,
125.61904717493));
#165174=CARTESIAN_POINT('Ctrl Pts',(-236.228215365815,2.99109150369809,
125.696901736135));
#165175=CARTESIAN_POINT('Ctrl Pts',(-236.220817451504,3.12490809913466,
125.780131329958));
#165176=CARTESIAN_POINT('Ctrl Pts',(-236.213420766591,3.25870245668095,
125.863347092532));
#165177=CARTESIAN_POINT('Ctrl Pts',(-236.206024081679,3.38921066771668,
125.951935917957));
#165178=CARTESIAN_POINT('Ctrl Pts',(-236.198627396767,3.51598172703827,
126.045599953524));
#165179=CARTESIAN_POINT('Ctrl Pts',(-236.191231039831,3.64274716519825,
126.13925983593));
#165180=CARTESIAN_POINT('Ctrl Pts',(-236.183834682896,3.7657754808919,126.237994259192));
#165181=CARTESIAN_POINT('Ctrl Pts',(-236.17643832596,3.88464640315174,126.341463253187));
#165182=CARTESIAN_POINT('Ctrl Pts',(-236.169040836624,4.00353552485323,
126.444948088549));
#165183=CARTESIAN_POINT('Ctrl Pts',(-236.161643347287,4.1182657041598,126.553168692862));
#165184=CARTESIAN_POINT('Ctrl Pts',(-236.154245857951,4.22845150251073,
126.665746301951));
#165185=CARTESIAN_POINT('Ctrl Pts',(-236.146845775435,4.33867592632261,
126.778363374946));
#165186=CARTESIAN_POINT('Ctrl Pts',(-236.139445692921,4.444352536527,126.895340227029));
#165187=CARTESIAN_POINT('Ctrl Pts',(-236.132045610406,4.54513445743372,
127.016263030868));
#165188=CARTESIAN_POINT('Ctrl Pts',(-236.124637390739,4.64602719842297,
127.137318801761));
#165189=CARTESIAN_POINT('Ctrl Pts',(-236.117229171072,4.74201426233549,
127.262328902701));
#165190=CARTESIAN_POINT('Ctrl Pts',(-236.109820951406,4.83279016570902,
127.390847796918));
#165191=CARTESIAN_POINT('Ctrl Pts',(-236.102408172104,4.92362194013614,
127.51944579237));
#165192=CARTESIAN_POINT('Ctrl Pts',(-236.094995392802,5.0092359603708,127.651556571839));
#165193=CARTESIAN_POINT('Ctrl Pts',(-236.0875826135,5.089371703596,127.78670818146));
#165194=CARTESIAN_POINT('Ctrl Pts',(-236.080159242471,5.16962194852946,
127.92205290204));
#165195=CARTESIAN_POINT('Ctrl Pts',(-236.072735871442,5.24437810599711,
128.0604468029));
#165196=CARTESIAN_POINT('Ctrl Pts',(-236.065312500413,5.31342659840628,
128.20139531894));
#165197=CARTESIAN_POINT('Ctrl Pts',(-236.061376450973,5.35003776587558,
128.276129604155));
#165198=CARTESIAN_POINT('Ctrl Pts',(-236.057440401532,5.38504511772872,
128.351581772324));
#165199=CARTESIAN_POINT('Ctrl Pts',(-236.053504352092,5.41842247308797,
128.427676274698));
#165200=CARTESIAN_POINT('Ctrl Pts',(-236.046081085686,5.48137112362688,
128.571188131354));
#165201=CARTESIAN_POINT('Ctrl Pts',(-236.038657819281,5.53870945822938,
128.717419600426));
#165202=CARTESIAN_POINT('Ctrl Pts',(-236.031234552875,5.59019407935361,
128.865891964825));
#165203=CARTESIAN_POINT('Ctrl Pts',(-236.023820060154,5.6416178499312,129.014188847219));
#165204=CARTESIAN_POINT('Ctrl Pts',(-236.016405567433,5.68720155744135,
129.164721003733));
#165205=CARTESIAN_POINT('Ctrl Pts',(-236.008991074712,5.72674878454648,
129.316987456185));
#165206=CARTESIAN_POINT('Ctrl Pts',(-236.001583728359,5.76625789454532,
129.469107148499));
#165207=CARTESIAN_POINT('Ctrl Pts',(-235.994176382005,5.7997420137932,129.62295745008));
#165208=CARTESIAN_POINT('Ctrl Pts',(-235.986769035651,5.82705374838034,
129.778019945086));
#165209=CARTESIAN_POINT('Ctrl Pts',(-235.979367213976,5.85434511284541,
129.932966788633));
#165210=CARTESIAN_POINT('Ctrl Pts',(-235.9719653923,5.8754731945584,130.089123659364));
#165211=CARTESIAN_POINT('Ctrl Pts',(-235.964563570625,5.890341160854,130.245959712079));
#165212=CARTESIAN_POINT('Ctrl Pts',(-235.957165656314,5.90520127846592,
130.402712972262));
#165213=CARTESIAN_POINT('Ctrl Pts',(-235.949767742002,5.91380782692023,
130.5601443297));
#165214=CARTESIAN_POINT('Ctrl Pts',(-235.942369827691,5.91611555093859,
130.717715649781));
#165215=CARTESIAN_POINT('Ctrl Pts',(-235.934973142779,5.91842289145508,
130.875260784366));
#165216=CARTESIAN_POINT('Ctrl Pts',(-235.927576457866,5.91443347956411,
131.032945462539));
#165217=CARTESIAN_POINT('Ctrl Pts',(-235.920179772954,5.90415412785713,
131.190229244183));
#165218=CARTESIAN_POINT('Ctrl Pts',(-235.912783416019,5.89387523194739,
131.3475060517));
#165219=CARTESIAN_POINT('Ctrl Pts',(-235.905387059083,5.87730697511917,
131.504381625531));
#165220=CARTESIAN_POINT('Ctrl Pts',(-235.897990702148,5.85450821714245,
131.660318617652));
#165221=CARTESIAN_POINT('Ctrl Pts',(-235.890593212811,5.83170596861762,
131.816279484125));
#165222=CARTESIAN_POINT('Ctrl Pts',(-235.883195723475,5.80267137359861,
131.971301113369));
#165223=CARTESIAN_POINT('Ctrl Pts',(-235.875798234138,5.76751475815558,
132.124854493719));
#165224=CARTESIAN_POINT('Ctrl Pts',(-235.868398151623,5.73234581861565,
132.278461701968));
#165225=CARTESIAN_POINT('Ctrl Pts',(-235.860998069108,5.69105066911282,
132.430599272918));
#165226=CARTESIAN_POINT('Ctrl Pts',(-235.853597986593,5.64378997951745,
132.580751686447));
#165227=CARTESIAN_POINT('Ctrl Pts',(-235.846189766927,5.59647732193529,
132.73106920799));
#165228=CARTESIAN_POINT('Ctrl Pts',(-235.83878154726,5.54318613620419,132.879396856454));
#165229=CARTESIAN_POINT('Ctrl Pts',(-235.831373327594,5.48412614375368,
133.025236796442));
#165230=CARTESIAN_POINT('Ctrl Pts',(-235.823960548292,5.42502980086329,
133.171166498479));
#165231=CARTESIAN_POINT('Ctrl Pts',(-235.81654776899,5.36015772970096,133.314605101705));
#165232=CARTESIAN_POINT('Ctrl Pts',(-235.809134989688,5.28976617947242,
133.455078318305));
#165233=CARTESIAN_POINT('Ctrl Pts',(-235.801711618659,5.21927405049578,
133.595752249624));
#165234=CARTESIAN_POINT('Ctrl Pts',(-235.794288247631,5.143246871316,133.733452005979));
#165235=CARTESIAN_POINT('Ctrl Pts',(-235.786864876602,5.06198528965285,
133.867730573976));
#165236=CARTESIAN_POINT('Ctrl Pts',(-235.782928827161,5.01889844920773,
133.938928292703));
#165237=CARTESIAN_POINT('Ctrl Pts',(-235.77899277772,4.974340731985,134.009164709201));
#165238=CARTESIAN_POINT('Ctrl Pts',(-235.775056728279,4.92836154788358,
134.078376960812));
#165239=CARTESIAN_POINT('Ctrl Pts',(-235.767633461873,4.84164624163427,
134.208909107304));
#165240=CARTESIAN_POINT('Ctrl Pts',(-235.760210195468,4.74961033563306,
134.336191153046));
#165241=CARTESIAN_POINT('Ctrl Pts',(-235.752786929062,4.65252502580741,
134.459759562515));
#165242=CARTESIAN_POINT('Ctrl Pts',(-235.745372436341,4.55555446275527,
134.583181924386));
#165243=CARTESIAN_POINT('Ctrl Pts',(-235.73795794362,4.45354660354109,134.70289909606));
#165244=CARTESIAN_POINT('Ctrl Pts',(-235.730543450899,4.34681676692741,
134.818475035125));
#165245=CARTESIAN_POINT('Ctrl Pts',(-235.723136104546,4.24018980054857,
134.933939577749));
#165246=CARTESIAN_POINT('Ctrl Pts',(-235.715728758192,4.12885016890964,
135.045270561599));
#165247=CARTESIAN_POINT('Ctrl Pts',(-235.708321411838,4.0131543599336,135.152063763578));
#165248=CARTESIAN_POINT('Ctrl Pts',(-235.700919590163,3.89754484125719,
135.258777315158));
#165249=CARTESIAN_POINT('Ctrl Pts',(-235.693517768487,3.77758588756741,
135.360959571655));
#165250=CARTESIAN_POINT('Ctrl Pts',(-235.686115946812,3.65367177354376,
135.458242130208));
#165251=CARTESIAN_POINT('Ctrl Pts',(-235.6787180325,3.52982307281566,135.555473334056));
#165252=CARTESIAN_POINT('Ctrl Pts',(-235.671320118189,3.40202366278135,
135.647809761191));
#165253=CARTESIAN_POINT('Ctrl Pts',(-235.663922203878,3.27070182974663,
135.734922462163));
#165254=CARTESIAN_POINT('Ctrl Pts',(-235.656525518966,3.13940182001869,
135.822020686584));
#165255=CARTESIAN_POINT('Ctrl Pts',(-235.649128834053,3.00458085983532,
135.903896701589));
#165256=CARTESIAN_POINT('Ctrl Pts',(-235.641732149141,2.86669731914428,
135.98026411772));
#165257=CARTESIAN_POINT('Ctrl Pts',(-235.634335792206,2.72881989235394,
136.056628147641));
#165258=CARTESIAN_POINT('Ctrl Pts',(-235.62693943527,2.58788048162462,136.127483883488));
#165259=CARTESIAN_POINT('Ctrl Pts',(-235.619543078335,2.44436298821062,
136.192590395922));
#165260=CARTESIAN_POINT('Ctrl Pts',(-235.612145588998,2.300823521902,136.25770687633));
#165261=CARTESIAN_POINT('Ctrl Pts',(-235.604748099661,2.15470552696101,
136.317072226458));
#165262=CARTESIAN_POINT('Ctrl Pts',(-235.597350610325,2.00651370981995,
136.370493323027));
#165263=CARTESIAN_POINT('Ctrl Pts',(-235.58995052781,1.85826994426732,136.423933146279));
#165264=CARTESIAN_POINT('Ctrl Pts',(-235.582550445295,1.70795126007021,
136.471424440728));
#165265=CARTESIAN_POINT('Ctrl Pts',(-235.57515036278,1.55607822489781,136.512823731268));
#165266=CARTESIAN_POINT('Ctrl Pts',(-235.567742143113,1.40403818971008,
136.554268544584));
#165267=CARTESIAN_POINT('Ctrl Pts',(-235.560333923447,1.25044075060268,
136.589607877842));
#165268=CARTESIAN_POINT('Ctrl Pts',(-235.552925703781,1.09581811014864,
136.61874908343));
#165269=CARTESIAN_POINT('Ctrl Pts',(-235.545512924479,0.941100302038981,
136.647908224943));
#165270=CARTESIAN_POINT('Ctrl Pts',(-235.538100145176,0.785356403699778,
136.670861582928));
#165271=CARTESIAN_POINT('Ctrl Pts',(-235.530687365874,0.629123955857885,
136.687568382949));
#165272=CARTESIAN_POINT('Ctrl Pts',(-235.523263994846,0.472668275768163,
136.70429905443));
#165273=CARTESIAN_POINT('Ctrl Pts',(-235.515840623817,0.315723023472359,
136.714765317198));
#165274=CARTESIAN_POINT('Ctrl Pts',(-235.508417252788,0.158826791435676,
136.718978493035));
#165275=CARTESIAN_POINT('Ctrl Pts',(-235.504481203347,0.0756366445359733,
136.721212419958));
#165276=CARTESIAN_POINT('Ctrl Pts',(-235.500545153907,-0.00753977640015259,
136.721689249256));
#165277=CARTESIAN_POINT('Ctrl Pts',(-235.496609104466,-0.0906228759804562,
136.720416572072));
#165278=CARTESIAN_POINT('Ctrl Pts',(-235.48918583806,-0.247315008852205,
136.718016342623));
#165279=CARTESIAN_POINT('Ctrl Pts',(-235.481762571655,-0.404148654045105,
136.709382983073));
#165280=CARTESIAN_POINT('Ctrl Pts',(-235.474339305249,-0.560587237971028,
136.694494105962));
#165281=CARTESIAN_POINT('Ctrl Pts',(-235.466924812529,-0.716840924482166,
136.679622826267));
#165282=CARTESIAN_POINT('Ctrl Pts',(-235.459510319808,-0.872700111162586,
136.658510780843));
#165283=CARTESIAN_POINT('Ctrl Pts',(-235.452095827087,-1.02762750568826,
136.631187564718));
#165284=CARTESIAN_POINT('Ctrl Pts',(-235.444688480733,-1.18240557535861,
136.603890683737));
#165285=CARTESIAN_POINT('Ctrl Pts',(-235.437281134379,-1.33625327565069,
136.570394614519));
#165286=CARTESIAN_POINT('Ctrl Pts',(-235.429873788025,-1.48863783179452,
136.530780787991));
#165287=CARTESIAN_POINT('Ctrl Pts',(-235.42247196635,-1.64090873378724,
136.491196506949));
#165288=CARTESIAN_POINT('Ctrl Pts',(-235.415070144675,-1.79171830475907,
136.445503647373));
#165289=CARTESIAN_POINT('Ctrl Pts',(-235.407668322999,-1.9405434818548,
136.393834792972));
#165290=CARTESIAN_POINT('Ctrl Pts',(-235.400270408688,-2.08929009529841,
136.342193214157));
#165291=CARTESIAN_POINT('Ctrl Pts',(-235.392872494377,-2.23605404934729,
136.284582045337));
#165292=CARTESIAN_POINT('Ctrl Pts',(-235.385474580065,-2.38032709030358,
136.221183810699));
#165293=CARTESIAN_POINT('Ctrl Pts',(-235.378077895153,-2.52457615569723,
136.157796111698));
#165294=CARTESIAN_POINT('Ctrl Pts',(-235.370681210241,-2.66633478813374,
136.088623405612));
#165295=CARTESIAN_POINT('Ctrl Pts',(-235.363284525329,-2.80511427989841,
136.013896531562));
#165296=CARTESIAN_POINT('Ctrl Pts',(-235.355888168393,-2.94388761803537,
135.939172970979));
#165297=CARTESIAN_POINT('Ctrl Pts',(-235.348491811458,-3.07968174947808,
135.858895909095));
#165298=CARTESIAN_POINT('Ctrl Pts',(-235.341095454522,-3.21203241310078,
135.773342237545));
#165299=CARTESIAN_POINT('Ctrl Pts',(-235.333697965186,-3.34440333994796,
135.68777546751));
#165300=CARTESIAN_POINT('Ctrl Pts',(-235.326300475849,-3.47332943572068,
135.596930681914));
#165301=CARTESIAN_POINT('Ctrl Pts',(-235.318902986513,-3.59837541417954,
135.501128116722));
#165302=CARTESIAN_POINT('Ctrl Pts',(-235.311502903998,-3.72346522731249,
135.405291968089));
#165303=CARTESIAN_POINT('Ctrl Pts',(-235.304102821483,-3.84467191890259,
135.304494806518));
#165304=CARTESIAN_POINT('Ctrl Pts',(-235.296702738968,-3.96159339973869,
135.199097048531));
#165305=CARTESIAN_POINT('Ctrl Pts',(-235.289294519302,-4.07864344776264,
135.093583394873));
#165306=CARTESIAN_POINT('Ctrl Pts',(-235.281886299635,-4.19139859735822,
134.983459292085));
#165307=CARTESIAN_POINT('Ctrl Pts',(-235.274478079969,-4.29949323297398,
134.869122418965));
#165308=CARTESIAN_POINT('Ctrl Pts',(-235.267065300667,-4.40765439903461,
134.754715173407));
#165309=CARTESIAN_POINT('Ctrl Pts',(-235.259652521364,-4.51114909048871,
134.636090271496));
#165310=CARTESIAN_POINT('Ctrl Pts',(-235.252239742062,-4.60965244875596,
134.513677921893));
#165311=CARTESIAN_POINT('Ctrl Pts',(-235.244816371034,-4.70829655324043,
134.391090663784));
#165312=CARTESIAN_POINT('Ctrl Pts',(-235.237393000005,-4.80193485899353,
134.264705448787));
#165313=CARTESIAN_POINT('Ctrl Pts',(-235.229969628976,-4.89028576896841,
134.134981529697));
#165314=CARTESIAN_POINT('Ctrl Pts',(-235.226033579535,-4.93713154139312,
134.066198795105));
#165315=CARTESIAN_POINT('Ctrl Pts',(-235.222097530094,-4.98249159860291,
133.996477854369));
#165316=CARTESIAN_POINT('Ctrl Pts',(-235.218161480653,-5.0263293039892,
133.925889776546));
#165317=CARTESIAN_POINT('Ctrl Pts',(-235.210525599101,-5.11137384696384,
133.788949880512));
#165318=CARTESIAN_POINT('Ctrl Pts',(-235.202889717548,-5.19093130654541,
133.648350491407));
#165319=CARTESIAN_POINT('Ctrl Pts',(-235.195253835996,-5.2646814211652,
133.504556924529));
#165320=CARTESIAN_POINT('Ctrl Pts',(-235.187628600606,-5.33832871128587,
133.360963838716));
#165321=CARTESIAN_POINT('Ctrl Pts',(-235.180003365216,-5.40618462981095,
133.214185750204));
#165322=CARTESIAN_POINT('Ctrl Pts',(-235.172378129827,-5.46797246205113,
133.064716279127));
#165323=CARTESIAN_POINT('Ctrl Pts',(-235.164762379847,-5.52968343332797,
132.915432740573));
#165324=CARTESIAN_POINT('Ctrl Pts',(-235.157146629867,-5.58534122619445,
132.763464805689));
#165325=CARTESIAN_POINT('Ctrl Pts',(-235.149530879888,-5.63471520293158,
132.609330186382));
#165326=CARTESIAN_POINT('Ctrl Pts',(-235.141926012989,-5.68401862312512,
132.455415828976));
#165327=CARTESIAN_POINT('Ctrl Pts',(-235.134321146091,-5.72705602833567,
132.299341287442));
#165328=CARTESIAN_POINT('Ctrl Pts',(-235.126716279192,-5.76364514583061,
132.141643383268));
#165329=CARTESIAN_POINT('Ctrl Pts',(-235.119117783915,-5.800203607694,131.984077603866));
#165330=CARTESIAN_POINT('Ctrl Pts',(-235.111519288638,-5.83032446630871,
131.824891505164));
#165331=CARTESIAN_POINT('Ctrl Pts',(-235.103920793361,-5.85387520708344,
131.664637097771));
#165332=CARTESIAN_POINT('Ctrl Pts',(-235.096328880991,-5.87740554482536,
131.504521525753));
#165333=CARTESIAN_POINT('Ctrl Pts',(-235.088736968622,-5.8943770629967,
131.343339830038));
#165334=CARTESIAN_POINT('Ctrl Pts',(-235.081145056252,-5.90470830302427,
131.181654162033));
#165335=CARTESIAN_POINT('Ctrl Pts',(-235.075221768238,-5.91276884261537,
131.055505343034));
#165336=CARTESIAN_POINT('Ctrl Pts',(-235.069298480223,-5.91678826105314,
130.929050024163));
#165337=CARTESIAN_POINT('Ctrl Pts',(-235.063375192209,-5.91674972543052,
130.802558086599));
#165338=CARTESIAN_POINT('',(-233.313375192209,-5.92110108695772,130.799604953112));
#165339=CARTESIAN_POINT('Ctrl Pts',(-235.063373960744,-5.9074389915308,
130.802534666533));
#165340=CARTESIAN_POINT('Ctrl Pts',(-235.02215392611,-5.90982138573415,
129.923664387846));
#165341=CARTESIAN_POINT('Ctrl Pts',(-234.88811801687,-5.31313791815044,
127.068909389366));
#165342=CARTESIAN_POINT('Ctrl Pts',(-234.661266233027,-0.886879056514751,
123.862386397694));
#165343=CARTESIAN_POINT('Ctrl Pts',(-234.382818609214,5.36109972483852,
126.305897516605));
#165344=CARTESIAN_POINT('Ctrl Pts',(-234.104370985401,6.68248976334735,
132.88327646317));
#165345=CARTESIAN_POINT('Ctrl Pts',(-233.825923361589,1.86299816711319,
137.550233308306));
#165346=CARTESIAN_POINT('Ctrl Pts',(-233.562258097191,-4.32175058245946,
136.099403303978));
#165347=CARTESIAN_POINT('Ctrl Pts',(-233.391408707398,-5.90662829739712,
132.453658602887));
#165348=CARTESIAN_POINT('Ctrl Pts',(-233.313375192209,-5.92110108695772,
130.799604953112));
#165349=CARTESIAN_POINT('',(-231.563375192209,-5.92030054368718,130.808418273216));
#165350=CARTESIAN_POINT('Ctrl Pts',(-233.313375192209,-5.92110108695772,
130.799604953112));
#165351=CARTESIAN_POINT('Ctrl Pts',(-233.298592832794,-5.92384275477205,
130.486267594354));
#165352=CARTESIAN_POINT('Ctrl Pts',(-233.283810473378,-5.90112681262327,
130.173328526099));
#165353=CARTESIAN_POINT('Ctrl Pts',(-233.176212239358,-5.54038544735297,
127.926876459006));
#165354=CARTESIAN_POINT('Ctrl Pts',(-232.99058049015,-2.80141177327697,
124.391120203632));
#165355=CARTESIAN_POINT('Ctrl Pts',(-232.712132866337,3.88140930090627,
124.980940456769));
#165356=CARTESIAN_POINT('Ctrl Pts',(-232.433685242524,6.99740484494153,
130.922199347785));
#165357=CARTESIAN_POINT('Ctrl Pts',(-232.155237618711,3.68312717870603,
136.755170202472));
#165358=CARTESIAN_POINT('Ctrl Pts',(-231.876789994898,-3.0157644339933,
137.119637761841));
#165359=CARTESIAN_POINT('Ctrl Pts',(-231.679502519397,-5.7985380671585,
133.265988781829));
#165360=CARTESIAN_POINT('Ctrl Pts',(-231.575030918501,-5.92484103517307,
131.055287059807));
#165361=CARTESIAN_POINT('Ctrl Pts',(-231.563375192209,-5.92290613080011,
130.808420059033));
#165362=CARTESIAN_POINT('',(-229.813375218367,-5.91200928751026,130.807165211494));
#165363=CARTESIAN_POINT('Ctrl Pts',(-231.563375192209,-5.91674861031638,
130.808415838792));
#165364=CARTESIAN_POINT('Ctrl Pts',(-231.556062235289,-5.91685465621581,
130.653690142413));
#165365=CARTESIAN_POINT('Ctrl Pts',(-231.548749278369,-5.91088733319179,
130.498726433687));
#165366=CARTESIAN_POINT('Ctrl Pts',(-231.541436321449,-5.89881716077939,
130.344049129338));
#165367=CARTESIAN_POINT('Ctrl Pts',(-231.534130820366,-5.88675929436655,
130.18952952438));
#165368=CARTESIAN_POINT('Ctrl Pts',(-231.526825319284,-5.86861098829339,
130.035296123186));
#165369=CARTESIAN_POINT('Ctrl Pts',(-231.519519818201,-5.84439477175359,
129.881874674909));
#165370=CARTESIAN_POINT('Ctrl Pts',(-231.512220066293,-5.82019761253225,
129.728573963966));
#165371=CARTESIAN_POINT('Ctrl Pts',(-231.504920314386,-5.78994210555702,
129.576084312388));
#165372=CARTESIAN_POINT('Ctrl Pts',(-231.497620562478,-5.75370268483897,
129.42492740897));
#165373=CARTESIAN_POINT('Ctrl Pts',(-231.490215320178,-5.71693955992359,
129.271586102403));
#165374=CARTESIAN_POINT('Ctrl Pts',(-231.482810077877,-5.67401825168733,
129.119616764242));
#165375=CARTESIAN_POINT('Ctrl Pts',(-231.475404835577,-5.62507056860757,
128.969554998247));
#165376=CARTESIAN_POINT('Ctrl Pts',(-231.468110520265,-5.5768560984118,
128.821741085741));
#165377=CARTESIAN_POINT('Ctrl Pts',(-231.460816204953,-5.52279467668824,
128.675778367587));
#165378=CARTESIAN_POINT('Ctrl Pts',(-231.453521889641,-5.46306277529751,
128.5321643946));
#165379=CARTESIAN_POINT('Ctrl Pts',(-231.446227859779,-5.40333321140892,
128.388556041692));
#165380=CARTESIAN_POINT('Ctrl Pts',(-231.438933829917,-5.33793375682769,
128.247296606419));
#165381=CARTESIAN_POINT('Ctrl Pts',(-231.431639800056,-5.26708912099379,
128.108863862975));
#165382=CARTESIAN_POINT('Ctrl Pts',(-231.424344521228,-5.19623235434514,
127.970407415522));
#165383=CARTESIAN_POINT('Ctrl Pts',(-231.4170492424,-5.11992872676776,127.834778965286));
#165384=CARTESIAN_POINT('Ctrl Pts',(-231.409753963573,-5.03844886050293,
127.702431597972));
#165385=CARTESIAN_POINT('Ctrl Pts',(-231.402265695548,-4.95481352707123,
127.566583115378));
#165386=CARTESIAN_POINT('Ctrl Pts',(-231.394777427523,-4.86572451460428,
127.434192088729));
#165387=CARTESIAN_POINT('Ctrl Pts',(-231.387289159498,-4.77152126524011,
127.305715825956));
#165388=CARTESIAN_POINT('Ctrl Pts',(-231.379983067157,-4.67960980635917,
127.180365152569));
#165389=CARTESIAN_POINT('Ctrl Pts',(-231.372676974816,-4.58283036123037,
127.058741230468));
#165390=CARTESIAN_POINT('Ctrl Pts',(-231.365370882475,-4.4815379056025,
126.941233831768));
#165391=CARTESIAN_POINT('Ctrl Pts',(-231.357791526608,-4.37645689484776,
126.819331404287));
#165392=CARTESIAN_POINT('Ctrl Pts',(-231.350212170741,-4.26651906354,126.701859738012));
#165393=CARTESIAN_POINT('Ctrl Pts',(-231.342632814874,-4.15216048765967,
126.589210104569));
#165394=CARTESIAN_POINT('Ctrl Pts',(-231.335053459007,-4.03780191177965,
126.476560471127));
#165395=CARTESIAN_POINT('Ctrl Pts',(-231.32747410314,-3.91902297669403,
126.368733121126));
#165396=CARTESIAN_POINT('Ctrl Pts',(-231.319894747273,-3.79629476082943,
126.266070559472));
#165397=CARTESIAN_POINT('Ctrl Pts',(-231.312471480867,-3.67609401319123,
126.165522233414));
#165398=CARTESIAN_POINT('Ctrl Pts',(-231.305048214462,-3.55171407794731,
126.069600604618));
#165399=CARTESIAN_POINT('Ctrl Pts',(-231.297624948057,-3.4235465731537,
125.978673161467));
#165400=CARTESIAN_POINT('Ctrl Pts',(-231.290210455336,-3.29553055170711,
125.887853187004));
#165401=CARTESIAN_POINT('Ctrl Pts',(-231.282795962614,-3.16373617288102,
125.802015862692));
#165402=CARTESIAN_POINT('Ctrl Pts',(-231.275381469893,-3.02858955858279,
125.721489790155));
#165403=CARTESIAN_POINT('Ctrl Pts',(-231.26797412354,-2.89357320367921,
125.641041331679));
#165404=CARTESIAN_POINT('Ctrl Pts',(-231.260566777186,-2.75521136414399,
125.565894123486));
#165405=CARTESIAN_POINT('Ctrl Pts',(-231.253159430832,-2.61396060553718,
125.496334570607));
#165406=CARTESIAN_POINT('Ctrl Pts',(-231.245757609157,-2.47281519707522,
125.426826897866));
#165407=CARTESIAN_POINT('Ctrl Pts',(-231.238355787481,-2.32878549322126,
125.362898746624));
#165408=CARTESIAN_POINT('Ctrl Pts',(-231.230953965806,-2.1823541242278,
125.30479144908));
#165409=CARTESIAN_POINT('Ctrl Pts',(-231.223556051494,-2.03600005521464,
125.246714825925));
#165410=CARTESIAN_POINT('Ctrl Pts',(-231.216158137183,-1.88724719208587,
125.194453074213));
#165411=CARTESIAN_POINT('Ctrl Pts',(-231.208760222872,-1.73659957864125,
125.148200041171));
#165412=CARTESIAN_POINT('Ctrl Pts',(-231.201363537959,-1.58597700009675,
125.101954694544));
#165413=CARTESIAN_POINT('Ctrl Pts',(-231.193966853047,-1.43346065267384,
125.061716194238));
#165414=CARTESIAN_POINT('Ctrl Pts',(-231.186570168135,-1.27957134548418,
125.027629038696));
#165415=CARTESIAN_POINT('Ctrl Pts',(-231.179173811199,-1.12568886190766,
124.993543394614));
#165416=CARTESIAN_POINT('Ctrl Pts',(-231.171777454264,-0.970433904074944,
124.965608633691));
#165417=CARTESIAN_POINT('Ctrl Pts',(-231.164381097328,-0.814338858108183,
124.943918416957));
#165418=CARTESIAN_POINT('Ctrl Pts',(-231.156983607992,-0.658219913591393,
124.922224879396));
#165419=CARTESIAN_POINT('Ctrl Pts',(-231.149586118655,-0.501260994610848,
124.906777841037));
#165420=CARTESIAN_POINT('Ctrl Pts',(-231.142188629319,-0.344000866660678,
124.897619217586));
#165421=CARTESIAN_POINT('Ctrl Pts',(-231.134788546804,-0.186685611416664,
124.888457383594));
#165422=CARTESIAN_POINT('Ctrl Pts',(-231.127388464289,-0.0290693094113907,
124.885588375131));
#165423=CARTESIAN_POINT('Ctrl Pts',(-231.119988381774,0.128308157965048,
124.889001999604));
#165424=CARTESIAN_POINT('Ctrl Pts',(-231.112580162107,0.285858678045888,
124.892419377708));
#165425=CARTESIAN_POINT('Ctrl Pts',(-231.105171942441,0.44316946558294,
124.902133177177));
#165426=CARTESIAN_POINT('Ctrl Pts',(-231.097763722774,0.599703910538144,
124.918081165978));
#165427=CARTESIAN_POINT('Ctrl Pts',(-231.090350943472,0.7563346998323,124.9340389705));
#165428=CARTESIAN_POINT('Ctrl Pts',(-231.08293816417,0.912187825705787,
124.956238557617));
#165429=CARTESIAN_POINT('Ctrl Pts',(-231.075525384868,1.06673628404196,
124.984566440552));
#165430=CARTESIAN_POINT('Ctrl Pts',(-231.068102013839,1.22150556846323,
125.012934799694));
#165431=CARTESIAN_POINT('Ctrl Pts',(-231.06067864281,1.37496609894559,125.047448861448));
#165432=CARTESIAN_POINT('Ctrl Pts',(-231.053255271781,1.52660465070735,
125.087944887151));
#165433=CARTESIAN_POINT('Ctrl Pts',(-231.049319222341,1.60700704936486,
125.109416851666));
#165434=CARTESIAN_POINT('Ctrl Pts',(-231.0453831729,1.68689752434762,125.132569742896));
#165435=CARTESIAN_POINT('Ctrl Pts',(-231.04144712346,1.76620190905187,125.15737368833));
#165436=CARTESIAN_POINT('Ctrl Pts',(-231.034023857054,1.91576750360562,
125.204153155317));
#165437=CARTESIAN_POINT('Ctrl Pts',(-231.026600590649,2.06369947970118,
125.25694953408));
#165438=CARTESIAN_POINT('Ctrl Pts',(-231.019177324243,2.20947697982862,
125.315631981706));
#165439=CARTESIAN_POINT('Ctrl Pts',(-231.011762831522,2.35508218305738,
125.374245071553));
#165440=CARTESIAN_POINT('Ctrl Pts',(-231.004348338801,2.4985376360528,125.438730244586));
#165441=CARTESIAN_POINT('Ctrl Pts',(-230.99693384608,2.63933654766249,125.508906609582));
#165442=CARTESIAN_POINT('Ctrl Pts',(-230.989526499726,2.77999975198019,
125.579015335955));
#165443=CARTESIAN_POINT('Ctrl Pts',(-230.982119153372,2.91801118045661,
125.654804168566));
#165444=CARTESIAN_POINT('Ctrl Pts',(-230.974711807019,3.05288308759154,
125.736043794794));
#165445=CARTESIAN_POINT('Ctrl Pts',(-230.967309985343,3.18765440217009,
125.817222829443));
#165446=CARTESIAN_POINT('Ctrl Pts',(-230.959908163668,3.31929053940336,
125.903844371151));
#165447=CARTESIAN_POINT('Ctrl Pts',(-230.952506341992,3.44732758623773,
125.995632815365));
#165448=CARTESIAN_POINT('Ctrl Pts',(-230.945108427681,3.57529704331208,
126.087372805174));
#165449=CARTESIAN_POINT('Ctrl Pts',(-230.93771051337,3.69967089116985,126.18427404846));
#165450=CARTESIAN_POINT('Ctrl Pts',(-230.930312599058,3.82001359266216,
126.286017258062));
#165451=CARTESIAN_POINT('Ctrl Pts',(-230.922915914146,3.9403362953802,126.387743559787));
#165452=CARTESIAN_POINT('Ctrl Pts',(-230.915519229233,4.05662889650189,
126.494309990067));
#165453=CARTESIAN_POINT('Ctrl Pts',(-230.908122544321,4.16848831534951,
126.605356482382));
#165454=CARTESIAN_POINT('Ctrl Pts',(-230.900726187386,4.28034277423328,
126.716398050779));
#165455=CARTESIAN_POINT('Ctrl Pts',(-230.89332983045,4.38776417677228,126.83191902323));
#165456=CARTESIAN_POINT('Ctrl Pts',(-230.885933473515,4.49038595558797,
126.951522114286));
#165457=CARTESIAN_POINT('Ctrl Pts',(-230.878535984178,4.59302344605999,
127.07114351688));
#165458=CARTESIAN_POINT('Ctrl Pts',(-230.871138494842,4.69085960655737,
127.194847999179));
#165459=CARTESIAN_POINT('Ctrl Pts',(-230.863741005505,4.78356795630168,
127.322204938975));
#165460=CARTESIAN_POINT('Ctrl Pts',(-230.85634092299,4.87630880481388,127.449606523548));
#165461=CARTESIAN_POINT('Ctrl Pts',(-230.848940840475,4.96391804411382,
127.580662813197));
#165462=CARTESIAN_POINT('Ctrl Pts',(-230.84154075796,5.04611243044084,127.714914081073));
#165463=CARTESIAN_POINT('Ctrl Pts',(-230.834132538294,5.12839719794553,
127.849312972019));
#165464=CARTESIAN_POINT('Ctrl Pts',(-230.826724318627,5.20525502653584,
127.986913538732));
#165465=CARTESIAN_POINT('Ctrl Pts',(-230.819316098961,5.27644822295134,
128.127230678057));
#165466=CARTESIAN_POINT('Ctrl Pts',(-230.811903319658,5.34768523759131,
128.26763418024));
#165467=CARTESIAN_POINT('Ctrl Pts',(-230.804490540357,5.41325051768329,
128.410757248119));
#165468=CARTESIAN_POINT('Ctrl Pts',(-230.797077761054,5.47295468426939,
128.55609515583));
#165469=CARTESIAN_POINT('Ctrl Pts',(-230.789654390026,5.53274415896865,
128.70164072916));
#165470=CARTESIAN_POINT('Ctrl Pts',(-230.782231018997,5.58665566653315,
128.849407113114));
#165471=CARTESIAN_POINT('Ctrl Pts',(-230.774807647968,5.6345495544069,128.9988740124));
#165472=CARTESIAN_POINT('Ctrl Pts',(-230.770871598528,5.65994404295338,
129.078124948804));
#165473=CARTESIAN_POINT('Ctrl Pts',(-230.766935549087,5.68364761299832,
129.15785377127));
#165474=CARTESIAN_POINT('Ctrl Pts',(-230.762999499647,5.7056453082692,129.237981934512));
#165475=CARTESIAN_POINT('Ctrl Pts',(-230.755576233241,5.74713227502902,
129.389101149686));
#165476=CARTESIAN_POINT('Ctrl Pts',(-230.748152966836,5.78267403282317,
129.54209824317));
#165477=CARTESIAN_POINT('Ctrl Pts',(-230.74072970043,5.81209912729416,129.696464279001));
#165478=CARTESIAN_POINT('Ctrl Pts',(-230.733315207709,5.84148944374708,
129.850647866996));
#165479=CARTESIAN_POINT('Ctrl Pts',(-230.725900714988,5.8647774177972,130.006196813632));
#165480=CARTESIAN_POINT('Ctrl Pts',(-230.718486222267,5.88184130535802,
130.162586965034));
#165481=CARTESIAN_POINT('Ctrl Pts',(-230.711078875914,5.89888874610166,
130.318826381721));
#165482=CARTESIAN_POINT('Ctrl Pts',(-230.70367152956,5.9097240029828,130.475905020456));
#165483=CARTESIAN_POINT('Ctrl Pts',(-230.696264183206,5.91427636484807,
130.633288578064));
#165484=CARTESIAN_POINT('Ctrl Pts',(-230.68886236153,5.91882533139009,130.790554753075));
#165485=CARTESIAN_POINT('Ctrl Pts',(-230.681460539855,5.91710072266801,
130.948125022599));
#165486=CARTESIAN_POINT('Ctrl Pts',(-230.67405871818,5.90908365626002,131.105460112452));
#165487=CARTESIAN_POINT('Ctrl Pts',(-230.666660803868,5.90107082199895,
131.262712146337));
#165488=CARTESIAN_POINT('Ctrl Pts',(-230.659262889557,5.88677216440396,
131.419728875929));
#165489=CARTESIAN_POINT('Ctrl Pts',(-230.651864975246,5.86622089033969,
131.575971288981));
#165490=CARTESIAN_POINT('Ctrl Pts',(-230.644468290333,5.84567303152436,
131.732187737379));
#165491=CARTESIAN_POINT('Ctrl Pts',(-230.637071605421,5.81887466712362,
131.887629754875));
#165492=CARTESIAN_POINT('Ctrl Pts',(-230.629674920509,5.78591085634493,
132.041763593532));
#165493=CARTESIAN_POINT('Ctrl Pts',(-230.622278563574,5.75294850721616,
132.195890597733));
#165494=CARTESIAN_POINT('Ctrl Pts',(-230.614882206638,5.71382133335572,
132.348709173387));
#165495=CARTESIAN_POINT('Ctrl Pts',(-230.607485849703,5.66866544364176,
132.499696174487));
#165496=CARTESIAN_POINT('Ctrl Pts',(-230.600088360366,5.62350264044593,
132.650706292083));
#165497=CARTESIAN_POINT('Ctrl Pts',(-230.59269087103,5.57230939052587,132.799883919105));
#165498=CARTESIAN_POINT('Ctrl Pts',(-230.585293381693,5.51527151770472,
132.946721616206));
#165499=CARTESIAN_POINT('Ctrl Pts',(-230.577893299178,5.45821365034543,
133.093610787036));
#165500=CARTESIAN_POINT('Ctrl Pts',(-230.570493216663,5.39530721597336,
133.238158047065));
#165501=CARTESIAN_POINT('Ctrl Pts',(-230.563093134148,5.32678589563614,
133.379876601704));
#165502=CARTESIAN_POINT('Ctrl Pts',(-230.555684914482,5.25818922906313,
133.521750990463));
#165503=CARTESIAN_POINT('Ctrl Pts',(-230.548276694815,5.1839655089468,133.660790125773));
#165504=CARTESIAN_POINT('Ctrl Pts',(-230.540868475149,5.1043943872987,133.796531819455));
#165505=CARTESIAN_POINT('Ctrl Pts',(-230.533455695847,5.02477429095271,
133.932357059885));
#165506=CARTESIAN_POINT('Ctrl Pts',(-230.526042916545,4.93980043590136,
134.064880501096));
#165507=CARTESIAN_POINT('Ctrl Pts',(-230.518630137243,4.84979509835615,
134.193669996549));
#165508=CARTESIAN_POINT('Ctrl Pts',(-230.511206766214,4.7596611569642,134.322643512472));
#165509=CARTESIAN_POINT('Ctrl Pts',(-230.503783395185,4.6644815998839,134.44787213056));
#165510=CARTESIAN_POINT('Ctrl Pts',(-230.496360024156,4.56461868066146,
134.56895712485));
#165511=CARTESIAN_POINT('Ctrl Pts',(-230.492423974715,4.51166896471087,
134.633159294218));
#165512=CARTESIAN_POINT('Ctrl Pts',(-230.488487925274,4.4574032069286,134.696197155051));
#165513=CARTESIAN_POINT('Ctrl Pts',(-230.484551875834,4.40187940545715,
134.758015668568));
#165514=CARTESIAN_POINT('Ctrl Pts',(-230.477128609428,4.29716324872232,
134.874603455768));
#165515=CARTESIAN_POINT('Ctrl Pts',(-230.469705343023,4.18765364911417,
134.987204409386));
#165516=CARTESIAN_POINT('Ctrl Pts',(-230.462282076617,4.07368611360614,
135.095399187692));
#165517=CARTESIAN_POINT('Ctrl Pts',(-230.454867583896,3.95985327826035,
135.203466088757));
#165518=CARTESIAN_POINT('Ctrl Pts',(-230.447453091175,3.8415732628944,135.307136926026));
#165519=CARTESIAN_POINT('Ctrl Pts',(-230.440038598454,3.71922124735563,
135.40602595478));
#165520=CARTESIAN_POINT('Ctrl Pts',(-230.432631252101,3.5969871592959,135.504819670565));
#165521=CARTESIAN_POINT('Ctrl Pts',(-230.425223905747,3.47068917284005,
135.598840520145));
#165522=CARTESIAN_POINT('Ctrl Pts',(-230.417816559393,3.34073859127704,
135.687740208306));
#165523=CARTESIAN_POINT('Ctrl Pts',(-230.410414737718,3.21088493176052,
135.776573591725));
#165524=CARTESIAN_POINT('Ctrl Pts',(-230.403012916042,3.07738440824752,
135.860293209109));
#165525=CARTESIAN_POINT('Ctrl Pts',(-230.395611094367,2.94068052097118,
135.938591683274));
#165526=CARTESIAN_POINT('Ctrl Pts',(-230.388213180055,2.80404879861284,
136.016848824284));
#165527=CARTESIAN_POINT('Ctrl Pts',(-230.380815265744,2.66421740336748,
136.089690336382));
#165528=CARTESIAN_POINT('Ctrl Pts',(-230.373417351433,2.52165777062691,
136.156852808157));
#165529=CARTESIAN_POINT('Ctrl Pts',(-230.36602066652,2.37912182871121,136.224004118748));
#165530=CARTESIAN_POINT('Ctrl Pts',(-230.358623981608,2.2338588864998,136.285478103147));
#165531=CARTESIAN_POINT('Ctrl Pts',(-230.351227296696,2.08636397782904,
136.341057820278));
#165532=CARTESIAN_POINT('Ctrl Pts',(-230.34383093976,1.93887560923709,136.396635072945));
#165533=CARTESIAN_POINT('Ctrl Pts',(-230.336434582825,1.78915582028648,
136.44631844638));
#165534=CARTESIAN_POINT('Ctrl Pts',(-230.32903822589,1.63771831870231,136.489939679639));
#165535=CARTESIAN_POINT('Ctrl Pts',(-230.321640736553,1.48625763165004,
136.533567591421));
#165536=CARTESIAN_POINT('Ctrl Pts',(-230.314243247217,1.3330790670597,136.571131411667));
#165537=CARTESIAN_POINT('Ctrl Pts',(-230.30684575788,1.17870999034055,136.60251319586));
#165538=CARTESIAN_POINT('Ctrl Pts',(-230.299445675365,1.02428679978196,
136.633905980888));
#165539=CARTESIAN_POINT('Ctrl Pts',(-230.29204559285,0.868672631776451,
136.659112340856));
#165540=CARTESIAN_POINT('Ctrl Pts',(-230.284645510335,0.712403350713097,
136.678065753883));
#165541=CARTESIAN_POINT('Ctrl Pts',(-230.277237290669,0.55596223550878,
136.697040008135));
#165542=CARTESIAN_POINT('Ctrl Pts',(-230.269829071002,0.39886493944161,
136.709747539131));
#165543=CARTESIAN_POINT('Ctrl Pts',(-230.262420851336,0.241651473258279,
136.716173802027));
#165544=CARTESIAN_POINT('Ctrl Pts',(-230.255008072034,0.084341244809761,
136.722604020182));
#165545=CARTESIAN_POINT('Ctrl Pts',(-230.247595292731,-0.0730849237969144,
136.722745266382));
#165546=CARTESIAN_POINT('Ctrl Pts',(-230.240182513429,-0.230089257275169,
136.716635094972));
#165547=CARTESIAN_POINT('Ctrl Pts',(-230.232759142401,-0.387317925907647,
136.710516193063));
#165548=CARTESIAN_POINT('Ctrl Pts',(-230.225335771372,-0.544123184456584,
136.698128063022));
#165549=CARTESIAN_POINT('Ctrl Pts',(-230.217912400343,-0.699973766585444,
136.679559957894));
#165550=CARTESIAN_POINT('Ctrl Pts',(-230.213976350902,-0.782609484814435,
136.66971470302));
#165551=CARTESIAN_POINT('Ctrl Pts',(-230.210040301461,-0.864976990053815,
136.658132887677));
#165552=CARTESIAN_POINT('Ctrl Pts',(-230.206104252021,-0.946998627205643,
136.64483355754));
#165553=CARTESIAN_POINT('Ctrl Pts',(-230.198680985615,-1.10168887506227,
136.619751435961));
#165554=CARTESIAN_POINT('Ctrl Pts',(-230.19125771921,-1.25561585987202,
136.588481474199));
#165555=CARTESIAN_POINT('Ctrl Pts',(-230.183834452805,-1.4082454278487,
136.551079279328));
#165556=CARTESIAN_POINT('Ctrl Pts',(-230.176419960084,-1.56069460035156,
136.513721290745));
#165557=CARTESIAN_POINT('Ctrl Pts',(-230.169005467363,-1.71184904931024,
136.470245583799));
#165558=CARTESIAN_POINT('Ctrl Pts',(-230.161590974642,-1.86118144289472,
136.420759303479));
#165559=CARTESIAN_POINT('Ctrl Pts',(-230.154183628288,-2.010369904296,136.371320719899));
#165560=CARTESIAN_POINT('Ctrl Pts',(-230.146776281935,-2.15773945453356,
136.315883212734));
#165561=CARTESIAN_POINT('Ctrl Pts',(-230.139368935581,-2.30277474350538,
136.254604561022));
#165562=CARTESIAN_POINT('Ctrl Pts',(-230.131967113906,-2.44770185968765,
136.193371613239));
#165563=CARTESIAN_POINT('Ctrl Pts',(-230.12456529223,-2.59029783874524,
136.126306340039));
#165564=CARTESIAN_POINT('Ctrl Pts',(-230.117163470555,-2.73006435283812,
136.053615725852));
#165565=CARTESIAN_POINT('Ctrl Pts',(-230.109765556244,-2.86975708527654,
135.980963484474));
#165566=CARTESIAN_POINT('Ctrl Pts',(-230.102367641932,-3.00662299708464,
135.902691987966));
#165567=CARTESIAN_POINT('Ctrl Pts',(-230.094969727621,-3.14018565043765,
135.819055487973));
#165568=CARTESIAN_POINT('Ctrl Pts',(-230.087573042709,-3.27372610809979,
135.73543288685));
#165569=CARTESIAN_POINT('Ctrl Pts',(-230.080176357797,-3.40396408071764,
135.646447249662));
#165570=CARTESIAN_POINT('Ctrl Pts',(-230.072779672885,-3.53044947173783,
135.552397800445));
#165571=CARTESIAN_POINT('Ctrl Pts',(-230.065383315949,-3.65692925426322,
135.45835252148));
#165572=CARTESIAN_POINT('Ctrl Pts',(-230.057986959014,-3.77965648647571,
135.359244099678));
#165573=CARTESIAN_POINT('Ctrl Pts',(-230.050590602079,-3.89821193410659,
135.255413782749));
#165574=CARTESIAN_POINT('Ctrl Pts',(-230.043193112742,-4.01678553287983,
135.151567569133));
#165575=CARTESIAN_POINT('Ctrl Pts',(-230.035795623406,-4.13118579447052,
135.042998266893));
#165576=CARTESIAN_POINT('Ctrl Pts',(-230.028398134069,-4.24102843493114,
134.93008581159));
#165577=CARTESIAN_POINT('Ctrl Pts',(-230.020998051554,-4.35090958055831,
134.817133775002));
#165578=CARTESIAN_POINT('Ctrl Pts',(-230.013597969039,-4.45622966397548,
134.699835821501));
#165579=CARTESIAN_POINT('Ctrl Pts',(-230.006197886524,-4.55664307064725,
134.578606832272));
#165580=CARTESIAN_POINT('Ctrl Pts',(-229.998789666858,-4.65716689218283,
134.457244539306));
#165581=CARTESIAN_POINT('Ctrl Pts',(-229.991381447192,-4.75277302374416,
134.331942865802));
#165582=CARTESIAN_POINT('Ctrl Pts',(-229.983973227525,-4.84315733934463,
134.203148276254));
#165583=CARTESIAN_POINT('Ctrl Pts',(-229.976560448223,-4.93359728498372,
134.074274415785));
#165584=CARTESIAN_POINT('Ctrl Pts',(-229.969147668921,-5.01880880889249,
133.941903668619));
#165585=CARTESIAN_POINT('Ctrl Pts',(-229.961734889619,-5.09853282592591,
133.806508779375));
#165586=CARTESIAN_POINT('Ctrl Pts',(-229.954311518591,-5.1783707563732,
133.670920431566));
#165587=CARTESIAN_POINT('Ctrl Pts',(-229.946888147562,-5.25270534414721,
133.532299639712));
#165588=CARTESIAN_POINT('Ctrl Pts',(-229.939464776533,-5.32132451793056,
133.391141616679));
#165589=CARTESIAN_POINT('Ctrl Pts',(-229.935528727092,-5.35770805037367,
133.316296245809));
#165590=CARTESIAN_POINT('Ctrl Pts',(-229.93159267765,-5.39248558963972,
133.240737876772));
#165591=CARTESIAN_POINT('Ctrl Pts',(-229.927656628208,-5.42563118491665,
133.164542137653));
#165592=CARTESIAN_POINT('Ctrl Pts',(-229.919453204097,-5.49471247556551,
133.005736723049));
#165593=CARTESIAN_POINT('Ctrl Pts',(-229.911249779985,-5.55688125103648,
132.843750280117));
#165594=CARTESIAN_POINT('Ctrl Pts',(-229.903046355874,-5.61186340173011,
132.679172534218));
#165595=CARTESIAN_POINT('Ctrl Pts',(-229.894874816899,-5.66663184734259,
132.515234470473));
#165596=CARTESIAN_POINT('Ctrl Pts',(-229.886703277925,-5.71426930736496,
132.348725421031));
#165597=CARTESIAN_POINT('Ctrl Pts',(-229.87853173895,-5.75455061996164,
132.180252228413));
#165598=CARTESIAN_POINT('Ctrl Pts',(-229.870380481584,-5.79473195508803,
132.012197183132));
#165599=CARTESIAN_POINT('Ctrl Pts',(-229.862229224218,-5.8275934947053,
131.842187947632));
#165600=CARTESIAN_POINT('Ctrl Pts',(-229.854077966851,-5.85295916047295,
131.670847563997));
#165601=CARTESIAN_POINT('Ctrl Pts',(-229.845960083918,-5.87822096929155,
131.500208714856));
#165602=CARTESIAN_POINT('Ctrl Pts',(-229.837842200985,-5.89604806700541,
131.328249822894));
#165603=CARTESIAN_POINT('Ctrl Pts',(-229.829724318052,-5.90631517593186,
131.155603560637));
#165604=CARTESIAN_POINT('Ctrl Pts',(-229.824274629052,-5.91320768116215,
131.039702845633));
#165605=CARTESIAN_POINT('Ctrl Pts',(-229.818824940053,-5.91669413707215,
130.923492707171));
#165606=CARTESIAN_POINT('Ctrl Pts',(-229.813375251053,-5.91674933390121,
130.807168157351));
#165607=CARTESIAN_POINT('',(-228.063375157888,-5.91524724934575,130.799300212791));
#165608=CARTESIAN_POINT('Ctrl Pts',(-229.813375192209,-5.90821578806308,
130.807162853899));
#165609=CARTESIAN_POINT('Ctrl Pts',(-229.758653129604,-5.90324637020015,
129.640793025429));
#165610=CARTESIAN_POINT('Ctrl Pts',(-229.611115192396,-5.00404810123538,
126.489038457145));
#165611=CARTESIAN_POINT('Ctrl Pts',(-229.370761380581,0.128487452770731,
123.807143206003));
#165612=CARTESIAN_POINT('Ctrl Pts',(-229.092313756769,5.95640778655091,
127.130293823035));
#165613=CARTESIAN_POINT('Ctrl Pts',(-228.813866132955,6.31068035119472,
133.829732336119));
#165614=CARTESIAN_POINT('Ctrl Pts',(-228.535418509144,0.865745966962777,
137.749002037465));
#165615=CARTESIAN_POINT('Ctrl Pts',(-228.285254862227,-4.7408718153285,
135.536621484418));
#165616=CARTESIAN_POINT('Ctrl Pts',(-228.127907089916,-5.90152179133772,
132.17219460905));
#165617=CARTESIAN_POINT('Ctrl Pts',(-228.063375192209,-5.91261418727021,
130.799303195672));
#165618=CARTESIAN_POINT('',(-226.313375192209,-5.92101946389561,130.803627806158));
#165619=CARTESIAN_POINT('Ctrl Pts',(-228.063375138329,-5.91674783454524,
130.799298512843));
#165620=CARTESIAN_POINT('Ctrl Pts',(-228.054506342384,-5.91658629655463,
130.610487808902));
#165621=CARTESIAN_POINT('Ctrl Pts',(-228.045637546438,-5.90738325424359,
130.422070303137));
#165622=CARTESIAN_POINT('Ctrl Pts',(-228.036768750493,-5.88927407511812,
130.234815684623));
#165623=CARTESIAN_POINT('Ctrl Pts',(-228.02782973436,-5.87102151351253,
130.046078446082));
#165624=CARTESIAN_POINT('Ctrl Pts',(-228.018890718226,-5.84372132038497,
129.858522591115));
#165625=CARTESIAN_POINT('Ctrl Pts',(-228.009951702093,-5.80756065119015,
129.672914708453));
#165626=CARTESIAN_POINT('Ctrl Pts',(-228.000937814618,-5.77109710774292,
129.485752212729));
#165627=CARTESIAN_POINT('Ctrl Pts',(-227.991923927143,-5.72562408790282,
129.300570461164));
#165628=CARTESIAN_POINT('Ctrl Pts',(-227.982910039668,-5.67138157104477,
129.118133575287));
#165629=CARTESIAN_POINT('Ctrl Pts',(-227.981447780285,-5.6625821901492,
129.088538126159));
#165630=CARTESIAN_POINT('Ctrl Pts',(-227.979985520901,-5.65355212979459,
129.059014865267));
#165631=CARTESIAN_POINT('Ctrl Pts',(-227.978523261518,-5.64429253147647,
129.029567000939));
#165632=CARTESIAN_POINT('Ctrl Pts',(-227.971099995113,-5.59728550528529,
128.880072769964));
#165633=CARTESIAN_POINT('Ctrl Pts',(-227.963676728707,-5.54426406037377,
128.73222131227));
#165634=CARTESIAN_POINT('Ctrl Pts',(-227.956253462302,-5.48535983216093,
128.586533285645));
#165635=CARTESIAN_POINT('Ctrl Pts',(-227.94883896958,-5.42652522385415,
128.441017450169));
#165636=CARTESIAN_POINT('Ctrl Pts',(-227.941424476859,-5.36182181071405,
128.297660298747));
#165637=CARTESIAN_POINT('Ctrl Pts',(-227.934009984138,-5.29143125500573,
128.156968346661));
#165638=CARTESIAN_POINT('Ctrl Pts',(-227.926602637784,-5.22110854436515,
128.016411998775));
#165639=CARTESIAN_POINT('Ctrl Pts',(-227.919195291431,-5.14510976961532,
127.878516067814));
#165640=CARTESIAN_POINT('Ctrl Pts',(-227.911787945077,-5.06366498537831,
127.743767949739));
#165641=CARTESIAN_POINT('Ctrl Pts',(-227.904386123401,-4.98228094573412,
127.609120331895));
#165642=CARTESIAN_POINT('Ctrl Pts',(-227.896984301726,-4.89545917653997,
127.477616170335));
#165643=CARTESIAN_POINT('Ctrl Pts',(-227.88958248005,-4.80347598802572,
127.349718958152));
#165644=CARTESIAN_POINT('Ctrl Pts',(-227.882184565739,-4.71154135672069,
127.221889261912));
#165645=CARTESIAN_POINT('Ctrl Pts',(-227.874786651427,-4.61445094982006,
127.097663025273));
#165646=CARTESIAN_POINT('Ctrl Pts',(-227.867388737116,-4.5125247169297,
126.977475298981));
#165647=CARTESIAN_POINT('Ctrl Pts',(-227.859992052204,-4.41061542232996,
126.857307545709));
#165648=CARTESIAN_POINT('Ctrl Pts',(-227.852595367291,-4.30387213790969,
126.741177255218));
#165649=CARTESIAN_POINT('Ctrl Pts',(-227.845198682379,-4.19265554319056,
126.629486959759));
#165650=CARTESIAN_POINT('Ctrl Pts',(-227.837802325444,-4.08144387993178,
126.517801616765));
#165651=CARTESIAN_POINT('Ctrl Pts',(-227.830405968508,-3.96575956416316,
126.410556141872));
#165652=CARTESIAN_POINT('Ctrl Pts',(-227.823009611573,-3.84600043872704,
126.308116497435));
#165653=CARTESIAN_POINT('Ctrl Pts',(-227.815612122236,-3.72622297786309,
126.205661169227));
#165654=CARTESIAN_POINT('Ctrl Pts',(-227.808214632899,-3.60236974882988,
126.108013379186));
#165655=CARTESIAN_POINT('Ctrl Pts',(-227.800817143563,-3.47487187018399,
126.015498952378));
#165656=CARTESIAN_POINT('Ctrl Pts',(-227.793417061048,-3.3473292973542,
125.922952094782));
#165657=CARTESIAN_POINT('Ctrl Pts',(-227.786016978533,-3.21613983311619,
125.835542402295));
#165658=CARTESIAN_POINT('Ctrl Pts',(-227.778616896018,-3.0817636348362,
125.753552418723));
#165659=CARTESIAN_POINT('Ctrl Pts',(-227.771208676351,-2.94723967611218,
125.671472278736));
#165660=CARTESIAN_POINT('Ctrl Pts',(-227.763800456684,-2.80952230420485,
125.594823943784));
#165661=CARTESIAN_POINT('Ctrl Pts',(-227.756392237018,-2.66909698343816,
125.523844368609));
#165662=CARTESIAN_POINT('Ctrl Pts',(-227.748979457716,-2.52858523322966,
125.452821106689));
#165663=CARTESIAN_POINT('Ctrl Pts',(-227.741566678414,-2.38536255188863,
125.387473711466));
#165664=CARTESIAN_POINT('Ctrl Pts',(-227.734153899112,-2.2399339528973,
125.327990793571));
#165665=CARTESIAN_POINT('Ctrl Pts',(-227.726730528083,-2.09429755870359,
125.268422883694));
#165666=CARTESIAN_POINT('Ctrl Pts',(-227.719307157054,-1.94644930172276,
125.21473631384));
#165667=CARTESIAN_POINT('Ctrl Pts',(-227.711883786025,-1.79690968917086,
125.167069944604));
#165668=CARTESIAN_POINT('Ctrl Pts',(-227.707947736585,-1.71762019845595,
125.141796091901));
#165669=CARTESIAN_POINT('Ctrl Pts',(-227.704011687145,-1.6378553955227,
125.118213883002));
#165670=CARTESIAN_POINT('Ctrl Pts',(-227.700075637705,-1.55769384832639,
125.09633815463));
#165671=CARTESIAN_POINT('Ctrl Pts',(-227.692652371299,-1.40651167204503,
125.055081213631));
#165672=CARTESIAN_POINT('Ctrl Pts',(-227.685229104894,-1.2534606672229,
125.019772332525));
#165673=CARTESIAN_POINT('Ctrl Pts',(-227.677805838488,-1.09905003016062,
124.990582190957));
#165674=CARTESIAN_POINT('Ctrl Pts',(-227.670391345767,-0.944821893647909,
124.961426549712));
#165675=CARTESIAN_POINT('Ctrl Pts',(-227.662976853046,-0.789237686801845,
124.938375321646));
#165676=CARTESIAN_POINT('Ctrl Pts',(-227.655562360325,-0.632821748164266,
124.921549453033));
#165677=CARTESIAN_POINT('Ctrl Pts',(-227.648155013972,-0.476556569097746,
124.904739801826));
#165678=CARTESIAN_POINT('Ctrl Pts',(-227.640747667618,-0.319461622840829,
124.894143604441));
#165679=CARTESIAN_POINT('Ctrl Pts',(-227.633340321264,-0.162071319561586,
124.88983075883));
#165680=CARTESIAN_POINT('Ctrl Pts',(-227.625938499589,-0.00479840390807593,
124.885521129903));
#165681=CARTESIAN_POINT('Ctrl Pts',(-227.618536677913,0.152769058592018,
124.887485531755));
#165682=CARTESIAN_POINT('Ctrl Pts',(-227.611134856238,0.310091765644128,
124.895742026103));
#165683=CARTESIAN_POINT('Ctrl Pts',(-227.603736941926,0.467331423263784,
124.903994161912));
#165684=CARTESIAN_POINT('Ctrl Pts',(-227.596339027615,0.624326210911163,
124.918531755683));
#165685=CARTESIAN_POINT('Ctrl Pts',(-227.588941113304,0.780537167497064,
124.939320780305));
#165686=CARTESIAN_POINT('Ctrl Pts',(-227.581544428391,0.936722164655714,
124.960106350168));
#165687=CARTESIAN_POINT('Ctrl Pts',(-227.574147743479,1.09212321960435,
124.987141239827));
#165688=CARTESIAN_POINT('Ctrl Pts',(-227.566751058567,1.24620671446836,
125.020339577899));
#165689=CARTESIAN_POINT('Ctrl Pts',(-227.559354701631,1.40028337710874,
125.053536443921));
#165690=CARTESIAN_POINT('Ctrl Pts',(-227.551958344696,1.55304223090366,
125.092896136331));
#165691=CARTESIAN_POINT('Ctrl Pts',(-227.54456198776,1.70396033758665,125.138281750269));
#165692=CARTESIAN_POINT('Ctrl Pts',(-227.537164498424,1.85490155021704,
125.18367431286));
#165693=CARTESIAN_POINT('Ctrl Pts',(-227.529767009087,2.00400109708265,
125.235094526453));
#165694=CARTESIAN_POINT('Ctrl Pts',(-227.52236951975,2.15075182221655,125.292355795205));
#165695=CARTESIAN_POINT('Ctrl Pts',(-227.514969437235,2.29755399058986,
125.349637136806));
#165696=CARTESIAN_POINT('Ctrl Pts',(-227.507569354721,2.44200535035133,
125.412763474657));
#165697=CARTESIAN_POINT('Ctrl Pts',(-227.500169272206,2.58361946309799,
125.481500387163));
#165698=CARTESIAN_POINT('Ctrl Pts',(-227.492761052539,2.72538929511969,
125.550312882971));
#165699=CARTESIAN_POINT('Ctrl Pts',(-227.485352832872,2.86431531355729,
125.624748111034));
#165700=CARTESIAN_POINT('Ctrl Pts',(-227.477944613206,2.99993575635128,
125.704525716291));
#165701=CARTESIAN_POINT('Ctrl Pts',(-227.470531833904,3.13563967126485,
125.784352423333));
#165702=CARTESIAN_POINT('Ctrl Pts',(-227.463119054602,3.26803364327327,
125.869527858104));
#165703=CARTESIAN_POINT('Ctrl Pts',(-227.4557062753,3.39668601678758,125.959729087113));
#165704=CARTESIAN_POINT('Ctrl Pts',(-227.448282904271,3.52552221484654,
126.050059199868));
#165705=CARTESIAN_POINT('Ctrl Pts',(-227.440859533242,3.6506058408394,126.145429223372));
#165706=CARTESIAN_POINT('Ctrl Pts',(-227.433436162213,3.77153872055182,
126.245476297705));
#165707=CARTESIAN_POINT('Ctrl Pts',(-227.429500112773,3.83566023511634,
126.298523657109));
#165708=CARTESIAN_POINT('Ctrl Pts',(-227.425564063332,3.89861543970226,
126.352885284942));
#165709=CARTESIAN_POINT('Ctrl Pts',(-227.421628013892,3.96034938385561,
126.408503099368));
#165710=CARTESIAN_POINT('Ctrl Pts',(-227.414204747486,4.07677767588481,
126.513396561609));
#165711=CARTESIAN_POINT('Ctrl Pts',(-227.406781481081,4.18921184414372,
126.623077393891));
#165712=CARTESIAN_POINT('Ctrl Pts',(-227.399358214675,4.29723305797474,
126.737209451461));
#165713=CARTESIAN_POINT('Ctrl Pts',(-227.391943721954,4.40512659970163,
126.851206614417));
#165714=CARTESIAN_POINT('Ctrl Pts',(-227.384529229233,4.50861731487337,
126.969644262183));
#165715=CARTESIAN_POINT('Ctrl Pts',(-227.377114736512,4.60732003017595,
127.092146628308));
#165716=CARTESIAN_POINT('Ctrl Pts',(-227.369707390158,4.70592761208543,
127.214530922041));
#165717=CARTESIAN_POINT('Ctrl Pts',(-227.362300043805,4.79975614875495,
127.340971845974));
#165718=CARTESIAN_POINT('Ctrl Pts',(-227.354892697451,4.88845797130749,
127.471057567248));
#165719=CARTESIAN_POINT('Ctrl Pts',(-227.347490875775,4.97709363669451,
127.601046265684));
#165720=CARTESIAN_POINT('Ctrl Pts',(-227.3400890541,5.06060999206217,127.734674041612));
#165721=CARTESIAN_POINT('Ctrl Pts',(-227.332687232425,5.13870033551353,
127.871496927537));
#165722=CARTESIAN_POINT('Ctrl Pts',(-227.325289318113,5.2167494556802,128.008247585724));
#165723=CARTESIAN_POINT('Ctrl Pts',(-227.317891403802,5.28937808384876,
128.148189671429));
#165724=CARTESIAN_POINT('Ctrl Pts',(-227.31049348949,5.35632352635789,128.290851348937));
#165725=CARTESIAN_POINT('Ctrl Pts',(-227.303096804578,5.42325784374888,
128.433489318662));
#165726=CARTESIAN_POINT('Ctrl Pts',(-227.295700119666,5.4845106914927,128.578845645601));
#165727=CARTESIAN_POINT('Ctrl Pts',(-227.288303434754,5.53986588211983,
128.726424966343));
#165728=CARTESIAN_POINT('Ctrl Pts',(-227.280907077818,5.59521861823997,
128.873997743264));
#165729=CARTESIAN_POINT('Ctrl Pts',(-227.273510720883,5.64467408610982,
129.023792968478));
#165730=CARTESIAN_POINT('Ctrl Pts',(-227.266114363947,5.68806480675869,
129.175296678792));
#165731=CARTESIAN_POINT('Ctrl Pts',(-227.258716874611,5.73146217063765,
129.326823584711));
#165732=CARTESIAN_POINT('Ctrl Pts',(-227.251319385274,5.76879283568528,
129.480059137663));
#165733=CARTESIAN_POINT('Ctrl Pts',(-227.243921895938,5.79993966008191,
129.634475793359));
#165734=CARTESIAN_POINT('Ctrl Pts',(-227.236521813423,5.83109740294951,
129.788946579575));
#165735=CARTESIAN_POINT('Ctrl Pts',(-227.229121730908,5.85606691545617,
129.944598927172));
#165736=CARTESIAN_POINT('Ctrl Pts',(-227.221721648393,5.87478249129061,
130.100896871147));
#165737=CARTESIAN_POINT('Ctrl Pts',(-227.214313428726,5.89351864682472,
130.25736668078));
#165738=CARTESIAN_POINT('Ctrl Pts',(-227.20690520906,5.90598708776309,130.414483133631));
#165739=CARTESIAN_POINT('Ctrl Pts',(-227.199496989393,5.91217409108498,
130.571706197441));
#165740=CARTESIAN_POINT('Ctrl Pts',(-227.192084210091,5.91836490240416,
130.729026029424));
#165741=CARTESIAN_POINT('Ctrl Pts',(-227.184671430789,5.91826657261066,
130.886452230686));
#165742=CARTESIAN_POINT('Ctrl Pts',(-227.177258651487,5.91191747440748,
131.043447083715));
#165743=CARTESIAN_POINT('Ctrl Pts',(-227.169835280458,5.90555930431503,
131.200666258352));
#165744=CARTESIAN_POINT('Ctrl Pts',(-227.16241190943,5.89293255770868,131.357452482698));
#165745=CARTESIAN_POINT('Ctrl Pts',(-227.154988538401,5.87412729602688,
131.513274626859));
#165746=CARTESIAN_POINT('Ctrl Pts',(-227.15105248896,5.86415629505729,131.595895266593));
#165747=CARTESIAN_POINT('Ctrl Pts',(-227.147116439519,5.85244914380482,
131.678245050899));
#165748=CARTESIAN_POINT('Ctrl Pts',(-227.143180390079,5.83902500609958,
131.760246353752));
#165749=CARTESIAN_POINT('Ctrl Pts',(-227.135757123673,5.81370750134011,
131.914898251763));
#165750=CARTESIAN_POINT('Ctrl Pts',(-227.128333857268,5.78220332512043,
132.068777470771));
#165751=CARTESIAN_POINT('Ctrl Pts',(-227.120910590862,5.74456889733928,
132.221349942234));
#165752=CARTESIAN_POINT('Ctrl Pts',(-227.113496098141,5.70697895032642,
132.373742085705));
#165753=CARTESIAN_POINT('Ctrl Pts',(-227.10608160542,5.6632732623841,132.524830197006));
#165754=CARTESIAN_POINT('Ctrl Pts',(-227.098667112699,5.61355978088494,
132.674087107973));
#165755=CARTESIAN_POINT('Ctrl Pts',(-227.091259766346,5.56389421511078,
132.823200159511));
#165756=CARTESIAN_POINT('Ctrl Pts',(-227.083852419992,5.50823250077247,
132.97048517265));
#165757=CARTESIAN_POINT('Ctrl Pts',(-227.076445073638,5.44673320099748,
133.115427037999));
#165758=CARTESIAN_POINT('Ctrl Pts',(-227.069043251963,5.38527976972049,
133.260260800236));
#165759=CARTESIAN_POINT('Ctrl Pts',(-227.061641430287,5.31799756737383,
133.402754552242));
#165760=CARTESIAN_POINT('Ctrl Pts',(-227.054239608612,5.24509433651822,
133.542410281748));
#165761=CARTESIAN_POINT('Ctrl Pts',(-227.0468416943,5.1722295907109,133.68199228808));
#165762=CARTESIAN_POINT('Ctrl Pts',(-227.039443779989,5.09374989822016,
133.818738925507));
#165763=CARTESIAN_POINT('Ctrl Pts',(-227.032045865678,5.00991023545401,
133.952174143681));
#165764=CARTESIAN_POINT('Ctrl Pts',(-227.024649180766,4.92608450531893,
134.085587187343));
#165765=CARTESIAN_POINT('Ctrl Pts',(-227.017252495853,4.83690077115004,
134.215689588156));
#165766=CARTESIAN_POINT('Ctrl Pts',(-227.009855810941,4.74265894160609,
134.342031705458));
#165767=CARTESIAN_POINT('Ctrl Pts',(-227.002459454006,4.64842129084362,
134.468368220617));
#165768=CARTESIAN_POINT('Ctrl Pts',(-226.99506309707,4.54912621385052,134.590944484567));
#165769=CARTESIAN_POINT('Ctrl Pts',(-226.987666740135,4.44511559594414,
134.709341782846));
#165770=CARTESIAN_POINT('Ctrl Pts',(-226.980269250798,4.34108905374633,
134.827757208054));
#165771=CARTESIAN_POINT('Ctrl Pts',(-226.972871761462,4.23234577950193,
134.941992113175));
#165772=CARTESIAN_POINT('Ctrl Pts',(-226.965474272125,4.11926629314812,
135.051662792904));
#165773=CARTESIAN_POINT('Ctrl Pts',(-226.95807418961,4.00614716695582,135.16137191752));
#165774=CARTESIAN_POINT('Ctrl Pts',(-226.950674107095,3.88868907004331,
135.266513371461));
#165775=CARTESIAN_POINT('Ctrl Pts',(-226.94327402458,3.76730740908115,135.366742171972));
#165776=CARTESIAN_POINT('Ctrl Pts',(-226.935865804914,3.64579227650426,
135.467081184352));
#165777=CARTESIAN_POINT('Ctrl Pts',(-226.928457585247,3.5203452518386,135.562496517387));
#165778=CARTESIAN_POINT('Ctrl Pts',(-226.921049365581,3.39141326188787,
135.652684724883));
#165779=CARTESIAN_POINT('Ctrl Pts',(-226.913636586279,3.26240191644866,
135.742928441716));
#165780=CARTESIAN_POINT('Ctrl Pts',(-226.906223806977,3.12990164513015,
135.827938421207));
#165781=CARTESIAN_POINT('Ctrl Pts',(-226.898811027675,2.99438558628782,
135.907456297948));
#165782=CARTESIAN_POINT('Ctrl Pts',(-226.891387656646,2.85867589574575,
135.98708779356));
#165783=CARTESIAN_POINT('Ctrl Pts',(-226.883964285617,2.71994213982124,
136.061211338007));
#165784=CARTESIAN_POINT('Ctrl Pts',(-226.876540914588,2.57867985354334,
136.129615613848));
#165785=CARTESIAN_POINT('Ctrl Pts',(-226.872604865148,2.50377919981375,
136.165885202239));
#165786=CARTESIAN_POINT('Ctrl Pts',(-226.868668815707,2.42816799279131,
136.200547714251));
#165787=CARTESIAN_POINT('Ctrl Pts',(-226.864732766266,2.35192189996657,
136.233577314195));
#165788=CARTESIAN_POINT('Ctrl Pts',(-226.85730949986,2.20812414846543,136.295870108869));
#165789=CARTESIAN_POINT('Ctrl Pts',(-226.849886233455,2.06163242665041,
136.352540229753));
#165790=CARTESIAN_POINT('Ctrl Pts',(-226.84246296705,1.91292655784591,136.403346467413));
#165791=CARTESIAN_POINT('Ctrl Pts',(-226.835048474329,1.76439644702866,
136.45409265632));
#165792=CARTESIAN_POINT('Ctrl Pts',(-226.827633981608,1.61365774805125,
136.498988637935));
#165793=CARTESIAN_POINT('Ctrl Pts',(-226.820219488887,1.46121233061102,
136.537840284171));
#165794=CARTESIAN_POINT('Ctrl Pts',(-226.812812142533,1.3089138458036,136.576654483728));
#165795=CARTESIAN_POINT('Ctrl Pts',(-226.805404796179,1.15491227671018,
136.609435854271));
#165796=CARTESIAN_POINT('Ctrl Pts',(-226.797997449826,0.999726706694797,
136.636039370243));
#165797=CARTESIAN_POINT('Ctrl Pts',(-226.79059562815,0.844656879932347,
136.662623044308));
#165798=CARTESIAN_POINT('Ctrl Pts',(-226.783193806475,0.688405176911631,
136.683037975506));
#165799=CARTESIAN_POINT('Ctrl Pts',(-226.7757919848,0.531502879386526,136.697189755739));
#165800=CARTESIAN_POINT('Ctrl Pts',(-226.768394070489,0.37468340936296,
136.711334065358));
#165801=CARTESIAN_POINT('Ctrl Pts',(-226.760996156177,0.217214399667312,
136.719221775157));
#165802=CARTESIAN_POINT('Ctrl Pts',(-226.753598241866,0.0596341859142466,
136.720810087169));
#165803=CARTESIAN_POINT('Ctrl Pts',(-226.746201556954,-0.0979198408663133,
136.722398135233));
#165804=CARTESIAN_POINT('Ctrl Pts',(-226.738804872042,-0.255584662113312,
136.71768885943));
#165805=CARTESIAN_POINT('Ctrl Pts',(-226.73140818713,-0.412819874445797,
136.706691539648));
#165806=CARTESIAN_POINT('Ctrl Pts',(-226.724011830194,-0.570048114804197,
136.695694707498));
#165807=CARTESIAN_POINT('Ctrl Pts',(-226.716615473259,-0.726846411736703,
136.678410411798));
#165808=CARTESIAN_POINT('Ctrl Pts',(-226.709219116323,-0.882677691542532,
136.654899964956));
#165809=CARTESIAN_POINT('Ctrl Pts',(-226.701821626987,-1.03853282951512,
136.631385918603));
#165810=CARTESIAN_POINT('Ctrl Pts',(-226.69442413765,-1.19342028642395,
136.601643878774));
#165811=CARTESIAN_POINT('Ctrl Pts',(-226.687026648314,-1.34681155980786,
136.565786585577));
#165812=CARTESIAN_POINT('Ctrl Pts',(-226.679626565799,-1.50025660426508,
136.529916722661));
#165813=CARTESIAN_POINT('Ctrl Pts',(-226.672226483284,-1.65220405768046,
136.487927423222));
#165814=CARTESIAN_POINT('Ctrl Pts',(-226.664826400769,-1.80213913883811,
136.439981709049));
#165815=CARTESIAN_POINT('Ctrl Pts',(-226.657418181103,-1.9522390890314,
136.391983273634));
#165816=CARTESIAN_POINT('Ctrl Pts',(-226.650009961436,-2.10032189206058,
136.338015457094));
#165817=CARTESIAN_POINT('Ctrl Pts',(-226.64260174177,-2.24589067519652,
136.278290251528));
#165818=CARTESIAN_POINT('Ctrl Pts',(-226.635188962468,-2.39154905348955,
136.218528286094));
#165819=CARTESIAN_POINT('Ctrl Pts',(-226.627776183166,-2.53468998998896,
136.153002025632));
#165820=CARTESIAN_POINT('Ctrl Pts',(-226.620363403864,-2.67484037172136,
136.081969882026));
#165821=CARTESIAN_POINT('Ctrl Pts',(-226.612940032835,-2.81519100689139,
136.010836244362));
#165822=CARTESIAN_POINT('Ctrl Pts',(-226.605516661807,-2.95254222795981,
135.934181192702));
#165823=CARTESIAN_POINT('Ctrl Pts',(-226.598093290778,-3.08644839879045,
135.852307412462));
#165824=CARTESIAN_POINT('Ctrl Pts',(-226.594157241336,-3.15744866361516,
135.808895969635));
#165825=CARTESIAN_POINT('Ctrl Pts',(-226.590221191895,-3.22748092097847,
135.76401805416));
#165826=CARTESIAN_POINT('Ctrl Pts',(-226.586285142453,-3.29648253445665,
135.71772336242));
#165827=CARTESIAN_POINT('Ctrl Pts',(-226.578887013369,-3.42617674971686,
135.630708676628));
#165828=CARTESIAN_POINT('Ctrl Pts',(-226.571488884284,-3.55262599635902,
135.53841925968));
#165829=CARTESIAN_POINT('Ctrl Pts',(-226.5640907552,-3.67536978180676,135.441125387261));
#165830=CARTESIAN_POINT('Ctrl Pts',(-226.556701385759,-3.79796823430501,
135.343946714201));
#165831=CARTESIAN_POINT('Ctrl Pts',(-226.549312016319,-3.91686966586141,
135.241775610162));
#165832=CARTESIAN_POINT('Ctrl Pts',(-226.541922646879,-4.03164112926855,
135.13492644287));
#165833=CARTESIAN_POINT('Ctrl Pts',(-226.534540385959,-4.14630218336419,
135.028180063698));
#165834=CARTESIAN_POINT('Ctrl Pts',(-226.527158125038,-4.25684090441604,
134.916764833901));
#165835=CARTESIAN_POINT('Ctrl Pts',(-226.519775864118,-4.3628562433914,
134.801036231373));
#165836=CARTESIAN_POINT('Ctrl Pts',(-226.512399066432,-4.46879312581351,
134.68539327369));
#165837=CARTESIAN_POINT('Ctrl Pts',(-226.505022268747,-4.57021303781855,
134.565443574654));
#165838=CARTESIAN_POINT('Ctrl Pts',(-226.497645471062,-4.66675085057975,
134.441580305887));
#165839=CARTESIAN_POINT('Ctrl Pts',(-226.489967542777,-4.76722946404511,
134.312660775302));
#165840=CARTESIAN_POINT('Ctrl Pts',(-226.482289614491,-4.86241866816122,
134.17950169917));
#165841=CARTESIAN_POINT('Ctrl Pts',(-226.474611686205,-4.95195177533823,
134.04258608489));
#165842=CARTESIAN_POINT('Ctrl Pts',(-226.467239868017,-5.03791530136331,
133.91112913737));
#165843=CARTESIAN_POINT('Ctrl Pts',(-226.459868049828,-5.11866481166663,
133.776209754528));
#165844=CARTESIAN_POINT('Ctrl Pts',(-226.452496231639,-5.19391926109291,
133.63828603503));
#165845=CARTESIAN_POINT('Ctrl Pts',(-226.445124560937,-5.2691722049107,
133.500365074958));
#165846=CARTESIAN_POINT('Ctrl Pts',(-226.437752890236,-5.33893012607006,
133.359440227836));
#165847=CARTESIAN_POINT('Ctrl Pts',(-226.430381219534,-5.40295766920539,
133.215994708235));
#165848=CARTESIAN_POINT('Ctrl Pts',(-226.423008214756,-5.46699679962502,
133.072523228805));
#165849=CARTESIAN_POINT('Ctrl Pts',(-226.415635209978,-5.5253033342825,
132.926530512276));
#165850=CARTESIAN_POINT('Ctrl Pts',(-226.4082622052,-5.57768992328781,132.778520105083));
#165851=CARTESIAN_POINT('Ctrl Pts',(-226.400886384224,-5.63009652191107,
132.630453163733));
#165852=CARTESIAN_POINT('Ctrl Pts',(-226.393510563247,-5.67657854823874,
132.480367351838));
#165853=CARTESIAN_POINT('Ctrl Pts',(-226.386134742271,-5.71699845977709,
132.328781548086));
#165854=CARTESIAN_POINT('Ctrl Pts',(-226.37875079904,-5.75746288172915,
132.17702881802));
#165855=CARTESIAN_POINT('Ctrl Pts',(-226.371366855808,-5.79185176377396,
132.023773161657));
#165856=CARTESIAN_POINT('Ctrl Pts',(-226.363982912577,-5.82007851800152,
131.869544454656));
#165857=CARTESIAN_POINT('Ctrl Pts',(-226.356594167713,-5.84832362752866,
131.715215455779));
#165858=CARTESIAN_POINT('Ctrl Pts',(-226.349205422849,-5.87039857370088,
131.559912516861));
#165859=CARTESIAN_POINT('Ctrl Pts',(-226.341816677986,-5.88626868280649,
131.404170217616));
#165860=CARTESIAN_POINT('Ctrl Pts',(-226.334417907912,-5.90216032482148,
131.24821660383));
#165861=CARTESIAN_POINT('Ctrl Pts',(-226.327019137838,-5.91183030008091,
131.091822813332));
#165862=CARTESIAN_POINT('Ctrl Pts',(-226.319620367765,-5.91529600517794,
130.935523621595));
#165863=CARTESIAN_POINT('Ctrl Pts',(-226.31753864258,-5.91627111935416,
130.891547128117));
#165864=CARTESIAN_POINT('Ctrl Pts',(-226.315456917394,-5.91675539410002,
130.847578092369));
#165865=CARTESIAN_POINT('Ctrl Pts',(-226.313375192209,-5.91674995468472,
130.803628334572));
#165866=CARTESIAN_POINT('',(-224.563375192209,-5.91483159952414,130.809774239277));
#165867=CARTESIAN_POINT('Ctrl Pts',(-226.313375192209,-5.92642165134677,
130.80362713756));
#165868=CARTESIAN_POINT('Ctrl Pts',(-226.311529301019,-5.92648962768387,
130.76459263781));
#165869=CARTESIAN_POINT('Ctrl Pts',(-226.30968340983,-5.92613747701628,
130.725559397462));
#165870=CARTESIAN_POINT('Ctrl Pts',(-226.30783751864,-5.92536146718798,
130.686534585569));
#165871=CARTESIAN_POINT('Ctrl Pts',(-226.215021644036,-5.88634181569524,
128.724272634618));
#165872=CARTESIAN_POINT('Ctrl Pts',(-226.029389894828,-3.66499790132608,
124.842368424212));
#165873=CARTESIAN_POINT('Ctrl Pts',(-225.750942271015,3.03497199644419,
124.498291674782));
#165874=CARTESIAN_POINT('Ctrl Pts',(-225.472494647202,6.94595089610799,
129.949184215175));
#165875=CARTESIAN_POINT('Ctrl Pts',(-225.194047023389,4.47394025081266,
136.185942091678));
#165876=CARTESIAN_POINT('Ctrl Pts',(-224.915599399576,-2.10940292084664,
137.477289498338));
#165877=CARTESIAN_POINT('Ctrl Pts',(-224.705375455848,-5.61623921853537,
133.822594326139));
#165878=CARTESIAN_POINT('Ctrl Pts',(-224.587967386727,-5.91948652701702,
131.332466920396));
#165879=CARTESIAN_POINT('Ctrl Pts',(-224.563375192209,-5.91483159952414,
130.809774239277));
#165880=CARTESIAN_POINT('',(-222.813375192209,-5.90733561507725,130.802750946968));
#165881=CARTESIAN_POINT('Ctrl Pts',(-224.563375192209,-5.91483159952414,
130.809774239277));
#165882=CARTESIAN_POINT('Ctrl Pts',(-224.495151512123,-5.90191789701304,
129.359719904591));
#165883=CARTESIAN_POINT('Ctrl Pts',(-224.334111957431,-4.63296812933935,
125.916704457217));
#165884=CARTESIAN_POINT('Ctrl Pts',(-224.080256528137,1.14114131736879,
123.899626225559));
#165885=CARTESIAN_POINT('Ctrl Pts',(-223.801808904323,6.42596335219761,
128.032257530277));
#165886=CARTESIAN_POINT('Ctrl Pts',(-223.523361280512,5.80563899211914,
134.712316147447));
#165887=CARTESIAN_POINT('Ctrl Pts',(-223.244913656698,-0.149783980485487,
137.801154546898));
#165888=CARTESIAN_POINT('Ctrl Pts',(-223.008251627265,-5.09451046644834,
134.961633525739));
#165889=CARTESIAN_POINT('Ctrl Pts',(-222.864405472434,-5.90469612405182,
131.890837229664));
#165890=CARTESIAN_POINT('Ctrl Pts',(-222.813375192209,-5.90733561507725,
130.802750946968));
#165891=CARTESIAN_POINT('',(-221.063375192209,-5.92075521056039,130.799502985017));
#165892=CARTESIAN_POINT('Ctrl Pts',(-222.813375192209,-5.90733561507725,
130.802750946968));
#165893=CARTESIAN_POINT('Ctrl Pts',(-222.77158959783,-5.90949693382502,
129.911783234133));
#165894=CARTESIAN_POINT('Ctrl Pts',(-222.636988128846,-5.30138420352635,
127.044562818406));
#165895=CARTESIAN_POINT('Ctrl Pts',(-222.40957078526,-0.844604857256582,
123.857116331848));
#165896=CARTESIAN_POINT('Ctrl Pts',(-222.131123161446,5.38838381779271,
126.338615398399));
#165897=CARTESIAN_POINT('Ctrl Pts',(-221.852675537634,6.66971100146858,
132.923916157578));
#165898=CARTESIAN_POINT('Ctrl Pts',(-221.574227913821,1.821899608298,137.561448921536));
#165899=CARTESIAN_POINT('Ctrl Pts',(-221.311127798679,-4.3406655091924,
136.076187875004));
#165900=CARTESIAN_POINT('Ctrl Pts',(-221.140843558142,-5.90619376265546,
132.441826029179));
#165901=CARTESIAN_POINT('Ctrl Pts',(-221.063375192209,-5.92075521056039,
130.799502985017));
#165902=CARTESIAN_POINT('',(-219.313375192209,-5.92045153616181,130.808269674344));
#165903=CARTESIAN_POINT('Ctrl Pts',(-221.063375192209,-5.92075521056039,
130.799502985017));
#165904=CARTESIAN_POINT('Ctrl Pts',(-221.048027683538,-5.92364002612731,
130.474137051998));
#165905=CARTESIAN_POINT('Ctrl Pts',(-221.032680174866,-5.89914275629101,
130.149205902182));
#165906=CARTESIAN_POINT('Ctrl Pts',(-220.924516791591,-5.52276673404195,
127.893203873355));
#165907=CARTESIAN_POINT('Ctrl Pts',(-220.738885042383,-2.76232065490982,
124.374186037525));
#165908=CARTESIAN_POINT('Ctrl Pts',(-220.46043741857,3.91678619878236,125.004675591346));
#165909=CARTESIAN_POINT('Ctrl Pts',(-220.181989794757,6.99655788143963,
130.964792353897));
#165910=CARTESIAN_POINT('Ctrl Pts',(-219.903542170944,3.64683467190507,
136.777480188288));
#165911=CARTESIAN_POINT('Ctrl Pts',(-219.625094547131,-3.05415144333025,
137.101162940295));
#165912=CARTESIAN_POINT('Ctrl Pts',(-219.428372220886,-5.80551108210207,
133.241733301106));
#165913=CARTESIAN_POINT('Ctrl Pts',(-219.324465769245,-5.92499839058684,
131.043137371517));
#165914=CARTESIAN_POINT('Ctrl Pts',(-219.313375192209,-5.92320801574442,
130.808271494346));
#165915=CARTESIAN_POINT('',(-217.563375219359,-5.91209744554343,130.80733573345));
#165916=CARTESIAN_POINT('Ctrl Pts',(-219.313375192209,-5.91674871030393,
130.808267229504));
#165917=CARTESIAN_POINT('Ctrl Pts',(-219.306059579814,-5.91685088830008,
130.653513817441));
#165918=CARTESIAN_POINT('Ctrl Pts',(-219.298743967419,-5.91087751960387,
130.498520301917));
#165919=CARTESIAN_POINT('Ctrl Pts',(-219.291428355024,-5.89879859397009,
130.343811260519));
#165920=CARTESIAN_POINT('Ctrl Pts',(-219.284120305473,-5.88673215546926,
130.189262156555));
#165921=CARTESIAN_POINT('Ctrl Pts',(-219.276812255921,-5.86857274844675,
130.034997321644));
#165922=CARTESIAN_POINT('Ctrl Pts',(-219.26950420637,-5.84434236784582,
129.88154273201));
#165923=CARTESIAN_POINT('Ctrl Pts',(-219.26220201398,-5.82013140710079,
129.7282111312));
#165924=CARTESIAN_POINT('Ctrl Pts',(-219.254899821591,-5.78985921545387,
129.575688861118));
#165925=CARTESIAN_POINT('Ctrl Pts',(-219.247597629202,-5.75359969604657,
129.424497906948));
#165926=CARTESIAN_POINT('Ctrl Pts',(-219.240122698798,-5.71648243459886,
129.269730434402));
#165927=CARTESIAN_POINT('Ctrl Pts',(-219.232647768394,-5.67309107105576,
129.116358458185));
#165928=CARTESIAN_POINT('Ctrl Pts',(-219.22517283799,-5.62356073441339,
128.964932655165));
#165929=CARTESIAN_POINT('Ctrl Pts',(-219.217876340133,-5.57521272639103,
128.817121506776));
#165930=CARTESIAN_POINT('Ctrl Pts',(-219.210579842277,-5.52101564217927,
128.67116505339));
#165931=CARTESIAN_POINT('Ctrl Pts',(-219.20328334442,-5.46114590788245,
128.527561123689));
#165932=CARTESIAN_POINT('Ctrl Pts',(-219.195987218609,-5.40127922631816,
128.383964516292));
#165933=CARTESIAN_POINT('Ctrl Pts',(-219.188691092798,-5.33574061779488,
128.242720548933));
#165934=CARTESIAN_POINT('Ctrl Pts',(-219.181394966987,-5.26475475767799,
128.104307302536));
#165935=CARTESIAN_POINT('Ctrl Pts',(-219.174097680021,-5.19375760038916,
127.965872028114));
#165936=CARTESIAN_POINT('Ctrl Pts',(-219.166800393055,-5.11731164224933,
127.830268713036));
#165937=CARTESIAN_POINT('Ctrl Pts',(-219.159503106089,-5.03568748843877,
127.697950779621));
#165938=CARTESIAN_POINT('Ctrl Pts',(-219.15189445554,-4.95058056232268,
127.559987051272));
#165939=CARTESIAN_POINT('Ctrl Pts',(-219.144285804991,-4.85984404607919,
127.425595645752));
#165940=CARTESIAN_POINT('Ctrl Pts',(-219.136677154443,-4.76383411652442,
127.295256020559));
#165941=CARTESIAN_POINT('Ctrl Pts',(-219.129369107119,-4.67161735558365,
127.170065864569));
#165942=CARTESIAN_POINT('Ctrl Pts',(-219.122061059795,-4.57453618848797,
127.048613716132));
#165943=CARTESIAN_POINT('Ctrl Pts',(-219.114753012472,-4.47294624763622,
126.931289171251));
#165944=CARTESIAN_POINT('Ctrl Pts',(-219.10744011649,-4.37128890507438,
126.813886785249));
#165945=CARTESIAN_POINT('Ctrl Pts',(-219.100127220508,-4.26511709451247,
126.700617734469));
#165946=CARTESIAN_POINT('Ctrl Pts',(-219.092814324526,-4.15482222848972,
126.591833726002));
#165947=CARTESIAN_POINT('Ctrl Pts',(-219.085491833986,-4.04438265502116,
126.482906992342));
#165948=CARTESIAN_POINT('Ctrl Pts',(-219.078169343447,-3.92980951568913,
126.378477298318));
#165949=CARTESIAN_POINT('Ctrl Pts',(-219.070846852907,-3.81152636629467,
126.278855416868));
#165950=CARTESIAN_POINT('Ctrl Pts',(-219.069964335106,-3.79727069955119,
126.266848834785));
#165951=CARTESIAN_POINT('Ctrl Pts',(-219.069081817305,-3.78296117632481,
126.254912035624));
#165952=CARTESIAN_POINT('Ctrl Pts',(-219.068199299505,-3.76859856456568,
126.24304551974));
#165953=CARTESIAN_POINT('Ctrl Pts',(-219.060776033099,-3.64778797777036,
126.143230752679));
#165954=CARTESIAN_POINT('Ctrl Pts',(-219.053352766694,-3.52282644481948,
126.048068037059));
#165955=CARTESIAN_POINT('Ctrl Pts',(-219.045929500288,-3.39410781351939,
125.957922470565));
#165956=CARTESIAN_POINT('Ctrl Pts',(-219.038515007567,-3.26554131695244,
125.867883448644));
#165957=CARTESIAN_POINT('Ctrl Pts',(-219.031100514847,-3.13322686381598,
125.782849984492));
#165958=CARTESIAN_POINT('Ctrl Pts',(-219.023686022126,-2.99759256841364,
125.703148079719));
#165959=CARTESIAN_POINT('Ctrl Pts',(-219.016278675772,-2.86208900245175,
125.623522994642));
#165960=CARTESIAN_POINT('Ctrl Pts',(-219.008871329418,-2.7232722840575,
125.549219426543));
#165961=CARTESIAN_POINT('Ctrl Pts',(-219.001463983064,-2.58160071376054,
125.480520995901));
#165962=CARTESIAN_POINT('Ctrl Pts',(-218.994062161389,-2.44003480746567,
125.41187380314));
#165963=CARTESIAN_POINT('Ctrl Pts',(-218.986660339714,-2.29561862334915,
125.348823586028));
#165964=CARTESIAN_POINT('Ctrl Pts',(-218.979258518039,-2.14883625177907,
125.291608734383));
#165965=CARTESIAN_POINT('Ctrl Pts',(-218.971860603727,-2.00213136547997,
125.234424086012));
#165966=CARTESIAN_POINT('Ctrl Pts',(-218.964462689416,-1.85306312628229,
125.183068803489));
#165967=CARTESIAN_POINT('Ctrl Pts',(-218.957064775104,-1.70213674865009,
125.13773366219));
#165968=CARTESIAN_POINT('Ctrl Pts',(-218.949668090192,-1.55123545224399,
125.092406054769));
#165969=CARTESIAN_POINT('Ctrl Pts',(-218.94227140528,-1.39847698742511,
125.053096710286));
#165970=CARTESIAN_POINT('Ctrl Pts',(-218.934874720368,-1.24438303325878,
125.019946954191));
#165971=CARTESIAN_POINT('Ctrl Pts',(-218.927478363433,-1.09029591177985,
124.986798667991));
#165972=CARTESIAN_POINT('Ctrl Pts',(-218.920082006497,-0.934873783645096,
124.95980950563));
#165973=CARTESIAN_POINT('Ctrl Pts',(-218.912685649562,-0.778649595254036,
124.939069885615));
#165974=CARTESIAN_POINT('Ctrl Pts',(-218.905288160225,-0.622401488541358,
124.918327090311));
#165975=CARTESIAN_POINT('Ctrl Pts',(-218.897890670889,-0.465351447141299,
124.90383579164));
#165976=CARTESIAN_POINT('Ctrl Pts',(-218.890493181552,-0.308038481718682,
124.895634624911));
#165977=CARTESIAN_POINT('Ctrl Pts',(-218.883093099037,-0.150670370479677,
124.887430583275));
#165978=CARTESIAN_POINT('Ctrl Pts',(-218.875693016523,0.00696047572782896,
124.885521083135));
#165979=CARTESIAN_POINT('Ctrl Pts',(-218.868292934008,0.164314247561687,
124.889892645673));
#165980=CARTESIAN_POINT('Ctrl Pts',(-218.860884714341,0.321841046044711,
124.894269015194));
#165981=CARTESIAN_POINT('Ctrl Pts',(-218.853476494675,0.479089788321696,
124.904940230102));
#165982=CARTESIAN_POINT('Ctrl Pts',(-218.846068275008,0.635524253120782,
124.921840793018));
#165983=CARTESIAN_POINT('Ctrl Pts',(-218.838655495706,0.792055000722703,
124.93875175795));
#165984=CARTESIAN_POINT('Ctrl Pts',(-218.831242716404,0.947770103810021,
124.961899655972));
#165985=CARTESIAN_POINT('Ctrl Pts',(-218.823829937102,1.1021432588565,124.991167794387));
#165986=CARTESIAN_POINT('Ctrl Pts',(-218.816406566073,1.25673698950607,
125.020477752491));
#165987=CARTESIAN_POINT('Ctrl Pts',(-218.808983195045,1.4099845798288,125.055925332584));
#165988=CARTESIAN_POINT('Ctrl Pts',(-218.801559824016,1.56137381127563,
125.097343674892));
#165989=CARTESIAN_POINT('Ctrl Pts',(-218.797623774575,1.64164401433556,
125.119304673807));
#165990=CARTESIAN_POINT('Ctrl Pts',(-218.793687725133,1.72139207092731,
125.142943452068));
#165991=CARTESIAN_POINT('Ctrl Pts',(-218.789751675692,1.80054399766364,
125.168229686246));
#165992=CARTESIAN_POINT('Ctrl Pts',(-218.782328409287,1.94982206121864,
125.215918734743));
#165993=CARTESIAN_POINT('Ctrl Pts',(-218.774905142881,2.09742990993292,
125.269614639238));
#165994=CARTESIAN_POINT('Ctrl Pts',(-218.767481876476,2.24284749242479,
125.329183388633));
#165995=CARTESIAN_POINT('Ctrl Pts',(-218.760067383755,2.38809320341033,
125.388681732714));
#165996=CARTESIAN_POINT('Ctrl Pts',(-218.752652891034,2.53115345895547,
125.454038965045));
#165997=CARTESIAN_POINT('Ctrl Pts',(-218.745238398313,2.67152257843374,
125.525071112773));
#165998=CARTESIAN_POINT('Ctrl Pts',(-218.737831051959,2.81175640486985,
125.596034797042));
#165999=CARTESIAN_POINT('Ctrl Pts',(-218.730423705605,2.94930392817718,
125.672662340198));
#166000=CARTESIAN_POINT('Ctrl Pts',(-218.723016359252,3.08367880778335,
125.754721464822));
#166001=CARTESIAN_POINT('Ctrl Pts',(-218.715614537576,3.21795346553502,
125.836719386655));
#166002=CARTESIAN_POINT('Ctrl Pts',(-218.708212715901,3.34905987394385,
125.924140629995));
#166003=CARTESIAN_POINT('Ctrl Pts',(-218.700810894226,3.47653580623464,
126.016706771425));
#166004=CARTESIAN_POINT('Ctrl Pts',(-218.693412979915,3.60394444497268,
126.10922404791));
#166005=CARTESIAN_POINT('Ctrl Pts',(-218.686015065603,3.72772612309777,
126.206880594752));
#166006=CARTESIAN_POINT('Ctrl Pts',(-218.678617151292,3.84744725512211,
126.309354479466));
#166007=CARTESIAN_POINT('Ctrl Pts',(-218.67122046638,3.96714849166643,126.411811334881));
#166008=CARTESIAN_POINT('Ctrl Pts',(-218.663823781468,4.08279023804669,
126.5190836968));
#166009=CARTESIAN_POINT('Ctrl Pts',(-218.656427096556,4.1939716128804,126.630809051711));
#166010=CARTESIAN_POINT('Ctrl Pts',(-218.64903073962,4.30514805781513,126.742529452602));
#166011=CARTESIAN_POINT('Ctrl Pts',(-218.641634382685,4.41186426113564,
126.858702189282));
#166012=CARTESIAN_POINT('Ctrl Pts',(-218.63423802575,4.51375608064432,126.978927752262));
#166013=CARTESIAN_POINT('Ctrl Pts',(-218.626840536413,4.61566350005128,
127.099171722084));
#166014=CARTESIAN_POINT('Ctrl Pts',(-218.619443047076,4.71274482357616,
127.223469468902));
#166015=CARTESIAN_POINT('Ctrl Pts',(-218.61204555774,4.80467619780906,127.351388391106));
#166016=CARTESIAN_POINT('Ctrl Pts',(-218.604645475225,4.89663979844203,
127.479352155088));
#166017=CARTESIAN_POINT('Ctrl Pts',(-218.59724539271,4.98344963771258,127.610939318872));
#166018=CARTESIAN_POINT('Ctrl Pts',(-218.589845310195,5.06482527559572,
127.745688439939));
#166019=CARTESIAN_POINT('Ctrl Pts',(-218.582437090529,5.14629039435869,
127.880585731519));
#166020=CARTESIAN_POINT('Ctrl Pts',(-218.575028870862,5.22230918524685,
128.018651604228));
#166021=CARTESIAN_POINT('Ctrl Pts',(-218.567620651196,5.29264691236428,
128.159399516994));
#166022=CARTESIAN_POINT('Ctrl Pts',(-218.560207871894,5.36302793117911,
128.300234057751));
#166023=CARTESIAN_POINT('Ctrl Pts',(-218.552795092592,5.42772076576185,
128.443753588359));
#166024=CARTESIAN_POINT('Ctrl Pts',(-218.54538231329,5.48653911307297,128.589452239501));
#166025=CARTESIAN_POINT('Ctrl Pts',(-218.537958942261,5.54544150279695,
128.735359071709));
#166026=CARTESIAN_POINT('Ctrl Pts',(-218.530535571233,5.59845251558682,
128.883450892541));
#166027=CARTESIAN_POINT('Ctrl Pts',(-218.523112200204,5.64543566865914,
129.033206566239));
#166028=CARTESIAN_POINT('Ctrl Pts',(-218.519176150762,5.67034726376772,
129.112610617786));
#166029=CARTESIAN_POINT('Ctrl Pts',(-218.515240101321,5.69356506267462,
129.19248225344));
#166030=CARTESIAN_POINT('Ctrl Pts',(-218.51130405188,5.71507458751184,129.272742838329));
#166031=CARTESIAN_POINT('Ctrl Pts',(-218.503880785474,5.75564088005899,
129.424111796556));
#166032=CARTESIAN_POINT('Ctrl Pts',(-218.496457519069,5.79025064261305,
129.577322408127));
#166033=CARTESIAN_POINT('Ctrl Pts',(-218.489034252663,5.81873552203086,
129.731864702816));
#166034=CARTESIAN_POINT('Ctrl Pts',(-218.481619759942,5.84718673468681,
129.886224341346));
#166035=CARTESIAN_POINT('Ctrl Pts',(-218.474205267221,5.86952740667652,
130.04191216653));
#166036=CARTESIAN_POINT('Ctrl Pts',(-218.4667907745,5.88563898684256,130.198403293112));
#166037=CARTESIAN_POINT('Ctrl Pts',(-218.459383428146,5.90173503806099,
130.354743587655));
#166038=CARTESIAN_POINT('Ctrl Pts',(-218.451976081792,5.91161391193149,
130.511885273371));
#166039=CARTESIAN_POINT('Ctrl Pts',(-218.444568735438,5.9152081510659,130.669293626545));
#166040=CARTESIAN_POINT('Ctrl Pts',(-218.437166913763,5.91879970948117,
130.82658457863));
#166041=CARTESIAN_POINT('Ctrl Pts',(-218.429765092087,5.91611595775744,
130.984141430561));
#166042=CARTESIAN_POINT('Ctrl Pts',(-218.422363270412,5.90714129653777,
131.141424803201));
#166043=CARTESIAN_POINT('Ctrl Pts',(-218.414965356101,5.8981713729719,131.298625147174));
#166044=CARTESIAN_POINT('Ctrl Pts',(-218.407567441789,5.8829171748978,131.455551927624));
#166045=CARTESIAN_POINT('Ctrl Pts',(-218.400169527478,5.86141518968541,
131.611666344429));
#166046=CARTESIAN_POINT('Ctrl Pts',(-218.392772842565,5.83991677771291,
131.767754817849));
#166047=CARTESIAN_POINT('Ctrl Pts',(-218.385376157653,5.81217269014303,
131.923030826115));
#166048=CARTESIAN_POINT('Ctrl Pts',(-218.377979472741,5.7782712336825,132.076961148957));
#166049=CARTESIAN_POINT('Ctrl Pts',(-218.370583115805,5.74437128044807,
132.230884646367));
#166050=CARTESIAN_POINT('Ctrl Pts',(-218.36318675887,5.70431458147778,132.383462212435));
#166051=CARTESIAN_POINT('Ctrl Pts',(-218.355790401934,5.65824042766622,
132.534171539379));
#166052=CARTESIAN_POINT('Ctrl Pts',(-218.348392912598,5.61215921978409,
132.684903940306));
#166053=CARTESIAN_POINT('Ctrl Pts',(-218.340995423261,5.56005883179809,
132.83376717557));
#166054=CARTESIAN_POINT('Ctrl Pts',(-218.333597933924,5.50212817301582,
132.980254946389));
#166055=CARTESIAN_POINT('Ctrl Pts',(-218.326197851409,5.44417720673067,
133.12679406827));
#166056=CARTESIAN_POINT('Ctrl Pts',(-218.318797768894,5.38039203766882,
133.270955720853));
#166057=CARTESIAN_POINT('Ctrl Pts',(-218.311397686379,5.31100930580515,
133.412254541051));
#166058=CARTESIAN_POINT('Ctrl Pts',(-218.303989466712,5.24155028049538,
133.553708733827));
#166059=CARTESIAN_POINT('Ctrl Pts',(-218.296581247046,5.16648156489098,
133.692293472212));
#166060=CARTESIAN_POINT('Ctrl Pts',(-218.28917302738,5.08608561929285,133.827548278913));
#166061=CARTESIAN_POINT('Ctrl Pts',(-218.281760248077,5.00564019133123,
133.962886332692));
#166062=CARTESIAN_POINT('Ctrl Pts',(-218.274347468775,4.91986120284593,
134.094890058577));
#166063=CARTESIAN_POINT('Ctrl Pts',(-218.266934689473,4.82907355467608,
134.223129279823));
#166064=CARTESIAN_POINT('Ctrl Pts',(-218.259511318444,4.73815618485739,
134.351551735281));
#166065=CARTESIAN_POINT('Ctrl Pts',(-218.252087947416,4.64221608908989,
134.476198648195));
#166066=CARTESIAN_POINT('Ctrl Pts',(-218.244664576387,4.54161794136622,
134.596673505127));
#166067=CARTESIAN_POINT('Ctrl Pts',(-218.240728526946,4.48827838963088,
134.660552165018));
#166068=CARTESIAN_POINT('Ctrl Pts',(-218.236792477506,4.43362990792399,
134.723258526826));
#166069=CARTESIAN_POINT('Ctrl Pts',(-218.232856428066,4.3777308283501,134.784737905841));
#166070=CARTESIAN_POINT('Ctrl Pts',(-218.22543316166,4.27230690881088,134.900686095971));
#166071=CARTESIAN_POINT('Ctrl Pts',(-218.218009895255,4.16211390419733,
135.012618347338));
#166072=CARTESIAN_POINT('Ctrl Pts',(-218.21058662885,4.04748986791888,135.12011736831));
#166073=CARTESIAN_POINT('Ctrl Pts',(-218.203172136129,3.93300130773237,
135.227489334366));
#166074=CARTESIAN_POINT('Ctrl Pts',(-218.195757643408,3.81409241000973,
135.33043824683));
#166075=CARTESIAN_POINT('Ctrl Pts',(-218.188343150687,3.6911406957847,135.428580651953));
#166076=CARTESIAN_POINT('Ctrl Pts',(-218.180935804333,3.56830748704985,
135.526628463731));
#166077=CARTESIAN_POINT('Ctrl Pts',(-218.173528457979,3.44143950900474,
135.619878759632));
#166078=CARTESIAN_POINT('Ctrl Pts',(-218.166121111625,3.31095017748968,
135.707985754613));
#166079=CARTESIAN_POINT('Ctrl Pts',(-218.15871928995,3.18055816984189,135.796027036073));
#166080=CARTESIAN_POINT('Ctrl Pts',(-218.151317468274,3.04655049471087,
135.878932446748));
#166081=CARTESIAN_POINT('Ctrl Pts',(-218.143915646599,2.90937251520491,
135.956397314861));
#166082=CARTESIAN_POINT('Ctrl Pts',(-218.136517732288,2.77226695088732,
136.033821289872));
#166083=CARTESIAN_POINT('Ctrl Pts',(-218.129119817976,2.63199473943562,
136.105810258993));
#166084=CARTESIAN_POINT('Ctrl Pts',(-218.121721903665,2.489028910967,136.172103685455));
#166085=CARTESIAN_POINT('Ctrl Pts',(-218.114325218753,2.34608684082479,
136.238386095153));
#166086=CARTESIAN_POINT('Ctrl Pts',(-218.106928533841,2.2004523804078,136.298974683822));
#166087=CARTESIAN_POINT('Ctrl Pts',(-218.099531848929,2.0526218749625,136.353655527816));
#166088=CARTESIAN_POINT('Ctrl Pts',(-218.092135491993,1.90479792447631,
136.408333947204));
#166089=CARTESIAN_POINT('Ctrl Pts',(-218.084739135058,1.75477847269028,
136.45710501327));
#166090=CARTESIAN_POINT('Ctrl Pts',(-218.077342778122,1.60307824206378,
136.499803595274));
#166091=CARTESIAN_POINT('Ctrl Pts',(-218.069945288786,1.45135478574513,
136.54250871454));
#166092=CARTESIAN_POINT('Ctrl Pts',(-218.062547799449,1.29795039756308,
136.579139397415));
#166093=CARTESIAN_POINT('Ctrl Pts',(-218.055150310113,1.14339315111778,
136.609580911791));
#166094=CARTESIAN_POINT('Ctrl Pts',(-218.047750227598,0.988781724870436,
136.640033097392));
#166095=CARTESIAN_POINT('Ctrl Pts',(-218.040350145083,0.833017001767469,
136.664291722736));
#166096=CARTESIAN_POINT('Ctrl Pts',(-218.032950062568,0.676635241207233,
136.682293529131));
#166097=CARTESIAN_POINT('Ctrl Pts',(-218.025541842902,0.520081522823261,
136.700315130363));
#166098=CARTESIAN_POINT('Ctrl Pts',(-218.018133623235,0.362909783057131,
136.712066130087));
#166099=CARTESIAN_POINT('Ctrl Pts',(-218.010725403569,0.205660111188952,
136.717535270928));
#166100=CARTESIAN_POINT('Ctrl Pts',(-218.003312624267,0.048313654771591,
136.723007777935));
#166101=CARTESIAN_POINT('Ctrl Pts',(-217.995899844964,-0.10911045689851,
136.722190723747));
#166102=CARTESIAN_POINT('Ctrl Pts',(-217.988487065662,-0.266074687102465,
136.715124935603));
#166103=CARTESIAN_POINT('Ctrl Pts',(-217.981063694634,-0.423263195158757,
136.70804905153));
#166104=CARTESIAN_POINT('Ctrl Pts',(-217.973640323605,-0.579990138405261,
136.694706632897));
#166105=CARTESIAN_POINT('Ctrl Pts',(-217.966216952576,-0.735724803657198,
136.675190165065));
#166106=CARTESIAN_POINT('Ctrl Pts',(-217.962280903136,-0.818299059977332,
136.664842065528));
#166107=CARTESIAN_POINT('Ctrl Pts',(-217.958344853695,-0.900594537340759,
136.652759070387));
#166108=CARTESIAN_POINT('Ctrl Pts',(-217.954408804254,-0.982533698024718,
136.63896069767));
#166109=CARTESIAN_POINT('Ctrl Pts',(-217.946985537848,-1.13706839784008,
136.612937397358));
#166110=CARTESIAN_POINT('Ctrl Pts',(-217.939562271443,-1.29080218161052,
136.580731017709));
#166111=CARTESIAN_POINT('Ctrl Pts',(-217.932139005037,-1.44320124394244,
136.542400416311));
#166112=CARTESIAN_POINT('Ctrl Pts',(-217.924724512316,-1.59542018323864,
136.504115118501));
#166113=CARTESIAN_POINT('Ctrl Pts',(-217.917310019595,-1.74630718269074,
136.459720097024));
#166114=CARTESIAN_POINT('Ctrl Pts',(-217.909895526874,-1.89533557246087,
136.409325704903));
#166115=CARTESIAN_POINT('Ctrl Pts',(-217.90248818052,-2.04422032305855,
136.358979884794));
#166116=CARTESIAN_POINT('Ctrl Pts',(-217.895080834166,-2.19124967904206,
136.302646324475));
#166117=CARTESIAN_POINT('Ctrl Pts',(-217.887673487812,-2.3359092603034,
136.240485937141));
#166118=CARTESIAN_POINT('Ctrl Pts',(-217.880271666137,-2.48046094899051,
136.17837191137));
#166119=CARTESIAN_POINT('Ctrl Pts',(-217.872869844462,-2.62264604072322,
136.110439858534));
#166120=CARTESIAN_POINT('Ctrl Pts',(-217.865468022786,-2.76196747686731,
136.036899792692));
#166121=CARTESIAN_POINT('Ctrl Pts',(-217.858070108475,-2.90121536631092,
135.963398548077));
#166122=CARTESIAN_POINT('Ctrl Pts',(-217.850672194163,-3.03760228149763,
135.884295360104));
#166123=CARTESIAN_POINT('Ctrl Pts',(-217.843274279852,-3.17065334113184,
135.799847375918));
#166124=CARTESIAN_POINT('Ctrl Pts',(-217.835877594939,-3.30368229009316,
135.715413425455));
#166125=CARTESIAN_POINT('Ctrl Pts',(-217.828480910027,-3.4333761688747,
135.625636641457));
#166126=CARTESIAN_POINT('Ctrl Pts',(-217.821084225115,-3.55928671072393,
135.530818982279));
#166127=CARTESIAN_POINT('Ctrl Pts',(-217.813687868179,-3.68519166956814,
135.436005527415));
#166128=CARTESIAN_POINT('Ctrl Pts',(-217.806291511244,-3.80731332683775,
135.336151866362));
#166129=CARTESIAN_POINT('Ctrl Pts',(-217.798895154308,-3.92523453330316,
135.231601792504));
#166130=CARTESIAN_POINT('Ctrl Pts',(-217.791497664971,-4.04317379380565,
135.127035711763));
#166131=CARTESIAN_POINT('Ctrl Pts',(-217.784100175635,-4.15691104366667,
135.017772034194));
#166132=CARTESIAN_POINT('Ctrl Pts',(-217.776702686298,-4.2660643188342,
134.904193027564));
#166133=CARTESIAN_POINT('Ctrl Pts',(-217.769302603783,-4.37525585751267,
134.79057420599));
#166134=CARTESIAN_POINT('Ctrl Pts',(-217.761902521268,-4.47985996365709,
134.672637312503));
#166135=CARTESIAN_POINT('Ctrl Pts',(-217.754502438753,-4.579533554635,134.550799324454));
#166136=CARTESIAN_POINT('Ctrl Pts',(-217.747094219086,-4.67931674697361,
134.428827363012));
#166137=CARTESIAN_POINT('Ctrl Pts',(-217.73968599942,-4.77415836032364,
134.302946029394));
#166138=CARTESIAN_POINT('Ctrl Pts',(-217.732277779753,-4.86375699208932,
134.173603631123));
#166139=CARTESIAN_POINT('Ctrl Pts',(-217.724865000451,-4.95341077031833,
134.044181624763));
#166140=CARTESIAN_POINT('Ctrl Pts',(-217.717452221149,-5.03781493714544,
133.911294623383));
#166141=CARTESIAN_POINT('Ctrl Pts',(-217.710039441847,-5.11671328995648,
133.775416939968));
#166142=CARTESIAN_POINT('Ctrl Pts',(-217.702616070818,-5.19572437643342,
133.639345108147));
#166143=CARTESIAN_POINT('Ctrl Pts',(-217.695192699789,-5.26921376285336,
133.500274388875));
#166144=CARTESIAN_POINT('Ctrl Pts',(-217.68776932876,-5.33697239632939,
133.358701276781));
#166145=CARTESIAN_POINT('Ctrl Pts',(-217.68383327932,-5.37289964963588,
133.283635815766));
#166146=CARTESIAN_POINT('Ctrl Pts',(-217.67989722988,-5.40721659929989,
133.207867145932));
#166147=CARTESIAN_POINT('Ctrl Pts',(-217.67596118044,-5.43989775535981,
133.131471051931));
#166148=CARTESIAN_POINT('Ctrl Pts',(-217.66772328069,-5.50829732488929,
132.971578913055));
#166149=CARTESIAN_POINT('Ctrl Pts',(-217.65948538094,-5.56970530852338,
132.808524925761));
#166150=CARTESIAN_POINT('Ctrl Pts',(-217.65124748119,-5.62384937071369,
132.642905916987));
#166151=CARTESIAN_POINT('Ctrl Pts',(-217.643042776513,-5.67777525641049,
132.47795427917));
#166152=CARTESIAN_POINT('Ctrl Pts',(-217.634838071835,-5.72449552927632,
132.310458456378));
#166153=CARTESIAN_POINT('Ctrl Pts',(-217.626633367158,-5.76378700476972,
132.141031828503));
#166154=CARTESIAN_POINT('Ctrl Pts',(-217.6184500779,-5.80297592405403,131.972047427662));
#166155=CARTESIAN_POINT('Ctrl Pts',(-217.610266788641,-5.83477465964333,
131.801142496242));
#166156=CARTESIAN_POINT('Ctrl Pts',(-217.602083499383,-5.85900923233826,
131.628946197039));
#166157=CARTESIAN_POINT('Ctrl Pts',(-217.59393521479,-5.88314013973657,
131.457486481091));
#166158=CARTESIAN_POINT('Ctrl Pts',(-217.585786930197,-5.89977136585755,
131.28474664181));
#166159=CARTESIAN_POINT('Ctrl Pts',(-217.577638645604,-5.90877981142748,
131.111365019109));
#166160=CARTESIAN_POINT('Ctrl Pts',(-217.572884181551,-5.91403617307598,
131.01019811911));
#166161=CARTESIAN_POINT('Ctrl Pts',(-217.568129717498,-5.91669817362437,
130.908813021326));
#166162=CARTESIAN_POINT('Ctrl Pts',(-217.563375253445,-5.91674925046863,
130.807338801387));
#166163=CARTESIAN_POINT('',(-215.813375157388,-5.91502029301215,130.799381620638));
#166164=CARTESIAN_POINT('Ctrl Pts',(-217.563375192209,-5.90839217088997,
130.807333289765));
#166165=CARTESIAN_POINT('Ctrl Pts',(-217.508087980348,-5.90305680765803,
129.629005570252));
#166166=CARTESIAN_POINT('Ctrl Pts',(-217.359984893885,-4.98979320465015,
126.464889769201));
#166167=CARTESIAN_POINT('Ctrl Pts',(-217.119065932814,0.171079120619924,
123.80805498781));
#166168=CARTESIAN_POINT('Ctrl Pts',(-216.840618309002,5.97866251551794,
127.16662023982));
#166169=CARTESIAN_POINT('Ctrl Pts',(-216.562170685189,6.2921471325479,133.868091185466));
#166170=CARTESIAN_POINT('Ctrl Pts',(-216.283723061376,0.823455923246531,
137.754143410778));
#166171=CARTESIAN_POINT('Ctrl Pts',(-216.034124563716,-4.7569552396461,
135.512749812486));
#166172=CARTESIAN_POINT('Ctrl Pts',(-215.87734194066,-5.90151798111243,
132.160438231407));
#166173=CARTESIAN_POINT('Ctrl Pts',(-215.813375192209,-5.91229507969721,
130.799384655716));
#166174=CARTESIAN_POINT('',(-214.063375192209,-5.92104864866457,130.803405895618));
#166175=CARTESIAN_POINT('Ctrl Pts',(-215.813375135314,-5.91674790344546,
130.799379696593));
#166176=CARTESIAN_POINT('Ctrl Pts',(-215.804563110474,-5.91658994349001,
130.611741860083));
#166177=CARTESIAN_POINT('Ctrl Pts',(-215.795751085635,-5.90750238473919,
130.424489465272));
#166178=CARTESIAN_POINT('Ctrl Pts',(-215.786939060796,-5.889617851042,130.238381703482));
#166179=CARTESIAN_POINT('Ctrl Pts',(-215.778062099627,-5.87160152516248,
130.050902502633));
#166180=CARTESIAN_POINT('Ctrl Pts',(-215.769185138457,-5.84465819380242,
129.864584895955));
#166181=CARTESIAN_POINT('Ctrl Pts',(-215.760308177288,-5.80897212291539,
129.680183835342));
#166182=CARTESIAN_POINT('Ctrl Pts',(-215.751359874733,-5.77299925413676,
129.494300800555));
#166183=CARTESIAN_POINT('Ctrl Pts',(-215.742411572178,-5.72814261072141,
129.310365266239));
#166184=CARTESIAN_POINT('Ctrl Pts',(-215.733463269623,-5.67463907513611,
129.129128714384));
#166185=CARTESIAN_POINT('Ctrl Pts',(-215.731251450999,-5.66141420754263,
129.084331125306));
#166186=CARTESIAN_POINT('Ctrl Pts',(-215.729039632374,-5.64766126993599,
129.039698330585));
#166187=CARTESIAN_POINT('Ctrl Pts',(-215.72682781375,-5.63338428331314,
128.995241473059));
#166188=CARTESIAN_POINT('Ctrl Pts',(-215.719404547345,-5.58546811424068,
128.846036156987));
#166189=CARTESIAN_POINT('Ctrl Pts',(-215.71198128094,-5.53154763790908,
128.698510195232));
#166190=CARTESIAN_POINT('Ctrl Pts',(-215.704558014535,-5.47175765669013,
128.553183434634));
#166191=CARTESIAN_POINT('Ctrl Pts',(-215.697143521814,-5.41203834226372,
128.408028438198));
#166192=CARTESIAN_POINT('Ctrl Pts',(-215.689729029094,-5.34646347226255,
128.265067810902));
#166193=CARTESIAN_POINT('Ctrl Pts',(-215.682314536373,-5.2752177888881,
128.124806952812));
#166194=CARTESIAN_POINT('Ctrl Pts',(-215.674907190019,-5.20404077478584,
127.984681283417));
#166195=CARTESIAN_POINT('Ctrl Pts',(-215.667499843666,-5.12720399645217,
127.847250533469));
#166196=CARTESIAN_POINT('Ctrl Pts',(-215.660092497313,-5.04494047116426,
127.713000689491));
#166197=CARTESIAN_POINT('Ctrl Pts',(-215.652690675638,-4.9627383011169,
127.57885097411));
#166198=CARTESIAN_POINT('Ctrl Pts',(-215.645288853963,-4.87511763737922,
127.447877757776));
#166199=CARTESIAN_POINT('Ctrl Pts',(-215.637887032288,-4.78235760647559,
127.320542843014));
#166200=CARTESIAN_POINT('Ctrl Pts',(-215.630489117977,-4.68964654287024,
127.193275147362));
#166201=CARTESIAN_POINT('Ctrl Pts',(-215.623091203666,-4.59180173447565,
127.069642229218));
#166202=CARTESIAN_POINT('Ctrl Pts',(-215.615693289355,-4.48914577324704,
126.95007718364));
#166203=CARTESIAN_POINT('Ctrl Pts',(-215.608296604443,-4.38650687157726,
126.830532007604));
#166204=CARTESIAN_POINT('Ctrl Pts',(-215.600899919531,-4.27905864683187,
126.715053645412));
#166205=CARTESIAN_POINT('Ctrl Pts',(-215.593503234619,-4.16716422217798,
126.604042426298));
#166206=CARTESIAN_POINT('Ctrl Pts',(-215.586106877684,-4.05527475904014,
126.493036129538));
#166207=CARTESIAN_POINT('Ctrl Pts',(-215.578710520749,-3.93893975299797,
126.386496844923));
#166208=CARTESIAN_POINT('Ctrl Pts',(-215.571314163814,-3.81855926723936,
126.284788106246));
#166209=CARTESIAN_POINT('Ctrl Pts',(-215.563916674478,-3.69816035092072,
126.1830637957));
#166210=CARTESIAN_POINT('Ctrl Pts',(-215.556519185141,-3.57371500679695,
126.086171744607));
#166211=CARTESIAN_POINT('Ctrl Pts',(-215.549121695805,-3.44565632882657,
125.994435147653));
#166212=CARTESIAN_POINT('Ctrl Pts',(-215.54172161329,-3.31755276008534,
125.902666392578));
#166213=CARTESIAN_POINT('Ctrl Pts',(-215.534321530776,-3.18583363888663,
125.816056907094));
#166214=CARTESIAN_POINT('Ctrl Pts',(-215.526921448261,-3.05096083399531,
125.734886428666));
#166215=CARTESIAN_POINT('Ctrl Pts',(-215.519513228595,-2.91593972258993,
125.653626694952));
#166216=CARTESIAN_POINT('Ctrl Pts',(-215.512105008929,-2.77775832210689,
125.577818104846));
#166217=CARTESIAN_POINT('Ctrl Pts',(-215.504696789263,-2.6369035302863,
125.507694653541));
#166218=CARTESIAN_POINT('Ctrl Pts',(-215.497284009961,-2.49596204469123,
125.437528042421));
#166219=CARTESIAN_POINT('Ctrl Pts',(-215.48987123066,-2.35234422880253,
125.373053695043));
#166220=CARTESIAN_POINT('Ctrl Pts',(-215.482458451358,-2.20655623487208,
125.314457144385));
#166221=CARTESIAN_POINT('Ctrl Pts',(-215.475035080329,-2.06055993221932,
125.255776868227));
#166222=CARTESIAN_POINT('Ctrl Pts',(-215.467611709301,-1.91238760914617,
125.202991287361));
#166223=CARTESIAN_POINT('Ctrl Pts',(-215.460188338273,-1.7625606085087,
125.156236091333));
#166224=CARTESIAN_POINT('Ctrl Pts',(-215.456252288828,-1.68311873763299,
125.131445364496));
#166225=CARTESIAN_POINT('Ctrl Pts',(-215.452316239383,-1.60321186086013,
125.108349143486));
#166226=CARTESIAN_POINT('Ctrl Pts',(-215.448380189938,-1.52291863500538,
125.086961786484));
#166227=CARTESIAN_POINT('Ctrl Pts',(-215.440956923532,-1.37148811706968,
125.046625898699));
#166228=CARTESIAN_POINT('Ctrl Pts',(-215.433533657127,-1.21822501274709,
125.012249336693));
#166229=CARTESIAN_POINT('Ctrl Pts',(-215.426110390721,-1.06363954787946,
124.983999677325));
#166230=CARTESIAN_POINT('Ctrl Pts',(-215.418695898,-0.90923679019333,124.955783406708));
#166231=CARTESIAN_POINT('Ctrl Pts',(-215.411281405279,-0.753515146594347,
124.933679690956));
#166232=CARTESIAN_POINT('Ctrl Pts',(-215.403866912558,-0.596999682143853,
124.917806282302));
#166233=CARTESIAN_POINT('Ctrl Pts',(-215.396459566204,-0.440635073191145,
124.901948173037));
#166234=CARTESIAN_POINT('Ctrl Pts',(-215.389052219851,-0.283478535478698,
124.892308453501));
#166235=CARTESIAN_POINT('Ctrl Pts',(-215.381644873497,-0.126064894761871,
124.888953767246));
#166236=CARTESIAN_POINT('Ctrl Pts',(-215.374243051821,0.0312313409228329,
124.885601583043));
#166237=CARTESIAN_POINT('Ctrl Pts',(-215.366841230146,0.188783926190721,
124.888525106367));
#166238=CARTESIAN_POINT('Ctrl Pts',(-215.359439408471,0.346053458792463,
124.897739115713));
#166239=CARTESIAN_POINT('Ctrl Pts',(-215.352041494159,0.50323997003168,
124.906948261054));
#166240=CARTESIAN_POINT('Ctrl Pts',(-215.344643579848,0.660143354468876,
124.92244125731));
#166241=CARTESIAN_POINT('Ctrl Pts',(-215.337245665537,0.816224868133231,
124.94418079719));
#166242=CARTESIAN_POINT('Ctrl Pts',(-215.329848980624,0.972280443881844,
124.965916724353));
#166243=CARTESIAN_POINT('Ctrl Pts',(-215.322452295712,1.12751405056174,
124.993897083447));
#166244=CARTESIAN_POINT('Ctrl Pts',(-215.3150556108,1.28139260290848,125.028032756398));
#166245=CARTESIAN_POINT('Ctrl Pts',(-215.307659253865,1.43526433211895,
125.062166915736));
#166246=CARTESIAN_POINT('Ctrl Pts',(-215.300262896929,1.5877807620265,125.102455765403));
#166247=CARTESIAN_POINT('Ctrl Pts',(-215.292866539994,1.73841979743222,
125.148759219802));
#166248=CARTESIAN_POINT('Ctrl Pts',(-215.285469050657,1.88908189605925,
125.195069763377));
#166249=CARTESIAN_POINT('Ctrl Pts',(-215.27807156132,2.03786567102082,125.247396635534));
#166250=CARTESIAN_POINT('Ctrl Pts',(-215.270674071984,2.18426511160827,
125.305550156683));
#166251=CARTESIAN_POINT('Ctrl Pts',(-215.263273989469,2.33071587229246,
125.36372406346));
#166252=CARTESIAN_POINT('Ctrl Pts',(-215.255873906954,2.4747802877687,125.427728548153));
#166253=CARTESIAN_POINT('Ctrl Pts',(-215.248473824439,2.61597335563737,
125.497326232423));
#166254=CARTESIAN_POINT('Ctrl Pts',(-215.241065604772,2.75732167979935,
125.567000446501));
#166255=CARTESIAN_POINT('Ctrl Pts',(-215.233657385106,2.89579201589938,
125.642279977557));
#166256=CARTESIAN_POINT('Ctrl Pts',(-215.226249165439,3.03092431703412,
125.722881664848));
#166257=CARTESIAN_POINT('Ctrl Pts',(-215.218836386137,3.16613978984541,
125.803532961134));
#166258=CARTESIAN_POINT('Ctrl Pts',(-215.211423606835,3.2980128218533,125.889512737487));
#166259=CARTESIAN_POINT('Ctrl Pts',(-215.204010827533,3.42611373125421,
125.98049543879));
#166260=CARTESIAN_POINT('Ctrl Pts',(-215.196587456504,3.55439767724162,
126.071608140442));
#166261=CARTESIAN_POINT('Ctrl Pts',(-215.189164085476,3.67889844132221,
126.167737816495));
#166262=CARTESIAN_POINT('Ctrl Pts',(-215.181740714447,3.79922006549019,
126.26851918995));
#166263=CARTESIAN_POINT('Ctrl Pts',(-215.177804665006,3.86301747770077,
126.321955892371));
#166264=CARTESIAN_POINT('Ctrl Pts',(-215.173868615565,3.92564060121673,
126.37669973921));
#166265=CARTESIAN_POINT('Ctrl Pts',(-215.169932566125,3.9870348401628,126.43269231521));
#166266=CARTESIAN_POINT('Ctrl Pts',(-215.162509299719,4.10282245876953,
126.538292566078));
#166267=CARTESIAN_POINT('Ctrl Pts',(-215.155086033314,4.21458688552747,
126.648655784924));
#166268=CARTESIAN_POINT('Ctrl Pts',(-215.147662766908,4.32191134374749,
126.763443283682));
#166269=CARTESIAN_POINT('Ctrl Pts',(-215.140248274187,4.42910895337063,
126.878095113148));
#166270=CARTESIAN_POINT('Ctrl Pts',(-215.132833781466,4.5318767875213,126.997160543898));
#166271=CARTESIAN_POINT('Ctrl Pts',(-215.125419288745,4.62983196741889,
127.120261471782));
#166272=CARTESIAN_POINT('Ctrl Pts',(-215.118011942391,4.72769273442615,
127.243243750357));
#166273=CARTESIAN_POINT('Ctrl Pts',(-215.110604596037,4.82074985087852,
127.370253492568));
#166274=CARTESIAN_POINT('Ctrl Pts',(-215.103197249683,4.90865816128401,
127.500876756827));
#166275=CARTESIAN_POINT('Ctrl Pts',(-215.095795428008,4.99650090635502,
127.631402597328));
#166276=CARTESIAN_POINT('Ctrl Pts',(-215.088393606332,5.07920228415796,
127.765536285204));
#166277=CARTESIAN_POINT('Ctrl Pts',(-215.080991784657,5.15645830103452,
127.902831994203));
#166278=CARTESIAN_POINT('Ctrl Pts',(-215.073593870346,5.23367353506112,
128.040055225867));
#166279=CARTESIAN_POINT('Ctrl Pts',(-215.066195956034,5.30544895039352,
128.180436829845));
#166280=CARTESIAN_POINT('Ctrl Pts',(-215.058798041723,5.37152473043544,
128.323503380073));
#166281=CARTESIAN_POINT('Ctrl Pts',(-215.05140135681,5.43758952988135,128.466546155237));
#166282=CARTESIAN_POINT('Ctrl Pts',(-215.044004671898,5.49795641753252,
128.612272652531));
#166283=CARTESIAN_POINT('Ctrl Pts',(-215.036607986986,5.55241222534259,
128.760186201728));
#166284=CARTESIAN_POINT('Ctrl Pts',(-215.02921163005,5.60686561852507,128.908093192284));
#166285=CARTESIAN_POINT('Ctrl Pts',(-215.021815273115,5.65540832404635,
129.058186691611));
#166286=CARTESIAN_POINT('Ctrl Pts',(-215.014418916179,5.69787599467857,
129.209951726545));
#166287=CARTESIAN_POINT('Ctrl Pts',(-215.007021426843,5.7403501672197,129.361739997094));
#166288=CARTESIAN_POINT('Ctrl Pts',(-214.999623937506,5.7767473523118,129.515199953302));
#166289=CARTESIAN_POINT('Ctrl Pts',(-214.992226448169,5.80695362161742,
129.669803347577));
#166290=CARTESIAN_POINT('Ctrl Pts',(-214.984826365654,5.83717047968395,
129.824460937833));
#166291=CARTESIAN_POINT('Ctrl Pts',(-214.977426283139,5.86119202954348,
129.980262398064));
#166292=CARTESIAN_POINT('Ctrl Pts',(-214.970026200624,5.87895582867323,
130.136671373225));
#166293=CARTESIAN_POINT('Ctrl Pts',(-214.962617980958,5.89673916092626,
130.293252336133));
#166294=CARTESIAN_POINT('Ctrl Pts',(-214.955209761291,5.90825095840889,
130.450441776919));
#166295=CARTESIAN_POINT('Ctrl Pts',(-214.947801541624,5.91348078568425,
130.607699589797));
#166296=CARTESIAN_POINT('Ctrl Pts',(-214.940388762322,5.91871383183104,
130.765054192235));
#166297=CARTESIAN_POINT('Ctrl Pts',(-214.93297598302,5.91765720588825,130.922476878194));
#166298=CARTESIAN_POINT('Ctrl Pts',(-214.925563203718,5.91035255308703,
131.079430173711));
#166299=CARTESIAN_POINT('Ctrl Pts',(-214.918139832689,5.90303746305534,
131.236607731456));
#166300=CARTESIAN_POINT('Ctrl Pts',(-214.91071646166,5.88945654814317,131.393314188327));
#166301=CARTESIAN_POINT('Ctrl Pts',(-214.903293090632,5.86970310125876,
131.5490189725));
#166302=CARTESIAN_POINT('Ctrl Pts',(-214.899357041192,5.85922934974553,
131.631577385136));
#166303=CARTESIAN_POINT('Ctrl Pts',(-214.895420991752,5.84702112889083,
131.713854378921));
#166304=CARTESIAN_POINT('Ctrl Pts',(-214.891484942312,5.83309807470133,
131.795772445928));
#166305=CARTESIAN_POINT('Ctrl Pts',(-214.884061675906,5.80683962901805,
131.950267363759));
#166306=CARTESIAN_POINT('Ctrl Pts',(-214.876638409501,5.77439933001569,
132.103951956879));
#166307=CARTESIAN_POINT('Ctrl Pts',(-214.869215143095,5.73583684757446,
132.256292510083));
#166308=CARTESIAN_POINT('Ctrl Pts',(-214.861800650374,5.69731994278507,
132.408453009404));
#166309=CARTESIAN_POINT('Ctrl Pts',(-214.854386157653,5.65269534839071,
132.559272272464));
#166310=CARTESIAN_POINT('Ctrl Pts',(-214.846971664932,5.60207421878622,
132.708223797973));
#166311=CARTESIAN_POINT('Ctrl Pts',(-214.839564318579,5.5515018797323,132.857031758395));
#166312=CARTESIAN_POINT('Ctrl Pts',(-214.832156972225,5.49494463099763,
133.003975214029));
#166313=CARTESIAN_POINT('Ctrl Pts',(-214.824749625871,5.43256416838892,
133.148540030247));
#166314=CARTESIAN_POINT('Ctrl Pts',(-214.817347804196,5.37023023148271,
133.292997024571));
#166315=CARTESIAN_POINT('Ctrl Pts',(-214.809945982521,5.30208187580697,
133.435078570634));
#166316=CARTESIAN_POINT('Ctrl Pts',(-214.802544160845,5.22832987161546,
133.574287929983));
#166317=CARTESIAN_POINT('Ctrl Pts',(-214.795146246534,5.15461680053308,
133.713423801795));
#166318=CARTESIAN_POINT('Ctrl Pts',(-214.787748332223,5.07530614649459,
133.849690177459));
#166319=CARTESIAN_POINT('Ctrl Pts',(-214.780350417911,4.99065577903745,
133.982612567563));
#166320=CARTESIAN_POINT('Ctrl Pts',(-214.772953732999,4.90601947893555,
134.115512868378));
#166321=CARTESIAN_POINT('Ctrl Pts',(-214.765557048087,4.81604542689396,
134.245069971992));
#166322=CARTESIAN_POINT('Ctrl Pts',(-214.758160363175,4.72103626310515,
134.370836071701));
#166323=CARTESIAN_POINT('Ctrl Pts',(-214.75076400624,4.62603131212223,134.496596594809));
#166324=CARTESIAN_POINT('Ctrl Pts',(-214.743367649304,4.52599191832748,
134.618566150388));
#166325=CARTESIAN_POINT('Ctrl Pts',(-214.735971292369,4.42126250953769,
134.736328112886));
#166326=CARTESIAN_POINT('Ctrl Pts',(-214.728573803032,4.31651706640775,
134.854108105042));
#166327=CARTESIAN_POINT('Ctrl Pts',(-214.721176313695,4.20708042663369,
134.96767894248));
#166328=CARTESIAN_POINT('Ctrl Pts',(-214.713778824359,4.09333543882564,
135.076659243336));
#166329=CARTESIAN_POINT('Ctrl Pts',(-214.706378741844,3.97955057788893,
135.185677747067));
#166330=CARTESIAN_POINT('Ctrl Pts',(-214.698978659329,3.86145463133097,
135.290102252206));
#166331=CARTESIAN_POINT('Ctrl Pts',(-214.691578576814,3.73946509813376,
135.389590311086));
#166332=CARTESIAN_POINT('Ctrl Pts',(-214.684170357148,3.61734142490346,
135.489187767315));
#166333=CARTESIAN_POINT('Ctrl Pts',(-214.676762137481,3.49131590426694,
135.583837700879));
#166334=CARTESIAN_POINT('Ctrl Pts',(-214.669353917815,3.36183730191046,
135.673239391779));
#166335=CARTESIAN_POINT('Ctrl Pts',(-214.661941138513,3.2322790076347,135.762696107928));
#166336=CARTESIAN_POINT('Ctrl Pts',(-214.654528359211,3.09926371136607,
135.846897945622));
#166337=CARTESIAN_POINT('Ctrl Pts',(-214.647115579909,2.96326611543749,
135.925589424366));
#166338=CARTESIAN_POINT('Ctrl Pts',(-214.63969220888,2.82707419976637,136.004393341186));
#166339=CARTESIAN_POINT('Ctrl Pts',(-214.632268837851,2.68789180320384,
136.077671000546));
#166340=CARTESIAN_POINT('Ctrl Pts',(-214.624845466822,2.54621573794707,
136.145214105383));
#166341=CARTESIAN_POINT('Ctrl Pts',(-214.620909417381,2.47109568866772,
136.181027080247));
#166342=CARTESIAN_POINT('Ctrl Pts',(-214.61697336794,2.39527488199036,136.215228683168));
#166343=CARTESIAN_POINT('Ctrl Pts',(-214.613037318499,2.3188291412728,136.247793539545));
#166344=CARTESIAN_POINT('Ctrl Pts',(-214.605614052093,2.17465486008611,
136.30920984235));
#166345=CARTESIAN_POINT('Ctrl Pts',(-214.598190785688,2.02782088530974,
136.364987176579));
#166346=CARTESIAN_POINT('Ctrl Pts',(-214.590767519282,1.87880849968838,
136.414887258087));
#166347=CARTESIAN_POINT('Ctrl Pts',(-214.583353026561,1.72997223433212,
136.464728361843));
#166348=CARTESIAN_POINT('Ctrl Pts',(-214.57593853384,1.57896303360794,136.508705922394));
#166349=CARTESIAN_POINT('Ctrl Pts',(-214.568524041119,1.42628393962747,
136.546628870274));
#166350=CARTESIAN_POINT('Ctrl Pts',(-214.561116694765,1.27375200350605,
136.584515266589));
#166351=CARTESIAN_POINT('Ctrl Pts',(-214.553709348411,1.11955373819532,
136.616358578508));
#166352=CARTESIAN_POINT('Ctrl Pts',(-214.546302002058,0.964209100253664,
136.642016942966));
#166353=CARTESIAN_POINT('Ctrl Pts',(-214.538900180382,0.808980324203797,
136.667656170448));
#166354=CARTESIAN_POINT('Ctrl Pts',(-214.531498358707,0.652607244681802,
136.687119574938));
#166355=CARTESIAN_POINT('Ctrl Pts',(-214.524096537031,0.495621708287031,
136.700315984152));
#166356=CARTESIAN_POINT('Ctrl Pts',(-214.51669862272,0.33871904333495,136.713505427084));
#166357=CARTESIAN_POINT('Ctrl Pts',(-214.509300708408,0.181204936444183,
136.720434432184));
#166358=CARTESIAN_POINT('Ctrl Pts',(-214.501902794097,0.0236179737786697,
136.72106347928));
#166359=CARTESIAN_POINT('Ctrl Pts',(-214.494506109185,-0.133942800792343,
136.72169242184));
#166360=CARTESIAN_POINT('Ctrl Pts',(-214.487109424272,-0.291576034179248,
136.71602348277));
#166361=CARTESIAN_POINT('Ctrl Pts',(-214.47971273936,-0.448741389502812,
136.704069231375));
#166362=CARTESIAN_POINT('Ctrl Pts',(-214.472316382425,-0.605899775949823,
136.692115510043));
#166363=CARTESIAN_POINT('Ctrl Pts',(-214.464920025489,-0.762589953361557,
136.673877058842));
#166364=CARTESIAN_POINT('Ctrl Pts',(-214.457523668554,-0.918275231213955,
136.649418458361));
#166365=CARTESIAN_POINT('Ctrl Pts',(-214.450126179217,-1.07398434487984,
136.624956113206));
#166366=CARTESIAN_POINT('Ctrl Pts',(-214.44272868988,-1.22868788384681,
136.594271780513));
#166367=CARTESIAN_POINT('Ctrl Pts',(-214.435331200544,-1.38185804172664,
136.557481415447));
#166368=CARTESIAN_POINT('Ctrl Pts',(-214.427931118029,-1.53508189316766,
136.520678153577));
#166369=CARTESIAN_POINT('Ctrl Pts',(-214.420531035514,-1.68677093056666,
136.477764684823));
#166370=CARTESIAN_POINT('Ctrl Pts',(-214.413130952999,-1.83641137460534,
136.428907161575));
#166371=CARTESIAN_POINT('Ctrl Pts',(-214.405722733332,-1.98621636369587,
136.379995914457));
#166372=CARTESIAN_POINT('Ctrl Pts',(-214.398314513666,-2.13396790567806,
136.32512767576));
#166373=CARTESIAN_POINT('Ctrl Pts',(-214.390906293999,-2.27917042748476,
136.26451745826));
#166374=CARTESIAN_POINT('Ctrl Pts',(-214.383493514697,-2.42446231902121,
136.203869936183));
#166375=CARTESIAN_POINT('Ctrl Pts',(-214.376080735395,-2.56720172650639,
136.137473550258));
#166376=CARTESIAN_POINT('Ctrl Pts',(-214.368667956093,-2.70691711875904,
136.065589587557));
#166377=CARTESIAN_POINT('Ctrl Pts',(-214.361244585064,-2.84683214291555,
135.993602913679));
#166378=CARTESIAN_POINT('Ctrl Pts',(-214.353821214035,-2.98371419812839,
135.916113186389));
#166379=CARTESIAN_POINT('Ctrl Pts',(-214.346397843006,-3.11711949905002,
135.833425798208));
#166380=CARTESIAN_POINT('Ctrl Pts',(-214.342461793566,-3.18785419060599,
135.789582960943));
#166381=CARTESIAN_POINT('Ctrl Pts',(-214.338525744126,-3.25761196580092,
135.744279570738));
#166382=CARTESIAN_POINT('Ctrl Pts',(-214.334589694686,-3.32633049188761,
135.697565704341));
#166383=CARTESIAN_POINT('Ctrl Pts',(-214.327198576855,-3.45537021335995,
135.609846356268));
#166384=CARTESIAN_POINT('Ctrl Pts',(-214.319807459024,-3.58114113330062,
135.516880709447));
#166385=CARTESIAN_POINT('Ctrl Pts',(-214.312416341193,-3.70318490983809,
135.418940997844));
#166386=CARTESIAN_POINT('Ctrl Pts',(-214.305033978144,-3.82508412546336,
135.321117295877));
#166387=CARTESIAN_POINT('Ctrl Pts',(-214.297651615096,-3.94326469299833,
135.218331488424));
#166388=CARTESIAN_POINT('Ctrl Pts',(-214.290269252047,-4.0572960434475,
135.110899759188));
#166389=CARTESIAN_POINT('Ctrl Pts',(-214.282893986435,-4.17121776365406,
135.00357131529));
#166390=CARTESIAN_POINT('Ctrl Pts',(-214.275518720823,-4.28099793458178,
134.891606097103));
#166391=CARTESIAN_POINT('Ctrl Pts',(-214.268143455211,-4.38623810574165,
134.775361227266));
#166392=CARTESIAN_POINT('Ctrl Pts',(-214.260773635606,-4.49140056598207,
134.659202194383));
#166393=CARTESIAN_POINT('Ctrl Pts',(-214.253403816001,-4.59202944872852,
134.53877007949));
#166394=CARTESIAN_POINT('Ctrl Pts',(-214.246033996395,-4.68776243321892,
134.414459498788));
#166395=CARTESIAN_POINT('Ctrl Pts',(-214.238423212888,-4.78662550701507,
134.286084454607));
#166396=CARTESIAN_POINT('Ctrl Pts',(-214.23081242938,-4.88026677970626,
134.153573287877));
#166397=CARTESIAN_POINT('Ctrl Pts',(-214.223201645872,-4.96833121822625,
134.017398972223));
#166398=CARTESIAN_POINT('Ctrl Pts',(-214.215836748133,-5.05355051050206,
133.885624115071));
#166399=CARTESIAN_POINT('Ctrl Pts',(-214.208471850393,-5.13354750807239,
133.75041947113));
#166400=CARTESIAN_POINT('Ctrl Pts',(-214.201106952653,-5.20804399196539,
133.612243866608));
#166401=CARTESIAN_POINT('Ctrl Pts',(-214.193742182749,-5.28253918279686,
133.47407066045));
#166402=CARTESIAN_POINT('Ctrl Pts',(-214.186377412844,-5.3515338706958,
133.332926927929));
#166403=CARTESIAN_POINT('Ctrl Pts',(-214.17901264294,-5.41479566029319,
133.18929636508));
#166404=CARTESIAN_POINT('Ctrl Pts',(-214.171646513804,-5.47806912539624,
133.045639293979));
#166405=CARTESIAN_POINT('Ctrl Pts',(-214.164280384668,-5.53560743415387,
132.899494823891));
#166406=CARTESIAN_POINT('Ctrl Pts',(-214.156914255532,-5.58722630848571,
132.751366714183));
#166407=CARTESIAN_POINT('Ctrl Pts',(-214.14954527951,-5.63886513264815,
132.603181355442));
#166408=CARTESIAN_POINT('Ctrl Pts',(-214.142176303489,-5.68457984454065,
132.453011186632));
#166409=CARTESIAN_POINT('Ctrl Pts',(-214.134807327467,-5.72423605993967,
132.301375010478));
#166410=CARTESIAN_POINT('Ctrl Pts',(-214.127430261279,-5.7639358126471,
132.149572357749));
#166411=CARTESIAN_POINT('Ctrl Pts',(-214.120053195091,-5.79756369440894,
131.996300849077));
#166412=CARTESIAN_POINT('Ctrl Pts',(-214.112676128903,-5.82503634052978,
131.842089962823));
#166413=CARTESIAN_POINT('Ctrl Pts',(-214.105294222152,-5.85252701320656,
131.687777888967));
#166414=CARTESIAN_POINT('Ctrl Pts',(-214.0979123154,-5.87385435360959,131.532525581733));
#166415=CARTESIAN_POINT('Ctrl Pts',(-214.090530408648,-5.8889869347913,
131.376866900813));
#166416=CARTESIAN_POINT('Ctrl Pts',(-214.083138624783,-5.90413976361654,
131.220999946007));
#166417=CARTESIAN_POINT('Ctrl Pts',(-214.075746840918,-5.91308126700828,
131.064725906564));
#166418=CARTESIAN_POINT('Ctrl Pts',(-214.068355057054,-5.91583208039486,
130.908578461868));
#166419=CARTESIAN_POINT('Ctrl Pts',(-214.066695102105,-5.9164498238755,
130.873512809487));
#166420=CARTESIAN_POINT('Ctrl Pts',(-214.065035147157,-5.91675557412369,
130.838453519149));
#166421=CARTESIAN_POINT('Ctrl Pts',(-214.063375192209,-5.91674992308523,
130.803406588753));
#166422=CARTESIAN_POINT('',(-212.313375192209,-5.91518716771215,130.809800676931));
#166423=CARTESIAN_POINT('Ctrl Pts',(-214.063375192209,-5.92634516172826,
130.803405041597));
#166424=CARTESIAN_POINT('Ctrl Pts',(-214.060964151763,-5.92645914177806,
130.752417734346));
#166425=CARTESIAN_POINT('Ctrl Pts',(-214.058553111318,-5.92585830881452,
130.701433182352));
#166426=CARTESIAN_POINT('Ctrl Pts',(-214.056142070873,-5.92453444346407,
130.650467411543));
#166427=CARTESIAN_POINT('Ctrl Pts',(-213.963326196269,-5.87357066946307,
128.688479340455));
#166428=CARTESIAN_POINT('Ctrl Pts',(-213.777694447059,-3.62863765870681,
124.820169003641));
#166429=CARTESIAN_POINT('Ctrl Pts',(-213.499246823247,3.07330259697371,
124.516883247605));
#166430=CARTESIAN_POINT('Ctrl Pts',(-213.220799199435,6.9510279052142,129.991482034214));
#166431=CARTESIAN_POINT('Ctrl Pts',(-212.942351575622,4.44109814515497,
136.213076527599));
#166432=CARTESIAN_POINT('Ctrl Pts',(-212.663903951809,-2.14998385059845,
137.464325330124));
#166433=CARTESIAN_POINT('Ctrl Pts',(-212.454245157338,-5.62514049150498,
133.79823295943));
#166434=CARTESIAN_POINT('Ctrl Pts',(-212.337402237471,-5.9197797619191,
131.320403388515));
#166435=CARTESIAN_POINT('Ctrl Pts',(-212.313375192209,-5.91518716771215,
130.809800676931));
#166436=CARTESIAN_POINT('',(-210.563375192209,-5.90724396466958,130.802943052422));
#166437=CARTESIAN_POINT('Ctrl Pts',(-212.313375192209,-5.91518716771215,
130.809800676931));
#166438=CARTESIAN_POINT('Ctrl Pts',(-212.244586362867,-5.90203868542103,
129.3479578908));
#166439=CARTESIAN_POINT('Ctrl Pts',(-212.082981658921,-4.61601153110151,
125.893005037876));
#166440=CARTESIAN_POINT('Ctrl Pts',(-211.828561080369,1.18315125270368,
123.906700605387));
#166441=CARTESIAN_POINT('Ctrl Pts',(-211.550113456557,6.44271887229008,
128.071425553759));
#166442=CARTESIAN_POINT('Ctrl Pts',(-211.271665832744,5.78174259255394,
134.747584314464));
#166443=CARTESIAN_POINT('Ctrl Pts',(-210.993218208931,-0.192372675911253,
137.800113134909));
#166444=CARTESIAN_POINT('Ctrl Pts',(-210.757121328754,-5.10795605870944,
134.937397303148));
#166445=CARTESIAN_POINT('Ctrl Pts',(-210.613840323178,-5.90494721591197,
131.879020657015));
#166446=CARTESIAN_POINT('Ctrl Pts',(-210.563375192209,-5.90724396466958,
130.802943052422));
#166447=CARTESIAN_POINT('',(-208.813375192209,-5.92040475870682,130.799408613133));
#166448=CARTESIAN_POINT('Ctrl Pts',(-210.563375192209,-5.90724396466958,
130.802943052422));
#166449=CARTESIAN_POINT('Ctrl Pts',(-210.521024448574,-5.90917141469214,
129.899890075305));
#166450=CARTESIAN_POINT('Ctrl Pts',(-210.385857830337,-5.28952247014664,
127.020214927324));
#166451=CARTESIAN_POINT('Ctrl Pts',(-210.157875337492,-0.802299360853992,
123.852103698697));
#166452=CARTESIAN_POINT('Ctrl Pts',(-209.87942771368,5.41546824219867,126.371498760019));
#166453=CARTESIAN_POINT('Ctrl Pts',(-209.600980089866,6.65668509099864,
132.964477311082));
#166454=CARTESIAN_POINT('Ctrl Pts',(-209.322532466054,1.78073353831976,
137.572414148371));
#166455=CARTESIAN_POINT('Ctrl Pts',(-209.059997500168,-4.35945843268618,
136.052938256508));
#166456=CARTESIAN_POINT('Ctrl Pts',(-208.890278408886,-5.90578069205309,
132.430000405375));
#166457=CARTESIAN_POINT('Ctrl Pts',(-208.813375192209,-5.92040475870682,
130.799408613133));
#166458=CARTESIAN_POINT('',(-207.063375192208,-5.92350094233479,130.808116397466));
#166459=CARTESIAN_POINT('Ctrl Pts',(-208.813375192209,-5.92040475870682,
130.799408613133));
#166460=CARTESIAN_POINT('Ctrl Pts',(-208.797462534282,-5.92343074097668,
130.462009860137));
#166461=CARTESIAN_POINT('Ctrl Pts',(-208.781549876355,-5.89708361299461,
130.125083613377));
#166462=CARTESIAN_POINT('Ctrl Pts',(-208.672821343824,-5.50494337257859,
127.859639161688));
#166463=CARTESIAN_POINT('Ctrl Pts',(-208.487189594614,-2.72312717773575,
124.3574901439));
#166464=CARTESIAN_POINT('Ctrl Pts',(-208.208741970802,3.95201795870991,
125.028625635385));
#166465=CARTESIAN_POINT('Ctrl Pts',(-207.93029434699,6.99545165791052,131.007379415155));
#166466=CARTESIAN_POINT('Ctrl Pts',(-207.651846723176,3.61040703030553,
136.799568837958));
#166467=CARTESIAN_POINT('Ctrl Pts',(-207.373399099364,-3.0924252799637,
137.082454788425));
#166468=CARTESIAN_POINT('Ctrl Pts',(-207.177241922374,-5.8124039569315,
133.217483732592));
#166469=CARTESIAN_POINT('Ctrl Pts',(-207.073900619989,-5.92514845404535,
131.030985187931));
#166470=CARTESIAN_POINT('Ctrl Pts',(-207.063375192208,-5.92350094233479,
130.808116397466));
#166471=CARTESIAN_POINT('',(-205.313375192208,-5.90857914829821,130.807499840963));
#166472=CARTESIAN_POINT('Ctrl Pts',(-207.063375192208,-5.92350094233479,
130.808116397466));
#166473=CARTESIAN_POINT('Ctrl Pts',(-206.981084745385,-5.91062028060458,
129.06567203012));
#166474=CARTESIAN_POINT('Ctrl Pts',(-206.805978423956,-4.17532705327718,
125.335613429113));
#166475=CARTESIAN_POINT('Ctrl Pts',(-206.538056227925,2.17024453367553,
124.150970564787));
#166476=CARTESIAN_POINT('Ctrl Pts',(-206.259608604111,6.77075566682168,
129.033928966654));
#166477=CARTESIAN_POINT('Ctrl Pts',(-205.981160980299,5.14927311196064,
135.543827565311));
#166478=CARTESIAN_POINT('Ctrl Pts',(-205.702713356486,-1.20413987681471,
137.698387574825));
#166479=CARTESIAN_POINT('Ctrl Pts',(-205.480118093789,-5.39856531937876,
134.356261281287));
#166480=CARTESIAN_POINT('Ctrl Pts',(-205.350338705697,-5.91235307129998,
131.595235086907));
#166481=CARTESIAN_POINT('Ctrl Pts',(-205.313375192208,-5.90857914829821,
130.807499840963));
#166482=CARTESIAN_POINT('',(-203.563375192208,-5.91198242686231,130.79947290462));
#166483=CARTESIAN_POINT('Ctrl Pts',(-205.313375192208,-5.90857914829821,
130.807499840963));
#166484=CARTESIAN_POINT('Ctrl Pts',(-205.257522831092,-5.90287670038602,
129.617221394239));
#166485=CARTESIAN_POINT('Ctrl Pts',(-205.108854595372,-4.97542928644342,
126.440754491598));
#166486=CARTESIAN_POINT('Ctrl Pts',(-204.867370485048,0.213664449080756,
123.809226020325));
#166487=CARTESIAN_POINT('Ctrl Pts',(-204.588922861234,6.00069570294186,
127.203081454398));
#166488=CARTESIAN_POINT('Ctrl Pts',(-204.310475237422,6.27338075607734,
133.906336507158));
#166489=CARTESIAN_POINT('Ctrl Pts',(-204.032027613609,0.781135366069192,
137.759027257328));
#166490=CARTESIAN_POINT('Ctrl Pts',(-203.782994265204,-4.77292417967637,
135.488857499412));
#166491=CARTESIAN_POINT('Ctrl Pts',(-203.626776791404,-5.90152837485451,
132.148681533904));
#166492=CARTESIAN_POINT('Ctrl Pts',(-203.563375192208,-5.91198242686231,
130.79947290462));
#166493=CARTESIAN_POINT('',(-201.813375867204,-5.92197308054016,130.803199987403));
#166494=CARTESIAN_POINT('Ctrl Pts',(-203.563375192208,-5.91198242686231,
130.79947290462));
#166495=CARTESIAN_POINT('Ctrl Pts',(-203.5339609168,-5.91683243646446,130.173526639722));
#166496=CARTESIAN_POINT('Ctrl Pts',(-203.504546641391,-5.82534361100667,
129.54896166662));
#166497=CARTESIAN_POINT('Ctrl Pts',(-203.382316491379,-5.02009495809496,
127.092968345155));
#166498=CARTESIAN_POINT('Ctrl Pts',(-203.196684742167,-1.76012566321133,
124.030918495546));
#166499=CARTESIAN_POINT('Ctrl Pts',(-202.918237118359,4.74729777661893,
125.662306130287));
#166500=CARTESIAN_POINT('Ctrl Pts',(-202.639789494544,6.89218647818192,
132.018990635446));
#166501=CARTESIAN_POINT('Ctrl Pts',(-202.361341870732,2.70349250829908,
137.25948949219));
#166502=CARTESIAN_POINT('Ctrl Pts',(-202.085870845849,-3.89824401710562,
136.575431840637));
#166503=CARTESIAN_POINT('Ctrl Pts',(-201.90321569557,-5.92108948216704,
132.703162475868));
#166504=CARTESIAN_POINT('Ctrl Pts',(-201.813376419895,-5.92624986544025,
130.803210827386));
#166505=CARTESIAN_POINT('',(-200.063375194059,-5.91567330630329,130.809819562943));
#166506=CARTESIAN_POINT('Ctrl Pts',(-201.813375192208,-5.91674988355362,
130.803186748634));
#166507=CARTESIAN_POINT('Ctrl Pts',(-201.810399002507,-5.91673741614191,
130.740346209347));
#166508=CARTESIAN_POINT('Ctrl Pts',(-201.807422812807,-5.9157238558129,
130.677516728804));
#166509=CARTESIAN_POINT('Ctrl Pts',(-201.804446623105,-5.91371007129092,
130.614719495411));
#166510=CARTESIAN_POINT('Ctrl Pts',(-201.7970233567,-5.90868725336307,130.458089495395));
#166511=CARTESIAN_POINT('Ctrl Pts',(-201.789600090295,-5.89742980985056,
130.301422341445));
#166512=CARTESIAN_POINT('Ctrl Pts',(-201.782176823889,-5.87992433832519,
130.145254906719));
#166513=CARTESIAN_POINT('Ctrl Pts',(-201.774762331168,-5.86243955681343,
129.989272048933));
#166514=CARTESIAN_POINT('Ctrl Pts',(-201.767347838447,-5.83872148765387,
129.833788102077));
#166515=CARTESIAN_POINT('Ctrl Pts',(-201.759933345726,-5.80880871565572,
129.679339787793));
#166516=CARTESIAN_POINT('Ctrl Pts',(-201.752525999373,-5.77892477471341,
129.52504033661));
#166517=CARTESIAN_POINT('Ctrl Pts',(-201.745118653019,-5.74285808789947,
129.371774894843));
#166518=CARTESIAN_POINT('Ctrl Pts',(-201.737711306665,-5.70069899303698,
129.220074799512));
#166519=CARTESIAN_POINT('Ctrl Pts',(-201.73030948499,-5.658571342018,129.068487847836));
#166520=CARTESIAN_POINT('Ctrl Pts',(-201.722907663315,-5.6103604300888,
128.918464276076));
#166521=CARTESIAN_POINT('Ctrl Pts',(-201.715505841639,-5.55620757811541,
128.770524854434));
#166522=CARTESIAN_POINT('Ctrl Pts',(-201.708107927328,-5.50208331301106,
128.622663528862));
#166523=CARTESIAN_POINT('Ctrl Pts',(-201.700710013017,-5.44202348275199,
128.476884511958));
#166524=CARTESIAN_POINT('Ctrl Pts',(-201.693312098705,-5.37621909378814,
128.333692930869));
#166525=CARTESIAN_POINT('Ctrl Pts',(-201.685915413793,-5.31042564032021,
128.190525145624));
#166526=CARTESIAN_POINT('Ctrl Pts',(-201.678518728881,-5.23888967855432,
128.049944281665));
#166527=CARTESIAN_POINT('Ctrl Pts',(-201.671122043969,-5.16185019591898,
127.912435114136));
#166528=CARTESIAN_POINT('Ctrl Pts',(-201.663725687034,-5.08481412929481,
127.774932043906));
#166529=CARTESIAN_POINT('Ctrl Pts',(-201.656329330098,-5.00227520947535,
127.640500724959));
#166530=CARTESIAN_POINT('Ctrl Pts',(-201.648932973163,-4.91451806073126,
127.509600718386));
#166531=CARTESIAN_POINT('Ctrl Pts',(-201.641535483827,-4.82674747614365,
127.378680670687));
#166532=CARTESIAN_POINT('Ctrl Pts',(-201.63413799449,-4.73375727975254,
127.251293321958));
#166533=CARTESIAN_POINT('Ctrl Pts',(-201.626740505153,-4.635874949064,127.127868536908));
#166534=CARTESIAN_POINT('Ctrl Pts',(-201.619340422639,-4.53795830587631,
127.004400485491));
#166535=CARTESIAN_POINT('Ctrl Pts',(-201.611940340124,-4.43514634578947,
126.884898055683));
#166536=CARTESIAN_POINT('Ctrl Pts',(-201.604540257609,-4.32780616554116,
126.76975724722));
#166537=CARTESIAN_POINT('Ctrl Pts',(-201.597132037942,-4.22034795372998,
126.654489829602));
#166538=CARTESIAN_POINT('Ctrl Pts',(-201.589723818276,-4.10835183258725,
126.543593884573));
#166539=CARTESIAN_POINT('Ctrl Pts',(-201.58231559861,-3.99222154535993,
126.437428319572));
#166540=CARTESIAN_POINT('Ctrl Pts',(-201.574902819308,-3.87601978187823,
126.331197411437));
#166541=CARTESIAN_POINT('Ctrl Pts',(-201.567490040006,-3.7556790667533,
126.22970292491));
#166542=CARTESIAN_POINT('Ctrl Pts',(-201.560077260704,-3.63163498628868,
126.133262471641));
#166543=CARTESIAN_POINT('Ctrl Pts',(-201.552653889675,-3.50741366582499,
126.03668421973));
#166544=CARTESIAN_POINT('Ctrl Pts',(-201.545230518646,-3.3794787144427,
125.945174640511));
#166545=CARTESIAN_POINT('Ctrl Pts',(-201.537807147618,-3.24829403434159,
125.859007603982));
#166546=CARTESIAN_POINT('Ctrl Pts',(-201.533871098176,-3.17873676920309,
125.813319773655));
#166547=CARTESIAN_POINT('Ctrl Pts',(-201.529935048734,-3.10826629928466,
125.769133155338));
#166548=CARTESIAN_POINT('Ctrl Pts',(-201.525998999293,-3.03695429695874,
125.726483190857));
#166549=CARTESIAN_POINT('Ctrl Pts',(-201.518575732887,-2.90246208617211,
125.646046688922));
#166550=CARTESIAN_POINT('Ctrl Pts',(-201.511152466482,-2.76456864931066,
125.570835471457));
#166551=CARTESIAN_POINT('Ctrl Pts',(-201.503729200076,-2.6237184286282,
125.50115100736));
#166552=CARTESIAN_POINT('Ctrl Pts',(-201.496314707355,-2.4830346812097,
125.431548904513));
#166553=CARTESIAN_POINT('Ctrl Pts',(-201.488900214634,-2.3394014374572,
125.367460716645));
#166554=CARTESIAN_POINT('Ctrl Pts',(-201.481485721913,-2.1932911125198,
125.30914409242));
#166555=CARTESIAN_POINT('Ctrl Pts',(-201.47407837556,-2.04732161421452,
125.250883675953));
#166556=CARTESIAN_POINT('Ctrl Pts',(-201.466671029206,-1.89888013215013,
125.198383886038));
#166557=CARTESIAN_POINT('Ctrl Pts',(-201.459263682852,-1.74846252501016,
125.151855919546));
#166558=CARTESIAN_POINT('Ctrl Pts',(-201.451861861177,-1.5981571049961,
125.105362655367));
#166559=CARTESIAN_POINT('Ctrl Pts',(-201.444460039501,-1.44587884966913,
125.064832455911));
#166560=CARTESIAN_POINT('Ctrl Pts',(-201.437058217826,-1.29214228512928,
125.030427912946));
#166561=CARTESIAN_POINT('Ctrl Pts',(-201.429660303514,-1.13848687692604,
124.996041531872));
#166562=CARTESIAN_POINT('Ctrl Pts',(-201.422262389203,-0.983375056028614,
124.967774448564));
#166563=CARTESIAN_POINT('Ctrl Pts',(-201.414864474892,-0.827335043864665,
124.94573899745));
#166564=CARTESIAN_POINT('Ctrl Pts',(-201.40746778998,-0.67132096271966,
124.923707208227));
#166565=CARTESIAN_POINT('Ctrl Pts',(-201.400071105067,-0.514379365714424,
124.907905048017));
#166566=CARTESIAN_POINT('Ctrl Pts',(-201.392674420155,-0.357047286449173,
124.898393482732));
#166567=CARTESIAN_POINT('Ctrl Pts',(-201.38527806322,-0.199722183453189,
124.8888823392));
#166568=CARTESIAN_POINT('Ctrl Pts',(-201.377881706284,-0.0420070052413085,
124.88566125851));
#166569=CARTESIAN_POINT('Ctrl Pts',(-201.370485349349,0.115557760055124,
124.888739182198));
#166570=CARTESIAN_POINT('Ctrl Pts',(-201.363087860012,0.273146648919818,
124.891817577123));
#166571=CARTESIAN_POINT('Ctrl Pts',(-201.355690370676,0.430584705765377,
124.90119688937));
#166572=CARTESIAN_POINT('Ctrl Pts',(-201.348292881339,0.587333263647712,
124.916833955213));
#166573=CARTESIAN_POINT('Ctrl Pts',(-201.340892798824,0.744136769493798,
124.932476502606));
#166574=CARTESIAN_POINT('Ctrl Pts',(-201.333492716309,0.900249923925743,
124.954381134094));
#166575=CARTESIAN_POINT('Ctrl Pts',(-201.326092633794,1.05514113639827,
124.982453048325));
#166576=CARTESIAN_POINT('Ctrl Pts',(-201.318684414127,1.21020266768233,
125.010555830512));
#166577=CARTESIAN_POINT('Ctrl Pts',(-201.311276194461,1.36403920610859,
125.044839372054));
#166578=CARTESIAN_POINT('Ctrl Pts',(-201.303867974794,1.51613055959717,
125.08515799056));
#166579=CARTESIAN_POINT('Ctrl Pts',(-201.296455195492,1.66831552277604,
125.125501424502));
#166580=CARTESIAN_POINT('Ctrl Pts',(-201.28904241619,1.81875280477592,125.171887227256));
#166581=CARTESIAN_POINT('Ctrl Pts',(-201.281629636888,1.96693974488418,
125.224120604583));
#166582=CARTESIAN_POINT('Ctrl Pts',(-201.274206265859,2.11533842144153,
125.276428615409));
#166583=CARTESIAN_POINT('Ctrl Pts',(-201.266782894831,2.26147998833225,
125.334600750501));
#166584=CARTESIAN_POINT('Ctrl Pts',(-201.259359523802,2.4048832805008,125.398394749225));
#166585=CARTESIAN_POINT('Ctrl Pts',(-201.255423474361,2.48091914692211,
125.432219858064));
#166586=CARTESIAN_POINT('Ctrl Pts',(-201.25148742492,2.55618561065255,125.467624713707));
#166587=CARTESIAN_POINT('Ctrl Pts',(-201.24755137548,2.63061411281273,125.504568173331));
#166588=CARTESIAN_POINT('Ctrl Pts',(-201.240128109074,2.77098394505528,
125.574242385217));
#166589=CARTESIAN_POINT('Ctrl Pts',(-201.232704842669,2.908796043259,125.649602538817));
#166590=CARTESIAN_POINT('Ctrl Pts',(-201.225281576263,3.04355654120713,
125.730437663581));
#166591=CARTESIAN_POINT('Ctrl Pts',(-201.217867083542,3.17815776343784,
125.81117724794));
#166592=CARTESIAN_POINT('Ctrl Pts',(-201.210452590821,3.30971424764855,
125.89737873283));
#166593=CARTESIAN_POINT('Ctrl Pts',(-201.2030380981,3.43775387479355,125.988783927403));
#166594=CARTESIAN_POINT('Ctrl Pts',(-201.195630751746,3.56567009252529,
126.080101022208));
#166595=CARTESIAN_POINT('Ctrl Pts',(-201.188223405393,3.69007589959199,
126.176611626323));
#166596=CARTESIAN_POINT('Ctrl Pts',(-201.180816059039,3.81052558635577,
126.27801271686));
#166597=CARTESIAN_POINT('Ctrl Pts',(-201.173414237363,3.93088543719886,
126.379338178638));
#166598=CARTESIAN_POINT('Ctrl Pts',(-201.166012415688,4.04729475848319,
126.485546624777));
#166599=CARTESIAN_POINT('Ctrl Pts',(-201.158610594013,4.15933864322472,
126.59629305472));
#166600=CARTESIAN_POINT('Ctrl Pts',(-201.151212679701,4.27132338087164,
126.706981022484));
#166601=CARTESIAN_POINT('Ctrl Pts',(-201.14381476539,4.37894700663587,126.822201941411));
#166602=CARTESIAN_POINT('Ctrl Pts',(-201.136416851079,4.48182949379902,
126.941572123354));
#166603=CARTESIAN_POINT('Ctrl Pts',(-201.129020166166,4.58469488375913,
127.060922468139));
#166604=CARTESIAN_POINT('Ctrl Pts',(-201.121623481254,4.68282045537774,
127.184420424934));
#166605=CARTESIAN_POINT('Ctrl Pts',(-201.114226796342,4.77586463652599,
127.311647125726));
#166606=CARTESIAN_POINT('Ctrl Pts',(-201.106830439406,4.86890469199773,
127.438868185153));
#166607=CARTESIAN_POINT('Ctrl Pts',(-201.099434082471,4.95686358463872,
127.569817358517));
#166608=CARTESIAN_POINT('Ctrl Pts',(-201.092037725536,5.03944164464534,
127.704044750962));
#166609=CARTESIAN_POINT('Ctrl Pts',(-201.084640236199,5.12203234756399,
127.838292693965));
#166610=CARTESIAN_POINT('Ctrl Pts',(-201.077242746863,5.19924038189781,
127.975819537438));
#166611=CARTESIAN_POINT('Ctrl Pts',(-201.069845257526,5.27081089987097,
128.11614875458));
#166612=CARTESIAN_POINT('Ctrl Pts',(-201.062445175011,5.34240650677816,
128.25652716391));
#166613=CARTESIAN_POINT('Ctrl Pts',(-201.055045092496,5.40836049318189,
128.399709570458));
#166614=CARTESIAN_POINT('Ctrl Pts',(-201.047645009981,5.46846528047079,
128.545197489595));
#166615=CARTESIAN_POINT('Ctrl Pts',(-201.040236790314,5.52863615915231,
128.690845387655));
#166616=CARTESIAN_POINT('Ctrl Pts',(-201.032828570648,5.58294485137867,
128.838803515936));
#166617=CARTESIAN_POINT('Ctrl Pts',(-201.025420350982,5.63123274734572,
128.988555477216));
#166618=CARTESIAN_POINT('Ctrl Pts',(-201.01800757168,5.67955036370688,129.138399608329));
#166619=CARTESIAN_POINT('Ctrl Pts',(-201.010594792377,5.72183969969134,
129.290039413705));
#166620=CARTESIAN_POINT('Ctrl Pts',(-201.003182013075,5.75799294081597,
129.442946699607));
#166621=CARTESIAN_POINT('Ctrl Pts',(-200.995758642047,5.79419783938699,
129.596072466609));
#166622=CARTESIAN_POINT('Ctrl Pts',(-200.988335271018,5.82424906122381,
129.750468965729));
#166623=CARTESIAN_POINT('Ctrl Pts',(-200.980911899989,5.84809034559499,
129.905600431388));
#166624=CARTESIAN_POINT('Ctrl Pts',(-200.976975850548,5.86073156663221,
129.987854856808));
#166625=CARTESIAN_POINT('Ctrl Pts',(-200.973039801108,5.8716278209937,130.070315853689));
#166626=CARTESIAN_POINT('Ctrl Pts',(-200.969103751667,5.88077666555392,
130.152903502802));
#166627=CARTESIAN_POINT('Ctrl Pts',(-200.961680485262,5.898031100869,130.308661231559));
#166628=CARTESIAN_POINT('Ctrl Pts',(-200.954257218856,5.90911927466106,
130.465340456614));
#166629=CARTESIAN_POINT('Ctrl Pts',(-200.946833952451,5.91395173567687,
130.622411639596));
#166630=CARTESIAN_POINT('Ctrl Pts',(-200.93941945973,5.91877848512508,130.779297177483));
#166631=CARTESIAN_POINT('Ctrl Pts',(-200.932004967009,5.91736422769598,
130.936573381693));
#166632=CARTESIAN_POINT('Ctrl Pts',(-200.924590474288,5.90967099478593,
131.093703486643));
#166633=CARTESIAN_POINT('Ctrl Pts',(-200.917183127934,5.90198517690339,
131.250682143683));
#166634=CARTESIAN_POINT('Ctrl Pts',(-200.90977578158,5.88803244983971,131.40751461145));
#166635=CARTESIAN_POINT('Ctrl Pts',(-200.902368435227,5.86782683838578,
131.563662110531));
#166636=CARTESIAN_POINT('Ctrl Pts',(-200.894966613551,5.84763629703924,
131.719693148917));
#166637=CARTESIAN_POINT('Ctrl Pts',(-200.887564791876,5.82120220493272,
131.87503986722));
#166638=CARTESIAN_POINT('Ctrl Pts',(-200.880162970201,5.78859055344715,
132.029166711216));
#166639=CARTESIAN_POINT('Ctrl Pts',(-200.872765055889,5.75599611739846,
132.183212192852));
#166640=CARTESIAN_POINT('Ctrl Pts',(-200.865367141578,5.71723069365822,
132.336038718374));
#166641=CARTESIAN_POINT('Ctrl Pts',(-200.857969227266,5.67241167620617,
132.487119167727));
#166642=CARTESIAN_POINT('Ctrl Pts',(-200.850572542354,5.62760010686179,
132.63817451025));
#166643=CARTESIAN_POINT('Ctrl Pts',(-200.843175857442,5.57673704647701,
132.787483994966));
#166644=CARTESIAN_POINT('Ctrl Pts',(-200.83577917253,5.51999027249402,132.934533839178));
#166645=CARTESIAN_POINT('Ctrl Pts',(-200.828382815595,5.46324601472245,
133.081577163045));
#166646=CARTESIAN_POINT('Ctrl Pts',(-200.820986458659,5.40061869648633,
133.226360697364));
#166647=CARTESIAN_POINT('Ctrl Pts',(-200.813590101724,5.33232484821961,
133.368389142282));
#166648=CARTESIAN_POINT('Ctrl Pts',(-200.806192612387,5.26402054399037,
133.510439332119));
#166649=CARTESIAN_POINT('Ctrl Pts',(-200.79879512305,5.1900481440821,133.649733256226));
#166650=CARTESIAN_POINT('Ctrl Pts',(-200.791397633714,5.11067081254324,
133.785798929576));
#166651=CARTESIAN_POINT('Ctrl Pts',(-200.783997551199,5.03126565540398,
133.921912300536));
#166652=CARTESIAN_POINT('Ctrl Pts',(-200.776597468684,4.94645198230616,
134.054794845375));
#166653=CARTESIAN_POINT('Ctrl Pts',(-200.769197386169,4.85653698117537,
134.18400247921));
#166654=CARTESIAN_POINT('Ctrl Pts',(-200.761789166503,4.76652310925724,
134.313352190122));
#166655=CARTESIAN_POINT('Ctrl Pts',(-200.754380946836,4.67139692025517,
134.439018613408));
#166656=CARTESIAN_POINT('Ctrl Pts',(-200.74697272717,4.57150714130225,134.560589180836));
#166657=CARTESIAN_POINT('Ctrl Pts',(-200.739559947868,4.47155588185713,
134.682234572919));
#166658=CARTESIAN_POINT('Ctrl Pts',(-200.732147168566,4.36683543800591,
134.799778807794));
#166659=CARTESIAN_POINT('Ctrl Pts',(-200.724734389264,4.25773191773792,
134.912845676462));
#166660=CARTESIAN_POINT('Ctrl Pts',(-200.717311018235,4.14847250524356,
135.026074100376));
#166661=CARTESIAN_POINT('Ctrl Pts',(-200.709887647206,4.03481777724236,
135.134812123521));
#166662=CARTESIAN_POINT('Ctrl Pts',(-200.702464276177,3.91718807819064,
135.238722817768));
#166663=CARTESIAN_POINT('Ctrl Pts',(-200.698528226736,3.85481798926586,
135.293818761162));
#166664=CARTESIAN_POINT('Ctrl Pts',(-200.694592177296,3.79133090880903,
135.347558271593));
#166665=CARTESIAN_POINT('Ctrl Pts',(-200.690656127855,3.72679275456151,
135.399896095293));
#166666=CARTESIAN_POINT('Ctrl Pts',(-200.683232861449,3.60507580982061,
135.498603597382));
#166667=CARTESIAN_POINT('Ctrl Pts',(-200.675809595044,3.4792505691735,135.592621340272));
#166668=CARTESIAN_POINT('Ctrl Pts',(-200.668386328638,3.34971419766227,
135.681587837666));
#166669=CARTESIAN_POINT('Ctrl Pts',(-200.660971835917,3.22033092738485,
135.770449184047));
#166670=CARTESIAN_POINT('Ctrl Pts',(-200.653557343196,3.08724556180289,
135.854270959279));
#166671=CARTESIAN_POINT('Ctrl Pts',(-200.646142850475,2.95088917404671,
135.93273108439));
#166672=CARTESIAN_POINT('Ctrl Pts',(-200.638735504121,2.81466421171077,
136.011115586678));
#166673=CARTESIAN_POINT('Ctrl Pts',(-200.631328157768,2.67517482505955,
136.084148541912));
#166674=CARTESIAN_POINT('Ctrl Pts',(-200.623920811414,2.53288188521501,
136.151550526111));
#166675=CARTESIAN_POINT('Ctrl Pts',(-200.616518989738,2.3906950728134,136.218902239368));
#166676=CARTESIAN_POINT('Ctrl Pts',(-200.609117168063,2.24570920658458,
136.280631184824));
#166677=CARTESIAN_POINT('Ctrl Pts',(-200.601715346387,2.09841053341921,
136.336503402757));
#166678=CARTESIAN_POINT('Ctrl Pts',(-200.594317432076,1.95118961807727,
136.39234612618));
#166679=CARTESIAN_POINT('Ctrl Pts',(-200.586919517765,1.80165867545395,
136.442338147334));
#166680=CARTESIAN_POINT('Ctrl Pts',(-200.579521603453,1.65032464089478,
136.486293311831));
#166681=CARTESIAN_POINT('Ctrl Pts',(-200.572124918541,1.49901575530602,
136.530241171777));
#166682=CARTESIAN_POINT('Ctrl Pts',(-200.564728233629,1.34590473061233,
136.568154062135));
#166683=CARTESIAN_POINT('Ctrl Pts',(-200.557331548716,1.19151451455393,
136.599895426719));
#166684=CARTESIAN_POINT('Ctrl Pts',(-200.549935191781,1.03713114431951,
136.631635383858));
#166685=CARTESIAN_POINT('Ctrl Pts',(-200.542538834845,0.881469061150174,
136.657204284162));
#166686=CARTESIAN_POINT('Ctrl Pts',(-200.53514247791,0.725062014826754,
136.676516579149));
#166687=CARTESIAN_POINT('Ctrl Pts',(-200.527744988573,0.568631022185253,
136.695831830898));
#166688=CARTESIAN_POINT('Ctrl Pts',(-200.520347499237,0.411455209797665,
136.708888524271));
#166689=CARTESIAN_POINT('Ctrl Pts',(-200.5129500099,0.254073918632435,136.715652947198));
#166690=CARTESIAN_POINT('Ctrl Pts',(-200.505549927385,0.0966374576993343,
136.722419741384));
#166691=CARTESIAN_POINT('Ctrl Pts',(-200.49814984487,-0.0610042527022276,
136.72288985748));
#166692=CARTESIAN_POINT('Ctrl Pts',(-200.490749762355,-0.218311548806333,
136.717081702664));
#166693=CARTESIAN_POINT('Ctrl Pts',(-200.483341542688,-0.375791820453863,
136.711267161183));
#166694=CARTESIAN_POINT('Ctrl Pts',(-200.475933323022,-0.532936570164552,
136.699160575621));
#166695=CARTESIAN_POINT('Ctrl Pts',(-200.468525103355,-0.689210197067142,
136.680832336783));
#166696=CARTESIAN_POINT('Ctrl Pts',(-200.461112324053,-0.845580007779526,
136.66249281722));
#166697=CARTESIAN_POINT('Ctrl Pts',(-200.453699544751,-1.00107725944581,
136.637924072098));
#166698=CARTESIAN_POINT('Ctrl Pts',(-200.446286765449,-1.15517673598396,
136.607247594851));
#166699=CARTESIAN_POINT('Ctrl Pts',(-200.43886339442,-1.30949639708053,
136.576527285615));
#166700=CARTESIAN_POINT('Ctrl Pts',(-200.431440023392,-1.4624139322289,
136.539681901662));
#166701=CARTESIAN_POINT('Ctrl Pts',(-200.424016652363,-1.61341866780536,
136.496882972803));
#166702=CARTESIAN_POINT('Ctrl Pts',(-200.420080602922,-1.69348500191474,
136.474189953777));
#166703=CARTESIAN_POINT('Ctrl Pts',(-200.416144553482,-1.77301389176252,
136.449823992991));
#166704=CARTESIAN_POINT('Ctrl Pts',(-200.412208504041,-1.85193163392452,
136.423816088141));
#166705=CARTESIAN_POINT('Ctrl Pts',(-200.404785237635,-2.00076803270955,
136.37476599127));
#166706=CARTESIAN_POINT('Ctrl Pts',(-200.39736197123,-2.14787943854751,
136.3197245393));
#166707=CARTESIAN_POINT('Ctrl Pts',(-200.389938704824,-2.29274704537207,
136.258830486255));
#166708=CARTESIAN_POINT('Ctrl Pts',(-200.382524212103,-2.43744343071588,
136.198008404924));
#166709=CARTESIAN_POINT('Ctrl Pts',(-200.375109719382,-2.57990095506391,
136.131347634659));
#166710=CARTESIAN_POINT('Ctrl Pts',(-200.367695226661,-2.71961563869954,
136.059036757942));
#166711=CARTESIAN_POINT('Ctrl Pts',(-200.360287880307,-2.85919566006293,
135.986795577171));
#166712=CARTESIAN_POINT('Ctrl Pts',(-200.352880533953,-2.99603777440594,
135.908915301869));
#166713=CARTESIAN_POINT('Ctrl Pts',(-200.3454731876,-3.1296577823218,135.825632640475));
#166714=CARTESIAN_POINT('Ctrl Pts',(-200.338071365924,-3.26317813139457,
135.742412094433));
#166715=CARTESIAN_POINT('Ctrl Pts',(-200.330669544249,-3.39348084363586,
135.653797381792));
#166716=CARTESIAN_POINT('Ctrl Pts',(-200.323267722573,-3.52010625378327,
135.560071134889));
#166717=CARTESIAN_POINT('Ctrl Pts',(-200.315869808262,-3.64666481936232,
135.466394365342));
#166718=CARTESIAN_POINT('Ctrl Pts',(-200.30847189395,-3.76954964959203,
135.367611656931));
#166719=CARTESIAN_POINT('Ctrl Pts',(-200.301073979639,-3.88833011657844,
135.264048887727));
#166720=CARTESIAN_POINT('Ctrl Pts',(-200.293677294726,-4.00709084440596,
135.160503328776));
#166721=CARTESIAN_POINT('Ctrl Pts',(-200.286280609814,-4.12174828160482,
135.052179530682));
#166722=CARTESIAN_POINT('Ctrl Pts',(-200.278883924902,-4.23190487356255,
134.939443652236));
#166723=CARTESIAN_POINT('Ctrl Pts',(-200.271487567967,-4.34205658106188,
134.826712772617));
#166724=CARTESIAN_POINT('Ctrl Pts',(-200.264091211031,-4.44770757924775,
134.709570468634));
#166725=CARTESIAN_POINT('Ctrl Pts',(-200.256694854095,-4.5484973889659,
134.588419558052));
#166726=CARTESIAN_POINT('Ctrl Pts',(-200.249297364759,-4.64930262986123,
134.467250098956));
#166727=CARTESIAN_POINT('Ctrl Pts',(-200.241899875422,-4.74524496160936,
134.342071098237));
#166728=CARTESIAN_POINT('Ctrl Pts',(-200.234502386085,-4.83600449432356,
134.21331809653));
#166729=CARTESIAN_POINT('Ctrl Pts',(-200.22710230357,-4.92679584265112,
134.084519960658));
#166730=CARTESIAN_POINT('Ctrl Pts',(-200.219702221055,-5.01240055972236,
133.952145634283));
#166731=CARTESIAN_POINT('Ctrl Pts',(-200.21230213854,-5.09254243056786,
133.816659101343));
#166732=CARTESIAN_POINT('Ctrl Pts',(-200.204893918873,-5.17277242563903,
133.681023587033));
#166733=CARTESIAN_POINT('Ctrl Pts',(-200.197485699207,-5.24752738802124,
133.542269353312));
#166734=CARTESIAN_POINT('Ctrl Pts',(-200.19007747954,-5.31657703414016,
133.400885064313));
#166735=CARTESIAN_POINT('Ctrl Pts',(-200.182664700238,-5.38566917916411,
133.259413755643));
#166736=CARTESIAN_POINT('Ctrl Pts',(-200.175251920936,-5.44904886082607,
133.115309507039));
#166737=CARTESIAN_POINT('Ctrl Pts',(-200.167839141634,-5.50653440287247,
132.969079867834));
#166738=CARTESIAN_POINT('Ctrl Pts',(-200.160415770605,-5.56410208295706,
132.822641288864));
#166739=CARTESIAN_POINT('Ctrl Pts',(-200.152992399576,-5.615758680887,132.674071605666));
#166740=CARTESIAN_POINT('Ctrl Pts',(-200.145569028547,-5.66137247798355,
132.523893178476));
#166741=CARTESIAN_POINT('Ctrl Pts',(-200.141632979107,-5.68555800768561,
132.44426497292));
#166742=CARTESIAN_POINT('Ctrl Pts',(-200.137696929668,-5.70804554235413,
132.364184668557));
#166743=CARTESIAN_POINT('Ctrl Pts',(-200.133760880228,-5.7288213227283,
132.283731029178));
#166744=CARTESIAN_POINT('Ctrl Pts',(-200.124071939592,-5.77996277961027,
132.085687140804));
#166745=CARTESIAN_POINT('Ctrl Pts',(-200.114382998956,-5.82085499360012,
131.88489595805));
#166746=CARTESIAN_POINT('Ctrl Pts',(-200.10469405832,-5.85125580823402,
131.682276347638));
#166747=CARTESIAN_POINT('Ctrl Pts',(-200.095203709521,-5.88103350483466,
131.483809781632));
#166748=CARTESIAN_POINT('Ctrl Pts',(-200.085713360723,-5.90074552551159,
131.283588737847));
#166749=CARTESIAN_POINT('Ctrl Pts',(-200.076223011924,-5.91020894769956,
131.082498635521));
#166750=CARTESIAN_POINT('Ctrl Pts',(-200.071940411166,-5.91447939759482,
130.991755013462));
#166751=CARTESIAN_POINT('Ctrl Pts',(-200.067657810408,-5.91666348839728,
130.900834742462));
#166752=CARTESIAN_POINT('Ctrl Pts',(-200.06337520965,-5.91674748049752,
130.809820885532));
#166753=CARTESIAN_POINT('',(-198.313375158537,-5.91281518750731,130.803135099679));
#166754=CARTESIAN_POINT('Ctrl Pts',(-200.063375192208,-5.91554583036233,
130.809819405987));
#166755=CARTESIAN_POINT('Ctrl Pts',(-199.994021213611,-5.90217632497919,
129.336193982877));
#166756=CARTESIAN_POINT('Ctrl Pts',(-199.831851360409,-4.59893760167832,
125.869330780398));
#166757=CARTESIAN_POINT('Ctrl Pts',(-199.576865632603,1.22511734593415,
123.91403058054));
#166758=CARTESIAN_POINT('Ctrl Pts',(-199.298418008789,6.45923565506566,
128.110694847157));
#166759=CARTESIAN_POINT('Ctrl Pts',(-199.019970384977,5.7576319483906,134.782706363876));
#166760=CARTESIAN_POINT('Ctrl Pts',(-198.741522761164,-0.234954242897439,
137.798812492739));
#166761=CARTESIAN_POINT('Ctrl Pts',(-198.505991030241,-5.12129580041003,
134.913151181637));
#166762=CARTESIAN_POINT('Ctrl Pts',(-198.363275173922,-5.90520520611573,
131.867199701326));
#166763=CARTESIAN_POINT('Ctrl Pts',(-198.313375192208,-5.90716405999748,
130.803136989425));
#166764=CARTESIAN_POINT('',(-196.563375192208,-5.91754067440713,130.799324060973));
#166765=CARTESIAN_POINT('Ctrl Pts',(-198.313375135094,-5.91674987280848,
130.803133783915));
#166766=CARTESIAN_POINT('Ctrl Pts',(-198.305494209198,-5.91671497079014,
130.634808997274));
#166767=CARTESIAN_POINT('Ctrl Pts',(-198.297613283303,-5.90949285436914,
130.466668773567));
#166768=CARTESIAN_POINT('Ctrl Pts',(-198.289732357408,-5.89515605919228,
130.29932042088));
#166769=CARTESIAN_POINT('Ctrl Pts',(-198.281836630896,-5.88079233908077,
130.131657782929));
#166770=CARTESIAN_POINT('Ctrl Pts',(-198.273940904384,-5.85928727531646,
129.964790277688));
#166771=CARTESIAN_POINT('Ctrl Pts',(-198.266045177872,-5.83076466142615,
129.799316327217));
#166772=CARTESIAN_POINT('Ctrl Pts',(-198.258126453544,-5.80215896996073,
129.633360402175));
#166773=CARTESIAN_POINT('Ctrl Pts',(-198.250207729216,-5.76649488777139,
129.468806441626));
#166774=CARTESIAN_POINT('Ctrl Pts',(-198.242289004889,-5.72394703223156,
129.306241485218));
#166775=CARTESIAN_POINT('Ctrl Pts',(-198.234357905677,-5.6813326855795,
129.143422482521));
#166776=CARTESIAN_POINT('Ctrl Pts',(-198.226426806465,-5.63181316657086,
128.982598970972));
#166777=CARTESIAN_POINT('Ctrl Pts',(-198.218495707253,-5.57561197482526,
128.824339994268));
#166778=CARTESIAN_POINT('Ctrl Pts',(-198.210545405859,-5.51927471297368,
128.665697852811));
#166779=CARTESIAN_POINT('Ctrl Pts',(-198.202595104465,-5.45622353317009,
128.509632936207));
#166780=CARTESIAN_POINT('Ctrl Pts',(-198.194644803071,-5.38672971531874,
128.356693659706));
#166781=CARTESIAN_POINT('Ctrl Pts',(-198.19130570656,-5.35754257470302,
128.292459742115));
#166782=CARTESIAN_POINT('Ctrl Pts',(-198.187966610049,-5.32721951801162,
128.228776855833));
#166783=CARTESIAN_POINT('Ctrl Pts',(-198.184627513538,-5.29578296029053,
128.165684169042));
#166784=CARTESIAN_POINT('Ctrl Pts',(-198.177204247133,-5.22589521009871,
128.025420531639));
#166785=CARTESIAN_POINT('Ctrl Pts',(-198.169780980727,-5.15032541721235,
127.887723278348));
#166786=CARTESIAN_POINT('Ctrl Pts',(-198.162357714322,-5.06928530351928,
127.753085953754));
#166787=CARTESIAN_POINT('Ctrl Pts',(-198.154943221601,-4.98834097251064,
127.618607759295));
#166788=CARTESIAN_POINT('Ctrl Pts',(-198.14752872888,-4.90193938086913,
127.487182611414));
#166789=CARTESIAN_POINT('Ctrl Pts',(-198.14011423616,-4.8103394376285,127.359282235686));
#166790=CARTESIAN_POINT('Ctrl Pts',(-198.132706889806,-4.71882778186184,
127.231505135156));
#166791=CARTESIAN_POINT('Ctrl Pts',(-198.125299543452,-4.62212796504708,
127.107246344862));
#166792=CARTESIAN_POINT('Ctrl Pts',(-198.117892197099,-4.52054368801486,
126.986951112778));
#166793=CARTESIAN_POINT('Ctrl Pts',(-198.110490375423,-4.41903517636901,
126.866745601416));
#166794=CARTESIAN_POINT('Ctrl Pts',(-198.103088553748,-4.31264969804995,
126.750498046109));
#166795=CARTESIAN_POINT('Ctrl Pts',(-198.095686732073,-4.20173288463405,
126.638622828328));
#166796=CARTESIAN_POINT('Ctrl Pts',(-198.088288817762,-4.09087462334089,
126.526806668604));
#166797=CARTESIAN_POINT('Ctrl Pts',(-198.080890903451,-3.97549005300435,
126.419358514093));
#166798=CARTESIAN_POINT('Ctrl Pts',(-198.07349298914,-3.85596343966191,
126.316657807164));
#166799=CARTESIAN_POINT('Ctrl Pts',(-198.066096304228,-3.736456689474,126.213974167229));
#166800=CARTESIAN_POINT('Ctrl Pts',(-198.058699619315,-3.61280954527593,
126.116036652106));
#166801=CARTESIAN_POINT('Ctrl Pts',(-198.051302934403,-3.48544139440895,
126.023186196083));
#166802=CARTESIAN_POINT('Ctrl Pts',(-198.043906577468,-3.35807889117926,
125.930339857147));
#166803=CARTESIAN_POINT('Ctrl Pts',(-198.036510220533,-3.22699601099537,
125.842580348711));
#166804=CARTESIAN_POINT('Ctrl Pts',(-198.029113863598,-3.09264310423706,
125.76020665557));
#166805=CARTESIAN_POINT('Ctrl Pts',(-198.021716374261,-2.95826962770573,
125.677820350807));
#166806=CARTESIAN_POINT('Ctrl Pts',(-198.014318884925,-2.82062544600519,
125.600821698323));
#166807=CARTESIAN_POINT('Ctrl Pts',(-198.006921395588,-2.68018747322264,
125.529464820407));
#166808=CARTESIAN_POINT('Ctrl Pts',(-197.999521313073,-2.53970027012625,
125.458082928449));
#166809=CARTESIAN_POINT('Ctrl Pts',(-197.992121230558,-2.39641765864562,
125.392346917666));
#166810=CARTESIAN_POINT('Ctrl Pts',(-197.984721148044,-2.2508384387309,
125.332463607823));
#166811=CARTESIAN_POINT('Ctrl Pts',(-197.977312928377,-2.10509913949819,
125.272514450125));
#166812=CARTESIAN_POINT('Ctrl Pts',(-197.969904708711,-1.95705853397072,
125.21843098787));
#166813=CARTESIAN_POINT('Ctrl Pts',(-197.962496489045,-1.80723326014781,
125.170371044811));
#166814=CARTESIAN_POINT('Ctrl Pts',(-197.955083709743,-1.65731577136839,
125.122281521658));
#166815=CARTESIAN_POINT('Ctrl Pts',(-197.947670930441,-1.50561178442189,
125.080223004612));
#166816=CARTESIAN_POINT('Ctrl Pts',(-197.940258151139,-1.35264965650991,
125.04430250421));
#166817=CARTESIAN_POINT('Ctrl Pts',(-197.93283478011,-1.19946896913657,
125.008330678912));
#166818=CARTESIAN_POINT('Ctrl Pts',(-197.925411409082,-1.04502691596486,
124.97851445706));
#166819=CARTESIAN_POINT('Ctrl Pts',(-197.917988038053,-0.889859347573362,
124.954909283976));
#166820=CARTESIAN_POINT('Ctrl Pts',(-197.91405198861,-0.807585779573266,
124.942393254802));
#166821=CARTESIAN_POINT('Ctrl Pts',(-197.910115939167,-0.725108295893379,
124.931622504652));
#166822=CARTESIAN_POINT('Ctrl Pts',(-197.906179889724,-0.642506819387798,
124.922599355024));
#166823=CARTESIAN_POINT('Ctrl Pts',(-197.898756623319,-0.486723012682509,
124.905581976438));
#166824=CARTESIAN_POINT('Ctrl Pts',(-197.891333356914,-0.330027094746583,
124.894732254595));
#166825=CARTESIAN_POINT('Ctrl Pts',(-197.883910090508,-0.172948739468105,
124.890138834777));
#166826=CARTESIAN_POINT('Ctrl Pts',(-197.876495597787,-0.0160560377610202,
124.885550844));
#166827=CARTESIAN_POINT('Ctrl Pts',(-197.869081105066,0.141217832067213,
124.887204447401));
#166828=CARTESIAN_POINT('Ctrl Pts',(-197.861666612345,0.298336047272165,
124.895136796674));
#166829=CARTESIAN_POINT('Ctrl Pts',(-197.854259265991,0.455302826025905,
124.90306150045));
#166830=CARTESIAN_POINT('Ctrl Pts',(-197.846851919638,0.612113878507934,
124.917252883675));
#166831=CARTESIAN_POINT('Ctrl Pts',(-197.839444573284,0.768230447271629,
124.937696101643));
#166832=CARTESIAN_POINT('Ctrl Pts',(-197.832042751609,0.924230578407954,
124.958124072289));
#166833=CARTESIAN_POINT('Ctrl Pts',(-197.824640929933,1.07953688863353,
124.984794545045));
#166834=CARTESIAN_POINT('Ctrl Pts',(-197.817239108258,1.23361392477094,
125.017640713587));
#166835=CARTESIAN_POINT('Ctrl Pts',(-197.809841193946,1.38760962484074,
125.050469542891));
#166836=CARTESIAN_POINT('Ctrl Pts',(-197.802443279635,1.54037697901615,
125.089467497698));
#166837=CARTESIAN_POINT('Ctrl Pts',(-197.795045365324,1.69138904650517,
125.134516381975));
#166838=CARTESIAN_POINT('Ctrl Pts',(-197.787648680412,1.84237601852799,
125.179557779945));
#166839=CARTESIAN_POINT('Ctrl Pts',(-197.780251995499,1.99160792542631,
125.23064800505));
#166840=CARTESIAN_POINT('Ctrl Pts',(-197.772855310587,2.1385712404262,125.287618498152));
#166841=CARTESIAN_POINT('Ctrl Pts',(-197.765458953652,2.2855280389187,125.344586465122));
#166842=CARTESIAN_POINT('Ctrl Pts',(-197.758062596717,2.43021609746273,
125.407434046729));
#166843=CARTESIAN_POINT('Ctrl Pts',(-197.750666239781,2.57214044630336,
125.475943959028));
#166844=CARTESIAN_POINT('Ctrl Pts',(-197.743268750445,2.71408652412452,
125.544464360369));
#166845=CARTESIAN_POINT('Ctrl Pts',(-197.735871261108,2.8532677135316,125.618648656259));
#166846=CARTESIAN_POINT('Ctrl Pts',(-197.728473771771,2.98921243053313,
125.698232964672));
#166847=CARTESIAN_POINT('Ctrl Pts',(-197.721073689256,3.12520480274389,
125.777845171241));
#166848=CARTESIAN_POINT('Ctrl Pts',(-197.713673606741,3.25795812173416,
125.862860970739));
#166849=CARTESIAN_POINT('Ctrl Pts',(-197.706273524226,3.38702877062359,
125.952972499772));
#166850=CARTESIAN_POINT('Ctrl Pts',(-197.69886530456,3.51624134596045,126.043183115696));
#166851=CARTESIAN_POINT('Ctrl Pts',(-197.691457084894,3.64176285786007,
126.138500437448));
#166852=CARTESIAN_POINT('Ctrl Pts',(-197.684048865227,3.76318126927204,
126.238575110438));
#166853=CARTESIAN_POINT('Ctrl Pts',(-197.676636085925,3.88467441169026,
126.33871137772));
#166854=CARTESIAN_POINT('Ctrl Pts',(-197.669223306623,4.002059143761,126.443610582622));
#166855=CARTESIAN_POINT('Ctrl Pts',(-197.661810527321,4.11495984451519,
126.552886045076));
#166856=CARTESIAN_POINT('Ctrl Pts',(-197.654387156293,4.2280218630853,126.662317645436));
#166857=CARTESIAN_POINT('Ctrl Pts',(-197.646963785264,4.33658679716489,
126.776137722587));
#166858=CARTESIAN_POINT('Ctrl Pts',(-197.639540414235,4.4403183587074,126.893925419813));
#166859=CARTESIAN_POINT('Ctrl Pts',(-197.635604364794,4.49531932164588,
126.956379283164));
#166860=CARTESIAN_POINT('Ctrl Pts',(-197.631668315353,4.54896215332004,
127.019948072493));
#166861=CARTESIAN_POINT('Ctrl Pts',(-197.627732265912,4.60120170033201,
127.084565801267));
#166862=CARTESIAN_POINT('Ctrl Pts',(-197.620308999507,4.69972385564997,
127.206432821078));
#166863=CARTESIAN_POINT('Ctrl Pts',(-197.612885733101,4.79355000507247,
127.332400995022));
#166864=CARTESIAN_POINT('Ctrl Pts',(-197.605462466696,4.88231926713834,
127.462072608398));
#166865=CARTESIAN_POINT('Ctrl Pts',(-197.598047973975,4.97098361130828,
127.591590960695));
#166866=CARTESIAN_POINT('Ctrl Pts',(-197.590633481254,5.05460275620507,
127.72480373464));
#166867=CARTESIAN_POINT('Ctrl Pts',(-197.583218988533,5.13285527925053,
127.861279367452));
#166868=CARTESIAN_POINT('Ctrl Pts',(-197.575811642179,5.21103237956813,
127.997623459912));
#166869=CARTESIAN_POINT('Ctrl Pts',(-197.568404295825,5.28385297112994,
128.137223828763));
#166870=CARTESIAN_POINT('Ctrl Pts',(-197.560996949471,5.35103833164711,
128.279619178182));
#166871=CARTESIAN_POINT('Ctrl Pts',(-197.553595127796,5.41817358278764,
128.421908323777));
#166872=CARTESIAN_POINT('Ctrl Pts',(-197.54619330612,5.47968181295513,128.566987963062));
#166873=CARTESIAN_POINT('Ctrl Pts',(-197.538791484445,5.53532980268285,
128.714371493663));
#166874=CARTESIAN_POINT('Ctrl Pts',(-197.531393570133,5.59094841626997,
128.861677221646));
#166875=CARTESIAN_POINT('Ctrl Pts',(-197.523995655822,5.64071281889356,
129.011284070463));
#166876=CARTESIAN_POINT('Ctrl Pts',(-197.516597741511,5.6844376278525,129.162684822059));
#166877=CARTESIAN_POINT('Ctrl Pts',(-197.509201056598,5.72815517054139,
129.314060413596));
#166878=CARTESIAN_POINT('Ctrl Pts',(-197.501804371686,5.76583500808062,
129.467228957956));
#166879=CARTESIAN_POINT('Ctrl Pts',(-197.494407686774,5.79734138028169,
129.621667300187));
#166880=CARTESIAN_POINT('Ctrl Pts',(-197.487011329838,5.82884635545729,
129.77609879446));
#166881=CARTESIAN_POINT('Ctrl Pts',(-197.479614972903,5.85417833496008,
129.93179960889));
#166882=CARTESIAN_POINT('Ctrl Pts',(-197.472218615968,5.87325258268416,
130.088235864123));
#166883=CARTESIAN_POINT('Ctrl Pts',(-197.464821126631,5.89232975072421,
130.244696070146));
#166884=CARTESIAN_POINT('Ctrl Pts',(-197.457423637294,5.90514723414698,
130.401891570591));
#166885=CARTESIAN_POINT('Ctrl Pts',(-197.450026147958,5.91167214170678,
130.559282973812));
#166886=CARTESIAN_POINT('Ctrl Pts',(-197.442626065443,5.91819933656282,
130.716729550346));
#166887=CARTESIAN_POINT('Ctrl Pts',(-197.435225982928,5.9184295482666,130.874371793638));
#166888=CARTESIAN_POINT('Ctrl Pts',(-197.427825900413,5.91238200524872,
131.03167006856));
#166889=CARTESIAN_POINT('Ctrl Pts',(-197.420417680746,5.9063278123356,131.189141309106));
#166890=CARTESIAN_POINT('Ctrl Pts',(-197.41300946108,5.89398209323351,131.346267452684));
#166891=CARTESIAN_POINT('Ctrl Pts',(-197.405601241413,5.87541605376114,
131.502513006165));
#166892=CARTESIAN_POINT('Ctrl Pts',(-197.398188462111,5.85683858720126,
131.658854726177));
#166893=CARTESIAN_POINT('Ctrl Pts',(-197.390775682809,5.83203323018161,
131.814314408332));
#166894=CARTESIAN_POINT('Ctrl Pts',(-197.383362903507,5.80112227528612,
131.96836702205));
#166895=CARTESIAN_POINT('Ctrl Pts',(-197.375939532478,5.77016715336866,
132.122639753366));
#166896=CARTESIAN_POINT('Ctrl Pts',(-197.368516161449,5.73308909762374,
132.275501039037));
#166897=CARTESIAN_POINT('Ctrl Pts',(-197.361092790421,5.69006041482304,
132.426440467069));
#166898=CARTESIAN_POINT('Ctrl Pts',(-197.35715674098,5.66724557474622,132.506472173542));
#166899=CARTESIAN_POINT('Ctrl Pts',(-197.35322069154,5.64275861274537,132.585963890444));
#166900=CARTESIAN_POINT('Ctrl Pts',(-197.3492846421,5.6166306386455,132.664841961608));
#166901=CARTESIAN_POINT('Ctrl Pts',(-197.341861375694,5.56735409491276,
132.813603542143));
#166902=CARTESIAN_POINT('Ctrl Pts',(-197.334438109289,5.51208882816386,
132.960631013906));
#166903=CARTESIAN_POINT('Ctrl Pts',(-197.327014842883,5.45097438179734,
133.105405782592));
#166904=CARTESIAN_POINT('Ctrl Pts',(-197.319600350162,5.38993216763119,
133.250009439524));
#166905=CARTESIAN_POINT('Ctrl Pts',(-197.312185857442,5.32305467845807,
133.392365352562));
#166906=CARTESIAN_POINT('Ctrl Pts',(-197.304771364721,5.25053126351302,
133.531969829563));
#166907=CARTESIAN_POINT('Ctrl Pts',(-197.297364018367,5.17807774936575,
133.671439750514));
#166908=CARTESIAN_POINT('Ctrl Pts',(-197.289956672013,5.09998931384532,
133.808163185873));
#166909=CARTESIAN_POINT('Ctrl Pts',(-197.282549325659,5.01650340198775,
133.941656297024));
#166910=CARTESIAN_POINT('Ctrl Pts',(-197.275147503984,4.93307975707299,
134.075049843976));
#166911=CARTESIAN_POINT('Ctrl Pts',(-197.267745682308,4.84426684850198,
134.20521754882));
#166912=CARTESIAN_POINT('Ctrl Pts',(-197.260343860633,4.75034800781524,
134.331700176943));
#166913=CARTESIAN_POINT('Ctrl Pts',(-197.252945946322,4.65647874615343,
134.458116035871));
#166914=CARTESIAN_POINT('Ctrl Pts',(-197.24554803201,4.55750914234047,134.580850393335));
#166915=CARTESIAN_POINT('Ctrl Pts',(-197.238150117699,4.453765729412,134.699473117869));
#166916=CARTESIAN_POINT('Ctrl Pts',(-197.230753432787,4.3500395567568,134.818076129458));
#166917=CARTESIAN_POINT('Ctrl Pts',(-197.223356747875,4.24154139500116,
134.932568583504));
#166918=CARTESIAN_POINT('Ctrl Pts',(-197.215960062963,4.12863800752296,
135.042553483085));
#166919=CARTESIAN_POINT('Ctrl Pts',(-197.208563706027,4.01573962629928,
135.152533505821));
#166920=CARTESIAN_POINT('Ctrl Pts',(-197.201167349092,3.89843667513432,
135.258006111018));
#166921=CARTESIAN_POINT('Ctrl Pts',(-197.193770992156,3.77713251991294,
135.35861143296));
#166922=CARTESIAN_POINT('Ctrl Pts',(-197.18637350282,3.65580979271537,135.459232157834));
#166923=CARTESIAN_POINT('Ctrl Pts',(-197.178976013483,3.53048492905807,
135.554983877352));
#166924=CARTESIAN_POINT('Ctrl Pts',(-197.171578524146,3.40159395588911,
135.645547364817));
#166925=CARTESIAN_POINT('Ctrl Pts',(-197.164178441631,3.27265780018913,
135.736142599172));
#166926=CARTESIAN_POINT('Ctrl Pts',(-197.156778359116,3.14015335129741,
135.821545765924));
#166927=CARTESIAN_POINT('Ctrl Pts',(-197.149378276601,3.00454501296717,
135.901481356528));
#166928=CARTESIAN_POINT('Ctrl Pts',(-197.141970056935,2.86878755932826,
135.981504844531));
#166929=CARTESIAN_POINT('Ctrl Pts',(-197.134561837268,2.72991972195824,
136.056048560025));
#166930=CARTESIAN_POINT('Ctrl Pts',(-197.127153617602,2.58843051487615,
136.124882963366));
#166931=CARTESIAN_POINT('Ctrl Pts',(-197.1197408383,2.44685422354838,136.193759733134));
#166932=CARTESIAN_POINT('Ctrl Pts',(-197.112328058998,2.3026536887318,136.256920039268));
#166933=CARTESIAN_POINT('Ctrl Pts',(-197.104915279696,2.15633673565307,
136.31418297813));
#166934=CARTESIAN_POINT('Ctrl Pts',(-197.097491908667,2.00981071804999,
136.371527736965));
#166935=CARTESIAN_POINT('Ctrl Pts',(-197.090068537638,1.86116259434809,
136.422958177311));
#166936=CARTESIAN_POINT('Ctrl Pts',(-197.08264516661,1.71091492463178,136.468343375588));
#166937=CARTESIAN_POINT('Ctrl Pts',(-197.078709117169,1.63125000500077,
136.492407696719));
#166938=CARTESIAN_POINT('Ctrl Pts',(-197.074773067728,1.55113557114578,
136.514773336763));
#166939=CARTESIAN_POINT('Ctrl Pts',(-197.070837018287,1.47065040770534,
136.535426656342));
#166940=CARTESIAN_POINT('Ctrl Pts',(-197.063413751881,1.31885790131885,
136.574378172499));
#166941=CARTESIAN_POINT('Ctrl Pts',(-197.055990485476,1.16528729868185,
136.607353878223));
#166942=CARTESIAN_POINT('Ctrl Pts',(-197.04856721907,1.01045033448641,136.634190862439));
#166943=CARTESIAN_POINT('Ctrl Pts',(-197.041152726349,0.855796374724231,
136.660996127568));
#166944=CARTESIAN_POINT('Ctrl Pts',(-197.033738233628,0.699879396883509,
136.681677050091));
#166945=CARTESIAN_POINT('Ctrl Pts',(-197.026323740907,0.543225519315743,
136.696120676976));
#166946=CARTESIAN_POINT('Ctrl Pts',(-197.018916394553,0.38672263065309,
136.71055038255));
#166947=CARTESIAN_POINT('Ctrl Pts',(-197.011509048199,0.229484625460507,
136.718754726634));
#166948=CARTESIAN_POINT('Ctrl Pts',(-197.004101701846,0.072046915710644,
136.720671951872));
#166949=CARTESIAN_POINT('Ctrl Pts',(-196.99669988017,-0.0852733710555033,
136.722587747171));
#166950=CARTESIAN_POINT('Ctrl Pts',(-196.989298058495,-0.242792694141263,
136.718225755868));
#166951=CARTESIAN_POINT('Ctrl Pts',(-196.981896236819,-0.399971538843124,
136.707576125289));
#166952=CARTESIAN_POINT('Ctrl Pts',(-196.974498322508,-0.557067410055896,
136.696932116566));
#166953=CARTESIAN_POINT('Ctrl Pts',(-196.967100408196,-0.71382278933619,
136.680007104075));
#166954=CARTESIAN_POINT('Ctrl Pts',(-196.959702493885,-0.869699295819346,
136.656843312743));
#166955=CARTESIAN_POINT('Ctrl Pts',(-196.952305808973,-1.02554989845523,
136.633683370814));
#166956=CARTESIAN_POINT('Ctrl Pts',(-196.944909124061,-1.18052154928376,
136.604286762546));
#166957=CARTESIAN_POINT('Ctrl Pts',(-196.937512439148,-1.33408199898751,
136.568747469823));
#166958=CARTESIAN_POINT('Ctrl Pts',(-196.930116082213,-1.48763563966,136.533209752951));
#166959=CARTESIAN_POINT('Ctrl Pts',(-196.922719725277,-1.63977783994152,
136.491529977363));
#166960=CARTESIAN_POINT('Ctrl Pts',(-196.915323368342,-1.7899878054991,
136.443852989993));
#166961=CARTESIAN_POINT('Ctrl Pts',(-196.907925879005,-1.94022076858587,
136.396168703155));
#166962=CARTESIAN_POINT('Ctrl Pts',(-196.900528389669,-2.08852055208359,
136.34248548924));
#166963=CARTESIAN_POINT('Ctrl Pts',(-196.893130900332,-2.23438289831461,
136.28299764024));
#166964=CARTESIAN_POINT('Ctrl Pts',(-196.885730817817,-2.38029637636477,
136.223488937868));
#166965=CARTESIAN_POINT('Ctrl Pts',(-196.878330735302,-2.52377037052379,
136.158171690011));
#166966=CARTESIAN_POINT('Ctrl Pts',(-196.870930652787,-2.66432206607766,
136.087287693602));
#166967=CARTESIAN_POINT('Ctrl Pts',(-196.86352243312,-2.80502831267005,
136.016325752951));
#166968=CARTESIAN_POINT('Ctrl Pts',(-196.856114213454,-2.9428055098375,
135.939785007485));
#166969=CARTESIAN_POINT('Ctrl Pts',(-196.848705993787,-3.07719621535446,
135.857952806763));
#166970=CARTESIAN_POINT('Ctrl Pts',(-196.841293214485,-3.21166963610861,
135.776070239686));
#166971=CARTESIAN_POINT('Ctrl Pts',(-196.833880435183,-3.3427521018158,
135.688889934013));
#166972=CARTESIAN_POINT('Ctrl Pts',(-196.826467655881,-3.47001692118132,
135.596741354654));
#166973=CARTESIAN_POINT('Ctrl Pts',(-196.819044284852,-3.59746358248833,
135.504461109084));
#166974=CARTESIAN_POINT('Ctrl Pts',(-196.811620913823,-3.72108141033138,
135.407198641944));
#166975=CARTESIAN_POINT('Ctrl Pts',(-196.804197542794,-3.84047779850241,
135.305322830439));
#166976=CARTESIAN_POINT('Ctrl Pts',(-196.800261493354,-3.90378462838005,
135.251305830709));
#166977=CARTESIAN_POINT('Ctrl Pts',(-196.796325443914,-3.96590528316954,
135.195992463312));
#166978=CARTESIAN_POINT('Ctrl Pts',(-196.792389394474,-4.02678570265285,
135.139441639578));
#166979=CARTESIAN_POINT('Ctrl Pts',(-196.78507668251,-4.13989428490648,
135.034376931548));
#166980=CARTESIAN_POINT('Ctrl Pts',(-196.777763970547,-4.24908372070728,
134.924700531894));
#166981=CARTESIAN_POINT('Ctrl Pts',(-196.770451258584,-4.35394615139191,
134.810740963125));
#166982=CARTESIAN_POINT('Ctrl Pts',(-196.763147289429,-4.45868321243069,
134.696917640204));
#166983=CARTESIAN_POINT('Ctrl Pts',(-196.755843320274,-4.55910330236656,
134.578821616739));
#166984=CARTESIAN_POINT('Ctrl Pts',(-196.748539351119,-4.65483230230702,
134.456820993792));
#166985=CARTESIAN_POINT('Ctrl Pts',(-196.741242407847,-4.75046921796755,
134.3349377265));
#166986=CARTESIAN_POINT('Ctrl Pts',(-196.733945464575,-4.84142378676094,
134.209157634796));
#166987=CARTESIAN_POINT('Ctrl Pts',(-196.726648521302,-4.92735958258975,
134.079884714006));
#166988=CARTESIAN_POINT('Ctrl Pts',(-196.719357248112,-5.01322860210467,
133.950712244595));
#166989=CARTESIAN_POINT('Ctrl Pts',(-196.712065974921,-5.09408640058275,
133.818052669374));
#166990=CARTESIAN_POINT('Ctrl Pts',(-196.704774701731,-5.16963782844034,
133.682341730301));
#166991=CARTESIAN_POINT('Ctrl Pts',(-196.697486477277,-5.24515766559986,
133.546687536724));
#166992=CARTESIAN_POINT('Ctrl Pts',(-196.690198252823,-5.31537535882009,
133.407984853367));
#166993=CARTESIAN_POINT('Ctrl Pts',(-196.682910028369,-5.38004001794075,
133.266696900013));
#166994=CARTESIAN_POINT('Ctrl Pts',(-196.675623313027,-5.44469128748668,
133.125438201984));
#166995=CARTESIAN_POINT('Ctrl Pts',(-196.668336597685,-5.50379165095616,
132.98159564949));
#166996=CARTESIAN_POINT('Ctrl Pts',(-196.661049882344,-5.5571371184965,
132.835655182303));
#166997=CARTESIAN_POINT('Ctrl Pts',(-196.653763137853,-5.61048279943774,
132.689714131302));
#166998=CARTESIAN_POINT('Ctrl Pts',(-196.646476393361,-5.65807340793315,
132.541675511368));
#166999=CARTESIAN_POINT('Ctrl Pts',(-196.63918964887,-5.69975396984224,
132.392042967965));
#167000=CARTESIAN_POINT('Ctrl Pts',(-196.631898500147,-5.74145972418876,
132.242319984118));
#167001=CARTESIAN_POINT('Ctrl Pts',(-196.624607351424,-5.77724819432482,
132.091001524323));
#167002=CARTESIAN_POINT('Ctrl Pts',(-196.617316202701,-5.80701487487784,
131.938604332756));
#167003=CARTESIAN_POINT('Ctrl Pts',(-196.61002256742,-5.83679170699883,
131.786155167962));
#167004=CARTESIAN_POINT('Ctrl Pts',(-196.602728932139,-5.86054259825711,
131.632626918938));
#167005=CARTESIAN_POINT('Ctrl Pts',(-196.595435296857,-5.87821471232728,
131.478543351162));
#167006=CARTESIAN_POINT('Ctrl Pts',(-196.58813424297,-5.89590480130939,
131.324303059717));
#167007=CARTESIAN_POINT('Ctrl Pts',(-196.580833189082,-5.90750373817299,
131.169506705419));
#167008=CARTESIAN_POINT('Ctrl Pts',(-196.573532135195,-5.91301075271542,
131.014680375962));
#167009=CARTESIAN_POINT('Ctrl Pts',(-196.570146487533,-5.91556446772689,
130.942884247832));
#167010=CARTESIAN_POINT('Ctrl Pts',(-196.56676083987,-5.91680893090054,
130.871081648203));
#167011=CARTESIAN_POINT('Ctrl Pts',(-196.563375192208,-5.91674785692228,
130.799324735758));
#167012=CARTESIAN_POINT('',(-194.813375192208,-5.92378430407072,130.807954965743));
#167013=CARTESIAN_POINT('Ctrl Pts',(-196.563375192208,-5.92005028606524,
130.799321924984));
#167014=CARTESIAN_POINT('Ctrl Pts',(-196.546897385026,-5.92321501407519,
130.449886125491));
#167015=CARTESIAN_POINT('Ctrl Pts',(-196.530419577843,-5.89494931063627,
130.100961680412));
#167016=CARTESIAN_POINT('Ctrl Pts',(-196.421125896056,-5.48691602341415,
127.826183567757));
#167017=CARTESIAN_POINT('Ctrl Pts',(-196.235494146848,-2.68383279408233,
124.341033141431));
#167018=CARTESIAN_POINT('Ctrl Pts',(-195.957046523035,3.98710327515676,
125.052789701408));
#167019=CARTESIAN_POINT('Ctrl Pts',(-195.678598899222,6.99408621534913,
131.049958953475));
#167020=CARTESIAN_POINT('Ctrl Pts',(-195.400151275409,3.57384560374378,
136.821435332985));
#167021=CARTESIAN_POINT('Ctrl Pts',(-195.121703651596,-3.13058452563971,
137.063513999468));
#167022=CARTESIAN_POINT('Ctrl Pts',(-194.926111623863,-5.81921701947016,
133.19324015144));
#167023=CARTESIAN_POINT('Ctrl Pts',(-194.823335470733,-5.92529114525991,
131.018830628555));
#167024=CARTESIAN_POINT('Ctrl Pts',(-194.813375192208,-5.92378430407072,
130.807954965743));
#167025=CARTESIAN_POINT('',(-193.063375192208,-5.90877653025682,130.807662282052));
#167026=CARTESIAN_POINT('Ctrl Pts',(-194.813375192208,-5.92378430407072,
130.807954965743));
#167027=CARTESIAN_POINT('Ctrl Pts',(-194.730519596129,-5.91124949145352,
129.053764187153));
#167028=CARTESIAN_POINT('Ctrl Pts',(-194.554848125446,-4.15536005181142,
125.312715685492));
#167029=CARTESIAN_POINT('Ctrl Pts',(-194.286360780158,2.21070539777845,
124.164304731159));
#167030=CARTESIAN_POINT('Ctrl Pts',(-194.007913156345,6.78140734036955,
129.075177280167));
#167031=CARTESIAN_POINT('Ctrl Pts',(-193.729465532532,5.12032722732323,
135.575084840937));
#167032=CARTESIAN_POINT('Ctrl Pts',(-193.451017908719,-1.24608346573943,
137.690929903266));
#167033=CARTESIAN_POINT('Ctrl Pts',(-193.228987795278,-5.40948930689292,
134.331882897925));
#167034=CARTESIAN_POINT('Ctrl Pts',(-193.099773556441,-5.91269277027163,
131.5832887094));
#167035=CARTESIAN_POINT('Ctrl Pts',(-193.063375192208,-5.90877653025682,
130.807662282052));
#167036=CARTESIAN_POINT('',(-191.313375192208,-5.91167657527647,130.799567797019));
#167037=CARTESIAN_POINT('Ctrl Pts',(-193.063375192208,-5.90877653025682,
130.807662282052));
#167038=CARTESIAN_POINT('Ctrl Pts',(-193.006957681836,-5.90270635330487,
129.605440343458));
#167039=CARTESIAN_POINT('Ctrl Pts',(-192.857724296862,-4.96095598029521,
126.416633059624));
#167040=CARTESIAN_POINT('Ctrl Pts',(-192.61567503728,0.256241860122023,
123.810656260109));
#167041=CARTESIAN_POINT('Ctrl Pts',(-192.337227413466,6.02250653238034,
127.239676115707));
#167042=CARTESIAN_POINT('Ctrl Pts',(-192.058779789655,6.25438191717603,
133.944466883987));
#167043=CARTESIAN_POINT('Ctrl Pts',(-191.780332165841,0.738785863635208,
137.763653396148));
#167044=CARTESIAN_POINT('Ctrl Pts',(-191.531863966693,-4.78877897888325,
135.464945051595));
#167045=CARTESIAN_POINT('Ctrl Pts',(-191.376211642148,-5.90155266118287,
132.136924284238));
#167046=CARTESIAN_POINT('Ctrl Pts',(-191.313375192208,-5.91167657527647,
130.799567797019));
#167047=CARTESIAN_POINT('',(-189.563375998339,-5.92191640313042,130.80298505409));
#167048=CARTESIAN_POINT('Ctrl Pts',(-191.313375192208,-5.91167657527647,
130.799567797019));
#167049=CARTESIAN_POINT('Ctrl Pts',(-191.283395767544,-5.91650671956634,
130.161511730902));
#167050=CARTESIAN_POINT('Ctrl Pts',(-191.160600468276,-5.52689340955663,
127.553783705044));
#167051=CARTESIAN_POINT('Ctrl Pts',(-190.944989294402,-1.71886118746277,
124.020329607269));
#167052=CARTESIAN_POINT('Ctrl Pts',(-190.66654167059,4.77851096535738,125.691299549647));
#167053=CARTESIAN_POINT('Ctrl Pts',(-190.388094046777,6.88466498425298,
132.060922826512));
#167054=CARTESIAN_POINT('Ctrl Pts',(-190.109646422965,2.66414821720038,
137.275826819836));
#167055=CARTESIAN_POINT('Ctrl Pts',(-189.834740626303,-3.91976489026385,
136.553081220811));
#167056=CARTESIAN_POINT('Ctrl Pts',(-189.65265070425,-5.9201422633631,132.691092662961));
#167057=CARTESIAN_POINT('Ctrl Pts',(-189.563376656799,-5.92613653540298,
130.802997987718));
#167058=CARTESIAN_POINT('',(-187.813375192208,-5.91590714834001,130.809830359851));
#167059=CARTESIAN_POINT('Ctrl Pts',(-189.563375192208,-5.91674983639772,
130.802969219882));
#167060=CARTESIAN_POINT('Ctrl Pts',(-189.559833853251,-5.91673225127943,
130.728190637922));
#167061=CARTESIAN_POINT('Ctrl Pts',(-189.556292514295,-5.91529709555501,
130.653430419199));
#167062=CARTESIAN_POINT('Ctrl Pts',(-189.552751175338,-5.91244610460354,
130.578724577319));
#167063=CARTESIAN_POINT('Ctrl Pts',(-189.545327908933,-5.90646992847011,
130.42212805461));
#167064=CARTESIAN_POINT('Ctrl Pts',(-189.537904642528,-5.89425901609847,
130.265532330591));
#167065=CARTESIAN_POINT('Ctrl Pts',(-189.530481376122,-5.87580323340804,
130.109474350058));
#167066=CARTESIAN_POINT('Ctrl Pts',(-189.523066883401,-5.85736926392009,
129.953600817098));
#167067=CARTESIAN_POINT('Ctrl Pts',(-189.51565239068,-5.832705159285,129.798264129616));
#167068=CARTESIAN_POINT('Ctrl Pts',(-189.508237897959,-5.80185277077408,
129.644000764434));
#167069=CARTESIAN_POINT('Ctrl Pts',(-189.500830551605,-5.77103011895677,
129.48988608409));
#167070=CARTESIAN_POINT('Ctrl Pts',(-189.493423205251,-5.73403113012844,
129.336843030134));
#167071=CARTESIAN_POINT('Ctrl Pts',(-189.486015858898,-5.69094937483769,
129.18540237983));
#167072=CARTESIAN_POINT('Ctrl Pts',(-189.478614037222,-5.64789975154543,
129.034074679676));
#167073=CARTESIAN_POINT('Ctrl Pts',(-189.471212215547,-5.59877649678882,
128.884347361008));
#167074=CARTESIAN_POINT('Ctrl Pts',(-189.463810393871,-5.54372409889164,
128.73674032412));
#167075=CARTESIAN_POINT('Ctrl Pts',(-189.45641247956,-5.48870076272677,
128.589211207839));
#167076=CARTESIAN_POINT('Ctrl Pts',(-189.449014565249,-5.42775464698324,
128.443800493114));
#167077=CARTESIAN_POINT('Ctrl Pts',(-189.441616650937,-5.36107982942442,
128.301012135025));
#167078=CARTESIAN_POINT('Ctrl Pts',(-189.434219966025,-5.29441609201077,
128.158247505772));
#167079=CARTESIAN_POINT('Ctrl Pts',(-189.426823281113,-5.22202570001855,
128.018104706153));
#167080=CARTESIAN_POINT('Ctrl Pts',(-189.419426596201,-5.14415058741227,
127.881067047545));
#167081=CARTESIAN_POINT('Ctrl Pts',(-189.412030239265,-5.06627892787009,
127.744035465331));
#167082=CARTESIAN_POINT('Ctrl Pts',(-189.40463388233,-4.98292321570959,
127.610109074916));
#167083=CARTESIAN_POINT('Ctrl Pts',(-189.397237525395,-4.89437086740681,
127.479745696289));
#167084=CARTESIAN_POINT('Ctrl Pts',(-189.389840036058,-4.80580496151345,
127.349362358695));
#167085=CARTESIAN_POINT('Ctrl Pts',(-189.382442546721,-4.71204104506515,
127.222543427878));
#167086=CARTESIAN_POINT('Ctrl Pts',(-189.375045057385,-4.61340920620913,
127.099716767131));
#167087=CARTESIAN_POINT('Ctrl Pts',(-189.36764497487,-4.51474279211475,
126.976847049689));
#167088=CARTESIAN_POINT('Ctrl Pts',(-189.360244892355,-4.41120529168435,
126.857972679567));
#167089=CARTESIAN_POINT('Ctrl Pts',(-189.35284480984,-4.30316620541695,
126.74348741454));
#167090=CARTESIAN_POINT('Ctrl Pts',(-189.345436590173,-4.19500831906767,
126.628876261194));
#167091=CARTESIAN_POINT('Ctrl Pts',(-189.338028370507,-4.08233921785816,
126.518664122988));
#167092=CARTESIAN_POINT('Ctrl Pts',(-189.33062015084,-3.96556482232641,
126.413207443008));
#167093=CARTESIAN_POINT('Ctrl Pts',(-189.323207371538,-3.84871855410236,
126.307685856202));
#167094=CARTESIAN_POINT('Ctrl Pts',(-189.315794592236,-3.72776224286292,
126.206925798223));
#167095=CARTESIAN_POINT('Ctrl Pts',(-189.308381812934,-3.6031334002335,
126.111242223297));
#167096=CARTESIAN_POINT('Ctrl Pts',(-189.300958441905,-3.4783264820694,
126.015421931193));
#167097=CARTESIAN_POINT('Ctrl Pts',(-189.293535070877,-3.349836856241,125.924692823797));
#167098=CARTESIAN_POINT('Ctrl Pts',(-189.286111699848,-3.21813008347746,
125.839325942126));
#167099=CARTESIAN_POINT('Ctrl Pts',(-189.282175650407,-3.14829599229798,
125.794062373115));
#167100=CARTESIAN_POINT('Ctrl Pts',(-189.278239600966,-3.07755785156217,
125.750305547236));
#167101=CARTESIAN_POINT('Ctrl Pts',(-189.274303551526,-3.00598754805893,
125.708090469368));
#167102=CARTESIAN_POINT('Ctrl Pts',(-189.26688028512,-2.8710081892836,125.628474149996));
#167103=CARTESIAN_POINT('Ctrl Pts',(-189.259457018715,-2.73265947523997,
125.55410372251));
#167104=CARTESIAN_POINT('Ctrl Pts',(-189.252033752309,-2.59138767507411,
125.485277944776));
#167105=CARTESIAN_POINT('Ctrl Pts',(-189.244619259588,-2.45028284644415,
125.416533513396));
#167106=CARTESIAN_POINT('Ctrl Pts',(-189.237204766867,-2.30626214089305,
125.353320849256));
#167107=CARTESIAN_POINT('Ctrl Pts',(-189.229790274146,-2.15979953319767,
125.295894720522));
#167108=CARTESIAN_POINT('Ctrl Pts',(-189.222382927793,-2.01347809167781,
125.238523941253));
#167109=CARTESIAN_POINT('Ctrl Pts',(-189.214975581439,-1.86471977876785,
125.186928729472));
#167110=CARTESIAN_POINT('Ctrl Pts',(-189.207568235085,-1.71402172957951,
125.141317259704));
#167111=CARTESIAN_POINT('Ctrl Pts',(-189.20016641341,-1.56343607668177,
125.09573980869));
#167112=CARTESIAN_POINT('Ctrl Pts',(-189.192764591734,-1.4109139238907,
125.056137321127));
#167113=CARTESIAN_POINT('Ctrl Pts',(-189.185362770059,-1.25697077751556,
125.022669253703));
#167114=CARTESIAN_POINT('Ctrl Pts',(-189.177964855747,-1.10310889652911,
124.989218853811));
#167115=CARTESIAN_POINT('Ctrl Pts',(-189.170566941436,-0.94782787973478,
124.961896503906));
#167116=CARTESIAN_POINT('Ctrl Pts',(-189.163169027125,-0.791656622585064,
124.940811320901));
#167117=CARTESIAN_POINT('Ctrl Pts',(-189.155772342213,-0.635511318265274,
124.919729641871));
#167118=CARTESIAN_POINT('Ctrl Pts',(-189.1483756573,-0.478476436789943,
124.904883122484));
#167119=CARTESIAN_POINT('Ctrl Pts',(-189.140978972388,-0.321089372926129,
124.896329458449));
#167120=CARTESIAN_POINT('Ctrl Pts',(-189.133582615453,-0.163709287769656,
124.887776173693));
#167121=CARTESIAN_POINT('Ctrl Pts',(-189.126186258517,-0.00597742402233353,
124.885515209737));
#167122=CARTESIAN_POINT('Ctrl Pts',(-189.118789901582,0.151565685768833,
124.889552217846));
#167123=CARTESIAN_POINT('Ctrl Pts',(-189.111392412245,0.309132915812747,
124.893589844031));
#167124=CARTESIAN_POINT('Ctrl Pts',(-189.103994922909,0.466510961159943,
124.90392735264));
#167125=CARTESIAN_POINT('Ctrl Pts',(-189.096597433572,0.623161427596432,
124.920518301727));
#167126=CARTESIAN_POINT('Ctrl Pts',(-189.089197351057,0.779866807610867,
124.937115066746));
#167127=CARTESIAN_POINT('Ctrl Pts',(-189.081797268542,0.935843729918489,
124.959969597473));
#167128=CARTESIAN_POINT('Ctrl Pts',(-189.074397186027,1.09056119090591,
124.988983858371));
#167129=CARTESIAN_POINT('Ctrl Pts',(-189.06698896636,1.24544877964724,125.018030023431));
#167130=CARTESIAN_POINT('Ctrl Pts',(-189.059580746694,1.39907377419055,
125.053249376451));
#167131=CARTESIAN_POINT('Ctrl Pts',(-189.052172527027,1.55091687890397,
125.094493071184));
#167132=CARTESIAN_POINT('Ctrl Pts',(-189.044759747725,1.7028534405147,125.135762150722));
#167133=CARTESIAN_POINT('Ctrl Pts',(-189.037346968423,1.85300557171295,
125.183062848489));
#167134=CARTESIAN_POINT('Ctrl Pts',(-189.029934189121,2.00087180686703,
125.236197314017));
#167135=CARTESIAN_POINT('Ctrl Pts',(-189.022510818092,2.14894932023193,
125.289407700562));
#167136=CARTESIAN_POINT('Ctrl Pts',(-189.015087447064,2.29473406916035,
125.348468363057));
#167137=CARTESIAN_POINT('Ctrl Pts',(-189.007664076035,2.43774637222091,
125.413134116368));
#167138=CARTESIAN_POINT('Ctrl Pts',(-189.003728026594,2.5135749268355,125.447421450406));
#167139=CARTESIAN_POINT('Ctrl Pts',(-188.999791977153,2.58862447664729,
125.483283818407));
#167140=CARTESIAN_POINT('Ctrl Pts',(-188.995855927713,2.66282671449517,
125.520679660972));
#167141=CARTESIAN_POINT('Ctrl Pts',(-188.988432661307,2.80276981930618,
125.591207052967));
#167142=CARTESIAN_POINT('Ctrl Pts',(-188.981009394902,2.94012062552616,
125.667404711676));
#167143=CARTESIAN_POINT('Ctrl Pts',(-188.973586128496,3.07438656032618,
125.749058664153));
#167144=CARTESIAN_POINT('Ctrl Pts',(-188.966171635775,3.20849380394173,
125.830616108438));
#167145=CARTESIAN_POINT('Ctrl Pts',(-188.958757143054,3.33952311781041,
125.917616817874));
#167146=CARTESIAN_POINT('Ctrl Pts',(-188.951342650333,3.46700396331473,
126.009799732473));
#167147=CARTESIAN_POINT('Ctrl Pts',(-188.943935303979,3.59436193798021,
126.101893797708));
#167148=CARTESIAN_POINT('Ctrl Pts',(-188.936527957626,3.71817795265517,
126.199159907163));
#167149=CARTESIAN_POINT('Ctrl Pts',(-188.929120611272,3.83800815054602,
126.301292330404));
#167150=CARTESIAN_POINT('Ctrl Pts',(-188.921718789596,3.95774897455468,
126.403348579431));
#167151=CARTESIAN_POINT('Ctrl Pts',(-188.914316967921,4.07350961808697,
126.510263674354));
#167152=CARTESIAN_POINT('Ctrl Pts',(-188.906915146246,4.1848772819624,126.62169009535));
#167153=CARTESIAN_POINT('Ctrl Pts',(-188.899517231934,4.29618615571496,
126.733057695206));
#167154=CARTESIAN_POINT('Ctrl Pts',(-188.892119317623,4.40310640502578,
126.848931614914));
#167155=CARTESIAN_POINT('Ctrl Pts',(-188.884721403311,4.50526034583612,
126.968925860105));
#167156=CARTESIAN_POINT('Ctrl Pts',(-188.877324718399,4.60739731051461,
127.08890016443));
#167157=CARTESIAN_POINT('Ctrl Pts',(-188.869928033487,4.70476929697789,
127.2129931513));
#167158=CARTESIAN_POINT('Ctrl Pts',(-188.862531348575,4.79703728919411,
127.340783881217));
#167159=CARTESIAN_POINT('Ctrl Pts',(-188.855134991639,4.88930119015086,
127.468568944758));
#167160=CARTESIAN_POINT('Ctrl Pts',(-188.847738634704,4.97646132833132,
127.600051122683));
#167161=CARTESIAN_POINT('Ctrl Pts',(-188.840342277768,5.05822077812171,
127.734778704295));
#167162=CARTESIAN_POINT('Ctrl Pts',(-188.832944788432,5.13999274549259,
127.869526913045));
#167163=CARTESIAN_POINT('Ctrl Pts',(-188.825547299095,5.21636218440918,
128.007521195684));
#167164=CARTESIAN_POINT('Ctrl Pts',(-188.818149809759,5.28707715257132,
128.148283482907));
#167165=CARTESIAN_POINT('Ctrl Pts',(-188.810749727244,5.35781690975603,
128.289095114132));
#167166=CARTESIAN_POINT('Ctrl Pts',(-188.803349644729,5.42289808223647,
128.432676348477));
#167167=CARTESIAN_POINT('Ctrl Pts',(-188.795949562214,5.48211612966465,
128.57852744696));
#167168=CARTESIAN_POINT('Ctrl Pts',(-188.788541342547,5.54139929342365,
128.724538923719));
#167169=CARTESIAN_POINT('Ctrl Pts',(-188.781133122881,5.59480631631315,
128.872824903103));
#167170=CARTESIAN_POINT('Ctrl Pts',(-188.773724903214,5.64218173492415,
129.022868031955));
#167171=CARTESIAN_POINT('Ctrl Pts',(-188.766312123912,5.68958631231479,
129.173003509849));
#167172=CARTESIAN_POINT('Ctrl Pts',(-188.75889934461,5.73095179023987,129.324897932882));
#167173=CARTESIAN_POINT('Ctrl Pts',(-188.751486565308,5.76617357147899,
129.478022460806));
#167174=CARTESIAN_POINT('Ctrl Pts',(-188.744063194279,5.80144567925094,
129.631365780237));
#167175=CARTESIAN_POINT('Ctrl Pts',(-188.73663982325,5.83055648899496,129.785942349065));
#167176=CARTESIAN_POINT('Ctrl Pts',(-188.729216452221,5.85345300237912,
129.941216069162));
#167177=CARTESIAN_POINT('Ctrl Pts',(-188.725280402781,5.86559328316901,
130.023545921295));
#167178=CARTESIAN_POINT('Ctrl Pts',(-188.72134435334,5.8759873721544,130.106071718954));
#167179=CARTESIAN_POINT('Ctrl Pts',(-188.7174083039,5.88463331274603,130.18871352952));
#167180=CARTESIAN_POINT('Ctrl Pts',(-188.709985037494,5.90093928687214,
130.344573405092));
#167181=CARTESIAN_POINT('Ctrl Pts',(-188.702561771089,5.91107350431225,
130.501317224105));
#167182=CARTESIAN_POINT('Ctrl Pts',(-188.695138504683,5.91494973892084,
130.658414913483));
#167183=CARTESIAN_POINT('Ctrl Pts',(-188.687724011962,5.91882139214203,
130.815326926438));
#167184=CARTESIAN_POINT('Ctrl Pts',(-188.680309519241,5.91644977602051,
130.972591607699));
#167185=CARTESIAN_POINT('Ctrl Pts',(-188.67289502652,5.90780019010058,131.1296719705));
#167186=CARTESIAN_POINT('Ctrl Pts',(-188.665487680167,5.89915894097722,
131.286600933333));
#167187=CARTESIAN_POINT('Ctrl Pts',(-188.658080333813,5.88425178867966,
131.443345561147));
#167188=CARTESIAN_POINT('Ctrl Pts',(-188.650672987459,5.86309603744215,
131.599367169885));
#167189=CARTESIAN_POINT('Ctrl Pts',(-188.643271165784,5.84195606496208,
131.75527241182));
#167190=CARTESIAN_POINT('Ctrl Pts',(-188.635869344108,5.81457682305113,
131.910455340087));
#167191=CARTESIAN_POINT('Ctrl Pts',(-188.628467522433,5.78102756193813,
132.064380812091));
#167192=CARTESIAN_POINT('Ctrl Pts',(-188.621069608122,5.74749601121893,
132.218225028037));
#167193=CARTESIAN_POINT('Ctrl Pts',(-188.61367169381,5.70780100727417,132.3708127459));
#167194=CARTESIAN_POINT('Ctrl Pts',(-188.606273779499,5.66206315063794,
132.521617570001));
#167195=CARTESIAN_POINT('Ctrl Pts',(-188.598877094587,5.61633289480377,
132.672397333077));
#167196=CARTESIAN_POINT('Ctrl Pts',(-188.591480409675,5.56456188758136,
132.821394433549));
#167197=CARTESIAN_POINT('Ctrl Pts',(-188.584083724762,5.50692103084546,
132.968096119547));
#167198=CARTESIAN_POINT('Ctrl Pts',(-188.576687367827,5.44928272996555,
133.114791300639));
#167199=CARTESIAN_POINT('Ctrl Pts',(-188.569291010892,5.38577523360099,
133.259190922191));
#167200=CARTESIAN_POINT('Ctrl Pts',(-188.561894653956,5.3166180832047,133.400801011613));
#167201=CARTESIAN_POINT('Ctrl Pts',(-188.55449716462,5.24745034467193,133.542432781902));
#167202=CARTESIAN_POINT('Ctrl Pts',(-188.547099675283,5.17263139364863,
133.681273834221));
#167203=CARTESIAN_POINT('Ctrl Pts',(-188.539702185946,5.09242726241424,
133.816853794242));
#167204=CARTESIAN_POINT('Ctrl Pts',(-188.532302103431,5.0121950157461,133.952481281607));
#167205=CARTESIAN_POINT('Ctrl Pts',(-188.524902020916,4.92657402028228,
134.084845079539));
#167206=CARTESIAN_POINT('Ctrl Pts',(-188.517501938401,4.83587416152764,
134.213502981324));
#167207=CARTESIAN_POINT('Ctrl Pts',(-188.510093718735,4.74507456895399,
134.342302355698));
#167208=CARTESIAN_POINT('Ctrl Pts',(-188.502685499068,4.64918517523304,
134.467387390564));
#167209=CARTESIAN_POINT('Ctrl Pts',(-188.495277279402,4.54855721245665,
134.588347648134));
#167210=CARTESIAN_POINT('Ctrl Pts',(-188.4878645001,4.44786731484825,134.709382354725));
#167211=CARTESIAN_POINT('Ctrl Pts',(-188.480451720798,4.34243328610366,
134.826286948712));
#167212=CARTESIAN_POINT('Ctrl Pts',(-188.473038941496,4.23264351714947,
134.938687578419));
#167213=CARTESIAN_POINT('Ctrl Pts',(-188.465615570467,4.12269687542492,
135.051248811416));
#167214=CARTESIAN_POINT('Ctrl Pts',(-188.458192199438,4.00838233397257,
135.159292971309));
#167215=CARTESIAN_POINT('Ctrl Pts',(-188.45076882841,3.89012228043788,135.262485694966));
#167216=CARTESIAN_POINT('Ctrl Pts',(-188.446832778969,3.82741796243955,
135.317200953127));
#167217=CARTESIAN_POINT('Ctrl Pts',(-188.442896729528,3.76360493059685,
135.370553004011));
#167218=CARTESIAN_POINT('Ctrl Pts',(-188.438960680087,3.69874937690234,
135.422496995951));
#167219=CARTESIAN_POINT('Ctrl Pts',(-188.431537413681,3.57643382671275,
135.520461743629));
#167220=CARTESIAN_POINT('Ctrl Pts',(-188.424114147276,3.45003860462953,
135.613711810634));
#167221=CARTESIAN_POINT('Ctrl Pts',(-188.41669088087,3.31996306880589,135.701888135025));
#167222=CARTESIAN_POINT('Ctrl Pts',(-188.409276388149,3.1900412714635,135.789960242322));
#167223=CARTESIAN_POINT('Ctrl Pts',(-188.401861895428,3.05644812470781,
135.872970336136));
#167224=CARTESIAN_POINT('Ctrl Pts',(-188.394447402707,2.91961665426848,
135.950598967528));
#167225=CARTESIAN_POINT('Ctrl Pts',(-188.387040056353,2.78291706715196,
136.028152777522));
#167226=CARTESIAN_POINT('Ctrl Pts',(-188.37963271,2.64298569258825,136.100335268136));
#167227=CARTESIAN_POINT('Ctrl Pts',(-188.372225363646,2.50028509409351,
136.16686982602));
#167228=CARTESIAN_POINT('Ctrl Pts',(-188.36482354197,2.35769092708891,136.233354759921));
#167229=CARTESIAN_POINT('Ctrl Pts',(-188.357421720295,2.2123319855006,136.294199991563));
#167230=CARTESIAN_POINT('Ctrl Pts',(-188.35001989862,2.06469593138949,136.349174525481));
#167231=CARTESIAN_POINT('Ctrl Pts',(-188.342621984308,1.91713781320257,
136.40412003877));
#167232=CARTESIAN_POINT('Ctrl Pts',(-188.335224069997,1.76730532541907,
136.453200896397));
#167233=CARTESIAN_POINT('Ctrl Pts',(-188.327826155686,1.61570652716677,
136.496234033285));
#167234=CARTESIAN_POINT('Ctrl Pts',(-188.320429470773,1.46413292188381,
136.539260018847));
#167235=CARTESIAN_POINT('Ctrl Pts',(-188.313032785861,1.31079394745819,
136.576240176501));
#167236=CARTESIAN_POINT('Ctrl Pts',(-188.305636100949,1.15621337319739,
136.607041135925));
#167237=CARTESIAN_POINT('Ctrl Pts',(-188.298239744013,1.00163965320169,
136.637840729602));
#167238=CARTESIAN_POINT('Ctrl Pts',(-188.290843387078,0.845824808937177,
136.662461596891));
#167239=CARTESIAN_POINT('Ctrl Pts',(-188.283447030143,0.689303101053426,
136.680821439981));
#167240=CARTESIAN_POINT('Ctrl Pts',(-188.276049540806,0.53275742929617,
136.69918409401));
#167241=CARTESIAN_POINT('Ctrl Pts',(-188.268652051469,0.375505049213833,
136.711283771691));
#167242=CARTESIAN_POINT('Ctrl Pts',(-188.261254562133,0.21808549699706,
136.7170900447));
#167243=CARTESIAN_POINT('Ctrl Pts',(-188.253854479618,0.060610761600514,
136.722898353089));
#167244=CARTESIAN_POINT('Ctrl Pts',(-188.246454397103,-0.0970308897949569,
136.72240885064));
#167245=CARTESIAN_POINT('Ctrl Pts',(-188.239054314588,-0.254299915471865,
136.715643229275));
#167246=CARTESIAN_POINT('Ctrl Pts',(-188.231646094921,-0.411741874610377,
136.708870168413));
#167247=CARTESIAN_POINT('Ctrl Pts',(-188.224237875255,-0.568810016570274,
136.695807222463));
#167248=CARTESIAN_POINT('Ctrl Pts',(-188.216829655588,-0.724969178892556,
136.676528041282));
#167249=CARTESIAN_POINT('Ctrl Pts',(-188.209416876286,-0.881224454573593,
136.657236994087));
#167250=CARTESIAN_POINT('Ctrl Pts',(-188.202004096984,-1.03656926831098,
136.631722148261));
#167251=CARTESIAN_POINT('Ctrl Pts',(-188.194591317682,-1.19047915331876,
136.600108192126));
#167252=CARTESIAN_POINT('Ctrl Pts',(-188.187167946653,-1.34460895198768,
136.568449064488));
#167253=CARTESIAN_POINT('Ctrl Pts',(-188.179744575625,-1.49729936561825,
136.530673510755));
#167254=CARTESIAN_POINT('Ctrl Pts',(-188.172321204596,-1.648040774199,136.486956166176));
#167255=CARTESIAN_POINT('Ctrl Pts',(-188.168385155155,-1.72796748601767,
136.463776181097));
#167256=CARTESIAN_POINT('Ctrl Pts',(-188.164449105714,-1.80734657986099,
136.438926556829));
#167257=CARTESIAN_POINT('Ctrl Pts',(-188.160513056274,-1.88610454236212,
136.412438739149));
#167258=CARTESIAN_POINT('Ctrl Pts',(-188.153089789868,-2.03463960169,136.36248354166));
#167259=CARTESIAN_POINT('Ctrl Pts',(-188.145666523463,-2.18141322895194,
136.306547600599));
#167260=CARTESIAN_POINT('Ctrl Pts',(-188.138243257057,-2.32590747232902,
136.244772825539));
#167261=CARTESIAN_POINT('Ctrl Pts',(-188.130828764336,-2.47023093550992,
136.183071063134));
#167262=CARTESIAN_POINT('Ctrl Pts',(-188.123414271615,-2.61228003741925,
136.115544348554));
#167263=CARTESIAN_POINT('Ctrl Pts',(-188.115999778894,-2.75155195563308,
136.042384328657));
#167264=CARTESIAN_POINT('Ctrl Pts',(-188.10859243254,-2.89068963832824,
135.969294823142));
#167265=CARTESIAN_POINT('Ctrl Pts',(-188.101185086187,-3.02705513796119,
135.890582993991));
#167266=CARTESIAN_POINT('Ctrl Pts',(-188.093777739833,-3.16016570500775,
135.80648849272));
#167267=CARTESIAN_POINT('Ctrl Pts',(-188.086375918158,-3.29317699317143,
135.722456712301));
#167268=CARTESIAN_POINT('Ctrl Pts',(-188.078974096482,-3.42293786829595,
135.633050451894));
#167269=CARTESIAN_POINT('Ctrl Pts',(-188.071572274807,-3.5489903940987,
135.53855513671));
#167270=CARTESIAN_POINT('Ctrl Pts',(-188.064174360495,-3.67497637775464,
135.444109704868));
#167271=CARTESIAN_POINT('Ctrl Pts',(-188.056776446184,-3.79725761282802,
135.344580791833));
#167272=CARTESIAN_POINT('Ctrl Pts',(-188.049378531873,-3.91540546311575,
135.240296890993));
#167273=CARTESIAN_POINT('Ctrl Pts',(-188.041981846961,-4.03353367937402,
135.136030320245));
#167274=CARTESIAN_POINT('Ctrl Pts',(-188.034585162048,-4.1475295945303,
135.027010576778));
#167275=CARTESIAN_POINT('Ctrl Pts',(-188.027188477136,-4.2569978902504,
134.913606232628));
#167276=CARTESIAN_POINT('Ctrl Pts',(-188.019792120201,-4.36646133203156,
134.800206916945));
#167277=CARTESIAN_POINT('Ctrl Pts',(-188.012395763265,-4.4713972942949,
134.682423655727));
#167278=CARTESIAN_POINT('Ctrl Pts',(-188.00499940633,-4.5714477566311,134.560661453614));
#167279=CARTESIAN_POINT('Ctrl Pts',(-187.997601916993,-4.67151353694821,
134.438880609397));
#167280=CARTESIAN_POINT('Ctrl Pts',(-187.990204427657,-4.76669209099886,
134.313119899753));
#167281=CARTESIAN_POINT('Ctrl Pts',(-187.98280693832,-4.85666618608259,
134.183816804508));
#167282=CARTESIAN_POINT('Ctrl Pts',(-187.975406855805,-4.94667182144627,
134.054468382263));
#167283=CARTESIAN_POINT('Ctrl Pts',(-187.96800677329,-5.03146915236339,
133.92157540827));
#167284=CARTESIAN_POINT('Ctrl Pts',(-187.960606690775,-5.11078479338413,
133.785603539271));
#167285=CARTESIAN_POINT('Ctrl Pts',(-187.953198471109,-5.19018765010589,
133.649482155223));
#167286=CARTESIAN_POINT('Ctrl Pts',(-187.945790251442,-5.26409659104829,
133.510275437626));
#167287=CARTESIAN_POINT('Ctrl Pts',(-187.938382031776,-5.3322843115409,
133.368473443359));
#167288=CARTESIAN_POINT('Ctrl Pts',(-187.930969252474,-5.40051400043771,
133.226584172331));
#167289=CARTESIAN_POINT('Ctrl Pts',(-187.923556473172,-5.46301530435872,
133.082096783536));
#167290=CARTESIAN_POINT('Ctrl Pts',(-187.91614369387,-5.51960964001329,
132.93551992282));
#167291=CARTESIAN_POINT('Ctrl Pts',(-187.908720322841,-5.57628484030872,
132.788733626212));
#167292=CARTESIAN_POINT('Ctrl Pts',(-187.901296951812,-5.62703609533202,
132.639852247296));
#167293=CARTESIAN_POINT('Ctrl Pts',(-187.893873580783,-5.67173486859993,
132.489398938438));
#167294=CARTESIAN_POINT('Ctrl Pts',(-187.889937531343,-5.6954352307193,
132.409624984003));
#167295=CARTESIAN_POINT('Ctrl Pts',(-187.886001481902,-5.71743487721036,
132.329409275315));
#167296=CARTESIAN_POINT('Ctrl Pts',(-187.882065432461,-5.73772052852476,
132.248830658462));
#167297=CARTESIAN_POINT('Ctrl Pts',(-187.872272656446,-5.78819063633813,
132.048353413881));
#167298=CARTESIAN_POINT('Ctrl Pts',(-187.862479880431,-5.82817280781611,
131.845137610024));
#167299=CARTESIAN_POINT('Ctrl Pts',(-187.852687104416,-5.85742459265489,
131.640128350768));
#167300=CARTESIAN_POINT('Ctrl Pts',(-187.843111607346,-5.88602734836112,
131.43966777059));
#167301=CARTESIAN_POINT('Ctrl Pts',(-187.833536110275,-5.90437066060156,
131.237492158579));
#167302=CARTESIAN_POINT('Ctrl Pts',(-187.823960613204,-5.91227224031638,
131.034507350944));
#167303=CARTESIAN_POINT('Ctrl Pts',(-187.820432147727,-5.915183885637,130.959709679258));
#167304=CARTESIAN_POINT('Ctrl Pts',(-187.81690368225,-5.91667814734567,
130.88480237372));
#167305=CARTESIAN_POINT('Ctrl Pts',(-187.813375216773,-5.91674747054566,
130.809831658736));
#167306=CARTESIAN_POINT('',(-186.063375192208,-5.90709598019638,130.803332506185));
#167307=CARTESIAN_POINT('Ctrl Pts',(-187.813375192208,-5.91590714834001,
130.809830359851));
#167308=CARTESIAN_POINT('Ctrl Pts',(-187.743456064355,-5.90233112363404,
129.324427893846));
#167309=CARTESIAN_POINT('Ctrl Pts',(-187.580721061896,-4.58174601807203,
125.845682237925));
#167310=CARTESIAN_POINT('Ctrl Pts',(-187.325170184835,1.26703804199676,
123.92161587942));
#167311=CARTESIAN_POINT('Ctrl Pts',(-187.046722561023,6.47551308848548,
128.150063955324));
#167312=CARTESIAN_POINT('Ctrl Pts',(-186.768274937209,5.73330795305963,
134.817680994228));
#167313=CARTESIAN_POINT('Ctrl Pts',(-186.489827313397,-0.277527103565456,
137.797252668579));
#167314=CARTESIAN_POINT('Ctrl Pts',(-186.254860731729,-5.1345300677341,
134.88889554915));
#167315=CARTESIAN_POINT('Ctrl Pts',(-186.112710024666,-5.90546980125088,
131.855374257204));
#167316=CARTESIAN_POINT('Ctrl Pts',(-186.063375192208,-5.90709598019638,
130.803332506185));
#167317=CARTESIAN_POINT('',(-184.313376079986,-5.91869333543885,130.799262689142));
#167318=CARTESIAN_POINT('Ctrl Pts',(-186.063375192208,-5.90709598019638,
130.803332506185));
#167319=CARTESIAN_POINT('Ctrl Pts',(-186.019894150062,-5.90852920600748,
129.876120039144));
#167320=CARTESIAN_POINT('Ctrl Pts',(-185.883597233311,-5.26549744303905,
126.971533866971));
#167321=CARTESIAN_POINT('Ctrl Pts',(-185.654484441958,-0.717600748298859,
123.842851463917));
#167322=CARTESIAN_POINT('Ctrl Pts',(-185.376036818144,5.46903407832205,
126.437757042646));
#167323=CARTESIAN_POINT('Ctrl Pts',(-185.097589194332,6.62989376413611,
133.045357986287));
#167324=CARTESIAN_POINT('Ctrl Pts',(-184.819141570519,1.69820496902565,
137.593591826879));
#167325=CARTESIAN_POINT('Ctrl Pts',(-184.557737350984,-4.39666896695656,
136.006341653894));
#167326=CARTESIAN_POINT('Ctrl Pts',(-184.389149006053,-5.90500976629783,
132.406387652391));
#167327=CARTESIAN_POINT('Ctrl Pts',(-184.313376535726,-5.91969208008458,
130.799271491783));
#167328=CARTESIAN_POINT('',(-182.56337376072,-5.92087641190242,130.807755266905));
#167329=CARTESIAN_POINT('Ctrl Pts',(-184.313375192208,-5.91674778898835,
130.799245541667));
#167330=CARTESIAN_POINT('Ctrl Pts',(-184.30222306504,-5.91654340696533,
130.56283128179));
#167331=CARTESIAN_POINT('Ctrl Pts',(-184.291070937872,-5.90216644403423,
130.327006005632));
#167332=CARTESIAN_POINT('Ctrl Pts',(-184.279918810703,-5.87384581741895,
130.093118130302));
#167333=CARTESIAN_POINT('Ctrl Pts',(-184.274027981434,-5.85888616230683,
129.969572772447));
#167334=CARTESIAN_POINT('Ctrl Pts',(-184.268137152164,-5.84003663158251,
129.846567305077));
#167335=CARTESIAN_POINT('Ctrl Pts',(-184.262246322894,-5.81733560061832,
129.724297160042));
#167336=CARTESIAN_POINT('Ctrl Pts',(-184.254823056489,-5.78872913575387,
129.570219725698));
#167337=CARTESIAN_POINT('Ctrl Pts',(-184.247399790083,-5.75395386469645,
129.417046595923));
#167338=CARTESIAN_POINT('Ctrl Pts',(-184.239976523677,-5.71307757234325,
129.265310516079));
#167339=CARTESIAN_POINT('Ctrl Pts',(-184.232562030956,-5.67224959237304,
129.11375377568));
#167340=CARTESIAN_POINT('Ctrl Pts',(-184.225147538235,-5.6253350405974,
128.963631061319));
#167341=CARTESIAN_POINT('Ctrl Pts',(-184.217733045514,-5.5724530706871,
128.815467121803));
#167342=CARTESIAN_POINT('Ctrl Pts',(-184.21032569916,-5.51962207041052,
128.66744598827));
#167343=CARTESIAN_POINT('Ctrl Pts',(-184.202918352807,-5.46083522698721,
128.521380220278));
#167344=CARTESIAN_POINT('Ctrl Pts',(-184.195511006453,-5.39626204145504,
128.377781432282));
#167345=CARTESIAN_POINT('Ctrl Pts',(-184.188109184777,-5.33173701704084,
128.23428974568));
#167346=CARTESIAN_POINT('Ctrl Pts',(-184.180707363102,-5.26143439604173,
128.093261714445));
#167347=CARTESIAN_POINT('Ctrl Pts',(-184.173305541426,-5.18557248352986,
127.955190812069));
#167348=CARTESIAN_POINT('Ctrl Pts',(-184.165907627115,-5.1097506179311,
127.817192796247));
#167349=CARTESIAN_POINT('Ctrl Pts',(-184.158509712804,-5.02837548473259,
127.682149126725));
#167350=CARTESIAN_POINT('Ctrl Pts',(-184.151111798492,-4.94171214425669,
127.550530313785));
#167351=CARTESIAN_POINT('Ctrl Pts',(-184.14371511358,-4.85506320565538,
127.418933373503));
#167352=CARTESIAN_POINT('Ctrl Pts',(-184.136318428668,-4.76312800903145,
127.290760471687));
#167353=CARTESIAN_POINT('Ctrl Pts',(-184.128921743756,-4.66621597412815,
127.166454757694));
#167354=CARTESIAN_POINT('Ctrl Pts',(-184.12152538682,-4.56930823640603,
127.042154555547));
#167355=CARTESIAN_POINT('Ctrl Pts',(-184.114129029885,-4.46742432870891,
126.921721494671));
#167356=CARTESIAN_POINT('Ctrl Pts',(-184.106732672949,-4.36091497905957,
126.80556691097));
#167357=CARTESIAN_POINT('Ctrl Pts',(-184.099335183613,-4.25438932255719,
126.689394543706));
#167358=CARTESIAN_POINT('Ctrl Pts',(-184.091937694276,-4.14323706635495,
126.577502233055));
#167359=CARTESIAN_POINT('Ctrl Pts',(-184.084540204939,-4.02784681849153,
126.470265490637));
#167360=CARTESIAN_POINT('Ctrl Pts',(-184.077140122424,-3.91241612075543,
126.362991156545));
#167361=CARTESIAN_POINT('Ctrl Pts',(-184.069740039909,-3.79274474677175,
126.260375893956));
#167362=CARTESIAN_POINT('Ctrl Pts',(-184.062339957394,-3.66925535844911,
126.1627557575));
#167363=CARTESIAN_POINT('Ctrl Pts',(-184.054931737728,-3.54563018084883,
126.065028277668));
#167364=CARTESIAN_POINT('Ctrl Pts',(-184.047523518061,-3.41817889765681,
125.972307124804));
#167365=CARTESIAN_POINT('Ctrl Pts',(-184.040115298395,-3.28735479886558,
125.884886154895));
#167366=CARTESIAN_POINT('Ctrl Pts',(-184.032702519093,-3.15645018002447,
125.797411378838));
#167367=CARTESIAN_POINT('Ctrl Pts',(-184.025289739791,-3.02216892674676,
125.715243480416));
#167368=CARTESIAN_POINT('Ctrl Pts',(-184.017876960489,-2.88498957422633,
125.638630686655));
#167369=CARTESIAN_POINT('Ctrl Pts',(-184.01045358946,-2.74761421341414,
125.561908424942));
#167370=CARTESIAN_POINT('Ctrl Pts',(-184.003030218431,-2.60733281501413,
125.490757289058));
#167371=CARTESIAN_POINT('Ctrl Pts',(-183.995606847402,-2.46464530350015,
125.425377991601));
#167372=CARTESIAN_POINT('Ctrl Pts',(-183.991670797962,-2.38898896116109,
125.390712319337));
#167373=CARTESIAN_POINT('Ctrl Pts',(-183.987734748521,-2.31265646397017,
125.357668496352));
#167374=CARTESIAN_POINT('Ctrl Pts',(-183.983798699081,-2.23572401264854,
125.326270740449));
#167375=CARTESIAN_POINT('Ctrl Pts',(-183.976375432675,-2.09063181042523,
125.267055552704));
#167376=CARTESIAN_POINT('Ctrl Pts',(-183.96895216627,-1.94296603481777,
125.213519155027));
#167377=CARTESIAN_POINT('Ctrl Pts',(-183.961528899864,-1.79321153898064,
125.165892479945));
#167378=CARTESIAN_POINT('Ctrl Pts',(-183.954114407143,-1.64363404052125,
125.118322095638));
#167379=CARTESIAN_POINT('Ctrl Pts',(-183.946699914422,-1.49197308804768,
125.076647642673));
#167380=CARTESIAN_POINT('Ctrl Pts',(-183.939285421701,-1.33873457306213,
125.04105251324));
#167381=CARTESIAN_POINT('Ctrl Pts',(-183.931878075348,-1.18564375512665,
125.005491691733));
#167382=CARTESIAN_POINT('Ctrl Pts',(-183.924470728994,-1.03097876289946,
124.975998612581));
#167383=CARTESIAN_POINT('Ctrl Pts',(-183.91706338264,-0.875261651561804,
124.95270720987));
#167384=CARTESIAN_POINT('Ctrl Pts',(-183.909661560965,-0.71966067992065,
124.929433178765));
#167385=CARTESIAN_POINT('Ctrl Pts',(-183.902259739289,-0.563009519234663,
124.912351669202));
#167386=CARTESIAN_POINT('Ctrl Pts',(-183.894857917614,-0.405841341951333,
124.901545749415));
#167387=CARTESIAN_POINT('Ctrl Pts',(-183.887460003302,-0.248756132525396,
124.890745533989));
#167388=CARTESIAN_POINT('Ctrl Pts',(-183.880062088991,-0.091154821529368,
124.886214336211));
#167389=CARTESIAN_POINT('Ctrl Pts',(-183.87266417468,0.066423465832265,
124.887983475625));
#167390=CARTESIAN_POINT('Ctrl Pts',(-183.865267489768,0.223975566541075,
124.889752321039));
#167391=CARTESIAN_POINT('Ctrl Pts',(-183.857870804855,0.38150427830029,
124.89781942147));
#167392=CARTESIAN_POINT('Ctrl Pts',(-183.850474119943,0.538469518075691,
124.912163986376));
#167393=CARTESIAN_POINT('Ctrl Pts',(-183.843077763008,0.695427797847872,
124.92650791523));
#167394=CARTESIAN_POINT('Ctrl Pts',(-183.835681406072,0.851822283566282,
124.947128721133));
#167395=CARTESIAN_POINT('Ctrl Pts',(-183.828285049137,1.00711732962266,
124.97395366377));
#167396=CARTESIAN_POINT('Ctrl Pts',(-183.8208875598,1.16243615174704,125.000782713374));
#167397=CARTESIAN_POINT('Ctrl Pts',(-183.813490070464,1.31665483117389,
125.033817727484));
#167398=CARTESIAN_POINT('Ctrl Pts',(-183.806092581127,1.46924738720576,
125.072934732353));
#167399=CARTESIAN_POINT('Ctrl Pts',(-183.798692498612,1.6218934343218,125.112065449627));
#167400=CARTESIAN_POINT('Ctrl Pts',(-183.791292416097,1.77291186172737,
125.157282309882));
#167401=CARTESIAN_POINT('Ctrl Pts',(-183.783892333582,1.92179147805772,
125.20841136142));
#167402=CARTESIAN_POINT('Ctrl Pts',(-183.776484113915,2.07083480283121,
125.259596634606));
#167403=CARTESIAN_POINT('Ctrl Pts',(-183.769075894249,2.21773426647063,
125.316706960799));
#167404=CARTESIAN_POINT('Ctrl Pts',(-183.761667674582,2.3619976252977,125.379519810631));
#167405=CARTESIAN_POINT('Ctrl Pts',(-183.75425489528,2.50634977581538,125.442371320724));
#167406=CARTESIAN_POINT('Ctrl Pts',(-183.746842115978,2.64806225327137,
125.510932185989));
#167407=CARTESIAN_POINT('Ctrl Pts',(-183.739429336676,2.7866675572784,125.584933973986));
#167408=CARTESIAN_POINT('Ctrl Pts',(-183.732005965648,2.92547090704354,
125.659041499208));
#167409=CARTESIAN_POINT('Ctrl Pts',(-183.724582594619,3.06115789516633,
125.738605285748));
#167410=CARTESIAN_POINT('Ctrl Pts',(-183.71715922359,3.19328943506455,125.823313223051));
#167411=CARTESIAN_POINT('Ctrl Pts',(-183.713223174149,3.26334874797098,
125.868227403948));
#167412=CARTESIAN_POINT('Ctrl Pts',(-183.709287124708,3.33240903135922,
125.914587102222));
#167413=CARTESIAN_POINT('Ctrl Pts',(-183.705351075268,3.40040872175365,
125.962341298364));
#167414=CARTESIAN_POINT('Ctrl Pts',(-183.697927808862,3.52865401564075,
126.052404221932));
#167415=CARTESIAN_POINT('Ctrl Pts',(-183.690504542457,3.65351266188925,
126.147701890419));
#167416=CARTESIAN_POINT('Ctrl Pts',(-183.683081276051,3.77452829544996,
126.247951207806));
#167417=CARTESIAN_POINT('Ctrl Pts',(-183.67566678333,3.89540089858187,126.348082038826));
#167418=CARTESIAN_POINT('Ctrl Pts',(-183.668252290609,4.01243924548009,
126.453152633621));
#167419=CARTESIAN_POINT('Ctrl Pts',(-183.660837797888,4.12521559638735,
126.562836499301));
#167420=CARTESIAN_POINT('Ctrl Pts',(-183.653430451534,4.23788324920132,
126.672414647542));
#167421=CARTESIAN_POINT('Ctrl Pts',(-183.646023105181,4.34629681818062,
126.786596956152));
#167422=CARTESIAN_POINT('Ctrl Pts',(-183.638615758827,4.45006143720835,
126.905016599969));
#167423=CARTESIAN_POINT('Ctrl Pts',(-183.631213937151,4.55374866466839,
127.023347921947));
#167424=CARTESIAN_POINT('Ctrl Pts',(-183.623812115476,4.65279360120558,
127.145910006866));
#167425=CARTESIAN_POINT('Ctrl Pts',(-183.616410293801,4.74683816642942,
127.272299182054));
#167426=CARTESIAN_POINT('Ctrl Pts',(-183.609012379489,4.84083308625904,
127.398621637381));
#167427=CARTESIAN_POINT('Ctrl Pts',(-183.601614465178,4.92983266949919,
127.528766860743));
#167428=CARTESIAN_POINT('Ctrl Pts',(-183.594216550867,5.01351915578842,
127.662298199815));
#167429=CARTESIAN_POINT('Ctrl Pts',(-183.586819865954,5.09719173490199,
127.795807348402));
#167430=CARTESIAN_POINT('Ctrl Pts',(-183.579423181042,5.17555277139587,
127.932701179883));
#167431=CARTESIAN_POINT('Ctrl Pts',(-183.57202649613,5.24832782886879,128.072514069309));
#167432=CARTESIAN_POINT('Ctrl Pts',(-183.564630139194,5.32109965941941,
128.212320759286));
#167433=CARTESIAN_POINT('Ctrl Pts',(-183.557233782259,5.38828583108009,
128.355045918725));
#167434=CARTESIAN_POINT('Ctrl Pts',(-183.549837425324,5.44965801280331,
128.500199575888));
#167435=CARTESIAN_POINT('Ctrl Pts',(-183.542439935987,5.5110395907644,128.645375456446));
#167436=CARTESIAN_POINT('Ctrl Pts',(-183.53504244665,5.56660526102463,128.7929802312));
#167437=CARTESIAN_POINT('Ctrl Pts',(-183.527644957314,5.61617502079312,
128.942504366853));
#167438=CARTESIAN_POINT('Ctrl Pts',(-183.520244874799,5.665762157164,129.09208091796));
#167439=CARTESIAN_POINT('Ctrl Pts',(-183.512844792284,5.70934908086662,
129.243577815451));
#167440=CARTESIAN_POINT('Ctrl Pts',(-183.505444709769,5.74680583097126,
129.396470954412));
#167441=CARTESIAN_POINT('Ctrl Pts',(-183.498036490102,5.78430376862334,
129.549532215098));
#167442=CARTESIAN_POINT('Ctrl Pts',(-183.490628270436,5.81565798206432,
129.703992420572));
#167443=CARTESIAN_POINT('Ctrl Pts',(-183.483220050769,5.84078962182305,
129.859317149728));
#167444=CARTESIAN_POINT('Ctrl Pts',(-183.475807271467,5.8659367296867,130.014737478662));
#167445=CARTESIAN_POINT('Ctrl Pts',(-183.468394492165,5.88485358757889,
130.17102302182));
#167446=CARTESIAN_POINT('Ctrl Pts',(-183.460981712863,5.89751333993616,
130.327635363594));
#167447=CARTESIAN_POINT('Ctrl Pts',(-183.453558341834,5.91019118114126,
130.484471480425));
#167448=CARTESIAN_POINT('Ctrl Pts',(-183.446134970806,5.91659404558043,
130.641634956467));
#167449=CARTESIAN_POINT('Ctrl Pts',(-183.438711599777,5.91674718368156,
130.798587672361));
#167450=CARTESIAN_POINT('Ctrl Pts',(-183.434775550336,5.91682838117727,
130.881807768356));
#167451=CARTESIAN_POINT('Ctrl Pts',(-183.430839500895,5.9151534241066,130.964968689975));
#167452=CARTESIAN_POINT('Ctrl Pts',(-183.426903451455,5.91173196006602,
131.04799106483));
#167453=CARTESIAN_POINT('Ctrl Pts',(-183.419480185049,5.90527918566564,
131.204568672769));
#167454=CARTESIAN_POINT('Ctrl Pts',(-183.412056918644,5.8925917063369,131.36112650563));
#167455=CARTESIAN_POINT('Ctrl Pts',(-183.404633652238,5.87366102232141,
131.517127590259));
#167456=CARTESIAN_POINT('Ctrl Pts',(-183.397219159517,5.85475271280228,
131.672944294561));
#167457=CARTESIAN_POINT('Ctrl Pts',(-183.389804666796,5.82961593096655,
131.828205193483));
#167458=CARTESIAN_POINT('Ctrl Pts',(-183.382390174075,5.79829416074255,
131.982373940071));
#167459=CARTESIAN_POINT('Ctrl Pts',(-183.374982827722,5.76700257961994,
132.136394093016));
#167460=CARTESIAN_POINT('Ctrl Pts',(-183.367575481368,5.72953795175678,
132.289323825892));
#167461=CARTESIAN_POINT('Ctrl Pts',(-183.360168135014,5.68599546277168,
132.44063264869));
#167462=CARTESIAN_POINT('Ctrl Pts',(-183.352766313339,5.64248544941762,
132.59182861966));
#167463=CARTESIAN_POINT('Ctrl Pts',(-183.345364491663,5.59290670374262,
132.741405730511));
#167464=CARTESIAN_POINT('Ctrl Pts',(-183.337962669988,5.5374052957988,132.888844523131));
#167465=CARTESIAN_POINT('Ctrl Pts',(-183.330564755676,5.48193318661622,
133.03620548396));
#167466=CARTESIAN_POINT('Ctrl Pts',(-183.323166841365,5.42054477297452,
133.181430026141));
#167467=CARTESIAN_POINT('Ctrl Pts',(-183.315768927054,5.35343566560404,
133.324014787634));
#167468=CARTESIAN_POINT('Ctrl Pts',(-183.308372242142,5.28633771054982,
133.466575854126));
#167469=CARTESIAN_POINT('Ctrl Pts',(-183.300975557229,5.21352110739003,
133.606497673161));
#167470=CARTESIAN_POINT('Ctrl Pts',(-183.293578872317,5.13522926000215,
133.743297671965));
#167471=CARTESIAN_POINT('Ctrl Pts',(-183.286182515382,5.05694088415682,
133.880091604913));
#167472=CARTESIAN_POINT('Ctrl Pts',(-183.278786158446,4.97317793223063,
134.013763668875));
#167473=CARTESIAN_POINT('Ctrl Pts',(-183.271389801511,4.88422921281487,
134.143856920781));
#167474=CARTESIAN_POINT('Ctrl Pts',(-183.263992312174,4.7952668751231,134.273970090296));
#167475=CARTESIAN_POINT('Ctrl Pts',(-183.256594822838,4.70111739978136,
134.400503048588));
#167476=CARTESIAN_POINT('Ctrl Pts',(-183.249197333501,4.60211217567657,
134.523028939021));
#167477=CARTESIAN_POINT('Ctrl Pts',(-183.241797250986,4.50307224544381,
134.645597780714));
#167478=CARTESIAN_POINT('Ctrl Pts',(-183.234397168471,4.39917341190046,
134.764156467682));
#167479=CARTESIAN_POINT('Ctrl Pts',(-183.226997085956,4.29078637229727,
134.878312368607));
#167480=CARTESIAN_POINT('Ctrl Pts',(-183.219588866289,4.18228015000174,
134.99259379568));
#167481=CARTESIAN_POINT('Ctrl Pts',(-183.212180646623,4.06927612283048,
135.102462497404));
#167482=CARTESIAN_POINT('Ctrl Pts',(-183.204772426956,3.95218129433147,
135.207563267824));
#167483=CARTESIAN_POINT('Ctrl Pts',(-183.197359647654,3.83501439591901,
135.312728726014));
#167484=CARTESIAN_POINT('Ctrl Pts',(-183.189946868352,3.71375196598444,
135.413120167876));
#167485=CARTESIAN_POINT('Ctrl Pts',(-183.18253408905,3.58883247273898,135.508423972275));
#167486=CARTESIAN_POINT('Ctrl Pts',(-183.175110718021,3.46373448866361,
135.603863951219));
#167487=CARTESIAN_POINT('Ctrl Pts',(-183.167687346993,3.33496930979695,
135.694201560142));
#167488=CARTESIAN_POINT('Ctrl Pts',(-183.160263975964,3.20300331966732,
135.779167176288));
#167489=CARTESIAN_POINT('Ctrl Pts',(-183.156327926523,3.13303178521975,
135.82421798469));
#167490=CARTESIAN_POINT('Ctrl Pts',(-183.152391877082,3.06216079141112,
135.867759305324));
#167491=CARTESIAN_POINT('Ctrl Pts',(-183.148455827642,2.99046233124018,
135.90975635227));
#167492=CARTESIAN_POINT('Ctrl Pts',(-183.141032561236,2.85524127299102,
135.988961472127));
#167493=CARTESIAN_POINT('Ctrl Pts',(-183.133609294831,2.71666684177059,
136.062910469239));
#167494=CARTESIAN_POINT('Ctrl Pts',(-183.126186028425,2.57518621397406,
136.131305945412));
#167495=CARTESIAN_POINT('Ctrl Pts',(-183.118771535704,2.43387280453034,
136.199620583812));
#167496=CARTESIAN_POINT('Ctrl Pts',(-183.111357042983,2.28966036846826,
136.262394605668));
#167497=CARTESIAN_POINT('Ctrl Pts',(-183.103942550262,2.14302365379594,
136.319374686612));
#167498=CARTESIAN_POINT('Ctrl Pts',(-183.096535203909,1.99652827310958,
136.376299848008));
#167499=CARTESIAN_POINT('Ctrl Pts',(-183.089127857555,1.84761361116126,
136.427442051669));
#167500=CARTESIAN_POINT('Ctrl Pts',(-183.081720511201,1.69677743437165,
136.472594637145));
#167501=CARTESIAN_POINT('Ctrl Pts',(-183.074318689525,1.54605375689342,
136.517713546118));
#167502=CARTESIAN_POINT('Ctrl Pts',(-183.06691686785,1.39341177422502,136.556851625278));
#167503=CARTESIAN_POINT('Ctrl Pts',(-183.059515046175,1.23936747561927,
136.589850987697));
#167504=CARTESIAN_POINT('Ctrl Pts',(-183.052117131863,1.08540449579967,
136.622832930009));
#167505=CARTESIAN_POINT('Ctrl Pts',(-183.044719217552,0.930041038421735,
136.649682531358));
#167506=CARTESIAN_POINT('Ctrl Pts',(-183.037321303241,0.773806328602494,
136.670292285112));
#167507=CARTESIAN_POINT('Ctrl Pts',(-183.029924618328,0.617597582157862,
136.690898613898));
#167508=CARTESIAN_POINT('Ctrl Pts',(-183.022527933416,0.460518240359305,
136.705267104356));
#167509=CARTESIAN_POINT('Ctrl Pts',(-183.015131248504,0.303105871090587,
136.713341696687));
#167510=CARTESIAN_POINT('Ctrl Pts',(-183.007734891569,0.145700481651279,
136.721415930983));
#167511=CARTESIAN_POINT('Ctrl Pts',(-183.000338534633,-0.012037533089414,
136.72319680293));
#167512=CARTESIAN_POINT('Ctrl Pts',(-182.992942177698,-0.169567625887687,
136.718680306486));
#167513=CARTESIAN_POINT('Ctrl Pts',(-182.985544688361,-0.327121836945322,
136.714163118556));
#167514=CARTESIAN_POINT('Ctrl Pts',(-182.978147199025,-0.484467689507502,
136.703346653195));
#167515=CARTESIAN_POINT('Ctrl Pts',(-182.970749709688,-0.641066933207348,
136.686278990822));
#167516=CARTESIAN_POINT('Ctrl Pts',(-182.963349627173,-0.797721072529536,
136.669205345406));
#167517=CARTESIAN_POINT('Ctrl Pts',(-182.955949544658,-0.953627711032837,
136.645876180442));
#167518=CARTESIAN_POINT('Ctrl Pts',(-182.948549462143,-1.10825614594989,
136.616391147206));
#167519=CARTESIAN_POINT('Ctrl Pts',(-182.941141242476,-1.26305461072711,
136.586873692145));
#167520=CARTESIAN_POINT('Ctrl Pts',(-182.93373302281,-1.41657169809388,
136.551186920619));
#167521=CARTESIAN_POINT('Ctrl Pts',(-182.926324803144,-1.56828856786049,
136.509481258746));
#167522=CARTESIAN_POINT('Ctrl Pts',(-182.918912023842,-1.7200988168289,
136.467749927734));
#167523=CARTESIAN_POINT('Ctrl Pts',(-182.911499244539,-1.8701062854791,
136.419992437623));
#167524=CARTESIAN_POINT('Ctrl Pts',(-182.904086465237,-2.01781011269092,
136.366408164254));
#167525=CARTESIAN_POINT('Ctrl Pts',(-182.896663094209,-2.1657249860579,
136.312747327163));
#167526=CARTESIAN_POINT('Ctrl Pts',(-182.88923972318,-2.31132929938075,
136.253243219605));
#167527=CARTESIAN_POINT('Ctrl Pts',(-182.881816352151,-2.45414411970913,
136.188142485565));
#167528=CARTESIAN_POINT('Ctrl Pts',(-182.87788030271,-2.52986796424262,
136.153624514306));
#167529=CARTESIAN_POINT('Ctrl Pts',(-182.873944253269,-2.60480801371997,
136.117533887402));
#167530=CARTESIAN_POINT('Ctrl Pts',(-182.870008203829,-2.67889608778898,
136.079912371964));
#167531=CARTESIAN_POINT('Ctrl Pts',(-182.862584937423,-2.81862388327062,
136.008959367975));
#167532=CARTESIAN_POINT('Ctrl Pts',(-182.855161671018,-2.95574213382726,
135.932344013602));
#167533=CARTESIAN_POINT('Ctrl Pts',(-182.847738404613,-3.08975892017157,
135.850281780022));
#167534=CARTESIAN_POINT('Ctrl Pts',(-182.840323911892,-3.22361730980421,
135.768316537187));
#167535=CARTESIAN_POINT('Ctrl Pts',(-182.832909419171,-3.35438121652008,
135.680917422574));
#167536=CARTESIAN_POINT('Ctrl Pts',(-182.82549492645,-3.48158089845803,
135.588346927119));
#167537=CARTESIAN_POINT('Ctrl Pts',(-182.818087580096,-3.60865798055354,
135.495865654593));
#167538=CARTESIAN_POINT('Ctrl Pts',(-182.810680233742,-3.7321773771412,
135.398223142311));
#167539=CARTESIAN_POINT('Ctrl Pts',(-182.803272887389,-3.85169616402163,
135.295726470239));
#167540=CARTESIAN_POINT('Ctrl Pts',(-182.795871065713,-3.97112580928161,
135.193306244053));
#167541=CARTESIAN_POINT('Ctrl Pts',(-182.788469244038,-4.08656050384569,
135.086039308776));
#167542=CARTESIAN_POINT('Ctrl Pts',(-182.781067422363,-4.19758850817627,
134.974274439041));
#167543=CARTESIAN_POINT('Ctrl Pts',(-182.773669508051,-4.30855790168761,
134.86256856911));
#167544=CARTESIAN_POINT('Ctrl Pts',(-182.76627159374,-4.4151249753976,134.746369757665));
#167545=CARTESIAN_POINT('Ctrl Pts',(-182.758873679429,-4.51691322183099,
134.626065146824));
#167546=CARTESIAN_POINT('Ctrl Pts',(-182.751476994517,-4.61868455290431,
134.505780528426));
#167547=CARTESIAN_POINT('Ctrl Pts',(-182.744080309604,-4.71567839198069,
134.381391749517));
#167548=CARTESIAN_POINT('Ctrl Pts',(-182.736683624692,-4.80755700579362,
134.253320779491));
#167549=CARTESIAN_POINT('Ctrl Pts',(-182.729287267757,-4.89943154561279,
134.125255488265));
#167550=CARTESIAN_POINT('Ctrl Pts',(-182.721890910821,-4.98619109355161,
133.993508633881));
#167551=CARTESIAN_POINT('Ctrl Pts',(-182.714494553886,-5.06754010022365,
133.858532828677));
#167552=CARTESIAN_POINT('Ctrl Pts',(-182.70709706455,-5.14890156163604,
133.723536358334));
#167553=CARTESIAN_POINT('Ctrl Pts',(-182.699699575213,-5.22485063968611,
133.585310272575));
#167554=CARTESIAN_POINT('Ctrl Pts',(-182.692302085877,-5.29513684831921,
133.444333405318));
#167555=CARTESIAN_POINT('Ctrl Pts',(-182.684902003362,-5.36544769567369,
133.303307118839));
#167556=CARTESIAN_POINT('Ctrl Pts',(-182.677501920847,-5.43009155481507,
133.159528464853));
#167557=CARTESIAN_POINT('Ctrl Pts',(-182.670101838332,-5.48886540737634,
133.013497802579));
#167558=CARTESIAN_POINT('Ctrl Pts',(-182.662693618666,-5.54770388783085,
132.867306564579));
#167559=CARTESIAN_POINT('Ctrl Pts',(-182.655285398999,-5.6006593318303,
132.718858719442));
#167560=CARTESIAN_POINT('Ctrl Pts',(-182.647877179333,-5.6475778513308,
132.568672091104));
#167561=CARTESIAN_POINT('Ctrl Pts',(-182.640464400031,-5.69452524839718,
132.418393025403));
#167562=CARTESIAN_POINT('Ctrl Pts',(-182.633051620729,-5.73542822034687,
132.26637340365));
#167563=CARTESIAN_POINT('Ctrl Pts',(-182.625638841427,-5.77018378005181,
132.113142382005));
#167564=CARTESIAN_POINT('Ctrl Pts',(-182.618215470398,-5.80498900013038,
131.959692416689));
#167565=CARTESIAN_POINT('Ctrl Pts',(-182.61079209937,-5.83362919713295,
131.80502796056));
#167566=CARTESIAN_POINT('Ctrl Pts',(-182.603368728341,-5.85605300467136,
131.649685270572));
#167567=CARTESIAN_POINT('Ctrl Pts',(-182.5994326789,-5.86794264548235,131.567318848928));
#167568=CARTESIAN_POINT('Ctrl Pts',(-182.595496629458,-5.87808550618547,
131.484761797472));
#167569=CARTESIAN_POINT('Ctrl Pts',(-182.591560580017,-5.88647987348797,
131.40209405441));
#167570=CARTESIAN_POINT('Ctrl Pts',(-182.582165450747,-5.90651675745441,
131.204770788007));
#167571=CARTESIAN_POINT('Ctrl Pts',(-182.572770321477,-5.91663410596626,
131.006423364004));
#167572=CARTESIAN_POINT('Ctrl Pts',(-182.563375192208,-5.91674901010249,
130.807783182575));
#167573=CARTESIAN_POINT('',(-180.813376354123,-5.91239331584027,130.807847145143));
#167574=CARTESIAN_POINT('Ctrl Pts',(-182.56337265757,-5.92405711974599,
130.807733754196));
#167575=CARTESIAN_POINT('Ctrl Pts',(-182.479952757115,-5.91188579994225,
129.041809576944));
#167576=CARTESIAN_POINT('Ctrl Pts',(-182.303716982053,-4.13524844748988,
125.289854803609));
#167577=CARTESIAN_POINT('Ctrl Pts',(-182.034665332392,2.25108434336954,
124.177884947263));
#167578=CARTESIAN_POINT('Ctrl Pts',(-181.756217708577,6.79180772637146,
129.116489669186));
#167579=CARTESIAN_POINT('Ctrl Pts',(-181.477770084765,5.09119160707943,
135.60616533563));
#167580=CARTESIAN_POINT('Ctrl Pts',(-181.199322460952,-1.28798088058456,
137.683217047348));
#167581=CARTESIAN_POINT('Ctrl Pts',(-180.977858187196,-5.42030405385856,
134.307513343875));
#167582=CARTESIAN_POINT('Ctrl Pts',(-180.849209788043,-5.91302735279117,
131.571366059404));
#167583=CARTESIAN_POINT('Ctrl Pts',(-180.813377263496,-5.90898434920711,
130.80786452556));
#167584=CARTESIAN_POINT('',(-179.063374001572,-5.91358993803376,130.79964208133));
#167585=CARTESIAN_POINT('Ctrl Pts',(-180.813375192208,-5.91674898580156,
130.807824938015));
#167586=CARTESIAN_POINT('Ctrl Pts',(-180.80590436759,-5.91684231226662,
130.648431696059));
#167587=CARTESIAN_POINT('Ctrl Pts',(-180.798433542972,-5.91049037800369,
130.489025468643));
#167588=CARTESIAN_POINT('Ctrl Pts',(-180.790962718354,-5.89771667312605,
130.330157490171));
#167589=CARTESIAN_POINT('Ctrl Pts',(-180.783490770938,-5.88494104847493,
130.171265635264));
#167590=CARTESIAN_POINT('Ctrl Pts',(-180.776018823522,-5.86574175873066,
130.012912552212));
#167591=CARTESIAN_POINT('Ctrl Pts',(-180.768546876106,-5.84019423006307,
129.855644686616));
#167592=CARTESIAN_POINT('Ctrl Pts',(-180.761072443837,-5.81463820537227,
129.698324520407));
#167593=CARTESIAN_POINT('Ctrl Pts',(-180.753598011569,-5.78272979363846,
129.542090648727));
#167594=CARTESIAN_POINT('Ctrl Pts',(-180.7461235793,-5.74459562263046,129.3874796434));
#167595=CARTESIAN_POINT('Ctrl Pts',(-180.738645298881,-5.70644181855295,
129.232789037847));
#167596=CARTESIAN_POINT('Ctrl Pts',(-180.731167018461,-5.66205595596423,
129.079723315102));
#167597=CARTESIAN_POINT('Ctrl Pts',(-180.723688738042,-5.61161462016539,
128.928804188864));
#167598=CARTESIAN_POINT('Ctrl Pts',(-180.716200537055,-5.56110636969527,
128.777684855721));
#167599=CARTESIAN_POINT('Ctrl Pts',(-180.708712336068,-5.50452671422177,
128.628718151764));
#167600=CARTESIAN_POINT('Ctrl Pts',(-180.701224135081,-5.4421008949015,
128.482407040896));
#167601=CARTESIAN_POINT('Ctrl Pts',(-180.693730469935,-5.37962952330192,
128.335989166437));
#167602=CARTESIAN_POINT('Ctrl Pts',(-180.686236804789,-5.31130363918635,
128.192231074739));
#167603=CARTESIAN_POINT('Ctrl Pts',(-180.678743139642,-5.23739446975496,
128.051611131928));
#167604=CARTESIAN_POINT('Ctrl Pts',(-180.67123737861,-5.16336599996819,
127.910764207684));
#167605=CARTESIAN_POINT('Ctrl Pts',(-180.663731617577,-5.0837364204128,
127.773065865971));
#167606=CARTESIAN_POINT('Ctrl Pts',(-180.656225856544,-4.99882089239424,
127.638966448073));
#167607=CARTESIAN_POINT('Ctrl Pts',(-180.651626308805,-4.9467844602118,
127.556790014292));
#167608=CARTESIAN_POINT('Ctrl Pts',(-180.647026761065,-4.89276383469503,
127.475964459253));
#167609=CARTESIAN_POINT('Ctrl Pts',(-180.642427213326,-4.83683886899804,
127.396587104281));
#167610=CARTESIAN_POINT('Ctrl Pts',(-180.63500394692,-4.74658088221714,
127.26847901934));
#167611=CARTESIAN_POINT('Ctrl Pts',(-180.627580680515,-4.65109331048002,
127.143765544506));
#167612=CARTESIAN_POINT('Ctrl Pts',(-180.62015741411,-4.55065994398724,
127.022902613477));
#167613=CARTESIAN_POINT('Ctrl Pts',(-180.612742921389,-4.45034528139318,
126.902182532395));
#167614=CARTESIAN_POINT('Ctrl Pts',(-180.605328428668,-4.34509669582955,
126.785304220586));
#167615=CARTESIAN_POINT('Ctrl Pts',(-180.597913935947,-4.23524133075553,
126.672694920446));
#167616=CARTESIAN_POINT('Ctrl Pts',(-180.590506589593,-4.12549184841834,
126.560194157389));
#167617=CARTESIAN_POINT('Ctrl Pts',(-180.583099243239,-4.01114468503391,
126.451954479988));
#167618=CARTESIAN_POINT('Ctrl Pts',(-180.575691896886,-3.89256726626094,
126.348370195658));
#167619=CARTESIAN_POINT('Ctrl Pts',(-180.56829007521,-3.77407828700056,
126.244863168396));
#167620=CARTESIAN_POINT('Ctrl Pts',(-180.560888253535,-3.65136561447588,
126.146004865181));
#167621=CARTESIAN_POINT('Ctrl Pts',(-180.55348643186,-3.52483346582677,
126.05215275167));
#167622=CARTESIAN_POINT('Ctrl Pts',(-180.546088517549,-3.39836811251472,
125.958350181959));
#167623=CARTESIAN_POINT('Ctrl Pts',(-180.538690603237,-3.26808759764599,
125.869548760655));
#167624=CARTESIAN_POINT('Ctrl Pts',(-180.531292688926,-3.13442905661681,
125.78606558324));
#167625=CARTESIAN_POINT('Ctrl Pts',(-180.523896004014,-3.00079272721176,
125.702596279216));
#167626=CARTESIAN_POINT('Ctrl Pts',(-180.516499319102,-2.86377980209576,
125.624443662571));
#167627=CARTESIAN_POINT('Ctrl Pts',(-180.50910263419,-2.72385632332298,
125.551881460787));
#167628=CARTESIAN_POINT('Ctrl Pts',(-180.501706277254,-2.58393904890388,
125.479322476488));
#167629=CARTESIAN_POINT('Ctrl Pts',(-180.494309920319,-2.44111180882452,
125.412353586024));
#167630=CARTESIAN_POINT('Ctrl Pts',(-180.486913563384,-2.29586492173638,
125.351202374526));
#167631=CARTESIAN_POINT('Ctrl Pts',(-180.479516074047,-2.15059579697861,
125.29004180062));
#167632=CARTESIAN_POINT('Ctrl Pts',(-180.472118584711,-2.0029066316598,
125.234700824044));
#167633=CARTESIAN_POINT('Ctrl Pts',(-180.464721095374,-1.85330723241896,
125.185358671956));
#167634=CARTESIAN_POINT('Ctrl Pts',(-180.457321012859,-1.70365539134041,
125.135999223054));
#167635=CARTESIAN_POINT('Ctrl Pts',(-180.449920930344,-1.55209233740366,
125.092642902312));
#167636=CARTESIAN_POINT('Ctrl Pts',(-180.442520847829,-1.39914237269438,
125.055418872912));
#167637=CARTESIAN_POINT('Ctrl Pts',(-180.435112628163,-1.24602422377592,
125.018153911864));
#167638=CARTESIAN_POINT('Ctrl Pts',(-180.427704408496,-1.0915164813912,
124.987034796868));
#167639=CARTESIAN_POINT('Ctrl Pts',(-180.42029618883,-0.936153686024078,
124.962139564007));
#167640=CARTESIAN_POINT('Ctrl Pts',(-180.412883409528,-0.780695267448333,
124.937229008546));
#167641=CARTESIAN_POINT('Ctrl Pts',(-180.405470630226,-0.624381117031028,
124.91855001255));
#167642=CARTESIAN_POINT('Ctrl Pts',(-180.398057850924,-0.467749690625702,
124.906128612175));
#167643=CARTESIAN_POINT('Ctrl Pts',(-180.390634479895,-0.310894461893262,
124.893689463521));
#167644=CARTESIAN_POINT('Ctrl Pts',(-180.383211108867,-0.153721423776527,
124.887525782551));
#167645=CARTESIAN_POINT('Ctrl Pts',(-180.375787737838,0.00323134341759472,
124.887611499941));
#167646=CARTESIAN_POINT('Ctrl Pts',(-180.371851688396,0.0864514666357916,
124.887656949358));
#167647=CARTESIAN_POINT('Ctrl Pts',(-180.367915638954,0.169609742978011,
124.889458461255));
#167648=CARTESIAN_POINT('Ctrl Pts',(-180.363979589513,0.252626814831058,
124.893006267256));
#167649=CARTESIAN_POINT('Ctrl Pts',(-180.356556323107,0.409194421432122,
124.899697318649));
#167650=CARTESIAN_POINT('Ctrl Pts',(-180.349133056702,0.565732764817981,
124.912623037657));
#167651=CARTESIAN_POINT('Ctrl Pts',(-180.341709790296,0.721704859521438,
124.931791106846));
#167652=CARTESIAN_POINT('Ctrl Pts',(-180.334295297575,0.877492608161631,
124.950936520968));
#167653=CARTESIAN_POINT('Ctrl Pts',(-180.326880804854,1.03271507339061,
124.976309554354));
#167654=CARTESIAN_POINT('Ctrl Pts',(-180.319466312133,1.18683597505039,
125.007865906896));
#167655=CARTESIAN_POINT('Ctrl Pts',(-180.31205896578,1.34080832918305,125.039391844237));
#167656=CARTESIAN_POINT('Ctrl Pts',(-180.304651619426,1.49368087018309,
125.077089161737));
#167657=CARTESIAN_POINT('Ctrl Pts',(-180.297244273072,1.6449232535122,125.120861866572));
#167658=CARTESIAN_POINT('Ctrl Pts',(-180.289842451397,1.79605283456535,
125.164601924071));
#167659=CARTESIAN_POINT('Ctrl Pts',(-180.282440629721,1.94555432179695,
125.214408243235));
#167660=CARTESIAN_POINT('Ctrl Pts',(-180.275038808046,2.09290847999003,
125.270133963653));
#167661=CARTESIAN_POINT('Ctrl Pts',(-180.267640893735,2.24018485107,125.325830266896));
#167662=CARTESIAN_POINT('Ctrl Pts',(-180.260242979423,2.38531580236709,
125.387439616482));
#167663=CARTESIAN_POINT('Ctrl Pts',(-180.252845065112,2.52779827011158,
125.454765635876));
#167664=CARTESIAN_POINT('Ctrl Pts',(-180.2454483802,2.67025705985461,125.522080466907));
#167665=CARTESIAN_POINT('Ctrl Pts',(-180.238051695287,2.81006790238803,
125.595109922935));
#167666=CARTESIAN_POINT('Ctrl Pts',(-180.230655010375,2.94674859591522,
125.673609865973));
#167667=CARTESIAN_POINT('Ctrl Pts',(-180.22325865344,3.08342322887723,125.752106328241));
#167668=CARTESIAN_POINT('Ctrl Pts',(-180.215862296504,3.21696766509498,
125.836072609297));
#167669=CARTESIAN_POINT('Ctrl Pts',(-180.208465939569,3.34692540154562,
125.925219205495));
#167670=CARTESIAN_POINT('Ctrl Pts',(-180.201068450232,3.47690303485747,
126.014379450264));
#167671=CARTESIAN_POINT('Ctrl Pts',(-180.193670960896,3.60329256715243,
126.108721378205));
#167672=CARTESIAN_POINT('Ctrl Pts',(-180.186273471559,3.72566764660411,
126.20791295121));
#167673=CARTESIAN_POINT('Ctrl Pts',(-180.178873389044,3.84808562445071,
126.307139295668));
#167674=CARTESIAN_POINT('Ctrl Pts',(-180.171473306529,3.96648605779236,
126.411218435038));
#167675=CARTESIAN_POINT('Ctrl Pts',(-180.164073224014,4.08047687990288,
126.519779074979));
#167676=CARTESIAN_POINT('Ctrl Pts',(-180.156665004348,4.19459304664037,
126.628459088503));
#167677=CARTESIAN_POINT('Ctrl Pts',(-180.149256784681,4.30428964824568,
126.741630186279));
#167678=CARTESIAN_POINT('Ctrl Pts',(-180.141848565015,4.40921209856459,
126.858884824665));
#167679=CARTESIAN_POINT('Ctrl Pts',(-180.134435785713,4.51419912690065,
126.976211631324));
#167680=CARTESIAN_POINT('Ctrl Pts',(-180.127023006411,4.61440591173413,
127.097626699522));
#167681=CARTESIAN_POINT('Ctrl Pts',(-180.119610227109,4.7095194995687,127.222691084278));
#167682=CARTESIAN_POINT('Ctrl Pts',(-180.11218685608,4.80476899015836,127.347934166893));
#167683=CARTESIAN_POINT('Ctrl Pts',(-180.104763485052,4.89491053578961,
127.476836675114));
#167684=CARTESIAN_POINT('Ctrl Pts',(-180.097340114023,4.97967522377445,
127.608931815632));
#167685=CARTESIAN_POINT('Ctrl Pts',(-180.093404064582,5.02461949524755,
127.678971828719));
#167686=CARTESIAN_POINT('Ctrl Pts',(-180.089468015141,5.06805291187504,
127.749909002942));
#167687=CARTESIAN_POINT('Ctrl Pts',(-180.0855319657,5.10994079734045,127.821671292448));
#167688=CARTESIAN_POINT('Ctrl Pts',(-180.078108699294,5.18894004204775,
127.957012730823));
#167689=CARTESIAN_POINT('Ctrl Pts',(-180.070685432889,5.2626780668334,128.095699539363));
#167690=CARTESIAN_POINT('Ctrl Pts',(-180.063262166483,5.33085815437477,
128.2372840896));
#167691=CARTESIAN_POINT('Ctrl Pts',(-180.055847673762,5.39895765871467,
128.378701298656));
#167692=CARTESIAN_POINT('Ctrl Pts',(-180.048433181041,5.46151214110167,
128.523009099099));
#167693=CARTESIAN_POINT('Ctrl Pts',(-180.04101868832,5.51826899994545,128.669732357952));
#167694=CARTESIAN_POINT('Ctrl Pts',(-180.033611341967,5.57497115439181,
128.816314199405));
#167695=CARTESIAN_POINT('Ctrl Pts',(-180.026203995613,5.62588667606558,
128.965306518641));
#167696=CARTESIAN_POINT('Ctrl Pts',(-180.018796649259,5.67080966227076,
129.116211235314));
#167697=CARTESIAN_POINT('Ctrl Pts',(-180.011394827583,5.71569914321786,
129.267003401556));
#167698=CARTESIAN_POINT('Ctrl Pts',(-180.003993005908,5.75460488194266,
129.419704768962));
#167699=CARTESIAN_POINT('Ctrl Pts',(-179.996591184232,5.78736977694945,
129.573799108599));
#167700=CARTESIAN_POINT('Ctrl Pts',(-179.989193269921,5.8201173756232,129.727812103033));
#167701=CARTESIAN_POINT('Ctrl Pts',(-179.98179535561,5.84673050914526,129.883216241026));
#167702=CARTESIAN_POINT('Ctrl Pts',(-179.974397441298,5.86710247640078,
130.039482134464));
#167703=CARTESIAN_POINT('Ctrl Pts',(-179.967000756386,5.88747105820495,
130.195722059347));
#167704=CARTESIAN_POINT('Ctrl Pts',(-179.959604071474,5.90160048400506,
130.352823085647));
#167705=CARTESIAN_POINT('Ctrl Pts',(-179.952207386562,5.9094355121563,130.51024756079));
#167706=CARTESIAN_POINT('Ctrl Pts',(-179.944811029626,5.91727019289419,
130.667665055567));
#167707=CARTESIAN_POINT('Ctrl Pts',(-179.937414672691,5.91881101237257,
130.825405597834));
#167708=CARTESIAN_POINT('Ctrl Pts',(-179.930018315755,5.91405478717383,
130.982928634877));
#167709=CARTESIAN_POINT('Ctrl Pts',(-179.922620826419,5.90929783378486,
131.140475789099));
#167710=CARTESIAN_POINT('Ctrl Pts',(-179.915223337082,5.89824192734704,
131.297804998638));
#167711=CARTESIAN_POINT('Ctrl Pts',(-179.907825847746,5.88093596734664,
131.454378086923));
#167712=CARTESIAN_POINT('Ctrl Pts',(-179.900425765231,5.86362394076881,
131.61100606166));
#167713=CARTESIAN_POINT('Ctrl Pts',(-179.893025682716,5.84005753945498,
131.766877016608));
#167714=CARTESIAN_POINT('Ctrl Pts',(-179.885625600201,5.81033722220633,
131.921460401266));
#167715=CARTESIAN_POINT('Ctrl Pts',(-179.878217380534,5.78058422441342,
132.076213766249));
#167716=CARTESIAN_POINT('Ctrl Pts',(-179.870809160868,5.74466386733851,
132.229676366655));
#167717=CARTESIAN_POINT('Ctrl Pts',(-179.863400941201,5.70272736651028,
132.381329591818));
#167718=CARTESIAN_POINT('Ctrl Pts',(-179.855988161899,5.66076505446567,
132.533076157011));
#167719=CARTESIAN_POINT('Ctrl Pts',(-179.848575382597,5.61277933382527,
132.683010773186));
#167720=CARTESIAN_POINT('Ctrl Pts',(-179.841162603295,5.55897034242447,
132.830632883217));
#167721=CARTESIAN_POINT('Ctrl Pts',(-179.833739232266,5.50508446621329,
132.978465922642));
#167722=CARTESIAN_POINT('Ctrl Pts',(-179.826315861237,5.44535884258079,
133.123979512235));
#167723=CARTESIAN_POINT('Ctrl Pts',(-179.818892490209,5.380040844081,133.266695094951));
#167724=CARTESIAN_POINT('Ctrl Pts',(-179.814956440768,5.34540767399451,
133.342366321317));
#167725=CARTESIAN_POINT('Ctrl Pts',(-179.811020391327,5.30920304288685,
133.417251360219));
#167726=CARTESIAN_POINT('Ctrl Pts',(-179.807084341887,5.27146882157906,
133.491282094949));
#167727=CARTESIAN_POINT('Ctrl Pts',(-179.799661075481,5.20030325783337,
133.630901750236));
#167728=CARTESIAN_POINT('Ctrl Pts',(-179.792237809076,5.12347932154279,
133.767903246486));
#167729=CARTESIAN_POINT('Ctrl Pts',(-179.784814542671,5.04121323225327,
133.901794992893));
#167730=CARTESIAN_POINT('Ctrl Pts',(-179.77740004995,4.95904437464975,134.035528490373));
#167731=CARTESIAN_POINT('Ctrl Pts',(-179.769985557229,4.87144636083707,
134.166159239093));
#167732=CARTESIAN_POINT('Ctrl Pts',(-179.762571064508,4.77868239631381,
134.293217897201));
#167733=CARTESIAN_POINT('Ctrl Pts',(-179.755163718154,4.68600784119206,
134.42015409139));
#167734=CARTESIAN_POINT('Ctrl Pts',(-179.7477563718,4.5881774664831,134.543524749663));
#167735=CARTESIAN_POINT('Ctrl Pts',(-179.740349025446,4.485499025852,134.662887415656));
#167736=CARTESIAN_POINT('Ctrl Pts',(-179.732947203771,4.38289716667605,
134.78216105647));
#167737=CARTESIAN_POINT('Ctrl Pts',(-179.725545382096,4.27545468365737,
134.897432375347));
#167738=CARTESIAN_POINT('Ctrl Pts',(-179.71814356042,4.16352097762122,135.008290164003));
#167739=CARTESIAN_POINT('Ctrl Pts',(-179.710745646109,4.05164636051687,
135.119089431696));
#167740=CARTESIAN_POINT('Ctrl Pts',(-179.703347731798,3.93528550668121,
135.225479547193));
#167741=CARTESIAN_POINT('Ctrl Pts',(-179.695949817487,3.81482613076614,
135.32708459262));
#167742=CARTESIAN_POINT('Ctrl Pts',(-179.688553132574,3.69438677301383,
135.428672753131));
#167743=CARTESIAN_POINT('Ctrl Pts',(-179.681156447662,3.56985053003108,
135.525477181344));
#167744=CARTESIAN_POINT('Ctrl Pts',(-179.67375976275,3.44163988469777,135.617160786548));
#167745=CARTESIAN_POINT('Ctrl Pts',(-179.666363405815,3.31343492435919,
135.708840326406));
#167746=CARTESIAN_POINT('Ctrl Pts',(-179.658967048879,3.18155618927124,
135.795399277593));
#167747=CARTESIAN_POINT('Ctrl Pts',(-179.651570691944,3.04645674102676,
135.876542779866));
#167748=CARTESIAN_POINT('Ctrl Pts',(-179.644173202607,2.91133660871186,
135.957698705416));
#167749=CARTESIAN_POINT('Ctrl Pts',(-179.636775713271,2.77299510144716,
136.033437338946));
#167750=CARTESIAN_POINT('Ctrl Pts',(-179.629378223934,2.63191143379257,
136.103508923395));
#167751=CARTESIAN_POINT('Ctrl Pts',(-179.621978141419,2.49077830947559,
136.17360507133));
#167752=CARTESIAN_POINT('Ctrl Pts',(-179.614578058904,2.3469014450307,136.23803004898));
#167753=CARTESIAN_POINT('Ctrl Pts',(-179.607177976389,2.20078150805586,
136.296581599673));
#167754=CARTESIAN_POINT('Ctrl Pts',(-179.599769756723,2.05450089718987,
136.355197533815));
#167755=CARTESIAN_POINT('Ctrl Pts',(-179.592361537056,1.90597263478008,
136.407927004143));
#167756=CARTESIAN_POINT('Ctrl Pts',(-179.58495331739,1.75571477835447,136.45461691083));
#167757=CARTESIAN_POINT('Ctrl Pts',(-179.577540538088,1.60536444072542,
136.501335554375));
#167758=CARTESIAN_POINT('Ctrl Pts',(-179.570127758786,1.45328274764712,
136.542007130973));
#167759=CARTESIAN_POINT('Ctrl Pts',(-179.562714979484,1.29999901139323,
136.576529458901));
#167760=CARTESIAN_POINT('Ctrl Pts',(-179.555291608455,1.14649625614847,
136.611101113949));
#167761=CARTESIAN_POINT('Ctrl Pts',(-179.547868237426,0.991788393612213,
136.639505904812));
#167762=CARTESIAN_POINT('Ctrl Pts',(-179.540444866397,0.836411758288183,
136.661693281253));
#167763=CARTESIAN_POINT('Ctrl Pts',(-179.536508816957,0.754027338025988,
136.673457560621));
#167764=CARTESIAN_POINT('Ctrl Pts',(-179.532572767516,0.671454946475021,
136.683474771799));
#167765=CARTESIAN_POINT('Ctrl Pts',(-179.528636718075,0.588774524354783,
136.691743323147));
#167766=CARTESIAN_POINT('Ctrl Pts',(-179.521213451669,0.432841828606704,
136.707337552936));
#167767=CARTESIAN_POINT('Ctrl Pts',(-179.513790185264,0.276053375632314,
136.716756054739));
#167768=CARTESIAN_POINT('Ctrl Pts',(-179.506366918858,0.118939626646369,
136.719915023343));
#167769=CARTESIAN_POINT('Ctrl Pts',(-179.498952426137,-0.0379884269357607,
136.723070258309));
#167770=CARTESIAN_POINT('Ctrl Pts',(-179.491537933416,-0.195240641656169,
136.7199806789));
#167771=CARTESIAN_POINT('Ctrl Pts',(-179.484123440695,-0.352279877922297,
136.710614036622));
#167772=CARTESIAN_POINT('Ctrl Pts',(-179.476716094341,-0.509167753859644,
136.701256422266));
#167773=CARTESIAN_POINT('Ctrl Pts',(-179.469308747988,-0.665842689874027,
136.685633811616));
#167774=CARTESIAN_POINT('Ctrl Pts',(-179.461901401634,-0.821766086522907,
136.663765968072));
#167775=CARTESIAN_POINT('Ctrl Pts',(-179.454499579958,-0.977573189619913,
136.641914434392));
#167776=CARTESIAN_POINT('Ctrl Pts',(-179.447097758283,-1.13262950134629,
136.61382699401));
#167777=CARTESIAN_POINT('Ctrl Pts',(-179.439695936607,-1.28640020084502,
136.579575339615));
#167778=CARTESIAN_POINT('Ctrl Pts',(-179.432298022296,-1.44008972598887,
136.545341766401));
#167779=CARTESIAN_POINT('Ctrl Pts',(-179.424900107985,-1.59249462705246,
136.504950540707));
#167780=CARTESIAN_POINT('Ctrl Pts',(-179.417502193673,-1.74308906444127,
136.458524665056));
#167781=CARTESIAN_POINT('Ctrl Pts',(-179.410105508761,-1.89365847576642,
136.412106504543));
#167782=CARTESIAN_POINT('Ctrl Pts',(-179.402708823849,-2.04241766416558,
136.3596557943));
#167783=CARTESIAN_POINT('Ctrl Pts',(-179.395312138936,-2.18885466336137,
136.301345775376));
#167784=CARTESIAN_POINT('Ctrl Pts',(-179.387915782001,-2.33528516938715,
136.243038341979));
#167785=CARTESIAN_POINT('Ctrl Pts',(-179.380519425065,-2.47939334413142,
136.178872254585));
#167786=CARTESIAN_POINT('Ctrl Pts',(-179.37312306813,-2.62068622246135,
136.109069307579));
#167787=CARTESIAN_POINT('Ctrl Pts',(-179.365725578793,-2.76200073309085,
136.039255673564));
#167788=CARTESIAN_POINT('Ctrl Pts',(-179.358328089457,-2.90049875436519,
135.963803626908));
#167789=CARTESIAN_POINT('Ctrl Pts',(-179.35093060012,-3.03571113142043,
135.882981344601));
#167790=CARTESIAN_POINT('Ctrl Pts',(-179.343530517605,-3.17097090696619,
135.802130730167));
#167791=CARTESIAN_POINT('Ctrl Pts',(-179.33613043509,-3.30294242489327,
135.715906323391));
#167792=CARTESIAN_POINT('Ctrl Pts',(-179.328730352575,-3.43118489787047,
135.624620025433));
#167793=CARTESIAN_POINT('Ctrl Pts',(-179.321322132908,-3.55956838662981,
135.533233348805));
#167794=CARTESIAN_POINT('Ctrl Pts',(-179.313913913242,-3.6842143372299,
135.4367738818));
#167795=CARTESIAN_POINT('Ctrl Pts',(-179.306505693575,-3.80471391970313,
135.335594726693));
#167796=CARTESIAN_POINT('Ctrl Pts',(-179.299092914273,-3.92528766765873,
135.234353297504));
#167797=CARTESIAN_POINT('Ctrl Pts',(-179.291680134971,-4.04170968684056,
135.128386642548));
#167798=CARTESIAN_POINT('Ctrl Pts',(-179.284267355669,-4.15360790265782,
135.018084855515));
#167799=CARTESIAN_POINT('Ctrl Pts',(-179.27684398464,-4.26566600389351,
134.907625464115));
#167800=CARTESIAN_POINT('Ctrl Pts',(-179.269420613611,-4.37318713756271,
134.792818841095));
#167801=CARTESIAN_POINT('Ctrl Pts',(-179.261997242582,-4.47583887241952,
134.674088896223));
#167802=CARTESIAN_POINT('Ctrl Pts',(-179.258061193142,-4.53026728532872,
134.611135430574));
#167803=CARTESIAN_POINT('Ctrl Pts',(-179.254125143702,-4.58332744336295,
134.547079486324));
#167804=CARTESIAN_POINT('Ctrl Pts',(-179.250189094261,-4.63497479752016,
134.481987459546));
#167805=CARTESIAN_POINT('Ctrl Pts',(-179.242405181676,-4.73711235857636,
134.35326177809));
#167806=CARTESIAN_POINT('Ctrl Pts',(-179.23462126909,-4.83405257557669,
134.220064488449));
#167807=CARTESIAN_POINT('Ctrl Pts',(-179.226837356504,-4.92538181691207,
134.082857913605));
#167808=CARTESIAN_POINT('Ctrl Pts',(-179.21943360423,-5.01225060826353,
133.952352402468));
#167809=CARTESIAN_POINT('Ctrl Pts',(-179.212029851955,-5.09404316262776,
133.818220254166));
#167810=CARTESIAN_POINT('Ctrl Pts',(-179.20462609968,-5.17044286712766,
133.680895185456));
#167811=CARTESIAN_POINT('Ctrl Pts',(-179.197229304088,-5.24677078525505,
133.543699149556));
#167812=CARTESIAN_POINT('Ctrl Pts',(-179.189832508496,-5.31771575753479,
133.403316488217));
#167813=CARTESIAN_POINT('Ctrl Pts',(-179.182435712904,-5.38300406071346,
133.260210337081));
#167814=CARTESIAN_POINT('Ctrl Pts',(-179.175044399858,-5.44824397184658,
133.117210257003));
#167815=CARTESIAN_POINT('Ctrl Pts',(-179.167653086811,-5.50783540530376,
132.971491044007));
#167816=CARTESIAN_POINT('Ctrl Pts',(-179.160261773764,-5.56155032784516,
132.82354077628));
#167817=CARTESIAN_POINT('Ctrl Pts',(-179.152874472875,-5.61523609281154,
132.67567081903));
#167818=CARTESIAN_POINT('Ctrl Pts',(-179.145487171987,-5.66305157103681,
132.525572568989));
#167819=CARTESIAN_POINT('Ctrl Pts',(-179.138099871098,-5.70481673901178,
132.373754302016));
#167820=CARTESIAN_POINT('Ctrl Pts',(-179.130714471695,-5.74657115666838,
132.221975112935));
#167821=CARTESIAN_POINT('Ctrl Pts',(-179.123329072291,-5.78227826278416,
132.068477147734));
#167822=CARTESIAN_POINT('Ctrl Pts',(-179.115943672887,-5.81180782512948,
131.913784056233));
#167823=CARTESIAN_POINT('Ctrl Pts',(-179.108559362774,-5.84133303208765,
131.759113780793));
#167824=CARTESIAN_POINT('Ctrl Pts',(-179.101175052661,-5.86468244308912,
131.603249097923));
#167825=CARTESIAN_POINT('Ctrl Pts',(-179.093790742548,-5.88177695426642,
131.446723772456));
#167826=CARTESIAN_POINT('Ctrl Pts',(-179.086404697669,-5.89887548138718,
131.290161675136));
#167827=CARTESIAN_POINT('Ctrl Pts',(-179.079018652791,-5.90971613497904,
131.132938997188));
#167828=CARTESIAN_POINT('Ctrl Pts',(-179.071632607912,-5.91427167588424,
130.975594686412));
#167829=CARTESIAN_POINT('Ctrl Pts',(-179.068880136011,-5.91596933661368,
130.916959002315));
#167830=CARTESIAN_POINT('Ctrl Pts',(-179.066127664109,-5.91679467625972,
130.858306445919));
#167831=CARTESIAN_POINT('Ctrl Pts',(-179.063375192208,-5.91674813668029,
130.799664918431));
#167832=CARTESIAN_POINT('',(-177.313376099405,-5.92185101381458,130.802772195749));
#167833=CARTESIAN_POINT('Ctrl Pts',(-179.063373167743,-5.91137817917409,
130.799626087985));
#167834=CARTESIAN_POINT('Ctrl Pts',(-179.032829268644,-5.91617425954304,
130.149473536606));
#167835=CARTESIAN_POINT('Ctrl Pts',(-178.909469494942,-5.51702945710787,
127.529389957826));
#167836=CARTESIAN_POINT('Ctrl Pts',(-178.693293846636,-1.67753301865071,
124.009992103728));
#167837=CARTESIAN_POINT('Ctrl Pts',(-178.414846222822,4.80954708459832,
125.720482435377));
#167838=CARTESIAN_POINT('Ctrl Pts',(-178.13639859901,6.87688837653484,132.102808455183));
#167839=CARTESIAN_POINT('Ctrl Pts',(-177.857950975197,2.62470520511161,
137.291924344931));
#167840=CARTESIAN_POINT('Ctrl Pts',(-177.583610388289,-3.94115904884794,
136.530682336505));
#167841=CARTESIAN_POINT('Ctrl Pts',(-177.402085675986,-5.91922248209783,
132.679038148341));
#167842=CARTESIAN_POINT('Ctrl Pts',(-177.313376838286,-5.92600578683143,
130.802786695663));
#167843=CARTESIAN_POINT('',(-175.563375192208,-5.91627067345725,130.809833481333));
#167844=CARTESIAN_POINT('Ctrl Pts',(-177.313375192207,-5.91674978197843,
130.802754392749));
#167845=CARTESIAN_POINT('Ctrl Pts',(-177.309268703995,-5.91672624024111,
130.716035169074));
#167846=CARTESIAN_POINT('Ctrl Pts',(-177.305162215783,-5.91479628735477,
130.629344163195));
#167847=CARTESIAN_POINT('Ctrl Pts',(-177.301055727571,-5.91096305005085,
130.542738020236));
#167848=CARTESIAN_POINT('Ctrl Pts',(-177.293632461165,-5.9040337371609,
130.386180777579));
#167849=CARTESIAN_POINT('Ctrl Pts',(-177.28620919476,-5.89086980840988,
130.229662286206));
#167850=CARTESIAN_POINT('Ctrl Pts',(-177.278785928355,-5.87146439844034,
130.073719542655));
#167851=CARTESIAN_POINT('Ctrl Pts',(-177.271371435634,-5.85208192405386,
129.917961110475));
#167852=CARTESIAN_POINT('Ctrl Pts',(-177.263956942913,-5.82647269788109,
129.762777438429));
#167853=CARTESIAN_POINT('Ctrl Pts',(-177.256542450192,-5.79468183610456,
129.608704738636));
#167854=CARTESIAN_POINT('Ctrl Pts',(-177.249135103838,-5.76292161555761,
129.454780539912));
#167855=CARTESIAN_POINT('Ctrl Pts',(-177.241727757484,-5.72499169572692,
129.301965544837));
#167856=CARTESIAN_POINT('Ctrl Pts',(-177.234320411131,-5.68098887641932,
129.15078995125));
#167857=CARTESIAN_POINT('Ctrl Pts',(-177.226918589455,-5.63701887607436,
128.999727110124));
#167858=CARTESIAN_POINT('Ctrl Pts',(-177.21951676778,-5.58698509877179,
128.850301592753));
#167859=CARTESIAN_POINT('Ctrl Pts',(-177.212114946105,-5.53103519493896,
128.703032410254));
#167860=CARTESIAN_POINT('Ctrl Pts',(-177.204717031793,-5.47511482662469,
128.555840970009));
#167861=CARTESIAN_POINT('Ctrl Pts',(-177.197319117482,-5.4132846837787,
128.410803945714));
#167862=CARTESIAN_POINT('Ctrl Pts',(-177.189921203171,-5.34574190828615,
128.268424101702));
#167863=CARTESIAN_POINT('Ctrl Pts',(-177.182524518258,-5.27821035717784,
128.126067918638));
#167864=CARTESIAN_POINT('Ctrl Pts',(-177.175127833346,-5.20496821741377,
127.986368376403));
#167865=CARTESIAN_POINT('Ctrl Pts',(-177.167731148434,-5.12626036052953,
127.849807304701));
#167866=CARTESIAN_POINT('Ctrl Pts',(-177.160334791499,-5.04755599363414,
127.713252288259));
#167867=CARTESIAN_POINT('Ctrl Pts',(-177.152938434563,-4.96338657791109,
127.57983578907));
#167868=CARTESIAN_POINT('Ctrl Pts',(-177.145542077628,-4.87404231139147,
127.450013869052));
#167869=CARTESIAN_POINT('Ctrl Pts',(-177.138144588291,-4.78468436603631,
127.320172072967));
#167870=CARTESIAN_POINT('Ctrl Pts',(-177.130747098955,-4.69015020398907,
127.193926259383));
#167871=CARTESIAN_POINT('Ctrl Pts',(-177.123349609618,-4.59077251180646,
127.071702274328));
#167872=CARTESIAN_POINT('Ctrl Pts',(-177.115949527103,-4.49135998292834,
126.949435443845));
#167873=CARTESIAN_POINT('Ctrl Pts',(-177.108549444588,-4.38710077877733,
126.831193538343));
#167874=CARTESIAN_POINT('Ctrl Pts',(-177.101149362073,-4.27836678992182,
126.717368059046));
#167875=CARTESIAN_POINT('Ctrl Pts',(-177.093741142407,-4.16951323686698,
126.603417416933));
#167876=CARTESIAN_POINT('Ctrl Pts',(-177.08633292274,-4.05617533058798,
126.4938931695));
#167877=CARTESIAN_POINT('Ctrl Pts',(-177.078924703074,-3.93876115387232,
126.389149282279));
#167878=CARTESIAN_POINT('Ctrl Pts',(-177.071511923772,-3.82127471069039,
126.284340926943));
#167879=CARTESIAN_POINT('Ctrl Pts',(-177.06409914447,-3.69970728542012,
126.184319031213));
#167880=CARTESIAN_POINT('Ctrl Pts',(-177.056686365168,-3.57449829879662,
126.089395880222));
#167881=CARTESIAN_POINT('Ctrl Pts',(-177.049262994139,-3.44911040770114,
125.994337098581));
#167882=CARTESIAN_POINT('Ctrl Pts',(-177.041839623111,-3.32007086865978,
125.904391825007));
#167883=CARTESIAN_POINT('Ctrl Pts',(-177.034416252082,-3.18784688367952,
125.819828261495));
#167884=CARTESIAN_POINT('Ctrl Pts',(-177.030480202641,-3.11773855416769,
125.774990631044));
#167885=CARTESIAN_POINT('Ctrl Pts',(-177.0265441532,-3.04673536382247,125.731665219015));
#167886=CARTESIAN_POINT('Ctrl Pts',(-177.022608103759,-2.9749094111855,
125.689886592044));
#167887=CARTESIAN_POINT('Ctrl Pts',(-177.015184837353,-2.8394479061316,
125.611093405447));
#167888=CARTESIAN_POINT('Ctrl Pts',(-177.007761570948,-2.70064904146863,
125.537566523763));
#167889=CARTESIAN_POINT('Ctrl Pts',(-177.000338304542,-2.55896089669827,
125.469601982757));
#167890=CARTESIAN_POINT('Ctrl Pts',(-176.992923811821,-2.41744021554856,
125.401717770194));
#167891=CARTESIAN_POINT('Ctrl Pts',(-176.985509319101,-2.27303738493946,
125.339382972151));
#167892=CARTESIAN_POINT('Ctrl Pts',(-176.97809482638,-2.12622792171232,
125.282849466855));
#167893=CARTESIAN_POINT('Ctrl Pts',(-176.970687480026,-1.9795599589727,
125.226370450678));
#167894=CARTESIAN_POINT('Ctrl Pts',(-176.963280133672,-1.83049032751116,
125.175681728911));
#167895=CARTESIAN_POINT('Ctrl Pts',(-176.955872787318,-1.67951742044608,
125.130988446016));
#167896=CARTESIAN_POINT('Ctrl Pts',(-176.948470965643,-1.52865711467097,
125.086328497058));
#167897=CARTESIAN_POINT('Ctrl Pts',(-176.941069143967,-1.3758967161798,
125.047655188872));
#167898=CARTESIAN_POINT('Ctrl Pts',(-176.933667322292,-1.22175269238884,
125.015124837159));
#167899=CARTESIAN_POINT('Ctrl Pts',(-176.926269407981,-1.06769004002861,
124.982611657967));
#167900=CARTESIAN_POINT('Ctrl Pts',(-176.918871493669,-0.912245581333441,
124.956235053905));
#167901=CARTESIAN_POINT('Ctrl Pts',(-176.911473579358,-0.755948866182213,
124.936100920329));
#167902=CARTESIAN_POINT('Ctrl Pts',(-176.904076894446,-0.599678124709309,
124.91597013268));
#167903=CARTESIAN_POINT('Ctrl Pts',(-176.896680209534,-0.44255577774917,
124.90207980426));
#167904=CARTESIAN_POINT('Ctrl Pts',(-176.889283524621,-0.285119561322315,
124.894484358434));
#167905=CARTESIAN_POINT('Ctrl Pts',(-176.881887167686,-0.127690325782278,
124.886889249398));
#167906=CARTESIAN_POINT('Ctrl Pts',(-176.87449081075,0.030052378688286,
124.885588485957));
#167907=CARTESIAN_POINT('Ctrl Pts',(-176.867094453815,0.187567995156329,
124.890584428895));
#167908=CARTESIAN_POINT('Ctrl Pts',(-176.859696964478,0.345107727667371,
124.895581136725));
#167909=CARTESIAN_POINT('Ctrl Pts',(-176.852299475142,0.502419929814423,
124.906876458634));
#167910=CARTESIAN_POINT('Ctrl Pts',(-176.844901985805,0.658966500063999,
124.924420676181));
#167911=CARTESIAN_POINT('Ctrl Pts',(-176.83750190329,0.815567947471321,
124.941971043826));
#167912=CARTESIAN_POINT('Ctrl Pts',(-176.830101820775,0.971402857872432,
124.96577462691));
#167913=CARTESIAN_POINT('Ctrl Pts',(-176.82270173826,1.12594083426236,124.995730159339));
#167914=CARTESIAN_POINT('Ctrl Pts',(-176.815293518594,1.280648741044,125.025718630956));
#167915=CARTESIAN_POINT('Ctrl Pts',(-176.807885298927,1.43405649907329,
125.061872490389));
#167916=CARTESIAN_POINT('Ctrl Pts',(-176.800477079261,1.58564572840909,
125.104039733047));
#167917=CARTESIAN_POINT('Ctrl Pts',(-176.793064299959,1.73732825838658,
125.14623292894));
#167918=CARTESIAN_POINT('Ctrl Pts',(-176.785651520657,1.88718967484081,
125.194446768976));
#167919=CARTESIAN_POINT('Ctrl Pts',(-176.778238741354,2.03472972580306,
125.248480353788));
#167920=CARTESIAN_POINT('Ctrl Pts',(-176.770815370326,2.18248058890885,
125.30259114432));
#167921=CARTESIAN_POINT('Ctrl Pts',(-176.763391999297,2.32790311776757,
125.362538145704));
#167922=CARTESIAN_POINT('Ctrl Pts',(-176.755968628268,2.47051913234672,
125.428073257388));
#167923=CARTESIAN_POINT('Ctrl Pts',(-176.752032578827,2.54613756530169,
125.462821546097));
#167924=CARTESIAN_POINT('Ctrl Pts',(-176.748096529386,2.62096742020819,
125.499140097564));
#167925=CARTESIAN_POINT('Ctrl Pts',(-176.744160479946,2.69494064415454,
125.536986937355));
#167926=CARTESIAN_POINT('Ctrl Pts',(-176.73673721354,2.8344518358904,125.608364896039));
#167927=CARTESIAN_POINT('Ctrl Pts',(-176.729313947135,2.97133626054164,
125.685397236324));
#167928=CARTESIAN_POINT('Ctrl Pts',(-176.721890680729,3.1051026569196,125.767866990796));
#167929=CARTESIAN_POINT('Ctrl Pts',(-176.714476188008,3.23871095252604,
125.850239272868));
#167930=CARTESIAN_POINT('Ctrl Pts',(-176.707061695287,3.36920824071257,
125.938035983006));
#167931=CARTESIAN_POINT('Ctrl Pts',(-176.699647202566,3.49612558072596,
126.030993201758));
#167932=CARTESIAN_POINT('Ctrl Pts',(-176.692239856212,3.6229205930287,126.123860824844));
#167933=CARTESIAN_POINT('Ctrl Pts',(-176.684832509859,3.74614222726404,
126.221878835408));
#167934=CARTESIAN_POINT('Ctrl Pts',(-176.677425163505,3.86534849593,126.324738806798));
#167935=CARTESIAN_POINT('Ctrl Pts',(-176.67002334183,3.98446585606339,126.42752206134));
#167936=CARTESIAN_POINT('Ctrl Pts',(-176.662621520154,4.09957353228987,
126.535139843268));
#167937=CARTESIAN_POINT('Ctrl Pts',(-176.655219698479,4.21026084852899,
126.64724212637));
#167938=CARTESIAN_POINT('Ctrl Pts',(-176.647821784167,4.32088973379546,
126.75928523155));
#167939=CARTESIAN_POINT('Ctrl Pts',(-176.640423869856,4.42710264468329,
126.875807858287));
#167940=CARTESIAN_POINT('Ctrl Pts',(-176.633025955545,4.5285242537886,126.996421720295));
#167941=CARTESIAN_POINT('Ctrl Pts',(-176.625629270632,4.62992900846261,
127.117015538468));
#167942=CARTESIAN_POINT('Ctrl Pts',(-176.61823258572,4.72654380161574,127.241698957101));
#167943=CARTESIAN_POINT('Ctrl Pts',(-176.610835900808,4.81803218587554,
127.370048980809));
#167944=CARTESIAN_POINT('Ctrl Pts',(-176.603439543872,4.90951651344424,
127.498393313341));
#167945=CARTESIAN_POINT('Ctrl Pts',(-176.596043186937,4.99587466741297,
127.630403623705));
#167946=CARTESIAN_POINT('Ctrl Pts',(-176.588646830002,5.0768124773605,127.765626402104));
#167947=CARTESIAN_POINT('Ctrl Pts',(-176.581249340665,5.15776267909337,
127.900869883456));
#167948=CARTESIAN_POINT('Ctrl Pts',(-176.573851851329,5.2332906926952,128.039326491832));
#167949=CARTESIAN_POINT('Ctrl Pts',(-176.566454361992,5.30314749067731,
128.180516633137));
#167950=CARTESIAN_POINT('Ctrl Pts',(-176.559054279477,5.37302877685177,
128.321756268428));
#167951=CARTESIAN_POINT('Ctrl Pts',(-176.551654196962,5.43723472380216,
128.465731010114));
#167952=CARTESIAN_POINT('Ctrl Pts',(-176.544254114447,5.49556383702317,
128.611939883377));
#167953=CARTESIAN_POINT('Ctrl Pts',(-176.53684589478,5.55395708910046,128.758309528326));
#167954=CARTESIAN_POINT('Ctrl Pts',(-176.529437675114,5.60646046363653,
128.90691786402));
#167955=CARTESIAN_POINT('Ctrl Pts',(-176.522029455448,5.65292164937822,
129.057246600539));
#167956=CARTESIAN_POINT('Ctrl Pts',(-176.514616676145,5.69941143120462,
129.207667861888));
#167957=CARTESIAN_POINT('Ctrl Pts',(-176.507203896843,5.73985151825766,
129.359811274075));
#167958=CARTESIAN_POINT('Ctrl Pts',(-176.499791117541,5.77414053445561,
129.513147369935));
#167959=CARTESIAN_POINT('Ctrl Pts',(-176.492367746513,5.80847854440786,
129.6667025596));
#167960=CARTESIAN_POINT('Ctrl Pts',(-176.484944375484,5.83664786334767,
129.821453470244));
#167961=CARTESIAN_POINT('Ctrl Pts',(-176.477521004455,5.85859875730653,
129.976863691054));
#167962=CARTESIAN_POINT('Ctrl Pts',(-176.473584955014,5.87023764798798,
130.059265919145));
#167963=CARTESIAN_POINT('Ctrl Pts',(-176.469648905573,5.8801291864416,130.141853459566));
#167964=CARTESIAN_POINT('Ctrl Pts',(-176.465712856133,5.88827190268693,
130.224546369269));
#167965=CARTESIAN_POINT('Ctrl Pts',(-176.458289589727,5.90362881140016,
130.380502616212));
#167966=CARTESIAN_POINT('Ctrl Pts',(-176.450866323322,5.91280869696112,
130.537305220984));
#167967=CARTESIAN_POINT('Ctrl Pts',(-176.443443056916,5.91572856152709,
130.694423595446));
#167968=CARTESIAN_POINT('Ctrl Pts',(-176.436028564195,5.91864497505563,
130.851356269038));
#167969=CARTESIAN_POINT('Ctrl Pts',(-176.428614071474,5.91531608812268,
131.008603599848));
#167970=CARTESIAN_POINT('Ctrl Pts',(-176.421199578753,5.90571046970631,
131.165628399829));
#167971=CARTESIAN_POINT('Ctrl Pts',(-176.413792232399,5.89611410954661,
131.322501853396));
#167972=CARTESIAN_POINT('Ctrl Pts',(-176.406384886046,5.88025308440494,
131.479152833029));
#167973=CARTESIAN_POINT('Ctrl Pts',(-176.398977539692,5.8581479773177,131.635042769986));
#167974=CARTESIAN_POINT('Ctrl Pts',(-176.391575718016,5.8360593570533,131.790816438346));
#167975=CARTESIAN_POINT('Ctrl Pts',(-176.384173896341,5.80773597988552,
131.945829826216));
#167976=CARTESIAN_POINT('Ctrl Pts',(-176.376772074666,5.77325035232502,
132.099548222463));
#167977=CARTESIAN_POINT('Ctrl Pts',(-176.369374160354,5.73878292945897,
132.253185471965));
#167978=CARTESIAN_POINT('Ctrl Pts',(-176.361976246043,5.69815981622234,
132.405528727975));
#167979=CARTESIAN_POINT('Ctrl Pts',(-176.354578331732,5.65150481523468,
132.556052338697));
#167980=CARTESIAN_POINT('Ctrl Pts',(-176.347181646819,5.60485756746171,
132.706550935126));
#167981=CARTESIAN_POINT('Ctrl Pts',(-176.339784961907,5.55218053179486,
132.855230130211));
#167982=CARTESIAN_POINT('Ctrl Pts',(-176.332388276995,5.49364772820861,
133.001578221912));
#167983=CARTESIAN_POINT('Ctrl Pts',(-176.32499192006,5.43511752002822,133.147919824385));
#167984=CARTESIAN_POINT('Ctrl Pts',(-176.317595563124,5.37073219882822,
133.291930182392));
#167985=CARTESIAN_POINT('Ctrl Pts',(-176.310199206189,5.30071430894531,
133.433116668903));
#167986=CARTESIAN_POINT('Ctrl Pts',(-176.302801716852,5.23068569914471,
133.574324771426));
#167987=CARTESIAN_POINT('Ctrl Pts',(-176.295404227515,5.15502296944984,
133.712707807152));
#167988=CARTESIAN_POINT('Ctrl Pts',(-176.288006738179,5.07399501051325,
133.847797029878));
#167989=CARTESIAN_POINT('Ctrl Pts',(-176.280606655664,4.99293864735137,
133.982933607922));
#167990=CARTESIAN_POINT('Ctrl Pts',(-176.273206573149,4.90651350223879,
134.114773754158));
#167991=CARTESIAN_POINT('Ctrl Pts',(-176.265806490634,4.81503214677668,
134.242877156425));
#167992=CARTESIAN_POINT('Ctrl Pts',(-176.258398270967,4.72345019815959,
134.371121421553));
#167993=CARTESIAN_POINT('Ctrl Pts',(-176.250990051301,4.62680115293626,
134.495620432926));
#167994=CARTESIAN_POINT('Ctrl Pts',(-176.243581831635,4.52543873514238,
134.615965898412));
#167995=CARTESIAN_POINT('Ctrl Pts',(-176.236169052333,4.42401393047166,
134.736385434524));
#167996=CARTESIAN_POINT('Ctrl Pts',(-176.22875627303,4.31787022373021,134.85264605568));
#167997=CARTESIAN_POINT('Ctrl Pts',(-176.221343493728,4.2073982743899,134.964376281378));
#167998=CARTESIAN_POINT('Ctrl Pts',(-176.2139201227,4.09676847754758,135.076266152462));
#167999=CARTESIAN_POINT('Ctrl Pts',(-176.206496751671,3.9817983586106,135.183612445486));
#168000=CARTESIAN_POINT('Ctrl Pts',(-176.199073380642,3.86291233276183,
135.286083374709));
#168001=CARTESIAN_POINT('Ctrl Pts',(-176.195137331201,3.7998761092251,135.34041592014));
#168002=CARTESIAN_POINT('Ctrl Pts',(-176.191201281761,3.73573949061561,
135.393378534495));
#168003=CARTESIAN_POINT('Ctrl Pts',(-176.18726523232,3.67056894072435,135.444926769868));
#168004=CARTESIAN_POINT('Ctrl Pts',(-176.179841965914,3.54765931753379,
135.542145133014));
#168005=CARTESIAN_POINT('Ctrl Pts',(-176.172418699509,3.42069879763591,
135.63462406872));
#168006=CARTESIAN_POINT('Ctrl Pts',(-176.164995433103,3.2900889174967,135.722006952701));
#168007=CARTESIAN_POINT('Ctrl Pts',(-176.157580940382,3.15963340738935,
135.809286557369));
#168008=CARTESIAN_POINT('Ctrl Pts',(-176.150166447661,3.02553742980314,
135.891481893796));
#168009=CARTESIAN_POINT('Ctrl Pts',(-176.14275195494,2.88823594702113,135.968276154911));
#168010=CARTESIAN_POINT('Ctrl Pts',(-176.135344608586,2.75106680057753,
136.044996398826));
#168011=CARTESIAN_POINT('Ctrl Pts',(-176.127937262233,2.6106986233099,136.116325750071));
#168012=CARTESIAN_POINT('Ctrl Pts',(-176.120529915879,2.46759565398815,
136.181990416178));
#168013=CARTESIAN_POINT('Ctrl Pts',(-176.113128094203,2.32459941625988,
136.247606107099));
#168014=CARTESIAN_POINT('Ctrl Pts',(-176.105726272528,2.17887278564117,
136.307565370285));
#168015=CARTESIAN_POINT('Ctrl Pts',(-176.098324450853,2.03090482129261,
136.361640183086));
#168016=CARTESIAN_POINT('Ctrl Pts',(-176.090926536541,1.88301496808065,
136.415686450215));
#168017=CARTESIAN_POINT('Ctrl Pts',(-176.08352862223,1.73288648723452,136.463854325608));
#168018=CARTESIAN_POINT('Ctrl Pts',(-176.076130707919,1.5810285428379,136.505963840277));
#168019=CARTESIAN_POINT('Ctrl Pts',(-176.068734023006,1.42919583447687,
136.54806635711));
#168020=CARTESIAN_POINT('Ctrl Pts',(-176.061337338094,1.27563459235188,
136.584112411747));
#168021=CARTESIAN_POINT('Ctrl Pts',(-176.053940653182,1.12086938792917,
136.61397182467));
#168022=CARTESIAN_POINT('Ctrl Pts',(-176.046544296246,0.966111045957819,
136.643829913595));
#168023=CARTESIAN_POINT('Ctrl Pts',(-176.039147939311,0.810149214374073,
136.667501835533));
#168024=CARTESIAN_POINT('Ctrl Pts',(-176.031751582376,0.653518644899017,
136.684908546396));
#168025=CARTESIAN_POINT('Ctrl Pts',(-176.024354093039,0.496864094883469,
136.702317922271));
#168026=CARTESIAN_POINT('Ctrl Pts',(-176.016956603702,0.339540974151185,
136.713460135902));
#168027=CARTESIAN_POINT('Ctrl Pts',(-176.009559114366,0.182088994122295,
136.718308043839));
#168028=CARTESIAN_POINT('Ctrl Pts',(-176.002159031851,0.0245818195456645,
136.723157651202));
#168029=CARTESIAN_POINT('Ctrl Pts',(-175.994758949336,-0.133053931375224,
136.721708548347));
#168030=CARTESIAN_POINT('Ctrl Pts',(-175.987358866821,-0.290278858964217,
136.713985711135));
#168031=CARTESIAN_POINT('Ctrl Pts',(-175.979950647154,-0.447676671523984,
136.706254381869));
#168032=CARTESIAN_POINT('Ctrl Pts',(-175.972542427488,-0.604662385515286,
136.692235559584));
#168033=CARTESIAN_POINT('Ctrl Pts',(-175.965134207821,-0.760701296722034,
136.672006150458));
#168034=CARTESIAN_POINT('Ctrl Pts',(-175.957721428519,-0.916836247274981,
136.651764290468));
#168035=CARTESIAN_POINT('Ctrl Pts',(-175.950308649217,-1.07202286672424,
136.625304289398));
#168036=CARTESIAN_POINT('Ctrl Pts',(-175.942895869915,-1.22573745701421,
136.592754025842));
#168037=CARTESIAN_POINT('Ctrl Pts',(-175.935472498886,-1.37967168191951,
136.560157252942));
#168038=CARTESIAN_POINT('Ctrl Pts',(-175.928049127857,-1.53212931603322,
136.521452929216));
#168039=CARTESIAN_POINT('Ctrl Pts',(-175.920625756829,-1.6826018118403,
136.476818788879));
#168040=CARTESIAN_POINT('Ctrl Pts',(-175.916689707388,-1.76238593965281,
136.453152696691));
#168041=CARTESIAN_POINT('Ctrl Pts',(-175.912753657947,-1.84161229606844,
136.427820329755));
#168042=CARTESIAN_POINT('Ctrl Pts',(-175.908817608507,-1.92020756050174,
136.400853580761));
#168043=CARTESIAN_POINT('Ctrl Pts',(-175.901394342101,-2.06843577635333,
136.34999513376));
#168044=CARTESIAN_POINT('Ctrl Pts',(-175.893971075696,-2.21486618629056,
136.293166776334));
#168045=CARTESIAN_POINT('Ctrl Pts',(-175.88654780929,-2.35898171193482,
136.230513568346));
#168046=CARTESIAN_POINT('Ctrl Pts',(-175.879133316569,-2.50292690499581,
136.167934411247));
#168047=CARTESIAN_POINT('Ctrl Pts',(-175.871718823848,-2.64456232078667,
136.099544254579));
#168048=CARTESIAN_POINT('Ctrl Pts',(-175.864304331127,-2.7833863128084,
136.025537802471));
#168049=CARTESIAN_POINT('Ctrl Pts',(-175.856896984773,-2.92207650103999,
135.951602680568));
#168050=CARTESIAN_POINT('Ctrl Pts',(-175.849489638419,-3.0579603328917,
135.872062214263));
#168051=CARTESIAN_POINT('Ctrl Pts',(-175.842082292066,-3.19055652661036,
135.787158989265));
#168052=CARTESIAN_POINT('Ctrl Pts',(-175.83468047039,-3.32305382508517,
135.702319088295));
#168053=CARTESIAN_POINT('Ctrl Pts',(-175.827278648715,-3.45226805475828,
135.612124593101));
#168054=CARTESIAN_POINT('Ctrl Pts',(-175.819876827039,-3.57774302529583,
135.516863711193));
#168055=CARTESIAN_POINT('Ctrl Pts',(-175.812478912728,-3.70315175857313,
135.421653116764));
#168056=CARTESIAN_POINT('Ctrl Pts',(-175.805080998417,-3.82482486731538,
135.321381687183));
#168057=CARTESIAN_POINT('Ctrl Pts',(-175.797683084105,-3.94233572289361,
135.216380518983));
#168058=CARTESIAN_POINT('Ctrl Pts',(-175.790286399193,-4.05982705029934,
135.111396800071));
#168059=CARTESIAN_POINT('Ctrl Pts',(-175.782889714281,-4.17315721925357,
135.001685150996));
#168060=CARTESIAN_POINT('Ctrl Pts',(-175.775493029369,-4.28193316234904,
134.887616543378));
#168061=CARTESIAN_POINT('Ctrl Pts',(-175.768096672433,-4.3907042822052,
134.773552993681));
#168062=CARTESIAN_POINT('Ctrl Pts',(-175.760700315498,-4.49492132010646,
134.655133139727));
#168063=CARTESIAN_POINT('Ctrl Pts',(-175.753303958562,-4.59422872765494,
134.532764158023));
#168064=CARTESIAN_POINT('Ctrl Pts',(-175.745906469226,-4.69355133942103,
134.410376441315));
#168065=CARTESIAN_POINT('Ctrl Pts',(-175.738508979889,-4.78796258889911,
134.284038682851));
#168066=CARTESIAN_POINT('Ctrl Pts',(-175.731111490553,-4.87714791233018,
134.154190285438));
#168067=CARTESIAN_POINT('Ctrl Pts',(-175.723711408037,-4.9663644995385,
134.024296369869));
#168068=CARTESIAN_POINT('Ctrl Pts',(-175.716311325522,-5.05035130210546,
133.890889672652));
#168069=CARTESIAN_POINT('Ctrl Pts',(-175.708911243007,-5.12883777423118,
133.754437506076));
#168070=CARTESIAN_POINT('Ctrl Pts',(-175.701503023341,-5.20741055030126,
133.617835296315));
#168071=CARTESIAN_POINT('Ctrl Pts',(-175.694094803674,-5.28047073108043,
133.478181253193));
#168072=CARTESIAN_POINT('Ctrl Pts',(-175.686686584008,-5.347793999225,133.33596680818));
#168073=CARTESIAN_POINT('Ctrl Pts',(-175.679273804706,-5.41515870371796,
133.193664832547));
#168074=CARTESIAN_POINT('Ctrl Pts',(-175.671861025404,-5.47677931388848,
133.048799657591));
#168075=CARTESIAN_POINT('Ctrl Pts',(-175.664448246102,-5.53248034602625,
132.901881006819));
#168076=CARTESIAN_POINT('Ctrl Pts',(-175.657024875073,-5.58826096641077,
132.75475243179));
#168077=CARTESIAN_POINT('Ctrl Pts',(-175.649601504044,-5.63810499791941,
132.605564874005));
#168078=CARTESIAN_POINT('Ctrl Pts',(-175.642178133015,-5.68188709102735,
132.454842258578));
#168079=CARTESIAN_POINT('Ctrl Pts',(-175.638242083575,-5.70510140732827,
132.374925511345));
#168080=CARTESIAN_POINT('Ctrl Pts',(-175.634306034134,-5.72661235042798,
132.294577370783));
#168081=CARTESIAN_POINT('Ctrl Pts',(-175.630369984694,-5.7464071209827,
132.213876762354));
#168082=CARTESIAN_POINT('Ctrl Pts',(-175.620466734164,-5.79621151875603,
132.010830953281));
#168083=CARTESIAN_POINT('Ctrl Pts',(-175.610563483633,-5.83527224067263,
131.805053969676));
#168084=CARTESIAN_POINT('Ctrl Pts',(-175.600660233103,-5.86334628783755,
131.597519410874));
#168085=CARTESIAN_POINT('Ctrl Pts',(-175.590995694119,-5.89074362797718,
131.394987340424));
#168086=CARTESIAN_POINT('Ctrl Pts',(-175.581331155135,-5.90767763415524,
131.1907810782));
#168087=CARTESIAN_POINT('Ctrl Pts',(-175.571666616152,-5.91396652719755,
130.985828184054));
#168088=CARTESIAN_POINT('Ctrl Pts',(-175.568902812819,-5.91576498479371,
130.927217060148));
#168089=CARTESIAN_POINT('Ctrl Pts',(-175.566139009486,-5.91669315462093,
130.868545037559));
#168090=CARTESIAN_POINT('Ctrl Pts',(-175.563375206154,-5.91674746817804,
130.809834218641));
#168091=CARTESIAN_POINT('',(-173.813375192207,-5.90703979259401,130.803529349416));
#168092=CARTESIAN_POINT('Ctrl Pts',(-175.563375192208,-5.91627067345725,
130.809833481333));
#168093=CARTESIAN_POINT('Ctrl Pts',(-175.492890915099,-5.90250338860239,
129.312659330916));
#168094=CARTESIAN_POINT('Ctrl Pts',(-175.329590763386,-4.56443645972603,
125.822059968559));
#168095=CARTESIAN_POINT('Ctrl Pts',(-175.073474737067,1.30891178749135,
123.929456220927));
#168096=CARTESIAN_POINT('Ctrl Pts',(-174.795027113256,6.49155056939029,
128.189531419434));
#168097=CARTESIAN_POINT('Ctrl Pts',(-174.516579489441,5.70877150789232,
134.852506909512));
#168098=CARTESIAN_POINT('Ctrl Pts',(-174.238131865631,-0.320089680364641,
137.795433720237));
#168099=CARTESIAN_POINT('Ctrl Pts',(-174.003730433218,-5.14765923758726,
134.864630788722));
#168100=CARTESIAN_POINT('Ctrl Pts',(-173.86214487541,-5.90574070942643,
131.843544224169));
#168101=CARTESIAN_POINT('Ctrl Pts',(-173.813375192207,-5.90703979259401,
130.803529349416));
#168102=CARTESIAN_POINT('',(-172.06337600335,-5.91851287666386,130.799189814356));
#168103=CARTESIAN_POINT('Ctrl Pts',(-173.813375192207,-5.90703979259401,
130.803529349416));
#168104=CARTESIAN_POINT('Ctrl Pts',(-173.769329000806,-5.90821305561495,
129.864243071036));
#168105=CARTESIAN_POINT('Ctrl Pts',(-173.632466934801,-5.25333338380343,
126.947201347647));
#168106=CARTESIAN_POINT('Ctrl Pts',(-173.40278899419,-0.675210770690227,
123.838612205118));
#168107=CARTESIAN_POINT('Ctrl Pts',(-173.124341370378,5.49551350513835,
126.471129508431));
#168108=CARTESIAN_POINT('Ctrl Pts',(-172.845893746565,6.61612934050591,
133.085674510926));
#168109=CARTESIAN_POINT('Ctrl Pts',(-172.567446122752,1.65684552783385,
137.603803493805));
#168110=CARTESIAN_POINT('Ctrl Pts',(-172.306607000367,-4.4150988260753,
135.982992920257));
#168111=CARTESIAN_POINT('Ctrl Pts',(-172.138583752587,-5.90466033572452,
132.394578448931));
#168112=CARTESIAN_POINT('Ctrl Pts',(-172.063376379411,-5.91933123059252,
130.799197074345));
#168113=CARTESIAN_POINT('',(-170.313373776064,-5.92100765474907,130.807582161906));
#168114=CARTESIAN_POINT('Ctrl Pts',(-172.063375192207,-5.91674772684328,
130.799174154912));
#168115=CARTESIAN_POINT('Ctrl Pts',(-172.052420060435,-5.91654410871785,
130.566885375217));
#168116=CARTESIAN_POINT('Ctrl Pts',(-172.041464928663,-5.90265803068872,
130.335172335765));
#168117=CARTESIAN_POINT('Ctrl Pts',(-172.03050979689,-5.87531071615658,
130.105322313096));
#168118=CARTESIAN_POINT('Ctrl Pts',(-172.023856822969,-5.85870288576437,
129.965736022543));
#168119=CARTESIAN_POINT('Ctrl Pts',(-172.017203849047,-5.83713132794981,
129.826836005019));
#168120=CARTESIAN_POINT('Ctrl Pts',(-172.010550875126,-5.81065316603754,
129.688905398152));
#168121=CARTESIAN_POINT('Ctrl Pts',(-172.003127608721,-5.78110931810908,
129.535004954177));
#168122=CARTESIAN_POINT('Ctrl Pts',(-171.995704342315,-5.74540228303988,
129.382046349289));
#168123=CARTESIAN_POINT('Ctrl Pts',(-171.988281075909,-5.70360308744345,
129.230561906356));
#168124=CARTESIAN_POINT('Ctrl Pts',(-171.980866583188,-5.66185329502501,
129.079256505455));
#168125=CARTESIAN_POINT('Ctrl Pts',(-171.973452090467,-5.61402577289467,
128.929422154712));
#168126=CARTESIAN_POINT('Ctrl Pts',(-171.966037597746,-5.56024286681052,
128.78158286789));
#168127=CARTESIAN_POINT('Ctrl Pts',(-171.958630251392,-5.50651179871599,
128.633886074139));
#168128=CARTESIAN_POINT('Ctrl Pts',(-171.951222905038,-5.44683690068766,
128.488180864608));
#168129=CARTESIAN_POINT('Ctrl Pts',(-171.943815558684,-5.38139078496531,
128.344977812472));
#168130=CARTESIAN_POINT('Ctrl Pts',(-171.936413737009,-5.31599348142539,
128.201881566576));
#168131=CARTESIAN_POINT('Ctrl Pts',(-171.929011915333,-5.24483368531546,
128.061284100271));
#168132=CARTESIAN_POINT('Ctrl Pts',(-171.921610093658,-5.16813270157619,
127.923677549022));
#168133=CARTESIAN_POINT('Ctrl Pts',(-171.914212179347,-5.09147220768898,
127.786143639199));
#168134=CARTESIAN_POINT('Ctrl Pts',(-171.906814265035,-5.00927653303559,
127.651597825255));
#168135=CARTESIAN_POINT('Ctrl Pts',(-171.899416350724,-4.92181359715705,
127.520508995257));
#168136=CARTESIAN_POINT('Ctrl Pts',(-171.892019665812,-4.83436519603208,
127.389441949846));
#168137=CARTESIAN_POINT('Ctrl Pts',(-171.884622980899,-4.74165147792062,
127.261831058413));
#168138=CARTESIAN_POINT('Ctrl Pts',(-171.877226295987,-4.64398455440899,
127.13811757858));
#168139=CARTESIAN_POINT('Ctrl Pts',(-171.869829939052,-4.54632196155081,
127.014409584333));
#168140=CARTESIAN_POINT('Ctrl Pts',(-171.862433582116,-4.44370683130106,
126.894598951067));
#168141=CARTESIAN_POINT('Ctrl Pts',(-171.85503722518,-4.33649238910272,
126.779094872084));
#168142=CARTESIAN_POINT('Ctrl Pts',(-171.847639735844,-4.22926153209957,
126.663573109131));
#168143=CARTESIAN_POINT('Ctrl Pts',(-171.840242246507,-4.11743021503611,
126.552359486918));
#168144=CARTESIAN_POINT('Ctrl Pts',(-171.832844757171,-4.00138932459684,
126.445827144538));
#168145=CARTESIAN_POINT('Ctrl Pts',(-171.825444674656,-3.88530775620348,
126.339257457412));
#168146=CARTESIAN_POINT('Ctrl Pts',(-171.818044592141,-3.76501395122304,
126.237372569665));
#168147=CARTESIAN_POINT('Ctrl Pts',(-171.810644509626,-3.64093260939317,
126.140505956842));
#168148=CARTESIAN_POINT('Ctrl Pts',(-171.803236289959,-3.5167148273719,
126.043532829219));
#168149=CARTESIAN_POINT('Ctrl Pts',(-171.795828070293,-3.38870148558098,
125.951589226399));
#168150=CARTESIAN_POINT('Ctrl Pts',(-171.788419850626,-3.25734765439931,
125.864966239621));
#168151=CARTESIAN_POINT('Ctrl Pts',(-171.781007071324,-3.12591297712631,
125.778289937839));
#168152=CARTESIAN_POINT('Ctrl Pts',(-171.773594292022,-2.99113403244836,
125.696940969901));
#168153=CARTESIAN_POINT('Ctrl Pts',(-171.76618151272,-2.85349085772153,
125.621164645253));
#168154=CARTESIAN_POINT('Ctrl Pts',(-171.758758141691,-2.71565101197164,
125.545280047839));
#168155=CARTESIAN_POINT('Ctrl Pts',(-171.751334770662,-2.57493909550023,
125.47498416291));
#168156=CARTESIAN_POINT('Ctrl Pts',(-171.743911399634,-2.43185624531328,
125.410474656162));
#168157=CARTESIAN_POINT('Ctrl Pts',(-171.739975350194,-2.35599028493666,
125.376270167808));
#168158=CARTESIAN_POINT('Ctrl Pts',(-171.736039300754,-2.27945805489288,
125.34369161463));
#168159=CARTESIAN_POINT('Ctrl Pts',(-171.732103251314,-2.20233590191188,
125.312762750128));
#168160=CARTESIAN_POINT('Ctrl Pts',(-171.724679984909,-2.05688592825637,
125.25443187692));
#168161=CARTESIAN_POINT('Ctrl Pts',(-171.717256718503,-1.90889699730604,
125.201795354637));
#168162=CARTESIAN_POINT('Ctrl Pts',(-171.709833452098,-1.75885535898401,
125.155081160089));
#168163=CARTESIAN_POINT('Ctrl Pts',(-171.702418959377,-1.6089910574183,
125.108422177839));
#168164=CARTESIAN_POINT('Ctrl Pts',(-171.695004466656,-1.45707923064753,
125.06767170027));
#168165=CARTESIAN_POINT('Ctrl Pts',(-171.687589973935,-1.30362687716122,
125.033010036667));
#168166=CARTESIAN_POINT('Ctrl Pts',(-171.680182627581,-1.15032242683059,
124.998381781281));
#168167=CARTESIAN_POINT('Ctrl Pts',(-171.672775281227,-0.995480767443993,
124.969830738274));
#168168=CARTESIAN_POINT('Ctrl Pts',(-171.665367934874,-0.839624759804996,
124.947487661353));
#168169=CARTESIAN_POINT('Ctrl Pts',(-171.657966113198,-0.683884995456607,
124.925161248741));
#168170=CARTESIAN_POINT('Ctrl Pts',(-171.650564291523,-0.527132757157224,
124.909033635737));
#168171=CARTESIAN_POINT('Ctrl Pts',(-171.643162469847,-0.369901713135807,
124.899184643463));
#168172=CARTESIAN_POINT('Ctrl Pts',(-171.635764555536,-0.212753670158198,
124.889340850396));
#168173=CARTESIAN_POINT('Ctrl Pts',(-171.628366641225,-0.0551276964624343,
124.885769100483));
#168174=CARTESIAN_POINT('Ctrl Pts',(-171.620968726913,0.102436902084779,
124.88849743088));
#168175=CARTESIAN_POINT('Ctrl Pts',(-171.613572042001,0.259975316254002,
124.891225307877));
#168176=CARTESIAN_POINT('Ctrl Pts',(-171.606175357089,0.417452002641037,
124.900251180824));
#168177=CARTESIAN_POINT('Ctrl Pts',(-171.598778672177,0.574327014776075,
124.915550971925));
#168178=CARTESIAN_POINT('Ctrl Pts',(-171.591382315241,0.731195070908682,
124.930850084617));
#168179=CARTESIAN_POINT('Ctrl Pts',(-171.583985958306,0.887461134301129,
124.952422526089));
#168180=CARTESIAN_POINT('Ctrl Pts',(-171.57658960137,1.04259001206037,124.980192296745));
#168181=CARTESIAN_POINT('Ctrl Pts',(-171.569192112034,1.19774264044638,
125.007966319024));
#168182=CARTESIAN_POINT('Ctrl Pts',(-171.561794622697,1.35175736905057,
125.041939493946));
#168183=CARTESIAN_POINT('Ctrl Pts',(-171.55439713336,1.50410898158405,125.081984648266));
#168184=CARTESIAN_POINT('Ctrl Pts',(-171.546997050845,1.65651400073979,
125.122043840354));
#168185=CARTESIAN_POINT('Ctrl Pts',(-171.53959696833,1.80725438226129,125.168179154876));
#168186=CARTESIAN_POINT('Ctrl Pts',(-171.532196885815,1.95582000314838,
125.220213531593));
#168187=CARTESIAN_POINT('Ctrl Pts',(-171.524788666149,2.10454898720834,
125.272305125455));
#168188=CARTESIAN_POINT('Ctrl Pts',(-171.517380446482,2.25109808237563,
125.330308612257));
#168189=CARTESIAN_POINT('Ctrl Pts',(-171.509972226816,2.39497640869152,
125.393998470324));
#168190=CARTESIAN_POINT('Ctrl Pts',(-171.502559447514,2.53894328971694,
125.457727528436));
#168191=CARTESIAN_POINT('Ctrl Pts',(-171.495146668212,2.68023579212227,
125.5271497675));
#168192=CARTESIAN_POINT('Ctrl Pts',(-171.487733888909,2.81838805820637,
125.601993914241));
#168193=CARTESIAN_POINT('Ctrl Pts',(-171.480310517881,2.95673772272675,
125.676945001809));
#168194=CARTESIAN_POINT('Ctrl Pts',(-171.472887146852,3.09193786953243,
125.757333279426));
#168195=CARTESIAN_POINT('Ctrl Pts',(-171.465463775823,3.22355132008199,
125.842843969474));
#168196=CARTESIAN_POINT('Ctrl Pts',(-171.461527726382,3.29333592958626,
125.888183789139));
#168197=CARTESIAN_POINT('Ctrl Pts',(-171.457591676941,3.36211272880741,
125.934963018023));
#168198=CARTESIAN_POINT('Ctrl Pts',(-171.4536556275,3.4298204659807,125.983130262808));
#168199=CARTESIAN_POINT('Ctrl Pts',(-171.446232361095,3.55751514520048,
126.073972183222));
#168200=CARTESIAN_POINT('Ctrl Pts',(-171.43880909469,3.68179137415032,126.170028136082));
#168201=CARTESIAN_POINT('Ctrl Pts',(-171.431385828284,3.80219451952221,
126.271012252592));
#168202=CARTESIAN_POINT('Ctrl Pts',(-171.423971335563,3.92245535837514,
126.371877014262));
#168203=CARTESIAN_POINT('Ctrl Pts',(-171.416556842842,4.03885194229015,
126.477658107978));
#168204=CARTESIAN_POINT('Ctrl Pts',(-171.409142350121,4.15095852688988,
126.588026443127));
#168205=CARTESIAN_POINT('Ctrl Pts',(-171.401735003767,4.26295705894264,
126.69828840112));
#168206=CARTESIAN_POINT('Ctrl Pts',(-171.394327657414,4.37067355914808,
126.813128538362));
#168207=CARTESIAN_POINT('Ctrl Pts',(-171.38692031106,4.47371540167417,126.932177632824));
#168208=CARTESIAN_POINT('Ctrl Pts',(-171.379518489384,4.57668039170655,
127.05113793598));
#168209=CARTESIAN_POINT('Ctrl Pts',(-171.372116667709,4.67497742297217,
127.174300664748));
#168210=CARTESIAN_POINT('Ctrl Pts',(-171.364714846034,4.76825087898503,
127.301259974199));
#168211=CARTESIAN_POINT('Ctrl Pts',(-171.357316931722,4.8614750966665,127.428152262819));
#168212=CARTESIAN_POINT('Ctrl Pts',(-171.349919017411,4.94968080003645,
127.558836840615));
#168213=CARTESIAN_POINT('Ctrl Pts',(-171.3425211031,5.03255289264745,127.692875129056));
#168214=CARTESIAN_POINT('Ctrl Pts',(-171.335124418187,5.11541121342024,
127.826891142766));
#168215=CARTESIAN_POINT('Ctrl Pts',(-171.327727733275,5.19293748645846,
127.964259443792));
#168216=CARTESIAN_POINT('Ctrl Pts',(-171.320331048363,5.26486011483673,
128.10451274524));
#168217=CARTESIAN_POINT('Ctrl Pts',(-171.312934691428,5.3367795540903,128.244759827711));
#168218=CARTESIAN_POINT('Ctrl Pts',(-171.305538334492,5.40309567239127,
128.387891324079));
#168219=CARTESIAN_POINT('Ctrl Pts',(-171.298141977557,5.46358312551962,
128.533415881771));
#168220=CARTESIAN_POINT('Ctrl Pts',(-171.29074448822,5.52407983943146,128.678962719643));
#168221=CARTESIAN_POINT('Ctrl Pts',(-171.283346998884,5.57874596802939,
128.826903003628));
#168222=CARTESIAN_POINT('Ctrl Pts',(-171.275949509547,5.62740461353139,
128.976726114142));
#168223=CARTESIAN_POINT('Ctrl Pts',(-171.268549427032,5.67608031624607,
129.126601744915));
#168224=CARTESIAN_POINT('Ctrl Pts',(-171.261149344517,5.71874422776907,
129.278361161495));
#168225=CARTESIAN_POINT('Ctrl Pts',(-171.253749262002,5.75526957995392,
129.43147947757));
#168226=CARTESIAN_POINT('Ctrl Pts',(-171.246341042336,5.79183509551844,
129.584766162974));
#168227=CARTESIAN_POINT('Ctrl Pts',(-171.238932822669,5.82224848492687,
129.739414368654));
#168228=CARTESIAN_POINT('Ctrl Pts',(-171.231524603003,5.84643415334193,
129.894889203426));
#168229=CARTESIAN_POINT('Ctrl Pts',(-171.224111823701,5.87063470763234,
130.050459730365));
#168230=CARTESIAN_POINT('Ctrl Pts',(-171.216699044399,5.88859986057887,
130.206857530197));
#168231=CARTESIAN_POINT('Ctrl Pts',(-171.209286265097,5.90030603460425,
130.363544033812));
#168232=CARTESIAN_POINT('Ctrl Pts',(-171.201862894068,5.91202893496002,
130.520454418451));
#168233=CARTESIAN_POINT('Ctrl Pts',(-171.194439523039,5.91747498208225,
130.67765395867));
#168234=CARTESIAN_POINT('Ctrl Pts',(-171.187016152011,5.91667270161625,
130.834604698789));
#168235=CARTESIAN_POINT('Ctrl Pts',(-171.18308010257,5.91624731326271,130.917823747185));
#168236=CARTESIAN_POINT('Ctrl Pts',(-171.179144053129,5.91406616309129,
131.000972932089));
#168237=CARTESIAN_POINT('Ctrl Pts',(-171.175208003688,5.91013938168198,
131.083972941314));
#168238=CARTESIAN_POINT('Ctrl Pts',(-171.167784737282,5.90273359449494,
131.240508368364));
#168239=CARTESIAN_POINT('Ctrl Pts',(-171.160361470877,5.88909333827066,
131.396986068284));
#168240=CARTESIAN_POINT('Ctrl Pts',(-171.152938204471,5.86921338211624,
131.552869026128));
#168241=CARTESIAN_POINT('Ctrl Pts',(-171.14552371175,5.849356922419,131.708567743261));
#168242=CARTESIAN_POINT('Ctrl Pts',(-171.138109219029,5.8232754891494,131.863672750833));
#168243=CARTESIAN_POINT('Ctrl Pts',(-171.130694726308,5.79101583032626,
132.017647976525));
#168244=CARTESIAN_POINT('Ctrl Pts',(-171.123287379954,5.75878726457693,
132.171474795098));
#168245=CARTESIAN_POINT('Ctrl Pts',(-171.115880033601,5.72039240415578,
132.324173636717));
#168246=CARTESIAN_POINT('Ctrl Pts',(-171.108472687247,5.67592966216109,
132.475214600624));
#168247=CARTESIAN_POINT('Ctrl Pts',(-171.101070865572,5.63150008215673,
132.626142912482));
#168248=CARTESIAN_POINT('Ctrl Pts',(-171.093669043896,5.58101173673197,
132.775415452119));
#168249=CARTESIAN_POINT('Ctrl Pts',(-171.086267222221,5.52461385532159,
132.922513660216));
#168250=CARTESIAN_POINT('Ctrl Pts',(-171.078869307909,5.4682457459138,133.069534216315));
#168251=CARTESIAN_POINT('Ctrl Pts',(-171.071471393598,5.40597444664899,
133.214382379123));
#168252=CARTESIAN_POINT('Ctrl Pts',(-171.064073479287,5.33799862874087,
133.356555986667));
#168253=CARTESIAN_POINT('Ctrl Pts',(-171.056676794374,5.27003410718058,
133.498705967536));
#168254=CARTESIAN_POINT('Ctrl Pts',(-171.049280109462,5.19636710931638,
133.638181938813));
#168255=CARTESIAN_POINT('Ctrl Pts',(-171.04188342455,5.11724397207349,133.774502818333));
#168256=CARTESIAN_POINT('Ctrl Pts',(-171.034487067614,5.03812434323341,
133.910817653242));
#168257=CARTESIAN_POINT('Ctrl Pts',(-171.027090710679,4.95354924344627,
134.043977351708));
#168258=CARTESIAN_POINT('Ctrl Pts',(-171.019694353743,4.86381025749459,
134.173526737185));
#168259=CARTESIAN_POINT('Ctrl Pts',(-171.012296864407,4.77405753227506,
134.303095957005));
#168260=CARTESIAN_POINT('Ctrl Pts',(-171.00489937507,4.67913955927308,134.429053456356));
#168261=CARTESIAN_POINT('Ctrl Pts',(-170.997501885733,4.57939031963322,
134.550974403767));
#168262=CARTESIAN_POINT('Ctrl Pts',(-170.990101803218,4.47960611305218,
134.672938090377));
#168263=CARTESIAN_POINT('Ctrl Pts',(-170.982701720704,4.37498750413481,
134.790862119037));
#168264=CARTESIAN_POINT('Ctrl Pts',(-170.975301638189,4.26590757332199,
134.904356122243));
#168265=CARTESIAN_POINT('Ctrl Pts',(-170.967893418522,4.15670769791139,
135.017974923773));
#168266=CARTESIAN_POINT('Ctrl Pts',(-170.960485198855,4.04303696247064,
135.127153702297));
#168267=CARTESIAN_POINT('Ctrl Pts',(-170.953076979189,3.92530452524635,
135.231539735987));
#168268=CARTESIAN_POINT('Ctrl Pts',(-170.945664199887,3.80749962567142,
135.335990017538));
#168269=CARTESIAN_POINT('Ctrl Pts',(-170.938251420585,3.68562833124752,
135.435641440549));
#168270=CARTESIAN_POINT('Ctrl Pts',(-170.930838641283,3.56013101116293,
135.530183058777));
#168271=CARTESIAN_POINT('Ctrl Pts',(-170.923415270254,3.43445437462199,
135.624859762503));
#168272=CARTESIAN_POINT('Ctrl Pts',(-170.915991899225,3.30514167080891,
135.714411867488));
#168273=CARTESIAN_POINT('Ctrl Pts',(-170.908568528196,3.17266091588127,
135.798572594979));
#168274=CARTESIAN_POINT('Ctrl Pts',(-170.904632478756,3.10241644079015,
135.843196632102));
#168275=CARTESIAN_POINT('Ctrl Pts',(-170.900696429315,3.03128171168346,
135.886305734158));
#168276=CARTESIAN_POINT('Ctrl Pts',(-170.896760379875,2.95932893197784,
135.927865554117));
#168277=CARTESIAN_POINT('Ctrl Pts',(-170.889337113469,2.82362823501603,
136.006246077524));
#168278=CARTESIAN_POINT('Ctrl Pts',(-170.881913847064,2.6846062227242,136.079350162637));
#168279=CARTESIAN_POINT('Ctrl Pts',(-170.874490580658,2.54271187355959,
136.146883138862));
#168280=CARTESIAN_POINT('Ctrl Pts',(-170.867076087937,2.40098523173209,
136.214336296718));
#168281=CARTESIAN_POINT('Ctrl Pts',(-170.859661595216,2.256393344304,136.276231293486));
#168282=CARTESIAN_POINT('Ctrl Pts',(-170.852247102495,2.10941249254478,
136.332317699418));
#168283=CARTESIAN_POINT('Ctrl Pts',(-170.844839756142,1.9625733064638,136.38835004716));
#168284=CARTESIAN_POINT('Ctrl Pts',(-170.837432409788,1.81335008644968,
136.43858481746));
#168285=CARTESIAN_POINT('Ctrl Pts',(-170.830025063434,1.66224184770144,
136.482818383742));
#168286=CARTESIAN_POINT('Ctrl Pts',(-170.822623241758,1.51124631117908,
136.527018958962));
#168287=CARTESIAN_POINT('Ctrl Pts',(-170.815221420083,1.35836891201696,
136.56522713791));
#168288=CARTESIAN_POINT('Ctrl Pts',(-170.807819598408,1.20412659101033,
136.597288177559));
#168289=CARTESIAN_POINT('Ctrl Pts',(-170.800421684096,1.0499656933239,136.629332292434));
#168290=CARTESIAN_POINT('Ctrl Pts',(-170.793023769785,0.89444167332675,
136.655235654859));
#168291=CARTESIAN_POINT('Ctrl Pts',(-170.785625855474,0.738084400753971,
136.674893981739));
#168292=CARTESIAN_POINT('Ctrl Pts',(-170.778229170562,0.581753111923507,
136.694549041761));
#168293=CARTESIAN_POINT('Ctrl Pts',(-170.770832485649,0.424589215361653,
136.707961079465));
#168294=CARTESIAN_POINT('Ctrl Pts',(-170.763435800737,0.267130610244179,
136.715077308423));
#168295=CARTESIAN_POINT('Ctrl Pts',(-170.756039443802,0.10967898700626,
136.722193221839));
#168296=CARTESIAN_POINT('Ctrl Pts',(-170.748643086866,-0.048066945887389,
136.723013864724));
#168297=CARTESIAN_POINT('Ctrl Pts',(-170.741246729931,-0.205566626822125,
136.717538521573));
#168298=CARTESIAN_POINT('Ctrl Pts',(-170.733849240594,-0.36309042136009,
136.712062340133));
#168299=CARTESIAN_POINT('Ctrl Pts',(-170.726451751258,-0.520367515773337,
136.700288266313));
#168300=CARTESIAN_POINT('Ctrl Pts',(-170.719054261921,-0.676859962346667,
136.682267656119));
#168301=CARTESIAN_POINT('Ctrl Pts',(-170.711654179406,-0.833407267104324,
136.664240728829));
#168302=CARTESIAN_POINT('Ctrl Pts',(-170.704254096891,-0.989169005769536,
136.639962948139));
#168303=CARTESIAN_POINT('Ctrl Pts',(-170.696854014376,-1.14361509201325,
136.609537194021));
#168304=CARTESIAN_POINT('Ctrl Pts',(-170.68944579471,-1.29823100760645,
136.579077983658));
#168305=CARTESIAN_POINT('Ctrl Pts',(-170.682037575043,-1.45152801514979,
136.542457371241));
#168306=CARTESIAN_POINT('Ctrl Pts',(-170.674629355377,-1.60298819975292,
136.499828938429));
#168307=CARTESIAN_POINT('Ctrl Pts',(-170.667216576075,-1.75454160557242,
136.457174268527));
#168308=CARTESIAN_POINT('Ctrl Pts',(-170.659803796773,-1.90425558153418,
136.408504525213));
#168309=CARTESIAN_POINT('Ctrl Pts',(-170.652391017471,-2.05163048945519,
136.354022129518));
#168310=CARTESIAN_POINT('Ctrl Pts',(-170.644967646442,-2.19921597355562,
136.29946188682));
#168311=CARTESIAN_POINT('Ctrl Pts',(-170.637544275413,-2.34445537077541,
136.239072546953));
#168312=CARTESIAN_POINT('Ctrl Pts',(-170.630120904384,-2.4868712584297,
136.173103664732));
#168313=CARTESIAN_POINT('Ctrl Pts',(-170.626184854943,-2.56238357928856,
136.138125380476));
#168314=CARTESIAN_POINT('Ctrl Pts',(-170.622248805503,-2.63710254641187,
136.101579240896));
#168315=CARTESIAN_POINT('Ctrl Pts',(-170.618312756062,-2.71096023495891,
136.06350742736));
#168316=CARTESIAN_POINT('Ctrl Pts',(-170.610889489656,-2.85025353053517,
135.991705175216));
#168317=CARTESIAN_POINT('Ctrl Pts',(-170.603466223251,-2.98690286120123,
135.914256562637));
#168318=CARTESIAN_POINT('Ctrl Pts',(-170.596042956845,-3.12041762841813,
135.831380051262));
#168319=CARTESIAN_POINT('Ctrl Pts',(-170.588628464124,-3.25377459226752,
135.748601493041));
#168320=CARTESIAN_POINT('Ctrl Pts',(-170.581213971403,-3.38400405301389,
135.660408000716));
#168321=CARTESIAN_POINT('Ctrl Pts',(-170.573799478682,-3.51063787535615,
135.56706491981));
#168322=CARTESIAN_POINT('Ctrl Pts',(-170.566392132329,-3.63714964325312,
135.47381180648));
#168323=CARTESIAN_POINT('Ctrl Pts',(-170.558984785975,-3.76007237362654,
135.375419205661));
#168324=CARTESIAN_POINT('Ctrl Pts',(-170.551577439621,-3.8789650197663,
135.272196887835));
#168325=CARTESIAN_POINT('Ctrl Pts',(-170.544175617946,-3.99776899128467,
135.169051557108));
#168326=CARTESIAN_POINT('Ctrl Pts',(-170.53677379627,-4.11254858283041,
135.061083925489));
#168327=CARTESIAN_POINT('Ctrl Pts',(-170.529371974595,-4.22289418558466,
134.948645267521));
#168328=CARTESIAN_POINT('Ctrl Pts',(-170.521974060284,-4.33318153775447,
134.836265965046));
#168329=CARTESIAN_POINT('Ctrl Pts',(-170.514576145972,-4.43903930187741,
134.719420602469));
#168330=CARTESIAN_POINT('Ctrl Pts',(-170.507178231661,-4.54009333409802,
134.598498606646));
#168331=CARTESIAN_POINT('Ctrl Pts',(-170.499781546749,-4.64113057297164,
134.477596705865));
#168332=CARTESIAN_POINT('Ctrl Pts',(-170.492384861837,-4.73736542517419,
134.352619802561));
#168333=CARTESIAN_POINT('Ctrl Pts',(-170.484988176925,-4.82846273234404,
134.223991914192));
#168334=CARTESIAN_POINT('Ctrl Pts',(-170.477591819989,-4.91955600016382,
134.095369729318));
#168335=CARTESIAN_POINT('Ctrl Pts',(-170.470195463054,-5.00551196015227,
133.963097185903));
#168336=CARTESIAN_POINT('Ctrl Pts',(-170.462799106118,-5.08603782357858,
133.827628686995));
#168337=CARTESIAN_POINT('Ctrl Pts',(-170.455401616782,-5.16657601572014,
133.692139447514));
#168338=CARTESIAN_POINT('Ctrl Pts',(-170.448004127445,-5.24168226519253,
133.553453599168));
#168339=CARTESIAN_POINT('Ctrl Pts',(-170.440606638109,-5.31110900537997,
133.412051491782));
#168340=CARTESIAN_POINT('Ctrl Pts',(-170.433206555594,-5.38056008300366,
133.270599816107));
#168341=CARTESIAN_POINT('Ctrl Pts',(-170.425806473079,-5.44432752296808,
133.126430320487));
#168342=CARTESIAN_POINT('Ctrl Pts',(-170.418406390564,-5.50221135649625,
132.980044590698));
#168343=CARTESIAN_POINT('Ctrl Pts',(-170.410998170897,-5.56015883925006,
132.833497894751));
#168344=CARTESIAN_POINT('Ctrl Pts',(-170.403589951231,-5.61220965793961,
132.684730445189));
#168345=CARTESIAN_POINT('Ctrl Pts',(-170.396181731564,-5.65821307951348,
132.534260993114));
#168346=CARTESIAN_POINT('Ctrl Pts',(-170.388768952262,-5.70424481542559,
132.383698929604));
#168347=CARTESIAN_POINT('Ctrl Pts',(-170.38135617296,-5.74422164295145,
132.231433136422));
#168348=CARTESIAN_POINT('Ctrl Pts',(-170.373943393658,-5.77804379799479,
132.077993386834));
#168349=CARTESIAN_POINT('Ctrl Pts',(-170.36652002263,-5.81191427971941,
131.924334395337));
#168350=CARTESIAN_POINT('Ctrl Pts',(-170.359096651601,-5.83961245964126,
131.769498463773));
#168351=CARTESIAN_POINT('Ctrl Pts',(-170.351673280572,-5.86109023667217,
131.614022151842));
#168352=CARTESIAN_POINT('Ctrl Pts',(-170.347737231131,-5.87247826940697,
131.531584880648));
#168353=CARTESIAN_POINT('Ctrl Pts',(-170.34380118169,-5.88211839398032,
131.44896761632));
#168354=CARTESIAN_POINT('Ctrl Pts',(-170.339865132249,-5.89000938373772,
131.366250306012));
#168355=CARTESIAN_POINT('Ctrl Pts',(-170.331035152235,-5.90771172281953,
131.180685513758));
#168356=CARTESIAN_POINT('Ctrl Pts',(-170.322205172221,-5.91664660285328,
130.994271132306));
#168357=CARTESIAN_POINT('Ctrl Pts',(-170.313375192207,-5.91674910785689,
130.807609798182));
#168358=CARTESIAN_POINT('',(-168.563376377968,-5.91250207745248,130.808001233738));
#168359=CARTESIAN_POINT('Ctrl Pts',(-170.31337267473,-5.92431952931233,
130.807560669157));
#168360=CARTESIAN_POINT('Ctrl Pts',(-170.229387619299,-5.91256351382009,
129.029879967327));
#168361=CARTESIAN_POINT('Ctrl Pts',(-170.052586689264,-4.11503221513579,
125.267038583023));
#168362=CARTESIAN_POINT('Ctrl Pts',(-169.782969884622,2.29137987422938,
124.191710709827));
#168363=CARTESIAN_POINT('Ctrl Pts',(-169.50452226081,6.80195643944412,129.157864602918));
#168364=CARTESIAN_POINT('Ctrl Pts',(-169.226074636996,5.06186733085566,
135.637067897668));
#168365=CARTESIAN_POINT('Ctrl Pts',(-168.947627013185,-1.32983056882352,
137.675249292881));
#168366=CARTESIAN_POINT('Ctrl Pts',(-168.726727900654,-5.43103555014988,
134.283132100589));
#168367=CARTESIAN_POINT('Ctrl Pts',(-168.598644662728,-5.91336715510493,
131.559408908431));
#168368=CARTESIAN_POINT('Ctrl Pts',(-168.563377299405,-5.90920193984457,
130.80801884743));
#168369=CARTESIAN_POINT('',(-166.813373979163,-5.91344434060639,130.799749243495));
#168370=CARTESIAN_POINT('Ctrl Pts',(-168.563375192207,-5.91674889385541,
130.807978567374));
#168371=CARTESIAN_POINT('Ctrl Pts',(-168.55591487972,-5.91684620926024,
130.648830197611));
#168372=CARTESIAN_POINT('Ctrl Pts',(-168.548454567234,-5.91051804296644,
130.489661439869));
#168373=CARTESIAN_POINT('Ctrl Pts',(-168.540994254747,-5.89778612679078,
130.33102208635));
#168374=CARTESIAN_POINT('Ctrl Pts',(-168.533533119083,-5.88505280576286,
130.172365228406));
#168375=CARTESIAN_POINT('Ctrl Pts',(-168.526071983418,-5.8659143555312,
130.014238254263));
#168376=CARTESIAN_POINT('Ctrl Pts',(-168.518610847753,-5.84044445990559,
129.857186360495));
#168377=CARTESIAN_POINT('Ctrl Pts',(-168.511147511828,-5.81496705330743,
129.700088152738));
#168378=CARTESIAN_POINT('Ctrl Pts',(-168.503684175904,-5.78315453978418,
129.544066016489));
#168379=CARTESIAN_POINT('Ctrl Pts',(-168.496220839979,-5.74513183840758,
129.389655446226));
#168380=CARTESIAN_POINT('Ctrl Pts',(-168.48875392566,-5.70709090654714,
129.235170841786));
#168381=CARTESIAN_POINT('Ctrl Pts',(-168.481287011341,-5.66283394199877,
129.082299695985));
#168382=CARTESIAN_POINT('Ctrl Pts',(-168.473820097022,-5.61253586847653,
128.931562794104));
#168383=CARTESIAN_POINT('Ctrl Pts',(-168.466343481839,-5.56217244871151,
128.780630057879));
#168384=CARTESIAN_POINT('Ctrl Pts',(-168.458866866655,-5.50575235689669,
128.631837450325));
#168385=CARTESIAN_POINT('Ctrl Pts',(-168.451390251472,-5.44349922980364,
128.485687139556));
#168386=CARTESIAN_POINT('Ctrl Pts',(-168.443908382716,-5.38120235948349,
128.339434133765));
#168387=CARTESIAN_POINT('Ctrl Pts',(-168.436426513961,-5.31306443944356,
128.19582745407));
#168388=CARTESIAN_POINT('Ctrl Pts',(-168.428944645206,-5.23935515865615,
128.055344778404));
#168389=CARTESIAN_POINT('Ctrl Pts',(-168.421450603008,-5.16552594851533,
127.914633529127));
#168390=CARTESIAN_POINT('Ctrl Pts',(-168.41395656081,-5.08610744715199,
127.777056754815));
#168391=CARTESIAN_POINT('Ctrl Pts',(-168.406462518613,-5.00141337865723,
127.643064241348));
#168392=CARTESIAN_POINT('Ctrl Pts',(-168.401218934261,-4.94215290473659,
127.549309625577));
#168393=CARTESIAN_POINT('Ctrl Pts',(-168.39597534991,-4.88031051355676,
127.457309165077));
#168394=CARTESIAN_POINT('Ctrl Pts',(-168.390731765558,-4.81600516896356,
127.367207031382));
#168395=CARTESIAN_POINT('Ctrl Pts',(-168.383308499153,-4.72496902417803,
127.239650745969));
#168396=CARTESIAN_POINT('Ctrl Pts',(-168.375885232747,-4.62872405528346,
127.115520841736));
#168397=CARTESIAN_POINT('Ctrl Pts',(-168.368461966342,-4.52755682262028,
126.995271516423));
#168398=CARTESIAN_POINT('Ctrl Pts',(-168.361047473621,-4.42650916122441,
126.875164315826));
#168399=CARTESIAN_POINT('Ctrl Pts',(-168.3536329809,-4.32055105421296,126.758928847513));
#168400=CARTESIAN_POINT('Ctrl Pts',(-168.346218488179,-4.21001223972966,
126.646990354548));
#168401=CARTESIAN_POINT('Ctrl Pts',(-168.338811141825,-4.09957996671779,
126.535159752117));
#168402=CARTESIAN_POINT('Ctrl Pts',(-168.331403795471,-3.98457603628079,
126.427618143785));
#168403=CARTESIAN_POINT('Ctrl Pts',(-168.323996449117,-3.86537026753099,
126.324757593035));
#168404=CARTESIAN_POINT('Ctrl Pts',(-168.316594627442,-3.7462534069409,
126.221973759565));
#168405=CARTESIAN_POINT('Ctrl Pts',(-168.309192805766,-3.62294122944443,
126.123864274832));
#168406=CARTESIAN_POINT('Ctrl Pts',(-168.301790984091,-3.49584012068717,
126.030784137285));
#168407=CARTESIAN_POINT('Ctrl Pts',(-168.29439306978,-3.36880610761551,
125.937753136017));
#168408=CARTESIAN_POINT('Ctrl Pts',(-168.286995155468,-3.237987447083,125.849746414469));
#168409=CARTESIAN_POINT('Ctrl Pts',(-168.279597241157,-3.103823196637,125.767078401279));
#168410=CARTESIAN_POINT('Ctrl Pts',(-168.272200556245,-2.96968124185563,
125.684424126014));
#168411=CARTESIAN_POINT('Ctrl Pts',(-168.264803871332,-2.8321951181089,
125.60710699392));
#168412=CARTESIAN_POINT('Ctrl Pts',(-168.25740718642,-2.69183252507318,
125.535397890477));
#168413=CARTESIAN_POINT('Ctrl Pts',(-168.250010829485,-2.55147615586194,
125.46369196669));
#168414=CARTESIAN_POINT('Ctrl Pts',(-168.242614472549,-2.40824390339317,
125.397593746954));
#168415=CARTESIAN_POINT('Ctrl Pts',(-168.235218115614,-2.26262746260918,
125.337327827473));
#168416=CARTESIAN_POINT('Ctrl Pts',(-168.227820626277,-2.11698872757636,
125.277052681127));
#168417=CARTESIAN_POINT('Ctrl Pts',(-168.220423136941,-1.968965422361,125.22261175576));
#168418=CARTESIAN_POINT('Ctrl Pts',(-168.213025647604,-1.81906843516317,
125.174181171874));
#168419=CARTESIAN_POINT('Ctrl Pts',(-168.205625565089,-1.66911890180864,
125.125733610722));
#168420=CARTESIAN_POINT('Ctrl Pts',(-168.198225482574,-1.51729473375126,
125.083300700601));
#168421=CARTESIAN_POINT('Ctrl Pts',(-168.190825400059,-1.36412100961559,
125.047008410724));
#168422=CARTESIAN_POINT('Ctrl Pts',(-168.183417180392,-1.21077885522382,
125.010676213744));
#168423=CARTESIAN_POINT('Ctrl Pts',(-168.176008960726,-1.05608454462107,
124.980498207797));
#168424=CARTESIAN_POINT('Ctrl Pts',(-168.168600741059,-0.900573083415225,
124.956549173622));
#168425=CARTESIAN_POINT('Ctrl Pts',(-168.161187961757,-0.744965907499412,
124.932585399215));
#168426=CARTESIAN_POINT('Ctrl Pts',(-168.153775182455,-0.588540948868006,
124.9148582779));
#168427=CARTESIAN_POINT('Ctrl Pts',(-168.146362403153,-0.431836811887692,
124.903390567617));
#168428=CARTESIAN_POINT('Ctrl Pts',(-168.138939032124,-0.274908768687989,
124.891906471731));
#168429=CARTESIAN_POINT('Ctrl Pts',(-168.131515661096,-0.117701122545321,
124.886699661856));
#168430=CARTESIAN_POINT('Ctrl Pts',(-168.124092290067,0.0392482148941711,
124.887740793703));
#168431=CARTESIAN_POINT('Ctrl Pts',(-168.120156240626,0.122466519541952,
124.88829282679));
#168432=CARTESIAN_POINT('Ctrl Pts',(-168.116220191186,0.205612288808921,
124.89060051334));
#168433=CARTESIAN_POINT('Ctrl Pts',(-168.112284141746,0.288606226015166,
124.894653602087));
#168434=CARTESIAN_POINT('Ctrl Pts',(-168.10486087534,0.44513020145275,124.902297600971));
#168435=CARTESIAN_POINT('Ctrl Pts',(-168.097437608935,0.601586962025899,
124.916175973822));
#168436=CARTESIAN_POINT('Ctrl Pts',(-168.090014342529,0.757439485450539,
124.936293134282));
#168437=CARTESIAN_POINT('Ctrl Pts',(-168.082599849808,0.913107804135237,
124.956386517928));
#168438=CARTESIAN_POINT('Ctrl Pts',(-168.075185357087,1.06817294059602,
124.982703964414));
#168439=CARTESIAN_POINT('Ctrl Pts',(-168.067770864366,1.22209889427824,
125.015197909963));
#168440=CARTESIAN_POINT('Ctrl Pts',(-168.060363518013,1.3758764883311,125.047660536624));
#168441=CARTESIAN_POINT('Ctrl Pts',(-168.052956171659,1.52851672268564,
125.086287734227));
#168442=CARTESIAN_POINT('Ctrl Pts',(-168.045548825305,1.67948984696516,
125.13098028337));
#168443=CARTESIAN_POINT('Ctrl Pts',(-168.03814700363,1.8303503697927,125.175639499124));
#168444=CARTESIAN_POINT('Ctrl Pts',(-168.030745181954,1.9795459019069,125.226354953478));
#168445=CARTESIAN_POINT('Ctrl Pts',(-168.023343360279,2.12655811169202,
125.282976628013));
#168446=CARTESIAN_POINT('Ctrl Pts',(-168.015945445968,2.27349271487594,
125.339568412406));
#168447=CARTESIAN_POINT('Ctrl Pts',(-168.008547531656,2.41824594363519,
125.402060073807));
#168448=CARTESIAN_POINT('Ctrl Pts',(-168.001149617345,2.56031593892036,
125.470252177029));
#168449=CARTESIAN_POINT('Ctrl Pts',(-167.993752932433,2.70236232474993,
125.53843294796));
#168450=CARTESIAN_POINT('Ctrl Pts',(-167.98635624752,2.84172602588579,125.612312119204));
#168451=CARTESIAN_POINT('Ctrl Pts',(-167.978959562608,2.97792633560266,
125.691642621996));
#168452=CARTESIAN_POINT('Ctrl Pts',(-167.971563205673,3.11412060605507,
125.770969607191));
#168453=CARTESIAN_POINT('Ctrl Pts',(-167.964166848737,3.24715144141897,
125.855747255434));
#168454=CARTESIAN_POINT('Ctrl Pts',(-167.956770491801,3.37656410942032,
125.945683289581));
#168455=CARTESIAN_POINT('Ctrl Pts',(-167.949373002465,3.50599659083153,
126.035633093164));
#168456=CARTESIAN_POINT('Ctrl Pts',(-167.941975513128,3.63180949532877,
126.130742642125));
#168457=CARTESIAN_POINT('Ctrl Pts',(-167.934578023792,3.75357850019519,
126.230677309184));
#168458=CARTESIAN_POINT('Ctrl Pts',(-167.927177941277,3.87539019099803,
126.330647008186));
#168459=CARTESIAN_POINT('Ctrl Pts',(-167.919777858762,3.99315487139164,
126.435444956255));
#168460=CARTESIAN_POINT('Ctrl Pts',(-167.912377776247,4.10648274208797,
126.544697479308));
#168461=CARTESIAN_POINT('Ctrl Pts',(-167.90496955658,4.21993522842804,126.654070136741));
#168462=CARTESIAN_POINT('Ctrl Pts',(-167.897561336914,4.32894089301561,
126.767906892069));
#168463=CARTESIAN_POINT('Ctrl Pts',(-167.890153117247,4.43314763709995,
126.885798050734));
#168464=CARTESIAN_POINT('Ctrl Pts',(-167.882740337945,4.5374185186965,127.003761769441));
#168465=CARTESIAN_POINT('Ctrl Pts',(-167.875327558643,4.63688435894883,
127.125784575242));
#168466=CARTESIAN_POINT('Ctrl Pts',(-167.867914779341,4.73123488214162,
127.251425626252));
#168467=CARTESIAN_POINT('Ctrl Pts',(-167.860491408312,4.82572021778669,
127.377246199087));
#168468=CARTESIAN_POINT('Ctrl Pts',(-167.853068037283,4.91507542714935,
127.506695036217));
#168469=CARTESIAN_POINT('Ctrl Pts',(-167.845644666255,4.99903444402728,
127.639303716035));
#168470=CARTESIAN_POINT('Ctrl Pts',(-167.841708616814,5.04355152934311,
127.709616019973));
#168471=CARTESIAN_POINT('Ctrl Pts',(-167.837772567373,5.08655232653177,
127.780816271422));
#168472=CARTESIAN_POINT('Ctrl Pts',(-167.833836517933,5.12800259848285,
127.85283221478));
#168473=CARTESIAN_POINT('Ctrl Pts',(-167.826413251527,5.20617651776695,
127.988652036417));
#168474=CARTESIAN_POINT('Ctrl Pts',(-167.818989985122,5.27906895038996,
128.127785139697));
#168475=CARTESIAN_POINT('Ctrl Pts',(-167.811566718716,5.34638590936825,
128.269782098244));
#168476=CARTESIAN_POINT('Ctrl Pts',(-167.804152225995,5.41362330529116,
128.411611228178));
#168477=CARTESIAN_POINT('Ctrl Pts',(-167.796737733274,5.47529818614745,
128.55629714182));
#168478=CARTESIAN_POINT('Ctrl Pts',(-167.789323240553,5.5311608472962,128.70336317734));
#168479=CARTESIAN_POINT('Ctrl Pts',(-167.781915894199,5.58696966590894,
128.850287465078));
#168480=CARTESIAN_POINT('Ctrl Pts',(-167.774508547846,5.63697728569962,
128.999586961062));
#168481=CARTESIAN_POINT('Ctrl Pts',(-167.767101201492,5.6809808397436,129.150762340787));
#168482=CARTESIAN_POINT('Ctrl Pts',(-167.759699379817,5.72495157427682,
129.30182496821));
#168483=CARTESIAN_POINT('Ctrl Pts',(-167.752297558141,5.76292705560328,
129.454760336687));
#168484=CARTESIAN_POINT('Ctrl Pts',(-167.744895736466,5.79475332757003,
129.609051270528));
#168485=CARTESIAN_POINT('Ctrl Pts',(-167.737497822154,5.82656279869564,
129.763260755387));
#168486=CARTESIAN_POINT('Ctrl Pts',(-167.730099907843,5.8522294500413,129.918824015798));
#168487=CARTESIAN_POINT('Ctrl Pts',(-167.722701993532,5.87164980500478,
130.075211023938));
#168488=CARTESIAN_POINT('Ctrl Pts',(-167.71530530862,5.8910669326575,130.231572043395));
#168489=CARTESIAN_POINT('Ctrl Pts',(-167.707908623707,5.9042397781346,130.388756168801));
#168490=CARTESIAN_POINT('Ctrl Pts',(-167.700511938795,5.91111637365859,
130.546225421273));
#168491=CARTESIAN_POINT('Ctrl Pts',(-167.69311558186,5.91799266426713,130.703687691393));
#168492=CARTESIAN_POINT('Ctrl Pts',(-167.685719224924,5.91857324374515,
130.861434690498));
#168493=CARTESIAN_POINT('Ctrl Pts',(-167.678322867989,5.9128582192318,131.01892585651));
#168494=CARTESIAN_POINT('Ctrl Pts',(-167.670925378652,5.90714231973359,
131.176441134822));
#168495=CARTESIAN_POINT('Ctrl Pts',(-167.663527889316,5.8951289105827,131.333700128975));
#168496=CARTESIAN_POINT('Ctrl Pts',(-167.656130399979,5.87687016639297,
131.490164970031));
#168497=CARTESIAN_POINT('Ctrl Pts',(-167.648730317464,5.85860502162885,
131.646684659595));
#168498=CARTESIAN_POINT('Ctrl Pts',(-167.641330234949,5.83409022620219,
131.802409271241));
#168499=CARTESIAN_POINT('Ctrl Pts',(-167.633930152434,5.80342946666439,
131.956808875819));
#168500=CARTESIAN_POINT('Ctrl Pts',(-167.626521932768,5.77273499246934,
132.111378258637));
#168501=CARTESIAN_POINT('Ctrl Pts',(-167.619113713101,5.73588113050957,
132.264619358327));
#168502=CARTESIAN_POINT('Ctrl Pts',(-167.611705493435,5.69302225044242,
132.416014494324));
#168503=CARTESIAN_POINT('Ctrl Pts',(-167.604292714133,5.65013699144985,
132.5675028115));
#168504=CARTESIAN_POINT('Ctrl Pts',(-167.596879934831,5.60123946530932,
132.717142547031));
#168505=CARTESIAN_POINT('Ctrl Pts',(-167.589467155529,5.54653285318143,
132.864434371362));
#168506=CARTESIAN_POINT('Ctrl Pts',(-167.5820437845,5.49174807368057,133.011936653159));
#168507=CARTESIAN_POINT('Ctrl Pts',(-167.574620413471,5.43113777410489,
133.157083979899));
#168508=CARTESIAN_POINT('Ctrl Pts',(-167.567197042443,5.36495223553776,
133.29939930923));
#168509=CARTESIAN_POINT('Ctrl Pts',(-167.563260993002,5.32985907488748,
133.374858311654));
#168510=CARTESIAN_POINT('Ctrl Pts',(-167.559324943561,5.29319926807747,
133.449521575252));
#168511=CARTESIAN_POINT('Ctrl Pts',(-167.55538889412,5.25501509979877,133.523321239456));
#168512=CARTESIAN_POINT('Ctrl Pts',(-167.547965627714,5.18300095011559,
133.662505102928));
#168513=CARTESIAN_POINT('Ctrl Pts',(-167.540542361309,5.10534447020123,
133.799036411753));
#168514=CARTESIAN_POINT('Ctrl Pts',(-167.533119094903,5.02226486804838,
133.93242490042));
#168515=CARTESIAN_POINT('Ctrl Pts',(-167.525704602182,4.93928345908594,
134.065655734971));
#168516=CARTESIAN_POINT('Ctrl Pts',(-167.518290109461,4.85089188181637,
134.195750829432));
#168517=CARTESIAN_POINT('Ctrl Pts',(-167.51087561674,4.75735619387874,134.322242452856));
#168518=CARTESIAN_POINT('Ctrl Pts',(-167.503468270387,4.6639106591587,134.448612158891));
#168519=CARTESIAN_POINT('Ctrl Pts',(-167.496060924033,4.56533110480596,
134.571385010133));
#168520=CARTESIAN_POINT('Ctrl Pts',(-167.488653577679,4.46192797214109,
134.690120431801));
#168521=CARTESIAN_POINT('Ctrl Pts',(-167.481251756004,4.35860196143375,
134.808767296112));
#168522=CARTESIAN_POINT('Ctrl Pts',(-167.473849934328,4.25045977983879,
134.92338244639));
#168523=CARTESIAN_POINT('Ctrl Pts',(-167.466448112653,4.13785332484944,
135.033556808869));
#168524=CARTESIAN_POINT('Ctrl Pts',(-167.459050198341,4.02530631393244,
135.143673011159));
#168525=CARTESIAN_POINT('Ctrl Pts',(-167.45165228403,3.90829998916464,135.249352833948));
#168526=CARTESIAN_POINT('Ctrl Pts',(-167.444254369719,3.78722434633334,
135.350222726456));
#168527=CARTESIAN_POINT('Ctrl Pts',(-167.436857684807,3.66616882407613,
135.451075856218));
#168528=CARTESIAN_POINT('Ctrl Pts',(-167.429460999894,3.54104561243058,
135.547120403411));
#168529=CARTESIAN_POINT('Ctrl Pts',(-167.422064314982,3.41227923841575,
135.638021855342));
#168530=CARTESIAN_POINT('Ctrl Pts',(-167.414667958047,3.28351857403687,
135.728919276607));
#168531=CARTESIAN_POINT('Ctrl Pts',(-167.407271601111,3.15111537345175,
135.814673840766));
#168532=CARTESIAN_POINT('Ctrl Pts',(-167.399875244176,3.0155244847571,135.89499345095));
#168533=CARTESIAN_POINT('Ctrl Pts',(-167.392477754839,2.87991283675123,
135.975325358272));
#168534=CARTESIAN_POINT('Ctrl Pts',(-167.385080265503,2.74111285007431,
136.05022046452));
#168535=CARTESIAN_POINT('Ctrl Pts',(-167.377682776166,2.59960525074963,
136.119431934376));
#168536=CARTESIAN_POINT('Ctrl Pts',(-167.370282693651,2.45804804615476,
136.188667666206));
#168537=CARTESIAN_POINT('Ctrl Pts',(-167.362882611136,2.31378167429036,
136.252215630898));
#168538=CARTESIAN_POINT('Ctrl Pts',(-167.355482528621,2.16730802467192,
136.309876623236));
#168539=CARTESIAN_POINT('Ctrl Pts',(-167.348074308955,2.0206733122185,136.367601019763));
#168540=CARTESIAN_POINT('Ctrl Pts',(-167.340666089288,1.87182682244108,
136.419425379445));
#168541=CARTESIAN_POINT('Ctrl Pts',(-167.333257869622,1.72128753523133,
136.465199758856));
#168542=CARTESIAN_POINT('Ctrl Pts',(-167.32584509032,1.57065559360219,136.511002311633));
#168543=CARTESIAN_POINT('Ctrl Pts',(-167.318432311018,1.41832913881467,
136.550747370249));
#168544=CARTESIAN_POINT('Ctrl Pts',(-167.311019531716,1.26483809534467,
136.584335976948));
#168545=CARTESIAN_POINT('Ctrl Pts',(-167.303596160687,1.11112773667353,
136.617972576623));
#168546=CARTESIAN_POINT('Ctrl Pts',(-167.296172789658,0.956249832491398,
136.645435090541));
#168547=CARTESIAN_POINT('Ctrl Pts',(-167.288749418629,0.800741015078611,
136.66667623422));
#168548=CARTESIAN_POINT('Ctrl Pts',(-167.284813369188,0.718286508702174,
136.677938798274));
#168549=CARTESIAN_POINT('Ctrl Pts',(-167.280877319748,0.635654669419594,
136.687453182271));
#168550=CARTESIAN_POINT('Ctrl Pts',(-167.276941270307,0.552925446158012,
136.695218281225));
#168551=CARTESIAN_POINT('Ctrl Pts',(-167.269518003901,0.396900712980493,
136.709863015512));
#168552=CARTESIAN_POINT('Ctrl Pts',(-167.262094737496,0.240057831841021,
136.718326926996));
#168553=CARTESIAN_POINT('Ctrl Pts',(-167.25467147109,0.0829277642722101,
136.720529441088));
#168554=CARTESIAN_POINT('Ctrl Pts',(-167.247256978369,-0.0740165886046808,
136.722729351991));
#168555=CARTESIAN_POINT('Ctrl Pts',(-167.239842485649,-0.231247082656321,
136.71868259096));
#168556=CARTESIAN_POINT('Ctrl Pts',(-167.232427992928,-0.388226391936349,
136.708360179821));
#168557=CARTESIAN_POINT('Ctrl Pts',(-167.225020646574,-0.545054398648819,
136.698047717809));
#168558=CARTESIAN_POINT('Ctrl Pts',(-167.21761330022,-0.701631332572941,
136.681471671805));
#168559=CARTESIAN_POINT('Ctrl Pts',(-167.210205953866,-0.857418724550655,
136.658655083451));
#168560=CARTESIAN_POINT('Ctrl Pts',(-167.202804132191,-1.01308992441347,
136.635855512569));
#168561=CARTESIAN_POINT('Ctrl Pts',(-167.195402310516,-1.16797238708205,
136.606824720804));
#168562=CARTESIAN_POINT('Ctrl Pts',(-167.18800048884,-1.32153173802212,
136.57163765512));
#168563=CARTESIAN_POINT('Ctrl Pts',(-167.180602574529,-1.47501002617788,
136.536469164414));
#168564=CARTESIAN_POINT('Ctrl Pts',(-167.173204660218,-1.62716623067609,
136.495150955186));
#168565=CARTESIAN_POINT('Ctrl Pts',(-167.165806745906,-1.77747527041611,
136.447809228616));
#168566=CARTESIAN_POINT('Ctrl Pts',(-167.158410060994,-1.92775933151911,
136.400475369382));
#168567=CARTESIAN_POINT('Ctrl Pts',(-167.151013376082,-2.07619648139296,
136.347120091528));
#168568=CARTESIAN_POINT('Ctrl Pts',(-167.14361669117,-2.22227581781325,
136.287919749377));
#168569=CARTESIAN_POINT('Ctrl Pts',(-167.136220334234,-2.3683486769231,
136.22872203223));
#168570=CARTESIAN_POINT('Ctrl Pts',(-167.128823977299,-2.51206358448913,
136.163679906325));
#168571=CARTESIAN_POINT('Ctrl Pts',(-167.121427620363,-2.65292893463741,
136.093018162753));
#168572=CARTESIAN_POINT('Ctrl Pts',(-167.114030131027,-2.7938158516292,
136.022345600689));
#168573=CARTESIAN_POINT('Ctrl Pts',(-167.106632641691,-2.93185200883081,
135.94605187522));
#168574=CARTESIAN_POINT('Ctrl Pts',(-167.099235152354,-3.06656989254012,
135.864408014248));
#168575=CARTESIAN_POINT('Ctrl Pts',(-167.091835069839,-3.20133500139531,
135.782735533146));
#168576=CARTESIAN_POINT('Ctrl Pts',(-167.084434987324,-3.33277920175647,
135.695709375824));
#168577=CARTESIAN_POINT('Ctrl Pts',(-167.077034904809,-3.46046361309011,
135.603644120859));
#168578=CARTESIAN_POINT('Ctrl Pts',(-167.069626685143,-3.58828842656047,
135.511477630682));
#168579=CARTESIAN_POINT('Ctrl Pts',(-167.062218465477,-3.71234489160475,
135.41426119557));
#168580=CARTESIAN_POINT('Ctrl Pts',(-167.05481024581,-3.83222633526381,
135.31235039992));
#168581=CARTESIAN_POINT('Ctrl Pts',(-167.047397466508,-3.95218156395179,
135.210376879876));
#168582=CARTESIAN_POINT('Ctrl Pts',(-167.039984687206,-4.06795637699756,
135.103703494364));
#168583=CARTESIAN_POINT('Ctrl Pts',(-167.032571907904,-4.17918108131504,
134.992722594769));
#168584=CARTESIAN_POINT('Ctrl Pts',(-167.025148536875,-4.2905647087055,
134.881583120461));
#168585=CARTESIAN_POINT('Ctrl Pts',(-167.017725165847,-4.39738498975635,
134.766124112885));
#168586=CARTESIAN_POINT('Ctrl Pts',(-167.010301794818,-4.49931207983995,
134.646771497561));
#168587=CARTESIAN_POINT('Ctrl Pts',(-167.006365745377,-4.55335626871649,
134.583487877081));
#168588=CARTESIAN_POINT('Ctrl Pts',(-167.002429695935,-4.60602551696784,
134.519110127383));
#168589=CARTESIAN_POINT('Ctrl Pts',(-166.998493646494,-4.65727568058904,
134.45370491449));
#168590=CARTESIAN_POINT('Ctrl Pts',(-166.990780377565,-4.75770792884831,
134.32553376118));
#168591=CARTESIAN_POINT('Ctrl Pts',(-166.983067108637,-4.85300887122969,
134.193004710594));
#168592=CARTESIAN_POINT('Ctrl Pts',(-166.975353839708,-4.94277941001957,
134.056569446406));
#168593=CARTESIAN_POINT('Ctrl Pts',(-166.96794177963,-5.02904434294246,
133.925462080091));
#168594=CARTESIAN_POINT('Ctrl Pts',(-166.960529719552,-5.11020235861462,
133.790748144403));
#168595=CARTESIAN_POINT('Ctrl Pts',(-166.953117659474,-5.1859386345529,
133.652863915993));
#168596=CARTESIAN_POINT('Ctrl Pts',(-166.945712645278,-5.26160291581968,
133.515110759908));
#168597=CARTESIAN_POINT('Ctrl Pts',(-166.938307631081,-5.33185553661064,
133.374193633447));
#168598=CARTESIAN_POINT('Ctrl Pts',(-166.930902616885,-5.39642472220652,
133.230577998606));
#168599=CARTESIAN_POINT('Ctrl Pts',(-166.923503181855,-5.46094525938241,
133.087070568222));
#168600=CARTESIAN_POINT('Ctrl Pts',(-166.916103746825,-5.51979073326164,
132.940869015276));
#168601=CARTESIAN_POINT('Ctrl Pts',(-166.908704311795,-5.57273518684203,
132.792463507216));
#168602=CARTESIAN_POINT('Ctrl Pts',(-166.901308993002,-5.62565018791908,
132.644140555748));
#168603=CARTESIAN_POINT('Ctrl Pts',(-166.893913674208,-5.67267058019892,
132.493616440793));
#168604=CARTESIAN_POINT('Ctrl Pts',(-166.886518355415,-5.71361851471088,
132.341401290695));
#168605=CARTESIAN_POINT('Ctrl Pts',(-166.879125157563,-5.75455470554994,
132.189229795179));
#168606=CARTESIAN_POINT('Ctrl Pts',(-166.871731959712,-5.78942180747217,
132.035368589346));
#168607=CARTESIAN_POINT('Ctrl Pts',(-166.864338761861,-5.81809183905864,
131.880342919827));
#168608=CARTESIAN_POINT('Ctrl Pts',(-166.856946750918,-5.84675726793967,
131.725342138229));
#168609=CARTESIAN_POINT('Ctrl Pts',(-166.849554739976,-5.86922754325991,
131.569177632432));
#168610=CARTESIAN_POINT('Ctrl Pts',(-166.842162729033,-5.88542585283588,
131.412384542483));
#168611=CARTESIAN_POINT('Ctrl Pts',(-166.83476927801,-5.90162731809879,
131.255560906759));
#168612=CARTESIAN_POINT('Ctrl Pts',(-166.827375826987,-5.91155434066848,
131.098108813454));
#168613=CARTESIAN_POINT('Ctrl Pts',(-166.819982375964,-5.91518199387662,
130.940568333272));
#168614=CARTESIAN_POINT('Ctrl Pts',(-166.817779981378,-5.9162626155997,
130.893639463454));
#168615=CARTESIAN_POINT('Ctrl Pts',(-166.815577586793,-5.9167846129143,
130.846702761056));
#168616=CARTESIAN_POINT('Ctrl Pts',(-166.813375192207,-5.91674822108608,
130.799772505246));
#168617=CARTESIAN_POINT('',(-165.063375192207,-5.92585842785378,130.802539843459));
#168618=CARTESIAN_POINT('Ctrl Pts',(-166.813373113621,-5.91108692821504,
130.799732645576));
#168619=CARTESIAN_POINT('Ctrl Pts',(-166.782264083308,-5.91584379486465,
130.13746865848));
#168620=CARTESIAN_POINT('Ctrl Pts',(-166.658339178391,-5.50708468086315,
127.505006129433));
#168621=CARTESIAN_POINT('Ctrl Pts',(-166.441598398868,-1.63614268822863,
123.999906368037));
#168622=CARTESIAN_POINT('Ctrl Pts',(-166.163150775056,4.84040498430027,
125.749853706071));
#168623=CARTESIAN_POINT('Ctrl Pts',(-165.884703151243,6.86885694319062,
132.144645969399));
#168624=CARTESIAN_POINT('Ctrl Pts',(-165.60625552743,2.58516493360408,137.307781470961));
#168625=CARTESIAN_POINT('Ctrl Pts',(-165.332479541084,-3.96244082963463,
136.508234171304));
#168626=CARTESIAN_POINT('Ctrl Pts',(-165.151519429344,-5.91834266072314,
132.666973356396));
#168627=CARTESIAN_POINT('Ctrl Pts',(-165.063375192207,-5.92585842785378,
130.802539843459));
#168628=CARTESIAN_POINT('',(-163.313375192207,-5.91663594861072,130.809828722829));
#168629=CARTESIAN_POINT('Ctrl Pts',(-165.063375192207,-5.92585842785378,
130.802539843459));
#168630=CARTESIAN_POINT('Ctrl Pts',(-165.058703554739,-5.92625676290626,
130.703725017464));
#168631=CARTESIAN_POINT('Ctrl Pts',(-165.054031917272,-5.92400007146822,
130.604928770715));
#168632=CARTESIAN_POINT('Ctrl Pts',(-165.049360279804,-5.91903141901539,
130.506269102489));
#168633=CARTESIAN_POINT('Ctrl Pts',(-164.9565444052,-5.82031446458566,128.546103430853));
#168634=CARTESIAN_POINT('Ctrl Pts',(-164.77091265599,-3.4818656310583,124.733596888215));
#168635=CARTESIAN_POINT('Ctrl Pts',(-164.492465032178,3.22547203558176,
124.593572368236));
#168636=CARTESIAN_POINT('Ctrl Pts',(-164.214017408366,6.96875847459233,
130.160958835515));
#168637=CARTESIAN_POINT('Ctrl Pts',(-163.935569784553,4.30809631822942,
136.319600108577));
#168638=CARTESIAN_POINT('Ctrl Pts',(-163.65712216074,-2.31149589238026,
137.410005723825));
#168639=CARTESIAN_POINT('Ctrl Pts',(-163.449723963291,-5.65986792970276,
133.700820216349));
#168640=CARTESIAN_POINT('Ctrl Pts',(-163.335141640447,-5.92090732989969,
131.272102409195));
#168641=CARTESIAN_POINT('Ctrl Pts',(-163.313375192207,-5.91663594861072,
130.809828722829));
#168642=CARTESIAN_POINT('',(-161.563375192207,-5.90699555269057,130.803727264571));
#168643=CARTESIAN_POINT('Ctrl Pts',(-163.313375192207,-5.91663594861072,
130.809828722829));
#168644=CARTESIAN_POINT('Ctrl Pts',(-163.242325765842,-5.90269342629282,
129.300887995441));
#168645=CARTESIAN_POINT('Ctrl Pts',(-163.078460464874,-4.54700860849117,
125.798464535153));
#168646=CARTESIAN_POINT('Ctrl Pts',(-162.8217792893,1.35073703078564,123.937551314553));
#168647=CARTESIAN_POINT('Ctrl Pts',(-162.543331665488,6.50734750349729,
128.229095776998));
#168648=CARTESIAN_POINT('Ctrl Pts',(-162.264884041675,5.68402352209907,
134.887182819252));
#168649=CARTESIAN_POINT('Ctrl Pts',(-161.986436417862,-0.36264039612703,
137.793355715106));
#168650=CARTESIAN_POINT('Ctrl Pts',(-161.752600134706,-5.16068368769393,
134.840357278418));
#168651=CARTESIAN_POINT('Ctrl Pts',(-161.611579726154,-5.90601764033103,
131.831709506599));
#168652=CARTESIAN_POINT('Ctrl Pts',(-161.563375192207,-5.90699555269057,
130.803727264571));
#168653=CARTESIAN_POINT('',(-159.813375923929,-5.91833122137932,130.799124748602));
#168654=CARTESIAN_POINT('Ctrl Pts',(-161.563375192207,-5.90699555269057,
130.803727264571));
#168655=CARTESIAN_POINT('Ctrl Pts',(-161.51876385155,-5.90790057090839,
129.852371401689));
#168656=CARTESIAN_POINT('Ctrl Pts',(-161.381336636286,-5.24106778416674,
126.922874610178));
#168657=CARTESIAN_POINT('Ctrl Pts',(-161.151093546426,-0.632795772907546,
123.834631064731));
#168658=CARTESIAN_POINT('Ctrl Pts',(-160.87264592261,5.52178929367618,126.504662543663));
#168659=CARTESIAN_POINT('Ctrl Pts',(-160.594198298798,6.6021197537721,133.125906500654));
#168660=CARTESIAN_POINT('Ctrl Pts',(-160.315750674985,1.61542469162351,
137.613763204867));
#168661=CARTESIAN_POINT('Ctrl Pts',(-160.055476648106,-4.43340787030794,
135.95961243181));
#168662=CARTESIAN_POINT('Ctrl Pts',(-159.888018495832,-5.90433120923933,
132.382774673116));
#168663=CARTESIAN_POINT('Ctrl Pts',(-159.813376218162,-5.91896798354517,
130.799130426129));
#168664=CARTESIAN_POINT('',(-158.06337382183,-5.9211331929274,130.807404054331));
#168665=CARTESIAN_POINT('Ctrl Pts',(-159.813375192207,-5.91674767081739,
130.79911062928));
#168666=CARTESIAN_POINT('Ctrl Pts',(-159.802601402648,-5.91654492606026,
130.570616868126));
#168667=CARTESIAN_POINT('Ctrl Pts',(-159.791827613089,-5.90310296772487,
130.342686443863));
#168668=CARTESIAN_POINT('Ctrl Pts',(-159.78105382353,-5.87663597283087,
130.116552355526));
#168669=CARTESIAN_POINT('Ctrl Pts',(-159.77365435814,-5.85845837509346,
129.961242902792));
#168670=CARTESIAN_POINT('Ctrl Pts',(-159.766254892749,-5.8341378241786,
129.806779859639));
#168671=CARTESIAN_POINT('Ctrl Pts',(-159.758855427359,-5.80375541556725,
129.653554969868));
#168672=CARTESIAN_POINT('Ctrl Pts',(-159.751432160953,-5.77327527933359,
129.499837219102));
#168673=CARTESIAN_POINT('Ctrl Pts',(-159.744008894548,-5.73663780339078,
129.347098807042));
#168674=CARTESIAN_POINT('Ctrl Pts',(-159.736585628143,-5.69391725343677,
129.195871614335));
#168675=CARTESIAN_POINT('Ctrl Pts',(-159.729171135422,-5.65124719562507,
129.044823159611));
#168676=CARTESIAN_POINT('Ctrl Pts',(-159.721756642701,-5.60250847540776,
128.895282724656));
#168677=CARTESIAN_POINT('Ctrl Pts',(-159.71434214998,-5.54782662609658,
128.74777356877));
#168678=CARTESIAN_POINT('Ctrl Pts',(-159.706934803626,-5.4931974812105,
128.600406587763));
#168679=CARTESIAN_POINT('Ctrl Pts',(-159.699527457272,-5.43263673985462,
128.455067335857));
#168680=CARTESIAN_POINT('Ctrl Pts',(-159.692120110918,-5.36632011907443,
128.312265326026));
#168681=CARTESIAN_POINT('Ctrl Pts',(-159.684718289243,-5.300052959732,128.169569823322));
#168682=CARTESIAN_POINT('Ctrl Pts',(-159.677316467568,-5.22803862536594,
128.02940813184));
#168683=CARTESIAN_POINT('Ctrl Pts',(-159.669914645892,-5.15050141258487,
127.892271030781));
#168684=CARTESIAN_POINT('Ctrl Pts',(-159.662516731581,-5.07300513109467,
127.75520632333));
#168685=CARTESIAN_POINT('Ctrl Pts',(-159.65511881727,-4.98999196078019,
127.621163350611));
#168686=CARTESIAN_POINT('Ctrl Pts',(-159.647720902958,-4.9017326704733,
127.490609361102));
#168687=CARTESIAN_POINT('Ctrl Pts',(-159.640324218046,-4.81348804725965,
127.360077067299));
#168688=CARTESIAN_POINT('Ctrl Pts',(-159.632927533134,-4.71999924320396,
127.233032914919));
#168689=CARTESIAN_POINT('Ctrl Pts',(-159.625530848222,-4.62158105017022,
127.109916253496));
#168690=CARTESIAN_POINT('Ctrl Pts',(-159.618134491286,-4.52316722110229,
126.986805051195));
#168691=CARTESIAN_POINT('Ctrl Pts',(-159.610738134351,-4.41982467074444,
126.867621285167));
#168692=CARTESIAN_POINT('Ctrl Pts',(-159.603341777415,-4.31190910887094,
126.752771990949));
#168693=CARTESIAN_POINT('Ctrl Pts',(-159.595944288079,-4.20397702484912,
126.637905113009));
#168694=CARTESIAN_POINT('Ctrl Pts',(-159.588546798742,-4.09147079087838,
126.527374300296));
#168695=CARTESIAN_POINT('Ctrl Pts',(-159.581149309405,-3.97478355780458,
126.421550305551));
#168696=CARTESIAN_POINT('Ctrl Pts',(-159.57374922689,-3.85805542020194,
126.315689214368));
#168697=CARTESIAN_POINT('Ctrl Pts',(-159.566349144375,-3.73714364175878,
126.214538476847));
#168698=CARTESIAN_POINT('Ctrl Pts',(-159.55894906186,-3.61247494430429,
126.118428977084));
#168699=CARTESIAN_POINT('Ctrl Pts',(-159.551540842194,-3.48766916080086,
126.022213795045));
#168700=CARTESIAN_POINT('Ctrl Pts',(-159.544132622527,-3.35909850399577,
125.931051149273));
#168701=CARTESIAN_POINT('Ctrl Pts',(-159.536724402861,-3.2272198077915,
125.84522935547));
#168702=CARTESIAN_POINT('Ctrl Pts',(-159.529311623559,-3.09525994245023,
125.759354739785));
#168703=CARTESIAN_POINT('Ctrl Pts',(-159.521898844257,-2.95998830065875,
125.678827716746));
#168704=CARTESIAN_POINT('Ctrl Pts',(-159.514486064955,-2.82188640414737,
125.60389066913));
#168705=CARTESIAN_POINT('Ctrl Pts',(-159.507062693926,-2.68358718117011,
125.528846547946));
#168706=CARTESIAN_POINT('Ctrl Pts',(-159.499639322897,-2.54244996076335,
125.45940851881));
#168707=CARTESIAN_POINT('Ctrl Pts',(-159.492215951869,-2.39897707389532,
125.395771193194));
#168708=CARTESIAN_POINT('Ctrl Pts',(-159.488279902428,-2.32290430669016,
125.362029156195));
#168709=CARTESIAN_POINT('Ctrl Pts',(-159.484343852987,-2.24617517969082,
125.32991708002));
#168710=CARTESIAN_POINT('Ctrl Pts',(-159.480407803546,-2.16886618280707,
125.299458252984));
#168711=CARTESIAN_POINT('Ctrl Pts',(-159.47298453714,-2.02306382742118,
125.242013855786));
#168712=CARTESIAN_POINT('Ctrl Pts',(-159.465561270735,-1.87475722491181,
125.190279159363));
#168713=CARTESIAN_POINT('Ctrl Pts',(-159.458138004329,-1.72443400395254,
125.14447917636));
#168714=CARTESIAN_POINT('Ctrl Pts',(-159.450723511608,-1.57428845255687,
125.098733325133));
#168715=CARTESIAN_POINT('Ctrl Pts',(-159.443309018888,-1.42213138063707,
125.058908332983));
#168716=CARTESIAN_POINT('Ctrl Pts',(-159.435894526167,-1.26847087488296,
125.025181419611));
#168717=CARTESIAN_POINT('Ctrl Pts',(-159.428487179813,-1.11495847290907,
124.991487013508));
#168718=CARTESIAN_POINT('Ctrl Pts',(-159.421079833459,-0.959945884076821,
124.963879064616));
#168719=CARTESIAN_POINT('Ctrl Pts',(-159.413672487105,-0.803956755437283,
124.942485141416));
#168720=CARTESIAN_POINT('Ctrl Pts',(-159.40627066543,-0.648083969375018,
124.921107174611));
#168721=CARTESIAN_POINT('Ctrl Pts',(-159.398868843755,-0.49123646197319,
124.90593405578));
#168722=CARTESIAN_POINT('Ctrl Pts',(-159.391467022079,-0.33394837746697,
124.897042355978));
#168723=CARTESIAN_POINT('Ctrl Pts',(-159.384069107768,-0.176743324116681,
124.888155350036));
#168724=CARTESIAN_POINT('Ctrl Pts',(-159.376671193457,-0.0190985286100915,
124.88554318034));
#168725=CARTESIAN_POINT('Ctrl Pts',(-159.369273279145,0.138446542508064,
124.889230600621));
#168726=CARTESIAN_POINT('Ctrl Pts',(-159.361876594233,0.295965432493784,
124.892917408119));
#168727=CARTESIAN_POINT('Ctrl Pts',(-159.354479909321,0.453384258152054,
124.902901719124));
#168728=CARTESIAN_POINT('Ctrl Pts',(-159.347083224409,0.610163229585403,
124.919156169481));
#168729=CARTESIAN_POINT('Ctrl Pts',(-159.339686867473,0.766935249274866,
124.935409899098));
#168730=CARTESIAN_POINT('Ctrl Pts',(-159.332290510538,0.923067099844836,
124.957933176764));
#168731=CARTESIAN_POINT('Ctrl Pts',(-159.324894153603,1.07802406094925,
124.986646746421));
#168732=CARTESIAN_POINT('Ctrl Pts',(-159.317496664266,1.23300474636,125.015364712198));
#168733=CARTESIAN_POINT('Ctrl Pts',(-159.31009917493,1.38680981706991,125.050274789043));
#168734=CARTESIAN_POINT('Ctrl Pts',(-159.302701685593,1.53891484066075,
125.091246608928));
#168735=CARTESIAN_POINT('Ctrl Pts',(-159.295301603078,1.69107318443204,
125.132232791421));
#168736=CARTESIAN_POINT('Ctrl Pts',(-159.287901520563,1.8415299343291,125.179284850651));
#168737=CARTESIAN_POINT('Ctrl Pts',(-159.280501438048,1.98977605461909,
125.232222624393));
#168738=CARTESIAN_POINT('Ctrl Pts',(-159.273093218382,2.13818518675821,
125.285218608659));
#168739=CARTESIAN_POINT('Ctrl Pts',(-159.265684998715,2.28437848302263,
125.344113106728));
#168740=CARTESIAN_POINT('Ctrl Pts',(-159.258276779049,2.42786644536294,
125.40867761298));
#168741=CARTESIAN_POINT('Ctrl Pts',(-159.250863999747,2.57144272215026,
125.473281857608));
#168742=CARTESIAN_POINT('Ctrl Pts',(-159.243451220445,2.71231001385916,
125.543562898004));
#168743=CARTESIAN_POINT('Ctrl Pts',(-159.236038441143,2.85000412273718,
125.619246630113));
#168744=CARTESIAN_POINT('Ctrl Pts',(-159.228615070114,2.98789497541499,
125.695038502687));
#168745=CARTESIAN_POINT('Ctrl Pts',(-159.221191699085,3.12260327101227,
125.776248292564));
#168746=CARTESIAN_POINT('Ctrl Pts',(-159.213768328056,3.25369375522823,
125.862558566726));
#168747=CARTESIAN_POINT('Ctrl Pts',(-159.209832278616,3.32320107543327,
125.908322345074));
#168748=CARTESIAN_POINT('Ctrl Pts',(-159.205896229175,3.39169184193513,
125.955519371145));
#168749=CARTESIAN_POINT('Ctrl Pts',(-159.201960179734,3.45910511694965,
126.004097879716));
#168750=CARTESIAN_POINT('Ctrl Pts',(-159.194536913329,3.5862444497292,126.095715430796));
#168751=CARTESIAN_POINT('Ctrl Pts',(-159.187113646923,3.70993365627935,
126.192526108641));
#168752=CARTESIAN_POINT('Ctrl Pts',(-159.179690380518,3.82971985187992,
126.294241282269));
#168753=CARTESIAN_POINT('Ctrl Pts',(-159.172275887797,3.94936447014524,
126.395836237009));
#168754=CARTESIAN_POINT('Ctrl Pts',(-159.164861395076,4.06511497795973,
126.502323909891));
#168755=CARTESIAN_POINT('Ctrl Pts',(-159.157446902355,4.17654764210205,
126.613372624771));
#168756=CARTESIAN_POINT('Ctrl Pts',(-159.150039556001,4.28787290324731,
126.724314306719));
#168757=CARTESIAN_POINT('Ctrl Pts',(-159.142632209647,4.39488834320481,
126.83980801715));
#168758=CARTESIAN_POINT('Ctrl Pts',(-159.135224863293,4.49720359097627,
126.959482150851));
#168759=CARTESIAN_POINT('Ctrl Pts',(-159.127823041618,4.59944252817581,
127.079067027068));
#168760=CARTESIAN_POINT('Ctrl Pts',(-159.120421219942,4.69698801173753,
127.202825835845));
#168761=CARTESIAN_POINT('Ctrl Pts',(-159.113019398267,4.78948690225745,
127.330350575035));
#168762=CARTESIAN_POINT('Ctrl Pts',(-159.105621483956,4.88193696333308,
127.457807994909));
#168763=CARTESIAN_POINT('Ctrl Pts',(-159.098223569644,4.96934551833801,
127.589027084575));
#168764=CARTESIAN_POINT('Ctrl Pts',(-159.090825655333,5.05140014641481,
127.723567355547));
#168765=CARTESIAN_POINT('Ctrl Pts',(-159.083428970421,5.13344113850094,
127.858085268367));
#168766=CARTESIAN_POINT('Ctrl Pts',(-159.076032285508,5.21012977531861,
127.995922948705));
#168767=CARTESIAN_POINT('Ctrl Pts',(-159.068635600596,5.28119730948246,
128.136611465038));
#168768=CARTESIAN_POINT('Ctrl Pts',(-159.061239243661,5.35226169243737,
128.277293743094));
#168769=CARTESIAN_POINT('Ctrl Pts',(-159.053842886725,5.41770530001016,
128.420826272603));
#168770=CARTESIAN_POINT('Ctrl Pts',(-159.04644652979,5.47730578315848,128.566716338357));
#168771=CARTESIAN_POINT('Ctrl Pts',(-159.039049040453,5.53691539129293,
128.712628740252));
#168772=CARTESIAN_POINT('Ctrl Pts',(-159.031651551117,5.59067995255489,
128.860899051487));
#168773=CARTESIAN_POINT('Ctrl Pts',(-159.02425406178,5.63842568072617,129.011015585112));
#168774=CARTESIAN_POINT('Ctrl Pts',(-159.016853979265,5.68618814608851,
129.161184741855));
#168775=CARTESIAN_POINT('Ctrl Pts',(-159.00945389675,5.72792746450482,129.313201054025));
#168776=CARTESIAN_POINT('Ctrl Pts',(-159.002053814235,5.7635200653093,129.466538873358));
#168777=CARTESIAN_POINT('Ctrl Pts',(-158.994645594568,5.79915180383733,
129.620045303386));
#168778=CARTESIAN_POINT('Ctrl Pts',(-158.987237374902,5.82862324223355,
129.774875778727));
#168779=CARTESIAN_POINT('Ctrl Pts',(-158.979829155236,5.85186204309573,
129.930494957939));
#168780=CARTESIAN_POINT('Ctrl Pts',(-158.972416375933,5.87511514705216,
130.086209918159));
#168781=CARTESIAN_POINT('Ctrl Pts',(-158.965003596631,5.8921279293473,130.242714179287));
#168782=CARTESIAN_POINT('Ctrl Pts',(-158.957590817329,5.90288009126378,
130.399469038669));
#168783=CARTESIAN_POINT('Ctrl Pts',(-158.950167446301,5.9136476163734,130.556447876744));
#168784=CARTESIAN_POINT('Ctrl Pts',(-158.942744075272,5.91813664437292,
130.713677656055));
#168785=CARTESIAN_POINT('Ctrl Pts',(-158.935320704243,5.91637897506805,
130.870620604532));
#168786=CARTESIAN_POINT('Ctrl Pts',(-158.931384654802,5.91544701662791,
130.953835521609));
#168787=CARTESIAN_POINT('Ctrl Pts',(-158.927448605361,5.9127597541791,131.036969888669));
#168788=CARTESIAN_POINT('Ctrl Pts',(-158.923512555921,5.90832780090972,
131.11994445666));
#168789=CARTESIAN_POINT('Ctrl Pts',(-158.916089289515,5.89996927536024,
131.276431902343));
#168790=CARTESIAN_POINT('Ctrl Pts',(-158.90866602311,5.88537674768521,131.432823670982));
#168791=CARTESIAN_POINT('Ctrl Pts',(-158.901242756704,5.86454825605106,
131.58858272574));
#168792=CARTESIAN_POINT('Ctrl Pts',(-158.893828263983,5.84374438196431,
131.74415768623));
#168793=CARTESIAN_POINT('Ctrl Pts',(-158.886413771262,5.8167192637182,131.899101054978));
#168794=CARTESIAN_POINT('Ctrl Pts',(-158.878999278541,5.78352291168975,
132.052877054166));
#168795=CARTESIAN_POINT('Ctrl Pts',(-158.871591932187,5.75035855555522,
132.206504838256));
#168796=CARTESIAN_POINT('Ctrl Pts',(-158.864184585834,5.71103488531188,
132.358967130306));
#168797=CARTESIAN_POINT('Ctrl Pts',(-158.85677723948,5.66565353789099,132.509734638443));
#168798=CARTESIAN_POINT('Ctrl Pts',(-158.849375417804,5.62030603759115,
132.660389698485));
#168799=CARTESIAN_POINT('Ctrl Pts',(-158.841973596129,5.5689099632813,132.809352135558));
#168800=CARTESIAN_POINT('Ctrl Pts',(-158.834571774453,5.5116176982491,132.956104308354));
#168801=CARTESIAN_POINT('Ctrl Pts',(-158.827173860142,5.45435567735766,
133.102779011821));
#168802=CARTESIAN_POINT('Ctrl Pts',(-158.819775945831,5.39120379995621,
133.247245427855));
#168803=CARTESIAN_POINT('Ctrl Pts',(-158.81237803152,5.32236379038003,133.389002613153));
#168804=CARTESIAN_POINT('Ctrl Pts',(-158.804981346607,5.25353522076465,
133.530736240978));
#168805=CARTESIAN_POINT('Ctrl Pts',(-158.797584661695,5.17902055795444,
133.669761196163));
#168806=CARTESIAN_POINT('Ctrl Pts',(-158.790187976783,5.09906906279423,
133.805597904978));
#168807=CARTESIAN_POINT('Ctrl Pts',(-158.782791619847,5.0191211127671,133.941428590652));
#168808=CARTESIAN_POINT('Ctrl Pts',(-158.775395262912,4.93373699908124,
134.074070989338));
#168809=CARTESIAN_POINT('Ctrl Pts',(-158.767998905977,4.8432110719056,134.203071707887));
#168810=CARTESIAN_POINT('Ctrl Pts',(-158.76060141664,4.75267128497914,134.332092176776));
#168811=CARTESIAN_POINT('Ctrl Pts',(-158.753203927303,4.65698833153793,
134.457469549783));
#168812=CARTESIAN_POINT('Ctrl Pts',(-158.745806437967,4.55649877260838,
134.578781036348));
#168813=CARTESIAN_POINT('Ctrl Pts',(-158.738406355452,4.45597398721988,
134.700135048466));
#168814=CARTESIAN_POINT('Ctrl Pts',(-158.731006272937,4.35063947960985,
134.817420049101));
#168815=CARTESIAN_POINT('Ctrl Pts',(-158.723606190422,4.24087069958465,
134.930247949026));
#168816=CARTESIAN_POINT('Ctrl Pts',(-158.716197970755,4.13098121750116,
135.043199914827));
#168817=CARTESIAN_POINT('Ctrl Pts',(-158.708789751089,4.01664798590246,
135.151684724491));
#168818=CARTESIAN_POINT('Ctrl Pts',(-158.701381531422,3.89828230257228,
135.255352153387));
#168819=CARTESIAN_POINT('Ctrl Pts',(-158.69396875212,3.77984376713906,135.359083387856));
#168820=CARTESIAN_POINT('Ctrl Pts',(-158.686555972818,3.65736812421176,
135.457991099397));
#168821=CARTESIAN_POINT('Ctrl Pts',(-158.679143193516,3.53129762763767,
135.55176702818));
#168822=CARTESIAN_POINT('Ctrl Pts',(-158.671719822487,3.40504699562614,
135.645676948408));
#168823=CARTESIAN_POINT('Ctrl Pts',(-158.664296451459,3.27519155859747,
135.734440231068));
#168824=CARTESIAN_POINT('Ctrl Pts',(-158.65687308043,3.14220094799595,135.817792951298));
#168825=CARTESIAN_POINT('Ctrl Pts',(-158.652937030989,3.07168613519026,
135.861988563585));
#168826=CARTESIAN_POINT('Ctrl Pts',(-158.649000981548,3.00029030670304,
135.904663849644));
#168827=CARTESIAN_POINT('Ctrl Pts',(-158.645064932108,2.92808587369328,
135.945784902604));
#168828=CARTESIAN_POINT('Ctrl Pts',(-158.637641665702,2.79191056645806,
136.023337925143));
#168829=CARTESIAN_POINT('Ctrl Pts',(-158.630218399297,2.65244612460663,
136.095594389359));
#168830=CARTESIAN_POINT('Ctrl Pts',(-158.622795132891,2.51014331202124,
136.162262363176));
#168831=CARTESIAN_POINT('Ctrl Pts',(-158.61538064017,2.3680086895428,136.228851540985));
#168832=CARTESIAN_POINT('Ctrl Pts',(-158.60796614745,2.22304270865427,136.289865219124));
#168833=CARTESIAN_POINT('Ctrl Pts',(-158.600551654729,2.07572316623768,
136.345055871742));
#168834=CARTESIAN_POINT('Ctrl Pts',(-158.593144308375,1.92854561594214,
136.400193329531));
#168835=CARTESIAN_POINT('Ctrl Pts',(-158.585736962021,1.77901936738352,
136.449518805002));
#168836=CARTESIAN_POINT('Ctrl Pts',(-158.578329615667,1.62764466604802,
136.492831713));
#168837=CARTESIAN_POINT('Ctrl Pts',(-158.570927793992,1.47638286567624,
136.536112316596));
#168838=CARTESIAN_POINT('Ctrl Pts',(-158.563525972316,1.32327571494822,
136.573389179515));
#168839=CARTESIAN_POINT('Ctrl Pts',(-158.556124150641,1.16884108704619,
136.60451070836));
#168840=CARTESIAN_POINT('Ctrl Pts',(-158.54872623633,1.01448798398213,136.635615808392));
#168841=CARTESIAN_POINT('Ctrl Pts',(-158.541328322018,0.858809164365971,
136.660571972034));
#168842=CARTESIAN_POINT('Ctrl Pts',(-158.533930407707,0.702335122916342,
136.679278143593));
#168843=CARTESIAN_POINT('Ctrl Pts',(-158.526533722795,0.545887084613451,
136.697981206525));
#168844=CARTESIAN_POINT('Ctrl Pts',(-158.519137037882,0.388644457054291,
136.710436294489));
#168845=CARTESIAN_POINT('Ctrl Pts',(-158.51174035297,0.231145450774582,
136.716593896378));
#168846=CARTESIAN_POINT('Ctrl Pts',(-158.504343996035,0.0736534281658596,
136.722751225232));
#168847=CARTESIAN_POINT('Ctrl Pts',(-158.496947639099,-0.0840945775471877,
136.722611608645));
#168848=CARTESIAN_POINT('Ctrl Pts',(-158.489551282164,-0.241558010409788,
136.716177621678));
#168849=CARTESIAN_POINT('Ctrl Pts',(-158.482153792827,-0.399045551325945,
136.709742649651));
#168850=CARTESIAN_POINT('Ctrl Pts',(-158.474756303491,-0.556248059629689,
136.697011403663));
#168851=CARTESIAN_POINT('Ctrl Pts',(-158.467358814154,-0.712627910191346,
136.678038513409));
#168852=CARTESIAN_POINT('Ctrl Pts',(-158.459958731639,-0.869062579466975,
136.659058972238));
#168853=CARTESIAN_POINT('Ctrl Pts',(-158.452558649124,-1.02467364648604,
136.633833475447));
#168854=CARTESIAN_POINT('Ctrl Pts',(-158.445158566609,-1.17893166100033,
136.602468127883));
#168855=CARTESIAN_POINT('Ctrl Pts',(-158.437750346943,-1.33335929805991,
136.571068290895));
#168856=CARTESIAN_POINT('Ctrl Pts',(-158.430342127276,-1.48643054530283,
136.533515194578));
#168857=CARTESIAN_POINT('Ctrl Pts',(-158.42293390761,-1.63762843232964,
136.489965570438));
#168858=CARTESIAN_POINT('Ctrl Pts',(-158.415521128308,-1.78891937913304,
136.446389142232));
#168859=CARTESIAN_POINT('Ctrl Pts',(-158.408108349006,-1.93833431469994,
136.39680894919));
#168860=CARTESIAN_POINT('Ctrl Pts',(-158.400695569704,-2.08537484229872,
136.341430450032));
#168861=CARTESIAN_POINT('Ctrl Pts',(-158.393272198675,-2.23262546829905,
136.285972823478));
#168862=CARTESIAN_POINT('Ctrl Pts',(-158.385848827646,-2.37749456751733,
136.22470048905));
#168863=CARTESIAN_POINT('Ctrl Pts',(-158.378425456617,-2.51950624522521,
136.15786590315));
#168864=CARTESIAN_POINT('Ctrl Pts',(-158.374489407176,-2.59480424427137,
136.12242860203));
#168865=CARTESIAN_POINT('Ctrl Pts',(-158.370553357736,-2.66929936030063,
136.085428304004));
#168866=CARTESIAN_POINT('Ctrl Pts',(-158.366617308295,-2.74292392650072,
136.046907603138));
#168867=CARTESIAN_POINT('Ctrl Pts',(-158.359194041889,-2.88177756060691,
135.974258763496));
#168868=CARTESIAN_POINT('Ctrl Pts',(-158.351770775484,-3.01795290779085,
135.895979762598));
#168869=CARTESIAN_POINT('Ctrl Pts',(-158.344347509078,-3.15096070844118,
135.812292044449));
#168870=CARTESIAN_POINT('Ctrl Pts',(-158.336933016357,-3.28381130491713,
135.728703238232));
#168871=CARTESIAN_POINT('Ctrl Pts',(-158.329518523636,-3.41350149399454,
135.639718636236));
#168872=CARTESIAN_POINT('Ctrl Pts',(-158.322104030915,-3.53956476427929,
135.54560642874));
#168873=CARTESIAN_POINT('Ctrl Pts',(-158.314696684561,-3.66550653003723,
135.451584930133));
#168874=CARTESIAN_POINT('Ctrl Pts',(-158.307289338207,-3.78782803924903,
135.352445886752));
#168875=CARTESIAN_POINT('Ctrl Pts',(-158.299881991854,-3.90609013903702,
135.248501748113));
#168876=CARTESIAN_POINT('Ctrl Pts',(-158.292480170178,-4.02426403448955,
135.144635134934));
#168877=CARTESIAN_POINT('Ctrl Pts',(-158.285078348503,-4.13838426981755,
135.035970807751));
#168878=CARTESIAN_POINT('Ctrl Pts',(-158.277676526827,-4.24804338209912,
134.922862528007));
#168879=CARTESIAN_POINT('Ctrl Pts',(-158.270278612516,-4.3576446061889,
134.809813957243));
#168880=CARTESIAN_POINT('Ctrl Pts',(-158.262880698205,-4.46278913812631,
134.692326373282));
#168881=CARTESIAN_POINT('Ctrl Pts',(-158.255482783893,-4.56310521153969,
134.570791473286));
#168882=CARTESIAN_POINT('Ctrl Pts',(-158.248086098981,-4.66340461424173,
134.449276770185));
#168883=CARTESIAN_POINT('Ctrl Pts',(-158.240689414069,-4.75887691355273,
134.323716373552));
#168884=CARTESIAN_POINT('Ctrl Pts',(-158.233292729156,-4.84918953843538,
134.194536333193));
#168885=CARTESIAN_POINT('Ctrl Pts',(-158.225896372221,-4.93949815876135,
134.065362020813));
#168886=CARTESIAN_POINT('Ctrl Pts',(-158.218500015286,-5.02464734566979,
133.932568689775));
#168887=CARTESIAN_POINT('Ctrl Pts',(-158.21110365835,-5.10434708193491,
133.796612516996));
#168888=CARTESIAN_POINT('Ctrl Pts',(-158.203706169013,-5.18405902043334,
133.66063552898));
#168889=CARTESIAN_POINT('Ctrl Pts',(-158.196308679677,-5.25831965823834,
133.521495057102));
#168890=CARTESIAN_POINT('Ctrl Pts',(-158.18891119034,-5.32688435734669,
133.379672949295));
#168891=CARTESIAN_POINT('Ctrl Pts',(-158.181511107825,-5.39547309170373,
133.237801125969));
#168892=CARTESIAN_POINT('Ctrl Pts',(-158.17411102531,-5.45836174956468,
133.093246130967));
#168893=CARTESIAN_POINT('Ctrl Pts',(-158.166710942795,-5.51535341915249,
132.946510758042));
#168894=CARTESIAN_POINT('Ctrl Pts',(-158.159302723129,-5.57240775693998,
132.79961403449));
#168895=CARTESIAN_POINT('Ctrl Pts',(-158.151894503462,-5.6235520215571,
132.650532493136));
#168896=CARTESIAN_POINT('Ctrl Pts',(-158.144486283796,-5.66863864053037,
132.499785793027));
#168897=CARTESIAN_POINT('Ctrl Pts',(-158.137073504493,-5.71375300956531,
132.348946310839));
#168898=CARTESIAN_POINT('Ctrl Pts',(-158.129660725191,-5.75280221131124,
132.196439988492));
#168899=CARTESIAN_POINT('Ctrl Pts',(-158.122247945889,-5.78568970840053,
132.042797196729));
#168900=CARTESIAN_POINT('Ctrl Pts',(-158.11482457486,-5.81862419668799,
131.888934872939));
#168901=CARTESIAN_POINT('Ctrl Pts',(-158.107401203832,-5.84537933316278,
131.733933203442));
#168902=CARTESIAN_POINT('Ctrl Pts',(-158.099977832803,-5.86591028381913,
131.578329030801));
#168903=CARTESIAN_POINT('Ctrl Pts',(-158.096041783362,-5.87679628648974,
131.495823964801));
#168904=CARTESIAN_POINT('Ctrl Pts',(-158.092105733922,-5.88593331771477,
131.413149549017));
#168905=CARTESIAN_POINT('Ctrl Pts',(-158.088169684481,-5.89332063752347,
131.330385736586));
#168906=CARTESIAN_POINT('Ctrl Pts',(-158.079904853723,-5.90883237051814,
131.156600088571));
#168907=CARTESIAN_POINT('Ctrl Pts',(-158.071640022965,-5.9166585591732,
130.982118301593));
#168908=CARTESIAN_POINT('Ctrl Pts',(-158.063375192207,-5.9167492034552,
130.807430782429));
#168909=CARTESIAN_POINT('',(-156.31337639652,-5.91261572195128,130.808150436615));
#168910=CARTESIAN_POINT('Ctrl Pts',(-158.063372747364,-5.92457053254746,
130.807383097723));
#168911=CARTESIAN_POINT('Ctrl Pts',(-157.978822518465,-5.913266273438,129.017939476383));
#168912=CARTESIAN_POINT('Ctrl Pts',(-157.801456414963,-4.0946913805117,
125.244264131813));
#168913=CARTESIAN_POINT('Ctrl Pts',(-157.531274436855,2.33159049714918,
124.205781506578));
#168914=CARTESIAN_POINT('Ctrl Pts',(-157.252826813043,6.81185310351898,
129.19930054815));
#168915=CARTESIAN_POINT('Ctrl Pts',(-156.97437918923,5.032355485277,135.667791381967));
#168916=CARTESIAN_POINT('Ctrl Pts',(-156.695931565417,-1.37163097969959,
137.667026935103));
#168917=CARTESIAN_POINT('Ctrl Pts',(-156.475597610672,-5.44167151906352,
134.25874964179));
#168918=CARTESIAN_POINT('Ctrl Pts',(-156.34807953053,-5.91370668157247,
131.547445981901));
#168919=CARTESIAN_POINT('Ctrl Pts',(-156.313377324993,-5.90942929569692,
130.808168187674));
#168920=CARTESIAN_POINT('',(-154.563373962346,-5.91330263212981,130.799862701196));
#168921=CARTESIAN_POINT('Ctrl Pts',(-156.313375192207,-5.91674880096835,
130.808127411907));
#168922=CARTESIAN_POINT('Ctrl Pts',(-156.30592501074,-5.91684996871559,
130.649216653056));
#168923=CARTESIAN_POINT('Ctrl Pts',(-156.298474829273,-5.91054481878383,
130.490278168592));
#168924=CARTESIAN_POINT('Ctrl Pts',(-156.291024647806,-5.89785334377332,
130.3318603553));
#168925=CARTESIAN_POINT('Ctrl Pts',(-156.283573932567,-5.8851609594741,
130.173431192064));
#168926=CARTESIAN_POINT('Ctrl Pts',(-156.276123217327,-5.86608136692814,
130.015523138905));
#168927=CARTESIAN_POINT('Ctrl Pts',(-156.268672502087,-5.8406865256537,
129.858680189754));
#168928=CARTESIAN_POINT('Ctrl Pts',(-156.261219862126,-5.81528512420402,
129.701796723821));
#168929=CARTESIAN_POINT('Ctrl Pts',(-156.253767222165,-5.78356528241957,
129.545979270953));
#168930=CARTESIAN_POINT('Ctrl Pts',(-156.246314582203,-5.74565022793222,
129.391762295054));
#168931=CARTESIAN_POINT('Ctrl Pts',(-156.238858625697,-5.70771830063484,
129.237476690117));
#168932=CARTESIAN_POINT('Ctrl Pts',(-156.231402669191,-5.66358575588237,
129.084793335707));
#168933=CARTESIAN_POINT('Ctrl Pts',(-156.223946712685,-5.61342587259247,
128.934232136576));
#168934=CARTESIAN_POINT('Ctrl Pts',(-156.216481268912,-5.56320216379481,
128.783479357156));
#168935=CARTESIAN_POINT('Ctrl Pts',(-156.209015825139,-5.50693591093644,
128.634854474635));
#168936=CARTESIAN_POINT('Ctrl Pts',(-156.201550381365,-5.44484916311179,
128.488858910924));
#168937=CARTESIAN_POINT('Ctrl Pts',(-156.194079889917,-5.38272043603389,
128.342764633963));
#168938=CARTESIAN_POINT('Ctrl Pts',(-156.186609398468,-5.3147635256011,
128.199303549248));
#168939=CARTESIAN_POINT('Ctrl Pts',(-156.179138907019,-5.24124659973601,
128.058952698284));
#168940=CARTESIAN_POINT('Ctrl Pts',(-156.171656160374,-5.16760907077987,
127.918371604472));
#168941=CARTESIAN_POINT('Ctrl Pts',(-156.164173413729,-5.08839348286153,
127.780911256275));
#168942=CARTESIAN_POINT('Ctrl Pts',(-156.156690667084,-5.00391214106337,
127.647020938815));
#168943=CARTESIAN_POINT('Ctrl Pts',(-156.150805883987,-4.93747204949496,
127.541723310216));
#168944=CARTESIAN_POINT('Ctrl Pts',(-156.144921100889,-4.86777598405215,
127.438633188503));
#168945=CARTESIAN_POINT('Ctrl Pts',(-156.139036317792,-4.79499301008061,
127.337954323466));
#168946=CARTESIAN_POINT('Ctrl Pts',(-156.131613051386,-4.70318208067051,
127.210954564228));
#168947=CARTESIAN_POINT('Ctrl Pts',(-156.124189784981,-4.60618328101365,
127.08741283028));
#168948=CARTESIAN_POINT('Ctrl Pts',(-156.116766518575,-4.50428593097169,
126.967781566569));
#168949=CARTESIAN_POINT('Ctrl Pts',(-156.109352025854,-4.40250901513543,
126.848291697077));
#168950=CARTESIAN_POINT('Ctrl Pts',(-156.101937533134,-4.2958453129962,
126.732703379411));
#168951=CARTESIAN_POINT('Ctrl Pts',(-156.094523040413,-4.18462714516366,
126.621439841546));
#168952=CARTESIAN_POINT('Ctrl Pts',(-156.087115694059,-4.07351617358825,
126.510283543668));
#168953=CARTESIAN_POINT('Ctrl Pts',(-156.079708347705,-3.95785973761438,
126.403443989399));
#168954=CARTESIAN_POINT('Ctrl Pts',(-156.072301001351,-3.8380300361042,
126.301310983766));
#168955=CARTESIAN_POINT('Ctrl Pts',(-156.064899179676,-3.71828970810598,
126.199254152782));
#168956=CARTESIAN_POINT('Ctrl Pts',(-156.057497358,-3.59438259501838,126.101897122016));
#168957=CARTESIAN_POINT('Ctrl Pts',(-156.050095536325,-3.4667172359339,
126.009592409552));
#168958=CARTESIAN_POINT('Ctrl Pts',(-156.042697622013,-3.33911927039982,
125.917336424029));
#168959=CARTESIAN_POINT('Ctrl Pts',(-156.035299707702,-3.20776731174243,
125.830127663359));
#168960=CARTESIAN_POINT('Ctrl Pts',(-156.027901793391,-3.07310232339073,
125.74827787769));
#168961=CARTESIAN_POINT('Ctrl Pts',(-156.020505108479,-2.93845971391682,
125.666441693971));
#168962=CARTESIAN_POINT('Ctrl Pts',(-156.013108423567,-2.80050548614263,
125.589962911443));
#168963=CARTESIAN_POINT('Ctrl Pts',(-156.005711738654,-2.65970898003594,
125.519109563546));
#168964=CARTESIAN_POINT('Ctrl Pts',(-155.998315381719,-2.51891871699388,
125.448259357362));
#168965=CARTESIAN_POINT('Ctrl Pts',(-155.990919024784,-2.37528675966399,
125.383034257648));
#168966=CARTESIAN_POINT('Ctrl Pts',(-155.983522667848,-2.22930616105943,
125.323655863361));
#168967=CARTESIAN_POINT('Ctrl Pts',(-155.976125178511,-2.08330321245213,
125.264268378091));
#168968=CARTESIAN_POINT('Ctrl Pts',(-155.968727689175,-1.93495125240191,
125.210729521261));
#168969=CARTESIAN_POINT('Ctrl Pts',(-155.961330199838,-1.78476223173872,
125.163212300188));
#168970=CARTESIAN_POINT('Ctrl Pts',(-155.953930117323,-1.63452056254781,
125.115678422027));
#168971=CARTESIAN_POINT('Ctrl Pts',(-155.946530034808,-1.4824409062747,
125.074170494894));
#168972=CARTESIAN_POINT('Ctrl Pts',(-155.939129952293,-1.32904909862578,
125.038811289363));
#168973=CARTESIAN_POINT('Ctrl Pts',(-155.931721732627,-1.17548862091464,
125.003413202751));
#168974=CARTESIAN_POINT('Ctrl Pts',(-155.92431351296,-1.02061347435243,
124.974177424108));
#168975=CARTESIAN_POINT('Ctrl Pts',(-155.916905293294,-0.864959109846162,
124.951175476056));
#168976=CARTESIAN_POINT('Ctrl Pts',(-155.909492513992,-0.709208942675329,
124.928159370688));
#168977=CARTESIAN_POINT('Ctrl Pts',(-155.90207973469,-0.552678972218055,
124.911384780937));
#168978=CARTESIAN_POINT('Ctrl Pts',(-155.894666955388,-0.395907931395946,
124.900871185683));
#168979=CARTESIAN_POINT('Ctrl Pts',(-155.887243584359,-0.238912888759547,
124.890342568111));
#168980=CARTESIAN_POINT('Ctrl Pts',(-155.87982021333,-0.0816764599822073,
124.886092822268));
#168981=CARTESIAN_POINT('Ctrl Pts',(-155.872396842301,0.0752636318832187,
124.888089329988));
#168982=CARTESIAN_POINT('Ctrl Pts',(-155.868460792861,0.158477034319438,
124.889147926287));
#168983=CARTESIAN_POINT('Ctrl Pts',(-155.86452474342,0.241607215557805,
124.891961701979));
#168984=CARTESIAN_POINT('Ctrl Pts',(-155.860588693979,0.324574942789907,
124.896519923284));
#168985=CARTESIAN_POINT('Ctrl Pts',(-155.853165427573,0.481049487009007,
124.905116586408));
#168986=CARTESIAN_POINT('Ctrl Pts',(-155.845742161168,0.63741886720515,
124.919947098834));
#168987=CARTESIAN_POINT('Ctrl Pts',(-155.838318894762,0.793146044176981,
124.941012605116));
#168988=CARTESIAN_POINT('Ctrl Pts',(-155.830904402041,0.948689164557967,
124.962053213718));
#168989=CARTESIAN_POINT('Ctrl Pts',(-155.82348990932,1.10359122625353,124.9893140981));
#168990=CARTESIAN_POINT('Ctrl Pts',(-155.816075416599,1.25731652817408,
125.022744432581));
#168991=CARTESIAN_POINT('Ctrl Pts',(-155.808668070246,1.41089366386142,
125.056142545647));
#168992=CARTESIAN_POINT('Ctrl Pts',(-155.801260723892,1.56329593543008,
125.095698192009));
#168993=CARTESIAN_POINT('Ctrl Pts',(-155.793853377538,1.71399420629504,
125.141308929361));
#168994=CARTESIAN_POINT('Ctrl Pts',(-155.786451555863,1.8645800807045,125.186885648504));
#168995=CARTESIAN_POINT('Ctrl Pts',(-155.779049734187,2.01346412920573,
125.238508358769));
#168996=CARTESIAN_POINT('Ctrl Pts',(-155.771647912512,2.16012894299117,
125.296023889283));
#168997=CARTESIAN_POINT('Ctrl Pts',(-155.7642499982,2.30671633356222,125.353509057796));
#168998=CARTESIAN_POINT('Ctrl Pts',(-155.756852083889,2.45108647589852,
125.41688071536));
#168999=CARTESIAN_POINT('Ctrl Pts',(-155.749454169578,2.59273873426755,
125.485936375525));
#169000=CARTESIAN_POINT('Ctrl Pts',(-155.742057484666,2.73436745260167,
125.554980559892));
#169001=CARTESIAN_POINT('Ctrl Pts',(-155.734660799753,2.87327884816594,
125.629706708731));
#169002=CARTESIAN_POINT('Ctrl Pts',(-155.727264114841,3.00899372711915,
125.709864831656));
#169003=CARTESIAN_POINT('Ctrl Pts',(-155.719867757906,3.14470258833241,
125.790019400285));
#169004=CARTESIAN_POINT('Ctrl Pts',(-155.71247140097,3.27721489333526,125.875605274249));
#169005=CARTESIAN_POINT('Ctrl Pts',(-155.705075044035,3.40607769745273,
125.96632741373));
#169006=CARTESIAN_POINT('Ctrl Pts',(-155.697677554698,3.53496023079448,
126.057063443003));
#169007=CARTESIAN_POINT('Ctrl Pts',(-155.690280065362,3.66019184545004,
126.152937088664));
#169008=CARTESIAN_POINT('Ctrl Pts',(-155.682882576025,3.78135026353552,
126.253611146659));
#169009=CARTESIAN_POINT('Ctrl Pts',(-155.67548249351,3.90255115351646,126.354320495789));
#169010=CARTESIAN_POINT('Ctrl Pts',(-155.668082410995,4.0196757171475,126.459833369229));
#169011=CARTESIAN_POINT('Ctrl Pts',(-155.66068232848,4.13233643702285,126.569773727));
#169012=CARTESIAN_POINT('Ctrl Pts',(-155.653274108814,4.24512103894167,
126.679834975497));
#169013=CARTESIAN_POINT('Ctrl Pts',(-155.645865889147,4.35343172726638,
126.794333170112));
#169014=CARTESIAN_POINT('Ctrl Pts',(-155.638457669481,4.45691890369688,
126.912856480556));
#169015=CARTESIAN_POINT('Ctrl Pts',(-155.631044890179,4.5604697747577,127.031452740119));
#169016=CARTESIAN_POINT('Ctrl Pts',(-155.623632110877,4.65919098468538,
127.154078761921));
#169017=CARTESIAN_POINT('Ctrl Pts',(-155.616219331575,4.75277494704296,
127.280291823507));
#169018=CARTESIAN_POINT('Ctrl Pts',(-155.608795960546,4.84649262655447,
127.406685224234));
#169019=CARTESIAN_POINT('Ctrl Pts',(-155.601372589517,4.93505818855841,
127.536675593498));
#169020=CARTESIAN_POINT('Ctrl Pts',(-155.593949218489,5.01820842319731,
127.669792898749));
#169021=CARTESIAN_POINT('Ctrl Pts',(-155.590013169048,5.06229667276761,
127.740374888102));
#169022=CARTESIAN_POINT('Ctrl Pts',(-155.586077119607,5.10486325711525,
127.81183557844));
#169023=CARTESIAN_POINT('Ctrl Pts',(-155.582141070166,5.14587437960451,
127.884102507085));
#169024=CARTESIAN_POINT('Ctrl Pts',(-155.57471780376,5.22322007670234,128.02039567913));
#169025=CARTESIAN_POINT('Ctrl Pts',(-155.567294537355,5.295264216107,128.159969921523));
#169026=CARTESIAN_POINT('Ctrl Pts',(-155.559871270949,5.36171555206768,
128.302374026632));
#169027=CARTESIAN_POINT('Ctrl Pts',(-155.552456778228,5.42808834806768,
128.444609821914));
#169028=CARTESIAN_POINT('Ctrl Pts',(-155.545042285507,5.48888134200826,
128.589668487366));
#169029=CARTESIAN_POINT('Ctrl Pts',(-155.537627792786,5.54384773545081,
128.737071849968));
#169030=CARTESIAN_POINT('Ctrl Pts',(-155.530220446432,5.59876115021375,
128.884333139659));
#169031=CARTESIAN_POINT('Ctrl Pts',(-155.522813100079,5.64785901507064,
129.033934280045));
#169032=CARTESIAN_POINT('Ctrl Pts',(-155.515405753725,5.69094150638549,
129.185374720963));
#169033=CARTESIAN_POINT('Ctrl Pts',(-155.50800393205,5.73399186515316,129.336702211888));
#169034=CARTESIAN_POINT('Ctrl Pts',(-155.500602110374,5.77103568188583,
129.489865914361));
#169035=CARTESIAN_POINT('Ctrl Pts',(-155.493200288699,5.80192215147819,
129.6443477251));
#169036=CARTESIAN_POINT('Ctrl Pts',(-155.485802374387,5.83279231634359,
129.798747986094));
#169037=CARTESIAN_POINT('Ctrl Pts',(-155.478404460076,5.85751153442523,
129.954464604469));
#169038=CARTESIAN_POINT('Ctrl Pts',(-155.471006545765,5.87597955746785,
130.110966932334));
#169039=CARTESIAN_POINT('Ctrl Pts',(-155.463609860852,5.89444451146012,
130.267443252351));
#169040=CARTESIAN_POINT('Ctrl Pts',(-155.45621317594,5.90666028848924,130.42470465235));
#169041=CARTESIAN_POINT('Ctrl Pts',(-155.448816491028,5.91257819657075,
130.58221284707));
#169042=CARTESIAN_POINT('Ctrl Pts',(-155.441420134092,5.918495842246,130.739714057713));
#169043=CARTESIAN_POINT('Ctrl Pts',(-155.434023777157,5.91811616020948,
130.897461668284));
#169044=CARTESIAN_POINT('Ctrl Pts',(-155.426627420222,5.91144254815312,
131.054915127374));
#169045=CARTESIAN_POINT('Ctrl Pts',(-155.419229930885,5.90476791434974,
131.21239269299));
#169046=CARTESIAN_POINT('Ctrl Pts',(-155.411832441548,5.89179744764637,
131.369575644466));
#169047=CARTESIAN_POINT('Ctrl Pts',(-155.404434952212,5.87258659585107,
131.525926440433));
#169048=CARTESIAN_POINT('Ctrl Pts',(-155.397034869697,5.85336900972132,
131.682332044931));
#169049=CARTESIAN_POINT('Ctrl Pts',(-155.389634787182,5.82790672858541,
131.837904542844));
#169050=CARTESIAN_POINT('Ctrl Pts',(-155.382234704667,5.7963066629028,131.992114646012));
#169051=CARTESIAN_POINT('Ctrl Pts',(-155.374826485,5.76467184969954,132.14649431904));
#169052=CARTESIAN_POINT('Ctrl Pts',(-155.367418265334,5.72688584848713,
132.299508239609));
#169053=CARTESIAN_POINT('Ctrl Pts',(-155.360010045667,5.68310617733135,
132.450639676437));
#169054=CARTESIAN_POINT('Ctrl Pts',(-155.352597266365,5.63929956051847,
132.601864132143));
#169055=CARTESIAN_POINT('Ctrl Pts',(-155.345184487063,5.58949204079213,
132.751203442076));
#169056=CARTESIAN_POINT('Ctrl Pts',(-155.337771707761,5.53388983510917,
132.898159522756));
#169057=CARTESIAN_POINT('Ctrl Pts',(-155.330348336732,5.47820818238717,
133.045325581176));
#169058=CARTESIAN_POINT('Ctrl Pts',(-155.322924965703,5.41671545280354,
133.190101266576));
#169059=CARTESIAN_POINT('Ctrl Pts',(-155.315501594675,5.34966482669673,
133.332011068974));
#169060=CARTESIAN_POINT('Ctrl Pts',(-155.311565545234,5.31411297587865,
133.407255051282));
#169061=CARTESIAN_POINT('Ctrl Pts',(-155.307629495793,5.27699935181552,
133.481693772887));
#169062=CARTESIAN_POINT('Ctrl Pts',(-155.303693446353,5.23836665150149,
133.555259631877));
#169063=CARTESIAN_POINT('Ctrl Pts',(-155.296270179947,5.16550658439187,
133.694002546025));
#169064=CARTESIAN_POINT('Ctrl Pts',(-155.288846913542,5.08702043844345,
133.830058608206));
#169065=CARTESIAN_POINT('Ctrl Pts',(-155.281423647136,5.0031304019728,133.962938896374));
#169066=CARTESIAN_POINT('Ctrl Pts',(-155.274009154415,4.91933951655838,
134.095662131076));
#169067=CARTESIAN_POINT('Ctrl Pts',(-155.266594661694,4.83015765121469,
134.225216750558));
#169068=CARTESIAN_POINT('Ctrl Pts',(-155.259180168973,4.73585370586237,
134.351136652104));
#169069=CARTESIAN_POINT('Ctrl Pts',(-155.25177282262,4.64164065420307,134.476935187307));
#169070=CARTESIAN_POINT('Ctrl Pts',(-155.244365476266,4.54231557310859,
134.599105682126));
#169071=CARTESIAN_POINT('Ctrl Pts',(-155.236958129912,4.43819158005151,
134.717209459683));
#169072=CARTESIAN_POINT('Ctrl Pts',(-155.229556308237,4.33414524659711,
134.835225150988));
#169073=CARTESIAN_POINT('Ctrl Pts',(-155.222154486561,4.22530737367528,
134.949179885558));
#169074=CARTESIAN_POINT('Ctrl Pts',(-155.214752664886,4.1120323424075,135.058666739308));
#169075=CARTESIAN_POINT('Ctrl Pts',(-155.207354750574,3.99881710814603,
135.168095795802));
#169076=CARTESIAN_POINT('Ctrl Pts',(-155.199956836263,3.88116964815559,
135.273061409881));
#169077=CARTESIAN_POINT('Ctrl Pts',(-155.192558921952,3.75948222490738,
135.373192411702));
#169078=CARTESIAN_POINT('Ctrl Pts',(-155.185162237039,3.63781502390215,
135.473306773566));
#169079=CARTESIAN_POINT('Ctrl Pts',(-155.177765552127,3.51210948008041,
135.568587880771));
#169080=CARTESIAN_POINT('Ctrl Pts',(-155.170368867215,3.38279214886937,
135.658703811042));
#169081=CARTESIAN_POINT('Ctrl Pts',(-155.162972510279,3.25348055172469,
135.748815745478));
#169082=CARTESIAN_POINT('Ctrl Pts',(-155.155576153344,3.12055779189248,
135.83376274494));
#169083=CARTESIAN_POINT('Ctrl Pts',(-155.148179796409,2.98448048711869,
135.913255486763));
#169084=CARTESIAN_POINT('Ctrl Pts',(-155.140782307072,2.84838234856177,
135.992760399128));
#169085=CARTESIAN_POINT('Ctrl Pts',(-155.133384817736,2.70912902575761,
136.066809202828));
#169086=CARTESIAN_POINT('Ctrl Pts',(-155.125987328399,2.56720273837941,
136.135157993434));
#169087=CARTESIAN_POINT('Ctrl Pts',(-155.118587245884,2.42522669896138,
136.203530743602));
#169088=CARTESIAN_POINT('Ctrl Pts',(-155.111187163369,2.2805761655214,136.266199340544));
#169089=CARTESIAN_POINT('Ctrl Pts',(-155.103787080854,2.13375423089479,
136.322967637878));
#169090=CARTESIAN_POINT('Ctrl Pts',(-155.096378861188,1.98677085045719,
136.379798357791));
#169091=CARTESIAN_POINT('Ctrl Pts',(-155.088970641521,1.83761164887359,
136.430715686456));
#169092=CARTESIAN_POINT('Ctrl Pts',(-155.081562421855,1.6867965091684,136.475572842404));
#169093=CARTESIAN_POINT('Ctrl Pts',(-155.074149642553,1.53588854526078,
136.520457607184));
#169094=CARTESIAN_POINT('Ctrl Pts',(-155.06673686325,1.38332297327647,136.55927467505));
#169095=CARTESIAN_POINT('Ctrl Pts',(-155.059324083948,1.22963031025704,
136.591928315883));
#169096=CARTESIAN_POINT('Ctrl Pts',(-155.05190071292,1.07571804395343,136.624628613768));
#169097=CARTESIAN_POINT('Ctrl Pts',(-155.044477341891,0.920675837183158,
136.651147833106));
#169098=CARTESIAN_POINT('Ctrl Pts',(-155.037053970862,0.765040600118077,
136.671441956926));
#169099=CARTESIAN_POINT('Ctrl Pts',(-155.033117921421,0.68251906300948,
136.682202388327));
#169100=CARTESIAN_POINT('Ctrl Pts',(-155.02918187198,0.599830837948508,
136.691213592585));
#169101=CARTESIAN_POINT('Ctrl Pts',(-155.02524582254,0.5170558791074,136.698474951406));
#169102=CARTESIAN_POINT('Ctrl Pts',(-155.017822556134,0.360944890052135,
136.712169647524));
#169103=CARTESIAN_POINT('Ctrl Pts',(-155.010399289729,0.204053392616007,
136.719678655057));
#169104=CARTESIAN_POINT('Ctrl Pts',(-155.002976023323,0.0469128289745836,
136.720924633021));
#169105=CARTESIAN_POINT('Ctrl Pts',(-154.995561530602,-0.110042007570774,
136.722169138343));
#169106=CARTESIAN_POINT('Ctrl Pts',(-154.988147037881,-0.267244954724259,
136.717165345645));
#169107=CARTESIAN_POINT('Ctrl Pts',(-154.98073254516,-0.424158520096556,
136.705887548143));
#169108=CARTESIAN_POINT('Ctrl Pts',(-154.973325198807,-0.580920846266409,
136.694620620608));
#169109=CARTESIAN_POINT('Ctrl Pts',(-154.965917852453,-0.73739397608614,
136.67709175348));
#169110=CARTESIAN_POINT('Ctrl Pts',(-154.958510506099,-0.893039590635261,
136.653327265792));
#169111=CARTESIAN_POINT('Ctrl Pts',(-154.951108684424,-1.04856911881288,
136.629580502555));
#169112=CARTESIAN_POINT('Ctrl Pts',(-154.943706862748,-1.20327199319958,
136.599607435151));
#169113=CARTESIAN_POINT('Ctrl Pts',(-154.936305041073,-1.35661430538524,
136.563486262047));
#169114=CARTESIAN_POINT('Ctrl Pts',(-154.928907126762,-1.50987566935792,
136.52738415703));
#169115=CARTESIAN_POINT('Ctrl Pts',(-154.92150921245,-1.66177753908607,
136.485140495328));
#169116=CARTESIAN_POINT('Ctrl Pts',(-154.914111298139,-1.81179561141999,
136.436884672103));
#169117=CARTESIAN_POINT('Ctrl Pts',(-154.906714613227,-1.96178875347212,
136.38863686812));
#169118=CARTESIAN_POINT('Ctrl Pts',(-154.899317928315,-2.10989836442982,
136.334378999752));
#169119=CARTESIAN_POINT('Ctrl Pts',(-154.891921243402,-2.25561462505338,
136.274290528063));
#169120=CARTESIAN_POINT('Ctrl Pts',(-154.884524886467,-2.40132442446565,
136.214204720759));
#169121=CARTESIAN_POINT('Ctrl Pts',(-154.877128529531,-2.5446407394465,
136.148288966499));
#169122=CARTESIAN_POINT('Ctrl Pts',(-154.869732172596,-2.6850733415975,
136.076771044756));
#169123=CARTESIAN_POINT('Ctrl Pts',(-154.862334683259,-2.82552744433759,
136.005242173437));
#169124=CARTESIAN_POINT('Ctrl Pts',(-154.854937193923,-2.96309662248831,
135.928109596246));
#169125=CARTESIAN_POINT('Ctrl Pts',(-154.847539704586,-3.09731502083322,
135.845647181948));
#169126=CARTESIAN_POINT('Ctrl Pts',(-154.840139622071,-3.23158046923057,
135.763155860578));
#169127=CARTESIAN_POINT('Ctrl Pts',(-154.832739539556,-3.36249248131584,
135.675331177492));
#169128=CARTESIAN_POINT('Ctrl Pts',(-154.825339457041,-3.48961409961607,
135.582490377028));
#169129=CARTESIAN_POINT('Ctrl Pts',(-154.817931237375,-3.6168755012035,
135.489547488561));
#169130=CARTESIAN_POINT('Ctrl Pts',(-154.810523017708,-3.74033788373541,
135.391577687729));
#169131=CARTESIAN_POINT('Ctrl Pts',(-154.803114798042,-3.85959674633049,
135.288939027876));
#169132=CARTESIAN_POINT('Ctrl Pts',(-154.79570201874,-3.9789290107659,135.186237195639));
#169133=CARTESIAN_POINT('Ctrl Pts',(-154.788289239438,-4.09405232759739,
135.078861032389));
#169134=CARTESIAN_POINT('Ctrl Pts',(-154.780876460135,-4.2045993989427,
134.967205132668));
#169135=CARTESIAN_POINT('Ctrl Pts',(-154.773453089107,-4.31530442512722,
134.855389693761));
#169136=CARTESIAN_POINT('Ctrl Pts',(-154.766029718078,-4.42141989529531,
134.739282580002));
#169137=CARTESIAN_POINT('Ctrl Pts',(-154.758606347049,-4.52261856366009,
134.619311716877));
#169138=CARTESIAN_POINT('Ctrl Pts',(-154.754670297609,-4.57627652585711,
134.555700286586));
#169139=CARTESIAN_POINT('Ctrl Pts',(-154.750734248168,-4.62855291262859,
134.491003117001));
#169140=CARTESIAN_POINT('Ctrl Pts',(-154.746798198727,-4.6794039866025,
134.42528714163));
#169141=CARTESIAN_POINT('Ctrl Pts',(-154.739155573455,-4.77814149203344,
134.297686464436));
#169142=CARTESIAN_POINT('Ctrl Pts',(-154.731512948183,-4.87181406104119,
134.165839883425));
#169143=CARTESIAN_POINT('Ctrl Pts',(-154.723870322912,-4.96003677850672,
134.030188529647));
#169144=CARTESIAN_POINT('Ctrl Pts',(-154.716449600915,-5.04569795340555,
133.898475806722));
#169145=CARTESIAN_POINT('Ctrl Pts',(-154.709028878919,-5.12622107821451,
133.763176497115));
#169146=CARTESIAN_POINT('Ctrl Pts',(-154.701608156922,-5.20129311617826,
133.624729473247));
#169147=CARTESIAN_POINT('Ctrl Pts',(-154.694194574293,-5.27629292843997,
133.486415647222));
#169148=CARTESIAN_POINT('Ctrl Pts',(-154.686780991664,-5.34585191604673,
133.344960458892));
#169149=CARTESIAN_POINT('Ctrl Pts',(-154.679367409035,-5.40970024717301,
133.200831731149));
#169150=CARTESIAN_POINT('Ctrl Pts',(-154.671959507099,-5.47349965420942,
133.056813442734));
#169151=CARTESIAN_POINT('Ctrl Pts',(-154.664551605163,-5.5315969659786,
132.910126031599));
#169152=CARTESIAN_POINT('Ctrl Pts',(-154.657143703227,-5.58376829481499,
132.761261788376));
#169153=CARTESIAN_POINT('Ctrl Pts',(-154.649740027136,-5.63590986246714,
132.612482464903));
#169154=CARTESIAN_POINT('Ctrl Pts',(-154.642336351045,-5.68213205602446,
132.461529132111));
#169155=CARTESIAN_POINT('Ctrl Pts',(-154.634932674954,-5.72225919274741,
132.3089138049));
#169156=CARTESIAN_POINT('Ctrl Pts',(-154.627531344331,-5.7623736172847,
132.156346825878));
#169157=CARTESIAN_POINT('Ctrl Pts',(-154.620130013707,-5.79639673423116,
132.002119259781));
#169158=CARTESIAN_POINT('Ctrl Pts',(-154.612728683084,-5.82420280300167,
131.846757985179));
#169159=CARTESIAN_POINT('Ctrl Pts',(-154.605328642872,-5.85200402382515,
131.691423797587));
#169160=CARTESIAN_POINT('Ctrl Pts',(-154.597928602659,-5.87359029279718,
131.534956661622));
#169161=CARTESIAN_POINT('Ctrl Pts',(-154.590528562447,-5.88888707822839,
131.377893129613));
#169162=CARTESIAN_POINT('Ctrl Pts',(-154.58312737356,-5.9041862381108,131.220805217338));
#169163=CARTESIAN_POINT('Ctrl Pts',(-154.575726184673,-5.9131939302452,
131.063121094403));
#169164=CARTESIAN_POINT('Ctrl Pts',(-154.568324995785,-5.9158875279668,
130.905381996228));
#169165=CARTESIAN_POINT('Ctrl Pts',(-154.566675061259,-5.91648800715306,
130.870217485747));
#169166=CARTESIAN_POINT('Ctrl Pts',(-154.565025126733,-5.91677489975811,
130.835050248019));
#169167=CARTESIAN_POINT('Ctrl Pts',(-154.563375192207,-5.91674830821855,
130.799886280413));
#169168=CARTESIAN_POINT('',(-152.813375192207,-5.92569483190729,130.802331264594));
#169169=CARTESIAN_POINT('Ctrl Pts',(-154.563373070317,-5.91080345335137,
130.799845598986));
#169170=CARTESIAN_POINT('Ctrl Pts',(-154.531698905183,-5.91551139364249,
130.125469392084));
#169171=CARTESIAN_POINT('Ctrl Pts',(-154.407208865444,-5.49704716835897,
127.480621738463));
#169172=CARTESIAN_POINT('Ctrl Pts',(-154.189902951101,-1.59469172994353,
123.990072773871));
#169173=CARTESIAN_POINT('Ctrl Pts',(-153.911455327288,4.87108352101917,
125.779412273391));
#169174=CARTESIAN_POINT('Ctrl Pts',(-153.633007703476,6.86057098182519,
132.186433818843));
#169175=CARTESIAN_POINT('Ctrl Pts',(-153.354560079662,2.54552886785856,
137.323397610345));
#169176=CARTESIAN_POINT('Ctrl Pts',(-153.081349242573,-3.98358274264103,
136.485740721758));
#169177=CARTESIAN_POINT('Ctrl Pts',(-152.900954280088,-5.91747741062501,
132.654946942402));
#169178=CARTESIAN_POINT('Ctrl Pts',(-152.813375192207,-5.92569483190729,
130.802331264594));
#169179=CARTESIAN_POINT('',(-151.063375192207,-5.91700250792318,130.809816046553));
#169180=CARTESIAN_POINT('Ctrl Pts',(-152.813375192207,-5.92569483190729,
130.802331264594));
#169181=CARTESIAN_POINT('Ctrl Pts',(-152.808138405483,-5.92618619215906,
130.691554212449));
#169182=CARTESIAN_POINT('Ctrl Pts',(-152.80290161876,-5.92335003819969,
130.580802825064));
#169183=CARTESIAN_POINT('Ctrl Pts',(-152.704848957432,-5.80645997517362,
128.51071536498));
#169184=CARTESIAN_POINT('Ctrl Pts',(-152.519217208224,-3.44484665824443,
124.71251426104));
#169185=CARTESIAN_POINT('Ctrl Pts',(-152.240769584411,3.26321910596172,
124.613321803534));
#169186=CARTESIAN_POINT('Ctrl Pts',(-151.962321960598,6.97254592890501,
130.203391567066));
#169187=CARTESIAN_POINT('Ctrl Pts',(-151.683874336785,4.27444367098919,
136.345722529034));
#169188=CARTESIAN_POINT('Ctrl Pts',(-151.405426712973,-2.3516635023825,
137.395812604943));
#169189=CARTESIAN_POINT('Ctrl Pts',(-151.198593664779,-5.66833219350764,
133.676476019849));
#169190=CARTESIAN_POINT('Ctrl Pts',(-151.084576491191,-5.92117706019566,
131.260015846219));
#169191=CARTESIAN_POINT('Ctrl Pts',(-151.063375192207,-5.91700250792318,
130.809816046553));
#169192=CARTESIAN_POINT('',(-149.313375192166,-5.91674998398419,130.803925275142));
#169193=CARTESIAN_POINT('Ctrl Pts',(-151.063375192207,-5.91674748517798,
130.809815811424));
#169194=CARTESIAN_POINT('Ctrl Pts',(-151.056065681028,-5.91689058382068,
130.65460986341));
#169195=CARTESIAN_POINT('Ctrl Pts',(-151.048756169849,-5.91092255348512,
130.499227142345));
#169196=CARTESIAN_POINT('Ctrl Pts',(-151.04144665867,-5.89882852235356,
130.344194749244));
#169197=CARTESIAN_POINT('Ctrl Pts',(-151.034142292742,-5.88674300435314,
130.189271485274));
#169198=CARTESIAN_POINT('Ctrl Pts',(-151.026837926814,-5.8685400977311,
130.03469843971));
#169199=CARTESIAN_POINT('Ctrl Pts',(-151.019533560886,-5.84425700214759,
129.881002260616));
#169200=CARTESIAN_POINT('Ctrl Pts',(-151.012231970289,-5.81998313304877,
129.727364479161));
#169201=CARTESIAN_POINT('Ctrl Pts',(-151.004930379692,-5.78963372854271,
129.574603280231));
#169202=CARTESIAN_POINT('Ctrl Pts',(-150.997628789094,-5.75329778200764,
129.423239625746));
#169203=CARTESIAN_POINT('Ctrl Pts',(-150.990328503748,-5.71696833097914,
129.271903029415));
#169204=CARTESIAN_POINT('Ctrl Pts',(-150.983028218402,-5.67465455591097,
129.121963853903));
#169205=CARTESIAN_POINT('Ctrl Pts',(-150.975727933055,-5.62649639284513,
128.973932005519));
#169206=CARTESIAN_POINT('Ctrl Pts',(-150.968427422173,-5.57833674197355,
128.825895583816));
#169207=CARTESIAN_POINT('Ctrl Pts',(-150.961126911291,-5.52433246254643,
128.67976697175));
#169208=CARTESIAN_POINT('Ctrl Pts',(-150.953826400408,-5.46467301493037,
128.536039784352));
#169209=CARTESIAN_POINT('Ctrl Pts',(-150.946524133204,-5.40499921473299,
128.392278019763));
#169210=CARTESIAN_POINT('Ctrl Pts',(-150.939221866,-5.33966768671681,128.250919183856));
#169211=CARTESIAN_POINT('Ctrl Pts',(-150.931919598796,-5.26891544568148,
128.112435546402));
#169212=CARTESIAN_POINT('Ctrl Pts',(-150.924609826913,-5.19809049121819,
127.973809586672));
#169213=CARTESIAN_POINT('Ctrl Pts',(-150.917300055029,-5.1218338728137,
127.838065068987));
#169214=CARTESIAN_POINT('Ctrl Pts',(-150.909990283146,-5.04042816247926,
127.705648868889));
#169215=CARTESIAN_POINT('Ctrl Pts',(-150.902676570827,-4.95897856924788,
127.573161287971));
#169216=CARTESIAN_POINT('Ctrl Pts',(-150.895362858508,-4.87237456954214,
127.444005916282));
#169217=CARTESIAN_POINT('Ctrl Pts',(-150.888049146189,-4.78094076898396,
127.318598731555));
#169218=CARTESIAN_POINT('Ctrl Pts',(-150.880724518015,-4.68937050173198,
127.19300437421));
#169219=CARTESIAN_POINT('Ctrl Pts',(-150.87339988984,-4.5929562729929,127.071169678463));
#169220=CARTESIAN_POINT('Ctrl Pts',(-150.866075261666,-4.49206204232252,
126.953476411254));
#169221=CARTESIAN_POINT('Ctrl Pts',(-150.860227329559,-4.41150879144472,
126.859510926636));
#169222=CARTESIAN_POINT('Ctrl Pts',(-150.854379397453,-4.32810063904638,
126.768184663981));
#169223=CARTESIAN_POINT('Ctrl Pts',(-150.848531465346,-4.24203829366849,
126.679673759446));
#169224=CARTESIAN_POINT('Ctrl Pts',(-150.84110819894,-4.13279220367148,
126.567319509743));
#169225=CARTESIAN_POINT('Ctrl Pts',(-150.833684932535,-4.01891413083966,
126.459138588643));
#169226=CARTESIAN_POINT('Ctrl Pts',(-150.826261666129,-3.90075590755898,
126.355536737916));
#169227=CARTESIAN_POINT('Ctrl Pts',(-150.818847173408,-3.78273733748545,
126.252057335973));
#169228=CARTESIAN_POINT('Ctrl Pts',(-150.811432680687,-3.66044896444028,
126.153146475329));
#169229=CARTESIAN_POINT('Ctrl Pts',(-150.804018187966,-3.53428093362584,
126.059174757696));
#169230=CARTESIAN_POINT('Ctrl Pts',(-150.796610841613,-3.40823450830928,
125.965293613542));
#169231=CARTESIAN_POINT('Ctrl Pts',(-150.789203495259,-3.27831616692556,
125.876342356604));
#169232=CARTESIAN_POINT('Ctrl Pts',(-150.781796148905,-3.14495066844497,
125.792652739452));
#169233=CARTESIAN_POINT('Ctrl Pts',(-150.774394327229,-3.01168463898511,
125.709025541175));
#169234=CARTESIAN_POINT('Ctrl Pts',(-150.766992505554,-2.87497688651215,
125.630652366382));
#169235=CARTESIAN_POINT('Ctrl Pts',(-150.759590683879,-2.73528272313482,
125.557822808018));
#169236=CARTESIAN_POINT('Ctrl Pts',(-150.752192769567,-2.59566230321896,
125.485031695811));
#169237=CARTESIAN_POINT('Ctrl Pts',(-150.744794855256,-2.45305894225528,
125.417778544041));
#169238=CARTESIAN_POINT('Ctrl Pts',(-150.737396940945,-2.30795412648063,
125.356307909253));
#169239=CARTESIAN_POINT('Ctrl Pts',(-150.730000256032,-2.16287342449411,
125.294847489769));
#169240=CARTESIAN_POINT('Ctrl Pts',(-150.72260357112,-2.01529243612141,
125.239167825537));
#169241=CARTESIAN_POINT('Ctrl Pts',(-150.715206886208,-1.86571438933428,
125.189466105651));
#169242=CARTESIAN_POINT('Ctrl Pts',(-150.707810529273,-1.71614297499406,
125.139766589592));
#169243=CARTESIAN_POINT('Ctrl Pts',(-150.700414172337,-1.56457503256302,
125.096044608544));
#169244=CARTESIAN_POINT('Ctrl Pts',(-150.693017815402,-1.41153052363258,
125.058447970879));
#169245=CARTESIAN_POINT('Ctrl Pts',(-150.685620326065,-1.25846258319711,
125.020845577074));
#169246=CARTESIAN_POINT('Ctrl Pts',(-150.678222836729,-1.10391798867733,
124.989370483008));
#169247=CARTESIAN_POINT('Ctrl Pts',(-150.670825347392,-0.948428358278844,
124.964119679753));
#169248=CARTESIAN_POINT('Ctrl Pts',(-150.663425264877,-0.792884221232128,
124.938860024867));
#169249=CARTESIAN_POINT('Ctrl Pts',(-150.656025182362,-0.636394756969904,
124.919829064768));
#169250=CARTESIAN_POINT('Ctrl Pts',(-150.648625099847,-0.479498041886692,
124.907072071944));
#169251=CARTESIAN_POINT('Ctrl Pts',(-150.641216880181,-0.3224288027352,
124.894301051494));
#169252=CARTESIAN_POINT('Ctrl Pts',(-150.633808660514,-0.16495179074682,
124.88781780609));
#169253=CARTESIAN_POINT('Ctrl Pts',(-150.626400440848,-0.00760716935874803,
124.887615507839));
#169254=CARTESIAN_POINT('Ctrl Pts',(-150.618987661546,0.149834295018352,
124.887413085078));
#169255=CARTESIAN_POINT('Ctrl Pts',(-150.611574882244,0.307142834273683,
124.8934992982));
#169256=CARTESIAN_POINT('Ctrl Pts',(-150.604162102942,0.463782579581826,
124.905815349334));
#169257=CARTESIAN_POINT('Ctrl Pts',(-150.596738731913,0.620646139103517,
124.918148998221));
#169258=CARTESIAN_POINT('Ctrl Pts',(-150.589315360884,0.77683862642008,
124.9367302194));
#169259=CARTESIAN_POINT('Ctrl Pts',(-150.581891989855,0.931832721620842,
124.961448814243));
#169260=CARTESIAN_POINT('Ctrl Pts',(-150.577955940415,1.0140143099217,124.974555206341));
#169261=CARTESIAN_POINT('Ctrl Pts',(-150.574019890974,1.09585920157823,
124.989386189939));
#169262=CARTESIAN_POINT('Ctrl Pts',(-150.570083841534,1.17729055566755,
125.005919662444));
#169263=CARTESIAN_POINT('Ctrl Pts',(-150.562660575129,1.33086754810704,
125.037101275599));
#169264=CARTESIAN_POINT('Ctrl Pts',(-150.555237308723,1.48343710086397,
125.074435693147));
#169265=CARTESIAN_POINT('Ctrl Pts',(-150.547814042318,1.63446767789529,
125.117846221874));
#169266=CARTESIAN_POINT('Ctrl Pts',(-150.540399549597,1.7853197493273,125.161205442961));
#169267=CARTESIAN_POINT('Ctrl Pts',(-150.532985056876,1.93463611037831,
125.210626378381));
#169268=CARTESIAN_POINT('Ctrl Pts',(-150.525570564155,2.08189408032096,
125.265981107202));
#169269=CARTESIAN_POINT('Ctrl Pts',(-150.518163217801,2.22901011748802,
125.321282483051));
#169270=CARTESIAN_POINT('Ctrl Pts',(-150.510755871447,2.37407136613012,
125.382506136005));
#169271=CARTESIAN_POINT('Ctrl Pts',(-150.503348525093,2.51656912081436,
125.449474024681));
#169272=CARTESIAN_POINT('Ctrl Pts',(-150.495946703418,2.65896059529662,
125.516391966178));
#169273=CARTESIAN_POINT('Ctrl Pts',(-150.488544881742,2.79879204637759,
125.589045454751));
#169274=CARTESIAN_POINT('Ctrl Pts',(-150.481143060067,2.93557372399401,
125.667207955488));
#169275=CARTESIAN_POINT('Ctrl Pts',(-150.473745145756,3.07228319562752,
125.745329194849));
#169276=CARTESIAN_POINT('Ctrl Pts',(-150.466347231444,3.20594577680103,
125.828953469883));
#169277=CARTESIAN_POINT('Ctrl Pts',(-150.458949317133,3.33609546009509,
125.917807881369));
#169278=CARTESIAN_POINT('Ctrl Pts',(-150.451552632221,3.46622351487314,
126.006647526864));
#169279=CARTESIAN_POINT('Ctrl Pts',(-150.444155947308,3.59283952240294,
126.100715373524));
#169280=CARTESIAN_POINT('Ctrl Pts',(-150.436759262396,3.71550557490402,
126.199694626926));
#169281=CARTESIAN_POINT('Ctrl Pts',(-150.429362905461,3.83816618826414,
126.298669491484));
#169282=CARTESIAN_POINT('Ctrl Pts',(-150.421966548525,3.95687690432722,
126.402555095354));
#169283=CARTESIAN_POINT('Ctrl Pts',(-150.41457019159,4.0712323157834,126.510993874156));
#169284=CARTESIAN_POINT('Ctrl Pts',(-150.407172702253,4.18560523534468,
126.619449255211));
#169285=CARTESIAN_POINT('Ctrl Pts',(-150.399775212916,4.29562125170189,
126.732458942347));
#169286=CARTESIAN_POINT('Ctrl Pts',(-150.39237772358,4.40091141089656,126.849628096151));
#169287=CARTESIAN_POINT('Ctrl Pts',(-150.384977641065,4.50623847939347,
126.96683832342));
#169288=CARTESIAN_POINT('Ctrl Pts',(-150.37757755855,4.60683614301077,127.088210642926));
#169289=CARTESIAN_POINT('Ctrl Pts',(-150.370177476035,4.70237546928901,
127.213316826643));
#169290=CARTESIAN_POINT('Ctrl Pts',(-150.362769256368,4.79801985087831,
127.33856057747));
#169291=CARTESIAN_POINT('Ctrl Pts',(-150.355361036702,4.88859456042188,
127.467546095133));
#169292=CARTESIAN_POINT('Ctrl Pts',(-150.347952817035,4.97381337088553,
127.599815234193));
#169293=CARTESIAN_POINT('Ctrl Pts',(-150.340540037733,5.05908463210483,
127.732165782699));
#169294=CARTESIAN_POINT('Ctrl Pts',(-150.333127258431,5.138993236577,127.86780365884));
#169295=CARTESIAN_POINT('Ctrl Pts',(-150.325714479129,5.21329900242612,
128.00624623931));
#169296=CARTESIAN_POINT('Ctrl Pts',(-150.3182911081,5.28771093983817,128.144886633031));
#169297=CARTESIAN_POINT('Ctrl Pts',(-150.310867737071,5.35650388682064,
128.286339400131));
#169298=CARTESIAN_POINT('Ctrl Pts',(-150.303444366042,5.41948552731017,
128.430101326382));
#169299=CARTESIAN_POINT('Ctrl Pts',(-150.299508316602,5.45287990431955,
128.506327349195));
#169300=CARTESIAN_POINT('Ctrl Pts',(-150.295572267161,5.48464134089764,
128.583202283417));
#169301=CARTESIAN_POINT('Ctrl Pts',(-150.291636217721,5.51474689818421,
128.660649533612));
#169302=CARTESIAN_POINT('Ctrl Pts',(-150.284212951315,5.57152503966739,
128.806712630441));
#169303=CARTESIAN_POINT('Ctrl Pts',(-150.27678968491,5.62258210680279,128.955253880797));
#169304=CARTESIAN_POINT('Ctrl Pts',(-150.269366418504,5.66769531554686,
129.1057846338));
#169305=CARTESIAN_POINT('Ctrl Pts',(-150.261951925783,5.71275520422461,
129.256137471953));
#169306=CARTESIAN_POINT('Ctrl Pts',(-150.254537433062,5.75188511198533,
129.408474778131));
#169307=CARTESIAN_POINT('Ctrl Pts',(-150.247122940341,5.78491014063071,
129.562287661847));
#169308=CARTESIAN_POINT('Ctrl Pts',(-150.239715593987,5.81790333851021,
129.715952294916));
#169309=CARTESIAN_POINT('Ctrl Pts',(-150.232308247634,5.84480329354514,
129.871089311639));
#169310=CARTESIAN_POINT('Ctrl Pts',(-150.22490090128,5.86548482928115,130.027174488011));
#169311=CARTESIAN_POINT('Ctrl Pts',(-150.217499079605,5.88615093994742,
130.183143250169));
#169312=CARTESIAN_POINT('Ctrl Pts',(-150.210097257929,5.9006078172398,130.340058395429));
#169313=CARTESIAN_POINT('Ctrl Pts',(-150.202695436254,5.90878132952298,
130.497385435539));
#169314=CARTESIAN_POINT('Ctrl Pts',(-150.195297521942,5.91695052707265,
130.654629423929));
#169315=CARTESIAN_POINT('Ctrl Pts',(-150.187899607631,5.91884294613844,
130.812284502283));
#169316=CARTESIAN_POINT('Ctrl Pts',(-150.18050169332,5.91443629617107,130.969811096666));
#169317=CARTESIAN_POINT('Ctrl Pts',(-150.173105008408,5.91003037850896,
131.127311512987));
#169318=CARTESIAN_POINT('Ctrl Pts',(-150.165708323495,5.89932747981234,
131.284683114927));
#169319=CARTESIAN_POINT('Ctrl Pts',(-150.158311638583,5.88235742834927,
131.441386243145));
#169320=CARTESIAN_POINT('Ctrl Pts',(-150.150915281648,5.86538812935606,
131.598082422982));
#169321=CARTESIAN_POINT('Ctrl Pts',(-150.143518924713,5.84215227033082,
131.754109816905));
#169322=CARTESIAN_POINT('Ctrl Pts',(-150.136122567777,5.81273154775772,
131.908934071983));
#169323=CARTESIAN_POINT('Ctrl Pts',(-150.128725078441,5.78330632079681,
132.063782031049));
#169324=CARTESIAN_POINT('Ctrl Pts',(-150.121327589104,5.74769441454144,
132.217426117738));
#169325=CARTESIAN_POINT('Ctrl Pts',(-150.113930099767,5.70602858994373,
132.369342500287));
#169326=CARTESIAN_POINT('Ctrl Pts',(-150.106530017252,5.66434815945597,
132.521312136888));
#169327=CARTESIAN_POINT('Ctrl Pts',(-150.099129934737,5.61660968403365,
132.671552503739));
#169328=CARTESIAN_POINT('Ctrl Pts',(-150.091729852222,5.56299564801337,
132.819555392937));
#169329=CARTESIAN_POINT('Ctrl Pts',(-150.084321632556,5.50932265784876,
132.967721026528));
#169330=CARTESIAN_POINT('Ctrl Pts',(-150.07691341289,5.44976133169865,133.113643917819));
#169331=CARTESIAN_POINT('Ctrl Pts',(-150.069505193223,5.38454240759331,
133.256835617098));
#169332=CARTESIAN_POINT('Ctrl Pts',(-150.062092413921,5.31928334232842,
133.400115448479));
#169333=CARTESIAN_POINT('Ctrl Pts',(-150.054679634619,5.24835990826135,
133.540660405744));
#169334=CARTESIAN_POINT('Ctrl Pts',(-150.047266855317,5.17204832587609,
133.678007547393));
#169335=CARTESIAN_POINT('Ctrl Pts',(-150.039843484288,5.09562770592314,
133.815550937079));
#169336=CARTESIAN_POINT('Ctrl Pts',(-150.03242011326,5.01380375501804,133.949887067486));
#169337=CARTESIAN_POINT('Ctrl Pts',(-150.024996742231,4.92689589001179,
134.080582138081));
#169338=CARTESIAN_POINT('Ctrl Pts',(-150.02106069279,4.88081525465654,134.149879800501));
#169339=CARTESIAN_POINT('Ctrl Pts',(-150.017124643349,4.83330602756548,
134.218154376355));
#169340=CARTESIAN_POINT('Ctrl Pts',(-150.013188593908,4.78442025163299,
134.285345164826));
#169341=CARTESIAN_POINT('Ctrl Pts',(-150.005765327502,4.69222320390343,
134.412064894922));
#169342=CARTESIAN_POINT('Ctrl Pts',(-149.998342061097,4.5948488349964,134.535310825654));
#169343=CARTESIAN_POINT('Ctrl Pts',(-149.990918794691,4.49258784052027,
134.654631394759));
#169344=CARTESIAN_POINT('Ctrl Pts',(-149.98350430197,4.39044771004737,134.773810936861));
#169345=CARTESIAN_POINT('Ctrl Pts',(-149.976089809249,4.28343269088841,
134.889074071511));
#169346=CARTESIAN_POINT('Ctrl Pts',(-149.968675316528,4.17187639027414,
134.999998584166));
#169347=CARTESIAN_POINT('Ctrl Pts',(-149.961267970175,4.06042761182244,
135.110816183599));
#169348=CARTESIAN_POINT('Ctrl Pts',(-149.953860623821,3.9444465287092,135.217303224587));
#169349=CARTESIAN_POINT('Ctrl Pts',(-149.946453277467,3.82430652450501,
135.319071036754));
#169350=CARTESIAN_POINT('Ctrl Pts',(-149.939051455792,3.70425612524892,
135.420762946648));
#169351=CARTESIAN_POINT('Ctrl Pts',(-149.931649634116,3.58005326477897,
135.517742395833));
#169352=CARTESIAN_POINT('Ctrl Pts',(-149.924247812441,3.45210755323912,
135.609658111309));
#169353=CARTESIAN_POINT('Ctrl Pts',(-149.916849898129,3.32422938324483,
135.701525305193));
#169354=CARTESIAN_POINT('Ctrl Pts',(-149.909451983818,3.19261259953175,
135.788333871739));
#169355=CARTESIAN_POINT('Ctrl Pts',(-149.902054069507,3.05769911234658,
135.869773404384));
#169356=CARTESIAN_POINT('Ctrl Pts',(-149.894657384595,2.92280804533483,
135.951199403256));
#169357=CARTESIAN_POINT('Ctrl Pts',(-149.887260699682,2.78462168144833,
136.027257946324));
#169358=CARTESIAN_POINT('Ctrl Pts',(-149.87986401477,2.64361017428252,136.0976824299));
#169359=CARTESIAN_POINT('Ctrl Pts',(-149.872467657835,2.5026049197143,136.168103790781));
#169360=CARTESIAN_POINT('Ctrl Pts',(-149.865071300899,2.35877510490991,
136.232891422106));
#169361=CARTESIAN_POINT('Ctrl Pts',(-149.857674943964,2.21261445506972,
136.291825226629));
#169362=CARTESIAN_POINT('Ctrl Pts',(-149.850277454627,2.06643142766174,
136.350768054068));
#169363=CARTESIAN_POINT('Ctrl Pts',(-149.842879965291,1.91791720090442,
136.403855130574));
#169364=CARTESIAN_POINT('Ctrl Pts',(-149.835482475954,1.76758424983121,
136.450915007833));
#169365=CARTESIAN_POINT('Ctrl Pts',(-149.828082393439,1.6171985997744,136.497991381861));
#169366=CARTESIAN_POINT('Ctrl Pts',(-149.820682310924,1.46499331207091,
136.539036238572));
#169367=CARTESIAN_POINT('Ctrl Pts',(-149.813282228409,1.31149459366289,
136.573928408423));
#169368=CARTESIAN_POINT('Ctrl Pts',(-149.805874008743,1.1578270876337,136.608858945802));
#169369=CARTESIAN_POINT('Ctrl Pts',(-149.798465789076,1.00286367478862,
136.637623202355));
#169370=CARTESIAN_POINT('Ctrl Pts',(-149.79105756941,0.847140021244748,
136.660151285521));
#169371=CARTESIAN_POINT('Ctrl Pts',(-149.783644790108,0.691320522390506,
136.682693234346));
#169372=CARTESIAN_POINT('Ctrl Pts',(-149.776232010806,0.534740220888373,
136.698991323012));
#169373=CARTESIAN_POINT('Ctrl Pts',(-149.768819231503,0.377937906451597,
136.709027712447));
#169374=CARTESIAN_POINT('Ctrl Pts',(-149.761395860475,0.220911545514431,
136.719078442345));
#169375=CARTESIAN_POINT('Ctrl Pts',(-149.753972489446,0.0636629102801282,
136.722849594901));
#169376=CARTESIAN_POINT('Ctrl Pts',(-149.746549118417,-0.0932703779676402,
136.720375424773));
#169377=CARTESIAN_POINT('Ctrl Pts',(-149.742613068976,-0.176480172958929,
136.719063560405));
#169378=CARTESIAN_POINT('Ctrl Pts',(-149.738677019535,-0.259601404975529,
136.71599677807));
#169379=CARTESIAN_POINT('Ctrl Pts',(-149.734740970095,-0.342554874245969,
136.711186052656));
#169380=CARTESIAN_POINT('Ctrl Pts',(-149.727317703689,-0.499002528400226,
136.702113174664));
#169381=CARTESIAN_POINT('Ctrl Pts',(-149.719894437284,-0.655326045325712,
136.686806796327));
#169382=CARTESIAN_POINT('Ctrl Pts',(-149.712471170878,-0.810988384824968,
136.665267407661));
#169383=CARTESIAN_POINT('Ctrl Pts',(-149.705056678157,-0.966466744365004,
136.643753476763));
#169384=CARTESIAN_POINT('Ctrl Pts',(-149.697642185437,-1.12128511580916,
136.61602125006));
#169385=CARTESIAN_POINT('Ctrl Pts',(-149.690227692716,-1.2749079552451,
136.582123183487));
#169386=CARTESIAN_POINT('Ctrl Pts',(-149.682820346362,-1.42838272720545,
136.548257789146));
#169387=CARTESIAN_POINT('Ctrl Pts',(-149.675413000008,-1.58066389907574,
136.508238465913));
#169388=CARTESIAN_POINT('Ctrl Pts',(-149.668005653654,-1.73122264852107,
136.462169266128));
#169389=CARTESIAN_POINT('Ctrl Pts',(-149.660603831979,-1.88166910556994,
136.416134426492));
#169390=CARTESIAN_POINT('Ctrl Pts',(-149.653202010304,-2.03039534267612,
136.36405880351));
#169391=CARTESIAN_POINT('Ctrl Pts',(-149.645800188628,-2.17688441962812,
136.306097142163));
#169392=CARTESIAN_POINT('Ctrl Pts',(-149.638402274317,-2.32329616613749,
136.248166078325));
#169393=CARTESIAN_POINT('Ctrl Pts',(-149.631004360006,-2.46747275823444,
136.184355301241));
#169394=CARTESIAN_POINT('Ctrl Pts',(-149.623606445694,-2.60891417880448,
136.11486882019));
#169395=CARTESIAN_POINT('Ctrl Pts',(-149.616209760782,-2.75033209437662,
136.045393886531));
#169396=CARTESIAN_POINT('Ctrl Pts',(-149.60881307587,-2.88901540582003,
135.970245285314));
#169397=CARTESIAN_POINT('Ctrl Pts',(-149.601416390958,-3.02448568239786,
135.889674464269));
#169398=CARTESIAN_POINT('Ctrl Pts',(-149.594020034022,-3.15994995208127,
135.809107215819));
#169399=CARTESIAN_POINT('Ctrl Pts',(-149.586623677087,-3.29220114933539,
135.72311841641));
#169400=CARTESIAN_POINT('Ctrl Pts',(-149.579227320152,-3.42078722958298,
135.632004483099));
#169401=CARTESIAN_POINT('Ctrl Pts',(-149.571829830815,-3.54939299668735,
135.540876600013));
#169402=CARTESIAN_POINT('Ctrl Pts',(-149.564432341479,-3.6743322248794,
135.444622236477));
#169403=CARTESIAN_POINT('Ctrl Pts',(-149.557034852142,-3.79518366456432,
135.34357988025));
#169404=CARTESIAN_POINT('Ctrl Pts',(-149.549634769627,-3.9160774685339,
135.242502103782));
#169405=CARTESIAN_POINT('Ctrl Pts',(-149.542234687112,-4.03288034475929,
135.13663323219));
#169406=CARTESIAN_POINT('Ctrl Pts',(-149.534834604598,-4.14520592216597,
135.026350483179));
#169407=CARTESIAN_POINT('Ctrl Pts',(-149.527426384931,-4.25765501309316,
134.915946466947));
#169408=CARTESIAN_POINT('Ctrl Pts',(-149.520018165265,-4.3656167066114,
134.801119142203));
#169409=CARTESIAN_POINT('Ctrl Pts',(-149.512609945598,-4.46874265950966,
134.682281401385));
#169410=CARTESIAN_POINT('Ctrl Pts',(-149.505197166296,-4.57193208471119,
134.563370517921));
#169411=CARTESIAN_POINT('Ctrl Pts',(-149.497784386994,-4.6702796059402,
134.440444590711));
#169412=CARTESIAN_POINT('Ctrl Pts',(-149.490371607692,-4.76347898567933,
134.313947276347));
#169413=CARTESIAN_POINT('Ctrl Pts',(-149.482948236663,-4.85681153306298,
134.187269216687));
#169414=CARTESIAN_POINT('Ctrl Pts',(-149.475524865635,-4.94498103886841,
134.057009886425));
#169415=CARTESIAN_POINT('Ctrl Pts',(-149.468101494606,-5.02772572507474,
133.923640117053));
#169416=CARTESIAN_POINT('Ctrl Pts',(-149.464165445165,-5.0715989431393,
133.852924265158));
#169417=CARTESIAN_POINT('Ctrl Pts',(-149.460229395723,-5.11394782856564,
133.781334347775));
#169418=CARTESIAN_POINT('Ctrl Pts',(-149.456293346282,-5.15473880542603,
133.708942930109));
#169419=CARTESIAN_POINT('Ctrl Pts',(-149.448532235494,-5.23517054168529,
133.566201376429));
#169420=CARTESIAN_POINT('Ctrl Pts',(-149.440771124706,-5.30976717986972,
133.419943423783));
#169421=CARTESIAN_POINT('Ctrl Pts',(-149.433010013918,-5.37822242016894,
133.270664362382));
#169422=CARTESIAN_POINT('Ctrl Pts',(-149.425261138445,-5.44656974145093,
133.121620637962));
#169423=CARTESIAN_POINT('Ctrl Pts',(-149.417512262972,-5.50879482582847,
132.969565589936));
#169424=CARTESIAN_POINT('Ctrl Pts',(-149.409763387499,-5.56463630721829,
132.815020541792));
#169425=CARTESIAN_POINT('Ctrl Pts',(-149.401731037891,-5.62252061607184,
132.654821831516));
#169426=CARTESIAN_POINT('Ctrl Pts',(-149.393698688284,-5.67354521648552,
132.491947762961));
#169427=CARTESIAN_POINT('Ctrl Pts',(-149.385666338676,-5.71747147437235,
132.327006506221));
#169428=CARTESIAN_POINT('Ctrl Pts',(-149.377943353434,-5.75970592107237,
132.168417929558));
#169429=CARTESIAN_POINT('Ctrl Pts',(-149.370220368192,-5.7953784543159,
132.00791877723));
#169430=CARTESIAN_POINT('Ctrl Pts',(-149.362497382951,-5.82432596352126,
131.846069613952));
#169431=CARTESIAN_POINT('Ctrl Pts',(-149.354782943143,-5.85324144249298,
131.684399535738));
#169432=CARTESIAN_POINT('Ctrl Pts',(-149.347068503335,-5.87544666835424,
131.52138274165));
#169433=CARTESIAN_POINT('Ctrl Pts',(-149.339354063527,-5.89082885337101,
131.357592922111));
#169434=CARTESIAN_POINT('Ctrl Pts',(-149.331649592881,-5.90619116040465,
131.194014763741));
#169435=CARTESIAN_POINT('Ctrl Pts',(-149.323945122236,-5.91474797918278,
131.029665894648));
#169436=CARTESIAN_POINT('Ctrl Pts',(-149.316240651591,-5.91643793876513,
130.865128036802));
#169437=CARTESIAN_POINT('Ctrl Pts',(-149.315285498462,-5.91664744961356,
130.844729639967));
#169438=CARTESIAN_POINT('Ctrl Pts',(-149.314330345334,-5.9167514851978,
130.824328347825));
#169439=CARTESIAN_POINT('Ctrl Pts',(-149.313375192206,-5.91674998398426,
130.803925276003));
#169440=CARTESIAN_POINT('',(-147.563375192206,-5.91701416015386,130.799054768139));
#169441=CARTESIAN_POINT('Ctrl Pts',(-149.313375192165,-5.9167499839842,
130.803925275142));
#169442=CARTESIAN_POINT('Ctrl Pts',(-149.305582974739,-5.91673773693701,
130.637475344648));
#169443=CARTESIAN_POINT('Ctrl Pts',(-149.297790757313,-5.90969735063202,
130.471177295381));
#169444=CARTESIAN_POINT('Ctrl Pts',(-149.289998539887,-5.8956928681459,
130.305626051896));
#169445=CARTESIAN_POINT('Ctrl Pts',(-149.282195001545,-5.88166803925994,
130.139834287436));
#169446=CARTESIAN_POINT('Ctrl Pts',(-149.274391463202,-5.86065894060254,
129.974791803421));
#169447=CARTESIAN_POINT('Ctrl Pts',(-149.26658792486,-5.8327810051871,129.8110850727));
#169448=CARTESIAN_POINT('Ctrl Pts',(-149.258764812563,-5.80483314233355,
129.646967709265));
#169449=CARTESIAN_POINT('Ctrl Pts',(-149.250941700266,-5.76998203666509,
129.484193106869));
#169450=CARTESIAN_POINT('Ctrl Pts',(-149.243118587969,-5.72839403677041,
129.323336538763));
#169451=CARTESIAN_POINT('Ctrl Pts',(-149.23528527844,-5.68675182795818,
129.162270298145));
#169452=CARTESIAN_POINT('Ctrl Pts',(-149.227451968912,-5.63835528362459,
129.003127379344));
#169453=CARTESIAN_POINT('Ctrl Pts',(-149.219618659384,-5.58341978017229,
128.846465288167));
#169454=CARTESIAN_POINT('Ctrl Pts',(-149.211766885304,-5.52835478363359,
128.689433915625));
#169455=CARTESIAN_POINT('Ctrl Pts',(-149.203915111225,-5.46672011538763,
128.534895355183));
#169456=CARTESIAN_POINT('Ctrl Pts',(-149.196063337145,-5.39877913040065,
128.383386750782));
#169457=CARTESIAN_POINT('Ctrl Pts',(-149.189990798919,-5.34623377896548,
128.266210456308));
#169458=CARTESIAN_POINT('Ctrl Pts',(-149.183918260694,-5.28991730978643,
128.150846052432));
#169459=CARTESIAN_POINT('Ctrl Pts',(-149.177845722469,-5.22996959741401,
128.037530559065));
#169460=CARTESIAN_POINT('Ctrl Pts',(-149.170422456063,-5.15668758208057,
127.899010048543));
#169461=CARTESIAN_POINT('Ctrl Pts',(-149.162999189657,-5.0777876918209,
127.763193501392));
#169462=CARTESIAN_POINT('Ctrl Pts',(-149.155575923252,-4.99349360203296,
127.630569161128));
#169463=CARTESIAN_POINT('Ctrl Pts',(-149.148161430531,-4.90929914085919,
127.498101571821));
#169464=CARTESIAN_POINT('Ctrl Pts',(-149.14074693781,-4.81972336890147,
127.368818991347));
#169465=CARTESIAN_POINT('Ctrl Pts',(-149.133332445089,-4.72503660349127,
127.243186701823));
#169466=CARTESIAN_POINT('Ctrl Pts',(-149.125925098735,-4.63044110075019,
127.117675501429));
#169467=CARTESIAN_POINT('Ctrl Pts',(-149.118517752381,-4.53074463475934,
126.995807883875));
#169468=CARTESIAN_POINT('Ctrl Pts',(-149.111110406027,-4.42626165672246,
126.878021570982));
#169469=CARTESIAN_POINT('Ctrl Pts',(-149.103708584351,-4.32185660603251,
126.760323107565));
#169470=CARTESIAN_POINT('Ctrl Pts',(-149.096306762676,-4.21267239822448,
126.646700165871));
#169471=CARTESIAN_POINT('Ctrl Pts',(-149.088904941,-4.09906465131535,126.537558589485));
#169472=CARTESIAN_POINT('Ctrl Pts',(-149.081507026689,-3.98551687705182,
126.428474628088));
#169473=CARTESIAN_POINT('Ctrl Pts',(-149.074109112378,-3.86755048277244,
126.323867578601));
#169474=CARTESIAN_POINT('Ctrl Pts',(-149.066711198066,-3.74555885884481,
126.224107415239));
#169475=CARTESIAN_POINT('Ctrl Pts',(-149.059314513154,-3.62358750771175,
126.124363830205));
#169476=CARTESIAN_POINT('Ctrl Pts',(-149.051917828242,-3.49759254323203,
126.029465768769));
#169477=CARTESIAN_POINT('Ctrl Pts',(-149.044521143329,-3.3680015291144,
125.939743853382));
#169478=CARTESIAN_POINT('Ctrl Pts',(-149.037124786394,-3.23841626119776,
125.850025916358));
#169479=CARTESIAN_POINT('Ctrl Pts',(-149.029728429458,-3.10523556760557,
125.765483881521));
#169480=CARTESIAN_POINT('Ctrl Pts',(-149.022332072523,-2.96891694456745,
125.68640568041));
#169481=CARTESIAN_POINT('Ctrl Pts',(-149.014934583186,-2.83257745080014,
125.607315372224));
#169482=CARTESIAN_POINT('Ctrl Pts',(-149.00753709385,-2.6930993939181,125.533690750727));
#169483=CARTESIAN_POINT('Ctrl Pts',(-149.000139604513,-2.55096573372212,
125.465774251507));
#169484=CARTESIAN_POINT('Ctrl Pts',(-148.992739521998,-2.4087822487921,
125.397833944263));
#169485=CARTESIAN_POINT('Ctrl Pts',(-148.985339439483,-2.26394164370845,
125.335605904064));
#169486=CARTESIAN_POINT('Ctrl Pts',(-148.977939356968,-2.11694760597834,
125.279284745142));
#169487=CARTESIAN_POINT('Ctrl Pts',(-148.970531137301,-1.96979193319219,
125.222901655316));
#169488=CARTESIAN_POINT('Ctrl Pts',(-148.963122917635,-1.82047844766713,
125.172438551798));
#169489=CARTESIAN_POINT('Ctrl Pts',(-148.955714697968,-1.66952747677182,
125.128040633033));
#169490=CARTESIAN_POINT('Ctrl Pts',(-148.948301918666,-1.51848359807267,
125.083615388091));
#169491=CARTESIAN_POINT('Ctrl Pts',(-148.940889139364,-1.365800586957,125.045262857144));
#169492=CARTESIAN_POINT('Ctrl Pts',(-148.933476360062,-1.2120092493786,
125.013077155161));
#169493=CARTESIAN_POINT('Ctrl Pts',(-148.926052989033,-1.05799816752519,
124.980845464738));
#169494=CARTESIAN_POINT('Ctrl Pts',(-148.918629618004,-0.902875963515867,
124.954798263382));
#169495=CARTESIAN_POINT('Ctrl Pts',(-148.911206246975,-0.747179679008069,
124.934977933691));
#169496=CARTESIAN_POINT('Ctrl Pts',(-148.907270197536,-0.664625773109596,
124.924468719309));
#169497=CARTESIAN_POINT('Ctrl Pts',(-148.903334148097,-0.581910504076674,
124.915709231308));
#169498=CARTESIAN_POINT('Ctrl Pts',(-148.899398098657,-0.499113827592994,
124.908699844624));
#169499=CARTESIAN_POINT('Ctrl Pts',(-148.891974832252,-0.342961879688421,
124.89548036009));
#169500=CARTESIAN_POINT('Ctrl Pts',(-148.884551565846,-0.186048254126534,
124.888448911088));
#169501=CARTESIAN_POINT('Ctrl Pts',(-148.877128299441,-0.0289046260206381,
124.887681220717));
#169502=CARTESIAN_POINT('Ctrl Pts',(-148.86971380672,0.12805327136725,124.886914437692));
#169503=CARTESIAN_POINT('Ctrl Pts',(-148.862299313999,0.285240260544175,
124.892396678909));
#169504=CARTESIAN_POINT('Ctrl Pts',(-148.854884821278,0.442118773367819,
124.90415201509));
#169505=CARTESIAN_POINT('Ctrl Pts',(-148.847477474924,0.598846080773985,
124.915896021035));
#169506=CARTESIAN_POINT('Ctrl Pts',(-148.84007012857,0.755265133979427,
124.933901057353));
#169507=CARTESIAN_POINT('Ctrl Pts',(-148.832662782216,0.910837696663221,
124.958139166677));
#169508=CARTESIAN_POINT('Ctrl Pts',(-148.825260960541,1.06629422746079,
124.982359198304));
#169509=CARTESIAN_POINT('Ctrl Pts',(-148.817859138866,1.22090515756829,
125.012802989209));
#169510=CARTESIAN_POINT('Ctrl Pts',(-148.81045731719,1.37413681905786,125.049390716254));
#169511=CARTESIAN_POINT('Ctrl Pts',(-148.803059402879,1.52728759074608,
125.085959128922));
#169512=CARTESIAN_POINT('Ctrl Pts',(-148.795661488567,1.67906018170088,
125.128664931993));
#169513=CARTESIAN_POINT('Ctrl Pts',(-148.788263574256,1.82893068503546,
125.17737713511));
#169514=CARTESIAN_POINT('Ctrl Pts',(-148.780866889344,1.97877628261109,
125.226081243142));
#169515=CARTESIAN_POINT('Ctrl Pts',(-148.773470204431,2.12672006524806,
125.2807896549));
#169516=CARTESIAN_POINT('Ctrl Pts',(-148.766073519519,2.2722527622858,125.341321358437));
#169517=CARTESIAN_POINT('Ctrl Pts',(-148.758677162584,2.41777900625125,
125.401850377935));
#169518=CARTESIAN_POINT('Ctrl Pts',(-148.751280805648,2.56089403251859,
125.468202032442));
#169519=CARTESIAN_POINT('Ctrl Pts',(-148.743884448712,2.70110830824247,
125.540147051453));
#169520=CARTESIAN_POINT('Ctrl Pts',(-148.736486959376,2.84134405112992,
125.612103085431));
#169521=CARTESIAN_POINT('Ctrl Pts',(-148.729089470039,2.97867782703762,
125.689654018606));
#169522=CARTESIAN_POINT('Ctrl Pts',(-148.721691980703,3.1126446164693,125.77252456558));
#169523=CARTESIAN_POINT('Ctrl Pts',(-148.714291898188,3.24665836775153,
125.855424162696));
#169524=CARTESIAN_POINT('Ctrl Pts',(-148.706891815673,3.3773024653361,125.943646890118));
#169525=CARTESIAN_POINT('Ctrl Pts',(-148.699491733158,3.50414091935663,
126.036874175027));
#169526=CARTESIAN_POINT('Ctrl Pts',(-148.692083513491,3.63111884529648,
126.130203972921));
#169527=CARTESIAN_POINT('Ctrl Pts',(-148.684675293824,3.75428246958552,
126.228549096987));
#169528=CARTESIAN_POINT('Ctrl Pts',(-148.677267074158,3.87322838300728,
126.33155026438));
#169529=CARTESIAN_POINT('Ctrl Pts',(-148.669854294856,3.99224750565403,
126.434614827273));
#169530=CARTESIAN_POINT('Ctrl Pts',(-148.662441515554,4.10704347313671,
126.542340888941));
#169531=CARTESIAN_POINT('Ctrl Pts',(-148.655028736252,4.21725019028441,
126.654332738738));
#169532=CARTESIAN_POINT('Ctrl Pts',(-148.647605365223,4.3276143759579,126.766484607743));
#169533=CARTESIAN_POINT('Ctrl Pts',(-148.640181994194,4.43337596449143,
126.882914162692));
#169534=CARTESIAN_POINT('Ctrl Pts',(-148.632758623165,4.53420901407189,
127.003192484056));
#169535=CARTESIAN_POINT('Ctrl Pts',(-148.628822573725,4.58767311641224,
127.066966936079));
#169536=CARTESIAN_POINT('Ctrl Pts',(-148.624886524284,4.63975234510969,
127.131822917325));
#169537=CARTESIAN_POINT('Ctrl Pts',(-148.620950474843,4.69040316671737,
127.197693361477));
#169538=CARTESIAN_POINT('Ctrl Pts',(-148.613527208438,4.78592903551642,
127.321922963407));
#169539=CARTESIAN_POINT('Ctrl Pts',(-148.606103942032,4.87666044014705,
127.450138170678));
#169540=CARTESIAN_POINT('Ctrl Pts',(-148.598680675627,4.96224628923592,
127.581932600144));
#169541=CARTESIAN_POINT('Ctrl Pts',(-148.591266182906,5.04773098295863,
127.71357125954));
#169542=CARTESIAN_POINT('Ctrl Pts',(-148.583851690185,5.12808202531325,
127.848780410589));
#169543=CARTESIAN_POINT('Ctrl Pts',(-148.576437197464,5.20298859620775,
127.987120792803));
#169544=CARTESIAN_POINT('Ctrl Pts',(-148.56902985111,5.27782296932904,128.125327837348));
#169545=CARTESIAN_POINT('Ctrl Pts',(-148.561622504757,5.34722314135069,
128.266659778754));
#169546=CARTESIAN_POINT('Ctrl Pts',(-148.554215158403,5.4109217037192,128.410648671922));
#169547=CARTESIAN_POINT('Ctrl Pts',(-148.546813336727,5.47457275729669,
128.55453017274));
#169548=CARTESIAN_POINT('Ctrl Pts',(-148.539411515052,5.5325305181004,128.701064339663));
#169549=CARTESIAN_POINT('Ctrl Pts',(-148.532009693377,5.58457368304614,
128.849759036392));
#169550=CARTESIAN_POINT('Ctrl Pts',(-148.524611779065,5.63658937481022,
128.998375238348));
#169551=CARTESIAN_POINT('Ctrl Pts',(-148.517213864754,5.68269656585787,
129.149149347248));
#169552=CARTESIAN_POINT('Ctrl Pts',(-148.509815950443,5.72272227761775,
129.301569781901));
#169553=CARTESIAN_POINT('Ctrl Pts',(-148.502419265531,5.76274133783043,
129.453964887044));
#169554=CARTESIAN_POINT('Ctrl Pts',(-148.495022580618,5.79668082983904,
129.608005414244));
#169555=CARTESIAN_POINT('Ctrl Pts',(-148.487625895706,5.82441777088901,
129.763165058292));
#169556=CARTESIAN_POINT('Ctrl Pts',(-148.480229538771,5.85215348205395,
129.918317822399));
#169557=CARTESIAN_POINT('Ctrl Pts',(-148.472833181835,5.87368712341728,
130.074589237215));
#169558=CARTESIAN_POINT('Ctrl Pts',(-148.4654368249,5.88894698228776,130.231443518586));
#169559=CARTESIAN_POINT('Ctrl Pts',(-148.458039335563,5.90420917748159,
130.388321814747));
#169560=CARTESIAN_POINT('Ctrl Pts',(-148.450641846227,5.91319564148672,
130.545782783581));
#169561=CARTESIAN_POINT('Ctrl Pts',(-148.44324435689,5.91588662531099,130.70328639253));
#169562=CARTESIAN_POINT('Ctrl Pts',(-148.435844274375,5.91857855245547,
130.860845214126));
#169563=CARTESIAN_POINT('Ctrl Pts',(-148.42844419186,5.91497059918249,131.018446332588));
#169564=CARTESIAN_POINT('Ctrl Pts',(-148.421044109345,5.90509512665435,
131.175550740903));
#169565=CARTESIAN_POINT('Ctrl Pts',(-148.413635889679,5.89520879502896,
131.332827901666));
#169566=CARTESIAN_POINT('Ctrl Pts',(-148.406227670013,5.87904120424122,
131.489606888725));
#169567=CARTESIAN_POINT('Ctrl Pts',(-148.398819450346,5.8566765765891,131.645354101329));
#169568=CARTESIAN_POINT('Ctrl Pts',(-148.391406671044,5.83429818388178,
131.801197173744));
#169569=CARTESIAN_POINT('Ctrl Pts',(-148.383993891742,5.80571522171299,
131.956006840065));
#169570=CARTESIAN_POINT('Ctrl Pts',(-148.37658111244,5.771062729272,132.109261202786));
#169571=CARTESIAN_POINT('Ctrl Pts',(-148.369157741411,5.73636072372482,
132.262734542528));
#169572=CARTESIAN_POINT('Ctrl Pts',(-148.361734370383,5.69557196366407,
132.414647780684));
#169573=CARTESIAN_POINT('Ctrl Pts',(-148.354310999354,5.64888113172408,
132.564494851695));
#169574=CARTESIAN_POINT('Ctrl Pts',(-148.350374949913,5.62412453229683,
132.643947364281));
#169575=CARTESIAN_POINT('Ctrl Pts',(-148.346438900472,5.59770945367184,
132.722819336412));
#169576=CARTESIAN_POINT('Ctrl Pts',(-148.342502851031,5.56966878975008,
132.801037891184));
#169577=CARTESIAN_POINT('Ctrl Pts',(-148.335079584625,5.51678497271598,
132.948555644358));
#169578=CARTESIAN_POINT('Ctrl Pts',(-148.32765631822,5.45795642803586,133.094193996082));
#169579=CARTESIAN_POINT('Ctrl Pts',(-148.320233051815,5.39333528389671,
133.237437903222));
#169580=CARTESIAN_POINT('Ctrl Pts',(-148.312818559094,5.32879051658329,
133.38051250796));
#169581=CARTESIAN_POINT('Ctrl Pts',(-148.305404066372,5.25846692955907,
133.521197964362));
#169582=CARTESIAN_POINT('Ctrl Pts',(-148.297989573651,5.18256607926244,
133.658995339659));
#169583=CARTESIAN_POINT('Ctrl Pts',(-148.290582227298,5.10673838506294,
133.796659900657));
#169584=CARTESIAN_POINT('Ctrl Pts',(-148.283174880944,5.02534430819991,
133.931441597449));
#169585=CARTESIAN_POINT('Ctrl Pts',(-148.27576753459,4.93863300328432,134.062862515888));
#169586=CARTESIAN_POINT('Ctrl Pts',(-148.268365712915,4.85198637093111,
134.194185415649));
#169587=CARTESIAN_POINT('Ctrl Pts',(-148.260963891239,4.76003061164661,
134.322152217781));
#169588=CARTESIAN_POINT('Ctrl Pts',(-148.253562069564,4.66306015391342,
134.446310722041));
#169589=CARTESIAN_POINT('Ctrl Pts',(-148.246164155252,4.56614088613032,
134.570403683993));
#169590=CARTESIAN_POINT('Ctrl Pts',(-148.238766240941,4.46421242115982,
134.690692058368));
#169591=CARTESIAN_POINT('Ctrl Pts',(-148.23136832663,4.35761166760262,134.806753791265));
#169592=CARTESIAN_POINT('Ctrl Pts',(-148.223971641717,4.25102862915689,
134.922796236808));
#169593=CARTESIAN_POINT('Ctrl Pts',(-148.216574956805,4.13977509541776,
135.034613160252));
#169594=CARTESIAN_POINT('Ctrl Pts',(-148.209178271893,4.02422738668002,
135.141816611901));
#169595=CARTESIAN_POINT('Ctrl Pts',(-148.201781914958,3.90868480144878,
135.249015310037));
#169596=CARTESIAN_POINT('Ctrl Pts',(-148.194385558022,3.78884869347208,
135.351600689231));
#169597=CARTESIAN_POINT('Ctrl Pts',(-148.186989201087,3.66513107067269,
135.44922281114));
#169598=CARTESIAN_POINT('Ctrl Pts',(-148.17959171175,3.54139450638942,135.546859879245));
#169599=CARTESIAN_POINT('Ctrl Pts',(-148.172194222414,3.41377553708434,
135.639531945775));
#169600=CARTESIAN_POINT('Ctrl Pts',(-148.164796733077,3.2827178326284,135.726930494555));
#169601=CARTESIAN_POINT('Ctrl Pts',(-148.157396650562,3.15161418609714,
135.814359680762));
#169602=CARTESIAN_POINT('Ctrl Pts',(-148.149996568047,3.01706971476592,
135.896511461641));
#169603=CARTESIAN_POINT('Ctrl Pts',(-148.142596485532,2.87955539249854,
135.973121717098));
#169604=CARTESIAN_POINT('Ctrl Pts',(-148.135188265865,2.7418898590968,136.049816213406));
#169605=CARTESIAN_POINT('Ctrl Pts',(-148.127780046199,2.60124827933473,
136.120956833432));
#169606=CARTESIAN_POINT('Ctrl Pts',(-148.120371826532,2.45812511084739,
136.186326011539));
#169607=CARTESIAN_POINT('Ctrl Pts',(-148.11295904723,2.314913852438,136.251735423284));
#169608=CARTESIAN_POINT('Ctrl Pts',(-148.105546267928,2.16921830649471,
136.311366173782));
#169609=CARTESIAN_POINT('Ctrl Pts',(-148.098133488626,2.0215505521491,136.365049776978));
#169610=CARTESIAN_POINT('Ctrl Pts',(-148.090710117598,1.87367180319136,
136.418810085824));
#169611=CARTESIAN_POINT('Ctrl Pts',(-148.083286746569,1.72381557238988,
136.466606162698));
#169612=CARTESIAN_POINT('Ctrl Pts',(-148.07586337554,1.57250745250771,136.508319845533));
#169613=CARTESIAN_POINT('Ctrl Pts',(-148.071927326099,1.49228025675812,
136.530437441078));
#169614=CARTESIAN_POINT('Ctrl Pts',(-148.067991276658,1.41164503761781,
136.550845914807));
#169615=CARTESIAN_POINT('Ctrl Pts',(-148.064055227218,1.33068088844758,
136.569533549545));
#169616=CARTESIAN_POINT('Ctrl Pts',(-148.056631960812,1.17798502991737,
136.604777845438));
#169617=CARTESIAN_POINT('Ctrl Pts',(-148.049208694407,1.02365709455418,
136.634004811209));
#169618=CARTESIAN_POINT('Ctrl Pts',(-148.041785428002,0.868212631733326,
136.657064043215));
#169619=CARTESIAN_POINT('Ctrl Pts',(-148.034370935281,0.712951891358672,
136.680096021123));
#169620=CARTESIAN_POINT('Ctrl Pts',(-148.02695644256,0.556577615933735,
136.696974721311));
#169621=CARTESIAN_POINT('Ctrl Pts',(-148.019541949839,0.399618517907053,
136.707600033569));
#169622=CARTESIAN_POINT('Ctrl Pts',(-148.012134603485,0.242810702968456,
136.71821510475));
#169623=CARTESIAN_POINT('Ctrl Pts',(-148.004727257131,0.0854195575373565,
136.722588762027));
#169624=CARTESIAN_POINT('Ctrl Pts',(-147.997319910777,-0.0720181615264252,
136.720672301961));
#169625=CARTESIAN_POINT('Ctrl Pts',(-147.989918089102,-0.229338457599992,
136.718757271263));
#169626=CARTESIAN_POINT('Ctrl Pts',(-147.982516267427,-0.386704886477705,
136.71056146897));
#169627=CARTESIAN_POINT('Ctrl Pts',(-147.975114445751,-0.543577853502071,
136.696088180826));
#169628=CARTESIAN_POINT('Ctrl Pts',(-147.96771653144,-0.700368008508242,
136.681622533019));
#169629=CARTESIAN_POINT('Ctrl Pts',(-147.960318617129,-0.856664849670433,
136.660886033232));
#169630=CARTESIAN_POINT('Ctrl Pts',(-147.952920702817,-1.01193118376104,
136.633934001771));
#169631=CARTESIAN_POINT('Ctrl Pts',(-147.945524017905,-1.16717171540351,
136.606986449249));
#169632=CARTESIAN_POINT('Ctrl Pts',(-147.938127332993,-1.32138171242044,
136.573825478853));
#169633=CARTESIAN_POINT('Ctrl Pts',(-147.930730648081,-1.47403137143431,
136.534558003218));
#169634=CARTESIAN_POINT('Ctrl Pts',(-147.923334291145,-1.62667426180234,
136.495292268743));
#169635=CARTESIAN_POINT('Ctrl Pts',(-147.91593793421,-1.77775659020682,
136.44992066041));
#169636=CARTESIAN_POINT('Ctrl Pts',(-147.908541577275,-1.92676124326431,
136.398600661929));
#169637=CARTESIAN_POINT('Ctrl Pts',(-147.901144087938,-2.07578870931458,
136.347272806226));
#169638=CARTESIAN_POINT('Ctrl Pts',(-147.893746598602,-2.22273751367075,
136.289994868594));
#169639=CARTESIAN_POINT('Ctrl Pts',(-147.886349109265,-2.36710827853568,
136.226973360533));
#169640=CARTESIAN_POINT('Ctrl Pts',(-147.87894902675,-2.51152965234864,
136.16392976038));
#169641=CARTESIAN_POINT('Ctrl Pts',(-147.871548944235,-2.65337084544653,
136.095138730387));
#169642=CARTESIAN_POINT('Ctrl Pts',(-147.86414886172,-2.79215507323656,
136.02085375084));
#169643=CARTESIAN_POINT('Ctrl Pts',(-147.856740642054,-2.93109190855221,
135.946487087322));
#169644=CARTESIAN_POINT('Ctrl Pts',(-147.849332422388,-3.06696473620898,
135.866614585924));
#169645=CARTESIAN_POINT('Ctrl Pts',(-147.841924202721,-3.19932324564573,
135.781534648316));
#169646=CARTESIAN_POINT('Ctrl Pts',(-147.834511423419,-3.3317632195369,
135.696402345426));
#169647=CARTESIAN_POINT('Ctrl Pts',(-147.827098644117,-3.46068426015495,
135.606056433519));
#169648=CARTESIAN_POINT('Ctrl Pts',(-147.819685864815,-3.58566782413148,
135.510836668444));
#169649=CARTESIAN_POINT('Ctrl Pts',(-147.812262493786,-3.71082997048519,
135.415480848903));
#169650=CARTESIAN_POINT('Ctrl Pts',(-147.804839122758,-3.83204311680381,
135.315237504817));
#169651=CARTESIAN_POINT('Ctrl Pts',(-147.797415751729,-3.94892375426819,
135.210484962779));
#169652=CARTESIAN_POINT('Ctrl Pts',(-147.793479702288,-4.01089667277319,
135.154942651479));
#169653=CARTESIAN_POINT('Ctrl Pts',(-147.789543652846,-4.07165220529871,
135.098133236456));
#169654=CARTESIAN_POINT('Ctrl Pts',(-147.785607603405,-4.13113774195879,
135.040116927774));
#169655=CARTESIAN_POINT('Ctrl Pts',(-147.778290858419,-4.24171574881784,
134.932270077268));
#169656=CARTESIAN_POINT('Ctrl Pts',(-147.770974113432,-4.34825821180401,
134.819904157256));
#169657=CARTESIAN_POINT('Ctrl Pts',(-147.763657368446,-4.45036514945744,
134.703358001381));
#169658=CARTESIAN_POINT('Ctrl Pts',(-147.756349411285,-4.55234945089338,
134.586951824042));
#169659=CARTESIAN_POINT('Ctrl Pts',(-147.749041454124,-4.64990857515767,
134.466375686573));
#169660=CARTESIAN_POINT('Ctrl Pts',(-147.741733496963,-4.74267725621687,
134.342007152462));
#169661=CARTESIAN_POINT('Ctrl Pts',(-147.734301900931,-4.83701543401553,
134.215534502969));
#169662=CARTESIAN_POINT('Ctrl Pts',(-147.7268703049,-4.92639929930953,134.085140227386));
#169663=CARTESIAN_POINT('Ctrl Pts',(-147.719438708868,-5.01048467166432,
133.951259713107));
#169664=CARTESIAN_POINT('Ctrl Pts',(-147.712143701413,-5.09302460192625,
133.819839847766));
#169665=CARTESIAN_POINT('Ctrl Pts',(-147.704848693958,-5.17045889754112,
133.685061122964));
#169666=CARTESIAN_POINT('Ctrl Pts',(-147.697553686503,-5.24250370133411,
133.547367271586));
#169667=CARTESIAN_POINT('Ctrl Pts',(-147.690261763559,-5.31451804279654,
133.409731640585));
#169668=CARTESIAN_POINT('Ctrl Pts',(-147.682969840614,-5.38114724798181,
133.269183675585));
#169669=CARTESIAN_POINT('Ctrl Pts',(-147.675677917669,-5.44215242935071,
133.126193406165));
#169670=CARTESIAN_POINT('Ctrl Pts',(-147.668387541704,-5.50314466848771,
132.98323347209));
#169671=CARTESIAN_POINT('Ctrl Pts',(-147.661097165738,-5.55851510777398,
132.83783261877));
#169672=CARTESIAN_POINT('Ctrl Pts',(-147.653806789773,-5.60807233973095,
132.690482351401));
#169673=CARTESIAN_POINT('Ctrl Pts',(-147.646270823309,-5.65929900346469,
132.538168303591));
#169674=CARTESIAN_POINT('Ctrl Pts',(-147.638734856845,-5.70431376762358,
132.383771600791));
#169675=CARTESIAN_POINT('Ctrl Pts',(-147.631198890381,-5.74296078845821,
132.227853485385));
#169676=CARTESIAN_POINT('Ctrl Pts',(-147.623904542744,-5.78036870507304,
132.076934430465));
#169677=CARTESIAN_POINT('Ctrl Pts',(-147.616610195108,-5.81181086636718,
131.924590415814));
#169678=CARTESIAN_POINT('Ctrl Pts',(-147.609315847471,-5.83719786223342,
131.771341320392));
#169679=CARTESIAN_POINT('Ctrl Pts',(-147.601659071593,-5.86384624084512,
131.610477863438));
#169680=CARTESIAN_POINT('Ctrl Pts',(-147.594002295716,-5.88382227129655,
131.448617561023));
#169681=CARTESIAN_POINT('Ctrl Pts',(-147.586345519838,-5.8970840217172,
131.286367467422));
#169682=CARTESIAN_POINT('Ctrl Pts',(-147.578688743961,-5.91034577213782,
131.124117373821));
#169683=CARTESIAN_POINT('Ctrl Pts',(-147.571031968084,-5.91689326760382,
130.961477977213));
#169684=CARTESIAN_POINT('Ctrl Pts',(-147.563375192206,-5.91674762120188,
130.799055007147));
#169685=CARTESIAN_POINT('',(-145.813375192206,-5.92480979664972,130.807250319294));
#169686=CARTESIAN_POINT('Ctrl Pts',(-147.563375192206,-5.9186030338184,
130.799053343379));
#169687=CARTESIAN_POINT('Ctrl Pts',(-147.544636788001,-5.92229012192935,
130.401427829348));
#169688=CARTESIAN_POINT('Ctrl Pts',(-147.525898383797,-5.88565898036021,
130.00447795396));
#169689=CARTESIAN_POINT('Ctrl Pts',(-147.414344104987,-5.41278022280702,
127.693477101972));
#169690=CARTESIAN_POINT('Ctrl Pts',(-147.228712355779,-2.52567537098746,
124.277606106268));
#169691=CARTESIAN_POINT('Ctrl Pts',(-146.950264731965,4.12595418657829,
125.151568158913));
#169692=CARTESIAN_POINT('Ctrl Pts',(-146.671817108153,6.98603341074523,
131.220170326794));
#169693=CARTESIAN_POINT('Ctrl Pts',(-146.39336948434,3.42628921714421,136.906663685328));
#169694=CARTESIAN_POINT('Ctrl Pts',(-146.114921860528,-3.2820473834807,
136.985438638666));
#169695=CARTESIAN_POINT('Ctrl Pts',(-145.921590429816,-5.84567763105308,
133.09632707134));
#169696=CARTESIAN_POINT('Ctrl Pts',(-145.821074873709,-5.92578672622296,
130.970191063743));
#169697=CARTESIAN_POINT('Ctrl Pts',(-145.813375192206,-5.92480979664972,
130.807250319294));
#169698=CARTESIAN_POINT('',(-144.063375192206,-5.90966590561723,130.808266582045));
#169699=CARTESIAN_POINT('Ctrl Pts',(-145.813375192206,-5.92480979664972,
130.807250319294));
#169700=CARTESIAN_POINT('Ctrl Pts',(-145.728258999105,-5.9140103205709,
129.00602050689));
#169701=CARTESIAN_POINT('Ctrl Pts',(-145.550326931398,-4.07424408851649,
125.221534978211));
#169702=CARTESIAN_POINT('Ctrl Pts',(-145.279578989089,2.37171472213127,
124.220096816113));
#169703=CARTESIAN_POINT('Ctrl Pts',(-145.001131365275,6.82149735186778,
129.240795969467));
#169704=CARTESIAN_POINT('Ctrl Pts',(-144.722683741463,5.00265716391772,
135.698334650054));
#169705=CARTESIAN_POINT('Ctrl Pts',(-144.44423611765,-1.41338056428836,
137.658550278703));
#169706=CARTESIAN_POINT('Ctrl Pts',(-144.22446660123,-5.45222549990329,
134.234355068096));
#169707=CARTESIAN_POINT('Ctrl Pts',(-144.097512959417,-5.91405090638656,
131.535446847972));
#169708=CARTESIAN_POINT('Ctrl Pts',(-144.063375192206,-5.90966590561723,
130.808266582045));
#169709=CARTESIAN_POINT('',(-142.313375175084,-5.91365185916051,130.800007985964));
#169710=CARTESIAN_POINT('Ctrl Pts',(-144.063375192206,-5.90966590561723,
130.808266582045));
#169711=CARTESIAN_POINT('Ctrl Pts',(-144.004697084812,-5.90212869486523,
129.558344128823));
#169712=CARTESIAN_POINT('Ctrl Pts',(-143.853203102813,-4.90196159472372,
126.320294665178));
#169713=CARTESIAN_POINT('Ctrl Pts',(-143.608893246212,0.426440781348736,
123.818968088136));
#169714=CARTESIAN_POINT('Ctrl Pts',(-143.330445622398,6.10751023032449,
127.387362034476));
#169715=CARTESIAN_POINT('Ctrl Pts',(-143.051997998586,6.17607614610116,
134.095810749031));
#169716=CARTESIAN_POINT('Ctrl Pts',(-142.773550374773,0.569129801701234,
137.77957758904));
#169717=CARTESIAN_POINT('Ctrl Pts',(-142.527342772645,-4.85106370396208,
135.369103867334));
#169718=CARTESIAN_POINT('Ctrl Pts',(-142.373951045124,-5.90178250636266,
132.089885314399));
#169719=CARTESIAN_POINT('Ctrl Pts',(-142.313375192206,-5.9105277485179,
130.80001065018));
#169720=CARTESIAN_POINT('',(-140.563375192206,-5.92111884170449,130.80212814766));
#169721=CARTESIAN_POINT('Ctrl Pts',(-142.313375158114,-5.91674839705925,
130.800005345262));
#169722=CARTESIAN_POINT('Ctrl Pts',(-142.304860995865,-5.91661480626093,
130.618518841854));
#169723=CARTESIAN_POINT('Ctrl Pts',(-142.296346833615,-5.90812709802129,
130.437370762715));
#169724=CARTESIAN_POINT('Ctrl Pts',(-142.287832671366,-5.89140221138,130.257267804374));
#169725=CARTESIAN_POINT('Ctrl Pts',(-142.279276745037,-5.8745952850168,
130.0762813963));
#169726=CARTESIAN_POINT('Ctrl Pts',(-142.270720818708,-5.84947027717438,
129.896350514552));
#169727=CARTESIAN_POINT('Ctrl Pts',(-142.262164892379,-5.81619531024774,
129.718173398182));
#169728=CARTESIAN_POINT('Ctrl Pts',(-142.253554344712,-5.782707914749,129.538858792766));
#169729=CARTESIAN_POINT('Ctrl Pts',(-142.244943797045,-5.74096625036584,
129.361320542769));
#169730=CARTESIAN_POINT('Ctrl Pts',(-142.236333249378,-5.69119024460289,
129.186249322804));
#169731=CARTESIAN_POINT('Ctrl Pts',(-142.229773875301,-5.65327169929296,
129.052882937033));
#169732=CARTESIAN_POINT('Ctrl Pts',(-142.223214501224,-5.6106917110202,
128.920947786416));
#169733=CARTESIAN_POINT('Ctrl Pts',(-142.216655127147,-5.56356579263376,
128.790740436515));
#169734=CARTESIAN_POINT('Ctrl Pts',(-142.209231860741,-5.51023322725657,
128.643384326779));
#169735=CARTESIAN_POINT('Ctrl Pts',(-142.201808594336,-5.45096168202031,
128.497925703494));
#169736=CARTESIAN_POINT('Ctrl Pts',(-142.19438532793,-5.38590485202148,
128.354879144382));
#169737=CARTESIAN_POINT('Ctrl Pts',(-142.186970835209,-5.32092491379289,
128.212001654423));
#169738=CARTESIAN_POINT('Ctrl Pts',(-142.179556342488,-5.25017345436617,
128.071530890473));
#169739=CARTESIAN_POINT('Ctrl Pts',(-142.172141849767,-5.17385354782587,
127.933965169522));
#169740=CARTESIAN_POINT('Ctrl Pts',(-142.164734503413,-5.09760720128489,
127.796532039593));
#169741=CARTESIAN_POINT('Ctrl Pts',(-142.157327157059,-5.01580327231036,
127.661998702671));
#169742=CARTESIAN_POINT('Ctrl Pts',(-142.149919810705,-4.92869236896547,
127.530842312347));
#169743=CARTESIAN_POINT('Ctrl Pts',(-142.14251798903,-4.84164643621855,
127.399783743408));
#169744=CARTESIAN_POINT('Ctrl Pts',(-142.135116167354,-4.74930161593849,
127.272097415708));
#169745=CARTESIAN_POINT('Ctrl Pts',(-142.127714345679,-4.65195371158615,
127.148234631258));
#169746=CARTESIAN_POINT('Ctrl Pts',(-142.120316431368,-4.55465719643503,
127.024437233007));
#169747=CARTESIAN_POINT('Ctrl Pts',(-142.112918517056,-4.45236308715456,
126.904459650984));
#169748=CARTESIAN_POINT('Ctrl Pts',(-142.105520602745,-4.34540957537183,
126.788722911701));
#169749=CARTESIAN_POINT('Ctrl Pts',(-142.098123917832,-4.23847383732228,
126.673005405764));
#169750=CARTESIAN_POINT('Ctrl Pts',(-142.09072723292,-4.12688048664842,
126.561527617734));
#169751=CARTESIAN_POINT('Ctrl Pts',(-142.083330548008,-4.0110070226874,
126.454676350122));
#169752=CARTESIAN_POINT('Ctrl Pts',(-142.075934191072,-3.8951386966772,
126.347829820406));
#169753=CARTESIAN_POINT('Ctrl Pts',(-142.068537834137,-3.77499090916475,
126.245609656272));
#169754=CARTESIAN_POINT('Ctrl Pts',(-142.061141477201,-3.65097673125637,
126.148364540428));
#169755=CARTESIAN_POINT('Ctrl Pts',(-142.053743987864,-3.52694356646076,
126.051104536109));
#169756=CARTESIAN_POINT('Ctrl Pts',(-142.046346498528,-3.39904312638324,
125.958821327073));
#169757=CARTESIAN_POINT('Ctrl Pts',(-142.038949009191,-3.26772001785685,
125.871822077686));
#169758=CARTESIAN_POINT('Ctrl Pts',(-142.031548926676,-3.13635087421852,
125.784792330848));
#169759=CARTESIAN_POINT('Ctrl Pts',(-142.024148844161,-3.00155698432438,
125.70305043758));
#169760=CARTESIAN_POINT('Ctrl Pts',(-142.016748761646,-2.86381012374739,
125.626859083271));
#169761=CARTESIAN_POINT('Ctrl Pts',(-142.009340541979,-2.72591179633629,
125.550583948736));
#169762=CARTESIAN_POINT('Ctrl Pts',(-142.001932322313,-2.58505434043865,
125.479871722819));
#169763=CARTESIAN_POINT('Ctrl Pts',(-141.994524102646,-2.44173287359424,
125.414938465191));
#169764=CARTESIAN_POINT('Ctrl Pts',(-141.987111323344,-2.29832319477843,
125.349965242227));
#169765=CARTESIAN_POINT('Ctrl Pts',(-141.979698544042,-2.15244682819286,
125.29077821506));
#169766=CARTESIAN_POINT('Ctrl Pts',(-141.97228576474,-2.00461636341079,
125.237544310372));
#169767=CARTESIAN_POINT('Ctrl Pts',(-141.964862393711,-1.85657467152787,
125.184234342584));
#169768=CARTESIAN_POINT('Ctrl Pts',(-141.957439022682,-1.7065736600313,
125.136894597918));
#169769=CARTESIAN_POINT('Ctrl Pts',(-141.950015651653,-1.55513927889432,
125.095641638168));
#169770=CARTESIAN_POINT('Ctrl Pts',(-141.946079602214,-1.4748451364164,
125.073768329062));
#169771=CARTESIAN_POINT('Ctrl Pts',(-141.942143552774,-1.3941481744168,
125.053605375738));
#169772=CARTESIAN_POINT('Ctrl Pts',(-141.938207503334,-1.31312752155294,
125.035164254584));
#169773=CARTESIAN_POINT('Ctrl Pts',(-141.930784236928,-1.16032509878548,
125.000384875608));
#169774=CARTESIAN_POINT('Ctrl Pts',(-141.923360970523,-1.00590892142774,
124.971627766364));
#169775=CARTESIAN_POINT('Ctrl Pts',(-141.915937704117,-0.850394994243977,
124.949041760641));
#169776=CARTESIAN_POINT('Ctrl Pts',(-141.908523211396,-0.695064871607517,
124.926482449701));
#169777=CARTESIAN_POINT('Ctrl Pts',(-141.901108718676,-0.538639947539334,
124.910079777198));
#169778=CARTESIAN_POINT('Ctrl Pts',(-141.893694225955,-0.381649236740049,
124.899932243659));
#169779=CARTESIAN_POINT('Ctrl Pts',(-141.886286879601,-0.224809839497981,
124.889794490695));
#169780=CARTESIAN_POINT('Ctrl Pts',(-141.878879533247,-0.067406111182322,
124.885899898183));
#169781=CARTESIAN_POINT('Ctrl Pts',(-141.871472186893,0.0900250455968013,
124.888295535633));
#169782=CARTESIAN_POINT('Ctrl Pts',(-141.864070365218,0.247338784279661,
124.890689386326));
#169783=CARTESIAN_POINT('Ctrl Pts',(-141.856668543542,0.404679539044736,
124.899364119935));
#169784=CARTESIAN_POINT('Ctrl Pts',(-141.849266721867,0.561507727734568,
124.91431480839));
#169785=CARTESIAN_POINT('Ctrl Pts',(-141.841868807556,0.718253128043891,
124.929257604492));
#169786=CARTESIAN_POINT('Ctrl Pts',(-141.834470893244,0.874486130477881,
124.95046972205));
#169787=CARTESIAN_POINT('Ctrl Pts',(-141.827072978933,1.02966971267315,
124.977894205983));
#169788=CARTESIAN_POINT('Ctrl Pts',(-141.819676294021,1.18482750617259,
125.005314132464));
#169789=CARTESIAN_POINT('Ctrl Pts',(-141.812279609108,1.33893585831316,
125.038944311447));
#169790=CARTESIAN_POINT('Ctrl Pts',(-141.804882924196,1.49146529357663,
125.078676218251));
#169791=CARTESIAN_POINT('Ctrl Pts',(-141.797486567261,1.6439879655251,125.118406363301));
#169792=CARTESIAN_POINT('Ctrl Pts',(-141.790090210325,1.79493149855872,
125.164237604115));
#169793=CARTESIAN_POINT('Ctrl Pts',(-141.78269385339,1.94377926101553,125.216010883794));
#169794=CARTESIAN_POINT('Ctrl Pts',(-141.775296364053,2.09264981244476,
125.267792090095));
#169795=CARTESIAN_POINT('Ctrl Pts',(-141.767898874717,2.23942360180544,
125.325517024033));
#169796=CARTESIAN_POINT('Ctrl Pts',(-141.76050138538,2.38360188216347,125.38897765513));
#169797=CARTESIAN_POINT('Ctrl Pts',(-141.753101302865,2.52783070399438,
125.452460532253));
#169798=CARTESIAN_POINT('Ctrl Pts',(-141.74570122035,2.669461863862,125.521682959412));
#169799=CARTESIAN_POINT('Ctrl Pts',(-141.738301137835,2.80801935088878,
125.596390006327));
#169800=CARTESIAN_POINT('Ctrl Pts',(-141.730892918169,2.9467291961164,125.671179201319));
#169801=CARTESIAN_POINT('Ctrl Pts',(-141.723484698502,3.08235829000079,
125.751464882904));
#169802=CARTESIAN_POINT('Ctrl Pts',(-141.716076478836,3.21445723229865,
125.836947280202));
#169803=CARTESIAN_POINT('Ctrl Pts',(-141.708663699534,3.34663747929169,
125.922482290489));
#169804=CARTESIAN_POINT('Ctrl Pts',(-141.701250920232,3.47528294087858,
126.013220175222));
#169805=CARTESIAN_POINT('Ctrl Pts',(-141.693838140929,3.5999761097295,126.108819906223));
#169806=CARTESIAN_POINT('Ctrl Pts',(-141.686414769901,3.72484744602743,
126.204556234603));
#169807=CARTESIAN_POINT('Ctrl Pts',(-141.678991398872,3.84575492463823,
126.305168045493));
#169808=CARTESIAN_POINT('Ctrl Pts',(-141.671568027843,3.96231619001513,
126.410275846781));
#169809=CARTESIAN_POINT('Ctrl Pts',(-141.667631978402,4.02411976976779,
126.466006525052));
#169810=CARTESIAN_POINT('Ctrl Pts',(-141.663695928961,4.08470211255227,
126.523000595873));
#169811=CARTESIAN_POINT('Ctrl Pts',(-141.659759879521,4.14401079198502,
126.581197689332));
#169812=CARTESIAN_POINT('Ctrl Pts',(-141.652336613115,4.25586511043332,
126.690955591325));
#169813=CARTESIAN_POINT('Ctrl Pts',(-141.64491334671,4.3635249965711,126.805326374652));
#169814=CARTESIAN_POINT('Ctrl Pts',(-141.637490080304,4.46658631913643,
126.923956358187));
#169815=CARTESIAN_POINT('Ctrl Pts',(-141.630075587583,4.56952583177748,
127.042446130935));
#169816=CARTESIAN_POINT('Ctrl Pts',(-141.622661094862,4.66787735705226,
127.165184804592));
#169817=CARTESIAN_POINT('Ctrl Pts',(-141.615246602141,4.76127207831011,
127.291780546051));
#169818=CARTESIAN_POINT('Ctrl Pts',(-141.607839255787,4.85457678221937,
127.418254269768));
#169819=CARTESIAN_POINT('Ctrl Pts',(-141.600431909434,4.94293397315485,
127.548577361921));
#169820=CARTESIAN_POINT('Ctrl Pts',(-141.59302456308,5.02601384122901,127.68232355336));
#169821=CARTESIAN_POINT('Ctrl Pts',(-141.585622741405,5.1090317452029,127.815969991843));
#169822=CARTESIAN_POINT('Ctrl Pts',(-141.578220919729,5.18677996734848,
127.953034130356));
#169823=CARTESIAN_POINT('Ctrl Pts',(-141.570819098054,5.25897099645432,
128.093059339406));
#169824=CARTESIAN_POINT('Ctrl Pts',(-141.563421183742,5.33112391647804,
128.233010630238));
#169825=CARTESIAN_POINT('Ctrl Pts',(-141.556023269431,5.39772531523721,
128.37591954761));
#169826=CARTESIAN_POINT('Ctrl Pts',(-141.54862535512,5.45853283694908,128.521303493785));
#169827=CARTESIAN_POINT('Ctrl Pts',(-141.541228670207,5.51933025355391,
128.666663279785));
#169828=CARTESIAN_POINT('Ctrl Pts',(-141.533831985295,5.57433556015751,
128.814496934219));
#169829=CARTESIAN_POINT('Ctrl Pts',(-141.526435300383,5.62335386719548,
128.964300334098));
#169830=CARTESIAN_POINT('Ctrl Pts',(-141.519038943448,5.67237000071036,
129.114097091537));
#169831=CARTESIAN_POINT('Ctrl Pts',(-141.511642586512,5.71539954641086,
129.265863065971));
#169832=CARTESIAN_POINT('Ctrl Pts',(-141.504246229577,5.75229707133786,
129.419077626413));
#169833=CARTESIAN_POINT('Ctrl Pts',(-141.49684874024,5.78920024537022,129.572315644396));
#169834=CARTESIAN_POINT('Ctrl Pts',(-141.489451250904,5.81996944189205,
129.727002327038));
#169835=CARTESIAN_POINT('Ctrl Pts',(-141.482053761567,5.84451009793547,
129.882605618865));
#169836=CARTESIAN_POINT('Ctrl Pts',(-141.474653679052,5.86905935666778,
130.038263457184));
#169837=CARTESIAN_POINT('Ctrl Pts',(-141.467253596537,5.88737566965912,
130.194838175915));
#169838=CARTESIAN_POINT('Ctrl Pts',(-141.459853514022,5.8994162214694,130.351791497581));
#169839=CARTESIAN_POINT('Ctrl Pts',(-141.452445294356,5.91147001310417,
130.508917405559));
#169840=CARTESIAN_POINT('Ctrl Pts',(-141.445037074689,5.9172342335473,130.666422375443));
#169841=CARTESIAN_POINT('Ctrl Pts',(-141.437628855023,5.91671817672114,
130.823766280598));
#169842=CARTESIAN_POINT('Ctrl Pts',(-141.430216075721,5.9162018022706,130.981207028302));
#169843=CARTESIAN_POINT('Ctrl Pts',(-141.422803296419,5.90939746434237,
131.138486141658));
#169844=CARTESIAN_POINT('Ctrl Pts',(-141.415390517117,5.8963664066898,131.295068025866));
#169845=CARTESIAN_POINT('Ctrl Pts',(-141.407967146088,5.88331672965098,
131.451873641612));
#169846=CARTESIAN_POINT('Ctrl Pts',(-141.400543775059,5.86402260919348,
131.607979669011));
#169847=CARTESIAN_POINT('Ctrl Pts',(-141.39312040403,5.83859665026538,131.762859296756));
#169848=CARTESIAN_POINT('Ctrl Pts',(-141.389184354589,5.82511519675411,
131.844980191673));
#169849=CARTESIAN_POINT('Ctrl Pts',(-141.385248305149,5.80991070689763,
131.926756519875));
#169850=CARTESIAN_POINT('Ctrl Pts',(-141.381312255708,5.79300563387162,
132.008111542148));
#169851=CARTESIAN_POINT('Ctrl Pts',(-141.373888989303,5.76112319373395,
132.161544575151));
#169852=CARTESIAN_POINT('Ctrl Pts',(-141.366465722897,5.72309261276887,
132.313942088495));
#169853=CARTESIAN_POINT('Ctrl Pts',(-141.359042456492,5.67899301010359,
132.464772901818));
#169854=CARTESIAN_POINT('Ctrl Pts',(-141.351627963771,5.63494552950641,
132.615425445645));
#169855=CARTESIAN_POINT('Ctrl Pts',(-141.34421347105,5.5848434089989,132.764514620489));
#169856=CARTESIAN_POINT('Ctrl Pts',(-141.336798978329,5.52881695446466,
132.911518335091));
#169857=CARTESIAN_POINT('Ctrl Pts',(-141.329391631975,5.47284450033665,
133.058380361978));
#169858=CARTESIAN_POINT('Ctrl Pts',(-141.321984285621,5.41095921191094,
133.203160583745));
#169859=CARTESIAN_POINT('Ctrl Pts',(-141.314576939267,5.34334145119713,
133.345351113105));
#169860=CARTESIAN_POINT('Ctrl Pts',(-141.307175117592,5.27577412236033,
133.487435591403));
#169861=CARTESIAN_POINT('Ctrl Pts',(-141.299773295917,5.20248299394662,
133.626933887483));
#169862=CARTESIAN_POINT('Ctrl Pts',(-141.292371474241,5.12369683444817,
133.763357290624));
#169863=CARTESIAN_POINT('Ctrl Pts',(-141.28497355993,5.04495226555005,133.899708676912));
#169864=CARTESIAN_POINT('Ctrl Pts',(-141.277575645619,4.9607186288334,134.032988080521));
#169865=CARTESIAN_POINT('Ctrl Pts',(-141.270177731307,4.87127094822071,
134.162730744803));
#169866=CARTESIAN_POINT('Ctrl Pts',(-141.262781046395,4.78183813218993,
134.292451848209));
#169867=CARTESIAN_POINT('Ctrl Pts',(-141.255384361483,4.68719320364637,
134.418637071745));
#169868=CARTESIAN_POINT('Ctrl Pts',(-141.247987676571,4.58765495296829,
134.540849958512));
#169869=CARTESIAN_POINT('Ctrl Pts',(-141.240591319635,4.48812111592056,
134.663057426232));
#169870=CARTESIAN_POINT('Ctrl Pts',(-141.2331949627,4.38369462389926,134.781292617962));
#169871=CARTESIAN_POINT('Ctrl Pts',(-141.225798605765,4.27473488843274,
134.895151763068));
#169872=CARTESIAN_POINT('Ctrl Pts',(-141.218401116428,4.16575847095225,
135.0090283403));
#169873=CARTESIAN_POINT('Ctrl Pts',(-141.211003627091,4.05224768618999,
135.118527267163));
#169874=CARTESIAN_POINT('Ctrl Pts',(-141.203606137755,3.93459905389209,
135.223281396174));
#169875=CARTESIAN_POINT('Ctrl Pts',(-141.19620605524,3.81690918004836,135.328072246582));
#169876=CARTESIAN_POINT('Ctrl Pts',(-141.188805972725,3.69507884932558,
135.428114739471));
#169877=CARTESIAN_POINT('Ctrl Pts',(-141.18140589021,3.56953778701891,135.523081900874));
#169878=CARTESIAN_POINT('Ctrl Pts',(-141.173997670543,3.44385867940884,
135.618153488433));
#169879=CARTESIAN_POINT('Ctrl Pts',(-141.166589450877,3.31446098942122,
135.708138373838));
#169880=CARTESIAN_POINT('Ctrl Pts',(-141.15918123121,3.1818041644834,135.792752424689));
#169881=CARTESIAN_POINT('Ctrl Pts',(-141.151768451908,3.04906569148296,
135.877418554077));
#169882=CARTESIAN_POINT('Ctrl Pts',(-141.144355672606,2.91306440818519,
135.956707074394));
#169883=CARTESIAN_POINT('Ctrl Pts',(-141.136942893304,2.7742840294092,136.030380009672));
#169884=CARTESIAN_POINT('Ctrl Pts',(-141.129519522275,2.63530535472006,
136.104158212294));
#169885=CARTESIAN_POINT('Ctrl Pts',(-141.122096151247,2.49353998932446,
136.172304643226));
#169886=CARTESIAN_POINT('Ctrl Pts',(-141.114672780218,2.34949202021907,
136.234629285821));
#169887=CARTESIAN_POINT('Ctrl Pts',(-141.110736730777,2.27311433061705,
136.267675306783));
#169888=CARTESIAN_POINT('Ctrl Pts',(-141.106800681336,2.19609519151904,
136.299085441743));
#169889=CARTESIAN_POINT('Ctrl Pts',(-141.102864631896,2.11851130228841,
136.328837101775));
#169890=CARTESIAN_POINT('Ctrl Pts',(-141.09544136549,1.97219050850881,136.384947804077));
#169891=CARTESIAN_POINT('Ctrl Pts',(-141.088018099085,1.823417706452,136.435326177708));
#169892=CARTESIAN_POINT('Ctrl Pts',(-141.08059483268,1.67268255902159,136.479751671867));
#169893=CARTESIAN_POINT('Ctrl Pts',(-141.073180339959,1.52212556801767,
136.524124658783));
#169894=CARTESIAN_POINT('Ctrl Pts',(-141.065765847238,1.3696112028514,136.562558666543));
#169895=CARTESIAN_POINT('Ctrl Pts',(-141.058351354517,1.21564914719937,
136.594881122099));
#169896=CARTESIAN_POINT('Ctrl Pts',(-141.050944008163,1.06183548597314,
136.627172424055));
#169897=CARTESIAN_POINT('Ctrl Pts',(-141.043536661809,0.906577274986908,
136.653363824539));
#169898=CARTESIAN_POINT('Ctrl Pts',(-141.036129315456,0.750399304271718,
136.673332541732));
#169899=CARTESIAN_POINT('Ctrl Pts',(-141.02872749378,0.594337816979347,
136.693286365502));
#169900=CARTESIAN_POINT('Ctrl Pts',(-141.021325672105,0.437358304549525,
136.707026699922));
#169901=CARTESIAN_POINT('Ctrl Pts',(-141.01392385043,0.279995588109698,
136.714481854321));
#169902=CARTESIAN_POINT('Ctrl Pts',(-141.006525936119,0.122715942222971,
136.721933073202));
#169903=CARTESIAN_POINT('Ctrl Pts',(-140.999128021807,-0.0349461328669095,
136.723105702193));
#169904=CARTESIAN_POINT('Ctrl Pts',(-140.991730107496,-0.192450967081312,
136.71797991439));
#169905=CARTESIAN_POINT('Ctrl Pts',(-140.984333422584,-0.349929626849472,
136.7128549784));
#169906=CARTESIAN_POINT('Ctrl Pts',(-140.976936737672,-0.507250724868555,
136.7014337151));
#169907=CARTESIAN_POINT('Ctrl Pts',(-140.96954005276,-0.663874743601535,
136.683748416249));
#169908=CARTESIAN_POINT('Ctrl Pts',(-140.962143695824,-0.820491817461393,
136.666063901584));
#169909=CARTESIAN_POINT('Ctrl Pts',(-140.954747338889,-0.976411502552809,
136.64211594552));
#169910=CARTESIAN_POINT('Ctrl Pts',(-140.947350981954,-1.13109982449628,
136.611988683268));
#169911=CARTESIAN_POINT('Ctrl Pts',(-140.939953492617,-1.28581182961674,
136.581856808454));
#169912=CARTESIAN_POINT('Ctrl Pts',(-140.932556003281,-1.43929172977447,
136.545543815072));
#169913=CARTESIAN_POINT('Ctrl Pts',(-140.925158513944,-1.59101630478494,
136.503184854232));
#169914=CARTESIAN_POINT('Ctrl Pts',(-140.917758431429,-1.74279406661019,
136.460811044523));
#169915=CARTESIAN_POINT('Ctrl Pts',(-140.910358348914,-1.89281491885331,
136.412387147954));
#169916=CARTESIAN_POINT('Ctrl Pts',(-140.902958266399,-2.04057149203691,
136.35809796717));
#169917=CARTESIAN_POINT('Ctrl Pts',(-140.895550046733,-2.18849053876267,
136.303749089851));
#169918=CARTESIAN_POINT('Ctrl Pts',(-140.888141827067,-2.33413998350985,
136.243522177097));
#169919=CARTESIAN_POINT('Ctrl Pts',(-140.8807336074,-2.47703243508653,136.177650194541));
#169920=CARTESIAN_POINT('Ctrl Pts',(-140.873320828098,-2.62001283458287,
136.111737668879));
#169921=CARTESIAN_POINT('Ctrl Pts',(-140.865908048796,-2.76023252793015,
136.040173319447));
#169922=CARTESIAN_POINT('Ctrl Pts',(-140.858495269494,-2.89722983953149,
135.9632354774));
#169923=CARTESIAN_POINT('Ctrl Pts',(-140.851071898466,-3.03442289931639,
135.886187702956));
#169924=CARTESIAN_POINT('Ctrl Pts',(-140.843648527437,-3.16838406447379,
135.803751296535));
#169925=CARTESIAN_POINT('Ctrl Pts',(-140.836225156408,-3.29868099728236,
135.716247652166));
#169926=CARTESIAN_POINT('Ctrl Pts',(-140.832289106967,-3.3677675575067,
135.669851120288));
#169927=CARTESIAN_POINT('Ctrl Pts',(-140.828353057525,-3.4358245196271,
135.622030682439));
#169928=CARTESIAN_POINT('Ctrl Pts',(-140.824417008083,-3.50279142106041,
135.572838658099));
#169929=CARTESIAN_POINT('Ctrl Pts',(-140.817061441009,-3.62793708869477,
135.48091012928));
#169930=CARTESIAN_POINT('Ctrl Pts',(-140.809705873935,-3.74966752560646,
135.383900102303));
#169931=CARTESIAN_POINT('Ctrl Pts',(-140.802350306861,-3.86753700508942,
135.282093087998));
#169932=CARTESIAN_POINT('Ctrl Pts',(-140.795003465457,-3.98526665985458,
135.180406844033));
#169933=CARTESIAN_POINT('Ctrl Pts',(-140.787656624052,-4.09914418577709,
135.073935182324));
#169934=CARTESIAN_POINT('Ctrl Pts',(-140.780309782647,-4.20875302359296,
134.963005655183));
#169935=CARTESIAN_POINT('Ctrl Pts',(-140.772969980566,-4.31825684047936,
134.852182414381));
#169936=CARTESIAN_POINT('Ctrl Pts',(-140.765630178486,-4.4234998433306,
134.736910077744));
#169937=CARTESIAN_POINT('Ctrl Pts',(-140.758290376405,-4.52409892771506,
134.6175560564));
#169938=CARTESIAN_POINT('Ctrl Pts',(-140.75095593373,-4.62462455626116,
134.49828918545));
#169939=CARTESIAN_POINT('Ctrl Pts',(-140.743621491055,-4.72051277178754,
134.374946852361));
#169940=CARTESIAN_POINT('Ctrl Pts',(-140.73628704838,-4.81141785660132,
134.247932712307));
#169941=CARTESIAN_POINT('Ctrl Pts',(-140.728955749256,-4.90228397938208,
134.120973010672));
#169942=CARTESIAN_POINT('Ctrl Pts',(-140.721624450132,-4.98817099931069,
133.990344941953));
#169943=CARTESIAN_POINT('Ctrl Pts',(-140.714293151009,-5.0687740522275,
133.856484496108));
#169944=CARTESIAN_POINT('Ctrl Pts',(-140.706963395188,-5.14936013749517,
133.72265222906));
#169945=CARTESIAN_POINT('Ctrl Pts',(-140.699633639367,-5.22466427218869,
133.585589264541));
#169946=CARTESIAN_POINT('Ctrl Pts',(-140.692303883546,-5.29442557038256,
133.445759573078));
#169947=CARTESIAN_POINT('Ctrl Pts',(-140.684974158339,-5.36418657720871,
133.305930465633));
#169948=CARTESIAN_POINT('Ctrl Pts',(-140.677644433132,-5.4284046235115,
133.163334994985));
#169949=CARTESIAN_POINT('Ctrl Pts',(-140.670314707924,-5.48686545862238,
133.018460434981));
#169950=CARTESIAN_POINT('Ctrl Pts',(-140.662983500884,-5.54533811261946,
132.873556586036));
#169951=CARTESIAN_POINT('Ctrl Pts',(-140.655652293844,-5.59805109692929,
132.726373083998));
#169952=CARTESIAN_POINT('Ctrl Pts',(-140.648321086804,-5.64483894244176,
132.577415573396));
#169953=CARTESIAN_POINT('Ctrl Pts',(-140.640982769134,-5.69167216807135,
132.428313587039));
#169954=CARTESIAN_POINT('Ctrl Pts',(-140.633644451465,-5.73256866190942,
132.27743451913));
#169955=CARTESIAN_POINT('Ctrl Pts',(-140.626306133795,-5.76741316800669,
132.125298130094));
#169956=CARTESIAN_POINT('Ctrl Pts',(-140.618964144388,-5.80227510859987,
131.973085619409));
#169957=CARTESIAN_POINT('Ctrl Pts',(-140.611622154982,-5.831078958612,131.819614908167));
#169958=CARTESIAN_POINT('Ctrl Pts',(-140.604280165575,-5.85376104713312,
131.665413557615));
#169959=CARTESIAN_POINT('Ctrl Pts',(-140.596927518036,-5.87647606251779,
131.510988357887));
#169960=CARTESIAN_POINT('Ctrl Pts',(-140.589574870498,-5.8930515219413,
131.355830778268));
#169961=CARTESIAN_POINT('Ctrl Pts',(-140.58222222296,-5.90347578439235,
131.200471997853));
#169962=CARTESIAN_POINT('Ctrl Pts',(-140.575939879375,-5.91238261665805,
131.067728352472));
#169963=CARTESIAN_POINT('Ctrl Pts',(-140.569657535791,-5.91679961509745,
130.934837971546));
#169964=CARTESIAN_POINT('Ctrl Pts',(-140.563375192206,-5.91674957945076,
130.802129795026));
#169965=CARTESIAN_POINT('',(-138.813375192206,-5.91736987688761,130.80979542472));
#169966=CARTESIAN_POINT('Ctrl Pts',(-140.563375192206,-5.92551577431234,
130.802126489862));
#169967=CARTESIAN_POINT('Ctrl Pts',(-140.557573256227,-5.92610769889885,
130.679384615503));
#169968=CARTESIAN_POINT('Ctrl Pts',(-140.551771320248,-5.92262577300941,
130.556676961143));
#169969=CARTESIAN_POINT('Ctrl Pts',(-140.545969384269,-5.91496369122512,
130.434230880662));
#169970=CARTESIAN_POINT('Ctrl Pts',(-140.453153509665,-5.79239032525184,
128.475412290975));
#169971=CARTESIAN_POINT('Ctrl Pts',(-140.267521760457,-3.40770003536918,
124.691657369469));
#169972=CARTESIAN_POINT('Ctrl Pts',(-139.989074136643,3.30084525658034,
124.633300650055));
#169973=CARTESIAN_POINT('Ctrl Pts',(-139.710626512832,6.97607501294665,
130.245846567736));
#169974=CARTESIAN_POINT('Ctrl Pts',(-139.432178889018,4.2406326326787,136.371639612287));
#169975=CARTESIAN_POINT('Ctrl Pts',(-139.153731265205,-2.39174397063631,
137.381375237385));
#169976=CARTESIAN_POINT('Ctrl Pts',(-138.947463366267,-5.67671014154374,
133.65213572739));
#169977=CARTESIAN_POINT('Ctrl Pts',(-138.834011341935,-5.92144161112725,
131.247924922634));
#169978=CARTESIAN_POINT('Ctrl Pts',(-138.813375192206,-5.91736987688761,
130.80979542472));
#169979=CARTESIAN_POINT('',(-137.063375192162,-5.91674999530446,130.804124896006));
#169980=CARTESIAN_POINT('Ctrl Pts',(-138.813375192206,-5.91674750446427,
130.809794853102));
#169981=CARTESIAN_POINT('Ctrl Pts',(-138.806067690693,-5.91688998265966,
130.65466585632));
#169982=CARTESIAN_POINT('Ctrl Pts',(-138.79876018918,-5.91092739121872,
130.499355244819));
#169983=CARTESIAN_POINT('Ctrl Pts',(-138.791452687668,-5.89884372612642,
130.344389686703));
#169984=CARTESIAN_POINT('Ctrl Pts',(-138.784150495039,-5.88676883979125,
130.189536710737));
#169985=CARTESIAN_POINT('Ctrl Pts',(-138.776848302411,-5.86858175993033,
130.035028670686));
#169986=CARTESIAN_POINT('Ctrl Pts',(-138.769546109782,-5.84431855243523,
129.881391918118));
#169987=CARTESIAN_POINT('Ctrl Pts',(-138.762246907774,-5.82006528196007,
129.727818087629));
#169988=CARTESIAN_POINT('Ctrl Pts',(-138.754947705765,-5.78974089254672,
129.575115213749));
#169989=CARTESIAN_POINT('Ctrl Pts',(-138.747648503757,-5.75343325457911,
129.423804082105));
#169990=CARTESIAN_POINT('Ctrl Pts',(-138.740350751801,-5.71713282945005,
129.272523009778));
#169991=CARTESIAN_POINT('Ctrl Pts',(-138.733052999844,-5.67485160934117,
129.122633503306));
#169992=CARTESIAN_POINT('Ctrl Pts',(-138.725755247888,-5.62672843348385,
128.974645421607));
#169993=CARTESIAN_POINT('Ctrl Pts',(-138.718457413593,-5.57860471467061,
128.826655670213));
#169994=CARTESIAN_POINT('Ctrl Pts',(-138.711159579299,-5.52463902766561,
128.680567751835));
#169995=CARTESIAN_POINT('Ctrl Pts',(-138.703861745005,-5.46501977561738,
128.536875355296));
#169996=CARTESIAN_POINT('Ctrl Pts',(-138.696562296083,-5.40538733295829,
128.393151167173));
#169997=CARTESIAN_POINT('Ctrl Pts',(-138.689262847161,-5.34009898392624,
128.251823910245));
#169998=CARTESIAN_POINT('Ctrl Pts',(-138.681963398239,-5.26939073775277,
128.113366040205));
#169999=CARTESIAN_POINT('Ctrl Pts',(-138.674656526794,-5.19861059113215,
127.974767377779));
#170000=CARTESIAN_POINT('Ctrl Pts',(-138.667349655348,-5.12239971494985,
127.839044272446));
#170001=CARTESIAN_POINT('Ctrl Pts',(-138.660042783902,-5.04103974336814,
127.706643899032));
#170002=CARTESIAN_POINT('Ctrl Pts',(-138.65273209628,-4.95963727972471,
127.574174376568));
#170003=CARTESIAN_POINT('Ctrl Pts',(-138.645421408657,-4.87308057835454,
127.445031361011));
#170004=CARTESIAN_POINT('Ctrl Pts',(-138.638110721035,-4.7816933820704,
127.319631221707));
#170005=CARTESIAN_POINT('Ctrl Pts',(-138.63078897038,-4.69016789243111,
127.194041318336));
#170006=CARTESIAN_POINT('Ctrl Pts',(-138.623467219725,-4.59379754355125,
127.072205906881));
#170007=CARTESIAN_POINT('Ctrl Pts',(-138.61614546907,-4.49294555443513,
126.954507268751));
#170008=CARTESIAN_POINT('Ctrl Pts',(-138.60970898524,-4.40428749602942,
126.85103947575));
#170009=CARTESIAN_POINT('Ctrl Pts',(-138.60327250141,-4.31216671313621,
126.7507681547));
#170010=CARTESIAN_POINT('Ctrl Pts',(-138.596836017579,-4.21685155889043,
126.65392768921));
#170011=CARTESIAN_POINT('Ctrl Pts',(-138.589412751174,-4.10692356076298,
126.54224053313));
#170012=CARTESIAN_POINT('Ctrl Pts',(-138.581989484768,-3.99238906985639,
126.434754824523));
#170013=CARTESIAN_POINT('Ctrl Pts',(-138.574566218363,-3.8736023819033,
126.331874155942));
#170014=CARTESIAN_POINT('Ctrl Pts',(-138.567151725642,-3.75495608995075,
126.229115083767));
#170015=CARTESIAN_POINT('Ctrl Pts',(-138.559737232921,-3.63206788414376,
126.130950459749));
#170016=CARTESIAN_POINT('Ctrl Pts',(-138.5523227402,-3.505330158414,126.037748503809));
#170017=CARTESIAN_POINT('Ctrl Pts',(-138.544915393846,-3.37871458727518,
125.944636379423));
#170018=CARTESIAN_POINT('Ctrl Pts',(-138.537508047492,-3.24825718142959,
125.856477620365));
#170019=CARTESIAN_POINT('Ctrl Pts',(-138.530100701139,-3.11438471144978,
125.773601387431));
#170020=CARTESIAN_POINT('Ctrl Pts',(-138.522698879463,-2.98061208860919,
125.690786966719));
#170021=CARTESIAN_POINT('Ctrl Pts',(-138.515297057788,-2.84342978925489,
125.613247422891));
#170022=CARTESIAN_POINT('Ctrl Pts',(-138.507895236112,-2.70329487989415,
125.541269571912));
#170023=CARTESIAN_POINT('Ctrl Pts',(-138.500497321801,-2.56323394666166,
125.469329717482));
#170024=CARTESIAN_POINT('Ctrl Pts',(-138.49309940749,-2.42022383878538,
125.402945878891));
#170025=CARTESIAN_POINT('Ctrl Pts',(-138.485701493178,-2.27474752226647,
125.342359677211));
#170026=CARTESIAN_POINT('Ctrl Pts',(-138.478304808266,-2.12929538127153,
125.281783543858));
#170027=CARTESIAN_POINT('Ctrl Pts',(-138.470908123354,-1.98137818931292,
125.227003278606));
#170028=CARTESIAN_POINT('Ctrl Pts',(-138.463511438442,-1.8315003653847,
125.178213003604));
#170029=CARTESIAN_POINT('Ctrl Pts',(-138.456115081506,-1.68162918719668,
125.129424892014));
#170030=CARTESIAN_POINT('Ctrl Pts',(-138.448718724571,-1.52979790486113,
125.086626358119));
#170031=CARTESIAN_POINT('Ctrl Pts',(-138.441322367636,-1.37652737008728,
125.049962042398));
#170032=CARTESIAN_POINT('Ctrl Pts',(-138.433924878299,-1.22323336920327,
125.013292113276));
#170033=CARTESIAN_POINT('Ctrl Pts',(-138.426527388962,-1.06850004020659,
124.982758359183));
#170034=CARTESIAN_POINT('Ctrl Pts',(-138.419129899626,-0.91285958186534,
124.95845453328));
#170035=CARTESIAN_POINT('Ctrl Pts',(-138.411729817111,-0.757164564002912,
124.934142187707));
#170036=CARTESIAN_POINT('Ctrl Pts',(-138.404329734596,-0.600562152272778,
124.916064175994));
#170037=CARTESIAN_POINT('Ctrl Pts',(-138.396929652081,-0.443590688686608,
124.904262494364));
#170038=CARTESIAN_POINT('Ctrl Pts',(-138.389521432415,-0.286446618838942,
124.892447835572));
#170039=CARTESIAN_POINT('Ctrl Pts',(-138.382113212748,-0.12893305918083,
124.886923317556));
#170040=CARTESIAN_POINT('Ctrl Pts',(-138.374704993082,0.0284098784218015,
124.887678824423));
#170041=CARTESIAN_POINT('Ctrl Pts',(-138.36729221378,0.185849657977568,
124.888434796293));
#170042=CARTESIAN_POINT('Ctrl Pts',(-138.359879434478,0.343118234162838,
124.895478478378));
#170043=CARTESIAN_POINT('Ctrl Pts',(-138.352466655175,0.499680105999917,
124.908747811914));
#170044=CARTESIAN_POINT('Ctrl Pts',(-138.345043284147,0.656465680781722,
124.922036105296));
#170045=CARTESIAN_POINT('Ctrl Pts',(-138.337619913118,0.812542165046005,
124.941567770211));
#170046=CARTESIAN_POINT('Ctrl Pts',(-138.330196542089,0.967382919462458,
124.967229400124));
#170047=CARTESIAN_POINT('Ctrl Pts',(-138.326260492648,1.04948320280673,
124.980835812047));
#170048=CARTESIAN_POINT('Ctrl Pts',(-138.322324443208,1.13123629766687,
124.996164733947));
#170049=CARTESIAN_POINT('Ctrl Pts',(-138.318388393767,1.21256549908842,
125.013193595892));
#170050=CARTESIAN_POINT('Ctrl Pts',(-138.310965127361,1.36594983477179,
125.045309498068));
#170051=CARTESIAN_POINT('Ctrl Pts',(-138.303541860956,1.51828929557144,
125.083571958067));
#170052=CARTESIAN_POINT('Ctrl Pts',(-138.296118594551,1.66905282214581,
125.127901048487));
#170053=CARTESIAN_POINT('Ctrl Pts',(-138.28870410183,1.8196381587519,125.172177745604));
#170054=CARTESIAN_POINT('Ctrl Pts',(-138.281289609109,1.96865091405452,
125.222506696438));
#170055=CARTESIAN_POINT('Ctrl Pts',(-138.273875116388,2.11556919570139,
125.278756800724));
#170056=CARTESIAN_POINT('Ctrl Pts',(-138.266467770034,2.26234587197746,
125.334952689041));
#170057=CARTESIAN_POINT('Ctrl Pts',(-138.25906042368,2.4070317472174,125.397058236656));
#170058=CARTESIAN_POINT('Ctrl Pts',(-138.251653077326,2.54911920920186,
125.46489230885));
#170059=CARTESIAN_POINT('Ctrl Pts',(-138.244251255651,2.69110069699652,
125.532675787834));
#170060=CARTESIAN_POINT('Ctrl Pts',(-138.236849433975,2.83048729491822,
125.606179124038));
#170061=CARTESIAN_POINT('Ctrl Pts',(-138.2294476123,2.96679064095992,125.685172805499));
#170062=CARTESIAN_POINT('Ctrl Pts',(-138.222049697989,3.10302203352585,
125.764124786811));
#170063=CARTESIAN_POINT('Ctrl Pts',(-138.214651783677,3.23617309354354,
125.84856115455));
#170064=CARTESIAN_POINT('Ctrl Pts',(-138.207253869366,3.3657794834426,125.938206177833));
#170065=CARTESIAN_POINT('Ctrl Pts',(-138.199857184454,3.49536433511115,
126.027836303739));
#170066=CARTESIAN_POINT('Ctrl Pts',(-138.192460499542,3.62140537905713,
126.122673155114));
#170067=CARTESIAN_POINT('Ctrl Pts',(-138.185063814629,3.74346664403109,
126.222397277738));
#170068=CARTESIAN_POINT('Ctrl Pts',(-138.177667457694,3.86552249668065,
126.32211697849));
#170069=CARTESIAN_POINT('Ctrl Pts',(-138.170271100758,3.98359863215166,
126.426723283421));
#170070=CARTESIAN_POINT('Ctrl Pts',(-138.162874743823,4.09729182724135,
126.535856166951));
#170071=CARTESIAN_POINT('Ctrl Pts',(-138.155477254486,4.21100242904946,
126.645005759003));
#170072=CARTESIAN_POINT('Ctrl Pts',(-138.14807976515,4.32032848502308,126.758683051048));
#170073=CARTESIAN_POINT('Ctrl Pts',(-138.140682275813,4.42490345153916,
126.876490965063));
#170074=CARTESIAN_POINT('Ctrl Pts',(-138.133282193298,4.5295150766481,126.994340176459));
#170075=CARTESIAN_POINT('Ctrl Pts',(-138.125882110783,4.62937204866553,
127.116322613748));
#170076=CARTESIAN_POINT('Ctrl Pts',(-138.118482028268,4.72414804797195,
127.242008054534));
#170077=CARTESIAN_POINT('Ctrl Pts',(-138.111073808602,4.81902826323241,
127.367831699382));
#170078=CARTESIAN_POINT('Ctrl Pts',(-138.103665588935,4.90881612317972,
127.497366181206));
#170079=CARTESIAN_POINT('Ctrl Pts',(-138.096257369269,4.99322819494413,
127.630151620711));
#170080=CARTESIAN_POINT('Ctrl Pts',(-138.088844589967,5.07769222093021,
127.763018787438));
#170081=CARTESIAN_POINT('Ctrl Pts',(-138.081431810664,5.15677367863044,
127.899140576879));
#170082=CARTESIAN_POINT('Ctrl Pts',(-138.074019031362,5.23023532848394,
128.038032912615));
#170083=CARTESIAN_POINT('Ctrl Pts',(-138.066595660334,5.30380194378787,
128.177123704234));
#170084=CARTESIAN_POINT('Ctrl Pts',(-138.059172289305,5.37173255305411,
128.318992612735));
#170085=CARTESIAN_POINT('Ctrl Pts',(-138.051748918276,5.43383790699033,
128.463135262532));
#170086=CARTESIAN_POINT('Ctrl Pts',(-138.047812868835,5.46676765584518,
128.53956315411));
#170087=CARTESIAN_POINT('Ctrl Pts',(-138.043876819394,5.4980605444152,128.616630004902));
#170088=CARTESIAN_POINT('Ctrl Pts',(-138.039940769954,5.52769410052333,
128.694259081256));
#170089=CARTESIAN_POINT('Ctrl Pts',(-138.032517503548,5.58358206251097,
128.840665096537));
#170090=CARTESIAN_POINT('Ctrl Pts',(-138.025094237143,5.63373397092519,
128.989514393627));
#170091=CARTESIAN_POINT('Ctrl Pts',(-138.017670970737,5.6779300204067,129.140316974549));
#170092=CARTESIAN_POINT('Ctrl Pts',(-138.010256478016,5.72207383382811,
129.290941319345));
#170093=CARTESIAN_POINT('Ctrl Pts',(-138.002841985295,5.76027569618112,
129.443513997921));
#170094=CARTESIAN_POINT('Ctrl Pts',(-137.995427492574,5.79236381026875,
129.597525064564));
#170095=CARTESIAN_POINT('Ctrl Pts',(-137.988020146221,5.82442099662392,
129.751387689543));
#170096=CARTESIAN_POINT('Ctrl Pts',(-137.980612799867,5.85037609021098,
129.906685579598));
#170097=CARTESIAN_POINT('Ctrl Pts',(-137.973205453513,5.87010710799512,
130.062893758452));
#170098=CARTESIAN_POINT('Ctrl Pts',(-137.965803631837,5.88982340964174,
130.218985431352));
#170099=CARTESIAN_POINT('Ctrl Pts',(-137.958401810162,5.90332483205459,
130.375985672453));
#170100=CARTESIAN_POINT('Ctrl Pts',(-137.950999988487,5.91054049855355,
130.533359552147));
#170101=CARTESIAN_POINT('Ctrl Pts',(-137.943602074175,5.91775235595837,
130.690650355395));
#170102=CARTESIAN_POINT('Ctrl Pts',(-137.936204159864,5.91868504875209,
130.848314032459));
#170103=CARTESIAN_POINT('Ctrl Pts',(-137.928806245553,5.91331957133809,
131.005810883711));
#170104=CARTESIAN_POINT('Ctrl Pts',(-137.92140956064,5.90795498556912,131.163281561843));
#170105=CARTESIAN_POINT('Ctrl Pts',(-137.914012875728,5.89629431956377,
131.32058509647));
#170106=CARTESIAN_POINT('Ctrl Pts',(-137.906616190816,5.87837068609705,
131.477182019823));
#170107=CARTESIAN_POINT('Ctrl Pts',(-137.899219833881,5.86044784738302,
131.633771999504));
#170108=CARTESIAN_POINT('Ctrl Pts',(-137.891823476945,5.83626263583146,
131.789655059332));
#170109=CARTESIAN_POINT('Ctrl Pts',(-137.88442712001,5.80589999917085,131.944297353586));
#170110=CARTESIAN_POINT('Ctrl Pts',(-137.877029630673,5.77553271391306,
132.09896332397));
#170111=CARTESIAN_POINT('Ctrl Pts',(-137.869632141336,5.73898619229852,
132.252387784208));
#170112=CARTESIAN_POINT('Ctrl Pts',(-137.862234652,5.69639638153221,132.404047720398));
#170113=CARTESIAN_POINT('Ctrl Pts',(-137.854834569485,5.65379164097407,
132.555760820742));
#170114=CARTESIAN_POINT('Ctrl Pts',(-137.84743448697,5.60513949427872,132.705707806337));
#170115=CARTESIAN_POINT('Ctrl Pts',(-137.840034404455,5.55062551600754,
132.853381589529));
#170116=CARTESIAN_POINT('Ctrl Pts',(-137.832626184789,5.49605159401254,
133.00121775523));
#170117=CARTESIAN_POINT('Ctrl Pts',(-137.825217965122,5.43560309733815,
133.14677537621));
#170118=CARTESIAN_POINT('Ctrl Pts',(-137.817809745456,5.36951373307164,
133.289567416377));
#170119=CARTESIAN_POINT('Ctrl Pts',(-137.810396966154,5.30338369190437,
133.432447342661));
#170120=CARTESIAN_POINT('Ctrl Pts',(-137.802984186852,5.23160603483752,
133.57255796488));
#170121=CARTESIAN_POINT('Ctrl Pts',(-137.79557140755,5.15445979529367,133.709438031543));
#170122=CARTESIAN_POINT('Ctrl Pts',(-137.788148036521,5.07720332558484,
133.846513678865));
#170123=CARTESIAN_POINT('Ctrl Pts',(-137.780724665492,4.99456314853259,
133.980349234721));
#170124=CARTESIAN_POINT('Ctrl Pts',(-137.773301294463,4.90686131573687,
134.110512850998));
#170125=CARTESIAN_POINT('Ctrl Pts',(-137.769365245022,4.86035969961123,
134.179528723582));
#170126=CARTESIAN_POINT('Ctrl Pts',(-137.765429195582,4.81243574603676,
134.247512832312));
#170127=CARTESIAN_POINT('Ctrl Pts',(-137.761493146141,4.76314186644666,
134.314404794297));
#170128=CARTESIAN_POINT('Ctrl Pts',(-137.754069879735,4.67017514795067,
134.440560946972));
#170129=CARTESIAN_POINT('Ctrl Pts',(-137.74664661333,4.57205235020373,134.56321184882));
#170130=CARTESIAN_POINT('Ctrl Pts',(-137.739223346924,4.46906691221595,
134.681907715492));
#170131=CARTESIAN_POINT('Ctrl Pts',(-137.731808854203,4.36620319446316,
134.800463293508));
#170132=CARTESIAN_POINT('Ctrl Pts',(-137.724394361482,4.25848851862847,
134.915072861803));
#170133=CARTESIAN_POINT('Ctrl Pts',(-137.716979868761,4.14625905590145,
135.025316244418));
#170134=CARTESIAN_POINT('Ctrl Pts',(-137.709572522408,4.03413776415629,
135.13545337031));
#170135=CARTESIAN_POINT('Ctrl Pts',(-137.702165176054,3.91751061306116,
135.241232428567));
#170136=CARTESIAN_POINT('Ctrl Pts',(-137.6947578297,3.79675334521557,135.342267028908));
#170137=CARTESIAN_POINT('Ctrl Pts',(-137.687356008025,3.67608614269556,
135.443226273832));
#170138=CARTESIAN_POINT('Ctrl Pts',(-137.679954186349,3.55129524198303,
135.539447868148));
#170139=CARTESIAN_POINT('Ctrl Pts',(-137.672552364674,3.42279238393125,
135.630583038777));
#170140=CARTESIAN_POINT('Ctrl Pts',(-137.665154450362,3.29435736153908,
135.721670099859));
#170141=CARTESIAN_POINT('Ctrl Pts',(-137.657756536051,3.1622145879964,135.807675869323));
#170142=CARTESIAN_POINT('Ctrl Pts',(-137.65035862174,3.02680785489518,135.888292636392));
#170143=CARTESIAN_POINT('Ctrl Pts',(-137.642961936828,2.89142362393589,
135.968896006417));
#170144=CARTESIAN_POINT('Ctrl Pts',(-137.635565251915,2.75277683038301,
136.044111960678));
#170145=CARTESIAN_POINT('Ctrl Pts',(-137.628168567003,2.61133924201346,
136.113676762384));
#170146=CARTESIAN_POINT('Ctrl Pts',(-137.620772210068,2.46990792513438,
136.183238479513));
#170147=CARTESIAN_POINT('Ctrl Pts',(-137.613375853132,2.32568639446254,
136.247149377567));
#170148=CARTESIAN_POINT('Ctrl Pts',(-137.605979496197,2.17916970584513,
136.305192368822));
#170149=CARTESIAN_POINT('Ctrl Pts',(-137.59858200686,2.0326305851495,136.363244246607));
#170150=CARTESIAN_POINT('Ctrl Pts',(-137.591184517524,1.88379595391424,
136.415426291281));
#170151=CARTESIAN_POINT('Ctrl Pts',(-137.583787028187,1.73317932133237,
136.461570177288));
#170152=CARTESIAN_POINT('Ctrl Pts',(-137.576386945672,1.58250989032193,
136.507730238962));
#170153=CARTESIAN_POINT('Ctrl Pts',(-137.568986863157,1.4300575709363,136.54784781842));
#170154=CARTESIAN_POINT('Ctrl Pts',(-137.561586780642,1.27634929796166,
136.581804951533));
#170155=CARTESIAN_POINT('Ctrl Pts',(-137.554178560976,1.12247200693996,
136.615799424005));
#170156=CARTESIAN_POINT('Ctrl Pts',(-137.546770341309,0.967336369014114,
136.643619841345));
#170157=CARTESIAN_POINT('Ctrl Pts',(-137.539362121642,0.811478465832407,
136.665199573039));
#170158=CARTESIAN_POINT('Ctrl Pts',(-137.53194934234,0.65552463471192,136.686792586698));
#170159=CARTESIAN_POINT('Ctrl Pts',(-137.524536563038,0.498848023188452,
136.70213722466));
#170160=CARTESIAN_POINT('Ctrl Pts',(-137.517123783736,0.341987519584247,
136.71121892795));
#170161=CARTESIAN_POINT('Ctrl Pts',(-137.509700412708,0.184902886336242,
136.720313607603));
#170162=CARTESIAN_POINT('Ctrl Pts',(-137.502277041679,0.0276342084789624,
136.723127473213));
#170163=CARTESIAN_POINT('Ctrl Pts',(-137.49485367065,-0.129281111182614,
136.719698051457));
#170164=CARTESIAN_POINT('Ctrl Pts',(-137.490917621209,-0.212481378797461,
136.717879689754));
#170165=CARTESIAN_POINT('Ctrl Pts',(-137.486981571768,-0.295582402394713,
136.714306981708));
#170166=CARTESIAN_POINT('Ctrl Pts',(-137.483045522328,-0.378505050477561,
136.708991384114));
#170167=CARTESIAN_POINT('Ctrl Pts',(-137.475622255922,-0.534894576835595,
136.698966332945));
#170168=CARTESIAN_POINT('Ctrl Pts',(-137.468198989517,-0.691122023178962,
136.682708652582));
#170169=CARTESIAN_POINT('Ctrl Pts',(-137.460775723111,-0.846650362243173,
136.660222102148));
#170170=CARTESIAN_POINT('Ctrl Pts',(-137.45336123039,-1.00199487972688,
136.637762128949));
#170171=CARTESIAN_POINT('Ctrl Pts',(-137.445946737669,-1.1566415688112,
136.60908799269));
#170172=CARTESIAN_POINT('Ctrl Pts',(-137.438532244948,-1.31005521482037,
136.574255408342));
#170173=CARTESIAN_POINT('Ctrl Pts',(-137.431124898595,-1.46332099498159,
136.53945639695));
#170174=CARTESIAN_POINT('Ctrl Pts',(-137.423717552241,-1.61535573645554,
136.498510836466));
#170175=CARTESIAN_POINT('Ctrl Pts',(-137.416310205887,-1.76563126010126,
136.451525996396));
#170176=CARTESIAN_POINT('Ctrl Pts',(-137.408908384212,-1.91579470259146,
136.404576199392));
#170177=CARTESIAN_POINT('Ctrl Pts',(-137.401506562536,-2.06420118504784,
136.351596202432));
#170178=CARTESIAN_POINT('Ctrl Pts',(-137.394104740861,-2.2103347188132,
136.292743894389));
#170179=CARTESIAN_POINT('Ctrl Pts',(-137.38670682655,-2.35639110982484,
136.233922654021));
#170180=CARTESIAN_POINT('Ctrl Pts',(-137.379308912238,-2.50017659635288,
136.169235415364));
#170181=CARTESIAN_POINT('Ctrl Pts',(-137.371910997927,-2.64119241240932,
136.098889227663));
#170182=CARTESIAN_POINT('Ctrl Pts',(-137.364514313015,-2.78218479419482,
136.028554730221));
#170183=CARTESIAN_POINT('Ctrl Pts',(-137.357117628103,-2.92040808529264,
135.952563316654));
#170184=CARTESIAN_POINT('Ctrl Pts',(-137.34972094319,-3.05538539446384,
135.871169342375));
#170185=CARTESIAN_POINT('Ctrl Pts',(-137.342324586255,-3.19035671859972,
135.789778977189));
#170186=CARTESIAN_POINT('Ctrl Pts',(-137.334928229319,-3.32208202731753,
135.702986720378));
#170187=CARTESIAN_POINT('Ctrl Pts',(-137.327531872384,-3.45011108879016,
135.611091735229));
#170188=CARTESIAN_POINT('Ctrl Pts',(-137.320134383047,-3.57815975183893,
135.519182680723));
#170189=CARTESIAN_POINT('Ctrl Pts',(-137.312736893711,-3.70251073756622,
135.422169560012));
#170190=CARTESIAN_POINT('Ctrl Pts',(-137.305339404374,-3.82274486465305,
135.32039341885));
#170191=CARTESIAN_POINT('Ctrl Pts',(-137.297939321859,-3.94302113962726,
135.218581600218));
#170192=CARTESIAN_POINT('Ctrl Pts',(-137.290539239344,-4.05917739789664,
135.112003677869));
#170193=CARTESIAN_POINT('Ctrl Pts',(-137.283139156829,-4.17082957177651,
135.001039214468));
#170194=CARTESIAN_POINT('Ctrl Pts',(-137.275730937163,-4.28260451869888,
134.889952734233));
#170195=CARTESIAN_POINT('Ctrl Pts',(-137.268322717496,-4.38986522541898,
134.774470343501));
#170196=CARTESIAN_POINT('Ctrl Pts',(-137.26091449783,-4.49226586857321,
134.655007047525));
#170197=CARTESIAN_POINT('Ctrl Pts',(-137.253501718528,-4.59472953761524,
134.535470223882));
#170198=CARTESIAN_POINT('Ctrl Pts',(-137.246088939226,-4.69232695168307,
134.411947904928));
#170199=CARTESIAN_POINT('Ctrl Pts',(-137.238676159924,-4.78475457959678,
134.284885603186));
#170200=CARTESIAN_POINT('Ctrl Pts',(-137.231252788895,-4.87731427243955,
134.15764174887));
#170201=CARTESIAN_POINT('Ctrl Pts',(-137.223829417866,-4.9646892191526,
134.026848119203));
#170202=CARTESIAN_POINT('Ctrl Pts',(-137.216406046837,-5.04662051265013,
133.892977130473));
#170203=CARTESIAN_POINT('Ctrl Pts',(-137.212469997396,-5.09006245037808,
133.821995520055));
#170204=CARTESIAN_POINT('Ctrl Pts',(-137.208533947955,-5.1319747630258,
133.75014913939));
#170205=CARTESIAN_POINT('Ctrl Pts',(-137.204597898515,-5.17232431701266,
133.677510756723));
#170206=CARTESIAN_POINT('Ctrl Pts',(-137.196816576985,-5.25209284071643,
133.533909254921));
#170207=CARTESIAN_POINT('Ctrl Pts',(-137.189035255457,-5.32597286795493,
133.386811640862));
#170208=CARTESIAN_POINT('Ctrl Pts',(-137.181253933927,-5.39366007775706,
133.236717813397));
#170209=CARTESIAN_POINT('Ctrl Pts',(-137.173485134107,-5.4612383652485,
133.086865517036));
#170210=CARTESIAN_POINT('Ctrl Pts',(-137.165716334287,-5.52264356596163,
132.934026908043));
#170211=CARTESIAN_POINT('Ctrl Pts',(-137.157947534466,-5.57761648533935,
132.778727580663));
#170212=CARTESIAN_POINT('Ctrl Pts',(-137.150066505945,-5.63338354789144,
132.621184786825));
#170213=CARTESIAN_POINT('Ctrl Pts',(-137.142185477423,-5.68253084916941,
132.461109897367));
#170214=CARTESIAN_POINT('Ctrl Pts',(-137.134304448901,-5.7248365729683,
132.299076903456));
#170215=CARTESIAN_POINT('Ctrl Pts',(-137.126562263329,-5.76639698142256,
132.139898503814));
#170216=CARTESIAN_POINT('Ctrl Pts',(-137.118820077758,-5.80135475029489,
131.978830741823));
#170217=CARTESIAN_POINT('Ctrl Pts',(-137.111077892186,-5.8295481012705,
131.816437441465));
#170218=CARTESIAN_POINT('Ctrl Pts',(-137.103127442189,-5.85849985205065,
131.649675769027));
#170219=CARTESIAN_POINT('Ctrl Pts',(-137.095176992192,-5.88031800224339,
131.481516547968));
#170220=CARTESIAN_POINT('Ctrl Pts',(-137.087226542196,-5.89488225293724,
131.312586735063));
#170221=CARTESIAN_POINT('Ctrl Pts',(-137.079276092199,-5.90944650363105,
131.143656922157));
#170222=CARTESIAN_POINT('Ctrl Pts',(-137.071325642203,-5.91675676133333,
130.973956878516));
#170223=CARTESIAN_POINT('Ctrl Pts',(-137.063375192206,-5.9167499953045,
130.80412489694));
#170224=CARTESIAN_POINT('',(-135.313375192206,-5.91688315261144,130.799007197003));
#170225=CARTESIAN_POINT('Ctrl Pts',(-137.063375192162,-5.91674999530446,
130.804124896005));
#170226=CARTESIAN_POINT('Ctrl Pts',(-137.05560354086,-5.9167433814115,130.638112287751));
#170227=CARTESIAN_POINT('Ctrl Pts',(-137.047831889558,-5.90974547835622,
130.472243404385));
#170228=CARTESIAN_POINT('Ctrl Pts',(-137.040060238256,-5.89581823969249,
130.307110331483));
#170229=CARTESIAN_POINT('Ctrl Pts',(-137.032278021656,-5.8818720674173,
130.141752765736));
#170230=CARTESIAN_POINT('Ctrl Pts',(-137.024495805056,-5.86097778122643,
129.97713331967));
#170231=CARTESIAN_POINT('Ctrl Pts',(-137.016713588456,-5.83324875759858,
129.813835759486));
#170232=CARTESIAN_POINT('Ctrl Pts',(-137.008912554227,-5.80545268437448,
129.650143340989));
#170233=CARTESIAN_POINT('Ctrl Pts',(-137.001111519998,-5.77078887560722,
129.487779511236));
#170234=CARTESIAN_POINT('Ctrl Pts',(-136.993310485769,-5.72942165030861,
129.327316909521));
#170235=CARTESIAN_POINT('Ctrl Pts',(-136.985499742625,-5.68800294069421,
129.166654601222));
#170236=CARTESIAN_POINT('Ctrl Pts',(-136.97768899948,-5.63986425109469,
129.007898544551));
#170237=CARTESIAN_POINT('Ctrl Pts',(-136.969878256335,-5.58521897036779,
128.851603690669));
#170238=CARTESIAN_POINT('Ctrl Pts',(-136.962049208225,-5.53044562501072,
128.69494255003));
#170239=CARTESIAN_POINT('Ctrl Pts',(-136.954220160116,-5.46913530667103,
128.540754440993));
#170240=CARTESIAN_POINT('Ctrl Pts',(-136.946391112006,-5.40154943985235,
128.3895740408));
#170241=CARTESIAN_POINT('Ctrl Pts',(-136.939644166238,-5.34330504388798,
128.259289241545));
#170242=CARTESIAN_POINT('Ctrl Pts',(-136.93289722047,-5.28040079509976,
128.13123788636));
#170243=CARTESIAN_POINT('Ctrl Pts',(-136.926150274702,-5.21303021830327,
128.005745512633));
#170244=CARTESIAN_POINT('Ctrl Pts',(-136.918727008296,-5.13890634705246,
127.867673657005));
#170245=CARTESIAN_POINT('Ctrl Pts',(-136.911303741891,-5.05918116475427,
127.732339912249));
#170246=CARTESIAN_POINT('Ctrl Pts',(-136.903880475485,-4.97408131473932,
127.600231151258));
#170247=CARTESIAN_POINT('Ctrl Pts',(-136.896465982764,-4.88908204567975,
127.468278531852));
#170248=CARTESIAN_POINT('Ctrl Pts',(-136.889051490043,-4.79872095359227,
127.339543619835));
#170249=CARTESIAN_POINT('Ctrl Pts',(-136.881636997322,-4.70327118310432,
127.214490043203));
#170250=CARTESIAN_POINT('Ctrl Pts',(-136.874229650968,-4.60791341069906,
127.089556997916));
#170251=CARTESIAN_POINT('Ctrl Pts',(-136.866822304615,-4.50747694907607,
126.968298518974));
#170252=CARTESIAN_POINT('Ctrl Pts',(-136.859414958261,-4.40227890815001,
126.851150405933));
#170253=CARTESIAN_POINT('Ctrl Pts',(-136.852013136585,-4.29715932789146,
126.734089666374));
#170254=CARTESIAN_POINT('Ctrl Pts',(-136.84461131491,-4.18728548791909,
126.621133465114));
#170255=CARTESIAN_POINT('Ctrl Pts',(-136.837209493234,-4.0730154701462,
126.51268547347));
#170256=CARTESIAN_POINT('Ctrl Pts',(-136.829811578923,-3.95880577462622,
126.404294730677));
#170257=CARTESIAN_POINT('Ctrl Pts',(-136.822413664612,-3.8402047931907,
126.300407714242));
#170258=CARTESIAN_POINT('Ctrl Pts',(-136.8150157503,-3.71760816105667,126.201391996845));
#170259=CARTESIAN_POINT('Ctrl Pts',(-136.807619065388,-3.59503190225895,
126.102392734063));
#170260=CARTESIAN_POINT('Ctrl Pts',(-136.800222380476,-3.46846160074031,
126.008263397979));
#170261=CARTESIAN_POINT('Ctrl Pts',(-136.792825695563,-3.33832682488041,
125.919332002216));
#170262=CARTESIAN_POINT('Ctrl Pts',(-136.785429338628,-3.20819781933284,
125.830404549765));
#170263=CARTESIAN_POINT('Ctrl Pts',(-136.778032981692,-3.07450496191039,
125.74667478998));
#170264=CARTESIAN_POINT('Ctrl Pts',(-136.770636624757,-2.9377074930873,
125.668427864155));
#170265=CARTESIAN_POINT('Ctrl Pts',(-136.76323913542,-2.80088908022252,
125.590168958526));
#170266=CARTESIAN_POINT('Ctrl Pts',(-136.755841646084,-2.66096543357956,
125.517394743643));
#170267=CARTESIAN_POINT('Ctrl Pts',(-136.748444156747,-2.51842097978532,
125.45034471069));
#170268=CARTESIAN_POINT('Ctrl Pts',(-136.741044074232,-2.37582655725316,
125.383271173452));
#170269=CARTESIAN_POINT('Ctrl Pts',(-136.733643991717,-2.23060983598848,
125.321925972068));
#170270=CARTESIAN_POINT('Ctrl Pts',(-136.726243909202,-2.08327567883836,
125.266500651075));
#170271=CARTESIAN_POINT('Ctrl Pts',(-136.718835689535,-1.93577951263676,
125.211014384245));
#170272=CARTESIAN_POINT('Ctrl Pts',(-136.711427469869,-1.7861616103125,
125.161461129258));
#170273=CARTESIAN_POINT('Ctrl Pts',(-136.704019250202,-1.63494317345788,
125.117982914488));
#170274=CARTESIAN_POINT('Ctrl Pts',(-136.6966064709,-1.4836316641786,125.074477939602));
#170275=CARTESIAN_POINT('Ctrl Pts',(-136.689193691598,-1.33071801918584,
125.037055544064));
#170276=CARTESIAN_POINT('Ctrl Pts',(-136.681780912296,-1.17673360750333,
125.00580660993));
#170277=CARTESIAN_POINT('Ctrl Pts',(-136.674357541267,-1.02252917567203,
124.974513025853));
#170278=CARTESIAN_POINT('Ctrl Pts',(-136.666934170238,-0.867251289011637,
124.949410579975));
#170279=CARTESIAN_POINT('Ctrl Pts',(-136.659510799209,-0.711437237224342,
124.930538384983));
#170280=CARTESIAN_POINT('Ctrl Pts',(-136.655574749769,-0.62882088827053,
124.920531894367));
#170281=CARTESIAN_POINT('Ctrl Pts',(-136.651638700329,-0.546053830252986,
124.912276079976));
#170282=CARTESIAN_POINT('Ctrl Pts',(-136.647702650889,-0.463216019656414,
124.905770830029));
#170283=CARTESIAN_POINT('Ctrl Pts',(-136.640279384483,-0.306986494131329,
124.89350213165));
#170284=CARTESIAN_POINT('Ctrl Pts',(-136.632856118078,-0.150032973389701,
124.887425990701));
#170285=CARTESIAN_POINT('Ctrl Pts',(-136.625432851672,0.00711241635787892,
124.88761489242));
#170286=CARTESIAN_POINT('Ctrl Pts',(-136.618018358951,0.164072073305337,
124.887803570873));
#170287=CARTESIAN_POINT('Ctrl Pts',(-136.61060386623,0.321222778213059,
124.894242552335));
#170288=CARTESIAN_POINT('Ctrl Pts',(-136.603189373509,0.478026826373297,
124.906952634751));
#170289=CARTESIAN_POINT('Ctrl Pts',(-136.595782027155,0.634679740887905,
124.919650466712));
#170290=CARTESIAN_POINT('Ctrl Pts',(-136.588374680802,0.790986294244059,
124.938607336612));
#170291=CARTESIAN_POINT('Ctrl Pts',(-136.580967334448,0.946408430277538,
124.963792011206));
#170292=CARTESIAN_POINT('Ctrl Pts',(-136.573565512772,1.10171464661822,
124.988957902119));
#170293=CARTESIAN_POINT('Ctrl Pts',(-136.566163691097,1.25613739214663,
125.020342289586));
#170294=CARTESIAN_POINT('Ctrl Pts',(-136.558761869422,1.40914349472865,
125.057862103361));
#170295=CARTESIAN_POINT('Ctrl Pts',(-136.55136395511,1.56206882657967,125.095362110717));
#170296=CARTESIAN_POINT('Ctrl Pts',(-136.543966040799,1.71357864319441,
125.138991005388));
#170297=CARTESIAN_POINT('Ctrl Pts',(-136.536568126488,1.86314984476834,
125.188614610272));
#170298=CARTESIAN_POINT('Ctrl Pts',(-136.529171441575,2.01269619032228,
125.238229968613));
#170299=CARTESIAN_POINT('Ctrl Pts',(-136.521774756663,2.16030420627278,
125.293837942547));
#170300=CARTESIAN_POINT('Ctrl Pts',(-136.514378071751,2.30546573326601,
125.355254423406));
#170301=CARTESIAN_POINT('Ctrl Pts',(-136.506981714815,2.45062082364502,
125.416668180993));
#170302=CARTESIAN_POINT('Ctrl Pts',(-136.49958535788,2.59332929696827,125.483889787944));
#170303=CARTESIAN_POINT('Ctrl Pts',(-136.492189000945,2.73310302509495,
125.556686998074));
#170304=CARTESIAN_POINT('Ctrl Pts',(-136.484791511608,2.87289815293663,
125.629495353642));
#170305=CARTESIAN_POINT('Ctrl Pts',(-136.477394022271,3.00975730982586,
125.707880839653));
#170306=CARTESIAN_POINT('Ctrl Pts',(-136.469996532935,3.14321716062246,
125.791565345099));
#170307=CARTESIAN_POINT('Ctrl Pts',(-136.46259645042,3.27672379556305,125.875279186019));
#170308=CARTESIAN_POINT('Ctrl Pts',(-136.455196367905,3.40682843583282,
125.964295546581));
#170309=CARTESIAN_POINT('Ctrl Pts',(-136.44779628539,3.53309703888642,126.058293205875));
#170310=CARTESIAN_POINT('Ctrl Pts',(-136.440388065723,3.65950448724962,
126.152394225259));
#170311=CARTESIAN_POINT('Ctrl Pts',(-136.432979846057,3.78206717491825,
126.251487259157));
#170312=CARTESIAN_POINT('Ctrl Pts',(-136.42557162639,3.90038388720675,126.355210575713));
#170313=CARTESIAN_POINT('Ctrl Pts',(-136.418158847088,4.01877342145743,
126.45899773224));
#170314=CARTESIAN_POINT('Ctrl Pts',(-136.410746067786,4.13291150292322,
126.56742059363));
#170315=CARTESIAN_POINT('Ctrl Pts',(-136.403333288484,4.24243445201907,
126.680081228046));
#170316=CARTESIAN_POINT('Ctrl Pts',(-136.395909917455,4.35211389264055,
126.792902837259));
#170317=CARTESIAN_POINT('Ctrl Pts',(-136.388486546426,4.45716478190906,
126.909974035845));
#170318=CARTESIAN_POINT('Ctrl Pts',(-136.381063175398,4.55726379500535,
127.030863928124));
#170319=CARTESIAN_POINT('Ctrl Pts',(-136.377127125957,4.61033869359071,
127.094962649721));
#170320=CARTESIAN_POINT('Ctrl Pts',(-136.373191076516,4.66202216061623,
127.160134450385));
#170321=CARTESIAN_POINT('Ctrl Pts',(-136.369255027076,4.71227107169331,
127.22631200004));
#170322=CARTESIAN_POINT('Ctrl Pts',(-136.36183176067,4.80703894977178,127.35112079336));
#170323=CARTESIAN_POINT('Ctrl Pts',(-136.354408494265,4.89698819100115,
127.479885932913));
#170324=CARTESIAN_POINT('Ctrl Pts',(-136.346985227859,4.98177018428258,
127.61219890589));
#170325=CARTESIAN_POINT('Ctrl Pts',(-136.339570735138,5.06645197228865,
127.74435549592));
#170326=CARTESIAN_POINT('Ctrl Pts',(-136.332156242417,5.14597846944518,
127.880051261458));
#170327=CARTESIAN_POINT('Ctrl Pts',(-136.324741749696,5.22004153532217,
128.018845058103));
#170328=CARTESIAN_POINT('Ctrl Pts',(-136.317334403343,5.29403321642806,
128.157505080061));
#170329=CARTESIAN_POINT('Ctrl Pts',(-136.309927056989,5.36257177498328,
128.29925686146));
#170330=CARTESIAN_POINT('Ctrl Pts',(-136.302519710635,5.42539265590344,
128.443630838076));
#170331=CARTESIAN_POINT('Ctrl Pts',(-136.29511788896,5.48816668264034,128.587897135134));
#170332=CARTESIAN_POINT('Ctrl Pts',(-136.287716067284,5.54523137455547,
128.734781392458));
#170333=CARTESIAN_POINT('Ctrl Pts',(-136.280314245609,5.59636842843825,
128.883790135735));
#170334=CARTESIAN_POINT('Ctrl Pts',(-136.272916331298,5.64747848746834,
129.032720218457));
#170335=CARTESIAN_POINT('Ctrl Pts',(-136.265518416986,5.69266701946077,
129.18377220142));
#170336=CARTESIAN_POINT('Ctrl Pts',(-136.258120502675,5.73176416318901,
129.336433459945));
#170337=CARTESIAN_POINT('Ctrl Pts',(-136.250723817763,5.77085480968132,
129.489069348938));
#170338=CARTESIAN_POINT('Ctrl Pts',(-136.24332713285,5.80385598445876,129.643313621445));
#170339=CARTESIAN_POINT('Ctrl Pts',(-136.235930447938,5.83064791081451,
129.798639233377));
#170340=CARTESIAN_POINT('Ctrl Pts',(-136.228534091003,5.85743864918818,
129.95395795801));
#170341=CARTESIAN_POINT('Ctrl Pts',(-136.221137734067,5.87802062312581,
130.110357558866));
#170342=CARTESIAN_POINT('Ctrl Pts',(-136.213741377132,5.89232538273506,
130.267301825183));
#170343=CARTESIAN_POINT('Ctrl Pts',(-136.206343887795,5.90663233243953,
130.424270120067));
#170344=CARTESIAN_POINT('Ctrl Pts',(-136.198946398459,5.91466012033609,
130.581782874671));
#170345=CARTESIAN_POINT('Ctrl Pts',(-136.191548909122,5.91639228512992,
130.739299946227));
#170346=CARTESIAN_POINT('Ctrl Pts',(-136.184148826607,5.91812505713144,
130.896872235147));
#170347=CARTESIAN_POINT('Ctrl Pts',(-136.176748744092,5.91355780796466,
131.054448470989));
#170348=CARTESIAN_POINT('Ctrl Pts',(-136.169348661577,5.90272617928099,
131.211489853719));
#170349=CARTESIAN_POINT('Ctrl Pts',(-136.161940441911,5.89188264010805,
131.368703919594));
#170350=CARTESIAN_POINT('Ctrl Pts',(-136.154532222244,5.87476099067463,
131.525381585189));
#170351=CARTESIAN_POINT('Ctrl Pts',(-136.147124002578,5.85144869989751,
131.680989772322));
#170352=CARTESIAN_POINT('Ctrl Pts',(-136.139711223276,5.82812206079434,
131.836693733698));
#170353=CARTESIAN_POINT('Ctrl Pts',(-136.132298443974,5.79859725782218,
131.99132653915));
#170354=CARTESIAN_POINT('Ctrl Pts',(-136.124885664672,5.76301250460659,
132.144367122867));
#170355=CARTESIAN_POINT('Ctrl Pts',(-136.117462293643,5.7273769062269,132.297626378146));
#170356=CARTESIAN_POINT('Ctrl Pts',(-136.110038922614,5.68566416288823,
132.449288508942));
#170357=CARTESIAN_POINT('Ctrl Pts',(-136.102615551585,5.63806203436787,
132.598848583288));
#170358=CARTESIAN_POINT('Ctrl Pts',(-136.098679502145,5.61282224362844,
132.678148923352));
#170359=CARTESIAN_POINT('Ctrl Pts',(-136.094743452704,5.58592753833369,
132.756858638084));
#170360=CARTESIAN_POINT('Ctrl Pts',(-136.090807403263,5.55741125539755,
132.834905052165));
#170361=CARTESIAN_POINT('Ctrl Pts',(-136.083384136857,5.50363043574379,
132.982098153372));
#170362=CARTESIAN_POINT('Ctrl Pts',(-136.075960870452,5.44391643903607,
133.127375700706));
#170363=CARTESIAN_POINT('Ctrl Pts',(-136.068537604047,5.37842452585654,
133.270223586623));
#170364=CARTESIAN_POINT('Ctrl Pts',(-136.061123111326,5.31301001867962,
133.412902638201));
#170365=CARTESIAN_POINT('Ctrl Pts',(-136.053708618605,5.24183134228407,
133.553157408393));
#170366=CARTESIAN_POINT('Ctrl Pts',(-136.046294125884,5.16509308651932,
133.690490200605));
#170367=CARTESIAN_POINT('Ctrl Pts',(-136.03888677953,5.08842879397484,133.8276906263));
#170368=CARTESIAN_POINT('Ctrl Pts',(-136.031479433176,5.00621577071171,
133.96197435705));
#170369=CARTESIAN_POINT('Ctrl Pts',(-136.024072086822,4.9187060759237,134.09286500424));
#170370=CARTESIAN_POINT('Ctrl Pts',(-136.016670265147,4.83126164916737,
134.223658028246));
#170371=CARTESIAN_POINT('Ctrl Pts',(-136.009268443472,4.73852862336444,
134.351062698642));
#170372=CARTESIAN_POINT('Ctrl Pts',(-136.001866621796,4.64080417421365,
134.474628615833));
#170373=CARTESIAN_POINT('Ctrl Pts',(-135.994468707485,4.54313131303917,
134.598129303537));
#170374=CARTESIAN_POINT('Ctrl Pts',(-135.987070793174,4.44047250709058,
134.71779498175));
#170375=CARTESIAN_POINT('Ctrl Pts',(-135.979672878862,4.33316722788835,
134.833205655248));
#170376=CARTESIAN_POINT('Ctrl Pts',(-135.97227619395,4.22587978087665,134.948597149586));
#170377=CARTESIAN_POINT('Ctrl Pts',(-135.964879509038,4.11394764705738,
135.059734769484));
#170378=CARTESIAN_POINT('Ctrl Pts',(-135.957482824126,3.99774950131289,
135.166232863202));
#170379=CARTESIAN_POINT('Ctrl Pts',(-135.95008646719,3.88155650791595,135.272726234684));
#170380=CARTESIAN_POINT('Ctrl Pts',(-135.942690110255,3.76109815390441,
135.374580236805));
#170381=CARTESIAN_POINT('Ctrl Pts',(-135.93529375332,3.6367885697415,135.471447445717));
#170382=CARTESIAN_POINT('Ctrl Pts',(-135.927896263983,3.5124599534639,135.568329485246));
#170383=CARTESIAN_POINT('Ctrl Pts',(-135.920498774646,3.38427922747028,
135.660222981888));
#170384=CARTESIAN_POINT('Ctrl Pts',(-135.91310128531,3.25269193143695,135.746822125931));
#170385=CARTESIAN_POINT('Ctrl Pts',(-135.905701202795,3.12105850768117,
135.833451627169));
#170386=CARTESIAN_POINT('Ctrl Pts',(-135.89830112028,2.98601644794011,135.91478287558));
#170387=CARTESIAN_POINT('Ctrl Pts',(-135.890901037765,2.84803832512546,
135.990554622915));
#170388=CARTESIAN_POINT('Ctrl Pts',(-135.883492818099,2.70990848118009,
136.066409689076));
#170389=CARTESIAN_POINT('Ctrl Pts',(-135.876084598432,2.56883645403495,
136.136692865816));
#170390=CARTESIAN_POINT('Ctrl Pts',(-135.868676378766,2.42531801654775,
136.201189601433));
#170391=CARTESIAN_POINT('Ctrl Pts',(-135.861263599464,2.28171124585702,
136.265726033715));
#170392=CARTESIAN_POINT('Ctrl Pts',(-135.853850820162,2.13565541001169,
136.324468789252));
#170393=CARTESIAN_POINT('Ctrl Pts',(-135.84643804086,1.98766360427814,136.377252502282));
#170394=CARTESIAN_POINT('Ctrl Pts',(-135.839014669831,1.83946034091221,
136.430111635156));
#170395=CARTESIAN_POINT('Ctrl Pts',(-135.831591298802,1.68931593831358,
136.476994609067));
#170396=CARTESIAN_POINT('Ctrl Pts',(-135.824167927773,1.53775669879329,
136.517786463573));
#170397=CARTESIAN_POINT('Ctrl Pts',(-135.820231878333,1.45739635338431,
136.539415283619));
#170398=CARTESIAN_POINT('Ctrl Pts',(-135.816295828892,1.37663839605393,
136.559332529761));
#170399=CARTESIAN_POINT('Ctrl Pts',(-135.812359779451,1.29556199002331,
136.577526966504));
#170400=CARTESIAN_POINT('Ctrl Pts',(-135.804936513045,1.14265441856021,
136.611841106371));
#170401=CARTESIAN_POINT('Ctrl Pts',(-135.79751324664,0.988151429699113,
136.640128092688));
#170402=CARTESIAN_POINT('Ctrl Pts',(-135.790089980234,0.832569478813058,
136.662240662894));
#170403=CARTESIAN_POINT('Ctrl Pts',(-135.782675487514,0.677171412872674,
136.684327097878));
#170404=CARTESIAN_POINT('Ctrl Pts',(-135.775260994793,0.520697289261222,
136.700253590744));
#170405=CARTESIAN_POINT('Ctrl Pts',(-135.767846502072,0.363676420030692,
136.709923251559));
#170406=CARTESIAN_POINT('Ctrl Pts',(-135.760439155718,0.206806893425211,
136.719583592391));
#170407=CARTESIAN_POINT('Ctrl Pts',(-135.753031809364,0.0493920403929515,
136.722999084059));
#170408=CARTESIAN_POINT('Ctrl Pts',(-135.74562446301,-0.108031095679464,
136.720124291418));
#170409=CARTESIAN_POINT('Ctrl Pts',(-135.738222641335,-0.265336819637314,
136.717251642906));
#170410=CARTESIAN_POINT('Ctrl Pts',(-135.730820819659,-0.422650442705173,
136.708098058343));
#170411=CARTESIAN_POINT('Ctrl Pts',(-135.723418997984,-0.579432400224242,
136.692670108079));
#170412=CARTESIAN_POINT('Ctrl Pts',(-135.716021083673,-0.736131593768324,
136.677250302111));
#170413=CARTESIAN_POINT('Ctrl Pts',(-135.708623169361,-0.892299310152501,
136.655562763288));
#170414=CARTESIAN_POINT('Ctrl Pts',(-135.70122525505,-1.04739870285251,
136.62766608094));
#170415=CARTESIAN_POINT('Ctrl Pts',(-135.693828570138,-1.20247232084702,
136.599774034515));
#170416=CARTESIAN_POINT('Ctrl Pts',(-135.686431885226,-1.35647760047121,
136.565674958492));
#170417=CARTESIAN_POINT('Ctrl Pts',(-135.679035200313,-1.50888539897116,
136.52547898859));
#170418=CARTESIAN_POINT('Ctrl Pts',(-135.671638843378,-1.66128643954961,
136.48528480102));
#170419=CARTESIAN_POINT('Ctrl Pts',(-135.664242486442,-1.81208977889087,
136.438994352301));
#170420=CARTESIAN_POINT('Ctrl Pts',(-135.656846129507,-1.96077927184045,
136.386768271045));
#170421=CARTESIAN_POINT('Ctrl Pts',(-135.64944864017,-2.10949152953099,
136.334534193842));
#170422=CARTESIAN_POINT('Ctrl Pts',(-135.642051150834,-2.25608894420267,
136.276362798356));
#170423=CARTESIAN_POINT('Ctrl Pts',(-135.634653661497,-2.40007340440478,
136.212463632115));
#170424=CARTESIAN_POINT('Ctrl Pts',(-135.627253578982,-2.54410833813682,
136.148542066119));
#170425=CARTESIAN_POINT('Ctrl Pts',(-135.619853496467,-2.68552815272177,
136.078888883061));
#170426=CARTESIAN_POINT('Ctrl Pts',(-135.612453413952,-2.82385761540701,
136.003760460856));
#170427=CARTESIAN_POINT('Ctrl Pts',(-135.605045194286,-2.96233918555689,
135.928549427228));
#170428=CARTESIAN_POINT('Ctrl Pts',(-135.597636974619,-3.09772328921889,
135.847851309213));
#170429=CARTESIAN_POINT('Ctrl Pts',(-135.590228754953,-3.22956144063075,
135.761967244124));
#170430=CARTESIAN_POINT('Ctrl Pts',(-135.582815975651,-3.36148073622497,
135.676030318825));
#170431=CARTESIAN_POINT('Ctrl Pts',(-135.575403196349,-3.48984942702584,
135.584901301852));
#170432=CARTESIAN_POINT('Ctrl Pts',(-135.567990417047,-3.61425104560988,
135.488922490549));
#170433=CARTESIAN_POINT('Ctrl Pts',(-135.560567046018,-3.73883041506059,
135.39280654022));
#170434=CARTESIAN_POINT('Ctrl Pts',(-135.553143674989,-3.85943110589282,
135.291827194583));
#170435=CARTESIAN_POINT('Ctrl Pts',(-135.54572030396,-3.97567191937431,
135.186365107751));
#170436=CARTESIAN_POINT('Ctrl Pts',(-135.54178425452,-4.03730558784453,
135.130446578782));
#170437=CARTESIAN_POINT('Ctrl Pts',(-135.537848205079,-4.09771417967086,
135.07326838014));
#170438=CARTESIAN_POINT('Ctrl Pts',(-135.533912155638,-4.15684545245782,
135.014891041026));
#170439=CARTESIAN_POINT('Ctrl Pts',(-135.526593680781,-4.26679090401356,
134.906347412467));
#170440=CARTESIAN_POINT('Ctrl Pts',(-135.519275205925,-4.37267110236618,
134.793307590097));
#170441=CARTESIAN_POINT('Ctrl Pts',(-135.511956731068,-4.47408803446405,
134.676113040225));
#170442=CARTESIAN_POINT('Ctrl Pts',(-135.504647058547,-4.57538298679652,
134.559059446733));
#170443=CARTESIAN_POINT('Ctrl Pts',(-135.497337386025,-4.67222510440882,
134.437861356091));
#170444=CARTESIAN_POINT('Ctrl Pts',(-135.490027713504,-4.76425133291557,
134.312898746091));
#170445=CARTESIAN_POINT('Ctrl Pts',(-135.482667191783,-4.85691773511574,
134.18706684288));
#170446=CARTESIAN_POINT('Ctrl Pts',(-135.475306670063,-4.94470068521811,
134.057418097223));
#170447=CARTESIAN_POINT('Ctrl Pts',(-135.467946148342,-5.02726830169465,
133.924377281829));
#170448=CARTESIAN_POINT('Ctrl Pts',(-135.460649442483,-5.10912005538388,
133.792489932805));
#170449=CARTESIAN_POINT('Ctrl Pts',(-135.453352736624,-5.18584633495802,
133.657269427338));
#170450=CARTESIAN_POINT('Ctrl Pts',(-135.446056030765,-5.2571654720375,
133.519161118914));
#170451=CARTESIAN_POINT('Ctrl Pts',(-135.438762445043,-5.32845411241422,
133.381111866841));
#170452=CARTESIAN_POINT('Ctrl Pts',(-135.43146885932,-5.3943400341916,133.240177609734));
#170453=CARTESIAN_POINT('Ctrl Pts',(-135.424175273598,-5.45458667183857,
133.096829767173));
#170454=CARTESIAN_POINT('Ctrl Pts',(-135.416883271381,-5.51482022938264,
132.953513046757));
#170455=CARTESIAN_POINT('Ctrl Pts',(-135.409591269164,-5.56941679093975,
132.807784138428));
#170456=CARTESIAN_POINT('Ctrl Pts',(-135.402299266947,-5.61818737844745,
132.660135696382));
#170457=CARTESIAN_POINT('Ctrl Pts',(-135.394888927385,-5.66774943332515,
132.510091160089));
#170458=CARTESIAN_POINT('Ctrl Pts',(-135.387478587823,-5.71129462244642,
132.358064624372));
#170459=CARTESIAN_POINT('Ctrl Pts',(-135.380068248262,-5.74867703636407,
132.20459020377));
#170460=CARTESIAN_POINT('Ctrl Pts',(-135.372772483496,-5.78548146294015,
132.053488724427));
#170461=CARTESIAN_POINT('Ctrl Pts',(-135.365476718731,-5.81631227136727,
131.900984201993));
#170462=CARTESIAN_POINT('Ctrl Pts',(-135.358180953966,-5.84108172357949,
131.747596993543));
#170463=CARTESIAN_POINT('Ctrl Pts',(-135.350713327006,-5.8664346557357,
131.590596529578));
#170464=CARTESIAN_POINT('Ctrl Pts',(-135.343245700046,-5.88543705467267,
131.432671700418));
#170465=CARTESIAN_POINT('Ctrl Pts',(-135.335778073086,-5.89805111906382,
131.2743856801));
#170466=CARTESIAN_POINT('Ctrl Pts',(-135.328310446126,-5.91066518345497,
131.116099659782));
#170467=CARTESIAN_POINT('Ctrl Pts',(-135.320842819166,-5.91689093509487,
130.957452878542));
#170468=CARTESIAN_POINT('Ctrl Pts',(-135.313375192206,-5.91674757824783,
130.799007319666));
#170469=CARTESIAN_POINT('',(-133.563375192206,-5.92503606369206,130.807060657761));
#170470=CARTESIAN_POINT('Ctrl Pts',(-135.313375192206,-5.91823652768249,
130.799005972509));
#170471=CARTESIAN_POINT('Ctrl Pts',(-135.294071638746,-5.92204404516267,
130.389322916598));
#170472=CARTESIAN_POINT('Ctrl Pts',(-135.274768085285,-5.88314771307888,
129.980358143981));
#170473=CARTESIAN_POINT('Ctrl Pts',(-135.16264865722,-5.39374310559234,
127.660585609891));
#170474=CARTESIAN_POINT('Ctrl Pts',(-134.977016908012,-2.48589836884803,
124.262352529057));
#170475=CARTESIAN_POINT('Ctrl Pts',(-134.698569284199,4.16028789435366,
125.176788746284));
#170476=CARTESIAN_POINT('Ctrl Pts',(-134.420121660386,6.9833728240057,131.262688591048));
#170477=CARTESIAN_POINT('Ctrl Pts',(-134.141674036573,3.38907928512634,
136.927407418748));
#170478=CARTESIAN_POINT('Ctrl Pts',(-133.86322641276,-3.31961255106015,
136.965345363627));
#170479=CARTESIAN_POINT('Ctrl Pts',(-133.670460131305,-5.8520964766113,
133.072114422921));
#170480=CARTESIAN_POINT('Ctrl Pts',(-133.570509724453,-5.9258914963796,
130.95802645762));
#170481=CARTESIAN_POINT('Ctrl Pts',(-133.563375192206,-5.92503606369206,
130.807060657761));
#170482=CARTESIAN_POINT('',(-131.813375192206,-5.90991206338681,130.808405239875));
#170483=CARTESIAN_POINT('Ctrl Pts',(-133.563375192206,-5.92503606369206,
130.807060657761));
#170484=CARTESIAN_POINT('Ctrl Pts',(-133.477693849849,-5.91476284346878,
128.994054291817));
#170485=CARTESIAN_POINT('Ctrl Pts',(-133.299196632889,-4.0536518896767,
125.19884575645));
#170486=CARTESIAN_POINT('Ctrl Pts',(-133.027883541321,2.41175106234068,
124.234656107945));
#170487=CARTESIAN_POINT('Ctrl Pts',(-132.749435917509,6.83088882713039,
129.282349329258));
#170488=CARTESIAN_POINT('Ctrl Pts',(-132.470988293696,4.97277346725347,
135.728696570128));
#170489=CARTESIAN_POINT('Ctrl Pts',(-132.192540669883,-1.45507777553816,
137.649819637784));
#170490=CARTESIAN_POINT('Ctrl Pts',(-131.97333630272,-5.46267151731689,
134.20997083825));
#170491=CARTESIAN_POINT('Ctrl Pts',(-131.846947810161,-5.91438909886242,
131.523472343736));
#170492=CARTESIAN_POINT('Ctrl Pts',(-131.813375192206,-5.90991206338681,
130.808405239875));
#170493=CARTESIAN_POINT('',(-130.063375158615,-5.91342694435326,130.800133359548));
#170494=CARTESIAN_POINT('Ctrl Pts',(-131.813375192206,-5.90991206338681,
130.808405239875));
#170495=CARTESIAN_POINT('Ctrl Pts',(-131.754131935556,-5.90201175123154,
129.546576209652));
#170496=CARTESIAN_POINT('Ctrl Pts',(-131.602072804305,-4.88693589981136,
126.296249162835));
#170497=CARTESIAN_POINT('Ctrl Pts',(-131.357197798442,0.468954947398858,
123.821693377335));
#170498=CARTESIAN_POINT('Ctrl Pts',(-131.078750174631,6.12819731254553,
127.424603491846));
#170499=CARTESIAN_POINT('Ctrl Pts',(-130.800302550819,6.15592572653701,
134.133345294561));
#170500=CARTESIAN_POINT('Ctrl Pts',(-130.521854927006,0.52665913153656,
137.782912809069));
#170501=CARTESIAN_POINT('Ctrl Pts',(-130.276212474135,-4.86635301707174,
135.345098168375));
#170502=CARTESIAN_POINT('Ctrl Pts',(-130.123385895868,-5.90187158747846,
132.078122015566));
#170503=CARTESIAN_POINT('Ctrl Pts',(-130.063375192206,-5.91026073634778,
130.800136338677));
#170504=CARTESIAN_POINT('',(-128.313375192206,-5.92111332573527,130.80192758));
#170505=CARTESIAN_POINT('Ctrl Pts',(-130.063375123377,-5.916748487671,130.800130234262));
#170506=CARTESIAN_POINT('Ctrl Pts',(-130.054904464835,-5.91661937012662,
130.619542334627));
#170507=CARTESIAN_POINT('Ctrl Pts',(-130.046433806292,-5.90821859595855,
130.43928493431));
#170508=CARTESIAN_POINT('Ctrl Pts',(-130.03796314775,-5.89166059700865,
130.260057418829));
#170509=CARTESIAN_POINT('Ctrl Pts',(-130.029453540339,-5.87502646285285,
130.080005798705));
#170510=CARTESIAN_POINT('Ctrl Pts',(-130.020943932927,-5.8501600223074,
129.900993696451));
#170511=CARTESIAN_POINT('Ctrl Pts',(-130.012434325516,-5.81722686199573,
129.723711646542));
#170512=CARTESIAN_POINT('Ctrl Pts',(-130.003872284472,-5.78409077749085,
129.545337238152));
#170513=CARTESIAN_POINT('Ctrl Pts',(-129.995310243429,-5.742788341951,129.368714407466));
#170514=CARTESIAN_POINT('Ctrl Pts',(-129.986748202385,-5.69353686693738,
129.194525685865));
#170515=CARTESIAN_POINT('Ctrl Pts',(-129.979485361383,-5.65175878735304,
129.046768278159));
#170516=CARTESIAN_POINT('Ctrl Pts',(-129.972222520382,-5.60426186830998,
128.900762007714));
#170517=CARTESIAN_POINT('Ctrl Pts',(-129.96495967938,-5.55120523506474,
128.756910740111));
#170518=CARTESIAN_POINT('Ctrl Pts',(-129.957536412975,-5.49697665935459,
128.609882011014));
#170519=CARTESIAN_POINT('Ctrl Pts',(-129.950113146569,-5.43682076436011,
128.464786885468));
#170520=CARTESIAN_POINT('Ctrl Pts',(-129.942689880164,-5.37089437471072,
128.322138996074));
#170521=CARTESIAN_POINT('Ctrl Pts',(-129.935275387444,-5.30504590457888,
128.179659704639));
#170522=CARTESIAN_POINT('Ctrl Pts',(-129.927860894723,-5.23344067060665,
128.039622227509));
#170523=CARTESIAN_POINT('Ctrl Pts',(-129.920446402002,-5.15628477651301,
127.902523636273));
#170524=CARTESIAN_POINT('Ctrl Pts',(-129.913039055649,-5.07920324817518,
127.765557185821));
#170525=CARTESIAN_POINT('Ctrl Pts',(-129.905631709295,-4.99658189223649,
127.63152430523));
#170526=CARTESIAN_POINT('Ctrl Pts',(-129.898224362942,-4.90867421668623,
127.500900613731));
#170527=CARTESIAN_POINT('Ctrl Pts',(-129.890822541267,-4.82083210599671,
127.370374346308));
#170528=CARTESIAN_POINT('Ctrl Pts',(-129.883420719591,-4.72771173374014,
127.243252513477));
#170529=CARTESIAN_POINT('Ctrl Pts',(-129.876018897916,-4.62961164510019,
127.119984608246));
#170530=CARTESIAN_POINT('Ctrl Pts',(-129.868620983605,-4.5315633427337,
126.996781775183));
#170531=CARTESIAN_POINT('Ctrl Pts',(-129.861223069294,-4.42854079113761,
126.877429109349));
#170532=CARTESIAN_POINT('Ctrl Pts',(-129.853825154983,-4.32088473858091,
126.762345570786));
#170533=CARTESIAN_POINT('Ctrl Pts',(-129.846428470071,-4.21324657650723,
126.647281157019));
#170534=CARTESIAN_POINT('Ctrl Pts',(-129.839031785159,-4.10097669647058,
126.536484734818));
#170535=CARTESIAN_POINT('Ctrl Pts',(-129.831635100247,-3.98445494539054,
126.430340801578));
#170536=CARTESIAN_POINT('Ctrl Pts',(-129.824238743312,-3.86793836100704,
126.324201574872));
#170537=CARTESIAN_POINT('Ctrl Pts',(-129.816842386377,-3.74717055641044,
126.222714678327));
#170538=CARTESIAN_POINT('Ctrl Pts',(-129.809446029442,-3.62256671758438,
126.126226273712));
#170539=CARTESIAN_POINT('Ctrl Pts',(-129.802048540105,-3.49794380159249,
126.029723096475));
#170540=CARTESIAN_POINT('Ctrl Pts',(-129.794651050769,-3.369483977136,125.938220163515));
#170541=CARTESIAN_POINT('Ctrl Pts',(-129.787253561433,-3.23763371260702,
125.852021927059));
#170542=CARTESIAN_POINT('Ctrl Pts',(-129.779853478918,-3.10573722817201,
125.765793473945));
#170543=CARTESIAN_POINT('Ctrl Pts',(-129.772453396403,-2.97044824959946,
125.684873623831));
#170544=CARTESIAN_POINT('Ctrl Pts',(-129.765053313888,-2.83224014276189,
125.609522185408));
#170545=CARTESIAN_POINT('Ctrl Pts',(-129.757645094222,-2.69388006190291,
125.534087890332));
#170546=CARTESIAN_POINT('Ctrl Pts',(-129.750236874556,-2.55259477038696,
125.464234413861));
#170547=CARTESIAN_POINT('Ctrl Pts',(-129.742828654889,-2.40888069179691,
125.400174797742));
#170548=CARTESIAN_POINT('Ctrl Pts',(-129.735415875588,-2.26507815958949,
125.336075753998));
#170549=CARTESIAN_POINT('Ctrl Pts',(-129.728003096286,-2.11884420753047,
125.277777814274));
#170550=CARTESIAN_POINT('Ctrl Pts',(-129.720590316984,-1.97069243182606,
125.225444781882));
#170551=CARTESIAN_POINT('Ctrl Pts',(-129.713166945956,-1.82232896991667,
125.173036973599));
#170552=CARTESIAN_POINT('Ctrl Pts',(-129.705743574927,-1.67204256713796,
125.126611204757));
#170553=CARTESIAN_POINT('Ctrl Pts',(-129.698320203899,-1.52035987326319,
125.086280833384));
#170554=CARTESIAN_POINT('Ctrl Pts',(-129.694384154454,-1.43993406932512,
125.06489670275));
#170555=CARTESIAN_POINT('Ctrl Pts',(-129.69044810501,-1.35911586474888,
125.045225348288));
#170556=CARTESIAN_POINT('Ctrl Pts',(-129.686512055566,-1.27798445658614,
125.027277764497));
#170557=CARTESIAN_POINT('Ctrl Pts',(-129.679088789161,-1.12497315294235,
124.99342918162));
#170558=CARTESIAN_POINT('Ctrl Pts',(-129.671665522755,-0.970384783872578,
124.965612580278));
#170559=CARTESIAN_POINT('Ctrl Pts',(-129.66424225635,-0.81473625057424,
124.943973650437));
#170560=CARTESIAN_POINT('Ctrl Pts',(-129.656827763629,-0.659271680916454,
124.922360296013));
#170561=CARTESIAN_POINT('Ctrl Pts',(-129.649413270908,-0.502749807316699,
124.906910130325));
#170562=CARTESIAN_POINT('Ctrl Pts',(-129.641998778187,-0.345700234274841,
124.897718431813));
#170563=CARTESIAN_POINT('Ctrl Pts',(-129.634591431833,-0.188802031523845,
124.888535592605));
#170564=CARTESIAN_POINT('Ctrl Pts',(-129.627184085479,-0.0313775120446858,
124.885599233421));
#170565=CARTESIAN_POINT('Ctrl Pts',(-129.619776739126,0.126036144974603,
124.888953154621));
#170566=CARTESIAN_POINT('Ctrl Pts',(-129.61237491745,0.283332396949609,
124.892304574341));
#170567=CARTESIAN_POINT('Ctrl Pts',(-129.604973095775,0.440617430989262,
124.90193692506));
#170568=CARTESIAN_POINT('Ctrl Pts',(-129.597571274099,0.597351704931872,
124.91784199421));
#170569=CARTESIAN_POINT('Ctrl Pts',(-129.590173359788,0.754003240070838,
124.933738667199));
#170570=CARTESIAN_POINT('Ctrl Pts',(-129.582775445477,0.910104223688883,
124.955901426375));
#170571=CARTESIAN_POINT('Ctrl Pts',(-129.575377531165,1.06511799007414,
124.984270048707));
#170572=CARTESIAN_POINT('Ctrl Pts',(-129.567980846253,1.22010599598387,
125.012633956689));
#170573=CARTESIAN_POINT('Ctrl Pts',(-129.560584161341,1.37400677640881,
125.047201613863));
#170574=CARTESIAN_POINT('Ctrl Pts',(-129.553187476429,1.5262915262612,125.087861274492));
#170575=CARTESIAN_POINT('Ctrl Pts',(-129.545791119493,1.6785695236482,125.12851913223));
#170576=CARTESIAN_POINT('Ctrl Pts',(-129.538394762558,1.82923127227653,
125.175268360025));
#170577=CARTESIAN_POINT('Ctrl Pts',(-129.530998405623,1.97776111828071,
125.227946759044));
#170578=CARTESIAN_POINT('Ctrl Pts',(-129.523600916286,2.1263137045835,125.28063322326));
#170579=CARTESIAN_POINT('Ctrl Pts',(-129.51620342695,2.27273338650872,125.339250541403));
#170580=CARTESIAN_POINT('Ctrl Pts',(-129.508805937613,2.41652269270348,
125.403587650837));
#170581=CARTESIAN_POINT('Ctrl Pts',(-129.501405855098,2.56036240401683,
125.467947313545));
#170582=CARTESIAN_POINT('Ctrl Pts',(-129.494005772583,2.7015695632254,125.538030607243));
#170583=CARTESIAN_POINT('Ctrl Pts',(-129.486605690068,2.83966972010401,
125.61357970876));
#170584=CARTESIAN_POINT('Ctrl Pts',(-129.479197470402,2.97792173230195,
125.68921188428));
#170585=CARTESIAN_POINT('Ctrl Pts',(-129.471789250735,3.11305959156186,
125.770321691148));
#170586=CARTESIAN_POINT('Ctrl Pts',(-129.464381031069,3.24463573075725,
125.856606628412));
#170587=CARTESIAN_POINT('Ctrl Pts',(-129.456968251767,3.37629285287084,
125.942944672614));
#170588=CARTESIAN_POINT('Ctrl Pts',(-129.449555472465,3.50438358369619,
126.034463977622));
#170589=CARTESIAN_POINT('Ctrl Pts',(-129.442142693163,3.62849249957423,
126.130820980093));
#170590=CARTESIAN_POINT('Ctrl Pts',(-129.434719322134,3.75277874809159,
126.227315661967));
#170591=CARTESIAN_POINT('Ctrl Pts',(-129.427295951105,3.87307153391706,
126.328661606893));
#170592=CARTESIAN_POINT('Ctrl Pts',(-129.419872580076,3.98899081866422,
126.434477002284));
#170593=CARTESIAN_POINT('Ctrl Pts',(-129.415936530635,4.05045400488321,
126.490582863926));
#170594=CARTESIAN_POINT('Ctrl Pts',(-129.412000481195,4.11068828613165,
126.547944660695));
#170595=CARTESIAN_POINT('Ctrl Pts',(-129.408064431754,4.16964160448611,
126.606501704663));
#170596=CARTESIAN_POINT('Ctrl Pts',(-129.400641165348,4.28082572303124,
126.716938462082));
#170597=CARTESIAN_POINT('Ctrl Pts',(-129.393217898943,4.38778740706093,
126.831962482668));
#170598=CARTESIAN_POINT('Ctrl Pts',(-129.385794632537,4.49012468575821,
126.951217631789));
#170599=CARTESIAN_POINT('Ctrl Pts',(-129.378380139816,4.59234101029095,
127.070331831227));
#170600=CARTESIAN_POINT('Ctrl Pts',(-129.370965647095,4.68994356819628,
127.193666924472));
#170601=CARTESIAN_POINT('Ctrl Pts',(-129.363551154374,4.78256593485623,
127.320828840583));
#170602=CARTESIAN_POINT('Ctrl Pts',(-129.35614380802,4.87509902859202,127.447868193251));
#170603=CARTESIAN_POINT('Ctrl Pts',(-129.348736461667,4.96266126882164,
127.578726726121));
#170604=CARTESIAN_POINT('Ctrl Pts',(-129.341329115313,5.04492544658949,
127.712976170291));
#170605=CARTESIAN_POINT('Ctrl Pts',(-129.333927293637,5.12712826862991,
127.847125486161));
#170606=CARTESIAN_POINT('Ctrl Pts',(-129.326525471962,5.20404070196677,
127.98466036069));
#170607=CARTESIAN_POINT('Ctrl Pts',(-129.319123650286,5.27537802034888,
128.125122422683));
#170608=CARTESIAN_POINT('Ctrl Pts',(-129.311725735975,5.34667768031591,
128.265510335847));
#170609=CARTESIAN_POINT('Ctrl Pts',(-129.304327821663,5.41240791796292,
128.408822027066));
#170610=CARTESIAN_POINT('Ctrl Pts',(-129.296929907352,5.47232931970685,
128.554573432258));
#170611=CARTESIAN_POINT('Ctrl Pts',(-129.28953322244,5.53224076360098,128.700300616211));
#170612=CARTESIAN_POINT('Ctrl Pts',(-129.282136537528,5.58634514566882,
128.848466364544));
#170613=CARTESIAN_POINT('Ctrl Pts',(-129.274739852615,5.63445064869656,
128.998565377262));
#170614=CARTESIAN_POINT('Ctrl Pts',(-129.26734349568,5.68255401867576,129.148657734433));
#170615=CARTESIAN_POINT('Ctrl Pts',(-129.259947138744,5.72465892457534,
129.300682830054));
#170616=CARTESIAN_POINT('Ctrl Pts',(-129.252550781809,5.76062310535929,
129.454119157493));
#170617=CARTESIAN_POINT('Ctrl Pts',(-129.245153292472,5.79659279235124,
129.607578976426));
#170618=CARTESIAN_POINT('Ctrl Pts',(-129.237755803135,5.82641979704802,
129.762450093916));
#170619=CARTESIAN_POINT('Ctrl Pts',(-129.230358313799,5.85001279700647,
129.918199888713));
#170620=CARTESIAN_POINT('Ctrl Pts',(-129.222958231284,5.87361406745445,
130.07400428136));
#170621=CARTESIAN_POINT('Ctrl Pts',(-129.215558148769,5.89097692633214,
130.230687595721));
#170622=CARTESIAN_POINT('Ctrl Pts',(-129.208158066254,5.90206183564049,
130.387711303663));
#170623=CARTESIAN_POINT('Ctrl Pts',(-129.200749846587,5.9131589339462,130.544907675314));
#170624=CARTESIAN_POINT('Ctrl Pts',(-129.193341626921,5.91796427013394,
130.702444815443));
#170625=CARTESIAN_POINT('Ctrl Pts',(-129.185933407254,5.91649042585801,
130.859782663996));
#170626=CARTESIAN_POINT('Ctrl Pts',(-129.178520627952,5.91501567445552,
131.01721735137));
#170627=CARTESIAN_POINT('Ctrl Pts',(-129.17110784865,5.90725405999082,131.174452130773));
#170628=CARTESIAN_POINT('Ctrl Pts',(-129.163695069348,5.89327008540014,
131.330951790135));
#170629=CARTESIAN_POINT('Ctrl Pts',(-129.156271698319,5.87926612985076,
131.48767506355));
#170630=CARTESIAN_POINT('Ctrl Pts',(-129.14884832729,5.85902210517054,131.643660749879));
#170631=CARTESIAN_POINT('Ctrl Pts',(-129.141424956261,5.83265382107117,
131.798382733036));
#170632=CARTESIAN_POINT('Ctrl Pts',(-129.137488906821,5.81867272414561,
131.880420040996));
#170633=CARTESIAN_POINT('Ctrl Pts',(-129.133552857381,5.80297072027464,
131.962102300013));
#170634=CARTESIAN_POINT('Ctrl Pts',(-129.129616807941,5.7855707293513,132.043352908976));
#170635=CARTESIAN_POINT('Ctrl Pts',(-129.122193541535,5.75275488950022,
132.196589021757));
#170636=CARTESIAN_POINT('Ctrl Pts',(-129.11477027513,5.7137973262347,132.348752208587));
#170637=CARTESIAN_POINT('Ctrl Pts',(-129.107347008724,5.66878039066167,
132.499311780564));
#170638=CARTESIAN_POINT('Ctrl Pts',(-129.099932516003,5.62381666136794,
132.649693403632));
#170639=CARTESIAN_POINT('Ctrl Pts',(-129.092518023282,5.57280792101309,
132.79847483037));
#170640=CARTESIAN_POINT('Ctrl Pts',(-129.085103530561,5.51588765118415,
132.945134772402));
#170641=CARTESIAN_POINT('Ctrl Pts',(-129.077696184208,5.45902224325428,
133.09165335806));
#170642=CARTESIAN_POINT('Ctrl Pts',(-129.070288837854,5.39625678311652,
133.236054184069));
#170643=CARTESIAN_POINT('Ctrl Pts',(-129.0628814915,5.32777472109283,133.377830470466));
#170644=CARTESIAN_POINT('Ctrl Pts',(-129.055479669825,5.25934373557468,
133.519501014759));
#170645=CARTESIAN_POINT('Ctrl Pts',(-129.048077848149,5.1852047993536,133.658550582357));
#170646=CARTESIAN_POINT('Ctrl Pts',(-129.040676026474,5.1055896516041,133.794491864173));
#170647=CARTESIAN_POINT('Ctrl Pts',(-129.033278112163,5.02601653207136,
133.930361383644));
#170648=CARTESIAN_POINT('Ctrl Pts',(-129.025880197851,4.94097314645032,
134.063125563839));
#170649=CARTESIAN_POINT('Ctrl Pts',(-129.01848228354,4.85073734267355,134.19232133087));
#170650=CARTESIAN_POINT('Ctrl Pts',(-129.011085598628,4.76051653445046,
134.321495627908));
#170651=CARTESIAN_POINT('Ctrl Pts',(-129.003688913716,4.66510523418736,
134.447102382981));
#170652=CARTESIAN_POINT('Ctrl Pts',(-128.996292228803,4.56482488319306,
134.568707087842));
#170653=CARTESIAN_POINT('Ctrl Pts',(-128.988895871868,4.46454897873461,
134.690306400624));
#170654=CARTESIAN_POINT('Ctrl Pts',(-128.981499514933,4.3594046903236,134.807903728032));
#170655=CARTESIAN_POINT('Ctrl Pts',(-128.974103157997,4.24975388069575,
134.921097494755));
#170656=CARTESIAN_POINT('Ctrl Pts',(-128.966705668661,4.14008628324903,
135.034308591733));
#170657=CARTESIAN_POINT('Ctrl Pts',(-128.959308179324,4.02591105053221,
135.14311451747));
#170658=CARTESIAN_POINT('Ctrl Pts',(-128.951910689988,3.90762692987578,
135.247150545011));
#170659=CARTESIAN_POINT('Ctrl Pts',(-128.944510607473,3.78930134490406,
135.351223042221));
#170660=CARTESIAN_POINT('Ctrl Pts',(-128.937110524958,3.66686428436636,
135.450522065752));
#170661=CARTESIAN_POINT('Ctrl Pts',(-128.929710442443,3.54074745597937,
135.544723263554));
#170662=CARTESIAN_POINT('Ctrl Pts',(-128.922302222776,3.41449194917462,
135.639028045257));
#170663=CARTESIAN_POINT('Ctrl Pts',(-128.91489400311,3.28454889308884,135.728223582984));
#170664=CARTESIAN_POINT('Ctrl Pts',(-128.907485783443,3.15137945623144,
135.812028546387));
#170665=CARTESIAN_POINT('Ctrl Pts',(-128.900073004141,3.01812805580732,
135.895885090347));
#170666=CARTESIAN_POINT('Ctrl Pts',(-128.892660224839,2.88164664057096,
135.974344263218));
#170667=CARTESIAN_POINT('Ctrl Pts',(-128.885247445537,2.74242036500662,
136.047171037951));
#170668=CARTESIAN_POINT('Ctrl Pts',(-128.877824074509,2.60299515641088,
136.120101870995));
#170669=CARTESIAN_POINT('Ctrl Pts',(-128.87040070348,2.46081759093237,136.187384073314));
#170670=CARTESIAN_POINT('Ctrl Pts',(-128.862977332451,2.31639290291346,
136.248830700304));
#170671=CARTESIAN_POINT('Ctrl Pts',(-128.85904128301,2.23981546789787,136.281411176328));
#170672=CARTESIAN_POINT('Ctrl Pts',(-128.855105233569,2.16260655337318,
136.312351891974));
#170673=CARTESIAN_POINT('Ctrl Pts',(-128.851169184128,2.0848429947869,136.341630725624));
#170674=CARTESIAN_POINT('Ctrl Pts',(-128.843745917723,1.93818335021957,
136.396849692123));
#170675=CARTESIAN_POINT('Ctrl Pts',(-128.836322651317,1.78910663711666,
136.446321510086));
#170676=CARTESIAN_POINT('Ctrl Pts',(-128.828899384912,1.63810385186479,
136.489828613519));
#170677=CARTESIAN_POINT('Ctrl Pts',(-128.821484892191,1.48727953936466,
136.533284295169));
#170678=CARTESIAN_POINT('Ctrl Pts',(-128.81407039947,1.33453404121955,136.570789192606));
#170679=CARTESIAN_POINT('Ctrl Pts',(-128.806655906749,1.18037808216392,
136.60217383857));
#170680=CARTESIAN_POINT('Ctrl Pts',(-128.799248560395,1.02637070442594,
136.63352823483));
#170681=CARTESIAN_POINT('Ctrl Pts',(-128.791841214041,0.870955935523697,
136.65877404925));
#170682=CARTESIAN_POINT('Ctrl Pts',(-128.784433867687,0.71465930317291,
136.677791696832));
#170683=CARTESIAN_POINT('Ctrl Pts',(-128.777032046012,0.558479242747264,
136.696795160335));
#170684=CARTESIAN_POINT('Ctrl Pts',(-128.769630224336,0.40141899746631,
136.709579661329));
#170685=CARTESIAN_POINT('Ctrl Pts',(-128.762228402661,0.244013814949968,
136.716076766081));
#170686=CARTESIAN_POINT('Ctrl Pts',(-128.75483048835,0.0866917254037876,
136.722570441062));
#170687=CARTESIAN_POINT('Ctrl Pts',(-128.747432574038,-0.0709745667012892,
136.722783314525));
#170688=CARTESIAN_POINT('Ctrl Pts',(-128.740034659727,-0.228445280593447,
136.716698845059));
#170689=CARTESIAN_POINT('Ctrl Pts',(-128.732637974815,-0.385889825709542,
136.710615386721));
#170690=CARTESIAN_POINT('Ctrl Pts',(-128.725241289902,-0.543138484464353,
136.698236676853));
#170691=CARTESIAN_POINT('Ctrl Pts',(-128.71784460499,-0.699651945885949,
136.679598290811));
#170692=CARTESIAN_POINT('Ctrl Pts',(-128.710448248055,-0.856158467336651,
136.660960731215));
#170693=CARTESIAN_POINT('Ctrl Pts',(-128.703051891119,-1.01192948559431,
136.636064091472));
#170694=CARTESIAN_POINT('Ctrl Pts',(-128.695655534184,-1.16643154832761,
136.604995755684));
#170695=CARTESIAN_POINT('Ctrl Pts',(-128.688258044847,-1.32095726572113,
136.573922663254));
#170696=CARTESIAN_POINT('Ctrl Pts',(-128.68086055551,-1.47421327475679,
136.536676066951));
#170697=CARTESIAN_POINT('Ctrl Pts',(-128.673463066174,-1.62567718764724,
136.493394300369));
#170698=CARTESIAN_POINT('Ctrl Pts',(-128.666062983659,-1.77719419597778,
136.45009736143));
#170699=CARTESIAN_POINT('Ctrl Pts',(-128.658662901144,-1.92691749868164,
136.400761142532));
#170700=CARTESIAN_POINT('Ctrl Pts',(-128.651262818629,-2.07434086062793,
136.345573531399));
#170701=CARTESIAN_POINT('Ctrl Pts',(-128.643854598962,-2.22192632971596,
136.290325235814));
#170702=CARTESIAN_POINT('Ctrl Pts',(-128.636446379296,-2.3672064576057,
136.229212829412));
#170703=CARTESIAN_POINT('Ctrl Pts',(-128.629038159629,-2.5096952802634,
136.162472240398));
#170704=CARTESIAN_POINT('Ctrl Pts',(-128.621625380327,-2.65227180241389,
136.095690573664));
#170705=CARTESIAN_POINT('Ctrl Pts',(-128.614212601025,-2.79205326530924,
136.023273993078));
#170706=CARTESIAN_POINT('Ctrl Pts',(-128.606799821723,-2.92857969618707,
135.945503634987));
#170707=CARTESIAN_POINT('Ctrl Pts',(-128.599376450694,-3.06530120243159,
135.867622154962));
#170708=CARTESIAN_POINT('Ctrl Pts',(-128.591953079665,-3.19875807179573,
135.784371816258));
#170709=CARTESIAN_POINT('Ctrl Pts',(-128.584529708637,-3.32851993098497,
135.696076638712));
#170710=CARTESIAN_POINT('Ctrl Pts',(-128.580593659196,-3.3973227823126,
135.649260416968));
#170711=CARTESIAN_POINT('Ctrl Pts',(-128.576657609756,-3.46508738689326,
135.601026583092));
#170712=CARTESIAN_POINT('Ctrl Pts',(-128.572721560316,-3.53175360174764,
135.551427823646));
#170713=CARTESIAN_POINT('Ctrl Pts',(-128.565370856845,-3.65625497916728,
135.458800487854));
#170714=CARTESIAN_POINT('Ctrl Pts',(-128.558020153374,-3.77731613250596,
135.361118238744));
#170715=CARTESIAN_POINT('Ctrl Pts',(-128.550669449903,-3.89449339699107,
135.258667717811));
#170716=CARTESIAN_POINT('Ctrl Pts',(-128.543327467855,-4.01153163363528,
135.156338751813));
#170717=CARTESIAN_POINT('Ctrl Pts',(-128.535985485806,-4.12469486664513,
135.049253019551));
#170718=CARTESIAN_POINT('Ctrl Pts',(-128.528643503758,-4.23356883529318,
134.937740043573));
#170719=CARTESIAN_POINT('Ctrl Pts',(-128.521308553125,-4.34233853535686,
134.826333863555));
#170720=CARTESIAN_POINT('Ctrl Pts',(-128.513973602492,-4.44682688166327,
134.710509148898));
#170721=CARTESIAN_POINT('Ctrl Pts',(-128.506638651858,-4.54665329278074,
134.590635092264));
#170722=CARTESIAN_POINT('Ctrl Pts',(-128.499309049148,-4.64640692032246,
134.470848435971));
#170723=CARTESIAN_POINT('Ctrl Pts',(-128.491979446438,-4.7415051355231,
134.347018606272));
#170724=CARTESIAN_POINT('Ctrl Pts',(-128.484649843727,-4.83160495263324,
134.219550823717));
#170725=CARTESIAN_POINT('Ctrl Pts',(-128.477323379202,-4.92166619330557,
134.092137616778));
#170726=CARTESIAN_POINT('Ctrl Pts',(-128.469996914678,-5.00673307380124,
133.961089866465));
#170727=CARTESIAN_POINT('Ctrl Pts',(-128.462670450153,-5.08650365374587,
133.826844884346));
#170728=CARTESIAN_POINT('Ctrl Pts',(-128.455345514147,-5.16625759116744,
133.692627909735));
#170729=CARTESIAN_POINT('Ctrl Pts',(-128.448020578142,-5.24071723147476,
133.555215357894));
#170730=CARTESIAN_POINT('Ctrl Pts',(-128.440695642136,-5.30962478121342,
133.415072253351));
#170731=CARTESIAN_POINT('Ctrl Pts',(-128.433370718813,-5.37853221164376,
133.274929391456));
#170732=CARTESIAN_POINT('Ctrl Pts',(-128.42604579549,-5.441887402354,133.132056328493));
#170733=CARTESIAN_POINT('Ctrl Pts',(-128.418720872167,-5.49947933825294,
132.986941101908));
#170734=CARTESIAN_POINT('Ctrl Pts',(-128.411394445916,-5.55708309087056,
132.841796100567));
#170735=CARTESIAN_POINT('Ctrl Pts',(-128.404068019664,-5.60892109517581,
132.69440837462));
#170736=CARTESIAN_POINT('Ctrl Pts',(-128.396741593413,-5.65483123213515,
132.545284021559));
#170737=CARTESIAN_POINT('Ctrl Pts',(-128.389408124028,-5.70078550401455,
132.396016310367));
#170738=CARTESIAN_POINT('Ctrl Pts',(-128.382074654642,-5.74080041454549,
132.245009002581));
#170739=CARTESIAN_POINT('Ctrl Pts',(-128.374741185257,-5.77476415054914,
132.092781964809));
#170740=CARTESIAN_POINT('Ctrl Pts',(-128.367404016875,-5.80874501783938,
131.940478143818));
#170741=CARTESIAN_POINT('Ctrl Pts',(-128.360066848492,-5.83666856210573,
131.786953741942));
#170742=CARTESIAN_POINT('Ctrl Pts',(-128.35272968011,-5.85847460091912,
131.632736083696));
#170743=CARTESIAN_POINT('Ctrl Pts',(-128.345382085172,-5.8803116274182,
131.478299272931));
#170744=CARTESIAN_POINT('Ctrl Pts',(-128.338034490234,-5.89601374437728,
131.323167616817));
#170745=CARTESIAN_POINT('Ctrl Pts',(-128.330686895297,-5.90557281670467,
131.167871647796));
#170746=CARTESIAN_POINT('Ctrl Pts',(-128.3249163276,-5.91308020850467,131.045907126086));
#170747=CARTESIAN_POINT('Ctrl Pts',(-128.319145759903,-5.91679959518812,
130.923841335279));
#170748=CARTESIAN_POINT('Ctrl Pts',(-128.313375192206,-5.91674950049016,
130.801929373134));
#170749=CARTESIAN_POINT('',(-126.563375192206,-5.9177375725148,130.809766839768));
#170750=CARTESIAN_POINT('Ctrl Pts',(-128.313375192206,-5.92532190149327,
130.801925850659));
#170751=CARTESIAN_POINT('Ctrl Pts',(-128.307008106971,-5.9260213244518,
130.66721635484));
#170752=CARTESIAN_POINT('Ctrl Pts',(-128.300641021737,-5.92182725011439,
130.532551188858));
#170753=CARTESIAN_POINT('Ctrl Pts',(-128.294273936502,-5.91260101588379,
130.398231675452));
#170754=CARTESIAN_POINT('Ctrl Pts',(-128.201458061898,-5.77810603617641,
128.440195517006));
#170755=CARTESIAN_POINT('Ctrl Pts',(-128.01582631269,-3.37042713891619,
124.671026986366));
#170756=CARTESIAN_POINT('Ctrl Pts',(-127.737378688876,3.3383490931192,124.653508167472));
#170757=CARTESIAN_POINT('Ctrl Pts',(-127.458931065064,6.97934559599797,
130.288322264368));
#170758=CARTESIAN_POINT('Ctrl Pts',(-127.180483441251,4.20666445614103,
136.397350397977));
#170759=CARTESIAN_POINT('Ctrl Pts',(-126.902035817438,-2.43173581192483,
137.366694156127));
#170760=CARTESIAN_POINT('Ctrl Pts',(-126.696333067756,-5.68500213269131,
133.627799485708));
#170761=CARTESIAN_POINT('Ctrl Pts',(-126.583446192679,-5.92170083184643,
131.235829725967));
#170762=CARTESIAN_POINT('Ctrl Pts',(-126.563375192206,-5.9177375725148,
130.809766839768));
#170763=CARTESIAN_POINT('',(-124.813375192206,-5.90693489644606,130.804324882377));
#170764=CARTESIAN_POINT('Ctrl Pts',(-126.563375192206,-5.9177375725148,
130.809766839768));
#170765=CARTESIAN_POINT('Ctrl Pts',(-126.490630318075,-5.90337322622243,
129.265554279451));
#170766=CARTESIAN_POINT('Ctrl Pts',(-126.325069569338,-4.49401215403822,
125.727844952722));
#170767=CARTESIAN_POINT('Ctrl Pts',(-126.066692945999,1.47590625823722,
123.963362061268));
#170768=CARTESIAN_POINT('Ctrl Pts',(-125.788245322187,6.55328921615238,
128.348355532103));
#170769=CARTESIAN_POINT('Ctrl Pts',(-125.509797698372,5.60851953039534,
134.990297693958));
#170770=CARTESIAN_POINT('Ctrl Pts',(-125.231350074562,-0.49020561238188,
137.785568177001));
#170771=CARTESIAN_POINT('Ctrl Pts',(-124.999209239171,-5.19913250634134,
134.767487955326));
#170772=CARTESIAN_POINT('Ctrl Pts',(-124.859884278386,-5.90688169119504,
131.796176362661));
#170773=CARTESIAN_POINT('Ctrl Pts',(-124.813375192206,-5.90693489644606,
130.804324882377));
#170774=CARTESIAN_POINT('',(-123.063375192206,-5.91786917663301,130.798966564578));
#170775=CARTESIAN_POINT('Ctrl Pts',(-124.813375192206,-5.90693489644606,
130.804324882377));
#170776=CARTESIAN_POINT('Ctrl Pts',(-124.767068403782,-5.90698787027343,
129.816787598437));
#170777=CARTESIAN_POINT('Ctrl Pts',(-124.627945740753,-5.20365792411555,
126.849932484951));
#170778=CARTESIAN_POINT('Ctrl Pts',(-124.396007203122,-0.505416379733264,
123.824237781003));
#170779=CARTESIAN_POINT('Ctrl Pts',(-124.117559579308,5.59938513102161,
126.606212611025));
#170780=CARTESIAN_POINT('Ctrl Pts',(-123.839111955496,6.55862525153711,
133.246080368117));
#170781=CARTESIAN_POINT('Ctrl Pts',(-123.560664331683,1.49080917254681,
137.642126959098));
#170782=CARTESIAN_POINT('Ctrl Pts',(-123.302085410586,-4.48761703300956,
135.889285280182));
#170783=CARTESIAN_POINT('Ctrl Pts',(-123.136322364094,-5.90346559078905,
132.347385160215));
#170784=CARTESIAN_POINT('Ctrl Pts',(-123.063375192206,-5.91786917663301,
130.798966564578));
#170785=CARTESIAN_POINT('',(-121.313375192206,-5.92147242173306,130.806864541253));
#170786=CARTESIAN_POINT('Ctrl Pts',(-123.063375192206,-5.91786917663301,
130.798966564578));
#170787=CARTESIAN_POINT('Ctrl Pts',(-123.04350648949,-5.92179229740345,
130.377222061529));
#170788=CARTESIAN_POINT('Ctrl Pts',(-122.930821912165,-5.68794946591629,
127.989632006443));
#170789=CARTESIAN_POINT('Ctrl Pts',(-122.725321460248,-2.44602925083019,
124.247341368356));
#170790=CARTESIAN_POINT('Ctrl Pts',(-122.44687383643,4.19446744113016,125.202217865403));
#170791=CARTESIAN_POINT('Ctrl Pts',(-122.16842621262,6.98045346581883,131.305189871789));
#170792=CARTESIAN_POINT('Ctrl Pts',(-121.889978588805,3.35174376952896,
136.947924260418));
#170793=CARTESIAN_POINT('Ctrl Pts',(-121.611530964993,-3.35705470917186,
136.945023791032));
#170794=CARTESIAN_POINT('Ctrl Pts',(-121.419329832793,-5.85843743252595,
133.0479081345));
#170795=CARTESIAN_POINT('Ctrl Pts',(-121.319944575197,-5.9259884994246,
130.945860215635));
#170796=CARTESIAN_POINT('Ctrl Pts',(-121.313375192206,-5.92524902604646,
130.806866138209));
#170797=CARTESIAN_POINT('',(-119.563375221739,-5.91298467060509,130.808541148921));
#170798=CARTESIAN_POINT('Ctrl Pts',(-121.313375192206,-5.91674947102406,
130.80686254413));
#170799=CARTESIAN_POINT('Ctrl Pts',(-121.306028534646,-5.91681510495363,
130.651646350502));
#170800=CARTESIAN_POINT('Ctrl Pts',(-121.298681877086,-5.91076878111168,
130.496180606544));
#170801=CARTESIAN_POINT('Ctrl Pts',(-121.291335219526,-5.89857784810465,
130.340992586354));
#170802=CARTESIAN_POINT('Ctrl Pts',(-121.283996845679,-5.88640066096616,
130.185979548188));
#170803=CARTESIAN_POINT('Ctrl Pts',(-121.276658471832,-5.86809268057159,
130.03124398736));
#170804=CARTESIAN_POINT('Ctrl Pts',(-121.269320097985,-5.84367323058927,
129.877314913949));
#170805=CARTESIAN_POINT('Ctrl Pts',(-121.261988318462,-5.81927572412734,
129.723524162481));
#170806=CARTESIAN_POINT('Ctrl Pts',(-121.254656538938,-5.78877773718004,
129.57053883055));
#170807=CARTESIAN_POINT('Ctrl Pts',(-121.247324759415,-5.75225051416586,
129.41888431507));
#170808=CARTESIAN_POINT('Ctrl Pts',(-121.239997890939,-5.71574775819199,
129.267331382377));
#170809=CARTESIAN_POINT('Ctrl Pts',(-121.232671022464,-5.67322389422861,
129.117107861219));
#170810=CARTESIAN_POINT('Ctrl Pts',(-121.225344153989,-5.62480147257169,
128.968730219949));
#170811=CARTESIAN_POINT('Ctrl Pts',(-121.21801976663,-5.57639544832839,
128.820402824195));
#170812=CARTESIAN_POINT('Ctrl Pts',(-121.210695379272,-5.52209495599299,
128.673920427593));
#170813=CARTESIAN_POINT('Ctrl Pts',(-121.203370991913,-5.46207273869829,
128.529785501271));
#170814=CARTESIAN_POINT('Ctrl Pts',(-121.19604772567,-5.40205970876471,
128.385672637106));
#170815=CARTESIAN_POINT('Ctrl Pts',(-121.188724459426,-5.3363268424924,
128.24390688063));
#170816=CARTESIAN_POINT('Ctrl Pts',(-121.181401193182,-5.26509537115889,
128.104971557964));
#170817=CARTESIAN_POINT('Ctrl Pts',(-121.174077531278,-5.19386005134228,
127.96602872892));
#170818=CARTESIAN_POINT('Ctrl Pts',(-121.166753869374,-5.11712570923675,
127.829916977633));
#170819=CARTESIAN_POINT('Ctrl Pts',(-121.15943020747,-5.03515983296668,
127.697095579147));
#170820=CARTESIAN_POINT('Ctrl Pts',(-121.152104633067,-4.9531725521544,
127.564239495725));
#170821=CARTESIAN_POINT('Ctrl Pts',(-121.144779058665,-4.86595121890948,
127.434675799529));
#170822=CARTESIAN_POINT('Ctrl Pts',(-121.137453484262,-4.77380683854971,
127.308835073286));
#170823=CARTESIAN_POINT('Ctrl Pts',(-121.130120271257,-4.68156637639744,
127.182863129029));
#170824=CARTESIAN_POINT('Ctrl Pts',(-121.122787058251,-4.58439284068438,
127.060622215841));
#170825=CARTESIAN_POINT('Ctrl Pts',(-121.115453845246,-4.48263815387548,
126.942510575951));
#170826=CARTESIAN_POINT('Ctrl Pts',(-121.108116577606,-4.38082720550211,
126.824333630512));
#170827=CARTESIAN_POINT('Ctrl Pts',(-121.100779309966,-4.27443032048298,
126.710290784522));
#170828=CARTESIAN_POINT('Ctrl Pts',(-121.093442042326,-4.16383600305346,
126.600743091889));
#170829=CARTESIAN_POINT('Ctrl Pts',(-121.086093879819,-4.05307746776123,
126.491032735493));
#170830=CARTESIAN_POINT('Ctrl Pts',(-121.078745717313,-3.93810933173165,
126.385831121878));
#170831=CARTESIAN_POINT('Ctrl Pts',(-121.071397554806,-3.81935351503993,
126.285459280996));
#170832=CARTESIAN_POINT('Ctrl Pts',(-121.065810275659,-3.72905585253458,
126.20914013415));
#170833=CARTESIAN_POINT('Ctrl Pts',(-121.060222996513,-3.63656901350179,
126.135612506084));
#170834=CARTESIAN_POINT('Ctrl Pts',(-121.054635717367,-3.54208899513348,
126.065000311253));
#170835=CARTESIAN_POINT('Ctrl Pts',(-121.047212450962,-3.41656271874957,
125.971184856541));
#170836=CARTESIAN_POINT('Ctrl Pts',(-121.039789184556,-3.28711687605227,
125.88221800333));
#170837=CARTESIAN_POINT('Ctrl Pts',(-121.032365918151,-3.15416262063407,
125.798445244221));
#170838=CARTESIAN_POINT('Ctrl Pts',(-121.02495142543,-3.02136550610423,
125.714771497555));
#170839=CARTESIAN_POINT('Ctrl Pts',(-121.017536932709,-2.88506854553574,
125.63627982236));
#170840=CARTESIAN_POINT('Ctrl Pts',(-121.010122439988,-2.74571521522359,
125.563274993443));
#170841=CARTESIAN_POINT('Ctrl Pts',(-121.002715093634,-2.60649619889814,
125.490340529328));
#170842=CARTESIAN_POINT('Ctrl Pts',(-120.99530774728,-2.46422700587418,
125.42288255534));
#170843=CARTESIAN_POINT('Ctrl Pts',(-120.987900400926,-2.31937919980076,
125.361162045951));
#170844=CARTESIAN_POINT('Ctrl Pts',(-120.980498579251,-2.1746394266855,
125.299487570047));
#170845=CARTESIAN_POINT('Ctrl Pts',(-120.973096757575,-2.02732521186773,
125.243542183947));
#170846=CARTESIAN_POINT('Ctrl Pts',(-120.9656949359,-1.87793167646206,125.193540429658));
#170847=CARTESIAN_POINT('Ctrl Pts',(-120.958297021589,-1.72861700474086,
125.143565070905));
#170848=CARTESIAN_POINT('Ctrl Pts',(-120.950899107277,-1.57722555156876,
125.099527213471));
#170849=CARTESIAN_POINT('Ctrl Pts',(-120.943501192966,-1.42427121927405,
125.061592813062));
#170850=CARTESIAN_POINT('Ctrl Pts',(-120.936104508054,-1.2713423052147,
125.023664716662));
#170851=CARTESIAN_POINT('Ctrl Pts',(-120.928707823141,-1.11685138947067,
124.991838154007));
#170852=CARTESIAN_POINT('Ctrl Pts',(-120.921311138229,-0.961326412262909,
124.966228888015));
#170853=CARTESIAN_POINT('Ctrl Pts',(-120.913914781294,-0.805808331195621,
124.940620757565));
#170854=CARTESIAN_POINT('Ctrl Pts',(-120.906518424358,-0.649256648170021,
124.921229436283));
#170855=CARTESIAN_POINT('Ctrl Pts',(-120.899122067423,-0.492208079267675,
124.908119292009));
#170856=CARTESIAN_POINT('Ctrl Pts',(-120.891724578086,-0.335135465828503,
124.895007140539));
#170857=CARTESIAN_POINT('Ctrl Pts',(-120.88432708875,-0.177566187066021,
124.888178111935));
#170858=CARTESIAN_POINT('Ctrl Pts',(-120.876929599413,-0.0200404953665216,
124.887644557027));
#170859=CARTESIAN_POINT('Ctrl Pts',(-120.869529516898,0.137540416720232,
124.887110815081));
#170860=CARTESIAN_POINT('Ctrl Pts',(-120.862129434383,0.295077338259973,
124.892876941955));
#170861=CARTESIAN_POINT('Ctrl Pts',(-120.854729351868,0.452031756016429,
124.904903197256));
#170862=CARTESIAN_POINT('Ctrl Pts',(-120.847321132202,0.609158761290738,
124.916942676661));
#170863=CARTESIAN_POINT('Ctrl Pts',(-120.839912912535,0.765701611180409,
124.935256003066));
#170864=CARTESIAN_POINT('Ctrl Pts',(-120.832504692869,0.921127908494123,
124.959751653855));
#170865=CARTESIAN_POINT('Ctrl Pts',(-120.825091913566,1.07664986809996,
124.984262381307));
#170866=CARTESIAN_POINT('Ctrl Pts',(-120.817679134264,1.23105354047714,
125.014962942686));
#170867=CARTESIAN_POINT('Ctrl Pts',(-120.810266354962,1.38381892657568,
125.051711163536));
#170868=CARTESIAN_POINT('Ctrl Pts',(-120.802842983934,1.53680259102208,
125.088511891967));
#170869=CARTESIAN_POINT('Ctrl Pts',(-120.795419612905,1.68814293574958,
125.131377436782));
#170870=CARTESIAN_POINT('Ctrl Pts',(-120.787996241876,1.83733647208646,
125.180116201572));
#170871=CARTESIAN_POINT('Ctrl Pts',(-120.784060192435,1.91644246490247,
125.205958664134));
#170872=CARTESIAN_POINT('Ctrl Pts',(-120.780124142994,1.99494525711013,
125.233451499228));
#170873=CARTESIAN_POINT('Ctrl Pts',(-120.776188093554,2.0727724291567,125.262560817914));
#170874=CARTESIAN_POINT('Ctrl Pts',(-120.768764827148,2.21955204673268,
125.317460084483));
#170875=CARTESIAN_POINT('Ctrl Pts',(-120.761341560743,2.36437101987972,
125.378277780744));
#170876=CARTESIAN_POINT('Ctrl Pts',(-120.753918294337,2.50671643732821,
125.444854738725));
#170877=CARTESIAN_POINT('Ctrl Pts',(-120.746503801616,2.64889361431474,
125.511353008271));
#170878=CARTESIAN_POINT('Ctrl Pts',(-120.739089308895,2.78860272008164,
125.583596833619));
#170879=CARTESIAN_POINT('Ctrl Pts',(-120.731674816174,2.92534762918201,
125.661377843831));
#170880=CARTESIAN_POINT('Ctrl Pts',(-120.72426746982,3.06196073839064,125.739083885776));
#170881=CARTESIAN_POINT('Ctrl Pts',(-120.716860123467,3.19561501636462,
125.822316304446));
#170882=CARTESIAN_POINT('Ctrl Pts',(-120.709452777113,3.3258360062163,125.910819423067));
#170883=CARTESIAN_POINT('Ctrl Pts',(-120.702050955438,3.45595987234043,
125.999256532723));
#170884=CARTESIAN_POINT('Ctrl Pts',(-120.694649133762,3.58265524158026,
126.092956306076));
#170885=CARTESIAN_POINT('Ctrl Pts',(-120.687247312087,3.70547398861345,
126.191618148903));
#170886=CARTESIAN_POINT('Ctrl Pts',(-120.679849397775,3.82822790058681,
126.290227908912));
#170887=CARTESIAN_POINT('Ctrl Pts',(-120.672451483464,3.94710897564502,
126.393794288467));
#170888=CARTESIAN_POINT('Ctrl Pts',(-120.665053569153,4.06169981378983,
126.501974630098));
#170889=CARTESIAN_POINT('Ctrl Pts',(-120.65765688424,4.17627160901574,126.610136994119));
#170890=CARTESIAN_POINT('Ctrl Pts',(-120.650260199328,4.28655431116285,
126.722911542422));
#170891=CARTESIAN_POINT('Ctrl Pts',(-120.642863514416,4.39216516102326,
126.839916676634));
#170892=CARTESIAN_POINT('Ctrl Pts',(-120.635467157481,4.49777132798792,
126.956916622715));
#170893=CARTESIAN_POINT('Ctrl Pts',(-120.628070800545,4.59870580443632,
127.078146504606));
#170894=CARTESIAN_POINT('Ctrl Pts',(-120.62067444361,4.69462432772869,127.203189560257));
#170895=CARTESIAN_POINT('Ctrl Pts',(-120.613276954273,4.79055753639185,
127.328251760319));
#170896=CARTESIAN_POINT('Ctrl Pts',(-120.605879464937,4.88147303557931,
127.457128000367));
#170897=CARTESIAN_POINT('Ctrl Pts',(-120.5984819756,4.96706841457714,127.589370426693));
#170898=CARTESIAN_POINT('Ctrl Pts',(-120.591081893085,5.05269379890177,
127.721659210395));
#170899=CARTESIAN_POINT('Ctrl Pts',(-120.58368181057,5.13299514720268,127.857316216583));
#170900=CARTESIAN_POINT('Ctrl Pts',(-120.576281728055,5.20771481463843,
127.995866898168));
#170901=CARTESIAN_POINT('Ctrl Pts',(-120.568873508389,5.28251664403043,
128.134569930472));
#170902=CARTESIAN_POINT('Ctrl Pts',(-120.561465288722,5.35172435800186,
128.276172663858));
#170903=CARTESIAN_POINT('Ctrl Pts',(-120.554057069056,5.41512718343709,
128.42017770728));
#170904=CARTESIAN_POINT('Ctrl Pts',(-120.546644289754,5.47856903225344,
128.564271383403));
#170905=CARTESIAN_POINT('Ctrl Pts',(-120.539231510452,5.53619873691977,
128.710769969241));
#170906=CARTESIAN_POINT('Ctrl Pts',(-120.53181873115,5.58785484064342,128.859159126101));
#170907=CARTESIAN_POINT('Ctrl Pts',(-120.524395360121,5.63958475303057,
129.007760308347));
#170908=CARTESIAN_POINT('Ctrl Pts',(-120.516971989092,5.68532390918129,
129.158257100569));
#170909=CARTESIAN_POINT('Ctrl Pts',(-120.509548618064,5.72496135665502,
129.310122340949));
#170910=CARTESIAN_POINT('Ctrl Pts',(-120.505612568623,5.74597808239354,
129.390644935357));
#170911=CARTESIAN_POINT('Ctrl Pts',(-120.501676519182,5.7652802583171,129.471552106675));
#170912=CARTESIAN_POINT('Ctrl Pts',(-120.497740469741,5.78285725161436,
129.552764608483));
#170913=CARTESIAN_POINT('Ctrl Pts',(-120.490317203336,5.81600691241305,
129.705928852335));
#170914=CARTESIAN_POINT('Ctrl Pts',(-120.48289393693,5.84311745448787,129.860642606314));
#170915=CARTESIAN_POINT('Ctrl Pts',(-120.475470670525,5.86404554929174,
130.016388309466));
#170916=CARTESIAN_POINT('Ctrl Pts',(-120.468056177804,5.88494890882558,
130.171949934132));
#170917=CARTESIAN_POINT('Ctrl Pts',(-120.460641685083,5.89968431676038,
130.328540713836));
#170918=CARTESIAN_POINT('Ctrl Pts',(-120.453227192362,5.90815891354594,
130.485630614605));
#170919=CARTESIAN_POINT('Ctrl Pts',(-120.445819846008,5.91662534219603,
130.642569106213));
#170920=CARTESIAN_POINT('Ctrl Pts',(-120.438412499654,5.91884295303603,
130.800005390914));
#170921=CARTESIAN_POINT('Ctrl Pts',(-120.431005153301,5.91477039864094,
130.957402095149));
#170922=CARTESIAN_POINT('Ctrl Pts',(-120.423603331625,5.91070088171053,
131.114681406986));
#170923=CARTESIAN_POINT('Ctrl Pts',(-120.41620150995,5.90035055045421,131.271920825569));
#170924=CARTESIAN_POINT('Ctrl Pts',(-120.408799688274,5.883730080621,131.428580851855));
#170925=CARTESIAN_POINT('Ctrl Pts',(-120.401401773963,5.86711838460459,
131.585158178531));
#170926=CARTESIAN_POINT('Ctrl Pts',(-120.394003859652,5.84424318123347,
131.741156351762));
#170927=CARTESIAN_POINT('Ctrl Pts',(-120.38660594534,5.81516714304668,131.896038986377));
#170928=CARTESIAN_POINT('Ctrl Pts',(-120.379209260428,5.78609593676982,
132.050895882309));
#170929=CARTESIAN_POINT('Ctrl Pts',(-120.371812575516,5.75082600965621,
132.204637241024));
#170930=CARTESIAN_POINT('Ctrl Pts',(-120.364415890604,5.70947152052425,
132.356734773117));
#170931=CARTESIAN_POINT('Ctrl Pts',(-120.357019533668,5.66811886509379,
132.508825561046));
#170932=CARTESIAN_POINT('Ctrl Pts',(-120.349623176733,5.62068228203217,
132.659272307061));
#170933=CARTESIAN_POINT('Ctrl Pts',(-120.342226819798,5.56732632268922,
132.807560103187));
#170934=CARTESIAN_POINT('Ctrl Pts',(-120.334829330461,5.51396219441252,
132.955870602553));
#170935=CARTESIAN_POINT('Ctrl Pts',(-120.327431841124,5.45467701174053,
133.102021142604));
#170936=CARTESIAN_POINT('Ctrl Pts',(-120.320034351788,5.38968410630416,
133.245515220772));
#170937=CARTESIAN_POINT('Ctrl Pts',(-120.312634269273,5.32466841770544,
133.389059600567));
#170938=CARTESIAN_POINT('Ctrl Pts',(-120.305234186758,5.25394117661835,
133.529945324598));
#170939=CARTESIAN_POINT('Ctrl Pts',(-120.297834104243,5.1777623696189,133.667699124669));
#170940=CARTESIAN_POINT('Ctrl Pts',(-120.290425884576,5.10149979619011,
133.805604399204));
#170941=CARTESIAN_POINT('Ctrl Pts',(-120.28301766491,5.0197738660886,133.940370545267));
#170942=CARTESIAN_POINT('Ctrl Pts',(-120.275609445243,4.93288912047083,
134.071551381455));
#170943=CARTESIAN_POINT('Ctrl Pts',(-120.268196665941,4.84595089874188,
134.202812957259));
#170944=CARTESIAN_POINT('Ctrl Pts',(-120.260783886639,4.7538477524764,134.330484524025));
#170945=CARTESIAN_POINT('Ctrl Pts',(-120.253371107337,4.65692513804388,
134.454152230954));
#170946=CARTESIAN_POINT('Ctrl Pts',(-120.245947736308,4.5598640360345,134.577996640102));
#170947=CARTESIAN_POINT('Ctrl Pts',(-120.23852436528,4.45796995358772,134.697825479856));
#170948=CARTESIAN_POINT('Ctrl Pts',(-120.231100994251,4.35162643436671,
134.813260458947));
#170949=CARTESIAN_POINT('Ctrl Pts',(-120.22716494481,4.29524054879861,134.874466854684));
#170950=CARTESIAN_POINT('Ctrl Pts',(-120.223228895369,4.23760435172856,
134.934438624318));
#170951=CARTESIAN_POINT('Ctrl Pts',(-120.219292845929,4.17877876812081,
134.993123987536));
#170952=CARTESIAN_POINT('Ctrl Pts',(-120.211869579523,4.06783555331918,
135.103802751059));
#170953=CARTESIAN_POINT('Ctrl Pts',(-120.204446313118,3.95232440057861,
135.210238181037));
#170954=CARTESIAN_POINT('Ctrl Pts',(-120.197023046713,3.83260327600736,
135.312029936764));
#170955=CARTESIAN_POINT('Ctrl Pts',(-120.189608553992,3.7130236518628,135.413701383089));
#170956=CARTESIAN_POINT('Ctrl Pts',(-120.18219406127,3.58924424193811,135.510739840486));
#170957=CARTESIAN_POINT('Ctrl Pts',(-120.174779568549,3.46166078596998,
135.602780687274));
#170958=CARTESIAN_POINT('Ctrl Pts',(-120.167372222196,3.33420029974052,
135.694732821629));
#170959=CARTESIAN_POINT('Ctrl Pts',(-120.159964875842,3.20294336742124,
135.781696717911));
#170960=CARTESIAN_POINT('Ctrl Pts',(-120.152557529488,3.06831974731346,
135.863347125825));
#170961=CARTESIAN_POINT('Ctrl Pts',(-120.145155707813,2.93379653457985,
135.944936635785));
#170962=CARTESIAN_POINT('Ctrl Pts',(-120.137753886137,2.79591195160947,
136.021220355493));
#170963=CARTESIAN_POINT('Ctrl Pts',(-120.130352064462,2.6551256647309,136.091915654347));
#170964=CARTESIAN_POINT('Ctrl Pts',(-120.12295415015,2.51441369783769,136.162573633703));
#170965=CARTESIAN_POINT('Ctrl Pts',(-120.115556235839,2.37080341041977,
136.227648900347));
#170966=CARTESIAN_POINT('Ctrl Pts',(-120.108158321528,2.22477995455184,
136.286904253172));
#170967=CARTESIAN_POINT('Ctrl Pts',(-120.100761636616,2.07878076513294,
136.346149758833));
#170968=CARTESIAN_POINT('Ctrl Pts',(-120.093364951703,1.93036954874399,
136.399577129983));
#170969=CARTESIAN_POINT('Ctrl Pts',(-120.085968266791,1.78005247585254,
136.446996858341));
#170970=CARTESIAN_POINT('Ctrl Pts',(-120.078571909856,1.62974206817806,
136.494414484059));
#170971=CARTESIAN_POINT('Ctrl Pts',(-120.07117555292,1.47752632803416,136.535824884343));
#170972=CARTESIAN_POINT('Ctrl Pts',(-120.063779195985,1.32392740610855,
136.571088180565));
#170973=CARTESIAN_POINT('Ctrl Pts',(-120.056381706648,1.17030496779544,
136.606356875688));
#170974=CARTESIAN_POINT('Ctrl Pts',(-120.048984217312,1.01529928989712,
136.635476509285));
#170975=CARTESIAN_POINT('Ctrl Pts',(-120.041586727975,0.859443405042454,
136.658358191534));
#170976=CARTESIAN_POINT('Ctrl Pts',(-120.03418664546,0.703532885148287,
136.681247894922));
#170977=CARTESIAN_POINT('Ctrl Pts',(-120.026786562945,0.546771934013165,
136.69789523906));
#170978=CARTESIAN_POINT('Ctrl Pts',(-120.01938648043,0.389699254668284,
136.708263144997));
#170979=CARTESIAN_POINT('Ctrl Pts',(-120.011978260763,0.232453857765671,
136.718642451513));
#170980=CARTESIAN_POINT('Ctrl Pts',(-120.004570041097,0.0748964208206027,
136.722728505713));
#170981=CARTESIAN_POINT('Ctrl Pts',(-119.99716182143,-0.0824330591834801,
136.720536354751));
#170982=CARTESIAN_POINT('Ctrl Pts',(-119.989749042128,-0.239859372857322,
136.718342854556));
#170983=CARTESIAN_POINT('Ctrl Pts',(-119.982336262826,-0.397057078125725,
136.709863469495));
#170984=CARTESIAN_POINT('Ctrl Pts',(-119.974923483524,-0.553491262984103,
136.695165145328));
#170985=CARTESIAN_POINT('Ctrl Pts',(-119.967500112495,-0.71014896834162,
136.680445819506));
#170986=CARTESIAN_POINT('Ctrl Pts',(-119.960076741466,-0.866040605419736,
136.659489857023));
#170987=CARTESIAN_POINT('Ctrl Pts',(-119.952653370438,-1.02064059234089,
136.632415468352));
#170988=CARTESIAN_POINT('Ctrl Pts',(-119.948717320997,-1.10261321498006,
136.618059977838));
#170989=CARTESIAN_POINT('Ctrl Pts',(-119.944781271556,-1.1842229356191,
136.60198521928));
#170990=CARTESIAN_POINT('Ctrl Pts',(-119.940845222116,-1.26539325858399,
136.584214462053));
#170991=CARTESIAN_POINT('Ctrl Pts',(-119.93342195571,-1.41847795446017,
136.550699368529));
#170992=CARTESIAN_POINT('Ctrl Pts',(-119.925998689305,-1.57046169568063,
136.511047514015));
#170993=CARTESIAN_POINT('Ctrl Pts',(-119.918575422899,-1.72081417484769,
136.465343671607));
#170994=CARTESIAN_POINT('Ctrl Pts',(-119.911160930178,-1.87098894987038,
136.419693847346));
#170995=CARTESIAN_POINT('Ctrl Pts',(-119.903746437457,-2.01953594689331,
136.36800638068));
#170996=CARTESIAN_POINT('Ctrl Pts',(-119.896331944736,-2.16593449237795,
136.310417131735));
#170997=CARTESIAN_POINT('Ctrl Pts',(-119.888924598383,-2.31219193343265,
136.252883389477));
#170998=CARTESIAN_POINT('Ctrl Pts',(-119.881517252029,-2.45630470036704,
136.189459325079));
#170999=CARTESIAN_POINT('Ctrl Pts',(-119.874109905675,-2.59776685603759,
136.120330700643));
#171000=CARTESIAN_POINT('Ctrl Pts',(-119.866708084,-2.73912350389537,136.051253634944));
#171001=CARTESIAN_POINT('Ctrl Pts',(-119.859306262324,-2.87783314286533,
135.976480644033));
#171002=CARTESIAN_POINT('Ctrl Pts',(-119.851904440649,-3.01340952693938,
135.896245689467));
#171003=CARTESIAN_POINT('Ctrl Pts',(-119.844506526338,-3.14891434129483,
135.81605309031));
#171004=CARTESIAN_POINT('Ctrl Pts',(-119.837108612027,-3.28128887437365,
135.730404459425));
#171005=CARTESIAN_POINT('Ctrl Pts',(-119.829710697715,-3.41007132562115,
135.639579756));
#171006=CARTESIAN_POINT('Ctrl Pts',(-119.822314012803,-3.53883237556252,
135.548770145992));
#171007=CARTESIAN_POINT('Ctrl Pts',(-119.814917327891,-3.66400222365588,
135.452786385564));
#171008=CARTESIAN_POINT('Ctrl Pts',(-119.807520642979,-3.7851478337164,
135.351951896409));
#171009=CARTESIAN_POINT('Ctrl Pts',(-119.800124286043,-3.90628807205363,
135.251121878362));
#171010=CARTESIAN_POINT('Ctrl Pts',(-119.792727929108,-4.02340414023981,
135.145441798064));
#171011=CARTESIAN_POINT('Ctrl Pts',(-119.785331572172,-4.13609611922292,
135.035275347864));
#171012=CARTESIAN_POINT('Ctrl Pts',(-119.777934082836,-4.24880535163569,
134.925092030898));
#171013=CARTESIAN_POINT('Ctrl Pts',(-119.770536593499,-4.35708887921984,
134.81042123734));
#171014=CARTESIAN_POINT('Ctrl Pts',(-119.763139104163,-4.46058379929442,
134.691663375517));
#171015=CARTESIAN_POINT('Ctrl Pts',(-119.755739021648,-4.56411499935235,
134.57286388331));
#171016=CARTESIAN_POINT('Ctrl Pts',(-119.748338939133,-4.66285400463935,
134.449974751562));
#171017=CARTESIAN_POINT('Ctrl Pts',(-119.740938856618,-4.75647843743766,
134.323429164311));
#171018=CARTESIAN_POINT('Ctrl Pts',(-119.733530636952,-4.85020581992532,
134.196744427177));
#171019=CARTESIAN_POINT('Ctrl Pts',(-119.726122417285,-4.93880717627017,
134.06639550532));
#171020=CARTESIAN_POINT('Ctrl Pts',(-119.718714197619,-5.02200328450927,
133.93284484685));
#171021=CARTESIAN_POINT('Ctrl Pts',(-119.711301418317,-5.10525059856455,
133.799211990178));
#171022=CARTESIAN_POINT('Ctrl Pts',(-119.703888639014,-5.1830858512289,
133.662373793921));
#171023=CARTESIAN_POINT('Ctrl Pts',(-119.696475859712,-5.25527623286301,
133.522816480516));
#171024=CARTESIAN_POINT('Ctrl Pts',(-119.689052488684,-5.32756976349968,
133.383059761077));
#171025=CARTESIAN_POINT('Ctrl Pts',(-119.681629117655,-5.39420215646452,
133.240576502124));
#171026=CARTESIAN_POINT('Ctrl Pts',(-119.674205746626,-5.4549887757349,
133.095872786224));
#171027=CARTESIAN_POINT('Ctrl Pts',(-119.670269697185,-5.48721929983094,
133.019147403926));
#171028=CARTESIAN_POINT('Ctrl Pts',(-119.666333647744,-5.51780719763373,
132.941798034986));
#171029=CARTESIAN_POINT('Ctrl Pts',(-119.662397598302,-5.54673069854685,
132.863901615045));
#171030=CARTESIAN_POINT('Ctrl Pts',(-119.653853459437,-5.60951609084795,
132.694808762161));
#171031=CARTESIAN_POINT('Ctrl Pts',(-119.645309320571,-5.6646129739838,
132.522714853274));
#171032=CARTESIAN_POINT('Ctrl Pts',(-119.636765181705,-5.71176372379817,
132.34827956816));
#171033=CARTESIAN_POINT('Ctrl Pts',(-119.628251478122,-5.75874651679441,
132.174465643164));
#171034=CARTESIAN_POINT('Ctrl Pts',(-119.619737774538,-5.79783959119408,
131.998327121539));
#171035=CARTESIAN_POINT('Ctrl Pts',(-119.611224070954,-5.82883457131893,
131.820538802087));
#171036=CARTESIAN_POINT('Ctrl Pts',(-119.602770336281,-5.8596112286944,
131.64400278977));
#171037=CARTESIAN_POINT('Ctrl Pts',(-119.594316601608,-5.882403397313,131.465840283061));
#171038=CARTESIAN_POINT('Ctrl Pts',(-119.585862866934,-5.89705423531172,
131.286731748846));
#171039=CARTESIAN_POINT('Ctrl Pts',(-119.578366998354,-5.91004503292618,
131.127917439438));
#171040=CARTESIAN_POINT('Ctrl Pts',(-119.570871129774,-5.91663550731186,
130.96835967698));
#171041=CARTESIAN_POINT('Ctrl Pts',(-119.563375261194,-5.91674852062905,
130.808544650777));
#171042=CARTESIAN_POINT('',(-117.813375192206,-5.91000238445492,130.800267657125));
#171043=CARTESIAN_POINT('Ctrl Pts',(-119.563375192206,-5.91016724854547,
130.808538527613));
#171044=CARTESIAN_POINT('Ctrl Pts',(-119.5035667863,-5.90190641363403,129.534810380383));
#171045=CARTESIAN_POINT('Ctrl Pts',(-119.35094250579,-4.87179864722807,
126.272220221406));
#171046=CARTESIAN_POINT('Ctrl Pts',(-119.105502350678,0.511451736149495,
123.824677411885));
#171047=CARTESIAN_POINT('Ctrl Pts',(-118.827054726865,6.14865731213414,
127.461970187318));
#171048=CARTESIAN_POINT('Ctrl Pts',(-118.54860710305,6.13554719689485,134.170756483371));
#171049=CARTESIAN_POINT('Ctrl Pts',(-118.270159479238,0.484168945789873,
137.785989436281));
#171050=CARTESIAN_POINT('Ctrl Pts',(-118.025082175625,-4.88153028890003,
135.32107526904));
#171051=CARTESIAN_POINT('Ctrl Pts',(-117.872820746612,-5.90197269538057,
132.066356888141));
#171052=CARTESIAN_POINT('Ctrl Pts',(-117.813375192206,-5.91000238445492,
130.800267657125));
#171053=CARTESIAN_POINT('',(-116.063375192205,-5.92511385651394,130.801729663424));
#171054=CARTESIAN_POINT('Ctrl Pts',(-117.813375192206,-5.91000238445492,
130.800267657125));
#171055=CARTESIAN_POINT('Ctrl Pts',(-117.780004872008,-5.9145099258207,
130.089536577909));
#171056=CARTESIAN_POINT('Ctrl Pts',(-117.653818677207,-5.46638774170925,
127.407478954535));
#171057=CARTESIAN_POINT('Ctrl Pts',(-117.4348166078,-1.46999045857098,123.962088437774));
#171058=CARTESIAN_POINT('Ctrl Pts',(-117.156368983987,4.96203161869359,
125.869200767536));
#171059=CARTESIAN_POINT('Ctrl Pts',(-116.877921360174,6.83418904709124,
132.311483903476));
#171060=CARTESIAN_POINT('Ctrl Pts',(-116.599473736361,2.42606060991088,
137.368794366749));
#171061=CARTESIAN_POINT('Ctrl Pts',(-116.327958347038,-4.04625026551561,
136.417986591368));
#171062=CARTESIAN_POINT('Ctrl Pts',(-116.14925883232,-5.91503838326621,
132.618953446528));
#171063=CARTESIAN_POINT('Ctrl Pts',(-116.063375192205,-5.92511385651394,
130.801729663424));
#171064=CARTESIAN_POINT('',(-114.313375192205,-5.91789950705419,130.809730098004));
#171065=CARTESIAN_POINT('Ctrl Pts',(-116.063375192205,-5.92511385651394,
130.801729663424));
#171066=CARTESIAN_POINT('Ctrl Pts',(-116.056442957715,-5.92592711434814,
130.655049558007));
#171067=CARTESIAN_POINT('Ctrl Pts',(-116.049510723225,-5.92095444110238,
130.508425518448));
#171068=CARTESIAN_POINT('Ctrl Pts',(-116.042578488735,-5.91001924693745,
130.3622475195));
#171069=CARTESIAN_POINT('Ctrl Pts',(-115.949762614131,-5.7636076372569,
128.405066348045));
#171070=CARTESIAN_POINT('Ctrl Pts',(-115.764130864921,-3.33302935004614,
124.650623876197));
#171071=CARTESIAN_POINT('Ctrl Pts',(-115.48568324111,3.37572922592766,124.673943606988));
#171072=CARTESIAN_POINT('Ctrl Pts',(-115.207235617296,6.98235755681463,
130.330817082983));
#171073=CARTESIAN_POINT('Ctrl Pts',(-114.928787993484,4.17254040011804,
136.422853933367));
#171074=CARTESIAN_POINT('Ctrl Pts',(-114.650340369671,-2.47163754435426,
137.351769905191));
#171075=CARTESIAN_POINT('Ctrl Pts',(-114.445202769245,-5.69320852440163,
133.603467437331));
#171076=CARTESIAN_POINT('Ctrl Pts',(-114.332881043423,-5.92195457526042,
131.22373034605));
#171077=CARTESIAN_POINT('Ctrl Pts',(-114.313375192205,-5.91810510348369,
130.809730284548));
#171078=CARTESIAN_POINT('',(-112.563375192235,-5.91674999772218,130.804524796032));
#171079=CARTESIAN_POINT('Ctrl Pts',(-114.313375192205,-5.91674756453265,
130.809729052814));
#171080=CARTESIAN_POINT('Ctrl Pts',(-114.306070857519,-5.91688819427679,
130.654735901592));
#171081=CARTESIAN_POINT('Ctrl Pts',(-114.298766522834,-5.91093444397203,
130.499551867607));
#171082=CARTESIAN_POINT('Ctrl Pts',(-114.291462188148,-5.89886813750953,
130.344702854905));
#171083=CARTESIAN_POINT('Ctrl Pts',(-114.284163478904,-5.88681112392603,
130.189973099337));
#171084=CARTESIAN_POINT('Ctrl Pts',(-114.27686476966,-5.86865095246589,
130.035578233295));
#171085=CARTESIAN_POINT('Ctrl Pts',(-114.269566060416,-5.84442151256597,
129.882044106841));
#171086=CARTESIAN_POINT('Ctrl Pts',(-114.262227687984,-5.82006040324443,
129.727675633835));
#171087=CARTESIAN_POINT('Ctrl Pts',(-114.254889315551,-5.78956386125597,
129.574177676706));
#171088=CARTESIAN_POINT('Ctrl Pts',(-114.247550943119,-5.75301928217937,
129.422080001565));
#171089=CARTESIAN_POINT('Ctrl Pts',(-114.240257380979,-5.71669785520761,
129.270911080214));
#171090=CARTESIAN_POINT('Ctrl Pts',(-114.232963818839,-5.67440215317019,
129.12112576259));
#171091=CARTESIAN_POINT('Ctrl Pts',(-114.225670256699,-5.62626920573315,
128.973233809527));
#171092=CARTESIAN_POINT('Ctrl Pts',(-114.218376881327,-5.57813749085329,
128.825345643585));
#171093=CARTESIAN_POINT('Ctrl Pts',(-114.211083505956,-5.52416894682227,
128.679351111731));
#171094=CARTESIAN_POINT('Ctrl Pts',(-114.203790130584,-5.46455023345578,
128.53574401079));
#171095=CARTESIAN_POINT('Ctrl Pts',(-114.196495407217,-5.40492050107706,
128.392110367707));
#171096=CARTESIAN_POINT('Ctrl Pts',(-114.189200683849,-5.33963866932655,
128.250865388737));
#171097=CARTESIAN_POINT('Ctrl Pts',(-114.181905960482,-5.26893909120866,
128.112481828387));
#171098=CARTESIAN_POINT('Ctrl Pts',(-114.174534223945,-5.19749311075687,
127.972637300162));
#171099=CARTESIAN_POINT('Ctrl Pts',(-114.167162487409,-5.12051451299327,
127.835715315378));
#171100=CARTESIAN_POINT('Ctrl Pts',(-114.159790750873,-5.03829170692901,
127.702176348637));
#171101=CARTESIAN_POINT('Ctrl Pts',(-114.152485137341,-4.95680642302291,
127.569835199772));
#171102=CARTESIAN_POINT('Ctrl Pts',(-114.14517952381,-4.870170894451,127.440816910365));
#171103=CARTESIAN_POINT('Ctrl Pts',(-114.137873910279,-4.77870783924653,
127.315538187343));
#171104=CARTESIAN_POINT('Ctrl Pts',(-114.13046911224,-4.68600303780323,
127.188558620383));
#171105=CARTESIAN_POINT('Ctrl Pts',(-114.123064314201,-4.5883389364067,
127.065421216274));
#171106=CARTESIAN_POINT('Ctrl Pts',(-114.115659516162,-4.486091339419,126.946522485025));
#171107=CARTESIAN_POINT('Ctrl Pts',(-114.108254718123,-4.3838437424313,
126.827623753776));
#171108=CARTESIAN_POINT('Ctrl Pts',(-114.100849920084,-4.27701297370974,
126.71296394576));
#171109=CARTESIAN_POINT('Ctrl Pts',(-114.093445122045,-4.16601025747249,
126.602897884525));
#171110=CARTESIAN_POINT('Ctrl Pts',(-114.086021855639,-4.05473068846847,
126.492557306642));
#171111=CARTESIAN_POINT('Ctrl Pts',(-114.078598589234,-3.9388961179316,
126.386473945882));
#171112=CARTESIAN_POINT('Ctrl Pts',(-114.071175322828,-3.81886572881143,
126.285047051568));
#171113=CARTESIAN_POINT('Ctrl Pts',(-114.063760830108,-3.69897720564364,
126.183740035422));
#171114=CARTESIAN_POINT('Ctrl Pts',(-114.056346337387,-3.57490301737353,
126.087078769448));
#171115=CARTESIAN_POINT('Ctrl Pts',(-114.048931844666,-3.44704001168771,
125.99542666914));
#171116=CARTESIAN_POINT('Ctrl Pts',(-114.041524498312,-3.31930024518073,
125.903862906577));
#171117=CARTESIAN_POINT('Ctrl Pts',(-114.034117151958,-3.18777923264967,
125.817298914059));
#171118=CARTESIAN_POINT('Ctrl Pts',(-114.026709805605,-3.05290772035521,
125.736058632335));
#171119=CARTESIAN_POINT('Ctrl Pts',(-114.019307983929,-2.91813680032266,
125.654878942679));
#171120=CARTESIAN_POINT('Ctrl Pts',(-114.011906162254,-2.78002067462342,
125.579015249553));
#171121=CARTESIAN_POINT('Ctrl Pts',(-114.004504340578,-2.63901986768726,
125.508748783184));
#171122=CARTESIAN_POINT('Ctrl Pts',(-113.997106426267,-2.49809349397873,
125.438519409935));
#171123=CARTESIAN_POINT('Ctrl Pts',(-113.989708511956,-2.35428580502743,
125.37388154503));
#171124=CARTESIAN_POINT('Ctrl Pts',(-113.982310597644,-2.20808267261941,
125.315070911841));
#171125=CARTESIAN_POINT('Ctrl Pts',(-113.974913912732,-2.06190383652064,
125.256270051913));
#171126=CARTESIAN_POINT('Ctrl Pts',(-113.96751722782,-1.91333069302429,
125.203294640926));
#171127=CARTESIAN_POINT('Ctrl Pts',(-113.960120542908,-1.76286998705137,
125.156332645676));
#171128=CARTESIAN_POINT('Ctrl Pts',(-113.952724185972,-1.61241595266338,
125.109372732769));
#171129=CARTESIAN_POINT('Ctrl Pts',(-113.945327829037,-1.46007487855918,
125.068425816648));
#171130=CARTESIAN_POINT('Ctrl Pts',(-113.937931472102,-1.30636933875029,
125.033630186046));
#171131=CARTESIAN_POINT('Ctrl Pts',(-113.930533982765,-1.15264026623131,
124.998829228143));
#171132=CARTESIAN_POINT('Ctrl Pts',(-113.923136493428,-0.997546676162303,
124.97018151339));
#171133=CARTESIAN_POINT('Ctrl Pts',(-113.915739004092,-0.841621869253158,
124.947774308828));
#171134=CARTESIAN_POINT('Ctrl Pts',(-113.908338921577,-0.685642403144888,
124.925359249456));
#171135=CARTESIAN_POINT('Ctrl Pts',(-113.900938839062,-0.528831509329074,
124.909189108839));
#171136=CARTESIAN_POINT('Ctrl Pts',(-113.893538756547,-0.371728001197229,
124.899299326129));
#171137=CARTESIAN_POINT('Ctrl Pts',(-113.886130536881,-0.214451741607334,
124.889398668587));
#171138=CARTESIAN_POINT('Ctrl Pts',(-113.878722317214,-0.0568825979155635,
124.885792183953));
#171139=CARTESIAN_POINT('Ctrl Pts',(-113.871314097548,0.100439481194228,
124.888463181579));
#171140=CARTESIAN_POINT('Ctrl Pts',(-113.863901318246,0.2578583894191,124.891135823159));
#171141=CARTESIAN_POINT('Ctrl Pts',(-113.856488538944,0.415029558226182,
124.900093624685));
#171142=CARTESIAN_POINT('Ctrl Pts',(-113.849075759642,0.571418281848443,
124.915268012617));
#171143=CARTESIAN_POINT('Ctrl Pts',(-113.841652388613,0.728030461012253,
124.930464082425));
#171144=CARTESIAN_POINT('Ctrl Pts',(-113.834229017584,0.883857593268391,
124.95189442836));
#171145=CARTESIAN_POINT('Ctrl Pts',(-113.826805646555,1.03837445896579,
124.979439240803));
#171146=CARTESIAN_POINT('Ctrl Pts',(-113.822869597114,1.1203030087511,124.994044161291));
#171147=CARTESIAN_POINT('Ctrl Pts',(-113.818933547673,1.2018634253566,125.010367237311));
#171148=CARTESIAN_POINT('Ctrl Pts',(-113.814997498232,1.2829792842865,125.02838496677));
#171149=CARTESIAN_POINT('Ctrl Pts',(-113.807574231826,1.43596126266911,
125.06236584221));
#171150=CARTESIAN_POINT('Ctrl Pts',(-113.800150965421,1.58782361330608,
125.102480099287));
#171151=CARTESIAN_POINT('Ctrl Pts',(-113.792727699015,1.7380362892762,125.148641351225));
#171152=CARTESIAN_POINT('Ctrl Pts',(-113.785313206294,1.8880714263377,125.194748044397));
#171153=CARTESIAN_POINT('Ctrl Pts',(-113.777898713573,2.0364604164326,125.246887397611));
#171154=CARTESIAN_POINT('Ctrl Pts',(-113.770484220852,2.18268300194557,
125.30492196662));
#171155=CARTESIAN_POINT('Ctrl Pts',(-113.763076874499,2.32876465262585,
125.362900599727));
#171156=CARTESIAN_POINT('Ctrl Pts',(-113.755669528145,2.47268371100539,
125.426763000039));
#171157=CARTESIAN_POINT('Ctrl Pts',(-113.748262181791,2.61393480768006,
125.496321866417));
#171158=CARTESIAN_POINT('Ctrl Pts',(-113.740860360116,2.75508055395652,
125.565828853168));
#171159=CARTESIAN_POINT('Ctrl Pts',(-113.73345853844,2.89356196716893,125.641023682162));
#171160=CARTESIAN_POINT('Ctrl Pts',(-113.726056716765,3.02889351565995,
125.721670912961));
#171161=CARTESIAN_POINT('Ctrl Pts',(-113.718658802454,3.16415362367994,
125.802275570715));
#171162=CARTESIAN_POINT('Ctrl Pts',(-113.711260888142,3.29626685863876,
125.888326707427));
#171163=CARTESIAN_POINT('Ctrl Pts',(-113.703862973831,3.42477227422022,
125.97954295964));
#171164=CARTESIAN_POINT('Ctrl Pts',(-113.696466288919,3.55325633453347,
126.070744053368));
#171165=CARTESIAN_POINT('Ctrl Pts',(-113.689069604007,3.67813346129888,
126.167108343168));
#171166=CARTESIAN_POINT('Ctrl Pts',(-113.681672919095,3.7989716047218,126.268311090828));
#171167=CARTESIAN_POINT('Ctrl Pts',(-113.674276562159,3.91980439005481,
126.369509351053));
#171168=CARTESIAN_POINT('Ctrl Pts',(-113.666880205224,4.03659826195533,
126.475545402873));
#171169=CARTESIAN_POINT('Ctrl Pts',(-113.659483848288,4.14895441017811,
126.58605433841));
#171170=CARTESIAN_POINT('Ctrl Pts',(-113.652086358952,4.26132776041402,
126.696580193148));
#171171=CARTESIAN_POINT('Ctrl Pts',(-113.644688869615,4.36926176798573,
126.811580033369));
#171172=CARTESIAN_POINT('Ctrl Pts',(-113.637291380279,4.47239475059848,
126.93065234805));
#171173=CARTESIAN_POINT('Ctrl Pts',(-113.629891297764,4.57556388631827,
127.049766403346));
#171174=CARTESIAN_POINT('Ctrl Pts',(-113.622491215249,4.67392840200823,
127.172955493448));
#171175=CARTESIAN_POINT('Ctrl Pts',(-113.615091132734,4.76716723990703,
127.299785455117));
#171176=CARTESIAN_POINT('Ctrl Pts',(-113.607682913067,4.86050860349341,
127.426754879367));
#171177=CARTESIAN_POINT('Ctrl Pts',(-113.600274693401,4.94871281216255,
127.557372869507));
#171178=CARTESIAN_POINT('Ctrl Pts',(-113.592866473734,5.03150205277778,
127.691176129716));
#171179=CARTESIAN_POINT('Ctrl Pts',(-113.585453694432,5.11434224878921,
127.825061743598));
#171180=CARTESIAN_POINT('Ctrl Pts',(-113.57804091513,5.19176065252689,127.962136209765));
#171181=CARTESIAN_POINT('Ctrl Pts',(-113.570628135828,5.26352593532371,
128.10191259944));
#171182=CARTESIAN_POINT('Ctrl Pts',(-113.5632047648,5.33539375972193,128.241888708175));
#171183=CARTESIAN_POINT('Ctrl Pts',(-113.555781393771,5.40159217402192,
128.384574113239));
#171184=CARTESIAN_POINT('Ctrl Pts',(-113.548358022742,5.46193808339751,
128.529462172441));
#171185=CARTESIAN_POINT('Ctrl Pts',(-113.544421973301,5.49393493253177,
128.606285297979));
#171186=CARTESIAN_POINT('Ctrl Pts',(-113.54048592386,5.52428726378068,128.683727407679));
#171187=CARTESIAN_POINT('Ctrl Pts',(-113.536549874419,5.55297354081431,
128.761711499994));
#171188=CARTESIAN_POINT('Ctrl Pts',(-113.529126608013,5.60707496402698,
128.908787064288));
#171189=CARTESIAN_POINT('Ctrl Pts',(-113.521703341608,5.65541101341678,
129.05823589664));
#171190=CARTESIAN_POINT('Ctrl Pts',(-113.514280075202,5.69776786531719,
129.209565359403));
#171191=CARTESIAN_POINT('Ctrl Pts',(-113.506865582481,5.74007465493617,
129.360715963308));
#171192=CARTESIAN_POINT('Ctrl Pts',(-113.49945108976,5.77641621416304,129.513742417257));
#171193=CARTESIAN_POINT('Ctrl Pts',(-113.492036597039,5.80662696678625,
129.668132721811));
#171194=CARTESIAN_POINT('Ctrl Pts',(-113.484629250685,5.83680860114866,
129.822374219178));
#171195=CARTESIAN_POINT('Ctrl Pts',(-113.477221904332,5.86087112156129,
129.977976586287));
#171196=CARTESIAN_POINT('Ctrl Pts',(-113.469814557978,5.87869894527026,
130.134413400706));
#171197=CARTESIAN_POINT('Ctrl Pts',(-113.462412736302,5.89651347231566,
130.290733538646));
#171198=CARTESIAN_POINT('Ctrl Pts',(-113.455010914627,5.90810251949215,
130.447886515388));
#171199=CARTESIAN_POINT('Ctrl Pts',(-113.447609092951,5.91340172778835,
130.605336578089));
#171200=CARTESIAN_POINT('Ctrl Pts',(-113.44021117864,5.91869813867371,130.762703524127));
#171201=CARTESIAN_POINT('Ctrl Pts',(-113.432813264329,5.91771131080386,
130.920366871648));
#171202=CARTESIAN_POINT('Ctrl Pts',(-113.425415350017,5.91042881047856,
131.077786729642));
#171203=CARTESIAN_POINT('Ctrl Pts',(-113.418018665105,5.90314752037266,
131.235180427313));
#171204=CARTESIAN_POINT('Ctrl Pts',(-113.410621980193,5.88957265149538,
131.39233034323));
#171205=CARTESIAN_POINT('Ctrl Pts',(-113.403225295281,5.86974388183291,
131.548697452732));
#171206=CARTESIAN_POINT('Ctrl Pts',(-113.395828938345,5.84991599139886,
131.705057628752));
#171207=CARTESIAN_POINT('Ctrl Pts',(-113.38843258141,5.82383479851612,131.860634697041));
#171208=CARTESIAN_POINT('Ctrl Pts',(-113.381036224474,5.79159174383815,
132.014895885621));
#171209=CARTESIAN_POINT('Ctrl Pts',(-113.373638735138,5.75934375266629,
132.169180691983));
#171210=CARTESIAN_POINT('Ctrl Pts',(-113.366241245801,5.72093209765044,
132.32214885207));
#171211=CARTESIAN_POINT('Ctrl Pts',(-113.358843756465,5.67649908327068,
132.473279045808));
#171212=CARTESIAN_POINT('Ctrl Pts',(-113.35144367395,5.63205049296629,132.624462218003));
#171213=CARTESIAN_POINT('Ctrl Pts',(-113.344043591435,5.58157644598328,
132.773805783143));
#171214=CARTESIAN_POINT('Ctrl Pts',(-113.33664350892,5.52526867658858,132.920804950406));
#171215=CARTESIAN_POINT('Ctrl Pts',(-113.329235289253,5.4688989910131,133.067965758364));
#171216=CARTESIAN_POINT('Ctrl Pts',(-113.321827069587,5.40668290590618,
133.212776671384));
#171217=CARTESIAN_POINT('Ctrl Pts',(-113.31441884992,5.33886004037904,133.354753534695));
#171218=CARTESIAN_POINT('Ctrl Pts',(-113.307006070618,5.27099543100986,
133.496817782398));
#171219=CARTESIAN_POINT('Ctrl Pts',(-113.299593291316,5.19751733874125,
133.636044175259));
#171220=CARTESIAN_POINT('Ctrl Pts',(-113.292180512014,5.11871039175003,
133.771974893022));
#171221=CARTESIAN_POINT('Ctrl Pts',(-113.284757140985,5.03979084169739,
133.908099834969));
#171222=CARTESIAN_POINT('Ctrl Pts',(-113.277333769957,4.9555274292701,134.040919382478));
#171223=CARTESIAN_POINT('Ctrl Pts',(-113.269910398928,4.8662474396675,134.170005640207));
#171224=CARTESIAN_POINT('Ctrl Pts',(-113.265974349487,4.8189090469383,134.238450271434));
#171225=CARTESIAN_POINT('Ctrl Pts',(-113.262038300047,4.77016098321603,
134.305845899249));
#171226=CARTESIAN_POINT('Ctrl Pts',(-113.258102250606,4.7200563911717,134.37213278331));
#171227=CARTESIAN_POINT('Ctrl Pts',(-113.250678984201,4.62556069428295,
134.497147777911));
#171228=CARTESIAN_POINT('Ctrl Pts',(-113.243255717795,4.52595197438324,
134.618595009587));
#171229=CARTESIAN_POINT('Ctrl Pts',(-113.23583245139,4.42152912456444,134.73602829975));
#171230=CARTESIAN_POINT('Ctrl Pts',(-113.228417958669,4.31722969388176,
134.853322793516));
#171231=CARTESIAN_POINT('Ctrl Pts',(-113.221003465948,4.20812770469415,
134.966612512778));
#171232=CARTESIAN_POINT('Ctrl Pts',(-113.213588973227,4.09456441864342,
135.075481405378));
#171233=CARTESIAN_POINT('Ctrl Pts',(-113.206181626873,3.9811105891637,135.18424536604));
#171234=CARTESIAN_POINT('Ctrl Pts',(-113.198774280519,3.8632042908697,135.28859672617));
#171235=CARTESIAN_POINT('Ctrl Pts',(-113.191366934165,3.74122594256215,
135.388153698542));
#171236=CARTESIAN_POINT('Ctrl Pts',(-113.18396511249,3.61933857030841,135.487636417567));
#171237=CARTESIAN_POINT('Ctrl Pts',(-113.176563290815,3.49338548324887,
135.58233163378));
#171238=CARTESIAN_POINT('Ctrl Pts',(-113.169161469139,3.36378263780546,
135.671895612622));
#171239=CARTESIAN_POINT('Ctrl Pts',(-113.161763554828,3.23424820869645,
135.761412311337));
#171240=CARTESIAN_POINT('Ctrl Pts',(-113.154365640517,3.10106816460101,
135.845802955578));
#171241=CARTESIAN_POINT('Ctrl Pts',(-113.146967726205,2.96469001039799,
135.924765260243));
#171242=CARTESIAN_POINT('Ctrl Pts',(-113.139571041293,2.82833451976945,
136.003714442805));
#171243=CARTESIAN_POINT('Ctrl Pts',(-113.132174356381,2.68878229657856,
136.077236889312));
#171244=CARTESIAN_POINT('Ctrl Pts',(-113.124777671469,2.54650828446141,
136.14507462598));
#171245=CARTESIAN_POINT('Ctrl Pts',(-113.117381314533,2.40424058092304,
136.212909354651));
#171246=CARTESIAN_POINT('Ctrl Pts',(-113.109984957598,2.25925166537939,
136.275059714012));
#171247=CARTESIAN_POINT('Ctrl Pts',(-113.102588600663,2.11203919988923,
136.331314659408));
#171248=CARTESIAN_POINT('Ctrl Pts',(-113.095191111326,1.96480419579437,
136.387578217579));
#171249=CARTESIAN_POINT('Ctrl Pts',(-113.087793621989,1.81534531263664,
136.437944431322));
#171250=CARTESIAN_POINT('Ctrl Pts',(-113.080396132653,1.66417807080576,
136.482251239192));
#171251=CARTESIAN_POINT('Ctrl Pts',(-113.072996050138,1.51295783753238,
136.526573578745));
#171252=CARTESIAN_POINT('Ctrl Pts',(-113.065595967623,1.36002841125942,
136.564832178397));
#171253=CARTESIAN_POINT('Ctrl Pts',(-113.058195885108,1.20591812385754,
136.596915497846));
#171254=CARTESIAN_POINT('Ctrl Pts',(-113.050787665441,1.05163837635196,
136.629034096203));
#171255=CARTESIAN_POINT('Ctrl Pts',(-113.043379445775,0.896175540257714,
136.654963777442));
#171256=CARTESIAN_POINT('Ctrl Pts',(-113.035971226108,0.740066468676722,
136.674644442428));
#171257=CARTESIAN_POINT('Ctrl Pts',(-113.028558446806,0.583861314566547,
136.694337220536));
#171258=CARTESIAN_POINT('Ctrl Pts',(-113.021145667504,0.427009503482,136.707773286638));
#171259=CARTESIAN_POINT('Ctrl Pts',(-113.013732888202,0.270050061054221,
136.714944643449));
#171260=CARTESIAN_POINT('Ctrl Pts',(-113.006309517173,0.112866347614659,
136.722126247031));
#171261=CARTESIAN_POINT('Ctrl Pts',(-112.998886146144,-0.0444249320157711,
136.723025261419));
#171262=CARTESIAN_POINT('Ctrl Pts',(-112.991462775116,-0.201286871721675,
136.717685753035));
#171263=CARTESIAN_POINT('Ctrl Pts',(-112.987526725675,-0.284458836002299,
136.714854617571));
#171264=CARTESIAN_POINT('Ctrl Pts',(-112.983590676234,-0.367510205607769,
136.710270474008));
#171265=CARTESIAN_POINT('Ctrl Pts',(-112.979654626794,-0.450361994384643,
136.703945741667));
#171266=CARTESIAN_POINT('Ctrl Pts',(-112.972231360388,-0.60661788230606,
136.69201749386));
#171267=CARTESIAN_POINT('Ctrl Pts',(-112.964808093983,-0.762635824064563,
136.673859051977));
#171268=CARTESIAN_POINT('Ctrl Pts',(-112.957384827577,-0.917878877959609,
136.649480712816));
#171269=CARTESIAN_POINT('Ctrl Pts',(-112.949970334856,-1.07293844745841,
136.625131186827));
#171270=CARTESIAN_POINT('Ctrl Pts',(-112.942555842135,-1.22722458692694,
136.594576453911));
#171271=CARTESIAN_POINT('Ctrl Pts',(-112.935141349414,-1.38020279964729,
136.557878740797));
#171272=CARTESIAN_POINT('Ctrl Pts',(-112.92773400306,-1.53303356620713,
136.52121639832));
#171273=CARTESIAN_POINT('Ctrl Pts',(-112.920326656706,-1.68455855512059,
136.478422949359));
#171274=CARTESIAN_POINT('Ctrl Pts',(-112.912919310352,-1.83425093232574,
136.429612085702));
#171275=CARTESIAN_POINT('Ctrl Pts',(-112.905517488676,-1.98383166330756,
136.380837627028));
#171276=CARTESIAN_POINT('Ctrl Pts',(-112.898115667001,-2.13158215074669,
136.326054805129));
#171277=CARTESIAN_POINT('Ctrl Pts',(-112.890713845326,-2.27698836641902,
136.265427779));
#171278=CARTESIAN_POINT('Ctrl Pts',(-112.883315931014,-2.42231782328193,
136.204832757406));
#171279=CARTESIAN_POINT('Ctrl Pts',(-112.875918016703,-2.5653051292881,
136.13839981902));
#171280=CARTESIAN_POINT('Ctrl Pts',(-112.868520102391,-2.70545407610144,
136.06634206989));
#171281=CARTESIAN_POINT('Ctrl Pts',(-112.861123417479,-2.84557973270179,
135.994296295452));
#171282=CARTESIAN_POINT('Ctrl Pts',(-112.853726732567,-2.98286763459972,
135.916627735978));
#171283=CARTESIAN_POINT('Ctrl Pts',(-112.846330047654,-3.11684402250852,
135.833596533871));
#171284=CARTESIAN_POINT('Ctrl Pts',(-112.838933690719,-3.25081446976426,
135.750569013454));
#171285=CARTESIAN_POINT('Ctrl Pts',(-112.831537333783,-3.38147337768759,
135.662179519848));
#171286=CARTESIAN_POINT('Ctrl Pts',(-112.824140976848,-3.50837418993428,
135.568732675446));
#171287=CARTESIAN_POINT('Ctrl Pts',(-112.816743487511,-3.63529443101929,
135.475271524093));
#171288=CARTESIAN_POINT('Ctrl Pts',(-112.809345998174,-3.75845513016968,
135.376751701586));
#171289=CARTESIAN_POINT('Ctrl Pts',(-112.801948508838,-3.87744128913971,
135.273519331661));
#171290=CARTESIAN_POINT('Ctrl Pts',(-112.794548426322,-3.99646915852248,
135.17025077379));
#171291=CARTESIAN_POINT('Ctrl Pts',(-112.787148343807,-4.11131929235792,
135.062266623909));
#171292=CARTESIAN_POINT('Ctrl Pts',(-112.779748261292,-4.22161227235034,
134.949951092328));
#171293=CARTESIAN_POINT('Ctrl Pts',(-112.772340041626,-4.33202653081314,
134.837512058274));
#171294=CARTESIAN_POINT('Ctrl Pts',(-112.764931821959,-4.43787336630588,
134.720732397407));
#171295=CARTESIAN_POINT('Ctrl Pts',(-112.757523602293,-4.53881203350988,
134.600031294398));
#171296=CARTESIAN_POINT('Ctrl Pts',(-112.750110822991,-4.63981282677959,
134.479255901874));
#171297=CARTESIAN_POINT('Ctrl Pts',(-112.742698043688,-4.73589920493002,
134.354554552856));
#171298=CARTESIAN_POINT('Ctrl Pts',(-112.735285264386,-4.82677308309787,
134.226376422144));
#171299=CARTESIAN_POINT('Ctrl Pts',(-112.727861893357,-4.91777680612428,
134.098015144508));
#171300=CARTESIAN_POINT('Ctrl Pts',(-112.720438522329,-5.00355295108318,
133.966167475469));
#171301=CARTESIAN_POINT('Ctrl Pts',(-112.7130151513,-5.08384838143384,133.831308948326));
#171302=CARTESIAN_POINT('Ctrl Pts',(-112.70907910186,-5.12642294526084,
133.759803721361));
#171303=CARTESIAN_POINT('Ctrl Pts',(-112.705143052419,-5.16745746935994,
133.687452410416));
#171304=CARTESIAN_POINT('Ctrl Pts',(-112.701207002979,-5.20691970851158,
133.614328181723));
#171305=CARTESIAN_POINT('Ctrl Pts',(-112.693383344829,-5.28535852734934,
133.468979659936));
#171306=CARTESIAN_POINT('Ctrl Pts',(-112.685559686679,-5.35779890327574,
133.320175471554));
#171307=CARTESIAN_POINT('Ctrl Pts',(-112.677736028528,-5.4239404560296,
133.168425018538));
#171308=CARTESIAN_POINT('Ctrl Pts',(-112.669925520726,-5.48997083515598,
133.01692963435));
#171309=CARTESIAN_POINT('Ctrl Pts',(-112.662115012924,-5.54972337017719,
132.86249814332));
#171310=CARTESIAN_POINT('Ctrl Pts',(-112.654304505122,-5.60294318882384,
132.705664955465));
#171311=CARTESIAN_POINT('Ctrl Pts',(-112.646511917776,-5.65604089973241,
132.549191606224));
#171312=CARTESIAN_POINT('Ctrl Pts',(-112.63871933043,-5.70263569018409,
132.390327847665));
#171313=CARTESIAN_POINT('Ctrl Pts',(-112.630926743085,-5.74252069389382,
132.229627835565));
#171314=CARTESIAN_POINT('Ctrl Pts',(-112.623144694277,-5.78235175792649,
132.069145150929));
#171315=CARTESIAN_POINT('Ctrl Pts',(-112.61536264547,-5.81549104384244,
131.906831464921));
#171316=CARTESIAN_POINT('Ctrl Pts',(-112.607580596663,-5.8417807737891,
131.743257818269));
#171317=CARTESIAN_POINT('Ctrl Pts',(-112.599813085406,-5.86802139221372,
131.57998974154));
#171318=CARTESIAN_POINT('Ctrl Pts',(-112.592045574148,-5.88743792681151,
131.41546670787));
#171319=CARTESIAN_POINT('Ctrl Pts',(-112.584278062891,-5.89992324519862,
131.250271217647));
#171320=CARTESIAN_POINT('Ctrl Pts',(-112.577310439339,-5.91112284254257,
131.102087333491));
#171321=CARTESIAN_POINT('Ctrl Pts',(-112.570342815787,-5.91674586775566,
130.95336270369));
#171322=CARTESIAN_POINT('Ctrl Pts',(-112.563375192235,-5.91674999772218,
130.804524796032));
#171323=CARTESIAN_POINT('',(-110.813375192205,-5.91674751312338,130.798935818188));
#171324=CARTESIAN_POINT('Ctrl Pts',(-112.563375192205,-5.9167499977222,
130.804524795383));
#171325=CARTESIAN_POINT('Ctrl Pts',(-112.555642867804,-5.91675458093688,
130.639351838401));
#171326=CARTESIAN_POINT('Ctrl Pts',(-112.547910543403,-5.90983835624213,
130.474306327478));
#171327=CARTESIAN_POINT('Ctrl Pts',(-112.540178219002,-5.89605913921249,
130.309974948873));
#171328=CARTESIAN_POINT('Ctrl Pts',(-112.532436725038,-5.88226358176701,
130.145448693951));
#171329=CARTESIAN_POINT('Ctrl Pts',(-112.524695231074,-5.8615888162922,
129.9816385811));
#171330=CARTESIAN_POINT('Ctrl Pts',(-112.51695373711,-5.83414414635372,
129.819123264404));
#171331=CARTESIAN_POINT('Ctrl Pts',(-112.509104207281,-5.80631647428949,
129.654339976844));
#171332=CARTESIAN_POINT('Ctrl Pts',(-112.501254677453,-5.77152862197727,
129.490888229268));
#171333=CARTESIAN_POINT('Ctrl Pts',(-112.493405147624,-5.72994687374479,
129.329355740773));
#171334=CARTESIAN_POINT('Ctrl Pts',(-112.485637347382,-5.68879807616569,
129.16950513434));
#171335=CARTESIAN_POINT('Ctrl Pts',(-112.477869547139,-5.64099635216969,
129.011534291415));
#171336=CARTESIAN_POINT('Ctrl Pts',(-112.470101746897,-5.58675172779189,
128.855993174163));
#171337=CARTESIAN_POINT('Ctrl Pts',(-112.462211352275,-5.53165099411291,
128.697997247816));
#171338=CARTESIAN_POINT('Ctrl Pts',(-112.454320957654,-5.4699024378795,
128.542508702172));
#171339=CARTESIAN_POINT('Ctrl Pts',(-112.446430563032,-5.40177507766933,
128.390078825237));
#171340=CARTESIAN_POINT('Ctrl Pts',(-112.438540168411,-5.33364771745899,
128.237648948302));
#171341=CARTESIAN_POINT('Ctrl Pts',(-112.430649773789,-5.25914176213731,
128.088278016487));
#171342=CARTESIAN_POINT('Ctrl Pts',(-112.422759379168,-5.17857258267913,
127.94248770487));
#171343=CARTESIAN_POINT('Ctrl Pts',(-112.415336112762,-5.10277327074935,
127.805328491124));
#171344=CARTESIAN_POINT('Ctrl Pts',(-112.407912846357,-5.02140639758439,
127.670975377606));
#171345=CARTESIAN_POINT('Ctrl Pts',(-112.400489579952,-4.93470451707544,
127.539912441893));
#171346=CARTESIAN_POINT('Ctrl Pts',(-112.393075087231,-4.84810511098886,
127.409004411686));
#171347=CARTESIAN_POINT('Ctrl Pts',(-112.38566059451,-4.75618345271013,
127.28137912707));
#171348=CARTESIAN_POINT('Ctrl Pts',(-112.378246101789,-4.65921831098971,
127.157496856327));
#171349=CARTESIAN_POINT('Ctrl Pts',(-112.370838755436,-4.56234662792355,
127.033733987981));
#171350=CARTESIAN_POINT('Ctrl Pts',(-112.363431409082,-4.46044136744951,
126.913707243357));
#171351=CARTESIAN_POINT('Ctrl Pts',(-112.356024062729,-4.35382492155404,
126.797848529109));
#171352=CARTESIAN_POINT('Ctrl Pts',(-112.348622241053,-4.24728799422634,
126.682076226661));
#171353=CARTESIAN_POINT('Ctrl Pts',(-112.341220419378,-4.13604712957681,
126.570466038308));
#171354=CARTESIAN_POINT('Ctrl Pts',(-112.333818597703,-4.020465297414,126.463417246041));
#171355=CARTESIAN_POINT('Ctrl Pts',(-112.326420683392,-3.90494448000071,
126.356424963998));
#171356=CARTESIAN_POINT('Ctrl Pts',(-112.31902276908,-3.78508753201583,
126.253989535557));
#171357=CARTESIAN_POINT('Ctrl Pts',(-112.311624854769,-3.66129453431139,
126.156473689561));
#171358=CARTESIAN_POINT('Ctrl Pts',(-112.304228169857,-3.53752210875751,
126.058974048929));
#171359=CARTESIAN_POINT('Ctrl Pts',(-112.296831484945,-3.40981522463513,
125.966392598926));
#171360=CARTESIAN_POINT('Ctrl Pts',(-112.289434800033,-3.27860741183864,
125.879052099155));
#171361=CARTESIAN_POINT('Ctrl Pts',(-112.282038443098,-3.14740541693406,
125.791715472153));
#171362=CARTESIAN_POINT('Ctrl Pts',(-112.274642086162,-3.01270311276057,
125.709619540167));
#171363=CARTESIAN_POINT('Ctrl Pts',(-112.267245729227,-2.87496317716572,
125.63304383241));
#171364=CARTESIAN_POINT('Ctrl Pts',(-112.259848239891,-2.73720215323548,
125.556456400716));
#171365=CARTESIAN_POINT('Ctrl Pts',(-112.252450750554,-2.59640289815762,
125.485391057476));
#171366=CARTESIAN_POINT('Ctrl Pts',(-112.245053261218,-2.45305271830573,
125.420081378549));
#171367=CARTESIAN_POINT('Ctrl Pts',(-112.237653178703,-2.3096522872699,
125.354748805414));
#171368=CARTESIAN_POINT('Ctrl Pts',(-112.230253096188,-2.16369949056062,
125.295176068368));
#171369=CARTESIAN_POINT('Ctrl Pts',(-112.222853013673,-2.01570148553828,
125.241548551381));
#171370=CARTESIAN_POINT('Ctrl Pts',(-112.215444794007,-1.86754074149505,
125.187862065425));
#171371=CARTESIAN_POINT('Ctrl Pts',(-112.20803657434,-1.71733064908698,
125.140133982357));
#171372=CARTESIAN_POINT('Ctrl Pts',(-112.200628354674,-1.56559410038212,
125.09849997474));
#171373=CARTESIAN_POINT('Ctrl Pts',(-112.193215575372,-1.41376416036338,
125.056840342086));
#171374=CARTESIAN_POINT('Ctrl Pts',(-112.18580279607,-1.26040625476733,
125.021282342947));
#171375=CARTESIAN_POINT('Ctrl Pts',(-112.178390016768,-1.10605281966712,
124.991910383576));
#171376=CARTESIAN_POINT('Ctrl Pts',(-112.17096664574,-0.951478837140164,
124.962496456172));
#171377=CARTESIAN_POINT('Ctrl Pts',(-112.163543274711,-0.795906852372275,
124.939286276748));
#171378=CARTESIAN_POINT('Ctrl Pts',(-112.156119903682,-0.639874591418284,
124.922312413942));
#171379=CARTESIAN_POINT('Ctrl Pts',(-112.15218385424,-0.557142542677966,
124.913312464596));
#171380=CARTESIAN_POINT('Ctrl Pts',(-112.148247804797,-0.474281109374064,
124.906064896517));
#171381=CARTESIAN_POINT('Ctrl Pts',(-112.144311755355,-0.391370240704987,
124.900568624517));
#171382=CARTESIAN_POINT('Ctrl Pts',(-112.136888488949,-0.235002930027058,
124.890202827062));
#171383=CARTESIAN_POINT('Ctrl Pts',(-112.129465222544,-0.0779870681005315,
124.886037942271));
#171384=CARTESIAN_POINT('Ctrl Pts',(-112.122041956138,0.0791443758398206,
124.888139971725));
#171385=CARTESIAN_POINT('Ctrl Pts',(-112.114627463417,0.23609010346239,
124.890239516755));
#171386=CARTESIAN_POINT('Ctrl Pts',(-112.107212970696,0.393150771559606,
124.898591227467));
#171387=CARTESIAN_POINT('Ctrl Pts',(-112.099798477975,0.54978846207174,
124.913209354063));
#171388=CARTESIAN_POINT('Ctrl Pts',(-112.092391131621,0.706275179280899,
124.927813391159));
#171389=CARTESIAN_POINT('Ctrl Pts',(-112.084983785268,0.862339361331365,
124.948671785618));
#171390=CARTESIAN_POINT('Ctrl Pts',(-112.077576438914,1.01744337217851,
124.975746756028));
#171391=CARTESIAN_POINT('Ctrl Pts',(-112.070174617238,1.17243170060306,
125.002801532904));
#171392=CARTESIAN_POINT('Ctrl Pts',(-112.062772795563,1.32646091758501,
125.036063589805));
#171393=CARTESIAN_POINT('Ctrl Pts',(-112.055370973887,1.47899890182926,
125.075443371621));
#171394=CARTESIAN_POINT('Ctrl Pts',(-112.047973059576,1.63145636245767,
125.114802365156));
#171395=CARTESIAN_POINT('Ctrl Pts',(-112.040575145265,1.78242379758288,
125.160272558826));
#171396=CARTESIAN_POINT('Ctrl Pts',(-112.033177230954,1.93137977968521,
125.211713417078));
#171397=CARTESIAN_POINT('Ctrl Pts',(-112.025780546041,2.08031100800629,
125.263145726793));
#171398=CARTESIAN_POINT('Ctrl Pts',(-112.018383861129,2.22723109422135,
125.320546610101));
#171399=CARTESIAN_POINT('Ctrl Pts',(-112.010987176217,2.37163415803816,
125.383725785471));
#171400=CARTESIAN_POINT('Ctrl Pts',(-112.003590819282,2.5160308188718,125.44690215941));
#171401=CARTESIAN_POINT('Ctrl Pts',(-111.996194462346,2.65791033722359,
125.515856166338));
#171402=CARTESIAN_POINT('Ctrl Pts',(-111.988798105411,2.7967874485724,125.590349634646));
#171403=CARTESIAN_POINT('Ctrl Pts',(-111.981400616074,2.93568582236149,
125.664854508095));
#171404=CARTESIAN_POINT('Ctrl Pts',(-111.974003126738,3.07158054488917,
125.744900355148));
#171405=CARTESIAN_POINT('Ctrl Pts',(-111.966605637401,3.20401170117158,
125.830203444611));
#171406=CARTESIAN_POINT('Ctrl Pts',(-111.959205554886,3.33648928099109,
125.915536436941));
#171407=CARTESIAN_POINT('Ctrl Pts',(-111.951805472371,3.46550056357364,
126.006130138896));
#171408=CARTESIAN_POINT('Ctrl Pts',(-111.944405389856,3.59061544919406,
126.101658069189));
#171409=CARTESIAN_POINT('Ctrl Pts',(-111.936997170189,3.71586791149281,
126.197291042262));
#171410=CARTESIAN_POINT('Ctrl Pts',(-111.929588950523,3.83721512353996,
126.297868852459));
#171411=CARTESIAN_POINT('Ctrl Pts',(-111.922180730857,3.95426030423132,
126.403024910206));
#171412=CARTESIAN_POINT('Ctrl Pts',(-111.914767951555,4.0713775242784,126.508245689753));
#171413=CARTESIAN_POINT('Ctrl Pts',(-111.907355172252,4.18418716995908,
126.618050071969));
#171414=CARTESIAN_POINT('Ctrl Pts',(-111.89994239295,4.29233043319898,126.73203572695));
#171415=CARTESIAN_POINT('Ctrl Pts',(-111.892519021922,4.40062821660466,
126.846184249979));
#171416=CARTESIAN_POINT('Ctrl Pts',(-111.885095650893,4.50424605572476,
126.964525697877));
#171417=CARTESIAN_POINT('Ctrl Pts',(-111.877672279864,4.60286589557306,
127.086625270628));
#171418=CARTESIAN_POINT('Ctrl Pts',(-111.873736230423,4.65515650101219,
127.151365393841));
#171419=CARTESIAN_POINT('Ctrl Pts',(-111.869800180983,4.70604271397878,
127.217161576831));
#171420=CARTESIAN_POINT('Ctrl Pts',(-111.865864131542,4.75548223297956,
127.2839459695));
#171421=CARTESIAN_POINT('Ctrl Pts',(-111.858440865136,4.84872362285936,
127.409899249804));
#171422=CARTESIAN_POINT('Ctrl Pts',(-111.851017598731,4.93709856708689,
127.539749919401));
#171423=CARTESIAN_POINT('Ctrl Pts',(-111.843594332325,5.02026345377358,
127.673085251648));
#171424=CARTESIAN_POINT('Ctrl Pts',(-111.836179839604,5.1033300464711,127.806262992605));
#171425=CARTESIAN_POINT('Ctrl Pts',(-111.828765346883,5.1811986432444,127.942916884508));
#171426=CARTESIAN_POINT('Ctrl Pts',(-111.821350854162,5.25356649714264,
128.082602064241));
#171427=CARTESIAN_POINT('Ctrl Pts',(-111.813943507808,5.32586460017808,
128.222152610137));
#171428=CARTESIAN_POINT('Ctrl Pts',(-111.806536161455,5.3926723446569,128.364728298163));
#171429=CARTESIAN_POINT('Ctrl Pts',(-111.799128815101,5.45373091173638,
128.509856378112));
#171430=CARTESIAN_POINT('Ctrl Pts',(-111.791726993425,5.51474393903293,
128.654876216064));
#171431=CARTESIAN_POINT('Ctrl Pts',(-111.78432517175,5.57001618268286,128.802444312871));
#171432=CARTESIAN_POINT('Ctrl Pts',(-111.776923350075,5.61933536337916,
128.952064573091));
#171433=CARTESIAN_POINT('Ctrl Pts',(-111.769525435763,5.66862850886386,
129.101605849941));
#171434=CARTESIAN_POINT('Ctrl Pts',(-111.762127521452,5.71197473341609,
129.253196779083));
#171435=CARTESIAN_POINT('Ctrl Pts',(-111.75472960714,5.74921042926596,129.406322705877));
#171436=CARTESIAN_POINT('Ctrl Pts',(-111.747332922228,5.78643993721887,
129.559423185921));
#171437=CARTESIAN_POINT('Ctrl Pts',(-111.739936237316,5.81756084373676,
129.71405779497));
#171438=CARTESIAN_POINT('Ctrl Pts',(-111.732539552404,5.84245979740451,
129.869698069792));
#171439=CARTESIAN_POINT('Ctrl Pts',(-111.725143195468,5.86735764702656,
130.025331443361));
#171440=CARTESIAN_POINT('Ctrl Pts',(-111.717746838533,5.88603403338742,
130.181970025428));
#171441=CARTESIAN_POINT('Ctrl Pts',(-111.710350481597,5.89842703968086,
130.339076811635));
#171442=CARTESIAN_POINT('Ctrl Pts',(-111.702952992261,5.91082194337521,
130.496207651292));
#171443=CARTESIAN_POINT('Ctrl Pts',(-111.695555502924,5.91693152217169,
130.653806465655));
#171444=CARTESIAN_POINT('Ctrl Pts',(-111.688158013587,5.91674589187827,
130.81133295158));
#171445=CARTESIAN_POINT('Ctrl Pts',(-111.680757931072,5.91656019651245,
130.968914658171));
#171446=CARTESIAN_POINT('Ctrl Pts',(-111.673357848557,5.91007489882196,
131.126423612777));
#171447=CARTESIAN_POINT('Ctrl Pts',(-111.665957766042,5.89733219735277,
131.28332148921));
#171448=CARTESIAN_POINT('Ctrl Pts',(-111.658549546376,5.88457548397331,
131.440391890988));
#171449=CARTESIAN_POINT('Ctrl Pts',(-111.651141326709,5.86554765592489,
131.596849500377));
#171450=CARTESIAN_POINT('Ctrl Pts',(-111.643733107043,5.84034266551811,
131.752162343577));
#171451=CARTESIAN_POINT('Ctrl Pts',(-111.636320327741,5.81512216186016,
131.907570779241));
#171452=CARTESIAN_POINT('Ctrl Pts',(-111.628907548438,5.78371699429802,
132.061832679798));
#171453=CARTESIAN_POINT('Ctrl Pts',(-111.621494769136,5.74627170984768,
132.214428700711));
#171454=CARTESIAN_POINT('Ctrl Pts',(-111.614071398108,5.70877292181908,
132.367242757974));
#171455=CARTESIAN_POINT('Ctrl Pts',(-111.606648027079,5.66521688314878,
132.518385823875));
#171456=CARTESIAN_POINT('Ctrl Pts',(-111.59922465605,5.61579748691372,132.66735528972));
#171457=CARTESIAN_POINT('Ctrl Pts',(-111.595288606609,5.58959413723057,
132.746342474975));
#171458=CARTESIAN_POINT('Ctrl Pts',(-111.591352557169,5.56174318611317,
132.824718931174));
#171459=CARTESIAN_POINT('Ctrl Pts',(-111.587416507729,5.53227885277902,
132.902412394237));
#171460=CARTESIAN_POINT('Ctrl Pts',(-111.579993241323,5.47671003965574,
133.048939840859));
#171461=CARTESIAN_POINT('Ctrl Pts',(-111.572569974918,5.4152318097948,133.193479643042));
#171462=CARTESIAN_POINT('Ctrl Pts',(-111.565146708512,5.34800567119306,
133.335519621538));
#171463=CARTESIAN_POINT('Ctrl Pts',(-111.557732215791,5.28085898830436,
133.477391720575));
#171464=CARTESIAN_POINT('Ctrl Pts',(-111.55031772307,5.20797807741091,133.616769542922));
#171465=CARTESIAN_POINT('Ctrl Pts',(-111.54290323035,5.12957357232856,133.753157919614));
#171466=CARTESIAN_POINT('Ctrl Pts',(-111.535495883996,5.05124463646009,
133.889414840055));
#171467=CARTESIAN_POINT('Ctrl Pts',(-111.528088537642,4.96740288993177,
134.022687729561));
#171468=CARTESIAN_POINT('Ctrl Pts',(-111.520681191288,4.87830617297523,
134.152503303476));
#171469=CARTESIAN_POINT('Ctrl Pts',(-111.513279369613,4.78927590771137,
134.282222056039));
#171470=CARTESIAN_POINT('Ctrl Pts',(-111.505877547938,4.69499868631527,
134.408488320888));
#171471=CARTESIAN_POINT('Ctrl Pts',(-111.498475726262,4.59577714578074,
134.530855349726));
#171472=CARTESIAN_POINT('Ctrl Pts',(-111.491077811951,4.49660798352456,
134.653157781964));
#171473=CARTESIAN_POINT('Ctrl Pts',(-111.483679897639,4.39249993472033,
134.771564788325));
#171474=CARTESIAN_POINT('Ctrl Pts',(-111.476281983328,4.2837975588958,134.885660537555));
#171475=CARTESIAN_POINT('Ctrl Pts',(-111.468885298416,4.17511324743484,
134.99973732614));
#171476=CARTESIAN_POINT('Ctrl Pts',(-111.461488613504,4.06183638150699,
135.109504009534));
#171477=CARTESIAN_POINT('Ctrl Pts',(-111.454091928591,3.94435030298717,
135.214579574696));
#171478=CARTESIAN_POINT('Ctrl Pts',(-111.446695571656,3.8268694339232,135.319650480696));
#171479=CARTESIAN_POINT('Ctrl Pts',(-111.439299214721,3.70518000162044,
135.420030433202));
#171480=CARTESIAN_POINT('Ctrl Pts',(-111.431902857785,3.57970033550769,
135.515377075876));
#171481=CARTESIAN_POINT('Ctrl Pts',(-111.424505368449,3.45420145813773,
135.610738316365));
#171482=CARTESIAN_POINT('Ctrl Pts',(-111.417107879112,3.32491148875949,
135.701064486766));
#171483=CARTESIAN_POINT('Ctrl Pts',(-111.409710389775,3.19227965706237,
135.786055224184));
#171484=CARTESIAN_POINT('Ctrl Pts',(-111.40231030726,3.05960133148206,135.871075754973));
#171485=CARTESIAN_POINT('Ctrl Pts',(-111.394910224745,2.92357912527311,
135.950756927688));
#171486=CARTESIAN_POINT('Ctrl Pts',(-111.38751014223,2.78468875685034,136.024843266706));
#171487=CARTESIAN_POINT('Ctrl Pts',(-111.380101922564,2.64564566418941,
136.09901107127));
#171488=CARTESIAN_POINT('Ctrl Pts',(-111.372693702898,2.503728440462,136.167571580201));
#171489=CARTESIAN_POINT('Ctrl Pts',(-111.365285483231,2.35943543380992,
136.230316293406));
#171490=CARTESIAN_POINT('Ctrl Pts',(-111.357872703929,2.21505361721908,
136.293099624936));
#171491=CARTESIAN_POINT('Ctrl Pts',(-111.350459924627,2.06829345117668,
136.350059893333));
#171492=CARTESIAN_POINT('Ctrl Pts',(-111.343047145325,1.91967000614294,
136.401037991689));
#171493=CARTESIAN_POINT('Ctrl Pts',(-111.335623774296,1.77083420096182,
136.452088929941));
#171494=CARTESIAN_POINT('Ctrl Pts',(-111.328200403268,1.62013015620956,
136.497140520032));
#171495=CARTESIAN_POINT('Ctrl Pts',(-111.320777032239,1.46808553476072,
136.53608421742));
#171496=CARTESIAN_POINT('Ctrl Pts',(-111.316840982798,1.38746782820295,
136.556733100218));
#171497=CARTESIAN_POINT('Ctrl Pts',(-111.312904933357,1.30647337647703,
136.575665695293));
#171498=CARTESIAN_POINT('Ctrl Pts',(-111.308968883916,1.22518147372208,
136.592871731743));
#171499=CARTESIAN_POINT('Ctrl Pts',(-111.30154561751,1.07186748216805,136.625321779503));
#171500=CARTESIAN_POINT('Ctrl Pts',(-111.294122351105,0.917031568081696,
136.651725697228));
#171501=CARTESIAN_POINT('Ctrl Pts',(-111.286699084699,0.761191941386301,
136.671942520775));
#171502=CARTESIAN_POINT('Ctrl Pts',(-111.279284591978,0.60553650418754,
136.692135449717));
#171503=CARTESIAN_POINT('Ctrl Pts',(-111.271870099257,0.448880082307066,
136.706155792758));
#171504=CARTESIAN_POINT('Ctrl Pts',(-111.264455606536,0.291753128140704,
136.713913111175));
#171505=CARTESIAN_POINT('Ctrl Pts',(-111.257048260182,0.134777618849387,
136.721662952796));
#171506=CARTESIAN_POINT('Ctrl Pts',(-111.249640913829,-0.0226671495244484,
136.723161769069));
#171507=CARTESIAN_POINT('Ctrl Pts',(-111.242233567475,-0.180043620251498,
136.718370666366));
#171508=CARTESIAN_POINT('Ctrl Pts',(-111.234831745799,-0.337302713669653,
136.713583137048));
#171509=CARTESIAN_POINT('Ctrl Pts',(-111.227429924124,-0.494493239348228,
136.702515040993));
#171510=CARTESIAN_POINT('Ctrl Pts',(-111.220028102449,-0.65107575260525,
136.685179516909));
#171511=CARTESIAN_POINT('Ctrl Pts',(-111.212630188137,-0.807575607171467,
136.667853144113));
#171512=CARTESIAN_POINT('Ctrl Pts',(-111.205232273826,-0.963467718441625,
136.644265973351));
#171513=CARTESIAN_POINT('Ctrl Pts',(-111.197834359514,-1.1182159929637,
136.61448312536));
#171514=CARTESIAN_POINT('Ctrl Pts',(-111.190437674602,-1.27293855113108,
136.584705226739));
#171515=CARTESIAN_POINT('Ctrl Pts',(-111.18304098969,-1.42651728360098,
136.54873376484));
#171516=CARTESIAN_POINT('Ctrl Pts',(-111.175644304778,-1.57842442766419,
136.506685309185));
#171517=CARTESIAN_POINT('Ctrl Pts',(-111.168247947842,-1.73032483600501,
136.464638718003));
#171518=CARTESIAN_POINT('Ctrl Pts',(-111.160851590907,-1.88055344354558,
136.416515768428));
#171519=CARTESIAN_POINT('Ctrl Pts',(-111.153455233971,-2.02859609893061,
136.362483360894));
#171520=CARTESIAN_POINT('Ctrl Pts',(-111.146057744635,-2.17666142002453,
136.308442680861));
#171521=CARTESIAN_POINT('Ctrl Pts',(-111.138660255298,-2.32253977188676,
136.248490869381));
#171522=CARTESIAN_POINT('Ctrl Pts',(-111.131262765961,-2.46573563108488,
136.182843522633));
#171523=CARTESIAN_POINT('Ctrl Pts',(-111.123862683446,-2.60898168737048,
136.117173163309));
#171524=CARTESIAN_POINT('Ctrl Pts',(-111.116462600931,-2.74954303964861,
136.045803449048));
#171525=CARTESIAN_POINT('Ctrl Pts',(-111.109062518416,-2.88694761161864,
135.968996524411));
#171526=CARTESIAN_POINT('Ctrl Pts',(-111.10165429875,-3.0245032740401,135.892105142665));
#171527=CARTESIAN_POINT('Ctrl Pts',(-111.094246079083,-3.15889489788458,
135.809764792797));
#171528=CARTESIAN_POINT('Ctrl Pts',(-111.086837859417,-3.28967769677574,
135.722282049821));
#171529=CARTESIAN_POINT('Ctrl Pts',(-111.079425080115,-3.4205409902974,
135.634745462677));
#171530=CARTESIAN_POINT('Ctrl Pts',(-111.072012300812,-3.54779073186089,
135.542060394921));
#171531=CARTESIAN_POINT('Ctrl Pts',(-111.06459952151,-3.67101465215211,
135.444574188748));
#171532=CARTESIAN_POINT('Ctrl Pts',(-111.057176150481,-3.7944146405591,
135.346948689713));
#171533=CARTESIAN_POINT('Ctrl Pts',(-111.049752779453,-3.9137770365694,
135.244508593591));
#171534=CARTESIAN_POINT('Ctrl Pts',(-111.042329408424,-4.02872530391475,
135.137639167128));
#171535=CARTESIAN_POINT('Ctrl Pts',(-111.038393358983,-4.08967363340134,
135.080974432926));
#171536=CARTESIAN_POINT('Ctrl Pts',(-111.034457309543,-4.1493816413853,
135.023065036908));
#171537=CARTESIAN_POINT('Ctrl Pts',(-111.030521260103,-4.20779782624605,
134.963972139804));
#171538=CARTESIAN_POINT('Ctrl Pts',(-111.023198451068,-4.3164780074149,
134.854032971776));
#171539=CARTESIAN_POINT('Ctrl Pts',(-111.015875642033,-4.42103274883604,
134.739643052212));
#171540=CARTESIAN_POINT('Ctrl Pts',(-111.008552832998,-4.52106797482426,
134.621149179894));
#171541=CARTESIAN_POINT('Ctrl Pts',(-111.00123885966,-4.62098249836996,
134.50279828221));
#171542=CARTESIAN_POINT('Ctrl Pts',(-110.993924886322,-4.71638811132162,
134.380353575008));
#171543=CARTESIAN_POINT('Ctrl Pts',(-110.986610912985,-4.80692618199845,
134.254199924449));
#171544=CARTESIAN_POINT('Ctrl Pts',(-110.979305281407,-4.89736099185748,
134.128190155122));
#171545=CARTESIAN_POINT('Ctrl Pts',(-110.971999649829,-4.98293909235842,
133.99848017652));
#171546=CARTESIAN_POINT('Ctrl Pts',(-110.964694018251,-5.06334123005648,
133.865488865534));
#171547=CARTESIAN_POINT('Ctrl Pts',(-110.957393102566,-5.14369146699154,
133.732583402397));
#171548=CARTESIAN_POINT('Ctrl Pts',(-110.950092186881,-5.21887218919547,
133.596401147546));
#171549=CARTESIAN_POINT('Ctrl Pts',(-110.942791271196,-5.28860661020286,
133.457391089502));
#171550=CARTESIAN_POINT('Ctrl Pts',(-110.935493534486,-5.35831066734712,
133.318441559419));
#171551=CARTESIAN_POINT('Ctrl Pts',(-110.928195797777,-5.42257296965475,
133.176667018737));
#171552=CARTESIAN_POINT('Ctrl Pts',(-110.920898061067,-5.48116212836772,
133.032542002698));
#171553=CARTESIAN_POINT('Ctrl Pts',(-110.91360196904,-5.53973808290514,
132.888449467958));
#171554=CARTESIAN_POINT('Ctrl Pts',(-110.906305877013,-5.59264329444742,
132.74200786814));
#171555=CARTESIAN_POINT('Ctrl Pts',(-110.899009784987,-5.63969419815228,
132.593712431444));
#171556=CARTESIAN_POINT('Ctrl Pts',(-110.891711309516,-5.6867604721658,
132.445368550479));
#171557=CARTESIAN_POINT('Ctrl Pts',(-110.884412834046,-5.72796849501785,
132.295169987417));
#171558=CARTESIAN_POINT('Ctrl Pts',(-110.877114358575,-5.76318429015178,
132.143628104011));
#171559=CARTESIAN_POINT('Ctrl Pts',(-110.86981486775,-5.79840498446254,
131.992065138289));
#171560=CARTESIAN_POINT('Ctrl Pts',(-110.862515376925,-5.82763171215511,
131.839158856489));
#171561=CARTESIAN_POINT('Ctrl Pts',(-110.855215886099,-5.85078163412601,
131.685430894147));
#171562=CARTESIAN_POINT('Ctrl Pts',(-110.847909803773,-5.87395246067146,
131.53156411416));
#171563=CARTESIAN_POINT('Ctrl Pts',(-110.840603721446,-5.89103546933593,
131.376874552918));
#171564=CARTESIAN_POINT('Ctrl Pts',(-110.833297639119,-5.90199966949726,
131.221889615067));
#171565=CARTESIAN_POINT('Ctrl Pts',(-110.826656823481,-5.91196550736092,
131.081017071772));
#171566=CARTESIAN_POINT('Ctrl Pts',(-110.820016007843,-5.91687675752732,
130.939900755746));
#171567=CARTESIAN_POINT('Ctrl Pts',(-110.813375192205,-5.91674751312338,
130.798935818188));
#171568=CARTESIAN_POINT('',(-109.063375192205,-5.92157197187691,130.806665548282));
#171569=CARTESIAN_POINT('Ctrl Pts',(-110.813375192205,-5.91750148305884,
130.798935126907));
#171570=CARTESIAN_POINT('Ctrl Pts',(-110.792941340233,-5.92153502060429,
130.365125357009));
#171571=CARTESIAN_POINT('Ctrl Pts',(-110.772507488262,-5.87789815567871,
129.932120052829));
#171572=CARTESIAN_POINT('Ctrl Pts',(-110.659257761686,-5.3550699825935,
127.595153321436));
#171573=CARTESIAN_POINT('Ctrl Pts',(-110.473626012476,-2.40606949429832,
124.232573180426));
#171574=CARTESIAN_POINT('Ctrl Pts',(-110.195178388666,4.22849156037399,
125.227854573977));
#171575=CARTESIAN_POINT('Ctrl Pts',(-109.916730764851,6.9772754443608,131.34767259412));
#171576=CARTESIAN_POINT('Ctrl Pts',(-109.638283141039,3.31428405383379,
136.968213450076));
#171577=CARTESIAN_POINT('Ctrl Pts',(-109.359835517226,-3.39437247038935,
136.924474673905));
#171578=CARTESIAN_POINT('Ctrl Pts',(-109.168199534281,-5.86470081146466,
133.023708255532));
#171579=CARTESIAN_POINT('Ctrl Pts',(-109.069379425941,-5.92607768413121,
130.933692464336));
#171580=CARTESIAN_POINT('Ctrl Pts',(-109.063375192205,-5.92544804556881,
130.806667057017));
#171581=CARTESIAN_POINT('',(-107.313375206758,-5.91311659137678,130.808668519379));
#171582=CARTESIAN_POINT('Ctrl Pts',(-109.063375192205,-5.91674955177621,
130.806663671189));
#171583=CARTESIAN_POINT('Ctrl Pts',(-109.056023423059,-5.91681000323962,
130.651358486149));
#171584=CARTESIAN_POINT('Ctrl Pts',(-109.048671653912,-5.9107514836903,
130.495803539147));
#171585=CARTESIAN_POINT('Ctrl Pts',(-109.041319884766,-5.89854122567361,
130.340526626219));
#171586=CARTESIAN_POINT('Ctrl Pts',(-109.033976470725,-5.88634484431719,
130.185426181713));
#171587=CARTESIAN_POINT('Ctrl Pts',(-109.026633056685,-5.86801066591285,
130.030603518659));
#171588=CARTESIAN_POINT('Ctrl Pts',(-109.019289642645,-5.8435578953709,
129.876588185367));
#171589=CARTESIAN_POINT('Ctrl Pts',(-109.011952897582,-5.81912733179754,
129.722712722265));
#171590=CARTESIAN_POINT('Ctrl Pts',(-109.004616152518,-5.78858929435041,
129.569643503627));
#171591=CARTESIAN_POINT('Ctrl Pts',(-108.997279407455,-5.75201490861492,
129.417906487935));
#171592=CARTESIAN_POINT('Ctrl Pts',(-108.989947651338,-5.71546539326063,
129.266272652579));
#171593=CARTESIAN_POINT('Ctrl Pts',(-108.982615895221,-5.67288778935029,
129.115969585884));
#171594=CARTESIAN_POINT('Ctrl Pts',(-108.975284139104,-5.62440453236753,
128.967514347792));
#171595=CARTESIAN_POINT('Ctrl Pts',(-108.96795496801,-5.57593836955698,
128.819111451881));
#171596=CARTESIAN_POINT('Ctrl Pts',(-108.960625796915,-5.52157081217014,
128.672555450604));
#171597=CARTESIAN_POINT('Ctrl Pts',(-108.95329662582,-5.46147449631298,
128.528349438195));
#171598=CARTESIAN_POINT('Ctrl Pts',(-108.945968652129,-5.40138799868857,
128.384166985436));
#171599=CARTESIAN_POINT('Ctrl Pts',(-108.938640678437,-5.33557475075789,
128.242334109451));
#171600=CARTESIAN_POINT('Ctrl Pts',(-108.931312704745,-5.26425589327723,
128.103334802696));
#171601=CARTESIAN_POINT('Ctrl Pts',(-108.923984414724,-5.19293395714485,
127.964329495698));
#171602=CARTESIAN_POINT('Ctrl Pts',(-108.916656124702,-5.1161061122852,
127.828158340491));
#171603=CARTESIAN_POINT('Ctrl Pts',(-108.909327834681,-5.03403978129622,
127.695281325745));
#171604=CARTESIAN_POINT('Ctrl Pts',(-108.901997714597,-4.95195295623358,
127.562371128192));
#171605=CARTESIAN_POINT('Ctrl Pts',(-108.894667594513,-4.86462524191013,
127.432757032239));
#171606=CARTESIAN_POINT('Ctrl Pts',(-108.887337474429,-4.77236761262287,
127.3068703842));
#171607=CARTESIAN_POINT('Ctrl Pts',(-108.879999739041,-4.68001413635613,
127.180852951802));
#171608=CARTESIAN_POINT('Ctrl Pts',(-108.872662003654,-4.58272074116282,
127.058571009372));
#171609=CARTESIAN_POINT('Ctrl Pts',(-108.865324268266,-4.48083937209908,
126.940423624815));
#171610=CARTESIAN_POINT('Ctrl Pts',(-108.857982558186,-4.37890281609824,
126.822212242373));
#171611=CARTESIAN_POINT('Ctrl Pts',(-108.850640848105,-4.27237359538035,
126.708140157104));
#171612=CARTESIAN_POINT('Ctrl Pts',(-108.843299138025,-4.16164029524909,
126.598569298984));
#171613=CARTESIAN_POINT('Ctrl Pts',(-108.835946378891,-4.05074034482209,
126.488833540008));
#171614=CARTESIAN_POINT('Ctrl Pts',(-108.828593619757,-3.93562395658254,
126.383612797555));
#171615=CARTESIAN_POINT('Ctrl Pts',(-108.821240860623,-3.81671324254075,
126.283229057136));
#171616=CARTESIAN_POINT('Ctrl Pts',(-108.815140663615,-3.71805928573641,
126.199945954592));
#171617=CARTESIAN_POINT('Ctrl Pts',(-108.809040466607,-3.6167943011096,
126.119991532806));
#171618=CARTESIAN_POINT('Ctrl Pts',(-108.802940269599,-3.51317353705052,
126.043526419543));
#171619=CARTESIAN_POINT('Ctrl Pts',(-108.795517003194,-3.38707850507706,
125.950476817087));
#171620=CARTESIAN_POINT('Ctrl Pts',(-108.788093736788,-3.25709349422422,
125.862299585812));
#171621=CARTESIAN_POINT('Ctrl Pts',(-108.780670470383,-3.1236317535783,
125.779337709107));
#171622=CARTESIAN_POINT('Ctrl Pts',(-108.773255977662,-2.99032775362614,
125.696473886451));
#171623=CARTESIAN_POINT('Ctrl Pts',(-108.765841484941,-2.85355551721927,
125.61881334381));
#171624=CARTESIAN_POINT('Ctrl Pts',(-108.75842699222,-2.71376036768682,
125.546658150778));
#171625=CARTESIAN_POINT('Ctrl Pts',(-108.751019645866,-2.57409995798308,
125.474572503637));
#171626=CARTESIAN_POINT('Ctrl Pts',(-108.743612299512,-2.43142276504334,
125.407981812447));
#171627=CARTESIAN_POINT('Ctrl Pts',(-108.736204953159,-2.28620193240537,
125.347144176305));
#171628=CARTESIAN_POINT('Ctrl Pts',(-108.728803131483,-2.14108941094326,
125.286351915167));
#171629=CARTESIAN_POINT('Ctrl Pts',(-108.721401309808,-1.99343737007284,
125.231304309045));
#171630=CARTESIAN_POINT('Ctrl Pts',(-108.713999488133,-1.84374222771336,
125.182212882025));
#171631=CARTESIAN_POINT('Ctrl Pts',(-108.706601573821,-1.69412610825474,
125.133147369988));
#171632=CARTESIAN_POINT('Ctrl Pts',(-108.69920365951,-1.54246938907896,
125.090031891219));
#171633=CARTESIAN_POINT('Ctrl Pts',(-108.691805745199,-1.3892869732124,
125.053029270081));
#171634=CARTESIAN_POINT('Ctrl Pts',(-108.684409060287,-1.23613001348369,
125.016032798108));
#171635=CARTESIAN_POINT('Ctrl Pts',(-108.677012375374,-1.08144822277829,
124.985147255178));
#171636=CARTESIAN_POINT('Ctrl Pts',(-108.669615690462,-0.925770236217381,
124.960485188347));
#171637=CARTESIAN_POINT('Ctrl Pts',(-108.662219333527,-0.770099152581536,
124.935824215057));
#171638=CARTESIAN_POINT('Ctrl Pts',(-108.654822976591,-0.613432329619568,
124.91738622758));
#171639=CARTESIAN_POINT('Ctrl Pts',(-108.647426619656,-0.45630686529425,
124.905232325421));
#171640=CARTESIAN_POINT('Ctrl Pts',(-108.640029130319,-0.299157344659222,
124.893076562469));
#171641=CARTESIAN_POINT('Ctrl Pts',(-108.632631640983,-0.141549415055182,
124.887206829314));
#171642=CARTESIAN_POINT('Ctrl Pts',(-108.625234151646,0.0159766059581922,
124.887632187888));
#171643=CARTESIAN_POINT('Ctrl Pts',(-108.617834069131,0.173557847473812,
124.88805769557));
#171644=CARTESIAN_POINT('Ctrl Pts',(-108.610433986616,0.331056750167858,
124.894782687566));
#171645=CARTESIAN_POINT('Ctrl Pts',(-108.603033904101,0.4879350526925,124.907764146138));
#171646=CARTESIAN_POINT('Ctrl Pts',(-108.595625684435,0.644985859038026,
124.920759879158));
#171647=CARTESIAN_POINT('Ctrl Pts',(-108.588217464768,0.80141433013455,
124.94002578702));
#171648=CARTESIAN_POINT('Ctrl Pts',(-108.580809245102,0.956688635779004,
124.965467107947));
#171649=CARTESIAN_POINT('Ctrl Pts',(-108.5733964658,1.11205851016769,124.990924087583));
#171650=CARTESIAN_POINT('Ctrl Pts',(-108.565983686498,1.26627243877102,
125.02256397913));
#171651=CARTESIAN_POINT('Ctrl Pts',(-108.558570907196,1.41881129762964,
125.060241445385));
#171652=CARTESIAN_POINT('Ctrl Pts',(-108.551147536167,1.57156811116338,
125.097972746971));
#171653=CARTESIAN_POINT('Ctrl Pts',(-108.543724165138,1.72264471716643,
125.14175874922));
#171654=CARTESIAN_POINT('Ctrl Pts',(-108.53630079411,1.87153880259726,125.191404794395));
#171655=CARTESIAN_POINT('Ctrl Pts',(-108.532364744669,1.95048601936168,
125.217728318788));
#171656=CARTESIAN_POINT('Ctrl Pts',(-108.528428695228,2.02882000040759,
125.245698513283));
#171657=CARTESIAN_POINT('Ctrl Pts',(-108.524492645787,2.10646853381558,
125.275281048728));
#171658=CARTESIAN_POINT('Ctrl Pts',(-108.517069379381,2.25291124448683,
125.331072787334));
#171659=CARTESIAN_POINT('Ctrl Pts',(-108.509646112976,2.39735731989397,
125.392770910978));
#171660=CARTESIAN_POINT('Ctrl Pts',(-108.502222846571,2.53929482717109,
125.4602131324));
#171661=CARTESIAN_POINT('Ctrl Pts',(-108.49480835385,2.68106457610179,125.527575642718));
#171662=CARTESIAN_POINT('Ctrl Pts',(-108.487393861129,2.8203313247116,125.600668578536));
#171663=CARTESIAN_POINT('Ctrl Pts',(-108.479979368408,2.95660022515872,
125.679280552719));
#171664=CARTESIAN_POINT('Ctrl Pts',(-108.472572022054,3.09273778450955,
125.757816757722));
#171665=CARTESIAN_POINT('Ctrl Pts',(-108.4651646757,3.22588292682234,125.841861225814));
#171666=CARTESIAN_POINT('Ctrl Pts',(-108.457757329346,3.35556276037715,
125.931155396803));
#171667=CARTESIAN_POINT('Ctrl Pts',(-108.450355507671,3.48514587381992,
126.020382968831));
#171668=CARTESIAN_POINT('Ctrl Pts',(-108.442953685995,3.61126851857284,
126.114852236817));
#171669=CARTESIAN_POINT('Ctrl Pts',(-108.43555186432,3.73348440741865,126.214259884242));
#171670=CARTESIAN_POINT('Ctrl Pts',(-108.428153950009,3.85563577944772,
126.313615055144));
#171671=CARTESIAN_POINT('Ctrl Pts',(-108.420756035697,3.97388421396637,
126.417903178699));
#171672=CARTESIAN_POINT('Ctrl Pts',(-108.413358121386,4.08781440456307,
126.526779062955));
#171673=CARTESIAN_POINT('Ctrl Pts',(-108.405961436474,4.20172566202916,
126.635636854015));
#171674=CARTESIAN_POINT('Ctrl Pts',(-108.398564751562,4.3113198302086,126.749080634977));
#171675=CARTESIAN_POINT('Ctrl Pts',(-108.391168066649,4.41621647988275,
126.866726484573));
#171676=CARTESIAN_POINT('Ctrl Pts',(-108.383771709714,4.52110847832952,
126.984367117629));
#171677=CARTESIAN_POINT('Ctrl Pts',(-108.376375352779,4.62130312399578,
127.106209170218));
#171678=CARTESIAN_POINT('Ctrl Pts',(-108.368978995843,4.71645869756903,
127.231833792387));
#171679=CARTESIAN_POINT('Ctrl Pts',(-108.361581506507,4.81162883970351,
127.357477648006));
#171680=CARTESIAN_POINT('Ctrl Pts',(-108.35418401717,4.9017581481849,127.486904928724));
#171681=CARTESIAN_POINT('Ctrl Pts',(-108.346786527833,4.98654694411484,
127.619665948271));
#171682=CARTESIAN_POINT('Ctrl Pts',(-108.339386445318,5.07136546262564,
127.752473506986));
#171683=CARTESIAN_POINT('Ctrl Pts',(-108.331986362803,5.15083954042843,
127.888616816865));
#171684=CARTESIAN_POINT('Ctrl Pts',(-108.324586280288,5.22471442615815,
128.027619771251));
#171685=CARTESIAN_POINT('Ctrl Pts',(-108.317178060622,5.29867054491936,
128.166775573676));
#171686=CARTESIAN_POINT('Ctrl Pts',(-108.309769840955,5.36701500060249,
128.308796970489));
#171687=CARTESIAN_POINT('Ctrl Pts',(-108.302361621289,5.42954005175752,
128.453185296825));
#171688=CARTESIAN_POINT('Ctrl Pts',(-108.294948841987,5.4921035860386,128.597662491768));
#171689=CARTESIAN_POINT('Ctrl Pts',(-108.287536062685,5.54884044448712,
128.744509171697));
#171690=CARTESIAN_POINT('Ctrl Pts',(-108.280123283383,5.59959230422747,
128.893210024615));
#171691=CARTESIAN_POINT('Ctrl Pts',(-108.272699912354,5.65041668060468,
129.042123348284));
#171692=CARTESIAN_POINT('Ctrl Pts',(-108.265276541325,5.69523887262437,
129.192895779375));
#171693=CARTESIAN_POINT('Ctrl Pts',(-108.257853170296,5.73395113888528,
129.344999490437));
#171694=CARTESIAN_POINT('Ctrl Pts',(-108.253917120855,5.75447731134562,
129.425648527723));
#171695=CARTESIAN_POINT('Ctrl Pts',(-108.249981071415,5.77328662472877,
129.506671697843));
#171696=CARTESIAN_POINT('Ctrl Pts',(-108.246045021974,5.79036892881588,
129.58798969112));
#171697=CARTESIAN_POINT('Ctrl Pts',(-108.238621755568,5.82258562120263,
129.741352888587));
#171698=CARTESIAN_POINT('Ctrl Pts',(-108.231198489163,5.84875387444842,
129.896228805643));
#171699=CARTESIAN_POINT('Ctrl Pts',(-108.223775222757,5.86873351320218,
130.052099018441));
#171700=CARTESIAN_POINT('Ctrl Pts',(-108.216360730036,5.88868953768214,
130.207785005593));
#171701=CARTESIAN_POINT('Ctrl Pts',(-108.208946237315,5.90247146008212,
130.364462582642));
#171702=CARTESIAN_POINT('Ctrl Pts',(-108.201531744594,5.90998964903964,
130.521601160174));
#171703=CARTESIAN_POINT('Ctrl Pts',(-108.194124398241,5.91750059168362,
130.678588281631));
#171704=CARTESIAN_POINT('Ctrl Pts',(-108.186717051887,5.91875980208571,
130.83603514863));
#171705=CARTESIAN_POINT('Ctrl Pts',(-108.179309705533,5.91372920473236,
130.993404145875));
#171706=CARTESIAN_POINT('Ctrl Pts',(-108.171907883857,5.90870235938832,
131.150655771385));
#171707=CARTESIAN_POINT('Ctrl Pts',(-108.164506062182,5.89739505892894,
131.307829271281));
#171708=CARTESIAN_POINT('Ctrl Pts',(-108.157104240507,5.87982126298926,
131.464385221501));
#171709=CARTESIAN_POINT('Ctrl Pts',(-108.149706326195,5.86225674411971,
131.620858527053));
#171710=CARTESIAN_POINT('Ctrl Pts',(-108.142308411884,5.83843235941513,
131.776714562144));
#171711=CARTESIAN_POINT('Ctrl Pts',(-108.134910497573,5.80841404538217,
131.931417333045));
#171712=CARTESIAN_POINT('Ctrl Pts',(-108.12751381266,5.77840071984838,132.086094395153));
#171713=CARTESIAN_POINT('Ctrl Pts',(-108.120117127748,5.74219557891749,
132.239618207339));
#171714=CARTESIAN_POINT('Ctrl Pts',(-108.112720442836,5.69991599514033,
132.391461184904));
#171715=CARTESIAN_POINT('Ctrl Pts',(-108.105324085901,5.65763828608422,
132.543297429592));
#171716=CARTESIAN_POINT('Ctrl Pts',(-108.097927728965,5.60928676986781,
132.693452628232));
#171717=CARTESIAN_POINT('Ctrl Pts',(-108.09053137203,5.55502912918315,132.84141288406));
#171718=CARTESIAN_POINT('Ctrl Pts',(-108.083133882693,5.50076318151534,
132.989395792979));
#171719=CARTESIAN_POINT('Ctrl Pts',(-108.075736393357,5.44058943744113,
133.135182739464));
#171720=CARTESIAN_POINT('Ctrl Pts',(-108.06833890402,5.37472424699098,133.278278528756));
#171721=CARTESIAN_POINT('Ctrl Pts',(-108.060938821505,5.30883596759976,
133.421424480057));
#171722=CARTESIAN_POINT('Ctrl Pts',(-108.05353873899,5.23725242553421,133.56187705701));
#171723=CARTESIAN_POINT('Ctrl Pts',(-108.046138656475,5.16023648347125,
133.699164582803));
#171724=CARTESIAN_POINT('Ctrl Pts',(-108.038730436808,5.0831358544629,133.836603070343));
#171725=CARTESIAN_POINT('Ctrl Pts',(-108.031322217142,5.00059107877114,
133.970869230568));
#171726=CARTESIAN_POINT('Ctrl Pts',(-108.023913997475,4.91290940794283,
134.101518744172));
#171727=CARTESIAN_POINT('Ctrl Pts',(-108.016501218173,4.82517377050918,
134.232248670372));
#171728=CARTESIAN_POINT('Ctrl Pts',(-108.009088438871,4.73229515763702,
134.359357213687));
#171729=CARTESIAN_POINT('Ctrl Pts',(-108.001675659569,4.63462153852264,
134.482432633876));
#171730=CARTESIAN_POINT('Ctrl Pts',(-107.994252288541,4.53680835876098,
134.605683909997));
#171731=CARTESIAN_POINT('Ctrl Pts',(-107.986828917512,4.43418673201651,
134.724890271399));
#171732=CARTESIAN_POINT('Ctrl Pts',(-107.979405546483,4.32714249761254,
134.839675768562));
#171733=CARTESIAN_POINT('Ctrl Pts',(-107.975469497042,4.27038507604071,
134.900537793397));
#171734=CARTESIAN_POINT('Ctrl Pts',(-107.971533447601,4.21238488165182,
134.960157604002));
#171735=CARTESIAN_POINT('Ctrl Pts',(-107.967597398161,4.15320315348277,
135.018483791893));
#171736=CARTESIAN_POINT('Ctrl Pts',(-107.960174131755,4.041588261154,135.128485161957));
#171737=CARTESIAN_POINT('Ctrl Pts',(-107.95275086535,3.92543134589529,135.23421547076));
#171738=CARTESIAN_POINT('Ctrl Pts',(-107.945327598944,3.80509280417013,
135.335276564055));
#171739=CARTESIAN_POINT('Ctrl Pts',(-107.937913106223,3.68489649260779,
135.436218211531));
#171740=CARTESIAN_POINT('Ctrl Pts',(-107.930498613502,3.56052867539627,
135.532501390628));
#171741=CARTESIAN_POINT('Ctrl Pts',(-107.923084120781,3.43238730449575,
135.623763895404));
#171742=CARTESIAN_POINT('Ctrl Pts',(-107.915676774428,3.30436944107258,
135.714938437942));
#171743=CARTESIAN_POINT('Ctrl Pts',(-107.908269428074,3.17258556671991,
135.801101724782));
#171744=CARTESIAN_POINT('Ctrl Pts',(-107.90086208172,3.03746741166749,135.881931127717));
#171745=CARTESIAN_POINT('Ctrl Pts',(-107.893460260045,2.90245003283244,
135.962700245034));
#171746=CARTESIAN_POINT('Ctrl Pts',(-107.886058438369,2.76410364389025,
136.038143208789));
#171747=CARTESIAN_POINT('Ctrl Pts',(-107.878656616694,2.62288962310563,
136.107980191735));
#171748=CARTESIAN_POINT('Ctrl Pts',(-107.871258702382,2.48175014810378,
136.177780308281));
#171749=CARTESIAN_POINT('Ctrl Pts',(-107.863860788071,2.33774638983323,
136.241980172649));
#171750=CARTESIAN_POINT('Ctrl Pts',(-107.85646287376,2.19136493529039,136.300345541388));
#171751=CARTESIAN_POINT('Ctrl Pts',(-107.849066188847,2.04500780668987,
136.358701210861));
#171752=CARTESIAN_POINT('Ctrl Pts',(-107.841669503935,1.89627411244474,
136.411224170927));
#171753=CARTESIAN_POINT('Ctrl Pts',(-107.834272819023,1.74567116723508,
136.45772799802));
#171754=CARTESIAN_POINT('Ctrl Pts',(-107.826876462088,1.59507489991783,
136.504229763085));
#171755=CARTESIAN_POINT('Ctrl Pts',(-107.819480105152,1.44260990311884,
136.544712815716));
#171756=CARTESIAN_POINT('Ctrl Pts',(-107.812083748217,1.28879916933246,
136.579040458356));
#171757=CARTESIAN_POINT('Ctrl Pts',(-107.80468625888,1.13496488673009,136.613373356646));
#171758=CARTESIAN_POINT('Ctrl Pts',(-107.797288769544,0.979784821253583,
136.641548887167));
#171759=CARTESIAN_POINT('Ctrl Pts',(-107.789891280207,0.823792536753465,
136.663481406463));
#171760=CARTESIAN_POINT('Ctrl Pts',(-107.782491197692,0.667745569400947,
136.68542161417));
#171761=CARTESIAN_POINT('Ctrl Pts',(-107.775091115177,0.510886185576555,
136.701114401467));
#171762=CARTESIAN_POINT('Ctrl Pts',(-107.767691032662,0.353753304040651,
136.71052596933));
#171763=CARTESIAN_POINT('Ctrl Pts',(-107.760282812996,0.196447638746722,
136.719947886179));
#171764=CARTESIAN_POINT('Ctrl Pts',(-107.752874593329,0.0388682480047973,
136.723074767836));
#171765=CARTESIAN_POINT('Ctrl Pts',(-107.745466373663,-0.11844497280288,
136.719924948289));
#171766=CARTESIAN_POINT('Ctrl Pts',(-107.738053594361,-0.275855017273053,
136.71677319008));
#171767=CARTESIAN_POINT('Ctrl Pts',(-107.730640815059,-0.432998193608058,
136.707337055073));
#171768=CARTESIAN_POINT('Ctrl Pts',(-107.723228035757,-0.589340007231835,
136.691686743948));
#171769=CARTESIAN_POINT('Ctrl Pts',(-107.715804664728,-0.745905209370844,
136.676014070924));
#171770=CARTESIAN_POINT('Ctrl Pts',(-107.708381293699,-0.901666393246402,
136.654109540064));
#171771=CARTESIAN_POINT('Ctrl Pts',(-107.70095792267,-1.05609870629948,
136.626094559018));
#171772=CARTESIAN_POINT('Ctrl Pts',(-107.69702187323,-1.13798242423446,
136.611240343857));
#171773=CARTESIAN_POINT('Ctrl Pts',(-107.693085823789,-1.21949278122046,
136.594669101593));
#171774=CARTESIAN_POINT('Ctrl Pts',(-107.689149774348,-1.30055342464799,
136.576404566821));
#171775=CARTESIAN_POINT('Ctrl Pts',(-107.681726507942,-1.4534312683332,
136.54195822426));
#171776=CARTESIAN_POINT('Ctrl Pts',(-107.674303241537,-1.60517082155485,
136.501381936232));
#171777=CARTESIAN_POINT('Ctrl Pts',(-107.666879975132,-1.7552423027785,
136.454763702394));
#171778=CARTESIAN_POINT('Ctrl Pts',(-107.659465482411,-1.90513641197444,
136.408200567438));
#171779=CARTESIAN_POINT('Ctrl Pts',(-107.65205098969,-2.05336602048654,
136.355609810687));
#171780=CARTESIAN_POINT('Ctrl Pts',(-107.644636496969,-2.19941129144228,
136.297130459238));
#171781=CARTESIAN_POINT('Ctrl Pts',(-107.637229150615,-2.34531579846778,
136.238707472389));
#171782=CARTESIAN_POINT('Ctrl Pts',(-107.629821804261,-2.48903981504603,
136.174407327774));
#171783=CARTESIAN_POINT('Ctrl Pts',(-107.622414457907,-2.63007854419395,
136.104418863838));
#171784=CARTESIAN_POINT('Ctrl Pts',(-107.615012636232,-2.77101208133618,
136.034482599938));
#171785=CARTESIAN_POINT('Ctrl Pts',(-107.607610814556,-2.90926398592004,
135.958866629453));
#171786=CARTESIAN_POINT('Ctrl Pts',(-107.600208992881,-3.04434944513681,
135.877807869524));
#171787=CARTESIAN_POINT('Ctrl Pts',(-107.59281107857,-3.17936359379116,
135.796791899882));
#171788=CARTESIAN_POINT('Ctrl Pts',(-107.585413164258,-3.3112143067519,
135.71033905451));
#171789=CARTESIAN_POINT('Ctrl Pts',(-107.578015249947,-3.43944149621148,
135.618732098522));
#171790=CARTESIAN_POINT('Ctrl Pts',(-107.570618565035,-3.5676473766379,
135.527140365947));
#171791=CARTESIAN_POINT('Ctrl Pts',(-107.563221880122,-3.69223062523073,
135.430396439482));
#171792=CARTESIAN_POINT('Ctrl Pts',(-107.55582519521,-3.81276018258793,
135.328826370843));
#171793=CARTESIAN_POINT('Ctrl Pts',(-107.548428838275,-3.93328439553861,
135.227260805926));
#171794=CARTESIAN_POINT('Ctrl Pts',(-107.541032481339,-4.04975498919121,
135.120869764886));
#171795=CARTESIAN_POINT('Ctrl Pts',(-107.533636124404,-4.16177426580181,
135.010019367751));
#171796=CARTESIAN_POINT('Ctrl Pts',(-107.526238635067,-4.27381069284995,
134.899151999137));
#171797=CARTESIAN_POINT('Ctrl Pts',(-107.518841145731,-4.3813941805237,
134.783824177595));
#171798=CARTESIAN_POINT('Ctrl Pts',(-107.511443656394,-4.48416427026502,
134.664438513124));
#171799=CARTESIAN_POINT('Ctrl Pts',(-107.504043573879,-4.58697038590184,
134.545010998194));
#171800=CARTESIAN_POINT('Ctrl Pts',(-107.496643491364,-4.68495950075922,
134.421523090944));
#171801=CARTESIAN_POINT('Ctrl Pts',(-107.489243408849,-4.77781188000648,
134.294409929792));
#171802=CARTESIAN_POINT('Ctrl Pts',(-107.481835189183,-4.87076635999004,
134.167156994652));
#171803=CARTESIAN_POINT('Ctrl Pts',(-107.474426969516,-4.95857260387171,
134.036271146253));
#171804=CARTESIAN_POINT('Ctrl Pts',(-107.46701874985,-5.04095420991477,
133.902216523841));
#171805=CARTESIAN_POINT('Ctrl Pts',(-107.459605970548,-5.12338652046197,
133.768079393045));
#171806=CARTESIAN_POINT('Ctrl Pts',(-107.452193191246,-5.20038735807925,
133.630769926805));
#171807=CARTESIAN_POINT('Ctrl Pts',(-107.444780411944,-5.27172687721469,
133.490775755729));
#171808=CARTESIAN_POINT('Ctrl Pts',(-107.437357040915,-5.34316832960026,
133.350581554417));
#171809=CARTESIAN_POINT('Ctrl Pts',(-107.429933669886,-5.40893215198175,
133.207695325058));
#171810=CARTESIAN_POINT('Ctrl Pts',(-107.422510298857,-5.46883679242566,
133.062624264776));
#171811=CARTESIAN_POINT('Ctrl Pts',(-107.418574249417,-5.50059967017909,
132.985704107687));
#171812=CARTESIAN_POINT('Ctrl Pts',(-107.414638199976,-5.53071615369011,
132.90816997465));
#171813=CARTESIAN_POINT('Ctrl Pts',(-107.410702150536,-5.55916494109477,
132.830098932404));
#171814=CARTESIAN_POINT('Ctrl Pts',(-107.402111129881,-5.621258703863,132.65969712556));
#171815=CARTESIAN_POINT('Ctrl Pts',(-107.393520109225,-5.67555971971428,
132.486312339245));
#171816=CARTESIAN_POINT('Ctrl Pts',(-107.38492908857,-5.72181188622781,
132.310614016275));
#171817=CARTESIAN_POINT('Ctrl Pts',(-107.376370430877,-5.767889817669,132.135577560896));
#171818=CARTESIAN_POINT('Ctrl Pts',(-107.367811773184,-5.80597933618538,
131.958245083306));
#171819=CARTESIAN_POINT('Ctrl Pts',(-107.359253115491,-5.83587378478307,
131.779300477548));
#171820=CARTESIAN_POINT('Ctrl Pts',(-107.350757783627,-5.86554704323359,
131.601679889645));
#171821=CARTESIAN_POINT('Ctrl Pts',(-107.342262451764,-5.8871459811393,
131.422471073596));
#171822=CARTESIAN_POINT('Ctrl Pts',(-107.3337671199,-5.90051563382055,131.242362692378));
#171823=CARTESIAN_POINT('Ctrl Pts',(-107.32696982208,-5.91121298060858,
131.098254101133));
#171824=CARTESIAN_POINT('Ctrl Pts',(-107.32017252426,-5.91664285591595,
130.953570016966));
#171825=CARTESIAN_POINT('Ctrl Pts',(-107.31337522644,-5.91674842950609,
130.80867158466));
#171826=CARTESIAN_POINT('',(-105.563375192205,-5.90975296513838,130.800404415155));
#171827=CARTESIAN_POINT('Ctrl Pts',(-107.313375192205,-5.91043119270566,
130.808666252895));
#171828=CARTESIAN_POINT('Ctrl Pts',(-107.253001637044,-5.90181299183432,
129.523046449566));
#171829=CARTESIAN_POINT('Ctrl Pts',(-107.099812207279,-4.8565494805829,
126.248208310993));
#171830=CARTESIAN_POINT('Ctrl Pts',(-106.85380690291,0.553929572890924,
123.827920081116));
#171831=CARTESIAN_POINT('Ctrl Pts',(-106.575359279096,6.16888947100959,
127.499460736355));
#171832=CARTESIAN_POINT('Ctrl Pts',(-106.296911655284,6.11494131227265,
134.208042929093));
#171833=CARTESIAN_POINT('Ctrl Pts',(-106.018464031471,0.441660819049746,
137.78880735666));
#171834=CARTESIAN_POINT('Ctrl Pts',(-105.773951877111,-4.8965958753672,
135.297035641043));
#171835=CARTESIAN_POINT('Ctrl Pts',(-105.622255597356,-5.90208552014624,
132.054589738716));
#171836=CARTESIAN_POINT('Ctrl Pts',(-105.563375192205,-5.90975296513838,
130.800404415155));
#171837=CARTESIAN_POINT('',(-103.813375192205,-5.92489227885479,130.801538229806));
#171838=CARTESIAN_POINT('Ctrl Pts',(-105.563375192205,-5.90975296513838,
130.800404415155));
#171839=CARTESIAN_POINT('Ctrl Pts',(-105.529439722752,-5.91417206423678,
130.077560072841));
#171840=CARTESIAN_POINT('Ctrl Pts',(-105.402688378692,-5.45597557692382,
127.383094551451));
#171841=CARTESIAN_POINT('Ctrl Pts',(-105.183121160033,-1.42831237022071,
123.953266960094));
#171842=CARTESIAN_POINT('Ctrl Pts',(-104.90467353622,4.99198140251171,125.899497499463));
#171843=CARTESIAN_POINT('Ctrl Pts',(-104.626225912407,6.82488813818383,
132.353057628482));
#171844=CARTESIAN_POINT('Ctrl Pts',(-104.347778288594,2.38605608918648,
137.383440862523));
#171845=CARTESIAN_POINT('Ctrl Pts',(-104.076828048526,-4.06688745323623,
136.395312951788));
#171846=CARTESIAN_POINT('Ctrl Pts',(-103.898693683064,-5.91427678181791,
132.606982621728));
#171847=CARTESIAN_POINT('Ctrl Pts',(-103.813375192205,-5.92489227885479,
130.801538229806));
#171848=CARTESIAN_POINT('',(-102.063375192205,-5.91808296072073,130.809685412516));
#171849=CARTESIAN_POINT('Ctrl Pts',(-103.813375192205,-5.92489227885479,
130.801538229806));
#171850=CARTESIAN_POINT('Ctrl Pts',(-103.805877808459,-5.92582511831476,
130.642884351829));
#171851=CARTESIAN_POINT('Ctrl Pts',(-103.798380424714,-5.92000731493553,
130.484299960519));
#171852=CARTESIAN_POINT('Ctrl Pts',(-103.698067166363,-5.74889566573683,
128.370026085815));
#171853=CARTESIAN_POINT('Ctrl Pts',(-103.512435417155,-3.29550805454775,
124.630448795005));
#171854=CARTESIAN_POINT('Ctrl Pts',(-103.233987793341,3.41298426984717,
124.694606211362));
#171855=CARTESIAN_POINT('Ctrl Pts',(-102.955540169529,6.98511078380345,
130.373329448925));
#171856=CARTESIAN_POINT('Ctrl Pts',(-102.677092545716,4.13826172907665,
136.448149273423));
#171857=CARTESIAN_POINT('Ctrl Pts',(-102.398644921904,-2.51144768934695,
137.336603037595));
#171858=CARTESIAN_POINT('Ctrl Pts',(-102.194072470733,-5.70132967268059,
133.57913972058));
#171859=CARTESIAN_POINT('Ctrl Pts',(-102.082315894167,-5.92220269805738,
131.211626874956));
#171860=CARTESIAN_POINT('Ctrl Pts',(-102.063375192205,-5.91847197029493,
130.809685762527));
#171861=CARTESIAN_POINT('',(-100.313375192239,-5.9167499888071,130.804724555984));
#171862=CARTESIAN_POINT('Ctrl Pts',(-102.063375192205,-5.91674760504896,
130.809684211029));
#171863=CARTESIAN_POINT('Ctrl Pts',(-102.056072017781,-5.91688700715738,
130.654749936505));
#171864=CARTESIAN_POINT('Ctrl Pts',(-102.048768843358,-5.91093665927345,
130.499620358955));
#171865=CARTESIAN_POINT('Ctrl Pts',(-102.041465668934,-5.89887734654449,
130.344821051343));
#171866=CARTESIAN_POINT('Ctrl Pts',(-102.034168273018,-5.88682757553336,
130.190144225944));
#171867=CARTESIAN_POINT('Ctrl Pts',(-102.026870877102,-5.86867848847835,
130.035797532258));
#171868=CARTESIAN_POINT('Ctrl Pts',(-102.019573481186,-5.84446293334446,
129.882306615209));
#171869=CARTESIAN_POINT('Ctrl Pts',(-102.012164155899,-5.8198759536767,
129.72646141423));
#171870=CARTESIAN_POINT('Ctrl Pts',(-102.004754830611,-5.78903486896265,
129.571498861028));
#171871=CARTESIAN_POINT('Ctrl Pts',(-101.997345505323,-5.75202887664798,
129.417964438724));
#171872=CARTESIAN_POINT('Ctrl Pts',(-101.990053608961,-5.71560938496194,
129.266863353011));
#171873=CARTESIAN_POINT('Ctrl Pts',(-101.982761712599,-5.67321906097977,
129.117145848256));
#171874=CARTESIAN_POINT('Ctrl Pts',(-101.975469816238,-5.62499442660723,
128.969321581704));
#171875=CARTESIAN_POINT('Ctrl Pts',(-101.96817822644,-5.57677181968034,
128.821503529935));
#171876=CARTESIAN_POINT('Ctrl Pts',(-101.960886636642,-5.52271550949202,
128.6755789241));
#171877=CARTESIAN_POINT('Ctrl Pts',(-101.953595046844,-5.46301166816555,
128.532041521139));
#171878=CARTESIAN_POINT('Ctrl Pts',(-101.94630222786,-5.40329776221654,
128.388479921246));
#171879=CARTESIAN_POINT('Ctrl Pts',(-101.939009408877,-5.33793457897994,
128.24730668025));
#171880=CARTESIAN_POINT('Ctrl Pts',(-101.931716589893,-5.26715601040432,
128.108994571078));
#171881=CARTESIAN_POINT('Ctrl Pts',(-101.924219346925,-5.19439345771586,
127.966805454603));
#171882=CARTESIAN_POINT('Ctrl Pts',(-101.916722103957,-5.11590766486404,
127.82764061171));
#171883=CARTESIAN_POINT('Ctrl Pts',(-101.909224860989,-5.03200221987744,
127.691984640656));
#171884=CARTESIAN_POINT('Ctrl Pts',(-101.901921253736,-4.95026385029387,
127.559832336357));
#171885=CARTESIAN_POINT('Ctrl Pts',(-101.894617646483,-4.86338260310448,
127.431010168018));
#171886=CARTESIAN_POINT('Ctrl Pts',(-101.88731403923,-4.7716815209098,127.305934396319));
#171887=CARTESIAN_POINT('Ctrl Pts',(-101.879719978405,-4.67633362338209,
127.175884547639));
#171888=CARTESIAN_POINT('Ctrl Pts',(-101.872125917579,-4.57577495020364,
127.049885568865));
#171889=CARTESIAN_POINT('Ctrl Pts',(-101.864531856754,-4.47041207257545,
126.928364427698));
#171890=CARTESIAN_POINT('Ctrl Pts',(-101.856937795929,-4.36504919494726,
126.806843286531));
#171891=CARTESIAN_POINT('Ctrl Pts',(-101.849343735103,-4.25488248181308,
126.68980026642));
#171892=CARTESIAN_POINT('Ctrl Pts',(-101.841749674278,-4.14035757478254,
126.577616041011));
#171893=CARTESIAN_POINT('Ctrl Pts',(-101.834326407872,-4.02840839311396,
126.467954897803));
#171894=CARTESIAN_POINT('Ctrl Pts',(-101.826903141467,-3.91193020919505,
126.362578620429));
#171895=CARTESIAN_POINT('Ctrl Pts',(-101.819479875061,-3.79128462966451,
126.261884264367));
#171896=CARTESIAN_POINT('Ctrl Pts',(-101.81206538234,-3.67078164318999,
126.161308920672));
#171897=CARTESIAN_POINT('Ctrl Pts',(-101.804650889619,-3.54612134916366,
126.065404720407));
#171898=CARTESIAN_POINT('Ctrl Pts',(-101.797236396898,-3.41770280013275,
125.974532656607));
#171899=CARTESIAN_POINT('Ctrl Pts',(-101.789829050545,-3.28940802573428,
125.883748178723));
#171900=CARTESIAN_POINT('Ctrl Pts',(-101.782421704191,-3.15736251038875,
125.797986395767));
#171901=CARTESIAN_POINT('Ctrl Pts',(-101.775014357837,-3.02199896429545,
125.717568620413));
#171902=CARTESIAN_POINT('Ctrl Pts',(-101.767612536161,-2.88673637744179,
125.637210823671));
#171903=CARTESIAN_POINT('Ctrl Pts',(-101.760210714486,-2.74816100688009,
125.562189288182));
#171904=CARTESIAN_POINT('Ctrl Pts',(-101.752808892811,-2.60673508043586,
125.49278243562));
#171905=CARTESIAN_POINT('Ctrl Pts',(-101.745410978499,-2.46538381163774,
125.423412222395));
#171906=CARTESIAN_POINT('Ctrl Pts',(-101.738013064188,-2.32118531807934,
125.359650953302));
#171907=CARTESIAN_POINT('Ctrl Pts',(-101.730615149876,-2.17462689745969,
125.301731389702));
#171908=CARTESIAN_POINT('Ctrl Pts',(-101.723218464964,-2.0280928321905,
125.243821451283));
#171909=CARTESIAN_POINT('Ctrl Pts',(-101.715821780052,-1.87919996504587,
125.191751428703));
#171910=CARTESIAN_POINT('Ctrl Pts',(-101.70842509514,-1.72845617576522,
125.145706200573));
#171911=CARTESIAN_POINT('Ctrl Pts',(-101.701028738204,-1.57771907062215,
125.099663014136));
#171912=CARTESIAN_POINT('Ctrl Pts',(-101.693632381269,-1.42513156354348,
125.059644200025));
#171913=CARTESIAN_POINT('Ctrl Pts',(-101.686236024333,-1.27121706066143,
125.025784863353));
#171914=CARTESIAN_POINT('Ctrl Pts',(-101.678838534997,-1.11727899307607,
124.99192034273));
#171915=CARTESIAN_POINT('Ctrl Pts',(-101.67144104566,-0.962013889759597,
124.964217257456));
#171916=CARTESIAN_POINT('Ctrl Pts',(-101.664043556324,-0.805955572760337,
124.942759626605));
#171917=CARTESIAN_POINT('Ctrl Pts',(-101.656643473808,-0.649842549759751,
124.921294473814));
#171918=CARTESIAN_POINT('Ctrl Pts',(-101.649243391293,-0.492936129049061,
124.906079185212));
#171919=CARTESIAN_POINT('Ctrl Pts',(-101.641843308778,-0.335775329764997,
124.897145919384));
#171920=CARTESIAN_POINT('Ctrl Pts',(-101.634435089112,-0.178441716025822,
124.888202830511));
#171921=CARTESIAN_POINT('Ctrl Pts',(-101.627026869445,-0.0208535380282623,
124.885555580799));
#171922=CARTESIAN_POINT('Ctrl Pts',(-101.619618649779,0.136449367148529,
124.889184193088));
#171923=CARTESIAN_POINT('Ctrl Pts',(-101.612205870477,0.293849089638717,
124.892815038726));
#171924=CARTESIAN_POINT('Ctrl Pts',(-101.604793091175,0.450962817748566,
124.902729419801));
#171925=CARTESIAN_POINT('Ctrl Pts',(-101.597380311873,0.607256273044526,
124.918855509137));
#171926=CARTESIAN_POINT('Ctrl Pts',(-101.589956940844,0.763773047759072,
124.935004640185));
#171927=CARTESIAN_POINT('Ctrl Pts',(-101.582533569815,0.919466840302727,
124.95738315305));
#171928=CARTESIAN_POINT('Ctrl Pts',(-101.575110198786,1.07381317007064,
124.985868043172));
#171929=CARTESIAN_POINT('Ctrl Pts',(-101.571174149346,1.15565129759787,
125.000971415399));
#171930=CARTESIAN_POINT('Ctrl Pts',(-101.567238099905,1.23711083986569,
125.017790670393));
#171931=CARTESIAN_POINT('Ctrl Pts',(-101.563302050465,1.31811551685823,
125.036301841278));
#171932=CARTESIAN_POINT('Ctrl Pts',(-101.555878784059,1.47088780960643,
125.071213331855));
#171933=CARTESIAN_POINT('Ctrl Pts',(-101.548455517654,1.62250315971815,
125.11225127494));
#171934=CARTESIAN_POINT('Ctrl Pts',(-101.541032251248,1.77243205595355,
125.159326058812));
#171935=CARTESIAN_POINT('Ctrl Pts',(-101.533617758527,1.92218374868442,
125.206345204198));
#171936=CARTESIAN_POINT('Ctrl Pts',(-101.526203265806,2.07025260243396,
125.259386877292));
#171937=CARTESIAN_POINT('Ctrl Pts',(-101.518788773085,2.21611920588817,
125.318310469436));
#171938=CARTESIAN_POINT('Ctrl Pts',(-101.511381426731,2.36184521761778,
125.377177268804));
#171939=CARTESIAN_POINT('Ctrl Pts',(-101.503974080378,2.50537286095345,
125.441914562052));
#171940=CARTESIAN_POINT('Ctrl Pts',(-101.496566734024,2.64619791600956,
125.512331975183));
#171941=CARTESIAN_POINT('Ctrl Pts',(-101.489164912348,2.78691793842699,
125.58269686835));
#171942=CARTESIAN_POINT('Ctrl Pts',(-101.481763090673,2.92493905363406,
125.658733279828));
#171943=CARTESIAN_POINT('Ctrl Pts',(-101.474361268997,3.05977717216197,
125.740202817969));
#171944=CARTESIAN_POINT('Ctrl Pts',(-101.466963354686,3.19454411069669,
125.821629348976));
#171945=CARTESIAN_POINT('Ctrl Pts',(-101.459565440375,3.3261310802111,125.908483102119));
#171946=CARTESIAN_POINT('Ctrl Pts',(-101.452167526063,3.45407885566847,
126.000479913247));
#171947=CARTESIAN_POINT('Ctrl Pts',(-101.444770841151,3.58200536852621,
126.092461436174));
#171948=CARTESIAN_POINT('Ctrl Pts',(-101.437374156239,3.70629358482421,
126.189584103082));
#171949=CARTESIAN_POINT('Ctrl Pts',(-101.429977471327,3.82651343954635,
126.291520551768));
#171950=CARTESIAN_POINT('Ctrl Pts',(-101.422581114391,3.9467279635945,126.393452480485));
#171951=CARTESIAN_POINT('Ctrl Pts',(-101.415184757456,4.06287420003124,
126.500197525152));
#171952=CARTESIAN_POINT('Ctrl Pts',(-101.40778840052,4.17455556729817,126.61138835698));
#171953=CARTESIAN_POINT('Ctrl Pts',(-101.400390911184,4.28625403326721,
126.722596212409));
#171954=CARTESIAN_POINT('Ctrl Pts',(-101.392993421847,4.39348600440325,
126.838250946889));
#171955=CARTESIAN_POINT('Ctrl Pts',(-101.385595932511,4.4958922492242,126.957948855174));
#171956=CARTESIAN_POINT('Ctrl Pts',(-101.378195849996,4.59833439239568,
127.077688723376));
#171957=CARTESIAN_POINT('Ctrl Pts',(-101.370795767481,4.69594719866225,
127.201474303797));
#171958=CARTESIAN_POINT('Ctrl Pts',(-101.363395684966,4.7884122590859,127.328869486872));
#171959=CARTESIAN_POINT('Ctrl Pts',(-101.355987465299,4.88097899434926,
127.456404754047));
#171960=CARTESIAN_POINT('Ctrl Pts',(-101.348579245633,4.96838646001872,
127.587557248193));
#171961=CARTESIAN_POINT('Ctrl Pts',(-101.341171025966,5.05035966831803,
127.721861990944));
#171962=CARTESIAN_POINT('Ctrl Pts',(-101.333758246664,5.1323833297595,127.856249396023));
#171963=CARTESIAN_POINT('Ctrl Pts',(-101.326345467362,5.20896588793141,
127.993792590317));
#171964=CARTESIAN_POINT('Ctrl Pts',(-101.31893268806,5.2798789825263,128.134003245906));
#171965=CARTESIAN_POINT('Ctrl Pts',(-101.311509317031,5.35089340107615,
128.274414241055));
#171966=CARTESIAN_POINT('Ctrl Pts',(-101.304085946002,5.41622202231293,
128.417499971028));
#171967=CARTESIAN_POINT('Ctrl Pts',(-101.296662574974,5.47568483887766,
128.56275268847));
#171968=CARTESIAN_POINT('Ctrl Pts',(-101.292726525533,5.50721345100937,
128.639769164545));
#171969=CARTESIAN_POINT('Ctrl Pts',(-101.288790476092,5.53709380779301,
128.717394602667));
#171970=CARTESIAN_POINT('Ctrl Pts',(-101.284854426652,5.56530484202796,
128.795551871617));
#171971=CARTESIAN_POINT('Ctrl Pts',(-101.277431160246,5.61850997216148,
128.94295404166));
#171972=CARTESIAN_POINT('Ctrl Pts',(-101.270007893841,5.6659353885349,129.092694340323));
#171973=CARTESIAN_POINT('Ctrl Pts',(-101.262584627435,5.70737027026856,
129.244278837481));
#171974=CARTESIAN_POINT('Ctrl Pts',(-101.255170134714,5.74875617941298,
129.395684174351));
#171975=CARTESIAN_POINT('Ctrl Pts',(-101.247755641993,5.78416554985556,
129.54892901446));
#171976=CARTESIAN_POINT('Ctrl Pts',(-101.240341149272,5.81343592513844,
129.703500359945));
#171977=CARTESIAN_POINT('Ctrl Pts',(-101.232933802919,5.84267808853162,
129.857922723748));
#171978=CARTESIAN_POINT('Ctrl Pts',(-101.225526456565,5.86579296734766,
130.013668683297));
#171979=CARTESIAN_POINT('Ctrl Pts',(-101.218119110211,5.88266818545696,
130.170211122327));
#171980=CARTESIAN_POINT('Ctrl Pts',(-101.210717288536,5.89953081739189,
130.326636806099));
#171981=CARTESIAN_POINT('Ctrl Pts',(-101.20331546686,5.9101630150755,130.483857416979));
#171982=CARTESIAN_POINT('Ctrl Pts',(-101.195913645185,5.91450368196843,
130.641336820279));
#171983=CARTESIAN_POINT('Ctrl Pts',(-101.188515730873,5.91884205745711,
130.798733091428));
#171984=CARTESIAN_POINT('Ctrl Pts',(-101.181117816562,5.91689550632446,
130.956387510711));
#171985=CARTESIAN_POINT('Ctrl Pts',(-101.173719902251,5.90865488157045,
131.113760121434));
#171986=CARTESIAN_POINT('Ctrl Pts',(-101.166323217338,5.90041562625877,
131.271106579684));
#171987=CARTESIAN_POINT('Ctrl Pts',(-101.158926532426,5.88588439274989,
131.428170949897));
#171988=CARTESIAN_POINT('Ctrl Pts',(-101.151529847514,5.865104139491,131.584414458929));
#171989=CARTESIAN_POINT('Ctrl Pts',(-101.144133490579,5.84432480765031,
131.74065103996));
#171990=CARTESIAN_POINT('Ctrl Pts',(-101.136737133643,5.81729705621921,
131.896066462142));
#171991=CARTESIAN_POINT('Ctrl Pts',(-101.129340776708,5.78411556729121,
132.050128519994));
#171992=CARTESIAN_POINT('Ctrl Pts',(-101.121943287371,5.75092899819263,
132.20421416514));
#171993=CARTESIAN_POINT('Ctrl Pts',(-101.114545798035,5.7115868942481,132.356945668434));
#171994=CARTESIAN_POINT('Ctrl Pts',(-101.107148308698,5.66623473072437,
132.50780258571));
#171995=CARTESIAN_POINT('Ctrl Pts',(-101.099748226183,5.62086666906996,
132.658712385644));
#171996=CARTESIAN_POINT('Ctrl Pts',(-101.092348143668,5.56948446058505,
132.807745933942));
#171997=CARTESIAN_POINT('Ctrl Pts',(-101.084948061153,5.51228290878922,
132.954399616275));
#171998=CARTESIAN_POINT('Ctrl Pts',(-101.077539841487,5.45501845800665,
133.101214559408));
#171999=CARTESIAN_POINT('Ctrl Pts',(-101.07013162182,5.39192202049038,133.245644062448));
#172000=CARTESIAN_POINT('Ctrl Pts',(-101.062723402154,5.32323615809954,
133.387205438224));
#172001=CARTESIAN_POINT('Ctrl Pts',(-101.055310622852,5.25450802070668,
133.528853942665));
#172002=CARTESIAN_POINT('Ctrl Pts',(-101.04789784355,5.18018377924718,133.66763047398));
#172003=CARTESIAN_POINT('Ctrl Pts',(-101.040485064248,5.1005508435062,133.803078953007));
#172004=CARTESIAN_POINT('Ctrl Pts',(-101.033061693219,5.02080412449189,
133.938720967173));
#172005=CARTESIAN_POINT('Ctrl Pts',(-101.02563832219,4.93573376298643,134.071025118535));
#172006=CARTESIAN_POINT('Ctrl Pts',(-101.018214951161,4.84566964284574,
134.199565511958));
#172007=CARTESIAN_POINT('Ctrl Pts',(-101.01427890172,4.79791548528698,134.267720712837));
#172008=CARTESIAN_POINT('Ctrl Pts',(-101.01034285228,4.7487580684344,134.334818348671));
#172009=CARTESIAN_POINT('Ctrl Pts',(-101.006406802839,4.69825089763084,
134.400799003721));
#172010=CARTESIAN_POINT('Ctrl Pts',(-100.998983536433,4.60299594977255,
134.525236459956));
#172011=CARTESIAN_POINT('Ctrl Pts',(-100.991560270028,4.50264979162134,
134.646075094947));
#172012=CARTESIAN_POINT('Ctrl Pts',(-100.984137003622,4.39751402674697,
134.762870557817));
#172013=CARTESIAN_POINT('Ctrl Pts',(-100.976722510901,4.2925025236157,134.879527978149));
#172014=CARTESIAN_POINT('Ctrl Pts',(-100.96930801818,4.18271292915891,134.99215146364));
#172015=CARTESIAN_POINT('Ctrl Pts',(-100.961893525459,4.06848903132321,
135.100327047195));
#172016=CARTESIAN_POINT('Ctrl Pts',(-100.954486179105,3.95437522678069,
135.208398367051));
#172017=CARTESIAN_POINT('Ctrl Pts',(-100.947078832752,3.83583589666972,
135.312030064689));
#172018=CARTESIAN_POINT('Ctrl Pts',(-100.939671486398,3.71325377678995,
135.410842675672));
#172019=CARTESIAN_POINT('Ctrl Pts',(-100.932269664722,3.59076308327994,
135.509581588483));
#172020=CARTESIAN_POINT('Ctrl Pts',(-100.924867843047,3.46423589318093,
135.603508338021));
#172021=CARTESIAN_POINT('Ctrl Pts',(-100.917466021372,3.33409024761793,
135.692281728145));
#172022=CARTESIAN_POINT('Ctrl Pts',(-100.91006810706,3.20401330492928,135.781008255485));
#172023=CARTESIAN_POINT('Ctrl Pts',(-100.902670192749,3.07032201854756,
135.864586631434));
#172024=CARTESIAN_POINT('Ctrl Pts',(-100.895272278438,2.93346572515558,
135.942717300576));
#172025=CARTESIAN_POINT('Ctrl Pts',(-100.887875593526,2.79663217479577,
136.02083498582));
#172026=CARTESIAN_POINT('Ctrl Pts',(-100.880478908613,2.6566349851843,136.093506576134));
#172027=CARTESIAN_POINT('Ctrl Pts',(-100.873082223701,2.51395066151732,
136.160476993631));
#172028=CARTESIAN_POINT('Ctrl Pts',(-100.865685866766,2.37127266462237,
136.227444441591));
#172029=CARTESIAN_POINT('Ctrl Pts',(-100.85828950983,2.22590810850929,136.288711060768));
#172030=CARTESIAN_POINT('Ctrl Pts',(-100.850893152895,2.07835593070503,
136.344068839829));
#172031=CARTESIAN_POINT('Ctrl Pts',(-100.843495663558,1.93078116228609,
136.399435094306));
#172032=CARTESIAN_POINT('Ctrl Pts',(-100.836098174222,1.78101845481702,
136.448890576236));
#172033=CARTESIAN_POINT('Ctrl Pts',(-100.828700684885,1.62958430565016,
136.492276365296));
#172034=CARTESIAN_POINT('Ctrl Pts',(-100.82130060237,1.47809707147727,136.535677363177));
#172035=CARTESIAN_POINT('Ctrl Pts',(-100.813900519855,1.32493758767808,
136.573004329161));
#172036=CARTESIAN_POINT('Ctrl Pts',(-100.80650043734,1.17063485531195,136.60414894112));
#172037=CARTESIAN_POINT('Ctrl Pts',(-100.799092217674,1.01616245122866,
136.635327799781));
#172038=CARTESIAN_POINT('Ctrl Pts',(-100.791683998007,0.860544654171698,
136.660310654194));
#172039=CARTESIAN_POINT('Ctrl Pts',(-100.784275778341,0.704318673136859,
136.679040674316));
#172040=CARTESIAN_POINT('Ctrl Pts',(-100.776862999039,0.547996537617463,
136.697782222452));
#172041=CARTESIAN_POINT('Ctrl Pts',(-100.769450219737,0.391065843486597,
136.710263238121));
#172042=CARTESIAN_POINT('Ctrl Pts',(-100.762037440434,0.23406565507024,
136.716479005387));
#172043=CARTESIAN_POINT('Ctrl Pts',(-100.754614069406,0.0768411374218717,
136.722703654033));
#172044=CARTESIAN_POINT('Ctrl Pts',(-100.747190698377,-0.0804527005207835,
136.722645175101));
#172045=CARTESIAN_POINT('Ctrl Pts',(-100.739767327348,-0.237279230834789,
136.716350902497));
#172046=CARTESIAN_POINT('Ctrl Pts',(-100.735831277907,-0.32043242020955,
136.713013528133));
#172047=CARTESIAN_POINT('Ctrl Pts',(-100.731895228467,-0.40345434608564,
136.707923912244));
#172048=CARTESIAN_POINT('Ctrl Pts',(-100.727959179026,-0.486266099372952,
136.701094954731));
#172049=CARTESIAN_POINT('Ctrl Pts',(-100.72053591262,-0.642446481603767,
136.688215753986));
#172050=CARTESIAN_POINT('Ctrl Pts',(-100.713112646215,-0.798350997120586,
136.669107923043));
#172051=CARTESIAN_POINT('Ctrl Pts',(-100.705689379809,-0.95344277685068,
136.643785027024));
#172052=CARTESIAN_POINT('Ctrl Pts',(-100.698274887088,-1.10835125097626,
136.618492060565));
#172053=CARTESIAN_POINT('Ctrl Pts',(-100.690860394367,-1.26244853654563,
136.586998710235));
#172054=CARTESIAN_POINT('Ctrl Pts',(-100.683445901647,-1.4152005255357,
136.549370455245));
#172055=CARTESIAN_POINT('Ctrl Pts',(-100.676038555293,-1.56780528640776,
136.511778467783));
#172056=CARTESIAN_POINT('Ctrl Pts',(-100.668631208939,-1.71906697204115,
136.468063436071));
#172057=CARTESIAN_POINT('Ctrl Pts',(-100.661223862585,-1.86845945020915,
136.418342256779));
#172058=CARTESIAN_POINT('Ctrl Pts',(-100.65382204091,-2.01774050583068,
136.368658161419));
#172059=CARTESIAN_POINT('Ctrl Pts',(-100.646420219234,-2.16515477720742,
136.312976955367));
#172060=CARTESIAN_POINT('Ctrl Pts',(-100.639018397559,-2.31018924492142,
136.251465923612));
#172061=CARTESIAN_POINT('Ctrl Pts',(-100.631620483248,-2.45514715007052,
136.18998736305));
#172062=CARTESIAN_POINT('Ctrl Pts',(-100.624222568936,-2.59772741070102,
136.122685251198));
#172063=CARTESIAN_POINT('Ctrl Pts',(-100.616824654625,-2.73743512490741,
136.049775710714));
#172064=CARTESIAN_POINT('Ctrl Pts',(-100.609427969713,-2.87711962222447,
135.976878286474));
#172065=CARTESIAN_POINT('Ctrl Pts',(-100.602031284801,-3.01393218992775,
135.898375455595));
#172066=CARTESIAN_POINT('Ctrl Pts',(-100.594634599888,-3.14740066106887,
135.814530239565));
#172067=CARTESIAN_POINT('Ctrl Pts',(-100.587238242953,-3.28086321407848,
135.73068874132));
#172068=CARTESIAN_POINT('Ctrl Pts',(-100.579841886018,-3.41098164925822,
135.64150552751));
#172069=CARTESIAN_POINT('Ctrl Pts',(-100.572445529082,-3.53731127286047,
135.547287933201));
#172070=CARTESIAN_POINT('Ctrl Pts',(-100.565048039746,-3.66366023785095,
135.453055913937));
#172071=CARTESIAN_POINT('Ctrl Pts',(-100.557650550409,-3.78621893699536,
135.353788202643));
#172072=CARTESIAN_POINT('Ctrl Pts',(-100.550253061073,-3.90457448669035,
135.249833442855));
#172073=CARTESIAN_POINT('Ctrl Pts',(-100.542852978558,-4.02297152573998,
135.145842241887));
#172074=CARTESIAN_POINT('Ctrl Pts',(-100.535452896042,-4.13716220149907,
135.037160967341));
#172075=CARTESIAN_POINT('Ctrl Pts',(-100.528052813527,-4.24676944149886,
134.924176132034));
#172076=CARTESIAN_POINT('Ctrl Pts',(-100.520644593861,-4.35649720592646,
134.811067058286));
#172077=CARTESIAN_POINT('Ctrl Pts',(-100.513236374195,-4.46163120938045,
134.693645241348));
#172078=CARTESIAN_POINT('Ctrl Pts',(-100.505828154528,-4.56183326455146,
134.572331932336));
#172079=CARTESIAN_POINT('Ctrl Pts',(-100.498415375226,-4.66209699241603,
134.450943957007));
#172080=CARTESIAN_POINT('Ctrl Pts',(-100.491002595924,-4.75742249780265,
134.325660013361));
#172081=CARTESIAN_POINT('Ctrl Pts',(-100.483589816622,-4.84751443562534,
134.196931082406));
#172082=CARTESIAN_POINT('Ctrl Pts',(-100.476166445593,-4.9377351010333,
134.068018217518));
#172083=CARTESIAN_POINT('Ctrl Pts',(-100.468743074565,-5.02270706257476,
133.935650847573));
#172084=CARTESIAN_POINT('Ctrl Pts',(-100.461319703536,-5.10218008310522,
133.800306037974));
#172085=CARTESIAN_POINT('Ctrl Pts',(-100.457383654095,-5.14431858552158,
133.728542972367));
#172086=CARTESIAN_POINT('Ctrl Pts',(-100.453447604654,-5.18491192638941,
133.655943213113));
#172087=CARTESIAN_POINT('Ctrl Pts',(-100.449511555213,-5.22392830647022,
133.582580121378));
#172088=CARTESIAN_POINT('Ctrl Pts',(-100.441665730885,-5.30170061818242,
133.436343663079));
#172089=CARTESIAN_POINT('Ctrl Pts',(-100.433819906556,-5.37341784873034,
133.286671693839));
#172090=CARTESIAN_POINT('Ctrl Pts',(-100.425974082228,-5.43878157850147,
133.134078519771));
#172091=CARTESIAN_POINT('Ctrl Pts',(-100.418141753343,-5.50403287744844,
132.981747818122));
#172092=CARTESIAN_POINT('Ctrl Pts',(-100.410309424458,-5.56295233934166,
132.826506211912));
#172093=CARTESIAN_POINT('Ctrl Pts',(-100.402477095573,-5.61528724153757,
132.668892665434));
#172094=CARTESIAN_POINT('Ctrl Pts',(-100.394663328559,-5.66749811501631,
132.511652647999));
#172095=CARTESIAN_POINT('Ctrl Pts',(-100.386849561545,-5.71315545719033,
132.352052196133));
#172096=CARTESIAN_POINT('Ctrl Pts',(-100.379035794531,-5.75205470421961,
132.190649635832));
#172097=CARTESIAN_POINT('Ctrl Pts',(-100.371233019106,-5.7908992318609,
132.029474119754));
#172098=CARTESIAN_POINT('Ctrl Pts',(-100.363430243681,-5.82300453863767,
131.866501847538));
#172099=CARTESIAN_POINT('Ctrl Pts',(-100.355627468256,-5.84821524401388,
131.702307733038));
#172100=CARTESIAN_POINT('Ctrl Pts',(-100.347839976852,-5.87337656684029,
131.538435240797));
#172101=CARTESIAN_POINT('Ctrl Pts',(-100.340052485449,-5.89167017837645,
131.373345985616));
#172102=CARTESIAN_POINT('Ctrl Pts',(-100.332264994045,-5.90299140926265,
131.20762601984));
#172103=CARTESIAN_POINT('Ctrl Pts',(-100.325968393443,-5.91214522600743,
131.073632621692));
#172104=CARTESIAN_POINT('Ctrl Pts',(-100.319671792841,-5.91674171556739,
130.939227231668));
#172105=CARTESIAN_POINT('Ctrl Pts',(-100.313375192239,-5.9167499888071,
130.804724555984));
#172106=CARTESIAN_POINT('',(-98.563375192205,-5.91674749124866,130.798912011994));
#172107=CARTESIAN_POINT('Ctrl Pts',(-100.313375192205,-5.91674998880715,
130.804724555263));
#172108=CARTESIAN_POINT('Ctrl Pts',(-100.305661661453,-5.91676012376195,
130.639954611816));
#172109=CARTESIAN_POINT('Ctrl Pts',(-100.297948130701,-5.90988315404377,
130.475303996975));
#172110=CARTESIAN_POINT('Ctrl Pts',(-100.29023459995,-5.89617484706362,
130.311356829189));
#172111=CARTESIAN_POINT('Ctrl Pts',(-100.282512544976,-5.88245139103566,
130.147228483414));
#172112=CARTESIAN_POINT('Ctrl Pts',(-100.274790490003,-5.8618815601619,
129.983805458956));
#172113=CARTESIAN_POINT('Ctrl Pts',(-100.267068435029,-5.83457264172292,
129.821663995531));
#172114=CARTESIAN_POINT('Ctrl Pts',(-100.259068059727,-5.8062794480888,
129.65367858699));
#172115=CARTESIAN_POINT('Ctrl Pts',(-100.251067684424,-5.77075242492543,
129.487069227152));
#172116=CARTESIAN_POINT('Ctrl Pts',(-100.243067309122,-5.72816741204176,
129.322460262575));
#172117=CARTESIAN_POINT('Ctrl Pts',(-100.235319847535,-5.68692862773064,
129.163055036975));
#172118=CARTESIAN_POINT('Ctrl Pts',(-100.227572385948,-5.63907146202288,
129.00552593413));
#172119=CARTESIAN_POINT('Ctrl Pts',(-100.219824924361,-5.584805069566,128.850420266007));
#172120=CARTESIAN_POINT('Ctrl Pts',(-100.2116980922,-5.52788141031746,128.687719526194));
#172121=CARTESIAN_POINT('Ctrl Pts',(-100.20357126004,-5.46390524848292,
128.527685917589));
#172122=CARTESIAN_POINT('Ctrl Pts',(-100.19544442788,-5.39317272883823,
128.370923032705));
#172123=CARTESIAN_POINT('Ctrl Pts',(-100.18731759572,-5.32244020919354,
128.21416014782));
#172124=CARTESIAN_POINT('Ctrl Pts',(-100.17919076356,-5.24495157963472,
128.060668314391));
#172125=CARTESIAN_POINT('Ctrl Pts',(-100.1710639314,-5.16105560301029,127.911017287587));
#172126=CARTESIAN_POINT('Ctrl Pts',(-100.163640664995,-5.08442276839887,
127.774322027004));
#172127=CARTESIAN_POINT('Ctrl Pts',(-100.156217398589,-5.00223955723448,
127.640466705985));
#172128=CARTESIAN_POINT('Ctrl Pts',(-100.148794132184,-4.9147414658173,
127.509933977515));
#172129=CARTESIAN_POINT('Ctrl Pts',(-100.141379639462,-4.82734678987766,
127.379555527891));
#172130=CARTESIAN_POINT('Ctrl Pts',(-100.133965146741,-4.73464994335874,
127.252492161096));
#172131=CARTESIAN_POINT('Ctrl Pts',(-100.12655065402,-4.63693249162979,
127.12920243994));
#172132=CARTESIAN_POINT('Ctrl Pts',(-100.119143307666,-4.53930922365981,
127.00603155006));
#172133=CARTESIAN_POINT('Ctrl Pts',(-100.111735961313,-4.43667521438776,
126.886627355494));
#172134=CARTESIAN_POINT('Ctrl Pts',(-100.104328614959,-4.32935547896536,
126.771419792405));
#172135=CARTESIAN_POINT('Ctrl Pts',(-100.096926793283,-4.22211578665059,
126.656298155462));
#172136=CARTESIAN_POINT('Ctrl Pts',(-100.089524971608,-4.11019758013669,
126.545367189702));
#172137=CARTESIAN_POINT('Ctrl Pts',(-100.082123149932,-3.99396625305007,
126.439023960217));
#172138=CARTESIAN_POINT('Ctrl Pts',(-100.074725235621,-3.87779628357628,
126.332736868495));
#172139=CARTESIAN_POINT('Ctrl Pts',(-100.067327321309,-3.75731800273049,
126.231032941206));
#172140=CARTESIAN_POINT('Ctrl Pts',(-100.059929406998,-3.63293369198555,
126.134272465064));
#172141=CARTESIAN_POINT('Ctrl Pts',(-100.052532722085,-3.50857005165668,
126.037528068759));
#172142=CARTESIAN_POINT('Ctrl Pts',(-100.045136037173,-3.3803019640779,
125.945725722126));
#172143=CARTESIAN_POINT('Ctrl Pts',(-100.037739352261,-3.24856491584063,
125.859185539769));
#172144=CARTESIAN_POINT('Ctrl Pts',(-100.030342995325,-3.11683370896214,
125.772649194694));
#172145=CARTESIAN_POINT('Ctrl Pts',(-100.02294663839,-2.98163415926531,
125.691374754914));
#172146=CARTESIAN_POINT('Ctrl Pts',(-100.015550281454,-2.84343063759905,
125.615638928011));
#172147=CARTESIAN_POINT('Ctrl Pts',(-100.008152792118,-2.70520595662081,
125.539891505759));
#172148=CARTESIAN_POINT('Ctrl Pts',(-100.000755302781,-2.56397671530603,
125.469684564225));
#172149=CARTESIAN_POINT('Ctrl Pts',(-99.9933578134444,-2.42023163284223,
125.405248708567));
#172150=CARTESIAN_POINT('Ctrl Pts',(-99.9859577309293,-2.27643616076282,
125.340790265021));
#172151=CARTESIAN_POINT('Ctrl Pts',(-99.9785576484144,-2.13012343205648,
125.282107087822));
#172152=CARTESIAN_POINT('Ctrl Pts',(-99.9711575658993,-1.98180172317201,
125.229381470293));
#172153=CARTESIAN_POINT('Ctrl Pts',(-99.9637493462328,-1.83331691932058,
125.176597875527));
#172154=CARTESIAN_POINT('Ctrl Pts',(-99.9563411265662,-1.68281907556357,
125.12978504822));
#172155=CARTESIAN_POINT('Ctrl Pts',(-99.9489329068996,-1.53083190015848,
125.089075475427));
#172156=CARTESIAN_POINT('Ctrl Pts',(-99.9415201275975,-1.37875117918209,
125.048340846571));
#172157=CARTESIAN_POINT('Ctrl Pts',(-99.9341073482953,-1.22517966331314,
125.013717039342));
#172158=CARTESIAN_POINT('Ctrl Pts',(-99.9266945689931,-1.07065029256481,
124.985285217339));
#172159=CARTESIAN_POINT('Ctrl Pts',(-99.9192711979643,-0.915900123005516,
124.956812770615));
#172160=CARTESIAN_POINT('Ctrl Pts',(-99.9118478269355,-0.760189733670803,
124.934550032053));
#172161=CARTESIAN_POINT('Ctrl Pts',(-99.9044244559067,-0.604057038907278,
124.918526296397));
#172162=CARTESIAN_POINT('Ctrl Pts',(-99.9004884064669,-0.521271737812884,
124.910030127271));
#172163=CARTESIAN_POINT('Ctrl Pts',(-99.8965523570271,-0.438367721794466,
124.903287094543));
#172164=CARTESIAN_POINT('Ctrl Pts',(-99.8926163075873,-0.355424931963131,
124.898295626369));
#172165=CARTESIAN_POINT('Ctrl Pts',(-99.8851930411819,-0.198997418857412,
124.888881873171));
#172166=CARTESIAN_POINT('Ctrl Pts',(-99.8777697747764,-0.0419591132346854,
124.885672865664));
#172167=CARTESIAN_POINT('Ctrl Pts',(-99.870346508371,0.1151566237746,124.888731359871));
#172168=CARTESIAN_POINT('Ctrl Pts',(-99.86293201565,0.272086663030391,124.891786239192));
#172169=CARTESIAN_POINT('Ctrl Pts',(-99.8555175229289,0.429093581924141,
124.901093868031));
#172170=CARTESIAN_POINT('Ctrl Pts',(-99.8481030302079,0.585639385617466,
124.916665221869));
#172171=CARTESIAN_POINT('Ctrl Pts',(-99.8406956838542,0.742034304571345,
124.93222156745));
#172172=CARTESIAN_POINT('Ctrl Pts',(-99.8332883375003,0.897968624146639,
124.954029582423));
#172173=CARTESIAN_POINT('Ctrl Pts',(-99.8258809911466,1.05290494824604,
124.982048213335));
#172174=CARTESIAN_POINT('Ctrl Pts',(-99.8184791694712,1.20772571498951,
125.010045946895));
#172175=CARTESIAN_POINT('Ctrl Pts',(-99.8110773477957,1.36154960258513,
125.04424500709));
#172176=CARTESIAN_POINT('Ctrl Pts',(-99.8036755261203,1.51384504474415,
125.084552601295));
#172177=CARTESIAN_POINT('Ctrl Pts',(-99.796277611809,1.66606009132429,125.124838917434));
#172178=CARTESIAN_POINT('Ctrl Pts',(-99.7888796974977,1.81674793939811,
125.171227250274));
#172179=CARTESIAN_POINT('Ctrl Pts',(-99.7814817831863,1.96538802658662,
125.223573892789));
#172180=CARTESIAN_POINT('Ctrl Pts',(-99.7740850982741,2.11400341248988,
125.275911836241));
#172181=CARTESIAN_POINT('Ctrl Pts',(-99.7666884133618,2.26057136114734,
125.334206000309));
#172182=CARTESIAN_POINT('Ctrl Pts',(-99.7592917284496,2.40458715993728,
125.398263027551));
#172183=CARTESIAN_POINT('Ctrl Pts',(-99.7518953715142,2.54859657291577,
125.462317214438));
#172184=CARTESIAN_POINT('Ctrl Pts',(-99.7444990145787,2.69005371995732,
125.532133604707));
#172185=CARTESIAN_POINT('Ctrl Pts',(-99.7371026576432,2.8284747953498,125.607471077219));
#172186=CARTESIAN_POINT('Ctrl Pts',(-99.7297051683066,2.96691706336229,
125.68282008409));
#172187=CARTESIAN_POINT('Ctrl Pts',(-99.7223076789701,3.10232200628499,
125.763691677827));
#172188=CARTESIAN_POINT('Ctrl Pts',(-99.7149101896335,3.23423144480751,
125.849799332859));
#172189=CARTESIAN_POINT('Ctrl Pts',(-99.7075101071185,3.36618712397941,
125.935937172796));
#172190=CARTESIAN_POINT('Ctrl Pts',(-99.7001100246035,3.49464454670415,
126.027314524554));
#172191=CARTESIAN_POINT('Ctrl Pts',(-99.6927099420885,3.61917560860956,
126.123602294757));
#172192=CARTESIAN_POINT('Ctrl Pts',(-99.685301722422,3.74384360521946,126.219995943262));
#172193=CARTESIAN_POINT('Ctrl Pts',(-99.6778935027555,3.86457632330588,
126.321310564907));
#172194=CARTESIAN_POINT('Ctrl Pts',(-99.670485283089,3.98097922065087,126.427177161593));
#172195=CARTESIAN_POINT('Ctrl Pts',(-99.6630725037869,4.09745376203722,
126.533108917403));
#172196=CARTESIAN_POINT('Ctrl Pts',(-99.6556597244847,4.20959290717608,
126.643597969532));
#172197=CARTESIAN_POINT('Ctrl Pts',(-99.6482469451826,4.31704030373725,
126.758239811361));
#172198=CARTESIAN_POINT('Ctrl Pts',(-99.6408235741538,4.42464122617726,
126.873045458829));
#172199=CARTESIAN_POINT('Ctrl Pts',(-99.633400203125,4.52753676751639,126.992015465332));
#172200=CARTESIAN_POINT('Ctrl Pts',(-99.6259768320962,4.62541152541234,
127.114713102818));
#172201=CARTESIAN_POINT('Ctrl Pts',(-99.6220407826556,4.67730707051926,
127.179770334301));
#172202=CARTESIAN_POINT('Ctrl Pts',(-99.618104733215,4.72779182063832,127.245875057057));
#172203=CARTESIAN_POINT('Ctrl Pts',(-99.6141686837743,4.77682388808281,
127.312959164748));
#172204=CARTESIAN_POINT('Ctrl Pts',(-99.6067454173689,4.86929683704776,
127.439477698233));
#172205=CARTESIAN_POINT('Ctrl Pts',(-99.5993221509635,4.95687970600967,
127.569863925366));
#172206=CARTESIAN_POINT('Ctrl Pts',(-99.5918988845581,5.03923140183056,
127.703703035487));
#172207=CARTESIAN_POINT('Ctrl Pts',(-99.5844843918371,5.12148576478588,
127.837383958894));
#172208=CARTESIAN_POINT('Ctrl Pts',(-99.5770698991162,5.19852106780652,
127.974509327165));
#172209=CARTESIAN_POINT('Ctrl Pts',(-99.5696554063952,5.27003727755891,
128.114632442519));
#172210=CARTESIAN_POINT('Ctrl Pts',(-99.5622480600415,5.3414845572958,128.25462050194));
#172211=CARTESIAN_POINT('Ctrl Pts',(-99.5548407136876,5.407423165301,128.397600226071));
#172212=CARTESIAN_POINT('Ctrl Pts',(-99.5474333673339,5.46759716529179,
128.543097297961));
#172213=CARTESIAN_POINT('Ctrl Pts',(-99.5400315456585,5.52772628524315,
128.688485852645));
#172214=CARTESIAN_POINT('Ctrl Pts',(-99.5326297239832,5.58209921593647,
128.83638767319));
#172215=CARTESIAN_POINT('Ctrl Pts',(-99.5252279023078,5.63050670187152,
128.986305381144));
#172216=CARTESIAN_POINT('Ctrl Pts',(-99.5178299879965,5.67888863387169,
129.136143948708));
#172217=CARTESIAN_POINT('Ctrl Pts',(-99.5104320736852,5.72131127830683,
129.287995929992));
#172218=CARTESIAN_POINT('Ctrl Pts',(-99.5030341593739,5.7576141632872,129.441345683967));
#172219=CARTESIAN_POINT('Ctrl Pts',(-99.4956374744617,5.79391101538663,
129.594669953994));
#172220=CARTESIAN_POINT('Ctrl Pts',(-99.4882407895495,5.82409004055069,
129.749491139811));
#172221=CARTESIAN_POINT('Ctrl Pts',(-99.4808441046373,5.84804110637009,
129.905280097976));
#172222=CARTESIAN_POINT('Ctrl Pts',(-99.4734477477019,5.87199111017406,
130.061062148295));
#172223=CARTESIAN_POINT('Ctrl Pts',(-99.4660513907665,5.88971364699685,
130.217811516675));
#172224=CARTESIAN_POINT('Ctrl Pts',(-99.4586550338311,5.90115007007733,
130.374990831803));
#172225=CARTESIAN_POINT('Ctrl Pts',(-99.4512575444945,5.91258824410341,
130.532194211485));
#172226=CARTESIAN_POINT('Ctrl Pts',(-99.4438600551579,5.91773836098938,
130.689827296646));
#172227=CARTESIAN_POINT('Ctrl Pts',(-99.4364625658214,5.91659382570492,
130.847349733985));
#172228=CARTESIAN_POINT('Ctrl Pts',(-99.4290624833064,5.91544888920539,
131.00492739057));
#172229=CARTESIAN_POINT('Ctrl Pts',(-99.4216624007915,5.90800490996031,
131.162393949051));
#172230=CARTESIAN_POINT('Ctrl Pts',(-99.4142623182765,5.8943073626781,131.319211350088));
#172231=CARTESIAN_POINT('Ctrl Pts',(-99.4068540986101,5.88059475353448,
131.476201187979));
#172232=CARTESIAN_POINT('Ctrl Pts',(-99.3994458789437,5.86061487615244,
131.632540070779));
#172233=CARTESIAN_POINT('Ctrl Pts',(-99.3920376592772,5.83446491937734,
131.787696606461));
#172234=CARTESIAN_POINT('Ctrl Pts',(-99.3846248799751,5.80829886774011,
131.942948638401));
#172235=CARTESIAN_POINT('Ctrl Pts',(-99.3772121006731,5.77595524607093,
132.097016508672));
#172236=CARTESIAN_POINT('Ctrl Pts',(-99.3697993213711,5.73758176010527,
132.249381762258));
#172237=CARTESIAN_POINT('Ctrl Pts',(-99.3623759503424,5.69915344430339,
132.401964722463));
#172238=CARTESIAN_POINT('Ctrl Pts',(-99.3549525793136,5.65467816188542,
132.552839850063));
#172239=CARTESIAN_POINT('Ctrl Pts',(-99.3475292082849,5.60435286185769,
132.701505725956));
#172240=CARTESIAN_POINT('Ctrl Pts',(-99.3435931588437,5.57766918024148,
132.78033194055));
#172241=CARTESIAN_POINT('Ctrl Pts',(-99.3396571094026,5.54934164539772,
132.858537407986));
#172242=CARTESIAN_POINT('Ctrl Pts',(-99.3357210599614,5.51940491580191,
132.936050073824));
#172243=CARTESIAN_POINT('Ctrl Pts',(-99.328297793556,5.46294517808277,133.082236542494));
#172244=CARTESIAN_POINT('Ctrl Pts',(-99.3208745271506,5.4005882324696,133.226399431254));
#172245=CARTESIAN_POINT('Ctrl Pts',(-99.3134512607452,5.33249870174735,
133.368027553493));
#172246=CARTESIAN_POINT('Ctrl Pts',(-99.3060367680242,5.26448964719574,
133.509488283052));
#172247=CARTESIAN_POINT('Ctrl Pts',(-99.2986222753032,5.19076165425145,
133.648419876261));
#172248=CARTESIAN_POINT('Ctrl Pts',(-99.2912077825821,5.11152836706183,
133.784328455517));
#172249=CARTESIAN_POINT('Ctrl Pts',(-99.2838004362284,5.03237144789747,
133.920106040968));
#172250=CARTESIAN_POINT('Ctrl Pts',(-99.2763930898745,4.94771998485609,
134.052866092728));
#172251=CARTESIAN_POINT('Ctrl Pts',(-99.2689857435207,4.85783469441018,
134.182136904457));
#172252=CARTESIAN_POINT('Ctrl Pts',(-99.2615839218453,4.76801644380481,
134.311311301138));
#172253=CARTESIAN_POINT('Ctrl Pts',(-99.2541821001699,4.67297235055375,
134.437001334361));
#172254=CARTESIAN_POINT('Ctrl Pts',(-99.2467802784945,4.57300776552732,
134.558762106342));
#172255=CARTESIAN_POINT('Ctrl Pts',(-99.2393823641832,4.47309595102777,
134.68045860176));
#172256=CARTESIAN_POINT('Ctrl Pts',(-99.2319844498718,4.36826905404935,
134.79822967907));
#172257=CARTESIAN_POINT('Ctrl Pts',(-99.2245865355605,4.25887415901876,
134.911661612154));
#172258=CARTESIAN_POINT('Ctrl Pts',(-99.2171898506483,4.14949744343463,
135.025074694909));
#172259=CARTESIAN_POINT('Ctrl Pts',(-99.209793165736,4.03555449530661,135.134149796146));
#172260=CARTESIAN_POINT('Ctrl Pts',(-99.2023964808238,3.91743096874174,
135.238508243395));
#172261=CARTESIAN_POINT('Ctrl Pts',(-99.1950001238883,3.79931267989816,
135.34286206328));
#172262=CARTESIAN_POINT('Ctrl Pts',(-99.187603766953,3.67701446095609,135.442499397863));
#172263=CARTESIAN_POINT('Ctrl Pts',(-99.1802074100175,3.55095671761385,
135.537080443642));
#172264=CARTESIAN_POINT('Ctrl Pts',(-99.1728099206809,3.42487967450857,
135.631675970021));
#172265=CARTESIAN_POINT('Ctrl Pts',(-99.1654124313443,3.29504225953587,
135.721213442148));
#172266=CARTESIAN_POINT('Ctrl Pts',(-99.1580149420076,3.16189552245616,
135.805395237279));
#172267=CARTESIAN_POINT('Ctrl Pts',(-99.1506148594926,3.02870211099436,
135.889606542208));
#172268=CARTESIAN_POINT('Ctrl Pts',(-99.1432147769776,2.89219738304632,
135.968458232839));
#172269=CARTESIAN_POINT('Ctrl Pts',(-99.1358146944626,2.75285860336558,
136.041697734114));
#172270=CARTESIAN_POINT('Ctrl Pts',(-99.1284064747961,2.61336660637241,
136.11501776975));
#172271=CARTESIAN_POINT('Ctrl Pts',(-99.1209982551296,2.47103466476383,
136.182713117992));
#172272=CARTESIAN_POINT('Ctrl Pts',(-99.1135900354632,2.32636238664759,
136.244578316196));
#172273=CARTESIAN_POINT('Ctrl Pts',(-99.1061772561611,2.18160106515775,
136.306481591398));
#172274=CARTESIAN_POINT('Ctrl Pts',(-99.098764476859,2.03449688491973,136.362547433667));
#172275=CARTESIAN_POINT('Ctrl Pts',(-99.0913516975569,1.8855658753796,136.412619874421));
#172276=CARTESIAN_POINT('Ctrl Pts',(-99.0839283265281,1.73642206622908,
136.462763861027));
#172277=CARTESIAN_POINT('Ctrl Pts',(-99.0765049554993,1.58544657185666,
136.506897238121));
#172278=CARTESIAN_POINT('Ctrl Pts',(-99.0690815844706,1.43316770610195,
136.544914675206));
#172279=CARTESIAN_POINT('Ctrl Pts',(-99.0651455350299,1.35242579760083,
136.565072432564));
#172280=CARTESIAN_POINT('Ctrl Pts',(-99.0612094855892,1.27131759844237,
136.583511640643));
#172281=CARTESIAN_POINT('Ctrl Pts',(-99.0572734361486,1.18992246381842,
136.600222511418));
#172282=CARTESIAN_POINT('Ctrl Pts',(-99.0498501697432,1.03641378016814,
136.631738692171));
#172283=CARTESIAN_POINT('Ctrl Pts',(-99.0424269033378,0.881420006692884,
136.657199590535));
#172284=CARTESIAN_POINT('Ctrl Pts',(-99.0350036369325,0.725460201803441,
136.676467399471));
#172285=CARTESIAN_POINT('Ctrl Pts',(-99.0275891442115,0.56968472845128,
136.695712435458));
#172286=CARTESIAN_POINT('Ctrl Pts',(-99.0201746514904,0.412945863245716,
136.708778906631));
#172287=CARTESIAN_POINT('Ctrl Pts',(-99.0127601587695,0.255774599280688,
136.715579604955));
#172288=CARTESIAN_POINT('Ctrl Pts',(-99.0053528124158,0.0987548228977118,
136.722373748509));
#172289=CARTESIAN_POINT('Ctrl Pts',(-98.997945466062,-0.0586961521079571,
136.72291412602));
#172290=CARTESIAN_POINT('Ctrl Pts',(-98.9905381197083,-0.216040542210129,
136.717165116839));
#172291=CARTESIAN_POINT('Ctrl Pts',(-98.983136298033,-0.373267578930346,
136.711420395486));
#172292=CARTESIAN_POINT('Ctrl Pts',(-98.9757344763576,-0.53038781758902,
136.699395641152));
#172293=CARTESIAN_POINT('Ctrl Pts',(-98.9683326546823,-0.686861903477895,
136.681107276054));
#172294=CARTESIAN_POINT('Ctrl Pts',(-98.960934740371,-0.843253387914375,
136.662828565242));
#172295=CARTESIAN_POINT('Ctrl Pts',(-98.9535368260596,-0.998999029060612,
136.638292871967));
#172296=CARTESIAN_POINT('Ctrl Pts',(-98.9461389117483,-1.15356313980562,
136.607568579115));
#172297=CARTESIAN_POINT('Ctrl Pts',(-98.9387422268362,-1.30810156479972,
136.576849392083));
#172298=CARTESIAN_POINT('Ctrl Pts',(-98.931345541924,-1.46145848331121,
136.539943719318));
#172299=CARTESIAN_POINT('Ctrl Pts',(-98.9239488570119,-1.61310685200084,
136.496971340822));
#172300=CARTESIAN_POINT('Ctrl Pts',(-98.9165525000764,-1.76474849644289,
136.454000867767));
#172301=CARTESIAN_POINT('Ctrl Pts',(-98.909156143141,-1.91468138254109,
136.404964325625));
#172302=CARTESIAN_POINT('Ctrl Pts',(-98.9017597862056,-2.06239238443654,
136.350031741525));
#172303=CARTESIAN_POINT('Ctrl Pts',(-98.8943622968691,-2.21012600126262,
136.295090747107));
#172304=CARTESIAN_POINT('Ctrl Pts',(-98.8869648075328,-2.35563670664166,
136.234252043465));
#172305=CARTESIAN_POINT('Ctrl Pts',(-98.8795673181963,-2.49843029871731,
136.167734239173));
#172306=CARTESIAN_POINT('Ctrl Pts',(-98.8721672356813,-2.64127394686632,
136.101193117168));
#172307=CARTESIAN_POINT('Ctrl Pts',(-98.8647671531664,-2.78139824715815,
136.028969088377));
#172308=CARTESIAN_POINT('Ctrl Pts',(-98.8573670706515,-2.918332727787,135.951327166168));
#172309=CARTESIAN_POINT('Ctrl Pts',(-98.8499588509851,-3.0554177819547,
135.873599868683));
#172310=CARTESIAN_POINT('Ctrl Pts',(-98.8425506313185,-3.18930568675224,
135.790442964435));
#172311=CARTESIAN_POINT('Ctrl Pts',(-98.8351424116521,-3.31955353025329,
135.702165730296));
#172312=CARTESIAN_POINT('Ctrl Pts',(-98.82772963235,-3.44988153912945,135.613834162992));
#172313=CARTESIAN_POINT('Ctrl Pts',(-98.8203168530479,-3.57656472273543,
135.520376207183));
#172314=CARTESIAN_POINT('Ctrl Pts',(-98.8129040737459,-3.69919293376609,
135.422141708228));
#172315=CARTESIAN_POINT('Ctrl Pts',(-98.8054807027171,-3.82199636173483,
135.323766847215));
#172316=CARTESIAN_POINT('Ctrl Pts',(-98.7980573316884,-3.94073296429517,
135.220602056289));
#172317=CARTESIAN_POINT('Ctrl Pts',(-98.7906339606597,-4.05502855738327,
135.113034887142));
#172318=CARTESIAN_POINT('Ctrl Pts',(-98.7866979112184,-4.11563082333166,
135.056000193014));
#172319=CARTESIAN_POINT('Ctrl Pts',(-98.7827618617771,-4.17498521414741,
134.997728410319));
#172320=CARTESIAN_POINT('Ctrl Pts',(-98.7788258123359,-4.23304060146686,
134.938281012159));
#172321=CARTESIAN_POINT('Ctrl Pts',(-98.771500395973,-4.34108799532415,
134.827642934639));
#172322=CARTESIAN_POINT('Ctrl Pts',(-98.76417497961,-4.44497946114729,134.712576679298));
#172323=CARTESIAN_POINT('Ctrl Pts',(-98.7568495632472,-4.54432289261208,
134.593431745188));
#172324=CARTESIAN_POINT('Ctrl Pts',(-98.7495330015686,-4.64354624152007,
134.474430828938));
#172325=CARTESIAN_POINT('Ctrl Pts',(-98.7422164398901,-4.73823225107807,
134.351361335499));
#172326=CARTESIAN_POINT('Ctrl Pts',(-98.7348998782115,-4.82802450097346,
134.224610605579));
#172327=CARTESIAN_POINT('Ctrl Pts',(-98.7275917009874,-4.9177138529426,
134.098005126359));
#172328=CARTESIAN_POINT('Ctrl Pts',(-98.7202835237632,-5.00252039296936,
133.967727122969));
#172329=CARTESIAN_POINT('Ctrl Pts',(-98.712975346539,-5.0821272954591,133.83419769491));
#172330=CARTESIAN_POINT('Ctrl Pts',(-98.7056719100402,-5.16168255792281,
133.700754885761));
#172331=CARTESIAN_POINT('Ctrl Pts',(-98.6983684735414,-5.23604469649038,
133.564065175827));
#172332=CARTESIAN_POINT('Ctrl Pts',(-98.6910650370426,-5.3049395390632,
133.424579510976));
#172333=CARTESIAN_POINT('Ctrl Pts',(-98.6837648057947,-5.37380414583459,
133.285155062041));
#172334=CARTESIAN_POINT('Ctrl Pts',(-98.6764645745468,-5.43720606106764,
133.142937443257));
#172335=CARTESIAN_POINT('Ctrl Pts',(-98.6691643432989,-5.49491666632617,
132.998402867075));
#172336=CARTESIAN_POINT('Ctrl Pts',(-98.6618657844603,-5.55261405066784,
132.853901402305));
#172337=CARTESIAN_POINT('Ctrl Pts',(-98.6545672256217,-5.60462257837086,
132.707084393212));
#172338=CARTESIAN_POINT('Ctrl Pts',(-98.647268666783,-5.650761579237,132.55844845377));
#172339=CARTESIAN_POINT('Ctrl Pts',(-98.6399678669216,-5.69691474708537,
132.409766875656));
#172340=CARTESIAN_POINT('Ctrl Pts',(-98.6326670670602,-5.73719466763828,
132.259265616628));
#172341=CARTESIAN_POINT('Ctrl Pts',(-98.6253662671987,-5.77147035984798,
132.107457102058));
#172342=CARTESIAN_POINT('Ctrl Pts',(-98.6180644732092,-5.80575071927642,
131.955627916176));
#172343=CARTESIAN_POINT('Ctrl Pts',(-98.6107626792195,-5.83402514580646,
131.802491496868));
#172344=CARTESIAN_POINT('Ctrl Pts',(-98.6034608852299,-5.85621385145219,
131.648570241155));
#172345=CARTESIAN_POINT('Ctrl Pts',(-98.5961528071448,-5.87842165321974,
131.494516517189));
#172346=CARTESIAN_POINT('Ctrl Pts',(-98.5888447290596,-5.89453322471738,
131.339676989102));
#172347=CARTESIAN_POINT('Ctrl Pts',(-98.5815366509744,-5.90452065747652,
131.184579459725));
#172348=CARTESIAN_POINT('Ctrl Pts',(-98.5754828313846,-5.9127939839769,
131.056100747439));
#172349=CARTESIAN_POINT('Ctrl Pts',(-98.5694290117949,-5.91686585467058,
130.927445169786));
#172350=CARTESIAN_POINT('Ctrl Pts',(-98.5633751922051,-5.91674749124866,
130.798912011994));
#172351=CARTESIAN_POINT('',(-96.8133751922048,-5.92166422711087,130.806462316915));
#172352=CARTESIAN_POINT('Ctrl Pts',(-98.563375192205,-5.91713394122631,
130.798911656121));
#172353=CARTESIAN_POINT('Ctrl Pts',(-98.5423761909776,-5.9212723605073,
130.353032893676));
#172354=CARTESIAN_POINT('Ctrl Pts',(-98.5213771897503,-5.87515968389772,
129.908001828249));
#172355=CARTESIAN_POINT('Ctrl Pts',(-98.4075623139186,-5.33543540985616,
127.56261494968));
#172356=CARTESIAN_POINT('Ctrl Pts',(-98.2219305647096,-2.36602057997696,
124.21804851249));
#172357=CARTESIAN_POINT('Ctrl Pts',(-97.9434829408973,4.26235899130877,
125.253697922036));
#172358=CARTESIAN_POINT('Ctrl Pts',(-97.6650353170831,6.97383887740406,
131.390135183845));
#172359=CARTESIAN_POINT('Ctrl Pts',(-97.3865876932723,3.27670152612622,
136.988274235881));
#172360=CARTESIAN_POINT('Ctrl Pts',(-97.1081400694582,-3.43156445187626,
136.903698773712));
#172361=CARTESIAN_POINT('Ctrl Pts',(-96.91706923577,-5.87088692384846,132.999514831838));
#172362=CARTESIAN_POINT('Ctrl Pts',(-96.818814276685,-5.92615900346599,
130.921523331019));
#172363=CARTESIAN_POINT('Ctrl Pts',(-96.8133751922048,-5.9256324804525,
130.806463725316));
#172364=CARTESIAN_POINT('',(-95.063375206451,-5.91325275216486,130.808790442179));
#172365=CARTESIAN_POINT('Ctrl Pts',(-96.8133751922048,-5.91674962734513,
130.80646057264));
#172366=CARTESIAN_POINT('Ctrl Pts',(-96.8060180359455,-5.916804781926,130.651059226289));
#172367=CARTESIAN_POINT('Ctrl Pts',(-96.7986608796862,-5.91073338293157,
130.49540813547));
#172368=CARTESIAN_POINT('Ctrl Pts',(-96.7913037234269,-5.89850259791408,
130.340035661419));
#172369=CARTESIAN_POINT('Ctrl Pts',(-96.7839549889756,-5.88628581359465,
130.184841043744));
#172370=CARTESIAN_POINT('Ctrl Pts',(-96.7766062545244,-5.86792370315422,
130.029924783744));
#172371=CARTESIAN_POINT('Ctrl Pts',(-96.7692575200732,-5.84343540412144,
129.875817005041));
#172372=CARTESIAN_POINT('Ctrl Pts',(-96.7619155248804,-5.81896956242183,
129.721850553008));
#172373=CARTESIAN_POINT('Ctrl Pts',(-96.7545735296877,-5.78838877287601,
129.568691479954));
#172374=CARTESIAN_POINT('Ctrl Pts',(-96.7472315344949,-5.75176409327423,
129.416866337282));
#172375=CARTESIAN_POINT('Ctrl Pts',(-96.7398946020873,-5.71516466878055,
129.265145887959));
#172376=CARTESIAN_POINT('Ctrl Pts',(-96.7325576696796,-5.67252973937426,
129.114757906376));
#172377=CARTESIAN_POINT('Ctrl Pts',(-96.725220737272,-5.62398167587752,
128.966220070194));
#172378=CARTESIAN_POINT('Ctrl Pts',(-96.7178864892326,-5.57545137469236,
128.817736579647));
#172379=CARTESIAN_POINT('Ctrl Pts',(-96.7105522411932,-5.52101235978126,
128.671102249299));
#172380=CARTESIAN_POINT('Ctrl Pts',(-96.7032179931538,-5.46083720911901,
128.526820818133));
#172381=CARTESIAN_POINT('Ctrl Pts',(-96.6958850156969,-5.40067248317853,
128.382564382231));
#172382=CARTESIAN_POINT('Ctrl Pts',(-96.6885520382401,-5.33477374453361,
128.240660385716));
#172383=CARTESIAN_POINT('Ctrl Pts',(-96.6812190607832,-5.26336209064202,
128.101593504903));
#172384=CARTESIAN_POINT('Ctrl Pts',(-96.6738858434829,-5.19194810105341,
127.962522075559));
#172385=CARTESIAN_POINT('Ctrl Pts',(-96.6665526261826,-5.11502101097641,
127.826288285204));
#172386=CARTESIAN_POINT('Ctrl Pts',(-96.6592194088823,-5.03284822279007,
127.69335285016));
#172387=CARTESIAN_POINT('Ctrl Pts',(-96.6518844413729,-4.95065582253505,
127.560385687595));
#172388=CARTESIAN_POINT('Ctrl Pts',(-96.6445494738636,-4.86321543263135,
127.430718770531));
#172389=CARTESIAN_POINT('Ctrl Pts',(-96.6372145063542,-4.77083803961927,
127.304784220026));
#172390=CARTESIAN_POINT('Ctrl Pts',(-96.6298719452267,-4.67836501173922,
127.178719294179));
#172391=CARTESIAN_POINT('Ctrl Pts',(-96.6225293840991,-4.58094499712026,
127.056394760042));
#172392=CARTESIAN_POINT('Ctrl Pts',(-96.6151868229715,-4.47893000454518,
126.938210520003));
#172393=CARTESIAN_POINT('Ctrl Pts',(-96.60784036526,-4.37686087418683,126.81996356141));
#172394=CARTESIAN_POINT('Ctrl Pts',(-96.6004939075486,-4.27019216761278,
126.705861551566));
#172395=CARTESIAN_POINT('Ctrl Pts',(-96.5931474498371,-4.1593125902904,
126.596267303635));
#172396=CARTESIAN_POINT('Ctrl Pts',(-96.5857897877326,-4.04826390584006,
126.486505908886));
#172397=CARTESIAN_POINT('Ctrl Pts',(-96.5784321256281,-3.93299180058921,
126.381266267863));
#172398=CARTESIAN_POINT('Ctrl Pts',(-96.5710744635236,-3.8139186156817,
126.280871327708));
#172399=CARTESIAN_POINT('Ctrl Pts',(-96.5644645829599,-3.70694720011512,
126.190679830165));
#172400=CARTESIAN_POINT('Ctrl Pts',(-96.5578547023961,-3.59690865649137,
126.104397861297));
#172401=CARTESIAN_POINT('Ctrl Pts',(-96.5512448218323,-3.48412789702929,
126.022228942294));
#172402=CARTESIAN_POINT('Ctrl Pts',(-96.5438215554269,-3.35746878196404,
125.929948640082));
#172403=CARTESIAN_POINT('Ctrl Pts',(-96.5363982890215,-3.22694941959803,
125.842564298181));
#172404=CARTESIAN_POINT('Ctrl Pts',(-96.5289750226161,-3.09298513919825,
125.760416378065));
#172405=CARTESIAN_POINT('Ctrl Pts',(-96.5215605298952,-2.95917919345286,
125.678365549968));
#172406=CARTESIAN_POINT('Ctrl Pts',(-96.5141460371742,-2.82193674935347,
125.60153901762));
#172407=CARTESIAN_POINT('Ctrl Pts',(-96.5067315444532,-2.68170496076179,
125.530236134211));
#172408=CARTESIAN_POINT('Ctrl Pts',(-96.4993241980994,-2.54160833284718,
125.459001975205));
#172409=CARTESIAN_POINT('Ctrl Pts',(-96.4919168517456,-2.39852842694709,
125.393281034356));
#172410=CARTESIAN_POINT('Ctrl Pts',(-96.4845095053919,-2.25293994895548,
125.333328525821));
#172411=CARTESIAN_POINT('Ctrl Pts',(-96.4771076837166,-2.10746005634475,
125.27342073213));
#172412=CARTESIAN_POINT('Ctrl Pts',(-96.4697058620412,-1.95947566072277,
125.219272945793));
#172413=CARTESIAN_POINT('Ctrl Pts',(-96.4623040403659,-1.80948445841844,
125.171093665145));
#172414=CARTESIAN_POINT('Ctrl Pts',(-96.4549061260546,-1.65957243530142,
125.122939817963));
#172415=CARTESIAN_POINT('Ctrl Pts',(-96.4475082117432,-1.50765606981616,
125.080748315519));
#172416=CARTESIAN_POINT('Ctrl Pts',(-96.4401102974319,-1.35425124660715,
125.044678844797));
#172417=CARTESIAN_POINT('Ctrl Pts',(-96.4327136125197,-1.20087191649693,
125.008615368168));
#172418=CARTESIAN_POINT('Ctrl Pts',(-96.4253169276075,-1.04600498262119,
124.97867198944));
#172419=CARTESIAN_POINT('Ctrl Pts',(-96.4179202426953,-0.890179755412589,
124.954958035631));
#172420=CARTESIAN_POINT('Ctrl Pts',(-96.4105238857599,-0.734361437657853,
124.931245133322));
#172421=CARTESIAN_POINT('Ctrl Pts',(-96.4031275288246,-0.577585280106661,
124.913761162877));
#172422=CARTESIAN_POINT('Ctrl Pts',(-96.3957311718892,-0.420388742700662,
124.902563953201));
#172423=CARTESIAN_POINT('Ctrl Pts',(-96.3883336825526,-0.263168138103033,
124.891365029203));
#172424=CARTESIAN_POINT('Ctrl Pts',(-96.380936193216,-0.105527397877214,
124.886454809003));
#172425=CARTESIAN_POINT('Ctrl Pts',(-96.3735387038794,0.0519931152654158,
124.887839065297));
#172426=CARTESIAN_POINT('Ctrl Pts',(-96.3661386213645,0.209568846979065,
124.88922380684));
#172427=CARTESIAN_POINT('Ctrl Pts',(-96.3587385388496,0.367023894647666,
124.896907414761));
#172428=CARTESIAN_POINT('Ctrl Pts',(-96.3513384563346,0.523820268757316,
124.910843595571));
#172429=CARTESIAN_POINT('Ctrl Pts',(-96.3439302366681,0.680789056599582,
124.924795100645));
#172430=CARTESIAN_POINT('Ctrl Pts',(-96.3365220170017,0.837097352389349,
124.945012876057));
#172431=CARTESIAN_POINT('Ctrl Pts',(-96.3291137973353,0.992213912618926,
124.971398924386));
#172432=CARTESIAN_POINT('Ctrl Pts',(-96.3217010180332,1.14742594450307,
124.997801212887));
#172433=CARTESIAN_POINT('Ctrl Pts',(-96.3142882387312,1.30144441487911,
125.030379262175));
#172434=CARTESIAN_POINT('Ctrl Pts',(-96.3068754594292,1.45375109411471,
125.068984577683));
#172435=CARTESIAN_POINT('Ctrl Pts',(-96.2994520884005,1.60627539627629,
125.107645054277));
#172436=CARTESIAN_POINT('Ctrl Pts',(-96.2920287173717,1.75708266535607,
125.152349891454));
#172437=CARTESIAN_POINT('Ctrl Pts',(-96.284605346343,1.90567178255613,125.202901377362));
#172438=CARTESIAN_POINT('Ctrl Pts',(-96.2806692969019,1.98445729784823,
125.229704988158));
#172439=CARTESIAN_POINT('Ctrl Pts',(-96.2767332474608,2.06261956503536,
125.258151505607));
#172440=CARTESIAN_POINT('Ctrl Pts',(-96.2727971980198,2.14008658250731,
125.288206161618));
#172441=CARTESIAN_POINT('Ctrl Pts',(-96.2653739316143,2.28618695978618,
125.344888304878));
#172442=CARTESIAN_POINT('Ctrl Pts',(-96.257950665209,2.43025478495182,125.407464569658));
#172443=CARTESIAN_POINT('Ctrl Pts',(-96.2505273988036,2.57177912251184,
125.475769555427));
#172444=CARTESIAN_POINT('Ctrl Pts',(-96.2431129060826,2.71313619005773,
125.543993810374));
#172445=CARTESIAN_POINT('Ctrl Pts',(-96.2356984133615,2.85195542093101,
125.617933148177));
#172446=CARTESIAN_POINT('Ctrl Pts',(-96.2282839206405,2.98774326323177,
125.697373173337));
#172447=CARTESIAN_POINT('Ctrl Pts',(-96.2208765742867,3.12340022809819,
125.77673663121));
#172448=CARTESIAN_POINT('Ctrl Pts',(-96.2134692279329,3.25603130100827,
125.861590034426));
#172449=CARTESIAN_POINT('Ctrl Pts',(-96.2060618815792,3.38516517293291,
125.951671948955));
#172450=CARTESIAN_POINT('Ctrl Pts',(-96.1986600599038,3.51420273194319,
126.041686676994));
#172451=CARTESIAN_POINT('Ctrl Pts',(-96.1912582382283,3.63974797868707,
126.136921939019));
#172452=CARTESIAN_POINT('Ctrl Pts',(-96.1838564165529,3.76135648058971,
126.237071707455));
#172453=CARTESIAN_POINT('Ctrl Pts',(-96.1764585022416,3.88290078631044,
126.337168607607));
#172454=CARTESIAN_POINT('Ctrl Pts',(-96.1690605879304,4.00051219855026,
126.442174610728));
#172455=CARTESIAN_POINT('Ctrl Pts',(-96.1616626736191,4.11377751987369,
126.551742003173));
#172456=CARTESIAN_POINT('Ctrl Pts',(-96.1542659887069,4.22702401855604,
126.661291187505));
#172457=CARTESIAN_POINT('Ctrl Pts',(-96.1468693037948,4.33592559171524,
126.775399997425));
#172458=CARTESIAN_POINT('Ctrl Pts',(-96.1394726188826,4.44010415421885,
126.893682202995));
#172459=CARTESIAN_POINT('Ctrl Pts',(-96.1320762619471,4.54427809733583,
127.011959163809));
#172460=CARTESIAN_POINT('Ctrl Pts',(-96.1246799050117,4.64372919947019,
127.134408872193));
#172461=CARTESIAN_POINT('Ctrl Pts',(-96.1172835480763,4.73811829729925,
127.260610405813));
#172462=CARTESIAN_POINT('Ctrl Pts',(-96.1098860587397,4.83252184633989,
127.38683126121));
#172463=CARTESIAN_POINT('Ctrl Pts',(-96.1024885694032,4.92186162434002,
127.516804786622));
#172464=CARTESIAN_POINT('Ctrl Pts',(-96.0950910800667,5.00584069532163,
127.65007947988));
#172465=CARTESIAN_POINT('Ctrl Pts',(-96.0876909975517,5.08984920503626,
127.783400892375));
#172466=CARTESIAN_POINT('Ctrl Pts',(-96.0802909150367,5.16849306739893,
127.920025461101));
#172467=CARTESIAN_POINT('Ctrl Pts',(-96.0728908325218,5.24152043396087,
128.059475537481));
#172468=CARTESIAN_POINT('Ctrl Pts',(-96.0654826128554,5.31462810162006,
128.199078953557));
#172469=CARTESIAN_POINT('Ctrl Pts',(-96.0580743931889,5.38210676648592,
128.341513751143));
#172470=CARTESIAN_POINT('Ctrl Pts',(-96.0506661735224,5.44375172647199,
128.48628001003));
#172471=CARTESIAN_POINT('Ctrl Pts',(-96.0432533942204,5.50543462790214,
128.631135370134));
#172472=CARTESIAN_POINT('Ctrl Pts',(-96.0358406149184,5.56127653772704,
128.778324702694));
#172473=CARTESIAN_POINT('Ctrl Pts',(-96.0284278356164,5.61112227285479,
128.927331741503));
#172474=CARTESIAN_POINT('Ctrl Pts',(-96.0210044645877,5.66103922990663,
129.076551688558));
#172475=CARTESIAN_POINT('Ctrl Pts',(-96.013581093559,5.70494279689298,129.22759417159));
#172476=CARTESIAN_POINT('Ctrl Pts',(-96.0061577225302,5.74272844744428,
129.379930717075));
#172477=CARTESIAN_POINT('Ctrl Pts',(-96.0022216730891,5.76276330602281,
129.460703208764));
#172478=CARTESIAN_POINT('Ctrl Pts',(-95.9982856236479,5.78107905988061,
129.541839375347));
#172479=CARTESIAN_POINT('Ctrl Pts',(-95.9943495742067,5.79766604176739,
129.623259846828));
#172480=CARTESIAN_POINT('Ctrl Pts',(-95.9869263078013,5.8289485719409,129.776816314981));
#172481=CARTESIAN_POINT('Ctrl Pts',(-95.9795030413958,5.85417356668348,
129.931848656131));
#172482=CARTESIAN_POINT('Ctrl Pts',(-95.9720797749903,5.87320400903427,
130.087837602748));
#172483=CARTESIAN_POINT('Ctrl Pts',(-95.9646652822693,5.89221195898259,
130.243642183384));
#172484=CARTESIAN_POINT('Ctrl Pts',(-95.9572507895483,5.90503988515356,
130.400400752035));
#172485=CARTESIAN_POINT('Ctrl Pts',(-95.9498362968273,5.91160138769369,
130.557582183504));
#172486=CARTESIAN_POINT('Ctrl Pts',(-95.9424289504735,5.91815656601064,
130.714612117592));
#172487=CARTESIAN_POINT('Ctrl Pts',(-95.9350216041198,5.91845732931424,
130.872063732636));
#172488=CARTESIAN_POINT('Ctrl Pts',(-95.927614257766,5.91246887541329,131.029399191524));
#172489=CARTESIAN_POINT('Ctrl Pts',(-95.9202124360906,5.9064848879272,131.186617303691));
#172490=CARTESIAN_POINT('Ctrl Pts',(-95.9128106144152,5.89422103726083,
131.343719060779));
#172491=CARTESIAN_POINT('Ctrl Pts',(-95.9054087927398,5.87569456641797,
131.500165133696));
#172492=CARTESIAN_POINT('Ctrl Pts',(-95.8980108784284,5.85717787555485,
131.656528619948));
#172493=CARTESIAN_POINT('Ctrl Pts',(-95.8906129641171,5.83240519233798,
131.812236741597));
#172494=CARTESIAN_POINT('Ctrl Pts',(-95.8832150498057,5.80144571479833,
131.966753916217));
#172495=CARTESIAN_POINT('Ctrl Pts',(-95.8758183648935,5.77049138216213,
132.121245412886));
#172496=CARTESIAN_POINT('Ctrl Pts',(-95.8684216799813,5.73335236900841,
132.274545989662));
#172497=CARTESIAN_POINT('Ctrl Pts',(-95.861024995069,5.69014925727116,132.426128786102));
#172498=CARTESIAN_POINT('Ctrl Pts',(-95.8536286381336,5.64694806120516,
132.577704861202));
#172499=CARTESIAN_POINT('Ctrl Pts',(-95.8462322811981,5.59768340351682,
132.727562948412));
#172500=CARTESIAN_POINT('Ctrl Pts',(-95.8388359242626,5.54252609202692,
132.875190181219));
#172501=CARTESIAN_POINT('Ctrl Pts',(-95.8314384349261,5.48736033581182,
133.022840016133));
#172502=CARTESIAN_POINT('Ctrl Pts',(-95.8240409455895,5.42630026009468,
133.168257966865));
#172503=CARTESIAN_POINT('Ctrl Pts',(-95.8166434562529,5.35956522528852,
133.310950164815));
#172504=CARTESIAN_POINT('Ctrl Pts',(-95.8092433737379,5.29280679661984,
133.453692383293));
#172505=CARTESIAN_POINT('Ctrl Pts',(-95.801843291223,5.22036960613111,133.593706608646));
#172506=CARTESIAN_POINT('Ctrl Pts',(-95.794443208708,5.14251938285965,133.730522772918));
#172507=CARTESIAN_POINT('Ctrl Pts',(-95.7870349890415,5.06458355526396,
133.867489380629));
#172508=CARTESIAN_POINT('Ctrl Pts',(-95.7796267693751,4.98122299270906,
134.001250579734));
#172509=CARTESIAN_POINT('Ctrl Pts',(-95.7722185497086,4.89274764574691,
134.131363929488));
#172510=CARTESIAN_POINT('Ctrl Pts',(-95.7648057704065,4.804217843685,134.261557361837));
#172511=CARTESIAN_POINT('Ctrl Pts',(-95.7573929911045,4.7105672058575,134.388098171646));
#172512=CARTESIAN_POINT('Ctrl Pts',(-95.7499802118024,4.61214620139334,
134.51057674449));
#172513=CARTESIAN_POINT('Ctrl Pts',(-95.7425568407737,4.51358456838238,
134.633230320463));
#172514=CARTESIAN_POINT('Ctrl Pts',(-95.7351334697449,4.41023920002195,
134.751809786278));
#172515=CARTESIAN_POINT('Ctrl Pts',(-95.7277100987161,4.3024982169981,134.865941548094));
#172516=CARTESIAN_POINT('Ctrl Pts',(-95.7237740492754,4.24537136259084,
134.926456946761));
#172517=CARTESIAN_POINT('Ctrl Pts',(-95.7198379998347,4.18700932010286,
134.985722589103));
#172518=CARTESIAN_POINT('Ctrl Pts',(-95.715901950394,4.12747364037448,135.043687440366));
#172519=CARTESIAN_POINT('Ctrl Pts',(-95.7084786839886,4.01519120644945,
135.15300734083));
#172520=CARTESIAN_POINT('Ctrl Pts',(-95.7010554175831,3.89839283290984,
135.258028610583));
#172521=CARTESIAN_POINT('Ctrl Pts',(-95.6936321511777,3.77744133321969,
135.358355296591));
#172522=CARTESIAN_POINT('Ctrl Pts',(-95.6862176584567,3.65663278815709,
135.458563404788));
#172523=CARTESIAN_POINT('Ctrl Pts',(-95.6788031657356,3.53168117215285,
135.554087737778));
#172524=CARTESIAN_POINT('Ctrl Pts',(-95.6713886730146,3.40298663464442,
135.644568518776));
#172525=CARTESIAN_POINT('Ctrl Pts',(-95.6639813266608,3.27441613777687,
135.73496209099));
#172526=CARTESIAN_POINT('Ctrl Pts',(-95.656573980307,3.14211020469109,135.820321575576));
#172527=CARTESIAN_POINT('Ctrl Pts',(-95.6491666339533,3.00650252154732,
135.900326978368));
#172528=CARTESIAN_POINT('Ctrl Pts',(-95.6417648122779,2.87099597973021,
135.980272710113));
#172529=CARTESIAN_POINT('Ctrl Pts',(-95.6343629906025,2.73219291129334,
136.054872122346));
#172530=CARTESIAN_POINT('Ctrl Pts',(-95.6269611689271,2.59055638934099,
136.123848201549));
#172531=CARTESIAN_POINT('Ctrl Pts',(-95.6195632546157,2.44899463620569,
136.192787868816));
#172532=CARTESIAN_POINT('Ctrl Pts',(-95.6121653403044,2.30460274319476,
136.25610995196));
#172533=CARTESIAN_POINT('Ctrl Pts',(-95.604767425993,2.15786871419567,136.313583173862));
#172534=CARTESIAN_POINT('Ctrl Pts',(-95.5973707410808,2.01115906973039,
136.371046844757));
#172535=CARTESIAN_POINT('Ctrl Pts',(-95.5899740561686,1.86210840901045,
136.422663447481));
#172536=CARTESIAN_POINT('Ctrl Pts',(-95.5825773712564,1.7112251721297,136.468249650092));
#172537=CARTESIAN_POINT('Ctrl Pts',(-95.5751810143209,1.56034862556979,
136.513833831363));
#172538=CARTESIAN_POINT('Ctrl Pts',(-95.5677846573855,1.40764002176226,
136.553388036227));
#172539=CARTESIAN_POINT('Ctrl Pts',(-95.5603883004501,1.25362317562847,
136.586778753262));
#172540=CARTESIAN_POINT('Ctrl Pts',(-95.5529908111135,1.09958274912191,
136.620174582502));
#172541=CARTESIAN_POINT('Ctrl Pts',(-95.5455933217769,0.944234046320716,
136.647404965891));
#172542=CARTESIAN_POINT('Ctrl Pts',(-95.5381958324403,0.788111142525765,
136.668387509517));
#172543=CARTESIAN_POINT('Ctrl Pts',(-95.5307957499253,0.631933510089578,
136.689377408541));
#172544=CARTESIAN_POINT('Ctrl Pts',(-95.5233956674102,0.474981506054996,
136.704115057496));
#172545=CARTESIAN_POINT('Ctrl Pts',(-95.5159955848952,0.317794244941677,
136.712569938535));
#172546=CARTESIAN_POINT('Ctrl Pts',(-95.5085873652287,0.160434140275297,
136.721034116584));
#172547=CARTESIAN_POINT('Ctrl Pts',(-95.5011791455624,0.00283863489836503,
136.723201709829));
#172548=CARTESIAN_POINT('Ctrl Pts',(-95.4937709258959,-0.154452497414042,
136.719094338415));
#172549=CARTESIAN_POINT('Ctrl Pts',(-95.4863581465939,-0.311840439794293,
136.714984438982));
#172550=CARTESIAN_POINT('Ctrl Pts',(-95.4789453672918,-0.468923264198511,
136.704591903687));
#172551=CARTESIAN_POINT('Ctrl Pts',(-95.4715325879897,-0.625166913285077,
136.687990185531));
#172552=CARTESIAN_POINT('Ctrl Pts',(-95.4641092169609,-0.781633810624336,
136.671364746062));
#172553=CARTESIAN_POINT('Ctrl Pts',(-95.4566858459322,-0.937258769509263,
136.648512458505));
#172554=CARTESIAN_POINT('Ctrl Pts',(-95.4492624749034,-1.09151768614798,
136.619557923189));
#172555=CARTESIAN_POINT('Ctrl Pts',(-95.4453264254626,-1.17330946514215,
136.60420553381));
#172556=CARTESIAN_POINT('Ctrl Pts',(-95.4413903760218,-1.25471743807355,
136.587138421895));
#172557=CARTESIAN_POINT('Ctrl Pts',(-95.437454326581,-1.33566539822654,
136.568380786379));
#172558=CARTESIAN_POINT('Ctrl Pts',(-95.4300310601755,-1.48833072477601,
136.533004471201));
#172559=CARTESIAN_POINT('Ctrl Pts',(-95.42260779377,-1.63982046723384,136.491505253228));
#172560=CARTESIAN_POINT('Ctrl Pts',(-95.4151845273645,-1.78960538956013,
136.443974355417));
#172561=CARTESIAN_POINT('Ctrl Pts',(-95.4077700346434,-1.93921327854795,
136.396499635179));
#172562=CARTESIAN_POINT('Ctrl Pts',(-95.4003555419223,-2.08712000584653,
136.343007537113));
#172563=CARTESIAN_POINT('Ctrl Pts',(-95.3929410492012,-2.23280659051213,
136.283640250133));
#172564=CARTESIAN_POINT('Ctrl Pts',(-95.3855337028474,-2.37835275696242,
136.224330183579));
#172565=CARTESIAN_POINT('Ctrl Pts',(-95.3781263564934,-2.52168269743741,
136.159156341415));
#172566=CARTESIAN_POINT('Ctrl Pts',(-95.3707190101396,-2.66229277381995,
136.088310631426));
#172567=CARTESIAN_POINT('Ctrl Pts',(-95.3633171884641,-2.80279797790181,
136.01751776084));
#172568=CARTESIAN_POINT('Ctrl Pts',(-95.3559153667888,-2.94058702512365,
135.94106161276));
#172569=CARTESIAN_POINT('Ctrl Pts',(-95.3485135451133,-3.07517655384108,
135.859182051129));
#172570=CARTESIAN_POINT('Ctrl Pts',(-95.3411156308019,-3.20969503379471,
135.77734571308));
#172571=CARTESIAN_POINT('Ctrl Pts',(-95.3337177164903,-3.34101704086007,
135.690091856765));
#172572=CARTESIAN_POINT('Ctrl Pts',(-95.3263198021788,-3.46868421702546,
135.597706042742));
#172573=CARTESIAN_POINT('Ctrl Pts',(-95.3189231172666,-3.59633017722139,
135.505335581566));
#172574=CARTESIAN_POINT('Ctrl Pts',(-95.3115264323544,-3.72032220983606,
135.407835073946));
#172575=CARTESIAN_POINT('Ctrl Pts',(-95.3041297474421,-3.84023124822334,
135.305533189538));
#172576=CARTESIAN_POINT('Ctrl Pts',(-95.2967333905066,-3.96013496971821,
135.203235841302));
#172577=CARTESIAN_POINT('Ctrl Pts',(-95.2893370335711,-4.07595577297636,
135.096137781879));
#172578=CARTESIAN_POINT('Ctrl Pts',(-95.2819406766356,-4.18729819629881,
134.984607545413));
#172579=CARTESIAN_POINT('Ctrl Pts',(-95.274543187299,-4.29865766643019,
134.873060233383));
#172580=CARTESIAN_POINT('Ctrl Pts',(-95.2671456979625,-4.40553712764686,
134.757079657373));
#172581=CARTESIAN_POINT('Ctrl Pts',(-95.2597482086259,-4.50757857887058,
134.637070614136));
#172582=CARTESIAN_POINT('Ctrl Pts',(-95.2523481261108,-4.60965580056727,
134.517019501914));
#172583=CARTESIAN_POINT('Ctrl Pts',(-95.2449480435957,-4.70689139397183,
134.392937395054));
#172584=CARTESIAN_POINT('Ctrl Pts',(-95.2375479610807,-4.79896827898857,
134.265261370226));
#172585=CARTESIAN_POINT('Ctrl Pts',(-95.2301397414141,-4.89114641200624,
134.137444952483));
#172586=CARTESIAN_POINT('Ctrl Pts',(-95.2227315217475,-4.9781542897327,
134.006027027566));
#172587=CARTESIAN_POINT('Ctrl Pts',(-95.215323302081,-5.05971834089961,
133.871473408655));
#172588=CARTESIAN_POINT('Ctrl Pts',(-95.2079105227789,-5.14133259337882,
133.736836974238));
#172589=CARTESIAN_POINT('Ctrl Pts',(-95.2004977434769,-5.21749616265445,
133.59906132607));
#172590=CARTESIAN_POINT('Ctrl Pts',(-95.1930849641748,-5.28798217577897,
133.458635484859));
#172591=CARTESIAN_POINT('Ctrl Pts',(-95.1856615931459,-5.35856890262481,
133.318008996621));
#172592=CARTESIAN_POINT('Ctrl Pts',(-95.1782382221169,-5.42346171752098,
133.174725091558));
#172593=CARTESIAN_POINT('Ctrl Pts',(-95.1708148510881,-5.48248215935056,
133.029292062555));
#172594=CARTESIAN_POINT('Ctrl Pts',(-95.1668788016479,-5.51377621377919,
132.952179980974));
#172595=CARTESIAN_POINT('Ctrl Pts',(-95.1629427522078,-5.54342016702373,
132.874463956889));
#172596=CARTESIAN_POINT('Ctrl Pts',(-95.1590067027677,-5.57139318674206,
132.796221185283));
#172597=CARTESIAN_POINT('Ctrl Pts',(-95.1503669630726,-5.63279475512309,
132.624476091636));
#172598=CARTESIAN_POINT('Ctrl Pts',(-95.1417272233776,-5.68629543393868,
132.449765875302));
#172599=CARTESIAN_POINT('Ctrl Pts',(-95.1330874836826,-5.73164059706365,
132.272770175078));
#172600=CARTESIAN_POINT('Ctrl Pts',(-95.1244822298778,-5.77680476303202,
132.096480960756));
#172601=CARTESIAN_POINT('Ctrl Pts',(-95.1158769760729,-5.81387830329087,
131.917924575233));
#172602=CARTESIAN_POINT('Ctrl Pts',(-95.1072717222681,-5.84265624027591,
131.737794396934));
#172603=CARTESIAN_POINT('Ctrl Pts',(-95.0987334134545,-5.87121029789798,
131.559065550134));
#172604=CARTESIAN_POINT('Ctrl Pts',(-95.0901951046409,-5.89159725125045,
131.378787421531));
#172605=CARTESIAN_POINT('Ctrl Pts',(-95.0816567958273,-5.90366397735691,
131.197657204073));
#172606=CARTESIAN_POINT('Ctrl Pts',(-95.0755629392138,-5.91227609250675,
131.068383175965));
#172607=CARTESIAN_POINT('Ctrl Pts',(-95.0694690826003,-5.91665103111156,
130.938675529287));
#172608=CARTESIAN_POINT('Ctrl Pts',(-95.0633752259867,-5.91674833943923,
130.808793477043));
#172609=CARTESIAN_POINT('',(-93.3133751922047,-5.90951273974424,130.800546416903));
#172610=CARTESIAN_POINT('Ctrl Pts',(-95.0633751922047,-5.91070361657871,
130.808788229024));
#172611=CARTESIAN_POINT('Ctrl Pts',(-95.0024364877883,-5.90173179602721,
129.511284220283));
#172612=CARTESIAN_POINT('Ctrl Pts',(-94.8486819087681,-4.84118804501417,
126.224213906414));
#172613=CARTESIAN_POINT('Ctrl Pts',(-94.6021114551422,0.596386883552906,
123.831421264929));
#172614=CARTESIAN_POINT('Ctrl Pts',(-94.3236638313295,6.18889303939605,
127.537073749649));
#172615=CARTESIAN_POINT('Ctrl Pts',(-94.0452162075165,6.09410883626184,
134.245203250136));
#172616=CARTESIAN_POINT('Ctrl Pts',(-93.7667685837036,0.399136326374221,
137.791366465805));
#172617=CARTESIAN_POINT('Ctrl Pts',(-93.5228215785999,-4.91155013382791,
135.272979751163));
#172618=CARTESIAN_POINT('Ctrl Pts',(-93.3716904481001,-5.90220975232409,
132.042820379345));
#172619=CARTESIAN_POINT('Ctrl Pts',(-93.3133751922047,-5.90951273974424,
130.800546416903));
#172620=CARTESIAN_POINT('',(-91.5633765517166,-5.92117668185514,130.801382376507));
#172621=CARTESIAN_POINT('Ctrl Pts',(-93.3133751922047,-5.90951273974424,
130.800546416903));
#172622=CARTESIAN_POINT('Ctrl Pts',(-93.2788745734958,-5.913833351573,130.065589163398));
#172623=CARTESIAN_POINT('Ctrl Pts',(-93.1515580801835,-5.44546871744137,
127.358710712193));
#172624=CARTESIAN_POINT('Ctrl Pts',(-92.9314257122645,-1.38658135523596,
123.944699352184));
#172625=CARTESIAN_POINT('Ctrl Pts',(-92.6529780884523,5.02174620662583,
125.929975982911));
#172626=CARTESIAN_POINT('Ctrl Pts',(-92.3745304646391,6.81533433053491,
132.394573965943));
#172627=CARTESIAN_POINT('Ctrl Pts',(-92.0960828408264,2.34596315227786,
137.397843568065));
#172628=CARTESIAN_POINT('Ctrl Pts',(-91.8256985594628,-4.08737977375717,
136.37259907124));
#172629=CARTESIAN_POINT('Ctrl Pts',(-91.6481301527034,-5.91352381113235,
132.595058967895));
#172630=CARTESIAN_POINT('Ctrl Pts',(-91.5633776205484,-5.9246574854241,
130.801403228907));
#172631=CARTESIAN_POINT('',(-89.8133744894949,-5.9182659565827,130.809617868958));
#172632=CARTESIAN_POINT('Ctrl Pts',(-91.5633751922047,-5.9167492370296,
130.801355853076));
#172633=CARTESIAN_POINT('Ctrl Pts',(-91.5553126592033,-5.91666269968621,
130.630953226781));
#172634=CARTESIAN_POINT('Ctrl Pts',(-91.5472501262019,-5.90921545676705,
130.460742668894));
#172635=CARTESIAN_POINT('Ctrl Pts',(-91.5391875932004,-5.89445284654217,
130.291178191531));
#172636=CARTESIAN_POINT('Ctrl Pts',(-91.531764326795,-5.88086074235885,
130.135058236659));
#172637=CARTESIAN_POINT('Ctrl Pts',(-91.5243410603895,-5.86104133235314,
129.979242582282));
#172638=CARTESIAN_POINT('Ctrl Pts',(-91.5169177939841,-5.83501063256916,
129.824268029947));
#172639=CARTESIAN_POINT('Ctrl Pts',(-91.5095033012632,-5.80901069891061,
129.669476644664));
#172640=CARTESIAN_POINT('Ctrl Pts',(-91.5020888085421,-5.77681414946191,
129.515524747181));
#172641=CARTESIAN_POINT('Ctrl Pts',(-91.4946743158212,-5.7384889012075,
129.362946141012));
#172642=CARTESIAN_POINT('Ctrl Pts',(-91.4872669694674,-5.70020059227029,
129.210514595849));
#172643=CARTESIAN_POINT('Ctrl Pts',(-91.4798596231137,-5.6557954346729,
129.059454066533));
#172644=CARTESIAN_POINT('Ctrl Pts',(-91.4724522767599,-5.60539272591123,
128.910290146121));
#172645=CARTESIAN_POINT('Ctrl Pts',(-91.4650504550845,-5.55502760939134,
128.761237477787));
#172646=CARTESIAN_POINT('Ctrl Pts',(-91.4576486334092,-5.49867396743771,
128.614078953904));
#172647=CARTESIAN_POINT('Ctrl Pts',(-91.4502468117338,-5.4365014254727,
128.469326824806));
#172648=CARTESIAN_POINT('Ctrl Pts',(-91.4428488974224,-5.37436170390846,
128.324651109229));
#172649=CARTESIAN_POINT('Ctrl Pts',(-91.4354509831112,-5.30640934682248,
128.182379600671));
#172650=CARTESIAN_POINT('Ctrl Pts',(-91.4280530687998,-5.23286273408415,
128.043006209176));
#172651=CARTESIAN_POINT('Ctrl Pts',(-91.4206563838876,-5.15932834345889,
127.903655979011));
#172652=CARTESIAN_POINT('Ctrl Pts',(-91.4132596989754,-5.08020171633685,
127.767203239874));
#172653=CARTESIAN_POINT('Ctrl Pts',(-91.4058630140632,-4.99574802713157,
127.634118952975));
#172654=CARTESIAN_POINT('Ctrl Pts',(-91.3984666571278,-4.91129808269137,
127.501040567172));
#172655=CARTESIAN_POINT('Ctrl Pts',(-91.3910703001923,-4.82152174584406,
127.371330651817));
#172656=CARTESIAN_POINT('Ctrl Pts',(-91.3836739432569,-4.72672837868967,
127.245432492893));
#172657=CARTESIAN_POINT('Ctrl Pts',(-91.3762764539203,-4.63192049842851,
127.119515058639));
#172658=CARTESIAN_POINT('Ctrl Pts',(-91.3688789645838,-4.53209428298416,
126.997410841056));
#172659=CARTESIAN_POINT('Ctrl Pts',(-91.3614814752472,-4.4276002572672,
126.879531127722));
#172660=CARTESIAN_POINT('Ctrl Pts',(-91.3540813927322,-4.32306960133165,
126.761610091838));
#172661=CARTESIAN_POINT('Ctrl Pts',(-91.3466813102172,-4.2138681247446,
126.64791678782));
#172662=CARTESIAN_POINT('Ctrl Pts',(-91.3392812277023,-4.10038405780983,
126.538826519594));
#172663=CARTESIAN_POINT('Ctrl Pts',(-91.3318730080358,-3.98677520347685,
126.429616295404));
#172664=CARTESIAN_POINT('Ctrl Pts',(-91.3244647883694,-3.8688746236027,
126.325019474033));
#172665=CARTESIAN_POINT('Ctrl Pts',(-91.3170565687029,-3.74710510889896,
126.225372316056));
#172666=CARTESIAN_POINT('Ctrl Pts',(-91.3096437894009,-3.62526064709075,
126.125663826916));
#172667=CARTESIAN_POINT('Ctrl Pts',(-91.3022310100988,-3.49954280290225,
126.030911295736));
#172668=CARTESIAN_POINT('Ctrl Pts',(-91.2948182307967,-3.37040390103012,
125.94140800558));
#172669=CARTESIAN_POINT('Ctrl Pts',(-91.287394859768,-3.24108047943916,
125.851776828926));
#172670=CARTESIAN_POINT('Ctrl Pts',(-91.2799714887392,-3.10832655162119,
125.767410072895));
#172671=CARTESIAN_POINT('Ctrl Pts',(-91.2725481177105,-2.97262032045786,
125.688555793992));
#172672=CARTESIAN_POINT('Ctrl Pts',(-91.2686120682695,-2.90066562046546,
125.646745363234));
#172673=CARTESIAN_POINT('Ctrl Pts',(-91.2646760188286,-2.82788128994348,
125.606483897824));
#172674=CARTESIAN_POINT('Ctrl Pts',(-91.2607399693877,-2.75434083446996,
125.567802861743));
#172675=CARTESIAN_POINT('Ctrl Pts',(-91.2533167029822,-2.61564583057169,
125.49485163489));
#172676=CARTESIAN_POINT('Ctrl Pts',(-91.2458934365767,-2.47384083239129,
125.427304098643));
#172677=CARTESIAN_POINT('Ctrl Pts',(-91.2384701701713,-2.32938612333577,
125.365436932598));
#172678=CARTESIAN_POINT('Ctrl Pts',(-91.2310556774503,-2.18510214775013,
125.303642888405));
#172679=CARTESIAN_POINT('Ctrl Pts',(-91.2236411847293,-2.03817503483164,
125.247515996236));
#172680=CARTESIAN_POINT('Ctrl Pts',(-91.2162266920083,-1.88909059938297,
125.197287649446));
#172681=CARTESIAN_POINT('Ctrl Pts',(-91.2088193456545,-1.74014985712612,
125.147107714627));
#172682=CARTESIAN_POINT('Ctrl Pts',(-91.2014119993007,-1.5890562832183,
125.10281512538));
#172683=CARTESIAN_POINT('Ctrl Pts',(-91.1940046529469,-1.43631655719245,
125.064593609225));
#172684=CARTESIAN_POINT('Ctrl Pts',(-91.1866028312715,-1.28369075021637,
125.02640060012));
#172685=CARTESIAN_POINT('Ctrl Pts',(-91.1792010095962,-1.12942159633595,
124.994269738407));
#172686=CARTESIAN_POINT('Ctrl Pts',(-91.1717991879207,-0.974031752950555,
124.968335197235));
#172687=CARTESIAN_POINT('Ctrl Pts',(-91.1644012736094,-0.818723938654372,
124.942414346706));
#172688=CARTESIAN_POINT('Ctrl Pts',(-91.157003359298,-0.662296980332273,
124.922683363683));
#172689=CARTESIAN_POINT('Ctrl Pts',(-91.1496054449866,-0.505284458147056,
124.909225489441));
#172690=CARTESIAN_POINT('Ctrl Pts',(-91.1422087600744,-0.348298028594753,
124.895769851653));
#172691=CARTESIAN_POINT('Ctrl Pts',(-91.1348120751622,-0.190726599881081,
124.888585285487));
#172692=CARTESIAN_POINT('Ctrl Pts',(-91.12741539025,-0.0331097382576597,
124.887703258234));
#172693=CARTESIAN_POINT('Ctrl Pts',(-91.1200190333145,0.124500134469396,
124.886821270092));
#172694=CARTESIAN_POINT('Ctrl Pts',(-91.1126226763791,0.28215506280889,
124.89224126729));
#172695=CARTESIAN_POINT('Ctrl Pts',(-91.1052263194436,0.439314879937609,
124.903942581633));
#172696=CARTESIAN_POINT('Ctrl Pts',(-91.097828830107,0.596498758635541,
124.915645687477));
#172697=CARTESIAN_POINT('Ctrl Pts',(-91.0904313407705,0.753187002897855,
124.933631997591));
#172698=CARTESIAN_POINT('Ctrl Pts',(-91.0830338514339,0.908844117561575,
124.957828916423));
#172699=CARTESIAN_POINT('Ctrl Pts',(-91.0756337689189,1.06455579758532,
124.982034317447));
#172700=CARTESIAN_POINT('Ctrl Pts',(-91.0682336864038,1.2192352597069,125.012454604511));
#172701=CARTESIAN_POINT('Ctrl Pts',(-91.0608336038888,1.37235690214343,
125.048966009406));
#172702=CARTESIAN_POINT('Ctrl Pts',(-91.0534253842223,1.52564691756732,
125.085517562343));
#172703=CARTESIAN_POINT('Ctrl Pts',(-91.0460171645559,1.67737532902632,
125.12817352244));
#172704=CARTESIAN_POINT('Ctrl Pts',(-91.0386089448894,1.82703070226985,
125.176759940949));
#172705=CARTESIAN_POINT('Ctrl Pts',(-91.0311961655873,1.97677818589847,
125.225376263588));
#172706=CARTESIAN_POINT('Ctrl Pts',(-91.0237833862852,2.12444973952501,
125.279930188856));
#172707=CARTESIAN_POINT('Ctrl Pts',(-91.0163706069831,2.26955412325322,
125.340199689837));
#172708=CARTESIAN_POINT('Ctrl Pts',(-91.0089472359544,2.4148658389294,125.400555306707));
#172709=CARTESIAN_POINT('Ctrl Pts',(-91.0015238649257,2.55760272085013,
125.466642653559));
#172710=CARTESIAN_POINT('Ctrl Pts',(-90.9941004938969,2.69729759171301,
125.538193485368));
#172711=CARTESIAN_POINT('Ctrl Pts',(-90.9901644444562,2.77136716417534,
125.576131453231));
#172712=CARTESIAN_POINT('Ctrl Pts',(-90.9862283950155,2.84458198378661,
125.615604666362));
#172713=CARTESIAN_POINT('Ctrl Pts',(-90.9822923455748,2.91687584745019,
125.656568289484));
#172714=CARTESIAN_POINT('Ctrl Pts',(-90.9748690791694,3.05321981810821,
125.733824404263));
#172715=CARTESIAN_POINT('Ctrl Pts',(-90.9674458127639,3.18669853869445,
125.816617872076));
#172716=CARTESIAN_POINT('Ctrl Pts',(-90.9600225463585,3.316830436404,125.904710995537));
#172717=CARTESIAN_POINT('Ctrl Pts',(-90.9526080536375,3.44680852901723,
125.992700000242));
#172718=CARTESIAN_POINT('Ctrl Pts',(-90.9451935609166,3.57344736642153,
126.08597598534));
#172719=CARTESIAN_POINT('Ctrl Pts',(-90.9377790681956,3.6962896760663,126.184255294837));
#172720=CARTESIAN_POINT('Ctrl Pts',(-90.9303717218418,3.81901358566811,
126.282439879036));
#172721=CARTESIAN_POINT('Ctrl Pts',(-90.922964375488,3.93794796279608,126.385617955562));
#172722=CARTESIAN_POINT('Ctrl Pts',(-90.9155570291342,4.05266435961837,
126.493462549787));
#172723=CARTESIAN_POINT('Ctrl Pts',(-90.9081552074588,4.1672951966239,126.601226709445));
#172724=CARTESIAN_POINT('Ctrl Pts',(-90.9007533857834,4.27771404648123,
126.713650202138));
#172725=CARTESIAN_POINT('Ctrl Pts',(-90.8933515641081,4.38352551643076,
126.830365825257));
#172726=CARTESIAN_POINT('Ctrl Pts',(-90.8859536497967,4.48928112932924,
126.947019835107));
#172727=CARTESIAN_POINT('Ctrl Pts',(-90.8785557354854,4.59043395607122,
127.067961187105));
#172728=CARTESIAN_POINT('Ctrl Pts',(-90.871157821174,4.68662555030327,127.19278595909));
#172729=CARTESIAN_POINT('Ctrl Pts',(-90.8637611362618,4.78280115923731,
127.317589987463));
#172730=CARTESIAN_POINT('Ctrl Pts',(-90.8563644513495,4.87401694434677,
127.446275859589));
#172731=CARTESIAN_POINT('Ctrl Pts',(-90.8489677664373,4.95995478256792,
127.578406631939));
#172732=CARTESIAN_POINT('Ctrl Pts',(-90.8415714095019,5.04588881021528,
127.710531545473));
#172733=CARTESIAN_POINT('Ctrl Pts',(-90.8341750525665,5.12654515277362,
127.84610074258));
#172734=CARTESIAN_POINT('Ctrl Pts',(-90.826778695631,5.2016492256185,127.98464859395));
#172735=CARTESIAN_POINT('Ctrl Pts',(-90.8193812062945,5.27676479708867,
128.12321765735));
#172736=CARTESIAN_POINT('Ctrl Pts',(-90.8119837169579,5.34632622833766,
128.264765954846));
#172737=CARTESIAN_POINT('Ctrl Pts',(-90.8045862276214,5.41010514784449,
128.408803719522));
#172738=CARTESIAN_POINT('Ctrl Pts',(-90.7971861451064,5.47390642495259,
128.552891976413));
#172739=CARTESIAN_POINT('Ctrl Pts',(-90.7897860625913,5.53192100343032,
128.69947109686));
#172740=CARTESIAN_POINT('Ctrl Pts',(-90.7823859800764,5.58396891237707,
128.848031977458));
#172741=CARTESIAN_POINT('Ctrl Pts',(-90.7749777604099,5.63607405335044,
128.996756216017));
#172742=CARTESIAN_POINT('Ctrl Pts',(-90.7675695407434,5.68219929860803,
129.14746621411));
#172743=CARTESIAN_POINT('Ctrl Pts',(-90.7601613210769,5.72221455345155,
129.299637664073));
#172744=CARTESIAN_POINT('Ctrl Pts',(-90.7527485417748,5.76225443701674,
129.451902773025));
#172745=CARTESIAN_POINT('Ctrl Pts',(-90.7453357624728,5.7961767564546,129.605630762527));
#172746=CARTESIAN_POINT('Ctrl Pts',(-90.7379229831707,5.82390278213553,
129.760288327572));
#172747=CARTESIAN_POINT('Ctrl Pts',(-90.730499612142,5.8516684240622,129.915166874598));
#172748=CARTESIAN_POINT('Ctrl Pts',(-90.7230762411133,5.87322003868459,
130.070977281123));
#172749=CARTESIAN_POINT('Ctrl Pts',(-90.7156528700845,5.88853078739758,
130.227181504664));
#172750=CARTESIAN_POINT('Ctrl Pts',(-90.7117168206436,5.89664891374179,
130.310004732056));
#172751=CARTESIAN_POINT('Ctrl Pts',(-90.7077807712027,5.90301337996738,
130.392938669234));
#172752=CARTESIAN_POINT('Ctrl Pts',(-90.7038447217618,5.90762612287072,
130.475903383096));
#172753=CARTESIAN_POINT('Ctrl Pts',(-90.6964214553564,5.91632561202739,
130.632372244197));
#172754=CARTESIAN_POINT('Ctrl Pts',(-90.688998188951,5.91881763159911,130.789423563835));
#172755=CARTESIAN_POINT('Ctrl Pts',(-90.6815749225456,5.91504186126461,
130.94652369993));
#172756=CARTESIAN_POINT('Ctrl Pts',(-90.6741604298246,5.91127055357707,
131.103438156711));
#172757=CARTESIAN_POINT('Ctrl Pts',(-90.6667459371035,5.90124621054413,
131.260400945556));
#172758=CARTESIAN_POINT('Ctrl Pts',(-90.6593314443825,5.88496031300223,
131.416874027124));
#172759=CARTESIAN_POINT('Ctrl Pts',(-90.6519240980287,5.86869011242153,
131.573196294046));
#172760=CARTESIAN_POINT('Ctrl Pts',(-90.6445167516749,5.84617041045668,
131.729029424547));
#172761=CARTESIAN_POINT('Ctrl Pts',(-90.6371094053211,5.81744471360352,
131.883836215561));
#172762=CARTESIAN_POINT('Ctrl Pts',(-90.6297075836457,5.78874044145883,
132.038527545829));
#172763=CARTESIAN_POINT('Ctrl Pts',(-90.6223057619704,5.75383945853556,
132.192193695336));
#172764=CARTESIAN_POINT('Ctrl Pts',(-90.614903940295,5.71283698334393,132.344303526975));
#172765=CARTESIAN_POINT('Ctrl Pts',(-90.6075060259836,5.6718561530398,132.496333061017));
#172766=CARTESIAN_POINT('Ctrl Pts',(-90.6001081116723,5.62478034201596,
132.646807553864));
#172767=CARTESIAN_POINT('Ctrl Pts',(-90.5927101973609,5.57175563241608,
132.795207104651));
#172768=CARTESIAN_POINT('Ctrl Pts',(-90.5853135124487,5.51873973456104,
132.943581994125));
#172769=CARTESIAN_POINT('Ctrl Pts',(-90.5779168275365,5.4597770256894,133.089882274714));
#172770=CARTESIAN_POINT('Ctrl Pts',(-90.5705201426243,5.39506316547971,
133.233604121825));
#172771=CARTESIAN_POINT('Ctrl Pts',(-90.5631237856889,5.3303521747504,133.377319596158));
#172772=CARTESIAN_POINT('Ctrl Pts',(-90.5557274287534,5.25989069299819,
133.518456523957));
#172773=CARTESIAN_POINT('Ctrl Pts',(-90.548331071818,5.18392204765302,133.656532205384));
#172774=CARTESIAN_POINT('Ctrl Pts',(-90.5409335824814,5.10794177131432,
133.794629026551));
#172775=CARTESIAN_POINT('Ctrl Pts',(-90.5335360931448,5.02645283249731,
133.929663341048));
#172776=CARTESIAN_POINT('Ctrl Pts',(-90.5261386038082,4.9397438455942,134.061178282467));
#172777=CARTESIAN_POINT('Ctrl Pts',(-90.5187385212932,4.85300446299003,
134.192739326246));
#172778=CARTESIAN_POINT('Ctrl Pts',(-90.5113384387783,4.7610415943726,134.320778229174));
#172779=CARTESIAN_POINT('Ctrl Pts',(-90.5039383562633,4.66418628418919,
134.444868393808));
#172780=CARTESIAN_POINT('Ctrl Pts',(-90.4965301365968,4.56722447163513,
134.569095008336));
#172781=CARTESIAN_POINT('Ctrl Pts',(-90.4891219169303,4.46535970364301,
134.689363918773));
#172782=CARTESIAN_POINT('Ctrl Pts',(-90.4817136972638,4.3589627757391,134.805282271663));
#172783=CARTESIAN_POINT('Ctrl Pts',(-90.4743009179617,4.2525003623014,134.921271970365));
#172784=CARTESIAN_POINT('Ctrl Pts',(-90.4668881386597,4.14150049318447,
135.032905511779));
#172785=CARTESIAN_POINT('Ctrl Pts',(-90.4594753593577,4.0263692977088,135.139828394054));
#172786=CARTESIAN_POINT('Ctrl Pts',(-90.4520519883289,3.91107359738209,
135.246904052757));
#172787=CARTESIAN_POINT('Ctrl Pts',(-90.4446286173001,3.79163506372278,
135.34925536712));
#172788=CARTESIAN_POINT('Ctrl Pts',(-90.4372052462713,3.66849186019001,
135.446568931959));
#172789=CARTESIAN_POINT('Ctrl Pts',(-90.4332691968306,3.60319837889668,
135.498166919043));
#172790=CARTESIAN_POINT('Ctrl Pts',(-90.4293331473898,3.53686385819526,
135.548349343547));
#172791=CARTESIAN_POINT('Ctrl Pts',(-90.425397097949,3.46955659495388,135.597074629158));
#172792=CARTESIAN_POINT('Ctrl Pts',(-90.4179738315436,3.34261719706789,
135.688968997157));
#172793=CARTESIAN_POINT('Ctrl Pts',(-90.4105505651382,3.2118324713806,135.775955678257));
#172794=CARTESIAN_POINT('Ctrl Pts',(-90.4031272987328,3.07761878148282,
135.857695476683));
#172795=CARTESIAN_POINT('Ctrl Pts',(-90.3957128060118,2.94356372102037,
135.939338665455));
#172796=CARTESIAN_POINT('Ctrl Pts',(-90.3882983132907,2.80608807908072,
136.015747123157));
#172797=CARTESIAN_POINT('Ctrl Pts',(-90.3808838205697,2.66563991858251,
136.08662285897));
#172798=CARTESIAN_POINT('Ctrl Pts',(-90.3734764742159,2.52532712730916,
136.15743028208));
#172799=CARTESIAN_POINT('Ctrl Pts',(-90.3660691278622,2.38204785220827,
136.222715432498));
#172800=CARTESIAN_POINT('Ctrl Pts',(-90.3586617815084,2.23627757375913,
136.28222454209));
#172801=CARTESIAN_POINT('Ctrl Pts',(-90.351259959833,2.09061601628326,136.341689267543));
#172802=CARTESIAN_POINT('Ctrl Pts',(-90.3438581381575,1.94246749887782,
136.395386389476));
#172803=CARTESIAN_POINT('Ctrl Pts',(-90.336456316482,1.79233035016364,136.443108925336));
#172804=CARTESIAN_POINT('Ctrl Pts',(-90.3290584021707,1.64227245768204,
136.490806268842));
#172805=CARTESIAN_POINT('Ctrl Pts',(-90.3216604878594,1.49022837944259,
136.532535194698));
#172806=CARTESIAN_POINT('Ctrl Pts',(-90.314262573548,1.33671448373252,136.568137586835));
#172807=CARTESIAN_POINT('Ctrl Pts',(-90.3068658886358,1.18322609924668,
136.603734062501));
#172808=CARTESIAN_POINT('Ctrl Pts',(-90.2994692037237,1.02826874535859,
136.633205940858));
#172809=CARTESIAN_POINT('Ctrl Pts',(-90.2920725188115,0.87237206280302,
136.656445506436));
#172810=CARTESIAN_POINT('Ctrl Pts',(-90.284676161876,0.716482292869719,
136.679684041548));
#172811=CARTESIAN_POINT('Ctrl Pts',(-90.2772798049405,0.559653646302565,
136.696690758313));
#172812=CARTESIAN_POINT('Ctrl Pts',(-90.2698834480051,0.402423756565,136.707409463938));
#172813=CARTESIAN_POINT('Ctrl Pts',(-90.2624859586685,0.245169794529927,
136.718129810624));
#172814=CARTESIAN_POINT('Ctrl Pts',(-90.255088469332,0.0875148394638481,
136.722560203893));
#172815=CARTESIAN_POINT('Ctrl Pts',(-90.2476909799954,-0.0700007308546633,
136.720696515753));
#172816=CARTESIAN_POINT('Ctrl Pts',(-90.2402908974804,-0.227571518012394,
136.718832174301));
#172817=CARTESIAN_POINT('Ctrl Pts',(-90.2328908149653,-0.385002450101525,
136.710669362966));
#172818=CARTESIAN_POINT('Ctrl Pts',(-90.2254907324503,-0.541755681001532,
136.696256012479));
#172819=CARTESIAN_POINT('Ctrl Pts',(-90.2180825127839,-0.698681278193312,
136.681826813033));
#172820=CARTESIAN_POINT('Ctrl Pts',(-90.2106742931175,-0.854927314020519,
136.661133382583));
#172821=CARTESIAN_POINT('Ctrl Pts',(-90.203266073451,-1.00996284570659,
136.63427533502));
#172822=CARTESIAN_POINT('Ctrl Pts',(-90.1958532941489,-1.16509379917596,
136.607400756778));
#172823=CARTESIAN_POINT('Ctrl Pts',(-90.1884405148468,-1.31901239977424,
136.574354079145));
#172824=CARTESIAN_POINT('Ctrl Pts',(-90.1810277355448,-1.47120087223584,
136.535285373313));
#172825=CARTESIAN_POINT('Ctrl Pts',(-90.173604364516,-1.62360679872362,
136.496160844282));
#172826=CARTESIAN_POINT('Ctrl Pts',(-90.1661809934872,-1.7742773031283,
136.450997208722));
#172827=CARTESIAN_POINT('Ctrl Pts',(-90.1587576224584,-1.92271187073998,
136.399993702804));
#172828=CARTESIAN_POINT('Ctrl Pts',(-90.1548215730176,-2.00141544012667,
136.372950420155));
#172829=CARTESIAN_POINT('Ctrl Pts',(-90.1508855235768,-2.07949076385258,
136.344266135415));
#172830=CARTESIAN_POINT('Ctrl Pts',(-90.146949474136,-2.15686594646315,
136.313975835663));
#172831=CARTESIAN_POINT('Ctrl Pts',(-90.1395262077306,-2.30279312606935,
136.256849275659));
#172832=CARTESIAN_POINT('Ctrl Pts',(-90.1321029413251,-2.4466698232985,
136.193834807825));
#172833=CARTESIAN_POINT('Ctrl Pts',(-90.1246796749197,-2.58798560844716,
136.125099387039));
#172834=CARTESIAN_POINT('Ctrl Pts',(-90.1172651821987,-2.72913437007332,
136.056445205812));
#172835=CARTESIAN_POINT('Ctrl Pts',(-90.1098506894776,-2.86772791203561,
135.982083692504));
#172836=CARTESIAN_POINT('Ctrl Pts',(-90.1024361967566,-3.00327333726637,
135.902230743821));
#172837=CARTESIAN_POINT('Ctrl Pts',(-90.0950288504028,-3.13868811871309,
135.822454760417));
#172838=CARTESIAN_POINT('Ctrl Pts',(-90.0876215040491,-3.27106031271403,
135.737198066874));
#172839=CARTESIAN_POINT('Ctrl Pts',(-90.0802141576953,-3.39991940813838,
135.646723530511));
#172840=CARTESIAN_POINT('Ctrl Pts',(-90.0728123360199,-3.52868239558817,
135.556316473471));
#172841=CARTESIAN_POINT('Ctrl Pts',(-90.0654105143445,-3.65393719743797,
135.460699536022));
#172842=CARTESIAN_POINT('Ctrl Pts',(-90.0580086926691,-3.77524031461416,
135.360180097024));
#172843=CARTESIAN_POINT('Ctrl Pts',(-90.0506107783577,-3.89647939681867,
135.259713721456));
#172844=CARTESIAN_POINT('Ctrl Pts',(-90.0432128640463,-4.0137706621383,
135.154350236032));
#172845=CARTESIAN_POINT('Ctrl Pts',(-90.0358149497349,-4.12670197337219,
135.044438610418));
#172846=CARTESIAN_POINT('Ctrl Pts',(-90.0284182648227,-4.2396145174711,
134.934545250122));
#172847=CARTESIAN_POINT('Ctrl Pts',(-90.0210215799105,-4.34816827824035,
134.820105509818));
#172848=CARTESIAN_POINT('Ctrl Pts',(-90.0136248949983,-4.45198634784982,
134.701506768413));
#172849=CARTESIAN_POINT('Ctrl Pts',(-90.0062285380629,-4.5557998140573,
134.5829132858));
#172850=CARTESIAN_POINT('Ctrl Pts',(-89.9988321811274,-4.65487776074972,
134.460161449648));
#172851=CARTESIAN_POINT('Ctrl Pts',(-89.9914358241919,-4.74888230731818,
134.333673212639));
#172852=CARTESIAN_POINT('Ctrl Pts',(-89.9840383348553,-4.8429012462227,
134.207165609957));
#172853=CARTESIAN_POINT('Ctrl Pts',(-89.9766408455187,-4.93184501570499,
134.07692076702));
#172854=CARTESIAN_POINT('Ctrl Pts',(-89.9692433561821,-5.01541805537971,
133.943391087675));
#172855=CARTESIAN_POINT('Ctrl Pts',(-89.9618432736671,-5.09902039145382,
133.809814599708));
#172856=CARTESIAN_POINT('Ctrl Pts',(-89.9544431911521,-5.1772480513532,
133.672951298951));
#172857=CARTESIAN_POINT('Ctrl Pts',(-89.9470431086371,-5.2498506415936,
133.533279598309));
#172858=CARTESIAN_POINT('Ctrl Pts',(-89.9396348889706,-5.32253306584581,
133.393454314273));
#172859=CARTESIAN_POINT('Ctrl Pts',(-89.9322266693041,-5.3895778956264,
133.25081479459));
#172860=CARTESIAN_POINT('Ctrl Pts',(-89.9248184496376,-5.45078195138222,
133.105861580196));
#172861=CARTESIAN_POINT('Ctrl Pts',(-89.9174056703355,-5.51202367721328,
132.960819149516));
#172862=CARTESIAN_POINT('Ctrl Pts',(-89.9099928910334,-5.56741733468471,
132.81346053516));
#172863=CARTESIAN_POINT('Ctrl Pts',(-89.9025801117313,-5.61680931276014,
132.664302473268));
#172864=CARTESIAN_POINT('Ctrl Pts',(-89.8951567407025,-5.66627186441004,
132.514931287341));
#172865=CARTESIAN_POINT('Ctrl Pts',(-89.8877333696738,-5.70971550667538,
132.363755876572));
#172866=CARTESIAN_POINT('Ctrl Pts',(-89.880309998645,-5.74703732216239,
132.211305030175));
#172867=CARTESIAN_POINT('Ctrl Pts',(-89.8763739492043,-5.76682624425736,
132.130471933412));
#172868=CARTESIAN_POINT('Ctrl Pts',(-89.8724378997637,-5.78489496269358,
132.049280395803));
#172869=CARTESIAN_POINT('Ctrl Pts',(-89.8685018503231,-5.80123405184049,
131.9678098164));
#172870=CARTESIAN_POINT('Ctrl Pts',(-89.8577895132931,-5.84570245406606,
131.746079800615));
#172871=CARTESIAN_POINT('Ctrl Pts',(-89.847077176263,-5.87746997319479,
131.521724546966));
#172872=CARTESIAN_POINT('Ctrl Pts',(-89.836364839233,-5.89629390879888,
131.295938387162));
#172873=CARTESIAN_POINT('Ctrl Pts',(-89.8287016235569,-5.90975986660081,
131.134419193508));
#172874=CARTESIAN_POINT('Ctrl Pts',(-89.8210384078808,-5.91660286006169,
130.972168001611));
#172875=CARTESIAN_POINT('Ctrl Pts',(-89.8133751922047,-5.91674765230671,
130.809631426141));
#172876=CARTESIAN_POINT('',(-88.0633751922046,-5.90698262932298,130.80492291423));
#172877=CARTESIAN_POINT('Ctrl Pts',(-89.8133742249814,-5.91883747551114,
130.809612765774));
#172878=CARTESIAN_POINT('Ctrl Pts',(-89.7389342254909,-5.90421827380185,
129.230170522338));
#172879=CARTESIAN_POINT('Ctrl Pts',(-89.5716783513963,-4.43993236803427,
125.657485558116));
#172880=CARTESIAN_POINT('Ctrl Pts',(-89.3116066026975,1.60058328561251,
123.991454213087));
#172881=CARTESIAN_POINT('Ctrl Pts',(-89.0331589788845,6.59704547191749,
128.468434340518));
#172882=CARTESIAN_POINT('Ctrl Pts',(-88.7547113550716,5.5311451531159,135.092016600209));
#172883=CARTESIAN_POINT('Ctrl Pts',(-88.4762637312587,-0.617607349934246,
137.775452475492));
#172884=CARTESIAN_POINT('Ctrl Pts',(-88.2458183436364,-5.23665250507847,
134.694553022179));
#172885=CARTESIAN_POINT('Ctrl Pts',(-88.1081888306183,-5.9077896589492,
131.760598074561));
#172886=CARTESIAN_POINT('Ctrl Pts',(-88.0633751922046,-5.90698262932298,
130.80492291423));
#172887=CARTESIAN_POINT('',(-86.3133751922044,-5.91676703712452,130.798896138361));
#172888=CARTESIAN_POINT('Ctrl Pts',(-88.0633751922046,-5.90698262932298,
130.80492291423));
#172889=CARTESIAN_POINT('Ctrl Pts',(-88.015372956014,-5.90611817760466,
129.781249175799));
#172890=CARTESIAN_POINT('Ctrl Pts',(-87.8745548452193,-5.16532046994545,
126.777054825752));
#172891=CARTESIAN_POINT('Ctrl Pts',(-87.6409208598199,-0.377868435225309,
123.81617229898));
#172892=CARTESIAN_POINT('Ctrl Pts',(-87.3624732360072,5.67511362901596,
126.709162719037));
#172893=CARTESIAN_POINT('Ctrl Pts',(-87.0840256121942,6.51294351290233,
133.365439946302));
#172894=CARTESIAN_POINT('Ctrl Pts',(-86.8055779883815,1.36569648341219,
137.668210386139));
#172895=CARTESIAN_POINT('Ctrl Pts',(-86.5486945150514,-4.54074141890726,
135.818696162511));
#172896=CARTESIAN_POINT('Ctrl Pts',(-86.3846269163258,-5.90276582907417,
132.312047574845));
#172897=CARTESIAN_POINT('Ctrl Pts',(-86.3133751922044,-5.91676703712452,
130.798896138361));
#172898=CARTESIAN_POINT('',(-84.5633751922045,-5.92580168545033,130.806256469132));
#172899=CARTESIAN_POINT('Ctrl Pts',(-86.3133751922044,-5.91676703712452,
130.798896138361));
#172900=CARTESIAN_POINT('Ctrl Pts',(-86.2918110417214,-5.92100446661924,
130.340944759889));
#172901=CARTESIAN_POINT('Ctrl Pts',(-86.1774310166342,-5.66290769290208,
127.916615574322));
#172902=CARTESIAN_POINT('Ctrl Pts',(-85.9702351169427,-2.3258839918925,
124.203767902776));
#172903=CARTESIAN_POINT('Ctrl Pts',(-85.6917874931298,4.29606847896242,
125.279746951938));
#172904=CARTESIAN_POINT('Ctrl Pts',(-85.4133398693169,6.97014389226581,
131.432576067439));
#172905=CARTESIAN_POINT('Ctrl Pts',(-85.134892245504,3.23899757903464,137.008105874533));
#172906=CARTESIAN_POINT('Ctrl Pts',(-84.8564446216911,-3.46862927549987,
136.88269686028));
#172907=CARTESIAN_POINT('Ctrl Pts',(-84.6659389372578,-5.87699607777005,
132.975327905718));
#172908=CARTESIAN_POINT('Ctrl Pts',(-84.5682491274291,-5.92623241459706,
130.909352943666));
#172909=CARTESIAN_POINT('Ctrl Pts',(-84.5633751922045,-5.92580168545033,
130.806256469132));
#172910=CARTESIAN_POINT('',(-82.813376411914,-5.91339316048575,130.808932093645));
#172911=CARTESIAN_POINT('Ctrl Pts',(-84.5633751922045,-5.92580168545033,
130.806256469132));
#172912=CARTESIAN_POINT('Ctrl Pts',(-84.4754332528247,-5.91802990458645,
128.946054497649));
#172913=CARTESIAN_POINT('Ctrl Pts',(-84.2946754388405,-3.9700232261154,
125.108533355109));
#172914=CARTESIAN_POINT('Ctrl Pts',(-84.0211017502524,2.57098795437597,
124.295322173311));
#172915=CARTESIAN_POINT('Ctrl Pts',(-83.7426541264397,6.86592017791128,
129.449111326519));
#172916=CARTESIAN_POINT('Ctrl Pts',(-83.4642065026265,4.85140717679743,
135.848308370593));
#172917=CARTESIAN_POINT('Ctrl Pts',(-83.1857588788137,-1.62131201537933,
137.612363840181));
#172918=CARTESIAN_POINT('Ctrl Pts',(-82.9688158071183,-5.50350238343903,
134.112443556921));
#172919=CARTESIAN_POINT('Ctrl Pts',(-82.8446886100276,-5.91572502166291,
131.475548415697));
#172920=CARTESIAN_POINT('Ctrl Pts',(-82.8133772875409,-5.91098454745023,
130.808948883669));
#172921=CARTESIAN_POINT('',(-81.0633739991884,-5.91254220191759,130.800666021097));
#172922=CARTESIAN_POINT('Ctrl Pts',(-82.8133751922044,-5.91674825198712,
130.808908705884));
#172923=CARTESIAN_POINT('Ctrl Pts',(-82.8056872104954,-5.91687418582307,
130.645077497767));
#172924=CARTESIAN_POINT('Ctrl Pts',(-82.7979992287864,-5.91019052118769,
130.48117042425));
#172925=CARTESIAN_POINT('Ctrl Pts',(-82.7903112470773,-5.89670961218577,
130.317794782292));
#172926=CARTESIAN_POINT('Ctrl Pts',(-82.7829152084456,-5.88374062662591,
130.160623159734));
#172927=CARTESIAN_POINT('Ctrl Pts',(-82.7755191698139,-5.86448120197058,
130.003943747025));
#172928=CARTESIAN_POINT('Ctrl Pts',(-82.7681231311822,-5.83899539068648,
129.848293993296));
#172929=CARTESIAN_POINT('Ctrl Pts',(-82.7607265983148,-5.81350787632902,
129.692633838371));
#172930=CARTESIAN_POINT('Ctrl Pts',(-82.7533300654475,-5.78179320650162,
129.538003847396));
#172931=CARTESIAN_POINT('Ctrl Pts',(-82.7459335325802,-5.74396684664459,
129.384932765526));
#172932=CARTESIAN_POINT('Ctrl Pts',(-82.7385350509601,-5.70613052073683,
129.231821354262));
#172933=CARTESIAN_POINT('Ctrl Pts',(-82.73113656934,-5.66217938781907,129.080270031722));
#172934=CARTESIAN_POINT('Ctrl Pts',(-82.7237380877199,-5.61227917682799,
128.930793697533));
#172935=CARTESIAN_POINT('Ctrl Pts',(-82.71633620194,-5.56235600595053,128.781248586888));
#172936=CARTESIAN_POINT('Ctrl Pts',(-82.70893431616,-5.50647842441477,128.633780718771));
#172937=CARTESIAN_POINT('Ctrl Pts',(-82.70153243038,-5.44486074827377,128.488886153356));
#172938=CARTESIAN_POINT('Ctrl Pts',(-82.6941216520159,-5.38316904500114,
128.343817512421));
#172939=CARTESIAN_POINT('Ctrl Pts',(-82.6867108736518,-5.31572362347877,
128.201328689992));
#172940=CARTESIAN_POINT('Ctrl Pts',(-82.6793000952876,-5.24278564009095,
128.061892879459));
#172941=CARTESIAN_POINT('Ctrl Pts',(-82.6718840542683,-5.16979586086856,
127.922358050639));
#172942=CARTESIAN_POINT('Ctrl Pts',(-82.664468013249,-5.09130593352807,
127.785880875214));
#172943=CARTESIAN_POINT('Ctrl Pts',(-82.6570519722298,-5.00762070700942,
127.652906125235));
#172944=CARTESIAN_POINT('Ctrl Pts',(-82.6496253628503,-4.92381622338038,
127.519741877241));
#172945=CARTESIAN_POINT('Ctrl Pts',(-82.6421987534708,-4.83480186949621,
127.390090325031));
#172946=CARTESIAN_POINT('Ctrl Pts',(-82.6347721440912,-4.74092356084927,
127.26436424007));
#172947=CARTESIAN_POINT('Ctrl Pts',(-82.6328026397902,-4.71602744430311,
127.231022232644));
#172948=CARTESIAN_POINT('Ctrl Pts',(-82.6308331354891,-4.69078945681863,
127.197956101158));
#172949=CARTESIAN_POINT('Ctrl Pts',(-82.6288636311881,-4.6652164826873,
127.165173107673));
#172950=CARTESIAN_POINT('Ctrl Pts',(-82.6214403647826,-4.56882928533186,
127.041610598019));
#172951=CARTESIAN_POINT('Ctrl Pts',(-82.6140170983771,-4.46738395023727,
126.92169324669));
#172952=CARTESIAN_POINT('Ctrl Pts',(-82.6065938319717,-4.36118612570389,
126.805862632138));
#172953=CARTESIAN_POINT('Ctrl Pts',(-82.5991793392506,-4.25511381817993,
126.690168919754));
#172954=CARTESIAN_POINT('Ctrl Pts',(-82.5917648465296,-4.1443004517905,
126.578552602109));
#172955=CARTESIAN_POINT('Ctrl Pts',(-82.5843503538085,-4.0290935800243,
126.471424489961));
#172956=CARTESIAN_POINT('Ctrl Pts',(-82.5769430074547,-3.91399774897824,
126.36439963192));
#172957=CARTESIAN_POINT('Ctrl Pts',(-82.5695356611009,-3.79451711439902,
126.261854619855));
#172958=CARTESIAN_POINT('Ctrl Pts',(-82.5621283147471,-3.67103786096599,
126.164165407679));
#172959=CARTESIAN_POINT('Ctrl Pts',(-82.5547264930717,-3.54765070301914,
126.066549055804));
#172960=CARTESIAN_POINT('Ctrl Pts',(-82.5473246713962,-3.42027115591953,
125.973781523261));
#172961=CARTESIAN_POINT('Ctrl Pts',(-82.5399228497208,-3.28932035877788,
125.886200174897));
#172962=CARTESIAN_POINT('Ctrl Pts',(-82.5325249354094,-3.15843868954236,
125.798665060046));
#172963=CARTESIAN_POINT('Ctrl Pts',(-82.5251270210979,-3.02398983431051,
125.716310884025));
#172964=CARTESIAN_POINT('Ctrl Pts',(-82.5177291067865,-2.88642584623075,
125.639433086931));
#172965=CARTESIAN_POINT('Ctrl Pts',(-82.5103324218743,-2.74888471878994,
125.562568065532));
#172966=CARTESIAN_POINT('Ctrl Pts',(-82.502935736962,-2.60822981148502,
125.491177798763));
#172967=CARTESIAN_POINT('Ctrl Pts',(-82.4955390520497,-2.46493993872728,
125.425513002977));
#172968=CARTESIAN_POINT('Ctrl Pts',(-82.4881426951142,-2.32165641959307,
125.359851118837));
#172969=CARTESIAN_POINT('Ctrl Pts',(-82.4807463381788,-2.17573850667814,
125.299914356412));
#172970=CARTESIAN_POINT('Ctrl Pts',(-82.4733499812433,-2.02768701603159,
125.245906162637));
#172971=CARTESIAN_POINT('Ctrl Pts',(-82.4659524919067,-1.87961285832387,
125.191889700071));
#172972=CARTESIAN_POINT('Ctrl Pts',(-82.4585550025701,-1.72940482318353,
125.143803741403));
#172973=CARTESIAN_POINT('Ctrl Pts',(-82.4511575132335,-1.57758083751009,
125.10180248427));
#172974=CARTESIAN_POINT('Ctrl Pts',(-82.4437574307184,-1.42570363017317,
125.059786503661));
#172975=CARTESIAN_POINT('Ctrl Pts',(-82.4363573482033,-1.27220970402733,
125.02385957081));
#172976=CARTESIAN_POINT('Ctrl Pts',(-82.4289572656882,-1.11762902715309,
124.994125173097));
#172977=CARTESIAN_POINT('Ctrl Pts',(-82.4215490460217,-0.962878372933568,
124.964358079357));
#172978=CARTESIAN_POINT('Ctrl Pts',(-82.4141408263552,-0.807038948306534,
124.940797189989));
#172979=CARTESIAN_POINT('Ctrl Pts',(-82.4067326066886,-0.650648458779961,
124.923494427489));
#172980=CARTESIAN_POINT('Ctrl Pts',(-82.3993198273866,-0.494161713517491,
124.906181015428));
#172981=CARTESIAN_POINT('Ctrl Pts',(-82.3919070480845,-0.337123599028448,
124.895133431512));
#172982=CARTESIAN_POINT('Ctrl Pts',(-82.3844942687825,-0.180073200227318,
124.89035146936));
#172983=CARTESIAN_POINT('Ctrl Pts',(-82.3770708977537,-0.0227984004507772,
124.885562674517));
#172984=CARTESIAN_POINT('Ctrl Pts',(-82.3696475267249,0.134488346401762,
124.88705737828));
#172985=CARTESIAN_POINT('Ctrl Pts',(-82.3622241556961,0.291250866976861,
124.894783348845));
#172986=CARTESIAN_POINT('Ctrl Pts',(-82.3582881062558,0.374370116840544,
124.89887984382));
#172987=CARTESIAN_POINT('Ctrl Pts',(-82.3543520568154,0.457342109213834,
124.904727308725));
#172988=CARTESIAN_POINT('Ctrl Pts',(-82.3504160073751,0.540088056083287,
124.912312123691));
#172989=CARTESIAN_POINT('Ctrl Pts',(-82.3429927409696,0.696144329485136,
124.926616848003));
#172990=CARTESIAN_POINT('Ctrl Pts',(-82.3355694745642,0.851867874952232,
124.947147423962));
#172991=CARTESIAN_POINT('Ctrl Pts',(-82.3281462081587,1.00672196965357,
124.973885384936));
#172992=CARTESIAN_POINT('Ctrl Pts',(-82.3207317154377,1.16139303967481,
125.00059174386));
#172993=CARTESIAN_POINT('Ctrl Pts',(-82.3133172227167,1.31519634014826,
125.033490821333));
#172994=CARTESIAN_POINT('Ctrl Pts',(-82.3059027299957,1.46759838319741,
125.072512264012));
#172995=CARTESIAN_POINT('Ctrl Pts',(-82.2984953836419,1.61985353541964,
125.111496096356));
#172996=CARTESIAN_POINT('Ctrl Pts',(-82.2910880372882,1.77070975976131,
125.156590454272));
#172997=CARTESIAN_POINT('Ctrl Pts',(-82.2836806909344,1.91964201329523,
125.207673641927));
#172998=CARTESIAN_POINT('Ctrl Pts',(-82.276278869259,2.06846318753557,125.258718729812));
#172999=CARTESIAN_POINT('Ctrl Pts',(-82.2688770475836,2.21536289660225,
125.315743633051));
#173000=CARTESIAN_POINT('Ctrl Pts',(-82.2614752259082,2.35982966991864,
125.378576389321));
#173001=CARTESIAN_POINT('Ctrl Pts',(-82.2540773115968,2.50422018034952,
125.441375976668));
#173002=CARTESIAN_POINT('Ctrl Pts',(-82.2466793972855,2.64617997137505,
125.509977162612));
#173003=CARTESIAN_POINT('Ctrl Pts',(-82.2392814829741,2.78521613510553,
125.584159314623));
#173004=CARTESIAN_POINT('Ctrl Pts',(-82.2318847980619,2.92422919354856,
125.658329138907));
#173005=CARTESIAN_POINT('Ctrl Pts',(-82.2244881131497,3.06031925994357,
125.738077912983));
#173006=CARTESIAN_POINT('Ctrl Pts',(-82.2170914282374,3.19301658863656,
125.823138315039));
#173007=CARTESIAN_POINT('Ctrl Pts',(-82.209695071302,3.32570803339095,125.908194945428));
#173008=CARTESIAN_POINT('Ctrl Pts',(-82.2022987143665,3.45500672529041,
125.998562534045));
#173009=CARTESIAN_POINT('Ctrl Pts',(-82.1949023574311,3.58047079535733,
126.093929698203));
#173010=CARTESIAN_POINT('Ctrl Pts',(-82.1875048680945,3.70595407429368,
126.189311463317));
#173011=CARTESIAN_POINT('Ctrl Pts',(-82.1801073787579,3.82760126521419,
126.289694102168));
#173012=CARTESIAN_POINT('Ctrl Pts',(-82.1727098894213,3.94500268514106,
126.394725215775));
#173013=CARTESIAN_POINT('Ctrl Pts',(-82.1653098069063,4.06244525995419,
126.499793147876));
#173014=CARTESIAN_POINT('Ctrl Pts',(-82.1579097243912,4.17563882244492,
126.609512550346));
#173015=CARTESIAN_POINT('Ctrl Pts',(-82.1505096418762,4.28420984505616,
126.723493483485));
#173016=CARTESIAN_POINT('Ctrl Pts',(-82.1431014222097,4.39290025266797,
126.837599750377));
#173017=CARTESIAN_POINT('Ctrl Pts',(-82.1356932025431,4.49695771177296,
126.955976635707));
#173018=CARTESIAN_POINT('Ctrl Pts',(-82.1282849828766,4.59604789554275,
127.078199817979));
#173019=CARTESIAN_POINT('Ctrl Pts',(-82.1208722035745,4.69519906766723,
127.200498226581));
#173020=CARTESIAN_POINT('Ctrl Pts',(-82.1134594242724,4.78937664965125,
127.326647350892));
#173021=CARTESIAN_POINT('Ctrl Pts',(-82.1060466449703,4.8782894265632,127.456193531953));
#173022=CARTESIAN_POINT('Ctrl Pts',(-82.0986232739415,4.96732924622026,
127.585924814673));
#173023=CARTESIAN_POINT('Ctrl Pts',(-82.0911999029128,5.05108903822848,
127.719062533285));
#173024=CARTESIAN_POINT('Ctrl Pts',(-82.083776531884,5.12932293189013,127.855127357397));
#173025=CARTESIAN_POINT('Ctrl Pts',(-82.0798404824434,5.17080441950393,
127.927272191968));
#173026=CARTESIAN_POINT('Ctrl Pts',(-82.0759044330027,5.21073317025427,
128.00023957666));
#173027=CARTESIAN_POINT('Ctrl Pts',(-82.0719683835621,5.24907805607844,
128.073955863011));
#173028=CARTESIAN_POINT('Ctrl Pts',(-82.0645451171567,5.32139531404309,
128.21298247847));
#173029=CARTESIAN_POINT('Ctrl Pts',(-82.0571218507514,5.38829473911661,
128.355094385383));
#173030=CARTESIAN_POINT('Ctrl Pts',(-82.0496985843459,5.44950175599861,
128.499830041968));
#173031=CARTESIAN_POINT('Ctrl Pts',(-82.042284091625,5.51063643126958,128.644394633025));
#173032=CARTESIAN_POINT('Ctrl Pts',(-82.0348695989041,5.56609194640114,
128.791576460628));
#173033=CARTESIAN_POINT('Ctrl Pts',(-82.0274551061831,5.61563912842514,
128.940888658614));
#173034=CARTESIAN_POINT('Ctrl Pts',(-82.0200477598293,5.66513855500982,
129.090056943883));
#173035=CARTESIAN_POINT('Ctrl Pts',(-82.0126404134756,5.70874086868112,
129.241351159836));
#173036=CARTESIAN_POINT('Ctrl Pts',(-82.0052330671218,5.74626465706431,
129.394263793418));
#173037=CARTESIAN_POINT('Ctrl Pts',(-81.9978312454464,5.78376045879044,
129.547062378988));
#173038=CARTESIAN_POINT('Ctrl Pts',(-81.9904294237709,5.81518667364236,
129.701476617752));
#173039=CARTESIAN_POINT('Ctrl Pts',(-81.9830276020955,5.84041151605071,
129.856983245194));
#173040=CARTESIAN_POINT('Ctrl Pts',(-81.9756296877842,5.86562304246124,
130.012407781899));
#173041=CARTESIAN_POINT('Ctrl Pts',(-81.9682317734728,5.88463965645102,
130.168923191279));
#173042=CARTESIAN_POINT('Ctrl Pts',(-81.9608338591614,5.89738055365975,
130.325995518697));
#173043=CARTESIAN_POINT('Ctrl Pts',(-81.9534371742492,5.91011933356242,
130.483041743543));
#173044=CARTESIAN_POINT('Ctrl Pts',(-81.9460404893371,5.91658443640106,
130.640644331031));
#173045=CARTESIAN_POINT('Ctrl Pts',(-81.9386438044249,5.91674685858663,
130.798263576871));
#173046=CARTESIAN_POINT('Ctrl Pts',(-81.9312474474895,5.91690927357023,
130.955875833708));
#173047=CARTESIAN_POINT('Ctrl Pts',(-81.9238510905539,5.91076956319177,
131.113504374131));
#173048=CARTESIAN_POINT('Ctrl Pts',(-81.9164547336185,5.89835086154906,
131.270609131305));
#173049=CARTESIAN_POINT('Ctrl Pts',(-81.9090572442819,5.8859302585715,131.427737941617));
#173050=CARTESIAN_POINT('Ctrl Pts',(-81.9016597549455,5.86722877961298,
131.584342436846));
#173051=CARTESIAN_POINT('Ctrl Pts',(-81.8942622656089,5.84232146425987,
131.739887458842));
#173052=CARTESIAN_POINT('Ctrl Pts',(-81.8868621830939,5.81740541768579,
131.895487006906));
#173053=CARTESIAN_POINT('Ctrl Pts',(-81.879462100579,5.78627926240652,132.050025973917));
#173054=CARTESIAN_POINT('Ctrl Pts',(-81.872062018064,5.74906916496555,132.202979328631));
#173055=CARTESIAN_POINT('Ctrl Pts',(-81.8646537983976,5.7118181511972,132.356100871283));
#173056=CARTESIAN_POINT('Ctrl Pts',(-81.857245578731,5.66846992335339,132.507632956724));
#173057=CARTESIAN_POINT('Ctrl Pts',(-81.8498373590646,5.61920076330784,
132.657064950195));
#173058=CARTESIAN_POINT('Ctrl Pts',(-81.8424245797625,5.56990127891637,
132.806588916563));
#173059=CARTESIAN_POINT('Ctrl Pts',(-81.8350118004604,5.51467373138314,
132.954009866587));
#173060=CARTESIAN_POINT('Ctrl Pts',(-81.8275990211583,5.45374238805491,
133.098837579149));
#173061=CARTESIAN_POINT('Ctrl Pts',(-81.8201756501296,5.39272398316602,
133.243872228337));
#173062=CARTESIAN_POINT('Ctrl Pts',(-81.812752279101,5.32598566336909,133.386305902533));
#173063=CARTESIAN_POINT('Ctrl Pts',(-81.8053289080722,5.25379780378184,
133.52567265397));
#173064=CARTESIAN_POINT('Ctrl Pts',(-81.8013928586312,5.21552206850281,
133.599568249645));
#173065=CARTESIAN_POINT('Ctrl Pts',(-81.7974568091902,5.17571500630908,
133.672602092252));
#173066=CARTESIAN_POINT('Ctrl Pts',(-81.7935207597492,5.13442175425764,
133.74470818408));
#173067=CARTESIAN_POINT('Ctrl Pts',(-81.7860974933438,5.05654396961077,
133.880698022907));
#173068=CARTESIAN_POINT('Ctrl Pts',(-81.7786742269383,4.9731419708674,134.013797360875));
#173069=CARTESIAN_POINT('Ctrl Pts',(-81.7712509605329,4.88445565154512,
134.143525715399));
#173070=CARTESIAN_POINT('Ctrl Pts',(-81.7638364678119,4.79587415208708,
134.273100741783));
#173071=CARTESIAN_POINT('Ctrl Pts',(-81.756421975091,4.70202097262363,134.39931241018));
#173072=CARTESIAN_POINT('Ctrl Pts',(-81.74900748237,4.60318185385699,134.521704747832));
#173073=CARTESIAN_POINT('Ctrl Pts',(-81.7416001360162,4.50443799995396,
134.643979119141));
#173074=CARTESIAN_POINT('Ctrl Pts',(-81.7341927896623,4.40071800678207,
134.762441199804));
#173075=CARTESIAN_POINT('Ctrl Pts',(-81.7267854433085,4.29235080162894,
134.87666403925));
#173076=CARTESIAN_POINT('Ctrl Pts',(-81.7193836216332,4.18406442082649,
134.990801686992));
#173077=CARTESIAN_POINT('Ctrl Pts',(-81.7119817999577,4.07113798527085,
135.100706119413));
#173078=CARTESIAN_POINT('Ctrl Pts',(-81.7045799782824,3.9539404989001,135.205983624328));
#173079=CARTESIAN_POINT('Ctrl Pts',(-81.6971820639711,3.83680488017047,
135.311205554068));
#173080=CARTESIAN_POINT('Ctrl Pts',(-81.6897841496598,3.71540297788113,
135.411805171867));
#173081=CARTESIAN_POINT('Ctrl Pts',(-81.6823862353485,3.59014034646083,
135.507425879203));
#173082=CARTESIAN_POINT('Ctrl Pts',(-81.6749895504363,3.46489853141684,
135.603030696113));
#173083=CARTESIAN_POINT('Ctrl Pts',(-81.6675928655241,3.33579755702844,
135.693658018427));
#173084=CARTESIAN_POINT('Ctrl Pts',(-81.6601961806119,3.20327581465295,
135.778991721252));
#173085=CARTESIAN_POINT('Ctrl Pts',(-81.6527998236765,3.07075994843001,
135.864321640292));
#173086=CARTESIAN_POINT('Ctrl Pts',(-81.645403466741,2.93482392966964,135.944358204454));
#173087=CARTESIAN_POINT('Ctrl Pts',(-81.6380071098055,2.79593463643932,
136.018828957796));
#173088=CARTESIAN_POINT('Ctrl Pts',(-81.630609620469,2.65702407890404,136.0933111128));
#173089=CARTESIAN_POINT('Ctrl Pts',(-81.6232121311324,2.51515967561123,
136.162225583847));
#173090=CARTESIAN_POINT('Ctrl Pts',(-81.6158146417959,2.37083223099745,
136.225346237817));
#173091=CARTESIAN_POINT('Ctrl Pts',(-81.6084145592809,2.22645419262149,
136.288489018633));
#173092=CARTESIAN_POINT('Ctrl Pts',(-81.6010144767658,2.0796117356769,136.345833789152));
#173093=CARTESIAN_POINT('Ctrl Pts',(-81.5936143942508,1.93081477991784,
136.397202904646));
#173094=CARTESIAN_POINT('Ctrl Pts',(-81.5862061745844,1.78185420660943,
136.448628505764));
#173095=CARTESIAN_POINT('Ctrl Pts',(-81.578797954918,1.63093519552675,136.494065207551));
#173096=CARTESIAN_POINT('Ctrl Pts',(-81.5713897352515,1.47858264281552,
136.533385310379));
#173097=CARTESIAN_POINT('Ctrl Pts',(-81.5639769559494,1.3261363196498,136.572729614075));
#173098=CARTESIAN_POINT('Ctrl Pts',(-81.5565641766474,1.17225506076626,
136.605949738655));
#173099=CARTESIAN_POINT('Ctrl Pts',(-81.5491513973453,1.01747252505441,
136.6329693901));
#173100=CARTESIAN_POINT('Ctrl Pts',(-81.5417280263166,0.86246882879718,
136.66002764849));
#173101=CARTESIAN_POINT('Ctrl Pts',(-81.5343046552877,0.706561652739749,
136.680867689957));
#173102=CARTESIAN_POINT('Ctrl Pts',(-81.526881284259,0.550289156290671,
136.695465132593));
#173103=CARTESIAN_POINT('Ctrl Pts',(-81.5229452348182,0.467429728965848,
136.703205046939));
#173104=CARTESIAN_POINT('Ctrl Pts',(-81.5190091853774,0.384467599300527,
136.709190814001));
#173105=CARTESIAN_POINT('Ctrl Pts',(-81.5150731359366,0.301482690721084,
136.713424735487));
#173106=CARTESIAN_POINT('Ctrl Pts',(-81.5076498695312,0.144975743012964,
136.721409779272));
#173107=CARTESIAN_POINT('Ctrl Pts',(-81.5002266031259,-0.0120853171151492,
136.723184758965));
#173108=CARTESIAN_POINT('Ctrl Pts',(-81.4928033367206,-0.169166577750935,
136.718691791204));
#173109=CARTESIAN_POINT('Ctrl Pts',(-81.4853888439996,-0.326062181382328,
136.714204133758));
#173110=CARTESIAN_POINT('Ctrl Pts',(-81.4779743512786,-0.482977568495968,
136.703463285476));
#173111=CARTESIAN_POINT('Ctrl Pts',(-81.4705598585576,-0.639374666465414,
136.686463183688));
#173112=CARTESIAN_POINT('Ctrl Pts',(-81.4631525122038,-0.795621023024034,
136.669479467239));
#173113=CARTESIAN_POINT('Ctrl Pts',(-81.4557451658501,-0.951349716316779,
136.646248547676));
#173114=CARTESIAN_POINT('Ctrl Pts',(-81.4483378194963,-1.106023747502,136.616816383631));
#173115=CARTESIAN_POINT('Ctrl Pts',(-81.4409359978209,-1.26058241695881,
136.587406171204));
#173116=CARTESIAN_POINT('Ctrl Pts',(-81.4335341761455,-1.41408762540887,
136.551803993017));
#173117=CARTESIAN_POINT('Ctrl Pts',(-81.4261323544702,-1.56600867599897,
136.510107491481));
#173118=CARTESIAN_POINT('Ctrl Pts',(-81.4187344401589,-1.7178495286477,
136.468433001205));
#173119=CARTESIAN_POINT('Ctrl Pts',(-81.4113365258476,-1.86810752982338,
136.420670693231));
#173120=CARTESIAN_POINT('Ctrl Pts',(-81.4039386115364,-2.01626345101585,
136.366969021777));
#173121=CARTESIAN_POINT('Ctrl Pts',(-81.3965419266242,-2.16439475138309,
136.313276274566));
#173122=CARTESIAN_POINT('Ctrl Pts',(-81.3891452417121,-2.31042431446803,
136.25364624989));
#173123=CARTESIAN_POINT('Ctrl Pts',(-81.3817485567999,-2.45384921420774,
136.188276905588));
#173124=CARTESIAN_POINT('Ctrl Pts',(-81.3743521998645,-2.59726775433709,
136.122910459832));
#173125=CARTESIAN_POINT('Ctrl Pts',(-81.3669558429291,-2.73808152108111,
136.051805355273));
#173126=CARTESIAN_POINT('Ctrl Pts',(-81.3595594859937,-2.87580893053838,
135.975207120561));
#173127=CARTESIAN_POINT('Ctrl Pts',(-81.3521619966572,-3.01355742641404,
135.898597158463));
#173128=CARTESIAN_POINT('Ctrl Pts',(-81.3447645073206,-3.14821829787595,
135.816492573096));
#173129=CARTESIAN_POINT('Ctrl Pts',(-81.337367017984,-3.27933600093747,
135.729184061656));
#173130=CARTESIAN_POINT('Ctrl Pts',(-81.3299669354691,-3.41049966710672,
135.641844944352));
#173131=CARTESIAN_POINT('Ctrl Pts',(-81.3225668529541,-3.53811738143704,
135.54929847572));
#173132=CARTESIAN_POINT('Ctrl Pts',(-81.3151667704391,-3.6617640623067,
135.451877644377));
#173133=CARTESIAN_POINT('Ctrl Pts',(-81.3077585507727,-3.78554670541263,
135.354349688815));
#173134=CARTESIAN_POINT('Ctrl Pts',(-81.3003503311062,-3.90534930135215,
135.251936897714));
#173135=CARTESIAN_POINT('Ctrl Pts',(-81.2929421114398,-4.02078069362285,
135.145011856296));
#173136=CARTESIAN_POINT('Ctrl Pts',(-81.2855293321378,-4.13628313198974,
135.0380210043));
#173137=CARTESIAN_POINT('Ctrl Pts',(-81.2781165528358,-4.24740874282639,
134.92651263184));
#173138=CARTESIAN_POINT('Ctrl Pts',(-81.2707037735337,-4.35380488214927,
134.810894482476));
#173139=CARTESIAN_POINT('Ctrl Pts',(-81.263280402505,-4.46035304526566,
134.695111132478));
#173140=CARTESIAN_POINT('Ctrl Pts',(-81.2558570314763,-4.56215799927547,
134.5752065612));
#173141=CARTESIAN_POINT('Ctrl Pts',(-81.2484336604476,-4.65890834268524,
134.451620358379));
#173142=CARTESIAN_POINT('Ctrl Pts',(-81.2444976110063,-4.71020769626048,
134.386091988225));
#173143=CARTESIAN_POINT('Ctrl Pts',(-81.240561561565,-4.76008674916817,
134.319529052227));
#173144=CARTESIAN_POINT('Ctrl Pts',(-81.2366255121237,-4.80850423733689,
134.252000036359));
#173145=CARTESIAN_POINT('Ctrl Pts',(-81.2291362145993,-4.90063036016376,
134.123509553982));
#173146=CARTESIAN_POINT('Ctrl Pts',(-81.2216469170749,-4.98773943234449,
133.991133385634));
#173147=CARTESIAN_POINT('Ctrl Pts',(-81.2141576195505,-5.06948932391224,
133.855296303096));
#173148=CARTESIAN_POINT('Ctrl Pts',(-81.206677475249,-5.15113930290757,
133.719625237076));
#173149=CARTESIAN_POINT('Ctrl Pts',(-81.1991973309475,-5.2274429538628,
133.580501986051));
#173150=CARTESIAN_POINT('Ctrl Pts',(-81.191717186646,-5.29809939888114,
133.438382888177));
#173151=CARTESIAN_POINT('Ctrl Pts',(-81.184244796432,-5.36868259982376,
133.296411114188));
#173152=CARTESIAN_POINT('Ctrl Pts',(-81.176772406218,-5.43363008903948,
133.151450000467));
#173153=CARTESIAN_POINT('Ctrl Pts',(-81.169300016004,-5.49268521580541,
133.003983240329));
#173154=CARTESIAN_POINT('Ctrl Pts',(-81.1618339858426,-5.55169007837193,
132.856641995097));
#173155=CARTESIAN_POINT('Ctrl Pts',(-81.1543679556812,-5.60481243076715,
132.706799687089));
#173156=CARTESIAN_POINT('Ctrl Pts',(-81.1469019255198,-5.65184238195513,
132.554962871659));
#173157=CARTESIAN_POINT('Ctrl Pts',(-81.1394413679871,-5.69883786000854,
132.403237353197));
#173158=CARTESIAN_POINT('Ctrl Pts',(-81.1319808104545,-5.7397497277019,
132.249520587567));
#173159=CARTESIAN_POINT('Ctrl Pts',(-81.1245202529218,-5.77441694790665,
132.094337157751));
#173160=CARTESIAN_POINT('Ctrl Pts',(-81.1170629530263,-5.80906903074052,
131.939221488464));
#173161=CARTESIAN_POINT('Ctrl Pts',(-81.1096056531308,-5.83748181760578,
131.782640785632));
#173162=CARTESIAN_POINT('Ctrl Pts',(-81.1021483532353,-5.85954464004648,
131.625132920828));
#173163=CARTESIAN_POINT('Ctrl Pts',(-81.0946921811703,-5.88160412574032,
131.467648877269));
#173164=CARTESIAN_POINT('Ctrl Pts',(-81.0872360091052,-5.897315504748,131.309238311168));
#173165=CARTESIAN_POINT('Ctrl Pts',(-81.0797798370402,-5.90661954331391,
131.150447504116));
#173166=CARTESIAN_POINT('Ctrl Pts',(-81.0743116220949,-5.91344294844644,
131.033993342823));
#173167=CARTESIAN_POINT('Ctrl Pts',(-81.0688434071496,-5.91682124838117,
130.917334873091));
#173168=CARTESIAN_POINT('Ctrl Pts',(-81.0633751922043,-5.91674886068838,
130.800688827439));
#173169=CARTESIAN_POINT('',(-79.3133766006371,-5.92105326280497,130.80120237523));
#173170=CARTESIAN_POINT('Ctrl Pts',(-81.0633730746496,-5.90928221278149,
130.800648347112));
#173171=CARTESIAN_POINT('Ctrl Pts',(-81.0283080125366,-5.91348873412656,
130.053593847611));
#173172=CARTESIAN_POINT('Ctrl Pts',(-80.9004270758182,-5.43485370113081,
127.334316820743));
#173173=CARTESIAN_POINT('Ctrl Pts',(-80.6797302644982,-1.34479895996363,
123.936385931571));
#173174=CARTESIAN_POINT('Ctrl Pts',(-80.4012826406847,5.05132492808504,
125.96063508846));
#173175=CARTESIAN_POINT('Ctrl Pts',(-80.1228350168721,6.80552797816757,
132.43603137747));
#173176=CARTESIAN_POINT('Ctrl Pts',(-79.8443873930591,2.30578328483937,
137.412001949667));
#173177=CARTESIAN_POINT('Ctrl Pts',(-79.5745682871991,-4.107765378118,136.349839717701));
#173178=CARTESIAN_POINT('Ctrl Pts',(-79.3975650559447,-5.91281211476802,
132.583114278618));
#173179=CARTESIAN_POINT('Ctrl Pts',(-79.3133776992939,-5.92441071902747,
130.801223821324));
#173180=CARTESIAN_POINT('',(-77.5633744091961,-5.91844797605931,130.809555611699));
#173181=CARTESIAN_POINT('Ctrl Pts',(-79.3133751922043,-5.91674914235768,
130.801174882221));
#173182=CARTESIAN_POINT('Ctrl Pts',(-79.3047475099473,-5.91665094697026,
130.618800199036));
#173183=CARTESIAN_POINT('Ctrl Pts',(-79.2961198276903,-5.90812140161666,
130.436657192634));
#173184=CARTESIAN_POINT('Ctrl Pts',(-79.2874921454338,-5.89121974889844,
130.255306492102));
#173185=CARTESIAN_POINT('Ctrl Pts',(-79.2800688790283,-5.87667755006802,
130.099272168765));
#173186=CARTESIAN_POINT('Ctrl Pts',(-79.2726456126227,-5.8559100131561,
129.943580047664));
#173187=CARTESIAN_POINT('Ctrl Pts',(-79.2652223462172,-5.82893642157347,
129.788766822905));
#173188=CARTESIAN_POINT('Ctrl Pts',(-79.2578078534961,-5.80199471053601,
129.634136574521));
#173189=CARTESIAN_POINT('Ctrl Pts',(-79.250393360775,-5.76886160871769,
129.480383518943));
#173190=CARTESIAN_POINT('Ctrl Pts',(-79.242978868054,-5.72960828125813,
129.328041036365));
#173191=CARTESIAN_POINT('Ctrl Pts',(-79.2355715217001,-5.69039278763345,
129.175845387207));
#173192=CARTESIAN_POINT('Ctrl Pts',(-79.2281641753463,-5.64506890444209,
129.025057963489));
#173193=CARTESIAN_POINT('Ctrl Pts',(-79.2207568289924,-5.59375912640378,
128.876203622331));
#173194=CARTESIAN_POINT('Ctrl Pts',(-79.2133550073169,-5.54248761713374,
128.727460302356));
#173195=CARTESIAN_POINT('Ctrl Pts',(-79.2059531856416,-5.48523922357823,
128.580647545591));
#173196=CARTESIAN_POINT('Ctrl Pts',(-79.1985513639661,-5.42218668623004,
128.436276560323));
#173197=CARTESIAN_POINT('Ctrl Pts',(-79.1911534496546,-5.35916743382533,
128.291981787373));
#173198=CARTESIAN_POINT('Ctrl Pts',(-79.1837555353432,-5.29035028868397,
128.15012656006));
#173199=CARTESIAN_POINT('Ctrl Pts',(-79.1763576210317,-5.21595663319991,
128.011203449937));
#173200=CARTESIAN_POINT('Ctrl Pts',(-79.1689609361195,-5.14157534059186,
127.872303426314));
#173201=CARTESIAN_POINT('Ctrl Pts',(-79.1615642512072,-5.06161955294839,
127.736334881567));
#173202=CARTESIAN_POINT('Ctrl Pts',(-79.1541675662949,-4.97635730664454,
127.603767153987));
#173203=CARTESIAN_POINT('Ctrl Pts',(-79.1467712093594,-4.89109884095829,
127.471205304599));
#173204=CARTESIAN_POINT('Ctrl Pts',(-79.1393748524239,-4.80053458638627,
127.342044286512));
#173205=CARTESIAN_POINT('Ctrl Pts',(-79.1319784954885,-4.70497659770437,
127.216725494319));
#173206=CARTESIAN_POINT('Ctrl Pts',(-79.1245810061518,-4.60940397885045,
127.0913875155));
#173207=CARTESIAN_POINT('Ctrl Pts',(-79.1171835168151,-4.50883632992364,
126.969893230733));
#173208=CARTESIAN_POINT('Ctrl Pts',(-79.1097860274785,-4.40362667296433,
126.85265178623));
#173209=CARTESIAN_POINT('Ctrl Pts',(-79.1023859449634,-4.29838013492272,
126.735369242921));
#173210=CARTESIAN_POINT('Ctrl Pts',(-79.0949858624484,-4.1884885981729,
126.62234278576));
#173211=CARTESIAN_POINT('Ctrl Pts',(-79.0875857799334,-4.07434257040716,
126.51394534845));
#173212=CARTESIAN_POINT('Ctrl Pts',(-79.0801775602668,-3.96007102734923,
126.405428717013));
#173213=CARTESIAN_POINT('Ctrl Pts',(-79.0727693406003,-3.84153592135824,
126.301551527873));
#173214=CARTESIAN_POINT('Ctrl Pts',(-79.0653611209337,-3.71916208222599,
126.202647461726));
#173215=CARTESIAN_POINT('Ctrl Pts',(-79.0579483416316,-3.59671292403768,
126.103682521776));
#173216=CARTESIAN_POINT('Ctrl Pts',(-79.0505355623296,-3.47042062355663,
126.009697026341));
#173217=CARTESIAN_POINT('Ctrl Pts',(-79.0431227830275,-3.34073928239624,
125.920981499624));
#173218=CARTESIAN_POINT('Ctrl Pts',(-79.0356994119986,-3.21087264645396,
125.832139212001));
#173219=CARTESIAN_POINT('Ctrl Pts',(-79.0282760409698,-3.07760761386653,
125.748582129929));
#173220=CARTESIAN_POINT('Ctrl Pts',(-79.020852669941,-2.94142388864598,
125.670555394361));
#173221=CARTESIAN_POINT('Ctrl Pts',(-79.0169166205008,-2.86921600986188,
125.629183746944));
#173222=CARTESIAN_POINT('Ctrl Pts',(-79.0129805710606,-2.79618794491139,
125.589366086373));
#173223=CARTESIAN_POINT('Ctrl Pts',(-79.0090445216204,-2.7224133895408,
125.551133428595));
#173224=CARTESIAN_POINT('Ctrl Pts',(-79.0016212552149,-2.58327688051581,
125.479027829214));
#173225=CARTESIAN_POINT('Ctrl Pts',(-78.9941979888094,-2.44106332862814,
125.412344751739));
#173226=CARTESIAN_POINT('Ctrl Pts',(-78.986774722404,-2.29623469298405,
125.351358068764));
#173227=CARTESIAN_POINT('Ctrl Pts',(-78.979360229683,-2.15157723276002,
125.290443466984));
#173228=CARTESIAN_POINT('Ctrl Pts',(-78.9719457369619,-2.00431118173726,
125.235212001756));
#173229=CARTESIAN_POINT('Ctrl Pts',(-78.9645312442409,-1.85492375427443,
125.185892104855));
#173230=CARTESIAN_POINT('Ctrl Pts',(-78.9571238978871,-1.70568031203854,
125.136619744327));
#173231=CARTESIAN_POINT('Ctrl Pts',(-78.9497165515334,-1.55431991598217,
125.093247725188));
#173232=CARTESIAN_POINT('Ctrl Pts',(-78.9423092051796,-1.40135035465225,
125.055956687255));
#173233=CARTESIAN_POINT('Ctrl Pts',(-78.9349073835042,-1.24849488379239,
125.018693462385));
#173234=CARTESIAN_POINT('Ctrl Pts',(-78.9275055618289,-1.09403299848743,
124.987502276109));
#173235=CARTESIAN_POINT('Ctrl Pts',(-78.9201037401535,-0.938488163203133,
124.962514117526));
#173236=CARTESIAN_POINT('Ctrl Pts',(-78.9127058258421,-0.783025438826628,
124.937539149997));
#173237=CARTESIAN_POINT('Ctrl Pts',(-78.9053079115308,-0.62648127063976,
124.918760747838));
#173238=CARTESIAN_POINT('Ctrl Pts',(-78.8979099972194,-0.469389735632584,
124.906258902727));
#173239=CARTESIAN_POINT('Ctrl Pts',(-78.8905133123072,-0.31232430638882,
124.893759135196));
#173240=CARTESIAN_POINT('Ctrl Pts',(-78.8831166273949,-0.154712062615261,
124.887533884154));
#173241=CARTESIAN_POINT('Ctrl Pts',(-78.8757199424827,0.00290724788302974,
124.887611331817));
#173242=CARTESIAN_POINT('Ctrl Pts',(-78.8683235855473,0.16051956937592,
124.887688776046));
#173243=CARTESIAN_POINT('Ctrl Pts',(-78.8609272286119,0.318138583672985,
124.894068363121));
#173244=CARTESIAN_POINT('Ctrl Pts',(-78.8535308716765,0.475224259772234,
124.906726137079));
#173245=CARTESIAN_POINT('Ctrl Pts',(-78.8461333823399,0.632333986089963,
124.919385848976));
#173246=CARTESIAN_POINT('Ctrl Pts',(-78.8387358930033,0.788909839507255,
124.938325631662));
#173247=CARTESIAN_POINT('Ctrl Pts',(-78.8313384036667,0.944416776692353,
124.963469631218));
#173248=CARTESIAN_POINT('Ctrl Pts',(-78.8239383211517,1.09997822659299,
124.988622444964));
#173249=CARTESIAN_POINT('Ctrl Pts',(-78.8165382386367,1.25446964594075,
125.019983746201));
#173250=CARTESIAN_POINT('Ctrl Pts',(-78.8091381561217,1.40736619610315,
125.057426569522));
#173251=CARTESIAN_POINT('Ctrl Pts',(-78.8017299364552,1.56043087174082,
125.094910565077));
#173252=CARTESIAN_POINT('Ctrl Pts',(-78.7943217167887,1.71189681308749,
125.138489348763));
#173253=CARTESIAN_POINT('Ctrl Pts',(-78.7869134971222,1.86125365424366,
125.187985861813));
#173254=CARTESIAN_POINT('Ctrl Pts',(-78.7795007178201,2.0107024220434,125.23751283914));
#173255=CARTESIAN_POINT('Ctrl Pts',(-78.772087938518,2.15803915443074,125.292964672311));
#173256=CARTESIAN_POINT('Ctrl Pts',(-78.7646751592159,2.30277397215182,
125.354116348207));
#173257=CARTESIAN_POINT('Ctrl Pts',(-78.7572517881872,2.44771559376764,
125.415355400485));
#173258=CARTESIAN_POINT('Ctrl Pts',(-78.7498284171585,2.59004753866645,
125.482310402806));
#173259=CARTESIAN_POINT('Ctrl Pts',(-78.7424050461297,2.72930427108517,
125.554710271273));
#173260=CARTESIAN_POINT('Ctrl Pts',(-78.738468996689,2.80314153203182,125.593098418744));
#173261=CARTESIAN_POINT('Ctrl Pts',(-78.7345329472482,2.87611471049029,
125.633016579915));
#173262=CARTESIAN_POINT('Ctrl Pts',(-78.7305968978075,2.9481578775156,125.674419517344));
#173263=CARTESIAN_POINT('Ctrl Pts',(-78.7231736314021,3.08402904213746,
125.752504165195));
#173264=CARTESIAN_POINT('Ctrl Pts',(-78.7157503649966,3.21700130233436,
125.836108621896));
#173265=CARTESIAN_POINT('Ctrl Pts',(-78.7083270985912,3.34659454115527,
125.924992262993));
#173266=CARTESIAN_POINT('Ctrl Pts',(-78.7009126058701,3.47603461152995,
126.013770851008));
#173267=CARTESIAN_POINT('Ctrl Pts',(-78.6934981131491,3.60210330521407,
126.107815994465));
#173268=CARTESIAN_POINT('Ctrl Pts',(-78.6860836204281,3.72434508482375,
126.20684125908));
#173269=CARTESIAN_POINT('Ctrl Pts',(-78.6786762740744,3.84646904320358,
126.305771079418));
#173270=CARTESIAN_POINT('Ctrl Pts',(-78.6712689277205,3.96477314251573,
126.409671231604));
#173271=CARTESIAN_POINT('Ctrl Pts',(-78.6638615813667,4.07883093325383,
126.518212138986));
#173272=CARTESIAN_POINT('Ctrl Pts',(-78.6564597596913,4.19280365538877,
126.626672092465));
#173273=CARTESIAN_POINT('Ctrl Pts',(-78.649057938016,4.30253610573119,126.739765653091));
#173274=CARTESIAN_POINT('Ctrl Pts',(-78.6416561163406,4.4076351341137,126.857123218191));
#173275=CARTESIAN_POINT('Ctrl Pts',(-78.6342582020292,4.51267868153692,
126.974418831145));
#173276=CARTESIAN_POINT('Ctrl Pts',(-78.6268602877179,4.61309342981408,
127.095973688346));
#173277=CARTESIAN_POINT('Ctrl Pts',(-78.6194623734066,4.70852339802178,
127.221381693154));
#173278=CARTESIAN_POINT('Ctrl Pts',(-78.6120656884944,4.80393750750017,
127.346768857426));
#173279=CARTESIAN_POINT('Ctrl Pts',(-78.6046690035822,4.8943682551633,127.476007601675));
#173280=CARTESIAN_POINT('Ctrl Pts',(-78.59727231867,4.9795001836408,127.608659053962));
#173281=CARTESIAN_POINT('Ctrl Pts',(-78.5898759617346,5.06462833727939,
127.741304624344));
#173282=CARTESIAN_POINT('Ctrl Pts',(-78.5824796047991,5.14445793728053,
127.877362287719));
#173283=CARTESIAN_POINT('Ctrl Pts',(-78.5750832478636,5.21871723852496,
128.016364751927));
#173284=CARTESIAN_POINT('Ctrl Pts',(-78.5676857585271,5.29298790905799,
128.155388497767));
#173285=CARTESIAN_POINT('Ctrl Pts',(-78.5602882691905,5.36168640683164,
128.297357612876));
#173286=CARTESIAN_POINT('Ctrl Pts',(-78.552890779854,5.42458734590637,128.441780949252));
#173287=CARTESIAN_POINT('Ctrl Pts',(-78.5454906973389,5.48751033480787,
128.586254913004));
#173288=CARTESIAN_POINT('Ctrl Pts',(-78.5380906148239,5.54463156969961,
128.733184468886));
#173289=CARTESIAN_POINT('Ctrl Pts',(-78.5306905323089,5.59577418207239,
128.88205942739));
#173290=CARTESIAN_POINT('Ctrl Pts',(-78.5232823126425,5.64697303100499,
129.031098089215));
#173291=CARTESIAN_POINT('Ctrl Pts',(-78.515874092976,5.6921800071335,129.182086072462));
#173292=CARTESIAN_POINT('Ctrl Pts',(-78.5084658733095,5.73126820977958,
129.334498287254));
#173293=CARTESIAN_POINT('Ctrl Pts',(-78.5010530940075,5.77038047056217,
129.487004309222));
#173294=CARTESIAN_POINT('Ctrl Pts',(-78.4936403147054,5.8033663755926,129.640935945287));
#173295=CARTESIAN_POINT('Ctrl Pts',(-78.4862275354033,5.83015044307889,
129.795759421073));
#173296=CARTESIAN_POINT('Ctrl Pts',(-78.4788041643746,5.85697278089689,
129.950804115902));
#173297=CARTESIAN_POINT('Ctrl Pts',(-78.4713807933459,5.87757553404887,
130.106742826417));
#173298=CARTESIAN_POINT('Ctrl Pts',(-78.4639574223171,5.89193513964429,
130.263037356727));
#173299=CARTESIAN_POINT('Ctrl Pts',(-78.4600213728763,5.89954894708507,
130.345908466935));
#173300=CARTESIAN_POINT('Ctrl Pts',(-78.4560853234354,5.90540845297665,
130.42887960985));
#173301=CARTESIAN_POINT('Ctrl Pts',(-78.4521492739946,5.90951608065499,
130.511870865643));
#173302=CARTESIAN_POINT('Ctrl Pts',(-78.4447260075892,5.91726293826161,
130.668389783998));
#173303=CARTESIAN_POINT('Ctrl Pts',(-78.4373027411837,5.91879889570283,
130.82545336347));
#173304=CARTESIAN_POINT('Ctrl Pts',(-78.4298794747783,5.91406688220579,
130.982527604678));
#173305=CARTESIAN_POINT('Ctrl Pts',(-78.4224649820572,5.90934046155575,
131.139416197177));
#173306=CARTESIAN_POINT('Ctrl Pts',(-78.4150504893362,5.89836082720356,
131.296315056844));
#173307=CARTESIAN_POINT('Ctrl Pts',(-78.4076359966152,5.8811227353417,131.452686102448));
#173308=CARTESIAN_POINT('Ctrl Pts',(-78.4002286502615,5.86390125820179,
131.608906431751));
#173309=CARTESIAN_POINT('Ctrl Pts',(-78.3928213039077,5.84043337297872,
131.764599591207));
#173310=CARTESIAN_POINT('Ctrl Pts',(-78.3854139575539,5.81076585546984,
131.91922865254));
#173311=CARTESIAN_POINT('Ctrl Pts',(-78.3780121358785,5.7811204651148,132.073742385684));
#173312=CARTESIAN_POINT('Ctrl Pts',(-78.3706103142031,5.74528471935816,
132.227193235924));
#173313=CARTESIAN_POINT('Ctrl Pts',(-78.3632084925277,5.70335706812827,
132.379050655615));
#173314=CARTESIAN_POINT('Ctrl Pts',(-78.3558105782163,5.66145155017911,
132.530827910957));
#173315=CARTESIAN_POINT('Ctrl Pts',(-78.348412663905,5.61346063041326,132.681013052036));
#173316=CARTESIAN_POINT('Ctrl Pts',(-78.3410147495937,5.55953355305193,
132.829087076866));
#173317=CARTESIAN_POINT('Ctrl Pts',(-78.3336180646815,5.5056154373926,132.977136494479));
#173318=CARTESIAN_POINT('Ctrl Pts',(-78.3262213797692,5.44576324963043,
133.123075141718));
#173319=CARTESIAN_POINT('Ctrl Pts',(-78.318824694857,5.38017571274215,133.266400394361));
#173320=CARTESIAN_POINT('Ctrl Pts',(-78.3114283379215,5.31459108407399,
133.409719291811));
#173321=CARTESIAN_POINT('Ctrl Pts',(-78.3040319809862,5.24327176727085,
133.550424685631));
#173322=CARTESIAN_POINT('Ctrl Pts',(-78.2966356240507,5.16646402358529,
133.688035366129));
#173323=CARTESIAN_POINT('Ctrl Pts',(-78.2892381347142,5.08964452043788,
133.825667115174));
#173324=CARTESIAN_POINT('Ctrl Pts',(-78.2818406453775,5.00733509922222,
133.960202881499));
#173325=CARTESIAN_POINT('Ctrl Pts',(-78.2744431560409,4.91982715005869,
134.091187564037));
#173326=CARTESIAN_POINT('Ctrl Pts',(-78.2670430735259,4.83228852511911,
134.222218163052));
#173327=CARTESIAN_POINT('Ctrl Pts',(-78.2596429910109,4.7395479512164,134.349694889633));
#173328=CARTESIAN_POINT('Ctrl Pts',(-78.2522429084959,4.64193906348408,
134.473193169401));
#173329=CARTESIAN_POINT('Ctrl Pts',(-78.2448346888294,4.54422284474539,
134.596827248223));
#173330=CARTESIAN_POINT('Ctrl Pts',(-78.2374264691629,4.44162785307719,
134.716473850599));
#173331=CARTESIAN_POINT('Ctrl Pts',(-78.2300182494964,4.33452726854626,
134.831742387492));
#173332=CARTESIAN_POINT('Ctrl Pts',(-78.2226054701944,4.22736076539261,
134.947081870245));
#173333=CARTESIAN_POINT('Ctrl Pts',(-78.2151926908923,4.11568340779413,
135.05803765564));
#173334=CARTESIAN_POINT('Ctrl Pts',(-78.2077799115902,3.99990347550006,
135.164257720616));
#173335=CARTESIAN_POINT('Ctrl Pts',(-78.2003565405614,3.88395811140934,
135.270629557802));
#173336=CARTESIAN_POINT('Ctrl Pts',(-78.1929331695327,3.76389874916808,
135.372251919577));
#173337=CARTESIAN_POINT('Ctrl Pts',(-78.185509798504,3.64016545190354,135.468814073789));
#173338=CARTESIAN_POINT('Ctrl Pts',(-78.1815737490633,3.57455908875558,
135.520013644928));
#173339=CARTESIAN_POINT('Ctrl Pts',(-78.1776376996226,3.50792032241883,
135.569791342611));
#173340=CARTESIAN_POINT('Ctrl Pts',(-78.1737016501818,3.44031770158284,
135.618106007039));
#173341=CARTESIAN_POINT('Ctrl Pts',(-78.1662783837764,3.31282126848915,
135.709225956304));
#173342=CARTESIAN_POINT('Ctrl Pts',(-78.158855117371,3.1815094533223,135.795414901996));
#173343=CARTESIAN_POINT('Ctrl Pts',(-78.1514318509655,3.04680067673981,
135.876336189147));
#173344=CARTESIAN_POINT('Ctrl Pts',(-78.1440173582445,2.912251114744,135.957161834058));
#173345=CARTESIAN_POINT('Ctrl Pts',(-78.1366028655235,2.77431289994026,
136.032732022835));
#173346=CARTESIAN_POINT('Ctrl Pts',(-78.1291883728024,2.63343590090035,
136.102751497668));
#173347=CARTESIAN_POINT('Ctrl Pts',(-78.1217810264487,2.49269468441605,
136.172703485095));
#173348=CARTESIAN_POINT('Ctrl Pts',(-78.1143736800949,2.34902065470756,
136.237115244315));
#173349=CARTESIAN_POINT('Ctrl Pts',(-78.1069663337411,2.20289082820329,
136.295735906282));
#173350=CARTESIAN_POINT('Ctrl Pts',(-78.0995645120657,2.05686999083637,
136.354312846747));
#173351=CARTESIAN_POINT('Ctrl Pts',(-78.0921626903903,1.90839734865715,
136.407107151722));
#173352=CARTESIAN_POINT('Ctrl Pts',(-78.0847608687149,1.75797248101512,
136.453914875956));
#173353=CARTESIAN_POINT('Ctrl Pts',(-78.0773629544035,1.60762702149025,
136.500697890757));
#173354=CARTESIAN_POINT('Ctrl Pts',(-78.069965040092,1.45533174445921,136.541500508014));
#173355=CARTESIAN_POINT('Ctrl Pts',(-78.0625671257807,1.30160397113954,
136.576167757866));
#173356=CARTESIAN_POINT('Ctrl Pts',(-78.0551704408685,1.1479017445871,136.610829246649));
#173357=CARTESIAN_POINT('Ctrl Pts',(-78.0477737559563,0.992767858011212,
136.639357309565));
#173358=CARTESIAN_POINT('Ctrl Pts',(-78.0403770710441,0.836732598028245,
136.661647457213));
#173359=CARTESIAN_POINT('Ctrl Pts',(-78.0329807141087,0.680704256812219,
136.683936616492));
#173360=CARTESIAN_POINT('Ctrl Pts',(-78.0255843571732,0.523774991204623,
136.699988357677));
#173361=CARTESIAN_POINT('Ctrl Pts',(-78.0181880002378,0.366482766769292,
136.709749761743));
#173362=CARTESIAN_POINT('Ctrl Pts',(-78.0107905109012,0.209166460492403,
136.719512660305));
#173363=CARTESIAN_POINT('Ctrl Pts',(-78.0033930215645,0.0514874573457338,
136.722983281029));
#173364=CARTESIAN_POINT('Ctrl Pts',(-77.9959955322279,-0.106013849775836,
136.720160785435));
#173365=CARTESIAN_POINT('Ctrl Pts',(-77.9885954497129,-0.263570368735784,
136.717337300419));
#173366=CARTESIAN_POINT('Ctrl Pts',(-77.981195367198,-0.420948694644431,
136.708216313554));
#173367=CARTESIAN_POINT('Ctrl Pts',(-77.973795284683,-0.577611283114258,
136.692849028705));
#173368=CARTESIAN_POINT('Ctrl Pts',(-77.9663870650165,-0.734446138206083,
136.677464845947));
#173369=CARTESIAN_POINT('Ctrl Pts',(-77.9589788453501,-0.890563312371909,
136.65582068493));
#173370=CARTESIAN_POINT('Ctrl Pts',(-77.9515706256836,-1.04543247905034,
136.628019389699));
#173371=CARTESIAN_POINT('Ctrl Pts',(-77.9441578463815,-1.20039696511673,
136.600200983235));
#173372=CARTESIAN_POINT('Ctrl Pts',(-77.9367450670794,-1.35411154945329,
136.566217971672));
#173373=CARTESIAN_POINT('Ctrl Pts',(-77.9293322877774,-1.50605937991354,
136.526223575264));
#173374=CARTESIAN_POINT('Ctrl Pts',(-77.9219089167486,-1.65822432055937,
136.486172032987));
#173375=CARTESIAN_POINT('Ctrl Pts',(-77.9144855457198,-1.80861710951992,
136.440092060079));
#173376=CARTESIAN_POINT('Ctrl Pts',(-77.907062174691,-1.95673845416578,
136.388185935794));
#173377=CARTESIAN_POINT('Ctrl Pts',(-77.9031261252503,-2.03527594521947,
136.360664063229));
#173378=CARTESIAN_POINT('Ctrl Pts',(-77.8991900758095,-2.11317521300684,
136.331505043287));
#173379=CARTESIAN_POINT('Ctrl Pts',(-77.8952540263687,-2.19036457638164,
136.300744300046));
#173380=CARTESIAN_POINT('Ctrl Pts',(-77.8878307599634,-2.3359413067075,
136.242730498304));
#173381=CARTESIAN_POINT('Ctrl Pts',(-77.8804074935581,-2.47943175128092,
136.17884137969));
#173382=CARTESIAN_POINT('Ctrl Pts',(-77.8729842271528,-2.62032650615729,
136.109247003119));
#173383=CARTESIAN_POINT('Ctrl Pts',(-77.8655697344319,-2.76105473513398,
136.039734881322));
#173384=CARTESIAN_POINT('Ctrl Pts',(-77.858155241711,-2.89919304963888,
135.964531087535));
#173385=CARTESIAN_POINT('Ctrl Pts',(-77.8507407489901,-3.03424987596111,
135.883854514868));
#173386=CARTESIAN_POINT('Ctrl Pts',(-77.8433334026365,-3.16917652942933,
135.80325570132));
#173387=CARTESIAN_POINT('Ctrl Pts',(-77.8359260562828,-3.30102728918574,
135.717194800271));
#173388=CARTESIAN_POINT('Ctrl Pts',(-77.8285187099291,-3.42933325296503,
135.625937538306));
#173389=CARTESIAN_POINT('Ctrl Pts',(-77.8211168882539,-3.55754352131619,
135.534748339449));
#173390=CARTESIAN_POINT('Ctrl Pts',(-77.8137150665785,-3.68221395504526,
135.438370712033));
#173391=CARTESIAN_POINT('Ctrl Pts',(-77.8063132449032,-3.802902934398,135.337114728926));
#173392=CARTESIAN_POINT('Ctrl Pts',(-77.798915330592,-3.92352820297763,
135.235912198064));
#173393=CARTESIAN_POINT('Ctrl Pts',(-77.7915174162808,-4.04017591771877,
135.12983667956));
#173394=CARTESIAN_POINT('Ctrl Pts',(-77.7841195019696,-4.15243607333393,
135.019239645412));
#173395=CARTESIAN_POINT('Ctrl Pts',(-77.7767228170575,-4.264677573348,134.908660990484));
#173396=CARTESIAN_POINT('Ctrl Pts',(-77.7693261321454,-4.37253269568519,
134.793562572933));
#173397=CARTESIAN_POINT('Ctrl Pts',(-77.7619294472333,-4.47562689758401,
134.674334058834));
#173398=CARTESIAN_POINT('Ctrl Pts',(-77.754533090298,-4.57871652817789,
134.555110831453));
#173399=CARTESIAN_POINT('Ctrl Pts',(-77.7471367333627,-4.67704541391682,
134.431758154029));
#173400=CARTESIAN_POINT('Ctrl Pts',(-77.7397403764274,-4.77027824899781,
134.3047000282));
#173401=CARTESIAN_POINT('Ctrl Pts',(-77.7323428870909,-4.86352535826413,
134.177622449448));
#173402=CARTESIAN_POINT('Ctrl Pts',(-77.7249453977545,-4.95167464249734,
134.046838593678));
#173403=CARTESIAN_POINT('Ctrl Pts',(-77.7175479084181,-5.03443330069878,
133.912802655519));
#173404=CARTESIAN_POINT('Ctrl Pts',(-77.7101478259032,-5.11722096981968,
133.77871973127));
#173405=CARTESIAN_POINT('Ctrl Pts',(-77.7027477433882,-5.19461405458396,
133.641382772306));
#173406=CARTESIAN_POINT('Ctrl Pts',(-77.6953476608733,-5.26636507838174,
133.501271706887));
#173407=CARTESIAN_POINT('Ctrl Pts',(-77.687939441207,-5.33819499980626,
133.361006574947));
#173408=CARTESIAN_POINT('Ctrl Pts',(-77.6805312215408,-5.4043703001598,
133.217961577139));
#173409=CARTESIAN_POINT('Ctrl Pts',(-77.6731230018744,-5.46469085058839,
133.072638481937));
#173410=CARTESIAN_POINT('Ctrl Pts',(-77.6657102225725,-5.52504852730944,
132.927225942794));
#173411=CARTESIAN_POINT('Ctrl Pts',(-77.6582974432705,-5.5795441447548,
132.77953286174));
#173412=CARTESIAN_POINT('Ctrl Pts',(-77.6508846639686,-5.62802724025374,
132.630076900416));
#173413=CARTESIAN_POINT('Ctrl Pts',(-77.64346129294,-5.6765796106731,132.480407389404));
#173414=CARTESIAN_POINT('Ctrl Pts',(-77.6360379219114,-5.71910220039589,
132.328970325788));
#173415=CARTESIAN_POINT('Ctrl Pts',(-77.6286145508828,-5.75549531282523,
132.176295115473));
#173416=CARTESIAN_POINT('Ctrl Pts',(-77.6246785014408,-5.77479181428223,
132.095343055546));
#173417=CARTESIAN_POINT('Ctrl Pts',(-77.6207424519988,-5.79236596201951,
132.014043032783));
#173418=CARTESIAN_POINT('Ctrl Pts',(-77.6168064025568,-5.80820881390571,
131.93247450214));
#173419=CARTESIAN_POINT('Ctrl Pts',(-77.6059178851201,-5.85203579615075,
131.70682683656));
#173420=CARTESIAN_POINT('Ctrl Pts',(-77.5950293676835,-5.88272376379399,
131.478551115798));
#173421=CARTESIAN_POINT('Ctrl Pts',(-77.5841408502469,-5.9000270659515,
131.248895412087));
#173422=CARTESIAN_POINT('Ctrl Pts',(-77.5772189642326,-5.9110268632979,
131.102902111082));
#173423=CARTESIAN_POINT('Ctrl Pts',(-77.5702970782184,-5.91661845541344,
130.956351474934));
#173424=CARTESIAN_POINT('Ctrl Pts',(-77.5633751922042,-5.91674770606937,
130.809570725322));
#173425=CARTESIAN_POINT('',(-75.8133751922041,-5.90702258126614,130.805121151015));
#173426=CARTESIAN_POINT('Ctrl Pts',(-77.5633740622052,-5.9192014526658,
130.809548914079));
#173427=CARTESIAN_POINT('Ctrl Pts',(-77.4883689677179,-5.90454020598336,
129.218368607907));
#173428=CARTESIAN_POINT('Ctrl Pts',(-77.3205479986255,-4.42166650021555,
125.634093850048));
#173429=CARTESIAN_POINT('Ctrl Pts',(-77.0599111549303,1.64202572553403,
124.00132364523));
#173430=CARTESIAN_POINT('Ctrl Pts',(-76.7814635311171,6.61114269020578,
128.508635708072));
#173431=CARTESIAN_POINT('Ctrl Pts',(-76.5030159073044,5.50494249485923,
135.125606810351));
#173432=CARTESIAN_POINT('Ctrl Pts',(-76.2245682834915,-0.66003092187362,
137.771563766067));
#173433=CARTESIAN_POINT('Ctrl Pts',(-75.9946880451241,-5.24895454444059,
134.670228436097));
#173434=CARTESIAN_POINT('Ctrl Pts',(-75.8576236813622,-5.90810076479692,
131.748728288428));
#173435=CARTESIAN_POINT('Ctrl Pts',(-75.8133751922041,-5.90702258126614,
130.805121151015));
#173436=CARTESIAN_POINT('',(-74.063375192204,-5.91640124831382,130.798888549479));
#173437=CARTESIAN_POINT('Ctrl Pts',(-75.8133751922041,-5.90702258126614,
130.805121151015));
#173438=CARTESIAN_POINT('Ctrl Pts',(-75.764807806758,-5.90583916108351,
129.76941275906));
#173439=CARTESIAN_POINT('Ctrl Pts',(-75.6234245467082,-5.1523334128451,
126.75277827436));
#173440=CARTESIAN_POINT('Ctrl Pts',(-75.3892254120525,-0.335322348419818,
123.814001581503));
#173441=CARTESIAN_POINT('Ctrl Pts',(-75.11077778824,5.69993711426887,126.743784621021));
#173442=CARTESIAN_POINT('Ctrl Pts',(-74.8323301644269,6.49723282634914,
133.405038631191));
#173443=CARTESIAN_POINT('Ctrl Pts',(-74.5538825406141,1.32388897848506,
137.676396597024));
#173444=CARTESIAN_POINT('Ctrl Pts',(-74.2975642165399,-4.55821169044833,
135.795110472929));
#173445=CARTESIAN_POINT('Ctrl Pts',(-74.1340617670698,-5.90256935525085,
132.300275173225));
#173446=CARTESIAN_POINT('Ctrl Pts',(-74.063375192204,-5.91640124831382,
130.798888549479));
#173447=CARTESIAN_POINT('',(-72.3133751922041,-5.92595501209889,130.806045629526));
#173448=CARTESIAN_POINT('Ctrl Pts',(-74.063375192204,-5.91640124831382,
130.798888549479));
#173449=CARTESIAN_POINT('Ctrl Pts',(-74.0412458924655,-5.92073149218436,
130.328861041661));
#173450=CARTESIAN_POINT('Ctrl Pts',(-73.9263007181233,-5.65438782062924,
127.892268950583));
#173451=CARTESIAN_POINT('Ctrl Pts',(-73.7185396691751,-2.28566121732441,
124.189731880434));
#173452=CARTESIAN_POINT('Ctrl Pts',(-73.4400920453628,4.32961877422029,
125.306000698443));
#173453=CARTESIAN_POINT('Ctrl Pts',(-73.1616444215496,6.96619062589002,
131.474993672292));
#173454=CARTESIAN_POINT('Ctrl Pts',(-72.8831967977369,3.20117360970058,
137.027707631104));
#173455=CARTESIAN_POINT('Ctrl Pts',(-72.6047491739239,-3.5055655677807,
136.861469711872));
#173456=CARTESIAN_POINT('Ctrl Pts',(-72.4148086387464,-5.88302857893171,
132.951147516027));
#173457=CARTESIAN_POINT('Ctrl Pts',(-72.3176839781731,-5.92629787890155,
130.897181430883));
#173458=CARTESIAN_POINT('Ctrl Pts',(-72.3133751922041,-5.92595501209889,
130.806045629526));
#173459=CARTESIAN_POINT('',(-70.5633763914996,-5.91353738369623,130.809041528552));
#173460=CARTESIAN_POINT('Ctrl Pts',(-72.3133751922041,-5.92595501209889,
130.806045629526));
#173461=CARTESIAN_POINT('Ctrl Pts',(-72.2248681035687,-5.9189121599564,
128.934018449121));
#173462=CARTESIAN_POINT('Ctrl Pts',(-72.0435451403292,-3.9487999677908,
125.086069876051));
#173463=CARTESIAN_POINT('Ctrl Pts',(-71.7694063024852,2.61056268441707,
124.311093104128));
#173464=CARTESIAN_POINT('Ctrl Pts',(-71.4909586786723,6.87404275541449,
129.490931241054));
#173465=CARTESIAN_POINT('Ctrl Pts',(-71.2125110548594,4.82061334984184,
135.877746810402));
#173466=CARTESIAN_POINT('Ctrl Pts',(-70.9340634310466,-1.66272422418068,
137.602368317227));
#173467=CARTESIAN_POINT('Ctrl Pts',(-70.717685491852,-5.51348031185306,
134.088059501253));
#173468=CARTESIAN_POINT('Ctrl Pts',(-70.5941234272619,-5.91605620421693,
131.463545541928));
#173469=CARTESIAN_POINT('Ctrl Pts',(-70.5633772372761,-5.91127305061012,
130.809057749741));
#173470=CARTESIAN_POINT('',(-68.8133740211525,-5.91243167929344,130.800818385325));
#173471=CARTESIAN_POINT('Ctrl Pts',(-70.5633751922041,-5.91674816655043,
130.809018527203));
#173472=CARTESIAN_POINT('Ctrl Pts',(-70.5556165668381,-5.91687830402043,
130.643710331672));
#173473=CARTESIAN_POINT('Ctrl Pts',(-70.547857941472,-5.91007539724289,
130.478317204947));
#173474=CARTESIAN_POINT('Ctrl Pts',(-70.5400993161061,-5.89635065780119,
130.313464006509));
#173475=CARTESIAN_POINT('Ctrl Pts',(-70.5327111471719,-5.88328124295133,
130.156482167337));
#173476=CARTESIAN_POINT('Ctrl Pts',(-70.5253229782378,-5.86393568336394,
129.9999903029));
#173477=CARTESIAN_POINT('Ctrl Pts',(-70.5179348093037,-5.83837699622299,
129.844524895958));
#173478=CARTESIAN_POINT('Ctrl Pts',(-70.5105463541655,-5.81281731898565,
129.689053466573));
#173479=CARTESIAN_POINT('Ctrl Pts',(-70.5031578990273,-5.78104409495704,
129.534608942759));
#173480=CARTESIAN_POINT('Ctrl Pts',(-70.4957694438891,-5.74317177248523,
129.381719217132));
#173481=CARTESIAN_POINT('Ctrl Pts',(-70.4883792401909,-5.70529048710717,
129.228793308451));
#173482=CARTESIAN_POINT('Ctrl Pts',(-70.4809890364927,-5.66130731908094,
129.077423293322));
#173483=CARTESIAN_POINT('Ctrl Pts',(-70.4735988327945,-5.61138700801363,
128.928123316797));
#173484=CARTESIAN_POINT('Ctrl Pts',(-70.4662054173999,-5.56144500216118,
128.778758456244));
#173485=CARTESIAN_POINT('Ctrl Pts',(-70.4588120020053,-5.50556083423948,
128.631465779532));
#173486=CARTESIAN_POINT('Ctrl Pts',(-70.4514185866107,-5.44394786519913,
128.486740673854));
#173487=CARTESIAN_POINT('Ctrl Pts',(-70.4440164177111,-5.38226194889408,
128.341844219501));
#173488=CARTESIAN_POINT('Ctrl Pts',(-70.4366142488115,-5.31483383449027,
128.199521749961));
#173489=CARTESIAN_POINT('Ctrl Pts',(-70.429212079912,-5.24192376487584,
128.060245859446));
#173490=CARTESIAN_POINT('Ctrl Pts',(-70.4218048048358,-5.16896340031444,
127.920873893403));
#173491=CARTESIAN_POINT('Ctrl Pts',(-70.4143975297596,-5.09051373203574,
127.784553016251));
#173492=CARTESIAN_POINT('Ctrl Pts',(-70.4069902546835,-5.00687873761646,
127.651727453161));
#173493=CARTESIAN_POINT('Ctrl Pts',(-70.3995723268131,-4.92312346328625,
127.518710866601));
#173494=CARTESIAN_POINT('Ctrl Pts',(-70.3921543989427,-4.83416818413982,
127.389199937277));
#173495=CARTESIAN_POINT('Ctrl Pts',(-70.3847364710722,-4.74035801715883,
127.263606964506));
#173496=CARTESIAN_POINT('Ctrl Pts',(-70.3822137085218,-4.70845412428677,
127.220894059522));
#173497=CARTESIAN_POINT('Ctrl Pts',(-70.3796909459713,-4.67598903149527,
127.178634002934));
#173498=CARTESIAN_POINT('Ctrl Pts',(-70.3771681834209,-4.6429772797318,
127.13684203651));
#173499=CARTESIAN_POINT('Ctrl Pts',(-70.3697449170155,-4.54583970814075,
127.013868552412));
#173500=CARTESIAN_POINT('Ctrl Pts',(-70.3623216506099,-4.44366628163952,
126.894570949422));
#173501=CARTESIAN_POINT('Ctrl Pts',(-70.3548983842045,-4.33676533087885,
126.779388937245));
#173502=CARTESIAN_POINT('Ctrl Pts',(-70.3474838914835,-4.22999072816441,
126.66434306064));
#173503=CARTESIAN_POINT('Ctrl Pts',(-70.3400693987625,-4.11849997468444,
126.553403363401));
#173504=CARTESIAN_POINT('Ctrl Pts',(-70.3326549060415,-4.00264311820997,
126.446978533017));
#173505=CARTESIAN_POINT('Ctrl Pts',(-70.3252475596877,-3.8868979289357,
126.340656278892));
#173506=CARTESIAN_POINT('Ctrl Pts',(-70.3178402133339,-3.76679528746255,
126.238840479285));
#173507=CARTESIAN_POINT('Ctrl Pts',(-70.3104328669801,-3.64272365985294,
126.141904730327));
#173508=CARTESIAN_POINT('Ctrl Pts',(-70.3030310453047,-3.51874456954415,
126.045041279709));
#173509=CARTESIAN_POINT('Ctrl Pts',(-70.2956292236293,-3.39080268019189,
125.953050861391));
#173510=CARTESIAN_POINT('Ctrl Pts',(-70.2882274019539,-3.25932117673971,
125.866268270378));
#173511=CARTESIAN_POINT('Ctrl Pts',(-70.2808294876426,-3.12790908134993,
125.779531491219));
#173512=CARTESIAN_POINT('Ctrl Pts',(-70.2734315733312,-2.99296140390075,
125.697997269374));
#173513=CARTESIAN_POINT('Ctrl Pts',(-70.2660336590199,-2.85493198759279,
125.621958287689));
#173514=CARTESIAN_POINT('Ctrl Pts',(-70.2586369741076,-2.71692550926932,
125.545931942302));
#173515=CARTESIAN_POINT('Ctrl Pts',(-70.2512402891954,-2.57583863515824,
125.475399204573));
#173516=CARTESIAN_POINT('Ctrl Pts',(-70.2438436042831,-2.4321516969811,
125.41060787153));
#173517=CARTESIAN_POINT('Ctrl Pts',(-70.2364472473477,-2.28847113003338,
125.345819411402));
#173518=CARTESIAN_POINT('Ctrl Pts',(-70.2290508904122,-2.14219106855501,
125.286772003218));
#173519=CARTESIAN_POINT('Ctrl Pts',(-70.2216545334767,-1.99381355775538,
125.233666041536));
#173520=CARTESIAN_POINT('Ctrl Pts',(-70.2142570441401,-1.84541332998005,
125.180551949195));
#173521=CARTESIAN_POINT('Ctrl Pts',(-70.2068595548035,-1.69491536496844,
125.133381240393));
#173522=CARTESIAN_POINT('Ctrl Pts',(-70.1994620654669,-1.54283851866879,
125.092304957139));
#173523=CARTESIAN_POINT('Ctrl Pts',(-70.1920619829519,-1.39070836206665,
125.051214274658));
#173524=CARTESIAN_POINT('Ctrl Pts',(-70.1846619004369,-1.23699858237161,
125.016222368545));
#173525=CARTESIAN_POINT('Ctrl Pts',(-70.1772618179219,-1.08223976780218,
124.987429498197));
#173526=CARTESIAN_POINT('Ctrl Pts',(-70.1698535982554,-0.927310780006325,
124.958604967127));
#173527=CARTESIAN_POINT('Ctrl Pts',(-70.1624453785889,-0.771330820902878,
124.935993153098));
#173528=CARTESIAN_POINT('Ctrl Pts',(-70.1550371589224,-0.61483790210435,
124.919642704477));
#173529=CARTESIAN_POINT('Ctrl Pts',(-70.1476243796204,-0.458248664525749,
124.903282192427));
#173530=CARTESIAN_POINT('Ctrl Pts',(-70.1402116003183,-0.301146209810517,
124.893190748772));
#173531=CARTESIAN_POINT('Ctrl Pts',(-70.1327988210163,-0.144069611628858,
124.889364885572));
#173532=CARTESIAN_POINT('Ctrl Pts',(-70.1253754499875,0.0132314249628933,
124.8855335558));
#173533=CARTESIAN_POINT('Ctrl Pts',(-70.1179520789587,0.170506158969827,
124.88798568094));
#173534=CARTESIAN_POINT('Ctrl Pts',(-70.1105287079299,0.327218744922378,
124.896665766317));
#173535=CARTESIAN_POINT('Ctrl Pts',(-70.1065926584892,0.410311518258836,
124.90126815586));
#173536=CARTESIAN_POINT('Ctrl Pts',(-70.1026566090485,0.493246378182262,
124.907620586494));
#173537=CARTESIAN_POINT('Ctrl Pts',(-70.0987205596078,0.575944621046976,
124.915708958995));
#173538=CARTESIAN_POINT('Ctrl Pts',(-70.0912972932024,0.731910926170226,
124.930963377105));
#173539=CARTESIAN_POINT('Ctrl Pts',(-70.0838740267969,0.887506610997351,
124.9524415061));
#173540=CARTESIAN_POINT('Ctrl Pts',(-70.0764507603915,1.04219507505318,
124.980121612508));
#173541=CARTESIAN_POINT('Ctrl Pts',(-70.0690362676705,1.19670071019079,
125.007769003329));
#173542=CARTESIAN_POINT('Ctrl Pts',(-70.0616217749495,1.35030089502287,
125.041603715604));
#173543=CARTESIAN_POINT('Ctrl Pts',(-70.0542072822284,1.50246257981797,
125.081552149799));
#173544=CARTESIAN_POINT('Ctrl Pts',(-70.0467999358747,1.65447760545227,
125.121462080189));
#173545=CARTESIAN_POINT('Ctrl Pts',(-70.0393925895208,1.80505653262137,
125.167473907267));
#173546=CARTESIAN_POINT('Ctrl Pts',(-70.0319852431671,1.95367506892302,
125.219462741367));
#173547=CARTESIAN_POINT('Ctrl Pts',(-70.0245834214917,2.10218275991302,
125.271412800234));
#173548=CARTESIAN_POINT('Ctrl Pts',(-70.0171815998163,2.24873262049636,
125.329330867157));
#173549=CARTESIAN_POINT('Ctrl Pts',(-70.0097797781409,2.39281423635623,
125.393041869535));
#173550=CARTESIAN_POINT('Ctrl Pts',(-70.0023818638296,2.53681979265281,
125.456719239371));
#173551=CARTESIAN_POINT('Ctrl Pts',(-69.9949839495182,2.67835935860231,
125.526183303835));
#173552=CARTESIAN_POINT('Ctrl Pts',(-69.9875860352068,2.81694137850027,
125.601210434014));
#173553=CARTESIAN_POINT('Ctrl Pts',(-69.9801893502947,2.95550036858065,
125.676225096046));
#173554=CARTESIAN_POINT('Ctrl Pts',(-69.9727926653825,3.09110246011843,
125.756800811423));
#173555=CARTESIAN_POINT('Ctrl Pts',(-69.9653959804703,3.22327954342664,
125.842667403811));
#173556=CARTESIAN_POINT('Ctrl Pts',(-69.9579996235349,3.35545076586466,
125.928530188783));
#173557=CARTESIAN_POINT('Ctrl Pts',(-69.9506032665994,3.48419696899745,
126.019683180935));
#173558=CARTESIAN_POINT('Ctrl Pts',(-69.9432069096639,3.60907818750902,
126.115812313565));
#173559=CARTESIAN_POINT('Ctrl Pts',(-69.9358094203273,3.73397852565341,
126.211956163811));
#173560=CARTESIAN_POINT('Ctrl Pts',(-69.9284119309909,3.85501240511799,
126.313077443782));
#173561=CARTESIAN_POINT('Ctrl Pts',(-69.9210144416543,3.97177229566804,
126.418821267171));
#173562=CARTESIAN_POINT('Ctrl Pts',(-69.9136143591393,4.08857311621772,
126.524602158894));
#173563=CARTESIAN_POINT('Ctrl Pts',(-69.9062142766242,4.20109668834899,
126.63500856986));
#173564=CARTESIAN_POINT('Ctrl Pts',(-69.8988141941091,4.308971865099,126.749648293826));
#173565=CARTESIAN_POINT('Ctrl Pts',(-69.8914059744427,4.41696566169522,
126.864414075955));
#173566=CARTESIAN_POINT('Ctrl Pts',(-69.8839977547763,4.52030059915588,
126.983422195323));
#173567=CARTESIAN_POINT('Ctrl Pts',(-69.8765895351098,4.61864493981229,
127.106246303156));
#173568=CARTESIAN_POINT('Ctrl Pts',(-69.8691767558078,4.71704980976927,
127.229146007177));
#173569=CARTESIAN_POINT('Ctrl Pts',(-69.8617639765057,4.81045774133546,
127.355866079909));
#173570=CARTESIAN_POINT('Ctrl Pts',(-69.8543511972036,4.89858028652564,
127.485951098088));
#173571=CARTESIAN_POINT('Ctrl Pts',(-69.8469278261749,4.98682874534118,
127.616221987842));
#173572=CARTESIAN_POINT('Ctrl Pts',(-69.8395044551461,5.06977653839243,
127.749867109348));
#173573=CARTESIAN_POINT('Ctrl Pts',(-69.8320810841174,5.14718071735724,
127.88640564441));
#173574=CARTESIAN_POINT('Ctrl Pts',(-69.8281450346766,5.18822227033221,
127.958801651897));
#173575=CARTESIAN_POINT('Ctrl Pts',(-69.8242089852357,5.22770610811614,
128.032010742314));
#173576=CARTESIAN_POINT('Ctrl Pts',(-69.8202729357949,5.26560155154211,
128.105959079081));
#173577=CARTESIAN_POINT('Ctrl Pts',(-69.8128496693895,5.33707117516701,
128.245423334375));
#173578=CARTESIAN_POINT('Ctrl Pts',(-69.8054264029841,5.40310428523581,
128.387939844073));
#173579=CARTESIAN_POINT('Ctrl Pts',(-69.7980031365786,5.46342912107124,
128.533045403526));
#173580=CARTESIAN_POINT('Ctrl Pts',(-69.7905886438576,5.52368265796054,
128.677979460258));
#173581=CARTESIAN_POINT('Ctrl Pts',(-69.7831741511366,5.57824120807032,
128.825496134384));
#173582=CARTESIAN_POINT('Ctrl Pts',(-69.7757596584156,5.62687856637098,
128.975107173722));
#173583=CARTESIAN_POINT('Ctrl Pts',(-69.7683523120618,5.67546904615455,
129.124574012308));
#173584=CARTESIAN_POINT('Ctrl Pts',(-69.760944965708,5.71814958114104,129.27613084479));
#173585=CARTESIAN_POINT('Ctrl Pts',(-69.7535376193542,5.7547418516929,129.429269063205));
#173586=CARTESIAN_POINT('Ctrl Pts',(-69.7461357976788,5.79130683034868,
129.582293065359));
#173587=CARTESIAN_POINT('Ctrl Pts',(-69.7387339760035,5.82179249964607,
129.736895743475));
#173588=CARTESIAN_POINT('Ctrl Pts',(-69.7313321543281,5.84607026171702,
129.892553040515));
#173589=CARTESIAN_POINT('Ctrl Pts',(-69.7239342400167,5.87033520774649,
130.04812816728));
#173590=CARTESIAN_POINT('Ctrl Pts',(-69.7165363257053,5.88839871568098,
130.204756436319));
#173591=CARTESIAN_POINT('Ctrl Pts',(-69.709138411394,5.90018323299076,130.361903411008));
#173592=CARTESIAN_POINT('Ctrl Pts',(-69.7017417264817,5.91196579192751,
130.519024270721));
#173593=CARTESIAN_POINT('Ctrl Pts',(-69.6943450415694,5.91747140329958,
130.676663293115));
#173594=CARTESIAN_POINT('Ctrl Pts',(-69.6869483566572,5.91667434938848,
130.834280607346));
#173595=CARTESIAN_POINT('Ctrl Pts',(-69.6795519997218,5.91587733081959,
130.991890932659));
#173596=CARTESIAN_POINT('Ctrl Pts',(-69.6721556427864,5.90877820452963,
131.14947917843));
#173597=CARTESIAN_POINT('Ctrl Pts',(-69.664759285851,5.89540339172789,131.306505428655));
#173598=CARTESIAN_POINT('Ctrl Pts',(-69.6573617965144,5.88202653120816,
131.463555719999));
#173599=CARTESIAN_POINT('Ctrl Pts',(-69.6499643071779,5.86237210273223,
131.6200434725));
#173600=CARTESIAN_POINT('Ctrl Pts',(-69.6425668178413,5.83651840215569,
131.77543399471));
#173601=CARTESIAN_POINT('Ctrl Pts',(-69.6351667353263,5.81065563860442,
131.930878988827));
#173602=CARTESIAN_POINT('Ctrl Pts',(-69.6277666528113,5.77858933746478,
132.085225618848));
#173603=CARTESIAN_POINT('Ctrl Pts',(-69.6203665702963,5.74044885895687,
132.237949631266));
#173604=CARTESIAN_POINT('Ctrl Pts',(-69.6129583506298,5.70226644107197,
132.390841579436));
#173605=CARTESIAN_POINT('Ctrl Pts',(-69.6055501309633,5.65799659755602,
132.542106984372));
#173606=CARTESIAN_POINT('Ctrl Pts',(-69.5981419112969,5.60781871539539,
132.691236293852));
#173607=CARTESIAN_POINT('Ctrl Pts',(-69.5907291319948,5.55760994958561,
132.840457389934));
#173608=CARTESIAN_POINT('Ctrl Pts',(-69.5833163526927,5.50148603212475,
132.987539422832));
#173609=CARTESIAN_POINT('Ctrl Pts',(-69.5759035733907,5.43967421031951,
133.13199354569));
#173610=CARTESIAN_POINT('Ctrl Pts',(-69.5684802023619,5.37777406888441,
133.276654071373));
#173611=CARTESIAN_POINT('Ctrl Pts',(-69.5610568313332,5.31016995139102,
133.418678851508));
#173612=CARTESIAN_POINT('Ctrl Pts',(-69.5536334603044,5.23713506430395,
133.557603592811));
#173613=CARTESIAN_POINT('Ctrl Pts',(-69.5496974108637,5.1984102147228,133.631264824103));
#173614=CARTESIAN_POINT('Ctrl Pts',(-69.5457613614229,5.1581593123346,133.704054996672));
#173615=CARTESIAN_POINT('Ctrl Pts',(-69.5418253119821,5.11642789510683,
133.775908388791));
#173616=CARTESIAN_POINT('Ctrl Pts',(-69.5344020455767,5.03772374460734,
133.911421643862));
#173617=CARTESIAN_POINT('Ctrl Pts',(-69.5269787791712,4.95351307766139,
134.044010824169));
#173618=CARTESIAN_POINT('Ctrl Pts',(-69.5195555127658,4.86403870817574,
134.17319691633));
#173619=CARTESIAN_POINT('Ctrl Pts',(-69.5121410200448,4.77467008996419,
134.302230321259));
#173620=CARTESIAN_POINT('Ctrl Pts',(-69.5047265273237,4.68005036313393,
134.427868340304));
#173621=CARTESIAN_POINT('Ctrl Pts',(-69.4973120346027,4.58046803872867,
134.54965674854));
#173622=CARTESIAN_POINT('Ctrl Pts',(-69.4899046882489,4.48098169551717,
134.671327772521));
#173623=CARTESIAN_POINT('Ctrl Pts',(-69.4824973418952,4.37654251172839,
134.789156285318));
#173624=CARTESIAN_POINT('Ctrl Pts',(-69.4750899955415,4.26748200752502,
134.902717346543));
#173625=CARTESIAN_POINT('Ctrl Pts',(-69.4676881738661,4.1585028447603,135.016193709644));
#173626=CARTESIAN_POINT('Ctrl Pts',(-69.4602863521906,4.04490948199505,
135.125408690525));
#173627=CARTESIAN_POINT('Ctrl Pts',(-69.4528845305152,3.92707331296834,
135.229970830528));
#173628=CARTESIAN_POINT('Ctrl Pts',(-69.4454866162039,3.80929934873836,
135.334477772991));
#173629=CARTESIAN_POINT('Ctrl Pts',(-69.4380887018926,3.68728731731776,
135.434336519075));
#173630=CARTESIAN_POINT('Ctrl Pts',(-69.4306907875812,3.56144493633774,
135.529192945589));
#173631=CARTESIAN_POINT('Ctrl Pts',(-69.423294102669,3.43562346807806,135.624033608687));
#173632=CARTESIAN_POINT('Ctrl Pts',(-69.4158974177568,3.30597321139763,
135.713873377613));
#173633=CARTESIAN_POINT('Ctrl Pts',(-69.4085007328446,3.17293447387337,
135.798398801942));
#173634=CARTESIAN_POINT('Ctrl Pts',(-69.4011043759092,3.03990163542576,
135.882920478326));
#173635=CARTESIAN_POINT('Ctrl Pts',(-69.3937080189737,2.90348092996179,
135.962128078467));
#173636=CARTESIAN_POINT('Ctrl Pts',(-69.3863116620382,2.76414088541546,
136.035751993488));
#173637=CARTESIAN_POINT('Ctrl Pts',(-69.3789141727016,2.62477950755278,
136.109387180519));
#173638=CARTESIAN_POINT('Ctrl Pts',(-69.371516683365,2.48249823073304,136.177436805853));
#173639=CARTESIAN_POINT('Ctrl Pts',(-69.3641191940284,2.33778922683581,
136.239677728222));
#173640=CARTESIAN_POINT('Ctrl Pts',(-69.3567191115135,2.19302949542282,
136.30194046905));
#173641=CARTESIAN_POINT('Ctrl Pts',(-69.3493190289986,2.04584068523556,
136.358390305388));
#173642=CARTESIAN_POINT('Ctrl Pts',(-69.3419189464837,1.89673378795444,
136.408852699828));
#173643=CARTESIAN_POINT('Ctrl Pts',(-69.3345107268172,1.74746293230992,
136.459370582858));
#173644=CARTESIAN_POINT('Ctrl Pts',(-69.3271025071507,1.59627013130651,
136.503887755952));
#173645=CARTESIAN_POINT('Ctrl Pts',(-69.3196942874842,1.44368104870872,
136.542279717039));
#173646=CARTESIAN_POINT('Ctrl Pts',(-69.3122815081821,1.29099805007645,
136.580695307738));
#173647=CARTESIAN_POINT('Ctrl Pts',(-69.30486872888,1.13691742192892,136.612978097926));
#173648=CARTESIAN_POINT('Ctrl Pts',(-69.297455949578,0.98197327769154,136.639055043532));
#173649=CARTESIAN_POINT('Ctrl Pts',(-69.2900325785492,0.826807741994932,
136.665169249101));
#173650=CARTESIAN_POINT('Ctrl Pts',(-69.2826092075204,0.670776595288852,
136.685059853217));
#173651=CARTESIAN_POINT('Ctrl Pts',(-69.2751858364916,0.514418135430624,
136.698705750356));
#173652=CARTESIAN_POINT('Ctrl Pts',(-69.2712497870508,0.431513128242939,
136.705941132447));
#173653=CARTESIAN_POINT('Ctrl Pts',(-69.26731373761,0.348516098610012,136.711421774576));
#173654=CARTESIAN_POINT('Ctrl Pts',(-69.2633776881692,0.26550695446625,
136.715150464924));
#173655=CARTESIAN_POINT('Ctrl Pts',(-69.2559544217638,0.108954299240561,
136.722182658552));
#173656=CARTESIAN_POINT('Ctrl Pts',(-69.2485311553583,-0.0481146557159442,
136.723001530107));
#173657=CARTESIAN_POINT('Ctrl Pts',(-69.2411078889529,-0.205165656030647,
136.717552447372));
#173658=CARTESIAN_POINT('Ctrl Pts',(-69.2336933962319,-0.362031035105474,
136.712109805));
#173659=CARTESIAN_POINT('Ctrl Pts',(-69.226278903511,-0.518878132348524,
136.700413967222));
#173660=CARTESIAN_POINT('Ctrl Pts',(-69.21886441079,-0.675168848197389,
136.68246214688));
#173661=CARTESIAN_POINT('Ctrl Pts',(-69.2114570644362,-0.831308925170076,
136.664527629179));
#173662=CARTESIAN_POINT('Ctrl Pts',(-69.2040497180825,-0.986893319969474,
136.640349175274));
#173663=CARTESIAN_POINT('Ctrl Pts',(-69.1966423717287,-1.14138532346651,
136.609976011809));
#173664=CARTESIAN_POINT('Ctrl Pts',(-69.1892405500533,-1.29576210099913,
136.579625501795));
#173665=CARTESIAN_POINT('Ctrl Pts',(-69.181838728378,-1.44904774479013,
136.54308955346));
#173666=CARTESIAN_POINT('Ctrl Pts',(-69.1744369067026,-1.60071216219591,
136.500469037909));
#173667=CARTESIAN_POINT('Ctrl Pts',(-69.1670389923912,-1.75229651713629,
136.457871021395));
#173668=CARTESIAN_POINT('Ctrl Pts',(-69.1596410780798,-1.9022609916559,
136.409194935244));
#173669=CARTESIAN_POINT('Ctrl Pts',(-69.1522431637685,-2.05008727054761,
136.354592391613));
#173670=CARTESIAN_POINT('Ctrl Pts',(-69.1448464788563,-2.19788898339319,
136.299998921933));
#173671=CARTESIAN_POINT('Ctrl Pts',(-69.1374497939441,-2.34355285600365,
136.239481078665));
#173672=CARTESIAN_POINT('Ctrl Pts',(-69.130053109032,-2.48657717665965,
136.173239877432));
#173673=CARTESIAN_POINT('Ctrl Pts',(-69.1226567520966,-2.6295951554672,
136.107001613403));
#173674=CARTESIAN_POINT('Ctrl Pts',(-69.1152603951612,-2.76997347630487,
136.035040652891));
#173675=CARTESIAN_POINT('Ctrl Pts',(-69.1078640382258,-2.90723205879644,
135.957605451533));
#173676=CARTESIAN_POINT('Ctrl Pts',(-69.1004665488893,-3.0445116559274,
135.880158394648));
#173677=CARTESIAN_POINT('Ctrl Pts',(-69.0930690595527,-3.17867023851975,
135.797235611542));
#173678=CARTESIAN_POINT('Ctrl Pts',(-69.0856715702162,-3.30925404058336,
135.709130567052));
#173679=CARTESIAN_POINT('Ctrl Pts',(-69.0782714877013,-3.43988361859653,
135.620994637475));
#173680=CARTESIAN_POINT('Ctrl Pts',(-69.0708714051863,-3.5669356118435,
135.527673038265));
#173681=CARTESIAN_POINT('Ctrl Pts',(-69.0634713226713,-3.68998697357453,
135.429501339463));
#173682=CARTESIAN_POINT('Ctrl Pts',(-69.0560631030049,-3.81317364292777,
135.331221690786));
#173683=CARTESIAN_POINT('Ctrl Pts',(-69.0486548833384,-3.93235060347521,
135.228081524749));
#173684=CARTESIAN_POINT('Ctrl Pts',(-69.0412466636719,-4.04712897399369,
135.120455800757));
#173685=CARTESIAN_POINT('Ctrl Pts',(-69.0338338843699,-4.1619779886842,
135.012763834926));
#173686=CARTESIAN_POINT('Ctrl Pts',(-69.0264211050679,-4.27242275750764,
134.900581075324));
#173687=CARTESIAN_POINT('Ctrl Pts',(-69.0190083257659,-4.37811312506494,
134.784317404597));
#173688=CARTESIAN_POINT('Ctrl Pts',(-69.0115849547371,-4.48395450797564,
134.667887610885));
#173689=CARTESIAN_POINT('Ctrl Pts',(-69.0041615837084,-4.58502768261678,
134.54736554551));
#173690=CARTESIAN_POINT('Ctrl Pts',(-68.9967382126797,-4.68102392917194,
134.423192685654));
#173691=CARTESIAN_POINT('Ctrl Pts',(-68.9928021632386,-4.73192344249798,
134.357353255865));
#173692=CARTESIAN_POINT('Ctrl Pts',(-68.9888661137975,-4.78139638377557,
134.290487925176));
#173693=CARTESIAN_POINT('Ctrl Pts',(-68.9849300643564,-4.82940190659136,
134.222665429474));
#173694=CARTESIAN_POINT('Ctrl Pts',(-68.9774294548569,-4.92088212955422,
134.093421611996));
#173695=CARTESIAN_POINT('Ctrl Pts',(-68.9699288453573,-5.00730510338989,
133.960313065865));
#173696=CARTESIAN_POINT('Ctrl Pts',(-68.9624282358577,-5.08833070564033,
133.823768041637));
#173697=CARTESIAN_POINT('Ctrl Pts',(-68.9549368819826,-5.16925632367674,
133.687391511645));
#173698=CARTESIAN_POINT('Ctrl Pts',(-68.9474455281075,-5.24479764593728,
133.547587254532));
#173699=CARTESIAN_POINT('Ctrl Pts',(-68.9399541742324,-5.31465601959238,
133.404814800187));
#173700=CARTESIAN_POINT('Ctrl Pts',(-68.9324706909269,-5.38444099861082,
133.262192345503));
#173701=CARTESIAN_POINT('Ctrl Pts',(-68.9249872076214,-5.44855475875408,
133.116608226452));
#173702=CARTESIAN_POINT('Ctrl Pts',(-68.917503724316,-5.50674305299424,
132.968549036073));
#173703=CARTESIAN_POINT('Ctrl Pts',(-68.9100267317162,-5.5648808783445,
132.820618262982));
#173704=CARTESIAN_POINT('Ctrl Pts',(-68.9025497391166,-5.61710334055933,
132.670217029963));
#173705=CARTESIAN_POINT('Ctrl Pts',(-68.8950727465169,-5.66320309338228,
132.517854500136));
#173706=CARTESIAN_POINT('Ctrl Pts',(-68.8876014915568,-5.70926747051557,
132.365608889148));
#173707=CARTESIAN_POINT('Ctrl Pts',(-68.8801302365967,-5.7492183963796,
132.211405327029));
#173708=CARTESIAN_POINT('Ctrl Pts',(-68.8726589816366,-5.7828974908347,
132.055770691442));
#173709=CARTESIAN_POINT('Ctrl Pts',(-68.8651911165758,-5.81656130422431,
131.900206671264));
#173710=CARTESIAN_POINT('Ctrl Pts',(-68.8577232515151,-5.84395887749384,
131.743213225079));
#173711=CARTESIAN_POINT('Ctrl Pts',(-68.8502553864543,-5.86498226780924,
131.585330246158));
#173712=CARTESIAN_POINT('Ctrl Pts',(-68.8427890124123,-5.88600146063689,
131.427478789834));
#173713=CARTESIAN_POINT('Ctrl Pts',(-68.8353226383703,-5.90064895462738,
131.268738513768));
#173714=CARTESIAN_POINT('Ctrl Pts',(-68.8278562643284,-5.90886828661765,
131.109657413986));
#173715=CARTESIAN_POINT('Ctrl Pts',(-68.823029240287,-5.9141820993062,131.006811201236));
#173716=CARTESIAN_POINT('Ctrl Pts',(-68.8182022162455,-5.91681021654618,
130.903822693668));
#173717=CARTESIAN_POINT('Ctrl Pts',(-68.8133751922041,-5.91674895302827,
130.80084076829));
#173718=CARTESIAN_POINT('',(-67.0633766192359,-5.92092402712534,130.801027289785));
#173719=CARTESIAN_POINT('Ctrl Pts',(-68.8133731068898,-5.90906110029032,
130.800800910513));
#173720=CARTESIAN_POINT('Ctrl Pts',(-68.7777428847743,-5.91314900340379,
130.04163462849));
#173721=CARTESIAN_POINT('Ctrl Pts',(-68.6492967880541,-5.42415644322105,
127.3099351127));
#173722=CARTESIAN_POINT('Ctrl Pts',(-68.4280348167307,-1.30296673267659,
123.928327006259));
#173723=CARTESIAN_POINT('Ctrl Pts',(-68.1495871929176,5.08071647084124,
125.991473680054));
#173724=CARTESIAN_POINT('Ctrl Pts',(-67.8711395691046,6.79546944445906,
132.477428326834));
#173725=CARTESIAN_POINT('Ctrl Pts',(-67.592691945292,2.26551797575204,137.425915482692));
#173726=CARTESIAN_POINT('Ctrl Pts',(-67.3234379964852,-4.12802629246645,
136.327038353622));
#173727=CARTESIAN_POINT('Ctrl Pts',(-67.146999922283,-5.91212555947519,
132.571180631677));
#173728=CARTESIAN_POINT('Ctrl Pts',(-67.0633777226851,-5.92415232255569,
130.801048813814));
#173729=CARTESIAN_POINT('',(-65.3133743315069,-5.91862889358278,130.80948552551));
#173730=CARTESIAN_POINT('Ctrl Pts',(-67.0633751922041,-5.91674904530173,
130.800999453909));
#173731=CARTESIAN_POINT('Ctrl Pts',(-67.0541823606914,-5.9166386387428,
130.60664774455));
#173732=CARTESIAN_POINT('Ctrl Pts',(-67.0449895291787,-5.90695304333343,
130.412571862945));
#173733=CARTESIAN_POINT('Ctrl Pts',(-67.035796697666,-5.88776834993849,
130.219455138055));
#173734=CARTESIAN_POINT('Ctrl Pts',(-67.0283734312605,-5.87227659532702,
130.063512228163));
#173735=CARTESIAN_POINT('Ctrl Pts',(-67.020950164855,-5.85056170105724,
129.907949409567));
#173736=CARTESIAN_POINT('Ctrl Pts',(-67.0135268984495,-5.822646217192,129.753303249046));
#173737=CARTESIAN_POINT('Ctrl Pts',(-67.0061124057283,-5.79476372711042,
129.598839867444));
#173738=CARTESIAN_POINT('Ctrl Pts',(-66.9986979130071,-5.76069530068166,
129.445291351149));
#173739=CARTESIAN_POINT('Ctrl Pts',(-66.991283420286,-5.72051534856346,
129.293190637269));
#173740=CARTESIAN_POINT('Ctrl Pts',(-66.9838760739322,-5.6803741233958,
129.141236523784));
#173741=CARTESIAN_POINT('Ctrl Pts',(-66.9764687275783,-5.63413319410368,
128.990727793149));
#173742=CARTESIAN_POINT('Ctrl Pts',(-66.9690613812244,-5.58191824809153,
128.842188547098));
#173743=CARTESIAN_POINT('Ctrl Pts',(-66.9616595595489,-5.52974224595615,
128.693760087222));
#173744=CARTESIAN_POINT('Ctrl Pts',(-66.9542577378734,-5.47160122215931,
128.547298537778));
#173745=CARTESIAN_POINT('Ctrl Pts',(-66.9468559161979,-5.40767102586325,
128.40331404606));
#173746=CARTESIAN_POINT('Ctrl Pts',(-66.9394580018865,-5.34377457782018,
128.259405562635));
#173747=CARTESIAN_POINT('Ctrl Pts',(-66.932060087575,-5.2740951946687,128.117971873066));
#173748=CARTESIAN_POINT('Ctrl Pts',(-66.9246621732635,-5.1988572531239,
127.979504192163));
#173749=CARTESIAN_POINT('Ctrl Pts',(-66.9172654883512,-5.12363181476004,
127.841059522076));
#173750=CARTESIAN_POINT('Ctrl Pts',(-66.9098688034391,-5.04284982938717,
127.705580210085));
#173751=CARTESIAN_POINT('Ctrl Pts',(-66.9024721185268,-4.95678218540968,
127.573533954171));
#173752=CARTESIAN_POINT('Ctrl Pts',(-66.8950757615912,-4.87071835776171,
127.441493553326));
#173753=CARTESIAN_POINT('Ctrl Pts',(-66.8876794046558,-4.77936954135731,
127.312886218616));
#173754=CARTESIAN_POINT('Ctrl Pts',(-66.8802830477202,-4.68305047208488,
127.18815143689));
#173755=CARTESIAN_POINT('Ctrl Pts',(-66.8728855583836,-4.58671665611692,
127.06339755795));
#173756=CARTESIAN_POINT('Ctrl Pts',(-66.8654880690468,-4.48541130027901,
126.942517708014));
#173757=CARTESIAN_POINT('Ctrl Pts',(-66.8580905797102,-4.37948991066,126.825918876768));
#173758=CARTESIAN_POINT('Ctrl Pts',(-66.8506904971951,-4.2735313904619,
126.709279171981));
#173759=CARTESIAN_POINT('Ctrl Pts',(-66.8432904146799,-4.16295386562101,
126.596923749914));
#173760=CARTESIAN_POINT('Ctrl Pts',(-66.8358903321648,-4.04815010674773,
126.489223160226));
#173761=CARTESIAN_POINT('Ctrl Pts',(-66.8284821124982,-3.93322010933962,
126.381404142669));
#173762=CARTESIAN_POINT('Ctrl Pts',(-66.8210738928317,-3.81405486959446,
126.278250434967));
#173763=CARTESIAN_POINT('Ctrl Pts',(-66.8136656731651,-3.69108124064205,
126.180093125575));
#173764=CARTESIAN_POINT('Ctrl Pts',(-66.806252893863,-3.56803192347277,
126.081875401998));
#173765=CARTESIAN_POINT('Ctrl Pts',(-66.7988401145608,-3.44116984650735,
125.988660424976));
#173766=CARTESIAN_POINT('Ctrl Pts',(-66.7914273352586,-3.31095087144901,
125.900735949083));
#173767=CARTESIAN_POINT('Ctrl Pts',(-66.7840039642298,-3.18054583341263,
125.812685842577));
#173768=CARTESIAN_POINT('Ctrl Pts',(-66.776580593201,-3.04677463424182,
125.729941530703));
#173769=CARTESIAN_POINT('Ctrl Pts',(-66.7691572221722,-2.91011846130336,
125.652745229779));
#173770=CARTESIAN_POINT('Ctrl Pts',(-66.7652211727325,-2.83766007941345,
125.611813898742));
#173771=CARTESIAN_POINT('Ctrl Pts',(-66.7612851232929,-2.76439098611254,
125.572441518465));
#173772=CARTESIAN_POINT('Ctrl Pts',(-66.7573490738532,-2.69038506458434,
125.534658655713));
#173773=CARTESIAN_POINT('Ctrl Pts',(-66.7499258074478,-2.55081220618745,
125.463401355704));
#173774=CARTESIAN_POINT('Ctrl Pts',(-66.7425025410424,-2.40819537036832,
125.397585207967));
#173775=CARTESIAN_POINT('Ctrl Pts',(-66.735079274637,-2.26299817481437,
125.337481267947));
#173776=CARTESIAN_POINT('Ctrl Pts',(-66.727664781916,-2.11797259028748,
125.277448365793));
#173777=CARTESIAN_POINT('Ctrl Pts',(-66.7202502891949,-1.97037305815825,
125.223114374127));
#173778=CARTESIAN_POINT('Ctrl Pts',(-66.7128357964739,-1.82068817428747,
125.174704754682));
#173779=CARTESIAN_POINT('Ctrl Pts',(-66.7054284501201,-1.67114756234329,
125.12634179425));
#173780=CARTESIAN_POINT('Ctrl Pts',(-66.6980211037663,-1.51952595285366,
125.083891952386));
#173781=CARTESIAN_POINT('Ctrl Pts',(-66.6906137574126,-1.36633222456315,
125.047532774507));
#173782=CARTESIAN_POINT('Ctrl Pts',(-66.6832119357372,-1.2132527539351,
125.011200714675));
#173783=CARTESIAN_POINT('Ctrl Pts',(-66.6758101140618,-1.05860386084746,
124.980950359637));
#173784=CARTESIAN_POINT('Ctrl Pts',(-66.6684082923864,-0.902909797435244,
124.956909509588));
#173785=CARTESIAN_POINT('Ctrl Pts',(-66.6610103780751,-0.747297923707401,
124.932881350516));
#173786=CARTESIAN_POINT('Ctrl Pts',(-66.6536124637637,-0.590642346458045,
124.915056225062));
#173787=CARTESIAN_POINT('Ctrl Pts',(-66.6462145494524,-0.433477619714073,
124.903510872342));
#173788=CARTESIAN_POINT('Ctrl Pts',(-66.6388178645402,-0.276339010896203,
124.891967438251));
#173789=CARTESIAN_POINT('Ctrl Pts',(-66.631421179628,-0.118691792442532,
124.886701733012));
#173790=CARTESIAN_POINT('Ctrl Pts',(-66.6240244947158,0.0389241262890107,
124.88773865272));
#173791=CARTESIAN_POINT('Ctrl Pts',(-66.6166281377804,0.196533056165548,
124.888775526451));
#173792=CARTESIAN_POINT('Ctrl Pts',(-66.6092317808449,0.354110315790006,
124.896114467004));
#173793=CARTESIAN_POINT('Ctrl Pts',(-66.6018354239094,0.511116029992645,
124.90972823154));
#173794=CARTESIAN_POINT('Ctrl Pts',(-66.5944379345729,0.668145782170946,
124.923344080378));
#173795=CARTESIAN_POINT('Ctrl Pts',(-66.5870404452363,0.824603442766855,
124.943236633815));
#173796=CARTESIAN_POINT('Ctrl Pts',(-66.5796429558997,0.979954440106066,
124.969326782376));
#173797=CARTESIAN_POINT('Ctrl Pts',(-66.5722428733847,1.13535989549657,
124.995426076798));
#173798=CARTESIAN_POINT('Ctrl Pts',(-66.5648427908696,1.28965754733386,
125.027727230101));
#173799=CARTESIAN_POINT('Ctrl Pts',(-66.5574427083546,1.44232333958396,
125.066100084391));
#173800=CARTESIAN_POINT('Ctrl Pts',(-66.5500344886882,1.59515700356729,
125.10451513358));
#173801=CARTESIAN_POINT('Ctrl Pts',(-66.5426262690219,1.74635486217521,
125.149015126028));
#173802=CARTESIAN_POINT('Ctrl Pts',(-66.5352180493554,1.8954076367711,125.199419899506));
#173803=CARTESIAN_POINT('Ctrl Pts',(-66.5278052700533,2.04455215086288,
125.249855696281));
#173804=CARTESIAN_POINT('Ctrl Pts',(-66.5203924907512,2.1915486023942,125.306203382567));
#173805=CARTESIAN_POINT('Ctrl Pts',(-66.5129797114491,2.33590849090625,
125.36823496738));
#173806=CARTESIAN_POINT('Ctrl Pts',(-66.5055563404204,2.4804746475966,125.43035518583));
#173807=CARTESIAN_POINT('Ctrl Pts',(-66.4981329693916,2.62239638131092,
125.498175362577));
#173808=CARTESIAN_POINT('Ctrl Pts',(-66.4907095983629,2.76120981507606,
125.571421584897));
#173809=CARTESIAN_POINT('Ctrl Pts',(-66.4867735489219,2.83481202844313,
125.610258489492));
#173810=CARTESIAN_POINT('Ctrl Pts',(-66.482837499481,2.90754086170374,125.650620119523));
#173811=CARTESIAN_POINT('Ctrl Pts',(-66.4789014500401,2.97933066250755,
125.69246083706));
#173812=CARTESIAN_POINT('Ctrl Pts',(-66.4714781836347,3.11472398633657,
125.771371124527));
#173813=CARTESIAN_POINT('Ctrl Pts',(-66.4640549172293,3.24718485880746,
125.85578347212));
#173814=CARTESIAN_POINT('Ctrl Pts',(-66.4566316508239,3.37623463661398,
125.945454337236));
#173815=CARTESIAN_POINT('Ctrl Pts',(-66.4492171581029,3.50513188830024,
126.035019218837));
#173816=CARTESIAN_POINT('Ctrl Pts',(-66.4418026653818,3.63062576674194,
126.129830035777));
#173817=CARTESIAN_POINT('Ctrl Pts',(-66.4343881726608,3.75226248660205,
126.229597586092));
#173818=CARTESIAN_POINT('Ctrl Pts',(-66.426980826307,3.87378196841203,126.329268976687));
#173819=CARTESIAN_POINT('Ctrl Pts',(-66.4195734799533,3.99145140610673,
126.433887354475));
#173820=CARTESIAN_POINT('Ctrl Pts',(-66.4121661335995,4.10484636430756,
126.543120552992));
#173821=CARTESIAN_POINT('Ctrl Pts',(-66.4047643119241,4.21815674827041,
126.652272281268));
#173822=CARTESIAN_POINT('Ctrl Pts',(-66.3973624902487,4.32719873292128,
126.766031719103));
#173823=CARTESIAN_POINT('Ctrl Pts',(-66.3899606685733,4.43158142525334,
126.884026877455));
#173824=CARTESIAN_POINT('Ctrl Pts',(-66.3825627542619,4.53590901477448,
127.001959747082));
#173825=CARTESIAN_POINT('Ctrl Pts',(-66.3751648399506,4.63558196368183,
127.124123605227));
#173826=CARTESIAN_POINT('Ctrl Pts',(-66.3677669256392,4.730246769673,127.250110195818));
#173827=CARTESIAN_POINT('Ctrl Pts',(-66.360370240727,4.82489584409095,127.376075849723));
#173828=CARTESIAN_POINT('Ctrl Pts',(-66.3529735558148,4.91453820336326,
127.505862677105));
#173829=CARTESIAN_POINT('Ctrl Pts',(-66.3455768709026,4.99886106750231,
127.63902989388));
#173830=CARTESIAN_POINT('Ctrl Pts',(-66.3381805139672,5.08318019267708,
127.772191205881));
#173831=CARTESIAN_POINT('Ctrl Pts',(-66.3307841570318,5.16218009200584,
127.908732293855));
#173832=CARTESIAN_POINT('Ctrl Pts',(-66.3233878000963,5.23559186994411,
128.048184220113));
#173833=CARTESIAN_POINT('Ctrl Pts',(-66.3159903107598,5.309014887413,128.187657496817));
#173834=CARTESIAN_POINT('Ctrl Pts',(-66.3085928214232,5.37684790606324,
128.330042168823));
#173835=CARTESIAN_POINT('Ctrl Pts',(-66.3011953320866,5.43886853388846,
128.474845725238));
#173836=CARTESIAN_POINT('Ctrl Pts',(-66.2937952495716,5.50091090294861,
128.619700042315));
#173837=CARTESIAN_POINT('Ctrl Pts',(-66.2863951670566,5.55713667760582,
128.766974589103));
#173838=CARTESIAN_POINT('Ctrl Pts',(-66.2789950845416,5.60737209829619,
128.916158108896));
#173839=CARTESIAN_POINT('Ctrl Pts',(-66.2715868648752,5.65766275799601,
129.065505671305));
#173840=CARTESIAN_POINT('Ctrl Pts',(-66.2641786452088,5.70194978983447,
129.216766044789));
#173841=CARTESIAN_POINT('Ctrl Pts',(-66.2567704255423,5.74010949185553,
129.369413376721));
#173842=CARTESIAN_POINT('Ctrl Pts',(-66.2493576462402,5.77829268053645,
129.522154660538));
#173843=CARTESIAN_POINT('Ctrl Pts',(-66.2419448669381,5.81034094885473,
129.676284239173));
#173844=CARTESIAN_POINT('Ctrl Pts',(-66.2345320876361,5.83618206565302,
129.83126788866));
#173845=CARTESIAN_POINT('Ctrl Pts',(-66.2271087166073,5.86206010545083,
129.986472986053));
#173846=CARTESIAN_POINT('Ctrl Pts',(-66.2196853455785,5.88171323368988,
130.142534222191));
#173847=CARTESIAN_POINT('Ctrl Pts',(-66.2122619745498,5.89512116406734,
130.298913267721));
#173848=CARTESIAN_POINT('Ctrl Pts',(-66.208325925109,5.90223037047237,130.381829189925));
#173849=CARTESIAN_POINT('Ctrl Pts',(-66.2043898756682,5.90758469890388,
130.464834464052));
#173850=CARTESIAN_POINT('Ctrl Pts',(-66.2004538262274,5.91118705914763,
130.547849186504));
#173851=CARTESIAN_POINT('Ctrl Pts',(-66.1930305598219,5.91798099814152,
130.704412362246));
#173852=CARTESIAN_POINT('Ctrl Pts',(-66.1856072934165,5.91856083653682,
130.861482381503));
#173853=CARTESIAN_POINT('Ctrl Pts',(-66.1781840270111,5.91287275522387,
131.018524907379));
#173854=CARTESIAN_POINT('Ctrl Pts',(-66.1707695342901,5.90719139675067,
131.175381822032));
#173855=CARTESIAN_POINT('Ctrl Pts',(-66.1633550415692,5.89525687793374,
131.332210938575));
#173856=CARTESIAN_POINT('Ctrl Pts',(-66.1559405488482,5.87706723051589,
131.488474153828));
#173857=CARTESIAN_POINT('Ctrl Pts',(-66.1485332024944,5.85889511496505,
131.64458675671));
#173858=CARTESIAN_POINT('Ctrl Pts',(-66.1411258561406,5.83447991609504,
131.800134175855));
#173859=CARTESIAN_POINT('Ctrl Pts',(-66.1337185097868,5.80387167727135,
131.954579777669));
#173860=CARTESIAN_POINT('Ctrl Pts',(-66.1263166881114,5.77328626722696,
132.108910188126));
#173861=CARTESIAN_POINT('Ctrl Pts',(-66.1189148664361,5.73651708654385,
132.262140052921));
#173862=CARTESIAN_POINT('Ctrl Pts',(-66.1115130447607,5.69366581292043,
132.413739433532));
#173863=CARTESIAN_POINT('Ctrl Pts',(-66.1041151304493,5.65083716015079,
132.565258786011));
#173864=CARTESIAN_POINT('Ctrl Pts',(-66.0967172161379,5.6019329099643,132.715149010157));
#173865=CARTESIAN_POINT('Ctrl Pts',(-66.0893193018265,5.54710546312941,
132.862892022092));
#173866=CARTESIAN_POINT('Ctrl Pts',(-66.0819226169143,5.49228712762151,
133.010610481819));
#173867=CARTESIAN_POINT('Ctrl Pts',(-66.0745259320022,5.43154767881375,
133.156182087898));
#173868=CARTESIAN_POINT('Ctrl Pts',(-66.06712924709,5.36508889561729,133.299105435102));
#173869=CARTESIAN_POINT('Ctrl Pts',(-66.0597328901545,5.29863305927292,
133.442022444936));
#173870=CARTESIAN_POINT('Ctrl Pts',(-66.052336533219,5.22645855018246,133.582291090886));
#173871=CARTESIAN_POINT('Ctrl Pts',(-66.0449401762836,5.14881455429579,
133.719431671241));
#173872=CARTESIAN_POINT('Ctrl Pts',(-66.037542686947,5.07115867091514,133.856593248168));
#173873=CARTESIAN_POINT('Ctrl Pts',(-66.0301451976104,4.98803181730729,
133.990625481047));
#173874=CARTESIAN_POINT('Ctrl Pts',(-66.0227477082739,4.89972814852321,
134.121075051018));
#173875=CARTESIAN_POINT('Ctrl Pts',(-66.0153476257589,4.8113935250248,134.251570349883));
#173876=CARTESIAN_POINT('Ctrl Pts',(-66.0079475432438,4.71787868237357,
134.378480176419));
#173877=CARTESIAN_POINT('Ctrl Pts',(-66.0005474607288,4.6195198340263,134.501381995045));
#173878=CARTESIAN_POINT('Ctrl Pts',(-65.9931392410623,4.52105283001387,
134.624418956855));
#173879=CARTESIAN_POINT('Ctrl Pts',(-65.9857310213959,4.41773141636521,
134.743438817623));
#173880=CARTESIAN_POINT('Ctrl Pts',(-65.9783228017295,4.30993114385929,
134.858053267199));
#173881=CARTESIAN_POINT('Ctrl Pts',(-65.9709100224274,4.20206452208423,
134.972738260057));
#173882=CARTESIAN_POINT('Ctrl Pts',(-65.9634972431253,4.08971381425009,
135.083012177924));
#173883=CARTESIAN_POINT('Ctrl Pts',(-65.9560844638232,3.97328943540592,
135.188525489579));
#173884=CARTESIAN_POINT('Ctrl Pts',(-65.9486610927945,3.85669870394948,
135.294189563601));
#173885=CARTESIAN_POINT('Ctrl Pts',(-65.9412377217657,3.73602296197024,
135.395079207134));
#173886=CARTESIAN_POINT('Ctrl Pts',(-65.933814350737,3.61170415595693,135.490886372573));
#173887=CARTESIAN_POINT('Ctrl Pts',(-65.9298783012961,3.54578734201899,
135.541685630551));
#173888=CARTESIAN_POINT('Ctrl Pts',(-65.9259422518553,3.47884679936752,
135.591056756885));
#173889=CARTESIAN_POINT('Ctrl Pts',(-65.9220062024144,3.41095132597342,
135.638959009815));
#173890=CARTESIAN_POINT('Ctrl Pts',(-65.914582936009,3.28290258209922,135.729301163862));
#173891=CARTESIAN_POINT('Ctrl Pts',(-65.9071596696035,3.15106854326037,
135.814689180383));
#173892=CARTESIAN_POINT('Ctrl Pts',(-65.8997364031981,3.01586967167639,
135.894788957692));
#173893=CARTESIAN_POINT('Ctrl Pts',(-65.8923219104771,2.88083059393067,
135.974794063717));
#173894=CARTESIAN_POINT('Ctrl Pts',(-65.8849074177562,2.74243491761407,
136.049523183289));
#173895=CARTESIAN_POINT('Ctrl Pts',(-65.8774929250351,2.60113430028143,
136.118683802544));
#173896=CARTESIAN_POINT('Ctrl Pts',(-65.8700855786814,2.45996987380385,
136.187777762191));
#173897=CARTESIAN_POINT('Ctrl Pts',(-65.8626782323275,2.31590641338194,
136.251313743412));
#173898=CARTESIAN_POINT('Ctrl Pts',(-65.8552708859738,2.16942245371716,
136.309043785543));
#173899=CARTESIAN_POINT('Ctrl Pts',(-65.8478690642984,2.02304774731602,
136.366730770431));
#173900=CARTESIAN_POINT('Ctrl Pts',(-65.840467242623,1.87425648207241,136.418620302134));
#173901=CARTESIAN_POINT('Ctrl Pts',(-65.8330654209476,1.72354946955238,
136.464511480264));
#173902=CARTESIAN_POINT('Ctrl Pts',(-65.8256675066363,1.57292201409094,
136.510378432799));
#173903=CARTESIAN_POINT('Ctrl Pts',(-65.8182695923248,1.42038118162624,
136.550253229501));
#173904=CARTESIAN_POINT('Ctrl Pts',(-65.8108716780135,1.26644522713655,
136.583984052459));
#173905=CARTESIAN_POINT('Ctrl Pts',(-65.8034749931013,1.11253485401004,
136.617709269966));
#173906=CARTESIAN_POINT('Ctrl Pts',(-65.7960783081892,0.957230183289539,
136.645292460324));
#173907=CARTESIAN_POINT('Ctrl Pts',(-65.788681623277,0.801062127823096,
136.666632364071));
#173908=CARTESIAN_POINT('Ctrl Pts',(-65.7812852663416,0.644900997011886,
136.687971321584));
#173909=CARTESIAN_POINT('Ctrl Pts',(-65.773888909406,0.487876927435477,
136.703067492386));
#173910=CARTESIAN_POINT('Ctrl Pts',(-65.7664925524706,0.330528196823573,
136.711871233181));
#173911=CARTESIAN_POINT('Ctrl Pts',(-65.759095063134,0.173155375719321,
136.720676321851));
#173912=CARTESIAN_POINT('Ctrl Pts',(-65.7516975737974,0.0154581673463709,
136.723187041426));
#173913=CARTESIAN_POINT('Ctrl Pts',(-65.7443000844609,-0.142023040308535,
136.719405842966));
#173914=CARTESIAN_POINT('Ctrl Pts',(-65.7369000019459,-0.299559452756658,
136.715623319011));
#173915=CARTESIAN_POINT('Ctrl Pts',(-65.7294999194308,-0.456879340773783,
136.705544494598));
#173916=CARTESIAN_POINT('Ctrl Pts',(-65.7220998369158,-0.613445481624306,
136.689223844828));
#173917=CARTESIAN_POINT('Ctrl Pts',(-65.7146916172494,-0.770183783042085,
136.672885248825));
#173918=CARTESIAN_POINT('Ctrl Pts',(-65.707283397583,-0.926166310566384,
136.650291159274));
#173919=CARTESIAN_POINT('Ctrl Pts',(-65.6998751779165,-1.08086337350242,
136.621547646562));
#173920=CARTESIAN_POINT('Ctrl Pts',(-65.6924623986145,-1.23565564989943,
136.592786442698));
#173921=CARTESIAN_POINT('Ctrl Pts',(-65.6850496193124,-1.38916052202344,
136.557868356457));
#173922=CARTESIAN_POINT('Ctrl Pts',(-65.6776368400104,-1.54086207999922,
136.516949751481));
#173923=CARTESIAN_POINT('Ctrl Pts',(-65.6702134689816,-1.69278039627535,
136.475972680083));
#173924=CARTESIAN_POINT('Ctrl Pts',(-65.662790097953,-1.84288989693174,
136.428978077337));
#173925=CARTESIAN_POINT('Ctrl Pts',(-65.6553667269242,-1.99069252992094,
136.376171258086));
#173926=CARTESIAN_POINT('Ctrl Pts',(-65.6514306774834,-2.06906103240837,
136.348171815437));
#173927=CARTESIAN_POINT('Ctrl Pts',(-65.6474946280425,-2.14678135767349,
136.31853914079));
#173928=CARTESIAN_POINT('Ctrl Pts',(-65.6435585786016,-2.22378204153457,
136.28730909391));
#173929=CARTESIAN_POINT('Ctrl Pts',(-65.6361353121962,-2.36900292818556,
136.228410200152));
#173930=CARTESIAN_POINT('Ctrl Pts',(-65.6287120457907,-2.51210180301667,
136.163648798191));
#173931=CARTESIAN_POINT('Ctrl Pts',(-65.6212887793853,-2.65257030671823,
136.093198044678));
#173932=CARTESIAN_POINT('Ctrl Pts',(-65.6138742866643,-2.7928727883138,
136.022830558105));
#173933=CARTESIAN_POINT('Ctrl Pts',(-65.6064597939433,-2.9305507565997,
135.946787270539));
#173934=CARTESIAN_POINT('Ctrl Pts',(-65.5990453012222,-3.06511397943727,
135.865290063385));
#173935=CARTESIAN_POINT('Ctrl Pts',(-65.5916379548685,-3.19954750517444,
135.783871406308));
#173936=CARTESIAN_POINT('Ctrl Pts',(-65.5842306085147,-3.33087194491194,
135.697009486768));
#173937=CARTESIAN_POINT('Ctrl Pts',(-65.5768232621609,-3.45862002262525,
135.604972880767));
#173938=CARTESIAN_POINT('Ctrl Pts',(-65.5694214404855,-3.58627282100237,
135.513004919139));
#173939=CARTESIAN_POINT('Ctrl Pts',(-65.5620196188102,-3.71035426690494,
135.41587017306));
#173940=CARTESIAN_POINT('Ctrl Pts',(-65.5546177971348,-3.83042463626246,
135.313881397917));
#173941=CARTESIAN_POINT('Ctrl Pts',(-65.5472198828235,-3.95043162140679,
135.211946461853));
#173942=CARTESIAN_POINT('Ctrl Pts',(-65.539821968512,-4.06643146314844,
135.105162840933));
#173943=CARTESIAN_POINT('Ctrl Pts',(-65.5324240542006,-4.17801630330618,
134.993884496458));
#173944=CARTESIAN_POINT('Ctrl Pts',(-65.5250273692884,-4.28958260008783,
134.882624644425));
#173945=CARTESIAN_POINT('Ctrl Pts',(-65.5176306843763,-4.39673508738394,
134.766871814636));
#173946=CARTESIAN_POINT('Ctrl Pts',(-65.510233999464,-4.4991016013804,134.647017945894));
#173947=CARTESIAN_POINT('Ctrl Pts',(-65.5028376425286,-4.60146357633835,
134.527169391599));
#173948=CARTESIAN_POINT('Ctrl Pts',(-65.4954412855931,-4.69903975751229,
134.403220443774));
#173949=CARTESIAN_POINT('Ctrl Pts',(-65.4880449286577,-4.79149742632994,
134.275597137306));
#173950=CARTESIAN_POINT('Ctrl Pts',(-65.4806474393211,-4.88396925065285,
134.147954291383));
#173951=CARTESIAN_POINT('Ctrl Pts',(-65.4732499499844,-4.9713207832332,
134.016636269019));
#173952=CARTESIAN_POINT('Ctrl Pts',(-65.4658524606479,-5.05326199330886,
133.88209903879));
#173953=CARTESIAN_POINT('Ctrl Pts',(-65.4584523781328,-5.13523192774869,
133.747514646744));
#173954=CARTESIAN_POINT('Ctrl Pts',(-65.4510522956179,-5.21178756954797,
133.609709118639));
#173955=CARTESIAN_POINT('Ctrl Pts',(-65.4436522131028,-5.2826843681415,
133.469163880303));
#173956=CARTESIAN_POINT('Ctrl Pts',(-65.4362439934364,-5.35365912505335,
133.328464098029));
#173957=CARTESIAN_POINT('Ctrl Pts',(-65.4288357737699,-5.41896244382849,
133.185018922674));
#173958=CARTESIAN_POINT('Ctrl Pts',(-65.4214275541034,-5.47839725372801,
133.039331331657));
#173959=CARTESIAN_POINT('Ctrl Pts',(-65.4140147748013,-5.53786864476129,
132.893554072359));
#173960=CARTESIAN_POINT('Ctrl Pts',(-65.4066019954993,-5.59146420282318,
132.745531997422));
#173961=CARTESIAN_POINT('Ctrl Pts',(-65.3991892161972,-5.63903661918401,
132.595783674803));
#173962=CARTESIAN_POINT('Ctrl Pts',(-65.3917658451685,-5.68667700924425,
132.445821384759));
#173963=CARTESIAN_POINT('Ctrl Pts',(-65.3843424741398,-5.72827697073119,
132.294128279844));
#173964=CARTESIAN_POINT('Ctrl Pts',(-65.376919103111,-5.76374003153909,
132.141234363039));
#173965=CARTESIAN_POINT('Ctrl Pts',(-65.3729830536703,-5.7825433973037,
132.06016633971));
#173966=CARTESIAN_POINT('Ctrl Pts',(-65.3690470042294,-5.79962232311235,
131.978760844448));
#173967=CARTESIAN_POINT('Ctrl Pts',(-65.3651109547887,-5.81496835066423,
131.89709738517));
#173968=CARTESIAN_POINT('Ctrl Pts',(-65.3540312620643,-5.8581663013949,
131.667220690471));
#173969=CARTESIAN_POINT('Ctrl Pts',(-65.34295156934,-5.8877428756825,131.434710068976));
#173970=CARTESIAN_POINT('Ctrl Pts',(-65.3318718766157,-5.90344880502964,
131.200873882028));
#173971=CARTESIAN_POINT('Ctrl Pts',(-65.3257063151452,-5.91218874712461,
131.070750112306));
#173972=CARTESIAN_POINT('Ctrl Pts',(-65.3195407536746,-5.91663417826577,
130.940216236482));
#173973=CARTESIAN_POINT('Ctrl Pts',(-65.3133751922041,-5.91674776606,130.809502146914));
#173974=CARTESIAN_POINT('',(-63.5633751922041,-5.90707449789702,130.805318407263));
#173975=CARTESIAN_POINT('Ctrl Pts',(-65.3133739040115,-5.91956322123172,
130.80947726991));
#173976=CARTESIAN_POINT('Ctrl Pts',(-65.2378037129995,-5.90488233384873,
129.206561386044));
#173977=CARTESIAN_POINT('Ctrl Pts',(-65.0694176473834,-4.40327992023266,
125.61073367988));
#173978=CARTESIAN_POINT('Ctrl Pts',(-64.8082157071628,1.68340731958302,
124.011445166397));
#173979=CARTESIAN_POINT('Ctrl Pts',(-64.5297680833501,6.62499493017222,
128.54892214456));
#173980=CARTESIAN_POINT('Ctrl Pts',(-64.2513204595371,5.47853584893362,
135.159036895121));
#173981=CARTESIAN_POINT('Ctrl Pts',(-63.9728728357242,-0.702430036122883,
137.767416884371));
#173982=CARTESIAN_POINT('Ctrl Pts',(-63.7435577466132,-5.2611549065832,
134.645897948005));
#173983=CARTESIAN_POINT('Ctrl Pts',(-63.6070585321065,-5.90841563450014,
131.736853223252));
#173984=CARTESIAN_POINT('Ctrl Pts',(-63.5633751922041,-5.90707449789702,
130.805318407263));
#173985=CARTESIAN_POINT('',(-61.813375192204,-5.91603704377717,130.798888855257));
#173986=CARTESIAN_POINT('Ctrl Pts',(-63.5633751922041,-5.90707449789702,
130.805318407263));
#173987=CARTESIAN_POINT('Ctrl Pts',(-63.5142426575023,-5.90556606376996,
129.757581059916));
#173988=CARTESIAN_POINT('Ctrl Pts',(-63.3722942481961,-5.13924177134339,
126.728510338679));
#173989=CARTESIAN_POINT('Ctrl Pts',(-63.1375299642854,-0.292763836116973,
123.812089894358));
#173990=CARTESIAN_POINT('Ctrl Pts',(-62.8590823404728,5.72454938625507,
126.778556989137));
#173991=CARTESIAN_POINT('Ctrl Pts',(-62.5806347166597,6.48128138244416,
133.444540947002));
#173992=CARTESIAN_POINT('Ctrl Pts',(-62.3021870928469,1.2820324163645,137.68432816209));
#173993=CARTESIAN_POINT('Ctrl Pts',(-62.0464339180284,-4.57556355584588,
135.771497744683));
#173994=CARTESIAN_POINT('Ctrl Pts',(-61.883496617814,-5.90239076361927,
132.288505652477));
#173995=CARTESIAN_POINT('Ctrl Pts',(-61.813375192204,-5.91603704377717,
130.798888855257));
#173996=CARTESIAN_POINT('',(-60.0633743488977,-5.92189398088504,130.805812684987));
#173997=CARTESIAN_POINT('Ctrl Pts',(-61.8133751713904,-5.9167474688621,
130.798887755983));
#173998=CARTESIAN_POINT('Ctrl Pts',(-61.8037869858401,-5.91655904331685,
130.595179631626));
#173999=CARTESIAN_POINT('Ctrl Pts',(-61.7941988002899,-5.9058470097901,
130.391941306513));
#174000=CARTESIAN_POINT('Ctrl Pts',(-61.7846106147396,-5.88477711978155,
130.190089656999));
#174001=CARTESIAN_POINT('Ctrl Pts',(-61.7747945288506,-5.86320642229021,
129.983440221809));
#174002=CARTESIAN_POINT('Ctrl Pts',(-61.7649784429615,-5.83077960451583,
129.778243866767));
#174003=CARTESIAN_POINT('Ctrl Pts',(-61.7551623570725,-5.78772236815066,
129.575458525571));
#174004=CARTESIAN_POINT('Ctrl Pts',(-61.7518721864553,-5.77329037809414,
129.507488626089));
#174005=CARTESIAN_POINT('Ctrl Pts',(-61.7485820158383,-5.75766448883687,
129.439789405312));
#174006=CARTESIAN_POINT('Ctrl Pts',(-61.7452918452211,-5.74085438261084,
129.372396400081));
#174007=CARTESIAN_POINT('Ctrl Pts',(-61.7378685788157,-5.70292750545467,
129.220344640489));
#174008=CARTESIAN_POINT('Ctrl Pts',(-61.7304453124103,-5.65889826191603,
129.069570793701));
#174009=CARTESIAN_POINT('Ctrl Pts',(-61.7230220460048,-5.60886672123866,
128.920602494589));
#174010=CARTESIAN_POINT('Ctrl Pts',(-61.7156075532838,-5.55889431368752,
128.771810263636));
#174011=CARTESIAN_POINT('Ctrl Pts',(-61.7081930605627,-5.50293384776418,
128.624819683024));
#174012=CARTESIAN_POINT('Ctrl Pts',(-61.7007785678417,-5.44113617986515,
128.48014728083));
#174013=CARTESIAN_POINT('Ctrl Pts',(-61.693371221488,-5.37939807488507,
128.335614319344));
#174014=CARTESIAN_POINT('Ctrl Pts',(-61.6859638751342,-5.31183411407088,
128.193395429116));
#174015=CARTESIAN_POINT('Ctrl Pts',(-61.6785565287805,-5.23864460889609,
128.053990965286));
#174016=CARTESIAN_POINT('Ctrl Pts',(-61.6711547071051,-5.16550969121563,
127.914690474564));
#174017=CARTESIAN_POINT('Ctrl Pts',(-61.6637528854297,-5.08675775624425,
127.77820055973));
#174018=CARTESIAN_POINT('Ctrl Pts',(-61.6563510637543,-5.00263672547793,
127.645000499536));
#174019=CARTESIAN_POINT('Ctrl Pts',(-61.648953149443,-4.91856010154895,
127.511870754617));
#174020=CARTESIAN_POINT('Ctrl Pts',(-61.6415552351315,-4.82912022530189,
127.382027720465));
#174021=CARTESIAN_POINT('Ctrl Pts',(-61.6341573208202,-4.73461028990158,
127.255924910771));
#174022=CARTESIAN_POINT('Ctrl Pts',(-61.626760635908,-4.64011606033782,
127.129843057076));
#174023=CARTESIAN_POINT('Ctrl Pts',(-61.6193639509958,-4.54055366749458,
127.007500492655));
#174024=CARTESIAN_POINT('Ctrl Pts',(-61.6119672660836,-4.436258917276,126.889320722317));
#174025=CARTESIAN_POINT('Ctrl Pts',(-61.6045709091481,-4.33196879159592,
126.771146192195));
#174026=CARTESIAN_POINT('Ctrl Pts',(-61.5971745522127,-4.22294697277507,
126.657134369035));
#174027=CARTESIAN_POINT('Ctrl Pts',(-61.5897781952773,-4.10956856309439,
126.547674490104));
#174028=CARTESIAN_POINT('Ctrl Pts',(-61.5823807059407,-3.99617279488974,
126.438197852587));
#174029=CARTESIAN_POINT('Ctrl Pts',(-61.5749832166041,-3.87841937630812,
126.333274806244));
#174030=CARTESIAN_POINT('Ctrl Pts',(-61.5675857272675,-3.75671904009221,
126.233256525959));
#174031=CARTESIAN_POINT('Ctrl Pts',(-61.5601856447525,-3.63497604201228,
126.13320318442));
#174032=CARTESIAN_POINT('Ctrl Pts',(-61.5527855622375,-3.50928365980766,
126.038058269039));
#174033=CARTESIAN_POINT('Ctrl Pts',(-61.5453854797225,-3.38008421662579,
125.948131499102));
#174034=CARTESIAN_POINT('Ctrl Pts',(-61.537977260056,-3.25074270537393,
125.858105845437));
#174035=CARTESIAN_POINT('Ctrl Pts',(-61.5305690403896,-3.1178867382884,
125.773310009541));
#174036=CARTESIAN_POINT('Ctrl Pts',(-61.5231608207231,-2.98198664269018,
125.69400972694));
#174037=CARTESIAN_POINT('Ctrl Pts',(-61.515748041421,-2.84600290285074,
125.614660636339));
#174038=CARTESIAN_POINT('Ctrl Pts',(-61.5083352621189,-2.70697163000957,
125.540814013635));
#174039=CARTESIAN_POINT('Ctrl Pts',(-61.5009224828169,-2.56538557406321,
125.472688514099));
#174040=CARTESIAN_POINT('Ctrl Pts',(-61.4934991117881,-2.4235972133204,
125.404465673654));
#174041=CARTESIAN_POINT('Ctrl Pts',(-61.4860757407594,-2.27924712048853,
125.341980430805));
#174042=CARTESIAN_POINT('Ctrl Pts',(-61.4786523697306,-2.13284650455696,
125.28540271317));
#174043=CARTESIAN_POINT('Ctrl Pts',(-61.4747163202899,-2.05522138515569,
125.255403849716));
#174044=CARTESIAN_POINT('Ctrl Pts',(-61.4707802708491,-1.97702002949481,
125.227064965853));
#174045=CARTESIAN_POINT('Ctrl Pts',(-61.4668442214083,-1.89831997046167,
125.200405598809));
#174046=CARTESIAN_POINT('Ctrl Pts',(-61.4594209550028,-1.74989411526949,
125.150126864576));
#174047=CARTESIAN_POINT('Ctrl Pts',(-61.4519976885974,-1.5992449262225,
125.105672967093));
#174048=CARTESIAN_POINT('Ctrl Pts',(-61.444574422192,-1.44687040735415,
125.067244914809));
#174049=CARTESIAN_POINT('Ctrl Pts',(-61.437159929471,-1.29467598251319,
125.028862281291));
#174050=CARTESIAN_POINT('Ctrl Pts',(-61.42974543675,-1.14076064531272,124.99649140689));
#174051=CARTESIAN_POINT('Ctrl Pts',(-61.4223309440289,-0.985640507020434,
124.970284567889));
#174052=CARTESIAN_POINT('Ctrl Pts',(-61.4149235976752,-0.830669879357381,
124.944102988025));
#174053=CARTESIAN_POINT('Ctrl Pts',(-61.4075162513212,-0.674497127998955,
124.924073677711));
#174054=CARTESIAN_POINT('Ctrl Pts',(-61.4001089049675,-0.517651489138725,
124.910298563406));
#174055=CARTESIAN_POINT('Ctrl Pts',(-61.3927070832921,-0.360922831673627,
124.8965337231));
#174056=CARTESIAN_POINT('Ctrl Pts',(-61.3853052616168,-0.203522656253442,
124.889013823443));
#174057=CARTESIAN_POINT('Ctrl Pts',(-61.3779034399413,-0.0459882012907073,
124.88778934293));
#174058=CARTESIAN_POINT('Ctrl Pts',(-61.37050552563,0.111463092459498,124.886565508812));
#174059=CARTESIAN_POINT('Ctrl Pts',(-61.3631076113186,0.269048152239418,
124.891630478216));
#174060=CARTESIAN_POINT('Ctrl Pts',(-61.3557096970073,0.426226946069279,
124.902982714657));
#174061=CARTESIAN_POINT('Ctrl Pts',(-61.3483130120951,0.583379619635344,
124.914333064562));
#174062=CARTESIAN_POINT('Ctrl Pts',(-61.340916327183,0.740125789283221,
124.931968580961));
#174063=CARTESIAN_POINT('Ctrl Pts',(-61.3335196422707,0.895927637127192,
124.955835655532));
#174064=CARTESIAN_POINT('Ctrl Pts',(-61.3261232853353,1.05172257655374,
124.979701671812));
#174065=CARTESIAN_POINT('Ctrl Pts',(-61.3187269283998,1.20657290843936,
125.009798640333));
#174066=CARTESIAN_POINT('Ctrl Pts',(-61.3113305714643,1.35994840450235,
125.046021369172));
#174067=CARTESIAN_POINT('Ctrl Pts',(-61.3039330821278,1.51334738274533,
125.082249643804));
#174068=CARTESIAN_POINT('Ctrl Pts',(-61.2965355927911,1.66527071223876,
125.124605460371));
#174069=CARTESIAN_POINT('Ctrl Pts',(-61.2891381034545,1.81520092852823,
125.172933076385));
#174070=CARTESIAN_POINT('Ctrl Pts',(-61.2817380209395,1.9651837026228,125.22127763357));
#174071=CARTESIAN_POINT('Ctrl Pts',(-61.2743379384246,2.11317161736641,
125.275598043705));
#174072=CARTESIAN_POINT('Ctrl Pts',(-61.2669378559096,2.25866501068448,
125.335689578638));
#174073=CARTESIAN_POINT('Ctrl Pts',(-61.2595296362431,2.40431838894559,
125.395847190391));
#174074=CARTESIAN_POINT('Ctrl Pts',(-61.2521214165766,2.54747142262499,
125.461788457622));
#174075=CARTESIAN_POINT('Ctrl Pts',(-61.2447131969101,2.68764631749271,
125.533261317176));
#174076=CARTESIAN_POINT('Ctrl Pts',(-61.2373004176081,2.82790748766928,
125.604778167084));
#174077=CARTESIAN_POINT('Ctrl Pts',(-61.229887638306,2.96518654179332,125.68183321112));
#174078=CARTESIAN_POINT('Ctrl Pts',(-61.222474859004,3.09903317563845,125.764130073356));
#174079=CARTESIAN_POINT('Ctrl Pts',(-61.2150514879752,3.23307105583081,
125.846544525207));
#174080=CARTESIAN_POINT('Ctrl Pts',(-61.2076281169464,3.36366641143666,
125.934215546467));
#174081=CARTESIAN_POINT('Ctrl Pts',(-61.2002047459177,3.49039995659213,
126.026804892562));
#174082=CARTESIAN_POINT('Ctrl Pts',(-61.1962686964769,3.55759712316341,
126.075897985512));
#174083=CARTESIAN_POINT('Ctrl Pts',(-61.1923326470361,3.62370917166573,
126.126373141864));
#174084=CARTESIAN_POINT('Ctrl Pts',(-61.1883965975953,3.68867775645533,
126.178175691352));
#174085=CARTESIAN_POINT('Ctrl Pts',(-61.1809733311899,3.81120647976808,
126.275873682984));
#174086=CARTESIAN_POINT('Ctrl Pts',(-61.1735500647845,3.93003636921133,
126.3785906949));
#174087=CARTESIAN_POINT('Ctrl Pts',(-61.166126798379,4.04472912733981,126.486016392177));
#174088=CARTESIAN_POINT('Ctrl Pts',(-61.158712305658,4.15928632815297,126.593315121202));
#174089=CARTESIAN_POINT('Ctrl Pts',(-61.151297812937,4.26971586092583,126.705311205181));
#174090=CARTESIAN_POINT('Ctrl Pts',(-61.143883320216,4.37561064056104,126.821652734139));
#174091=CARTESIAN_POINT('Ctrl Pts',(-61.1364759738622,4.48140335482078,
126.937882128752));
#174092=CARTESIAN_POINT('Ctrl Pts',(-61.1290686275084,4.58266976768811,
127.058448356044));
#174093=CARTESIAN_POINT('Ctrl Pts',(-61.1216612811546,4.67903806045666,
127.182961248358));
#174094=CARTESIAN_POINT('Ctrl Pts',(-61.1142594594792,4.7753344781167,127.30738127426));
#174095=CARTESIAN_POINT('Ctrl Pts',(-61.1068576378038,4.86673982220071,
127.435741810197));
#174096=CARTESIAN_POINT('Ctrl Pts',(-61.0994558161284,4.95292123323519,
127.567618147139));
#174097=CARTESIAN_POINT('Ctrl Pts',(-61.0920579018171,5.0390571497735,127.699424867588));
#174098=CARTESIAN_POINT('Ctrl Pts',(-61.0846599875057,5.11997442160667,
127.834743381103));
#174099=CARTESIAN_POINT('Ctrl Pts',(-61.0772620731944,5.1953824409474,127.973118512977));
#174100=CARTESIAN_POINT('Ctrl Pts',(-61.0698653882822,5.27077792884347,
128.111470649415));
#174101=CARTESIAN_POINT('Ctrl Pts',(-61.0624687033699,5.34066580286567,
128.252878068607));
#174102=CARTESIAN_POINT('Ctrl Pts',(-61.0550720184577,5.40480046150981,
128.396859312527));
#174103=CARTESIAN_POINT('Ctrl Pts',(-61.0476756615223,5.46893227635599,
128.540834172168));
#174104=CARTESIAN_POINT('Ctrl Pts',(-61.0402793045868,5.52731123116298,
128.687382288618));
#174105=CARTESIAN_POINT('Ctrl Pts',(-61.0328829476514,5.57973922553615,
128.836000707003));
#174106=CARTESIAN_POINT('Ctrl Pts',(-61.0254854583148,5.63217524676911,
128.984641879247));
#174107=CARTESIAN_POINT('Ctrl Pts',(-61.0180879689783,5.67865836923736,
129.135353632495));
#174108=CARTESIAN_POINT('Ctrl Pts',(-61.0106904796417,5.71903992132884,
129.287616426627));
#174109=CARTESIAN_POINT('Ctrl Pts',(-61.0032903971267,5.75943562911081,
129.439932596246));
#174110=CARTESIAN_POINT('Ctrl Pts',(-60.9958903146117,5.79372541235539,
129.593800528683));
#174111=CARTESIAN_POINT('Ctrl Pts',(-60.9884902320967,5.82181143509756,
129.748689183517));
#174112=CARTESIAN_POINT('Ctrl Pts',(-60.9810820124302,5.84992834130905,
129.90374815435));
#174113=CARTESIAN_POINT('Ctrl Pts',(-60.9736737927637,5.87182779704541,
130.059829721532));
#174114=CARTESIAN_POINT('Ctrl Pts',(-60.9662655730972,5.8874636107235,130.216395656955));
#174115=CARTESIAN_POINT('Ctrl Pts',(-60.9588527937952,5.90310904798401,
130.373057956098));
#174116=CARTESIAN_POINT('Ctrl Pts',(-60.9514400144931,5.91248313910554,
130.530204845753));
#174117=CARTESIAN_POINT('Ctrl Pts',(-60.944027235191,5.91559183311733,130.687297273792));
#174118=CARTESIAN_POINT('Ctrl Pts',(-60.9366038641623,5.9187049689769,130.844614162859));
#174119=CARTESIAN_POINT('Ctrl Pts',(-60.9291804931335,5.91553483549277,
131.001876062657));
#174120=CARTESIAN_POINT('Ctrl Pts',(-60.9217571221048,5.90613937315212,
131.158547386662));
#174121=CARTESIAN_POINT('Ctrl Pts',(-60.917821072664,5.90115767357812,131.241618281925));
#174122=CARTESIAN_POINT('Ctrl Pts',(-60.9138850232233,5.89442667210103,
131.324523275652));
#174123=CARTESIAN_POINT('Ctrl Pts',(-60.9099489737825,5.88596082711695,
131.407183729386));
#174124=CARTESIAN_POINT('Ctrl Pts',(-60.9025257073771,5.86999450768682,
131.563078765387));
#174125=CARTESIAN_POINT('Ctrl Pts',(-60.8951024409717,5.84780623429085,
131.718574770755));
#174126=CARTESIAN_POINT('Ctrl Pts',(-60.8876791745662,5.81942019001215,
131.873135249834));
#174127=CARTESIAN_POINT('Ctrl Pts',(-60.8802646818452,5.79106769568043,
132.027513051261));
#174128=CARTESIAN_POINT('Ctrl Pts',(-60.8728501891242,5.75653207818981,
132.180957163757));
#174129=CARTESIAN_POINT('Ctrl Pts',(-60.8654356964032,5.71588936993058,
132.332934879162));
#174130=CARTESIAN_POINT('Ctrl Pts',(-60.8580283500494,5.67528583464374,
132.484766112723));
#174131=CARTESIAN_POINT('Ctrl Pts',(-60.8506210036956,5.62858702273421,
132.635133404728));
#174132=CARTESIAN_POINT('Ctrl Pts',(-60.8432136573418,5.57592021620963,
132.783513038418));
#174133=CARTESIAN_POINT('Ctrl Pts',(-60.8358118356664,5.52329269057643,
132.93178200498));
#174134=CARTESIAN_POINT('Ctrl Pts',(-60.828410013991,5.46470615751025,133.078065914746));
#174135=CARTESIAN_POINT('Ctrl Pts',(-60.8210081923156,5.40033801807167,
133.221855158009));
#174136=CARTESIAN_POINT('Ctrl Pts',(-60.8136102780043,5.33600385807286,
133.365568496049));
#174137=CARTESIAN_POINT('Ctrl Pts',(-60.806212363693,5.26589432217311,133.506789450432));
#174138=CARTESIAN_POINT('Ctrl Pts',(-60.7988144493816,5.19023528113713,
133.645027491548));
#174139=CARTESIAN_POINT('Ctrl Pts',(-60.7914177644694,5.11458881326108,
133.78324256001));
#174140=CARTESIAN_POINT('Ctrl Pts',(-60.7840210795571,5.03339484964367,
133.918475371894));
#174141=CARTESIAN_POINT('Ctrl Pts',(-60.7766243946449,4.94692570094628,
134.050259055875));
#174142=CARTESIAN_POINT('Ctrl Pts',(-60.7692280377095,4.86046038638169,
134.18203689643));
#174143=CARTESIAN_POINT('Ctrl Pts',(-60.7618316807741,4.76872055661285,
134.310365601064));
#174144=CARTESIAN_POINT('Ctrl Pts',(-60.7544353238386,4.67202228371712,
134.434806642912));
#174145=CARTESIAN_POINT('Ctrl Pts',(-60.747037834502,4.57530920606894,134.559266737001));
#174146=CARTESIAN_POINT('Ctrl Pts',(-60.7396403451654,4.47363640279043,
134.679837688373));
#174147=CARTESIAN_POINT('Ctrl Pts',(-60.7322428558288,4.36736061706032,
134.796113591267));
#174148=CARTESIAN_POINT('Ctrl Pts',(-60.7248427733138,4.26104757651828,
134.912430254498));
#174149=CARTESIAN_POINT('Ctrl Pts',(-60.7174426907989,4.1501285926113,135.024448596194));
#174150=CARTESIAN_POINT('Ctrl Pts',(-60.7100426082839,4.03499756195621,
135.131799263868));
#174151=CARTESIAN_POINT('Ctrl Pts',(-60.7026343886174,3.91973993289699,
135.239267974637));
#174152=CARTESIAN_POINT('Ctrl Pts',(-60.6952261689509,3.80026128071653,
135.342058506539));
#174153=CARTESIAN_POINT('Ctrl Pts',(-60.6878179492845,3.67698946428683,
135.439841071847));
#174154=CARTESIAN_POINT('Ctrl Pts',(-60.6804051699824,3.55364177611101,
135.537683820693));
#174155=CARTESIAN_POINT('Ctrl Pts',(-60.6729923906803,3.42649657243919,
135.630512241426));
#174156=CARTESIAN_POINT('Ctrl Pts',(-60.6655796113782,3.29601058868899,
135.718039968292));
#174157=CARTESIAN_POINT('Ctrl Pts',(-60.6581562403495,3.16533816044602,
135.805692758878));
#174158=CARTESIAN_POINT('Ctrl Pts',(-60.6507328693208,3.03131573567422,
135.888029533972));
#174159=CARTESIAN_POINT('Ctrl Pts',(-60.643309498292,2.89442523673469,135.964809542946));
#174160=CARTESIAN_POINT('Ctrl Pts',(-60.6393734488512,2.82184260955433,
136.005520146015));
#174161=CARTESIAN_POINT('Ctrl Pts',(-60.6354373994104,2.7484540196275,136.044669338017));
#174162=CARTESIAN_POINT('Ctrl Pts',(-60.6315013499696,2.67433344283047,
136.082226777205));
#174163=CARTESIAN_POINT('Ctrl Pts',(-60.6240780835642,2.53454434821584,
136.153058935384));
#174164=CARTESIAN_POINT('Ctrl Pts',(-60.6166548171588,2.3917278512743,136.218440701675));
#174165=CARTESIAN_POINT('Ctrl Pts',(-60.6092315507533,2.24634839254537,
136.27810243298));
#174166=CARTESIAN_POINT('Ctrl Pts',(-60.6018170580324,2.10114076026364,
136.337693649073));
#174167=CARTESIAN_POINT('Ctrl Pts',(-60.5944025653114,1.95337653782512,
136.391578146863));
#174168=CARTESIAN_POINT('Ctrl Pts',(-60.5869880725904,1.8035450050554,136.439531952782));
#174169=CARTESIAN_POINT('Ctrl Pts',(-60.5795807262366,1.65385788555803,
136.487439539017));
#174170=CARTESIAN_POINT('Ctrl Pts',(-60.5721733798828,1.50210777565312,
136.529427700232));
#174171=CARTESIAN_POINT('Ctrl Pts',(-60.564766033529,1.34880409211538,136.565320440685));
#174172=CARTESIAN_POINT('Ctrl Pts',(-60.5573642118536,1.19561474824843,
136.601186410978));
#174173=CARTESIAN_POINT('Ctrl Pts',(-60.5499623901782,1.04087449980872,
136.630965927865));
#174174=CARTESIAN_POINT('Ctrl Pts',(-60.5425605685028,0.885107985482796,
136.654532787386));
#174175=CARTESIAN_POINT('Ctrl Pts',(-60.5351626541915,0.72942369908752,
136.678087206145));
#174176=CARTESIAN_POINT('Ctrl Pts',(-60.5277647398802,0.572714593905674,
136.695435443345));
#174177=CARTESIAN_POINT('Ctrl Pts',(-60.5203668255688,0.415515455055614,
136.706502387221));
#174178=CARTESIAN_POINT('Ctrl Pts',(-60.5129701406566,0.258342439850548,
136.717567491972));
#174179=CARTESIAN_POINT('Ctrl Pts',(-60.5055734557445,0.100679924612702,
136.722353348917));
#174180=CARTESIAN_POINT('Ctrl Pts',(-60.4981767708323,-0.0569321080256532,
136.720836705372));
#174181=CARTESIAN_POINT('Ctrl Pts',(-60.4907804138969,-0.214537151981316,
136.719320129076));
#174182=CARTESIAN_POINT('Ctrl Pts',(-60.4833840569614,-0.372091344508002,
136.711501611543));
#174183=CARTESIAN_POINT('Ctrl Pts',(-60.475987700026,-0.529054895854471,
136.697410038678));
#174184=CARTESIAN_POINT('Ctrl Pts',(-60.4685902106894,-0.68604247872136,
136.683316308358));
#174185=CARTESIAN_POINT('Ctrl Pts',(-60.4611927213528,-0.84243886852604,
136.662947643763));
#174186=CARTESIAN_POINT('Ctrl Pts',(-60.4537952320163,-0.997709736852333,
136.636384781052));
#174187=CARTESIAN_POINT('Ctrl Pts',(-60.4463951495013,-1.15303503514082,
136.609812606772));
#174188=CARTESIAN_POINT('Ctrl Pts',(-60.4389950669864,-1.30723365868226,
136.577041974109));
#174189=CARTESIAN_POINT('Ctrl Pts',(-60.4315949844714,-1.45978195002596,
136.538204635402));
#174190=CARTESIAN_POINT('Ctrl Pts',(-60.424186764805,-1.61249798389834,
136.499324591049));
#174191=CARTESIAN_POINT('Ctrl Pts',(-60.4167785451385,-1.76355969949811,
136.45436461045));
#174192=CARTESIAN_POINT('Ctrl Pts',(-60.4093703254721,-1.91245836889943,
136.40350640507));
#174193=CARTESIAN_POINT('Ctrl Pts',(-60.40195754617,-2.06144868294747,136.352616897313));
#174194=CARTESIAN_POINT('Ctrl Pts',(-60.3945447668679,-2.20827295062666,
136.295822065392));
#174195=CARTESIAN_POINT('Ctrl Pts',(-60.3871319875659,-2.35244336766703,
136.233351386062));
#174196=CARTESIAN_POINT('Ctrl Pts',(-60.3797086165371,-2.49681978215999,
136.170791445697));
#174197=CARTESIAN_POINT('Ctrl Pts',(-60.3722852455084,-2.63853443721335,
136.10253962215));
#174198=CARTESIAN_POINT('Ctrl Pts',(-60.3648618744796,-2.77712429169874,
136.028871238759));
#174199=CARTESIAN_POINT('Ctrl Pts',(-60.3609258250386,-2.85060795796856,
135.989810494234));
#174200=CARTESIAN_POINT('Ctrl Pts',(-60.3569897755977,-2.92321360743758,
135.949227689603));
#174201=CARTESIAN_POINT('Ctrl Pts',(-60.3530537261567,-2.9948757269657,
135.907168662411));
#174202=CARTESIAN_POINT('Ctrl Pts',(-60.3456304597512,-3.13002824789162,
135.827846649746));
#174203=CARTESIAN_POINT('Ctrl Pts',(-60.3382071933459,-3.26223158466391,
135.743031527813));
#174204=CARTESIAN_POINT('Ctrl Pts',(-60.3307839269404,-3.39100783745323,
135.652968294913));
#174205=CARTESIAN_POINT('Ctrl Pts',(-60.3233694342194,-3.51963188740615,
135.563011509275));
#174206=CARTESIAN_POINT('Ctrl Pts',(-60.3159549414983,-3.64483661305601,
135.467819171294));
#174207=CARTESIAN_POINT('Ctrl Pts',(-60.3085404487773,-3.76616911139899,
135.367681862761));
#174208=CARTESIAN_POINT('Ctrl Pts',(-60.3011331024234,-3.88738466491198,
135.267641070335));
#174209=CARTESIAN_POINT('Ctrl Pts',(-60.2937257560696,-4.00473513521546,
135.162665031839));
#174210=CARTESIAN_POINT('Ctrl Pts',(-60.2863184097158,-4.11779709989725,
135.053087204036));
#174211=CARTESIAN_POINT('Ctrl Pts',(-60.2789165880403,-4.23077473870035,
134.943591103511));
#174212=CARTESIAN_POINT('Ctrl Pts',(-60.2715147663649,-4.33946997367944,
134.829500306308));
#174213=CARTESIAN_POINT('Ctrl Pts',(-60.2641129446894,-4.44349304584495,
134.711187989492));
#174214=CARTESIAN_POINT('Ctrl Pts',(-60.256715030378,-4.54746120504037,
134.592938128826));
#174215=CARTESIAN_POINT('Ctrl Pts',(-60.2493171160666,-4.64676186750825,
134.470471466364));
#174216=CARTESIAN_POINT('Ctrl Pts',(-60.2419192017553,-4.74104277517465,
134.344197332227));
#174217=CARTESIAN_POINT('Ctrl Pts',(-60.234522516843,-4.83530801506436,
134.217944182561));
#174218=CARTESIAN_POINT('Ctrl Pts',(-60.2271258319308,-4.92455493266152,
134.087885115836));
#174219=CARTESIAN_POINT('Ctrl Pts',(-60.2197291470186,-5.00847209102242,
133.95446186609));
#174220=CARTESIAN_POINT('Ctrl Pts',(-60.2123327900831,-5.09238552840858,
133.82104453247));
#174221=CARTESIAN_POINT('Ctrl Pts',(-60.2049364331476,-5.1709694777115,
133.684263628425));
#174222=CARTESIAN_POINT('Ctrl Pts',(-60.1975400762121,-5.24395647191723,
133.544588907898));
#174223=CARTESIAN_POINT('Ctrl Pts',(-60.1901425868755,-5.31695464061809,
133.404892802816));
#174224=CARTESIAN_POINT('Ctrl Pts',(-60.1827450975389,-5.38435397510693,
133.26230232995));
#174225=CARTESIAN_POINT('Ctrl Pts',(-60.1753476082023,-5.44593358344121,
133.117310674797));
#174226=CARTESIAN_POINT('Ctrl Pts',(-60.1679475256873,-5.50753477841182,
132.972268193045));
#174227=CARTESIAN_POINT('Ctrl Pts',(-60.1605474431723,-5.56331203957477,
132.824823196505));
#174228=CARTESIAN_POINT('Ctrl Pts',(-60.1531473606573,-5.61309316426054,
132.675487468379));
#174229=CARTESIAN_POINT('Ctrl Pts',(-60.1457391409908,-5.66292902841053,
132.525987530267));
#174230=CARTESIAN_POINT('Ctrl Pts',(-60.1383309213242,-5.70675547056859,
132.374593062919));
#174231=CARTESIAN_POINT('Ctrl Pts',(-60.1309227016577,-5.74445038986613,
132.221830293032));
#174232=CARTESIAN_POINT('Ctrl Pts',(-60.1235099223556,-5.78216850975747,
132.06897350021));
#174233=CARTESIAN_POINT('Ctrl Pts',(-60.1160971430536,-5.81374751221079,
131.914747091587));
#174234=CARTESIAN_POINT('Ctrl Pts',(-60.1086843637515,-5.83911679239732,
131.759685508503));
#174235=CARTESIAN_POINT('Ctrl Pts',(-60.1012609927227,-5.86452232140111,
131.604402366157));
#174236=CARTESIAN_POINT('Ctrl Pts',(-60.093837621694,-5.88370036188762,
131.448282035521));
#174237=CARTESIAN_POINT('Ctrl Pts',(-60.0864142506652,-5.89663226613734,
131.2918629052));
#174238=CARTESIAN_POINT('Ctrl Pts',(-60.0824782012247,-5.90348907206677,
131.208925729084));
#174239=CARTESIAN_POINT('Ctrl Pts',(-60.0785421517842,-5.90859073619492,
131.125904542705));
#174240=CARTESIAN_POINT('Ctrl Pts',(-60.0746061023437,-5.91194041149315,
131.042879240433));
#174241=CARTESIAN_POINT('Ctrl Pts',(-60.0708624656306,-5.91512633880762,
130.963912607924));
#174242=CARTESIAN_POINT('Ctrl Pts',(-60.0671188289174,-5.916730195719,130.884881716305));
#174243=CARTESIAN_POINT('Ctrl Pts',(-60.0633751922041,-5.91674981773242,
130.80582924392));
#174244=CARTESIAN_POINT('',(-58.3133751922041,-5.91156881184207,130.80911788525));
#174245=CARTESIAN_POINT('Ctrl Pts',(-60.0633736607459,-5.92609170103476,
130.80579917263));
#174246=CARTESIAN_POINT('Ctrl Pts',(-59.9743019333409,-5.91980991597853,
128.921945335877));
#174247=CARTESIAN_POINT('Ctrl Pts',(-59.7924143313318,-3.92743761287679,
125.063652292068));
#174248=CARTESIAN_POINT('Ctrl Pts',(-59.5177108547178,2.6500406791028,124.327104645363));
#174249=CARTESIAN_POINT('Ctrl Pts',(-59.2392632309052,6.8819106127336,129.532799825198));
#174250=CARTESIAN_POINT('Ctrl Pts',(-58.960815607092,4.78964089328673,135.906997254022));
#174251=CARTESIAN_POINT('Ctrl Pts',(-58.6823679832794,-1.70407482012499,
137.5921208916));
#174252=CARTESIAN_POINT('Ctrl Pts',(-58.4665545116499,-5.52337744944411,
134.063665339323));
#174253=CARTESIAN_POINT('Ctrl Pts',(-58.3435569146249,-5.9163895394015,
131.451508990351));
#174254=CARTESIAN_POINT('Ctrl Pts',(-58.3133751922041,-5.91156881184207,
130.80911788525));
#174255=CARTESIAN_POINT('',(-56.5633751922042,-5.90884967465456,130.801001847959));
#174256=CARTESIAN_POINT('Ctrl Pts',(-58.3133751922041,-5.91156881184207,
130.80911788525));
#174257=CARTESIAN_POINT('Ctrl Pts',(-58.2507410400206,-5.90156467160833,
129.476005689816));
#174258=CARTESIAN_POINT('Ctrl Pts',(-58.095291013233,-4.79442660150182,
126.152340551137));
#174259=CARTESIAN_POINT('Ctrl Pts',(-57.8470251118403,0.723619930605998,
123.843474558564));
#174260=CARTESIAN_POINT('Ctrl Pts',(-57.5685774880279,6.24752483186355,
127.65063361518));
#174261=CARTESIAN_POINT('Ctrl Pts',(-57.2901298642149,6.03025962119851,
134.355913718856));
#174262=CARTESIAN_POINT('Ctrl Pts',(-57.0116822404018,0.271480413209222,
137.797490025462));
#174263=CARTESIAN_POINT('Ctrl Pts',(-56.7694306830652,-4.95574853847363,
135.200719103271));
#174264=CARTESIAN_POINT('Ctrl Pts',(-56.6199950003325,-5.90264780731658,
132.007497243329));
#174265=CARTESIAN_POINT('Ctrl Pts',(-56.5633751922042,-5.90884967465456,
130.801001847959));
#174266=CARTESIAN_POINT('',(-54.8133751922042,-5.92388329333877,130.80082555441));
#174267=CARTESIAN_POINT('Ctrl Pts',(-56.5633751922042,-5.90884967465456,
130.801001847959));
#174268=CARTESIAN_POINT('Ctrl Pts',(-56.5271791257282,-5.91281442144304,
130.02971015734));
#174269=CARTESIAN_POINT('Ctrl Pts',(-56.3981671846476,-5.41337615916817,
127.285565116781));
#174270=CARTESIAN_POINT('Ctrl Pts',(-56.1763393689635,-1.26108622347638,
123.9205228749));
#174271=CARTESIAN_POINT('Ctrl Pts',(-55.8978917451504,5.10991974578196,
126.022490614944));
#174272=CARTESIAN_POINT('Ctrl Pts',(-55.6194441213376,6.78515910212911,
132.518763280054));
#174273=CARTESIAN_POINT('Ctrl Pts',(-55.3409964975246,2.22516871706598,
137.439583651567));
#174274=CARTESIAN_POINT('Ctrl Pts',(-55.0723068544802,-4.14818251483082,
136.304192128701));
#174275=CARTESIAN_POINT('Ctrl Pts',(-54.89643308604,-5.91148057148662,132.559222115526));
#174276=CARTESIAN_POINT('Ctrl Pts',(-54.8133751922042,-5.92388329333877,
130.80082555441));
#174277=CARTESIAN_POINT('',(-53.0633751922041,-5.91880835334059,130.809427504538));
#174278=CARTESIAN_POINT('Ctrl Pts',(-54.8133751922042,-5.92388329333877,
130.80082555441));
#174279=CARTESIAN_POINT('Ctrl Pts',(-54.8036172114357,-5.92534041578338,
130.59424194105));
#174280=CARTESIAN_POINT('Ctrl Pts',(-54.7010433560634,-5.82163645082206,
128.424157715391));
#174281=CARTESIAN_POINT('Ctrl Pts',(-54.5056536260855,-3.14421568114513,
124.552043584596));
#174282=CARTESIAN_POINT('Ctrl Pts',(-54.2272060022732,3.56072601726273,
124.779512838547));
#174283=CARTESIAN_POINT('Ctrl Pts',(-53.9487583784601,6.99353445694264,
130.543522871244));
#174284=CARTESIAN_POINT('Ctrl Pts',(-53.6703107546473,3.99962638384432,
136.547230050173));
#174285=CARTESIAN_POINT('Ctrl Pts',(-53.3918631308343,-2.66974294339494,
137.27352077531));
#174286=CARTESIAN_POINT('Ctrl Pts',(-53.1895512766867,-5.7329688978399,
133.481874791569));
#174287=CARTESIAN_POINT('Ctrl Pts',(-53.0800552971433,-5.92313625057596,
131.163173995511));
#174288=CARTESIAN_POINT('Ctrl Pts',(-53.0633751922041,-5.9199225285852,
130.809428458345));
#174289=CARTESIAN_POINT('',(-51.313375216539,-5.9114707548659,130.80551579402));
#174290=CARTESIAN_POINT('Ctrl Pts',(-53.0633751922041,-5.91674783196214,
130.809425740597));
#174291=CARTESIAN_POINT('Ctrl Pts',(-53.0560738687434,-5.91688031615351,
130.654666310814));
#174292=CARTESIAN_POINT('Ctrl Pts',(-53.0487725452826,-5.91093678929377,
130.499695394686));
#174293=CARTESIAN_POINT('Ctrl Pts',(-53.0414712218218,-5.89889421094919,
130.345037582513));
#174294=CARTESIAN_POINT('Ctrl Pts',(-53.0341762556043,-5.88686211804603,
130.190514430493));
#174295=CARTESIAN_POINT('Ctrl Pts',(-53.0268812893869,-5.86874157038524,
130.036304221831));
#174296=CARTESIAN_POINT('Ctrl Pts',(-53.0195863231694,-5.84456157651281,
129.882932084879));
#174297=CARTESIAN_POINT('Ctrl Pts',(-53.0122960072682,-5.82039699664201,
129.729657717942));
#174298=CARTESIAN_POINT('Ctrl Pts',(-53.0050056913671,-5.79018071829052,
129.577220738767));
#174299=CARTESIAN_POINT('Ctrl Pts',(-52.9977153754659,-5.75399360318452,
129.426141412573));
#174300=CARTESIAN_POINT('Ctrl Pts',(-52.9904271935296,-5.71781708049078,
129.27510630915));
#174301=CARTESIAN_POINT('Ctrl Pts',(-52.9831390115933,-5.67567328381649,
129.125428443235));
#174302=CARTESIAN_POINT('Ctrl Pts',(-52.975850829657,-5.62769420842712,
128.977618036101));
#174303=CARTESIAN_POINT('Ctrl Pts',(-52.9685634929614,-5.57972069737013,
128.829824771154));
#174304=CARTESIAN_POINT('Ctrl Pts',(-52.9612761562658,-5.52591337242735,
128.683898900805));
#174305=CARTESIAN_POINT('Ctrl Pts',(-52.9539888195702,-5.46645404004436,
128.540335266431));
#174306=CARTESIAN_POINT('Ctrl Pts',(-52.9467007900094,-5.40698905438916,
128.396757982319));
#174307=CARTESIAN_POINT('Ctrl Pts',(-52.9394127604487,-5.34187113974337,
128.255543737113));
#174308=CARTESIAN_POINT('Ctrl Pts',(-52.9321247308879,-5.27133003934232,
128.117166880816));
#174309=CARTESIAN_POINT('Ctrl Pts',(-52.9248344699682,-5.20076734153747,
127.978747658001));
#174310=CARTESIAN_POINT('Ctrl Pts',(-52.9175442090485,-5.12477832970221,
127.843167895492));
#174311=CARTESIAN_POINT('Ctrl Pts',(-52.9102539481288,-5.04363827206326,
127.71087657153));
#174312=CARTESIAN_POINT('Ctrl Pts',(-52.9029560283258,-4.96241297162721,
127.578446267109));
#174313=CARTESIAN_POINT('Ctrl Pts',(-52.8956581085228,-4.8760260235918,
127.44931162676));
#174314=CARTESIAN_POINT('Ctrl Pts',(-52.8883601887198,-4.78479581982511,
127.323892326505));
#174315=CARTESIAN_POINT('Ctrl Pts',(-52.8810578861492,-4.69351082773637,
127.198397705657));
#174316=CARTESIAN_POINT('Ctrl Pts',(-52.8737555835786,-4.59737702659977,
127.076623169065));
#174317=CARTESIAN_POINT('Ctrl Pts',(-52.866453281008,-4.49675195989873,
126.958953958492));
#174318=CARTESIAN_POINT('Ctrl Pts',(-52.8591408388067,-4.39598717000699,
126.84112135804));
#174319=CARTESIAN_POINT('Ctrl Pts',(-52.8518283966053,-4.29071892636813,
126.727405744225));
#174320=CARTESIAN_POINT('Ctrl Pts',(-52.844515954404,-4.18134074351241,
126.618154680307));
#174321=CARTESIAN_POINT('Ctrl Pts',(-52.8413332640055,-4.13373463835684,
126.570603902799));
#174322=CARTESIAN_POINT('Ctrl Pts',(-52.8381505736071,-4.08535037470118,
126.523898349799));
#174323=CARTESIAN_POINT('Ctrl Pts',(-52.8349678832086,-4.03622221003705,
126.478064183697));
#174324=CARTESIAN_POINT('Ctrl Pts',(-52.8275446168032,-3.92163630671296,
126.371161160517));
#174325=CARTESIAN_POINT('Ctrl Pts',(-52.8201213503977,-3.8026270667802,
126.268652000085));
#174326=CARTESIAN_POINT('Ctrl Pts',(-52.8126980839923,-3.67956565674869,
126.170924836186));
#174327=CARTESIAN_POINT('Ctrl Pts',(-52.8052835912713,-3.55664969508404,
126.073313177678));
#174328=CARTESIAN_POINT('Ctrl Pts',(-52.7978690985503,-3.42969138598225,
125.980472495404));
#174329=CARTESIAN_POINT('Ctrl Pts',(-52.7904546058293,-3.29909845275371,
125.892753959706));
#174330=CARTESIAN_POINT('Ctrl Pts',(-52.7830472594756,-3.16863138991114,
125.805119970434));
#174331=CARTESIAN_POINT('Ctrl Pts',(-52.7756399131217,-3.0345369849,125.722598506056));
#174332=CARTESIAN_POINT('Ctrl Pts',(-52.7682325667679,-2.89725564261266,
125.645500248856));
#174333=CARTESIAN_POINT('Ctrl Pts',(-52.7608307450925,-2.76007668992973,
125.568459494444));
#174334=CARTESIAN_POINT('Ctrl Pts',(-52.7534289234172,-2.61971585685554,
125.49683407541));
#174335=CARTESIAN_POINT('Ctrl Pts',(-52.7460271017418,-2.47664201289675,
125.430891077087));
#174336=CARTESIAN_POINT('Ctrl Pts',(-52.7386291874304,-2.3336436965067,
125.36498288956));
#174337=CARTESIAN_POINT('Ctrl Pts',(-52.731231273119,-2.18793555964505,
125.304751304547));
#174338=CARTESIAN_POINT('Ctrl Pts',(-52.7238333588077,-2.04001042257452,
125.250417150237));
#174339=CARTESIAN_POINT('Ctrl Pts',(-52.7164366738955,-1.89210986797813,
125.196092025277));
#174340=CARTESIAN_POINT('Ctrl Pts',(-52.7090399889834,-1.74199339445259,
125.147662514501));
#174341=CARTESIAN_POINT('Ctrl Pts',(-52.7016433040712,-1.59017323240424,
125.105301076427));
#174342=CARTESIAN_POINT('Ctrl Pts',(-52.6942469471357,-1.43835980222074,
125.062941516704));
#174343=CARTESIAN_POINT('Ctrl Pts',(-52.6868505902002,-1.28484319328321,
125.02664959502));
#174344=CARTESIAN_POINT('Ctrl Pts',(-52.6794542332648,-1.13014994595898,
124.996547633133));
#174345=CARTESIAN_POINT('Ctrl Pts',(-52.6720567439282,-0.97543301470345,
124.966441062559));
#174346=CARTESIAN_POINT('Ctrl Pts',(-52.6646592545916,-0.819539452814311,
124.942526410084));
#174347=CARTESIAN_POINT('Ctrl Pts',(-52.657261765255,-0.663004969701697,
124.924874672974));
#174348=CARTESIAN_POINT('Ctrl Pts',(-52.64986168274,-0.50641561366891,124.907216748076));
#174349=CARTESIAN_POINT('Ctrl Pts',(-52.6424616002251,-0.349185259803934,
124.895826151482));
#174350=CARTESIAN_POINT('Ctrl Pts',(-52.6350615177101,-0.191853550423675,
124.890721908811));
#174351=CARTESIAN_POINT('Ctrl Pts',(-52.6276532980436,-0.034348838654634,
124.8856120535));
#174352=CARTESIAN_POINT('Ctrl Pts',(-52.6202450783771,0.123257077873727,
124.886802368925));
#174353=CARTESIAN_POINT('Ctrl Pts',(-52.6128368587106,0.280425008487276,
124.894259740498));
#174354=CARTESIAN_POINT('Ctrl Pts',(-52.6054240794086,0.43768967333963,
124.90172170196));
#174355=CARTESIAN_POINT('Ctrl Pts',(-52.5980113001065,0.594515444107284,
124.915458373162));
#174356=CARTESIAN_POINT('Ctrl Pts',(-52.5905985208045,0.750369949499985,
124.935384940211));
#174357=CARTESIAN_POINT('Ctrl Pts',(-52.5831751497757,0.906447147118842,
124.955339979273));
#174358=CARTESIAN_POINT('Ctrl Pts',(-52.5757517787469,1.06154994051297,
124.981502516532));
#174359=CARTESIAN_POINT('Ctrl Pts',(-52.5683284077181,1.21515699932609,
125.013736814426));
#174360=CARTESIAN_POINT('Ctrl Pts',(-52.5643923582773,1.29660314766047,
125.030828212621));
#174361=CARTESIAN_POINT('Ctrl Pts',(-52.5604563088365,1.37762904656777,
125.049625767575));
#174362=CARTESIAN_POINT('Ctrl Pts',(-52.5565202593957,1.45815902216238,
125.070103662338));
#174363=CARTESIAN_POINT('Ctrl Pts',(-52.5490969929903,1.61003604287771,
125.108724332765));
#174364=CARTESIAN_POINT('Ctrl Pts',(-52.5416737265848,1.76060730390585,
125.153441471698));
#174365=CARTESIAN_POINT('Ctrl Pts',(-52.5342504601794,1.90934563273537,
125.204152602032));
#174366=CARTESIAN_POINT('Ctrl Pts',(-52.5268359674584,2.05790816521238,
125.254803796021));
#174367=CARTESIAN_POINT('Ctrl Pts',(-52.5194214747373,2.204641727793,125.311434760585));
#174368=CARTESIAN_POINT('Ctrl Pts',(-52.5120069820163,2.34903048651398,
125.373892282705));
#174369=CARTESIAN_POINT('Ctrl Pts',(-52.5045996356626,2.49328007791296,
125.436289605913));
#174370=CARTESIAN_POINT('Ctrl Pts',(-52.4971922893088,2.63518902437024,
125.504502159405));
#174371=CARTESIAN_POINT('Ctrl Pts',(-52.489784942955,2.77425789047849,125.578327349434));
#174372=CARTESIAN_POINT('Ctrl Pts',(-52.4823831212796,2.91322303377983,
125.652097477852));
#174373=CARTESIAN_POINT('Ctrl Pts',(-52.4749812996041,3.04935198613164,
125.731471733407));
#174374=CARTESIAN_POINT('Ctrl Pts',(-52.4675794779287,3.18216660565613,
125.81620000905));
#174375=CARTESIAN_POINT('Ctrl Pts',(-52.4601815636174,3.31491111337623,
125.900883557297));
#174376=CARTESIAN_POINT('Ctrl Pts',(-52.4527836493061,3.44434445878719,
125.990915296569));
#174377=CARTESIAN_POINT('Ctrl Pts',(-52.4453857349948,3.57001447149046,
126.085999966254));
#174378=CARTESIAN_POINT('Ctrl Pts',(-52.4379890500826,3.69566360011804,
126.181068834592));
#174379=CARTESIAN_POINT('Ctrl Pts',(-52.4305923651704,3.8175503398691,126.281188741757));
#174380=CARTESIAN_POINT('Ctrl Pts',(-52.4231956802582,3.93525272345958,
126.386021951845));
#174381=CARTESIAN_POINT('Ctrl Pts',(-52.4157993233228,4.05294988800302,
126.490850513518));
#174382=CARTESIAN_POINT('Ctrl Pts',(-52.4084029663873,4.16646278653926,
126.600391714284));
#174383=CARTESIAN_POINT('Ctrl Pts',(-52.4010066094519,4.27540389837806,
126.714268678717));
#174384=CARTESIAN_POINT('Ctrl Pts',(-52.3936091201153,4.38436168937888,
126.828163078004));
#174385=CARTESIAN_POINT('Ctrl Pts',(-52.3862116307787,4.48874604191685,
126.946394292946));
#174386=CARTESIAN_POINT('Ctrl Pts',(-52.3788141414421,4.58820765995969,
127.0685499918));
#174387=CARTESIAN_POINT('Ctrl Pts',(-52.3714140589272,4.68770414411854,
127.190748512145));
#174388=CARTESIAN_POINT('Ctrl Pts',(-52.3640139764122,4.78227422246028,
127.316873966156));
#174389=CARTESIAN_POINT('Ctrl Pts',(-52.3566138938972,4.8716101983397,127.446482621281));
#174390=CARTESIAN_POINT('Ctrl Pts',(-52.3492056742307,4.96104440830883,
127.576233794447));
#174391=CARTESIAN_POINT('Ctrl Pts',(-52.3417974545643,5.04523280985229,
127.709475510216));
#174392=CARTESIAN_POINT('Ctrl Pts',(-52.3343892348978,5.12391181748065,
127.845736232961));
#174393=CARTESIAN_POINT('Ctrl Pts',(-52.3269764555957,5.20263925072538,
127.982080821906));
#174394=CARTESIAN_POINT('Ctrl Pts',(-52.3195636762936,5.27585035998211,
128.121447790711));
#174395=CARTESIAN_POINT('Ctrl Pts',(-52.3121508969916,5.34332874189719,
128.26334339635));
#174396=CARTESIAN_POINT('Ctrl Pts',(-52.3047275259628,5.41090354008868,
128.405441749085));
#174397=CARTESIAN_POINT('Ctrl Pts',(-52.2973041549342,5.47272910495652,
128.55007561235));
#174398=CARTESIAN_POINT('Ctrl Pts',(-52.2898807839054,5.52863784456495,
128.696733006686));
#174399=CARTESIAN_POINT('Ctrl Pts',(-52.2859447344646,5.55828199981758,
128.77449427616));
#174400=CARTESIAN_POINT('Ctrl Pts',(-52.2820086850237,5.58626356198724,
128.852824197292));
#174401=CARTESIAN_POINT('Ctrl Pts',(-52.2780726355828,5.61256334802277,
128.931645148806));
#174402=CARTESIAN_POINT('Ctrl Pts',(-52.2706493691774,5.6621639236969,129.080299003443));
#174403=CARTESIAN_POINT('Ctrl Pts',(-52.2632261027721,5.70592957275061,
129.231149575616));
#174404=CARTESIAN_POINT('Ctrl Pts',(-52.2558028363666,5.74366156245514,
129.383697948782));
#174405=CARTESIAN_POINT('Ctrl Pts',(-52.2483883436456,5.78134895608134,
129.53606602244));
#174406=CARTESIAN_POINT('Ctrl Pts',(-52.2409738509246,5.81301679646227,
129.690127543985));
#174407=CARTESIAN_POINT('Ctrl Pts',(-52.2335593582035,5.83851516519413,
129.845365712315));
#174408=CARTESIAN_POINT('Ctrl Pts',(-52.2261520118498,5.86398895763818,
130.000454256253));
#174409=CARTESIAN_POINT('Ctrl Pts',(-52.2187446654959,5.88330505638482,
130.156716823324));
#174410=CARTESIAN_POINT('Ctrl Pts',(-52.2113373191421,5.89636395225233,
130.313623717507));
#174411=CARTESIAN_POINT('Ctrl Pts',(-52.2039354974668,5.90941310830254,
130.470413584608));
#174412=CARTESIAN_POINT('Ctrl Pts',(-52.1965336757915,5.91621432298951,
130.627846451544));
#174413=CARTESIAN_POINT('Ctrl Pts',(-52.1891318541161,5.91671957109146,
130.785384855043));
#174414=CARTESIAN_POINT('Ctrl Pts',(-52.1817339398047,5.91722455247687,
130.942840095246));
#174415=CARTESIAN_POINT('Ctrl Pts',(-52.1743360254934,5.91144018517517,
131.100400388709));
#174416=CARTESIAN_POINT('Ctrl Pts',(-52.166938111182,5.89937047115848,131.257525716093));
#174417=CARTESIAN_POINT('Ctrl Pts',(-52.1595414262698,5.88730276290932,
131.414624932099));
#174418=CARTESIAN_POINT('Ctrl Pts',(-52.1521447413576,5.86895180955259,
131.571288953651));
#174419=CARTESIAN_POINT('Ctrl Pts',(-52.1447480564454,5.84437367424631,
131.726980213216));
#174420=CARTESIAN_POINT('Ctrl Pts',(-52.1373516995099,5.81979662876026,
131.882664569267));
#174421=CARTESIAN_POINT('Ctrl Pts',(-52.1299553425744,5.78899300855361,
132.037375880365));
#174422=CARTESIAN_POINT('Ctrl Pts',(-52.122558985639,5.75207042519614,132.190584404003));
#174423=CARTESIAN_POINT('Ctrl Pts',(-52.1151614963024,5.71514218889695,
132.343816384257));
#174424=CARTESIAN_POINT('Ctrl Pts',(-52.1077640069658,5.6720932115609,132.495544756));
#174425=CARTESIAN_POINT('Ctrl Pts',(-52.1003665176293,5.62308159652317,
132.645252771208));
#174426=CARTESIAN_POINT('Ctrl Pts',(-52.0929664351143,5.57405280053977,
132.79501326633));
#174427=CARTESIAN_POINT('Ctrl Pts',(-52.0855663525993,5.51905732136755,
132.942751640281));
#174428=CARTESIAN_POINT('Ctrl Pts',(-52.0781662700843,5.45830216621815,
133.087969170878));
#174429=CARTESIAN_POINT('Ctrl Pts',(-52.0707580504178,5.3974802045298,133.233346383078));
#174430=CARTESIAN_POINT('Ctrl Pts',(-52.0633498307514,5.33088606290201,
133.376196871619));
#174431=CARTESIAN_POINT('Ctrl Pts',(-52.0559416110849,5.25877398321794,
133.516043998038));
#174432=CARTESIAN_POINT('Ctrl Pts',(-52.0485288317828,5.18661751975208,
133.655977198031));
#174433=CARTESIAN_POINT('Ctrl Pts',(-52.0411160524808,5.1089365346525,133.792903028561));
#174434=CARTESIAN_POINT('Ctrl Pts',(-52.0337032731787,5.02602945661223,
133.926372543194));
#174435=CARTESIAN_POINT('Ctrl Pts',(-52.02627990215,4.94300391705102,134.060032765329));
#174436=CARTESIAN_POINT('Ctrl Pts',(-52.0188565311212,4.85473757962601,
134.190226500017));
#174437=CARTESIAN_POINT('Ctrl Pts',(-52.0114331600925,4.76157059962359,
134.316536010012));
#174438=CARTESIAN_POINT('Ctrl Pts',(-52.0074971106516,4.71217123131458,
134.383508342967));
#174439=CARTESIAN_POINT('Ctrl Pts',(-52.0035610612108,4.66139476808778,
134.449389259386));
#174440=CARTESIAN_POINT('Ctrl Pts',(-51.9996250117699,4.60929614601334,
134.514120663829));
#174441=CARTESIAN_POINT('Ctrl Pts',(-51.9922017453645,4.51103977072458,
134.636202072408));
#174442=CARTESIAN_POINT('Ctrl Pts',(-51.9847784789591,4.40778131439432,
134.754561771454));
#174443=CARTESIAN_POINT('Ctrl Pts',(-51.9773552125536,4.29983310974557,
134.868762884915));
#174444=CARTESIAN_POINT('Ctrl Pts',(-51.9699407198326,4.19201249091017,
134.982829022145));
#174445=CARTESIAN_POINT('Ctrl Pts',(-51.9625262271117,4.07951341084149,
135.092746088694));
#174446=CARTESIAN_POINT('Ctrl Pts',(-51.9551117343906,3.96268963438439,
135.198108610344));
#174447=CARTESIAN_POINT('Ctrl Pts',(-51.9477043880368,3.84597845708105,
135.30336957963));
#174448=CARTESIAN_POINT('Ctrl Pts',(-51.9402970416831,3.72495115701242,
135.404084494993));
#174449=CARTESIAN_POINT('Ctrl Pts',(-51.9328896953293,3.5999995952991,135.499883322904));
#174450=CARTESIAN_POINT('Ctrl Pts',(-51.9254878736538,3.47514122717394,
135.595610700435));
#174451=CARTESIAN_POINT('Ctrl Pts',(-51.9180860519783,3.3463647201556,135.686429065064));
#174452=CARTESIAN_POINT('Ctrl Pts',(-51.9106842303029,3.21409629851096,
135.772007499783));
#174453=CARTESIAN_POINT('Ctrl Pts',(-51.9032863159915,3.08189770033766,
135.857540758312));
#174454=CARTESIAN_POINT('Ctrl Pts',(-51.8958884016802,2.94621117129102,
135.937839393519));
#174455=CARTESIAN_POINT('Ctrl Pts',(-51.8884904873688,2.80749320809699,
136.012614878735));
#174456=CARTESIAN_POINT('Ctrl Pts',(-51.8810938024566,2.66879829731183,
136.087377937623));
#174457=CARTESIAN_POINT('Ctrl Pts',(-51.8736971175444,2.52707328048832,
136.156619491218));
#174458=CARTESIAN_POINT('Ctrl Pts',(-51.8663004326322,2.38280073192316,
136.220096138661));
#174459=CARTESIAN_POINT('Ctrl Pts',(-51.8589040756968,2.23853458055379,
136.283569971483));
#174460=CARTESIAN_POINT('Ctrl Pts',(-51.8515077187613,2.09172146373359,
136.341279256081));
#174461=CARTESIAN_POINT('Ctrl Pts',(-51.8441113618258,1.94286523551681,
136.393028190353));
#174462=CARTESIAN_POINT('Ctrl Pts',(-51.8367138724892,1.79398621703191,
136.444785047519));
#174463=CARTESIAN_POINT('Ctrl Pts',(-51.8293163831528,1.64306381693422,
136.490579614774));
#174464=CARTESIAN_POINT('Ctrl Pts',(-51.8219188938162,1.49061824868513,
136.530265594003));
#174465=CARTESIAN_POINT('Ctrl Pts',(-51.8145188113012,1.33811924087842,
136.569965485091));
#174466=CARTESIAN_POINT('Ctrl Pts',(-51.8071187287862,1.18409636287308,
136.603552430741));
#174467=CARTESIAN_POINT('Ctrl Pts',(-51.7997186462712,1.02908109622292,
136.630931020461));
#174468=CARTESIAN_POINT('Ctrl Pts',(-51.7923104266047,0.87389537435112,
136.658339715755));
#174469=CARTESIAN_POINT('Ctrl Pts',(-51.7849022069383,0.717715452403777,
136.679526356733));
#174470=CARTESIAN_POINT('Ctrl Pts',(-51.7774939872719,0.561079763766469,
136.69444720956));
#174471=CARTESIAN_POINT('Ctrl Pts',(-51.7700812079698,0.404347668476189,
136.709377245923));
#174472=CARTESIAN_POINT('Ctrl Pts',(-51.7626684286677,0.247159619399972,
136.718033789121));
#174473=CARTESIAN_POINT('Ctrl Pts',(-51.7552556493657,0.0900546358877009,
136.720425249148));
#174474=CARTESIAN_POINT('Ctrl Pts',(-51.7478322783369,-0.0672748265925056,
136.722820126206));
#174475=CARTESIAN_POINT('Ctrl Pts',(-51.7404089073082,-0.224520614267026,
136.718932050455));
#174476=CARTESIAN_POINT('Ctrl Pts',(-51.7329855362795,-0.381147410718013,
136.708821406986));
#174477=CARTESIAN_POINT('Ctrl Pts',(-51.7290494868387,-0.464194696405279,
136.703460501218));
#174478=CARTESIAN_POINT('Ctrl Pts',(-51.7251134373979,-0.54706809589055,
136.696351069196));
#174479=CARTESIAN_POINT('Ctrl Pts',(-51.7211773879571,-0.629689037547038,
136.687507928189));
#174480=CARTESIAN_POINT('Ctrl Pts',(-51.7137541215516,-0.785509554999487,
136.670830040235));
#174481=CARTESIAN_POINT('Ctrl Pts',(-51.7063308551461,-0.940902639802616,
136.647932084924));
#174482=CARTESIAN_POINT('Ctrl Pts',(-51.6989075887406,-1.09533191229578,
136.618840694444));
#174483=CARTESIAN_POINT('Ctrl Pts',(-51.6914930960196,-1.24957866221319,
136.589783687571));
#174484=CARTESIAN_POINT('Ctrl Pts',(-51.6840786032987,-1.40286350403403,
136.554547884713));
#174485=CARTESIAN_POINT('Ctrl Pts',(-51.6766641105777,-1.55465408227488,
136.513211749533));
#174486=CARTESIAN_POINT('Ctrl Pts',(-51.6692567642239,-1.7062983590414,
136.471915455677));
#174487=CARTESIAN_POINT('Ctrl Pts',(-51.6618494178702,-1.85645088167409,
136.424530632311));
#174488=CARTESIAN_POINT('Ctrl Pts',(-51.6544420715164,-2.00458851997636,
136.371186951132));
#174489=CARTESIAN_POINT('Ctrl Pts',(-51.6470402498409,-2.15261567164096,
136.317883055682));
#174490=CARTESIAN_POINT('Ctrl Pts',(-51.6396384281654,-2.2986305814974,
136.25862927763));
#174491=CARTESIAN_POINT('Ctrl Pts',(-51.6322366064899,-2.44212445506916,
136.193605342799));
#174492=CARTESIAN_POINT('Ctrl Pts',(-51.6248386921785,-2.58554257934057,
136.128615733598));
#174493=CARTESIAN_POINT('Ctrl Pts',(-51.6174407778672,-2.72644197859387,
136.057862187601));
#174494=CARTESIAN_POINT('Ctrl Pts',(-51.6100428635558,-2.86433315953933,
135.981572812721));
#174495=CARTESIAN_POINT('Ctrl Pts',(-51.6026461786436,-3.00220142547232,
135.905296115751));
#174496=CARTESIAN_POINT('Ctrl Pts',(-51.5952494937313,-3.13706213895409,
135.823485596273));
#174497=CARTESIAN_POINT('Ctrl Pts',(-51.587852808819,-3.26844967675284,
135.7364156936));
#174498=CARTESIAN_POINT('Ctrl Pts',(-51.5804564518836,-3.39983138869029,
135.649349651698));
#174499=CARTESIAN_POINT('Ctrl Pts',(-51.5730600949482,-3.52773991998567,
135.557024896506));
#174500=CARTESIAN_POINT('Ctrl Pts',(-51.5656637380127,-3.65173819136145,
135.459759498892));
#174501=CARTESIAN_POINT('Ctrl Pts',(-51.5582662486762,-3.77575544718895,
135.362479209697));
#174502=CARTESIAN_POINT('Ctrl Pts',(-51.5508687593395,-3.89586095732777,
135.260257002346));
#174503=CARTESIAN_POINT('Ctrl Pts',(-51.543471270003,-4.01165044894745,
135.153451469452));
#174504=CARTESIAN_POINT('Ctrl Pts',(-51.5360711874879,-4.12748053039493,
135.046608496043));
#174505=CARTESIAN_POINT('Ctrl Pts',(-51.5286711049729,-4.23899130678344,
134.935179251152));
#174506=CARTESIAN_POINT('Ctrl Pts',(-51.5212710224578,-4.34581522780061,
134.819559313561));
#174507=CARTESIAN_POINT('Ctrl Pts',(-51.5138628027913,-4.45275661269994,
134.703812239962));
#174508=CARTESIAN_POINT('Ctrl Pts',(-51.5064545831248,-4.55500059651085,
134.583865545343));
#174509=CARTESIAN_POINT('Ctrl Pts',(-51.4990463634584,-4.65221934832278,
134.460148589754));
#174510=CARTESIAN_POINT('Ctrl Pts',(-51.4916335841563,-4.74949793665456,
134.336355488442));
#174511=CARTESIAN_POINT('Ctrl Pts',(-51.4842208048541,-4.84174491166975,
134.208787804002));
#174512=CARTESIAN_POINT('Ctrl Pts',(-51.476808025552,-4.92867599581161,
134.077903574488));
#174513=CARTESIAN_POINT('Ctrl Pts',(-51.4693846545233,-5.01573129116279,
133.946832331448));
#174514=CARTESIAN_POINT('Ctrl Pts',(-51.4619612834945,-5.09745533209747,
133.812435396931));
#174515=CARTESIAN_POINT('Ctrl Pts',(-51.4545379124658,-5.1736095707027,
133.675195787414));
#174516=CARTESIAN_POINT('Ctrl Pts',(-51.4506018630252,-5.21398837530511,
133.602428053432));
#174517=CARTESIAN_POINT('Ctrl Pts',(-51.4466658135846,-5.25280210551076,
133.528861493687));
#174518=CARTESIAN_POINT('Ctrl Pts',(-51.442729764144,-5.29002075762279,
133.454570221809));
#174519=CARTESIAN_POINT('Ctrl Pts',(-51.4347880966952,-5.3651158910625,
133.304674600701));
#174520=CARTESIAN_POINT('Ctrl Pts',(-51.4268464292464,-5.43391710599038,
133.151423594091));
#174521=CARTESIAN_POINT('Ctrl Pts',(-51.4189047617976,-5.49613374452766,
132.995352270851));
#174522=CARTESIAN_POINT('Ctrl Pts',(-51.4109782153217,-5.55823192228682,
132.839578108159));
#174523=CARTESIAN_POINT('Ctrl Pts',(-51.4030516688456,-5.61377041282377,
132.680994606987));
#174524=CARTESIAN_POINT('Ctrl Pts',(-51.3951251223697,-5.66250500041385,
132.520160047216));
#174525=CARTESIAN_POINT('Ctrl Pts',(-51.3872200850336,-5.71110734389741,
132.359761921275));
#174526=CARTESIAN_POINT('Ctrl Pts',(-51.3793150476975,-5.75294252721499,
132.197125200942));
#174527=CARTESIAN_POINT('Ctrl Pts',(-51.3714100103613,-5.78781509037246,
132.03282593745));
#174528=CARTESIAN_POINT('Ctrl Pts',(-51.3635181584019,-5.82262948708961,
131.868800720441));
#174529=CARTESIAN_POINT('Ctrl Pts',(-51.3556263064426,-5.85050435298047,
131.70311877322));
#174530=CARTESIAN_POINT('Ctrl Pts',(-51.3477344544831,-5.87129377485024,
131.536371527256));
#174531=CARTESIAN_POINT('Ctrl Pts',(-51.3398611043402,-5.89203445758117,
131.370015206889));
#174532=CARTESIAN_POINT('Ctrl Pts',(-51.3319877541973,-5.90572279094747,
131.202598859044));
#174533=CARTESIAN_POINT('Ctrl Pts',(-51.3241144040543,-5.91226381036876,
131.034723807125));
#174534=CARTESIAN_POINT('Ctrl Pts',(-51.3205346847667,-5.9152377684626,
130.958397268821));
#174535=CARTESIAN_POINT('Ctrl Pts',(-51.3169549654791,-5.91673493774469,
130.881976074287));
#174536=CARTESIAN_POINT('Ctrl Pts',(-51.3133752461914,-5.91674988690743,
130.805517458505));
#174537=CARTESIAN_POINT('',(-49.5633751912882,-5.91573782775675,130.798896933973));
#174538=CARTESIAN_POINT('Ctrl Pts',(-51.3133751922042,-5.9071383279532,
130.805514428026));
#174539=CARTESIAN_POINT('Ctrl Pts',(-51.2636775082465,-5.90529917539433,
129.745753984472));
#174540=CARTESIAN_POINT('Ctrl Pts',(-51.1211639496847,-5.12604516750494,
126.704251395053));
#174541=CARTESIAN_POINT('Ctrl Pts',(-50.8858345165182,-0.250194475344861,
123.810437308373));
#174542=CARTESIAN_POINT('Ctrl Pts',(-50.6073868927055,5.74894953295976,
126.81347853489));
#174543=CARTESIAN_POINT('Ctrl Pts',(-50.3289392688926,6.46508977227328,
133.483945429956));
#174544=CARTESIAN_POINT('Ctrl Pts',(-50.0504916450797,1.24012834806205,
137.692004787431));
#174545=CARTESIAN_POINT('Ctrl Pts',(-49.7953036195168,-4.59279733233232,
135.747858542419));
#174546=CARTESIAN_POINT('Ctrl Pts',(-49.6329314685584,-5.902229748077,132.27673871186));
#174547=CARTESIAN_POINT('Ctrl Pts',(-49.5633751922042,-5.91567488377501,
130.798897011574));
#174548=CARTESIAN_POINT('',(-47.8133744782874,-5.92195381510691,130.805598640966));
#174549=CARTESIAN_POINT('Ctrl Pts',(-49.5633751765939,-5.91674747619486,
130.798895689225));
#174550=CARTESIAN_POINT('Ctrl Pts',(-49.5538760923211,-5.91656103173357,
130.597036721113));
#174551=CARTESIAN_POINT('Ctrl Pts',(-49.5443770080484,-5.9060410641023,
130.395639713077));
#174552=CARTESIAN_POINT('Ctrl Pts',(-49.5348779237755,-5.88534989114146,
130.195601862934));
#174553=CARTESIAN_POINT('Ctrl Pts',(-49.5251696431194,-5.86420304072518,
129.991158620273));
#174554=CARTESIAN_POINT('Ctrl Pts',(-49.5154613624632,-5.83243204681259,
129.788134809279));
#174555=CARTESIAN_POINT('Ctrl Pts',(-49.5057530818071,-5.79025820845633,
129.587462741036));
#174556=CARTESIAN_POINT('Ctrl Pts',(-49.5017008536894,-5.77265488407041,
129.503702389828));
#174557=CARTESIAN_POINT('Ctrl Pts',(-49.4976486255716,-5.7532397230529,
129.420351485477));
#174558=CARTESIAN_POINT('Ctrl Pts',(-49.4935963974539,-5.73203124524393,
129.337476720985));
#174559=CARTESIAN_POINT('Ctrl Pts',(-49.4861731310485,-5.69317948856694,
129.185658650227));
#174560=CARTESIAN_POINT('Ctrl Pts',(-49.4787498646431,-5.64823325758814,
129.035155615431));
#174561=CARTESIAN_POINT('Ctrl Pts',(-49.4713265982376,-5.59729583156049,
128.886494632546));
#174562=CARTESIAN_POINT('Ctrl Pts',(-49.4639121055166,-5.54641860934023,
128.738009354597));
#174563=CARTESIAN_POINT('Ctrl Pts',(-49.4564976127956,-5.48956440684963,
128.591362144619));
#174564=CARTESIAN_POINT('Ctrl Pts',(-49.4490831200745,-5.42688722194317,
128.447068602815));
#174565=CARTESIAN_POINT('Ctrl Pts',(-49.4416757737207,-5.36427044766719,
128.302914136558));
#174566=CARTESIAN_POINT('Ctrl Pts',(-49.434268427367,-5.29584201190525,
128.161109162323));
#174567=CARTESIAN_POINT('Ctrl Pts',(-49.4268610810132,-5.2218052682233,
128.022152806626));
#174568=CARTESIAN_POINT('Ctrl Pts',(-49.4194592593378,-5.14782374393836,
127.883300089822));
#174569=CARTESIAN_POINT('Ctrl Pts',(-49.4120574376624,-5.06824241520598,
127.747292089211));
#174570=CARTESIAN_POINT('Ctrl Pts',(-49.4046556159871,-4.98331211643455,
127.614606565496));
#174571=CARTESIAN_POINT('Ctrl Pts',(-49.3972577016757,-4.89842665170675,
127.481991085436));
#174572=CARTESIAN_POINT('Ctrl Pts',(-49.3898597873643,-4.80819804117083,
127.352694902888));
#174573=CARTESIAN_POINT('Ctrl Pts',(-49.382461873053,-4.71292223322602,
127.227169738389));
#174574=CARTESIAN_POINT('Ctrl Pts',(-49.3750651881408,-4.61766225839188,
127.101665433896));
#174575=CARTESIAN_POINT('Ctrl Pts',(-49.3676685032286,-4.51735697629474,
126.979931200743));
#174576=CARTESIAN_POINT('Ctrl Pts',(-49.3602718183164,-4.41234476461102,
126.86238849175));
#174577=CARTESIAN_POINT('Ctrl Pts',(-49.352875461381,-4.30733720927881,
126.744850994724));
#174578=CARTESIAN_POINT('Ctrl Pts',(-49.3454791044454,-4.19762338805193,
126.631504930694));
#174579=CARTESIAN_POINT('Ctrl Pts',(-49.33808274751,-4.0835807656593,126.522737246362));
#174580=CARTESIAN_POINT('Ctrl Pts',(-49.3306852581734,-3.96952068304989,
126.41395290942));
#174581=CARTESIAN_POINT('Ctrl Pts',(-49.3232877688369,-3.85113074980261,
126.30974860554));
#174582=CARTESIAN_POINT('Ctrl Pts',(-49.3158902795003,-3.72882382875141,
126.210473002851));
#174583=CARTESIAN_POINT('Ctrl Pts',(-49.3084901969853,-3.60647403319846,
126.111162599253));
#174584=CARTESIAN_POINT('Ctrl Pts',(-49.3010901144702,-3.48020480567695,
126.016784571892));
#174585=CARTESIAN_POINT('Ctrl Pts',(-49.2936900319552,-3.35046034648829,
125.927645941771));
#174586=CARTESIAN_POINT('Ctrl Pts',(-49.2862818122888,-3.22057321992887,
125.838409294564));
#174587=CARTESIAN_POINT('Ctrl Pts',(-49.2788735926223,-3.08720353803567,
125.754423761719));
#174588=CARTESIAN_POINT('Ctrl Pts',(-49.2714653729558,-2.95082323702318,
125.675952210824));
#174589=CARTESIAN_POINT('Ctrl Pts',(-49.2640525936537,-2.81435899621084,
125.597432361999));
#174590=CARTESIAN_POINT('Ctrl Pts',(-49.2566398143518,-2.67488077394437,
125.524433430321));
#174591=CARTESIAN_POINT('Ctrl Pts',(-49.2492270350497,-2.5328826420075,
125.457171067502));
#174592=CARTESIAN_POINT('Ctrl Pts',(-49.2418036640209,-2.39068161648087,
125.389812597064));
#174593=CARTESIAN_POINT('Ctrl Pts',(-49.2343802929921,-2.24595383271325,
125.328207211908));
#174594=CARTESIAN_POINT('Ctrl Pts',(-49.2269569219633,-2.09921152462009,
125.27252172463));
#174595=CARTESIAN_POINT('Ctrl Pts',(-49.2230208725225,-2.02140523183575,
125.24299594312));
#174596=CARTESIAN_POINT('Ctrl Pts',(-49.2190848230818,-1.94303281823506,
125.215133618159));
#174597=CARTESIAN_POINT('Ctrl Pts',(-49.215148773641,-1.86417193419749,
125.188953814649));
#174598=CARTESIAN_POINT('Ctrl Pts',(-49.2077255072355,-1.71544276806656,
125.139579522273));
#174599=CARTESIAN_POINT('Ctrl Pts',(-49.2003022408301,-1.56452576670862,
125.09604349279));
#174600=CARTESIAN_POINT('Ctrl Pts',(-49.1928789744247,-1.41192014852576,
125.058543699434));
#174601=CARTESIAN_POINT('Ctrl Pts',(-49.1854644817037,-1.25949489751027,
125.02108822772));
#174602=CARTESIAN_POINT('Ctrl Pts',(-49.1780499889827,-1.10538536130388,
124.98965487942));
#174603=CARTESIAN_POINT('Ctrl Pts',(-49.1706354962616,-0.950108568560871,
124.964392786281));
#174604=CARTESIAN_POINT('Ctrl Pts',(-49.1632281499079,-0.794981437436779,
124.939155041698));
#174605=CARTESIAN_POINT('Ctrl Pts',(-49.155820803554,-0.638689655500852,
124.920076770346));
#174606=CARTESIAN_POINT('Ctrl Pts',(-49.1484134572003,-0.481763069596425,
124.907256675183));
#174607=CARTESIAN_POINT('Ctrl Pts',(-49.1410116355249,-0.324953525460267,
124.89444614173));
#174608=CARTESIAN_POINT('Ctrl Pts',(-49.1336098138495,-0.167510490536946,
124.887884520943));
#174609=CARTESIAN_POINT('Ctrl Pts',(-49.1262079921741,-0.00997150056215477,
124.887619020058));
#174610=CARTESIAN_POINT('Ctrl Pts',(-49.1188100778627,0.14748432580611,
124.88735365933));
#174611=CARTESIAN_POINT('Ctrl Pts',(-49.1114121635514,0.305035633993691,
124.893377799879));
#174612=CARTESIAN_POINT('Ctrl Pts',(-49.10401424924,0.46214241137939,124.90568661792));
#174613=CARTESIAN_POINT('Ctrl Pts',(-49.0966175643278,0.61922308046867,
124.917993390458));
#174614=CARTESIAN_POINT('Ctrl Pts',(-49.0892208794156,0.775858993578949,
124.936582738537));
#174615=CARTESIAN_POINT('Ctrl Pts',(-49.0818241945034,0.931512669118098,
124.961397780976));
#174616=CARTESIAN_POINT('Ctrl Pts',(-49.0744278375679,1.08715944281038,
124.98621172309));
#174617=CARTESIAN_POINT('Ctrl Pts',(-49.0670314806325,1.24182369688828,
125.017250751906));
#174618=CARTESIAN_POINT('Ctrl Pts',(-49.059635123697,1.39497585322708,125.0544064498));
#174619=CARTESIAN_POINT('Ctrl Pts',(-49.0522376343605,1.54815145755176,
125.091567836326));
#174620=CARTESIAN_POINT('Ctrl Pts',(-49.0448401450239,1.69981414038029,
125.134847668565));
#174621=CARTESIAN_POINT('Ctrl Pts',(-49.0374426556873,1.84944739489439,
125.184087056963));
#174622=CARTESIAN_POINT('Ctrl Pts',(-49.0300425731723,1.99913310311389,
125.233343706151));
#174623=CARTESIAN_POINT('Ctrl Pts',(-49.0226424906573,2.1467876122295,125.288563954295));
#174624=CARTESIAN_POINT('Ctrl Pts',(-49.0152424081423,2.29191251566261,
125.349540035453));
#174625=CARTESIAN_POINT('Ctrl Pts',(-49.0078341884759,2.43719699884644,
125.410583166079));
#174626=CARTESIAN_POINT('Ctrl Pts',(-49.0004259688094,2.57994597702167,
125.477394624718));
#174627=CARTESIAN_POINT('Ctrl Pts',(-48.9930177491429,2.71968319919072,
125.549719444418));
#174628=CARTESIAN_POINT('Ctrl Pts',(-48.9856049698408,2.85950642728856,
125.622088778838));
#174629=CARTESIAN_POINT('Ctrl Pts',(-48.9781921905387,2.99631388202598,
125.699978051789));
#174630=CARTESIAN_POINT('Ctrl Pts',(-48.9707794112367,3.12965707164409,
125.783088151706));
#174631=CARTESIAN_POINT('Ctrl Pts',(-48.9633560402079,3.26319078826452,
125.86631700323));
#174632=CARTESIAN_POINT('Ctrl Pts',(-48.9559326691793,3.39325004585048,
125.954781371145));
#174633=CARTESIAN_POINT('Ctrl Pts',(-48.9485092981505,3.51941762529719,
126.048140464835));
#174634=CARTESIAN_POINT('Ctrl Pts',(-48.9445732487097,3.58631470326899,
126.097641696429));
#174635=CARTESIAN_POINT('Ctrl Pts',(-48.9406371992689,3.65211827026437,
126.148518360397));
#174636=CARTESIAN_POINT('Ctrl Pts',(-48.9367011498281,3.71677031451401,
126.200715432319));
#174637=CARTESIAN_POINT('Ctrl Pts',(-48.9292778834227,3.83870205224826,
126.29915748095));
#174638=CARTESIAN_POINT('Ctrl Pts',(-48.9218546170173,3.9569044724428,126.402595941023));
#174639=CARTESIAN_POINT('Ctrl Pts',(-48.9144313506119,4.07094117486974,
126.510717815323));
#174640=CARTESIAN_POINT('Ctrl Pts',(-48.9070168578909,4.18484309538457,
126.618711898548));
#174641=CARTESIAN_POINT('Ctrl Pts',(-48.8996023651697,4.29458883020234,
126.731378123408));
#174642=CARTESIAN_POINT('Ctrl Pts',(-48.8921878724487,4.39977344394399,
126.848362108407));
#174643=CARTESIAN_POINT('Ctrl Pts',(-48.884780526095,4.50485667679494,126.965233339838));
#174644=CARTESIAN_POINT('Ctrl Pts',(-48.8773731797412,4.6053872925839,127.086413770715));
#174645=CARTESIAN_POINT('Ctrl Pts',(-48.8699658333874,4.70099585455471,
127.211510977244));
#174646=CARTESIAN_POINT('Ctrl Pts',(-48.862564011712,4.79653310805277,127.336514881557));
#174647=CARTESIAN_POINT('Ctrl Pts',(-48.8551621900366,4.88715539159204,
127.465429449544));
#174648=CARTESIAN_POINT('Ctrl Pts',(-48.8477603683612,4.97253243719055,
127.597827953833));
#174649=CARTESIAN_POINT('Ctrl Pts',(-48.8403624540499,5.05786441291127,
127.730156565981));
#174650=CARTESIAN_POINT('Ctrl Pts',(-48.8329645397386,5.1379564633351,127.865965138759));
#174651=CARTESIAN_POINT('Ctrl Pts',(-48.8255666254272,5.21252075683664,
128.004796736879));
#174652=CARTESIAN_POINT('Ctrl Pts',(-48.818169940515,5.28707265910534,128.143605263706));
#174653=CARTESIAN_POINT('Ctrl Pts',(-48.8107732556028,5.3560984511702,128.285435490272));
#174654=CARTESIAN_POINT('Ctrl Pts',(-48.8033765706906,5.41935546684912,
128.429804472424));
#174655=CARTESIAN_POINT('Ctrl Pts',(-48.7959802137552,5.48260967764568,
128.574167053104));
#174656=CARTESIAN_POINT('Ctrl Pts',(-48.7885838568196,5.54009547084567,
128.721067823624));
#174657=CARTESIAN_POINT('Ctrl Pts',(-48.7811874998842,5.59161781135387,
128.870002632536));
#174658=CARTESIAN_POINT('Ctrl Pts',(-48.7737900105476,5.64314804006392,
129.018960243747));
#174659=CARTESIAN_POINT('Ctrl Pts',(-48.7663925212111,5.68871287608846,
129.169952160615));
#174660=CARTESIAN_POINT('Ctrl Pts',(-48.7589950318745,5.7281668131581,129.32245794764));
#174661=CARTESIAN_POINT('Ctrl Pts',(-48.7515949493595,5.76763458074427,
129.475017195332));
#174662=CARTESIAN_POINT('Ctrl Pts',(-48.7441948668445,5.80098709090098,
129.629091008595));
#174663=CARTESIAN_POINT('Ctrl Pts',(-48.7367947843294,5.82812974206965,
129.784147761294));
#174664=CARTESIAN_POINT('Ctrl Pts',(-48.729386564663,5.85530223937357,129.939375014832));
#174665=CARTESIAN_POINT('Ctrl Pts',(-48.7219783449966,5.8762511765631,130.095586998386));
#174666=CARTESIAN_POINT('Ctrl Pts',(-48.7145701253302,5.89093363925821,
130.252245212641));
#174667=CARTESIAN_POINT('Ctrl Pts',(-48.7071573460281,5.90562513876414,
130.408999847412));
#174668=CARTESIAN_POINT('Ctrl Pts',(-48.6997445667261,5.91404245848461,
130.566200888252));
#174669=CARTESIAN_POINT('Ctrl Pts',(-48.692331787424,5.91619482870196,130.723309329235));
#174670=CARTESIAN_POINT('Ctrl Pts',(-48.6849084163952,5.91835027432682,
130.880642254125));
#174671=CARTESIAN_POINT('Ctrl Pts',(-48.6774850453664,5.91422290175767,
131.037881942723));
#174672=CARTESIAN_POINT('Ctrl Pts',(-48.6700616743377,5.90387391067542,
131.194493171125));
#174673=CARTESIAN_POINT('Ctrl Pts',(-48.6661256248968,5.89838662728293,
131.277532202259));
#174674=CARTESIAN_POINT('Ctrl Pts',(-48.662189575456,5.89115108428755,131.360394686433));
#174675=CARTESIAN_POINT('Ctrl Pts',(-48.6582535260152,5.8821822185121,131.443002074661));
#174676=CARTESIAN_POINT('Ctrl Pts',(-48.6508302596098,5.86526721756844,
131.598797030769));
#174677=CARTESIAN_POINT('Ctrl Pts',(-48.6434069932043,5.84213280695006,
131.754155088839));
#174678=CARTESIAN_POINT('Ctrl Pts',(-48.6359837267989,5.81280643509335,
131.908539910361));
#174679=CARTESIAN_POINT('Ctrl Pts',(-48.6285692340779,5.78351472457273,
132.062742261845));
#174680=CARTESIAN_POINT('Ctrl Pts',(-48.6211547413569,5.74804568908171,
132.215973303271));
#174681=CARTESIAN_POINT('Ctrl Pts',(-48.6137402486358,5.70647860234763,
132.36770079918));
#174682=CARTESIAN_POINT('Ctrl Pts',(-48.6063329022821,5.66495157953671,
132.519282054416));
#174683=CARTESIAN_POINT('Ctrl Pts',(-48.5989255559283,5.61733830446223,
132.66936229154));
#174684=CARTESIAN_POINT('Ctrl Pts',(-48.5915182095745,5.56376924478614,
132.817418578299));
#174685=CARTESIAN_POINT('Ctrl Pts',(-48.5841163878991,5.51024013893581,
132.965364439094));
#174686=CARTESIAN_POINT('Ctrl Pts',(-48.5767145662237,5.45076421966322,
133.111289005703));
#174687=CARTESIAN_POINT('Ctrl Pts',(-48.5693127445483,5.38552198688106,
133.25468375775));
#174688=CARTESIAN_POINT('Ctrl Pts',(-48.5619148302369,5.32031419496584,
133.398002812823));
#174689=CARTESIAN_POINT('Ctrl Pts',(-48.5545169159256,5.24934630600076,
133.538794374064));
#174690=CARTESIAN_POINT('Ctrl Pts',(-48.5471190016142,5.17284717255866,
133.676569295892));
#174691=CARTESIAN_POINT('Ctrl Pts',(-48.539722316702,5.09636075188458,133.814321322027));
#174692=CARTESIAN_POINT('Ctrl Pts',(-48.5323256317898,5.01434509209365,
133.949057377659));
#174693=CARTESIAN_POINT('Ctrl Pts',(-48.5249289468776,4.92707534078023,
134.080312257743));
#174694=CARTESIAN_POINT('Ctrl Pts',(-48.5175325899421,4.83980945909903,
134.211561317848));
#174695=CARTESIAN_POINT('Ctrl Pts',(-48.5101362330066,4.74729015580746,
134.339329198466));
#174696=CARTESIAN_POINT('Ctrl Pts',(-48.5027398760712,4.64983616656427,
134.463179304876));
#174697=CARTESIAN_POINT('Ctrl Pts',(-48.4953423867346,4.55236725686655,
134.587048373054));
#174698=CARTESIAN_POINT('Ctrl Pts',(-48.487944897398,4.44996238774628,134.706998179314));
#174699=CARTESIAN_POINT('Ctrl Pts',(-48.4805474080615,4.34298076663618,
134.822624997012));
#174700=CARTESIAN_POINT('Ctrl Pts',(-48.4731473255465,4.23596164328465,
134.938292347512));
#174701=CARTESIAN_POINT('Ctrl Pts',(-48.4657472430314,4.12436282700883,
135.04963341843));
#174702=CARTESIAN_POINT('Ctrl Pts',(-48.4583471605164,4.00858045548097,
135.156281261883));
#174703=CARTESIAN_POINT('Ctrl Pts',(-48.45093894085,3.89267076933289,135.263046375604));
#174704=CARTESIAN_POINT('Ctrl Pts',(-48.4435307211835,3.77256861567195,
135.365107702568));
#174705=CARTESIAN_POINT('Ctrl Pts',(-48.436122501517,3.6487038529544,135.462138065656));
#174706=CARTESIAN_POINT('Ctrl Pts',(-48.4287097222149,3.52476285354219,
135.559228149314));
#174707=CARTESIAN_POINT('Ctrl Pts',(-48.4212969429129,3.3970549326316,135.651280881209));
#174708=CARTESIAN_POINT('Ctrl Pts',(-48.4138841636108,3.26603856036764,
135.738012681169));
#174709=CARTESIAN_POINT('Ctrl Pts',(-48.4064607925821,3.13483498576692,
135.824868407592));
#174710=CARTESIAN_POINT('Ctrl Pts',(-48.3990374215534,3.00031383680022,
135.906387824636));
#174711=CARTESIAN_POINT('Ctrl Pts',(-48.3916140505246,2.86295849241714,
135.982333119733));
#174712=CARTESIAN_POINT('Ctrl Pts',(-48.3876780010838,2.79012939302957,
136.022601137475));
#174713=CARTESIAN_POINT('Ctrl Pts',(-48.3837419516431,2.71650385058052,
136.061302866956));
#174714=CARTESIAN_POINT('Ctrl Pts',(-48.3798059022023,2.64215602427448,
136.098408417302));
#174715=CARTESIAN_POINT('Ctrl Pts',(-48.3723826357969,2.50193834417637,
136.16838832723));
#174716=CARTESIAN_POINT('Ctrl Pts',(-48.3649593693915,2.35872649592454,
136.232899517595));
#174717=CARTESIAN_POINT('Ctrl Pts',(-48.357536102986,2.21298655284755,136.291675177477));
#174718=CARTESIAN_POINT('Ctrl Pts',(-48.350121610265,2.06741886228034,136.350381369411));
#174719=CARTESIAN_POINT('Ctrl Pts',(-48.342707117544,1.91932936733809,136.403365386084));
#174720=CARTESIAN_POINT('Ctrl Pts',(-48.335292624823,1.76920870217187,136.450406236462));
#174721=CARTESIAN_POINT('Ctrl Pts',(-48.3278852784692,1.61923272895446,
136.497401747098));
#174722=CARTESIAN_POINT('Ctrl Pts',(-48.3204779321155,1.46722983677219,
136.538465384379));
#174723=CARTESIAN_POINT('Ctrl Pts',(-48.3130705857617,1.31371050429746,
136.573424256788));
#174724=CARTESIAN_POINT('Ctrl Pts',(-48.3056687640863,1.16030567233307,
136.608357055552));
#174725=CARTESIAN_POINT('Ctrl Pts',(-48.2982669424109,1.00538701450003,
136.63719407288));
#174726=CARTESIAN_POINT('Ctrl Pts',(-48.2908651207355,0.849479928003844,
136.659812300777));
#174727=CARTESIAN_POINT('Ctrl Pts',(-48.2834672064241,0.693655143644823,
136.682418588688));
#174728=CARTESIAN_POINT('Ctrl Pts',(-48.2760692921128,0.536843338275426,
136.698812571662));
#174729=CARTESIAN_POINT('Ctrl Pts',(-48.2686713778014,0.379579744332311,
136.708922394717));
#174730=CARTESIAN_POINT('Ctrl Pts',(-48.2612746928892,0.222342284745682,
136.719030537702));
#174731=CARTESIAN_POINT('Ctrl Pts',(-48.253878007977,0.0646535577592358,
136.722856569496));
#174732=CARTESIAN_POINT('Ctrl Pts',(-48.2464813230648,-0.092946322453696,
136.720380524872));
#174733=CARTESIAN_POINT('Ctrl Pts',(-48.2390849661294,-0.250539214522786,
136.717904590039));
#174734=CARTESIAN_POINT('Ctrl Pts',(-48.2316886091939,-0.408042894400034,
136.709127140275));
#174735=CARTESIAN_POINT('Ctrl Pts',(-48.2242922522585,-0.56491775817197,
136.694080346806));
#174736=CARTESIAN_POINT('Ctrl Pts',(-48.2168947629219,-0.721816639886255,
136.679031249635));
#174737=CARTESIAN_POINT('Ctrl Pts',(-48.2094972735853,-0.87808614218579,
136.657710933208));
#174738=CARTESIAN_POINT('Ctrl Pts',(-48.2020997842487,-1.03319243801818,
136.630203384799));
#174739=CARTESIAN_POINT('Ctrl Pts',(-48.1946997017337,-1.18835310612214,
136.602686193662));
#174740=CARTESIAN_POINT('Ctrl Pts',(-48.1872996192187,-1.34234938857821,
136.568977517374));
#174741=CARTESIAN_POINT('Ctrl Pts',(-48.1798995367037,-1.49465843965174,
136.529212293485));
#174742=CARTESIAN_POINT('Ctrl Pts',(-48.1724913170373,-1.64713497018445,
136.489403343645));
#174743=CARTESIAN_POINT('Ctrl Pts',(-48.1650830973708,-1.7979202027976,
136.443524640511));
#174744=CARTESIAN_POINT('Ctrl Pts',(-48.1576748777043,-1.94650652512017,
136.391760988952));
#174745=CARTESIAN_POINT('Ctrl Pts',(-48.1502620984023,-2.09518429984484,
136.339965477729));
#174746=CARTESIAN_POINT('Ctrl Pts',(-48.1428493191002,-2.24166012094816,
136.282277937093));
#174747=CARTESIAN_POINT('Ctrl Pts',(-48.1354365397981,-2.38544759008819,
136.218930808952));
#174748=CARTESIAN_POINT('Ctrl Pts',(-48.1280131687694,-2.5294405095073,
136.155493167463));
#174749=CARTESIAN_POINT('Ctrl Pts',(-48.1205897977406,-2.67073707069456,
136.086379951135));
#174750=CARTESIAN_POINT('Ctrl Pts',(-48.1131664267119,-2.80887591707196,
136.011869296867));
#174751=CARTESIAN_POINT('Ctrl Pts',(-48.109230377271,-2.88212044801796,
135.972361960115));
#174752=CARTESIAN_POINT('Ctrl Pts',(-48.1052943278302,-2.95447771321897,
135.931337936195));
#174753=CARTESIAN_POINT('Ctrl Pts',(-48.1013582783894,-3.02588247977486,
135.888843460598));
#174754=CARTESIAN_POINT('Ctrl Pts',(-48.093935011984,-3.16054964103153,
135.808700205831));
#174755=CARTESIAN_POINT('Ctrl Pts',(-48.0865117455786,-3.2922342346609,
135.723081896093));
#174756=CARTESIAN_POINT('Ctrl Pts',(-48.0790884791732,-3.42045986106223,
135.632236434254));
#174757=CARTESIAN_POINT('Ctrl Pts',(-48.0716739864521,-3.54853393542182,
135.541498344207));
#174758=CARTESIAN_POINT('Ctrl Pts',(-48.0642594937311,-3.67315687853743,
135.445545613218));
#174759=CARTESIAN_POINT('Ctrl Pts',(-48.0568450010101,-3.79387756465029,
135.344671574642));
#174760=CARTESIAN_POINT('Ctrl Pts',(-48.0494376546563,-3.91448189562082,
135.243894762262));
#174761=CARTESIAN_POINT('Ctrl Pts',(-48.0420303083026,-4.03119117274931,
135.138206323109));
#174762=CARTESIAN_POINT('Ctrl Pts',(-48.0346229619488,-4.14358401131458,
135.02794228526));
#174763=CARTESIAN_POINT('Ctrl Pts',(-48.0272211402734,-4.2558930230605,
134.91776048649));
#174764=CARTESIAN_POINT('Ctrl Pts',(-48.019819318598,-4.36389174110269,
134.80301014438));
#174765=CARTESIAN_POINT('Ctrl Pts',(-48.0124174969226,-4.46719268530761,
134.684066801652));
#174766=CARTESIAN_POINT('Ctrl Pts',(-48.0050195826113,-4.57043909774833,
134.565186248188));
#174767=CARTESIAN_POINT('Ctrl Pts',(-47.9976216682999,-4.66899243107006,
134.442117383433));
#174768=CARTESIAN_POINT('Ctrl Pts',(-47.9902237539885,-4.76250292543401,
134.31527167422));
#174769=CARTESIAN_POINT('Ctrl Pts',(-47.9828270690763,-4.85599788005013,
134.188447044462));
#174770=CARTESIAN_POINT('Ctrl Pts',(-47.9754303841641,-4.94445143765424,
134.057847116112));
#174771=CARTESIAN_POINT('Ctrl Pts',(-47.9680336992519,-5.0275548560333,
133.923915510828));
#174772=CARTESIAN_POINT('Ctrl Pts',(-47.9606373423165,-5.11065458951971,
133.789989844212));
#174773=CARTESIAN_POINT('Ctrl Pts',(-47.953240985381,-5.18840445865811,
133.652733111597));
#174774=CARTESIAN_POINT('Ctrl Pts',(-47.9458446284456,-5.26053986091569,
133.512616686371));
#174775=CARTESIAN_POINT('Ctrl Pts',(-47.938447139109,-5.33268630728741,
133.372478808962));
#174776=CARTESIAN_POINT('Ctrl Pts',(-47.9310496497725,-5.39921640434239,
133.229480699089));
#174777=CARTESIAN_POINT('Ctrl Pts',(-47.9236521604359,-5.45991226639079,
133.084116877743));
#174778=CARTESIAN_POINT('Ctrl Pts',(-47.9162520779209,-5.52062940527981,
132.938702099334));
#174779=CARTESIAN_POINT('Ctrl Pts',(-47.9088519954058,-5.57550809347577,
132.790920302588));
#174780=CARTESIAN_POINT('Ctrl Pts',(-47.9014519128908,-5.62437924686929,
132.641284309472));
#174781=CARTESIAN_POINT('Ctrl Pts',(-47.8940436932243,-5.67330413911991,
132.491483776199));
#174782=CARTESIAN_POINT('Ctrl Pts',(-47.8866354735579,-5.71620818818213,
132.339825329848));
#174783=CARTESIAN_POINT('Ctrl Pts',(-47.8792272538914,-5.75297249874091,
132.18683593063));
#174784=CARTESIAN_POINT('Ctrl Pts',(-47.8718144745894,-5.78975943711944,
132.033752368989));
#174785=CARTESIAN_POINT('Ctrl Pts',(-47.8644016952873,-5.82039903456348,
131.879336587473));
#174786=CARTESIAN_POINT('Ctrl Pts',(-47.8569889159853,-5.84482394084855,
131.724123447313));
#174787=CARTESIAN_POINT('Ctrl Pts',(-47.8495655449565,-5.86928374658509,
131.568688531339));
#174788=CARTESIAN_POINT('Ctrl Pts',(-47.8421421739278,-5.88751108298261,
131.412454351077));
#174789=CARTESIAN_POINT('Ctrl Pts',(-47.8347188028991,-5.89949057999138,
131.255959398668));
#174790=CARTESIAN_POINT('Ctrl Pts',(-47.8307827534583,-5.9058423967496,
131.172982019855));
#174791=CARTESIAN_POINT('Ctrl Pts',(-47.8268467040173,-5.91043859283062,
131.089931316381));
#174792=CARTESIAN_POINT('Ctrl Pts',(-47.8229106545765,-5.91328280748709,
131.006887161944));
#174793=CARTESIAN_POINT('Ctrl Pts',(-47.8197321671191,-5.91557960297907,
130.939826316479));
#174794=CARTESIAN_POINT('Ctrl Pts',(-47.8165536796616,-5.91673566589503,
130.872726177956));
#174795=CARTESIAN_POINT('Ctrl Pts',(-47.8133751922042,-5.91674986753237,
130.805612638189));
#174796=CARTESIAN_POINT('',(-46.0633751922042,-5.91187214664006,130.80921511903));
#174797=CARTESIAN_POINT('Ctrl Pts',(-47.8133738942076,-5.92621134272425,
130.805587189359));
#174798=CARTESIAN_POINT('Ctrl Pts',(-47.7237369397262,-5.92074740615048,
128.909881288281));
#174799=CARTESIAN_POINT('Ctrl Pts',(-47.5412841106406,-3.90596225253313,
125.041284327674));
#174800=CARTESIAN_POINT('Ctrl Pts',(-47.2660154069507,2.68942047555363,
124.343356203699));
#174801=CARTESIAN_POINT('Ctrl Pts',(-46.9875677831378,6.88952345832453,
129.574715527493));
#174802=CARTESIAN_POINT('Ctrl Pts',(-46.7091201593249,4.75849095482671,
135.936058617563));
#174803=CARTESIAN_POINT('Ctrl Pts',(-46.4306725355122,-1.74536227095043,
137.58162194302));
#174804=CARTESIAN_POINT('Ctrl Pts',(-46.2154242131385,-5.53317027689218,
134.039283239287));
#174805=CARTESIAN_POINT('Ctrl Pts',(-46.0929917653692,-5.91671613064816,
131.43949600246));
#174806=CARTESIAN_POINT('Ctrl Pts',(-46.0633751922042,-5.91187214664006,
130.80921511903));
#174807=CARTESIAN_POINT('',(-44.3133751922042,-5.90864861670285,130.801162763788));
#174808=CARTESIAN_POINT('Ctrl Pts',(-46.0633751922042,-5.91187214664006,
130.80921511903));
#174809=CARTESIAN_POINT('Ctrl Pts',(-46.0001758907649,-5.90153548804726,
129.464248187122));
#174810=CARTESIAN_POINT('Ctrl Pts',(-45.8441607147213,-4.77861257565497,
126.128421018115));
#174811=CARTESIAN_POINT('Ctrl Pts',(-45.5953296640732,0.765979412781536,
123.848008407568));
#174812=CARTESIAN_POINT('Ctrl Pts',(-45.3168820402607,6.26660671109677,
127.688722503348));
#174813=CARTESIAN_POINT('Ctrl Pts',(-45.0384344164476,6.00852858267546,
134.39255581871));
#174814=CARTESIAN_POINT('Ctrl Pts',(-44.7599867926347,0.228906219712464,
137.799013037303));
#174815=CARTESIAN_POINT('Ctrl Pts',(-44.5183003845536,-4.97026108933638,
135.176602734102));
#174816=CARTESIAN_POINT('Ctrl Pts',(-44.3694298510767,-5.90281458641276,
131.995717272823));
#174817=CARTESIAN_POINT('Ctrl Pts',(-44.3133751922042,-5.90864861670285,
130.801162763788));
#174818=CARTESIAN_POINT('',(-42.5633751922041,-5.92360350378115,130.800661905678));
#174819=CARTESIAN_POINT('Ctrl Pts',(-44.3133751922042,-5.90864861670285,
130.801162763788));
#174820=CARTESIAN_POINT('Ctrl Pts',(-44.2766139764725,-5.9124746331374,
130.017761760318));
#174821=CARTESIAN_POINT('Ctrl Pts',(-44.1470368861364,-5.4024867072948,
127.261186095784));
#174822=CARTESIAN_POINT('Ctrl Pts',(-43.924643921196,-1.21915898426497,
123.912973826689));
#174823=CARTESIAN_POINT('Ctrl Pts',(-43.6461962973832,5.13893367076999,
126.053684743782));
#174824=CARTESIAN_POINT('Ctrl Pts',(-43.3677486735701,6.77459733323286,
132.560034705456));
#174825=CARTESIAN_POINT('Ctrl Pts',(-43.0893010497574,2.18473700393284,
137.453005949813));
#174826=CARTESIAN_POINT('Ctrl Pts',(-42.8211765559688,-4.16819407011025,
136.281308753027));
#174827=CARTESIAN_POINT('Ctrl Pts',(-42.6458679367842,-5.91084275337813,
132.547310458652));
#174828=CARTESIAN_POINT('Ctrl Pts',(-42.5633751922041,-5.92360350378115,
130.800661905678));
#174829=CARTESIAN_POINT('',(-40.8133751922042,-5.91898627828404,130.809343451928));
#174830=CARTESIAN_POINT('Ctrl Pts',(-42.5633751922041,-5.92360350378115,
130.800661905678));
#174831=CARTESIAN_POINT('Ctrl Pts',(-42.55305206218,-5.92520038222528,130.582086560529));
#174832=CARTESIAN_POINT('Ctrl Pts',(-42.4499130575518,-5.81485187816171,
128.399916294978));
#174833=CARTESIAN_POINT('Ctrl Pts',(-42.2539581783187,-3.10609779771171,
124.533019692256));
#174834=CARTESIAN_POINT('Ctrl Pts',(-41.9755105545057,3.59733500374434,
124.801299614947));
#174835=CARTESIAN_POINT('Ctrl Pts',(-41.697062930693,6.99499267634301,130.586099333203));
#174836=CARTESIAN_POINT('Ctrl Pts',(-41.4186153068799,3.96459380377209,
136.571470509137));
#174837=CARTESIAN_POINT('Ctrl Pts',(-41.1401676830672,-2.70907309328813,
137.257149433693));
#174838=CARTESIAN_POINT('Ctrl Pts',(-40.9384209781752,-5.74066911494575,
133.457570663198));
#174839=CARTESIAN_POINT('Ctrl Pts',(-40.8294901478875,-5.92335425468506,
131.151051523995));
#174840=CARTESIAN_POINT('Ctrl Pts',(-40.8133751922042,-5.92027830700173,
130.809344539608));
#174841=CARTESIAN_POINT('',(-39.0633752204132,-5.91150858312851,130.805710542273));
#174842=CARTESIAN_POINT('Ctrl Pts',(-40.8133751922042,-5.91674790342102,
130.809341567576));
#174843=CARTESIAN_POINT('Ctrl Pts',(-40.806073639501,-5.9168781620269,130.654610576157));
#174844=CARTESIAN_POINT('Ctrl Pts',(-40.7987720867977,-5.91093464250606,
130.499664442865));
#174845=CARTESIAN_POINT('Ctrl Pts',(-40.7914705340945,-5.89889343352436,
130.345027598479));
#174846=CARTESIAN_POINT('Ctrl Pts',(-40.7841754751059,-5.88686293352173,
130.190528282039));
#174847=CARTESIAN_POINT('Ctrl Pts',(-40.7768804161173,-5.8687455646891,
130.036338088981));
#174848=CARTESIAN_POINT('Ctrl Pts',(-40.7695853571287,-5.84456946063665,
129.882982094757));
#174849=CARTESIAN_POINT('Ctrl Pts',(-40.762295084242,-5.82040921790863,
129.729726713484));
#174850=CARTESIAN_POINT('Ctrl Pts',(-40.7550048113552,-5.79019821096416,
129.577304821114));
#174851=CARTESIAN_POINT('Ctrl Pts',(-40.7477145384685,-5.75401643453495,
129.426236735761));
#174852=CARTESIAN_POINT('Ctrl Pts',(-40.7404265740672,-5.71784611516684,
129.275216486541));
#174853=CARTESIAN_POINT('Ctrl Pts',(-40.7331386096659,-5.67570887379195,
129.125549566526));
#174854=CARTESIAN_POINT('Ctrl Pts',(-40.7258506452646,-5.62773585583999,
128.977746345369));
#174855=CARTESIAN_POINT('Ctrl Pts',(-40.7185636482984,-5.57976920602881,
128.829962744236));
#174856=CARTESIAN_POINT('Ctrl Pts',(-40.7112766513322,-5.5259684392141,
128.684042716502));
#174857=CARTESIAN_POINT('Ctrl Pts',(-40.703989654366,-5.46651454289294,
128.540481355141));
#174858=CARTESIAN_POINT('Ctrl Pts',(-40.6967020865158,-5.40705598878513,
128.396908746776));
#174859=CARTESIAN_POINT('Ctrl Pts',(-40.6894145186656,-5.3419435716094,
128.255695528562));
#174860=CARTESIAN_POINT('Ctrl Pts',(-40.6821269508155,-5.27140625812483,
128.117316400531));
#174861=CARTESIAN_POINT('Ctrl Pts',(-40.6748372734662,-5.20084852652484,
127.978897216523));
#174862=CARTESIAN_POINT('Ctrl Pts',(-40.6675475961168,-5.12486294960536,
127.843314097973));
#174863=CARTESIAN_POINT('Ctrl Pts',(-40.6602579187675,-5.04372407249495,
127.711016465514));
#174864=CARTESIAN_POINT('Ctrl Pts',(-40.6529606389673,-4.96250057513231,
127.578580859011));
#174865=CARTESIAN_POINT('Ctrl Pts',(-40.645663359167,-4.87611324910678,
127.449437908301));
#174866=CARTESIAN_POINT('Ctrl Pts',(-40.6383660793667,-4.78487983439095,
127.324007828991));
#174867=CARTESIAN_POINT('Ctrl Pts',(-40.6310645260418,-4.69359299041688,
127.198504293743));
#174868=CARTESIAN_POINT('Ctrl Pts',(-40.6237629727168,-4.59745464492467,
127.07671826108));
#174869=CARTESIAN_POINT('Ctrl Pts',(-40.6164614193919,-4.49682176573284,
126.959035589726));
#174870=CARTESIAN_POINT('Ctrl Pts',(-40.6091495810276,-4.39604713408348,
126.841187149411));
#174871=CARTESIAN_POINT('Ctrl Pts',(-40.6018377426631,-4.2907655900787,
126.727453891566));
#174872=CARTESIAN_POINT('Ctrl Pts',(-40.5945259042988,-4.18137019794758,
126.618184100717));
#174873=CARTESIAN_POINT('Ctrl Pts',(-40.590774748013,-4.12524762078129,
126.562125960156));
#174874=CARTESIAN_POINT('Ctrl Pts',(-40.5870235917272,-4.06804283219271,
126.507241923182));
#174875=CARTESIAN_POINT('Ctrl Pts',(-40.5832724354414,-4.00981203384433,
126.45357470974));
#174876=CARTESIAN_POINT('Ctrl Pts',(-40.575849169036,-3.89457750448703,
126.347371184142));
#174877=CARTESIAN_POINT('Ctrl Pts',(-40.5684259026306,-3.77494646716493,
126.24558836599));
#174878=CARTESIAN_POINT('Ctrl Pts',(-40.5610026362251,-3.6512924441916,
126.148612122481));
#174879=CARTESIAN_POINT('Ctrl Pts',(-40.5535881435041,-3.52778457000442,
126.051750496838));
#174880=CARTESIAN_POINT('Ctrl Pts',(-40.5461736507831,-3.40026346556194,
125.959684365949));
#174881=CARTESIAN_POINT('Ctrl Pts',(-40.5387591580621,-3.26913898429393,
125.872762411723));
#174882=CARTESIAN_POINT('Ctrl Pts',(-40.5313518117083,-3.13814088573771,
125.78592423615));
#174883=CARTESIAN_POINT('Ctrl Pts',(-40.5239444653546,-3.0035466336093,
125.704220571407));
#174884=CARTESIAN_POINT('Ctrl Pts',(-40.5165371190008,-2.86579851585264,
125.627959413154));
#174885=CARTESIAN_POINT('Ctrl Pts',(-40.5091352973254,-2.72815313583895,
125.55175513335));
#174886=CARTESIAN_POINT('Ctrl Pts',(-40.50173347565,-2.58735889907036,125.480985457599));
#174887=CARTESIAN_POINT('Ctrl Pts',(-40.4943316539745,-2.44388629219069,
125.415914612145));
#174888=CARTESIAN_POINT('Ctrl Pts',(-40.4869337396632,-2.30048942338301,
125.350878117083));
#174889=CARTESIAN_POINT('Ctrl Pts',(-40.4795358253518,-2.1544173394011,
125.291534614808));
#174890=CARTESIAN_POINT('Ctrl Pts',(-40.4721379110404,-2.00616419562074,
125.238101929479));
#174891=CARTESIAN_POINT('Ctrl Pts',(-40.4647412261282,-1.85793568882392,
125.184678123693));
#174892=CARTESIAN_POINT('Ctrl Pts',(-40.4573445412159,-1.70752719243071,
125.137163311785));
#174893=CARTESIAN_POINT('Ctrl Pts',(-40.4499478563037,-1.55545197716094,
125.095726830989));
#174894=CARTESIAN_POINT('Ctrl Pts',(-40.4425514993683,-1.40338350506558,
125.05429218753));
#174895=CARTESIAN_POINT('Ctrl Pts',(-40.4351551424328,-1.24964882120708,
125.018935437423));
#174896=CARTESIAN_POINT('Ctrl Pts',(-40.4277587854974,-1.09477520080447,
124.989775694959));
#174897=CARTESIAN_POINT('Ctrl Pts',(-40.4203612961608,-0.939877868855211,
124.960611488065));
#174898=CARTESIAN_POINT('Ctrl Pts',(-40.4129638068242,-0.783841620035531,
124.937646247032));
#174899=CARTESIAN_POINT('Ctrl Pts',(-40.4055663174876,-0.627202586010622,
124.920947706797));
#174900=CARTESIAN_POINT('Ctrl Pts',(-40.3981662349727,-0.470508642415827,
124.904243312915));
#174901=CARTESIAN_POINT('Ctrl Pts',(-40.3907661524578,-0.313211863871322,
124.893810033153));
#174902=CARTESIAN_POINT('Ctrl Pts',(-40.3833660699428,-0.155851998510028,
124.889663607823));
#174903=CARTESIAN_POINT('Ctrl Pts',(-40.3759578502763,0.0016809002008922,
124.885512623072));
#174904=CARTESIAN_POINT('Ctrl Pts',(-40.3685496306099,0.15927665086858,
124.887662308391));
#174905=CARTESIAN_POINT('Ctrl Pts',(-40.3611414109434,0.316396274386738,
124.8960762676));
#174906=CARTESIAN_POINT('Ctrl Pts',(-40.3537286316413,0.473612602411938,
124.90449540546));
#174907=CARTESIAN_POINT('Ctrl Pts',(-40.3463158523392,0.630351848544956,
124.919186465133));
#174908=CARTESIAN_POINT('Ctrl Pts',(-40.3389030730371,0.7860821676454,124.9400613936));
#174909=CARTESIAN_POINT('Ctrl Pts',(-40.3314797020083,0.94203500152858,
124.960966149143));
#174910=CARTESIAN_POINT('Ctrl Pts',(-40.3240563309797,1.09697566243705,
124.988072356398));
#174911=CARTESIAN_POINT('Ctrl Pts',(-40.316632959951,1.25038365594666,125.021241106831));
#174912=CARTESIAN_POINT('Ctrl Pts',(-40.3126969105101,1.33172425508061,
125.038827974184));
#174913=CARTESIAN_POINT('Ctrl Pts',(-40.3087608610692,1.41263422671327,
125.058118408508));
#174914=CARTESIAN_POINT('Ctrl Pts',(-40.3048248116284,1.49303805551621,
125.079086132681));
#174915=CARTESIAN_POINT('Ctrl Pts',(-40.2974015452229,1.64467716731935,
125.11863060609));
#174916=CARTESIAN_POINT('Ctrl Pts',(-40.2899782788175,1.79497343269383,
125.164263486521));
#174917=CARTESIAN_POINT('Ctrl Pts',(-40.282555012412,1.94340031270272,125.215879089719));
#174918=CARTESIAN_POINT('Ctrl Pts',(-40.275140519691,2.09165176446553,125.267433687561));
#174919=CARTESIAN_POINT('Ctrl Pts',(-40.26772602697,2.2380378796578,125.324956811728));
#174920=CARTESIAN_POINT('Ctrl Pts',(-40.260311534249,2.3820437665246,125.388292112011));
#174921=CARTESIAN_POINT('Ctrl Pts',(-40.2529041878953,2.52591085509611,
125.451566367348));
#174922=CARTESIAN_POINT('Ctrl Pts',(-40.2454968415414,2.66740194313536,
125.520641497054));
#174923=CARTESIAN_POINT('Ctrl Pts',(-40.2380894951876,2.80601883773402,
125.595311870935));
#174924=CARTESIAN_POINT('Ctrl Pts',(-40.2306876735123,2.94453234662277,
125.669926552833));
#174925=CARTESIAN_POINT('Ctrl Pts',(-40.2232858518369,3.08017560319755,
125.750127993337));
#174926=CARTESIAN_POINT('Ctrl Pts',(-40.2158840301616,3.21247199691197,
125.835663179448));
#174927=CARTESIAN_POINT('Ctrl Pts',(-40.2084861158502,3.34469855238976,
125.921153212201));
#174928=CARTESIAN_POINT('Ctrl Pts',(-40.2010882015388,3.47358145094979,
126.011971180905));
#174929=CARTESIAN_POINT('Ctrl Pts',(-40.1936902872275,3.59867032790635,
126.107819077928));
#174930=CARTESIAN_POINT('Ctrl Pts',(-40.1862936023153,3.7237384173609,126.203651046769));
#174931=CARTESIAN_POINT('Ctrl Pts',(-40.1788969174032,3.84501344054032,
126.304511058125));
#174932=CARTESIAN_POINT('Ctrl Pts',(-40.171500232491,3.96207549387292,126.410058813712));
#174933=CARTESIAN_POINT('Ctrl Pts',(-40.1641038755556,4.07913235655157,
126.515601889202));
#174934=CARTESIAN_POINT('Ctrl Pts',(-40.1567075186201,4.19197634357601,
126.625832045655));
#174935=CARTESIAN_POINT('Ctrl Pts',(-40.1493111616847,4.30022223558357,
126.740370055681));
#174936=CARTESIAN_POINT('Ctrl Pts',(-40.1419136723481,4.40848470031338,
126.854925601768));
#174937=CARTESIAN_POINT('Ctrl Pts',(-40.1345161830116,4.51214741188774,
126.973790043341));
#174938=CARTESIAN_POINT('Ctrl Pts',(-40.1271186936751,4.61086359072635,
127.096548930032));
#174939=CARTESIAN_POINT('Ctrl Pts',(-40.1197186111601,4.70961437436899,
127.219350849661));
#174940=CARTESIAN_POINT('Ctrl Pts',(-40.112318528645,4.8034149391095,127.34604964177));
#174941=CARTESIAN_POINT('Ctrl Pts',(-40.1049184461299,4.89196029512963,
127.47619970899));
#174942=CARTESIAN_POINT('Ctrl Pts',(-40.0975102264635,4.98060301587099,
127.606492889587));
#174943=CARTESIAN_POINT('Ctrl Pts',(-40.090102006797,5.06397877745584,127.740244615392));
#174944=CARTESIAN_POINT('Ctrl Pts',(-40.0826937871306,5.14182686964955,
127.876981754991));
#174945=CARTESIAN_POINT('Ctrl Pts',(-40.0752810078285,5.21972287604515,
128.013803054019));
#174946=CARTESIAN_POINT('Ctrl Pts',(-40.0678682285265,5.29208426257341,
128.153613097479));
#174947=CARTESIAN_POINT('Ctrl Pts',(-40.0604554492244,5.35869763544404,
128.295916834184));
#174948=CARTESIAN_POINT('Ctrl Pts',(-40.0530320781957,5.4254061886257,128.438423901142));
#174949=CARTESIAN_POINT('Ctrl Pts',(-40.0456087071669,5.48635018063139,
128.583431434439));
#174950=CARTESIAN_POINT('Ctrl Pts',(-40.0381853361381,5.54136513919476,
128.73042644392));
#174951=CARTESIAN_POINT('Ctrl Pts',(-40.0342492866973,5.57053539029118,
128.808366725044));
#174952=CARTESIAN_POINT('Ctrl Pts',(-40.0303132372565,5.5980396175646,128.886865526615));
#174953=CARTESIAN_POINT('Ctrl Pts',(-40.0263771878157,5.62385911082201,
128.965845112022));
#174954=CARTESIAN_POINT('Ctrl Pts',(-40.0189539214102,5.67255386930616,
129.11479814523));
#174955=CARTESIAN_POINT('Ctrl Pts',(-40.0115306550048,5.71540043723443,
129.265912336419));
#174956=CARTESIAN_POINT('Ctrl Pts',(-40.0041073885994,5.7522031226067,129.418687568548));
#174957=CARTESIAN_POINT('Ctrl Pts',(-39.9966928958784,5.78896231026119,
129.571282233041));
#174958=CARTESIAN_POINT('Ctrl Pts',(-39.9892784031574,5.81969174770084,
129.725533671315));
#174959=CARTESIAN_POINT('Ctrl Pts',(-39.9818639104363,5.84424466521449,
129.880924179249));
#174960=CARTESIAN_POINT('Ctrl Pts',(-39.9744565640826,5.86877391770181,
130.03616491596));
#174961=CARTESIAN_POINT('Ctrl Pts',(-39.9670492177287,5.88713844396749,
130.192542170424));
#174962=CARTESIAN_POINT('Ctrl Pts',(-39.9596418713749,5.89924196108349,
130.349525650691));
#174963=CARTESIAN_POINT('Ctrl Pts',(-39.9522400496995,5.91133645093981,
130.506392046757));
#174964=CARTESIAN_POINT('Ctrl Pts',(-39.9448382280241,5.91717920107018,
130.663863397752));
#174965=CARTESIAN_POINT('Ctrl Pts',(-39.9374364063487,5.9167254588341,130.821401958019));
#174966=CARTESIAN_POINT('Ctrl Pts',(-39.9300384920374,5.91627195612501,
130.978857354905));
#174967=CARTESIAN_POINT('Ctrl Pts',(-39.9226405777261,5.90952858176699,
131.136379518053));
#174968=CARTESIAN_POINT('Ctrl Pts',(-39.9152426634148,5.89650262490897,
131.293428462493));
#174969=CARTESIAN_POINT('Ctrl Pts',(-39.9078459785026,5.88347883272858,
131.450451308248));
#174970=CARTESIAN_POINT('Ctrl Pts',(-39.9004492935904,5.86417456100677,
131.607000719717));
#174971=CARTESIAN_POINT('Ctrl Pts',(-39.8930526086781,5.83864914418897,
131.762539480598));
#174972=CARTESIAN_POINT('Ctrl Pts',(-39.8856562517427,5.81312485919486,
131.918071344728));
#174973=CARTESIAN_POINT('Ctrl Pts',(-39.8782598948072,5.78138003804499,
132.072592279003));
#174974=CARTESIAN_POINT('Ctrl Pts',(-39.8708635378717,5.74352551500831,
132.225573205798));
#174975=CARTESIAN_POINT('Ctrl Pts',(-39.8634660485352,5.70566519634756,
132.378577554362));
#174976=CARTESIAN_POINT('Ctrl Pts',(-39.8560685591986,5.6616934029449,132.530041063586));
#174977=CARTESIAN_POINT('Ctrl Pts',(-39.8486710698621,5.61177138079809,
132.67944795744));
#174978=CARTESIAN_POINT('Ctrl Pts',(-39.841270987347,5.56183185856352,132.82890722565));
#174979=CARTESIAN_POINT('Ctrl Pts',(-39.833870904832,5.5059380729144,132.976308089261));
#174980=CARTESIAN_POINT('Ctrl Pts',(-39.8264708223169,5.44430006309049,
133.12115309544));
#174981=CARTESIAN_POINT('Ctrl Pts',(-39.8190626026505,5.3825942759386,133.266157373593));
#174982=CARTESIAN_POINT('Ctrl Pts',(-39.811654382984,5.31513179667647,133.408599838003));
#174983=CARTESIAN_POINT('Ctrl Pts',(-39.8042461633175,5.2421697639104,133.548005406682));
#174984=CARTESIAN_POINT('Ctrl Pts',(-39.7968333840154,5.16916282423029,
133.687496777163));
#174985=CARTESIAN_POINT('Ctrl Pts',(-39.7894206047134,5.09064977198451,
133.823947204571));
#174986=CARTESIAN_POINT('Ctrl Pts',(-39.7820078254113,5.00693176320131,
133.956909567407));
#174987=CARTESIAN_POINT('Ctrl Pts',(-39.7745844543825,4.9230941342013,134.090061913103));
#174988=CARTESIAN_POINT('Ctrl Pts',(-39.7671610833537,4.83403690593031,
134.219715933354));
#174989=CARTESIAN_POINT('Ctrl Pts',(-39.7597377123249,4.74010277025761,
134.345455969275));
#174990=CARTESIAN_POINT('Ctrl Pts',(-39.7558016628841,4.69029663760551,
134.412126353411));
#174991=CARTESIAN_POINT('Ctrl Pts',(-39.7518656134434,4.63912007931228,
134.477696958464));
#174992=CARTESIAN_POINT('Ctrl Pts',(-39.7479295640026,4.58662838407366,
134.542110024483));
#174993=CARTESIAN_POINT('Ctrl Pts',(-39.7405062975972,4.48763068506306,
134.663591056732));
#174994=CARTESIAN_POINT('Ctrl Pts',(-39.7330830311917,4.38365365279023,
134.781319999315));
#174995=CARTESIAN_POINT('Ctrl Pts',(-39.7256597647863,4.27501227357988,
134.894861885533));
#174996=CARTESIAN_POINT('Ctrl Pts',(-39.7182452720653,4.1664992994575,135.008269574671));
#174997=CARTESIAN_POINT('Ctrl Pts',(-39.7108307793442,4.05333320735376,
135.11749979088));
#174998=CARTESIAN_POINT('Ctrl Pts',(-39.7034162866232,3.93587022379573,
135.222149220922));
#174999=CARTESIAN_POINT('Ctrl Pts',(-39.6960089402695,3.81852045548382,
135.326697785902));
#175000=CARTESIAN_POINT('Ctrl Pts',(-39.6886015939158,3.69688231749495,
135.426674107724));
#175001=CARTESIAN_POINT('Ctrl Pts',(-39.681194247562,3.57134991618857,135.521710545082));
#175002=CARTESIAN_POINT('Ctrl Pts',(-39.6737924258866,3.4459111416828,135.616676100681));
#175003=CARTESIAN_POINT('Ctrl Pts',(-39.6663906042111,3.3165841834328,135.706708883505));
#175004=CARTESIAN_POINT('Ctrl Pts',(-39.6589887825357,3.18379727219426,
135.791480577229));
#175005=CARTESIAN_POINT('Ctrl Pts',(-39.6515908682243,3.05108045813274,
135.876207520635));
#175006=CARTESIAN_POINT('Ctrl Pts',(-39.644192953913,2.91490764245909,135.95567870568));
#175007=CARTESIAN_POINT('Ctrl Pts',(-39.6367950396016,2.77573706978512,
136.029608389865));
#175008=CARTESIAN_POINT('Ctrl Pts',(-39.6293983546894,2.63658962473572,
136.103525788278));
#175009=CARTESIAN_POINT('Ctrl Pts',(-39.6220016697772,2.4944457407587,136.171903338584));
#175010=CARTESIAN_POINT('Ctrl Pts',(-39.614604984865,2.34978946485991,136.234500581999));
#175011=CARTESIAN_POINT('Ctrl Pts',(-39.6072086279296,2.2051396031722,136.297095049787));
#175012=CARTESIAN_POINT('Ctrl Pts',(-39.5998122709942,2.05797791366424,
136.353909572053));
#175013=CARTESIAN_POINT('Ctrl Pts',(-39.5924159140587,1.90880943295803,
136.404751417425));
#175014=CARTESIAN_POINT('Ctrl Pts',(-39.5850184247221,1.75961811417598,
136.455601046815));
#175015=CARTESIAN_POINT('Ctrl Pts',(-39.5776209353856,1.60841974579123,
136.500476058116));
#175016=CARTESIAN_POINT('Ctrl Pts',(-39.5702234460491,1.45573542218498,
136.539233322613));
#175017=CARTESIAN_POINT('Ctrl Pts',(-39.562823363534,1.30299757532557,136.578004173409));
#175018=CARTESIAN_POINT('Ctrl Pts',(-39.555423281019,1.14877309773524,136.610652915796));
#175019=CARTESIAN_POINT('Ctrl Pts',(-39.548023198504,0.993594041911419,
136.637087376328));
#175020=CARTESIAN_POINT('Ctrl Pts',(-39.5406149788375,0.838244350763372,
136.663550904266));
#175021=CARTESIAN_POINT('Ctrl Pts',(-39.533206759171,0.681938353370654,
136.683786441191));
#175022=CARTESIAN_POINT('Ctrl Pts',(-39.5257985395045,0.525214739363178,
136.697753531674));
#175023=CARTESIAN_POINT('Ctrl Pts',(-39.5183857602024,0.36839466458613,
136.711729218668));
#175024=CARTESIAN_POINT('Ctrl Pts',(-39.5109729809004,0.211156833004429,
136.719428753209));
#175025=CARTESIAN_POINT('Ctrl Pts',(-39.5035602015983,0.0540402027871688,
136.720863826302));
#175026=CARTESIAN_POINT('Ctrl Pts',(-39.4961368305695,-0.103300923039385,
136.722300949894));
#175027=CARTESIAN_POINT('Ctrl Pts',(-39.4887134595408,-0.260520129493493,
136.717455746439));
#175028=CARTESIAN_POINT('Ctrl Pts',(-39.481290088512,-0.417082477656666,
136.706391858531));
#175029=CARTESIAN_POINT('Ctrl Pts',(-39.4773540390713,-0.500095591313523,
136.700525519688));
#175030=CARTESIAN_POINT('Ctrl Pts',(-39.4734179896306,-0.582924178214504,
136.692911745483));
#175031=CARTESIAN_POINT('Ctrl Pts',(-39.4694819401898,-0.665489758385496,
136.683565831197));
#175032=CARTESIAN_POINT('Ctrl Pts',(-39.4620586737844,-0.821205865806332,
136.665939728528));
#175033=CARTESIAN_POINT('Ctrl Pts',(-39.454635407379,-0.976456685181706,
136.64209627565));
#175034=CARTESIAN_POINT('Ctrl Pts',(-39.4472121409736,-1.13070600890658,
136.612065369352));
#175035=CARTESIAN_POINT('Ctrl Pts',(-39.4397976482526,-1.28477302274064,
136.582069957092));
#175036=CARTESIAN_POINT('Ctrl Pts',(-39.4323831555316,-1.43784053421516,
136.545901718732));
#175037=CARTESIAN_POINT('Ctrl Pts',(-39.4249686628106,-1.58937667534061,
136.503642357082));
#175038=CARTESIAN_POINT('Ctrl Pts',(-39.4175613164568,-1.74076676022715,
136.461423726596));
#175039=CARTESIAN_POINT('Ctrl Pts',(-39.410153970103,-1.89062805601135,
136.413125760138));
#175040=CARTESIAN_POINT('Ctrl Pts',(-39.4027466237493,-2.03843823153748,
136.358881311443));
#175041=CARTESIAN_POINT('Ctrl Pts',(-39.395344802074,-2.18613816465772,
136.304677320305));
#175042=CARTESIAN_POINT('Ctrl Pts',(-39.3879429803987,-2.33178967462792,
136.24453580589));
#175043=CARTESIAN_POINT('Ctrl Pts',(-39.3805411587234,-2.47488507044041,
136.178639587866));
#175044=CARTESIAN_POINT('Ctrl Pts',(-39.373143244412,-2.61790492730954,
136.112778155942));
#175045=CARTESIAN_POINT('Ctrl Pts',(-39.3657453301005,-2.7583710191074,
136.04116822621));
#175046=CARTESIAN_POINT('Ctrl Pts',(-39.3583474157891,-2.89579525017106,
135.964040882038));
#175047=CARTESIAN_POINT('Ctrl Pts',(-39.3509507308769,-3.03319664381967,
135.886926355033));
#175048=CARTESIAN_POINT('Ctrl Pts',(-39.3435540459648,-3.16755685479181,
135.804296415874));
#175049=CARTESIAN_POINT('Ctrl Pts',(-39.3361573610526,-3.29841193907253,
135.71642833317));
#175050=CARTESIAN_POINT('Ctrl Pts',(-39.3287610041172,-3.4292612211017,
135.62856414663));
#175051=CARTESIAN_POINT('Ctrl Pts',(-39.3213646471817,-3.5566053755584,
135.535462486468));
#175052=CARTESIAN_POINT('Ctrl Pts',(-39.3139682902462,-3.68000926745085,
135.437444078284));
#175053=CARTESIAN_POINT('Ctrl Pts',(-39.3065708009097,-3.80343205279366,
135.339410663231));
#175054=CARTESIAN_POINT('Ctrl Pts',(-39.2991733115732,-3.92291308206493,
135.236459233492));
#175055=CARTESIAN_POINT('Ctrl Pts',(-39.2917758222367,-4.03805027277946,
135.128950835957));
#175056=CARTESIAN_POINT('Ctrl Pts',(-39.2843757397216,-4.15322782465886,
135.02140475152));
#175057=CARTESIAN_POINT('Ctrl Pts',(-39.2769756572065,-4.2640582335698,
134.909298773409));
#175058=CARTESIAN_POINT('Ctrl Pts',(-39.2695755746915,-4.37017636401009,
134.79303071046));
#175059=CARTESIAN_POINT('Ctrl Pts',(-39.262167355025,-4.47641118224341,
134.676634798824));
#175060=CARTESIAN_POINT('Ctrl Pts',(-39.2547591353586,-4.57792312213516,
134.55606793839));
#175061=CARTESIAN_POINT('Ctrl Pts',(-39.2473509156921,-4.67438697248521,
134.431761476854));
#175062=CARTESIAN_POINT('Ctrl Pts',(-39.23993813639,-4.77091019472571,134.307378506764));
#175063=CARTESIAN_POINT('Ctrl Pts',(-39.232525357088,-4.86237891991497,
134.179251652339));
#175064=CARTESIAN_POINT('Ctrl Pts',(-39.225112577786,-4.94851166397086,
134.047840673624));
#175065=CARTESIAN_POINT('Ctrl Pts',(-39.2176892067572,-5.03476747853081,
133.916241928739));
#175066=CARTESIAN_POINT('Ctrl Pts',(-39.2102658357284,-5.11567189302207,
133.781350006852));
#175067=CARTESIAN_POINT('Ctrl Pts',(-39.2028424646996,-5.19098930420983,
133.643649367602));
#175068=CARTESIAN_POINT('Ctrl Pts',(-39.1989064152588,-5.23092440283896,
133.570637184588));
#175069=CARTESIAN_POINT('Ctrl Pts',(-39.1949703658178,-5.26928959338914,
133.496835717663));
#175070=CARTESIAN_POINT('Ctrl Pts',(-39.1910343163769,-5.30605532387013,
133.422319261726));
#175071=CARTESIAN_POINT('Ctrl Pts',(-39.1830667672712,-5.38047836337056,
133.271479306388));
#175072=CARTESIAN_POINT('Ctrl Pts',(-39.1750992181656,-5.44854441786373,
133.117303859407));
#175073=CARTESIAN_POINT('Ctrl Pts',(-39.1671316690599,-5.50996474576556,
132.960333498407));
#175074=CARTESIAN_POINT('Ctrl Pts',(-39.1591797189277,-5.57126482413259,
132.803670456067));
#175075=CARTESIAN_POINT('Ctrl Pts',(-39.1512277687956,-5.62594501497068,
132.644223678088));
#175076=CARTESIAN_POINT('Ctrl Pts',(-39.1432758186635,-5.67376320284541,
132.482556577678));
#175077=CARTESIAN_POINT('Ctrl Pts',(-39.1353462269315,-5.72144694091106,
132.321344034661));
#175078=CARTESIAN_POINT('Ctrl Pts',(-39.1274166351995,-5.76230707955355,
132.157923897655));
#175079=CARTESIAN_POINT('Ctrl Pts',(-39.1194870434675,-5.79615040522259,
131.992876937411));
#175080=CARTESIAN_POINT('Ctrl Pts',(-39.1115712989339,-5.8299346313491,
131.828118193519));
#175081=CARTESIAN_POINT('Ctrl Pts',(-39.1036555544003,-5.85672641306675,
131.661738570411));
#175082=CARTESIAN_POINT('Ctrl Pts',(-39.0957398098666,-5.87638217084346,
131.494333910305));
#175083=CARTESIAN_POINT('Ctrl Pts',(-39.0878434404491,-5.8959898178472,
131.327339001259));
#175084=CARTESIAN_POINT('Ctrl Pts',(-39.0799470710314,-5.9084962433274,
131.159324344707));
#175085=CARTESIAN_POINT('Ctrl Pts',(-39.0720507016138,-5.91380886971371,
130.990895373029));
#175086=CARTESIAN_POINT('Ctrl Pts',(-39.0691588860228,-5.91575446458157,
130.929213161808));
#175087=CARTESIAN_POINT('Ctrl Pts',(-39.0662670704316,-5.91673573397632,
130.867475498038));
#175088=CARTESIAN_POINT('Ctrl Pts',(-39.0633752548405,-5.91674984556424,
130.805712473904));
#175089=CARTESIAN_POINT('',(-37.3133751886983,-5.91555801160614,130.798912666527));
#175090=CARTESIAN_POINT('Ctrl Pts',(-39.0633751922042,-5.90721400833861,
130.805708959537));
#175091=CARTESIAN_POINT('Ctrl Pts',(-39.0131123589908,-5.90503878728851,
129.733931433989));
#175092=CARTESIAN_POINT('Ctrl Pts',(-38.870033651173,-5.11274322411047,
126.68000182472));
#175093=CARTESIAN_POINT('Ctrl Pts',(-38.6341390687512,-0.207615843526837,
123.809043884792));
#175094=CARTESIAN_POINT('Ctrl Pts',(-38.3556914449382,5.77313665022518,
126.848547964243));
#175095=CARTESIAN_POINT('Ctrl Pts',(-38.0772438211253,6.44865859582369,
133.523250619913));
#175096=CARTESIAN_POINT('Ctrl Pts',(-37.7987961973124,1.19817832634459,
137.699426188581));
#175097=CARTESIAN_POINT('Ctrl Pts',(-37.5441733210053,-4.60991333961225,
135.724193425928));
#175098=CARTESIAN_POINT('Ctrl Pts',(-37.3823663193026,-5.90208600168968,
132.264974056485));
#175099=CARTESIAN_POINT('Ctrl Pts',(-37.3133751922042,-5.91531521970268,
130.798912964642));
#175100=CARTESIAN_POINT('',(-35.5633751921759,-5.91674990983146,130.805393579034));
#175101=CARTESIAN_POINT('Ctrl Pts',(-37.3133751715223,-5.91674749050639,
130.798911206011));
#175102=CARTESIAN_POINT('Ctrl Pts',(-37.3039607718894,-5.91656319311221,
130.598808656684));
#175103=CARTESIAN_POINT('Ctrl Pts',(-37.2945463722564,-5.90622431910606,
130.399160275082));
#175104=CARTESIAN_POINT('Ctrl Pts',(-37.2851319726236,-5.88588985533355,
130.20084493974));
#175105=CARTESIAN_POINT('Ctrl Pts',(-37.2755249102599,-5.86513925314817,
129.998471143363));
#175106=CARTESIAN_POINT('Ctrl Pts',(-37.2659178478962,-5.83397976607423,
129.797485305177));
#175107=CARTESIAN_POINT('Ctrl Pts',(-37.2563107855325,-5.7926285272159,
129.598796306472));
#175108=CARTESIAN_POINT('Ctrl Pts',(-37.2515075069172,-5.77195399489752,
129.499457030589));
#175109=CARTESIAN_POINT('Ctrl Pts',(-37.2467042283019,-5.74873253607829,
129.400691536482));
#175110=CARTESIAN_POINT('Ctrl Pts',(-37.2419009496867,-5.72299570535111,
129.302611397812));
#175111=CARTESIAN_POINT('Ctrl Pts',(-37.2344776832812,-5.68322050881899,
129.15103264156));
#175112=CARTESIAN_POINT('Ctrl Pts',(-37.2270544168757,-5.63735895589863,
129.0008059957));
#175113=CARTESIAN_POINT('Ctrl Pts',(-37.2196311504702,-5.5855175320251,
128.852457837728));
#175114=CARTESIAN_POINT('Ctrl Pts',(-37.2122166577491,-5.53373738040943,
128.704285014958));
#175115=CARTESIAN_POINT('Ctrl Pts',(-37.2048021650281,-5.4759915481044,
128.55798660968));
#175116=CARTESIAN_POINT('Ctrl Pts',(-37.197387672307,-5.41243716871604,
128.414077275114));
#175117=CARTESIAN_POINT('Ctrl Pts',(-37.1899803259532,-5.34894404543122,
128.270306645783));
#175118=CARTESIAN_POINT('Ctrl Pts',(-37.1825729795993,-5.27965367036182,
128.128920842176));
#175119=CARTESIAN_POINT('Ctrl Pts',(-37.1751656332455,-5.20477243163089,
127.99041774369));
#175120=CARTESIAN_POINT('Ctrl Pts',(-37.1677638115701,-5.12994704215301,
127.852017946041));
#175121=CARTESIAN_POINT('Ctrl Pts',(-37.1603619898947,-5.04953926857393,
127.716496899478));
#175122=CARTESIAN_POINT('Ctrl Pts',(-37.1529601682192,-4.96380284891965,
127.584330828953));
#175123=CARTESIAN_POINT('Ctrl Pts',(-37.1455622539078,-4.87811168885406,
127.452234527867));
#175124=CARTESIAN_POINT('Ctrl Pts',(-37.1381643395965,-4.7870976874825,
127.323489988039));
#175125=CARTESIAN_POINT('Ctrl Pts',(-37.1307664252851,-4.69105953747209,
127.198547120116));
#175126=CARTESIAN_POINT('Ctrl Pts',(-37.1233697403728,-4.59503734725976,
127.073625015431));
#175127=CARTESIAN_POINT('Ctrl Pts',(-37.1159730554605,-4.49399289275658,
126.952503624453));
#175128=CARTESIAN_POINT('Ctrl Pts',(-37.1085763705483,-4.38826711087254,
126.835602332392));
#175129=CARTESIAN_POINT('Ctrl Pts',(-37.1011800136128,-4.28254601698046,
126.718706223858));
#175130=CARTESIAN_POINT('Ctrl Pts',(-37.0937836566772,-4.1721442588322,
126.606030119038));
#175131=CARTESIAN_POINT('Ctrl Pts',(-37.0863872997417,-4.05744164961755,
126.497958659731));
#175132=CARTESIAN_POINT('Ctrl Pts',(-37.0789898104051,-3.94272147914044,
126.389870654407));
#175133=CARTESIAN_POINT('Ctrl Pts',(-37.0715923210685,-3.82369941820876,
126.286388954317));
#175134=CARTESIAN_POINT('Ctrl Pts',(-37.0641948317318,-3.70079044444893,
126.187859707919));
#175135=CARTESIAN_POINT('Ctrl Pts',(-37.0567947492168,-3.57783838513889,
126.089295922245));
#175136=CARTESIAN_POINT('Ctrl Pts',(-37.0493946667017,-3.4509969912524,
125.995688280118));
#175137=CARTESIAN_POINT('Ctrl Pts',(-37.0419945841867,-3.32071232378487,
125.907341092879));
#175138=CARTESIAN_POINT('Ctrl Pts',(-37.0345863645201,-3.19028439493188,
125.818896758826));
#175139=CARTESIAN_POINT('Ctrl Pts',(-37.0271781448536,-3.05640594029233,
125.735724641147));
#175140=CARTESIAN_POINT('Ctrl Pts',(-37.0197699251871,-2.91955048748648,
125.65808472975));
#175141=CARTESIAN_POINT('Ctrl Pts',(-37.012357145885,-2.78261080243258,
125.580397032283));
#175142=CARTESIAN_POINT('Ctrl Pts',(-37.0049443665829,-2.64269079915634,
125.508248496634));
#175143=CARTESIAN_POINT('Ctrl Pts',(-36.9975315872807,-2.50028585302065,
125.441851762964));
#175144=CARTESIAN_POINT('Ctrl Pts',(-36.9901082162519,-2.35767743202019,
125.375360158527));
#175145=CARTESIAN_POINT('Ctrl Pts',(-36.982684845223,-2.21257732025677,
125.314636913875));
#175146=CARTESIAN_POINT('Ctrl Pts',(-36.9752614741942,-2.06549875759093,
125.2598457204));
#175147=CARTESIAN_POINT('Ctrl Pts',(-36.9713254247541,-1.98751417457693,
125.230794114928));
#175148=CARTESIAN_POINT('Ctrl Pts',(-36.967389375314,-1.90897360716784,
125.203409381323));
#175149=CARTESIAN_POINT('Ctrl Pts',(-36.9634533258738,-1.82995482035788,
125.177710111452));
#175150=CARTESIAN_POINT('Ctrl Pts',(-36.9560300594683,-1.6809278545018,
125.129242090516));
#175151=CARTESIAN_POINT('Ctrl Pts',(-36.9486067930629,-1.52974863311755,
125.086625542278));
#175152=CARTESIAN_POINT('Ctrl Pts',(-36.9411835266575,-1.37691757047712,
125.050055397419));
#175153=CARTESIAN_POINT('Ctrl Pts',(-36.9337690339364,-1.22426714146091,
125.013528475434));
#175154=CARTESIAN_POINT('Ctrl Pts',(-36.9263545412154,-1.0699691168342,
124.983033818009));
#175155=CARTESIAN_POINT('Ctrl Pts',(-36.9189400484944,-0.914541423479221,
124.958717406829));
#175156=CARTESIAN_POINT('Ctrl Pts',(-36.9115327021406,-0.759263537186846,
124.93442443272));
#175157=CARTESIAN_POINT('Ctrl Pts',(-36.9041253557868,-0.60285851612274,
124.916297907282));
#175158=CARTESIAN_POINT('Ctrl Pts',(-36.896718009433,-0.445856798146332,
124.904433306315));
#175159=CARTESIAN_POINT('Ctrl Pts',(-36.8893161877575,-0.288972177974303,
124.892577554415));
#175160=CARTESIAN_POINT('Ctrl Pts',(-36.8819143660822,-0.131492117657274,
124.886974455641));
#175161=CARTESIAN_POINT('Ctrl Pts',(-36.8745125444067,0.0260455696644963,
124.887667944222));
#175162=CARTESIAN_POINT('Ctrl Pts',(-36.8671146300954,0.183500094066952,
124.888361066717));
#175163=CARTESIAN_POINT('Ctrl Pts',(-36.859716715784,0.341011812540219,
124.895344155183));
#175164=CARTESIAN_POINT('Ctrl Pts',(-36.8523188014726,0.498040751832022,
124.908609098717));
#175165=CARTESIAN_POINT('Ctrl Pts',(-36.8449221165604,0.655043595763134,
124.921871837857));
#175166=CARTESIAN_POINT('Ctrl Pts',(-36.8375254316482,0.811563448135018,
124.94141432878));
#175167=CARTESIAN_POINT('Ctrl Pts',(-36.830128746736,0.967063183565719,
124.967176419557));
#175168=CARTESIAN_POINT('Ctrl Pts',(-36.8227323898005,1.1225560239752,124.992937368015));
#175169=CARTESIAN_POINT('Ctrl Pts',(-36.8153360328651,1.27702846910446,
125.024917306963));
#175170=CARTESIAN_POINT('Ctrl Pts',(-36.8079396759296,1.42995161060948,
125.063004597094));
#175171=CARTESIAN_POINT('Ctrl Pts',(-36.8005421865931,1.58289816503785,
125.101097718485));
#175172=CARTESIAN_POINT('Ctrl Pts',(-36.7931446972564,1.73429458128532,
125.145299962647));
#175173=CARTESIAN_POINT('Ctrl Pts',(-36.7857472079199,1.88362532930908,
125.195449298844));
#175174=CARTESIAN_POINT('Ctrl Pts',(-36.7783471254048,2.03300842499507,
125.245616214813));
#175175=CARTESIAN_POINT('Ctrl Pts',(-36.7709470428898,2.18032405709106,
125.301734254761));
#175176=CARTESIAN_POINT('Ctrl Pts',(-36.7635469603748,2.32507509298301,
125.363592622651));
#175177=CARTESIAN_POINT('Ctrl Pts',(-36.7561387407084,2.46998529751969,
125.425519010176));
#175178=CARTESIAN_POINT('Ctrl Pts',(-36.7487305210419,2.61232493057494,
125.493198184501));
#175179=CARTESIAN_POINT('Ctrl Pts',(-36.7413223013754,2.7516193020312,125.566372284323));
#175180=CARTESIAN_POINT('Ctrl Pts',(-36.7339095220733,2.89099940684923,
125.639591421583));
#175181=CARTESIAN_POINT('Ctrl Pts',(-36.7264967427712,3.02733019274953,
125.718312037234));
#175182=CARTESIAN_POINT('Ctrl Pts',(-36.7190839634691,3.16016499705973,
125.802232295156));
#175183=CARTESIAN_POINT('Ctrl Pts',(-36.7116605924404,3.29318960196728,
125.886272462277));
#175184=CARTESIAN_POINT('Ctrl Pts',(-36.7042372214116,3.42270794213975,
125.975526898769));
#175185=CARTESIAN_POINT('Ctrl Pts',(-36.6968138503828,3.54830488069168,
126.069652280597));
#175186=CARTESIAN_POINT('Ctrl Pts',(-36.6928778009421,3.61489939116719,
126.119559816549));
#175187=CARTESIAN_POINT('Ctrl Pts',(-36.6889417515014,3.68039203827932,
126.170836102878));
#175188=CARTESIAN_POINT('Ctrl Pts',(-36.6850057020607,3.7447251462828,126.223425763052));
#175189=CARTESIAN_POINT('Ctrl Pts',(-36.6775824356553,3.86605538021307,
126.322608220877));
#175190=CARTESIAN_POINT('Ctrl Pts',(-36.6701591692499,3.98362595112466,
126.426764296155));
#175191=CARTESIAN_POINT('Ctrl Pts',(-36.6627359028445,4.09700237217803,
126.535578340983));
#175192=CARTESIAN_POINT('Ctrl Pts',(-36.6553214101235,4.21024479171705,
126.644263776647));
#175193=CARTESIAN_POINT('Ctrl Pts',(-36.6479069174025,4.31930266191125,
126.7575959675));
#175194=CARTESIAN_POINT('Ctrl Pts',(-36.6404924246815,4.42377321210486,
126.875218073656));
#175195=CARTESIAN_POINT('Ctrl Pts',(-36.6330850783277,4.52814306964896,
126.992726811197));
#175196=CARTESIAN_POINT('Ctrl Pts',(-36.6256777319739,4.62793416316039,
127.114516955274));
#175197=CARTESIAN_POINT('Ctrl Pts',(-36.6182703856201,4.72277945152285,
127.240193840495));
#175198=CARTESIAN_POINT('Ctrl Pts',(-36.6108685639448,4.81755400069094,
127.365776991154));
#175199=CARTESIAN_POINT('Ctrl Pts',(-36.6034667422694,4.9073898656435,127.495240814215));
#175200=CARTESIAN_POINT('Ctrl Pts',(-36.596064920594,4.99195938212829,127.628156579775));
#175201=CARTESIAN_POINT('Ctrl Pts',(-36.5886670062826,5.07648425502363,
127.761002180137));
#175202=CARTESIAN_POINT('Ctrl Pts',(-36.5812690919713,5.15574811619767,
127.89729577974));
#175203=CARTESIAN_POINT('Ctrl Pts',(-36.5738711776599,5.22946592085267,
128.03657869965));
#175204=CARTESIAN_POINT('Ctrl Pts',(-36.5664744927477,5.30317147494592,
128.175838473267));
#175205=CARTESIAN_POINT('Ctrl Pts',(-36.5590778078356,5.37133262727738,
128.318086251635));
#175206=CARTESIAN_POINT('Ctrl Pts',(-36.5516811229234,5.43370965597914,
128.462837622373));
#175207=CARTESIAN_POINT('Ctrl Pts',(-36.5442847659879,5.49608391881808,
128.607582574683));
#175208=CARTESIAN_POINT('Ctrl Pts',(-36.5368884090525,5.55267442025389,
128.754830555812));
#175209=CARTESIAN_POINT('Ctrl Pts',(-36.529492052117,5.60328919771785,128.904076236417));
#175210=CARTESIAN_POINT('Ctrl Pts',(-36.5220945627804,5.65391172443346,
129.053344766917));
#175211=CARTESIAN_POINT('Ctrl Pts',(-36.5146970734439,5.69855658559252,
129.204611252345));
#175212=CARTESIAN_POINT('Ctrl Pts',(-36.5072995841073,5.73708144566016,
129.357354381103));
#175213=CARTESIAN_POINT('Ctrl Pts',(-36.4998995015923,5.77561981055778,
129.510151053729));
#175214=CARTESIAN_POINT('Ctrl Pts',(-36.4924994190774,5.80803381173699,
129.664425038557));
#175215=CARTESIAN_POINT('Ctrl Pts',(-36.4850993365624,5.83423208555115,
129.819644143435));
#175216=CARTESIAN_POINT('Ctrl Pts',(-36.4776911168959,5.86045916706061,
129.975033927675));
#175217=CARTESIAN_POINT('Ctrl Pts',(-36.4702828972295,5.88045680943273,
130.13137053911));
#175218=CARTESIAN_POINT('Ctrl Pts',(-36.462874677563,5.89418537708077,130.288115227168));
#175219=CARTESIAN_POINT('Ctrl Pts',(-36.4554618982609,5.90792239443314,
130.444956388966));
#175220=CARTESIAN_POINT('Ctrl Pts',(-36.4480491189589,5.91538263084562,
130.60220575585));
#175221=CARTESIAN_POINT('Ctrl Pts',(-36.4406363396568,5.9165785975116,130.759324388065));
#175222=CARTESIAN_POINT('Ctrl Pts',(-36.4332129686281,5.91777627303084,
130.91666751875));
#175223=CARTESIAN_POINT('Ctrl Pts',(-36.4257895975994,5.91269181431795,
131.073879169572));
#175224=CARTESIAN_POINT('Ctrl Pts',(-36.4183662265706,5.90138967797973,
131.230424499084));
#175225=CARTESIAN_POINT('Ctrl Pts',(-36.4144301771298,5.89539701410207,
131.313428589046));
#175226=CARTESIAN_POINT('Ctrl Pts',(-36.4104941276889,5.88765719770414,
131.396245493168));
#175227=CARTESIAN_POINT('Ctrl Pts',(-36.406558078248,5.878185643482,131.478796754841));
#175228=CARTESIAN_POINT('Ctrl Pts',(-36.3991348118426,5.86032258781643,
131.634485858017));
#175229=CARTESIAN_POINT('Ctrl Pts',(-36.3917115454372,5.83624289722977,
131.789700211938));
#175230=CARTESIAN_POINT('Ctrl Pts',(-36.3842882790318,5.80597728449461,
131.943903655118));
#175231=CARTESIAN_POINT('Ctrl Pts',(-36.3768737863108,5.77574744320025,
132.097924842633));
#175232=CARTESIAN_POINT('Ctrl Pts',(-36.3694592935897,5.73934630402704,
132.250937134956));
#175233=CARTESIAN_POINT('Ctrl Pts',(-36.3620448008687,5.69685637910187,
132.402408789051));
#175234=CARTESIAN_POINT('Ctrl Pts',(-36.354637454515,5.65440740756607,132.553734449062));
#175235=CARTESIAN_POINT('Ctrl Pts',(-36.3472301081612,5.60588143365416,
132.703522070027));
#175236=CARTESIAN_POINT('Ctrl Pts',(-36.3398227618075,5.55141210584787,
132.851249523576));
#175237=CARTESIAN_POINT('Ctrl Pts',(-36.3324209401321,5.49698340332128,
132.998866796416));
#175238=CARTESIAN_POINT('Ctrl Pts',(-36.3250191184567,5.43662030174455,
133.144426612578));
#175239=CARTESIAN_POINT('Ctrl Pts',(-36.3176172967813,5.37050639319398,
133.287421559863));
#175240=CARTESIAN_POINT('Ctrl Pts',(-36.3102193824699,5.30442738566111,
133.430341021229));
#175241=CARTESIAN_POINT('Ctrl Pts',(-36.3028214681585,5.23260377337199,
133.570697972246));
#175242=CARTESIAN_POINT('Ctrl Pts',(-36.2954235538471,5.15526738222731,
133.708004669485));
#175243=CARTESIAN_POINT('Ctrl Pts',(-36.2880268689349,5.07794384298792,
133.845288548842));
#175244=CARTESIAN_POINT('Ctrl Pts',(-36.2806301840228,4.99510952614419,
133.979522855525));
#175245=CARTESIAN_POINT('Ctrl Pts',(-36.2732334991106,4.90704240602778,
134.110244068014));
#175246=CARTESIAN_POINT('Ctrl Pts',(-36.2658371421751,4.81897919089976,
134.240959484187));
#175247=CARTESIAN_POINT('Ctrl Pts',(-36.2584407852398,4.72568384242273,
134.368161806303));
#175248=CARTESIAN_POINT('Ctrl Pts',(-36.2510444283043,4.62747774802602,
134.491416387964));
#175249=CARTESIAN_POINT('Ctrl Pts',(-36.2436469389678,4.52925661802541,
134.614689840216));
#175250=CARTESIAN_POINT('Ctrl Pts',(-36.2362494496312,4.42612347771388,
134.73401405658));
#175251=CARTESIAN_POINT('Ctrl Pts',(-36.2288519602946,4.31843998546752,
134.848987504488));
#175252=CARTESIAN_POINT('Ctrl Pts',(-36.2214518777796,4.21071874494005,
134.96400125616));
#175253=CARTESIAN_POINT('Ctrl Pts',(-36.2140517952646,4.09844423163117,
135.074660930516));
#175254=CARTESIAN_POINT('Ctrl Pts',(-36.2066517127496,3.98201480958954,
135.180601997873));
#175255=CARTESIAN_POINT('Ctrl Pts',(-36.1992434930831,3.86545736142897,
135.286659558325));
#175256=CARTESIAN_POINT('Ctrl Pts',(-36.1918352734167,3.74473615671733,
135.38798789843));
#175257=CARTESIAN_POINT('Ctrl Pts',(-36.1844270537503,3.62028303756659,
135.484262463802));
#175258=CARTESIAN_POINT('Ctrl Pts',(-36.1770142744482,3.49575331959763,
135.580596284564));
#175259=CARTESIAN_POINT('Ctrl Pts',(-36.1696014951461,3.36748741371257,
135.671869916572));
#175260=CARTESIAN_POINT('Ctrl Pts',(-36.162188715844,3.23594550779504,135.757802575748));
#175261=CARTESIAN_POINT('Ctrl Pts',(-36.1547653448153,3.10421564863363,
135.843858019538));
#175262=CARTESIAN_POINT('Ctrl Pts',(-36.1473419737866,2.96920076020303,
135.9245570578));
#175263=CARTESIAN_POINT('Ctrl Pts',(-36.1399186027578,2.83138566012953,
135.999664824839));
#175264=CARTESIAN_POINT('Ctrl Pts',(-36.1359825533169,2.75831278724038,
136.039488765111));
#175265=CARTESIAN_POINT('Ctrl Pts',(-36.132046503876,2.68445302048714,136.077741597966));
#175266=CARTESIAN_POINT('Ctrl Pts',(-36.1281104544351,2.60988069965456,
136.114393884512));
#175267=CARTESIAN_POINT('Ctrl Pts',(-36.1206871880297,2.4692396298907,136.183518953057));
#175268=CARTESIAN_POINT('Ctrl Pts',(-36.1132639216242,2.3256377370963,136.24715717701));
#175269=CARTESIAN_POINT('Ctrl Pts',(-36.1058406552187,2.17954271011847,
136.305044587516));
#175270=CARTESIAN_POINT('Ctrl Pts',(-36.0984261624977,2.0336203553301,136.362863579911));
#175271=CARTESIAN_POINT('Ctrl Pts',(-36.0910116697768,1.88521107539483,
136.414945152124));
#175272=CARTESIAN_POINT('Ctrl Pts',(-36.0835971770557,1.73480684060859,
136.461071303846));
#175273=CARTESIAN_POINT('Ctrl Pts',(-36.0761898307019,1.58454757108623,
136.507152997447));
#175274=CARTESIAN_POINT('Ctrl Pts',(-36.0687824843481,1.4322975291499,136.547290589165));
#175275=CARTESIAN_POINT('Ctrl Pts',(-36.0613751379943,1.27856823645375,
136.581314298117));
#175276=CARTESIAN_POINT('Ctrl Pts',(-36.0539733163189,1.12495360086441,
136.615312630903));
#175277=CARTESIAN_POINT('Ctrl Pts',(-36.0465714946436,0.969862274205898,
136.643206080106));
#175278=CARTESIAN_POINT('Ctrl Pts',(-36.0391696729682,0.813820392733913,
136.664874838253));
#175279=CARTESIAN_POINT('Ctrl Pts',(-36.0317717586568,0.657860884556308,
136.68653215763));
#175280=CARTESIAN_POINT('Ctrl Pts',(-36.0243738443455,0.50095218971895,
136.701971278895));
#175281=CARTESIAN_POINT('Ctrl Pts',(-36.0169759300341,0.343629968143567,
136.711123606505));
#175282=CARTESIAN_POINT('Ctrl Pts',(-36.0095792451219,0.186333890667293,
136.720274413164));
#175283=CARTESIAN_POINT('Ctrl Pts',(-36.0021825602096,0.0286247951460516,
136.723140478031));
#175284=CARTESIAN_POINT('Ctrl Pts',(-35.9947858752974,-0.128957092719909,
136.719705124079));
#175285=CARTESIAN_POINT('Ctrl Pts',(-35.9873895183619,-0.286531993239603,
136.716269922455));
#175286=CARTESIAN_POINT('Ctrl Pts',(-35.9799931614266,-0.443979324110384,
136.706533865713));
#175287=CARTESIAN_POINT('Ctrl Pts',(-35.9725968044911,-0.600759687251767,
136.690532409204));
#175288=CARTESIAN_POINT('Ctrl Pts',(-35.9651993151545,-0.757564053867211,
136.674528502831));
#175289=CARTESIAN_POINT('Ctrl Pts',(-35.957801825818,-0.913700878037255,
136.652257324605));
#175290=CARTESIAN_POINT('Ctrl Pts',(-35.9504043364814,-1.06863685385445,
136.6238061098));
#175291=CARTESIAN_POINT('Ctrl Pts',(-35.9430042539664,-1.22362714223779,
136.595344921466));
#175292=CARTESIAN_POINT('Ctrl Pts',(-35.9356041714513,-1.37741537721916,
136.560699450641));
#175293=CARTESIAN_POINT('Ctrl Pts',(-35.9282040889363,-1.52947954415417,
136.520007815086));
#175294=CARTESIAN_POINT('Ctrl Pts',(-35.9207958692699,-1.68171092127329,
136.479271434894));
#175295=CARTESIAN_POINT('Ctrl Pts',(-35.9133876496034,-1.83221408349758,
136.432475709276));
#175296=CARTESIAN_POINT('Ctrl Pts',(-35.905979429937,-1.98048255282059,
136.37980852966));
#175297=CARTESIAN_POINT('Ctrl Pts',(-35.8985666506349,-2.12884227891269,
136.327108934273));
#175298=CARTESIAN_POINT('Ctrl Pts',(-35.8911538713328,-2.27496422572512,
136.268530822556));
#175299=CARTESIAN_POINT('Ctrl Pts',(-35.8837410920307,-2.41836341886766,
136.204309592953));
#175300=CARTESIAN_POINT('Ctrl Pts',(-35.8763177210019,-2.56196750750212,
136.139996601046));
#175301=CARTESIAN_POINT('Ctrl Pts',(-35.8688943499732,-2.70284073902702,
136.070024552953));
#175302=CARTESIAN_POINT('Ctrl Pts',(-35.8614709789445,-2.84052345851048,
135.994674388828));
#175303=CARTESIAN_POINT('Ctrl Pts',(-35.8575349295037,-2.91352614003103,
135.954721923807));
#175304=CARTESIAN_POINT('Ctrl Pts',(-35.8535988800629,-2.98563233974033,
135.913258200757));
#175305=CARTESIAN_POINT('Ctrl Pts',(-35.8496628306222,-3.05677710739541,
135.870329851405));
#175306=CARTESIAN_POINT('Ctrl Pts',(-35.8422395642167,-3.19095391884254,
135.789368324273));
#175307=CARTESIAN_POINT('Ctrl Pts',(-35.8348162978114,-3.3221148897088,
135.702949999345));
#175308=CARTESIAN_POINT('Ctrl Pts',(-35.827393031406,-3.4497851382752,135.61132567488));
#175309=CARTESIAN_POINT('Ctrl Pts',(-35.819978538685,-3.57730449121032,
135.519809642757));
#175310=CARTESIAN_POINT('Ctrl Pts',(-35.8125640459639,-3.70134103384341,
135.423100074323));
#175311=CARTESIAN_POINT('Ctrl Pts',(-35.8051495532429,-3.82144543437741,
135.321493043627));
#175312=CARTESIAN_POINT('Ctrl Pts',(-35.7977422068891,-3.94143407376832,
135.219983945614));
#175313=CARTESIAN_POINT('Ctrl Pts',(-35.7903348605353,-4.05749783301726,
135.113587022127));
#175314=CARTESIAN_POINT('Ctrl Pts',(-35.7829275141815,-4.16921738070859,
135.002640860105));
#175315=CARTESIAN_POINT('Ctrl Pts',(-35.7755256925061,-4.28085360374616,
134.891777445918));
#175316=CARTESIAN_POINT('Ctrl Pts',(-35.7681238708307,-4.38815180291972,
134.776371811015));
#175317=CARTESIAN_POINT('Ctrl Pts',(-35.7607220491553,-4.49072679131001,
134.656801849864));
#175318=CARTESIAN_POINT('Ctrl Pts',(-35.7533241348439,-4.59324763116238,
134.537295008765));
#175319=CARTESIAN_POINT('Ctrl Pts',(-35.7459262205326,-4.69104998340803,
134.413628502078));
#175320=CARTESIAN_POINT('Ctrl Pts',(-35.7385283062212,-4.78378659940384,
134.286215918101));
#175321=CARTESIAN_POINT('Ctrl Pts',(-35.731131621309,-4.87650780425661,
134.158824507784));
#175322=CARTESIAN_POINT('Ctrl Pts',(-35.7237349363968,-4.96416472418869,
134.027688557237));
#175323=CARTESIAN_POINT('Ctrl Pts',(-35.7163382514846,-5.04645132315826,
133.8932535593));
#175324=CARTESIAN_POINT('Ctrl Pts',(-35.7089418945492,-5.1287342734538,
133.758824522352));
#175325=CARTESIAN_POINT('Ctrl Pts',(-35.7015455376137,-5.20564718137771,
133.621097047265));
#175326=CARTESIAN_POINT('Ctrl Pts',(-35.6941491806782,-5.27692831868325,
133.480544109403));
#175327=CARTESIAN_POINT('Ctrl Pts',(-35.6867516913416,-5.34822036931299,
133.339969652527));
#175328=CARTESIAN_POINT('Ctrl Pts',(-35.6793542020051,-5.41387876363703,
133.196569204493));
#175329=CARTESIAN_POINT('Ctrl Pts',(-35.6719567126685,-5.4736886302921,
133.050838603461));
#175330=CARTESIAN_POINT('Ctrl Pts',(-35.6645566301535,-5.53351946320322,
132.905056916793));
#175331=CARTESIAN_POINT('Ctrl Pts',(-35.6571565476384,-5.58749754488179,
132.75694379595));
#175332=CARTESIAN_POINT('Ctrl Pts',(-35.6497564651234,-5.63545691604405,
132.607013082661));
#175333=CARTESIAN_POINT('Ctrl Pts',(-35.6423482454569,-5.68346902346516,
132.456917505138));
#175334=CARTESIAN_POINT('Ctrl Pts',(-35.6349400257905,-5.72544908960591,
132.305000699543));
#175335=CARTESIAN_POINT('Ctrl Pts',(-35.627531806124,-5.76128142911044,
132.15179034007));
#175336=CARTESIAN_POINT('Ctrl Pts',(-35.6201190268219,-5.79713582282209,
131.998485682177));
#175337=CARTESIAN_POINT('Ctrl Pts',(-35.6127062475199,-5.82683487989473,
131.843886249702));
#175338=CARTESIAN_POINT('Ctrl Pts',(-35.6052934682178,-5.85031450720381,
131.688527303944));
#175339=CARTESIAN_POINT('Ctrl Pts',(-35.597870097189,-5.87382768330547,
131.532946374039));
#175340=CARTESIAN_POINT('Ctrl Pts',(-35.5904467261602,-5.89110364019271,
131.376604133463));
#175341=CARTESIAN_POINT('Ctrl Pts',(-35.5830233551314,-5.90213028605508,
131.220039157945));
#175342=CARTESIAN_POINT('Ctrl Pts',(-35.5790873056907,-5.90797687827193,
131.137024651201));
#175343=CARTESIAN_POINT('Ctrl Pts',(-35.57515125625,-5.91206743599125,131.053947508116));
#175344=CARTESIAN_POINT('Ctrl Pts',(-35.5712152068093,-5.91440608461213,
130.970887578756));
#175345=CARTESIAN_POINT('Ctrl Pts',(-35.5686018686076,-5.91595882927992,
130.915739977158));
#175346=CARTESIAN_POINT('Ctrl Pts',(-35.5659885304059,-5.91674027688676,
130.86057055656));
#175347=CARTESIAN_POINT('Ctrl Pts',(-35.5633751922042,-5.91674990983136,
130.805393579632));
#175348=CARTESIAN_POINT('',(-33.8133752151521,-5.91399190468965,130.809307765289));
#175349=CARTESIAN_POINT('Ctrl Pts',(-35.5633751921759,-5.91674990983146,
130.805393579034));
#175350=CARTESIAN_POINT('Ctrl Pts',(-35.5559869379694,-5.91677714342954,
130.649400936515));
#175351=CARTESIAN_POINT('Ctrl Pts',(-35.5485986837629,-5.9106310999208,
130.493162228736));
#175352=CARTESIAN_POINT('Ctrl Pts',(-35.5412104295564,-5.89827942929397,
130.337209318234));
#175353=CARTESIAN_POINT('Ctrl Pts',(-35.5338308523911,-5.88594226492956,
130.181439564643));
#175354=CARTESIAN_POINT('Ctrl Pts',(-35.5264512752258,-5.8674140075802,
130.025955312578));
#175355=CARTESIAN_POINT('Ctrl Pts',(-35.5190716980605,-5.84271427044327,
129.871290139811));
#175356=CARTESIAN_POINT('Ctrl Pts',(-35.5116991387766,-5.81803802243363,
129.716772051602));
#175357=CARTESIAN_POINT('Ctrl Pts',(-35.5043265794927,-5.78720203589756,
129.563071862187));
#175358=CARTESIAN_POINT('Ctrl Pts',(-35.4969540202089,-5.75027783723711,
129.410719574442));
#175359=CARTESIAN_POINT('Ctrl Pts',(-35.489586825525,-5.71338050625557,
129.258478144955));
#175360=CARTESIAN_POINT('Ctrl Pts',(-35.4822196308411,-5.67040387116845,
129.107583029565));
#175361=CARTESIAN_POINT('Ctrl Pts',(-35.4748524361572,-5.6214707734391,
128.958555398733));
#175362=CARTESIAN_POINT('Ctrl Pts',(-35.4672655672755,-5.57107859400335,
128.805084078457));
#175363=CARTESIAN_POINT('Ctrl Pts',(-35.4596786983938,-5.51436926674348,
128.653593749841));
#175364=CARTESIAN_POINT('Ctrl Pts',(-35.4520918295121,-5.45153285809808,
128.504638882317));
#175365=CARTESIAN_POINT('Ctrl Pts',(-35.4447293484672,-5.39055488750217,
128.360089476522));
#175366=CARTESIAN_POINT('Ctrl Pts',(-35.4373668674222,-5.32380729160206,
128.217928046068));
#175367=CARTESIAN_POINT('Ctrl Pts',(-35.4300043863773,-5.25151313802298,
128.078642304227));
#175368=CARTESIAN_POINT('Ctrl Pts',(-35.4226419565869,-5.1792194877258,
127.939357532036));
#175369=CARTESIAN_POINT('Ctrl Pts',(-35.4152795267965,-5.10137952996784,
127.802948743642));
#175370=CARTESIAN_POINT('Ctrl Pts',(-35.4079170970061,-5.01826264884636,
127.669879711627));
#175371=CARTESIAN_POINT('Ctrl Pts',(-35.4005532295195,-4.93512953710119,
127.536784694598));
#175372=CARTESIAN_POINT('Ctrl Pts',(-35.3931893620328,-4.84671765065185,
127.407031052028));
#175373=CARTESIAN_POINT('Ctrl Pts',(-35.3858254945462,-4.75333999936162,
127.281054015385));
#175374=CARTESIAN_POINT('Ctrl Pts',(-35.3784586997688,-4.65992522850938,
127.155026900246));
#175375=CARTESIAN_POINT('Ctrl Pts',(-35.3710919049914,-4.5615409878702,
127.032779682138));
#175376=CARTESIAN_POINT('Ctrl Pts',(-35.363725110214,-4.45854075467284,
126.914714759468));
#175377=CARTESIAN_POINT('Ctrl Pts',(-35.356350135751,-4.35542615565569,
126.796518743971));
#175378=CARTESIAN_POINT('Ctrl Pts',(-35.348975161288,-4.24768557986087,
126.682514578862));
#175379=CARTESIAN_POINT('Ctrl Pts',(-35.341600186825,-4.13570998790208,
126.573068443954));
#175380=CARTESIAN_POINT('Ctrl Pts',(-35.3342202982419,-4.02365978395514,
126.463549382496));
#175381=CARTESIAN_POINT('Ctrl Pts',(-35.3268404096588,-3.90736922166183,
126.358594652872));
#175382=CARTESIAN_POINT('Ctrl Pts',(-35.3194605210757,-3.78726204666404,
126.258529917639));
#175383=CARTESIAN_POINT('Ctrl Pts',(-35.3120707249736,-3.66699362748174,
126.158330845248));
#175384=CARTESIAN_POINT('Ctrl Pts',(-35.3046809288715,-3.54289866613725,
126.063035098984));
#175385=CARTESIAN_POINT('Ctrl Pts',(-35.2972911327694,-3.41542997607893,
125.972925153752));
#175386=CARTESIAN_POINT('Ctrl Pts',(-35.2957832828451,-3.38942064483255,
125.95453868243));
#175387=CARTESIAN_POINT('Ctrl Pts',(-35.2942754329207,-3.36327093207583,
125.936367965198));
#175388=CARTESIAN_POINT('Ctrl Pts',(-35.2927675829964,-3.33698480487009,
125.918415164067));
#175389=CARTESIAN_POINT('Ctrl Pts',(-35.2853443165909,-3.20757608728912,
125.830032080732));
#175390=CARTESIAN_POINT('Ctrl Pts',(-35.2779210501855,-3.07445790372475,
125.746660164798));
#175391=CARTESIAN_POINT('Ctrl Pts',(-35.27049778378,-2.9380557519732,125.668627080787));
#175392=CARTESIAN_POINT('Ctrl Pts',(-35.263083291059,-2.80181481623773,
125.590686225401));
#175393=CARTESIAN_POINT('Ctrl Pts',(-35.2556687983381,-2.66229795907687,
125.518071825293));
#175394=CARTESIAN_POINT('Ctrl Pts',(-35.2482543056171,-2.51996123713822,
125.451069487259));
#175395=CARTESIAN_POINT('Ctrl Pts',(-35.2408469592633,-2.37776170469086,
125.384131728601));
#175396=CARTESIAN_POINT('Ctrl Pts',(-35.2334396129094,-2.23274805373423,
125.322795421452));
#175397=CARTESIAN_POINT('Ctrl Pts',(-35.2260322665556,-2.08540253695233,
125.267301215557));
#175398=CARTESIAN_POINT('Ctrl Pts',(-35.2186304448803,-1.93816691601608,
125.211848399335));
#175399=CARTESIAN_POINT('Ctrl Pts',(-35.2112286232049,-1.78860324006258,
125.162229139482));
#175400=CARTESIAN_POINT('Ctrl Pts',(-35.2038268015295,-1.63721531991091,
125.118636691912));
#175401=CARTESIAN_POINT('Ctrl Pts',(-35.1964288872181,-1.48590731626454,
125.075067256457));
#175402=CARTESIAN_POINT('Ctrl Pts',(-35.1890309729068,-1.33277734410326,
125.037518400195));
#175403=CARTESIAN_POINT('Ctrl Pts',(-35.1816330585955,-1.1783459087153,
125.006134036799));
#175404=CARTESIAN_POINT('Ctrl Pts',(-35.1742363736833,-1.02394013702934,
124.974754888914));
#175405=CARTESIAN_POINT('Ctrl Pts',(-35.1668396887712,-0.86823369682951,
124.949538274981));
#175406=CARTESIAN_POINT('Ctrl Pts',(-35.1594430038589,-0.711758980423895,
124.930577363454));
#175407=CARTESIAN_POINT('Ctrl Pts',(-35.1520466469235,-0.555291202270955,
124.911617292674));
#175408=CARTESIAN_POINT('Ctrl Pts',(-35.144650289988,-0.398055586234015,
124.898912417671));
#175409=CARTESIAN_POINT('Ctrl Pts',(-35.1372539330525,-0.24059110316989,
124.892504184636));
#175410=CARTESIAN_POINT('Ctrl Pts',(-35.129856443716,-0.0831025118918699,
124.886094970484));
#175411=CARTESIAN_POINT('Ctrl Pts',(-35.1224589543793,0.0746146431697645,
124.885984332997));
#175412=CARTESIAN_POINT('Ctrl Pts',(-35.1150614650428,0.232020073902628,
124.892161597928));
#175413=CARTESIAN_POINT('Ctrl Pts',(-35.1076613825278,0.389480682865451,
124.89834102829));
#175414=CARTESIAN_POINT('Ctrl Pts',(-35.1002613000128,0.546628977156729,
124.910812735017));
#175415=CARTESIAN_POINT('Ctrl Pts',(-35.0928612174978,0.70292862523581,
124.929514074011));
#175416=CARTESIAN_POINT('Ctrl Pts',(-35.0854529978313,0.859400140845949,
124.948235977049));
#175417=CARTESIAN_POINT('Ctrl Pts',(-35.0780447781649,1.01502077575306,
124.973201148121));
#175418=CARTESIAN_POINT('Ctrl Pts',(-35.0706365584984,1.16926251474753,
125.00429546844));
#175419=CARTESIAN_POINT('Ctrl Pts',(-35.0632237791963,1.32359918695913,
125.035408926794));
#175420=CARTESIAN_POINT('Ctrl Pts',(-35.0558109998942,1.47655491028574,
125.072658963228));
#175421=CARTESIAN_POINT('Ctrl Pts',(-35.0483982205921,1.62761621409,125.115881381238));
#175422=CARTESIAN_POINT('Ctrl Pts',(-35.0409748495634,1.778893361369,125.159165557466));
#175423=CARTESIAN_POINT('Ctrl Pts',(-35.0335514785346,1.9282703293981,125.208439042192));
#175424=CARTESIAN_POINT('Ctrl Pts',(-35.0261281075058,2.07525224822536,
125.263488965133));
#175425=CARTESIAN_POINT('Ctrl Pts',(-35.022192058065,2.15318558836977,125.292677755181));
#175426=CARTESIAN_POINT('Ctrl Pts',(-35.0182560086243,2.23044597228738,
125.323489724327));
#175427=CARTESIAN_POINT('Ctrl Pts',(-35.0143199591835,2.30696248977542,
125.355887929439));
#175428=CARTESIAN_POINT('Ctrl Pts',(-35.0068966927781,2.4512702537599,125.416989933166));
#175429=CARTESIAN_POINT('Ctrl Pts',(-34.9994734263727,2.59336703765948,
125.483921474066));
#175430=CARTESIAN_POINT('Ctrl Pts',(-34.9920501599673,2.73274717607931,
125.556501679472));
#175431=CARTESIAN_POINT('Ctrl Pts',(-34.9846356672463,2.87196257875034,
125.628996101103));
#175432=CARTESIAN_POINT('Ctrl Pts',(-34.9772211745252,3.00846739929175,
125.707125727391));
#175433=CARTESIAN_POINT('Ctrl Pts',(-34.9698066818042,3.14177483886011,
125.790661242413));
#175434=CARTESIAN_POINT('Ctrl Pts',(-34.9623993354504,3.27495379169927,
125.874116242761));
#175435=CARTESIAN_POINT('Ctrl Pts',(-34.9549919890966,3.40494118453581,
125.962966562074));
#175436=CARTESIAN_POINT('Ctrl Pts',(-34.9475846427429,3.53127388256734,
126.056936544577));
#175437=CARTESIAN_POINT('Ctrl Pts',(-34.9401828210675,3.65751235690642,
126.150836440721));
#175438=CARTESIAN_POINT('Ctrl Pts',(-34.9327809993921,3.78010126566057,
126.249848175196));
#175439=CARTESIAN_POINT('Ctrl Pts',(-34.9253791777167,3.89860569510034,
126.353652337232));
#175440=CARTESIAN_POINT('Ctrl Pts',(-34.9179812634053,4.01704756697493,
126.45740170186));
#175441=CARTESIAN_POINT('Ctrl Pts',(-34.9105833490939,4.13140897354866,
126.565938210315));
#175442=CARTESIAN_POINT('Ctrl Pts',(-34.9031854347825,4.24128749035135,
126.678901735612));
#175443=CARTESIAN_POINT('Ctrl Pts',(-34.8957887498703,4.35114774733716,
126.79184648842));
#175444=CARTESIAN_POINT('Ctrl Pts',(-34.8883920649582,4.45652633307937,
126.909216530615));
#175445=CARTESIAN_POINT('Ctrl Pts',(-34.880995380046,4.55705709127248,127.030614305294));
#175446=CARTESIAN_POINT('Ctrl Pts',(-34.8735990231105,4.65758339182656,
127.15200669707));
#175447=CARTESIAN_POINT('Ctrl Pts',(-34.8662026661751,4.75326205414824,
127.277426178712));
#175448=CARTESIAN_POINT('Ctrl Pts',(-34.8588063092396,4.84376688147076,
127.406441701455));
#175449=CARTESIAN_POINT('Ctrl Pts',(-34.851408819903,4.93428556531351,127.535476976803));
#175450=CARTESIAN_POINT('Ctrl Pts',(-34.8440113305665,5.01962862253187,
127.668109083874));
#175451=CARTESIAN_POINT('Ctrl Pts',(-34.8366138412299,5.09951299474849,
127.803877693287));
#175452=CARTESIAN_POINT('Ctrl Pts',(-34.8292137587149,5.17942537030761,
127.939693896174));
#175453=CARTESIAN_POINT('Ctrl Pts',(-34.8218136761999,5.25387506184623,
128.078648468956));
#175454=CARTESIAN_POINT('Ctrl Pts',(-34.8144135936849,5.32262487331873,
128.220256320052));
#175455=CARTESIAN_POINT('Ctrl Pts',(-34.8070053740185,5.3914502822767,128.362019883539));
#175456=CARTESIAN_POINT('Ctrl Pts',(-34.799597154352,5.45456313121603,128.506442215864));
#175457=CARTESIAN_POINT('Ctrl Pts',(-34.7921889346856,5.51177402638542,
128.653017398885));
#175458=CARTESIAN_POINT('Ctrl Pts',(-34.7847761553835,5.56902013390633,
128.799682796487));
#175459=CARTESIAN_POINT('Ctrl Pts',(-34.7773633760815,5.62035692788746,
128.948503333028));
#175460=CARTESIAN_POINT('Ctrl Pts',(-34.7699505967795,5.66564500807687,
129.098958258897));
#175461=CARTESIAN_POINT('Ctrl Pts',(-34.7625272257507,5.71099779799906,
129.24962816182));
#175462=CARTESIAN_POINT('Ctrl Pts',(-34.7551038547219,5.75028451975687,
129.401936757664));
#175463=CARTESIAN_POINT('Ctrl Pts',(-34.7476804836931,5.78341677785059,
129.555352636736));
#175464=CARTESIAN_POINT('Ctrl Pts',(-34.7437444342523,5.80098429608973,
129.636697416985));
#175465=CARTESIAN_POINT('Ctrl Pts',(-34.7398083848115,5.81682243850423,
129.718353388052));
#175466=CARTESIAN_POINT('Ctrl Pts',(-34.7358723353706,5.83092395770166,
129.800240922509));
#175467=CARTESIAN_POINT('Ctrl Pts',(-34.7284490689652,5.85751898281439,
129.954678256872));
#175468=CARTESIAN_POINT('Ctrl Pts',(-34.7210258025597,5.87801436445953,
130.110406438308));
#175469=CARTESIAN_POINT('Ctrl Pts',(-34.7136025361543,5.89228895143836,
130.266902270103));
#175470=CARTESIAN_POINT('Ctrl Pts',(-34.7061880434332,5.90654666704081,
130.423213136822));
#175471=CARTESIAN_POINT('Ctrl Pts',(-34.6987735507123,5.91459818951644,
130.580289479792));
#175472=CARTESIAN_POINT('Ctrl Pts',(-34.6913590579912,5.91637332218163,
130.737597790502));
#175473=CARTESIAN_POINT('Ctrl Pts',(-34.6839517116374,5.91814674390712,
130.89475448154));
#175474=CARTESIAN_POINT('Ctrl Pts',(-34.6765443652836,5.91365581484407,
131.052142324447));
#175475=CARTESIAN_POINT('Ctrl Pts',(-34.6691370189298,5.9028821163297,131.209222672117));
#175476=CARTESIAN_POINT('Ctrl Pts',(-34.6617351972544,5.8921164532462,131.366185863336));
#175477=CARTESIAN_POINT('Ctrl Pts',(-34.654333375579,5.87507737645693,131.522841645149));
#175478=CARTESIAN_POINT('Ctrl Pts',(-34.6469315539036,5.85179853379275,
131.678651462995));
#175479=CARTESIAN_POINT('Ctrl Pts',(-34.6395336395921,5.82853197984821,
131.834379030052));
#175480=CARTESIAN_POINT('Ctrl Pts',(-34.6321357252807,5.79903227505665,
131.989261154258));
#175481=CARTESIAN_POINT('Ctrl Pts',(-34.6247378109693,5.76338488419449,
132.142764607077));
#175482=CARTESIAN_POINT('Ctrl Pts',(-34.6173411260571,5.72774341728218,
132.296242550405));
#175483=CARTESIAN_POINT('Ctrl Pts',(-34.6099444411449,5.68595637629979,
132.448341913797));
#175484=CARTESIAN_POINT('Ctrl Pts',(-34.6025477562326,5.63816032070145,
132.598539750364));
#175485=CARTESIAN_POINT('Ctrl Pts',(-34.5951513992972,5.59036638443037,
132.748730927002));
#175486=CARTESIAN_POINT('Ctrl Pts',(-34.5877550423618,5.53656407652576,
132.897020388743));
#175487=CARTESIAN_POINT('Ctrl Pts',(-34.5803586854263,5.47693973320394,
133.042900704621));
#175488=CARTESIAN_POINT('Ctrl Pts',(-34.5729611960897,5.41730626124269,
133.188803355149));
#175489=CARTESIAN_POINT('Ctrl Pts',(-34.5655637067531,5.35184912027339,
133.332295779819));
#175490=CARTESIAN_POINT('Ctrl Pts',(-34.5581662174165,5.28080259847433,
133.472891014329));
#175491=CARTESIAN_POINT('Ctrl Pts',(-34.5507661349015,5.2097311714274,133.61353553428));
#175492=CARTESIAN_POINT('Ctrl Pts',(-34.5433660523864,5.13306663075884,
133.751280509039));
#175493=CARTESIAN_POINT('Ctrl Pts',(-34.5359659698714,5.0510888874963,133.885664175009));
#175494=CARTESIAN_POINT('Ctrl Pts',(-34.5285577502049,4.96902100127764,
134.020195609635));
#175495=CARTESIAN_POINT('Ctrl Pts',(-34.5211495305385,4.88162843930775,
134.151358035229));
#175496=CARTESIAN_POINT('Ctrl Pts',(-34.513741310872,4.78923447289869,134.278718648354));
#175497=CARTESIAN_POINT('Ctrl Pts',(-34.5063285315699,4.69678363954498,
134.40615764981));
#175498=CARTESIAN_POINT('Ctrl Pts',(-34.4989157522677,4.59932549845371,
134.529789883664));
#175499=CARTESIAN_POINT('Ctrl Pts',(-34.4915029729657,4.49722282177984,
134.64921659065));
#175500=CARTESIAN_POINT('Ctrl Pts',(-34.4840796019369,4.39497425601324,
134.768813940116));
#175501=CARTESIAN_POINT('Ctrl Pts',(-34.4766562309081,4.28806815346692,
134.884193488187));
#175502=CARTESIAN_POINT('Ctrl Pts',(-34.4692328598794,4.17690382423927,
134.994993625305));
#175503=CARTESIAN_POINT('Ctrl Pts',(-34.4652968104388,4.11796182953463,
135.053742516615));
#175504=CARTESIAN_POINT('Ctrl Pts',(-34.4613607609982,4.05782325130584,
135.111204641304));
#175505=CARTESIAN_POINT('Ctrl Pts',(-34.4574247115576,3.99655116497038,
135.167330861365));
#175506=CARTESIAN_POINT('Ctrl Pts',(-34.4500014451522,3.88099392237199,
135.273183160767));
#175507=CARTESIAN_POINT('Ctrl Pts',(-34.4425781787468,3.76105364728595,
135.374601391742));
#175508=CARTESIAN_POINT('Ctrl Pts',(-34.4351549123414,3.6371050347427,135.471200825753));
#175509=CARTESIAN_POINT('Ctrl Pts',(-34.4277404196204,3.513302919166,135.567686087255));
#175510=CARTESIAN_POINT('Ctrl Pts',(-34.4203259268994,3.38550218775947,
135.659363661323));
#175511=CARTESIAN_POINT('Ctrl Pts',(-34.4129114341784,3.25411375332225,
135.745886115116));
#175512=CARTESIAN_POINT('Ctrl Pts',(-34.4055040878246,3.12285195600464,
135.832325175311));
#175513=CARTESIAN_POINT('Ctrl Pts',(-34.3980967414708,2.98800964945674,
135.913618803003));
#175514=CARTESIAN_POINT('Ctrl Pts',(-34.3906893951171,2.8500300570067,135.989460350132));
#175515=CARTESIAN_POINT('Ctrl Pts',(-34.3832875734416,2.71215337494198,
136.065245331774));
#175516=CARTESIAN_POINT('Ctrl Pts',(-34.3758857517661,2.57114439177295,
136.1355861505));
#175517=CARTESIAN_POINT('Ctrl Pts',(-34.3684839300907,2.42747439617799,
136.200220013288));
#175518=CARTESIAN_POINT('Ctrl Pts',(-34.3610860157793,2.28388024285558,
136.264819756363));
#175519=CARTESIAN_POINT('Ctrl Pts',(-34.353688101468,2.13762821426212,136.323718390586));
#175520=CARTESIAN_POINT('Ctrl Pts',(-34.3462901871567,1.98921312646629,
136.376699596845));
#175521=CARTESIAN_POINT('Ctrl Pts',(-34.3388935022444,1.84082270256573,
136.429671998589));
#175522=CARTESIAN_POINT('Ctrl Pts',(-34.3314968173322,1.69027028411111,
136.476728798687));
#175523=CARTESIAN_POINT('Ctrl Pts',(-34.32410013242,1.5380696548491,136.517702222908));
#175524=CARTESIAN_POINT('Ctrl Pts',(-34.3167037754845,1.38587577432272,
136.558673830325));
#175525=CARTESIAN_POINT('Ctrl Pts',(-34.3093074185491,1.23203418876763,
136.593562501167));
#175526=CARTESIAN_POINT('Ctrl Pts',(-34.3019110616137,1.07707253350351,
136.622250726538));
#175527=CARTESIAN_POINT('Ctrl Pts',(-34.2945135722771,0.922087153214153,
136.65094334415));
#175528=CARTESIAN_POINT('Ctrl Pts',(-34.2871160829405,0.765981728849491,
136.673433558141));
#175529=CARTESIAN_POINT('Ctrl Pts',(-34.2797185936039,0.609292595753247,
136.689655265692));
#175530=CARTESIAN_POINT('Ctrl Pts',(-34.272318511089,0.452548535524518,
136.705882659737));
#175531=CARTESIAN_POINT('Ctrl Pts',(-34.264918428574,0.295220730252588,
136.715837133886));
#175532=CARTESIAN_POINT('Ctrl Pts',(-34.257518346059,0.137848973478393,
136.719504590709));
#175533=CARTESIAN_POINT('Ctrl Pts',(-34.2501101263925,-0.0196958297208099,
136.723176080278));
#175534=CARTESIAN_POINT('Ctrl Pts',(-34.242701906726,-0.177284307513279,
136.720546737662));
#175535=CARTESIAN_POINT('Ctrl Pts',(-34.2352936870595,-0.334377594066704,
136.711654599339));
#175536=CARTESIAN_POINT('Ctrl Pts',(-34.2278809077575,-0.491567568916312,
136.702756988053));
#175537=CARTESIAN_POINT('Ctrl Pts',(-34.2204681284555,-0.648261374510992,
136.687588936078));
#175538=CARTESIAN_POINT('Ctrl Pts',(-34.2130553491534,-0.803927436176936,
136.66624011478));
#175539=CARTESIAN_POINT('Ctrl Pts',(-34.2056319781247,-0.959815920812247,
136.644860789286));
#175540=CARTESIAN_POINT('Ctrl Pts',(-34.1982086070959,-1.11467336207536,
136.61728312151));
#175541=CARTESIAN_POINT('Ctrl Pts',(-34.1907852360671,-1.26797969074281,
136.58364760355));
#175542=CARTESIAN_POINT('Ctrl Pts',(-34.1868491866263,-1.34926638473693,
136.565813244854));
#175543=CARTESIAN_POINT('Ctrl Pts',(-34.1829131371856,-1.43011726815256,
136.546276637761));
#175544=CARTESIAN_POINT('Ctrl Pts',(-34.1789770877448,-1.51045690598956,
136.525064289113));
#175545=CARTESIAN_POINT('Ctrl Pts',(-34.1715538213394,-1.66197495563588,
136.485058461576));
#175546=CARTESIAN_POINT('Ctrl Pts',(-34.1641305549339,-1.81213163405688,
136.438968342382));
#175547=CARTESIAN_POINT('Ctrl Pts',(-34.1567072885285,-1.96040072642103,
136.386901217897));
#175548=CARTESIAN_POINT('Ctrl Pts',(-34.1492927958075,-2.1084945770312,
136.33489563243));
#175549=CARTESIAN_POINT('Ctrl Pts',(-34.1418783030866,-2.25470493356989,
136.276927225726));
#175550=CARTESIAN_POINT('Ctrl Pts',(-34.1344638103656,-2.39851738254339,
136.213153914424));
#175551=CARTESIAN_POINT('Ctrl Pts',(-34.1270564640119,-2.54219121966432,
136.14944207024));
#175552=CARTESIAN_POINT('Ctrl Pts',(-34.1196491176581,-2.68347141139231,
136.079936610284));
#175553=CARTESIAN_POINT('Ctrl Pts',(-34.1122417713044,-2.82186039299421,
136.004844680127));
#175554=CARTESIAN_POINT('Ctrl Pts',(-34.104839949629,-2.96014615887172,
135.929808756365));
#175555=CARTESIAN_POINT('Ctrl Pts',(-34.0974381279536,-3.09554468155867,
135.849194835935));
#175556=CARTESIAN_POINT('Ctrl Pts',(-34.0900363062783,-3.22758012280086,
135.763257381303));
#175557=CARTESIAN_POINT('Ctrl Pts',(-34.0826383919669,-3.35954586356231,
135.677365292384));
#175558=CARTESIAN_POINT('Ctrl Pts',(-34.0752404776555,-3.48815174648927,
135.586155469132));
#175559=CARTESIAN_POINT('Ctrl Pts',(-34.0678425633441,-3.61294831601482,
135.489927288557));
#175560=CARTESIAN_POINT('Ctrl Pts',(-34.0604458784319,-3.73772414661438,
135.393715099361));
#175561=CARTESIAN_POINT('Ctrl Pts',(-34.0530491935198,-3.85869162487618,
135.292486435728));
#175562=CARTESIAN_POINT('Ctrl Pts',(-34.0456525086076,-3.9754318849244,
135.186582872407));
#175563=CARTESIAN_POINT('Ctrl Pts',(-34.0382561516722,-4.09216696858683,
135.080684004962));
#175564=CARTESIAN_POINT('Ctrl Pts',(-34.0308597947367,-4.20467493024666,
134.970110900808));
#175565=CARTESIAN_POINT('Ctrl Pts',(-34.0234634378013,-4.31257170656327,
134.855243958055));
#175566=CARTESIAN_POINT('Ctrl Pts',(-34.0160659484648,-4.42048500215193,
134.740359428879));
#175567=CARTESIAN_POINT('Ctrl Pts',(-34.0086684591282,-4.52378545109523,
134.621180024243));
#175568=CARTESIAN_POINT('Ctrl Pts',(-34.0012709697916,-4.62212753686347,
134.498121248071));
#175569=CARTESIAN_POINT('Ctrl Pts',(-33.9938708872767,-4.72050409629728,
134.375019333836));
#175570=CARTESIAN_POINT('Ctrl Pts',(-33.9864708047617,-4.81391859901877,
134.248035631935));
#175571=CARTESIAN_POINT('Ctrl Pts',(-33.9790707222467,-4.90206741286746,
134.117616665958));
#175572=CARTESIAN_POINT('Ctrl Pts',(-33.9716625025803,-4.99031315539914,
133.987054290919));
#175573=CARTESIAN_POINT('Ctrl Pts',(-33.9642542829138,-5.07328143654858,
133.853049417505));
#175574=CARTESIAN_POINT('Ctrl Pts',(-33.9568460632474,-5.15071298733801,
133.716075968449));
#175575=CARTESIAN_POINT('Ctrl Pts',(-33.9494332839453,-5.22819219595495,
133.57901821452));
#175576=CARTESIAN_POINT('Ctrl Pts',(-33.9420205046432,-5.30012771363057,
133.438988575482));
#175577=CARTESIAN_POINT('Ctrl Pts',(-33.9346077253412,-5.36630765432855,
133.296482749725));
#175578=CARTESIAN_POINT('Ctrl Pts',(-33.9271843543124,-5.43258215602942,
133.153773304961));
#175579=CARTESIAN_POINT('Ctrl Pts',(-33.9197609832837,-5.49308451269598,
133.008580950781));
#175580=CARTESIAN_POINT('Ctrl Pts',(-33.9123376122549,-5.54765181418925,
132.861419175562));
#175581=CARTESIAN_POINT('Ctrl Pts',(-33.9084015628139,-5.57658470676673,
132.783390471238));
#175582=CARTESIAN_POINT('Ctrl Pts',(-33.904465513373,-5.60384988329389,
132.704808319859));
#175583=CARTESIAN_POINT('Ctrl Pts',(-33.900529463932,-5.62942887026787,
132.625750514621));
#175584=CARTESIAN_POINT('Ctrl Pts',(-33.891614366256,-5.68736492283714,
132.44668567656));
#175585=CARTESIAN_POINT('Ctrl Pts',(-33.88269926858,-5.73679017535818,132.264740894172));
#175586=CARTESIAN_POINT('Ctrl Pts',(-33.8737841709039,-5.77745654700139,
132.080654631503));
#175587=CARTESIAN_POINT('Ctrl Pts',(-33.864918132021,-5.81789913611463,
131.897581375107));
#175588=CARTESIAN_POINT('Ctrl Pts',(-33.856052093138,-5.84967891348687,
131.71239016528));
#175589=CARTESIAN_POINT('Ctrl Pts',(-33.847186054255,-5.87259860290424,
131.525828712264));
#175590=CARTESIAN_POINT('Ctrl Pts',(-33.8384101721643,-5.89528522705938,
131.341164361481));
#175591=CARTESIAN_POINT('Ctrl Pts',(-33.8296342900738,-5.90929097733084,
131.155157536546));
#175592=CARTESIAN_POINT('Ctrl Pts',(-33.8208584079831,-5.91447133257009,
130.968553853439));
#175593=CARTESIAN_POINT('Ctrl Pts',(-33.8183640220233,-5.91594375497067,
130.915515127262));
#175594=CARTESIAN_POINT('Ctrl Pts',(-33.8158696360635,-5.91670348892751,
130.862428307846));
#175595=CARTESIAN_POINT('Ctrl Pts',(-33.8133752501038,-5.91674792922998,
130.809310814809));
#175596=CARTESIAN_POINT('',(-32.0633751628002,-5.91238878816303,130.801325224237));
#175597=CARTESIAN_POINT('Ctrl Pts',(-33.8133751922042,-5.91218240422062,
130.80930576309));
#175598=CARTESIAN_POINT('Ctrl Pts',(-33.7496107415092,-5.90152008560987,
129.452491318376));
#175599=CARTESIAN_POINT('Ctrl Pts',(-33.5930304162097,-4.76268453244047,
126.104521439791));
#175600=CARTESIAN_POINT('Ctrl Pts',(-33.3436342163061,0.808310511306774,
123.852800026758));
#175601=CARTESIAN_POINT('Ctrl Pts',(-33.0651865924932,6.28545637891517,
127.726926842634));
#175602=CARTESIAN_POINT('Ctrl Pts',(-32.7867389686805,5.98657489591573,
134.429064956672));
#175603=CARTESIAN_POINT('Ctrl Pts',(-32.5082913448675,0.186323544011373,
137.800276859724));
#175604=CARTESIAN_POINT('Ctrl Pts',(-32.2671700860422,-4.98466412141571,
135.152472362352));
#175605=CARTESIAN_POINT('Ctrl Pts',(-32.118864701821,-5.90299123506428,
131.98393423347));
#175606=CARTESIAN_POINT('Ctrl Pts',(-32.0633751922042,-5.90845789250784,
130.801327869466));
#175607=CARTESIAN_POINT('',(-30.3133751922042,-5.92024601756991,130.800506515061));
#175608=CARTESIAN_POINT('Ctrl Pts',(-32.0633751301833,-5.9167492198897,
130.801322289959));
#175609=CARTESIAN_POINT('Ctrl Pts',(-32.0552226912489,-5.91665987366913,
130.627332105479));
#175610=CARTESIAN_POINT('Ctrl Pts',(-32.0470702523146,-5.90889181901625,
130.453606855061));
#175611=CARTESIAN_POINT('Ctrl Pts',(-32.0389178133802,-5.89353951184319,
130.280793444375));
#175612=CARTESIAN_POINT('Ctrl Pts',(-32.0307233044932,-5.87810798042311,
130.107088245101));
#175613=CARTESIAN_POINT('Ctrl Pts',(-32.0225287956061,-5.85501380044389,
129.934304547922));
#175614=CARTESIAN_POINT('Ctrl Pts',(-32.0143342867191,-5.82440321666261,
129.763083645656));
#175615=CARTESIAN_POINT('Ctrl Pts',(-32.0061184001803,-5.79371277667428,
129.591416066125));
#175616=CARTESIAN_POINT('Ctrl Pts',(-31.9979025136416,-5.75546677692304,
129.421319658769));
#175617=CARTESIAN_POINT('Ctrl Pts',(-31.9896866271029,-5.70986156687168,
129.253421724617));
#175618=CARTESIAN_POINT('Ctrl Pts',(-31.981440949994,-5.66409099363012,
129.084914997348));
#175619=CARTESIAN_POINT('Ctrl Pts',(-31.9731952728851,-5.61090785806304,
128.918622924254));
#175620=CARTESIAN_POINT('Ctrl Pts',(-31.9649495957763,-5.55055821384193,
128.755157338911));
#175621=CARTESIAN_POINT('Ctrl Pts',(-31.9604317629314,-5.51749245086869,
128.665594022192));
#175622=CARTESIAN_POINT('Ctrl Pts',(-31.9559139300866,-5.48227613873368,
128.576878802306));
#175623=CARTESIAN_POINT('Ctrl Pts',(-31.9513960972417,-5.44495557469001,
128.489109151277));
#175624=CARTESIAN_POINT('Ctrl Pts',(-31.9439728308363,-5.38363402986731,
128.344894541248));
#175625=CARTESIAN_POINT('Ctrl Pts',(-31.936549564431,-5.31648631935658,
128.202899780306));
#175626=CARTESIAN_POINT('Ctrl Pts',(-31.9291262980256,-5.24369408515371,
128.063630258004));
#175627=CARTESIAN_POINT('Ctrl Pts',(-31.9217118053046,-5.17098788532654,
127.924525340712));
#175628=CARTESIAN_POINT('Ctrl Pts',(-31.9142973125836,-5.09265061241143,
127.788139578232));
#175629=CARTESIAN_POINT('Ctrl Pts',(-31.9068828198626,-5.00891232289246,
127.654959419866));
#175630=CARTESIAN_POINT('Ctrl Pts',(-31.8994754735088,-4.92525474348962,
127.52190762555));
#175631=CARTESIAN_POINT('Ctrl Pts',(-31.8920681271552,-4.83620670838022,
127.392055598298));
#175632=CARTESIAN_POINT('Ctrl Pts',(-31.8846607808014,-4.74204457783254,
127.265866052875));
#175633=CARTESIAN_POINT('Ctrl Pts',(-31.8772589591261,-4.6479526769545,
127.139770624376));
#175634=CARTESIAN_POINT('Ctrl Pts',(-31.8698571374507,-4.54875449768384,
127.017332536583));
#175635=CARTESIAN_POINT('Ctrl Pts',(-31.8624553157753,-4.44477011228294,
126.898986216634));
#175636=CARTESIAN_POINT('Ctrl Pts',(-31.855057401464,-4.34084061942953,
126.780702370786));
#175637=CARTESIAN_POINT('Ctrl Pts',(-31.8476594871526,-4.2321301980658,
126.666506270731));
#175638=CARTESIAN_POINT('Ctrl Pts',(-31.8402615728413,-4.11899958718184,
126.556799792422));
#175639=CARTESIAN_POINT('Ctrl Pts',(-31.8328648879291,-4.00588777655302,
126.44711154534));
#175640=CARTESIAN_POINT('Ctrl Pts',(-31.8254682030169,-3.88835750200238,
126.341911698849));
#175641=CARTESIAN_POINT('Ctrl Pts',(-31.8180715181047,-3.7668068771992,
126.241565803816));
#175642=CARTESIAN_POINT('Ctrl Pts',(-31.8106751611693,-3.64526164207828,
126.141224358225));
#175643=CARTESIAN_POINT('Ctrl Pts',(-31.8032788042339,-3.51969669903321,
126.045736673799));
#175644=CARTESIAN_POINT('Ctrl Pts',(-31.7958824472985,-3.39054359274896,
125.955428290943));
#175645=CARTESIAN_POINT('Ctrl Pts',(-31.7884849579619,-3.26137071279423,
125.865106081643));
#175646=CARTESIAN_POINT('Ctrl Pts',(-31.7810874686253,-3.12860888170464,
125.779964966739));
#175647=CARTESIAN_POINT('Ctrl Pts',(-31.7736899792888,-2.9927188590947,
125.700287303739));
#175648=CARTESIAN_POINT('Ctrl Pts',(-31.7662898967738,-2.85678120044799,
125.620581709858));
#175649=CARTESIAN_POINT('Ctrl Pts',(-31.7588898142588,-2.71771348881668,
125.546343569736));
#175650=CARTESIAN_POINT('Ctrl Pts',(-31.7514897317438,-2.57600117619034,
125.477809340917));
#175651=CARTESIAN_POINT('Ctrl Pts',(-31.7440815120773,-2.43413303630788,
125.409199751669));
#175652=CARTESIAN_POINT('Ctrl Pts',(-31.736673292411,-2.28961482420962,
125.346306762018));
#175653=CARTESIAN_POINT('Ctrl Pts',(-31.7292650727446,-2.1429527456763,
125.289318995575));
#175654=CARTESIAN_POINT('Ctrl Pts',(-31.7218522934425,-1.99620039908083,
125.232296154112));
#175655=CARTESIAN_POINT('Ctrl Pts',(-31.7144395141404,-1.84730190901101,
125.1811858991));
#175656=CARTESIAN_POINT('Ctrl Pts',(-31.7070267348384,-1.6967782366183,
125.136126838139));
#175657=CARTESIAN_POINT('Ctrl Pts',(-31.6996033638096,-1.54603948894339,
125.091003394678));
#175658=CARTESIAN_POINT('Ctrl Pts',(-31.6921799927809,-1.39367128176785,
125.051948506168));
#175659=CARTESIAN_POINT('Ctrl Pts',(-31.6847566217521,-1.24020515869239,
125.019049759293));
#175660=CARTESIAN_POINT('Ctrl Pts',(-31.680820572311,-1.15883373786127,
125.001606054303));
#175661=CARTESIAN_POINT('Ctrl Pts',(-31.6768845228699,-1.07715375838786,
124.985892196715));
#175662=CARTESIAN_POINT('Ctrl Pts',(-31.6729484734287,-0.995244858637009,
124.971915312734));
#175663=CARTESIAN_POINT('Ctrl Pts',(-31.6655252070233,-0.840767230009799,
124.945555345751));
#175664=CARTESIAN_POINT('Ctrl Pts',(-31.6581019406178,-0.685008038423174,
124.925296979622));
#175665=CARTESIAN_POINT('Ctrl Pts',(-31.6506786742124,-0.52849066435613,
124.911260569188));
#175666=CARTESIAN_POINT('Ctrl Pts',(-31.6432641814914,-0.37215828082705,
124.897240748626));
#175667=CARTESIAN_POINT('Ctrl Pts',(-31.6358496887704,-0.21506986670196,
124.889428278929));
#175668=CARTESIAN_POINT('Ctrl Pts',(-31.6284351960493,-0.0577590367029607,
124.88789254479));
#175669=CARTESIAN_POINT('Ctrl Pts',(-31.6210278496956,0.0994001711954374,
124.886358290849));
#175670=CARTESIAN_POINT('Ctrl Pts',(-31.6136205033418,0.256780997419503,
124.891088732216));
#175671=CARTESIAN_POINT('Ctrl Pts',(-31.606213156988,0.413844767457253,
124.902101467804));
#175672=CARTESIAN_POINT('Ctrl Pts',(-31.5988113353126,0.570791393409633,
124.913105989678));
#175673=CARTESIAN_POINT('Ctrl Pts',(-31.5914095136372,0.727421063243341,
124.930383450169));
#175674=CARTESIAN_POINT('Ctrl Pts',(-31.5840076919618,0.88319527422838,
124.953899381896));
#175675=CARTESIAN_POINT('Ctrl Pts',(-31.5766097776504,1.03888725321998,
124.977402899745));
#175676=CARTESIAN_POINT('Ctrl Pts',(-31.5692118633392,1.19372430454489,
125.007138274604));
#175677=CARTESIAN_POINT('Ctrl Pts',(-31.5618139490278,1.34717333034709,
125.043019230311));
#175678=CARTESIAN_POINT('Ctrl Pts',(-31.5544172641156,1.50059685570483,
125.078894223254));
#175679=CARTESIAN_POINT('Ctrl Pts',(-31.5470205792033,1.65263245020395,
125.120912685186));
#175680=CARTESIAN_POINT('Ctrl Pts',(-31.5396238942911,1.80275737538391,
125.168937260976));
#175681=CARTESIAN_POINT('Ctrl Pts',(-31.5322275373557,1.95287564386758,
125.216959707306));
#175682=CARTESIAN_POINT('Ctrl Pts',(-31.5248311804202,2.10108305593801,
125.270987624226));
#175683=CARTESIAN_POINT('Ctrl Pts',(-31.5174348234848,2.24687246478841,
125.330833903511));
#175684=CARTESIAN_POINT('Ctrl Pts',(-31.5100373341482,2.39268419436928,
125.390689345414));
#175685=CARTESIAN_POINT('Ctrl Pts',(-31.5026398448117,2.5360768382514,125.456364781628));
#175686=CARTESIAN_POINT('Ctrl Pts',(-31.4952423554751,2.67656378924137,
125.527625183169));
#175687=CARTESIAN_POINT('Ctrl Pts',(-31.4878422729601,2.81709998771423,
125.598910564933));
#175688=CARTESIAN_POINT('Ctrl Pts',(-31.4804421904451,2.95472813258679,
125.675784641228));
#175689=CARTESIAN_POINT('Ctrl Pts',(-31.4730421079302,3.08898688677217,
125.757966798625));
#175690=CARTESIAN_POINT('Ctrl Pts',(-31.4656338882637,3.2233932722601,125.840239323752));
#175691=CARTESIAN_POINT('Ctrl Pts',(-31.4582256685972,3.35442254936867,
125.927831391406));
#175692=CARTESIAN_POINT('Ctrl Pts',(-31.4508174489307,3.48164240712283,
126.020419071997));
#175693=CARTESIAN_POINT('Ctrl Pts',(-31.4434046696286,3.60894056657666,
126.11306373876));
#175694=CARTESIAN_POINT('Ctrl Pts',(-31.4359918903266,3.73242434256604,
126.21070991421));
#175695=CARTESIAN_POINT('Ctrl Pts',(-31.4285791110246,3.85169552836548,
126.312994219768));
#175696=CARTESIAN_POINT('Ctrl Pts',(-31.4211557399958,3.97113713442844,
126.415424673939));
#175697=CARTESIAN_POINT('Ctrl Pts',(-31.413732368967,4.08635385600204,126.52250624072));
#175698=CARTESIAN_POINT('Ctrl Pts',(-31.4063089979383,4.19698469163003,
126.633839060168));
#175699=CARTESIAN_POINT('Ctrl Pts',(-31.4023729484975,4.25564381523029,
126.692870392433));
#175700=CARTESIAN_POINT('Ctrl Pts',(-31.3984368990568,4.31301435270298,
126.753096348597));
#175701=CARTESIAN_POINT('Ctrl Pts',(-31.394500849616,4.36904726208884,126.814453778537));
#175702=CARTESIAN_POINT('Ctrl Pts',(-31.3870775832105,4.47472358046362,
126.930171976502));
#175703=CARTESIAN_POINT('Ctrl Pts',(-31.3796543168051,4.57595916531729,
127.050266453983));
#175704=CARTESIAN_POINT('Ctrl Pts',(-31.3722310503997,4.67236985877937,
127.17436193089));
#175705=CARTESIAN_POINT('Ctrl Pts',(-31.3648165576787,4.76866660280833,
127.298310737249));
#175706=CARTESIAN_POINT('Ctrl Pts',(-31.3574020649576,4.86014957975774,
127.426250838326));
#175707=CARTESIAN_POINT('Ctrl Pts',(-31.3499875722366,4.94647198252855,
127.557770793064));
#175708=CARTESIAN_POINT('Ctrl Pts',(-31.3425802258828,5.03271118451759,
127.689163983918));
#175709=CARTESIAN_POINT('Ctrl Pts',(-31.3351728795291,5.11379951103673,
127.824129849383));
#175710=CARTESIAN_POINT('Ctrl Pts',(-31.3277655331753,5.1894309888911,127.962224699979));
#175711=CARTESIAN_POINT('Ctrl Pts',(-31.3203637114999,5.26500605793588,
128.100216554226));
#175712=CARTESIAN_POINT('Ctrl Pts',(-31.3129618898245,5.33513220353953,
128.24133242086));
#175713=CARTESIAN_POINT('Ctrl Pts',(-31.3055600681491,5.399547350206,128.385100611824));
#175714=CARTESIAN_POINT('Ctrl Pts',(-31.2981621538377,5.46392849261786,
128.528792908678));
#175715=CARTESIAN_POINT('Ctrl Pts',(-31.2907642395263,5.52260448794614,
128.675134401609));
#175716=CARTESIAN_POINT('Ctrl Pts',(-31.2833663252149,5.57535977035532,
128.823629945919));
#175717=CARTESIAN_POINT('Ctrl Pts',(-31.2759696403027,5.62810628579372,
128.972100812964));
#175718=CARTESIAN_POINT('Ctrl Pts',(-31.2685729553906,5.67493391624791,
129.12272466952));
#175719=CARTESIAN_POINT('Ctrl Pts',(-31.2611762704784,5.71567566957414,
129.274987477113));
#175720=CARTESIAN_POINT('Ctrl Pts',(-31.2537799135429,5.75641561636833,
129.427243533214));
#175721=CARTESIAN_POINT('Ctrl Pts',(-31.2463835566075,5.79107012610512,
129.581138035241));
#175722=CARTESIAN_POINT('Ctrl Pts',(-31.238987199672,5.8195224929958,129.736143169658));
#175723=CARTESIAN_POINT('Ctrl Pts',(-31.2315897103355,5.84797921601649,
129.891172035756));
#175724=CARTESIAN_POINT('Ctrl Pts',(-31.2241922209989,5.87023183808305,
130.04731150563));
#175725=CARTESIAN_POINT('Ctrl Pts',(-31.2167947316623,5.88621507266181,
130.204025143961));
#175726=CARTESIAN_POINT('Ctrl Pts',(-31.2093946491473,5.90220391013868,
130.360793718014));
#175727=CARTESIAN_POINT('Ctrl Pts',(-31.2019945666322,5.91191894662271,
130.518136490118));
#175728=CARTESIAN_POINT('Ctrl Pts',(-31.1945944841172,5.91534690617494,
130.675513645904));
#175729=CARTESIAN_POINT('Ctrl Pts',(-31.1871862644508,5.9187786351211,130.833063854051));
#175730=CARTESIAN_POINT('Ctrl Pts',(-31.1797780447843,5.91590947271245,
130.990648147946));
#175731=CARTESIAN_POINT('Ctrl Pts',(-31.1723698251179,5.90677827544612,
131.147727720268));
#175732=CARTESIAN_POINT('Ctrl Pts',(-31.1649570458158,5.89764145808025,
131.304903972445));
#175733=CARTESIAN_POINT('Ctrl Pts',(-31.1575442665136,5.88223496237197,
131.461574513398));
#175734=CARTESIAN_POINT('Ctrl Pts',(-31.1501314872116,5.86064926854897,
131.617207905534));
#175735=CARTESIAN_POINT('Ctrl Pts',(-31.1427081161828,5.83903273207435,
131.773063673959));
#175736=CARTESIAN_POINT('Ctrl Pts',(-31.1352847451541,5.81121942956898,
131.927878967384));
#175737=CARTESIAN_POINT('Ctrl Pts',(-31.1278613741253,5.7773506444235,132.081133930993));
#175738=CARTESIAN_POINT('Ctrl Pts',(-31.1239253246845,5.75939260186919,
132.16239339));
#175739=CARTESIAN_POINT('Ctrl Pts',(-31.1199892752438,5.73973297611782,
132.243214448401));
#175740=CARTESIAN_POINT('Ctrl Pts',(-31.1160532258031,5.71839838878044,
132.323521711622));
#175741=CARTESIAN_POINT('Ctrl Pts',(-31.1086299593976,5.67816202289149,
132.474978703754));
#175742=CARTESIAN_POINT('Ctrl Pts',(-31.1012066929921,5.6318434441649,132.625065066981));
#175743=CARTESIAN_POINT('Ctrl Pts',(-31.0937834265867,5.57955073965454,
132.773254750352));
#175744=CARTESIAN_POINT('Ctrl Pts',(-31.0863689338657,5.5273198407782,132.921269285825));
#175745=CARTESIAN_POINT('Ctrl Pts',(-31.0789544411448,5.46912899392726,
133.067391255007));
#175746=CARTESIAN_POINT('Ctrl Pts',(-31.0715399484237,5.40513689840729,
133.211106485325));
#175747=CARTESIAN_POINT('Ctrl Pts',(-31.06413260207,5.34120648087834,133.354683197493));
#175748=CARTESIAN_POINT('Ctrl Pts',(-31.0567252557161,5.27148609700651,
133.495857450143));
#175749=CARTESIAN_POINT('Ctrl Pts',(-31.0493179093623,5.19618364933253,
133.634131994358));
#175750=CARTESIAN_POINT('Ctrl Pts',(-31.0419160876869,5.1209373650649,133.772303408201));
#175751=CARTESIAN_POINT('Ctrl Pts',(-31.0345142660115,5.04011748448139,
133.907579093436));
#175752=CARTESIAN_POINT('Ctrl Pts',(-31.0271124443361,4.95397919389765,
134.039483599607));
#175753=CARTESIAN_POINT('Ctrl Pts',(-31.0197145300247,4.86788637504713,
134.171318474416));
#175754=CARTESIAN_POINT('Ctrl Pts',(-31.0123166157134,4.77648094115402,
134.299785402595));
#175755=CARTESIAN_POINT('Ctrl Pts',(-31.0049187014021,4.68006295287517,
134.424435384698));
#175756=CARTESIAN_POINT('Ctrl Pts',(-30.9975220164899,4.58366098751677,
134.549064652235));
#175757=CARTESIAN_POINT('Ctrl Pts',(-30.9901253315777,4.48224834919548,
134.669877937625));
#175758=CARTESIAN_POINT('Ctrl Pts',(-30.9827286466655,4.3761672497064,134.786456895294));
#175759=CARTESIAN_POINT('Ctrl Pts',(-30.97533228973,4.27009085396444,134.903030683731));
#175760=CARTESIAN_POINT('Ctrl Pts',(-30.9679359327946,4.15934665988656,
135.015370241667));
#175761=CARTESIAN_POINT('Ctrl Pts',(-30.9605395758591,4.04431564962055,
135.123092085108));
#175762=CARTESIAN_POINT('Ctrl Pts',(-30.9531420865225,3.92926702781321,
135.230830421038));
#175763=CARTESIAN_POINT('Ctrl Pts',(-30.9457445971859,3.80993055548604,
135.333949379595));
#175764=CARTESIAN_POINT('Ctrl Pts',(-30.9383471078494,3.68672226190013,
135.432104076976));
#175765=CARTESIAN_POINT('Ctrl Pts',(-30.9309470253344,3.5634707778379,135.530293182333));
#175766=CARTESIAN_POINT('Ctrl Pts',(-30.9235469428194,3.43634506201051,
135.623514329305));
#175767=CARTESIAN_POINT('Ctrl Pts',(-30.9161468603044,3.30579209956626,
135.711464565614));
#175768=CARTESIAN_POINT('Ctrl Pts',(-30.9087386406379,3.17509558071863,
135.799511512249));
#175769=CARTESIAN_POINT('Ctrl Pts',(-30.9013304209715,3.04096459888016,
135.882275764717));
#175770=CARTESIAN_POINT('Ctrl Pts',(-30.8939222013051,2.90387347079756,
135.959498775569));
#175771=CARTESIAN_POINT('Ctrl Pts',(-30.886509422003,2.76669796541292,136.036769315896));
#175772=CARTESIAN_POINT('Ctrl Pts',(-30.8790966427009,2.62655901491376,
136.108491648998));
#175773=CARTESIAN_POINT('Ctrl Pts',(-30.8716838633989,2.48395263957195,
136.174454643453));
#175774=CARTESIAN_POINT('Ctrl Pts',(-30.8642604923701,2.34114250155346,
136.240511888927));
#175775=CARTESIAN_POINT('Ctrl Pts',(-30.8568371213413,2.1958582412163,136.300793217486));
#175776=CARTESIAN_POINT('Ctrl Pts',(-30.8494137503126,2.04861359426401,
136.35513650062));
#175777=CARTESIAN_POINT('Ctrl Pts',(-30.8454777008717,1.97054094936247,
136.383950613288));
#175778=CARTESIAN_POINT('Ctrl Pts',(-30.8415416514309,1.89191739602549,
136.411096169584));
#175779=CARTESIAN_POINT('Ctrl Pts',(-30.8376056019901,1.81282075547442,
136.436554814415));
#175780=CARTESIAN_POINT('Ctrl Pts',(-30.8301823355846,1.66364695991792,
136.48456902403));
#175781=CARTESIAN_POINT('Ctrl Pts',(-30.8227590691793,1.51233872867243,
136.526725237324));
#175782=CARTESIAN_POINT('Ctrl Pts',(-30.8153358027739,1.359397066994,136.56283004761));
#175783=CARTESIAN_POINT('Ctrl Pts',(-30.8079213100529,1.20663616965867,
136.598892185008));
#175784=CARTESIAN_POINT('Ctrl Pts',(-30.8005068173318,1.05224604448269,
136.628917071073));
#175785=CARTESIAN_POINT('Ctrl Pts',(-30.7930923246108,0.896745060267345,
136.652760301188));
#175786=CARTESIAN_POINT('Ctrl Pts',(-30.785684978257,0.74139395375487,136.6765805503));
#175787=CARTESIAN_POINT('Ctrl Pts',(-30.7782776319032,0.584934486240059,
136.694230948695));
#175788=CARTESIAN_POINT('Ctrl Pts',(-30.7708702855494,0.427897383720886,
136.705617635482));
#175789=CARTESIAN_POINT('Ctrl Pts',(-30.7634684638741,0.270977405397665,
136.716995829649));
#175790=CARTESIAN_POINT('Ctrl Pts',(-30.7560666421986,0.113481020612778,
136.722119587338));
#175791=CARTESIAN_POINT('Ctrl Pts',(-30.7486648205232,-0.0440538262639501,
136.720946611439));
#175792=CARTESIAN_POINT('Ctrl Pts',(-30.7412669062119,-0.201505511721036,
136.719774254745));
#175793=CARTESIAN_POINT('Ctrl Pts',(-30.7338689919006,-0.358995246491254,
136.712311787134));
#175794=CARTESIAN_POINT('Ctrl Pts',(-30.7264710775893,-0.515983084510254,
136.698568962967));
#175795=CARTESIAN_POINT('Ctrl Pts',(-30.719074392677,-0.67294483399885,
136.684828422609));
#175796=CARTESIAN_POINT('Ctrl Pts',(-30.7116777077649,-0.829404480761122,
136.664809629616));
#175797=CARTESIAN_POINT('Ctrl Pts',(-30.7042810228527,-0.984825084984825,
136.638574370462));
#175798=CARTESIAN_POINT('Ctrl Pts',(-30.6968846659172,-1.14023879769607,
136.612340274608));
#175799=CARTESIAN_POINT('Ctrl Pts',(-30.6894883089817,-1.29461319138569,
136.579890322802));
#175800=CARTESIAN_POINT('Ctrl Pts',(-30.6820919520463,-1.44741969995118,
136.54133776365));
#175801=CARTESIAN_POINT('Ctrl Pts',(-30.6746944627097,-1.60024960358324,
136.502779302003));
#175802=CARTESIAN_POINT('Ctrl Pts',(-30.6672969733732,-1.75151078214626,
136.45811646397));
#175803=CARTESIAN_POINT('Ctrl Pts',(-30.6598994840366,-1.90068820115118,
136.407512848632));
#175804=CARTESIAN_POINT('Ctrl Pts',(-30.6524994015216,-2.04991791406908,
136.356891494276));
#175805=CARTESIAN_POINT('Ctrl Pts',(-30.6450993190067,-2.19706205979905,
136.300325336154));
#175806=CARTESIAN_POINT('Ctrl Pts',(-30.6376992364917,-2.34162414962036,
136.238026682426));
#175807=CARTESIAN_POINT('Ctrl Pts',(-30.6302910168252,-2.48634520032076,
136.175659524925));
#175808=CARTESIAN_POINT('Ctrl Pts',(-30.6228827971588,-2.62847818194231,
136.107547431205));
#175809=CARTESIAN_POINT('Ctrl Pts',(-30.6154745774923,-2.7675491914073,
136.033949706169));
#175810=CARTESIAN_POINT('Ctrl Pts',(-30.6080617981902,-2.90670579675828,
135.960306682962));
#175811=CARTESIAN_POINT('Ctrl Pts',(-30.6006490188882,-3.042796352708,135.881171487923));
#175812=CARTESIAN_POINT('Ctrl Pts',(-30.5932362395861,-3.17537511733832,
135.796847315264));
#175813=CARTESIAN_POINT('Ctrl Pts',(-30.5858128685574,-3.30814331672487,
135.712402656272));
#175814=CARTESIAN_POINT('Ctrl Pts',(-30.5783894975286,-3.43738939717479,
135.622754423926));
#175815=CARTESIAN_POINT('Ctrl Pts',(-30.5709661264999,-3.56269926868576,
135.528247204203));
#175816=CARTESIAN_POINT('Ctrl Pts',(-30.567030077059,-3.62914156933087,
135.478137208635));
#175817=CARTESIAN_POINT('Ctrl Pts',(-30.5630940276182,-3.69447784571092,
135.426661822723));
#175818=CARTESIAN_POINT('Ctrl Pts',(-30.5591579781774,-3.75865059089494,
135.373876598287));
#175819=CARTESIAN_POINT('Ctrl Pts',(-30.5518356192568,-3.87803320542091,
135.275678553566));
#175820=CARTESIAN_POINT('Ctrl Pts',(-30.5445132603363,-3.99376921053319,
135.172630614569));
#175821=CARTESIAN_POINT('Ctrl Pts',(-30.5371909014158,-4.10543114346578,
135.065037287857));
#175822=CARTESIAN_POINT('Ctrl Pts',(-30.5298772454647,-4.21696036091817,
134.957571840894));
#175823=CARTESIAN_POINT('Ctrl Pts',(-30.5225635895135,-4.32442486623985,
134.845572018463));
#175824=CARTESIAN_POINT('Ctrl Pts',(-30.5152499335623,-4.42742852318782,
134.729383832091));
#175825=CARTESIAN_POINT('Ctrl Pts',(-30.5079432704593,-4.53033369465485,
134.6133067374));
#175826=CARTESIAN_POINT('Ctrl Pts',(-30.5006366073561,-4.62878625187513,
134.493049533255));
#175827=CARTESIAN_POINT('Ctrl Pts',(-30.493329944253,-4.72242553994323,
134.368996304728));
#175828=CARTESIAN_POINT('Ctrl Pts',(-30.4858318295843,-4.8185183951257,
134.241692593117));
#175829=CARTESIAN_POINT('Ctrl Pts',(-30.4783337149157,-4.9095419668824,
134.110391462067));
#175830=CARTESIAN_POINT('Ctrl Pts',(-30.470835600247,-4.99514875989112,
133.975546425597));
#175831=CARTESIAN_POINT('Ctrl Pts',(-30.4635374611051,-5.078472410499,133.844297720791));
#175832=CARTESIAN_POINT('Ctrl Pts',(-30.4562393219631,-5.15666431666376,
133.709692083498));
#175833=CARTESIAN_POINT('Ctrl Pts',(-30.4489411828212,-5.22944681245081,
133.572178638724));
#175834=CARTESIAN_POINT('Ctrl Pts',(-30.441644464302,-5.30221514072616,
133.434691961696));
#175835=CARTESIAN_POINT('Ctrl Pts',(-30.4343477457829,-5.36957597382484,
133.294298942816));
#175836=CARTESIAN_POINT('Ctrl Pts',(-30.4270510272637,-5.43129716072561,
133.151474103189));
#175837=CARTESIAN_POINT('Ctrl Pts',(-30.4197541965348,-5.49301929678201,
133.008647067185));
#175838=CARTESIAN_POINT('Ctrl Pts',(-30.4124573658057,-5.54910146225589,
132.863388489118));
#175839=CARTESIAN_POINT('Ctrl Pts',(-30.4051605350768,-5.59935941978715,
132.716193416359));
#175840=CARTESIAN_POINT('Ctrl Pts',(-30.3975117565041,-5.65204146805617,
132.561898687544));
#175841=CARTESIAN_POINT('Ctrl Pts',(-30.3898629779314,-5.69832334402539,
132.405476452916));
#175842=CARTESIAN_POINT('Ctrl Pts',(-30.3822141993587,-5.73805168600958,
132.247514597979));
#175843=CARTESIAN_POINT('Ctrl Pts',(-30.3749091742947,-5.77599454592966,
132.096651908141));
#175844=CARTESIAN_POINT('Ctrl Pts',(-30.3676041492307,-5.80796004342863,
131.944385359264));
#175845=CARTESIAN_POINT('Ctrl Pts',(-30.3602991241668,-5.83386718326425,
131.791236623218));
#175846=CARTESIAN_POINT('Ctrl Pts',(-30.3529901493464,-5.8597883308398,
131.638005081133));
#175847=CARTESIAN_POINT('Ctrl Pts',(-30.345681174526,-5.87964454851776,
131.483890782082));
#175848=CARTESIAN_POINT('Ctrl Pts',(-30.3383721997057,-5.89340677965082,
131.329419749537));
#175849=CARTESIAN_POINT('Ctrl Pts',(-30.331054809785,-5.90718485576337,
131.174770868624));
#175850=CARTESIAN_POINT('Ctrl Pts',(-30.3237374198642,-5.91485492660111,
131.019764816672));
#175851=CARTESIAN_POINT('Ctrl Pts',(-30.3164200299435,-5.91643999844559,
130.86492717016));
#175852=CARTESIAN_POINT('Ctrl Pts',(-30.3154050840304,-5.9166598530943,
130.843450682202));
#175853=CARTESIAN_POINT('Ctrl Pts',(-30.3143901381173,-5.91676272238497,
130.821977425223));
#175854=CARTESIAN_POINT('Ctrl Pts',(-30.3133751922042,-5.91674874622358,
130.800508791798));
#175855=CARTESIAN_POINT('',(-28.5633751922042,-5.92063026149449,130.809252908732));
#175856=CARTESIAN_POINT('Ctrl Pts',(-30.3133751922042,-5.92331393100809,
130.800504517838));
#175857=CARTESIAN_POINT('Ctrl Pts',(-30.3024869129242,-5.92505294868337,
130.569933512729));
#175858=CARTESIAN_POINT('Ctrl Pts',(-30.1987827590407,-5.80798761008149,
128.375668861247));
#175859=CARTESIAN_POINT('Ctrl Pts',(-30.0022627305509,-3.06786481668135,
124.514228186764));
#175860=CARTESIAN_POINT('Ctrl Pts',(-29.7238151067389,3.63381068965364,
124.823308836979));
#175861=CARTESIAN_POINT('Ctrl Pts',(-29.4453674829254,6.99619169371812,
130.628683882915));
#175862=CARTESIAN_POINT('Ctrl Pts',(-29.166919859113,3.92941431422043,136.595497265716));
#175863=CARTESIAN_POINT('Ctrl Pts',(-28.8884722352998,-2.74830285748438,
137.240538981617));
#175864=CARTESIAN_POINT('Ctrl Pts',(-28.6872906796637,-5.74828619175598,
133.433271609878));
#175865=CARTESIAN_POINT('Ctrl Pts',(-28.5789249986318,-5.92356585908216,
131.138925557496));
#175866=CARTESIAN_POINT('Ctrl Pts',(-28.5633751922042,-5.92063026149449,
130.809252908732));
#175867=CARTESIAN_POINT('',(-26.8133751922042,-5.90730146414194,130.80590174944));
#175868=CARTESIAN_POINT('Ctrl Pts',(-28.5633751922042,-5.92063026149449,
130.809252908732));
#175869=CARTESIAN_POINT('Ctrl Pts',(-28.4861091240275,-5.90604345075803,
129.171129021212));
#175870=CARTESIAN_POINT('Ctrl Pts',(-28.3160271812466,-4.34740652689545,
125.540851770958));
#175871=CARTESIAN_POINT('Ctrl Pts',(-28.0531293638612,1.80717170404076,
124.043318466945));
#175872=CARTESIAN_POINT('Ctrl Pts',(-27.7746817400483,6.66507669263684,
128.670276923891));
#175873=CARTESIAN_POINT('Ctrl Pts',(-27.4962341162354,5.39810180779896,
135.258354039539));
#175874=CARTESIAN_POINT('Ctrl Pts',(-27.2177864924227,-0.829464926472844,
137.753428790069));
#175875=CARTESIAN_POINT('Ctrl Pts',(-26.9901668510788,-5.29714975403036,
134.572874387029));
#175876=CARTESIAN_POINT('Ctrl Pts',(-26.8553630843394,-5.90938010162537,
131.701195839402));
#175877=CARTESIAN_POINT('Ctrl Pts',(-26.8133751922042,-5.90730146414194,
130.80590174944));
#175878=CARTESIAN_POINT('',(-25.0633751922042,-5.91495849395119,130.798936651208));
#175879=CARTESIAN_POINT('Ctrl Pts',(-26.8133751922042,-5.90730146414194,
130.80590174944));
#175880=CARTESIAN_POINT('Ctrl Pts',(-26.7625472097351,-5.90478519232655,
129.722113304836));
#175881=CARTESIAN_POINT('Ctrl Pts',(-26.6189033526615,-5.09933556471253,
126.655762013877));
#175882=CARTESIAN_POINT('Ctrl Pts',(-26.3824436209839,-0.165029518421817,
123.807909675237));
#175883=CARTESIAN_POINT('Ctrl Pts',(-26.103995997171,5.79710984178776,126.883763977695));
#175884=CARTESIAN_POINT('Ctrl Pts',(-25.8255483733581,6.43198846195871,
133.562455060395));
#175885=CARTESIAN_POINT('Ctrl Pts',(-25.5471007495452,1.15618390569174,
137.706592090545));
#175886=CARTESIAN_POINT('Ctrl Pts',(-25.2930430224939,-4.62691189982062,
135.700502950123));
#175887=CARTESIAN_POINT('Ctrl Pts',(-25.1318011700469,-5.90195921676385,
132.253211397296));
#175888=CARTESIAN_POINT('Ctrl Pts',(-25.0633751922042,-5.91495849395119,
130.798936651208));
#175889=CARTESIAN_POINT('',(-23.3133751922042,-5.92204637845178,130.805173195123));
#175890=CARTESIAN_POINT('Ctrl Pts',(-25.0633751922042,-5.91495849395119,
130.798936651208));
#175891=CARTESIAN_POINT('Ctrl Pts',(-25.0389852954426,-5.9195919831401,
130.280571959342));
#175892=CARTESIAN_POINT('Ctrl Pts',(-24.9217795240766,-5.61943562007176,
127.794847517694));
#175893=CARTESIAN_POINT('Ctrl Pts',(-24.7117578781066,-2.12393811031069,
124.136043930883));
#175894=CARTESIAN_POINT('Ctrl Pts',(-24.4333102542936,4.46220325635265,
125.413043280463));
#175895=CARTESIAN_POINT('Ctrl Pts',(-24.1548626304806,6.9477978211794,131.644399882352));
#175896=CARTESIAN_POINT('Ctrl Pts',(-23.8764150066679,3.04870560713308,
137.103801438095));
#175897=CARTESIAN_POINT('Ctrl Pts',(-23.5979673828549,-3.65199812231858,
136.774324624571));
#175898=CARTESIAN_POINT('Ctrl Pts',(-23.4102874447005,-5.90639808632494,
132.854491977135));
#175899=CARTESIAN_POINT('Ctrl Pts',(-23.3154233811502,-5.92647964306893,
130.84848671572));
#175900=CARTESIAN_POINT('Ctrl Pts',(-23.3133751922042,-5.92639646612977,
130.805173792008));
#175901=CARTESIAN_POINT('',(-21.5633752135755,-5.91415027995088,130.809391528846));
#175902=CARTESIAN_POINT('Ctrl Pts',(-23.3133751922042,-5.91674994430204,
130.805172468387));
#175903=CARTESIAN_POINT('Ctrl Pts',(-23.3059798793106,-5.9167713677538,
130.649038849046));
#175904=CARTESIAN_POINT('Ctrl Pts',(-23.2985845664169,-5.91060834918149,
130.492660650871));
#175905=CARTESIAN_POINT('Ctrl Pts',(-23.2911892535234,-5.89822880539483,
130.336570577366));
#175906=CARTESIAN_POINT('Ctrl Pts',(-23.2838026511675,-5.88586384280095,
130.180664353886));
#175907=CARTESIAN_POINT('Ctrl Pts',(-23.2764160488116,-5.86729695721436,
130.025045951154));
#175908=CARTESIAN_POINT('Ctrl Pts',(-23.2690294464557,-5.84254802841723,
129.870249757904));
#175909=CARTESIAN_POINT('Ctrl Pts',(-23.2616499014213,-5.81782274528825,
129.715601460325));
#175910=CARTESIAN_POINT('Ctrl Pts',(-23.2542703563871,-5.78692723508014,
129.561774177723));
#175911=CARTESIAN_POINT('Ctrl Pts',(-23.2468908113527,-5.74993328836115,
129.409298704282));
#175912=CARTESIAN_POINT('Ctrl Pts',(-23.2395166762504,-5.71296646184232,
129.256935010354));
#175913=CARTESIAN_POINT('Ctrl Pts',(-23.2321425411481,-5.66991018801461,
129.105921516842));
#175914=CARTESIAN_POINT('Ctrl Pts',(-23.2247684060458,-5.62088757009435,
128.956780176324));
#175915=CARTESIAN_POINT('Ctrl Pts',(-23.2171143947618,-5.57000435931385,
128.801978360599));
#175916=CARTESIAN_POINT('Ctrl Pts',(-23.2094603834777,-5.51269307061477,
128.649194014824));
#175917=CARTESIAN_POINT('Ctrl Pts',(-23.2018063721937,-5.44914883316946,
128.498995666746));
#175918=CARTESIAN_POINT('Ctrl Pts',(-23.1944370770504,-5.38796833277387,
128.354384440561));
#175919=CARTESIAN_POINT('Ctrl Pts',(-23.187067781907,-5.32101042755766,
128.212170651381));
#175920=CARTESIAN_POINT('Ctrl Pts',(-23.1796984867637,-5.24849883706996,
128.072842629382));
#175921=CARTESIAN_POINT('Ctrl Pts',(-23.1723292880499,-5.17598819541877,
127.933516430533));
#175922=CARTESIAN_POINT('Ctrl Pts',(-23.1649600893362,-5.09792418648816,
127.797076257873));
#175923=CARTESIAN_POINT('Ctrl Pts',(-23.1575908906224,-5.01457683741423,
127.663986483141));
#175924=CARTESIAN_POINT('Ctrl Pts',(-23.1502203047479,-4.93121379922998,
127.5308716559));
#175925=CARTESIAN_POINT('Ctrl Pts',(-23.1428497188733,-4.84256564093685,
127.40110880106));
#175926=CARTESIAN_POINT('Ctrl Pts',(-23.1354791329987,-4.74894601112439,
127.27513374105));
#175927=CARTESIAN_POINT('Ctrl Pts',(-23.1281056757768,-4.65528991006212,
127.149109605136));
#175928=CARTESIAN_POINT('Ctrl Pts',(-23.1207322185549,-4.55665870647836,
127.026876503302));
#175929=CARTESIAN_POINT('Ctrl Pts',(-23.1133587613329,-4.45340651845562,
126.908837424993));
#175930=CARTESIAN_POINT('Ctrl Pts',(-23.1059771282012,-4.35003984132017,
126.790667461424));
#175931=CARTESIAN_POINT('Ctrl Pts',(-23.0985954950695,-4.24204219768873,
126.676701089374));
#175932=CARTESIAN_POINT('Ctrl Pts',(-23.0912138619378,-4.1298052089831,
126.567305095348));
#175933=CARTESIAN_POINT('Ctrl Pts',(-23.0838273751285,-4.01749442059947,
126.457837169696));
#175934=CARTESIAN_POINT('Ctrl Pts',(-23.0764408883193,-3.90093901295938,
126.352945859601));
#175935=CARTESIAN_POINT('Ctrl Pts',(-23.0690544015101,-3.78056341408622,
126.252957445513));
#175936=CARTESIAN_POINT('Ctrl Pts',(-23.0616578881235,-3.66002441476484,
126.152833304984));
#175937=CARTESIAN_POINT('Ctrl Pts',(-23.0542613747369,-3.53565517005978,
126.057625573558));
#175938=CARTESIAN_POINT('Ctrl Pts',(-23.0468648613503,-3.40790924259743,
125.967617378906));
#175939=CARTESIAN_POINT('Ctrl Pts',(-23.0449339526433,-3.37456032389313,
125.944120144781));
#175940=CARTESIAN_POINT('Ctrl Pts',(-23.0430030439361,-3.34098141257093,
125.92097701851));
#175941=CARTESIAN_POINT('Ctrl Pts',(-23.0410721352291,-3.30718084149768,
125.898192515663));
#175942=CARTESIAN_POINT('Ctrl Pts',(-23.0336488688237,-3.1772365086463,
125.810598817457));
#175943=CARTESIAN_POINT('Ctrl Pts',(-23.0262256024183,-3.04361328293765,
125.728038774378));
#175944=CARTESIAN_POINT('Ctrl Pts',(-23.0188023360128,-2.9067386488714,
125.650837454752));
#175945=CARTESIAN_POINT('Ctrl Pts',(-23.0113878432918,-2.7700257892559,
125.573727380675));
#175946=CARTESIAN_POINT('Ctrl Pts',(-23.0039733505708,-2.63006949255535,
125.501963604653));
#175947=CARTESIAN_POINT('Ctrl Pts',(-22.9965588578498,-2.48732754553731,
125.435828952044));
#175948=CARTESIAN_POINT('Ctrl Pts',(-22.989151511496,-2.34472317858195,
125.369758042503));
#175949=CARTESIAN_POINT('Ctrl Pts',(-22.9817441651423,-2.19933884288163,
125.309305611026));
#175950=CARTESIAN_POINT('Ctrl Pts',(-22.9743368187885,-2.05165824708864,
125.254709367293));
#175951=CARTESIAN_POINT('Ctrl Pts',(-22.9669349971132,-1.90408779705587,
125.200153843499));
#175952=CARTESIAN_POINT('Ctrl Pts',(-22.9595331754377,-1.75422484565269,
125.151445939522));
#175953=CARTESIAN_POINT('Ctrl Pts',(-22.9521313537623,-1.60257437076737,
125.108775840859));
#175954=CARTESIAN_POINT('Ctrl Pts',(-22.9447334394509,-1.45100395098642,
125.066128267408));
#175955=CARTESIAN_POINT('Ctrl Pts',(-22.9373355251395,-1.2976482454218,
125.029512252444));
#175956=CARTESIAN_POINT('Ctrl Pts',(-22.9299376108281,-1.14302862576133,
124.999068538507));
#175957=CARTESIAN_POINT('Ctrl Pts',(-22.9225409259159,-0.988434701077222,
124.968629883763));
#175958=CARTESIAN_POINT('Ctrl Pts',(-22.9151442410038,-0.832577645070909,
124.944361566332));
#175959=CARTESIAN_POINT('Ctrl Pts',(-22.9077475560916,-0.675990407329334,
124.926353512118));
#175960=CARTESIAN_POINT('Ctrl Pts',(-22.9003511991562,-0.519410112829972,
124.9083462564));
#175961=CARTESIAN_POINT('Ctrl Pts',(-22.8929548422207,-0.362100071825017,
124.896598754613));
#175962=CARTESIAN_POINT('Ctrl Pts',(-22.8855584852852,-0.204599497480111,
124.89114917131));
#175963=CARTESIAN_POINT('Ctrl Pts',(-22.8781609959487,-0.0470748093954174,
124.885698753662));
#175964=CARTESIAN_POINT('Ctrl Pts',(-22.8707635066121,0.110640097014221,
124.886548187313));
#175965=CARTESIAN_POINT('Ctrl Pts',(-22.8633660172756,0.268005008623873,
124.893683509328));
#175966=CARTESIAN_POINT('Ctrl Pts',(-22.8559659347606,0.425425084259119,
124.900821332619));
#175967=CARTESIAN_POINT('Ctrl Pts',(-22.8485658522456,0.582494548137099,
124.914249414544));
#175968=CARTESIAN_POINT('Ctrl Pts',(-22.8411657697306,0.738677459986535,
124.933901847367));
#175969=CARTESIAN_POINT('Ctrl Pts',(-22.8337575500642,0.895032111003989,
124.95357589006));
#175970=CARTESIAN_POINT('Ctrl Pts',(-22.8263493303977,1.05049789253869,
124.97948790556));
#175971=CARTESIAN_POINT('Ctrl Pts',(-22.8189411107313,1.20454749383738,
125.011520563017));
#175972=CARTESIAN_POINT('Ctrl Pts',(-22.8115283314292,1.35869191009564,
125.04357293604));
#175973=CARTESIAN_POINT('Ctrl Pts',(-22.8041155521271,1.51141804796216,
125.081753367219));
#175974=CARTESIAN_POINT('Ctrl Pts',(-22.796702772825,1.66221344582373,125.12589453745));
#175975=CARTESIAN_POINT('Ctrl Pts',(-22.7892794017963,1.81322430722093,
125.170098778655));
#175976=CARTESIAN_POINT('Ctrl Pts',(-22.7818560307675,1.96229856595337,
125.22028065046));
#175977=CARTESIAN_POINT('Ctrl Pts',(-22.7744326597387,2.10894265703972,
125.276224274112));
#175978=CARTESIAN_POINT('Ctrl Pts',(-22.7704966102979,2.18669687281173,
125.305886925721));
#175979=CARTESIAN_POINT('Ctrl Pts',(-22.7665605608571,2.26376826407334,
125.33716862988));
#175980=CARTESIAN_POINT('Ctrl Pts',(-22.7626245114162,2.34008614681892,
125.370032012488));
#175981=CARTESIAN_POINT('Ctrl Pts',(-22.7552012450108,2.48401929187543,
125.432011326455));
#175982=CARTESIAN_POINT('Ctrl Pts',(-22.7477779786054,2.62570601176396,
125.499806610725));
#175983=CARTESIAN_POINT('Ctrl Pts',(-22.7403547121999,2.76464175148176,
125.573233917852));
#175984=CARTESIAN_POINT('Ctrl Pts',(-22.7329402194789,2.9034132806931,125.646574439999));
#175985=CARTESIAN_POINT('Ctrl Pts',(-22.7255257267578,3.03943997490544,
125.725533562314));
#175986=CARTESIAN_POINT('Ctrl Pts',(-22.7181112340368,3.17223644020566,
125.809879009838));
#175987=CARTESIAN_POINT('Ctrl Pts',(-22.710703887683,3.3049049112733,125.894143162045));
#175988=CARTESIAN_POINT('Ctrl Pts',(-22.7032965413292,3.4343490386326,125.983783105323));
#175989=CARTESIAN_POINT('Ctrl Pts',(-22.6958891949754,3.56010737405691,
126.07852036977));
#175990=CARTESIAN_POINT('Ctrl Pts',(-22.6884873733,3.68577191416971,126.173186975592));
#175991=CARTESIAN_POINT('Ctrl Pts',(-22.6810855516246,3.80775583910473,
126.272943109091));
#175992=CARTESIAN_POINT('Ctrl Pts',(-22.6736837299492,3.9256261875345,126.377466717974));
#175993=CARTESIAN_POINT('Ctrl Pts',(-22.6662858156379,4.04343431312467,
126.481935149658));
#175994=CARTESIAN_POINT('Ctrl Pts',(-22.6588879013265,4.15713290831237,
126.591165797524));
#175995=CARTESIAN_POINT('Ctrl Pts',(-22.6514899870152,4.26632174827858,
126.704796091587));
#175996=CARTESIAN_POINT('Ctrl Pts',(-22.644093302103,4.37549244304063,126.818407502357));
#175997=CARTESIAN_POINT('Ctrl Pts',(-22.6366966171908,4.4801546116015,126.936416839318));
#175998=CARTESIAN_POINT('Ctrl Pts',(-22.6292999322785,4.57994452448142,
127.058424324038));
#175999=CARTESIAN_POINT('Ctrl Pts',(-22.6219035753431,4.67973001257203,
127.180426398817));
#176000=CARTESIAN_POINT('Ctrl Pts',(-22.6145072184076,4.7746434382067,127.306425979902));
#176001=CARTESIAN_POINT('Ctrl Pts',(-22.6071108614722,4.8643612345785,127.435990040858));
#176002=CARTESIAN_POINT('Ctrl Pts',(-22.5997133721356,4.95409276697384,
127.565573938403));
#176003=CARTESIAN_POINT('Ctrl Pts',(-22.5923158827991,5.03862687370157,
127.69872309552));
#176004=CARTESIAN_POINT('Ctrl Pts',(-22.5849183934625,5.11768330378438,
127.834975468303));
#176005=CARTESIAN_POINT('Ctrl Pts',(-22.5775183109475,5.19676744697631,
127.971275604143));
#176006=CARTESIAN_POINT('Ctrl Pts',(-22.5701182284326,5.27036990321027,
128.110680798823));
#176007=CARTESIAN_POINT('Ctrl Pts',(-22.5627181459176,5.33825643372543,
128.25270452587));
#176008=CARTESIAN_POINT('Ctrl Pts',(-22.5553099262511,5.40621761245989,
128.394884422606));
#176009=CARTESIAN_POINT('Ctrl Pts',(-22.5479017065846,5.46845015233561,
128.539688264945));
#176010=CARTESIAN_POINT('Ctrl Pts',(-22.5404934869181,5.52476774277762,
128.686608991226));
#176011=CARTESIAN_POINT('Ctrl Pts',(-22.533080707616,5.58111999575693,128.833620144763));
#176012=CARTESIAN_POINT('Ctrl Pts',(-22.5256679283139,5.63154992573988,
128.982750425641));
#176013=CARTESIAN_POINT('Ctrl Pts',(-22.5182551490118,5.67592130500799,
129.133478245328));
#176014=CARTESIAN_POINT('Ctrl Pts',(-22.510831777983,5.72035608418356,129.284421431992));
#176015=CARTESIAN_POINT('Ctrl Pts',(-22.5034084069543,5.75871493239599,
129.436966355337));
#176016=CARTESIAN_POINT('Ctrl Pts',(-22.4959850359255,5.79091269062497,
129.590581077428));
#176017=CARTESIAN_POINT('Ctrl Pts',(-22.4920489864848,5.80798471461218,
129.672031289013));
#176018=CARTESIAN_POINT('Ctrl Pts',(-22.4881129370441,5.82332550050936,
129.753782158449));
#176019=CARTESIAN_POINT('Ctrl Pts',(-22.4841768876034,5.83692828577312,
129.835754015667));
#176020=CARTESIAN_POINT('Ctrl Pts',(-22.476753621198,5.86258271425269,129.99035038013));
#176021=CARTESIAN_POINT('Ctrl Pts',(-22.4693303547925,5.88212975452446,
130.146200437488));
#176022=CARTESIAN_POINT('Ctrl Pts',(-22.4619070883871,5.89545144248125,
130.30278026324));
#176023=CARTESIAN_POINT('Ctrl Pts',(-22.4544925956661,5.90875738530923,
130.459175024642));
#176024=CARTESIAN_POINT('Ctrl Pts',(-22.4470781029451,5.91585259032555,
130.616297469254));
#176025=CARTESIAN_POINT('Ctrl Pts',(-22.439663610224,5.91667010976492,130.773613671142));
#176026=CARTESIAN_POINT('Ctrl Pts',(-22.4322562638703,5.91748684124827,
130.930778245751));
#176027=CARTESIAN_POINT('Ctrl Pts',(-22.4248489175164,5.91203793091999,
131.088135835065));
#176028=CARTESIAN_POINT('Ctrl Pts',(-22.4174415711627,5.9003082393564,131.245147689839));
#176029=CARTESIAN_POINT('Ctrl Pts',(-22.4100397494873,5.88858729623937,
131.402042439247));
#176030=CARTESIAN_POINT('Ctrl Pts',(-22.402637927812,5.87059492693678,131.558591596893));
#176031=CARTESIAN_POINT('Ctrl Pts',(-22.3952361061366,5.84636805699052,
131.714256823021));
#176032=CARTESIAN_POINT('Ctrl Pts',(-22.3878381918252,5.82215397622001,
131.869839874689));
#176033=CARTESIAN_POINT('Ctrl Pts',(-22.3804402775138,5.79171200653895,
132.024539556212));
#176034=CARTESIAN_POINT('Ctrl Pts',(-22.3730423632024,5.75513085705372,
132.177823169181));
#176035=CARTESIAN_POINT('Ctrl Pts',(-22.3656456782902,5.71855578669215,
132.331081309193));
#176036=CARTESIAN_POINT('Ctrl Pts',(-22.3582489933779,5.67584364793114,
132.482923484956));
#176037=CARTESIAN_POINT('Ctrl Pts',(-22.3508523084657,5.62713418102083,
132.632827590548));
#176038=CARTESIAN_POINT('Ctrl Pts',(-22.3434559515303,5.57842687393939,
132.782725049235));
#176039=CARTESIAN_POINT('Ctrl Pts',(-22.3360595945949,5.523722882824,132.930684253597));
#176040=CARTESIAN_POINT('Ctrl Pts',(-22.3286632376594,5.46321162931493,
133.076198916349));
#176041=CARTESIAN_POINT('Ctrl Pts',(-22.3212657483228,5.40269111137829,
133.221735857768));
#176042=CARTESIAN_POINT('Ctrl Pts',(-22.3138682589862,5.33636170406164,
133.36482716766));
#176043=CARTESIAN_POINT('Ctrl Pts',(-22.3064707696496,5.26446065549238,
133.504987316922));
#176044=CARTESIAN_POINT('Ctrl Pts',(-22.2990706871346,5.19253440212221,
133.645196599106));
#176045=CARTESIAN_POINT('Ctrl Pts',(-22.2916706046196,5.11503278911246,
133.782472342951));
#176046=CARTESIAN_POINT('Ctrl Pts',(-22.2842705221046,5.03223853319076,
133.916354497311));
#176047=CARTESIAN_POINT('Ctrl Pts',(-22.2768623024381,4.94935323647323,
134.050383868863));
#176048=CARTESIAN_POINT('Ctrl Pts',(-22.2694540827717,4.8611638707726,134.181011880992));
#176049=CARTESIAN_POINT('Ctrl Pts',(-22.2620458631052,4.76799633600885,
134.307807706121));
#176050=CARTESIAN_POINT('Ctrl Pts',(-22.2546330838032,4.67477145818217,
134.434681571965));
#176051=CARTESIAN_POINT('Ctrl Pts',(-22.2472203045011,4.57656253826667,
134.557718259832));
#176052=CARTESIAN_POINT('Ctrl Pts',(-22.2398075251991,4.47373476905679,
134.676521226145));
#176053=CARTESIAN_POINT('Ctrl Pts',(-22.2323841541703,4.37076007470783,
134.795493943708));
#176054=CARTESIAN_POINT('Ctrl Pts',(-22.2249607831415,4.26315360482678,
134.910220586273));
#176055=CARTESIAN_POINT('Ctrl Pts',(-22.2175374121128,4.15131686333376,
135.020341981697));
#176056=CARTESIAN_POINT('Ctrl Pts',(-22.213601362672,4.09201833950854,135.078730987877));
#176057=CARTESIAN_POINT('Ctrl Pts',(-22.2096653132312,4.03153108724262,
135.135825967334));
#176058=CARTESIAN_POINT('Ctrl Pts',(-22.2057292637905,3.96991847990183,
135.191578166928));
#176059=CARTESIAN_POINT('Ctrl Pts',(-22.198305997385,3.85371902532059,135.296725075398));
#176060=CARTESIAN_POINT('Ctrl Pts',(-22.1908827309796,3.73316361089217,
135.39741131683));
#176061=CARTESIAN_POINT('Ctrl Pts',(-22.1834594645742,3.60862926665662,
135.493254450692));
#176062=CARTESIAN_POINT('Ctrl Pts',(-22.1760449718532,3.48424211167366,
135.588984305929));
#176063=CARTESIAN_POINT('Ctrl Pts',(-22.1686304791322,3.35588568070393,
135.679882222098));
#176064=CARTESIAN_POINT('Ctrl Pts',(-22.1612159864112,3.22397299385564,
135.765603274138));
#176065=CARTESIAN_POINT('Ctrl Pts',(-22.1538086400574,3.09218744942174,
135.851241705));
#176066=CARTESIAN_POINT('Ctrl Pts',(-22.1464012937036,2.95685278380421,
135.931713003117));
#176067=CARTESIAN_POINT('Ctrl Pts',(-22.1389939473499,2.81841407877306,
136.006713224135));
#176068=CARTESIAN_POINT('Ctrl Pts',(-22.1315921256745,2.68007862655091,
136.081657507159));
#176069=CARTESIAN_POINT('Ctrl Pts',(-22.1241903039991,2.53864407142366,
136.151138660928));
#176070=CARTESIAN_POINT('Ctrl Pts',(-22.1167884823237,2.39458329303352,
136.214896766158));
#176071=CARTESIAN_POINT('Ctrl Pts',(-22.1093905680123,2.2505985632061,136.278621213982));
#176072=CARTESIAN_POINT('Ctrl Pts',(-22.1019926537009,2.10399071161964,
136.33662847934));
#176073=CARTESIAN_POINT('Ctrl Pts',(-22.0945947393895,1.95525586197085,
136.388705259216));
#176074=CARTESIAN_POINT('Ctrl Pts',(-22.0871980544773,1.8065457293568,136.440773384876));
#176075=CARTESIAN_POINT('Ctrl Pts',(-22.0798013695651,1.65570965219169,
136.486912857817));
#176076=CARTESIAN_POINT('Ctrl Pts',(-22.072404684653,1.50326242599239,136.526959034465));
#176077=CARTESIAN_POINT('Ctrl Pts',(-22.0650083277175,1.35082195946285,
136.567003435425));
#176078=CARTESIAN_POINT('Ctrl Pts',(-22.057611970782,1.19677084699426,136.600954982464));
#176079=CARTESIAN_POINT('Ctrl Pts',(-22.0502156138466,1.0416374294404,136.62869938073));
#176080=CARTESIAN_POINT('Ctrl Pts',(-22.04281812451,0.88648026056494,136.656448026734));
#176081=CARTESIAN_POINT('Ctrl Pts',(-22.0354206351736,0.730240824157295,
136.677987566008));
#176082=CARTESIAN_POINT('Ctrl Pts',(-22.028023145837,0.573455848010767,
136.693255161781));
#176083=CARTESIAN_POINT('Ctrl Pts',(-22.020623063322,0.416615911133003,
136.708528109586));
#176084=CARTESIAN_POINT('Ctrl Pts',(-22.0132229808071,0.259230425071346,
136.717524700296));
#176085=CARTESIAN_POINT('Ctrl Pts',(-22.0058228982921,0.101839259180674,
136.720234122619));
#176086=CARTESIAN_POINT('Ctrl Pts',(-21.9984146786257,-0.0557249744771007,
136.722946524231));
#176087=CARTESIAN_POINT('Ctrl Pts',(-21.9910064589591,-0.213294526965045,
136.719357944537));
#176088=CARTESIAN_POINT('Ctrl Pts',(-21.9835982392927,-0.370330773973643,
136.709509699541));
#176089=CARTESIAN_POINT('Ctrl Pts',(-21.9761854599906,-0.527463674171985,
136.699655393114));
#176090=CARTESIAN_POINT('Ctrl Pts',(-21.9687726806886,-0.684062244356029,
136.683533782499));
#176091=CARTESIAN_POINT('Ctrl Pts',(-21.9613599013866,-0.839595465555872,
136.661237773245));
#176092=CARTESIAN_POINT('Ctrl Pts',(-21.9539365303578,-0.99535091991573,
136.638909906408));
#176093=CARTESIAN_POINT('Ctrl Pts',(-21.9465131593291,-1.15003761893748,
136.610390088384));
#176094=CARTESIAN_POINT('Ctrl Pts',(-21.9390897883003,-1.30313635824861,
136.575821974476));
#176095=CARTESIAN_POINT('Ctrl Pts',(-21.9351537388594,-1.38431298338782,
136.557493131032));
#176096=CARTESIAN_POINT('Ctrl Pts',(-21.9312176894186,-1.46504344395392,
136.53746472363));
#176097=CARTESIAN_POINT('Ctrl Pts',(-21.9272816399777,-1.54525246769907,
136.515763717818));
#176098=CARTESIAN_POINT('Ctrl Pts',(-21.9198583735721,-1.69652418324068,
136.474836298123));
#176099=CARTESIAN_POINT('Ctrl Pts',(-21.9124351071667,-1.84639751596973,
136.42783298655));
#176100=CARTESIAN_POINT('Ctrl Pts',(-21.9050118407613,-1.99434691388684,
136.374864270699));
#176101=CARTESIAN_POINT('Ctrl Pts',(-21.8975973480402,-2.14212144790203,
136.321958159472));
#176102=CARTESIAN_POINT('Ctrl Pts',(-21.8901828553191,-2.28797622535719,
136.263100802848));
#176103=CARTESIAN_POINT('Ctrl Pts',(-21.8827683625981,-2.43139780357286,
136.198453245922));
#176104=CARTESIAN_POINT('Ctrl Pts',(-21.8753610162443,-2.5746811466707,
136.133867998745));
#176105=CARTESIAN_POINT('Ctrl Pts',(-21.8679536698907,-2.71553562134067,
136.063503813937));
#176106=CARTESIAN_POINT('Ctrl Pts',(-21.8605463235369,-2.85346493302224,
135.987570862049));
#176107=CARTESIAN_POINT('Ctrl Pts',(-21.8531445018615,-2.99129137182076,
135.911694543821));
